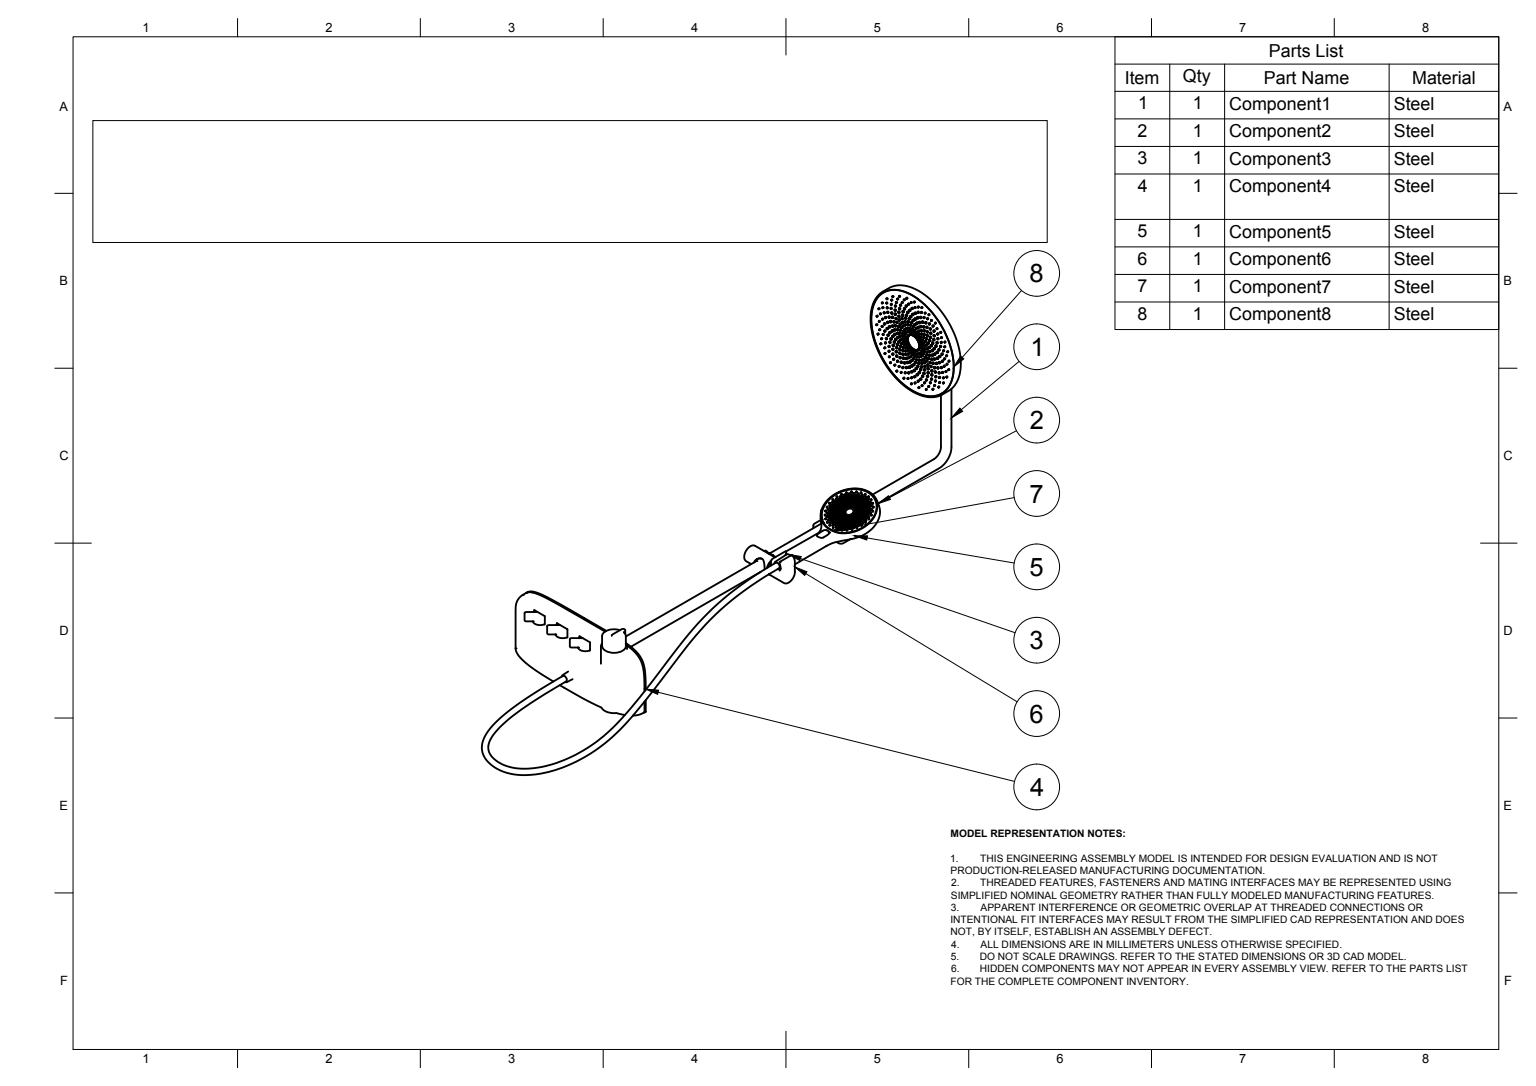
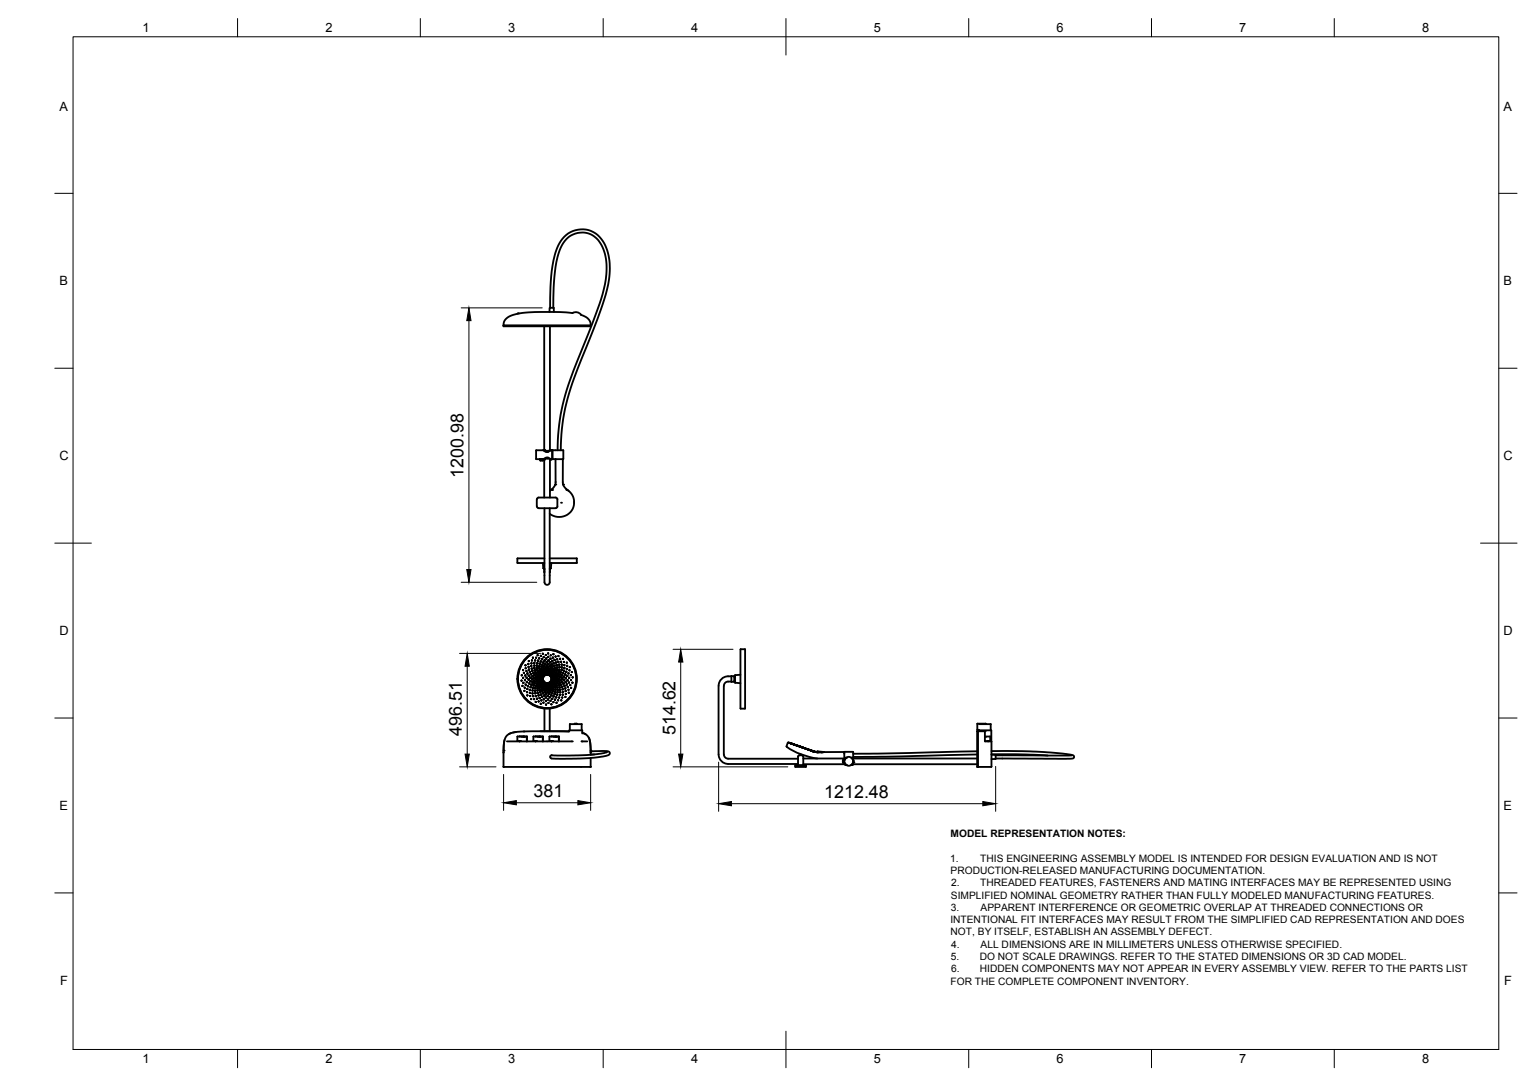
ISO-10303-21;
HEADER;
/* Generated by software containing ST-Developer
 * from STEP Tools, Inc. (www.steptools.com) 
 */

FILE_DESCRIPTION(
/* description */ ('STEP AP214'),
/* implementation_level */ '2;1');

FILE_NAME(
/* name */ 'MAS-616',
/* time_stamp */ '2026-10-06T11:02:40-07:00',
/* author */ (''),
/* organization */ (''),
/* preprocessor_version */ 'ST-DEVELOPER v20.2',
/* originating_system */ 'Autodesk Translation Framework v15.15.0.0',
/* authorisation */ '');

FILE_SCHEMA (('AUTOMOTIVE_DESIGN { 1 0 10303 214 3 1 1 }'));
ENDSEC;

DATA;
#10=MECHANICAL_DESIGN_GEOMETRIC_PRESENTATION_REPRESENTATION('',(#2936,#2937,
#2938,#2939,#2940,#2941,#2942,#2943),#130910);
#11=ITEM_DEFINED_TRANSFORMATION($,$,#45550,#51593);
#12=ITEM_DEFINED_TRANSFORMATION($,$,#45568,#51594);
#13=ITEM_DEFINED_TRANSFORMATION($,$,#48137,#51595);
#14=ITEM_DEFINED_TRANSFORMATION($,$,#48162,#51596);
#15=ITEM_DEFINED_TRANSFORMATION($,$,#48574,#51597);
#16=ITEM_DEFINED_TRANSFORMATION($,$,#48753,#51598);
#17=ITEM_DEFINED_TRANSFORMATION($,$,#48892,#51599);
#18=ITEM_DEFINED_TRANSFORMATION($,$,#48902,#51600);
#19=(
REPRESENTATION_RELATIONSHIP($,$,#130942,#130941)
REPRESENTATION_RELATIONSHIP_WITH_TRANSFORMATION(#11)
SHAPE_REPRESENTATION_RELATIONSHIP()
);
#20=(
REPRESENTATION_RELATIONSHIP($,$,#130943,#130941)
REPRESENTATION_RELATIONSHIP_WITH_TRANSFORMATION(#12)
SHAPE_REPRESENTATION_RELATIONSHIP()
);
#21=(
REPRESENTATION_RELATIONSHIP($,$,#130944,#130941)
REPRESENTATION_RELATIONSHIP_WITH_TRANSFORMATION(#13)
SHAPE_REPRESENTATION_RELATIONSHIP()
);
#22=(
REPRESENTATION_RELATIONSHIP($,$,#130945,#130941)
REPRESENTATION_RELATIONSHIP_WITH_TRANSFORMATION(#14)
SHAPE_REPRESENTATION_RELATIONSHIP()
);
#23=(
REPRESENTATION_RELATIONSHIP($,$,#130946,#130941)
REPRESENTATION_RELATIONSHIP_WITH_TRANSFORMATION(#15)
SHAPE_REPRESENTATION_RELATIONSHIP()
);
#24=(
REPRESENTATION_RELATIONSHIP($,$,#130947,#130941)
REPRESENTATION_RELATIONSHIP_WITH_TRANSFORMATION(#16)
SHAPE_REPRESENTATION_RELATIONSHIP()
);
#25=(
REPRESENTATION_RELATIONSHIP($,$,#130948,#130941)
REPRESENTATION_RELATIONSHIP_WITH_TRANSFORMATION(#17)
SHAPE_REPRESENTATION_RELATIONSHIP()
);
#26=(
REPRESENTATION_RELATIONSHIP($,$,#130949,#130941)
REPRESENTATION_RELATIONSHIP_WITH_TRANSFORMATION(#18)
SHAPE_REPRESENTATION_RELATIONSHIP()
);
#27=CONTEXT_DEPENDENT_SHAPE_REPRESENTATION(#19,#130933);
#28=CONTEXT_DEPENDENT_SHAPE_REPRESENTATION(#20,#130934);
#29=CONTEXT_DEPENDENT_SHAPE_REPRESENTATION(#21,#130935);
#30=CONTEXT_DEPENDENT_SHAPE_REPRESENTATION(#22,#130936);
#31=CONTEXT_DEPENDENT_SHAPE_REPRESENTATION(#23,#130937);
#32=CONTEXT_DEPENDENT_SHAPE_REPRESENTATION(#24,#130938);
#33=CONTEXT_DEPENDENT_SHAPE_REPRESENTATION(#25,#130939);
#34=CONTEXT_DEPENDENT_SHAPE_REPRESENTATION(#26,#130940);
#35=NEXT_ASSEMBLY_USAGE_OCCURRENCE('Component1:1','Component1:1',
'Component1:1',#130951,#130952,'Component1:1');
#36=NEXT_ASSEMBLY_USAGE_OCCURRENCE('Component2:1','Component2:1',
'Component2:1',#130951,#130953,'Component2:1');
#37=NEXT_ASSEMBLY_USAGE_OCCURRENCE('Component3:1','Component3:1',
'Component3:1',#130951,#130954,'Component3:1');
#38=NEXT_ASSEMBLY_USAGE_OCCURRENCE('Component4:1','Component4:1',
'Component4:1',#130951,#130955,'Component4:1');
#39=NEXT_ASSEMBLY_USAGE_OCCURRENCE('Component5:1','Component5:1',
'Component5:1',#130951,#130956,'Component5:1');
#40=NEXT_ASSEMBLY_USAGE_OCCURRENCE('Component6:1','Component6:1',
'Component6:1',#130951,#130957,'Component6:1');
#41=NEXT_ASSEMBLY_USAGE_OCCURRENCE('Component7:1','Component7:1',
'Component7:1',#130951,#130958,'Component7:1');
#42=NEXT_ASSEMBLY_USAGE_OCCURRENCE('Component8:1','Component8:1',
'Component8:1',#130951,#130959,'Component8:1');
#43=(
BOUNDED_CURVE()
B_SPLINE_CURVE(3,(#103309,#103310,#103311,#103312,#103313,#103314,#103315,
#103316,#103317,#103318,#103319,#103320,#103321,#103322,#103323,#103324,
#103325,#103326),.UNSPECIFIED.,.F.,.F.)
B_SPLINE_CURVE_WITH_KNOTS((4,2,2,2,2,2,2,2,4),(0.,0.392699081698724,0.785398163397448,
1.17809724509617,1.5707963267949,1.96349540849362,2.35619449019234,2.74889357189107,
3.14159265358979),.UNSPECIFIED.)
CURVE()
GEOMETRIC_REPRESENTATION_ITEM()
RATIONAL_B_SPLINE_CURVE((1.,1.,1.,1.,1.,1.,1.,1.,1.,1.,1.,1.,1.,1.,1.,1.,
1.,1.))
REPRESENTATION_ITEM('')
);
#44=(
BOUNDED_CURVE()
B_SPLINE_CURVE(3,(#103476,#103477,#103478,#103479,#103480,#103481,#103482,
#103483,#103484,#103485,#103486,#103487,#103488,#103489,#103490,#103491,
#103492,#103493),.UNSPECIFIED.,.F.,.F.)
B_SPLINE_CURVE_WITH_KNOTS((4,2,2,2,2,2,2,2,4),(3.14159265358979,3.53429173528852,
3.92699081698724,4.31968989868597,4.71238898038469,5.10508806208341,5.49778714378214,
5.89048622548086,6.28318530717959),.UNSPECIFIED.)
CURVE()
GEOMETRIC_REPRESENTATION_ITEM()
RATIONAL_B_SPLINE_CURVE((1.,1.,1.,1.,1.,1.,1.,1.,1.,1.,1.,1.,1.,1.,1.,1.,
1.,1.))
REPRESENTATION_ITEM('')
);
#45=B_SPLINE_SURFACE_WITH_KNOTS('',5,5,((#80582,#80583,#80584,#80585,#80586,
#80587),(#80588,#80589,#80590,#80591,#80592,#80593),(#80594,#80595,#80596,
#80597,#80598,#80599),(#80600,#80601,#80602,#80603,#80604,#80605),(#80606,
#80607,#80608,#80609,#80610,#80611),(#80612,#80613,#80614,#80615,#80616,
#80617),(#80618,#80619,#80620,#80621,#80622,#80623),(#80624,#80625,#80626,
#80627,#80628,#80629),(#80630,#80631,#80632,#80633,#80634,#80635),(#80636,
#80637,#80638,#80639,#80640,#80641),(#80642,#80643,#80644,#80645,#80646,
#80647),(#80648,#80649,#80650,#80651,#80652,#80653),(#80654,#80655,#80656,
#80657,#80658,#80659),(#80660,#80661,#80662,#80663,#80664,#80665),(#80666,
#80667,#80668,#80669,#80670,#80671),(#80672,#80673,#80674,#80675,#80676,
#80677),(#80678,#80679,#80680,#80681,#80682,#80683),(#80684,#80685,#80686,
#80687,#80688,#80689),(#80690,#80691,#80692,#80693,#80694,#80695),(#80696,
#80697,#80698,#80699,#80700,#80701),(#80702,#80703,#80704,#80705,#80706,
#80707),(#80708,#80709,#80710,#80711,#80712,#80713)),.UNSPECIFIED.,.F.,
 .F.,.F.,(6,4,4,4,4,6),(6,6),(0.,0.25,0.375,0.5,0.75,1.),(-5.17415755595432E-6,
1.),.UNSPECIFIED.);
#46=B_SPLINE_SURFACE_WITH_KNOTS('',5,5,((#80915,#80916,#80917,#80918,#80919,
#80920),(#80921,#80922,#80923,#80924,#80925,#80926),(#80927,#80928,#80929,
#80930,#80931,#80932),(#80933,#80934,#80935,#80936,#80937,#80938),(#80939,
#80940,#80941,#80942,#80943,#80944),(#80945,#80946,#80947,#80948,#80949,
#80950),(#80951,#80952,#80953,#80954,#80955,#80956),(#80957,#80958,#80959,
#80960,#80961,#80962),(#80963,#80964,#80965,#80966,#80967,#80968),(#80969,
#80970,#80971,#80972,#80973,#80974),(#80975,#80976,#80977,#80978,#80979,
#80980),(#80981,#80982,#80983,#80984,#80985,#80986),(#80987,#80988,#80989,
#80990,#80991,#80992),(#80993,#80994,#80995,#80996,#80997,#80998),(#80999,
#81000,#81001,#81002,#81003,#81004),(#81005,#81006,#81007,#81008,#81009,
#81010),(#81011,#81012,#81013,#81014,#81015,#81016),(#81017,#81018,#81019,
#81020,#81021,#81022),(#81023,#81024,#81025,#81026,#81027,#81028),(#81029,
#81030,#81031,#81032,#81033,#81034),(#81035,#81036,#81037,#81038,#81039,
#81040),(#81041,#81042,#81043,#81044,#81045,#81046)),.UNSPECIFIED.,.F.,
 .F.,.F.,(6,4,4,4,4,6),(6,6),(0.,0.25,0.5,0.625,0.75,1.),(-4.87729692394977E-6,
1.),.UNSPECIFIED.);
#47=B_SPLINE_SURFACE_WITH_KNOTS('',5,5,((#81337,#81338,#81339,#81340,#81341,
#81342),(#81343,#81344,#81345,#81346,#81347,#81348),(#81349,#81350,#81351,
#81352,#81353,#81354),(#81355,#81356,#81357,#81358,#81359,#81360),(#81361,
#81362,#81363,#81364,#81365,#81366),(#81367,#81368,#81369,#81370,#81371,
#81372),(#81373,#81374,#81375,#81376,#81377,#81378),(#81379,#81380,#81381,
#81382,#81383,#81384),(#81385,#81386,#81387,#81388,#81389,#81390),(#81391,
#81392,#81393,#81394,#81395,#81396),(#81397,#81398,#81399,#81400,#81401,
#81402),(#81403,#81404,#81405,#81406,#81407,#81408),(#81409,#81410,#81411,
#81412,#81413,#81414),(#81415,#81416,#81417,#81418,#81419,#81420),(#81421,
#81422,#81423,#81424,#81425,#81426),(#81427,#81428,#81429,#81430,#81431,
#81432),(#81433,#81434,#81435,#81436,#81437,#81438),(#81439,#81440,#81441,
#81442,#81443,#81444),(#81445,#81446,#81447,#81448,#81449,#81450),(#81451,
#81452,#81453,#81454,#81455,#81456),(#81457,#81458,#81459,#81460,#81461,
#81462),(#81463,#81464,#81465,#81466,#81467,#81468),(#81469,#81470,#81471,
#81472,#81473,#81474),(#81475,#81476,#81477,#81478,#81479,#81480),(#81481,
#81482,#81483,#81484,#81485,#81486),(#81487,#81488,#81489,#81490,#81491,
#81492),(#81493,#81494,#81495,#81496,#81497,#81498),(#81499,#81500,#81501,
#81502,#81503,#81504),(#81505,#81506,#81507,#81508,#81509,#81510),(#81511,
#81512,#81513,#81514,#81515,#81516),(#81517,#81518,#81519,#81520,#81521,
#81522),(#81523,#81524,#81525,#81526,#81527,#81528),(#81529,#81530,#81531,
#81532,#81533,#81534),(#81535,#81536,#81537,#81538,#81539,#81540),(#81541,
#81542,#81543,#81544,#81545,#81546),(#81547,#81548,#81549,#81550,#81551,
#81552),(#81553,#81554,#81555,#81556,#81557,#81558),(#81559,#81560,#81561,
#81562,#81563,#81564),(#81565,#81566,#81567,#81568,#81569,#81570),(#81571,
#81572,#81573,#81574,#81575,#81576),(#81577,#81578,#81579,#81580,#81581,
#81582),(#81583,#81584,#81585,#81586,#81587,#81588),(#81589,#81590,#81591,
#81592,#81593,#81594),(#81595,#81596,#81597,#81598,#81599,#81600),(#81601,
#81602,#81603,#81604,#81605,#81606),(#81607,#81608,#81609,#81610,#81611,
#81612)),.UNSPECIFIED.,.F.,.F.,.F.,(6,4,4,4,4,4,4,4,4,4,4,6),(6,6),(0.,
0.0625,0.125,0.25,0.3125,0.375,0.5,0.625,0.6875,0.75,0.875,1.),(0.,1.),
 .UNSPECIFIED.);
#48=B_SPLINE_SURFACE_WITH_KNOTS('',5,5,((#82412,#82413,#82414,#82415,#82416,
#82417),(#82418,#82419,#82420,#82421,#82422,#82423),(#82424,#82425,#82426,
#82427,#82428,#82429),(#82430,#82431,#82432,#82433,#82434,#82435),(#82436,
#82437,#82438,#82439,#82440,#82441),(#82442,#82443,#82444,#82445,#82446,
#82447),(#82448,#82449,#82450,#82451,#82452,#82453),(#82454,#82455,#82456,
#82457,#82458,#82459),(#82460,#82461,#82462,#82463,#82464,#82465),(#82466,
#82467,#82468,#82469,#82470,#82471)),.UNSPECIFIED.,.F.,.F.,.F.,(6,4,6),
(6,6),(0.,0.5,1.),(-3.3767936030343E-7,1.),.UNSPECIFIED.);
#49=B_SPLINE_SURFACE_WITH_KNOTS('',5,5,((#83493,#83494,#83495,#83496,#83497,
#83498),(#83499,#83500,#83501,#83502,#83503,#83504),(#83505,#83506,#83507,
#83508,#83509,#83510),(#83511,#83512,#83513,#83514,#83515,#83516),(#83517,
#83518,#83519,#83520,#83521,#83522),(#83523,#83524,#83525,#83526,#83527,
#83528),(#83529,#83530,#83531,#83532,#83533,#83534),(#83535,#83536,#83537,
#83538,#83539,#83540),(#83541,#83542,#83543,#83544,#83545,#83546),(#83547,
#83548,#83549,#83550,#83551,#83552)),.UNSPECIFIED.,.F.,.F.,.F.,(6,4,6),
(6,6),(0.,0.5,1.),(0.,1.),.UNSPECIFIED.);
#50=B_SPLINE_SURFACE_WITH_KNOTS('',3,1,((#87618,#87619),(#87620,#87621),
(#87622,#87623),(#87624,#87625)),.UNSPECIFIED.,.F.,.F.,.F.,(4,4),(2,2),
(0.0749476459249852,1.),(0.,0.360000000000005),.UNSPECIFIED.);
#51=B_SPLINE_SURFACE_WITH_KNOTS('',3,1,((#88063,#88064),(#88065,#88066),
(#88067,#88068),(#88069,#88070)),.UNSPECIFIED.,.F.,.F.,.F.,(4,4),(2,2),
(0.,0.925052354075012),(0.,0.360000000000003),.UNSPECIFIED.);
#52=B_SPLINE_SURFACE_WITH_KNOTS('',3,1,((#96549,#96550),(#96551,#96552),
(#96553,#96554),(#96555,#96556)),.UNSPECIFIED.,.F.,.F.,.F.,(4,4),(2,2),
(0.0749476459249852,1.),(0.,3.46611820003485),.UNSPECIFIED.);
#53=B_SPLINE_SURFACE_WITH_KNOTS('',3,1,((#96558,#96559),(#96560,#96561),
(#96562,#96563),(#96564,#96565)),.UNSPECIFIED.,.F.,.F.,.F.,(4,4),(2,2),
(0.309194334580351,0.92505235407501),(0.,1.8569103791729),.UNSPECIFIED.);
#54=B_SPLINE_SURFACE_WITH_KNOTS('',3,1,((#96571,#96572),(#96573,#96574),
(#96575,#96576),(#96577,#96578)),.UNSPECIFIED.,.F.,.F.,.F.,(4,4),(2,2),
(0.62139116379009,1.),(0.,13.1529900906224),.UNSPECIFIED.);
#55=B_SPLINE_SURFACE_WITH_KNOTS('',3,1,((#96579,#96580),(#96581,#96582),
(#96583,#96584),(#96585,#96586)),.UNSPECIFIED.,.F.,.F.,.F.,(4,4),(2,2),
(0.,1.),(0.,13.1529900906224),.UNSPECIFIED.);
#56=B_SPLINE_SURFACE_WITH_KNOTS('',3,1,((#96901,#96902),(#96903,#96904),
(#96905,#96906),(#96907,#96908)),.UNSPECIFIED.,.F.,.F.,.F.,(4,4),(2,2),
(0.,0.448741420101952),(0.,13.1529900906224),.UNSPECIFIED.);
#57=B_SPLINE_SURFACE_WITH_KNOTS('',3,1,((#96909,#96910),(#96911,#96912),
(#96913,#96914),(#96915,#96916)),.UNSPECIFIED.,.F.,.F.,.F.,(4,4),(2,2),
(0.,0.274332977827422),(0.,3.42421373123634),.UNSPECIFIED.);
#58=SPHERICAL_SURFACE('',#47449,40.9182954767619);
#59=SPHERICAL_SURFACE('',#47518,216.25);
#60=SPHERICAL_SURFACE('',#48303,0.5);
#61=SPHERICAL_SURFACE('',#48305,0.5);
#62=SPHERICAL_SURFACE('',#48314,0.5);
#63=SPHERICAL_SURFACE('',#48316,0.5);
#64=SPHERICAL_SURFACE('',#48525,1.);
#65=SPHERICAL_SURFACE('',#48533,1.);
#66=SPHERICAL_SURFACE('',#48870,0.5);
#67=SPHERICAL_SURFACE('',#48880,0.5);
#68=SPHERICAL_SURFACE('',#48882,0.5);
#69=SPHERICAL_SURFACE('',#48888,0.5);
#70=SPHERICAL_SURFACE('',#50902,14.1583614602198);
#71=CONICAL_SURFACE('',#47414,8.99091713639496,1.30899693899566);
#72=CONICAL_SURFACE('',#47466,6.3031389659941,0.785398163397445);
#73=CONICAL_SURFACE('',#47469,6.3031389659941,0.785398163397445);
#74=CONICAL_SURFACE('',#47523,22.9751982564137,0.00349065850398867);
#75=CONICAL_SURFACE('',#47530,22.9751982564137,0.00349065850398867);
#76=CONICAL_SURFACE('',#48147,9.47320447306899,0.0418325464020223);
#77=CONICAL_SURFACE('',#48154,8.94802844775792,0.0407936828678657);
#78=CONICAL_SURFACE('',#48628,2.99999999999998,0.78539816339745);
#79=CONICAL_SURFACE('',#48632,2.99999999999998,0.78539816339745);
#80=CONICAL_SURFACE('',#48637,3.00000000000006,0.785398163397453);
#81=CONICAL_SURFACE('',#48641,3.00000000000006,0.785398163397453);
#82=CONICAL_SURFACE('',#50915,18.5103550292801,0.080595262641945);
#83=FACE_BOUND('',#13544,.T.);
#84=FACE_BOUND('',#13545,.T.);
#85=FACE_BOUND('',#13546,.T.);
#86=FACE_BOUND('',#13547,.T.);
#87=FACE_BOUND('',#13548,.T.);
#88=FACE_BOUND('',#13549,.T.);
#89=FACE_BOUND('',#13550,.T.);
#90=FACE_BOUND('',#13551,.T.);
#91=FACE_BOUND('',#13552,.T.);
#92=FACE_BOUND('',#13553,.T.);
#93=FACE_BOUND('',#13554,.T.);
#94=FACE_BOUND('',#13555,.T.);
#95=FACE_BOUND('',#13556,.T.);
#96=FACE_BOUND('',#13557,.T.);
#97=FACE_BOUND('',#13558,.T.);
#98=FACE_BOUND('',#13559,.T.);
#99=FACE_BOUND('',#13560,.T.);
#100=FACE_BOUND('',#13561,.T.);
#101=FACE_BOUND('',#13562,.T.);
#102=FACE_BOUND('',#13563,.T.);
#103=FACE_BOUND('',#13564,.T.);
#104=FACE_BOUND('',#13565,.T.);
#105=FACE_BOUND('',#13566,.T.);
#106=FACE_BOUND('',#13567,.T.);
#107=FACE_BOUND('',#13568,.T.);
#108=FACE_BOUND('',#13569,.T.);
#109=FACE_BOUND('',#13570,.T.);
#110=FACE_BOUND('',#13571,.T.);
#111=FACE_BOUND('',#13572,.T.);
#112=FACE_BOUND('',#13573,.T.);
#113=FACE_BOUND('',#13574,.T.);
#114=FACE_BOUND('',#13575,.T.);
#115=FACE_BOUND('',#13576,.T.);
#116=FACE_BOUND('',#13577,.T.);
#117=FACE_BOUND('',#13578,.T.);
#118=FACE_BOUND('',#13579,.T.);
#119=FACE_BOUND('',#13580,.T.);
#120=FACE_BOUND('',#13581,.T.);
#121=FACE_BOUND('',#13582,.T.);
#122=FACE_BOUND('',#13583,.T.);
#123=FACE_BOUND('',#13584,.T.);
#124=FACE_BOUND('',#13585,.T.);
#125=FACE_BOUND('',#13586,.T.);
#126=FACE_BOUND('',#13587,.T.);
#127=FACE_BOUND('',#13588,.T.);
#128=FACE_BOUND('',#13589,.T.);
#129=FACE_BOUND('',#13590,.T.);
#130=FACE_BOUND('',#13591,.T.);
#131=FACE_BOUND('',#13605,.T.);
#132=FACE_BOUND('',#13670,.T.);
#133=FACE_BOUND('',#13671,.T.);
#134=FACE_BOUND('',#13672,.T.);
#135=FACE_BOUND('',#13673,.T.);
#136=FACE_BOUND('',#13674,.T.);
#137=FACE_BOUND('',#13675,.T.);
#138=FACE_BOUND('',#13676,.T.);
#139=FACE_BOUND('',#13677,.T.);
#140=FACE_BOUND('',#13678,.T.);
#141=FACE_BOUND('',#13679,.T.);
#142=FACE_BOUND('',#13680,.T.);
#143=FACE_BOUND('',#13681,.T.);
#144=FACE_BOUND('',#13682,.T.);
#145=FACE_BOUND('',#13683,.T.);
#146=FACE_BOUND('',#13684,.T.);
#147=FACE_BOUND('',#13685,.T.);
#148=FACE_BOUND('',#13686,.T.);
#149=FACE_BOUND('',#13687,.T.);
#150=FACE_BOUND('',#13689,.T.);
#151=FACE_BOUND('',#13690,.T.);
#152=FACE_BOUND('',#13691,.T.);
#153=FACE_BOUND('',#13692,.T.);
#154=FACE_BOUND('',#13693,.T.);
#155=FACE_BOUND('',#13694,.T.);
#156=FACE_BOUND('',#13695,.T.);
#157=FACE_BOUND('',#13696,.T.);
#158=FACE_BOUND('',#13697,.T.);
#159=FACE_BOUND('',#13698,.T.);
#160=FACE_BOUND('',#13699,.T.);
#161=FACE_BOUND('',#13700,.T.);
#162=FACE_BOUND('',#13701,.T.);
#163=FACE_BOUND('',#13702,.T.);
#164=FACE_BOUND('',#13703,.T.);
#165=FACE_BOUND('',#13704,.T.);
#166=FACE_BOUND('',#13705,.T.);
#167=FACE_BOUND('',#13706,.T.);
#168=FACE_BOUND('',#13707,.T.);
#169=FACE_BOUND('',#13708,.T.);
#170=FACE_BOUND('',#13709,.T.);
#171=FACE_BOUND('',#13710,.T.);
#172=FACE_BOUND('',#13711,.T.);
#173=FACE_BOUND('',#13712,.T.);
#174=FACE_BOUND('',#13713,.T.);
#175=FACE_BOUND('',#13714,.T.);
#176=FACE_BOUND('',#13715,.T.);
#177=FACE_BOUND('',#13716,.T.);
#178=FACE_BOUND('',#13717,.T.);
#179=FACE_BOUND('',#13718,.T.);
#180=FACE_BOUND('',#13719,.T.);
#181=FACE_BOUND('',#13720,.T.);
#182=FACE_BOUND('',#13721,.T.);
#183=FACE_BOUND('',#13722,.T.);
#184=FACE_BOUND('',#13723,.T.);
#185=FACE_BOUND('',#13724,.T.);
#186=FACE_BOUND('',#13725,.T.);
#187=FACE_BOUND('',#13726,.T.);
#188=FACE_BOUND('',#13727,.T.);
#189=FACE_BOUND('',#13728,.T.);
#190=FACE_BOUND('',#13729,.T.);
#191=FACE_BOUND('',#13730,.T.);
#192=FACE_BOUND('',#13731,.T.);
#193=FACE_BOUND('',#13732,.T.);
#194=FACE_BOUND('',#13733,.T.);
#195=FACE_BOUND('',#13734,.T.);
#196=FACE_BOUND('',#13735,.T.);
#197=FACE_BOUND('',#13736,.T.);
#198=FACE_BOUND('',#13737,.T.);
#199=FACE_BOUND('',#13738,.T.);
#200=FACE_BOUND('',#13739,.T.);
#201=FACE_BOUND('',#13740,.T.);
#202=FACE_BOUND('',#13741,.T.);
#203=FACE_BOUND('',#13742,.T.);
#204=FACE_BOUND('',#13743,.T.);
#205=FACE_BOUND('',#13744,.T.);
#206=FACE_BOUND('',#13745,.T.);
#207=FACE_BOUND('',#13746,.T.);
#208=FACE_BOUND('',#13747,.T.);
#209=FACE_BOUND('',#13748,.T.);
#210=FACE_BOUND('',#13749,.T.);
#211=FACE_BOUND('',#13750,.T.);
#212=FACE_BOUND('',#13751,.T.);
#213=FACE_BOUND('',#13752,.T.);
#214=FACE_BOUND('',#13753,.T.);
#215=FACE_BOUND('',#13754,.T.);
#216=FACE_BOUND('',#13755,.T.);
#217=FACE_BOUND('',#13756,.T.);
#218=FACE_BOUND('',#13757,.T.);
#219=FACE_BOUND('',#13758,.T.);
#220=FACE_BOUND('',#13759,.T.);
#221=FACE_BOUND('',#13760,.T.);
#222=FACE_BOUND('',#13761,.T.);
#223=FACE_BOUND('',#13762,.T.);
#224=FACE_BOUND('',#13763,.T.);
#225=FACE_BOUND('',#13764,.T.);
#226=FACE_BOUND('',#13765,.T.);
#227=FACE_BOUND('',#13766,.T.);
#228=FACE_BOUND('',#13767,.T.);
#229=FACE_BOUND('',#13768,.T.);
#230=FACE_BOUND('',#13769,.T.);
#231=FACE_BOUND('',#13770,.T.);
#232=FACE_BOUND('',#13771,.T.);
#233=FACE_BOUND('',#13772,.T.);
#234=FACE_BOUND('',#13773,.T.);
#235=FACE_BOUND('',#13774,.T.);
#236=FACE_BOUND('',#13775,.T.);
#237=FACE_BOUND('',#13776,.T.);
#238=FACE_BOUND('',#13777,.T.);
#239=FACE_BOUND('',#13778,.T.);
#240=FACE_BOUND('',#13779,.T.);
#241=FACE_BOUND('',#13780,.T.);
#242=FACE_BOUND('',#13781,.T.);
#243=FACE_BOUND('',#13782,.T.);
#244=FACE_BOUND('',#13783,.T.);
#245=FACE_BOUND('',#13784,.T.);
#246=FACE_BOUND('',#13785,.T.);
#247=FACE_BOUND('',#13786,.T.);
#248=FACE_BOUND('',#13787,.T.);
#249=FACE_BOUND('',#13788,.T.);
#250=FACE_BOUND('',#13789,.T.);
#251=FACE_BOUND('',#13790,.T.);
#252=FACE_BOUND('',#13791,.T.);
#253=FACE_BOUND('',#13792,.T.);
#254=FACE_BOUND('',#13793,.T.);
#255=FACE_BOUND('',#13794,.T.);
#256=FACE_BOUND('',#13795,.T.);
#257=FACE_BOUND('',#13796,.T.);
#258=FACE_BOUND('',#13797,.T.);
#259=FACE_BOUND('',#13798,.T.);
#260=FACE_BOUND('',#13799,.T.);
#261=FACE_BOUND('',#13800,.T.);
#262=FACE_BOUND('',#13801,.T.);
#263=FACE_BOUND('',#13802,.T.);
#264=FACE_BOUND('',#13803,.T.);
#265=FACE_BOUND('',#13804,.T.);
#266=FACE_BOUND('',#13805,.T.);
#267=FACE_BOUND('',#13806,.T.);
#268=FACE_BOUND('',#13807,.T.);
#269=FACE_BOUND('',#13808,.T.);
#270=FACE_BOUND('',#13809,.T.);
#271=FACE_BOUND('',#13810,.T.);
#272=FACE_BOUND('',#13811,.T.);
#273=FACE_BOUND('',#13812,.T.);
#274=FACE_BOUND('',#13813,.T.);
#275=FACE_BOUND('',#13814,.T.);
#276=FACE_BOUND('',#13815,.T.);
#277=FACE_BOUND('',#13816,.T.);
#278=FACE_BOUND('',#13817,.T.);
#279=FACE_BOUND('',#13818,.T.);
#280=FACE_BOUND('',#13819,.T.);
#281=FACE_BOUND('',#13820,.T.);
#282=FACE_BOUND('',#13821,.T.);
#283=FACE_BOUND('',#13822,.T.);
#284=FACE_BOUND('',#13823,.T.);
#285=FACE_BOUND('',#13824,.T.);
#286=FACE_BOUND('',#13825,.T.);
#287=FACE_BOUND('',#13826,.T.);
#288=FACE_BOUND('',#13827,.T.);
#289=FACE_BOUND('',#13828,.T.);
#290=FACE_BOUND('',#13829,.T.);
#291=FACE_BOUND('',#13830,.T.);
#292=FACE_BOUND('',#13831,.T.);
#293=FACE_BOUND('',#13832,.T.);
#294=FACE_BOUND('',#13833,.T.);
#295=FACE_BOUND('',#13834,.T.);
#296=FACE_BOUND('',#13835,.T.);
#297=FACE_BOUND('',#13836,.T.);
#298=FACE_BOUND('',#13837,.T.);
#299=FACE_BOUND('',#13838,.T.);
#300=FACE_BOUND('',#13839,.T.);
#301=FACE_BOUND('',#13840,.T.);
#302=FACE_BOUND('',#13841,.T.);
#303=FACE_BOUND('',#13842,.T.);
#304=FACE_BOUND('',#13843,.T.);
#305=FACE_BOUND('',#13844,.T.);
#306=FACE_BOUND('',#13845,.T.);
#307=FACE_BOUND('',#13846,.T.);
#308=FACE_BOUND('',#13847,.T.);
#309=FACE_BOUND('',#13848,.T.);
#310=FACE_BOUND('',#13849,.T.);
#311=FACE_BOUND('',#13850,.T.);
#312=FACE_BOUND('',#13851,.T.);
#313=FACE_BOUND('',#13852,.T.);
#314=FACE_BOUND('',#13853,.T.);
#315=FACE_BOUND('',#13854,.T.);
#316=FACE_BOUND('',#13855,.T.);
#317=FACE_BOUND('',#13856,.T.);
#318=FACE_BOUND('',#13857,.T.);
#319=FACE_BOUND('',#13858,.T.);
#320=FACE_BOUND('',#13859,.T.);
#321=FACE_BOUND('',#13860,.T.);
#322=FACE_BOUND('',#13861,.T.);
#323=FACE_BOUND('',#13862,.T.);
#324=FACE_BOUND('',#13863,.T.);
#325=FACE_BOUND('',#13864,.T.);
#326=FACE_BOUND('',#13865,.T.);
#327=FACE_BOUND('',#13866,.T.);
#328=FACE_BOUND('',#13867,.T.);
#329=FACE_BOUND('',#13868,.T.);
#330=FACE_BOUND('',#13869,.T.);
#331=FACE_BOUND('',#13870,.T.);
#332=FACE_BOUND('',#13871,.T.);
#333=FACE_BOUND('',#13872,.T.);
#334=FACE_BOUND('',#13873,.T.);
#335=FACE_BOUND('',#13874,.T.);
#336=FACE_BOUND('',#13875,.T.);
#337=FACE_BOUND('',#13876,.T.);
#338=FACE_BOUND('',#13877,.T.);
#339=FACE_BOUND('',#13878,.T.);
#340=FACE_BOUND('',#13879,.T.);
#341=FACE_BOUND('',#13880,.T.);
#342=FACE_BOUND('',#13881,.T.);
#343=FACE_BOUND('',#13882,.T.);
#344=FACE_BOUND('',#13883,.T.);
#345=FACE_BOUND('',#13884,.T.);
#346=FACE_BOUND('',#13885,.T.);
#347=FACE_BOUND('',#13886,.T.);
#348=FACE_BOUND('',#13887,.T.);
#349=FACE_BOUND('',#13888,.T.);
#350=FACE_BOUND('',#13889,.T.);
#351=FACE_BOUND('',#13890,.T.);
#352=FACE_BOUND('',#13891,.T.);
#353=FACE_BOUND('',#13892,.T.);
#354=FACE_BOUND('',#13893,.T.);
#355=FACE_BOUND('',#13894,.T.);
#356=FACE_BOUND('',#13895,.T.);
#357=FACE_BOUND('',#13896,.T.);
#358=FACE_BOUND('',#13897,.T.);
#359=FACE_BOUND('',#13898,.T.);
#360=FACE_BOUND('',#13899,.T.);
#361=FACE_BOUND('',#13900,.T.);
#362=FACE_BOUND('',#13901,.T.);
#363=FACE_BOUND('',#13902,.T.);
#364=FACE_BOUND('',#13903,.T.);
#365=FACE_BOUND('',#13904,.T.);
#366=FACE_BOUND('',#13905,.T.);
#367=FACE_BOUND('',#13906,.T.);
#368=FACE_BOUND('',#13907,.T.);
#369=FACE_BOUND('',#13908,.T.);
#370=FACE_BOUND('',#13909,.T.);
#371=FACE_BOUND('',#13910,.T.);
#372=FACE_BOUND('',#13911,.T.);
#373=FACE_BOUND('',#13912,.T.);
#374=FACE_BOUND('',#13913,.T.);
#375=FACE_BOUND('',#13914,.T.);
#376=FACE_BOUND('',#13915,.T.);
#377=FACE_BOUND('',#13916,.T.);
#378=FACE_BOUND('',#13917,.T.);
#379=FACE_BOUND('',#13918,.T.);
#380=FACE_BOUND('',#13919,.T.);
#381=FACE_BOUND('',#13920,.T.);
#382=FACE_BOUND('',#13921,.T.);
#383=FACE_BOUND('',#13922,.T.);
#384=FACE_BOUND('',#13923,.T.);
#385=FACE_BOUND('',#13924,.T.);
#386=FACE_BOUND('',#13933,.T.);
#387=FACE_BOUND('',#13936,.T.);
#388=FACE_BOUND('',#13939,.T.);
#389=FACE_BOUND('',#13942,.T.);
#390=FACE_BOUND('',#13945,.T.);
#391=FACE_BOUND('',#13948,.T.);
#392=FACE_BOUND('',#13951,.T.);
#393=FACE_BOUND('',#13954,.T.);
#394=FACE_BOUND('',#13957,.T.);
#395=FACE_BOUND('',#13960,.T.);
#396=FACE_BOUND('',#13963,.T.);
#397=FACE_BOUND('',#13966,.T.);
#398=FACE_BOUND('',#13969,.T.);
#399=FACE_BOUND('',#13972,.T.);
#400=FACE_BOUND('',#13975,.T.);
#401=FACE_BOUND('',#13978,.T.);
#402=FACE_BOUND('',#13981,.T.);
#403=FACE_BOUND('',#13984,.T.);
#404=FACE_BOUND('',#13987,.T.);
#405=FACE_BOUND('',#13990,.T.);
#406=FACE_BOUND('',#13993,.T.);
#407=FACE_BOUND('',#13996,.T.);
#408=FACE_BOUND('',#13999,.T.);
#409=FACE_BOUND('',#14002,.T.);
#410=FACE_BOUND('',#14005,.T.);
#411=FACE_BOUND('',#14008,.T.);
#412=FACE_BOUND('',#14011,.T.);
#413=FACE_BOUND('',#14014,.T.);
#414=FACE_BOUND('',#14017,.T.);
#415=FACE_BOUND('',#14020,.T.);
#416=FACE_BOUND('',#14023,.T.);
#417=FACE_BOUND('',#14026,.T.);
#418=FACE_BOUND('',#14029,.T.);
#419=FACE_BOUND('',#14032,.T.);
#420=FACE_BOUND('',#14035,.T.);
#421=FACE_BOUND('',#14038,.T.);
#422=FACE_BOUND('',#14041,.T.);
#423=FACE_BOUND('',#14044,.T.);
#424=FACE_BOUND('',#14047,.T.);
#425=FACE_BOUND('',#14050,.T.);
#426=FACE_BOUND('',#14053,.T.);
#427=FACE_BOUND('',#14056,.T.);
#428=FACE_BOUND('',#14059,.T.);
#429=FACE_BOUND('',#14062,.T.);
#430=FACE_BOUND('',#14065,.T.);
#431=FACE_BOUND('',#14068,.T.);
#432=FACE_BOUND('',#14071,.T.);
#433=FACE_BOUND('',#14074,.T.);
#434=FACE_BOUND('',#14077,.T.);
#435=FACE_BOUND('',#14080,.T.);
#436=FACE_BOUND('',#14083,.T.);
#437=FACE_BOUND('',#14086,.T.);
#438=FACE_BOUND('',#14089,.T.);
#439=FACE_BOUND('',#14092,.T.);
#440=FACE_BOUND('',#14095,.T.);
#441=FACE_BOUND('',#14098,.T.);
#442=FACE_BOUND('',#14101,.T.);
#443=FACE_BOUND('',#14104,.T.);
#444=FACE_BOUND('',#14107,.T.);
#445=FACE_BOUND('',#14110,.T.);
#446=FACE_BOUND('',#14113,.T.);
#447=FACE_BOUND('',#14116,.T.);
#448=FACE_BOUND('',#14119,.T.);
#449=FACE_BOUND('',#14122,.T.);
#450=FACE_BOUND('',#14125,.T.);
#451=FACE_BOUND('',#14128,.T.);
#452=FACE_BOUND('',#14131,.T.);
#453=FACE_BOUND('',#14134,.T.);
#454=FACE_BOUND('',#14137,.T.);
#455=FACE_BOUND('',#14140,.T.);
#456=FACE_BOUND('',#14143,.T.);
#457=FACE_BOUND('',#14146,.T.);
#458=FACE_BOUND('',#14149,.T.);
#459=FACE_BOUND('',#14152,.T.);
#460=FACE_BOUND('',#14155,.T.);
#461=FACE_BOUND('',#14158,.T.);
#462=FACE_BOUND('',#14161,.T.);
#463=FACE_BOUND('',#14164,.T.);
#464=FACE_BOUND('',#14167,.T.);
#465=FACE_BOUND('',#14170,.T.);
#466=FACE_BOUND('',#14173,.T.);
#467=FACE_BOUND('',#14176,.T.);
#468=FACE_BOUND('',#14179,.T.);
#469=FACE_BOUND('',#14182,.T.);
#470=FACE_BOUND('',#14185,.T.);
#471=FACE_BOUND('',#14188,.T.);
#472=FACE_BOUND('',#14191,.T.);
#473=FACE_BOUND('',#14194,.T.);
#474=FACE_BOUND('',#14197,.T.);
#475=FACE_BOUND('',#14200,.T.);
#476=FACE_BOUND('',#14203,.T.);
#477=FACE_BOUND('',#14206,.T.);
#478=FACE_BOUND('',#14209,.T.);
#479=FACE_BOUND('',#14212,.T.);
#480=FACE_BOUND('',#14215,.T.);
#481=FACE_BOUND('',#14218,.T.);
#482=FACE_BOUND('',#14221,.T.);
#483=FACE_BOUND('',#14224,.T.);
#484=FACE_BOUND('',#14227,.T.);
#485=FACE_BOUND('',#14230,.T.);
#486=FACE_BOUND('',#14233,.T.);
#487=FACE_BOUND('',#14236,.T.);
#488=FACE_BOUND('',#14239,.T.);
#489=FACE_BOUND('',#14242,.T.);
#490=FACE_BOUND('',#14245,.T.);
#491=FACE_BOUND('',#14248,.T.);
#492=FACE_BOUND('',#14251,.T.);
#493=FACE_BOUND('',#14254,.T.);
#494=FACE_BOUND('',#14257,.T.);
#495=FACE_BOUND('',#14260,.T.);
#496=FACE_BOUND('',#14263,.T.);
#497=FACE_BOUND('',#14266,.T.);
#498=FACE_BOUND('',#14269,.T.);
#499=FACE_BOUND('',#14272,.T.);
#500=FACE_BOUND('',#14275,.T.);
#501=FACE_BOUND('',#14278,.T.);
#502=FACE_BOUND('',#14281,.T.);
#503=FACE_BOUND('',#14284,.T.);
#504=FACE_BOUND('',#14287,.T.);
#505=FACE_BOUND('',#14290,.T.);
#506=FACE_BOUND('',#14293,.T.);
#507=FACE_BOUND('',#14296,.T.);
#508=FACE_BOUND('',#14299,.T.);
#509=FACE_BOUND('',#14302,.T.);
#510=FACE_BOUND('',#14305,.T.);
#511=FACE_BOUND('',#14308,.T.);
#512=FACE_BOUND('',#14311,.T.);
#513=FACE_BOUND('',#14314,.T.);
#514=FACE_BOUND('',#14317,.T.);
#515=FACE_BOUND('',#14320,.T.);
#516=FACE_BOUND('',#14323,.T.);
#517=FACE_BOUND('',#14326,.T.);
#518=FACE_BOUND('',#14329,.T.);
#519=FACE_BOUND('',#14332,.T.);
#520=FACE_BOUND('',#14335,.T.);
#521=FACE_BOUND('',#14338,.T.);
#522=FACE_BOUND('',#14341,.T.);
#523=FACE_BOUND('',#14344,.T.);
#524=FACE_BOUND('',#14347,.T.);
#525=FACE_BOUND('',#14350,.T.);
#526=FACE_BOUND('',#14353,.T.);
#527=FACE_BOUND('',#14356,.T.);
#528=FACE_BOUND('',#14359,.T.);
#529=FACE_BOUND('',#14362,.T.);
#530=FACE_BOUND('',#14365,.T.);
#531=FACE_BOUND('',#14368,.T.);
#532=FACE_BOUND('',#14371,.T.);
#533=FACE_BOUND('',#14374,.T.);
#534=FACE_BOUND('',#14377,.T.);
#535=FACE_BOUND('',#14380,.T.);
#536=FACE_BOUND('',#14383,.T.);
#537=FACE_BOUND('',#14386,.T.);
#538=FACE_BOUND('',#14389,.T.);
#539=FACE_BOUND('',#14392,.T.);
#540=FACE_BOUND('',#14395,.T.);
#541=FACE_BOUND('',#14398,.T.);
#542=FACE_BOUND('',#14401,.T.);
#543=FACE_BOUND('',#14404,.T.);
#544=FACE_BOUND('',#14407,.T.);
#545=FACE_BOUND('',#14410,.T.);
#546=FACE_BOUND('',#14413,.T.);
#547=FACE_BOUND('',#14416,.T.);
#548=FACE_BOUND('',#14419,.T.);
#549=FACE_BOUND('',#14422,.T.);
#550=FACE_BOUND('',#14425,.T.);
#551=FACE_BOUND('',#14428,.T.);
#552=FACE_BOUND('',#14431,.T.);
#553=FACE_BOUND('',#14434,.T.);
#554=FACE_BOUND('',#14437,.T.);
#555=FACE_BOUND('',#14440,.T.);
#556=FACE_BOUND('',#14443,.T.);
#557=FACE_BOUND('',#14446,.T.);
#558=FACE_BOUND('',#14449,.T.);
#559=FACE_BOUND('',#14452,.T.);
#560=FACE_BOUND('',#14455,.T.);
#561=FACE_BOUND('',#14458,.T.);
#562=FACE_BOUND('',#14461,.T.);
#563=FACE_BOUND('',#14464,.T.);
#564=FACE_BOUND('',#14467,.T.);
#565=FACE_BOUND('',#14470,.T.);
#566=FACE_BOUND('',#14473,.T.);
#567=FACE_BOUND('',#14476,.T.);
#568=FACE_BOUND('',#14479,.T.);
#569=FACE_BOUND('',#14482,.T.);
#570=FACE_BOUND('',#14485,.T.);
#571=FACE_BOUND('',#14488,.T.);
#572=FACE_BOUND('',#14491,.T.);
#573=FACE_BOUND('',#14494,.T.);
#574=FACE_BOUND('',#14497,.T.);
#575=FACE_BOUND('',#14500,.T.);
#576=FACE_BOUND('',#14503,.T.);
#577=FACE_BOUND('',#14506,.T.);
#578=FACE_BOUND('',#14509,.T.);
#579=FACE_BOUND('',#14512,.T.);
#580=FACE_BOUND('',#14515,.T.);
#581=FACE_BOUND('',#14518,.T.);
#582=FACE_BOUND('',#14521,.T.);
#583=FACE_BOUND('',#14524,.T.);
#584=FACE_BOUND('',#14527,.T.);
#585=FACE_BOUND('',#14530,.T.);
#586=FACE_BOUND('',#14533,.T.);
#587=FACE_BOUND('',#14536,.T.);
#588=FACE_BOUND('',#14539,.T.);
#589=FACE_BOUND('',#14542,.T.);
#590=FACE_BOUND('',#14545,.T.);
#591=FACE_BOUND('',#14548,.T.);
#592=FACE_BOUND('',#14551,.T.);
#593=FACE_BOUND('',#14554,.T.);
#594=FACE_BOUND('',#14557,.T.);
#595=FACE_BOUND('',#14560,.T.);
#596=FACE_BOUND('',#14563,.T.);
#597=FACE_BOUND('',#14566,.T.);
#598=FACE_BOUND('',#14569,.T.);
#599=FACE_BOUND('',#14572,.T.);
#600=FACE_BOUND('',#14575,.T.);
#601=FACE_BOUND('',#14578,.T.);
#602=FACE_BOUND('',#14581,.T.);
#603=FACE_BOUND('',#14584,.T.);
#604=FACE_BOUND('',#14587,.T.);
#605=FACE_BOUND('',#14590,.T.);
#606=FACE_BOUND('',#14593,.T.);
#607=FACE_BOUND('',#14596,.T.);
#608=FACE_BOUND('',#14599,.T.);
#609=FACE_BOUND('',#14602,.T.);
#610=FACE_BOUND('',#14605,.T.);
#611=FACE_BOUND('',#14608,.T.);
#612=FACE_BOUND('',#14611,.T.);
#613=FACE_BOUND('',#14614,.T.);
#614=FACE_BOUND('',#14617,.T.);
#615=FACE_BOUND('',#14620,.T.);
#616=FACE_BOUND('',#14623,.T.);
#617=FACE_BOUND('',#14626,.T.);
#618=FACE_BOUND('',#14629,.T.);
#619=FACE_BOUND('',#14632,.T.);
#620=FACE_BOUND('',#14635,.T.);
#621=FACE_BOUND('',#14638,.T.);
#622=FACE_BOUND('',#14641,.T.);
#623=FACE_BOUND('',#14644,.T.);
#624=FACE_BOUND('',#14647,.T.);
#625=FACE_BOUND('',#14650,.T.);
#626=FACE_BOUND('',#14653,.T.);
#627=FACE_BOUND('',#14656,.T.);
#628=FACE_BOUND('',#14659,.T.);
#629=FACE_BOUND('',#14662,.T.);
#630=FACE_BOUND('',#14665,.T.);
#631=FACE_BOUND('',#14668,.T.);
#632=FACE_BOUND('',#14671,.T.);
#633=FACE_BOUND('',#14674,.T.);
#634=FACE_BOUND('',#14677,.T.);
#635=FACE_BOUND('',#14680,.T.);
#636=FACE_BOUND('',#14683,.T.);
#637=FACE_BOUND('',#14686,.T.);
#638=FACE_BOUND('',#14689,.T.);
#639=FACE_BOUND('',#14692,.T.);
#640=FACE_BOUND('',#14695,.T.);
#641=FACE_BOUND('',#14698,.T.);
#642=FACE_BOUND('',#14701,.T.);
#643=FACE_BOUND('',#14704,.T.);
#644=FACE_BOUND('',#14707,.T.);
#645=FACE_BOUND('',#14710,.T.);
#646=FACE_BOUND('',#14713,.T.);
#647=FACE_BOUND('',#14716,.T.);
#648=FACE_BOUND('',#14719,.T.);
#649=FACE_BOUND('',#14722,.T.);
#650=FACE_BOUND('',#14725,.T.);
#651=FACE_BOUND('',#14728,.T.);
#652=FACE_BOUND('',#14731,.T.);
#653=FACE_BOUND('',#14734,.T.);
#654=FACE_BOUND('',#14737,.T.);
#655=FACE_BOUND('',#14740,.T.);
#656=FACE_BOUND('',#14743,.T.);
#657=FACE_BOUND('',#14746,.T.);
#658=FACE_BOUND('',#14749,.T.);
#659=FACE_BOUND('',#14752,.T.);
#660=FACE_BOUND('',#14755,.T.);
#661=FACE_BOUND('',#14758,.T.);
#662=FACE_BOUND('',#14761,.T.);
#663=FACE_BOUND('',#14764,.T.);
#664=FACE_BOUND('',#14767,.T.);
#665=FACE_BOUND('',#14770,.T.);
#666=FACE_BOUND('',#14773,.T.);
#667=FACE_BOUND('',#14776,.T.);
#668=FACE_BOUND('',#14779,.T.);
#669=FACE_BOUND('',#14782,.T.);
#670=FACE_BOUND('',#14785,.T.);
#671=FACE_BOUND('',#14788,.T.);
#672=FACE_BOUND('',#14791,.T.);
#673=FACE_BOUND('',#14794,.T.);
#674=FACE_BOUND('',#14797,.T.);
#675=FACE_BOUND('',#14800,.T.);
#676=FACE_BOUND('',#14803,.T.);
#677=FACE_BOUND('',#14806,.T.);
#678=FACE_BOUND('',#14809,.T.);
#679=FACE_BOUND('',#14812,.T.);
#680=FACE_BOUND('',#14815,.T.);
#681=FACE_BOUND('',#14818,.T.);
#682=FACE_BOUND('',#14821,.T.);
#683=FACE_BOUND('',#14824,.T.);
#684=FACE_BOUND('',#14827,.T.);
#685=FACE_BOUND('',#14830,.T.);
#686=FACE_BOUND('',#14833,.T.);
#687=FACE_BOUND('',#14836,.T.);
#688=FACE_BOUND('',#14839,.T.);
#689=FACE_BOUND('',#14842,.T.);
#690=FACE_BOUND('',#14845,.T.);
#691=FACE_BOUND('',#14848,.T.);
#692=FACE_BOUND('',#14851,.T.);
#693=FACE_BOUND('',#14854,.T.);
#694=FACE_BOUND('',#14857,.T.);
#695=FACE_BOUND('',#14860,.T.);
#696=FACE_BOUND('',#14863,.T.);
#697=FACE_BOUND('',#14866,.T.);
#698=FACE_BOUND('',#14869,.T.);
#699=FACE_BOUND('',#14872,.T.);
#700=FACE_BOUND('',#14875,.T.);
#701=FACE_BOUND('',#14878,.T.);
#702=FACE_BOUND('',#14881,.T.);
#703=FACE_BOUND('',#14884,.T.);
#704=FACE_BOUND('',#14887,.T.);
#705=FACE_BOUND('',#14890,.T.);
#706=FACE_BOUND('',#14893,.T.);
#707=FACE_BOUND('',#14896,.T.);
#708=FACE_BOUND('',#14899,.T.);
#709=FACE_BOUND('',#14901,.T.);
#710=FACE_BOUND('',#14904,.T.);
#711=FACE_BOUND('',#14907,.T.);
#712=FACE_BOUND('',#14910,.T.);
#713=FACE_BOUND('',#14913,.T.);
#714=FACE_BOUND('',#14916,.T.);
#715=FACE_BOUND('',#14926,.T.);
#716=FACE_BOUND('',#14930,.T.);
#717=FACE_BOUND('',#15125,.T.);
#718=FACE_BOUND('',#15135,.T.);
#719=FACE_BOUND('',#15136,.T.);
#720=FACE_BOUND('',#15137,.T.);
#721=FACE_BOUND('',#15164,.T.);
#722=FACE_BOUND('',#15172,.T.);
#723=FACE_BOUND('',#15175,.T.);
#724=FACE_BOUND('',#15265,.T.);
#725=FACE_BOUND('',#15266,.T.);
#726=FACE_BOUND('',#15267,.T.);
#727=FACE_BOUND('',#15278,.T.);
#728=FACE_BOUND('',#15280,.T.);
#729=FACE_BOUND('',#15289,.T.);
#730=FACE_BOUND('',#15291,.T.);
#731=FACE_BOUND('',#15335,.T.);
#732=FACE_BOUND('',#15338,.T.);
#733=FACE_BOUND('',#15339,.T.);
#734=FACE_BOUND('',#15340,.T.);
#735=FACE_BOUND('',#15341,.T.);
#736=FACE_BOUND('',#15342,.T.);
#737=FACE_BOUND('',#15343,.T.);
#738=FACE_BOUND('',#15344,.T.);
#739=FACE_BOUND('',#15345,.T.);
#740=FACE_BOUND('',#15346,.T.);
#741=FACE_BOUND('',#15347,.T.);
#742=FACE_BOUND('',#15348,.T.);
#743=FACE_BOUND('',#15349,.T.);
#744=FACE_BOUND('',#15350,.T.);
#745=FACE_BOUND('',#15351,.T.);
#746=FACE_BOUND('',#15352,.T.);
#747=FACE_BOUND('',#15353,.T.);
#748=FACE_BOUND('',#15354,.T.);
#749=FACE_BOUND('',#15355,.T.);
#750=FACE_BOUND('',#15356,.T.);
#751=FACE_BOUND('',#15357,.T.);
#752=FACE_BOUND('',#15358,.T.);
#753=FACE_BOUND('',#15359,.T.);
#754=FACE_BOUND('',#15360,.T.);
#755=FACE_BOUND('',#15361,.T.);
#756=FACE_BOUND('',#15362,.T.);
#757=FACE_BOUND('',#15363,.T.);
#758=FACE_BOUND('',#15364,.T.);
#759=FACE_BOUND('',#15365,.T.);
#760=FACE_BOUND('',#15366,.T.);
#761=FACE_BOUND('',#15367,.T.);
#762=FACE_BOUND('',#15368,.T.);
#763=FACE_BOUND('',#15369,.T.);
#764=FACE_BOUND('',#15370,.T.);
#765=FACE_BOUND('',#15371,.T.);
#766=FACE_BOUND('',#15372,.T.);
#767=FACE_BOUND('',#15373,.T.);
#768=FACE_BOUND('',#15374,.T.);
#769=FACE_BOUND('',#15375,.T.);
#770=FACE_BOUND('',#15376,.T.);
#771=FACE_BOUND('',#15377,.T.);
#772=FACE_BOUND('',#15378,.T.);
#773=FACE_BOUND('',#15379,.T.);
#774=FACE_BOUND('',#15380,.T.);
#775=FACE_BOUND('',#15381,.T.);
#776=FACE_BOUND('',#15382,.T.);
#777=FACE_BOUND('',#15383,.T.);
#778=FACE_BOUND('',#15384,.T.);
#779=FACE_BOUND('',#15385,.T.);
#780=FACE_BOUND('',#15386,.T.);
#781=FACE_BOUND('',#15387,.T.);
#782=FACE_BOUND('',#15388,.T.);
#783=FACE_BOUND('',#15389,.T.);
#784=FACE_BOUND('',#15390,.T.);
#785=FACE_BOUND('',#15391,.T.);
#786=FACE_BOUND('',#15392,.T.);
#787=FACE_BOUND('',#15393,.T.);
#788=FACE_BOUND('',#15394,.T.);
#789=FACE_BOUND('',#15395,.T.);
#790=FACE_BOUND('',#15396,.T.);
#791=FACE_BOUND('',#15397,.T.);
#792=FACE_BOUND('',#16183,.T.);
#793=FACE_BOUND('',#16193,.T.);
#794=FACE_BOUND('',#16196,.T.);
#795=FACE_BOUND('',#16198,.T.);
#796=FACE_BOUND('',#16200,.T.);
#797=FACE_BOUND('',#16203,.T.);
#798=FACE_BOUND('',#16205,.T.);
#799=FACE_BOUND('',#16206,.T.);
#800=FACE_BOUND('',#16207,.T.);
#801=FACE_BOUND('',#16208,.T.);
#802=FACE_BOUND('',#16209,.T.);
#803=FACE_BOUND('',#16210,.T.);
#804=FACE_BOUND('',#16211,.T.);
#805=FACE_BOUND('',#16212,.T.);
#806=FACE_BOUND('',#16213,.T.);
#807=FACE_BOUND('',#16214,.T.);
#808=FACE_BOUND('',#16215,.T.);
#809=FACE_BOUND('',#16216,.T.);
#810=FACE_BOUND('',#16217,.T.);
#811=FACE_BOUND('',#16218,.T.);
#812=FACE_BOUND('',#16219,.T.);
#813=FACE_BOUND('',#16220,.T.);
#814=FACE_BOUND('',#16221,.T.);
#815=FACE_BOUND('',#16222,.T.);
#816=FACE_BOUND('',#16223,.T.);
#817=FACE_BOUND('',#16224,.T.);
#818=FACE_BOUND('',#16225,.T.);
#819=FACE_BOUND('',#16226,.T.);
#820=FACE_BOUND('',#16227,.T.);
#821=FACE_BOUND('',#16228,.T.);
#822=FACE_BOUND('',#16229,.T.);
#823=FACE_BOUND('',#16230,.T.);
#824=FACE_BOUND('',#16231,.T.);
#825=FACE_BOUND('',#16232,.T.);
#826=FACE_BOUND('',#16233,.T.);
#827=FACE_BOUND('',#16234,.T.);
#828=FACE_BOUND('',#16235,.T.);
#829=FACE_BOUND('',#16236,.T.);
#830=FACE_BOUND('',#16237,.T.);
#831=FACE_BOUND('',#16238,.T.);
#832=FACE_BOUND('',#16239,.T.);
#833=FACE_BOUND('',#16240,.T.);
#834=FACE_BOUND('',#16241,.T.);
#835=FACE_BOUND('',#16242,.T.);
#836=FACE_BOUND('',#16243,.T.);
#837=FACE_BOUND('',#16244,.T.);
#838=FACE_BOUND('',#16245,.T.);
#839=FACE_BOUND('',#16246,.T.);
#840=FACE_BOUND('',#16247,.T.);
#841=FACE_BOUND('',#16248,.T.);
#842=FACE_BOUND('',#16249,.T.);
#843=FACE_BOUND('',#16250,.T.);
#844=FACE_BOUND('',#16251,.T.);
#845=FACE_BOUND('',#16252,.T.);
#846=FACE_BOUND('',#16253,.T.);
#847=FACE_BOUND('',#16254,.T.);
#848=FACE_BOUND('',#16255,.T.);
#849=FACE_BOUND('',#16256,.T.);
#850=FACE_BOUND('',#16257,.T.);
#851=FACE_BOUND('',#16258,.T.);
#852=FACE_BOUND('',#16259,.T.);
#853=FACE_BOUND('',#16260,.T.);
#854=FACE_BOUND('',#16261,.T.);
#855=FACE_BOUND('',#16262,.T.);
#856=FACE_BOUND('',#16263,.T.);
#857=FACE_BOUND('',#16264,.T.);
#858=FACE_BOUND('',#16265,.T.);
#859=FACE_BOUND('',#16266,.T.);
#860=FACE_BOUND('',#16267,.T.);
#861=FACE_BOUND('',#16268,.T.);
#862=FACE_BOUND('',#16269,.T.);
#863=FACE_BOUND('',#16270,.T.);
#864=FACE_BOUND('',#16271,.T.);
#865=FACE_BOUND('',#16272,.T.);
#866=FACE_BOUND('',#16273,.T.);
#867=FACE_BOUND('',#16274,.T.);
#868=FACE_BOUND('',#16275,.T.);
#869=FACE_BOUND('',#16276,.T.);
#870=FACE_BOUND('',#16277,.T.);
#871=FACE_BOUND('',#16278,.T.);
#872=FACE_BOUND('',#16279,.T.);
#873=FACE_BOUND('',#16280,.T.);
#874=FACE_BOUND('',#16281,.T.);
#875=FACE_BOUND('',#16282,.T.);
#876=FACE_BOUND('',#16283,.T.);
#877=FACE_BOUND('',#16284,.T.);
#878=FACE_BOUND('',#16285,.T.);
#879=FACE_BOUND('',#16286,.T.);
#880=FACE_BOUND('',#16287,.T.);
#881=FACE_BOUND('',#16288,.T.);
#882=FACE_BOUND('',#16289,.T.);
#883=FACE_BOUND('',#16290,.T.);
#884=FACE_BOUND('',#16291,.T.);
#885=FACE_BOUND('',#16292,.T.);
#886=FACE_BOUND('',#16293,.T.);
#887=FACE_BOUND('',#16294,.T.);
#888=FACE_BOUND('',#16295,.T.);
#889=FACE_BOUND('',#16296,.T.);
#890=FACE_BOUND('',#16297,.T.);
#891=FACE_BOUND('',#16298,.T.);
#892=FACE_BOUND('',#16299,.T.);
#893=FACE_BOUND('',#16300,.T.);
#894=FACE_BOUND('',#16301,.T.);
#895=FACE_BOUND('',#16302,.T.);
#896=FACE_BOUND('',#16303,.T.);
#897=FACE_BOUND('',#16304,.T.);
#898=FACE_BOUND('',#16305,.T.);
#899=FACE_BOUND('',#16306,.T.);
#900=FACE_BOUND('',#16307,.T.);
#901=FACE_BOUND('',#16308,.T.);
#902=FACE_BOUND('',#16309,.T.);
#903=FACE_BOUND('',#16310,.T.);
#904=FACE_BOUND('',#16311,.T.);
#905=FACE_BOUND('',#16312,.T.);
#906=FACE_BOUND('',#16313,.T.);
#907=FACE_BOUND('',#16314,.T.);
#908=FACE_BOUND('',#16315,.T.);
#909=FACE_BOUND('',#16316,.T.);
#910=FACE_BOUND('',#16317,.T.);
#911=FACE_BOUND('',#16318,.T.);
#912=FACE_BOUND('',#16319,.T.);
#913=FACE_BOUND('',#16320,.T.);
#914=FACE_BOUND('',#16321,.T.);
#915=FACE_BOUND('',#16322,.T.);
#916=FACE_BOUND('',#16323,.T.);
#917=FACE_BOUND('',#16324,.T.);
#918=FACE_BOUND('',#16325,.T.);
#919=FACE_BOUND('',#16326,.T.);
#920=FACE_BOUND('',#16327,.T.);
#921=FACE_BOUND('',#16328,.T.);
#922=FACE_BOUND('',#16329,.T.);
#923=FACE_BOUND('',#16330,.T.);
#924=FACE_BOUND('',#16331,.T.);
#925=FACE_BOUND('',#16332,.T.);
#926=FACE_BOUND('',#16333,.T.);
#927=FACE_BOUND('',#16334,.T.);
#928=FACE_BOUND('',#16335,.T.);
#929=FACE_BOUND('',#16336,.T.);
#930=FACE_BOUND('',#16337,.T.);
#931=FACE_BOUND('',#16338,.T.);
#932=FACE_BOUND('',#16339,.T.);
#933=FACE_BOUND('',#16340,.T.);
#934=FACE_BOUND('',#16341,.T.);
#935=FACE_BOUND('',#16342,.T.);
#936=FACE_BOUND('',#16343,.T.);
#937=FACE_BOUND('',#16344,.T.);
#938=FACE_BOUND('',#16345,.T.);
#939=FACE_BOUND('',#16346,.T.);
#940=FACE_BOUND('',#16347,.T.);
#941=FACE_BOUND('',#16348,.T.);
#942=FACE_BOUND('',#16349,.T.);
#943=FACE_BOUND('',#16350,.T.);
#944=FACE_BOUND('',#16351,.T.);
#945=FACE_BOUND('',#16352,.T.);
#946=FACE_BOUND('',#16353,.T.);
#947=FACE_BOUND('',#16354,.T.);
#948=FACE_BOUND('',#16355,.T.);
#949=FACE_BOUND('',#16356,.T.);
#950=FACE_BOUND('',#16357,.T.);
#951=FACE_BOUND('',#16358,.T.);
#952=FACE_BOUND('',#16359,.T.);
#953=FACE_BOUND('',#16360,.T.);
#954=FACE_BOUND('',#16361,.T.);
#955=FACE_BOUND('',#16362,.T.);
#956=FACE_BOUND('',#16363,.T.);
#957=FACE_BOUND('',#16364,.T.);
#958=FACE_BOUND('',#16365,.T.);
#959=FACE_BOUND('',#16366,.T.);
#960=FACE_BOUND('',#16367,.T.);
#961=FACE_BOUND('',#16368,.T.);
#962=FACE_BOUND('',#16369,.T.);
#963=FACE_BOUND('',#16370,.T.);
#964=FACE_BOUND('',#16371,.T.);
#965=FACE_BOUND('',#16372,.T.);
#966=FACE_BOUND('',#16373,.T.);
#967=FACE_BOUND('',#16374,.T.);
#968=FACE_BOUND('',#16375,.T.);
#969=FACE_BOUND('',#16376,.T.);
#970=FACE_BOUND('',#16377,.T.);
#971=FACE_BOUND('',#16378,.T.);
#972=FACE_BOUND('',#16379,.T.);
#973=FACE_BOUND('',#16380,.T.);
#974=FACE_BOUND('',#16381,.T.);
#975=FACE_BOUND('',#16382,.T.);
#976=FACE_BOUND('',#16383,.T.);
#977=FACE_BOUND('',#16384,.T.);
#978=FACE_BOUND('',#16385,.T.);
#979=FACE_BOUND('',#16386,.T.);
#980=FACE_BOUND('',#16387,.T.);
#981=FACE_BOUND('',#16388,.T.);
#982=FACE_BOUND('',#16389,.T.);
#983=FACE_BOUND('',#16390,.T.);
#984=FACE_BOUND('',#16391,.T.);
#985=FACE_BOUND('',#16392,.T.);
#986=FACE_BOUND('',#16393,.T.);
#987=FACE_BOUND('',#16394,.T.);
#988=FACE_BOUND('',#16395,.T.);
#989=FACE_BOUND('',#16396,.T.);
#990=FACE_BOUND('',#16397,.T.);
#991=FACE_BOUND('',#16398,.T.);
#992=FACE_BOUND('',#16399,.T.);
#993=FACE_BOUND('',#16400,.T.);
#994=FACE_BOUND('',#16401,.T.);
#995=FACE_BOUND('',#16402,.T.);
#996=FACE_BOUND('',#16403,.T.);
#997=FACE_BOUND('',#16404,.T.);
#998=FACE_BOUND('',#16405,.T.);
#999=FACE_BOUND('',#16406,.T.);
#1000=FACE_BOUND('',#16407,.T.);
#1001=FACE_BOUND('',#16408,.T.);
#1002=FACE_BOUND('',#16409,.T.);
#1003=FACE_BOUND('',#16410,.T.);
#1004=FACE_BOUND('',#16411,.T.);
#1005=FACE_BOUND('',#16412,.T.);
#1006=FACE_BOUND('',#16413,.T.);
#1007=FACE_BOUND('',#16414,.T.);
#1008=FACE_BOUND('',#16415,.T.);
#1009=FACE_BOUND('',#16416,.T.);
#1010=FACE_BOUND('',#16417,.T.);
#1011=FACE_BOUND('',#16418,.T.);
#1012=FACE_BOUND('',#16419,.T.);
#1013=FACE_BOUND('',#16420,.T.);
#1014=FACE_BOUND('',#16421,.T.);
#1015=FACE_BOUND('',#16422,.T.);
#1016=FACE_BOUND('',#16423,.T.);
#1017=FACE_BOUND('',#16424,.T.);
#1018=FACE_BOUND('',#16425,.T.);
#1019=FACE_BOUND('',#16426,.T.);
#1020=FACE_BOUND('',#16427,.T.);
#1021=FACE_BOUND('',#16428,.T.);
#1022=FACE_BOUND('',#16429,.T.);
#1023=FACE_BOUND('',#16430,.T.);
#1024=FACE_BOUND('',#16431,.T.);
#1025=FACE_BOUND('',#16432,.T.);
#1026=FACE_BOUND('',#16433,.T.);
#1027=FACE_BOUND('',#16434,.T.);
#1028=FACE_BOUND('',#16435,.T.);
#1029=FACE_BOUND('',#16436,.T.);
#1030=FACE_BOUND('',#16437,.T.);
#1031=FACE_BOUND('',#16438,.T.);
#1032=FACE_BOUND('',#16439,.T.);
#1033=FACE_BOUND('',#16440,.T.);
#1034=FACE_BOUND('',#16441,.T.);
#1035=FACE_BOUND('',#16442,.T.);
#1036=FACE_BOUND('',#16443,.T.);
#1037=FACE_BOUND('',#16444,.T.);
#1038=FACE_BOUND('',#16445,.T.);
#1039=FACE_BOUND('',#16446,.T.);
#1040=FACE_BOUND('',#16447,.T.);
#1041=FACE_BOUND('',#16448,.T.);
#1042=FACE_BOUND('',#16449,.T.);
#1043=FACE_BOUND('',#16450,.T.);
#1044=FACE_BOUND('',#16451,.T.);
#1045=FACE_BOUND('',#16452,.T.);
#1046=FACE_BOUND('',#16453,.T.);
#1047=FACE_BOUND('',#16454,.T.);
#1048=FACE_BOUND('',#16455,.T.);
#1049=FACE_BOUND('',#16456,.T.);
#1050=FACE_BOUND('',#16457,.T.);
#1051=FACE_BOUND('',#16458,.T.);
#1052=FACE_BOUND('',#16459,.T.);
#1053=FACE_BOUND('',#16460,.T.);
#1054=FACE_BOUND('',#16461,.T.);
#1055=FACE_BOUND('',#16462,.T.);
#1056=FACE_BOUND('',#16463,.T.);
#1057=FACE_BOUND('',#16464,.T.);
#1058=FACE_BOUND('',#16465,.T.);
#1059=FACE_BOUND('',#16466,.T.);
#1060=FACE_BOUND('',#16467,.T.);
#1061=FACE_BOUND('',#16468,.T.);
#1062=FACE_BOUND('',#16469,.T.);
#1063=FACE_BOUND('',#16470,.T.);
#1064=FACE_BOUND('',#16471,.T.);
#1065=FACE_BOUND('',#16472,.T.);
#1066=FACE_BOUND('',#16473,.T.);
#1067=FACE_BOUND('',#16474,.T.);
#1068=FACE_BOUND('',#16476,.T.);
#1069=FACE_BOUND('',#16477,.T.);
#1070=FACE_BOUND('',#16478,.T.);
#1071=FACE_BOUND('',#16479,.T.);
#1072=FACE_BOUND('',#16480,.T.);
#1073=FACE_BOUND('',#16481,.T.);
#1074=FACE_BOUND('',#16482,.T.);
#1075=FACE_BOUND('',#16483,.T.);
#1076=FACE_BOUND('',#16484,.T.);
#1077=FACE_BOUND('',#16485,.T.);
#1078=FACE_BOUND('',#16486,.T.);
#1079=FACE_BOUND('',#16487,.T.);
#1080=FACE_BOUND('',#16488,.T.);
#1081=FACE_BOUND('',#16489,.T.);
#1082=FACE_BOUND('',#16490,.T.);
#1083=FACE_BOUND('',#16491,.T.);
#1084=FACE_BOUND('',#16492,.T.);
#1085=FACE_BOUND('',#16493,.T.);
#1086=FACE_BOUND('',#16494,.T.);
#1087=FACE_BOUND('',#16495,.T.);
#1088=FACE_BOUND('',#16496,.T.);
#1089=FACE_BOUND('',#16497,.T.);
#1090=FACE_BOUND('',#16498,.T.);
#1091=FACE_BOUND('',#16499,.T.);
#1092=FACE_BOUND('',#16500,.T.);
#1093=FACE_BOUND('',#16501,.T.);
#1094=FACE_BOUND('',#16502,.T.);
#1095=FACE_BOUND('',#16503,.T.);
#1096=FACE_BOUND('',#16504,.T.);
#1097=FACE_BOUND('',#16505,.T.);
#1098=FACE_BOUND('',#16506,.T.);
#1099=FACE_BOUND('',#16507,.T.);
#1100=FACE_BOUND('',#16508,.T.);
#1101=FACE_BOUND('',#16509,.T.);
#1102=FACE_BOUND('',#16510,.T.);
#1103=FACE_BOUND('',#16511,.T.);
#1104=FACE_BOUND('',#16512,.T.);
#1105=FACE_BOUND('',#16513,.T.);
#1106=FACE_BOUND('',#16514,.T.);
#1107=FACE_BOUND('',#16515,.T.);
#1108=FACE_BOUND('',#16516,.T.);
#1109=FACE_BOUND('',#16517,.T.);
#1110=FACE_BOUND('',#16518,.T.);
#1111=FACE_BOUND('',#16519,.T.);
#1112=FACE_BOUND('',#16520,.T.);
#1113=FACE_BOUND('',#16521,.T.);
#1114=FACE_BOUND('',#16522,.T.);
#1115=FACE_BOUND('',#16523,.T.);
#1116=FACE_BOUND('',#16524,.T.);
#1117=FACE_BOUND('',#16525,.T.);
#1118=FACE_BOUND('',#16526,.T.);
#1119=FACE_BOUND('',#16527,.T.);
#1120=FACE_BOUND('',#16528,.T.);
#1121=FACE_BOUND('',#16529,.T.);
#1122=FACE_BOUND('',#16530,.T.);
#1123=FACE_BOUND('',#16531,.T.);
#1124=FACE_BOUND('',#16532,.T.);
#1125=FACE_BOUND('',#16533,.T.);
#1126=FACE_BOUND('',#16534,.T.);
#1127=FACE_BOUND('',#16535,.T.);
#1128=FACE_BOUND('',#16538,.T.);
#1129=FACE_BOUND('',#16541,.T.);
#1130=FACE_BOUND('',#16544,.T.);
#1131=FACE_BOUND('',#16547,.T.);
#1132=FACE_BOUND('',#16550,.T.);
#1133=FACE_BOUND('',#16553,.T.);
#1134=FACE_BOUND('',#16556,.T.);
#1135=FACE_BOUND('',#16559,.T.);
#1136=FACE_BOUND('',#16562,.T.);
#1137=FACE_BOUND('',#16565,.T.);
#1138=FACE_BOUND('',#16568,.T.);
#1139=FACE_BOUND('',#16571,.T.);
#1140=FACE_BOUND('',#16574,.T.);
#1141=FACE_BOUND('',#16577,.T.);
#1142=FACE_BOUND('',#16580,.T.);
#1143=FACE_BOUND('',#16583,.T.);
#1144=FACE_BOUND('',#16586,.T.);
#1145=FACE_BOUND('',#16589,.T.);
#1146=FACE_BOUND('',#16592,.T.);
#1147=FACE_BOUND('',#16595,.T.);
#1148=FACE_BOUND('',#16598,.T.);
#1149=FACE_BOUND('',#16601,.T.);
#1150=FACE_BOUND('',#16604,.T.);
#1151=FACE_BOUND('',#16607,.T.);
#1152=FACE_BOUND('',#16610,.T.);
#1153=FACE_BOUND('',#16613,.T.);
#1154=FACE_BOUND('',#16616,.T.);
#1155=FACE_BOUND('',#16619,.T.);
#1156=FACE_BOUND('',#16622,.T.);
#1157=FACE_BOUND('',#16625,.T.);
#1158=FACE_BOUND('',#16628,.T.);
#1159=FACE_BOUND('',#16631,.T.);
#1160=FACE_BOUND('',#16634,.T.);
#1161=FACE_BOUND('',#16637,.T.);
#1162=FACE_BOUND('',#16640,.T.);
#1163=FACE_BOUND('',#16643,.T.);
#1164=FACE_BOUND('',#16646,.T.);
#1165=FACE_BOUND('',#16649,.T.);
#1166=FACE_BOUND('',#16652,.T.);
#1167=FACE_BOUND('',#16655,.T.);
#1168=FACE_BOUND('',#16658,.T.);
#1169=FACE_BOUND('',#16661,.T.);
#1170=FACE_BOUND('',#16664,.T.);
#1171=FACE_BOUND('',#16667,.T.);
#1172=FACE_BOUND('',#16670,.T.);
#1173=FACE_BOUND('',#16673,.T.);
#1174=FACE_BOUND('',#16676,.T.);
#1175=FACE_BOUND('',#16679,.T.);
#1176=FACE_BOUND('',#16682,.T.);
#1177=FACE_BOUND('',#16685,.T.);
#1178=FACE_BOUND('',#16688,.T.);
#1179=FACE_BOUND('',#16691,.T.);
#1180=FACE_BOUND('',#16694,.T.);
#1181=FACE_BOUND('',#16697,.T.);
#1182=FACE_BOUND('',#16700,.T.);
#1183=FACE_BOUND('',#16703,.T.);
#1184=FACE_BOUND('',#16706,.T.);
#1185=FACE_BOUND('',#16709,.T.);
#1186=FACE_BOUND('',#16712,.T.);
#1187=FACE_BOUND('',#16715,.T.);
#1188=FACE_BOUND('',#16718,.T.);
#1189=FACE_BOUND('',#16721,.T.);
#1190=FACE_BOUND('',#16724,.T.);
#1191=FACE_BOUND('',#16727,.T.);
#1192=FACE_BOUND('',#16730,.T.);
#1193=FACE_BOUND('',#16733,.T.);
#1194=FACE_BOUND('',#16736,.T.);
#1195=FACE_BOUND('',#16739,.T.);
#1196=FACE_BOUND('',#16742,.T.);
#1197=FACE_BOUND('',#16745,.T.);
#1198=FACE_BOUND('',#16748,.T.);
#1199=FACE_BOUND('',#16751,.T.);
#1200=FACE_BOUND('',#16754,.T.);
#1201=FACE_BOUND('',#16757,.T.);
#1202=FACE_BOUND('',#16760,.T.);
#1203=FACE_BOUND('',#16763,.T.);
#1204=FACE_BOUND('',#16766,.T.);
#1205=FACE_BOUND('',#16769,.T.);
#1206=FACE_BOUND('',#16772,.T.);
#1207=FACE_BOUND('',#16775,.T.);
#1208=FACE_BOUND('',#16778,.T.);
#1209=FACE_BOUND('',#16781,.T.);
#1210=FACE_BOUND('',#16784,.T.);
#1211=FACE_BOUND('',#16787,.T.);
#1212=FACE_BOUND('',#16790,.T.);
#1213=FACE_BOUND('',#16793,.T.);
#1214=FACE_BOUND('',#16796,.T.);
#1215=FACE_BOUND('',#16799,.T.);
#1216=FACE_BOUND('',#16802,.T.);
#1217=FACE_BOUND('',#16805,.T.);
#1218=FACE_BOUND('',#16808,.T.);
#1219=FACE_BOUND('',#16811,.T.);
#1220=FACE_BOUND('',#16814,.T.);
#1221=FACE_BOUND('',#16817,.T.);
#1222=FACE_BOUND('',#16820,.T.);
#1223=FACE_BOUND('',#16823,.T.);
#1224=FACE_BOUND('',#16826,.T.);
#1225=FACE_BOUND('',#16829,.T.);
#1226=FACE_BOUND('',#16832,.T.);
#1227=FACE_BOUND('',#16835,.T.);
#1228=FACE_BOUND('',#16838,.T.);
#1229=FACE_BOUND('',#16841,.T.);
#1230=FACE_BOUND('',#16844,.T.);
#1231=FACE_BOUND('',#16847,.T.);
#1232=FACE_BOUND('',#16850,.T.);
#1233=FACE_BOUND('',#16853,.T.);
#1234=FACE_BOUND('',#16856,.T.);
#1235=FACE_BOUND('',#16859,.T.);
#1236=FACE_BOUND('',#16862,.T.);
#1237=FACE_BOUND('',#16865,.T.);
#1238=FACE_BOUND('',#16868,.T.);
#1239=FACE_BOUND('',#16871,.T.);
#1240=FACE_BOUND('',#16874,.T.);
#1241=FACE_BOUND('',#16877,.T.);
#1242=FACE_BOUND('',#16880,.T.);
#1243=FACE_BOUND('',#16883,.T.);
#1244=FACE_BOUND('',#16886,.T.);
#1245=FACE_BOUND('',#16889,.T.);
#1246=FACE_BOUND('',#16892,.T.);
#1247=FACE_BOUND('',#16895,.T.);
#1248=FACE_BOUND('',#16898,.T.);
#1249=FACE_BOUND('',#16901,.T.);
#1250=FACE_BOUND('',#16904,.T.);
#1251=FACE_BOUND('',#16907,.T.);
#1252=FACE_BOUND('',#16910,.T.);
#1253=FACE_BOUND('',#16913,.T.);
#1254=FACE_BOUND('',#16916,.T.);
#1255=FACE_BOUND('',#16919,.T.);
#1256=FACE_BOUND('',#16922,.T.);
#1257=FACE_BOUND('',#16925,.T.);
#1258=FACE_BOUND('',#16928,.T.);
#1259=FACE_BOUND('',#16931,.T.);
#1260=FACE_BOUND('',#16934,.T.);
#1261=FACE_BOUND('',#16937,.T.);
#1262=FACE_BOUND('',#16940,.T.);
#1263=FACE_BOUND('',#16943,.T.);
#1264=FACE_BOUND('',#16946,.T.);
#1265=FACE_BOUND('',#16949,.T.);
#1266=FACE_BOUND('',#16952,.T.);
#1267=FACE_BOUND('',#16955,.T.);
#1268=FACE_BOUND('',#16958,.T.);
#1269=FACE_BOUND('',#16961,.T.);
#1270=FACE_BOUND('',#16964,.T.);
#1271=FACE_BOUND('',#16967,.T.);
#1272=FACE_BOUND('',#16970,.T.);
#1273=FACE_BOUND('',#16973,.T.);
#1274=FACE_BOUND('',#16976,.T.);
#1275=FACE_BOUND('',#16979,.T.);
#1276=FACE_BOUND('',#16982,.T.);
#1277=FACE_BOUND('',#16985,.T.);
#1278=FACE_BOUND('',#16988,.T.);
#1279=FACE_BOUND('',#16991,.T.);
#1280=FACE_BOUND('',#16994,.T.);
#1281=FACE_BOUND('',#16997,.T.);
#1282=FACE_BOUND('',#17000,.T.);
#1283=FACE_BOUND('',#17003,.T.);
#1284=FACE_BOUND('',#17006,.T.);
#1285=FACE_BOUND('',#17009,.T.);
#1286=FACE_BOUND('',#17012,.T.);
#1287=FACE_BOUND('',#17015,.T.);
#1288=FACE_BOUND('',#17018,.T.);
#1289=FACE_BOUND('',#17021,.T.);
#1290=FACE_BOUND('',#17024,.T.);
#1291=FACE_BOUND('',#17027,.T.);
#1292=FACE_BOUND('',#17030,.T.);
#1293=FACE_BOUND('',#17033,.T.);
#1294=FACE_BOUND('',#17036,.T.);
#1295=FACE_BOUND('',#17039,.T.);
#1296=FACE_BOUND('',#17042,.T.);
#1297=FACE_BOUND('',#17045,.T.);
#1298=FACE_BOUND('',#17048,.T.);
#1299=FACE_BOUND('',#17051,.T.);
#1300=FACE_BOUND('',#17054,.T.);
#1301=FACE_BOUND('',#17057,.T.);
#1302=FACE_BOUND('',#17060,.T.);
#1303=FACE_BOUND('',#17063,.T.);
#1304=FACE_BOUND('',#17066,.T.);
#1305=FACE_BOUND('',#17069,.T.);
#1306=FACE_BOUND('',#17072,.T.);
#1307=FACE_BOUND('',#17075,.T.);
#1308=FACE_BOUND('',#17078,.T.);
#1309=FACE_BOUND('',#17081,.T.);
#1310=FACE_BOUND('',#17084,.T.);
#1311=FACE_BOUND('',#17087,.T.);
#1312=FACE_BOUND('',#17090,.T.);
#1313=FACE_BOUND('',#17093,.T.);
#1314=FACE_BOUND('',#17096,.T.);
#1315=FACE_BOUND('',#17099,.T.);
#1316=FACE_BOUND('',#17102,.T.);
#1317=FACE_BOUND('',#17105,.T.);
#1318=FACE_BOUND('',#17108,.T.);
#1319=FACE_BOUND('',#17111,.T.);
#1320=FACE_BOUND('',#17114,.T.);
#1321=FACE_BOUND('',#17117,.T.);
#1322=FACE_BOUND('',#17120,.T.);
#1323=FACE_BOUND('',#17123,.T.);
#1324=FACE_BOUND('',#17126,.T.);
#1325=FACE_BOUND('',#17129,.T.);
#1326=FACE_BOUND('',#17132,.T.);
#1327=FACE_BOUND('',#17135,.T.);
#1328=FACE_BOUND('',#17138,.T.);
#1329=FACE_BOUND('',#17141,.T.);
#1330=FACE_BOUND('',#17144,.T.);
#1331=FACE_BOUND('',#17147,.T.);
#1332=FACE_BOUND('',#17150,.T.);
#1333=FACE_BOUND('',#17153,.T.);
#1334=FACE_BOUND('',#17156,.T.);
#1335=FACE_BOUND('',#17159,.T.);
#1336=FACE_BOUND('',#17162,.T.);
#1337=FACE_BOUND('',#17165,.T.);
#1338=FACE_BOUND('',#17168,.T.);
#1339=FACE_BOUND('',#17171,.T.);
#1340=FACE_BOUND('',#17174,.T.);
#1341=FACE_BOUND('',#17177,.T.);
#1342=FACE_BOUND('',#17180,.T.);
#1343=FACE_BOUND('',#17183,.T.);
#1344=FACE_BOUND('',#17186,.T.);
#1345=FACE_BOUND('',#17189,.T.);
#1346=FACE_BOUND('',#17192,.T.);
#1347=FACE_BOUND('',#17195,.T.);
#1348=FACE_BOUND('',#17198,.T.);
#1349=FACE_BOUND('',#17201,.T.);
#1350=FACE_BOUND('',#17204,.T.);
#1351=FACE_BOUND('',#17207,.T.);
#1352=FACE_BOUND('',#17210,.T.);
#1353=FACE_BOUND('',#17213,.T.);
#1354=FACE_BOUND('',#17216,.T.);
#1355=FACE_BOUND('',#17219,.T.);
#1356=FACE_BOUND('',#17222,.T.);
#1357=FACE_BOUND('',#17225,.T.);
#1358=FACE_BOUND('',#17228,.T.);
#1359=FACE_BOUND('',#17231,.T.);
#1360=FACE_BOUND('',#17234,.T.);
#1361=FACE_BOUND('',#17237,.T.);
#1362=FACE_BOUND('',#17240,.T.);
#1363=FACE_BOUND('',#17243,.T.);
#1364=FACE_BOUND('',#17246,.T.);
#1365=FACE_BOUND('',#17249,.T.);
#1366=FACE_BOUND('',#17252,.T.);
#1367=FACE_BOUND('',#17255,.T.);
#1368=FACE_BOUND('',#17258,.T.);
#1369=FACE_BOUND('',#17261,.T.);
#1370=FACE_BOUND('',#17264,.T.);
#1371=FACE_BOUND('',#17267,.T.);
#1372=FACE_BOUND('',#17270,.T.);
#1373=FACE_BOUND('',#17273,.T.);
#1374=FACE_BOUND('',#17276,.T.);
#1375=FACE_BOUND('',#17279,.T.);
#1376=FACE_BOUND('',#17282,.T.);
#1377=FACE_BOUND('',#17285,.T.);
#1378=FACE_BOUND('',#17288,.T.);
#1379=FACE_BOUND('',#17291,.T.);
#1380=FACE_BOUND('',#17294,.T.);
#1381=FACE_BOUND('',#17297,.T.);
#1382=FACE_BOUND('',#17300,.T.);
#1383=FACE_BOUND('',#17303,.T.);
#1384=FACE_BOUND('',#17306,.T.);
#1385=FACE_BOUND('',#17309,.T.);
#1386=FACE_BOUND('',#17312,.T.);
#1387=FACE_BOUND('',#17315,.T.);
#1388=FACE_BOUND('',#17318,.T.);
#1389=FACE_BOUND('',#17321,.T.);
#1390=FACE_BOUND('',#17324,.T.);
#1391=FACE_BOUND('',#17327,.T.);
#1392=FACE_BOUND('',#17330,.T.);
#1393=FACE_BOUND('',#17333,.T.);
#1394=FACE_BOUND('',#17336,.T.);
#1395=FACE_BOUND('',#17339,.T.);
#1396=FACE_BOUND('',#17342,.T.);
#1397=FACE_BOUND('',#17345,.T.);
#1398=FACE_BOUND('',#17348,.T.);
#1399=FACE_BOUND('',#17351,.T.);
#1400=FACE_BOUND('',#17354,.T.);
#1401=FACE_BOUND('',#17357,.T.);
#1402=FACE_BOUND('',#17360,.T.);
#1403=FACE_BOUND('',#17363,.T.);
#1404=FACE_BOUND('',#17366,.T.);
#1405=FACE_BOUND('',#17369,.T.);
#1406=FACE_BOUND('',#17372,.T.);
#1407=FACE_BOUND('',#17375,.T.);
#1408=FACE_BOUND('',#17378,.T.);
#1409=FACE_BOUND('',#17381,.T.);
#1410=FACE_BOUND('',#17384,.T.);
#1411=FACE_BOUND('',#17387,.T.);
#1412=FACE_BOUND('',#17390,.T.);
#1413=FACE_BOUND('',#17393,.T.);
#1414=FACE_BOUND('',#17396,.T.);
#1415=FACE_BOUND('',#17399,.T.);
#1416=FACE_BOUND('',#17402,.T.);
#1417=FACE_BOUND('',#17405,.T.);
#1418=FACE_BOUND('',#17408,.T.);
#1419=FACE_BOUND('',#17411,.T.);
#1420=FACE_BOUND('',#17414,.T.);
#1421=FACE_BOUND('',#17417,.T.);
#1422=FACE_BOUND('',#17420,.T.);
#1423=FACE_BOUND('',#17423,.T.);
#1424=FACE_BOUND('',#17426,.T.);
#1425=FACE_BOUND('',#17429,.T.);
#1426=FACE_BOUND('',#17432,.T.);
#1427=FACE_BOUND('',#17435,.T.);
#1428=FACE_BOUND('',#17438,.T.);
#1429=FACE_BOUND('',#17441,.T.);
#1430=FACE_BOUND('',#17444,.T.);
#1431=FACE_BOUND('',#17447,.T.);
#1432=FACE_BOUND('',#17450,.T.);
#1433=FACE_BOUND('',#17453,.T.);
#1434=FACE_BOUND('',#17456,.T.);
#1435=FACE_BOUND('',#17459,.T.);
#1436=FACE_BOUND('',#17462,.T.);
#1437=FACE_BOUND('',#17465,.T.);
#1438=FACE_BOUND('',#17468,.T.);
#1439=FACE_BOUND('',#17471,.T.);
#1440=FACE_BOUND('',#17474,.T.);
#1441=FACE_BOUND('',#17477,.T.);
#1442=FACE_BOUND('',#17480,.T.);
#1443=FACE_BOUND('',#17483,.T.);
#1444=FACE_BOUND('',#17486,.T.);
#1445=FACE_BOUND('',#17489,.T.);
#1446=FACE_BOUND('',#17492,.T.);
#1447=FACE_BOUND('',#17495,.T.);
#1448=FACE_BOUND('',#17498,.T.);
#1449=FACE_BOUND('',#17501,.T.);
#1450=FACE_BOUND('',#17504,.T.);
#1451=FACE_BOUND('',#17507,.T.);
#1452=FACE_BOUND('',#17510,.T.);
#1453=FACE_BOUND('',#17513,.T.);
#1454=FACE_BOUND('',#17516,.T.);
#1455=FACE_BOUND('',#17519,.T.);
#1456=FACE_BOUND('',#17522,.T.);
#1457=FACE_BOUND('',#17525,.T.);
#1458=FACE_BOUND('',#17528,.T.);
#1459=FACE_BOUND('',#17531,.T.);
#1460=FACE_BOUND('',#17534,.T.);
#1461=FACE_BOUND('',#17537,.T.);
#1462=FACE_BOUND('',#17540,.T.);
#1463=FACE_BOUND('',#17543,.T.);
#1464=FACE_BOUND('',#17546,.T.);
#1465=FACE_BOUND('',#17549,.T.);
#1466=FACE_BOUND('',#17552,.T.);
#1467=FACE_BOUND('',#17555,.T.);
#1468=FACE_BOUND('',#17558,.T.);
#1469=FACE_BOUND('',#17561,.T.);
#1470=FACE_BOUND('',#17564,.T.);
#1471=FACE_BOUND('',#17567,.T.);
#1472=FACE_BOUND('',#17570,.T.);
#1473=FACE_BOUND('',#17573,.T.);
#1474=FACE_BOUND('',#17576,.T.);
#1475=FACE_BOUND('',#17579,.T.);
#1476=FACE_BOUND('',#17582,.T.);
#1477=FACE_BOUND('',#17585,.T.);
#1478=FACE_BOUND('',#17588,.T.);
#1479=FACE_BOUND('',#17591,.T.);
#1480=FACE_BOUND('',#17594,.T.);
#1481=FACE_BOUND('',#17597,.T.);
#1482=FACE_BOUND('',#17600,.T.);
#1483=FACE_BOUND('',#17603,.T.);
#1484=FACE_BOUND('',#17606,.T.);
#1485=FACE_BOUND('',#17609,.T.);
#1486=FACE_BOUND('',#17612,.T.);
#1487=FACE_BOUND('',#17615,.T.);
#1488=FACE_BOUND('',#17618,.T.);
#1489=FACE_BOUND('',#17621,.T.);
#1490=FACE_BOUND('',#17624,.T.);
#1491=FACE_BOUND('',#17627,.T.);
#1492=FACE_BOUND('',#17630,.T.);
#1493=FACE_BOUND('',#17633,.T.);
#1494=FACE_BOUND('',#17636,.T.);
#1495=FACE_BOUND('',#17639,.T.);
#1496=FACE_BOUND('',#17642,.T.);
#1497=FACE_BOUND('',#17645,.T.);
#1498=FACE_BOUND('',#17648,.T.);
#1499=FACE_BOUND('',#17651,.T.);
#1500=FACE_BOUND('',#17654,.T.);
#1501=FACE_BOUND('',#17657,.T.);
#1502=FACE_BOUND('',#17660,.T.);
#1503=FACE_BOUND('',#17663,.T.);
#1504=FACE_BOUND('',#17666,.T.);
#1505=FACE_BOUND('',#17669,.T.);
#1506=FACE_BOUND('',#17672,.T.);
#1507=FACE_BOUND('',#17675,.T.);
#1508=FACE_BOUND('',#17678,.T.);
#1509=FACE_BOUND('',#17681,.T.);
#1510=FACE_BOUND('',#17684,.T.);
#1511=FACE_BOUND('',#17687,.T.);
#1512=FACE_BOUND('',#17690,.T.);
#1513=FACE_BOUND('',#17693,.T.);
#1514=FACE_BOUND('',#17696,.T.);
#1515=FACE_BOUND('',#17699,.T.);
#1516=FACE_BOUND('',#17702,.T.);
#1517=(
BOUNDED_SURFACE()
B_SPLINE_SURFACE(2,2,((#77343,#77344,#77345,#77346,#77347,#77348,#77349,
#77350,#77351),(#77352,#77353,#77354,#77355,#77356,#77357,#77358,#77359,
#77360),(#77361,#77362,#77363,#77364,#77365,#77366,#77367,#77368,#77369)),
 .UNSPECIFIED.,.F.,.F.,.F.)
B_SPLINE_SURFACE_WITH_KNOTS((3,3),(3,2,2,2,3),(1.3311777581657,1.5707963267949),
(-2.52686466384705,-1.26345162727942,-3.85907117990136E-5,1.26337444585582,
2.52678748242345),.UNSPECIFIED.)
GEOMETRIC_REPRESENTATION_ITEM()
RATIONAL_B_SPLINE_SURFACE(((1.,0.807020945928444,1.,0.807020945928444,1.,
0.807020945928444,1.,0.807020945928444,1.),(0.992831448793889,0.801235774953152,
0.992831448793889,0.801235774953152,0.992831448793889,0.801235774953152,
0.992831448793889,0.801235774953152,0.992831448793889),(1.,0.807020945928444,
1.,0.807020945928444,1.,0.807020945928444,1.,0.807020945928444,1.)))
REPRESENTATION_ITEM('')
SURFACE()
);
#1518=(
BOUNDED_SURFACE()
B_SPLINE_SURFACE(2,3,((#77987,#77988,#77989,#77990),(#77991,#77992,#77993,
#77994),(#77995,#77996,#77997,#77998)),.UNSPECIFIED.,.F.,.F.,.F.)
B_SPLINE_SURFACE_WITH_KNOTS((3,3),(4,4),(0.122256864728636,0.285813497577799),
(0.,1.),.UNSPECIFIED.)
GEOMETRIC_REPRESENTATION_ITEM()
RATIONAL_B_SPLINE_SURFACE(((1.,0.999857188395218,0.999857188395218,1.),
(1.,0.999857188395218,0.999857188395218,1.),(1.,0.999857188395218,0.999857188395218,
1.)))
REPRESENTATION_ITEM('')
SURFACE()
);
#1519=(
BOUNDED_SURFACE()
B_SPLINE_SURFACE(3,2,((#78330,#78331,#78332),(#78333,#78334,#78335),(#78336,
#78337,#78338),(#78339,#78340,#78341),(#78342,#78343,#78344),(#78345,#78346,
#78347),(#78348,#78349,#78350),(#78351,#78352,#78353)),.UNSPECIFIED.,.F.,
 .F.,.F.)
B_SPLINE_SURFACE_WITH_KNOTS((4,2,2,4),(3,3),(-0.000825561057166025,0.00287128254447656,
0.00574256508895301,0.012310691235072),(0.,1.00082556105717),
 .UNSPECIFIED.)
GEOMETRIC_REPRESENTATION_ITEM()
RATIONAL_B_SPLINE_SURFACE(((1.,0.548378337711978,1.00074568251392),(1.,
0.548355519536473,1.00074572018951),(1.,0.548039556019421,1.00074624188386),
(1.,0.550338775294527,1.00074244559207),(1.,0.552341143417591,1.00073913943778),
(1.,0.563047839052552,1.00072146137585),(1.,0.577111435906181,1.00069824066007),
(1.,0.593159390799436,1.00067174352686)))
REPRESENTATION_ITEM('')
SURFACE()
);
#1520=(
BOUNDED_SURFACE()
B_SPLINE_SURFACE(3,2,((#78409,#78410,#78411),(#78412,#78413,#78414),(#78415,
#78416,#78417),(#78418,#78419,#78420),(#78421,#78422,#78423),(#78424,#78425,
#78426),(#78427,#78428,#78429),(#78430,#78431,#78432),(#78433,#78434,#78435),
(#78436,#78437,#78438),(#78439,#78440,#78441),(#78442,#78443,#78444),(#78445,
#78446,#78447),(#78448,#78449,#78450),(#78451,#78452,#78453),(#78454,#78455,
#78456),(#78457,#78458,#78459),(#78460,#78461,#78462),(#78463,#78464,#78465),
(#78466,#78467,#78468),(#78469,#78470,#78471),(#78472,#78473,#78474),(#78475,
#78476,#78477),(#78478,#78479,#78480),(#78481,#78482,#78483),(#78484,#78485,
#78486),(#78487,#78488,#78489),(#78490,#78491,#78492),(#78493,#78494,#78495),
(#78496,#78497,#78498),(#78499,#78500,#78501),(#78502,#78503,#78504),(#78505,
#78506,#78507),(#78508,#78509,#78510),(#78511,#78512,#78513),(#78514,#78515,
#78516),(#78517,#78518,#78519),(#78520,#78521,#78522),(#78523,#78524,#78525),
(#78526,#78527,#78528),(#78529,#78530,#78531),(#78532,#78533,#78534),(#78535,
#78536,#78537),(#78538,#78539,#78540),(#78541,#78542,#78543),(#78544,#78545,
#78546),(#78547,#78548,#78549),(#78550,#78551,#78552),(#78553,#78554,#78555),
(#78556,#78557,#78558)),.UNSPECIFIED.,.F.,.F.,.F.)
B_SPLINE_SURFACE_WITH_KNOTS((4,2,2,2,2,2,2,2,2,2,2,2,2,2,2,2,2,2,2,2,2,
2,2,2,4),(3,3),(-8.67361737988404E-19,0.00173990906147062,0.00260986359220593,
0.00347981812294124,0.00521972718441186,0.00608968171514717,0.00695963624588248,
0.00869954530735309,0.0095694998380884,0.0104394543688237,0.011309408899559,
0.0121793634302943,0.013919272491765,0.0147892270225003,0.0156591815532356,
0.0173990906147062,0.0182690451454415,0.0191389996761768,0.0200089542069121,
0.0208789087376474,0.022618817799118,0.0234887723298534,0.0243587268605887,
0.0260986359220593,0.0278385449835299),(0.,1.),.UNSPECIFIED.)
GEOMETRIC_REPRESENTATION_ITEM()
RATIONAL_B_SPLINE_SURFACE(((1.,0.587551834406292,1.),(1.,0.594699344437623,
1.),(1.,0.60382457287242,1.),(1.,0.618585716818677,1.),(1.,0.623688783259158,
1.),(1.,0.63402443640501,1.),(1.,0.639270861094579,1.),(1.,0.654612725815785,
1.),(1.,0.664393776262156,1.),(1.,0.677891309661685,1.),(1.,0.682215510713266,
1.),(1.,0.690382450875376,1.),(1.,0.694194502561824,1.),(1.,0.70485633352738,
1.),(1.,0.710933841358089,1.),(1.,0.718683431814466,1.),(1.,0.721040520492153,
1.),(1.,0.72523171526594,1.),(1.,0.727081934015882,1.),(1.,0.730342541173125,
1.),(1.,0.731752928390573,1.),(1.,0.734165338317436,1.),(1.,0.735170559598651,
1.),(1.,0.73756891973958,1.),(1.,0.738337302433501,1.),(1.,0.738350513419653,
1.),(1.,0.738161957403833,1.),(1.,0.737381790844921,1.),(1.,0.736790346153837,
1.),(1.,0.734428150437933,1.),(1.,0.732073793565705,1.),(1.,0.727166869065942,
1.),(1.,0.72528892033234,1.),(1.,0.721100474370705,1.),(1.,0.718783894149779,
1.),(1.,0.713670637512177,1.),(1.,0.710873855381012,1.),(1.,0.704754666210018,
1.),(1.,0.701414681407374,1.),(1.,0.690657616069657,1.),(1.,0.682568234525227,
1.),(1.,0.66911478968892,1.),(1.,0.664412058412855,1.),(1.,0.654618386970392,
1.),(1.,0.64955633063672,1.),(1.,0.634259701134918,1.),(1.,0.623798684793027,
1.),(1.,0.603998854527123,1.),(1.,0.594654550866798,1.),(1.,0.587551863023681,
1.)))
REPRESENTATION_ITEM('')
SURFACE()
);
#1521=(
BOUNDED_SURFACE()
B_SPLINE_SURFACE(3,2,((#78907,#78908,#78909),(#78910,#78911,#78912),(#78913,
#78914,#78915),(#78916,#78917,#78918),(#78919,#78920,#78921),(#78922,#78923,
#78924),(#78925,#78926,#78927),(#78928,#78929,#78930)),.UNSPECIFIED.,.F.,
 .F.,.F.)
B_SPLINE_SURFACE_WITH_KNOTS((4,2,2,4),(3,3),(-0.000839894778808834,0.00577703258153561,
0.00866554887230341,0.0123250319154216),(0.,1.00083989477881),
 .UNSPECIFIED.)
GEOMETRIC_REPRESENTATION_ITEM()
RATIONAL_B_SPLINE_SURFACE(((1.,0.59326054090623,1.00068323669606),(1.,0.577077765226871,
1.00071042035366),(1.,0.562913931262478,1.00073421261405),(1.,0.552227354080058,
1.0007521638148),(1.,0.550251225165873,1.00075548329552),(1.,0.548035546079893,
1.00075920517011),(1.,0.548356794981543,1.00075866553956),(1.,0.548365499452713,
1.00075865091788)))
REPRESENTATION_ITEM('')
SURFACE()
);
#1522=(
BOUNDED_SURFACE()
B_SPLINE_SURFACE(3,2,((#79061,#79062,#79063),(#79064,#79065,#79066),(#79067,
#79068,#79069),(#79070,#79071,#79072)),.UNSPECIFIED.,.F.,.F.,.F.)
B_SPLINE_SURFACE_WITH_KNOTS((4,4),(3,3),(0.,0.00312507179263297),(0.,1.),
 .UNSPECIFIED.)
GEOMETRIC_REPRESENTATION_ITEM()
RATIONAL_B_SPLINE_SURFACE(((1.,0.705667563680649,1.),(1.,0.683141011037701,
1.),(1.,0.667195074226265,1.),(1.,0.657315835427036,1.)))
REPRESENTATION_ITEM('')
SURFACE()
);
#1523=(
BOUNDED_SURFACE()
B_SPLINE_SURFACE(3,2,((#79086,#79087,#79088),(#79089,#79090,#79091),(#79092,
#79093,#79094),(#79095,#79096,#79097),(#79098,#79099,#79100),(#79101,#79102,
#79103),(#79104,#79105,#79106),(#79107,#79108,#79109),(#79110,#79111,#79112),
(#79113,#79114,#79115),(#79116,#79117,#79118),(#79119,#79120,#79121),(#79122,
#79123,#79124),(#79125,#79126,#79127),(#79128,#79129,#79130),(#79131,#79132,
#79133),(#79134,#79135,#79136),(#79137,#79138,#79139),(#79140,#79141,#79142),
(#79143,#79144,#79145),(#79146,#79147,#79148),(#79149,#79150,#79151),(#79152,
#79153,#79154),(#79155,#79156,#79157),(#79158,#79159,#79160),(#79161,#79162,
#79163),(#79164,#79165,#79166),(#79167,#79168,#79169),(#79170,#79171,#79172),
(#79173,#79174,#79175),(#79176,#79177,#79178),(#79179,#79180,#79181),(#79182,
#79183,#79184),(#79185,#79186,#79187),(#79188,#79189,#79190),(#79191,#79192,
#79193),(#79194,#79195,#79196),(#79197,#79198,#79199)),.UNSPECIFIED.,.F.,
 .F.,.F.)
B_SPLINE_SURFACE_WITH_KNOTS((4,2,2,2,2,2,2,2,2,2,2,2,2,2,2,2,2,2,4),(3,
3),(0.177629622043919,0.182227008052906,0.186824394061894,0.191421780070882,
0.19601916607987,0.200616552088858,0.205213938097846,0.209811324106834,
0.212110017111328,0.214408710115822,0.21900609612481,0.223603482133797,
0.228200868142785,0.230499561147279,0.232798254151773,0.237395640160761,
0.241993026169749,0.246590412178737,0.251187798187725),(-0.0011272803117177,
1.),.UNSPECIFIED.)
GEOMETRIC_REPRESENTATION_ITEM()
RATIONAL_B_SPLINE_SURFACE(((1.00066433836603,0.705335771802172,1.),(1.0006672369253,
0.704050129161315,1.),(1.00067174234902,0.702051769185273,1.),(1.00067937529164,
0.698666212576715,1.),(1.00068246888629,0.697294062890189,1.),(1.00068363404296,
0.696777263006209,1.),(1.00068168398229,0.697642203450054,1.),(1.00067057469206,
0.702569678060129,1.),(1.0006614418033,0.706620528884515,1.),(1.00063696614129,
0.717476596249883,1.),(1.0006216381699,0.724275247496527,1.),(1.00058883922152,
0.738823070267793,1.),(1.00057145082916,0.746535611763709,1.),(1.00054028106102,
0.760360819129251,1.),(1.00052657168104,0.766441551595995,1.),(1.00051230540889,
0.772769291024644,1.),(1.00050858517592,0.774419383257745,1.),(1.00050358230416,
0.776638384027486,1.),(1.00050231593974,0.777200074144778,1.),(1.00050237161857,
0.777175378053496,1.),(1.00050761438758,0.774849971960635,1.),(1.00052653204965,
0.766459129919287,1.),(1.00054018535901,0.760403267317986,1.),(1.00057139341204,
0.746561078861873,1.),(1.00058887691054,0.738806353479752,1.),(1.00061367660858,
0.727806561420185,1.),(1.00062171490961,0.724241209950337,1.),(1.00063661263986,
0.717633390187928,1.),(1.0006434784523,0.714588090641112,1.),(1.00066174186374,
0.706487438457221,1.),(1.00067070720977,0.702510900441748,1.),(1.00068161675471,
0.69767202193592,1.),(1.00068360383072,0.696790663504269,1.),(1.00068252855983,
0.697267594964546,1.),(1.00067947813414,0.698620597255677,1.),(1.00067181783581,
0.702018287367237,1.),(1.00066724002584,0.704048753932027,1.),(1.00066433837343,
0.705335768520302,1.)))
REPRESENTATION_ITEM('')
SURFACE()
);
#1524=(
BOUNDED_SURFACE()
B_SPLINE_SURFACE(3,2,((#79482,#79483,#79484),(#79485,#79486,#79487),(#79488,
#79489,#79490),(#79491,#79492,#79493)),.UNSPECIFIED.,.F.,.F.,.F.)
B_SPLINE_SURFACE_WITH_KNOTS((4,4),(3,3),(-2.75071984392645E-5,0.00458060955690249),
(0.,1.),.UNSPECIFIED.)
GEOMETRIC_REPRESENTATION_ITEM()
RATIONAL_B_SPLINE_SURFACE(((1.,0.641978469944238,1.),(1.,0.641650471821333,
1.),(1.,0.64244455436399,1.),(1.,0.657315835410222,1.)))
REPRESENTATION_ITEM('')
SURFACE()
);
#1525=(
BOUNDED_SURFACE()
B_SPLINE_SURFACE(3,2,((#79501,#79502,#79503),(#79504,#79505,#79506),(#79507,
#79508,#79509),(#79510,#79511,#79512)),.UNSPECIFIED.,.F.,.F.,.F.)
B_SPLINE_SURFACE_WITH_KNOTS((4,4),(3,3),(-2.46898855527089E-13,0.00312495174925659),
(0.,1.),.UNSPECIFIED.)
GEOMETRIC_REPRESENTATION_ITEM()
RATIONAL_B_SPLINE_SURFACE(((1.,0.657316968304524,1.),(1.,0.667197332814039,
1.),(1.,0.683144406660839,1.),(1.,0.7056675669599,1.)))
REPRESENTATION_ITEM('')
SURFACE()
);
#1526=(
BOUNDED_SURFACE()
B_SPLINE_SURFACE(3,2,((#79523,#79524,#79525),(#79526,#79527,#79528),(#79529,
#79530,#79531),(#79532,#79533,#79534)),.UNSPECIFIED.,.F.,.F.,.F.)
B_SPLINE_SURFACE_WITH_KNOTS((4,4),(3,3),(-2.7488975911652E-5,0.00458149598527533),
(0.,1.),.UNSPECIFIED.)
GEOMETRIC_REPRESENTATION_ITEM()
RATIONAL_B_SPLINE_SURFACE(((1.,0.641978587954326,1.),(1.,0.641650294890703,
1.),(1.,0.642442143358719,1.),(1.,0.657316968289027,1.)))
REPRESENTATION_ITEM('')
SURFACE()
);
#1527=(
BOUNDED_SURFACE()
B_SPLINE_SURFACE(3,2,((#79542,#79543,#79544),(#79545,#79546,#79547),(#79548,
#79549,#79550),(#79551,#79552,#79553),(#79554,#79555,#79556),(#79557,#79558,
#79559),(#79560,#79561,#79562),(#79563,#79564,#79565)),.UNSPECIFIED.,.F.,
 .F.,.F.)
B_SPLINE_SURFACE_WITH_KNOTS((4,2,2,4),(3,3),(0.,0.000314760444717589,0.000629520889435179,
0.00125904177887036),(0.,1.),.UNSPECIFIED.)
GEOMETRIC_REPRESENTATION_ITEM()
RATIONAL_B_SPLINE_SURFACE(((1.,0.705871570678672,1.),(1.,0.705832198773769,
1.),(1.,0.705802677875688,1.),(1.,0.705762810535011,1.),(1.,0.705752530546662,
1.),(1.,0.705752443860712,1.),(1.,0.705792484302677,1.),(1.,0.705871570678672,
1.)))
REPRESENTATION_ITEM('')
SURFACE()
);
#1528=(
BOUNDED_SURFACE()
B_SPLINE_SURFACE(3,2,((#79592,#79593,#79594),(#79595,#79596,#79597),(#79598,
#79599,#79600),(#79601,#79602,#79603),(#79604,#79605,#79606),(#79607,#79608,
#79609),(#79610,#79611,#79612),(#79613,#79614,#79615)),.UNSPECIFIED.,.F.,
 .F.,.F.)
B_SPLINE_SURFACE_WITH_KNOTS((4,2,2,4),(3,3),(0.,0.000314760444717589,0.000629520889435178,
0.00125904177887036),(0.,1.),.UNSPECIFIED.)
GEOMETRIC_REPRESENTATION_ITEM()
RATIONAL_B_SPLINE_SURFACE(((1.,0.705871570678664,1.),(1.,0.705832198778323,
1.),(1.,0.705802677887727,1.),(1.,0.705762810539017,1.),(1.,0.705752530546526,
1.),(1.,0.705752443861208,1.),(1.,0.705792484282721,1.),(1.,0.705871570678672,
1.)))
REPRESENTATION_ITEM('')
SURFACE()
);
#1529=(
BOUNDED_SURFACE()
B_SPLINE_SURFACE(3,2,((#79636,#79637,#79638),(#79639,#79640,#79641),(#79642,
#79643,#79644),(#79645,#79646,#79647),(#79648,#79649,#79650),(#79651,#79652,
#79653),(#79654,#79655,#79656),(#79657,#79658,#79659)),.UNSPECIFIED.,.F.,
 .F.,.F.)
B_SPLINE_SURFACE_WITH_KNOTS((4,2,2,4),(3,3),(0.,0.000314760444717595,0.000629520889435189,
0.00125904177887038),(0.,1.),.UNSPECIFIED.)
GEOMETRIC_REPRESENTATION_ITEM()
RATIONAL_B_SPLINE_SURFACE(((1.,0.705871570678672,1.),(1.,0.705832198778314,
1.),(1.,0.705802677887727,1.),(1.,0.705762810539017,1.),(1.,0.705752530546536,
1.),(1.,0.7057524438612,1.),(1.,0.705792484282725,1.),(1.,0.705871570678672,
1.)))
REPRESENTATION_ITEM('')
SURFACE()
);
#1530=(
BOUNDED_SURFACE()
B_SPLINE_SURFACE(3,2,((#79683,#79684,#79685),(#79686,#79687,#79688),(#79689,
#79690,#79691),(#79692,#79693,#79694),(#79695,#79696,#79697),(#79698,#79699,
#79700),(#79701,#79702,#79703),(#79704,#79705,#79706)),.UNSPECIFIED.,.F.,
 .F.,.F.)
B_SPLINE_SURFACE_WITH_KNOTS((4,2,2,4),(3,3),(-1.36609473733174E-17,0.000314760444717569,
0.000629520889435153,0.00125904177887032),(0.,1.),.UNSPECIFIED.)
GEOMETRIC_REPRESENTATION_ITEM()
RATIONAL_B_SPLINE_SURFACE(((1.,0.705871570678672,1.),(1.,0.705832198773852,
1.),(1.,0.705802677875577,1.),(1.,0.705762810535121,1.),(1.,0.705752530546451,
1.),(1.,0.705752443861133,1.),(1.,0.705792484302369,1.),(1.,0.705871570678672,
1.)))
REPRESENTATION_ITEM('')
SURFACE()
);
#1531=(
BOUNDED_SURFACE()
B_SPLINE_SURFACE(3,2,((#79724,#79725,#79726),(#79727,#79728,#79729),(#79730,
#79731,#79732),(#79733,#79734,#79735),(#79736,#79737,#79738),(#79739,#79740,
#79741),(#79742,#79743,#79744),(#79745,#79746,#79747),(#79748,#79749,#79750),
(#79751,#79752,#79753),(#79754,#79755,#79756),(#79757,#79758,#79759),(#79760,
#79761,#79762),(#79763,#79764,#79765)),.UNSPECIFIED.,.F.,.F.,.F.)
B_SPLINE_SURFACE_WITH_KNOTS((4,2,2,2,2,2,4),(3,3),(0.0964178567359105,0.0969969483064025,
0.097141430047764,0.0974303935304871,0.0980083204959333,0.0991641744268257,
0.101910812839202),(-0.0156147939957968,0.908717315728862),
 .UNSPECIFIED.)
GEOMETRIC_REPRESENTATION_ITEM()
RATIONAL_B_SPLINE_SURFACE(((1.01039996590636,0.697849574056477,0.945601885810221),
(1.00920776855038,0.732486508654537,0.951837799321068),(1.00928443570073,
0.730259096339428,0.951436783737236),(1.00928198827333,0.730330201498752,
0.951449585263377),(1.00928121023475,0.730352805869793,0.9514536548759),
(1.00927803608829,0.730445024412888,0.951470257582389),(1.00927479988541,
0.730539045882487,0.951487184881511),(1.00926195866405,0.73091212215395,
0.951554352238807),(1.00924922181827,0.731282165999437,0.951620973648653),
(1.00920031293424,0.73270311682538,0.951876796704491),(1.00915348816192,
0.734063517910211,0.952121718595055),(1.00896275601819,0.739604862851685,
0.953119363109207),(1.00877459790181,0.745071424523457,0.954103543902988),
(1.00857970487406,0.750733655715106,0.955122952358132)))
REPRESENTATION_ITEM('')
SURFACE()
);
#1532=(
BOUNDED_SURFACE()
B_SPLINE_SURFACE(3,2,((#79838,#79839,#79840),(#79841,#79842,#79843),(#79844,
#79845,#79846),(#79847,#79848,#79849),(#79850,#79851,#79852),(#79853,#79854,
#79855),(#79856,#79857,#79858),(#79859,#79860,#79861),(#79862,#79863,#79864),
(#79865,#79866,#79867),(#79868,#79869,#79870),(#79871,#79872,#79873),(#79874,
#79875,#79876),(#79877,#79878,#79879)),.UNSPECIFIED.,.F.,.F.,.F.)
B_SPLINE_SURFACE_WITH_KNOTS((4,2,2,2,2,2,4),(3,3),(0.0924478328249838,0.0927448966007841,
0.0928885691804298,0.0931759143397212,0.0937506046583039,0.0948999852954695,
0.0973806489601807),(0.0912830955164557,1.),.UNSPECIFIED.)
GEOMETRIC_REPRESENTATION_ITEM()
RATIONAL_B_SPLINE_SURFACE(((0.950792246120108,0.730466229253696,1.),(0.951545496940602,
0.734592134582775,1.),(0.951441568640601,0.734022870912366,1.),(0.951449313493617,
0.734065293077013,1.),(0.951453334853521,0.734087319936867,1.),(0.951469744567059,
0.734177203575482,1.),(0.951486478882703,0.734268865210911,1.),(0.951552891707438,
0.734632639162483,1.),(0.951618775955208,0.734993517851996,1.),(0.951871831973123,
0.736379623441885,1.),(0.9521141728944,0.737707037460359,1.),(0.95303809490497,
0.742767788332922,1.),(0.953900490476868,0.747491530264648,1.),(0.954811659448391,
0.752482426806707,1.)))
REPRESENTATION_ITEM('')
SURFACE()
);
#1533=(
BOUNDED_SURFACE()
B_SPLINE_SURFACE(3,2,((#79936,#79937,#79938),(#79939,#79940,#79941),(#79942,
#79943,#79944),(#79945,#79946,#79947),(#79948,#79949,#79950),(#79951,#79952,
#79953),(#79954,#79955,#79956),(#79957,#79958,#79959),(#79960,#79961,#79962),
(#79963,#79964,#79965),(#79966,#79967,#79968),(#79969,#79970,#79971),(#79972,
#79973,#79974),(#79975,#79976,#79977),(#79978,#79979,#79980),(#79981,#79982,
#79983),(#79984,#79985,#79986),(#79987,#79988,#79989),(#79990,#79991,#79992),
(#79993,#79994,#79995),(#79996,#79997,#79998),(#79999,#80000,#80001),(#80002,
#80003,#80004),(#80005,#80006,#80007),(#80008,#80009,#80010),(#80011,#80012,
#80013)),.UNSPECIFIED.,.F.,.F.,.F.)
B_SPLINE_SURFACE_WITH_KNOTS((4,2,2,2,2,2,2,2,2,2,2,2,4),(3,3),(0.0594208250393089,
0.0624427293703808,0.0654646337014528,0.0684865380325247,0.0715084423635966,
0.0745303466946686,0.0775522510257405,0.0835960596878844,0.0896398683500283,
0.0956836770121721,0.101727485674316,0.104749390005388,0.10777129433646),
(0.,1.),.UNSPECIFIED.)
GEOMETRIC_REPRESENTATION_ITEM()
RATIONAL_B_SPLINE_SURFACE(((1.,0.910520832001509,1.),(1.,0.9105597736334,
1.),(1.,0.910319336406336,1.),(1.,0.908142721689739,1.),(1.,0.906245529262798,
1.),(1.,0.901234434942702,1.),(1.,0.898144388409968,1.),(1.,0.891406127314929,
1.),(1.,0.887761424599258,1.),(1.,0.880392731230951,1.),(1.,0.876718575830069,
1.),(1.,0.869691185417515,1.),(1.,0.866327693994065,1.),(1.,0.856764909704854,
1.),(1.,0.851141864877978,1.),(1.,0.840201694261591,1.),(1.,0.834927827340277,
1.),(1.,0.822462805562699,1.),(1.,0.815237195282872,1.),(1.,0.796337704941202,
1.),(1.,0.784465640270227,1.),(1.,0.763309807388115,1.),(1.,0.755741399790356,
1.),(1.,0.740595302762885,1.),(1.,0.733036463112068,1.),(1.,0.726414797481264,
1.)))
REPRESENTATION_ITEM('')
SURFACE()
);
#1534=(
BOUNDED_SURFACE()
B_SPLINE_SURFACE(3,2,((#80259,#80260,#80261),(#80262,#80263,#80264),(#80265,
#80266,#80267),(#80268,#80269,#80270),(#80271,#80272,#80273),(#80274,#80275,
#80276),(#80277,#80278,#80279),(#80280,#80281,#80282),(#80283,#80284,#80285),
(#80286,#80287,#80288),(#80289,#80290,#80291),(#80292,#80293,#80294),(#80295,
#80296,#80297),(#80298,#80299,#80300),(#80301,#80302,#80303),(#80304,#80305,
#80306),(#80307,#80308,#80309),(#80310,#80311,#80312),(#80313,#80314,#80315),
(#80316,#80317,#80318),(#80319,#80320,#80321),(#80322,#80323,#80324),(#80325,
#80326,#80327),(#80328,#80329,#80330)),.UNSPECIFIED.,.F.,.F.,.F.)
B_SPLINE_SURFACE_WITH_KNOTS((4,2,2,2,2,2,2,2,2,2,2,4),(3,3),(0.0606605585620472,
0.0636555247412189,0.0666504909203906,0.0696454570995622,0.0726404232787339,
0.0786303556370772,0.0846202879954206,0.0906102203537639,0.0966001527121072,
0.102590085070451,0.105585051249622,0.108580017428794),(0.,1.),
 .UNSPECIFIED.)
GEOMETRIC_REPRESENTATION_ITEM()
RATIONAL_B_SPLINE_SURFACE(((1.,0.910520832008251,1.),(1.,0.910557149201625,
1.),(1.,0.910326426062521,1.),(1.,0.908197427220197,1.),(1.,0.906334049728144,
1.),(1.,0.901360304418425,1.),(1.,0.898273108952946,1.),(1.,0.891491725305196,
1.),(1.,0.887782421911941,1.),(1.,0.876777623836887,1.),(1.,0.869626693180036,
1.),(1.,0.856891658692805,1.),(1.,0.851262654293129,1.),(1.,0.8403112833867,
1.),(1.,0.835034820594825,1.),(1.,0.822574702116822,1.),(1.,0.815355066496494,
1.),(1.,0.796454715054513,1.),(1.,0.784574360623197,1.),(1.,0.763378174579001,
1.),(1.,0.755789676929053,1.),(1.,0.740619606484873,1.),(1.,0.733047686471531,
1.),(1.,0.726415577619866,1.)))
REPRESENTATION_ITEM('')
SURFACE()
);
#1535=(
BOUNDED_SURFACE()
B_SPLINE_SURFACE(3,2,((#82000,#82001,#82002),(#82003,#82004,#82005),(#82006,
#82007,#82008),(#82009,#82010,#82011)),.UNSPECIFIED.,.F.,.F.,.F.)
B_SPLINE_SURFACE_WITH_KNOTS((4,4),(3,3),(0.216396890133946,0.218669589029756),
(-1.61816610990125E-8,1.00000001618164),.UNSPECIFIED.)
GEOMETRIC_REPRESENTATION_ITEM()
RATIONAL_B_SPLINE_SURFACE(((1.00000000633075,0.804385064253204,1.00000000633074),
(1.0000000063304,0.804395878645463,1.00000000633039),(1.00000000633075,
0.804385034103866,1.00000000633074),(1.00000000632997,0.804409130794161,
1.00000000632996)))
REPRESENTATION_ITEM('')
SURFACE()
);
#1536=(
BOUNDED_SURFACE()
B_SPLINE_SURFACE(3,2,((#82049,#82050,#82051),(#82052,#82053,#82054),(#82055,
#82056,#82057),(#82058,#82059,#82060),(#82061,#82062,#82063),(#82064,#82065,
#82066),(#82067,#82068,#82069),(#82070,#82071,#82072),(#82073,#82074,#82075),
(#82076,#82077,#82078),(#82079,#82080,#82081),(#82082,#82083,#82084),(#82085,
#82086,#82087),(#82088,#82089,#82090),(#82091,#82092,#82093),(#82094,#82095,
#82096),(#82097,#82098,#82099),(#82100,#82101,#82102),(#82103,#82104,#82105),
(#82106,#82107,#82108),(#82109,#82110,#82111),(#82112,#82113,#82114),(#82115,
#82116,#82117),(#82118,#82119,#82120),(#82121,#82122,#82123),(#82124,#82125,
#82126),(#82127,#82128,#82129),(#82130,#82131,#82132),(#82133,#82134,#82135),
(#82136,#82137,#82138),(#82139,#82140,#82141),(#82142,#82143,#82144)),
 .UNSPECIFIED.,.F.,.F.,.F.)
B_SPLINE_SURFACE_WITH_KNOTS((4,2,2,2,2,2,2,2,2,2,2,2,2,2,2,4),(3,3),(0.0174491083826989,
0.0224393045100345,0.0274148701487939,0.0373660014263126,0.0473171327038314,
0.0572682639813502,0.0622438296201096,0.067219395258869,0.0721949608976284,
0.0771705265363878,0.0796583093557675,0.0821460921751472,0.0871216578139065,
0.0896094406332862,0.0920972234526659,0.0970881741758769),(-1.53850844515961E-5,
1.),.UNSPECIFIED.)
GEOMETRIC_REPRESENTATION_ITEM()
RATIONAL_B_SPLINE_SURFACE(((1.00000601573862,0.804494455691282,1.),(1.00000601347822,
0.804567916370663,1.),(1.00000598439474,0.80551310069534,1.),(1.00000592861333,
0.807325941125275,1.),(1.00000590213421,0.808186486425802,1.),(1.00000584309961,
0.8101050523979,1.),(1.00000582785138,0.810600604914554,1.),(1.00000576773212,
0.812554421336114,1.),(1.00000572109564,0.814070060616225,1.),(1.00000555112649,
0.819593889563631,1.),(1.00000542866216,0.823573859054488,1.),(1.00000517883153,
0.831693106854347,1.),(1.00000508467203,0.834753197277551,1.),(1.00000487522662,
0.841559965551597,1.),(1.00000475986163,0.845309213420213,1.),(1.00000450905516,
0.853460175211236,1.),(1.00000437351983,0.857864939115207,1.),(1.00000408592671,
0.867211430603691,1.),(1.00000393358681,0.872162326389599,1.),(1.00000370102243,
0.879720438187042,1.),(1.00000362262617,0.882268239125395,1.),(1.00000347023075,
0.887220939280501,1.),(1.00000339603593,0.889632197256966,1.),(1.00000318536523,
0.896478786368241,1.),(1.00000306133323,0.900509703409517,1.),(1.00000292228749,
0.90502855208934,1.),(1.00000288369192,0.906282870115633,1.),(1.00000282289798,
0.908258612681891,1.),(1.00000280075343,0.908978288843577,1.),(1.00000275537084,
0.910453178046207,1.),(1.00000275328214,0.910521058617971,1.),(1.000002752855,
0.910534940276836,0.999999999999999)))
REPRESENTATION_ITEM('')
SURFACE()
);
#1537=(
BOUNDED_SURFACE()
B_SPLINE_SURFACE(3,2,((#82158,#82159,#82160),(#82161,#82162,#82163),(#82164,
#82165,#82166),(#82167,#82168,#82169),(#82170,#82171,#82172),(#82173,#82174,
#82175),(#82176,#82177,#82178),(#82179,#82180,#82181),(#82182,#82183,#82184),
(#82185,#82186,#82187),(#82188,#82189,#82190),(#82191,#82192,#82193),(#82194,
#82195,#82196),(#82197,#82198,#82199),(#82200,#82201,#82202),(#82203,#82204,
#82205),(#82206,#82207,#82208),(#82209,#82210,#82211),(#82212,#82213,#82214),
(#82215,#82216,#82217),(#82218,#82219,#82220),(#82221,#82222,#82223),(#82224,
#82225,#82226),(#82227,#82228,#82229),(#82230,#82231,#82232),(#82233,#82234,
#82235),(#82236,#82237,#82238),(#82239,#82240,#82241),(#82242,#82243,#82244),
(#82245,#82246,#82247),(#82248,#82249,#82250),(#82251,#82252,#82253),(#82254,
#82255,#82256),(#82257,#82258,#82259),(#82260,#82261,#82262),(#82263,#82264,
#82265),(#82266,#82267,#82268),(#82269,#82270,#82271),(#82272,#82273,#82274),
(#82275,#82276,#82277),(#82278,#82279,#82280),(#82281,#82282,#82283)),
 .UNSPECIFIED.,.F.,.F.,.F.)
B_SPLINE_SURFACE_WITH_KNOTS((4,2,2,2,2,2,2,2,2,2,2,2,2,2,2,2,2,2,2,2,4),
(3,3),(0.0202219973471745,0.0205361900892103,0.0206932864602282,0.0208503828312461,
0.0214787683153177,0.0227355392834609,0.0252490812197474,0.0302761650923202,
0.0403303328374658,0.0503845005826114,0.060438668327757,0.0654657522003299,
0.0704928360729027,0.0755199199454755,0.0805470038180483,0.0830605457543347,
0.0855740876906211,0.0906011715631939,0.0956282554357667,0.0981417973720531,
0.10065533930834),(0.,1.),.UNSPECIFIED.)
GEOMETRIC_REPRESENTATION_ITEM()
RATIONAL_B_SPLINE_SURFACE(((1.,0.807165688592199,1.),(1.,0.806582212610433,
1.),(1.,0.805998311839245,1.),(1.,0.805121971305601,1.),(1.,0.804829775055439,
1.),(1.,0.804245234526162,1.),(1.,0.804494537678017,1.),(1.,0.804512504992895,
1.),(1.,0.804541617021244,1.),(1.,0.804665694249588,1.),(1.,0.804797226303217,
1.),(1.,0.805283123878148,1.),(1.,0.805724879158345,1.),(1.,0.807081366668598,
1.),(1.,0.807987348168922,1.),(1.,0.810007014899584,1.),(1.,0.810518600716015,
1.),(1.,0.812400911040395,1.),(1.,0.813844794272986,1.),(1.,0.819230623807962,
1.),(1.,0.823143123389045,1.),(1.,0.831181433207098,1.),(1.,0.834218469870357,
1.),(1.,0.840986673920921,1.),(1.,0.844720392224904,1.),(1.,0.852849711004914,
1.),(1.,0.85724827861479,1.),(1.,0.866596658340533,1.),(1.,0.871555644103613,
1.),(1.,0.879143902650669,1.),(1.,0.881695428003563,1.),(1.,0.886744320440305,
1.),(1.,0.88920804734286,1.),(1.,0.896192729532698,1.),(1.,0.900300234614913,
1.),(1.,0.906436112516518,1.),(1.,0.908421979022621,1.),(1.,0.909940953080824,
1.),(1.,0.910217476180097,1.),(1.,0.910507345346127,1.),(1.,0.910523722940057,
1.),(1.,0.910536186741694,1.)))
REPRESENTATION_ITEM('')
SURFACE()
);
#1538=(
BOUNDED_SURFACE()
B_SPLINE_SURFACE(3,2,((#82322,#82323,#82324),(#82325,#82326,#82327),(#82328,
#82329,#82330),(#82331,#82332,#82333)),.UNSPECIFIED.,.F.,.F.,.F.)
B_SPLINE_SURFACE_WITH_KNOTS((4,4),(3,3),(0.216508113827287,0.218767312738254),
(0.,1.),.UNSPECIFIED.)
GEOMETRIC_REPRESENTATION_ITEM()
RATIONAL_B_SPLINE_SURFACE(((1.,0.804378955100775,1.),(1.,0.804378707109012,
1.),(1.,0.804379610342439,1.),(1.,0.804401469359353,1.)))
REPRESENTATION_ITEM('')
SURFACE()
);
#1539=(
BOUNDED_SURFACE()
B_SPLINE_SURFACE(3,2,((#82334,#82335,#82336),(#82337,#82338,#82339),(#82340,
#82341,#82342),(#82343,#82344,#82345)),.UNSPECIFIED.,.F.,.F.,.F.)
B_SPLINE_SURFACE_WITH_KNOTS((4,4),(3,3),(0.10574004256303,0.205836563902916),
(-5.04238789072631E-7,1.00000050424698),.UNSPECIFIED.)
GEOMETRIC_REPRESENTATION_ITEM()
RATIONAL_B_SPLINE_SURFACE(((1.00000008857927,0.912165313998971,1.00000008858071),
(1.00000008909479,0.91165412809819,1.00000008909623),(1.00000008961932,
0.911134000853112,1.00000008962078),(1.00000009015337,0.910604444656701,
1.00000009015483)))
REPRESENTATION_ITEM('')
SURFACE()
);
#1540=(
BOUNDED_SURFACE()
B_SPLINE_SURFACE(3,2,((#82358,#82359,#82360),(#82361,#82362,#82363),(#82364,
#82365,#82366),(#82367,#82368,#82369)),.UNSPECIFIED.,.F.,.F.,.F.)
B_SPLINE_SURFACE_WITH_KNOTS((4,4),(3,3),(0.115644169265868,0.215740688922389),
(-5.04243592763465E-7,1.00000050424162),.UNSPECIFIED.)
GEOMETRIC_REPRESENTATION_ITEM()
RATIONAL_B_SPLINE_SURFACE(((1.00000009015423,0.910604444683308,1.00000009015387),
(1.00000008962018,0.911134000870471,1.00000008961982),(1.00000008909563,
0.911654128106663,1.00000008909529),(1.00000008858011,0.912165313998868,
1.00000008857976)))
REPRESENTATION_ITEM('')
SURFACE()
);
#1541=(
BOUNDED_SURFACE()
B_SPLINE_SURFACE(3,2,((#82378,#82379,#82380),(#82381,#82382,#82383),(#82384,
#82385,#82386),(#82387,#82388,#82389)),.UNSPECIFIED.,.F.,.F.,.F.)
B_SPLINE_SURFACE_WITH_KNOTS((4,4),(3,3),(0.10574004257307,0.205836562229605),
(-5.04246958612367E-7,1.00000050424698),.UNSPECIFIED.)
GEOMETRIC_REPRESENTATION_ITEM()
RATIONAL_B_SPLINE_SURFACE(((1.0000000885807,0.9121653139981,1.00000008858071),
(1.00000008909623,0.911654128105911,1.00000008909623),(1.00000008962077,
0.911134000869722,1.00000008962078),(1.00000009015483,0.910604444682528,
1.00000009015483)))
REPRESENTATION_ITEM('')
SURFACE()
);
#1542=(
BOUNDED_SURFACE()
B_SPLINE_SURFACE(3,2,((#82394,#82395,#82396),(#82397,#82398,#82399),(#82400,
#82401,#82402),(#82403,#82404,#82405)),.UNSPECIFIED.,.F.,.F.,.F.)
B_SPLINE_SURFACE_WITH_KNOTS((4,4),(3,3),(0.11564416787367,0.21574068893074),
(-5.04246457809262E-7,1.00000050424698),.UNSPECIFIED.)
GEOMETRIC_REPRESENTATION_ITEM()
RATIONAL_B_SPLINE_SURFACE(((1.00000009015474,0.910604444660476,1.00000009015483),
(1.00000008962069,0.911134000855317,1.00000008962078),(1.00000008909614,
0.911654128098913,1.00000008909623),(1.00000008858061,0.912165313998272,
1.00000008858071)))
REPRESENTATION_ITEM('')
SURFACE()
);
#1543=(
BOUNDED_SURFACE()
B_SPLINE_SURFACE(3,2,((#82662,#82663,#82664),(#82665,#82666,#82667),(#82668,
#82669,#82670),(#82671,#82672,#82673),(#82674,#82675,#82676),(#82677,#82678,
#82679),(#82680,#82681,#82682),(#82683,#82684,#82685),(#82686,#82687,#82688),
(#82689,#82690,#82691),(#82692,#82693,#82694),(#82695,#82696,#82697),(#82698,
#82699,#82700),(#82701,#82702,#82703),(#82704,#82705,#82706),(#82707,#82708,
#82709),(#82710,#82711,#82712),(#82713,#82714,#82715),(#82716,#82717,#82718),
(#82719,#82720,#82721),(#82722,#82723,#82724),(#82725,#82726,#82727),(#82728,
#82729,#82730),(#82731,#82732,#82733),(#82734,#82735,#82736),(#82737,#82738,
#82739),(#82740,#82741,#82742),(#82743,#82744,#82745),(#82746,#82747,#82748),
(#82749,#82750,#82751),(#82752,#82753,#82754),(#82755,#82756,#82757),(#82758,
#82759,#82760),(#82761,#82762,#82763),(#82764,#82765,#82766),(#82767,#82768,
#82769),(#82770,#82771,#82772),(#82773,#82774,#82775)),.UNSPECIFIED.,.F.,
 .F.,.F.)
B_SPLINE_SURFACE_WITH_KNOTS((4,2,2,2,2,2,2,2,2,2,2,2,2,2,2,2,2,2,4),(3,
3),(-0.000153005044684754,0.00487935154325309,0.00975870308650617,0.0146380546297593,
0.0195174061730123,0.0219570819446389,0.0243967577162654,0.0292761092595185,
0.0341554608027716,0.0390348123460247,0.0414744881176512,0.0439141638892778,
0.0487935154325309,0.0536728669757839,0.058552218519037,0.0634315700622901,
0.0683109216055432,0.0731902731487963,0.0782226297367341),(-0.0169255195142288,
1.00015300504468),.UNSPECIFIED.)
GEOMETRIC_REPRESENTATION_ITEM()
RATIONAL_B_SPLINE_SURFACE(((1.0100822613812,0.702111663841635,1.00008963941067),
(1.0100867902307,0.701977855424187,1.00008967967579),(1.01004679985172,
0.703159402599464,1.00008932412916),(1.00994454152905,0.706180705107466,
1.00008841497045),(1.00988572291064,0.707918547414101,1.00008789202564),
(1.00982367182762,0.709751895427783,1.00008734034161),(1.00982036137587,
0.70984970532654,1.00008731090904),(1.00991672914796,0.707002443764782,
1.00008816769602),(1.01001697409506,0.704040628020217,1.0000890589542),
(1.01025875007564,0.696897166662037,1.00009120853708),(1.0103545597349,
0.694066394982443,1.00009206036199),(1.01057160703966,0.68765356178565,
1.00009399008705),(1.01069283755543,0.684071710922103,1.00009506792382),
(1.01108293972011,0.672545835885354,1.00009853624574),(1.01137949432823,
0.663783896926268,1.00010117285466),(1.01194225591252,0.647156663644023,
1.00010617625765),(1.01220631384047,0.639354864639494,1.00010852394495),
(1.01258477234773,0.628173010611811,1.0001118887454),(1.01269712171499,
0.624853560260868,1.00011288762161),(1.01270485754633,0.624624999044277,
1.00011295639937),(1.0126812274977,0.625323167401867,1.00011274630924),
(1.01258396260394,0.628196935128459,1.00011188154612),(1.01251079042069,
0.630358864788737,1.00011123098658),(1.01223331549631,0.638557079497002,
1.00010876401139),(1.01197060246929,0.646319142346594,1.00010642828133),
(1.01140779312517,0.662947786730735,1.00010142445372),(1.01110987446146,
0.671750027784363,1.00009877571724),(1.01058580635657,0.687234031808314,
1.0000941163304),(1.01036033377541,0.693895796417769,1.00009211169785),
(1.0100292848136,0.703676898165709,1.00008916840639),(1.00992329109318,
0.706808565936043,1.00008822603699),(1.0098208881916,0.709834140141601,
1.00008731559285),(1.00982288319264,0.709775196268177,1.00008733333001),
(1.00988403419022,0.707968441985946,1.00008787701155),(1.00994325766289,
0.706218637942392,1.00008840355585),(1.01004641341464,0.703170820186587,
1.00008932069343),(1.010086856497,0.701975897534046,1.00008968026495),(1.01008225630153,
0.7021118139247,1.00008963936551)))
REPRESENTATION_ITEM('')
SURFACE()
);
#1544=(
BOUNDED_SURFACE()
B_SPLINE_SURFACE(3,2,((#82814,#82815,#82816),(#82817,#82818,#82819),(#82820,
#82821,#82822),(#82823,#82824,#82825),(#82826,#82827,#82828),(#82829,#82830,
#82831),(#82832,#82833,#82834),(#82835,#82836,#82837),(#82838,#82839,#82840),
(#82841,#82842,#82843),(#82844,#82845,#82846),(#82847,#82848,#82849),(#82850,
#82851,#82852),(#82853,#82854,#82855),(#82856,#82857,#82858),(#82859,#82860,
#82861),(#82862,#82863,#82864),(#82865,#82866,#82867),(#82868,#82869,#82870),
(#82871,#82872,#82873),(#82874,#82875,#82876),(#82877,#82878,#82879),(#82880,
#82881,#82882),(#82883,#82884,#82885),(#82886,#82887,#82888),(#82889,#82890,
#82891),(#82892,#82893,#82894),(#82895,#82896,#82897),(#82898,#82899,#82900),
(#82901,#82902,#82903),(#82904,#82905,#82906),(#82907,#82908,#82909),(#82910,
#82911,#82912),(#82913,#82914,#82915),(#82916,#82917,#82918),(#82919,#82920,
#82921),(#82922,#82923,#82924),(#82925,#82926,#82927),(#82928,#82929,#82930),
(#82931,#82932,#82933),(#82934,#82935,#82936),(#82937,#82938,#82939),(#82940,
#82941,#82942),(#82943,#82944,#82945),(#82946,#82947,#82948),(#82949,#82950,
#82951),(#82952,#82953,#82954),(#82955,#82956,#82957),(#82958,#82959,#82960),
(#82961,#82962,#82963),(#82964,#82965,#82966),(#82967,#82968,#82969),(#82970,
#82971,#82972),(#82973,#82974,#82975),(#82976,#82977,#82978),(#82979,#82980,
#82981),(#82982,#82983,#82984),(#82985,#82986,#82987),(#82988,#82989,#82990),
(#82991,#82992,#82993),(#82994,#82995,#82996),(#82997,#82998,#82999),(#83000,
#83001,#83002),(#83003,#83004,#83005),(#83006,#83007,#83008),(#83009,#83010,
#83011),(#83012,#83013,#83014),(#83015,#83016,#83017),(#83018,#83019,#83020),
(#83021,#83022,#83023),(#83024,#83025,#83026),(#83027,#83028,#83029),(#83030,
#83031,#83032),(#83033,#83034,#83035),(#83036,#83037,#83038),(#83039,#83040,
#83041),(#83042,#83043,#83044),(#83045,#83046,#83047),(#83048,#83049,#83050),
(#83051,#83052,#83053),(#83054,#83055,#83056),(#83057,#83058,#83059),(#83060,
#83061,#83062),(#83063,#83064,#83065)),.UNSPECIFIED.,.F.,.F.,.F.)
B_SPLINE_SURFACE_WITH_KNOTS((4,2,2,2,2,2,2,2,2,2,2,2,2,2,2,2,2,2,2,2,2,
2,2,2,2,2,2,2,2,2,2,2,2,2,2,2,2,2,2,2,2,4),(3,3),(0.143336734946112,0.145077233025809,
0.14676220431832,0.14844717561083,0.149289661257085,0.150132146903341,0.150974632549596,
0.151395875372724,0.151817118195851,0.152238361018979,0.152659603842107,
0.153080846665234,0.153502089488362,0.154344575134617,0.155187060780872,
0.156029546427128,0.156872032073383,0.158557003365894,0.160241974658404,
0.163611917243425,0.166981859828446,0.170351802413467,0.173721744998489,
0.17709168758351,0.180461630168531,0.182146601461041,0.183831572753552,
0.184674058399807,0.185516544046062,0.186359029692318,0.187201515338573,
0.187622758161701,0.188044000984828,0.188465243807956,0.188886486631084,
0.189728972277339,0.190571457923594,0.191413943569849,0.192256429216105,
0.193941400508615,0.195626371801126,0.197366417069027),(-5.55267871867606E-5,
1.),.UNSPECIFIED.)
GEOMETRIC_REPRESENTATION_ITEM()
RATIONAL_B_SPLINE_SURFACE(((1.0000007961373,0.992831051955489,1.),(1.00000079614004,
0.99283102735741,1.),(1.00000079610334,0.992831357779363,1.),(1.00000079553568,
0.992836469390048,1.),(1.00000079502573,0.992841061353999,1.),(1.00000079388901,
0.992851297090919,1.),(1.00000079321307,0.992857383722212,1.),(1.00000079328263,
0.992856757367858,1.),(1.00000079349646,0.992854831864327,1.),(1.00000079489792,
0.99284221223048,1.),(1.0000007960679,0.992831676885065,1.),(1.00000080065879,
0.992790337525115,1.),(1.00000080402759,0.99276000259259,1.),(1.00000081291108,
0.99268000979147,1.),(1.0000008165308,0.992647415417328,1.),(1.00000082570108,
0.992564840127059,1.),(1.00000083126436,0.992514744632364,1.),(1.00000084494363,
0.992391567460146,1.),(1.00000085308652,0.992318243506232,1.),(1.00000087193122,
0.992148553332822,1.),(1.00000088262546,0.992052255238254,1.),(1.00000090544812,
0.99184674487725,1.),(1.00000091755832,0.99173769661988,1.),(1.00000094174194,
0.9915199312853,1.),(1.00000095374568,0.991411841667855,1.),(1.0000009885794,
0.991098175741489,1.),(1.00000101018179,0.990903653484852,1.),(1.0000010498042,
0.990546867101254,1.),(1.00000106791611,0.990383775459736,1.),(1.00000110147245,
0.990081611875504,1.),(1.000001116925,0.989942466912265,1.),(1.00000114577958,
0.989682641089782,1.),(1.00000115917998,0.989561975013968,1.),(1.00000119692308,
0.989222111151196,1.),(1.00000121884368,0.98902472358164,1.),(1.0000012581359,
0.988670910349041,1.),(1.00000127548289,0.988514706508194,1.),(1.00000132214589,
0.98809452195995,1.),(1.00000134616352,0.987878251318118,1.),(1.0000013836916,
0.987540323616174,1.),(1.00000139708822,0.987419691529657,1.),(1.00000141461613,
0.987261858649905,1.),(1.00000141873575,0.987224762828979,1.),(1.00000141813951,
0.987230131741563,1.),(1.00000141342297,0.987272602591746,1.),(1.00000139474718,
0.987440771836899,1.),(1.00000138080777,0.987566291546218,1.),(1.00000134224022,
0.987913579257289,1.),(1.00000131768873,0.988134657203702,1.),(1.00000127005862,
0.98856355026087,1.),(1.00000125236095,0.988722911871249,1.),(1.00000121226484,
0.98908396376986,1.),(1.0000011898936,0.989285409256699,1.),(1.00000115132915,
0.989632669120568,1.),(1.00000113763001,0.989756025257267,1.),(1.00000110810876,
0.990021854183857,1.),(1.00000109228755,0.990164318811314,1.),(1.00000105790784,
0.990473896506666,1.),(1.00000103933542,0.990641134935092,1.),(1.00000099876335,
0.991006472756129,1.),(1.00000097663901,0.991205694949805,1.),(1.00000094145119,
0.991522549380576,1.),(1.00000092941198,0.991630958408669,1.),(1.00000090553833,
0.991845932574461,1.),(1.00000089369581,0.991952570533307,1.),(1.00000087196574,
0.992148242439595,1.),(1.00000086207814,0.992237276976211,1.),(1.00000084501282,
0.992390944434512,1.),(1.0000008378228,0.992455688157901,1.),(1.00000081985816,
0.992617453680996,1.),(1.00000081255367,0.992683228105805,1.),(1.0000008023705,
0.992774924164358,1.),(1.00000079947944,0.992800957134375,1.),(1.00000079555182,
0.992836324009601,1.),(1.00000079455633,0.992845288063244,1.),(1.00000079339196,
0.992855772879035,1.),(1.00000079324102,0.992857132057369,1.),(1.00000079329672,
0.992856630423569,1.),(1.00000079396815,0.992850584467251,1.),(1.00000079508137,
0.992840560290287,1.),(1.00000079556752,0.992836182715642,1.),(1.00000079610664,
0.99283132804581,1.),(1.00000079613978,0.992831029688952,1.),(1.00000079613732,
0.992831051827691,1.)))
REPRESENTATION_ITEM('')
SURFACE()
);
#1545=(
BOUNDED_SURFACE()
B_SPLINE_SURFACE(3,2,((#83553,#83554,#83555),(#83556,#83557,#83558),(#83559,
#83560,#83561),(#83562,#83563,#83564),(#83565,#83566,#83567),(#83568,#83569,
#83570),(#83571,#83572,#83573),(#83574,#83575,#83576),(#83577,#83578,#83579),
(#83580,#83581,#83582),(#83583,#83584,#83585),(#83586,#83587,#83588),(#83589,
#83590,#83591),(#83592,#83593,#83594),(#83595,#83596,#83597),(#83598,#83599,
#83600),(#83601,#83602,#83603),(#83604,#83605,#83606),(#83607,#83608,#83609),
(#83610,#83611,#83612),(#83613,#83614,#83615),(#83616,#83617,#83618),(#83619,
#83620,#83621),(#83622,#83623,#83624),(#83625,#83626,#83627),(#83628,#83629,
#83630),(#83631,#83632,#83633),(#83634,#83635,#83636),(#83637,#83638,#83639),
(#83640,#83641,#83642),(#83643,#83644,#83645),(#83646,#83647,#83648),(#83649,
#83650,#83651),(#83652,#83653,#83654),(#83655,#83656,#83657),(#83658,#83659,
#83660),(#83661,#83662,#83663),(#83664,#83665,#83666),(#83667,#83668,#83669),
(#83670,#83671,#83672),(#83673,#83674,#83675),(#83676,#83677,#83678),(#83679,
#83680,#83681),(#83682,#83683,#83684),(#83685,#83686,#83687),(#83688,#83689,
#83690)),.UNSPECIFIED.,.F.,.F.,.F.)
B_SPLINE_SURFACE_WITH_KNOTS((4,2,2,2,2,2,2,2,2,2,2,2,2,2,2,2,2,2,2,2,2,
2,4),(3,3),(0.,0.00173795884810334,0.00260693827215501,0.00347591769620668,
0.00521387654431002,0.00608285596836169,0.00695183539241337,0.00868979424051671,
0.01042775308862,0.0112967325126717,0.0121657119367234,0.0139036707848267,
0.0147726502088784,0.0156416296329301,0.0173795884810334,0.0191175473291368,
0.0199865267531884,0.0208555061772401,0.0225934650253434,0.0234624444493951,
0.0243314238734468,0.0260693827215501,0.0278073415696535),(0.,1.),
 .UNSPECIFIED.)
GEOMETRIC_REPRESENTATION_ITEM()
RATIONAL_B_SPLINE_SURFACE(((1.,0.548774182857018,1.),(1.,0.548893499031212,
1.),(1.,0.551454790284224,1.),(1.,0.558414139525284,1.),(1.,0.561252468336352,
1.),(1.,0.567859325258193,1.),(1.,0.571621573059519,1.),(1.,0.583808409735634,
1.),(1.,0.593194455071645,1.),(1.,0.608188368401722,1.),(1.,0.613360873897966,
1.),(1.,0.62366572039419,1.),(1.,0.628817963503084,1.),(1.,0.644073171070199,
1.),(1.,0.654001656968634,1.),(1.,0.67225025019413,1.),(1.,0.68032620635555,
1.),(1.,0.690419184626026,1.),(1.,0.693446892845268,1.),(1.,0.698746884637556,
1.),(1.,0.7010212029547,1.),(1.,0.70645959379097,1.),(1.,0.708316472383437,
1.),(1.,0.70835119300799,1.),(1.,0.70789791374197,1.),(1.,0.706062313929642,
1.),(1.,0.70469165429023,1.),(1.,0.699305887702423,1.),(1.,0.69401802314486,
1.),(1.,0.680392676022202,1.),(1.,0.672280667494579,1.),(1.,0.658740368498969,
1.),(1.,0.653997319012882,1.),(1.,0.644149376735424,1.),(1.,0.639064976044898,
1.),(1.,0.623754379898659,1.),(1.,0.613373212611566,1.),(1.,0.598394950949806,
1.),(1.,0.593477175295379,1.),(1.,0.584180333306127,1.),(1.,0.579796878582778,
1.),(1.,0.567666674638681,1.),(1.,0.560935688280663,1.),(1.,0.551485305881092,
1.),(1.,0.548874864843112,1.),(1.,0.548774182857018,1.)))
REPRESENTATION_ITEM('')
SURFACE()
);
#1546=(
BOUNDED_SURFACE()
B_SPLINE_SURFACE(2,3,((#84213,#84214,#84215,#84216),(#84217,#84218,#84219,
#84220),(#84221,#84222,#84223,#84224)),.UNSPECIFIED.,.F.,.F.,.F.)
B_SPLINE_SURFACE_WITH_KNOTS((3,3),(4,4),(0.119519500000458,0.283084102927177),
(0.,1.),.UNSPECIFIED.)
GEOMETRIC_REPRESENTATION_ITEM()
RATIONAL_B_SPLINE_SURFACE(((1.,0.999857616157758,0.999857616157758,1.),
(1.,0.999857616157758,0.999857616157758,1.),(1.,0.999857616157758,0.999857616157758,
1.)))
REPRESENTATION_ITEM('')
SURFACE()
);
#1547=(
BOUNDED_SURFACE()
B_SPLINE_SURFACE(2,3,((#84226,#84227,#84228,#84229),(#84230,#84231,#84232,
#84233),(#84234,#84235,#84236,#84237)),.UNSPECIFIED.,.F.,.F.,.F.)
B_SPLINE_SURFACE_WITH_KNOTS((3,3),(4,4),(0.446518847929411,0.592183392830318),
(0.,1.),.UNSPECIFIED.)
GEOMETRIC_REPRESENTATION_ITEM()
RATIONAL_B_SPLINE_SURFACE(((1.,0.999895190835713,0.999895190835713,1.),
(1.,0.999895190835713,0.999895190835713,1.),(1.,0.999895190835713,0.999895190835713,
1.)))
REPRESENTATION_ITEM('')
SURFACE()
);
#1548=(
BOUNDED_SURFACE()
B_SPLINE_SURFACE(2,3,((#84239,#84240,#84241,#84242),(#84243,#84244,#84245,
#84246),(#84247,#84248,#84249,#84250)),.UNSPECIFIED.,.F.,.F.,.F.)
B_SPLINE_SURFACE_WITH_KNOTS((3,3),(4,4),(0.444107179195925,0.589622570294522),
(0.,1.),.UNSPECIFIED.)
GEOMETRIC_REPRESENTATION_ITEM()
RATIONAL_B_SPLINE_SURFACE(((1.,0.999894134350414,0.999894134350414,1.),
(1.,0.999894134350414,0.999894134350414,1.),(1.,0.999894134350414,0.999894134350414,
1.)))
REPRESENTATION_ITEM('')
SURFACE()
);
#1549=(
BOUNDED_SURFACE()
B_SPLINE_SURFACE(2,3,((#84252,#84253,#84254,#84255),(#84256,#84257,#84258,
#84259),(#84260,#84261,#84262,#84263)),.UNSPECIFIED.,.F.,.F.,.F.)
B_SPLINE_SURFACE_WITH_KNOTS((3,3),(4,4),(0.116491116663128,0.280009921526958),
(0.,1.),.UNSPECIFIED.)
GEOMETRIC_REPRESENTATION_ITEM()
RATIONAL_B_SPLINE_SURFACE(((1.,0.999856284631683,0.999856284631683,1.),
(1.,0.999856284631683,0.999856284631683,1.),(1.,0.999856284631683,0.999856284631683,
1.)))
REPRESENTATION_ITEM('')
SURFACE()
);
#1550=(
BOUNDED_SURFACE()
B_SPLINE_SURFACE(2,3,((#84265,#84266,#84267,#84268),(#84269,#84270,#84271,
#84272),(#84273,#84274,#84275,#84276)),.UNSPECIFIED.,.F.,.F.,.F.)
B_SPLINE_SURFACE_WITH_KNOTS((3,3),(4,4),(0.4413524597824,0.586836701733118),
(0.,1.),.UNSPECIFIED.)
GEOMETRIC_REPRESENTATION_ITEM()
RATIONAL_B_SPLINE_SURFACE(((1.,0.99989457919486,0.99989457919486,1.),(1.,
0.99989457919486,0.99989457919486,1.),(1.,0.99989457919486,0.99989457919486,
1.)))
REPRESENTATION_ITEM('')
SURFACE()
);
#1551=(
BOUNDED_SURFACE()
B_SPLINE_SURFACE(2,3,((#84278,#84279,#84280,#84281),(#84282,#84283,#84284,
#84285),(#84286,#84287,#84288,#84289)),.UNSPECIFIED.,.F.,.F.,.F.)
B_SPLINE_SURFACE_WITH_KNOTS((3,3),(4,4),(0.11378820966997,0.27774209483516),
(0.,1.),.UNSPECIFIED.)
GEOMETRIC_REPRESENTATION_ITEM()
RATIONAL_B_SPLINE_SURFACE(((1.,0.99985641298154,0.99985641298154,1.),(1.,
0.99985641298154,0.99985641298154,1.),(1.,0.99985641298154,0.99985641298154,
1.)))
REPRESENTATION_ITEM('')
SURFACE()
);
#1552=(
BOUNDED_SURFACE()
B_SPLINE_SURFACE(2,3,((#84291,#84292,#84293,#84294),(#84295,#84296,#84297,
#84298),(#84299,#84300,#84301,#84302)),.UNSPECIFIED.,.F.,.F.,.F.)
B_SPLINE_SURFACE_WITH_KNOTS((3,3),(4,4),(0.439204842985634,0.585079578178692),
(0.,1.),.UNSPECIFIED.)
GEOMETRIC_REPRESENTATION_ITEM()
RATIONAL_B_SPLINE_SURFACE(((1.,0.999894006880548,0.999894006880548,1.),
(1.,0.999894006880548,0.999894006880548,1.),(1.,0.999894006880548,0.999894006880548,
1.)))
REPRESENTATION_ITEM('')
SURFACE()
);
#1553=(
BOUNDED_SURFACE()
B_SPLINE_SURFACE(2,3,((#84304,#84305,#84306,#84307),(#84308,#84309,#84310,
#84311),(#84312,#84313,#84314,#84315)),.UNSPECIFIED.,.F.,.F.,.F.)
B_SPLINE_SURFACE_WITH_KNOTS((3,3),(4,4),(0.111781170302558,0.275355623142002),
(0.,1.),.UNSPECIFIED.)
GEOMETRIC_REPRESENTATION_ITEM()
RATIONAL_B_SPLINE_SURFACE(((1.,0.999855716855875,0.999855716855875,1.),
(1.,0.999855716855875,0.999855716855875,1.),(1.,0.999855716855875,0.999855716855875,
1.)))
REPRESENTATION_ITEM('')
SURFACE()
);
#1554=(
BOUNDED_SURFACE()
B_SPLINE_SURFACE(2,3,((#84317,#84318,#84319,#84320),(#84321,#84322,#84323,
#84324),(#84325,#84326,#84327,#84328)),.UNSPECIFIED.,.F.,.F.,.F.)
B_SPLINE_SURFACE_WITH_KNOTS((3,3),(4,4),(0.437631507199148,0.58331506862024),
(0.,1.),.UNSPECIFIED.)
GEOMETRIC_REPRESENTATION_ITEM()
RATIONAL_B_SPLINE_SURFACE(((1.,0.999893875799735,0.999893875799735,1.),
(1.,0.999893875799735,0.999893875799735,1.),(1.,0.999893875799735,0.999893875799735,
1.)))
REPRESENTATION_ITEM('')
SURFACE()
);
#1555=(
BOUNDED_SURFACE()
B_SPLINE_SURFACE(2,3,((#84330,#84331,#84332,#84333),(#84334,#84335,#84336,
#84337),(#84338,#84339,#84340,#84341)),.UNSPECIFIED.,.F.,.F.,.F.)
B_SPLINE_SURFACE_WITH_KNOTS((3,3),(4,4),(0.109326350548543,0.273102821567692),
(0.,1.),.UNSPECIFIED.)
GEOMETRIC_REPRESENTATION_ITEM()
RATIONAL_B_SPLINE_SURFACE(((1.,0.999856457285684,0.999856457285684,1.),
(1.,0.999856457285684,0.999856457285684,1.),(1.,0.999856457285684,0.999856457285684,
1.)))
REPRESENTATION_ITEM('')
SURFACE()
);
#1556=(
BOUNDED_SURFACE()
B_SPLINE_SURFACE(2,3,((#84343,#84344,#84345,#84346),(#84347,#84348,#84349,
#84350),(#84351,#84352,#84353,#84354)),.UNSPECIFIED.,.F.,.F.,.F.)
B_SPLINE_SURFACE_WITH_KNOTS((3,3),(4,4),(0.4362431045186,0.582003553328225),
(0.,1.),.UNSPECIFIED.)
GEOMETRIC_REPRESENTATION_ITEM()
RATIONAL_B_SPLINE_SURFACE(((1.,0.999894314506178,0.999894314506178,1.),
(1.,0.999894314506178,0.999894314506178,1.),(1.,0.999894314506178,0.999894314506178,
1.)))
REPRESENTATION_ITEM('')
SURFACE()
);
#1557=(
BOUNDED_SURFACE()
B_SPLINE_SURFACE(2,3,((#84356,#84357,#84358,#84359),(#84360,#84361,#84362,
#84363),(#84364,#84365,#84366,#84367)),.UNSPECIFIED.,.F.,.F.,.F.)
B_SPLINE_SURFACE_WITH_KNOTS((3,3),(4,4),(0.107751460645953,0.271675591859108),
(0.,1.),.UNSPECIFIED.)
GEOMETRIC_REPRESENTATION_ITEM()
RATIONAL_B_SPLINE_SURFACE(((1.,0.999855488146839,0.999855488146839,1.),
(1.,0.999855488146839,0.999855488146839,1.),(1.,0.999855488146839,0.999855488146839,
1.)))
REPRESENTATION_ITEM('')
SURFACE()
);
#1558=(
BOUNDED_SURFACE()
B_SPLINE_SURFACE(2,3,((#84369,#84370,#84371,#84372),(#84373,#84374,#84375,
#84376),(#84377,#84378,#84379,#84380)),.UNSPECIFIED.,.F.,.F.,.F.)
B_SPLINE_SURFACE_WITH_KNOTS((3,3),(4,4),(0.435648728780737,0.581287225202112),
(0.,1.),.UNSPECIFIED.)
GEOMETRIC_REPRESENTATION_ITEM()
RATIONAL_B_SPLINE_SURFACE(((1.,0.999893801137434,0.999893801137434,1.),
(1.,0.999893801137434,0.999893801137434,1.),(1.,0.999893801137434,0.999893801137434,
1.)))
REPRESENTATION_ITEM('')
SURFACE()
);
#1559=(
BOUNDED_SURFACE()
B_SPLINE_SURFACE(2,3,((#84382,#84383,#84384,#84385),(#84386,#84387,#84388,
#84389),(#84390,#84391,#84392,#84393)),.UNSPECIFIED.,.F.,.F.,.F.)
B_SPLINE_SURFACE_WITH_KNOTS((3,3),(4,4),(0.106721261020608,0.270558651464622),
(0.,1.),.UNSPECIFIED.)
GEOMETRIC_REPRESENTATION_ITEM()
RATIONAL_B_SPLINE_SURFACE(((1.,0.999855390875252,0.999855390875252,1.),
(1.,0.999855390875252,0.999855390875252,1.),(1.,0.999855390875252,0.999855390875252,
1.)))
REPRESENTATION_ITEM('')
SURFACE()
);
#1560=(
BOUNDED_SURFACE()
B_SPLINE_SURFACE(2,3,((#84397,#84398,#84399,#84400),(#84401,#84402,#84403,
#84404),(#84405,#84406,#84407,#84408)),.UNSPECIFIED.,.F.,.F.,.F.)
B_SPLINE_SURFACE_WITH_KNOTS((3,3),(4,4),(0.435592989219888,0.580856308187753),
(0.,1.),.UNSPECIFIED.)
GEOMETRIC_REPRESENTATION_ITEM()
RATIONAL_B_SPLINE_SURFACE(((1.,0.999893836126727,0.999893836126727,1.),
(1.,0.999893836126727,0.999893836126727,1.),(1.,0.999893836126727,0.999893836126727,
1.)))
REPRESENTATION_ITEM('')
SURFACE()
);
#1561=(
BOUNDED_SURFACE()
B_SPLINE_SURFACE(2,3,((#84410,#84411,#84412,#84413),(#84414,#84415,#84416,
#84417),(#84418,#84419,#84420,#84421)),.UNSPECIFIED.,.F.,.F.,.F.)
B_SPLINE_SURFACE_WITH_KNOTS((3,3),(4,4),(0.106356611558605,0.270154561740801),
(0.,1.),.UNSPECIFIED.)
GEOMETRIC_REPRESENTATION_ITEM()
RATIONAL_B_SPLINE_SURFACE(((1.,0.999856152844613,0.999856152844613,1.),
(1.,0.999856152844613,0.999856152844613,1.),(1.,0.999856152844613,0.999856152844613,
1.)))
REPRESENTATION_ITEM('')
SURFACE()
);
#1562=(
BOUNDED_SURFACE()
B_SPLINE_SURFACE(2,3,((#84425,#84426,#84427,#84428),(#84429,#84430,#84431,
#84432),(#84433,#84434,#84435,#84436)),.UNSPECIFIED.,.F.,.F.,.F.)
B_SPLINE_SURFACE_WITH_KNOTS((3,3),(4,4),(0.435593699966305,0.581365752295347),
(0.,1.),.UNSPECIFIED.)
GEOMETRIC_REPRESENTATION_ITEM()
RATIONAL_B_SPLINE_SURFACE(((1.,0.999894372975926,0.999894372975926,1.),
(1.,0.999894372975926,0.999894372975926,1.),(1.,0.999894372975926,0.999894372975926,
1.)))
REPRESENTATION_ITEM('')
SURFACE()
);
#1563=(
BOUNDED_SURFACE()
B_SPLINE_SURFACE(2,3,((#84438,#84439,#84440,#84441),(#84442,#84443,#84444,
#84445),(#84446,#84447,#84448,#84449)),.UNSPECIFIED.,.F.,.F.,.F.)
B_SPLINE_SURFACE_WITH_KNOTS((3,3),(4,4),(0.10645020218376,0.269987102818262),
(0.,1.),.UNSPECIFIED.)
GEOMETRIC_REPRESENTATION_ITEM()
RATIONAL_B_SPLINE_SURFACE(((1.,0.999855425942098,0.999855425942098,1.),
(1.,0.999855425942098,0.999855425942098,1.),(1.,0.999855425942098,0.999855425942098,
1.)))
REPRESENTATION_ITEM('')
SURFACE()
);
#1564=(
BOUNDED_SURFACE()
B_SPLINE_SURFACE(2,3,((#84455,#84456,#84457,#84458),(#84459,#84460,#84461,
#84462),(#84463,#84464,#84465,#84466)),.UNSPECIFIED.,.F.,.F.,.F.)
B_SPLINE_SURFACE_WITH_KNOTS((3,3),(4,4),(0.43676522787172,0.582408838010634),
(0.,1.),.UNSPECIFIED.)
GEOMETRIC_REPRESENTATION_ITEM()
RATIONAL_B_SPLINE_SURFACE(((1.,0.999893765134106,0.999893765134106,1.),
(1.,0.999893765134106,0.999893765134106,1.),(1.,0.999893765134106,0.999893765134106,
1.)))
REPRESENTATION_ITEM('')
SURFACE()
);
#1565=(
BOUNDED_SURFACE()
B_SPLINE_SURFACE(2,3,((#84468,#84469,#84470,#84471),(#84472,#84473,#84474,
#84475),(#84476,#84477,#84478,#84479)),.UNSPECIFIED.,.F.,.F.,.F.)
B_SPLINE_SURFACE_WITH_KNOTS((3,3),(4,4),(0.106848672671777,0.270925177669003),
(0.,1.),.UNSPECIFIED.)
GEOMETRIC_REPRESENTATION_ITEM()
RATIONAL_B_SPLINE_SURFACE(((1.,0.999855651237632,0.999855651237632,1.),
(1.,0.999855651237632,0.999855651237632,1.),(1.,0.999855651237632,0.999855651237632,
1.)))
REPRESENTATION_ITEM('')
SURFACE()
);
#1566=(
BOUNDED_SURFACE()
B_SPLINE_SURFACE(2,3,((#84485,#84486,#84487,#84488),(#84489,#84490,#84491,
#84492),(#84493,#84494,#84495,#84496)),.UNSPECIFIED.,.F.,.F.,.F.)
B_SPLINE_SURFACE_WITH_KNOTS((3,3),(4,4),(0.437930879651441,0.583845036959533),
(0.,1.),.UNSPECIFIED.)
GEOMETRIC_REPRESENTATION_ITEM()
RATIONAL_B_SPLINE_SURFACE(((1.,0.999894219919845,0.999894219919845,1.),
(1.,0.999894219919845,0.999894219919845,1.),(1.,0.999894219919845,0.999894219919845,
1.)))
REPRESENTATION_ITEM('')
SURFACE()
);
#1567=(
BOUNDED_SURFACE()
B_SPLINE_SURFACE(2,3,((#84498,#84499,#84500,#84501),(#84502,#84503,#84504,
#84505),(#84506,#84507,#84508,#84509)),.UNSPECIFIED.,.F.,.F.,.F.)
B_SPLINE_SURFACE_WITH_KNOTS((3,3),(4,4),(0.108080512552553,0.271754524433647),
(0.,1.),.UNSPECIFIED.)
GEOMETRIC_REPRESENTATION_ITEM()
RATIONAL_B_SPLINE_SURFACE(((1.,0.999855950268206,0.999855950268206,1.),
(1.,0.999855950268206,0.999855950268206,1.),(1.,0.999855950268206,0.999855950268206,
1.)))
REPRESENTATION_ITEM('')
SURFACE()
);
#1568=(
BOUNDED_SURFACE()
B_SPLINE_SURFACE(2,3,((#84511,#84512,#84513,#84514),(#84515,#84516,#84517,
#84518),(#84519,#84520,#84521,#84522)),.UNSPECIFIED.,.F.,.F.,.F.)
B_SPLINE_SURFACE_WITH_KNOTS((3,3),(4,4),(0.439818550318335,0.585360171796468),
(0.,1.),.UNSPECIFIED.)
GEOMETRIC_REPRESENTATION_ITEM()
RATIONAL_B_SPLINE_SURFACE(((1.,0.999894184107649,0.999894184107649,1.),
(1.,0.999894184107649,0.999894184107649,1.),(1.,0.999894184107649,0.999894184107649,
1.)))
REPRESENTATION_ITEM('')
SURFACE()
);
#1569=(
BOUNDED_SURFACE()
B_SPLINE_SURFACE(2,3,((#84524,#84525,#84526,#84527),(#84528,#84529,#84530,
#84531),(#84532,#84533,#84534,#84535)),.UNSPECIFIED.,.F.,.F.,.F.)
B_SPLINE_SURFACE_WITH_KNOTS((3,3),(4,4),(0.110237303004777,0.27386314548445),
(0.,1.),.UNSPECIFIED.)
GEOMETRIC_REPRESENTATION_ITEM()
RATIONAL_B_SPLINE_SURFACE(((1.,0.999855610234961,0.999855610234961,1.),
(1.,0.999855610234961,0.999855610234961,1.),(1.,0.999855610234961,0.999855610234961,
1.)))
REPRESENTATION_ITEM('')
SURFACE()
);
#1570=(
BOUNDED_SURFACE()
B_SPLINE_SURFACE(2,3,((#84537,#84538,#84539,#84540),(#84541,#84542,#84543,
#84544),(#84545,#84546,#84547,#84548)),.UNSPECIFIED.,.F.,.F.,.F.)
B_SPLINE_SURFACE_WITH_KNOTS((3,3),(4,4),(0.442417506739257,0.587930688159455),
(0.,1.),.UNSPECIFIED.)
GEOMETRIC_REPRESENTATION_ITEM()
RATIONAL_B_SPLINE_SURFACE(((1.,0.999894126686531,0.999894126686531,1.),
(1.,0.999894126686531,0.999894126686531,1.),(1.,0.999894126686531,0.999894126686531,
1.)))
REPRESENTATION_ITEM('')
SURFACE()
);
#1571=(
BOUNDED_SURFACE()
B_SPLINE_SURFACE(2,3,((#84550,#84551,#84552,#84553),(#84554,#84555,#84556,
#84557),(#84558,#84559,#84560,#84561)),.UNSPECIFIED.,.F.,.F.,.F.)
B_SPLINE_SURFACE_WITH_KNOTS((3,3),(4,4),(0.112034372975308,0.275982742979846),
(0.,1.),.UNSPECIFIED.)
GEOMETRIC_REPRESENTATION_ITEM()
RATIONAL_B_SPLINE_SURFACE(((1.,0.99985664856181,0.99985664856181,1.),(1.,
0.99985664856181,0.99985664856181,1.),(1.,0.99985664856181,0.99985664856181,
1.)))
REPRESENTATION_ITEM('')
SURFACE()
);
#1572=(
BOUNDED_SURFACE()
B_SPLINE_SURFACE(2,3,((#84563,#84564,#84565,#84566),(#84567,#84568,#84569,
#84570),(#84571,#84572,#84573,#84574)),.UNSPECIFIED.,.F.,.F.,.F.)
B_SPLINE_SURFACE_WITH_KNOTS((3,3),(4,4),(0.444647530372542,0.590398629876671),
(0.,1.),.UNSPECIFIED.)
GEOMETRIC_REPRESENTATION_ITEM()
RATIONAL_B_SPLINE_SURFACE(((1.,0.999894743750065,0.999894743750065,1.),
(1.,0.999894743750065,0.999894743750065,1.),(1.,0.999894743750065,0.999894743750065,
1.)))
REPRESENTATION_ITEM('')
SURFACE()
);
#1573=(
BOUNDED_SURFACE()
B_SPLINE_SURFACE(2,3,((#84576,#84577,#84578,#84579),(#84580,#84581,#84582,
#84583),(#84584,#84585,#84586,#84587)),.UNSPECIFIED.,.F.,.F.,.F.)
B_SPLINE_SURFACE_WITH_KNOTS((3,3),(4,4),(0.114586911656446,0.278222488663965),
(0.,1.),.UNSPECIFIED.)
GEOMETRIC_REPRESENTATION_ITEM()
RATIONAL_B_SPLINE_SURFACE(((1.,0.99985598038009,0.99985598038009,1.),(1.,
0.99985598038009,0.99985598038009,1.),(1.,0.99985598038009,0.99985598038009,
1.)))
REPRESENTATION_ITEM('')
SURFACE()
);
#1574=(
BOUNDED_SURFACE()
B_SPLINE_SURFACE(2,3,((#84589,#84590,#84591,#84592),(#84593,#84594,#84595,
#84596),(#84597,#84598,#84599,#84600)),.UNSPECIFIED.,.F.,.F.,.F.)
B_SPLINE_SURFACE_WITH_KNOTS((3,3),(4,4),(0.447384652812814,0.592887765650982),
(0.,1.),.UNSPECIFIED.)
GEOMETRIC_REPRESENTATION_ITEM()
RATIONAL_B_SPLINE_SURFACE(((1.,0.999894664792425,0.999894664792425,1.),
(1.,0.999894664792425,0.999894664792425,1.),(1.,0.999894664792425,0.999894664792425,
1.)))
REPRESENTATION_ITEM('')
SURFACE()
);
#1575=(
BOUNDED_SURFACE()
B_SPLINE_SURFACE(2,3,((#84602,#84603,#84604,#84605),(#84606,#84607,#84608,
#84609),(#84610,#84611,#84612,#84613)),.UNSPECIFIED.,.F.,.F.,.F.)
B_SPLINE_SURFACE_WITH_KNOTS((3,3),(4,4),(0.117361364034985,0.281017412150302),
(0.,1.),.UNSPECIFIED.)
GEOMETRIC_REPRESENTATION_ITEM()
RATIONAL_B_SPLINE_SURFACE(((1.,0.99985654046593,0.99985654046593,1.),(1.,
0.99985654046593,0.99985654046593,1.),(1.,0.99985654046593,0.99985654046593,
1.)))
REPRESENTATION_ITEM('')
SURFACE()
);
#1576=(
BOUNDED_SURFACE()
B_SPLINE_SURFACE(2,3,((#84615,#84616,#84617,#84618),(#84619,#84620,#84621,
#84622),(#84623,#84624,#84625,#84626)),.UNSPECIFIED.,.F.,.F.,.F.)
B_SPLINE_SURFACE_WITH_KNOTS((3,3),(4,4),(0.450061410330926,0.59563674968253),
(0.,1.),.UNSPECIFIED.)
GEOMETRIC_REPRESENTATION_ITEM()
RATIONAL_B_SPLINE_SURFACE(((1.,0.999895034648578,0.999895034648578,1.),
(1.,0.999895034648578,0.999895034648578,1.),(1.,0.999895034648578,0.999895034648578,
1.)))
REPRESENTATION_ITEM('')
SURFACE()
);
#1577=(
BOUNDED_SURFACE()
B_SPLINE_SURFACE(2,3,((#84628,#84629,#84630,#84631),(#84632,#84633,#84634,
#84635),(#84636,#84637,#84638,#84639)),.UNSPECIFIED.,.F.,.F.,.F.)
B_SPLINE_SURFACE_WITH_KNOTS((3,3),(4,4),(0.120146383290712,0.283727976150696),
(0.,1.),.UNSPECIFIED.)
GEOMETRIC_REPRESENTATION_ITEM()
RATIONAL_B_SPLINE_SURFACE(((1.,0.999857826216213,0.999857826216213,1.),
(1.,0.999857826216213,0.999857826216213,1.),(1.,0.999857826216213,0.999857826216213,
1.)))
REPRESENTATION_ITEM('')
SURFACE()
);
#1578=(
BOUNDED_SURFACE()
B_SPLINE_SURFACE(2,3,((#84641,#84642,#84643,#84644),(#84645,#84646,#84647,
#84648),(#84649,#84650,#84651,#84652)),.UNSPECIFIED.,.F.,.F.,.F.)
B_SPLINE_SURFACE_WITH_KNOTS((3,3),(4,4),(0.452662415799281,0.598065007501956),
(0.,1.),.UNSPECIFIED.)
GEOMETRIC_REPRESENTATION_ITEM()
RATIONAL_B_SPLINE_SURFACE(((1.,0.999894544464411,0.999894544464411,1.),
(1.,0.999894544464411,0.999894544464411,1.),(1.,0.999894544464411,0.999894544464411,
1.)))
REPRESENTATION_ITEM('')
SURFACE()
);
#1579=(
BOUNDED_SURFACE()
B_SPLINE_SURFACE(2,3,((#84654,#84655,#84656,#84657),(#84658,#84659,#84660,
#84661),(#84662,#84663,#84664,#84665)),.UNSPECIFIED.,.F.,.F.,.F.)
B_SPLINE_SURFACE_WITH_KNOTS((3,3),(4,4),(0.123248945302883,0.286626574700324),
(0.,1.),.UNSPECIFIED.)
GEOMETRIC_REPRESENTATION_ITEM()
RATIONAL_B_SPLINE_SURFACE(((1.,0.999857334762909,0.999857334762909,1.),
(1.,0.999857334762909,0.999857334762909,1.),(1.,0.999857334762909,0.999857334762909,
1.)))
REPRESENTATION_ITEM('')
SURFACE()
);
#1580=(
BOUNDED_SURFACE()
B_SPLINE_SURFACE(2,3,((#84667,#84668,#84669,#84670),(#84671,#84672,#84673,
#84674),(#84675,#84676,#84677,#84678)),.UNSPECIFIED.,.F.,.F.,.F.)
B_SPLINE_SURFACE_WITH_KNOTS((3,3),(4,4),(0.455532155630731,0.600703145607525),
(0.,1.),.UNSPECIFIED.)
GEOMETRIC_REPRESENTATION_ITEM()
RATIONAL_B_SPLINE_SURFACE(((1.,0.999895073920667,0.999895073920667,1.),
(1.,0.999895073920667,0.999895073920667,1.),(1.,0.999895073920667,0.999895073920667,
1.)))
REPRESENTATION_ITEM('')
SURFACE()
);
#1581=(
BOUNDED_SURFACE()
B_SPLINE_SURFACE(2,3,((#84680,#84681,#84682,#84683),(#84684,#84685,#84686,
#84687),(#84688,#84689,#84690,#84691)),.UNSPECIFIED.,.F.,.F.,.F.)
B_SPLINE_SURFACE_WITH_KNOTS((3,3),(4,4),(0.125578640126081,0.289268722273738),
(0.,1.),.UNSPECIFIED.)
GEOMETRIC_REPRESENTATION_ITEM()
RATIONAL_B_SPLINE_SURFACE(((1.,0.999857143537026,0.999857143537026,1.),
(1.,0.999857143537026,0.999857143537026,1.),(1.,0.999857143537026,0.999857143537026,
1.)))
REPRESENTATION_ITEM('')
SURFACE()
);
#1582=(
BOUNDED_SURFACE()
B_SPLINE_SURFACE(2,3,((#84693,#84694,#84695,#84696),(#84697,#84698,#84699,
#84700),(#84701,#84702,#84703,#84704)),.UNSPECIFIED.,.F.,.F.,.F.)
B_SPLINE_SURFACE_WITH_KNOTS((3,3),(4,4),(0.45725674537802,0.602810602402847),
(0.,1.),.UNSPECIFIED.)
GEOMETRIC_REPRESENTATION_ITEM()
RATIONAL_B_SPLINE_SURFACE(((1.,0.999895364461255,0.999895364461255,1.),
(1.,0.999895364461255,0.999895364461255,1.),(1.,0.999895364461255,0.999895364461255,
1.)))
REPRESENTATION_ITEM('')
SURFACE()
);
#1583=(
BOUNDED_SURFACE()
B_SPLINE_SURFACE(2,3,((#84706,#84707,#84708,#84709),(#84710,#84711,#84712,
#84713),(#84714,#84715,#84716,#84717)),.UNSPECIFIED.,.F.,.F.,.F.)
B_SPLINE_SURFACE_WITH_KNOTS((3,3),(4,4),(0.128000754786,0.291182820426702),
(0.,1.),.UNSPECIFIED.)
GEOMETRIC_REPRESENTATION_ITEM()
RATIONAL_B_SPLINE_SURFACE(((1.,0.999856825985705,0.999856825985705,1.),
(1.,0.999856825985705,0.999856825985705,1.),(1.,0.999856825985705,0.999856825985705,
1.)))
REPRESENTATION_ITEM('')
SURFACE()
);
#1584=(
BOUNDED_SURFACE()
B_SPLINE_SURFACE(2,3,((#84719,#84720,#84721,#84722),(#84723,#84724,#84725,
#84726),(#84727,#84728,#84729,#84730)),.UNSPECIFIED.,.F.,.F.,.F.)
B_SPLINE_SURFACE_WITH_KNOTS((3,3),(4,4),(0.459038110287163,0.604290998985184),
(0.,1.),.UNSPECIFIED.)
GEOMETRIC_REPRESENTATION_ITEM()
RATIONAL_B_SPLINE_SURFACE(((1.,0.999895063286365,0.999895063286365,1.),
(1.,0.999895063286365,0.999895063286365,1.),(1.,0.999895063286365,0.999895063286365,
1.)))
REPRESENTATION_ITEM('')
SURFACE()
);
#1585=(
BOUNDED_SURFACE()
B_SPLINE_SURFACE(2,3,((#84732,#84733,#84734,#84735),(#84736,#84737,#84738,
#84739),(#84740,#84741,#84742,#84743)),.UNSPECIFIED.,.F.,.F.,.F.)
B_SPLINE_SURFACE_WITH_KNOTS((3,3),(4,4),(0.130338341892577,0.293624277563459),
(0.,1.),.UNSPECIFIED.)
GEOMETRIC_REPRESENTATION_ITEM()
RATIONAL_B_SPLINE_SURFACE(((1.,0.99985730936314,0.99985730936314,1.),(1.,
0.99985730936314,0.99985730936314,1.),(1.,0.99985730936314,0.99985730936314,
1.)))
REPRESENTATION_ITEM('')
SURFACE()
);
#1586=(
BOUNDED_SURFACE()
B_SPLINE_SURFACE(2,3,((#84745,#84746,#84747,#84748),(#84749,#84750,#84751,
#84752),(#84753,#84754,#84755,#84756)),.UNSPECIFIED.,.F.,.F.,.F.)
B_SPLINE_SURFACE_WITH_KNOTS((3,3),(4,4),(0.46039588922153,0.605713534640108),
(0.,1.),.UNSPECIFIED.)
GEOMETRIC_REPRESENTATION_ITEM()
RATIONAL_B_SPLINE_SURFACE(((1.,0.999895090466177,0.999895090466177,1.),
(1.,0.999895090466177,0.999895090466177,1.),(1.,0.999895090466177,0.999895090466177,
1.)))
REPRESENTATION_ITEM('')
SURFACE()
);
#1587=(
BOUNDED_SURFACE()
B_SPLINE_SURFACE(2,3,((#84758,#84759,#84760,#84761),(#84762,#84763,#84764,
#84765),(#84766,#84767,#84768,#84769)),.UNSPECIFIED.,.F.,.F.,.F.)
B_SPLINE_SURFACE_WITH_KNOTS((3,3),(4,4),(0.131726348549557,0.295159314599406),
(0.,1.),.UNSPECIFIED.)
GEOMETRIC_REPRESENTATION_ITEM()
RATIONAL_B_SPLINE_SURFACE(((1.,0.999857853682077,0.999857853682077,1.),
(1.,0.999857853682077,0.999857853682077,1.),(1.,0.999857853682077,0.999857853682077,
1.)))
REPRESENTATION_ITEM('')
SURFACE()
);
#1588=(
BOUNDED_SURFACE()
B_SPLINE_SURFACE(2,3,((#84771,#84772,#84773,#84774),(#84775,#84776,#84777,
#84778),(#84779,#84780,#84781,#84782)),.UNSPECIFIED.,.F.,.F.,.F.)
B_SPLINE_SURFACE_WITH_KNOTS((3,3),(4,4),(0.461107076972092,0.606286854344933),
(0.,1.),.UNSPECIFIED.)
GEOMETRIC_REPRESENTATION_ITEM()
RATIONAL_B_SPLINE_SURFACE(((1.,0.999895120190421,0.999895120190421,1.),
(1.,0.999895120190421,0.999895120190421,1.),(1.,0.999895120190421,0.999895120190421,
1.)))
REPRESENTATION_ITEM('')
SURFACE()
);
#1589=(
BOUNDED_SURFACE()
B_SPLINE_SURFACE(2,3,((#84784,#84785,#84786,#84787),(#84788,#84789,#84790,
#84791),(#84792,#84793,#84794,#84795)),.UNSPECIFIED.,.F.,.F.,.F.)
B_SPLINE_SURFACE_WITH_KNOTS((3,3),(4,4),(0.132862776548585,0.29611733043446),
(0.,1.),.UNSPECIFIED.)
GEOMETRIC_REPRESENTATION_ITEM()
RATIONAL_B_SPLINE_SURFACE(((1.,0.999857587798397,0.999857587798397,1.),
(1.,0.999857587798397,0.999857587798397,1.),(1.,0.999857587798397,0.999857587798397,
1.)))
REPRESENTATION_ITEM('')
SURFACE()
);
#1590=(
BOUNDED_SURFACE()
B_SPLINE_SURFACE(2,3,((#84797,#84798,#84799,#84800),(#84801,#84802,#84803,
#84804),(#84805,#84806,#84807,#84808)),.UNSPECIFIED.,.F.,.F.,.F.)
B_SPLINE_SURFACE_WITH_KNOTS((3,3),(4,4),(0.46154805509299,0.606328036429091),
(0.,1.),.UNSPECIFIED.)
GEOMETRIC_REPRESENTATION_ITEM()
RATIONAL_B_SPLINE_SURFACE(((1.,0.999895578580056,0.999895578580056,1.),
(1.,0.999895578580056,0.999895578580056,1.),(1.,0.999895578580056,0.999895578580056,
1.)))
REPRESENTATION_ITEM('')
SURFACE()
);
#1591=(
BOUNDED_SURFACE()
B_SPLINE_SURFACE(2,3,((#84810,#84811,#84812,#84813),(#84814,#84815,#84816,
#84817),(#84818,#84819,#84820,#84821)),.UNSPECIFIED.,.F.,.F.,.F.)
B_SPLINE_SURFACE_WITH_KNOTS((3,3),(4,4),(0.133282157276565,0.296502083979664),
(0.,1.),.UNSPECIFIED.)
GEOMETRIC_REPRESENTATION_ITEM()
RATIONAL_B_SPLINE_SURFACE(((1.,0.999857405537845,0.999857405537845,1.),
(1.,0.999857405537845,0.999857405537845,1.),(1.,0.999857405537845,0.999857405537845,
1.)))
REPRESENTATION_ITEM('')
SURFACE()
);
#1592=(
BOUNDED_SURFACE()
B_SPLINE_SURFACE(2,3,((#84823,#84824,#84825,#84826),(#84827,#84828,#84829,
#84830),(#84831,#84832,#84833,#84834)),.UNSPECIFIED.,.F.,.F.,.F.)
B_SPLINE_SURFACE_WITH_KNOTS((3,3),(4,4),(0.461051817256631,0.606319374173236),
(0.,1.),.UNSPECIFIED.)
GEOMETRIC_REPRESENTATION_ITEM()
RATIONAL_B_SPLINE_SURFACE(((1.,0.999895294476726,0.999895294476726,1.),
(1.,0.999895294476726,0.999895294476726,1.),(1.,0.999895294476726,0.999895294476726,
1.)))
REPRESENTATION_ITEM('')
SURFACE()
);
#1593=(
BOUNDED_SURFACE()
B_SPLINE_SURFACE(2,3,((#84836,#84837,#84838,#84839),(#84840,#84841,#84842,
#84843),(#84844,#84845,#84846,#84847)),.UNSPECIFIED.,.F.,.F.,.F.)
B_SPLINE_SURFACE_WITH_KNOTS((3,3),(4,4),(0.133462377346205,0.296408008484315),
(0.,1.),.UNSPECIFIED.)
GEOMETRIC_REPRESENTATION_ITEM()
RATIONAL_B_SPLINE_SURFACE(((1.,0.99985728327432,0.99985728327432,1.),(1.,
0.99985728327432,0.99985728327432,1.),(1.,0.99985728327432,0.99985728327432,
1.)))
REPRESENTATION_ITEM('')
SURFACE()
);
#1594=(
BOUNDED_SURFACE()
B_SPLINE_SURFACE(2,3,((#84849,#84850,#84851,#84852),(#84853,#84854,#84855,
#84856),(#84857,#84858,#84859,#84860)),.UNSPECIFIED.,.F.,.F.,.F.)
B_SPLINE_SURFACE_WITH_KNOTS((3,3),(4,4),(0.459951997369159,0.605164063679616),
(0.,1.),.UNSPECIFIED.)
GEOMETRIC_REPRESENTATION_ITEM()
RATIONAL_B_SPLINE_SURFACE(((1.,0.999894901788882,0.999894901788882,1.),
(1.,0.999894901788882,0.999894901788882,1.),(1.,0.999894901788882,0.999894901788882,
1.)))
REPRESENTATION_ITEM('')
SURFACE()
);
#1595=(
BOUNDED_SURFACE()
B_SPLINE_SURFACE(2,3,((#84862,#84863,#84864,#84865),(#84866,#84867,#84868,
#84869),(#84870,#84871,#84872,#84873)),.UNSPECIFIED.,.F.,.F.,.F.)
B_SPLINE_SURFACE_WITH_KNOTS((3,3),(4,4),(0.132492075185841,0.296014197565379),
(0.,1.),.UNSPECIFIED.)
GEOMETRIC_REPRESENTATION_ITEM()
RATIONAL_B_SPLINE_SURFACE(((1.,0.999857956642642,0.999857956642642,1.),
(1.,0.999857956642642,0.999857956642642,1.),(1.,0.999857956642642,0.999857956642642,
1.)))
REPRESENTATION_ITEM('')
SURFACE()
);
#1596=(
BOUNDED_SURFACE()
B_SPLINE_SURFACE(2,3,((#84875,#84876,#84877,#84878),(#84879,#84880,#84881,
#84882),(#84883,#84884,#84885,#84886)),.UNSPECIFIED.,.F.,.F.,.F.)
B_SPLINE_SURFACE_WITH_KNOTS((3,3),(4,4),(0.458503447428235,0.604044265656637),
(0.,1.),.UNSPECIFIED.)
GEOMETRIC_REPRESENTATION_ITEM()
RATIONAL_B_SPLINE_SURFACE(((1.,0.99989525299666,0.99989525299666,1.),(1.,
0.99989525299666,0.99989525299666,1.),(1.,0.99989525299666,0.99989525299666,
1.)))
REPRESENTATION_ITEM('')
SURFACE()
);
#1597=(
BOUNDED_SURFACE()
B_SPLINE_SURFACE(2,3,((#84888,#84889,#84890,#84891),(#84892,#84893,#84894,
#84895),(#84896,#84897,#84898,#84899)),.UNSPECIFIED.,.F.,.F.,.F.)
B_SPLINE_SURFACE_WITH_KNOTS((3,3),(4,4),(0.13173580484991,0.294818644607769),
(0.,1.),.UNSPECIFIED.)
GEOMETRIC_REPRESENTATION_ITEM()
RATIONAL_B_SPLINE_SURFACE(((1.,0.999857776424627,0.999857776424627,1.),
(1.,0.999857776424627,0.999857776424627,1.),(1.,0.999857776424627,0.999857776424627,
1.)))
REPRESENTATION_ITEM('')
SURFACE()
);
#1598=(
BOUNDED_SURFACE()
B_SPLINE_SURFACE(2,3,((#84901,#84902,#84903,#84904),(#84905,#84906,#84907,
#84908),(#84909,#84910,#84911,#84912)),.UNSPECIFIED.,.F.,.F.,.F.)
B_SPLINE_SURFACE_WITH_KNOTS((3,3),(4,4),(0.457070219990733,0.602201786761517),
(0.,1.),.UNSPECIFIED.)
GEOMETRIC_REPRESENTATION_ITEM()
RATIONAL_B_SPLINE_SURFACE(((1.,0.999895375004805,0.999895375004805,1.),
(1.,0.999895375004805,0.999895375004805,1.),(1.,0.999895375004805,0.999895375004805,
1.)))
REPRESENTATION_ITEM('')
SURFACE()
);
#1599=(
BOUNDED_SURFACE()
B_SPLINE_SURFACE(2,3,((#84914,#84915,#84916,#84917),(#84918,#84919,#84920,
#84921),(#84922,#84923,#84924,#84925)),.UNSPECIFIED.,.F.,.F.,.F.)
B_SPLINE_SURFACE_WITH_KNOTS((3,3),(4,4),(0.129525912426222,0.29278263731982),
(0.,1.),.UNSPECIFIED.)
GEOMETRIC_REPRESENTATION_ITEM()
RATIONAL_B_SPLINE_SURFACE(((1.,0.999856990812476,0.999856990812476,1.),
(1.,0.999856990812476,0.999856990812476,1.),(1.,0.999856990812476,0.999856990812476,
1.)))
REPRESENTATION_ITEM('')
SURFACE()
);
#1600=(
BOUNDED_SURFACE()
B_SPLINE_SURFACE(2,3,((#84927,#84928,#84929,#84930),(#84931,#84932,#84933,
#84934),(#84935,#84936,#84937,#84938)),.UNSPECIFIED.,.F.,.F.,.F.)
B_SPLINE_SURFACE_WITH_KNOTS((3,3),(4,4),(0.454381854054376,0.599708978407689),
(0.,1.),.UNSPECIFIED.)
GEOMETRIC_REPRESENTATION_ITEM()
RATIONAL_B_SPLINE_SURFACE(((1.,0.999894752812304,0.999894752812304,1.),
(1.,0.999894752812304,0.999894752812304,1.),(1.,0.999894752812304,0.999894752812304,
1.)))
REPRESENTATION_ITEM('')
SURFACE()
);
#1601=(
BOUNDED_SURFACE()
B_SPLINE_SURFACE(2,3,((#84940,#84941,#84942,#84943),(#84944,#84945,#84946,
#84947),(#84948,#84949,#84950,#84951)),.UNSPECIFIED.,.F.,.F.,.F.)
B_SPLINE_SURFACE_WITH_KNOTS((3,3),(4,4),(0.127384118218686,0.29096643518866),
(0.,1.),.UNSPECIFIED.)
GEOMETRIC_REPRESENTATION_ITEM()
RATIONAL_B_SPLINE_SURFACE(((1.,0.999857013359022,0.999857013359022,1.),
(1.,0.999857013359022,0.999857013359022,1.),(1.,0.999857013359022,0.999857013359022,
1.)))
REPRESENTATION_ITEM('')
SURFACE()
);
#1602=(
BOUNDED_SURFACE()
B_SPLINE_SURFACE(2,3,((#84953,#84954,#84955,#84956),(#84957,#84958,#84959,
#84960),(#84961,#84962,#84963,#84964)),.UNSPECIFIED.,.F.,.F.,.F.)
B_SPLINE_SURFACE_WITH_KNOTS((3,3),(4,4),(0.451885461485502,0.597476529771293),
(0.,1.),.UNSPECIFIED.)
GEOMETRIC_REPRESENTATION_ITEM()
RATIONAL_B_SPLINE_SURFACE(((1.,0.999894655481396,0.999894655481396,1.),
(1.,0.999894655481396,0.999894655481396,1.),(1.,0.999894655481396,0.999894655481396,
1.)))
REPRESENTATION_ITEM('')
SURFACE()
);
#1603=(
BOUNDED_SURFACE()
B_SPLINE_SURFACE(2,3,((#84966,#84967,#84968,#84969),(#84970,#84971,#84972,
#84973),(#84974,#84975,#84976,#84977)),.UNSPECIFIED.,.F.,.F.,.F.)
B_SPLINE_SURFACE_WITH_KNOTS((3,3),(4,4),(0.125053932102849,0.288479498956097),
(0.,1.),.UNSPECIFIED.)
GEOMETRIC_REPRESENTATION_ITEM()
RATIONAL_B_SPLINE_SURFACE(((1.,0.999857122345165,0.999857122345165,1.),
(1.,0.999857122345165,0.999857122345165,1.),(1.,0.999857122345165,0.999857122345165,
1.)))
REPRESENTATION_ITEM('')
SURFACE()
);
#1604=(
BOUNDED_SURFACE()
B_SPLINE_SURFACE(2,3,((#84979,#84980,#84981,#84982),(#84983,#84984,#84985,
#84986),(#84987,#84988,#84989,#84990)),.UNSPECIFIED.,.F.,.F.,.F.)
B_SPLINE_SURFACE_WITH_KNOTS((3,3),(4,4),(0.449312907381874,0.594798425786394),
(0.,1.),.UNSPECIFIED.)
GEOMETRIC_REPRESENTATION_ITEM()
RATIONAL_B_SPLINE_SURFACE(((1.,0.999894852716433,0.999894852716433,1.),
(1.,0.999894852716433,0.999894852716433,1.),(1.,0.999894852716433,0.999894852716433,
1.)))
REPRESENTATION_ITEM('')
SURFACE()
);
#1605=(
BOUNDED_SURFACE()
B_SPLINE_SURFACE(3,3,((#85020,#85021,#85022,#85023,#85024,#85025,#85026,
#85027,#85028,#85029,#85030,#85031,#85032,#85033,#85034,#85035,#85036,#85037,
#85038,#85039,#85040,#85041,#85042,#85043,#85044,#85045,#85046,#85047,#85048,
#85049,#85050,#85051,#85052,#85053,#85054,#85055,#85056,#85057,#85058,#85059,
#85060,#85061,#85062,#85063,#85064,#85065,#85066,#85067,#85068,#85069,#85070,
#85071,#85072,#85073),(#85074,#85075,#85076,#85077,#85078,#85079,#85080,
#85081,#85082,#85083,#85084,#85085,#85086,#85087,#85088,#85089,#85090,#85091,
#85092,#85093,#85094,#85095,#85096,#85097,#85098,#85099,#85100,#85101,#85102,
#85103,#85104,#85105,#85106,#85107,#85108,#85109,#85110,#85111,#85112,#85113,
#85114,#85115,#85116,#85117,#85118,#85119,#85120,#85121,#85122,#85123,#85124,
#85125,#85126,#85127),(#85128,#85129,#85130,#85131,#85132,#85133,#85134,
#85135,#85136,#85137,#85138,#85139,#85140,#85141,#85142,#85143,#85144,#85145,
#85146,#85147,#85148,#85149,#85150,#85151,#85152,#85153,#85154,#85155,#85156,
#85157,#85158,#85159,#85160,#85161,#85162,#85163,#85164,#85165,#85166,#85167,
#85168,#85169,#85170,#85171,#85172,#85173,#85174,#85175,#85176,#85177,#85178,
#85179,#85180,#85181),(#85182,#85183,#85184,#85185,#85186,#85187,#85188,
#85189,#85190,#85191,#85192,#85193,#85194,#85195,#85196,#85197,#85198,#85199,
#85200,#85201,#85202,#85203,#85204,#85205,#85206,#85207,#85208,#85209,#85210,
#85211,#85212,#85213,#85214,#85215,#85216,#85217,#85218,#85219,#85220,#85221,
#85222,#85223,#85224,#85225,#85226,#85227,#85228,#85229,#85230,#85231,#85232,
#85233,#85234,#85235),(#85236,#85237,#85238,#85239,#85240,#85241,#85242,
#85243,#85244,#85245,#85246,#85247,#85248,#85249,#85250,#85251,#85252,#85253,
#85254,#85255,#85256,#85257,#85258,#85259,#85260,#85261,#85262,#85263,#85264,
#85265,#85266,#85267,#85268,#85269,#85270,#85271,#85272,#85273,#85274,#85275,
#85276,#85277,#85278,#85279,#85280,#85281,#85282,#85283,#85284,#85285,#85286,
#85287,#85288,#85289),(#85290,#85291,#85292,#85293,#85294,#85295,#85296,
#85297,#85298,#85299,#85300,#85301,#85302,#85303,#85304,#85305,#85306,#85307,
#85308,#85309,#85310,#85311,#85312,#85313,#85314,#85315,#85316,#85317,#85318,
#85319,#85320,#85321,#85322,#85323,#85324,#85325,#85326,#85327,#85328,#85329,
#85330,#85331,#85332,#85333,#85334,#85335,#85336,#85337,#85338,#85339,#85340,
#85341,#85342,#85343),(#85344,#85345,#85346,#85347,#85348,#85349,#85350,
#85351,#85352,#85353,#85354,#85355,#85356,#85357,#85358,#85359,#85360,#85361,
#85362,#85363,#85364,#85365,#85366,#85367,#85368,#85369,#85370,#85371,#85372,
#85373,#85374,#85375,#85376,#85377,#85378,#85379,#85380,#85381,#85382,#85383,
#85384,#85385,#85386,#85387,#85388,#85389,#85390,#85391,#85392,#85393,#85394,
#85395,#85396,#85397)),.UNSPECIFIED.,.T.,.F.,.F.)
B_SPLINE_SURFACE_WITH_KNOTS((4,3,4),(4,2,2,2,2,2,2,2,2,2,2,2,2,2,2,2,2,
2,2,2,2,2,2,2,2,2,4),(0.,0.5,1.),(0.,0.00855967103632646,0.0171193420726529,
0.0342386841453058,0.0684773682906117,0.136954736581223,0.171193420726529,
0.205432104871835,0.239670789017141,0.273909473162447,0.302569805907928,
0.316899972280669,0.324065055467039,0.33123013865341,0.358116418237434,
0.385002697821458,0.438775256989507,0.492547816157555,0.546320375325604,
0.555016077087237,0.563711778848869,0.581103182372135,0.615885989418665,
0.711914492063999,0.807942994709333,0.903971497354666,1.),.UNSPECIFIED.)
GEOMETRIC_REPRESENTATION_ITEM()
RATIONAL_B_SPLINE_SURFACE(((1.,1.,1.,1.,1.,1.,1.,1.,1.,1.,1.,1.,1.,1.,1.,
1.,1.,1.,1.,1.,1.,1.,1.,1.,1.,1.,1.,1.,1.,1.,1.,1.,1.,1.,1.,1.,1.,1.,1.,
1.,1.,1.,1.,1.,1.,1.,1.,1.,1.,1.,1.,1.,1.,1.),(0.333333333333333,0.333333333333333,
0.333333333333333,0.333333333333333,0.333333333333333,0.333333333333333,
0.333333333333333,0.333333333333333,0.333333333333333,0.333333333333333,
0.333333333333333,0.333333333333333,0.333333333333333,0.333333333333333,
0.333333333333333,0.333333333333333,0.333333333333333,0.333333333333333,
0.333333333333333,0.333333333333333,0.333333333333333,0.333333333333333,
0.333333333333333,0.333333333333333,0.333333333333333,0.333333333333333,
0.333333333333333,0.333333333333333,0.333333333333333,0.333333333333333,
0.333333333333333,0.333333333333333,0.333333333333333,0.333333333333333,
0.333333333333333,0.333333333333333,0.333333333333333,0.333333333333333,
0.333333333333333,0.333333333333333,0.333333333333333,0.333333333333333,
0.333333333333333,0.333333333333333,0.333333333333333,0.333333333333333,
0.333333333333333,0.333333333333333,0.333333333333333,0.333333333333333,
0.333333333333333,0.333333333333333,0.333333333333333,0.333333333333333),
(0.333333333333333,0.333333333333333,0.333333333333333,0.333333333333333,
0.333333333333333,0.333333333333333,0.333333333333333,0.333333333333333,
0.333333333333333,0.333333333333333,0.333333333333333,0.333333333333333,
0.333333333333333,0.333333333333333,0.333333333333333,0.333333333333333,
0.333333333333333,0.333333333333333,0.333333333333333,0.333333333333333,
0.333333333333333,0.333333333333333,0.333333333333333,0.333333333333333,
0.333333333333333,0.333333333333333,0.333333333333333,0.333333333333333,
0.333333333333333,0.333333333333333,0.333333333333333,0.333333333333333,
0.333333333333333,0.333333333333333,0.333333333333333,0.333333333333333,
0.333333333333333,0.333333333333333,0.333333333333333,0.333333333333333,
0.333333333333333,0.333333333333333,0.333333333333333,0.333333333333333,
0.333333333333333,0.333333333333333,0.333333333333333,0.333333333333333,
0.333333333333333,0.333333333333333,0.333333333333333,0.333333333333333,
0.333333333333333,0.333333333333333),(1.,1.,1.,1.,1.,1.,1.,1.,1.,1.,1.,
1.,1.,1.,1.,1.,1.,1.,1.,1.,1.,1.,1.,1.,1.,1.,1.,1.,1.,1.,1.,1.,1.,1.,1.,
1.,1.,1.,1.,1.,1.,1.,1.,1.,1.,1.,1.,1.,1.,1.,1.,1.,1.,1.),(0.333333333333333,
0.333333333333333,0.333333333333333,0.333333333333333,0.333333333333333,
0.333333333333333,0.333333333333333,0.333333333333333,0.333333333333333,
0.333333333333333,0.333333333333333,0.333333333333333,0.333333333333333,
0.333333333333333,0.333333333333333,0.333333333333333,0.333333333333333,
0.333333333333333,0.333333333333333,0.333333333333333,0.333333333333333,
0.333333333333333,0.333333333333333,0.333333333333333,0.333333333333333,
0.333333333333333,0.333333333333333,0.333333333333333,0.333333333333333,
0.333333333333333,0.333333333333333,0.333333333333333,0.333333333333333,
0.333333333333333,0.333333333333333,0.333333333333333,0.333333333333333,
0.333333333333333,0.333333333333333,0.333333333333333,0.333333333333333,
0.333333333333333,0.333333333333333,0.333333333333333,0.333333333333333,
0.333333333333333,0.333333333333333,0.333333333333333,0.333333333333333,
0.333333333333333,0.333333333333333,0.333333333333333,0.333333333333333,
0.333333333333333),(0.333333333333333,0.333333333333333,0.333333333333333,
0.333333333333333,0.333333333333333,0.333333333333333,0.333333333333333,
0.333333333333333,0.333333333333333,0.333333333333333,0.333333333333333,
0.333333333333333,0.333333333333333,0.333333333333333,0.333333333333333,
0.333333333333333,0.333333333333333,0.333333333333333,0.333333333333333,
0.333333333333333,0.333333333333333,0.333333333333333,0.333333333333333,
0.333333333333333,0.333333333333333,0.333333333333333,0.333333333333333,
0.333333333333333,0.333333333333333,0.333333333333333,0.333333333333333,
0.333333333333333,0.333333333333333,0.333333333333333,0.333333333333333,
0.333333333333333,0.333333333333333,0.333333333333333,0.333333333333333,
0.333333333333333,0.333333333333333,0.333333333333333,0.333333333333333,
0.333333333333333,0.333333333333333,0.333333333333333,0.333333333333333,
0.333333333333333,0.333333333333333,0.333333333333333,0.333333333333333,
0.333333333333333,0.333333333333333,0.333333333333333),(1.,1.,1.,1.,1.,
1.,1.,1.,1.,1.,1.,1.,1.,1.,1.,1.,1.,1.,1.,1.,1.,1.,1.,1.,1.,1.,1.,1.,1.,
1.,1.,1.,1.,1.,1.,1.,1.,1.,1.,1.,1.,1.,1.,1.,1.,1.,1.,1.,1.,1.,1.,1.,1.,
1.)))
REPRESENTATION_ITEM('')
SURFACE()
);
#1606=(
BOUNDED_SURFACE()
B_SPLINE_SURFACE(3,3,((#85525,#85526,#85527,#85528,#85529,#85530,#85531,
#85532,#85533,#85534,#85535,#85536,#85537,#85538,#85539,#85540,#85541,#85542,
#85543,#85544,#85545,#85546,#85547,#85548,#85549,#85550,#85551,#85552,#85553,
#85554,#85555,#85556,#85557,#85558,#85559,#85560,#85561,#85562,#85563,#85564,
#85565,#85566,#85567,#85568,#85569,#85570,#85571,#85572,#85573,#85574,#85575,
#85576,#85577,#85578),(#85579,#85580,#85581,#85582,#85583,#85584,#85585,
#85586,#85587,#85588,#85589,#85590,#85591,#85592,#85593,#85594,#85595,#85596,
#85597,#85598,#85599,#85600,#85601,#85602,#85603,#85604,#85605,#85606,#85607,
#85608,#85609,#85610,#85611,#85612,#85613,#85614,#85615,#85616,#85617,#85618,
#85619,#85620,#85621,#85622,#85623,#85624,#85625,#85626,#85627,#85628,#85629,
#85630,#85631,#85632),(#85633,#85634,#85635,#85636,#85637,#85638,#85639,
#85640,#85641,#85642,#85643,#85644,#85645,#85646,#85647,#85648,#85649,#85650,
#85651,#85652,#85653,#85654,#85655,#85656,#85657,#85658,#85659,#85660,#85661,
#85662,#85663,#85664,#85665,#85666,#85667,#85668,#85669,#85670,#85671,#85672,
#85673,#85674,#85675,#85676,#85677,#85678,#85679,#85680,#85681,#85682,#85683,
#85684,#85685,#85686),(#85687,#85688,#85689,#85690,#85691,#85692,#85693,
#85694,#85695,#85696,#85697,#85698,#85699,#85700,#85701,#85702,#85703,#85704,
#85705,#85706,#85707,#85708,#85709,#85710,#85711,#85712,#85713,#85714,#85715,
#85716,#85717,#85718,#85719,#85720,#85721,#85722,#85723,#85724,#85725,#85726,
#85727,#85728,#85729,#85730,#85731,#85732,#85733,#85734,#85735,#85736,#85737,
#85738,#85739,#85740),(#85741,#85742,#85743,#85744,#85745,#85746,#85747,
#85748,#85749,#85750,#85751,#85752,#85753,#85754,#85755,#85756,#85757,#85758,
#85759,#85760,#85761,#85762,#85763,#85764,#85765,#85766,#85767,#85768,#85769,
#85770,#85771,#85772,#85773,#85774,#85775,#85776,#85777,#85778,#85779,#85780,
#85781,#85782,#85783,#85784,#85785,#85786,#85787,#85788,#85789,#85790,#85791,
#85792,#85793,#85794),(#85795,#85796,#85797,#85798,#85799,#85800,#85801,
#85802,#85803,#85804,#85805,#85806,#85807,#85808,#85809,#85810,#85811,#85812,
#85813,#85814,#85815,#85816,#85817,#85818,#85819,#85820,#85821,#85822,#85823,
#85824,#85825,#85826,#85827,#85828,#85829,#85830,#85831,#85832,#85833,#85834,
#85835,#85836,#85837,#85838,#85839,#85840,#85841,#85842,#85843,#85844,#85845,
#85846,#85847,#85848),(#85849,#85850,#85851,#85852,#85853,#85854,#85855,
#85856,#85857,#85858,#85859,#85860,#85861,#85862,#85863,#85864,#85865,#85866,
#85867,#85868,#85869,#85870,#85871,#85872,#85873,#85874,#85875,#85876,#85877,
#85878,#85879,#85880,#85881,#85882,#85883,#85884,#85885,#85886,#85887,#85888,
#85889,#85890,#85891,#85892,#85893,#85894,#85895,#85896,#85897,#85898,#85899,
#85900,#85901,#85902)),.UNSPECIFIED.,.T.,.F.,.F.)
B_SPLINE_SURFACE_WITH_KNOTS((4,3,4),(4,2,2,2,2,2,2,2,2,2,2,2,2,2,2,2,2,
2,2,2,2,2,2,2,2,2,4),(0.,0.5,1.),(0.,0.00855967103632646,0.0171193420726529,
0.0342386841453058,0.0684773682906117,0.136954736581223,0.171193420726529,
0.205432104871835,0.239670789017141,0.273909473162447,0.302569805907928,
0.316899972280669,0.324065055467039,0.33123013865341,0.358116418237434,
0.385002697821458,0.438775256989507,0.492547816157555,0.546320375325604,
0.555016077087237,0.563711778848869,0.581103182372135,0.615885989418665,
0.711914492063999,0.807942994709333,0.903971497354666,1.),.UNSPECIFIED.)
GEOMETRIC_REPRESENTATION_ITEM()
RATIONAL_B_SPLINE_SURFACE(((1.,1.,1.,1.,1.,1.,1.,1.,1.,1.,1.,1.,1.,1.,1.,
1.,1.,1.,1.,1.,1.,1.,1.,1.,1.,1.,1.,1.,1.,1.,1.,1.,1.,1.,1.,1.,1.,1.,1.,
1.,1.,1.,1.,1.,1.,1.,1.,1.,1.,1.,1.,1.,1.,1.),(0.333333333333333,0.333333333333333,
0.333333333333333,0.333333333333333,0.333333333333333,0.333333333333333,
0.333333333333333,0.333333333333333,0.333333333333333,0.333333333333333,
0.333333333333333,0.333333333333333,0.333333333333333,0.333333333333333,
0.333333333333333,0.333333333333333,0.333333333333333,0.333333333333333,
0.333333333333333,0.333333333333333,0.333333333333333,0.333333333333333,
0.333333333333333,0.333333333333333,0.333333333333333,0.333333333333333,
0.333333333333333,0.333333333333333,0.333333333333333,0.333333333333333,
0.333333333333333,0.333333333333333,0.333333333333333,0.333333333333333,
0.333333333333333,0.333333333333333,0.333333333333333,0.333333333333333,
0.333333333333333,0.333333333333333,0.333333333333333,0.333333333333333,
0.333333333333333,0.333333333333333,0.333333333333333,0.333333333333333,
0.333333333333333,0.333333333333333,0.333333333333333,0.333333333333333,
0.333333333333333,0.333333333333333,0.333333333333333,0.333333333333333),
(0.333333333333333,0.333333333333333,0.333333333333333,0.333333333333333,
0.333333333333333,0.333333333333333,0.333333333333333,0.333333333333333,
0.333333333333333,0.333333333333333,0.333333333333333,0.333333333333333,
0.333333333333333,0.333333333333333,0.333333333333333,0.333333333333333,
0.333333333333333,0.333333333333333,0.333333333333333,0.333333333333333,
0.333333333333333,0.333333333333333,0.333333333333333,0.333333333333333,
0.333333333333333,0.333333333333333,0.333333333333333,0.333333333333333,
0.333333333333333,0.333333333333333,0.333333333333333,0.333333333333333,
0.333333333333333,0.333333333333333,0.333333333333333,0.333333333333333,
0.333333333333333,0.333333333333333,0.333333333333333,0.333333333333333,
0.333333333333333,0.333333333333333,0.333333333333333,0.333333333333333,
0.333333333333333,0.333333333333333,0.333333333333333,0.333333333333333,
0.333333333333333,0.333333333333333,0.333333333333333,0.333333333333333,
0.333333333333333,0.333333333333333),(1.,1.,1.,1.,1.,1.,1.,1.,1.,1.,1.,
1.,1.,1.,1.,1.,1.,1.,1.,1.,1.,1.,1.,1.,1.,1.,1.,1.,1.,1.,1.,1.,1.,1.,1.,
1.,1.,1.,1.,1.,1.,1.,1.,1.,1.,1.,1.,1.,1.,1.,1.,1.,1.,1.),(0.333333333333333,
0.333333333333333,0.333333333333333,0.333333333333333,0.333333333333333,
0.333333333333333,0.333333333333333,0.333333333333333,0.333333333333333,
0.333333333333333,0.333333333333333,0.333333333333333,0.333333333333333,
0.333333333333333,0.333333333333333,0.333333333333333,0.333333333333333,
0.333333333333333,0.333333333333333,0.333333333333333,0.333333333333333,
0.333333333333333,0.333333333333333,0.333333333333333,0.333333333333333,
0.333333333333333,0.333333333333333,0.333333333333333,0.333333333333333,
0.333333333333333,0.333333333333333,0.333333333333333,0.333333333333333,
0.333333333333333,0.333333333333333,0.333333333333333,0.333333333333333,
0.333333333333333,0.333333333333333,0.333333333333333,0.333333333333333,
0.333333333333333,0.333333333333333,0.333333333333333,0.333333333333333,
0.333333333333333,0.333333333333333,0.333333333333333,0.333333333333333,
0.333333333333333,0.333333333333333,0.333333333333333,0.333333333333333,
0.333333333333333),(0.333333333333333,0.333333333333333,0.333333333333333,
0.333333333333333,0.333333333333333,0.333333333333333,0.333333333333333,
0.333333333333333,0.333333333333333,0.333333333333333,0.333333333333333,
0.333333333333333,0.333333333333333,0.333333333333333,0.333333333333333,
0.333333333333333,0.333333333333333,0.333333333333333,0.333333333333333,
0.333333333333333,0.333333333333333,0.333333333333333,0.333333333333333,
0.333333333333333,0.333333333333333,0.333333333333333,0.333333333333333,
0.333333333333333,0.333333333333333,0.333333333333333,0.333333333333333,
0.333333333333333,0.333333333333333,0.333333333333333,0.333333333333333,
0.333333333333333,0.333333333333333,0.333333333333333,0.333333333333333,
0.333333333333333,0.333333333333333,0.333333333333333,0.333333333333333,
0.333333333333333,0.333333333333333,0.333333333333333,0.333333333333333,
0.333333333333333,0.333333333333333,0.333333333333333,0.333333333333333,
0.333333333333333,0.333333333333333,0.333333333333333),(1.,1.,1.,1.,1.,
1.,1.,1.,1.,1.,1.,1.,1.,1.,1.,1.,1.,1.,1.,1.,1.,1.,1.,1.,1.,1.,1.,1.,1.,
1.,1.,1.,1.,1.,1.,1.,1.,1.,1.,1.,1.,1.,1.,1.,1.,1.,1.,1.,1.,1.,1.,1.,1.,
1.)))
REPRESENTATION_ITEM('')
SURFACE()
);
#1607=(
BOUNDED_SURFACE()
B_SPLINE_SURFACE(3,2,((#88517,#88518,#88519),(#88520,#88521,#88522),(#88523,
#88524,#88525),(#88526,#88527,#88528),(#88529,#88530,#88531),(#88532,#88533,
#88534),(#88535,#88536,#88537),(#88538,#88539,#88540),(#88541,#88542,#88543),
(#88544,#88545,#88546),(#88547,#88548,#88549),(#88550,#88551,#88552),(#88553,
#88554,#88555),(#88556,#88557,#88558),(#88559,#88560,#88561),(#88562,#88563,
#88564),(#88565,#88566,#88567),(#88568,#88569,#88570),(#88571,#88572,#88573),
(#88574,#88575,#88576),(#88577,#88578,#88579),(#88580,#88581,#88582),(#88583,
#88584,#88585),(#88586,#88587,#88588),(#88589,#88590,#88591),(#88592,#88593,
#88594),(#88595,#88596,#88597),(#88598,#88599,#88600),(#88601,#88602,#88603),
(#88604,#88605,#88606),(#88607,#88608,#88609),(#88610,#88611,#88612),(#88613,
#88614,#88615),(#88616,#88617,#88618),(#88619,#88620,#88621),(#88622,#88623,
#88624),(#88625,#88626,#88627),(#88628,#88629,#88630),(#88631,#88632,#88633),
(#88634,#88635,#88636),(#88637,#88638,#88639),(#88640,#88641,#88642),(#88643,
#88644,#88645),(#88646,#88647,#88648),(#88649,#88650,#88651),(#88652,#88653,
#88654),(#88655,#88656,#88657),(#88658,#88659,#88660),(#88661,#88662,#88663),
(#88664,#88665,#88666),(#88667,#88668,#88669),(#88670,#88671,#88672),(#88673,
#88674,#88675),(#88676,#88677,#88678),(#88679,#88680,#88681),(#88682,#88683,
#88684),(#88685,#88686,#88687),(#88688,#88689,#88690)),.UNSPECIFIED.,.F.,
 .F.,.F.)
B_SPLINE_SURFACE_WITH_KNOTS((4,2,2,2,2,2,2,2,2,2,2,2,2,2,2,2,2,2,2,2,2,
2,2,2,2,2,2,2,4),(3,3),(0.,0.0321349777273596,0.0642699554547192,0.080337444318399,
0.0964049331820788,0.112472422045759,0.128539910909438,0.136573655341278,
0.140590527557198,0.144607399773118,0.152641144204958,0.156658016420878,
0.160674888636798,0.168708633068638,0.172725505284558,0.174733941392518,
0.176742377500478,0.184776121932318,0.186784558040278,0.188792994148238,
0.192809866364158,0.200843610795998,0.204860483011918,0.208877355227837,
0.216911099659677,0.224944844091517,0.232978588523357,0.241012332955197,
0.25739509415827),(0.295972225728062,1.),.UNSPECIFIED.)
GEOMETRIC_REPRESENTATION_ITEM()
RATIONAL_B_SPLINE_SURFACE(((0.877938117508499,0.793795039059425,1.),(0.877938117508499,
0.793795039059425,1.),(0.877938117508498,0.793795039059421,1.),(0.877938117508498,
0.793795039059421,1.),(0.877938117508498,0.793795039059421,1.),(0.877938117508498,
0.793795039059421,1.),(0.877938117508498,0.793795039059421,1.),(0.877938117508498,
0.793795039059421,1.),(0.877938117508499,0.793795039059425,1.),(0.877938117508499,
0.793795039059425,1.),(0.877938117508489,0.793795039059407,1.),(0.877938117508489,
0.793795039059407,1.),(0.877938117508506,0.793795039059435,1.),(0.877938117508506,
0.793795039059435,1.),(0.877938117508499,0.793795039059425,1.),(0.877938117508499,
0.793795039059425,1.),(0.877938117508499,0.793795039059425,1.),(0.877938117508499,
0.793795039059425,1.),(0.877938117508498,0.793795039059421,1.),(0.877938117508498,
0.793795039059421,1.),(0.877938117508485,0.793795039059401,1.),(0.877938117508485,
0.793795039059401,1.),(0.877938117508505,0.793795039059434,1.),(0.877938117508505,
0.793795039059434,1.),(0.87793811750849,0.793795039059408,1.),(0.87793811750849,
0.793795039059408,1.),(0.87793811750849,0.793795039059409,1.),(0.87793811750849,
0.793795039059409,1.),(0.877938117508486,0.793795039059402,1.),(0.877938117508486,
0.793795039059402,1.),(0.877938117508504,0.793795039059432,1.),(0.877938117508504,
0.793795039059432,1.),(0.877938117508498,0.793795039059421,1.),(0.877938117508498,
0.793795039059421,1.),(0.877938117508506,0.793795039059436,1.),(0.877938117508506,
0.793795039059436,1.),(0.877938117508498,0.793795039059421,1.),(0.877938117508498,
0.793795039059421,1.),(0.877938117508493,0.793795039059414,1.),(0.877938117508493,
0.793795039059414,1.),(0.877938117508498,0.793795039059421,1.),(0.877938117508498,
0.793795039059421,1.),(0.877938117508498,0.793795039059421,1.),(0.877938117508498,
0.793795039059421,1.),(0.877938117508489,0.793795039059408,1.),(0.877938117508489,
0.793795039059408,1.),(0.877938117508506,0.793795039059435,1.),(0.877938117508506,
0.793795039059435,1.),(0.877938117508489,0.793795039059408,1.),(0.877938117508489,
0.793795039059408,1.),(0.877938117508498,0.793795039059421,1.),(0.877938117508498,
0.793795039059421,1.),(0.877938117508506,0.793795039059435,1.),(0.877938117508506,
0.793795039059435,1.),(0.877938117508506,0.793795039059435,1.),(0.877938117508506,
0.793795039059435,1.),(0.877938117508499,0.793795039059424,1.),(0.877938117508499,
0.793795039059425,1.)))
REPRESENTATION_ITEM('')
SURFACE()
);
#1608=(
BOUNDED_SURFACE()
B_SPLINE_SURFACE(3,2,((#88828,#88829,#88830),(#88831,#88832,#88833),(#88834,
#88835,#88836),(#88837,#88838,#88839),(#88840,#88841,#88842),(#88843,#88844,
#88845),(#88846,#88847,#88848),(#88849,#88850,#88851),(#88852,#88853,#88854),
(#88855,#88856,#88857),(#88858,#88859,#88860),(#88861,#88862,#88863),(#88864,
#88865,#88866),(#88867,#88868,#88869),(#88870,#88871,#88872),(#88873,#88874,
#88875),(#88876,#88877,#88878),(#88879,#88880,#88881),(#88882,#88883,#88884),
(#88885,#88886,#88887),(#88888,#88889,#88890),(#88891,#88892,#88893),(#88894,
#88895,#88896),(#88897,#88898,#88899),(#88900,#88901,#88902),(#88903,#88904,
#88905),(#88906,#88907,#88908),(#88909,#88910,#88911),(#88912,#88913,#88914),
(#88915,#88916,#88917),(#88918,#88919,#88920),(#88921,#88922,#88923),(#88924,
#88925,#88926),(#88927,#88928,#88929),(#88930,#88931,#88932),(#88933,#88934,
#88935),(#88936,#88937,#88938),(#88939,#88940,#88941),(#88942,#88943,#88944),
(#88945,#88946,#88947),(#88948,#88949,#88950),(#88951,#88952,#88953),(#88954,
#88955,#88956),(#88957,#88958,#88959),(#88960,#88961,#88962),(#88963,#88964,
#88965),(#88966,#88967,#88968),(#88969,#88970,#88971),(#88972,#88973,#88974),
(#88975,#88976,#88977),(#88978,#88979,#88980),(#88981,#88982,#88983),(#88984,
#88985,#88986),(#88987,#88988,#88989),(#88990,#88991,#88992),(#88993,#88994,
#88995)),.UNSPECIFIED.,.F.,.F.,.F.)
B_SPLINE_SURFACE_WITH_KNOTS((4,2,2,2,2,2,2,2,2,2,2,2,2,2,2,2,2,2,2,2,2,
2,2,2,2,2,2,4),(3,3),(0.,0.0161428187212414,0.0242142280818621,0.0322856374424828,
0.0403570468031035,0.0484284561637242,0.0564998655243449,0.0605355702046552,
0.0645712748849656,0.0686069795652759,0.0706248319054311,0.0726426842455863,
0.0807140936062069,0.0847497982865173,0.0867676506266725,0.0887855029668276,
0.0968569123274483,0.100892617007759,0.104928321688069,0.11299973104869,
0.12107114040931,0.129142549769931,0.145285368491173,0.161428187212414,
0.177571005933655,0.193713824654897,0.225999462097379,0.258285099539862),
(0.296287498067819,1.),.UNSPECIFIED.)
GEOMETRIC_REPRESENTATION_ITEM()
RATIONAL_B_SPLINE_SURFACE(((0.877862815112484,0.793887380189833,1.),(0.877862815112484,
0.793887380189833,1.),(0.877862815112466,0.793887380189802,1.),(0.877862815112466,
0.793887380189802,1.),(0.87786281511247,0.793887380189809,1.),(0.87786281511247,
0.793887380189809,1.),(0.877862815112476,0.793887380189819,1.),(0.877862815112476,
0.793887380189819,1.),(0.877862815112474,0.793887380189816,1.),(0.877862815112474,
0.793887380189816,1.),(0.877862815112474,0.793887380189816,1.),(0.877862815112474,
0.793887380189816,1.),(0.877862815112476,0.793887380189819,1.),(0.877862815112476,
0.793887380189819,1.),(0.877862815112474,0.793887380189816,1.),(0.877862815112474,
0.793887380189816,1.),(0.877862815112481,0.793887380189828,1.),(0.877862815112481,
0.793887380189828,1.),(0.877862815112485,0.793887380189834,1.),(0.877862815112485,
0.793887380189834,1.),(0.877862815112478,0.793887380189823,1.),(0.877862815112478,
0.793887380189823,1.),(0.877862815112464,0.7938873801898,1.),(0.877862815112464,
0.7938873801898,1.),(0.877862815112474,0.793887380189816,1.),(0.877862815112474,
0.793887380189816,1.),(0.877862815112474,0.793887380189816,1.),(0.877862815112474,
0.793887380189816,1.),(0.877862815112474,0.793887380189816,1.),(0.877862815112474,
0.793887380189816,1.),(0.877862815112474,0.793887380189816,1.),(0.877862815112474,
0.793887380189816,1.),(0.877862815112472,0.793887380189812,1.),(0.877862815112472,
0.793887380189812,1.),(0.877862815112482,0.793887380189829,1.),(0.877862815112482,
0.793887380189829,1.),(0.877862815112466,0.793887380189802,1.),(0.877862815112466,
0.793887380189802,1.),(0.877862815112476,0.793887380189819,1.),(0.877862815112476,
0.793887380189819,1.),(0.877862815112466,0.793887380189802,1.),(0.877862815112466,
0.793887380189802,1.),(0.877862815112474,0.793887380189816,1.),(0.877862815112474,
0.793887380189816,1.),(0.877862815112474,0.793887380189815,1.),(0.877862815112474,
0.793887380189815,1.),(0.877862815112484,0.793887380189833,1.),(0.877862815112484,
0.793887380189833,1.),(0.877862815112461,0.793887380189795,1.),(0.877862815112461,
0.793887380189795,1.),(0.877862815112466,0.793887380189802,1.),(0.877862815112466,
0.793887380189802,1.),(0.877862815112474,0.793887380189816,1.),(0.877862815112474,
0.793887380189816,1.),(0.877862815112476,0.793887380189819,1.),(0.877862815112476,
0.793887380189819,1.)))
REPRESENTATION_ITEM('')
SURFACE()
);
#1609=(
BOUNDED_SURFACE()
B_SPLINE_SURFACE(3,2,((#89355,#89356,#89357),(#89358,#89359,#89360),(#89361,
#89362,#89363),(#89364,#89365,#89366),(#89367,#89368,#89369),(#89370,#89371,
#89372),(#89373,#89374,#89375),(#89376,#89377,#89378),(#89379,#89380,#89381),
(#89382,#89383,#89384),(#89385,#89386,#89387),(#89388,#89389,#89390),(#89391,
#89392,#89393),(#89394,#89395,#89396),(#89397,#89398,#89399),(#89400,#89401,
#89402),(#89403,#89404,#89405),(#89406,#89407,#89408),(#89409,#89410,#89411),
(#89412,#89413,#89414),(#89415,#89416,#89417),(#89418,#89419,#89420),(#89421,
#89422,#89423),(#89424,#89425,#89426),(#89427,#89428,#89429),(#89430,#89431,
#89432),(#89433,#89434,#89435),(#89436,#89437,#89438),(#89439,#89440,#89441),
(#89442,#89443,#89444),(#89445,#89446,#89447),(#89448,#89449,#89450),(#89451,
#89452,#89453),(#89454,#89455,#89456),(#89457,#89458,#89459),(#89460,#89461,
#89462),(#89463,#89464,#89465),(#89466,#89467,#89468),(#89469,#89470,#89471),
(#89472,#89473,#89474),(#89475,#89476,#89477),(#89478,#89479,#89480),(#89481,
#89482,#89483),(#89484,#89485,#89486),(#89487,#89488,#89489),(#89490,#89491,
#89492),(#89493,#89494,#89495),(#89496,#89497,#89498),(#89499,#89500,#89501),
(#89502,#89503,#89504),(#89505,#89506,#89507),(#89508,#89509,#89510),(#89511,
#89512,#89513),(#89514,#89515,#89516),(#89517,#89518,#89519),(#89520,#89521,
#89522)),.UNSPECIFIED.,.F.,.F.,.F.)
B_SPLINE_SURFACE_WITH_KNOTS((4,2,2,2,2,2,2,2,2,2,2,2,2,2,2,2,2,2,2,2,2,
2,2,2,2,2,2,4),(3,3),(0.,0.0161428187212413,0.024214228081862,0.0322856374424827,
0.0403570468031034,0.048428456163724,0.0564998655243447,0.060535570204655,
0.0645712748849654,0.0686069795652757,0.0706248319054309,0.072642684245586,
0.0807140936062067,0.084749798286517,0.0867676506266722,0.0887855029668274,
0.0968569123274481,0.100892617007758,0.104928321688069,0.112999731048689,
0.12107114040931,0.129142549769931,0.145285368491172,0.161428187212413,
0.177571005933655,0.193713824654896,0.225999462097379,0.258285099539862),
(0.,1.),.UNSPECIFIED.)
GEOMETRIC_REPRESENTATION_ITEM()
RATIONAL_B_SPLINE_SURFACE(((1.,0.707106781186543,1.),(1.,0.707106781186543,
1.),(1.,0.707106781186528,1.),(1.,0.707106781186528,1.),(1.,0.707106781186548,
1.),(1.,0.707106781186548,1.),(1.,0.707106781186548,1.),(1.,0.707106781186548,
1.),(1.,0.707106781186533,1.),(1.,0.707106781186533,1.),(1.,0.707106781186557,
1.),(1.,0.707106781186557,1.),(1.,0.707106781186548,1.),(1.,0.707106781186548,
1.),(1.,0.707106781186548,1.),(1.,0.707106781186548,1.),(1.,0.707106781186548,
1.),(1.,0.707106781186548,1.),(1.,0.707106781186548,1.),(1.,0.707106781186548,
1.),(1.,0.707106781186564,1.),(1.,0.707106781186564,1.),(1.,0.707106781186562,
1.),(1.,0.707106781186562,1.),(1.,0.707106781186548,1.),(1.,0.707106781186548,
1.),(1.,0.707106781186559,1.),(1.,0.707106781186559,1.),(1.,0.707106781186537,
1.),(1.,0.707106781186537,1.),(1.,0.707106781186579,1.),(1.,0.707106781186579,
1.),(1.,0.707106781186543,1.),(1.,0.707106781186543,1.),(1.,0.707106781186548,
1.),(1.,0.707106781186548,1.),(1.,0.707106781186562,1.),(1.,0.707106781186562,
1.),(1.,0.707106781186533,1.),(1.,0.707106781186533,1.),(1.,0.707106781186562,
1.),(1.,0.707106781186562,1.),(1.,0.707106781186548,1.),(1.,0.707106781186548,
1.),(1.,0.707106781186548,1.),(1.,0.707106781186548,1.),(1.,0.707106781186547,
1.),(1.,0.707106781186547,1.),(1.,0.707106781186548,1.),(1.,0.707106781186548,
1.),(1.,0.707106781186548,1.),(1.,0.707106781186548,1.),(1.,0.707106781186543,
1.),(1.,0.707106781186543,1.),(1.,0.707106781186543,1.),(1.,0.707106781186543,
1.)))
REPRESENTATION_ITEM('')
SURFACE()
);
#1610=(
BOUNDED_SURFACE()
B_SPLINE_SURFACE(3,2,((#89524,#89525,#89526),(#89527,#89528,#89529),(#89530,
#89531,#89532),(#89533,#89534,#89535),(#89536,#89537,#89538),(#89539,#89540,
#89541),(#89542,#89543,#89544),(#89545,#89546,#89547),(#89548,#89549,#89550),
(#89551,#89552,#89553),(#89554,#89555,#89556),(#89557,#89558,#89559),(#89560,
#89561,#89562),(#89563,#89564,#89565),(#89566,#89567,#89568),(#89569,#89570,
#89571),(#89572,#89573,#89574),(#89575,#89576,#89577),(#89578,#89579,#89580),
(#89581,#89582,#89583),(#89584,#89585,#89586),(#89587,#89588,#89589),(#89590,
#89591,#89592),(#89593,#89594,#89595),(#89596,#89597,#89598),(#89599,#89600,
#89601),(#89602,#89603,#89604),(#89605,#89606,#89607),(#89608,#89609,#89610),
(#89611,#89612,#89613),(#89614,#89615,#89616),(#89617,#89618,#89619),(#89620,
#89621,#89622),(#89623,#89624,#89625),(#89626,#89627,#89628),(#89629,#89630,
#89631),(#89632,#89633,#89634),(#89635,#89636,#89637),(#89638,#89639,#89640),
(#89641,#89642,#89643),(#89644,#89645,#89646),(#89647,#89648,#89649),(#89650,
#89651,#89652),(#89653,#89654,#89655),(#89656,#89657,#89658),(#89659,#89660,
#89661),(#89662,#89663,#89664),(#89665,#89666,#89667),(#89668,#89669,#89670),
(#89671,#89672,#89673),(#89674,#89675,#89676),(#89677,#89678,#89679),(#89680,
#89681,#89682),(#89683,#89684,#89685),(#89686,#89687,#89688),(#89689,#89690,
#89691),(#89692,#89693,#89694),(#89695,#89696,#89697)),.UNSPECIFIED.,.F.,
 .F.,.F.)
B_SPLINE_SURFACE_WITH_KNOTS((4,2,2,2,2,2,2,2,2,2,2,2,2,2,2,2,2,2,2,2,2,
2,2,2,2,2,2,2,4),(3,3),(0.,0.0321349777273597,0.0642699554547194,0.0803374443183993,
0.0964049331820791,0.112472422045759,0.128539910909439,0.136573655341279,
0.140590527557199,0.144607399773119,0.152641144204959,0.156658016420879,
0.160674888636799,0.168708633068638,0.172725505284558,0.174733941392518,
0.176742377500478,0.184776121932318,0.186784558040278,0.188792994148238,
0.192809866364158,0.200843610795998,0.204860483011918,0.208877355227838,
0.216911099659678,0.224944844091518,0.232978588523358,0.241012332955198,
0.257079821818878),(0.,1.),.UNSPECIFIED.)
GEOMETRIC_REPRESENTATION_ITEM()
RATIONAL_B_SPLINE_SURFACE(((1.,0.707106781186543,1.),(1.,0.707106781186543,
1.),(1.,0.707106781186543,1.),(1.,0.707106781186543,1.),(1.,0.707106781186548,
1.),(1.,0.707106781186548,1.),(1.,0.707106781186548,1.),(1.,0.707106781186548,
1.),(1.,0.707106781186548,1.),(1.,0.707106781186548,1.),(1.,0.707106781186553,
1.),(1.,0.707106781186553,1.),(1.,0.707106781186567,1.),(1.,0.707106781186567,
1.),(1.,0.707106781186533,1.),(1.,0.707106781186533,1.),(1.,0.707106781186552,
1.),(1.,0.707106781186552,1.),(1.,0.707106781186572,1.),(1.,0.707106781186572,
1.),(1.,0.707106781186552,1.),(1.,0.707106781186552,1.),(1.,0.707106781186552,
1.),(1.,0.707106781186552,1.),(1.,0.707106781186561,1.),(1.,0.707106781186561,
1.),(1.,0.707106781186543,1.),(1.,0.707106781186543,1.),(1.,0.707106781186552,
1.),(1.,0.707106781186552,1.),(1.,0.707106781186558,1.),(1.,0.707106781186558,
1.),(1.,0.707106781186543,1.),(1.,0.707106781186543,1.),(1.,0.707106781186552,
1.),(1.,0.707106781186552,1.),(1.,0.707106781186532,1.),(1.,0.707106781186532,
1.),(1.,0.707106781186533,1.),(1.,0.707106781186533,1.),(1.,0.707106781186543,
1.),(1.,0.707106781186543,1.),(1.,0.707106781186543,1.),(1.,0.707106781186543,
1.),(1.,0.707106781186543,1.),(1.,0.707106781186543,1.),(1.,0.707106781186543,
1.),(1.,0.707106781186543,1.),(1.,0.707106781186538,1.),(1.,0.707106781186538,
1.),(1.,0.707106781186552,1.),(1.,0.707106781186552,1.),(1.,0.707106781186572,
1.),(1.,0.707106781186572,1.),(1.,0.707106781186552,1.),(1.,0.707106781186552,
1.),(1.,0.707106781186528,1.),(1.,0.707106781186528,1.)))
REPRESENTATION_ITEM('')
SURFACE()
);
#1611=(
BOUNDED_SURFACE()
B_SPLINE_SURFACE(3,2,((#89728,#89729,#89730),(#89731,#89732,#89733),(#89734,
#89735,#89736),(#89737,#89738,#89739),(#89740,#89741,#89742),(#89743,#89744,
#89745),(#89746,#89747,#89748),(#89749,#89750,#89751),(#89752,#89753,#89754),
(#89755,#89756,#89757),(#89758,#89759,#89760),(#89761,#89762,#89763)),
 .UNSPECIFIED.,.F.,.F.,.F.)
B_SPLINE_SURFACE_WITH_KNOTS((4,2,2,2,2,4),(3,3),(0.000926277054046903,0.00147787442090103,
0.00175367310432809,0.00202947178775516,0.00258106915460929,0.00313266652146341),
(0.,1.),.UNSPECIFIED.)
GEOMETRIC_REPRESENTATION_ITEM()
RATIONAL_B_SPLINE_SURFACE(((1.,0.775937515965206,1.),(1.,0.775965554436259,
1.),(1.,0.773720199380605,1.),(1.,0.767576773145645,1.),(1.,0.765096790635356,
1.),(1.,0.759365493434644,1.),(1.,0.756099558648518,1.),(1.,0.745708436761125,
1.),(1.,0.737726760693873,1.),(1.,0.721983931595965,1.),(1.,0.714015299600668,
1.),(1.,0.707106781186543,1.)))
REPRESENTATION_ITEM('')
SURFACE()
);
#1612=(
BOUNDED_SURFACE()
B_SPLINE_SURFACE(3,2,((#89809,#89810,#89811),(#89812,#89813,#89814),(#89815,
#89816,#89817),(#89818,#89819,#89820),(#89821,#89822,#89823),(#89824,#89825,
#89826),(#89827,#89828,#89829),(#89830,#89831,#89832),(#89833,#89834,#89835),
(#89836,#89837,#89838),(#89839,#89840,#89841),(#89842,#89843,#89844)),
 .UNSPECIFIED.,.F.,.F.,.F.)
B_SPLINE_SURFACE_WITH_KNOTS((4,2,2,2,2,4),(3,3),(0.000925070050461762,0.00147866127618651,
0.00175545688904888,0.00203225250191126,0.00258584372763601,0.00313943495336076),
(0.,1.),.UNSPECIFIED.)
GEOMETRIC_REPRESENTATION_ITEM()
RATIONAL_B_SPLINE_SURFACE(((1.,0.775937515965214,1.),(1.,0.775948908187678,
1.),(1.,0.7742815251738,1.),(1.,0.769435561772286,1.),(1.,0.767450319305812,
1.),(1.,0.762709308920971,1.),(1.,0.75994120696576,1.),(1.,0.750761268625032,
1.),(1.,0.743229618394193,1.),(1.,0.726398019745837,1.),(1.,0.716867225806667,
1.),(1.,0.707106781186526,1.)))
REPRESENTATION_ITEM('')
SURFACE()
);
#1613=(
BOUNDED_SURFACE()
B_SPLINE_SURFACE(3,2,((#89924,#89925,#89926),(#89927,#89928,#89929),(#89930,
#89931,#89932),(#89933,#89934,#89935),(#89936,#89937,#89938),(#89939,#89940,
#89941),(#89942,#89943,#89944),(#89945,#89946,#89947),(#89948,#89949,#89950),
(#89951,#89952,#89953),(#89954,#89955,#89956),(#89957,#89958,#89959)),
 .UNSPECIFIED.,.F.,.F.,.F.)
B_SPLINE_SURFACE_WITH_KNOTS((4,2,2,2,2,4),(3,3),(0.000954052972318673,0.00150562533929701,
0.00178141152278617,0.00205719770627534,0.00260877007325367,0.003160342440232),
(0.,1.),.UNSPECIFIED.)
GEOMETRIC_REPRESENTATION_ITEM()
RATIONAL_B_SPLINE_SURFACE(((1.,0.707106781186548,1.),(1.,0.714095715093505,
1.),(1.,0.721962502896922,1.),(1.,0.733852450860903,1.),(1.,0.737775695415353,
1.),(1.,0.745441210409867,1.),(1.,0.749210335263833,1.),(1.,0.759607646869478,
1.),(1.,0.765574863587299,1.),(1.,0.773709421852012,1.),(1.,0.775971965811445,
1.),(1.,0.775937515965212,1.)))
REPRESENTATION_ITEM('')
SURFACE()
);
#1614=(
BOUNDED_SURFACE()
B_SPLINE_SURFACE(3,2,((#90005,#90006,#90007),(#90008,#90009,#90010),(#90011,
#90012,#90013),(#90014,#90015,#90016),(#90017,#90018,#90019),(#90020,#90021,
#90022),(#90023,#90024,#90025),(#90026,#90027,#90028),(#90029,#90030,#90031),
(#90032,#90033,#90034),(#90035,#90036,#90037),(#90038,#90039,#90040)),
 .UNSPECIFIED.,.F.,.F.,.F.)
B_SPLINE_SURFACE_WITH_KNOTS((4,2,2,2,2,4),(3,3),(0.000982297288438947,0.0015357772992534,
0.00181251730466063,0.00208925731006786,0.00264273732088231,0.00319621733169676),
(0.,1.),.UNSPECIFIED.)
GEOMETRIC_REPRESENTATION_ITEM()
RATIONAL_B_SPLINE_SURFACE(((1.,0.707106781186548,1.),(1.,0.716971715675457,
1.),(1.,0.726372587537382,1.),(1.,0.739082989278526,1.),(1.,0.743030515251258,
1.),(1.,0.75040043255623,1.),(1.,0.753848954137035,1.),(1.,0.763039215535026,
1.),(1.,0.767853458839658,1.),(1.,0.774273736205767,1.),(1.,0.7759516406652,
1.),(1.,0.775937515965214,1.)))
REPRESENTATION_ITEM('')
SURFACE()
);
#1615=(
BOUNDED_SURFACE()
B_SPLINE_SURFACE(3,2,((#90152,#90153,#90154),(#90155,#90156,#90157),(#90158,
#90159,#90160),(#90161,#90162,#90163),(#90164,#90165,#90166),(#90167,#90168,
#90169),(#90170,#90171,#90172),(#90173,#90174,#90175),(#90176,#90177,#90178),
(#90179,#90180,#90181)),.UNSPECIFIED.,.F.,.F.,.F.)
B_SPLINE_SURFACE_WITH_KNOTS((4,2,2,2,4),(3,3),(0.000653855251160619,0.00105056734621481,
0.00144727944126899,0.00184399153632318,0.00224070363137736),(0.,1.),
 .UNSPECIFIED.)
GEOMETRIC_REPRESENTATION_ITEM()
RATIONAL_B_SPLINE_SURFACE(((1.,0.797116436093323,1.),(1.,0.797153870787656,
1.),(1.,0.794288909474886,1.),(1.,0.78384172562724,1.),(1.,0.776220388773547,
1.),(1.,0.758398453086649,1.),(1.,0.748065045409874,1.),(1.,0.727318436656279,
1.),(1.,0.716633802230093,1.),(1.,0.707106781186546,1.)))
REPRESENTATION_ITEM('')
SURFACE()
);
#1616=(
BOUNDED_SURFACE()
B_SPLINE_SURFACE(3,2,((#90227,#90228,#90229),(#90230,#90231,#90232),(#90233,
#90234,#90235),(#90236,#90237,#90238),(#90239,#90240,#90241),(#90242,#90243,
#90244),(#90245,#90246,#90247),(#90248,#90249,#90250),(#90251,#90252,#90253),
(#90254,#90255,#90256)),.UNSPECIFIED.,.F.,.F.,.F.)
B_SPLINE_SURFACE_WITH_KNOTS((4,2,2,2,4),(3,3),(0.000346079680846979,0.000742789375765937,
0.0011394990706849,0.00153620876560385,0.00193291846052281),(0.,1.),
 .UNSPECIFIED.)
GEOMETRIC_REPRESENTATION_ITEM()
RATIONAL_B_SPLINE_SURFACE(((1.,0.707106781186546,1.),(1.,0.716758952028491,
1.),(1.,0.727288011548078,1.),(1.,0.748184897298097,1.),(1.,0.758437122287583,
1.),(1.,0.776285930138696,1.),(1.,0.783895918656499,1.),(1.,0.794279688273945,
1.),(1.,0.797152913684426,1.),(1.,0.797116436093324,1.)))
REPRESENTATION_ITEM('')
SURFACE()
);
#1617=(
BOUNDED_SURFACE()
B_SPLINE_SURFACE(3,2,((#90319,#90320,#90321),(#90322,#90323,#90324),(#90325,
#90326,#90327),(#90328,#90329,#90330),(#90331,#90332,#90333),(#90334,#90335,
#90336),(#90337,#90338,#90339),(#90340,#90341,#90342),(#90343,#90344,#90345),
(#90346,#90347,#90348)),.UNSPECIFIED.,.F.,.F.,.F.)
B_SPLINE_SURFACE_WITH_KNOTS((4,2,2,2,4),(3,3),(0.000652435349851691,0.00105161226574612,
0.00145078918164054,0.00184996609753497,0.00224914301342939),(0.,1.),
 .UNSPECIFIED.)
GEOMETRIC_REPRESENTATION_ITEM()
RATIONAL_B_SPLINE_SURFACE(((1.,0.797116436093325,1.),(1.,0.797133991687376,
1.),(1.,0.794952627585106,1.),(1.,0.786540751799673,1.),(1.,0.780263959283907,
1.),(1.,0.764334803592024,1.),(1.,0.754537231252642,1.),(1.,0.73252430168142,
1.),(1.,0.720028936379281,1.),(1.,0.707106781186558,1.)))
REPRESENTATION_ITEM('')
SURFACE()
);
#1618=(
BOUNDED_SURFACE()
B_SPLINE_SURFACE(3,2,((#90394,#90395,#90396),(#90397,#90398,#90399),(#90400,
#90401,#90402),(#90403,#90404,#90405),(#90406,#90407,#90408),(#90409,#90410,
#90411),(#90412,#90413,#90414),(#90415,#90416,#90417),(#90418,#90419,#90420),
(#90421,#90422,#90423)),.UNSPECIFIED.,.F.,.F.,.F.)
B_SPLINE_SURFACE_WITH_KNOTS((4,2,2,2,4),(3,3),(0.000364014256986725,0.000763079051988796,
0.00116214384699087,0.00156120864199294,0.00196027343699501),(0.,1.),
 .UNSPECIFIED.)
GEOMETRIC_REPRESENTATION_ITEM()
RATIONAL_B_SPLINE_SURFACE(((1.,0.707106781186567,1.),(1.,0.720184284287166,
1.),(1.,0.73248314811275,1.),(1.,0.754654774294656,1.),(1.,0.764346716512339,
1.),(1.,0.780321857768423,1.),(1.,0.786575289610347,1.),(1.,0.794947899012155,
1.),(1.,0.797127700950814,1.),(1.,0.797116436093325,1.)))
REPRESENTATION_ITEM('')
SURFACE()
);
#1619=(
BOUNDED_SURFACE()
B_SPLINE_SURFACE(3,2,((#90516,#90517,#90518),(#90519,#90520,#90521),(#90522,
#90523,#90524),(#90525,#90526,#90527),(#90528,#90529,#90530),(#90531,#90532,
#90533),(#90534,#90535,#90536),(#90537,#90538,#90539),(#90540,#90541,#90542),
(#90543,#90544,#90545)),.UNSPECIFIED.,.F.,.F.,.F.)
B_SPLINE_SURFACE_WITH_KNOTS((4,2,2,2,4),(3,3),(0.000653855251160618,0.0010505673462148,
0.00144727944126899,0.00184399153632318,0.00224070363137736),(0.,1.),
 .UNSPECIFIED.)
GEOMETRIC_REPRESENTATION_ITEM()
RATIONAL_B_SPLINE_SURFACE(((1.,0.797116436093328,1.),(1.,0.797153870787879,
1.),(1.,0.794288909474585,1.),(1.,0.783841725627543,1.),(1.,0.776220388773417,
1.),(1.,0.758398453086769,1.),(1.,0.748065045410025,1.),(1.,0.727318436656137,
1.),(1.,0.7166338022302,1.),(1.,0.707106781186548,1.)))
REPRESENTATION_ITEM('')
SURFACE()
);
#1620=(
BOUNDED_SURFACE()
B_SPLINE_SURFACE(3,2,((#90591,#90592,#90593),(#90594,#90595,#90596),(#90597,
#90598,#90599),(#90600,#90601,#90602),(#90603,#90604,#90605),(#90606,#90607,
#90608),(#90609,#90610,#90611),(#90612,#90613,#90614),(#90615,#90616,#90617),
(#90618,#90619,#90620)),.UNSPECIFIED.,.F.,.F.,.F.)
B_SPLINE_SURFACE_WITH_KNOTS((4,2,2,2,4),(3,3),(0.000346079680846979,0.000742789375765937,
0.0011394990706849,0.00153620876560385,0.00193291846052281),(0.,1.),
 .UNSPECIFIED.)
GEOMETRIC_REPRESENTATION_ITEM()
RATIONAL_B_SPLINE_SURFACE(((1.,0.707106781186542,1.),(1.,0.716758952028229,
1.),(1.,0.727288011548429,1.),(1.,0.748184897297752,1.),(1.,0.758437122287011,
1.),(1.,0.776285930139258,1.),(1.,0.783895918655783,1.),(1.,0.794279688274653,
1.),(1.,0.797152913683895,1.),(1.,0.79711643609332,1.)))
REPRESENTATION_ITEM('')
SURFACE()
);
#1621=(
BOUNDED_SURFACE()
B_SPLINE_SURFACE(3,2,((#90683,#90684,#90685),(#90686,#90687,#90688),(#90689,
#90690,#90691),(#90692,#90693,#90694),(#90695,#90696,#90697),(#90698,#90699,
#90700),(#90701,#90702,#90703),(#90704,#90705,#90706),(#90707,#90708,#90709),
(#90710,#90711,#90712)),.UNSPECIFIED.,.F.,.F.,.F.)
B_SPLINE_SURFACE_WITH_KNOTS((4,2,2,2,4),(3,3),(0.000652435349851691,0.00105161226574612,
0.00145078918164054,0.00184996609753497,0.00224914301342939),(0.,1.),
 .UNSPECIFIED.)
GEOMETRIC_REPRESENTATION_ITEM()
RATIONAL_B_SPLINE_SURFACE(((1.,0.797116436093328,1.),(1.,0.797133991687402,
1.),(1.,0.79495262758507,1.),(1.,0.786540751799712,1.),(1.,0.780263959283842,
1.),(1.,0.764334803592092,1.),(1.,0.754537231252535,1.),(1.,0.732524301681536,
1.),(1.,0.720028936379193,1.),(1.,0.707106781186563,1.)))
REPRESENTATION_ITEM('')
SURFACE()
);
#1622=(
BOUNDED_SURFACE()
B_SPLINE_SURFACE(3,2,((#90758,#90759,#90760),(#90761,#90762,#90763),(#90764,
#90765,#90766),(#90767,#90768,#90769),(#90770,#90771,#90772),(#90773,#90774,
#90775),(#90776,#90777,#90778),(#90779,#90780,#90781),(#90782,#90783,#90784),
(#90785,#90786,#90787)),.UNSPECIFIED.,.F.,.F.,.F.)
B_SPLINE_SURFACE_WITH_KNOTS((4,2,2,2,4),(3,3),(0.000364014256986725,0.000763079051988796,
0.00116214384699087,0.00156120864199294,0.00196027343699501),(0.,1.),
 .UNSPECIFIED.)
GEOMETRIC_REPRESENTATION_ITEM()
RATIONAL_B_SPLINE_SURFACE(((1.,0.707106781186571,1.),(1.,0.72018428428724,
1.),(1.,0.732483148112645,1.),(1.,0.75465477429476,1.),(1.,0.764346716512432,
1.),(1.,0.780321857768337,1.),(1.,0.786575289610486,1.),(1.,0.794947899012013,
1.),(1.,0.797127700950917,1.),(1.,0.797116436093326,1.)))
REPRESENTATION_ITEM('')
SURFACE()
);
#1623=(
BOUNDED_SURFACE()
B_SPLINE_SURFACE(3,2,((#90880,#90881,#90882),(#90883,#90884,#90885),(#90886,
#90887,#90888),(#90889,#90890,#90891),(#90892,#90893,#90894),(#90895,#90896,
#90897),(#90898,#90899,#90900),(#90901,#90902,#90903),(#90904,#90905,#90906),
(#90907,#90908,#90909)),.UNSPECIFIED.,.F.,.F.,.F.)
B_SPLINE_SURFACE_WITH_KNOTS((4,2,2,2,4),(3,3),(0.000653855251160619,0.00105056734621481,
0.00144727944126899,0.00184399153632318,0.00224070363137737),(0.,1.),
 .UNSPECIFIED.)
GEOMETRIC_REPRESENTATION_ITEM()
RATIONAL_B_SPLINE_SURFACE(((1.,0.797116436093321,1.),(1.,0.797153870787877,
1.),(1.,0.794288909474591,1.),(1.,0.783841725627535,1.),(1.,0.776220388773692,
1.),(1.,0.7583984530865,1.),(1.,0.748065045409612,1.),(1.,0.727318436656547,
1.),(1.,0.716633802229892,1.),(1.,0.707106781186553,1.)))
REPRESENTATION_ITEM('')
SURFACE()
);
#1624=(
BOUNDED_SURFACE()
B_SPLINE_SURFACE(3,2,((#90955,#90956,#90957),(#90958,#90959,#90960),(#90961,
#90962,#90963),(#90964,#90965,#90966),(#90967,#90968,#90969),(#90970,#90971,
#90972),(#90973,#90974,#90975),(#90976,#90977,#90978),(#90979,#90980,#90981),
(#90982,#90983,#90984)),.UNSPECIFIED.,.F.,.F.,.F.)
B_SPLINE_SURFACE_WITH_KNOTS((4,2,2,2,4),(3,3),(0.000346079680846979,0.000742789375765937,
0.0011394990706849,0.00153620876560385,0.00193291846052281),(0.,1.),
 .UNSPECIFIED.)
GEOMETRIC_REPRESENTATION_ITEM()
RATIONAL_B_SPLINE_SURFACE(((1.,0.707106781186546,1.),(1.,0.716758952028333,
1.),(1.,0.727288011548303,1.),(1.,0.748184897297863,1.),(1.,0.758437122288391,
1.),(1.,0.776285930137885,1.),(1.,0.783895918656293,1.),(1.,0.79427968827415,
1.),(1.,0.797152913684263,1.),(1.,0.797116436093329,1.)))
REPRESENTATION_ITEM('')
SURFACE()
);
#1625=(
BOUNDED_SURFACE()
B_SPLINE_SURFACE(3,2,((#91047,#91048,#91049),(#91050,#91051,#91052),(#91053,
#91054,#91055),(#91056,#91057,#91058),(#91059,#91060,#91061),(#91062,#91063,
#91064),(#91065,#91066,#91067),(#91068,#91069,#91070),(#91071,#91072,#91073),
(#91074,#91075,#91076)),.UNSPECIFIED.,.F.,.F.,.F.)
B_SPLINE_SURFACE_WITH_KNOTS((4,2,2,2,4),(3,3),(0.000652435349851691,0.00105161226574612,
0.00145078918164054,0.00184996609753497,0.00224914301342939),(0.,1.),
 .UNSPECIFIED.)
GEOMETRIC_REPRESENTATION_ITEM()
RATIONAL_B_SPLINE_SURFACE(((1.,0.797116436093322,1.),(1.,0.79713399168744,
1.),(1.,0.794952627585016,1.),(1.,0.786540751799761,1.),(1.,0.780263959283671,
1.),(1.,0.764334803592261,1.),(1.,0.754537231253279,1.),(1.,0.732524301680786,
1.),(1.,0.720028936379745,1.),(1.,0.707106781186564,1.)))
REPRESENTATION_ITEM('')
SURFACE()
);
#1626=(
BOUNDED_SURFACE()
B_SPLINE_SURFACE(3,2,((#91122,#91123,#91124),(#91125,#91126,#91127),(#91128,
#91129,#91130),(#91131,#91132,#91133),(#91134,#91135,#91136),(#91137,#91138,
#91139),(#91140,#91141,#91142),(#91143,#91144,#91145),(#91146,#91147,#91148),
(#91149,#91150,#91151)),.UNSPECIFIED.,.F.,.F.,.F.)
B_SPLINE_SURFACE_WITH_KNOTS((4,2,2,2,4),(3,3),(0.000364014256986725,0.000763079051988796,
0.00116214384699087,0.00156120864199294,0.00196027343699501),(0.,1.),
 .UNSPECIFIED.)
GEOMETRIC_REPRESENTATION_ITEM()
RATIONAL_B_SPLINE_SURFACE(((1.,0.707106781186567,1.),(1.,0.720184284287246,
1.),(1.,0.732483148112649,1.),(1.,0.754654774294764,1.),(1.,0.76434671651307,
1.),(1.,0.780321857767699,1.),(1.,0.786575289610259,1.),(1.,0.79494789901223,
1.),(1.,0.797127700950757,1.),(1.,0.797116436093331,1.)))
REPRESENTATION_ITEM('')
SURFACE()
);
#1627=(
BOUNDED_SURFACE()
B_SPLINE_SURFACE(2,2,((#91239,#91240,#91241),(#91242,#91243,#91244),(#91245,
#91246,#91247)),.UNSPECIFIED.,.F.,.F.,.F.)
B_SPLINE_SURFACE_WITH_KNOTS((3,3),(3,3),(-1.11976951499864,0.),(0.,1.5707963267949),
 .UNSPECIFIED.)
GEOMETRIC_REPRESENTATION_ITEM()
RATIONAL_B_SPLINE_SURFACE(((1.,0.707106781186548,1.),(0.847316320613008,
0.599143116115493,0.847316320613008),(1.,0.707106781186548,1.)))
REPRESENTATION_ITEM('')
SURFACE()
);
#1628=(
BOUNDED_SURFACE()
B_SPLINE_SURFACE(3,2,((#91251,#91252,#91253),(#91254,#91255,#91256),(#91257,
#91258,#91259),(#91260,#91261,#91262),(#91263,#91264,#91265),(#91266,#91267,
#91268),(#91269,#91270,#91271),(#91272,#91273,#91274),(#91275,#91276,#91277),
(#91278,#91279,#91280),(#91281,#91282,#91283),(#91284,#91285,#91286),(#91287,
#91288,#91289),(#91290,#91291,#91292),(#91293,#91294,#91295),(#91296,#91297,
#91298),(#91299,#91300,#91301),(#91302,#91303,#91304),(#91305,#91306,#91307),
(#91308,#91309,#91310),(#91311,#91312,#91313),(#91314,#91315,#91316),(#91317,
#91318,#91319),(#91320,#91321,#91322),(#91323,#91324,#91325),(#91326,#91327,
#91328),(#91329,#91330,#91331),(#91332,#91333,#91334),(#91335,#91336,#91337),
(#91338,#91339,#91340),(#91341,#91342,#91343),(#91344,#91345,#91346),(#91347,
#91348,#91349),(#91350,#91351,#91352),(#91353,#91354,#91355),(#91356,#91357,
#91358),(#91359,#91360,#91361),(#91362,#91363,#91364),(#91365,#91366,#91367),
(#91368,#91369,#91370),(#91371,#91372,#91373),(#91374,#91375,#91376),(#91377,
#91378,#91379),(#91380,#91381,#91382),(#91383,#91384,#91385),(#91386,#91387,
#91388)),.UNSPECIFIED.,.F.,.F.,.F.)
B_SPLINE_SURFACE_WITH_KNOTS((4,2,2,2,2,2,2,2,2,2,2,2,2,2,2,2,2,2,2,2,2,
2,4),(3,3),(-0.000517275538890252,0.0157285769420072,0.0235928654130109,
0.0314571538840145,0.0393214423550181,0.0471857308260217,0.0550500192970254,
0.0570160914147763,0.0589821635325272,0.062914307768029,0.0707785962390326,
0.0727446683567835,0.0747107404745344,0.0786428847100362,0.082575028945538,
0.0845411010632889,0.0865071731810398,0.0943714616520435,0.102235750123047,
0.106167894358549,0.110100038594051,0.117964327065054,0.126345891074948),
(0.295770222528606,1.),.UNSPECIFIED.)
GEOMETRIC_REPRESENTATION_ITEM()
RATIONAL_B_SPLINE_SURFACE(((0.877986426924503,0.793735873692126,1.),(0.877986426924503,
0.793735873692126,1.),(0.877986426924503,0.793735873692126,1.),(0.877986426924503,
0.793735873692126,1.),(0.877986426924503,0.793735873692126,1.),(0.877986426924503,
0.793735873692126,1.),(0.877986426924503,0.793735873692126,1.),(0.877986426924503,
0.793735873692126,1.),(0.877986426924505,0.793735873692129,1.),(0.877986426924505,
0.793735873692129,1.),(0.877986426924511,0.793735873692139,1.),(0.877986426924511,
0.793735873692139,1.),(0.877986426924503,0.793735873692126,1.),(0.877986426924503,
0.793735873692126,1.),(0.877986426924503,0.793735873692126,1.),(0.877986426924503,
0.793735873692126,1.),(0.877986426924503,0.793735873692126,1.),(0.877986426924503,
0.793735873692126,1.),(0.877986426924503,0.793735873692126,1.),(0.877986426924503,
0.793735873692126,1.),(0.877986426924503,0.793735873692126,1.),(0.877986426924503,
0.793735873692126,1.),(0.877986426924492,0.793735873692107,1.),(0.877986426924492,
0.793735873692107,1.),(0.877986426924499,0.793735873692119,1.),(0.877986426924499,
0.793735873692119,1.),(0.877986426924505,0.793735873692129,1.),(0.877986426924505,
0.793735873692129,1.),(0.877986426924504,0.793735873692127,1.),(0.877986426924504,
0.793735873692127,1.),(0.877986426924488,0.793735873692099,1.),(0.877986426924488,
0.793735873692099,1.),(0.877986426924506,0.79373587369213,1.),(0.877986426924506,
0.79373587369213,1.),(0.877986426924503,0.793735873692126,1.),(0.877986426924503,
0.793735873692126,1.),(0.877986426924499,0.793735873692119,1.),(0.877986426924499,
0.793735873692119,1.),(0.877986426924503,0.793735873692126,1.),(0.877986426924503,
0.793735873692126,1.),(0.877986426924507,0.793735873692132,1.),(0.877986426924507,
0.793735873692132,1.),(0.877986426924503,0.793735873692126,1.),(0.877986426924503,
0.793735873692126,1.),(0.877986426924498,0.793735873692118,1.),(0.877986426924499,
0.793735873692119,1.)))
REPRESENTATION_ITEM('')
SURFACE()
);
#1629=(
BOUNDED_SURFACE()
B_SPLINE_SURFACE(3,2,((#91399,#91400,#91401),(#91402,#91403,#91404),(#91405,
#91406,#91407),(#91408,#91409,#91410),(#91411,#91412,#91413),(#91414,#91415,
#91416)),.UNSPECIFIED.,.F.,.F.,.F.)
B_SPLINE_SURFACE_WITH_KNOTS((4,2,4),(3,3),(0.,0.00187370917737372,0.00374741835474743),
(0.,0.715643358171679),.UNSPECIFIED.)
GEOMETRIC_REPRESENTATION_ITEM()
RATIONAL_B_SPLINE_SURFACE(((1.,0.868676996939189,0.925314863709635),(1.,
0.862154096139035,0.921605203376613),(1.,0.852620844137825,0.916183516327079),
(1.,0.826855889165617,0.901530644181569),(1.,0.81063530623189,0.892305783198504),
(1.,0.790392913302621,0.880793665446632)))
REPRESENTATION_ITEM('')
SURFACE()
);
#1630=(
BOUNDED_SURFACE()
B_SPLINE_SURFACE(2,2,((#91432,#91433,#91434),(#91435,#91436,#91437),(#91438,
#91439,#91440)),.UNSPECIFIED.,.F.,.F.,.F.)
B_SPLINE_SURFACE_WITH_KNOTS((3,3),(3,3),(-1.11976951499864,0.),(-1.5707963267949,
0.),.UNSPECIFIED.)
GEOMETRIC_REPRESENTATION_ITEM()
RATIONAL_B_SPLINE_SURFACE(((1.,0.707106781186548,1.),(0.847316320613008,
0.599143116115493,0.847316320613008),(1.,0.707106781186548,1.)))
REPRESENTATION_ITEM('')
SURFACE()
);
#1631=(
BOUNDED_SURFACE()
B_SPLINE_SURFACE(3,2,((#91444,#91445,#91446),(#91447,#91448,#91449),(#91450,
#91451,#91452),(#91453,#91454,#91455),(#91456,#91457,#91458),(#91459,#91460,
#91461)),.UNSPECIFIED.,.F.,.F.,.F.)
B_SPLINE_SURFACE_WITH_KNOTS((4,2,4),(3,3),(0.,0.00204073705610436,0.00408147411220872),
(0.,0.735738848586875),.UNSPECIFIED.)
GEOMETRIC_REPRESENTATION_ITEM()
RATIONAL_B_SPLINE_SURFACE(((1.,0.864989405740761,0.928643889816166),(1.,
0.872322079329199,0.932519371347001),(1.,0.875877893683041,0.934398698537716),
(1.,0.875878347808356,0.934398938553073),(1.,0.872319864193714,0.932518200598494),
(1.,0.864989405740073,0.928643889815803)))
REPRESENTATION_ITEM('')
SURFACE()
);
#1632=(
BOUNDED_SURFACE()
B_SPLINE_SURFACE(3,2,((#91474,#91475,#91476),(#91477,#91478,#91479),(#91480,
#91481,#91482),(#91483,#91484,#91485),(#91486,#91487,#91488),(#91489,#91490,
#91491)),.UNSPECIFIED.,.F.,.F.,.F.)
B_SPLINE_SURFACE_WITH_KNOTS((4,2,4),(3,3),(-4.33680868994202E-19,0.00187190510061502,
0.00374381020123004),(0.,0.715644139044445),.UNSPECIFIED.)
GEOMETRIC_REPRESENTATION_ITEM()
RATIONAL_B_SPLINE_SURFACE(((1.,0.790392684589732,0.880793862727862),(1.,
0.810642558292627,0.892310203269917),(1.,0.826863334737431,0.901535148972577),
(1.,0.852626485765744,0.916186954955745),(1.,0.862156703884265,0.921606901712117),
(1.,0.86867685364703,0.925314987310818)))
REPRESENTATION_ITEM('')
SURFACE()
);
#1633=(
BOUNDED_SURFACE()
B_SPLINE_SURFACE(3,2,((#91511,#91512,#91513),(#91514,#91515,#91516),(#91517,
#91518,#91519),(#91520,#91521,#91522),(#91523,#91524,#91525),(#91526,#91527,
#91528),(#91529,#91530,#91531),(#91532,#91533,#91534),(#91535,#91536,#91537),
(#91538,#91539,#91540),(#91541,#91542,#91543),(#91544,#91545,#91546),(#91547,
#91548,#91549),(#91550,#91551,#91552)),.UNSPECIFIED.,.F.,.F.,.F.)
B_SPLINE_SURFACE_WITH_KNOTS((4,2,2,2,2,2,4),(3,3),(-9.89281647458895E-5,
0.0149256238360901,0.0298512476721802,0.0447768715082703,0.0597024953443604,
0.0895537430165406,0.119503918899356),(0.296188569857101,1.),
 .UNSPECIFIED.)
GEOMETRIC_REPRESENTATION_ITEM()
RATIONAL_B_SPLINE_SURFACE(((0.877886431452041,0.793858404787744,1.),(0.877886431452041,
0.793858404787744,1.),(0.877886431452049,0.793858404787757,1.),(0.877886431452049,
0.793858404787757,1.),(0.877886431452045,0.79385840478775,1.),(0.877886431452045,
0.79385840478775,1.),(0.877886431452041,0.793858404787744,1.),(0.877886431452041,
0.793858404787744,1.),(0.877886431452041,0.793858404787744,1.),(0.877886431452041,
0.793858404787744,1.),(0.877886431452037,0.793858404787737,1.),(0.877886431452037,
0.793858404787737,1.),(0.877886431452041,0.793858404787744,1.),(0.877886431452041,
0.793858404787744,1.)))
REPRESENTATION_ITEM('')
SURFACE()
);
#1634=(
BOUNDED_SURFACE()
B_SPLINE_SURFACE(3,2,((#91583,#91584,#91585),(#91586,#91587,#91588),(#91589,
#91590,#91591),(#91592,#91593,#91594),(#91595,#91596,#91597),(#91598,#91599,
#91600),(#91601,#91602,#91603),(#91604,#91605,#91606),(#91607,#91608,#91609),
(#91610,#91611,#91612),(#91613,#91614,#91615),(#91616,#91617,#91618),(#91619,
#91620,#91621),(#91622,#91623,#91624),(#91625,#91626,#91627),(#91628,#91629,
#91630),(#91631,#91632,#91633),(#91634,#91635,#91636),(#91637,#91638,#91639),
(#91640,#91641,#91642),(#91643,#91644,#91645),(#91646,#91647,#91648),(#91649,
#91650,#91651),(#91652,#91653,#91654),(#91655,#91656,#91657),(#91658,#91659,
#91660),(#91661,#91662,#91663),(#91664,#91665,#91666),(#91667,#91668,#91669),
(#91670,#91671,#91672),(#91673,#91674,#91675),(#91676,#91677,#91678),(#91679,
#91680,#91681),(#91682,#91683,#91684),(#91685,#91686,#91687),(#91688,#91689,
#91690),(#91691,#91692,#91693),(#91694,#91695,#91696),(#91697,#91698,#91699),
(#91700,#91701,#91702),(#91703,#91704,#91705),(#91706,#91707,#91708),(#91709,
#91710,#91711),(#91712,#91713,#91714),(#91715,#91716,#91717),(#91718,#91719,
#91720),(#91721,#91722,#91723),(#91724,#91725,#91726),(#91727,#91728,#91729),
(#91730,#91731,#91732),(#91733,#91734,#91735),(#91736,#91737,#91738),(#91739,
#91740,#91741),(#91742,#91743,#91744),(#91745,#91746,#91747),(#91748,#91749,
#91750),(#91751,#91752,#91753),(#91754,#91755,#91756)),.UNSPECIFIED.,.F.,
 .F.,.F.)
B_SPLINE_SURFACE_WITH_KNOTS((4,2,2,2,2,2,2,2,2,2,2,2,2,2,2,2,2,2,2,2,2,
2,2,2,2,2,2,2,4),(3,3),(-0.000108339933889343,0.0321349777273597,0.0642699554547194,
0.0803374443183993,0.0964049331820792,0.112472422045759,0.128539910909439,
0.136573655341279,0.140590527557199,0.144607399773119,0.152641144204959,
0.156658016420879,0.160674888636799,0.168708633068639,0.172725505284558,
0.174733941392518,0.176742377500478,0.184776121932318,0.186784558040278,
0.188792994148238,0.192809866364158,0.200843610795998,0.204860483011918,
0.208877355227838,0.216911099659678,0.224944844091518,0.232978588523358,
0.241012332955198,0.257188161752767),(0.296179158133916,1.),
 .UNSPECIFIED.)
GEOMETRIC_REPRESENTATION_ITEM()
RATIONAL_B_SPLINE_SURFACE(((0.877888678834658,0.793855648157845,1.),(0.877888678834658,
0.793855648157845,1.),(0.877888678834658,0.793855648157845,1.),(0.877888678834658,
0.793855648157845,1.),(0.877888678834658,0.793855648157845,1.),(0.877888678834658,
0.793855648157845,1.),(0.877888678834658,0.793855648157845,1.),(0.877888678834658,
0.793855648157845,1.),(0.877888678834658,0.793855648157845,1.),(0.877888678834658,
0.793855648157845,1.),(0.877888678834658,0.793855648157846,1.),(0.877888678834658,
0.793855648157846,1.),(0.877888678834658,0.793855648157845,1.),(0.877888678834658,
0.793855648157845,1.),(0.877888678834649,0.793855648157832,1.),(0.877888678834649,
0.793855648157832,1.),(0.877888678834662,0.793855648157852,1.),(0.877888678834662,
0.793855648157852,1.),(0.87788867883467,0.793855648157866,1.),(0.87788867883467,
0.793855648157866,1.),(0.877888678834662,0.793855648157852,1.),(0.877888678834662,
0.793855648157852,1.),(0.877888678834658,0.793855648157845,1.),(0.877888678834658,
0.793855648157845,1.),(0.877888678834669,0.793855648157865,1.),(0.877888678834669,
0.793855648157865,1.),(0.877888678834662,0.793855648157852,1.),(0.877888678834662,
0.793855648157852,1.),(0.877888678834662,0.793855648157852,1.),(0.877888678834662,
0.793855648157852,1.),(0.877888678834667,0.793855648157861,1.),(0.877888678834667,
0.793855648157861,1.),(0.877888678834668,0.793855648157862,1.),(0.877888678834668,
0.793855648157862,1.),(0.877888678834658,0.793855648157845,1.),(0.877888678834658,
0.793855648157845,1.),(0.877888678834658,0.793855648157845,1.),(0.877888678834658,
0.793855648157845,1.),(0.877888678834658,0.793855648157845,1.),(0.877888678834658,
0.793855648157845,1.),(0.877888678834656,0.793855648157842,1.),(0.877888678834656,
0.793855648157842,1.),(0.877888678834663,0.793855648157855,1.),(0.877888678834663,
0.793855648157855,1.),(0.877888678834658,0.793855648157845,1.),(0.877888678834658,
0.793855648157845,1.),(0.877888678834662,0.793855648157852,1.),(0.877888678834662,
0.793855648157852,1.),(0.877888678834658,0.793855648157845,1.),(0.877888678834658,
0.793855648157845,1.),(0.877888678834662,0.793855648157852,1.),(0.877888678834662,
0.793855648157852,1.),(0.877888678834658,0.793855648157845,1.),(0.877888678834658,
0.793855648157845,1.),(0.877888678834664,0.793855648157856,1.),(0.877888678834664,
0.793855648157856,1.),(0.877888678834649,0.793855648157831,1.),(0.877888678834649,
0.793855648157831,1.)))
REPRESENTATION_ITEM('')
SURFACE()
);
#1635=(
BOUNDED_SURFACE()
B_SPLINE_SURFACE(3,2,((#91965,#91966,#91967),(#91968,#91969,#91970),(#91971,
#91972,#91973),(#91974,#91975,#91976),(#91977,#91978,#91979),(#91980,#91981,
#91982),(#91983,#91984,#91985),(#91986,#91987,#91988),(#91989,#91990,#91991),
(#91992,#91993,#91994),(#91995,#91996,#91997),(#91998,#91999,#92000),(#92001,
#92002,#92003),(#92004,#92005,#92006),(#92007,#92008,#92009),(#92010,#92011,
#92012),(#92013,#92014,#92015),(#92016,#92017,#92018),(#92019,#92020,#92021),
(#92022,#92023,#92024),(#92025,#92026,#92027),(#92028,#92029,#92030),(#92031,
#92032,#92033),(#92034,#92035,#92036),(#92037,#92038,#92039),(#92040,#92041,
#92042),(#92043,#92044,#92045),(#92046,#92047,#92048),(#92049,#92050,#92051),
(#92052,#92053,#92054),(#92055,#92056,#92057),(#92058,#92059,#92060),(#92061,
#92062,#92063),(#92064,#92065,#92066),(#92067,#92068,#92069),(#92070,#92071,
#92072),(#92073,#92074,#92075),(#92076,#92077,#92078),(#92079,#92080,#92081),
(#92082,#92083,#92084),(#92085,#92086,#92087),(#92088,#92089,#92090)),
 .UNSPECIFIED.,.F.,.F.,.F.)
B_SPLINE_SURFACE_WITH_KNOTS((4,2,2,2,2,2,2,2,2,2,2,2,2,2,2,2,2,2,2,2,4),
(3,3),(0.,0.0265419162547455,0.053083832509491,0.0796257487642365,0.0928967068916092,
0.106167665018982,0.119438623146355,0.132709581273727,0.139345060337414,
0.1459805394011,0.159251497528473,0.165886976592159,0.172522455655846,0.179157934719532,
0.185793413783218,0.189111153315062,0.192428892846905,0.199064371910591,
0.205699850974278,0.209017590506121,0.212335330037964),(0.,1.),
 .UNSPECIFIED.)
GEOMETRIC_REPRESENTATION_ITEM()
RATIONAL_B_SPLINE_SURFACE(((1.,0.707106781186547,1.),(1.,0.707106781186547,
1.),(1.,0.707106781186548,1.),(1.,0.707106781186548,1.),(1.,0.707106781186548,
1.),(1.,0.707106781186548,1.),(1.,0.707106781186543,1.),(1.,0.707106781186543,
1.),(1.,0.707106781186552,1.),(1.,0.707106781186552,1.),(1.,0.707106781186548,
1.),(1.,0.707106781186548,1.),(1.,0.707106781186548,1.),(1.,0.707106781186548,
1.),(1.,0.707106781186547,1.),(1.,0.707106781186547,1.),(1.,0.707106781186543,
1.),(1.,0.707106781186543,1.),(1.,0.707106781186548,1.),(1.,0.707106781186548,
1.),(1.,0.707106781186552,1.),(1.,0.707106781186552,1.),(1.,0.707106781186543,
1.),(1.,0.707106781186543,1.),(1.,0.707106781186547,1.),(1.,0.707106781186547,
1.),(1.,0.707106781186548,1.),(1.,0.707106781186548,1.),(1.,0.707106781186531,
1.),(1.,0.707106781186531,1.),(1.,0.707106781186543,1.),(1.,0.707106781186543,
1.),(1.,0.707106781186557,1.),(1.,0.707106781186557,1.),(1.,0.707106781186538,
1.),(1.,0.707106781186538,1.),(1.,0.707106781186548,1.),(1.,0.707106781186548,
1.),(1.,0.707106781186557,1.),(1.,0.707106781186557,1.),(1.,0.707106781186548,
1.),(1.,0.707106781186548,1.)))
REPRESENTATION_ITEM('')
SURFACE()
);
#1636=(
BOUNDED_SURFACE()
B_SPLINE_SURFACE(3,2,((#92408,#92409,#92410),(#92411,#92412,#92413),(#92414,
#92415,#92416),(#92417,#92418,#92419),(#92420,#92421,#92422),(#92423,#92424,
#92425),(#92426,#92427,#92428),(#92429,#92430,#92431),(#92432,#92433,#92434),
(#92435,#92436,#92437),(#92438,#92439,#92440),(#92441,#92442,#92443)),
 .UNSPECIFIED.,.F.,.F.,.F.)
B_SPLINE_SURFACE_WITH_KNOTS((4,2,2,2,2,4),(3,3),(0.,0.0276588530591966,
0.0553177061183932,0.0829765591775898,0.0968059857071881,0.110635412236786),
(0.,1.),.UNSPECIFIED.)
GEOMETRIC_REPRESENTATION_ITEM()
RATIONAL_B_SPLINE_SURFACE(((1.,0.707106781186547,1.),(1.,0.707106781186547,
1.),(1.,0.707106781186553,1.),(1.,0.707106781186553,1.),(1.,0.707106781186543,
1.),(1.,0.707106781186543,1.),(1.,0.707106781186548,1.),(1.,0.707106781186548,
1.),(1.,0.707106781186543,1.),(1.,0.707106781186543,1.),(1.,0.707106781186543,
1.),(1.,0.707106781186543,1.)))
REPRESENTATION_ITEM('')
SURFACE()
);
#1637=(
BOUNDED_SURFACE()
B_SPLINE_SURFACE(3,2,((#92543,#92544,#92545),(#92546,#92547,#92548),(#92549,
#92550,#92551),(#92552,#92553,#92554),(#92555,#92556,#92557),(#92558,#92559,
#92560),(#92561,#92562,#92563),(#92564,#92565,#92566),(#92567,#92568,#92569),
(#92570,#92571,#92572),(#92573,#92574,#92575),(#92576,#92577,#92578),(#92579,
#92580,#92581),(#92582,#92583,#92584)),.UNSPECIFIED.,.F.,.F.,.F.)
B_SPLINE_SURFACE_WITH_KNOTS((4,2,2,2,2,2,4),(3,3),(-2.75387351811318E-17,
0.000503019152578121,0.00100603830515627,0.00150905745773442,0.00201207661031257,
0.00301811491546887,0.00402415322062516),(0.,1.),.UNSPECIFIED.)
GEOMETRIC_REPRESENTATION_ITEM()
RATIONAL_B_SPLINE_SURFACE(((1.,0.947539216237274,1.),(1.,0.947529154337319,
1.),(1.,0.945092080349251,1.),(1.,0.936003138514207,1.),(1.,0.92961504518381,
1.),(1.,0.914166261177696,1.),(1.,0.905357494770243,1.),(1.,0.8860141198597,
1.),(1.,0.875396745378908,1.),(1.,0.842143074103383,1.),(1.,0.817763975573635,
1.),(1.,0.764845303360259,1.),(1.,0.736920996311044,1.),(1.,0.707106781186552,
1.)))
REPRESENTATION_ITEM('')
SURFACE()
);
#1638=(
BOUNDED_SURFACE()
B_SPLINE_SURFACE(3,2,((#92663,#92664,#92665),(#92666,#92667,#92668),(#92669,
#92670,#92671),(#92672,#92673,#92674),(#92675,#92676,#92677),(#92678,#92679,
#92680),(#92681,#92682,#92683),(#92684,#92685,#92686),(#92687,#92688,#92689),
(#92690,#92691,#92692),(#92693,#92694,#92695),(#92696,#92697,#92698),(#92699,
#92700,#92701),(#92702,#92703,#92704),(#92705,#92706,#92707),(#92708,#92709,
#92710),(#92711,#92712,#92713),(#92714,#92715,#92716),(#92717,#92718,#92719),
(#92720,#92721,#92722),(#92723,#92724,#92725),(#92726,#92727,#92728),(#92729,
#92730,#92731),(#92732,#92733,#92734),(#92735,#92736,#92737),(#92738,#92739,
#92740),(#92741,#92742,#92743),(#92744,#92745,#92746)),.UNSPECIFIED.,.F.,
 .F.,.F.)
B_SPLINE_SURFACE_WITH_KNOTS((4,2,2,2,2,2,2,2,2,2,2,2,2,4),(3,3),(0.,0.00784373710475995,
0.0117656056571399,0.0137265399333299,0.0156874742095199,0.0235312113142798,
0.0254921455904698,0.0274530798666598,0.0313749484190398,0.0392186855237997,
0.0431405540761797,0.0470624226285597,0.0549061597333196,0.0627498968380796),
(0.,1.),.UNSPECIFIED.)
GEOMETRIC_REPRESENTATION_ITEM()
RATIONAL_B_SPLINE_SURFACE(((1.,0.707106781186548,1.),(1.,0.707106781186548,
1.),(1.,0.707106781186548,1.),(1.,0.707106781186548,1.),(1.,0.707106781186548,
1.),(1.,0.707106781186548,1.),(1.,0.707106781186548,1.),(1.,0.707106781186548,
1.),(1.,0.707106781186539,1.),(1.,0.707106781186539,1.),(1.,0.707106781186558,
1.),(1.,0.707106781186558,1.),(1.,0.707106781186545,1.),(1.,0.707106781186545,
1.),(1.,0.70710678118655,1.),(1.,0.70710678118655,1.),(1.,0.707106781186557,
1.),(1.,0.707106781186557,1.),(1.,0.707106781186552,1.),(1.,0.707106781186552,
1.),(1.,0.707106781186543,1.),(1.,0.707106781186543,1.),(1.,0.707106781186538,
1.),(1.,0.707106781186538,1.),(1.,0.707106781186552,1.),(1.,0.707106781186552,
1.),(1.,0.707106781186552,1.),(1.,0.707106781186552,1.)))
REPRESENTATION_ITEM('')
SURFACE()
);
#1639=(
BOUNDED_SURFACE()
B_SPLINE_SURFACE(3,2,((#92883,#92884,#92885),(#92886,#92887,#92888),(#92889,
#92890,#92891),(#92892,#92893,#92894),(#92895,#92896,#92897),(#92898,#92899,
#92900),(#92901,#92902,#92903),(#92904,#92905,#92906),(#92907,#92908,#92909),
(#92910,#92911,#92912),(#92913,#92914,#92915),(#92916,#92917,#92918)),
 .UNSPECIFIED.,.F.,.F.,.F.)
B_SPLINE_SURFACE_WITH_KNOTS((4,2,2,2,2,4),(3,3),(-1.51788304147971E-17,
0.001026154090376,0.00205230818075201,0.00307846227112803,0.00359153931631603,
0.00410461636150404),(0.,1.),.UNSPECIFIED.)
GEOMETRIC_REPRESENTATION_ITEM()
RATIONAL_B_SPLINE_SURFACE(((1.,0.707106781186551,1.),(1.,0.737458539324085,
1.),(1.,0.765604818101815,1.),(1.,0.818578626740854,1.),(1.,0.843670764069377,
1.),(1.,0.88861714259258,1.),(1.,0.909068963683481,1.),(1.,0.932796796200486,
1.),(1.,0.939529068116547,1.),(1.,0.948990840857779,1.),(1.,0.951717595991349,
1.),(1.,0.951672260128341,1.)))
REPRESENTATION_ITEM('')
SURFACE()
);
#1640=(
BOUNDED_SURFACE()
B_SPLINE_SURFACE(3,2,((#93010,#93011,#93012),(#93013,#93014,#93015),(#93016,
#93017,#93018),(#93019,#93020,#93021),(#93022,#93023,#93024),(#93025,#93026,
#93027),(#93028,#93029,#93030),(#93031,#93032,#93033),(#93034,#93035,#93036),
(#93037,#93038,#93039),(#93040,#93041,#93042),(#93043,#93044,#93045),(#93046,
#93047,#93048),(#93049,#93050,#93051)),.UNSPECIFIED.,.F.,.F.,.F.)
B_SPLINE_SURFACE_WITH_KNOTS((4,2,2,2,2,2,4),(3,3),(-8.43509290193722E-17,
0.000727263540504352,0.00109089531075657,0.00145452708100879,0.00181815885126101,
0.00218179062151323,0.00290905416201766),(0.,1.),.UNSPECIFIED.)
GEOMETRIC_REPRESENTATION_ITEM()
RATIONAL_B_SPLINE_SURFACE(((1.,0.725721029069481,1.),(1.,0.724034693474907,
1.),(1.,0.721379296500622,1.),(1.,0.716422727384689,1.),(1.,0.714644097901878,
1.),(1.,0.710947104597259,1.),(1.,0.709008369219941,1.),(1.,0.705233944978655,
1.),(1.,0.703402722400818,1.),(1.,0.699997845626205,1.),(1.,0.698413596841744,
1.),(1.,0.694441904737375,1.),(1.,0.692773088959507,1.),(1.,0.69256010548478,
1.)))
REPRESENTATION_ITEM('')
SURFACE()
);
#1641=(
BOUNDED_SURFACE()
B_SPLINE_SURFACE(3,2,((#93095,#93096,#93097),(#93098,#93099,#93100),(#93101,
#93102,#93103),(#93104,#93105,#93106)),.UNSPECIFIED.,.F.,.F.,.F.)
B_SPLINE_SURFACE_WITH_KNOTS((4,4),(3,3),(-2.84494650060196E-16,0.00346720850760631),
(0.,1.),.UNSPECIFIED.)
GEOMETRIC_REPRESENTATION_ITEM()
RATIONAL_B_SPLINE_SURFACE(((1.,0.69256010548478,1.),(1.,0.692352515709661,
1.),(1.,0.693728033206585,1.),(1.,0.696613144076467,1.)))
REPRESENTATION_ITEM('')
SURFACE()
);
#1642=(
BOUNDED_SURFACE()
B_SPLINE_SURFACE(3,2,((#93116,#93117,#93118),(#93119,#93120,#93121),(#93122,
#93123,#93124),(#93125,#93126,#93127),(#93128,#93129,#93130),(#93131,#93132,
#93133),(#93134,#93135,#93136),(#93137,#93138,#93139)),.UNSPECIFIED.,.F.,
 .F.,.F.)
B_SPLINE_SURFACE_WITH_KNOTS((4,2,2,4),(3,3),(-2.56413813792822E-15,0.00117043131394467,
0.00175564697091828,0.0023408626278919),(0.,1.),.UNSPECIFIED.)
GEOMETRIC_REPRESENTATION_ITEM()
RATIONAL_B_SPLINE_SURFACE(((1.,0.829660876349343,1.),(1.,0.821608938591335,
1.),(1.,0.808805545265545,1.),(1.,0.782695994949833,1.),(1.,0.772729068233022,
1.),(1.,0.750888902265591,1.),(1.,0.738815967034684,1.),(1.,0.725721029069557,
1.)))
REPRESENTATION_ITEM('')
SURFACE()
);
#1643=(
BOUNDED_SURFACE()
B_SPLINE_SURFACE(3,2,((#93182,#93183,#93184),(#93185,#93186,#93187),(#93188,
#93189,#93190),(#93191,#93192,#93193),(#93194,#93195,#93196),(#93197,#93198,
#93199),(#93200,#93201,#93202),(#93203,#93204,#93205),(#93206,#93207,#93208),
(#93209,#93210,#93211),(#93212,#93213,#93214),(#93215,#93216,#93217),(#93218,
#93219,#93220),(#93221,#93222,#93223),(#93224,#93225,#93226),(#93227,#93228,
#93229),(#93230,#93231,#93232),(#93233,#93234,#93235),(#93236,#93237,#93238),
(#93239,#93240,#93241),(#93242,#93243,#93244),(#93245,#93246,#93247),(#93248,
#93249,#93250),(#93251,#93252,#93253),(#93254,#93255,#93256),(#93257,#93258,
#93259),(#93260,#93261,#93262),(#93263,#93264,#93265),(#93266,#93267,#93268),
(#93269,#93270,#93271)),.UNSPECIFIED.,.F.,.F.,.F.)
B_SPLINE_SURFACE_WITH_KNOTS((4,2,2,2,2,2,2,2,2,2,2,2,2,2,4),(3,3),(-2.39565312032397E-15,
0.00505776268902388,0.00758664403353702,0.0101155253780502,0.0151732880670764,
0.0177021694115896,0.0189666100838462,0.0202310507561027,0.025288813445129,
0.0278176947896421,0.0290821354618987,0.0303465761341553,0.0354043388231816,
0.0379332201676947,0.0404621015122078),(0.,1.),.UNSPECIFIED.)
GEOMETRIC_REPRESENTATION_ITEM()
RATIONAL_B_SPLINE_SURFACE(((1.,0.696613144076472,1.),(1.,0.696599130026136,
1.),(1.,0.696575727272268,1.),(1.,0.696538360390545,1.),(1.,0.696525560572403,
1.),(1.,0.696502310365975,1.),(1.,0.696491830261394,1.),(1.,0.696470340381519,
1.),(1.,0.696468946397757,1.),(1.,0.696519595395987,1.),(1.,0.696545414772987,
1.),(1.,0.696603616414338,1.),(1.,0.696626278754734,1.),(1.,0.696679373029936,
1.),(1.,0.696709897027162,1.),(1.,0.69688419627133,1.),(1.,0.697091091364156,
1.),(1.,0.697570485772635,1.),(1.,0.697758737895884,1.),(1.,0.698095724987984,
1.),(1.,0.698217184521284,1.),(1.,0.698480760086518,1.),(1.,0.698623206103489,
1.),(1.,0.699386462708979,1.),(1.,0.700161541053975,1.),(1.,0.701679166289421,
1.),(1.,0.702244592832563,1.),(1.,0.703518483373878,1.),(1.,0.704229250046039,
1.),(1.,0.705017710605485,1.)))
REPRESENTATION_ITEM('')
SURFACE()
);
#1644=(
BOUNDED_SURFACE()
B_SPLINE_SURFACE(3,2,((#93358,#93359,#93360),(#93361,#93362,#93363),(#93364,
#93365,#93366),(#93367,#93368,#93369),(#93370,#93371,#93372),(#93373,#93374,
#93375),(#93376,#93377,#93378),(#93379,#93380,#93381),(#93382,#93383,#93384),
(#93385,#93386,#93387),(#93388,#93389,#93390),(#93391,#93392,#93393)),
 .UNSPECIFIED.,.F.,.F.,.F.)
B_SPLINE_SURFACE_WITH_KNOTS((4,2,2,2,2,4),(3,3),(0.,0.00381964231177775,
0.0076392846235555,0.00954910577944438,0.0114589269353332,0.015278569247111),
(0.,1.),.UNSPECIFIED.)
GEOMETRIC_REPRESENTATION_ITEM()
RATIONAL_B_SPLINE_SURFACE(((1.,0.781244946784369,1.),(1.,0.781562440256923,
1.),(1.,0.783026424270278,1.),(1.,0.787952903484347,1.),(1.,0.791415097203598,
1.),(1.,0.797906633970797,1.),(1.,0.800295219844003,1.),(1.,0.805396324076371,
1.),(1.,0.808114271065591,1.),(1.,0.816694595542238,1.),(1.,0.822982727529132,
1.),(1.,0.829660876349356,1.)))
REPRESENTATION_ITEM('')
SURFACE()
);
#1645=(
BOUNDED_SURFACE()
B_SPLINE_SURFACE(3,2,((#93427,#93428,#93429),(#93430,#93431,#93432),(#93433,
#93434,#93435),(#93436,#93437,#93438),(#93439,#93440,#93441),(#93442,#93443,
#93444)),.UNSPECIFIED.,.F.,.F.,.F.)
B_SPLINE_SURFACE_WITH_KNOTS((4,2,4),(3,3),(0.00622093395683224,0.00836137417484186,
0.0105018143928515),(0.215795545199942,1.),.UNSPECIFIED.)
GEOMETRIC_REPRESENTATION_ITEM()
RATIONAL_B_SPLINE_SURFACE(((0.900161575810827,0.768673574571085,1.),(0.906212716749595,
0.782694116406556,1.),(0.909226759580194,0.789677677693251,1.),(0.909711211930778,
0.790800157654861,1.),(0.907180359960508,0.784936153446793,1.),(0.901691029052784,
0.772217329935776,1.)))
REPRESENTATION_ITEM('')
SURFACE()
);
#1646=(
BOUNDED_SURFACE()
B_SPLINE_SURFACE(3,2,((#93446,#93447,#93448),(#93449,#93450,#93451),(#93452,
#93453,#93454),(#93455,#93456,#93457),(#93458,#93459,#93460),(#93461,#93462,
#93463),(#93464,#93465,#93466),(#93467,#93468,#93469),(#93470,#93471,#93472),
(#93473,#93474,#93475),(#93476,#93477,#93478),(#93479,#93480,#93481),(#93482,
#93483,#93484),(#93485,#93486,#93487),(#93488,#93489,#93490),(#93491,#93492,
#93493),(#93494,#93495,#93496),(#93497,#93498,#93499),(#93500,#93501,#93502),
(#93503,#93504,#93505),(#93506,#93507,#93508),(#93509,#93510,#93511),(#93512,
#93513,#93514),(#93515,#93516,#93517)),.UNSPECIFIED.,.F.,.F.,.F.)
B_SPLINE_SURFACE_WITH_KNOTS((4,2,2,2,2,2,2,2,2,2,2,4),(3,3),(0.044623233310389,
0.0484077487639251,0.0503000064906932,0.0521922642174613,0.0559767796709975,
0.0578690373977656,0.0597612951245336,0.0635458105780698,0.067330326031606,
0.0692225837583741,0.0711148414851421,0.0748993569386783),(0.,1.),
 .UNSPECIFIED.)
GEOMETRIC_REPRESENTATION_ITEM()
RATIONAL_B_SPLINE_SURFACE(((1.,0.709536628273658,1.),(1.,0.711112477964268,
1.),(1.,0.712886961021962,1.),(1.,0.715904125550345,1.),(1.,0.716973272082696,
1.),(1.,0.71921250292588,1.),(1.,0.720383423890183,1.),(1.,0.724054149508398,
1.),(1.,0.726712444737782,1.),(1.,0.731025306021556,1.),(1.,0.732517045915888,
1.),(1.,0.735608355478324,1.),(1.,0.737211774675347,1.),(1.,0.742154682346366,
1.),(1.,0.74559035921566,1.),(1.,0.752655465612555,1.),(1.,0.756285259234572,
1.),(1.,0.761780390504015,1.),(1.,0.76362016208338,1.),(1.,0.767295160021535,
1.),(1.,0.769124263260604,1.),(1.,0.774512328170999,1.),(1.,0.77798836077047,
1.),(1.,0.781244946784368,1.)))
REPRESENTATION_ITEM('')
SURFACE()
);
#1647=(
BOUNDED_SURFACE()
B_SPLINE_SURFACE(3,2,((#93592,#93593,#93594),(#93595,#93596,#93597),(#93598,
#93599,#93600),(#93601,#93602,#93603),(#93604,#93605,#93606),(#93607,#93608,
#93609),(#93610,#93611,#93612),(#93613,#93614,#93615),(#93616,#93617,#93618),
(#93619,#93620,#93621),(#93622,#93623,#93624),(#93625,#93626,#93627),(#93628,
#93629,#93630),(#93631,#93632,#93633),(#93634,#93635,#93636),(#93637,#93638,
#93639),(#93640,#93641,#93642),(#93643,#93644,#93645),(#93646,#93647,#93648),
(#93649,#93650,#93651),(#93652,#93653,#93654),(#93655,#93656,#93657),(#93658,
#93659,#93660),(#93661,#93662,#93663),(#93664,#93665,#93666),(#93667,#93668,
#93669),(#93670,#93671,#93672),(#93673,#93674,#93675),(#93676,#93677,#93678),
(#93679,#93680,#93681),(#93682,#93683,#93684),(#93685,#93686,#93687),(#93688,
#93689,#93690),(#93691,#93692,#93693),(#93694,#93695,#93696),(#93697,#93698,
#93699),(#93700,#93701,#93702),(#93703,#93704,#93705),(#93706,#93707,#93708),
(#93709,#93710,#93711),(#93712,#93713,#93714),(#93715,#93716,#93717),(#93718,
#93719,#93720),(#93721,#93722,#93723),(#93724,#93725,#93726),(#93727,#93728,
#93729),(#93730,#93731,#93732),(#93733,#93734,#93735),(#93736,#93737,#93738),
(#93739,#93740,#93741),(#93742,#93743,#93744),(#93745,#93746,#93747)),
 .UNSPECIFIED.,.F.,.F.,.F.)
B_SPLINE_SURFACE_WITH_KNOTS((4,2,2,2,2,2,2,2,2,2,2,2,2,2,2,2,2,2,2,2,2,
2,2,2,2,4),(3,3),(0.,0.0246541424270968,0.0493082848541936,0.0739624272812903,
0.0862894984948387,0.0986165697083871,0.110943640921935,0.123270712135484,
0.129434247742258,0.135597783349032,0.141761318955806,0.144843086759194,
0.147924854562581,0.154088390169355,0.160251925776129,0.163333693579516,
0.16487457748121,0.166415461382903,0.172578996989677,0.175660764793065,
0.178742532596452,0.184906068203226,0.187987836006613,0.189528719908306,
0.19106960381,0.197233139416774),(0.,1.),.UNSPECIFIED.)
GEOMETRIC_REPRESENTATION_ITEM()
RATIONAL_B_SPLINE_SURFACE(((1.,0.709074301978794,1.),(1.,0.709074301978794,
1.),(1.,0.708963390930669,1.),(1.,0.710109418369442,1.),(1.,0.711345435969898,
1.),(1.,0.716322609340493,1.),(1.,0.720058949582277,1.),(1.,0.72837691193742,
1.),(1.,0.731601440707376,1.),(1.,0.739089721988529,1.),(1.,0.743354004659929,
1.),(1.,0.753044180212456,1.),(1.,0.758471196283739,1.),(1.,0.770572077971438,
1.),(1.,0.777247974837517,1.),(1.,0.788198389680482,1.),(1.,0.792007762550323,
1.),(1.,0.79989916400913,1.),(1.,0.803980722224322,1.),(1.,0.812377434705544,
1.),(1.,0.816692624895053,1.),(1.,0.82329981820533,1.),(1.,0.825524485365509,
1.),(1.,0.830009997246824,1.),(1.,0.832273217353446,1.),(1.,0.839066413030268,
1.),(1.,0.843609213674719,1.),(1.,0.852620563957069,1.),(1.,0.857088966114341,
1.),(1.,0.863655694461054,1.),(1.,0.86582194782431,1.),(1.,0.869027054063668,
1.),(1.,0.8700880407856,1.),(1.,0.872193462935808,1.),(1.,0.873239200602622,
1.),(1.,0.878385612494048,1.),(1.,0.882266154343622,1.),(1.,0.887638176463745,
1.),(1.,0.889353780493633,1.),(1.,0.892609052853279,1.),(1.,0.894152648985923,
1.),(1.,0.898377291742568,1.),(1.,0.900580262495945,1.),(1.,0.903583189673952,
1.),(1.,0.904578419755403,1.),(1.,0.906308844732561,1.),(1.,0.90692493411477,
1.),(1.,0.908224668315115,1.),(1.,0.90890921926144,1.),(1.,0.912472172767833,
1.),(1.,0.915754136767764,1.),(1.,0.918929033017135,1.)))
REPRESENTATION_ITEM('')
SURFACE()
);
#1648=(
BOUNDED_SURFACE()
B_SPLINE_SURFACE(3,2,((#94143,#94144,#94145),(#94146,#94147,#94148),(#94149,
#94150,#94151),(#94152,#94153,#94154),(#94155,#94156,#94157),(#94158,#94159,
#94160),(#94161,#94162,#94163),(#94164,#94165,#94166),(#94167,#94168,#94169),
(#94170,#94171,#94172),(#94173,#94174,#94175),(#94176,#94177,#94178),(#94179,
#94180,#94181),(#94182,#94183,#94184)),.UNSPECIFIED.,.F.,.F.,.F.)
B_SPLINE_SURFACE_WITH_KNOTS((4,2,2,2,2,2,4),(3,3),(0.00157084992542587,
0.00258948856452903,0.00355026347239947,0.00403065092633469,0.00451103838026991,
0.00499142583420513,0.00552967701937307),(0.,1.00005786373123),
 .UNSPECIFIED.)
GEOMETRIC_REPRESENTATION_ITEM()
RATIONAL_B_SPLINE_SURFACE(((1.,0.704737095511617,1.0000341700267),(1.,0.736101336346774,
1.00003054032269),(1.,0.764731830804985,1.00002722698822),(1.,0.815971505611802,
1.00002129715068),(1.,0.839121073814733,1.00001861810989),(1.,0.868723144579927,
1.00001519233736),(1.,0.877891123385711,1.00001413135044),(1.,0.893882869863667,
1.00001228066619),(1.,0.900743560306276,1.0000114866959),(1.,0.911766049485974,
1.0000102110912),(1.,0.915689588589873,1.00000975702997),(1.,0.920335904299819,
1.00000921932364),(1.,0.920452978363282,1.00000920577496),(1.,0.918312342823876,
1.00000945350528)))
REPRESENTATION_ITEM('')
SURFACE()
);
#1649=(
BOUNDED_SURFACE()
B_SPLINE_SURFACE(3,2,((#94281,#94282,#94283),(#94284,#94285,#94286),(#94287,
#94288,#94289),(#94290,#94291,#94292),(#94293,#94294,#94295),(#94296,#94297,
#94298),(#94299,#94300,#94301),(#94302,#94303,#94304),(#94305,#94306,#94307),
(#94308,#94309,#94310),(#94311,#94312,#94313),(#94314,#94315,#94316)),
 .UNSPECIFIED.,.F.,.F.,.F.)
B_SPLINE_SURFACE_WITH_KNOTS((4,2,2,2,2,4),(3,3),(0.,0.0240998197753932,
0.0481996395507863,0.0722994593261795,0.0843493692138761,0.0963992791015727),
(0.,1.),.UNSPECIFIED.)
GEOMETRIC_REPRESENTATION_ITEM()
RATIONAL_B_SPLINE_SURFACE(((1.,0.709074301978794,1.),(1.,0.709074301978794,
1.),(1.,0.708967090641946,1.),(1.,0.710030391587723,1.),(1.,0.711181727679598,
1.),(1.,0.715829967728869,1.),(1.,0.719322261302017,1.),(1.,0.727098307859076,
1.),(1.,0.730113359209246,1.),(1.,0.737118658661219,1.),(1.,0.741109043083379,
1.),(1.,0.745647926668359,1.)))
REPRESENTATION_ITEM('')
SURFACE()
);
#1650=(
BOUNDED_SURFACE()
B_SPLINE_SURFACE(3,2,((#94357,#94358,#94359),(#94360,#94361,#94362),(#94363,
#94364,#94365),(#94366,#94367,#94368)),.UNSPECIFIED.,.F.,.F.,.F.)
B_SPLINE_SURFACE_WITH_KNOTS((4,4),(3,3),(0.,0.000852897709755378),(0.,1.),
 .UNSPECIFIED.)
GEOMETRIC_REPRESENTATION_ITEM()
RATIONAL_B_SPLINE_SURFACE(((1.,0.707106781186548,1.),(1.,0.708115545993389,
1.),(1.,0.709103409674823,1.),(1.,0.710072428249471,1.)))
REPRESENTATION_ITEM('')
SURFACE()
);
#1651=(
BOUNDED_SURFACE()
B_SPLINE_SURFACE(3,2,((#94374,#94375,#94376),(#94377,#94378,#94379),(#94380,
#94381,#94382),(#94383,#94384,#94385),(#94386,#94387,#94388),(#94389,#94390,
#94391),(#94392,#94393,#94394),(#94395,#94396,#94397),(#94398,#94399,#94400),
(#94401,#94402,#94403),(#94404,#94405,#94406),(#94407,#94408,#94409),(#94410,
#94411,#94412),(#94413,#94414,#94415),(#94416,#94417,#94418),(#94419,#94420,
#94421)),.UNSPECIFIED.,.F.,.F.,.F.)
B_SPLINE_SURFACE_WITH_KNOTS((4,2,2,2,2,2,2,4),(3,3),(0.00112108086692784,
0.00160664620305947,0.00209221153919109,0.00257777687532272,0.00306334221145435,
0.00354890754758597,0.0040344728837176,0.00500560355598086),(0.,1.),
 .UNSPECIFIED.)
GEOMETRIC_REPRESENTATION_ITEM()
RATIONAL_B_SPLINE_SURFACE(((1.,0.918929033017135,1.),(1.,0.920406077770156,
1.),(1.,0.92007472019659,1.),(1.,0.915695855491378,1.),(1.,0.911745925902294,
1.),(1.,0.900758581231695,1.),(1.,0.893857751485131,1.),(1.,0.877902801467609,
1.),(1.,0.868723355189685,1.),(1.,0.849021030588752,1.),(1.,0.838418680991936,
1.),(1.,0.815752189451713,1.),(1.,0.803660285004169,1.),(1.,0.766185207769967,
1.),(1.,0.739276146867789,1.),(1.,0.710072428249468,1.)))
REPRESENTATION_ITEM('')
SURFACE()
);
#1652=(
BOUNDED_SURFACE()
B_SPLINE_SURFACE(3,2,((#94571,#94572,#94573),(#94574,#94575,#94576),(#94577,
#94578,#94579),(#94580,#94581,#94582),(#94583,#94584,#94585),(#94586,#94587,
#94588),(#94589,#94590,#94591),(#94592,#94593,#94594),(#94595,#94596,#94597),
(#94598,#94599,#94600),(#94601,#94602,#94603),(#94604,#94605,#94606),(#94607,
#94608,#94609),(#94610,#94611,#94612),(#94613,#94614,#94615),(#94616,#94617,
#94618),(#94619,#94620,#94621),(#94622,#94623,#94624),(#94625,#94626,#94627),
(#94628,#94629,#94630),(#94631,#94632,#94633),(#94634,#94635,#94636),(#94637,
#94638,#94639),(#94640,#94641,#94642),(#94643,#94644,#94645),(#94646,#94647,
#94648),(#94649,#94650,#94651),(#94652,#94653,#94654),(#94655,#94656,#94657),
(#94658,#94659,#94660),(#94661,#94662,#94663),(#94664,#94665,#94666)),
 .UNSPECIFIED.,.F.,.F.,.F.)
B_SPLINE_SURFACE_WITH_KNOTS((4,2,2,2,2,2,2,2,2,2,2,2,2,2,2,4),(3,3),(0.,
0.0224324402603045,0.044864880520609,0.0672973207809135,0.0785135409110657,
0.089729761041218,0.112162201301522,0.123378421431675,0.134594641561827,
0.140202751626903,0.145810861691979,0.157027081822131,0.168243301952284,
0.171047356984822,0.17385141201736,0.179459522082436),(0.,1.),
 .UNSPECIFIED.)
GEOMETRIC_REPRESENTATION_ITEM()
RATIONAL_B_SPLINE_SURFACE(((1.,0.707106781186547,1.),(1.,0.707106781186547,
1.),(1.,0.707106781186548,1.),(1.,0.707106781186548,1.),(1.,0.707106781186548,
1.),(1.,0.707106781186548,1.),(1.,0.707106781186548,1.),(1.,0.707106781186548,
1.),(1.,0.707106781186548,1.),(1.,0.707106781186548,1.),(1.,0.707106781186548,
1.),(1.,0.707106781186548,1.),(1.,0.707106781186548,1.),(1.,0.707106781186548,
1.),(1.,0.707106781186548,1.),(1.,0.707106781186548,1.),(1.,0.707106781186548,
1.),(1.,0.707106781186548,1.),(1.,0.707106781186548,1.),(1.,0.707106781186548,
1.),(1.,0.707106781186548,1.),(1.,0.707106781186548,1.),(1.,0.707106781186548,
1.),(1.,0.707106781186548,1.),(1.,0.707106781186548,1.),(1.,0.707106781186548,
1.),(1.,0.707106781186557,1.),(1.,0.707106781186557,1.),(1.,0.707106781186548,
1.),(1.,0.707106781186548,1.),(1.,0.707106781186554,1.),(1.,0.707106781186554,
1.)))
REPRESENTATION_ITEM('')
SURFACE()
);
#1653=(
BOUNDED_SURFACE()
B_SPLINE_SURFACE(3,2,((#94746,#94747,#94748),(#94749,#94750,#94751),(#94752,
#94753,#94754),(#94755,#94756,#94757)),.UNSPECIFIED.,.F.,.F.,.F.)
B_SPLINE_SURFACE_WITH_KNOTS((4,4),(3,3),(0.,0.000852980308014371),(0.,1.),
 .UNSPECIFIED.)
GEOMETRIC_REPRESENTATION_ITEM()
RATIONAL_B_SPLINE_SURFACE(((1.,0.70710678118654,1.),(1.,0.708115537335819,
1.),(1.,0.709103401373757,1.),(1.,0.710072428249464,1.)))
REPRESENTATION_ITEM('')
SURFACE()
);
#1654=(
BOUNDED_SURFACE()
B_SPLINE_SURFACE(3,2,((#94763,#94764,#94765),(#94766,#94767,#94768),(#94769,
#94770,#94771),(#94772,#94773,#94774),(#94775,#94776,#94777),(#94778,#94779,
#94780),(#94781,#94782,#94783),(#94784,#94785,#94786),(#94787,#94788,#94789),
(#94790,#94791,#94792)),.UNSPECIFIED.,.F.,.F.,.F.)
B_SPLINE_SURFACE_WITH_KNOTS((4,2,2,2,4),(3,3),(-9.09012448646607E-14,0.0074893773271988,
0.0149787546544885,0.0224681319817782,0.0299575093090679),(0.,1.),
 .UNSPECIFIED.)
GEOMETRIC_REPRESENTATION_ITEM()
RATIONAL_B_SPLINE_SURFACE(((1.,0.707106781186548,1.),(1.,0.707106781186548,
1.),(1.,0.707106781186553,1.),(1.,0.707106781186553,1.),(1.,0.707106781186547,
1.),(1.,0.707106781186547,1.),(1.,0.707106781186548,1.),(1.,0.707106781186548,
1.),(1.,0.707106781186548,1.),(1.,0.707106781186548,1.)))
REPRESENTATION_ITEM('')
SURFACE()
);
#1655=(
BOUNDED_SURFACE()
B_SPLINE_SURFACE(3,2,((#94873,#94874,#94875),(#94876,#94877,#94878),(#94879,
#94880,#94881),(#94882,#94883,#94884),(#94885,#94886,#94887),(#94888,#94889,
#94890),(#94891,#94892,#94893),(#94894,#94895,#94896),(#94897,#94898,#94899),
(#94900,#94901,#94902),(#94903,#94904,#94905),(#94906,#94907,#94908),(#94909,
#94910,#94911),(#94912,#94913,#94914),(#94915,#94916,#94917),(#94918,#94919,
#94920),(#94921,#94922,#94923),(#94924,#94925,#94926),(#94927,#94928,#94929),
(#94930,#94931,#94932),(#94933,#94934,#94935),(#94936,#94937,#94938),(#94939,
#94940,#94941),(#94942,#94943,#94944),(#94945,#94946,#94947),(#94948,#94949,
#94950),(#94951,#94952,#94953),(#94954,#94955,#94956),(#94957,#94958,#94959),
(#94960,#94961,#94962),(#94963,#94964,#94965),(#94966,#94967,#94968),(#94969,
#94970,#94971),(#94972,#94973,#94974),(#94975,#94976,#94977),(#94978,#94979,
#94980),(#94981,#94982,#94983),(#94984,#94985,#94986),(#94987,#94988,#94989),
(#94990,#94991,#94992),(#94993,#94994,#94995),(#94996,#94997,#94998),(#94999,
#95000,#95001),(#95002,#95003,#95004),(#95005,#95006,#95007),(#95008,#95009,
#95010),(#95011,#95012,#95013),(#95014,#95015,#95016),(#95017,#95018,#95019),
(#95020,#95021,#95022),(#95023,#95024,#95025),(#95026,#95027,#95028),(#95029,
#95030,#95031),(#95032,#95033,#95034),(#95035,#95036,#95037),(#95038,#95039,
#95040),(#95041,#95042,#95043),(#95044,#95045,#95046),(#95047,#95048,#95049),
(#95050,#95051,#95052),(#95053,#95054,#95055),(#95056,#95057,#95058),(#95059,
#95060,#95061),(#95062,#95063,#95064),(#95065,#95066,#95067),(#95068,#95069,
#95070),(#95071,#95072,#95073),(#95074,#95075,#95076),(#95077,#95078,#95079),
(#95080,#95081,#95082),(#95083,#95084,#95085),(#95086,#95087,#95088),(#95089,
#95090,#95091),(#95092,#95093,#95094),(#95095,#95096,#95097),(#95098,#95099,
#95100),(#95101,#95102,#95103),(#95104,#95105,#95106),(#95107,#95108,#95109),
(#95110,#95111,#95112),(#95113,#95114,#95115),(#95116,#95117,#95118),(#95119,
#95120,#95121),(#95122,#95123,#95124),(#95125,#95126,#95127),(#95128,#95129,
#95130),(#95131,#95132,#95133),(#95134,#95135,#95136),(#95137,#95138,#95139),
(#95140,#95141,#95142),(#95143,#95144,#95145),(#95146,#95147,#95148),(#95149,
#95150,#95151),(#95152,#95153,#95154),(#95155,#95156,#95157),(#95158,#95159,
#95160),(#95161,#95162,#95163),(#95164,#95165,#95166),(#95167,#95168,#95169),
(#95170,#95171,#95172),(#95173,#95174,#95175),(#95176,#95177,#95178),(#95179,
#95180,#95181),(#95182,#95183,#95184),(#95185,#95186,#95187),(#95188,#95189,
#95190),(#95191,#95192,#95193),(#95194,#95195,#95196),(#95197,#95198,#95199),
(#95200,#95201,#95202),(#95203,#95204,#95205),(#95206,#95207,#95208),(#95209,
#95210,#95211),(#95212,#95213,#95214),(#95215,#95216,#95217),(#95218,#95219,
#95220)),.UNSPECIFIED.,.F.,.F.,.F.)
B_SPLINE_SURFACE_WITH_KNOTS((4,2,2,2,2,2,2,2,2,2,2,2,2,2,2,2,2,2,2,2,2,
2,2,2,2,2,2,2,2,2,2,2,2,2,2,2,2,2,2,2,2,2,2,2,2,2,2,2,2,2,2,2,2,2,2,2,2,
4),(3,3),(-0.000159417639105601,5.25012345884415E-5,0.000105002469176911,
0.000210004938353849,0.000420009876707727,0.000840019753415481,0.00168003950683099,
0.00336007901366201,0.00504011852049303,0.00672015802732404,0.0100802370409861,
0.0134403160546481,0.0168003950683101,0.0201604740819722,0.0235205530956342,
0.0268806321092963,0.0302407111229583,0.0336007901366203,0.0369608691502824,
0.0403209481639444,0.0436810271776064,0.0453610666844374,0.0470411061912685,
0.0487211456980995,0.0504011852049305,0.051241204958346,0.0520812247117615,
0.052921244465177,0.0537612642185925,0.054601283972008,0.0550212938487158,
0.0554413037254236,0.0558613136021313,0.0562813234788391,0.0567013333555468,
0.0571213432322546,0.0579613629856701,0.0588013827390856,0.0596414024925011,
0.0604814222459166,0.0621614617527476,0.0638415012595786,0.0655215407664097,
0.0672015802732407,0.0705616592869027,0.0739217383005648,0.0772818173142268,
0.0806418963278888,0.0873620543552129,0.094082212382537,0.100802370409861,
0.107522528437185,0.120962844491833,0.134403160546481,0.14784347660113,
0.161283792655778,0.188164424765074,0.215204474513476),(0.,1.00049765253644),
 .UNSPECIFIED.)
GEOMETRIC_REPRESENTATION_ITEM()
RATIONAL_B_SPLINE_SURFACE(((1.,0.999949367340627,1.00000005039494),(1.,
1.00000292399598,0.999999997089732),(1.,1.00000065570695,0.999999999347372),
(1.,0.999995149653455,1.00000000482757),(1.,0.999993866690958,1.00000000610451),
(1.,0.999989925403203,1.0000000100273),(1.,0.999987096878001,1.00000001284254),
(1.,0.99997833469904,1.00000002156358),(1.,0.999972169356053,1.00000002769998),
(1.,0.999953092103803,1.00000004668767),(1.,0.999939523207601,1.00000006019286),
(1.,0.999896582312161,1.00000010293215),(1.,0.999865028402933,1.00000013433792),
(1.,0.99976109014112,1.00000023778819),(1.,0.999679452472188,1.00000031904258),
(1.,0.99948567066185,1.0000005119146),(1.,0.99937353290825,1.00000062352587),
(1.,0.999110700111499,1.00000088512469),(1.,0.998960025063699,1.00000103509233),
(1.,0.998434367260317,1.00000155828221),(1.,0.997987950051853,1.00000200260352),
(1.,0.996776052520384,1.00000320881128),(1.,0.996011341315486,1.00000396993222),
(1.,0.993955400376975,1.00000601622067),(1.,0.992659906297562,1.0000073056325),
(1.,0.989276125492113,1.0000106735267),(1.,0.987170900665479,1.00001276886765),
(1.,0.98215667507351,1.00001775955182),(1.,0.979261511224488,1.00002064112308),
(1.,0.973160709403129,1.00002671328208),(1.,0.969970805398307,1.00002988820972),
(1.,0.9635930773515,1.0000362359948),(1.,0.960398704296731,1.00003941537051),
(1.,0.954031963961403,1.00004575221946),(1.,0.95085609693907,1.00004891317602),
(1.,0.9444675189357,1.00005527176011),(1.,0.941254261837805,1.0000584699312),
(1.,0.934708472493586,1.00006498498854),(1.,0.931376690992807,1.00006830112757),
(1.,0.924480383729073,1.00007516505718),(1.,0.920918391836673,1.00007871032578),
(1.,0.915258653779197,1.00008434349178),(1.,0.913318538561208,1.0000862744983),
(1.,0.909289199099064,1.0000902849203),(1.,0.907200548321262,1.00009236376502),
(1.,0.902807624646881,1.00009673606423),(1.,0.900504791744677,1.0000990280855),
(1.,0.895564714735884,1.00010394496921),(1.,0.892926137783545,1.00010657115824),
(1.,0.888550840104385,1.00011092591421),(1.,0.887026301150163,1.00011244329557),
(1.,0.883791478576254,1.00011566293089),(1.,0.88208209272103,1.0001173642913),
(1.,0.878387519679857,1.00012104151859),(1.,0.876404617983387,1.00012301511071),
(1.,0.871992495379262,1.00012740651872),(1.,0.869569843109419,1.00012981779681),
(1.,0.863909422913507,1.00013545164175),(1.,0.860681833252753,1.00013866407811),
(1.,0.854578489267958,1.00014473876734),(1.,0.85234061153918,1.00014696613839),
(1.,0.847339711856798,1.00015194355922),(1.,0.844566230719838,1.00015470401906),
(1.,0.838556583919586,1.00016068545101),(1.,0.835325483162265,1.00016390138198),
(1.,0.828864063959496,1.00017033246529),(1.,0.825653137654185,1.00017352831653),
(1.,0.819601311538472,1.00017955172977),(1.,0.816754485958108,1.00018238518971),
(1.,0.811453866107576,1.00018766092354),(1.,0.808994767190061,1.00019010847716),
(1.,0.802099709928181,1.00019697116263),(1.,0.798172772551782,1.00020087966333),
(1.,0.791166169096681,1.00020785337129),(1.,0.788081780349506,1.00021092327906),
(1.,0.782459542826891,1.00021651912058),(1.,0.779924928789769,1.00021904183479),
(1.,0.775247221203772,1.00022369758088),(1.,0.773105531885213,1.00022582921512),
(1.,0.76712446186861,1.00023178220445),(1.,0.763721566682336,1.00023516912329),
(1.,0.757649562702981,1.00024121261966),(1.,0.754986501187558,1.00024386317829),
(1.,0.750176146086482,1.00024865094913),(1.,0.748029059539643,1.00025078795526),
(1.,0.744138354127913,1.00025466039409),(1.,0.742391880608881,1.00025639866805),
(1.,0.737599380181131,1.00026116866803),(1.,0.734992429078544,1.00026376337969),
(1.,0.730493964703101,1.0002682407241),(1.,0.728608199101415,1.00027011763617),
(1.,0.725314975577855,1.00027339539825),(1.,0.723909745358972,1.00027479403102),
(1.,0.721433553601674,1.00027725859724),(1.,0.720363611737886,1.0002783235158),
(1.,0.717515918379571,1.00028115783945),(1.,0.716092416594757,1.00028257465799),
(1.,0.713767134874405,1.00028488902269),(1.,0.712870679247257,1.00028578126952),
(1.,0.71140011759095,1.000287244927),(1.,0.710826151043487,1.00028781619881),
(1.,0.709874603825523,1.00028876327859),(1.,0.709498188857635,1.00028913792631),
(1.,0.708557794279807,1.00029007390581),(1.,0.708176463449255,1.00029045344632),
(1.,0.707619701944943,1.00029100759387),(1.,0.707449638803699,1.00029117685857),
(1.,0.707205802728201,1.00029141954986),(1.,0.707133872162536,1.00029149114271),
(1.,0.707034573241446,1.00029158997543),(1.,0.707007932052635,1.00029161649154),
(1.,0.706956830206343,1.00029166735347),(1.,0.706958779087662,1.00029166541374),
(1.,0.7069598146507,1.00029166438304),(1.,0.706961036516168,1.00029166316691),
(0.999999999999999,0.706961022005169,1.00029166318135)))
REPRESENTATION_ITEM('')
SURFACE()
);
#1656=(
BOUNDED_SURFACE()
B_SPLINE_SURFACE(3,2,((#95897,#95898,#95899),(#95900,#95901,#95902),(#95903,
#95904,#95905),(#95906,#95907,#95908),(#95909,#95910,#95911),(#95912,#95913,
#95914),(#95915,#95916,#95917),(#95918,#95919,#95920),(#95921,#95922,#95923),
(#95924,#95925,#95926),(#95927,#95928,#95929),(#95930,#95931,#95932),(#95933,
#95934,#95935),(#95936,#95937,#95938),(#95939,#95940,#95941),(#95942,#95943,
#95944),(#95945,#95946,#95947),(#95948,#95949,#95950),(#95951,#95952,#95953),
(#95954,#95955,#95956),(#95957,#95958,#95959),(#95960,#95961,#95962),(#95963,
#95964,#95965),(#95966,#95967,#95968),(#95969,#95970,#95971),(#95972,#95973,
#95974),(#95975,#95976,#95977),(#95978,#95979,#95980),(#95981,#95982,#95983),
(#95984,#95985,#95986),(#95987,#95988,#95989),(#95990,#95991,#95992),(#95993,
#95994,#95995),(#95996,#95997,#95998),(#95999,#96000,#96001),(#96002,#96003,
#96004),(#96005,#96006,#96007),(#96008,#96009,#96010),(#96011,#96012,#96013),
(#96014,#96015,#96016),(#96017,#96018,#96019),(#96020,#96021,#96022),(#96023,
#96024,#96025),(#96026,#96027,#96028),(#96029,#96030,#96031),(#96032,#96033,
#96034),(#96035,#96036,#96037),(#96038,#96039,#96040),(#96041,#96042,#96043),
(#96044,#96045,#96046),(#96047,#96048,#96049),(#96050,#96051,#96052),(#96053,
#96054,#96055),(#96056,#96057,#96058),(#96059,#96060,#96061),(#96062,#96063,
#96064),(#96065,#96066,#96067),(#96068,#96069,#96070),(#96071,#96072,#96073),
(#96074,#96075,#96076),(#96077,#96078,#96079),(#96080,#96081,#96082),(#96083,
#96084,#96085),(#96086,#96087,#96088),(#96089,#96090,#96091),(#96092,#96093,
#96094),(#96095,#96096,#96097),(#96098,#96099,#96100),(#96101,#96102,#96103),
(#96104,#96105,#96106),(#96107,#96108,#96109),(#96110,#96111,#96112),(#96113,
#96114,#96115),(#96116,#96117,#96118),(#96119,#96120,#96121),(#96122,#96123,
#96124),(#96125,#96126,#96127),(#96128,#96129,#96130),(#96131,#96132,#96133),
(#96134,#96135,#96136),(#96137,#96138,#96139),(#96140,#96141,#96142),(#96143,
#96144,#96145),(#96146,#96147,#96148),(#96149,#96150,#96151),(#96152,#96153,
#96154),(#96155,#96156,#96157),(#96158,#96159,#96160),(#96161,#96162,#96163),
(#96164,#96165,#96166),(#96167,#96168,#96169),(#96170,#96171,#96172),(#96173,
#96174,#96175),(#96176,#96177,#96178)),.UNSPECIFIED.,.F.,.F.,.F.)
B_SPLINE_SURFACE_WITH_KNOTS((4,2,2,2,2,2,2,2,2,2,2,2,2,2,2,2,2,2,2,2,2,
2,2,2,2,2,2,2,2,2,2,2,2,2,2,2,2,2,2,2,2,2,2,2,2,2,4),(3,3),(-0.000455987201348429,
6.77530739903753E-5,0.000135506147980765,0.000271012295961543,0.0005420245919231,
0.00108404918384621,0.00216809836769244,0.0043361967353849,0.00650429510307735,
0.00867239347076981,0.0130085902061547,0.0151766885738472,0.0173447869415396,
0.0195128853092321,0.0216809836769245,0.023849082044617,0.0260171804123094,
0.0303533771476944,0.0346895738830793,0.0390257706184642,0.0433619673538491,
0.0455300657215415,0.047698164089234,0.0498662624569264,0.0509503116407727,
0.0520343608246189,0.0531184100084651,0.0536604346003882,0.0542024591923114,
0.0547444837842345,0.055015496080196,0.0552865083761576,0.0555575206721191,
0.0558285329680807,0.0560995452640423,0.0563705575600038,0.0569125821519269,
0.05745460674385,0.0579966313357732,0.0585386559276963,0.0596227051115425,
0.0607067542953887,0.0617908034792349,0.0628748526630812,0.0650429510307736,
0.0672110493984661,0.0693791477661585),(-0.00105667980444056,1.),
 .UNSPECIFIED.)
GEOMETRIC_REPRESENTATION_ITEM()
RATIONAL_B_SPLINE_SURFACE(((1.00000122872547,0.999418591393398,1.),(0.999999970682267,
1.00001387257154,1.),(0.999999984891384,1.00000714909853,1.),(1.0000000133113,
0.999993701353975,1.),(1.0000000169606,0.999991974577991,1.),(1.00000002816705,
0.999986671909136,1.),(1.00000003618925,0.999982875963573,1.),(1.00000006084249,
0.99997121053403,1.),(1.00000007816967,0.99996301165573,1.),(1.00000013222322,
0.999937434583641,1.),(1.00000017108158,0.999919047579035,1.),(1.00000029529396,
0.999860272733172,1.),(1.00000038845866,0.999816189039171,1.),(1.00000070251841,
0.999667582170744,1.),(1.00000095771891,0.99954682633964,1.),(1.00000159059792,
0.999247360501307,1.),(1.00000196820243,0.999068685507852,1.),(1.0000028904322,
0.998632304607156,1.),(1.00000343484386,0.998374699769646,1.),(1.00000541275052,
0.99743879342894,1.),(1.00000717381538,0.996605492340337,1.),(1.00001110917801,
0.994743356518011,1.),(1.00001264120727,0.994018430551732,1.),(1.00001629437776,
0.992289822476323,1.),(1.00001841824292,0.991284851457104,1.),(1.00002338906489,
0.988932756739908,1.),(1.00002624044633,0.987583539396207,1.),(1.00003266989126,
0.984541253121083,1.),(1.00003624703493,0.982848619430627,1.),(1.00004391733999,
0.979219182668691,1.),(1.00004800332235,0.977285776567571,1.),(1.00005640354012,
0.973310959535482,1.),(1.00006071496906,0.97127087656586,1.),(1.00007372132053,
0.96511652809888,1.),(1.00008246110805,0.960981033372461,1.),(1.00009983287502,
0.952761056566164,1.),(1.00010849085217,0.94866427288905,1.),(1.00012601542624,
0.940371990780815,1.),(1.00013488263451,0.936176203071392,1.),(1.00015325734255,
0.927481654375009,1.),(1.00016275199041,0.922988974649895,1.),(1.0001780326614,
0.915758463134714,1.),(1.00018330226891,0.913264989006041,1.),(1.00019438183262,
0.90802235842585,1.),(1.00020018692943,0.905275501342365,1.),(1.00021268132342,
0.8993634010367,1.),(1.00021935337707,0.896206317112169,1.),(1.00023061024255,
0.890879790841062,1.),(1.00023457668858,0.889002946966943,1.),(1.0002430696063,
0.884984266152402,1.),(1.00024759861899,0.882841226853296,1.),(1.00025759604395,
0.878110642946419,1.),(1.00026304750707,0.875531118337484,1.),(1.00027254695219,
0.871036168645314,1.),(1.0002759382853,0.869431456840574,1.),(1.00028339567493,
0.865902767449779,1.),(1.00028745809758,0.863980509341721,1.),(1.00029664982192,
0.859631167041402,1.),(1.00030180427318,0.857192182572172,1.),(1.00031072607401,
0.852970562746628,1.),(1.00031389851946,0.851469424257118,1.),(1.0003207022979,
0.848250010763257,1.),(1.00032433622182,0.846530509782674,1.),(1.00033205991999,
0.842875808456326,1.),(1.00033615148806,0.840939759307718,1.),(1.00034464121058,
0.836922590395633,1.),(1.00034903560759,0.83484324857865,1.),(1.0003578501401,
0.830672385995587,1.),(1.00036226481903,0.828583447176264,1.),(1.00037087202048,
0.824510689556839,1.),(1.00037506411381,0.822527073841625,1.),(1.00038714159423,
0.816812248801122,1.),(1.00039451387087,0.81332383319144,1.),(1.00040797039675,
0.806956471094042,1.),(1.00041408703279,0.804062199804767,1.),(1.00042528086499,
0.798765499632482,1.),(1.00043037654998,0.796354322200385,1.),(1.00043983949878,
0.791876641849007,1.),(1.00044420538629,0.789810790164972,1.),(1.00045647509847,
0.78400500485181,1.),(1.0004635657767,0.780649836045255,1.),(1.00047637896645,
0.774586887889098,1.),(1.00048209039966,0.771884350569236,1.),(1.00049254768431,
0.766936170141906,1.),(1.00049728941638,0.764692476240422,1.),(1.00050605146711,
0.760546447002399,1.),(1.0005100700131,0.758644950456529,1.),(1.00052128416306,
0.753338636324398,1.),(1.00052765962714,0.750321892724031,1.),(1.00053892919238,
0.744989357174405,1.),(1.00054380318641,0.742683079527015,1.),(1.00055251252087,
0.73856199458653,1.),(1.00055634149899,0.736750197813865,1.),(1.00055979741554,
0.735114926399246,1.)))
REPRESENTATION_ITEM('')
SURFACE()
);
#1657=(
BOUNDED_SURFACE()
B_SPLINE_SURFACE(3,2,((#96588,#96589,#96590),(#96591,#96592,#96593),(#96594,
#96595,#96596),(#96597,#96598,#96599),(#96600,#96601,#96602),(#96603,#96604,
#96605),(#96606,#96607,#96608),(#96609,#96610,#96611),(#96612,#96613,#96614),
(#96615,#96616,#96617),(#96618,#96619,#96620),(#96621,#96622,#96623),(#96624,
#96625,#96626),(#96627,#96628,#96629),(#96630,#96631,#96632),(#96633,#96634,
#96635),(#96636,#96637,#96638),(#96639,#96640,#96641),(#96642,#96643,#96644),
(#96645,#96646,#96647),(#96648,#96649,#96650),(#96651,#96652,#96653),(#96654,
#96655,#96656),(#96657,#96658,#96659),(#96660,#96661,#96662),(#96663,#96664,
#96665)),.UNSPECIFIED.,.F.,.F.,.F.)
B_SPLINE_SURFACE_WITH_KNOTS((4,2,2,2,2,2,2,2,2,2,2,2,4),(3,3),(0.155017009813997,
0.160281319258347,0.165545628702697,0.170809938147046,0.173442092869221,
0.174758170230309,0.176074247591396,0.181338557035746,0.18397071175792,
0.185286789119008,0.186602866480095,0.191867175924445,0.19714352226199),
(0.,1.0000120368932),.UNSPECIFIED.)
GEOMETRIC_REPRESENTATION_ITEM()
RATIONAL_B_SPLINE_SURFACE(((1.,0.850111718516678,1.00000360837847),(1.,
0.853975052401841,1.0000035153734),(1.,0.85784940533772,1.00000342210305),
(1.,0.865373998108453,1.00000324095761),(1.,0.869032295171854,1.00000315288855),
(1.,0.876071575182358,1.00000298342643),(1.,0.87945336507496,1.00000290201394),
(1.,0.884260511104441,1.00000278628773),(1.,0.885818521137499,1.00000274878053),
(1.,0.888078501958785,1.00000269437424),(1.,0.888819457713693,1.00000267653663),
(1.,0.890260900245237,1.00000264183565),(1.,0.890962995541521,1.00000262493355),
(1.,0.894376106658767,1.00000254276705),(1.,0.896789199731204,1.00000248467476),
(1.,0.899867832814397,1.0000024105604),(1.,0.900801953241813,1.00000238807259),
(1.,0.9021344685165,1.0000023559939),(1.,0.902568647198769,1.00000234554158),
(1.,0.903435292916418,1.00000232467813),(1.,0.90386932572828,1.00000231422932),
(1.,0.906115157049724,1.00000226016365),(1.,0.908273545910519,1.00000220820306),
(1.,0.913356587833321,1.000002085835),(1.,0.916197241241691,1.00000201744971),
(1.,0.918946876765757,1.00000195125558)))
REPRESENTATION_ITEM('')
SURFACE()
);
#1658=(
BOUNDED_SURFACE()
B_SPLINE_SURFACE(3,2,((#96751,#96752,#96753),(#96754,#96755,#96756),(#96757,
#96758,#96759),(#96760,#96761,#96762),(#96763,#96764,#96765),(#96766,#96767,
#96768),(#96769,#96770,#96771),(#96772,#96773,#96774),(#96775,#96776,#96777),
(#96778,#96779,#96780),(#96781,#96782,#96783),(#96784,#96785,#96786)),
 .UNSPECIFIED.,.F.,.F.,.F.)
B_SPLINE_SURFACE_WITH_KNOTS((4,2,2,2,2,4),(3,3),(0.0678369045371883,0.0816632472223668,
0.0954895899075452,0.123142275277902,0.150794960648259,0.178447646018616),
(0.,1.),.UNSPECIFIED.)
GEOMETRIC_REPRESENTATION_ITEM()
RATIONAL_B_SPLINE_SURFACE(((1.,0.707106781186538,1.),(1.,0.707106781186538,
1.),(1.,0.707106781186548,1.),(1.,0.707106781186548,1.),(1.,0.707106781186548,
1.),(1.,0.707106781186548,1.),(1.,0.707106781186548,1.),(1.,0.707106781186548,
1.),(1.,0.707106781186547,1.),(1.,0.707106781186547,1.),(1.,0.707106781186547,
1.),(1.,0.707106781186547,1.)))
REPRESENTATION_ITEM('')
SURFACE()
);
#1659=(
BOUNDED_SURFACE()
B_SPLINE_SURFACE(3,2,((#96801,#96802,#96803),(#96804,#96805,#96806),(#96807,
#96808,#96809),(#96810,#96811,#96812),(#96813,#96814,#96815),(#96816,#96817,
#96818),(#96819,#96820,#96821),(#96822,#96823,#96824),(#96825,#96826,#96827),
(#96828,#96829,#96830),(#96831,#96832,#96833),(#96834,#96835,#96836),(#96837,
#96838,#96839),(#96840,#96841,#96842)),.UNSPECIFIED.,.F.,.F.,.F.)
B_SPLINE_SURFACE_WITH_KNOTS((4,2,2,2,2,2,4),(3,3),(0.118318550770891,0.130409364032191,
0.142500177293491,0.154590990554791,0.166681803816091,0.190863430338691,
0.215045056861291),(0.,0.0769991253144525),.UNSPECIFIED.)
GEOMETRIC_REPRESENTATION_ITEM()
RATIONAL_B_SPLINE_SURFACE(((1.,0.977533303103487,0.958526438226447),(1.,
0.977510801002336,0.958484899308358),(1.,0.977496043811651,0.958457657508537),
(1.,0.977474369053602,0.958417645867262),(1.,0.977467466178115,0.958404903147037),
(1.,0.977457506956036,0.958386518405656),(1.,0.977454497282011,0.958380962542142),
(1.,0.977450352423876,0.958373311126773),(1.,0.977449238571154,0.9583712549527),
(1.,0.97744714373703,0.958367387885243),(1.,0.977447298282621,0.958367673176674),
(1.,0.977447427205131,0.958367911167852),(1.,0.97744747834083,0.958368005564442),
(1.,0.97744747834083,0.958368005564442)))
REPRESENTATION_ITEM('')
SURFACE()
);
#1660=(
BOUNDED_SURFACE()
B_SPLINE_SURFACE(3,2,((#97421,#97422,#97423),(#97424,#97425,#97426),(#97427,
#97428,#97429),(#97430,#97431,#97432),(#97433,#97434,#97435),(#97436,#97437,
#97438),(#97439,#97440,#97441),(#97442,#97443,#97444),(#97445,#97446,#97447),
(#97448,#97449,#97450),(#97451,#97452,#97453),(#97454,#97455,#97456),(#97457,
#97458,#97459),(#97460,#97461,#97462),(#97463,#97464,#97465),(#97466,#97467,
#97468),(#97469,#97470,#97471),(#97472,#97473,#97474),(#97475,#97476,#97477),
(#97478,#97479,#97480),(#97481,#97482,#97483),(#97484,#97485,#97486),(#97487,
#97488,#97489),(#97490,#97491,#97492),(#97493,#97494,#97495),(#97496,#97497,
#97498),(#97499,#97500,#97501),(#97502,#97503,#97504),(#97505,#97506,#97507),
(#97508,#97509,#97510),(#97511,#97512,#97513),(#97514,#97515,#97516),(#97517,
#97518,#97519),(#97520,#97521,#97522),(#97523,#97524,#97525),(#97526,#97527,
#97528),(#97529,#97530,#97531),(#97532,#97533,#97534),(#97535,#97536,#97537),
(#97538,#97539,#97540),(#97541,#97542,#97543),(#97544,#97545,#97546),(#97547,
#97548,#97549),(#97550,#97551,#97552),(#97553,#97554,#97555),(#97556,#97557,
#97558),(#97559,#97560,#97561),(#97562,#97563,#97564),(#97565,#97566,#97567),
(#97568,#97569,#97570),(#97571,#97572,#97573),(#97574,#97575,#97576),(#97577,
#97578,#97579),(#97580,#97581,#97582),(#97583,#97584,#97585),(#97586,#97587,
#97588),(#97589,#97590,#97591),(#97592,#97593,#97594),(#97595,#97596,#97597),
(#97598,#97599,#97600)),.UNSPECIFIED.,.F.,.F.,.F.)
B_SPLINE_SURFACE_WITH_KNOTS((4,2,2,2,2,2,2,2,2,2,2,2,2,2,2,2,2,2,2,2,2,
2,2,2,2,2,2,2,2,4),(3,3),(-0.00058262743669386,0.00319856320703094,0.00399820400878867,
0.00479784481054641,0.00639712641406187,0.00719676721581961,0.00799640801757734,
0.00959568962109281,0.0111949712246083,0.0127942528281237,0.0159928160351547,
0.0175920976386702,0.0191913792421856,0.0223899424492166,0.023989224052732,
0.0255885056562475,0.027187787259763,0.0279874280615207,0.0287870688632784,
0.0319856320703094,0.0335849136738248,0.0351841952773403,0.0367834768808558,
0.0383827584843712,0.0399820400878867,0.0415813216914022,0.0447798848984331,
0.0463791665019486,0.047978448105464,0.0517596387491888),(0.,1.00058262743669),
 .UNSPECIFIED.)
GEOMETRIC_REPRESENTATION_ITEM()
RATIONAL_B_SPLINE_SURFACE(((1.,0.372615622620617,1.00073106270323),(1.,
0.349888963005402,1.0007575450541),(1.,0.33336913321619,1.00077679486627),
(1.,0.327705676201969,1.00078339423716),(1.,0.327251477944985,1.00078392349389),
(1.,0.327438578938257,1.00078370547354),(1.,0.328073122498965,1.00078296606857),
(1.,0.331521383799571,1.00077894796528),(1.,0.335886927429418,1.00077386099429),
(1.,0.345028662937665,1.00076320854244),(1.,0.348522443164058,1.00075913739801),
(1.,0.356175477316151,1.00075021966266),(1.,0.360329629032238,1.00074537901713),
(1.,0.373578575616019,1.00072994061756),(1.,0.383450575672534,1.00071843722138),
(1.,0.404468341585455,1.00069394616722),(1.,0.415617057266219,1.00068095507195),
(1.,0.438646408868145,1.00065412000776),(1.,0.450439636237964,1.00064037789209),
(1.,0.485738524418637,1.00059924569062),(1.,0.509290450787533,1.00057180169364),
(1.,0.543406923368721,1.0005320473077),(1.,0.554585702870248,1.00051902118041),
(1.,0.576402400431413,1.00049359916725),(1.,0.586915261405066,1.00048134900477),
(1.,0.616896247011513,1.00044641351518),(1.,0.634916789357006,1.00042541499039),
(1.,0.658271057878159,1.00039820131519),(1.,0.665440397537911,1.00038984720721),
(1.,0.678364602785122,1.00037478721406),(1.,0.684003905064955,1.00036821598959),
(1.,0.693490447304963,1.00035716175002),(1.,0.697353099044676,1.00035266077625),
(1.,0.701751933579305,1.00034753501288),(1.,0.702985302217132,1.00034609782406),
(1.,0.704968511748717,1.00034378687949),(1.,0.705717903905829,1.00034291364662),
(1.,0.708180950178283,1.00034004356995),(1.,0.706146530160687,1.00034241418779),
(1.,0.69729017361677,1.00035273410042),(1.,0.693336856914947,1.00035734072197),
(1.,0.683762701080569,1.00036849705371),(1.,0.678128040418911,1.00037506286951),
(1.,0.665292401063798,1.00039001966082),(1.,0.658088068918505,1.00039841454396),
(1.,0.642209400675926,1.00041691723951),(1.,0.633656376746873,1.00042688369233),
(1.,0.615478575266067,1.00044806546409),(1.,0.605853070392858,1.00045928163056),
(1.,0.585652603574339,1.00048282032296),(1.,0.575043134289062,1.00049518305875),
(1.,0.542192039840224,1.00053346295665),(1.,0.519160353863195,1.00056030074098),
(1.,0.483909414581263,1.00060137706977),(1.,0.472043707472279,1.0006152036428),
(1.,0.448330324994361,1.0006428357773),(1.,0.43649600801918,1.00065662577283),
(1.,0.398029999848111,1.00070144847631),(1.,0.372846379395456,1.00073079381277),
(1.,0.353825408000619,1.00075295809239)))
REPRESENTATION_ITEM('')
SURFACE()
);
#1661=(
BOUNDED_SURFACE()
B_SPLINE_SURFACE(3,2,((#97849,#97850,#97851),(#97852,#97853,#97854),(#97855,
#97856,#97857),(#97858,#97859,#97860),(#97861,#97862,#97863),(#97864,#97865,
#97866),(#97867,#97868,#97869),(#97870,#97871,#97872),(#97873,#97874,#97875),
(#97876,#97877,#97878),(#97879,#97880,#97881),(#97882,#97883,#97884),(#97885,
#97886,#97887),(#97888,#97889,#97890),(#97891,#97892,#97893),(#97894,#97895,
#97896),(#97897,#97898,#97899),(#97900,#97901,#97902),(#97903,#97904,#97905),
(#97906,#97907,#97908),(#97909,#97910,#97911),(#97912,#97913,#97914),(#97915,
#97916,#97917),(#97918,#97919,#97920),(#97921,#97922,#97923),(#97924,#97925,
#97926),(#97927,#97928,#97929),(#97930,#97931,#97932),(#97933,#97934,#97935),
(#97936,#97937,#97938),(#97939,#97940,#97941),(#97942,#97943,#97944),(#97945,
#97946,#97947),(#97948,#97949,#97950),(#97951,#97952,#97953),(#97954,#97955,
#97956),(#97957,#97958,#97959),(#97960,#97961,#97962),(#97963,#97964,#97965),
(#97966,#97967,#97968),(#97969,#97970,#97971),(#97972,#97973,#97974),(#97975,
#97976,#97977),(#97978,#97979,#97980),(#97981,#97982,#97983),(#97984,#97985,
#97986),(#97987,#97988,#97989),(#97990,#97991,#97992),(#97993,#97994,#97995),
(#97996,#97997,#97998),(#97999,#98000,#98001),(#98002,#98003,#98004)),
 .UNSPECIFIED.,.F.,.F.,.F.)
B_SPLINE_SURFACE_WITH_KNOTS((4,2,2,2,2,2,2,2,2,2,2,2,2,2,2,2,2,2,2,2,2,
2,2,2,2,4),(3,3),(0.,0.00315886476497431,0.00473829714746146,0.00631772952994861,
0.00789716191243577,0.00947659429492292,0.0126354590598972,0.0142148914423844,
0.0157943238248715,0.0189531885898458,0.0221120533548201,0.0236914857373073,
0.0252709181197944,0.0268503505022816,0.0284297828847688,0.0315886476497431,
0.0331680800322302,0.0347475124147174,0.0363269447972045,0.0379063771796917,
0.041065241944666,0.0426446743271531,0.0442241067096403,0.0473829714746146,
0.0489624038571017,0.0509081571689574),(-0.000366320929394054,1.),
 .UNSPECIFIED.)
GEOMETRIC_REPRESENTATION_ITEM()
RATIONAL_B_SPLINE_SURFACE(((1.00005042977931,0.931167215319011,1.),(1.00004802363142,
0.934451422823265,1.),(1.00004766638974,0.934939030352376,1.),(1.00005016915153,
0.931522952280194,1.),(1.00005152792892,0.92966832525533,1.),(1.00005514272126,
0.924734410684191,1.),(1.00005739708062,0.921657382894737,1.),(1.00006270960761,
0.914406190616929,1.),(1.00006578664498,0.910206270369143,1.),(1.00007258454286,
0.900927660639692,1.),(1.00007629268405,0.89586633205052,1.),(1.0000882084061,
0.879602284474657,1.),(1.00009720731593,0.867319462069032,1.),(1.00011185421907,
0.847327561573564,1.),(1.00011692583641,0.840405192509689,1.),(1.00012717668813,
0.826413565365098,1.),(1.00013237821318,0.819313882232296,1.),(1.00014804138246,
0.797934856318314,1.),(1.00015859373613,0.783531702112416,1.),(1.00017861952009,
0.756198041441388,1.),(1.00018776819113,0.743710806479728,1.),(1.00019903767144,
0.728328829354908,1.),(1.00020239085733,0.723751987553838,1.),(1.00020800234017,
0.716092743446008,1.),(1.00021021837205,0.713068029719533,1.),(1.00021337561237,
0.708758638603594,1.),(1.00021431665381,0.707474189140747,1.),(1.00021485246247,
0.70674285137928,1.),(1.0002144426404,0.707302227096993,1.),(1.00021115809343,
0.711785382037871,1.),(1.00020631623579,0.718394146723749,1.),(1.00019606386371,
0.732387849048684,1.),(1.0001921234338,0.737766233939451,1.),(1.0001836019673,
0.74939738277055,1.),(1.00017901501663,0.755658218975225,1.),(1.00016939628292,
0.768787053474939,1.),(1.00016436417741,0.775655491921232,1.),(1.00015402891774,
0.789762329443024,1.),(1.00014872894768,0.796996382481174,1.),(1.00013293409498,
0.818555146164889,1.),(1.00012245640244,0.832856393646782,1.),(1.00010747739276,
0.853301594132862,1.),(1.0001025893796,0.859973357550685,1.),(1.00009330215817,
0.872649703192738,1.),(1.00008888539535,0.878678246012862,1.),(1.00007641546784,
0.895698741577217,1.),(1.00006912991505,0.905642962900587,1.),(1.00006026267051,
0.917746072269067,1.),(1.00005766031332,0.921298090426901,1.),(1.00005289421335,
0.927803451699111,1.),(1.00005093853036,0.930472809118457,1.),(1.00004972550474,
0.932128496152477,1.)))
REPRESENTATION_ITEM('')
SURFACE()
);
#1662=(
BOUNDED_SURFACE()
B_SPLINE_SURFACE(3,2,((#98299,#98300,#98301),(#98302,#98303,#98304),(#98305,
#98306,#98307),(#98308,#98309,#98310),(#98311,#98312,#98313),(#98314,#98315,
#98316),(#98317,#98318,#98319),(#98320,#98321,#98322),(#98323,#98324,#98325),
(#98326,#98327,#98328),(#98329,#98330,#98331),(#98332,#98333,#98334),(#98335,
#98336,#98337),(#98338,#98339,#98340),(#98341,#98342,#98343),(#98344,#98345,
#98346),(#98347,#98348,#98349),(#98350,#98351,#98352),(#98353,#98354,#98355),
(#98356,#98357,#98358),(#98359,#98360,#98361),(#98362,#98363,#98364),(#98365,
#98366,#98367),(#98368,#98369,#98370),(#98371,#98372,#98373),(#98374,#98375,
#98376),(#98377,#98378,#98379),(#98380,#98381,#98382),(#98383,#98384,#98385),
(#98386,#98387,#98388),(#98389,#98390,#98391),(#98392,#98393,#98394),(#98395,
#98396,#98397),(#98398,#98399,#98400),(#98401,#98402,#98403),(#98404,#98405,
#98406),(#98407,#98408,#98409),(#98410,#98411,#98412),(#98413,#98414,#98415),
(#98416,#98417,#98418),(#98419,#98420,#98421),(#98422,#98423,#98424),(#98425,
#98426,#98427),(#98428,#98429,#98430),(#98431,#98432,#98433),(#98434,#98435,
#98436),(#98437,#98438,#98439),(#98440,#98441,#98442),(#98443,#98444,#98445),
(#98446,#98447,#98448)),.UNSPECIFIED.,.F.,.F.,.F.)
B_SPLINE_SURFACE_WITH_KNOTS((4,2,2,2,2,2,2,2,2,2,2,2,2,2,2,2,2,2,2,2,2,
2,2,2,4),(3,3),(0.,0.0025187116162184,0.00377806742432761,0.00503742323243681,
0.00629677904054601,0.00755613484865521,0.0100748464648736,0.0113342022729828,
0.012593558081092,0.0151122696973104,0.0163716255054196,0.0176309813135288,
0.018890337121638,0.0201496929297472,0.0226684045459656,0.0239277603540748,
0.025187116162184,0.0264464719702932,0.0277058277784024,0.0302245393946208,
0.0327432510108392,0.0352619626270576,0.0365213184351669,0.0377806742432761,
0.0402993858594945),(0.,1.),.UNSPECIFIED.)
GEOMETRIC_REPRESENTATION_ITEM()
RATIONAL_B_SPLINE_SURFACE(((1.,0.444837807664136,1.),(1.,0.443889729175589,
1.),(1.,0.447748071183855,1.),(1.,0.459453142902776,1.),(1.,0.464367346379585,
1.),(1.,0.475717163519536,1.),(1.,0.48211295799902,1.),(1.,0.495944712524718,
1.),(1.,0.503380981743553,1.),(1.,0.518962657925113,1.),(1.,0.527139185789211,
1.),(1.,0.551895636149689,1.),(1.,0.568781778812327,1.),(1.,0.593444445481799,
1.),(1.,0.601597343431266,1.),(1.,0.61732836948322,1.),(1.,0.624889681210996,
1.),(1.,0.646485984307859,1.),(1.,0.659441840352202,1.),(1.,0.675982223306384,
1.),(1.,0.68102172685123,1.),(1.,0.689763664719054,1.),(1.,0.693504359158594,
1.),(1.,0.69968025928586,1.),(1.,0.702115682658639,1.),(1.,0.705612781075522,
1.),(1.,0.706675637348199,1.),(1.,0.707648224727786,1.),(1.,0.705356532405246,
1.),(1.,0.697802511437167,1.),(1.,0.69458157237586,1.),(1.,0.686829651284654,
1.),(1.,0.682347030399091,1.),(1.,0.672289714801745,1.),(1.,0.666714572428337,
1.),(1.,0.654569105179005,1.),(1.,0.647967838573232,1.),(1.,0.627025457575446,
1.),(1.,0.611679454062546,1.),(1.,0.579351199094756,1.),(1.,0.56222647842645,
1.),(1.,0.529022354961919,1.),(1.,0.512804015742491,1.),(1.,0.490778638607675,
1.),(1.,0.48379298434534,1.),(1.,0.471266214350623,1.),(1.,0.46570913806108,
1.),(1.,0.451670624760032,1.),(1.,0.445830006853561,1.),(1.,0.444857616465186,
1.)))
REPRESENTATION_ITEM('')
SURFACE()
);
#1663=(
BOUNDED_SURFACE()
B_SPLINE_SURFACE(3,2,((#99274,#99275,#99276),(#99277,#99278,#99279),(#99280,
#99281,#99282),(#99283,#99284,#99285),(#99286,#99287,#99288),(#99289,#99290,
#99291),(#99292,#99293,#99294),(#99295,#99296,#99297),(#99298,#99299,#99300),
(#99301,#99302,#99303),(#99304,#99305,#99306),(#99307,#99308,#99309),(#99310,
#99311,#99312),(#99313,#99314,#99315),(#99316,#99317,#99318),(#99319,#99320,
#99321),(#99322,#99323,#99324),(#99325,#99326,#99327),(#99328,#99329,#99330),
(#99331,#99332,#99333),(#99334,#99335,#99336),(#99337,#99338,#99339),(#99340,
#99341,#99342),(#99343,#99344,#99345),(#99346,#99347,#99348),(#99349,#99350,
#99351),(#99352,#99353,#99354),(#99355,#99356,#99357),(#99358,#99359,#99360),
(#99361,#99362,#99363),(#99364,#99365,#99366),(#99367,#99368,#99369),(#99370,
#99371,#99372),(#99373,#99374,#99375),(#99376,#99377,#99378),(#99379,#99380,
#99381),(#99382,#99383,#99384),(#99385,#99386,#99387),(#99388,#99389,#99390),
(#99391,#99392,#99393),(#99394,#99395,#99396),(#99397,#99398,#99399),(#99400,
#99401,#99402),(#99403,#99404,#99405),(#99406,#99407,#99408),(#99409,#99410,
#99411)),.UNSPECIFIED.,.F.,.F.,.F.)
B_SPLINE_SURFACE_WITH_KNOTS((4,2,2,2,2,2,2,2,2,2,2,2,2,2,2,2,2,2,2,2,2,
2,4),(3,3),(0.,0.00125459591840773,0.0018818938776116,0.00250919183681547,
0.0037637877552232,0.00439108571442707,0.00501838367363094,0.00564568163283481,
0.00627297959203867,0.00752757551044641,0.00878217142885414,0.0100367673472619,
0.0106640653064657,0.0112913632656696,0.0125459591840773,0.0138005551024851,
0.0144278530616889,0.0150551510208928,0.0163097469393006,0.0169370448985044,
0.0175643428577083,0.018818938776116,0.0200735346945238),(0.,1.),
 .UNSPECIFIED.)
GEOMETRIC_REPRESENTATION_ITEM()
RATIONAL_B_SPLINE_SURFACE(((1.,0.753501700966988,1.),(1.,0.758919966590289,
1.),(1.,0.762624474007346,1.),(1.,0.765493967892479,1.),(1.,0.766001864196328,
1.),(1.,0.766081899420437,1.),(1.,0.765645177532698,1.),(1.,0.762965796826428,
1.),(1.,0.75937217675435,1.),(1.,0.751475581705692,1.),(1.,0.748410443135639,
1.),(1.,0.741628592661977,1.),(1.,0.737899758372927,1.),(1.,0.729842420453465,
1.),(1.,0.725513701271151,1.),(1.,0.716322621401233,1.),(1.,0.71144077787533,
1.),(1.,0.696381444937169,1.),(1.,0.685722488457871,1.),(1.,0.663879284854164,
1.),(1.,0.652645530876282,1.),(1.,0.631293420609983,1.),(1.,0.621067849093089,
1.),(1.,0.607073245214128,1.),(1.,0.602619800288969,1.),(1.,0.594464909703987,
1.),(1.,0.590739984910806,1.),(1.,0.580731511515441,1.),(1.,0.575617470391927,
1.),(1.,0.569031517938587,1.),(1.,0.567674325666079,1.),(1.,0.568262977064503,
1.),(1.,0.568891116188093,1.),(1.,0.570935397635918,1.),(1.,0.572362568136071,
1.),(1.,0.577560685048605,1.),(1.,0.582247188120323,1.),(1.,0.59023516464793,
1.),(1.,0.593074756205356,1.),(1.,0.598856135494127,1.),(1.,0.601790038290455,
1.),(1.,0.610522818926502,1.),(1.,0.616249874441583,1.),(1.,0.626614400505202,
1.),(1.,0.631088239307343,1.),(1.,0.634563057406884,1.)))
REPRESENTATION_ITEM('')
SURFACE()
);
#1664=(
BOUNDED_SURFACE()
B_SPLINE_SURFACE(3,2,((#99754,#99755,#99756),(#99757,#99758,#99759),(#99760,
#99761,#99762),(#99763,#99764,#99765),(#99766,#99767,#99768),(#99769,#99770,
#99771),(#99772,#99773,#99774),(#99775,#99776,#99777),(#99778,#99779,#99780),
(#99781,#99782,#99783),(#99784,#99785,#99786),(#99787,#99788,#99789),(#99790,
#99791,#99792),(#99793,#99794,#99795),(#99796,#99797,#99798),(#99799,#99800,
#99801),(#99802,#99803,#99804),(#99805,#99806,#99807),(#99808,#99809,#99810),
(#99811,#99812,#99813),(#99814,#99815,#99816),(#99817,#99818,#99819),(#99820,
#99821,#99822),(#99823,#99824,#99825),(#99826,#99827,#99828),(#99829,#99830,
#99831),(#99832,#99833,#99834),(#99835,#99836,#99837),(#99838,#99839,#99840),
(#99841,#99842,#99843),(#99844,#99845,#99846),(#99847,#99848,#99849),(#99850,
#99851,#99852),(#99853,#99854,#99855),(#99856,#99857,#99858),(#99859,#99860,
#99861),(#99862,#99863,#99864),(#99865,#99866,#99867),(#99868,#99869,#99870),
(#99871,#99872,#99873),(#99874,#99875,#99876),(#99877,#99878,#99879),(#99880,
#99881,#99882),(#99883,#99884,#99885),(#99886,#99887,#99888),(#99889,#99890,
#99891),(#99892,#99893,#99894),(#99895,#99896,#99897),(#99898,#99899,#99900),
(#99901,#99902,#99903),(#99904,#99905,#99906),(#99907,#99908,#99909),(#99910,
#99911,#99912),(#99913,#99914,#99915)),.UNSPECIFIED.,.F.,.F.,.F.)
B_SPLINE_SURFACE_WITH_KNOTS((4,2,2,2,2,2,2,2,2,2,2,2,2,2,2,2,2,2,2,2,2,
2,2,2,2,2,4),(3,3),(-7.78153428745613E-5,0.00257554787859691,0.00386332181789536,
0.00515109575719382,0.00643886969649227,0.00772664363579073,0.0103021915143876,
0.0115899654536861,0.0128777393929845,0.0154532872715815,0.0167410612108799,
0.0180288351501784,0.0193166090894768,0.0206043830287753,0.0231799309073722,
0.0244677048466706,0.0257554787859691,0.0270432527252676,0.028331026664566,
0.0309065745431629,0.0321943484824614,0.0334821224217598,0.0347698963610583,
0.0360576703003567,0.0386332181789536,0.0399209921182521,0.0412865814003949),
(-5.57615391788296E-5,1.00007781534287),.UNSPECIFIED.)
GEOMETRIC_REPRESENTATION_ITEM()
RATIONAL_B_SPLINE_SURFACE(((1.00006499666788,0.417145519460541,1.00009070498426),
(1.00006613373744,0.406948903154154,1.00009229180215),(1.00006666002296,
0.402229463167758,1.00009302625088),(1.00006643124968,0.404280976494946,
1.00009270699026),(1.00006619616633,0.406389075066969,1.00009237892372),
(1.00006542207527,0.413330699283567,1.00009129865423),(1.00006489161556,
0.418087571101604,1.00009055838029),(1.00006360370812,0.429636818858515,
1.00008876106317),(1.00006284644101,0.436427575124811,1.00008770427205),
(1.00006116075035,0.451543924676617,1.00008535183539),(1.00006022957763,
0.459894171148586,1.00008405235327),(1.00005731845811,0.485999494820791,
1.0000799897904),(1.00005520865809,0.504919024658453,1.00007704549518),
(1.00005200598796,0.533638814326789,1.00007257606387),(1.00005092886496,
0.543297862838644,1.00007107290335),(1.00004879117353,0.562467507505169,
1.00006808968476),(1.00004774201681,0.571875769700711,1.00006662555212),
(1.00004468046442,0.599330092951599,1.00006235305522),(1.00004275366152,
0.616608604952205,1.0000596641385),(1.00004012772931,0.640156525218429,
1.00005599956388),(1.00003929341804,0.647638171228524,1.00005483525511),
(1.00003776153149,0.661375289848644,1.00005269745713),(1.00003706001501,
0.667666105061143,1.00005171846784),(1.00003579596344,0.679001426435143,
1.00004995444238),(1.00003523337831,0.684046381465567,1.00004916933635),
(1.00003426031965,0.692772237972241,1.00004781140104),(1.00003384837915,
0.696466294543873,1.00004723652454),(1.00003288787868,0.705079536093434,
1.0000458961146),(1.00003260121688,0.707650161916355,1.00004549606865),
(1.00003271698939,0.706611977550149,1.00004565763299),(1.0000328491286,
0.705427025561222,1.00004584203759),(1.0000332924415,0.701451638594737,
1.00004646069529),(1.00003360204356,0.6986752970103,1.00004689275514),(1.00003438648853,
0.691640824637982,1.00004798747386),(1.00003486136748,0.687382370582247,
1.00004865018302),(1.00003596953549,0.677444927484954,1.00005019666787),
(1.0000366053434,0.671743350745739,1.00005108395868),(1.00003869257694,
0.653026184786068,1.00005399676162),(1.00004033354564,0.638310877237478,
1.00005628678732),(1.00004309135935,0.613580315885842,1.00006013540692),
(1.00004405946053,0.604898915345222,1.0000614864239),(1.00004604481265,
0.587095366038472,1.00006425704798),(1.00004706626934,0.577935502541562,
1.00006568252433),(1.00004914915559,0.559257320686793,1.00006858926048),
(1.00005021068348,0.549738120586547,1.00007007065751),(1.00005235335541,
0.530523813480548,1.00007306082655),(1.00005343979317,0.520781235371959,
1.00007457698611),(1.00005663467271,0.492131307351429,1.00007903554542),
(1.00005869139382,0.4736877601911,1.00008190576725),(1.00006143077889,0.449122456788815,
1.00008572866908),(1.00006228506745,0.44146166545061,1.00008692085681),
(1.00006386334166,0.427308567599321,1.0000891233903),(1.00006457824779,
0.420897681437532,1.00009012106528),(1.00006512941961,0.415955074725545,
1.00009089024365)))
REPRESENTATION_ITEM('')
SURFACE()
);
#1665=(
BOUNDED_SURFACE()
B_SPLINE_SURFACE(3,2,((#100046,#100047,#100048),(#100049,#100050,#100051),
(#100052,#100053,#100054),(#100055,#100056,#100057),(#100058,#100059,#100060),
(#100061,#100062,#100063),(#100064,#100065,#100066),(#100067,#100068,#100069),
(#100070,#100071,#100072),(#100073,#100074,#100075),(#100076,#100077,#100078),
(#100079,#100080,#100081),(#100082,#100083,#100084),(#100085,#100086,#100087),
(#100088,#100089,#100090),(#100091,#100092,#100093),(#100094,#100095,#100096),
(#100097,#100098,#100099),(#100100,#100101,#100102),(#100103,#100104,#100105),
(#100106,#100107,#100108),(#100109,#100110,#100111),(#100112,#100113,#100114),
(#100115,#100116,#100117),(#100118,#100119,#100120),(#100121,#100122,#100123),
(#100124,#100125,#100126),(#100127,#100128,#100129),(#100130,#100131,#100132),
(#100133,#100134,#100135),(#100136,#100137,#100138),(#100139,#100140,#100141),
(#100142,#100143,#100144),(#100145,#100146,#100147),(#100148,#100149,#100150),
(#100151,#100152,#100153),(#100154,#100155,#100156),(#100157,#100158,#100159),
(#100160,#100161,#100162),(#100163,#100164,#100165),(#100166,#100167,#100168),
(#100169,#100170,#100171),(#100172,#100173,#100174),(#100175,#100176,#100177),
(#100178,#100179,#100180),(#100181,#100182,#100183),(#100184,#100185,#100186),
(#100187,#100188,#100189),(#100190,#100191,#100192),(#100193,#100194,#100195),
(#100196,#100197,#100198),(#100199,#100200,#100201),(#100202,#100203,#100204),
(#100205,#100206,#100207)),.UNSPECIFIED.,.F.,.F.,.F.)
B_SPLINE_SURFACE_WITH_KNOTS((4,2,2,2,2,2,2,2,2,2,2,2,2,2,2,2,2,2,2,2,2,
2,2,2,2,2,4),(3,3),(-7.78153430528562E-5,0.00257554787859691,0.00386332181789536,
0.00515109575719382,0.00643886969649227,0.00772664363579073,0.0103021915143876,
0.0115899654536861,0.0128777393929845,0.0154532872715815,0.0167410612108799,
0.0180288351501784,0.0193166090894768,0.0206043830287753,0.0231799309073722,
0.0244677048466706,0.0257554787859691,0.0270432527252676,0.028331026664566,
0.0309065745431629,0.0321943484824614,0.0334821224217598,0.0347698963610583,
0.0360576703003567,0.0386332181789536,0.0399209921182521,0.0412865814005733),
(-5.57615387946816E-5,1.00007781534305),.UNSPECIFIED.)
GEOMETRIC_REPRESENTATION_ITEM()
RATIONAL_B_SPLINE_SURFACE(((1.00006499666744,0.417145519462717,1.00009070498446),
(1.00006613373698,0.406948903154911,1.00009229180236),(1.0000666600225,
0.402229463167788,1.00009302625109),(1.00006643124922,0.404280976495069,
1.00009270699047),(1.00006619616587,0.406389075067091,1.00009237892394),
(1.00006542207482,0.413330699283688,1.00009129865444),(1.00006489161511,
0.418087571101724,1.0000905583805),(1.00006360370768,0.429636818858632,
1.00008876106337),(1.00006284644058,0.436427575124927,1.00008770427225),
(1.00006116074993,0.45154392467673,1.00008535183558),(1.00006022957721,
0.459894171148698,1.00008405235346),(1.00005731845772,0.485999494820897,
1.00007998979058),(1.00005520865771,0.504919024658555,1.00007704549536),
(1.0000520059876,0.533638814326885,1.00007257606403),(1.00005092886461,
0.543297862838738,1.00007107290351),(1.00004879117319,0.562467507505259,
1.00006808968492),(1.00004774201649,0.571875769700799,1.00006662555227),
(1.00004468046411,0.599330092951681,1.00006235305536),(1.00004275366122,
0.616608604952284,1.00005966413864),(1.00004012772903,0.640156525218503,
1.00005599956401),(1.00003929341777,0.647638171228596,1.00005483525523),
(1.00003776153123,0.661375289848713,1.00005269745725),(1.00003706001475,
0.667666105061211,1.00005171846796),(1.00003579596319,0.679001426435209,
1.00004995444249),(1.00003523337806,0.684046381465632,1.00004916933646),
(1.00003426031941,0.692772237972305,1.00004781140115),(1.00003384837891,
0.696466294543935,1.00004723652465),(1.00003288787845,0.705079536093495,
1.00004589611471),(1.00003260121666,0.707650161916415,1.00004549606876),
(1.00003271698917,0.706611977550209,1.00004565763309),(1.00003284912838,
0.705427025561283,1.0000458420377),(1.00003329244127,0.701451638594799,
1.0000464606954),(1.00003360204333,0.698675297010362,1.00004689275525),
(1.00003438648829,0.691640824638045,1.00004798747396),(1.00003486136724,
0.687382370582311,1.00004865018313),(1.00003596953524,0.677444927485021,
1.00005019666798),(1.00003660534315,0.671743350745806,1.0000510839588),
(1.00003869257667,0.653026184786139,1.00005399676175),(1.00004033354536,
0.638310877237552,1.00005628678745),(1.00004309135906,0.613580315885922,
1.00006013540706),(1.00004405946023,0.604898915345303,1.00006148642404),
(1.00004604481234,0.587095366038557,1.00006425704813),(1.00004706626902,
0.577935502541649,1.00006568252448),(1.00004914915525,0.559257320686884,
1.00006858926064),(1.00005021068313,0.54973812058664,1.00007007065767),
(1.00005235335505,0.530523813480645,1.00007306082672),(1.0000534397928,
0.520781235372058,1.00007457698628),(1.00005663467232,0.492131307351533,
1.0000790355456),(1.00005869139341,0.473687760191208,1.00008190576744),
(1.00006143077847,0.449122456788928,1.00008572866928),(1.00006228506702,
0.441461665450725,1.000086920857),(1.00006386334123,0.427308567598488,1.00008912339051),
(1.00006457824735,0.420897681435977,1.00009012106548),(1.00006512941917,
0.415955074723729,1.00009089024386)))
REPRESENTATION_ITEM('')
SURFACE()
);
#1666=(
BOUNDED_SURFACE()
B_SPLINE_SURFACE(3,2,((#101435,#101436,#101437),(#101438,#101439,#101440),
(#101441,#101442,#101443),(#101444,#101445,#101446),(#101447,#101448,#101449),
(#101450,#101451,#101452),(#101453,#101454,#101455),(#101456,#101457,#101458),
(#101459,#101460,#101461),(#101462,#101463,#101464),(#101465,#101466,#101467),
(#101468,#101469,#101470),(#101471,#101472,#101473),(#101474,#101475,#101476),
(#101477,#101478,#101479),(#101480,#101481,#101482),(#101483,#101484,#101485),
(#101486,#101487,#101488),(#101489,#101490,#101491),(#101492,#101493,#101494),
(#101495,#101496,#101497),(#101498,#101499,#101500),(#101501,#101502,#101503),
(#101504,#101505,#101506),(#101507,#101508,#101509),(#101510,#101511,#101512),
(#101513,#101514,#101515),(#101516,#101517,#101518),(#101519,#101520,#101521),
(#101522,#101523,#101524),(#101525,#101526,#101527),(#101528,#101529,#101530),
(#101531,#101532,#101533),(#101534,#101535,#101536),(#101537,#101538,#101539),
(#101540,#101541,#101542),(#101543,#101544,#101545),(#101546,#101547,#101548),
(#101549,#101550,#101551),(#101552,#101553,#101554),(#101555,#101556,#101557),
(#101558,#101559,#101560),(#101561,#101562,#101563),(#101564,#101565,#101566),
(#101567,#101568,#101569),(#101570,#101571,#101572),(#101573,#101574,#101575),
(#101576,#101577,#101578),(#101579,#101580,#101581),(#101582,#101583,#101584),
(#101585,#101586,#101587),(#101588,#101589,#101590),(#101591,#101592,#101593),
(#101594,#101595,#101596),(#101597,#101598,#101599),(#101600,#101601,#101602),
(#101603,#101604,#101605),(#101606,#101607,#101608),(#101609,#101610,#101611),
(#101612,#101613,#101614)),.UNSPECIFIED.,.F.,.F.,.F.)
B_SPLINE_SURFACE_WITH_KNOTS((4,2,2,2,2,2,2,2,2,2,2,2,2,2,2,2,2,2,2,2,2,
2,2,2,2,2,2,2,2,4),(3,3),(-0.000582627436703559,0.00319856320703094,0.00399820400878867,
0.00479784481054641,0.00639712641406187,0.00719676721581961,0.00799640801757734,
0.00959568962109281,0.0111949712246083,0.0127942528281237,0.0159928160351547,
0.0175920976386702,0.0191913792421856,0.0223899424492166,0.023989224052732,
0.0255885056562475,0.027187787259763,0.0279874280615207,0.0287870688632784,
0.0319856320703094,0.0335849136738248,0.0351841952773403,0.0367834768808558,
0.0383827584843712,0.0399820400878867,0.0415813216914022,0.0447798848984331,
0.0463791665019486,0.047978448105464,0.0517596387491986),(-0.000582627436703563,
1.),.UNSPECIFIED.)
GEOMETRIC_REPRESENTATION_ITEM()
RATIONAL_B_SPLINE_SURFACE(((1.00073106270324,0.372615622620786,1.),(1.00075754505411,
0.34988896300548,1.),(1.00077679486628,0.333369133216196,1.),(1.00078339423717,
0.327705676201963,1.),(1.0007839234939,0.327251477944978,1.),(1.00078370547356,
0.327438578938251,1.),(1.00078296606858,0.328073122498959,1.),(1.0007789479653,
0.331521383799564,1.),(1.00077386099431,0.335886927429411,1.),(1.00076320854245,
0.345028662937659,1.),(1.00075913739802,0.348522443164051,1.),(1.00075021966268,
0.356175477316145,1.),(1.00074537901714,0.360329629032232,1.),(1.00072994061757,
0.373578575616013,1.),(1.00071843722139,0.383450575672528,1.),(1.00069394616724,
0.404468341585449,1.),(1.00068095507196,0.415617057266214,1.),(1.00065412000777,
0.438646408868139,1.),(1.0006403778921,0.450439636237959,1.),(1.00059924569063,
0.485738524418632,1.),(1.00057180169365,0.509290450787528,1.),(1.00053204730771,
0.543406923368716,1.),(1.00051902118042,0.554585702870244,1.),(1.00049359916726,
0.576402400431409,1.),(1.00048134900478,0.586915261405062,1.),(1.00044641351519,
0.616896247011509,1.),(1.0004254149904,0.634916789357002,1.),(1.00039820131519,
0.658271057878156,1.),(1.00038984720721,0.665440397537908,1.),(1.00037478721406,
0.678364602785118,1.),(1.0003682159896,0.684003905064952,1.),(1.00035716175002,
0.69349044730496,1.),(1.00035266077626,0.697353099044673,1.),(1.00034753501288,
0.701751933579303,1.),(1.00034609782407,0.702985302217129,1.),(1.00034378687949,
0.704968511748714,1.),(1.00034291364663,0.705717903905826,1.),(1.00034004356996,
0.70818095017828,1.),(1.0003424141878,0.706146530160684,1.),(1.00035273410042,
0.697290173616767,1.),(1.00035734072197,0.693336856914944,1.),(1.00036849705372,
0.683762701080566,1.),(1.00037506286951,0.678128040418907,1.),(1.00039001966083,
0.665292401063795,1.),(1.00039841454397,0.658088068918501,1.),(1.00041691723952,
0.642209400675922,1.),(1.00042688369234,0.633656376746869,1.),(1.0004480654641,
0.615478575266063,1.),(1.00045928163056,0.605853070392854,1.),(1.00048282032297,
0.585652603574335,1.),(1.00049518305876,0.575043134289058,1.),(1.00053346295666,
0.542192039840219,1.),(1.00056030074099,0.51916035386319,1.),(1.00060137706978,
0.483909414581257,1.),(1.00061520364281,0.472043707472274,1.),(1.00064283577731,
0.448330324994356,1.),(1.00065662577284,0.436496008019175,1.),(1.00070144847632,
0.398029999848035,1.),(1.00073079381278,0.37284637939532,1.),(1.0007529580924,
0.353825408000466,1.)))
REPRESENTATION_ITEM('')
SURFACE()
);
#1667=(
BOUNDED_SURFACE()
B_SPLINE_SURFACE(3,2,((#101803,#101804,#101805),(#101806,#101807,#101808),
(#101809,#101810,#101811),(#101812,#101813,#101814),(#101815,#101816,#101817),
(#101818,#101819,#101820),(#101821,#101822,#101823),(#101824,#101825,#101826),
(#101827,#101828,#101829),(#101830,#101831,#101832),(#101833,#101834,#101835),
(#101836,#101837,#101838),(#101839,#101840,#101841),(#101842,#101843,#101844),
(#101845,#101846,#101847),(#101848,#101849,#101850),(#101851,#101852,#101853),
(#101854,#101855,#101856),(#101857,#101858,#101859),(#101860,#101861,#101862),
(#101863,#101864,#101865),(#101866,#101867,#101868),(#101869,#101870,#101871),
(#101872,#101873,#101874),(#101875,#101876,#101877),(#101878,#101879,#101880),
(#101881,#101882,#101883),(#101884,#101885,#101886),(#101887,#101888,#101889),
(#101890,#101891,#101892),(#101893,#101894,#101895),(#101896,#101897,#101898),
(#101899,#101900,#101901),(#101902,#101903,#101904),(#101905,#101906,#101907),
(#101908,#101909,#101910),(#101911,#101912,#101913),(#101914,#101915,#101916),
(#101917,#101918,#101919),(#101920,#101921,#101922),(#101923,#101924,#101925),
(#101926,#101927,#101928),(#101929,#101930,#101931),(#101932,#101933,#101934),
(#101935,#101936,#101937),(#101938,#101939,#101940),(#101941,#101942,#101943),
(#101944,#101945,#101946),(#101947,#101948,#101949),(#101950,#101951,#101952),
(#101953,#101954,#101955),(#101956,#101957,#101958)),.UNSPECIFIED.,.F.,
 .F.,.F.)
B_SPLINE_SURFACE_WITH_KNOTS((4,2,2,2,2,2,2,2,2,2,2,2,2,2,2,2,2,2,2,2,2,
2,2,2,2,4),(3,3),(0.,0.00315886476497431,0.00473829714746146,0.00631772952994861,
0.00789716191243577,0.00947659429492292,0.0126354590598972,0.0142148914423844,
0.0157943238248715,0.0189531885898458,0.0221120533548201,0.0236914857373073,
0.0252709181197944,0.0268503505022816,0.0284297828847688,0.0315886476497431,
0.0331680800322302,0.0347475124147174,0.0363269447972045,0.0379063771796917,
0.041065241944666,0.0426446743271531,0.0442241067096403,0.0473829714746146,
0.0489624038571017,0.0509081571686288),(0.,1.00036632092907),
 .UNSPECIFIED.)
GEOMETRIC_REPRESENTATION_ITEM()
RATIONAL_B_SPLINE_SURFACE(((1.,0.931167215319034,1.00005042977927),(1.,
0.934451422823286,1.00004802363138),(1.,0.934939030352398,1.00004766638969),
(1.,0.931522952280216,1.00005016915148),(1.,0.929668325255353,1.00005152792887),
(1.,0.924734410684215,1.00005514272121),(1.,0.921657382894763,1.00005739708057),
(1.,0.914406190616957,1.00006270960755),(1.,0.910206270369172,1.00006578664493),
(1.,0.900927660639724,1.0000725845428),(1.,0.895866332050554,1.00007629268398),
(1.,0.879602284474697,1.00008820840602),(1.,0.867319462069075,1.00009720731585),
(1.,0.847327561573614,1.00011185421897),(1.,0.840405192509742,1.00011692583631),
(1.,0.826413565365155,1.00012717668802),(1.,0.819313882232356,1.00013237821306),
(1.,0.797934856318381,1.00014804138233),(1.,0.783531702112487,1.00015859373599),
(1.,0.756198041441468,1.00017861951993),(1.,0.743710806479812,1.00018776819096),
(1.,0.728328829354997,1.00019903767126),(1.,0.723751987553928,1.00020239085714),
(1.,0.716092743446101,1.00020800233998),(1.,0.713068029719627,1.00021021837186),
(1.,0.708758638603689,1.00021337561218),(1.,0.707474189140843,1.00021431665362),
(1.,0.706742851379377,1.00021485246228),(1.,0.70730222709709,1.00021444264021),
(1.,0.711785382037965,1.00021115809324),(1.,0.718394146723841,1.0002063162356),
(1.,0.732387849048772,1.00019606386353),(1.,0.737766233939537,1.00019212343363),
(1.,0.749397382770632,1.00018360196714),(1.,0.755658218975305,1.00017901501647),
(1.,0.768787053475015,1.00016939628277),(1.,0.775655491921306,1.00016436417726),
(1.,0.789762329443093,1.00015402891761),(1.,0.79699638248124,1.00014872894755),
(1.,0.818555146164949,1.00013293409486),(1.,0.832856393646837,1.00012245640233),
(1.,0.85330159413291,1.00010747739266),(1.,0.859973357550731,1.00010258937951),
(1.,0.872649703192779,1.00009330215809),(1.,0.878678246012902,1.00008888539527),
(1.,0.895698741577251,1.00007641546778),(1.,0.905642962900618,1.00006912991499),
(1.,0.917746072269094,1.00006026267045),(1.,0.921298090426927,1.00005766031327),
(1.,0.927803451698529,1.0000528942133),(1.,0.930472809117578,1.00005093853032),
(1.,0.93212849615166,1.00004972550469)))
REPRESENTATION_ITEM('')
SURFACE()
);
#1668=(
BOUNDED_SURFACE()
B_SPLINE_SURFACE(3,2,((#102253,#102254,#102255),(#102256,#102257,#102258),
(#102259,#102260,#102261),(#102262,#102263,#102264),(#102265,#102266,#102267),
(#102268,#102269,#102270),(#102271,#102272,#102273),(#102274,#102275,#102276),
(#102277,#102278,#102279),(#102280,#102281,#102282),(#102283,#102284,#102285),
(#102286,#102287,#102288),(#102289,#102290,#102291),(#102292,#102293,#102294),
(#102295,#102296,#102297),(#102298,#102299,#102300),(#102301,#102302,#102303),
(#102304,#102305,#102306),(#102307,#102308,#102309),(#102310,#102311,#102312),
(#102313,#102314,#102315),(#102316,#102317,#102318),(#102319,#102320,#102321),
(#102322,#102323,#102324),(#102325,#102326,#102327),(#102328,#102329,#102330),
(#102331,#102332,#102333),(#102334,#102335,#102336),(#102337,#102338,#102339),
(#102340,#102341,#102342),(#102343,#102344,#102345),(#102346,#102347,#102348),
(#102349,#102350,#102351),(#102352,#102353,#102354),(#102355,#102356,#102357),
(#102358,#102359,#102360),(#102361,#102362,#102363),(#102364,#102365,#102366),
(#102367,#102368,#102369),(#102370,#102371,#102372),(#102373,#102374,#102375),
(#102376,#102377,#102378),(#102379,#102380,#102381),(#102382,#102383,#102384),
(#102385,#102386,#102387),(#102388,#102389,#102390),(#102391,#102392,#102393),
(#102394,#102395,#102396),(#102397,#102398,#102399),(#102400,#102401,#102402)),
 .UNSPECIFIED.,.F.,.F.,.F.)
B_SPLINE_SURFACE_WITH_KNOTS((4,2,2,2,2,2,2,2,2,2,2,2,2,2,2,2,2,2,2,2,2,
2,2,2,4),(3,3),(0.,0.0025187116162184,0.00377806742432761,0.00503742323243681,
0.00629677904054601,0.00755613484865521,0.0100748464648736,0.0113342022729828,
0.012593558081092,0.0151122696973104,0.0163716255054196,0.0176309813135288,
0.018890337121638,0.0201496929297472,0.0226684045459656,0.0239277603540748,
0.025187116162184,0.0264464719702932,0.0277058277784024,0.0302245393946208,
0.0327432510108392,0.0352619626270576,0.0365213184351669,0.0377806742432761,
0.0402993858594945),(0.,1.),.UNSPECIFIED.)
GEOMETRIC_REPRESENTATION_ITEM()
RATIONAL_B_SPLINE_SURFACE(((1.,0.444837807664136,1.),(1.,0.443889729175589,
1.),(1.,0.447748071183855,1.),(1.,0.459453142902776,1.),(1.,0.464367346379585,
1.),(1.,0.475717163519536,1.),(1.,0.48211295799902,1.),(1.,0.495944712524718,
1.),(1.,0.503380981743553,1.),(1.,0.518962657925113,1.),(1.,0.527139185789211,
1.),(1.,0.551895636149689,1.),(1.,0.568781778812327,1.),(1.,0.593444445481799,
1.),(1.,0.601597343431266,1.),(1.,0.61732836948322,1.),(1.,0.624889681210996,
1.),(1.,0.646485984307859,1.),(1.,0.659441840352202,1.),(1.,0.675982223306384,
1.),(1.,0.68102172685123,1.),(1.,0.689763664719054,1.),(1.,0.693504359158594,
1.),(1.,0.69968025928586,1.),(1.,0.702115682658639,1.),(1.,0.705612781075522,
1.),(1.,0.706675637348199,1.),(1.,0.707648224727786,1.),(1.,0.705356532405246,
1.),(1.,0.697802511437167,1.),(1.,0.69458157237586,1.),(1.,0.686829651284654,
1.),(1.,0.682347030399091,1.),(1.,0.672289714801745,1.),(1.,0.666714572428337,
1.),(1.,0.654569105179005,1.),(1.,0.647967838573232,1.),(1.,0.627025457575446,
1.),(1.,0.611679454062546,1.),(1.,0.579351199094756,1.),(1.,0.56222647842645,
1.),(1.,0.529022354961919,1.),(1.,0.512804015742491,1.),(1.,0.490778638607675,
1.),(1.,0.48379298434534,1.),(1.,0.471266214350623,1.),(1.,0.46570913806108,
1.),(1.,0.451670624760032,1.),(1.,0.445830006853561,1.),(1.,0.444857616465186,
1.)))
REPRESENTATION_ITEM('')
SURFACE()
);
#1669=(
BOUNDED_SURFACE()
B_SPLINE_SURFACE(3,2,((#103225,#103226,#103227),(#103228,#103229,#103230),
(#103231,#103232,#103233),(#103234,#103235,#103236),(#103237,#103238,#103239),
(#103240,#103241,#103242),(#103243,#103244,#103245),(#103246,#103247,#103248),
(#103249,#103250,#103251),(#103252,#103253,#103254),(#103255,#103256,#103257),
(#103258,#103259,#103260),(#103261,#103262,#103263),(#103264,#103265,#103266),
(#103267,#103268,#103269),(#103270,#103271,#103272),(#103273,#103274,#103275),
(#103276,#103277,#103278)),.UNSPECIFIED.,.F.,.F.,.F.)
B_SPLINE_SURFACE_WITH_KNOTS((4,2,2,2,2,2,2,2,4),(3,3),(0.,0.392699081698724,
0.785398163397448,1.17809724509617,1.5707963267949,1.96349540849362,2.35619449019234,
2.74889357189107,3.14159265358979),(0.,1.),.UNSPECIFIED.)
GEOMETRIC_REPRESENTATION_ITEM()
RATIONAL_B_SPLINE_SURFACE(((1.,0.766044443118988,1.),(1.,0.766049891332403,
1.),(1.,0.764573371724783,1.),(1.,0.758863530286151,1.),(1.,0.754625142483316,
1.),(1.,0.74389933443991,1.),(1.,0.737413012003865,1.),(1.,0.723033687231336,
1.),(1.,0.715143224098042,1.),(1.,0.699070338275054,1.),(1.,0.690892921248369,
1.),(1.,0.675524086364245,1.),(1.,0.668340746363067,1.),(1.,0.656206116553444,
1.),(1.,0.651264584058791,1.),(1.,0.644551763110563,1.),(1.,0.642777121345109,
1.),(1.,0.642787609686527,1.)))
REPRESENTATION_ITEM('')
SURFACE()
);
#1670=(
BOUNDED_SURFACE()
B_SPLINE_SURFACE(3,2,((#103526,#103527,#103528),(#103529,#103530,#103531),
(#103532,#103533,#103534),(#103535,#103536,#103537),(#103538,#103539,#103540),
(#103541,#103542,#103543),(#103544,#103545,#103546),(#103547,#103548,#103549),
(#103550,#103551,#103552),(#103553,#103554,#103555),(#103556,#103557,#103558),
(#103559,#103560,#103561),(#103562,#103563,#103564),(#103565,#103566,#103567),
(#103568,#103569,#103570),(#103571,#103572,#103573),(#103574,#103575,#103576),
(#103577,#103578,#103579)),.UNSPECIFIED.,.F.,.F.,.F.)
B_SPLINE_SURFACE_WITH_KNOTS((4,2,2,2,2,2,2,2,4),(3,3),(3.14159265358979,
3.53429173528852,3.92699081698724,4.31968989868597,4.71238898038469,5.10508806208341,
5.49778714378214,5.89048622548086,6.28318530717959),(0.,1.),
 .UNSPECIFIED.)
GEOMETRIC_REPRESENTATION_ITEM()
RATIONAL_B_SPLINE_SURFACE(((1.,0.642787609686527,1.),(1.,0.642777121345374,
1.),(1.,0.64455176311021,1.),(1.,0.651264584059143,1.),(1.,0.656206116553373,
1.),(1.,0.668340746363138,1.),(1.,0.675524086364297,1.),(1.,0.690892921248316,
1.),(1.,0.699070338275045,1.),(1.,0.71514322409805,1.),(1.,0.723033687231423,
1.),(1.,0.737413012003777,1.),(1.,0.74389933443967,1.),(1.,0.754625142483555,
1.),(1.,0.758863530286359,1.),(1.,0.764573371724574,1.),(1.,0.76604989133256,
1.),(1.,0.766044443118988,1.)))
REPRESENTATION_ITEM('')
SURFACE()
);
#1671=(
BOUNDED_SURFACE()
B_SPLINE_SURFACE(3,2,((#104053,#104054,#104055),(#104056,#104057,#104058),
(#104059,#104060,#104061),(#104062,#104063,#104064),(#104065,#104066,#104067),
(#104068,#104069,#104070),(#104071,#104072,#104073),(#104074,#104075,#104076),
(#104077,#104078,#104079),(#104080,#104081,#104082),(#104083,#104084,#104085),
(#104086,#104087,#104088),(#104089,#104090,#104091),(#104092,#104093,#104094),
(#104095,#104096,#104097),(#104098,#104099,#104100),(#104101,#104102,#104103),
(#104104,#104105,#104106),(#104107,#104108,#104109),(#104110,#104111,#104112),
(#104113,#104114,#104115),(#104116,#104117,#104118),(#104119,#104120,#104121),
(#104122,#104123,#104124),(#104125,#104126,#104127),(#104128,#104129,#104130),
(#104131,#104132,#104133),(#104134,#104135,#104136),(#104137,#104138,#104139),
(#104140,#104141,#104142),(#104143,#104144,#104145),(#104146,#104147,#104148),
(#104149,#104150,#104151),(#104152,#104153,#104154),(#104155,#104156,#104157),
(#104158,#104159,#104160),(#104161,#104162,#104163),(#104164,#104165,#104166),
(#104167,#104168,#104169),(#104170,#104171,#104172),(#104173,#104174,#104175),
(#104176,#104177,#104178),(#104179,#104180,#104181),(#104182,#104183,#104184),
(#104185,#104186,#104187),(#104188,#104189,#104190),(#104191,#104192,#104193),
(#104194,#104195,#104196),(#104197,#104198,#104199),(#104200,#104201,#104202)),
 .UNSPECIFIED.,.F.,.F.,.F.)
B_SPLINE_SURFACE_WITH_KNOTS((4,2,2,2,2,2,2,2,2,2,2,2,2,2,2,2,2,2,2,2,2,
2,2,2,4),(3,3),(0.0401498964591801,0.0428180974757128,0.044077453283822,
0.0453368090919312,0.0478555207081496,0.0503742323243681,0.0516335881324773,
0.0528929439405865,0.0554116555568049,0.0566710113649141,0.0579303671730233,
0.0604490787892417,0.0617084345973509,0.0629677904054601,0.0642271462135693,
0.0654865020216785,0.0680052136378969,0.0692645694460061,0.0705239252541153,
0.0717832810622245,0.0730426368703337,0.0755613484865521,0.0768207042946613,
0.0780800601027705,0.0807482611193032),(-0.000149489400314319,1.00005043309073),
 .UNSPECIFIED.)
GEOMETRIC_REPRESENTATION_ITEM()
RATIONAL_B_SPLINE_SURFACE(((1.00016593113143,0.444979039486126,1.00005597447691),
(1.00016643634691,0.443289150557816,1.00005614490407),(1.00016529660589,
0.447101455982151,1.00005576042886),(1.00016168673046,0.459176083043693,
1.00005454268938),(1.00016023845558,0.464020399532478,1.00005405413471),
(1.0001568480558,0.475360905223927,1.00005291043219),(1.00015492735237,
0.481785442045407,1.00005226251055),(1.00014872412617,0.502534535585041,
1.00005016994155),(1.00014399003011,0.518369554110557,1.00004857296244),
(1.00013406108711,0.551580751016643,1.00004522357655),(1.00012899351324,
0.568531215324515,1.00004351410351),(1.00012163222129,0.593153908442809,
1.00004103087771),(1.00011921529229,0.601238263928208,1.00004021556153),
(1.00011450349337,0.616998701048742,1.00003862610404),(1.00011220865661,
0.624674671757922,1.00003785197391),(1.00010570995292,0.646412104231448,
1.00003565972984),(1.00010183928869,0.659359040447713,1.00003435401702),
(1.00009691980327,0.675814165548792,1.00003269449948),(1.00009542797567,
0.680804160975152,1.00003219125293),(1.0000927816452,0.689655838565047,
1.00003129855147),(1.00009164983775,0.693441607130467,1.00003091675252),
(1.0000888664481,0.702751732254162,1.00002997781612),(1.00008780970836,
0.706286407750837,1.00002962134019),(1.000087517189,0.707264852088577,1.000029522663),
(1.00008764050632,0.706852369539625,1.00002956426232),(1.00008831781664,
0.704586842745149,1.0000297927432),(1.00008886935843,0.702741997522547,
1.00002997879788),(1.00009037928611,0.697691459383048,1.00003048815023),
(1.00009133772998,0.694485572475585,1.00003081146747),(1.00009365026412,
0.686750406029988,1.00003159156755),(1.00009500848198,0.682207320168808,
1.00003204974277),(1.00009954618833,0.667029203085519,1.00003358047265),
(1.0001032112903,0.654769849490324,1.000034816842),(1.00010947933538,0.633803944091153,
1.00003693127671),(1.00011169564763,0.626390629056982,1.00003767891772),
(1.0001162633142,0.61111229843889,1.00003921975424),(1.00011862464285,0.603213919841106,
1.00004001631445),(1.00012345746406,0.587048676802423,1.00004164659706),
(1.00012592916457,0.578781116742047,1.00004248038963),(1.00013093264633,
0.562045033359206,1.00004416824212),(1.00013347588336,0.553538191714369,
1.0000450261665),(1.00014096760153,0.528479237548492,1.0000475533897),(1.00014581500858,
0.512265206506655,1.00004918859264),(1.00015235765643,0.490380785760463,
1.00005139566065),(1.00015441501403,0.483499156141063,1.0000520896806),
(1.00015816391477,0.470959505082299,1.00005335431825),(1.00015984343524,
0.465341698114523,1.00005392088029),(1.00016419732593,0.450778423751254,
1.0000553896026),(1.00016593013437,0.44498237454662,1.00005597414056),(1.00016604025919,
0.444614019388471,1.00005601128959)))
REPRESENTATION_ITEM('')
SURFACE()
);
#1672=(
BOUNDED_SURFACE()
B_SPLINE_SURFACE(3,2,((#104203,#104204,#104205),(#104206,#104207,#104208),
(#104209,#104210,#104211),(#104212,#104213,#104214),(#104215,#104216,#104217),
(#104218,#104219,#104220),(#104221,#104222,#104223),(#104224,#104225,#104226),
(#104227,#104228,#104229),(#104230,#104231,#104232),(#104233,#104234,#104235),
(#104236,#104237,#104238),(#104239,#104240,#104241),(#104242,#104243,#104244),
(#104245,#104246,#104247),(#104248,#104249,#104250),(#104251,#104252,#104253),
(#104254,#104255,#104256),(#104257,#104258,#104259),(#104260,#104261,#104262),
(#104263,#104264,#104265),(#104266,#104267,#104268),(#104269,#104270,#104271),
(#104272,#104273,#104274),(#104275,#104276,#104277),(#104278,#104279,#104280),
(#104281,#104282,#104283),(#104284,#104285,#104286),(#104287,#104288,#104289),
(#104290,#104291,#104292),(#104293,#104294,#104295),(#104296,#104297,#104298),
(#104299,#104300,#104301),(#104302,#104303,#104304),(#104305,#104306,#104307),
(#104308,#104309,#104310),(#104311,#104312,#104313),(#104314,#104315,#104316),
(#104317,#104318,#104319),(#104320,#104321,#104322),(#104323,#104324,#104325),
(#104326,#104327,#104328),(#104329,#104330,#104331),(#104332,#104333,#104334),
(#104335,#104336,#104337),(#104338,#104339,#104340),(#104341,#104342,#104343),
(#104344,#104345,#104346),(#104347,#104348,#104349),(#104350,#104351,#104352),
(#104353,#104354,#104355),(#104356,#104357,#104358),(#104359,#104360,#104361),
(#104362,#104363,#104364),(#104365,#104366,#104367),(#104368,#104369,#104370),
(#104371,#104372,#104373),(#104374,#104375,#104376)),.UNSPECIFIED.,.F.,
 .F.,.F.)
B_SPLINE_SURFACE_WITH_KNOTS((4,2,2,2,2,2,2,2,2,2,2,2,2,2,2,2,2,2,2,2,2,
2,2,2,2,2,2,2,4),(3,3),(0.0492257416356437,0.05212126862205,0.0537007010045366,
0.0568595657695099,0.0576492819607532,0.0584389981519965,0.0600184305344832,
0.0615978629169698,0.0631772952994565,0.0663361600644298,0.0679155924469164,
0.0694950248294031,0.0726538895943764,0.0734436057856197,0.074233321976863,
0.0758127543593496,0.0773921867418363,0.0781819029330796,0.0789716191243229,
0.0821304838892962,0.0852893486542695,0.0868687810367562,0.0884482134192428,
0.0900276458017295,0.0916070781842161,0.0947659429491894,0.096345375331676,
0.0979248077141627,0.102399767083081),(-0.00131609460394527,1.),
 .UNSPECIFIED.)
GEOMETRIC_REPRESENTATION_ITEM()
RATIONAL_B_SPLINE_SURFACE(((1.00019594420023,0.925558466828159,1.),(1.00018290788058,
0.930511119781782,1.),(1.0001751814063,0.933446499297356,1.),(1.00017321277706,
0.934194404970496,1.),(1.0001744476356,0.933725267517896,1.),(1.00018352032596,
0.930278444495986,1.),(1.00019661401617,0.925303995782883,1.),(1.00022056253643,
0.916205667977813,1.),(1.00022574524419,0.914236695630683,1.),(1.00023669726237,
0.910075893610628,1.),(1.00024248153479,0.907878379693053,1.),(1.00026068949453,
0.90096095913229,1.),(1.00027396619521,0.89591698256937,1.),(1.00030249814301,
0.885077356102603,1.),(1.00031775500613,0.879281092265426,1.),(1.0003500033902,
0.867029547437474,1.),(1.00036707393448,0.860544244548642,1.),(1.00041973886326,
0.840536211453396,1.),(1.00045688450781,0.826424139102216,1.),(1.00051343672853,
0.804939277545135,1.),(1.00053242174643,0.797726643344391,1.),(1.00057017087807,
0.783385299064109,1.),(1.00058872431045,0.776336629339777,1.),(1.00064219262702,
0.756023379667273,1.),(1.00067513352966,0.743508738794324,1.),(1.00070920004036,
0.730566466029059,1.),(1.00071565293189,0.728114935756786,1.),(1.00072756192772,
0.723590566538064,1.),(1.0007330434182,0.721508083078691,1.),(1.00074797494598,
0.715835418009637,1.),(1.00075591036059,0.712820659575825,1.),(1.000767275578,
0.708502878251978,1.),(1.00077070476305,0.707200090045197,1.),(1.00077216358358,
0.706645866767436,1.),(1.00077203127614,0.706696131940276,1.),(1.00077052239234,
0.707269374848357,1.),(1.00076915238989,0.707789855080943,1.),(1.00075935410316,
0.711512340799273,1.),(1.00074204927767,0.718086649909378,1.),(1.00069241079651,
0.736944899541594,1.),(1.00066105961441,0.748855586662284,1.),(1.00060901661395,
0.768627341787248,1.),(1.00059072235101,0.77557754995927,1.),(1.00055350269926,
0.789717738526475,1.),(1.00053461513014,0.796893350775199,1.),(1.00049682155246,
0.81125158063532,1.),(1.00047791391785,0.818434816002099,1.),(1.00044051452833,
0.832643289086462,1.),(1.00042195785068,0.839693191730224,1.),(1.0003679404696,
0.860215037543297,1.),(1.00033443596869,0.87294379610312,1.),(1.00028952640061,
0.890005475388769,1.),(1.00027544616487,0.895354724483665,1.),(1.00024937271555,
0.905260338122725,1.),(1.00023733657422,0.909833011429418,1.),(1.00019681928589,
0.925226011375529,1.),(1.00017807148057,0.932348525694257,1.),(1.00017411585802,
0.93385131376765,1.)))
REPRESENTATION_ITEM('')
SURFACE()
);
#1673=(
BOUNDED_SURFACE()
B_SPLINE_SURFACE(3,2,((#104377,#104378,#104379),(#104380,#104381,#104382),
(#104383,#104384,#104385),(#104386,#104387,#104388),(#104389,#104390,#104391),
(#104392,#104393,#104394),(#104395,#104396,#104397),(#104398,#104399,#104400),
(#104401,#104402,#104403),(#104404,#104405,#104406),(#104407,#104408,#104409),
(#104410,#104411,#104412),(#104413,#104414,#104415),(#104416,#104417,#104418),
(#104419,#104420,#104421),(#104422,#104423,#104424),(#104425,#104426,#104427),
(#104428,#104429,#104430),(#104431,#104432,#104433),(#104434,#104435,#104436),
(#104437,#104438,#104439),(#104440,#104441,#104442),(#104443,#104444,#104445),
(#104446,#104447,#104448),(#104449,#104450,#104451),(#104452,#104453,#104454),
(#104455,#104456,#104457),(#104458,#104459,#104460),(#104461,#104462,#104463),
(#104464,#104465,#104466),(#104467,#104468,#104469),(#104470,#104471,#104472),
(#104473,#104474,#104475),(#104476,#104477,#104478),(#104479,#104480,#104481),
(#104482,#104483,#104484),(#104485,#104486,#104487),(#104488,#104489,#104490),
(#104491,#104492,#104493),(#104494,#104495,#104496),(#104497,#104498,#104499),
(#104500,#104501,#104502),(#104503,#104504,#104505),(#104506,#104507,#104508),
(#104509,#104510,#104511),(#104512,#104513,#104514),(#104515,#104516,#104517),
(#104518,#104519,#104520),(#104521,#104522,#104523),(#104524,#104525,#104526),
(#104527,#104528,#104529),(#104530,#104531,#104532),(#104533,#104534,#104535),
(#104536,#104537,#104538),(#104539,#104540,#104541),(#104542,#104543,#104544)),
 .UNSPECIFIED.,.F.,.F.,.F.)
B_SPLINE_SURFACE_WITH_KNOTS((4,2,2,2,2,2,2,2,2,2,2,2,2,2,2,2,2,2,2,2,2,
2,2,2,2,2,2,4),(3,3),(0.0511475161399861,0.0543755745194946,0.0559748561230095,
0.0575741377265244,0.0591734193300392,0.0607727009335541,0.062371982537069,
0.0639712641405839,0.0671698273476136,0.0687691089511285,0.0703683905546434,
0.0735669537616731,0.0743665945634306,0.075166235365188,0.0767655169687029,
0.0783647985722178,0.0799640801757326,0.0831626433827624,0.0839622841845198,
0.0847619249862773,0.0863612065897922,0.087960488193307,0.0895597697968219,
0.0911590514003368,0.0927583330038517,0.0959568962108814,0.0991554594179112,
0.102525861223953),(0.,1.00017183859901),.UNSPECIFIED.)
GEOMETRIC_REPRESENTATION_ITEM()
RATIONAL_B_SPLINE_SURFACE(((0.999999999999999,0.363791624139497,1.00021865031197),
(1.,0.345907098152807,1.00022479681575),(1.,0.333093359896291,1.00022920060541),
(1.,0.326997783970327,1.00023129551587),(1.,0.327177805749954,1.00023123364649),
(1.,0.331655133124558,1.00022969489116),(1.,0.33594526264938,1.00022822047147),
(1.,0.347973250814003,1.0002240867262),(1.,0.355767139651311,1.00022140814432),
(1.,0.373420234385515,1.00021534117819),(1.,0.383300909504948,1.00021194541545),
(1.,0.404353607436141,1.00020471008321),(1.,0.415539518961281,1.00020086574048),
(1.,0.438608462395935,1.00019293747064),(1.,0.450347915466347,1.0001889028883),
(1.,0.48562633119133,1.00017677850123),(1.,0.509203616458581,1.0001686755259),
(1.,0.543403436110305,1.00015692182771),(1.,0.554652013302503,1.00015305594821),
(1.,0.576466905683596,1.00014555866713),(1.,0.58694153284502,1.00014195877661),
(1.,0.616911695858428,1.00013165871496),(1.,0.634969557244847,1.00012545263976),
(1.,0.654503005935658,1.00011873943885),(1.,0.65825654007911,1.00011744943475),
(1.,0.665435063621704,1.00011498233989),(1.,0.668871309120368,1.00011380138067),
(1.,0.678546034793369,1.00011047639806),(1.,0.684157382338495,1.00010854790585),
(1.,0.693634268435882,1.00010529091619),(1.,0.697500232426135,1.00010396227252),
(1.,0.703370534929454,1.00010194478341),(1.,0.705371444929301,1.00010125711626),
(1.,0.708290812429381,1.00010025379622),(1.,0.706260755280861,1.00010095148057),
(1.,0.69882470043928,1.00010350708307),(1.,0.697084750890873,1.00010410506405),
(1.,0.693165330790786,1.00010545207937),(1.,0.690982356485942,1.00010620231786),
(1.,0.68379338348011,1.00010867300396),(1.,0.678148780393404,1.00011061292534),
(1.,0.665272843129722,1.00011503809138),(1.,0.658004130630274,1.00011753618212),
(1.,0.642133827810631,1.00012299044333),(1.,0.6335794985508,1.00012593037124),
(1.,0.615382081200458,1.00013218440864),(1.,0.605738300581893,1.00013549875614),
(1.,0.585480053220422,1.00014246105383),(1.,0.57481870187419,1.00014612511719),
(1.,0.54200218601379,1.00015740340541),(1.,0.51896068005778,1.00016532224562),
(1.,0.471865311436787,1.00018150784994),(1.,0.447600125261933,1.00018984724114),
(1.,0.400739305781053,1.00020595223628),(1.,0.378121326325834,1.00021372552008),
(1.,0.360032870100529,1.00021994211003)))
REPRESENTATION_ITEM('')
SURFACE()
);
#1674=(
BOUNDED_SURFACE()
B_SPLINE_SURFACE(3,2,((#104546,#104547,#104548),(#104549,#104550,#104551),
(#104552,#104553,#104554),(#104555,#104556,#104557),(#104558,#104559,#104560),
(#104561,#104562,#104563),(#104564,#104565,#104566),(#104567,#104568,#104569),
(#104570,#104571,#104572),(#104573,#104574,#104575),(#104576,#104577,#104578),
(#104579,#104580,#104581),(#104582,#104583,#104584),(#104585,#104586,#104587),
(#104588,#104589,#104590),(#104591,#104592,#104593),(#104594,#104595,#104596),
(#104597,#104598,#104599),(#104600,#104601,#104602),(#104603,#104604,#104605),
(#104606,#104607,#104608),(#104609,#104610,#104611),(#104612,#104613,#104614),
(#104615,#104616,#104617),(#104618,#104619,#104620),(#104621,#104622,#104623),
(#104624,#104625,#104626),(#104627,#104628,#104629),(#104630,#104631,#104632),
(#104633,#104634,#104635),(#104636,#104637,#104638),(#104639,#104640,#104641),
(#104642,#104643,#104644),(#104645,#104646,#104647),(#104648,#104649,#104650),
(#104651,#104652,#104653),(#104654,#104655,#104656),(#104657,#104658,#104659),
(#104660,#104661,#104662),(#104663,#104664,#104665),(#104666,#104667,#104668),
(#104669,#104670,#104671),(#104672,#104673,#104674),(#104675,#104676,#104677),
(#104678,#104679,#104680),(#104681,#104682,#104683),(#104684,#104685,#104686),
(#104687,#104688,#104689),(#104690,#104691,#104692),(#104693,#104694,#104695)),
 .UNSPECIFIED.,.F.,.F.,.F.)
B_SPLINE_SURFACE_WITH_KNOTS((4,2,2,2,2,2,2,2,2,2,2,2,2,2,2,2,2,2,2,2,2,
2,2,2,4),(3,3),(0.0411832956025613,0.0424965399968198,0.0437843139361192,
0.0463598618147179,0.0476476357540172,0.0489354096933166,0.0515109575719153,
0.054086505450514,0.0553742793898133,0.0566620533291127,0.0592376012077114,
0.0618131490863101,0.0631009230256095,0.0643886969649088,0.0656764709042082,
0.0669642448435075,0.0695397927221063,0.0708275666614056,0.072115340600705,
0.0734031145400043,0.0746908884793037,0.0772664363579024,0.0785542102972017,
0.0798419842365011,0.0824175321150998),(-2.54704549892859E-5,1.),
 .UNSPECIFIED.)
GEOMETRIC_REPRESENTATION_ITEM()
RATIONAL_B_SPLINE_SURFACE(((1.00002969011113,0.41716567016007,1.),(1.00002994384796,
0.412184667121395,1.),(1.0000301347314,0.408437513003748,1.),(1.00003036746518,
0.403868812055419,1.),(1.00003041084928,0.403017156769614,1.),(1.00003031596223,
0.404879845196922,1.),(1.00002995641597,0.411937949549854,1.),(1.00002907725759,
0.42919634528864,1.),(1.0000287281148,0.436050223421914,1.),(1.0000279625118,
0.45107946022051,1.),(1.00002754420566,0.459291055676708,1.),(1.00002621873246,
0.485310873574663,1.),(1.00002523535442,0.504615162293121,1.),(1.00002327853494,
0.543028678709834,1.),(1.00002229863343,0.562264721202267,1.),(1.00002088610616,
0.58999346174123,1.),(1.00002042575008,0.599030522075286,1.),(1.00001954857755,
0.616249934281681,1.),(1.00001912948864,0.624476895847254,1.),(1.00001793948785,
0.647837310828753,1.),(1.0000172350414,0.661666008506602,1.),(1.00001606044591,
0.68472400830539,1.),(1.00001561170694,0.693533018117966,1.),(1.00001517175011,
0.702169629233436,1.),(1.00001506362195,0.704292248448626,1.),(1.00001493152404,
0.706885408022375,1.),(1.0000149083449,0.70734042817065,1.),(1.00001494501072,
0.706620656543938,1.),(1.00001500486264,0.705445728351282,1.),(1.00001520669394,
0.701483661229885,1.),(1.00001534974885,0.698675409330837,1.),(1.00001589553929,
0.687961222177015,1.),(1.0000164072945,0.677915166725478,1.),(1.00001736385409,
0.659137339788157,1.),(1.00001771630397,0.652218541517549,1.),(1.00001846671731,
0.637487486635047,1.),(1.00001886535688,0.629661957539986,1.),(1.00001970257416,
0.613226890341952,1.),(1.0000201411837,0.604616727276649,1.),(1.00002105184036,
0.586740001976879,1.),(1.00002152598384,0.577432286849769,1.),(1.00002296522561,
0.549179124901904,1.),(1.00002395181897,0.529811717588144,1.),(1.00002540634078,
0.501258599676148,1.),(1.00002588670869,0.491828695166698,1.),(1.00002682175625,
0.473473162191487,1.),(1.000027272038,0.464633866720484,1.),(1.0000285273913,
0.439990543645249,1.),(1.00002924391365,0.425924788916652,1.),(1.00002973290203,
0.416325659622527,1.)))
REPRESENTATION_ITEM('')
SURFACE()
);
#1675=(
BOUNDED_SURFACE()
B_SPLINE_SURFACE(3,2,((#104696,#104697,#104698),(#104699,#104700,#104701),
(#104702,#104703,#104704),(#104705,#104706,#104707),(#104708,#104709,#104710),
(#104711,#104712,#104713),(#104714,#104715,#104716),(#104717,#104718,#104719),
(#104720,#104721,#104722),(#104723,#104724,#104725),(#104726,#104727,#104728),
(#104729,#104730,#104731),(#104732,#104733,#104734),(#104735,#104736,#104737),
(#104738,#104739,#104740),(#104741,#104742,#104743),(#104744,#104745,#104746),
(#104747,#104748,#104749),(#104750,#104751,#104752),(#104753,#104754,#104755),
(#104756,#104757,#104758),(#104759,#104760,#104761),(#104762,#104763,#104764),
(#104765,#104766,#104767),(#104768,#104769,#104770),(#104771,#104772,#104773),
(#104774,#104775,#104776),(#104777,#104778,#104779),(#104780,#104781,#104782),
(#104783,#104784,#104785),(#104786,#104787,#104788),(#104789,#104790,#104791),
(#104792,#104793,#104794),(#104795,#104796,#104797),(#104798,#104799,#104800),
(#104801,#104802,#104803),(#104804,#104805,#104806),(#104807,#104808,#104809),
(#104810,#104811,#104812),(#104813,#104814,#104815),(#104816,#104817,#104818),
(#104819,#104820,#104821),(#104822,#104823,#104824),(#104825,#104826,#104827),
(#104828,#104829,#104830),(#104831,#104832,#104833),(#104834,#104835,#104836),
(#104837,#104838,#104839),(#104840,#104841,#104842),(#104843,#104844,#104845)),
 .UNSPECIFIED.,.F.,.F.,.F.)
B_SPLINE_SURFACE_WITH_KNOTS((4,2,2,2,2,2,2,2,2,2,2,2,2,2,2,2,2,2,2,2,2,
2,2,2,4),(3,3),(0.0411832956025262,0.0424965399968198,0.0437843139361192,
0.0463598618147179,0.0476476357540172,0.0489354096933166,0.0515109575719153,
0.054086505450514,0.0553742793898133,0.0566620533291127,0.0592376012077114,
0.0618131490863101,0.0631009230256095,0.0643886969649088,0.0656764709042082,
0.0669642448435075,0.0695397927221063,0.0708275666614056,0.072115340600705,
0.0734031145400043,0.0746908884793037,0.0772664363579024,0.0785542102972017,
0.0798419842365011,0.0824175321150998),(-2.54704550244023E-5,1.),
 .UNSPECIFIED.)
GEOMETRIC_REPRESENTATION_ITEM()
RATIONAL_B_SPLINE_SURFACE(((1.00002969011117,0.417165670160449,1.),(1.000029943848,
0.412184667121575,1.),(1.00003013473144,0.408437513003789,1.),(1.00003036746522,
0.403868812055398,1.),(1.00003041084932,0.403017156769593,1.),(1.00003031596227,
0.404879845196902,1.),(1.00002995641602,0.411937949549833,1.),(1.00002907725763,
0.42919634528862,1.),(1.00002872811484,0.436050223421894,1.),(1.00002796251184,
0.451079460220491,1.),(1.0000275442057,0.459291055676689,1.),(1.00002621873249,
0.485310873574645,1.),(1.00002523535446,0.504615162293104,1.),(1.00002327853497,
0.543028678709818,1.),(1.00002229863346,0.562264721202251,1.),(1.00002088610619,
0.589993461741216,1.),(1.00002042575011,0.599030522075271,1.),(1.00001954857758,
0.616249934281668,1.),(1.00001912948867,0.624476895847241,1.),(1.00001793948787,
0.64783731082874,1.),(1.00001723504143,0.66166600850659,1.),(1.00001606044593,
0.684724008305379,1.),(1.00001561170696,0.693533018117955,1.),(1.00001517175013,
0.702169629233425,1.),(1.00001506362197,0.704292248448615,1.),(1.00001493152406,
0.706885408022364,1.),(1.00001490834492,0.70734042817064,1.),(1.00001494501075,
0.706620656543927,1.),(1.00001500486266,0.705445728351272,1.),(1.00001520669396,
0.701483661229874,1.),(1.00001534974887,0.698675409330827,1.),(1.00001589553931,
0.687961222177005,1.),(1.00001640729452,0.677915166725467,1.),(1.00001736385411,
0.659137339788145,1.),(1.00001771630399,0.652218541517537,1.),(1.00001846671733,
0.637487486635034,1.),(1.00001886535691,0.629661957539973,1.),(1.00001970257419,
0.613226890341938,1.),(1.00002014118373,0.604616727276635,1.),(1.00002105184039,
0.586740001976865,1.),(1.00002152598387,0.577432286849754,1.),(1.00002296522565,
0.549179124901888,1.),(1.000023951819,0.529811717588127,1.),(1.00002540634081,
0.50125859967613,1.),(1.00002588670873,0.49182869516668,1.),(1.00002682175628,
0.473473162191469,1.),(1.00002727203804,0.464633866720466,1.),(1.00002852739134,
0.439990543645229,1.),(1.00002924391369,0.425924788916632,1.),(1.00002973290207,
0.416325659622506,1.)))
REPRESENTATION_ITEM('')
SURFACE()
);
#1676=(
BOUNDED_SURFACE()
B_SPLINE_SURFACE(3,2,((#105057,#105058,#105059),(#105060,#105061,#105062),
(#105063,#105064,#105065),(#105066,#105067,#105068),(#105069,#105070,#105071),
(#105072,#105073,#105074),(#105075,#105076,#105077),(#105078,#105079,#105080),
(#105081,#105082,#105083),(#105084,#105085,#105086),(#105087,#105088,#105089),
(#105090,#105091,#105092),(#105093,#105094,#105095),(#105096,#105097,#105098),
(#105099,#105100,#105101),(#105102,#105103,#105104),(#105105,#105106,#105107),
(#105108,#105109,#105110),(#105111,#105112,#105113),(#105114,#105115,#105116),
(#105117,#105118,#105119),(#105120,#105121,#105122),(#105123,#105124,#105125),
(#105126,#105127,#105128),(#105129,#105130,#105131),(#105132,#105133,#105134),
(#105135,#105136,#105137),(#105138,#105139,#105140),(#105141,#105142,#105143),
(#105144,#105145,#105146),(#105147,#105148,#105149),(#105150,#105151,#105152),
(#105153,#105154,#105155),(#105156,#105157,#105158),(#105159,#105160,#105161),
(#105162,#105163,#105164),(#105165,#105166,#105167),(#105168,#105169,#105170),
(#105171,#105172,#105173),(#105174,#105175,#105176),(#105177,#105178,#105179),
(#105180,#105181,#105182)),.UNSPECIFIED.,.F.,.F.,.F.)
B_SPLINE_SURFACE_WITH_KNOTS((4,2,2,2,2,2,2,2,2,2,2,2,2,2,2,2,2,2,2,2,4),
(3,3),(0.0200568639003605,0.0213281306129126,0.0225827265313192,0.0232100244905226,
0.0238373224497259,0.0250919183681325,0.0263465142865391,0.0269738122457424,
0.0276011102049457,0.0288557061233524,0.030110302041759,0.0313648979601656,
0.0326194938785723,0.0332467918377756,0.0338740897969789,0.0351286857153855,
0.0363832816337921,0.0376378775521988,0.0382651755114021,0.0388924734706054,
0.040147069389012),(-1.6670794163376E-5,1.),.UNSPECIFIED.)
GEOMETRIC_REPRESENTATION_ITEM()
RATIONAL_B_SPLINE_SURFACE(((1.00001218909147,0.634417792362364,1.),(1.00001207070658,
0.637968459699978,1.),(1.00001198539686,0.640527117559773,1.),(1.00001190087293,
0.643062207776934,1.),(1.00001189940874,0.643106122556049,1.),(1.00001195795143,
0.641350276625085,1.),(1.00001198783686,0.640453935716271,1.),(1.0000120665277,
0.638093795110533,1.),(1.00001211511354,0.636636580788178,1.),(1.00001228558705,
0.631523641684606,1.),(1.0000124323333,0.627122344191632,1.),(1.00001277455001,
0.616858384702073,1.),(1.00001296504766,0.611144870017612,1.),(1.00001325563189,
0.602429501679159,1.),(1.00001335337752,0.599497858598228,1.),(1.00001354628551,
0.593712051753561,1.),(1.0000136417071,0.590850112792402,1.),(1.00001391054031,
0.582787113346938,1.),(1.00001406873562,0.578042429230547,1.),(1.00001430529436,
0.570947423996434,1.),(1.00001438238684,0.568635222351684,1.),(1.00001441730522,
0.56758793028365,1.),(1.00001437708325,0.568794290657144,1.),(1.00001416717897,
0.575089859693509,1.),(1.0000139997862,0.580110399619696,1.),(1.00001367027674,
0.589993235888577,1.),(1.00001354728695,0.593682016041953,1.),(1.00001327743302,
0.601775629678951,1.),(1.0000131303487,0.606187066817002,1.),(1.00001266743157,
0.620071142126849,1.),(1.00001232742341,0.630268861450101,1.),(1.00001161384565,
0.6516708939964,1.),(1.0000112397551,0.662890831923292,1.),(1.00001051322695,
0.684681280272715,1.),(1.0000101570569,0.69536373622251,1.),(1.00000965159222,
0.710523921999963,1.),(1.00000948811148,0.715427130046569,1.),(1.00000918068499,
0.724647641305723,1.),(1.00000903576729,0.728994095987094,1.),(1.00000863062084,
0.741145479997482,1.),(1.00000839984957,0.748066904027392,1.),(1.00000821878182,
0.753497591644584,1.)))
REPRESENTATION_ITEM('')
SURFACE()
);
#1677=(
BOUNDED_SURFACE()
B_SPLINE_SURFACE(3,2,((#105445,#105446,#105447),(#105448,#105449,#105450),
(#105451,#105452,#105453),(#105454,#105455,#105456),(#105457,#105458,#105459),
(#105460,#105461,#105462),(#105463,#105464,#105465),(#105466,#105467,#105468),
(#105469,#105470,#105471),(#105472,#105473,#105474),(#105475,#105476,#105477),
(#105478,#105479,#105480),(#105481,#105482,#105483),(#105484,#105485,#105486),
(#105487,#105488,#105489),(#105490,#105491,#105492),(#105493,#105494,#105495),
(#105496,#105497,#105498),(#105499,#105500,#105501),(#105502,#105503,#105504),
(#105505,#105506,#105507),(#105508,#105509,#105510),(#105511,#105512,#105513),
(#105514,#105515,#105516),(#105517,#105518,#105519),(#105520,#105521,#105522),
(#105523,#105524,#105525),(#105526,#105527,#105528),(#105529,#105530,#105531),
(#105532,#105533,#105534),(#105535,#105536,#105537),(#105538,#105539,#105540),
(#105541,#105542,#105543),(#105544,#105545,#105546),(#105547,#105548,#105549),
(#105550,#105551,#105552),(#105553,#105554,#105555),(#105556,#105557,#105558),
(#105559,#105560,#105561),(#105562,#105563,#105564),(#105565,#105566,#105567),
(#105568,#105569,#105570),(#105571,#105572,#105573),(#105574,#105575,#105576),
(#105577,#105578,#105579),(#105580,#105581,#105582),(#105583,#105584,#105585),
(#105586,#105587,#105588),(#105589,#105590,#105591),(#105592,#105593,#105594)),
 .UNSPECIFIED.,.F.,.F.,.F.)
B_SPLINE_SURFACE_WITH_KNOTS((4,2,2,2,2,2,2,2,2,2,2,2,2,2,2,2,2,2,2,2,2,
2,2,2,4),(3,3),(0.0401498964592781,0.0428180974757128,0.044077453283822,
0.0453368090919312,0.0478555207081496,0.0503742323243681,0.0516335881324773,
0.0528929439405865,0.0554116555568049,0.0566710113649141,0.0579303671730233,
0.0604490787892417,0.0617084345973509,0.0629677904054601,0.0642271462135693,
0.0654865020216785,0.0680052136378969,0.0692645694460061,0.0705239252541153,
0.0717832810622245,0.0730426368703337,0.0755613484865521,0.0768207042946613,
0.0780800601027705,0.0807482611192052),(-5.04330907357126E-5,1.00014948940022),
 .UNSPECIFIED.)
GEOMETRIC_REPRESENTATION_ITEM()
RATIONAL_B_SPLINE_SURFACE(((1.00005597447691,0.444979039485992,1.00016593113132),
(1.00005614490408,0.443289150558148,1.0001664363468),(1.00005576042886,
0.447101455982505,1.00016529660579),(1.00005454268939,0.459176083043744,
1.00016168673036),(1.00005405413472,0.464020399532528,1.00016023845548),
(1.00005291043219,0.475360905223976,1.0001568480557),(1.00005226251056,
0.481785442045456,1.00015492735227),(1.00005016994156,0.502534535585088,
1.00014872412607),(1.00004857296245,0.518369554110602,1.00014399003002),
(1.00004522357656,0.551580751016686,1.00013406108703),(1.00004351410351,
0.568531215324555,1.00012899351315),(1.00004103087771,0.593153908442847,
1.00012163222121),(1.00004021556153,0.601238263928246,1.00011921529221),
(1.00003862610404,0.616998701048778,1.0001145034933),(1.00003785197391,
0.624674671757957,1.00011220865653),(1.00003565972984,0.646412104231481,
1.00010570995285),(1.00003435401702,0.659359040447745,1.00010183928863),
(1.00003269449948,0.675814165548823,1.00009691980321),(1.00003219125293,
0.680804160975182,1.00009542797561),(1.00003129855147,0.689655838565076,
1.00009278164514),(1.00003091675253,0.693441607130496,1.00009164983769),
(1.00002997781612,0.70275173225419,1.00008886644804),(1.0000296213402,0.706286407750865,
1.0000878097083),(1.000029522663,0.707264852088604,1.00008751718895),(1.00002956426232,
0.706852369539653,1.00008764050626),(1.0000297927432,0.704586842745177,
1.00008831781658),(1.00002997879788,0.702741997522575,1.00008886935837),
(1.00003048815023,0.697691459383076,1.00009037928605),(1.00003081146747,
0.694485572475614,1.00009133772992),(1.00003159156755,0.686750406030017,
1.00009365026406),(1.00003204974278,0.682207320168837,1.00009500848191),
(1.00003358047265,0.66702920308555,1.00009954618827),(1.000034816842,0.654769849490357,
1.00010321129023),(1.00003693127672,0.633803944091187,1.00010947933531),
(1.00003767891773,0.626390629057017,1.00011169564756),(1.00003921975424,
0.611112298438927,1.00011626331412),(1.00004001631445,0.603213919841143,
1.00011862464277),(1.00004164659707,0.587048676802461,1.00012345746397),
(1.00004248038963,0.578781116742087,1.00012592916449),(1.00004416824212,
0.562045033359247,1.00013093264624),(1.0000450261665,0.553538191714411,
1.00013347588327),(1.00004755338971,0.528479237548537,1.00014096760144),
(1.00004918859265,0.512265206506701,1.00014581500849),(1.00005139566065,
0.490380785760511,1.00015235765633),(1.0000520896806,0.483499156141111,
1.00015441501393),(1.00005335431826,0.470959505082348,1.00015816391466),
(1.0000539208803,0.465341698114573,1.00015984343514),(1.0000553896026,0.450778423751669,
1.00016419732582),(1.00005597414057,0.444982374547099,1.00016593013426),
(1.00005601128959,0.444614019388563,1.00016604025909)))
REPRESENTATION_ITEM('')
SURFACE()
);
#1678=(
BOUNDED_SURFACE()
B_SPLINE_SURFACE(3,2,((#105595,#105596,#105597),(#105598,#105599,#105600),
(#105601,#105602,#105603),(#105604,#105605,#105606),(#105607,#105608,#105609),
(#105610,#105611,#105612),(#105613,#105614,#105615),(#105616,#105617,#105618),
(#105619,#105620,#105621),(#105622,#105623,#105624),(#105625,#105626,#105627),
(#105628,#105629,#105630),(#105631,#105632,#105633),(#105634,#105635,#105636),
(#105637,#105638,#105639),(#105640,#105641,#105642),(#105643,#105644,#105645),
(#105646,#105647,#105648),(#105649,#105650,#105651),(#105652,#105653,#105654),
(#105655,#105656,#105657),(#105658,#105659,#105660),(#105661,#105662,#105663),
(#105664,#105665,#105666),(#105667,#105668,#105669),(#105670,#105671,#105672),
(#105673,#105674,#105675),(#105676,#105677,#105678),(#105679,#105680,#105681),
(#105682,#105683,#105684),(#105685,#105686,#105687),(#105688,#105689,#105690),
(#105691,#105692,#105693),(#105694,#105695,#105696),(#105697,#105698,#105699),
(#105700,#105701,#105702),(#105703,#105704,#105705),(#105706,#105707,#105708),
(#105709,#105710,#105711),(#105712,#105713,#105714),(#105715,#105716,#105717),
(#105718,#105719,#105720),(#105721,#105722,#105723),(#105724,#105725,#105726),
(#105727,#105728,#105729),(#105730,#105731,#105732),(#105733,#105734,#105735),
(#105736,#105737,#105738),(#105739,#105740,#105741),(#105742,#105743,#105744),
(#105745,#105746,#105747),(#105748,#105749,#105750),(#105751,#105752,#105753),
(#105754,#105755,#105756),(#105757,#105758,#105759),(#105760,#105761,#105762),
(#105763,#105764,#105765),(#105766,#105767,#105768)),.UNSPECIFIED.,.F.,
 .F.,.F.)
B_SPLINE_SURFACE_WITH_KNOTS((4,2,2,2,2,2,2,2,2,2,2,2,2,2,2,2,2,2,2,2,2,
2,2,2,2,2,2,2,4),(3,3),(0.0492257416375651,0.05212126862205,0.0537007010045366,
0.0568595657695099,0.0576492819607532,0.0584389981519965,0.0600184305344832,
0.0615978629169698,0.0631772952994565,0.0663361600644298,0.0679155924469164,
0.0694950248294031,0.0726538895943764,0.0734436057856197,0.074233321976863,
0.0758127543593496,0.0773921867418363,0.0781819029330796,0.0789716191243229,
0.0821304838892962,0.0852893486542695,0.0868687810367562,0.0884482134192428,
0.0900276458017295,0.0916070781842161,0.0947659429491894,0.096345375331676,
0.0979248077141627,0.10239976708116),(0.,1.00131609460202),
 .UNSPECIFIED.)
GEOMETRIC_REPRESENTATION_ITEM()
RATIONAL_B_SPLINE_SURFACE(((1.,0.925558466838161,1.00019594419992),(1.,
0.930511119785811,1.0001829078803),(1.,0.933446499297804,1.00017518140604),
(1.,0.934194404970622,1.0001732127768),(1.,0.933725267518023,1.00017444763534),
(1.,0.93027844449612,1.00018352032569),(1.,0.925303995783027,1.00019661401589),
(1.,0.916205667977974,1.00022056253611),(1.,0.914236695630848,1.00022574524386),
(1.,0.910075893610801,1.00023669726202),(1.,0.907878379693229,1.00024248153443),
(1.,0.90096095913248,1.00026068949415),(1.,0.895916982569569,1.00027396619481),
(1.,0.885077356102823,1.00030249814257),(1.,0.879281092265658,1.00031775500566),
(1.,0.867029547437729,1.00035000338969),(1.,0.86054424454891,1.00036707393394),
(1.,0.840536211453702,1.00041973886265),(1.,0.826424139102549,1.00045688450714),
(1.,0.804939277545509,1.00051343672778),(1.,0.797726643344779,1.00053242174565),
(1.,0.783385299064525,1.00057017087724),(1.,0.776336629340206,1.00058872430959),
(1.,0.756023379667741,1.00064219262608),(1.,0.743508738794816,1.00067513352868),
(1.,0.730566466029576,1.00070920003933),(1.,0.728114935757307,1.00071565293084),
(1.,0.723590566538595,1.00072756192665),(1.,0.721508083079225,1.00073304341713),
(1.,0.715835418010182,1.00074797494489),(1.,0.712820659576376,1.00075591035949),
(1.,0.708502878252537,1.00076727557687),(1.,0.707200090045759,1.00077070476193),
(1.,0.706645866767999,1.00077216358246),(1.,0.706696131940839,1.00077203127501),
(1.,0.707269374848919,1.00077052239122),(1.,0.707789855081503,1.00076915238877),
(1.,0.711512340799826,1.00075935410205),(1.,0.718086649909919,1.00074204927658),
(1.,0.736944899542099,1.0006924107955),(1.,0.748855586662766,1.00066105961344),
(1.,0.768627341787692,1.00060901661306),(1.,0.7755775499597,1.00059072235014),
(1.,0.789717738526879,1.00055350269845),(1.,0.796893350775588,1.00053461512936),
(1.,0.811251580635682,1.00049682155173),(1.,0.818434816002448,1.00047791391715),
(1.,0.832643289086783,1.00044051452769),(1.,0.839693191730531,1.00042195785006),
(1.,0.860215037543565,1.00036794046907),(1.,0.872943796103364,1.0003344359682),
(1.,0.89000547538898,1.00028952640019),(1.,0.895354724483866,1.00027544616447),
(1.,0.905260338122907,1.00024937271519),(1.,0.909833011429591,1.00023733657388),
(1.,0.925226011370787,1.00019681928561),(1.,0.93234852568827,1.00017807148032),
(1.,0.933851313765841,1.00017411585777)))
REPRESENTATION_ITEM('')
SURFACE()
);
#1679=(
BOUNDED_SURFACE()
B_SPLINE_SURFACE(3,2,((#105769,#105770,#105771),(#105772,#105773,#105774),
(#105775,#105776,#105777),(#105778,#105779,#105780),(#105781,#105782,#105783),
(#105784,#105785,#105786),(#105787,#105788,#105789),(#105790,#105791,#105792),
(#105793,#105794,#105795),(#105796,#105797,#105798),(#105799,#105800,#105801),
(#105802,#105803,#105804),(#105805,#105806,#105807),(#105808,#105809,#105810),
(#105811,#105812,#105813),(#105814,#105815,#105816),(#105817,#105818,#105819),
(#105820,#105821,#105822),(#105823,#105824,#105825),(#105826,#105827,#105828),
(#105829,#105830,#105831),(#105832,#105833,#105834),(#105835,#105836,#105837),
(#105838,#105839,#105840),(#105841,#105842,#105843),(#105844,#105845,#105846),
(#105847,#105848,#105849),(#105850,#105851,#105852),(#105853,#105854,#105855),
(#105856,#105857,#105858),(#105859,#105860,#105861),(#105862,#105863,#105864),
(#105865,#105866,#105867),(#105868,#105869,#105870),(#105871,#105872,#105873),
(#105874,#105875,#105876),(#105877,#105878,#105879),(#105880,#105881,#105882),
(#105883,#105884,#105885),(#105886,#105887,#105888),(#105889,#105890,#105891),
(#105892,#105893,#105894),(#105895,#105896,#105897),(#105898,#105899,#105900),
(#105901,#105902,#105903),(#105904,#105905,#105906),(#105907,#105908,#105909),
(#105910,#105911,#105912),(#105913,#105914,#105915),(#105916,#105917,#105918),
(#105919,#105920,#105921),(#105922,#105923,#105924),(#105925,#105926,#105927),
(#105928,#105929,#105930),(#105931,#105932,#105933),(#105934,#105935,#105936)),
 .UNSPECIFIED.,.F.,.F.,.F.)
B_SPLINE_SURFACE_WITH_KNOTS((4,2,2,2,2,2,2,2,2,2,2,2,2,2,2,2,2,2,2,2,2,
2,2,2,2,2,2,4),(3,3),(0.0511475161397767,0.0543755745194946,0.0559748561230095,
0.0575741377265244,0.0591734193300392,0.0607727009335541,0.062371982537069,
0.0639712641405839,0.0671698273476136,0.0687691089511285,0.0703683905546434,
0.0735669537616731,0.0743665945634306,0.075166235365188,0.0767655169687029,
0.0783647985722178,0.0799640801757326,0.0831626433827624,0.0839622841845198,
0.0847619249862773,0.0863612065897922,0.087960488193307,0.0895597697968219,
0.0911590514003368,0.0927583330038517,0.0959568962108814,0.0991554594179112,
0.102525861223878),(-0.000171838598937368,1.),.UNSPECIFIED.)
GEOMETRIC_REPRESENTATION_ITEM()
RATIONAL_B_SPLINE_SURFACE(((1.00021865031188,0.363791624143024,1.),(1.00022479681566,
0.345907098154518,1.),(1.00022920060531,0.333093359896605,1.),(1.00023129551577,
0.326997783970377,1.),(1.00023123364639,0.327177805750004,1.),(1.00022969489106,
0.331655133124608,1.),(1.00022822047137,0.33594526264943,1.),(1.0002240867261,
0.347973250814052,1.),(1.00022140814422,0.35576713965136,1.),(1.00021534117809,
0.373420234385561,1.),(1.00021194541535,0.383300909504994,1.),(1.00020471008312,
0.404353607436186,1.),(1.00020086574039,0.415539518961325,1.),(1.00019293747055,
0.438608462395977,1.),(1.00018890288822,0.450347915466388,1.),(1.00017677850116,
0.485626331191368,1.),(1.00016867552582,0.509203616458618,1.),(1.00015692182764,
0.543403436110339,1.),(1.00015305594815,0.554652013302536,1.),(1.00014555866706,
0.576466905683628,1.),(1.00014195877655,0.586941532845051,1.),(1.00013165871491,
0.616911695858456,1.),(1.0001254526397,0.634969557244874,1.),(1.00011873943879,
0.654503005935684,1.),(1.0001174494347,0.658256540079135,1.),(1.00011498233984,
0.665435063621729,1.),(1.00011380138062,0.668871309120393,1.),(1.00011047639801,
0.678546034793393,1.),(1.00010854790581,0.684157382338519,1.),(1.00010529091615,
0.693634268435905,1.),(1.00010396227248,0.697500232426158,1.),(1.00010194478336,
0.703370534929476,1.),(1.00010125711622,0.705371444929324,1.),(1.00010025379618,
0.708290812429403,1.),(1.00010095148053,0.706260755280883,1.),(1.00010350708302,
0.698824700439302,1.),(1.00010410506401,0.697084750890896,1.),(1.00010545207932,
0.693165330790809,1.),(1.00010620231782,0.690982356485965,1.),(1.00010867300391,
0.683793383480134,1.),(1.00011061292529,0.678148780393428,1.),(1.00011503809133,
0.665272843129747,1.),(1.00011753618207,0.658004130630299,1.),(1.00012299044327,
0.642133827810658,1.),(1.00012593037118,0.633579498550827,1.),(1.00013218440859,
0.615382081200487,1.),(1.00013549875609,0.605738300581923,1.),(1.00014246105377,
0.585480053220453,1.),(1.00014612511713,0.574818701874222,1.),(1.00015740340534,
0.542002186013824,1.),(1.00016532224555,0.518960680057816,1.),(1.00018150784987,
0.471865311436827,1.),(1.00018984724106,0.447600125261974,1.),(1.00020595223619,
0.400739305781631,1.),(1.00021372551999,0.378121326326883,1.),(1.00021994210994,
0.36003287010178,1.)))
REPRESENTATION_ITEM('')
SURFACE()
);
#1680=(
BOUNDED_SURFACE()
B_SPLINE_SURFACE(3,2,((#106162,#106163,#106164),(#106165,#106166,#106167),
(#106168,#106169,#106170),(#106171,#106172,#106173),(#106174,#106175,#106176),
(#106177,#106178,#106179),(#106180,#106181,#106182),(#106183,#106184,#106185),
(#106186,#106187,#106188),(#106189,#106190,#106191),(#106192,#106193,#106194),
(#106195,#106196,#106197)),.UNSPECIFIED.,.F.,.F.,.F.)
B_SPLINE_SURFACE_WITH_KNOTS((4,2,2,2,2,4),(3,3),(0.0020168056312046,0.00318801267491835,
0.00435921971863209,0.00670163380605957,0.00904404789348706,0.0113864619809145),
(0.,1.),.UNSPECIFIED.)
GEOMETRIC_REPRESENTATION_ITEM()
RATIONAL_B_SPLINE_SURFACE(((1.,0.707106781186548,1.),(1.,0.734176096219266,
1.),(1.,0.758590233751572,1.),(1.,0.803187254291515,1.),(1.,0.823368840149339,
1.),(1.,0.878495386168538,1.),(1.,0.908178291941153,1.),(1.,0.954777204682283,
1.),(1.,0.971753344320815,1.),(1.,0.994387335841996,1.),(1.,0.999999540046553,
1.),(1.,1.,1.)))
REPRESENTATION_ITEM('')
SURFACE()
);
#1681=(
BOUNDED_SURFACE()
B_SPLINE_SURFACE(3,2,((#106201,#106202,#106203),(#106204,#106205,#106206),
(#106207,#106208,#106209),(#106210,#106211,#106212),(#106213,#106214,#106215),
(#106216,#106217,#106218),(#106219,#106220,#106221),(#106222,#106223,#106224),
(#106225,#106226,#106227),(#106228,#106229,#106230),(#106231,#106232,#106233),
(#106234,#106235,#106236)),.UNSPECIFIED.,.F.,.F.,.F.)
B_SPLINE_SURFACE_WITH_KNOTS((4,2,2,2,2,4),(3,3),(0.00201680563120466,0.00318801267491843,
0.00435921971863221,0.00670163380605975,0.0090440478934873,0.0113864619809148),
(0.,1.),.UNSPECIFIED.)
GEOMETRIC_REPRESENTATION_ITEM()
RATIONAL_B_SPLINE_SURFACE(((1.,0.707106781186548,1.),(1.,0.734176096219302,
1.),(1.,0.758590233751572,1.),(1.,0.803187254291516,1.),(1.,0.823368840149552,
1.),(1.,0.878495386168105,1.),(1.,0.908178291940607,1.),(1.,0.954777204682866,
1.),(1.,0.971753344320825,1.),(1.,0.994387335842007,1.),(1.,0.999999540046577,
1.),(1.,1.,1.)))
REPRESENTATION_ITEM('')
SURFACE()
);
#1682=(
BOUNDED_SURFACE()
B_SPLINE_SURFACE(3,2,((#106403,#106404,#106405),(#106406,#106407,#106408),
(#106409,#106410,#106411),(#106412,#106413,#106414),(#106415,#106416,#106417),
(#106418,#106419,#106420),(#106421,#106422,#106423),(#106424,#106425,#106426),
(#106427,#106428,#106429),(#106430,#106431,#106432)),.UNSPECIFIED.,.F.,
 .F.,.F.)
B_SPLINE_SURFACE_WITH_KNOTS((4,2,2,2,4),(3,3),(0.,0.000214020122328381,
0.000428040244656761,0.000642060366985142,0.000856080489313522),(0.,1.),
 .UNSPECIFIED.)
GEOMETRIC_REPRESENTATION_ITEM()
RATIONAL_B_SPLINE_SURFACE(((1.,0.707106781186548,1.),(1.,0.68347722662262,
1.),(1.,0.659481175544654,1.),(1.,0.610508879439021,1.),(1.,0.585996172067873,
1.),(1.,0.540858044367121,1.),(1.,0.519989927806179,1.),(1.,0.489650895143399,
1.),(1.,0.480786371092266,1.),(1.,0.480804881866771,1.)))
REPRESENTATION_ITEM('')
SURFACE()
);
#1683=(
BOUNDED_SURFACE()
B_SPLINE_SURFACE(3,2,((#106441,#106442,#106443),(#106444,#106445,#106446),
(#106447,#106448,#106449),(#106450,#106451,#106452),(#106453,#106454,#106455),
(#106456,#106457,#106458),(#106459,#106460,#106461),(#106462,#106463,#106464),
(#106465,#106466,#106467),(#106468,#106469,#106470),(#106471,#106472,#106473),
(#106474,#106475,#106476),(#106477,#106478,#106479),(#106480,#106481,#106482)),
 .UNSPECIFIED.,.F.,.F.,.F.)
B_SPLINE_SURFACE_WITH_KNOTS((4,2,2,2,2,2,4),(3,3),(-8.59074174355445E-5,
0.000107384271794359,0.000214768543588717,0.000322152815383076,0.000429537087177435,
0.000644305630766152,0.000944981591790375),(-0.00127279735662637,1.),
 .UNSPECIFIED.)
GEOMETRIC_REPRESENTATION_ITEM()
RATIONAL_B_SPLINE_SURFACE(((1.0013127144284,0.484319156713673,1.),(1.00132886473298,
0.477974743557733,1.),(1.0013261987696,0.47902202864576,1.),(1.00129711892767,
0.490445623210585,1.),(1.00128159687351,0.496543237288905,1.),(1.00124353256439,
0.511496249612038,1.),(1.00122061910444,0.520497470359364,1.),(1.00117008762078,
0.540348031566809,1.),(1.0011427053451,0.551104761827022,1.),(1.00105582580784,
0.585234129241031,1.),(1.00099333442134,0.609782964990972,1.),(1.00084281910852,
0.668910724817792,1.),(1.00075790617431,0.70226754071777,1.),(1.00067489566942,
0.734877014827455,1.)))
REPRESENTATION_ITEM('')
SURFACE()
);
#1684=(
BOUNDED_SURFACE()
B_SPLINE_SURFACE(3,2,((#106494,#106495,#106496),(#106497,#106498,#106499),
(#106500,#106501,#106502),(#106503,#106504,#106505),(#106506,#106507,#106508),
(#106509,#106510,#106511),(#106512,#106513,#106514),(#106515,#106516,#106517),
(#106518,#106519,#106520),(#106521,#106522,#106523)),.UNSPECIFIED.,.F.,
 .F.,.F.)
B_SPLINE_SURFACE_WITH_KNOTS((4,2,2,2,4),(3,3),(0.,0.000214020122328381,
0.000428040244656761,0.000642060366985142,0.000856080489313522),(0.,1.),
 .UNSPECIFIED.)
GEOMETRIC_REPRESENTATION_ITEM()
RATIONAL_B_SPLINE_SURFACE(((1.,0.707106781186548,1.),(1.,0.68347722662262,
1.),(1.,0.659481175544654,1.),(1.,0.610508879439021,1.),(1.,0.585996172067677,
1.),(1.,0.540858044367307,1.),(1.,0.519989927806563,1.),(1.,0.489650895143026,
1.),(1.,0.480786371092547,1.),(1.,0.480804881866766,1.)))
REPRESENTATION_ITEM('')
SURFACE()
);
#1685=(
BOUNDED_SURFACE()
B_SPLINE_SURFACE(3,2,((#106531,#106532,#106533),(#106534,#106535,#106536),
(#106537,#106538,#106539),(#106540,#106541,#106542),(#106543,#106544,#106545),
(#106546,#106547,#106548),(#106549,#106550,#106551),(#106552,#106553,#106554),
(#106555,#106556,#106557),(#106558,#106559,#106560),(#106561,#106562,#106563),
(#106564,#106565,#106566),(#106567,#106568,#106569),(#106570,#106571,#106572)),
 .UNSPECIFIED.,.F.,.F.,.F.)
B_SPLINE_SURFACE_WITH_KNOTS((4,2,2,2,2,2,4),(3,3),(-8.59074174354856E-5,
0.000107384271794357,0.000214768543588714,0.000322152815383071,0.000429537087177428,
0.000644305630766142,0.00094498159179036),(0.,1.00128352994005),
 .UNSPECIFIED.)
GEOMETRIC_REPRESENTATION_ITEM()
RATIONAL_B_SPLINE_SURFACE(((1.,0.484313629162157,1.00132379779329),(1.,
0.477969147999695,1.00134008445634),(1.,0.47901644431411,1.00133739598399),
(1.,0.490440161327499,1.00130807061837),(1.,0.496537840765783,1.00129241751012),
(1.,0.511491013369546,1.00125403182065),(1.,0.520492330600339,1.00123092490032),
(1.,0.540343104584769,1.00117996677483),(1.,0.551099950145726,1.00115235330815),
(1.,0.585229683390388,1.00106474023922),(1.,0.609778782278141,1.00100172123238),
(1.,0.668907175891151,1.00084993510536),(1.,0.702264349342087,1.00076430524368),
(1.,0.734874172989235,1.0006805938737)))
REPRESENTATION_ITEM('')
SURFACE()
);
#1686=(
BOUNDED_SURFACE()
B_SPLINE_SURFACE(2,3,((#106592,#106593,#106594,#106595),(#106596,#106597,
#106598,#106599),(#106600,#106601,#106602,#106603)),.UNSPECIFIED.,.F.,.F.,
 .F.)
B_SPLINE_SURFACE_WITH_KNOTS((3,3),(4,4),(0.,0.976475345222878),(0.,1.),
 .UNSPECIFIED.)
GEOMETRIC_REPRESENTATION_ITEM()
RATIONAL_B_SPLINE_SURFACE(((1.,0.333333333333333,0.333333333333333,1.),
(1.,0.333333333333333,0.333333333333333,1.),(1.,0.333333333333333,0.333333333333333,
1.)))
REPRESENTATION_ITEM('')
SURFACE()
);
#1687=(
BOUNDED_SURFACE()
B_SPLINE_SURFACE(3,3,((#128284,#128285,#128286,#128287),(#128288,#128289,
#128290,#128291),(#128292,#128293,#128294,#128295),(#128296,#128297,#128298,
#128299)),.UNSPECIFIED.,.F.,.F.,.F.)
B_SPLINE_SURFACE_WITH_KNOTS((4,4),(4,4),(0.847987177476328,0.924268857153948),
(0.,1.),.UNSPECIFIED.)
GEOMETRIC_REPRESENTATION_ITEM()
RATIONAL_B_SPLINE_SURFACE(((1.,0.999906698612453,0.999906698612453,1.),
(1.,0.999906698612453,0.999906698612453,1.),(1.,0.999906698612453,0.999906698612453,
1.),(1.,0.999906698612453,0.999906698612453,1.)))
REPRESENTATION_ITEM('')
SURFACE()
);
#1688=(
BOUNDED_SURFACE()
B_SPLINE_SURFACE(2,3,((#128308,#128309,#128310,#128311),(#128312,#128313,
#128314,#128315),(#128316,#128317,#128318,#128319)),.UNSPECIFIED.,.F.,.F.,
 .F.)
B_SPLINE_SURFACE_WITH_KNOTS((3,3),(4,4),(0.,0.976475345222877),(0.,1.),
 .UNSPECIFIED.)
GEOMETRIC_REPRESENTATION_ITEM()
RATIONAL_B_SPLINE_SURFACE(((1.,0.333333333333333,0.333333333333333,1.),
(1.,0.333333333333333,0.333333333333333,1.),(1.,0.333333333333333,0.333333333333333,
1.)))
REPRESENTATION_ITEM('')
SURFACE()
);
#1689=(
BOUNDED_SURFACE()
B_SPLINE_SURFACE(3,3,((#128861,#128862,#128863,#128864),(#128865,#128866,
#128867,#128868),(#128869,#128870,#128871,#128872),(#128873,#128874,#128875,
#128876)),.UNSPECIFIED.,.F.,.F.,.F.)
B_SPLINE_SURFACE_WITH_KNOTS((4,4),(4,4),(0.485044458534508,0.53777950288349),
(0.,1.),.UNSPECIFIED.)
GEOMETRIC_REPRESENTATION_ITEM()
RATIONAL_B_SPLINE_SURFACE(((1.,0.999962226576742,0.999962226576742,1.),
(1.,0.999962226576742,0.999962226576742,1.),(1.,0.999962226576742,0.999962226576742,
1.),(1.,0.999962226576742,0.999962226576742,1.)))
REPRESENTATION_ITEM('')
SURFACE()
);
#1690=(
BOUNDED_SURFACE()
B_SPLINE_SURFACE(3,3,((#128878,#128879,#128880,#128881),(#128882,#128883,
#128884,#128885),(#128886,#128887,#128888,#128889),(#128890,#128891,#128892,
#128893)),.UNSPECIFIED.,.F.,.F.,.F.)
B_SPLINE_SURFACE_WITH_KNOTS((4,4),(4,4),(0.320611406771219,0.371419418548152),
(0.,1.),.UNSPECIFIED.)
GEOMETRIC_REPRESENTATION_ITEM()
RATIONAL_B_SPLINE_SURFACE(((1.,0.999967235134602,0.999967235134602,1.),
(1.,0.999967235134602,0.999967235134602,1.),(1.,0.999967235134602,0.999967235134602,
1.),(1.,0.999967235134602,0.999967235134602,1.)))
REPRESENTATION_ITEM('')
SURFACE()
);
#1691=(
BOUNDED_SURFACE()
B_SPLINE_SURFACE(3,3,((#128895,#128896,#128897,#128898),(#128899,#128900,
#128901,#128902),(#128903,#128904,#128905,#128906),(#128907,#128908,#128909,
#128910)),.UNSPECIFIED.,.F.,.F.,.F.)
B_SPLINE_SURFACE_WITH_KNOTS((4,4),(4,4),(0.675456663809549,0.739075881246651),
(0.,1.),.UNSPECIFIED.)
GEOMETRIC_REPRESENTATION_ITEM()
RATIONAL_B_SPLINE_SURFACE(((1.,0.999940066556315,0.999940066556315,1.),
(1.,0.999940066556315,0.999940066556315,1.),(1.,0.999940066556315,0.999940066556315,
1.),(1.,0.999940066556315,0.999940066556315,1.)))
REPRESENTATION_ITEM('')
SURFACE()
);
#1692=(
BOUNDED_SURFACE()
B_SPLINE_SURFACE(3,3,((#128912,#128913,#128914,#128915),(#128916,#128917,
#128918,#128919),(#128920,#128921,#128922,#128923),(#128924,#128925,#128926,
#128927)),.UNSPECIFIED.,.F.,.F.,.F.)
B_SPLINE_SURFACE_WITH_KNOTS((4,4),(4,4),(0.848056712870581,0.924286002747189),
(0.,1.),.UNSPECIFIED.)
GEOMETRIC_REPRESENTATION_ITEM()
RATIONAL_B_SPLINE_SURFACE(((1.,0.999906141303136,0.999906141303136,1.),
(1.,0.999906141303136,0.999906141303136,1.),(1.,0.999906141303136,0.999906141303136,
1.),(1.,0.999906141303136,0.999906141303136,1.)))
REPRESENTATION_ITEM('')
SURFACE()
);
#1693=(
BOUNDED_SURFACE()
B_SPLINE_SURFACE(3,3,((#128929,#128930,#128931,#128932),(#128933,#128934,
#128935,#128936),(#128937,#128938,#128939,#128940),(#128941,#128942,#128943,
#128944)),.UNSPECIFIED.,.F.,.F.,.F.)
B_SPLINE_SURFACE_WITH_KNOTS((4,4),(4,4),(0.320500925502344,0.371279762151148),
(0.,1.),.UNSPECIFIED.)
GEOMETRIC_REPRESENTATION_ITEM()
RATIONAL_B_SPLINE_SURFACE(((1.,0.999967409032415,0.999967409032415,1.),
(1.,0.999967409032415,0.999967409032415,1.),(1.,0.999967409032415,0.999967409032415,
1.),(1.,0.999967409032415,0.999967409032415,1.)))
REPRESENTATION_ITEM('')
SURFACE()
);
#1694=(
BOUNDED_SURFACE()
B_SPLINE_SURFACE(3,3,((#128946,#128947,#128948,#128949),(#128950,#128951,
#128952,#128953),(#128954,#128955,#128956,#128957),(#128958,#128959,#128960,
#128961)),.UNSPECIFIED.,.F.,.F.,.F.)
B_SPLINE_SURFACE_WITH_KNOTS((4,4),(4,4),(0.485038746158877,0.537899824885899),
(0.,1.),.UNSPECIFIED.)
GEOMETRIC_REPRESENTATION_ITEM()
RATIONAL_B_SPLINE_SURFACE(((1.,0.999962208905504,0.999962208905504,1.),
(1.,0.999962208905504,0.999962208905504,1.),(1.,0.999962208905504,0.999962208905504,
1.),(1.,0.999962208905504,0.999962208905504,1.)))
REPRESENTATION_ITEM('')
SURFACE()
);
#1695=(
BOUNDED_SURFACE()
B_SPLINE_SURFACE(3,3,((#128963,#128964,#128965,#128966),(#128967,#128968,
#128969,#128970),(#128971,#128972,#128973,#128974),(#128975,#128976,#128977,
#128978)),.UNSPECIFIED.,.F.,.F.,.F.)
B_SPLINE_SURFACE_WITH_KNOTS((4,4),(4,4),(0.675591945838646,0.739081108319602),
(0.,1.),.UNSPECIFIED.)
GEOMETRIC_REPRESENTATION_ITEM()
RATIONAL_B_SPLINE_SURFACE(((1.,0.999939919244887,0.999939919244887,1.),
(1.,0.999939919244887,0.999939919244887,1.),(1.,0.999939919244887,0.999939919244887,
1.),(1.,0.999939919244887,0.999939919244887,1.)))
REPRESENTATION_ITEM('')
SURFACE()
);
#1696=(
BOUNDED_SURFACE()
B_SPLINE_SURFACE(3,3,((#128980,#128981,#128982,#128983),(#128984,#128985,
#128986,#128987),(#128988,#128989,#128990,#128991),(#128992,#128993,#128994,
#128995)),.UNSPECIFIED.,.F.,.F.,.F.)
B_SPLINE_SURFACE_WITH_KNOTS((4,4),(4,4),(0.847948073492975,0.924101847380027),
(0.,1.),.UNSPECIFIED.)
GEOMETRIC_REPRESENTATION_ITEM()
RATIONAL_B_SPLINE_SURFACE(((1.,0.999906397449935,0.999906397449935,1.),
(1.,0.999906397449935,0.999906397449935,1.),(1.,0.999906397449935,0.999906397449935,
1.),(1.,0.999906397449935,0.999906397449935,1.)))
REPRESENTATION_ITEM('')
SURFACE()
);
#1697=(
BOUNDED_SURFACE()
B_SPLINE_SURFACE(3,3,((#128997,#128998,#128999,#129000),(#129001,#129002,
#129003,#129004),(#129005,#129006,#129007,#129008),(#129009,#129010,#129011,
#129012)),.UNSPECIFIED.,.F.,.F.,.F.)
B_SPLINE_SURFACE_WITH_KNOTS((4,4),(4,4),(0.320502373890073,0.371416725883164),
(0.,1.),.UNSPECIFIED.)
GEOMETRIC_REPRESENTATION_ITEM()
RATIONAL_B_SPLINE_SURFACE(((1.,0.999967412958646,0.999967412958646,1.),
(1.,0.999967412958646,0.999967412958646,1.),(1.,0.999967412958646,0.999967412958646,
1.),(1.,0.999967412958646,0.999967412958646,1.)))
REPRESENTATION_ITEM('')
SURFACE()
);
#1698=(
BOUNDED_SURFACE()
B_SPLINE_SURFACE(3,3,((#129014,#129015,#129016,#129017),(#129018,#129019,
#129020,#129021),(#129022,#129023,#129024,#129025),(#129026,#129027,#129028,
#129029)),.UNSPECIFIED.,.F.,.F.,.F.)
B_SPLINE_SURFACE_WITH_KNOTS((4,4),(4,4),(0.485176572716987,0.537896306928668),
(0.,1.),.UNSPECIFIED.)
GEOMETRIC_REPRESENTATION_ITEM()
RATIONAL_B_SPLINE_SURFACE(((1.,0.999962047914293,0.999962047914293,1.),
(1.,0.999962047914293,0.999962047914293,1.),(1.,0.999962047914293,0.999962047914293,
1.),(1.,0.999962047914293,0.999962047914293,1.)))
REPRESENTATION_ITEM('')
SURFACE()
);
#1699=(
BOUNDED_SURFACE()
B_SPLINE_SURFACE(3,3,((#129031,#129032,#129033,#129034),(#129035,#129036,
#129037,#129038),(#129039,#129040,#129041,#129042),(#129043,#129044,#129045,
#129046)),.UNSPECIFIED.,.F.,.F.,.F.)
B_SPLINE_SURFACE_WITH_KNOTS((4,4),(4,4),(0.675443757413942,0.738914540526937),
(0.,1.),.UNSPECIFIED.)
GEOMETRIC_REPRESENTATION_ITEM()
RATIONAL_B_SPLINE_SURFACE(((1.,0.999940218802441,0.999940218802441,1.),
(1.,0.999940218802441,0.999940218802441,1.),(1.,0.999940218802441,0.999940218802441,
1.),(1.,0.999940218802441,0.999940218802441,1.)))
REPRESENTATION_ITEM('')
SURFACE()
);
#1700=(
BOUNDED_SURFACE()
B_SPLINE_SURFACE(3,3,((#129048,#129049,#129050,#129051),(#129052,#129053,
#129054,#129055),(#129056,#129057,#129058,#129059),(#129060,#129061,#129062,
#129063)),.UNSPECIFIED.,.F.,.F.,.F.)
B_SPLINE_SURFACE_WITH_KNOTS((4,4),(4,4),(0.847942166937427,0.924299897199325),
(0.,1.),.UNSPECIFIED.)
GEOMETRIC_REPRESENTATION_ITEM()
RATIONAL_B_SPLINE_SURFACE(((1.,0.999906256993129,0.999906256993129,1.),
(1.,0.999906256993129,0.999906256993129,1.),(1.,0.999906256993129,0.999906256993129,
1.),(1.,0.999906256993129,0.999906256993129,1.)))
REPRESENTATION_ITEM('')
SURFACE()
);
#1701=(
BOUNDED_SURFACE()
B_SPLINE_SURFACE(3,3,((#129065,#129066,#129067,#129068),(#129069,#129070,
#129071,#129072),(#129073,#129074,#129075,#129076),(#129077,#129078,#129079,
#129080)),.UNSPECIFIED.,.F.,.F.,.F.)
B_SPLINE_SURFACE_WITH_KNOTS((4,4),(4,4),(0.320591553275913,0.371408509515467),
(0.,1.),.UNSPECIFIED.)
GEOMETRIC_REPRESENTATION_ITEM()
RATIONAL_B_SPLINE_SURFACE(((1.,0.999967222717093,0.999967222717093,1.),
(1.,0.999967222717093,0.999967222717093,1.),(1.,0.999967222717093,0.999967222717093,
1.),(1.,0.999967222717093,0.999967222717093,1.)))
REPRESENTATION_ITEM('')
SURFACE()
);
#1702=(
BOUNDED_SURFACE()
B_SPLINE_SURFACE(3,3,((#129082,#129083,#129084,#129085),(#129086,#129087,
#129088,#129089),(#129090,#129091,#129092,#129093),(#129094,#129095,#129096,
#129097)),.UNSPECIFIED.,.F.,.F.,.F.)
B_SPLINE_SURFACE_WITH_KNOTS((4,4),(4,4),(0.485044526648914,0.537808799135296),
(0.,1.),.UNSPECIFIED.)
GEOMETRIC_REPRESENTATION_ITEM()
RATIONAL_B_SPLINE_SURFACE(((1.,0.999962197880072,0.999962197880072,1.),
(1.,0.999962197880072,0.999962197880072,1.),(1.,0.999962197880072,0.999962197880072,
1.),(1.,0.999962197880072,0.999962197880072,1.)))
REPRESENTATION_ITEM('')
SURFACE()
);
#1703=(
BOUNDED_SURFACE()
B_SPLINE_SURFACE(3,3,((#129099,#129100,#129101,#129102),(#129103,#129104,
#129105,#129106),(#129107,#129108,#129109,#129110),(#129111,#129112,#129113,
#129114)),.UNSPECIFIED.,.F.,.F.,.F.)
B_SPLINE_SURFACE_WITH_KNOTS((4,4),(4,4),(0.675446956850003,0.739072743686735),
(0.,1.),.UNSPECIFIED.)
GEOMETRIC_REPRESENTATION_ITEM()
RATIONAL_B_SPLINE_SURFACE(((1.,0.999940262362188,0.999940262362188,1.),
(1.,0.999940262362188,0.999940262362188,1.),(1.,0.999940262362188,0.999940262362188,
1.),(1.,0.999940262362188,0.999940262362188,1.)))
REPRESENTATION_ITEM('')
SURFACE()
);
#1704=(
BOUNDED_SURFACE()
B_SPLINE_SURFACE(3,3,((#129116,#129117,#129118,#129119),(#129120,#129121,
#129122,#129123),(#129124,#129125,#129126,#129127),(#129128,#129129,#129130,
#129131)),.UNSPECIFIED.,.F.,.F.,.F.)
B_SPLINE_SURFACE_WITH_KNOTS((4,4),(4,4),(0.848119490523076,0.924292153421624),
(0.,1.),.UNSPECIFIED.)
GEOMETRIC_REPRESENTATION_ITEM()
RATIONAL_B_SPLINE_SURFACE(((1.,0.999905838370628,0.999905838370628,1.),
(1.,0.999905838370628,0.999905838370628,1.),(1.,0.999905838370628,0.999905838370628,
1.),(1.,0.999905838370628,0.999905838370628,1.)))
REPRESENTATION_ITEM('')
SURFACE()
);
#1705=(
BOUNDED_SURFACE()
B_SPLINE_SURFACE(3,3,((#129133,#129134,#129135,#129136),(#129137,#129138,
#129139,#129140),(#129141,#129142,#129143,#129144),(#129145,#129146,#129147,
#129148)),.UNSPECIFIED.,.F.,.F.,.F.)
B_SPLINE_SURFACE_WITH_KNOTS((4,4),(4,4),(0.320518889190736,0.371365428236457),
(0.,1.),.UNSPECIFIED.)
GEOMETRIC_REPRESENTATION_ITEM()
RATIONAL_B_SPLINE_SURFACE(((1.,0.999967318979484,0.999967318979484,1.),
(1.,0.999967318979484,0.999967318979484,1.),(1.,0.999967318979484,0.999967318979484,
1.),(1.,0.999967318979484,0.999967318979484,1.)))
REPRESENTATION_ITEM('')
SURFACE()
);
#1706=(
BOUNDED_SURFACE()
B_SPLINE_SURFACE(3,3,((#129150,#129151,#129152,#129153),(#129154,#129155,
#129156,#129157),(#129158,#129159,#129160,#129161),(#129162,#129163,#129164,
#129165)),.UNSPECIFIED.,.F.,.F.,.F.)
B_SPLINE_SURFACE_WITH_KNOTS((4,4),(4,4),(0.485053151926106,0.537874785203655),
(0.,1.),.UNSPECIFIED.)
GEOMETRIC_REPRESENTATION_ITEM()
RATIONAL_B_SPLINE_SURFACE(((1.,0.999962225139893,0.999962225139893,1.),
(1.,0.999962225139893,0.999962225139893,1.),(1.,0.999962225139893,0.999962225139893,
1.),(1.,0.999962225139893,0.999962225139893,1.)))
REPRESENTATION_ITEM('')
SURFACE()
);
#1707=(
BOUNDED_SURFACE()
B_SPLINE_SURFACE(3,3,((#129167,#129168,#129169,#129170),(#129171,#129172,
#129173,#129174),(#129175,#129176,#129177,#129178),(#129179,#129180,#129181,
#129182)),.UNSPECIFIED.,.F.,.F.,.F.)
B_SPLINE_SURFACE_WITH_KNOTS((4,4),(4,4),(0.675540106157524,0.739058970060862),
(0.,1.),.UNSPECIFIED.)
GEOMETRIC_REPRESENTATION_ITEM()
RATIONAL_B_SPLINE_SURFACE(((1.,0.999939959405442,0.999939959405442,1.),
(1.,0.999939959405442,0.999939959405442,1.),(1.,0.999939959405442,0.999939959405442,
1.),(1.,0.999939959405442,0.999939959405442,1.)))
REPRESENTATION_ITEM('')
SURFACE()
);
#1708=(
BOUNDED_SURFACE()
B_SPLINE_SURFACE(3,3,((#129184,#129185,#129186,#129187),(#129188,#129189,
#129190,#129191),(#129192,#129193,#129194,#129195),(#129196,#129197,#129198,
#129199)),.UNSPECIFIED.,.F.,.F.,.F.)
B_SPLINE_SURFACE_WITH_KNOTS((4,4),(4,4),(0.847959162456777,0.924189890634277),
(0.,1.),.UNSPECIFIED.)
GEOMETRIC_REPRESENTATION_ITEM()
RATIONAL_B_SPLINE_SURFACE(((1.,0.999906054677511,0.999906054677511,1.),
(1.,0.999906054677511,0.999906054677511,1.),(1.,0.999906054677511,0.999906054677511,
1.),(1.,0.999906054677511,0.999906054677511,1.)))
REPRESENTATION_ITEM('')
SURFACE()
);
#1709=(
BOUNDED_SURFACE()
B_SPLINE_SURFACE(3,3,((#129201,#129202,#129203,#129204),(#129205,#129206,
#129207,#129208),(#129209,#129210,#129211,#129212),(#129213,#129214,#129215,
#129216)),.UNSPECIFIED.,.F.,.F.,.F.)
B_SPLINE_SURFACE_WITH_KNOTS((4,4),(4,4),(0.320639964684793,0.371314507617759),
(0.,1.),.UNSPECIFIED.)
GEOMETRIC_REPRESENTATION_ITEM()
RATIONAL_B_SPLINE_SURFACE(((1.,0.999967350702174,0.999967350702174,1.),
(1.,0.999967350702174,0.999967350702174,1.),(1.,0.999967350702174,0.999967350702174,
1.),(1.,0.999967350702174,0.999967350702174,1.)))
REPRESENTATION_ITEM('')
SURFACE()
);
#1710=(
BOUNDED_SURFACE()
B_SPLINE_SURFACE(3,3,((#129218,#129219,#129220,#129221),(#129222,#129223,
#129224,#129225),(#129226,#129227,#129228,#129229),(#129230,#129231,#129232,
#129233)),.UNSPECIFIED.,.F.,.F.,.F.)
B_SPLINE_SURFACE_WITH_KNOTS((4,4),(4,4),(0.485088192372813,0.537796433966225),
(0.,1.),.UNSPECIFIED.)
GEOMETRIC_REPRESENTATION_ITEM()
RATIONAL_B_SPLINE_SURFACE(((1.,0.999962120409815,0.999962120409815,1.),
(1.,0.999962120409815,0.999962120409815,1.),(1.,0.999962120409815,0.999962120409815,
1.),(1.,0.999962120409815,0.999962120409815,1.)))
REPRESENTATION_ITEM('')
SURFACE()
);
#1711=(
BOUNDED_SURFACE()
B_SPLINE_SURFACE(3,3,((#129235,#129236,#129237,#129238),(#129239,#129240,
#129241,#129242),(#129243,#129244,#129245,#129246),(#129247,#129248,#129249,
#129250)),.UNSPECIFIED.,.F.,.F.,.F.)
B_SPLINE_SURFACE_WITH_KNOTS((4,4),(4,4),(0.675478450031988,0.739029557635334),
(0.,1.),.UNSPECIFIED.)
GEOMETRIC_REPRESENTATION_ITEM()
RATIONAL_B_SPLINE_SURFACE(((1.,0.999940036715462,0.999940036715462,1.),
(1.,0.999940036715462,0.999940036715462,1.),(1.,0.999940036715462,0.999940036715462,
1.),(1.,0.999940036715462,0.999940036715462,1.)))
REPRESENTATION_ITEM('')
SURFACE()
);
#1712=(
BOUNDED_SURFACE()
B_SPLINE_SURFACE(3,3,((#129252,#129253,#129254,#129255),(#129256,#129257,
#129258,#129259),(#129260,#129261,#129262,#129263),(#129264,#129265,#129266,
#129267)),.UNSPECIFIED.,.F.,.F.,.F.)
B_SPLINE_SURFACE_WITH_KNOTS((4,4),(4,4),(0.847977146575099,0.924247070973153),
(0.,1.),.UNSPECIFIED.)
GEOMETRIC_REPRESENTATION_ITEM()
RATIONAL_B_SPLINE_SURFACE(((1.,0.9999062633542,0.9999062633542,1.),(1.,
0.9999062633542,0.9999062633542,1.),(1.,0.9999062633542,0.9999062633542,
1.),(1.,0.9999062633542,0.9999062633542,1.)))
REPRESENTATION_ITEM('')
SURFACE()
);
#1713=(
BOUNDED_SURFACE()
B_SPLINE_SURFACE(3,3,((#129269,#129270,#129271,#129272),(#129273,#129274,
#129275,#129276),(#129277,#129278,#129279,#129280),(#129281,#129282,#129283,
#129284)),.UNSPECIFIED.,.F.,.F.,.F.)
B_SPLINE_SURFACE_WITH_KNOTS((4,4),(4,4),(0.320583334123496,0.371380663507137),
(0.,1.),.UNSPECIFIED.)
GEOMETRIC_REPRESENTATION_ITEM()
RATIONAL_B_SPLINE_SURFACE(((1.,0.99996730938274,0.99996730938274,1.),(1.,
0.99996730938274,0.99996730938274,1.),(1.,0.99996730938274,0.99996730938274,
1.),(1.,0.99996730938274,0.99996730938274,1.)))
REPRESENTATION_ITEM('')
SURFACE()
);
#1714=(
BOUNDED_SURFACE()
B_SPLINE_SURFACE(3,3,((#129286,#129287,#129288,#129289),(#129290,#129291,
#129292,#129293),(#129294,#129295,#129296,#129297),(#129298,#129299,#129300,
#129301)),.UNSPECIFIED.,.F.,.F.,.F.)
B_SPLINE_SURFACE_WITH_KNOTS((4,4),(4,4),(0.485126102700377,0.537860300944991),
(0.,1.),.UNSPECIFIED.)
GEOMETRIC_REPRESENTATION_ITEM()
RATIONAL_B_SPLINE_SURFACE(((1.,0.999962137299808,0.999962137299808,1.),
(1.,0.999962137299808,0.999962137299808,1.),(1.,0.999962137299808,0.999962137299808,
1.),(1.,0.999962137299808,0.999962137299808,1.)))
REPRESENTATION_ITEM('')
SURFACE()
);
#1715=(
BOUNDED_SURFACE()
B_SPLINE_SURFACE(3,3,((#129303,#129304,#129305,#129306),(#129307,#129308,
#129309,#129310),(#129311,#129312,#129313,#129314),(#129315,#129316,#129317,
#129318)),.UNSPECIFIED.,.F.,.F.,.F.)
B_SPLINE_SURFACE_WITH_KNOTS((4,4),(4,4),(0.675620555481706,0.738956525898373),
(0.,1.),.UNSPECIFIED.)
GEOMETRIC_REPRESENTATION_ITEM()
RATIONAL_B_SPLINE_SURFACE(((1.,0.999940072974474,0.999940072974474,1.),
(1.,0.999940072974474,0.999940072974474,1.),(1.,0.999940072974474,0.999940072974474,
1.),(1.,0.999940072974474,0.999940072974474,1.)))
REPRESENTATION_ITEM('')
SURFACE()
);
#1716=(
BOUNDED_SURFACE()
B_SPLINE_SURFACE(3,3,((#129320,#129321,#129322,#129323),(#129324,#129325,
#129326,#129327),(#129328,#129329,#129330,#129331),(#129332,#129333,#129334,
#129335)),.UNSPECIFIED.,.F.,.F.,.F.)
B_SPLINE_SURFACE_WITH_KNOTS((4,4),(4,4),(0.84799244392776,0.924142505922786),
(0.,1.),.UNSPECIFIED.)
GEOMETRIC_REPRESENTATION_ITEM()
RATIONAL_B_SPLINE_SURFACE(((1.,0.999906153501141,0.999906153501141,1.),
(1.,0.999906153501141,0.999906153501141,1.),(1.,0.999906153501141,0.999906153501141,
1.),(1.,0.999906153501141,0.999906153501141,1.)))
REPRESENTATION_ITEM('')
SURFACE()
);
#1717=(
BOUNDED_SURFACE()
B_SPLINE_SURFACE(3,3,((#129337,#129338,#129339,#129340),(#129341,#129342,
#129343,#129344),(#129345,#129346,#129347,#129348),(#129349,#129350,#129351,
#129352)),.UNSPECIFIED.,.F.,.F.,.F.)
B_SPLINE_SURFACE_WITH_KNOTS((4,4),(4,4),(0.320518100436019,0.371362835533565),
(0.,1.),.UNSPECIFIED.)
GEOMETRIC_REPRESENTATION_ITEM()
RATIONAL_B_SPLINE_SURFACE(((1.,0.999967298407033,0.999967298407033,1.),
(1.,0.999967298407033,0.999967298407033,1.),(1.,0.999967298407033,0.999967298407033,
1.),(1.,0.999967298407033,0.999967298407033,1.)))
REPRESENTATION_ITEM('')
SURFACE()
);
#1718=(
BOUNDED_SURFACE()
B_SPLINE_SURFACE(3,3,((#129354,#129355,#129356,#129357),(#129358,#129359,
#129360,#129361),(#129362,#129363,#129364,#129365),(#129366,#129367,#129368,
#129369)),.UNSPECIFIED.,.F.,.F.,.F.)
B_SPLINE_SURFACE_WITH_KNOTS((4,4),(4,4),(0.485111695336929,0.537875420193652),
(0.,1.),.UNSPECIFIED.)
GEOMETRIC_REPRESENTATION_ITEM()
RATIONAL_B_SPLINE_SURFACE(((1.,0.999962111917502,0.999962111917502,1.),
(1.,0.999962111917502,0.999962111917502,1.),(1.,0.999962111917502,0.999962111917502,
1.),(1.,0.999962111917502,0.999962111917502,1.)))
REPRESENTATION_ITEM('')
SURFACE()
);
#1719=(
BOUNDED_SURFACE()
B_SPLINE_SURFACE(3,3,((#129371,#129372,#129373,#129374),(#129375,#129376,
#129377,#129378),(#129379,#129380,#129381,#129382),(#129383,#129384,#129385,
#129386)),.UNSPECIFIED.,.F.,.F.,.F.)
B_SPLINE_SURFACE_WITH_KNOTS((4,4),(4,4),(0.67554330969252,0.739050792335592),
(0.,1.),.UNSPECIFIED.)
GEOMETRIC_REPRESENTATION_ITEM()
RATIONAL_B_SPLINE_SURFACE(((1.,0.999940183216014,0.999940183216014,1.),
(1.,0.999940183216014,0.999940183216014,1.),(1.,0.999940183216014,0.999940183216014,
1.),(1.,0.999940183216014,0.999940183216014,1.)))
REPRESENTATION_ITEM('')
SURFACE()
);
#1720=(
BOUNDED_SURFACE()
B_SPLINE_SURFACE(3,3,((#129388,#129389,#129390,#129391),(#129392,#129393,
#129394,#129395),(#129396,#129397,#129398,#129399),(#129400,#129401,#129402,
#129403)),.UNSPECIFIED.,.F.,.F.,.F.)
B_SPLINE_SURFACE_WITH_KNOTS((4,4),(4,4),(0.848082295900864,0.924212909944339),
(0.,1.),.UNSPECIFIED.)
GEOMETRIC_REPRESENTATION_ITEM()
RATIONAL_B_SPLINE_SURFACE(((1.,0.999906015094081,0.999906015094081,1.),
(1.,0.999906015094081,0.999906015094081,1.),(1.,0.999906015094081,0.999906015094081,
1.),(1.,0.999906015094081,0.999906015094081,1.)))
REPRESENTATION_ITEM('')
SURFACE()
);
#1721=(
BOUNDED_SURFACE()
B_SPLINE_SURFACE(3,3,((#129405,#129406,#129407,#129408),(#129409,#129410,
#129411,#129412),(#129413,#129414,#129415,#129416),(#129417,#129418,#129419,
#129420)),.UNSPECIFIED.,.F.,.F.,.F.)
B_SPLINE_SURFACE_WITH_KNOTS((4,4),(4,4),(0.320600960423681,0.371411458072819),
(0.,1.),.UNSPECIFIED.)
GEOMETRIC_REPRESENTATION_ITEM()
RATIONAL_B_SPLINE_SURFACE(((1.,0.999967243891018,0.999967243891018,1.),
(1.,0.999967243891018,0.999967243891018,1.),(1.,0.999967243891018,0.999967243891018,
1.),(1.,0.999967243891018,0.999967243891018,1.)))
REPRESENTATION_ITEM('')
SURFACE()
);
#1722=(
BOUNDED_SURFACE()
B_SPLINE_SURFACE(3,3,((#129422,#129423,#129424,#129425),(#129426,#129427,
#129428,#129429),(#129430,#129431,#129432,#129433),(#129434,#129435,#129436,
#129437)),.UNSPECIFIED.,.F.,.F.,.F.)
B_SPLINE_SURFACE_WITH_KNOTS((4,4),(4,4),(0.48504256867854,0.537887934754555),
(0.,1.),.UNSPECIFIED.)
GEOMETRIC_REPRESENTATION_ITEM()
RATIONAL_B_SPLINE_SURFACE(((1.,0.999962231855016,0.999962231855016,1.),
(1.,0.999962231855016,0.999962231855016,1.),(1.,0.999962231855016,0.999962231855016,
1.),(1.,0.999962231855016,0.999962231855016,1.)))
REPRESENTATION_ITEM('')
SURFACE()
);
#1723=(
BOUNDED_SURFACE()
B_SPLINE_SURFACE(3,3,((#129439,#129440,#129441,#129442),(#129443,#129444,
#129445,#129446),(#129447,#129448,#129449,#129450),(#129451,#129452,#129453,
#129454)),.UNSPECIFIED.,.F.,.F.,.F.)
B_SPLINE_SURFACE_WITH_KNOTS((4,4),(4,4),(0.675450724081424,0.73897092350891),
(0.,1.),.UNSPECIFIED.)
GEOMETRIC_REPRESENTATION_ITEM()
RATIONAL_B_SPLINE_SURFACE(((1.,0.99994009649207,0.99994009649207,1.),(1.,
0.99994009649207,0.99994009649207,1.),(1.,0.99994009649207,0.99994009649207,
1.),(1.,0.99994009649207,0.99994009649207,1.)))
REPRESENTATION_ITEM('')
SURFACE()
);
#1724=(
BOUNDED_SURFACE()
B_SPLINE_SURFACE(3,3,((#129456,#129457,#129458,#129459),(#129460,#129461,
#129462,#129463),(#129464,#129465,#129466,#129467),(#129468,#129469,#129470,
#129471)),.UNSPECIFIED.,.F.,.F.,.F.)
B_SPLINE_SURFACE_WITH_KNOTS((4,4),(4,4),(0.848090733102027,0.924284397580542),
(0.,1.),.UNSPECIFIED.)
GEOMETRIC_REPRESENTATION_ITEM()
RATIONAL_B_SPLINE_SURFACE(((1.,0.999905868674041,0.999905868674041,1.),
(1.,0.999905868674041,0.999905868674041,1.),(1.,0.999905868674041,0.999905868674041,
1.),(1.,0.999905868674041,0.999905868674041,1.)))
REPRESENTATION_ITEM('')
SURFACE()
);
#1725=(
BOUNDED_SURFACE()
B_SPLINE_SURFACE(3,3,((#129473,#129474,#129475,#129476),(#129477,#129478,
#129479,#129480),(#129481,#129482,#129483,#129484),(#129485,#129486,#129487,
#129488)),.UNSPECIFIED.,.F.,.F.,.F.)
B_SPLINE_SURFACE_WITH_KNOTS((4,4),(4,4),(0.320500281417297,0.37141920772819),
(0.,1.),.UNSPECIFIED.)
GEOMETRIC_REPRESENTATION_ITEM()
RATIONAL_B_SPLINE_SURFACE(((1.,0.999967398958956,0.999967398958956,1.),
(1.,0.999967398958956,0.999967398958956,1.),(1.,0.999967398958956,0.999967398958956,
1.),(1.,0.999967398958956,0.999967398958956,1.)))
REPRESENTATION_ITEM('')
SURFACE()
);
#1726=(
BOUNDED_SURFACE()
B_SPLINE_SURFACE(3,3,((#129490,#129491,#129492,#129493),(#129494,#129495,
#129496,#129497),(#129498,#129499,#129500,#129501),(#129502,#129503,#129504,
#129505)),.UNSPECIFIED.,.F.,.F.,.F.)
B_SPLINE_SURFACE_WITH_KNOTS((4,4),(4,4),(0.485039113478553,0.537770836541586),
(0.,1.),.UNSPECIFIED.)
GEOMETRIC_REPRESENTATION_ITEM()
RATIONAL_B_SPLINE_SURFACE(((1.,0.999962216400084,0.999962216400084,1.),
(1.,0.999962216400084,0.999962216400084,1.),(1.,0.999962216400084,0.999962216400084,
1.),(1.,0.999962216400084,0.999962216400084,1.)))
REPRESENTATION_ITEM('')
SURFACE()
);
#1727=(
BOUNDED_SURFACE()
B_SPLINE_SURFACE(3,3,((#129507,#129508,#129509,#129510),(#129511,#129512,
#129513,#129514),(#129515,#129516,#129517,#129518),(#129519,#129520,#129521,
#129522)),.UNSPECIFIED.,.F.,.F.,.F.)
B_SPLINE_SURFACE_WITH_KNOTS((4,4),(4,4),(0.675616885244456,0.739079678101414),
(0.,1.),.UNSPECIFIED.)
GEOMETRIC_REPRESENTATION_ITEM()
RATIONAL_B_SPLINE_SURFACE(((1.,0.999939908563371,0.999939908563371,1.),
(1.,0.999939908563371,0.999939908563371,1.),(1.,0.999939908563371,0.999939908563371,
1.),(1.,0.999939908563371,0.999939908563371,1.)))
REPRESENTATION_ITEM('')
SURFACE()
);
#1728=(
BOUNDED_SURFACE()
B_SPLINE_SURFACE(3,3,((#129524,#129525,#129526,#129527),(#129528,#129529,
#129530,#129531),(#129532,#129533,#129534,#129535),(#129536,#129537,#129538,
#129539)),.UNSPECIFIED.,.F.,.F.,.F.)
B_SPLINE_SURFACE_WITH_KNOTS((4,4),(4,4),(0.847942523738152,0.924296420006828),
(0.,1.),.UNSPECIFIED.)
GEOMETRIC_REPRESENTATION_ITEM()
RATIONAL_B_SPLINE_SURFACE(((1.,0.999906356251184,0.999906356251184,1.),
(1.,0.999906356251184,0.999906356251184,1.),(1.,0.999906356251184,0.999906356251184,
1.),(1.,0.999906356251184,0.999906356251184,1.)))
REPRESENTATION_ITEM('')
SURFACE()
);
#1729=(
BOUNDED_SURFACE()
B_SPLINE_SURFACE(3,3,((#129541,#129542,#129543,#129544),(#129545,#129546,
#129547,#129548),(#129549,#129550,#129551,#129552),(#129553,#129554,#129555,
#129556)),.UNSPECIFIED.,.F.,.F.,.F.)
B_SPLINE_SURFACE_WITH_KNOTS((4,4),(4,4),(0.320503220290746,0.371278341845292),
(0.,1.),.UNSPECIFIED.)
GEOMETRIC_REPRESENTATION_ITEM()
RATIONAL_B_SPLINE_SURFACE(((1.,0.999967413248699,0.999967413248699,1.),
(1.,0.999967413248699,0.999967413248699,1.),(1.,0.999967413248699,0.999967413248699,
1.),(1.,0.999967413248699,0.999967413248699,1.)))
REPRESENTATION_ITEM('')
SURFACE()
);
#1730=(
BOUNDED_SURFACE()
B_SPLINE_SURFACE(3,3,((#129558,#129559,#129560,#129561),(#129562,#129563,
#129564,#129565),(#129566,#129567,#129568,#129569),(#129570,#129571,#129572,
#129573)),.UNSPECIFIED.,.F.,.F.,.F.)
B_SPLINE_SURFACE_WITH_KNOTS((4,4),(4,4),(0.485167461585208,0.537898795794421),
(0.,1.),.UNSPECIFIED.)
GEOMETRIC_REPRESENTATION_ITEM()
RATIONAL_B_SPLINE_SURFACE(((1.,0.999962048910248,0.999962048910248,1.),
(1.,0.999962048910248,0.999962048910248,1.),(1.,0.999962048910248,0.999962048910248,
1.),(1.,0.999962048910248,0.999962048910248,1.)))
REPRESENTATION_ITEM('')
SURFACE()
);
#1731=(
BOUNDED_SURFACE()
B_SPLINE_SURFACE(3,3,((#129575,#129576,#129577,#129578),(#129579,#129580,
#129581,#129582),(#129583,#129584,#129585,#129586),(#129587,#129588,#129589,
#129590)),.UNSPECIFIED.,.F.,.F.,.F.)
B_SPLINE_SURFACE_WITH_KNOTS((4,4),(4,4),(0.675444558331159,0.739082790885492),
(0.,1.),.UNSPECIFIED.)
GEOMETRIC_REPRESENTATION_ITEM()
RATIONAL_B_SPLINE_SURFACE(((1.,0.999940167892219,0.999940167892219,1.),
(1.,0.999940167892219,0.999940167892219,1.),(1.,0.999940167892219,0.999940167892219,
1.),(1.,0.999940167892219,0.999940167892219,1.)))
REPRESENTATION_ITEM('')
SURFACE()
);
#1732=(
BOUNDED_SURFACE()
B_SPLINE_SURFACE(3,3,((#129592,#129593,#129594,#129595),(#129596,#129597,
#129598,#129599),(#129600,#129601,#129602,#129603),(#129604,#129605,#129606,
#129607)),.UNSPECIFIED.,.F.,.F.,.F.)
B_SPLINE_SURFACE_WITH_KNOTS((4,4),(4,4),(0.847944615083763,0.924067134683459),
(0.,1.),.UNSPECIFIED.)
GEOMETRIC_REPRESENTATION_ITEM()
RATIONAL_B_SPLINE_SURFACE(((1.,0.999906379098947,0.999906379098947,1.),
(1.,0.999906379098947,0.999906379098947,1.),(1.,0.999906379098947,0.999906379098947,
1.),(1.,0.999906379098947,0.999906379098947,1.)))
REPRESENTATION_ITEM('')
SURFACE()
);
#1733=(
BOUNDED_SURFACE()
B_SPLINE_SURFACE(3,3,((#129609,#129610,#129611,#129612),(#129613,#129614,
#129615,#129616),(#129617,#129618,#129619,#129620),(#129621,#129622,#129623,
#129624)),.UNSPECIFIED.,.F.,.F.,.F.)
B_SPLINE_SURFACE_WITH_KNOTS((4,4),(4,4),(0.320579981379885,0.371413971104649),
(0.,1.),.UNSPECIFIED.)
GEOMETRIC_REPRESENTATION_ITEM()
RATIONAL_B_SPLINE_SURFACE(((1.,0.999967229881466,0.999967229881466,1.),
(1.,0.999967229881466,0.999967229881466,1.),(1.,0.999967229881466,0.999967229881466,
1.),(1.,0.999967229881466,0.999967229881466,1.)))
REPRESENTATION_ITEM('')
SURFACE()
);
#1734=(
BOUNDED_SURFACE()
B_SPLINE_SURFACE(3,3,((#129626,#129627,#129628,#129629),(#129630,#129631,
#129632,#129633),(#129634,#129635,#129636,#129637),(#129638,#129639,#129640,
#129641)),.UNSPECIFIED.,.F.,.F.,.F.)
B_SPLINE_SURFACE_WITH_KNOTS((4,4),(4,4),(0.485048076032685,0.537894489611572),
(0.,1.),.UNSPECIFIED.)
GEOMETRIC_REPRESENTATION_ITEM()
RATIONAL_B_SPLINE_SURFACE(((1.,0.999962180624942,0.999962180624942,1.),
(1.,0.999962180624942,0.999962180624942,1.),(1.,0.999962180624942,0.999962180624942,
1.),(1.,0.999962180624942,0.999962180624942,1.)))
REPRESENTATION_ITEM('')
SURFACE()
);
#1735=(
BOUNDED_SURFACE()
B_SPLINE_SURFACE(3,3,((#129643,#129644,#129645,#129646),(#129647,#129648,
#129649,#129650),(#129651,#129652,#129653,#129654),(#129655,#129656,#129657,
#129658)),.UNSPECIFIED.,.F.,.F.,.F.)
B_SPLINE_SURFACE_WITH_KNOTS((4,4),(4,4),(0.675453398131279,0.738944677678275),
(0.,1.),.UNSPECIFIED.)
GEOMETRIC_REPRESENTATION_ITEM()
RATIONAL_B_SPLINE_SURFACE(((1.,0.9999402244459,0.9999402244459,1.),(1.,
0.9999402244459,0.9999402244459,1.),(1.,0.9999402244459,0.9999402244459,
1.),(1.,0.9999402244459,0.9999402244459,1.)))
REPRESENTATION_ITEM('')
SURFACE()
);
#1736=(
BOUNDED_SURFACE()
B_SPLINE_SURFACE(3,3,((#129660,#129661,#129662,#129663),(#129664,#129665,
#129666,#129667),(#129668,#129669,#129670,#129671),(#129672,#129673,#129674,
#129675)),.UNSPECIFIED.,.F.,.F.,.F.)
B_SPLINE_SURFACE_WITH_KNOTS((4,4),(4,4),(0.848081923661779,0.924293307560431),
(0.,1.),.UNSPECIFIED.)
GEOMETRIC_REPRESENTATION_ITEM()
RATIONAL_B_SPLINE_SURFACE(((1.,0.999905876932681,0.999905876932681,1.),
(1.,0.999905876932681,0.999905876932681,1.),(1.,0.999905876932681,0.999905876932681,
1.),(1.,0.999905876932681,0.999905876932681,1.)))
REPRESENTATION_ITEM('')
SURFACE()
);
#1737=(
BOUNDED_SURFACE()
B_SPLINE_SURFACE(3,3,((#129677,#129678,#129679,#129680),(#129681,#129682,
#129683,#129684),(#129685,#129686,#129687,#129688),(#129689,#129690,#129691,
#129692)),.UNSPECIFIED.,.F.,.F.,.F.)
B_SPLINE_SURFACE_WITH_KNOTS((4,4),(4,4),(0.320532095739598,0.371399682963038),
(0.,1.),.UNSPECIFIED.)
GEOMETRIC_REPRESENTATION_ITEM()
RATIONAL_B_SPLINE_SURFACE(((1.,0.999967407141921,0.999967407141921,1.),
(1.,0.999967407141921,0.999967407141921,1.),(1.,0.999967407141921,0.999967407141921,
1.),(1.,0.999967407141921,0.999967407141921,1.)))
REPRESENTATION_ITEM('')
SURFACE()
);
#1738=(
BOUNDED_SURFACE()
B_SPLINE_SURFACE(3,3,((#129694,#129695,#129696,#129697),(#129698,#129699,
#129700,#129701),(#129702,#129703,#129704,#129705),(#129706,#129707,#129708,
#129709)),.UNSPECIFIED.,.F.,.F.,.F.)
B_SPLINE_SURFACE_WITH_KNOTS((4,4),(4,4),(0.485063242836078,0.537827571850851),
(0.,1.),.UNSPECIFIED.)
GEOMETRIC_REPRESENTATION_ITEM()
RATIONAL_B_SPLINE_SURFACE(((1.,0.999962210107628,0.999962210107628,1.),
(1.,0.999962210107628,0.999962210107628,1.),(1.,0.999962210107628,0.999962210107628,
1.),(1.,0.999962210107628,0.999962210107628,1.)))
REPRESENTATION_ITEM('')
SURFACE()
);
#1739=(
BOUNDED_SURFACE()
B_SPLINE_SURFACE(3,3,((#129711,#129712,#129713,#129714),(#129715,#129716,
#129717,#129718),(#129719,#129720,#129721,#129722),(#129723,#129724,#129725,
#129726)),.UNSPECIFIED.,.F.,.F.,.F.)
B_SPLINE_SURFACE_WITH_KNOTS((4,4),(4,4),(0.675517041172354,0.739061923565337),
(0.,1.),.UNSPECIFIED.)
GEOMETRIC_REPRESENTATION_ITEM()
RATIONAL_B_SPLINE_SURFACE(((1.,0.999940001666099,0.999940001666099,1.),
(1.,0.999940001666099,0.999940001666099,1.),(1.,0.999940001666099,0.999940001666099,
1.),(1.,0.999940001666099,0.999940001666099,1.)))
REPRESENTATION_ITEM('')
SURFACE()
);
#1740=(
BOUNDED_SURFACE()
B_SPLINE_SURFACE(3,3,((#129728,#129729,#129730,#129731),(#129732,#129733,
#129734,#129735),(#129736,#129737,#129738,#129739),(#129740,#129741,#129742,
#129743)),.UNSPECIFIED.,.F.,.F.,.F.)
B_SPLINE_SURFACE_WITH_KNOTS((4,4),(4,4),(0.847973179754561,0.924280871374564),
(0.,1.),.UNSPECIFIED.)
GEOMETRIC_REPRESENTATION_ITEM()
RATIONAL_B_SPLINE_SURFACE(((1.,0.999906008444178,0.999906008444178,1.),
(1.,0.999906008444178,0.999906008444178,1.),(1.,0.999906008444178,0.999906008444178,
1.),(1.,0.999906008444178,0.999906008444178,1.)))
REPRESENTATION_ITEM('')
SURFACE()
);
#1741=(
BOUNDED_SURFACE()
B_SPLINE_SURFACE(3,3,((#129745,#129746,#129747,#129748),(#129749,#129750,
#129751,#129752),(#129753,#129754,#129755,#129756),(#129757,#129758,#129759,
#129760)),.UNSPECIFIED.,.F.,.F.,.F.)
B_SPLINE_SURFACE_WITH_KNOTS((4,4),(4,4),(0.320557075856707,0.371389535077562),
(0.,1.),.UNSPECIFIED.)
GEOMETRIC_REPRESENTATION_ITEM()
RATIONAL_B_SPLINE_SURFACE(((1.,0.999967354745893,0.999967354745893,1.),
(1.,0.999967354745893,0.999967354745893,1.),(1.,0.999967354745893,0.999967354745893,
1.),(1.,0.999967354745893,0.999967354745893,1.)))
REPRESENTATION_ITEM('')
SURFACE()
);
#1742=(
BOUNDED_SURFACE()
B_SPLINE_SURFACE(3,3,((#129762,#129763,#129764,#129765),(#129766,#129767,
#129768,#129769),(#129770,#129771,#129772,#129773),(#129774,#129775,#129776,
#129777)),.UNSPECIFIED.,.F.,.F.,.F.)
B_SPLINE_SURFACE_WITH_KNOTS((4,4),(4,4),(0.485068338493211,0.537857806791834),
(0.,1.),.UNSPECIFIED.)
GEOMETRIC_REPRESENTATION_ITEM()
RATIONAL_B_SPLINE_SURFACE(((1.,0.999962427563455,0.999962427563455,1.),
(1.,0.999962427563455,0.999962427563455,1.),(1.,0.999962427563455,0.999962427563455,
1.),(1.,0.999962427563455,0.999962427563455,1.)))
REPRESENTATION_ITEM('')
SURFACE()
);
#1743=(
BOUNDED_SURFACE()
B_SPLINE_SURFACE(3,3,((#129779,#129780,#129781,#129782),(#129783,#129784,
#129785,#129786),(#129787,#129788,#129789,#129790),(#129791,#129792,#129793,
#129794)),.UNSPECIFIED.,.F.,.F.,.F.)
B_SPLINE_SURFACE_WITH_KNOTS((4,4),(4,4),(0.675489981246965,0.739042440925566),
(0.,1.),.UNSPECIFIED.)
GEOMETRIC_REPRESENTATION_ITEM()
RATIONAL_B_SPLINE_SURFACE(((1.,0.999940192796421,0.999940192796421,1.),
(1.,0.999940192796421,0.999940192796421,1.),(1.,0.999940192796421,0.999940192796421,
1.),(1.,0.999940192796421,0.999940192796421,1.)))
REPRESENTATION_ITEM('')
SURFACE()
);
#1744=(
BOUNDED_SURFACE()
B_SPLINE_SURFACE(3,3,((#129796,#129797,#129798,#129799),(#129800,#129801,
#129802,#129803),(#129804,#129805,#129806,#129807),(#129808,#129809,#129810,
#129811)),.UNSPECIFIED.,.F.,.F.,.F.)
B_SPLINE_SURFACE_WITH_KNOTS((4,4),(4,4),(0.847997664137825,0.924222883197149),
(0.,1.),.UNSPECIFIED.)
GEOMETRIC_REPRESENTATION_ITEM()
RATIONAL_B_SPLINE_SURFACE(((1.,0.999906130607457,0.999906130607457,1.),
(1.,0.999906130607457,0.999906130607457,1.),(1.,0.999906130607457,0.999906130607457,
1.),(1.,0.999906130607457,0.999906130607457,1.)))
REPRESENTATION_ITEM('')
SURFACE()
);
#1745=(
BOUNDED_SURFACE()
B_SPLINE_SURFACE(3,3,((#129813,#129814,#129815,#129816),(#129817,#129818,
#129819,#129820),(#129821,#129822,#129823,#129824),(#129825,#129826,#129827,
#129828)),.UNSPECIFIED.,.F.,.F.,.F.)
B_SPLINE_SURFACE_WITH_KNOTS((4,4),(4,4),(0.320507814263771,0.371406373023686),
(0.,1.),.UNSPECIFIED.)
GEOMETRIC_REPRESENTATION_ITEM()
RATIONAL_B_SPLINE_SURFACE(((1.,0.999967375144329,0.999967375144329,1.),
(1.,0.999967375144329,0.999967375144329,1.),(1.,0.999967375144329,0.999967375144329,
1.),(1.,0.999967375144329,0.999967375144329,1.)))
REPRESENTATION_ITEM('')
SURFACE()
);
#1746=(
BOUNDED_SURFACE()
B_SPLINE_SURFACE(3,3,((#129830,#129831,#129832,#129833),(#129834,#129835,
#129836,#129837),(#129838,#129839,#129840,#129841),(#129842,#129843,#129844,
#129845)),.UNSPECIFIED.,.F.,.F.,.F.)
B_SPLINE_SURFACE_WITH_KNOTS((4,4),(4,4),(0.485052737431369,0.53783191570572),
(0.,1.),.UNSPECIFIED.)
GEOMETRIC_REPRESENTATION_ITEM()
RATIONAL_B_SPLINE_SURFACE(((1.,0.999962226594182,0.999962226594182,1.),
(1.,0.999962226594182,0.999962226594182,1.),(1.,0.999962226594182,0.999962226594182,
1.),(1.,0.999962226594182,0.999962226594182,1.)))
REPRESENTATION_ITEM('')
SURFACE()
);
#1747=(
BOUNDED_SURFACE()
B_SPLINE_SURFACE(3,3,((#129847,#129848,#129849,#129850),(#129851,#129852,
#129853,#129854),(#129855,#129856,#129857,#129858),(#129859,#129860,#129861,
#129862)),.UNSPECIFIED.,.F.,.F.,.F.)
B_SPLINE_SURFACE_WITH_KNOTS((4,4),(4,4),(0.675526759490361,0.739051034903929),
(0.,1.),.UNSPECIFIED.)
GEOMETRIC_REPRESENTATION_ITEM()
RATIONAL_B_SPLINE_SURFACE(((1.,0.999940214293996,0.999940214293996,1.),
(1.,0.999940214293996,0.999940214293996,1.),(1.,0.999940214293996,0.999940214293996,
1.),(1.,0.999940214293996,0.999940214293996,1.)))
REPRESENTATION_ITEM('')
SURFACE()
);
#1748=(
BOUNDED_SURFACE()
B_SPLINE_SURFACE(3,3,((#129864,#129865,#129866,#129867),(#129868,#129869,
#129870,#129871),(#129872,#129873,#129874,#129875),(#129876,#129877,#129878,
#129879)),.UNSPECIFIED.,.F.,.F.,.F.)
B_SPLINE_SURFACE_WITH_KNOTS((4,4),(4,4),(0.847972351420996,0.924252627795196),
(0.,1.),.UNSPECIFIED.)
GEOMETRIC_REPRESENTATION_ITEM()
RATIONAL_B_SPLINE_SURFACE(((1.,0.999906726046663,0.999906726046663,1.),
(1.,0.999906726046663,0.999906726046663,1.),(1.,0.999906726046663,0.999906726046663,
1.),(1.,0.999906726046663,0.999906726046663,1.)))
REPRESENTATION_ITEM('')
SURFACE()
);
#1749=(
BOUNDED_SURFACE()
B_SPLINE_SURFACE(3,3,((#129881,#129882,#129883,#129884),(#129885,#129886,
#129887,#129888),(#129889,#129890,#129891,#129892),(#129893,#129894,#129895,
#129896)),.UNSPECIFIED.,.F.,.F.,.F.)
B_SPLINE_SURFACE_WITH_KNOTS((4,4),(4,4),(0.320502655600432,0.371307521287429),
(0.,1.),.UNSPECIFIED.)
GEOMETRIC_REPRESENTATION_ITEM()
RATIONAL_B_SPLINE_SURFACE(((1.,0.999967242859915,0.999967242859915,1.),
(1.,0.999967242859915,0.999967242859915,1.),(1.,0.999967242859915,0.999967242859915,
1.),(1.,0.999967242859915,0.999967242859915,1.)))
REPRESENTATION_ITEM('')
SURFACE()
);
#1750=(
BOUNDED_SURFACE()
B_SPLINE_SURFACE(3,3,((#129898,#129899,#129900,#129901),(#129902,#129903,
#129904,#129905),(#129906,#129907,#129908,#129909),(#129910,#129911,#129912,
#129913)),.UNSPECIFIED.,.F.,.F.,.F.)
B_SPLINE_SURFACE_WITH_KNOTS((4,4),(4,4),(0.485155008733541,0.537892550151409),
(0.,1.),.UNSPECIFIED.)
GEOMETRIC_REPRESENTATION_ITEM()
RATIONAL_B_SPLINE_SURFACE(((1.,0.999962141529141,0.999962141529141,1.),
(1.,0.999962141529141,0.999962141529141,1.),(1.,0.999962141529141,0.999962141529141,
1.),(1.,0.999962141529141,0.999962141529141,1.)))
REPRESENTATION_ITEM('')
SURFACE()
);
#1751=(
BOUNDED_SURFACE()
B_SPLINE_SURFACE(3,3,((#129915,#129916,#129917,#129918),(#129919,#129920,
#129921,#129922),(#129923,#129924,#129925,#129926),(#129927,#129928,#129929,
#129930)),.UNSPECIFIED.,.F.,.F.,.F.)
B_SPLINE_SURFACE_WITH_KNOTS((4,4),(4,4),(0.675449354058364,0.739068188298896),
(0.,1.),.UNSPECIFIED.)
GEOMETRIC_REPRESENTATION_ITEM()
RATIONAL_B_SPLINE_SURFACE(((1.,0.999940252055417,0.999940252055417,1.),
(1.,0.999940252055417,0.999940252055417,1.),(1.,0.999940252055417,0.999940252055417,
1.),(1.,0.999940252055417,0.999940252055417,1.)))
REPRESENTATION_ITEM('')
SURFACE()
);
#1752=(
BOUNDED_SURFACE()
B_SPLINE_SURFACE(3,3,((#129932,#129933,#129934,#129935),(#129936,#129937,
#129938,#129939),(#129940,#129941,#129942,#129943),(#129944,#129945,#129946,
#129947)),.UNSPECIFIED.,.F.,.F.,.F.)
B_SPLINE_SURFACE_WITH_KNOTS((4,4),(4,4),(0.847955892602436,0.924180945781555),
(0.,1.),.UNSPECIFIED.)
GEOMETRIC_REPRESENTATION_ITEM()
RATIONAL_B_SPLINE_SURFACE(((1.,0.999906284659141,0.999906284659141,1.),
(1.,0.999906284659141,0.999906284659141,1.),(1.,0.999906284659141,0.999906284659141,
1.),(1.,0.999906284659141,0.999906284659141,1.)))
REPRESENTATION_ITEM('')
SURFACE()
);
#1753=(
BOUNDED_SURFACE()
B_SPLINE_SURFACE(3,3,((#129949,#129950,#129951,#129952),(#129953,#129954,
#129955,#129956),(#129957,#129958,#129959,#129960),(#129961,#129962,#129963,
#129964)),.UNSPECIFIED.,.F.,.F.,.F.)
B_SPLINE_SURFACE_WITH_KNOTS((4,4),(4,4),(0.320636407294544,0.371421293305274),
(0.,1.),.UNSPECIFIED.)
GEOMETRIC_REPRESENTATION_ITEM()
RATIONAL_B_SPLINE_SURFACE(((1.,0.999967341957925,0.999967341957925,1.),
(1.,0.999967341957925,0.999967341957925,1.),(1.,0.999967341957925,0.999967341957925,
1.),(1.,0.999967341957925,0.999967341957925,1.)))
REPRESENTATION_ITEM('')
SURFACE()
);
#1754=(
BOUNDED_SURFACE()
B_SPLINE_SURFACE(3,3,((#129966,#129967,#129968,#129969),(#129970,#129971,
#129972,#129973),(#129974,#129975,#129976,#129977),(#129978,#129979,#129980,
#129981)),.UNSPECIFIED.,.F.,.F.,.F.)
B_SPLINE_SURFACE_WITH_KNOTS((4,4),(4,4),(0.485037430561784,0.537898553504801),
(0.,1.),.UNSPECIFIED.)
GEOMETRIC_REPRESENTATION_ITEM()
RATIONAL_B_SPLINE_SURFACE(((1.,0.999962289386236,0.999962289386236,1.),
(1.,0.999962289386236,0.999962289386236,1.),(1.,0.999962289386236,0.999962289386236,
1.),(1.,0.999962289386236,0.999962289386236,1.)))
REPRESENTATION_ITEM('')
SURFACE()
);
#1755=(
BOUNDED_SURFACE()
B_SPLINE_SURFACE(3,3,((#129983,#129984,#129985,#129986),(#129987,#129988,
#129989,#129990),(#129991,#129992,#129993,#129994),(#129995,#129996,#129997,
#129998)),.UNSPECIFIED.,.F.,.F.,.F.)
B_SPLINE_SURFACE_WITH_KNOTS((4,4),(4,4),(0.675444462502036,0.738927835629777),
(0.,1.),.UNSPECIFIED.)
GEOMETRIC_REPRESENTATION_ITEM()
RATIONAL_B_SPLINE_SURFACE(((1.,0.999939938463589,0.999939938463589,1.),
(1.,0.999939938463589,0.999939938463589,1.),(1.,0.999939938463589,0.999939938463589,
1.),(1.,0.999939938463589,0.999939938463589,1.)))
REPRESENTATION_ITEM('')
SURFACE()
);
#1756=(
BOUNDED_SURFACE()
B_SPLINE_SURFACE(3,3,((#130000,#130001,#130002,#130003),(#130004,#130005,
#130006,#130007),(#130008,#130009,#130010,#130011),(#130012,#130013,#130014,
#130015)),.UNSPECIFIED.,.F.,.F.,.F.)
B_SPLINE_SURFACE_WITH_KNOTS((4,4),(4,4),(0.848132173016768,0.924294320658525),
(0.,1.),.UNSPECIFIED.)
GEOMETRIC_REPRESENTATION_ITEM()
RATIONAL_B_SPLINE_SURFACE(((1.,0.999906066464898,0.999906066464898,1.),
(1.,0.999906066464898,0.999906066464898,1.),(1.,0.999906066464898,0.999906066464898,
1.),(1.,0.999906066464898,0.999906066464898,1.)))
REPRESENTATION_ITEM('')
SURFACE()
);
#1757=(
BOUNDED_SURFACE()
B_SPLINE_SURFACE(3,3,((#130017,#130018,#130019,#130020),(#130021,#130022,
#130023,#130024),(#130025,#130026,#130027,#130028),(#130029,#130030,#130031,
#130032)),.UNSPECIFIED.,.F.,.F.,.F.)
B_SPLINE_SURFACE_WITH_KNOTS((4,4),(4,4),(0.320505725021218,0.371419722674487),
(0.,1.),.UNSPECIFIED.)
GEOMETRIC_REPRESENTATION_ITEM()
RATIONAL_B_SPLINE_SURFACE(((1.,0.999967360975282,0.999967360975282,1.),
(1.,0.999967360975282,0.999967360975282,1.),(1.,0.999967360975282,0.999967360975282,
1.),(1.,0.999967360975282,0.999967360975282,1.)))
REPRESENTATION_ITEM('')
SURFACE()
);
#1758=(
BOUNDED_SURFACE()
B_SPLINE_SURFACE(3,3,((#130034,#130035,#130036,#130037),(#130038,#130039,
#130040,#130041),(#130042,#130043,#130044,#130045),(#130046,#130047,#130048,
#130049)),.UNSPECIFIED.,.F.,.F.,.F.)
B_SPLINE_SURFACE_WITH_KNOTS((4,4),(4,4),(0.485041236272929,0.537757161067977),
(0.,1.),.UNSPECIFIED.)
GEOMETRIC_REPRESENTATION_ITEM()
RATIONAL_B_SPLINE_SURFACE(((1.,0.999962057900831,0.999962057900831,1.),
(1.,0.999962057900831,0.999962057900831,1.),(1.,0.999962057900831,0.999962057900831,
1.),(1.,0.999962057900831,0.999962057900831,1.)))
REPRESENTATION_ITEM('')
SURFACE()
);
#1759=(
BOUNDED_SURFACE()
B_SPLINE_SURFACE(3,3,((#130051,#130052,#130053,#130054),(#130055,#130056,
#130057,#130058),(#130059,#130060,#130061,#130062),(#130063,#130064,#130065,
#130066)),.UNSPECIFIED.,.F.,.F.,.F.)
B_SPLINE_SURFACE_WITH_KNOTS((4,4),(4,4),(0.675602722634434,0.739081859127056),
(0.,1.),.UNSPECIFIED.)
GEOMETRIC_REPRESENTATION_ITEM()
RATIONAL_B_SPLINE_SURFACE(((1.,0.99994018156245,0.99994018156245,1.),(1.,
0.99994018156245,0.99994018156245,1.),(1.,0.99994018156245,0.99994018156245,
1.),(1.,0.99994018156245,0.99994018156245,1.)))
REPRESENTATION_ITEM('')
SURFACE()
);
#1760=(
BOUNDED_SURFACE()
B_SPLINE_SURFACE(3,3,((#130068,#130069,#130070,#130071),(#130072,#130073,
#130074,#130075),(#130076,#130077,#130078,#130079),(#130080,#130081,#130082,
#130083)),.UNSPECIFIED.,.F.,.F.,.F.)
B_SPLINE_SURFACE_WITH_KNOTS((4,4),(4,4),(0.847942716817777,0.924300472680093),
(0.,1.),.UNSPECIFIED.)
GEOMETRIC_REPRESENTATION_ITEM()
RATIONAL_B_SPLINE_SURFACE(((1.,0.99990624222844,0.99990624222844,1.),(1.,
0.99990624222844,0.99990624222844,1.),(1.,0.99990624222844,0.99990624222844,
1.),(1.,0.99990624222844,0.99990624222844,1.)))
REPRESENTATION_ITEM('')
SURFACE()
);
#1761=(
BOUNDED_SURFACE()
B_SPLINE_SURFACE(3,3,((#130085,#130086,#130087,#130088),(#130089,#130090,
#130091,#130092),(#130093,#130094,#130095,#130096),(#130097,#130098,#130099,
#130100)),.UNSPECIFIED.,.F.,.F.,.F.)
B_SPLINE_SURFACE_WITH_KNOTS((4,4),(4,4),(0.320514009564598,0.371328550441877),
(0.,1.),.UNSPECIFIED.)
GEOMETRIC_REPRESENTATION_ITEM()
RATIONAL_B_SPLINE_SURFACE(((1.,0.999967231313903,0.999967231313903,1.),
(1.,0.999967231313903,0.999967231313903,1.),(1.,0.999967231313903,0.999967231313903,
1.),(1.,0.999967231313903,0.999967231313903,1.)))
REPRESENTATION_ITEM('')
SURFACE()
);
#1762=(
BOUNDED_SURFACE()
B_SPLINE_SURFACE(3,3,((#130102,#130103,#130104,#130105),(#130106,#130107,
#130108,#130109),(#130110,#130111,#130112,#130113),(#130114,#130115,#130116,
#130117)),.UNSPECIFIED.,.F.,.F.,.F.)
B_SPLINE_SURFACE_WITH_KNOTS((4,4),(4,4),(0.48512402908949,0.537892318607367),
(0.,1.),.UNSPECIFIED.)
GEOMETRIC_REPRESENTATION_ITEM()
RATIONAL_B_SPLINE_SURFACE(((1.,0.999962289571751,0.999962289571751,1.),
(1.,0.999962289571751,0.999962289571751,1.),(1.,0.999962289571751,0.999962289571751,
1.),(1.,0.999962289571751,0.999962289571751,1.)))
REPRESENTATION_ITEM('')
SURFACE()
);
#1763=(
BOUNDED_SURFACE()
B_SPLINE_SURFACE(3,3,((#130119,#130120,#130121,#130122),(#130123,#130124,
#130125,#130126),(#130127,#130128,#130129,#130130),(#130131,#130132,#130133,
#130134)),.UNSPECIFIED.,.F.,.F.,.F.)
B_SPLINE_SURFACE_WITH_KNOTS((4,4),(4,4),(0.675452991908006,0.739078420574732),
(0.,1.),.UNSPECIFIED.)
GEOMETRIC_REPRESENTATION_ITEM()
RATIONAL_B_SPLINE_SURFACE(((1.,0.999940089902897,0.999940089902897,1.),
(1.,0.999940089902897,0.999940089902897,1.),(1.,0.999940089902897,0.999940089902897,
1.),(1.,0.999940089902897,0.999940089902897,1.)))
REPRESENTATION_ITEM('')
SURFACE()
);
#1764=(
BOUNDED_SURFACE()
B_SPLINE_SURFACE(3,3,((#130136,#130137,#130138,#130139),(#130140,#130141,
#130142,#130143),(#130144,#130145,#130146,#130147),(#130148,#130149,#130150,
#130151)),.UNSPECIFIED.,.F.,.F.,.F.)
B_SPLINE_SURFACE_WITH_KNOTS((4,4),(4,4),(0.847950520319574,0.924115043194035),
(0.,1.),.UNSPECIFIED.)
GEOMETRIC_REPRESENTATION_ITEM()
RATIONAL_B_SPLINE_SURFACE(((1.,0.999905876767882,0.999905876767882,1.),
(1.,0.999905876767882,0.999905876767882,1.),(1.,0.999905876767882,0.999905876767882,
1.),(1.,0.999905876767882,0.999905876767882,1.)))
REPRESENTATION_ITEM('')
SURFACE()
);
#1765=(
BOUNDED_SURFACE()
B_SPLINE_SURFACE(3,3,((#130153,#130154,#130155,#130156),(#130157,#130158,
#130159,#130160),(#130161,#130162,#130163,#130164),(#130165,#130166,#130167,
#130168)),.UNSPECIFIED.,.F.,.F.,.F.)
B_SPLINE_SURFACE_WITH_KNOTS((4,4),(4,4),(0.320554317164351,0.371402703199328),
(0.,1.),.UNSPECIFIED.)
GEOMETRIC_REPRESENTATION_ITEM()
RATIONAL_B_SPLINE_SURFACE(((1.,0.999967393810812,0.999967393810812,1.),
(1.,0.999967393810812,0.999967393810812,1.),(1.,0.999967393810812,0.999967393810812,
1.),(1.,0.999967393810812,0.999967393810812,1.)))
REPRESENTATION_ITEM('')
SURFACE()
);
#1766=(
BOUNDED_SURFACE()
B_SPLINE_SURFACE(3,3,((#130170,#130171,#130172,#130173),(#130174,#130175,
#130176,#130177),(#130178,#130179,#130180,#130181),(#130182,#130183,#130184,
#130185)),.UNSPECIFIED.,.F.,.F.,.F.)
B_SPLINE_SURFACE_WITH_KNOTS((4,4),(4,4),(0.485062342489115,0.537883560988347),
(0.,1.),.UNSPECIFIED.)
GEOMETRIC_REPRESENTATION_ITEM()
RATIONAL_B_SPLINE_SURFACE(((1.,0.999962138574809,0.999962138574809,1.),
(1.,0.999962138574809,0.999962138574809,1.),(1.,0.999962138574809,0.999962138574809,
1.),(1.,0.999962138574809,0.999962138574809,1.)))
REPRESENTATION_ITEM('')
SURFACE()
);
#1767=(
BOUNDED_SURFACE()
B_SPLINE_SURFACE(3,3,((#130187,#130188,#130189,#130190),(#130191,#130192,
#130193,#130194),(#130195,#130196,#130197,#130198),(#130199,#130200,#130201,
#130202)),.UNSPECIFIED.,.F.,.F.,.F.)
B_SPLINE_SURFACE_WITH_KNOTS((4,4),(4,4),(0.675466656549766,0.738982296165968),
(0.,1.),.UNSPECIFIED.)
GEOMETRIC_REPRESENTATION_ITEM()
RATIONAL_B_SPLINE_SURFACE(((1.,0.999939980433748,0.999939980433748,1.),
(1.,0.999939980433748,0.999939980433748,1.),(1.,0.999939980433748,0.999939980433748,
1.),(1.,0.999939980433748,0.999939980433748,1.)))
REPRESENTATION_ITEM('')
SURFACE()
);
#1768=(
BOUNDED_SURFACE()
B_SPLINE_SURFACE(3,3,((#130204,#130205,#130206,#130207),(#130208,#130209,
#130210,#130211),(#130212,#130213,#130214,#130215),(#130216,#130217,#130218,
#130219)),.UNSPECIFIED.,.F.,.F.,.F.)
B_SPLINE_SURFACE_WITH_KNOTS((4,4),(4,4),(0.84804648712844,0.924282372382723),
(0.,1.),.UNSPECIFIED.)
GEOMETRIC_REPRESENTATION_ITEM()
RATIONAL_B_SPLINE_SURFACE(((1.,0.999906415714148,0.999906415714148,1.),
(1.,0.999906415714148,0.999906415714148,1.),(1.,0.999906415714148,0.999906415714148,
1.),(1.,0.999906415714148,0.999906415714148,1.)))
REPRESENTATION_ITEM('')
SURFACE()
);
#1769=(
BOUNDED_SURFACE()
B_SPLINE_SURFACE(3,3,((#130221,#130222,#130223,#130224),(#130225,#130226,
#130227,#130228),(#130229,#130230,#130231,#130232),(#130233,#130234,#130235,
#130236)),.UNSPECIFIED.,.F.,.F.,.F.)
B_SPLINE_SURFACE_WITH_KNOTS((4,4),(4,4),(0.320604734130633,0.371278297272317),
(0.,1.),.UNSPECIFIED.)
GEOMETRIC_REPRESENTATION_ITEM()
RATIONAL_B_SPLINE_SURFACE(((1.,0.999967281636602,0.999967281636602,1.),
(1.,0.999967281636602,0.999967281636602,1.),(1.,0.999967281636602,0.999967281636602,
1.),(1.,0.999967281636602,0.999967281636602,1.)))
REPRESENTATION_ITEM('')
SURFACE()
);
#1770=(
BOUNDED_SURFACE()
B_SPLINE_SURFACE(3,3,((#130238,#130239,#130240,#130241),(#130242,#130243,
#130244,#130245),(#130246,#130247,#130248,#130249),(#130250,#130251,#130252,
#130253)),.UNSPECIFIED.,.F.,.F.,.F.)
B_SPLINE_SURFACE_WITH_KNOTS((4,4),(4,4),(0.485137973433402,0.537847298674517),
(0.,1.),.UNSPECIFIED.)
GEOMETRIC_REPRESENTATION_ITEM()
RATIONAL_B_SPLINE_SURFACE(((1.,0.99996212094789,0.99996212094789,1.),(1.,
0.99996212094789,0.99996212094789,1.),(1.,0.99996212094789,0.99996212094789,
1.),(1.,0.99996212094789,0.99996212094789,1.)))
REPRESENTATION_ITEM('')
SURFACE()
);
#1771=(
BOUNDED_SURFACE()
B_SPLINE_SURFACE(3,3,((#130255,#130256,#130257,#130258),(#130259,#130260,
#130261,#130262),(#130263,#130264,#130265,#130266),(#130267,#130268,#130269,
#130270)),.UNSPECIFIED.,.F.,.F.,.F.)
B_SPLINE_SURFACE_WITH_KNOTS((4,4),(4,4),(0.675493277798674,0.739045612587958),
(0.,1.),.UNSPECIFIED.)
GEOMETRIC_REPRESENTATION_ITEM()
RATIONAL_B_SPLINE_SURFACE(((1.,0.999940222070666,0.999940222070666,1.),
(1.,0.999940222070666,0.999940222070666,1.),(1.,0.999940222070666,0.999940222070666,
1.),(1.,0.999940222070666,0.999940222070666,1.)))
REPRESENTATION_ITEM('')
SURFACE()
);
#1772=(
BOUNDED_SURFACE()
B_SPLINE_SURFACE(3,3,((#130272,#130273,#130274,#130275),(#130276,#130277,
#130278,#130279),(#130280,#130281,#130282,#130283),(#130284,#130285,#130286,
#130287)),.UNSPECIFIED.,.F.,.F.,.F.)
B_SPLINE_SURFACE_WITH_KNOTS((4,4),(4,4),(0.84799348482738,0.92426372810007),
(0.,1.),.UNSPECIFIED.)
GEOMETRIC_REPRESENTATION_ITEM()
RATIONAL_B_SPLINE_SURFACE(((1.,0.999905944721945,0.999905944721945,1.),
(1.,0.999905944721945,0.999905944721945,1.),(1.,0.999905944721945,0.999905944721945,
1.),(1.,0.999905944721945,0.999905944721945,1.)))
REPRESENTATION_ITEM('')
SURFACE()
);
#1773=(
BOUNDED_SURFACE()
B_SPLINE_SURFACE(3,3,((#130289,#130290,#130291,#130292),(#130293,#130294,
#130295,#130296),(#130297,#130298,#130299,#130300),(#130301,#130302,#130303,
#130304)),.UNSPECIFIED.,.F.,.F.,.F.)
B_SPLINE_SURFACE_WITH_KNOTS((4,4),(4,4),(0.3205402280231,0.371335872514157),
(0.,1.),.UNSPECIFIED.)
GEOMETRIC_REPRESENTATION_ITEM()
RATIONAL_B_SPLINE_SURFACE(((1.,0.99996727377962,0.99996727377962,1.),(1.,
0.99996727377962,0.99996727377962,1.),(1.,0.99996727377962,0.99996727377962,
1.),(1.,0.99996727377962,0.99996727377962,1.)))
REPRESENTATION_ITEM('')
SURFACE()
);
#1774=(
BOUNDED_SURFACE()
B_SPLINE_SURFACE(3,3,((#130306,#130307,#130308,#130309),(#130310,#130311,
#130312,#130313),(#130314,#130315,#130316,#130317),(#130318,#130319,#130320,
#130321)),.UNSPECIFIED.,.F.,.F.,.F.)
B_SPLINE_SURFACE_WITH_KNOTS((4,4),(4,4),(0.485075837246189,0.537808186355769),
(0.,1.),.UNSPECIFIED.)
GEOMETRIC_REPRESENTATION_ITEM()
RATIONAL_B_SPLINE_SURFACE(((1.,0.999962230795869,0.999962230795869,1.),
(1.,0.999962230795869,0.999962230795869,1.),(1.,0.999962230795869,0.999962230795869,
1.),(1.,0.999962230795869,0.999962230795869,1.)))
REPRESENTATION_ITEM('')
SURFACE()
);
#1775=(
BOUNDED_SURFACE()
B_SPLINE_SURFACE(3,3,((#130323,#130324,#130325,#130326),(#130327,#130328,
#130329,#130330),(#130331,#130332,#130333,#130334),(#130335,#130336,#130337,
#130338)),.UNSPECIFIED.,.F.,.F.,.F.)
B_SPLINE_SURFACE_WITH_KNOTS((4,4),(4,4),(0.675564486464684,0.738898139890546),
(0.,1.),.UNSPECIFIED.)
GEOMETRIC_REPRESENTATION_ITEM()
RATIONAL_B_SPLINE_SURFACE(((1.,0.999939996666824,0.999939996666824,1.),
(1.,0.999939996666824,0.999939996666824,1.),(1.,0.999939996666824,0.999939996666824,
1.),(1.,0.999939996666824,0.999939996666824,1.)))
REPRESENTATION_ITEM('')
SURFACE()
);
#1776=(
BOUNDED_SURFACE()
B_SPLINE_SURFACE(3,3,((#130340,#130341,#130342,#130343),(#130344,#130345,
#130346,#130347),(#130348,#130349,#130350,#130351),(#130352,#130353,#130354,
#130355)),.UNSPECIFIED.,.F.,.F.,.F.)
B_SPLINE_SURFACE_WITH_KNOTS((4,4),(4,4),(0.84809304582895,0.924247716835722),
(0.,1.),.UNSPECIFIED.)
GEOMETRIC_REPRESENTATION_ITEM()
RATIONAL_B_SPLINE_SURFACE(((1.,0.999905933509504,0.999905933509504,1.),
(1.,0.999905933509504,0.999905933509504,1.),(1.,0.999905933509504,0.999905933509504,
1.),(1.,0.999905933509504,0.999905933509504,1.)))
REPRESENTATION_ITEM('')
SURFACE()
);
#1777=(
BOUNDED_SURFACE()
B_SPLINE_SURFACE(3,3,((#130357,#130358,#130359,#130360),(#130361,#130362,
#130363,#130364),(#130365,#130366,#130367,#130368),(#130369,#130370,#130371,
#130372)),.UNSPECIFIED.,.F.,.F.,.F.)
B_SPLINE_SURFACE_WITH_KNOTS((4,4),(4,4),(0.320557294445702,0.371402834588606),
(0.,1.),.UNSPECIFIED.)
GEOMETRIC_REPRESENTATION_ITEM()
RATIONAL_B_SPLINE_SURFACE(((1.,0.999967373265669,0.999967373265669,1.),
(1.,0.999967373265669,0.999967373265669,1.),(1.,0.999967373265669,0.999967373265669,
1.),(1.,0.999967373265669,0.999967373265669,1.)))
REPRESENTATION_ITEM('')
SURFACE()
);
#1778=(
BOUNDED_SURFACE()
B_SPLINE_SURFACE(3,3,((#130374,#130375,#130376,#130377),(#130378,#130379,
#130380,#130381),(#130382,#130383,#130384,#130385),(#130386,#130387,#130388,
#130389)),.UNSPECIFIED.,.F.,.F.,.F.)
B_SPLINE_SURFACE_WITH_KNOTS((4,4),(4,4),(0.485061470768506,0.537824685725865),
(0.,1.),.UNSPECIFIED.)
GEOMETRIC_REPRESENTATION_ITEM()
RATIONAL_B_SPLINE_SURFACE(((1.,0.999962123207486,0.999962123207486,1.),
(1.,0.999962123207486,0.999962123207486,1.),(1.,0.999962123207486,0.999962123207486,
1.),(1.,0.999962123207486,0.999962123207486,1.)))
REPRESENTATION_ITEM('')
SURFACE()
);
#1779=(
BOUNDED_SURFACE()
B_SPLINE_SURFACE(3,3,((#130391,#130392,#130393,#130394),(#130395,#130396,
#130397,#130398),(#130399,#130400,#130401,#130402),(#130403,#130404,#130405,
#130406)),.UNSPECIFIED.,.F.,.F.,.F.)
B_SPLINE_SURFACE_WITH_KNOTS((4,4),(4,4),(0.675473799809187,0.738977929617164),
(0.,1.),.UNSPECIFIED.)
GEOMETRIC_REPRESENTATION_ITEM()
RATIONAL_B_SPLINE_SURFACE(((1.,0.999940012441812,0.999940012441812,1.),
(1.,0.999940012441812,0.999940012441812,1.),(1.,0.999940012441812,0.999940012441812,
1.),(1.,0.999940012441812,0.999940012441812,1.)))
REPRESENTATION_ITEM('')
SURFACE()
);
#1780=(
BOUNDED_SURFACE()
B_SPLINE_SURFACE(3,3,((#130408,#130409,#130410,#130411),(#130412,#130413,
#130414,#130415),(#130416,#130417,#130418,#130419),(#130420,#130421,#130422,
#130423)),.UNSPECIFIED.,.F.,.F.,.F.)
B_SPLINE_SURFACE_WITH_KNOTS((4,4),(4,4),(0.848025753359781,0.924153418178438),
(0.,1.),.UNSPECIFIED.)
GEOMETRIC_REPRESENTATION_ITEM()
RATIONAL_B_SPLINE_SURFACE(((1.,0.99990637728161,0.99990637728161,1.),(1.,
0.99990637728161,0.99990637728161,1.),(1.,0.99990637728161,0.99990637728161,
1.),(1.,0.99990637728161,0.99990637728161,1.)))
REPRESENTATION_ITEM('')
SURFACE()
);
#1781=(
BOUNDED_SURFACE()
B_SPLINE_SURFACE(3,3,((#130425,#130426,#130427,#130428),(#130429,#130430,
#130431,#130432),(#130433,#130434,#130435,#130436),(#130437,#130438,#130439,
#130440)),.UNSPECIFIED.,.F.,.F.,.F.)
B_SPLINE_SURFACE_WITH_KNOTS((4,4),(4,4),(0.320510703809115,0.371320148131838),
(0.,1.),.UNSPECIFIED.)
GEOMETRIC_REPRESENTATION_ITEM()
RATIONAL_B_SPLINE_SURFACE(((1.,0.999967253008905,0.999967253008905,1.),
(1.,0.999967253008905,0.999967253008905,1.),(1.,0.999967253008905,0.999967253008905,
1.),(1.,0.999967253008905,0.999967253008905,1.)))
REPRESENTATION_ITEM('')
SURFACE()
);
#1782=(
BOUNDED_SURFACE()
B_SPLINE_SURFACE(3,3,((#130442,#130443,#130444,#130445),(#130446,#130447,
#130448,#130449),(#130450,#130451,#130452,#130453),(#130454,#130455,#130456,
#130457)),.UNSPECIFIED.,.F.,.F.,.F.)
B_SPLINE_SURFACE_WITH_KNOTS((4,4),(4,4),(0.485049233505636,0.537894115044618),
(0.,1.),.UNSPECIFIED.)
GEOMETRIC_REPRESENTATION_ITEM()
RATIONAL_B_SPLINE_SURFACE(((1.,0.999962145144179,0.999962145144179,1.),
(1.,0.999962145144179,0.999962145144179,1.),(1.,0.999962145144179,0.999962145144179,
1.),(1.,0.999962145144179,0.999962145144179,1.)))
REPRESENTATION_ITEM('')
SURFACE()
);
#1783=(
BOUNDED_SURFACE()
B_SPLINE_SURFACE(3,3,((#130459,#130460,#130461,#130462),(#130463,#130464,
#130465,#130466),(#130467,#130468,#130469,#130470),(#130471,#130472,#130473,
#130474)),.UNSPECIFIED.,.F.,.F.,.F.)
B_SPLINE_SURFACE_WITH_KNOTS((4,4),(4,4),(0.67554993384203,0.739074174432657),
(0.,1.),.UNSPECIFIED.)
GEOMETRIC_REPRESENTATION_ITEM()
RATIONAL_B_SPLINE_SURFACE(((1.,0.999940279534679,0.999940279534679,1.),
(1.,0.999940279534679,0.999940279534679,1.),(1.,0.999940279534679,0.999940279534679,
1.),(1.,0.999940279534679,0.999940279534679,1.)))
REPRESENTATION_ITEM('')
SURFACE()
);
#1784=(
BOUNDED_SURFACE()
B_SPLINE_SURFACE(3,3,((#130476,#130477,#130478,#130479),(#130480,#130481,
#130482,#130483),(#130484,#130485,#130486,#130487),(#130488,#130489,#130490,
#130491)),.UNSPECIFIED.,.F.,.F.,.F.)
B_SPLINE_SURFACE_WITH_KNOTS((4,4),(4,4),(0.847957765543921,0.924145861363742),
(0.,1.),.UNSPECIFIED.)
GEOMETRIC_REPRESENTATION_ITEM()
RATIONAL_B_SPLINE_SURFACE(((1.,0.9999059073186,0.9999059073186,1.),(1.,
0.9999059073186,0.9999059073186,1.),(1.,0.9999059073186,0.9999059073186,
1.),(1.,0.9999059073186,0.9999059073186,1.)))
REPRESENTATION_ITEM('')
SURFACE()
);
#1785=(
BOUNDED_SURFACE()
B_SPLINE_SURFACE(3,3,((#130493,#130494,#130495,#130496),(#130497,#130498,
#130499,#130500),(#130501,#130502,#130503,#130504),(#130505,#130506,#130507,
#130508)),.UNSPECIFIED.,.F.,.F.,.F.)
B_SPLINE_SURFACE_WITH_KNOTS((4,4),(4,4),(0.320502991162247,0.371421831902603),
(0.,1.),.UNSPECIFIED.)
GEOMETRIC_REPRESENTATION_ITEM()
RATIONAL_B_SPLINE_SURFACE(((1.,0.999967329307079,0.999967329307079,1.),
(1.,0.999967329307079,0.999967329307079,1.),(1.,0.999967329307079,0.999967329307079,
1.),(1.,0.999967329307079,0.999967329307079,1.)))
REPRESENTATION_ITEM('')
SURFACE()
);
#1786=(
BOUNDED_SURFACE()
B_SPLINE_SURFACE(3,3,((#130510,#130511,#130512,#130513),(#130514,#130515,
#130516,#130517),(#130518,#130519,#130520,#130521),(#130522,#130523,#130524,
#130525)),.UNSPECIFIED.,.F.,.F.,.F.)
B_SPLINE_SURFACE_WITH_KNOTS((4,4),(4,4),(0.485162005966803,0.537898074092653),
(0.,1.),.UNSPECIFIED.)
GEOMETRIC_REPRESENTATION_ITEM()
RATIONAL_B_SPLINE_SURFACE(((1.,0.999962283120094,0.999962283120094,1.),
(1.,0.999962283120094,0.999962283120094,1.),(1.,0.999962283120094,0.999962283120094,
1.),(1.,0.999962283120094,0.999962283120094,1.)))
REPRESENTATION_ITEM('')
SURFACE()
);
#1787=(
BOUNDED_SURFACE()
B_SPLINE_SURFACE(3,3,((#130527,#130528,#130529,#130530),(#130531,#130532,
#130533,#130534),(#130535,#130536,#130537,#130538),(#130539,#130540,#130541,
#130542)),.UNSPECIFIED.,.F.,.F.,.F.)
B_SPLINE_SURFACE_WITH_KNOTS((4,4),(4,4),(0.675446019028147,0.738904200659153),
(0.,1.),.UNSPECIFIED.)
GEOMETRIC_REPRESENTATION_ITEM()
RATIONAL_B_SPLINE_SURFACE(((1.,0.999939928462316,0.999939928462316,1.),
(1.,0.999939928462316,0.999939928462316,1.),(1.,0.999939928462316,0.999939928462316,
1.),(1.,0.999939928462316,0.999939928462316,1.)))
REPRESENTATION_ITEM('')
SURFACE()
);
#1788=(
BOUNDED_SURFACE()
B_SPLINE_SURFACE(3,3,((#130544,#130545,#130546,#130547),(#130548,#130549,
#130550,#130551),(#130552,#130553,#130554,#130555),(#130556,#130557,#130558,
#130559)),.UNSPECIFIED.,.F.,.F.,.F.)
B_SPLINE_SURFACE_WITH_KNOTS((4,4),(4,4),(0.847946092181821,0.924299972364549),
(0.,1.),.UNSPECIFIED.)
GEOMETRIC_REPRESENTATION_ITEM()
RATIONAL_B_SPLINE_SURFACE(((1.,0.999906151714093,0.999906151714093,1.),
(1.,0.999906151714093,0.999906151714093,1.),(1.,0.999906151714093,0.999906151714093,
1.),(1.,0.999906151714093,0.999906151714093,1.)))
REPRESENTATION_ITEM('')
SURFACE()
);
#1789=(
BOUNDED_SURFACE()
B_SPLINE_SURFACE(3,3,((#130561,#130562,#130563,#130564),(#130565,#130566,
#130567,#130568),(#130569,#130570,#130571,#130572),(#130573,#130574,#130575,
#130576)),.UNSPECIFIED.,.F.,.F.,.F.)
B_SPLINE_SURFACE_WITH_KNOTS((4,4),(4,4),(0.320639346010966,0.371419107445367),
(0.,1.),.UNSPECIFIED.)
GEOMETRIC_REPRESENTATION_ITEM()
RATIONAL_B_SPLINE_SURFACE(((1.,0.999967363082376,0.999967363082376,1.),
(1.,0.999967363082376,0.999967363082376,1.),(1.,0.999967363082376,0.999967363082376,
1.),(1.,0.999967363082376,0.999967363082376,1.)))
REPRESENTATION_ITEM('')
SURFACE()
);
#1790=(
BOUNDED_SURFACE()
B_SPLINE_SURFACE(3,3,((#130578,#130579,#130580,#130581),(#130582,#130583,
#130584,#130585),(#130586,#130587,#130588,#130589),(#130590,#130591,#130592,
#130593)),.UNSPECIFIED.,.F.,.F.,.F.)
B_SPLINE_SURFACE_WITH_KNOTS((4,4),(4,4),(0.485038469133326,0.53776448421819),
(0.,1.),.UNSPECIFIED.)
GEOMETRIC_REPRESENTATION_ITEM()
RATIONAL_B_SPLINE_SURFACE(((1.,0.999962058707067,0.999962058707067,1.),
(1.,0.999962058707067,0.999962058707067,1.),(1.,0.999962058707067,0.999962058707067,
1.),(1.,0.999962058707067,0.999962058707067,1.)))
REPRESENTATION_ITEM('')
SURFACE()
);
#1791=(
BOUNDED_SURFACE()
B_SPLINE_SURFACE(3,3,((#130595,#130596,#130597,#130598),(#130599,#130600,
#130601,#130602),(#130603,#130604,#130605,#130606),(#130607,#130608,#130609,
#130610)),.UNSPECIFIED.,.F.,.F.,.F.)
B_SPLINE_SURFACE_WITH_KNOTS((4,4),(4,4),(0.675442877290701,0.739081132522842),
(0.,1.),.UNSPECIFIED.)
GEOMETRIC_REPRESENTATION_ITEM()
RATIONAL_B_SPLINE_SURFACE(((1.,0.999940234359194,0.999940234359194,1.),
(1.,0.999940234359194,0.999940234359194,1.),(1.,0.999940234359194,0.999940234359194,
1.),(1.,0.999940234359194,0.999940234359194,1.)))
REPRESENTATION_ITEM('')
SURFACE()
);
#1792=(
BOUNDED_SURFACE()
B_SPLINE_SURFACE(3,3,((#130612,#130613,#130614,#130615),(#130616,#130617,
#130618,#130619),(#130620,#130621,#130622,#130623),(#130624,#130625,#130626,
#130627)),.UNSPECIFIED.,.F.,.F.,.F.)
B_SPLINE_SURFACE_WITH_KNOTS((4,4),(4,4),(0.848165051389747,0.924298160543409),
(0.,1.),.UNSPECIFIED.)
GEOMETRIC_REPRESENTATION_ITEM()
RATIONAL_B_SPLINE_SURFACE(((1.,0.999906139404426,0.999906139404426,1.),
(1.,0.999906139404426,0.999906139404426,1.),(1.,0.999906139404426,0.999906139404426,
1.),(1.,0.999906139404426,0.999906139404426,1.)))
REPRESENTATION_ITEM('')
SURFACE()
);
#1793=(
BOUNDED_SURFACE()
B_SPLINE_SURFACE(3,3,((#130629,#130630,#130631,#130632),(#130633,#130634,
#130635,#130636),(#130637,#130638,#130639,#130640),(#130641,#130642,#130643,
#130644)),.UNSPECIFIED.,.F.,.F.,.F.)
B_SPLINE_SURFACE_WITH_KNOTS((4,4),(4,4),(0.32050822714455,0.371339675656775),
(0.,1.),.UNSPECIFIED.)
GEOMETRIC_REPRESENTATION_ITEM()
RATIONAL_B_SPLINE_SURFACE(((1.,0.999967238121568,0.999967238121568,1.),
(1.,0.999967238121568,0.999967238121568,1.),(1.,0.999967238121568,0.999967238121568,
1.),(1.,0.999967238121568,0.999967238121568,1.)))
REPRESENTATION_ITEM('')
SURFACE()
);
#1794=(
BOUNDED_SURFACE()
B_SPLINE_SURFACE(3,3,((#130646,#130647,#130648,#130649),(#130650,#130651,
#130652,#130653),(#130654,#130655,#130656,#130657),(#130658,#130659,#130660,
#130661)),.UNSPECIFIED.,.F.,.F.,.F.)
B_SPLINE_SURFACE_WITH_KNOTS((4,4),(4,4),(0.48504281620503,0.537888955734494),
(0.,1.),.UNSPECIFIED.)
GEOMETRIC_REPRESENTATION_ITEM()
RATIONAL_B_SPLINE_SURFACE(((1.,0.999962273981182,0.999962273981182,1.),
(1.,0.999962273981182,0.999962273981182,1.),(1.,0.999962273981182,0.999962273981182,
1.),(1.,0.999962273981182,0.999962273981182,1.)))
REPRESENTATION_ITEM('')
SURFACE()
);
#1795=(
BOUNDED_SURFACE()
B_SPLINE_SURFACE(3,3,((#130663,#130664,#130665,#130666),(#130667,#130668,
#130669,#130670),(#130671,#130672,#130673,#130674),(#130675,#130676,#130677,
#130678)),.UNSPECIFIED.,.F.,.F.,.F.)
B_SPLINE_SURFACE_WITH_KNOTS((4,4),(4,4),(0.675575393990298,0.739072202256826),
(0.,1.),.UNSPECIFIED.)
GEOMETRIC_REPRESENTATION_ITEM()
RATIONAL_B_SPLINE_SURFACE(((1.,0.999940054601015,0.999940054601015,1.),
(1.,0.999940054601015,0.999940054601015,1.),(1.,0.999940054601015,0.999940054601015,
1.),(1.,0.999940054601015,0.999940054601015,1.)))
REPRESENTATION_ITEM('')
SURFACE()
);
#1796=(
BOUNDED_SURFACE()
B_SPLINE_SURFACE(3,3,((#130680,#130681,#130682,#130683),(#130684,#130685,
#130686,#130687),(#130688,#130689,#130690,#130691),(#130692,#130693,#130694,
#130695)),.UNSPECIFIED.,.F.,.F.,.F.)
B_SPLINE_SURFACE_WITH_KNOTS((4,4),(4,4),(0.847948974964019,0.924153056993776),
(0.,1.),.UNSPECIFIED.)
GEOMETRIC_REPRESENTATION_ITEM()
RATIONAL_B_SPLINE_SURFACE(((1.,0.999905914043422,0.999905914043422,1.),
(1.,0.999905914043422,0.999905914043422,1.),(1.,0.999905914043422,0.999905914043422,
1.),(1.,0.999905914043422,0.999905914043422,1.)))
REPRESENTATION_ITEM('')
SURFACE()
);
#1797=(
BOUNDED_SURFACE()
B_SPLINE_SURFACE(3,3,((#130697,#130698,#130699,#130700),(#130701,#130702,
#130703,#130704),(#130705,#130706,#130707,#130708),(#130709,#130710,#130711,
#130712)),.UNSPECIFIED.,.F.,.F.,.F.)
B_SPLINE_SURFACE_WITH_KNOTS((4,4),(4,4),(0.320522498194537,0.37138906164921),
(0.,1.),.UNSPECIFIED.)
GEOMETRIC_REPRESENTATION_ITEM()
RATIONAL_B_SPLINE_SURFACE(((1.,0.999967455651376,0.999967455651376,1.),
(1.,0.999967455651376,0.999967455651376,1.),(1.,0.999967455651376,0.999967455651376,
1.),(1.,0.999967455651376,0.999967455651376,1.)))
REPRESENTATION_ITEM('')
SURFACE()
);
#1798=(
BOUNDED_SURFACE()
B_SPLINE_SURFACE(3,3,((#130714,#130715,#130716,#130717),(#130718,#130719,
#130720,#130721),(#130722,#130723,#130724,#130725),(#130726,#130727,#130728,
#130729)),.UNSPECIFIED.,.F.,.F.,.F.)
B_SPLINE_SURFACE_WITH_KNOTS((4,4),(4,4),(0.485106664599375,0.537873353821538),
(0.,1.),.UNSPECIFIED.)
GEOMETRIC_REPRESENTATION_ITEM()
RATIONAL_B_SPLINE_SURFACE(((1.,0.999962124007028,0.999962124007028,1.),
(1.,0.999962124007028,0.999962124007028,1.),(1.,0.999962124007028,0.999962124007028,
1.),(1.,0.999962124007028,0.999962124007028,1.)))
REPRESENTATION_ITEM('')
SURFACE()
);
#1799=(
BOUNDED_SURFACE()
B_SPLINE_SURFACE(3,3,((#130731,#130732,#130733,#130734),(#130735,#130736,
#130737,#130738),(#130739,#130740,#130741,#130742),(#130743,#130744,#130745,
#130746)),.UNSPECIFIED.,.F.,.F.,.F.)
B_SPLINE_SURFACE_WITH_KNOTS((4,4),(4,4),(0.675463196603712,0.739005452081438),
(0.,1.),.UNSPECIFIED.)
GEOMETRIC_REPRESENTATION_ITEM()
RATIONAL_B_SPLINE_SURFACE(((1.,0.999940012325831,0.999940012325831,1.),
(1.,0.999940012325831,0.999940012325831,1.),(1.,0.999940012325831,0.999940012325831,
1.),(1.,0.999940012325831,0.999940012325831,1.)))
REPRESENTATION_ITEM('')
SURFACE()
);
#1800=(
BOUNDED_SURFACE()
B_SPLINE_SURFACE(3,3,((#130748,#130749,#130750,#130751),(#130752,#130753,
#130754,#130755),(#130756,#130757,#130758,#130759),(#130760,#130761,#130762,
#130763)),.UNSPECIFIED.,.F.,.F.,.F.)
B_SPLINE_SURFACE_WITH_KNOTS((4,4),(4,4),(0.847961069051777,0.924267936729202),
(0.,1.),.UNSPECIFIED.)
GEOMETRIC_REPRESENTATION_ITEM()
RATIONAL_B_SPLINE_SURFACE(((1.,0.999906371282588,0.999906371282588,1.),
(1.,0.999906371282588,0.999906371282588,1.),(1.,0.999906371282588,0.999906371282588,
1.),(1.,0.999906371282588,0.999906371282588,1.)))
REPRESENTATION_ITEM('')
SURFACE()
);
#1801=(
BOUNDED_SURFACE()
B_SPLINE_SURFACE(3,3,((#130765,#130766,#130767,#130768),(#130769,#130770,
#130771,#130772),(#130773,#130774,#130775,#130776),(#130777,#130778,#130779,
#130780)),.UNSPECIFIED.,.F.,.F.,.F.)
B_SPLINE_SURFACE_WITH_KNOTS((4,4),(4,4),(0.320531188332224,0.371363614789913),
(0.,1.),.UNSPECIFIED.)
GEOMETRIC_REPRESENTATION_ITEM()
RATIONAL_B_SPLINE_SURFACE(((1.,0.999967376576078,0.999967376576078,1.),
(1.,0.999967376576078,0.999967376576078,1.),(1.,0.999967376576078,0.999967376576078,
1.),(1.,0.999967376576078,0.999967376576078,1.)))
REPRESENTATION_ITEM('')
SURFACE()
);
#1802=(
BOUNDED_SURFACE()
B_SPLINE_SURFACE(3,3,((#130782,#130783,#130784,#130785),(#130786,#130787,
#130788,#130789),(#130790,#130791,#130792,#130793),(#130794,#130795,#130796,
#130797)),.UNSPECIFIED.,.F.,.F.,.F.)
B_SPLINE_SURFACE_WITH_KNOTS((4,4),(4,4),(0.485078772666084,0.537867979489318),
(0.,1.),.UNSPECIFIED.)
GEOMETRIC_REPRESENTATION_ITEM()
RATIONAL_B_SPLINE_SURFACE(((1.,0.999962406883938,0.999962406883938,1.),
(1.,0.999962406883938,0.999962406883938,1.),(1.,0.999962406883938,0.999962406883938,
1.),(1.,0.999962406883938,0.999962406883938,1.)))
REPRESENTATION_ITEM('')
SURFACE()
);
#1803=(
BOUNDED_SURFACE()
B_SPLINE_SURFACE(3,3,((#130799,#130800,#130801,#130802),(#130803,#130804,
#130805,#130806),(#130807,#130808,#130809,#130810),(#130811,#130812,#130813,
#130814)),.UNSPECIFIED.,.F.,.F.,.F.)
B_SPLINE_SURFACE_WITH_KNOTS((4,4),(4,4),(0.675482427883467,0.739033730461373),
(0.,1.),.UNSPECIFIED.)
GEOMETRIC_REPRESENTATION_ITEM()
RATIONAL_B_SPLINE_SURFACE(((1.,0.999940312318114,0.999940312318114,1.),
(1.,0.999940312318114,0.999940312318114,1.),(1.,0.999940312318114,0.999940312318114,
1.),(1.,0.999940312318114,0.999940312318114,1.)))
REPRESENTATION_ITEM('')
SURFACE()
);
#1804=(
BOUNDED_SURFACE()
B_SPLINE_SURFACE(3,3,((#130816,#130817,#130818,#130819),(#130820,#130821,
#130822,#130823),(#130824,#130825,#130826,#130827),(#130828,#130829,#130830,
#130831)),.UNSPECIFIED.,.F.,.F.,.F.)
B_SPLINE_SURFACE_WITH_KNOTS((4,4),(4,4),(0.848015663369457,0.924242408791934),
(0.,1.),.UNSPECIFIED.)
GEOMETRIC_REPRESENTATION_ITEM()
RATIONAL_B_SPLINE_SURFACE(((1.,0.999905933188592,0.999905933188592,1.),
(1.,0.999905933188592,0.999905933188592,1.),(1.,0.999905933188592,0.999905933188592,
1.),(1.,0.999905933188592,0.999905933188592,1.)))
REPRESENTATION_ITEM('')
SURFACE()
);
#1805=(
BOUNDED_SURFACE()
B_SPLINE_SURFACE(3,3,((#130833,#130834,#130835,#130836),(#130837,#130838,
#130839,#130840),(#130841,#130842,#130843,#130844),(#130845,#130846,#130847,
#130848)),.UNSPECIFIED.,.F.,.F.,.F.)
B_SPLINE_SURFACE_WITH_KNOTS((4,4),(4,4),(0.320515186267197,0.371414001692915),
(0.,1.),.UNSPECIFIED.)
GEOMETRIC_REPRESENTATION_ITEM()
RATIONAL_B_SPLINE_SURFACE(((1.,0.999967299513002,0.999967299513002,1.),
(1.,0.999967299513002,0.999967299513002,1.),(1.,0.999967299513002,0.999967299513002,
1.),(1.,0.999967299513002,0.999967299513002,1.)))
REPRESENTATION_ITEM('')
SURFACE()
);
#1806=(
BOUNDED_SURFACE()
B_SPLINE_SURFACE(3,3,((#130850,#130851,#130852,#130853),(#130854,#130855,
#130856,#130857),(#130858,#130859,#130860,#130861),(#130862,#130863,#130864,
#130865)),.UNSPECIFIED.,.F.,.F.,.F.)
B_SPLINE_SURFACE_WITH_KNOTS((4,4),(4,4),(0.485104001865671,0.537883970557087),
(0.,1.),.UNSPECIFIED.)
GEOMETRIC_REPRESENTATION_ITEM()
RATIONAL_B_SPLINE_SURFACE(((1.,0.999962204175861,0.999962204175861,1.),
(1.,0.999962204175861,0.999962204175861,1.),(1.,0.999962204175861,0.999962204175861,
1.),(1.,0.999962204175861,0.999962204175861,1.)))
REPRESENTATION_ITEM('')
SURFACE()
);
#1807=(
BOUNDED_SURFACE()
B_SPLINE_SURFACE(3,3,((#130867,#130868,#130869,#130870),(#130871,#130872,
#130873,#130874),(#130875,#130876,#130877,#130878),(#130879,#130880,#130881,
#130882)),.UNSPECIFIED.,.F.,.F.,.F.)
B_SPLINE_SURFACE_WITH_KNOTS((4,4),(4,4),(0.675472893615401,0.738995723881163),
(0.,1.),.UNSPECIFIED.)
GEOMETRIC_REPRESENTATION_ITEM()
RATIONAL_B_SPLINE_SURFACE(((1.,0.999940268417788,0.999940268417788,1.),
(1.,0.999940268417788,0.999940268417788,1.),(1.,0.999940268417788,0.999940268417788,
1.),(1.,0.999940268417788,0.999940268417788,1.)))
REPRESENTATION_ITEM('')
SURFACE()
);
#1808=B_SPLINE_CURVE_WITH_KNOTS('',3,(#65625,#65626,#65627,#65628,#65629,
#65630,#65631,#65632,#65633,#65634,#65635,#65636,#65637,#65638,#65639,#65640,
#65641,#65642,#65643,#65644,#65645),.UNSPECIFIED.,.F.,.F.,(4,2,2,2,2,2,
2,2,3,4),(-0.301207075635748,-0.262710648076985,-0.224963089028706,-0.187920887348923,
-0.151298118741226,-0.114507144214601,-0.0770611386627541,-0.0389186460799617,
0.,0.000154759158804522),.UNSPECIFIED.);
#1809=B_SPLINE_CURVE_WITH_KNOTS('',3,(#65648,#65649,#65650,#65651,#65652,
#65653,#65654,#65655,#65656,#65657,#65658,#65659,#65660,#65661,#65662,#65663,
#65664,#65665,#65666,#65667,#65668,#65669,#65670,#65671,#65672,#65673,#65674,
#65675,#65676,#65677,#65678,#65679,#65680,#65681,#65682,#65683),
 .UNSPECIFIED.,.T.,.F.,(4,2,2,2,2,2,2,2,2,2,2,2,2,2,2,2,2,4),(0.,0.0355202696276814,
0.0730229242192624,0.109881947978595,0.147332215352117,0.185244244852364,
0.223245130807779,0.259644256147526,0.294838797511801,0.330228485407574,
0.366554345821638,0.404791218300025,0.442165216596553,0.480056587425708,
0.518291371447407,0.552548743077857,0.58852966840272,0.599949959198704),
 .UNSPECIFIED.);
#1810=B_SPLINE_CURVE_WITH_KNOTS('',3,(#65684,#65685,#65686,#65687,#65688,
#65689,#65690,#65691,#65692,#65693,#65694,#65695,#65696,#65697,#65698,#65699,
#65700,#65701,#65702,#65703),.UNSPECIFIED.,.F.,.F.,(4,2,2,2,2,2,2,2,2,4),
(0.000154759158804522,0.0372889614373737,0.0752199300055963,0.112924529730869,
0.149859365579758,0.187155736640999,0.224850670418274,0.262646502930588,
0.300853550272872,0.301114086264827),.UNSPECIFIED.);
#1811=B_SPLINE_CURVE_WITH_KNOTS('',3,(#65709,#65710,#65711,#65712,#65713,
#65714,#65715,#65716,#65717,#65718,#65719,#65720,#65721,#65722,#65723,#65724,
#65725,#65726,#65727,#65728,#65729,#65730,#65731,#65732,#65733,#65734,#65735,
#65736,#65737,#65738,#65739,#65740,#65741,#65742),.UNSPECIFIED.,.T.,.F.,
(4,2,2,2,2,2,2,2,2,2,2,2,2,2,2,2,4),(-0.31764321474939,-0.297585218798245,
-0.277672851988763,-0.258107799080609,-0.238754678175866,-0.21934156864919,
-0.199630721249192,-0.179486526168813,-0.159056300074024,-0.13875563311955,
-0.118621969325576,-0.0989972178555827,-0.0795589853250667,-0.0601192898607882,
-0.040316055511345,-0.0202331842178355,0.),.UNSPECIFIED.);
#1812=B_SPLINE_CURVE_WITH_KNOTS('',3,(#65746,#65747,#65748,#65749,#65750,
#65751,#65752,#65753,#65754,#65755,#65756,#65757,#65758,#65759,#65760,#65761,
#65762,#65763,#65764,#65765),.UNSPECIFIED.,.F.,.F.,(4,2,2,2,2,2,2,2,2,4),
(-0.322456793629602,-0.321930945694818,-0.281120714431957,-0.240874004386435,
-0.200756138465722,-0.160810087223787,-0.12089229981328,-0.0807982385809383,
-0.0404605678798725,-5.67197663269965E-6),.UNSPECIFIED.);
#1813=B_SPLINE_CURVE_WITH_KNOTS('',3,(#65768,#65769,#65770,#65771,#65772,
#65773,#65774,#65775,#65776,#65777,#65778,#65779,#65780,#65781,#65782,#65783,
#65784,#65785,#65786,#65787,#65788,#65789,#65790,#65791,#65792,#65793,#65794,
#65795,#65796,#65797,#65798,#65799,#65800,#65801,#65802,#65803),
 .UNSPECIFIED.,.T.,.F.,(4,2,2,2,2,2,2,2,2,2,2,2,2,2,2,2,2,4),(0.,0.0399541104209996,
0.0799101633968203,0.120042188030658,0.160349494009884,0.200700062460061,
0.240669149748206,0.281146928547698,0.321688268052451,0.361827692829584,
0.401937446248238,0.441912733331546,0.482224630786286,0.523014478227826,
0.563360237934725,0.603655558776063,0.623959945525968,0.644496878439197),
 .UNSPECIFIED.);
#1814=B_SPLINE_CURVE_WITH_KNOTS('',3,(#65804,#65805,#65806,#65807,#65808,
#65809,#65810,#65811,#65812,#65813,#65814,#65815,#65816,#65817,#65818,#65819,
#65820,#65821,#65822,#65823,#65824),.UNSPECIFIED.,.F.,.F.,(4,3,2,2,2,2,
2,2,2,4),(-5.67197663269965E-6,0.,0.0395310619276315,0.0803390393793353,
0.120710239662218,0.161056371560083,0.201562793815772,0.242068779839465,
0.282414440590624,0.322260650653274),.UNSPECIFIED.);
#1815=B_SPLINE_CURVE_WITH_KNOTS('',3,(#65830,#65831,#65832,#65833,#65834,
#65835,#65836,#65837,#65838,#65839,#65840,#65841,#65842,#65843,#65844,#65845,
#65846,#65847,#65848,#65849,#65850,#65851,#65852,#65853,#65854,#65855,#65856,
#65857,#65858,#65859,#65860,#65861,#65862,#65863),.UNSPECIFIED.,.T.,.F.,
(4,2,2,2,2,2,2,2,2,2,2,2,2,2,2,2,4),(-0.315589981954352,-0.297256657266753,
-0.277538667548594,-0.257873603172813,-0.238278181150012,-0.218708538295045,
-0.199094835855894,-0.179399406131129,-0.159642486979386,-0.139670907982114,
-0.119619104317766,-0.0996819381389054,-0.0797621233342936,-0.0598091169008165,
-0.039854339317345,-0.0199328473099917,0.),.UNSPECIFIED.);
#1816=B_SPLINE_CURVE_WITH_KNOTS('',3,(#65867,#65868,#65869,#65870,#65871,
#65872,#65873,#65874,#65875,#65876,#65877,#65878,#65879,#65880,#65881,#65882,
#65883,#65884,#65885,#65886,#65887,#65888,#65889),.UNSPECIFIED.,.F.,.F.,
(4,2,2,2,2,2,2,2,2,3,4),(-0.301165935385473,-0.300788234391116,-0.262281544053756,
-0.22421926833655,-0.186818821875507,-0.15004770924054,-0.113427897963337,
-0.0763613905919923,-0.0385473925034182,0.,0.000181127945344951),
 .UNSPECIFIED.);
#1817=B_SPLINE_CURVE_WITH_KNOTS('',3,(#65892,#65893,#65894,#65895,#65896,
#65897,#65898,#65899,#65900,#65901,#65902,#65903,#65904,#65905,#65906,#65907,
#65908,#65909,#65910,#65911,#65912,#65913,#65914,#65915,#65916,#65917,#65918,
#65919,#65920,#65921,#65922,#65923,#65924,#65925,#65926,#65927),
 .UNSPECIFIED.,.T.,.F.,(4,2,2,2,2,2,2,2,2,2,2,2,2,2,2,2,2,4),(0.,0.0355202696276384,
0.0730229242190651,0.109881947978276,0.14733221535191,0.18524424485214,
0.223245130807427,0.259644256147236,0.294838797511598,0.330228485407464,
0.366554345821612,0.4047912183001,0.442165216596848,0.480056587426246,0.518291371448191,
0.552548743078774,0.588529668403866,0.599949959199946),.UNSPECIFIED.);
#1818=B_SPLINE_CURVE_WITH_KNOTS('',3,(#65928,#65929,#65930,#65931,#65932,
#65933,#65934,#65935,#65936,#65937,#65938,#65939,#65940,#65941,#65942,#65943,
#65944,#65945),.UNSPECIFIED.,.F.,.F.,(4,2,2,2,2,2,2,2,4),(0.000181127945344951,
0.0376469167067535,0.0758399504044883,0.113626377029077,0.151312096065185,
0.18817171823677,0.225871250407431,0.263579914127532,0.301176733243773),
 .UNSPECIFIED.);
#1819=B_SPLINE_CURVE_WITH_KNOTS('',3,(#65951,#65952,#65953,#65954,#65955,
#65956,#65957,#65958,#65959,#65960,#65961,#65962,#65963,#65964,#65965,#65966,
#65967,#65968,#65969,#65970,#65971,#65972,#65973,#65974,#65975,#65976,#65977,
#65978,#65979,#65980,#65981,#65982,#65983,#65984),.UNSPECIFIED.,.T.,.F.,
(4,2,2,2,2,2,2,2,2,2,2,2,2,2,2,2,4),(-0.317651970798428,-0.29815178689123,
-0.277708377482877,-0.257961131709923,-0.238526287372716,-0.219184977021519,
-0.19965572209791,-0.179773340350517,-0.159321772514999,-0.13892751869627,
-0.118697905777899,-0.0986211371345974,-0.0791085006013058,-0.0596989356638533,
-0.0401874040480438,-0.0201536713619323,0.),.UNSPECIFIED.);
#1820=B_SPLINE_CURVE_WITH_KNOTS('',3,(#65988,#65989,#65990,#65991,#65992,
#65993,#65994,#65995,#65996,#65997,#65998,#65999,#66000,#66001,#66002,#66003,
#66004,#66005,#66006,#66007),.UNSPECIFIED.,.F.,.F.,(4,2,2,2,2,2,2,2,2,4),
(-0.322457248719835,-0.321529294029697,-0.281003068363887,-0.240747294879843,
-0.20053995746929,-0.160507771051919,-0.120603186514104,-0.0806274654213206,
-0.0404172639125648,-3.12966711858995E-5),.UNSPECIFIED.);
#1821=B_SPLINE_CURVE_WITH_KNOTS('',3,(#66010,#66011,#66012,#66013,#66014,
#66015,#66016,#66017,#66018,#66019,#66020,#66021,#66022,#66023,#66024,#66025,
#66026,#66027,#66028,#66029,#66030,#66031,#66032,#66033,#66034,#66035,#66036,
#66037,#66038,#66039,#66040,#66041,#66042,#66043,#66044,#66045),
 .UNSPECIFIED.,.T.,.F.,(4,2,2,2,2,2,2,2,2,2,2,2,2,2,2,2,2,4),(0.,0.0399541104211576,
0.0799101633974278,0.120042188031722,0.160349494011448,0.20070006246199,
0.240669149750381,0.281146928550143,0.321688268055072,0.361827692832458,
0.401937446251656,0.44191273333538,0.482224630790607,0.523014478232421,
0.563360237939489,0.603655558781071,0.623959945531265,0.644496878444614),
 .UNSPECIFIED.);
#1822=B_SPLINE_CURVE_WITH_KNOTS('',3,(#66046,#66047,#66048,#66049,#66050,
#66051,#66052,#66053,#66054,#66055,#66056,#66057,#66058,#66059,#66060,#66061,
#66062,#66063,#66064,#66065,#66066),.UNSPECIFIED.,.F.,.F.,(4,3,2,2,2,2,
2,2,2,4),(-3.12966711858995E-5,0.,0.0394735202592785,0.0806056751944302,
0.121148951974962,0.161462087232505,0.201894298596311,0.242442947719733,
0.282882236373443,0.322267164573172),.UNSPECIFIED.);
#1823=B_SPLINE_CURVE_WITH_KNOTS('',3,(#66072,#66073,#66074,#66075,#66076,
#66077,#66078,#66079,#66080,#66081,#66082,#66083,#66084,#66085,#66086,#66087,
#66088,#66089,#66090,#66091,#66092,#66093,#66094,#66095,#66096,#66097,#66098,
#66099,#66100,#66101,#66102,#66103,#66104,#66105),.UNSPECIFIED.,.T.,.F.,
(4,2,2,2,2,2,2,2,2,2,2,2,2,2,2,2,4),(-0.315593239578836,-0.297155229491326,
-0.277429616910152,-0.257728814722726,-0.238097547859077,-0.218523354285244,
-0.198942519291424,-0.179292718177143,-0.159563077843648,-0.139793456325068,
-0.119664685919836,-0.0996815350600369,-0.0797642526410489,-0.0598256812499414,
-0.0398597186100538,-0.0199163208441135,0.),.UNSPECIFIED.);
#1824=B_SPLINE_CURVE_WITH_KNOTS('',3,(#66109,#66110,#66111,#66112,#66113,
#66114,#66115,#66116,#66117,#66118,#66119,#66120,#66121,#66122,#66123,#66124,
#66125,#66126,#66127,#66128,#66129,#66130,#66131),.UNSPECIFIED.,.F.,.F.,
(4,2,2,2,2,2,2,2,2,3,4),(-0.301161917452386,-0.300838295583177,-0.262579133327298,
-0.223756342411398,-0.185991834148995,-0.14894433741301,-0.112334627077444,
-0.0755690315276266,-0.0381431397130738,0.,0.000141379885012664),
 .UNSPECIFIED.);
#1825=B_SPLINE_CURVE_WITH_KNOTS('',3,(#66134,#66135,#66136,#66137,#66138,
#66139,#66140,#66141,#66142,#66143,#66144,#66145,#66146,#66147,#66148,#66149,
#66150,#66151,#66152,#66153,#66154,#66155,#66156,#66157,#66158,#66159,#66160,
#66161,#66162,#66163,#66164,#66165,#66166,#66167,#66168,#66169),
 .UNSPECIFIED.,.T.,.F.,(4,2,2,2,2,2,2,2,2,2,2,2,2,2,2,2,2,4),(0.,0.035520269627735,
0.0730229242195194,0.109881947979011,0.147332215352631,0.185244244852754,
0.223245130808132,0.259644256148007,0.294838797512386,0.330228485408292,
0.366554345822388,0.404791218300835,0.442165216597801,0.480056587427053,
0.518291371449001,0.552548743079509,0.588529668404388,0.599949959200391),
 .UNSPECIFIED.);
#1826=B_SPLINE_CURVE_WITH_KNOTS('',3,(#66170,#66171,#66172,#66173,#66174,
#66175,#66176,#66177,#66178,#66179,#66180,#66181,#66182,#66183,#66184,#66185,
#66186,#66187),.UNSPECIFIED.,.F.,.F.,(4,2,2,2,2,2,2,2,4),(0.000141379885012664,
0.0375906403896581,0.0761417945336856,0.114138356543264,0.151831601486628,
0.188756872156502,0.226035096963817,0.263685590536988,0.301167081091413),
 .UNSPECIFIED.);
#1827=B_SPLINE_CURVE_WITH_KNOTS('',3,(#66193,#66194,#66195,#66196,#66197,
#66198,#66199,#66200,#66201,#66202,#66203,#66204,#66205,#66206,#66207,#66208,
#66209,#66210,#66211,#66212,#66213,#66214,#66215,#66216,#66217,#66218,#66219,
#66220,#66221,#66222,#66223,#66224,#66225,#66226),.UNSPECIFIED.,.T.,.F.,
(4,2,2,2,2,2,2,2,2,2,2,2,2,2,2,2,4),(-0.317642803625192,-0.297848684457,
-0.277420857385532,-0.257494471404098,-0.237922107431991,-0.218574026097491,
-0.199176141984307,-0.179480980704758,-0.159354591123693,-0.138883902901578,
-0.118529867925916,-0.0983635747576582,-0.0787362066700163,-0.0593026472197343,
-0.0398721579205076,-0.0200860310405472,0.),.UNSPECIFIED.);
#1828=B_SPLINE_CURVE_WITH_KNOTS('',3,(#66230,#66231,#66232,#66233,#66234,
#66235,#66236,#66237,#66238,#66239,#66240,#66241,#66242,#66243,#66244,#66245,
#66246,#66247,#66248,#66249,#66250,#66251,#66252),.UNSPECIFIED.,.F.,.F.,
(4,2,2,2,2,2,2,2,2,3,4),(-0.322302397770585,-0.321865205480829,-0.281475562271467,
-0.240625403307893,-0.200376862230115,-0.160259298530777,-0.120320752093,
-0.0804184780332567,-0.0403383378354368,0.,0.000100255797653548),
 .UNSPECIFIED.);
#1829=B_SPLINE_CURVE_WITH_KNOTS('',3,(#66255,#66256,#66257,#66258,#66259,
#66260,#66261,#66262,#66263,#66264,#66265,#66266,#66267,#66268,#66269,#66270,
#66271,#66272,#66273,#66274,#66275,#66276,#66277,#66278,#66279,#66280,#66281,
#66282,#66283,#66284,#66285,#66286,#66287,#66288,#66289,#66290),
 .UNSPECIFIED.,.T.,.F.,(4,2,2,2,2,2,2,2,2,2,2,2,2,2,2,2,2,4),(0.,0.0399541104210705,
0.0799101633969787,0.120042188030797,0.160349494010289,0.200700062460403,
0.240669149748371,0.281146928547758,0.321688268052559,0.361827692829776,
0.401937446248424,0.441912733331591,0.482224630786227,0.523014478227558,
0.56336023793413,0.603655558775227,0.623959945525105,0.64449687843833),
 .UNSPECIFIED.);
#1830=B_SPLINE_CURVE_WITH_KNOTS('',3,(#66291,#66292,#66293,#66294,#66295,
#66296,#66297,#66298,#66299,#66300,#66301,#66302,#66303,#66304,#66305,#66306,
#66307,#66308),.UNSPECIFIED.,.F.,.F.,(4,2,2,2,2,2,2,2,4),(0.000100255797653548,
0.0395671716758544,0.0800121271978018,0.120938471359253,0.16136281430439,
0.201675954298304,0.242101002732803,0.282537408146094,0.322421957479456),
 .UNSPECIFIED.);
#1831=B_SPLINE_CURVE_WITH_KNOTS('',3,(#66314,#66315,#66316,#66317,#66318,
#66319,#66320,#66321,#66322,#66323,#66324,#66325,#66326,#66327,#66328,#66329,
#66330,#66331,#66332,#66333,#66334,#66335,#66336,#66337,#66338,#66339,#66340,
#66341,#66342,#66343,#66344,#66345,#66346,#66347),.UNSPECIFIED.,.T.,.F.,
(4,2,2,2,2,2,2,2,2,2,2,2,2,2,2,2,4),(-0.315594444981776,-0.297150257709209,
-0.277089673960405,-0.257371001063089,-0.237708755743781,-0.218118780490078,
-0.198554739122427,-0.178943293168605,-0.159244534976724,-0.139480293177502,
-0.119705544795745,-0.0996065223937357,-0.0796463317455234,-0.0597393894595519,
-0.0398237825108839,-0.019905987916103,0.),.UNSPECIFIED.);
#1832=B_SPLINE_CURVE_WITH_KNOTS('',3,(#66351,#66352,#66353,#66354,#66355,
#66356,#66357,#66358,#66359,#66360,#66361,#66362,#66363,#66364,#66365,#66366,
#66367,#66368,#66369,#66370,#66371,#66372,#66373),.UNSPECIFIED.,.F.,.F.,
(4,2,2,2,2,2,2,2,2,3,4),(-0.301138647978451,-0.300148980683225,-0.262187460405049,
-0.223694248594581,-0.185606204515038,-0.148180061349361,-0.111404035321645,
-0.0748077387741857,-0.0377816370688137,0.,9.36180134758838E-5),
 .UNSPECIFIED.);
#1833=B_SPLINE_CURVE_WITH_KNOTS('',3,(#66376,#66377,#66378,#66379,#66380,
#66381,#66382,#66383,#66384,#66385,#66386,#66387,#66388,#66389,#66390,#66391,
#66392,#66393,#66394,#66395,#66396,#66397,#66398,#66399,#66400,#66401,#66402,
#66403,#66404,#66405,#66406,#66407,#66408,#66409,#66410,#66411),
 .UNSPECIFIED.,.T.,.F.,(4,2,2,2,2,2,2,2,2,2,2,2,2,2,2,2,2,4),(0.,0.0355202696276501,
0.0730229242191375,0.109881947978365,0.147332215351896,0.185244244852142,
0.223245130807564,0.259644256147409,0.294838797511695,0.330228485407438,
0.366554345821406,0.404791218299827,0.442165216596728,0.48005658742597,
0.518291371447828,0.552548743078327,0.588529668403252,0.599949959199292),
 .UNSPECIFIED.);
#1834=B_SPLINE_CURVE_WITH_KNOTS('',3,(#66412,#66413,#66414,#66415,#66416,
#66417,#66418,#66419,#66420,#66421,#66422,#66423,#66424,#66425,#66426,#66427,
#66428,#66429),.UNSPECIFIED.,.F.,.F.,(4,2,2,2,2,2,2,2,4),(9.36180134758838E-5,
0.0374299437225984,0.0762103935681948,0.114435762991268,0.152233330864938,
0.189908215887392,0.226754855658746,0.264441309346417,0.301150344435867),
 .UNSPECIFIED.);
#1835=B_SPLINE_CURVE_WITH_KNOTS('',3,(#66435,#66436,#66437,#66438,#66439,
#66440,#66441,#66442,#66443,#66444,#66445,#66446,#66447,#66448,#66449,#66450,
#66451,#66452,#66453,#66454,#66455,#66456,#66457,#66458,#66459,#66460,#66461,
#66462,#66463,#66464,#66465,#66466,#66467,#66468),.UNSPECIFIED.,.T.,.F.,
(4,2,2,2,2,2,2,2,2,2,2,2,2,2,2,2,4),(-0.317624209562258,-0.298289597345508,
-0.277972697831312,-0.257527888571395,-0.237763251490301,-0.218322761768441,
-0.198992662014899,-0.179486146547689,-0.159624742417884,-0.139172721329641,
-0.118765873430163,-0.0985217268535809,-0.0784385072884339,-0.0589223902968011,
-0.0395209714294252,-0.0200261862458832,0.),.UNSPECIFIED.);
#1836=B_SPLINE_CURVE_WITH_KNOTS('',3,(#66472,#66473,#66474,#66475,#66476,
#66477,#66478,#66479,#66480,#66481,#66482,#66483,#66484,#66485,#66486,#66487,
#66488,#66489,#66490,#66491,#66492,#66493,#66494),.UNSPECIFIED.,.F.,.F.,
(4,2,2,2,2,2,2,2,2,3,4),(-0.322297560764302,-0.321398021306828,-0.281085553827047,
-0.240561930877692,-0.200304325379963,-0.16008994753857,-0.120052587150318,
-0.0801539535150511,-0.0401950225836323,0.,7.70459312222638E-5),
 .UNSPECIFIED.);
#1837=B_SPLINE_CURVE_WITH_KNOTS('',3,(#66497,#66498,#66499,#66500,#66501,
#66502,#66503,#66504,#66505,#66506,#66507,#66508,#66509,#66510,#66511,#66512,
#66513,#66514,#66515,#66516,#66517,#66518,#66519,#66520,#66521,#66522,#66523,
#66524,#66525,#66526,#66527,#66528,#66529,#66530,#66531,#66532),
 .UNSPECIFIED.,.T.,.F.,(4,2,2,2,2,2,2,2,2,2,2,2,2,2,2,2,2,4),(0.,0.0399541104210288,
0.0799101633969753,0.120042188031154,0.160349494011009,0.200700062461553,
0.240669149749968,0.281146928549773,0.321688268054745,0.361827692832095,
0.401937446251242,0.441912733335269,0.482224630790471,0.523014478232509,
0.563360237939814,0.603655558781587,0.623959945531849,0.644496878445225),
 .UNSPECIFIED.);
#1838=B_SPLINE_CURVE_WITH_KNOTS('',3,(#66533,#66534,#66535,#66536,#66537,
#66538,#66539,#66540,#66541,#66542,#66543,#66544,#66545,#66546,#66547,#66548,
#66549,#66550),.UNSPECIFIED.,.F.,.F.,(4,2,2,2,2,2,2,2,4),(7.70459312222638E-5,
0.0397955677791879,0.0802687034398072,0.121068716980965,0.161667866029956,
0.201985897549818,0.242384262176046,0.282897418235116,0.322422982766503),
 .UNSPECIFIED.);
#1839=B_SPLINE_CURVE_WITH_KNOTS('',3,(#66556,#66557,#66558,#66559,#66560,
#66561,#66562,#66563,#66564,#66565,#66566,#66567,#66568,#66569,#66570,#66571,
#66572,#66573,#66574,#66575,#66576,#66577,#66578,#66579,#66580,#66581,#66582,
#66583,#66584,#66585,#66586,#66587,#66588,#66589),.UNSPECIFIED.,.T.,.F.,
(4,2,2,2,2,2,2,2,2,2,2,2,2,2,2,2,4),(-0.315594596112197,-0.297212238945519,
-0.277244382715483,-0.257516629840736,-0.237813342886634,-0.218181203303342,
-0.198609433310666,-0.179033482143113,-0.159387625583977,-0.139657909631806,
-0.119884576737678,-0.0997305737884784,-0.0797274953574875,-0.0598072340293335,
-0.0398813658942522,-0.0199326208918523,0.),.UNSPECIFIED.);
#1840=B_SPLINE_CURVE_WITH_KNOTS('',3,(#66593,#66594,#66595,#66596,#66597,
#66598,#66599,#66600,#66601,#66602,#66603,#66604,#66605,#66606,#66607,#66608,
#66609,#66610,#66611,#66612,#66613,#66614,#66615),.UNSPECIFIED.,.F.,.F.,
(4,2,2,2,2,2,2,2,2,3,4),(-0.301061346698403,-0.300154233107256,-0.262390271276384,
-0.224265876054378,-0.185595957927573,-0.147776554844827,-0.110684741630273,
-0.0740733635944757,-0.0373547309855255,0.,9.9963037913639E-5),
 .UNSPECIFIED.);
#1841=B_SPLINE_CURVE_WITH_KNOTS('',3,(#66618,#66619,#66620,#66621,#66622,
#66623,#66624,#66625,#66626,#66627,#66628,#66629,#66630,#66631,#66632,#66633,
#66634,#66635,#66636,#66637,#66638,#66639,#66640,#66641,#66642,#66643,#66644,
#66645,#66646,#66647,#66648,#66649,#66650,#66651,#66652,#66653),
 .UNSPECIFIED.,.T.,.F.,(4,2,2,2,2,2,2,2,2,2,2,2,2,2,2,2,2,4),(0.,0.0355202696277959,
0.0730229242197281,0.109881947979451,0.14733221535353,0.185244244854458,
0.223245130810672,0.259644256151418,0.294838797516899,0.330228485413916,
0.366554345829066,0.404791218309081,0.442165216607522,0.480056587438502,
0.518291371462249,0.552548743094609,0.588529668421804,0.59994995921808),
 .UNSPECIFIED.);
#1842=B_SPLINE_CURVE_WITH_KNOTS('',3,(#66654,#66655,#66656,#66657,#66658,
#66659,#66660,#66661,#66662,#66663,#66664,#66665,#66666,#66667,#66668,#66669,
#66670,#66671),.UNSPECIFIED.,.F.,.F.,(4,2,2,2,2,2,2,2,4),(9.9963037913639E-5,
0.0375956597039427,0.0765101512186815,0.114950962752918,0.152884443087743,
0.190596119807599,0.227522757249408,0.264361209646464,0.301167798081618),
 .UNSPECIFIED.);
#1843=B_SPLINE_CURVE_WITH_KNOTS('',3,(#66677,#66678,#66679,#66680,#66681,
#66682,#66683,#66684,#66685,#66686,#66687,#66688,#66689,#66690,#66691,#66692,
#66693,#66694,#66695,#66696,#66697,#66698,#66699,#66700,#66701,#66702,#66703,
#66704,#66705,#66706,#66707,#66708,#66709,#66710),.UNSPECIFIED.,.T.,.F.,
(4,2,2,2,2,2,2,2,2,2,2,2,2,2,2,2,4),(-0.317595599740568,-0.297703490970376,
-0.277509143763147,-0.257154452491718,-0.237202102860055,-0.217609159241214,
-0.198259786702619,-0.178882547663072,-0.159219940579443,-0.139111795431245,
-0.118694444304224,-0.0983996654619764,-0.0782652805385247,-0.0586175735931439,
-0.0391812471909454,-0.0197681563368876,0.),.UNSPECIFIED.);
#1844=B_SPLINE_CURVE_WITH_KNOTS('',3,(#66714,#66715,#66716,#66717,#66718,
#66719,#66720,#66721,#66722,#66723,#66724,#66725,#66726,#66727,#66728,#66729,
#66730,#66731,#66732,#66733,#66734,#66735,#66736),.UNSPECIFIED.,.F.,.F.,
(4,2,2,2,2,2,2,2,2,3,4),(-0.322354039166853,-0.321726786837625,-0.28131793661759,
-0.241002699918155,-0.200356598490939,-0.160084029752791,-0.119921696599811,
-0.0799481541673699,-0.0400452631944034,0.,7.17856074681361E-6),
 .UNSPECIFIED.);
#1845=B_SPLINE_CURVE_WITH_KNOTS('',3,(#66739,#66740,#66741,#66742,#66743,
#66744,#66745,#66746,#66747,#66748,#66749,#66750,#66751,#66752,#66753,#66754,
#66755,#66756,#66757,#66758,#66759,#66760,#66761,#66762,#66763,#66764,#66765,
#66766,#66767,#66768,#66769,#66770,#66771,#66772,#66773,#66774),
 .UNSPECIFIED.,.T.,.F.,(4,2,2,2,2,2,2,2,2,2,2,2,2,2,2,2,2,4),(0.,0.0399541104211525,
0.0799101633973132,0.120042188031252,0.160349494010639,0.200700062460746,
0.24066914974878,0.281146928548183,0.321688268052773,0.361827692829693,
0.401937446248195,0.441912733331337,0.482224630785847,0.523014478227025,
0.563360237933407,0.603655558774048,0.623959945523888,0.644496878437146),
 .UNSPECIFIED.);
#1846=B_SPLINE_CURVE_WITH_KNOTS('',3,(#66775,#66776,#66777,#66778,#66779,
#66780,#66781,#66782,#66783,#66784,#66785,#66786,#66787,#66788,#66789,#66790,
#66791,#66792),.UNSPECIFIED.,.F.,.F.,(4,2,2,2,2,2,2,2,4),(7.17856074681361E-6,
0.0390237938020301,0.0794667944515802,0.120295929995562,0.16108166723615,
0.201434585894493,0.241793385121914,0.282373009958602,0.322362267042215),
 .UNSPECIFIED.);
#1847=B_SPLINE_CURVE_WITH_KNOTS('',3,(#66798,#66799,#66800,#66801,#66802,
#66803,#66804,#66805,#66806,#66807,#66808,#66809,#66810,#66811,#66812,#66813,
#66814,#66815,#66816,#66817,#66818,#66819,#66820,#66821,#66822,#66823,#66824,
#66825,#66826,#66827,#66828,#66829,#66830,#66831),.UNSPECIFIED.,.T.,.F.,
(4,2,2,2,2,2,2,2,2,2,2,2,2,2,2,2,4),(-0.315594622373487,-0.297533870662118,
-0.277622157510714,-0.257651723875446,-0.237921713542688,-0.218237311660376,
-0.198628601130043,-0.179061340536985,-0.159464238093167,-0.139788278396831,
-0.120041716967774,-0.0998694200192435,-0.0798494940937937,-0.0599296759610903,
-0.0399990336273364,-0.0200054074132563,0.),.UNSPECIFIED.);
#1848=B_SPLINE_CURVE_WITH_KNOTS('',3,(#66835,#66836,#66837,#66838,#66839,
#66840,#66841,#66842,#66843,#66844,#66845,#66846,#66847,#66848,#66849,#66850,
#66851,#66852,#66853,#66854),.UNSPECIFIED.,.F.,.F.,(4,2,2,2,2,2,2,2,2,4),
(-0.301147961624379,-0.300062316631199,-0.262394637047186,-0.224420968944876,
-0.185887448097902,-0.1477829056142,-0.110335991047362,-0.0735563535339244,
-0.036984133703636,-4.35690811094724E-5),.UNSPECIFIED.);
#1849=B_SPLINE_CURVE_WITH_KNOTS('',3,(#66857,#66858,#66859,#66860,#66861,
#66862,#66863,#66864,#66865,#66866,#66867,#66868,#66869,#66870,#66871,#66872,
#66873,#66874,#66875,#66876,#66877,#66878,#66879,#66880,#66881,#66882,#66883,
#66884,#66885,#66886,#66887,#66888,#66889,#66890,#66891,#66892),
 .UNSPECIFIED.,.T.,.F.,(4,2,2,2,2,2,2,2,2,2,2,2,2,2,2,2,2,4),(0.,0.0355202696275203,
0.0730229242186996,0.109881947977571,0.147332215350384,0.185244244849724,
0.223245130804017,0.259644256142594,0.294838797505521,0.330228485399748,
0.366554345812062,0.40479121828863,0.442165216583351,0.48005658741036,0.518291371429938,
0.552548743058257,0.588529668380768,0.599949959176512),.UNSPECIFIED.);
#1850=B_SPLINE_CURVE_WITH_KNOTS('',3,(#66893,#66894,#66895,#66896,#66897,
#66898,#66899,#66900,#66901,#66902,#66903,#66904,#66905,#66906,#66907,#66908,
#66909,#66910,#66911,#66912,#66913),.UNSPECIFIED.,.F.,.F.,(4,3,2,2,2,2,
2,2,2,4),(-4.35690811094724E-5,0.,0.0365327773178391,0.0750112777319575,
0.113889864865708,0.152210652521084,0.190038882754267,0.227668024742707,
0.264502667827508,0.301030361353156),.UNSPECIFIED.);
#1851=B_SPLINE_CURVE_WITH_KNOTS('',3,(#66919,#66920,#66921,#66922,#66923,
#66924,#66925,#66926,#66927,#66928,#66929,#66930,#66931,#66932,#66933,#66934,
#66935,#66936,#66937,#66938,#66939,#66940,#66941,#66942,#66943,#66944,#66945,
#66946,#66947,#66948,#66949,#66950,#66951,#66952),.UNSPECIFIED.,.T.,.F.,
(4,2,2,2,2,2,2,2,2,2,2,2,2,2,2,2,4),(-0.31757151244209,-0.298332728669395,
-0.27818234576115,-0.2578362591579,-0.23736096878236,-0.217588804779534,
-0.198148148450172,-0.178828387511107,-0.159338797938639,-0.139491768304976,
-0.119229310805976,-0.098777940027667,-0.078489708879422,-0.0583916924149346,
-0.0388763803889898,-0.0194825025044759,0.),.UNSPECIFIED.);
#1852=B_SPLINE_CURVE_WITH_KNOTS('',3,(#66956,#66957,#66958,#66959,#66960,
#66961,#66962,#66963,#66964,#66965,#66966,#66967,#66968,#66969,#66970,#66971,
#66972,#66973,#66974,#66975),.UNSPECIFIED.,.F.,.F.,(4,2,2,2,2,2,2,2,2,4),
(-0.322405728416197,-0.321546706061062,-0.281198364753022,-0.2408951979842,
-0.200323869063384,-0.160069256043837,-0.119861454351153,-0.0798327506359469,
-0.0399463257727349,-5.45498490094123E-5),.UNSPECIFIED.);
#1853=B_SPLINE_CURVE_WITH_KNOTS('',3,(#66978,#66979,#66980,#66981,#66982,
#66983,#66984,#66985,#66986,#66987,#66988,#66989,#66990,#66991,#66992,#66993,
#66994,#66995,#66996,#66997,#66998,#66999,#67000,#67001,#67002,#67003,#67004,
#67005,#67006,#67007,#67008,#67009,#67010,#67011,#67012,#67013),
 .UNSPECIFIED.,.T.,.F.,(4,2,2,2,2,2,2,2,2,2,2,2,2,2,2,2,2,4),(0.,0.0399541104209913,
0.0799101633967558,0.120042188030517,0.1603494940098,0.200700062459717,
0.240669149747544,0.281146928546853,0.321688268051145,0.361827692827755,
0.401937446246095,0.4419127333289,0.482224630783017,0.523014478224009,0.563360237930216,
0.603655558770796,0.623959945520647,0.644496878433936),.UNSPECIFIED.);
#1854=B_SPLINE_CURVE_WITH_KNOTS('',3,(#67014,#67015,#67016,#67017,#67018,
#67019,#67020,#67021,#67022,#67023,#67024,#67025,#67026,#67027,#67028,#67029,
#67030,#67031,#67032,#67033,#67034),.UNSPECIFIED.,.F.,.F.,(4,3,2,2,2,2,
2,2,2,4),(-5.45498490094123E-5,0.,0.0396635395521475,0.080088963912866,
0.12057975818371,0.161389406329886,0.202107242285931,0.242444716121441,
0.282765523937027,0.322306952019563),.UNSPECIFIED.);
#1855=B_SPLINE_CURVE_WITH_KNOTS('',3,(#67040,#67041,#67042,#67043,#67044,
#67045,#67046,#67047,#67048,#67049,#67050,#67051,#67052,#67053,#67054,#67055,
#67056,#67057,#67058,#67059,#67060,#67061,#67062,#67063,#67064,#67065,#67066,
#67067,#67068,#67069,#67070,#67071,#67072,#67073),.UNSPECIFIED.,.T.,.F.,
(4,2,2,2,2,2,2,2,2,2,2,2,2,2,2,2,4),(-0.315593063776311,-0.29700803323264,
-0.277101906790985,-0.25710555612465,-0.237377416904486,-0.217678261420823,
-0.198052738861469,-0.178487401632928,-0.158914692523433,-0.139266634878621,
-0.119529894293757,-0.0997490751108272,-0.0797713096896962,-0.05971623206454,
-0.0397855249884807,-0.0198939142348958,0.),.UNSPECIFIED.);
#1856=B_SPLINE_CURVE_WITH_KNOTS('',3,(#67077,#67078,#67079,#67080,#67081,
#67082,#67083,#67084,#67085,#67086,#67087,#67088,#67089,#67090,#67091,#67092,
#67093,#67094,#67095,#67096),.UNSPECIFIED.,.F.,.F.,(4,2,2,2,2,2,2,2,2,4),
(-0.301118946487766,-0.300527485838102,-0.262862138850157,-0.22510653196151,
-0.186960746251741,-0.148254876835345,-0.110408214249886,-0.0732924492929095,
-0.0366839954349046,-4.93896356226975E-5),.UNSPECIFIED.);
#1857=B_SPLINE_CURVE_WITH_KNOTS('',3,(#67099,#67100,#67101,#67102,#67103,
#67104,#67105,#67106,#67107,#67108,#67109,#67110,#67111,#67112,#67113,#67114,
#67115,#67116,#67117,#67118,#67119,#67120,#67121,#67122,#67123,#67124,#67125,
#67126,#67127,#67128,#67129,#67130,#67131,#67132,#67133,#67134),
 .UNSPECIFIED.,.T.,.F.,(4,2,2,2,2,2,2,2,2,2,2,2,2,2,2,2,2,4),(0.,0.0355202696277843,
0.0730229242196146,0.10988194797903,0.147332215352703,0.185244244852949,
0.223245130808307,0.25964425614813,0.294838797512346,0.330228485408035,
0.366554345822135,0.404791218300662,0.442165216597325,0.480056587426433,
0.51829137144813,0.552548743078511,0.588529668403261,0.599949959199294),
 .UNSPECIFIED.);
#1858=B_SPLINE_CURVE_WITH_KNOTS('',3,(#67135,#67136,#67137,#67138,#67139,
#67140,#67141,#67142,#67143,#67144,#67145,#67146,#67147,#67148,#67149,#67150,
#67151,#67152,#67153,#67154,#67155),.UNSPECIFIED.,.F.,.F.,(4,3,2,2,2,2,
2,2,2,4),(-4.93896356226975E-5,0.,0.0365695267012744,0.074616322225757,
0.113601961148227,0.152149562549399,0.190151155062694,0.227853759249584,
0.264779511262172,0.301013530103241),.UNSPECIFIED.);
#1859=B_SPLINE_CURVE_WITH_KNOTS('',3,(#67161,#67162,#67163,#67164,#67165,
#67166,#67167,#67168,#67169,#67170,#67171,#67172,#67173,#67174,#67175,#67176,
#67177,#67178,#67179,#67180,#67181,#67182,#67183,#67184,#67185,#67186,#67187,
#67188,#67189,#67190,#67191,#67192,#67193,#67194),.UNSPECIFIED.,.T.,.F.,
(4,2,2,2,2,2,2,2,2,2,2,2,2,2,2,2,4),(-0.317551766644571,-0.298486525081855,
-0.278428882026584,-0.258221088221274,-0.237842005071232,-0.217867604593861,
-0.198254586659461,-0.178902478996899,-0.159544153524827,-0.139911897737489,
-0.119838709236774,-0.0993894180525655,-0.0790440450201523,-0.0588750365855975,
-0.0388400330894688,-0.0194039455565196,0.),.UNSPECIFIED.);
#1860=B_SPLINE_CURVE_WITH_KNOTS('',3,(#67198,#67199,#67200,#67201,#67202,
#67203,#67204,#67205,#67206,#67207,#67208,#67209,#67210,#67211,#67212,#67213,
#67214,#67215,#67216,#67217),.UNSPECIFIED.,.F.,.F.,(4,2,2,2,2,2,2,2,2,4),
(-0.322355554522363,-0.322178904200381,-0.281704619582365,-0.241356636912598,
-0.201005058459337,-0.16025826339261,-0.119996742027504,-0.0798488072456165,
-0.0398898126128195,-2.20474994749807E-6),.UNSPECIFIED.);
#1861=B_SPLINE_CURVE_WITH_KNOTS('',3,(#67220,#67221,#67222,#67223,#67224,
#67225,#67226,#67227,#67228,#67229,#67230,#67231,#67232,#67233,#67234,#67235,
#67236,#67237,#67238,#67239,#67240,#67241,#67242,#67243,#67244,#67245,#67246,
#67247,#67248,#67249,#67250,#67251,#67252,#67253,#67254,#67255),
 .UNSPECIFIED.,.T.,.F.,(4,2,2,2,2,2,2,2,2,2,2,2,2,2,2,2,2,4),(0.,0.0399541104211012,
0.0799101633971579,0.120042188031192,0.160349494010781,0.200700062461153,
0.240669149749436,0.281146928549182,0.321688268054342,0.361827692831924,
0.401937446250896,0.441912733334278,0.482224630789236,0.523014478230996,
0.563360237938004,0.603655558779501,0.623959945529625,0.644496878442948),
 .UNSPECIFIED.);
#1862=B_SPLINE_CURVE_WITH_KNOTS('',3,(#67256,#67257,#67258,#67259,#67260,
#67261,#67262,#67263,#67264,#67265,#67266,#67267,#67268,#67269,#67270,#67271,
#67272,#67273,#67274,#67275,#67276),.UNSPECIFIED.,.F.,.F.,(4,3,2,2,2,2,
2,2,2,4),(-2.20474994749807E-6,0.,0.0391360015106571,0.0794317419925186,
0.119897010292482,0.160355079753466,0.201332782499759,0.241783415181495,
0.282097330185288,0.32235683326756),.UNSPECIFIED.);
#1863=B_SPLINE_CURVE_WITH_KNOTS('',3,(#67282,#67283,#67284,#67285,#67286,
#67287,#67288,#67289,#67290,#67291,#67292,#67293,#67294,#67295,#67296,#67297,
#67298,#67299,#67300,#67301,#67302,#67303,#67304,#67305,#67306,#67307,#67308,
#67309,#67310,#67311,#67312,#67313,#67314,#67315),.UNSPECIFIED.,.T.,.F.,
(4,2,2,2,2,2,2,2,2,2,2,2,2,2,2,2,4),(-0.315592915588056,-0.297157230115009,
-0.277242481766554,-0.257314550571046,-0.237282993015635,-0.217557856490286,
-0.197884126696601,-0.178286261599438,-0.158724647806166,-0.139124925349899,
-0.119439049162832,-0.0996807653366323,-0.0799033227642352,-0.0598016412664598,
-0.0398382198951536,-0.0199265333829655,0.),.UNSPECIFIED.);
#1864=B_SPLINE_CURVE_WITH_KNOTS('',3,(#67319,#67320,#67321,#67322,#67323,
#67324,#67325,#67326,#67327,#67328,#67329,#67330,#67331,#67332,#67333,#67334,
#67335,#67336,#67337,#67338),.UNSPECIFIED.,.F.,.F.,(4,2,2,2,2,2,2,2,2,4),
(-0.301058381607661,-0.300695934659419,-0.263083586410712,-0.225429745929767,
-0.187495787142987,-0.149014527999422,-0.110874845528449,-0.0733724375687369,
-0.0365583584387441,-2.17004182293026E-6),.UNSPECIFIED.);
#1865=B_SPLINE_CURVE_WITH_KNOTS('',3,(#67341,#67342,#67343,#67344,#67345,
#67346,#67347,#67348,#67349,#67350,#67351,#67352,#67353,#67354,#67355,#67356,
#67357,#67358,#67359,#67360,#67361,#67362,#67363,#67364,#67365,#67366,#67367,
#67368,#67369,#67370,#67371,#67372,#67373,#67374,#67375,#67376),
 .UNSPECIFIED.,.T.,.F.,(4,2,2,2,2,2,2,2,2,2,2,2,2,2,2,2,2,4),(0.,0.0355202696277563,
0.0730229242195573,0.109881947979313,0.147332215353586,0.185244244854587,
0.223245130811004,0.259644256151833,0.294838797517268,0.330228485414355,
0.366554345829942,0.404791218310431,0.442165216609281,0.480056587440684,
0.518291371464912,0.552548743097934,0.588529668425773,0.599949959222132),
 .UNSPECIFIED.);
#1866=B_SPLINE_CURVE_WITH_KNOTS('',3,(#67377,#67378,#67379,#67380,#67381,
#67382,#67383,#67384,#67385,#67386,#67387,#67388,#67389,#67390,#67391,#67392,
#67393,#67394,#67395,#67396,#67397),.UNSPECIFIED.,.F.,.F.,(4,3,2,2,2,2,
2,2,2,4),(-2.17004182293026E-6,0.,0.0357498274067009,0.0734077363203498,
0.111837190993789,0.150741885695325,0.189101783842794,0.226953230384565,
0.264585676093243,0.301058061735977),.UNSPECIFIED.);
#1867=B_SPLINE_CURVE_WITH_KNOTS('',3,(#67403,#67404,#67405,#67406,#67407,
#67408,#67409,#67410,#67411,#67412,#67413,#67414,#67415,#67416,#67417,#67418,
#67419,#67420,#67421,#67422,#67423,#67424,#67425,#67426,#67427,#67428,#67429,
#67430,#67431,#67432,#67433,#67434,#67435,#67436),.UNSPECIFIED.,.T.,.F.,
(4,2,2,2,2,2,2,2,2,2,2,2,2,2,2,2,4),(-0.31754433338207,-0.298803281332166,
-0.278807800538721,-0.258673081016315,-0.238343826302372,-0.217876028762562,
-0.19807748660554,-0.178620027297595,-0.159304922169407,-0.139840169793005,
-0.120023736794459,-0.0997855989498413,-0.0793300681815676,-0.0590301788462695,
-0.0389218783466252,-0.0193925721148871,0.),.UNSPECIFIED.);
#1868=B_SPLINE_CURVE_WITH_KNOTS('',3,(#67440,#67441,#67442,#67443,#67444,
#67445,#67446,#67447,#67448,#67449,#67450,#67451,#67452,#67453,#67454,#67455,
#67456,#67457,#67458,#67459),.UNSPECIFIED.,.F.,.F.,(4,2,2,2,2,2,2,2,2,4),
(-0.322354756361963,-0.322205918870643,-0.281689949818391,-0.241237699113221,
-0.20092186741425,-0.160456629709274,-0.120204465960691,-0.0799716249211841,
-0.039906809364872,-5.39397368838195E-6),.UNSPECIFIED.);
#1869=B_SPLINE_CURVE_WITH_KNOTS('',3,(#67462,#67463,#67464,#67465,#67466,
#67467,#67468,#67469,#67470,#67471,#67472,#67473,#67474,#67475,#67476,#67477,
#67478,#67479,#67480,#67481,#67482,#67483,#67484,#67485,#67486,#67487,#67488,
#67489,#67490,#67491,#67492,#67493,#67494,#67495,#67496,#67497),
 .UNSPECIFIED.,.T.,.F.,(4,2,2,2,2,2,2,2,2,2,2,2,2,2,2,2,2,4),(0.,0.0399541104210428,
0.0799101633969861,0.120042188031056,0.160349494010698,0.200700062460998,
0.240669149749349,0.281146928549081,0.321688268054021,0.361827692831356,
0.401937446250295,0.44191273333395,0.482224630789036,0.52301447823097,0.563360237938078,
0.603655558779622,0.623959945529193,0.644496878442225),.UNSPECIFIED.);
#1870=B_SPLINE_CURVE_WITH_KNOTS('',3,(#67498,#67499,#67500,#67501,#67502,
#67503,#67504,#67505,#67506,#67507,#67508,#67509,#67510,#67511,#67512,#67513,
#67514,#67515,#67516,#67517,#67518),.UNSPECIFIED.,.F.,.F.,(4,3,2,2,2,2,
2,2,2,4),(-5.39397368838195E-6,0.,0.0393075887039707,0.0794597964783887,
0.119850067157852,0.160325694985967,0.201138041009554,0.241798684361789,
0.282127159463835,0.322359660598591),.UNSPECIFIED.);
#1871=B_SPLINE_CURVE_WITH_KNOTS('',3,(#67524,#67525,#67526,#67527,#67528,
#67529,#67530,#67531,#67532,#67533,#67534,#67535,#67536,#67537,#67538,#67539,
#67540,#67541,#67542,#67543,#67544,#67545,#67546,#67547,#67548,#67549,#67550,
#67551,#67552,#67553,#67554,#67555,#67556,#67557),.UNSPECIFIED.,.T.,.F.,
(4,2,2,2,2,2,2,2,2,2,2,2,2,2,2,2,4),(-0.315593410768126,-0.29754747075378,
-0.277605746518463,-0.257690189723362,-0.237736453581343,-0.217652321280653,
-0.197942437206122,-0.178301549934773,-0.15872624759116,-0.139155513391519,
-0.119520099622689,-0.099798701851234,-0.080027130270589,-0.0598618542633545,
-0.0398484241333443,-0.0199251752696053,0.),.UNSPECIFIED.);
#1872=B_SPLINE_CURVE_WITH_KNOTS('',3,(#67561,#67562,#67563,#67564,#67565,
#67566,#67567,#67568,#67569,#67570,#67571,#67572,#67573,#67574,#67575,#67576,
#67577,#67578,#67579,#67580,#67581),.UNSPECIFIED.,.F.,.F.,(4,2,2,2,2,2,
2,2,3,4),(-0.300978142018712,-0.263914525329246,-0.226284750703183,-0.188545296544232,
-0.150403990415101,-0.111688584966917,-0.0737943243144371,-0.0366264406025384,
0.,8.00110665434538E-5),.UNSPECIFIED.);
#1873=B_SPLINE_CURVE_WITH_KNOTS('',3,(#67584,#67585,#67586,#67587,#67588,
#67589,#67590,#67591,#67592,#67593,#67594,#67595,#67596,#67597,#67598,#67599,
#67600,#67601,#67602,#67603,#67604,#67605,#67606,#67607,#67608,#67609,#67610,
#67611,#67612,#67613,#67614,#67615,#67616,#67617,#67618,#67619),
 .UNSPECIFIED.,.T.,.F.,(4,2,2,2,2,2,2,2,2,2,2,2,2,2,2,2,2,4),(0.,0.0355202696274643,
0.0730229242183205,0.109881947976405,0.147332215348248,0.185244244846206,
0.223245130798705,0.259644256135453,0.294838797496282,0.330228485388232,
0.366554345798093,0.404791218271537,0.442165216563109,0.480056587386566,
0.518291371402324,0.55254874302685,0.58852966834476,0.599949959139978),
 .UNSPECIFIED.);
#1874=B_SPLINE_CURVE_WITH_KNOTS('',3,(#67620,#67621,#67622,#67623,#67624,
#67625,#67626,#67627,#67628,#67629,#67630,#67631,#67632,#67633,#67634,#67635,
#67636,#67637,#67638,#67639),.UNSPECIFIED.,.F.,.F.,(4,2,2,2,2,2,2,2,2,4),
(8.00110665434538E-5,0.0353108547782378,0.0725312692972248,0.110518938547593,
0.149564323404323,0.188222355253345,0.226307975094044,0.264023560479495,
0.300970351665515,0.301144794938351),.UNSPECIFIED.);
#1875=B_SPLINE_CURVE_WITH_KNOTS('',3,(#67645,#67646,#67647,#67648,#67649,
#67650,#67651,#67652,#67653,#67654,#67655,#67656,#67657,#67658,#67659,#67660,
#67661,#67662,#67663,#67664,#67665,#67666,#67667,#67668,#67669,#67670,#67671,
#67672,#67673,#67674,#67675,#67676,#67677,#67678),.UNSPECIFIED.,.T.,.F.,
(4,2,2,2,2,2,2,2,2,2,2,2,2,2,2,2,4),(-0.31754678186458,-0.298854543535332,
-0.279132590217806,-0.25908366028776,-0.238869461524636,-0.218473096805952,
-0.198477657185613,-0.17884202633409,-0.159481005232111,-0.140133917139174,
-0.120526215304075,-0.100546056505587,-0.0800747095050212,-0.0596878946432227,
-0.0394856419211679,-0.019444442213569,0.),.UNSPECIFIED.);
#1876=B_SPLINE_CURVE_WITH_KNOTS('',3,(#67682,#67683,#67684,#67685,#67686,
#67687,#67688,#67689,#67690,#67691,#67692,#67693,#67694,#67695,#67696,#67697,
#67698,#67699),.UNSPECIFIED.,.F.,.F.,(4,2,2,2,2,2,2,2,4),(-0.322410599568958,
-0.282381736564621,-0.241782820187053,-0.201359211265473,-0.161045994561305,
-0.120443581321846,-0.0801730862382622,-0.0399924380800003,-6.45926737957721E-5),
 .UNSPECIFIED.);
#1877=B_SPLINE_CURVE_WITH_KNOTS('',3,(#67702,#67703,#67704,#67705,#67706,
#67707,#67708,#67709,#67710,#67711,#67712,#67713,#67714,#67715,#67716,#67717,
#67718,#67719,#67720,#67721,#67722,#67723,#67724,#67725,#67726,#67727,#67728,
#67729,#67730,#67731,#67732,#67733,#67734,#67735,#67736,#67737),
 .UNSPECIFIED.,.T.,.F.,(4,2,2,2,2,2,2,2,2,2,2,2,2,2,2,2,2,4),(0.,0.0399541104209861,
0.0799101633967313,0.120042188030496,0.160349494009841,0.200700062459914,
0.240669149747714,0.281146928546904,0.321688268051343,0.361827692828311,
0.401937446247057,0.441912733330249,0.482224630784895,0.523014478226398,
0.563360237933181,0.603655558774504,0.623959945523992,0.644496878437005),
 .UNSPECIFIED.);
#1878=B_SPLINE_CURVE_WITH_KNOTS('',3,(#67738,#67739,#67740,#67741,#67742,
#67743,#67744,#67745,#67746,#67747,#67748,#67749,#67750,#67751,#67752,#67753,
#67754,#67755,#67756,#67757,#67758,#67759,#67760),.UNSPECIFIED.,.F.,.F.,
(4,3,2,2,2,2,2,2,2,2,4),(-6.45926737957721E-5,0.,0.0390108812553356,0.0790243539467953,
0.119283184671902,0.159719989985786,0.200170808743092,0.241073441282928,
0.281478872292121,0.321809987466221,0.322307943731577),.UNSPECIFIED.);
#1879=B_SPLINE_CURVE_WITH_KNOTS('',3,(#67766,#67767,#67768,#67769,#67770,
#67771,#67772,#67773,#67774,#67775,#67776,#67777,#67778,#67779,#67780,#67781,
#67782,#67783,#67784,#67785,#67786,#67787,#67788,#67789,#67790,#67791,#67792,
#67793,#67794,#67795,#67796,#67797,#67798,#67799),.UNSPECIFIED.,.T.,.F.,
(4,2,2,2,2,2,2,2,2,2,2,2,2,2,2,2,4),(-0.31559325345182,-0.297317730854205,
-0.277323673584106,-0.257372580958333,-0.237457900008399,-0.217484430544864,
-0.197755119221471,-0.178067553902672,-0.158455097163848,-0.138887603657002,
-0.119294455824915,-0.0996233242918477,-0.0798789996652367,-0.0599063556623395,
-0.0398565846628778,-0.0199228180997341,0.),.UNSPECIFIED.);
#1880=B_SPLINE_CURVE_WITH_KNOTS('',3,(#67803,#67804,#67805,#67806,#67807,
#67808,#67809,#67810,#67811,#67812,#67813,#67814,#67815,#67816,#67817,#67818,
#67819,#67820,#67821,#67822,#67823,#67824,#67825),.UNSPECIFIED.,.F.,.F.,
(4,2,2,2,2,2,2,2,2,3,4),(-0.301050544014646,-0.300701045912431,-0.263849573346669,
-0.226560847894422,-0.188894701836328,-0.151018078542583,-0.112639483085741,
-0.0744561853366415,-0.0368753905065712,0.,7.74278383810611E-6),
 .UNSPECIFIED.);
#1881=B_SPLINE_CURVE_WITH_KNOTS('',3,(#67828,#67829,#67830,#67831,#67832,
#67833,#67834,#67835,#67836,#67837,#67838,#67839,#67840,#67841,#67842,#67843,
#67844,#67845,#67846,#67847,#67848,#67849,#67850,#67851,#67852,#67853,#67854,
#67855,#67856,#67857,#67858,#67859,#67860,#67861,#67862,#67863),
 .UNSPECIFIED.,.T.,.F.,(4,2,2,2,2,2,2,2,2,2,2,2,2,2,2,2,2,4),(0.,0.0355202696275411,
0.0730229242188105,0.10988194797803,0.147332215351439,0.185244244851336,
0.223245130806424,0.259644256145998,0.294838797510073,0.330228485405602,
0.366554345819332,0.404791218297467,0.442165216593924,0.480056587422867,
0.518291371444443,0.552548743074661,0.588529668399372,0.599949959195358),
 .UNSPECIFIED.);
#1882=B_SPLINE_CURVE_WITH_KNOTS('',3,(#67864,#67865,#67866,#67867,#67868,
#67869,#67870,#67871,#67872,#67873,#67874,#67875,#67876,#67877,#67878,#67879,
#67880,#67881),.UNSPECIFIED.,.F.,.F.,(4,2,2,2,2,2,2,2,4),(7.74278383810611E-6,
0.0358556004554429,0.0727165890303891,0.110307479935514,0.148690120729207,
0.187575552003323,0.225931327919466,0.263793633053924,0.301107698759479),
 .UNSPECIFIED.);
#1883=B_SPLINE_CURVE_WITH_KNOTS('',3,(#67887,#67888,#67889,#67890,#67891,
#67892,#67893,#67894,#67895,#67896,#67897,#67898,#67899,#67900,#67901,#67902,
#67903,#67904,#67905,#67906,#67907,#67908,#67909,#67910,#67911,#67912,#67913,
#67914,#67915,#67916,#67917,#67918,#67919,#67920),.UNSPECIFIED.,.T.,.F.,
(4,2,2,2,2,2,2,2,2,2,2,2,2,2,2,2,4),(-0.317562554188654,-0.298753170810319,
-0.279306735529762,-0.259305046894606,-0.239193146172324,-0.21890439655601,
-0.198468405269086,-0.178635579958314,-0.159150751579314,-0.139831347137531,
-0.120387634799293,-0.100604124620228,-0.0803902771831579,-0.0599545013953302,
-0.0396660633012328,-0.0195543258745943,0.),.UNSPECIFIED.);
#1884=B_SPLINE_CURVE_WITH_KNOTS('',3,(#67924,#67925,#67926,#67927,#67928,
#67929,#67930,#67931,#67932,#67933,#67934,#67935,#67936,#67937,#67938,#67939,
#67940,#67941),.UNSPECIFIED.,.F.,.F.,(4,2,2,2,2,2,2,2,4),(-0.322408809219383,
-0.282264936011648,-0.241770195002564,-0.201321774169933,-0.161005070722384,
-0.120554276389559,-0.0803107265542591,-0.0400757886480797,-8.3535166333862E-5),
 .UNSPECIFIED.);
#1885=B_SPLINE_CURVE_WITH_KNOTS('',3,(#67944,#67945,#67946,#67947,#67948,
#67949,#67950,#67951,#67952,#67953,#67954,#67955,#67956,#67957,#67958,#67959,
#67960,#67961,#67962,#67963,#67964,#67965,#67966,#67967,#67968,#67969,#67970,
#67971,#67972,#67973,#67974,#67975,#67976,#67977,#67978,#67979),
 .UNSPECIFIED.,.T.,.F.,(4,2,2,2,2,2,2,2,2,2,2,2,2,2,2,2,2,4),(0.,0.0399541104210371,
0.0799101633969276,0.120042188030811,0.160349494010247,0.200700062460135,
0.240669149748269,0.281146928547783,0.321688268052386,0.361827692829341,
0.401937446247806,0.441912733330861,0.48222463078534,0.5230144782264,0.563360237932858,
0.603655558773727,0.623959945523498,0.644496878436718),.UNSPECIFIED.);
#1886=B_SPLINE_CURVE_WITH_KNOTS('',3,(#67980,#67981,#67982,#67983,#67984,
#67985,#67986,#67987,#67988,#67989,#67990,#67991,#67992,#67993,#67994,#67995,
#67996,#67997,#67998,#67999,#68000,#68001,#68002),.UNSPECIFIED.,.F.,.F.,
(4,3,2,2,2,2,2,2,2,2,4),(-8.3535166333862E-5,0.,0.0393019758222067,0.0792300811977625,
0.119369024266062,0.159749636133907,0.200224937322439,0.241039083207198,
0.281753542603645,0.322095726126061,0.322313417546895),.UNSPECIFIED.);
#1887=B_SPLINE_CURVE_WITH_KNOTS('',3,(#68008,#68009,#68010,#68011,#68012,
#68013,#68014,#68015,#68016,#68017,#68018,#68019,#68020,#68021,#68022,#68023,
#68024,#68025,#68026,#68027,#68028,#68029,#68030,#68031,#68032,#68033,#68034,
#68035,#68036,#68037,#68038,#68039,#68040,#68041),.UNSPECIFIED.,.T.,.F.,
(4,2,2,2,2,2,2,2,2,2,2,2,2,2,2,2,4),(-0.315593216159719,-0.297386462000642,
-0.277445073116452,-0.257509675245072,-0.23759598204093,-0.217641702014589,
-0.197556079016382,-0.177846611841745,-0.158203876776851,-0.138626450407983,
-0.119055296324289,-0.0994213253944243,-0.0797018271356818,-0.0599314841789836,
-0.0399559588412318,-0.0199275817504349,0.),.UNSPECIFIED.);
#1888=B_SPLINE_CURVE_WITH_KNOTS('',3,(#68045,#68046,#68047,#68048,#68049,
#68050,#68051,#68052,#68053,#68054,#68055,#68056,#68057,#68058,#68059,#68060,
#68061,#68062),.UNSPECIFIED.,.F.,.F.,(4,2,2,2,2,2,2,2,4),(-0.301100921471536,
-0.264139472742094,-0.227310847047349,-0.18966289503287,-0.151936985647909,
-0.113847516176928,-0.0751904625710873,-0.0372387069697444,-4.04142026933364E-5),
 .UNSPECIFIED.);
#1889=B_SPLINE_CURVE_WITH_KNOTS('',3,(#68065,#68066,#68067,#68068,#68069,
#68070,#68071,#68072,#68073,#68074,#68075,#68076,#68077,#68078,#68079,#68080,
#68081,#68082,#68083,#68084,#68085,#68086,#68087,#68088,#68089,#68090,#68091,
#68092,#68093,#68094,#68095,#68096,#68097,#68098,#68099,#68100),
 .UNSPECIFIED.,.T.,.F.,(4,2,2,2,2,2,2,2,2,2,2,2,2,2,2,2,2,4),(0.,0.0355202696276432,
0.0730229242191987,0.10988194797855,0.14733221535206,0.185244244852172,
0.223245130807611,0.259644256147649,0.294838797512173,0.330228485408115,
0.366554345822225,0.404791218300779,0.442165216597644,0.48005658742687,
0.518291371448558,0.552548743079322,0.588529668404772,0.59994995920088),
 .UNSPECIFIED.);
#1890=B_SPLINE_CURVE_WITH_KNOTS('',3,(#68101,#68102,#68103,#68104,#68105,
#68106,#68107,#68108,#68109,#68110,#68111,#68112,#68113,#68114,#68115,#68116,
#68117,#68118,#68119,#68120,#68121,#68122,#68123),.UNSPECIFIED.,.F.,.F.,
(4,3,2,2,2,2,2,2,2,2,4),(-4.04142026933364E-5,0.,0.03615915200202,0.0727912610659081,
0.109971042269411,0.147916803776992,0.186554927423317,0.225238144277993,
0.263352588611955,0.301088646814997,0.301107134483528),.UNSPECIFIED.);
#1891=B_SPLINE_CURVE_WITH_KNOTS('',3,(#68129,#68130,#68131,#68132,#68133,
#68134,#68135,#68136,#68137,#68138,#68139,#68140,#68141,#68142,#68143,#68144,
#68145,#68146,#68147,#68148,#68149,#68150,#68151,#68152,#68153,#68154,#68155,
#68156,#68157,#68158,#68159,#68160,#68161,#68162),.UNSPECIFIED.,.T.,.F.,
(4,2,2,2,2,2,2,2,2,2,2,2,2,2,2,2,4),(-0.317584181788589,-0.298794557913286,
-0.279396413811771,-0.259685398425666,-0.239643320269254,-0.219448537685349,
-0.199071862622537,-0.179049482147542,-0.159380904563574,-0.140000463388759,
-0.120658150946535,-0.101075283083877,-0.0811229435079882,-0.0606564184644852,
-0.0402655107884883,-0.0200531994927753,0.),.UNSPECIFIED.);
#1892=B_SPLINE_CURVE_WITH_KNOTS('',3,(#68166,#68167,#68168,#68169,#68170,
#68171,#68172,#68173,#68174,#68175,#68176,#68177,#68178,#68179,#68180,#68181,
#68182,#68183),.UNSPECIFIED.,.F.,.F.,(4,2,2,2,2,2,2,2,4),(-0.322367453094563,
-0.282589671050591,-0.242222087757724,-0.201802504566437,-0.161472574115384,
-0.121132041451418,-0.0804114872777562,-0.0401588574067352,-6.49995567824529E-5),
 .UNSPECIFIED.);
#1893=B_SPLINE_CURVE_WITH_KNOTS('',3,(#68186,#68187,#68188,#68189,#68190,
#68191,#68192,#68193,#68194,#68195,#68196,#68197,#68198,#68199,#68200,#68201,
#68202,#68203,#68204,#68205,#68206,#68207,#68208,#68209,#68210,#68211,#68212,
#68213,#68214,#68215,#68216,#68217,#68218,#68219,#68220,#68221),
 .UNSPECIFIED.,.T.,.F.,(4,2,2,2,2,2,2,2,2,2,2,2,2,2,2,2,2,4),(0.,0.0399541104210577,
0.0799101633970396,0.120042188031162,0.160349494011025,0.200700062461786,
0.240669149750123,0.281146928549829,0.321688268054903,0.361827692832479,
0.401937446251727,0.441912733335557,0.482224630790908,0.523014478233397,
0.563360237941084,0.603655558783352,0.623959945533176,0.644496878446289),
 .UNSPECIFIED.);
#1894=B_SPLINE_CURVE_WITH_KNOTS('',3,(#68222,#68223,#68224,#68225,#68226,
#68227,#68228,#68229,#68230,#68231,#68232,#68233,#68234,#68235,#68236,#68237,
#68238,#68239,#68240,#68241,#68242,#68243,#68244),.UNSPECIFIED.,.F.,.F.,
(4,3,2,2,2,2,2,2,2,2,4),(-6.49995567824529E-5,0.,0.0390494216426324,0.0789385757792174,
0.118952328471186,0.159225359712887,0.199685658614001,0.240152451429887,
0.281286390433688,0.321830207846101,0.322355904221303),.UNSPECIFIED.);
#1895=B_SPLINE_CURVE_WITH_KNOTS('',3,(#68250,#68251,#68252,#68253,#68254,
#68255,#68256,#68257,#68258,#68259,#68260,#68261,#68262,#68263,#68264,#68265,
#68266,#68267,#68268,#68269,#68270,#68271,#68272,#68273,#68274,#68275,#68276,
#68277,#68278,#68279,#68280,#68281,#68282,#68283),.UNSPECIFIED.,.T.,.F.,
(4,2,2,2,2,2,2,2,2,2,2,2,2,2,2,2,4),(-0.315592124455107,-0.297184981883786,
-0.277286589738207,-0.257382966676634,-0.237485648421939,-0.217559378959289,
-0.19751848279024,-0.177796769809496,-0.158121997499943,-0.138520769293498,
-0.118957847887096,-0.0993605170780253,-0.0796782175625232,-0.0599216742760547,
-0.0401442832093851,-0.0199940413345806,0.),.UNSPECIFIED.);
#1896=B_SPLINE_CURVE_WITH_KNOTS('',3,(#68287,#68288,#68289,#68290,#68291,
#68292,#68293,#68294,#68295,#68296,#68297,#68298,#68299,#68300,#68301,#68302,
#68303,#68304),.UNSPECIFIED.,.F.,.F.,(4,2,2,2,2,2,2,2,4),(-0.301134002178748,
-0.264338890436258,-0.227452398713043,-0.190161791067931,-0.152441756292719,
-0.114634728995588,-0.0764184751015692,-0.0376670804260189,-7.69005437173066E-5),
 .UNSPECIFIED.);
#1897=B_SPLINE_CURVE_WITH_KNOTS('',3,(#68307,#68308,#68309,#68310,#68311,
#68312,#68313,#68314,#68315,#68316,#68317,#68318,#68319,#68320,#68321,#68322,
#68323,#68324,#68325,#68326,#68327,#68328,#68329,#68330,#68331,#68332,#68333,
#68334,#68335,#68336,#68337,#68338,#68339,#68340,#68341,#68342),
 .UNSPECIFIED.,.T.,.F.,(4,2,2,2,2,2,2,2,2,2,2,2,2,2,2,2,2,4),(0.,0.0355202696275121,
0.0730229242186736,0.109881947977543,0.147332215350511,0.185244244850115,
0.223245130804628,0.259644256143591,0.29483879750692,0.330228485401583,
0.366554345814411,0.404791218291486,0.442165216586747,0.480056587414318,
0.518291371434548,0.552548743063418,0.588529668386507,0.599949959182332),
 .UNSPECIFIED.);
#1898=B_SPLINE_CURVE_WITH_KNOTS('',3,(#68343,#68344,#68345,#68346,#68347,
#68348,#68349,#68350,#68351,#68352,#68353,#68354,#68355,#68356,#68357,#68358,
#68359,#68360,#68361,#68362,#68363,#68364,#68365),.UNSPECIFIED.,.F.,.F.,
(4,3,2,2,2,2,2,2,2,2,4),(-7.69005437173066E-5,0.,0.0360098100406934,0.0725977261367332,
0.109413926555899,0.146922956928712,0.185251849369556,0.224065827656858,
0.262360606682867,0.300207053497309,0.301127729713689),.UNSPECIFIED.);
#1899=B_SPLINE_CURVE_WITH_KNOTS('',3,(#68371,#68372,#68373,#68374,#68375,
#68376,#68377,#68378,#68379,#68380,#68381,#68382,#68383,#68384,#68385,#68386,
#68387,#68388,#68389,#68390,#68391,#68392,#68393,#68394,#68395,#68396,#68397,
#68398,#68399,#68400,#68401,#68402,#68403,#68404),.UNSPECIFIED.,.T.,.F.,
(4,2,2,2,2,2,2,2,2,2,2,2,2,2,2,2,4),(-0.317612772210092,-0.29817683215515,
-0.278761042396339,-0.259321595298189,-0.239494618350438,-0.219410736380407,
-0.199190916813444,-0.178820497886802,-0.158948070546673,-0.139427101945941,
-0.120094699680415,-0.100667107706439,-0.0809176240818496,-0.0607258855069793,
-0.0403404075805791,-0.0200982006130535,0.),.UNSPECIFIED.);
#1900=B_SPLINE_CURVE_WITH_KNOTS('',3,(#68408,#68409,#68410,#68411,#68412,
#68413,#68414,#68415,#68416,#68417,#68418,#68419,#68420,#68421,#68422,#68423,
#68424,#68425,#68426,#68427,#68428),.UNSPECIFIED.,.F.,.F.,(4,2,2,2,2,2,
2,2,3,4),(-0.322272493248835,-0.283311097305131,-0.242918471103494,-0.202337942338775,
-0.161792707575712,-0.121445031217079,-0.0810725197347086,-0.0402471007473572,
0.,8.22734960809895E-6),.UNSPECIFIED.);
#1901=B_SPLINE_CURVE_WITH_KNOTS('',3,(#68431,#68432,#68433,#68434,#68435,
#68436,#68437,#68438,#68439,#68440,#68441,#68442,#68443,#68444,#68445,#68446,
#68447,#68448,#68449,#68450,#68451,#68452,#68453,#68454,#68455,#68456,#68457,
#68458,#68459,#68460,#68461,#68462,#68463,#68464,#68465,#68466),
 .UNSPECIFIED.,.T.,.F.,(4,2,2,2,2,2,2,2,2,2,2,2,2,2,2,2,2,4),(0.,0.0399541104210513,
0.0799101633969759,0.120042188030928,0.160349494010625,0.200700062460617,
0.240669149748604,0.281146928548014,0.321688268052903,0.361827692830282,
0.401937446249133,0.441912733332665,0.482224630787743,0.523014478229303,
0.563360237936166,0.603655558777767,0.623959945527549,0.644496878440685),
 .UNSPECIFIED.);
#1902=B_SPLINE_CURVE_WITH_KNOTS('',3,(#68467,#68468,#68469,#68470,#68471,
#68472,#68473,#68474,#68475,#68476,#68477,#68478,#68479,#68480,#68481,#68482,
#68483,#68484,#68485,#68486),.UNSPECIFIED.,.F.,.F.,(4,2,2,2,2,2,2,2,2,4),
(8.22734960809895E-6,0.0388137442425556,0.0787567868575889,0.118683761763293,
0.158793716743972,0.19913884956911,0.239593065809621,0.280403847371113,
0.321081099617034,0.322446122896613),.UNSPECIFIED.);
#1903=B_SPLINE_CURVE_WITH_KNOTS('',3,(#68492,#68493,#68494,#68495,#68496,
#68497,#68498,#68499,#68500,#68501,#68502,#68503,#68504,#68505,#68506,#68507,
#68508,#68509,#68510,#68511,#68512,#68513,#68514,#68515,#68516,#68517,#68518,
#68519,#68520,#68521,#68522,#68523,#68524,#68525),.UNSPECIFIED.,.T.,.F.,
(4,2,2,2,2,2,2,2,2,2,2,2,2,2,2,2,4),(-0.315589991769754,-0.297543654155397,
-0.277607478676899,-0.257621899085537,-0.237642557654303,-0.21771469574947,
-0.197788689069841,-0.177759014798792,-0.158043966994748,-0.138388532458108,
-0.118799826628472,-0.0992263512383482,-0.0796005434512017,-0.0598945213917012,
-0.04013518410926,-0.0199929772862508,0.),.UNSPECIFIED.);
#1904=B_SPLINE_CURVE_WITH_KNOTS('',3,(#68529,#68530,#68531,#68532,#68533,
#68534,#68535,#68536,#68537,#68538,#68539,#68540,#68541,#68542,#68543,#68544,
#68545,#68546),.UNSPECIFIED.,.F.,.F.,(4,2,2,2,2,2,2,2,4),(-0.301156891144586,
-0.264547753021578,-0.226893649082149,-0.190048717511566,-0.152393534543418,
-0.114675560216569,-0.0766170892067709,-0.0379948570526523,-0.000119814599371271),
 .UNSPECIFIED.);
#1905=B_SPLINE_CURVE_WITH_KNOTS('',3,(#68549,#68550,#68551,#68552,#68553,
#68554,#68555,#68556,#68557,#68558,#68559,#68560,#68561,#68562,#68563,#68564,
#68565,#68566,#68567,#68568,#68569,#68570,#68571,#68572,#68573,#68574,#68575,
#68576,#68577,#68578,#68579,#68580,#68581,#68582,#68583,#68584),
 .UNSPECIFIED.,.T.,.F.,(4,2,2,2,2,2,2,2,2,2,2,2,2,2,2,2,2,4),(0.,0.0355202696278532,
0.0730229242199749,0.109881947980052,0.147332215354528,0.185244244855757,
0.223245130812486,0.259644256153658,0.294838797519483,0.330228485416982,
0.366554345832849,0.40479121831343,0.44216521661239,0.480056587444108,0.518291371468795,
0.552548743101786,0.588529668429641,0.599949959225988),.UNSPECIFIED.);
#1906=B_SPLINE_CURVE_WITH_KNOTS('',3,(#68585,#68586,#68587,#68588,#68589,
#68590,#68591,#68592,#68593,#68594,#68595,#68596,#68597,#68598,#68599,#68600,
#68601,#68602,#68603,#68604,#68605,#68606,#68607),.UNSPECIFIED.,.F.,.F.,
(4,3,2,2,2,2,2,2,2,2,4),(-0.000119814599371271,0.,0.0361408497492226,0.0728594924793139,
0.109485135803451,0.14661099959075,0.18449654911239,0.223091526309962,0.261828300698411,
0.299996368157121,0.301150010874056),.UNSPECIFIED.);
#1907=B_SPLINE_CURVE_WITH_KNOTS('',3,(#68613,#68614,#68615,#68616,#68617,
#68618,#68619,#68620,#68621,#68622,#68623,#68624,#68625,#68626,#68627,#68628,
#68629,#68630,#68631,#68632,#68633,#68634,#68635,#68636,#68637,#68638,#68639,
#68640,#68641,#68642,#68643,#68644,#68645,#68646),.UNSPECIFIED.,.T.,.F.,
(4,2,2,2,2,2,2,2,2,2,2,2,2,2,2,2,4),(-0.317634341816681,-0.298273465275683,
-0.278787654783001,-0.25938260516859,-0.239674569645085,-0.219635485556022,
-0.199447957928304,-0.179077235091592,-0.159038453352017,-0.139345729329634,
-0.119946990249479,-0.100601607582497,-0.0810308238562121,-0.06109602261861,
-0.0406271433249967,-0.0202254737216437,0.),.UNSPECIFIED.);
#1908=B_SPLINE_CURVE_WITH_KNOTS('',3,(#68650,#68651,#68652,#68653,#68654,
#68655,#68656,#68657,#68658,#68659,#68660,#68661,#68662,#68663,#68664,#68665,
#68666,#68667),.UNSPECIFIED.,.F.,.F.,(4,2,2,2,2,2,2,2,4),(-0.322263458289222,
-0.282900889548461,-0.242587226965438,-0.202121378962893,-0.161558213341175,
-0.121131727269642,-0.0808194109808987,-0.0402525098016497,-1.03876710068041E-5),
 .UNSPECIFIED.);
#1909=B_SPLINE_CURVE_WITH_KNOTS('',3,(#68670,#68671,#68672,#68673,#68674,
#68675,#68676,#68677,#68678,#68679,#68680,#68681,#68682,#68683,#68684,#68685,
#68686,#68687,#68688,#68689,#68690,#68691,#68692,#68693,#68694,#68695,#68696,
#68697,#68698,#68699,#68700,#68701,#68702,#68703,#68704,#68705),
 .UNSPECIFIED.,.T.,.F.,(4,2,2,2,2,2,2,2,2,2,2,2,2,2,2,2,2,4),(0.,0.0399541104210523,
0.0799101633969911,0.120042188030941,0.160349494010304,0.200700062459907,
0.240669149747547,0.281146928546813,0.321688268051475,0.361827692828482,
0.401937446246947,0.441912733330034,0.482224630784599,0.523014478226203,
0.563360237932926,0.603655558773891,0.623959945523787,0.644496878437038),
 .UNSPECIFIED.);
#1910=B_SPLINE_CURVE_WITH_KNOTS('',3,(#68706,#68707,#68708,#68709,#68710,
#68711,#68712,#68713,#68714,#68715,#68716,#68717,#68718,#68719,#68720,#68721,
#68722,#68723,#68724,#68725,#68726,#68727,#68728),.UNSPECIFIED.,.F.,.F.,
(4,3,2,2,2,2,2,2,2,2,4),(-1.03876710068041E-5,0.,0.0392625678077015,0.0792796756538265,
0.119187885161736,0.159187268402346,0.199422118099274,0.239844848466983,
0.280293454869346,0.321327404961611,0.322443487755003),.UNSPECIFIED.);
#1911=B_SPLINE_CURVE_WITH_KNOTS('',3,(#68734,#68735,#68736,#68737,#68738,
#68739,#68740,#68741,#68742,#68743,#68744,#68745,#68746,#68747,#68748,#68749,
#68750,#68751,#68752,#68753,#68754,#68755,#68756,#68757,#68758,#68759,#68760,
#68761,#68762,#68763,#68764,#68765,#68766,#68767),.UNSPECIFIED.,.T.,.F.,
(4,2,2,2,2,2,2,2,2,2,2,2,2,2,2,2,4),(-0.315584858250283,-0.297326864181455,
-0.27741097433004,-0.257461582863128,-0.237487701039889,-0.217544474680261,
-0.197628413501937,-0.177651504562011,-0.157929072796535,-0.138241416178837,
-0.118623507039874,-0.0990510100831163,-0.0794575655906757,-0.0597904016325671,
-0.0400512984940925,-0.0200862920905489,0.),.UNSPECIFIED.);
#1912=B_SPLINE_CURVE_WITH_KNOTS('',3,(#68771,#68772,#68773,#68774,#68775,
#68776,#68777,#68778,#68779,#68780,#68781,#68782,#68783,#68784,#68785,#68786,
#68787,#68788),.UNSPECIFIED.,.F.,.F.,(4,2,2,2,2,2,2,2,4),(-0.301172697629259,
-0.264933081927209,-0.227255014847489,-0.190345810670057,-0.152699661165205,
-0.115048750531758,-0.077207473536471,-0.0388798599000017,-0.000160983825265968),
 .UNSPECIFIED.);
#1913=B_SPLINE_CURVE_WITH_KNOTS('',3,(#68791,#68792,#68793,#68794,#68795,
#68796,#68797,#68798,#68799,#68800,#68801,#68802,#68803,#68804,#68805,#68806,
#68807,#68808,#68809,#68810,#68811,#68812,#68813,#68814,#68815,#68816,#68817,
#68818,#68819,#68820,#68821,#68822,#68823,#68824,#68825,#68826),
 .UNSPECIFIED.,.T.,.F.,(4,2,2,2,2,2,2,2,2,2,2,2,2,2,2,2,2,4),(0.,0.0355202696277295,
0.0730229242194867,0.109881947979006,0.147332215352552,0.185244244852634,
0.223245130807763,0.259644256147242,0.294838797511455,0.330228485407204,
0.366554345821095,0.404791218299421,0.44216521659611,0.480056587425235,
0.518291371446824,0.552548743077254,0.588529668402066,0.599949959198078),
 .UNSPECIFIED.);
#1914=B_SPLINE_CURVE_WITH_KNOTS('',3,(#68827,#68828,#68829,#68830,#68831,
#68832,#68833,#68834,#68835,#68836,#68837,#68838,#68839,#68840,#68841,#68842,
#68843,#68844,#68845,#68846,#68847,#68848,#68849),.UNSPECIFIED.,.F.,.F.,
(4,3,2,2,2,2,2,2,2,2,4),(-0.000160983825265968,0.,0.0358793027228612,0.0728886733477424,
0.10949360406576,0.14629244320943,0.183767821004726,0.2219434550389,0.260934846486396,
0.299438510889526,0.301156987828858),.UNSPECIFIED.);
#1915=B_SPLINE_CURVE_WITH_KNOTS('',3,(#68855,#68856,#68857,#68858,#68859,
#68860,#68861,#68862,#68863,#68864,#68865,#68866,#68867,#68868,#68869,#68870,
#68871,#68872,#68873,#68874,#68875,#68876,#68877,#68878,#68879,#68880,#68881,
#68882,#68883,#68884,#68885,#68886,#68887,#68888),.UNSPECIFIED.,.T.,.F.,
(4,2,2,2,2,2,2,2,2,2,2,2,2,2,2,2,4),(-0.317647719239506,-0.298200520794536,
-0.278596926941396,-0.25917026528438,-0.239726352873434,-0.21973739477608,
-0.199634745171728,-0.179348387513285,-0.158901547715117,-0.139020909227822,
-0.119487985266671,-0.100147621029955,-0.0807199456085233,-0.060975594285225,
-0.0408050752255367,-0.0203363613524164,0.),.UNSPECIFIED.);
#1916=B_SPLINE_CURVE_WITH_KNOTS('',3,(#68892,#68893,#68894,#68895,#68896,
#68897,#68898,#68899,#68900,#68901,#68902,#68903,#68904,#68905,#68906,#68907,
#68908,#68909),.UNSPECIFIED.,.F.,.F.,(4,2,2,2,2,2,2,2,4),(-0.322308096898006,
-0.283403399723437,-0.243105674074854,-0.202689452701646,-0.162028412209055,
-0.121388392100284,-0.0810028958206459,-0.0406912162856388,-6.69647710747405E-5),
 .UNSPECIFIED.);
#1917=B_SPLINE_CURVE_WITH_KNOTS('',3,(#68912,#68913,#68914,#68915,#68916,
#68917,#68918,#68919,#68920,#68921,#68922,#68923,#68924,#68925,#68926,#68927,
#68928,#68929,#68930,#68931,#68932,#68933,#68934,#68935,#68936,#68937,#68938,
#68939,#68940,#68941,#68942,#68943,#68944,#68945,#68946,#68947),
 .UNSPECIFIED.,.T.,.F.,(4,2,2,2,2,2,2,2,2,2,2,2,2,2,2,2,2,4),(0.,0.0399541104210872,
0.0799101633970701,0.120042188030963,0.160349494010509,0.200700062460821,
0.240669149749049,0.281146928548708,0.32168826805372,0.361827692831149,
0.401937446250155,0.441912733333774,0.482224630788839,0.523014478230791,
0.563360237937848,0.603655558779499,0.623959945529538,0.644496878442784),
 .UNSPECIFIED.);
#1918=B_SPLINE_CURVE_WITH_KNOTS('',3,(#68948,#68949,#68950,#68951,#68952,
#68953,#68954,#68955,#68956,#68957,#68958,#68959,#68960,#68961,#68962,#68963,
#68964,#68965,#68966,#68967,#68968,#68969,#68970),.UNSPECIFIED.,.F.,.F.,
(4,3,2,2,2,2,2,2,2,2,4),(-6.69647710747405E-5,0.,0.0389899751502963,0.0791272762346116,
0.119095234364202,0.159026497444346,0.199115825652264,0.239429199251524,
0.279858625606866,0.320661061518468,0.322378864463958),.UNSPECIFIED.);
#1919=B_SPLINE_CURVE_WITH_KNOTS('',3,(#68976,#68977,#68978,#68979,#68980,
#68981,#68982,#68983,#68984,#68985,#68986,#68987,#68988,#68989,#68990,#68991,
#68992,#68993,#68994,#68995,#68996,#68997,#68998,#68999,#69000,#69001,#69002,
#69003,#69004,#69005,#69006,#69007,#69008,#69009),.UNSPECIFIED.,.T.,.F.,
(4,2,2,2,2,2,2,2,2,2,2,2,2,2,2,2,4),(-0.315576748184792,-0.297053244765837,
-0.277151967701907,-0.257199189469323,-0.237571593074575,-0.217547892466614,
-0.197602911587109,-0.177701138303981,-0.157724828227981,-0.138006616652287,
-0.118340280590273,-0.0987405684270933,-0.079163582765697,-0.0595443936454144,
-0.0398513567435344,-0.0201041897531687,0.),.UNSPECIFIED.);
#1920=B_SPLINE_CURVE_WITH_KNOTS('',3,(#69013,#69014,#69015,#69016,#69017,
#69018,#69019,#69020,#69021,#69022,#69023,#69024,#69025,#69026,#69027,#69028,
#69029,#69030),.UNSPECIFIED.,.F.,.F.,(4,2,2,2,2,2,2,2,4),(-0.301120281951729,
-0.263576382922298,-0.225818802173902,-0.188754997605974,-0.151895401076345,
-0.114142761407066,-0.0764203504572131,-0.0384663620558447,-0.000147603040413052),
 .UNSPECIFIED.);
#1921=B_SPLINE_CURVE_WITH_KNOTS('',3,(#69033,#69034,#69035,#69036,#69037,
#69038,#69039,#69040,#69041,#69042,#69043,#69044,#69045,#69046,#69047,#69048,
#69049,#69050,#69051,#69052,#69053,#69054,#69055,#69056,#69057,#69058,#69059,
#69060,#69061,#69062,#69063,#69064,#69065,#69066,#69067,#69068),
 .UNSPECIFIED.,.T.,.F.,(4,2,2,2,2,2,2,2,2,2,2,2,2,2,2,2,2,4),(0.,0.0355202696276992,
0.0730229242193473,0.109881947978628,0.147332215351885,0.185244244851691,
0.223245130806753,0.259644256146375,0.294838797510505,0.330228485406038,
0.366554345819724,0.404791218297806,0.442165216594333,0.480056587423189,
0.518291371444511,0.552548743074586,0.588529668399033,0.599949959194981),
 .UNSPECIFIED.);
#1922=B_SPLINE_CURVE_WITH_KNOTS('',3,(#69069,#69070,#69071,#69072,#69073,
#69074,#69075,#69076,#69077,#69078,#69079,#69080,#69081,#69082,#69083,#69084,
#69085,#69086,#69087,#69088,#69089,#69090,#69091),.UNSPECIFIED.,.F.,.F.,
(4,3,2,2,2,2,2,2,2,2,4),(-0.000147603040413052,0.,0.0377539037831993,0.0751281221644984,
0.111887841210243,0.148520861419402,0.185616402493165,0.223453147294145,
0.262021736554917,0.300656505695179,0.301204822429525),.UNSPECIFIED.);
#1923=B_SPLINE_CURVE_WITH_KNOTS('',3,(#69097,#69098,#69099,#69100,#69101,
#69102,#69103,#69104,#69105,#69106,#69107,#69108,#69109,#69110,#69111,#69112,
#69113,#69114,#69115,#69116,#69117,#69118,#69119,#69120,#69121,#69122,#69123,
#69124,#69125,#69126,#69127,#69128,#69129,#69130),.UNSPECIFIED.,.T.,.F.,
(4,2,2,2,2,2,2,2,2,2,2,2,2,2,2,2,4),(-0.31764769122437,-0.298126594757583,
-0.278061059087757,-0.25855168614256,-0.239139946378455,-0.219621724224507,
-0.199578995246519,-0.179441223078379,-0.159144891999467,-0.138727517362643,
-0.119005202378359,-0.0995832877709888,-0.080234028709081,-0.060680702994594,
-0.0407740894175593,-0.0203443038622857,0.),.UNSPECIFIED.);
#1924=B_SPLINE_CURVE_WITH_KNOTS('',3,(#69134,#69135,#69136,#69137,#69138,
#69139,#69140,#69141,#69142,#69143,#69144,#69145,#69146,#69147,#69148,#69149,
#69150,#69151),.UNSPECIFIED.,.F.,.F.,(4,2,2,2,2,2,2,2,4),(-0.322294993083104,
-0.283085587582025,-0.242573319111423,-0.202265149720554,-0.161825459085777,
-0.121278611006667,-0.0808520831048596,-0.0405436064875047,-6.00049658257628E-5),
 .UNSPECIFIED.);
#1925=B_SPLINE_CURVE_WITH_KNOTS('',3,(#69154,#69155,#69156,#69157,#69158,
#69159,#69160,#69161,#69162,#69163,#69164,#69165,#69166,#69167,#69168,#69169,
#69170,#69171,#69172,#69173,#69174,#69175,#69176,#69177,#69178,#69179,#69180,
#69181,#69182,#69183,#69184,#69185,#69186,#69187,#69188,#69189),
 .UNSPECIFIED.,.T.,.F.,(4,2,2,2,2,2,2,2,2,2,2,2,2,2,2,2,2,4),(0.,0.0399541104211089,
0.0799101633971605,0.120042188031111,0.160349494010587,0.200700062460756,
0.240669149748765,0.281146928548236,0.321688268053059,0.361827692830262,
0.401937446248863,0.441912733332053,0.482224630786682,0.523014478228254,
0.563360237935002,0.603655558776195,0.623959945526125,0.644496878439372),
 .UNSPECIFIED.);
#1926=B_SPLINE_CURVE_WITH_KNOTS('',3,(#69190,#69191,#69192,#69193,#69194,
#69195,#69196,#69197,#69198,#69199,#69200,#69201,#69202,#69203,#69204,#69205,
#69206,#69207,#69208,#69209,#69210,#69211,#69212),.UNSPECIFIED.,.F.,.F.,
(4,3,2,2,2,2,2,2,2,2,4),(-6.00049658257628E-5,0.,0.0392897850588587,0.079479345871773,
0.119504351273332,0.159417323923056,0.199410327075563,0.239631683305099,
0.280043161873825,0.320485699897508,0.322364974673507),.UNSPECIFIED.);
#1927=B_SPLINE_CURVE_WITH_KNOTS('',3,(#69218,#69219,#69220,#69221,#69222,
#69223,#69224,#69225,#69226,#69227,#69228,#69229,#69230,#69231,#69232,#69233,
#69234,#69235,#69236,#69237,#69238,#69239,#69240,#69241,#69242,#69243,#69244,
#69245,#69246,#69247,#69248,#69249,#69250,#69251),.UNSPECIFIED.,.T.,.F.,
(4,2,2,2,2,2,2,2,2,2,2,2,2,2,2,2,4),(-0.315565835813836,-0.296977761293976,
-0.27700797437709,-0.257093427677873,-0.237151911102798,-0.217186116270328,
-0.197247154373207,-0.177332194059719,-0.157355502362145,-0.137638223444148,
-0.117952752060795,-0.098333751530719,-0.078758992743179,-0.0591645986628483,
-0.039498859894482,-0.0197630645862081,0.),.UNSPECIFIED.);
#1928=B_SPLINE_CURVE_WITH_KNOTS('',3,(#69255,#69256,#69257,#69258,#69259,
#69260,#69261,#69262,#69263,#69264,#69265,#69266,#69267,#69268,#69269,#69270,
#69271,#69272),.UNSPECIFIED.,.F.,.F.,(4,2,2,2,2,2,2,2,4),(-0.301047223106738,
-0.263578632733685,-0.225649522088337,-0.18795353439141,-0.151022848397426,
-0.113722078451354,-0.076039607899864,-0.0382349400305562,-9.66538702340807E-5),
 .UNSPECIFIED.);
#1929=B_SPLINE_CURVE_WITH_KNOTS('',3,(#69275,#69276,#69277,#69278,#69279,
#69280,#69281,#69282,#69283,#69284,#69285,#69286,#69287,#69288,#69289,#69290,
#69291,#69292,#69293,#69294,#69295,#69296,#69297,#69298,#69299,#69300,#69301,
#69302,#69303,#69304,#69305,#69306,#69307,#69308,#69309,#69310),
 .UNSPECIFIED.,.T.,.F.,(4,2,2,2,2,2,2,2,2,2,2,2,2,2,2,2,2,4),(0.,0.0355202696276597,
0.0730229242192084,0.109881947978522,0.147332215351905,0.185244244851805,
0.223245130806825,0.259644256146175,0.29483879750995,0.330228485405148,
0.366554345818643,0.404791218296623,0.442165216592673,0.480056587420968,
0.518291371441852,0.552548743071643,0.588529668395749,0.599949959191659),
 .UNSPECIFIED.);
#1930=B_SPLINE_CURVE_WITH_KNOTS('',3,(#69311,#69312,#69313,#69314,#69315,
#69316,#69317,#69318,#69319,#69320,#69321,#69322,#69323,#69324,#69325,#69326,
#69327,#69328,#69329,#69330,#69331,#69332,#69333),.UNSPECIFIED.,.F.,.F.,
(4,3,2,2,2,2,2,2,2,2,4),(-9.66538702340807E-5,0.,0.0375393633518907,0.0752835051296635,
0.112326473702278,0.148951470060482,0.18574314538863,0.223186825882593,
0.261324249138133,0.300258541488849,0.301234911690416),.UNSPECIFIED.);
#1931=B_SPLINE_CURVE_WITH_KNOTS('',3,(#69339,#69340,#69341,#69342,#69343,
#69344,#69345,#69346,#69347,#69348,#69349,#69350,#69351,#69352,#69353,#69354,
#69355,#69356,#69357,#69358,#69359,#69360,#69361,#69362,#69363,#69364,#69365,
#69366,#69367,#69368,#69369,#69370,#69371,#69372),.UNSPECIFIED.,.T.,.F.,
(4,2,2,2,2,2,2,2,2,2,2,2,2,2,2,2,4),(-0.317629464904961,-0.297714272038367,
-0.277577500901888,-0.257956254729707,-0.238517861015399,-0.219074978638032,
-0.199269307107419,-0.179183937587056,-0.158941321785611,-0.138538737217386,
-0.11863886681209,-0.099083234988701,-0.0797310797511626,-0.0603101816157416,
-0.0405879439157434,-0.0204362250140278,0.),.UNSPECIFIED.);
#1932=B_SPLINE_CURVE_WITH_KNOTS('',3,(#69376,#69377,#69378,#69379,#69380,
#69381,#69382,#69383,#69384,#69385,#69386,#69387,#69388,#69389,#69390,#69391,
#69392,#69393),.UNSPECIFIED.,.F.,.F.,(4,2,2,2,2,2,2,2,4),(-0.322273280496128,
-0.283164066278084,-0.242313649635905,-0.201927757921193,-0.161607273321421,
-0.121157355445028,-0.080708923195034,-0.0403897617268959,-4.12631041346659E-5),
 .UNSPECIFIED.);
#1933=B_SPLINE_CURVE_WITH_KNOTS('',3,(#69396,#69397,#69398,#69399,#69400,
#69401,#69402,#69403,#69404,#69405,#69406,#69407,#69408,#69409,#69410,#69411,
#69412,#69413,#69414,#69415,#69416,#69417,#69418,#69419,#69420,#69421,#69422,
#69423,#69424,#69425,#69426,#69427,#69428,#69429,#69430,#69431),
 .UNSPECIFIED.,.T.,.F.,(4,2,2,2,2,2,2,2,2,2,2,2,2,2,2,2,2,4),(0.,0.0399541104210812,
0.0799101633970315,0.120042188030822,0.160349494010275,0.200700062460568,
0.240669149748756,0.281146928548416,0.321688268053484,0.361827692830935,
0.401937446249939,0.441912733333782,0.482224630788817,0.523014478230698,
0.563360237937675,0.603655558779108,0.623959945529211,0.644496878442527),
 .UNSPECIFIED.);
#1934=B_SPLINE_CURVE_WITH_KNOTS('',3,(#69432,#69433,#69434,#69435,#69436,
#69437,#69438,#69439,#69440,#69441,#69442,#69443,#69444,#69445,#69446,#69447,
#69448,#69449,#69450,#69451,#69452,#69453,#69454),.UNSPECIFIED.,.F.,.F.,
(4,3,2,2,2,2,2,2,2,2,4),(-4.12631041346659E-5,0.,0.0399675679442238,0.0801897951235173,
0.120290688199724,0.160233372859482,0.200158067921408,0.240260671009271,
0.280600379519264,0.321053048499667,0.322354423090216),.UNSPECIFIED.);
#1935=B_SPLINE_CURVE_WITH_KNOTS('',3,(#69460,#69461,#69462,#69463,#69464,
#69465,#69466,#69467,#69468,#69469,#69470,#69471,#69472,#69473,#69474,#69475,
#69476,#69477,#69478,#69479,#69480,#69481,#69482,#69483,#69484,#69485,#69486,
#69487,#69488,#69489,#69490,#69491,#69492,#69493),.UNSPECIFIED.,.T.,.F.,
(4,2,2,2,2,2,2,2,2,2,2,2,2,2,2,2,4),(-0.315553268146494,-0.297304300154847,
-0.277232874841197,-0.257288395179118,-0.237380069391282,-0.217453712880523,
-0.197526993272217,-0.177618574645662,-0.157675821289914,-0.137607666323394,
-0.117904352341964,-0.0982559940572506,-0.0786687230926247,-0.0590935104011807,
-0.0394653656100249,-0.0197579638748003,0.),.UNSPECIFIED.);
#1936=B_SPLINE_CURVE_WITH_KNOTS('',3,(#69497,#69498,#69499,#69500,#69501,
#69502,#69503,#69504,#69505,#69506,#69507,#69508,#69509,#69510,#69511,#69512,
#69513,#69514),.UNSPECIFIED.,.F.,.F.,(4,2,2,2,2,2,2,2,4),(-0.301109175947192,
-0.262812042982321,-0.224724316953933,-0.186970956972154,-0.149886488164483,
-0.11301762842648,-0.0756285515230846,-0.0379138418272327,-0.000181832202353105),
 .UNSPECIFIED.);
#1937=B_SPLINE_CURVE_WITH_KNOTS('',3,(#69517,#69518,#69519,#69520,#69521,
#69522,#69523,#69524,#69525,#69526,#69527,#69528,#69529,#69530,#69531,#69532,
#69533,#69534,#69535,#69536,#69537,#69538,#69539,#69540,#69541,#69542,#69543,
#69544,#69545,#69546,#69547,#69548,#69549,#69550,#69551,#69552),
 .UNSPECIFIED.,.T.,.F.,(4,2,2,2,2,2,2,2,2,2,2,2,2,2,2,2,2,4),(0.,0.0355202696277283,
0.0730229242195419,0.109881947979107,0.147332215352648,0.185244244852912,
0.223245130808583,0.25964425614879,0.294838797513527,0.330228485409711,
0.366554345824243,0.404791218303629,0.442165216601193,0.480056587431119,
0.518291371453736,0.552548743085037,0.588529668410891,0.59994995920701),
 .UNSPECIFIED.);
#1938=B_SPLINE_CURVE_WITH_KNOTS('',3,(#69553,#69554,#69555,#69556,#69557,
#69558,#69559,#69560,#69561,#69562,#69563,#69564,#69565,#69566,#69567,#69568,
#69569,#69570,#69571,#69572,#69573,#69574,#69575,#69576,#69577),
 .UNSPECIFIED.,.F.,.F.,(4,3,2,2,2,2,2,2,2,2,2,4),(-0.000181832202353105,
0.,9.38366536167301E-5,0.0385047798493244,0.0765518818810497,0.113953342602953,
0.150737446188046,0.187371554731283,0.224440136490084,0.262235508831512,
0.300767100191795,0.301097788245665),.UNSPECIFIED.);
#1939=B_SPLINE_CURVE_WITH_KNOTS('',3,(#69583,#69584,#69585,#69586,#69587,
#69588,#69589,#69590,#69591,#69592,#69593,#69594,#69595,#69596,#69597,#69598,
#69599,#69600,#69601,#69602,#69603,#69604,#69605,#69606,#69607,#69608,#69609,
#69610,#69611,#69612,#69613,#69614,#69615,#69616),.UNSPECIFIED.,.T.,.F.,
(4,2,2,2,2,2,2,2,2,2,2,2,2,2,2,2,4),(-0.317594533089036,-0.297902075164115,
-0.277717583659871,-0.257653287417695,-0.238130426363534,-0.218714109872533,
-0.199204998726052,-0.179166112450341,-0.159044764786859,-0.138770672776784,
-0.118368847123579,-0.0986295682412476,-0.0791930104351003,-0.0598423732615011,
-0.0403036962525294,-0.0204206770504485,0.),.UNSPECIFIED.);
#1940=B_SPLINE_CURVE_WITH_KNOTS('',3,(#69620,#69621,#69622,#69623,#69624,
#69625,#69626,#69627,#69628,#69629,#69630,#69631,#69632,#69633,#69634,#69635,
#69636,#69637,#69638,#69639,#69640),.UNSPECIFIED.,.F.,.F.,(4,2,2,2,2,2,
2,2,3,4),(-0.322212451494843,-0.283737281153516,-0.242722123714327,-0.202268209971048,
-0.161970355596362,-0.121472143151954,-0.0808174241678842,-0.0403032184405623,
0.,3.41805086617603E-5),.UNSPECIFIED.);
#1941=B_SPLINE_CURVE_WITH_KNOTS('',3,(#69643,#69644,#69645,#69646,#69647,
#69648,#69649,#69650,#69651,#69652,#69653,#69654,#69655,#69656,#69657,#69658,
#69659,#69660,#69661,#69662,#69663,#69664,#69665,#69666,#69667,#69668,#69669,
#69670,#69671,#69672,#69673,#69674,#69675,#69676,#69677,#69678),
 .UNSPECIFIED.,.T.,.F.,(4,2,2,2,2,2,2,2,2,2,2,2,2,2,2,2,2,4),(0.,0.0399541104211557,
0.0799101633973391,0.120042188031283,0.160349494010752,0.200700062461029,
0.240669149749152,0.281146928548658,0.321688268053438,0.361827692830745,
0.401937446249819,0.441912733333285,0.482224630788115,0.523014478229936,
0.563360237936776,0.603655558778112,0.623959945528129,0.644496878441407),
 .UNSPECIFIED.);
#1942=B_SPLINE_CURVE_WITH_KNOTS('',3,(#69679,#69680,#69681,#69682,#69683,
#69684,#69685,#69686,#69687,#69688,#69689,#69690,#69691,#69692,#69693,#69694,
#69695,#69696,#69697,#69698),.UNSPECIFIED.,.F.,.F.,(4,2,2,2,2,2,2,2,2,4),
(3.41805086617603E-5,0.0394732086774792,0.079701088033428,0.119906369771394,
0.159959613748505,0.199889421771116,0.239872401764791,0.280061608671928,
0.320438058972153,0.32238398619812),.UNSPECIFIED.);
#1943=B_SPLINE_CURVE_WITH_KNOTS('',3,(#69704,#69705,#69706,#69707,#69708,
#69709,#69710,#69711,#69712,#69713,#69714,#69715,#69716,#69717,#69718,#69719,
#69720,#69721,#69722,#69723,#69724,#69725,#69726,#69727,#69728,#69729,#69730,
#69731,#69732,#69733,#69734,#69735,#69736,#69737),.UNSPECIFIED.,.T.,.F.,
(4,2,2,2,2,2,2,2,2,2,2,2,2,2,2,2,4),(-0.315539422451451,-0.29764665964427,
-0.277579650597126,-0.25764437253977,-0.237734954471469,-0.217762026234666,
-0.19774279120852,-0.17776218314531,-0.157848862492919,-0.137922119941295,
-0.117871746268506,-0.0981780349529489,-0.078545939200476,-0.0589630124018614,
-0.0393717766439356,-0.0197194318849499,0.),.UNSPECIFIED.);
#1944=B_SPLINE_CURVE_WITH_KNOTS('',3,(#69741,#69742,#69743,#69744,#69745,
#69746,#69747,#69748,#69749,#69750,#69751,#69752,#69753,#69754,#69755,#69756,
#69757,#69758),.UNSPECIFIED.,.F.,.F.,(4,2,2,2,2,2,2,2,4),(-0.301006762787625,
-0.264925988556105,-0.226376240130882,-0.188384262261974,-0.150702655161475,
-0.113069725454281,-0.0754287199925444,-0.0377927671943644,-6.79809902074358E-5),
 .UNSPECIFIED.);
#1945=B_SPLINE_CURVE_WITH_KNOTS('',3,(#69761,#69762,#69763,#69764,#69765,
#69766,#69767,#69768,#69769,#69770,#69771,#69772,#69773,#69774,#69775,#69776,
#69777,#69778,#69779,#69780,#69781,#69782,#69783,#69784,#69785,#69786,#69787,
#69788,#69789,#69790,#69791,#69792,#69793,#69794,#69795,#69796),
 .UNSPECIFIED.,.T.,.F.,(4,2,2,2,2,2,2,2,2,2,2,2,2,2,2,2,2,4),(0.,0.0355202696277629,
0.0730229242196933,0.109881947979405,0.147332215353019,0.185244244853643,
0.223245130809453,0.259644256149627,0.294838797514426,0.330228485410828,
0.366554345825704,0.404791218305273,0.442165216603097,0.480056587433275,
0.518291371456087,0.552548743087593,0.58852966841366,0.599949959209818),
 .UNSPECIFIED.);
#1946=B_SPLINE_CURVE_WITH_KNOTS('',3,(#69797,#69798,#69799,#69800,#69801,
#69802,#69803,#69804,#69805,#69806,#69807,#69808,#69809,#69810,#69811,#69812,
#69813,#69814,#69815,#69816,#69817,#69818,#69819),.UNSPECIFIED.,.F.,.F.,
(4,3,2,2,2,2,2,2,2,2,4),(-6.79809902074358E-5,0.,0.0356803651782013,0.0744612460975631,
0.112238318105394,0.14932462663091,0.185963804099021,0.222722923188193,
0.260104146420146,0.298186022335344,0.301109163651249),.UNSPECIFIED.);
#1947=B_SPLINE_CURVE_WITH_KNOTS('',3,(#69825,#69826,#69827,#69828,#69829,
#69830,#69831,#69832,#69833,#69834,#69835,#69836,#69837,#69838,#69839,#69840,
#69841,#69842,#69843,#69844,#69845,#69846,#69847,#69848,#69849,#69850,#69851,
#69852,#69853,#69854,#69855,#69856,#69857,#69858),.UNSPECIFIED.,.T.,.F.,
(4,2,2,2,2,2,2,2,2,2,2,2,2,2,2,2,4),(-0.317546919319209,-0.298237181118452,
-0.27788599623212,-0.257722699827236,-0.237703531338022,-0.218259701974539,
-0.198818616029039,-0.178839663119116,-0.158758082875245,-0.138499360197678,
-0.118073251856203,-0.0981722626108359,-0.0786104829396448,-0.0592550425800418,
-0.0398390935163074,-0.0201296135639513,0.),.UNSPECIFIED.);
#1948=B_SPLINE_CURVE_WITH_KNOTS('',3,(#69862,#69863,#69864,#69865,#69866,
#69867,#69868,#69869,#69870,#69871,#69872,#69873,#69874,#69875,#69876,#69877,
#69878,#69879),.UNSPECIFIED.,.F.,.F.,(4,2,2,2,2,2,2,2,4),(-0.322300981754088,
-0.28318251522055,-0.242774753788783,-0.201858981303984,-0.16144569609712,
-0.121144311498917,-0.0807322407035335,-0.0403094094323443,-4.72125003703735E-5),
 .UNSPECIFIED.);
#1949=B_SPLINE_CURVE_WITH_KNOTS('',3,(#69882,#69883,#69884,#69885,#69886,
#69887,#69888,#69889,#69890,#69891,#69892,#69893,#69894,#69895,#69896,#69897,
#69898,#69899,#69900,#69901,#69902,#69903,#69904,#69905,#69906,#69907,#69908,
#69909,#69910,#69911,#69912,#69913,#69914,#69915,#69916,#69917),
 .UNSPECIFIED.,.T.,.F.,(4,2,2,2,2,2,2,2,2,2,2,2,2,2,2,2,2,4),(0.,0.0399541104209768,
0.0799101633966359,0.120042188030262,0.160349494009563,0.200700062459491,
0.240669149747351,0.281146928546543,0.321688268050956,0.361827692827786,
0.401937446246216,0.441912733329095,0.482224630783251,0.523014478224417,
0.563360237930717,0.603655558771478,0.623959945521238,0.644496878434432),
 .UNSPECIFIED.);
#1950=B_SPLINE_CURVE_WITH_KNOTS('',3,(#69918,#69919,#69920,#69921,#69922,
#69923,#69924,#69925,#69926,#69927,#69928,#69929,#69930,#69931,#69932,#69933,
#69934,#69935,#69936,#69937,#69938,#69939,#69940),.UNSPECIFIED.,.F.,.F.,
(4,3,2,2,2,2,2,2,2,2,4),(-4.72125003703735E-5,0.,0.0401541608355253,0.0803379018857595,
0.120550355458553,0.160650987023366,0.200596462646156,0.2405175782139,0.280609074525696,
0.320937808358075,0.322266789344037),.UNSPECIFIED.);
#1951=B_SPLINE_CURVE_WITH_KNOTS('',3,(#69946,#69947,#69948,#69949,#69950,
#69951,#69952,#69953,#69954,#69955,#69956,#69957,#69958,#69959,#69960,#69961,
#69962,#69963,#69964,#69965,#69966,#69967,#69968,#69969,#69970,#69971,#69972,
#69973,#69974,#69975,#69976,#69977,#69978,#69979),.UNSPECIFIED.,.T.,.F.,
(4,2,2,2,2,2,2,2,2,2,2,2,2,2,2,2,4),(-0.31552451047958,-0.297280907827344,
-0.277523391905511,-0.257428902418356,-0.237473497248995,-0.217571624881194,
-0.197661500232289,-0.177749354472922,-0.157848485240125,-0.137907777204664,
-0.117838620146662,-0.09813907693786,-0.0784912592307547,-0.0589032081742604,
-0.0393286932776206,-0.0197035504924225,0.),.UNSPECIFIED.);
#1952=B_SPLINE_CURVE_WITH_KNOTS('',3,(#69983,#69984,#69985,#69986,#69987,
#69988,#69989,#69990,#69991,#69992,#69993,#69994,#69995,#69996,#69997,#69998,
#69999,#70000),.UNSPECIFIED.,.F.,.F.,(4,2,2,2,2,2,2,2,4),(-0.301015621190795,
-0.26464913614506,-0.225860948774485,-0.187630348606652,-0.149844101969181,
-0.112198999979826,-0.0753249907283473,-0.037674212913492,-9.15455865655557E-5),
 .UNSPECIFIED.);
#1953=B_SPLINE_CURVE_WITH_KNOTS('',3,(#70003,#70004,#70005,#70006,#70007,
#70008,#70009,#70010,#70011,#70012,#70013,#70014,#70015,#70016,#70017,#70018,
#70019,#70020,#70021,#70022,#70023,#70024,#70025,#70026,#70027,#70028,#70029,
#70030,#70031,#70032,#70033,#70034,#70035,#70036,#70037,#70038),
 .UNSPECIFIED.,.T.,.F.,(4,2,2,2,2,2,2,2,2,2,2,2,2,2,2,2,2,4),(0.,0.0355202696278056,
0.0730229242197536,0.109881947979361,0.147332215353219,0.185244244853985,
0.223245130809959,0.259644256150568,0.29483879751575,0.330228485412583,
0.366554345827937,0.404791218307693,0.442165216605726,0.48005658743653,
0.518291371460154,0.552548743092215,0.588529668419006,0.599949959215237),
 .UNSPECIFIED.);
#1954=B_SPLINE_CURVE_WITH_KNOTS('',3,(#70039,#70040,#70041,#70042,#70043,
#70044,#70045,#70046,#70047,#70048,#70049,#70050,#70051,#70052,#70053,#70054,
#70055,#70056,#70057,#70058,#70059,#70060,#70061),.UNSPECIFIED.,.F.,.F.,
(4,3,2,2,2,2,2,2,2,2,4),(-9.15455865655557E-5,0.,0.0367498513809987,0.0752209939176623,
0.113273329807805,0.15070796959203,0.187516731080181,0.224138077913942,
0.261156975549728,0.298894829763992,0.300991424502598),.UNSPECIFIED.);
#1955=B_SPLINE_CURVE_WITH_KNOTS('',3,(#70067,#70068,#70069,#70070,#70071,
#70072,#70073,#70074,#70075,#70076,#70077,#70078,#70079,#70080,#70081,#70082,
#70083,#70084,#70085,#70086,#70087,#70088,#70089,#70090,#70091,#70092,#70093,
#70094,#70095,#70096,#70097,#70098,#70099,#70100),.UNSPECIFIED.,.T.,.F.,
(4,2,2,2,2,2,2,2,2,2,2,2,2,2,2,2,4),(-0.317488428877463,-0.298036515488589,
-0.277628055879793,-0.25738424350405,-0.237308164390969,-0.21778572227554,
-0.198368809302504,-0.178862365231032,-0.158846741703291,-0.138701111469329,
-0.11837423341009,-0.0979264050779261,-0.078190697669169,-0.0587545592685796,
-0.0394060149601878,-0.0198735656069791,0.),.UNSPECIFIED.);
#1956=B_SPLINE_CURVE_WITH_KNOTS('',3,(#70104,#70105,#70106,#70107,#70108,
#70109,#70110,#70111,#70112,#70113,#70114,#70115,#70116,#70117,#70118,#70119,
#70120,#70121),.UNSPECIFIED.,.F.,.F.,(4,2,2,2,2,2,2,2,4),(-0.322341080919583,
-0.283397192137026,-0.242965114707,-0.202207166282649,-0.161620101984401,
-0.12131449207317,-0.0809262451179171,-0.0404192807283227,-7.52860376557503E-5),
 .UNSPECIFIED.);
#1957=B_SPLINE_CURVE_WITH_KNOTS('',3,(#70124,#70125,#70126,#70127,#70128,
#70129,#70130,#70131,#70132,#70133,#70134,#70135,#70136,#70137,#70138,#70139,
#70140,#70141,#70142,#70143,#70144,#70145,#70146,#70147,#70148,#70149,#70150,
#70151,#70152,#70153,#70154,#70155,#70156,#70157,#70158,#70159,#70160,#70161,
#70162,#70163,#70164,#70165,#70166,#70167,#70168,#70169,#70170,#70171),
 .UNSPECIFIED.,.T.,.F.,(4,2,2,2,2,2,2,2,2,2,2,2,2,2,2,2,2,2,2,2,2,2,2,4),
(0.,0.0335113392274846,0.0695662695919637,0.108091819664512,0.148791621535511,
0.188697016176582,0.228911969541493,0.248549485762229,0.261288477298313,
0.266974681879587,0.279405337299656,0.297653721121311,0.335724703623805,
0.370458461479632,0.40772209622371,0.447602408687505,0.488121713087397,
0.527106132404311,0.559214002352181,0.575561093124945,0.587383293115077,
0.599420863476123,0.616221156668834,0.644049639714414),.UNSPECIFIED.);
#1958=B_SPLINE_CURVE_WITH_KNOTS('',3,(#70172,#70173,#70174,#70175,#70176,
#70177,#70178,#70179,#70180,#70181,#70182,#70183,#70184,#70185,#70186,#70187,
#70188,#70189,#70190,#70191,#70192,#70193,#70194),.UNSPECIFIED.,.F.,.F.,
(4,3,2,2,2,2,2,2,2,2,4),(-7.52860376557503E-5,0.,0.0397392322804878,0.0802354008620384,
0.120447425093409,0.16063007506737,0.200664146488323,0.240582108771279,
0.280562031686767,0.320758571866905,0.322205986735066),.UNSPECIFIED.);
#1959=B_SPLINE_CURVE_WITH_KNOTS('',3,(#70200,#70201,#70202,#70203,#70204,
#70205,#70206,#70207,#70208,#70209,#70210,#70211,#70212,#70213,#70214,#70215,
#70216,#70217,#70218,#70219,#70220,#70221,#70222,#70223,#70224,#70225,#70226,
#70227,#70228,#70229,#70230,#70231,#70232,#70233),.UNSPECIFIED.,.T.,.F.,
(4,2,2,2,2,2,2,2,2,2,2,2,2,2,2,2,4),(-0.315511801736032,-0.297322926516652,
-0.277567954138442,-0.257424067681664,-0.237430365844225,-0.217516351887858,
-0.197593634790712,-0.177646959906082,-0.157717567973084,-0.137807467592321,
-0.117838533294104,-0.0981312561837001,-0.0784480093982619,-0.0588252961267834,
-0.0392478427160484,-0.0196569263325427,0.),.UNSPECIFIED.);
#1960=B_SPLINE_CURVE_WITH_KNOTS('',3,(#70237,#70238,#70239,#70240,#70241,
#70242,#70243,#70244,#70245,#70246,#70247,#70248,#70249,#70250,#70251,#70252,
#70253,#70254),.UNSPECIFIED.,.F.,.F.,(4,2,2,2,2,2,2,2,4),(-0.301008850825269,
-0.26442428051724,-0.225539555035701,-0.187129468600546,-0.14922300031385,
-0.111530253351743,-0.0745692246178906,-0.0377021715762848,-9.92896090334623E-5),
 .UNSPECIFIED.);
#1961=B_SPLINE_CURVE_WITH_KNOTS('',3,(#70257,#70258,#70259,#70260,#70261,
#70262,#70263,#70264,#70265,#70266,#70267,#70268,#70269,#70270,#70271,#70272,
#70273,#70274,#70275,#70276,#70277,#70278,#70279,#70280,#70281,#70282,#70283,
#70284,#70285,#70286,#70287,#70288,#70289,#70290,#70291,#70292),
 .UNSPECIFIED.,.T.,.F.,(4,2,2,2,2,2,2,2,2,2,2,2,2,2,2,2,2,4),(0.,0.0355202696276149,
0.0730229242189981,0.109881947977939,0.147332215351036,0.185244244850885,
0.223245130805628,0.259644256144758,0.294838797508318,0.330228485403177,
0.366554345816096,0.404791218293387,0.442165216588983,0.480056587416825,
0.51829137143723,0.552548743066467,0.588529668389975,0.599949959185819),
 .UNSPECIFIED.);
#1962=B_SPLINE_CURVE_WITH_KNOTS('',3,(#70293,#70294,#70295,#70296,#70297,
#70298,#70299,#70300,#70301,#70302,#70303,#70304,#70305,#70306,#70307,#70308,
#70309,#70310,#70311,#70312,#70313,#70314,#70315),.UNSPECIFIED.,.F.,.F.,
(4,3,2,2,2,2,2,2,2,2,4),(-9.92896090334623E-5,0.,0.0371215071931662,0.0751963489563421,
0.113814279468518,0.151609467281234,0.18872289670269,0.22537433686428,0.262116084041776,
0.299451874579786,0.3008946113259),.UNSPECIFIED.);
#1963=B_SPLINE_CURVE_WITH_KNOTS('',3,(#70321,#70322,#70323,#70324,#70325,
#70326,#70327,#70328,#70329,#70330,#70331,#70332,#70333,#70334,#70335,#70336,
#70337,#70338,#70339,#70340,#70341,#70342,#70343,#70344,#70345,#70346,#70347,
#70348,#70349,#70350,#70351,#70352,#70353,#70354),.UNSPECIFIED.,.T.,.F.,
(4,2,2,2,2,2,2,2,2,2,2,2,2,2,2,2,4),(-0.31742888296956,-0.297614680988988,
-0.277216006988426,-0.256943128376054,-0.236826826287557,-0.217180233857531,
-0.197728370920642,-0.178297477151747,-0.158518654238573,-0.138464191712988,
-0.118284269507906,-0.0979458955695503,-0.078023359766043,-0.0584366788244967,
-0.0390722257779513,-0.0196727140138107,0.),.UNSPECIFIED.);
#1964=B_SPLINE_CURVE_WITH_KNOTS('',3,(#70360,#70361,#70362,#70363,#70364,
#70365,#70366,#70367,#70368,#70369,#70370,#70371,#70372,#70373,#70374,#70375,
#70376,#70377,#70378,#70379,#70380,#70381,#70382,#70383,#70384,#70385,#70386,
#70387,#70388,#70389,#70390,#70391,#70392,#70393,#70394,#70395,#70396,#70397,
#70398,#70399,#70400,#70401,#70402,#70403),.UNSPECIFIED.,.T.,.F.,(4,2,2,
2,2,2,2,2,2,2,2,2,2,2,2,2,2,2,2,2,2,4),(0.,0.0127770956840893,0.0401769293152859,
0.0780448846179358,0.139821331639922,0.195108267791615,0.25352997178776,
0.31553240477771,0.376490923311257,0.438446166471974,0.474035280748466,
0.500390883434378,0.526892757452704,0.56201393628215,0.624036266196096,
0.678511078694792,0.736162275713911,0.797543466099766,0.858642911548674,
0.920080478592296,0.956389836746744,0.97628076565265),.UNSPECIFIED.);
#1965=B_SPLINE_CURVE_WITH_KNOTS('',3,(#70415,#70416,#70417,#70418,#70419,
#70420,#70421,#70422,#70423,#70424,#70425,#70426,#70427,#70428,#70429,#70430,
#70431,#70432,#70433,#70434,#70435,#70436,#70437,#70438,#70439,#70440,#70441,
#70442,#70443,#70444,#70445,#70446,#70447,#70448,#70449,#70450,#70451,#70452,
#70453,#70454,#70455,#70456,#70457,#70458,#70459,#70460),.UNSPECIFIED.,
 .T.,.F.,(4,2,2,2,2,2,2,2,2,2,2,2,2,2,2,2,2,2,2,2,2,2,4),(0.,0.00956491245687488,
0.030883344589073,0.0618829516961483,0.112184753046831,0.156999876022228,
0.204430459079411,0.254727738816217,0.304367474343013,0.353938489206773,
0.383699609227687,0.404561462882039,0.414031956382108,0.435291839053782,
0.466616523466818,0.517017233475614,0.561720661065273,0.609373928277655,
0.659517635087295,0.708833303469572,0.754032026996831,0.78008309963919,
0.793860837770021),.UNSPECIFIED.);
#1966=B_SPLINE_CURVE_WITH_KNOTS('',3,(#70470,#70471,#70472,#70473,#70474,
#70475,#70476,#70477,#70478,#70479,#70480,#70481,#70482,#70483,#70484,#70485,
#70486,#70487),.UNSPECIFIED.,.F.,.F.,(4,2,2,2,2,2,2,2,4),(-0.32228159478291,
-0.283799439738403,-0.243381635204158,-0.202597493718955,-0.161764444001045,
-0.121394670185239,-0.0810652882896529,-0.0405499785426211,-6.66314878022331E-6),
 .UNSPECIFIED.);
#1967=B_SPLINE_CURVE_WITH_KNOTS('',3,(#70490,#70491,#70492,#70493,#70494,
#70495,#70496,#70497,#70498,#70499,#70500,#70501,#70502,#70503,#70504,#70505,
#70506,#70507,#70508,#70509,#70510,#70511,#70512,#70513,#70514,#70515,#70516,
#70517,#70518,#70519,#70520,#70521,#70522,#70523,#70524,#70525,#70526,#70527,
#70528,#70529,#70530,#70531,#70532,#70533,#70534,#70535,#70536,#70537,#70538,
#70539,#70540,#70541),.UNSPECIFIED.,.T.,.F.,(4,2,2,2,2,2,2,2,2,2,2,2,2,
2,2,2,2,2,2,2,2,2,2,2,2,4),(0.,0.0282895937381302,0.0604612061645479,0.0955483414317913,
0.133156791658192,0.173259107140958,0.2138054447814,0.252451243352889,0.283476215783229,
0.297624487910025,0.307274542296832,0.311654955761004,0.321804811499666,
0.337921929043092,0.375015994336447,0.40903555725717,0.446013229785303,
0.486013466010895,0.526529373075068,0.564703570234459,0.599506180594163,
0.613229117562791,0.622237737759,0.626302999451298,0.635646637048587,0.644410107943693),
 .UNSPECIFIED.);
#1968=B_SPLINE_CURVE_WITH_KNOTS('',3,(#70542,#70543,#70544,#70545,#70546,
#70547,#70548,#70549,#70550,#70551,#70552,#70553,#70554,#70555,#70556,#70557,
#70558,#70559,#70560,#70561,#70562,#70563,#70564),.UNSPECIFIED.,.F.,.F.,
(4,3,2,2,2,2,2,2,2,2,4),(-6.66314878022331E-6,0.,0.0391495632548314,0.0794647813952141,
0.120127711159877,0.160348499619285,0.200480693554725,0.240456530427129,
0.280381832209827,0.32044609784586,0.322252227541039),.UNSPECIFIED.);
#1969=B_SPLINE_CURVE_WITH_KNOTS('',3,(#70570,#70571,#70572,#70573,#70574,
#70575,#70576,#70577,#70578,#70579,#70580,#70581,#70582,#70583,#70584,#70585,
#70586,#70587,#70588,#70589,#70590,#70591,#70592,#70593,#70594,#70595,#70596,
#70597,#70598,#70599,#70600,#70601,#70602,#70603),.UNSPECIFIED.,.T.,.F.,
(4,2,2,2,2,2,2,2,2,2,2,2,2,2,2,2,4),(-0.315502449039155,-0.297515748826024,
-0.277778880448211,-0.257824981175595,-0.237783331527644,-0.217855184230197,
-0.197937909351415,-0.177974799956127,-0.158002028094032,-0.138072732783704,
-0.118158524215663,-0.0981590114967407,-0.0784549137780755,-0.0587934272076247,
-0.0391924430371145,-0.0196151302800391,0.),.UNSPECIFIED.);
#1970=B_SPLINE_CURVE_WITH_KNOTS('',3,(#70607,#70608,#70609,#70610,#70611,
#70612,#70613,#70614,#70615,#70616,#70617,#70618,#70619,#70620,#70621,#70622,
#70623,#70624,#70625,#70626,#70627),.UNSPECIFIED.,.F.,.F.,(4,2,2,2,2,2,
2,2,3,4),(-0.300867269446679,-0.266056862620371,-0.227808585743502,-0.188962005203739,
-0.150665481576804,-0.11285491655002,-0.0752335214926206,-0.037614382743869,
0.,4.23225959967841E-5),.UNSPECIFIED.);
#1971=B_SPLINE_CURVE_WITH_KNOTS('',3,(#70630,#70631,#70632,#70633,#70634,
#70635,#70636,#70637,#70638,#70639,#70640,#70641,#70642,#70643,#70644,#70645,
#70646,#70647,#70648,#70649,#70650,#70651,#70652,#70653,#70654,#70655,#70656,
#70657,#70658,#70659,#70660,#70661,#70662,#70663,#70664,#70665,#70666,#70667,
#70668,#70669,#70670,#70671,#70672,#70673,#70674,#70675,#70676,#70677,#70678,
#70679,#70680,#70681,#70682,#70683),.UNSPECIFIED.,.T.,.F.,(4,2,2,2,2,2,
2,2,2,2,2,2,2,2,2,2,2,2,2,2,2,2,2,2,2,2,4),(0.,0.029081491771507,0.0612502674553373,
0.0961097574703367,0.133607299680108,0.171385053584874,0.206641008499803,
0.237112772984767,0.249042656047471,0.256728934232189,0.260169709018563,
0.267882879740654,0.279907399797955,0.312932772577639,0.343668137806066,
0.377290154421155,0.413624402754248,0.451812104238219,0.488740715671467,
0.523779739364488,0.54324113697516,0.552348398814064,0.556143993023423,
0.559504603731152,0.5668581250006,0.578100823004826,0.599543898462904),
 .UNSPECIFIED.);
#1972=B_SPLINE_CURVE_WITH_KNOTS('',3,(#70684,#70685,#70686,#70687,#70688,
#70689,#70690,#70691,#70692,#70693,#70694,#70695,#70696,#70697,#70698,#70699,
#70700,#70701,#70702,#70703),.UNSPECIFIED.,.F.,.F.,(4,2,2,2,2,2,2,2,2,4),
(4.23225959967841E-5,0.0357919825936412,0.0736951427824967,0.11213398720573,
0.150200682323832,0.187678724930752,0.224519795797413,0.261130708849028,
0.29809507630152,0.300954458020331),.UNSPECIFIED.);
#1973=B_SPLINE_CURVE_WITH_KNOTS('',3,(#70709,#70710,#70711,#70712,#70713,
#70714,#70715,#70716,#70717,#70718,#70719,#70720,#70721,#70722,#70723,#70724,
#70725,#70726,#70727,#70728,#70729,#70730,#70731,#70732,#70733,#70734,#70735,
#70736,#70737,#70738,#70739,#70740,#70741,#70742),.UNSPECIFIED.,.T.,.F.,
(4,2,2,2,2,2,2,2,2,2,2,2,2,2,2,2,4),(-0.317382584107991,-0.298404141251476,
-0.278172891490457,-0.257747654398373,-0.237483739094739,-0.217400881549399,
-0.197870634374672,-0.178454632462585,-0.158961383169832,-0.138962436628909,
-0.118826492452815,-0.0985020845516959,-0.0780507441744616,-0.0583017008699032,
-0.0388560211137377,-0.0195122248887286,0.),.UNSPECIFIED.);
#1974=B_SPLINE_CURVE_WITH_KNOTS('',3,(#70748,#70749,#70750,#70751,#70752,
#70753,#70754,#70755,#70756,#70757,#70758,#70759,#70760,#70761,#70762,#70763,
#70764,#70765,#70766,#70767,#70768,#70769,#70770,#70771,#70772,#70773,#70774,
#70775,#70776,#70777,#70778,#70779,#70780,#70781,#70782,#70783,#70784,#70785,
#70786,#70787,#70788,#70789,#70790,#70791,#70792,#70793,#70794,#70795),
 .UNSPECIFIED.,.T.,.F.,(4,2,2,2,2,2,2,2,2,2,2,2,2,2,2,2,2,2,2,2,2,2,2,4),
(0.,0.0282046675723413,0.0672171199264202,0.129041618802007,0.184527661316184,
0.24325253918707,0.304784892317842,0.365588080179233,0.423060617652659,
0.457593113565745,0.47215336749717,0.485219180055195,0.513137775499108,
0.551542455419591,0.613353262192266,0.66846001838336,0.726644630290134,
0.788438287740315,0.849529302645522,0.908974797531781,0.944754831213901,
0.959764451759562,0.967998471593533,0.976310474265571),.UNSPECIFIED.);
#1975=B_SPLINE_CURVE_WITH_KNOTS('',3,(#70807,#70808,#70809,#70810,#70811,
#70812,#70813,#70814,#70815,#70816,#70817,#70818,#70819,#70820,#70821,#70822,
#70823,#70824,#70825,#70826,#70827,#70828,#70829,#70830,#70831,#70832,#70833,
#70834,#70835,#70836,#70837,#70838,#70839,#70840,#70841,#70842,#70843,#70844,
#70845,#70846,#70847,#70848,#70849,#70850,#70851,#70852),.UNSPECIFIED.,
 .T.,.F.,(4,2,2,2,2,2,2,2,2,2,2,2,2,2,2,2,2,2,2,2,2,2,4),(0.,0.0111055104419066,
0.0368929406912385,0.074670643681405,0.125120054145412,0.171409106180065,
0.220390846274497,0.270537305216151,0.319819552908647,0.35954184970516,
0.386169475565741,0.397831092450577,0.408798696086061,0.434213522740755,
0.471993677197715,0.522392420649816,0.568316684839256,0.617007335876734,
0.66731342361697,0.716761752372739,0.755752478614718,0.782476626020418,
0.794702189516223),.UNSPECIFIED.);
#1976=B_SPLINE_CURVE_WITH_KNOTS('',3,(#70862,#70863,#70864,#70865,#70866,
#70867,#70868,#70869,#70870,#70871,#70872,#70873,#70874,#70875,#70876,#70877,
#70878,#70879,#70880,#70881,#70882),.UNSPECIFIED.,.F.,.F.,(4,2,2,2,2,2,
2,2,3,4),(-0.322218774969075,-0.28335234068869,-0.24295415460927,-0.202510991809381,
-0.161749409589793,-0.121051618638299,-0.0807274114131348,-0.0404085956102785,
0.,5.45605715912487E-5),.UNSPECIFIED.);
#1977=B_SPLINE_CURVE_WITH_KNOTS('',3,(#70885,#70886,#70887,#70888,#70889,
#70890,#70891,#70892,#70893,#70894,#70895,#70896,#70897,#70898,#70899,#70900,
#70901,#70902,#70903,#70904,#70905,#70906,#70907,#70908,#70909,#70910,#70911,
#70912,#70913,#70914,#70915,#70916,#70917,#70918,#70919,#70920,#70921,#70922,
#70923,#70924,#70925,#70926,#70927,#70928,#70929,#70930),.UNSPECIFIED.,
 .T.,.F.,(4,2,2,2,2,2,2,2,2,2,2,2,2,2,2,2,2,2,2,2,2,2,4),(0.,0.00873810502121739,
0.0297335652237157,0.0616990112040461,0.0970631346087308,0.134531567849255,
0.174349671243284,0.215481948596841,0.255760444392016,0.290213292281182,
0.312334523108192,0.321849300142609,0.33060135081765,0.350070743937972,
0.378009519424791,0.418839524570214,0.455810185569734,0.495264052732823,
0.536510600809825,0.576903924585634,0.610567503992075,0.632496660166461,
0.646225650111759),.UNSPECIFIED.);
#1978=B_SPLINE_CURVE_WITH_KNOTS('',3,(#70931,#70932,#70933,#70934,#70935,
#70936,#70937,#70938,#70939,#70940,#70941,#70942,#70943,#70944,#70945,#70946,
#70947,#70948,#70949,#70950),.UNSPECIFIED.,.F.,.F.,(4,2,2,2,2,2,2,2,2,4),
(5.45605715912487E-5,0.039878400931096,0.0801684025650735,0.120697106682991,
0.160900180797334,0.201072985262158,0.241099781645388,0.281010189203807,
0.320981648387607,0.322308412283677),.UNSPECIFIED.);
#1979=B_SPLINE_CURVE_WITH_KNOTS('',3,(#70956,#70957,#70958,#70959,#70960,
#70961,#70962,#70963,#70964,#70965,#70966,#70967,#70968,#70969,#70970,#70971,
#70972,#70973,#70974,#70975,#70976,#70977,#70978,#70979,#70980,#70981,#70982,
#70983,#70984,#70985,#70986,#70987,#70988,#70989),.UNSPECIFIED.,.T.,.F.,
(4,2,2,2,2,2,2,2,2,2,2,2,2,2,2,2,4),(-0.315496151749696,-0.297141575074231,
-0.277415457408466,-0.25765681663082,-0.237703025077304,-0.217662758313652,
-0.197739942938581,-0.177848166453009,-0.157949624971573,-0.138056146550069,
-0.118152621681464,-0.0981620045445807,-0.0784580509416342,-0.058779887561761,
-0.039162115708029,-0.0195886853957665,0.),.UNSPECIFIED.);
#1980=B_SPLINE_CURVE_WITH_KNOTS('',3,(#70993,#70994,#70995,#70996,#70997,
#70998,#70999,#71000,#71001,#71002,#71003,#71004,#71005,#71006,#71007,#71008,
#71009,#71010,#71011,#71012,#71013),.UNSPECIFIED.,.F.,.F.,(4,2,2,2,2,2,
2,2,3,4),(-0.300833207677732,-0.264750113783143,-0.226774592484691,-0.187880911782623,
-0.149445134550555,-0.111523025139705,-0.0738351531346529,-0.0368602858553398,
0.,4.89537572855928E-5),.UNSPECIFIED.);
#1981=B_SPLINE_CURVE_WITH_KNOTS('',3,(#71016,#71017,#71018,#71019,#71020,
#71021,#71022,#71023,#71024,#71025,#71026,#71027,#71028,#71029,#71030,#71031,
#71032,#71033,#71034,#71035,#71036,#71037,#71038,#71039,#71040,#71041,#71042,
#71043,#71044,#71045,#71046,#71047,#71048,#71049,#71050,#71051,#71052,#71053,
#71054,#71055,#71056,#71057,#71058,#71059,#71060,#71061,#71062,#71063,#71064,
#71065),.UNSPECIFIED.,.T.,.F.,(4,2,2,2,2,2,2,2,2,2,2,2,2,2,2,2,2,2,2,2,
2,2,2,2,4),(0.,0.0174902552738314,0.0550858062300793,0.0874413426616621,
0.122435820544715,0.160114672538892,0.198542604931461,0.235366820436462,
0.265053282103129,0.280633075883739,0.29213323641515,0.297515032600734,
0.310503863061896,0.331904262314661,0.369614127865018,0.402708235043435,
0.438605222741391,0.477283719499992,0.515058936087459,0.552237125762763,
0.571453983183572,0.583426564445621,0.588721291414423,0.593833968276376,
0.601312691951912),.UNSPECIFIED.);
#1982=B_SPLINE_CURVE_WITH_KNOTS('',3,(#71066,#71067,#71068,#71069,#71070,
#71071,#71072,#71073,#71074,#71075,#71076,#71077,#71078,#71079,#71080,#71081,
#71082,#71083,#71084,#71085),.UNSPECIFIED.,.F.,.F.,(4,2,2,2,2,2,2,2,2,4),
(4.89537572855928E-5,0.0370578863318484,0.0747718108286307,0.112802698338598,
0.151373421073754,0.189198820460287,0.226350822172125,0.263015487542908,
0.299729496728428,0.30092650203114),.UNSPECIFIED.);
#1983=B_SPLINE_CURVE_WITH_KNOTS('',3,(#71091,#71092,#71093,#71094,#71095,
#71096,#71097,#71098,#71099,#71100,#71101,#71102,#71103,#71104,#71105,#71106,
#71107,#71108,#71109,#71110,#71111,#71112,#71113,#71114,#71115,#71116,#71117,
#71118,#71119,#71120,#71121,#71122,#71123,#71124),.UNSPECIFIED.,.T.,.F.,
(4,2,2,2,2,2,2,2,2,2,2,2,2,2,2,2,4),(-0.317346030989117,-0.297995934362178,
-0.277928934514266,-0.25753190568753,-0.237254031147267,-0.217134005118395,
-0.197471893982024,-0.178012846903565,-0.158589272536198,-0.138829010197109,
-0.118785798049446,-0.0986237170224576,-0.0783022451151404,-0.0583630651928147,
-0.0387567340203183,-0.0193856473349845,0.),.UNSPECIFIED.);
#1984=B_SPLINE_CURVE_WITH_KNOTS('',3,(#71130,#71131,#71132,#71133,#71134,
#71135,#71136,#71137,#71138,#71139,#71140,#71141,#71142,#71143,#71144,#71145,
#71146,#71147,#71148,#71149,#71150,#71151,#71152,#71153,#71154,#71155,#71156,
#71157,#71158,#71159,#71160,#71161,#71162,#71163,#71164,#71165,#71166,#71167,
#71168,#71169,#71170,#71171,#71172,#71173,#71174,#71175,#71176,#71177),
 .UNSPECIFIED.,.T.,.F.,(4,2,2,2,2,2,2,2,2,2,2,2,2,2,2,2,2,2,2,2,2,2,2,4),
(0.,0.0228087393460127,0.0549366750067231,0.105316123466778,0.150464710355334,
0.198392767561193,0.248535673308152,0.297889317955252,0.342588836115512,
0.369689349930825,0.38118255907791,0.391575762926861,0.41409606552552,0.445762906742391,
0.49601844873358,0.540990902106172,0.5885466312523,0.639053432053313,0.688811270073417,
0.738067260149195,0.767321634856702,0.778057915095754,0.786088157672185,
0.794230570233434),.UNSPECIFIED.);
#1985=B_SPLINE_CURVE_WITH_KNOTS('',3,(#71187,#71188,#71189,#71190,#71191,
#71192,#71193,#71194,#71195,#71196,#71197,#71198,#71199,#71200,#71201,#71202,
#71203,#71204),.UNSPECIFIED.,.F.,.F.,(4,2,2,2,2,2,2,2,4),(-0.322324642448947,
-0.283170110480757,-0.242893701651131,-0.20248068587249,-0.162079642170941,
-0.121214233737345,-0.0808314172024501,-0.0405092858788416,-5.16185884715199E-5),
 .UNSPECIFIED.);
#1986=B_SPLINE_CURVE_WITH_KNOTS('',3,(#71207,#71208,#71209,#71210,#71211,
#71212,#71213,#71214,#71215,#71216,#71217,#71218,#71219,#71220,#71221,#71222,
#71223,#71224,#71225,#71226,#71227,#71228,#71229,#71230,#71231,#71232,#71233,
#71234,#71235,#71236,#71237,#71238,#71239,#71240,#71241,#71242,#71243,#71244,
#71245,#71246,#71247,#71248,#71249,#71250,#71251,#71252),.UNSPECIFIED.,
 .T.,.F.,(4,2,2,2,2,2,2,2,2,2,2,2,2,2,2,2,2,2,2,2,2,2,4),(0.,0.0199662620991212,
0.0456036708902883,0.0866788818107017,0.123725228190072,0.163049723108265,
0.204263320607153,0.244685065062753,0.282205616781563,0.306135095944507,
0.316400114302969,0.325778046773526,0.346228604908454,0.374648057812432,
0.415526278856,0.452824745585227,0.492421691123166,0.533724430707627,0.574202604793491,
0.609288763055298,0.632836882279711,0.639650492487668,0.646612817989489),
 .UNSPECIFIED.);
#1987=B_SPLINE_CURVE_WITH_KNOTS('',3,(#71253,#71254,#71255,#71256,#71257,
#71258,#71259,#71260,#71261,#71262,#71263,#71264,#71265,#71266,#71267,#71268,
#71269,#71270,#71271,#71272,#71273,#71274,#71275),.UNSPECIFIED.,.F.,.F.,
(4,3,2,2,2,2,2,2,2,2,4),(-5.16185884715199E-5,0.,0.0397076196931033,0.0800974819415304,
0.12040505293073,0.161034734354159,0.201254995785147,0.241394874061776,
0.281378594841956,0.321302725625809,0.322201573923194),.UNSPECIFIED.);
#1988=B_SPLINE_CURVE_WITH_KNOTS('',3,(#71281,#71282,#71283,#71284,#71285,
#71286,#71287,#71288,#71289,#71290,#71291,#71292,#71293,#71294,#71295,#71296,
#71297,#71298,#71299,#71300,#71301,#71302,#71303,#71304,#71305,#71306,#71307,
#71308,#71309,#71310,#71311,#71312,#71313,#71314),.UNSPECIFIED.,.T.,.F.,
(4,2,2,2,2,2,2,2,2,2,2,2,2,2,2,2,4),(-0.315495812936942,-0.297578610010775,
-0.277904381048878,-0.25817151629882,-0.238219344577973,-0.218169621207347,
-0.198238419757734,-0.17832335818959,-0.158361527849011,-0.138384955393027,
-0.11845118141045,-0.0985400198722068,-0.0785529006156278,-0.0588481937293625,
-0.0391823435752262,-0.0195772166611429,0.),.UNSPECIFIED.);
#1989=B_SPLINE_CURVE_WITH_KNOTS('',3,(#71318,#71319,#71320,#71321,#71322,
#71323,#71324,#71325,#71326,#71327,#71328,#71329,#71330,#71331,#71332,#71333,
#71334,#71335,#71336,#71337,#71338),.UNSPECIFIED.,.F.,.F.,(4,2,2,2,2,2,
2,2,3,4),(-0.300885931061383,-0.266181870099638,-0.228550611403087,-0.190322958570215,
-0.151381013671441,-0.112981195344573,-0.0751269286008902,-0.0375398082342578,
0.,1.71168970408003E-6),.UNSPECIFIED.);
#1990=B_SPLINE_CURVE_WITH_KNOTS('',3,(#71341,#71342,#71343,#71344,#71345,
#71346,#71347,#71348,#71349,#71350,#71351,#71352,#71353,#71354,#71355,#71356,
#71357,#71358,#71359,#71360,#71361,#71362,#71363,#71364,#71365,#71366,#71367,
#71368,#71369,#71370,#71371,#71372,#71373,#71374,#71375,#71376,#71377,#71378,
#71379,#71380,#71381,#71382,#71383,#71384),.UNSPECIFIED.,.T.,.F.,(4,2,2,
2,2,2,2,2,2,2,2,2,2,2,2,2,2,2,2,2,2,4),(0.,0.0203990498424528,0.0469460048503852,
0.0848738261531423,0.120105716086176,0.157717798457702,0.196702634118489,
0.234570083384929,0.26706804740395,0.289415373886137,0.299224543866209,
0.308435731691215,0.329423643581651,0.359480802783041,0.392724216440543,
0.428045328293282,0.465901370645603,0.504950277233587,0.542785883592349,
0.572721848192345,0.594147464046836,0.603455879224188),.UNSPECIFIED.);
#1991=B_SPLINE_CURVE_WITH_KNOTS('',3,(#71385,#71386,#71387,#71388,#71389,
#71390,#71391,#71392,#71393,#71394,#71395,#71396,#71397,#71398,#71399,#71400,
#71401,#71402,#71403,#71404),.UNSPECIFIED.,.F.,.F.,(4,2,2,2,2,2,2,2,2,4),
(1.71168970408003E-6,0.03560475636088,0.0732078587183183,0.111112077341659,
0.149581682513832,0.187656524414964,0.225160409956919,0.262020719057387,
0.298624458310984,0.300851400504656),.UNSPECIFIED.);
#1992=B_SPLINE_CURVE_WITH_KNOTS('',3,(#71410,#71411,#71412,#71413,#71414,
#71415,#71416,#71417,#71418,#71419,#71420,#71421,#71422,#71423,#71424,#71425,
#71426,#71427,#71428,#71429,#71430,#71431,#71432,#71433,#71434,#71435,#71436,
#71437,#71438,#71439,#71440,#71441,#71442,#71443),.UNSPECIFIED.,.T.,.F.,
(4,2,2,2,2,2,2,2,2,2,2,2,2,2,2,2,4),(-0.317333830607944,-0.299024107107697,
-0.279222039008183,-0.259023226107041,-0.238552477892511,-0.218235524773687,
-0.198127155821481,-0.178585612581037,-0.15916910395986,-0.139501687049666,
-0.119527020809853,-0.0993901227013666,-0.0790439448424767,-0.0585635571160489,
-0.0387971326001783,-0.0193396977379661,0.),.UNSPECIFIED.);
#1993=B_SPLINE_CURVE_WITH_KNOTS('',3,(#71449,#71450,#71451,#71452,#71453,
#71454,#71455,#71456,#71457,#71458,#71459,#71460,#71461,#71462,#71463,#71464,
#71465,#71466,#71467,#71468,#71469,#71470,#71471,#71472,#71473,#71474,#71475,
#71476,#71477,#71478,#71479,#71480,#71481,#71482,#71483,#71484,#71485,#71486,
#71487,#71488,#71489,#71490,#71491,#71492,#71493,#71494,#71495,#71496,#71497,
#71498),.UNSPECIFIED.,.T.,.F.,(4,2,2,2,2,2,2,2,2,2,2,2,2,2,2,2,2,2,2,2,
2,2,2,2,4),(0.,0.015737764201583,0.0227091894460013,0.0379800462074193,
0.0610465319914851,0.109245059961081,0.151423734853957,0.196523645677437,
0.244746836023321,0.294515239039496,0.343325882195566,0.373646972099584,
0.391245029174184,0.398851690056153,0.40592016688941,0.42227530229542,0.447514818143624,
0.497644663183851,0.54189375504281,0.588933970108545,0.63880092723784,0.688513444191969,
0.736651553710438,0.778315039794088,0.793270637567377),.UNSPECIFIED.);
#1994=B_SPLINE_CURVE_WITH_KNOTS('',3,(#71508,#71509,#71510,#71511,#71512,
#71513,#71514,#71515,#71516,#71517,#71518,#71519,#71520,#71521,#71522,#71523,
#71524,#71525,#71526,#71527,#71528),.UNSPECIFIED.,.F.,.F.,(4,2,2,2,2,2,
2,2,3,4),(-0.322273947232433,-0.283099340074154,-0.242930612661278,-0.202553329014119,
-0.162116370789489,-0.121350728416329,-0.0806718074596314,-0.0403491998561452,
0.,4.9818029130011E-6),.UNSPECIFIED.);
#1995=B_SPLINE_CURVE_WITH_KNOTS('',3,(#71531,#71532,#71533,#71534,#71535,
#71536,#71537,#71538,#71539,#71540,#71541,#71542,#71543,#71544,#71545,#71546,
#71547,#71548,#71549,#71550,#71551,#71552,#71553,#71554,#71555,#71556,#71557,
#71558,#71559,#71560,#71561,#71562,#71563,#71564,#71565,#71566,#71567,#71568,
#71569,#71570,#71571,#71572,#71573,#71574,#71575,#71576,#71577,#71578),
 .UNSPECIFIED.,.T.,.F.,(4,2,2,2,2,2,2,2,2,2,2,2,2,2,2,2,2,2,2,2,2,2,2,4),
(0.,0.00669853431147558,0.012713180910249,0.0259817703783651,0.0457978017341711,
0.0862472748334269,0.121364061808267,0.159062921898553,0.19950502707867,
0.239781234850052,0.279191609031118,0.303790559229149,0.318543386024955,
0.331106263508047,0.345588545654211,0.368909480379511,0.409771179994493,
0.445823314050088,0.48429238576702,0.525273376653319,0.565632394938103,
0.604062186616965,0.630829326260229,0.644914916016497),.UNSPECIFIED.);
#1996=B_SPLINE_CURVE_WITH_KNOTS('',3,(#71579,#71580,#71581,#71582,#71583,
#71584,#71585,#71586,#71587,#71588,#71589,#71590,#71591,#71592,#71593,#71594,
#71595,#71596,#71597,#71598),.UNSPECIFIED.,.F.,.F.,(4,2,2,2,2,2,2,2,2,4),
(4.9818029130011E-6,0.0399314412331601,0.0803482982070822,0.12064699164969,
0.161109119663353,0.201310573704939,0.241498999732639,0.28154854111158,
0.3214703171836,0.322256971972009),.UNSPECIFIED.);
#1997=B_SPLINE_CURVE_WITH_KNOTS('',3,(#71604,#71605,#71606,#71607,#71608,
#71609,#71610,#71611,#71612,#71613,#71614,#71615,#71616,#71617,#71618,#71619,
#71620,#71621,#71622,#71623,#71624,#71625,#71626,#71627,#71628,#71629,#71630,
#71631,#71632,#71633,#71634,#71635,#71636,#71637),.UNSPECIFIED.,.T.,.F.,
(4,2,2,2,2,2,2,2,2,2,2,2,2,2,2,2,4),(-0.315499076058523,-0.2972402057324,
-0.277597963621351,-0.257882336638775,-0.238128502172578,-0.21817417918185,
-0.198149453137237,-0.178227840344242,-0.15831825446875,-0.1383881085649,
-0.118467083477265,-0.0985607662514616,-0.0785988845860134,-0.0588944188066577,
-0.0392078558436279,-0.0195791697313611,0.),.UNSPECIFIED.);
#1998=B_SPLINE_CURVE_WITH_KNOTS('',3,(#71641,#71642,#71643,#71644,#71645,
#71646,#71647,#71648,#71649,#71650,#71651,#71652,#71653,#71654,#71655,#71656,
#71657,#71658),.UNSPECIFIED.,.F.,.F.,(4,2,2,2,2,2,2,2,4),(-0.300918316190137,
-0.265745760462606,-0.228515752189276,-0.190575887865076,-0.151992690861013,
-0.113365511833562,-0.0753078026554617,-0.0376144696996458,-2.55858819131527E-5),
 .UNSPECIFIED.);
#1999=B_SPLINE_CURVE_WITH_KNOTS('',3,(#71661,#71662,#71663,#71664,#71665,
#71666,#71667,#71668,#71669,#71670,#71671,#71672,#71673,#71674,#71675,#71676,
#71677,#71678,#71679,#71680,#71681,#71682,#71683,#71684,#71685,#71686,#71687,
#71688,#71689,#71690,#71691,#71692,#71693,#71694,#71695,#71696,#71697,#71698,
#71699,#71700,#71701,#71702,#71703,#71704,#71705,#71706),.UNSPECIFIED.,
 .T.,.F.,(4,2,2,2,2,2,2,2,2,2,2,2,2,2,2,2,2,2,2,2,2,2,4),(0.,0.00760469797038185,
0.0225312774191947,0.0419560879026201,0.0780731809945311,0.111552300436574,
0.147532803522562,0.185950797597975,0.223692437106523,0.260678361683232,
0.284505934676511,0.300664678877027,0.307944044053357,0.323797732599743,
0.34634348054576,0.384453328157906,0.418674376842058,0.455279169648842,
0.4942078035792,0.531921981089708,0.568780963126567,0.59189655980923,0.602188976422285),
 .UNSPECIFIED.);
#2000=B_SPLINE_CURVE_WITH_KNOTS('',3,(#71707,#71708,#71709,#71710,#71711,
#71712,#71713,#71714,#71715,#71716,#71717,#71718,#71719,#71720,#71721,#71722,
#71723,#71724,#71725,#71726,#71727,#71728,#71729),.UNSPECIFIED.,.F.,.F.,
(4,3,2,2,2,2,2,2,2,2,4),(-2.55858819131527E-5,0.,0.035530362708851,0.0731447096843527,
0.110848045581484,0.148930238186376,0.187583389005476,0.22544323105114,
0.262636684542578,0.299315223853983,0.300828949622202),.UNSPECIFIED.);
#2001=B_SPLINE_CURVE_WITH_KNOTS('',3,(#71735,#71736,#71737,#71738,#71739,
#71740,#71741,#71742,#71743,#71744,#71745,#71746,#71747,#71748,#71749,#71750,
#71751,#71752,#71753,#71754,#71755,#71756,#71757,#71758,#71759,#71760,#71761,
#71762,#71763,#71764,#71765,#71766,#71767,#71768),.UNSPECIFIED.,.T.,.F.,
(4,2,2,2,2,2,2,2,2,2,2,2,2,2,2,2,4),(-0.317339667561293,-0.298795703489905,
-0.279184279507441,-0.259230080396284,-0.238777447832178,-0.218410892308438,
-0.198226466872123,-0.17819786279233,-0.158733004447799,-0.139311936420403,
-0.119571300281915,-0.0995322929494558,-0.0793315274247309,-0.0589518315551108,
-0.0389982306107753,-0.0193762192206639,0.),.UNSPECIFIED.);
#2002=B_SPLINE_CURVE_WITH_KNOTS('',3,(#71772,#71773,#71774,#71775,#71776,
#71777,#71778,#71779,#71780,#71781,#71782,#71783,#71784,#71785,#71786,#71787,
#71788,#71789,#71790,#71791,#71792),.UNSPECIFIED.,.F.,.F.,(4,2,2,2,2,2,
2,2,3,4),(-0.322274258494419,-0.282879524331831,-0.242837204088746,-0.202563596153524,
-0.162140589147018,-0.121726321036062,-0.0807483977258747,-0.0403043194683415,
0.,1.88449534006124E-5),.UNSPECIFIED.);
#2003=B_SPLINE_CURVE_WITH_KNOTS('',3,(#71795,#71796,#71797,#71798,#71799,
#71800,#71801,#71802,#71803,#71804,#71805,#71806,#71807,#71808,#71809,#71810,
#71811,#71812,#71813,#71814,#71815,#71816,#71817,#71818,#71819,#71820,#71821,
#71822,#71823,#71824,#71825,#71826,#71827,#71828,#71829,#71830,#71831,#71832,
#71833,#71834,#71835,#71836,#71837,#71838,#71839,#71840,#71841,#71842,#71843,
#71844,#71845,#71846),.UNSPECIFIED.,.T.,.F.,(4,2,2,2,2,2,2,2,2,2,2,2,2,
2,2,2,2,2,2,2,2,2,2,2,2,4),(0.,0.0269134229306956,0.0409782021484428,0.0467989934801527,
0.0519956902626756,0.0634124484114814,0.0804691074750597,0.117157819874466,
0.151328717625095,0.188057436113526,0.227289028229523,0.267875360744782,
0.307235789391439,0.342887885734985,0.359578238118146,0.370976269015013,
0.376151692845378,0.388053248420623,0.406799989243721,0.44617600536186,
0.481057576445251,0.518571261952553,0.558803877079373,0.59508754338857,
0.616643521243479,0.643958608562694),.UNSPECIFIED.);
#2004=B_SPLINE_CURVE_WITH_KNOTS('',3,(#71847,#71848,#71849,#71850,#71851,
#71852,#71853,#71854,#71855,#71856,#71857,#71858,#71859,#71860,#71861,#71862,
#71863,#71864,#71865,#71866),.UNSPECIFIED.,.F.,.F.,(4,2,2,2,2,2,2,2,2,4),
(1.88449534006124E-5,0.0395684033320943,0.0800690626690298,0.120435494836762,
0.160752649183436,0.201406338324787,0.241624765872817,0.281764951499659,
0.321747064678894,0.322268162535351),.UNSPECIFIED.);
#2005=B_SPLINE_CURVE_WITH_KNOTS('',3,(#71872,#71873,#71874,#71875,#71876,
#71877,#71878,#71879,#71880,#71881,#71882,#71883,#71884,#71885,#71886,#71887,
#71888,#71889,#71890,#71891,#71892,#71893,#71894,#71895,#71896,#71897,#71898,
#71899,#71900,#71901,#71902,#71903,#71904,#71905),.UNSPECIFIED.,.T.,.F.,
(4,2,2,2,2,2,2,2,2,2,2,2,2,2,2,2,4),(-0.315507475062968,-0.297429255241995,
-0.27782589295879,-0.258150653180531,-0.238413338898343,-0.218658308519064,
-0.198562599760213,-0.178604336309516,-0.158695105820558,-0.138763144550359,
-0.118818027328735,-0.0988989879663173,-0.0789817611557068,-0.0589745295578617,
-0.0392695744228467,-0.0196038790058241,0.),.UNSPECIFIED.);
#2006=B_SPLINE_CURVE_WITH_KNOTS('',3,(#71909,#71910,#71911,#71912,#71913,
#71914,#71915,#71916,#71917,#71918,#71919,#71920,#71921,#71922,#71923,#71924,
#71925,#71926),.UNSPECIFIED.,.F.,.F.,(4,2,2,2,2,2,2,2,4),(-0.300983756064892,
-0.265266012119335,-0.228384761090753,-0.190829162479439,-0.152502737010859,
-0.113726790690218,-0.0754803593170012,-0.0376768011524792,-5.89284099797474E-5),
 .UNSPECIFIED.);
#2007=B_SPLINE_CURVE_WITH_KNOTS('',3,(#71929,#71930,#71931,#71932,#71933,
#71934,#71935,#71936,#71937,#71938,#71939,#71940,#71941,#71942,#71943,#71944,
#71945,#71946,#71947,#71948,#71949,#71950,#71951,#71952,#71953,#71954,#71955,
#71956,#71957,#71958,#71959,#71960,#71961,#71962,#71963,#71964,#71965,#71966,
#71967,#71968,#71969,#71970,#71971,#71972,#71973,#71974,#71975,#71976,#71977,
#71978,#71979,#71980,#71981,#71982,#71983,#71984),.UNSPECIFIED.,.T.,.F.,
(4,2,2,2,2,2,2,2,2,2,2,2,2,2,2,2,2,2,2,2,2,2,2,2,2,2,2,4),(0.,0.0195543842904808,
0.027312393989098,0.0324982300196665,0.0348519738504469,0.0403876189278208,
0.0496853599646738,0.082443001531438,0.112274367628169,0.145234456597813,
0.180889844249304,0.219274867422076,0.256429259960666,0.288239963951727,
0.314854389628641,0.324153776360445,0.329896973336055,0.332440267879227,
0.338012281194982,0.34657211619618,0.37067856846271,0.39932757792812,0.431417294726784,
0.466348706046538,0.50396323936281,0.542162628101251,0.565650967054169,
0.599691088329776),.UNSPECIFIED.);
#2008=B_SPLINE_CURVE_WITH_KNOTS('',3,(#71985,#71986,#71987,#71988,#71989,
#71990,#71991,#71992,#71993,#71994,#71995,#71996,#71997,#71998,#71999,#72000,
#72001,#72002,#72003,#72004,#72005,#72006,#72007),.UNSPECIFIED.,.F.,.F.,
(4,3,2,2,2,2,2,2,2,2,4),(-5.89284099797474E-5,0.,0.0356142768925199,0.072932941351032,
0.110609867053781,0.148407439096288,0.186642520710408,0.225409711009659,
0.2629940508189,0.299916704084242,0.300810914179693),.UNSPECIFIED.);
#2009=B_SPLINE_CURVE_WITH_KNOTS('',3,(#72013,#72014,#72015,#72016,#72017,
#72018,#72019,#72020,#72021,#72022,#72023,#72024,#72025,#72026,#72027,#72028,
#72029,#72030,#72031,#72032,#72033,#72034,#72035,#72036,#72037,#72038,#72039,
#72040,#72041,#72042,#72043,#72044,#72045,#72046),.UNSPECIFIED.,.T.,.F.,
(4,2,2,2,2,2,2,2,2,2,2,2,2,2,2,2,4),(-0.317367226772087,-0.29856007747775,
-0.279107507122395,-0.259344623570977,-0.239162101406073,-0.218785432411179,
-0.198555314522819,-0.178473874575583,-0.15889896570101,-0.139474421591269,
-0.120014537391426,-0.100004403392165,-0.0799235976831349,-0.0596943289774754,
-0.0393180790414062,-0.0194978929382608,0.),.UNSPECIFIED.);
#2010=B_SPLINE_CURVE_WITH_KNOTS('',3,(#72050,#72051,#72052,#72053,#72054,
#72055,#72056,#72057,#72058,#72059,#72060,#72061,#72062,#72063,#72064,#72065,
#72066,#72067,#72068,#72069,#72070),.UNSPECIFIED.,.F.,.F.,(4,2,2,2,2,2,
2,2,3,4),(-0.322235936119025,-0.282555513840953,-0.242603866140275,-0.202466099519466,
-0.162118431397947,-0.121692507545716,-0.0809194365641546,-0.0403047888943224,
0.,8.24103542715754E-5),.UNSPECIFIED.);
#2011=B_SPLINE_CURVE_WITH_KNOTS('',3,(#72073,#72074,#72075,#72076,#72077,
#72078,#72079,#72080,#72081,#72082,#72083,#72084,#72085,#72086,#72087,#72088,
#72089,#72090,#72091,#72092,#72093,#72094,#72095,#72096,#72097,#72098,#72099,
#72100,#72101,#72102,#72103,#72104,#72105,#72106,#72107,#72108),
 .UNSPECIFIED.,.T.,.F.,(4,2,2,2,2,2,2,2,2,2,2,2,2,2,2,2,2,4),(0.,0.0399541104210797,
0.0799101633971029,0.120042188031122,0.160349494010668,0.200700062460712,
0.24066914974901,0.281146928548852,0.321688268053878,0.361827692831203,
0.401937446249913,0.441912733333203,0.482224630787991,0.523014478229367,
0.563360237936025,0.603655558777084,0.623959945526864,0.644496878440061),
 .UNSPECIFIED.);
#2012=B_SPLINE_CURVE_WITH_KNOTS('',3,(#72109,#72110,#72111,#72112,#72113,
#72114,#72115,#72116,#72117,#72118,#72119,#72120,#72121,#72122,#72123,#72124,
#72125,#72126,#72127,#72128),.UNSPECIFIED.,.F.,.F.,(4,2,2,2,2,2,2,2,2,4),
(8.24103542715754E-5,0.0391110548112336,0.0796930627605846,0.12022456504364,
0.160555221999647,0.200926013596631,0.241765756700222,0.281979900518358,
0.322064242067825,0.322325169710773),.UNSPECIFIED.);
#2013=B_SPLINE_CURVE_WITH_KNOTS('',3,(#72134,#72135,#72136,#72137,#72138,
#72139,#72140,#72141,#72142,#72143,#72144,#72145,#72146,#72147,#72148,#72149,
#72150,#72151,#72152,#72153,#72154,#72155,#72156,#72157,#72158,#72159,#72160,
#72161,#72162,#72163,#72164,#72165,#72166,#72167),.UNSPECIFIED.,.T.,.F.,
(4,2,2,2,2,2,2,2,2,2,2,2,2,2,2,2,4),(-0.315519596162171,-0.297809213750164,
-0.278229052184091,-0.258601131851469,-0.238901505305988,-0.219155579631688,
-0.19901849790277,-0.179030986117222,-0.15911985913336,-0.139182788191571,
-0.11919620309571,-0.0992213413463237,-0.0793002802766647,-0.0593770243920267,
-0.0393451090122846,-0.0196454507796741,0.),.UNSPECIFIED.);
#2014=B_SPLINE_CURVE_WITH_KNOTS('',3,(#72171,#72172,#72173,#72174,#72175,
#72176,#72177,#72178,#72179,#72180,#72181,#72182,#72183,#72184,#72185,#72186,
#72187,#72188),.UNSPECIFIED.,.F.,.F.,(4,2,2,2,2,2,2,2,4),(-0.300994263979636,
-0.264790681083084,-0.228121553138037,-0.190934646109778,-0.153029416903194,
-0.114459349502728,-0.0758034579641479,-0.0377146753865591,-9.89973092749212E-6),
 .UNSPECIFIED.);
#2015=B_SPLINE_CURVE_WITH_KNOTS('',3,(#72191,#72192,#72193,#72194,#72195,
#72196,#72197,#72198,#72199,#72200,#72201,#72202,#72203,#72204,#72205,#72206,
#72207,#72208,#72209,#72210,#72211,#72212,#72213,#72214,#72215,#72216,#72217,
#72218,#72219,#72220,#72221,#72222,#72223,#72224,#72225,#72226,#72227,#72228,
#72229,#72230,#72231,#72232,#72233,#72234,#72235,#72236,#72237,#72238,#72239,
#72240),.UNSPECIFIED.,.T.,.F.,(4,2,2,2,2,2,2,2,2,2,2,2,2,2,2,2,2,2,2,2,
2,2,2,2,4),(0.,0.0307690129943918,0.0457737289117332,0.0564496066162463,
0.067013357847641,0.0815094903801632,0.112271321654035,0.143533118871858,
0.177384865979269,0.213742800882818,0.251861559810511,0.288869905007967,
0.326261511254301,0.342991018079337,0.354087677704956,0.359080348486155,
0.370267767881213,0.38720643207021,0.422871977549177,0.455142045306466,
0.489970533764269,0.527422511009619,0.559321254860859,0.577641902721842,
0.599527726299083),.UNSPECIFIED.);
#2016=B_SPLINE_CURVE_WITH_KNOTS('',3,(#72241,#72242,#72243,#72244,#72245,
#72246,#72247,#72248,#72249,#72250,#72251,#72252,#72253,#72254,#72255,#72256,
#72257,#72258,#72259,#72260,#72261,#72262,#72263),.UNSPECIFIED.,.F.,.F.,
(4,3,2,2,2,2,2,2,2,2,4),(-9.89973092749212E-6,0.,0.0355811345666444,0.073230471527062,
0.110862998883392,0.148561283179237,0.186608826750277,0.225220645754983,
0.263129936848216,0.300376106774349,0.300875213706327),.UNSPECIFIED.);
#2017=B_SPLINE_CURVE_WITH_KNOTS('',3,(#72269,#72270,#72271,#72272,#72273,
#72274,#72275,#72276,#72277,#72278,#72279,#72280,#72281,#72282,#72283,#72284,
#72285,#72286,#72287,#72288,#72289,#72290,#72291,#72292,#72293,#72294,#72295,
#72296,#72297,#72298,#72299,#72300,#72301,#72302),.UNSPECIFIED.,.T.,.F.,
(4,2,2,2,2,2,2,2,2,2,2,2,2,2,2,2,4),(-0.317410329630175,-0.298796136347515,
-0.279435032432556,-0.259850090267512,-0.239920497281374,-0.219468774491086,
-0.199092484550111,-0.178893042770457,-0.158849925953669,-0.139369604600803,
-0.119951222078813,-0.100224265505886,-0.0801908841414913,-0.0600071079341823,
-0.0396435087199044,-0.0196564465565322,0.),.UNSPECIFIED.);
#2018=B_SPLINE_CURVE_WITH_KNOTS('',3,(#72306,#72307,#72308,#72309,#72310,
#72311,#72312,#72313,#72314,#72315,#72316,#72317,#72318,#72319,#72320,#72321,
#72322,#72323,#72324,#72325,#72326),.UNSPECIFIED.,.F.,.F.,(4,2,2,2,2,2,
2,2,3,4),(-0.322296005070645,-0.282691705710254,-0.242785602353315,-0.202757253805612,
-0.162487760230491,-0.122052055744033,-0.0816187550391033,-0.0405188529317101,
0.,6.19087250895434E-5),.UNSPECIFIED.);
#2019=B_SPLINE_CURVE_WITH_KNOTS('',3,(#72329,#72330,#72331,#72332,#72333,
#72334,#72335,#72336,#72337,#72338,#72339,#72340,#72341,#72342,#72343,#72344,
#72345,#72346,#72347,#72348,#72349,#72350,#72351,#72352,#72353,#72354,#72355,
#72356,#72357,#72358,#72359,#72360,#72361,#72362,#72363,#72364),
 .UNSPECIFIED.,.T.,.F.,(4,2,2,2,2,2,2,2,2,2,2,2,2,2,2,2,2,4),(0.,0.0399541104210688,
0.079910163397041,0.120042188031002,0.160349494010565,0.200700062460793,
0.240669149749168,0.281146928548791,0.321688268053567,0.361827692830774,
0.401937446249555,0.441912733332932,0.482224630787771,0.52301447822922,
0.563360237936112,0.603655558777431,0.623959945527353,0.644496878440584),
 .UNSPECIFIED.);
#2020=B_SPLINE_CURVE_WITH_KNOTS('',3,(#72365,#72366,#72367,#72368,#72369,
#72370,#72371,#72372,#72373,#72374,#72375,#72376,#72377,#72378,#72379,#72380,
#72381,#72382,#72383,#72384),.UNSPECIFIED.,.F.,.F.,(4,2,2,2,2,2,2,2,2,4),
(6.19087250895434E-5,0.0393985606342027,0.0797735668134333,0.120209511040999,
0.160547540179541,0.200870649931096,0.241547367613034,0.281769090282563,
0.321913645565474,0.322291378416777),.UNSPECIFIED.);
#2021=B_SPLINE_CURVE_WITH_KNOTS('',3,(#72390,#72391,#72392,#72393,#72394,
#72395,#72396,#72397,#72398,#72399,#72400,#72401,#72402,#72403,#72404,#72405,
#72406,#72407,#72408,#72409,#72410,#72411,#72412,#72413,#72414,#72415,#72416,
#72417,#72418,#72419,#72420,#72421,#72422,#72423),.UNSPECIFIED.,.T.,.F.,
(4,2,2,2,2,2,2,2,2,2,2,2,2,2,2,2,4),(-0.315533165774014,-0.297436528606874,
-0.277865413070616,-0.258265642221209,-0.238590196427937,-0.218847406594884,
-0.199084884742368,-0.178940376230227,-0.158949603464515,-0.139041131952,
-0.119136887716367,-0.0992245788045587,-0.0793233934924771,-0.0594023812818215,
-0.0393747941743775,-0.0196670977017911,0.),.UNSPECIFIED.);
#2022=B_SPLINE_CURVE_WITH_KNOTS('',3,(#72427,#72428,#72429,#72430,#72431,
#72432,#72433,#72434,#72435,#72436,#72437,#72438,#72439,#72440,#72441,#72442,
#72443,#72444,#72445,#72446,#72447),.UNSPECIFIED.,.F.,.F.,(4,2,2,2,2,2,
2,2,3,4),(-0.30096860817143,-0.264198560924269,-0.227582862782118,-0.19073044092391,
-0.153208886894111,-0.115042102447996,-0.0761891983612259,-0.0378539075755994,
0.,0.000101239354754264),.UNSPECIFIED.);
#2023=B_SPLINE_CURVE_WITH_KNOTS('',3,(#72450,#72451,#72452,#72453,#72454,
#72455,#72456,#72457,#72458,#72459,#72460,#72461,#72462,#72463,#72464,#72465,
#72466,#72467,#72468,#72469,#72470,#72471,#72472,#72473,#72474,#72475,#72476,
#72477,#72478,#72479,#72480,#72481,#72482,#72483,#72484,#72485),
 .UNSPECIFIED.,.T.,.F.,(4,2,2,2,2,2,2,2,2,2,2,2,2,2,2,2,2,4),(0.,0.0355202696275906,
0.0730229242189133,0.109881947977843,0.147332215350788,0.185244244850189,
0.223245130804677,0.259644256143498,0.29483879750671,0.330228485401298,
0.366554345813953,0.404791218290754,0.442165216585822,0.480056587413159,
0.518291371432835,0.552548743061451,0.588529668384299,0.599949959180055),
 .UNSPECIFIED.);
#2024=B_SPLINE_CURVE_WITH_KNOTS('',3,(#72486,#72487,#72488,#72489,#72490,
#72491,#72492,#72493,#72494,#72495,#72496,#72497,#72498,#72499,#72500,#72501,
#72502,#72503,#72504,#72505),.UNSPECIFIED.,.F.,.F.,(4,2,2,2,2,2,2,2,2,4),
(0.000101239354754264,0.036436712581457,0.0733520329498323,0.110663930226565,
0.14833558961367,0.186139232912933,0.224385561227797,0.263172520415901,
0.300809097706522,0.30100062624167),.UNSPECIFIED.);
#2025=B_SPLINE_CURVE_WITH_KNOTS('',3,(#72511,#72512,#72513,#72514,#72515,
#72516,#72517,#72518,#72519,#72520,#72521,#72522,#72523,#72524,#72525,#72526,
#72527,#72528,#72529,#72530,#72531,#72532,#72533,#72534,#72535,#72536,#72537,
#72538,#72539,#72540,#72541,#72542,#72543,#72544),.UNSPECIFIED.,.T.,.F.,
(4,2,2,2,2,2,2,2,2,2,2,2,2,2,2,2,4),(-0.317465401521424,-0.298534881991798,
-0.279185985931209,-0.259748990694432,-0.24000764059935,-0.219844234330012,
-0.199433889771009,-0.179162910845198,-0.159055689337048,-0.13946094284028,
-0.120029518902961,-0.100576113834194,-0.0805716695602433,-0.060486845933592,
-0.0402456000833756,-0.0198516982892401,0.),.UNSPECIFIED.);
#2026=B_SPLINE_CURVE_WITH_KNOTS('',3,(#72548,#72549,#72550,#72551,#72552,
#72553,#72554,#72555,#72556,#72557,#72558,#72559,#72560,#72561,#72562,#72563,
#72564,#72565,#72566,#72567),.UNSPECIFIED.,.F.,.F.,(4,2,2,2,2,2,2,2,2,4),
(-0.32240779513704,-0.322309948170045,-0.282207124514264,-0.242258251398018,
-0.202316548946315,-0.162196977851497,-0.121858894724617,-0.0814269356067834,
-0.0406404219381981,-1.19643287557059E-5),.UNSPECIFIED.);
#2027=B_SPLINE_CURVE_WITH_KNOTS('',3,(#72570,#72571,#72572,#72573,#72574,
#72575,#72576,#72577,#72578,#72579,#72580,#72581,#72582,#72583,#72584,#72585,
#72586,#72587,#72588,#72589,#72590,#72591,#72592,#72593,#72594,#72595,#72596,
#72597,#72598,#72599,#72600,#72601,#72602,#72603,#72604,#72605),
 .UNSPECIFIED.,.T.,.F.,(4,2,2,2,2,2,2,2,2,2,2,2,2,2,2,2,2,4),(0.,0.0399541104211151,
0.0799101633971823,0.120042188031122,0.160349494010512,0.200700062460637,
0.240669149748722,0.281146928548262,0.321688268053098,0.361827692830207,
0.401937446248661,0.441912733331772,0.482224630786321,0.523014478227461,
0.563360237933615,0.603655558774151,0.623959945524341,0.64449687843778),
 .UNSPECIFIED.);
#2028=B_SPLINE_CURVE_WITH_KNOTS('',3,(#72606,#72607,#72608,#72609,#72610,
#72611,#72612,#72613,#72614,#72615,#72616,#72617,#72618,#72619,#72620,#72621,
#72622,#72623,#72624,#72625,#72626),.UNSPECIFIED.,.F.,.F.,(4,3,2,2,2,2,
2,2,2,4),(-1.19643287557059E-5,0.,0.0390447294337543,0.0794373447788432,
0.120030120161568,0.160589432579093,0.200937759073155,0.241289481748733,
0.282079104740989,0.322210485893345),.UNSPECIFIED.);
#2029=B_SPLINE_CURVE_WITH_KNOTS('',3,(#72632,#72633,#72634,#72635,#72636,
#72637,#72638,#72639,#72640,#72641,#72642,#72643,#72644,#72645,#72646,#72647,
#72648,#72649,#72650,#72651,#72652,#72653,#72654,#72655,#72656,#72657,#72658,
#72659,#72660,#72661,#72662,#72663,#72664,#72665),.UNSPECIFIED.,.T.,.F.,
(4,2,2,2,2,2,2,2,2,2,2,2,2,2,2,2,4),(-0.315548571684421,-0.297773351174838,
-0.278176003062129,-0.258598189537295,-0.238976726468293,-0.219281852001301,
-0.199535221016545,-0.179391819962517,-0.159399197996224,-0.139486889367128,
-0.11954902226534,-0.0995560164366063,-0.0795697129165012,-0.059641377251603,
-0.0397234123798072,-0.0197072139785503,0.),.UNSPECIFIED.);
#2030=B_SPLINE_CURVE_WITH_KNOTS('',3,(#72669,#72670,#72671,#72672,#72673,
#72674,#72675,#72676,#72677,#72678,#72679,#72680,#72681,#72682,#72683,#72684,
#72685,#72686,#72687,#72688,#72689,#72690,#72691),.UNSPECIFIED.,.F.,.F.,
(4,2,2,2,2,2,2,2,2,3,4),(-0.301044807969637,-0.301018227949179,-0.263705218785146,
-0.226969493307541,-0.190315888874966,-0.153176105293676,-0.115309971137163,
-0.0767479418711244,-0.0380966018702412,0.,0.000121343267829525),
 .UNSPECIFIED.);
#2031=B_SPLINE_CURVE_WITH_KNOTS('',3,(#72694,#72695,#72696,#72697,#72698,
#72699,#72700,#72701,#72702,#72703,#72704,#72705,#72706,#72707,#72708,#72709,
#72710,#72711,#72712,#72713,#72714,#72715,#72716,#72717,#72718,#72719,#72720,
#72721,#72722,#72723,#72724,#72725,#72726,#72727,#72728,#72729),
 .UNSPECIFIED.,.T.,.F.,(4,2,2,2,2,2,2,2,2,2,2,2,2,2,2,2,2,4),(0.,0.035520269627724,
0.0730229242195072,0.109881947979195,0.147332215353038,0.185244244853688,
0.223245130809801,0.259644256150227,0.294838797515063,0.330228485411425,
0.366554345826138,0.404791218305404,0.442165216602898,0.480056587432884,
0.518291371455665,0.55254874308709,0.588529668413202,0.599949959209379),
 .UNSPECIFIED.);
#2032=B_SPLINE_CURVE_WITH_KNOTS('',3,(#72730,#72731,#72732,#72733,#72734,
#72735,#72736,#72737,#72738,#72739,#72740,#72741,#72742,#72743,#72744,#72745,
#72746,#72747),.UNSPECIFIED.,.F.,.F.,(4,2,2,2,2,2,2,2,4),(0.000121343267829525,
0.0366203311667738,0.0742978920120693,0.111163641608319,0.148850930352528,
0.186555371217545,0.224549916816768,0.263085201813925,0.301031791575559),
 .UNSPECIFIED.);
#2033=B_SPLINE_CURVE_WITH_KNOTS('',3,(#72753,#72754,#72755,#72756,#72757,
#72758,#72759,#72760,#72761,#72762,#72763,#72764,#72765,#72766,#72767,#72768,
#72769,#72770,#72771,#72772,#72773,#72774,#72775,#72776,#72777,#72778,#72779,
#72780,#72781,#72782,#72783,#72784,#72785,#72786),.UNSPECIFIED.,.T.,.F.,
(4,2,2,2,2,2,2,2,2,2,2,2,2,2,2,2,4),(-0.317520789214244,-0.298884746791165,
-0.279463280388508,-0.260109693987934,-0.240554297200441,-0.220653647372428,
-0.200213118904547,-0.179844668128175,-0.159642952730947,-0.139584427087022,
-0.120082689424148,-0.100665871473826,-0.0809522571001296,-0.0609189321719877,
-0.0407632761903409,-0.0204362576967705,0.),.UNSPECIFIED.);
#2034=B_SPLINE_CURVE_WITH_KNOTS('',3,(#72790,#72791,#72792,#72793,#72794,
#72795,#72796,#72797,#72798,#72799,#72800,#72801,#72802,#72803,#72804,#72805,
#72806,#72807,#72808,#72809,#72810,#72811,#72812),.UNSPECIFIED.,.F.,.F.,
(4,2,2,2,2,2,2,2,2,3,4),(-0.322425076967677,-0.32231349089565,-0.282145629075095,
-0.242145113385566,-0.202238999895162,-0.162228469192213,-0.121978668171416,
-0.0815481694877585,-0.0411040729638831,0.,7.74523776212593E-6),
 .UNSPECIFIED.);
#2035=B_SPLINE_CURVE_WITH_KNOTS('',3,(#72815,#72816,#72817,#72818,#72819,
#72820,#72821,#72822,#72823,#72824,#72825,#72826,#72827,#72828,#72829,#72830,
#72831,#72832,#72833,#72834,#72835,#72836,#72837,#72838,#72839,#72840,#72841,
#72842,#72843,#72844,#72845,#72846,#72847,#72848,#72849,#72850),
 .UNSPECIFIED.,.T.,.F.,(4,2,2,2,2,2,2,2,2,2,2,2,2,2,2,2,2,4),(0.,0.0399541104210824,
0.0799101633971159,0.120042188031233,0.160349494011014,0.200700062461302,
0.240669149749529,0.281146928549236,0.321688268054275,0.361827692831736,
0.401937446250701,0.441912733334188,0.482224630789035,0.523014478230616,
0.56336023793752,0.603655558779058,0.623959945529218,0.644496878442553),
 .UNSPECIFIED.);
#2036=B_SPLINE_CURVE_WITH_KNOTS('',3,(#72851,#72852,#72853,#72854,#72855,
#72856,#72857,#72858,#72859,#72860,#72861,#72862,#72863,#72864,#72865,#72866,
#72867,#72868),.UNSPECIFIED.,.F.,.F.,(4,2,2,2,2,2,2,2,4),(7.74523776212593E-6,
0.0396065933934371,0.0799124406986436,0.120313242028674,0.160793977016685,
0.201168607760791,0.24148430748624,0.282102424584037,0.322225812953619),
 .UNSPECIFIED.);
#2037=B_SPLINE_CURVE_WITH_KNOTS('',3,(#72874,#72875,#72876,#72877,#72878,
#72879,#72880,#72881,#72882,#72883,#72884,#72885,#72886,#72887,#72888,#72889,
#72890,#72891,#72892,#72893,#72894,#72895,#72896,#72897,#72898,#72899,#72900,
#72901,#72902,#72903,#72904,#72905,#72906,#72907),.UNSPECIFIED.,.T.,.F.,
(4,2,2,2,2,2,2,2,2,2,2,2,2,2,2,2,4),(-0.315562181390567,-0.297399338673171,
-0.277783079139259,-0.258210583754242,-0.238617327429595,-0.218950639127311,
-0.19921201502306,-0.179446456268321,-0.159308096556667,-0.139319421594417,
-0.119405860207257,-0.0994866391650725,-0.0795530415751003,-0.0596365801854092,
-0.0397191192000682,-0.0197147983578177,0.),.UNSPECIFIED.);
#2038=B_SPLINE_CURVE_WITH_KNOTS('',3,(#72911,#72912,#72913,#72914,#72915,
#72916,#72917,#72918,#72919,#72920,#72921,#72922,#72923,#72924,#72925,#72926,
#72927,#72928,#72929,#72930,#72931),.UNSPECIFIED.,.F.,.F.,(4,2,2,2,2,2,
2,2,3,4),(-0.301143817833422,-0.263550055241862,-0.226554857552283,-0.189938047509704,
-0.153112323520037,-0.115617591452942,-0.0774492295109371,-0.0384767409856328,
0.,0.000115639545563484),.UNSPECIFIED.);
#2039=B_SPLINE_CURVE_WITH_KNOTS('',3,(#72934,#72935,#72936,#72937,#72938,
#72939,#72940,#72941,#72942,#72943,#72944,#72945,#72946,#72947,#72948,#72949,
#72950,#72951,#72952,#72953,#72954,#72955,#72956,#72957,#72958,#72959,#72960,
#72961,#72962,#72963,#72964,#72965,#72966,#72967,#72968,#72969),
 .UNSPECIFIED.,.T.,.F.,(4,2,2,2,2,2,2,2,2,2,2,2,2,2,2,2,2,4),(0.,0.0355202696276797,
0.0730229242192678,0.109881947978633,0.147332215352278,0.185244244852624,
0.223245130807942,0.259644256147764,0.294838797512181,0.330228485408057,
0.366554345822135,0.404791218300789,0.442165216597746,0.480056587427034,
0.518291371449068,0.552548743079712,0.588529668404829,0.599949959200832),
 .UNSPECIFIED.);
#2040=B_SPLINE_CURVE_WITH_KNOTS('',3,(#72970,#72971,#72972,#72973,#72974,
#72975,#72976,#72977,#72978,#72979,#72980,#72981,#72982,#72983,#72984,#72985,
#72986,#72987,#72988,#72989),.UNSPECIFIED.,.F.,.F.,(4,2,2,2,2,2,2,2,2,4),
(0.000115639545563484,0.0353759396023698,0.0730488697140438,0.110680865125456,
0.14831820650525,0.185958002516291,0.223780919085869,0.262084290340789,
0.300943211829805,0.301033737001698),.UNSPECIFIED.);
#2041=B_SPLINE_CURVE_WITH_KNOTS('',3,(#72995,#72996,#72997,#72998,#72999,
#73000,#73001,#73002,#73003,#73004,#73005,#73006,#73007,#73008,#73009,#73010,
#73011,#73012,#73013,#73014,#73015,#73016,#73017,#73018,#73019,#73020,#73021,
#73022,#73023,#73024,#73025,#73026,#73027,#73028),.UNSPECIFIED.,.T.,.F.,
(4,2,2,2,2,2,2,2,2,2,2,2,2,2,2,2,4),(-0.317575567098843,-0.298445182096447,
-0.278896806076191,-0.259545627203428,-0.240120965983672,-0.220394138326682,
-0.200247246637959,-0.179781459930513,-0.159442591673954,-0.13929341444518,
-0.11968545437467,-0.100250205219309,-0.080800551891539,-0.0608164077051777,
-0.0407200069083776,-0.020440667324873,0.),.UNSPECIFIED.);
#2042=B_SPLINE_CURVE_WITH_KNOTS('',3,(#73032,#73033,#73034,#73035,#73036,
#73037,#73038,#73039,#73040,#73041,#73042,#73043,#73044,#73045,#73046,#73047,
#73048,#73049,#73050,#73051,#73052,#73053,#73054),.UNSPECIFIED.,.F.,.F.,
(4,2,2,2,2,2,2,2,2,3,4),(-0.301177822624064,-0.30086554318467,-0.262823177269621,
-0.225437092346638,-0.188664030260345,-0.152025487199693,-0.114937899685909,
-0.0771209266757964,-0.0385646913814458,0.,0.000147036074768649),
 .UNSPECIFIED.);
#2043=B_SPLINE_CURVE_WITH_KNOTS('',3,(#73057,#73058,#73059,#73060,#73061,
#73062,#73063,#73064,#73065,#73066,#73067,#73068,#73069,#73070,#73071,#73072,
#73073,#73074,#73075,#73076,#73077,#73078,#73079,#73080,#73081,#73082,#73083,
#73084,#73085,#73086,#73087,#73088,#73089,#73090,#73091,#73092),
 .UNSPECIFIED.,.T.,.F.,(4,2,2,2,2,2,2,2,2,2,2,2,2,2,2,2,2,4),(0.,0.0355202696277128,
0.0730229242193518,0.109881947978684,0.147332215352392,0.185244244852654,
0.223245130808227,0.259644256148146,0.294838797512514,0.330228485408397,
0.366554345822571,0.404791218301228,0.442165216598115,0.480056587427485,
0.518291371449575,0.552548743080241,0.588529668405412,0.599949959201459),
 .UNSPECIFIED.);
#2044=B_SPLINE_CURVE_WITH_KNOTS('',3,(#73093,#73094,#73095,#73096,#73097,
#73098,#73099,#73100,#73101,#73102,#73103,#73104,#73105,#73106,#73107,#73108,
#73109,#73110,#73111,#73112),.UNSPECIFIED.,.F.,.F.,(4,2,2,2,2,2,2,2,2,4),
(0.000147036074768649,0.0002632003303773,0.0382957067158387,0.076039995313587,
0.11311569401633,0.149980240799155,0.1873806962898,0.225106586749685,0.26300984239388,
0.301085178106991),.UNSPECIFIED.);
#2045=B_SPLINE_CURVE_WITH_KNOTS('',3,(#73118,#73119,#73120,#73121,#73122,
#73123,#73124,#73125,#73126,#73127,#73128,#73129,#73130,#73131,#73132,#73133,
#73134,#73135,#73136,#73137,#73138,#73139,#73140,#73141,#73142,#73143,#73144,
#73145,#73146,#73147,#73148,#73149,#73150,#73151),.UNSPECIFIED.,.T.,.F.,
(4,2,2,2,2,2,2,2,2,2,2,2,2,2,2,2,4),(-0.317617838667146,-0.297749119122409,
-0.27801232301177,-0.25857847777276,-0.239227863669495,-0.219685791919498,
-0.199797683321152,-0.179390605497121,-0.159080534568315,-0.138922841472281,
-0.118864173739561,-0.0993487487947275,-0.0799339791397019,-0.0604183948867128,
-0.0403723235572229,-0.0202583353081762,0.),.UNSPECIFIED.);
#2046=B_SPLINE_CURVE_WITH_KNOTS('',3,(#73155,#73156,#73157,#73158,#73159,
#73160,#73161,#73162,#73163,#73164,#73165,#73166,#73167,#73168,#73169,#73170,
#73171,#73172,#73173,#73174,#73175,#73176,#73177),.UNSPECIFIED.,.F.,.F.,
(4,2,2,2,2,2,2,2,2,3,4),(-0.322386353128523,-0.321924747431815,-0.281676040704693,
-0.241548845237877,-0.201587824271888,-0.16165494878838,-0.121556749590579,
-0.081233967950947,-0.0408003840156776,0.,6.67458284606265E-5),
 .UNSPECIFIED.);
#2047=B_SPLINE_CURVE_WITH_KNOTS('',3,(#73180,#73181,#73182,#73183,#73184,
#73185,#73186,#73187,#73188,#73189,#73190,#73191,#73192,#73193,#73194,#73195,
#73196,#73197,#73198,#73199,#73200,#73201,#73202,#73203,#73204,#73205,#73206,
#73207,#73208,#73209,#73210,#73211,#73212,#73213,#73214,#73215),
 .UNSPECIFIED.,.T.,.F.,(4,2,2,2,2,2,2,2,2,2,2,2,2,2,2,2,2,4),(0.,0.0399541104211141,
0.0799101633971717,0.120042188031049,0.160349494010557,0.200700062460784,
0.240669149748917,0.281146928548468,0.321688268053327,0.361827692830636,
0.401937446249474,0.441912733332744,0.482224630787451,0.523014478229153,
0.56336023793604,0.603655558777477,0.623959945527602,0.644496878440942),
 .UNSPECIFIED.);
#2048=B_SPLINE_CURVE_WITH_KNOTS('',3,(#73216,#73217,#73218,#73219,#73220,
#73221,#73222,#73223,#73224,#73225,#73226,#73227,#73228,#73229,#73230,#73231,
#73232,#73233),.UNSPECIFIED.,.F.,.F.,(4,2,2,2,2,2,2,2,4),(6.67458284606265E-5,
0.0393826488471203,0.0796914813289635,0.120093624542018,0.160725370013617,
0.201339688030563,0.24171722174321,0.282040571557513,0.322293513905308),
 .UNSPECIFIED.);
#2049=B_SPLINE_CURVE_WITH_KNOTS('',3,(#73239,#73240,#73241,#73242,#73243,
#73244,#73245,#73246,#73247,#73248,#73249,#73250,#73251,#73252,#73253,#73254,
#73255,#73256,#73257,#73258,#73259,#73260,#73261,#73262,#73263,#73264,#73265,
#73266,#73267,#73268,#73269,#73270,#73271,#73272),.UNSPECIFIED.,.T.,.F.,
(4,2,2,2,2,2,2,2,2,2,2,2,2,2,2,2,4),(-0.315575068397107,-0.297725501979271,
-0.278054313638465,-0.258450452345541,-0.238874557421568,-0.219261153221667,
-0.199573893731351,-0.179829007564642,-0.159694178352794,-0.139711485464633,
-0.119804488965712,-0.0998605425660636,-0.0798476482302862,-0.0598364031986145,
-0.0398950310581945,-0.0199874120120488,0.),.UNSPECIFIED.);
#2050=B_SPLINE_CURVE_WITH_KNOTS('',3,(#73375,#73376,#73377,#73378,#73379,
#73380,#73381,#73382,#73383,#73384,#73385,#73386,#73387,#73388,#73389,#73390,
#73391,#73392,#73393,#73394,#73395,#73396,#73397,#73398,#73399),
 .UNSPECIFIED.,.F.,.F.,(4,2,2,2,3,2,2,2,2,2,2,4),(-0.163168148872215,-0.149527097306421,
-0.099418871001962,-0.0495338134349146,0.,0.0181167695460887,0.0672138706813057,
0.116111680955948,0.165495495020991,0.211936470057348,0.257662170504295,
0.287380385163945),.UNSPECIFIED.);
#2051=B_SPLINE_CURVE_WITH_KNOTS('',3,(#73402,#73403,#73404,#73405,#73406,
#73407,#73408,#73409),.UNSPECIFIED.,.F.,.F.,(4,2,2,4),(-0.287435863143152,
-0.242415728675084,-0.196766145639793,-0.163168148872215),.UNSPECIFIED.);
#2052=B_SPLINE_CURVE_WITH_KNOTS('',3,(#73518,#73519,#73520,#73521,#73522,
#73523,#73524,#73525,#73526,#73527,#73528,#73529,#73530,#73531,#73532,#73533,
#73534,#73535,#73536,#73537,#73538,#73539,#73540),.UNSPECIFIED.,.F.,.F.,
(4,2,2,3,2,2,2,2,2,2,4),(-0.136734216111625,-0.0994188710018493,-0.0495338134348796,
0.,0.0181167695462525,0.0672138706826966,0.11611168095846,0.165495495024581,
0.211936470061975,0.257662170509725,0.287380385169817),.UNSPECIFIED.);
#2053=B_SPLINE_CURVE_WITH_KNOTS('',3,(#73543,#73544,#73545,#73546,#73547,
#73548,#73549,#73550,#73551,#73552),.UNSPECIFIED.,.F.,.F.,(4,2,2,2,4),(-0.287435863144066,
-0.242415728675624,-0.196766145640031,-0.149527097306449,-0.136734216111625),
 .UNSPECIFIED.);
#2054=B_SPLINE_CURVE_WITH_KNOTS('',3,(#73649,#73650,#73651,#73652,#73653,
#73654,#73655,#73656,#73657,#73658,#73659,#73660,#73661,#73662,#73663,#73664,
#73665,#73666,#73667,#73668,#73669,#73670,#73671),.UNSPECIFIED.,.F.,.F.,
(4,2,2,3,2,2,2,2,2,2,4),(-0.110237651798014,-0.0994188710015688,-0.0495338134348444,
0.,0.018116769546061,0.0672138706809179,0.116111680955262,0.165495495019963,
0.21193647005629,0.257662170503162,0.287380385162707),.UNSPECIFIED.);
#2055=B_SPLINE_CURVE_WITH_KNOTS('',3,(#73674,#73675,#73676,#73677,#73678,
#73679,#73680,#73681,#73682,#73683),.UNSPECIFIED.,.F.,.F.,(4,2,2,2,4),(-0.287435863141549,
-0.242415728673738,-0.196766145638641,-0.149527097305494,-0.110237651798014),
 .UNSPECIFIED.);
#2056=B_SPLINE_CURVE_WITH_KNOTS('',3,(#73792,#73793,#73794,#73795,#73796,
#73797,#73798,#73799,#73800,#73801,#73802,#73803,#73804,#73805,#73806,#73807,
#73808,#73809,#73810,#73811,#73812),.UNSPECIFIED.,.F.,.F.,(4,2,3,2,2,2,
2,2,2,4),(-0.0838008711994917,-0.0495338134349723,0.,0.0181167695463933,
0.0672138706835067,0.116111680959761,0.165495495026224,0.211936470064241,
0.25766217051282,0.287380385173364),.UNSPECIFIED.);
#2057=B_SPLINE_CURVE_WITH_KNOTS('',3,(#73815,#73816,#73817,#73818,#73819,
#73820,#73821,#73822,#73823,#73824,#73825,#73826),.UNSPECIFIED.,.F.,.F.,
(4,2,2,2,2,4),(-0.28743586314397,-0.242415728675305,-0.196766145639633,
-0.149527097306083,-0.0994188710019063,-0.0838008711994917),
 .UNSPECIFIED.);
#2058=B_SPLINE_CURVE_WITH_KNOTS('',3,(#73935,#73936,#73937,#73938,#73939,
#73940,#73941,#73942,#73943,#73944,#73945,#73946,#73947,#73948,#73949,#73950,
#73951,#73952,#73953,#73954,#73955),.UNSPECIFIED.,.F.,.F.,(4,2,3,2,2,2,
2,2,2,4),(-0.0573096617767208,-0.0495338134349582,0.,0.0181167695464065,
0.067213870683422,0.11611168095957,0.165495495026031,0.211936470063854,
0.257662170511938,0.287380385172065),.UNSPECIFIED.);
#2059=B_SPLINE_CURVE_WITH_KNOTS('',3,(#73958,#73959,#73960,#73961,#73962,
#73963,#73964,#73965,#73966,#73967,#73968,#73969),.UNSPECIFIED.,.F.,.F.,
(4,2,2,2,2,4),(-0.287435863144792,-0.24241572867618,-0.196766145640472,
-0.149527097306765,-0.0994188710021029,-0.0573096617767208),
 .UNSPECIFIED.);
#2060=B_SPLINE_CURVE_WITH_KNOTS('',3,(#74078,#74079,#74080,#74081,#74082,
#74083,#74084,#74085,#74086,#74087,#74088,#74089,#74090,#74091,#74092,#74093,
#74094,#74095,#74096),.UNSPECIFIED.,.F.,.F.,(4,3,2,2,2,2,2,2,4),(-0.030871330269263,
0.,0.0181167695458699,0.0672138706791213,0.116111680952223,0.165495495015657,
0.211936470050785,0.257662170496474,0.287380385155237),.UNSPECIFIED.);
#2061=B_SPLINE_CURVE_WITH_KNOTS('',3,(#74099,#74100,#74101,#74102,#74103,
#74104,#74105,#74106,#74107,#74108,#74109,#74110,#74111,#74112),
 .UNSPECIFIED.,.F.,.F.,(4,2,2,2,2,2,4),(-0.287435863140128,-0.242415728672749,
-0.196766145638088,-0.149527097305286,-0.0994188710013708,-0.0495338134347677,
-0.030871330269263),.UNSPECIFIED.);
#2062=B_SPLINE_CURVE_WITH_KNOTS('',3,(#74221,#74222,#74223,#74224,#74225,
#74226,#74227,#74228,#74229,#74230,#74231,#74232,#74233,#74234,#74235,#74236,
#74237,#74238,#74239),.UNSPECIFIED.,.F.,.F.,(4,3,2,2,2,2,2,2,4),(-0.0043909955767957,
0.,0.0181167695464896,0.0672138706846621,0.116111680961959,0.165495495029324,
0.211936470068035,0.257662170516974,0.287380385177773),.UNSPECIFIED.);
#2063=B_SPLINE_CURVE_WITH_KNOTS('',3,(#74242,#74243,#74244,#74245,#74246,
#74247,#74248,#74249,#74250,#74251,#74252,#74253,#74254,#74255),
 .UNSPECIFIED.,.F.,.F.,(4,2,2,2,2,2,4),(-0.287435863146267,-0.242415728677103,
-0.196766145640964,-0.149527097306892,-0.0994188710022298,-0.0495338134350148,
-0.0043909955767957),.UNSPECIFIED.);
#2064=B_SPLINE_CURVE_WITH_KNOTS('',3,(#74352,#74353,#74354,#74355,#74356,
#74357,#74358,#74359,#74360,#74361,#74362,#74363,#74364,#74365),
 .UNSPECIFIED.,.F.,.F.,(4,2,2,2,2,2,4),(0.0219992412523513,0.0672138706833701,
0.116111680959517,0.165495495025897,0.211936470063604,0.257662170511581,
0.287380385171759),.UNSPECIFIED.);
#2065=B_SPLINE_CURVE_WITH_KNOTS('',3,(#74368,#74369,#74370,#74371,#74372,
#74373,#74374,#74375,#74376,#74377,#74378,#74379,#74380,#74381,#74382,#74383,
#74384,#74385,#74386),.UNSPECIFIED.,.F.,.F.,(4,2,2,2,2,2,3,2,4),(-0.287435863143863,
-0.242415728675397,-0.196766145639793,-0.149527097306269,-0.0994188710018298,
-0.0495338134348875,0.,0.0181167695463815,0.0219992412523513),
 .UNSPECIFIED.);
#2066=B_SPLINE_CURVE_WITH_KNOTS('',3,(#74495,#74496,#74497,#74498,#74499,
#74500,#74501,#74502,#74503,#74504,#74505,#74506,#74507,#74508),
 .UNSPECIFIED.,.F.,.F.,(4,2,2,2,2,2,4),(0.0484769366691737,0.0672138706802703,
0.116111680953911,0.165495495018043,0.211936470053924,0.2576621705003,0.287380385159541),
 .UNSPECIFIED.);
#2067=B_SPLINE_CURVE_WITH_KNOTS('',3,(#74511,#74512,#74513,#74514,#74515,
#74516,#74517,#74518,#74519,#74520,#74521,#74522,#74523,#74524,#74525,#74526,
#74527,#74528,#74529),.UNSPECIFIED.,.F.,.F.,(4,2,2,2,2,2,3,2,4),(-0.28743586314069,
-0.242415728673121,-0.196766145638307,-0.149527097305332,-0.0994188710013639,
-0.0495338134347652,0.,0.0181167695459964,0.0484769366691737),
 .UNSPECIFIED.);
#2068=B_SPLINE_CURVE_WITH_KNOTS('',3,(#74638,#74639,#74640,#74641,#74642,
#74643,#74644,#74645,#74646,#74647,#74648,#74649),.UNSPECIFIED.,.F.,.F.,
(4,2,2,2,2,4),(0.074915383377095,0.116111680950963,0.165495495013905,0.211936470048695,
0.257662170494074,0.287380385152742),.UNSPECIFIED.);
#2069=B_SPLINE_CURVE_WITH_KNOTS('',3,(#74652,#74653,#74654,#74655,#74656,
#74657,#74658,#74659,#74660,#74661,#74662,#74663,#74664,#74665,#74666,#74667,
#74668,#74669,#74670,#74671,#74672),.UNSPECIFIED.,.F.,.F.,(4,2,2,2,2,2,
3,2,2,4),(-0.287435863139544,-0.242415728672318,-0.196766145637718,-0.149527097305004,
-0.099418871001249,-0.0495338134347465,0.,0.0181167695457953,0.067213870678527,
0.074915383377095),.UNSPECIFIED.);
#2070=B_SPLINE_CURVE_WITH_KNOTS('',3,(#74781,#74782,#74783,#74784,#74785,
#74786,#74787,#74788,#74789,#74790,#74791,#74792),.UNSPECIFIED.,.F.,.F.,
(4,2,2,2,2,4),(0.101402925040076,0.116111680956364,0.165495495021304,0.211936470057817,
0.257662170504839,0.287380385164579),.UNSPECIFIED.);
#2071=B_SPLINE_CURVE_WITH_KNOTS('',3,(#74795,#74796,#74797,#74798,#74799,
#74800,#74801,#74802,#74803,#74804,#74805,#74806,#74807,#74808,#74809,#74810,
#74811,#74812,#74813,#74814,#74815),.UNSPECIFIED.,.F.,.F.,(4,2,2,2,2,2,
3,2,2,4),(-0.28743586314205,-0.242415728673942,-0.196766145638722,-0.14952709730564,
-0.0994188710015697,-0.0495338134348303,0.,0.0181167695460824,0.0672138706815053,
0.101402925040076),.UNSPECIFIED.);
#2072=B_SPLINE_CURVE_WITH_KNOTS('',3,(#74924,#74925,#74926,#74927,#74928,
#74929,#74930,#74931,#74932,#74933),.UNSPECIFIED.,.F.,.F.,(4,2,2,2,4),(0.127838203298608,
0.165495495016154,0.211936470051326,0.257662170497038,0.287380385156003),
 .UNSPECIFIED.);
#2073=B_SPLINE_CURVE_WITH_KNOTS('',3,(#74936,#74937,#74938,#74939,#74940,
#74941,#74942,#74943,#74944,#74945,#74946,#74947,#74948,#74949,#74950,#74951,
#74952,#74953,#74954,#74955,#74956,#74957,#74958),.UNSPECIFIED.,.F.,.F.,
(4,2,2,2,2,2,3,2,2,2,4),(-0.287435863140559,-0.242415728672966,-0.196766145638107,
-0.149527097305205,-0.0994188710012938,-0.0495338134347454,0.,0.0181167695458621,
0.0672138706792296,0.116111680952409,0.127838203298608),.UNSPECIFIED.);
#2074=B_SPLINE_CURVE_WITH_KNOTS('',3,(#75055,#75056,#75057,#75058,#75059,
#75060,#75061,#75062,#75063,#75064),.UNSPECIFIED.,.F.,.F.,(4,2,2,2,4),(0.154331148598444,
0.165495495019413,0.211936470055537,0.257662170502203,0.287380385161736),
 .UNSPECIFIED.);
#2075=B_SPLINE_CURVE_WITH_KNOTS('',3,(#75067,#75068,#75069,#75070,#75071,
#75072,#75073,#75074,#75075,#75076,#75077,#75078,#75079,#75080,#75081,#75082,
#75083,#75084,#75085,#75086,#75087,#75088,#75089),.UNSPECIFIED.,.F.,.F.,
(4,2,2,2,2,2,3,2,2,2,4),(-0.2874358631423,-0.242415728674201,-0.196766145638911,
-0.149527097305732,-0.0994188710014949,-0.0495338134347817,0.,0.018116769546075,
0.0672138706808332,0.116111680954877,0.154331148598444),.UNSPECIFIED.);
#2076=B_SPLINE_CURVE_WITH_KNOTS('',3,(#75198,#75199,#75200,#75201,#75202,
#75203,#75204,#75205),.UNSPECIFIED.,.F.,.F.,(4,2,2,4),(0.180763661414687,
0.211936470057055,0.257662170504015,0.287380385163549),.UNSPECIFIED.);
#2077=B_SPLINE_CURVE_WITH_KNOTS('',3,(#75208,#75209,#75210,#75211,#75212,
#75213,#75214,#75215,#75216,#75217,#75218,#75219,#75220,#75221,#75222,#75223,
#75224,#75225,#75226,#75227,#75228,#75229,#75230,#75231,#75232),
 .UNSPECIFIED.,.F.,.F.,(4,2,2,2,2,2,3,2,2,2,2,4),(-0.287435863142792,-0.242415728674566,
-0.196766145639177,-0.149527097305729,-0.0994188710016275,-0.0495338134348599,
0.,0.0181167695461263,0.0672138706812888,0.116111680955793,0.165495495020501,
0.180763661414687),.UNSPECIFIED.);
#2078=B_SPLINE_CURVE_WITH_KNOTS('',3,(#75341,#75342,#75343,#75344,#75345,
#75346,#75347,#75348),.UNSPECIFIED.,.F.,.F.,(4,2,2,4),(0.20723494990689,
0.211936470059604,0.25766217050719,0.28738038516735),.UNSPECIFIED.);
#2079=B_SPLINE_CURVE_WITH_KNOTS('',3,(#75351,#75352,#75353,#75354,#75355,
#75356,#75357,#75358,#75359,#75360,#75361,#75362,#75363,#75364,#75365,#75366,
#75367,#75368,#75369,#75370,#75371,#75372,#75373,#75374,#75375),
 .UNSPECIFIED.,.F.,.F.,(4,2,2,2,2,2,3,2,2,2,2,4),(-0.287435863143056,-0.242415728674689,
-0.196766145639263,-0.14952709730598,-0.099418871001769,-0.0495338134348932,
0.,0.0181167695462657,0.0672138706821976,0.116111680957489,0.165495495022889,
0.20723494990689),.UNSPECIFIED.);
#2080=B_SPLINE_CURVE_WITH_KNOTS('',3,(#75484,#75485,#75486,#75487,#75488,
#75489),.UNSPECIFIED.,.F.,.F.,(4,2,4),(0.233673284093007,0.257662170504296,
0.287380385164373),.UNSPECIFIED.);
#2081=B_SPLINE_CURVE_WITH_KNOTS('',3,(#75492,#75493,#75494,#75495,#75496,
#75497,#75498,#75499,#75500,#75501,#75502,#75503,#75504,#75505,#75506,#75507,
#75508,#75509,#75510,#75511,#75512,#75513,#75514,#75515,#75516,#75517,#75518),
 .UNSPECIFIED.,.F.,.F.,(4,2,2,2,2,2,3,2,2,2,2,2,4),(-0.287435863141504,
-0.242415728674061,-0.196766145638992,-0.149527097305872,-0.0994188710018303,
-0.0495338134349093,0.,0.0181167695460408,0.0672138706811696,0.116111680955736,
0.165495495020723,0.211936470057386,0.233673284093007),.UNSPECIFIED.);
#2082=B_SPLINE_CURVE_WITH_KNOTS('',3,(#75627,#75628,#75629,#75630),
 .UNSPECIFIED.,.F.,.F.,(4,4),(0.260117487351587,0.287380385169054),
 .UNSPECIFIED.);
#2083=B_SPLINE_CURVE_WITH_KNOTS('',3,(#75633,#75634,#75635,#75636,#75637,
#75638,#75639,#75640,#75641,#75642,#75643,#75644,#75645,#75646,#75647,#75648,
#75649,#75650,#75651,#75652,#75653,#75654,#75655,#75656,#75657,#75658,#75659,
#75660,#75661),.UNSPECIFIED.,.F.,.F.,(4,2,2,2,2,2,3,2,2,2,2,2,2,4),(-0.287435863143853,
-0.242415728675398,-0.19676614563975,-0.149527097306065,-0.0994188710017117,
-0.0495338134348613,0.,0.0181167695462665,0.0672138706825982,0.116111680958237,
0.165495495023962,0.211936470061099,0.257662170508858,0.260117487351587),
 .UNSPECIFIED.);
#2084=B_SPLINE_CURVE_WITH_KNOTS('',3,(#75758,#75759,#75760,#75761),
 .UNSPECIFIED.,.F.,.F.,(4,4),(0.286585728945047,0.287380385163699),
 .UNSPECIFIED.);
#2085=B_SPLINE_CURVE_WITH_KNOTS('',3,(#75764,#75765,#75766,#75767,#75768,
#75769,#75770,#75771,#75772,#75773,#75774,#75775,#75776,#75777,#75778,#75779,
#75780,#75781,#75782,#75783,#75784,#75785,#75786,#75787,#75788,#75789,#75790,
#75791,#75792),.UNSPECIFIED.,.F.,.F.,(4,2,2,2,2,2,3,2,2,2,2,2,2,4),(-0.287435863142645,
-0.242415728674694,-0.196766145639482,-0.149527097306091,-0.099418871001846,
-0.0495338134349094,0.,0.0181167695460932,0.0672138706811363,0.116111680955706,
0.165495495020644,0.211936470057252,0.257662170504159,0.286585728945047),
 .UNSPECIFIED.);
#2086=B_SPLINE_CURVE_WITH_KNOTS('',3,(#75903,#75904,#75905,#75906,#75907,
#75908,#75909,#75910,#75911,#75912,#75913,#75914,#75915,#75916,#75917,#75918,
#75919,#75920,#75921,#75922,#75923,#75924,#75925,#75926,#75927,#75928,#75929,
#75930,#75931),.UNSPECIFIED.,.F.,.F.,(4,2,2,2,2,2,2,3,2,2,2,2,2,4),(0.50632031739344,
0.53603853205329,0.581764232500794,0.628205207537996,0.677589021603566,
0.726486831878774,0.775583933014714,0.793700702560937,0.843234515995651,
0.893119573562134,0.94322779986628,0.990466848199578,1.0361164312349,1.08113656570317),
 .UNSPECIFIED.);
#2087=B_SPLINE_CURVE_WITH_KNOTS('',3,(#76031,#76032,#76033,#76034,#76035,
#76036,#76037,#76038,#76039,#76040,#76041,#76042),.UNSPECIFIED.,.F.,.F.,
(4,2,2,2,2,4),(0.,0.0190658252712468,0.0452304041939831,0.0568941639977528,
0.0817283147450615,0.110084577318765),.UNSPECIFIED.);
#2088=B_SPLINE_CURVE_WITH_KNOTS('',3,(#76058,#76059,#76060,#76061,#76062,
#76063,#76064,#76065,#76066,#76067,#76068,#76069,#76070,#76071,#76072,#76073,
#76074,#76075,#76076,#76077,#76078,#76079,#76080,#76081,#76082,#76083,#76084,
#76085,#76086,#76087,#76088,#76089,#76090,#76091,#76092,#76093),
 .UNSPECIFIED.,.F.,.F.,(4,2,2,2,2,2,2,2,2,2,2,2,2,2,2,2,2,4),(0.,0.0308101291271131,
0.0585102160249069,0.107376034221475,0.153242377810569,0.196274905402532,
0.246470222643019,0.271920550681864,0.288008391296742,0.294995460635489,
0.310418509414427,0.333264464530267,0.381330610566836,0.423929647067707,
0.469249423768235,0.517202341943224,0.551749790166704,0.59009865246996),
 .UNSPECIFIED.);
#2089=B_SPLINE_CURVE_WITH_KNOTS('',3,(#76181,#76182,#76183,#76184,#76185,
#76186,#76187,#76188,#76189,#76190,#76191,#76192,#76193,#76194),
 .UNSPECIFIED.,.F.,.F.,(4,2,2,2,2,2,4),(0.,0.0755351073398052,0.117972466547439,
0.150106900517715,0.182308953145744,0.22500423988959,0.300408947780656),
 .UNSPECIFIED.);
#2090=B_SPLINE_CURVE_WITH_KNOTS('',3,(#76366,#76367,#76368,#76369,#76370,
#76371,#76372,#76373,#76374,#76375,#76376,#76377,#76378,#76379,#76380,#76381,
#76382,#76383,#76384,#76385,#76386,#76387,#76388,#76389),.UNSPECIFIED.,
 .F.,.F.,(4,2,2,2,2,2,2,2,2,2,2,4),(0.,0.0432252777893914,0.0917875128943153,
0.153562045824851,0.189491598602029,0.215103697999651,0.226790580176592,
0.253342417228272,0.292964110987221,0.354939922037077,0.394370298538859,
0.430153691883516),.UNSPECIFIED.);
#2091=B_SPLINE_CURVE_WITH_KNOTS('',3,(#76597,#76598,#76599,#76600,#76601,
#76602,#76603,#76604,#76605,#76606),.UNSPECIFIED.,.F.,.F.,(4,2,2,2,4),(0.115471253326685,
0.14952709730731,0.196766145641448,0.242415728677503,0.287435863146423),
 .UNSPECIFIED.);
#2092=B_SPLINE_CURVE_WITH_KNOTS('',3,(#76608,#76609,#76610,#76611,#76612,
#76613,#76614,#76615,#76616,#76617,#76618,#76619,#76620,#76621,#76622,#76623,
#76624,#76625,#76626,#76627,#76628,#76629,#76630,#76631,#76632,#76633,#76634,
#76635),.UNSPECIFIED.,.F.,.F.,(4,2,2,2,2,2,2,2,2,2,2,2,2,4),(0.,0.0337497043514118,
0.064125244377998,0.112622372775232,0.158167577684873,0.200871358502125,
0.246447408502993,0.269509078364172,0.2859826603936,0.293562975218655,0.311533142617737,
0.3405100735619,0.374412159077522,0.401781469644215),.UNSPECIFIED.);
#2093=B_SPLINE_CURVE_WITH_KNOTS('',3,(#76747,#76748,#76749,#76750,#76751,
#76752,#76753,#76754,#76755,#76756,#76757,#76758,#76759,#76760,#76761,#76762,
#76763,#76764,#76765,#76766,#76767,#76768,#76769,#76770,#76771,#76772,#76773,
#76774,#76775),.UNSPECIFIED.,.F.,.F.,(4,2,2,2,2,2,2,3,2,2,2,2,2,4),(0.506320317396995,
0.536038532057083,0.581764232504992,0.628205207542535,0.677589021608681,
0.726486831884498,0.775583933021264,0.793700702567583,0.843234516002442,
0.893119573569278,0.943227799873571,0.990466848207139,1.03611643124272,
1.08113656571108),.UNSPECIFIED.);
#2094=B_SPLINE_CURVE_WITH_KNOTS('',3,(#76885,#76886,#76887,#76888,#76889,
#76890,#76891,#76892,#76893,#76894,#76895,#76896,#76897,#76898,#76899,#76900,
#76901,#76902,#76903,#76904,#76905,#76906,#76907,#76908,#76909,#76910,#76911,
#76912,#76913),.UNSPECIFIED.,.F.,.F.,(4,2,2,2,2,2,3,2,2,2,2,2,2,4),(-0.268990399052299,
-0.242415728673278,-0.196766145638393,-0.149527097305505,-0.0994188710015041,
-0.0495338134348189,0.,0.0181167695460229,0.0672138706805404,0.116111680954595,
0.165495495019033,0.211936470055113,0.257662170501655,0.287380385160891),
 .UNSPECIFIED.);
#2095=B_SPLINE_CURVE_WITH_KNOTS('',3,(#76916,#76917,#76918,#76919),
 .UNSPECIFIED.,.F.,.F.,(4,4),(-0.287435863140965,-0.268990399052299),
 .UNSPECIFIED.);
#2096=B_SPLINE_CURVE_WITH_KNOTS('',3,(#77016,#77017,#77018,#77019,#77020,
#77021,#77022,#77023,#77024,#77025,#77026,#77027,#77028,#77029,#77030,#77031,
#77032,#77033,#77034,#77035,#77036,#77037,#77038,#77039,#77040,#77041,#77042,
#77043,#77044),.UNSPECIFIED.,.F.,.F.,(4,2,2,2,2,2,3,2,2,2,2,2,2,4),(-0.242533959473534,
-0.242415728674442,-0.196766145639165,-0.149527097305957,-0.099418871001771,
-0.0495338134348831,0.,0.0181167695462372,0.067213870681872,0.116111680956732,
0.165495495021875,0.211936470058645,0.257662170505937,0.287380385164999),
 .UNSPECIFIED.);
#2097=B_SPLINE_CURVE_WITH_KNOTS('',3,(#77047,#77048,#77049,#77050),
 .UNSPECIFIED.,.F.,.F.,(4,4),(-0.287435863143146,-0.242533959473534),
 .UNSPECIFIED.);
#2098=B_SPLINE_CURVE_WITH_KNOTS('',3,(#77159,#77160,#77161,#77162,#77163,
#77164,#77165,#77166,#77167,#77168,#77169,#77170,#77171,#77172,#77173,#77174,
#77175,#77176,#77177,#77178,#77179,#77180,#77181,#77182,#77183,#77184,#77185),
 .UNSPECIFIED.,.F.,.F.,(4,2,2,2,2,3,2,2,2,2,2,2,4),(-0.216081250737383,
-0.196766145639079,-0.149527097305844,-0.0994188710017439,-0.0495338134348963,
0.,0.0181167695460728,0.067213870681023,0.116111680955563,0.165495495020394,
0.211936470056958,0.25766217050386,0.287380385163262),.UNSPECIFIED.);
#2099=B_SPLINE_CURVE_WITH_KNOTS('',3,(#77188,#77189,#77190,#77191,#77192,
#77193),.UNSPECIFIED.,.F.,.F.,(4,2,4),(-0.287435863142567,-0.242415728674427,
-0.216081250737383),.UNSPECIFIED.);
#2100=B_SPLINE_CURVE_WITH_KNOTS('',3,(#77302,#77303,#77304,#77305,#77306,
#77307,#77308,#77309,#77310,#77311,#77312,#77313,#77314,#77315,#77316,#77317,
#77318,#77319,#77320,#77321,#77322,#77323,#77324,#77325,#77326),
 .UNSPECIFIED.,.F.,.F.,(4,2,2,2,3,2,2,2,2,2,2,4),(-0.189647450541698,-0.149527097305893,
-0.0994188710016985,-0.0495338134348624,0.,0.0181167695462411,0.0672138706819809,
0.11611168095712,0.165495495022401,0.211936470059391,0.25766217050701,0.287380385166855),
 .UNSPECIFIED.);
#2101=B_SPLINE_CURVE_WITH_KNOTS('',3,(#77329,#77330,#77331,#77332,#77333,
#77334,#77335,#77336),.UNSPECIFIED.,.F.,.F.,(4,2,2,4),(-0.287435863142678,
-0.242415728674601,-0.19676614563926,-0.189647450541698),.UNSPECIFIED.);
#2102=B_SPLINE_CURVE_WITH_KNOTS('',3,(#77403,#77404,#77405,#77406,#77407,
#77408,#77409,#77410,#77411,#77412,#77413,#77414,#77415,#77416,#77417,#77418,
#77419,#77420,#77421,#77422,#77423,#77424,#77425),.UNSPECIFIED.,.F.,.F.,
(4,2,2,2,2,2,3,2,2,2,4),(0.46489444415617,0.482224630787222,0.523014478228721,
0.563360237935425,0.603655558776688,0.623959945526705,0.644496878439993,
0.684450988861052,0.72440704183694,0.76453906647082,0.78715174771853),
 .UNSPECIFIED.);
#2103=B_SPLINE_CURVE_WITH_KNOTS('',3,(#77426,#77427,#77428,#77429,#77430,
#77431,#77432,#77433,#77434,#77435,#77436,#77437,#77438,#77439,#77440,#77441,
#77442,#77443,#77444,#77445),.UNSPECIFIED.,.F.,.F.,(4,2,2,2,2,2,2,2,2,4),
(0.78715174771853,0.804846372450503,0.845196940900909,0.88516602818916,
0.925643806988713,0.96618514649351,1.00632457127068,1.04643432468934,1.08640961177265,
1.10939132259616),.UNSPECIFIED.);
#2104=B_SPLINE_CURVE_WITH_KNOTS('',3,(#77453,#77454,#77455,#77456),
 .UNSPECIFIED.,.F.,.F.,(4,4),(0.,0.000964377926953999),.UNSPECIFIED.);
#2105=B_SPLINE_CURVE_WITH_KNOTS('',3,(#77458,#77459,#77460,#77461),
 .UNSPECIFIED.,.F.,.F.,(4,4),(0.000964426268463036,0.0153569489639517),
 .UNSPECIFIED.);
#2106=B_SPLINE_CURVE_WITH_KNOTS('',3,(#77463,#77464,#77465,#77466,#77467,
#77468,#77469,#77470,#77471,#77472,#77473,#77474,#77475,#77476,#77477,#77478,
#77479,#77480,#77481,#77482,#77483,#77484,#77485,#77486,#77487,#77488,#77489,
#77490,#77491,#77492,#77493,#77494,#77495,#77496,#77497,#77498,#77499,#77500,
#77501,#77502,#77503,#77504,#77505,#77506,#77507,#77508,#77509,#77510,#77511,
#77512,#77513,#77514,#77515,#77516,#77517,#77518,#77519,#77520,#77521,#77522,
#77523,#77524,#77525,#77526,#77527,#77528,#77529,#77530,#77531,#77532,#77533,
#77534,#77535,#77536,#77537,#77538,#77539,#77540,#77541,#77542,#77543,#77544,
#77545,#77546,#77547,#77548,#77549,#77550,#77551,#77552,#77553,#77554,#77555,
#77556,#77557,#77558,#77559,#77560,#77561,#77562,#77563,#77564,#77565,#77566,
#77567,#77568,#77569,#77570,#77571,#77572,#77573,#77574,#77575,#77576,#77577,
#77578,#77579,#77580,#77581,#77582,#77583,#77584,#77585,#77586,#77587,#77588,
#77589,#77590,#77591,#77592,#77593,#77594,#77595,#77596,#77597,#77598,#77599,
#77600,#77601,#77602,#77603,#77604,#77605,#77606,#77607,#77608,#77609,#77610,
#77611,#77612,#77613,#77614,#77615,#77616,#77617,#77618,#77619,#77620,#77621,
#77622),.UNSPECIFIED.,.F.,.F.,(4,3,3,3,3,3,3,3,3,3,3,3,3,3,3,3,3,3,3,3,
3,3,3,3,3,3,3,3,3,3,3,3,3,3,3,3,3,3,3,3,3,3,3,3,3,3,3,3,3,3,3,3,3,4),(0.0153569489639517,
0.0219282083148865,0.0294333381847798,0.0381269700773983,0.0456471396536513,
0.0550333230967721,0.0644194943084723,0.0738056535444641,0.0831918010597966,
0.0925779371097566,0.101964061949826,0.111350175835289,0.120736279021378,
0.130122371763683,0.139508454317902,0.148894526938201,0.158280589880695,
0.167666643401077,0.177052687754107,0.186438723195174,0.196237513095298,
0.205730090811043,0.21511647703801,0.224502831755281,0.233889155984714,
0.243275450747821,0.252661717066159,0.262047955961215,0.271434168454673,
0.280820355568032,0.290206518322942,0.29959265774067,0.308978774842652,
0.318364870650084,0.327750946184637,0.337137002467656,0.346523040520444,
0.356115350487863,0.365501714783882,0.374888018497213,0.384274265714455,
0.39366046052189,0.403046607005449,0.412432709250706,0.42181877134353,0.431591424925482,
0.440977743225469,0.450363950600201,0.459750063393973,0.469064457894216,
0.47842434354882,0.48778780374317,0.497151365244305,0.499999999999145),
 .UNSPECIFIED.);
#2107=B_SPLINE_CURVE_WITH_KNOTS('',3,(#77624,#77625,#77626,#77627,#77628,
#77629,#77630,#77631,#77632,#77633,#77634,#77635,#77636,#77637,#77638,#77639,
#77640,#77641,#77642,#77643,#77644,#77645,#77646,#77647,#77648,#77649,#77650,
#77651,#77652,#77653,#77654,#77655,#77656,#77657,#77658,#77659,#77660,#77661,
#77662,#77663,#77664,#77665,#77666,#77667,#77668,#77669,#77670,#77671,#77672,
#77673,#77674,#77675,#77676,#77677,#77678,#77679,#77680,#77681,#77682,#77683,
#77684,#77685,#77686,#77687,#77688,#77689,#77690,#77691,#77692,#77693,#77694,
#77695,#77696,#77697,#77698,#77699,#77700,#77701,#77702,#77703,#77704,#77705,
#77706,#77707,#77708,#77709,#77710,#77711,#77712,#77713,#77714,#77715,#77716,
#77717,#77718,#77719,#77720,#77721,#77722,#77723,#77724,#77725,#77726,#77727,
#77728,#77729,#77730,#77731,#77732,#77733,#77734,#77735,#77736,#77737,#77738,
#77739,#77740,#77741,#77742,#77743,#77744,#77745,#77746,#77747,#77748,#77749,
#77750,#77751,#77752,#77753,#77754,#77755,#77756,#77757,#77758,#77759,#77760,
#77761,#77762,#77763,#77764,#77765,#77766,#77767,#77768,#77769,#77770,#77771,
#77772,#77773,#77774,#77775,#77776,#77777,#77778,#77779,#77780,#77781,#77782,
#77783),.UNSPECIFIED.,.F.,.F.,(4,3,3,3,3,3,3,3,3,3,3,3,3,3,3,3,3,3,3,3,
3,3,3,3,3,3,3,3,3,3,3,3,3,3,3,3,3,3,3,3,3,3,3,3,3,3,3,3,3,3,3,3,3,4),(0.499999999999145,
0.509363634815052,0.518727213283903,0.528087636608761,0.537479514573638,
0.546865650705078,0.556251775624736,0.565637889587881,0.575023992849933,
0.584410085666254,0.593796168292422,0.60318224098332,0.612568303994555,
0.621954357581328,0.631340401999322,0.64072643750358,0.650527332785632,
0.66002195009012,0.669408336532774,0.678794691458984,0.688181015890325,
0.697567310848398,0.706953577354932,0.716339816431409,0.725726029099394,
0.735112216380421,0.744498379295462,0.753884518867239,0.763270636116398,
0.772656732063998,0.78204280773193,0.791428864141412,0.800814902313632,
0.810411163827108,0.819797528518683,0.829183832601694,0.838570080162811,
0.847956275288611,0.857342422064618,0.866728524576365,0.876114586909905,
0.885894649362323,0.895280968320628,0.904667176263448,0.914053289534979,
0.923439324478087,0.932825563338133,0.942211619595582,0.951597722715543,
0.954355086529251,0.963248944870356,0.971455195139771,0.978625769560708,
0.984645425631258),.UNSPECIFIED.);
#2108=B_SPLINE_CURVE_WITH_KNOTS('',3,(#77785,#77786,#77787,#77788),
 .UNSPECIFIED.,.F.,.F.,(4,4),(0.984645425631258,0.999035201896067),
 .UNSPECIFIED.);
#2109=B_SPLINE_CURVE_WITH_KNOTS('',3,(#77790,#77791,#77792,#77793),
 .UNSPECIFIED.,.F.,.F.,(4,4),(0.999035250238492,1.),.UNSPECIFIED.);
#2110=B_SPLINE_CURVE_WITH_KNOTS('',3,(#77818,#77819,#77820,#77821,#77822,
#77823,#77824,#77825,#77826,#77827),.UNSPECIFIED.,.F.,.F.,(4,2,2,2,4),(0.,
0.221863776616433,0.443727553232867,0.6655913298493,0.887455106465734),
 .UNSPECIFIED.);
#2111=B_SPLINE_CURVE_WITH_KNOTS('',3,(#77830,#77831,#77832,#77833,#77834,
#77835,#77836,#77837,#77838,#77839),.UNSPECIFIED.,.F.,.F.,(4,2,2,2,4),(0.,
0.22177646038554,0.443552920771081,0.665329381156621,0.887105841542162),
 .UNSPECIFIED.);
#2112=B_SPLINE_CURVE_WITH_KNOTS('',3,(#77861,#77862,#77863,#77864,#77865,
#77866,#77867,#77868,#77869,#77870,#77871,#77872,#77873,#77874,#77875,#77876,
#77877,#77878,#77879,#77880,#77881,#77882,#77883,#77884,#77885,#77886,#77887,
#77888,#77889,#77890,#77891),.UNSPECIFIED.,.F.,.F.,(4,3,3,3,3,3,3,3,3,3,
4),(0.0219302008781805,0.110889998370047,0.208167498777535,0.309406295627344,
0.422707248982262,0.5,0.625,0.72740110002725,0.823316949159066,0.912880322251734,
1.),.UNSPECIFIED.);
#2113=B_SPLINE_CURVE_WITH_KNOTS('',3,(#77908,#77909,#77910,#77911,#77912,
#77913,#77914,#77915,#77916,#77917,#77918,#77919,#77920,#77921,#77922,#77923,
#77924,#77925,#77926,#77927,#77928,#77929,#77930,#77931,#77932,#77933,#77934,
#77935,#77936,#77937,#77938,#77939,#77940,#77941),.UNSPECIFIED.,.T.,.F.,
(4,2,2,2,2,2,2,2,2,2,2,2,2,2,2,2,4),(-0.315583874891462,-0.29738266229352,
-0.27768463654161,-0.258053667090507,-0.238476218724991,-0.218890293083453,
-0.199237519662791,-0.179509847947857,-0.159745824539116,-0.139647939264777,
-0.119687705010333,-0.0997724646185103,-0.0798173438841853,-0.0598300512340101,
-0.0398741605185745,-0.0199587807235321,0.),.UNSPECIFIED.);
#2114=B_SPLINE_CURVE_WITH_KNOTS('',3,(#77945,#77946,#77947,#77948,#77949,
#77950,#77951,#77952,#77953,#77954,#77955,#77956,#77957,#77958,#77959,#77960,
#77961,#77962,#77963,#77964,#77965,#77966,#77967),.UNSPECIFIED.,.F.,.F.,
(4,2,2,2,2,2,2,2,2,3,4),(-0.322394442933457,-0.321463867844831,-0.281213098456134,
-0.241013349314738,-0.200984471704924,-0.161071936773251,-0.121080015185152,
-0.080858754962794,-0.0404461452144988,0.,6.19698534856371E-5),
 .UNSPECIFIED.);
#2115=B_SPLINE_CURVE_WITH_KNOTS('',3,(#77969,#77970,#77971,#77972,#77973,
#77974,#77975,#77976,#77977,#77978,#77979,#77980,#77981,#77982,#77983,#77984,
#77985,#77986),.UNSPECIFIED.,.F.,.F.,(4,2,2,2,2,2,2,2,4),(6.19698534856371E-5,
0.04009610250426,0.0805804917540971,0.120891813402526,0.161364748502932,
0.201955855009439,0.242412218648003,0.282721308068169,0.322308248865181),
 .UNSPECIFIED.);
#2116=B_SPLINE_CURVE_WITH_KNOTS('',3,(#78006,#78007,#78008,#78009,#78010,
#78011,#78012,#78013,#78014,#78015,#78016,#78017,#78018,#78019,#78020,#78021,
#78022,#78023,#78024,#78025,#78026,#78027),.UNSPECIFIED.,.F.,.F.,(4,3,3,
3,3,3,3,4),(0.000407408283309958,0.00497275683192009,0.005742565261487,
0.00594626923060788,0.00861384760452239,0.00871569970425684,0.0108497382981234,
0.0114851301779058),.UNSPECIFIED.);
#2117=B_SPLINE_CURVE_WITH_KNOTS('',3,(#78031,#78032,#78033,#78034,#78035,
#78036,#78037,#78038),.UNSPECIFIED.,.F.,.F.,(4,2,2,4),(-0.0450504263378443,
-0.043734901660658,-0.0225288176281075,0.),.UNSPECIFIED.);
#2118=B_SPLINE_CURVE_WITH_KNOTS('',3,(#78047,#78048,#78049,#78050,#78051,
#78052,#78053,#78054,#78055,#78056,#78057,#78058,#78059,#78060,#78061,#78062,
#78063,#78064,#78065,#78066,#78067,#78068),.UNSPECIFIED.,.F.,.F.,(4,3,3,
3,3,3,3,4),(2.91329505494903E-9,0.000660163016541207,0.00123543637619839,
0.0017900655732896,0.00185315456429469,0.00211503954798182,0.00237836381180336,
0.00247087275239099),.UNSPECIFIED.);
#2119=B_SPLINE_CURVE_WITH_KNOTS('',3,(#78072,#78073,#78074,#78075,#78076,
#78077,#78078,#78079,#78080,#78081,#78082,#78083,#78084,#78085,#78086,#78087,
#78088,#78089),.UNSPECIFIED.,.F.,.F.,(4,2,2,2,2,2,2,2,4),(-0.31597704258338,
-0.275100125004532,-0.244154449549492,-0.223290285080556,-0.213738196895435,
-0.192181551009235,-0.15769667845806,-0.0892749983694439,-1.39001374278569E-6),
 .UNSPECIFIED.);
#2120=B_SPLINE_CURVE_WITH_KNOTS('',3,(#78105,#78106,#78107,#78108,#78109,
#78110),.UNSPECIFIED.,.F.,.F.,(4,2,4),(1.13372962259874E-5,0.075979708245961,
0.132752016386919),.UNSPECIFIED.);
#2121=B_SPLINE_CURVE_WITH_KNOTS('',3,(#78116,#78117,#78118,#78119,#78120,
#78121,#78122,#78123,#78124,#78125,#78126,#78127,#78128,#78129,#78130,#78131,
#78132,#78133,#78134),.UNSPECIFIED.,.F.,.F.,(4,3,3,3,3,3,4),(0.,0.00276943641060585,
0.00281960538769298,0.00553887282121171,0.00570812155224864,0.0103685864131738,
0.0110777456424234),.UNSPECIFIED.);
#2122=B_SPLINE_CURVE_WITH_KNOTS('',3,(#78136,#78137,#78138,#78139,#78140,
#78141,#78142,#78143,#78144,#78145),.UNSPECIFIED.,.F.,.F.,(4,3,3,4),(5.53618044130801E-9,
0.000299661069992586,0.000432086313124671,0.000450310767172612),
 .UNSPECIFIED.);
#2123=B_SPLINE_CURVE_WITH_KNOTS('',3,(#78171,#78172,#78173,#78174,#78175,
#78176,#78177,#78178,#78179,#78180,#78181,#78182,#78183),.UNSPECIFIED.,
 .F.,.F.,(4,3,3,3,4),(2.55408693138011E-10,0.000328350173161266,0.00065542770044065,
0.000980575591406873,0.00121964937926107),.UNSPECIFIED.);
#2124=B_SPLINE_CURVE_WITH_KNOTS('',3,(#78191,#78192,#78193,#78194,#78195,
#78196),.UNSPECIFIED.,.F.,.F.,(4,2,4),(-0.12344151138567,-0.0612593453644722,
-1.69855123624801E-5),.UNSPECIFIED.);
#2125=B_SPLINE_CURVE_WITH_KNOTS('',3,(#78197,#78198,#78199,#78200,#78201,
#78202,#78203,#78204,#78205,#78206,#78207,#78208,#78209,#78210,#78211,#78212,
#78213,#78214,#78215,#78216,#78217,#78218,#78219,#78220,#78221,#78222,#78223,
#78224,#78225,#78226,#78227,#78228,#78229,#78230,#78231,#78232,#78233,#78234,
#78235,#78236,#78237,#78238,#78239,#78240,#78241,#78242,#78243,#78244,#78245,
#78246,#78247,#78248,#78249,#78250,#78251,#78252,#78253,#78254,#78255,#78256,
#78257,#78258,#78259,#78260,#78261,#78262,#78263,#78264,#78265,#78266,#78267,
#78268,#78269,#78270,#78271,#78272,#78273,#78274,#78275,#78276,#78277,#78278,
#78279,#78280,#78281,#78282,#78283,#78284,#78285,#78286,#78287,#78288,#78289,
#78290,#78291,#78292,#78293),.UNSPECIFIED.,.F.,.F.,(4,3,3,3,3,3,3,3,3,3,
3,3,3,3,3,3,3,3,3,3,3,3,3,3,3,3,3,3,3,3,3,3,4),(0.00488558905517301,0.0051934316125717,
0.00550131709313176,0.0056266698314079,0.00611648667187354,0.00636775060764279,
0.00686005421483842,0.00735498318747559,0.00784991216011275,0.00819113275196426,
0.00853283329082221,0.00859099293634774,0.00908351642592215,0.00933207371258273,
0.00982197624572552,0.0103181057553891,0.0108142352650527,0.0113008118805492,
0.0117986043490359,0.0122963968175226,0.0127889568608241,0.0130374775937576,
0.0133803810095318,0.0137227757530312,0.0137785583699925,0.0142670392354198,
0.0147638795789411,0.0152607199224624,0.0157505715721473,0.0160018006986973,
0.0163098524339766,0.016617784004579,0.016742881472115),.UNSPECIFIED.);
#2126=B_SPLINE_CURVE_WITH_KNOTS('',3,(#78306,#78307,#78308,#78309,#78310,
#78311,#78312,#78313,#78314,#78315,#78316,#78317,#78318,#78319,#78320,#78321,
#78322,#78323),.UNSPECIFIED.,.F.,.F.,(4,2,2,2,2,2,2,2,4),(-0.314107268919085,
-0.223401463457807,-0.156175714250431,-0.122651406592743,-0.10167412033179,
-0.092313374585261,-0.0715343781050509,-0.0401556420432856,-1.88820737717577E-5),
 .UNSPECIFIED.);
#2127=B_SPLINE_CURVE_WITH_KNOTS('',3,(#78357,#78358,#78359,#78360),
 .UNSPECIFIED.,.F.,.F.,(4,4),(0.,0.000407408044724523),.UNSPECIFIED.);
#2128=B_SPLINE_CURVE_WITH_KNOTS('',3,(#78363,#78364,#78365,#78366,#78367,
#78368,#78369,#78370,#78371,#78372,#78373,#78374,#78375,#78376,#78377,#78378,
#78379,#78380,#78381,#78382,#78383,#78384,#78385,#78386,#78387,#78388,#78389,
#78390,#78391,#78392,#78393,#78394,#78395,#78396,#78397,#78398,#78399,#78400,
#78401,#78402,#78403,#78404,#78405,#78406,#78407,#78408),.UNSPECIFIED.,
 .F.,.F.,(4,3,3,3,3,3,3,3,3,3,3,3,3,3,3,4),(1.47097541858838E-9,0.000771492196635795,
0.00152729150168422,0.00226483520945305,0.00286070517058098,0.00360261249656041,
0.00434678131828715,0.0050965673029855,0.00572141034116197,0.00654881697400354,
0.00740654146015019,0.00829947330035251,0.00925690323311813,0.010261775897808,
0.0113497658956453,0.0114428206823239),.UNSPECIFIED.);
#2129=B_SPLINE_CURVE_WITH_KNOTS('',3,(#78562,#78563,#78564,#78565,#78566,
#78567,#78568,#78569,#78570,#78571,#78572,#78573,#78574,#78575,#78576,#78577,
#78578,#78579,#78580,#78581,#78582,#78583,#78584,#78585,#78586,#78587,#78588,
#78589,#78590,#78591,#78592,#78593,#78594,#78595,#78596,#78597,#78598,#78599,
#78600,#78601,#78602,#78603,#78604,#78605,#78606,#78607,#78608,#78609,#78610,
#78611,#78612,#78613,#78614,#78615,#78616,#78617,#78618,#78619,#78620,#78621,
#78622,#78623,#78624,#78625,#78626,#78627,#78628,#78629,#78630,#78631,#78632,
#78633,#78634,#78635,#78636,#78637,#78638,#78639,#78640,#78641,#78642,#78643,
#78644,#78645,#78646,#78647,#78648,#78649,#78650,#78651,#78652,#78653,#78654,
#78655,#78656,#78657,#78658,#78659,#78660,#78661,#78662,#78663,#78664,#78665,
#78666,#78667,#78668,#78669,#78670,#78671,#78672,#78673,#78674,#78675,#78676,
#78677,#78678,#78679,#78680,#78681,#78682,#78683,#78684,#78685,#78686,#78687,
#78688,#78689,#78690,#78691,#78692,#78693,#78694,#78695,#78696,#78697,#78698,
#78699,#78700,#78701,#78702,#78703,#78704,#78705,#78706,#78707,#78708,#78709,
#78710,#78711,#78712,#78713,#78714,#78715,#78716,#78717,#78718,#78719,#78720,
#78721,#78722,#78723,#78724,#78725,#78726,#78727,#78728,#78729,#78730,#78731,
#78732,#78733,#78734,#78735,#78736,#78737,#78738,#78739),.UNSPECIFIED.,
 .F.,.F.,(4,3,3,3,3,3,3,3,3,3,3,3,3,3,3,3,3,3,3,3,3,3,3,3,3,3,3,3,3,3,3,
3,3,3,3,3,3,3,3,3,3,3,3,3,3,3,3,3,3,3,3,3,3,3,3,3,3,3,3,4),(0.,0.000926416342889362,
0.00173634802732097,0.00175238767688987,0.00260794610843211,0.00262858151533464,
0.00340413825758895,0.00348157049108613,0.00350477535377941,0.00497295805954557,
0.00523349326742887,0.00525716303066868,0.00611135611184734,0.0069897893210327,
0.00700955070755794,0.00850723651272925,0.00874742345145967,0.0087619383844472,
0.00962649083989963,0.00963813222289174,0.0105052986518987,0.0105143260613363,
0.0113839108634704,0.0113905198997808,0.0122624548555008,0.0122667137382254,
0.0135264537493205,0.0140191014151145,0.014019137693761,0.0148952952535591,
0.014897467492945,0.0157714890920036,0.0157758871470558,0.0169878014714307,
0.0175238767688928,0.0175330131040703,0.0184000706073373,0.0184119417422983,
0.0192762644457819,0.0192908621262671,0.0201524582842264,0.0201697828683268,
0.0208826521471334,0.0210286521226709,0.0210487131721851,0.0221316423632042,
0.02278103979956,0.0228048120482523,0.0236572336380045,0.0236815439919199,
0.024533427476449,0.0245569736992918,0.0257675221065015,0.0262858151533381,
0.0263020749158942,0.0267918500587691,0.0271620089917824,0.0275476169326534,
0.0279235134160577,0.0280382028302268),.UNSPECIFIED.);
#2130=B_SPLINE_CURVE_WITH_KNOTS('',3,(#78740,#78741,#78742,#78743,#78744,
#78745,#78746,#78747,#78748,#78749,#78750,#78751,#78752,#78753,#78754,#78755,
#78756,#78757,#78758,#78759,#78760,#78761,#78762,#78763,#78764,#78765,#78766,
#78767,#78768,#78769,#78770,#78771,#78772,#78773,#78774,#78775,#78776,#78777,
#78778,#78779,#78780,#78781,#78782,#78783,#78784,#78785,#78786,#78787,#78788,
#78789,#78790,#78791,#78792,#78793,#78794,#78795,#78796,#78797,#78798,#78799,
#78800,#78801,#78802,#78803,#78804,#78805,#78806,#78807,#78808,#78809,#78810,
#78811,#78812,#78813,#78814,#78815,#78816,#78817,#78818,#78819,#78820,#78821,
#78822,#78823,#78824,#78825,#78826,#78827,#78828,#78829,#78830,#78831,#78832,
#78833,#78834,#78835,#78836,#78837,#78838,#78839,#78840,#78841,#78842,#78843,
#78844,#78845,#78846,#78847,#78848,#78849,#78850,#78851,#78852,#78853,#78854,
#78855,#78856,#78857,#78858,#78859,#78860,#78861,#78862,#78863,#78864,#78865,
#78866,#78867,#78868,#78869,#78870,#78871,#78872,#78873,#78874,#78875,#78876,
#78877,#78878,#78879,#78880,#78881,#78882,#78883,#78884,#78885,#78886,#78887,
#78888,#78889,#78890,#78891,#78892,#78893,#78894,#78895,#78896,#78897,#78898,
#78899,#78900,#78901,#78902),.UNSPECIFIED.,.F.,.F.,(4,3,3,3,3,3,3,3,3,3,
3,3,3,3,3,3,3,3,3,3,3,3,3,3,3,3,3,3,3,3,3,3,3,3,3,3,3,3,3,3,3,3,3,3,3,3,
3,3,3,3,3,3,3,3,4),(0.,0.000368128432020981,0.000744995308322254,0.000832257560475207,
0.0013051293478806,0.00166426378958133,0.00166451512095041,0.00296289381169945,
0.00332903024190082,0.00333012447958715,0.00416335856250361,0.00499354536285123,
0.00499658605666537,0.00656887393213025,0.00665806048380164,0.00666253488292151,
0.00749031804427697,0.00749514135964159,0.0083225756047523,0.00832744533043317,
0.00915483316522763,0.0091594350159297,0.00998709072570296,0.00999111303251047,
0.0116516058466535,0.0116538603965027,0.0124838634071288,0.0124849548202084,
0.0133160095344897,0.0133161209676041,0.0148710898848926,0.0149782215041487,
0.0149806360885546,0.0158094588117832,0.0158128936490299,0.0166409414709503,
0.0166451512095052,0.0174726683061663,0.0174774087699804,0.0183046496274646,
0.0183096663304557,0.0199695592386629,0.0199741814514062,0.0208024587002455,
0.021635565418514,0.0216386965723568,0.0231473042510861,0.0233019830100467,
0.0233032116933073,0.0241350880431039,0.0241354692537826,0.0249677268142579,
0.0249679138728332,0.0260382453062477,0.0266322419352084),.UNSPECIFIED.);
#2131=B_SPLINE_CURVE_WITH_KNOTS('',3,(#78933,#78934,#78935,#78936,#78937,
#78938,#78939,#78940,#78941,#78942,#78943,#78944,#78945,#78946,#78947,#78948,
#78949,#78950,#78951,#78952,#78953,#78954,#78955,#78956,#78957,#78958,#78959,
#78960,#78961,#78962,#78963,#78964,#78965,#78966,#78967,#78968,#78969,#78970,
#78971,#78972,#78973,#78974,#78975,#78976,#78977,#78978),.UNSPECIFIED.,
 .F.,.F.,(4,3,3,3,3,3,3,3,3,3,3,3,3,3,3,4),(0.,0.00106719154926921,0.00206281499229115,
0.00297783614552313,0.00385877869507663,0.00471036156803993,0.00552671449927665,
0.00572149247899258,0.00647690763549953,0.00722797363372799,0.00797355695846304,
0.00858223871848886,0.00932082492988301,0.0100699874777538,0.0108423688248513,
0.0114429849579852),.UNSPECIFIED.);
#2132=B_SPLINE_CURVE_WITH_KNOTS('',3,(#78979,#78980,#78981,#78982),
 .UNSPECIFIED.,.F.,.F.,(4,4),(0.011077745885897,0.0114851542376453),
 .UNSPECIFIED.);
#2133=B_SPLINE_CURVE_WITH_KNOTS('',3,(#78988,#78989,#78990,#78991,#78992,
#78993,#78994,#78995,#78996,#78997,#78998,#78999,#79000,#79001,#79002,#79003,
#79004,#79005,#79006,#79007,#79008,#79009,#79010,#79011,#79012,#79013,#79014,
#79015,#79016,#79017,#79018,#79019,#79020,#79021,#79022,#79023,#79024,#79025,
#79026,#79027,#79028,#79029,#79030,#79031,#79032,#79033,#79034,#79035,#79036,
#79037,#79038,#79039,#79040,#79041,#79042,#79043,#79044,#79045,#79046,#79047,
#79048,#79049,#79050,#79051,#79052,#79053,#79054,#79055,#79056,#79057,#79058,
#79059,#79060),.UNSPECIFIED.,.F.,.F.,(4,3,3,3,3,3,3,3,3,3,3,3,3,3,3,3,3,
3,3,3,3,3,3,3,4),(0.00723577310341842,0.00746729739937353,0.00813249812078954,
0.00829755964440309,0.00874410725636207,0.00949827503482505,0.00995736819421411,
0.010252442813288,0.0113395003728997,0.0116156878478535,0.011760778370214,
0.0124443236839924,0.0132691139271399,0.0132728091843271,0.0147774494840659,
0.0149301313935435,0.0155316172625289,0.0157589738467299,0.0162857850409919,
0.0165883666173337,0.0177941205979179,0.0182480168910559,0.018548288376381,
0.0191055922868745,0.0193024561548439),.UNSPECIFIED.);
#2134=B_SPLINE_CURVE_WITH_KNOTS('',3,(#79076,#79077,#79078,#79079),
 .UNSPECIFIED.,.F.,.F.,(4,4),(0.,0.00312907272408999),.UNSPECIFIED.);
#2135=B_SPLINE_CURVE_WITH_KNOTS('',3,(#79082,#79083,#79084,#79085),
 .UNSPECIFIED.,.F.,.F.,(4,4),(0.,1.),.UNSPECIFIED.);
#2136=B_SPLINE_CURVE_WITH_KNOTS('',3,(#79204,#79205,#79206,#79207,#79208,
#79209,#79210,#79211,#79212,#79213,#79214,#79215,#79216,#79217,#79218,#79219,
#79220,#79221,#79222,#79223,#79224,#79225,#79226,#79227,#79228),
 .UNSPECIFIED.,.F.,.F.,(4,3,3,3,3,3,3,3,4),(0.,0.125,0.25,0.258487929334817,
0.437367182643581,0.5,0.562763102241527,0.867038912738001,0.999999776819451),
 .UNSPECIFIED.);
#2137=B_SPLINE_CURVE_WITH_KNOTS('',3,(#79230,#79231,#79232,#79233,#79234,
#79235,#79236,#79237,#79238,#79239,#79240,#79241,#79242,#79243,#79244,#79245,
#79246,#79247,#79248,#79249,#79250,#79251,#79252,#79253,#79254,#79255,#79256,
#79257,#79258,#79259,#79260,#79261,#79262,#79263,#79264,#79265,#79266,#79267,
#79268,#79269,#79270,#79271,#79272,#79273,#79274,#79275,#79276,#79277,#79278,
#79279,#79280,#79281,#79282,#79283,#79284,#79285,#79286,#79287,#79288,#79289,
#79290,#79291,#79292,#79293,#79294,#79295,#79296,#79297,#79298,#79299),
 .UNSPECIFIED.,.F.,.F.,(4,3,3,3,3,3,3,3,3,3,3,3,3,3,3,3,3,3,3,3,3,3,3,4),
(0.,0.0141557809778879,0.0625000000000003,0.0746323172226332,0.125000000000001,
0.13511093095757,0.250000000000001,0.256066251541517,0.375000000000001,
0.3770215763065,0.487187056529488,0.497976862476372,0.500000000000001,0.558454572926683,
0.562500000000001,0.618932222315836,0.625000000000001,0.739887548974724,
0.750000000000001,0.860842875279398,0.875,0.941938525686023,0.981797501825127,
0.999999999378131),.UNSPECIFIED.);
#2138=B_SPLINE_CURVE_WITH_KNOTS('',3,(#79300,#79301,#79302,#79303,#79304,
#79305,#79306,#79307,#79308,#79309,#79310,#79311,#79312,#79313,#79314,#79315,
#79316,#79317,#79318,#79319,#79320,#79321),.UNSPECIFIED.,.F.,.F.,(4,3,3,
3,3,3,3,4),(1.32021523337872E-9,0.130874672952653,0.432343443865136,0.500000000000005,
0.733812423852511,0.750000000000002,0.964531007757503,0.999999999999006),
 .UNSPECIFIED.);
#2139=B_SPLINE_CURVE_WITH_KNOTS('',3,(#79322,#79323,#79324,#79325,#79326,
#79327,#79328,#79329,#79330,#79331,#79332,#79333,#79334,#79335,#79336,#79337,
#79338,#79339,#79340,#79341,#79342,#79343,#79344,#79345,#79346,#79347,#79348,
#79349,#79350,#79351,#79352,#79353,#79354,#79355,#79356,#79357,#79358,#79359,
#79360,#79361,#79362,#79363,#79364,#79365,#79366,#79367,#79368,#79369,#79370,
#79371,#79372,#79373,#79374,#79375,#79376,#79377,#79378,#79379,#79380,#79381,
#79382,#79383,#79384,#79385,#79386,#79387,#79388,#79389,#79390,#79391,#79392,
#79393,#79394,#79395,#79396,#79397,#79398,#79399,#79400,#79401,#79402,#79403,
#79404,#79405,#79406,#79407,#79408,#79409,#79410,#79411,#79412,#79413,#79414,
#79415,#79416,#79417,#79418,#79419,#79420,#79421,#79422,#79423,#79424,#79425,
#79426,#79427,#79428,#79429,#79430,#79431,#79432,#79433,#79434,#79435,#79436,
#79437,#79438,#79439,#79440,#79441,#79442,#79443,#79444,#79445,#79446,#79447,
#79448,#79449,#79450,#79451,#79452,#79453,#79454,#79455,#79456,#79457,#79458,
#79459,#79460,#79461,#79462,#79463,#79464,#79465,#79466,#79467,#79468,#79469,
#79470,#79471,#79472,#79473,#79474,#79475,#79476,#79477,#79478,#79479,#79480,
#79481),.UNSPECIFIED.,.F.,.F.,(4,3,3,3,3,3,3,3,3,3,3,3,3,3,3,3,3,3,3,3,
3,3,3,3,3,3,3,3,3,3,3,3,3,3,3,3,3,3,3,3,3,3,3,3,3,3,3,3,3,3,3,3,3,4),(2.91264979220492E-15,
0.00300575703219071,0.00458596257778495,0.00462972345140002,0.00757533490906404,
0.00918741237741677,0.00925944690279713,0.0126379912408766,0.0138046411776548,
0.0138891703541942,0.0172144086662736,0.0184304802702438,0.0185188938055914,
0.0219135792309688,0.023059852717408,0.0231486172569885,0.026176380485865,
0.0276962761650712,0.0277783407083856,0.0309338119603887,0.0323414639693572,
0.0324080641597827,0.0344028998389768,0.0346670786726838,0.0347229258854812,
0.0365283926285558,0.036993641415406,0.0370377876111798,0.040278050293859,
0.041644475594072,0.0416675110625769,0.0449242871498441,0.0462888090190751,
0.046297234513974,0.0493505573314523,0.0509248440873743,0.0509269579653712,
0.0532400429443998,0.0532418196910697,0.0555542205796149,0.0555566814167682,
0.0588514339459642,0.0601819075336434,0.0601864048681651,0.0640737496238627,
0.0648116186367275,0.064816128319562,0.0689095202840357,0.0694454977932579,
0.0694458517709589,0.0709188654315961,0.0723842403891683,0.0737814416001958,
0.0740755752223558),.UNSPECIFIED.);
#2140=B_SPLINE_CURVE_WITH_KNOTS('',3,(#79494,#79495,#79496,#79497,#79498,
#79499,#79500),.UNSPECIFIED.,.F.,.F.,(4,3,4),(0.,0.00276685003849761,0.00458363052137194),
 .UNSPECIFIED.);
#2141=B_SPLINE_CURVE_WITH_KNOTS('',3,(#79515,#79516,#79517,#79518),
 .UNSPECIFIED.,.F.,.F.,(4,4),(0.,1.),.UNSPECIFIED.);
#2142=B_SPLINE_CURVE_WITH_KNOTS('',3,(#79519,#79520,#79521,#79522),
 .UNSPECIFIED.,.F.,.F.,(4,4),(0.,0.00312895336538498),.UNSPECIFIED.);
#2143=B_SPLINE_CURVE_WITH_KNOTS('',3,(#79535,#79536,#79537,#79538,#79539,
#79540,#79541),.UNSPECIFIED.,.F.,.F.,(4,3,4),(5.87409092738369E-11,0.00293217098656389,
0.00458274107704695),.UNSPECIFIED.);
#2144=B_SPLINE_CURVE_WITH_KNOTS('',3,(#79570,#79571,#79572,#79573,#79574,
#79575,#79576,#79577,#79578,#79579,#79580,#79581,#79582,#79583,#79584,#79585),
 .UNSPECIFIED.,.F.,.F.,(4,3,3,3,3,4),(0.,0.000314760444717577,0.000629520889435155,
0.000835315943262965,0.00104717886106664,0.00125904177887031),
 .UNSPECIFIED.);
#2145=B_SPLINE_CURVE_WITH_KNOTS('',3,(#79619,#79620,#79621,#79622,#79623,
#79624,#79625,#79626,#79627,#79628,#79629,#79630,#79631,#79632,#79633,#79634),
 .UNSPECIFIED.,.F.,.F.,(4,3,3,3,3,4),(0.,0.000314760444717579,0.000629520889435158,
0.000835315943339465,0.00104717886110491,0.00125904177887035),
 .UNSPECIFIED.);
#2146=B_SPLINE_CURVE_WITH_KNOTS('',3,(#79661,#79662,#79663,#79664,#79665,
#79666,#79667,#79668,#79669,#79670,#79671,#79672,#79673,#79674,#79675,#79676),
 .UNSPECIFIED.,.F.,.F.,(4,3,3,3,3,4),(0.,0.000314760444717591,0.000629520889435182,
0.000835315943223551,0.00104717886104696,0.00125904177887036),
 .UNSPECIFIED.);
#2147=B_SPLINE_CURVE_WITH_KNOTS('',3,(#79708,#79709,#79710,#79711,#79712,
#79713,#79714,#79715,#79716,#79717,#79718,#79719,#79720,#79721,#79722,#79723),
 .UNSPECIFIED.,.F.,.F.,(4,3,3,3,3,4),(0.,0.000314760444717582,0.000629520889435164,
0.000835315943184375,0.00104717886102734,0.0012590417788703),
 .UNSPECIFIED.);
#2148=B_SPLINE_CURVE_WITH_KNOTS('',3,(#79767,#79768,#79769,#79770,#79771,
#79772,#79773,#79774,#79775,#79776,#79777,#79778,#79779,#79780,#79781,#79782,
#79783,#79784,#79785,#79786,#79787,#79788,#79789,#79790,#79791,#79792,#79793,
#79794,#79795,#79796,#79797,#79798,#79799,#79800,#79801,#79802,#79803,#79804,
#79805,#79806,#79807,#79808,#79809,#79810,#79811,#79812,#79813,#79814,#79815),
 .UNSPECIFIED.,.F.,.F.,(4,3,3,3,3,3,3,3,3,3,3,3,3,3,3,3,4),(6.4247391107438E-15,
0.0672804347847839,0.137054964536528,0.212077380895502,0.227495036868895,
0.298907893425271,0.372169120979542,0.447629859322508,0.454990073737789,
0.529338104220492,0.605911607413588,0.6782088495798,0.682485110606684,0.757595417712821,
0.829409200582694,0.897759011016633,0.909980147475578),.UNSPECIFIED.);
#2149=B_SPLINE_CURVE_WITH_KNOTS('',3,(#79816,#79817,#79818,#79819,#79820,
#79821,#79822,#79823,#79824,#79825,#79826,#79827,#79828,#79829,#79830,#79831,
#79832,#79833,#79834,#79835,#79836,#79837),.UNSPECIFIED.,.F.,.F.,(4,3,3,
3,3,3,3,4),(0.,0.000855980888566154,0.00166641330334462,0.00241857507887524,
0.00314395788179104,0.00384525579784931,0.00451678851924274,0.0046334773523488),
 .UNSPECIFIED.);
#2150=B_SPLINE_CURVE_WITH_KNOTS('',3,(#79882,#79883,#79884,#79885,#79886,
#79887,#79888,#79889,#79890,#79891,#79892,#79893,#79894,#79895,#79896,#79897,
#79898,#79899,#79900,#79901,#79902,#79903,#79904,#79905,#79906),
 .UNSPECIFIED.,.F.,.F.,(4,3,3,3,3,3,3,3,4),(-6.00000001243266E-8,0.000118874083410464,
0.00026625895319811,0.000560941736381697,0.00114958238230934,0.00232100875268056,
0.00261300899752845,0.003820437717179,0.00463423520310888),
 .UNSPECIFIED.);
#2151=B_SPLINE_CURVE_WITH_KNOTS('',3,(#79909,#79910,#79911,#79912,#79913,
#79914),.UNSPECIFIED.,.F.,.F.,(4,2,4),(0.00373703492180183,0.0175573755935873,
0.0313777749446053),.UNSPECIFIED.);
#2152=B_SPLINE_CURVE_WITH_KNOTS('',3,(#79916,#79917,#79918,#79919,#79920,
#79921,#79922),.UNSPECIFIED.,.F.,.F.,(4,3,4),(0.,0.00190419423264558,0.00234423638057238),
 .UNSPECIFIED.);
#2153=B_SPLINE_CURVE_WITH_KNOTS('',3,(#79926,#79927,#79928,#79929),
 .UNSPECIFIED.,.F.,.F.,(4,4),(0.,0.00234424630178264),.UNSPECIFIED.);
#2154=B_SPLINE_CURVE_WITH_KNOTS('',3,(#79930,#79931,#79932,#79933,#79934,
#79935),.UNSPECIFIED.,.F.,.F.,(4,2,4),(0.00236563017817001,0.0161860243951214,
0.0300063042511233),.UNSPECIFIED.);
#2155=B_SPLINE_CURVE_WITH_KNOTS('',3,(#80015,#80016,#80017,#80018,#80019,
#80020,#80021,#80022,#80023,#80024,#80025,#80026,#80027,#80028,#80029,#80030,
#80031,#80032,#80033,#80034,#80035,#80036,#80037,#80038,#80039,#80040,#80041,
#80042,#80043,#80044,#80045,#80046,#80047,#80048,#80049,#80050,#80051,#80052,
#80053,#80054,#80055,#80056,#80057,#80058,#80059,#80060,#80061,#80062,#80063,
#80064,#80065,#80066,#80067,#80068,#80069,#80070,#80071,#80072,#80073,#80074,
#80075,#80076,#80077,#80078,#80079,#80080,#80081,#80082,#80083,#80084,#80085,
#80086,#80087,#80088,#80089,#80090,#80091,#80092,#80093,#80094,#80095,#80096,
#80097,#80098,#80099,#80100,#80101,#80102,#80103,#80104,#80105,#80106,#80107,
#80108,#80109,#80110,#80111,#80112,#80113,#80114,#80115,#80116,#80117,#80118,
#80119,#80120,#80121,#80122,#80123,#80124,#80125,#80126,#80127,#80128,#80129),
 .UNSPECIFIED.,.F.,.F.,(4,3,3,3,3,3,3,3,3,3,3,3,3,3,3,3,3,3,3,3,3,3,3,3,
3,3,3,3,3,3,3,3,3,3,3,3,3,3,4),(0.00311905352256314,0.0053801116275994,
0.00602984295399501,0.00807521049387905,0.00859175969223719,0.0109929812518547,
0.0120513367482218,0.0140644658619112,0.0165539281004915,0.0180279533176651,
0.0195371720315853,0.0213524177914092,0.0222735251164223,0.0239416797884228,
0.0250098782012593,0.0268439228031144,0.0286311930298163,0.0297781443204118,
0.0304825843709334,0.0326614314275284,0.0332189374557705,0.0342821935385057,
0.0345871139981891,0.0355175999826488,0.0359552905406078,0.0371490638991439,
0.03834283725768,0.0394975346329774,0.0406635361544574,0.0411512932950454,
0.0414279967102819,0.0423661024051587,0.0433094733853823,0.0439784633754719,
0.0441643497951191,0.0449939343403188,0.0457876834631741,0.0465442361737627,
0.0469007028799563),.UNSPECIFIED.);
#2156=B_SPLINE_CURVE_WITH_KNOTS('',3,(#80131,#80132,#80133,#80134,#80135,
#80136,#80137,#80138,#80139,#80140,#80141,#80142,#80143,#80144,#80145,#80146,
#80147,#80148,#80149,#80150,#80151,#80152,#80153,#80154,#80155,#80156,#80157,
#80158,#80159,#80160,#80161,#80162,#80163,#80164,#80165,#80166,#80167,#80168,
#80169,#80170,#80171,#80172,#80173,#80174,#80175,#80176,#80177,#80178,#80179,
#80180,#80181,#80182,#80183,#80184,#80185,#80186,#80187,#80188,#80189,#80190,
#80191,#80192,#80193,#80194,#80195,#80196,#80197,#80198,#80199,#80200,#80201,
#80202,#80203,#80204,#80205,#80206,#80207,#80208,#80209,#80210,#80211,#80212,
#80213,#80214,#80215,#80216,#80217,#80218,#80219,#80220,#80221,#80222,#80223,
#80224,#80225,#80226,#80227,#80228,#80229,#80230,#80231,#80232,#80233,#80234,
#80235,#80236,#80237,#80238,#80239,#80240,#80241,#80242,#80243,#80244,#80245,
#80246,#80247,#80248,#80249,#80250,#80251,#80252,#80253,#80254,#80255,#80256,
#80257),.UNSPECIFIED.,.F.,.F.,(4,3,3,3,3,3,3,3,3,3,3,3,3,3,3,3,3,3,3,3,
3,3,3,3,3,3,3,3,3,3,3,3,3,3,3,3,3,3,3,3,3,3,4),(0.,0.000768003065203817,
0.00156145589592255,0.00241145844771756,0.00290679751418499,0.00294209519057979,
0.00392936817884266,0.0049005686379947,0.00578940001938904,0.00581359502836999,
0.00691978270676153,0.00802064641753534,0.00861020326582181,0.00872039254255498,
0.00999358199255706,0.011283185442689,0.0114371426134103,0.01162719005674,
0.0129550959660898,0.0142810553350758,0.0157391861777158,0.0171489834289433,
0.01744078508511,0.0191831843701593,0.0210590838955528,0.0229349834209464,
0.0232543801134799,0.0252635651010464,0.0273699950355587,0.028769893630631,
0.0290679751418499,0.0320087732834693,0.0346366633260412,0.0348815701702199,
0.0373829744484225,0.0398598781887525,0.0405367165403877,0.0406951651985899,
0.0429951987229959,0.0435089813873852,0.0436019627127749,0.0450961502804854,
0.0465087602269599),.UNSPECIFIED.);
#2157=B_SPLINE_CURVE_WITH_KNOTS('',3,(#80332,#80333,#80334,#80335,#80336,
#80337,#80338,#80339,#80340,#80341,#80342,#80343,#80344,#80345,#80346,#80347,
#80348,#80349,#80350,#80351,#80352,#80353,#80354,#80355,#80356,#80357,#80358,
#80359,#80360,#80361,#80362,#80363,#80364,#80365,#80366,#80367,#80368,#80369,
#80370,#80371,#80372,#80373,#80374,#80375,#80376,#80377,#80378,#80379,#80380,
#80381,#80382,#80383,#80384,#80385,#80386,#80387,#80388,#80389,#80390,#80391,
#80392,#80393,#80394,#80395,#80396,#80397,#80398,#80399,#80400,#80401,#80402,
#80403,#80404,#80405,#80406,#80407,#80408,#80409,#80410,#80411,#80412,#80413,
#80414,#80415,#80416,#80417,#80418,#80419,#80420,#80421,#80422,#80423,#80424,
#80425,#80426,#80427,#80428,#80429,#80430,#80431,#80432,#80433,#80434,#80435,
#80436,#80437,#80438,#80439,#80440,#80441,#80442,#80443,#80444,#80445,#80446,
#80447,#80448,#80449),.UNSPECIFIED.,.F.,.F.,(4,3,3,3,3,3,3,3,3,3,3,3,3,
3,3,3,3,3,3,3,3,3,3,3,3,3,3,3,3,3,3,3,3,3,3,3,3,3,3,4),(0.,0.000726143059507885,
0.00147913467854374,0.00229201659693578,0.00272869752028247,0.00289529540141928,
0.00384720949917479,0.00478654822520129,0.00545739504056494,0.00570254014808291,
0.00675424881063688,0.00778705433857549,0.00818609256084741,0.00849911281909295,
0.00934447282246815,0.00955044132098881,0.0104584755543277,0.0109147900811302,
0.0113219360486972,0.0135942089848239,0.0157324884413447,0.0163721851216964,
0.0170495208719571,0.0188101707222918,0.0206158981728578,0.0218295801622627,
0.0228747183578681,0.0245582776825458,0.0263139312909912,0.0272869752028289,
0.02877680882973,0.0313209150461057,0.032744370243395,0.0347410550859414,
0.037138016640503,0.0382017652839612,0.0403769928727384,0.0407493932180728,
0.0431136999609109,0.0436591603245274),.UNSPECIFIED.);
#2158=B_SPLINE_CURVE_WITH_KNOTS('',3,(#80452,#80453,#80454,#80455,#80456,
#80457,#80458,#80459,#80460,#80461,#80462,#80463,#80464,#80465,#80466,#80467,
#80468,#80469,#80470,#80471,#80472,#80473,#80474,#80475,#80476,#80477,#80478,
#80479,#80480,#80481,#80482,#80483,#80484,#80485,#80486,#80487,#80488,#80489,
#80490,#80491,#80492,#80493,#80494,#80495,#80496,#80497,#80498,#80499,#80500,
#80501,#80502,#80503,#80504,#80505,#80506,#80507,#80508,#80509,#80510,#80511,
#80512,#80513,#80514,#80515,#80516,#80517,#80518,#80519,#80520,#80521,#80522,
#80523,#80524,#80525,#80526,#80527,#80528,#80529,#80530,#80531,#80532,#80533,
#80534,#80535,#80536,#80537,#80538,#80539,#80540,#80541,#80542,#80543,#80544,
#80545,#80546,#80547,#80548,#80549,#80550,#80551,#80552,#80553,#80554,#80555,
#80556,#80557,#80558,#80559,#80560,#80561,#80562,#80563,#80564,#80565,#80566,
#80567,#80568,#80569,#80570,#80571,#80572,#80573,#80574,#80575,#80576,#80577,
#80578,#80579,#80580,#80581),.UNSPECIFIED.,.F.,.F.,(4,3,3,3,3,3,3,3,3,3,
3,3,3,3,3,3,3,3,3,3,3,3,3,3,3,3,3,3,3,3,3,3,3,3,3,3,3,3,3,3,3,3,3,4),(0.,
0.0014880631106233,0.00289325796053988,0.00298895696726662,0.00546149369419472,
0.00578651592107976,0.00595032476225151,0.00839147043197193,0.0108596509061964,
0.0115730318421595,0.0118288390287403,0.014754677083364,0.0173595477632393,
0.0176745278189992,0.0196969647367931,0.0216224066731238,0.0231460636843191,
0.0234885065984452,0.0252834612916259,0.0271080204485124,0.0287938721334718,
0.0289325796053988,0.0292532769261303,0.030987394920195,0.0326942847566698,
0.0343658661896815,0.0347190955264786,0.034944203878361,0.035728171147985,
0.0361657245067487,0.0376123534870188,0.0377582145051172,0.0387818159471292,
0.0398198044369845,0.0405056114475593,0.0405598044644439,0.0415184848666389,
0.0425122980456137,0.0433815323903777,0.0433988694080998,0.0442301226091971,
0.0450135032249515,0.0457477991098854,0.0462921273686404),.UNSPECIFIED.);
#2159=B_SPLINE_CURVE_WITH_KNOTS('',3,(#80715,#80716,#80717,#80718,#80719,
#80720,#80721,#80722,#80723,#80724,#80725,#80726,#80727,#80728,#80729,#80730,
#80731,#80732,#80733,#80734,#80735,#80736,#80737,#80738,#80739,#80740,#80741,
#80742,#80743,#80744,#80745,#80746,#80747,#80748,#80749,#80750,#80751,#80752,
#80753,#80754,#80755,#80756,#80757,#80758,#80759,#80760,#80761,#80762,#80763,
#80764,#80765,#80766,#80767,#80768,#80769,#80770,#80771,#80772,#80773,#80774,
#80775,#80776,#80777,#80778,#80779,#80780,#80781,#80782,#80783,#80784,#80785,
#80786,#80787,#80788,#80789,#80790,#80791,#80792,#80793,#80794,#80795,#80796,
#80797,#80798,#80799,#80800,#80801,#80802,#80803,#80804,#80805,#80806,#80807,
#80808,#80809,#80810,#80811,#80812,#80813,#80814,#80815,#80816,#80817,#80818,
#80819,#80820,#80821,#80822,#80823,#80824,#80825,#80826,#80827,#80828,#80829,
#80830,#80831,#80832,#80833,#80834,#80835,#80836,#80837,#80838,#80839,#80840,
#80841,#80842,#80843,#80844,#80845,#80846,#80847,#80848,#80849,#80850,#80851,
#80852,#80853,#80854,#80855,#80856,#80857,#80858,#80859,#80860,#80861,#80862,
#80863,#80864,#80865,#80866,#80867,#80868,#80869,#80870,#80871,#80872,#80873,
#80874,#80875,#80876,#80877,#80878,#80879,#80880,#80881,#80882,#80883,#80884,
#80885,#80886,#80887,#80888,#80889,#80890,#80891,#80892,#80893,#80894,#80895,
#80896,#80897,#80898,#80899,#80900,#80901,#80902,#80903,#80904,#80905,#80906,
#80907,#80908,#80909,#80910,#80911,#80912,#80913),.UNSPECIFIED.,.F.,.F.,
(4,3,3,3,3,3,3,3,3,3,3,3,3,3,3,3,3,3,3,3,3,3,3,3,3,3,3,3,3,3,3,3,3,3,3,
3,3,3,3,3,3,3,3,3,3,3,3,3,3,3,3,3,3,3,3,3,3,3,3,3,3,3,3,3,3,3,4),(-5.59795119973968E-8,
3.77153166948725E-5,5.42420177488181E-5,0.000132553837957507,0.000150709093707369,
0.000302142533558002,0.000604345067115865,0.000786478784293366,0.0012087501342316,
0.00205947175303894,0.00241756026846307,0.00432788328869313,0.00460569556319153,
0.00483518053692602,0.00765167798628207,0.0096704210738519,0.00968212413977662,
0.0121986817239082,0.0147309548882147,0.0172905697838751,0.0193409021477037,
0.0197246627808341,0.0225497079721102,0.0254165723872828,0.0283511952458422,
0.0290113832215555,0.0296334023415766,0.032598479695546,0.0356401719954766,
0.0384990492010592,0.0386818642954072,0.0394311552495718,0.0420390225446679,
0.0435171048323331,0.0442854463712337,0.0465596741328543,0.048352345369259,
0.0491025292327438,0.0511450575694643,0.0530508480161911,0.0531875859061849,
0.0538733380029565,0.0557095849073245,0.0575121872200063,0.0580228264431107,
0.0585879878559654,0.0604404467115735,0.0609228364106318,0.0616492568458051,
0.0628580669800366,0.0632453611893526,0.0645539017016228,0.0658671302108557,
0.0671869467768509,0.0676933075169628,0.0678750498154547,0.0692097954598117,
0.0705855751610864,0.0720100465266797,0.0725285480538889,0.0725479710459296,
0.0738436643829537,0.0749312406649937,0.0749461683223518,0.0759822319304995,
0.0769769212816998,0.0773637885908147),.UNSPECIFIED.);
#2160=B_SPLINE_CURVE_WITH_KNOTS('',3,(#81049,#81050,#81051,#81052,#81053,
#81054,#81055,#81056,#81057,#81058,#81059,#81060,#81061,#81062,#81063,#81064,
#81065,#81066,#81067,#81068,#81069,#81070,#81071,#81072,#81073,#81074,#81075,
#81076,#81077,#81078,#81079,#81080,#81081,#81082,#81083,#81084,#81085,#81086,
#81087,#81088),.UNSPECIFIED.,.F.,.F.,(4,2,2,2,2,2,2,2,2,2,2,2,2,2,2,2,2,
2,2,4),(0.,0.00488270447985229,0.00732405671977861,0.00976540895970492,
0.0146481134395579,0.0170894656794843,0.0183101417994474,0.0195308179194105,
0.0244135223992626,0.0292962268791146,0.0341789313589667,0.0390616358388187,
0.0488270447985229,0.058592453758227,0.0683578627179311,0.073240567197783,
0.0756819194377091,0.0769025955576723,0.0775129336176539,0.0781232716776354),
 .UNSPECIFIED.);
#2161=B_SPLINE_CURVE_WITH_KNOTS('',3,(#81092,#81093,#81094,#81095,#81096,
#81097,#81098,#81099,#81100,#81101,#81102,#81103,#81104,#81105,#81106,#81107,
#81108,#81109,#81110,#81111,#81112,#81113,#81114,#81115,#81116,#81117,#81118,
#81119,#81120,#81121,#81122,#81123,#81124,#81125,#81126,#81127,#81128,#81129,
#81130,#81131,#81132,#81133,#81134,#81135,#81136,#81137,#81138,#81139,#81140,
#81141,#81142,#81143,#81144,#81145,#81146,#81147,#81148,#81149,#81150,#81151,
#81152,#81153,#81154,#81155,#81156,#81157,#81158,#81159,#81160,#81161,#81162,
#81163,#81164,#81165,#81166,#81167,#81168,#81169,#81170,#81171,#81172,#81173,
#81174,#81175,#81176,#81177,#81178,#81179,#81180,#81181,#81182,#81183,#81184,
#81185,#81186,#81187,#81188,#81189,#81190,#81191,#81192,#81193,#81194,#81195,
#81196,#81197,#81198,#81199,#81200,#81201,#81202,#81203,#81204,#81205,#81206,
#81207,#81208,#81209,#81210,#81211,#81212,#81213,#81214,#81215,#81216,#81217,
#81218,#81219,#81220,#81221,#81222,#81223,#81224,#81225,#81226,#81227,#81228,
#81229,#81230,#81231,#81232,#81233,#81234,#81235,#81236,#81237,#81238,#81239,
#81240,#81241,#81242,#81243,#81244,#81245,#81246,#81247,#81248,#81249,#81250,
#81251,#81252,#81253,#81254,#81255,#81256,#81257,#81258,#81259,#81260,#81261,
#81262,#81263,#81264,#81265,#81266,#81267,#81268,#81269,#81270,#81271,#81272,
#81273,#81274,#81275,#81276,#81277,#81278,#81279,#81280,#81281,#81282,#81283,
#81284,#81285,#81286,#81287,#81288,#81289,#81290,#81291,#81292,#81293,#81294,
#81295,#81296,#81297,#81298,#81299,#81300,#81301,#81302,#81303,#81304,#81305,
#81306,#81307,#81308,#81309,#81310,#81311,#81312,#81313,#81314,#81315,#81316,
#81317,#81318,#81319,#81320,#81321,#81322,#81323,#81324,#81325,#81326,#81327,
#81328,#81329,#81330,#81331,#81332,#81333,#81334,#81335),.UNSPECIFIED.,
 .F.,.F.,(4,3,3,3,3,3,3,3,3,3,3,3,3,3,3,3,3,3,3,3,3,3,3,3,3,3,3,3,3,3,3,
3,3,3,3,3,3,3,3,3,3,3,3,3,3,3,3,3,3,3,3,3,3,3,3,3,3,3,3,3,3,3,3,3,3,3,3,
3,3,3,3,3,3,3,3,3,3,3,3,3,3,4),(0.0138213625150584,0.0153557252057815,0.016967809312913,
0.0186005460987653,0.0203100782662155,0.0218040616343076,0.0236391782065667,
0.0256135223282299,0.0278020457228518,0.0297867607535567,0.0324211420232949,
0.0346222226998159,0.0366314376259851,0.0385183080194414,0.0402765202164955,
0.0419783697096923,0.0436039474387354,0.0449779475927287,0.0457521589920549,
0.0471616940402511,0.0485724556204019,0.0499853340506432,0.0513995226194317,
0.0528159415151625,0.0537348581113041,0.0551463951926526,0.0565385724899381,
0.0577262076709287,0.0590012271883266,0.060299813065953,0.0613266973480848,
0.0617175572305534,0.0633557013899515,0.0649958419736401,0.0666385396463259,
0.0682825571558663,0.0699276823934046,0.0715737010877966,0.0732206481682718,
0.0748679134463574,0.0765153305568312,0.0776771708855837,0.0776829554690519,
0.0798220465852468,0.0820269821662078,0.0841070044248161,0.0856656545883011,
0.0875503928177031,0.0892804802057929,0.0909480261844515,0.0925357499280549,
0.0936483537075503,0.0940287551521221,0.095402302693789,0.0968005776623906,
0.0982387635443414,0.0997005647312465,0.10119455705148,0.1016310528268,
0.103158876473257,0.10470000813583,0.105775168386768,0.10731195168399,0.107618077166237,
0.108766337718664,0.109613751946049,0.110371017456633,0.112612002482226,
0.11491420298544,0.117283745588801,0.119769286762534,0.122334997043814,
0.125039715440694,0.125579150184548,0.128267344839129,0.129570499744172,
0.131236775216371,0.132915090511205,0.133561849303797,0.136328208654542,
0.139188103873677,0.14154453702431),.UNSPECIFIED.);
#2162=B_SPLINE_CURVE_WITH_KNOTS('',3,(#81614,#81615,#81616,#81617),
 .UNSPECIFIED.,.F.,.F.,(4,4),(0.,0.00229184701740597),.UNSPECIFIED.);
#2163=B_SPLINE_CURVE_WITH_KNOTS('',3,(#81619,#81620,#81621,#81622,#81623,
#81624,#81625),.UNSPECIFIED.,.F.,.F.,(4,3,4),(-5.9999999698125E-8,0.00114592679117705,
0.0022919135823538),.UNSPECIFIED.);
#2164=B_SPLINE_CURVE_WITH_KNOTS('',3,(#81627,#81628,#81629,#81630,#81631,
#81632,#81633,#81634,#81635,#81636,#81637,#81638,#81639,#81640,#81641,#81642,
#81643,#81644,#81645,#81646,#81647,#81648,#81649,#81650,#81651,#81652,#81653,
#81654,#81655,#81656,#81657,#81658,#81659,#81660,#81661,#81662,#81663,#81664,
#81665,#81666,#81667,#81668,#81669,#81670,#81671,#81672,#81673,#81674,#81675,
#81676,#81677,#81678,#81679,#81680,#81681,#81682,#81683,#81684,#81685,#81686,
#81687,#81688,#81689,#81690,#81691,#81692,#81693,#81694,#81695,#81696,#81697,
#81698,#81699,#81700,#81701,#81702,#81703,#81704,#81705,#81706,#81707,#81708,
#81709,#81710,#81711,#81712,#81713,#81714,#81715,#81716,#81717,#81718,#81719,
#81720,#81721,#81722,#81723,#81724,#81725,#81726,#81727,#81728,#81729,#81730,
#81731,#81732,#81733,#81734,#81735,#81736,#81737,#81738,#81739,#81740,#81741,
#81742,#81743,#81744,#81745,#81746,#81747,#81748,#81749,#81750,#81751,#81752,
#81753,#81754,#81755,#81756,#81757,#81758,#81759,#81760,#81761,#81762,#81763,
#81764,#81765,#81766,#81767,#81768,#81769,#81770,#81771,#81772,#81773,#81774,
#81775,#81776,#81777),.UNSPECIFIED.,.F.,.F.,(4,3,3,3,3,3,3,3,3,3,3,3,3,
3,3,3,3,3,3,3,3,3,3,3,3,3,3,3,3,3,3,3,3,3,3,3,3,3,3,3,3,3,3,3,3,3,3,3,3,
3,4),(0.,0.00254964314673973,0.00496070222628838,0.00501980874154407,0.00826545197487785,
0.00992140445257675,0.0100311925058059,0.0136136254161935,0.0174983629157502,
0.0198428089051537,0.0200323843653405,0.0251558497217403,0.0297642133577307,
0.0300168623559456,0.0348512400831266,0.0388899647682047,0.0396856178103077,
0.0399877547963082,0.0442724564177337,0.0446463200365963,0.044965125921608,
0.0478278095482398,0.0496070222628849,0.0499357590496292,0.0522517417694013,
0.0543924576210147,0.0545677244891735,0.0548913186057754,0.0568663425859277,
0.0587651627048331,0.0595284267154621,0.0598185736751817,0.0612486302751543,
0.0620087778286062,0.0622677632564443,0.0638697876314808,0.0644891289417504,
0.0647077384064401,0.0662847719523633,0.0678876752602966,0.0694498311680387,
0.0695699086585862,0.0710966014883998,0.0719301822811829,0.0720034895600447,
0.0734239213479113,0.074410533394327,0.0744472360436,0.0763835183275585,
0.077890280957556,0.079371235620615),.UNSPECIFIED.);
#2165=B_SPLINE_CURVE_WITH_KNOTS('',5,(#81779,#81780,#81781,#81782,#81783,
#81784,#81785,#81786,#81787,#81788,#81789,#81790,#81791,#81792,#81793,#81794,
#81795,#81796,#81797),.UNSPECIFIED.,.F.,.F.,(6,1,2,3,3,3,1,6),(0.026904580241564,
0.0624999999998681,0.124999999999887,0.249999999999925,0.500000000000001,
0.750000000000077,0.875000000000115,0.97309541975779),.UNSPECIFIED.);
#2166=B_SPLINE_CURVE_WITH_KNOTS('',3,(#81798,#81799,#81800,#81801,#81802,
#81803,#81804,#81805,#81806,#81807,#81808,#81809,#81810,#81811,#81812,#81813,
#81814,#81815,#81816,#81817,#81818,#81819,#81820,#81821,#81822,#81823,#81824,
#81825,#81826,#81827,#81828,#81829,#81830,#81831,#81832,#81833,#81834,#81835,
#81836,#81837,#81838,#81839,#81840,#81841,#81842,#81843,#81844,#81845,#81846,
#81847,#81848,#81849,#81850,#81851,#81852,#81853,#81854,#81855,#81856,#81857,
#81858,#81859,#81860,#81861,#81862,#81863,#81864,#81865,#81866,#81867,#81868,
#81869,#81870,#81871,#81872,#81873,#81874,#81875,#81876,#81877,#81878,#81879,
#81880,#81881,#81882,#81883,#81884,#81885,#81886,#81887,#81888,#81889,#81890,
#81891,#81892,#81893,#81894,#81895,#81896,#81897,#81898,#81899,#81900,#81901,
#81902,#81903,#81904,#81905,#81906,#81907,#81908,#81909,#81910,#81911,#81912,
#81913,#81914,#81915,#81916,#81917,#81918,#81919,#81920,#81921,#81922,#81923,
#81924,#81925,#81926,#81927,#81928,#81929,#81930,#81931,#81932,#81933,#81934,
#81935,#81936,#81937,#81938,#81939,#81940,#81941,#81942,#81943,#81944,#81945,
#81946,#81947,#81948,#81949,#81950,#81951,#81952,#81953,#81954,#81955,#81956,
#81957,#81958,#81959,#81960),.UNSPECIFIED.,.F.,.F.,(4,3,3,3,3,3,3,3,3,3,
3,3,3,3,3,3,3,3,3,3,3,3,3,3,3,3,3,3,3,3,3,3,3,3,3,3,3,3,3,3,3,3,3,3,3,3,
3,3,3,3,3,3,3,3,4),(0.,0.00140947603978418,0.0024756341357668,0.00248033423984031,
0.00401846206250739,0.00494329357891454,0.00495126827153361,0.00676698994228475,
0.00838410792447671,0.00982709094185986,0.00990253654306755,0.0114864206850264,
0.0130928099150335,0.0146991991450405,0.0148538048146015,0.0167010364617009,
0.0171457642489763,0.0173294389503683,0.0194739265126486,0.0196023111933348,
0.0198050730861351,0.0217052560346576,0.0236804462177422,0.0245443401511237,
0.0247563413576684,0.0269124535382796,0.0291847695784314,0.0295139096563174,
0.0297076096292018,0.0325507544885065,0.034497823346557,0.0346588779007351,
0.0378033430080754,0.0394883310170963,0.0396101461722684,0.0429789048814282,
0.0468219392681408,0.049498571171444,0.0495126827153351,0.0556179629347513,
0.0594152192584017,0.0595245880574298,0.0637007112342887,0.0643664875299352,
0.0666105083933754,0.0686940084843271,0.0693177558014686,0.0695562768533866,
0.0719529892403943,0.0742690240730021,0.0746112540765943,0.0771545039955694,
0.0784302024647239,0.0790690551790372,0.0792202923445355),.UNSPECIFIED.);
#2167=B_SPLINE_CURVE_WITH_KNOTS('',3,(#81962,#81963,#81964,#81965,#81966,
#81967,#81968,#81969,#81970,#81971,#81972,#81973,#81974,#81975,#81976,#81977,
#81978,#81979,#81980,#81981,#81982,#81983,#81984,#81985,#81986,#81987,#81988,
#81989,#81990,#81991,#81992,#81993,#81994,#81995,#81996,#81997,#81998),
 .UNSPECIFIED.,.F.,.F.,(4,3,3,3,3,3,3,3,3,3,3,3,4),(0.,0.0797408492149254,
0.161855164948292,0.248717931187981,0.338623906203558,0.432533374925927,
0.5,0.594371835892723,0.686236776709294,0.772607332273767,0.856209295506246,
0.93626015886546,1.),.UNSPECIFIED.);
#2168=B_SPLINE_CURVE_WITH_KNOTS('',3,(#82012,#82013,#82014,#82015,#82016,
#82017,#82018,#82019,#82020,#82021,#82022,#82023,#82024,#82025,#82026,#82027,
#82028,#82029,#82030,#82031,#82032,#82033,#82034,#82035,#82036,#82037,#82038,
#82039,#82040,#82041,#82042,#82043,#82044,#82045,#82046,#82047,#82048),
 .UNSPECIFIED.,.F.,.F.,(4,3,3,3,3,3,3,3,3,3,3,3,4),(0.,0.0797761540364943,
0.161934993682177,0.248863688029891,0.338853887792259,0.432867845144356,
0.5,0.594694033641728,0.686818625637526,0.773322404313094,0.857008887365513,
0.937104727272101,1.),.UNSPECIFIED.);
#2169=B_SPLINE_CURVE_WITH_KNOTS('',3,(#82147,#82148,#82149,#82150),
 .UNSPECIFIED.,.F.,.F.,(4,4),(0.,0.0994990093838759),.UNSPECIFIED.);
#2170=B_SPLINE_CURVE_WITH_KNOTS('',3,(#82151,#82152,#82153,#82154,#82155,
#82156,#82157),.UNSPECIFIED.,.F.,.F.,(4,3,4),(0.000501749122919644,0.0788687616003136,
0.100000758506779),.UNSPECIFIED.);
#2171=B_SPLINE_CURVE_WITH_KNOTS('',3,(#82285,#82286,#82287,#82288,#82289,
#82290,#82291,#82292,#82293,#82294,#82295,#82296,#82297,#82298,#82299,#82300,
#82301,#82302,#82303,#82304,#82305,#82306,#82307,#82308,#82309,#82310,#82311,
#82312,#82313,#82314,#82315,#82316,#82317,#82318,#82319,#82320,#82321),
 .UNSPECIFIED.,.F.,.F.,(4,3,3,3,3,3,3,3,3,3,3,3,4),(0.,0.0798162266516071,
0.161952526089989,0.248677675875237,0.338294947140869,0.431635010482063,
0.5,0.593343691841967,0.684478682447239,0.770593179237603,0.854107271329051,
0.934207928070758,1.),.UNSPECIFIED.);
#2172=B_SPLINE_CURVE_WITH_KNOTS('',3,(#82346,#82347,#82348,#82349),
 .UNSPECIFIED.,.F.,.F.,(4,4),(0.000501748999621204,0.100000733467173),
 .UNSPECIFIED.);
#2173=B_SPLINE_CURVE_WITH_KNOTS('',3,(#82350,#82351,#82352,#82353,#82354,
#82355,#82356),.UNSPECIFIED.,.F.,.F.,(4,3,4),(0.,0.0156807264631829,0.0994990093838759),
 .UNSPECIFIED.);
#2174=B_SPLINE_CURVE_WITH_KNOTS('',3,(#82370,#82371,#82372,#82373),
 .UNSPECIFIED.,.F.,.F.,(4,4),(0.000501749122919617,0.100000758506779),
 .UNSPECIFIED.);
#2175=B_SPLINE_CURVE_WITH_KNOTS('',3,(#82374,#82375,#82376,#82377),
 .UNSPECIFIED.,.F.,.F.,(4,4),(0.,0.0994989844675695),.UNSPECIFIED.);
#2176=B_SPLINE_CURVE_WITH_KNOTS('',3,(#82390,#82391,#82392,#82393),
 .UNSPECIFIED.,.F.,.F.,(4,4),(0.000501748999621204,0.100000733467173),
 .UNSPECIFIED.);
#2177=B_SPLINE_CURVE_WITH_KNOTS('',3,(#82406,#82407,#82408,#82409),
 .UNSPECIFIED.,.F.,.F.,(4,4),(0.,0.0994989844675695),.UNSPECIFIED.);
#2178=B_SPLINE_CURVE_WITH_KNOTS('',3,(#82475,#82476,#82477,#82478,#82479,
#82480,#82481,#82482,#82483,#82484,#82485,#82486,#82487,#82488,#82489,#82490,
#82491,#82492,#82493,#82494,#82495,#82496,#82497,#82498,#82499,#82500,#82501,
#82502,#82503,#82504,#82505,#82506,#82507,#82508,#82509,#82510,#82511,#82512,
#82513,#82514,#82515,#82516,#82517,#82518,#82519,#82520,#82521,#82522,#82523,
#82524,#82525,#82526,#82527,#82528,#82529,#82530,#82531,#82532,#82533,#82534,
#82535,#82536,#82537,#82538,#82539,#82540,#82541,#82542,#82543,#82544,#82545,
#82546,#82547,#82548,#82549,#82550,#82551,#82552,#82553,#82554,#82555,#82556,
#82557,#82558,#82559,#82560,#82561,#82562,#82563,#82564,#82565,#82566,#82567,
#82568,#82569,#82570,#82571,#82572,#82573,#82574,#82575,#82576,#82577,#82578,
#82579,#82580,#82581,#82582,#82583,#82584,#82585,#82586,#82587,#82588,#82589,
#82590,#82591,#82592,#82593,#82594,#82595,#82596,#82597,#82598,#82599,#82600,
#82601,#82602,#82603,#82604,#82605,#82606,#82607,#82608,#82609,#82610,#82611,
#82612,#82613,#82614,#82615,#82616,#82617,#82618,#82619,#82620,#82621,#82622,
#82623,#82624,#82625,#82626,#82627,#82628,#82629,#82630,#82631,#82632,#82633,
#82634,#82635,#82636,#82637,#82638,#82639,#82640,#82641,#82642,#82643,#82644,
#82645,#82646,#82647,#82648,#82649,#82650,#82651,#82652,#82653,#82654,#82655,
#82656,#82657,#82658,#82659,#82660,#82661),.UNSPECIFIED.,.F.,.F.,(4,3,3,
3,3,3,3,3,3,3,3,3,3,3,3,3,3,3,3,3,3,3,3,3,3,3,3,3,3,3,3,3,3,3,3,3,3,3,3,
3,3,3,3,3,3,3,3,3,3,3,3,3,3,3,3,3,3,3,3,3,3,3,4),(0.,0.00129806474652078,
0.00173826111454353,0.00175748537690092,0.00253439280672143,0.00260848340217944,
0.00263622806535153,0.00347971001178824,0.00351497075380215,0.00459045036182651,
0.00522713955700752,0.00527245613070368,0.00593919936703502,0.00610334028621381,
0.00615119881915445,0.00698136154947715,0.00702994150760521,0.00761773897739526,
0.00790868419605598,0.00836503337917805,0.00874285200622063,0.00878742688450675,
0.0102952263202082,0.0105106640972962,0.0105449122614081,0.0113430190056926,
0.0113966380311906,0.0114236549498588,0.0122838726044989,0.0123023976383095,
0.0140595560052317,0.0140598830152109,0.014764174565025,0.0149386257036616,
0.0149478752944383,0.0158173683921124,0.0158357198344066,0.0169081214885754,
0.0175748537690138,0.0176088189027247,0.0187941931735089,0.0193323391459153,
0.0193769020438058,0.0202110818343661,0.020258524249687,0.0209265199003004,
0.021089824522817,0.0211384645734138,0.0221119423053973,0.0228473098997184,
0.022892870910804,0.0236593526447152,0.0237260525881691,0.0237673174050347,
0.0246047952766199,0.0246402836506722,0.0258895920454538,0.0263622806535216,
0.0263820780204341,0.0268115506812034,0.0272410233419727,0.0276803946861982,
0.0281197660304237),.UNSPECIFIED.);
#2179=B_SPLINE_CURVE_WITH_KNOTS('',3,(#82776,#82777,#82778,#82779,#82780,
#82781,#82782,#82783,#82784,#82785,#82786,#82787,#82788,#82789,#82790,#82791,
#82792,#82793,#82794,#82795,#82796,#82797,#82798,#82799,#82800,#82801,#82802,
#82803,#82804,#82805,#82806,#82807,#82808,#82809,#82810,#82811,#82812,#82813),
 .UNSPECIFIED.,.F.,.F.,(4,2,2,2,2,2,2,2,2,2,2,2,2,2,2,2,2,2,4),(1.69183768239892E-7,
0.0048773097517895,0.00975461950357901,0.0146319292553685,0.019509239007158,
0.0219478938830527,0.0243865487589474,0.0292638585107367,0.034141168262526,
0.0390184780143152,0.0414571328902099,0.0438957877661045,0.0487730975178938,
0.0536504072696831,0.0585277170214724,0.0634050267732618,0.0682823365250511,
0.0731596462768404,0.078036786716835),.UNSPECIFIED.);
#2180=B_SPLINE_CURVE_WITH_KNOTS('',3,(#83066,#83067,#83068,#83069,#83070,
#83071,#83072,#83073,#83074,#83075,#83076,#83077,#83078,#83079,#83080,#83081,
#83082,#83083,#83084,#83085,#83086,#83087,#83088,#83089,#83090),
 .UNSPECIFIED.,.F.,.F.,(4,3,3,3,3,3,3,3,4),(0.0299184616875247,0.0303501458310297,
0.0337269825420159,0.0352479488762528,0.037103821794114,0.0379126924706169,
0.0387922400745739,0.0404806582791753,0.0405774360649809),.UNSPECIFIED.);
#2181=B_SPLINE_CURVE_WITH_KNOTS('',3,(#83091,#83092,#83093,#83094,#83095,
#83096,#83097,#83098,#83099,#83100,#83101,#83102,#83103,#83104,#83105,#83106),
 .UNSPECIFIED.,.F.,.F.,(4,3,3,3,3,4),(0.0170041804055748,0.0202196292169069,
0.0221201639002461,0.0235964706859312,0.0269733085854605,0.0272361473949173),
 .UNSPECIFIED.);
#2182=B_SPLINE_CURVE_WITH_KNOTS('',3,(#83107,#83108,#83109,#83110,#83111,
#83112,#83113,#83114,#83115,#83116,#83117,#83118,#83119,#83120,#83121,#83122,
#83123,#83124,#83125,#83126,#83127,#83128,#83129,#83130,#83131,#83132,#83133,
#83134,#83135,#83136,#83137,#83138,#83139,#83140,#83141,#83142,#83143,#83144,
#83145,#83146,#83147,#83148,#83149,#83150,#83151,#83152,#83153,#83154,#83155,
#83156,#83157,#83158,#83159,#83160,#83161,#83162,#83163,#83164,#83165,#83166,
#83167,#83168,#83169,#83170,#83171,#83172,#83173,#83174,#83175,#83176),
 .UNSPECIFIED.,.F.,.F.,(4,3,3,3,3,3,3,3,3,3,3,3,3,3,3,3,3,3,3,3,3,3,3,4),
(0.0019251675425492,0.00334378906625673,0.00447186156832812,0.00493983969368741,
0.00502452477533919,0.00586801927215848,0.00644718237437487,0.00671228437311717,
0.00755649345598186,0.00795452505506233,0.00840082127134725,0.00882308249445703,
0.00924513359857515,0.00946186773574978,0.00966686202115364,0.0100888830220607,
0.0108460286904892,0.0109333300155275,0.0109692104164372,0.0117775399721665,
0.0124765530971247,0.0126217496304117,0.0134659578750993,0.0139838957778122),
 .UNSPECIFIED.);
#2183=B_SPLINE_CURVE_WITH_KNOTS('',3,(#83177,#83178,#83179,#83180,#83181,
#83182,#83183,#83184,#83185,#83186,#83187,#83188,#83189,#83190,#83191,#83192,
#83193,#83194,#83195,#83196,#83197,#83198,#83199,#83200,#83201,#83202,#83203,
#83204,#83205,#83206,#83207,#83208,#83209,#83210,#83211,#83212,#83213,#83214,
#83215,#83216,#83217,#83218,#83219,#83220,#83221,#83222,#83223,#83224,#83225,
#83226,#83227,#83228,#83229,#83230,#83231,#83232,#83233,#83234,#83235,#83236,
#83237,#83238,#83239,#83240,#83241,#83242,#83243,#83244,#83245,#83246,#83247,
#83248,#83249,#83250,#83251,#83252,#83253,#83254,#83255,#83256,#83257,#83258,
#83259,#83260,#83261,#83262,#83263,#83264,#83265,#83266,#83267,#83268,#83269,
#83270,#83271,#83272,#83273,#83274,#83275,#83276,#83277,#83278,#83279,#83280,
#83281,#83282,#83283,#83284,#83285,#83286,#83287,#83288,#83289,#83290,#83291,
#83292,#83293,#83294,#83295,#83296,#83297,#83298,#83299,#83300,#83301,#83302,
#83303,#83304,#83305,#83306,#83307,#83308,#83309,#83310,#83311,#83312,#83313,
#83314,#83315,#83316,#83317,#83318,#83319,#83320,#83321,#83322,#83323,#83324,
#83325,#83326,#83327,#83328,#83329,#83330,#83331,#83332,#83333,#83334,#83335,
#83336,#83337,#83338,#83339,#83340,#83341,#83342,#83343,#83344,#83345,#83346,
#83347,#83348,#83349,#83350,#83351,#83352,#83353,#83354,#83355,#83356,#83357,
#83358,#83359,#83360,#83361,#83362,#83363,#83364,#83365,#83366,#83367,#83368,
#83369,#83370,#83371,#83372,#83373,#83374,#83375,#83376,#83377,#83378,#83379,
#83380,#83381,#83382,#83383,#83384,#83385,#83386,#83387,#83388,#83389,#83390,
#83391,#83392,#83393,#83394,#83395,#83396,#83397,#83398,#83399,#83400,#83401,
#83402,#83403,#83404,#83405,#83406,#83407,#83408,#83409,#83410,#83411,#83412,
#83413,#83414,#83415,#83416,#83417,#83418,#83419,#83420,#83421,#83422,#83423,
#83424,#83425,#83426,#83427,#83428,#83429,#83430,#83431,#83432),
 .UNSPECIFIED.,.F.,.F.,(4,3,3,3,3,3,3,3,3,3,3,3,3,3,3,3,3,3,3,3,3,3,3,3,
3,3,3,3,3,3,3,3,3,3,3,3,3,3,3,3,3,3,3,3,3,3,3,3,3,3,3,3,3,3,3,3,3,3,3,3,
3,3,3,3,3,3,3,3,3,3,3,3,3,3,3,3,3,3,3,3,3,3,3,3,3,4),(0.,0.000671271444715106,
0.00133573398492509,0.00199656612730211,0.00267564160261107,0.00334004269519932,
0.00402645536186862,0.00471286802853793,0.00547920794335988,0.00628429962118388,
0.00716079437273603,0.00808586384770316,0.00908883320141247,0.00942573605707585,
0.0104652026191,0.0115317045578357,0.0126000266263672,0.013666613817005,
0.0141386040856138,0.0151515096840178,0.0161699677133158,0.0171934455273772,
0.018228269718743,0.0188514721141517,0.0197328956913815,0.0206287034168766,
0.0212079061284207,0.0222544789108859,0.0233470560080171,0.0235643401426896,
0.0246626218613768,0.0258454200191195,0.0271492080637942,0.0282772081712275,
0.0296408732222399,0.030981969144124,0.0322417032554741,0.0329900761997653,
0.0341682932068998,0.0352934947584113,0.0363996004210637,0.0374869166232296,
0.0377029442283032,0.0378307562325676,0.0389450672375698,0.0400593782425721,
0.0410084966162602,0.0419734390593707,0.0424158122568411,0.0436667633990814,
0.0449613146661833,0.046274937431326,0.0471286802853789,0.048395788287793,
0.0495938760100985,0.0507177121620077,0.0518415483139168,0.0529519305126435,
0.0540079497098051,0.0550392316356208,0.0560406255956614,0.0565544163424547,
0.0575733034733135,0.0585697691399218,0.0589108503567236,0.0597776382715151,
0.0606400134853726,0.0612672843709925,0.0623243005149662,0.0633870339544853,
0.0644492360151451,0.0654931261235198,0.0659801523995304,0.0669869888480002,
0.0679134967430172,0.0687682851712823,0.0695816398702095,0.0703432939240617,
0.0706930204280682,0.0713654965182033,0.0720302304898885,0.0726900854517225,
0.0733690266256629,0.0740291640074781,0.074717507077481,0.0754058501474839),
 .UNSPECIFIED.);
#2184=B_SPLINE_CURVE_WITH_KNOTS('',3,(#83433,#83434,#83435,#83436,#83437,
#83438,#83439,#83440,#83441,#83442,#83443,#83444,#83445,#83446,#83447,#83448,
#83449,#83450,#83451,#83452,#83453,#83454),.UNSPECIFIED.,.F.,.F.,(4,3,3,
3,3,3,3,4),(0.0477477555525722,0.0480785186018883,0.0489227697563253,0.0493078116841327,
0.0506111708367689,0.0508678770957731,0.0522995954683137,0.0539880079190539),
 .UNSPECIFIED.);
#2185=B_SPLINE_CURVE_WITH_KNOTS('',3,(#83455,#83456,#83457,#83458,#83459,
#83460,#83461,#83462,#83463,#83464,#83465,#83466,#83467,#83468,#83469,#83470,
#83471,#83472,#83473,#83474,#83475,#83476,#83477,#83478,#83479,#83480,#83481,
#83482,#83483,#83484,#83485,#83486,#83487,#83488),.UNSPECIFIED.,.F.,.F.,
(4,3,3,3,3,3,3,3,3,3,3,4),(0.0416412057894145,0.0421690766487205,0.0427185744702001,
0.0430132854152916,0.0437959431509857,0.0438574958856639,0.0442796014294634,
0.0447017045928652,0.0448733118317713,0.0451238084081384,0.0455459138152578,
0.0459506805125569),.UNSPECIFIED.);
#2186=B_SPLINE_CURVE_WITH_KNOTS('',3,(#85402,#85403,#85404,#85405,#85406,
#85407,#85408,#85409,#85410,#85411,#85412,#85413,#85414,#85415,#85416,#85417,
#85418,#85419,#85420,#85421,#85422,#85423,#85424,#85425,#85426,#85427,#85428,
#85429,#85430,#85431,#85432,#85433,#85434,#85435,#85436,#85437,#85438,#85439,
#85440,#85441,#85442,#85443,#85444,#85445,#85446,#85447,#85448,#85449,#85450,
#85451,#85452,#85453,#85454,#85455),.UNSPECIFIED.,.F.,.F.,(4,2,2,2,2,2,
2,2,2,2,2,2,2,2,2,2,2,2,2,2,2,2,2,2,2,2,4),(0.,0.00855967103632646,0.0171193420726529,
0.0342386841453058,0.0684773682906117,0.136954736581223,0.171193420726529,
0.205432104871835,0.239670789017141,0.273909473162447,0.302569805907928,
0.316899972280669,0.324065055467039,0.33123013865341,0.358116418237434,
0.385002697821458,0.438775256989507,0.492547816157555,0.546320375325604,
0.555016077087237,0.563711778848869,0.581103182372135,0.615885989418665,
0.711914492063999,0.807942994709333,0.903971497354666,1.),.UNSPECIFIED.);
#2187=B_SPLINE_CURVE_WITH_KNOTS('',3,(#85458,#85459,#85460,#85461,#85462,
#85463,#85464,#85465,#85466,#85467,#85468,#85469,#85470,#85471,#85472,#85473,
#85474,#85475,#85476,#85477,#85478,#85479,#85480,#85481,#85482,#85483,#85484,
#85485,#85486,#85487,#85488,#85489,#85490,#85491,#85492,#85493,#85494,#85495,
#85496,#85497,#85498,#85499,#85500,#85501,#85502,#85503,#85504,#85505,#85506,
#85507,#85508,#85509,#85510,#85511),.UNSPECIFIED.,.F.,.F.,(4,2,2,2,2,2,
2,2,2,2,2,2,2,2,2,2,2,2,2,2,2,2,2,2,2,2,4),(0.,0.00855967103632646,0.0171193420726529,
0.0342386841453058,0.0684773682906117,0.136954736581223,0.171193420726529,
0.205432104871835,0.239670789017141,0.273909473162447,0.302569805907928,
0.316899972280669,0.324065055467039,0.33123013865341,0.358116418237434,
0.385002697821458,0.438775256989507,0.492547816157555,0.546320375325604,
0.555016077087237,0.563711778848869,0.581103182372135,0.615885989418665,
0.711914492063999,0.807942994709333,0.903971497354666,1.),.UNSPECIFIED.);
#2188=B_SPLINE_CURVE_WITH_KNOTS('',3,(#85962,#85963,#85964,#85965,#85966,
#85967,#85968,#85969,#85970,#85971,#85972,#85973,#85974,#85975,#85976,#85977,
#85978,#85979,#85980,#85981,#85982,#85983,#85984,#85985,#85986,#85987,#85988,
#85989,#85990,#85991,#85992,#85993,#85994,#85995,#85996,#85997,#85998,#85999,
#86000,#86001,#86002,#86003,#86004,#86005,#86006,#86007,#86008,#86009,#86010,
#86011,#86012,#86013,#86014,#86015,#86016),.UNSPECIFIED.,.F.,.F.,(4,3,3,
3,3,3,3,3,3,3,3,3,3,3,3,3,3,3,4),(0.000201753170275764,0.000391372308539321,
0.000584482554336057,0.000714496028078632,0.0008767415620752,0.0010625312444393,
0.00107365626679827,0.00127227482719147,0.00143589683236403,0.00155172995387464,
0.00173223334765279,0.00179960500601608,0.00198632247061839,0.00216599342059071,
0.00222671834567407,0.00240462689396127,0.00258342197686667,0.00276178812585047,
0.00290170673747351),.UNSPECIFIED.);
#2189=B_SPLINE_CURVE_WITH_KNOTS('',3,(#86022,#86023,#86024,#86025,#86026,
#86027,#86028,#86029,#86030,#86031,#86032,#86033,#86034,#86035,#86036,#86037,
#86038,#86039,#86040,#86041,#86042,#86043,#86044,#86045,#86046,#86047,#86048,
#86049,#86050,#86051,#86052,#86053,#86054,#86055,#86056,#86057,#86058,#86059,
#86060,#86061,#86062,#86063,#86064,#86065,#86066,#86067,#86068,#86069,#86070,
#86071,#86072,#86073,#86074,#86075,#86076,#86077,#86078,#86079),
 .UNSPECIFIED.,.F.,.F.,(4,3,3,3,3,3,3,3,3,3,3,3,3,3,3,3,3,3,3,4),(0.,0.000522356852536227,
0.000973581345339098,0.000984510290454162,0.00147422172391699,0.00195092533138153,
0.00196902058090832,0.00225002553935448,0.00244233119126233,0.00246127572613544,
0.00274151904332241,0.00293687568327876,0.00295353087136256,0.00317316065111924,
0.00336741647887176,0.00343557230408307,0.00344578601658967,0.00363646086434783,
0.00381869545059764,0.00393804116181679),.UNSPECIFIED.);
#2190=B_SPLINE_CURVE_WITH_KNOTS('',3,(#86087,#86088,#86089,#86090,#86091,
#86092,#86093,#86094,#86095,#86096,#86097,#86098,#86099,#86100,#86101,#86102,
#86103,#86104,#86105,#86106,#86107,#86108,#86109,#86110,#86111,#86112,#86113,
#86114,#86115,#86116,#86117,#86118,#86119,#86120,#86121,#86122,#86123,#86124,
#86125,#86126,#86127,#86128,#86129,#86130,#86131,#86132,#86133,#86134,#86135,
#86136,#86137,#86138,#86139,#86140,#86141),.UNSPECIFIED.,.F.,.F.,(4,3,3,
3,3,3,3,3,3,3,3,3,3,3,3,3,3,3,4),(0.,0.000132978696347368,0.000270241287995725,
0.000411196528084791,0.000507024332052189,0.000517726876311709,0.000779514505849355,
0.00101404866410438,0.00103112302519988,0.00132345052735938,0.00162877172921639,
0.0019603915463655,0.00202809732820876,0.00204614960503823,0.0024101150598867,
0.0028021558357775,0.00304214599231314,0.0030527561475232,0.00405619465641752),
 .UNSPECIFIED.);
#2191=B_SPLINE_CURVE_WITH_KNOTS('',3,(#86147,#86148,#86149,#86150,#86151,
#86152,#86153,#86154,#86155,#86156,#86157,#86158,#86159,#86160,#86161,#86162,
#86163,#86164,#86165,#86166,#86167,#86168,#86169,#86170,#86171,#86172,#86173,
#86174,#86175,#86176,#86177,#86178,#86179,#86180,#86181,#86182,#86183),
 .UNSPECIFIED.,.F.,.F.,(4,3,3,3,3,3,3,3,3,3,3,3,4),(0.,0.000314989845557401,
0.000586378060207524,0.000591775134429816,0.000903988302624528,0.00117275612041505,
0.00118112606261453,0.00147953454208657,0.00175913418062257,0.00192133188362462,
0.00208133452678515,0.00223644178065543,0.0023455122408301),
 .UNSPECIFIED.);
#2192=B_SPLINE_CURVE_WITH_KNOTS('',3,(#86190,#86191,#86192,#86193,#86194,
#86195,#86196,#86197,#86198,#86199,#86200,#86201),.UNSPECIFIED.,.F.,.F.,
(4,2,2,2,2,4),(0.00051471383035223,0.0041158554304885,0.00591642623055662,
0.00771699703062475,0.0113181386307609,0.0149192802308972),
 .UNSPECIFIED.);
#2193=B_SPLINE_CURVE_WITH_KNOTS('',3,(#86203,#86204,#86205,#86206,#86207,
#86208,#86209,#86210,#86211,#86212,#86213,#86214,#86215,#86216,#86217,#86218,
#86219,#86220,#86221,#86222,#86223,#86224,#86225,#86226,#86227,#86228,#86229,
#86230,#86231,#86232,#86233,#86234,#86235,#86236,#86237,#86238,#86239,#86240,
#86241,#86242,#86243,#86244,#86245,#86246,#86247,#86248,#86249,#86250,#86251,
#86252,#86253,#86254,#86255,#86256,#86257,#86258,#86259,#86260,#86261,#86262,
#86263,#86264,#86265,#86266),.UNSPECIFIED.,.F.,.F.,(4,3,3,3,3,3,3,3,3,3,
3,3,3,3,3,3,3,3,3,3,3,4),(0.,0.00369526538577179,0.0036953789086402,0.00554306836296028,
0.00554307302616271,0.00739075781728036,0.00739094612820333,0.0110861367259205,
0.0110867689982037,0.0147815156345607,0.0147825819056023,0.0166292050888808,
0.0166304351141471,0.018476894543201,0.0184782074975879,0.0221722734518412,
0.0221734986832148,0.0240199629061612,0.0240210156826648,0.0258676523604813,
0.025868445268313,0.0295630312691215),.UNSPECIFIED.);
#2194=B_SPLINE_CURVE_WITH_KNOTS('',3,(#86268,#86269,#86270,#86271,#86272,
#86273),.UNSPECIFIED.,.F.,.F.,(4,2,4),(0.,0.00201691944843358,0.00403383889686717),
 .UNSPECIFIED.);
#2195=B_SPLINE_CURVE_WITH_KNOTS('',3,(#86275,#86276,#86277,#86278,#86279,
#86280,#86281,#86282,#86283,#86284,#86285,#86286,#86287,#86288,#86289,#86290,
#86291,#86292,#86293,#86294,#86295,#86296,#86297,#86298,#86299,#86300,#86301,
#86302,#86303,#86304,#86305,#86306,#86307,#86308,#86309,#86310,#86311,#86312,
#86313,#86314,#86315,#86316,#86317,#86318,#86319,#86320,#86321,#86322,#86323,
#86324,#86325,#86326,#86327,#86328,#86329,#86330,#86331,#86332,#86333,#86334,
#86335,#86336,#86337,#86338,#86339,#86340,#86341,#86342,#86343,#86344,#86345,
#86346,#86347,#86348,#86349,#86350,#86351,#86352,#86353,#86354,#86355,#86356,
#86357,#86358,#86359,#86360,#86361,#86362,#86363,#86364,#86365,#86366,#86367,
#86368),.UNSPECIFIED.,.F.,.F.,(4,3,3,3,3,3,3,3,3,3,3,3,3,3,3,3,3,3,3,3,
3,3,3,3,3,3,3,3,3,3,3,4),(0.0336249043084812,0.0343340923276341,0.0348588967541102,
0.0357053672787823,0.0360928891997393,0.0360932923083427,0.0385608740909975,
0.0385615770429876,0.0434968438735138,0.043497886927775,0.0447308363191429,
0.0447319180031058,0.045964828764772,0.0459659358769334,0.0484328136560302,
0.0484339372781486,0.0533687834385465,0.0533698239727818,0.0546027758841757,
0.0546037755549375,0.0558367683298048,0.055837722246927,0.058304753221063,
0.0583056028338379,0.0632407230035794,0.0632413203753338,0.0657087078948376,
0.0657091630133129,0.0681766927860958,0.0681770006224813,0.0720142225821143,
0.0731126625686122),.UNSPECIFIED.);
#2196=B_SPLINE_CURVE_WITH_KNOTS('',3,(#86370,#86371,#86372,#86373,#86374,
#86375,#86376),.UNSPECIFIED.,.F.,.F.,(4,3,4),(0.,0.0026726882593627,0.00335009582233665),
 .UNSPECIFIED.);
#2197=B_SPLINE_CURVE_WITH_KNOTS('',3,(#86389,#86390,#86391,#86392,#86393,
#86394,#86395,#86396,#86397,#86398),.UNSPECIFIED.,.F.,.F.,(4,2,2,2,4),(0.,
0.0376344322078685,0.075268864415737,0.113378213559111,0.151487562702486),
 .UNSPECIFIED.);
#2198=B_SPLINE_CURVE_WITH_KNOTS('',3,(#86402,#86403,#86404,#86405,#86406,
#86407,#86408,#86409,#86410,#86411),.UNSPECIFIED.,.F.,.F.,(4,2,2,2,4),(0.455861178528749,
0.493970527672123,0.532079876815497,0.569714309023366,0.607348741231234),
 .UNSPECIFIED.);
#2199=B_SPLINE_CURVE_WITH_KNOTS('',3,(#86420,#86421,#86422,#86423,#86424,
#86425,#86426,#86427,#86428,#86429),.UNSPECIFIED.,.F.,.F.,(4,2,2,2,4),(0.,
0.0376344322078685,0.075268864415737,0.113378213559111,0.151487562702485),
 .UNSPECIFIED.);
#2200=B_SPLINE_CURVE_WITH_KNOTS('',3,(#86433,#86434,#86435,#86436,#86437,
#86438,#86439,#86440,#86441,#86442),.UNSPECIFIED.,.F.,.F.,(4,2,2,2,4),(0.455861178528749,
0.493970527672123,0.532079876815497,0.569714309023366,0.607348741231234),
 .UNSPECIFIED.);
#2201=B_SPLINE_CURVE_WITH_KNOTS('',3,(#86451,#86452,#86453,#86454,#86455,
#86456,#86457,#86458,#86459,#86460),.UNSPECIFIED.,.F.,.F.,(4,2,2,2,4),(0.,
0.0376344322078685,0.075268864415737,0.113378213559111,0.151487562702486),
 .UNSPECIFIED.);
#2202=B_SPLINE_CURVE_WITH_KNOTS('',3,(#86464,#86465,#86466,#86467,#86468,
#86469,#86470,#86471,#86472,#86473),.UNSPECIFIED.,.F.,.F.,(4,2,2,2,4),(0.455861178528749,
0.493970527672123,0.532079876815497,0.569714309023366,0.607348741231234),
 .UNSPECIFIED.);
#2203=B_SPLINE_CURVE_WITH_KNOTS('',3,(#86486,#86487,#86488,#86489,#86490,
#86491,#86492,#86493,#86494,#86495,#86496,#86497,#86498,#86499,#86500,#86501,
#86502,#86503,#86504,#86505,#86506,#86507,#86508,#86509,#86510,#86511,#86512,
#86513,#86514,#86515,#86516,#86517,#86518,#86519,#86520,#86521,#86522,#86523,
#86524,#86525,#86526,#86527,#86528,#86529,#86530,#86531,#86532,#86533,#86534),
 .UNSPECIFIED.,.F.,.F.,(4,3,3,3,3,3,3,3,3,3,3,3,3,3,3,3,4),(0.,0.000109821895971414,
0.000223718409793574,0.000340120943679785,0.000386128285975577,0.000392555857712287,
0.000584663348330143,0.000759528189981808,0.000776770838947999,0.000785111715424574,
0.000978472745646417,0.00117183377586826,0.00117766757313686,0.00129027810656827,
0.00140353834105485,0.00151434258567243,0.00157022343084915),
 .UNSPECIFIED.);
#2204=B_SPLINE_CURVE_WITH_KNOTS('',3,(#86538,#86539,#86540,#86541,#86542,
#86543,#86544,#86545,#86546,#86547,#86548,#86549,#86550,#86551,#86552,#86553,
#86554,#86555,#86556,#86557,#86558,#86559,#86560,#86561,#86562,#86563,#86564,
#86565,#86566,#86567,#86568,#86569,#86570,#86571,#86572,#86573,#86574,#86575,
#86576,#86577,#86578,#86579,#86580,#86581,#86582,#86583,#86584,#86585,#86586,
#86587,#86588,#86589,#86590,#86591,#86592,#86593,#86594,#86595),
 .UNSPECIFIED.,.F.,.F.,(4,3,3,3,3,3,3,3,3,3,3,3,3,3,3,3,3,3,3,4),(0.,0.000111469447673193,
0.000178663865080732,0.000294336346988578,0.000331041450458318,0.000388183044974913,
0.000398191848878749,0.000413182492575923,0.000536788127134726,0.000600678349583499,
0.000694426278087287,0.000788174206591076,0.000795149710050332,0.000971945613108558,
0.00115606563722798,0.00118226130988662,0.00118727564039461,0.00131748712639905,
0.00144691776979061,0.00157634841318217),.UNSPECIFIED.);
#2205=B_SPLINE_CURVE_WITH_KNOTS('',3,(#86617,#86618,#86619,#86620,#86621,
#86622,#86623,#86624,#86625,#86626,#86627,#86628,#86629,#86630,#86631,#86632,
#86633,#86634,#86635,#86636,#86637,#86638,#86639,#86640,#86641,#86642,#86643,
#86644,#86645,#86646,#86647,#86648,#86649,#86650,#86651,#86652,#86653,#86654,
#86655,#86656,#86657,#86658,#86659),.UNSPECIFIED.,.F.,.F.,(4,3,3,3,3,3,
3,3,3,3,3,3,3,3,4),(0.,9.24121435778908E-5,0.000182286807566461,0.00022129722760121,
0.000307679864338664,0.000389567696567305,0.000421720982923359,0.000436387456642549,
0.000526984691978052,0.000610982297301783,0.000642714900038087,0.000669097214438017,
0.000737690381912385,0.000803424779895835,0.000843441965846719),
 .UNSPECIFIED.);
#2206=B_SPLINE_CURVE_WITH_KNOTS('',3,(#86662,#86663,#86664,#86665,#86666,
#86667,#86668,#86669,#86670,#86671,#86672,#86673,#86674,#86675,#86676,#86677,
#86678,#86679,#86680,#86681,#86682,#86683,#86684,#86685,#86686,#86687,#86688,
#86689,#86690,#86691,#86692,#86693,#86694,#86695,#86696,#86697,#86698,#86699,
#86700,#86701,#86702,#86703,#86704,#86705,#86706,#86707),.UNSPECIFIED.,
 .F.,.F.,(4,3,3,3,3,3,3,3,3,3,3,3,3,3,3,4),(0.,6.65927751009938E-5,0.000136207087983939,
0.00015351019459415,0.000200453902910958,0.000220309690001092,0.000313539212629657,
0.000400256492199074,0.000406768735258222,0.000420708176221917,0.000497485021765038,
0.000579980519596234,0.000621930854547057,0.000707656251985938,0.000795542926537232,
0.000841416352443835),.UNSPECIFIED.);
#2207=B_SPLINE_CURVE_WITH_KNOTS('',3,(#86729,#86730,#86731,#86732,#86733,
#86734,#86735,#86736,#86737,#86738,#86739,#86740,#86741,#86742,#86743,#86744,
#86745,#86746,#86747,#86748,#86749,#86750,#86751,#86752,#86753,#86754,#86755,
#86756,#86757,#86758,#86759,#86760,#86761,#86762,#86763,#86764,#86765,#86766,
#86767,#86768,#86769,#86770,#86771,#86772,#86773,#86774,#86775,#86776,#86777),
 .UNSPECIFIED.,.F.,.F.,(4,3,3,3,3,3,3,3,3,3,3,3,3,3,3,3,4),(0.,0.000109821895962571,
0.000223718409775525,0.000340120943651616,0.000386128285975588,0.000392555857712286,
0.000584663348330096,0.000759528190225243,0.000776770838947905,0.000785111715424573,
0.000978472745646407,0.00117183377586824,0.00117766757313686,0.00129027810657364,
0.00140353834106094,0.00151434258567274,0.00157022343084915),
 .UNSPECIFIED.);
#2208=B_SPLINE_CURVE_WITH_KNOTS('',3,(#86781,#86782,#86783,#86784,#86785,
#86786,#86787,#86788,#86789,#86790,#86791,#86792,#86793,#86794,#86795,#86796,
#86797,#86798,#86799,#86800,#86801,#86802,#86803,#86804,#86805,#86806,#86807,
#86808,#86809,#86810,#86811,#86812,#86813,#86814,#86815,#86816,#86817,#86818,
#86819,#86820,#86821,#86822,#86823,#86824,#86825,#86826,#86827,#86828,#86829,
#86830,#86831,#86832,#86833,#86834,#86835,#86836,#86837,#86838),
 .UNSPECIFIED.,.F.,.F.,(4,3,3,3,3,3,3,3,3,3,3,3,3,3,3,3,3,3,3,4),(0.,0.00011146944768469,
0.000178663865080786,0.000294336346967297,0.000331041450458361,0.000388183044974952,
0.000398191848878757,0.00041318249257596,0.00053678812714408,0.000600678349583523,
0.000694426278087305,0.000788174206591086,0.000795149710050351,0.000971945613065413,
0.00115606563713422,0.00118226130988663,0.00118727564039461,0.00131748712642929,
0.00144691776980573,0.00157634841318217),.UNSPECIFIED.);
#2209=B_SPLINE_CURVE_WITH_KNOTS('',3,(#86860,#86861,#86862,#86863,#86864,
#86865,#86866,#86867,#86868,#86869,#86870,#86871,#86872,#86873,#86874,#86875,
#86876,#86877,#86878,#86879,#86880,#86881,#86882,#86883,#86884,#86885,#86886,
#86887,#86888,#86889,#86890,#86891,#86892,#86893,#86894,#86895,#86896,#86897,
#86898,#86899,#86900,#86901,#86902),.UNSPECIFIED.,.F.,.F.,(4,3,3,3,3,3,
3,3,3,3,3,3,3,3,4),(0.,9.2412143565261E-5,0.000182286807543989,0.000221297227600963,
0.000307679864329089,0.000389567696548903,0.000421720982923359,0.000436387456642595,
0.00052698469192393,0.000610982297301772,0.000642714900038126,0.000669097214438008,
0.000737690381855536,0.000803424779780432,0.000843441965846718),
 .UNSPECIFIED.);
#2210=B_SPLINE_CURVE_WITH_KNOTS('',3,(#86905,#86906,#86907,#86908,#86909,
#86910,#86911,#86912,#86913,#86914,#86915,#86916,#86917,#86918,#86919,#86920,
#86921,#86922,#86923,#86924,#86925,#86926,#86927,#86928,#86929,#86930,#86931,
#86932,#86933,#86934,#86935,#86936,#86937,#86938,#86939,#86940,#86941,#86942,
#86943,#86944,#86945,#86946,#86947,#86948,#86949,#86950),.UNSPECIFIED.,
 .F.,.F.,(4,3,3,3,3,3,3,3,3,3,3,3,3,3,3,4),(0.,6.65927750353964E-5,0.00013620708785258,
0.000153510194594128,0.000200453902910995,0.000220309690001075,0.000313539212629635,
0.000400256492216322,0.000406768735258194,0.000420708176221917,0.00049748502176149,
0.000579980519588019,0.000621930854547426,0.000707656251980385,0.000795542926521112,
0.000841416352443835),.UNSPECIFIED.);
#2211=B_SPLINE_CURVE_WITH_KNOTS('',3,(#86972,#86973,#86974,#86975,#86976,
#86977,#86978,#86979,#86980,#86981,#86982,#86983,#86984,#86985,#86986,#86987,
#86988,#86989,#86990,#86991,#86992,#86993,#86994,#86995,#86996,#86997,#86998,
#86999,#87000,#87001,#87002,#87003,#87004,#87005,#87006,#87007,#87008,#87009,
#87010,#87011,#87012,#87013,#87014,#87015,#87016,#87017,#87018,#87019,#87020),
 .UNSPECIFIED.,.F.,.F.,(4,3,3,3,3,3,3,3,3,3,3,3,3,3,3,3,4),(0.,0.000109821895955179,
0.000223718409760101,0.000340120943627297,0.000386128285975582,0.000392555857712287,
0.000584663348330105,0.000759528190240281,0.000776770838947923,0.000785111715424574,
0.000978472745646415,0.00117183377586826,0.00117766757313686,0.0012902781065717,
0.00140353834105677,0.00151434258566574,0.00157022343084915),
 .UNSPECIFIED.);
#2212=B_SPLINE_CURVE_WITH_KNOTS('',3,(#87024,#87025,#87026,#87027,#87028,
#87029,#87030,#87031,#87032,#87033,#87034,#87035,#87036,#87037,#87038,#87039,
#87040,#87041,#87042,#87043,#87044,#87045,#87046,#87047,#87048,#87049,#87050,
#87051,#87052,#87053,#87054,#87055,#87056,#87057,#87058,#87059,#87060,#87061,
#87062,#87063,#87064,#87065,#87066,#87067,#87068,#87069,#87070,#87071,#87072,
#87073,#87074,#87075,#87076,#87077,#87078,#87079,#87080,#87081),
 .UNSPECIFIED.,.F.,.F.,(4,3,3,3,3,3,3,3,3,3,3,3,3,3,3,3,3,3,3,4),(0.,0.000111469447679236,
0.000178663865080771,0.000294336346982952,0.000331041450458349,0.000388183044974941,
0.000398191848878742,0.00041318249257595,0.000536788127148723,0.000600678349583517,
0.000694426278087301,0.000788174206591084,0.000795149710050379,0.000971945613071812,
0.00115606563714846,0.00118226130988662,0.00118727564039459,0.00131748712641446,
0.00144691776979831,0.00157634841318216),.UNSPECIFIED.);
#2213=B_SPLINE_CURVE_WITH_KNOTS('',3,(#87103,#87104,#87105,#87106,#87107,
#87108,#87109,#87110,#87111,#87112,#87113,#87114,#87115,#87116,#87117,#87118,
#87119,#87120,#87121,#87122,#87123,#87124,#87125,#87126,#87127,#87128,#87129,
#87130,#87131,#87132,#87133,#87134,#87135,#87136,#87137,#87138,#87139,#87140,
#87141,#87142,#87143,#87144,#87145),.UNSPECIFIED.,.F.,.F.,(4,3,3,3,3,3,
3,3,3,3,3,3,3,3,4),(0.,9.24121435661261E-5,0.000182286807546301,0.000221297227601306,
0.00030767986433129,0.000389567696553656,0.000421720982923359,0.000436387456642586,
0.000526984691977222,0.000610982297301761,0.000642714900038117,0.000669097214438,
0.000737690381925544,0.000803424779913494,0.000843441965846718),
 .UNSPECIFIED.);
#2214=B_SPLINE_CURVE_WITH_KNOTS('',3,(#87148,#87149,#87150,#87151,#87152,
#87153,#87154,#87155,#87156,#87157,#87158,#87159,#87160,#87161,#87162,#87163,
#87164,#87165,#87166,#87167,#87168,#87169,#87170,#87171,#87172,#87173,#87174,
#87175,#87176,#87177,#87178,#87179,#87180,#87181,#87182,#87183,#87184,#87185,
#87186,#87187,#87188,#87189,#87190,#87191,#87192,#87193),.UNSPECIFIED.,
 .F.,.F.,(4,3,3,3,3,3,3,3,3,3,3,3,3,3,3,4),(0.,6.65927750433562E-5,0.000136207087870291,
0.000153510194594151,0.000200453902910911,0.000220309690001092,0.000313539212629646,
0.000400256492213659,0.000406768735258199,0.000420708176221917,0.000497485021762217,
0.000579980519589639,0.000621930854547661,0.000707656251980853,0.000795542926521681,
0.000841416352443835),.UNSPECIFIED.);
#2215=B_SPLINE_CURVE_WITH_KNOTS('',3,(#87214,#87215,#87216,#87217,#87218,
#87219,#87220,#87221,#87222,#87223,#87224,#87225,#87226,#87227,#87228,#87229,
#87230,#87231,#87232,#87233,#87234,#87235,#87236,#87237,#87238,#87239,#87240,
#87241,#87242,#87243,#87244,#87245,#87246,#87247,#87248,#87249,#87250,#87251,
#87252,#87253,#87254,#87255,#87256,#87257,#87258,#87259,#87260,#87261,#87262,
#87263,#87264,#87265,#87266,#87267,#87268,#87269,#87270,#87271),
 .UNSPECIFIED.,.F.,.F.,(4,3,3,3,3,3,3,3,3,3,3,3,3,3,3,3,3,3,3,4),(0.,0.000142427063094415,
0.000289764879815003,0.0004406238037737,0.000539597691306959,0.000547604890660785,
0.000777640858258875,0.000994951020817798,0.0010850065158908,0.00109520978132157,
0.00129973831583479,0.00135974988827171,0.00136901222665201,0.0016002541036825,
0.00163575977437615,0.00164281467198245,0.00178996226046791,0.00193796990731151,
0.00208341869133047,0.00219041956264326),.UNSPECIFIED.);
#2216=B_SPLINE_CURVE_WITH_KNOTS('',3,(#87275,#87276,#87277,#87278,#87279,
#87280,#87281,#87282,#87283,#87284,#87285,#87286,#87287,#87288,#87289,#87290,
#87291,#87292,#87293,#87294,#87295,#87296,#87297,#87298,#87299,#87300,#87301,
#87302,#87303,#87304,#87305,#87306,#87307,#87308,#87309,#87310,#87311,#87312,
#87313,#87314,#87315,#87316,#87317,#87318,#87319,#87320,#87321,#87322,#87323,
#87324,#87325,#87326,#87327,#87328,#87329),.UNSPECIFIED.,.F.,.F.,(4,3,3,
3,3,3,3,3,3,3,3,3,3,3,3,3,3,3,4),(0.,0.000149745139195585,0.000303435116966849,
0.000457535596445036,0.00054874626362146,0.00055385056701855,0.000825671547130735,
0.00109749252724292,0.00110571813660245,0.0012824107487252,0.00137186565905368,
0.00137959364926584,0.00162472087354463,0.00164623879086444,0.00165222802848104,
0.00181217997322851,0.00197175562074787,0.00212790425251907,0.00219498505448598),
 .UNSPECIFIED.);
#2217=B_SPLINE_CURVE_WITH_KNOTS('',3,(#87335,#87336,#87337,#87338,#87339,
#87340,#87341,#87342,#87343,#87344,#87345,#87346,#87347,#87348,#87349,#87350,
#87351,#87352,#87353,#87354,#87355,#87356,#87357,#87358,#87359,#87360,#87361,
#87362,#87363,#87364,#87365,#87366,#87367,#87368,#87369,#87370,#87371,#87372,
#87373,#87374,#87375,#87376,#87377,#87378,#87379,#87380,#87381,#87382,#87383),
 .UNSPECIFIED.,.F.,.F.,(4,3,3,3,3,3,3,3,3,3,3,3,3,3,3,3,4),(0.,8.13766152637004E-5,
0.000166095243180767,0.000231150059491329,0.000279600583482743,0.000370403859907583,
0.000403777499519012,0.000524287940974636,0.000564363768371529,0.000576404939546696,
0.000685318810052787,0.000709431730850445,0.000855957854003566,0.000864607409320044,
0.000958227502067959,0.00105551869058068,0.00115280987909339),
 .UNSPECIFIED.);
#2218=B_SPLINE_CURVE_WITH_KNOTS('',3,(#87386,#87387,#87388,#87389,#87390,
#87391,#87392,#87393,#87394,#87395,#87396,#87397,#87398,#87399,#87400,#87401,
#87402,#87403,#87404,#87405,#87406,#87407,#87408,#87409,#87410,#87411,#87412,
#87413,#87414,#87415,#87416,#87417,#87418,#87419,#87420,#87421,#87422,#87423,
#87424,#87425,#87426,#87427,#87428),.UNSPECIFIED.,.F.,.F.,(4,3,3,3,3,3,
3,3,3,3,3,3,3,3,4),(0.,9.08098863106932E-5,0.000185034709549021,0.000277456643574092,
0.000285171347001819,0.000417664071564358,0.000524072108197603,0.00055944501884406,
0.000570342694003638,0.000673602018050586,0.000783825143420611,0.000848914171300631,
0.000962109447417837,0.00107297388323492,0.00114068538800723),
 .UNSPECIFIED.);
#2219=B_SPLINE_CURVE_WITH_KNOTS('',3,(#87434,#87435,#87436,#87437,#87438,
#87439,#87440,#87441,#87442,#87443,#87444,#87445,#87446,#87447,#87448,#87449,
#87450,#87451,#87452,#87453,#87454,#87455,#87456,#87457,#87458,#87459,#87460,
#87461,#87462,#87463,#87464,#87465,#87466,#87467,#87468,#87469,#87470,#87471,
#87472,#87473,#87474,#87475,#87476,#87477,#87478,#87479,#87480,#87481,#87482,
#87483,#87484,#87485,#87486,#87487,#87488,#87489,#87490,#87491,#87492,#87493,
#87494,#87495,#87496,#87497,#87498,#87499,#87500,#87501,#87502,#87503,#87504,
#87505,#87506,#87507,#87508,#87509,#87510,#87511,#87512,#87513,#87514,#87515,
#87516,#87517,#87518),.UNSPECIFIED.,.F.,.F.,(4,3,3,3,3,3,3,3,3,3,3,3,3,
3,3,3,3,3,3,3,3,3,3,3,3,3,3,3,4),(0.,0.015926332992886,0.023889499489329,
0.031852665985772,0.039815832482215,0.0477789989786579,0.0517605822268794,
0.0557421654751008,0.0637053319715438,0.0676869152197653,0.0696777068438761,
0.0716684984679868,0.0796316649644298,0.0816224565885406,0.0836132482126513,
0.0875948314608729,0.0955579979573159,0.0995395812055374,0.103521164453759,
0.111484330950202,0.115465914198423,0.119447497446645,0.127410663943087,
0.143336996935973,0.159263329928859,0.175189662921744,0.19111599591463,
0.222968661900401,0.254821327886172),.UNSPECIFIED.);
#2220=B_SPLINE_CURVE_WITH_KNOTS('',3,(#87520,#87521,#87522,#87523,#87524,
#87525,#87526,#87527,#87528,#87529,#87530,#87531,#87532,#87533,#87534,#87535,
#87536,#87537,#87538,#87539,#87540,#87541,#87542,#87543,#87544,#87545,#87546,
#87547,#87548,#87549,#87550,#87551,#87552,#87553,#87554,#87555,#87556,#87557,
#87558,#87559,#87560,#87561,#87562,#87563,#87564,#87565,#87566,#87567,#87568,
#87569,#87570,#87571,#87572,#87573,#87574,#87575,#87576,#87577,#87578,#87579,
#87580,#87581,#87582,#87583,#87584,#87585,#87586,#87587,#87588,#87589,#87590,
#87591,#87592,#87593,#87594,#87595,#87596,#87597,#87598,#87599,#87600,#87601),
 .UNSPECIFIED.,.F.,.F.,(4,3,3,3,3,3,3,3,3,3,3,3,3,3,3,3,3,3,3,3,3,3,3,3,
3,3,3,4),(0.,0.0319823773664769,0.0639647547329538,0.0799559434161923,0.0959471320994307,
0.111938320782669,0.127929509465908,0.135925103807527,0.143920698149146,
0.151916292490765,0.155914089661575,0.159911886832385,0.167907481174004,
0.169906379759409,0.171905278344814,0.175903075515623,0.183898669857243,
0.185897568442648,0.187896467028052,0.191894264198862,0.195892061369672,
0.199889858540482,0.207885452882102,0.215881047223722,0.223876641565341,
0.231872235906961,0.239867830248581,0.25585901893182),.UNSPECIFIED.);
#2221=B_SPLINE_CURVE_WITH_KNOTS('',3,(#87629,#87630,#87631,#87632,#87633,
#87634,#87635,#87636,#87637,#87638,#87639,#87640,#87641,#87642,#87643,#87644,
#87645,#87646,#87647,#87648,#87649,#87650,#87651,#87652,#87653,#87654,#87655,
#87656,#87657,#87658,#87659,#87660,#87661,#87662,#87663,#87664,#87665,#87666,
#87667,#87668,#87669,#87670,#87671,#87672,#87673,#87674,#87675,#87676,#87677,
#87678,#87679,#87680,#87681,#87682,#87683,#87684,#87685,#87686,#87687,#87688,
#87689,#87690,#87691,#87692,#87693,#87694,#87695,#87696,#87697,#87698,#87699,
#87700,#87701,#87702,#87703,#87704,#87705,#87706,#87707,#87708,#87709,#87710,
#87711,#87712,#87713,#87714,#87715,#87716,#87717,#87718,#87719,#87720,#87721,
#87722,#87723,#87724,#87725,#87726,#87727,#87728,#87729,#87730,#87731,#87732,
#87733,#87734,#87735,#87736,#87737,#87738,#87739,#87740,#87741,#87742,#87743,
#87744,#87745,#87746,#87747,#87748,#87749,#87750,#87751,#87752,#87753,#87754,
#87755,#87756,#87757,#87758,#87759,#87760,#87761,#87762,#87763,#87764,#87765,
#87766,#87767,#87768,#87769,#87770,#87771,#87772,#87773,#87774,#87775,#87776,
#87777,#87778,#87779,#87780,#87781,#87782,#87783,#87784,#87785,#87786,#87787,
#87788,#87789,#87790,#87791,#87792,#87793,#87794,#87795,#87796,#87797,#87798,
#87799,#87800,#87801,#87802,#87803,#87804,#87805,#87806,#87807,#87808,#87809,
#87810,#87811,#87812,#87813,#87814,#87815,#87816,#87817,#87818,#87819,#87820,
#87821,#87822,#87823,#87824,#87825,#87826,#87827,#87828,#87829,#87830),
 .UNSPECIFIED.,.F.,.F.,(4,3,3,3,3,3,3,3,3,3,3,3,3,3,3,3,3,3,3,3,3,3,3,3,
3,3,3,3,3,3,3,3,3,3,3,3,3,3,3,3,3,3,3,3,3,3,3,3,3,3,3,3,3,3,3,3,3,3,3,3,
3,3,3,3,3,3,3,4),(0.,0.0321347663513911,0.0495590544123357,0.0642731458325226,
0.08034498525143,0.0862931788198439,0.096420051205167,0.104175959222532,
0.112500619108118,0.118863546557499,0.127099328679868,0.128591290601529,
0.134437145537029,0.13664323902993,0.137833345962692,0.140671729597307,
0.141438649477965,0.144702441480307,0.145881989700091,0.150173982122068,
0.15277262499039,0.153697717723032,0.156609795436613,0.156813504295752,
0.157452006785746,0.160140339134182,0.160859452487887,0.161815966928969,
0.165392978615863,0.168754753105444,0.168969990302757,0.172572899244027,
0.173035427576007,0.17347524134314,0.174874914490513,0.175070484733593,
0.175252929180179,0.175430745910084,0.176752761163085,0.177106662985369,
0.177544810736285,0.180196510461824,0.182865217256473,0.185255162170941,
0.187290885676172,0.188723431177471,0.189325249765294,0.191782739905368,
0.193388999062593,0.196260693769467,0.199201867815336,0.201293292290039,
0.201495395322361,0.203648653929001,0.205190627207978,0.20553912739097,
0.208511016314483,0.20957779685043,0.213946752277146,0.217643568734126,
0.223067791290745,0.225698462781859,0.232343117717054,0.23374618069259,
0.240117376236147,0.24178905493371,0.252643459611325,0.257865728390371),
 .UNSPECIFIED.);
#2222=B_SPLINE_CURVE_WITH_KNOTS('',3,(#87831,#87832,#87833,#87834,#87835,
#87836,#87837,#87838,#87839,#87840,#87841,#87842,#87843,#87844,#87845,#87846,
#87847,#87848,#87849,#87850,#87851,#87852,#87853,#87854,#87855,#87856,#87857,
#87858,#87859,#87860,#87861,#87862,#87863,#87864,#87865,#87866,#87867,#87868,
#87869,#87870,#87871,#87872,#87873,#87874,#87875,#87876,#87877,#87878,#87879,
#87880,#87881,#87882,#87883,#87884,#87885,#87886,#87887,#87888,#87889,#87890,
#87891,#87892,#87893,#87894,#87895,#87896,#87897,#87898,#87899,#87900,#87901,
#87902,#87903,#87904,#87905,#87906,#87907,#87908,#87909,#87910,#87911,#87912,
#87913,#87914,#87915,#87916,#87917,#87918,#87919,#87920,#87921,#87922,#87923,
#87924,#87925,#87926,#87927,#87928,#87929,#87930,#87931,#87932,#87933,#87934,
#87935,#87936,#87937,#87938,#87939,#87940,#87941,#87942,#87943,#87944,#87945,
#87946,#87947,#87948,#87949,#87950,#87951,#87952,#87953,#87954,#87955,#87956,
#87957,#87958,#87959,#87960,#87961,#87962,#87963,#87964,#87965,#87966,#87967,
#87968,#87969,#87970,#87971,#87972,#87973,#87974,#87975,#87976,#87977,#87978,
#87979,#87980,#87981,#87982,#87983,#87984,#87985,#87986,#87987,#87988,#87989,
#87990,#87991,#87992,#87993,#87994,#87995,#87996,#87997,#87998,#87999,#88000,
#88001,#88002,#88003,#88004,#88005,#88006,#88007,#88008,#88009,#88010,#88011,
#88012,#88013,#88014,#88015,#88016,#88017,#88018,#88019,#88020,#88021,#88022,
#88023,#88024,#88025,#88026,#88027,#88028,#88029,#88030,#88031,#88032,#88033,
#88034,#88035,#88036,#88037,#88038,#88039,#88040,#88041,#88042,#88043,#88044,
#88045,#88046,#88047,#88048,#88049,#88050,#88051,#88052,#88053),
 .UNSPECIFIED.,.F.,.F.,(4,3,3,3,3,3,3,3,3,3,3,3,3,3,3,3,3,3,3,3,3,3,3,3,
3,3,3,3,3,3,3,3,3,3,3,3,3,3,3,3,3,3,3,3,3,3,3,3,3,3,3,3,3,3,3,3,3,3,3,3,
3,3,3,3,3,3,3,3,3,3,3,3,3,3,4),(1.38777878078145E-17,0.0106941639093447,
0.0161523461777034,0.0227402015251543,0.024233158169914,0.0280246446205861,
0.032318957692043,0.0343085312999032,0.039439559310476,0.040412204119208,
0.0438163939820961,0.0480516959393415,0.0485168201369417,0.0521392406465668,
0.0556011264251879,0.0566387545963194,0.0595190127146115,0.0607085988403213,
0.0641053404658499,0.0647854729869067,0.0683552918842684,0.0688694798512335,
0.0705958462991164,0.0709138855415459,0.0721915283538115,0.0729595587907659,
0.0756454538405821,0.0783958280485235,0.0811462022564649,0.083190893065739,
0.084213238470376,0.0847448494708462,0.085235583875013,0.0862567993079951,
0.0867688029516202,0.0869883753967039,0.0871941013119647,0.0872780147409773,
0.0882984146107854,0.0889848264050506,0.0893188144805935,0.0925804399340324,
0.095871378192766,0.0974647550772858,0.0994966706183769,0.100770759871012,
0.101528586159468,0.103558015878763,0.104572730738411,0.105084838473142,
0.105497282385778,0.105587445598059,0.109640760080191,0.111667417321258,
0.11305254753347,0.113694074562324,0.119113264047518,0.121790080016155,
0.128084746183264,0.129879086061019,0.138165401946804,0.144801674340403,
0.146044239431815,0.15806298841324,0.162199498439194,0.170274193011518,
0.174902658669718,0.177996378870079,0.178348887583842,0.189957445534057,
0.19449377824725,0.210635725330604,0.221799181517672,0.226777672413958,
0.259058112487482),.UNSPECIFIED.);
#2223=B_SPLINE_CURVE_WITH_KNOTS('',3,(#88071,#88072,#88073,#88074,#88075,
#88076,#88077,#88078,#88079,#88080,#88081,#88082,#88083,#88084,#88085,#88086,
#88087,#88088,#88089,#88090,#88091,#88092,#88093,#88094,#88095,#88096,#88097,
#88098,#88099,#88100,#88101,#88102,#88103,#88104,#88105,#88106,#88107,#88108,
#88109,#88110,#88111,#88112,#88113,#88114,#88115,#88116,#88117,#88118,#88119,
#88120,#88121,#88122,#88123,#88124,#88125,#88126,#88127,#88128,#88129,#88130,
#88131,#88132,#88133,#88134,#88135,#88136,#88137,#88138,#88139,#88140,#88141,
#88142,#88143,#88144,#88145,#88146,#88147,#88148,#88149,#88150,#88151,#88152,
#88153,#88154,#88155,#88156,#88157,#88158,#88159,#88160,#88161,#88162,#88163,
#88164,#88165,#88166,#88167,#88168,#88169,#88170,#88171,#88172,#88173,#88174,
#88175,#88176,#88177,#88178,#88179,#88180,#88181,#88182,#88183,#88184,#88185,
#88186,#88187,#88188,#88189,#88190,#88191,#88192,#88193,#88194,#88195,#88196,
#88197,#88198,#88199,#88200,#88201,#88202,#88203,#88204,#88205,#88206,#88207,
#88208,#88209,#88210,#88211,#88212,#88213,#88214,#88215,#88216,#88217,#88218,
#88219,#88220,#88221,#88222,#88223,#88224,#88225,#88226,#88227,#88228,#88229,
#88230,#88231,#88232,#88233,#88234,#88235,#88236,#88237,#88238,#88239,#88240,
#88241,#88242,#88243,#88244,#88245,#88246,#88247,#88248,#88249,#88250,#88251,
#88252,#88253,#88254,#88255,#88256,#88257,#88258,#88259,#88260,#88261,#88262,
#88263,#88264,#88265,#88266,#88267,#88268,#88269,#88270,#88271,#88272,#88273,
#88274,#88275,#88276,#88277,#88278,#88279,#88280,#88281,#88282,#88283,#88284,
#88285,#88286,#88287,#88288,#88289,#88290,#88291,#88292,#88293),
 .UNSPECIFIED.,.F.,.F.,(4,3,3,3,3,3,3,3,3,3,3,3,3,3,3,3,3,3,3,3,3,3,3,3,
3,3,3,3,3,3,3,3,3,3,3,3,3,3,3,3,3,3,3,3,3,3,3,3,3,3,3,3,3,3,3,3,3,3,3,3,
3,3,3,3,3,3,3,3,3,3,3,3,3,3,4),(0.,0.0106941636076985,0.0161523461777031,
0.0227402277212279,0.0242331581699135,0.028024634482012,0.0323189576920425,
0.0343085308806789,0.0394395588329036,0.0404122041192073,0.043816391934837,
0.0480516939348734,0.048516820136941,0.0521392405666208,0.0556011263566289,
0.0566387545963185,0.059519013554307,0.0607085988403205,0.0641053384666623,
0.0647854729869058,0.0683553012725267,0.0688694798512329,0.0705958456560103,
0.0709138855415449,0.0721915282587155,0.0729595587907649,0.0756454538060452,
0.078395828031255,0.0811462022564647,0.0831908930657383,0.0842132384703751,
0.0847448494807507,0.0852355838750119,0.0862567993079953,0.0867688029457022,
0.0869883753565705,0.0871941012416039,0.0872780147409787,0.0882984146107866,
0.0889848263941232,0.0893188144805945,0.0925804399957425,0.0958713775988918,
0.0974647550772867,0.0994966706183765,0.100770759912968,0.101528586159466,
0.10355801587876,0.104572730738408,0.105084838501772,0.105497282404785,
0.105587445598055,0.109640760080188,0.111667417321254,0.113052547649134,
0.113694074562321,0.119113264976225,0.121790080016154,0.128084747049764,
0.129879086061018,0.138165402400325,0.14480167568036,0.146044239431815,
0.158062989096084,0.162199498439194,0.170274193011518,0.174902656539617,
0.17799637619432,0.178348887583842,0.189957483032288,0.194493778247249,
0.210635725330603,0.22179915802068,0.226777672413957,0.259058112487481),
 .UNSPECIFIED.);
#2224=B_SPLINE_CURVE_WITH_KNOTS('',3,(#88294,#88295,#88296,#88297,#88298,
#88299,#88300,#88301,#88302,#88303,#88304,#88305,#88306,#88307,#88308,#88309,
#88310,#88311,#88312,#88313,#88314,#88315,#88316,#88317,#88318,#88319,#88320,
#88321,#88322,#88323,#88324,#88325,#88326,#88327,#88328,#88329,#88330,#88331,
#88332,#88333,#88334,#88335,#88336,#88337,#88338,#88339,#88340,#88341,#88342,
#88343,#88344,#88345,#88346,#88347,#88348,#88349,#88350,#88351,#88352,#88353,
#88354,#88355,#88356,#88357,#88358,#88359,#88360,#88361,#88362,#88363,#88364,
#88365,#88366,#88367,#88368,#88369,#88370,#88371,#88372,#88373,#88374,#88375,
#88376,#88377,#88378,#88379,#88380,#88381,#88382,#88383,#88384,#88385,#88386,
#88387,#88388,#88389,#88390,#88391,#88392,#88393,#88394,#88395,#88396,#88397,
#88398,#88399,#88400,#88401,#88402,#88403,#88404,#88405,#88406,#88407,#88408,
#88409,#88410,#88411,#88412,#88413,#88414,#88415,#88416,#88417,#88418,#88419,
#88420,#88421,#88422,#88423,#88424,#88425,#88426,#88427,#88428,#88429,#88430,
#88431,#88432,#88433,#88434,#88435,#88436,#88437,#88438,#88439,#88440,#88441,
#88442,#88443,#88444,#88445,#88446,#88447,#88448,#88449,#88450,#88451,#88452,
#88453,#88454,#88455,#88456,#88457,#88458,#88459,#88460,#88461,#88462,#88463,
#88464,#88465,#88466,#88467,#88468,#88469,#88470,#88471,#88472,#88473,#88474,
#88475,#88476,#88477,#88478,#88479,#88480,#88481,#88482,#88483,#88484,#88485,
#88486,#88487,#88488,#88489,#88490,#88491,#88492,#88493,#88494,#88495),
 .UNSPECIFIED.,.F.,.F.,(4,3,3,3,3,3,3,3,3,3,3,3,3,3,3,3,3,3,3,3,3,3,3,3,
3,3,3,3,3,3,3,3,3,3,3,3,3,3,3,3,3,3,3,3,3,3,3,3,3,3,3,3,3,3,3,3,3,3,3,3,
3,3,3,3,3,3,3,4),(6.16297582203915E-33,0.0321347663513911,0.0495589744394204,
0.0642731458325225,0.0803449852514303,0.0862931668316303,0.0964200512051673,
0.104175946597151,0.112500619108118,0.11886353125611,0.127099313737542,
0.12859129060153,0.134437149230977,0.136643239029932,0.137833345642357,
0.140671729597306,0.14143864949136,0.144702441480305,0.145881990070148,
0.150173982655845,0.152772624990387,0.15369771794186,0.156609795765364,
0.156813504295751,0.157452006799269,0.160140339164123,0.160859452487887,
0.161815966913,0.165392978607879,0.168754753103115,0.168969990302757,0.17257289992554,
0.173035427576007,0.173475241346685,0.174874914500988,0.175070484733593,
0.17525292917881,0.175430745909119,0.176752761147611,0.177106662985368,
0.177544810722352,0.180196510450715,0.18286521724812,0.185255162170942,
0.187290885676172,0.188723431189574,0.189325249765294,0.191782743547589,
0.193388999062593,0.196260694481045,0.199201866898202,0.201293290007858,
0.201495395322361,0.203648653861136,0.205190627103753,0.20553912739097,
0.208511015022924,0.20957779685043,0.213946752579418,0.217643568734125,
0.223067792625719,0.225698462781859,0.232343125900126,0.23374618069259,
0.240117367875956,0.24178905493371,0.252643459758372,0.257865728390371),
 .UNSPECIFIED.);
#2225=B_SPLINE_CURVE_WITH_KNOTS('',3,(#88693,#88694,#88695,#88696,#88697,
#88698,#88699,#88700,#88701,#88702,#88703,#88704,#88705,#88706,#88707,#88708,
#88709,#88710,#88711,#88712,#88713,#88714,#88715,#88716,#88717,#88718,#88719,
#88720,#88721,#88722,#88723,#88724,#88725,#88726,#88727,#88728,#88729,#88730,
#88731,#88732),.UNSPECIFIED.,.F.,.F.,(4,3,3,3,3,3,3,3,3,3,3,3,3,4),(0.000395514605004968,
0.00735803993026417,0.0147386515350848,0.0193564268053037,0.0234273968067644,
0.0287669019918199,0.0316481254819651,0.0395037906813469,0.0451972349114162,
0.0555782389740722,0.060131141684423,0.0877234345305647,0.0899989552304367,
0.11986676877645),.UNSPECIFIED.);
#2226=B_SPLINE_CURVE_WITH_KNOTS('',3,(#88734,#88735,#88736,#88737),
 .UNSPECIFIED.,.F.,.F.,(4,4),(3.69657704960075E-5,0.00377790776151813),
 .UNSPECIFIED.);
#2227=B_SPLINE_CURVE_WITH_KNOTS('',3,(#88739,#88740,#88741,#88742,#88743,
#88744,#88745,#88746,#88747,#88748,#88749,#88750,#88751,#88752,#88753,#88754,
#88755,#88756),.UNSPECIFIED.,.F.,.F.,(4,2,2,2,2,2,2,2,4),(3.84557724733612E-8,
0.0945840906584437,0.156697190455936,0.184260984131437,0.204445099552682,
0.225130065891661,0.254993330497327,0.329798839730618,0.408766486569211),
 .UNSPECIFIED.);
#2228=B_SPLINE_CURVE_WITH_KNOTS('',3,(#88758,#88759,#88760,#88761,#88762,
#88763,#88764,#88765,#88766,#88767,#88768,#88769,#88770,#88771,#88772,#88773,
#88774,#88775,#88776,#88777,#88778,#88779,#88780,#88781,#88782),
 .UNSPECIFIED.,.F.,.F.,(4,3,3,3,3,3,3,3,4),(5.10853787706198E-5,0.00062493792641946,
0.000987407891113938,0.00133852883324268,0.00149214424542401,0.00192050093150165,
0.00259944460152424,0.00332768414277843,0.00379637501318569),
 .UNSPECIFIED.);
#2229=B_SPLINE_CURVE_WITH_KNOTS('',3,(#88784,#88785,#88786,#88787,#88788,
#88789,#88790,#88791,#88792,#88793,#88794,#88795,#88796,#88797,#88798,#88799,
#88800,#88801,#88802,#88803,#88804,#88805,#88806,#88807,#88808,#88809,#88810,
#88811,#88812,#88813,#88814,#88815,#88816,#88817,#88818,#88819,#88820,#88821,
#88822,#88823,#88824,#88825),.UNSPECIFIED.,.F.,.F.,(4,2,2,2,2,2,2,2,2,2,
2,2,2,2,2,2,2,2,2,2,4),(0.00244866002632205,0.0182112504277692,0.0260925456284927,
0.0339738408292162,0.0418551360299397,0.0497364312306633,0.0576177264313868,
0.0654990216321103,0.0694396692324721,0.0733803168328338,0.0773209644331956,
0.0792912882333765,0.0812616120335574,0.0891429072342809,0.0930835548346426,
0.0970242024350043,0.104905497635728,0.112786792836451,0.116727440436813,
0.120668088037175,0.128549383237898),.UNSPECIFIED.);
#2230=B_SPLINE_CURVE_WITH_KNOTS('',3,(#88997,#88998,#88999,#89000,#89001,
#89002,#89003,#89004,#89005,#89006,#89007,#89008,#89009,#89010,#89011,#89012,
#89013,#89014,#89015,#89016,#89017,#89018,#89019,#89020,#89021,#89022,#89023,
#89024,#89025,#89026,#89027,#89028,#89029,#89030,#89031,#89032,#89033,#89034,
#89035,#89036,#89037,#89038,#89039,#89040,#89041,#89042,#89043,#89044,#89045,
#89046,#89047,#89048,#89049,#89050,#89051,#89052,#89053,#89054,#89055,#89056,
#89057,#89058,#89059,#89060,#89061,#89062,#89063,#89064,#89065,#89066,#89067,
#89068,#89069,#89070,#89071,#89072,#89073,#89074,#89075,#89076,#89077,#89078,
#89079,#89080,#89081,#89082,#89083,#89084,#89085,#89086,#89087,#89088,#89089,
#89090,#89091,#89092,#89093,#89094,#89095,#89096,#89097,#89098,#89099,#89100,
#89101,#89102,#89103,#89104,#89105,#89106,#89107,#89108,#89109,#89110,#89111,
#89112,#89113,#89114,#89115,#89116,#89117,#89118,#89119,#89120,#89121,#89122,
#89123,#89124,#89125,#89126,#89127,#89128,#89129,#89130,#89131,#89132,#89133,
#89134,#89135,#89136,#89137,#89138,#89139,#89140,#89141,#89142,#89143,#89144,
#89145,#89146,#89147,#89148,#89149,#89150,#89151,#89152,#89153,#89154,#89155,
#89156,#89157,#89158,#89159,#89160,#89161,#89162,#89163,#89164,#89165,#89166,
#89167,#89168,#89169,#89170,#89171,#89172,#89173,#89174,#89175,#89176,#89177,
#89178,#89179,#89180,#89181,#89182,#89183,#89184,#89185,#89186,#89187,#89188,
#89189,#89190,#89191,#89192,#89193,#89194,#89195,#89196,#89197,#89198,#89199,
#89200,#89201,#89202,#89203,#89204,#89205,#89206,#89207,#89208,#89209,#89210,
#89211,#89212,#89213,#89214,#89215,#89216,#89217,#89218,#89219,#89220,#89221,
#89222,#89223,#89224,#89225,#89226,#89227,#89228,#89229,#89230,#89231,#89232,
#89233,#89234,#89235,#89236,#89237,#89238,#89239,#89240,#89241,#89242,#89243,
#89244,#89245,#89246,#89247,#89248,#89249,#89250,#89251,#89252,#89253,#89254,
#89255,#89256,#89257,#89258,#89259,#89260,#89261,#89262,#89263,#89264),
 .UNSPECIFIED.,.F.,.F.,(4,3,3,3,3,3,3,3,3,3,3,3,3,3,3,3,3,3,3,3,3,3,3,3,
3,3,3,3,3,3,3,3,3,3,3,3,3,3,3,3,3,3,3,3,3,3,3,3,3,3,3,3,3,3,3,3,3,3,3,3,
3,3,3,3,3,3,3,3,3,3,3,3,3,3,3,3,3,3,3,3,3,3,3,3,3,3,3,3,3,4),(0.00290000689679031,
0.0348826539958882,0.0350963826156628,0.0668668642324351,0.0672927583345353,
0.082860078071171,0.0833909461939715,0.0945706526654511,0.0988570416155822,
0.0994891340534077,0.110217632937352,0.114848443355895,0.115587321912844,
0.123621459932078,0.130825599159465,0.13168550977228,0.137907945927169,
0.138805785100152,0.139734603701998,0.142569338258938,0.145202261479709,
0.146788974383255,0.147783697631716,0.151528124751556,0.154835996905122,
0.155832791561434,0.157625464684268,0.158877559866273,0.159857338526293,
0.161374923374203,0.162784053106398,0.162892508222113,0.163881885491152,
0.166084679257195,0.168252123500641,0.170375742136789,0.170967585801291,
0.17193097942087,0.172948658231983,0.17300624347377,0.174025064253037,0.174961804199926,
0.175043885032305,0.175955526385729,0.176776567282671,0.177588295814947,
0.177967799868159,0.179058628275698,0.179980073350588,0.181933154415629,
0.183873304502664,0.185793614314497,0.187147307106593,0.188029167280306,
0.188897271074614,0.189178590123301,0.190041440762736,0.191196751699605,
0.192053714245165,0.194476618658257,0.195242705240045,0.196078261210024,
0.197610910808871,0.199202289441857,0.199305039765874,0.200979572980401,
0.20270812750911,0.203367880943842,0.204127355139742,0.205268535517417,
0.206139628622172,0.208151902104601,0.210715513500852,0.211463812165016,
0.21217644906946,0.215080533727073,0.218147052981163,0.219623796694952,
0.220225542999178,0.223743899304297,0.227811751274587,0.228274636928896,
0.234017162824901,0.235987273171213,0.236323730858614,0.243348196588658,
0.244153738737961,0.244372824788332,0.25381684351193,0.260471012647768),
 .UNSPECIFIED.);
#2231=B_SPLINE_CURVE_WITH_KNOTS('',3,(#89277,#89278,#89279,#89280,#89281,
#89282),.UNSPECIFIED.,.F.,.F.,(4,2,4),(-0.370409044038645,-0.349794382456071,
-0.288542083039148),.UNSPECIFIED.);
#2232=B_SPLINE_CURVE_WITH_KNOTS('',3,(#89290,#89291,#89292,#89293,#89294,
#89295,#89296,#89297),.UNSPECIFIED.,.F.,.F.,(4,2,2,4),(-0.28854208306912,
-0.285779192265103,-0.236097520538759,-0.207305103379315),.UNSPECIFIED.);
#2233=B_SPLINE_CURVE_WITH_KNOTS('',3,(#89301,#89302,#89303,#89304,#89305,
#89306),.UNSPECIFIED.,.F.,.F.,(4,2,4),(-0.370409029704745,-0.349794370647721,
-0.288542073385836),.UNSPECIFIED.);
#2234=B_SPLINE_CURVE_WITH_KNOTS('',3,(#89311,#89312,#89313,#89314,#89315,
#89316,#89317,#89318),.UNSPECIFIED.,.F.,.F.,(4,2,2,4),(-0.288542084579862,
-0.285779193751398,-0.236097521603963,-0.20730510422017),.UNSPECIFIED.);
#2235=B_SPLINE_CURVE_WITH_KNOTS('',3,(#89321,#89322,#89323,#89324,#89325,
#89326),.UNSPECIFIED.,.F.,.F.,(4,2,4),(0.0586376217690057,0.0656506321388606,
0.0726636425083133),.UNSPECIFIED.);
#2236=B_SPLINE_CURVE_WITH_KNOTS('',3,(#89329,#89330,#89331,#89332,#89333,
#89334),.UNSPECIFIED.,.F.,.F.,(4,2,4),(0.0586376217689954,0.0656506321388567,
0.0726636425085365),.UNSPECIFIED.);
#2237=B_SPLINE_CURVE_WITH_KNOTS('',3,(#89766,#89767,#89768,#89769,#89770,
#89771,#89772,#89773,#89774,#89775,#89776,#89777,#89778,#89779,#89780,#89781,
#89782,#89783,#89784,#89785,#89786,#89787,#89788,#89789,#89790,#89791,#89792,
#89793,#89794,#89795,#89796,#89797,#89798,#89799,#89800,#89801,#89802,#89803,
#89804,#89805,#89806,#89807,#89808),.UNSPECIFIED.,.F.,.F.,(4,3,3,3,3,3,
3,3,3,3,3,3,3,3,4),(0.,8.9705753555212E-5,0.000183089135322613,0.000276472517090014,
0.000281553305630493,0.000416119195405342,0.000530992189354976,0.000557015156113086,
0.000563106611260986,0.000666450358589742,0.000774434672098113,0.000842506489703533,
0.000949864819656856,0.00104944593936403,0.00112621322252192),
 .UNSPECIFIED.);
#2238=B_SPLINE_CURVE_WITH_KNOTS('',3,(#89847,#89848,#89849,#89850,#89851,
#89852,#89853,#89854,#89855,#89856,#89857,#89858,#89859,#89860,#89861,#89862,
#89863,#89864,#89865,#89866,#89867,#89868,#89869,#89870,#89871,#89872,#89873,
#89874,#89875,#89876,#89877,#89878,#89879,#89880,#89881,#89882,#89883,#89884,
#89885,#89886,#89887,#89888,#89889,#89890,#89891,#89892,#89893,#89894,#89895,
#89896,#89897,#89898,#89899,#89900,#89901),.UNSPECIFIED.,.F.,.F.,(4,3,3,
3,3,3,3,3,3,3,3,3,3,3,3,3,3,3,4),(0.,0.000143392181484494,0.000291008849434949,
0.000439783745059069,0.000555292712107868,0.000556789243875147,0.00099691583468798,
0.00111258082262434,0.00111357848775029,0.0013912248898476,0.00139197310968786,
0.00166986892675867,0.00167036773162542,0.00178582121038124,0.00190189432266007,
0.00194876235356299,0.00206633842710468,0.00218183211487081,0.00222715697550056),
 .UNSPECIFIED.);
#2239=B_SPLINE_CURVE_WITH_KNOTS('',3,(#89962,#89963,#89964,#89965,#89966,
#89967,#89968,#89969,#89970,#89971,#89972,#89973,#89974,#89975,#89976,#89977,
#89978,#89979,#89980,#89981,#89982,#89983,#89984,#89985,#89986,#89987,#89988,
#89989,#89990,#89991,#89992,#89993,#89994,#89995,#89996,#89997,#89998,#89999,
#90000,#90001,#90002,#90003,#90004),.UNSPECIFIED.,.F.,.F.,(4,3,3,3,3,3,
3,3,3,3,3,3,3,3,4),(0.,9.05348581213434E-5,0.000186230685823136,0.000281926513524929,
0.000285981344804193,0.000428798602281781,0.000551039228772444,0.000563853027049858,
0.000571011012586812,0.000700764976115681,0.000820908721173626,0.000852457805291007,
0.000968426992556637,0.00107689164183138,0.00112770605409983),
 .UNSPECIFIED.);
#2240=B_SPLINE_CURVE_WITH_KNOTS('',3,(#90043,#90044,#90045,#90046,#90047,
#90048,#90049,#90050,#90051,#90052,#90053,#90054,#90055,#90056,#90057,#90058,
#90059,#90060,#90061,#90062,#90063,#90064,#90065,#90066,#90067,#90068,#90069,
#90070,#90071,#90072,#90073,#90074,#90075,#90076,#90077,#90078,#90079,#90080,
#90081,#90082,#90083,#90084,#90085,#90086,#90087,#90088,#90089,#90090,#90091,
#90092,#90093,#90094,#90095,#90096,#90097,#90098,#90099,#90100,#90101,#90102,
#90103),.UNSPECIFIED.,.F.,.F.,(4,3,3,3,3,3,3,3,3,3,3,3,3,3,3,3,3,3,3,3,
4),(0.,0.000156013234498623,0.00031658985362754,0.000479148774670394,0.000556927769468564,
0.00055839865504465,0.000679544683456882,0.000802052832349284,0.000837597982566976,
0.000954893942540085,0.00107174028492991,0.00111581667603572,0.0011167973100893,
0.00139526120827785,0.00139599663761163,0.00167470569152652,0.00167519596513395,
0.00183768579152785,0.0020007981043495,0.00216182265289023,0.00223359462017865),
 .UNSPECIFIED.);
#2241=B_SPLINE_CURVE_WITH_KNOTS('',3,(#90184,#90185,#90186,#90187,#90188,
#90189,#90190,#90191,#90192,#90193,#90194,#90195,#90196,#90197,#90198,#90199,
#90200,#90201,#90202,#90203,#90204,#90205,#90206,#90207,#90208,#90209,#90210,
#90211,#90212,#90213,#90214,#90215,#90216,#90217,#90218,#90219,#90220,#90221,
#90222,#90223,#90224,#90225,#90226),.UNSPECIFIED.,.F.,.F.,(4,3,3,3,3,3,
3,3,3,3,3,3,3,3,4),(0.,6.67265512522049E-5,0.000136622019400954,0.000153029544754912,
0.00019924472822554,0.000217818617549667,0.000312328270306139,0.000403808730923921,
0.000412185835933932,0.000489165233070777,0.00057076509789447,0.000614356689352663,
0.000696473891804212,0.000772875577879106,0.000824371671867865),
 .UNSPECIFIED.);
#2242=B_SPLINE_CURVE_WITH_KNOTS('',3,(#90259,#90260,#90261,#90262,#90263,
#90264,#90265,#90266,#90267,#90268,#90269,#90270,#90271,#90272,#90273,#90274,
#90275,#90276,#90277,#90278,#90279,#90280,#90281,#90282,#90283,#90284,#90285,
#90286,#90287,#90288,#90289,#90290,#90291,#90292,#90293,#90294,#90295,#90296,
#90297,#90298),.UNSPECIFIED.,.F.,.F.,(4,3,3,3,3,3,3,3,3,3,3,3,3,4),(0.,
8.52389357182548E-5,0.000172733323547372,0.000211640487491587,0.000298212835710885,
0.000380876745557343,0.000413153329460335,0.000422318843197918,0.000516826234508421,
0.000606276517040864,0.000627441770070006,0.00071476091751551,0.000798063637109017,
0.00082630665892067),.UNSPECIFIED.);
#2243=B_SPLINE_CURVE_WITH_KNOTS('',3,(#90351,#90352,#90353,#90354,#90355,
#90356,#90357,#90358,#90359,#90360,#90361,#90362,#90363,#90364,#90365,#90366,
#90367,#90368,#90369,#90370,#90371,#90372,#90373,#90374,#90375,#90376,#90377,
#90378,#90379,#90380,#90381,#90382,#90383,#90384,#90385,#90386,#90387,#90388,
#90389,#90390),.UNSPECIFIED.,.F.,.F.,(4,3,3,3,3,3,3,3,3,3,3,3,3,4),(0.,
0.00011221574809149,0.000227726453824885,0.000343358926450897,0.000400006487034198,
0.000401026826947022,0.000801373468181378,0.000802053653894043,0.00120274039453808,
0.00120308048084106,0.00131908058326075,0.001435186796666,0.00154804834527591,
0.00160410730778809),.UNSPECIFIED.);
#2244=B_SPLINE_CURVE_WITH_KNOTS('',3,(#90426,#90427,#90428,#90429,#90430,
#90431,#90432,#90433,#90434,#90435,#90436,#90437,#90438,#90439,#90440,#90441,
#90442,#90443,#90444,#90445,#90446,#90447,#90448,#90449,#90450,#90451,#90452,
#90453,#90454,#90455,#90456,#90457,#90458,#90459,#90460,#90461,#90462,#90463,
#90464,#90465,#90466,#90467,#90468,#90469,#90470,#90471,#90472,#90473,#90474,
#90475,#90476,#90477,#90478,#90479,#90480),.UNSPECIFIED.,.F.,.F.,(4,3,3,
3,3,3,3,3,3,3,3,3,3,3,3,3,3,3,4),(0.,0.000114915791844144,0.000172822750101235,
0.000292298157290126,0.00033117836085677,0.000390561714890095,0.000402052540286958,
0.000416541932279675,0.000550281559212149,0.000611393562701525,0.000745898236157288,
0.000805581435491517,0.000806245193123375,0.00116372865527049,0.00120903591007228,
0.00120936778968506,0.0013421660310875,0.00147732820866712,0.00161249038624675),
 .UNSPECIFIED.);
#2245=B_SPLINE_CURVE_WITH_KNOTS('',3,(#90548,#90549,#90550,#90551,#90552,
#90553,#90554,#90555,#90556,#90557,#90558,#90559,#90560,#90561,#90562,#90563,
#90564,#90565,#90566,#90567,#90568,#90569,#90570,#90571,#90572,#90573,#90574,
#90575,#90576,#90577,#90578,#90579,#90580,#90581,#90582,#90583,#90584,#90585,
#90586,#90587,#90588,#90589,#90590),.UNSPECIFIED.,.F.,.F.,(4,3,3,3,3,3,
3,3,3,3,3,3,3,3,4),(0.,6.67265512633752E-5,0.000136622019425751,0.000153029544754895,
0.000199244728225524,0.000217818617549654,0.000312328270310071,0.000403808730923931,
0.000412185835933931,0.000489165233073854,0.000570765097900325,0.0006143566893525,
0.000696473891807362,0.000772875577886235,0.000824371671867863),
 .UNSPECIFIED.);
#2246=B_SPLINE_CURVE_WITH_KNOTS('',3,(#90623,#90624,#90625,#90626,#90627,
#90628,#90629,#90630,#90631,#90632,#90633,#90634,#90635,#90636,#90637,#90638,
#90639,#90640,#90641,#90642,#90643,#90644,#90645,#90646,#90647,#90648,#90649,
#90650,#90651,#90652,#90653,#90654,#90655,#90656,#90657,#90658,#90659,#90660,
#90661,#90662),.UNSPECIFIED.,.F.,.F.,(4,3,3,3,3,3,3,3,3,3,3,3,3,4),(0.,
8.52389357147525E-5,0.000172733323539415,0.000211640487491721,0.000298212835707085,
0.000380876745550233,0.000413153329460335,0.000422318843197926,0.000516826234503452,
0.000606276517025046,0.000627441770069871,0.000714760917507696,0.000798063637099582,
0.00082630665892067),.UNSPECIFIED.);
#2247=B_SPLINE_CURVE_WITH_KNOTS('',3,(#90715,#90716,#90717,#90718,#90719,
#90720,#90721,#90722,#90723,#90724,#90725,#90726,#90727,#90728,#90729,#90730,
#90731,#90732,#90733,#90734,#90735,#90736,#90737,#90738,#90739,#90740,#90741,
#90742,#90743,#90744,#90745,#90746,#90747,#90748,#90749,#90750,#90751,#90752,
#90753,#90754),.UNSPECIFIED.,.F.,.F.,(4,3,3,3,3,3,3,3,3,3,3,3,3,4),(0.,
0.000112215748106196,0.000227726453854894,0.000343358926496841,0.000400006487034196,
0.000401026826947021,0.000801373468181415,0.000802053653894042,0.00120274039453804,
0.00120308048084106,0.00131908058325572,0.00143518679665637,0.00154804834526206,
0.00160410730778808),.UNSPECIFIED.);
#2248=B_SPLINE_CURVE_WITH_KNOTS('',3,(#90790,#90791,#90792,#90793,#90794,
#90795,#90796,#90797,#90798,#90799,#90800,#90801,#90802,#90803,#90804,#90805,
#90806,#90807,#90808,#90809,#90810,#90811,#90812,#90813,#90814,#90815,#90816,
#90817,#90818,#90819,#90820,#90821,#90822,#90823,#90824,#90825,#90826,#90827,
#90828,#90829,#90830,#90831,#90832,#90833,#90834,#90835,#90836,#90837,#90838,
#90839,#90840,#90841,#90842,#90843,#90844),.UNSPECIFIED.,.F.,.F.,(4,3,3,
3,3,3,3,3,3,3,3,3,3,3,3,3,3,3,4),(0.,0.000114915791837638,0.000172822750101249,
0.000292298157306797,0.00033117836085678,0.000390561714890105,0.000402052540286979,
0.000416541932279684,0.000550281559217109,0.00061139356270153,0.000745898236163757,
0.00080558143549149,0.000806245193123376,0.00116372865379815,0.00120903591007227,
0.00120936778968506,0.00134216603106807,0.00147732820865741,0.00161249038624675),
 .UNSPECIFIED.);
#2249=B_SPLINE_CURVE_WITH_KNOTS('',3,(#90912,#90913,#90914,#90915,#90916,
#90917,#90918,#90919,#90920,#90921,#90922,#90923,#90924,#90925,#90926,#90927,
#90928,#90929,#90930,#90931,#90932,#90933,#90934,#90935,#90936,#90937,#90938,
#90939,#90940,#90941,#90942,#90943,#90944,#90945,#90946,#90947,#90948,#90949,
#90950,#90951,#90952,#90953,#90954),.UNSPECIFIED.,.F.,.F.,(4,3,3,3,3,3,
3,3,3,3,3,3,3,3,4),(0.,6.67265512482609E-5,0.000136622019394041,0.000153029544754874,
0.000199244728225511,0.000217818617549638,0.000312328270301001,0.000403808730923887,
0.000412185835933931,0.000489165233063715,0.000570765097881359,0.000614356689352532,
0.00069647389179857,0.000772875577868274,0.000824371671867862),
 .UNSPECIFIED.);
#2250=B_SPLINE_CURVE_WITH_KNOTS('',3,(#90987,#90988,#90989,#90990,#90991,
#90992,#90993,#90994,#90995,#90996,#90997,#90998,#90999,#91000,#91001,#91002,
#91003,#91004,#91005,#91006,#91007,#91008,#91009,#91010,#91011,#91012,#91013,
#91014,#91015,#91016,#91017,#91018,#91019,#91020,#91021,#91022,#91023,#91024,
#91025,#91026),.UNSPECIFIED.,.F.,.F.,(4,3,3,3,3,3,3,3,3,3,3,3,3,4),(0.,
8.5238935718577E-5,0.000172733323546976,0.000211640487491245,0.000298212835710136,
0.000380876745556722,0.000413153329460335,0.000422318843197919,0.000516826234506355,
0.000606276517037616,0.000627441770070124,0.000714760917514443,0.000798063637110687,
0.00082630665892067),.UNSPECIFIED.);
#2251=B_SPLINE_CURVE_WITH_KNOTS('',3,(#91079,#91080,#91081,#91082,#91083,
#91084,#91085,#91086,#91087,#91088,#91089,#91090,#91091,#91092,#91093,#91094,
#91095,#91096,#91097,#91098,#91099,#91100,#91101,#91102,#91103,#91104,#91105,
#91106,#91107,#91108,#91109,#91110,#91111,#91112,#91113,#91114,#91115,#91116,
#91117,#91118),.UNSPECIFIED.,.F.,.F.,(4,3,3,3,3,3,3,3,3,3,3,3,3,4),(0.,
0.000112215748089412,0.000227726453820774,0.000343358926444529,0.000400006487034207,
0.000401026826947022,0.000801373468181404,0.000802053653894045,0.00120274039453804,
0.00120308048084107,0.00131908058325539,0.00143518679665721,0.00154804834526584,
0.00160410730778809),.UNSPECIFIED.);
#2252=B_SPLINE_CURVE_WITH_KNOTS('',3,(#91154,#91155,#91156,#91157,#91158,
#91159,#91160,#91161,#91162,#91163,#91164,#91165,#91166,#91167,#91168,#91169,
#91170,#91171,#91172,#91173,#91174,#91175,#91176,#91177,#91178,#91179,#91180,
#91181,#91182,#91183,#91184,#91185,#91186,#91187,#91188,#91189,#91190,#91191,
#91192,#91193,#91194,#91195,#91196,#91197,#91198,#91199,#91200,#91201,#91202,
#91203,#91204,#91205,#91206,#91207,#91208),.UNSPECIFIED.,.F.,.F.,(4,3,3,
3,3,3,3,3,3,3,3,3,3,3,3,3,3,3,4),(0.,0.000114915791794343,0.000172822750101289,
0.000292298157340931,0.000331178360856813,0.000390561714890135,0.00040205254028697,
0.000416541932279713,0.00055028155921315,0.000611393562701549,0.000745898236154648,
0.000805581435491558,0.000806245193123386,0.00116372865600683,0.00120903591007228,
0.00120936778968507,0.00134216603108612,0.00147732820866644,0.00161249038624675),
 .UNSPECIFIED.);
#2253=B_SPLINE_CURVE_WITH_KNOTS('',3,(#91391,#91392,#91393,#91394),
 .UNSPECIFIED.,.F.,.F.,(4,4),(-0.92505235407501,-0.312867444040557),
 .UNSPECIFIED.);
#2254=B_SPLINE_CURVE_WITH_KNOTS('',3,(#91419,#91420,#91421,#91422,#91423,
#91424,#91425,#91426,#91427,#91428,#91429,#91430,#91431),.UNSPECIFIED.,
 .F.,.F.,(4,3,3,3,4),(2.77555756156289E-17,0.00107584967114952,0.00186640722503582,
0.00326502442945365,0.00374644515873592),.UNSPECIFIED.);
#2255=B_SPLINE_CURVE_WITH_KNOTS('',3,(#91464,#91465,#91466,#91467,#91468,
#91469),.UNSPECIFIED.,.F.,.F.,(4,2,4),(0.,0.00205629279785326,0.00411258559570652),
 .UNSPECIFIED.);
#2256=B_SPLINE_CURVE_WITH_KNOTS('',3,(#91494,#91495,#91496,#91497,#91498,
#91499,#91500,#91501,#91502,#91503,#91504,#91505,#91506),.UNSPECIFIED.,
 .F.,.F.,(4,3,3,3,4),(0.,0.00135643839013762,0.00187754543955613,0.00293345159169245,
0.00374102163234538),.UNSPECIFIED.);
#2257=B_SPLINE_CURVE_WITH_KNOTS('',3,(#91555,#91556,#91557,#91558,#91559,
#91560,#91561,#91562,#91563,#91564,#91565,#91566,#91567,#91568,#91569,#91570,
#91571,#91572,#91573,#91574,#91575,#91576,#91577,#91578,#91579,#91580,#91581,
#91582),.UNSPECIFIED.,.F.,.F.,(4,3,3,3,3,3,3,3,3,4),(0.,0.00952633528178463,
0.0149413816810589,0.027827346998543,0.0298764199626499,0.044807721980472,
0.0597366932955049,0.0825180253977875,0.0895905783515619,0.119441539355168),
 .UNSPECIFIED.);
#2258=B_SPLINE_CURVE_WITH_KNOTS('',3,(#91757,#91758,#91759,#91760,#91761,
#91762,#91763,#91764,#91765,#91766,#91767,#91768,#91769,#91770,#91771,#91772,
#91773,#91774,#91775,#91776,#91777,#91778,#91779,#91780,#91781,#91782,#91783,
#91784,#91785,#91786,#91787,#91788,#91789,#91790,#91791,#91792,#91793,#91794,
#91795,#91796,#91797,#91798,#91799,#91800,#91801,#91802,#91803,#91804,#91805,
#91806,#91807,#91808,#91809,#91810,#91811,#91812,#91813,#91814,#91815,#91816,
#91817,#91818,#91819,#91820,#91821,#91822,#91823,#91824,#91825,#91826,#91827,
#91828,#91829,#91830,#91831,#91832,#91833,#91834,#91835,#91836,#91837,#91838,
#91839,#91840,#91841,#91842,#91843,#91844,#91845,#91846,#91847,#91848,#91849,
#91850,#91851,#91852,#91853,#91854,#91855,#91856,#91857,#91858,#91859,#91860,
#91861,#91862,#91863,#91864,#91865,#91866,#91867,#91868,#91869,#91870,#91871,
#91872,#91873,#91874,#91875,#91876,#91877,#91878,#91879,#91880,#91881,#91882,
#91883,#91884,#91885,#91886,#91887,#91888,#91889,#91890,#91891,#91892,#91893,
#91894,#91895,#91896,#91897,#91898,#91899,#91900,#91901,#91902,#91903,#91904,
#91905,#91906,#91907,#91908,#91909,#91910,#91911,#91912,#91913,#91914,#91915,
#91916,#91917,#91918,#91919,#91920,#91921,#91922,#91923,#91924,#91925,#91926,
#91927,#91928,#91929,#91930,#91931,#91932,#91933,#91934,#91935,#91936,#91937,
#91938,#91939,#91940,#91941,#91942,#91943,#91944,#91945,#91946,#91947,#91948,
#91949,#91950,#91951,#91952,#91953,#91954,#91955,#91956,#91957,#91958),
 .UNSPECIFIED.,.F.,.F.,(4,3,3,3,3,3,3,3,3,3,3,3,3,3,3,3,3,3,3,3,3,3,3,3,
3,3,3,3,3,3,3,3,3,3,3,3,3,3,3,3,3,3,3,3,3,3,3,3,3,3,3,3,3,3,3,3,3,3,3,3,
3,3,3,3,3,3,3,4),(0.,0.0321347663513911,0.0495590971962858,0.0642731458325224,
0.0803449852514299,0.0862931845746985,0.0964200512051668,0.10417597746563,
0.112500619108118,0.1188635453537,0.127099327263411,0.12859129060153,0.134437158235721,
0.136643239029931,0.137833345921669,0.140671729597307,0.141438649477679,
0.144702441480307,0.145881989724134,0.150173982146214,0.15277262499039,
0.153697717707011,0.156609795439022,0.156813504295751,0.157452006796345,
0.160140339175471,0.160859452487887,0.161815966934324,0.165392978618541,
0.168754753030431,0.168969990302759,0.172572893113886,0.173035427576006,
0.17347524133991,0.174874914476304,0.175070484733593,0.17525292917978,0.175430745909724,
0.176752761166982,0.177106662985369,0.177544810746771,0.180196510508637,
0.182865217339906,0.185255162170942,0.187290885676172,0.188723430659198,
0.189325249765294,0.191782738213962,0.193388999062593,0.196260696109834,
0.199201866293497,0.201293287365534,0.201495395322362,0.203648653252632,
0.205190626206137,0.20553912739097,0.208511013889035,0.20957779685043,0.213946752682742,
0.217643568734126,0.2230677928992,0.22569846278186,0.23234312451842,0.233746180692591,
0.24011738396337,0.24178905493371,0.25264345913106,0.257865728390371),
 .UNSPECIFIED.);
#2259=B_SPLINE_CURVE_WITH_KNOTS('',3,(#92094,#92095,#92096,#92097,#92098,
#92099,#92100,#92101,#92102,#92103,#92104,#92105,#92106,#92107,#92108,#92109,
#92110,#92111,#92112,#92113,#92114,#92115,#92116,#92117,#92118,#92119,#92120,
#92121,#92122,#92123,#92124,#92125,#92126,#92127,#92128,#92129,#92130,#92131,
#92132,#92133,#92134,#92135,#92136,#92137,#92138,#92139,#92140,#92141,#92142,
#92143,#92144,#92145,#92146,#92147,#92148,#92149,#92150,#92151,#92152,#92153,
#92154,#92155,#92156,#92157,#92158,#92159,#92160,#92161,#92162,#92163,#92164,
#92165,#92166,#92167,#92168,#92169,#92170,#92171,#92172,#92173,#92174,#92175,
#92176,#92177,#92178,#92179,#92180,#92181,#92182,#92183,#92184,#92185,#92186,
#92187,#92188,#92189,#92190,#92191,#92192,#92193,#92194,#92195,#92196,#92197,
#92198,#92199,#92200,#92201,#92202,#92203,#92204,#92205,#92206,#92207,#92208,
#92209,#92210,#92211,#92212,#92213,#92214,#92215,#92216,#92217,#92218,#92219,
#92220,#92221,#92222,#92223,#92224,#92225,#92226,#92227,#92228,#92229,#92230,
#92231,#92232,#92233,#92234,#92235,#92236,#92237,#92238,#92239,#92240,#92241,
#92242,#92243,#92244,#92245,#92246,#92247,#92248,#92249,#92250,#92251,#92252,
#92253,#92254,#92255,#92256,#92257,#92258,#92259,#92260,#92261,#92262,#92263,
#92264,#92265,#92266,#92267,#92268,#92269,#92270,#92271,#92272,#92273,#92274,
#92275,#92276,#92277,#92278,#92279,#92280,#92281,#92282,#92283,#92284,#92285,
#92286,#92287,#92288,#92289,#92290,#92291,#92292,#92293,#92294,#92295,#92296,
#92297,#92298,#92299,#92300,#92301,#92302,#92303,#92304,#92305,#92306,#92307,
#92308,#92309,#92310,#92311,#92312,#92313,#92314,#92315,#92316,#92317,#92318,
#92319,#92320,#92321,#92322,#92323,#92324,#92325,#92326,#92327,#92328,#92329,
#92330,#92331,#92332,#92333,#92334,#92335,#92336,#92337,#92338,#92339,#92340,
#92341,#92342,#92343),.UNSPECIFIED.,.F.,.F.,(4,3,3,3,3,3,3,3,3,3,3,3,3,
3,3,3,3,3,3,3,3,3,3,3,3,3,3,3,3,3,3,3,3,3,3,3,3,3,3,3,3,3,3,3,3,3,3,3,3,
3,3,3,3,3,3,3,3,3,3,3,3,3,3,3,3,3,3,3,3,3,3,3,3,3,3,3,3,3,3,3,3,3,3,4),
(-5.99999999961901E-8,0.00205213753470555,0.00346047691825982,0.00549976480516702,
0.00684933075492668,0.00692828170882304,0.00947037504164401,0.0116737828388313,
0.0127754867374249,0.0134477508061639,0.0137277075245536,0.0138771906360185,
0.0147454865964315,0.0152762362074286,0.0156228660994763,0.0176161119027071,
0.0192198351110147,0.0202986140975471,0.0208235583193224,0.0225611142429988,
0.0236071707918062,0.0239227132772834,0.0242885895794692,0.025152866209584,
0.0255712676146208,0.0266029893184477,0.0268886660138179,0.0271218002136788,
0.0272592346694993,0.0277456960999287,0.0299580577697661,0.032296502762021,
0.0335558689820468,0.0343992850002989,0.0346349477542758,0.0377731272866975,
0.040976446705338,0.0414941580473473,0.0449116181533913,0.0473261513120718,
0.0480896243204303,0.0483290782594353,0.0500331936258331,0.0510138895980884,
0.0534411134522563,0.0551455397250265,0.0597641814744442,0.0642522681203356,
0.0665629408104305,0.0677395126638232,0.0685561850589512,0.068740354766227,
0.0721325097284016,0.073828587209489,0.0746119055671886,0.0750773246746244,
0.0755246646905763,0.0789136615920156,0.0808492608585523,0.082302658493455,
0.0899824409819067,0.095845006466064,0.102609655818586,0.106117423701975,
0.108183528611815,0.109374305171108,0.116134326690507,0.119525294284937,
0.122087358326956,0.122894348209906,0.12964774211714,0.133677826490132,
0.136177104645105,0.136401136024373,0.147704077365847,0.15553974506886,
0.159457578920367,0.161717990371485,0.163099656918869,0.163375412771874,
0.181117111195966,0.190331075834418,0.210237730720008,0.217279461675811),
 .UNSPECIFIED.);
#2260=B_SPLINE_CURVE_WITH_KNOTS('',3,(#92344,#92345,#92346,#92347,#92348,
#92349,#92350,#92351,#92352,#92353,#92354,#92355,#92356,#92357,#92358,#92359,
#92360,#92361,#92362,#92363,#92364,#92365,#92366,#92367,#92368,#92369,#92370,
#92371,#92372,#92373,#92374,#92375,#92376,#92377,#92378,#92379,#92380,#92381,
#92382,#92383,#92384,#92385,#92386,#92387,#92388,#92389,#92390,#92391,#92392,
#92393,#92394,#92395,#92396,#92397,#92398,#92399,#92400,#92401,#92402,#92403,
#92404,#92405,#92406,#92407),.UNSPECIFIED.,.F.,.F.,(4,3,3,3,3,3,3,3,3,3,
3,3,3,3,3,3,3,3,3,3,3,4),(0.,0.0265419162547455,0.0530838325094911,0.0796257487642366,
0.0928967068916094,0.106167665018982,0.119438623146355,0.132709581273728,
0.139345060337414,0.145980539401101,0.159251497528473,0.16588697659216,
0.172522455655846,0.179157934719533,0.185793413783219,0.189111153315062,
0.192428892846905,0.199064371910592,0.205699850974278,0.209017590506122,
0.21076098823351,0.212335330037965),.UNSPECIFIED.);
#2261=B_SPLINE_CURVE_WITH_KNOTS('',3,(#92447,#92448,#92449,#92450,#92451,
#92452,#92453,#92454,#92455,#92456,#92457,#92458,#92459,#92460,#92461,#92462,
#92463,#92464,#92465,#92466,#92467,#92468,#92469,#92470,#92471,#92472,#92473,
#92474,#92475,#92476,#92477,#92478,#92479,#92480,#92481,#92482,#92483,#92484,
#92485,#92486,#92487,#92488,#92489),.UNSPECIFIED.,.F.,.F.,(4,3,3,3,3,3,
3,3,3,3,3,3,3,3,4),(0.,0.0174818147702963,0.0276661561951365,0.0466085742141883,
0.0553487132947371,0.0706615640779338,0.083047726575705,0.0850821797454832,
0.0909913302116415,0.0939459054447206,0.0954294830608625,0.0964768515157899,
0.0969004806777997,0.107725903082733,0.110740358368174),.UNSPECIFIED.);
#2262=B_SPLINE_CURVE_WITH_KNOTS('',3,(#92490,#92491,#92492,#92493,#92494,
#92495,#92496,#92497,#92498,#92499,#92500,#92501,#92502,#92503,#92504,#92505,
#92506,#92507,#92508,#92509,#92510,#92511,#92512,#92513,#92514,#92515,#92516,
#92517,#92518,#92519,#92520,#92521,#92522,#92523),.UNSPECIFIED.,.F.,.F.,
(4,3,3,3,3,3,3,3,3,3,3,4),(0.,0.00853528476678784,0.0138219837281452,0.0138424585775806,
0.0212354389568398,0.0276642139270636,0.0276849171551612,0.0553560321602673,
0.0553698343103225,0.0830478503904525,0.0830547514654838,0.110739668620645),
 .UNSPECIFIED.);
#2263=B_SPLINE_CURVE_WITH_KNOTS('',3,(#92587,#92588,#92589,#92590,#92591,
#92592,#92593,#92594,#92595,#92596,#92597,#92598,#92599,#92600,#92601,#92602,
#92603,#92604,#92605,#92606,#92607,#92608,#92609,#92610,#92611,#92612,#92613,
#92614,#92615,#92616,#92617,#92618,#92619,#92620,#92621,#92622,#92623,#92624,
#92625,#92626,#92627,#92628,#92629,#92630,#92631,#92632,#92633,#92634,#92635,
#92636,#92637,#92638,#92639,#92640,#92641,#92642,#92643,#92644,#92645,#92646,
#92647,#92648,#92649,#92650,#92651,#92652,#92653,#92654,#92655,#92656,#92657,
#92658,#92659,#92660,#92661,#92662),.UNSPECIFIED.,.F.,.F.,(4,3,3,3,3,3,
3,3,3,3,3,3,3,3,3,3,3,3,3,3,3,3,3,3,3,4),(2.00078531959267E-15,6.27245974407096E-5,
0.00012523366663523,0.000168194487246218,0.000208019821857731,0.000263919656744897,
0.000292924598205694,0.000363889403564607,0.000377194267852935,0.000453363357768638,
0.000533936193646606,0.000576783819641349,0.000670776831385002,0.000735149291962565,
0.000856545197961509,0.000932596455777723,0.00105992985614175,0.00120019572685142,
0.00131573376212713,0.00147029858392507,0.00170701877802783,0.00195809484060081,
0.00211995765409861,0.00220544787588757,0.00284725701195324,0.00294057482639061),
 .UNSPECIFIED.);
#2264=B_SPLINE_CURVE_WITH_KNOTS('',3,(#92750,#92751,#92752,#92753,#92754,
#92755,#92756,#92757,#92758,#92759,#92760,#92761,#92762,#92763,#92764,#92765,
#92766,#92767,#92768,#92769,#92770,#92771,#92772,#92773,#92774,#92775,#92776,
#92777),.UNSPECIFIED.,.F.,.F.,(4,2,2,2,2,2,2,2,2,2,2,2,2,4),(1.73472347597681E-18,
0.00801632890443165,0.0160326578088633,0.0200408222610791,0.0240489867132949,
0.0320653156177267,0.0360734800699425,0.0380775622960505,0.0400816445221584,
0.0480979734265901,0.0501020556526981,0.052106137878806,0.0561143023310219,
0.0641306312354537),.UNSPECIFIED.);
#2265=B_SPLINE_CURVE_WITH_KNOTS('',3,(#92778,#92779,#92780,#92781,#92782,
#92783,#92784,#92785,#92786,#92787,#92788,#92789,#92790,#92791,#92792,#92793,
#92794,#92795,#92796,#92797,#92798,#92799,#92800,#92801,#92802,#92803,#92804,
#92805,#92806,#92807,#92808,#92809,#92810,#92811,#92812,#92813,#92814,#92815,
#92816,#92817,#92818,#92819,#92820,#92821,#92822,#92823,#92824,#92825,#92826,
#92827,#92828,#92829,#92830,#92831,#92832,#92833,#92834,#92835,#92836,#92837,
#92838,#92839,#92840,#92841,#92842,#92843,#92844,#92845,#92846,#92847,#92848,
#92849,#92850,#92851,#92852,#92853,#92854,#92855,#92856,#92857,#92858,#92859,
#92860,#92861,#92862,#92863,#92864,#92865,#92866,#92867,#92868,#92869,#92870,
#92871),.UNSPECIFIED.,.F.,.F.,(4,3,3,3,3,3,3,3,3,3,3,3,3,3,3,3,3,3,3,3,
3,3,3,3,3,3,3,3,3,3,3,4),(0.,0.00674763364146324,0.00782968911952726,0.00784373710529933,
0.0117445336792909,0.0117656056534845,0.0137019559591727,0.0137265401335389,
0.0156593782390545,0.0156874742092816,0.0234890673585819,0.0235312113204749,
0.0254464896384637,0.0254921454471888,0.0274039119183456,0.0274530829252165,
0.0303049604471932,0.0313187564781093,0.0313749484131831,0.0391484455976365,
0.0392186860654585,0.0416267378991184,0.0430632901574002,0.0431404818311709,
0.0469781347171638,0.0470560909016423,0.0506039903695911,0.0542607409119146,
0.0548078238366911,0.0548609217456285,0.0590992763654095,0.0626375129562184),
 .UNSPECIFIED.);
#2266=B_SPLINE_CURVE_WITH_KNOTS('',3,(#92921,#92922,#92923,#92924,#92925,
#92926,#92927,#92928,#92929,#92930,#92931,#92932,#92933,#92934,#92935,#92936,
#92937,#92938,#92939,#92940,#92941,#92942,#92943,#92944,#92945,#92946,#92947,
#92948,#92949,#92950,#92951,#92952,#92953,#92954,#92955,#92956,#92957,#92958,
#92959,#92960,#92961,#92962,#92963,#92964,#92965,#92966,#92967,#92968,#92969,
#92970,#92971,#92972,#92973,#92974,#92975,#92976,#92977,#92978,#92979,#92980,
#92981,#92982,#92983,#92984,#92985,#92986,#92987,#92988,#92989,#92990,#92991,
#92992,#92993),.UNSPECIFIED.,.F.,.F.,(4,3,3,3,3,3,3,3,3,3,3,3,3,3,3,3,3,
3,3,3,3,3,3,3,4),(2.53193767630367E-8,0.000761602148823654,0.000848295295233062,
0.00109951708486985,0.00132392636131809,0.0015232042976473,0.00168207255245941,
0.00185215920385473,0.00190400537205915,0.00204222878317895,0.00217140981375754,
0.00228480644647099,0.00238367032878988,0.00244986162048359,0.0025321966759578,
0.00260949404176403,0.00266560752088284,0.00272802392810674,0.00276080778948581,
0.0027758345451979,0.00282959836697759,0.00285600805808879,0.00290360819239027,
0.00297598425714359,0.00304640859529444),.UNSPECIFIED.);
#2267=B_SPLINE_CURVE_WITH_KNOTS('',3,(#93054,#93055,#93056,#93057,#93058,
#93059,#93060,#93061,#93062,#93063,#93064,#93065,#93066,#93067,#93068,#93069,
#93070,#93071,#93072,#93073,#93074,#93075,#93076,#93077,#93078,#93079,#93080,
#93081,#93082,#93083,#93084,#93085,#93086,#93087,#93088,#93089,#93090),
 .UNSPECIFIED.,.F.,.F.,(4,3,3,3,3,3,3,3,3,3,3,3,4),(1.83990108477198E-9,
0.000128387533529865,0.00025794985788125,0.000364723131813831,0.000364936417772228,
0.000547613913069482,0.000729446263627662,0.000730277175766961,0.000912528804080312,
0.00109439518681158,0.00127664385703345,0.00144798651104331,0.00145889252725532),
 .UNSPECIFIED.);
#2268=B_SPLINE_CURVE_WITH_KNOTS('',3,(#93109,#93110,#93111,#93112,#93113,
#93114,#93115),.UNSPECIFIED.,.F.,.F.,(4,3,4),(2.41016821063581E-15,0.00262158494557133,
0.00335832469594566),.UNSPECIFIED.);
#2269=B_SPLINE_CURVE_WITH_KNOTS('',3,(#93142,#93143,#93144,#93145,#93146,
#93147,#93148,#93149,#93150,#93151,#93152,#93153,#93154,#93155,#93156,#93157,
#93158,#93159,#93160,#93161,#93162,#93163,#93164,#93165,#93166,#93167,#93168,
#93169,#93170,#93171,#93172,#93173,#93174,#93175,#93176,#93177,#93178,#93179,
#93180,#93181),.UNSPECIFIED.,.F.,.F.,(4,3,3,3,3,3,3,3,3,3,3,3,3,4),(4.75463922286045E-13,
0.000114874771772721,0.000233668770413462,0.00035889395548095,0.000488266865941692,
0.000623835778388218,0.000646036121242161,0.000676434176771284,0.000814383672645379,
0.00095995065267877,0.000993298115721985,0.00115816801506027,0.00133156200529955,
0.00135286835354256),.UNSPECIFIED.);
#2270=B_SPLINE_CURVE_WITH_KNOTS('',3,(#93273,#93274,#93275,#93276,#93277,
#93278,#93279,#93280,#93281,#93282,#93283,#93284,#93285,#93286,#93287,#93288,
#93289,#93290,#93291,#93292,#93293,#93294,#93295,#93296,#93297,#93298,#93299,
#93300,#93301,#93302,#93303,#93304,#93305,#93306,#93307,#93308,#93309,#93310,
#93311,#93312,#93313,#93314,#93315,#93316,#93317,#93318,#93319,#93320,#93321,
#93322,#93323,#93324,#93325,#93326,#93327,#93328,#93329,#93330,#93331,#93332,
#93333,#93334,#93335,#93336,#93337,#93338,#93339,#93340,#93341,#93342,#93343,
#93344,#93345,#93346,#93347,#93348,#93349,#93350,#93351,#93352,#93353,#93354,
#93355,#93356,#93357),.UNSPECIFIED.,.F.,.F.,(4,3,3,3,3,3,3,3,3,3,3,3,3,
3,3,3,3,3,3,3,3,3,3,3,3,3,3,3,4),(1.04083408558608E-17,0.00306132087462231,
0.00458763228313725,0.00505755460700053,0.00737727473051059,0.00758657165052886,
0.0091752645662745,0.0101149087127913,0.0114690807078431,0.0137628968494117,
0.0151702835088379,0.0176976693841385,0.0183505291325489,0.0189612134424709,
0.0202246504480127,0.0206443452741175,0.0227077461535235,0.0229381614156862,
0.0252770618598094,0.0275257936988233,0.0278023764522136,0.0290648438726516,
0.0298196098403919,0.0303268301110632,0.0318006663681232,0.0321134259819605,
0.0348081739351341,0.0353740968812584,0.0367010582650977),.UNSPECIFIED.);
#2271=B_SPLINE_CURVE_WITH_KNOTS('',3,(#93396,#93397,#93398,#93399,#93400,
#93401,#93402,#93403,#93404,#93405,#93406,#93407,#93408,#93409,#93410,#93411,
#93412,#93413,#93414,#93415,#93416,#93417,#93418,#93419,#93420,#93421,#93422,
#93423,#93424,#93425,#93426),.UNSPECIFIED.,.F.,.F.,(4,3,3,3,3,3,3,3,3,3,
4),(1.38777878078145E-17,0.00369677025853092,0.00369698575261873,0.00739308614352542,
0.00739397150523745,0.00924116752762853,0.00924246438154679,0.0110896622905033,
0.0110909572578561,0.0145604524022874,0.0147879430104749),.UNSPECIFIED.);
#2272=B_SPLINE_CURVE_WITH_KNOTS('',3,(#93518,#93519,#93520,#93521,#93522,
#93523,#93524,#93525,#93526,#93527,#93528,#93529,#93530,#93531,#93532,#93533,
#93534,#93535,#93536,#93537,#93538,#93539,#93540,#93541,#93542,#93543,#93544,
#93545,#93546,#93547,#93548,#93549,#93550,#93551,#93552,#93553,#93554,#93555,
#93556,#93557,#93558,#93559,#93560,#93561,#93562,#93563,#93564,#93565,#93566,
#93567,#93568,#93569,#93570,#93571,#93572,#93573,#93574,#93575,#93576,#93577,
#93578,#93579,#93580,#93581,#93582,#93583,#93584,#93585,#93586,#93587,#93588,
#93589,#93590),.UNSPECIFIED.,.F.,.F.,(4,3,3,3,3,3,3,3,3,3,3,3,3,3,3,3,3,
3,3,3,3,3,3,3,4),(0.0483087273746794,0.0483353046476464,0.0499595272800289,
0.0502196409139219,0.0516103271853785,0.052103792003993,0.0549119269960775,
0.0558715388891371,0.0575187227537936,0.0577552750749259,0.0582135268067766,
0.0592308700721096,0.0596389008572866,0.0598643267121261,0.0615151266174756,
0.063406623077028,0.0671759109819169,0.0681183262388737,0.0690610075966447,
0.0697691261442232,0.0708751300026104,0.0709471315103791,0.0714199260495728,
0.0743329760918185,0.0747215258602685),.UNSPECIFIED.);
#2273=B_SPLINE_CURVE_WITH_KNOTS('',3,(#93752,#93753,#93754,#93755,#93756,
#93757,#93758,#93759,#93760,#93761,#93762,#93763,#93764,#93765,#93766,#93767,
#93768,#93769,#93770,#93771,#93772,#93773,#93774,#93775,#93776,#93777,#93778,
#93779,#93780,#93781,#93782,#93783,#93784,#93785,#93786,#93787,#93788,#93789,
#93790,#93791,#93792,#93793,#93794,#93795,#93796,#93797,#93798,#93799,#93800,
#93801,#93802,#93803,#93804,#93805,#93806,#93807,#93808,#93809,#93810,#93811,
#93812,#93813,#93814,#93815,#93816,#93817,#93818,#93819,#93820,#93821,#93822,
#93823,#93824,#93825,#93826,#93827,#93828,#93829,#93830,#93831,#93832,#93833,
#93834,#93835,#93836,#93837,#93838,#93839,#93840,#93841,#93842,#93843,#93844,
#93845,#93846,#93847,#93848,#93849,#93850,#93851,#93852,#93853,#93854,#93855,
#93856,#93857,#93858,#93859,#93860,#93861,#93862,#93863,#93864,#93865,#93866,
#93867,#93868,#93869,#93870,#93871,#93872,#93873,#93874,#93875,#93876,#93877,
#93878,#93879,#93880,#93881,#93882,#93883,#93884,#93885,#93886,#93887,#93888,
#93889,#93890,#93891,#93892,#93893,#93894,#93895,#93896,#93897,#93898,#93899,
#93900,#93901,#93902,#93903,#93904,#93905,#93906,#93907,#93908,#93909,#93910,
#93911,#93912,#93913,#93914,#93915,#93916,#93917,#93918,#93919,#93920,#93921,
#93922,#93923,#93924,#93925,#93926,#93927,#93928,#93929,#93930,#93931,#93932,
#93933,#93934,#93935,#93936,#93937,#93938,#93939,#93940,#93941,#93942,#93943,
#93944,#93945,#93946,#93947,#93948,#93949,#93950,#93951,#93952,#93953,#93954,
#93955,#93956,#93957,#93958,#93959,#93960,#93961,#93962,#93963,#93964,#93965),
 .UNSPECIFIED.,.F.,.F.,(4,3,3,3,3,3,3,3,3,3,3,3,3,3,3,3,3,3,3,3,3,3,3,3,
3,3,3,3,3,3,3,3,3,3,3,3,3,3,3,3,3,3,3,3,3,3,3,3,3,3,3,3,3,3,3,3,3,3,3,3,
3,3,3,3,3,3,3,3,3,3,3,4),(0.,0.0016184602718221,0.00319828590087957,0.004726552519676,
0.0062296665305914,0.00624571575272172,0.0077129297625436,0.00780714469090215,
0.00780777507546303,0.00880374169768939,0.00936857362908258,0.00939497775797128,
0.0110637108063712,0.0124914315054434,0.0125796213647023,0.014886037330468,
0.0172473351707312,0.0187371472581651,0.0189513025431913,0.0199039933520977,
0.0202985761963456,0.0213604955378055,0.021860005134526,0.0221313353710413,
0.023934479755877,0.0249828630108868,0.0253066784590323,0.0290723120433818,
0.0312285787636085,0.0316436340020624,0.0332250107158749,0.0343514366399693,
0.0348052706445514,0.0374742945163301,0.0379625216831405,0.0417199791548649,
0.0437200102690518,0.0442643097824748,0.0482414580560455,0.0499657260217734,
0.0505499917372572,0.0530885838981343,0.053687282245013,0.0562114417744951,
0.0568213808126068,0.0613502593264657,0.0624571575272168,0.0630810366667805,
0.0680308152815377,0.0687028732799386,0.0693306751795749,0.0735190343863351,
0.0749485890326603,0.0755720956952829,0.0811367906296009,0.0871241069005245,
0.0874400205381038,0.0880368539666603,0.0960156407501182,0.0999314520435472,
0.100484493326179,0.110352684692032,0.112422883548991,0.112920779842532,
0.124914315054434,0.125349598801627,0.142221446158236,0.149897178065321,
0.150194407331914,0.174880041076208,0.175030605012004,0.199862904087095),
 .UNSPECIFIED.);
#2274=B_SPLINE_CURVE_WITH_KNOTS('',3,(#93968,#93969,#93970,#93971,#93972,
#93973,#93974,#93975,#93976,#93977,#93978,#93979,#93980,#93981,#93982,#93983,
#93984,#93985,#93986,#93987,#93988,#93989,#93990,#93991,#93992,#93993,#93994,
#93995,#93996,#93997,#93998,#93999,#94000,#94001,#94002,#94003,#94004,#94005,
#94006,#94007,#94008,#94009,#94010,#94011,#94012,#94013,#94014,#94015,#94016,
#94017,#94018,#94019,#94020,#94021,#94022,#94023,#94024,#94025,#94026,#94027,
#94028,#94029,#94030,#94031,#94032,#94033,#94034,#94035,#94036,#94037,#94038,
#94039,#94040,#94041,#94042,#94043,#94044,#94045,#94046,#94047,#94048,#94049,
#94050,#94051,#94052,#94053,#94054,#94055,#94056,#94057,#94058,#94059,#94060,
#94061,#94062,#94063,#94064,#94065,#94066,#94067,#94068,#94069,#94070,#94071,
#94072,#94073,#94074,#94075,#94076,#94077,#94078,#94079,#94080,#94081,#94082,
#94083,#94084,#94085,#94086,#94087,#94088,#94089,#94090,#94091,#94092,#94093,
#94094,#94095,#94096,#94097,#94098,#94099,#94100,#94101,#94102,#94103,#94104,
#94105,#94106,#94107,#94108,#94109,#94110,#94111,#94112,#94113,#94114,#94115,
#94116,#94117,#94118,#94119,#94120,#94121,#94122,#94123,#94124,#94125,#94126,
#94127,#94128,#94129,#94130,#94131,#94132,#94133,#94134,#94135,#94136,#94137,
#94138,#94139,#94140,#94141,#94142),.UNSPECIFIED.,.F.,.F.,(4,3,3,3,3,3,
3,3,3,3,3,3,3,3,3,3,3,3,3,3,3,3,3,3,3,3,3,3,3,3,3,3,3,3,3,3,3,3,3,3,3,3,
3,3,3,3,3,3,3,3,3,3,3,3,3,3,3,3,4),(0.,0.0246446543849258,0.0246541408539193,
0.0492893087698515,0.0493082813931077,0.0739339631547773,0.0739624219187268,
0.0862562903472402,0.0862894922015488,0.0985786175397031,0.0986165624711814,
0.110900944732166,0.110943632741705,0.123223271924629,0.123270703016623,
0.12938443552086,0.129434238115484,0.135545599117092,0.135597773279537,
0.141706762713323,0.141761308417236,0.144787344511439,0.144843075947332,
0.147867926309555,0.147924844511973,0.15366260629182,0.154029089905786,
0.154088378680815,0.160190253502018,0.160251913829296,0.163270835300134,
0.163333681393769,0.164811126199191,0.164874564889871,0.166351417098249,
0.166415452062168,0.170160979779983,0.17251258069448,0.172578984095756,
0.175593162492596,0.175660751383538,0.177765246175035,0.178673744290712,
0.178742525402502,0.181788716644722,0.184834907886943,0.184906054338471,
0.187915489685058,0.187987822676343,0.189057434582198,0.189455780584116,
0.189527858303638,0.190809262316065,0.190996071483174,0.191062726298861,
0.192788975213052,0.194560412577886,0.196416249655382,0.197157235079405),
 .UNSPECIFIED.);
#2275=B_SPLINE_CURVE_WITH_KNOTS('',3,(#94188,#94189,#94190,#94191,#94192,
#94193,#94194,#94195,#94196,#94197,#94198,#94199,#94200,#94201,#94202,#94203,
#94204,#94205,#94206,#94207,#94208,#94209,#94210,#94211,#94212,#94213,#94214,
#94215,#94216,#94217,#94218,#94219,#94220,#94221,#94222,#94223,#94224,#94225,
#94226,#94227,#94228,#94229,#94230,#94231,#94232,#94233,#94234,#94235,#94236,
#94237,#94238,#94239,#94240,#94241,#94242,#94243,#94244,#94245,#94246,#94247,
#94248,#94249,#94250,#94251,#94252,#94253,#94254,#94255,#94256,#94257,#94258,
#94259,#94260,#94261,#94262,#94263,#94264,#94265,#94266),.UNSPECIFIED.,
 .F.,.F.,(4,3,3,3,3,3,3,3,3,3,3,3,3,3,3,3,3,3,3,3,3,3,3,3,3,3,4),(0.,0.000336250842231429,
0.000672501684462858,0.000787345219381404,0.000973846749200159,0.00114945806151638,
0.0013133825161952,0.00134500336892572,0.00148679920422429,0.00153267447151819,
0.00165410437577115,0.00168125421115719,0.00178334395389124,0.00187375941124646,
0.00197323383655314,0.00201750505338867,0.00209923935339125,0.00218097365339383,
0.00225620497656911,0.00232840090118059,0.00235375589562014,0.00242936444625713,
0.00244707680874984,0.00251502720952607,0.0025826808988154,0.00265019823541125,
0.00269000673785162),.UNSPECIFIED.);
#2276=B_SPLINE_CURVE_WITH_KNOTS('',3,(#94267,#94268,#94269,#94270,#94271,
#94272,#94273,#94274,#94275,#94276,#94277,#94278,#94279,#94280),
 .UNSPECIFIED.,.F.,.F.,(4,2,2,2,2,2,4),(0.,0.000499758886231802,0.000999517772463604,
0.00149927665869541,0.00199903554492721,0.00299855331739082,0.00399807108985443),
 .UNSPECIFIED.);
#2277=B_SPLINE_CURVE_WITH_KNOTS('',3,(#94317,#94318,#94319,#94320,#94321,
#94322,#94323,#94324,#94325,#94326,#94327,#94328,#94329,#94330,#94331,#94332,
#94333,#94334,#94335,#94336,#94337,#94338,#94339,#94340,#94341,#94342,#94343,
#94344),.UNSPECIFIED.,.F.,.F.,(4,3,3,3,3,3,3,3,3,4),(0.102333040030003,
0.113924927639759,0.114433131497043,0.126097619555127,0.126533222964083,
0.150443003704343,0.150733405898164,0.174788387734704,0.174933588832244,
0.199133771766325),.UNSPECIFIED.);
#2278=B_SPLINE_CURVE_WITH_KNOTS('',3,(#94345,#94346,#94347,#94348,#94349,
#94350,#94351,#94352,#94353,#94354,#94355,#94356),.UNSPECIFIED.,.F.,.F.,
(4,2,2,2,2,4),(6.16297582203915E-33,0.0239358211212684,0.0478716422425369,
0.0718074633638053,0.0837753739244396,0.0957432844850738),.UNSPECIFIED.);
#2279=B_SPLINE_CURVE_WITH_KNOTS('',3,(#94426,#94427,#94428,#94429,#94430,
#94431,#94432,#94433,#94434,#94435,#94436,#94437,#94438,#94439,#94440,#94441,
#94442,#94443,#94444,#94445,#94446,#94447,#94448,#94449,#94450,#94451,#94452,
#94453,#94454,#94455,#94456,#94457,#94458,#94459,#94460,#94461,#94462,#94463,
#94464,#94465,#94466,#94467,#94468,#94469,#94470,#94471,#94472,#94473,#94474,
#94475,#94476,#94477,#94478,#94479,#94480,#94481,#94482,#94483,#94484,#94485,
#94486,#94487,#94488,#94489,#94490,#94491,#94492,#94493,#94494,#94495,#94496,
#94497,#94498,#94499,#94500,#94501,#94502,#94503,#94504,#94505,#94506,#94507),
 .UNSPECIFIED.,.F.,.F.,(4,3,3,3,3,3,3,3,3,3,3,3,3,3,3,3,3,3,3,3,3,3,3,3,
3,3,3,4),(0.,0.000336813957898486,0.000673627915796972,0.000788294450931827,
0.000965405233874476,0.0011241828986832,0.00117000317678504,0.00133401990639404,
0.00134725583159394,0.00149483781156424,0.00153477011657144,0.00165318596336469,
0.00168406978949244,0.00178416166633809,0.00187612406911513,0.00197204161846305,
0.00202088374739094,0.00210969879246536,0.00218359020102549,0.00227031653218695,
0.00231573286521894,0.00235731345133549,0.0023805412898631,0.00245198186431492,
0.00252610468423863,0.00259198145108106,0.00265777781837003,0.00269451166318783),
 .UNSPECIFIED.);
#2280=B_SPLINE_CURVE_WITH_KNOTS('',3,(#94510,#94511,#94512,#94513,#94514,
#94515,#94516,#94517,#94518,#94519,#94520,#94521,#94522,#94523,#94524,#94525,
#94526,#94527,#94528,#94529,#94530,#94531,#94532,#94533,#94534,#94535,#94536,
#94537,#94538,#94539,#94540,#94541,#94542,#94543,#94544,#94545,#94546,#94547,
#94548,#94549,#94550,#94551,#94552,#94553,#94554,#94555,#94556,#94557,#94558,
#94559,#94560,#94561,#94562,#94563,#94564,#94565,#94566,#94567,#94568,#94569,
#94570),.UNSPECIFIED.,.F.,.F.,(4,3,3,3,3,3,3,3,3,3,3,3,3,3,3,3,3,3,3,3,
4),(0.,0.000740904719734282,0.000992426177924283,0.000994381157584888,0.00134969342662063,
0.00148863926688639,0.00149340155200891,0.00198485235584851,0.00199238270471871,
0.00229592938464614,0.00249083959038169,0.00275696980167887,0.00297727853377274,
0.00298709774675677,0.00319310808437571,0.00338978198634247,0.00347349162273481,
0.00348023433971105,0.00372496952570397,0.00395655830428439,0.00396970471169688),
 .UNSPECIFIED.);
#2281=B_SPLINE_CURVE_WITH_KNOTS('',3,(#94670,#94671,#94672,#94673,#94674,
#94675,#94676,#94677,#94678,#94679,#94680,#94681,#94682,#94683,#94684,#94685,
#94686,#94687,#94688,#94689,#94690,#94691,#94692,#94693,#94694,#94695,#94696,
#94697,#94698,#94699,#94700,#94701,#94702,#94703,#94704,#94705,#94706,#94707,
#94708,#94709,#94710,#94711,#94712,#94713,#94714,#94715),.UNSPECIFIED.,
 .F.,.F.,(4,3,3,3,3,3,3,3,3,3,3,3,3,3,3,4),(0.,0.0056591289497744,0.00848869342466156,
0.0113182578995487,0.0226365157990974,0.033954773698646,0.0396139026484203,
0.0452730315981947,0.0565912894977434,0.0679095473972921,0.0905460631963896,
0.101864321095938,0.113182578995487,0.135819094794585,0.158455610593682,
0.18109212639278),.UNSPECIFIED.);
#2282=B_SPLINE_CURVE_WITH_KNOTS('',3,(#94716,#94717,#94718,#94719,#94720,
#94721,#94722,#94723,#94724,#94725,#94726,#94727,#94728,#94729,#94730,#94731,
#94732,#94733,#94734,#94735,#94736,#94737,#94738,#94739,#94740,#94741,#94742,
#94743,#94744,#94745),.UNSPECIFIED.,.F.,.F.,(4,2,2,2,2,2,2,2,2,2,2,2,2,
2,4),(0.,0.0225170076686272,0.0450340153372545,0.0675510230058817,0.0788095268401953,
0.0900680306745089,0.112585038343136,0.12384354217745,0.135102046011763,
0.146360549846077,0.15761905368039,0.168877557514704,0.171692183473282,
0.174506809431861,0.180136061349017),.UNSPECIFIED.);
#2283=B_SPLINE_CURVE_WITH_KNOTS('',3,(#94793,#94794,#94795,#94796,#94797,
#94798,#94799,#94800,#94801,#94802,#94803,#94804,#94805,#94806,#94807,#94808,
#94809,#94810,#94811,#94812,#94813,#94814,#94815,#94816,#94817,#94818,#94819,
#94820),.UNSPECIFIED.,.F.,.F.,(4,3,3,3,3,3,3,3,3,4),(0.152124875880697,
0.156978231818529,0.158991212459818,0.164515562446826,0.165857549038938,
0.170542889642604,0.172052891500496,0.172723885618059,0.177134015604045,
0.17959022219718),.UNSPECIFIED.);
#2284=B_SPLINE_CURVE_WITH_KNOTS('',3,(#94821,#94822,#94823,#94824,#94825,
#94826,#94827,#94828,#94829,#94830),.UNSPECIFIED.,.F.,.F.,(4,2,2,2,4),(6.20633538311818E-17,
0.00753427253238126,0.0150685450647625,0.0226028175971437,0.0301370901295249),
 .UNSPECIFIED.);
#2285=B_SPLINE_CURVE_WITH_KNOTS('',3,(#94834,#94835,#94836,#94837,#94838,
#94839,#94840,#94841,#94842,#94843,#94844,#94845,#94846,#94847,#94848,#94849,
#94850,#94851,#94852,#94853,#94854,#94855,#94856,#94857,#94858,#94859,#94860,
#94861,#94862,#94863,#94864),.UNSPECIFIED.,.F.,.F.,(4,3,3,3,3,3,3,3,3,3,
4),(0.,0.0270705423331218,0.0278297418200406,0.0541410846662436,0.0556594833976957,
0.0812116269993654,0.083489181931652,0.0930720176545818,0.0947468981659263,
0.0974041311753799,0.108282169332487),.UNSPECIFIED.);
#2286=B_SPLINE_CURVE_WITH_KNOTS('',3,(#95223,#95224,#95225,#95226,#95227,
#95228,#95229,#95230,#95231,#95232,#95233,#95234,#95235,#95236,#95237,#95238,
#95239,#95240,#95241,#95242,#95243,#95244,#95245,#95246,#95247,#95248,#95249,
#95250,#95251,#95252,#95253,#95254,#95255,#95256,#95257,#95258,#95259,#95260,
#95261,#95262,#95263,#95264,#95265,#95266,#95267,#95268,#95269,#95270,#95271,
#95272,#95273,#95274,#95275,#95276,#95277,#95278,#95279,#95280,#95281,#95282,
#95283,#95284,#95285,#95286,#95287,#95288,#95289,#95290,#95291,#95292,#95293,
#95294,#95295,#95296,#95297,#95298,#95299,#95300,#95301,#95302,#95303,#95304,
#95305,#95306,#95307,#95308,#95309,#95310,#95311,#95312,#95313,#95314,#95315,
#95316,#95317,#95318,#95319,#95320,#95321,#95322,#95323,#95324,#95325,#95326,
#95327,#95328,#95329,#95330,#95331,#95332,#95333,#95334,#95335,#95336,#95337,
#95338,#95339,#95340,#95341,#95342,#95343,#95344,#95345,#95346,#95347,#95348,
#95349,#95350,#95351,#95352,#95353,#95354,#95355,#95356,#95357,#95358,#95359,
#95360,#95361,#95362,#95363,#95364,#95365,#95366,#95367,#95368,#95369,#95370,
#95371,#95372,#95373,#95374,#95375,#95376,#95377,#95378,#95379,#95380,#95381,
#95382,#95383,#95384,#95385,#95386,#95387,#95388,#95389,#95390,#95391,#95392,
#95393,#95394,#95395,#95396,#95397,#95398,#95399,#95400,#95401,#95402,#95403,
#95404,#95405,#95406,#95407,#95408,#95409,#95410,#95411,#95412,#95413,#95414,
#95415,#95416,#95417,#95418,#95419,#95420,#95421,#95422,#95423,#95424,#95425,
#95426,#95427,#95428,#95429,#95430,#95431,#95432,#95433,#95434,#95435,#95436,
#95437,#95438,#95439,#95440,#95441,#95442,#95443,#95444,#95445,#95446,#95447,
#95448,#95449,#95450,#95451,#95452,#95453,#95454,#95455,#95456,#95457,#95458,
#95459,#95460,#95461,#95462,#95463,#95464,#95465,#95466,#95467,#95468,#95469,
#95470,#95471,#95472,#95473,#95474,#95475,#95476,#95477,#95478,#95479,#95480,
#95481,#95482,#95483,#95484,#95485,#95486,#95487,#95488,#95489,#95490,#95491,
#95492,#95493,#95494,#95495,#95496,#95497,#95498,#95499,#95500,#95501,#95502,
#95503,#95504,#95505,#95506,#95507,#95508,#95509,#95510,#95511,#95512,#95513,
#95514,#95515,#95516,#95517,#95518,#95519,#95520,#95521,#95522,#95523,#95524,
#95525,#95526,#95527,#95528,#95529,#95530,#95531,#95532,#95533,#95534,#95535,
#95536,#95537,#95538,#95539,#95540,#95541,#95542,#95543,#95544,#95545,#95546,
#95547,#95548,#95549,#95550,#95551,#95552,#95553,#95554,#95555,#95556,#95557,
#95558,#95559,#95560,#95561,#95562,#95563,#95564,#95565,#95566,#95567,#95568,
#95569,#95570,#95571,#95572,#95573,#95574,#95575,#95576,#95577,#95578,#95579,
#95580,#95581,#95582,#95583,#95584,#95585,#95586,#95587,#95588,#95589,#95590,
#95591,#95592,#95593,#95594,#95595,#95596,#95597,#95598,#95599,#95600,#95601),
 .UNSPECIFIED.,.F.,.F.,(4,3,3,3,3,3,3,3,3,3,3,3,3,3,3,3,3,3,3,3,3,3,3,3,
3,3,3,3,3,3,3,3,3,3,3,3,3,3,3,3,3,3,3,3,3,3,3,3,3,3,3,3,3,3,3,3,3,3,3,3,
3,3,3,3,3,3,3,3,3,3,3,3,3,3,3,3,3,3,3,3,3,3,3,3,3,3,3,3,3,3,3,3,3,3,3,3,
3,3,3,3,3,3,3,3,3,3,3,3,3,3,3,3,3,3,3,3,3,3,3,3,3,3,3,3,3,3,4),(0.,6.3863872932077E-5,
0.000127727745864154,0.000255455491728355,0.000510910983456715,0.00102182196691343,
0.00204364393382687,0.00395866138431376,0.00408728786765373,0.00729301756278118,
0.00817457573530746,0.0109725858555631,0.0137315028763566,0.0163491514706149,
0.0188948101717854,0.0214185435272282,0.0239103168830918,0.0245237272059223,
0.0268730591163259,0.0292008190500179,0.0314952438282925,0.0326983029412297,
0.0348110563874667,0.0369036365300053,0.0389623250662188,0.0408728786765371,
0.042768391397286,0.0446313687617704,0.0464752601039315,0.0482907238196907,
0.0490474544118446,0.0507095387659064,0.0523399285160803,0.0539528973554379,
0.055587463751295,0.057222030147152,0.0585122437009908,0.0597920455722731,
0.0610597218698551,0.0613093180148057,0.0631588971570508,0.0649809589485905,
0.0653966058824594,0.0672599831382585,0.0691003001841124,0.0694838937501131,
0.0704474234477631,0.0714030435344079,0.0723553074864157,0.0733045284193833,
0.0735711816177668,0.0751256651782625,0.0766739942267828,0.0776584694854205,
0.079205276027418,0.0807467960809093,0.0817457573530743,0.0833266384402915,
0.0837894012869011,0.0846318113552563,0.0854751143109977,0.0858330452207279,
0.087426131113557,0.0890419747830855,0.0899203330883816,0.0914954629283162,
0.0931453244021594,0.0947560270353013,0.0964254679294951,0.0980949088236888,
0.100273110033121,0.102182196691342,0.103761745158836,0.105357246450793,
0.106269484558996,0.108028728367388,0.109807518376732,0.111597064178548,
0.113402460236553,0.114444060294304,0.11648770422813,0.118525317988821,
0.12058098272364,0.122618636029611,0.124886611197948,0.12716589682006,0.129461943442204,
0.130793211764918,0.134072565285742,0.137393966194065,0.138967787500226,
0.141523871414855,0.144091743727972,0.146675795174257,0.147142363235533,
0.149988497106441,0.152848718747428,0.155730243243085,0.158623557998049,
0.16153491316658,0.163491514706148,0.16674704306941,0.170024638087439,0.173314174255391,
0.176623301543565,0.179840666176763,0.183487414628456,0.187155087402397,
0.190834713137538,0.19453197048957,0.196189817647378,0.200362893445446,
0.204549745330657,0.208750511135911,0.212965303417563,0.217201799274002,
0.221450368174175,0.225717874822285,0.228888120588607,0.233645051531473,
0.238413896994045,0.243200551547939,0.245237272059222,0.250355598656634,
0.255485848524186,0.260633046954424,0.261586423529837),.UNSPECIFIED.);
#2287=B_SPLINE_CURVE_WITH_KNOTS('',3,(#95602,#95603,#95604,#95605,#95606,
#95607,#95608,#95609,#95610,#95611,#95612,#95613,#95614,#95615,#95616,#95617,
#95618,#95619,#95620,#95621,#95622,#95623,#95624,#95625,#95626,#95627,#95628,
#95629,#95630,#95631,#95632,#95633,#95634,#95635,#95636,#95637,#95638,#95639,
#95640,#95641,#95642,#95643,#95644,#95645,#95646,#95647,#95648,#95649,#95650,
#95651,#95652,#95653,#95654,#95655,#95656,#95657,#95658,#95659,#95660,#95661,
#95662,#95663,#95664,#95665,#95666,#95667,#95668,#95669,#95670,#95671,#95672,
#95673,#95674,#95675,#95676,#95677,#95678,#95679,#95680,#95681,#95682,#95683,
#95684,#95685,#95686,#95687,#95688,#95689,#95690,#95691,#95692,#95693,#95694,
#95695,#95696,#95697,#95698,#95699,#95700,#95701,#95702,#95703,#95704,#95705,
#95706,#95707,#95708,#95709,#95710,#95711,#95712,#95713,#95714,#95715,#95716,
#95717,#95718,#95719,#95720,#95721,#95722,#95723,#95724,#95725,#95726,#95727,
#95728,#95729,#95730,#95731,#95732,#95733,#95734,#95735,#95736,#95737,#95738,
#95739,#95740,#95741,#95742,#95743,#95744,#95745,#95746,#95747,#95748,#95749,
#95750,#95751,#95752,#95753,#95754,#95755,#95756,#95757,#95758,#95759,#95760,
#95761,#95762,#95763,#95764,#95765,#95766,#95767,#95768,#95769,#95770,#95771,
#95772,#95773,#95774,#95775,#95776,#95777,#95778,#95779,#95780,#95781,#95782,
#95783,#95784,#95785,#95786,#95787,#95788,#95789,#95790,#95791,#95792,#95793,
#95794,#95795,#95796,#95797,#95798,#95799,#95800,#95801,#95802,#95803,#95804,
#95805,#95806,#95807,#95808,#95809,#95810,#95811,#95812,#95813,#95814,#95815,
#95816,#95817,#95818,#95819,#95820,#95821,#95822,#95823,#95824,#95825,#95826,
#95827,#95828,#95829,#95830,#95831,#95832,#95833,#95834,#95835,#95836,#95837,
#95838,#95839,#95840,#95841,#95842,#95843,#95844,#95845,#95846,#95847,#95848,
#95849,#95850,#95851,#95852,#95853,#95854,#95855,#95856,#95857,#95858,#95859,
#95860,#95861,#95862,#95863,#95864,#95865,#95866,#95867,#95868,#95869,#95870,
#95871,#95872,#95873,#95874,#95875,#95876,#95877,#95878,#95879,#95880,#95881,
#95882,#95883,#95884,#95885,#95886,#95887,#95888,#95889,#95890,#95891,#95892,
#95893,#95894,#95895,#95896),.UNSPECIFIED.,.F.,.F.,(4,3,3,3,3,3,3,3,3,3,
3,3,3,3,3,3,3,3,3,3,3,3,3,3,3,3,3,3,3,3,3,3,3,3,3,3,3,3,3,3,3,3,3,3,3,3,
3,3,3,3,3,3,3,3,3,3,3,3,3,3,3,3,3,3,3,3,3,3,3,3,3,3,3,3,3,3,3,3,3,3,3,3,
3,3,3,3,3,3,3,3,3,3,3,3,3,3,3,3,4),(0.1827680134667,0.1837097763468,0.183788376881043,
0.1848114574746,0.185834538068157,0.186450425254853,0.187665846450934,0.187847001796835,
0.189183047116277,0.189834967005636,0.190132837043007,0.191684431947844,
0.193343346752475,0.193763845867017,0.195709116538605,0.197497660619314,
0.197664069537048,0.199428846362787,0.201037120742463,0.201573334879782,
0.203004814586262,0.204361491262147,0.20486248419562,0.205540372303086,
0.206882660228423,0.208197711507143,0.208544895983774,0.209619358449715,
0.211014679742743,0.212227307771927,0.213385155422244,0.213865693507827,
0.214928865854929,0.215909719560081,0.217074197422792,0.218129218846608,
0.218238675285504,0.219212653160603,0.219592131348234,0.220477427707672,
0.221340257489479,0.222173866721717,0.222523667053981,0.223274543136388,
0.224537890016825,0.225767044721813,0.226557950821135,0.226956954924541,
0.227791691781628,0.228649200114669,0.228798160818618,0.229998539586015,
0.230362152850368,0.230639366712694,0.231774149191568,0.232961266775828,
0.234037876499932,0.234321778500848,0.235846026650995,0.236162984394925,
0.236957113549215,0.237648448805943,0.238004190289001,0.238546786721677,
0.23892479323604,0.239291967104069,0.239471814281867,0.239740665904253,
0.239845396183078,0.240033003014875,0.240209425489808,0.240305697656597,
0.240424316420931,0.240595157775524,0.240755298158673,0.240765999130116,
0.240868186286462,0.240934658995761,0.241007569397729,0.241076617911449,
0.241145342671251,0.241214156232952,0.241226300603636,0.241227953670809,
0.241269769601594,0.241310756863425,0.241351708284969,0.241393277997084,
0.241408856129991,0.24144045251339,0.241456451340395,0.241496529999511,
0.241528523246559,0.241561898975136,0.241571526708775,0.241603871867202,
0.241636532552263,0.241670569204549,0.241686602077155),.UNSPECIFIED.);
#2288=B_SPLINE_CURVE_WITH_KNOTS('',3,(#96180,#96181,#96182,#96183,#96184,
#96185,#96186,#96187,#96188,#96189,#96190,#96191,#96192,#96193,#96194,#96195,
#96196,#96197,#96198,#96199,#96200,#96201,#96202,#96203,#96204,#96205,#96206,
#96207,#96208,#96209,#96210,#96211,#96212,#96213,#96214,#96215,#96216,#96217,
#96218,#96219,#96220,#96221,#96222,#96223,#96224,#96225,#96226,#96227,#96228,
#96229,#96230,#96231,#96232,#96233,#96234,#96235,#96236,#96237),
 .UNSPECIFIED.,.F.,.F.,(4,2,2,2,2,2,2,2,2,2,2,2,2,2,2,2,2,2,2,2,2,2,2,2,
2,2,2,2,4),(0.152635115845842,0.155960973078063,0.159286830310285,0.165938544774729,
0.172590259239172,0.175916116471394,0.179241973703615,0.185893688168059,
0.18755661678417,0.189219545400281,0.192545402632502,0.199197117096946,
0.202522974329168,0.20584883156139,0.212500546025834,0.219152260490277,
0.225803974954721,0.232455689419165,0.239107403883608,0.245759118348052,
0.252410832812496,0.255736690044718,0.257399618660829,0.258231082968884,
0.258646815122912,0.258854681199926,0.258958614238433,0.259010580757686,
0.25906254727694),.UNSPECIFIED.);
#2289=B_SPLINE_CURVE_WITH_KNOTS('',3,(#96238,#96239,#96240,#96241,#96242,
#96243,#96244,#96245,#96246,#96247,#96248,#96249,#96250,#96251,#96252,#96253,
#96254,#96255,#96256,#96257,#96258,#96259,#96260,#96261,#96262,#96263),
 .UNSPECIFIED.,.F.,.F.,(4,2,2,2,2,2,2,2,2,2,2,2,4),(0.155674698583529,0.158344544285759,
0.161014389987988,0.166354081392447,0.171693772796906,0.174363618499135,
0.177033464201365,0.182373155605823,0.185043001308053,0.186377924159168,
0.187712847010282,0.193052538414741,0.1983922298192),.UNSPECIFIED.);
#2290=B_SPLINE_CURVE_WITH_KNOTS('',3,(#96265,#96266,#96267,#96268,#96269,
#96270,#96271,#96272,#96273,#96274,#96275,#96276,#96277,#96278,#96279,#96280,
#96281,#96282,#96283,#96284,#96285,#96286,#96287,#96288,#96289,#96290,#96291,
#96292,#96293,#96294,#96295,#96296,#96297,#96298,#96299,#96300,#96301,#96302,
#96303,#96304,#96305,#96306,#96307,#96308,#96309,#96310,#96311,#96312,#96313,
#96314,#96315,#96316,#96317,#96318,#96319,#96320,#96321,#96322,#96323,#96324,
#96325,#96326,#96327,#96328,#96329,#96330,#96331,#96332,#96333,#96334,#96335,
#96336,#96337,#96338,#96339,#96340,#96341,#96342,#96343,#96344,#96345,#96346,
#96347,#96348,#96349,#96350,#96351,#96352,#96353,#96354,#96355,#96356,#96357,
#96358,#96359,#96360,#96361,#96362,#96363,#96364,#96365,#96366,#96367,#96368,
#96369,#96370,#96371,#96372,#96373,#96374,#96375,#96376,#96377,#96378,#96379,
#96380,#96381,#96382,#96383,#96384,#96385,#96386,#96387,#96388,#96389,#96390,
#96391,#96392,#96393,#96394,#96395,#96396,#96397,#96398,#96399,#96400,#96401,
#96402,#96403,#96404,#96405,#96406,#96407,#96408,#96409,#96410,#96411,#96412,
#96413,#96414,#96415,#96416,#96417,#96418,#96419,#96420,#96421,#96422,#96423,
#96424,#96425,#96426,#96427,#96428,#96429,#96430,#96431,#96432,#96433,#96434,
#96435,#96436,#96437,#96438,#96439,#96440,#96441,#96442,#96443,#96444,#96445,
#96446,#96447,#96448,#96449,#96450,#96451,#96452,#96453,#96454,#96455,#96456,
#96457,#96458,#96459,#96460,#96461,#96462,#96463,#96464,#96465,#96466,#96467,
#96468,#96469,#96470,#96471,#96472,#96473,#96474,#96475,#96476,#96477,#96478,
#96479,#96480,#96481,#96482,#96483,#96484,#96485,#96486,#96487,#96488,#96489,
#96490,#96491,#96492,#96493,#96494,#96495,#96496,#96497,#96498,#96499,#96500,
#96501,#96502,#96503,#96504,#96505,#96506,#96507,#96508,#96509,#96510,#96511,
#96512,#96513,#96514,#96515,#96516,#96517,#96518,#96519,#96520,#96521,#96522,
#96523,#96524,#96525,#96526,#96527,#96528,#96529,#96530,#96531,#96532,#96533,
#96534,#96535,#96536,#96537,#96538,#96539,#96540,#96541,#96542,#96543,#96544),
 .UNSPECIFIED.,.F.,.F.,(4,3,3,3,3,3,3,3,3,3,3,3,3,3,3,3,3,3,3,3,3,3,3,3,
3,3,3,3,3,3,3,3,3,3,3,3,3,3,3,3,3,3,3,3,3,3,3,3,3,3,3,3,3,3,3,3,3,3,3,3,
3,3,3,3,3,3,3,3,3,3,3,3,3,3,3,3,3,3,3,3,3,3,3,3,3,3,3,3,3,3,3,3,3,4),(-5.99999997357394E-8,
4.38639073236214E-5,9.45970100728408E-5,0.000143126291908774,0.000186981185804612,
0.000191655573744707,0.000238520430505583,0.000270886863781888,0.000302536470316016,
0.000334074906589417,0.000343491009070944,0.000385878567015112,0.000429046783158217,
0.000477100861010902,0.00053209145428618,0.000565495260578844,0.000644015141512509,
0.000724439418075443,0.000806876778552401,0.00089462570938181,0.000937236773082297,
0.000954261722021523,0.00108689662222606,0.00122328225306106,0.00136816856359854,
0.00143142258303214,0.00159703908410309,0.00182842102722904,0.00190858344404277,
0.00248987825450814,0.00283814937392281,0.002862905166064,0.0032727783285689,
0.00369274471980585,0.00381722688808523,0.00453462896213004,0.0052489820951574,
0.00572587033212766,0.00670618958050466,0.00763451377617009,0.00765380603805355,
0.00886989494599809,0.0100859838539426,0.0112427315510617,0.0114518006642549,
0.012508327049095,0.0135431991630298,0.01455216354716,0.0150992258566461,
0.0152690875523398,0.0165866437037344,0.0177273665533294,0.0189215940108622,
0.0190863744404246,0.0201406885427821,0.0204648227868727,0.0213971958834355,
0.0223802573823971,0.0229036613285095,0.0233008123087915,0.0243620918098927,
0.0255722010062106,0.0261934427647077,0.0267209482165943,0.0279206208184966,
0.0290918341054633,0.0303053741212861,0.0305382351046792,0.0319468973072417,
0.0336437380028234,0.034355521992764,0.0357530268846585,0.0371798114132647,
0.0374722459149548,0.0381728088808489,0.0396630234973826,0.0412451663134016,
0.0428139984561576,0.0446963350828273,0.0458073826570186,0.0478860358725533,
0.0480757277027665,0.0499768000329801,0.0516885463137229,0.0533471197081705,
0.0534419564331883,0.0548581550144974,0.0560142987512958,0.0572592433212732,
0.058412277998669,0.058721495098687,0.0597401974867129,0.0607272993377569,
0.0610765302093581),.UNSPECIFIED.);
#2291=B_SPLINE_CURVE_WITH_KNOTS('',3,(#96666,#96667,#96668,#96669,#96670,
#96671,#96672,#96673,#96674,#96675,#96676,#96677,#96678,#96679,#96680,#96681,
#96682,#96683,#96684,#96685,#96686,#96687,#96688,#96689,#96690,#96691,#96692,
#96693,#96694,#96695,#96696,#96697,#96698,#96699,#96700,#96701,#96702,#96703,
#96704,#96705,#96706,#96707,#96708,#96709,#96710,#96711,#96712,#96713,#96714,
#96715,#96716,#96717,#96718,#96719,#96720,#96721,#96722,#96723,#96724,#96725,
#96726,#96727,#96728,#96729,#96730,#96731,#96732,#96733,#96734,#96735,#96736,
#96737,#96738,#96739,#96740,#96741,#96742,#96743,#96744,#96745,#96746,#96747),
 .UNSPECIFIED.,.F.,.F.,(4,3,3,3,3,3,3,3,3,3,3,3,3,3,3,3,3,3,3,3,3,3,3,3,
3,3,3,4),(0.,0.00184488703262337,0.00351661220106541,0.00518833736950746,
0.00531158003263634,0.00840640040076616,0.0103766747390149,0.0106295342414134,
0.0119592317531148,0.0129708434237686,0.0132884192546281,0.0148093646562269,
0.0155650121085223,0.0159474718369938,0.0207533494780297,0.0212654877795165,
0.0225952604584355,0.0233475181627834,0.0239242929808601,0.0254892764424578,
0.025941686847537,0.0265833716869893,0.0311300242170443,0.0319013210682786,
0.0363183615865516,0.0372192739307114,0.041056774429001,0.0415066989560588),
 .UNSPECIFIED.);
#2292=B_SPLINE_CURVE_WITH_KNOTS('',3,(#96787,#96788,#96789,#96790,#96791,
#96792,#96793,#96794,#96795,#96796,#96797,#96798),.UNSPECIFIED.,.F.,.F.,
(4,2,2,2,2,4),(0.0690311453325833,0.082781586176973,0.0965320270213627,
0.124032908710142,0.151533790398921,0.179034672087701),.UNSPECIFIED.);
#2293=B_SPLINE_CURVE_WITH_KNOTS('',3,(#96843,#96844,#96845,#96846,#96847,
#96848,#96849,#96850,#96851,#96852,#96853,#96854,#96855,#96856,#96857,#96858,
#96859,#96860,#96861,#96862,#96863,#96864,#96865,#96866,#96867,#96868,#96869,
#96870,#96871,#96872,#96873,#96874,#96875,#96876,#96877,#96878,#96879,#96880,
#96881,#96882,#96883,#96884,#96885,#96886,#96887,#96888,#96889,#96890,#96891,
#96892,#96893,#96894,#96895,#96896,#96897,#96898,#96899,#96900),
 .UNSPECIFIED.,.F.,.F.,(4,3,3,3,3,3,3,3,3,3,3,3,3,3,3,3,3,3,3,4),(6.16297582203915E-33,
0.0119699703913031,0.022367524718284,0.0239399407826063,0.0240424455537452,
0.0334984644888833,0.0423205469418825,0.0479759496178658,0.0480848911074903,
0.055447210326906,0.0600524042179919,0.0667007954868039,0.0721273366612355,
0.0721894789266184,0.0776788850245133,0.0829468346892967,0.0844114653878106,
0.0892194993938014,0.0938779179888398,0.0961697822083357),.UNSPECIFIED.);
#2294=B_SPLINE_CURVE_WITH_KNOTS('',3,(#97323,#97324,#97325,#97326,#97327,
#97328,#97329,#97330,#97331,#97332,#97333,#97334,#97335,#97336,#97337,#97338,
#97339,#97340,#97341,#97342,#97343,#97344,#97345,#97346,#97347,#97348,#97349,
#97350,#97351,#97352,#97353,#97354,#97355,#97356,#97357,#97358,#97359),
 .UNSPECIFIED.,.F.,.F.,(4,3,3,3,3,3,3,3,3,3,3,3,4),(-2.78934132800095E-5,
0.00121588438262122,0.00221227975556897,0.00221609308686091,0.00384184723093993,
0.00445245292441795,0.00445837553689522,0.00611808335700871,0.00669262609326693,
0.00669744820440185,0.00781574891708038,0.00880510804235627,0.00893279926211591),
 .UNSPECIFIED.);
#2295=B_SPLINE_CURVE_WITH_KNOTS('',3,(#97363,#97364,#97365,#97366,#97367,
#97368,#97369,#97370,#97371,#97372,#97373,#97374,#97375,#97376,#97377,#97378,
#97379,#97380,#97381,#97382,#97383,#97384,#97385,#97386,#97387,#97388,#97389,
#97390,#97391,#97392,#97393,#97394,#97395,#97396,#97397,#97398,#97399,#97400,
#97401,#97402,#97403,#97404,#97405),.UNSPECIFIED.,.F.,.F.,(4,3,3,3,3,3,
3,3,3,3,3,3,3,3,4),(0.,0.000981863058810054,0.00110848267565544,0.00221820625791767,
0.00222304486987606,0.00387027745216958,0.00444010558372466,0.00444608973975211,
0.00605994093001663,0.00666519007157424,0.00666913460962817,0.00778065704456617,
0.00833641826203515,0.00866716277185096,0.00889217947950412),
 .UNSPECIFIED.);
#2296=B_SPLINE_CURVE_WITH_KNOTS('',3,(#97603,#97604,#97605,#97606,#97607,
#97608,#97609,#97610,#97611,#97612,#97613,#97614,#97615,#97616,#97617,#97618,
#97619,#97620,#97621,#97622,#97623,#97624,#97625,#97626,#97627,#97628,#97629,
#97630,#97631,#97632,#97633,#97634,#97635,#97636,#97637,#97638,#97639,#97640,
#97641,#97642,#97643,#97644,#97645,#97646,#97647,#97648,#97649,#97650,#97651,
#97652,#97653,#97654,#97655,#97656,#97657,#97658,#97659,#97660,#97661,#97662,
#97663,#97664,#97665,#97666,#97667,#97668,#97669,#97670,#97671,#97672,#97673,
#97674,#97675,#97676,#97677,#97678,#97679,#97680,#97681,#97682,#97683,#97684,
#97685,#97686,#97687,#97688,#97689,#97690,#97691,#97692,#97693,#97694,#97695,
#97696,#97697,#97698,#97699,#97700,#97701,#97702,#97703,#97704,#97705,#97706,
#97707,#97708,#97709,#97710,#97711,#97712,#97713,#97714,#97715,#97716,#97717,
#97718,#97719,#97720,#97721,#97722,#97723,#97724,#97725,#97726,#97727,#97728,
#97729,#97730,#97731,#97732,#97733,#97734,#97735,#97736,#97737,#97738,#97739,
#97740,#97741,#97742,#97743,#97744,#97745,#97746,#97747,#97748,#97749,#97750,
#97751,#97752,#97753,#97754,#97755,#97756,#97757,#97758,#97759,#97760,#97761,
#97762,#97763,#97764,#97765,#97766,#97767,#97768,#97769,#97770,#97771,#97772,
#97773,#97774,#97775,#97776,#97777),.UNSPECIFIED.,.F.,.F.,(4,3,3,3,3,3,
3,3,3,3,3,3,3,3,3,3,3,3,3,3,3,3,3,3,3,3,3,3,3,3,3,3,3,3,3,3,3,3,3,3,3,3,
3,3,3,3,3,3,3,3,3,3,3,3,3,3,3,3,4),(0.,7.00136229228457E-5,0.000880271419196664,
0.0019798005518509,0.00250406869828295,0.00300266268960072,0.00331712911283043,
0.00413059578319972,0.00532772256795508,0.0057574742158991,0.00600532537920143,
0.00738304200408563,0.00900794430850163,0.00900798806880215,0.0112899391799351,
0.0120106507584029,0.012257034623011,0.0135119821032032,0.0138815868497288,
0.0147250110536992,0.0150133134480036,0.0155067088258864,0.0168452146168024,
0.0180159761376041,0.0187586550708965,0.0195173074824044,0.0203855296680284,
0.0210186388272047,0.0220135800001955,0.0236425023713016,0.0240213015168053,
0.0244570699511878,0.0252717472664166,0.0255226328616056,0.0270239642064059,
0.0285252955512062,0.0285300848199135,0.0293428874314649,0.0300266268960065,
0.0301588925271162,0.0313458910919412,0.0317871551652159,0.033029289585607,
0.0334140923804464,0.0345306209304072,0.0350404780787164,0.0360319522752075,
0.0366663282699642,0.0375332836200077,0.0382915981957547,0.039034614964808,
0.0412861444649818,0.0415405183457811,0.0420372776544085,0.0431651404778179,
0.0447901356468785,0.045039940344009,0.0470573761230531,0.0480426030336095),
 .UNSPECIFIED.);
#2297=B_SPLINE_CURVE_WITH_KNOTS('',3,(#97781,#97782,#97783,#97784,#97785,
#97786,#97787,#97788,#97789,#97790,#97791,#97792,#97793,#97794,#97795,#97796,
#97797,#97798,#97799,#97800,#97801,#97802,#97803,#97804,#97805,#97806,#97807,
#97808,#97809,#97810,#97811,#97812,#97813,#97814,#97815,#97816,#97817,#97818,
#97819,#97820,#97821,#97822,#97823,#97824,#97825,#97826,#97827,#97828,#97829,
#97830,#97831,#97832,#97833,#97834,#97835,#97836,#97837,#97838),
 .UNSPECIFIED.,.F.,.F.,(4,2,2,2,2,2,2,2,2,2,2,2,2,2,2,2,2,2,2,2,2,2,2,2,
2,2,2,2,4),(0.0557463281926296,0.0589772878231815,0.0605927676384573,0.0622082474537332,
0.0654392070842851,0.067054686899561,0.068670166714837,0.0702856465301129,
0.0719011263453888,0.0735166061606648,0.0751320859759407,0.0783630456064926,
0.0791707855141306,0.0799785254217686,0.0815940052370446,0.0832094850523206,
0.0848249648675966,0.0880559244981484,0.0896714043134243,0.0912868841287003,
0.0945178437592521,0.096133323574528,0.0977488033898038,0.0993642832050797,
0.100979763020356,0.102595242835631,0.103402982743269,0.104210722650907,
0.107441682281459),.UNSPECIFIED.);
#2298=B_SPLINE_CURVE_WITH_KNOTS('',3,(#97841,#97842,#97843,#97844,#97845,
#97846,#97847,#97848),.UNSPECIFIED.,.F.,.F.,(4,2,2,4),(0.100097362857501,
0.102091718402555,0.103088896175082,0.104086073947609),.UNSPECIFIED.);
#2299=B_SPLINE_CURVE_WITH_KNOTS('',3,(#98007,#98008,#98009,#98010,#98011,
#98012,#98013,#98014,#98015,#98016,#98017,#98018,#98019,#98020,#98021,#98022,
#98023,#98024,#98025,#98026,#98027,#98028,#98029,#98030,#98031,#98032,#98033,
#98034,#98035,#98036,#98037,#98038,#98039,#98040,#98041,#98042,#98043,#98044,
#98045,#98046,#98047,#98048,#98049,#98050,#98051,#98052,#98053,#98054,#98055,
#98056,#98057,#98058,#98059,#98060),.UNSPECIFIED.,.F.,.F.,(4,2,2,2,2,2,
2,2,2,2,2,2,2,2,2,2,2,2,2,2,2,2,2,2,2,2,4),(0.,0.00156341081501294,0.00312682163002588,
0.00469023244503882,0.00625364326005176,0.00938046489007764,0.0109438757050905,
0.0125072865201034,0.0156341081501293,0.0171975189651422,0.0187609297801551,
0.021887751410181,0.0226694568176875,0.023451162225194,0.0250145730402071,
0.0265779838552202,0.0281413946702332,0.0312682163002594,0.0328316271152726,
0.0343950379302857,0.037521859560312,0.0406486811903383,0.0422120920053514,
0.0437755028203645,0.0469023244503908,0.0484657352654039,0.050029146080417),
 .UNSPECIFIED.);
#2300=B_SPLINE_CURVE_WITH_KNOTS('',3,(#98064,#98065,#98066,#98067,#98068,
#98069,#98070,#98071,#98072,#98073,#98074,#98075,#98076,#98077,#98078,#98079,
#98080,#98081,#98082,#98083,#98084,#98085,#98086,#98087,#98088,#98089,#98090,
#98091,#98092,#98093,#98094,#98095,#98096,#98097,#98098,#98099,#98100,#98101,
#98102,#98103,#98104,#98105,#98106,#98107,#98108,#98109,#98110,#98111,#98112,
#98113,#98114,#98115,#98116,#98117,#98118,#98119,#98120,#98121,#98122,#98123,
#98124,#98125,#98126,#98127,#98128,#98129,#98130,#98131,#98132,#98133,#98134,
#98135,#98136,#98137,#98138,#98139,#98140,#98141,#98142,#98143,#98144,#98145,
#98146,#98147,#98148,#98149,#98150,#98151,#98152,#98153,#98154,#98155,#98156,
#98157,#98158,#98159,#98160,#98161,#98162,#98163,#98164,#98165,#98166,#98167,
#98168,#98169,#98170,#98171,#98172,#98173,#98174,#98175,#98176,#98177,#98178,
#98179,#98180,#98181,#98182,#98183,#98184,#98185,#98186,#98187,#98188,#98189,
#98190,#98191,#98192,#98193,#98194,#98195,#98196,#98197,#98198,#98199,#98200,
#98201,#98202,#98203,#98204,#98205,#98206,#98207,#98208,#98209,#98210,#98211,
#98212,#98213,#98214,#98215,#98216,#98217,#98218,#98219,#98220,#98221,#98222,
#98223,#98224,#98225,#98226,#98227,#98228,#98229,#98230,#98231,#98232,#98233,
#98234,#98235,#98236,#98237,#98238,#98239,#98240,#98241,#98242,#98243,#98244,
#98245,#98246,#98247,#98248,#98249,#98250,#98251,#98252,#98253,#98254,#98255,
#98256,#98257,#98258,#98259,#98260,#98261,#98262,#98263,#98264,#98265,#98266,
#98267,#98268,#98269,#98270,#98271,#98272,#98273,#98274,#98275,#98276,#98277,
#98278,#98279,#98280,#98281,#98282,#98283,#98284,#98285,#98286),
 .UNSPECIFIED.,.F.,.F.,(4,3,3,3,3,3,3,3,3,3,3,3,3,3,3,3,3,3,3,3,3,3,3,3,
3,3,3,3,3,3,3,3,3,3,3,3,3,3,3,3,3,3,3,3,3,3,3,3,3,3,3,3,3,3,3,3,3,3,3,3,
3,3,3,3,3,3,3,3,3,3,3,3,3,3,4),(0.0536197899396224,0.0552276244004005,0.0552355709876449,
0.0564636360418572,0.056836730186764,0.0568513520356673,0.0585010989847782,
0.0600604289236084,0.0600829141317123,0.0616747375677009,0.0616986951797348,
0.0631694062564205,0.0632905117196436,0.0633144762277572,0.0653332916269836,
0.0665264501713466,0.0665460383238021,0.0680226211562579,0.0681465613676236,
0.0681618193718244,0.06976797630888,0.0697776004198467,0.0713906714255839,
0.0713933814678691,0.0730091625158914,0.0730146093723317,0.0752607556615613,
0.0762407246119361,0.0762648548190899,0.0777231476585644,0.0778565056599585,
0.0778906973850273,0.0791924472927823,0.0794722867079808,0.0795162256569394,
0.0810880677560031,0.0811414459847621,0.0823878645715334,0.0827038488040255,
0.082765970222281,0.0844200933214001,0.0859354109000701,0.0860114915248442,
0.0868961672851169,0.0875511919480923,0.0887466775681185,0.0891669729961145,
0.0892519026800105,0.0907827540441368,0.090869989342466,0.0922381233776412,
0.092398535092159,0.0924866314778508,0.0942502320947687,0.0956300971882036,
0.0957154955381664,0.0971616980108514,0.0972458782362259,0.0973274461005371,
0.0983010085687395,0.0988616592842482,0.0989376222126474,0.0999829246183408,
0.10047744033227,0.100546243852972,0.101152494922683,0.101724341209355,
0.102093221380293,0.102150357244739,0.102702522250809,0.102901111904304,
0.103522312960999,0.103709002428315,0.104937728080031,0.105324783476337),
 .UNSPECIFIED.);
#2301=B_SPLINE_CURVE_WITH_KNOTS('',3,(#98289,#98290,#98291,#98292,#98293,
#98294,#98295,#98296,#98297,#98298),.UNSPECIFIED.,.F.,.F.,(4,3,3,4),(0.101994009991496,
0.102941137438368,0.103427904624697,0.103888264885239),.UNSPECIFIED.);
#2302=B_SPLINE_CURVE_WITH_KNOTS('',3,(#98451,#98452,#98453,#98454,#98455,
#98456,#98457,#98458,#98459,#98460,#98461,#98462,#98463,#98464,#98465,#98466,
#98467,#98468,#98469,#98470,#98471,#98472,#98473,#98474,#98475,#98476,#98477,
#98478,#98479,#98480,#98481,#98482,#98483,#98484,#98485,#98486,#98487,#98488,
#98489,#98490,#98491,#98492,#98493,#98494,#98495,#98496,#98497,#98498,#98499,
#98500,#98501,#98502,#98503,#98504,#98505,#98506,#98507,#98508,#98509,#98510,
#98511,#98512,#98513,#98514,#98515,#98516,#98517,#98518,#98519,#98520,#98521,
#98522,#98523,#98524,#98525,#98526,#98527,#98528,#98529,#98530,#98531,#98532,
#98533,#98534,#98535,#98536,#98537,#98538,#98539,#98540,#98541,#98542,#98543,
#98544,#98545,#98546,#98547,#98548,#98549,#98550,#98551,#98552,#98553,#98554,
#98555,#98556,#98557,#98558,#98559,#98560,#98561,#98562,#98563,#98564,#98565,
#98566,#98567,#98568,#98569,#98570,#98571,#98572,#98573,#98574,#98575,#98576,
#98577,#98578,#98579,#98580,#98581,#98582,#98583,#98584,#98585,#98586,#98587,
#98588,#98589,#98590,#98591,#98592,#98593,#98594,#98595,#98596,#98597,#98598,
#98599,#98600,#98601,#98602,#98603,#98604,#98605,#98606,#98607,#98608,#98609,
#98610,#98611,#98612,#98613,#98614,#98615,#98616,#98617,#98618,#98619,#98620,
#98621,#98622,#98623,#98624,#98625,#98626,#98627,#98628,#98629,#98630,#98631,
#98632,#98633,#98634,#98635,#98636,#98637,#98638,#98639,#98640,#98641,#98642,
#98643,#98644,#98645,#98646,#98647,#98648,#98649,#98650,#98651,#98652,#98653,
#98654,#98655,#98656,#98657,#98658,#98659,#98660,#98661,#98662,#98663,#98664),
 .UNSPECIFIED.,.F.,.F.,(4,3,3,3,3,3,3,3,3,3,3,3,3,3,3,3,3,3,3,3,3,3,3,3,
3,3,3,3,3,3,3,3,3,3,3,3,3,3,3,3,3,3,3,3,3,3,3,3,3,3,3,3,3,3,3,3,3,3,3,3,
3,3,3,3,3,3,3,3,3,3,3,4),(0.,0.000919480979115724,0.00186665391132834,0.00222303890370072,
0.00246023501007185,0.00308006741790905,0.00345996891983424,0.00369035251510777,
0.00469778641362988,0.00492047002014368,0.00577875096527111,0.00593619564291903,
0.0061505875251796,0.00691217011934619,0.00717505541494653,0.00738070503021552,
0.00841742521904112,0.00946182449544975,0.00965322408999175,0.00984094004028725,
0.0105271968013281,0.0108924604402717,0.0110710575453231,0.0121313588744037,
0.012301175050359,0.0135614282722711,0.014608084951402,0.0147614100604307,
0.0155427428163806,0.0158457881834858,0.0159915275654665,0.0170831200839182,
0.0172216450705023,0.0180163683085217,0.0183201098374356,0.0184517625755382,
0.0191739816007994,0.0195568018131331,0.019681880080574,0.0208560722381215,
0.022030264395669,0.0221421150906457,0.0229078739324747,0.0232673524625759,
0.0233722325956815,0.0245048134750372,0.0246023501007174,0.0254360756730852,
0.0257427490373535,0.0258324676057532,0.026634352472142,0.0269811460780055,
0.027062585110789,0.0284787188530985,0.0294588729843419,0.0295228201208608,
0.0310014861472265,0.0319371442892161,0.0319830551309325,0.0335148785821422,
0.0344145418676413,0.0344432901410042,0.0353749506244627,0.0356525636344977,
0.0356734076460401,0.0368901184213511,0.036903525151076,0.0375185839035939,
0.0381336426561119,0.0385671407304436,0.0389938437394034,0.0393637601611478),
 .UNSPECIFIED.);
#2303=B_SPLINE_CURVE_WITH_KNOTS('',3,(#98668,#98669,#98670,#98671,#98672,
#98673,#98674,#98675,#98676,#98677,#98678,#98679,#98680,#98681,#98682,#98683,
#98684,#98685,#98686,#98687,#98688,#98689,#98690,#98691,#98692,#98693,#98694,
#98695,#98696,#98697,#98698,#98699,#98700,#98701,#98702,#98703,#98704,#98705,
#98706,#98707,#98708,#98709,#98710,#98711,#98712,#98713,#98714,#98715,#98716,
#98717,#98718,#98719,#98720,#98721,#98722,#98723,#98724,#98725,#98726,#98727,
#98728,#98729,#98730,#98731,#98732,#98733,#98734,#98735,#98736,#98737,#98738,
#98739,#98740,#98741,#98742,#98743,#98744,#98745,#98746,#98747,#98748,#98749,
#98750,#98751,#98752,#98753,#98754,#98755,#98756,#98757,#98758,#98759,#98760,
#98761,#98762,#98763,#98764,#98765,#98766,#98767,#98768,#98769,#98770,#98771,
#98772,#98773,#98774,#98775,#98776,#98777,#98778,#98779,#98780,#98781,#98782,
#98783,#98784,#98785,#98786,#98787,#98788,#98789,#98790,#98791,#98792,#98793,
#98794,#98795,#98796,#98797,#98798,#98799,#98800,#98801,#98802,#98803,#98804,
#98805,#98806,#98807,#98808,#98809,#98810,#98811,#98812,#98813,#98814,#98815,
#98816,#98817,#98818,#98819,#98820,#98821,#98822,#98823,#98824,#98825,#98826,
#98827,#98828,#98829,#98830,#98831,#98832,#98833,#98834,#98835,#98836,#98837,
#98838,#98839,#98840,#98841,#98842,#98843,#98844,#98845,#98846,#98847,#98848,
#98849,#98850,#98851,#98852,#98853,#98854,#98855,#98856,#98857,#98858,#98859,
#98860,#98861,#98862,#98863,#98864,#98865,#98866),.UNSPECIFIED.,.F.,.F.,
(4,3,3,3,3,3,3,3,3,3,3,3,3,3,3,3,3,3,3,3,3,3,3,3,3,3,3,3,3,3,3,3,3,3,3,
3,3,3,3,3,3,3,3,3,3,3,3,3,3,3,3,3,3,3,3,3,3,3,3,3,3,3,3,3,3,3,4),(0.0415609574076441,
0.0419999079181991,0.0424456108255438,0.0428514400237989,0.0434891733075762,
0.0441269065913535,0.0441419226399537,0.0454112381061315,0.0454324052561084,
0.0465323604471359,0.0466965822688831,0.0467228878722632,0.0484820040278885,
0.0492715033675918,0.0493038531045728,0.0507359116685006,0.0518516607057079,
0.0518848183368824,0.0535408116929441,0.0544369446773842,0.054465783569192,
0.0555110612925173,0.0557314168323167,0.0557562661853469,0.0570268987744937,
0.0570467488015017,0.0580899941195753,0.0583234009749456,0.0583372314176566,
0.0593028016533825,0.0596206777396424,0.0596277140338114,0.0622086792661211,
0.0622163187211141,0.063499161882276,0.0635142754825525,0.0647896444984309,
0.0648116296745799,0.0660801271145858,0.0661083966471777,0.0673706097307407,
0.0674045134523431,0.0688635319843868,0.0699515749630503,0.0699933139595394,
0.0712420575792051,0.0712859635838355,0.0722808578694621,0.0725325401953599,
0.0725774037566074,0.0740349703453863,0.0751135054276695,0.0751563211290189,
0.0761837854504516,0.0764039880438243,0.0764437283836802,0.07758048125962,
0.0776944706599792,0.0777298862469095,0.078984953276134,0.0790147568862244,
0.0801773798799933,0.0802754358922888,0.0802979121042526,0.0811942832430352,
0.082067096754397,0.0828564011245984),.UNSPECIFIED.);
#2304=B_SPLINE_CURVE_WITH_KNOTS('',3,(#98873,#98874,#98875,#98876,#98877,
#98878,#98879,#98880,#98881,#98882,#98883,#98884,#98885,#98886,#98887,#98888,
#98889,#98890,#98891,#98892,#98893,#98894,#98895,#98896,#98897,#98898),
 .UNSPECIFIED.,.F.,.F.,(4,2,2,2,2,2,2,2,2,2,2,2,4),(0.,0.24105520274149,
0.482110405482979,0.964220810965958,1.44228868010388,1.68132261467284,1.9203565492418,
2.15939048381076,2.39842441837972,2.87649228751764,3.35860269300062,3.59965789574211,
3.8407130984836),.UNSPECIFIED.);
#2305=B_SPLINE_CURVE_WITH_KNOTS('',3,(#98902,#98903,#98904,#98905,#98906,
#98907,#98908,#98909,#98910,#98911,#98912,#98913,#98914,#98915,#98916,#98917,
#98918,#98919,#98920,#98921,#98922,#98923,#98924,#98925,#98926,#98927,#98928,
#98929,#98930,#98931,#98932,#98933,#98934,#98935,#98936,#98937,#98938,#98939,
#98940,#98941,#98942,#98943,#98944,#98945,#98946,#98947,#98948,#98949,#98950,
#98951,#98952,#98953),.UNSPECIFIED.,.F.,.F.,(4,2,2,2,2,2,2,2,2,2,2,2,2,
2,2,2,2,2,2,2,2,2,2,2,2,4),(0.0396248818917768,0.0420848252462827,0.0433147969235357,
0.0445447686007886,0.0457747402780416,0.0470047119552946,0.0494646553098004,
0.0506946269870533,0.0519245986643062,0.0543845420188121,0.055614513696065,
0.0568444853733179,0.0593044287278237,0.0605344004050766,0.0617643720823295,
0.0629943437595824,0.0642243154368353,0.0666842587913412,0.0679142304685941,
0.069144202145847,0.0703741738231,0.0716041455003529,0.0740640888548589,
0.075294060532112,0.076524032209365,0.078983975563871),.UNSPECIFIED.);
#2306=B_SPLINE_CURVE_WITH_KNOTS('',3,(#98954,#98955,#98956,#98957,#98958,
#98959,#98960,#98961,#98962,#98963,#98964,#98965,#98966,#98967,#98968,#98969,
#98970,#98971,#98972,#98973,#98974,#98975,#98976,#98977,#98978,#98979),
 .UNSPECIFIED.,.F.,.F.,(4,2,2,2,2,2,2,2,2,2,2,2,4),(3.8407130984836,4.08176830122509,
4.32282350396658,4.80493390944956,5.28300177858748,5.52203571315644,5.7610696477254,
6.00010358229436,6.23913751686332,6.71720538600124,7.19931579148422,7.4403709942257,
7.68142619696719),.UNSPECIFIED.);
#2307=B_SPLINE_CURVE_WITH_KNOTS('',3,(#98982,#98983,#98984,#98985,#98986,
#98987,#98988,#98989,#98990,#98991,#98992,#98993,#98994,#98995,#98996,#98997,
#98998,#98999,#99000,#99001,#99002,#99003,#99004,#99005,#99006,#99007,#99008,
#99009,#99010,#99011,#99012,#99013,#99014,#99015,#99016,#99017,#99018,#99019,
#99020,#99021,#99022,#99023,#99024,#99025,#99026,#99027,#99028,#99029,#99030,
#99031,#99032,#99033,#99034,#99035,#99036,#99037,#99038,#99039,#99040,#99041,
#99042,#99043,#99044,#99045,#99046,#99047,#99048,#99049,#99050,#99051,#99052,
#99053,#99054,#99055,#99056,#99057,#99058,#99059,#99060,#99061,#99062,#99063,
#99064,#99065,#99066,#99067,#99068,#99069,#99070,#99071,#99072,#99073,#99074,
#99075,#99076,#99077,#99078,#99079,#99080,#99081,#99082,#99083,#99084,#99085,
#99086,#99087,#99088,#99089,#99090,#99091,#99092,#99093,#99094,#99095,#99096,
#99097,#99098,#99099,#99100,#99101,#99102,#99103,#99104,#99105,#99106,#99107,
#99108,#99109,#99110,#99111,#99112,#99113,#99114,#99115,#99116,#99117,#99118,
#99119,#99120,#99121,#99122,#99123,#99124,#99125,#99126,#99127,#99128,#99129,
#99130,#99131,#99132,#99133,#99134,#99135,#99136,#99137,#99138,#99139,#99140,
#99141,#99142,#99143,#99144,#99145,#99146,#99147,#99148,#99149,#99150,#99151,
#99152,#99153,#99154,#99155,#99156,#99157,#99158,#99159,#99160,#99161,#99162,
#99163,#99164,#99165,#99166,#99167,#99168,#99169,#99170,#99171,#99172,#99173,
#99174,#99175,#99176,#99177,#99178,#99179,#99180,#99181,#99182,#99183,#99184,
#99185,#99186),.UNSPECIFIED.,.F.,.F.,(4,3,3,3,3,3,3,3,3,3,3,3,3,3,3,3,3,
3,3,3,3,3,3,3,3,3,3,3,3,3,3,3,3,3,3,3,3,3,3,3,3,3,3,3,3,3,3,3,3,3,3,3,3,
3,3,3,3,3,3,3,3,3,3,3,3,3,3,3,4),(0.051952788832463,0.0523437358727679,
0.0530396348010571,0.0532815940436916,0.0535165769936827,0.0550803651549024,
0.0565315459304904,0.0566441533161221,0.0573435791058262,0.0581553062489573,
0.0582079414773418,0.0597781972481067,0.0613355177997813,0.0614004919138027,
0.0627595431985349,0.0628993059610011,0.0630224461823626,0.0644630941222208,
0.0662665572770309,0.0675906704446604,0.0678890579253496,0.0688036127964488,
0.0691544586058802,0.0695121857757964,0.0705623247810647,0.0707182467671,
0.0722820349283198,0.0727603963114584,0.0735729358548261,0.0738458230895395,
0.0743855823551034,0.0760111644019605,0.0769733994119791,0.0775954188217194,
0.0776371348320698,0.077755293492589,0.0783329590758319,0.0784502993253913,
0.078537187573199,0.079263366729678,0.0801009757344188,0.0816647638956387,
0.0825143971297319,0.0832285520568585,0.0853698372313069,0.0857634780397393,
0.0863561283792982,0.0870860429658391,0.087387128745137,0.087919916540518,
0.0890096229688163,0.0894837047017378,0.0904433744731794,0.0906319233369377,
0.0910474928629577,0.0918522904268007,0.0922540308854936,0.0926112810241775,
0.0947257451244876,0.0954981621844028,0.095738857346617,0.0966800930537362,
0.0971208482525779,0.0973026455078367,0.0981728563859435,0.0987443411160432,
0.0988664336690564,0.100855253342667,0.101994009991496),.UNSPECIFIED.);
#2308=B_SPLINE_CURVE_WITH_KNOTS('',3,(#99189,#99190,#99191,#99192,#99193,
#99194,#99195,#99196,#99197,#99198),.UNSPECIFIED.,.F.,.F.,(4,2,2,2,4),(0.0480426030336095,
0.0490467205767583,0.050050838119907,0.0510549556630558,0.0520590732062046),
 .UNSPECIFIED.);
#2309=B_SPLINE_CURVE_WITH_KNOTS('',3,(#99199,#99200,#99201,#99202,#99203,
#99204,#99205,#99206,#99207,#99208,#99209,#99210,#99211,#99212,#99213,#99214,
#99215,#99216,#99217,#99218,#99219,#99220,#99221,#99222,#99223,#99224,#99225,
#99226,#99227,#99228,#99229,#99230,#99231,#99232,#99233,#99234,#99235,#99236,
#99237,#99238,#99239,#99240,#99241,#99242,#99243,#99244,#99245,#99246,#99247,
#99248),.UNSPECIFIED.,.F.,.F.,(4,2,2,2,2,2,2,2,2,2,2,2,2,2,2,2,2,2,2,2,
2,2,2,2,4),(0.0520590732062046,0.0550614663094106,0.0558120645852121,0.0565626628610136,
0.0580638594126164,0.0595650559642193,0.0610662525158222,0.0640686456190281,
0.0655698421706311,0.0670710387222342,0.0700734318254403,0.0715746283770435,
0.0730758249286465,0.0760782180318527,0.0775794145834557,0.0790806111350588,
0.0805818076866618,0.0820830042382648,0.0850853973414709,0.0880877904446769,
0.0910901835478829,0.094092576651089,0.095593773202692,0.097094969754295,
0.100097362857501),.UNSPECIFIED.);
#2310=B_SPLINE_CURVE_WITH_KNOTS('',3,(#99249,#99250,#99251,#99252,#99253,
#99254,#99255,#99256,#99257,#99258,#99259,#99260,#99261,#99262,#99263,#99264,
#99265,#99266,#99267,#99268,#99269,#99270,#99271,#99272,#99273),
 .UNSPECIFIED.,.F.,.F.,(4,3,3,3,3,3,3,3,4),(0.050029146080417,0.0504604958563201,
0.0505100567684285,0.0509435518624639,0.05099096745644,0.0514718781444515,
0.0516554513507709,0.0517123334884572,0.0519527888232233),.UNSPECIFIED.);
#2311=B_SPLINE_CURVE_WITH_KNOTS('',3,(#99414,#99415,#99416,#99417,#99418,
#99419,#99420,#99421,#99422,#99423,#99424,#99425,#99426,#99427,#99428,#99429,
#99430,#99431,#99432,#99433,#99434,#99435,#99436,#99437,#99438,#99439,#99440,
#99441,#99442,#99443,#99444,#99445,#99446,#99447,#99448,#99449,#99450,#99451,
#99452,#99453,#99454,#99455,#99456,#99457,#99458,#99459,#99460,#99461,#99462,
#99463,#99464,#99465,#99466,#99467,#99468,#99469,#99470,#99471,#99472,#99473,
#99474,#99475,#99476,#99477,#99478,#99479,#99480,#99481,#99482,#99483,#99484,
#99485,#99486,#99487,#99488,#99489,#99490,#99491,#99492,#99493,#99494,#99495,
#99496,#99497,#99498,#99499,#99500,#99501,#99502,#99503,#99504,#99505,#99506,
#99507,#99508,#99509,#99510,#99511,#99512,#99513,#99514,#99515,#99516,#99517,
#99518,#99519,#99520,#99521,#99522,#99523,#99524,#99525,#99526,#99527,#99528,
#99529,#99530,#99531,#99532,#99533,#99534,#99535,#99536,#99537,#99538,#99539,
#99540,#99541,#99542,#99543,#99544,#99545,#99546,#99547,#99548,#99549,#99550,
#99551,#99552,#99553,#99554,#99555,#99556,#99557,#99558),.UNSPECIFIED.,
 .F.,.F.,(4,3,3,3,3,3,3,3,3,3,3,3,3,3,3,3,3,3,3,3,3,3,3,3,3,3,3,3,3,3,3,
3,3,3,3,3,3,3,3,3,3,3,3,3,3,3,3,3,4),(0.0203612017522921,0.0208877325613553,
0.0214142633704186,0.0215214199490211,0.0222272019780885,0.022467324988545,
0.0226816347878761,0.0232615135447818,0.0235203866066714,0.0238415310374913,
0.0244196285836592,0.0245734482247979,0.0250017753684234,0.0250999790338611,
0.0254745069658603,0.0255817617933977,0.0256265098429244,0.0261621061518675,
0.0266795714610508,0.027093539205275,0.0273236651342074,0.0277326330791773,
0.0284867951362316,0.0287856946973038,0.0290694919072253,0.0296527825000932,
0.0298387563154302,0.030424002716454,0.0308207212525154,0.0308918179335567,
0.0314448180467838,0.0319448795516832,0.0319897325623951,0.0328989778740624,
0.0329979411698097,0.033158038557521,0.0337415514971665,0.0340510027879362,
0.0343244349253117,0.034906676680582,0.0351040644060626,0.0354884218747967,
0.0359549037492386,0.0361571260241891,0.0364421515354402,0.0366539939248379,
0.0369320907835768,0.0371958940818509,0.0372101876423156),.UNSPECIFIED.);
#2312=B_SPLINE_CURVE_WITH_KNOTS('',3,(#99562,#99563,#99564,#99565,#99566,
#99567,#99568,#99569,#99570,#99571,#99572,#99573,#99574,#99575,#99576,#99577,
#99578,#99579,#99580,#99581,#99582,#99583,#99584,#99585,#99586,#99587,#99588,
#99589,#99590,#99591,#99592,#99593,#99594,#99595,#99596,#99597,#99598,#99599,
#99600,#99601,#99602,#99603,#99604,#99605,#99606,#99607,#99608,#99609,#99610,
#99611,#99612,#99613,#99614,#99615,#99616,#99617,#99618,#99619,#99620,#99621,
#99622,#99623,#99624,#99625,#99626,#99627,#99628,#99629,#99630,#99631,#99632,
#99633,#99634,#99635,#99636,#99637,#99638,#99639,#99640,#99641,#99642,#99643,
#99644,#99645,#99646,#99647,#99648,#99649,#99650,#99651,#99652,#99653,#99654,
#99655,#99656,#99657,#99658,#99659,#99660,#99661,#99662,#99663,#99664,#99665,
#99666,#99667,#99668,#99669,#99670,#99671,#99672,#99673,#99674,#99675,#99676,
#99677,#99678,#99679,#99680,#99681,#99682,#99683,#99684,#99685,#99686,#99687,
#99688,#99689,#99690,#99691,#99692,#99693,#99694,#99695,#99696,#99697,#99698,
#99699,#99700,#99701,#99702,#99703,#99704,#99705,#99706,#99707,#99708,#99709,
#99710,#99711,#99712,#99713,#99714,#99715,#99716,#99717,#99718,#99719,#99720,
#99721,#99722,#99723,#99724,#99725,#99726,#99727,#99728,#99729,#99730,#99731,
#99732,#99733,#99734,#99735,#99736,#99737,#99738,#99739,#99740,#99741,#99742,
#99743,#99744,#99745),.UNSPECIFIED.,.F.,.F.,(4,3,3,3,3,3,3,3,3,3,3,3,3,
3,3,3,3,3,3,3,3,3,3,3,3,3,3,3,3,3,3,3,3,3,3,3,3,3,3,3,3,3,3,3,3,3,3,3,3,
3,3,3,3,3,3,3,3,3,3,3,3,4),(0.0393915580945953,0.0406020192817889,0.0406842633633433,
0.0406958727203922,0.0411897366401807,0.041347511295112,0.0417997522419474,
0.0419769686320912,0.042001060508596,0.0427295402264934,0.0432696739008392,
0.0433092324285996,0.0438450851123192,0.0439160265352132,0.043962195669524,
0.0444511285765506,0.0445623791695872,0.044613777558144,0.0452087318039612,
0.0452639875668987,0.0457762976609016,0.0458550844383352,0.0459128163539046,
0.0466311140589519,0.0471477897070833,0.047205819393466,0.047825754424214,
0.0484404949758313,0.0484929313137353,0.0492161864185054,0.0497332002445794,
0.0497750420548443,0.0502299672427955,0.0503795528789534,0.0504143578583252,
0.0509624748546795,0.0510259055133274,0.0510532316307843,0.0523186107820755,
0.0523300368138618,0.053160842001516,0.0536076953320472,0.0536113160508235,
0.0542478903539933,0.0542576686851976,0.0547677584017706,0.0548891050414737,
0.0549040213195716,0.0557559568875907,0.0561762838139536,0.0561967265883197,
0.0567415483777051,0.0568222920920382,0.0568430792226938,0.0574699119703464,
0.0574894318570679,0.0582050150642818,0.0587698423842959,0.058782137125816,
0.0593635404971942,0.0599514576204697,0.0600748423945641),.UNSPECIFIED.);
#2313=B_SPLINE_CURVE_WITH_KNOTS('',3,(#99748,#99749,#99750,#99751,#99752,
#99753),.UNSPECIFIED.,.F.,.F.,(4,2,4),(1.4304896245382E-17,0.000879674198175861,
0.00175934839635171),.UNSPECIFIED.);
#2314=B_SPLINE_CURVE_WITH_KNOTS('',3,(#99918,#99919,#99920,#99921,#99922,
#99923,#99924,#99925,#99926,#99927,#99928,#99929,#99930,#99931,#99932,#99933,
#99934,#99935,#99936,#99937,#99938,#99939,#99940,#99941,#99942,#99943,#99944,
#99945,#99946,#99947,#99948,#99949,#99950,#99951,#99952,#99953,#99954,#99955,
#99956,#99957,#99958,#99959,#99960,#99961,#99962,#99963,#99964,#99965,#99966,
#99967,#99968,#99969,#99970,#99971),.UNSPECIFIED.,.F.,.F.,(4,2,2,2,2,2,
2,2,2,2,2,2,2,2,2,2,2,2,2,2,2,2,2,2,2,2,4),(0.0425666836577637,0.0437586716581344,
0.0449506596585051,0.0473346356592465,0.0485266236596173,0.0497186116599881,
0.0521025876607297,0.0532945756611006,0.0544865636614714,0.0556785516618422,
0.056870539662213,0.0592545156629546,0.0604465036633254,0.0616384916636961,
0.0628304796640669,0.0640224676644376,0.066406443665179,0.0675984316655497,
0.0687904196659204,0.0711743956666619,0.0723663836670326,0.0735583716674033,
0.0759423476681446,0.0771343356685152,0.0783263236688858,0.0795183116692565,
0.0807102996696271),.UNSPECIFIED.);
#2315=B_SPLINE_CURVE_WITH_KNOTS('',3,(#99975,#99976,#99977,#99978,#99979,
#99980,#99981,#99982,#99983,#99984,#99985,#99986,#99987,#99988,#99989,#99990,
#99991,#99992,#99993,#99994,#99995,#99996,#99997,#99998,#99999,#100000,
#100001,#100002,#100003,#100004,#100005,#100006,#100007,#100008,#100009,
#100010,#100011,#100012,#100013,#100014,#100015,#100016,#100017,#100018,
#100019,#100020,#100021,#100022,#100023,#100024,#100025,#100026,#100027,
#100028,#100029,#100030),.UNSPECIFIED.,.F.,.F.,(4,2,2,2,2,2,2,2,2,2,2,2,
2,2,2,2,2,2,2,2,2,2,2,2,2,2,2,4),(0.0826968326824961,0.0840239767822064,
0.0853511208819168,0.0866782649816271,0.0880054090813374,0.0893325531810478,
0.0906596972807581,0.0933139854801787,0.0946411295798889,0.0959682736795991,
0.0986225618790196,0.0999497059787299,0.10127685007844,0.10260399417815,
0.103931138277861,0.106585426477281,0.107912570576991,0.109239714676702,
0.110566858776412,0.111894002876122,0.114548291075542,0.115875435175253,
0.117202579274963,0.118529723374673,0.119856867474383,0.122511155673804,
0.123838299773514,0.125165443873224),.UNSPECIFIED.);
#2316=B_SPLINE_CURVE_WITH_KNOTS('',3,(#100033,#100034,#100035,#100036,#100037,
#100038,#100039,#100040,#100041,#100042,#100043,#100044,#100045),
 .UNSPECIFIED.,.F.,.F.,(4,3,3,3,4),(5.74602846774033E-18,0.00103091965574787,
0.00109496199515262,0.00213421079951866,0.00218992399030524),
 .UNSPECIFIED.);
#2317=B_SPLINE_CURVE_WITH_KNOTS('',3,(#100210,#100211,#100212,#100213,#100214,
#100215,#100216,#100217,#100218,#100219,#100220,#100221,#100222,#100223,
#100224,#100225,#100226,#100227,#100228,#100229,#100230,#100231,#100232,
#100233,#100234,#100235,#100236,#100237,#100238,#100239,#100240,#100241,
#100242,#100243,#100244,#100245,#100246,#100247,#100248,#100249,#100250,
#100251,#100252,#100253,#100254,#100255,#100256,#100257,#100258,#100259,
#100260,#100261,#100262,#100263),.UNSPECIFIED.,.F.,.F.,(4,2,2,2,2,2,2,2,
2,2,2,2,2,2,2,2,2,2,2,2,2,2,2,2,2,2,4),(0.0425666836577637,0.0437586716581344,
0.0449506596585051,0.0473346356592465,0.0485266236596173,0.0497186116599881,
0.0521025876607297,0.0532945756611006,0.0544865636614714,0.0556785516618422,
0.056870539662213,0.0592545156629546,0.0604465036633254,0.0616384916636961,
0.0628304796640669,0.0640224676644376,0.066406443665179,0.0675984316655497,
0.0687904196659204,0.0711743956666619,0.0723663836670326,0.0735583716674033,
0.0759423476681446,0.0771343356685152,0.0783263236688858,0.0795183116692565,
0.0807102996696271),.UNSPECIFIED.);
#2318=B_SPLINE_CURVE_WITH_KNOTS('',3,(#100267,#100268,#100269,#100270,#100271,
#100272,#100273,#100274,#100275,#100276,#100277,#100278,#100279,#100280,
#100281,#100282,#100283,#100284,#100285,#100286,#100287,#100288,#100289,
#100290,#100291,#100292,#100293,#100294,#100295,#100296,#100297,#100298,
#100299,#100300,#100301,#100302,#100303,#100304,#100305,#100306,#100307,
#100308,#100309,#100310,#100311,#100312,#100313,#100314,#100315,#100316,
#100317,#100318,#100319,#100320,#100321,#100322),.UNSPECIFIED.,.F.,.F.,
(4,2,2,2,2,2,2,2,2,2,2,2,2,2,2,2,2,2,2,2,2,2,2,2,2,2,2,4),(0.0826968326824961,
0.0840239767822064,0.0853511208819168,0.0866782649816271,0.0880054090813374,
0.0893325531810478,0.0906596972807581,0.0933139854801787,0.0946411295798889,
0.0959682736795991,0.0986225618790196,0.0999497059787299,0.10127685007844,
0.10260399417815,0.103931138277861,0.106585426477281,0.107912570576991,
0.109239714676702,0.110566858776412,0.111894002876122,0.114548291075542,
0.115875435175253,0.117202579274963,0.118529723374673,0.119856867474383,
0.122511155673804,0.123838299773514,0.125165443873224),.UNSPECIFIED.);
#2319=B_SPLINE_CURVE_WITH_KNOTS('',3,(#100325,#100326,#100327,#100328,#100329,
#100330,#100331,#100332,#100333,#100334,#100335,#100336,#100337),
 .UNSPECIFIED.,.F.,.F.,(4,3,3,3,4),(5.74602846774033E-18,0.00103091965584011,
0.00109496199515262,0.00213421079971333,0.00218992399030524),
 .UNSPECIFIED.);
#2320=B_SPLINE_CURVE_WITH_KNOTS('',3,(#100352,#100353,#100354,#100355,#100356,
#100357,#100358,#100359,#100360,#100361,#100362,#100363,#100364,#100365,
#100366,#100367,#100368,#100369,#100370,#100371,#100372,#100373,#100374,
#100375,#100376,#100377,#100378,#100379,#100380,#100381,#100382,#100383,
#100384,#100385,#100386,#100387,#100388,#100389,#100390,#100391,#100392,
#100393,#100394,#100395,#100396,#100397,#100398,#100399,#100400,#100401,
#100402,#100403,#100404,#100405,#100406,#100407,#100408,#100409,#100410,
#100411,#100412,#100413,#100414,#100415,#100416,#100417,#100418,#100419,
#100420,#100421,#100422,#100423,#100424,#100425,#100426,#100427,#100428,
#100429,#100430,#100431,#100432,#100433,#100434,#100435,#100436,#100437,
#100438,#100439,#100440,#100441,#100442,#100443,#100444,#100445,#100446,
#100447,#100448,#100449,#100450,#100451,#100452,#100453,#100454,#100455,
#100456,#100457,#100458,#100459,#100460,#100461,#100462,#100463,#100464,
#100465,#100466,#100467,#100468,#100469,#100470,#100471,#100472,#100473,
#100474,#100475,#100476,#100477,#100478,#100479,#100480,#100481,#100482,
#100483,#100484,#100485,#100486,#100487,#100488,#100489,#100490,#100491,
#100492,#100493,#100494,#100495,#100496,#100497,#100498,#100499,#100500,
#100501,#100502,#100503,#100504,#100505,#100506,#100507,#100508,#100509,
#100510,#100511,#100512,#100513,#100514,#100515,#100516,#100517,#100518,
#100519,#100520,#100521,#100522,#100523,#100524,#100525,#100526,#100527,
#100528,#100529,#100530,#100531,#100532,#100533,#100534,#100535,#100536,
#100537,#100538,#100539,#100540,#100541,#100542,#100543,#100544),
 .UNSPECIFIED.,.F.,.F.,(4,3,3,3,3,3,3,3,3,3,3,3,3,3,3,3,3,3,3,3,3,3,3,3,
3,3,3,3,3,3,3,3,3,3,3,3,3,3,3,3,3,3,3,3,3,3,3,3,3,3,3,3,3,3,3,3,3,3,3,3,
3,3,3,3,4),(0.00218992399030524,0.00308955832189556,0.004018478740376,0.00457303964936322,
0.00471820601332814,0.00528919436517401,0.00576459747889221,0.00599015957137656,
0.0064977592807818,0.00695615530842121,0.00724973709061845,0.00855234536231135,
0.0093392709674792,0.00977080820653486,0.0105308287970081,0.0110350977515803,
0.0117223866265371,0.012299424271805,0.0131312412090355,0.0135628412595257,
0.0141055022855951,0.0148235883463824,0.0156561031455178,0.0164886179446531,
0.0171451126945242,0.0173447902188242,0.0176801757741821,0.0181792030037352,
0.0186034896216875,0.0188717336037111,0.0196753837693712,0.0198625075997739,
0.0206539618856476,0.0211202966732222,0.0212548492627691,0.0219966235055716,
0.0223781033376274,0.0231455767622806,0.0236379649218272,0.0245470980206528,
0.0248989158279885,0.0258457255439288,0.0260210805808852,0.0274226554767584,
0.0284041962399432,0.0286863596781406,0.0299508419517926,0.0307873118990013,
0.0320722689041744,0.0324806915917337,0.0331704275580593,0.0337099622359248,
0.0342395035047979,0.0343619853875884,0.0350082143941416,0.0355535432171174,
0.0362707981721182,0.0367451010466465,0.0372671387162966,0.0375316513660662,
0.0379366588761756,0.0389074701956465,0.0398687342463795,0.0400497152061118,
0.0403197745314809),.UNSPECIFIED.);
#2321=B_SPLINE_CURVE_WITH_KNOTS('',3,(#100547,#100548,#100549,#100550,#100551,
#100552),.UNSPECIFIED.,.F.,.F.,(4,2,4),(0.0403197745352163,0.04144322909649,
0.0425666836577637),.UNSPECIFIED.);
#2322=B_SPLINE_CURVE_WITH_KNOTS('',3,(#100553,#100554,#100555,#100556,#100557,
#100558,#100559,#100560,#100561,#100562,#100563,#100564,#100565,#100566,
#100567,#100568,#100569,#100570,#100571,#100572,#100573,#100574,#100575,
#100576,#100577,#100578,#100579,#100580,#100581,#100582,#100583,#100584,
#100585,#100586,#100587,#100588,#100589,#100590,#100591,#100592,#100593,
#100594,#100595,#100596,#100597,#100598,#100599,#100600,#100601,#100602,
#100603,#100604,#100605,#100606,#100607,#100608,#100609,#100610,#100611,
#100612,#100613,#100614,#100615,#100616,#100617,#100618,#100619,#100620,
#100621,#100622,#100623,#100624,#100625,#100626,#100627,#100628,#100629,
#100630,#100631,#100632,#100633,#100634,#100635,#100636,#100637,#100638,
#100639,#100640,#100641,#100642,#100643,#100644,#100645,#100646,#100647,
#100648,#100649,#100650,#100651,#100652,#100653,#100654,#100655,#100656,
#100657,#100658,#100659,#100660,#100661,#100662,#100663,#100664,#100665,
#100666,#100667,#100668,#100669,#100670,#100671,#100672,#100673,#100674,
#100675,#100676,#100677,#100678,#100679,#100680,#100681,#100682,#100683,
#100684,#100685,#100686,#100687,#100688,#100689,#100690,#100691,#100692,
#100693,#100694,#100695,#100696,#100697,#100698,#100699,#100700,#100701,
#100702,#100703,#100704,#100705,#100706,#100707,#100708,#100709,#100710,
#100711,#100712,#100713,#100714,#100715,#100716,#100717,#100718,#100719,
#100720,#100721,#100722,#100723,#100724,#100725,#100726,#100727,#100728,
#100729,#100730,#100731,#100732,#100733,#100734,#100735,#100736,#100737,
#100738,#100739,#100740,#100741,#100742,#100743,#100744,#100745),
 .UNSPECIFIED.,.F.,.F.,(4,3,3,3,3,3,3,3,3,3,3,3,3,3,3,3,3,3,3,3,3,3,3,3,
3,3,3,3,3,3,3,3,3,3,3,3,3,3,3,3,3,3,3,3,3,3,3,3,3,3,3,3,3,3,3,3,3,3,3,3,
3,3,3,3,4),(0.00218992399030524,0.00308955832192262,0.00401847874043237,
0.0045730396493621,0.00471820601332802,0.00528919436515712,0.00576459747889057,
0.00599015957137656,0.00649775928078463,0.00695615530841904,0.00724973709061851,
0.00855234536240134,0.00933927096747599,0.00977080820653491,0.0105308287970044,
0.0110350977515804,0.0117223866265329,0.0122994242718053,0.0131312412090609,
0.0135628412595259,0.0141055022855899,0.0148235883463828,0.0156561031455148,
0.0164886179446468,0.0171451126945234,0.0173447902188245,0.0176801757741753,
0.0181792030037235,0.0186034896216878,0.0188717336037037,0.0196753837693461,
0.0198625075997741,0.0206539618856354,0.0211202966732224,0.0212548492627606,
0.0219966235055572,0.0223781033376276,0.0231455767622747,0.0236379649218175,
0.0245470980206775,0.0248989158279887,0.0258457255439675,0.0260210805808744,
0.0274226554767585,0.0284041962399313,0.0286863596781406,0.0299508419517927,
0.0307873118989883,0.0320722689041961,0.0324806915917337,0.0331704275580452,
0.0337099622359205,0.0342395035047928,0.0343619853875737,0.0350082143941417,
0.0355535432171022,0.0362707981721182,0.0367451010466307,0.0372671387162828,
0.0375316513660662,0.0379366588761592,0.0389074701956399,0.0398687342463254,
0.0400497152061118,0.0403197745314634),.UNSPECIFIED.);
#2323=B_SPLINE_CURVE_WITH_KNOTS('',3,(#100746,#100747,#100748,#100749,#100750,
#100751),.UNSPECIFIED.,.F.,.F.,(4,2,4),(0.0403197745352337,0.0414432290964987,
0.0425666836577637),.UNSPECIFIED.);
#2324=B_SPLINE_CURVE_WITH_KNOTS('',3,(#100754,#100755,#100756,#100757,#100758,
#100759,#100760,#100761,#100762,#100763,#100764,#100765,#100766,#100767,
#100768,#100769,#100770,#100771,#100772,#100773,#100774,#100775,#100776,
#100777,#100778,#100779,#100780,#100781,#100782,#100783,#100784,#100785,
#100786,#100787,#100788,#100789,#100790,#100791,#100792,#100793,#100794,
#100795,#100796,#100797,#100798,#100799,#100800,#100801,#100802,#100803,
#100804,#100805,#100806,#100807,#100808,#100809,#100810,#100811,#100812,
#100813,#100814,#100815,#100816,#100817,#100818,#100819,#100820,#100821,
#100822,#100823,#100824,#100825,#100826,#100827,#100828,#100829,#100830,
#100831,#100832,#100833,#100834,#100835,#100836,#100837,#100838,#100839,
#100840,#100841,#100842,#100843,#100844,#100845,#100846,#100847,#100848,
#100849,#100850,#100851,#100852,#100853,#100854,#100855,#100856,#100857,
#100858,#100859,#100860,#100861,#100862,#100863,#100864,#100865,#100866,
#100867,#100868,#100869,#100870,#100871,#100872,#100873,#100874,#100875,
#100876,#100877,#100878,#100879,#100880,#100881,#100882,#100883,#100884,
#100885,#100886,#100887,#100888,#100889,#100890,#100891,#100892,#100893,
#100894,#100895,#100896,#100897,#100898,#100899,#100900,#100901,#100902,
#100903,#100904,#100905,#100906,#100907,#100908,#100909,#100910,#100911,
#100912,#100913,#100914,#100915,#100916,#100917,#100918,#100919,#100920,
#100921,#100922,#100923,#100924,#100925,#100926,#100927,#100928,#100929,
#100930,#100931,#100932,#100933,#100934,#100935,#100936,#100937,#100938,
#100939,#100940,#100941,#100942,#100943,#100944,#100945,#100946,#100947,
#100948,#100949,#100950,#100951,#100952,#100953,#100954,#100955,#100956,
#100957,#100958,#100959,#100960,#100961,#100962,#100963,#100964,#100965,
#100966,#100967,#100968,#100969,#100970,#100971,#100972,#100973),
 .UNSPECIFIED.,.F.,.F.,(4,3,3,3,3,3,3,3,3,3,3,3,3,3,3,3,3,3,3,3,3,3,3,3,
3,3,3,3,3,3,3,3,3,3,3,3,3,3,3,3,3,3,3,3,3,3,3,3,3,3,3,3,3,3,3,3,3,3,3,3,
3,3,3,3,3,3,3,3,3,3,3,3,3,4),(0.00398066249725657,0.00520970825651315,0.00650636077682542,
0.00721601660321733,0.00723521461508359,0.00790676989862768,0.00859462407436548,
0.0088336936561977,0.00953736387305569,0.010259563370406,0.0104513707091781,
0.0104840369026883,0.0122603887891099,0.0136867248151388,0.0137089680572726,
0.0147832361856882,0.0153044018681193,0.0153241614395351,0.0169220789210998,
0.0169382407877385,0.0185397559740803,0.0185508989686889,0.0201574330270607,
0.0201622062086101,0.0217724235733863,0.0217751100800412,0.0225771129414008,
0.0225839486065314,0.0233815379211718,0.0233927871330216,0.0251680184799019,
0.0265986566873695,0.0266281412389824,0.0276739747417877,0.0282071183667835,
0.0282458182919628,0.0298163947543849,0.0298634953449433,0.0314265764578142,
0.0314811723979237,0.0322320258870935,0.033037874608938,0.0330988494509041,
0.0353209486500281,0.0362648283008095,0.0363342035568649,0.0372867356601343,
0.0378804048033753,0.0379518806098454,0.0388901500916239,0.0394973460129241,
0.0395695576628258,0.0417194838636053,0.0427357414432794,0.0428049117687866,
0.0443574142826654,0.0459808396568091,0.0460402658747474,0.0470431195999113,
0.0476060477279055,0.0476579429277278,0.0487984511437497,0.0492332173564472,
0.0492756199807082,0.0505099933557396,0.0508616218729735,0.0520424580018409,
0.0524903086159866,0.0525109740866689,0.0535033159543337,0.0541286511396493,
0.0546624608776011,0.0552149480467196,0.0557463281926296),.UNSPECIFIED.);
#2325=B_SPLINE_CURVE_WITH_KNOTS('',3,(#100976,#100977,#100978,#100979,#100980,
#100981,#100982,#100983,#100984,#100985,#100986,#100987,#100988,#100989,
#100990,#100991,#100992,#100993,#100994,#100995,#100996,#100997,#100998,
#100999,#101000,#101001,#101002,#101003,#101004,#101005,#101006,#101007,
#101008,#101009,#101010,#101011,#101012,#101013,#101014,#101015,#101016,
#101017,#101018,#101019,#101020,#101021,#101022,#101023,#101024,#101025,
#101026,#101027,#101028,#101029,#101030,#101031,#101032,#101033,#101034,
#101035,#101036,#101037,#101038,#101039,#101040,#101041,#101042,#101043,
#101044,#101045,#101046,#101047,#101048,#101049,#101050,#101051,#101052,
#101053,#101054,#101055,#101056,#101057,#101058,#101059,#101060,#101061,
#101062,#101063,#101064,#101065,#101066,#101067,#101068,#101069,#101070,
#101071,#101072,#101073,#101074,#101075,#101076,#101077,#101078,#101079,
#101080,#101081,#101082,#101083,#101084,#101085,#101086,#101087,#101088,
#101089,#101090,#101091,#101092,#101093,#101094,#101095,#101096,#101097,
#101098,#101099,#101100,#101101,#101102,#101103,#101104,#101105,#101106,
#101107,#101108,#101109,#101110,#101111,#101112,#101113,#101114,#101115,
#101116,#101117,#101118,#101119,#101120,#101121,#101122,#101123,#101124,
#101125,#101126,#101127,#101128,#101129,#101130,#101131,#101132,#101133,
#101134,#101135,#101136,#101137,#101138,#101139,#101140,#101141,#101142,
#101143,#101144,#101145,#101146,#101147,#101148,#101149,#101150,#101151,
#101152,#101153,#101154,#101155,#101156,#101157,#101158,#101159,#101160,
#101161,#101162,#101163,#101164,#101165,#101166,#101167,#101168,#101169,
#101170,#101171,#101172,#101173,#101174,#101175,#101176,#101177,#101178,
#101179,#101180,#101181,#101182,#101183,#101184,#101185,#101186,#101187,
#101188,#101189,#101190,#101191,#101192,#101193,#101194,#101195),
 .UNSPECIFIED.,.F.,.F.,(4,3,3,3,3,3,3,3,3,3,3,3,3,3,3,3,3,3,3,3,3,3,3,3,
3,3,3,3,3,3,3,3,3,3,3,3,3,3,3,3,3,3,3,3,3,3,3,3,3,3,3,3,3,3,3,3,3,3,3,3,
3,3,3,3,3,3,3,3,3,3,3,3,3,4),(0.00398066249725657,0.00520970825644499,0.00650636077671913,
0.00721601660321733,0.00723521461508372,0.00790676989864398,0.00859462407441027,
0.0088336936561977,0.00953736387311957,0.0102595633704823,0.0104513707091781,
0.0104840369026883,0.0122603887890039,0.0136867248151388,0.0137089680572725,
0.0147832361856785,0.0153044018681193,0.015324161439535,0.0169220789210998,
0.0169382407877384,0.0185397559740803,0.0185508989686889,0.0201574330270607,
0.0201622062086101,0.0217724235733863,0.0217751100800412,0.0225771129414007,
0.0225839486065314,0.0233815379211717,0.0233927871330216,0.0251680184799104,
0.0265986566873695,0.0266281412389824,0.027673974741794,0.0282071183667836,
0.0282458182919628,0.0298163947543848,0.0298634953449433,0.0314265764578142,
0.0314811723979237,0.0322320258870934,0.0330378746089379,0.0330988494509041,
0.0353209486498751,0.0362648283008094,0.0363342035568649,0.0372867356600656,
0.0378804048033753,0.0379518806098454,0.0388901500916096,0.0394973460129241,
0.0395695576628258,0.0417194838637361,0.0427357414432794,0.0428049117687866,
0.0443574142826654,0.045980839656809,0.0460402658747474,0.0470431195998788,
0.0476060477279055,0.0476579429277278,0.0487984511436461,0.0492332173564472,
0.0492756199807082,0.0505099933557137,0.0508616218729735,0.0520424580018639,
0.0524903086159865,0.0525109740866689,0.0535033159542304,0.0541286511396493,
0.0546624608775954,0.0552149480467123,0.0557463281926296),.UNSPECIFIED.);
#2326=B_SPLINE_CURVE_WITH_KNOTS('',3,(#101196,#101197,#101198,#101199,#101200,
#101201,#101202,#101203,#101204,#101205,#101206,#101207,#101208,#101209,
#101210,#101211,#101212,#101213,#101214,#101215,#101216,#101217,#101218,
#101219,#101220,#101221,#101222,#101223,#101224,#101225,#101226,#101227,
#101228,#101229,#101230,#101231,#101232,#101233,#101234,#101235,#101236,
#101237,#101238,#101239,#101240,#101241,#101242,#101243,#101244,#101245,
#101246,#101247,#101248,#101249,#101250,#101251,#101252,#101253),
 .UNSPECIFIED.,.F.,.F.,(4,2,2,2,2,2,2,2,2,2,2,2,2,2,2,2,2,2,2,2,2,2,2,2,
2,2,2,2,4),(0.0557463281926296,0.0589772878231815,0.0605927676384573,0.0622082474537332,
0.0654392070842851,0.067054686899561,0.068670166714837,0.0702856465301129,
0.0719011263453888,0.0735166061606648,0.0751320859759407,0.0783630456064926,
0.0791707855141306,0.0799785254217686,0.0815940052370446,0.0832094850523206,
0.0848249648675966,0.0880559244981484,0.0896714043134243,0.0912868841287003,
0.0945178437592521,0.096133323574528,0.0977488033898038,0.0993642832050797,
0.100979763020356,0.102595242835631,0.103402982743269,0.104210722650907,
0.107441682281459),.UNSPECIFIED.);
#2327=B_SPLINE_CURVE_WITH_KNOTS('',3,(#101254,#101255,#101256,#101257,#101258,
#101259,#101260,#101261,#101262,#101263,#101264,#101265,#101266,#101267,
#101268,#101269,#101270,#101271,#101272,#101273,#101274,#101275,#101276,
#101277,#101278,#101279,#101280,#101281,#101282,#101283,#101284,#101285,
#101286,#101287,#101288,#101289,#101290,#101291,#101292,#101293,#101294,
#101295,#101296,#101297,#101298,#101299,#101300,#101301,#101302,#101303,
#101304,#101305,#101306,#101307,#101308,#101309,#101310,#101311,#101312,
#101313,#101314,#101315,#101316,#101317,#101318,#101319,#101320,#101321,
#101322,#101323,#101324,#101325,#101326,#101327,#101328,#101329,#101330,
#101331,#101332,#101333,#101334,#101335,#101336,#101337,#101338,#101339,
#101340,#101341,#101342,#101343,#101344,#101345,#101346,#101347,#101348,
#101349,#101350,#101351,#101352,#101353,#101354,#101355,#101356,#101357,
#101358,#101359,#101360,#101361,#101362,#101363,#101364,#101365,#101366,
#101367,#101368,#101369,#101370,#101371,#101372,#101373,#101374,#101375,
#101376,#101377,#101378,#101379,#101380,#101381,#101382,#101383,#101384,
#101385,#101386,#101387,#101388,#101389,#101390,#101391,#101392,#101393,
#101394,#101395,#101396,#101397,#101398,#101399,#101400,#101401,#101402,
#101403,#101404,#101405,#101406,#101407,#101408,#101409,#101410,#101411,
#101412,#101413,#101414,#101415,#101416,#101417,#101418,#101419,#101420,
#101421,#101422,#101423,#101424,#101425,#101426,#101427,#101428,#101429,
#101430,#101431,#101432,#101433,#101434),.UNSPECIFIED.,.F.,.F.,(4,3,3,3,
3,3,3,3,3,3,3,3,3,3,3,3,3,3,3,3,3,3,3,3,3,3,3,3,3,3,3,3,3,3,3,3,3,3,3,3,
3,3,3,3,3,3,3,3,3,3,3,3,3,3,3,3,3,3,3,3,4),(0.0187002242979963,0.0189846710771926,
0.0192766768141431,0.01934682847914,0.0196838394086382,0.0199934326602836,
0.0200088365092078,0.0211598636679579,0.021286641022571,0.0213183403852421,
0.0219730079604549,0.0225798493848584,0.0226270459403006,0.0237548263912282,
0.0238730577471458,0.0239321804060318,0.0248848375890449,0.0251662661094332,
0.0252323362288836,0.0258128702905769,0.0258800535176497,0.0263231529799011,
0.0264594744717206,0.0265261910961018,0.0271926230304998,0.0277526828340081,
0.0278136196686285,0.0283474366902465,0.0288971381406126,0.0290458911962956,
0.0290951190771367,0.0297446067327393,0.0303390995585831,0.0303729190324874,
0.0306881476849833,0.0309857037397268,0.0313980451165654,0.0316323079208706,
0.0316493951147151,0.0322789121020143,0.0322880973836838,0.0328405965385594,
0.0329255162831581,0.0329273016035652,0.0340932297430462,0.034209139758673,
0.0342187246454456,0.0345492922426382,0.0348653288265893,0.0351986616609935,
0.0354959079175446,0.035511933007733,0.0365799882698762,0.0367886773665346,
0.0368051413700205,0.0374373369862022,0.0374517455511642,0.0380873647343798,
0.0380983497323079,0.0391442500642898,0.0393915580945953),.UNSPECIFIED.);
#2328=B_SPLINE_CURVE_WITH_KNOTS('',3,(#101618,#101619,#101620,#101621,#101622,
#101623,#101624,#101625,#101626,#101627,#101628,#101629,#101630,#101631,
#101632,#101633,#101634,#101635,#101636,#101637,#101638,#101639,#101640,
#101641,#101642,#101643,#101644,#101645,#101646,#101647,#101648,#101649,
#101650,#101651,#101652,#101653,#101654,#101655,#101656,#101657,#101658,
#101659,#101660,#101661,#101662,#101663,#101664,#101665,#101666,#101667,
#101668,#101669,#101670,#101671,#101672,#101673,#101674,#101675,#101676,
#101677,#101678,#101679,#101680,#101681,#101682,#101683,#101684,#101685,
#101686,#101687,#101688,#101689,#101690,#101691,#101692,#101693,#101694,
#101695,#101696,#101697,#101698,#101699,#101700,#101701,#101702,#101703,
#101704,#101705,#101706,#101707,#101708,#101709,#101710,#101711,#101712,
#101713,#101714,#101715,#101716,#101717,#101718,#101719,#101720,#101721,
#101722,#101723,#101724,#101725,#101726,#101727,#101728,#101729,#101730,
#101731,#101732,#101733,#101734,#101735,#101736,#101737,#101738,#101739,
#101740,#101741,#101742,#101743,#101744,#101745,#101746,#101747,#101748,
#101749,#101750,#101751,#101752,#101753,#101754,#101755,#101756,#101757,
#101758,#101759,#101760,#101761,#101762,#101763,#101764,#101765,#101766,
#101767,#101768,#101769,#101770,#101771,#101772,#101773,#101774,#101775,
#101776,#101777,#101778,#101779,#101780,#101781,#101782,#101783,#101784,
#101785,#101786,#101787,#101788,#101789,#101790,#101791,#101792),
 .UNSPECIFIED.,.F.,.F.,(4,3,3,3,3,3,3,3,3,3,3,3,3,3,3,3,3,3,3,3,3,3,3,3,
3,3,3,3,3,3,3,3,3,3,3,3,3,3,3,3,3,3,3,3,3,3,3,3,3,3,3,3,3,3,3,3,3,3,4),
(0.,7.00136229228461E-5,0.000880271419196672,0.00197980055185577,0.00250406869828298,
0.00300266268960072,0.00331712911283045,0.00413059578319974,0.00532772256794858,
0.0057574742158991,0.00600532537920143,0.00738304200408561,0.00900794430850162,
0.00900798806880215,0.0112899391783712,0.0120106507584029,0.0122570346230108,
0.0135119821032032,0.0138815868497288,0.0147250110537092,0.0150133134480036,
0.0155067088258865,0.016845214616771,0.0180159761376041,0.0187586550708964,
0.0195173074824044,0.0203855296680284,0.0210186388272047,0.0220135800001955,
0.0236425023713017,0.0240213015168053,0.0244570699511879,0.0252717472664166,
0.0255226328616056,0.0270239642064059,0.0285252955512062,0.0285300848199135,
0.0293428874314582,0.0300266268960065,0.0301588925271162,0.0313458910919184,
0.031787155165216,0.033029289585607,0.0334140923804464,0.0345306209304072,
0.0350404780787163,0.0360319522752075,0.0366663282699641,0.0375332836200077,
0.0382915981957545,0.039034614964808,0.0412861444660561,0.041540518345781,
0.0420372776544085,0.0431651404778179,0.0447901356468785,0.045039940344009,
0.0470573761227504,0.0480426030336095),.UNSPECIFIED.);
#2329=B_SPLINE_CURVE_WITH_KNOTS('',3,(#101794,#101795,#101796,#101797,#101798,
#101799,#101800,#101801),.UNSPECIFIED.,.F.,.F.,(4,2,2,4),(0.100097362857501,
0.102091718402555,0.103088896175082,0.104086073947609),.UNSPECIFIED.);
#2330=B_SPLINE_CURVE_WITH_KNOTS('',3,(#101961,#101962,#101963,#101964,#101965,
#101966,#101967,#101968,#101969,#101970,#101971,#101972,#101973,#101974,
#101975,#101976,#101977,#101978,#101979,#101980,#101981,#101982,#101983,
#101984,#101985,#101986,#101987,#101988,#101989,#101990,#101991,#101992,
#101993,#101994,#101995,#101996,#101997,#101998,#101999,#102000,#102001,
#102002,#102003,#102004,#102005,#102006,#102007,#102008,#102009,#102010,
#102011,#102012,#102013,#102014,#102015,#102016,#102017,#102018,#102019,
#102020,#102021,#102022,#102023,#102024,#102025,#102026,#102027,#102028,
#102029,#102030,#102031,#102032,#102033,#102034,#102035,#102036,#102037,
#102038,#102039,#102040,#102041,#102042,#102043,#102044,#102045,#102046,
#102047,#102048,#102049,#102050,#102051,#102052,#102053,#102054,#102055,
#102056,#102057,#102058,#102059,#102060,#102061,#102062,#102063,#102064,
#102065,#102066,#102067,#102068,#102069,#102070,#102071,#102072,#102073,
#102074,#102075,#102076,#102077,#102078,#102079,#102080,#102081,#102082,
#102083,#102084,#102085,#102086,#102087,#102088,#102089,#102090,#102091,
#102092,#102093,#102094,#102095,#102096,#102097,#102098,#102099,#102100,
#102101,#102102,#102103,#102104,#102105,#102106,#102107,#102108,#102109,
#102110,#102111,#102112,#102113,#102114,#102115,#102116,#102117,#102118,
#102119,#102120,#102121,#102122,#102123,#102124,#102125,#102126,#102127,
#102128,#102129,#102130,#102131,#102132,#102133,#102134,#102135,#102136,
#102137,#102138,#102139,#102140,#102141,#102142,#102143,#102144,#102145,
#102146,#102147,#102148,#102149,#102150,#102151,#102152,#102153,#102154,
#102155,#102156,#102157,#102158,#102159,#102160,#102161,#102162,#102163,
#102164,#102165,#102166,#102167,#102168,#102169,#102170,#102171,#102172,
#102173,#102174,#102175,#102176,#102177,#102178,#102179,#102180,#102181,
#102182,#102183),.UNSPECIFIED.,.F.,.F.,(4,3,3,3,3,3,3,3,3,3,3,3,3,3,3,3,
3,3,3,3,3,3,3,3,3,3,3,3,3,3,3,3,3,3,3,3,3,3,3,3,3,3,3,3,3,3,3,3,3,3,3,3,
3,3,3,3,3,3,3,3,3,3,3,3,3,3,3,3,3,3,3,3,3,3,4),(0.0536197899396224,0.0552276244004006,
0.0552355709876449,0.0564636360413837,0.056836730186764,0.0568513520356673,
0.0585010989846075,0.0600604289236084,0.0600829141317123,0.0616747375677009,
0.0616986951797348,0.0631694062564402,0.0632905117196437,0.0633144762277572,
0.0653332916274416,0.0665264501713466,0.0665460383238021,0.0680226211568013,
0.0681465613676236,0.0681618193718244,0.0697679763088799,0.0697776004198467,
0.0713906714255839,0.0713933814678691,0.0730091625158914,0.0730146093723318,
0.0752607556604403,0.0762407246119361,0.0762648548190898,0.0777231476585592,
0.0778565056599585,0.0778906973850273,0.0791924472928067,0.0794722867079808,
0.0795162256569394,0.0810880677560031,0.0811414459847621,0.0823878645714303,
0.0827038488040255,0.082765970222281,0.0844200933214862,0.0859354109000701,
0.0860114915248442,0.0868961672850943,0.0875511919480923,0.0887466775684487,
0.0891669729961145,0.0892519026800103,0.0907827540441368,0.090869989342466,
0.0922381233782822,0.092398535092159,0.0924866314778507,0.0942502320947376,
0.0956300971882036,0.0957154955381666,0.0971616980126198,0.0972458782362259,
0.097327446100537,0.0983010085687495,0.0988616592842482,0.0989376222126474,
0.0999829246184123,0.10047744033227,0.100546243852972,0.101152494922671,
0.101724341209343,0.102093221380293,0.102150357244739,0.102702522250806,
0.102901111904304,0.103522312960998,0.103709002428315,0.104937728080333,
0.105324783476337),.UNSPECIFIED.);
#2331=B_SPLINE_CURVE_WITH_KNOTS('',3,(#102187,#102188,#102189,#102190,#102191,
#102192,#102193,#102194,#102195,#102196,#102197,#102198,#102199,#102200,
#102201,#102202,#102203,#102204,#102205,#102206,#102207,#102208,#102209,
#102210,#102211,#102212,#102213,#102214,#102215,#102216,#102217,#102218,
#102219,#102220,#102221,#102222,#102223,#102224,#102225,#102226,#102227,
#102228,#102229,#102230,#102231,#102232,#102233,#102234,#102235,#102236,
#102237,#102238,#102239,#102240),.UNSPECIFIED.,.F.,.F.,(4,2,2,2,2,2,2,2,
2,2,2,2,2,2,2,2,2,2,2,2,2,2,2,2,2,2,4),(0.,0.00156341081501294,0.00312682163002588,
0.00469023244503882,0.00625364326005176,0.00938046489007764,0.0109438757050905,
0.0125072865201034,0.0156341081501293,0.0171975189651422,0.0187609297801551,
0.021887751410181,0.0226694568176875,0.023451162225194,0.0250145730402071,
0.0265779838552202,0.0281413946702332,0.0312682163002594,0.0328316271152726,
0.0343950379302857,0.037521859560312,0.0406486811903383,0.0422120920053514,
0.0437755028203645,0.0469023244503908,0.0484657352654039,0.050029146080417),
 .UNSPECIFIED.);
#2332=B_SPLINE_CURVE_WITH_KNOTS('',3,(#102242,#102243,#102244,#102245,#102246,
#102247,#102248,#102249,#102250,#102251),.UNSPECIFIED.,.F.,.F.,(4,3,3,4),
(0.101994009991496,0.102941137438368,0.1034279046247,0.103888264885239),
 .UNSPECIFIED.);
#2333=B_SPLINE_CURVE_WITH_KNOTS('',3,(#102405,#102406,#102407,#102408,#102409,
#102410,#102411,#102412,#102413,#102414,#102415,#102416,#102417,#102418,
#102419,#102420,#102421,#102422,#102423,#102424,#102425,#102426,#102427,
#102428,#102429,#102430,#102431,#102432,#102433,#102434,#102435,#102436,
#102437,#102438,#102439,#102440,#102441,#102442,#102443,#102444,#102445,
#102446,#102447,#102448,#102449,#102450,#102451,#102452,#102453,#102454,
#102455,#102456,#102457,#102458,#102459,#102460,#102461,#102462,#102463,
#102464,#102465,#102466,#102467,#102468,#102469,#102470,#102471,#102472,
#102473,#102474,#102475,#102476,#102477,#102478,#102479,#102480,#102481,
#102482,#102483,#102484,#102485,#102486,#102487,#102488,#102489,#102490,
#102491,#102492,#102493,#102494,#102495,#102496,#102497,#102498,#102499,
#102500,#102501,#102502,#102503,#102504,#102505,#102506,#102507,#102508,
#102509,#102510,#102511,#102512,#102513,#102514,#102515,#102516,#102517,
#102518,#102519,#102520,#102521,#102522,#102523,#102524,#102525,#102526,
#102527,#102528,#102529,#102530,#102531,#102532,#102533,#102534,#102535,
#102536,#102537,#102538,#102539,#102540,#102541,#102542,#102543,#102544,
#102545,#102546,#102547,#102548,#102549,#102550,#102551,#102552,#102553,
#102554,#102555,#102556,#102557,#102558,#102559,#102560,#102561,#102562,
#102563,#102564,#102565,#102566,#102567,#102568,#102569,#102570,#102571,
#102572,#102573,#102574,#102575,#102576,#102577,#102578,#102579,#102580,
#102581,#102582,#102583,#102584,#102585,#102586,#102587,#102588,#102589,
#102590,#102591,#102592,#102593,#102594,#102595,#102596,#102597,#102598,
#102599,#102600,#102601,#102602,#102603),.UNSPECIFIED.,.F.,.F.,(4,3,3,3,
3,3,3,3,3,3,3,3,3,3,3,3,3,3,3,3,3,3,3,3,3,3,3,3,3,3,3,3,3,3,3,3,3,3,3,3,
3,3,3,3,3,3,3,3,3,3,3,3,3,3,3,3,3,3,3,3,3,3,3,3,3,3,4),(0.0415609574076441,
0.0419999079181986,0.0424456108255441,0.0428514400237989,0.0434891733075762,
0.0441269065913535,0.0441419226399537,0.0454112381061315,0.0454324052561084,
0.0465323604473209,0.0466965822688831,0.0467228878722632,0.0484820040281491,
0.0492715033675918,0.0493038531045728,0.050735911668559,0.0518516607057079,
0.0518848183368824,0.0535408116928349,0.0544369446773842,0.054465783569192,
0.0555110612923409,0.0557314168323167,0.0557562661853469,0.0570268987744937,
0.0570467488015017,0.0580899941196728,0.0583234009749456,0.0583372314176566,
0.0593028016534022,0.0596206777396424,0.0596277140338114,0.0622086792661211,
0.0622163187211141,0.063499161882276,0.0635142754825525,0.0647896444984309,
0.0648116296745799,0.0660801271145858,0.0661083966471777,0.0673706097307407,
0.0674045134523431,0.0688635319844597,0.0699515749630503,0.0699933139595394,
0.0712420575792051,0.0712859635838356,0.0722808578696521,0.0725325401953599,
0.0725774037566074,0.0740349703455224,0.0751135054276695,0.0751563211290189,
0.0761837854504818,0.0764039880438243,0.0764437283836802,0.0775804812596956,
0.0776944706599792,0.0777298862469096,0.078984953276134,0.0790147568862244,
0.0801773798800301,0.0802754358922888,0.0802979121042526,0.0811942832430378,
0.0820670967544178,0.0828564011245984),.UNSPECIFIED.);
#2334=B_SPLINE_CURVE_WITH_KNOTS('',3,(#102607,#102608,#102609,#102610,#102611,
#102612,#102613,#102614,#102615,#102616,#102617,#102618,#102619,#102620,
#102621,#102622,#102623,#102624,#102625,#102626,#102627,#102628,#102629,
#102630,#102631,#102632,#102633,#102634,#102635,#102636,#102637,#102638,
#102639,#102640,#102641,#102642,#102643,#102644,#102645,#102646,#102647,
#102648,#102649,#102650,#102651,#102652,#102653,#102654,#102655,#102656,
#102657,#102658,#102659,#102660,#102661,#102662,#102663,#102664,#102665,
#102666,#102667,#102668,#102669,#102670,#102671,#102672,#102673,#102674,
#102675,#102676,#102677,#102678,#102679,#102680,#102681,#102682,#102683,
#102684,#102685,#102686,#102687,#102688,#102689,#102690,#102691,#102692,
#102693,#102694,#102695,#102696,#102697,#102698,#102699,#102700,#102701,
#102702,#102703,#102704,#102705,#102706,#102707,#102708,#102709,#102710,
#102711,#102712,#102713,#102714,#102715,#102716,#102717,#102718,#102719,
#102720,#102721,#102722,#102723,#102724,#102725,#102726,#102727,#102728,
#102729,#102730,#102731,#102732,#102733,#102734,#102735,#102736,#102737,
#102738,#102739,#102740,#102741,#102742,#102743,#102744,#102745,#102746,
#102747,#102748,#102749,#102750,#102751,#102752,#102753,#102754,#102755,
#102756,#102757,#102758,#102759,#102760,#102761,#102762,#102763,#102764,
#102765,#102766,#102767,#102768,#102769,#102770,#102771,#102772,#102773,
#102774,#102775,#102776,#102777,#102778,#102779,#102780,#102781,#102782,
#102783,#102784,#102785,#102786,#102787,#102788,#102789,#102790,#102791,
#102792,#102793,#102794,#102795,#102796,#102797,#102798,#102799,#102800,
#102801,#102802,#102803,#102804,#102805,#102806,#102807,#102808,#102809,
#102810,#102811,#102812,#102813,#102814,#102815,#102816,#102817,#102818,
#102819,#102820),.UNSPECIFIED.,.F.,.F.,(4,3,3,3,3,3,3,3,3,3,3,3,3,3,3,3,
3,3,3,3,3,3,3,3,3,3,3,3,3,3,3,3,3,3,3,3,3,3,3,3,3,3,3,3,3,3,3,3,3,3,3,3,
3,3,3,3,3,3,3,3,3,3,3,3,3,3,3,3,3,3,3,4),(0.,0.000919480979116562,0.00186665391132835,
0.00222303890370072,0.00246023501007185,0.00308006741789906,0.00345996891983423,
0.00369035251510777,0.00469778641362987,0.00492047002014368,0.00577875096523307,
0.00593619564291911,0.0061505875251796,0.00691217011921717,0.00717505541494648,
0.00738070503021552,0.00841742521903872,0.00946182449544707,0.00965322408999174,
0.00984094004028725,0.010527196801318,0.0108924604402717,0.0110710575453231,
0.0121313588744037,0.012301175050359,0.0135614282722574,0.014608084951402,
0.0147614100604307,0.0155427428164244,0.0158457881834858,0.0159915275654665,
0.0170831200839182,0.0172216450705023,0.0180163683085078,0.0183201098374356,
0.0184517625755382,0.0191739816007739,0.0195568018131331,0.019681880080574,
0.0208560722381215,0.022030264395669,0.0221421150906457,0.0229078739325012,
0.0232673524625759,0.0233722325956815,0.0245048134750371,0.0246023501007174,
0.0254360756729617,0.0257427490373535,0.0258324676057532,0.026634352472116,
0.0269811460780054,0.027062585110789,0.028478718853076,0.0294588729843419,
0.0295228201208608,0.0310014861472409,0.0319371442892162,0.0319830551309325,
0.0335148785822243,0.0344145418676412,0.0344432901410042,0.0353749506243358,
0.0356525636344977,0.0356734076460401,0.0368901184213511,0.036903525151076,
0.0375185839035939,0.0381336426561119,0.0385671407304433,0.0389938437394035,
0.0393637601611478),.UNSPECIFIED.);
#2335=B_SPLINE_CURVE_WITH_KNOTS('',3,(#102826,#102827,#102828,#102829,#102830,
#102831,#102832,#102833,#102834,#102835,#102836,#102837,#102838,#102839,
#102840,#102841,#102842,#102843,#102844,#102845,#102846,#102847,#102848,
#102849,#102850,#102851,#102852,#102853,#102854,#102855,#102856,#102857,
#102858,#102859,#102860,#102861,#102862,#102863,#102864,#102865,#102866,
#102867,#102868,#102869,#102870,#102871,#102872,#102873,#102874,#102875),
 .UNSPECIFIED.,.T.,.F.,(4,2,2,2,2,2,2,2,2,2,2,2,2,2,2,2,2,2,2,2,2,2,2,2,
4),(-7.68142619696719,-7.4403709942257,-7.19931579148422,-6.71720538600124,
-6.23913751686332,-6.00010358229436,-5.7610696477254,-5.52203571315644,
-5.28300177858748,-4.80493390944956,-4.32282350396658,-4.08176830122509,
-3.8407130984836,-3.59965789574211,-3.35860269300062,-2.87649228751764,
-2.39842441837972,-2.15939048381076,-1.9203565492418,-1.68132261467284,
-1.44228868010388,-0.964220810965958,-0.482110405482979,-0.24105520274149,
0.),.UNSPECIFIED.);
#2336=B_SPLINE_CURVE_WITH_KNOTS('',3,(#102878,#102879,#102880,#102881,#102882,
#102883,#102884,#102885,#102886,#102887,#102888,#102889,#102890,#102891,
#102892,#102893,#102894,#102895,#102896,#102897,#102898,#102899,#102900,
#102901,#102902,#102903,#102904,#102905,#102906,#102907,#102908,#102909,
#102910,#102911,#102912,#102913,#102914,#102915,#102916,#102917,#102918,
#102919,#102920,#102921,#102922,#102923,#102924,#102925,#102926,#102927,
#102928,#102929),.UNSPECIFIED.,.F.,.F.,(4,2,2,2,2,2,2,2,2,2,2,2,2,2,2,2,
2,2,2,2,2,2,2,2,2,4),(0.0396248818917468,0.0420848252462546,0.0433147969235084,
0.0445447686007623,0.0457747402780162,0.04700471195527,0.0494646553097779,
0.0506946269870318,0.0519245986642857,0.0543845420187934,0.0556145136960473,
0.0568444853733012,0.059304428727809,0.0605344004050629,0.0617643720823168,
0.0629943437595707,0.0642243154368246,0.0666842587913323,0.0679142304685862,
0.0691442021458401,0.0703741738230939,0.0716041455003478,0.0740640888548556,
0.0752940605321094,0.0765240322093633,0.078983975563871),.UNSPECIFIED.);
#2337=B_SPLINE_CURVE_WITH_KNOTS('',3,(#102933,#102934,#102935,#102936,#102937,
#102938,#102939,#102940,#102941,#102942,#102943,#102944,#102945,#102946,
#102947,#102948,#102949,#102950,#102951,#102952,#102953,#102954,#102955,
#102956,#102957),.UNSPECIFIED.,.F.,.F.,(4,3,3,3,3,3,3,3,4),(0.050029146080417,
0.0504604958563081,0.0505100567684285,0.0509435518624711,0.05099096745644,
0.0514718781444515,0.0516554513507709,0.0517123334884572,0.0519527888232233),
 .UNSPECIFIED.);
#2338=B_SPLINE_CURVE_WITH_KNOTS('',3,(#102960,#102961,#102962,#102963,#102964,
#102965,#102966,#102967,#102968,#102969,#102970,#102971,#102972,#102973,
#102974,#102975,#102976,#102977,#102978,#102979,#102980,#102981,#102982,
#102983,#102984,#102985,#102986,#102987,#102988,#102989,#102990,#102991,
#102992,#102993,#102994,#102995,#102996,#102997,#102998,#102999,#103000,
#103001,#103002,#103003,#103004,#103005,#103006,#103007,#103008,#103009),
 .UNSPECIFIED.,.F.,.F.,(4,2,2,2,2,2,2,2,2,2,2,2,2,2,2,2,2,2,2,2,2,2,2,2,
4),(0.0520590732062046,0.0550614663094106,0.0558120645852121,0.0565626628610136,
0.0580638594126165,0.0595650559642194,0.0610662525158222,0.0640686456190281,
0.0655698421706312,0.0670710387222342,0.0700734318254404,0.0715746283770435,
0.0730758249286466,0.0760782180318527,0.0775794145834557,0.0790806111350588,
0.0805818076866618,0.0820830042382649,0.0850853973414709,0.0880877904446769,
0.0910901835478829,0.094092576651089,0.095593773202692,0.097094969754295,
0.100097362857501),.UNSPECIFIED.);
#2339=B_SPLINE_CURVE_WITH_KNOTS('',3,(#103010,#103011,#103012,#103013,#103014,
#103015,#103016,#103017,#103018,#103019),.UNSPECIFIED.,.F.,.F.,(4,2,2,2,
4),(0.0480426030336095,0.0490467205767583,0.050050838119907,0.0510549556630558,
0.0520590732062046),.UNSPECIFIED.);
#2340=B_SPLINE_CURVE_WITH_KNOTS('',3,(#103020,#103021,#103022,#103023,#103024,
#103025,#103026,#103027,#103028,#103029,#103030,#103031,#103032,#103033,
#103034,#103035,#103036,#103037,#103038,#103039,#103040,#103041,#103042,
#103043,#103044,#103045,#103046,#103047,#103048,#103049,#103050,#103051,
#103052,#103053,#103054,#103055,#103056,#103057,#103058,#103059,#103060,
#103061,#103062,#103063,#103064,#103065,#103066,#103067,#103068,#103069,
#103070,#103071,#103072,#103073,#103074,#103075,#103076,#103077,#103078,
#103079,#103080,#103081,#103082,#103083,#103084,#103085,#103086,#103087,
#103088,#103089,#103090,#103091,#103092,#103093,#103094,#103095,#103096,
#103097,#103098,#103099,#103100,#103101,#103102,#103103,#103104,#103105,
#103106,#103107,#103108,#103109,#103110,#103111,#103112,#103113,#103114,
#103115,#103116,#103117,#103118,#103119,#103120,#103121,#103122,#103123,
#103124,#103125,#103126,#103127,#103128,#103129,#103130,#103131,#103132,
#103133,#103134,#103135,#103136,#103137,#103138,#103139,#103140,#103141,
#103142,#103143,#103144,#103145,#103146,#103147,#103148,#103149,#103150,
#103151,#103152,#103153,#103154,#103155,#103156,#103157,#103158,#103159,
#103160,#103161,#103162,#103163,#103164,#103165,#103166,#103167,#103168,
#103169,#103170,#103171,#103172,#103173,#103174,#103175,#103176,#103177,
#103178,#103179,#103180,#103181,#103182,#103183,#103184,#103185,#103186,
#103187,#103188,#103189,#103190,#103191,#103192,#103193,#103194,#103195,
#103196,#103197,#103198,#103199,#103200,#103201,#103202,#103203,#103204,
#103205,#103206,#103207,#103208,#103209,#103210,#103211,#103212,#103213,
#103214,#103215,#103216,#103217,#103218,#103219,#103220,#103221,#103222,
#103223,#103224),.UNSPECIFIED.,.F.,.F.,(4,3,3,3,3,3,3,3,3,3,3,3,3,3,3,3,
3,3,3,3,3,3,3,3,3,3,3,3,3,3,3,3,3,3,3,3,3,3,3,3,3,3,3,3,3,3,3,3,3,3,3,3,
3,3,3,3,3,3,3,3,3,3,3,3,3,3,3,3,4),(0.051952788832463,0.0523437358727679,
0.0530396348010499,0.0532815940436916,0.0535165769936827,0.0550803651549024,
0.0565315459304904,0.0566441533161221,0.0573435791058262,0.0581553062489572,
0.0582079414773418,0.0597781972481066,0.0613355177997813,0.0614004919138027,
0.0627595431987245,0.0628993059610011,0.0630224461823624,0.0644630941222208,
0.066266557277031,0.0675906704446604,0.0678890579253495,0.0688036127964717,
0.0691544586058802,0.0695121857757964,0.0705623247811663,0.0707182467671,
0.0722820349283198,0.0727603963114585,0.0735729358548261,0.0738458230895395,
0.0743855823551034,0.0760111644019604,0.0769733994119791,0.0775954188216906,
0.0776371348320698,0.077755293492589,0.0783329590757904,0.0784502993253913,
0.078537187573199,0.079263366729678,0.0801009757344188,0.0816647638956387,
0.0825143971297319,0.0832285520568585,0.0853698372315117,0.0857634780397394,
0.0863561283792982,0.0870860429658589,0.087387128745137,0.087919916540518,
0.0890096229688163,0.0894837047017378,0.0904433744732693,0.0906319233369378,
0.0910474928629577,0.0918522904268146,0.0922540308854937,0.0926112810241775,
0.0947257451253502,0.0954981621844028,0.095738857346617,0.0966800930537847,
0.0971208482525778,0.0973026455078367,0.098172856385979,0.0987443411160432,
0.0988664336690564,0.100855253343851,0.101994009991496),.UNSPECIFIED.);
#2341=B_SPLINE_CURVE_WITH_KNOTS('',3,(#103281,#103282,#103283,#103284,#103285,
#103286,#103287,#103288,#103289,#103290,#103291,#103292,#103293,#103294,
#103295,#103296,#103297,#103298,#103299,#103300,#103301,#103302,#103303,
#103304,#103305),.UNSPECIFIED.,.F.,.F.,(4,3,3,3,3,3,3,3,4),(3.14159265358979,
3.53429173528852,3.92699081698724,4.31968989868597,4.71238898038469,5.10508806208341,
5.49778714378214,5.89048622548086,6.28318530717959),.UNSPECIFIED.);
#2342=B_SPLINE_CURVE_WITH_KNOTS('',3,(#103330,#103331,#103332,#103333,#103334,
#103335,#103336,#103337,#103338,#103339,#103340,#103341,#103342,#103343,
#103344,#103345,#103346,#103347,#103348,#103349,#103350,#103351,#103352,
#103353,#103354,#103355,#103356,#103357,#103358,#103359,#103360,#103361,
#103362,#103363,#103364,#103365,#103366,#103367,#103368,#103369,#103370,
#103371,#103372,#103373,#103374,#103375,#103376,#103377,#103378,#103379,
#103380,#103381,#103382,#103383,#103384,#103385,#103386,#103387,#103388,
#103389,#103390,#103391,#103392,#103393,#103394,#103395,#103396,#103397,
#103398,#103399,#103400,#103401,#103402,#103403,#103404,#103405,#103406,
#103407,#103408,#103409,#103410,#103411,#103412,#103413,#103414,#103415,
#103416,#103417,#103418,#103419,#103420,#103421,#103422,#103423,#103424,
#103425,#103426,#103427,#103428,#103429,#103430,#103431,#103432,#103433,
#103434,#103435,#103436,#103437,#103438,#103439,#103440,#103441,#103442,
#103443,#103444,#103445,#103446,#103447,#103448,#103449,#103450,#103451,
#103452,#103453,#103454,#103455,#103456,#103457,#103458,#103459,#103460,
#103461,#103462,#103463,#103464,#103465,#103466,#103467,#103468,#103469,
#103470,#103471,#103472,#103473,#103474),.UNSPECIFIED.,.F.,.F.,(4,3,3,3,
3,3,3,3,3,3,3,3,3,3,3,3,3,3,3,3,3,3,3,3,3,3,3,3,3,3,3,3,3,3,3,3,3,3,3,3,
3,3,3,3,3,3,3,3,4),(0.00175934839635171,0.00264937165101398,0.00281190034136253,
0.0029216913114692,0.00345298327300805,0.00350284378635125,0.00386445228637335,
0.00408494443402798,0.0045643909026228,0.0050528930166323,0.00525444258302874,
0.00573754835263548,0.00596955617639502,0.00642216793328342,0.00688988455817184,
0.00702210812140589,0.00759015068768004,0.00807466006641675,0.00817328490518593,
0.00875592930808911,0.00912721201142762,0.00950595668589702,0.00965348798393305,
0.0099194404906703,0.0101797639564385,0.0106406398760054,0.0110804857260411,
0.0112323159014494,0.0116411351505613,0.0120566663811269,0.0122406856381238,
0.0122848678464602,0.0133374197914711,0.013400690819128,0.0139807325781765,
0.014389971736482,0.014560858934484,0.0150704291285518,0.0154425236814929,
0.015721211993778,0.0159687996539983,0.0164950756265037,0.0168813629537642,
0.0174094393522003,0.0174613379315374,0.0175476275715146,0.0180410999382036,
0.0185583303726384,0.0186001795165254),.UNSPECIFIED.);
#2343=B_SPLINE_CURVE_WITH_KNOTS('',3,(#103494,#103495,#103496,#103497,#103498,
#103499),.UNSPECIFIED.,.F.,.F.,(4,2,4),(0.0186001795165254,0.0194806906344087,
0.0203612017522921),.UNSPECIFIED.);
#2344=B_SPLINE_CURVE_WITH_KNOTS('',3,(#103501,#103502,#103503,#103504,#103505,
#103506,#103507,#103508,#103509,#103510,#103511,#103512,#103513,#103514,
#103515,#103516,#103517,#103518,#103519,#103520,#103521,#103522,#103523,
#103524,#103525),.UNSPECIFIED.,.F.,.F.,(4,3,3,3,3,3,3,3,4),(0.,0.392699081698723,
0.785398163397448,1.17809724509617,1.5707963267949,1.96349540849362,2.35619449019234,
2.74889357189107,3.14159265358979),.UNSPECIFIED.);
#2345=B_SPLINE_CURVE_WITH_KNOTS('',3,(#103581,#103582,#103583,#103584,#103585,
#103586,#103587,#103588,#103589,#103590,#103591,#103592,#103593,#103594,
#103595,#103596,#103597,#103598,#103599,#103600,#103601,#103602,#103603,
#103604,#103605,#103606,#103607,#103608,#103609,#103610,#103611,#103612,
#103613,#103614,#103615,#103616,#103617,#103618,#103619,#103620,#103621,
#103622,#103623,#103624,#103625,#103626,#103627,#103628,#103629,#103630,
#103631,#103632,#103633,#103634,#103635,#103636,#103637,#103638,#103639,
#103640,#103641,#103642,#103643,#103644,#103645,#103646,#103647,#103648,
#103649,#103650,#103651,#103652,#103653,#103654,#103655,#103656,#103657,
#103658,#103659,#103660,#103661,#103662,#103663,#103664,#103665,#103666,
#103667,#103668,#103669,#103670,#103671,#103672,#103673,#103674,#103675,
#103676,#103677,#103678,#103679,#103680,#103681,#103682,#103683,#103684,
#103685,#103686,#103687,#103688,#103689,#103690,#103691,#103692,#103693,
#103694,#103695,#103696,#103697,#103698,#103699,#103700,#103701,#103702,
#103703,#103704,#103705,#103706,#103707,#103708,#103709,#103710,#103711,
#103712,#103713,#103714,#103715,#103716,#103717,#103718,#103719,#103720,
#103721,#103722,#103723,#103724,#103725,#103726,#103727,#103728,#103729,
#103730,#103731,#103732,#103733,#103734,#103735,#103736,#103737,#103738,
#103739,#103740,#103741,#103742,#103743,#103744,#103745,#103746,#103747,
#103748,#103749,#103750,#103751,#103752,#103753,#103754,#103755,#103756,
#103757,#103758,#103759,#103760,#103761,#103762,#103763,#103764,#103765,
#103766,#103767,#103768,#103769,#103770,#103771,#103772,#103773,#103774,
#103775,#103776,#103777,#103778,#103779,#103780,#103781,#103782,#103783,
#103784,#103785,#103786,#103787,#103788,#103789,#103790,#103791),
 .UNSPECIFIED.,.F.,.F.,(4,3,3,3,3,3,3,3,3,3,3,3,3,3,3,3,3,3,3,3,3,3,3,3,
3,3,3,3,3,3,3,3,3,3,3,3,3,3,3,3,3,3,3,3,3,3,3,3,3,3,3,3,3,3,3,3,3,3,3,3,
3,3,3,3,3,3,3,3,3,3,4),(0.040185803323384,0.0413856421772186,0.0414967660328816,
0.0415142729908562,0.0422433040571364,0.0428064492703943,0.0428427426583284,
0.0441360070801344,0.0454292715019403,0.0454996819932728,0.0464712818980196,
0.0467431693953829,0.046828151660745,0.0477888706112027,0.0480601760161093,
0.0481566213282172,0.0494297557376454,0.0505688592524304,0.0507028901470736,
0.0508135606631617,0.05208542808009,0.0533572954970183,0.0534704999981061,
0.0543381547764814,0.0546885729894539,0.0547989696655784,0.0560224031717165,
0.0561274393330507,0.0570603085182229,0.0579546885749173,0.0586976832404988,
0.0587843786679952,0.0596803976577506,0.0605641633514876,0.0613811379148684,
0.0614413180029398,0.0626283973946032,0.0627251289020388,0.062769787670412,
0.0640695304066911,0.0640982573378843,0.0654135246131901,0.0654267270053565,
0.06664916102305,0.0667551966728288,0.0667570806288456,0.0685560798819261,
0.0694121360077733,0.069439147524414,0.0705885834253151,0.0707406056752456,
0.0707771747906088,0.0719257582233479,0.0720690753427178,0.072112636943896,
0.0733975450101901,0.0734454921936495,0.0745326321982652,0.0747260146776624,
0.0747757157272833,0.0763275630104522,0.0773829540126069,0.0774278153549588,
0.0787114236800792,0.0787493996324898,0.0798784815282868,0.0800398933475515,
0.0800679872775242,0.0812906359372778,0.0824788066968498,0.0826968326824961),
 .UNSPECIFIED.);
#2346=B_SPLINE_CURVE_WITH_KNOTS('',3,(#103793,#103794,#103795,#103796,#103797,
#103798,#103799,#103800,#103801,#103802,#103803,#103804,#103805,#103806,
#103807,#103808,#103809,#103810,#103811,#103812,#103813,#103814,#103815,
#103816,#103817,#103818,#103819,#103820,#103821,#103822,#103823,#103824,
#103825,#103826,#103827,#103828,#103829,#103830,#103831,#103832,#103833,
#103834,#103835,#103836,#103837,#103838,#103839,#103840,#103841,#103842,
#103843,#103844,#103845,#103846,#103847,#103848,#103849,#103850,#103851,
#103852,#103853,#103854,#103855,#103856,#103857,#103858,#103859,#103860,
#103861,#103862,#103863,#103864,#103865,#103866,#103867,#103868,#103869,
#103870,#103871,#103872,#103873,#103874,#103875,#103876,#103877,#103878,
#103879,#103880,#103881,#103882,#103883,#103884,#103885,#103886,#103887,
#103888,#103889,#103890,#103891,#103892,#103893,#103894,#103895,#103896,
#103897,#103898,#103899,#103900,#103901,#103902,#103903,#103904,#103905,
#103906,#103907,#103908,#103909,#103910,#103911,#103912,#103913,#103914,
#103915,#103916,#103917,#103918,#103919,#103920,#103921,#103922,#103923,
#103924,#103925,#103926,#103927,#103928,#103929,#103930,#103931,#103932,
#103933,#103934,#103935,#103936,#103937,#103938,#103939,#103940,#103941,
#103942,#103943,#103944,#103945,#103946,#103947,#103948,#103949,#103950,
#103951,#103952,#103953,#103954,#103955,#103956,#103957,#103958,#103959,
#103960,#103961,#103962,#103963,#103964,#103965,#103966,#103967,#103968,
#103969,#103970,#103971,#103972,#103973,#103974,#103975,#103976,#103977,
#103978,#103979,#103980,#103981,#103982,#103983,#103984,#103985,#103986,
#103987,#103988,#103989,#103990,#103991,#103992,#103993,#103994,#103995,
#103996,#103997,#103998,#103999,#104000),.UNSPECIFIED.,.F.,.F.,(4,3,3,3,
3,3,3,3,3,3,3,3,3,3,3,3,3,3,3,3,3,3,3,3,3,3,3,3,3,3,3,3,3,3,3,3,3,3,3,3,
3,3,3,3,3,3,3,3,3,3,3,3,3,3,3,3,3,3,3,3,3,3,3,3,3,3,3,3,3,4),(0.00187081090387685,
0.00271260435667731,0.00362268902859222,0.00470889615954381,0.0051051220936109,
0.00599081910916758,0.00672227768847788,0.00778276880661964,0.00833943328334486,
0.00942599481829403,0.0104998696456864,0.0115737444730788,0.0123823222705124,
0.0131909000679459,0.0142060282593073,0.014808055662813,0.01570812992925,
0.0164252112576801,0.0170970893496278,0.0177619833705879,0.0180423668525471,
0.0190026734096154,0.019950368561138,0.0208795972594237,0.0212766780422811,
0.0222765344942613,0.0232692933815865,0.0242499722556784,0.0245109892320151,
0.0253195670294486,0.025748847290095,0.0261281448268821,0.0270598184241075,
0.027745300421749,0.0287399757306573,0.029362456016616,0.0299897241643628,
0.0306190954857662,0.030979611611483,0.0318533830950452,0.032738324644238,
0.0336403396115833,0.034213922801217,0.0352558542716105,0.035831078396084,
0.0367181867272328,0.0374482339909511,0.038496060625361,0.0395893029030231,
0.0406825451806851,0.0413774134031154,0.0420918307001871,0.0422997007755522,
0.0433943605093511,0.0439168563704194,0.0450236020511531,0.0455340119652865,
0.04634258976272,0.0470220692265429,0.0471511675601536,0.048029000435268,
0.0488603746190341,0.0496350381747758,0.050385478749888,0.0511032328730903,
0.0517960284135848,0.0520026343447552,0.0527090367424346,0.0534533603415312,
0.0536197899396224),.UNSPECIFIED.);
#2347=B_SPLINE_CURVE_WITH_KNOTS('',3,(#104001,#104002,#104003,#104004,#104005,
#104006,#104007,#104008,#104009,#104010,#104011,#104012,#104013,#104014,
#104015,#104016,#104017,#104018,#104019,#104020,#104021,#104022,#104023,
#104024,#104025,#104026,#104027,#104028,#104029,#104030,#104031,#104032,
#104033,#104034,#104035,#104036,#104037,#104038,#104039,#104040,#104041,
#104042,#104043,#104044,#104045,#104046,#104047,#104048,#104049,#104050,
#104051,#104052),.UNSPECIFIED.,.F.,.F.,(4,2,2,2,2,2,2,2,2,2,2,2,2,2,2,2,
2,2,2,2,2,2,2,2,2,4),(0.000252666121810611,0.00283443432717517,0.00412531842985747,
0.00541620253253977,0.00799797073790439,0.00928885484058674,0.0105797389432691,
0.0118706230459514,0.0131615071486338,0.0157432753539985,0.0170341594566808,
0.018325043559363,0.0196159276620453,0.0209068117647276,0.0234885799700922,
0.0247794640727745,0.0260703481754568,0.0286521163808214,0.0299430004835037,
0.031233884586186,0.0338156527915506,0.0363974209969151,0.0376883050995973,
0.0389791892022796,0.0402700733049619,0.0415609574076441),.UNSPECIFIED.);
#2348=B_SPLINE_CURVE_WITH_KNOTS('',3,(#104846,#104847,#104848,#104849,#104850,
#104851,#104852,#104853,#104854,#104855,#104856,#104857,#104858,#104859,
#104860,#104861,#104862,#104863,#104864,#104865,#104866,#104867,#104868,
#104869,#104870,#104871,#104872,#104873,#104874,#104875,#104876,#104877,
#104878,#104879,#104880,#104881,#104882,#104883,#104884,#104885,#104886,
#104887,#104888,#104889,#104890,#104891,#104892,#104893,#104894,#104895,
#104896,#104897,#104898,#104899,#104900,#104901,#104902,#104903,#104904,
#104905,#104906,#104907,#104908,#104909,#104910,#104911,#104912,#104913,
#104914,#104915,#104916,#104917,#104918,#104919,#104920,#104921,#104922,
#104923,#104924,#104925,#104926,#104927,#104928,#104929,#104930,#104931,
#104932,#104933,#104934,#104935,#104936,#104937,#104938,#104939,#104940,
#104941,#104942,#104943,#104944,#104945,#104946,#104947,#104948,#104949,
#104950,#104951,#104952,#104953,#104954,#104955,#104956,#104957,#104958,
#104959,#104960,#104961,#104962,#104963,#104964,#104965,#104966,#104967,
#104968,#104969,#104970,#104971,#104972,#104973,#104974,#104975,#104976,
#104977,#104978,#104979,#104980,#104981,#104982,#104983,#104984,#104985,
#104986,#104987,#104988,#104989,#104990,#104991,#104992,#104993,#104994,
#104995,#104996,#104997,#104998,#104999,#105000,#105001,#105002,#105003,
#105004,#105005,#105006,#105007,#105008,#105009,#105010,#105011,#105012,
#105013,#105014,#105015,#105016,#105017,#105018,#105019,#105020,#105021,
#105022,#105023,#105024,#105025,#105026,#105027,#105028,#105029,#105030,
#105031,#105032,#105033,#105034,#105035,#105036,#105037,#105038,#105039,
#105040,#105041,#105042,#105043,#105044,#105045,#105046,#105047,#105048,
#105049,#105050,#105051,#105052,#105053,#105054,#105055,#105056),
 .UNSPECIFIED.,.F.,.F.,(4,3,3,3,3,3,3,3,3,3,3,3,3,3,3,3,3,3,3,3,3,3,3,3,
3,3,3,3,3,3,3,3,3,3,3,3,3,3,3,3,3,3,3,3,3,3,3,3,3,3,3,3,3,3,3,3,3,3,3,3,
3,3,3,3,3,3,3,3,3,3,4),(0.040185803323384,0.041385642177111,0.0414967660328816,
0.0415142729908562,0.0422433040571271,0.0428064492703943,0.0428427426583284,
0.0441360070801344,0.0454292715019403,0.0454996819932728,0.0464712818980038,
0.046743169395383,0.046828151660745,0.0477888706109921,0.0480601760161093,
0.0481566213282172,0.0494297557376455,0.050568859252351,0.0507028901470738,
0.0508135606631617,0.05208542808009,0.0533572954970184,0.0534704999981061,
0.0543381547765564,0.0546885729894539,0.0547989696655784,0.0560224031717167,
0.0561274393330507,0.0570603085182185,0.0579546885749104,0.0586976832404988,
0.0587843786679952,0.0596803976577581,0.0605641633515005,0.0613811379148684,
0.0614413180029398,0.062628397394844,0.0627251289020388,0.062769787670412,
0.0640695304066911,0.0640982573378843,0.0654135246131901,0.0654267270053565,
0.0666491610230946,0.0667551966728288,0.0667570806288456,0.0685560798820927,
0.0694121360077733,0.069439147524414,0.0705885834257307,0.0707406056752456,
0.0707771747906088,0.071925758222996,0.0720690753427178,0.072112636943896,
0.0733975450101901,0.0734454921936494,0.0745326321983655,0.0747260146776624,
0.0747757157272833,0.0763275630090201,0.0773829540126069,0.0774278153549589,
0.0787114236800792,0.0787493996324898,0.0798784815281566,0.0800398933475515,
0.0800679872775241,0.0812906359372127,0.0824788066966756,0.0826968326824961),
 .UNSPECIFIED.);
#2349=B_SPLINE_CURVE_WITH_KNOTS('',3,(#105185,#105186,#105187,#105188,#105189,
#105190,#105191,#105192,#105193,#105194,#105195,#105196,#105197,#105198,
#105199,#105200,#105201,#105202,#105203,#105204,#105205,#105206,#105207,
#105208,#105209,#105210,#105211,#105212,#105213,#105214,#105215,#105216,
#105217,#105218,#105219,#105220,#105221,#105222,#105223,#105224,#105225,
#105226,#105227,#105228,#105229,#105230,#105231,#105232,#105233,#105234,
#105235,#105236,#105237,#105238,#105239,#105240,#105241,#105242,#105243,
#105244,#105245,#105246,#105247,#105248,#105249,#105250,#105251,#105252,
#105253,#105254,#105255,#105256,#105257,#105258,#105259,#105260,#105261,
#105262,#105263,#105264,#105265,#105266,#105267,#105268,#105269,#105270,
#105271,#105272,#105273,#105274,#105275,#105276,#105277,#105278,#105279,
#105280,#105281,#105282,#105283,#105284,#105285,#105286,#105287,#105288,
#105289,#105290,#105291,#105292,#105293,#105294,#105295,#105296,#105297,
#105298,#105299,#105300,#105301,#105302,#105303,#105304,#105305,#105306,
#105307,#105308,#105309,#105310,#105311,#105312,#105313,#105314,#105315,
#105316,#105317,#105318,#105319,#105320,#105321,#105322,#105323,#105324,
#105325,#105326,#105327,#105328,#105329,#105330,#105331,#105332,#105333,
#105334,#105335,#105336,#105337,#105338,#105339,#105340,#105341,#105342,
#105343,#105344,#105345,#105346,#105347,#105348,#105349,#105350,#105351,
#105352,#105353,#105354,#105355,#105356,#105357,#105358,#105359,#105360,
#105361,#105362,#105363,#105364,#105365,#105366,#105367,#105368,#105369,
#105370,#105371,#105372,#105373,#105374,#105375,#105376,#105377,#105378,
#105379,#105380,#105381,#105382,#105383,#105384,#105385,#105386,#105387,
#105388,#105389,#105390,#105391,#105392),.UNSPECIFIED.,.F.,.F.,(4,3,3,3,
3,3,3,3,3,3,3,3,3,3,3,3,3,3,3,3,3,3,3,3,3,3,3,3,3,3,3,3,3,3,3,3,3,3,3,3,
3,3,3,3,3,3,3,3,3,3,3,3,3,3,3,3,3,3,3,3,3,3,3,3,3,3,3,3,3,4),(0.00187081090387685,
0.00271260435668075,0.00362268902859932,0.0047088961595475,0.0051051220936109,
0.00599081910917896,0.00672227768847788,0.00778276880660481,0.00833943328334486,
0.00942599481828414,0.0104998696456815,0.0115737444730788,0.0123823222705124,
0.0131909000679459,0.0142060282592838,0.014808055662813,0.0157081299291953,
0.0164252112576801,0.0170970893496155,0.0177619833705849,0.0180423668525471,
0.0190026734096196,0.0199503685611344,0.0208795972594173,0.0212766780422811,
0.0222765344942665,0.0232692933815988,0.0242499722556933,0.0245109892320151,
0.0253195670294486,0.0257488472900959,0.0261281448268821,0.0270598184241087,
0.027745300421749,0.0287399757306378,0.029362456016616,0.0299897241643665,
0.0306190954857663,0.030979611611483,0.0318533830950635,0.0327383246442732,
0.0336403396115905,0.034213922801217,0.0352558542716055,0.035831078396084,
0.0367181867272809,0.0374482339909511,0.0384960606253587,0.0395893029030219,
0.0406825451806851,0.0413774134031492,0.0420918307002056,0.0422997007755522,
0.0433943605093599,0.0439168563704194,0.045023602051156,0.0455340119652865,
0.04634258976272,0.0470220692264879,0.0471511675601536,0.04802900043527,
0.0488603746190379,0.0496350381747814,0.050385478749888,0.0511032328730951,
0.0517960284135882,0.0520026343447552,0.0527090367424356,0.0534533603415317,
0.0536197899396224),.UNSPECIFIED.);
#2350=B_SPLINE_CURVE_WITH_KNOTS('',3,(#105393,#105394,#105395,#105396,#105397,
#105398,#105399,#105400,#105401,#105402,#105403,#105404,#105405,#105406,
#105407,#105408,#105409,#105410,#105411,#105412,#105413,#105414,#105415,
#105416,#105417,#105418,#105419,#105420,#105421,#105422,#105423,#105424,
#105425,#105426,#105427,#105428,#105429,#105430,#105431,#105432,#105433,
#105434,#105435,#105436,#105437,#105438,#105439,#105440,#105441,#105442,
#105443,#105444),.UNSPECIFIED.,.F.,.F.,(4,2,2,2,2,2,2,2,2,2,2,2,2,2,2,2,
2,2,2,2,2,2,2,2,2,4),(0.000252666121810611,0.00283443432717517,0.00412531842985747,
0.00541620253253977,0.00799797073790439,0.00928885484058674,0.0105797389432691,
0.0118706230459514,0.0131615071486338,0.0157432753539985,0.0170341594566808,
0.018325043559363,0.0196159276620453,0.0209068117647276,0.0234885799700922,
0.0247794640727745,0.0260703481754568,0.0286521163808214,0.0299430004835037,
0.031233884586186,0.0338156527915506,0.0363974209969151,0.0376883050995973,
0.0389791892022796,0.0402700733049619,0.0415609574076441),.UNSPECIFIED.);
#2351=B_SPLINE_CURVE_WITH_KNOTS('',3,(#105992,#105993,#105994,#105995,#105996,
#105997),.UNSPECIFIED.,.F.,.F.,(4,2,4),(0.,0.000429537087177428,0.000859074174354856),
 .UNSPECIFIED.);
#2352=B_SPLINE_CURVE_WITH_KNOTS('',3,(#106005,#106006,#106007,#106008,#106009,
#106010,#106011,#106012,#106013,#106014,#106015,#106016,#106017,#106018,
#106019,#106020,#106021,#106022,#106023,#106024,#106025,#106026),
 .UNSPECIFIED.,.F.,.F.,(4,3,3,3,3,3,3,4),(1.38777878078145E-17,0.000188059268556367,
0.000214020122328391,0.000428040244656768,0.000642060366985145,0.000721468200741508,
0.000798165243973893,0.000856080489313522),.UNSPECIFIED.);
#2353=B_SPLINE_CURVE_WITH_KNOTS('',3,(#106031,#106032,#106033,#106034,#106035,
#106036,#106037,#106038,#106039,#106040,#106041,#106042,#106043,#106044,
#106045,#106046,#106047,#106048,#106049,#106050,#106051,#106052),
 .UNSPECIFIED.,.F.,.F.,(4,3,3,3,3,3,3,4),(0.,7.79304036744801E-5,0.000158641952040327,
0.00021866555281504,0.000437331105630081,0.000655996658445121,0.000848137862261846,
0.000874662211260162),.UNSPECIFIED.);
#2354=B_SPLINE_CURVE_WITH_KNOTS('',3,(#106060,#106061,#106062,#106063,#106064,
#106065),.UNSPECIFIED.,.F.,.F.,(4,2,4),(1.38777878078145E-17,0.000428854539313667,
0.00085770907862732),.UNSPECIFIED.);
#2355=B_SPLINE_CURVE_WITH_KNOTS('',3,(#106068,#106069,#106070,#106071,#106072,
#106073,#106074,#106075,#106076,#106077,#106078,#106079,#106080,#106081,
#106082,#106083,#106084,#106085,#106086,#106087,#106088,#106089,#106090,
#106091,#106092,#106093,#106094,#106095,#106096,#106097,#106098,#106099,
#106100,#106101,#106102,#106103,#106104,#106105,#106106,#106107,#106108,
#106109,#106110,#106111,#106112,#106113,#106114,#106115,#106116),
 .UNSPECIFIED.,.F.,.F.,(4,3,3,3,3,3,3,3,3,3,3,3,3,3,3,3,4),(0.,0.000172655359583005,
0.000214472733930129,0.000345356453129998,0.00040194427569836,0.000426371089395591,
0.000551635597584684,0.000633757499696936,0.000803888551396719,0.000836019899938085,
0.00100450939519915,0.00116399791926213,0.00120583282709508,0.00122724609507386,
0.00139282382099101,0.00156108680528541,0.00160777710279344),
 .UNSPECIFIED.);
#2356=B_SPLINE_CURVE_WITH_KNOTS('',3,(#106119,#106120,#106121,#106122,#106123,
#106124,#106125,#106126,#106127,#106128,#106129,#106130,#106131,#106132,
#106133,#106134,#106135,#106136,#106137,#106138,#106139,#106140,#106141,
#106142,#106143,#106144,#106145,#106146,#106147,#106148,#106149,#106150,
#106151,#106152,#106153,#106154,#106155,#106156,#106157,#106158,#106159,
#106160,#106161),.UNSPECIFIED.,.F.,.F.,(4,3,3,3,3,3,3,3,3,3,3,3,3,3,4),
(0.,0.00097071180919006,0.00109494777504685,0.00211704535126196,0.00219853891044863,
0.00223735799194462,0.00296830632650111,0.00376840487765825,0.00443540273119751,
0.00447471598388924,0.00577557119702807,0.00668663775574798,0.00671207397583386,
0.00820153167491206,0.00894943196777848),.UNSPECIFIED.);
#2357=B_SPLINE_CURVE_WITH_KNOTS('',3,(#106237,#106238,#106239,#106240,#106241,
#106242,#106243,#106244,#106245,#106246,#106247,#106248,#106249,#106250,
#106251,#106252,#106253,#106254,#106255,#106256,#106257,#106258,#106259,
#106260,#106261,#106262,#106263,#106264,#106265,#106266,#106267,#106268,
#106269,#106270,#106271,#106272,#106273,#106274,#106275,#106276,#106277,
#106278,#106279),.UNSPECIFIED.,.F.,.F.,(4,3,3,3,3,3,3,3,3,3,3,3,3,3,4),
(0.,0.000970711791819082,0.0010949477750237,0.00211704534669127,0.00219853891044869,
0.00223735799194468,0.00296830632781392,0.0037684048802517,0.00443540273119768,
0.00447471598388935,0.00577557115859329,0.0066866377557481,0.00671207397583403,
0.00820153142505179,0.00894943196777871),.UNSPECIFIED.);
#2358=B_SPLINE_CURVE_WITH_KNOTS('',3,(#106281,#106282,#106283,#106284,#106285,
#106286,#106287,#106288,#106289,#106290,#106291,#106292,#106293,#106294,
#106295,#106296,#106297,#106298,#106299,#106300,#106301,#106302,#106303,
#106304,#106305,#106306,#106307,#106308,#106309,#106310,#106311,#106312,
#106313,#106314,#106315,#106316,#106317,#106318,#106319,#106320,#106321,
#106322,#106323,#106324,#106325,#106326,#106327,#106328,#106329,#106330,
#106331,#106332,#106333,#106334,#106335),.UNSPECIFIED.,.F.,.F.,(4,3,3,3,
3,3,3,3,3,3,3,3,3,3,3,3,3,3,4),(0.,0.00011263901958812,0.000224528452761069,
0.000335876538867614,0.000378780084712497,0.000403082142219989,0.000535803330753571,
0.000671115250426468,0.000770572167488891,0.000806164284439978,0.000922051893666942,
0.000990761403542633,0.00108645700528024,0.00114554120348879,0.00118215260701784,
0.00126269703837782,0.00139376821745601,0.00152129814935798,0.00161232856888021),
 .UNSPECIFIED.);
#2359=B_SPLINE_CURVE_WITH_KNOTS('',3,(#106339,#106340,#106341,#106342,#106343,
#106344,#106345,#106346,#106347,#106348,#106349,#106350,#106351,#106352,
#106353,#106354,#106355,#106356,#106357,#106358,#106359,#106360,#106361,
#106362,#106363,#106364,#106365,#106366,#106367,#106368,#106369,#106370,
#106371,#106372,#106373,#106374,#106375,#106376,#106377,#106378,#106379,
#106380,#106381,#106382,#106383,#106384,#106385,#106386,#106387),
 .UNSPECIFIED.,.F.,.F.,(4,3,3,3,3,3,3,3,3,3,3,3,3,3,3,3,4),(0.,0.000167524699450898,
0.000332355096398968,0.00037843928853009,0.000399734851137576,0.000557949097585033,
0.000724839875838272,0.000767514974710719,0.000799469702275151,0.000968665570301764,
0.001093241519164,0.00117491201007438,0.00119920455341273,0.00132936882535921,
0.00138564559355697,0.00155735189376102,0.0015989394045503),
 .UNSPECIFIED.);
#2360=B_SPLINE_CURVE_WITH_KNOTS('',3,(#106393,#106394,#106395,#106396,#106397,
#106398,#106399,#106400,#106401,#106402),.UNSPECIFIED.,.F.,.F.,(4,2,2,2,
4),(0.,0.000406430200333951,0.000812860400667902,0.00121929060100185,0.0016257208013358),
 .UNSPECIFIED.);
#2361=B_SPLINE_CURVE_WITH_KNOTS('',2,(#106608,#106609,#106610),
 .UNSPECIFIED.,.F.,.F.,(3,3),(0.,0.976475345222877),.UNSPECIFIED.);
#2362=B_SPLINE_CURVE_WITH_KNOTS('',2,(#106613,#106614,#106615),
 .UNSPECIFIED.,.F.,.F.,(3,3),(0.,0.976475345222875),.UNSPECIFIED.);
#2363=B_SPLINE_CURVE_WITH_KNOTS('',3,(#106618,#106619,#106620,#106621,#106622,
#106623,#106624,#106625,#106626,#106627,#106628,#106629,#106630,#106631,
#106632,#106633,#106634,#106635,#106636,#106637,#106638,#106639,#106640,
#106641,#106642,#106643,#106644,#106645,#106646,#106647),.UNSPECIFIED.,
 .F.,.F.,(4,2,2,2,2,2,2,2,2,2,2,2,2,2,4),(0.344961523665507,0.345864796648895,
0.383397870327102,0.424095939866412,0.467988143099323,0.511077186362632,
0.54898968974865,0.584500295299886,0.594525424662999,0.600320181695393,
0.604744384514621,0.610406509282569,0.620117456540854,0.65644704575773,
0.689892766641171),.UNSPECIFIED.);
#2364=B_SPLINE_CURVE_WITH_KNOTS('',3,(#106648,#106649,#106650,#106651,#106652,
#106653,#106654,#106655,#106656,#106657,#106658,#106659,#106660,#106661,
#106662,#106663,#106664,#106665,#106666,#106667,#106668,#106669,#106670,
#106671,#106672,#106673,#106674,#106675,#106676,#106677,#106678),
 .UNSPECIFIED.,.F.,.F.,(4,3,2,2,2,2,2,2,2,2,2,2,2,2,4),(0.689892766641171,
0.689896902267116,0.727453888182981,0.768250651128135,0.812331190066408,
0.855408230286001,0.893310548156423,0.92927077257846,0.939389872106851,
0.945235691660359,0.949698027562582,0.955408685939896,0.965204348659296,
1.00190831825778,1.03485842593262),.UNSPECIFIED.);
#2365=B_SPLINE_CURVE_WITH_KNOTS('',3,(#106681,#106682,#106683,#106684,#106685,
#106686,#106687,#106688,#106689,#106690,#106691,#106692,#106693,#106694,
#106695,#106696,#106697,#106698,#106699,#106700,#106701,#106702,#106703,
#106704,#106705,#106706,#106707,#106708,#106709,#106710),.UNSPECIFIED.,
 .F.,.F.,(4,2,2,2,2,2,2,2,2,2,2,2,2,2,4),(0.345009231853205,0.378244613783399,
0.420328023332794,0.464149227428814,0.506016437255813,0.543856281234535,
0.565813314722034,0.573688761513894,0.578687760592208,0.583312543899507,
0.589347859881529,0.601974028845171,0.645360854368571,0.669727951332881,
0.689924578750462),.UNSPECIFIED.);
#2366=B_SPLINE_CURVE_WITH_KNOTS('',3,(#106711,#106712,#106713,#106714,#106715,
#106716,#106717,#106718,#106719,#106720,#106721,#106722,#106723,#106724,
#106725,#106726,#106727,#106728,#106729,#106730,#106731,#106732,#106733,
#106734,#106735,#106736,#106737,#106738,#106739,#106740,#106741,#106742,
#106743),.UNSPECIFIED.,.F.,.F.,(4,3,2,2,2,2,2,2,2,2,2,2,2,2,2,4),(0.689924578750462,
0.68993991408243,0.729536128270215,0.772335318064264,0.815994793172523,
0.857023119234385,0.897080615078242,0.913006093260828,0.919873093228367,
0.924198675336843,0.928927860867944,0.935400644318752,0.950143092826215,
0.993632031191612,1.02921319219025,1.03494914593564),.UNSPECIFIED.);
#2367=B_SPLINE_CURVE_WITH_KNOTS('',3,(#106746,#106747,#106748,#106749,#106750,
#106751,#106752,#106753,#106754,#106755,#106756,#106757,#106758,#106759,
#106760,#106761,#106762,#106763,#106764,#106765,#106766,#106767,#106768,
#106769,#106770,#106771,#106772,#106773,#106774,#106775),.UNSPECIFIED.,
 .F.,.F.,(4,2,2,2,2,2,2,2,2,2,2,2,2,2,4),(0.346938551924172,0.378440651179373,
0.421240632795595,0.464958543144959,0.506100204098339,0.54769824656266,
0.561705730881516,0.567440855372351,0.572216908670401,0.577088174639597,
0.584110215881562,0.601759745786392,0.645470178035154,0.67174709596461,
0.693868053317107),.UNSPECIFIED.);
#2368=B_SPLINE_CURVE_WITH_KNOTS('',3,(#106776,#106777,#106778,#106779,#106780,
#106781,#106782,#106783,#106784,#106785,#106786,#106787,#106788,#106789,
#106790,#106791,#106792,#106793,#106794,#106795,#106796,#106797,#106798,
#106799,#106800,#106801,#106802,#106803,#106804,#106805,#106806,#106807,
#106808),.UNSPECIFIED.,.F.,.F.,(4,3,2,2,2,2,2,2,2,2,2,2,2,2,2,4),(0.693868053317107,
0.693886488938521,0.734477998053822,0.778249159437278,0.82165549791726,
0.860952275386496,0.900557922887624,0.9098397687485,0.915807211744923,0.920529512902708,
0.925787413564647,0.934409438144411,0.963342903225506,0.99595895476539,
1.03255538373466,1.04082504086269),.UNSPECIFIED.);
#2369=B_SPLINE_CURVE_WITH_KNOTS('',3,(#106811,#106812,#106813,#106814,#106815,
#106816,#106817,#106818,#106819,#106820,#106821,#106822,#106823,#106824,
#106825,#106826,#106827,#106828,#106829,#106830,#106831,#106832,#106833,
#106834,#106835,#106836,#106837,#106838,#106839,#106840),.UNSPECIFIED.,
 .F.,.F.,(4,2,2,2,2,2,2,2,2,2,2,2,2,2,4),(0.40209989847735,0.40660288487618,
0.45450907004254,0.50530634558164,0.554814904564047,0.59717232465397,0.631280174008838,
0.641914587848182,0.648218209580416,0.653710157873207,0.660536877518756,
0.673512975029444,0.724577287352579,0.76556777577582,0.80412687291917),
 .UNSPECIFIED.);
#2370=B_SPLINE_CURVE_WITH_KNOTS('',3,(#106841,#106842,#106843,#106844,#106845,
#106846,#106847,#106848,#106849,#106850,#106851,#106852,#106853,#106854,
#106855,#106856,#106857,#106858,#106859,#106860,#106861,#106862,#106863,
#106864,#106865,#106866,#106867,#106868,#106869,#106870,#106871),
 .UNSPECIFIED.,.F.,.F.,(4,3,2,2,2,2,2,2,2,2,2,2,2,2,4),(0.80412687291917,
0.804148773323481,0.852022764489678,0.902845917375077,0.952486292226827,
0.993805484048557,1.03219252264168,1.04331428445352,1.04983910175525,1.0553827665417,
1.06210101783198,1.07437911638428,1.12547022180492,1.16619918742605,1.20624867180083),
 .UNSPECIFIED.);
#2371=B_SPLINE_CURVE_WITH_KNOTS('',3,(#106874,#106875,#106876,#106877,#106878,
#106879,#106880,#106881,#106882,#106883,#106884,#106885,#106886,#106887,
#106888,#106889,#106890,#106891,#106892,#106893,#106894,#106895,#106896,
#106897,#106898,#106899,#106900,#106901,#106902,#106903),.UNSPECIFIED.,
 .F.,.F.,(4,2,2,2,2,2,2,2,2,2,2,2,2,2,4),(0.465633214662796,0.465954622179084,
0.521966589812807,0.580586441169497,0.637296003323887,0.689137640373933,
0.718928717554103,0.730000425807782,0.737142867836688,0.743827353101546,
0.75265656150245,0.771478832925962,0.830418451259722,0.87860301952136,0.931247240689163),
 .UNSPECIFIED.);
#2372=B_SPLINE_CURVE_WITH_KNOTS('',3,(#106904,#106905,#106906,#106907,#106908,
#106909,#106910,#106911,#106912,#106913,#106914,#106915,#106916,#106917,
#106918,#106919,#106920,#106921,#106922,#106923,#106924,#106925,#106926,
#106927,#106928,#106929,#106930,#106931,#106932,#106933,#106934),
 .UNSPECIFIED.,.F.,.F.,(4,3,2,2,2,2,2,2,2,2,2,2,2,2,4),(0.931247240689163,
0.931260314529748,0.987731629074412,1.04629867668198,1.1027854627381,1.15459842582523,
1.18443011275622,1.19558842708719,1.20281567458219,1.20960223615331,1.21860242711111,
1.23793740883115,1.29692637503074,1.34499044045235,1.39689352919254),
 .UNSPECIFIED.);
#2373=B_SPLINE_CURVE_WITH_KNOTS('',3,(#106937,#106938,#106939,#106940,#106941,
#106942,#106943,#106944,#106945,#106946,#106947,#106948,#106949,#106950,
#106951,#106952,#106953,#106954,#106955,#106956,#106957,#106958,#106959,
#106960,#106961,#106962,#106963,#106964,#106965,#106966),.UNSPECIFIED.,
 .F.,.F.,(4,2,2,2,2,2,2,2,2,2,2,2,2,2,4),(0.465633282607765,0.476375394601976,
0.528663123786714,0.584725991294486,0.64333981569091,0.700032605532688,
0.75318841685325,0.780812469598235,0.792201294755606,0.799151250192924,
0.806562525317479,0.816363786652937,0.837233438559275,0.896272823761712,
0.931207257834669),.UNSPECIFIED.);
#2374=B_SPLINE_CURVE_WITH_KNOTS('',3,(#106967,#106968,#106969,#106970,#106971,
#106972,#106973,#106974,#106975,#106976,#106977,#106978,#106979,#106980,
#106981,#106982,#106983,#106984,#106985,#106986,#106987,#106988,#106989,
#106990,#106991,#106992,#106993,#106994,#106995,#106996,#106997),
 .UNSPECIFIED.,.F.,.F.,(4,3,2,2,2,2,2,2,2,2,2,2,2,2,4),(0.931207257834669,
0.931212131173444,0.982986506311894,1.03869641281129,1.09737760956241,1.15460057349639,
1.20473347532919,1.24264303882272,1.25581895302213,1.26401634376283,1.27147456569156,
1.28101576638611,1.3002403817436,1.35942112225154,1.39684541378121),
 .UNSPECIFIED.);
#2375=B_SPLINE_CURVE_WITH_KNOTS('',3,(#107000,#107001,#107002,#107003,#107004,
#107005,#107006,#107007,#107008,#107009,#107010,#107011,#107012,#107013,
#107014,#107015,#107016,#107017,#107018,#107019,#107020,#107021,#107022,
#107023,#107024,#107025,#107026,#107027,#107028,#107029),.UNSPECIFIED.,
 .F.,.F.,(4,2,2,2,2,2,2,2,2,2,2,2,2,2,4),(0.402110712104017,0.41872237939637,
0.463540332761411,0.511693032899096,0.562458220229975,0.611784757547159,
0.655989679395872,0.685075113511474,0.695759884692332,0.702594719239558,
0.708942989788131,0.717248297339878,0.734614608729777,0.757078010388911,
0.804098343149695),.UNSPECIFIED.);
#2376=B_SPLINE_CURVE_WITH_KNOTS('',3,(#107030,#107031,#107032,#107033,#107034,
#107035,#107036,#107037,#107038,#107039,#107040,#107041,#107042,#107043,
#107044,#107045,#107046,#107047,#107048,#107049,#107050,#107051,#107052,
#107053,#107054,#107055,#107056,#107057,#107058,#107059,#107060),
 .UNSPECIFIED.,.F.,.F.,(4,3,2,2,2,2,2,2,2,2,2,2,2,2,4),(0.804098343149695,
0.804102668688614,0.84772337182573,0.894852633655198,0.945590312254206,
0.995686686428953,1.04088233415374,1.08317466217842,1.0957257184503,1.10311305075802,
1.10939434530366,1.11700267358253,1.1308607530412,1.18173687996318,1.20621338079263),
 .UNSPECIFIED.);
#2377=B_SPLINE_CURVE_WITH_KNOTS('',3,(#107063,#107064,#107065,#107066,#107067,
#107068,#107069,#107070,#107071,#107072,#107073,#107074,#107075,#107076,
#107077,#107078,#107079,#107080,#107081,#107082,#107083,#107084,#107085,
#107086,#107087,#107088,#107089,#107090,#107091,#107092),.UNSPECIFIED.,
 .F.,.F.,(4,2,2,2,2,2,2,2,2,2,2,2,2,2,4),(0.346992260168847,0.349530800286321,
0.38627866048027,0.426164077376898,0.469071116498728,0.512754181117553,
0.553769559902602,0.597242326448665,0.60786359204204,0.614714583583491,
0.620138976121923,0.626171706766658,0.636023024924637,0.668251949000156,
0.693906585258332),.UNSPECIFIED.);
#2378=B_SPLINE_CURVE_WITH_KNOTS('',3,(#107093,#107094,#107095,#107096,#107097,
#107098,#107099,#107100,#107101,#107102,#107103,#107104,#107105,#107106,
#107107,#107108,#107109,#107110,#107111,#107112,#107113,#107114,#107115,
#107116,#107117,#107118,#107119,#107120,#107121,#107122,#107123),
 .UNSPECIFIED.,.F.,.F.,(4,3,2,2,2,2,2,2,2,2,2,2,2,2,4),(0.693906585258332,
0.693912249614694,0.730513622803473,0.770348783422489,0.813285096596775,
0.857012732304838,0.898242274447473,0.940578720860681,0.953105519851957,
0.959832426695438,0.965425958564593,0.971115461808322,0.979275907192453,
0.999461241194498,1.04090450978354),.UNSPECIFIED.);
#2379=B_SPLINE_CURVE_WITH_KNOTS('',3,(#107126,#107127,#107128,#107129,#107130,
#107131,#107132,#107133,#107134,#107135,#107136,#107137,#107138,#107139,
#107140,#107141,#107142,#107143,#107144,#107145,#107146,#107147,#107148,
#107149,#107150,#107151,#107152,#107153,#107154,#107155),.UNSPECIFIED.,
 .F.,.F.,(4,2,2,2,2,2,2,2,2,2,2,2,2,2,4),(0.344951413336473,0.351263812252431,
0.387082240635607,0.426231505582015,0.468477015007063,0.512252444209689,
0.553957162909252,0.593842901031732,0.61206567233696,0.620069861726783,
0.62514830287496,0.630721476371493,0.638371191430603,0.655771612190609,
0.689837953066993),.UNSPECIFIED.);
#2380=B_SPLINE_CURVE_WITH_KNOTS('',3,(#107156,#107157,#107158,#107159,#107160,
#107161,#107162,#107163,#107164,#107165,#107166,#107167,#107168,#107169,
#107170,#107171,#107172,#107173,#107174,#107175,#107176,#107177,#107178,
#107179,#107180,#107181,#107182,#107183,#107184,#107185,#107186),
 .UNSPECIFIED.,.F.,.F.,(4,3,2,2,2,2,2,2,2,2,2,2,2,2,4),(0.689837953066993,
0.689842314231483,0.725044567858473,0.763732437183778,0.805601673607611,
0.849510712956202,0.891773097528399,0.92955257745313,0.954274008555207,
0.963486286429678,0.969426005177119,0.974977209335325,0.982290928535058,
0.997772229719781,1.03479372756796),.UNSPECIFIED.);
#2381=B_SPLINE_CURVE_WITH_KNOTS('',3,(#107189,#107190,#107191,#107192,#107193,
#107194,#107195,#107196,#107197,#107198,#107199,#107200,#107201,#107202,
#107203,#107204,#107205,#107206,#107207,#107208,#107209,#107210,#107211,
#107212,#107213,#107214,#107215,#107216,#107217,#107218),.UNSPECIFIED.,
 .F.,.F.,(4,2,2,2,2,2,2,2,2,2,2,2,2,2,4),(0.465611109415691,0.467801168335867,
0.521727320971316,0.579585905539099,0.637746437962676,0.691244410595713,
0.743421186764121,0.756490984203512,0.765054461682126,0.771929024386779,
0.779678856588505,0.792584330974367,0.837109914470849,0.88241247221796,
0.931180169103219),.UNSPECIFIED.);
#2382=B_SPLINE_CURVE_WITH_KNOTS('',3,(#107219,#107220,#107221,#107222,#107223,
#107224,#107225,#107226,#107227,#107228,#107229,#107230,#107231,#107232,
#107233,#107234,#107235,#107236,#107237,#107238,#107239,#107240,#107241,
#107242,#107243,#107244,#107245,#107246,#107247,#107248,#107249),
 .UNSPECIFIED.,.F.,.F.,(4,3,2,2,2,2,2,2,2,2,2,2,2,2,4),(0.931180169103219,
0.931190700960073,0.985359391461488,1.04360629966377,1.1017009783728,1.15517235673943,
1.20857836605825,1.22186490429068,1.23055817840862,1.23753111124902,1.24538769484831,
1.25846672994737,1.30364877307048,1.34893703322522,1.39680181037576),
 .UNSPECIFIED.);
#2383=B_SPLINE_CURVE_WITH_KNOTS('',3,(#107252,#107253,#107254,#107255,#107256,
#107257,#107258,#107259,#107260,#107261,#107262,#107263,#107264,#107265,
#107266,#107267,#107268,#107269,#107270,#107271,#107272,#107273,#107274,
#107275,#107276,#107277,#107278,#107279,#107280,#107281),.UNSPECIFIED.,
 .F.,.F.,(4,2,2,2,2,2,2,2,2,2,2,2,2,2,4),(0.402104921302211,0.40543549785947,
0.451285049701036,0.500507144213953,0.551060081418048,0.599064996386686,
0.647473246556257,0.664439861589408,0.672224467659491,0.678150589012572,
0.684415149542514,0.693989426680647,0.721067191394358,0.757870178076073,
0.804134169471361),.UNSPECIFIED.);
#2384=B_SPLINE_CURVE_WITH_KNOTS('',3,(#107282,#107283,#107284,#107285,#107286,
#107287,#107288,#107289,#107290,#107291,#107292,#107293,#107294,#107295,
#107296,#107297,#107298,#107299,#107300,#107301,#107302,#107303,#107304,
#107305,#107306,#107307,#107308,#107309,#107310,#107311,#107312),
 .UNSPECIFIED.,.F.,.F.,(4,3,2,2,2,2,2,2,2,2,2,2,2,2,4),(0.804134169471361,
0.804148839679616,0.849980894175911,0.899293831723779,0.949871636716832,
0.998054666218493,1.04512970460772,1.06464658368308,1.07326751351405,1.07931411697895,
1.08546450846965,1.09429459053202,1.11625370584153,1.16727831526251,1.20625376098183),
 .UNSPECIFIED.);
#2385=B_SPLINE_CURVE_WITH_KNOTS('',3,(#107315,#107316,#107317,#107318,#107319,
#107320,#107321,#107322,#107323,#107324,#107325,#107326,#107327,#107328,
#107329,#107330,#107331,#107332,#107333,#107334,#107335,#107336,#107337,
#107338,#107339,#107340,#107341,#107342,#107343,#107344,#107345,#107346),
 .UNSPECIFIED.,.F.,.F.,(4,2,2,2,2,2,2,2,2,2,2,2,2,2,2,4),(0.346968393948669,
0.349681440565168,0.38848093502615,0.43028464532601,0.474246146607666,0.516732383605594,
0.554321336137149,0.579626948171219,0.588407112189454,0.593879794000829,
0.598870391068503,0.605276295008421,0.618284444515363,0.634910302035259,
0.666887126081608,0.693786984354256),.UNSPECIFIED.);
#2386=B_SPLINE_CURVE_WITH_KNOTS('',3,(#107347,#107348,#107349,#107350,#107351,
#107352,#107353,#107354,#107355,#107356,#107357,#107358,#107359,#107360,
#107361,#107362,#107363,#107364,#107365,#107366,#107367,#107368,#107369,
#107370,#107371,#107372,#107373,#107374,#107375,#107376,#107377),
 .UNSPECIFIED.,.F.,.F.,(4,3,2,2,2,2,2,2,2,2,2,2,2,2,4),(0.693786984354256,
0.693797831240842,0.732509231161277,0.774310918514032,0.818303801091492,
0.860899596877086,0.89782782159184,0.925658037889556,0.934852364047167,
0.940451300977366,0.945471484446629,0.951800265319109,0.964281244127681,
1.00801838154444,1.04076622518951),.UNSPECIFIED.);
#2387=B_SPLINE_CURVE_WITH_KNOTS('',3,(#107380,#107381,#107382,#107383,#107384,
#107385,#107386,#107387,#107388,#107389,#107390,#107391,#107392,#107393,
#107394,#107395,#107396,#107397,#107398,#107399,#107400,#107401,#107402,
#107403,#107404,#107405,#107406,#107407,#107408,#107409),.UNSPECIFIED.,
 .F.,.F.,(4,2,2,2,2,2,2,2,2,2,2,2,2,2,4),(0.235057050857596,0.292167847167887,
0.348533232507195,0.401524038651083,0.427641552568632,0.43803416448635,
0.444965886579442,0.451624678980447,0.460685531955045,0.481055806932457,
0.540180732620175,0.588617276937645,0.641338245174112,0.698017197142133,
0.700679974573688),.UNSPECIFIED.);
#2388=B_SPLINE_CURVE_WITH_KNOTS('',3,(#107410,#107411,#107412,#107413,#107414,
#107415,#107416,#107417,#107418,#107419,#107420,#107421,#107422,#107423,
#107424,#107425,#107426,#107427,#107428,#107429,#107430,#107431,#107432,
#107433,#107434,#107435,#107436,#107437,#107438,#107439,#107440,#107441,
#107442),.UNSPECIFIED.,.F.,.F.,(4,2,2,2,2,2,2,2,2,3,2,2,2,2,2,4),(0.700679974573688,
0.75654544780487,0.81278852129577,0.865332254711976,0.892716069810879,0.903401685258624,
0.910463492023461,0.917199943822292,0.92629568345056,0.93118074096206,0.964614669288399,
1.00756753716764,1.05596925831,1.1084746812396,1.1647789115579,1.16623779181966),
 .UNSPECIFIED.);
#2389=B_SPLINE_CURVE_WITH_KNOTS('',3,(#107445,#107446,#107447,#107448,#107449,
#107450,#107451,#107452,#107453,#107454,#107455,#107456,#107457,#107458,
#107459,#107460,#107461,#107462,#107463,#107464,#107465,#107466,#107467,
#107468,#107469,#107470,#107471,#107472),.UNSPECIFIED.,.F.,.F.,(4,2,2,2,
2,2,2,2,2,2,2,2,2,4),(0.402076330997609,0.452506126987892,0.501960460596592,
0.544174046662978,0.578024001620107,0.588408509033419,0.594526453801688,
0.599886720261833,0.606484916474157,0.61902420194864,0.670057777031238,
0.710940214646799,0.755738002101945,0.804142170440177),.UNSPECIFIED.);
#2390=B_SPLINE_CURVE_WITH_KNOTS('',3,(#107473,#107474,#107475,#107476,#107477,
#107478,#107479,#107480,#107481,#107482,#107483,#107484,#107485,#107486,
#107487,#107488,#107489,#107490,#107491,#107492,#107493,#107494,#107495,
#107496,#107497,#107498,#107499,#107500,#107501,#107502,#107503,#107504,
#107505),.UNSPECIFIED.,.F.,.F.,(4,3,2,2,2,2,2,2,2,2,2,2,2,2,2,4),(0.804142170440177,
0.80418148149889,0.854955500213731,0.904274720656576,0.946542921138172,
0.980094405895,0.990499100597637,0.996663986623071,1.0020365722695,1.00872009768154,
1.02145302090351,1.07252538866429,1.11332010049143,1.15793086937237,1.20589739254531,
1.2062578124965),.UNSPECIFIED.);
#2391=B_SPLINE_CURVE_WITH_KNOTS('',3,(#107508,#107509,#107510,#107511,#107512,
#107513,#107514,#107515,#107516,#107517,#107518,#107519,#107520,#107521,
#107522,#107523,#107524,#107525,#107526,#107527,#107528,#107529,#107530,
#107531,#107532,#107533,#107534,#107535,#107536,#107537),.UNSPECIFIED.,
 .F.,.F.,(4,2,2,2,2,2,2,2,2,2,2,2,2,2,4),(0.346941605198609,0.373567910257419,
0.417315713383248,0.458600424228201,0.499168359176905,0.514509718036955,
0.521095418591649,0.525235214587882,0.529755122461575,0.535931877421553,
0.549970599447536,0.593803901426271,0.629554481206799,0.663265304325165,
0.693877848521967),.UNSPECIFIED.);
#2392=B_SPLINE_CURVE_WITH_KNOTS('',3,(#107538,#107539,#107540,#107541,#107542,
#107543,#107544,#107545,#107546,#107547,#107548,#107549,#107550,#107551,
#107552,#107553,#107554,#107555,#107556,#107557,#107558,#107559,#107560,
#107561,#107562,#107563,#107564,#107565,#107566,#107567,#107568,#107569,
#107570),.UNSPECIFIED.,.F.,.F.,(4,3,2,2,2,2,2,2,2,2,2,2,2,2,2,4),(0.693877848521967,
0.693902648209849,0.738154480356306,0.781315453318249,0.81887107307235,
0.855429713474733,0.86408961971932,0.869698324340631,0.874166418409527,
0.879174671198948,0.887469616252308,0.916149834072149,0.948595112072686,
0.985080349849095,1.02476161037089,1.04084425340846),.UNSPECIFIED.);
#2393=B_SPLINE_CURVE_WITH_KNOTS('',3,(#107573,#107574,#107575,#107576,#107577,
#107578,#107579,#107580,#107581,#107582,#107583,#107584,#107585,#107586,
#107587,#107588,#107589,#107590,#107591,#107592,#107593,#107594,#107595,
#107596,#107597,#107598,#107599,#107600,#107601,#107602),.UNSPECIFIED.,
 .F.,.F.,(4,2,2,2,2,2,2,2,2,2,2,2,2,2,4),(0.345013218218888,0.376774001203925,
0.42054829328545,0.462160314370201,0.500129576849606,0.520667701551143,
0.52798814139206,0.532626762104135,0.536915397032792,0.542511761139062,
0.554238383666024,0.597657877890008,0.632740518823297,0.662888343785372,
0.689951584416554),.UNSPECIFIED.);
#2394=B_SPLINE_CURVE_WITH_KNOTS('',3,(#107603,#107604,#107605,#107606,#107607,
#107608,#107609,#107610,#107611,#107612,#107613,#107614,#107615,#107616,
#107617,#107618,#107619,#107620,#107621,#107622,#107623,#107624,#107625,
#107626,#107627,#107628,#107629,#107630,#107631,#107632,#107633,#107634,
#107635),.UNSPECIFIED.,.F.,.F.,(4,3,2,2,2,2,2,2,2,2,2,2,2,2,2,4),(0.689951584416554,
0.690031175819254,0.733367493896147,0.77682341922442,0.816779853506336,
0.859352194286298,0.869120219591277,0.874371575626691,0.878753589986668,
0.883235408613554,0.889725075757398,0.906246615748049,0.949592112952706,
0.985377265897947,1.02453248644676,1.03504439403814),.UNSPECIFIED.);
#2395=B_SPLINE_CURVE_WITH_KNOTS('',3,(#107638,#107639,#107640,#107641,#107642,
#107643,#107644,#107645,#107646,#107647,#107648,#107649,#107650,#107651,
#107652,#107653,#107654,#107655,#107656,#107657,#107658,#107659,#107660,
#107661,#107662,#107663,#107664,#107665,#107666,#107667),.UNSPECIFIED.,
 .F.,.F.,(4,2,2,2,2,2,2,2,2,2,2,2,2,2,4),(0.465678353925176,0.47947283256797,
0.538189478865465,0.595588351848854,0.645484311587241,0.685163547761563,
0.697581925416736,0.704952011159827,0.711377663530687,0.719369776764823,
0.734570748252662,0.793813012992343,0.841382671384268,0.888689663004795,
0.931208999842379),.UNSPECIFIED.);
#2396=B_SPLINE_CURVE_WITH_KNOTS('',3,(#107668,#107669,#107670,#107671,#107672,
#107673,#107674,#107675,#107676,#107677,#107678,#107679,#107680,#107681,
#107682,#107683,#107684,#107685,#107686,#107687,#107688,#107689,#107690,
#107691,#107692,#107693,#107694,#107695,#107696,#107697,#107698),
 .UNSPECIFIED.,.F.,.F.,(4,3,2,2,2,2,2,2,2,2,2,2,2,2,4),(0.931208999842379,
0.931226011304187,0.990115852016496,1.04793975658026,1.09935327814772,1.14838855309107,
1.16193535150595,1.16970866979478,1.17627256265779,1.18405220552771,1.19799767304289,
1.25690684108002,1.30400469548165,1.35545656622951,1.39690436522936),
 .UNSPECIFIED.);
#2397=B_SPLINE_CURVE_WITH_KNOTS('',3,(#107701,#107702,#107703,#107704,#107705,
#107706,#107707,#107708,#107709,#107710,#107711,#107712,#107713,#107714,
#107715,#107716,#107717,#107718,#107719,#107720,#107721,#107722,#107723,
#107724,#107725,#107726,#107727,#107728,#107729,#107730),.UNSPECIFIED.,
 .F.,.F.,(4,2,2,2,2,2,2,2,2,2,2,2,2,2,4),(0.345014549679634,0.386080567219748,
0.430067136651455,0.472735539508552,0.507148500076332,0.54032355653713,
0.549335158653087,0.554493138732614,0.558409474651096,0.563401158008921,
0.571922511028402,0.603836011650846,0.636683621167115,0.665362157489524,
0.689861699781107),.UNSPECIFIED.);
#2398=B_SPLINE_CURVE_WITH_KNOTS('',3,(#107731,#107732,#107733,#107734,#107735,
#107736,#107737,#107738,#107739,#107740,#107741,#107742,#107743,#107744,
#107745,#107746,#107747,#107748,#107749,#107750,#107751,#107752,#107753,
#107754,#107755,#107756,#107757,#107758,#107759,#107760,#107761,#107762,
#107763),.UNSPECIFIED.,.F.,.F.,(4,3,2,2,2,2,2,2,2,2,2,2,2,2,2,4),(0.689861699781107,
0.689885375867946,0.731365309643938,0.775350418287857,0.81793713912826,
0.854547668609502,0.885597013512973,0.894397666004993,0.899531658955586,
0.903879917755934,0.909136579589272,0.918721215817642,0.961979632551239,
0.996553294581035,1.0346901002883,1.03489992554758),.UNSPECIFIED.);
#2399=B_SPLINE_CURVE_WITH_KNOTS('',3,(#107766,#107767,#107768,#107769,#107770,
#107771,#107772,#107773,#107774,#107775,#107776,#107777,#107778,#107779,
#107780,#107781,#107782,#107783,#107784,#107785,#107786,#107787,#107788,
#107789,#107790,#107791,#107792,#107793,#107794,#107795),.UNSPECIFIED.,
 .F.,.F.,(4,2,2,2,2,2,2,2,2,2,2,2,2,2,4),(0.346984223850431,0.383731720043479,
0.427698885613696,0.470189395445113,0.506972584188474,0.533779035203666,
0.542258080208027,0.547330337125225,0.551374818695336,0.556768695551526,
0.566676832623525,0.610454623908707,0.645453349283034,0.670975380391931,
0.693877493439465),.UNSPECIFIED.);
#2400=B_SPLINE_CURVE_WITH_KNOTS('',3,(#107796,#107797,#107798,#107799,#107800,
#107801,#107802,#107803,#107804,#107805,#107806,#107807,#107808,#107809,
#107810,#107811,#107812,#107813,#107814,#107815,#107816,#107817,#107818,
#107819,#107820,#107821,#107822,#107823,#107824,#107825,#107826,#107827,
#107828),.UNSPECIFIED.,.F.,.F.,(4,3,2,2,2,2,2,2,2,2,2,2,2,2,2,4),(0.693877493439465,
0.693901141466938,0.73629287301764,0.780170172633046,0.82212462450606,0.860287561330358,
0.882073393862794,0.889866480431594,0.894811040195521,0.899385691506485,
0.905358118387944,0.917873381778568,0.961665207927685,0.997075301414317,
1.03584749510858,1.04088536531737),.UNSPECIFIED.);
#2401=B_SPLINE_CURVE_WITH_KNOTS('',3,(#107831,#107832,#107833,#107834,#107835,
#107836,#107837,#107838,#107839,#107840,#107841,#107842,#107843,#107844,
#107845,#107846,#107847,#107848,#107849,#107850,#107851,#107852,#107853,
#107854,#107855,#107856,#107857,#107858,#107859,#107860),.UNSPECIFIED.,
 .F.,.F.,(4,2,2,2,2,2,2,2,2,2,2,2,2,2,4),(0.402049162873731,0.433559116857739,
0.484300694332918,0.533445518859648,0.576861073004399,0.606036271221772,
0.615810656424386,0.621810686769589,0.627224521241337,0.634098780951983,
0.64782988545491,0.698680764045257,0.739769115378164,0.773562070585536,
0.804032136336491),.UNSPECIFIED.);
#2402=B_SPLINE_CURVE_WITH_KNOTS('',3,(#107861,#107862,#107863,#107864,#107865,
#107866,#107867,#107868,#107869,#107870,#107871,#107872,#107873,#107874,
#107875,#107876,#107877,#107878,#107879,#107880,#107881,#107882,#107883,
#107884,#107885,#107886,#107887,#107888,#107889,#107890,#107891,#107892,
#107893),.UNSPECIFIED.,.F.,.F.,(4,3,2,2,2,2,2,2,2,2,2,2,2,2,2,4),(0.804032136336491,
0.804062641115949,0.85398261454777,0.904386995172918,0.951492381667235,
1.00139949755574,1.01359242137182,1.02087251185226,1.02641430638157,1.03227768692638,
1.04126037251219,1.06694413485489,1.1031299344385,1.14435539546706,1.18931296399841,
1.20611180398968),.UNSPECIFIED.);
#2403=B_SPLINE_CURVE_WITH_KNOTS('',3,(#107896,#107897,#107898,#107899,#107900,
#107901,#107902,#107903,#107904,#107905,#107906,#107907,#107908,#107909,
#107910,#107911,#107912,#107913,#107914,#107915,#107916,#107917,#107918,
#107919,#107920,#107921,#107922,#107923),.UNSPECIFIED.,.F.,.F.,(4,2,2,2,
2,2,2,2,2,2,2,2,2,4),(0.346923834548804,0.347492471562536,0.358682387319118,
0.381656594144265,0.4255057126124,0.463082280883045,0.503624903071197,0.547176174235262,
0.590646242398574,0.630908946566644,0.663727463065525,0.677240358541954,
0.686199062140188,0.693838455970793),.UNSPECIFIED.);
#2404=B_SPLINE_CURVE_WITH_KNOTS('',3,(#107924,#107925,#107926,#107927,#107928,
#107929,#107930,#107931,#107932,#107933,#107934,#107935,#107936,#107937,
#107938,#107939,#107940,#107941,#107942,#107943,#107944,#107945,#107946,
#107947,#107948,#107949),.UNSPECIFIED.,.F.,.F.,(4,2,2,2,2,2,2,2,2,2,2,2,
4),(0.693839419404206,0.704606750411996,0.725889158263226,0.769735770694385,
0.807180923266053,0.847680428772612,0.891263177530282,0.934787064816284,
0.975315507846382,1.00980363380315,1.02369855675641,1.03279737143398,1.0407622905196),
 .UNSPECIFIED.);
#2405=B_SPLINE_CURVE_WITH_KNOTS('',3,(#107952,#107953,#107954,#107955,#107956,
#107957,#107958,#107959,#107960,#107961,#107962,#107963,#107964,#107965,
#107966,#107967,#107968,#107969,#107970,#107971,#107972,#107973,#107974,
#107975,#107976,#107977,#107978,#107979),.UNSPECIFIED.,.F.,.F.,(4,2,2,2,
2,2,2,2,2,2,2,2,2,4),(0.402045801646055,0.426921368863666,0.477783146629179,
0.521019108342606,0.567585276430284,0.617510190643648,0.66788189707345,
0.715127898259456,0.756057910476084,0.771905472506671,0.782049634113368,
0.791401874899713,0.803445023961482,0.804097435867718),.UNSPECIFIED.);
#2406=B_SPLINE_CURVE_WITH_KNOTS('',3,(#107980,#107981,#107982,#107983,#107984,
#107985,#107986,#107987,#107988,#107989,#107990,#107991,#107992,#107993,
#107994,#107995,#107996,#107997,#107998,#107999,#108000,#108001,#108002,
#108003,#108004,#108005,#108006,#108007,#108008,#108009,#108010),
 .UNSPECIFIED.,.F.,.F.,(4,3,2,2,2,2,2,2,2,2,2,2,2,2,4),(0.804097435867718,
0.804103776346135,0.829254561954751,0.880091094347011,0.923508652442152,
0.970360729707258,1.02070692826603,1.07099893487689,1.11789119350307,1.1582226578329,
1.17400850621127,1.18420897271328,1.19368863158308,1.20600944477179,1.20614957799219),
 .UNSPECIFIED.);
#2407=B_SPLINE_CURVE_WITH_KNOTS('',3,(#108013,#108014,#108015,#108016,#108017,
#108018,#108019,#108020,#108021,#108022,#108023,#108024,#108025,#108026,
#108027,#108028,#108029,#108030,#108031,#108032,#108033,#108034,#108035,
#108036,#108037,#108038,#108039,#108040,#108041,#108042,#108043),
 .UNSPECIFIED.,.F.,.F.,(4,2,2,2,2,2,2,2,2,2,2,2,2,3,4),(0.465705745830445,
0.470774723111983,0.52973002499315,0.578949941471191,0.632027677515685,
0.688850530102868,0.747336217373916,0.803360293533464,0.858785062007324,
0.878232653829143,0.889966032860068,0.900224687334042,0.912925016678726,
0.931340862153995,0.931356284564515),.UNSPECIFIED.);
#2408=B_SPLINE_CURVE_WITH_KNOTS('',3,(#108044,#108045,#108046,#108047,#108048,
#108049,#108050,#108051,#108052,#108053,#108054,#108055,#108056,#108057,
#108058,#108059,#108060,#108061,#108062,#108063,#108064,#108065,#108066,
#108067,#108068,#108069),.UNSPECIFIED.,.F.,.F.,(4,2,2,2,2,2,2,2,2,2,2,2,
4),(0.931356284564515,0.99029013163098,1.03925563042585,1.09229320421292,
1.1492159206642,1.20771402926609,1.26396011211653,1.32304991410423,1.34320598478706,
1.35520274265849,1.3656980982517,1.37850099915017,1.39704660798444),
 .UNSPECIFIED.);
#2409=B_SPLINE_CURVE_WITH_KNOTS('',3,(#108072,#108073,#108074,#108075,#108076,
#108077,#108078,#108079,#108080,#108081,#108082,#108083,#108084,#108085,
#108086,#108087,#108088,#108089,#108090,#108091,#108092,#108093,#108094,
#108095,#108096,#108097,#108098,#108099,#108100,#108101,#108102),
 .UNSPECIFIED.,.F.,.F.,(4,2,2,2,2,2,2,2,2,2,2,2,2,3,4),(0.465625642587795,
0.46963582819796,0.486523139143415,0.521324663550571,0.580567805094179,
0.631598103689096,0.68626244179692,0.744842955132037,0.802806095596914,
0.856101750172039,0.894199625898987,0.912116560013009,0.92483196746483,
0.93121746950414,0.931219179268937),.UNSPECIFIED.);
#2410=B_SPLINE_CURVE_WITH_KNOTS('',3,(#108103,#108104,#108105,#108106,#108107,
#108108,#108109,#108110,#108111,#108112,#108113,#108114,#108115,#108116,
#108117,#108118,#108119,#108120,#108121,#108122,#108123,#108124,#108125,
#108126,#108127,#108128),.UNSPECIFIED.,.F.,.F.,(4,2,2,2,2,2,2,2,2,2,2,2,
4),(0.931219179268937,0.945898873169598,0.971610242714637,1.03089218876425,
1.08093500745788,1.13484629914441,1.19265752748803,1.25095610952642,1.30630408366767,
1.3543436424464,1.37459191685001,1.38807682528934,1.39684311209194),
 .UNSPECIFIED.);
#2411=B_SPLINE_CURVE_WITH_KNOTS('',3,(#108131,#108132,#108133,#108134,#108135,
#108136,#108137,#108138,#108139,#108140,#108141,#108142,#108143,#108144,
#108145,#108146,#108147,#108148,#108149,#108150,#108151,#108152,#108153,
#108154,#108155,#108156,#108157,#108158,#108159,#108160),.UNSPECIFIED.,
 .F.,.F.,(4,2,2,2,2,2,2,2,2,2,2,2,2,2,4),(0.344929353748955,0.356066387985214,
0.389855717107168,0.427273389355083,0.46783456176705,0.511548842370844,
0.554747413930576,0.593618559643077,0.627942429506497,0.63944129776671,
0.646393342871627,0.651954413439602,0.659369265155035,0.672885808948647,
0.689779825813832),.UNSPECIFIED.);
#2412=B_SPLINE_CURVE_WITH_KNOTS('',3,(#108161,#108162,#108163,#108164,#108165,
#108166,#108167,#108168,#108169,#108170,#108171,#108172,#108173,#108174,
#108175,#108176,#108177,#108178,#108179,#108180,#108181,#108182,#108183,
#108184,#108185,#108186,#108187,#108188,#108189,#108190,#108191),
 .UNSPECIFIED.,.F.,.F.,(4,3,2,2,2,2,2,2,2,2,2,2,2,2,4),(0.689779825813832,
0.689781272935385,0.722061177204161,0.758341904221671,0.797942076641633,
0.840714760187093,0.884384308283039,0.925587030298816,0.968028390553152,
0.980740789559616,0.988792848857853,0.995059183993389,1.00190661459628,
1.01279771322258,1.03471062668434),.UNSPECIFIED.);
#2413=B_SPLINE_CURVE_WITH_KNOTS('',3,(#108194,#108195,#108196,#108197,#108198,
#108199,#108200,#108201,#108202,#108203,#108204,#108205,#108206,#108207,
#108208,#108209,#108210,#108211,#108212,#108213,#108214,#108215,#108216,
#108217,#108218,#108219,#108220,#108221,#108222,#108223),.UNSPECIFIED.,
 .F.,.F.,(4,2,2,2,2,2,2,2,2,2,2,2,2,2,4),(0.346946091970032,0.362169661154315,
0.397913330429784,0.436911788404973,0.478890702759673,0.522820047512213,
0.565181015061556,0.604959042354894,0.625937529042244,0.635004093110909,
0.640690484113908,0.646869824701532,0.655230741674527,0.673680600425937,
0.693804801232447),.UNSPECIFIED.);
#2414=B_SPLINE_CURVE_WITH_KNOTS('',3,(#108224,#108225,#108226,#108227,#108228,
#108229,#108230,#108231,#108232,#108233,#108234,#108235,#108236,#108237,
#108238,#108239,#108240,#108241,#108242,#108243,#108244,#108245,#108246,
#108247,#108248,#108249,#108250,#108251,#108252,#108253,#108254),
 .UNSPECIFIED.,.F.,.F.,(4,3,2,2,2,2,2,2,2,2,2,2,2,2,4),(0.693804801232447,
0.693806115099353,0.727855665576057,0.765538671741975,0.806334052799794,
0.850308183137197,0.893628499506294,0.932649719620875,0.967659922220942,
0.979166044414383,0.986074731355195,0.991577842716568,0.998889785880524,
1.01215643999181,1.04075220706938),.UNSPECIFIED.);
#2415=B_SPLINE_CURVE_WITH_KNOTS('',3,(#108257,#108258,#108259,#108260,#108261,
#108262,#108263,#108264,#108265,#108266,#108267,#108268,#108269,#108270,
#108271,#108272,#108273,#108274,#108275,#108276,#108277,#108278,#108279,
#108280,#108281,#108282,#108283,#108284,#108285,#108286),.UNSPECIFIED.,
 .F.,.F.,(4,2,2,2,2,2,2,2,2,2,2,2,2,2,4),(0.402056392934123,0.415725541001598,
0.458014623602486,0.503818281659996,0.552968951849433,0.603544598861705,
0.651759339635257,0.701442307487862,0.717795138271998,0.726389516260717,
0.733336281403097,0.741203550532206,0.754346536834056,0.799145653455496,
0.804125925786716),.UNSPECIFIED.);
#2416=B_SPLINE_CURVE_WITH_KNOTS('',3,(#108287,#108288,#108289,#108290,#108291,
#108292,#108293,#108294,#108295,#108296,#108297,#108298,#108299,#108300,
#108301,#108302,#108303,#108304,#108305,#108306,#108307,#108308,#108309,
#108310,#108311,#108312,#108313,#108314,#108315,#108316,#108317),
 .UNSPECIFIED.,.F.,.F.,(4,3,2,2,2,2,2,2,2,2,2,2,2,2,4),(0.804125925786716,
0.804128615238701,0.845155185705043,0.890014570959388,0.93831179499375,
0.989084952746491,1.03844854652443,1.08299792990404,1.11259388513163,1.12407593396706,
1.13161574664347,1.13875379755981,1.14828275904418,1.16884243501129,1.20618500817282),
 .UNSPECIFIED.);
#2417=B_SPLINE_CURVE_WITH_KNOTS('',3,(#108320,#108321,#108322,#108323,#108324,
#108325,#108326,#108327,#108328,#108329,#108330,#108331,#108332,#108333,
#108334,#108335,#108336,#108337,#108338,#108339,#108340,#108341,#108342,
#108343,#108344,#108345,#108346,#108347,#108348,#108349),.UNSPECIFIED.,
 .F.,.F.,(4,2,2,2,2,2,2,2,2,2,2,2,2,2,4),(0.465633555653808,0.48902304098224,
0.539900733776193,0.594559743378545,0.653268263770176,0.711087177306013,
0.762115182186353,0.805365665617788,0.820017835174731,0.828957198199194,
0.836960392683509,0.847007604204608,0.866574886846893,0.891177068870352,
0.931115281912586),.UNSPECIFIED.);
#2418=B_SPLINE_CURVE_WITH_KNOTS('',3,(#108350,#108351,#108352,#108353,#108354,
#108355,#108356,#108357,#108358,#108359,#108360,#108361,#108362,#108363,
#108364,#108365,#108366,#108367,#108368,#108369,#108370,#108371,#108372,
#108373,#108374,#108375,#108376,#108377,#108378,#108379,#108380),
 .UNSPECIFIED.,.F.,.F.,(4,3,2,2,2,2,2,2,2,2,2,2,2,2,4),(0.931115281912586,
0.931118834265423,0.980185404156724,1.03339735797292,1.09056474151636,1.14899276356096,
1.20469552616681,1.26194703525585,1.28158858556552,1.29173091397475,1.29984279634438,
1.30894160242414,1.32394974737251,1.3737045459604,1.39675238991923),
 .UNSPECIFIED.);
#2419=B_SPLINE_CURVE_WITH_KNOTS('',3,(#108383,#108384,#108385,#108386,#108387,
#108388,#108389,#108390,#108391,#108392,#108393,#108394,#108395,#108396,
#108397,#108398,#108399,#108400,#108401,#108402,#108403,#108404,#108405,
#108406,#108407,#108408,#108409,#108410,#108411,#108412,#108413),
 .UNSPECIFIED.,.F.,.F.,(4,2,2,2,2,2,2,2,2,2,2,2,2,3,4),(0.465589681684986,
0.496128546877633,0.544999613356941,0.597826659970873,0.65441740735428,
0.712942957110809,0.769128685328421,0.827041610036713,0.844828954473707,
0.856270447579278,0.865269152346198,0.875183138738762,0.891087651752675,
0.931218391145373,0.931220143022425),.UNSPECIFIED.);
#2420=B_SPLINE_CURVE_WITH_KNOTS('',3,(#108414,#108415,#108416,#108417,#108418,
#108419,#108420,#108421,#108422,#108423,#108424,#108425,#108426,#108427,
#108428,#108429,#108430,#108431,#108432,#108433,#108434,#108435,#108436,
#108437,#108438,#108439,#108440,#108441),.UNSPECIFIED.,.F.,.F.,(4,2,2,2,
2,2,2,2,2,2,2,2,2,4),(0.931220143022425,0.976984089799801,1.02746543549214,
1.08190728792339,1.14042373752107,1.19843917110758,1.25168121512924,1.29873019007383,
1.31517435472236,1.3252999622728,1.33441215374149,1.34589730846604,1.36832488468541,
1.39680807283036),.UNSPECIFIED.);
#2421=B_SPLINE_CURVE_WITH_KNOTS('',3,(#108444,#108445,#108446,#108447,#108448,
#108449,#108450,#108451,#108452,#108453,#108454,#108455,#108456,#108457,
#108458,#108459,#108460,#108461,#108462,#108463,#108464,#108465,#108466,
#108467,#108468,#108469,#108470,#108471),.UNSPECIFIED.,.F.,.F.,(4,2,2,2,
2,2,2,2,2,2,2,2,2,4),(0.402063646876575,0.441646596742676,0.483924716415397,
0.529687053017377,0.578771335705642,0.62936790151733,0.677767564968129,
0.728753561348022,0.744574570083672,0.753834238490205,0.760926103248254,
0.769993393033367,0.785403526963908,0.804156206519059),.UNSPECIFIED.);
#2422=B_SPLINE_CURVE_WITH_KNOTS('',3,(#108472,#108473,#108474,#108475,#108476,
#108477,#108478,#108479,#108480,#108481,#108482,#108483,#108484,#108485,
#108486,#108487,#108488,#108489,#108490,#108491,#108492,#108493,#108494,
#108495,#108496,#108497,#108498,#108499,#108500,#108501,#108502),
 .UNSPECIFIED.,.F.,.F.,(4,3,2,2,2,2,2,2,2,2,2,2,2,2,4),(0.804156206519059,
0.804157258093312,0.854950961196192,0.898407721114375,0.945342475157257,
0.995820010661875,1.0460439587594,1.0923382436039,1.13368877110193,1.14817489104761,
1.15708729909082,1.16509903970329,1.17518134959325,1.19480243396671,1.20622090496989),
 .UNSPECIFIED.);
#2423=B_SPLINE_CURVE_WITH_KNOTS('',3,(#108505,#108506,#108507,#108508,#108509,
#108510,#108511,#108512,#108513,#108514,#108515,#108516,#108517,#108518,
#108519,#108520,#108521,#108522,#108523,#108524,#108525,#108526,#108527,
#108528,#108529,#108530,#108531,#108532),.UNSPECIFIED.,.F.,.F.,(4,2,2,2,
2,2,2,2,2,2,2,2,2,4),(0.346979838988578,0.389336004351652,0.425577187134249,
0.46496713826328,0.507320727156668,0.55117060783772,0.593174276350411,0.635676681418817,
0.651757495702357,0.660344238561706,0.667330683117476,0.675272687128708,
0.688553176936598,0.693939839454841),.UNSPECIFIED.);
#2424=B_SPLINE_CURVE_WITH_KNOTS('',3,(#108533,#108534,#108535,#108536,#108537,
#108538,#108539,#108540,#108541,#108542,#108543,#108544,#108545,#108546,
#108547,#108548,#108549,#108550,#108551,#108552,#108553,#108554,#108555,
#108556,#108557,#108558,#108559,#108560),.UNSPECIFIED.,.F.,.F.,(4,2,2,2,
2,2,2,2,2,2,2,2,2,4),(0.693940241893941,0.737947156937577,0.774444412995097,
0.814135349753758,0.856885167708674,0.900674824035094,0.942337766572511,
0.986246565510725,1.00029536137702,1.0084596027801,1.01549910539396,1.02397712029396,
1.03938606723986,1.04092008088252),.UNSPECIFIED.);
#2425=B_SPLINE_CURVE_WITH_KNOTS('',3,(#108563,#108564,#108565,#108566,#108567,
#108568,#108569,#108570,#108571,#108572,#108573,#108574,#108575,#108576,
#108577,#108578,#108579,#108580,#108581,#108582,#108583,#108584,#108585,
#108586,#108587,#108588,#108589,#108590),.UNSPECIFIED.,.F.,.F.,(4,2,2,2,
2,2,2,2,2,2,2,2,2,4),(0.344885080154984,0.354876053781735,0.398358879728667,
0.434465989334581,0.473802837102125,0.516196923660638,0.55993729649274,
0.601593803249262,0.644356926525559,0.659194193979544,0.667768322580426,
0.674987214089382,0.683465605510929,0.689844673350394),.UNSPECIFIED.);
#2426=B_SPLINE_CURVE_WITH_KNOTS('',3,(#108591,#108592,#108593,#108594,#108595,
#108596,#108597,#108598,#108599,#108600,#108601,#108602,#108603,#108604,
#108605,#108606,#108607,#108608,#108609,#108610,#108611,#108612,#108613,
#108614,#108615,#108616,#108617,#108618,#108619,#108620,#108621),
 .UNSPECIFIED.,.F.,.F.,(4,3,2,2,2,2,2,2,2,2,2,2,2,2,4),(0.689844673350394,
0.689846634861934,0.715465196018713,0.748402202680178,0.785108152470509,
0.825054217672711,0.868162581283261,0.911721478265126,0.952519282856293,
0.99187467863693,1.00547719556773,1.01371135701474,1.02028401069715,1.02900997080457,
1.03473171501692),.UNSPECIFIED.);
#2427=B_SPLINE_CURVE_WITH_KNOTS('',3,(#108624,#108625,#108626,#108627,#108628,
#108629,#108630,#108631,#108632,#108633,#108634,#108635,#108636,#108637,
#108638,#108639,#108640,#108641,#108642,#108643,#108644,#108645,#108646,
#108647,#108648,#108649,#108650,#108651,#108652,#108653),.UNSPECIFIED.,
 .F.,.F.,(4,2,2,2,2,2,2,2,2,2,2,2,2,2,4),(0.23513087161813,0.257665545269238,
0.314319195769947,0.366535179018702,0.395398201653438,0.406406232789782,
0.413600810132003,0.42040112084831,0.429482432095946,0.449207525765485,
0.508236859979792,0.556589804879141,0.609236088900844,0.665834302352657,
0.700744682332408),.UNSPECIFIED.);
#2428=B_SPLINE_CURVE_WITH_KNOTS('',3,(#108654,#108655,#108656,#108657,#108658,
#108659,#108660,#108661,#108662,#108663,#108664,#108665,#108666,#108667,
#108668,#108669,#108670,#108671,#108672,#108673,#108674,#108675,#108676,
#108677,#108678,#108679,#108680,#108681,#108682,#108683,#108684,#108685,
#108686),.UNSPECIFIED.,.F.,.F.,(4,2,2,2,2,2,2,2,2,2,3,2,2,2,2,4),(0.700744682332408,
0.724377815208848,0.780725936511176,0.833217266124318,0.86120641695614,
0.872169246047208,0.879420403240007,0.886340189619999,0.895684963280036,
0.916407130769888,0.931141466796302,0.973719157965918,1.02185187591133,
1.07413019711891,1.13019606874401,1.16627233841443),.UNSPECIFIED.);
#2429=B_SPLINE_CURVE_WITH_KNOTS('',3,(#108689,#108690,#108691,#108692,#108693,
#108694,#108695,#108696,#108697,#108698,#108699,#108700,#108701,#108702,
#108703,#108704,#108705,#108706,#108707,#108708,#108709,#108710,#108711,
#108712,#108713,#108714,#108715,#108716,#108717,#108718),.UNSPECIFIED.,
 .F.,.F.,(4,2,2,2,2,2,2,2,2,2,2,2,2,2,4),(0.402049576064962,0.442924940773306,
0.490985398883326,0.538391239477101,0.556366477228441,0.564315810841895,
0.569899087317611,0.575587236270038,0.583774297354325,0.604278587837761,
0.655331441968366,0.69752209930774,0.743402415341105,0.773581410804251,
0.804039827553986),.UNSPECIFIED.);
#2430=B_SPLINE_CURVE_WITH_KNOTS('',3,(#108719,#108720,#108721,#108722,#108723,
#108724,#108725,#108726,#108727,#108728,#108729,#108730,#108731,#108732,
#108733,#108734,#108735,#108736,#108737,#108738,#108739,#108740,#108741,
#108742,#108743,#108744,#108745,#108746,#108747,#108748,#108749,#108750,
#108751),.UNSPECIFIED.,.F.,.F.,(4,3,2,2,2,2,2,2,2,2,2,2,2,2,2,4),(0.804039827553986,
0.804063550621079,0.854373442811622,0.900881225382939,0.949678790887404,
0.96080284686332,0.967871450737339,0.973410881050953,0.979522490884367,
0.989418941157237,1.02159380938173,1.05923062921021,1.10145952242515,1.14725276098453,
1.19642197418901,1.20611312668604),.UNSPECIFIED.);
#2431=B_SPLINE_CURVE_WITH_KNOTS('',3,(#108754,#108755,#108756,#108757,#108758,
#108759,#108760,#108761,#108762,#108763,#108764,#108765,#108766,#108767,
#108768,#108769,#108770,#108771,#108772,#108773,#108774,#108775,#108776,
#108777,#108778,#108779,#108780,#108781,#108782,#108783),.UNSPECIFIED.,
 .F.,.F.,(4,2,2,2,2,2,2,2,2,2,2,2,2,2,4),(0.346993950805442,0.380996151679775,
0.423508224638363,0.460147398068903,0.487374610716494,0.495858524682818,
0.500900558944594,0.505305062634139,0.51079885501452,0.52131419844937,0.565233428154864,
0.600368372516561,0.638991123740337,0.66668600193962,0.693883548523562),
 .UNSPECIFIED.);
#2432=B_SPLINE_CURVE_WITH_KNOTS('',3,(#108784,#108785,#108786,#108787,#108788,
#108789,#108790,#108791,#108792,#108793,#108794,#108795,#108796,#108797,
#108798,#108799,#108800,#108801,#108802,#108803,#108804,#108805,#108806,
#108807,#108808,#108809,#108810,#108811,#108812,#108813,#108814,#108815,
#108816),.UNSPECIFIED.,.F.,.F.,(4,3,2,2,2,2,2,2,2,2,2,2,2,2,2,4),(0.693883548523562,
0.693911449692292,0.737714685061078,0.779272180174301,0.818589460670165,
0.836942720435357,0.844132912473772,0.848432810651463,0.852961474627973,
0.858870645041464,0.871244658654114,0.915042137758771,0.950422336714534,
0.989171528292634,1.03093524701467,1.04090540049773),.UNSPECIFIED.);
#2433=B_SPLINE_CURVE_WITH_KNOTS('',3,(#108819,#108820,#108821,#108822,#108823,
#108824,#108825,#108826,#108827,#108828,#108829,#108830,#108831,#108832,
#108833,#108834,#108835,#108836,#108837,#108838,#108839,#108840,#108841,
#108842,#108843,#108844,#108845,#108846,#108847,#108848),.UNSPECIFIED.,
 .F.,.F.,(4,2,2,2,2,2,2,2,2,2,2,2,2,2,4),(0.3449473234351,0.383972379609475,
0.426630739903034,0.463495506028656,0.49478654096451,0.503410679492906,
0.508385006664272,0.512183429878956,0.517050806941317,0.525433985800617,
0.557706502535248,0.590555291519674,0.627396944749139,0.659553333722666,
0.68982195704123),.UNSPECIFIED.);
#2434=B_SPLINE_CURVE_WITH_KNOTS('',3,(#108849,#108850,#108851,#108852,#108853,
#108854,#108855,#108856,#108857,#108858,#108859,#108860,#108861,#108862,
#108863,#108864,#108865,#108866,#108867,#108868,#108869,#108870,#108871,
#108872,#108873,#108874,#108875,#108876,#108877,#108878,#108879,#108880,
#108881),.UNSPECIFIED.,.F.,.F.,(4,3,2,2,2,2,2,2,2,2,2,2,2,2,2,4),(0.68982195704123,
0.689915857735377,0.733838749870872,0.776100520611407,0.811923867201258,
0.840265609412777,0.848576158635835,0.853501218510488,0.857761720827947,
0.862941916004609,0.872615795928119,0.915883691423952,0.950464809790433,
0.988612423914805,1.02990109317486,1.03486318117048),.UNSPECIFIED.);
#2435=B_SPLINE_CURVE_WITH_KNOTS('',3,(#108884,#108885,#108886,#108887,#108888,
#108889,#108890,#108891,#108892,#108893,#108894,#108895,#108896,#108897,
#108898,#108899,#108900,#108901,#108902,#108903,#108904,#108905,#108906,
#108907,#108908,#108909,#108910,#108911,#108912,#108913,#108914),
 .UNSPECIFIED.,.F.,.F.,(4,2,2,2,2,2,2,2,2,2,2,2,2,3,4),(0.344948818872903,
0.34648558610318,0.35379420124694,0.363486809549799,0.380807029707963,0.424289830006885,
0.460871612859494,0.500666448418649,0.543589083599318,0.587222639540401,
0.628438882135512,0.668029692054682,0.682703378839969,0.689884357221945,
0.689885383506442),.UNSPECIFIED.);
#2436=B_SPLINE_CURVE_WITH_KNOTS('',3,(#108915,#108916,#108917,#108918,#108919,
#108920,#108921,#108922,#108923,#108924,#108925,#108926,#108927,#108928,
#108929,#108930,#108931,#108932,#108933,#108934,#108935,#108936,#108937,
#108938,#108939,#108940),.UNSPECIFIED.,.F.,.F.,(4,2,2,2,2,2,2,2,2,2,2,2,
4),(0.689885383506442,0.698053478442917,0.707526032156531,0.723721892194936,
0.767089663931964,0.803365942675116,0.842817653261609,0.885307866396609,
0.929024686839016,0.970639482202589,1.01223872953034,1.02722931611229,1.03483317609485),
 .UNSPECIFIED.);
#2437=B_SPLINE_CURVE_WITH_KNOTS('',3,(#108943,#108944,#108945,#108946,#108947,
#108948,#108949,#108950,#108951,#108952,#108953,#108954,#108955,#108956,
#108957,#108958,#108959,#108960,#108961,#108962,#108963,#108964,#108965,
#108966,#108967,#108968,#108969,#108970),.UNSPECIFIED.,.F.,.F.,(4,2,2,2,
2,2,2,2,2,2,2,2,2,4),(0.344882043626189,0.352989105107807,0.363926627501424,
0.3711716185643,0.378060236624948,0.387276828919064,0.407094714992322,0.450659584359954,
0.487474857318371,0.527535978355668,0.570775578744059,0.614277204715927,
0.65477324729973,0.689797023258215),.UNSPECIFIED.);
#2438=B_SPLINE_CURVE_WITH_KNOTS('',3,(#108971,#108972,#108973,#108974,#108975,
#108976,#108977,#108978,#108979,#108980,#108981,#108982,#108983,#108984,
#108985,#108986,#108987,#108988,#108989,#108990,#108991,#108992,#108993,
#108994,#108995,#108996,#108997,#108998),.UNSPECIFIED.,.F.,.F.,(4,2,2,2,
2,2,2,2,2,2,2,2,2,4),(0.689797333961378,0.703450158460547,0.71220221069754,
0.719066574503029,0.726610076636724,0.738671816952097,0.775294349047951,
0.80986862415414,0.847901887648394,0.889027092265501,0.933366718957538,
0.976197876803047,1.01535724395698,1.0346790668844),.UNSPECIFIED.);
#2439=B_SPLINE_CURVE_WITH_KNOTS('',3,(#109001,#109002,#109003,#109004,#109005,
#109006,#109007,#109008,#109009,#109010,#109011,#109012,#109013,#109014,
#109015,#109016,#109017,#109018,#109019,#109020,#109021,#109022,#109023,
#109024,#109025,#109026,#109027,#109028),.UNSPECIFIED.,.F.,.F.,(4,2,2,2,
2,2,2,2,2,2,2,2,2,4),(0.346869666639179,0.354370653515026,0.362541062299255,
0.370355651574061,0.38085124734922,0.403385681755292,0.447233199907815,
0.484762146264627,0.52536318975603,0.569075144213089,0.612537491684678,
0.652657149294534,0.687070443946799,0.693791313456527),.UNSPECIFIED.);
#2440=B_SPLINE_CURVE_WITH_KNOTS('',3,(#109029,#109030,#109031,#109032,#109033,
#109034,#109035,#109036,#109037,#109038,#109039,#109040,#109041,#109042,
#109043,#109044,#109045,#109046,#109047,#109048,#109049,#109050,#109051,
#109052,#109053,#109054,#109055,#109056,#109057,#109058,#109059),
 .UNSPECIFIED.,.F.,.F.,(4,3,2,2,2,2,2,2,2,2,2,2,2,2,4),(0.693791313456527,
0.693794119363892,0.704023311866356,0.711876653713803,0.720190462252714,
0.732808907987192,0.766691935276412,0.80138404315909,0.839422665010973,
0.880425923133339,0.924528249546443,0.967721377887932,1.00633946370428,
1.03596310622201,1.04066378600307),.UNSPECIFIED.);
#2441=B_SPLINE_CURVE_WITH_KNOTS('',3,(#109062,#109063,#109064,#109065,#109066,
#109067,#109068,#109069,#109070,#109071,#109072,#109073,#109074,#109075,
#109076,#109077,#109078,#109079,#109080,#109081,#109082,#109083,#109084,
#109085,#109086,#109087,#109088,#109089,#109090,#109091,#109092),
 .UNSPECIFIED.,.F.,.F.,(4,2,2,2,2,2,2,2,2,2,2,2,2,3,4),(0.402095295909212,
0.405579891764716,0.415766170466332,0.4284730590739,0.45249443113515,0.503327000412256,
0.546700481715136,0.593473225181061,0.643696040678488,0.694046096415582,
0.741373026361261,0.781608430858166,0.798286582163595,0.804144678533662,
0.804146349058566),.UNSPECIFIED.);
#2442=B_SPLINE_CURVE_WITH_KNOTS('',3,(#109093,#109094,#109095,#109096,#109097,
#109098,#109099,#109100,#109101,#109102,#109103,#109104,#109105,#109106,
#109107,#109108,#109109,#109110,#109111,#109112,#109113,#109114,#109115,
#109116,#109117,#109118),.UNSPECIFIED.,.F.,.F.,(4,2,2,2,2,2,2,2,2,2,2,2,
4),(0.804146349058566,0.814450657715169,0.825919625880521,0.844245346091432,
0.89509135649372,0.937392406014544,0.983081672039519,1.03202864527732,1.0826698233326,
1.13145421224722,1.18006724600391,1.19837326252841,1.20623997444287),
 .UNSPECIFIED.);
#2443=B_SPLINE_CURVE_WITH_KNOTS('',3,(#109121,#109122,#109123,#109124,#109125,
#109126,#109127,#109128,#109129,#109130,#109131,#109132,#109133,#109134,
#109135,#109136,#109137,#109138,#109139,#109140,#109141,#109142,#109143,
#109144,#109145,#109146,#109147,#109148,#109149,#109150),.UNSPECIFIED.,
 .F.,.F.,(4,2,2,2,2,2,2,2,2,2,2,2,2,2,4),(0.465630957639009,0.481933210616303,
0.535242614313078,0.563024946110058,0.574648402499332,0.581809656529143,
0.589496546094033,0.599743139456495,0.621829787220229,0.680864997484433,
0.729716870256327,0.782756962199145,0.83974870019235,0.881827618684303,
0.931138912205881),.UNSPECIFIED.);
#2444=B_SPLINE_CURVE_WITH_KNOTS('',3,(#109151,#109152,#109153,#109154,#109155,
#109156,#109157,#109158,#109159,#109160,#109161,#109162,#109163,#109164,
#109165,#109166,#109167,#109168,#109169,#109170,#109171,#109172,#109173,
#109174,#109175,#109176,#109177,#109178,#109179,#109180,#109181),
 .UNSPECIFIED.,.F.,.F.,(4,3,2,2,2,2,2,2,2,2,2,2,2,2,4),(0.931138912205881,
0.931141638331543,0.980504007870222,1.02323155336671,1.0374278068647,1.0460417539728,
1.05373254085545,1.06337028302394,1.08213318737524,1.14131516052482,1.18943829620451,
1.24168287524649,1.29769743121417,1.35631949893545,1.39677259597055),
 .UNSPECIFIED.);
#2445=B_SPLINE_CURVE_WITH_KNOTS('',3,(#109184,#109185,#109186,#109187,#109188,
#109189,#109190,#109191,#109192,#109193,#109194,#109195,#109196,#109197,
#109198,#109199,#109200,#109201,#109202,#109203,#109204,#109205,#109206,
#109207,#109208,#109209,#109210,#109211,#109212,#109213),.UNSPECIFIED.,
 .F.,.F.,(4,2,2,2,2,2,2,2,2,2,2,2,2,2,4),(0.402124309272361,0.421627341777243,
0.464872714227461,0.496765510113577,0.507624575968613,0.514319250314185,
0.520371390461007,0.528062884199748,0.543405344995164,0.594209088483205,
0.635662749000266,0.680906583862294,0.729607600766311,0.764590820032904,
0.804073160672369),.UNSPECIFIED.);
#2446=B_SPLINE_CURVE_WITH_KNOTS('',3,(#109214,#109215,#109216,#109217,#109218,
#109219,#109220,#109221,#109222,#109223,#109224,#109225,#109226,#109227,
#109228,#109229,#109230,#109231,#109232,#109233,#109234,#109235,#109236,
#109237,#109238,#109239,#109240,#109241,#109242,#109243,#109244),
 .UNSPECIFIED.,.F.,.F.,(4,3,2,2,2,2,2,2,2,2,2,2,2,2,4),(0.804073160672369,
0.804085254144401,0.850050308649933,0.895243952982647,0.907843732340252,
0.915061602581693,0.921143593411249,0.928331556329836,0.94114401239225,
0.991985862136534,1.0328415254673,1.0774801344348,1.12546183964273,1.17625016754876,
1.20620956341676),.UNSPECIFIED.);
#2447=B_SPLINE_CURVE_WITH_KNOTS('',3,(#109247,#109248,#109249,#109250,#109251,
#109252,#109253,#109254,#109255,#109256,#109257,#109258,#109259,#109260,
#109261,#109262,#109263,#109264,#109265,#109266,#109267,#109268,#109269,
#109270,#109271,#109272,#109273,#109274,#109275,#109276),.UNSPECIFIED.,
 .F.,.F.,(4,2,2,2,2,2,2,2,2,2,2,2,2,2,4),(0.346994532186391,0.382164652532166,
0.420784033011186,0.442103361704628,0.45010253341702,0.455291674197675,
0.460170465296368,0.466649939984645,0.480606624884645,0.524360787319406,
0.560151349727645,0.599306476742075,0.64155218827536,0.666590950965648,
0.693872421523419),.UNSPECIFIED.);
#2448=B_SPLINE_CURVE_WITH_KNOTS('',3,(#109277,#109278,#109279,#109280,#109281,
#109282,#109283,#109284,#109285,#109286,#109287,#109288,#109289,#109290,
#109291,#109292,#109293,#109294,#109295,#109296,#109297,#109298,#109299,
#109300,#109301,#109302,#109303,#109304,#109305,#109306,#109307,#109308,
#109309),.UNSPECIFIED.,.F.,.F.,(4,3,2,2,2,2,2,2,2,2,2,2,2,2,2,4),(0.693872421523419,
0.693884091081668,0.7351695103979,0.776128574475123,0.791745968454944,0.797891390586484,
0.802453862835923,0.807407685914084,0.814124184856907,0.829141438103611,
0.872882271954203,0.908751433499746,0.947896971802218,0.990049089273971,
1.03394297490375,1.04087862326806),.UNSPECIFIED.);
#2449=B_SPLINE_CURVE_WITH_KNOTS('',3,(#109312,#109313,#109314,#109315,#109316,
#109317,#109318,#109319,#109320,#109321,#109322,#109323,#109324,#109325,
#109326,#109327,#109328,#109329,#109330,#109331,#109332,#109333,#109334,
#109335,#109336,#109337,#109338,#109339,#109340,#109341),.UNSPECIFIED.,
 .F.,.F.,(4,2,2,2,2,2,2,2,2,2,2,2,2,2,4),(0.344999942815522,0.381943582058605,
0.418154029345294,0.44831722446467,0.45712008470837,0.462312727341851,0.46678675019175,
0.472201183473186,0.482227764720134,0.525498069008382,0.560258776784043,
0.598611000252602,0.640171561678573,0.664290716544723,0.68990424298228),
 .UNSPECIFIED.);
#2450=B_SPLINE_CURVE_WITH_KNOTS('',3,(#109342,#109343,#109344,#109345,#109346,
#109347,#109348,#109349,#109350,#109351,#109352,#109353,#109354,#109355,
#109356,#109357,#109358,#109359,#109360,#109361,#109362,#109363,#109364,
#109365,#109366,#109367,#109368,#109369,#109370,#109371,#109372,#109373,
#109374),.UNSPECIFIED.,.F.,.F.,(4,3,2,2,2,2,2,2,2,2,2,2,2,2,2,4),(0.68990424298228,
0.689921489597089,0.732017271454668,0.768741909879443,0.794320223466152,
0.802659448183967,0.807720878420951,0.811799401099935,0.817294338043404,
0.827565067504058,0.870910623355331,0.90565267068528,0.943924419349473,
0.985327674934479,1.0292961171375,1.03492143241261),.UNSPECIFIED.);
#2451=B_SPLINE_CURVE_WITH_KNOTS('',3,(#109377,#109378,#109379,#109380,#109381,
#109382,#109383,#109384,#109385,#109386,#109387,#109388,#109389,#109390,
#109391,#109392,#109393,#109394,#109395,#109396,#109397,#109398,#109399,
#109400,#109401,#109402,#109403,#109404,#109405,#109406),.UNSPECIFIED.,
 .F.,.F.,(4,2,2,2,2,2,2,2,2,2,2,2,2,2,4),(0.235147519047353,0.270079203343737,
0.321248161065438,0.360484158913179,0.373462373146903,0.381345721820111,
0.388394617326011,0.397247094673285,0.414563352645265,0.473778780166836,
0.521797219958211,0.574157167267294,0.630455746779035,0.689053581599555,
0.700757096167161),.UNSPECIFIED.);
#2452=B_SPLINE_CURVE_WITH_KNOTS('',3,(#109407,#109408,#109409,#109410,#109411,
#109412,#109413,#109414,#109415,#109416,#109417,#109418,#109419,#109420,
#109421,#109422,#109423,#109424,#109425,#109426,#109427,#109428,#109429,
#109430,#109431,#109432,#109433,#109434,#109435,#109436,#109437),
 .UNSPECIFIED.,.F.,.F.,(4,2,2,2,2,2,2,2,2,3,2,2,2,2,4),(0.700757096167161,
0.74574592571697,0.797562147829136,0.828614623243329,0.840400148080654,
0.848080143967425,0.855320592607384,0.864958909385184,0.885761885582985,
0.931172598139542,0.978100519054367,1.02940050406239,1.0844850950303,1.1437492669342,
1.16632011718689),.UNSPECIFIED.);
#2453=B_SPLINE_CURVE_WITH_KNOTS('',3,(#109440,#109441,#109442,#109443,#109444,
#109445,#109446,#109447,#109448,#109449,#109450,#109451,#109452,#109453,
#109454,#109455,#109456,#109457,#109458,#109459,#109460,#109461,#109462,
#109463,#109464,#109465,#109466,#109467,#109468,#109469),.UNSPECIFIED.,
 .F.,.F.,(4,2,2,2,2,2,2,2,2,2,2,2,2,2,4),(0.402068706671266,0.403065557403745,
0.452265829927698,0.495942952564712,0.525036207784967,0.535088757160506,
0.541344128236347,0.547042238725329,0.554348485704057,0.569162218753928,
0.619983909342393,0.661298627530047,0.706438874571811,0.755042332304185,
0.804117029823683),.UNSPECIFIED.);
#2454=B_SPLINE_CURVE_WITH_KNOTS('',3,(#109470,#109471,#109472,#109473,#109474,
#109475,#109476,#109477,#109478,#109479,#109480,#109481,#109482,#109483,
#109484,#109485,#109486,#109487,#109488,#109489,#109490,#109491,#109492,
#109493,#109494,#109495,#109496,#109497,#109498,#109499,#109500),
 .UNSPECIFIED.,.F.,.F.,(4,3,2,2,2,2,2,2,2,2,2,2,2,2,4),(0.804117029823683,
0.804148478785509,0.853289954180878,0.89669726254831,0.926741624702312,
0.936995948249101,0.943342218262998,0.949101125759267,0.956456433532982,
0.971280891051743,1.02210639107617,1.06328898116581,1.10820381165191,1.15646537383303,
1.20621718545677),.UNSPECIFIED.);
#2455=B_SPLINE_CURVE_WITH_KNOTS('',3,(#109503,#109504,#109505,#109506,#109507,
#109508,#109509,#109510,#109511,#109512,#109513,#109514,#109515,#109516,
#109517,#109518,#109519,#109520,#109521,#109522,#109523,#109524,#109525,
#109526,#109527,#109528,#109529,#109530,#109531,#109532,#109533,#109534),
 .UNSPECIFIED.,.F.,.F.,(4,2,2,2,2,2,2,2,2,2,2,2,2,2,2,4),(0.347000201591407,
0.349957219711082,0.39293291266258,0.428785611965772,0.46239565443992,0.47172731156569,
0.477108289343941,0.481213483526896,0.486467015331691,0.495487378786048,
0.529647560730359,0.56320586320055,0.600581178594504,0.641128658155968,
0.667016278770337,0.69380582230332),.UNSPECIFIED.);
#2456=B_SPLINE_CURVE_WITH_KNOTS('',3,(#109535,#109536,#109537,#109538,#109539,
#109540,#109541,#109542,#109543,#109544,#109545,#109546,#109547,#109548,
#109549,#109550,#109551,#109552,#109553,#109554,#109555,#109556,#109557,
#109558,#109559,#109560,#109561,#109562,#109563,#109564,#109565),
 .UNSPECIFIED.,.F.,.F.,(4,3,2,2,2,2,2,2,2,2,2,2,2,2,4),(0.69380582230332,
0.693823417159995,0.736887921450666,0.77375096897562,0.8088488216942,0.818398781231576,
0.823859998204031,0.828463261660433,0.833911929852199,0.843668681036052,
0.885405269817422,0.920052462661799,0.958204970860161,0.99939121812381,
1.0408236187514),.UNSPECIFIED.);
#2457=B_SPLINE_CURVE_WITH_KNOTS('',3,(#109568,#109569,#109570,#109571,#109572,
#109573,#109574,#109575,#109576,#109577,#109578,#109579,#109580,#109581,
#109582,#109583,#109584,#109585,#109586,#109587,#109588,#109589,#109590,
#109591,#109592,#109593,#109594,#109595,#109596,#109597),.UNSPECIFIED.,
 .F.,.F.,(4,2,2,2,2,2,2,2,2,2,2,2,2,2,4),(0.344994788972036,0.371998850508981,
0.41383828389175,0.451257335147389,0.473742260370782,0.481413353641608,
0.486172059564842,0.490502237936666,0.496054570065859,0.50734469069417,
0.5507443601542,0.585751946465345,0.624314672083482,0.657180388120093,0.689930754578743),
 .UNSPECIFIED.);
#2458=B_SPLINE_CURVE_WITH_KNOTS('',3,(#109598,#109599,#109600,#109601,#109602,
#109603,#109604,#109605,#109606,#109607,#109608,#109609,#109610,#109611,
#109612,#109613,#109614,#109615,#109616,#109617,#109618,#109619,#109620,
#109621,#109622,#109623,#109624,#109625,#109626,#109627,#109628,#109629,
#109630),.UNSPECIFIED.,.F.,.F.,(4,3,2,2,2,2,2,2,2,2,2,2,2,2,2,4),(0.689930754578743,
0.68995605109708,0.733315175883505,0.772752808703065,0.814476102512377,
0.823487197603381,0.829129592965408,0.833502545720314,0.838281230189835,
0.845927355678044,0.870210369956026,0.901450945282902,0.937040898848585,
0.976028236344697,1.01813254197155,1.03495084006912),.UNSPECIFIED.);
#2459=B_SPLINE_CURVE_WITH_KNOTS('',3,(#109633,#109634,#109635,#109636,#109637,
#109638,#109639,#109640,#109641,#109642,#109643,#109644,#109645,#109646,
#109647,#109648,#109649,#109650,#109651,#109652,#109653,#109654,#109655,
#109656,#109657,#109658,#109659,#109660,#109661,#109662,#109663,#109664),
 .UNSPECIFIED.,.F.,.F.,(4,2,2,2,2,2,2,2,2,2,2,2,2,2,2,4),(0.344971545335952,
0.345545647028644,0.384764681179798,0.40424327008886,0.412309880833698,
0.417253957091865,0.422545454073276,0.429579981909098,0.444717699179436,
0.488060634823621,0.523877930949446,0.563102095839794,0.605510165502449,
0.643225963532927,0.664545274820508,0.689824776316506),.UNSPECIFIED.);
#2460=B_SPLINE_CURVE_WITH_KNOTS('',3,(#109665,#109666,#109667,#109668,#109669,
#109670,#109671,#109672,#109673,#109674,#109675,#109676,#109677,#109678,
#109679,#109680,#109681,#109682,#109683,#109684,#109685,#109686,#109687,
#109688,#109689,#109690,#109691,#109692,#109693,#109694,#109695),
 .UNSPECIFIED.,.F.,.F.,(4,3,2,2,2,2,2,2,2,2,2,2,2,2,4),(0.689824776316506,
0.689830282259499,0.728867836398559,0.74884817389962,0.757049758657684,
0.762048740226498,0.767378328492543,0.77442980694277,0.789487509518511,
0.832830212937649,0.868546979352336,0.907616287512977,0.949786922410696,
0.993585378979441,1.03480182759545),.UNSPECIFIED.);
#2461=B_SPLINE_CURVE_WITH_KNOTS('',3,(#109698,#109699,#109700,#109701,#109702,
#109703,#109704,#109705,#109706,#109707,#109708,#109709,#109710,#109711,
#109712,#109713,#109714,#109715,#109716,#109717,#109718,#109719,#109720,
#109721,#109722,#109723,#109724,#109725,#109726,#109727),.UNSPECIFIED.,
 .F.,.F.,(4,2,2,2,2,2,2,2,2,2,2,2,2,2,4),(0.346991000077703,0.369652304047158,
0.393534285289892,0.402847338016846,0.408986699981362,0.414819000879822,
0.422638624902608,0.439658747555291,0.483358554520194,0.51977654113599,
0.559441391326081,0.602191731812778,0.641992454894118,0.665097906765919,
0.693832015935598),.UNSPECIFIED.);
#2462=B_SPLINE_CURVE_WITH_KNOTS('',3,(#109728,#109729,#109730,#109731,#109732,
#109733,#109734,#109735,#109736,#109737,#109738,#109739,#109740,#109741,
#109742,#109743,#109744,#109745,#109746,#109747,#109748,#109749,#109750,
#109751,#109752,#109753,#109754,#109755,#109756,#109757,#109758),
 .UNSPECIFIED.,.F.,.F.,(4,3,2,2,2,2,2,2,2,2,2,2,2,2,4),(0.693832015935598,
0.693838450061331,0.735157906153247,0.747030826425598,0.753866318900802,
0.759637840977357,0.766464847112779,0.778622940969573,0.82230777596829,
0.857791368445199,0.896584070116107,0.938366691203684,0.982333997742008,
1.02487382026543,1.04082945013903),.UNSPECIFIED.);
#2463=B_SPLINE_CURVE_WITH_KNOTS('',3,(#109761,#109762,#109763,#109764,#109765,
#109766,#109767,#109768,#109769,#109770,#109771,#109772,#109773,#109774,
#109775,#109776,#109777,#109778,#109779,#109780,#109781,#109782,#109783,
#109784,#109785,#109786,#109787,#109788,#109789,#109790),.UNSPECIFIED.,
 .F.,.F.,(4,2,2,2,2,2,2,2,2,2,2,2,2,2,4),(0.402070660444346,0.430721222203059,
0.448436737907617,0.457639121252569,0.465012884527248,0.473287523239665,
0.486915648254195,0.531388130722923,0.571962836637525,0.616435337523612,
0.664342021409311,0.715164441118493,0.752777285105839,0.775342417317356,
0.803996534145188),.UNSPECIFIED.);
#2464=B_SPLINE_CURVE_WITH_KNOTS('',3,(#109791,#109792,#109793,#109794,#109795,
#109796,#109797,#109798,#109799,#109800,#109801,#109802,#109803,#109804,
#109805,#109806,#109807,#109808,#109809,#109810,#109811,#109812,#109813,
#109814,#109815,#109816,#109817,#109818),.UNSPECIFIED.,.F.,.F.,(4,2,2,2,
2,2,2,2,2,2,2,2,2,4),(0.80399666330925,0.840948073023333,0.85411547906342,
0.862340222843209,0.869827285138543,0.879389422933621,0.898503079269372,
0.949541782070688,0.991673901808353,1.03732980012108,1.08631662695951,1.13693275473247,
1.18540913330378,1.20606719458953),.UNSPECIFIED.);
#2465=B_SPLINE_CURVE_WITH_KNOTS('',3,(#109821,#109822,#109823,#109824,#109825,
#109826,#109827,#109828,#109829,#109830,#109831,#109832,#109833,#109834,
#109835,#109836,#109837,#109838,#109839,#109840,#109841,#109842,#109843,
#109844,#109845,#109846,#109847,#109848,#109849,#109850,#109851),
 .UNSPECIFIED.,.F.,.F.,(4,2,2,2,2,2,2,2,2,2,2,2,2,3,4),(0.46556985358348,
0.477882011556651,0.488346204604764,0.499686903254209,0.514866865476111,
0.547047227056689,0.606163109414153,0.656953163861814,0.711606625070641,
0.770301819100196,0.828283906607871,0.881749498431883,0.924288167774753,
0.931164974956878,0.931170439482049),.UNSPECIFIED.);
#2466=B_SPLINE_CURVE_WITH_KNOTS('',3,(#109852,#109853,#109854,#109855,#109856,
#109857,#109858,#109859,#109860,#109861,#109862,#109863,#109864,#109865,
#109866,#109867,#109868,#109869,#109870,#109871,#109872,#109873,#109874,
#109875,#109876,#109877,#109878,#109879),.UNSPECIFIED.,.F.,.F.,(4,2,2,2,
2,2,2,2,2,2,2,2,2,4),(0.931170439482049,0.946077334530951,0.957538186455137,
0.969659736733055,0.987988431122021,1.03634818069539,1.08369048993003,1.13512985187121,
1.19024389724709,1.24943791437987,1.30707512832393,1.36096869048164,1.39504142334864,
1.39673482854036),.UNSPECIFIED.);
#2467=B_SPLINE_CURVE_WITH_KNOTS('',3,(#109882,#109883,#109884,#109885,#109886,
#109887,#109888,#109889,#109890,#109891,#109892,#109893,#109894,#109895,
#109896,#109897,#109898,#109899,#109900,#109901,#109902,#109903,#109904,
#109905,#109906,#109907,#109908,#109909),.UNSPECIFIED.,.F.,.F.,(4,2,2,2,
2,2,2,2,2,2,2,2,2,4),(0.402035858284301,0.415800106188637,0.426509562079159,
0.43449821732174,0.44316499473855,0.454821097473714,0.479978494161069,0.530831774585308,
0.574142313470446,0.620921348665322,0.671202766396292,0.721509774951859,
0.768376054624899,0.804067995108011),.UNSPECIFIED.);
#2468=B_SPLINE_CURVE_WITH_KNOTS('',3,(#109910,#109911,#109912,#109913,#109914,
#109915,#109916,#109917,#109918,#109919,#109920,#109921,#109922,#109923,
#109924,#109925,#109926,#109927,#109928,#109929,#109930,#109931,#109932,
#109933,#109934,#109935,#109936,#109937),.UNSPECIFIED.,.F.,.F.,(4,2,2,2,
2,2,2,2,2,2,2,2,2,4),(0.804068015337196,0.820830037169018,0.831725865127309,
0.840355281596958,0.849911251608451,0.865314090182635,0.912359544350536,
0.953570658305018,0.998400421083362,1.04651355615953,1.09728907212346,1.14674897700792,
1.19347446440925,1.20610385339231),.UNSPECIFIED.);
#2469=B_SPLINE_CURVE_WITH_KNOTS('',3,(#109940,#109941,#109942,#109943,#109944,
#109945,#109946,#109947,#109948,#109949,#109950,#109951,#109952,#109953,
#109954,#109955,#109956,#109957,#109958,#109959,#109960,#109961,#109962,
#109963,#109964,#109965,#109966,#109967,#109968,#109969),.UNSPECIFIED.,
 .F.,.F.,(4,2,2,2,2,2,2,2,2,2,2,2,2,2,4),(0.34693956539501,0.36351871144698,
0.376402246255229,0.383922554697919,0.390434897410649,0.398320444565317,
0.41279772900145,0.456696958114542,0.492818163098098,0.532197319465947,
0.574634286636639,0.61850585479356,0.649183604204981,0.668216244832537,
0.693788573117956),.UNSPECIFIED.);
#2470=B_SPLINE_CURVE_WITH_KNOTS('',3,(#109970,#109971,#109972,#109973,#109974,
#109975,#109976,#109977,#109978,#109979,#109980,#109981,#109982,#109983,
#109984,#109985,#109986,#109987,#109988,#109989,#109990,#109991,#109992,
#109993,#109994,#109995,#109996,#109997),.UNSPECIFIED.,.F.,.F.,(4,2,2,2,
2,2,2,2,2,2,2,2,2,4),(0.693788666223921,0.716636792221272,0.726516620727249,
0.732704302176124,0.739415944795447,0.748466294242799,0.768259990862704,
0.812205377250718,0.849077532443543,0.88904156018983,0.932010512859336,
0.975680172894089,1.01671881686369,1.04072813851297),.UNSPECIFIED.);
#2471=B_SPLINE_CURVE_WITH_KNOTS('',3,(#110000,#110001,#110002,#110003,#110004,
#110005,#110006,#110007,#110008,#110009,#110010,#110011,#110012,#110013,
#110014,#110015,#110016,#110017,#110018,#110019,#110020,#110021,#110022,
#110023,#110024,#110025,#110026,#110027,#110028,#110029),.UNSPECIFIED.,
 .F.,.F.,(4,2,2,2,2,2,2,2,2,2,2,2,2,2,4),(0.344949052494914,0.36277009235622,
0.381467624672727,0.388884092762833,0.394389517740211,0.400354875245585,
0.408399545858477,0.426069166833454,0.469389147836557,0.505710222697627,
0.545356716966147,0.588183386073944,0.630668972094002,0.656032036251321,
0.6898186201039),.UNSPECIFIED.);
#2472=B_SPLINE_CURVE_WITH_KNOTS('',3,(#110030,#110031,#110032,#110033,#110034,
#110035,#110036,#110037,#110038,#110039,#110040,#110041,#110042,#110043,
#110044,#110045,#110046,#110047,#110048,#110049,#110050,#110051,#110052,
#110053,#110054,#110055,#110056,#110057,#110058,#110059,#110060),
 .UNSPECIFIED.,.F.,.F.,(4,3,2,2,2,2,2,2,2,2,2,2,2,2,4),(0.6898186201039,
0.689820287363217,0.720993326898501,0.731680371989911,0.738253283448811,
0.744176013144634,0.751666615512782,0.766445212379684,0.809788249849371,
0.845546547900242,0.884630535928773,0.926803266506532,0.970599772849603,
1.01242230839075,1.03476933985813),.UNSPECIFIED.);
#2473=B_SPLINE_CURVE_WITH_KNOTS('',3,(#110063,#110064,#110065,#110066,#110067,
#110068,#110069,#110070,#110071,#110072,#110073,#110074,#110075,#110076,
#110077,#110078,#110079,#110080,#110081,#110082,#110083,#110084,#110085,
#110086,#110087,#110088,#110089,#110090,#110091,#110092),.UNSPECIFIED.,
 .F.,.F.,(4,2,2,2,2,2,2,2,2,2,2,2,2,2,4),(0.344940008736965,0.378978791644863,
0.42186508520073,0.431590749918263,0.437742985858769,0.442544553022841,
0.44782033022748,0.456311381108014,0.48343211103597,0.515569701577298,0.551845082220461,
0.591482902943101,0.634321511103674,0.660439052235908,0.689822751077019),
 .UNSPECIFIED.);
#2474=B_SPLINE_CURVE_WITH_KNOTS('',3,(#110093,#110094,#110095,#110096,#110097,
#110098,#110099,#110100,#110101,#110102,#110103,#110104,#110105,#110106,
#110107,#110108,#110109,#110110,#110111,#110112,#110113,#110114,#110115,
#110116,#110117,#110118,#110119,#110120,#110121,#110122,#110123,#110124,
#110125),.UNSPECIFIED.,.F.,.F.,(4,3,2,2,2,2,2,2,2,2,2,2,2,2,2,4),(0.689822751077019,
0.689835002982984,0.728744495340446,0.76747936074641,0.776814384144543,
0.782869367749044,0.787694633017288,0.793101248828574,0.802041370620515,
0.832608555074118,0.865362173435765,0.902043132002549,0.941969769687353,
0.985027673395759,1.02852816507098,1.03477501171995),.UNSPECIFIED.);
#2475=B_SPLINE_CURVE_WITH_KNOTS('',3,(#110128,#110129,#110130,#110131,#110132,
#110133,#110134,#110135,#110136,#110137,#110138,#110139,#110140,#110141,
#110142,#110143,#110144,#110145,#110146,#110147,#110148,#110149,#110150,
#110151,#110152,#110153,#110154,#110155,#110156,#110157,#110158,#110159,
#110160),.UNSPECIFIED.,.F.,.F.,(4,2,2,2,2,2,2,2,2,2,2,2,2,2,3,4),(0.347023138138081,
0.354237651152506,0.392088742983375,0.417111712806915,0.426077762137051,
0.43174994473942,0.436977598867684,0.44376256853267,0.45778036032763,0.501521672898848,
0.537374603000262,0.576570640714205,0.618850505784507,0.653291130836709,
0.693855228776299,0.693903487772775),.UNSPECIFIED.);
#2476=B_SPLINE_CURVE_WITH_KNOTS('',3,(#110161,#110162,#110163,#110164,#110165,
#110166,#110167,#110168,#110169,#110170,#110171,#110172,#110173,#110174,
#110175,#110176,#110177,#110178,#110179,#110180,#110181,#110182,#110183,
#110184,#110185,#110186,#110187,#110188),.UNSPECIFIED.,.F.,.F.,(4,2,2,2,
2,2,2,2,2,2,2,2,2,4),(0.693903487772775,0.729687754639204,0.761874414282563,
0.771942093684843,0.777899539963646,0.783079765382483,0.789502118333581,
0.801642899823187,0.845596548586892,0.881045805067327,0.91982886691259,
0.961612807804786,1.00557856818985,1.04087836691438),.UNSPECIFIED.);
#2477=B_SPLINE_CURVE_WITH_KNOTS('',3,(#110191,#110192,#110193,#110194,#110195,
#110196,#110197,#110198,#110199,#110200,#110201,#110202,#110203,#110204,
#110205,#110206,#110207,#110208,#110209,#110210,#110211,#110212,#110213,
#110214,#110215,#110216,#110217,#110218,#110219,#110220),.UNSPECIFIED.,
 .F.,.F.,(4,2,2,2,2,2,2,2,2,2,2,2,2,2,4),(0.402082644734097,0.408816886367671,
0.457317700146456,0.475413758181528,0.484000465094417,0.490648854483846,
0.497776850058018,0.508849809023471,0.540995027585967,0.579223696731807,
0.621922224793676,0.668212867966239,0.718001195146057,0.756613895926381,
0.804035907610257),.UNSPECIFIED.);
#2478=B_SPLINE_CURVE_WITH_KNOTS('',3,(#110221,#110222,#110223,#110224,#110225,
#110226,#110227,#110228,#110229,#110230,#110231,#110232,#110233,#110234,
#110235,#110236,#110237,#110238,#110239,#110240,#110241,#110242,#110243,
#110244,#110245,#110246,#110247,#110248,#110249,#110250,#110251),
 .UNSPECIFIED.,.F.,.F.,(4,3,2,2,2,2,2,2,2,2,2,2,2,2,4),(0.804035907610257,
0.804040984651415,0.850086369432104,0.873922371268176,0.884014085041587,
0.89028098025585,0.897048185533734,0.906140890385097,0.926032251354922,
0.977055761637495,1.0191917936117,1.06487574383506,1.11390884249085,1.16451044494518,
1.20612362938551),.UNSPECIFIED.);
#2479=B_SPLINE_CURVE_WITH_KNOTS('',3,(#110254,#110255,#110256,#110257,#110258,
#110259,#110260,#110261,#110262,#110263,#110264,#110265,#110266,#110267,
#110268,#110269,#110270,#110271,#110272,#110273,#110274,#110275,#110276,
#110277,#110278,#110279,#110280,#110281,#110282,#110283,#110284,#110285,
#110286),.UNSPECIFIED.,.F.,.F.,(4,2,2,2,2,2,2,2,2,2,2,2,2,2,3,4),(0.465697318151285,
0.500096550816189,0.530152083768842,0.542887027000964,0.550777921662509,
0.55927272797757,0.570621274065763,0.595067159352315,0.65402940437608,0.703342238243548,
0.756754657905659,0.814127098826639,0.865095529254773,0.894692705834994,
0.931141236328648,0.931163109251236),.UNSPECIFIED.);
#2480=B_SPLINE_CURVE_WITH_KNOTS('',3,(#110287,#110288,#110289,#110290,#110291,
#110292,#110293,#110294,#110295,#110296,#110297,#110298,#110299,#110300,
#110301,#110302,#110303,#110304,#110305,#110306,#110307,#110308,#110309,
#110310,#110311,#110312,#110313,#110314),.UNSPECIFIED.,.F.,.F.,(4,2,2,2,
2,2,2,2,2,2,2,2,2,4),(0.931163109251236,0.986893757473382,1.00378700412891,
1.01368892697709,1.02129904029214,1.03107558281521,1.04786913337837,1.10678708647645,
1.15462078504369,1.20659986804395,1.26232717177621,1.32099255779553,1.37806644213216,
1.39683855447993),.UNSPECIFIED.);
#2481=B_SPLINE_CURVE_WITH_KNOTS('',3,(#110317,#110318,#110319,#110320,#110321,
#110322,#110323,#110324,#110325,#110326,#110327,#110328,#110329,#110330,
#110331,#110332,#110333,#110334,#110335,#110336,#110337,#110338,#110339,
#110340,#110341,#110342,#110343,#110344),.UNSPECIFIED.,.F.,.F.,(4,2,2,2,
2,2,2,2,2,2,2,2,2,4),(0.4655389112447,0.488133130774159,0.506318884175181,
0.517142152662043,0.526626059065126,0.538230532411421,0.559797581148832,
0.618783918753435,0.667805538713148,0.720924860650082,0.777953615959564,
0.83642444066412,0.875349746240229,0.93113996876562),.UNSPECIFIED.);
#2482=B_SPLINE_CURVE_WITH_KNOTS('',3,(#110345,#110346,#110347,#110348,#110349,
#110350,#110351,#110352,#110353,#110354,#110355,#110356,#110357,#110358,
#110359,#110360,#110361,#110362,#110363,#110364,#110365,#110366,#110367,
#110368,#110369,#110370,#110371,#110372),.UNSPECIFIED.,.F.,.F.,(4,2,2,2,
2,2,2,2,2,2,2,2,2,4),(0.93113999918218,0.963154453507864,0.977016717729584,
0.986854762909184,0.996911582350658,1.01135266092654,1.04654269594155,1.09119591127059,
1.14061195756702,1.19389677378683,1.25097456683904,1.30939222705096,1.3649241947938,
1.39667888001032),.UNSPECIFIED.);
#2483=B_SPLINE_CURVE_WITH_KNOTS('',3,(#110382,#110383,#110384,#110385,#110386,
#110387,#110388,#110389,#110390,#110391,#110392,#110393,#110394,#110395,
#110396,#110397,#110398,#110399,#110400,#110401,#110402,#110403,#110404,
#110405,#110406,#110407,#110408,#110409,#110410,#110411,#110412,#110413,
#110414,#110415,#110416,#110417,#110418,#110419),.UNSPECIFIED.,.T.,.F.,
(4,2,2,2,2,2,2,2,2,2,2,2,2,2,2,2,2,2,4),(0.,0.0253587207966879,0.0757398285085816,
0.126070132097997,0.176266080606921,0.226299383634684,0.276249073740046,
0.326254642699978,0.376402382431699,0.401502370508004,0.426571573512854,
0.477394582349303,0.528028902540467,0.57881116631453,0.629741966063948,
0.68057107151679,0.731217559248426,0.7819629019431,0.804608887664541),
 .UNSPECIFIED.);
#2484=B_SPLINE_CURVE_WITH_KNOTS('',3,(#110423,#110424,#110425,#110426,#110427,
#110428,#110429,#110430,#110431,#110432,#110433,#110434,#110435,#110436,
#110437,#110438,#110439,#110440,#110441,#110442,#110443,#110444,#110445),
 .UNSPECIFIED.,.F.,.F.,(4,2,2,2,2,2,2,2,2,3,4),(0.213085231160066,0.229427465846964,
0.256360845004798,0.282978089057426,0.309527611387396,0.336016212989723,
0.362490334276596,0.389007528718512,0.415593427837248,0.42617576632081,
0.42617835082105),.UNSPECIFIED.);
#2485=B_SPLINE_CURVE_WITH_KNOTS('',3,(#110449,#110450,#110451,#110452,#110453,
#110454,#110455,#110456,#110457,#110458,#110459,#110460,#110461,#110462,
#110463,#110464,#110465,#110466,#110467,#110468),.UNSPECIFIED.,.F.,.F.,
(4,2,2,2,2,2,2,2,2,4),(0.42617835082105,0.439441496185428,0.466455555306613,
0.493421519222728,0.520432879955794,0.547485339174318,0.574506555632534,
0.6014753733821,0.628473697232218,0.639260997480876),.UNSPECIFIED.);
#2486=B_SPLINE_CURVE_WITH_KNOTS('',3,(#110472,#110473,#110474,#110475,#110476,
#110477,#110478,#110479,#110480,#110481,#110482,#110483,#110484,#110485,
#110486,#110487,#110488,#110489,#110490,#110491,#110492,#110493,#110494,
#110495,#110496,#110497,#110498,#110499,#110500,#110501,#110502,#110503,
#110504,#110505,#110506,#110507,#110508,#110509),.UNSPECIFIED.,.T.,.F.,
(4,2,2,2,2,2,2,2,2,2,2,2,2,2,2,2,2,2,4),(0.,0.0215934538029461,0.0661140688763958,
0.109673264959663,0.152976786454784,0.196013449229872,0.238933453610375,
0.281964346413397,0.325260417404302,0.347000989066419,0.368728099328494,
0.412825446316775,0.456665802011567,0.500491031429621,0.544396329252895,
0.587414183713088,0.631225382181991,0.675103653567844,0.694395412341892),
 .UNSPECIFIED.);
#2487=B_SPLINE_CURVE_WITH_KNOTS('',3,(#110513,#110514,#110515,#110516,#110517,
#110518,#110519,#110520,#110521,#110522,#110523,#110524,#110525,#110526,
#110527,#110528,#110529,#110530,#110531,#110532,#110533,#110534),
 .UNSPECIFIED.,.F.,.F.,(4,2,2,2,2,2,2,2,2,2,4),(0.157591377093445,0.158341318200066,
0.16816064064739,0.188318306898892,0.2082429048757,0.227875908952582,0.247403814330963,
0.266900129823757,0.28645832978064,0.306134210260318,0.315207466804691),
 .UNSPECIFIED.);
#2488=B_SPLINE_CURVE_WITH_KNOTS('',3,(#110538,#110539,#110540,#110541,#110542,
#110543,#110544,#110545,#110546,#110547,#110548,#110549,#110550,#110551,
#110552,#110553,#110554,#110555,#110556,#110557,#110558,#110559,#110560),
 .UNSPECIFIED.,.F.,.F.,(4,3,2,2,2,2,2,2,2,2,4),(0.315207466804691,0.315229215381257,
0.325074413465618,0.345142403734454,0.36514541055531,0.385129442882843,
0.404649613884746,0.424165788062158,0.443755125331743,0.463768996929674,
0.472820592474702),.UNSPECIFIED.);
#2489=B_SPLINE_CURVE_WITH_KNOTS('',3,(#110564,#110565,#110566,#110567,#110568,
#110569,#110570,#110571,#110572,#110573,#110574,#110575,#110576,#110577,
#110578,#110579,#110580,#110581,#110582,#110583,#110584,#110585,#110586,
#110587,#110588,#110589,#110590,#110591,#110592,#110593,#110594,#110595,
#110596,#110597,#110598,#110599,#110600,#110601),.UNSPECIFIED.,.T.,.F.,
(4,2,2,2,2,2,2,2,2,2,2,2,2,2,2,2,2,2,4),(0.,0.0214612457013718,0.0430041716204019,
0.0873575122693011,0.130712730392479,0.173621420731722,0.2161633020124,
0.258638327861848,0.301388430216311,0.344585415156887,0.366255653226389,
0.387851313185509,0.431696072327512,0.475306021742627,0.518888272730588,
0.561418888334619,0.604005607771101,0.647584473031916,0.690474393099494),
 .UNSPECIFIED.);
#2490=B_SPLINE_CURVE_WITH_KNOTS('',3,(#110605,#110606,#110607,#110608,#110609,
#110610,#110611,#110612,#110613,#110614,#110615,#110616,#110617,#110618,
#110619,#110620,#110621,#110622,#110623,#110624,#110625,#110626,#110627,
#110628,#110629),.UNSPECIFIED.,.F.,.F.,(4,2,2,2,2,2,2,2,2,2,3,4),(0.155294477826636,
0.155659400125146,0.165338299598688,0.175034361113789,0.194920097606448,
0.214541319872842,0.233821348963659,0.252953941695607,0.272074687541761,
0.29132605951052,0.310584998214978,0.310589086453876),.UNSPECIFIED.);
#2491=B_SPLINE_CURVE_WITH_KNOTS('',3,(#110633,#110634,#110635,#110636,#110637,
#110638,#110639,#110640,#110641,#110642,#110643,#110644,#110645,#110646,
#110647,#110648,#110649,#110650,#110651,#110652),.UNSPECIFIED.,.F.,.F.,
(4,2,2,2,2,2,2,2,2,4),(0.310589086453876,0.320305218454811,0.330010867645859,
0.349792458885214,0.369503570696552,0.388938417010325,0.408070037520553,
0.427213089555852,0.446492546606876,0.465879476041615),.UNSPECIFIED.);
#2492=B_SPLINE_CURVE_WITH_KNOTS('',3,(#110656,#110657,#110658,#110659,#110660,
#110661,#110662,#110663,#110664,#110665,#110666,#110667,#110668,#110669,
#110670,#110671,#110672,#110673,#110674,#110675,#110676,#110677,#110678,
#110679,#110680,#110681,#110682,#110683,#110684,#110685,#110686,#110687,
#110688,#110689,#110690,#110691,#110692,#110693),.UNSPECIFIED.,.T.,.F.,
(4,2,2,2,2,2,2,2,2,2,2,2,2,2,2,2,2,2,4),(0.,0.0582499854078214,0.116522238011401,
0.174719222883445,0.232763101450122,0.290685326407376,0.348596993560137,
0.406576740290978,0.435566714351364,0.494495631365087,0.552987315365781,
0.611558833999642,0.670345355331475,0.729066826381109,0.78756171029075,
0.846156998753239,0.874931172542359,0.903174012205886,0.93172187928848),
 .UNSPECIFIED.);
#2493=B_SPLINE_CURVE_WITH_KNOTS('',3,(#110697,#110698,#110699,#110700,#110701,
#110702,#110703,#110704,#110705,#110706,#110707,#110708,#110709,#110710,
#110711,#110712,#110713,#110714,#110715,#110716,#110717,#110718),
 .UNSPECIFIED.,.F.,.F.,(4,2,2,2,2,2,2,2,2,2,4),(0.276825859161365,0.297043390131478,
0.331626580694953,0.366194217943258,0.400710187129129,0.435170426794847,
0.469611031748545,0.504073425287484,0.521299803107865,0.537372852441424,
0.55357036764084),.UNSPECIFIED.);
#2494=B_SPLINE_CURVE_WITH_KNOTS('',3,(#110722,#110723,#110724,#110725,#110726,
#110727,#110728,#110729,#110730,#110731,#110732,#110733,#110734,#110735,
#110736,#110737,#110738,#110739,#110740,#110741),.UNSPECIFIED.,.F.,.F.,
(4,2,2,2,2,2,2,2,2,4),(0.553570660833043,0.588585516849723,0.623535548686362,
0.658551470263866,0.693596719240443,0.728577625844064,0.763532714810859,
0.798639038192274,0.816043463348951,0.830396226802205),.UNSPECIFIED.);
#2495=B_SPLINE_CURVE_WITH_KNOTS('',3,(#110745,#110746,#110747,#110748,#110749,
#110750,#110751,#110752,#110753,#110754,#110755,#110756,#110757,#110758,
#110759,#110760,#110761,#110762,#110763,#110764,#110765,#110766,#110767,
#110768,#110769,#110770,#110771,#110772,#110773,#110774,#110775,#110776,
#110777,#110778,#110779,#110780),.UNSPECIFIED.,.T.,.F.,(4,2,2,2,2,2,2,2,
2,2,2,2,2,2,2,2,2,4),(0.,0.0503768236674881,0.100697265705858,0.150882364943078,
0.200910039641612,0.250863071799662,0.300878991841609,0.351037208469142,
0.376138911045814,0.401180140933725,0.45196140826745,0.502592407894745,
0.553406592994723,0.60437887729313,0.655232719281932,0.70587844620255,0.756604415957716,
0.804713332817945),.UNSPECIFIED.);
#2496=B_SPLINE_CURVE_WITH_KNOTS('',3,(#110784,#110785,#110786,#110787,#110788,
#110789,#110790,#110791,#110792,#110793,#110794,#110795,#110796,#110797,
#110798,#110799,#110800,#110801,#110802,#110803,#110804,#110805,#110806,
#110807,#110808),.UNSPECIFIED.,.F.,.F.,(4,2,2,2,2,2,2,2,2,2,3,4),(0.213125454324095,
0.215371214439484,0.242304080051861,0.26891712435903,0.295463050658844,
0.321950717827531,0.348427104398956,0.374948460855996,0.401537986608032,
0.413805283512627,0.426168952202461,0.426174000047882),.UNSPECIFIED.);
#2497=B_SPLINE_CURVE_WITH_KNOTS('',3,(#110812,#110813,#110814,#110815,#110816,
#110817,#110818,#110819,#110820,#110821,#110822,#110823,#110824,#110825,
#110826,#110827,#110828,#110829),.UNSPECIFIED.,.F.,.F.,(4,2,2,2,2,2,2,2,
4),(0.426174000047882,0.453163023079439,0.480127907810925,0.507155788480461,
0.533952061349386,0.560478308801999,0.587447628308409,0.614431474663807,
0.639294406526556),.UNSPECIFIED.);
#2498=B_SPLINE_CURVE_WITH_KNOTS('',3,(#110833,#110834,#110835,#110836,#110837,
#110838,#110839,#110840,#110841,#110842,#110843,#110844,#110845,#110846,
#110847,#110848,#110849,#110850,#110851,#110852,#110853,#110854,#110855,
#110856,#110857,#110858,#110859,#110860,#110861,#110862,#110863,#110864,
#110865,#110866,#110867,#110868,#110869,#110870),.UNSPECIFIED.,.T.,.F.,
(4,2,2,2,2,2,2,2,2,2,2,2,2,2,2,2,2,2,4),(0.,0.0444221121400932,0.0879541817963996,
0.131227015999418,0.174246979918824,0.217174048974236,0.260231920457301,
0.303559228338858,0.325306871790306,0.346970541213297,0.390946973288773,
0.434747171355873,0.478633478836622,0.521609326830897,0.564635515872938,
0.608480355472813,0.652299252145619,0.673231330408672,0.694389830450528),
 .UNSPECIFIED.);
#2499=B_SPLINE_CURVE_WITH_KNOTS('',3,(#110874,#110875,#110876,#110877,#110878,
#110879,#110880,#110881,#110882,#110883,#110884,#110885,#110886,#110887,
#110888,#110889,#110890,#110891,#110892,#110893,#110894,#110895),
 .UNSPECIFIED.,.F.,.F.,(4,2,2,2,2,2,2,2,2,2,4),(0.157589267359033,0.158005279271924,
0.178114857305211,0.198037545113508,0.217659078264535,0.237181560870524,
0.256681548189167,0.276250496936562,0.295938152700304,0.305537860047768,
0.315206514186509),.UNSPECIFIED.);
#2500=B_SPLINE_CURVE_WITH_KNOTS('',3,(#110899,#110900,#110901,#110902,#110903,
#110904,#110905,#110906,#110907,#110908,#110909,#110910,#110911,#110912,
#110913,#110914,#110915,#110916,#110917,#110918,#110919,#110920,#110921),
 .UNSPECIFIED.,.F.,.F.,(4,3,2,2,2,2,2,2,2,2,4),(0.315206514186509,0.315228106062157,
0.335243855233202,0.355229872898987,0.375034891987949,0.39454965103334,
0.414070002826143,0.43367079485033,0.453658486096216,0.463440026256045,
0.472817373421189),.UNSPECIFIED.);
#2501=B_SPLINE_CURVE_WITH_KNOTS('',3,(#110925,#110926,#110927,#110928,#110929,
#110930,#110931,#110932,#110933,#110934,#110935,#110936,#110937,#110938,
#110939,#110940,#110941,#110942,#110943,#110944,#110945,#110946,#110947,
#110948,#110949,#110950,#110951,#110952,#110953,#110954,#110955,#110956,
#110957,#110958,#110959,#110960,#110961,#110962),.UNSPECIFIED.,.T.,.F.,
(4,2,2,2,2,2,2,2,2,2,2,2,2,2,2,2,2,2,4),(0.,0.0215520464773449,0.065916778292889,
0.109258524694745,0.152151785274527,0.194685629726144,0.237165327483375,
0.279930295138766,0.323143228583621,0.344811565913954,0.366403507243528,
0.410241083863158,0.453847992476275,0.497429011858637,0.539957033885482,
0.582551741103232,0.626132369502366,0.6698761895927,0.69048940316824),
 .UNSPECIFIED.);
#2502=B_SPLINE_CURVE_WITH_KNOTS('',3,(#110966,#110967,#110968,#110969,#110970,
#110971,#110972,#110973,#110974,#110975,#110976,#110977,#110978,#110979,
#110980,#110981,#110982,#110983,#110984,#110985,#110986,#110987),
 .UNSPECIFIED.,.F.,.F.,(4,2,2,2,2,2,2,2,2,2,4),(0.15527235737458,0.15562510787596,
0.165323609967748,0.185212103287073,0.204826616573261,0.224100586518285,
0.243230509120738,0.26235370154504,0.28161134459152,0.30106539687992,0.31057081404642),
 .UNSPECIFIED.);
#2503=B_SPLINE_CURVE_WITH_KNOTS('',3,(#110991,#110992,#110993,#110994,#110995,
#110996,#110997,#110998,#110999,#111000,#111001,#111002,#111003,#111004,
#111005,#111006,#111007,#111008,#111009,#111010,#111011,#111012,#111013),
 .UNSPECIFIED.,.F.,.F.,(4,3,2,2,2,2,2,2,2,2,4),(0.31057081404642,0.310589850236165,
0.32029547338224,0.340076326550382,0.359786151240218,0.379216021927432,
0.398345929856394,0.417491927740968,0.436777439352559,0.456533677744053,
0.465862207610745),.UNSPECIFIED.);
#2504=B_SPLINE_CURVE_WITH_KNOTS('',3,(#111017,#111018,#111019,#111020,#111021,
#111022,#111023,#111024,#111025,#111026,#111027,#111028,#111029,#111030,
#111031,#111032,#111033,#111034,#111035,#111036,#111037,#111038,#111039,
#111040,#111041,#111042,#111043,#111044,#111045,#111046,#111047,#111048,
#111049,#111050,#111051,#111052,#111053,#111054),.UNSPECIFIED.,.T.,.F.,
(4,2,2,2,2,2,2,2,2,2,2,2,2,2,2,2,2,2,4),(0.,0.0582371853616322,0.116450034307396,
0.174555153981211,0.23253603852723,0.290470301636954,0.348447688277155,
0.377437572006861,0.406430276039093,0.465167898343824,0.523607434262112,
0.582288349171024,0.641268831623812,0.700144809512642,0.758670415181914,
0.817168437078618,0.845875575798632,0.875163161983379,0.931710252415266),
 .UNSPECIFIED.);
#2505=B_SPLINE_CURVE_WITH_KNOTS('',3,(#111058,#111059,#111060,#111061,#111062,
#111063,#111064,#111065,#111066,#111067,#111068,#111069,#111070,#111071,
#111072,#111073,#111074,#111075,#111076,#111077,#111078,#111079,#111080,
#111081,#111082),.UNSPECIFIED.,.F.,.F.,(4,2,2,2,2,2,2,2,2,2,3,4),(0.276799012407407,
0.279373782652995,0.313936794852817,0.348484301688893,0.382991613305011,
0.417459748808092,0.45192017602727,0.48640262407376,0.50363241062791,0.520852093736164,
0.553556515029853,0.55355923315894),.UNSPECIFIED.);
#2506=B_SPLINE_CURVE_WITH_KNOTS('',3,(#111086,#111087,#111088,#111089,#111090,
#111091,#111092,#111093,#111094,#111095,#111096,#111097,#111098,#111099,
#111100,#111101,#111102,#111103,#111104,#111105),.UNSPECIFIED.,.F.,.F.,
(4,2,2,2,2,2,2,2,2,4),(0.55355923315894,0.588486820049772,0.623528572740515,
0.658687237671087,0.693800354600396,0.728770060347164,0.763712953575019,
0.780829430331441,0.798001660236641,0.83035552743726),.UNSPECIFIED.);
#2507=B_SPLINE_CURVE_WITH_KNOTS('',3,(#111109,#111110,#111111,#111112,#111113,
#111114,#111115,#111116,#111117,#111118,#111119,#111120,#111121,#111122,
#111123,#111124,#111125,#111126,#111127,#111128,#111129,#111130,#111131,
#111132,#111133,#111134,#111135,#111136,#111137,#111138,#111139,#111140,
#111141,#111142,#111143,#111144),.UNSPECIFIED.,.T.,.F.,(4,2,2,2,2,2,2,2,
2,2,2,2,2,2,2,2,2,4),(0.,0.0503765293579072,0.100656386784499,0.150767302359921,
0.200734910020674,0.250685919670086,0.300751653603399,0.35095811132866,
0.376056517716232,0.426926457491189,0.477568603688572,0.528302799585843,
0.579143561840979,0.629894549187007,0.680535051806248,0.73136306480552,
0.782694491287284,0.80473018173603),.UNSPECIFIED.);
#2508=B_SPLINE_CURVE_WITH_KNOTS('',3,(#111148,#111149,#111150,#111151,#111152,
#111153,#111154,#111155,#111156,#111157,#111158,#111159,#111160,#111161,
#111162,#111163,#111164,#111165,#111166,#111167),.UNSPECIFIED.,.F.,.F.,
(4,2,2,2,2,2,2,2,2,4),(0.213098726156546,0.215970507757757,0.242617902005601,
0.269207806476468,0.295724361337248,0.322195200337876,0.348679383881839,
0.375225908894206,0.401835845995312,0.426189984379948),.UNSPECIFIED.);
#2509=B_SPLINE_CURVE_WITH_KNOTS('',3,(#111171,#111172,#111173,#111174,#111175,
#111176,#111177,#111178,#111179,#111180,#111181,#111182,#111183,#111184,
#111185,#111186,#111187,#111188,#111189,#111190,#111191),.UNSPECIFIED.,
 .F.,.F.,(4,3,2,2,2,2,2,2,2,4),(0.426189984379948,0.426215668917109,0.453208711882292,
0.480176759933483,0.507173805734186,0.534171874901274,0.561140699681476,
0.588130649676459,0.615239336311902,0.639314395073655),.UNSPECIFIED.);
#2510=B_SPLINE_CURVE_WITH_KNOTS('',3,(#111195,#111196,#111197,#111198,#111199,
#111200,#111201,#111202,#111203,#111204,#111205,#111206,#111207,#111208,
#111209,#111210,#111211,#111212,#111213,#111214,#111215,#111216,#111217,
#111218,#111219,#111220,#111221,#111222,#111223,#111224,#111225,#111226,
#111227,#111228,#111229,#111230,#111231,#111232),.UNSPECIFIED.,.T.,.F.,
(4,2,2,2,2,2,2,2,2,2,2,2,2,2,2,2,2,2,4),(0.,0.0436396354015875,0.0870799379946624,
0.130235175112472,0.173181603494129,0.216128697217889,0.259286147781706,
0.302719831957823,0.324465331746154,0.368595894415476,0.412446137360158,
0.456247245545887,0.500100201234702,0.543937122812399,0.58773303976263,
0.63165494060563,0.653207446330335,0.673701504443971,0.694392975330147),
 .UNSPECIFIED.);
#2511=B_SPLINE_CURVE_WITH_KNOTS('',3,(#111236,#111237,#111238,#111239,#111240,
#111241,#111242,#111243,#111244,#111245,#111246,#111247,#111248,#111249,
#111250,#111251,#111252,#111253,#111254,#111255,#111256,#111257),
 .UNSPECIFIED.,.F.,.F.,(4,2,2,2,2,2,2,2,2,2,4),(0.157608270286503,0.168928237568431,
0.188674330321961,0.208302465762515,0.227826612069672,0.247322672121388,
0.266884223982705,0.286564705052486,0.296430638563966,0.305790479364867,
0.315202716294224),.UNSPECIFIED.);
#2512=B_SPLINE_CURVE_WITH_KNOTS('',3,(#111261,#111262,#111263,#111264,#111265,
#111266,#111267,#111268,#111269,#111270,#111271,#111272,#111273,#111274,
#111275,#111276,#111277,#111278,#111279,#111280,#111281,#111282,#111283),
 .UNSPECIFIED.,.F.,.F.,(4,3,2,2,2,2,2,2,2,2,4),(0.315202716294224,0.315228523372249,
0.335270894652026,0.355254388730732,0.375013449023108,0.394520810149056,
0.414067151678346,0.434066258167069,0.454138928812652,0.463973627677658,
0.472836793658752),.UNSPECIFIED.);
#2513=B_SPLINE_CURVE_WITH_KNOTS('',3,(#111287,#111288,#111289,#111290,#111291,
#111292,#111293,#111294,#111295,#111296,#111297,#111298,#111299,#111300,
#111301,#111302,#111303,#111304,#111305,#111306,#111307,#111308,#111309,
#111310,#111311,#111312,#111313,#111314,#111315,#111316,#111317,#111318,
#111319,#111320,#111321,#111322,#111323,#111324),.UNSPECIFIED.,.T.,.F.,
(4,2,2,2,2,2,2,2,2,2,2,2,2,2,2,2,2,2,4),(0.,0.044308474695846,0.0876221732407881,
0.13048794984384,0.173010584725196,0.215501776298411,0.258294467524509,
0.301535055508773,0.323165493512123,0.34471113614295,0.38847500202065,0.432069843045601,
0.475261647497953,0.517783869440572,0.560390231176503,0.603979847218741,
0.647677207401233,0.668966276445715,0.690485997484513),.UNSPECIFIED.);
#2514=B_SPLINE_CURVE_WITH_KNOTS('',3,(#111328,#111329,#111330,#111331,#111332,
#111333,#111334,#111335,#111336,#111337,#111338,#111339,#111340,#111341,
#111342,#111343,#111344,#111345,#111346,#111347,#111348,#111349),
 .UNSPECIFIED.,.F.,.F.,(4,2,2,2,2,2,2,2,2,2,4),(0.155266549715351,0.155540359583602,
0.175401508132681,0.195010291008741,0.214273102592753,0.233399032217858,
0.252527597849283,0.271796998188979,0.291262445086705,0.300880271086537,
0.310565043388772),.UNSPECIFIED.);
#2515=B_SPLINE_CURVE_WITH_KNOTS('',3,(#111353,#111354,#111355,#111356,#111357,
#111358,#111359,#111360,#111361,#111362,#111363,#111364,#111365,#111366,
#111367,#111368,#111369,#111370,#111371,#111372,#111373,#111374,#111375),
 .UNSPECIFIED.,.F.,.F.,(4,3,2,2,2,2,2,2,2,2,4),(0.310565043388772,0.310589642487775,
0.330339397260518,0.350044366011474,0.369470075015529,0.388596515754746,
0.407748711655326,0.427046686185302,0.446782028837706,0.456448834828453,
0.465856192203126),.UNSPECIFIED.);
#2516=B_SPLINE_CURVE_WITH_KNOTS('',3,(#111379,#111380,#111381,#111382,#111383,
#111384,#111385,#111386,#111387,#111388,#111389,#111390,#111391,#111392,
#111393,#111394,#111395,#111396,#111397,#111398,#111399,#111400,#111401,
#111402,#111403,#111404,#111405,#111406,#111407,#111408,#111409,#111410,
#111411,#111412,#111413,#111414,#111415,#111416),.UNSPECIFIED.,.T.,.F.,
(4,2,2,2,2,2,2,2,2,2,2,2,2,2,2,2,2,2,4),(0.,0.0582746652411334,0.116465563883562,
0.174498657639209,0.232413193768181,0.290323519241188,0.348304847203968,
0.37729479476534,0.436198928686154,0.49468657172654,0.553261258987217,0.612031433556264,
0.670719397047039,0.729201952557845,0.787836578600544,0.816640912143595,
0.845923968771257,0.90415568160122,0.931717558493197),.UNSPECIFIED.);
#2517=B_SPLINE_CURVE_WITH_KNOTS('',3,(#111420,#111421,#111422,#111423,#111424,
#111425,#111426,#111427,#111428,#111429,#111430,#111431,#111432,#111433,
#111434,#111435,#111436,#111437,#111438,#111439,#111440,#111441),
 .UNSPECIFIED.,.F.,.F.,(4,2,2,2,2,2,2,2,2,2,4),(0.276824259036896,0.296611116807084,
0.331178721594792,0.365691854475663,0.400148469904013,0.434586793442788,
0.469048541672308,0.486274882510752,0.503503889308575,0.53860420639192,
0.553568065350035),.UNSPECIFIED.);
#2518=B_SPLINE_CURVE_WITH_KNOTS('',3,(#111445,#111446,#111447,#111448,#111449,
#111450,#111451,#111452,#111453,#111454,#111455,#111456,#111457,#111458,
#111459,#111460,#111461,#111462,#111463,#111464),.UNSPECIFIED.,.F.,.F.,
(4,2,2,2,2,2,2,2,2,4),(0.553568655458047,0.588517511821428,0.623525749772073,
0.658555918364597,0.693525509166112,0.728486932769869,0.763618198128497,
0.781022020612757,0.815594259375338,0.830392914494943),.UNSPECIFIED.);
#2519=B_SPLINE_CURVE_WITH_KNOTS('',3,(#111468,#111469,#111470,#111471,#111472,
#111473,#111474,#111475,#111476,#111477,#111478,#111479,#111480,#111481,
#111482,#111483,#111484,#111485,#111486,#111487,#111488,#111489,#111490,
#111491,#111492,#111493,#111494,#111495,#111496,#111497,#111498,#111499,
#111500,#111501,#111502,#111503),.UNSPECIFIED.,.T.,.F.,(4,2,2,2,2,2,2,2,
2,2,2,2,2,2,2,2,2,4),(0.,0.0503397569852893,0.100535814375046,0.150559311436999,
0.20049644388078,0.250492956056916,0.300635695532588,0.325734796020786,
0.350832855894969,0.401702116132417,0.452343313876895,0.503069511784625,
0.553891621921385,0.60462388767292,0.655263863923187,0.706116496828786,
0.757483229007975,0.804696187913725),.UNSPECIFIED.);
#2520=B_SPLINE_CURVE_WITH_KNOTS('',3,(#111507,#111508,#111509,#111510,#111511,
#111512,#111513,#111514,#111515,#111516,#111517,#111518,#111519,#111520,
#111521,#111522,#111523,#111524,#111525,#111526,#111527,#111528,#111529),
 .UNSPECIFIED.,.F.,.F.,(4,2,2,2,2,2,2,2,2,3,4),(0.213084510884075,0.228781186975439,
0.255371494150004,0.281887710763666,0.308357606751256,0.334840690693978,
0.361386330906224,0.387995767314121,0.41510213099284,0.426162916715676,
0.426168100816612),.UNSPECIFIED.);
#2521=B_SPLINE_CURVE_WITH_KNOTS('',3,(#111533,#111534,#111535,#111536,#111537,
#111538,#111539,#111540,#111541,#111542,#111543,#111544,#111545,#111546,
#111547,#111548,#111549,#111550,#111551,#111552),.UNSPECIFIED.,.F.,.F.,
(4,2,2,2,2,2,2,2,2,4),(0.426168100816612,0.453130885029272,0.480106246397837,
0.507100150030191,0.53407533862366,0.561043554729105,0.588091928815527,
0.601349529885376,0.628296013507661,0.639247427599751),.UNSPECIFIED.);
#2522=B_SPLINE_CURVE_WITH_KNOTS('',3,(#111556,#111557,#111558,#111559,#111560,
#111561,#111562,#111563,#111564,#111565,#111566,#111567,#111568,#111569,
#111570,#111571,#111572,#111573,#111574,#111575,#111576,#111577,#111578,
#111579,#111580,#111581,#111582,#111583,#111584,#111585,#111586,#111587,
#111588,#111589,#111590,#111591,#111592,#111593),.UNSPECIFIED.,.T.,.F.,
(4,2,2,2,2,2,2,2,2,2,2,2,2,2,2,2,2,2,4),(0.,0.0435250099426588,0.0867875676414407,
0.129798831049099,0.172723528677881,0.215785743787518,0.259119343545877,
0.280868720015448,0.302536290796754,0.346522406274042,0.390327377842269,
0.434204529765891,0.477178955585274,0.520208273340797,0.564038055478109,
0.607876492390102,0.6293685607735,0.650934887956273,0.694354039347353),
 .UNSPECIFIED.);
#2523=B_SPLINE_CURVE_WITH_KNOTS('',3,(#111597,#111598,#111599,#111600,#111601,
#111602,#111603,#111604,#111605,#111606,#111607,#111608,#111609,#111610,
#111611,#111612,#111613,#111614,#111615,#111616,#111617,#111618,#111619,
#111620,#111621),.UNSPECIFIED.,.F.,.F.,(4,2,2,2,2,2,2,2,2,2,3,4),(0.157609960982023,
0.158131914212271,0.178047596316255,0.197664157824957,0.21718321769825,
0.236683024193072,0.256254661663229,0.275945553163195,0.2857852745923,0.295605663211171,
0.315211906754256,0.315215197496655),.UNSPECIFIED.);
#2524=B_SPLINE_CURVE_WITH_KNOTS('',3,(#111625,#111626,#111627,#111628,#111629,
#111630,#111631,#111632,#111633,#111634,#111635,#111636,#111637,#111638,
#111639,#111640,#111641,#111642,#111643,#111644),.UNSPECIFIED.,.F.,.F.,
(4,2,2,2,2,2,2,2,2,4),(0.315215197496655,0.335200466876354,0.354999433605467,
0.374512449736718,0.394033699253622,0.413636951394353,0.433631734481444,
0.443418967878,0.453219950155937,0.472821867736279),.UNSPECIFIED.);
#2525=B_SPLINE_CURVE_WITH_KNOTS('',3,(#111648,#111649,#111650,#111651,#111652,
#111653,#111654,#111655,#111656,#111657,#111658,#111659,#111660,#111661,
#111662,#111663,#111664,#111665,#111666,#111667,#111668,#111669,#111670,
#111671,#111672,#111673,#111674,#111675,#111676,#111677,#111678,#111679,
#111680,#111681,#111682,#111683,#111684,#111685),.UNSPECIFIED.,.T.,.F.,
(4,2,2,2,2,2,2,2,2,2,2,2,2,2,2,2,2,2,4),(0.,0.0435158903681535,0.0866337303822979,
0.129311950410083,0.17176772862335,0.214353892471028,0.257343254730134,
0.300752733852546,0.322381697566155,0.366274614380129,0.409883810353136,
0.453406609581401,0.495934191090317,0.538530090897993,0.582105934721859,
0.625923161624818,0.64744336097096,0.66884623605417,0.69046738873967),
 .UNSPECIFIED.);
#2526=B_SPLINE_CURVE_WITH_KNOTS('',3,(#111689,#111690,#111691,#111692,#111693,
#111694,#111695,#111696,#111697,#111698,#111699,#111700,#111701,#111702,
#111703,#111704,#111705,#111706,#111707,#111708,#111709,#111710,#111711,
#111712,#111713),.UNSPECIFIED.,.F.,.F.,(4,2,2,2,2,2,2,2,2,2,3,4),(0.15531487351589,
0.166145970728797,0.185609441146789,0.204874632650298,0.223999607628438,
0.243124535499743,0.262389220003626,0.281850923436399,0.291587450265206,
0.301045446444696,0.310583538395292,0.310587695933181),.UNSPECIFIED.);
#2527=B_SPLINE_CURVE_WITH_KNOTS('',3,(#111717,#111718,#111719,#111720,#111721,
#111722,#111723,#111724,#111725,#111726,#111727,#111728,#111729,#111730,
#111731,#111732,#111733,#111734,#111735,#111736),.UNSPECIFIED.,.F.,.F.,
(4,2,2,2,2,2,2,2,2,4),(0.310587695933181,0.330338548490155,0.35001160002629,
0.36918336873163,0.388303018538272,0.407509226017143,0.427247589363119,
0.447088430248727,0.456810155929384,0.465898411911182),.UNSPECIFIED.);
#2528=B_SPLINE_CURVE_WITH_KNOTS('',3,(#111740,#111741,#111742,#111743,#111744,
#111745,#111746,#111747,#111748,#111749,#111750,#111751,#111752,#111753,
#111754,#111755,#111756,#111757,#111758,#111759,#111760,#111761,#111762,
#111763,#111764,#111765,#111766,#111767,#111768,#111769,#111770,#111771,
#111772,#111773,#111774,#111775,#111776,#111777),.UNSPECIFIED.,.T.,.F.,
(4,2,2,2,2,2,2,2,2,2,2,2,2,2,2,2,2,2,4),(0.,0.0579456402909644,0.0869299048751541,
0.115920063309306,0.174806990420041,0.233290522899272,0.291875001059739,
0.350660758745357,0.409359852180272,0.467844120994597,0.526472280441444,
0.555272349874393,0.584555610575361,0.642786260517934,0.701059261140235,
0.759300709458156,0.817409370762721,0.875368479051853,0.931707159703552),
 .UNSPECIFIED.);
#2529=B_SPLINE_CURVE_WITH_KNOTS('',3,(#111781,#111782,#111783,#111784,#111785,
#111786,#111787,#111788,#111789,#111790,#111791,#111792,#111793,#111794,
#111795,#111796,#111797,#111798,#111799,#111800),.UNSPECIFIED.,.F.,.F.,
(4,2,2,2,2,2,2,2,2,4),(1.00000028111068E-6,0.0347832075796592,0.0692716651495764,
0.103819772803296,0.13840130343469,0.172863389577014,0.190089620355572,
0.207318502211029,0.242417063886181,0.276778761880576),.UNSPECIFIED.);
#2530=B_SPLINE_CURVE_WITH_KNOTS('',3,(#111804,#111805,#111806,#111807,#111808,
#111809,#111810,#111811,#111812,#111813,#111814,#111815,#111816,#111817,
#111818,#111819,#111820,#111821,#111822,#111823,#111824,#111825,#111826,
#111827,#111828,#111829,#111830,#111831,#111832,#111833,#111834,#111835,
#111836,#111837,#111838,#111839,#111840,#111841,#111842,#111843,#111844,
#111845,#111846,#111847,#111848,#111849,#111850,#111851,#111852,#111853,
#111854,#111855,#111856,#111857,#111858,#111859,#111860,#111861,#111862,
#111863,#111864,#111865,#111866,#111867,#111868,#111869,#111870,#111871,
#111872,#111873,#111874,#111875,#111876,#111877,#111878,#111879,#111880,
#111881,#111882),.UNSPECIFIED.,.F.,.F.,(4,3,3,3,3,3,3,3,3,3,3,3,3,3,3,3,
3,3,3,3,3,3,3,3,3,3,4),(0.00274647550789723,0.00284764836235053,0.00294876159984055,
0.00304994614202459,0.00308970325655458,0.00318942908487613,0.00328907626887442,
0.00338877449852303,0.00343293100521208,0.00354315533571446,0.00365327844248592,
0.00376338004483701,0.00377615875386958,0.0039686408465685,0.00411938650252707,
0.00426424510927638,0.00441595944867224,0.00446261425118457,0.00458541711012655,
0.00470860724668196,0.00480584199984207,0.00493281230714532,0.00505965424824699,
0.00518600265972549,0.00531190386550827,0.00543695346148025,0.00549229749715719),
 .UNSPECIFIED.);
#2531=B_SPLINE_CURVE_WITH_KNOTS('',3,(#111886,#111887,#111888,#111889,#111890,
#111891,#111892,#111893,#111894,#111895,#111896,#111897,#111898,#111899,
#111900,#111901,#111902,#111903,#111904,#111905,#111906,#111907,#111908,
#111909,#111910,#111911,#111912,#111913,#111914,#111915,#111916,#111917,
#111918,#111919,#111920,#111921),.UNSPECIFIED.,.T.,.F.,(4,2,2,2,2,2,2,2,
2,2,2,2,2,2,2,2,2,4),(0.,0.050238053143519,0.100318703593234,0.150284930734814,
0.200263745526201,0.250367992087392,0.30059723478709,0.351510110444586,
0.402132532931605,0.452865784267353,0.503834596479786,0.554795405381783,
0.605516639507723,0.656143227180573,0.680951395143589,0.705853156657982,
0.756739251203461,0.804680497302985),.UNSPECIFIED.);
#2532=B_SPLINE_CURVE_WITH_KNOTS('',3,(#111925,#111926,#111927,#111928,#111929,
#111930,#111931,#111932,#111933,#111934,#111935,#111936,#111937,#111938,
#111939,#111940,#111941,#111942,#111943,#111944,#111945,#111946,#111947),
 .UNSPECIFIED.,.F.,.F.,(4,2,2,2,2,2,2,2,2,3,4),(0.2131238921346,0.214468422234068,
0.241041142260569,0.267548108379182,0.294021969529815,0.320519566555282,
0.347081755444668,0.373699970899426,0.400716003372662,0.426139175217478,
0.426214998931696),.UNSPECIFIED.);
#2533=B_SPLINE_CURVE_WITH_KNOTS('',3,(#111951,#111952,#111953,#111954,#111955,
#111956,#111957,#111958,#111959,#111960,#111961,#111962,#111963,#111964,
#111965,#111966,#111967,#111968,#111969,#111970),.UNSPECIFIED.,.F.,.F.,
(4,2,2,2,2,2,2,2,2,4),(0.426214998931696,0.453141486117911,0.479941628222141,
0.506446749253699,0.533446181809698,0.560399835109198,0.573588277851575,
0.586799440471832,0.61397554918602,0.639263067352078),.UNSPECIFIED.);
#2534=B_SPLINE_CURVE_WITH_KNOTS('',3,(#111974,#111975,#111976,#111977,#111978,
#111979,#111980,#111981,#111982,#111983,#111984,#111985,#111986,#111987,
#111988,#111989,#111990,#111991,#111992,#111993,#111994,#111995,#111996,
#111997,#111998,#111999,#112000,#112001,#112002,#112003,#112004,#112005,
#112006,#112007,#112008,#112009,#112010,#112011),.UNSPECIFIED.,.T.,.F.,
(4,2,2,2,2,2,2,2,2,2,2,2,2,2,2,2,2,2,4),(0.,0.0434332594561585,0.0865773364499496,
0.129513968405876,0.17245727714254,0.215616554324647,0.259052653928386,
0.280820020239544,0.324985455094301,0.368839855016106,0.412603610869772,
0.456387211561026,0.500159730990598,0.543941426909056,0.587917004107691,
0.609507132339805,0.631194826658406,0.675273884169567,0.694350838467621),
 .UNSPECIFIED.);
#2535=B_SPLINE_CURVE_WITH_KNOTS('',3,(#112015,#112016,#112017,#112018,#112019,
#112020,#112021,#112022,#112023,#112024,#112025,#112026,#112027,#112028,
#112029,#112030,#112031,#112032,#112033,#112034,#112035,#112036),
 .UNSPECIFIED.,.F.,.F.,(4,2,2,2,2,2,2,2,2,2,4),(0.157597789128493,0.169083802496607,
0.18870673517436,0.208226233094476,0.227720441582404,0.247283245699002,
0.266966206820028,0.276841811354643,0.286707833757665,0.306807298818768,
0.315181555765077),.UNSPECIFIED.);
#2536=B_SPLINE_CURVE_WITH_KNOTS('',3,(#112040,#112041,#112042,#112043,#112044,
#112045,#112046,#112047,#112048,#112049,#112050,#112051,#112052,#112053,
#112054,#112055,#112056,#112057,#112058,#112059,#112060,#112061,#112062),
 .UNSPECIFIED.,.F.,.F.,(4,3,2,2,2,2,2,2,2,2,4),(0.315181555765077,0.315211081404571,
0.335185778257555,0.355123769487627,0.374629687959294,0.394580515763128,
0.414589339174075,0.43469511893165,0.44454832600833,0.46455224696731,0.472808870533064),
 .UNSPECIFIED.);
#2537=B_SPLINE_CURVE_WITH_KNOTS('',3,(#112066,#112067,#112068,#112069,#112070,
#112071,#112072,#112073,#112074,#112075,#112076,#112077,#112078,#112079,
#112080,#112081,#112082,#112083,#112084,#112085,#112086,#112087,#112088,
#112089,#112090,#112091,#112092,#112093,#112094,#112095,#112096,#112097,
#112098,#112099,#112100,#112101),.UNSPECIFIED.,.T.,.F.,(4,2,2,2,2,2,2,2,
2,2,2,2,2,2,2,2,2,4),(0.,0.0433164111904613,0.0861802904256355,0.128695730684266,
0.17117710467452,0.213959992111218,0.257192364442634,0.278872188929985,
0.300475215881829,0.344325448282991,0.387923981596494,0.43146876574843,
0.473989434020882,0.516592272710811,0.560170910964625,0.603968557707506,
0.648131236112833,0.690514011068081),.UNSPECIFIED.);
#2538=B_SPLINE_CURVE_WITH_KNOTS('',3,(#112105,#112106,#112107,#112108,#112109,
#112110,#112111,#112112,#112113,#112114,#112115,#112116,#112117,#112118,
#112119,#112120,#112121,#112122,#112123,#112124,#112125,#112126),
 .UNSPECIFIED.,.F.,.F.,(4,2,2,2,2,2,2,2,2,2,4),(0.155287089809751,0.156239702321605,
0.175693722579379,0.194950054784518,0.214071007842835,0.233198182186066,
0.252469243668368,0.271936827701031,0.281664497015936,0.291376767571409,
0.310561645694942),.UNSPECIFIED.);
#2539=B_SPLINE_CURVE_WITH_KNOTS('',3,(#112130,#112131,#112132,#112133,#112134,
#112135,#112136,#112137,#112138,#112139,#112140,#112141,#112142,#112143,
#112144,#112145,#112146,#112147,#112148,#112149,#112150),.UNSPECIFIED.,
 .F.,.F.,(4,3,2,2,2,2,2,2,2,4),(0.310561645694942,0.310600891687435,0.330305486834909,
0.349720687016697,0.368845270661463,0.387995078999074,0.40729029280085,
0.427067810869433,0.446935487204266,0.465887981497185),.UNSPECIFIED.);
#2540=B_SPLINE_CURVE_WITH_KNOTS('',3,(#112154,#112155,#112156,#112157,#112158,
#112159,#112160,#112161,#112162,#112163,#112164,#112165,#112166,#112167,
#112168,#112169,#112170,#112171,#112172,#112173,#112174,#112175,#112176,
#112177,#112178,#112179,#112180,#112181,#112182,#112183,#112184,#112185,
#112186,#112187,#112188,#112189,#112190,#112191),.UNSPECIFIED.,.T.,.F.,
(4,2,2,2,2,2,2,2,2,2,2,2,2,2,2,2,2,2,4),(0.,0.0580082234967378,0.0870003549736756,
0.145722824454584,0.204170932747089,0.262860983195594,0.32181813325465,
0.380645368506535,0.439147647867318,0.497686767907287,0.526427549115819,
0.555714243195097,0.61393184666816,0.672175661372658,0.730386137666084,
0.78847933364516,0.846448163441301,0.904377989258386,0.93172076410077),
 .UNSPECIFIED.);
#2541=B_SPLINE_CURVE_WITH_KNOTS('',3,(#112195,#112196,#112197,#112198,#112199,
#112200,#112201,#112202,#112203,#112204,#112205,#112206,#112207,#112208,
#112209,#112210,#112211,#112212,#112213,#112214,#112215,#112216),
 .UNSPECIFIED.,.F.,.F.,(4,2,2,2,2,2,2,2,2,2,4),(0.276825419382499,0.296324142535683,
0.330827915139416,0.365291806459535,0.399749802742698,0.434231353821986,
0.451460874855943,0.468676585515715,0.503676193620126,0.538615895182268,
0.553565879266481),.UNSPECIFIED.);
#2542=B_SPLINE_CURVE_WITH_KNOTS('',3,(#112220,#112221,#112222,#112223,#112224,
#112225,#112226,#112227,#112228,#112229,#112230,#112231,#112232,#112233,
#112234,#112235,#112236,#112237,#112238,#112239),.UNSPECIFIED.,.F.,.F.,
(4,2,2,2,2,2,2,2,2,4),(0.553566629579059,0.588673847195773,0.623808685061497,
0.658827117911204,0.693760556057172,0.728808292162389,0.74621422278564,
0.780776959390752,0.815342636920125,0.830391298648981),.UNSPECIFIED.);
#2543=B_SPLINE_CURVE_WITH_KNOTS('',3,(#112243,#112244,#112245,#112246,#112247,
#112248,#112249,#112250,#112251,#112252,#112253,#112254,#112255,#112256,
#112257,#112258,#112259,#112260,#112261,#112262,#112263,#112264,#112265,
#112266,#112267,#112268,#112269,#112270,#112271,#112272,#112273,#112274,
#112275,#112276,#112277,#112278),.UNSPECIFIED.,.T.,.F.,(4,2,2,2,2,2,2,2,
2,2,2,2,2,2,2,2,2,4),(0.,0.0501941079062752,0.100208029985453,0.150133961016788,
0.200122562975031,0.250261040409613,0.300503454318807,0.351402927886362,
0.402040021073659,0.452714837694694,0.503452587635481,0.55411839025828,
0.604764231782756,0.655704733278668,0.681060469351491,0.731450356759017,
0.781833273489143,0.804680564507272),.UNSPECIFIED.);
#2544=B_SPLINE_CURVE_WITH_KNOTS('',3,(#112282,#112283,#112284,#112285,#112286,
#112287,#112288,#112289,#112290,#112291,#112292,#112293,#112294,#112295,
#112296,#112297,#112298,#112299,#112300,#112301,#112302,#112303,#112304,
#112305,#112306),.UNSPECIFIED.,.F.,.F.,(4,2,2,2,2,2,2,2,2,2,3,4),(0.213115940430313,
0.228240783603859,0.25475654265634,0.281222254477514,0.307699372237131,
0.334239639354176,0.347526280393058,0.360821523860804,0.387448044952019,
0.41444762115626,0.42607809063124,0.426122798621427),.UNSPECIFIED.);
#2545=B_SPLINE_CURVE_WITH_KNOTS('',3,(#112310,#112311,#112312,#112313,#112314,
#112315,#112316,#112317,#112318,#112319,#112320,#112321,#112322,#112323,
#112324,#112325,#112326,#112327,#112328,#112329),.UNSPECIFIED.,.F.,.F.,
(4,2,2,2,2,2,2,2,2,4),(0.426122798621427,0.453022011122751,0.479971032167598,
0.506914688870937,0.533886525204312,0.560974013753547,0.574405821463177,
0.601073035300724,0.627725348855489,0.639194031061553),.UNSPECIFIED.);
#2546=B_SPLINE_CURVE_WITH_KNOTS('',3,(#112333,#112334,#112335,#112336,#112337,
#112338,#112339,#112340,#112341,#112342,#112343,#112344,#112345,#112346,
#112347,#112348,#112349,#112350,#112351,#112352,#112353,#112354,#112355,
#112356,#112357,#112358,#112359,#112360,#112361,#112362,#112363,#112364,
#112365,#112366,#112367,#112368,#112369,#112370),.UNSPECIFIED.,.T.,.F.,
(4,2,2,2,2,2,2,2,2,2,2,2,2,2,2,2,2,2,4),(0.,0.0432546244612286,0.086255807439944,
0.129173083664551,0.172232566355353,0.215565601873972,0.23731502413423,
0.259009358276642,0.30304397619408,0.346860989813651,0.390696968675583,
0.434168192850255,0.477198720502358,0.521002216775895,0.564898011457953,
0.586432590869027,0.608052372281735,0.652125519462753,0.694293106594506),
 .UNSPECIFIED.);
#2547=B_SPLINE_CURVE_WITH_KNOTS('',3,(#112374,#112375,#112376,#112377,#112378,
#112379,#112380,#112381,#112382,#112383,#112384,#112385,#112386,#112387,
#112388,#112389,#112390,#112391,#112392,#112393,#112394,#112395),
 .UNSPECIFIED.,.F.,.F.,(4,2,2,2,2,2,2,2,2,2,4),(0.157571090181139,0.158533388827235,
0.178145141731992,0.197659871594592,0.217157670328134,0.236729740971422,
0.256421770612226,0.266273321120224,0.276108275501286,0.296155698892633,
0.315156398956201),.UNSPECIFIED.);
#2548=B_SPLINE_CURVE_WITH_KNOTS('',3,(#112399,#112400,#112401,#112402,#112403,
#112404,#112405,#112406,#112407,#112408,#112409,#112410,#112411,#112412,
#112413,#112414,#112415,#112416,#112417,#112418,#112419,#112420,#112421),
 .UNSPECIFIED.,.F.,.F.,(4,3,2,2,2,2,2,2,2,2,4),(0.315156398956201,0.315184248085558,
0.33516826884962,0.354679961794265,0.37420007938843,0.394184451236293,0.414202323850884,
0.4240062685368,0.433828109433089,0.453986817846637,0.472755338266697),
 .UNSPECIFIED.);
#2549=B_SPLINE_CURVE_WITH_KNOTS('',3,(#112425,#112426,#112427,#112428,#112429,
#112430,#112431,#112432,#112433,#112434,#112435,#112436,#112437,#112438,
#112439,#112440,#112441,#112442,#112443,#112444,#112445,#112446,#112447,
#112448,#112449,#112450,#112451,#112452,#112453,#112454,#112455,#112456,
#112457,#112458,#112459,#112460),.UNSPECIFIED.,.T.,.F.,(4,2,2,2,2,2,2,2,
2,2,2,2,2,2,2,2,2,4),(0.,0.0430585199525399,0.0856946946073311,0.128146367850984,
0.170765293674358,0.21380192121876,0.258059130523452,0.279602698825103,
0.32336245007672,0.366948239185581,0.41010425798879,0.452616352668395,0.495235832149333,
0.53881891492568,0.582560673493689,0.626639303656973,0.670992351859876,
0.690486283458249),.UNSPECIFIED.);
#2550=B_SPLINE_CURVE_WITH_KNOTS('',3,(#112464,#112465,#112466,#112467,#112468,
#112469,#112470,#112471,#112472,#112473,#112474,#112475,#112476,#112477,
#112478,#112479,#112480,#112481,#112482,#112483,#112484,#112485,#112486),
 .UNSPECIFIED.,.F.,.F.,(4,2,2,2,2,2,2,2,2,3,4),(0.15531757295188,0.156219469888912,
0.175559071474778,0.194724030140012,0.21382905049678,0.233024066023952,
0.252406525118312,0.272263835569533,0.292052092223187,0.310621714473832,
0.310623433033234),.UNSPECIFIED.);
#2551=B_SPLINE_CURVE_WITH_KNOTS('',3,(#112490,#112491,#112492,#112493,#112494,
#112495,#112496,#112497,#112498,#112499,#112500,#112501,#112502,#112503,
#112504,#112505,#112506,#112507),.UNSPECIFIED.,.F.,.F.,(4,2,2,2,2,2,2,2,
4),(0.310623433033234,0.330112775227974,0.349270594235827,0.36839029551999,
0.387608771293272,0.407326728692038,0.42711301933763,0.446969017839007,
0.465939287425712),.UNSPECIFIED.);
#2552=B_SPLINE_CURVE_WITH_KNOTS('',3,(#112511,#112512,#112513,#112514,#112515,
#112516,#112517,#112518,#112519,#112520,#112521,#112522,#112523,#112524,
#112525,#112526,#112527,#112528,#112529,#112530,#112531,#112532,#112533,
#112534,#112535,#112536,#112537,#112538,#112539,#112540,#112541,#112542,
#112543,#112544,#112545,#112546),.UNSPECIFIED.,.T.,.F.,(4,2,2,2,2,2,2,2,
2,2,2,2,2,2,2,2,2,4),(0.,0.0580987417317566,0.116047179752343,0.173942504194012,
0.231890034901526,0.260874895236775,0.289864886177479,0.348715623176785,
0.40719421054338,0.465783055157053,0.524545288006566,0.583199724794616,
0.641672766601171,0.700361462609497,0.759142645252055,0.817380642606661,
0.875659937599892,0.931838431390136),.UNSPECIFIED.);
#2553=B_SPLINE_CURVE_WITH_KNOTS('',3,(#112550,#112551,#112552,#112553,#112554,
#112555,#112556,#112557,#112558,#112559,#112560,#112561,#112562,#112563,
#112564,#112565,#112566,#112567,#112568,#112569,#112570,#112571),
 .UNSPECIFIED.,.F.,.F.,(4,2,2,2,2,2,2,2,2,2,4),(0.139807847310764,0.172892344288993,
0.207349020107777,0.241786047442339,0.276246202522754,0.293472315492746,
0.31070131942903,0.345811547283687,0.380767382220101,0.41573982156058,0.416591164797455),
 .UNSPECIFIED.);
#2554=B_SPLINE_CURVE_WITH_KNOTS('',3,(#112575,#112576,#112577,#112578,#112579,
#112580,#112581,#112582,#112583,#112584,#112585,#112586,#112587,#112588,
#112589,#112590,#112591,#112592,#112593,#112594,#112595,#112596,#112597),
 .UNSPECIFIED.,.F.,.F.,(4,2,2,2,3,2,2,2,2,2,4),(0.416591164797455,0.450764532772226,
0.485758661251731,0.52070521808968,0.553554982405065,0.570960064057211,
0.588202925424454,0.622775829172639,0.657363001084429,0.691932699501471,
0.69336282971583),.UNSPECIFIED.);
#2555=B_SPLINE_CURVE_WITH_KNOTS('',3,(#112601,#112602,#112603,#112604,#112605,
#112606,#112607,#112608,#112609,#112610,#112611,#112612,#112613,#112614,
#112615,#112616,#112617,#112618,#112619,#112620,#112621,#112622,#112623,
#112624,#112625,#112626,#112627,#112628,#112629,#112630,#112631,#112632,
#112633,#112634,#112635,#112636),.UNSPECIFIED.,.T.,.F.,(4,2,2,2,2,2,2,2,
2,2,2,2,2,2,2,2,2,4),(0.,0.0500751837172648,0.100032835755184,0.150004622813311,
0.200104477996478,0.250330155712872,0.301275718890895,0.351916973449905,
0.402634777221146,0.453544462099944,0.504429457760046,0.555113620900938,
0.605779259382996,0.630621781652347,0.655571265702426,0.706455348933985,
0.756802298634988,0.804652792367142),.UNSPECIFIED.);
#2556=B_SPLINE_CURVE_WITH_KNOTS('',3,(#112640,#112641,#112642,#112643,#112644,
#112645,#112646,#112647,#112648,#112649,#112650,#112651,#112652,#112653,
#112654,#112655,#112656,#112657,#112658,#112659,#112660,#112661,#112662,
#112663,#112664),.UNSPECIFIED.,.F.,.F.,(4,2,2,2,2,2,2,2,2,2,3,4),(0.213076432906529,
0.214625312887961,0.241130224916482,0.267600798364176,0.294095401469753,
0.320655354479264,0.333945803383919,0.347229432506566,0.374268970490067,
0.401233145512626,0.426062397290551,0.426094069355307),.UNSPECIFIED.);
#2557=B_SPLINE_CURVE_WITH_KNOTS('',3,(#112668,#112669,#112670,#112671,#112672,
#112673,#112674,#112675,#112676,#112677,#112678,#112679,#112680,#112681,
#112682,#112683,#112684,#112685,#112686,#112687),.UNSPECIFIED.,.F.,.F.,
(4,2,2,2,2,2,2,2,2,4),(0.426094069355307,0.453108809523285,0.480148392673564,
0.507128954570031,0.534100718191605,0.547305148979544,0.560538665060336,
0.58748104776454,0.614114710291041,0.63913883019708),.UNSPECIFIED.);
#2558=B_SPLINE_CURVE_WITH_KNOTS('',3,(#112691,#112692,#112693,#112694,#112695,
#112696,#112697,#112698,#112699,#112700,#112701,#112702,#112703,#112704,
#112705,#112706,#112707,#112708,#112709,#112710,#112711,#112712,#112713,
#112714,#112715,#112716,#112717,#112718,#112719,#112720,#112721,#112722,
#112723,#112724,#112725,#112726,#112727,#112728),.UNSPECIFIED.,.T.,.F.,
(4,2,2,2,2,2,2,2,2,2,2,2,2,2,2,2,2,2,4),(0.,0.0431036505402475,0.086030227698429,
0.12899757453654,0.172198322896197,0.215665127366231,0.237347439199144,
0.28136115483838,0.325171935923412,0.369015030741623,0.412483731024054,
0.455518305292952,0.499321306509743,0.54321713079997,0.564752036213917,
0.58637219462266,0.63043986218883,0.673944869558154,0.694276631667984),
 .UNSPECIFIED.);
#2559=B_SPLINE_CURVE_WITH_KNOTS('',3,(#112732,#112733,#112734,#112735,#112736,
#112737,#112738,#112739,#112740,#112741,#112742,#112743,#112744,#112745,
#112746,#112747,#112748,#112749,#112750,#112751,#112752,#112753),
 .UNSPECIFIED.,.F.,.F.,(4,2,2,2,2,2,2,2,2,2,4),(0.157610394168263,0.167948182018796,
0.187461103302467,0.206959039117144,0.226532732494941,0.246226517887538,
0.256075595964361,0.265907492794962,0.285949702319035,0.305941086537169,
0.315175721481595),.UNSPECIFIED.);
#2560=B_SPLINE_CURVE_WITH_KNOTS('',3,(#112757,#112758,#112759,#112760,#112761,
#112762,#112763,#112764,#112765,#112766,#112767,#112768,#112769,#112770,
#112771,#112772,#112773,#112774,#112775,#112776),.UNSPECIFIED.,.F.,.F.,
(4,2,2,2,2,2,2,2,2,4),(0.315176131159691,0.334712905302903,0.354217365440266,
0.373772274158537,0.393765409621518,0.413813284197024,0.423632882046344,
0.443787520663527,0.46351526610713,0.472786115649858),.UNSPECIFIED.);
#2561=B_SPLINE_CURVE_WITH_KNOTS('',3,(#112780,#112781,#112782,#112783,#112784,
#112785,#112786,#112787,#112788,#112789,#112790,#112791,#112792,#112793,
#112794,#112795,#112796,#112797,#112798,#112799,#112800,#112801,#112802,
#112803,#112804,#112805,#112806,#112807,#112808,#112809,#112810,#112811,
#112812,#112813,#112814,#112815,#112816,#112817),.UNSPECIFIED.,.T.,.F.,
(4,2,2,2,2,2,2,2,2,2,2,2,2,2,2,2,2,2,4),(0.,0.0428352656493673,0.0853323262706088,
0.12781305629003,0.170609089855836,0.213855236814163,0.23554467169079,0.257156357809307,
0.301012526245623,0.344596881047352,0.388103409972812,0.43061567105667,
0.473223348968646,0.51680383210501,0.56065107298488,0.582188244212754,0.626563562308793,
0.67003492597377,0.69032599641099),.UNSPECIFIED.);
#2562=B_SPLINE_CURVE_WITH_KNOTS('',3,(#112821,#112822,#112823,#112824,#112825,
#112826,#112827,#112828,#112829,#112830,#112831,#112832,#112833,#112834,
#112835,#112836,#112837,#112838,#112839,#112840),.UNSPECIFIED.,.F.,.F.,
(4,2,2,2,2,2,2,2,2,4),(0.155279913630204,0.16580783098891,0.184973337282856,
0.204075159603871,0.223264401799693,0.242640837393322,0.262555404900247,
0.282398648796319,0.3021371068126,0.310566010568874),.UNSPECIFIED.);
#2563=B_SPLINE_CURVE_WITH_KNOTS('',3,(#112844,#112845,#112846,#112847,#112848,
#112849,#112850,#112851,#112852,#112853,#112854,#112855,#112856,#112857,
#112858,#112859,#112860,#112861,#112862,#112863),.UNSPECIFIED.,.F.,.F.,
(4,2,2,2,2,2,2,2,2,4),(0.31056680619282,0.329971810180022,0.349091924172357,
0.368241538651675,0.387939228916316,0.407735663979358,0.417440913787486,
0.437356634777529,0.457031325949547,0.465846719823024),.UNSPECIFIED.);
#2564=B_SPLINE_CURVE_WITH_KNOTS('',3,(#112868,#112869,#112870,#112871,#112872,
#112873,#112874,#112875,#112876,#112877,#112878,#112879,#112880,#112881,
#112882,#112883,#112884,#112885,#112886,#112887,#112888,#112889,#112890,
#112891,#112892,#112893,#112894,#112895,#112896,#112897,#112898,#112899,
#112900,#112901,#112902,#112903,#112904,#112905,#112906,#112907,#112908,
#112909,#112910,#112911,#112912,#112913,#112914,#112915,#112916,#112917,
#112918,#112919,#112920,#112921,#112922,#112923,#112924,#112925,#112926,
#112927,#112928,#112929,#112930,#112931,#112932,#112933,#112934,#112935,
#112936,#112937,#112938,#112939,#112940,#112941,#112942,#112943,#112944,
#112945,#112946,#112947,#112948,#112949,#112950,#112951,#112952,#112953,
#112954,#112955,#112956,#112957,#112958,#112959,#112960,#112961,#112962,
#112963,#112964,#112965,#112966,#112967,#112968,#112969,#112970,#112971,
#112972,#112973,#112974,#112975,#112976,#112977,#112978,#112979,#112980,
#112981,#112982,#112983,#112984,#112985,#112986,#112987,#112988,#112989,
#112990,#112991),.UNSPECIFIED.,.F.,.F.,(4,3,3,3,3,3,3,3,3,3,3,3,3,3,3,3,
3,3,3,3,3,3,3,3,3,3,3,3,3,3,3,3,3,3,3,3,3,3,3,3,3,4),(0.,0.000132727827510117,
0.000266773740721149,0.000288916803381741,0.000405384809022413,0.000521742841023505,
0.000577833606763482,0.000712486468141431,0.000847464610128366,0.000866750410145223,
0.000975173680697608,0.00108362607993552,0.00115566721352696,0.00130437632058373,
0.00145300072902973,0.00160173866912145,0.00173350082029021,0.0018816218515353,
0.00202963491476389,0.00217772706204638,0.00231133442705345,0.00242041547284975,
0.0025294417699843,0.00260025123043525,0.0027352309774238,0.00287005073028349,
0.00288916803381705,0.00300322542298272,0.00311737920790335,0.00317808483719885,
0.00331233809713726,0.00344542767765184,0.00346700164058064,0.00367446908522699,
0.00389243458456527,0.00404483524734448,0.00417937562109319,0.00431434174898983,
0.00433375205072634,0.00444167959104199,0.00454961794032719,0.00462266885410819),
 .UNSPECIFIED.);
#2565=B_SPLINE_CURVE_WITH_KNOTS('',3,(#112992,#112993,#112994,#112995,#112996,
#112997,#112998,#112999,#113000,#113001,#113002,#113003,#113004,#113005,
#113006,#113007,#113008,#113009,#113010,#113011,#113012,#113013),
 .UNSPECIFIED.,.F.,.F.,(4,2,2,2,2,2,2,2,2,2,4),(1.00000008493243E-6,0.029653429365995,
0.0602604700157899,0.11533078437385,0.17381113667683,0.232718531946666,
0.29151133439998,0.349760765588745,0.405060944992747,0.435860211986261,
0.465679959802954),.UNSPECIFIED.);
#2566=B_SPLINE_CURVE_WITH_KNOTS('',3,(#113017,#113018,#113019,#113020,#113021,
#113022,#113023,#113024,#113025,#113026,#113027,#113028,#113029,#113030,
#113031,#113032,#113033,#113034,#113035,#113036,#113037,#113038),
 .UNSPECIFIED.,.F.,.F.,(4,2,2,2,2,2,2,2,2,2,4),(0.139778603637599,0.155618232301033,
0.190078361151525,0.224525782933454,0.258996784686075,0.276224747417236,
0.293454286943181,0.328509035327943,0.363455338377977,0.398466352212045,
0.416560896929866),.UNSPECIFIED.);
#2567=B_SPLINE_CURVE_WITH_KNOTS('',3,(#113042,#113043,#113044,#113045,#113046,
#113047,#113048,#113049,#113050,#113051,#113052,#113053,#113054,#113055,
#113056,#113057,#113058,#113059,#113060,#113061,#113062,#113063,#113064),
 .UNSPECIFIED.,.F.,.F.,(4,2,2,2,2,3,2,2,2,2,4),(0.416560896929866,0.433550062973671,
0.468586736901151,0.503537705167099,0.538545078807563,0.553571177289101,
0.5709760822326,0.605544501529132,0.640121440384529,0.674680233623428,0.6933497809267),
 .UNSPECIFIED.);
#2568=B_SPLINE_CURVE_WITH_KNOTS('',3,(#113068,#113069,#113070,#113071,#113072,
#113073,#113074,#113075,#113076,#113077,#113078,#113079,#113080,#113081,
#113082,#113083,#113084,#113085,#113086,#113087,#113088,#113089,#113090,
#113091,#113092,#113093,#113094,#113095,#113096,#113097,#113098,#113099,
#113100,#113101,#113102,#113103),.UNSPECIFIED.,.T.,.F.,(4,2,2,2,2,2,2,2,
2,2,2,2,2,2,2,2,2,4),(0.,0.0500013751008811,0.0999335696666295,0.149942216996394,
0.200099464079681,0.250344942531881,0.301166873531067,0.35180215134918,
0.402535817466994,0.453341707681982,0.504043858657694,0.554688223342568,
0.605603037386339,0.630958857926489,0.681344686655627,0.731710165394641,
0.781959095477368,0.8046581519998),.UNSPECIFIED.);
#2569=B_SPLINE_CURVE_WITH_KNOTS('',3,(#113107,#113108,#113109,#113110,#113111,
#113112,#113113,#113114,#113115,#113116,#113117,#113118,#113119,#113120,
#113121,#113122,#113123,#113124,#113125,#113126,#113127,#113128,#113129,
#113130,#113131),.UNSPECIFIED.,.F.,.F.,(4,2,2,2,2,2,2,2,2,2,3,4),(0.21306639715026,
0.227818517188535,0.254284620692242,0.280769692590348,0.307320004030579,
0.320608781865553,0.333904721980843,0.360999127823795,0.387980630115309,
0.414943709069341,0.426070661041189,0.426071735170524),.UNSPECIFIED.);
#2570=B_SPLINE_CURVE_WITH_KNOTS('',3,(#113135,#113136,#113137,#113138,#113139,
#113140,#113141,#113142,#113143,#113144,#113145,#113146,#113147,#113148,
#113149,#113150,#113151,#113152,#113153,#113154),.UNSPECIFIED.,.F.,.F.,
(4,2,2,2,2,2,2,2,2,4),(0.426071735170524,0.453056419326165,0.480023136717187,
0.506993993658203,0.534059802781662,0.547491641042938,0.574156120741799,
0.600799182590686,0.627381165688696,0.639137058191448),.UNSPECIFIED.);
#2571=B_SPLINE_CURVE_WITH_KNOTS('',3,(#113158,#113159,#113160,#113161,#113162,
#113163,#113164,#113165,#113166,#113167,#113168,#113169,#113170,#113171,
#113172,#113173,#113174,#113175,#113176,#113177,#113178,#113179,#113180,
#113181,#113182,#113183,#113184,#113185,#113186,#113187,#113188,#113189,
#113190,#113191,#113192,#113193,#113194,#113195),.UNSPECIFIED.,.T.,.F.,
(4,2,2,2,2,2,2,2,2,2,2,2,2,2,2,2,2,2,4),(0.,0.0429891853374796,0.0859005999535319,
0.128961697155561,0.172298985504059,0.194049435970534,0.215763342582676,
0.259828801018375,0.30364808584257,0.34744608553005,0.391291350030285,0.435107609405515,
0.478899297207649,0.522858735862178,0.544436771053145,0.566107742248526,
0.610164662353544,0.653665850718197,0.694242334530551),.UNSPECIFIED.);
#2572=B_SPLINE_CURVE_WITH_KNOTS('',3,(#113199,#113200,#113201,#113202,#113203,
#113204,#113205,#113206,#113207,#113208,#113209,#113210,#113211,#113212,
#113213,#113214,#113215,#113216,#113217,#113218,#113219,#113220),
 .UNSPECIFIED.,.F.,.F.,(4,2,2,2,2,2,2,2,2,2,4),(0.157585769628841,0.158225301867115,
0.177736895355939,0.197232454756444,0.216803549637752,0.236495203073658,
0.246357547652047,0.256205161209479,0.276272029703586,0.296265613933276,
0.315159925279468),.UNSPECIFIED.);
#2573=B_SPLINE_CURVE_WITH_KNOTS('',3,(#113224,#113225,#113226,#113227,#113228,
#113229,#113230,#113231,#113232,#113233,#113234,#113235,#113236,#113237,
#113238,#113239,#113240,#113241,#113242,#113243),.UNSPECIFIED.,.F.,.F.,
(4,2,2,2,2,2,2,2,2,4),(0.315160050285981,0.334670430203605,0.354189141254802,
0.374168068425965,0.394206586146733,0.404024624906889,0.413863252447633,
0.434047259293593,0.453776342647583,0.47274569490831),.UNSPECIFIED.);
#2574=B_SPLINE_CURVE_WITH_KNOTS('',3,(#113247,#113248,#113249,#113250,#113251,
#113252,#113253,#113254,#113255,#113256,#113257,#113258,#113259,#113260,
#113261,#113262,#113263,#113264,#113265,#113266,#113267,#113268,#113269,
#113270,#113271,#113272,#113273,#113274,#113275,#113276,#113277,#113278,
#113279,#113280,#113281,#113282),.UNSPECIFIED.,.T.,.F.,(4,2,2,2,2,2,2,2,
2,2,2,2,2,2,2,2,2,4),(0.,0.0426100058611737,0.0850537338212922,0.127683673144397,
0.170738592765703,0.21499975720634,0.258917600876533,0.302551931591063,
0.346114098909498,0.388667892881555,0.431196440879394,0.473979898101083,
0.517628800858337,0.539043319669517,0.560533654325841,0.604811095552307,
0.648250315521968,0.690350009265023),.UNSPECIFIED.);
#2575=B_SPLINE_CURVE_WITH_KNOTS('',3,(#113286,#113287,#113288,#113289,#113290,
#113291,#113292,#113293,#113294,#113295,#113296,#113297,#113298,#113299,
#113300,#113301,#113302,#113303,#113304,#113305),.UNSPECIFIED.,.F.,.F.,
(4,2,2,2,2,2,2,2,2,4),(0.155247189447164,0.15543816107154,0.174597755768616,
0.193700166759114,0.212895298509184,0.232278832018566,0.252145502041954,
0.271941852319901,0.291661619042685,0.310534450795838),.UNSPECIFIED.);
#2576=B_SPLINE_CURVE_WITH_KNOTS('',3,(#113309,#113310,#113311,#113312,#113313,
#113314,#113315,#113316,#113317,#113318,#113319,#113320,#113321,#113322,
#113323,#113324,#113325,#113326,#113327,#113328),.UNSPECIFIED.,.F.,.F.,
(4,2,2,2,2,2,2,2,2,4),(0.310534954456055,0.329684905209518,0.348803441508971,
0.368026285193018,0.387750202801044,0.397415039714546,0.407097339812214,
0.426966474822227,0.446639471435926,0.465781640243002),.UNSPECIFIED.);
#2577=B_SPLINE_CURVE_WITH_KNOTS('',3,(#113331,#113332,#113333,#113334,#113335,
#113336,#113337,#113338,#113339,#113340,#113341,#113342,#113343,#113344,
#113345,#113346,#113347,#113348,#113349,#113350,#113351,#113352,#113353,
#113354,#113355,#113356,#113357,#113358,#113359,#113360,#113361,#113362,
#113363,#113364,#113365,#113366,#113367,#113368,#113369,#113370,#113371,
#113372,#113373,#113374,#113375,#113376,#113377,#113378,#113379,#113380,
#113381,#113382),.UNSPECIFIED.,.T.,.F.,(4,2,2,2,2,2,2,2,2,2,2,2,2,2,2,2,
2,2,2,2,2,2,2,2,2,4),(0.,0.0149121900649762,0.0263730121522091,0.0384946282833061,
0.0568236080976033,0.105185035310543,0.15252757552285,0.203967129899997,
0.259081364502726,0.318275621652717,0.375912708112063,0.429806971717993,
0.463877271061734,0.477882387809619,0.488346463978146,0.499687248960309,
0.514867691809364,0.547050340458692,0.606166413599678,0.656956780260717,
0.711610535401277,0.770306075356335,0.828288024650288,0.881752841068639,
0.924288918494816,0.931164985314503),.UNSPECIFIED.);
#2578=B_SPLINE_CURVE_WITH_KNOTS('',3,(#113385,#113386,#113387,#113388,#113389,
#113390,#113391,#113392,#113393,#113394,#113395,#113396,#113397,#113398,
#113399,#113400,#113401,#113402,#113403,#113404,#113405,#113406,#113407,
#113408,#113409,#113410,#113411,#113412,#113413,#113414,#113415,#113416,
#113417,#113418,#113419,#113420),.UNSPECIFIED.,.T.,.F.,(4,2,2,2,2,2,2,2,
2,2,2,2,2,2,2,2,2,4),(0.,0.0579392178980262,0.115832358242759,0.173782569200263,
0.202768105596445,0.231758126402807,0.290580147948642,0.349055239233202,
0.407648475424486,0.466395965739747,0.525022431850849,0.583492702203568,
0.642227911139218,0.701011634440832,0.759255031074558,0.817537947627413,
0.875769434518001,0.931837689371155),.UNSPECIFIED.);
#2579=B_SPLINE_CURVE_WITH_KNOTS('',3,(#113424,#113425,#113426,#113427,#113428,
#113429,#113430,#113431,#113432,#113433,#113434,#113435,#113436,#113437,
#113438,#113439,#113440,#113441,#113442,#113443,#113444,#113445),
 .UNSPECIFIED.,.F.,.F.,(4,2,2,2,2,2,2,2,2,2,4),(0.139755173621917,0.172696789744073,
0.207132505990929,0.241593382301936,0.258819812106426,0.276048929239917,
0.311151713616841,0.346105311669953,0.381075529717181,0.41609094289428,
0.416542789415429),.UNSPECIFIED.);
#2580=B_SPLINE_CURVE_WITH_KNOTS('',3,(#113449,#113450,#113451,#113452,#113453,
#113454,#113455,#113456,#113457,#113458,#113459,#113460,#113461,#113462,
#113463,#113464,#113465,#113466,#113467,#113468,#113469),.UNSPECIFIED.,
 .F.,.F.,(4,2,2,2,3,2,2,2,2,4),(0.416542789415429,0.451073116937688,0.486019624601739,
0.521078658759031,0.553639441035905,0.588214628645733,0.622803758665613,
0.657372419330951,0.691883255250138,0.693394614657822),.UNSPECIFIED.);
#2581=B_SPLINE_CURVE_WITH_KNOTS('',3,(#113472,#113473,#113474,#113475,#113476,
#113477,#113478,#113479,#113480,#113481,#113482,#113483,#113484,#113485,
#113486,#113487,#113488,#113489,#113490,#113491,#113492,#113493,#113494,
#113495,#113496,#113497,#113498,#113499,#113500,#113501,#113502,#113503,
#113504,#113505,#113506,#113507,#113508,#113509,#113510,#113511,#113512,
#113513,#113514,#113515,#113516,#113517,#113518,#113519,#113520,#113521),
 .UNSPECIFIED.,.T.,.F.,(4,2,2,2,2,2,2,2,2,2,2,2,2,2,2,2,2,2,2,2,2,2,2,2,
4),(0.,0.0103059827755144,0.021774930988132,0.0401005683710028,0.090946545392836,
0.133247576820222,0.17893682677858,0.227883783029288,0.278524964641298,
0.327309372403573,0.37592257094133,0.394228620230764,0.40557993585886,0.415766213194267,
0.428473089004967,0.452494405415434,0.503326975354497,0.546700448497774,
0.593473184390451,0.643695991372201,0.694046049974661,0.741372994330537,
0.781608468235862,0.798286634292714,0.804144679584088),.UNSPECIFIED.);
#2582=B_SPLINE_CURVE_WITH_KNOTS('',3,(#113524,#113525,#113526,#113527,#113528,
#113529,#113530,#113531,#113532,#113533,#113534,#113535,#113536,#113537,
#113538,#113539,#113540,#113541,#113542,#113543,#113544,#113545,#113546,
#113547,#113548,#113549,#113550,#113551,#113552,#113553,#113554,#113555,
#113556,#113557,#113558,#113559,#113560,#113561),.UNSPECIFIED.,.T.,.F.,
(4,2,2,2,2,2,2,2,2,2,2,2,2,2,2,2,2,2,4),(0.,0.0499381989460856,0.0998725123828674,
0.149935465327738,0.175016839438851,0.20011500129057,0.250360066695874,
0.301079010812412,0.351683677823475,0.402342546584077,0.452986451623471,
0.503593628908851,0.55440362747551,0.579355474490794,0.604708961736832,
0.655104047538882,0.705491754668316,0.755762117527372,0.80452176568964),
 .UNSPECIFIED.);
#2583=B_SPLINE_CURVE_WITH_KNOTS('',3,(#113565,#113566,#113567,#113568,#113569,
#113570,#113571,#113572,#113573,#113574,#113575,#113576,#113577,#113578,
#113579,#113580,#113581,#113582,#113583,#113584,#113585,#113586),
 .UNSPECIFIED.,.F.,.F.,(4,2,2,2,2,2,2,2,2,2,4),(0.213036061661774,0.214062815800093,
0.240524020727665,0.266997646133557,0.29353628989623,0.306823019148326,
0.320117997400603,0.346744786261035,0.373746339552302,0.400671850422301,
0.426054641361433),.UNSPECIFIED.);
#2584=B_SPLINE_CURVE_WITH_KNOTS('',3,(#113590,#113591,#113592,#113593,#113594,
#113595,#113596,#113597,#113598,#113599,#113600,#113601,#113602,#113603,
#113604,#113605,#113606,#113607,#113608,#113609),.UNSPECIFIED.,.F.,.F.,
(4,2,2,2,2,2,2,2,2,4),(0.426054687950607,0.452967716227119,0.479908637510472,
0.506954984943613,0.520385011281766,0.533687129977179,0.560356541301992,
0.587011391805014,0.613604928441249,0.639090749612381),.UNSPECIFIED.);
#2585=B_SPLINE_CURVE_WITH_KNOTS('',3,(#113613,#113614,#113615,#113616,#113617,
#113618,#113619,#113620,#113621,#113622,#113623,#113624,#113625,#113626,
#113627,#113628,#113629,#113630,#113631,#113632,#113633,#113634,#113635,
#113636,#113637,#113638,#113639,#113640,#113641,#113642,#113643,#113644,
#113645,#113646,#113647,#113648,#113649,#113650),.UNSPECIFIED.,.T.,.F.,
(4,2,2,2,2,2,2,2,2,2,2,2,2,2,2,2,2,2,4),(0.,0.0429187561003746,0.0858896515884315,
0.129100841751142,0.172575064704186,0.194263906971067,0.238287259078713,
0.282096822611242,0.325917945154874,0.369798678855887,0.413639582963019,
0.457434972396386,0.501380295514906,0.52294868181926,0.544607783282859,
0.588658005732957,0.63214369771093,0.675352452131438,0.694246639445642),
 .UNSPECIFIED.);
#2586=B_SPLINE_CURVE_WITH_KNOTS('',3,(#113654,#113655,#113656,#113657,#113658,
#113659,#113660,#113661,#113662,#113663,#113664,#113665,#113666,#113667,
#113668,#113669,#113670,#113671,#113672,#113673,#113674,#113675),
 .UNSPECIFIED.,.F.,.F.,(4,2,2,2,2,2,2,2,2,2,4),(0.157602878251341,0.167966818930531,
0.187464755105539,0.207042369642738,0.226740593720201,0.236595153449156,
0.246433052495769,0.266483796840619,0.286473869825833,0.306251221539351,
0.31516019215871),.UNSPECIFIED.);
#2587=B_SPLINE_CURVE_WITH_KNOTS('',3,(#113679,#113680,#113681,#113682,#113683,
#113684,#113685,#113686,#113687,#113688,#113689,#113690,#113691,#113692,
#113693,#113694,#113695,#113696,#113697,#113698),.UNSPECIFIED.,.F.,.F.,
(4,2,2,2,2,2,2,2,2,4),(0.315160208779593,0.334664476111517,0.354222134261767,
0.374222014056629,0.394291801029766,0.40412343171917,0.424295177671824,
0.44401709971294,0.463618758444822,0.472763087030934),.UNSPECIFIED.);
#2588=B_SPLINE_CURVE_WITH_KNOTS('',3,(#113702,#113703,#113704,#113705,#113706,
#113707,#113708,#113709,#113710,#113711,#113712,#113713,#113714,#113715,
#113716,#113717,#113718,#113719,#113720,#113721,#113722,#113723,#113724,
#113725,#113726,#113727,#113728,#113729,#113730,#113731,#113732,#113733,
#113734,#113735,#113736,#113737),.UNSPECIFIED.,.T.,.F.,(4,2,2,2,2,2,2,2,
2,2,2,2,2,2,2,2,2,4),(0.,0.0424789666300493,0.0849679774709149,0.127790667162137,
0.171061745642256,0.215259555594848,0.259077282811308,0.302642339527092,
0.346144078161022,0.38864715447244,0.431272128189375,0.474862210112901,
0.518734949851575,0.54028507684164,0.584672370605554,0.628106698383023,
0.671112016502596,0.690344504645899),.UNSPECIFIED.);
#2589=B_SPLINE_CURVE_WITH_KNOTS('',3,(#113741,#113742,#113743,#113744,#113745,
#113746,#113747,#113748,#113749,#113750,#113751,#113752,#113753,#113754,
#113755,#113756,#113757,#113758,#113759,#113760,#113761,#113762),
 .UNSPECIFIED.,.F.,.F.,(4,2,2,2,2,2,2,2,2,2,4),(0.155262427717209,0.165532373530381,
0.184632674841114,0.203829217875136,0.223215778643951,0.232952142141799,
0.24268393600619,0.262519622819918,0.282251093096163,0.301905988234787,
0.310480476684161),.UNSPECIFIED.);
#2590=B_SPLINE_CURVE_WITH_KNOTS('',3,(#113766,#113767,#113768,#113769,#113770,
#113771,#113772,#113773,#113774,#113775,#113776,#113777,#113778,#113779,
#113780,#113781,#113782,#113783,#113784,#113785),.UNSPECIFIED.,.F.,.F.,
(4,2,2,2,2,2,2,2,2,4),(0.310481108556768,0.329596553706086,0.348750568027949,
0.368451085094143,0.388251140444173,0.39795747456272,0.417871174091899,
0.437531059277961,0.456858480786928,0.465742904401369),.UNSPECIFIED.);
#2591=B_SPLINE_CURVE_WITH_KNOTS('',3,(#113788,#113789,#113790,#113791,#113792,
#113793,#113794,#113795,#113796,#113797,#113798,#113799,#113800,#113801,
#113802,#113803,#113804,#113805,#113806,#113807,#113808,#113809,#113810,
#113811,#113812,#113813,#113814,#113815,#113816,#113817,#113818,#113819,
#113820,#113821,#113822,#113823,#113824,#113825,#113826,#113827,#113828,
#113829,#113830,#113831,#113832,#113833,#113834,#113835,#113836,#113837,
#113838,#113839),.UNSPECIFIED.,.T.,.F.,(4,2,2,2,2,2,2,2,2,2,2,2,2,2,2,2,
2,2,2,2,2,2,2,2,2,4),(0.,0.0320144497702016,0.0458767136401181,0.0557147592155635,
0.0657715796145349,0.0802126605367964,0.115402705682847,0.160055925397762,
0.209471976042195,0.262756796732718,0.319834594604882,0.378252258368803,
0.433784228024685,0.488133124396683,0.506318876043764,0.517142144121038,
0.526626050564159,0.538230524464352,0.559797575654237,0.61878391320983,
0.667805533571324,0.720924855856359,0.777953611535871,0.836424436159223,
0.875349742476717,0.931139968817718),.UNSPECIFIED.);
#2592=B_SPLINE_CURVE_WITH_KNOTS('',3,(#113842,#113843,#113844,#113845,#113846,
#113847,#113848,#113849,#113850,#113851,#113852,#113853,#113854,#113855,
#113856,#113857,#113858,#113859,#113860,#113861,#113862,#113863,#113864,
#113865,#113866,#113867,#113868,#113869,#113870,#113871,#113872,#113873,
#113874,#113875,#113876,#113877),.UNSPECIFIED.,.T.,.F.,(4,2,2,2,2,2,2,2,
2,2,2,2,2,2,2,2,2,4),(0.,0.057912290383271,0.115844267345691,0.173845899019275,
0.202836343323089,0.261569328211721,0.320036860000859,0.378698392235191,
0.437537296788471,0.496221105841023,0.554691820018049,0.613381775757485,
0.672164534867042,0.730400175357851,0.788666822605191,0.846880699532441,
0.904953792012004,0.931852649550286),.UNSPECIFIED.);
#2593=B_SPLINE_CURVE_WITH_KNOTS('',3,(#113881,#113882,#113883,#113884,#113885,
#113886,#113887,#113888,#113889,#113890,#113891,#113892,#113893,#113894,
#113895,#113896,#113897,#113898,#113899,#113900),.UNSPECIFIED.,.F.,.F.,
(4,2,2,2,2,2,2,2,2,4),(0.139754715013795,0.172609259421165,0.207064650854054,
0.24155037115346,0.258779798092583,0.293833199650583,0.328780765782036,
0.363788421544044,0.398858105741495,0.416586635623603),.UNSPECIFIED.);
#2594=B_SPLINE_CURVE_WITH_KNOTS('',3,(#113904,#113905,#113906,#113907,#113908,
#113909,#113910,#113911,#113912,#113913,#113914,#113915,#113916,#113917,
#113918,#113919,#113920,#113921,#113922,#113923,#113924,#113925,#113926),
 .UNSPECIFIED.,.F.,.F.,(4,2,2,2,2,3,2,2,2,2,4),(0.416586635623603,0.433877760225201,
0.468826219581986,0.503854463105767,0.538780024933523,0.553655470180159,
0.588232581400899,0.6228064666686,0.657341280871621,0.691819483465528,0.693410185193954),
 .UNSPECIFIED.);
#2595=B_SPLINE_CURVE_WITH_KNOTS('',3,(#113929,#113930,#113931,#113932,#113933,
#113934,#113935,#113936,#113937,#113938,#113939,#113940,#113941,#113942,
#113943,#113944,#113945,#113946,#113947,#113948,#113949,#113950,#113951,
#113952,#113953,#113954,#113955,#113956,#113957,#113958,#113959,#113960,
#113961,#113962,#113963,#113964,#113965,#113966,#113967,#113968,#113969,
#113970,#113971,#113972,#113973,#113974,#113975,#113976,#113977,#113978,
#113979,#113980),.UNSPECIFIED.,.T.,.F.,(4,2,2,2,2,2,2,2,2,2,2,2,2,2,2,2,
2,2,2,2,2,2,2,2,2,4),(0.,0.0167619929348656,0.0276578117894851,0.0362872275608602,
0.0458432035478929,0.061246066336341,0.108291688612086,0.149502826269685,
0.194332609410432,0.242445764956923,0.293221281057508,0.342681173875022,
0.389406729870615,0.415800156239406,0.426509574580191,0.434498220080772,
0.44316500485031,0.454821148519414,0.479978746987761,0.530832024838283,
0.57414259102436,0.620921651218219,0.671203097113141,0.72151009555737,0.768376318472014,
0.804067995997234),.UNSPECIFIED.);
#2596=B_SPLINE_CURVE_WITH_KNOTS('',3,(#113983,#113984,#113985,#113986,#113987,
#113988,#113989,#113990,#113991,#113992,#113993,#113994,#113995,#113996,
#113997,#113998,#113999,#114000,#114001,#114002,#114003,#114004,#114005,
#114006,#114007,#114008,#114009,#114010,#114011,#114012,#114013,#114014,
#114015,#114016,#114017,#114018,#114019,#114020),.UNSPECIFIED.,.T.,.F.,
(4,2,2,2,2,2,2,2,2,2,2,2,2,2,2,2,2,2,4),(0.,0.0499483525656873,0.099989590289901,
0.150174211793659,0.175276943687537,0.226175081735644,0.276808377411066,
0.32754657529046,0.378464849820159,0.429330158496053,0.479996567083159,
0.530683580160234,0.5555461562912,0.580523336179942,0.631403252897784,0.681741873714619,
0.731957307096482,0.782008216404938,0.804543742961689),.UNSPECIFIED.);
#2597=B_SPLINE_CURVE_WITH_KNOTS('',3,(#114024,#114025,#114026,#114027,#114028,
#114029,#114030,#114031,#114032,#114033,#114034,#114035,#114036,#114037,
#114038,#114039,#114040,#114041,#114042,#114043,#114044,#114045),
 .UNSPECIFIED.,.F.,.F.,(4,2,2,2,2,2,2,2,2,2,4),(0.21306486411963,0.227332866823859,
0.253831618810689,0.280397178858473,0.293689043125694,0.306966278490336,
0.33399561376579,0.360958674455788,0.387958258092557,0.415007997854744,
0.426072187027784),.UNSPECIFIED.);
#2598=B_SPLINE_CURVE_WITH_KNOTS('',3,(#114049,#114050,#114051,#114052,#114053,
#114054,#114055,#114056,#114057,#114058,#114059,#114060,#114061,#114062,
#114063,#114064,#114065,#114066,#114067,#114068),.UNSPECIFIED.,.F.,.F.,
(4,2,2,2,2,2,2,2,2,4),(0.426072562334217,0.453077952711787,0.480040917586814,
0.507059803852167,0.520299739781239,0.547239747248079,0.573869121368994,
0.600435778555616,0.62693553674137,0.639137426453847),.UNSPECIFIED.);
#2599=B_SPLINE_CURVE_WITH_KNOTS('',3,(#114071,#114072,#114073,#114074,#114075,
#114076,#114077,#114078,#114079,#114080,#114081,#114082,#114083,#114084,
#114085,#114086,#114087,#114088,#114089,#114090,#114091,#114092,#114093,
#114094,#114095,#114096,#114097,#114098,#114099,#114100,#114101,#114102,
#114103,#114104,#114105,#114106,#114107,#114108,#114109,#114110,#114111,
#114112,#114113,#114114,#114115,#114116,#114117,#114118,#114119,#114120,
#114121,#114122),.UNSPECIFIED.,.T.,.F.,(4,2,2,2,2,2,2,2,2,2,2,2,2,2,2,2,
2,2,2,2,2,2,2,2,2,4),(0.,0.0102292473935223,0.018082598833696,0.0263963859846061,
0.0390147385032582,0.0728971977507561,0.107589219061119,0.145627768693997,
0.186630958119302,0.230733204186149,0.273926375893012,0.312544707081939,
0.342168896043744,0.354370671563563,0.362541105016026,0.370355680991137,
0.380851202731197,0.403385275933281,0.447232798198564,0.484761694810815,
0.525362691985882,0.569074594761023,0.612536964225629,0.652656732784191,
0.687070434853681,0.693794119617982),.UNSPECIFIED.);
#2600=B_SPLINE_CURVE_WITH_KNOTS('',3,(#114125,#114126,#114127,#114128,#114129,
#114130,#114131,#114132,#114133,#114134,#114135,#114136,#114137,#114138,
#114139,#114140,#114141,#114142,#114143,#114144,#114145,#114146,#114147,
#114148,#114149,#114150,#114151,#114152,#114153,#114154,#114155,#114156,
#114157,#114158,#114159,#114160),.UNSPECIFIED.,.T.,.F.,(4,2,2,2,2,2,2,2,
2,2,2,2,2,2,2,2,2,4),(0.,0.0429106502366654,0.0859817598443145,0.129331618969271,
0.151085232625045,0.172807852044397,0.21688288321358,0.260697808811353,
0.304470070080087,0.348270726520065,0.392048555605167,0.435841729163604,
0.479853272526997,0.524250865104275,0.567905223640583,0.611392741401498,
0.654598658582422,0.694333300491708),.UNSPECIFIED.);
#2601=B_SPLINE_CURVE_WITH_KNOTS('',3,(#114164,#114165,#114166,#114167,#114168,
#114169,#114170,#114171,#114172,#114173,#114174,#114175,#114176,#114177,
#114178,#114179,#114180,#114181,#114182,#114183,#114184,#114185),
 .UNSPECIFIED.,.F.,.F.,(4,2,2,2,2,2,2,2,2,2,4),(0.157555629279167,0.158070011383171,
0.177565895247574,0.197140695879063,0.216836715527659,0.226706323780034,
0.236561509314436,0.256637830271492,0.276629064151961,0.296577893477034,
0.315128960060253),.UNSPECIFIED.);
#2602=B_SPLINE_CURVE_WITH_KNOTS('',3,(#114189,#114190,#114191,#114192,#114193,
#114194,#114195,#114196,#114197,#114198,#114199,#114200,#114201,#114202,
#114203,#114204,#114205,#114206,#114207,#114208,#114209,#114210,#114211),
 .UNSPECIFIED.,.F.,.F.,(4,3,2,2,2,2,2,2,2,2,4),(0.315128960060253,0.31515595446884,
0.334676647783077,0.354656565529836,0.374714656610475,0.384544781031409,
0.394396710796161,0.41438903597914,0.434114151291953,0.453717853798424,
0.472711583748007),.UNSPECIFIED.);
#2603=B_SPLINE_CURVE_WITH_KNOTS('',3,(#114214,#114215,#114216,#114217,#114218,
#114219,#114220,#114221,#114222,#114223,#114224,#114225,#114226,#114227,
#114228,#114229,#114230,#114231,#114232,#114233,#114234,#114235,#114236,
#114237,#114238,#114239,#114240,#114241,#114242,#114243,#114244,#114245,
#114246,#114247,#114248,#114249,#114250,#114251,#114252,#114253,#114254,
#114255,#114256,#114257,#114258,#114259,#114260,#114261,#114262,#114263),
 .UNSPECIFIED.,.T.,.F.,(4,2,2,2,2,2,2,2,2,2,2,2,2,2,2,2,2,2,2,2,2,2,2,2,
4),(0.,0.00816912193231024,0.0176416594614524,0.0338374510674327,0.0772052149196674,
0.113481480317982,0.152933178844101,0.195423379618985,0.239140203807657,
0.28075501503573,0.3223543759762,0.3373449838732,0.346485616157516,0.353794230672201,
0.363486832242064,0.380807023601717,0.424289821313145,0.460871598877258,
0.500666429588826,0.54358905970758,0.587222617397712,0.628438867274253,
0.668029721109657,0.682703416332507,0.689884358287045),.UNSPECIFIED.);
#2604=B_SPLINE_CURVE_WITH_KNOTS('',3,(#114266,#114267,#114268,#114269,#114270,
#114271,#114272,#114273,#114274,#114275,#114276,#114277,#114278,#114279,
#114280,#114281,#114282,#114283,#114284,#114285,#114286,#114287,#114288,
#114289,#114290,#114291,#114292,#114293,#114294,#114295,#114296,#114297,
#114298,#114299,#114300,#114301,#114302,#114303),.UNSPECIFIED.,.T.,.F.,
(4,2,2,2,2,2,2,2,2,2,2,2,2,2,2,2,2,2,4),(0.,0.0424329954915689,0.0850548921633571,
0.128105489804561,0.149803496669879,0.171520604045967,0.215603286957798,
0.259291508388645,0.302760327587543,0.3461701106744,0.388697344372228,0.432199116431131,
0.47596752314268,0.497471190734652,0.519075683971176,0.563108028735137,
0.606545409681133,0.649549890723535,0.690224907908624),.UNSPECIFIED.);
#2605=B_SPLINE_CURVE_WITH_KNOTS('',3,(#114307,#114308,#114309,#114310,#114311,
#114312,#114313,#114314,#114315,#114316,#114317,#114318,#114319,#114320,
#114321,#114322,#114323,#114324,#114325,#114326,#114327,#114328),
 .UNSPECIFIED.,.F.,.F.,(4,2,2,2,2,2,2,2,2,2,4),(0.155239472480513,0.155629710387306,
0.174728016684647,0.193920885494023,0.213303831703006,0.223055692389348,
0.23280748114644,0.252679804558889,0.272421255492315,0.292053011218848,
0.310471145323146),.UNSPECIFIED.);
#2606=B_SPLINE_CURVE_WITH_KNOTS('',3,(#114332,#114333,#114334,#114335,#114336,
#114337,#114338,#114339,#114340,#114341,#114342,#114343,#114344,#114345,
#114346,#114347,#114348,#114349,#114350,#114351),.UNSPECIFIED.,.F.,.F.,
(4,2,2,2,2,2,2,2,2,4),(0.310471318769338,0.329587743034597,0.348807224721795,
0.368577426857687,0.378277472762051,0.388005564817206,0.407959259227537,
0.427615216256153,0.44694589841925,0.465710791249851),.UNSPECIFIED.);
#2607=B_SPLINE_CURVE_WITH_KNOTS('',3,(#114354,#114355,#114356,#114357,#114358,
#114359,#114360,#114361,#114362,#114363,#114364,#114365,#114366,#114367,
#114368,#114369,#114370,#114371,#114372,#114373,#114374,#114375,#114376,
#114377,#114378,#114379,#114380,#114381,#114382,#114383,#114384,#114385,
#114386,#114387,#114388,#114389,#114390,#114391,#114392,#114393,#114394,
#114395,#114396,#114397,#114398,#114399,#114400,#114401,#114402,#114403,
#114404,#114405),.UNSPECIFIED.,.T.,.F.,(4,2,2,2,2,2,2,2,2,2,2,2,2,2,2,2,
2,2,2,2,2,2,2,2,2,4),(0.,0.0525083345848551,0.108779286030152,0.167362101081689,
0.223884663346406,0.279431074018823,0.303364169525237,0.314486881214728,
0.322976133922097,0.331946667594864,0.345595995515426,0.383174082493277,
0.427903989648404,0.477632626158776,0.531410548614856,0.589183859623761,
0.647452074973242,0.702210239020413,0.756794536135306,0.773516436584552,
0.783377035922492,0.791753189623331,0.801870707780898,0.820156312424674,
0.879246497783655,0.931260216792454),.UNSPECIFIED.);
#2608=B_SPLINE_CURVE_WITH_KNOTS('',3,(#114408,#114409,#114410,#114411,#114412,
#114413,#114414,#114415,#114416,#114417,#114418,#114419,#114420,#114421,
#114422,#114423,#114424,#114425,#114426,#114427,#114428,#114429,#114430,
#114431,#114432,#114433,#114434,#114435,#114436,#114437,#114438,#114439,
#114440,#114441),.UNSPECIFIED.,.T.,.F.,(4,2,2,2,2,2,2,2,2,2,2,2,2,2,2,2,
4),(0.,0.0579319231973149,0.115920382400655,0.17394883011719,0.232575230845978,
0.29104002295107,0.349793697557817,0.408751929036138,0.467508142527154,
0.525973906050046,0.58459684254218,0.643901563943303,0.702126116460104,
0.760371269954299,0.818562878710026,0.876625675277847,0.931980461253038),
 .UNSPECIFIED.);
#2609=B_SPLINE_CURVE_WITH_KNOTS('',3,(#114445,#114446,#114447,#114448,#114449,
#114450,#114451,#114452,#114453,#114454,#114455,#114456,#114457,#114458,
#114459,#114460,#114461,#114462,#114463,#114464),.UNSPECIFIED.,.F.,.F.,
(4,2,2,2,2,2,2,2,2,4),(0.139799730781408,0.172534688541551,0.20701737584227,
0.224247110424717,0.241456599860779,0.27645017850127,0.311393660872747,
0.346452033300128,0.381592642182531,0.416592031663367),.UNSPECIFIED.);
#2610=B_SPLINE_CURVE_WITH_KNOTS('',3,(#114468,#114469,#114470,#114471,#114472,
#114473,#114474,#114475,#114476,#114477,#114478,#114479,#114480,#114481,
#114482,#114483,#114484,#114485,#114486,#114487,#114488,#114489,#114490),
 .UNSPECIFIED.,.F.,.F.,(4,2,2,2,2,3,2,2,2,2,4),(0.416592031663367,0.416659563180101,
0.451607079053152,0.486590699737675,0.521807059609053,0.553638721576443,
0.588205308843122,0.62275164209292,0.657252949664438,0.691715150272187,
0.693438452357851),.UNSPECIFIED.);
#2611=B_SPLINE_CURVE_WITH_KNOTS('',3,(#114493,#114494,#114495,#114496,#114497,
#114498,#114499,#114500,#114501,#114502,#114503,#114504,#114505,#114506,
#114507,#114508,#114509,#114510,#114511,#114512,#114513,#114514,#114515,
#114516,#114517,#114518,#114519,#114520,#114521,#114522,#114523,#114524,
#114525,#114526,#114527,#114528,#114529,#114530,#114531,#114532,#114533,
#114534,#114535,#114536,#114537,#114538,#114539,#114540,#114541,#114542,
#114543,#114544,#114545,#114546),.UNSPECIFIED.,.T.,.F.,(4,2,2,2,2,2,2,2,
2,2,2,2,2,2,2,2,2,2,2,2,2,2,2,2,2,2,4),(0.,0.0369491160369705,0.0501161427537167,
0.0583408003539779,0.0658278867613358,0.0753901969450591,0.0945046567240877,
0.145543352718396,0.187675607865597,0.233331625629896,0.282318578506677,
0.332934697685839,0.381410945852096,0.430720162800404,0.448434472729937,
0.45763659248232,0.465010329741499,0.473285136007353,0.486913981469558,
0.531392119941888,0.57196763051739,0.616440783205194,0.66434809866151,0.715170452984358,
0.752780603211039,0.775344267167268,0.803996562106116),.UNSPECIFIED.);
#2612=B_SPLINE_CURVE_WITH_KNOTS('',3,(#114549,#114550,#114551,#114552,#114553,
#114554,#114555,#114556,#114557,#114558,#114559,#114560,#114561,#114562,
#114563,#114564,#114565,#114566,#114567,#114568,#114569,#114570,#114571,
#114572,#114573,#114574,#114575,#114576,#114577,#114578,#114579,#114580,
#114581,#114582,#114583,#114584,#114585,#114586),.UNSPECIFIED.,.T.,.F.,
(4,2,2,2,2,2,2,2,2,2,2,2,2,2,2,2,2,2,4),(0.,0.0499637560937677,0.100062844084125,
0.125152294272686,0.150253945446171,0.201248481135741,0.251911968622351,
0.30259118437123,0.353387136819273,0.404139339396542,0.454777727746519,
0.505547296964785,0.530469187635523,0.555824699095162,0.606213141707336,
0.656572148122596,0.706804639103619,0.75685973914386,0.804538060714784),
 .UNSPECIFIED.);
#2613=B_SPLINE_CURVE_WITH_KNOTS('',3,(#114590,#114591,#114592,#114593,#114594,
#114595,#114596,#114597,#114598,#114599,#114600,#114601,#114602,#114603,
#114604,#114605,#114606,#114607,#114608,#114609,#114610,#114611),
 .UNSPECIFIED.,.F.,.F.,(4,2,2,2,2,2,2,2,2,2,4),(0.213035334055591,0.213498058337152,
0.239986509786572,0.266541736009027,0.279831953885245,0.293128400800926,
0.320214748878366,0.347192802047242,0.374155977515257,0.401138870741644,
0.42606188797298),.UNSPECIFIED.);
#2614=B_SPLINE_CURVE_WITH_KNOTS('',3,(#114615,#114616,#114617,#114618,#114619,
#114620,#114621,#114622,#114623,#114624,#114625,#114626,#114627,#114628,
#114629,#114630,#114631,#114632,#114633,#114634),.UNSPECIFIED.,.F.,.F.,
(4,2,2,2,2,2,2,2,2,4),(0.42606268775071,0.453023220919234,0.480038654483965,
0.493275670389338,0.506707490462197,0.533372517385062,0.560013344973749,
0.586590984961471,0.613095139159837,0.639098021806301),.UNSPECIFIED.);
#2615=B_SPLINE_CURVE_WITH_KNOTS('',3,(#114637,#114638,#114639,#114640,#114641,
#114642,#114643,#114644,#114645,#114646,#114647,#114648,#114649,#114650,
#114651,#114652,#114653,#114654,#114655,#114656,#114657,#114658,#114659,
#114660,#114661,#114662,#114663,#114664,#114665,#114666,#114667,#114668,
#114669,#114670,#114671,#114672,#114673,#114674,#114675,#114676,#114677,
#114678,#114679,#114680,#114681,#114682,#114683,#114684,#114685,#114686,
#114687,#114688,#114689,#114690),.UNSPECIFIED.,.T.,.F.,(4,2,2,2,2,2,2,2,
2,2,2,2,2,2,2,2,2,2,2,2,2,2,2,2,2,2,4),(0.,0.0228480468435155,0.0327278613357826,
0.0389155412692941,0.0456271880868092,0.0546775533820688,0.0744713233992156,
0.118416720185575,0.155288894882617,0.195252941934963,0.238221915332059,
0.281891583999893,0.322930222568161,0.363518611295154,0.3764021328255,0.383922438192359,
0.390434781093071,0.398320332011738,0.412797633133752,0.456696864945195,
0.492818073211253,0.532197232422632,0.574634202506513,0.618505769963775,
0.64918353719598,0.668216196324756,0.693788572706354),.UNSPECIFIED.);
#2616=B_SPLINE_CURVE_WITH_KNOTS('',3,(#114693,#114694,#114695,#114696,#114697,
#114698,#114699,#114700,#114701,#114702,#114703,#114704,#114705,#114706,
#114707,#114708,#114709,#114710,#114711,#114712,#114713,#114714,#114715,
#114716,#114717,#114718,#114719,#114720,#114721,#114722,#114723,#114724,
#114725,#114726,#114727,#114728),.UNSPECIFIED.,.T.,.F.,(4,2,2,2,2,2,2,2,
2,2,2,2,2,2,2,2,2,4),(0.,0.0429881271999506,0.0862259450153807,0.12971880175422,
0.151383394484505,0.195368245878792,0.239171549410387,0.283012428053759,
0.32647532705118,0.370326496748914,0.414125196034328,0.458075699664007,
0.502382022531898,0.546417694371204,0.589878387317715,0.633059308295633,
0.676015445526238,0.694361023560929),.UNSPECIFIED.);
#2617=B_SPLINE_CURVE_WITH_KNOTS('',3,(#114732,#114733,#114734,#114735,#114736,
#114737,#114738,#114739,#114740,#114741,#114742,#114743,#114744,#114745,
#114746,#114747,#114748,#114749,#114750,#114751,#114752,#114753),
 .UNSPECIFIED.,.F.,.F.,(4,2,2,2,2,2,2,2,2,2,4),(0.157606273259384,0.167943647681616,
0.187531534785128,0.207239841218768,0.217088558581301,0.226918881348354,
0.246957240578774,0.266944508893794,0.286716039025147,0.306221084842367,
0.315164770989864),.UNSPECIFIED.);
#2618=B_SPLINE_CURVE_WITH_KNOTS('',3,(#114757,#114758,#114759,#114760,#114761,
#114762,#114763,#114764,#114765,#114766,#114767,#114768,#114769,#114770,
#114771,#114772,#114773,#114774,#114775,#114776),.UNSPECIFIED.,.F.,.F.,
(4,2,2,2,2,2,2,2,2,4),(0.315165008584859,0.33473120703126,0.354732300285761,
0.374800531585434,0.384630520973591,0.404797893462523,0.42451030767009,
0.444102244164262,0.463606440620998,0.472771281844243),.UNSPECIFIED.);
#2619=B_SPLINE_CURVE_WITH_KNOTS('',3,(#114779,#114780,#114781,#114782,#114783,
#114784,#114785,#114786,#114787,#114788,#114789,#114790,#114791,#114792,
#114793,#114794,#114795,#114796,#114797,#114798,#114799,#114800,#114801,
#114802,#114803,#114804,#114805,#114806,#114807,#114808,#114809,#114810,
#114811,#114812,#114813,#114814,#114815,#114816,#114817,#114818,#114819,
#114820,#114821,#114822,#114823,#114824,#114825,#114826,#114827,#114828,
#114829,#114830),.UNSPECIFIED.,.T.,.F.,(4,2,2,2,2,2,2,2,2,2,2,2,2,2,2,2,
2,2,2,2,2,2,2,2,2,4),(0.,0.0136527846687363,0.0224048280718145,0.0292691959298057,
0.0368127137003927,0.0488745028759635,0.085497339849254,0.12007168662968,
0.158105018498429,0.199230292707366,0.243569997033518,0.286401168138391,
0.325560442066355,0.352989103119234,0.363926580530411,0.371171561415239,
0.378060184528038,0.387276805864347,0.407094836053811,0.450659703174363,
0.487474997610149,0.527536138269538,0.570775759477264,0.614277377050491,
0.654773380862052,0.689797023507),.UNSPECIFIED.);
#2620=B_SPLINE_CURVE_WITH_KNOTS('',3,(#114833,#114834,#114835,#114836,#114837,
#114838,#114839,#114840,#114841,#114842,#114843,#114844,#114845,#114846,
#114847,#114848,#114849,#114850,#114851,#114852,#114853,#114854,#114855,
#114856,#114857,#114858,#114859,#114860,#114861,#114862,#114863,#114864,
#114865,#114866,#114867,#114868,#114869,#114870),.UNSPECIFIED.,.T.,.F.,
(4,2,2,2,2,2,2,2,2,2,2,2,2,2,2,2,2,2,4),(0.,0.0425200356386948,0.0854005081350503,
0.128721173636264,0.150328968556923,0.194198532515018,0.237811372563917,
0.281382187239665,0.323917849204456,0.36645979650346,0.41002400041801,0.45368714777466,
0.475110659146658,0.496611135342448,0.540900250276031,0.584295227160176,
0.627255306982154,0.669821335667285,0.690233235741649),.UNSPECIFIED.);
#2621=B_SPLINE_CURVE_WITH_KNOTS('',3,(#114874,#114875,#114876,#114877,#114878,
#114879,#114880,#114881,#114882,#114883,#114884,#114885,#114886,#114887,
#114888,#114889,#114890,#114891,#114892,#114893,#114894,#114895),
 .UNSPECIFIED.,.F.,.F.,(4,2,2,2,2,2,2,2,2,2,4),(0.155262278701396,0.165381853607852,
0.184598949561035,0.204009403841683,0.213725435380747,0.223428918096119,
0.243208588599942,0.262918832679783,0.282370974502219,0.301506216814708,
0.310476735734228),.UNSPECIFIED.);
#2622=B_SPLINE_CURVE_WITH_KNOTS('',3,(#114899,#114900,#114901,#114902,#114903,
#114904,#114905,#114906,#114907,#114908,#114909,#114910,#114911,#114912,
#114913,#114914,#114915,#114916,#114917,#114918),.UNSPECIFIED.,.F.,.F.,
(4,2,2,2,2,2,2,2,2,4),(0.310476868687956,0.329646504529723,0.349347797550038,
0.369112205680196,0.378795195849324,0.3986619979492,0.418308071473111,0.437611587488503,
0.456753059132737,0.465739147389351),.UNSPECIFIED.);
#2623=B_SPLINE_CURVE_WITH_KNOTS('',3,(#114921,#114922,#114923,#114924,#114925,
#114926,#114927,#114928,#114929,#114930,#114931,#114932,#114933,#114934,
#114935,#114936,#114937,#114938,#114939,#114940,#114941,#114942,#114943,
#114944,#114945,#114946,#114947,#114948,#114949,#114950,#114951,#114952,
#114953,#114954,#114955,#114956,#114957,#114958,#114959,#114960,#114961,
#114962,#114963,#114964,#114965,#114966,#114967,#114968,#114969,#114970,
#114971,#114972,#114973,#114974),.UNSPECIFIED.,.T.,.F.,(4,2,2,2,2,2,2,2,
2,2,2,2,2,2,2,2,2,2,2,2,2,2,2,2,2,2,4),(0.,0.0493622911687678,0.0920897389128855,
0.106285977716751,0.114899921438983,0.122590708880221,0.132228456506715,
0.150991386280156,0.210173358576881,0.25829649839813,0.310541080858129,
0.366555640333151,0.425177707499093,0.481933053819406,0.535242472646899,
0.563024761787985,0.574648209252878,0.581809461553343,0.589496352209351,
0.59974295206476,0.621829632667757,0.680864842162272,0.729716719843076,
0.782756815964081,0.839748558376594,0.881827529122477,0.931141638313032),
 .UNSPECIFIED.);
#2624=B_SPLINE_CURVE_WITH_KNOTS('',3,(#114977,#114978,#114979,#114980,#114981,
#114982,#114983,#114984,#114985,#114986,#114987,#114988,#114989,#114990,
#114991,#114992,#114993,#114994,#114995,#114996,#114997,#114998,#114999,
#115000,#115001,#115002,#115003,#115004,#115005,#115006,#115007,#115008,
#115009,#115010,#115011,#115012),.UNSPECIFIED.,.T.,.F.,(4,2,2,2,2,2,2,2,
2,2,2,2,2,2,2,2,2,4),(0.,0.0579192164299872,0.115915121999537,0.173939752951927,
0.232491074358606,0.290999738521068,0.349702831816148,0.408399067865895,
0.466900664533333,0.525466259798678,0.554212336114783,0.612999379812414,
0.671249213282526,0.729534399890861,0.787757602555752,0.845825377259922,
0.903751470504909,0.931850859346782),.UNSPECIFIED.);
#2625=B_SPLINE_CURVE_WITH_KNOTS('',3,(#115016,#115017,#115018,#115019,#115020,
#115021,#115022,#115023,#115024,#115025,#115026,#115027,#115028,#115029,
#115030,#115031,#115032,#115033,#115034,#115035),.UNSPECIFIED.,.F.,.F.,
(4,2,2,2,2,2,2,2,2,4),(0.139799547746219,0.172474352311618,0.206955199528419,
0.241453517992284,0.276447794358104,0.311395446051869,0.346393507325481,
0.381392485264966,0.416340784159462,0.416668190260015),.UNSPECIFIED.);
#2626=B_SPLINE_CURVE_WITH_KNOTS('',3,(#115039,#115040,#115041,#115042,#115043,
#115044,#115045,#115046,#115047,#115048,#115049,#115050,#115051,#115052,
#115053,#115054,#115055,#115056,#115057,#115058,#115059),.UNSPECIFIED.,
 .F.,.F.,(4,2,2,2,3,2,2,2,2,4),(0.416668190260015,0.451332143736155,0.486542632424401,
0.521110864132053,0.553717878818723,0.588300910930042,0.622838001130257,
0.657310553681014,0.691745956896247,0.693517426564942),.UNSPECIFIED.);
#2627=B_SPLINE_CURVE_WITH_KNOTS('',3,(#115062,#115063,#115064,#115065,#115066,
#115067,#115068,#115069,#115070,#115071,#115072,#115073,#115074,#115075,
#115076,#115077,#115078,#115079,#115080,#115081,#115082,#115083,#115084,
#115085,#115086,#115087,#115088,#115089,#115090,#115091,#115092,#115093,
#115094,#115095,#115096,#115097,#115098,#115099,#115100,#115101,#115102,
#115103,#115104,#115105,#115106,#115107,#115108,#115109,#115110,#115111,
#115112,#115113,#115114,#115115),.UNSPECIFIED.,.T.,.F.,(4,2,2,2,2,2,2,2,
2,2,2,2,2,2,2,2,2,2,2,2,2,2,2,2,2,2,4),(0.,0.0460454477309475,0.0698812709915654,
0.0799729491598215,0.0862398375617845,0.0930070476114817,0.102099779915382,
0.12199128194129,0.173014803100763,0.21515085683549,0.260834825677685,0.309867943965691,
0.360469541845697,0.408816940310194,0.457317861799748,0.475413690833949,
0.484000351732,0.490648733697361,0.497776749178407,0.508849795549764,0.540995625074898,
0.579224411541502,0.621923026586917,0.668213746346409,0.718002156860292,
0.756614424716887,0.804040984351295),.UNSPECIFIED.);
#2628=B_SPLINE_CURVE_WITH_KNOTS('',3,(#115118,#115119,#115120,#115121,#115122,
#115123,#115124,#115125,#115126,#115127,#115128,#115129,#115130,#115131,
#115132,#115133,#115134,#115135,#115136,#115137,#115138,#115139,#115140,
#115141,#115142,#115143,#115144,#115145,#115146,#115147,#115148,#115149,
#115150,#115151,#115152,#115153,#115154,#115155),.UNSPECIFIED.,.T.,.F.,
(4,2,2,2,2,2,2,2,2,2,2,2,2,2,2,2,2,2,4),(0.,0.0500536302415826,0.100248886721465,
0.125348489355815,0.176214379653189,0.226845565123319,0.277601849505133,
0.328529501083987,0.379384828230058,0.430042925474586,0.480747127831807,
0.505624113439625,0.530982199089092,0.581360554251538,0.631694084279792,
0.681899084709615,0.731940525776284,0.781889300824048,0.804562731596483),
 .UNSPECIFIED.);
#2629=B_SPLINE_CURVE_WITH_KNOTS('',3,(#115159,#115160,#115161,#115162,#115163,
#115164,#115165,#115166,#115167,#115168,#115169,#115170,#115171,#115172,
#115173,#115174,#115175,#115176,#115177,#115178,#115179,#115180),
 .UNSPECIFIED.,.F.,.F.,(4,2,2,2,2,2,2,2,2,2,4),(0.21303360006203,0.226832685951809,
0.253402905279486,0.266696066155347,0.279968866775037,0.306991635605764,
0.333954950569698,0.360959243335334,0.388011844627178,0.415040640294028,
0.426047300578329),.UNSPECIFIED.);
#2630=B_SPLINE_CURVE_WITH_KNOTS('',3,(#115184,#115185,#115186,#115187,#115188,
#115189,#115190,#115191,#115192,#115193,#115194,#115195,#115196,#115197,
#115198,#115199,#115200,#115201,#115202,#115203,#115204,#115205,#115206),
 .UNSPECIFIED.,.F.,.F.,(4,3,2,2,2,2,2,2,2,2,4),(0.426047300578329,0.426084033079102,
0.453047560010972,0.4800723465664,0.493315909525459,0.520255179816914,0.5468823927282,
0.573445726460533,0.599943230326549,0.626413995982194,0.639117633141133),
 .UNSPECIFIED.);
#2631=B_SPLINE_CURVE_WITH_KNOTS('',3,(#115209,#115210,#115211,#115212,#115213,
#115214,#115215,#115216,#115217,#115218,#115219,#115220,#115221,#115222,
#115223,#115224,#115225,#115226,#115227,#115228,#115229,#115230,#115231,
#115232,#115233,#115234,#115235,#115236,#115237,#115238,#115239,#115240,
#115241,#115242,#115243,#115244,#115245,#115246,#115247,#115248,#115249,
#115250,#115251,#115252,#115253,#115254,#115255,#115256,#115257,#115258,
#115259,#115260,#115261,#115262),.UNSPECIFIED.,.T.,.F.,(4,2,2,2,2,2,2,2,
2,2,2,2,2,2,2,2,2,2,2,2,2,2,2,2,2,2,4),(0.,0.0413227067380907,0.0531960655412227,
0.060031662678502,0.0658031849778232,0.07263008717472,0.0847877219638444,
0.128472435213838,0.163955924831537,0.202748540799982,0.24453107733556,
0.288498399386162,0.331038302481138,0.369654939117629,0.393537949750696,
0.40285118334134,0.408990585916016,0.414822866875922,0.422642375189097,
0.439661907426131,0.483361718793369,0.519779614744175,0.559444385853513,
0.602194643829491,0.641994578407272,0.665099346451145,0.693838467012807),
 .UNSPECIFIED.);
#2632=B_SPLINE_CURVE_WITH_KNOTS('',3,(#115265,#115266,#115267,#115268,#115269,
#115270,#115271,#115272,#115273,#115274,#115275,#115276,#115277,#115278,
#115279,#115280,#115281,#115282,#115283,#115284,#115285,#115286,#115287,
#115288,#115289,#115290,#115291,#115292,#115293,#115294,#115295,#115296,
#115297,#115298,#115299,#115300),.UNSPECIFIED.,.T.,.F.,(4,2,2,2,2,2,2,2,
2,2,2,2,2,2,2,2,2,4),(0.,0.0431187333258002,0.0865147403830464,0.108243472874369,
0.12987976773851,0.173823473750012,0.217625265484648,0.261500895168154,
0.30446942925918,0.347533682276283,0.391335394292735,0.435259987839497,
0.479528027047697,0.523564188295094,0.567017611697541,0.610192543513944,
0.65314862373146,0.69437312784443),.UNSPECIFIED.);
#2633=B_SPLINE_CURVE_WITH_KNOTS('',3,(#115304,#115305,#115306,#115307,#115308,
#115309,#115310,#115311,#115312,#115313,#115314,#115315,#115316,#115317,
#115318,#115319,#115320,#115321,#115322,#115323,#115324,#115325,#115326),
 .UNSPECIFIED.,.F.,.F.,(4,2,2,2,2,2,2,2,2,3,4),(0.157667239710267,0.158554027511542,
0.17815254113598,0.1978706695312,0.217965348217132,0.237985776857621,0.257972625908517,
0.277739830800538,0.297244191330894,0.315264873286815,0.315290356393478),
 .UNSPECIFIED.);
#2634=B_SPLINE_CURVE_WITH_KNOTS('',3,(#115330,#115331,#115332,#115333,#115334,
#115335,#115336,#115337,#115338,#115339,#115340,#115341,#115342,#115343,
#115344,#115345,#115346,#115347),.UNSPECIFIED.,.F.,.F.,(4,2,2,2,2,2,2,2,
4),(0.315290356393478,0.335251799150366,0.35527186304086,0.37536599132469,
0.395521932534894,0.415225521851564,0.434809279024896,0.454311174901168,
0.472932112997082),.UNSPECIFIED.);
#2635=B_SPLINE_CURVE_WITH_KNOTS('',3,(#115350,#115351,#115352,#115353,#115354,
#115355,#115356,#115357,#115358,#115359,#115360,#115361,#115362,#115363,
#115364,#115365,#115366,#115367,#115368,#115369,#115370,#115371,#115372,
#115373,#115374,#115375,#115376,#115377,#115378,#115379,#115380,#115381,
#115382,#115383,#115384,#115385,#115386,#115387,#115388,#115389,#115390,
#115391,#115392,#115393,#115394,#115395,#115396,#115397,#115398,#115399,
#115400,#115401,#115402,#115403),.UNSPECIFIED.,.T.,.F.,(4,2,2,2,2,2,2,2,
2,2,2,2,2,2,2,2,2,2,2,2,2,2,2,2,2,2,4),(0.,0.0311731506870284,0.0418602132086393,
0.048433128696634,0.0543558575881586,0.0618464529327373,0.0766250168557595,
0.119968052551404,0.155726344679955,0.19481032757455,0.236983053010675,
0.280779560740691,0.322602102638611,0.362770152170366,0.381467742535013,
0.388884220477945,0.394389648003183,0.400355003625582,0.408399663589159,
0.426069229886513,0.469389210961475,0.505710277303957,0.545356763992023,
0.588183425258028,0.630669016411542,0.656032073470706,0.689820287540479),
 .UNSPECIFIED.);
#2636=B_SPLINE_CURVE_WITH_KNOTS('',3,(#115406,#115407,#115408,#115409,#115410,
#115411,#115412,#115413,#115414,#115415,#115416,#115417,#115418,#115419,
#115420,#115421,#115422,#115423,#115424,#115425,#115426,#115427,#115428,
#115429,#115430,#115431,#115432,#115433,#115434,#115435,#115436,#115437,
#115438,#115439,#115440,#115441,#115442,#115443),.UNSPECIFIED.,.T.,.F.,
(4,2,2,2,2,2,2,2,2,2,2,2,2,2,2,2,2,2,4),(0.,0.0426685344635419,0.0857754965458324,
0.107489611928664,0.129156562111911,0.173132822929053,0.216777258109929,
0.260284069552824,0.303288551242756,0.345834109097685,0.389370602799947,
0.433121652565274,0.454607365601712,0.476184832899817,0.520605100709639,
0.564002866904102,0.606959572147738,0.649520039161279,0.690276797053979),
 .UNSPECIFIED.);
#2637=B_SPLINE_CURVE_WITH_KNOTS('',3,(#115447,#115448,#115449,#115450,#115451,
#115452,#115453,#115454,#115455,#115456,#115457,#115458,#115459,#115460,
#115461,#115462,#115463,#115464,#115465,#115466,#115467,#115468,#115469,
#115470,#115471),.UNSPECIFIED.,.F.,.F.,(4,2,2,2,2,2,2,2,2,2,3,4),(0.155275981907625,
0.155530727882454,0.174743293281782,0.194149185772797,0.203888255648882,
0.213620765996803,0.233452450372135,0.253177159350054,0.272625126802198,
0.29176374553163,0.310495193130836,0.310519740065872),.UNSPECIFIED.);
#2638=B_SPLINE_CURVE_WITH_KNOTS('',3,(#115475,#115476,#115477,#115478,#115479,
#115480,#115481,#115482,#115483,#115484,#115485,#115486,#115487,#115488,
#115489,#115490,#115491,#115492,#115493,#115494),.UNSPECIFIED.,.F.,.F.,
(4,2,2,2,2,2,2,2,2,4),(0.310519740065872,0.329735065471992,0.349497188529111,
0.359187916628613,0.368901622450452,0.388823108609513,0.408466318982931,
0.427776988505657,0.446921682939557,0.465771175038461),.UNSPECIFIED.);
#2639=B_SPLINE_CURVE_WITH_KNOTS('',3,(#115497,#115498,#115499,#115500,#115501,
#115502,#115503,#115504,#115505,#115506,#115507,#115508,#115509,#115510,
#115511,#115512,#115513,#115514,#115515,#115516,#115517,#115518,#115519,
#115520,#115521,#115522,#115523,#115524,#115525,#115526,#115527,#115528,
#115529,#115530,#115531,#115532,#115533,#115534,#115535,#115536,#115537,
#115538,#115539,#115540,#115541,#115542,#115543,#115544,#115545,#115546,
#115547,#115548,#115549,#115550,#115551,#115552),.UNSPECIFIED.,.T.,.F.,
(4,2,2,2,2,2,2,2,2,2,2,2,2,2,2,2,2,2,2,2,2,2,2,2,2,2,2,4),(0.,0.0556753555883514,
0.111295357417788,0.132652566908597,0.14142414914753,0.1487293705942,0.156174104643047,
0.166882176783822,0.193563212831233,0.2306943281175,0.277656076892647,0.328982761782772,
0.384093225685445,0.443390367350251,0.500873838595757,0.551867915029868,
0.590932224647382,0.603885289668247,0.611762893866178,0.618812845921861,
0.627674925944102,0.645036014643981,0.704250219211749,0.752276706881969,
0.804643362721499,0.860948773120595,0.894503008286371,0.931042954406025),
 .UNSPECIFIED.);
#2640=B_SPLINE_CURVE_WITH_KNOTS('',3,(#115555,#115556,#115557,#115558,#115559,
#115560,#115561,#115562,#115563,#115564,#115565,#115566,#115567,#115568,
#115569,#115570,#115571,#115572,#115573,#115574,#115575,#115576,#115577,
#115578,#115579,#115580,#115581,#115582,#115583,#115584,#115585,#115586,
#115587,#115588,#115589,#115590),.UNSPECIFIED.,.T.,.F.,(4,2,2,2,2,2,2,2,
2,2,2,2,2,2,2,2,2,4),(0.,0.0579994311336097,0.116029404790947,0.174596164903087,
0.233073341184589,0.291880997534754,0.350877078588918,0.409632811124117,
0.468086866237769,0.526716683879389,0.555532242001599,0.614327126259762,
0.672562416696001,0.730782847087877,0.788903549501615,0.84689624499945,
0.904830147920778,0.931861761959869),.UNSPECIFIED.);
#2641=B_SPLINE_CURVE_WITH_KNOTS('',3,(#115594,#115595,#115596,#115597,#115598,
#115599,#115600,#115601,#115602,#115603,#115604,#115605,#115606,#115607,
#115608,#115609,#115610,#115611),.UNSPECIFIED.,.F.,.F.,(4,2,2,2,2,2,2,2,
4),(0.139799327221814,0.172451176872989,0.206950960902435,0.241917535014109,
0.276864920489073,0.311948417753927,0.347111913059652,0.382185271834272,
0.416673693505186),.UNSPECIFIED.);
#2642=B_SPLINE_CURVE_WITH_KNOTS('',3,(#115615,#115616,#115617,#115618,#115619,
#115620,#115621,#115622,#115623,#115624,#115625,#115626,#115627,#115628,
#115629,#115630,#115631,#115632,#115633,#115634,#115635,#115636,#115637,
#115638,#115639),.UNSPECIFIED.,.F.,.F.,(4,2,2,2,2,2,3,2,2,2,2,4),(0.416673693505186,
0.417127062322145,0.452103545097567,0.469249909212646,0.504177842204279,
0.538741036337965,0.553651070766805,0.588191271421502,0.622688360343799,
0.657151199404152,0.691614448294263,0.693450397988619),.UNSPECIFIED.);
#2643=B_SPLINE_CURVE_WITH_KNOTS('',3,(#115642,#115643,#115644,#115645,#115646,
#115647,#115648,#115649,#115650,#115651,#115652,#115653,#115654,#115655,
#115656,#115657,#115658,#115659,#115660,#115661,#115662,#115663,#115664,
#115665,#115666,#115667,#115668,#115669,#115670,#115671,#115672,#115673,
#115674,#115675,#115676,#115677,#115678,#115679,#115680,#115681,#115682,
#115683,#115684,#115685,#115686,#115687,#115688,#115689,#115690,#115691,
#115692,#115693,#115694,#115695),.UNSPECIFIED.,.T.,.F.,(4,2,2,2,2,2,2,2,
2,2,2,2,2,2,2,2,2,2,2,2,2,2,2,2,2,2,4),(0.,0.0459650663680729,0.0911587487632471,
0.103758532892469,0.11097640426392,0.117058395098765,0.124246356906787,
0.137058808038479,0.187900652546287,0.228756314324871,0.273394922041315,
0.32137662602244,0.372164954082387,0.421627383459268,0.464872751605755,
0.4967655638021,0.507624632110352,0.514319307018795,0.520371447043926,0.528062939766105,
0.543405395719753,0.594209139288907,0.635662798972432,0.680906633143842,
0.729607649348098,0.764590848895352,0.804085254219191),.UNSPECIFIED.);
#2644=B_SPLINE_CURVE_WITH_KNOTS('',3,(#115698,#115699,#115700,#115701,#115702,
#115703,#115704,#115705,#115706,#115707,#115708,#115709,#115710,#115711,
#115712,#115713,#115714,#115715,#115716,#115717,#115718,#115719,#115720,
#115721,#115722,#115723,#115724,#115725,#115726,#115727,#115728,#115729,
#115730,#115731,#115732,#115733,#115734,#115735),.UNSPECIFIED.,.T.,.F.,
(4,2,2,2,2,2,2,2,2,2,2,2,2,2,2,2,2,2,4),(0.,0.050121484155583,0.075216166844529,
0.100319777381396,0.151235204038981,0.20188109216132,0.252602851798492,
0.30345847426458,0.3542470207301,0.404892138611418,0.455654054509687,0.480571332706012,
0.505928132668391,0.556314256329173,0.606659368692688,0.656872239708216,
0.706914001750365,0.756857068749588,0.804567373387168),.UNSPECIFIED.);
#2645=B_SPLINE_CURVE_WITH_KNOTS('',3,(#115739,#115740,#115741,#115742,#115743,
#115744,#115745,#115746,#115747,#115748,#115749,#115750,#115751,#115752,
#115753,#115754,#115755,#115756,#115757,#115758,#115759,#115760),
 .UNSPECIFIED.,.F.,.F.,(4,2,2,2,2,2,2,2,2,2,4),(0.213043644044945,0.213108864360279,
0.23967407776299,0.252966657113423,0.266258274056565,0.293313125821752,
0.320284000338968,0.347266237832029,0.374279444703112,0.401275655429572,
0.426078427446025),.UNSPECIFIED.);
#2646=B_SPLINE_CURVE_WITH_KNOTS('',3,(#115764,#115765,#115766,#115767,#115768,
#115769,#115770,#115771,#115772,#115773,#115774,#115775,#115776,#115777,
#115778,#115779,#115780,#115781,#115782,#115783),.UNSPECIFIED.,.F.,.F.,
(4,2,2,2,2,2,2,2,2,4),(0.426078993093609,0.453084151464664,0.466313597304974,
0.479578787641244,0.506518893015236,0.533152886075883,0.559722291205634,
0.586222004888706,0.612690373328852,0.639122637138555),.UNSPECIFIED.);
#2647=B_SPLINE_CURVE_WITH_KNOTS('',3,(#115786,#115787,#115788,#115789,#115790,
#115791,#115792,#115793,#115794,#115795,#115796,#115797,#115798,#115799,
#115800,#115801,#115802,#115803,#115804,#115805,#115806,#115807,#115808,
#115809,#115810,#115811,#115812,#115813,#115814,#115815,#115816,#115817,
#115818,#115819,#115820,#115821,#115822,#115823,#115824,#115825,#115826,
#115827,#115828,#115829,#115830,#115831,#115832,#115833,#115834,#115835,
#115836,#115837,#115838,#115839),.UNSPECIFIED.,.T.,.F.,(4,2,2,2,2,2,2,2,
2,2,2,2,2,2,2,2,2,2,2,2,2,2,2,2,2,2,4),(0.,0.0358323773236018,0.0680188975168841,
0.0780865576065245,0.0840439994585673,0.0892242253478545,0.0956465843966478,
0.107787393851632,0.151741050997288,0.187190313612102,0.225973380531026,
0.267757326418516,0.311723085858284,0.354237392706437,0.392088501575104,
0.417111408422495,0.426077447776635,0.431749628100514,0.436977282925462,
0.443762257478613,0.457780073244758,0.501521385415829,0.537374319538356,
0.576570360647237,0.618850229147283,0.653290957580071,0.693855228535154),
 .UNSPECIFIED.);
#2648=B_SPLINE_CURVE_WITH_KNOTS('',3,(#115842,#115843,#115844,#115845,#115846,
#115847,#115848,#115849,#115850,#115851,#115852,#115853,#115854,#115855,
#115856,#115857,#115858,#115859,#115860,#115861,#115862,#115863,#115864,
#115865,#115866,#115867,#115868,#115869,#115870,#115871,#115872,#115873,
#115874,#115875,#115876,#115877),.UNSPECIFIED.,.T.,.F.,(4,2,2,2,2,2,2,2,
2,2,2,2,2,2,2,2,2,4),(0.,0.0432393772392339,0.0867357606147896,0.108454670231706,
0.152516802376092,0.196322221380555,0.240080495751704,0.283855323105076,
0.327612995695394,0.371423848910237,0.415499999521694,0.437148924076865,
0.481248840441568,0.524832181184604,0.568165199922297,0.611217062785529,
0.654126345857691,0.694403285213169),.UNSPECIFIED.);
#2649=B_SPLINE_CURVE_WITH_KNOTS('',3,(#115881,#115882,#115883,#115884,#115885,
#115886,#115887,#115888,#115889,#115890,#115891,#115892,#115893,#115894,
#115895,#115896,#115897,#115898,#115899,#115900),.UNSPECIFIED.,.F.,.F.,
(4,2,2,2,2,2,2,2,2,4),(0.157626892744907,0.158356648238268,0.178006478909925,
0.197765608415954,0.217893227495238,0.237918399467858,0.257873965262179,
0.277802919510397,0.297312155754085,0.315258042050784),.UNSPECIFIED.);
#2650=B_SPLINE_CURVE_WITH_KNOTS('',3,(#115904,#115905,#115906,#115907,#115908,
#115909,#115910,#115911,#115912,#115913,#115914,#115915,#115916,#115917,
#115918,#115919,#115920,#115921,#115922,#115923,#115924),.UNSPECIFIED.,
 .F.,.F.,(4,3,2,2,2,2,2,2,2,4),(0.315258042050784,0.315279326727019,0.335308798957692,
0.35544106154069,0.375647730314253,0.395414743460894,0.415069475378914,
0.434609381924642,0.454099654500455,0.472906219471926),.UNSPECIFIED.);
#2651=B_SPLINE_CURVE_WITH_KNOTS('',3,(#115927,#115928,#115929,#115930,#115931,
#115932,#115933,#115934,#115935,#115936,#115937,#115938,#115939,#115940,
#115941,#115942,#115943,#115944,#115945,#115946,#115947,#115948,#115949,
#115950,#115951,#115952,#115953,#115954,#115955,#115956,#115957,#115958,
#115959,#115960,#115961,#115962,#115963,#115964,#115965,#115966,#115967,
#115968,#115969,#115970,#115971,#115972,#115973,#115974,#115975,#115976,
#115977,#115978,#115979,#115980,#115981,#115982),.UNSPECIFIED.,.T.,.F.,
(4,2,2,2,2,2,2,2,2,2,2,2,2,2,2,2,2,2,2,2,2,2,2,2,2,2,2,4),(0.,0.0390375792045744,
0.0590178458522155,0.0672194166711689,0.0722183955160815,0.0775479853100994,
0.0845994732587413,0.0996572237805605,0.14299992688214,0.178716701234394,
0.217786016234129,0.259956657972089,0.303755112722266,0.345545654433592,
0.38476471673647,0.404243229009083,0.412309823986064,0.417253897181447,
0.422545396002088,0.429579934992201,0.444717708915258,0.488060644137423,
0.523877949673102,0.563102122736068,0.605510200655335,0.643225976330391,
0.664545279498856,0.689830282636683),.UNSPECIFIED.);
#2652=B_SPLINE_CURVE_WITH_KNOTS('',3,(#115985,#115986,#115987,#115988,#115989,
#115990,#115991,#115992,#115993,#115994,#115995,#115996,#115997,#115998,
#115999,#116000,#116001,#116002,#116003,#116004,#116005,#116006,#116007,
#116008,#116009,#116010,#116011,#116012,#116013,#116014,#116015,#116016,
#116017,#116018,#116019,#116020,#116021,#116022),.UNSPECIFIED.,.T.,.F.,
(4,2,2,2,2,2,2,2,2,2,2,2,2,2,2,2,2,2,4),(0.,0.0429286760162795,0.0862893470429538,
0.107869956323031,0.15168893150141,0.195288381210701,0.238885645590843,
0.281412823568044,0.323975646504692,0.367552260777747,0.411219341914282,
0.432643267861024,0.454142634616226,0.498425946874695,0.541789855901478,
0.584712513093188,0.627258856393838,0.669718871101792,0.69031086887045),
 .UNSPECIFIED.);
#2653=B_SPLINE_CURVE_WITH_KNOTS('',3,(#116026,#116027,#116028,#116029,#116030,
#116031,#116032,#116033,#116034,#116035,#116036,#116037,#116038,#116039,
#116040,#116041,#116042,#116043,#116044,#116045,#116046,#116047),
 .UNSPECIFIED.,.F.,.F.,(4,2,2,2,2,2,2,2,2,2,4),(0.155281525707715,0.165407413678005,
0.184837154921267,0.194547083649518,0.204241569791125,0.224004541735763,
0.243710040103625,0.263152667016854,0.282283166620068,0.301416643807714,
0.310510623695354),.UNSPECIFIED.);
#2654=B_SPLINE_CURVE_WITH_KNOTS('',3,(#116051,#116052,#116053,#116054,#116055,
#116056,#116057,#116058,#116059,#116060,#116061,#116062,#116063,#116064,
#116065,#116066,#116067,#116068,#116069,#116070),.UNSPECIFIED.,.F.,.F.,
(4,2,2,2,2,2,2,2,2,4),(0.310510783932394,0.33021534549801,0.349975556798286,
0.359654748676357,0.37951365110717,0.399147572564983,0.418436153684863,
0.43757097487398,0.456683395879265,0.465792149403069),.UNSPECIFIED.);
#2655=B_SPLINE_CURVE_WITH_KNOTS('',3,(#116073,#116074,#116075,#116076,#116077,
#116078,#116079,#116080,#116081,#116082,#116083,#116084,#116085,#116086,
#116087,#116088,#116089,#116090,#116091,#116092,#116093,#116094,#116095,
#116096,#116097,#116098,#116099,#116100,#116101,#116102,#116103,#116104,
#116105,#116106,#116107,#116108,#116109,#116110,#116111,#116112,#116113,
#116114,#116115,#116116,#116117,#116118,#116119,#116120,#116121,#116122,
#116123,#116124,#116125,#116126),.UNSPECIFIED.,.T.,.F.,(4,2,2,2,2,2,2,2,
2,2,2,2,2,2,2,2,2,2,2,2,2,2,2,2,2,2,4),(0.,0.0577066589623385,0.108220241511108,
0.155025064619134,0.168566924488323,0.176486388257448,0.183196502035754,
0.19130287220519,0.206035894029007,0.26494305616825,0.312215986498219,0.36379987608317,
0.419167761629723,0.477871964115765,0.535180527979754,0.584787120836968,
0.622981568939877,0.63542970577016,0.642952510898312,0.648987621127709,
0.657075914044929,0.672025070963926,0.731047633253834,0.778568461524894,
0.83053501913079,0.880505757758383,0.931203521812045),.UNSPECIFIED.);
#2656=B_SPLINE_CURVE_WITH_KNOTS('',3,(#116129,#116130,#116131,#116132,#116133,
#116134,#116135,#116136,#116137,#116138,#116139,#116140,#116141,#116142,
#116143,#116144,#116145,#116146,#116147,#116148,#116149,#116150,#116151,
#116152,#116153,#116154,#116155,#116156,#116157,#116158,#116159,#116160,
#116161,#116162,#116163,#116164),.UNSPECIFIED.,.T.,.F.,(4,2,2,2,2,2,2,2,
2,2,2,2,2,2,2,2,2,4),(0.,0.0580062210999761,0.116027500581797,0.174539501268387,
0.233085095091822,0.291851800270691,0.350586183609165,0.4090941168664,0.467658902805053,
0.496406714569538,0.525691391466127,0.583914495393509,0.642183460479962,
0.700438611055605,0.758574908135443,0.816555683924175,0.874457701625133,
0.931848830026075),.UNSPECIFIED.);
#2657=B_SPLINE_CURVE_WITH_KNOTS('',3,(#116168,#116169,#116170,#116171,#116172,
#116173,#116174,#116175,#116176,#116177,#116178,#116179,#116180,#116181,
#116182,#116183,#116184,#116185),.UNSPECIFIED.,.F.,.F.,(4,2,2,2,2,2,2,2,
4),(0.139756359393238,0.172379146205813,0.206875888117782,0.241848498189916,
0.276811650419912,0.311843728956546,0.346869648108179,0.381826442196638,
0.416625798777337),.UNSPECIFIED.);
#2658=B_SPLINE_CURVE_WITH_KNOTS('',3,(#116189,#116190,#116191,#116192,#116193,
#116194,#116195,#116196,#116197,#116198,#116199,#116200,#116201,#116202,
#116203,#116204,#116205,#116206,#116207,#116208,#116209,#116210,#116211,
#116212,#116213),.UNSPECIFIED.,.F.,.F.,(4,2,2,2,2,2,3,2,2,2,2,4),(0.416625798777337,
0.416811988200141,0.433955298027859,0.4513600485358,0.48592734829649,0.520509887106317,
0.553630915158508,0.588160307888751,0.622630239726201,0.657069905215908,
0.69152400979313,0.693387274551746),.UNSPECIFIED.);
#2659=B_SPLINE_CURVE_WITH_KNOTS('',3,(#116216,#116217,#116218,#116219,#116220,
#116221,#116222,#116223,#116224,#116225,#116226,#116227,#116228,#116229,
#116230,#116231,#116232,#116233,#116234,#116235,#116236,#116237,#116238,
#116239,#116240,#116241,#116242,#116243,#116244,#116245,#116246,#116247,
#116248,#116249,#116250,#116251,#116252,#116253,#116254,#116255,#116256,
#116257,#116258,#116259,#116260,#116261,#116262,#116263,#116264,#116265,
#116266,#116267,#116268,#116269),.UNSPECIFIED.,.T.,.F.,(4,2,2,2,2,2,2,2,
2,2,2,2,2,2,2,2,2,2,2,2,2,2,2,2,2,2,4),(0.,0.0491414753089632,0.0925487839832437,
0.122593144975948,0.132847468349746,0.139193738324383,0.14495264583004,
0.152307953678182,0.167132411558137,0.217957911591671,0.25914050175531,
0.304055332305895,0.35231689455287,0.403065556918838,0.452265829412814,
0.495942952242087,0.525036206824292,0.535088756106163,0.54134412715987,
0.547042237653256,0.554348484673671,0.56916221793295,0.619983908515213,
0.661298626737727,0.706438873808049,0.755042331569686,0.804148478915545),
 .UNSPECIFIED.);
#2660=B_SPLINE_CURVE_WITH_KNOTS('',3,(#116272,#116273,#116274,#116275,#116276,
#116277,#116278,#116279,#116280,#116281,#116282,#116283,#116284,#116285,
#116286,#116287,#116288,#116289,#116290,#116291,#116292,#116293,#116294,
#116295,#116296,#116297,#116298,#116299,#116300,#116301,#116302,#116303,
#116304,#116305,#116306,#116307,#116308,#116309),.UNSPECIFIED.,.T.,.F.,
(4,2,2,2,2,2,2,2,2,2,2,2,2,2,2,2,2,2,4),(0.,0.0501833807776728,0.0752864723656921,
0.12626759651476,0.176927418053835,0.227597522568229,0.278358481987529,
0.329065980432407,0.379699791417318,0.430534861965737,0.455501787095014,
0.480856165965872,0.531251764035078,0.581611739513776,0.63183513372458,
0.681877255988317,0.731811481032622,0.781785602018675,0.804591288052395),
 .UNSPECIFIED.);
#2661=B_SPLINE_CURVE_WITH_KNOTS('',3,(#116313,#116314,#116315,#116316,#116317,
#116318,#116319,#116320,#116321,#116322,#116323,#116324,#116325,#116326,
#116327,#116328,#116329,#116330,#116331,#116332,#116333,#116334),
 .UNSPECIFIED.,.F.,.F.,(4,2,2,2,2,2,2,2,2,2,4),(0.213057265421291,0.226444841366151,
0.239736816501714,0.253034106200005,0.280126668221598,0.3071042938041,0.334056714793563,
0.36101913045305,0.387974252130544,0.414936420729693,0.42607613571615),
 .UNSPECIFIED.);
#2662=B_SPLINE_CURVE_WITH_KNOTS('',3,(#116338,#116339,#116340,#116341,#116342,
#116343,#116344,#116345,#116346,#116347,#116348,#116349,#116350,#116351,
#116352,#116353,#116354,#116355,#116356,#116357,#116358,#116359,#116360),
 .UNSPECIFIED.,.F.,.F.,(4,3,2,2,2,2,2,2,2,2,4),(0.42607613571615,0.426097060646127,
0.453209656703842,0.466641094363468,0.493308893322814,0.519950454049193,
0.546525916596096,0.57302682164241,0.599491300460783,0.625982272547063,
0.639154326067418),.UNSPECIFIED.);
#2663=B_SPLINE_CURVE_WITH_KNOTS('',3,(#116363,#116364,#116365,#116366,#116367,
#116368,#116369,#116370,#116371,#116372,#116373,#116374,#116375,#116376,
#116377,#116378,#116379,#116380,#116381,#116382,#116383,#116384,#116385,
#116386,#116387,#116388,#116389,#116390,#116391,#116392,#116393,#116394,
#116395,#116396,#116397,#116398,#116399,#116400,#116401,#116402,#116403,
#116404,#116405,#116406,#116407,#116408,#116409,#116410,#116411,#116412,
#116413,#116414,#116415,#116416,#116417,#116418),.UNSPECIFIED.,.T.,.F.,
(4,2,2,2,2,2,2,2,2,2,2,2,2,2,2,2,2,2,2,2,2,2,2,2,2,2,2,4),(0.,0.041285253628399,
0.0822448660680709,0.0978610724808867,0.10400629769675,0.108568719624014,
0.113522581485496,0.120239297953382,0.13525770505281,0.178998524482636,
0.214867867279051,0.254013558218206,0.296165829644769,0.340059680648694,
0.382165264453309,0.420785265606447,0.442102674108075,0.450101530221598,
0.455290600040355,0.460169421252104,0.466649080514575,0.480606708590981,
0.524360856110365,0.560151574991358,0.599306833792761,0.6415526782016,0.666591170965427,
0.693884097625634),.UNSPECIFIED.);
#2664=B_SPLINE_CURVE_WITH_KNOTS('',3,(#116421,#116422,#116423,#116424,#116425,
#116426,#116427,#116428,#116429,#116430,#116431,#116432,#116433,#116434,
#116435,#116436,#116437,#116438,#116439,#116440,#116441,#116442,#116443,
#116444,#116445,#116446,#116447,#116448,#116449,#116450,#116451,#116452,
#116453,#116454,#116455,#116456),.UNSPECIFIED.,.T.,.F.,(4,2,2,2,2,2,2,2,
2,2,2,2,2,2,2,2,2,4),(0.,0.043430317645468,0.0876189818453222,0.131490406017855,
0.17529842262449,0.219243734427261,0.262215746345614,0.305308136875401,
0.34910933896524,0.393004507675874,0.414540236113842,0.45894962553968,0.502489821198032,
0.545774652003282,0.588801627501863,0.63172385035613,0.674765513237447,
0.694442278112711),.UNSPECIFIED.);
#2665=B_SPLINE_CURVE_WITH_KNOTS('',3,(#116460,#116461,#116462,#116463,#116464,
#116465,#116466,#116467,#116468,#116469,#116470,#116471,#116472,#116473,
#116474,#116475,#116476,#116477,#116478,#116479),.UNSPECIFIED.,.F.,.F.,
(4,2,2,2,2,2,2,2,2,4),(0.157627193529841,0.167716827321412,0.187814282331985,
0.207836144110288,0.227821673078062,0.247827083298905,0.267342985260238,
0.28685856777808,0.306450487286998,0.315250728700652),.UNSPECIFIED.);
#2666=B_SPLINE_CURVE_WITH_KNOTS('',3,(#116483,#116484,#116485,#116486,#116487,
#116488,#116489,#116490,#116491,#116492,#116493,#116494,#116495,#116496,
#116497,#116498,#116499,#116500,#116501,#116502,#116503,#116504,#116505),
 .UNSPECIFIED.,.F.,.F.,(4,3,2,2,2,2,2,2,2,2,4),(0.315250728700652,0.315252659637721,
0.335252771579398,0.345044128740003,0.365147854527748,0.385081661646758,
0.404715888785962,0.424245396326341,0.443741595607751,0.463297264804012,
0.472879853167562),.UNSPECIFIED.);
#2667=B_SPLINE_CURVE_WITH_KNOTS('',3,(#116508,#116509,#116510,#116511,#116512,
#116513,#116514,#116515,#116516,#116517,#116518,#116519,#116520,#116521,
#116522,#116523,#116524,#116525,#116526,#116527,#116528,#116529,#116530,
#116531,#116532,#116533,#116534,#116535,#116536,#116537,#116538,#116539,
#116540,#116541,#116542,#116543,#116544,#116545,#116546,#116547,#116548,
#116549,#116550,#116551,#116552,#116553,#116554,#116555,#116556,#116557,
#116558,#116559,#116560,#116561,#116562,#116563),.UNSPECIFIED.,.T.,.F.,
(4,2,2,2,2,2,2,2,2,2,2,2,2,2,2,2,2,2,2,2,2,2,2,2,2,2,2,4),(0.,0.0389094768208776,
0.077644299909024,0.0869793188239608,0.0930343010064621,0.0978595661268027,
0.103266182813461,0.112206308441846,0.142773526660472,0.175527151159333,
0.212208114415353,0.252134756286138,0.29519266441111,0.338693154248625,
0.378978774214529,0.421865026269376,0.431590686763012,0.437742921379179,
0.442544488371915,0.447820266261681,0.456311320145132,0.483432074234788,
0.51556966970483,0.551845054032032,0.591482878005452,0.63432148952688,0.660439037839305,
0.689835002387049),.UNSPECIFIED.);
#2668=B_SPLINE_CURVE_WITH_KNOTS('',3,(#116566,#116567,#116568,#116569,#116570,
#116571,#116572,#116573,#116574,#116575,#116576,#116577,#116578,#116579,
#116580,#116581,#116582,#116583,#116584,#116585,#116586,#116587,#116588,
#116589,#116590,#116591,#116592,#116593,#116594,#116595,#116596,#116597,
#116598,#116599,#116600,#116601,#116602,#116603),.UNSPECIFIED.,.T.,.F.,
(4,2,2,2,2,2,2,2,2,2,2,2,2,2,2,2,2,2,4),(0.,0.0431561762404372,0.0648561590452176,
0.0864916690642867,0.130405697248895,0.174030302676733,0.217566990876258,
0.260102189498512,0.302668301258938,0.346227368299971,0.389977906413364,
0.411459041889591,0.433027647489369,0.477425144947406,0.520797890347173,
0.563724989172446,0.606272249689026,0.648733187794411,0.690383069014513),
 .UNSPECIFIED.);
#2669=B_SPLINE_CURVE_WITH_KNOTS('',3,(#116607,#116608,#116609,#116610,#116611,
#116612,#116613,#116614,#116615,#116616,#116617,#116618,#116619,#116620,
#116621,#116622,#116623,#116624,#116625,#116626,#116627,#116628),
 .UNSPECIFIED.,.F.,.F.,(4,2,2,2,2,2,2,2,2,2,4),(0.155275319539932,0.155472519940377,
0.174899463638446,0.184631482355954,0.194352939394403,0.214162137141302,
0.233879076545751,0.253319079372333,0.272453534450712,0.291587356219028,
0.310541455171113),.UNSPECIFIED.);
#2670=B_SPLINE_CURVE_WITH_KNOTS('',3,(#116632,#116633,#116634,#116635,#116636,
#116637,#116638,#116639,#116640,#116641,#116642,#116643,#116644,#116645,
#116646,#116647,#116648,#116649,#116650,#116651,#116652,#116653,#116654),
 .UNSPECIFIED.,.F.,.F.,(4,3,2,2,2,2,2,2,2,2,4),(0.310541455171113,0.310542742432682,
0.330303977577274,0.339991361015711,0.349699012642844,0.369606133275464,
0.389237991660081,0.408533484226866,0.42767172155954,0.446783628648094,
0.465818061972614),.UNSPECIFIED.);
#2671=B_SPLINE_CURVE_WITH_KNOTS('',3,(#116657,#116658,#116659,#116660,#116661,
#116662,#116663,#116664,#116665,#116666,#116667,#116668,#116669,#116670,
#116671,#116672,#116673,#116674,#116675,#116676,#116677,#116678,#116679,
#116680,#116681,#116682,#116683,#116684,#116685,#116686,#116687,#116688,
#116689,#116690,#116691,#116692,#116693,#116694,#116695,#116696,#116697,
#116698,#116699,#116700,#116701,#116702,#116703,#116704,#116705,#116706,
#116707,#116708,#116709,#116710,#116711,#116712),.UNSPECIFIED.,.T.,.F.,
(4,2,2,2,2,2,2,2,2,2,2,2,2,2,2,2,2,2,2,2,2,2,2,2,2,2,2,4),(0.,0.0584891512695919,
0.114492542178861,0.167895255153171,0.192926962144756,0.203201312515091,
0.209475661727826,0.216178889385321,0.225078797588162,0.244244249149783,
0.303228610481566,0.351253205348421,0.40344779802583,0.459430920400994,
0.518055048404651,0.574790904207356,0.626379818080268,0.656739046234691,
0.667820528375868,0.674906502512356,0.681494594812286,0.690134018443859,
0.708330275060749,0.767556059783576,0.81565597509107,0.86809846809008,0.89975349026725,
0.931147159319543),.UNSPECIFIED.);
#2672=B_SPLINE_CURVE_WITH_KNOTS('',3,(#116715,#116716,#116717,#116718,#116719,
#116720,#116721,#116722,#116723,#116724,#116725,#116726,#116727,#116728,
#116729,#116730,#116731,#116732,#116733,#116734,#116735,#116736,#116737,
#116738,#116739,#116740,#116741,#116742,#116743,#116744,#116745,#116746,
#116747,#116748,#116749,#116750),.UNSPECIFIED.,.T.,.F.,(4,2,2,2,2,2,2,2,
2,2,2,2,2,2,2,2,2,4),(0.,0.0580273876658578,0.116624709778379,0.175109980248094,
0.233875067237791,0.292781005354475,0.351458258505243,0.409917402953638,
0.468652301333266,0.497938514908916,0.556156374039708,0.614407784487279,
0.672639310224047,0.730758072220705,0.788738683692563,0.846658543028034,
0.904617546167748,0.931861050654944),.UNSPECIFIED.);
#2673=B_SPLINE_CURVE_WITH_KNOTS('',3,(#116754,#116755,#116756,#116757,#116758,
#116759,#116760,#116761,#116762,#116763,#116764,#116765,#116766,#116767,
#116768,#116769,#116770,#116771),.UNSPECIFIED.,.F.,.F.,(4,2,2,2,2,2,2,2,
4),(0.13975667624528,0.172385107747455,0.207377997148642,0.242328900489864,
0.277382835898854,0.312493359299448,0.347523544103189,0.382466335247368,
0.416631398225218),.UNSPECIFIED.);
#2674=B_SPLINE_CURVE_WITH_KNOTS('',3,(#116775,#116776,#116777,#116778,#116779,
#116780,#116781,#116782,#116783,#116784,#116785,#116786,#116787,#116788,
#116789,#116790,#116791,#116792,#116793,#116794,#116795,#116796,#116797,
#116798,#116799),.UNSPECIFIED.,.F.,.F.,(4,2,2,2,2,2,3,2,2,2,2,4),(0.416631398225218,
0.417494170154389,0.434899729575189,0.469463645133473,0.504035272545212,
0.538595601414024,0.55364530802227,0.588140235067004,0.6225958952251,0.657050905834583,
0.691532621286376,0.69340198426755),.UNSPECIFIED.);
#2675=B_SPLINE_CURVE_WITH_KNOTS('',3,(#116802,#116803,#116804,#116805,#116806,
#116807,#116808,#116809,#116810,#116811,#116812,#116813,#116814,#116815,
#116816,#116817,#116818,#116819,#116820,#116821,#116822,#116823,#116824,
#116825,#116826,#116827,#116828,#116829,#116830,#116831,#116832,#116833,
#116834,#116835,#116836,#116837,#116838,#116839,#116840,#116841,#116842,
#116843,#116844,#116845,#116846,#116847,#116848,#116849,#116850,#116851,
#116852,#116853,#116854,#116855,#116856,#116857),.UNSPECIFIED.,.T.,.F.,
(4,2,2,2,2,2,2,2,2,2,2,2,2,2,2,2,2,2,2,2,2,2,2,2,2,2,2,4),(0.,0.050309885077182,
0.0968176213990348,0.14561500811571,0.156739046106578,0.163807644338246,
0.16934707395481,0.175458686824546,0.185355150398173,0.217530128519313,
0.25516696991148,0.297395878474636,0.343189130145614,0.392358357282366,
0.442924870955592,0.490985306930195,0.538391227704406,0.55636629273847,
0.564315592840812,0.569898862718201,0.575587019218597,0.583774116525507,
0.604278624054994,0.655331471969062,0.697522159209062,0.743402500798943,
0.773581445154641,0.804063549998697),.UNSPECIFIED.);
#2676=B_SPLINE_CURVE_WITH_KNOTS('',3,(#116860,#116861,#116862,#116863,#116864,
#116865,#116866,#116867,#116868,#116869,#116870,#116871,#116872,#116873,
#116874,#116875,#116876,#116877,#116878,#116879,#116880,#116881,#116882,
#116883,#116884,#116885,#116886,#116887,#116888,#116889,#116890,#116891,
#116892,#116893,#116894,#116895),.UNSPECIFIED.,.T.,.F.,(4,2,2,2,2,2,2,2,
2,2,2,2,2,2,2,2,2,4),(0.,0.0251012805543509,0.0501415752591219,0.100917082239335,
0.151542035486755,0.202362336623636,0.253360602597951,0.304245574169001,
0.354898572509294,0.405593370032142,0.45672129467809,0.507094850947286,
0.557408623612551,0.607586772950294,0.657611039698548,0.707566257516175,
0.757588498528219,0.804710998356802),.UNSPECIFIED.);
#2677=B_SPLINE_CURVE_WITH_KNOTS('',3,(#116899,#116900,#116901,#116902,#116903,
#116904,#116905,#116906,#116907,#116908,#116909,#116910,#116911,#116912,
#116913,#116914,#116915,#116916,#116917,#116918),.UNSPECIFIED.,.F.,.F.,
(4,2,2,2,2,2,2,2,2,4),(0.213045309439027,0.225903171160768,0.23915487036106,
0.266145051380448,0.293105692945154,0.320136249990941,0.34662148809123,
0.373143786348127,0.400118964953456,0.426087518215633),.UNSPECIFIED.);
#2678=B_SPLINE_CURVE_WITH_KNOTS('',3,(#116922,#116923,#116924,#116925,#116926,
#116927,#116928,#116929,#116930,#116931,#116932,#116933,#116934,#116935,
#116936,#116937,#116938,#116939,#116940,#116941,#116942,#116943,#116944,
#116945,#116946),.UNSPECIFIED.,.F.,.F.,(4,3,2,2,2,2,2,2,2,2,2,4),(0.426087518215633,
0.426092043059227,0.439294541944362,0.452527327986773,0.479465410345481,
0.506084663851214,0.532639176079408,0.559132814855581,0.58560811112673,
0.612122033742717,0.638703850902336,0.639137352498254),.UNSPECIFIED.);
#2679=B_SPLINE_CURVE_WITH_KNOTS('',3,(#116949,#116950,#116951,#116952,#116953,
#116954,#116955,#116956,#116957,#116958,#116959,#116960,#116961,#116962,
#116963,#116964,#116965,#116966,#116967,#116968,#116969,#116970,#116971,
#116972,#116973,#116974,#116975,#116976,#116977,#116978,#116979,#116980,
#116981,#116982,#116983,#116984,#116985,#116986,#116987,#116988,#116989,
#116990,#116991,#116992,#116993,#116994,#116995,#116996,#116997,#116998,
#116999,#117000,#117001,#117002,#117003,#117004),.UNSPECIFIED.,.T.,.F.,
(4,2,2,2,2,2,2,2,2,2,2,2,2,2,2,2,2,2,2,2,2,2,2,2,2,2,2,4),(0.,0.04306450588528,
0.0799275659781319,0.115025434929688,0.124575396355486,0.130036613772263,
0.134639877230734,0.140088544983391,0.149845294197815,0.191581859546887,
0.22622904912325,0.264381554721172,0.305567799522646,0.349957215317373,
0.392932910186313,0.428785627015779,0.462395684866412,0.471727343819009,
0.477108322028563,0.481213516207419,0.486467047619745,0.495487409345996,
0.529647573843035,0.563205873397388,0.600581186566829,0.641128664104466,
0.667016282704079,0.693823417143794),.UNSPECIFIED.);
#2680=B_SPLINE_CURVE_WITH_KNOTS('',3,(#117007,#117008,#117009,#117010,#117011,
#117012,#117013,#117014,#117015,#117016,#117017,#117018,#117019,#117020,
#117021,#117022,#117023,#117024,#117025,#117026,#117027,#117028,#117029,
#117030,#117031,#117032,#117033,#117034,#117035,#117036,#117037,#117038,
#117039,#117040,#117041,#117042),.UNSPECIFIED.,.T.,.F.,(4,2,2,2,2,2,2,2,
2,2,2,2,2,2,2,2,2,4),(0.,0.0435201388237783,0.0876896865062443,0.131556050902525,
0.175347888012368,0.219184263957841,0.263011932322101,0.306802442037427,
0.350712621875749,0.372257866489833,0.393892414057866,0.437988072782709,
0.481550707432859,0.524854944245018,0.567888576652302,0.610803761428183,
0.653830385515191,0.69446576879133),.UNSPECIFIED.);
#2681=B_SPLINE_CURVE_WITH_KNOTS('',3,(#117046,#117047,#117048,#117049,#117050,
#117051,#117052,#117053,#117054,#117055,#117056,#117057,#117058,#117059,
#117060,#117061,#117062,#117063,#117064,#117065,#117066),.UNSPECIFIED.,
 .F.,.F.,(4,2,2,2,2,2,2,2,3,4),(0.157656823790096,0.177236697355346,0.197336849182283,
0.217351967607823,0.237321518579206,0.256846128436631,0.276358786518457,
0.296332744546969,0.315265150459455,0.315307705902751),.UNSPECIFIED.);
#2682=B_SPLINE_CURVE_WITH_KNOTS('',3,(#117070,#117071,#117072,#117073,#117074,
#117075,#117076,#117077,#117078,#117079,#117080,#117081,#117082,#117083,
#117084,#117085,#117086,#117087,#117088,#117089,#117090,#117091),
 .UNSPECIFIED.,.F.,.F.,(4,2,2,2,2,2,2,2,2,2,4),(0.315307705902751,0.325075072158519,
0.33490628806666,0.355089026447615,0.374851285877192,0.394499906238306,
0.4140370791025,0.433530763726022,0.453075863775059,0.472735940924408,0.472921974249551),
 .UNSPECIFIED.);
#2683=B_SPLINE_CURVE_WITH_KNOTS('',3,(#117094,#117095,#117096,#117097,#117098,
#117099,#117100,#117101,#117102,#117103,#117104,#117105,#117106,#117107,
#117108,#117109,#117110,#117111,#117112,#117113,#117114,#117115,#117116,
#117117,#117118,#117119,#117120,#117121,#117122,#117123,#117124,#117125,
#117126,#117127,#117128,#117129,#117130,#117131,#117132,#117133,#117134,
#117135,#117136,#117137,#117138,#117139,#117140,#117141,#117142,#117143,
#117144,#117145,#117146,#117147,#117148,#117149),.UNSPECIFIED.,.T.,.F.,
(4,2,2,2,2,2,2,2,2,2,2,2,2,2,2,2,2,2,2,2,2,2,2,2,2,2,2,4),(0.,0.0420957482556104,
0.0788204825590171,0.10439842115468,0.112737593521854,0.117799011810767,
0.121877536406845,0.127372490945778,0.137643300991004,0.180988892763695,
0.215730960955723,0.25400272679975,0.295405998843111,0.339374438240802,
0.381943378576841,0.418153695727972,0.448316824505312,0.457119676510764,
0.462312317182371,0.466786340130831,0.472200775743362,0.482227367612323,
0.525497676632813,0.560258387201869,0.598610612973799,0.640171176621586,
0.664290506141458,0.689921488883007),.UNSPECIFIED.);
#2684=B_SPLINE_CURVE_WITH_KNOTS('',3,(#117152,#117153,#117154,#117155,#117156,
#117157,#117158,#117159,#117160,#117161,#117162,#117163,#117164,#117165,
#117166,#117167,#117168,#117169,#117170,#117171,#117172,#117173,#117174,
#117175,#117176,#117177,#117178,#117179,#117180,#117181,#117182,#117183,
#117184,#117185,#117186,#117187,#117188,#117189),.UNSPECIFIED.,.T.,.F.,
(4,2,2,2,2,2,2,2,2,2,2,2,2,2,2,2,2,2,4),(0.,0.0433710488880423,0.0650253824547739,
0.108968254486875,0.152596643322638,0.196107206689574,0.238642946636128,
0.281214225978943,0.32477135649117,0.368564045409551,0.390072545346376,
0.411672777792178,0.455677790431156,0.499049066862304,0.541971910087472,
0.584515751159163,0.626977488416304,0.669703944754416,0.690418361534604),
 .UNSPECIFIED.);
#2685=B_SPLINE_CURVE_WITH_KNOTS('',3,(#117193,#117194,#117195,#117196,#117197,
#117198,#117199,#117200,#117201,#117202,#117203,#117204,#117205,#117206,
#117207,#117208,#117209,#117210,#117211,#117212,#117213,#117214),
 .UNSPECIFIED.,.F.,.F.,(4,2,2,2,2,2,2,2,2,2,4),(0.155304109067118,0.165313690891263,
0.175054466501976,0.184785723582231,0.204609586111903,0.224327485013603,
0.243761651045815,0.262895169247043,0.282030889979258,0.301296683977728,
0.310555525369536),.UNSPECIFIED.);
#2686=B_SPLINE_CURVE_WITH_KNOTS('',3,(#117218,#117219,#117220,#117221,#117222,
#117223,#117224,#117225,#117226,#117227,#117228,#117229,#117230,#117231,
#117232,#117233,#117234,#117235,#117236,#117237,#117238,#117239,#117240),
 .UNSPECIFIED.,.F.,.F.,(4,3,2,2,2,2,2,2,2,2,4),(0.310555525369536,0.31055833948538,
0.330390740094614,0.340111031893878,0.360037161153345,0.37966238872268,
0.398954774450647,0.418091310700888,0.437204580349564,0.456440316485847,
0.465862448552498),.UNSPECIFIED.);
#2687=B_SPLINE_CURVE_WITH_KNOTS('',3,(#117243,#117244,#117245,#117246,#117247,
#117248,#117249,#117250,#117251,#117252,#117253,#117254,#117255,#117256,
#117257,#117258,#117259,#117260,#117261,#117262,#117263,#117264,#117265,
#117266,#117267,#117268,#117269,#117270,#117271,#117272,#117273,#117274,
#117275,#117276,#117277,#117278,#117279,#117280,#117281,#117282,#117283,
#117284,#117285,#117286,#117287,#117288,#117289,#117290,#117291,#117292,
#117293,#117294,#117295,#117296),.UNSPECIFIED.,.T.,.F.,(4,2,2,2,2,2,2,2,
2,2,2,2,2,2,2,2,2,2,2,2,2,2,2,2,2,2,4),(0.,0.0588899148675681,0.116713784598351,
0.168127032983557,0.217161756198921,0.230708488164785,0.238481790712691,
0.245045683531671,0.252825342057254,0.266770879667179,0.325680310196297,
0.372778207213426,0.424230111324823,0.479472421391073,0.538189063657707,
0.59558791103362,0.645483611950939,0.685162679203097,0.697581033759298,
0.704951114140878,0.711376767007497,0.719368887500008,0.734569892864707,
0.793812168199268,0.841381833347496,0.888689256421084,0.931225999577531),
 .UNSPECIFIED.);
#2688=B_SPLINE_CURVE_WITH_KNOTS('',3,(#117299,#117300,#117301,#117302,#117303,
#117304,#117305,#117306,#117307,#117308,#117309,#117310,#117311,#117312,
#117313,#117314,#117315,#117316,#117317,#117318,#117319,#117320,#117321,
#117322,#117323,#117324,#117325,#117326,#117327,#117328,#117329,#117330,
#117331,#117332,#117333,#117334,#117335,#117336),.UNSPECIFIED.,.T.,.F.,
(4,2,2,2,2,2,2,2,2,2,2,2,2,2,2,2,2,2,4),(0.,0.0586869128804075,0.117101756083158,
0.175809300555675,0.234870079029752,0.293836105351144,0.352394127952532,
0.410832470887651,0.439493106921451,0.468301655288093,0.527096860275995,
0.585318822752492,0.643517734326523,0.701618600084167,0.759606971398693,
0.817555987879628,0.875547839400924,0.903528726059672,0.931729138475359),
 .UNSPECIFIED.);
#2689=B_SPLINE_CURVE_WITH_KNOTS('',3,(#117340,#117341,#117342,#117343,#117344,
#117345,#117346,#117347,#117348,#117349,#117350,#117351,#117352,#117353,
#117354,#117355,#117356,#117357,#117358,#117359),.UNSPECIFIED.,.F.,.F.,
(4,2,2,2,2,2,2,2,2,4),(0.139842570142282,0.172920078696101,0.207831273050215,
0.242880597158898,0.278083844108549,0.3132558378693,0.348251982782376,0.383159208999535,
0.400246012749396,0.416635718978169),.UNSPECIFIED.);
#2690=B_SPLINE_CURVE_WITH_KNOTS('',3,(#117363,#117364,#117365,#117366,#117367,
#117368,#117369,#117370,#117371,#117372,#117373,#117374,#117375,#117376,
#117377,#117378,#117379,#117380,#117381,#117382,#117383,#117384,#117385),
 .UNSPECIFIED.,.F.,.F.,(4,2,2,2,2,3,2,2,2,2,4),(0.416635718978169,0.417378505027386,
0.45230554511966,0.486859439730073,0.521400572944025,0.553633145844837,
0.588108965928037,0.622576103225218,0.657062747984201,0.691566133172587,
0.69347571598712),.UNSPECIFIED.);
#2691=B_SPLINE_CURVE_WITH_KNOTS('',3,(#117388,#117389,#117390,#117391,#117392,
#117393,#117394,#117395,#117396,#117397,#117398,#117399,#117400,#117401,
#117402,#117403,#117404,#117405,#117406,#117407,#117408,#117409,#117410,
#117411,#117412,#117413,#117414,#117415,#117416,#117417,#117418,#117419,
#117420,#117421,#117422,#117423,#117424,#117425,#117426,#117427,#117428,
#117429,#117430,#117431,#117432,#117433,#117434,#117435,#117436,#117437,
#117438,#117439,#117440,#117441),.UNSPECIFIED.,.T.,.F.,(4,2,2,2,2,2,2,2,
2,2,2,2,2,2,2,2,2,2,2,2,2,2,2,2,2,2,4),(0.,0.0507741420462431,0.100094123453666,
0.142359412560989,0.175922593461849,0.186328843425225,0.19249408395989,
0.197866628454765,0.204549652896258,0.217280256032914,0.268351707683292,
0.309145879302129,0.353756216170168,0.401722317023322,0.45251258636343,
0.501967269874822,0.544179399225482,0.578035171108809,0.588420444970115,
0.594538564389574,0.599898813169662,0.60649676894749,0.619034943707488,
0.670068082662381,0.710950255764047,0.755747830094524,0.804181423392594),
 .UNSPECIFIED.);
#2692=B_SPLINE_CURVE_WITH_KNOTS('',3,(#117444,#117445,#117446,#117447,#117448,
#117449,#117450,#117451,#117452,#117453,#117454,#117455,#117456,#117457,
#117458,#117459,#117460,#117461,#117462,#117463,#117464,#117465,#117466,
#117467,#117468,#117469,#117470,#117471,#117472,#117473,#117474,#117475,
#117476,#117477,#117478,#117479),.UNSPECIFIED.,.T.,.F.,(4,2,2,2,2,2,2,2,
2,2,2,2,2,2,2,2,2,4),(0.,0.0250756242963306,0.0759095369482803,0.126546430158223,
0.177318372769854,0.228228295543835,0.279038395635305,0.329682630992297,
0.380447242003444,0.431684110304875,0.482066275987924,0.532392855418118,
0.582579304112608,0.632602831630785,0.68254973102261,0.73256082187328,0.782716074484924,
0.804734027170493),.UNSPECIFIED.);
#2693=B_SPLINE_CURVE_WITH_KNOTS('',3,(#117483,#117484,#117485,#117486,#117487,
#117488,#117489,#117490,#117491,#117492,#117493,#117494,#117495,#117496,
#117497,#117498,#117499,#117500,#117501,#117502),.UNSPECIFIED.,.F.,.F.,
(4,2,2,2,2,2,2,2,2,4),(0.213048682846188,0.226000664813719,0.253024885755239,
0.279991915565222,0.306995259686518,0.334036256070164,0.361049651624042,
0.388018253154667,0.415023294971757,0.426106451248178),.UNSPECIFIED.);
#2694=B_SPLINE_CURVE_WITH_KNOTS('',3,(#117506,#117507,#117508,#117509,#117510,
#117511,#117512,#117513,#117514,#117515,#117516,#117517,#117518,#117519,
#117520,#117521,#117522,#117523,#117524,#117525,#117526,#117527,#117528,
#117529,#117530),.UNSPECIFIED.,.F.,.F.,(4,3,2,2,2,2,2,2,2,2,2,4),(0.426106451248178,
0.426109299341064,0.43936868528645,0.466306397762246,0.492932086443071,
0.519491619644926,0.545986019938596,0.57245772480979,0.598965803631853,
0.625542456621915,0.638837591160798,0.639157982187252),.UNSPECIFIED.);
#2695=B_SPLINE_CURVE_WITH_KNOTS('',3,(#117533,#117534,#117535,#117536,#117537,
#117538,#117539,#117540,#117541,#117542,#117543,#117544,#117545,#117546,
#117547,#117548,#117549,#117550,#117551,#117552,#117553,#117554,#117555,
#117556,#117557,#117558,#117559,#117560,#117561,#117562,#117563,#117564,
#117565,#117566,#117567,#117568,#117569,#117570,#117571,#117572,#117573,
#117574,#117575,#117576,#117577,#117578,#117579,#117580,#117581,#117582,
#117583,#117584,#117585,#117586,#117587,#117588),.UNSPECIFIED.,.T.,.F.,
(4,2,2,2,2,2,2,2,2,2,2,2,2,2,2,2,2,2,2,2,2,2,2,2,2,2,2,4),(0.,0.0438032399281999,
0.0853607593781,0.124677963323405,0.143031430545011,0.150221652844284,0.154521557014495,
0.159050218307573,0.16495937041696,0.17733329248977,0.221130773605562,0.256510956710958,
0.295260135268376,0.337023841203116,0.380996197810603,0.423508283158955,
0.460147416455634,0.487374794940251,0.495858730912228,0.500900770187446,
0.505305273252891,0.510799058391344,0.521314368148725,0.565233583186423,
0.600368519153137,0.638991263532745,0.66668607501751,0.693911448956519),
 .UNSPECIFIED.);
#2696=B_SPLINE_CURVE_WITH_KNOTS('',3,(#117591,#117592,#117593,#117594,#117595,
#117596,#117597,#117598,#117599,#117600,#117601,#117602,#117603,#117604,
#117605,#117606,#117607,#117608,#117609,#117610,#117611,#117612,#117613,
#117614,#117615,#117616,#117617,#117618,#117619,#117620,#117621,#117622,
#117623,#117624,#117625,#117626,#117627,#117628),.UNSPECIFIED.,.T.,.F.,
(4,2,2,2,2,2,2,2,2,2,2,2,2,2,2,2,2,2,4),(0.,0.021720404281955,0.0658046663067377,
0.109640478743245,0.153471770102935,0.196955906477114,0.239974074579092,
0.283788922227855,0.327660640057054,0.349176397554091,0.370772527384884,
0.415295853168791,0.458843328684095,0.502130984362252,0.545156609874512,
0.588077379151349,0.631120466938282,0.674432102515339,0.694392108277034),
 .UNSPECIFIED.);
#2697=B_SPLINE_CURVE_WITH_KNOTS('',3,(#117632,#117633,#117634,#117635,#117636,
#117637,#117638,#117639,#117640,#117641,#117642,#117643,#117644,#117645,
#117646,#117647,#117648,#117649,#117650,#117651,#117652,#117653,#117654,
#117655,#117656),.UNSPECIFIED.,.F.,.F.,(4,2,2,2,2,2,2,2,2,2,3,4),(0.157639235373943,
0.157642233535094,0.167484880448895,0.187547965451918,0.207549295069419,
0.227535872366622,0.24705560360124,0.266571987452983,0.286162045201152,
0.306173181062702,0.315228898222867,0.315250512378167),.UNSPECIFIED.);
#2698=B_SPLINE_CURVE_WITH_KNOTS('',3,(#117660,#117661,#117662,#117663,#117664,
#117665,#117666,#117667,#117668,#117669,#117670,#117671,#117672,#117673,
#117674,#117675,#117676,#117677,#117678,#117679),.UNSPECIFIED.,.F.,.F.,
(4,2,2,2,2,2,2,2,2,4),(0.315250512378167,0.325044189685063,0.345194921525286,
0.365124037617517,0.38476096157514,0.404291501464033,0.423787526395124,
0.443342675224153,0.463014699867811,0.47286813359681),.UNSPECIFIED.);
#2699=B_SPLINE_CURVE_WITH_KNOTS('',3,(#117682,#117683,#117684,#117685,#117686,
#117687,#117688,#117689,#117690,#117691,#117692,#117693,#117694,#117695,
#117696,#117697,#117698,#117699,#117700,#117701,#117702,#117703,#117704,
#117705,#117706,#117707,#117708,#117709,#117710,#117711,#117712,#117713,
#117714,#117715,#117716,#117717,#117718,#117719,#117720,#117721,#117722,
#117723,#117724,#117725,#117726,#117727,#117728,#117729,#117730,#117731,
#117732,#117733,#117734,#117735,#117736,#117737),.UNSPECIFIED.,.T.,.F.,
(4,2,2,2,2,2,2,2,2,2,2,2,2,2,2,2,2,2,2,2,2,2,2,2,2,2,2,4),(0.,0.043359114946712,
0.0827966930249876,0.124519807183276,0.133530885608685,0.139173275794822,
0.143546227845922,0.14832491485639,0.155971051546056,0.180254156404085,
0.211494752418665,0.247084720750642,0.286072070810718,0.328176388927468,
0.371998745260341,0.413838162940434,0.451257260030457,0.473742030125035,
0.481413100726095,0.486171801486404,0.490501981131898,0.496054323204978,
0.5073444923318,0.550744168012344,0.585751764291186,0.624314498227347,0.65718029277283,
0.689956049972293),.UNSPECIFIED.);
#2700=B_SPLINE_CURVE_WITH_KNOTS('',3,(#117740,#117741,#117742,#117743,#117744,
#117745,#117746,#117747,#117748,#117749,#117750,#117751,#117752,#117753,
#117754,#117755,#117756,#117757,#117758,#117759,#117760,#117761,#117762,
#117763,#117764,#117765,#117766,#117767,#117768,#117769,#117770,#117771,
#117772,#117773,#117774,#117775,#117776,#117777),.UNSPECIFIED.,.T.,.F.,
(4,2,2,2,2,2,2,2,2,2,2,2,2,2,2,2,2,2,4),(0.,0.0216485531474219,0.0432173037461375,
0.0870175786107822,0.130618682039334,0.174231294254911,0.216757996492257,
0.259351610024986,0.30293769448103,0.34664050390938,0.368085861126179,0.389609200257064,
0.433928919817407,0.477263108896134,0.520150204902444,0.562682206963715,
0.605164701416418,0.64793524162617,0.690474681070088),.UNSPECIFIED.);
#2701=B_SPLINE_CURVE_WITH_KNOTS('',3,(#117781,#117782,#117783,#117784,#117785,
#117786,#117787,#117788,#117789,#117790,#117791,#117792,#117793,#117794,
#117795,#117796,#117797,#117798,#117799,#117800),.UNSPECIFIED.,.F.,.F.,
(4,2,2,2,2,2,2,2,2,4),(0.155292405987498,0.164791612401374,0.174486676683334,
0.194251067647735,0.213959456186071,0.233396530522292,0.252527635537242,
0.271671379434195,0.290952375222479,0.310581312971656),.UNSPECIFIED.);
#2702=B_SPLINE_CURVE_WITH_KNOTS('',3,(#117804,#117805,#117806,#117807,#117808,
#117809,#117810,#117811,#117812,#117813,#117814,#117815,#117816,#117817,
#117818,#117819,#117820,#117821,#117822,#117823,#117824,#117825,#117826,
#117827,#117828),.UNSPECIFIED.,.F.,.F.,(4,3,2,2,2,2,2,2,2,2,2,4),(0.310581312971656,
0.310585453103689,0.320254584528652,0.329939011021033,0.349806464126837,
0.369431787280329,0.38871220797298,0.407845471371859,0.426966696725866,
0.446218186332258,0.465665653817226,0.465877859091187),.UNSPECIFIED.);
#2703=B_SPLINE_CURVE_WITH_KNOTS('',3,(#117831,#117832,#117833,#117834,#117835,
#117836,#117837,#117838,#117839,#117840,#117841,#117842,#117843,#117844,
#117845,#117846,#117847,#117848,#117849,#117850,#117851,#117852,#117853,
#117854,#117855,#117856,#117857,#117858,#117859,#117860,#117861,#117862,
#117863,#117864,#117865,#117866,#117867,#117868,#117869,#117870,#117871,
#117872,#117873,#117874,#117875,#117876,#117877,#117878,#117879,#117880,
#117881,#117882,#117883,#117884),.UNSPECIFIED.,.T.,.F.,(4,2,2,2,2,2,2,2,
2,2,2,2,2,2,2,2,2,2,2,2,2,2,2,2,2,2,4),(0.,0.0564712967416743,0.115038347531717,
0.171525153227716,0.223338045127873,0.253169957371529,0.264328308664071,
0.271555564478627,0.278342122584976,0.287342292159235,0.306677164918464,
0.365666117627072,0.413730164621536,0.465954645778289,0.521966597945684,
0.580586451721482,0.637296030517189,0.689137603931885,0.718928884525764,
0.730000625988998,0.737143075518541,0.743827557819252,0.752656747560013,
0.771478924689879,0.830418531004859,0.878603082634546,0.931260313331436),
 .UNSPECIFIED.);
#2704=B_SPLINE_CURVE_WITH_KNOTS('',3,(#117888,#117889,#117890,#117891,#117892,
#117893,#117894,#117895,#117896,#117897,#117898,#117899,#117900,#117901,
#117902,#117903,#117904,#117905,#117906,#117907,#117908,#117909,#117910,
#117911,#117912,#117913,#117914,#117915,#117916,#117917,#117918,#117919,
#117920,#117921,#117922,#117923,#117924,#117925,#117926,#117927,#117928,
#117929,#117930,#117931,#117932,#117933,#117934,#117935,#117936,#117937,
#117938,#117939,#117940,#117941,#117942,#117943,#117944,#117945,#117946,
#117947,#117948,#117949,#117950,#117951,#117952,#117953,#117954,#117955,
#117956,#117957,#117958,#117959,#117960,#117961,#117962,#117963,#117964,
#117965,#117966,#117967,#117968,#117969,#117970,#117971,#117972,#117973,
#117974,#117975,#117976,#117977,#117978,#117979,#117980,#117981,#117982,
#117983,#117984,#117985,#117986,#117987,#117988,#117989,#117990,#117991,
#117992,#117993,#117994,#117995,#117996,#117997,#117998,#117999,#118000,
#118001,#118002,#118003,#118004,#118005,#118006,#118007,#118008,#118009,
#118010,#118011),.UNSPECIFIED.,.F.,.F.,(4,3,3,3,3,3,3,3,3,3,3,3,3,3,3,3,
3,3,3,3,3,3,3,3,3,3,3,3,3,3,3,3,3,3,3,3,3,3,3,3,3,4),(0.,0.000132780866822235,
0.000266873743469484,0.000288904340061033,0.000405509517205523,0.000522002177348785,
0.000577808680122067,0.000712482869108472,0.00084747631154527,0.0008667130201831,
0.000975050275463839,0.00108341287396082,0.00115561736024413,0.00130428113167908,
0.00145285915006363,0.00160154905450121,0.00173342604036622,0.00188138755364419,
0.00202924107209608,0.00217717427357142,0.00231123472048831,0.00242030735385376,
0.0025293260926867,0.00260013906054927,0.00273508332987814,0.00286987804292202,
0.00288904340061024,0.00300313603185183,0.0031173273659021,0.0031779477406712,
0.00331220596338911,0.00344530795511321,0.00346685208073216,0.00367373680256345,
0.00389128296162316,0.004044660760854,0.00417924015261657,0.00431424687026292,
0.00433356510091496,0.00444155537662282,0.00454955744617284,0.00462246944097592),
 .UNSPECIFIED.);
#2705=B_SPLINE_CURVE_WITH_KNOTS('',3,(#118012,#118013,#118014,#118015,#118016,
#118017,#118018,#118019,#118020,#118021,#118022,#118023,#118024,#118025,
#118026,#118027,#118028,#118029,#118030,#118031),.UNSPECIFIED.,.F.,.F.,
(4,2,2,2,2,2,2,2,2,4),(1.00000017144998E-6,0.0589091086023463,0.116821182098481,
0.174782248585886,0.232882215848222,0.290811365541089,0.348733625156973,
0.406721474339845,0.436820554289351,0.465866613116424),.UNSPECIFIED.);
#2706=B_SPLINE_CURVE_WITH_KNOTS('',3,(#118035,#118036,#118037,#118038,#118039,
#118040,#118041,#118042,#118043,#118044,#118045,#118046,#118047,#118048,
#118049,#118050,#118051,#118052,#118053,#118054,#118055,#118056),
 .UNSPECIFIED.,.F.,.F.,(4,2,2,2,2,2,2,2,2,2,4),(0.139811245314732,0.155709821294679,
0.1906606447556,0.225651069631098,0.260726976222177,0.295779710904132,0.330740401449915,
0.365720622817098,0.38286162399923,0.4002666603197,0.416590733425148),
 .UNSPECIFIED.);
#2707=B_SPLINE_CURVE_WITH_KNOTS('',3,(#118060,#118061,#118062,#118063,#118064,
#118065,#118066,#118067,#118068,#118069,#118070,#118071,#118072,#118073,
#118074,#118075,#118076,#118077,#118078,#118079,#118080,#118081,#118082),
 .UNSPECIFIED.,.F.,.F.,(4,2,2,2,2,3,2,2,2,2,4),(0.416590733425148,0.434833062902334,
0.469409572199181,0.503972722175614,0.538489176242052,0.553563397262184,
0.588014339663571,0.62246556895172,0.656945200368898,0.674174237448786,
0.693374642576916),.UNSPECIFIED.);
#2708=B_SPLINE_CURVE_WITH_KNOTS('',3,(#118085,#118086,#118087,#118088,#118089,
#118090,#118091,#118092,#118093,#118094,#118095,#118096,#118097,#118098,
#118099,#118100,#118101,#118102,#118103,#118104,#118105,#118106,#118107,
#118108,#118109,#118110,#118111,#118112,#118113,#118114,#118115,#118116,
#118117,#118118,#118119,#118120,#118121,#118122,#118123,#118124,#118125,
#118126,#118127,#118128,#118129,#118130,#118131,#118132,#118133,#118134,
#118135,#118136,#118137,#118138,#118139,#118140),.UNSPECIFIED.,.T.,.F.,
(4,2,2,2,2,2,2,2,2,2,2,2,2,2,2,2,2,2,2,2,2,2,2,2,2,2,2,4),(0.,0.0499191511799086,
0.100323798483693,0.147430853941386,0.19733219387334,0.209533422841237,
0.21681600564989,0.222358234196958,0.228220671789085,0.23719913857369,0.262853256702964,
0.299031751002697,0.340252278981359,0.385205828086949,0.433510601774857,
0.484252817009215,0.533401629552871,0.576802914325161,0.606031391015876,
0.615813482963946,0.621815274859459,0.627228741894021,0.63409986671774,
0.647815955990171,0.69869320668563,0.739781768645123,0.773567944088127,
0.804062709433453),.UNSPECIFIED.);
#2709=B_SPLINE_CURVE_WITH_KNOTS('',3,(#118143,#118144,#118145,#118146,#118147,
#118148,#118149,#118150,#118151,#118152,#118153,#118154,#118155,#118156,
#118157,#118158,#118159,#118160,#118161,#118162,#118163,#118164,#118165,
#118166,#118167,#118168,#118169,#118170,#118171,#118172,#118173,#118174,
#118175,#118176,#118177,#118178),.UNSPECIFIED.,.T.,.F.,(4,2,2,2,2,2,2,2,
2,2,2,2,2,2,2,2,2,4),(0.,0.0508102428370469,0.101446446049902,0.15223400388986,
0.203157794195011,0.253970631498262,0.304612808351331,0.355379759922047,
0.406622741889554,0.45700292782468,0.507323471911212,0.557501934458369,
0.607520193736365,0.657468271381405,0.707486102342854,0.75764833283291,
0.781103021944058,0.80473316872163),.UNSPECIFIED.);
#2710=B_SPLINE_CURVE_WITH_KNOTS('',3,(#118182,#118183,#118184,#118185,#118186,
#118187,#118188,#118189,#118190,#118191,#118192,#118193,#118194,#118195,
#118196,#118197,#118198,#118199,#118200,#118201,#118202),.UNSPECIFIED.,
 .F.,.F.,(4,2,2,2,2,2,2,2,3,4),(0.213076350460928,0.239748662991589,0.266715218453498,
0.293725024577096,0.32077322414254,0.347789969932072,0.37475820239879,0.401761549963476,
0.426157396856437,0.426182397841807),.UNSPECIFIED.);
#2711=B_SPLINE_CURVE_WITH_KNOTS('',3,(#118206,#118207,#118208,#118209,#118210,
#118211,#118212,#118213,#118214,#118215,#118216,#118217,#118218,#118219,
#118220,#118221,#118222,#118223,#118224,#118225,#118226,#118227),
 .UNSPECIFIED.,.F.,.F.,(4,2,2,2,2,2,2,2,2,2,4),(0.426182397841807,0.453093828382958,
0.479716429177484,0.506272416039609,0.532764847505401,0.559237494928504,
0.585748871646683,0.612328914248202,0.625624663661876,0.638890854983996,
0.639233747317365),.UNSPECIFIED.);
#2712=B_SPLINE_CURVE_WITH_KNOTS('',3,(#118230,#118231,#118232,#118233,#118234,
#118235,#118236,#118237,#118238,#118239,#118240,#118241,#118242,#118243,
#118244,#118245,#118246,#118247,#118248,#118249,#118250,#118251,#118252,
#118253,#118254,#118255,#118256,#118257,#118258,#118259,#118260,#118261,
#118262,#118263,#118264,#118265,#118266,#118267,#118268,#118269,#118270,
#118271,#118272,#118273,#118274,#118275,#118276,#118277,#118278,#118279,
#118280,#118281,#118282,#118283,#118284,#118285),.UNSPECIFIED.,.T.,.F.,
(4,2,2,2,2,2,2,2,2,2,2,2,2,2,2,2,2,2,2,2,2,2,2,2,2,2,2,4),(0.,0.0442480422944534,
0.0874111550741445,0.124982769447723,0.161567305412722,0.17022981975583,
0.175839348378204,0.18030752670857,0.185315270085969,0.193607980645255,
0.222268058354423,0.254709421019499,0.291191815675512,0.330870616067579,
0.373576985297977,0.417325574307142,0.458614686770495,0.499167985772272,
0.514540802408916,0.521132469232114,0.525273371147843,0.529792346622681,
0.535963995927171,0.549975098997772,0.593804620572848,0.629550277964284,
0.663265595848305,0.693902648410645),.UNSPECIFIED.);
#2713=B_SPLINE_CURVE_WITH_KNOTS('',3,(#118288,#118289,#118290,#118291,#118292,
#118293,#118294,#118295,#118296,#118297,#118298,#118299,#118300,#118301,
#118302,#118303,#118304,#118305,#118306,#118307,#118308,#118309,#118310,
#118311,#118312,#118313,#118314,#118315,#118316,#118317,#118318,#118319,
#118320,#118321,#118322,#118323,#118324,#118325),.UNSPECIFIED.,.T.,.F.,
(4,2,2,2,2,2,2,2,2,2,2,2,2,2,2,2,2,2,4),(0.,0.0439639503368589,0.0877604826916409,
0.131653516194325,0.174628164548689,0.217655865061386,0.261503244306837,
0.305316782533662,0.326788961668223,0.348329007627559,0.39274923929494,
0.436273490381119,0.479536625012623,0.522550458846832,0.565478794845261,
0.608544620564116,0.651881382844738,0.673041580934267,0.69438925335854),
 .UNSPECIFIED.);
#2714=B_SPLINE_CURVE_WITH_KNOTS('',3,(#118329,#118330,#118331,#118332,#118333,
#118334,#118335,#118336,#118337,#118338,#118339,#118340,#118341,#118342,
#118343,#118344,#118345,#118346,#118347,#118348),.UNSPECIFIED.,.F.,.F.,
(4,2,2,2,2,2,2,2,2,4),(0.157613569881594,0.177590621004305,0.197575064366368,
0.21738044374067,0.236894863818513,0.256415359500327,0.276016696532489,
0.296001655089685,0.305565247158479,0.315223462967867),.UNSPECIFIED.);
#2715=B_SPLINE_CURVE_WITH_KNOTS('',3,(#118352,#118353,#118354,#118355,#118356,
#118357,#118358,#118359,#118360,#118361,#118362,#118363,#118364,#118365,
#118366,#118367,#118368,#118369,#118370,#118371,#118372,#118373,#118374,
#118375,#118376),.UNSPECIFIED.,.F.,.F.,(4,3,2,2,2,2,2,2,2,2,2,4),(0.315223462967867,
0.315228090781128,0.335331383930744,0.355256493204118,0.374879646147263,
0.394403179322639,0.413902980207927,0.433470625988996,0.453156745636569,
0.462992521725115,0.472807666153366,0.472841660662722),.UNSPECIFIED.);
#2716=B_SPLINE_CURVE_WITH_KNOTS('',3,(#118379,#118380,#118381,#118382,#118383,
#118384,#118385,#118386,#118387,#118388,#118389,#118390,#118391,#118392,
#118393,#118394,#118395,#118396,#118397,#118398,#118399,#118400,#118401,
#118402,#118403,#118404,#118405,#118406,#118407,#118408,#118409,#118410,
#118411,#118412,#118413,#118414,#118415,#118416,#118417,#118418,#118419,
#118420,#118421,#118422,#118423,#118424,#118425,#118426,#118427,#118428,
#118429,#118430,#118431,#118432,#118433,#118434),.UNSPECIFIED.,.T.,.F.,
(4,2,2,2,2,2,2,2,2,2,2,2,2,2,2,2,2,2,2,2,2,2,2,2,2,2,2,4),(0.,0.0439238371863919,
0.0861902321541546,0.122000766940326,0.150399248999695,0.158716774702034,
0.16364349810409,0.167903904328712,0.173082066416487,0.182746594055837,
0.22600984128997,0.260588517680107,0.298734181935875,0.340021026144596,
0.384008664161648,0.426668835524534,0.460906519679387,0.494393680768921,
0.502475247123739,0.507752815267995,0.511987106073311,0.516766095538759,
0.524760138175885,0.553180307333632,0.585302647338573,0.621597531052235,
0.656973501569907,0.689916370643902),.UNSPECIFIED.);
#2717=B_SPLINE_CURVE_WITH_KNOTS('',3,(#118437,#118438,#118439,#118440,#118441,
#118442,#118443,#118444,#118445,#118446,#118447,#118448,#118449,#118450,
#118451,#118452,#118453,#118454,#118455,#118456,#118457,#118458,#118459,
#118460,#118461,#118462,#118463,#118464,#118465,#118466,#118467,#118468,
#118469,#118470,#118471,#118472,#118473,#118474),.UNSPECIFIED.,.T.,.F.,
(4,2,2,2,2,2,2,2,2,2,2,2,2,2,2,2,2,2,4),(0.,0.0215971103688694,0.0654425307483053,
0.109049877051987,0.152622345814217,0.195150110292293,0.237745904043596,
0.28132562175596,0.325081612743124,0.346562119435945,0.368126525189833,
0.412507376679562,0.455838675269931,0.498719845806797,0.54124703606024,
0.583729631416507,0.626505135491807,0.669729282213455,0.690488132151514),
 .UNSPECIFIED.);
#2718=B_SPLINE_CURVE_WITH_KNOTS('',3,(#118478,#118479,#118480,#118481,#118482,
#118483,#118484,#118485,#118486,#118487,#118488,#118489,#118490,#118491,
#118492,#118493,#118494,#118495,#118496,#118497,#118498,#118499,#118500),
 .UNSPECIFIED.,.F.,.F.,(4,2,2,2,2,2,2,2,2,3,4),(0.155318197570125,0.164879844339497,
0.184666529440326,0.204377543531482,0.223808485417644,0.242939179394705,
0.262083926601905,0.281366837067981,0.301126438334268,0.310590172209869,
0.310609150032715),.UNSPECIFIED.);
#2719=B_SPLINE_CURVE_WITH_KNOTS('',3,(#118504,#118505,#118506,#118507,#118508,
#118509,#118510,#118511,#118512,#118513,#118514,#118515,#118516,#118517,
#118518,#118519,#118520,#118521,#118522,#118523,#118524,#118525),
 .UNSPECIFIED.,.F.,.F.,(4,2,2,2,2,2,2,2,2,2,4),(0.310609150032715,0.320291308615886,
0.340184624148909,0.359802870962863,0.379081454733931,0.398213338810906,
0.417334739031231,0.436587884463708,0.456037397362742,0.46576085708419,
0.465908369779994),.UNSPECIFIED.);
#2720=B_SPLINE_CURVE_WITH_KNOTS('',3,(#118528,#118529,#118530,#118531,#118532,
#118533,#118534,#118535,#118536,#118537,#118538,#118539,#118540,#118541,
#118542,#118543,#118544,#118545,#118546,#118547,#118548,#118549,#118550,
#118551,#118552,#118553,#118554,#118555,#118556,#118557,#118558,#118559,
#118560,#118561,#118562,#118563,#118564,#118565,#118566,#118567,#118568,
#118569,#118570,#118571,#118572,#118573,#118574,#118575,#118576,#118577,
#118578,#118579,#118580,#118581),.UNSPECIFIED.,.T.,.F.,(4,2,2,2,2,2,2,2,
2,2,2,2,2,2,2,2,2,2,2,2,2,2,2,2,2,2,4),(0.,0.0541686820922835,0.112415580690374,
0.170510262941422,0.223981665771125,0.277387759445974,0.290674307093365,
0.299367584212841,0.306340517334599,0.31419709898001,0.327276125557507,
0.372458093488531,0.417746341578146,0.467801168688974,0.521727313250452,
0.579585888464177,0.637746424232553,0.691244422142438,0.743421281273534,
0.756491088086435,0.765054568557719,0.771929131539263,0.77967896178005,
0.792584427627161,0.837109936091434,0.882412481374293,0.931190701269262),
 .UNSPECIFIED.);
#2721=B_SPLINE_CURVE_WITH_KNOTS('',3,(#118585,#118586,#118587,#118588,#118589,
#118590,#118591,#118592,#118593,#118594,#118595,#118596,#118597,#118598,
#118599,#118600,#118601,#118602,#118603,#118604,#118605,#118606,#118607,
#118608,#118609,#118610,#118611,#118612,#118613,#118614,#118615,#118616,
#118617,#118618,#118619,#118620,#118621,#118622,#118623,#118624,#118625,
#118626,#118627,#118628,#118629,#118630,#118631,#118632,#118633,#118634,
#118635,#118636,#118637,#118638,#118639,#118640,#118641,#118642,#118643,
#118644,#118645,#118646,#118647,#118648,#118649,#118650,#118651,#118652,
#118653,#118654,#118655,#118656,#118657,#118658,#118659,#118660,#118661,
#118662,#118663,#118664,#118665,#118666,#118667,#118668,#118669,#118670,
#118671,#118672,#118673,#118674,#118675,#118676,#118677,#118678,#118679,
#118680,#118681,#118682,#118683,#118684,#118685,#118686,#118687,#118688,
#118689,#118690,#118691,#118692,#118693,#118694,#118695,#118696,#118697,
#118698,#118699,#118700,#118701,#118702,#118703,#118704,#118705,#118706,
#118707,#118708),.UNSPECIFIED.,.F.,.F.,(4,3,3,3,3,3,3,3,3,3,3,3,3,3,3,3,
3,3,3,3,3,3,3,3,3,3,3,3,3,3,3,3,3,3,3,3,3,3,3,3,3,4),(0.,0.00013277251793653,
0.000266857202581178,0.000288907094292459,0.000405479252460701,0.000521939192059059,
0.000577814188584917,0.000712479190419921,0.000847463317123744,0.000866721282877376,
0.00097506874242616,0.00108344212283471,0.00115562837716983,0.00130427764647303,
0.00145284128808089,0.00160151709564146,0.00173344256575487,0.00188142671647943,
0.00202930303207845,0.00217725917594754,0.0023112567543399,0.00242030890240509,
0.00252930785338822,0.00260016384863234,0.0027351175251363,0.00286991989522071,
0.00288907094292478,0.00300323587270697,0.00311750014522043,0.00317797803721722,
0.00331224152428824,0.00344534695923621,0.00346688513150965,0.00367342646213443,
0.00389049440139844,0.00404469932009453,0.00417928189170992,0.00431428786646436,
0.00433360641438694,0.00444159423475505,0.00454959321591867,0.00462251350867935),
 .UNSPECIFIED.);
#2722=B_SPLINE_CURVE_WITH_KNOTS('',3,(#118709,#118710,#118711,#118712,#118713,
#118714,#118715,#118716,#118717,#118718,#118719,#118720,#118721,#118722,
#118723,#118724,#118725,#118726,#118727,#118728),.UNSPECIFIED.,.F.,.F.,
(4,2,2,2,2,2,2,2,2,4),(1.0000001659162E-6,0.0587516845672802,0.116678515181389,
0.174707853111328,0.232881544735254,0.29079726537627,0.3487559236141,0.377742355197926,
0.423463627058049,0.465815224763171),.UNSPECIFIED.);
#2723=B_SPLINE_CURVE_WITH_KNOTS('',3,(#118732,#118733,#118734,#118735,#118736,
#118737,#118738,#118739,#118740,#118741,#118742,#118743,#118744,#118745,
#118746,#118747,#118748,#118749,#118750,#118751),.UNSPECIFIED.,.F.,.F.,
(4,2,2,2,2,2,2,2,2,4),(0.139779656786197,0.173396151004641,0.208397696003322,
0.243489615098716,0.27855188804276,0.313513313892874,0.348489752671695,
0.365628705522415,0.383033972564603,0.416570719226277),.UNSPECIFIED.);
#2724=B_SPLINE_CURVE_WITH_KNOTS('',3,(#118755,#118756,#118757,#118758,#118759,
#118760,#118761,#118762,#118763,#118764,#118765,#118766,#118767,#118768,
#118769,#118770,#118771,#118772,#118773,#118774,#118775,#118776,#118777,
#118778,#118779),.UNSPECIFIED.,.F.,.F.,(4,2,2,2,2,3,2,2,2,2,2,4),(0.416570719226277,
0.417599765181018,0.45217391626731,0.486733498952397,0.521247003328364,
0.553550457873372,0.587998762871438,0.622466686453937,0.639693726684147,
0.656923100441351,0.692000901398468,0.69333011465957),.UNSPECIFIED.);
#2725=B_SPLINE_CURVE_WITH_KNOTS('',3,(#118782,#118783,#118784,#118785,#118786,
#118787,#118788,#118789,#118790,#118791,#118792,#118793,#118794,#118795,
#118796,#118797,#118798,#118799,#118800,#118801,#118802,#118803,#118804,
#118805,#118806,#118807,#118808,#118809,#118810,#118811,#118812,#118813,
#118814,#118815,#118816,#118817,#118818,#118819,#118820,#118821,#118822,
#118823,#118824,#118825,#118826,#118827,#118828,#118829,#118830,#118831,
#118832,#118833,#118834,#118835),.UNSPECIFIED.,.T.,.F.,(4,2,2,2,2,2,2,2,
2,2,2,2,2,2,2,2,2,2,2,2,2,2,2,2,2,2,4),(0.,0.0478739945692769,0.0986971471010809,
0.148337519565137,0.189656688812435,0.228043708382913,0.239165467815064,
0.245690284550349,0.251233949360227,0.25795220129384,0.270230302745385,
0.321321411721412,0.362050378315662,0.406602849867675,0.454509035792872,
0.505306311247286,0.554814869634011,0.597172283297015,0.631280129484872,
0.641914542897276,0.648218164531197,0.653710112834502,0.660536832617733,
0.673512930764169,0.724577243318909,0.765567731891649,0.804148773373606),
 .UNSPECIFIED.);
#2726=B_SPLINE_CURVE_WITH_KNOTS('',3,(#118838,#118839,#118840,#118841,#118842,
#118843,#118844,#118845,#118846,#118847,#118848,#118849,#118850,#118851,
#118852,#118853,#118854,#118855,#118856,#118857,#118858,#118859,#118860,
#118861,#118862,#118863,#118864,#118865,#118866,#118867,#118868,#118869,
#118870,#118871),.UNSPECIFIED.,.T.,.F.,(4,2,2,2,2,2,2,2,2,2,2,2,2,2,2,2,
4),(0.,0.0507036982380927,0.101367967769165,0.15217435009708,0.202988254858527,
0.253660615022253,0.304349675621658,0.355417624755026,0.406309245550189,
0.456681959570615,0.506950514497502,0.557047627860013,0.607008171588907,
0.65696367342519,0.707040719162867,0.757254767928788,0.80482271556345),
 .UNSPECIFIED.);
#2727=B_SPLINE_CURVE_WITH_KNOTS('',3,(#118875,#118876,#118877,#118878,#118879,
#118880,#118881,#118882,#118883,#118884,#118885,#118886,#118887,#118888,
#118889,#118890,#118891,#118892,#118893,#118894,#118895,#118896,#118897),
 .UNSPECIFIED.,.F.,.F.,(4,2,2,2,2,2,2,2,2,3,4),(0.213107054482159,0.226203862898588,
0.253173118245501,0.28015352143344,0.307156285370326,0.334139138956564,
0.361106824850293,0.38814457612529,0.415330879616146,0.42617130555841,0.426197129198138),
 .UNSPECIFIED.);
#2728=B_SPLINE_CURVE_WITH_KNOTS('',3,(#118901,#118902,#118903,#118904,#118905,
#118906,#118907,#118908,#118909,#118910,#118911,#118912,#118913,#118914,
#118915,#118916,#118917,#118918,#118919,#118920),.UNSPECIFIED.,.F.,.F.,
(4,2,2,2,2,2,2,2,2,4),(0.426197129198138,0.452822943590338,0.479420811937044,
0.505945019640447,0.532418265293895,0.558897919334064,0.58543642024838,
0.612041061741514,0.625328210873673,0.639278360040569),.UNSPECIFIED.);
#2729=B_SPLINE_CURVE_WITH_KNOTS('',3,(#118923,#118924,#118925,#118926,#118927,
#118928,#118929,#118930,#118931,#118932,#118933,#118934,#118935,#118936,
#118937,#118938,#118939,#118940,#118941,#118942,#118943,#118944,#118945,
#118946,#118947,#118948,#118949,#118950,#118951,#118952,#118953,#118954,
#118955,#118956,#118957,#118958,#118959,#118960,#118961,#118962,#118963,
#118964,#118965,#118966,#118967,#118968,#118969,#118970,#118971,#118972,
#118973,#118974,#118975,#118976,#118977,#118978),.UNSPECIFIED.,.T.,.F.,
(4,2,2,2,2,2,2,2,2,2,2,2,2,2,2,2,2,2,2,2,2,2,2,2,2,2,2,4),(0.,0.0423917071008588,
0.0862690124816813,0.128223494874909,0.166386336836243,0.188172470137429,
0.195965603192946,0.200910173484711,0.205484821318604,0.211457224587722,
0.223972369869265,0.267764198510775,0.303174271614316,0.341946448532938,
0.383731798431802,0.42769896692924,0.470189492903271,0.506972629115825,
0.533779293250024,0.542258367054284,0.547330630539367,0.55137511128395,
0.556768979326987,0.566677076478627,0.610454812685682,0.645453523164812,
0.670975464062507,0.69390114019026),.UNSPECIFIED.);
#2730=B_SPLINE_CURVE_WITH_KNOTS('',3,(#118981,#118982,#118983,#118984,#118985,
#118986,#118987,#118988,#118989,#118990,#118991,#118992,#118993,#118994,
#118995,#118996,#118997,#118998,#118999,#119000,#119001,#119002,#119003,
#119004,#119005,#119006,#119007,#119008,#119009,#119010,#119011,#119012,
#119013,#119014,#119015,#119016,#119017,#119018),.UNSPECIFIED.,.T.,.F.,
(4,2,2,2,2,2,2,2,2,2,2,2,2,2,2,2,2,2,4),(0.,0.0439285969839785,0.0877338055835913,
0.131600288228661,0.174581723094377,0.218417405783077,0.262237812383161,
0.306273059701853,0.327893564393435,0.371979478856129,0.415515580695926,
0.458786565242884,0.501799585059231,0.544720010296071,0.587775168317762,
0.631102572848802,0.652852121001093,0.673538591001646,0.694388197397481),
 .UNSPECIFIED.);
#2731=B_SPLINE_CURVE_WITH_KNOTS('',3,(#119022,#119023,#119024,#119025,#119026,
#119027,#119028,#119029,#119030,#119031,#119032,#119033,#119034,#119035,
#119036,#119037,#119038,#119039,#119040,#119041,#119042,#119043,#119044,
#119045,#119046),.UNSPECIFIED.,.F.,.F.,(4,2,2,2,2,2,2,2,2,2,3,4),(0.157664314186863,
0.167520999539812,0.187522964929857,0.207504733138004,0.227022893262324,
0.246540738053684,0.266134356212337,0.286153085842429,0.295957890558149,
0.30554520497725,0.315225351986019,0.315251153228398),.UNSPECIFIED.);
#2732=B_SPLINE_CURVE_WITH_KNOTS('',3,(#119050,#119051,#119052,#119053,#119054,
#119055,#119056,#119057,#119058,#119059,#119060,#119061,#119062,#119063,
#119064,#119065,#119066,#119067,#119068,#119069),.UNSPECIFIED.,.F.,.F.,
(4,2,2,2,2,2,2,2,2,4),(0.315251153228398,0.335201080329252,0.354894727899546,
0.374468684471932,0.393968635000947,0.413485447868118,0.433100328931788,
0.452833383067246,0.462678741523263,0.472889666172882),.UNSPECIFIED.);
#2733=B_SPLINE_CURVE_WITH_KNOTS('',3,(#119072,#119073,#119074,#119075,#119076,
#119077,#119078,#119079,#119080,#119081,#119082,#119083,#119084,#119085,
#119086,#119087,#119088,#119089,#119090,#119091,#119092,#119093,#119094,
#119095,#119096,#119097,#119098,#119099,#119100,#119101,#119102,#119103,
#119104,#119105,#119106,#119107,#119108,#119109,#119110,#119111,#119112,
#119113,#119114,#119115,#119116,#119117,#119118,#119119,#119120,#119121,
#119122,#119123,#119124,#119125,#119126,#119127),.UNSPECIFIED.,.T.,.F.,
(4,2,2,2,2,2,2,2,2,2,2,2,2,2,2,2,2,2,2,2,2,2,2,2,2,2,2,4),(0.,0.0433357033279547,
0.0867918942096803,0.12674974376004,0.169317740075874,0.179091766390012,
0.184344749294548,0.188727191507819,0.193208494521891,0.199695700510524,
0.216202111608105,0.259547133084174,0.295329969828243,0.334483203156315,
0.376753899026277,0.420528758464677,0.462143525407209,0.500104687054551,
0.520667413014844,0.527991625556146,0.532631100199553,0.536919456730402,
0.542513918627149,0.554231014573357,0.597650721490353,0.632731625953485,
0.662884793490238,0.690031112817339),.UNSPECIFIED.);
#2734=B_SPLINE_CURVE_WITH_KNOTS('',3,(#119130,#119131,#119132,#119133,#119134,
#119135,#119136,#119137,#119138,#119139,#119140,#119141,#119142,#119143,
#119144,#119145,#119146,#119147,#119148,#119149,#119150,#119151,#119152,
#119153,#119154,#119155,#119156,#119157,#119158,#119159,#119160,#119161,
#119162,#119163,#119164,#119165,#119166,#119167),.UNSPECIFIED.,.T.,.F.,
(4,2,2,2,2,2,2,2,2,2,2,2,2,2,2,2,2,2,4),(0.,0.0437846598539115,0.0873818383118426,
0.130569174600926,0.173091910935896,0.215698254859366,0.25928498636956,
0.303005395562776,0.324461683296978,0.345997226871332,0.390332486539213,
0.433644313592107,0.476506969627738,0.519027119267212,0.561518089693932,
0.604312670966229,0.647555474893121,0.668924190877181,0.690483896486725),
 .UNSPECIFIED.);
#2735=B_SPLINE_CURVE_WITH_KNOTS('',3,(#119171,#119172,#119173,#119174,#119175,
#119176,#119177,#119178,#119179,#119180,#119181,#119182,#119183,#119184,
#119185,#119186,#119187,#119188,#119189,#119190,#119191,#119192,#119193),
 .UNSPECIFIED.,.F.,.F.,(4,2,2,2,2,2,2,2,2,3,4),(0.155323839065176,0.174895282975292,
0.194601807476139,0.214028772431744,0.233156373086578,0.252306343141429,
0.271599920800694,0.291343602566944,0.300917682052659,0.310590124203141,
0.310614889159676),.UNSPECIFIED.);
#2736=B_SPLINE_CURVE_WITH_KNOTS('',3,(#119197,#119198,#119199,#119200,#119201,
#119202,#119203,#119204,#119205,#119206,#119207,#119208,#119209,#119210,
#119211,#119212,#119213,#119214,#119215,#119216,#119217,#119218),
 .UNSPECIFIED.,.F.,.F.,(4,2,2,2,2,2,2,2,2,2,4),(0.310614889159676,0.330461615882692,
0.350073356350718,0.369341148381857,0.38846889618466,0.407595133318853,
0.426859384772424,0.446319865203601,0.45603054018867,0.465724013336885,
0.465913963268316),.UNSPECIFIED.);
#2737=B_SPLINE_CURVE_WITH_KNOTS('',3,(#119222,#119223,#119224,#119225,#119226,
#119227,#119228,#119229,#119230,#119231,#119232,#119233,#119234,#119235,
#119236,#119237,#119238,#119239,#119240,#119241,#119242,#119243,#119244,
#119245,#119246,#119247,#119248,#119249,#119250,#119251),.UNSPECIFIED.,
 .F.,.F.,(4,2,2,2,2,2,2,2,2,2,2,2,2,2,4),(1.00000010940975E-6,0.0384609387804645,
0.0726049480932644,0.12998621409426,0.183385238805886,0.232646795046144,
0.285302749131523,0.314403553947751,0.326074174045375,0.333858467758951,
0.341326316436165,0.351457949388285,0.37402026617642,0.433053304401173,
0.465421514323042),.UNSPECIFIED.);
#2738=B_SPLINE_CURVE_WITH_KNOTS('',3,(#119255,#119256,#119257,#119258,#119259,
#119260,#119261,#119262,#119263,#119264,#119265,#119266,#119267,#119268,
#119269,#119270,#119271,#119272,#119273,#119274,#119275,#119276,#119277,
#119278,#119279,#119280,#119281,#119282,#119283,#119284,#119285,#119286,
#119287,#119288,#119289,#119290,#119291,#119292,#119293,#119294,#119295,
#119296,#119297,#119298,#119299,#119300,#119301,#119302,#119303,#119304,
#119305,#119306,#119307,#119308,#119309,#119310,#119311,#119312,#119313,
#119314,#119315,#119316,#119317,#119318,#119319,#119320,#119321,#119322,
#119323,#119324,#119325,#119326,#119327,#119328,#119329,#119330,#119331,
#119332,#119333,#119334,#119335,#119336,#119337,#119338,#119339,#119340,
#119341,#119342,#119343,#119344,#119345,#119346,#119347,#119348,#119349,
#119350,#119351,#119352,#119353,#119354,#119355,#119356,#119357,#119358,
#119359,#119360,#119361,#119362,#119363,#119364,#119365,#119366,#119367,
#119368,#119369,#119370,#119371,#119372,#119373,#119374,#119375,#119376,
#119377,#119378),.UNSPECIFIED.,.F.,.F.,(4,3,3,3,3,3,3,3,3,3,3,3,3,3,3,3,
3,3,3,3,3,3,3,3,3,3,3,3,3,3,3,3,3,3,3,3,3,3,3,3,3,4),(0.,0.00013276129913434,
0.000266835524831858,0.000288910361442746,0.00040545879614334,0.000521895356260907,
0.000577820722885491,0.00071247778923503,0.000847454257176977,0.000866731084328237,
0.000975087715605292,0.00108347076913653,0.00115564144577098,0.00130428008995543,
0.00145283323966009,0.00160149883572666,0.00173346216865647,0.00188146410637275,
0.00202935838489384,0.00217733269970768,0.00231128289154197,0.00242032515157694,
0.00252931477079484,0.00260019325298471,0.00273515651973894,0.00286996752096618,
0.00288910361442745,0.0030033190459749,0.00311763416070541,0.00317801397587019,
0.00331228109060909,0.00344538869240954,0.00346692433731293,0.00367323273482719,
0.00388991397652125,0.00404474506019841,0.00417932605144588,0.00431432738910213,
0.00433365542164112,0.00444162789512621,0.0045496106988975,0.00462256578308383),
 .UNSPECIFIED.);
#2739=B_SPLINE_CURVE_WITH_KNOTS('',3,(#119379,#119380,#119381,#119382,#119383,
#119384,#119385,#119386,#119387,#119388,#119389,#119390,#119391,#119392,
#119393,#119394,#119395,#119396,#119397,#119398),.UNSPECIFIED.,.F.,.F.,
(4,2,2,2,2,2,2,2,2,4),(1.00000016868767E-6,0.0585541366944336,0.116515904932218,
0.174631749418359,0.232879705095392,0.290789101013029,0.348769985500845,
0.377759774398062,0.42345230050058,0.465809052198513),.UNSPECIFIED.);
#2740=B_SPLINE_CURVE_WITH_KNOTS('',3,(#119399,#119400,#119401,#119402,#119403,
#119404,#119405,#119406,#119407,#119408,#119409,#119410,#119411,#119412,
#119413,#119414,#119415,#119416,#119417,#119418,#119419,#119420,#119421,
#119422,#119423,#119424,#119425,#119426,#119427,#119428,#119429,#119430,
#119431,#119432,#119433,#119434,#119435,#119436,#119437,#119438,#119439,
#119440,#119441,#119442,#119443,#119444,#119445,#119446,#119447,#119448,
#119449,#119450,#119451,#119452,#119453,#119454,#119455,#119456,#119457,
#119458,#119459,#119460,#119461,#119462,#119463,#119464,#119465,#119466,
#119467,#119468,#119469,#119470,#119471,#119472,#119473,#119474,#119475,
#119476,#119477,#119478,#119479,#119480,#119481,#119482,#119483,#119484,
#119485,#119486,#119487,#119488,#119489,#119490,#119491,#119492,#119493,
#119494,#119495,#119496,#119497,#119498,#119499,#119500,#119501,#119502,
#119503,#119504,#119505,#119506,#119507,#119508,#119509,#119510,#119511,
#119512,#119513,#119514,#119515,#119516,#119517,#119518,#119519,#119520,
#119521,#119522),.UNSPECIFIED.,.F.,.F.,(4,3,3,3,3,3,3,3,3,3,3,3,3,3,3,3,
3,3,3,3,3,3,3,3,3,3,3,3,3,3,3,3,3,3,3,3,3,3,3,3,3,4),(0.,0.000132745935003127,
0.000266814935045813,0.000288919615584892,0.000405543240980673,0.00052205660558132,
0.000577839231169785,0.000712522167078833,0.000847534928045407,0.000866758846754677,
0.00097514847331441,0.00108356503212164,0.00115567846233957,0.00130446679715503,
0.00145316983239142,0.00160198502321772,0.00173351769350932,0.00188149019865714,
0.00202935391483387,0.0021772961594043,0.00231135692467908,0.00242052512897724,
0.00252963569872571,0.00260027654026395,0.00273521641874506,0.00287000951803308,
0.00288919615584882,0.00300295417106767,0.00311680707883515,0.00317811577143369,
0.00331235835362441,0.00344545082104483,0.00346703538701856,0.003675605881335,
0.0038952874317491,0.0040448746181883,0.00417940787509396,0.00431437880260212,
0.00433379423377317,0.0044417693386194,0.00454975693031286,0.00462271384935804),
 .UNSPECIFIED.);
#2741=B_SPLINE_CURVE_WITH_KNOTS('',3,(#119526,#119527,#119528,#119529,#119530,
#119531,#119532,#119533,#119534,#119535,#119536,#119537,#119538,#119539,
#119540,#119541,#119542,#119543,#119544,#119545,#119546,#119547),
 .UNSPECIFIED.,.F.,.F.,(4,2,2,2,2,2,2,2,2,2,4),(0.139827597716775,0.156235126594654,
0.191204336808387,0.226231673968276,0.261235307761556,0.296182933144171,
0.33120275340376,0.34837260812873,0.365776511367808,0.400348110030799,0.41660864742562),
 .UNSPECIFIED.);
#2742=B_SPLINE_CURVE_WITH_KNOTS('',3,(#119551,#119552,#119553,#119554,#119555,
#119556,#119557,#119558,#119559,#119560,#119561,#119562,#119563,#119564,
#119565,#119566,#119567,#119568,#119569,#119570,#119571,#119572,#119573),
 .UNSPECIFIED.,.F.,.F.,(4,2,2,2,2,3,2,2,2,2,4),(0.41660864742562,0.434934002630221,
0.469503712280229,0.504019646860705,0.538477704551985,0.553565728510636,
0.588009075052285,0.622483929180438,0.639712551567059,0.67484049808458,
0.69339332622741),.UNSPECIFIED.);
#2743=B_SPLINE_CURVE_WITH_KNOTS('',3,(#119576,#119577,#119578,#119579,#119580,
#119581,#119582,#119583,#119584,#119585,#119586,#119587,#119588,#119589,
#119590,#119591,#119592,#119593,#119594,#119595,#119596,#119597,#119598,
#119599,#119600,#119601,#119602,#119603,#119604,#119605,#119606,#119607,
#119608,#119609,#119610,#119611,#119612,#119613,#119614,#119615,#119616,
#119617,#119618,#119619,#119620,#119621,#119622,#119623,#119624,#119625,
#119626,#119627,#119628,#119629),.UNSPECIFIED.,.T.,.F.,(4,2,2,2,2,2,2,2,
2,2,2,2,2,2,2,2,2,2,2,2,2,2,2,2,2,2,4),(0.,0.0458320233936563,0.0951449281800662,
0.145722741215669,0.193905817750798,0.24098068927026,0.260497956547193,
0.269118961822078,0.275165580221845,0.281315954994347,0.290145956654934,
0.312104595695031,0.36312921663319,0.405435175946239,0.451284673710212,
0.500506710518771,0.551059662709869,0.599064670783345,0.647472573581018,
0.664439886250511,0.672224627284561,0.67815077226323,0.684415281967539,
0.693989332263362,0.721065537010137,0.757868161553381,0.80414884601772),
 .UNSPECIFIED.);
#2744=B_SPLINE_CURVE_WITH_KNOTS('',3,(#119632,#119633,#119634,#119635,#119636,
#119637,#119638,#119639,#119640,#119641,#119642,#119643,#119644,#119645,
#119646,#119647,#119648,#119649,#119650,#119651,#119652,#119653,#119654,
#119655,#119656,#119657,#119658,#119659,#119660,#119661,#119662,#119663,
#119664,#119665,#119666,#119667),.UNSPECIFIED.,.T.,.F.,(4,2,2,2,2,2,2,2,
2,2,2,2,2,2,2,2,2,4),(0.,0.0506382155192934,0.101412301739861,0.152300545666833,
0.203076346321417,0.253714832497476,0.304525318114152,0.329477947350912,
0.380367701352928,0.430730790890535,0.480986961082011,0.531075489416336,
0.581036229250358,0.631000474534633,0.681089122694047,0.731309856554222,
0.782321329423195,0.804714418336591),.UNSPECIFIED.);
#2745=B_SPLINE_CURVE_WITH_KNOTS('',3,(#119671,#119672,#119673,#119674,#119675,
#119676,#119677,#119678,#119679,#119680,#119681,#119682,#119683,#119684,
#119685,#119686,#119687,#119688,#119689,#119690),.UNSPECIFIED.,.F.,.F.,
(4,2,2,2,2,2,2,2,2,4),(0.213039430164029,0.239784499091426,0.266784297866583,
0.29381362797788,0.320813732727093,0.347781018775311,0.374802890367102,
0.388043853196362,0.414989929726265,0.426095694247663),.UNSPECIFIED.);
#2746=B_SPLINE_CURVE_WITH_KNOTS('',3,(#119694,#119695,#119696,#119697,#119698,
#119699,#119700,#119701,#119702,#119703,#119704,#119705,#119706,#119707,
#119708,#119709,#119710,#119711,#119712,#119713,#119714,#119715,#119716,
#119717,#119718),.UNSPECIFIED.,.F.,.F.,(4,3,2,2,2,2,2,2,2,2,2,4),(0.426095694247663,
0.426100860962362,0.452722929227169,0.479276968030936,0.505766829860246,
0.532237790565919,0.55874892707621,0.585329286001983,0.59862501203735,0.611895650008454,
0.638918112912157,0.639140291126391),.UNSPECIFIED.);
#2747=B_SPLINE_CURVE_WITH_KNOTS('',3,(#119721,#119722,#119723,#119724,#119725,
#119726,#119727,#119728,#119729,#119730,#119731,#119732,#119733,#119734,
#119735,#119736,#119737,#119738,#119739,#119740,#119741,#119742,#119743,
#119744,#119745,#119746,#119747,#119748,#119749,#119750,#119751,#119752,
#119753,#119754,#119755,#119756,#119757,#119758,#119759,#119760,#119761,
#119762,#119763,#119764,#119765,#119766,#119767,#119768,#119769,#119770,
#119771,#119772,#119773,#119774,#119775,#119776),.UNSPECIFIED.,.T.,.F.,
(4,2,2,2,2,2,2,2,2,2,2,2,2,2,2,2,2,2,2,2,2,2,2,2,2,2,2,4),(0.,0.0405914926291309,
0.0843626355691103,0.127768982513206,0.167065813577391,0.206671614216115,
0.215953475712915,0.221920923639481,0.226643225345449,0.231901123126324,
0.240523135098381,0.269456491599303,0.302072522394008,0.338668936139127,
0.378440679256369,0.421240646865564,0.46495856166125,0.50610024767708,0.547698204088174,
0.561705855753858,0.567441009098402,0.572217070056482,0.577088327121725,
0.584110325732133,0.60175959891513,0.645470033107342,0.671747046627922,
0.693886489051851),.UNSPECIFIED.);
#2748=B_SPLINE_CURVE_WITH_KNOTS('',3,(#119779,#119780,#119781,#119782,#119783,
#119784,#119785,#119786,#119787,#119788,#119789,#119790,#119791,#119792,
#119793,#119794,#119795,#119796,#119797,#119798,#119799,#119800,#119801,
#119802,#119803,#119804,#119805,#119806,#119807,#119808,#119809,#119810,
#119811,#119812,#119813,#119814,#119815,#119816),.UNSPECIFIED.,.T.,.F.,
(4,2,2,2,2,2,2,2,2,2,2,2,2,2,2,2,2,2,4),(0.,0.0438175087151928,0.0876691144818819,
0.131147129449532,0.174176486018958,0.217992008349161,0.261863242175615,
0.283379432303044,0.304976216118143,0.349059089995391,0.392583706563762,
0.435842850089949,0.478849630518895,0.52177211286288,0.564835596442599,
0.608171918261097,0.629922691866238,0.651607491185624,0.694352304660229),
 .UNSPECIFIED.);
#2749=B_SPLINE_CURVE_WITH_KNOTS('',3,(#119820,#119821,#119822,#119823,#119824,
#119825,#119826,#119827,#119828,#119829,#119830,#119831,#119832,#119833,
#119834,#119835,#119836,#119837,#119838,#119839),.UNSPECIFIED.,.F.,.F.,
(4,2,2,2,2,2,2,2,2,4),(0.157606167153757,0.177533160499949,0.197526249232083,
0.21704082507597,0.236560887844295,0.256160878575661,0.27616865652419,0.285965370433475,
0.29577830412786,0.315209094655922),.UNSPECIFIED.);
#2750=B_SPLINE_CURVE_WITH_KNOTS('',3,(#119843,#119844,#119845,#119846,#119847,
#119848,#119849,#119850,#119851,#119852,#119853,#119854,#119855,#119856,
#119857,#119858,#119859,#119860,#119861,#119862,#119863,#119864,#119865,
#119866,#119867),.UNSPECIFIED.,.F.,.F.,(4,3,2,2,2,2,2,2,2,2,2,4),(0.315209094655922,
0.315212335396961,0.335131144657127,0.354754972246871,0.374277570779983,
0.39377515829634,0.413340082716485,0.433023708581587,0.442873251294654,
0.452706286471694,0.472750995875536,0.472818502550718),.UNSPECIFIED.);
#2751=B_SPLINE_CURVE_WITH_KNOTS('',3,(#119870,#119871,#119872,#119873,#119874,
#119875,#119876,#119877,#119878,#119879,#119880,#119881,#119882,#119883,
#119884,#119885,#119886,#119887,#119888,#119889,#119890,#119891,#119892,
#119893,#119894,#119895,#119896,#119897,#119898,#119899,#119900,#119901,
#119902,#119903,#119904,#119905,#119906,#119907,#119908,#119909,#119910,
#119911,#119912,#119913,#119914,#119915,#119916,#119917,#119918,#119919,
#119920,#119921,#119922,#119923,#119924,#119925),.UNSPECIFIED.,.T.,.F.,
(4,2,2,2,2,2,2,2,2,2,2,2,2,2,2,2,2,2,2,2,2,2,2,2,2,2,2,4),(0.,0.0414795115022862,
0.0854646868492746,0.128051759118891,0.164665226970607,0.195716497055745,
0.204517379482455,0.209651426874716,0.213999683797992,0.219256285248534,
0.228840648703378,0.272097887192487,0.306671347087566,0.344807987469752,
0.386083672854091,0.430070266056682,0.472738795403928,0.507152959663538,
0.540328694973379,0.549340374995075,0.554498373378035,0.558414709258595,
0.563406376511839,0.571927658782594,0.603840451269834,0.636687933284218,
0.665364108131361,0.689885376340169),.UNSPECIFIED.);
#2752=B_SPLINE_CURVE_WITH_KNOTS('',3,(#119928,#119929,#119930,#119931,#119932,
#119933,#119934,#119935,#119936,#119937,#119938,#119939,#119940,#119941,
#119942,#119943,#119944,#119945,#119946,#119947,#119948,#119949,#119950,
#119951,#119952,#119953,#119954,#119955,#119956,#119957,#119958,#119959,
#119960,#119961,#119962,#119963),.UNSPECIFIED.,.T.,.F.,(4,2,2,2,2,2,2,2,
2,2,2,2,2,2,2,2,2,4),(0.,0.0437203941025976,0.0872619187212367,0.130314443853127,
0.172840099632362,0.216371752952188,0.260051472953626,0.304070571832068,
0.348437356049367,0.39193122891185,0.435014940311694,0.477666783665775,
0.520120318579686,0.562730177846754,0.605754886603923,0.649188896287545,
0.669804552140718,0.690576832826956),.UNSPECIFIED.);
#2753=B_SPLINE_CURVE_WITH_KNOTS('',3,(#119967,#119968,#119969,#119970,#119971,
#119972,#119973,#119974,#119975,#119976,#119977,#119978,#119979,#119980,
#119981,#119982,#119983,#119984,#119985,#119986),.UNSPECIFIED.,.F.,.F.,
(4,2,2,2,2,2,2,2,2,4),(0.155313790581586,0.165349433967049,0.185058166819829,
0.204477450512361,0.223605464026358,0.242753401686118,0.262450452504133,
0.282242587220628,0.302131095225523,0.310630462500323),.UNSPECIFIED.);
#2754=B_SPLINE_CURVE_WITH_KNOTS('',3,(#119990,#119991,#119992,#119993,#119994,
#119995,#119996,#119997,#119998,#119999,#120000,#120001,#120002,#120003,
#120004,#120005,#120006,#120007,#120008,#120009,#120010,#120011,#120012),
 .UNSPECIFIED.,.F.,.F.,(4,3,2,2,2,2,2,2,2,2,4),(0.310630462500323,0.310634616707648,
0.330337216979212,0.349710864965688,0.368898762124798,0.388004166232081,
0.407178443301545,0.426532516796507,0.446452164049864,0.4561765436671,0.465948407289234),
 .UNSPECIFIED.);
#2755=B_SPLINE_CURVE_WITH_KNOTS('',3,(#120015,#120016,#120017,#120018,#120019,
#120020,#120021,#120022,#120023,#120024,#120025,#120026,#120027,#120028,
#120029,#120030,#120031,#120032,#120033,#120034,#120035,#120036,#120037,
#120038,#120039,#120040,#120041,#120042,#120043,#120044,#120045,#120046,
#120047,#120048,#120049,#120050,#120051,#120052,#120053,#120054,#120055,
#120056,#120057,#120058,#120059,#120060,#120061,#120062,#120063,#120064,
#120065,#120066,#120067,#120068),.UNSPECIFIED.,.T.,.F.,(4,2,2,2,2,2,2,2,
2,2,2,2,2,2,2,2,2,2,2,2,2,2,2,2,2,2,4),(0.,0.0540423596745269,0.106458768986388,
0.122382214139942,0.131786992503092,0.139792246283686,0.149487906352155,
0.167103867927491,0.226190960021578,0.274156863496862,0.326257305107725,
0.382114137371328,0.440761445270956,0.497701345644869,0.55092190315513,
0.580002255699023,0.59223296424121,0.599783921991879,0.607895871128139,
0.6187122561808,0.641990799106262,0.70098574657611,0.750074000444414,0.803304704986148,
0.860492178265741,0.893904470056555,0.931148964406098),.UNSPECIFIED.);
#2756=B_SPLINE_CURVE_WITH_KNOTS('',3,(#120071,#120072,#120073,#120074,#120075,
#120076,#120077,#120078,#120079,#120080,#120081,#120082,#120083,#120084,
#120085,#120086,#120087,#120088,#120089,#120090,#120091,#120092,#120093,
#120094,#120095,#120096,#120097,#120098,#120099,#120100,#120101,#120102,
#120103,#120104,#120105,#120106,#120107,#120108),.UNSPECIFIED.,.T.,.F.,
(4,2,2,2,2,2,2,2,2,2,2,2,2,2,2,2,2,2,4),(0.,0.0586300084882738,0.117483040973624,
0.17622629878783,0.234715123518207,0.293318069965833,0.322102318538047,
0.351386546001824,0.409612976636273,0.467874879536276,0.526102208109452,
0.584201159872194,0.642161284355705,0.700072909012953,0.758033873788971,
0.787020936942943,0.816011821099062,0.874804862256184,0.931703358703855),
 .UNSPECIFIED.);
#2757=B_SPLINE_CURVE_WITH_KNOTS('',3,(#120112,#120113,#120114,#120115,#120116,
#120117,#120118,#120119,#120120,#120121,#120122,#120123,#120124,#120125,
#120126,#120127,#120128,#120129,#120130,#120131),.UNSPECIFIED.,.F.,.F.,
(4,2,2,2,2,2,2,2,2,4),(0.139767201099283,0.173948087346139,0.209027502769792,
0.244070694700763,0.279025309570312,0.31402030403869,0.331173399059848,
0.348578268416969,0.38314632638829,0.416559483837296),.UNSPECIFIED.);
#2758=B_SPLINE_CURVE_WITH_KNOTS('',3,(#120135,#120136,#120137,#120138,#120139,
#120140,#120141,#120142,#120143,#120144,#120145,#120146,#120147,#120148,
#120149,#120150,#120151,#120152,#120153,#120154,#120155,#120156,#120157,
#120158,#120159),.UNSPECIFIED.,.F.,.F.,(4,2,2,2,2,3,2,2,2,2,2,4),(0.416559483837296,
0.417723433981753,0.452283374405963,0.486794062508417,0.521254824770743,
0.553553763071154,0.588021449246394,0.605248660316662,0.622478045168663,
0.657553404742335,0.692501114966837,0.693320964170437),.UNSPECIFIED.);
#2759=B_SPLINE_CURVE_WITH_KNOTS('',3,(#120162,#120163,#120164,#120165,#120166,
#120167,#120168,#120169,#120170,#120171,#120172,#120173,#120174,#120175,
#120176,#120177,#120178,#120179,#120180,#120181,#120182,#120183,#120184,
#120185,#120186,#120187,#120188,#120189,#120190,#120191,#120192,#120193,
#120194,#120195,#120196,#120197,#120198,#120199,#120200,#120201,#120202,
#120203,#120204,#120205,#120206,#120207,#120208,#120209,#120210,#120211,
#120212,#120213,#120214,#120215),.UNSPECIFIED.,.T.,.F.,(4,2,2,2,2,2,2,2,
2,2,2,2,2,2,2,2,2,2,2,2,2,2,2,2,2,2,4),(0.,0.0436206699491311,0.090749901183791,
0.14148754427114,0.191583934327092,0.236779691637168,0.279072297635201,
0.291623391075206,0.299010732283145,0.305292026455287,0.312900344618033,
0.326758378813266,0.377634492790539,0.418722650965157,0.463540596216931,
0.511693288303611,0.562458476750911,0.611785021190842,0.655989914646358,
0.685075451837005,0.695760239918773,0.702595078313781,0.70894334751278,
0.717248646167864,0.734614913634257,0.7570782451133,0.804102668187989),
 .UNSPECIFIED.);
#2760=B_SPLINE_CURVE_WITH_KNOTS('',3,(#120218,#120219,#120220,#120221,#120222,
#120223,#120224,#120225,#120226,#120227,#120228,#120229,#120230,#120231,
#120232,#120233,#120234,#120235,#120236,#120237,#120238,#120239,#120240,
#120241,#120242,#120243,#120244,#120245,#120246,#120247,#120248,#120249,
#120250,#120251,#120252,#120253),.UNSPECIFIED.,.T.,.F.,(4,2,2,2,2,2,2,2,
2,2,2,2,2,2,2,2,2,4),(0.,0.0507228794267668,0.10166597248895,0.1526015226544,
0.20331343587648,0.253951968982878,0.27876966200945,0.303684210636509,0.354570883308706,
0.404917178454264,0.455153400555304,0.505229442536965,0.555191945447311,
0.605170640049558,0.655277164146098,0.705507445865675,0.756424092950211,
0.804681319466827),.UNSPECIFIED.);
#2761=B_SPLINE_CURVE_WITH_KNOTS('',3,(#120257,#120258,#120259,#120260,#120261,
#120262,#120263,#120264,#120265,#120266,#120267,#120268,#120269,#120270,
#120271,#120272,#120273,#120274,#120275,#120276,#120277,#120278),
 .UNSPECIFIED.,.F.,.F.,(4,2,2,2,2,2,2,2,2,2,4),(0.213065565020054,0.2132216265088,
0.240218856302912,0.267018454471732,0.293523298289317,0.320516778459753,
0.34747669940655,0.360670422284557,0.373888860401591,0.401079646648718,
0.426100077448779),.UNSPECIFIED.);
#2762=B_SPLINE_CURVE_WITH_KNOTS('',3,(#120282,#120283,#120284,#120285,#120286,
#120287,#120288,#120289,#120290,#120291,#120292,#120293,#120294,#120295,
#120296,#120297,#120298,#120299,#120300,#120301,#120302),.UNSPECIFIED.,
 .F.,.F.,(4,3,2,2,2,2,2,2,2,4),(0.426100077448779,0.426138379615387,0.452716978378953,
0.479228067467344,0.505701620846424,0.532194452261604,0.558750452815834,
0.585365281292561,0.612400917766107,0.639203944635441),.UNSPECIFIED.);
#2763=B_SPLINE_CURVE_WITH_KNOTS('',3,(#120305,#120306,#120307,#120308,#120309,
#120310,#120311,#120312,#120313,#120314,#120315,#120316,#120317,#120318,
#120319,#120320,#120321,#120322,#120323,#120324,#120325,#120326,#120327,
#120328,#120329,#120330,#120331,#120332,#120333,#120334,#120335,#120336,
#120337,#120338,#120339,#120340,#120341,#120342,#120343,#120344,#120345,
#120346,#120347,#120348,#120349,#120350,#120351,#120352,#120353,#120354,
#120355,#120356,#120357,#120358,#120359,#120360),.UNSPECIFIED.,.T.,.F.,
(4,2,2,2,2,2,2,2,2,2,2,2,2,2,2,2,2,2,2,2,2,2,2,2,2,2,2,4),(0.,0.0387113895615106,
0.0805130667469615,0.124505950972711,0.167101755822628,0.204029948058607,
0.231860291834698,0.241054636366574,0.246653577504196,0.251673760202214,
0.25800253399371,0.270483479280963,0.314220613655029,0.349681497508595,
0.388480986665803,0.430284691736075,0.474246193962455,0.516732436076201,
0.554321371029958,0.579627049069653,0.588407223118832,0.593879907222584,
0.598870503701298,0.605276403150402,0.618284530922307,0.634910354183487,
0.666887166430965,0.693797831079255),.UNSPECIFIED.);
#2764=B_SPLINE_CURVE_WITH_KNOTS('',3,(#120363,#120364,#120365,#120366,#120367,
#120368,#120369,#120370,#120371,#120372,#120373,#120374,#120375,#120376,
#120377,#120378,#120379,#120380,#120381,#120382,#120383,#120384,#120385,
#120386,#120387,#120388,#120389,#120390,#120391,#120392,#120393,#120394,
#120395,#120396,#120397,#120398,#120399,#120400),.UNSPECIFIED.,.T.,.F.,
(4,2,2,2,2,2,2,2,2,2,2,2,2,2,2,2,2,2,4),(0.,0.0437823947455483,0.0875527147869647,
0.131334832842352,0.175097356688018,0.218947594184666,0.263105738677232,
0.284797487459486,0.32887262269309,0.37240987695627,0.415675530898497,0.458678387410487,
0.501589552021586,0.544639998300872,0.587966065552883,0.609716214397085,
0.631470618066917,0.675605980504124,0.694348679609398),.UNSPECIFIED.);
#2765=B_SPLINE_CURVE_WITH_KNOTS('',3,(#120404,#120405,#120406,#120407,#120408,
#120409,#120410,#120411,#120412,#120413,#120414,#120415,#120416,#120417,
#120418,#120419,#120420,#120421,#120422,#120423,#120424,#120425,#120426,
#120427,#120428),.UNSPECIFIED.,.F.,.F.,(4,2,2,2,2,2,2,2,2,2,3,4),(0.157655388235319,
0.167606622324439,0.18755797051286,0.207290121019144,0.226806056807627,
0.246779384867164,0.266832954580611,0.276661997683397,0.286514670215304,
0.30652070403251,0.315210277187737,0.315239843192017),.UNSPECIFIED.);
#2766=B_SPLINE_CURVE_WITH_KNOTS('',3,(#120432,#120433,#120434,#120435,#120436,
#120437,#120438,#120439,#120440,#120441,#120442,#120443,#120444,#120445,
#120446,#120447,#120448,#120449,#120450,#120451),.UNSPECIFIED.,.F.,.F.,
(4,2,2,2,2,2,2,2,2,4),(0.315239843192017,0.334905849086587,0.354479560933382,
0.37397666178475,0.393489039425844,0.413099451365576,0.432829362268491,
0.442698129027635,0.462806348593131,0.472865665423056),.UNSPECIFIED.);
#2767=B_SPLINE_CURVE_WITH_KNOTS('',3,(#120454,#120455,#120456,#120457,#120458,
#120459,#120460,#120461,#120462,#120463,#120464,#120465,#120466,#120467,
#120468,#120469,#120470,#120471,#120472,#120473,#120474,#120475,#120476,
#120477,#120478,#120479,#120480,#120481,#120482,#120483,#120484,#120485,
#120486,#120487,#120488,#120489,#120490,#120491,#120492,#120493,#120494,
#120495,#120496,#120497,#120498,#120499,#120500,#120501,#120502,#120503,
#120504,#120505,#120506,#120507,#120508,#120509),.UNSPECIFIED.,.T.,.F.,
(4,2,2,2,2,2,2,2,2,2,2,2,2,2,2,2,2,2,2,2,2,2,2,2,2,2,2,4),(0.,0.039596158659987,
0.0823952911968967,0.126054785698637,0.167083206104417,0.207140413493102,
0.223066542451077,0.229933665475212,0.234259270307438,0.238988436149959,
0.245461112639432,0.260202981801162,0.303691845955503,0.339272904760605,
0.378244153279671,0.420327476204424,0.464148702486995,0.506016018533843,
0.543855540127323,0.565813628575552,0.573689239620962,0.578688275946453,
0.583313046972282,0.589348279542586,0.601974032650628,0.645360865220518,
0.669727977192671,0.689939909009643),.UNSPECIFIED.);
#2768=B_SPLINE_CURVE_WITH_KNOTS('',3,(#120512,#120513,#120514,#120515,#120516,
#120517,#120518,#120519,#120520,#120521,#120522,#120523,#120524,#120525,
#120526,#120527,#120528,#120529,#120530,#120531,#120532,#120533,#120534,
#120535,#120536,#120537,#120538,#120539,#120540,#120541,#120542,#120543,
#120544,#120545,#120546,#120547),.UNSPECIFIED.,.T.,.F.,(4,2,2,2,2,2,2,2,
2,2,2,2,2,2,2,2,2,4),(0.,0.0435930401462006,0.0871572230823697,0.129674587861441,
0.172285514734114,0.215867409321496,0.259652335979,0.303793851724133,0.347750906264732,
0.391036793565589,0.433869767017643,0.476371911416724,0.518865596090745,
0.561678995218631,0.604941064761695,0.62660055680218,0.648177684239587,
0.690509480107086),.UNSPECIFIED.);
#2769=B_SPLINE_CURVE_WITH_KNOTS('',3,(#120551,#120552,#120553,#120554,#120555,
#120556,#120557,#120558,#120559,#120560,#120561,#120562,#120563,#120564,
#120565,#120566,#120567,#120568,#120569,#120570,#120571,#120572,#120573),
 .UNSPECIFIED.,.F.,.F.,(4,2,2,2,2,2,2,2,2,3,4),(0.15531965076079,0.174754840487143,
0.19417250033404,0.213297327409549,0.232446865721418,0.251741462324811,
0.271508668310458,0.281196368653977,0.290901690065796,0.310557892572504,
0.310597054279583),.UNSPECIFIED.);
#2770=B_SPLINE_CURVE_WITH_KNOTS('',3,(#120577,#120578,#120579,#120580,#120581,
#120582,#120583,#120584,#120585,#120586,#120587,#120588,#120589,#120590,
#120591,#120592,#120593,#120594,#120595,#120596,#120597,#120598),
 .UNSPECIFIED.,.F.,.F.,(4,2,2,2,2,2,2,2,2,2,4),(0.310597054279583,0.330158543285891,
0.349421041224732,0.36854476073145,0.38766961382693,0.406934670947526,0.426396249473789,
0.436119083138285,0.445826468337623,0.465607794634539,0.465877543333294),
 .UNSPECIFIED.);
#2771=B_SPLINE_CURVE_WITH_KNOTS('',3,(#120601,#120602,#120603,#120604,#120605,
#120606,#120607,#120608,#120609,#120610,#120611,#120612,#120613,#120614,
#120615,#120616,#120617,#120618,#120619,#120620,#120621,#120622,#120623,
#120624,#120625,#120626,#120627,#120628,#120629,#120630,#120631,#120632,
#120633,#120634,#120635,#120636,#120637,#120638,#120639,#120640,#120641,
#120642,#120643,#120644,#120645,#120646,#120647,#120648,#120649,#120650,
#120651,#120652),.UNSPECIFIED.,.T.,.F.,(4,2,2,2,2,2,2,2,2,2,2,2,2,2,2,2,
2,2,2,2,2,2,2,2,2,4),(0.,0.0457657280663599,0.0962470966331294,0.150688970124808,
0.209205444217228,0.267220868171189,0.320462850227009,0.367511629141848,
0.383955761133481,0.39408136108263,0.403193554022451,0.414678721773825,
0.437106357996681,0.496128410031509,0.544999485599928,0.597826540018831,
0.654417295736584,0.712942843780337,0.769128561133749,0.827041531221436,
0.84482879582721,0.856270263279855,0.865268964852738,0.875182965117314,
0.891087537723763,0.931218391002395),.UNSPECIFIED.);
#2772=B_SPLINE_CURVE_WITH_KNOTS('',3,(#120655,#120656,#120657,#120658,#120659,
#120660,#120661,#120662,#120663,#120664,#120665,#120666,#120667,#120668,
#120669,#120670,#120671,#120672,#120673,#120674,#120675,#120676,#120677,
#120678,#120679,#120680,#120681,#120682,#120683,#120684,#120685,#120686,
#120687,#120688,#120689,#120690,#120691,#120692),.UNSPECIFIED.,.T.,.F.,
(4,2,2,2,2,2,2,2,2,2,2,2,2,2,2,2,2,2,4),(0.,0.058920779517719,0.117921436837851,
0.176593233578414,0.235023562463093,0.293771351172449,0.323059071245716,
0.381271618805364,0.439504199673013,0.497700513711045,0.555783874858827,
0.613753712690792,0.671694751020526,0.729686214224615,0.758678280096495,
0.787653234155945,0.846285702672291,0.904728850431761,0.931714763997535),
 .UNSPECIFIED.);
#2773=B_SPLINE_CURVE_WITH_KNOTS('',3,(#120696,#120697,#120698,#120699,#120700,
#120701,#120702,#120703,#120704,#120705,#120706,#120707,#120708,#120709,
#120710,#120711,#120712,#120713,#120714,#120715,#120716,#120717),
 .UNSPECIFIED.,.F.,.F.,(4,2,2,2,2,2,2,2,2,2,4),(0.13982808209604,0.156684952645851,
0.191864559984887,0.226983871072615,0.261948168518473,0.296885504504634,
0.314000364276795,0.331172042431347,0.366100387596459,0.400659900140943,
0.416615012156061),.UNSPECIFIED.);
#2774=B_SPLINE_CURVE_WITH_KNOTS('',3,(#120721,#120722,#120723,#120724,#120725,
#120726,#120727,#120728,#120729,#120730,#120731,#120732,#120733,#120734,
#120735,#120736,#120737,#120738,#120739,#120740,#120741,#120742,#120743),
 .UNSPECIFIED.,.F.,.F.,(4,2,2,2,2,3,2,2,2,2,4),(0.416615012156061,0.435202420474221,
0.469705730447166,0.504173728227007,0.53863810543123,0.553572697693693,
0.588069349484204,0.605280113114109,0.640265555971116,0.675195238381487,
0.693400779789733),.UNSPECIFIED.);
#2775=B_SPLINE_CURVE_WITH_KNOTS('',3,(#120746,#120747,#120748,#120749,#120750,
#120751,#120752,#120753,#120754,#120755,#120756,#120757,#120758,#120759,
#120760,#120761,#120762,#120763,#120764,#120765,#120766,#120767,#120768,
#120769,#120770,#120771,#120772,#120773,#120774,#120775,#120776,#120777,
#120778,#120779,#120780,#120781,#120782,#120783,#120784,#120785,#120786,
#120787,#120788,#120789,#120790,#120791,#120792,#120793,#120794,#120795,
#120796,#120797,#120798,#120799),.UNSPECIFIED.,.T.,.F.,(4,2,2,2,2,2,2,2,
2,2,2,2,2,2,2,2,2,2,2,2,2,2,2,2,2,2,4),(0.,0.0410256960338938,0.0858843637209721,
0.134180876844018,0.184954132352005,0.234318315071286,0.278865232377034,
0.308469870893335,0.319953448457986,0.327493605622781,0.334631495158405,
0.344159506408106,0.364714387064434,0.415726230703315,0.458014625617533,
0.503817689631654,0.552967727939839,0.603543528547655,0.651759195827544,
0.701438514782395,0.717798245396003,0.726394137160027,0.733341030655905,
0.741207260526554,0.754345756228916,0.799107153766506,0.804128273467629),
 .UNSPECIFIED.);
#2776=B_SPLINE_CURVE_WITH_KNOTS('',3,(#120802,#120803,#120804,#120805,#120806,
#120807,#120808,#120809,#120810,#120811,#120812,#120813,#120814,#120815,
#120816,#120817,#120818,#120819,#120820,#120821,#120822,#120823,#120824,
#120825,#120826,#120827,#120828,#120829,#120830,#120831,#120832,#120833,
#120834,#120835,#120836,#120837),.UNSPECIFIED.,.T.,.F.,(4,2,2,2,2,2,2,2,
2,2,2,2,2,2,2,2,2,4),(0.,0.050671481475036,0.101404234134367,0.152066263127611,
0.202712434371903,0.253657694987048,0.279013189545143,0.32940308141885,
0.379786196260612,0.430059917310446,0.480151651481399,0.530099594615151,
0.580042077960693,0.630109747347428,0.680318594563881,0.730564119609313,
0.781277800571749,0.80467565281243),.UNSPECIFIED.);
#2777=B_SPLINE_CURVE_WITH_KNOTS('',3,(#120841,#120842,#120843,#120844,#120845,
#120846,#120847,#120848,#120849,#120850,#120851,#120852,#120853,#120854,
#120855,#120856,#120857,#120858,#120859,#120860,#120861,#120862),
 .UNSPECIFIED.,.F.,.F.,(4,2,2,2,2,2,2,2,2,2,4),(0.213054899584985,0.213240549849428,
0.240182910677569,0.267129686203949,0.294071943340295,0.321044789490067,
0.348135746666136,0.361567634376776,0.388235323149757,0.414887993400968,
0.426100610580404),.UNSPECIFIED.);
#2778=B_SPLINE_CURVE_WITH_KNOTS('',3,(#120866,#120867,#120868,#120869,#120870,
#120871,#120872,#120873,#120874,#120875,#120876,#120877,#120878,#120879,
#120880,#120881,#120882,#120883,#120884,#120885,#120886),.UNSPECIFIED.,
 .F.,.F.,(4,3,2,2,2,2,2,2,2,4),(0.426100610580404,0.426145242037738,0.452705254015028,
0.47919324694378,0.505655512683507,0.532155454420269,0.558727065325242,
0.585349496759048,0.612421136299796,0.639200141622723),.UNSPECIFIED.);
#2779=B_SPLINE_CURVE_WITH_KNOTS('',3,(#120889,#120890,#120891,#120892,#120893,
#120894,#120895,#120896,#120897,#120898,#120899,#120900,#120901,#120902,
#120903,#120904,#120905,#120906,#120907,#120908,#120909,#120910,#120911,
#120912,#120913,#120914,#120915,#120916,#120917,#120918,#120919,#120920,
#120921,#120922,#120923,#120924,#120925,#120926,#120927,#120928,#120929,
#120930,#120931,#120932,#120933,#120934,#120935,#120936,#120937,#120938,
#120939,#120940,#120941,#120942),.UNSPECIFIED.,.T.,.F.,(4,2,2,2,2,2,2,2,
2,2,2,2,2,2,2,2,2,2,2,2,2,2,2,2,2,2,4),(0.,0.0366013559564401,0.0764365014300665,
0.119372798610828,0.16310043928206,0.204330007717561,0.246666363043394,
0.259193316849719,0.265920265998224,0.271513809212394,0.277203299739624,
0.285363684119845,0.305548661058766,0.349530477740465,0.38627829019971,
0.426163665012696,0.469070659303587,0.51275373872358,0.553769200036606,
0.597242402126746,0.607863717680535,0.614714725095663,0.620139119416996,
0.626171840821019,0.636023118823449,0.668251715399877,0.693912250555093),
 .UNSPECIFIED.);
#2780=B_SPLINE_CURVE_WITH_KNOTS('',3,(#120945,#120946,#120947,#120948,#120949,
#120950,#120951,#120952,#120953,#120954,#120955,#120956,#120957,#120958,
#120959,#120960,#120961,#120962,#120963,#120964,#120965,#120966,#120967,
#120968,#120969,#120970,#120971,#120972,#120973,#120974,#120975,#120976,
#120977,#120978,#120979,#120980,#120981,#120982),.UNSPECIFIED.,.T.,.F.,
(4,2,2,2,2,2,2,2,2,2,2,2,2,2,2,2,2,2,4),(0.,0.043813290614458,0.0876872070663863,
0.13153218183437,0.175328457737809,0.2192572073628,0.240814554252403,0.26246165039269,
0.306530340064736,0.350044147248009,0.393286106662586,0.43627728806497,
0.479194135759194,0.522262928847021,0.565607803967553,0.587360629268619,
0.609062896535199,0.653109830395691,0.69429306613882),.UNSPECIFIED.);
#2781=B_SPLINE_CURVE_WITH_KNOTS('',3,(#120986,#120987,#120988,#120989,#120990,
#120991,#120992,#120993,#120994,#120995,#120996,#120997,#120998,#120999,
#121000,#121001,#121002,#121003,#121004,#121005,#121006,#121007,#121008,
#121009,#121010),.UNSPECIFIED.,.F.,.F.,(4,2,2,2,2,2,2,2,2,2,3,4),(0.157621952213009,
0.157653184764648,0.17762672741589,0.197139809159047,0.216658658704082,
0.236639750750289,0.256668741552331,0.266480438865674,0.27631172587911,
0.29648603104283,0.31518544605496,0.315213231454912),.UNSPECIFIED.);
#2782=B_SPLINE_CURVE_WITH_KNOTS('',3,(#121014,#121015,#121016,#121017,#121018,
#121019,#121020,#121021,#121022,#121023,#121024,#121025,#121026,#121027,
#121028,#121029,#121030,#121031,#121032,#121033),.UNSPECIFIED.,.F.,.F.,
(4,2,2,2,2,2,2,2,2,4),(0.315213231454912,0.334806435763938,0.354325740797582,
0.373820720858293,0.393384197724592,0.413067020071531,0.422927128560577,
0.432773257208208,0.452840403179137,0.472807398267969),.UNSPECIFIED.);
#2783=B_SPLINE_CURVE_WITH_KNOTS('',3,(#121036,#121037,#121038,#121039,#121040,
#121041,#121042,#121043,#121044,#121045,#121046,#121047,#121048,#121049,
#121050,#121051,#121052,#121053,#121054,#121055,#121056,#121057,#121058,
#121059,#121060,#121061,#121062,#121063,#121064,#121065,#121066,#121067,
#121068,#121069,#121070,#121071,#121072,#121073,#121074,#121075,#121076,
#121077,#121078,#121079,#121080,#121081,#121082,#121083,#121084,#121085,
#121086,#121087,#121088,#121089),.UNSPECIFIED.,.T.,.F.,(4,2,2,2,2,2,2,2,
2,2,2,2,2,2,2,2,2,2,2,2,2,2,2,2,2,2,4),(0.,0.037556946163732,0.078353672010978,
0.122434169468536,0.165511233753611,0.20341370217087,0.239374223192113,
0.249493359317307,0.255339187545231,0.259801523354461,0.265512173804729,
0.275307801757659,0.312011429228339,0.345864756632766,0.383397787727872,
0.424095817779774,0.467987976817719,0.511077045633704,0.548989716122193,
0.584500641602089,0.594525810714392,0.60032057717742,0.604744779895977,
0.610406896041102,0.620117805489341,0.656447023762833,0.689896900949306),
 .UNSPECIFIED.);
#2784=B_SPLINE_CURVE_WITH_KNOTS('',3,(#121092,#121093,#121094,#121095,#121096,
#121097,#121098,#121099,#121100,#121101,#121102,#121103,#121104,#121105,
#121106,#121107,#121108,#121109,#121110,#121111,#121112,#121113,#121114,
#121115,#121116,#121117,#121118,#121119,#121120,#121121,#121122,#121123,
#121124,#121125),.UNSPECIFIED.,.T.,.F.,(4,2,2,2,2,2,2,2,2,2,2,2,2,2,2,2,
4),(0.,0.043596439164069,0.0861642710137229,0.128693297937725,0.171468209427599,
0.2150813225096,0.258933409386575,0.303127744859599,0.346899194209671,0.389933113733483,
0.432552889836591,0.475005878811627,0.517643008156437,0.560703769720036,
0.604908662276928,0.648772568902826,0.690554784558767),.UNSPECIFIED.);
#2785=B_SPLINE_CURVE_WITH_KNOTS('',3,(#121129,#121130,#121131,#121132,#121133,
#121134,#121135,#121136,#121137,#121138,#121139,#121140,#121141,#121142,
#121143,#121144,#121145,#121146,#121147,#121148),.UNSPECIFIED.,.F.,.F.,
(4,2,2,2,2,2,2,2,2,4),(0.15526622356778,0.16514719842404,0.184370089139019,
0.203490683518605,0.222647435046449,0.241956293352432,0.261690989855888,
0.28149517603416,0.301354306664443,0.31055959145846),.UNSPECIFIED.);
#2786=B_SPLINE_CURVE_WITH_KNOTS('',3,(#121152,#121153,#121154,#121155,#121156,
#121157,#121158,#121159,#121160,#121161,#121162,#121163,#121164,#121165,
#121166,#121167,#121168,#121169,#121170,#121171,#121172,#121173,#121174),
 .UNSPECIFIED.,.F.,.F.,(4,3,2,2,2,2,2,2,2,2,4),(0.31055959145846,0.310586625858458,
0.329931516356413,0.349100382910039,0.368205489314063,0.387396736722476,
0.406773990247626,0.426614881078628,0.436294287031581,0.456033588890424,
0.465852849426238),.UNSPECIFIED.);
#2787=B_SPLINE_CURVE_WITH_KNOTS('',3,(#121177,#121178,#121179,#121180,#121181,
#121182,#121183,#121184,#121185,#121186,#121187,#121188,#121189,#121190,
#121191,#121192,#121193,#121194,#121195,#121196,#121197,#121198,#121199,
#121200,#121201,#121202,#121203,#121204,#121205,#121206,#121207,#121208,
#121209,#121210,#121211,#121212,#121213,#121214,#121215,#121216,#121217,
#121218,#121219,#121220,#121221,#121222,#121223,#121224,#121225,#121226),
 .UNSPECIFIED.,.T.,.F.,(4,2,2,2,2,2,2,2,2,2,2,2,2,2,2,2,2,2,2,2,2,2,2,2,
4),(0.,0.0589492574510598,0.107914736457218,0.160952293016516,0.217874991214115,
0.276373103612947,0.332619207687263,0.391709189818869,0.41186529192147,
0.423862057197878,0.434357412140907,0.447160303263547,0.470774846569851,
0.529730149181218,0.578950059106104,0.63202778938777,0.688850635712996,
0.747336324371342,0.803360408965686,0.858785238766215,0.878232841788907,
0.889966223471808,0.900224877634544,0.912925203241937,0.931340863912512),
 .UNSPECIFIED.);
#2788=B_SPLINE_CURVE_WITH_KNOTS('',3,(#121229,#121230,#121231,#121232,#121233,
#121234,#121235,#121236,#121237,#121238,#121239,#121240,#121241,#121242,
#121243,#121244,#121245,#121246,#121247,#121248,#121249,#121250,#121251,
#121252,#121253,#121254,#121255,#121256,#121257,#121258,#121259,#121260,
#121261,#121262,#121263,#121264),.UNSPECIFIED.,.T.,.F.,(4,2,2,2,2,2,2,2,
2,2,2,2,2,2,2,2,2,4),(0.,0.058754774143773,0.117403197632285,0.175875621269893,
0.234569790357621,0.293351237166583,0.351590064970777,0.409870781021814,
0.468108002533021,0.526201151535928,0.584144950061525,0.642039413541678,
0.699988642810973,0.728973944077931,0.75796401140306,0.816798564560837,
0.87527518388624,0.931839180559051),.UNSPECIFIED.);
#2789=B_SPLINE_CURVE_WITH_KNOTS('',3,(#121268,#121269,#121270,#121271,#121272,
#121273,#121274,#121275,#121276,#121277,#121278,#121279,#121280,#121281,
#121282,#121283,#121284,#121285),.UNSPECIFIED.,.F.,.F.,(4,2,2,2,2,2,2,2,
4),(0.139818026634276,0.174512333238167,0.209502003810185,0.244448225294873,
0.279493276844203,0.314418985135482,0.348993948138227,0.383582033172368,
0.416694165602581),.UNSPECIFIED.);
#2790=B_SPLINE_CURVE_WITH_KNOTS('',3,(#121289,#121290,#121291,#121292,#121293,
#121294,#121295,#121296,#121297,#121298,#121299,#121300,#121301,#121302,
#121303,#121304,#121305,#121306,#121307,#121308,#121309,#121310,#121311,
#121312,#121313),.UNSPECIFIED.,.F.,.F.,(4,2,2,2,2,3,2,2,2,2,2,4),(0.416694165602581,
0.418149030337749,0.452658452441695,0.487111215703082,0.521548035500538,
0.55363961027923,0.570865744607261,0.588094764652048,0.6232050832238,0.658160766047363,
0.693131459530335,0.693457636913506),.UNSPECIFIED.);
#2791=B_SPLINE_CURVE_WITH_KNOTS('',3,(#121316,#121317,#121318,#121319,#121320,
#121321,#121322,#121323,#121324,#121325,#121326,#121327,#121328,#121329,
#121330,#121331,#121332,#121333,#121334,#121335,#121336,#121337,#121338,
#121339,#121340,#121341,#121342,#121343,#121344,#121345,#121346,#121347,
#121348,#121349,#121350,#121351,#121352,#121353,#121354,#121355,#121356,
#121357,#121358,#121359,#121360,#121361,#121362,#121363,#121364,#121365,
#121366,#121367),.UNSPECIFIED.,.T.,.F.,(4,2,2,2,2,2,2,2,2,2,2,2,2,2,2,2,
2,2,2,2,2,2,2,2,2,4),(0.,0.0507937034377209,0.0942504582104237,0.141185207519934,
0.191662737622325,0.241886687841347,0.288180985331185,0.32953155683084,
0.344017684193696,0.352930093965412,0.360941834251172,0.371024141212346,
0.390645212147654,0.441646633380299,0.483924750998178,0.529687085817695,
0.578771366615263,0.629367932882979,0.677767598915435,0.728753614508766,
0.744574626260671,0.753834295400635,0.760926160148939,0.769993449257638,
0.785403580290456,0.804157258531139),.UNSPECIFIED.);
#2792=B_SPLINE_CURVE_WITH_KNOTS('',3,(#121370,#121371,#121372,#121373,#121374,
#121375,#121376,#121377,#121378,#121379,#121380,#121381,#121382,#121383,
#121384,#121385,#121386,#121387,#121388,#121389,#121390,#121391,#121392,
#121393,#121394,#121395,#121396,#121397,#121398,#121399,#121400,#121401,
#121402,#121403,#121404,#121405),.UNSPECIFIED.,.T.,.F.,(4,2,2,2,2,2,2,2,
2,2,2,2,2,2,2,2,2,4),(0.,0.050833907134388,0.101649533693549,0.152311708696542,
0.203013209115999,0.227882884844094,0.252867746078267,0.303753702130619,
0.354114469975017,0.404361960576347,0.454437938512487,0.504389486437119,
0.554352331677784,0.604444370792824,0.654665986279593,0.705665420859672,
0.75632877106835,0.804655263691419),.UNSPECIFIED.);
#2793=B_SPLINE_CURVE_WITH_KNOTS('',3,(#121409,#121410,#121411,#121412,#121413,
#121414,#121415,#121416,#121417,#121418,#121419,#121420,#121421,#121422,
#121423,#121424,#121425,#121426,#121427,#121428,#121429,#121430),
 .UNSPECIFIED.,.F.,.F.,(4,2,2,2,2,2,2,2,2,2,4),(0.213066841557169,0.213662545774583,
0.240669569811573,0.267670841941382,0.294638476552452,0.321631963442581,
0.334853033549719,0.348108184038777,0.375050927422802,0.401690612064548,
0.426093389507995),.UNSPECIFIED.);
#2794=B_SPLINE_CURVE_WITH_KNOTS('',3,(#121434,#121435,#121436,#121437,#121438,
#121439,#121440,#121441,#121442,#121443,#121444,#121445,#121446,#121447,
#121448,#121449,#121450,#121451,#121452,#121453,#121454),.UNSPECIFIED.,
 .F.,.F.,(4,3,2,2,2,2,2,2,2,4),(0.426093389507995,0.426125083936875,0.452637149993507,
0.479106168396101,0.505591290010395,0.532139726713557,0.558750010866693,
0.585835324843181,0.612814653428274,0.639191925494045),.UNSPECIFIED.);
#2795=B_SPLINE_CURVE_WITH_KNOTS('',3,(#121457,#121458,#121459,#121460,#121461,
#121462,#121463,#121464,#121465,#121466,#121467,#121468,#121469,#121470,
#121471,#121472,#121473,#121474,#121475,#121476,#121477,#121478,#121479,
#121480,#121481,#121482,#121483,#121484,#121485,#121486,#121487,#121488,
#121489,#121490,#121491,#121492,#121493,#121494,#121495,#121496,#121497,
#121498,#121499,#121500,#121501,#121502,#121503,#121504,#121505,#121506,
#121507,#121508,#121509,#121510),.UNSPECIFIED.,.T.,.F.,(4,2,2,2,2,2,2,2,
2,2,2,2,2,2,2,2,2,2,2,2,2,2,2,2,2,2,4),(0.,0.0340495896964589,0.0717326270132875,
0.11252803704836,0.156502200310784,0.199822500511049,0.238843623221006,
0.273853576148806,0.285359660224145,0.292268338347826,0.297771450755393,
0.305083405497963,0.318350110983871,0.362169458367038,0.397913138379148,
0.436911605435009,0.478890528871826,0.522819871797262,0.565180829903189,
0.6049588927033,0.625937273272207,0.635003816763026,0.640690203873801,0.646869547498752,
0.655230481335403,0.673680426876438,0.693806114392571),.UNSPECIFIED.);
#2796=B_SPLINE_CURVE_WITH_KNOTS('',3,(#121513,#121514,#121515,#121516,#121517,
#121518,#121519,#121520,#121521,#121522,#121523,#121524,#121525,#121526,
#121527,#121528,#121529,#121530,#121531,#121532,#121533,#121534,#121535,
#121536,#121537,#121538,#121539,#121540,#121541,#121542,#121543,#121544,
#121545,#121546,#121547,#121548,#121549,#121550),.UNSPECIFIED.,.T.,.F.,
(4,2,2,2,2,2,2,2,2,2,2,2,2,2,2,2,2,2,4),(0.,0.0439347739032266,0.0869159744428171,
0.13077627881111,0.174581205598091,0.218579365897418,0.240178093592474,
0.284240919487602,0.327731207437498,0.370950319256991,0.413931398391036,
0.456855715235624,0.499944459043748,0.543309401480821,0.565046800844102,
0.586695146990834,0.630653497733593,0.674454613655654,0.694278240948528),
 .UNSPECIFIED.);
#2797=B_SPLINE_CURVE_WITH_KNOTS('',3,(#121554,#121555,#121556,#121557,#121558,
#121559,#121560,#121561,#121562,#121563,#121564,#121565,#121566,#121567,
#121568,#121569,#121570,#121571,#121572,#121573,#121574,#121575),
 .UNSPECIFIED.,.F.,.F.,(4,2,2,2,2,2,2,2,2,2,4),(0.157610631276741,0.167958486015372,
0.187466426098309,0.206990222488691,0.22660072328568,0.246603187530971,
0.256396456163226,0.266205345368447,0.286342556288682,0.306065981237513,
0.315177053872359),.UNSPECIFIED.);
#2798=B_SPLINE_CURVE_WITH_KNOTS('',3,(#121579,#121580,#121581,#121582,#121583,
#121584,#121585,#121586,#121587,#121588,#121589,#121590,#121591,#121592,
#121593,#121594,#121595,#121596,#121597,#121598),.UNSPECIFIED.,.F.,.F.,
(4,2,2,2,2,2,2,2,2,4),(0.315177875652213,0.334731312382099,0.354225127407107,
0.373752029378928,0.393385414052036,0.413517586583673,0.423338460875682,
0.443362292717093,0.463349884707035,0.472788506928953),.UNSPECIFIED.);
#2799=B_SPLINE_CURVE_WITH_KNOTS('',3,(#121601,#121602,#121603,#121604,#121605,
#121606,#121607,#121608,#121609,#121610,#121611,#121612,#121613,#121614,
#121615,#121616,#121617,#121618,#121619,#121620,#121621,#121622,#121623,
#121624,#121625,#121626,#121627,#121628,#121629,#121630,#121631,#121632,
#121633,#121634,#121635,#121636,#121637,#121638,#121639,#121640,#121641,
#121642,#121643,#121644,#121645,#121646,#121647,#121648,#121649,#121650,
#121651,#121652,#121653,#121654),.UNSPECIFIED.,.T.,.F.,(4,2,2,2,2,2,2,2,
2,2,2,2,2,2,2,2,2,2,2,2,2,2,2,2,2,2,4),(0.,0.0352022673375941,0.0738901483084225,
0.1157593961888,0.159668433184647,0.201930806507174,0.239710322409318,0.264431621656874,
0.2736438776145,0.279583591391943,0.285134797469431,0.292448528839575,0.307929890803635,
0.351263787235359,0.387082225605215,0.426231499198338,0.468477017309043,
0.512252444068684,0.553957151412746,0.593842927431791,0.612065599873391,
0.620069770023004,0.625148207635513,0.630721384385979,0.638371116778437,
0.655771630237812,0.689842314476748),.UNSPECIFIED.);
#2800=B_SPLINE_CURVE_WITH_KNOTS('',3,(#121657,#121658,#121659,#121660,#121661,
#121662,#121663,#121664,#121665,#121666,#121667,#121668,#121669,#121670,
#121671,#121672,#121673,#121674,#121675,#121676,#121677,#121678,#121679,
#121680,#121681,#121682,#121683,#121684,#121685,#121686,#121687,#121688,
#121689,#121690,#121691,#121692),.UNSPECIFIED.,.T.,.F.,(4,2,2,2,2,2,2,2,
2,2,2,2,2,2,2,2,2,4),(0.,0.0435016177078772,0.0860121887793504,0.12862128786204,
0.172202755572531,0.216057150084804,0.237598491123779,0.281980320515373,
0.325446999346799,0.368494831481356,0.411117560750869,0.453561023893441,
0.496180500458554,0.539222786240642,0.58266489810085,0.626698842331351,
0.67038314380947,0.690425413549481),.UNSPECIFIED.);
#2801=B_SPLINE_CURVE_WITH_KNOTS('',3,(#121696,#121697,#121698,#121699,#121700,
#121701,#121702,#121703,#121704,#121705,#121706,#121707,#121708,#121709,
#121710,#121711,#121712,#121713,#121714,#121715,#121716,#121717),
 .UNSPECIFIED.,.F.,.F.,(4,2,2,2,2,2,2,2,2,2,4),(0.155304341878299,0.155614346327306,
0.175017713542264,0.194137740808806,0.213289212695199,0.232988751462658,
0.252789069790465,0.262496324252049,0.282415062372032,0.302087245052277,
0.310566042860497),.UNSPECIFIED.);
#2802=B_SPLINE_CURVE_WITH_KNOTS('',3,(#121721,#121722,#121723,#121724,#121725,
#121726,#121727,#121728,#121729,#121730,#121731,#121732,#121733,#121734,
#121735,#121736,#121737,#121738),.UNSPECIFIED.,.F.,.F.,(4,2,2,2,2,2,2,2,
4),(0.310566841812876,0.329820690946879,0.348938270234188,0.368061455771084,
0.38732839010858,0.406792237945073,0.426685381368033,0.446482972279099,
0.465870384738796),.UNSPECIFIED.);
#2803=B_SPLINE_CURVE_WITH_KNOTS('',3,(#121741,#121742,#121743,#121744,#121745,
#121746,#121747,#121748,#121749,#121750,#121751,#121752,#121753,#121754,
#121755,#121756,#121757,#121758,#121759,#121760,#121761,#121762,#121763,
#121764,#121765,#121766,#121767,#121768,#121769,#121770,#121771,#121772,
#121773,#121774,#121775,#121776,#121777,#121778,#121779,#121780,#121781,
#121782,#121783,#121784,#121785,#121786,#121787,#121788,#121789,#121790),
 .UNSPECIFIED.,.T.,.F.,(4,2,2,2,2,2,2,2,2,2,2,2,2,2,2,2,2,2,2,2,2,2,2,2,
4),(0.,0.0146814900877869,0.0403932201823766,0.0996751527325199,0.149718027008705,
0.203629369858852,0.261440655475543,0.319739221183558,0.375087111970191,
0.423126186803048,0.443374355706851,0.456859239591619,0.469635723415156,
0.486523100520705,0.521324927686473,0.580568089427896,0.631598426631969,
0.686262802022563,0.744843360768508,0.802806482356597,0.856102034365298,
0.894199591680106,0.912116451169146,0.924831843263324,0.931217467582355),
 .UNSPECIFIED.);
#2804=B_SPLINE_CURVE_WITH_KNOTS('',3,(#121793,#121794,#121795,#121796,#121797,
#121798,#121799,#121800,#121801,#121802,#121803,#121804,#121805,#121806,
#121807,#121808,#121809,#121810,#121811,#121812,#121813,#121814,#121815,
#121816,#121817,#121818,#121819,#121820,#121821,#121822,#121823,#121824,
#121825,#121826,#121827,#121828),.UNSPECIFIED.,.T.,.F.,(4,2,2,2,2,2,2,2,
2,2,2,2,2,2,2,2,2,4),(0.,0.0587304660413623,0.117261312681522,0.175782378681062,
0.234811396887744,0.293027463812867,0.351294329347738,0.409567101310013,
0.467736885839166,0.525743559075219,0.583645163091547,0.641559649632323,
0.699549298941314,0.728539390326633,0.78735949377363,0.845834430734695,
0.904430972318154,0.93184955269919),.UNSPECIFIED.);
#2805=B_SPLINE_CURVE_WITH_KNOTS('',3,(#121832,#121833,#121834,#121835,#121836,
#121837,#121838,#121839,#121840,#121841,#121842,#121843,#121844,#121845,
#121846,#121847,#121848,#121849,#121850,#121851),.UNSPECIFIED.,.F.,.F.,
(4,2,2,2,2,2,2,2,2,4),(0.139782642488671,0.157277236176017,0.192263350991827,
0.227209833005202,0.262263155174017,0.297189356143265,0.331765243145084,
0.366353631343455,0.40091932638502,0.416650087036247),.UNSPECIFIED.);
#2806=B_SPLINE_CURVE_WITH_KNOTS('',3,(#121855,#121856,#121857,#121858,#121859,
#121860,#121861,#121862,#121863,#121864,#121865,#121866,#121867,#121868,
#121869,#121870,#121871,#121872,#121873,#121874,#121875,#121876,#121877),
 .UNSPECIFIED.,.F.,.F.,(4,2,2,2,2,3,2,2,2,2,4),(0.416650087036247,0.43542645929999,
0.469877637670099,0.504314536277139,0.538777951627268,0.553655749381749,
0.57088485344067,0.605987902900473,0.640941818311758,0.675913700988461,
0.693438391870421),.UNSPECIFIED.);
#2807=B_SPLINE_CURVE_WITH_KNOTS('',3,(#121880,#121881,#121882,#121883,#121884,
#121885,#121886,#121887,#121888,#121889,#121890,#121891,#121892,#121893,
#121894,#121895,#121896,#121897,#121898,#121899,#121900,#121901,#121902,
#121903,#121904,#121905,#121906,#121907,#121908,#121909,#121910,#121911,
#121912,#121913,#121914,#121915,#121916,#121917,#121918,#121919,#121920,
#121921,#121922,#121923,#121924,#121925,#121926,#121927,#121928,#121929,
#121930,#121931),.UNSPECIFIED.,.T.,.F.,(4,2,2,2,2,2,2,2,2,2,2,2,2,2,2,2,
2,2,2,2,2,2,2,2,2,4),(0.,0.0251512584232482,0.0759877853106741,0.119405408870884,
0.16625754672263,0.216603813925032,0.266895795796829,0.313787921137438,
0.354118828253151,0.36990456778704,0.380105008924405,0.389584676639667,
0.401905547614001,0.426921516051744,0.477783291068181,0.521019289601979,
0.567585491492379,0.617510443801545,0.667882138154644,0.715128069050405,
0.756057760669801,0.771905259786264,0.782049406675469,0.791401652048583,
0.803444832488867,0.804103777769588),.UNSPECIFIED.);
#2808=B_SPLINE_CURVE_WITH_KNOTS('',3,(#121934,#121935,#121936,#121937,#121938,
#121939,#121940,#121941,#121942,#121943,#121944,#121945,#121946,#121947,
#121948,#121949,#121950,#121951,#121952,#121953,#121954,#121955,#121956,
#121957,#121958,#121959,#121960,#121961,#121962,#121963,#121964,#121965,
#121966,#121967,#121968,#121969,#121970,#121971),.UNSPECIFIED.,.T.,.F.,
(4,2,2,2,2,2,2,2,2,2,2,2,2,2,2,2,2,2,4),(0.,0.0508792217220559,0.10162781996598,
0.15226341389946,0.203118878795053,0.22810150196294,0.278985025900999,0.329338017561462,
0.379573992903277,0.429640500475744,0.479590456671073,0.529560364764325,
0.579662501253364,0.604751617442169,0.629853487047417,0.680809050484543,
0.731459039231061,0.782167614091922,0.804545530220026),.UNSPECIFIED.);
#2809=B_SPLINE_CURVE_WITH_KNOTS('',3,(#121975,#121976,#121977,#121978,#121979,
#121980,#121981,#121982,#121983,#121984,#121985,#121986,#121987,#121988,
#121989,#121990,#121991,#121992,#121993,#121994,#121995,#121996),
 .UNSPECIFIED.,.F.,.F.,(4,2,2,2,2,2,2,2,2,2,4),(0.213062544082035,0.227396210814127,
0.254408164208183,0.281378412056288,0.308367215720059,0.32158497568968,
0.334835900148672,0.361777221247026,0.388412697486444,0.414986226725616,
0.426072215562033),.UNSPECIFIED.);
#2810=B_SPLINE_CURVE_WITH_KNOTS('',3,(#122000,#122001,#122002,#122003,#122004,
#122005,#122006,#122007,#122008,#122009,#122010,#122011,#122012,#122013,
#122014,#122015,#122016,#122017,#122018,#122019),.UNSPECIFIED.,.F.,.F.,
(4,2,2,2,2,2,2,2,2,4),(0.426073055069735,0.45255530258914,0.479026549487086,
0.50554445216474,0.532131476024713,0.545427554156093,0.572495206369301,
0.599468234270871,0.626448478859957,0.63913559915177),.UNSPECIFIED.);
#2811=B_SPLINE_CURVE_WITH_KNOTS('',3,(#122022,#122023,#122024,#122025,#122026,
#122027,#122028,#122029,#122030,#122031,#122032,#122033,#122034,#122035,
#122036,#122037,#122038,#122039,#122040,#122041,#122042,#122043,#122044,
#122045,#122046,#122047,#122048,#122049,#122050,#122051,#122052,#122053,
#122054,#122055,#122056,#122057,#122058,#122059,#122060,#122061,#122062,
#122063,#122064,#122065,#122066,#122067,#122068,#122069,#122070,#122071,
#122072,#122073),.UNSPECIFIED.,.T.,.F.,(4,2,2,2,2,2,2,2,2,2,2,2,2,2,2,2,
2,2,2,2,2,2,2,2,2,4),(0.,0.0440069107173191,0.0805041598387523,0.120195090458515,
0.162944901989734,0.206734560097777,0.248397511361373,0.29230637149236,
0.306355177191658,0.314519420881693,0.321558923387898,0.3300369356061,0.34544587077815,
0.38933609730284,0.425577319914237,0.464967314809013,0.507320950852571,
0.551170882890177,0.593174602554415,0.635677047601321,0.651757900842182,
0.660344658217508,0.667331111227712,0.675273121184593,0.688553612441433,
0.693940242356045),.UNSPECIFIED.);
#2812=B_SPLINE_CURVE_WITH_KNOTS('',3,(#122076,#122077,#122078,#122079,#122080,
#122081,#122082,#122083,#122084,#122085,#122086,#122087,#122088,#122089,
#122090,#122091,#122092,#122093,#122094,#122095,#122096,#122097,#122098,
#122099,#122100,#122101,#122102,#122103,#122104,#122105,#122106,#122107,
#122108,#122109,#122110,#122111,#122112,#122113),.UNSPECIFIED.,.T.,.F.,
(4,2,2,2,2,2,2,2,2,2,2,2,2,2,2,2,2,2,4),(0.,0.0438389442248891,0.0876506808071734,
0.131441119700838,0.175401927756875,0.196981044998168,0.218653481449126,
0.262711426228952,0.306215256616897,0.349443427925576,0.392423288200706,
0.435336799977891,0.478410083186314,0.521761202550275,0.543514873045346,
0.565221898322078,0.609273798985652,0.65308768053503,0.694240451037776),
 .UNSPECIFIED.);
#2813=B_SPLINE_CURVE_WITH_KNOTS('',3,(#122117,#122118,#122119,#122120,#122121,
#122122,#122123,#122124,#122125,#122126,#122127,#122128,#122129,#122130,
#122131,#122132,#122133,#122134,#122135,#122136,#122137,#122138),
 .UNSPECIFIED.,.F.,.F.,(4,2,2,2,2,2,2,2,2,2,4),(0.157584368232204,0.158006990486079,
0.177516943435242,0.19703668521392,0.217016218832852,0.237058339849597,
0.246878518641527,0.256719439219093,0.276906190297129,0.296633512619878,
0.315161445165693),.UNSPECIFIED.);
#2814=B_SPLINE_CURVE_WITH_KNOTS('',3,(#122142,#122143,#122144,#122145,#122146,
#122147,#122148,#122149,#122150,#122151,#122152,#122153,#122154,#122155,
#122156,#122157,#122158,#122159,#122160,#122161),.UNSPECIFIED.,.F.,.F.,
(4,2,2,2,2,2,2,2,2,4),(0.315161496914806,0.334675383606245,0.35416969963247,
0.373736756484906,0.393424082824057,0.403288169457306,0.413138376950184,
0.433210368829472,0.453206070159705,0.47274586514701),.UNSPECIFIED.);
#2815=B_SPLINE_CURVE_WITH_KNOTS('',3,(#122164,#122165,#122166,#122167,#122168,
#122169,#122170,#122171,#122172,#122173,#122174,#122175,#122176,#122177,
#122178,#122179,#122180,#122181,#122182,#122183,#122184,#122185,#122186,
#122187,#122188,#122189,#122190,#122191,#122192,#122193,#122194,#122195,
#122196,#122197,#122198,#122199,#122200,#122201,#122202,#122203,#122204,
#122205,#122206,#122207,#122208,#122209,#122210,#122211,#122212,#122213,
#122214,#122215,#122216,#122217),.UNSPECIFIED.,.T.,.F.,(4,2,2,2,2,2,2,2,
2,2,2,2,2,2,2,2,2,2,2,2,2,2,2,2,2,2,4),(0.,0.0322798876799803,0.0685606018541347,
0.108160762822184,0.150933434540211,0.194602986518808,0.23580572634401,
0.278247026689384,0.290959529057898,0.299011621102778,0.305277960644338,
0.312125374882226,0.323016402638355,0.356065834727992,0.389855079384049,
0.427272683016013,0.46783379181312,0.511548002156746,0.554746610986197,
0.593617964666262,0.627942371636709,0.639441324513358,0.646393389257674,
0.651954457241392,0.65936928222828,0.672885707450089,0.689781272001862),
 .UNSPECIFIED.);
#2816=B_SPLINE_CURVE_WITH_KNOTS('',3,(#122220,#122221,#122222,#122223,#122224,
#122225,#122226,#122227,#122228,#122229,#122230,#122231,#122232,#122233,
#122234,#122235,#122236,#122237,#122238,#122239,#122240,#122241,#122242,
#122243,#122244,#122245,#122246,#122247,#122248,#122249,#122250,#122251,
#122252,#122253,#122254,#122255),.UNSPECIFIED.,.T.,.F.,(4,2,2,2,2,2,2,2,
2,2,2,2,2,2,2,2,2,4),(0.,0.0430238998492563,0.0855495432772724,0.129093659280037,
0.172765482913272,0.194198251448662,0.215713043540718,0.260038404831785,
0.303483524869659,0.346505583580621,0.38911120796889,0.431553960019549,
0.474187363803603,0.517247893807355,0.560698863378657,0.604659525929812,
0.648310276563095,0.69036198545067),.UNSPECIFIED.);
#2817=B_SPLINE_CURVE_WITH_KNOTS('',3,(#122259,#122260,#122261,#122262,#122263,
#122264,#122265,#122266,#122267,#122268,#122269,#122270,#122271,#122272,
#122273,#122274,#122275,#122276,#122277,#122278,#122279,#122280),
 .UNSPECIFIED.,.F.,.F.,(4,2,2,2,2,2,2,2,2,2,4),(0.155290377429681,0.155736107592449,
0.17488551807521,0.194003788295001,0.213226575722084,0.232961080634223,
0.242634223098727,0.252327558687821,0.272217875481461,0.291885970236276,
0.310528859738257),.UNSPECIFIED.);
#2818=B_SPLINE_CURVE_WITH_KNOTS('',3,(#122284,#122285,#122286,#122287,#122288,
#122289,#122290,#122291,#122292,#122293,#122294,#122295,#122296,#122297,
#122298,#122299,#122300,#122301),.UNSPECIFIED.,.F.,.F.,(4,2,2,2,2,2,2,2,
4),(0.310529493700324,0.329692092162944,0.348793029124575,0.3679828392031,
0.387359973042316,0.407247623417337,0.427064981708464,0.446792783922369,
0.465819871130005),.UNSPECIFIED.);
#2819=B_SPLINE_CURVE_WITH_KNOTS('',3,(#122305,#122306,#122307,#122308,#122309,
#122310,#122311,#122312,#122313,#122314,#122315,#122316,#122317,#122318,
#122319,#122320,#122321,#122322,#122323,#122324,#122325,#122326,#122327,
#122328,#122329,#122330,#122331,#122332,#122333,#122334,#122335,#122336,
#122337,#122338,#122339,#122340),.UNSPECIFIED.,.T.,.F.,(4,2,2,2,2,2,2,2,
2,2,2,2,2,2,2,2,2,4),(0.,0.0586757670894926,0.117148553828277,0.175835299561973,
0.234617343239876,0.292853783791768,0.35112523429996,0.40934790866558,0.467429051180109,
0.525371799214443,0.583276714932037,0.641239111551701,0.670226582819686,
0.699216950303947,0.757975002952515,0.816444247800303,0.875085664577425,
0.931838732230833),.UNSPECIFIED.);
#2820=B_SPLINE_CURVE_WITH_KNOTS('',3,(#122344,#122345,#122346,#122347,#122348,
#122349,#122350,#122351,#122352,#122353,#122354,#122355,#122356,#122357,
#122358,#122359,#122360,#122361,#122362,#122363),.UNSPECIFIED.,.F.,.F.,
(4,2,2,2,2,2,2,2,2,4),(0.139760712682487,0.140067134145623,0.175076082565958,
0.210024263823074,0.245061416664295,0.27998722238202,0.314560327877607,
0.349142502650659,0.383701322132445,0.416632407884874),.UNSPECIFIED.);
#2821=B_SPLINE_CURVE_WITH_KNOTS('',3,(#122367,#122368,#122369,#122370,#122371,
#122372,#122373,#122374,#122375,#122376,#122377,#122378,#122379,#122380,
#122381,#122382,#122383,#122384,#122385,#122386,#122387,#122388,#122389),
 .UNSPECIFIED.,.F.,.F.,(4,2,2,2,2,2,3,2,2,2,4),(0.416632407884874,0.418204784014263,
0.452657939033403,0.487101288526142,0.521571286252258,0.537552757131005,
0.553655480527853,0.588723712999936,0.623672800339298,0.658668999727483,
0.69341619321034),.UNSPECIFIED.);
#2822=B_SPLINE_CURVE_WITH_KNOTS('',3,(#122393,#122394,#122395,#122396,#122397,
#122398,#122399,#122400,#122401,#122402,#122403,#122404,#122405,#122406,
#122407,#122408,#122409,#122410,#122411,#122412,#122413,#122414,#122415,
#122416,#122417,#122418,#122419,#122420,#122421,#122422,#122423,#122424,
#122425,#122426,#122427,#122428,#122429,#122430),.UNSPECIFIED.,.T.,.F.,
(4,2,2,2,2,2,2,2,2,2,2,2,2,2,2,2,2,2,4),(0.,0.050673276883592,0.101289176630062,
0.152081759329459,0.177020645452896,0.202374739783901,0.252767720361165,
0.303150046715415,0.353415021404996,0.403493331193659,0.45343162999718,
0.503373416551825,0.553446254375365,0.578529932675748,0.603629101080887,
0.653871646642357,0.704574133420325,0.75519545932242,0.804523692757691),
 .UNSPECIFIED.);
#2823=B_SPLINE_CURVE_WITH_KNOTS('',3,(#122434,#122435,#122436,#122437,#122438,
#122439,#122440,#122441,#122442,#122443,#122444,#122445,#122446,#122447,
#122448,#122449,#122450,#122451,#122452,#122453,#122454,#122455,#122456,
#122457,#122458),.UNSPECIFIED.,.F.,.F.,(4,2,2,2,2,2,2,2,2,2,3,4),(0.213033721720665,
0.213549478728336,0.24047802645704,0.267424502166104,0.294464476694524,
0.307719796467723,0.321150652985462,0.347819019993753,0.374470148743606,
0.401059222374504,0.426055563255932,0.426056605130622),.UNSPECIFIED.);
#2824=B_SPLINE_CURVE_WITH_KNOTS('',3,(#122462,#122463,#122464,#122465,#122466,
#122467,#122468,#122469,#122470,#122471,#122472,#122473,#122474,#122475,
#122476,#122477,#122478,#122479,#122480,#122481),.UNSPECIFIED.,.F.,.F.,
(4,2,2,2,2,2,2,2,2,4),(0.426056605130622,0.452518691987417,0.478993507171365,
0.50553229834979,0.5188187144497,0.532113581809939,0.5587398015711,0.585740731909802,
0.612676088223349,0.639089284976597),.UNSPECIFIED.);
#2825=B_SPLINE_CURVE_WITH_KNOTS('',3,(#122484,#122485,#122486,#122487,#122488,
#122489,#122490,#122491,#122492,#122493,#122494,#122495,#122496,#122497,
#122498,#122499,#122500,#122501,#122502,#122503,#122504,#122505,#122506,
#122507,#122508,#122509,#122510,#122511,#122512,#122513,#122514,#122515,
#122516,#122517,#122518,#122519,#122520,#122521,#122522,#122523,#122524,
#122525,#122526,#122527,#122528,#122529,#122530,#122531,#122532,#122533),
 .UNSPECIFIED.,.T.,.F.,(4,2,2,2,2,2,2,2,2,2,2,2,2,2,2,2,2,2,2,2,2,2,2,2,
4),(0.,0.0107674088208145,0.032050092364627,0.0758968238756297,0.113342112075795,
0.153841759557963,0.197424662011024,0.24094865716672,0.281477151458961,
0.315965112974783,0.329860021699639,0.338958849354584,0.347492432482236,
0.358682378546163,0.381656726340758,0.425505843569457,0.463082431170076,
0.503625071404071,0.547176362783087,0.590646422407844,0.630909084266853,
0.663727441955104,0.677240304474487,0.686199000451462,0.693838454416704),
 .UNSPECIFIED.);
#2826=B_SPLINE_CURVE_WITH_KNOTS('',3,(#122536,#122537,#122538,#122539,#122540,
#122541,#122542,#122543,#122544,#122545,#122546,#122547,#122548,#122549,
#122550,#122551,#122552,#122553,#122554,#122555,#122556,#122557,#122558,
#122559,#122560,#122561,#122562,#122563,#122564,#122565,#122566,#122567,
#122568,#122569,#122570,#122571,#122572,#122573),.UNSPECIFIED.,.T.,.F.,
(4,2,2,2,2,2,2,2,2,2,2,2,2,2,2,2,2,2,4),(0.,0.0438243930740146,0.0876062081298315,
0.131457732547539,0.175607022982147,0.197291180384503,0.241342381381052,
0.284837958123228,0.328055583488919,0.371028367060835,0.413942440611152,
0.457022969056832,0.500382292840913,0.522137595971807,0.543841887873517,
0.587887555125371,0.631697460152709,0.675489393505295,0.694245519838248),
 .UNSPECIFIED.);
#2827=B_SPLINE_CURVE_WITH_KNOTS('',3,(#122577,#122578,#122579,#122580,#122581,
#122582,#122583,#122584,#122585,#122586,#122587,#122588,#122589,#122590,
#122591,#122592,#122593,#122594,#122595,#122596,#122597,#122598),
 .UNSPECIFIED.,.F.,.F.,(4,2,2,2,2,2,2,2,2,2,4),(0.157602387106129,0.167770702836318,
0.187291656000666,0.207271901672337,0.227319605740903,0.237143104959657,
0.246987541016024,0.267178023530022,0.286901794386752,0.306504569661967,
0.315162938093162),.UNSPECIFIED.);
#2828=B_SPLINE_CURVE_WITH_KNOTS('',3,(#122602,#122603,#122604,#122605,#122606,
#122607,#122608,#122609,#122610,#122611,#122612,#122613,#122614,#122615,
#122616,#122617,#122618,#122619,#122620,#122621),.UNSPECIFIED.,.F.,.F.,
(4,2,2,2,2,2,2,2,2,4),(0.315162961924269,0.334653864296084,0.354176529092422,
0.373805857336121,0.393549777338162,0.403400597304252,0.423472399890395,
0.443466235193495,0.463424991039942,0.472765325199292),.UNSPECIFIED.);
#2829=B_SPLINE_CURVE_WITH_KNOTS('',3,(#122624,#122625,#122626,#122627,#122628,
#122629,#122630,#122631,#122632,#122633,#122634,#122635,#122636,#122637,
#122638,#122639,#122640,#122641,#122642,#122643,#122644,#122645,#122646,
#122647,#122648,#122649,#122650,#122651,#122652,#122653,#122654,#122655,
#122656,#122657,#122658,#122659,#122660,#122661,#122662,#122663,#122664,
#122665,#122666,#122667,#122668,#122669,#122670,#122671,#122672,#122673,
#122674,#122675),.UNSPECIFIED.,.T.,.F.,(4,2,2,2,2,2,2,2,2,2,2,2,2,2,2,2,
2,2,2,2,2,2,2,2,2,4),(0.,0.0256189301624599,0.0585560093974178,0.0952620183024296,
0.135208137493268,0.178316557997087,0.221875433422912,0.262673142368552,
0.302028045604151,0.315630477424899,0.323864618891318,0.33043727500203,
0.3391632615135,0.354876094361664,0.398358935388055,0.434466067107987,0.473802934543292,
0.516197041102924,0.559937408000424,0.601593888860772,0.644357103880208,
0.659194186873084,0.667768270573467,0.674987161506823,0.683465595734622,
0.689846633560524),.UNSPECIFIED.);
#2830=B_SPLINE_CURVE_WITH_KNOTS('',3,(#122678,#122679,#122680,#122681,#122682,
#122683,#122684,#122685,#122686,#122687,#122688,#122689,#122690,#122691,
#122692,#122693,#122694,#122695,#122696,#122697,#122698,#122699,#122700,
#122701,#122702,#122703,#122704,#122705,#122706,#122707,#122708,#122709,
#122710,#122711,#122712,#122713,#122714,#122715),.UNSPECIFIED.,.T.,.F.,
(4,2,2,2,2,2,2,2,2,2,2,2,2,2,2,2,2,2,4),(0.,0.0425025968360725,0.0851241096660763,
0.128708281636964,0.17255349411788,0.19408748717439,0.238446766102907,0.281883879757632,
0.324894484406876,0.367490323725331,0.409929583877134,0.452566309918705,
0.495632893687133,0.517333643790689,0.538995930030127,0.58297389480917,
0.626627855561898,0.670154211137559,0.690235808572164),.UNSPECIFIED.);
#2831=B_SPLINE_CURVE_WITH_KNOTS('',3,(#122719,#122720,#122721,#122722,#122723,
#122724,#122725,#122726,#122727,#122728,#122729,#122730,#122731,#122732,
#122733,#122734,#122735,#122736,#122737,#122738,#122739,#122740),
 .UNSPECIFIED.,.F.,.F.,(4,2,2,2,2,2,2,2,2,2,4),(0.155260120941377,0.165093014777806,
0.184211383687861,0.203435996037152,0.223178890816999,0.232858171175101,
0.242559308220261,0.262463457205943,0.282125538253841,0.301453343875752,
0.31047848171439),.UNSPECIFIED.);
#2832=B_SPLINE_CURVE_WITH_KNOTS('',3,(#122744,#122745,#122746,#122747,#122748,
#122749,#122750,#122751,#122752,#122753,#122754,#122755,#122756,#122757,
#122758,#122759,#122760,#122761,#122762,#122763),.UNSPECIFIED.,.F.,.F.,
(4,2,2,2,2,2,2,2,2,4),(0.310479060901921,0.329589414222322,0.348718434799171,
0.367999675413274,0.387476460125835,0.39720372215973,0.417032430741726,
0.436763267001542,0.456424627637958,0.465739181843299),.UNSPECIFIED.);
#2833=B_SPLINE_CURVE_WITH_KNOTS('',3,(#122767,#122768,#122769,#122770,#122771,
#122772,#122773,#122774,#122775,#122776,#122777,#122778,#122779,#122780,
#122781,#122782,#122783,#122784,#122785,#122786,#122787,#122788,#122789,
#122790,#122791,#122792,#122793,#122794,#122795,#122796,#122797,#122798,
#122799,#122800),.UNSPECIFIED.,.T.,.F.,(4,2,2,2,2,2,2,2,2,2,2,2,2,2,2,2,
4),(0.,0.0585926765660801,0.117060852770377,0.175963863544342,0.234757324802159,
0.292998945417122,0.351235837265488,0.409377235300801,0.467380436815063,
0.525306461368404,0.583257580760452,0.641271299034342,0.700216836299,0.75869435519625,
0.817268571442382,0.876149337626487,0.931978006137413),.UNSPECIFIED.);
#2834=B_SPLINE_CURVE_WITH_KNOTS('',3,(#122804,#122805,#122806,#122807,#122808,
#122809,#122810,#122811,#122812,#122813,#122814,#122815,#122816,#122817,
#122818,#122819,#122820,#122821,#122822,#122823),.UNSPECIFIED.,.F.,.F.,
(4,2,2,2,2,2,2,2,2,4),(0.139772579008333,0.140146289744173,0.17514281240646,
0.210084776298185,0.245174835201649,0.28010335525236,0.314672240383326,
0.34923361254127,0.383757569691577,0.416643770851934),.UNSPECIFIED.);
#2835=B_SPLINE_CURVE_WITH_KNOTS('',3,(#122827,#122828,#122829,#122830,#122831,
#122832,#122833,#122834,#122835,#122836,#122837,#122838,#122839,#122840,
#122841,#122842,#122843,#122844,#122845,#122846,#122847),.UNSPECIFIED.,
 .F.,.F.,(4,2,2,2,2,3,2,2,2,4),(0.416643770851934,0.418233336826679,0.452686571599011,
0.487154891484257,0.521648920350911,0.553720957181638,0.588667950785789,
0.623652766915587,0.658756034818722,0.693493536189971),.UNSPECIFIED.);
#2836=B_SPLINE_CURVE_WITH_KNOTS('',3,(#122851,#122852,#122853,#122854,#122855,
#122856,#122857,#122858,#122859,#122860,#122861,#122862,#122863,#122864,
#122865,#122866,#122867,#122868,#122869,#122870,#122871,#122872,#122873,
#122874,#122875,#122876,#122877,#122878,#122879,#122880,#122881,#122882,
#122883,#122884,#122885,#122886,#122887,#122888),.UNSPECIFIED.,.T.,.F.,
(4,2,2,2,2,2,2,2,2,2,2,2,2,2,2,2,2,2,4),(0.,0.0507229383181265,0.101364562659594,
0.152264741697718,0.177621136402009,0.228004403729544,0.278358115075993,
0.328590359266365,0.378650356083607,0.428595870888352,0.478566224724603,
0.528671625350514,0.553761862420612,0.578863709834058,0.62981803707715,
0.680469487571423,0.731173027366969,0.782017463135863,0.804541332944367),
 .UNSPECIFIED.);
#2837=B_SPLINE_CURVE_WITH_KNOTS('',3,(#122892,#122893,#122894,#122895,#122896,
#122897,#122898,#122899,#122900,#122901,#122902,#122903,#122904,#122905,
#122906,#122907,#122908,#122909,#122910,#122911,#122912,#122913,#122914,
#122915,#122916),.UNSPECIFIED.,.F.,.F.,(4,2,2,2,2,2,2,2,2,2,3,4),(0.213066867406632,
0.227903691482098,0.254869439722097,0.28187163635418,0.295099259249335,
0.308362448361286,0.335302105137811,0.361936581907251,0.38850722497422,
0.415007489812642,0.426072923770395,0.426074041187361),.UNSPECIFIED.);
#2838=B_SPLINE_CURVE_WITH_KNOTS('',3,(#122920,#122921,#122922,#122923,#122924,
#122925,#122926,#122927,#122928,#122929,#122930,#122931,#122932,#122933,
#122934,#122935,#122936,#122937,#122938,#122939),.UNSPECIFIED.,.F.,.F.,
(4,2,2,2,2,2,2,2,2,4),(0.426074041187361,0.452544161682515,0.479064421758956,
0.505653908774553,0.51895026828597,0.546020643171311,0.572994766851648,
0.599970746744037,0.626979273531269,0.639139791177027),.UNSPECIFIED.);
#2839=B_SPLINE_CURVE_WITH_KNOTS('',3,(#122943,#122944,#122945,#122946,#122947,
#122948,#122949,#122950,#122951,#122952,#122953,#122954,#122955,#122956,
#122957,#122958,#122959,#122960,#122961,#122962,#122963,#122964,#122965,
#122966,#122967,#122968,#122969,#122970,#122971,#122972,#122973,#122974,
#122975,#122976,#122977,#122978,#122979,#122980),.UNSPECIFIED.,.T.,.F.,
(4,2,2,2,2,2,2,2,2,2,2,2,2,2,2,2,2,2,4),(0.,0.0437776276195715,0.0875679900144141,
0.131571445742023,0.153177954178476,0.175159227728739,0.218816832071539,
0.262314817569206,0.305533297393407,0.348505149880481,0.39141745318968,
0.43449638406335,0.477854755514743,0.499610120533722,0.52132723824042,0.565391550289609,
0.609202037344911,0.652974164254737,0.694228661865369),.UNSPECIFIED.);
#2840=B_SPLINE_CURVE_WITH_KNOTS('',3,(#122984,#122985,#122986,#122987,#122988,
#122989,#122990,#122991,#122992,#122993,#122994,#122995,#122996,#122997,
#122998,#122999,#123000,#123001,#123002,#123003,#123004,#123005),
 .UNSPECIFIED.,.F.,.F.,(4,2,2,2,2,2,2,2,2,2,4),(0.157582047532889,0.158016502864322,
0.177538316893226,0.197519409217786,0.217579884773166,0.227411236627675,
0.237264279446347,0.257255031976338,0.276977952611641,0.296579243132181,
0.315156893082293),.UNSPECIFIED.);
#2841=B_SPLINE_CURVE_WITH_KNOTS('',3,(#123009,#123010,#123011,#123012,#123013,
#123014,#123015,#123016,#123017,#123018,#123019,#123020,#123021,#123022,
#123023,#123024,#123025,#123026,#123027,#123028),.UNSPECIFIED.,.F.,.F.,
(4,2,2,2,2,2,2,2,2,4),(0.315157288501979,0.334652252907642,0.354224086191744,
0.373916998640349,0.383787341684051,0.393643851193707,0.413723260089021,
0.433716344820741,0.453665515143594,0.472739336034868),.UNSPECIFIED.);
#2842=B_SPLINE_CURVE_WITH_KNOTS('',3,(#123032,#123033,#123034,#123035,#123036,
#123037,#123038,#123039,#123040,#123041,#123042,#123043,#123044,#123045,
#123046,#123047,#123048,#123049,#123050,#123051,#123052,#123053,#123054,
#123055,#123056,#123057,#123058,#123059,#123060,#123061,#123062,#123063,
#123064,#123065,#123066,#123067,#123068,#123069),.UNSPECIFIED.,.T.,.F.,
(4,2,2,2,2,2,2,2,2,2,2,2,2,2,2,2,2,2,4),(0.,0.0425264858563654,0.0860379263816963,
0.129775411807249,0.151257181847517,0.172834633622422,0.217270439947479,
0.26070584185836,0.303710158081262,0.346298776724129,0.388734672817207,
0.431373528152147,0.474445047486068,0.496148628393663,0.517840489242917,
0.561870047910052,0.60553584876945,0.649023088411614,0.690222497519466),
 .UNSPECIFIED.);
#2843=B_SPLINE_CURVE_WITH_KNOTS('',3,(#123073,#123074,#123075,#123076,#123077,
#123078,#123079,#123080,#123081,#123082,#123083,#123084,#123085,#123086,
#123087,#123088,#123089,#123090,#123091,#123092,#123093,#123094),
 .UNSPECIFIED.,.F.,.F.,(4,2,2,2,2,2,2,2,2,2,4),(0.155239240071724,0.155545159095705,
0.174663418665415,0.193888856365997,0.213651467942332,0.223344964073576,
0.233063963677857,0.252999263159233,0.272652527427125,0.291976817994604,
0.310472561331592),.UNSPECIFIED.);
#2844=B_SPLINE_CURVE_WITH_KNOTS('',3,(#123098,#123099,#123100,#123101,#123102,
#123103,#123104,#123105,#123106,#123107,#123108,#123109,#123110,#123111,
#123112,#123113,#123114,#123115,#123116,#123117),.UNSPECIFIED.,.F.,.F.,
(4,2,2,2,2,2,2,2,2,4),(0.310472731789002,0.329571781965114,0.348764795900237,
0.368147384944638,0.377891730151636,0.387634194863333,0.407490285800687,
0.427228176729605,0.4468714803911,0.465711801403316),.UNSPECIFIED.);
#2845=B_SPLINE_CURVE_WITH_KNOTS('',3,(#123121,#123122,#123123,#123124,#123125,
#123126,#123127,#123128,#123129,#123130,#123131,#123132,#123133,#123134,
#123135,#123136,#123137,#123138,#123139,#123140,#123141,#123142,#123143,
#123144,#123145,#123146,#123147,#123148,#123149,#123150,#123151,#123152,
#123153,#123154),.UNSPECIFIED.,.T.,.F.,(4,2,2,2,2,2,2,2,2,2,2,2,2,2,2,2,
4),(0.,0.0584699775520228,0.117165575370348,0.175948938510645,0.234185086571246,
0.292451210877633,0.350662965265276,0.408733587688452,0.466673944838772,
0.524585872842989,0.582557670909233,0.640581469672834,0.699285196519633,
0.757754370947284,0.816432379354141,0.875275608146019,0.931978925642126),
 .UNSPECIFIED.);
#2846=B_SPLINE_CURVE_WITH_KNOTS('',3,(#123158,#123159,#123160,#123161,#123162,
#123163,#123164,#123165,#123166,#123167,#123168,#123169,#123170,#123171,
#123172,#123173,#123174,#123175,#123176,#123177),.UNSPECIFIED.,.F.,.F.,
(4,2,2,2,2,2,2,2,2,4),(0.139770748206514,0.140049608785387,0.174997299730298,
0.210031400032424,0.244957219954342,0.279529040299516,0.314107503356081,
0.348661078446231,0.383160589516241,0.416637496476957),.UNSPECIFIED.);
#2847=B_SPLINE_CURVE_WITH_KNOTS('',3,(#123181,#123182,#123183,#123184,#123185,
#123186,#123187,#123188,#123189,#123190,#123191,#123192,#123193,#123194,
#123195,#123196,#123197,#123198,#123199,#123200,#123201),.UNSPECIFIED.,
 .F.,.F.,(4,2,2,2,2,3,2,2,2,4),(0.416637496476957,0.417613792200944,0.452061028986347,
0.486535436540338,0.521032083188937,0.553718729366543,0.588666002789255,
0.623678907144246,0.658750981999921,0.693489477573057),.UNSPECIFIED.);
#2848=B_SPLINE_CURVE_WITH_KNOTS('',3,(#123205,#123206,#123207,#123208,#123209,
#123210,#123211,#123212,#123213,#123214,#123215,#123216,#123217,#123218,
#123219,#123220,#123221,#123222,#123223,#123224,#123225,#123226,#123227,
#123228,#123229,#123230,#123231,#123232,#123233,#123234,#123235,#123236,
#123237,#123238,#123239,#123240,#123241,#123242),.UNSPECIFIED.,.T.,.F.,
(4,2,2,2,2,2,2,2,2,2,2,2,2,2,2,2,2,2,4),(0.,0.050638733810621,0.101400253214682,
0.12631607681873,0.151671805389745,0.202060284621524,0.252423238238989,
0.302663024997971,0.352724854939833,0.402666384079521,0.452629817735602,
0.502729034043684,0.52781857736665,0.552920189788985,0.603916159489469,
0.654579944565998,0.705256808810519,0.7560470808032,0.804537568823649),
 .UNSPECIFIED.);
#2849=B_SPLINE_CURVE_WITH_KNOTS('',3,(#123246,#123247,#123248,#123249,#123250,
#123251,#123252,#123253,#123254,#123255,#123256,#123257,#123258,#123259,
#123260,#123261,#123262,#123263,#123264,#123265,#123266,#123267),
 .UNSPECIFIED.,.F.,.F.,(4,2,2,2,2,2,2,2,2,2,4),(0.213045628511085,0.214611385801652,
0.241571963452503,0.268595658943336,0.281838232681206,0.29526966423576,
0.321934713953309,0.348573294216842,0.375146966582712,0.401647612531603,
0.426064000816764),.UNSPECIFIED.);
#2850=B_SPLINE_CURVE_WITH_KNOTS('',3,(#123271,#123272,#123273,#123274,#123275,
#123276,#123277,#123278,#123279,#123280,#123281,#123282,#123283,#123284,
#123285,#123286,#123287,#123288,#123289,#123290),.UNSPECIFIED.,.F.,.F.,
(4,2,2,2,2,2,2,2,2,4),(0.426064655025976,0.452551754020046,0.479105237030249,
0.492395062055931,0.505691423761415,0.532783295767128,0.55976324004501,
0.586724469365241,0.613704084643966,0.639109629327848),.UNSPECIFIED.);
#2851=B_SPLINE_CURVE_WITH_KNOTS('',3,(#123294,#123295,#123296,#123297,#123298,
#123299,#123300,#123301,#123302,#123303,#123304,#123305,#123306,#123307,
#123308,#123309,#123310,#123311,#123312,#123313,#123314,#123315,#123316,
#123317,#123318,#123319,#123320,#123321,#123322,#123323,#123324,#123325,
#123326,#123327,#123328,#123329),.UNSPECIFIED.,.T.,.F.,(4,2,2,2,2,2,2,2,
2,2,2,2,2,2,2,2,2,4),(0.,0.043833939544088,0.0876547626552344,0.13171418373345,
0.176143188576216,0.219711530800857,0.263036228023697,0.306089647100756,
0.349005450632323,0.392008244919775,0.435266561780069,0.478772277691574,
0.500403324464899,0.544338765949995,0.588137875440213,0.63201610258223,
0.674982061745284,0.694353973193238),.UNSPECIFIED.);
#2852=B_SPLINE_CURVE_WITH_KNOTS('',3,(#123333,#123334,#123335,#123336,#123337,
#123338,#123339,#123340,#123341,#123342,#123343,#123344,#123345,#123346,
#123347,#123348,#123349,#123350,#123351,#123352),.UNSPECIFIED.,.F.,.F.,
(4,2,2,2,2,2,2,2,2,4),(0.157606283114567,0.167956263024278,0.18794232221838,
0.20795897095516,0.228048601843927,0.248201222227485,0.26790407483132,0.287487183630145,
0.306988348642051,0.31521639087299),.UNSPECIFIED.);
#2853=B_SPLINE_CURVE_WITH_KNOTS('',3,(#123356,#123357,#123358,#123359,#123360,
#123361,#123362,#123363,#123364,#123365,#123366,#123367,#123368,#123369,
#123370,#123371,#123372,#123373,#123374,#123375),.UNSPECIFIED.,.F.,.F.,
(4,2,2,2,2,2,2,2,2,4),(0.315216519374046,0.334753816642054,0.354403128902944,
0.374535263751892,0.384354671581488,0.404377048151514,0.424363772031088,
0.444136761249955,0.463641311616163,0.472822673987557),.UNSPECIFIED.);
#2854=B_SPLINE_CURVE_WITH_KNOTS('',3,(#123379,#123380,#123381,#123382,#123383,
#123384,#123385,#123386,#123387,#123388,#123389,#123390,#123391,#123392,
#123393,#123394,#123395,#123396,#123397,#123398,#123399,#123400,#123401,
#123402,#123403,#123404,#123405,#123406,#123407,#123408,#123409,#123410,
#123411,#123412,#123413,#123414,#123415,#123416),.UNSPECIFIED.,.T.,.F.,
(4,2,2,2,2,2,2,2,2,2,2,2,2,2,2,2,2,2,4),(0.,0.0426485590853426,0.0862402884782325,
0.130075390184566,0.151600424496342,0.195934123792694,0.239336229067572,
0.282303133840975,0.324871762696591,0.367316422243404,0.409987876619906,
0.453097218074252,0.474786527840847,0.496414747803411,0.540321419594795,
0.583944828411629,0.62749138901914,0.670027574651375,0.69023199317909),
 .UNSPECIFIED.);
#2855=B_SPLINE_CURVE_WITH_KNOTS('',3,(#123420,#123421,#123422,#123423,#123424,
#123425,#123426,#123427,#123428,#123429,#123430,#123431,#123432,#123433,
#123434,#123435,#123436,#123437,#123438,#123439,#123440,#123441),
 .UNSPECIFIED.,.F.,.F.,(4,2,2,2,2,2,2,2,2,2,4),(0.155261651907409,0.16527671528697,
0.184519016768904,0.204259152541559,0.213934192699869,0.223628296706432,
0.24351518419013,0.263160537961134,0.282467130496838,0.301609884756148,
0.310478261413411),.UNSPECIFIED.);
#2856=B_SPLINE_CURVE_WITH_KNOTS('',3,(#123445,#123446,#123447,#123448,#123449,
#123450,#123451,#123452,#123453,#123454,#123455,#123456,#123457,#123458,
#123459,#123460,#123461,#123462,#123463,#123464),.UNSPECIFIED.,.F.,.F.,
(4,2,2,2,2,2,2,2,2,4),(0.310478282765048,0.329618019148117,0.348918877254669,
0.368809358815657,0.378523932330328,0.398324219984893,0.418040807624495,
0.43749361537484,0.456631081663014,0.46573991332082),.UNSPECIFIED.);
#2857=B_SPLINE_CURVE_WITH_KNOTS('',3,(#123468,#123469,#123470,#123471,#123472,
#123473,#123474,#123475,#123476,#123477,#123478,#123479,#123480,#123481,
#123482,#123483,#123484,#123485,#123486,#123487,#123488,#123489,#123490,
#123491,#123492,#123493,#123494,#123495,#123496,#123497,#123498,#123499,
#123500,#123501),.UNSPECIFIED.,.T.,.F.,(4,2,2,2,2,2,2,2,2,2,2,2,2,2,2,2,
4),(0.,0.058563364489267,0.117704649598256,0.175927357335253,0.234203267650359,
0.29247366123109,0.350626680658072,0.408614250475086,0.466507970326649,
0.524426802488493,0.582422733706092,0.640447373658858,0.698997907681633,
0.757505974204621,0.816205252734419,0.874894888625525,0.931980995563416),
 .UNSPECIFIED.);
#2858=B_SPLINE_CURVE_WITH_KNOTS('',3,(#123505,#123506,#123507,#123508,#123509,
#123510,#123511,#123512,#123513,#123514,#123515,#123516,#123517,#123518,
#123519,#123520,#123521,#123522,#123523,#123524),.UNSPECIFIED.,.F.,.F.,
(4,2,2,2,2,2,2,2,2,4),(0.139768652132161,0.139884269762596,0.174878693268074,
0.2100959056963,0.244664521169186,0.279252724422164,0.313834457306522,0.348367398742558,
0.382835795250566,0.416634411007083),.UNSPECIFIED.);
#2859=B_SPLINE_CURVE_WITH_KNOTS('',3,(#123528,#123529,#123530,#123531,#123532,
#123533,#123534,#123535,#123536,#123537,#123538,#123539,#123540,#123541,
#123542,#123543,#123544,#123545,#123546,#123547,#123548),.UNSPECIFIED.,
 .F.,.F.,(4,2,2,2,2,3,2,2,2,4),(0.416634411007083,0.417269899088962,0.451717700829539,
0.48620037123172,0.520698761065574,0.55371684967054,0.588663626154184,0.623659124796111,
0.658654452558276,0.693485501802701),.UNSPECIFIED.);
#2860=B_SPLINE_CURVE_WITH_KNOTS('',3,(#123552,#123553,#123554,#123555,#123556,
#123557,#123558,#123559,#123560,#123561,#123562,#123563,#123564,#123565,
#123566,#123567,#123568,#123569,#123570,#123571,#123572,#123573,#123574,
#123575,#123576,#123577,#123578,#123579,#123580,#123581,#123582,#123583,
#123584,#123585,#123586,#123587,#123588,#123589),.UNSPECIFIED.,.T.,.F.,
(4,2,2,2,2,2,2,2,2,2,2,2,2,2,2,2,2,2,4),(0.,0.0506163528267545,0.101414878043581,
0.126365601401302,0.177244213141222,0.227568438122892,0.277767225411541,
0.327809330368101,0.377764479210017,0.427767296504768,0.477908463703247,
0.503005947479194,0.52806740581208,0.578867942145032,0.62948374284351,0.680281858769973,
0.73128102309058,0.782192581946867,0.804565921037956),.UNSPECIFIED.);
#2861=B_SPLINE_CURVE_WITH_KNOTS('',3,(#123593,#123594,#123595,#123596,#123597,
#123598,#123599,#123600,#123601,#123602,#123603,#123604,#123605,#123606,
#123607,#123608,#123609,#123610,#123611,#123612,#123613,#123614,#123615,
#123616,#123617),.UNSPECIFIED.,.F.,.F.,(4,2,2,2,2,2,2,2,2,2,3,4),(0.213105558873963,
0.227668433906905,0.254627533146885,0.267825149105576,0.281051705768159,
0.307989464834126,0.334608596622551,0.36116368773351,0.387657442427522,
0.414131180745578,0.426078364283007,0.426115006982538),.UNSPECIFIED.);
#2862=B_SPLINE_CURVE_WITH_KNOTS('',3,(#123621,#123622,#123623,#123624,#123625,
#123626,#123627,#123628,#123629,#123630,#123631,#123632,#123633,#123634,
#123635,#123636,#123637,#123638,#123639,#123640),.UNSPECIFIED.,.F.,.F.,
(4,2,2,2,2,2,2,2,2,4),(0.426115006982538,0.452619111505283,0.479224276888074,
0.492480316918045,0.51947355541356,0.546429257856091,0.573453669608358,
0.600249948544724,0.626767102937182,0.63918392315697),.UNSPECIFIED.);
#2863=B_SPLINE_CURVE_WITH_KNOTS('',3,(#123644,#123645,#123646,#123647,#123648,
#123649,#123650,#123651,#123652,#123653,#123654,#123655,#123656,#123657,
#123658,#123659,#123660,#123661,#123662,#123663,#123664,#123665,#123666,
#123667,#123668,#123669,#123670,#123671,#123672,#123673,#123674,#123675,
#123676,#123677,#123678,#123679),.UNSPECIFIED.,.T.,.F.,(4,2,2,2,2,2,2,2,
2,2,2,2,2,2,2,2,2,4),(0.,0.0438004959938472,0.0877618839639682,0.132083039219552,
0.176121014722894,0.219586138844758,0.262771060863382,0.305729705032781,
0.348658957103483,0.391776284984157,0.435171792857276,0.456919677130482,
0.478577335014969,0.522551998360091,0.566354050965616,0.610193917091003,
0.654085372794423,0.694370484526123),.UNSPECIFIED.);
#2864=B_SPLINE_CURVE_WITH_KNOTS('',3,(#123683,#123684,#123685,#123686,#123687,
#123688,#123689,#123690,#123691,#123692,#123693,#123694,#123695,#123696,
#123697,#123698,#123699,#123700,#123701,#123702),.UNSPECIFIED.,.F.,.F.,
(4,2,2,2,2,2,2,2,2,4),(0.157563609058178,0.15782359728517,0.17781025817529,
0.197849116873822,0.217969925178253,0.238143964435893,0.257850129783055,
0.277435616699145,0.296937498491984,0.315195637226173),.UNSPECIFIED.);
#2865=B_SPLINE_CURVE_WITH_KNOTS('',3,(#123706,#123707,#123708,#123709,#123710,
#123711,#123712,#123713,#123714,#123715,#123716,#123717,#123718,#123719,
#123720,#123721,#123722,#123723,#123724,#123725,#123726,#123727,#123728),
 .UNSPECIFIED.,.F.,.F.,(4,3,2,2,2,2,2,2,2,2,4),(0.315195637226173,0.315221189479864,
0.334810208300643,0.354519738182407,0.364371264592903,0.374204660308851,
0.394247715670578,0.414236021170778,0.434007786695688,0.453513973251726,
0.472784798538042),.UNSPECIFIED.);
#2866=B_SPLINE_CURVE_WITH_KNOTS('',3,(#123732,#123733,#123734,#123735,#123736,
#123737,#123738,#123739,#123740,#123741,#123742,#123743,#123744,#123745,
#123746,#123747,#123748,#123749,#123750,#123751,#123752,#123753,#123754,
#123755,#123756,#123757,#123758,#123759,#123760,#123761,#123762,#123763,
#123764,#123765,#123766,#123767,#123768,#123769),.UNSPECIFIED.,.T.,.F.,
(4,2,2,2,2,2,2,2,2,2,2,2,2,2,2,2,2,2,4),(0.,0.0435335379564071,0.0872805418243845,
0.10876424930064,0.130340015627335,0.1747602629752,0.218165610708909,0.261131650700908,
0.3036977785209,0.346142301938299,0.38881760853067,0.431932992538991,0.453649473472543,
0.475314817814312,0.519285676559382,0.562925631864407,0.606429094795108,
0.649431149953087,0.69027309180811),.UNSPECIFIED.);
#2867=B_SPLINE_CURVE_WITH_KNOTS('',3,(#123773,#123774,#123775,#123776,#123777,
#123778,#123779,#123780,#123781,#123782,#123783,#123784,#123785,#123786,
#123787,#123788,#123789,#123790,#123791,#123792,#123793,#123794),
 .UNSPECIFIED.,.F.,.F.,(4,2,2,2,2,2,2,2,2,2,4),(0.155223965039871,0.155362142301834,
0.174603165145324,0.194367025915675,0.204058790757966,0.213773625392455,
0.233696561634035,0.253338083772129,0.272647283209335,0.291791090103793,
0.31047162775744),.UNSPECIFIED.);
#2868=B_SPLINE_CURVE_WITH_KNOTS('',3,(#123798,#123799,#123800,#123801,#123802,
#123803,#123804,#123805,#123806,#123807,#123808,#123809,#123810,#123811,
#123812,#123813,#123814,#123815,#123816,#123817,#123818,#123819,#123820),
 .UNSPECIFIED.,.F.,.F.,(4,3,2,2,2,2,2,2,2,2,4),(0.31047162775744,0.310496225533347,
0.329706636164436,0.349109981103316,0.358849708851866,0.368583376798189,
0.38841786259702,0.408144271063843,0.427594276693172,0.446734179455907,
0.465720190573218),.UNSPECIFIED.);
#2869=B_SPLINE_CURVE_WITH_KNOTS('',3,(#123824,#123825,#123826,#123827,#123828,
#123829,#123830,#123831,#123832,#123833,#123834,#123835,#123836,#123837,
#123838,#123839,#123840,#123841,#123842,#123843,#123844,#123845,#123846,
#123847,#123848,#123849,#123850,#123851,#123852,#123853,#123854,#123855,
#123856,#123857,#123858,#123859),.UNSPECIFIED.,.T.,.F.,(4,2,2,2,2,2,2,2,
2,2,2,2,2,2,2,2,2,4),(0.,0.0586079814967797,0.0874078554054557,0.146201962571134,
0.204435711225752,0.262657544525573,0.320782955246569,0.378780112689523,
0.436715022410588,0.494682759830729,0.552706578295632,0.611539730354419,
0.669983012530477,0.728607350829478,0.787564378993769,0.846487759981544,
0.905061888398866,0.931862013437082),.UNSPECIFIED.);
#2870=B_SPLINE_CURVE_WITH_KNOTS('',3,(#123863,#123864,#123865,#123866,#123867,
#123868,#123869,#123870,#123871,#123872,#123873,#123874,#123875,#123876,
#123877,#123878,#123879,#123880,#123881,#123882,#123883,#123884),
 .UNSPECIFIED.,.F.,.F.,(4,2,2,2,2,2,2,2,2,2,4),(0.139816053457858,0.140268245540218,
0.175242647417502,0.192387726565067,0.227315557315772,0.261878269111605,
0.29643087927095,0.330947507666127,0.365421949126044,0.399880936816061,
0.416635497165623),.UNSPECIFIED.);
#2871=B_SPLINE_CURVE_WITH_KNOTS('',3,(#123888,#123889,#123890,#123891,#123892,
#123893,#123894,#123895,#123896,#123897,#123898,#123899,#123900,#123901,
#123902,#123903,#123904,#123905,#123906,#123907,#123908),.UNSPECIFIED.,
 .F.,.F.,(4,2,2,2,2,3,2,2,2,4),(0.416635497165623,0.434357841681837,0.468856471627119,
0.503897324003799,0.53882431509626,0.553651505064719,0.588736869748285,
0.623903021104051,0.658978159339036,0.693467558522578),.UNSPECIFIED.);
#2872=B_SPLINE_CURVE_WITH_KNOTS('',3,(#123912,#123913,#123914,#123915,#123916,
#123917,#123918,#123919,#123920,#123921,#123922,#123923,#123924,#123925,
#123926,#123927,#123928,#123929,#123930,#123931,#123932,#123933,#123934,
#123935,#123936,#123937,#123938,#123939,#123940,#123941,#123942,#123943,
#123944,#123945,#123946,#123947,#123948,#123949),.UNSPECIFIED.,.T.,.F.,
(4,2,2,2,2,2,2,2,2,2,2,2,2,2,2,2,2,2,4),(0.,0.0507410411059291,0.0756428906135374,
0.101000376964068,0.151385667510921,0.201733650877737,0.251953710970444,
0.302003032346441,0.35194855798103,0.401931246270778,0.452052993923605,
0.477147607318242,0.502251198424077,0.553162007043944,0.603806479049535,
0.6545319614579,0.705395871704498,0.756192455948636,0.804565083083937),
 .UNSPECIFIED.);
#2873=B_SPLINE_CURVE_WITH_KNOTS('',3,(#123953,#123954,#123955,#123956,#123957,
#123958,#123959,#123960,#123961,#123962,#123963,#123964,#123965,#123966,
#123967,#123968,#123969,#123970,#123971,#123972,#123973,#123974),
 .UNSPECIFIED.,.F.,.F.,(4,2,2,2,2,2,2,2,2,2,4),(0.213054244451595,0.215140827835265,
0.242150406659373,0.25538302799454,0.268815218273894,0.295477383870316,
0.322106682092898,0.348669736568472,0.375165012920701,0.401633838738512,
0.426079206306101),.UNSPECIFIED.);
#2874=B_SPLINE_CURVE_WITH_KNOTS('',3,(#123978,#123979,#123980,#123981,#123982,
#123983,#123984,#123985,#123986,#123987,#123988,#123989,#123990,#123991,
#123992,#123993,#123994,#123995,#123996,#123997),.UNSPECIFIED.,.F.,.F.,
(4,2,2,2,2,2,2,2,2,4),(0.426079625809021,0.452645595099671,0.465938337013661,
0.479227879223233,0.506279278725265,0.533249557531349,0.560234630804096,
0.587252678468645,0.614252916234622,0.639133450757696),.UNSPECIFIED.);
#2875=B_SPLINE_CURVE_WITH_KNOTS('',3,(#124001,#124002,#124003,#124004,#124005,
#124006,#124007,#124008,#124009,#124010,#124011,#124012,#124013,#124014,
#124015,#124016,#124017,#124018,#124019,#124020,#124021,#124022,#124023,
#124024,#124025,#124026,#124027,#124028,#124029,#124030,#124031,#124032,
#124033,#124034,#124035,#124036),.UNSPECIFIED.,.T.,.F.,(4,2,2,2,2,2,2,2,
2,2,2,2,2,2,2,2,2,4),(0.,0.0439031127094954,0.065447765592922,0.109902791721661,
0.153561484989613,0.19704719047054,0.240247824587854,0.28320987925128,0.326130003594881,
0.369231772635403,0.412614437139118,0.456180877068987,0.500239656278008,
0.544042664929523,0.587798556171279,0.631569949867552,0.67532475002012,
0.694414801328956),.UNSPECIFIED.);
#2876=B_SPLINE_CURVE_WITH_KNOTS('',3,(#124040,#124041,#124042,#124043,#124044,
#124045,#124046,#124047,#124048,#124049,#124050,#124051,#124052,#124053,
#124054,#124055,#124056,#124057,#124058,#124059,#124060,#124061,#124062,
#124063,#124064),.UNSPECIFIED.,.F.,.F.,(4,2,2,2,2,2,2,2,2,2,3,4),(0.157670270859278,
0.158917049885251,0.178952570765188,0.188772784740277,0.198617965338202,
0.218827169194992,0.238590756353538,0.258240538801305,0.277776837156618,
0.29726705640842,0.315235161822161,0.315256462625511),.UNSPECIFIED.);
#2877=B_SPLINE_CURVE_WITH_KNOTS('',3,(#124068,#124069,#124070,#124071,#124072,
#124073,#124074,#124075,#124076,#124077,#124078,#124079,#124080,#124081,
#124082,#124083,#124084,#124085),.UNSPECIFIED.,.F.,.F.,(4,2,2,2,2,2,2,2,
4),(0.315256462625511,0.334880195493556,0.354636232285665,0.374768960524188,
0.394798226033378,0.414755231257366,0.434683621715996,0.454191919873264,
0.472905432681439),.UNSPECIFIED.);
#2878=B_SPLINE_CURVE_WITH_KNOTS('',3,(#124089,#124090,#124091,#124092,#124093,
#124094,#124095,#124096,#124097,#124098,#124099,#124100,#124101,#124102,
#124103,#124104,#124105,#124106,#124107,#124108,#124109,#124110,#124111,
#124112,#124113,#124114,#124115,#124116,#124117,#124118,#124119,#124120,
#124121,#124122,#124123,#124124,#124125,#124126),.UNSPECIFIED.,.T.,.F.,
(4,2,2,2,2,2,2,2,2,2,2,2,2,2,2,2,2,2,4),(0.,0.0435871080099574,0.0873540036482257,
0.108835854513303,0.153089303041548,0.196450323283551,0.239370816524269,
0.281917126448144,0.324379281818892,0.367100824058561,0.410266027335005,
0.431906304365628,0.453468385800544,0.497254546642128,0.540844614594443,
0.584460030183684,0.626983036772123,0.669548662465944,0.690304813988971),
 .UNSPECIFIED.);
#2879=B_SPLINE_CURVE_WITH_KNOTS('',3,(#124130,#124131,#124132,#124133,#124134,
#124135,#124136,#124137,#124138,#124139,#124140,#124141,#124142,#124143,
#124144,#124145,#124146,#124147,#124148,#124149,#124150,#124151),
 .UNSPECIFIED.,.F.,.F.,(4,2,2,2,2,2,2,2,2,2,4),(0.155277913628404,0.165292665851862,
0.185011545100367,0.19466938884267,0.204340835104207,0.224186417404708,
0.24382080194478,0.263107290942695,0.282241250383083,0.301354342848805,
0.31051158851085),.UNSPECIFIED.);
#2880=B_SPLINE_CURVE_WITH_KNOTS('',3,(#124155,#124156,#124157,#124158,#124159,
#124160,#124161,#124162,#124163,#124164,#124165,#124166,#124167,#124168,
#124169,#124170,#124171,#124172,#124173,#124174),.UNSPECIFIED.,.F.,.F.,
(4,2,2,2,2,2,2,2,2,4),(0.310511631495674,0.329840353193037,0.349688712066573,
0.359376076106975,0.37912670235507,0.398829574981945,0.418273867256278,
0.437404148789155,0.4565385186502,0.465789545124077),.UNSPECIFIED.);
#2881=B_SPLINE_CURVE_WITH_KNOTS('',3,(#124178,#124179,#124180,#124181,#124182,
#124183,#124184,#124185,#124186,#124187,#124188,#124189,#124190,#124191,
#124192,#124193,#124194,#124195,#124196,#124197,#124198,#124199,#124200,
#124201,#124202,#124203,#124204,#124205,#124206,#124207,#124208,#124209,
#124210,#124211,#124212,#124213),.UNSPECIFIED.,.T.,.F.,(4,2,2,2,2,2,2,2,
2,2,2,2,2,2,2,2,2,4),(0.,0.0287048976197577,0.0579909299519489,0.116207370107013,
0.174459798915435,0.232700244737173,0.290833045742682,0.348822778718614,
0.406740374765474,0.46469012417934,0.522704198390246,0.581625693995376,
0.640106014433827,0.698690856835086,0.757547003621423,0.816366942407726,
0.874903135177207,0.931848802228483),.UNSPECIFIED.);
#2882=B_SPLINE_CURVE_WITH_KNOTS('',3,(#124217,#124218,#124219,#124220,#124221,
#124222,#124223,#124224,#124225,#124226,#124227,#124228,#124229,#124230,
#124231,#124232,#124233,#124234,#124235,#124236,#124237,#124238),
 .UNSPECIFIED.,.F.,.F.,(4,2,2,2,2,2,2,2,2,2,4),(0.276840898672623,0.279628334212692,
0.296758473080632,0.314164071599323,0.348729292078658,0.38330329595071,
0.41786548372865,0.452383753230674,0.486851783291951,0.521300673093516,
0.55360078593496),.UNSPECIFIED.);
#2883=B_SPLINE_CURVE_WITH_KNOTS('',3,(#124242,#124243,#124244,#124245,#124246,
#124247,#124248,#124249,#124250,#124251,#124252,#124253,#124254,#124255,
#124256,#124257,#124258,#124259,#124260,#124261,#124262),.UNSPECIFIED.,
 .F.,.F.,(4,3,2,2,2,2,2,2,2,4),(0.55360078593496,0.55363816449267,0.588131209987963,
0.623227027140864,0.658175347111053,0.693169329612643,0.728259424581328,
0.763330988935877,0.798299689355572,0.830479063165293),.UNSPECIFIED.);
#2884=B_SPLINE_CURVE_WITH_KNOTS('',3,(#124266,#124267,#124268,#124269,#124270,
#124271,#124272,#124273,#124274,#124275,#124276,#124277,#124278,#124279,
#124280,#124281,#124282,#124283,#124284,#124285,#124286,#124287,#124288,
#124289,#124290,#124291,#124292,#124293,#124294,#124295,#124296,#124297,
#124298,#124299,#124300,#124301,#124302,#124303),.UNSPECIFIED.,.T.,.F.,
(4,2,2,2,2,2,2,2,2,2,2,2,2,2,2,2,2,2,4),(0.,0.0510429338667782,0.076397917131576,
0.126793391862614,0.177157527703175,0.227388740140887,0.277437957066358,
0.327373639274449,0.377342839915421,0.427453608676605,0.452546874856284,
0.477649776776157,0.528631836304232,0.579291425945068,0.6299594819957,0.68071679986447,
0.731420932397828,0.78205413142032,0.80458996698247),.UNSPECIFIED.);
#2885=B_SPLINE_CURVE_WITH_KNOTS('',3,(#124307,#124308,#124309,#124310,#124311,
#124312,#124313,#124314,#124315,#124316,#124317,#124318,#124319,#124320,
#124321,#124322,#124323,#124324,#124325,#124326,#124327,#124328,#124329,
#124330,#124331),.UNSPECIFIED.,.F.,.F.,(4,2,2,2,2,2,2,2,2,2,3,4),(0.213098728070289,
0.228843062715118,0.242103271971766,0.255533998221794,0.282201549216426,
0.308839793496936,0.335409925514743,0.361906495950229,0.3883705405282,0.414865169494334,
0.42609769849922,0.426118424467579),.UNSPECIFIED.);
#2886=B_SPLINE_CURVE_WITH_KNOTS('',3,(#124335,#124336,#124337,#124338,#124339,
#124340,#124341,#124342,#124343,#124344,#124345,#124346,#124347,#124348,
#124349,#124350,#124351,#124352,#124353,#124354),.UNSPECIFIED.,.F.,.F.,
(4,2,2,2,2,2,2,2,2,4),(0.426118424467579,0.452690856909965,0.465988190892994,
0.493083182685766,0.520061578949307,0.547013033000589,0.573973789465176,
0.600927728790317,0.627889696575217,0.639196426569509),.UNSPECIFIED.);
#2887=B_SPLINE_CURVE_WITH_KNOTS('',3,(#124358,#124359,#124360,#124361,#124362,
#124363,#124364,#124365,#124366,#124367,#124368,#124369,#124370,#124371,
#124372,#124373,#124374,#124375,#124376,#124377,#124378,#124379,#124380,
#124381,#124382,#124383,#124384,#124385,#124386,#124387,#124388,#124389,
#124390,#124391,#124392,#124393),.UNSPECIFIED.,.T.,.F.,(4,2,2,2,2,2,2,2,
2,2,2,2,2,2,2,2,2,4),(0.,0.0439191898210743,0.0654694974190781,0.109907007449981,
0.153463834912755,0.196769506044468,0.239810145530631,0.282730920257517,
0.325757072673901,0.369045496294376,0.412571123326874,0.45662283646866,
0.500442890777996,0.544288582176787,0.587775210315516,0.63078465200412,
0.674618447999147,0.694439725374071),.UNSPECIFIED.);
#2888=B_SPLINE_CURVE_WITH_KNOTS('',3,(#124397,#124398,#124399,#124400,#124401,
#124402,#124403,#124404,#124405,#124406,#124407,#124408,#124409,#124410,
#124411,#124412,#124413,#124414,#124415,#124416,#124417,#124418,#124419,
#124420,#124421),.UNSPECIFIED.,.F.,.F.,(4,2,2,2,2,2,2,2,2,2,3,4),(0.157675809345969,
0.158611419670666,0.178629032205577,0.188431328274174,0.208556988599352,
0.228485012656645,0.248116540522748,0.267643763056576,0.287139442297717,
0.306696505525884,0.315254903066365,0.315278867342973),.UNSPECIFIED.);
#2889=B_SPLINE_CURVE_WITH_KNOTS('',3,(#124425,#124426,#124427,#124428,#124429,
#124430,#124431,#124432,#124433,#124434,#124435,#124436,#124437,#124438,
#124439,#124440,#124441,#124442),.UNSPECIFIED.,.F.,.F.,(4,2,2,2,2,2,2,2,
4),(0.315278867342973,0.334979822168361,0.355060989011452,0.375072649078575,
0.395061815886258,0.414829311844664,0.43433498391426,0.453877529419646,
0.472930712412335),.UNSPECIFIED.);
#2890=B_SPLINE_CURVE_WITH_KNOTS('',3,(#124446,#124447,#124448,#124449,#124450,
#124451,#124452,#124453,#124454,#124455,#124456,#124457,#124458,#124459,
#124460,#124461,#124462,#124463,#124464,#124465,#124466,#124467,#124468,
#124469,#124470,#124471,#124472,#124473,#124474,#124475,#124476,#124477,
#124478,#124479,#124480,#124481,#124482,#124483),.UNSPECIFIED.,.T.,.F.,
(4,2,2,2,2,2,2,2,2,2,2,2,2,2,2,2,2,2,4),(0.,0.0437215782121247,0.0651830243893058,
0.0867281067522949,0.131089093155095,0.174465295391611,0.217398166083778,
0.259950071597516,0.302411478707208,0.345128929837316,0.38829073955286,
0.409975559561997,0.43159220439922,0.475473805177582,0.5190906858709,0.562648790415719,
0.605181447805459,0.647749615983058,0.690381534302931),.UNSPECIFIED.);
#2891=B_SPLINE_CURVE_WITH_KNOTS('',3,(#124487,#124488,#124489,#124490,#124491,
#124492,#124493,#124494,#124495,#124496,#124497,#124498,#124499,#124500,
#124501,#124502,#124503,#124504,#124505,#124506,#124507,#124508,#124509,
#124510,#124511),.UNSPECIFIED.,.F.,.F.,(4,2,2,2,2,2,2,2,2,2,3,4),(0.155271413259303,
0.155351020020443,0.175102755092281,0.184783290700741,0.194482425574497,
0.21437504374942,0.2340065060019,0.253298723705622,0.272435688303237,0.291548990163982,
0.31054439799597,0.310545731557595),.UNSPECIFIED.);
#2892=B_SPLINE_CURVE_WITH_KNOTS('',3,(#124515,#124516,#124517,#124518,#124519,
#124520,#124521,#124522,#124523,#124524,#124525,#124526,#124527,#124528,
#124529,#124530,#124531,#124532,#124533,#124534),.UNSPECIFIED.,.F.,.F.,
(4,2,2,2,2,2,2,2,2,4),(0.310545731557595,0.329972473025655,0.339697811404467,
0.349411125640383,0.369206800889191,0.388921424958359,0.408363687262648,
0.427498048467781,0.446632485253342,0.465815811255273),.UNSPECIFIED.);
#2893=B_SPLINE_CURVE_WITH_KNOTS('',3,(#124538,#124539,#124540,#124541,#124542,
#124543,#124544,#124545,#124546,#124547,#124548,#124549,#124550,#124551,
#124552,#124553,#124554,#124555,#124556,#124557,#124558,#124559,#124560,
#124561,#124562,#124563,#124564,#124565,#124566,#124567,#124568,#124569,
#124570,#124571,#124572,#124573),.UNSPECIFIED.,.T.,.F.,(4,2,2,2,2,2,2,2,
2,2,2,2,2,2,2,2,2,4),(0.,0.0292857032011709,0.0875046671306897,0.145761743962781,
0.204003525537326,0.262132469964737,0.320116278552626,0.378029949376738,
0.435978624454139,0.493992508043103,0.552906912724376,0.611388834361421,
0.669975114270796,0.728816779746512,0.787608935744797,0.846130493044841,
0.904669723525998,0.931860524916837),.UNSPECIFIED.);
#2894=B_SPLINE_CURVE_WITH_KNOTS('',3,(#124577,#124578,#124579,#124580,#124581,
#124582,#124583,#124584,#124585,#124586,#124587,#124588,#124589,#124590,
#124591,#124592,#124593,#124594,#124595,#124596,#124597,#124598),
 .UNSPECIFIED.,.F.,.F.,(4,2,2,2,2,2,2,2,2,2,4),(0.276760272839279,0.279486310257967,
0.296891678680277,0.331458165558293,0.366034485059258,0.400597852950089,
0.43511518918133,0.469581034947741,0.504027951985929,0.538494797944952,
0.553534858849661),.UNSPECIFIED.);
#2895=B_SPLINE_CURVE_WITH_KNOTS('',3,(#124602,#124603,#124604,#124605,#124606,
#124607,#124608,#124609,#124610,#124611,#124612,#124613,#124614,#124615,
#124616,#124617,#124618,#124619,#124620,#124621,#124622,#124623,#124624),
 .UNSPECIFIED.,.F.,.F.,(4,3,2,2,2,2,2,2,2,2,4),(0.553534858849661,0.553571407556779,
0.57080071510399,0.605899668347728,0.640850429205566,0.675842030038425,
0.710921555264802,0.745979016681533,0.780941869360024,0.815919166540209,
0.830331680396058),.UNSPECIFIED.);
#2896=B_SPLINE_CURVE_WITH_KNOTS('',3,(#124628,#124629,#124630,#124631,#124632,
#124633,#124634,#124635,#124636,#124637,#124638,#124639,#124640,#124641,
#124642,#124643,#124644,#124645,#124646,#124647,#124648,#124649,#124650,
#124651,#124652,#124653,#124654,#124655,#124656,#124657,#124658,#124659,
#124660,#124661,#124662,#124663,#124664,#124665),.UNSPECIFIED.,.T.,.F.,
(4,2,2,2,2,2,2,2,2,2,2,2,2,2,2,2,2,2,4),(0.,0.0248933932359958,0.0502522570920565,
0.100634389368853,0.150969557978298,0.201172913172633,0.251211890868952,
0.301161391274955,0.351160968415509,0.401301682580004,0.42640034086851,
0.451484147713581,0.502328460810631,0.552963491530814,0.603732474844502,
0.654653180071778,0.705482878991501,0.756131972743015,0.804589874132826),
 .UNSPECIFIED.);
#2897=B_SPLINE_CURVE_WITH_KNOTS('',3,(#124669,#124670,#124671,#124672,#124673,
#124674,#124675,#124676,#124677,#124678,#124679,#124680,#124681,#124682,
#124683,#124684,#124685,#124686,#124687,#124688,#124689,#124690,#124691),
 .UNSPECIFIED.,.F.,.F.,(4,2,2,2,2,2,2,2,2,3,4),(0.213062242779274,0.215594286347048,
0.242723114912628,0.26965769329563,0.296277525050163,0.322829978657394,
0.349320058762837,0.375793067010212,0.402307147515523,0.42615612595573,
0.426158064897884),.UNSPECIFIED.);
#2898=B_SPLINE_CURVE_WITH_KNOTS('',3,(#124695,#124696,#124697,#124698,#124699,
#124700,#124701,#124702,#124703,#124704,#124705,#124706,#124707,#124708,
#124709,#124710,#124711,#124712,#124713,#124714),.UNSPECIFIED.,.F.,.F.,
(4,2,2,2,2,2,2,2,2,4),(0.426158064897884,0.439451111668312,0.452721748725907,
0.479742872920943,0.50670905019566,0.533715458489057,0.56076305839436,0.587782693638629,
0.614752016947225,0.639218368735004),.UNSPECIFIED.);
#2899=B_SPLINE_CURVE_WITH_KNOTS('',3,(#124718,#124719,#124720,#124721,#124722,
#124723,#124724,#124725,#124726,#124727,#124728,#124729,#124730,#124731,
#124732,#124733,#124734,#124735,#124736,#124737,#124738,#124739,#124740,
#124741,#124742,#124743,#124744,#124745,#124746,#124747,#124748,#124749,
#124750,#124751,#124752,#124753,#124754,#124755),.UNSPECIFIED.,.T.,.F.,
(4,2,2,2,2,2,2,2,2,2,2,2,2,2,2,2,2,2,4),(0.,0.0439678896202485,0.0655655029275496,
0.110009025062157,0.15338644656328,0.196316281992617,0.238864267606157,
0.281325189401524,0.324046767682901,0.36721469666785,0.388931797762863,
0.410585946819287,0.454527722035373,0.498154390781355,0.54166243443166,
0.584196741622454,0.62676799340196,0.670324587180314,0.690419290830314),
 .UNSPECIFIED.);
#2900=B_SPLINE_CURVE_WITH_KNOTS('',3,(#124759,#124760,#124761,#124762,#124763,
#124764,#124765,#124766,#124767,#124768,#124769,#124770,#124771,#124772,
#124773,#124774,#124775,#124776,#124777,#124778,#124779,#124780,#124781,
#124782,#124783),.UNSPECIFIED.,.F.,.F.,(4,2,2,2,2,2,2,2,2,2,3,4),(0.155303368541285,
0.165953518380685,0.175653526394182,0.185375252576559,0.20530184599077,
0.224787768869467,0.24407598561316,0.263210264313593,0.282324346612549,
0.301563317562167,0.310561428945123,0.310564213819402),.UNSPECIFIED.);
#2901=B_SPLINE_CURVE_WITH_KNOTS('',3,(#124787,#124788,#124789,#124790,#124791,
#124792,#124793,#124794,#124795,#124796,#124797,#124798,#124799,#124800,
#124801,#124802,#124803,#124804,#124805,#124806),.UNSPECIFIED.,.F.,.F.,
(4,2,2,2,2,2,2,2,2,4),(0.310564213819402,0.330488585935209,0.340220314466039,
0.360044613831472,0.379762342175092,0.399195717228921,0.41832915217723,
0.437465757350788,0.456733128657656,0.465864797486408),.UNSPECIFIED.);
#2902=B_SPLINE_CURVE_WITH_KNOTS('',3,(#124810,#124811,#124812,#124813,#124814,
#124815,#124816,#124817,#124818,#124819,#124820,#124821,#124822,#124823,
#124824,#124825,#124826,#124827,#124828,#124829,#124830,#124831,#124832,
#124833,#124834,#124835,#124836,#124837,#124838,#124839,#124840,#124841,
#124842,#124843,#124844,#124845),.UNSPECIFIED.,.T.,.F.,(4,2,2,2,2,2,2,2,
2,2,2,2,2,2,2,2,2,4),(0.,0.0215162851055023,0.0431138208697561,0.0876446091306586,
0.131214824931109,0.174533219411644,0.217580020450594,0.260498958605342,
0.303517942761,0.346798698928251,0.390321256126534,0.434453407875001,0.478306337336134,
0.522117779247078,0.565997578097342,0.60900882863582,0.65281351297531,0.694470762403534),
 .UNSPECIFIED.);
#2903=B_SPLINE_CURVE_WITH_KNOTS('',3,(#124849,#124850,#124851,#124852,#124853,
#124854,#124855,#124856,#124857,#124858,#124859,#124860,#124861,#124862,
#124863,#124864,#124865,#124866,#124867,#124868,#124869,#124870),
 .UNSPECIFIED.,.F.,.F.,(4,2,2,2,2,2,2,2,2,2,4),(0.157596843449002,0.158418367788362,
0.168222589374335,0.178045702719235,0.198211232858027,0.217965980314702,
0.237605523059871,0.2571371745784,0.276632033627272,0.296184226993561,0.315204316067632),
 .UNSPECIFIED.);
#2904=B_SPLINE_CURVE_WITH_KNOTS('',3,(#124874,#124875,#124876,#124877,#124878,
#124879,#124880,#124881,#124882,#124883,#124884,#124885,#124886,#124887,
#124888,#124889,#124890,#124891,#124892,#124893,#124894,#124895,#124896),
 .UNSPECIFIED.,.F.,.F.,(4,3,2,2,2,2,2,2,2,2,4),(0.315204316067632,0.315219848506788,
0.325082339394274,0.33493357406727,0.355013881071206,0.375021647425745,
0.395000614069428,0.41452308079024,0.434037261815992,0.45362137049485,0.47281669195579),
 .UNSPECIFIED.);
#2905=B_SPLINE_CURVE_WITH_KNOTS('',3,(#128198,#128199,#128200,#128201,#128202,
#128203,#128204,#128205,#128206,#128207,#128208,#128209,#128210,#128211,
#128212,#128213,#128214,#128215,#128216,#128217,#128218,#128219),
 .UNSPECIFIED.,.F.,.F.,(4,2,2,2,2,2,2,2,2,2,4),(0.276798234884123,0.279451999398466,
0.314379791973188,0.348934706381492,0.383475726766096,0.417982346714956,
0.45245551940928,0.486923657573857,0.521413018577935,0.537430969346281,
0.553574548070559),.UNSPECIFIED.);
#2906=B_SPLINE_CURVE_WITH_KNOTS('',3,(#128223,#128224,#128225,#128226,#128227,
#128228,#128229,#128230,#128231,#128232,#128233,#128234,#128235,#128236,
#128237,#128238,#128239,#128240,#128241,#128242),.UNSPECIFIED.,.F.,.F.,
(4,2,2,2,2,2,2,2,2,4),(0.553575400065736,0.58855639024539,0.623472209566331,
0.658530105742964,0.693733478557596,0.728894593312329,0.763880944627597,
0.798792653463988,0.815885151458029,0.830372782954682),.UNSPECIFIED.);
#2907=B_SPLINE_CURVE_WITH_KNOTS('',3,(#128246,#128247,#128248,#128249,#128250,
#128251,#128252,#128253,#128254,#128255,#128256,#128257,#128258,#128259,
#128260,#128261,#128262,#128263,#128264,#128265,#128266,#128267,#128268,
#128269,#128270,#128271,#128272,#128273,#128274,#128275,#128276,#128277,
#128278,#128279,#128280,#128281,#128282,#128283),.UNSPECIFIED.,.T.,.F.,
(4,2,2,2,2,2,2,2,2,2,2,2,2,2,2,2,2,2,4),(0.,0.0587946924940988,0.117017440565929,
0.175220198207046,0.233326761370365,0.29131841207302,0.349265888456903,
0.40725387524115,0.436245732062709,0.465239839112465,0.523939722158812,
0.582356104658916,0.641055278220904,0.700106923889623,0.75907025217679,
0.817630646713495,0.876070888006275,0.903750502884322,0.931728974146718),
 .UNSPECIFIED.);
#2908=ORIENTED_CLOSED_SHELL('',*,#45449,.F.);
#2909=ORIENTED_CLOSED_SHELL('',*,#45450,.F.);
#2910=ORIENTED_CLOSED_SHELL('',*,#45453,.F.);
#2911=ORIENTED_CLOSED_SHELL('',*,#45454,.F.);
#2912=ELLIPSE('',#45570,8.34154176961301,8.30313896599411);
#2913=ELLIPSE('',#45577,8.31271199747688,8.30313896599411);
#2914=ELLIPSE('',#45578,8.3415417696134,8.3031389659941);
#2915=ELLIPSE('',#47457,8.31271199747759,8.3031389659941);
#2916=ELLIPSE('',#47528,19.6143071532144,16.9851908864685);
#2917=ELLIPSE('',#47529,19.614307153188,16.9851908864196);
#2918=BREP_WITH_VOIDS('Body1',#45451,(#2908,#2909));
#2919=BREP_WITH_VOIDS('Body1',#45455,(#2910,#2911));
#2920=SHAPE_REPRESENTATION_RELATIONSHIP('SRR','None',#130942,#2928);
#2921=SHAPE_REPRESENTATION_RELATIONSHIP('SRR','None',#130943,#2929);
#2922=SHAPE_REPRESENTATION_RELATIONSHIP('SRR','None',#130944,#2930);
#2923=SHAPE_REPRESENTATION_RELATIONSHIP('SRR','None',#130945,#2931);
#2924=SHAPE_REPRESENTATION_RELATIONSHIP('SRR','None',#130946,#2932);
#2925=SHAPE_REPRESENTATION_RELATIONSHIP('SRR','None',#130947,#2933);
#2926=SHAPE_REPRESENTATION_RELATIONSHIP('SRR','None',#130948,#2934);
#2927=SHAPE_REPRESENTATION_RELATIONSHIP('SRR','None',#130949,#2935);
#2928=ADVANCED_BREP_SHAPE_REPRESENTATION('',(#2944),#130902);
#2929=ADVANCED_BREP_SHAPE_REPRESENTATION('',(#2918),#130903);
#2930=ADVANCED_BREP_SHAPE_REPRESENTATION('',(#2945),#130904);
#2931=ADVANCED_BREP_SHAPE_REPRESENTATION('',(#2919),#130905);
#2932=ADVANCED_BREP_SHAPE_REPRESENTATION('',(#2946),#130906);
#2933=ADVANCED_BREP_SHAPE_REPRESENTATION('',(#2947),#130907);
#2934=ADVANCED_BREP_SHAPE_REPRESENTATION('',(#2948),#130908);
#2935=ADVANCED_BREP_SHAPE_REPRESENTATION('',(#2949),#130909);
#2936=STYLED_ITEM('',(#130991),#2944);
#2937=STYLED_ITEM('',(#130991),#2918);
#2938=STYLED_ITEM('',(#130991),#2945);
#2939=STYLED_ITEM('',(#130991),#2919);
#2940=STYLED_ITEM('',(#130991),#2946);
#2941=STYLED_ITEM('',(#130991),#2947);
#2942=STYLED_ITEM('',(#130991),#2948);
#2943=STYLED_ITEM('',(#130991),#2949);
#2944=MANIFOLD_SOLID_BREP('Body1',#45448);
#2945=MANIFOLD_SOLID_BREP('Body1',#45452);
#2946=MANIFOLD_SOLID_BREP('Body1',#45456);
#2947=MANIFOLD_SOLID_BREP('Body1',#45457);
#2948=MANIFOLD_SOLID_BREP('Body1',#45458);
#2949=MANIFOLD_SOLID_BREP('Body1',#45459);
#2950=PLANE('',#45566);
#2951=PLANE('',#45567);
#2952=PLANE('',#45569);
#2953=PLANE('',#45571);
#2954=PLANE('',#45574);
#2955=PLANE('',#45575);
#2956=PLANE('',#45579);
#2957=PLANE('',#45580);
#2958=PLANE('',#45581);
#2959=PLANE('',#47448);
#2960=PLANE('',#47450);
#2961=PLANE('',#47461);
#2962=PLANE('',#47462);
#2963=PLANE('',#47465);
#2964=PLANE('',#47472);
#2965=PLANE('',#47525);
#2966=PLANE('',#47526);
#2967=PLANE('',#47527);
#2968=PLANE('',#47531);
#2969=PLANE('',#47532);
#2970=PLANE('',#47535);
#2971=PLANE('',#47536);
#2972=PLANE('',#47538);
#2973=PLANE('',#47539);
#2974=PLANE('',#47540);
#2975=PLANE('',#47541);
#2976=PLANE('',#47542);
#2977=PLANE('',#47543);
#2978=PLANE('',#47544);
#2979=PLANE('',#47545);
#2980=PLANE('',#47546);
#2981=PLANE('',#47547);
#2982=PLANE('',#47548);
#2983=PLANE('',#47549);
#2984=PLANE('',#47550);
#2985=PLANE('',#47551);
#2986=PLANE('',#47552);
#2987=PLANE('',#47553);
#2988=PLANE('',#47554);
#2989=PLANE('',#47555);
#2990=PLANE('',#47556);
#2991=PLANE('',#47557);
#2992=PLANE('',#47558);
#2993=PLANE('',#47559);
#2994=PLANE('',#47560);
#2995=PLANE('',#47561);
#2996=PLANE('',#47562);
#2997=PLANE('',#47563);
#2998=PLANE('',#47564);
#2999=PLANE('',#47565);
#3000=PLANE('',#47566);
#3001=PLANE('',#47567);
#3002=PLANE('',#47568);
#3003=PLANE('',#47569);
#3004=PLANE('',#47570);
#3005=PLANE('',#47571);
#3006=PLANE('',#47572);
#3007=PLANE('',#47573);
#3008=PLANE('',#47574);
#3009=PLANE('',#47575);
#3010=PLANE('',#47576);
#3011=PLANE('',#47577);
#3012=PLANE('',#47578);
#3013=PLANE('',#47579);
#3014=PLANE('',#47580);
#3015=PLANE('',#47581);
#3016=PLANE('',#47582);
#3017=PLANE('',#47583);
#3018=PLANE('',#47584);
#3019=PLANE('',#47585);
#3020=PLANE('',#47586);
#3021=PLANE('',#47587);
#3022=PLANE('',#47588);
#3023=PLANE('',#47589);
#3024=PLANE('',#47590);
#3025=PLANE('',#47591);
#3026=PLANE('',#47592);
#3027=PLANE('',#47593);
#3028=PLANE('',#47594);
#3029=PLANE('',#47595);
#3030=PLANE('',#47596);
#3031=PLANE('',#47597);
#3032=PLANE('',#47598);
#3033=PLANE('',#47599);
#3034=PLANE('',#47600);
#3035=PLANE('',#47601);
#3036=PLANE('',#47602);
#3037=PLANE('',#47603);
#3038=PLANE('',#47604);
#3039=PLANE('',#47605);
#3040=PLANE('',#47606);
#3041=PLANE('',#47607);
#3042=PLANE('',#47608);
#3043=PLANE('',#47609);
#3044=PLANE('',#47610);
#3045=PLANE('',#47611);
#3046=PLANE('',#47612);
#3047=PLANE('',#47613);
#3048=PLANE('',#47614);
#3049=PLANE('',#47615);
#3050=PLANE('',#47616);
#3051=PLANE('',#47617);
#3052=PLANE('',#47618);
#3053=PLANE('',#47619);
#3054=PLANE('',#47620);
#3055=PLANE('',#47621);
#3056=PLANE('',#47622);
#3057=PLANE('',#47623);
#3058=PLANE('',#47624);
#3059=PLANE('',#47625);
#3060=PLANE('',#47626);
#3061=PLANE('',#47627);
#3062=PLANE('',#47628);
#3063=PLANE('',#47629);
#3064=PLANE('',#47630);
#3065=PLANE('',#47631);
#3066=PLANE('',#47632);
#3067=PLANE('',#47633);
#3068=PLANE('',#47634);
#3069=PLANE('',#47635);
#3070=PLANE('',#47636);
#3071=PLANE('',#47637);
#3072=PLANE('',#47638);
#3073=PLANE('',#47639);
#3074=PLANE('',#47640);
#3075=PLANE('',#47641);
#3076=PLANE('',#47642);
#3077=PLANE('',#47643);
#3078=PLANE('',#47644);
#3079=PLANE('',#47645);
#3080=PLANE('',#47646);
#3081=PLANE('',#47647);
#3082=PLANE('',#47648);
#3083=PLANE('',#47649);
#3084=PLANE('',#47650);
#3085=PLANE('',#47651);
#3086=PLANE('',#47652);
#3087=PLANE('',#47653);
#3088=PLANE('',#47654);
#3089=PLANE('',#47655);
#3090=PLANE('',#47656);
#3091=PLANE('',#47657);
#3092=PLANE('',#47658);
#3093=PLANE('',#47659);
#3094=PLANE('',#47660);
#3095=PLANE('',#47661);
#3096=PLANE('',#47662);
#3097=PLANE('',#47663);
#3098=PLANE('',#47664);
#3099=PLANE('',#47665);
#3100=PLANE('',#47666);
#3101=PLANE('',#47667);
#3102=PLANE('',#47668);
#3103=PLANE('',#47669);
#3104=PLANE('',#47670);
#3105=PLANE('',#47671);
#3106=PLANE('',#47672);
#3107=PLANE('',#47673);
#3108=PLANE('',#47674);
#3109=PLANE('',#47675);
#3110=PLANE('',#47676);
#3111=PLANE('',#47677);
#3112=PLANE('',#47678);
#3113=PLANE('',#47679);
#3114=PLANE('',#47680);
#3115=PLANE('',#47681);
#3116=PLANE('',#47682);
#3117=PLANE('',#47683);
#3118=PLANE('',#47684);
#3119=PLANE('',#47685);
#3120=PLANE('',#47686);
#3121=PLANE('',#47687);
#3122=PLANE('',#47688);
#3123=PLANE('',#47689);
#3124=PLANE('',#47690);
#3125=PLANE('',#47691);
#3126=PLANE('',#47692);
#3127=PLANE('',#47693);
#3128=PLANE('',#47694);
#3129=PLANE('',#47695);
#3130=PLANE('',#47696);
#3131=PLANE('',#47697);
#3132=PLANE('',#47698);
#3133=PLANE('',#47699);
#3134=PLANE('',#47700);
#3135=PLANE('',#47701);
#3136=PLANE('',#47702);
#3137=PLANE('',#47703);
#3138=PLANE('',#47704);
#3139=PLANE('',#47705);
#3140=PLANE('',#47706);
#3141=PLANE('',#47707);
#3142=PLANE('',#47708);
#3143=PLANE('',#47709);
#3144=PLANE('',#47710);
#3145=PLANE('',#47711);
#3146=PLANE('',#47712);
#3147=PLANE('',#47713);
#3148=PLANE('',#47714);
#3149=PLANE('',#47715);
#3150=PLANE('',#47716);
#3151=PLANE('',#47717);
#3152=PLANE('',#47718);
#3153=PLANE('',#47719);
#3154=PLANE('',#47720);
#3155=PLANE('',#47721);
#3156=PLANE('',#47722);
#3157=PLANE('',#47723);
#3158=PLANE('',#47724);
#3159=PLANE('',#47725);
#3160=PLANE('',#47726);
#3161=PLANE('',#47727);
#3162=PLANE('',#47728);
#3163=PLANE('',#47729);
#3164=PLANE('',#47730);
#3165=PLANE('',#47731);
#3166=PLANE('',#47732);
#3167=PLANE('',#47733);
#3168=PLANE('',#47734);
#3169=PLANE('',#47735);
#3170=PLANE('',#47736);
#3171=PLANE('',#47737);
#3172=PLANE('',#47738);
#3173=PLANE('',#47739);
#3174=PLANE('',#47740);
#3175=PLANE('',#47741);
#3176=PLANE('',#47742);
#3177=PLANE('',#47743);
#3178=PLANE('',#47744);
#3179=PLANE('',#47745);
#3180=PLANE('',#47746);
#3181=PLANE('',#47747);
#3182=PLANE('',#47748);
#3183=PLANE('',#47749);
#3184=PLANE('',#47750);
#3185=PLANE('',#47751);
#3186=PLANE('',#47752);
#3187=PLANE('',#47753);
#3188=PLANE('',#47754);
#3189=PLANE('',#47755);
#3190=PLANE('',#47756);
#3191=PLANE('',#47757);
#3192=PLANE('',#47758);
#3193=PLANE('',#47759);
#3194=PLANE('',#47760);
#3195=PLANE('',#47761);
#3196=PLANE('',#47762);
#3197=PLANE('',#47763);
#3198=PLANE('',#47764);
#3199=PLANE('',#47765);
#3200=PLANE('',#47766);
#3201=PLANE('',#47767);
#3202=PLANE('',#47768);
#3203=PLANE('',#47769);
#3204=PLANE('',#47770);
#3205=PLANE('',#47771);
#3206=PLANE('',#47772);
#3207=PLANE('',#47773);
#3208=PLANE('',#47774);
#3209=PLANE('',#47775);
#3210=PLANE('',#47776);
#3211=PLANE('',#47777);
#3212=PLANE('',#47778);
#3213=PLANE('',#47779);
#3214=PLANE('',#47780);
#3215=PLANE('',#47781);
#3216=PLANE('',#47782);
#3217=PLANE('',#47783);
#3218=PLANE('',#47784);
#3219=PLANE('',#47785);
#3220=PLANE('',#47786);
#3221=PLANE('',#47787);
#3222=PLANE('',#47788);
#3223=PLANE('',#47789);
#3224=PLANE('',#47790);
#3225=PLANE('',#47791);
#3226=PLANE('',#47792);
#3227=PLANE('',#47793);
#3228=PLANE('',#47794);
#3229=PLANE('',#47795);
#3230=PLANE('',#47796);
#3231=PLANE('',#47797);
#3232=PLANE('',#47798);
#3233=PLANE('',#47799);
#3234=PLANE('',#47800);
#3235=PLANE('',#47801);
#3236=PLANE('',#47802);
#3237=PLANE('',#47803);
#3238=PLANE('',#47804);
#3239=PLANE('',#47805);
#3240=PLANE('',#47806);
#3241=PLANE('',#47807);
#3242=PLANE('',#47808);
#3243=PLANE('',#47809);
#3244=PLANE('',#47810);
#3245=PLANE('',#47811);
#3246=PLANE('',#47812);
#3247=PLANE('',#47813);
#3248=PLANE('',#47814);
#3249=PLANE('',#47815);
#3250=PLANE('',#47816);
#3251=PLANE('',#47817);
#3252=PLANE('',#47818);
#3253=PLANE('',#47819);
#3254=PLANE('',#47820);
#3255=PLANE('',#47821);
#3256=PLANE('',#47822);
#3257=PLANE('',#47823);
#3258=PLANE('',#47824);
#3259=PLANE('',#47825);
#3260=PLANE('',#47826);
#3261=PLANE('',#47827);
#3262=PLANE('',#47828);
#3263=PLANE('',#47829);
#3264=PLANE('',#47830);
#3265=PLANE('',#47831);
#3266=PLANE('',#47832);
#3267=PLANE('',#47833);
#3268=PLANE('',#47834);
#3269=PLANE('',#47835);
#3270=PLANE('',#47836);
#3271=PLANE('',#47837);
#3272=PLANE('',#47838);
#3273=PLANE('',#47839);
#3274=PLANE('',#47840);
#3275=PLANE('',#47841);
#3276=PLANE('',#47842);
#3277=PLANE('',#47843);
#3278=PLANE('',#47844);
#3279=PLANE('',#47845);
#3280=PLANE('',#47846);
#3281=PLANE('',#47847);
#3282=PLANE('',#47848);
#3283=PLANE('',#47849);
#3284=PLANE('',#47850);
#3285=PLANE('',#47851);
#3286=PLANE('',#47852);
#3287=PLANE('',#47853);
#3288=PLANE('',#47854);
#3289=PLANE('',#47855);
#3290=PLANE('',#47856);
#3291=PLANE('',#47857);
#3292=PLANE('',#47858);
#3293=PLANE('',#47859);
#3294=PLANE('',#47860);
#3295=PLANE('',#47861);
#3296=PLANE('',#47862);
#3297=PLANE('',#47863);
#3298=PLANE('',#47864);
#3299=PLANE('',#47865);
#3300=PLANE('',#47866);
#3301=PLANE('',#47867);
#3302=PLANE('',#47868);
#3303=PLANE('',#47869);
#3304=PLANE('',#47870);
#3305=PLANE('',#47871);
#3306=PLANE('',#47872);
#3307=PLANE('',#47873);
#3308=PLANE('',#47874);
#3309=PLANE('',#47875);
#3310=PLANE('',#47876);
#3311=PLANE('',#47877);
#3312=PLANE('',#47878);
#3313=PLANE('',#47879);
#3314=PLANE('',#47880);
#3315=PLANE('',#47881);
#3316=PLANE('',#47882);
#3317=PLANE('',#47883);
#3318=PLANE('',#47884);
#3319=PLANE('',#47885);
#3320=PLANE('',#47886);
#3321=PLANE('',#47887);
#3322=PLANE('',#47888);
#3323=PLANE('',#47889);
#3324=PLANE('',#47890);
#3325=PLANE('',#47891);
#3326=PLANE('',#47892);
#3327=PLANE('',#47893);
#3328=PLANE('',#47894);
#3329=PLANE('',#47895);
#3330=PLANE('',#47896);
#3331=PLANE('',#47897);
#3332=PLANE('',#47898);
#3333=PLANE('',#47899);
#3334=PLANE('',#47900);
#3335=PLANE('',#47901);
#3336=PLANE('',#47902);
#3337=PLANE('',#47903);
#3338=PLANE('',#47904);
#3339=PLANE('',#47905);
#3340=PLANE('',#47906);
#3341=PLANE('',#47907);
#3342=PLANE('',#47908);
#3343=PLANE('',#47909);
#3344=PLANE('',#47910);
#3345=PLANE('',#47911);
#3346=PLANE('',#47912);
#3347=PLANE('',#47913);
#3348=PLANE('',#47914);
#3349=PLANE('',#47915);
#3350=PLANE('',#47916);
#3351=PLANE('',#47917);
#3352=PLANE('',#47918);
#3353=PLANE('',#47919);
#3354=PLANE('',#47920);
#3355=PLANE('',#47921);
#3356=PLANE('',#47922);
#3357=PLANE('',#47923);
#3358=PLANE('',#47924);
#3359=PLANE('',#47925);
#3360=PLANE('',#47926);
#3361=PLANE('',#47927);
#3362=PLANE('',#47928);
#3363=PLANE('',#47929);
#3364=PLANE('',#47930);
#3365=PLANE('',#47931);
#3366=PLANE('',#47932);
#3367=PLANE('',#47933);
#3368=PLANE('',#47934);
#3369=PLANE('',#47935);
#3370=PLANE('',#47936);
#3371=PLANE('',#47937);
#3372=PLANE('',#47938);
#3373=PLANE('',#47939);
#3374=PLANE('',#47940);
#3375=PLANE('',#47941);
#3376=PLANE('',#47942);
#3377=PLANE('',#47943);
#3378=PLANE('',#47944);
#3379=PLANE('',#47945);
#3380=PLANE('',#47946);
#3381=PLANE('',#47947);
#3382=PLANE('',#47948);
#3383=PLANE('',#47949);
#3384=PLANE('',#47950);
#3385=PLANE('',#47951);
#3386=PLANE('',#47952);
#3387=PLANE('',#47953);
#3388=PLANE('',#47954);
#3389=PLANE('',#47955);
#3390=PLANE('',#47956);
#3391=PLANE('',#47957);
#3392=PLANE('',#47958);
#3393=PLANE('',#47959);
#3394=PLANE('',#47960);
#3395=PLANE('',#47961);
#3396=PLANE('',#47962);
#3397=PLANE('',#47963);
#3398=PLANE('',#47964);
#3399=PLANE('',#47965);
#3400=PLANE('',#47966);
#3401=PLANE('',#47967);
#3402=PLANE('',#47968);
#3403=PLANE('',#47969);
#3404=PLANE('',#47970);
#3405=PLANE('',#47971);
#3406=PLANE('',#47972);
#3407=PLANE('',#47973);
#3408=PLANE('',#47974);
#3409=PLANE('',#47975);
#3410=PLANE('',#47976);
#3411=PLANE('',#47977);
#3412=PLANE('',#47978);
#3413=PLANE('',#47979);
#3414=PLANE('',#47980);
#3415=PLANE('',#47981);
#3416=PLANE('',#47982);
#3417=PLANE('',#47983);
#3418=PLANE('',#47984);
#3419=PLANE('',#47985);
#3420=PLANE('',#47986);
#3421=PLANE('',#47987);
#3422=PLANE('',#47988);
#3423=PLANE('',#47989);
#3424=PLANE('',#47990);
#3425=PLANE('',#47991);
#3426=PLANE('',#47992);
#3427=PLANE('',#47993);
#3428=PLANE('',#47994);
#3429=PLANE('',#47995);
#3430=PLANE('',#47996);
#3431=PLANE('',#47997);
#3432=PLANE('',#47998);
#3433=PLANE('',#47999);
#3434=PLANE('',#48000);
#3435=PLANE('',#48001);
#3436=PLANE('',#48002);
#3437=PLANE('',#48003);
#3438=PLANE('',#48004);
#3439=PLANE('',#48005);
#3440=PLANE('',#48006);
#3441=PLANE('',#48007);
#3442=PLANE('',#48008);
#3443=PLANE('',#48009);
#3444=PLANE('',#48010);
#3445=PLANE('',#48011);
#3446=PLANE('',#48012);
#3447=PLANE('',#48013);
#3448=PLANE('',#48014);
#3449=PLANE('',#48015);
#3450=PLANE('',#48016);
#3451=PLANE('',#48017);
#3452=PLANE('',#48018);
#3453=PLANE('',#48019);
#3454=PLANE('',#48020);
#3455=PLANE('',#48021);
#3456=PLANE('',#48022);
#3457=PLANE('',#48023);
#3458=PLANE('',#48024);
#3459=PLANE('',#48025);
#3460=PLANE('',#48026);
#3461=PLANE('',#48027);
#3462=PLANE('',#48028);
#3463=PLANE('',#48029);
#3464=PLANE('',#48030);
#3465=PLANE('',#48031);
#3466=PLANE('',#48032);
#3467=PLANE('',#48033);
#3468=PLANE('',#48034);
#3469=PLANE('',#48035);
#3470=PLANE('',#48036);
#3471=PLANE('',#48037);
#3472=PLANE('',#48038);
#3473=PLANE('',#48039);
#3474=PLANE('',#48040);
#3475=PLANE('',#48041);
#3476=PLANE('',#48042);
#3477=PLANE('',#48043);
#3478=PLANE('',#48044);
#3479=PLANE('',#48045);
#3480=PLANE('',#48046);
#3481=PLANE('',#48047);
#3482=PLANE('',#48048);
#3483=PLANE('',#48049);
#3484=PLANE('',#48050);
#3485=PLANE('',#48051);
#3486=PLANE('',#48052);
#3487=PLANE('',#48053);
#3488=PLANE('',#48054);
#3489=PLANE('',#48055);
#3490=PLANE('',#48056);
#3491=PLANE('',#48057);
#3492=PLANE('',#48058);
#3493=PLANE('',#48059);
#3494=PLANE('',#48060);
#3495=PLANE('',#48061);
#3496=PLANE('',#48062);
#3497=PLANE('',#48063);
#3498=PLANE('',#48064);
#3499=PLANE('',#48065);
#3500=PLANE('',#48066);
#3501=PLANE('',#48067);
#3502=PLANE('',#48068);
#3503=PLANE('',#48069);
#3504=PLANE('',#48070);
#3505=PLANE('',#48071);
#3506=PLANE('',#48072);
#3507=PLANE('',#48073);
#3508=PLANE('',#48074);
#3509=PLANE('',#48075);
#3510=PLANE('',#48076);
#3511=PLANE('',#48077);
#3512=PLANE('',#48078);
#3513=PLANE('',#48079);
#3514=PLANE('',#48080);
#3515=PLANE('',#48081);
#3516=PLANE('',#48082);
#3517=PLANE('',#48083);
#3518=PLANE('',#48084);
#3519=PLANE('',#48085);
#3520=PLANE('',#48086);
#3521=PLANE('',#48087);
#3522=PLANE('',#48088);
#3523=PLANE('',#48089);
#3524=PLANE('',#48090);
#3525=PLANE('',#48091);
#3526=PLANE('',#48092);
#3527=PLANE('',#48093);
#3528=PLANE('',#48094);
#3529=PLANE('',#48095);
#3530=PLANE('',#48096);
#3531=PLANE('',#48097);
#3532=PLANE('',#48098);
#3533=PLANE('',#48099);
#3534=PLANE('',#48100);
#3535=PLANE('',#48101);
#3536=PLANE('',#48102);
#3537=PLANE('',#48103);
#3538=PLANE('',#48104);
#3539=PLANE('',#48105);
#3540=PLANE('',#48106);
#3541=PLANE('',#48107);
#3542=PLANE('',#48108);
#3543=PLANE('',#48109);
#3544=PLANE('',#48110);
#3545=PLANE('',#48111);
#3546=PLANE('',#48112);
#3547=PLANE('',#48113);
#3548=PLANE('',#48114);
#3549=PLANE('',#48115);
#3550=PLANE('',#48116);
#3551=PLANE('',#48117);
#3552=PLANE('',#48118);
#3553=PLANE('',#48119);
#3554=PLANE('',#48120);
#3555=PLANE('',#48121);
#3556=PLANE('',#48122);
#3557=PLANE('',#48123);
#3558=PLANE('',#48124);
#3559=PLANE('',#48125);
#3560=PLANE('',#48126);
#3561=PLANE('',#48127);
#3562=PLANE('',#48128);
#3563=PLANE('',#48129);
#3564=PLANE('',#48130);
#3565=PLANE('',#48131);
#3566=PLANE('',#48132);
#3567=PLANE('',#48133);
#3568=PLANE('',#48134);
#3569=PLANE('',#48135);
#3570=PLANE('',#48136);
#3571=PLANE('',#48156);
#3572=PLANE('',#48157);
#3573=PLANE('',#48160);
#3574=PLANE('',#48161);
#3575=PLANE('',#48166);
#3576=PLANE('',#48170);
#3577=PLANE('',#48171);
#3578=PLANE('',#48172);
#3579=PLANE('',#48173);
#3580=PLANE('',#48176);
#3581=PLANE('',#48179);
#3582=PLANE('',#48182);
#3583=PLANE('',#48275);
#3584=PLANE('',#48284);
#3585=PLANE('',#48285);
#3586=PLANE('',#48286);
#3587=PLANE('',#48365);
#3588=PLANE('',#48366);
#3589=PLANE('',#48369);
#3590=PLANE('',#48370);
#3591=PLANE('',#48371);
#3592=PLANE('',#48400);
#3593=PLANE('',#48401);
#3594=PLANE('',#48403);
#3595=PLANE('',#48404);
#3596=PLANE('',#48405);
#3597=PLANE('',#48434);
#3598=PLANE('',#48435);
#3599=PLANE('',#48437);
#3600=PLANE('',#48438);
#3601=PLANE('',#48439);
#3602=PLANE('',#48468);
#3603=PLANE('',#48469);
#3604=PLANE('',#48471);
#3605=PLANE('',#48472);
#3606=PLANE('',#48473);
#3607=PLANE('',#48474);
#3608=PLANE('',#48475);
#3609=PLANE('',#48476);
#3610=PLANE('',#48544);
#3611=PLANE('',#48557);
#3612=PLANE('',#48563);
#3613=PLANE('',#48564);
#3614=PLANE('',#48565);
#3615=PLANE('',#48567);
#3616=PLANE('',#48568);
#3617=PLANE('',#48573);
#3618=PLANE('',#48578);
#3619=PLANE('',#48591);
#3620=PLANE('',#48592);
#3621=PLANE('',#48593);
#3622=PLANE('',#48594);
#3623=PLANE('',#48595);
#3624=PLANE('',#48600);
#3625=PLANE('',#48601);
#3626=PLANE('',#48604);
#3627=PLANE('',#48605);
#3628=PLANE('',#48608);
#3629=PLANE('',#48627);
#3630=PLANE('',#48631);
#3631=PLANE('',#48635);
#3632=PLANE('',#48636);
#3633=PLANE('',#48640);
#3634=PLANE('',#48644);
#3635=PLANE('',#48825);
#3636=PLANE('',#48828);
#3637=PLANE('',#48834);
#3638=PLANE('',#48837);
#3639=PLANE('',#48843);
#3640=PLANE('',#48844);
#3641=PLANE('',#48847);
#3642=PLANE('',#48848);
#3643=PLANE('',#48899);
#3644=PLANE('',#48900);
#3645=PLANE('',#48901);
#3646=PLANE('',#50926);
#3647=PLANE('',#50927);
#3648=PLANE('',#50928);
#3649=PLANE('',#50929);
#3650=PLANE('',#50930);
#3651=PLANE('',#50931);
#3652=PLANE('',#50932);
#3653=PLANE('',#50934);
#3654=PLANE('',#50935);
#3655=PLANE('',#50936);
#3656=PLANE('',#50937);
#3657=PLANE('',#50938);
#3658=PLANE('',#50939);
#3659=PLANE('',#50940);
#3660=PLANE('',#50941);
#3661=PLANE('',#50942);
#3662=PLANE('',#50943);
#3663=PLANE('',#50944);
#3664=PLANE('',#50945);
#3665=PLANE('',#50946);
#3666=PLANE('',#50947);
#3667=PLANE('',#50948);
#3668=PLANE('',#50949);
#3669=PLANE('',#50950);
#3670=PLANE('',#50951);
#3671=PLANE('',#50952);
#3672=PLANE('',#50953);
#3673=PLANE('',#50954);
#3674=PLANE('',#50955);
#3675=PLANE('',#50956);
#3676=PLANE('',#50957);
#3677=PLANE('',#50958);
#3678=PLANE('',#50959);
#3679=PLANE('',#50960);
#3680=PLANE('',#50961);
#3681=PLANE('',#50962);
#3682=PLANE('',#50963);
#3683=PLANE('',#50964);
#3684=PLANE('',#50965);
#3685=PLANE('',#50966);
#3686=PLANE('',#50967);
#3687=PLANE('',#50968);
#3688=PLANE('',#50969);
#3689=PLANE('',#50970);
#3690=PLANE('',#50971);
#3691=PLANE('',#50972);
#3692=PLANE('',#50973);
#3693=PLANE('',#50974);
#3694=PLANE('',#50975);
#3695=PLANE('',#50976);
#3696=PLANE('',#50977);
#3697=PLANE('',#50978);
#3698=PLANE('',#50979);
#3699=PLANE('',#50980);
#3700=PLANE('',#50981);
#3701=PLANE('',#50982);
#3702=PLANE('',#50983);
#3703=PLANE('',#50984);
#3704=PLANE('',#50985);
#3705=PLANE('',#50986);
#3706=PLANE('',#50987);
#3707=PLANE('',#50988);
#3708=PLANE('',#50989);
#3709=PLANE('',#50990);
#3710=PLANE('',#50991);
#3711=PLANE('',#50992);
#3712=PLANE('',#50993);
#3713=PLANE('',#50994);
#3714=PLANE('',#50995);
#3715=PLANE('',#50996);
#3716=PLANE('',#50997);
#3717=PLANE('',#50998);
#3718=PLANE('',#50999);
#3719=PLANE('',#51000);
#3720=PLANE('',#51001);
#3721=PLANE('',#51002);
#3722=PLANE('',#51003);
#3723=PLANE('',#51004);
#3724=PLANE('',#51005);
#3725=PLANE('',#51006);
#3726=PLANE('',#51007);
#3727=PLANE('',#51008);
#3728=PLANE('',#51009);
#3729=PLANE('',#51010);
#3730=PLANE('',#51011);
#3731=PLANE('',#51012);
#3732=PLANE('',#51013);
#3733=PLANE('',#51014);
#3734=PLANE('',#51015);
#3735=PLANE('',#51016);
#3736=PLANE('',#51017);
#3737=PLANE('',#51018);
#3738=PLANE('',#51019);
#3739=PLANE('',#51020);
#3740=PLANE('',#51021);
#3741=PLANE('',#51022);
#3742=PLANE('',#51023);
#3743=PLANE('',#51024);
#3744=PLANE('',#51025);
#3745=PLANE('',#51026);
#3746=PLANE('',#51027);
#3747=PLANE('',#51028);
#3748=PLANE('',#51029);
#3749=PLANE('',#51030);
#3750=PLANE('',#51031);
#3751=PLANE('',#51032);
#3752=PLANE('',#51033);
#3753=PLANE('',#51034);
#3754=PLANE('',#51035);
#3755=PLANE('',#51036);
#3756=PLANE('',#51037);
#3757=PLANE('',#51038);
#3758=PLANE('',#51039);
#3759=PLANE('',#51040);
#3760=PLANE('',#51041);
#3761=PLANE('',#51042);
#3762=PLANE('',#51043);
#3763=PLANE('',#51044);
#3764=PLANE('',#51045);
#3765=PLANE('',#51046);
#3766=PLANE('',#51047);
#3767=PLANE('',#51048);
#3768=PLANE('',#51049);
#3769=PLANE('',#51050);
#3770=PLANE('',#51051);
#3771=PLANE('',#51052);
#3772=PLANE('',#51053);
#3773=PLANE('',#51054);
#3774=PLANE('',#51055);
#3775=PLANE('',#51056);
#3776=PLANE('',#51057);
#3777=PLANE('',#51058);
#3778=PLANE('',#51059);
#3779=PLANE('',#51060);
#3780=PLANE('',#51061);
#3781=PLANE('',#51062);
#3782=PLANE('',#51063);
#3783=PLANE('',#51064);
#3784=PLANE('',#51065);
#3785=PLANE('',#51066);
#3786=PLANE('',#51067);
#3787=PLANE('',#51068);
#3788=PLANE('',#51069);
#3789=PLANE('',#51070);
#3790=PLANE('',#51071);
#3791=PLANE('',#51072);
#3792=PLANE('',#51073);
#3793=PLANE('',#51074);
#3794=PLANE('',#51075);
#3795=PLANE('',#51076);
#3796=PLANE('',#51077);
#3797=PLANE('',#51078);
#3798=PLANE('',#51079);
#3799=PLANE('',#51080);
#3800=PLANE('',#51081);
#3801=PLANE('',#51082);
#3802=PLANE('',#51083);
#3803=PLANE('',#51084);
#3804=PLANE('',#51085);
#3805=PLANE('',#51086);
#3806=PLANE('',#51087);
#3807=PLANE('',#51088);
#3808=PLANE('',#51089);
#3809=PLANE('',#51090);
#3810=PLANE('',#51091);
#3811=PLANE('',#51092);
#3812=PLANE('',#51093);
#3813=PLANE('',#51094);
#3814=PLANE('',#51095);
#3815=PLANE('',#51096);
#3816=PLANE('',#51097);
#3817=PLANE('',#51098);
#3818=PLANE('',#51099);
#3819=PLANE('',#51100);
#3820=PLANE('',#51101);
#3821=PLANE('',#51102);
#3822=PLANE('',#51103);
#3823=PLANE('',#51104);
#3824=PLANE('',#51105);
#3825=PLANE('',#51106);
#3826=PLANE('',#51107);
#3827=PLANE('',#51108);
#3828=PLANE('',#51109);
#3829=PLANE('',#51110);
#3830=PLANE('',#51111);
#3831=PLANE('',#51112);
#3832=PLANE('',#51113);
#3833=PLANE('',#51114);
#3834=PLANE('',#51115);
#3835=PLANE('',#51116);
#3836=PLANE('',#51117);
#3837=PLANE('',#51118);
#3838=PLANE('',#51119);
#3839=PLANE('',#51120);
#3840=PLANE('',#51121);
#3841=PLANE('',#51122);
#3842=PLANE('',#51123);
#3843=PLANE('',#51124);
#3844=PLANE('',#51125);
#3845=PLANE('',#51126);
#3846=PLANE('',#51127);
#3847=PLANE('',#51128);
#3848=PLANE('',#51129);
#3849=PLANE('',#51130);
#3850=PLANE('',#51131);
#3851=PLANE('',#51132);
#3852=PLANE('',#51133);
#3853=PLANE('',#51134);
#3854=PLANE('',#51135);
#3855=PLANE('',#51136);
#3856=PLANE('',#51137);
#3857=PLANE('',#51138);
#3858=PLANE('',#51139);
#3859=PLANE('',#51140);
#3860=PLANE('',#51141);
#3861=PLANE('',#51142);
#3862=PLANE('',#51143);
#3863=PLANE('',#51144);
#3864=PLANE('',#51145);
#3865=PLANE('',#51146);
#3866=PLANE('',#51147);
#3867=PLANE('',#51148);
#3868=PLANE('',#51149);
#3869=PLANE('',#51150);
#3870=PLANE('',#51151);
#3871=PLANE('',#51152);
#3872=PLANE('',#51153);
#3873=PLANE('',#51154);
#3874=PLANE('',#51155);
#3875=PLANE('',#51156);
#3876=PLANE('',#51157);
#3877=PLANE('',#51158);
#3878=PLANE('',#51159);
#3879=PLANE('',#51160);
#3880=PLANE('',#51161);
#3881=PLANE('',#51162);
#3882=PLANE('',#51163);
#3883=PLANE('',#51164);
#3884=PLANE('',#51165);
#3885=PLANE('',#51166);
#3886=PLANE('',#51167);
#3887=PLANE('',#51168);
#3888=PLANE('',#51169);
#3889=PLANE('',#51170);
#3890=PLANE('',#51171);
#3891=PLANE('',#51172);
#3892=PLANE('',#51173);
#3893=PLANE('',#51174);
#3894=PLANE('',#51175);
#3895=PLANE('',#51176);
#3896=PLANE('',#51177);
#3897=PLANE('',#51178);
#3898=PLANE('',#51179);
#3899=PLANE('',#51180);
#3900=PLANE('',#51181);
#3901=PLANE('',#51182);
#3902=PLANE('',#51183);
#3903=PLANE('',#51184);
#3904=PLANE('',#51185);
#3905=PLANE('',#51186);
#3906=PLANE('',#51187);
#3907=PLANE('',#51188);
#3908=PLANE('',#51189);
#3909=PLANE('',#51190);
#3910=PLANE('',#51191);
#3911=PLANE('',#51192);
#3912=PLANE('',#51193);
#3913=PLANE('',#51194);
#3914=PLANE('',#51195);
#3915=PLANE('',#51196);
#3916=PLANE('',#51197);
#3917=PLANE('',#51198);
#3918=PLANE('',#51199);
#3919=PLANE('',#51200);
#3920=PLANE('',#51201);
#3921=PLANE('',#51202);
#3922=PLANE('',#51203);
#3923=PLANE('',#51204);
#3924=PLANE('',#51205);
#3925=PLANE('',#51206);
#3926=PLANE('',#51207);
#3927=PLANE('',#51208);
#3928=PLANE('',#51209);
#3929=PLANE('',#51210);
#3930=PLANE('',#51211);
#3931=PLANE('',#51212);
#3932=PLANE('',#51213);
#3933=PLANE('',#51214);
#3934=PLANE('',#51215);
#3935=PLANE('',#51216);
#3936=PLANE('',#51217);
#3937=PLANE('',#51218);
#3938=PLANE('',#51219);
#3939=PLANE('',#51220);
#3940=PLANE('',#51221);
#3941=PLANE('',#51222);
#3942=PLANE('',#51223);
#3943=PLANE('',#51224);
#3944=PLANE('',#51225);
#3945=PLANE('',#51226);
#3946=PLANE('',#51227);
#3947=PLANE('',#51228);
#3948=PLANE('',#51229);
#3949=PLANE('',#51230);
#3950=PLANE('',#51231);
#3951=PLANE('',#51232);
#3952=PLANE('',#51233);
#3953=PLANE('',#51234);
#3954=PLANE('',#51235);
#3955=PLANE('',#51236);
#3956=PLANE('',#51237);
#3957=PLANE('',#51238);
#3958=PLANE('',#51239);
#3959=PLANE('',#51240);
#3960=PLANE('',#51241);
#3961=PLANE('',#51242);
#3962=PLANE('',#51243);
#3963=PLANE('',#51244);
#3964=PLANE('',#51245);
#3965=PLANE('',#51246);
#3966=PLANE('',#51247);
#3967=PLANE('',#51248);
#3968=PLANE('',#51249);
#3969=PLANE('',#51250);
#3970=PLANE('',#51251);
#3971=PLANE('',#51252);
#3972=PLANE('',#51253);
#3973=PLANE('',#51254);
#3974=PLANE('',#51255);
#3975=PLANE('',#51256);
#3976=PLANE('',#51257);
#3977=PLANE('',#51258);
#3978=PLANE('',#51259);
#3979=PLANE('',#51260);
#3980=PLANE('',#51261);
#3981=PLANE('',#51262);
#3982=PLANE('',#51263);
#3983=PLANE('',#51264);
#3984=PLANE('',#51265);
#3985=PLANE('',#51266);
#3986=PLANE('',#51267);
#3987=PLANE('',#51268);
#3988=PLANE('',#51269);
#3989=PLANE('',#51270);
#3990=PLANE('',#51271);
#3991=PLANE('',#51272);
#3992=PLANE('',#51273);
#3993=PLANE('',#51274);
#3994=PLANE('',#51275);
#3995=PLANE('',#51276);
#3996=PLANE('',#51277);
#3997=PLANE('',#51278);
#3998=PLANE('',#51279);
#3999=PLANE('',#51280);
#4000=PLANE('',#51281);
#4001=PLANE('',#51282);
#4002=PLANE('',#51283);
#4003=PLANE('',#51284);
#4004=PLANE('',#51285);
#4005=PLANE('',#51286);
#4006=PLANE('',#51287);
#4007=PLANE('',#51288);
#4008=PLANE('',#51289);
#4009=PLANE('',#51290);
#4010=PLANE('',#51291);
#4011=PLANE('',#51292);
#4012=PLANE('',#51293);
#4013=PLANE('',#51294);
#4014=PLANE('',#51295);
#4015=PLANE('',#51296);
#4016=PLANE('',#51297);
#4017=PLANE('',#51298);
#4018=PLANE('',#51299);
#4019=PLANE('',#51300);
#4020=PLANE('',#51301);
#4021=PLANE('',#51302);
#4022=PLANE('',#51303);
#4023=PLANE('',#51304);
#4024=PLANE('',#51305);
#4025=PLANE('',#51306);
#4026=PLANE('',#51307);
#4027=PLANE('',#51308);
#4028=PLANE('',#51309);
#4029=PLANE('',#51310);
#4030=PLANE('',#51311);
#4031=PLANE('',#51312);
#4032=PLANE('',#51313);
#4033=PLANE('',#51314);
#4034=PLANE('',#51315);
#4035=PLANE('',#51316);
#4036=PLANE('',#51317);
#4037=PLANE('',#51318);
#4038=PLANE('',#51319);
#4039=PLANE('',#51320);
#4040=PLANE('',#51321);
#4041=PLANE('',#51322);
#4042=PLANE('',#51323);
#4043=PLANE('',#51324);
#4044=PLANE('',#51325);
#4045=PLANE('',#51326);
#4046=PLANE('',#51327);
#4047=PLANE('',#51328);
#4048=PLANE('',#51329);
#4049=PLANE('',#51330);
#4050=PLANE('',#51331);
#4051=PLANE('',#51332);
#4052=PLANE('',#51333);
#4053=PLANE('',#51334);
#4054=PLANE('',#51335);
#4055=PLANE('',#51336);
#4056=PLANE('',#51337);
#4057=PLANE('',#51338);
#4058=PLANE('',#51339);
#4059=PLANE('',#51340);
#4060=PLANE('',#51341);
#4061=PLANE('',#51342);
#4062=PLANE('',#51343);
#4063=PLANE('',#51344);
#4064=PLANE('',#51345);
#4065=PLANE('',#51346);
#4066=PLANE('',#51347);
#4067=PLANE('',#51348);
#4068=PLANE('',#51349);
#4069=PLANE('',#51350);
#4070=PLANE('',#51351);
#4071=PLANE('',#51352);
#4072=PLANE('',#51353);
#4073=PLANE('',#51354);
#4074=PLANE('',#51355);
#4075=PLANE('',#51356);
#4076=PLANE('',#51357);
#4077=PLANE('',#51358);
#4078=PLANE('',#51359);
#4079=PLANE('',#51360);
#4080=PLANE('',#51361);
#4081=PLANE('',#51362);
#4082=PLANE('',#51363);
#4083=PLANE('',#51364);
#4084=PLANE('',#51365);
#4085=PLANE('',#51366);
#4086=PLANE('',#51367);
#4087=PLANE('',#51368);
#4088=PLANE('',#51369);
#4089=PLANE('',#51370);
#4090=PLANE('',#51371);
#4091=PLANE('',#51372);
#4092=PLANE('',#51373);
#4093=PLANE('',#51374);
#4094=PLANE('',#51375);
#4095=PLANE('',#51376);
#4096=PLANE('',#51377);
#4097=PLANE('',#51378);
#4098=PLANE('',#51379);
#4099=PLANE('',#51380);
#4100=PLANE('',#51381);
#4101=PLANE('',#51382);
#4102=PLANE('',#51383);
#4103=PLANE('',#51384);
#4104=PLANE('',#51385);
#4105=PLANE('',#51386);
#4106=PLANE('',#51387);
#4107=PLANE('',#51388);
#4108=PLANE('',#51389);
#4109=PLANE('',#51390);
#4110=PLANE('',#51391);
#4111=PLANE('',#51392);
#4112=PLANE('',#51393);
#4113=PLANE('',#51394);
#4114=PLANE('',#51395);
#4115=PLANE('',#51396);
#4116=PLANE('',#51397);
#4117=PLANE('',#51398);
#4118=PLANE('',#51399);
#4119=PLANE('',#51400);
#4120=PLANE('',#51401);
#4121=PLANE('',#51402);
#4122=PLANE('',#51403);
#4123=PLANE('',#51404);
#4124=PLANE('',#51405);
#4125=PLANE('',#51406);
#4126=PLANE('',#51407);
#4127=PLANE('',#51408);
#4128=PLANE('',#51409);
#4129=PLANE('',#51410);
#4130=PLANE('',#51411);
#4131=PLANE('',#51412);
#4132=PLANE('',#51413);
#4133=PLANE('',#51414);
#4134=PLANE('',#51415);
#4135=PLANE('',#51416);
#4136=PLANE('',#51417);
#4137=PLANE('',#51418);
#4138=PLANE('',#51419);
#4139=PLANE('',#51420);
#4140=PLANE('',#51421);
#4141=PLANE('',#51422);
#4142=PLANE('',#51423);
#4143=PLANE('',#51424);
#4144=PLANE('',#51425);
#4145=PLANE('',#51426);
#4146=PLANE('',#51427);
#4147=PLANE('',#51428);
#4148=PLANE('',#51429);
#4149=PLANE('',#51430);
#4150=PLANE('',#51431);
#4151=PLANE('',#51432);
#4152=PLANE('',#51433);
#4153=PLANE('',#51434);
#4154=PLANE('',#51435);
#4155=PLANE('',#51436);
#4156=PLANE('',#51437);
#4157=PLANE('',#51438);
#4158=PLANE('',#51439);
#4159=PLANE('',#51440);
#4160=PLANE('',#51441);
#4161=PLANE('',#51442);
#4162=PLANE('',#51443);
#4163=PLANE('',#51444);
#4164=PLANE('',#51445);
#4165=PLANE('',#51446);
#4166=PLANE('',#51447);
#4167=PLANE('',#51448);
#4168=PLANE('',#51449);
#4169=PLANE('',#51450);
#4170=PLANE('',#51451);
#4171=PLANE('',#51452);
#4172=PLANE('',#51453);
#4173=PLANE('',#51454);
#4174=PLANE('',#51455);
#4175=PLANE('',#51456);
#4176=PLANE('',#51457);
#4177=PLANE('',#51458);
#4178=PLANE('',#51459);
#4179=PLANE('',#51460);
#4180=PLANE('',#51461);
#4181=PLANE('',#51462);
#4182=PLANE('',#51463);
#4183=PLANE('',#51464);
#4184=PLANE('',#51465);
#4185=PLANE('',#51466);
#4186=PLANE('',#51467);
#4187=PLANE('',#51468);
#4188=PLANE('',#51469);
#4189=PLANE('',#51470);
#4190=PLANE('',#51471);
#4191=PLANE('',#51472);
#4192=PLANE('',#51473);
#4193=PLANE('',#51474);
#4194=PLANE('',#51475);
#4195=PLANE('',#51476);
#4196=PLANE('',#51477);
#4197=PLANE('',#51478);
#4198=PLANE('',#51479);
#4199=PLANE('',#51480);
#4200=PLANE('',#51481);
#4201=PLANE('',#51482);
#4202=PLANE('',#51483);
#4203=PLANE('',#51484);
#4204=PLANE('',#51485);
#4205=PLANE('',#51486);
#4206=PLANE('',#51487);
#4207=PLANE('',#51488);
#4208=PLANE('',#51489);
#4209=PLANE('',#51490);
#4210=PLANE('',#51491);
#4211=PLANE('',#51492);
#4212=PLANE('',#51493);
#4213=PLANE('',#51494);
#4214=PLANE('',#51495);
#4215=PLANE('',#51496);
#4216=PLANE('',#51497);
#4217=PLANE('',#51498);
#4218=PLANE('',#51499);
#4219=PLANE('',#51500);
#4220=PLANE('',#51501);
#4221=PLANE('',#51502);
#4222=PLANE('',#51503);
#4223=PLANE('',#51504);
#4224=PLANE('',#51505);
#4225=PLANE('',#51506);
#4226=PLANE('',#51507);
#4227=PLANE('',#51508);
#4228=PLANE('',#51509);
#4229=PLANE('',#51510);
#4230=PLANE('',#51511);
#4231=PLANE('',#51512);
#4232=PLANE('',#51513);
#4233=PLANE('',#51514);
#4234=PLANE('',#51515);
#4235=PLANE('',#51516);
#4236=PLANE('',#51517);
#4237=PLANE('',#51518);
#4238=PLANE('',#51519);
#4239=PLANE('',#51520);
#4240=PLANE('',#51521);
#4241=PLANE('',#51522);
#4242=PLANE('',#51523);
#4243=PLANE('',#51524);
#4244=PLANE('',#51525);
#4245=PLANE('',#51526);
#4246=PLANE('',#51527);
#4247=PLANE('',#51528);
#4248=PLANE('',#51529);
#4249=PLANE('',#51530);
#4250=PLANE('',#51531);
#4251=PLANE('',#51532);
#4252=PLANE('',#51533);
#4253=PLANE('',#51534);
#4254=PLANE('',#51535);
#4255=PLANE('',#51536);
#4256=PLANE('',#51537);
#4257=PLANE('',#51538);
#4258=PLANE('',#51539);
#4259=PLANE('',#51540);
#4260=PLANE('',#51541);
#4261=PLANE('',#51542);
#4262=PLANE('',#51543);
#4263=PLANE('',#51544);
#4264=PLANE('',#51545);
#4265=PLANE('',#51546);
#4266=PLANE('',#51547);
#4267=PLANE('',#51548);
#4268=PLANE('',#51549);
#4269=PLANE('',#51550);
#4270=PLANE('',#51551);
#4271=PLANE('',#51552);
#4272=PLANE('',#51553);
#4273=PLANE('',#51554);
#4274=PLANE('',#51555);
#4275=PLANE('',#51556);
#4276=PLANE('',#51557);
#4277=PLANE('',#51558);
#4278=PLANE('',#51559);
#4279=PLANE('',#51560);
#4280=PLANE('',#51561);
#4281=PLANE('',#51562);
#4282=PLANE('',#51563);
#4283=PLANE('',#51564);
#4284=PLANE('',#51565);
#4285=PLANE('',#51566);
#4286=PLANE('',#51567);
#4287=PLANE('',#51568);
#4288=PLANE('',#51569);
#4289=PLANE('',#51570);
#4290=PLANE('',#51571);
#4291=PLANE('',#51572);
#4292=PLANE('',#51573);
#4293=PLANE('',#51574);
#4294=PLANE('',#51575);
#4295=PLANE('',#51576);
#4296=PLANE('',#51577);
#4297=PLANE('',#51578);
#4298=PLANE('',#51579);
#4299=PLANE('',#51580);
#4300=PLANE('',#51581);
#4301=PLANE('',#51582);
#4302=PLANE('',#51583);
#4303=PLANE('',#51584);
#4304=PLANE('',#51585);
#4305=PLANE('',#51586);
#4306=PLANE('',#51587);
#4307=PLANE('',#51588);
#4308=PLANE('',#51589);
#4309=PLANE('',#51590);
#4310=PLANE('',#51591);
#4311=PLANE('',#51592);
#4312=LINE('',#65500,#6086);
#4313=LINE('',#65502,#6087);
#4314=LINE('',#65505,#6088);
#4315=LINE('',#65513,#6089);
#4316=LINE('',#65517,#6090);
#4317=LINE('',#65518,#6091);
#4318=LINE('',#65521,#6092);
#4319=LINE('',#65524,#6093);
#4320=LINE('',#65526,#6094);
#4321=LINE('',#65527,#6095);
#4322=LINE('',#65533,#6096);
#4323=LINE('',#65537,#6097);
#4324=LINE('',#65541,#6098);
#4325=LINE('',#65542,#6099);
#4326=LINE('',#65545,#6100);
#4327=LINE('',#65546,#6101);
#4328=LINE('',#65554,#6102);
#4329=LINE('',#65560,#6103);
#4330=LINE('',#65566,#6104);
#4331=LINE('',#65572,#6105);
#4332=LINE('',#65578,#6106);
#4333=LINE('',#65584,#6107);
#4334=LINE('',#65590,#6108);
#4335=LINE('',#65596,#6109);
#4336=LINE('',#65602,#6110);
#4337=LINE('',#65608,#6111);
#4338=LINE('',#65614,#6112);
#4339=LINE('',#65620,#6113);
#4340=LINE('',#65647,#6114);
#4341=LINE('',#65708,#6115);
#4342=LINE('',#65767,#6116);
#4343=LINE('',#65829,#6117);
#4344=LINE('',#65891,#6118);
#4345=LINE('',#65950,#6119);
#4346=LINE('',#66009,#6120);
#4347=LINE('',#66071,#6121);
#4348=LINE('',#66133,#6122);
#4349=LINE('',#66192,#6123);
#4350=LINE('',#66254,#6124);
#4351=LINE('',#66313,#6125);
#4352=LINE('',#66375,#6126);
#4353=LINE('',#66434,#6127);
#4354=LINE('',#66496,#6128);
#4355=LINE('',#66555,#6129);
#4356=LINE('',#66617,#6130);
#4357=LINE('',#66676,#6131);
#4358=LINE('',#66738,#6132);
#4359=LINE('',#66797,#6133);
#4360=LINE('',#66856,#6134);
#4361=LINE('',#66918,#6135);
#4362=LINE('',#66977,#6136);
#4363=LINE('',#67039,#6137);
#4364=LINE('',#67098,#6138);
#4365=LINE('',#67160,#6139);
#4366=LINE('',#67219,#6140);
#4367=LINE('',#67281,#6141);
#4368=LINE('',#67340,#6142);
#4369=LINE('',#67402,#6143);
#4370=LINE('',#67461,#6144);
#4371=LINE('',#67523,#6145);
#4372=LINE('',#67583,#6146);
#4373=LINE('',#67644,#6147);
#4374=LINE('',#67701,#6148);
#4375=LINE('',#67765,#6149);
#4376=LINE('',#67827,#6150);
#4377=LINE('',#67886,#6151);
#4378=LINE('',#67943,#6152);
#4379=LINE('',#68007,#6153);
#4380=LINE('',#68064,#6154);
#4381=LINE('',#68128,#6155);
#4382=LINE('',#68185,#6156);
#4383=LINE('',#68249,#6157);
#4384=LINE('',#68306,#6158);
#4385=LINE('',#68370,#6159);
#4386=LINE('',#68430,#6160);
#4387=LINE('',#68491,#6161);
#4388=LINE('',#68548,#6162);
#4389=LINE('',#68612,#6163);
#4390=LINE('',#68669,#6164);
#4391=LINE('',#68733,#6165);
#4392=LINE('',#68790,#6166);
#4393=LINE('',#68854,#6167);
#4394=LINE('',#68911,#6168);
#4395=LINE('',#68975,#6169);
#4396=LINE('',#69032,#6170);
#4397=LINE('',#69096,#6171);
#4398=LINE('',#69153,#6172);
#4399=LINE('',#69217,#6173);
#4400=LINE('',#69274,#6174);
#4401=LINE('',#69338,#6175);
#4402=LINE('',#69395,#6176);
#4403=LINE('',#69459,#6177);
#4404=LINE('',#69516,#6178);
#4405=LINE('',#69582,#6179);
#4406=LINE('',#69642,#6180);
#4407=LINE('',#69703,#6181);
#4408=LINE('',#69760,#6182);
#4409=LINE('',#69824,#6183);
#4410=LINE('',#69881,#6184);
#4411=LINE('',#69945,#6185);
#4412=LINE('',#70002,#6186);
#4413=LINE('',#70066,#6187);
#4414=LINE('',#70123,#6188);
#4415=LINE('',#70199,#6189);
#4416=LINE('',#70256,#6190);
#4417=LINE('',#70320,#6191);
#4418=LINE('',#70359,#6192);
#4419=LINE('',#70408,#6193);
#4420=LINE('',#70414,#6194);
#4421=LINE('',#70465,#6195);
#4422=LINE('',#70489,#6196);
#4423=LINE('',#70569,#6197);
#4424=LINE('',#70629,#6198);
#4425=LINE('',#70708,#6199);
#4426=LINE('',#70747,#6200);
#4427=LINE('',#70800,#6201);
#4428=LINE('',#70806,#6202);
#4429=LINE('',#70857,#6203);
#4430=LINE('',#70884,#6204);
#4431=LINE('',#70955,#6205);
#4432=LINE('',#71015,#6206);
#4433=LINE('',#71090,#6207);
#4434=LINE('',#71129,#6208);
#4435=LINE('',#71182,#6209);
#4436=LINE('',#71206,#6210);
#4437=LINE('',#71280,#6211);
#4438=LINE('',#71340,#6212);
#4439=LINE('',#71409,#6213);
#4440=LINE('',#71448,#6214);
#4441=LINE('',#71503,#6215);
#4442=LINE('',#71530,#6216);
#4443=LINE('',#71603,#6217);
#4444=LINE('',#71660,#6218);
#4445=LINE('',#71734,#6219);
#4446=LINE('',#71794,#6220);
#4447=LINE('',#71871,#6221);
#4448=LINE('',#71928,#6222);
#4449=LINE('',#72012,#6223);
#4450=LINE('',#72072,#6224);
#4451=LINE('',#72133,#6225);
#4452=LINE('',#72190,#6226);
#4453=LINE('',#72268,#6227);
#4454=LINE('',#72328,#6228);
#4455=LINE('',#72389,#6229);
#4456=LINE('',#72449,#6230);
#4457=LINE('',#72510,#6231);
#4458=LINE('',#72569,#6232);
#4459=LINE('',#72631,#6233);
#4460=LINE('',#72693,#6234);
#4461=LINE('',#72752,#6235);
#4462=LINE('',#72814,#6236);
#4463=LINE('',#72873,#6237);
#4464=LINE('',#72933,#6238);
#4465=LINE('',#72994,#6239);
#4466=LINE('',#73056,#6240);
#4467=LINE('',#73117,#6241);
#4468=LINE('',#73179,#6242);
#4469=LINE('',#73238,#6243);
#4470=LINE('',#73277,#6244);
#4471=LINE('',#73283,#6245);
#4472=LINE('',#73289,#6246);
#4473=LINE('',#73295,#6247);
#4474=LINE('',#73301,#6248);
#4475=LINE('',#73307,#6249);
#4476=LINE('',#73313,#6250);
#4477=LINE('',#73319,#6251);
#4478=LINE('',#73325,#6252);
#4479=LINE('',#73331,#6253);
#4480=LINE('',#73337,#6254);
#4481=LINE('',#73343,#6255);
#4482=LINE('',#73349,#6256);
#4483=LINE('',#73355,#6257);
#4484=LINE('',#73361,#6258);
#4485=LINE('',#73367,#6259);
#4486=LINE('',#73373,#6260);
#4487=LINE('',#73414,#6261);
#4488=LINE('',#73420,#6262);
#4489=LINE('',#73426,#6263);
#4490=LINE('',#73432,#6264);
#4491=LINE('',#73438,#6265);
#4492=LINE('',#73444,#6266);
#4493=LINE('',#73450,#6267);
#4494=LINE('',#73456,#6268);
#4495=LINE('',#73462,#6269);
#4496=LINE('',#73468,#6270);
#4497=LINE('',#73474,#6271);
#4498=LINE('',#73480,#6272);
#4499=LINE('',#73486,#6273);
#4500=LINE('',#73492,#6274);
#4501=LINE('',#73498,#6275);
#4502=LINE('',#73504,#6276);
#4503=LINE('',#73510,#6277);
#4504=LINE('',#73516,#6278);
#4505=LINE('',#73557,#6279);
#4506=LINE('',#73563,#6280);
#4507=LINE('',#73569,#6281);
#4508=LINE('',#73575,#6282);
#4509=LINE('',#73581,#6283);
#4510=LINE('',#73587,#6284);
#4511=LINE('',#73593,#6285);
#4512=LINE('',#73599,#6286);
#4513=LINE('',#73605,#6287);
#4514=LINE('',#73611,#6288);
#4515=LINE('',#73617,#6289);
#4516=LINE('',#73623,#6290);
#4517=LINE('',#73629,#6291);
#4518=LINE('',#73635,#6292);
#4519=LINE('',#73641,#6293);
#4520=LINE('',#73647,#6294);
#4521=LINE('',#73688,#6295);
#4522=LINE('',#73694,#6296);
#4523=LINE('',#73700,#6297);
#4524=LINE('',#73706,#6298);
#4525=LINE('',#73712,#6299);
#4526=LINE('',#73718,#6300);
#4527=LINE('',#73724,#6301);
#4528=LINE('',#73730,#6302);
#4529=LINE('',#73736,#6303);
#4530=LINE('',#73742,#6304);
#4531=LINE('',#73748,#6305);
#4532=LINE('',#73754,#6306);
#4533=LINE('',#73760,#6307);
#4534=LINE('',#73766,#6308);
#4535=LINE('',#73772,#6309);
#4536=LINE('',#73778,#6310);
#4537=LINE('',#73784,#6311);
#4538=LINE('',#73790,#6312);
#4539=LINE('',#73831,#6313);
#4540=LINE('',#73837,#6314);
#4541=LINE('',#73843,#6315);
#4542=LINE('',#73849,#6316);
#4543=LINE('',#73855,#6317);
#4544=LINE('',#73861,#6318);
#4545=LINE('',#73867,#6319);
#4546=LINE('',#73873,#6320);
#4547=LINE('',#73879,#6321);
#4548=LINE('',#73885,#6322);
#4549=LINE('',#73891,#6323);
#4550=LINE('',#73897,#6324);
#4551=LINE('',#73903,#6325);
#4552=LINE('',#73909,#6326);
#4553=LINE('',#73915,#6327);
#4554=LINE('',#73921,#6328);
#4555=LINE('',#73927,#6329);
#4556=LINE('',#73933,#6330);
#4557=LINE('',#73974,#6331);
#4558=LINE('',#73980,#6332);
#4559=LINE('',#73986,#6333);
#4560=LINE('',#73992,#6334);
#4561=LINE('',#73998,#6335);
#4562=LINE('',#74004,#6336);
#4563=LINE('',#74010,#6337);
#4564=LINE('',#74016,#6338);
#4565=LINE('',#74022,#6339);
#4566=LINE('',#74028,#6340);
#4567=LINE('',#74034,#6341);
#4568=LINE('',#74040,#6342);
#4569=LINE('',#74046,#6343);
#4570=LINE('',#74052,#6344);
#4571=LINE('',#74058,#6345);
#4572=LINE('',#74064,#6346);
#4573=LINE('',#74070,#6347);
#4574=LINE('',#74076,#6348);
#4575=LINE('',#74117,#6349);
#4576=LINE('',#74123,#6350);
#4577=LINE('',#74129,#6351);
#4578=LINE('',#74135,#6352);
#4579=LINE('',#74141,#6353);
#4580=LINE('',#74147,#6354);
#4581=LINE('',#74153,#6355);
#4582=LINE('',#74159,#6356);
#4583=LINE('',#74165,#6357);
#4584=LINE('',#74171,#6358);
#4585=LINE('',#74177,#6359);
#4586=LINE('',#74183,#6360);
#4587=LINE('',#74189,#6361);
#4588=LINE('',#74195,#6362);
#4589=LINE('',#74201,#6363);
#4590=LINE('',#74207,#6364);
#4591=LINE('',#74213,#6365);
#4592=LINE('',#74219,#6366);
#4593=LINE('',#74260,#6367);
#4594=LINE('',#74266,#6368);
#4595=LINE('',#74272,#6369);
#4596=LINE('',#74278,#6370);
#4597=LINE('',#74284,#6371);
#4598=LINE('',#74290,#6372);
#4599=LINE('',#74296,#6373);
#4600=LINE('',#74302,#6374);
#4601=LINE('',#74308,#6375);
#4602=LINE('',#74314,#6376);
#4603=LINE('',#74320,#6377);
#4604=LINE('',#74326,#6378);
#4605=LINE('',#74332,#6379);
#4606=LINE('',#74338,#6380);
#4607=LINE('',#74344,#6381);
#4608=LINE('',#74350,#6382);
#4609=LINE('',#74391,#6383);
#4610=LINE('',#74397,#6384);
#4611=LINE('',#74403,#6385);
#4612=LINE('',#74409,#6386);
#4613=LINE('',#74415,#6387);
#4614=LINE('',#74421,#6388);
#4615=LINE('',#74427,#6389);
#4616=LINE('',#74433,#6390);
#4617=LINE('',#74439,#6391);
#4618=LINE('',#74445,#6392);
#4619=LINE('',#74451,#6393);
#4620=LINE('',#74457,#6394);
#4621=LINE('',#74463,#6395);
#4622=LINE('',#74469,#6396);
#4623=LINE('',#74475,#6397);
#4624=LINE('',#74481,#6398);
#4625=LINE('',#74487,#6399);
#4626=LINE('',#74493,#6400);
#4627=LINE('',#74534,#6401);
#4628=LINE('',#74540,#6402);
#4629=LINE('',#74546,#6403);
#4630=LINE('',#74552,#6404);
#4631=LINE('',#74558,#6405);
#4632=LINE('',#74564,#6406);
#4633=LINE('',#74570,#6407);
#4634=LINE('',#74576,#6408);
#4635=LINE('',#74582,#6409);
#4636=LINE('',#74588,#6410);
#4637=LINE('',#74594,#6411);
#4638=LINE('',#74600,#6412);
#4639=LINE('',#74606,#6413);
#4640=LINE('',#74612,#6414);
#4641=LINE('',#74618,#6415);
#4642=LINE('',#74624,#6416);
#4643=LINE('',#74630,#6417);
#4644=LINE('',#74636,#6418);
#4645=LINE('',#74677,#6419);
#4646=LINE('',#74683,#6420);
#4647=LINE('',#74689,#6421);
#4648=LINE('',#74695,#6422);
#4649=LINE('',#74701,#6423);
#4650=LINE('',#74707,#6424);
#4651=LINE('',#74713,#6425);
#4652=LINE('',#74719,#6426);
#4653=LINE('',#74725,#6427);
#4654=LINE('',#74731,#6428);
#4655=LINE('',#74737,#6429);
#4656=LINE('',#74743,#6430);
#4657=LINE('',#74749,#6431);
#4658=LINE('',#74755,#6432);
#4659=LINE('',#74761,#6433);
#4660=LINE('',#74767,#6434);
#4661=LINE('',#74773,#6435);
#4662=LINE('',#74779,#6436);
#4663=LINE('',#74820,#6437);
#4664=LINE('',#74826,#6438);
#4665=LINE('',#74832,#6439);
#4666=LINE('',#74838,#6440);
#4667=LINE('',#74844,#6441);
#4668=LINE('',#74850,#6442);
#4669=LINE('',#74856,#6443);
#4670=LINE('',#74862,#6444);
#4671=LINE('',#74868,#6445);
#4672=LINE('',#74874,#6446);
#4673=LINE('',#74880,#6447);
#4674=LINE('',#74886,#6448);
#4675=LINE('',#74892,#6449);
#4676=LINE('',#74898,#6450);
#4677=LINE('',#74904,#6451);
#4678=LINE('',#74910,#6452);
#4679=LINE('',#74916,#6453);
#4680=LINE('',#74922,#6454);
#4681=LINE('',#74963,#6455);
#4682=LINE('',#74969,#6456);
#4683=LINE('',#74975,#6457);
#4684=LINE('',#74981,#6458);
#4685=LINE('',#74987,#6459);
#4686=LINE('',#74993,#6460);
#4687=LINE('',#74999,#6461);
#4688=LINE('',#75005,#6462);
#4689=LINE('',#75011,#6463);
#4690=LINE('',#75017,#6464);
#4691=LINE('',#75023,#6465);
#4692=LINE('',#75029,#6466);
#4693=LINE('',#75035,#6467);
#4694=LINE('',#75041,#6468);
#4695=LINE('',#75047,#6469);
#4696=LINE('',#75053,#6470);
#4697=LINE('',#75094,#6471);
#4698=LINE('',#75100,#6472);
#4699=LINE('',#75106,#6473);
#4700=LINE('',#75112,#6474);
#4701=LINE('',#75118,#6475);
#4702=LINE('',#75124,#6476);
#4703=LINE('',#75130,#6477);
#4704=LINE('',#75136,#6478);
#4705=LINE('',#75142,#6479);
#4706=LINE('',#75148,#6480);
#4707=LINE('',#75154,#6481);
#4708=LINE('',#75160,#6482);
#4709=LINE('',#75166,#6483);
#4710=LINE('',#75172,#6484);
#4711=LINE('',#75178,#6485);
#4712=LINE('',#75184,#6486);
#4713=LINE('',#75190,#6487);
#4714=LINE('',#75196,#6488);
#4715=LINE('',#75237,#6489);
#4716=LINE('',#75243,#6490);
#4717=LINE('',#75249,#6491);
#4718=LINE('',#75255,#6492);
#4719=LINE('',#75261,#6493);
#4720=LINE('',#75267,#6494);
#4721=LINE('',#75273,#6495);
#4722=LINE('',#75279,#6496);
#4723=LINE('',#75285,#6497);
#4724=LINE('',#75291,#6498);
#4725=LINE('',#75297,#6499);
#4726=LINE('',#75303,#6500);
#4727=LINE('',#75309,#6501);
#4728=LINE('',#75315,#6502);
#4729=LINE('',#75321,#6503);
#4730=LINE('',#75327,#6504);
#4731=LINE('',#75333,#6505);
#4732=LINE('',#75339,#6506);
#4733=LINE('',#75380,#6507);
#4734=LINE('',#75386,#6508);
#4735=LINE('',#75392,#6509);
#4736=LINE('',#75398,#6510);
#4737=LINE('',#75404,#6511);
#4738=LINE('',#75410,#6512);
#4739=LINE('',#75416,#6513);
#4740=LINE('',#75422,#6514);
#4741=LINE('',#75428,#6515);
#4742=LINE('',#75434,#6516);
#4743=LINE('',#75440,#6517);
#4744=LINE('',#75446,#6518);
#4745=LINE('',#75452,#6519);
#4746=LINE('',#75458,#6520);
#4747=LINE('',#75464,#6521);
#4748=LINE('',#75470,#6522);
#4749=LINE('',#75476,#6523);
#4750=LINE('',#75482,#6524);
#4751=LINE('',#75523,#6525);
#4752=LINE('',#75529,#6526);
#4753=LINE('',#75535,#6527);
#4754=LINE('',#75541,#6528);
#4755=LINE('',#75547,#6529);
#4756=LINE('',#75553,#6530);
#4757=LINE('',#75559,#6531);
#4758=LINE('',#75565,#6532);
#4759=LINE('',#75571,#6533);
#4760=LINE('',#75577,#6534);
#4761=LINE('',#75583,#6535);
#4762=LINE('',#75589,#6536);
#4763=LINE('',#75595,#6537);
#4764=LINE('',#75601,#6538);
#4765=LINE('',#75607,#6539);
#4766=LINE('',#75613,#6540);
#4767=LINE('',#75619,#6541);
#4768=LINE('',#75625,#6542);
#4769=LINE('',#75666,#6543);
#4770=LINE('',#75672,#6544);
#4771=LINE('',#75678,#6545);
#4772=LINE('',#75684,#6546);
#4773=LINE('',#75690,#6547);
#4774=LINE('',#75696,#6548);
#4775=LINE('',#75702,#6549);
#4776=LINE('',#75708,#6550);
#4777=LINE('',#75714,#6551);
#4778=LINE('',#75720,#6552);
#4779=LINE('',#75726,#6553);
#4780=LINE('',#75732,#6554);
#4781=LINE('',#75738,#6555);
#4782=LINE('',#75744,#6556);
#4783=LINE('',#75750,#6557);
#4784=LINE('',#75756,#6558);
#4785=LINE('',#75797,#6559);
#4786=LINE('',#75803,#6560);
#4787=LINE('',#75809,#6561);
#4788=LINE('',#75815,#6562);
#4789=LINE('',#75821,#6563);
#4790=LINE('',#75827,#6564);
#4791=LINE('',#75833,#6565);
#4792=LINE('',#75839,#6566);
#4793=LINE('',#75845,#6567);
#4794=LINE('',#75851,#6568);
#4795=LINE('',#75857,#6569);
#4796=LINE('',#75863,#6570);
#4797=LINE('',#75869,#6571);
#4798=LINE('',#75875,#6572);
#4799=LINE('',#75881,#6573);
#4800=LINE('',#75887,#6574);
#4801=LINE('',#75893,#6575);
#4802=LINE('',#75899,#6576);
#4803=LINE('',#75937,#6577);
#4804=LINE('',#75943,#6578);
#4805=LINE('',#75949,#6579);
#4806=LINE('',#75955,#6580);
#4807=LINE('',#75961,#6581);
#4808=LINE('',#75967,#6582);
#4809=LINE('',#75973,#6583);
#4810=LINE('',#75979,#6584);
#4811=LINE('',#75985,#6585);
#4812=LINE('',#75991,#6586);
#4813=LINE('',#75997,#6587);
#4814=LINE('',#76003,#6588);
#4815=LINE('',#76009,#6589);
#4816=LINE('',#76015,#6590);
#4817=LINE('',#76021,#6591);
#4818=LINE('',#76027,#6592);
#4819=LINE('',#76048,#6593);
#4820=LINE('',#76054,#6594);
#4821=LINE('',#76099,#6595);
#4822=LINE('',#76105,#6596);
#4823=LINE('',#76111,#6597);
#4824=LINE('',#76117,#6598);
#4825=LINE('',#76123,#6599);
#4826=LINE('',#76129,#6600);
#4827=LINE('',#76135,#6601);
#4828=LINE('',#76141,#6602);
#4829=LINE('',#76147,#6603);
#4830=LINE('',#76153,#6604);
#4831=LINE('',#76159,#6605);
#4832=LINE('',#76165,#6606);
#4833=LINE('',#76171,#6607);
#4834=LINE('',#76177,#6608);
#4835=LINE('',#76200,#6609);
#4836=LINE('',#76206,#6610);
#4837=LINE('',#76212,#6611);
#4838=LINE('',#76218,#6612);
#4839=LINE('',#76224,#6613);
#4840=LINE('',#76230,#6614);
#4841=LINE('',#76236,#6615);
#4842=LINE('',#76242,#6616);
#4843=LINE('',#76248,#6617);
#4844=LINE('',#76254,#6618);
#4845=LINE('',#76260,#6619);
#4846=LINE('',#76266,#6620);
#4847=LINE('',#76272,#6621);
#4848=LINE('',#76278,#6622);
#4849=LINE('',#76284,#6623);
#4850=LINE('',#76290,#6624);
#4851=LINE('',#76296,#6625);
#4852=LINE('',#76302,#6626);
#4853=LINE('',#76308,#6627);
#4854=LINE('',#76314,#6628);
#4855=LINE('',#76320,#6629);
#4856=LINE('',#76326,#6630);
#4857=LINE('',#76332,#6631);
#4858=LINE('',#76338,#6632);
#4859=LINE('',#76344,#6633);
#4860=LINE('',#76350,#6634);
#4861=LINE('',#76356,#6635);
#4862=LINE('',#76362,#6636);
#4863=LINE('',#76395,#6637);
#4864=LINE('',#76401,#6638);
#4865=LINE('',#76407,#6639);
#4866=LINE('',#76413,#6640);
#4867=LINE('',#76419,#6641);
#4868=LINE('',#76425,#6642);
#4869=LINE('',#76431,#6643);
#4870=LINE('',#76437,#6644);
#4871=LINE('',#76443,#6645);
#4872=LINE('',#76449,#6646);
#4873=LINE('',#76455,#6647);
#4874=LINE('',#76461,#6648);
#4875=LINE('',#76467,#6649);
#4876=LINE('',#76473,#6650);
#4877=LINE('',#76479,#6651);
#4878=LINE('',#76485,#6652);
#4879=LINE('',#76491,#6653);
#4880=LINE('',#76497,#6654);
#4881=LINE('',#76503,#6655);
#4882=LINE('',#76509,#6656);
#4883=LINE('',#76515,#6657);
#4884=LINE('',#76521,#6658);
#4885=LINE('',#76527,#6659);
#4886=LINE('',#76533,#6660);
#4887=LINE('',#76539,#6661);
#4888=LINE('',#76545,#6662);
#4889=LINE('',#76551,#6663);
#4890=LINE('',#76557,#6664);
#4891=LINE('',#76563,#6665);
#4892=LINE('',#76569,#6666);
#4893=LINE('',#76575,#6667);
#4894=LINE('',#76581,#6668);
#4895=LINE('',#76587,#6669);
#4896=LINE('',#76593,#6670);
#4897=LINE('',#76641,#6671);
#4898=LINE('',#76647,#6672);
#4899=LINE('',#76653,#6673);
#4900=LINE('',#76659,#6674);
#4901=LINE('',#76665,#6675);
#4902=LINE('',#76671,#6676);
#4903=LINE('',#76677,#6677);
#4904=LINE('',#76683,#6678);
#4905=LINE('',#76689,#6679);
#4906=LINE('',#76695,#6680);
#4907=LINE('',#76701,#6681);
#4908=LINE('',#76707,#6682);
#4909=LINE('',#76713,#6683);
#4910=LINE('',#76719,#6684);
#4911=LINE('',#76725,#6685);
#4912=LINE('',#76731,#6686);
#4913=LINE('',#76737,#6687);
#4914=LINE('',#76743,#6688);
#4915=LINE('',#76781,#6689);
#4916=LINE('',#76787,#6690);
#4917=LINE('',#76793,#6691);
#4918=LINE('',#76799,#6692);
#4919=LINE('',#76805,#6693);
#4920=LINE('',#76811,#6694);
#4921=LINE('',#76817,#6695);
#4922=LINE('',#76823,#6696);
#4923=LINE('',#76829,#6697);
#4924=LINE('',#76835,#6698);
#4925=LINE('',#76841,#6699);
#4926=LINE('',#76847,#6700);
#4927=LINE('',#76853,#6701);
#4928=LINE('',#76859,#6702);
#4929=LINE('',#76865,#6703);
#4930=LINE('',#76871,#6704);
#4931=LINE('',#76877,#6705);
#4932=LINE('',#76883,#6706);
#4933=LINE('',#76924,#6707);
#4934=LINE('',#76930,#6708);
#4935=LINE('',#76936,#6709);
#4936=LINE('',#76942,#6710);
#4937=LINE('',#76948,#6711);
#4938=LINE('',#76954,#6712);
#4939=LINE('',#76960,#6713);
#4940=LINE('',#76966,#6714);
#4941=LINE('',#76972,#6715);
#4942=LINE('',#76978,#6716);
#4943=LINE('',#76984,#6717);
#4944=LINE('',#76990,#6718);
#4945=LINE('',#76996,#6719);
#4946=LINE('',#77002,#6720);
#4947=LINE('',#77008,#6721);
#4948=LINE('',#77014,#6722);
#4949=LINE('',#77055,#6723);
#4950=LINE('',#77061,#6724);
#4951=LINE('',#77067,#6725);
#4952=LINE('',#77073,#6726);
#4953=LINE('',#77079,#6727);
#4954=LINE('',#77085,#6728);
#4955=LINE('',#77091,#6729);
#4956=LINE('',#77097,#6730);
#4957=LINE('',#77103,#6731);
#4958=LINE('',#77109,#6732);
#4959=LINE('',#77115,#6733);
#4960=LINE('',#77121,#6734);
#4961=LINE('',#77127,#6735);
#4962=LINE('',#77133,#6736);
#4963=LINE('',#77139,#6737);
#4964=LINE('',#77145,#6738);
#4965=LINE('',#77151,#6739);
#4966=LINE('',#77157,#6740);
#4967=LINE('',#77198,#6741);
#4968=LINE('',#77204,#6742);
#4969=LINE('',#77210,#6743);
#4970=LINE('',#77216,#6744);
#4971=LINE('',#77222,#6745);
#4972=LINE('',#77228,#6746);
#4973=LINE('',#77234,#6747);
#4974=LINE('',#77240,#6748);
#4975=LINE('',#77246,#6749);
#4976=LINE('',#77252,#6750);
#4977=LINE('',#77258,#6751);
#4978=LINE('',#77264,#6752);
#4979=LINE('',#77270,#6753);
#4980=LINE('',#77276,#6754);
#4981=LINE('',#77282,#6755);
#4982=LINE('',#77288,#6756);
#4983=LINE('',#77294,#6757);
#4984=LINE('',#77300,#6758);
#4985=LINE('',#77341,#6759);
#4986=LINE('',#77800,#6760);
#4987=LINE('',#77856,#6761);
#4988=LINE('',#77859,#6762);
#4989=LINE('',#77897,#6763);
#4990=LINE('',#77907,#6764);
#4991=LINE('',#77968,#6765);
#4992=LINE('',#78004,#6766);
#4993=LINE('',#78029,#6767);
#4994=LINE('',#78040,#6768);
#4995=LINE('',#78041,#6769);
#4996=LINE('',#78069,#6770);
#4997=LINE('',#78096,#6771);
#4998=LINE('',#78099,#6772);
#4999=LINE('',#78102,#6773);
#5000=LINE('',#78115,#6774);
#5001=LINE('',#78135,#6775);
#5002=LINE('',#78149,#6776);
#5003=LINE('',#78153,#6777);
#5004=LINE('',#78158,#6778);
#5005=LINE('',#78160,#6779);
#5006=LINE('',#78161,#6780);
#5007=LINE('',#78162,#6781);
#5008=LINE('',#78166,#6782);
#5009=LINE('',#78187,#6783);
#5010=LINE('',#78295,#6784);
#5011=LINE('',#78296,#6785);
#5012=LINE('',#78906,#6786);
#5013=LINE('',#78986,#6787);
#5014=LINE('',#79681,#6788);
#5015=LINE('',#79682,#6789);
#5016=LINE('',#80914,#6790);
#5017=LINE('',#81048,#6791);
#5018=LINE('',#83692,#6792);
#5019=LINE('',#83694,#6793);
#5020=LINE('',#85019,#6794);
#5021=LINE('',#85521,#6795);
#5022=LINE('',#85910,#6796);
#5023=LINE('',#85914,#6797);
#5024=LINE('',#85919,#6798);
#5025=LINE('',#85920,#6799);
#5026=LINE('',#85921,#6800);
#5027=LINE('',#85925,#6801);
#5028=LINE('',#85929,#6802);
#5029=LINE('',#85930,#6803);
#5030=LINE('',#85938,#6804);
#5031=LINE('',#85941,#6805);
#5032=LINE('',#85944,#6806);
#5033=LINE('',#85946,#6807);
#5034=LINE('',#85947,#6808);
#5035=LINE('',#85951,#6809);
#5036=LINE('',#85954,#6810);
#5037=LINE('',#85955,#6811);
#5038=LINE('',#86018,#6812);
#5039=LINE('',#86081,#6813);
#5040=LINE('',#86085,#6814);
#5041=LINE('',#86145,#6815);
#5042=LINE('',#86187,#6816);
#5043=LINE('',#86387,#6817);
#5044=LINE('',#86412,#6818);
#5045=LINE('',#86418,#6819);
#5046=LINE('',#86443,#6820);
#5047=LINE('',#86449,#6821);
#5048=LINE('',#86474,#6822);
#5049=LINE('',#86480,#6823);
#5050=LINE('',#86484,#6824);
#5051=LINE('',#86597,#6825);
#5052=LINE('',#86605,#6826);
#5053=LINE('',#86608,#6827);
#5054=LINE('',#86723,#6828);
#5055=LINE('',#86727,#6829);
#5056=LINE('',#86840,#6830);
#5057=LINE('',#86848,#6831);
#5058=LINE('',#86851,#6832);
#5059=LINE('',#86966,#6833);
#5060=LINE('',#86970,#6834);
#5061=LINE('',#87083,#6835);
#5062=LINE('',#87091,#6836);
#5063=LINE('',#87094,#6837);
#5064=LINE('',#87208,#6838);
#5065=LINE('',#87212,#6839);
#5066=LINE('',#87331,#6840);
#5067=LINE('',#87605,#6841);
#5068=LINE('',#87607,#6842);
#5069=LINE('',#87608,#6843);
#5070=LINE('',#87612,#6844);
#5071=LINE('',#87616,#6845);
#5072=LINE('',#87628,#6846);
#5073=LINE('',#88057,#6847);
#5074=LINE('',#88061,#6848);
#5075=LINE('',#88499,#6849);
#5076=LINE('',#88501,#6850);
#5077=LINE('',#88503,#6851);
#5078=LINE('',#88504,#6852);
#5079=LINE('',#88507,#6853);
#5080=LINE('',#88509,#6854);
#5081=LINE('',#88510,#6855);
#5082=LINE('',#88514,#6856);
#5083=LINE('',#88515,#6857);
#5084=LINE('',#88516,#6858);
#5085=LINE('',#89284,#6859);
#5086=LINE('',#89287,#6860);
#5087=LINE('',#89319,#6861);
#5088=LINE('',#89711,#6862);
#5089=LINE('',#89712,#6863);
#5090=LINE('',#89717,#6864);
#5091=LINE('',#89718,#6865);
#5092=LINE('',#89726,#6866);
#5093=LINE('',#89906,#6867);
#5094=LINE('',#89907,#6868);
#5095=LINE('',#89916,#6869);
#5096=LINE('',#89917,#6870);
#5097=LINE('',#90113,#6871);
#5098=LINE('',#90114,#6872);
#5099=LINE('',#90116,#6873);
#5100=LINE('',#90118,#6874);
#5101=LINE('',#90119,#6875);
#5102=LINE('',#90123,#6876);
#5103=LINE('',#90124,#6877);
#5104=LINE('',#90126,#6878);
#5105=LINE('',#90127,#6879);
#5106=LINE('',#90135,#6880);
#5107=LINE('',#90136,#6881);
#5108=LINE('',#90144,#6882);
#5109=LINE('',#90145,#6883);
#5110=LINE('',#90302,#6884);
#5111=LINE('',#90307,#6885);
#5112=LINE('',#90308,#6886);
#5113=LINE('',#90313,#6887);
#5114=LINE('',#90314,#6888);
#5115=LINE('',#90318,#6889);
#5116=LINE('',#90482,#6890);
#5117=LINE('',#90483,#6891);
#5118=LINE('',#90485,#6892);
#5119=LINE('',#90486,#6893);
#5120=LINE('',#90490,#6894);
#5121=LINE('',#90491,#6895);
#5122=LINE('',#90499,#6896);
#5123=LINE('',#90500,#6897);
#5124=LINE('',#90508,#6898);
#5125=LINE('',#90509,#6899);
#5126=LINE('',#90666,#6900);
#5127=LINE('',#90671,#6901);
#5128=LINE('',#90672,#6902);
#5129=LINE('',#90677,#6903);
#5130=LINE('',#90678,#6904);
#5131=LINE('',#90682,#6905);
#5132=LINE('',#90846,#6906);
#5133=LINE('',#90847,#6907);
#5134=LINE('',#90849,#6908);
#5135=LINE('',#90850,#6909);
#5136=LINE('',#90854,#6910);
#5137=LINE('',#90855,#6911);
#5138=LINE('',#90863,#6912);
#5139=LINE('',#90864,#6913);
#5140=LINE('',#90872,#6914);
#5141=LINE('',#90873,#6915);
#5142=LINE('',#91030,#6916);
#5143=LINE('',#91035,#6917);
#5144=LINE('',#91036,#6918);
#5145=LINE('',#91041,#6919);
#5146=LINE('',#91042,#6920);
#5147=LINE('',#91046,#6921);
#5148=LINE('',#91210,#6922);
#5149=LINE('',#91211,#6923);
#5150=LINE('',#91213,#6924);
#5151=LINE('',#91214,#6925);
#5152=LINE('',#91218,#6926);
#5153=LINE('',#91219,#6927);
#5154=LINE('',#91224,#6928);
#5155=LINE('',#91226,#6929);
#5156=LINE('',#91228,#6930);
#5157=LINE('',#91234,#6931);
#5158=LINE('',#91398,#6932);
#5159=LINE('',#91473,#6933);
#5160=LINE('',#91961,#6934);
#5161=LINE('',#91963,#6935);
#5162=LINE('',#92536,#6936);
#5163=LINE('',#92875,#6937);
#5164=LINE('',#92881,#6938);
#5165=LINE('',#92882,#6939);
#5166=LINE('',#93005,#6940);
#5167=LINE('',#93094,#6941);
#5168=LINE('',#94832,#6942);
#5169=LINE('',#94833,#6943);
#5170=LINE('',#94865,#6944);
#5171=LINE('',#94866,#6945);
#5172=LINE('',#94869,#6946);
#5173=LINE('',#94871,#6947);
#5174=LINE('',#96547,#6948);
#5175=LINE('',#96548,#6949);
#5176=LINE('',#96557,#6950);
#5177=LINE('',#96568,#6951);
#5178=LINE('',#96570,#6952);
#5179=LINE('',#96587,#6953);
#5180=LINE('',#96749,#6954);
#5181=LINE('',#96750,#6955);
#5182=LINE('',#96918,#6956);
#5183=LINE('',#96920,#6957);
#5184=LINE('',#96922,#6958);
#5185=LINE('',#96924,#6959);
#5186=LINE('',#96931,#6960);
#5187=LINE('',#96938,#6961);
#5188=LINE('',#96942,#6962);
#5189=LINE('',#96946,#6963);
#5190=LINE('',#96949,#6964);
#5191=LINE('',#96952,#6965);
#5192=LINE('',#96956,#6966);
#5193=LINE('',#96960,#6967);
#5194=LINE('',#96964,#6968);
#5195=LINE('',#96968,#6969);
#5196=LINE('',#96972,#6970);
#5197=LINE('',#96976,#6971);
#5198=LINE('',#96980,#6972);
#5199=LINE('',#96985,#6973);
#5200=LINE('',#96987,#6974);
#5201=LINE('',#96989,#6975);
#5202=LINE('',#96990,#6976);
#5203=LINE('',#96994,#6977);
#5204=LINE('',#96996,#6978);
#5205=LINE('',#96998,#6979);
#5206=LINE('',#96999,#6980);
#5207=LINE('',#97003,#6981);
#5208=LINE('',#97005,#6982);
#5209=LINE('',#97007,#6983);
#5210=LINE('',#97008,#6984);
#5211=LINE('',#97012,#6985);
#5212=LINE('',#97014,#6986);
#5213=LINE('',#97016,#6987);
#5214=LINE('',#97017,#6988);
#5215=LINE('',#97023,#6989);
#5216=LINE('',#97027,#6990);
#5217=LINE('',#97031,#6991);
#5218=LINE('',#97034,#6992);
#5219=LINE('',#97038,#6993);
#5220=LINE('',#97040,#6994);
#5221=LINE('',#97042,#6995);
#5222=LINE('',#97043,#6996);
#5223=LINE('',#97047,#6997);
#5224=LINE('',#97049,#6998);
#5225=LINE('',#97051,#6999);
#5226=LINE('',#97055,#7000);
#5227=LINE('',#97060,#7001);
#5228=LINE('',#97062,#7002);
#5229=LINE('',#97064,#7003);
#5230=LINE('',#97065,#7004);
#5231=LINE('',#97069,#7005);
#5232=LINE('',#97071,#7006);
#5233=LINE('',#97073,#7007);
#5234=LINE('',#97077,#7008);
#5235=LINE('',#97082,#7009);
#5236=LINE('',#97084,#7010);
#5237=LINE('',#97086,#7011);
#5238=LINE('',#97087,#7012);
#5239=LINE('',#97109,#7013);
#5240=LINE('',#97111,#7014);
#5241=LINE('',#97113,#7015);
#5242=LINE('',#97114,#7016);
#5243=LINE('',#97118,#7017);
#5244=LINE('',#97124,#7018);
#5245=LINE('',#97125,#7019);
#5246=LINE('',#97126,#7020);
#5247=LINE('',#97130,#7021);
#5248=LINE('',#97135,#7022);
#5249=LINE('',#97137,#7023);
#5250=LINE('',#97138,#7024);
#5251=LINE('',#97142,#7025);
#5252=LINE('',#97144,#7026);
#5253=LINE('',#97146,#7027);
#5254=LINE('',#97147,#7028);
#5255=LINE('',#97151,#7029);
#5256=LINE('',#97157,#7030);
#5257=LINE('',#97158,#7031);
#5258=LINE('',#97159,#7032);
#5259=LINE('',#97163,#7033);
#5260=LINE('',#97168,#7034);
#5261=LINE('',#97170,#7035);
#5262=LINE('',#97171,#7036);
#5263=LINE('',#97319,#7037);
#5264=LINE('',#97321,#7038);
#5265=LINE('',#97406,#7039);
#5266=LINE('',#97420,#7040);
#5267=LINE('',#98900,#7041);
#5268=LINE('',#99188,#7042);
#5269=LINE('',#100546,#7043);
#5270=LINE('',#100753,#7044);
#5271=LINE('',#102877,#7045);
#5272=LINE('',#102959,#7046);
#5273=LINE('',#103475,#7047);
#5274=LINE('',#105942,#7048);
#5275=LINE('',#105945,#7049);
#5276=LINE('',#105948,#7050);
#5277=LINE('',#105951,#7051);
#5278=LINE('',#105953,#7052);
#5279=LINE('',#105956,#7053);
#5280=LINE('',#105961,#7054);
#5281=LINE('',#105963,#7055);
#5282=LINE('',#105966,#7056);
#5283=LINE('',#105967,#7057);
#5284=LINE('',#105973,#7058);
#5285=LINE('',#105976,#7059);
#5286=LINE('',#105978,#7060);
#5287=LINE('',#105979,#7061);
#5288=LINE('',#105984,#7062);
#5289=LINE('',#105985,#7063);
#5290=LINE('',#105987,#7064);
#5291=LINE('',#105988,#7065);
#5292=LINE('',#105999,#7066);
#5293=LINE('',#106001,#7067);
#5294=LINE('',#106003,#7068);
#5295=LINE('',#106027,#7069);
#5296=LINE('',#106054,#7070);
#5297=LINE('',#106056,#7071);
#5298=LINE('',#106058,#7072);
#5299=LINE('',#106066,#7073);
#5300=LINE('',#106580,#7074);
#5301=LINE('',#106586,#7075);
#5302=LINE('',#110381,#7076);
#5303=LINE('',#110447,#7077);
#5304=LINE('',#110471,#7078);
#5305=LINE('',#110536,#7079);
#5306=LINE('',#110563,#7080);
#5307=LINE('',#110631,#7081);
#5308=LINE('',#110655,#7082);
#5309=LINE('',#110720,#7083);
#5310=LINE('',#110744,#7084);
#5311=LINE('',#110810,#7085);
#5312=LINE('',#110832,#7086);
#5313=LINE('',#110897,#7087);
#5314=LINE('',#110924,#7088);
#5315=LINE('',#110989,#7089);
#5316=LINE('',#111016,#7090);
#5317=LINE('',#111084,#7091);
#5318=LINE('',#111108,#7092);
#5319=LINE('',#111169,#7093);
#5320=LINE('',#111194,#7094);
#5321=LINE('',#111259,#7095);
#5322=LINE('',#111286,#7096);
#5323=LINE('',#111351,#7097);
#5324=LINE('',#111378,#7098);
#5325=LINE('',#111443,#7099);
#5326=LINE('',#111467,#7100);
#5327=LINE('',#111531,#7101);
#5328=LINE('',#111555,#7102);
#5329=LINE('',#111623,#7103);
#5330=LINE('',#111647,#7104);
#5331=LINE('',#111715,#7105);
#5332=LINE('',#111739,#7106);
#5333=LINE('',#111802,#7107);
#5334=LINE('',#111885,#7108);
#5335=LINE('',#111949,#7109);
#5336=LINE('',#111973,#7110);
#5337=LINE('',#112038,#7111);
#5338=LINE('',#112065,#7112);
#5339=LINE('',#112128,#7113);
#5340=LINE('',#112153,#7114);
#5341=LINE('',#112218,#7115);
#5342=LINE('',#112242,#7116);
#5343=LINE('',#112308,#7117);
#5344=LINE('',#112332,#7118);
#5345=LINE('',#112397,#7119);
#5346=LINE('',#112424,#7120);
#5347=LINE('',#112488,#7121);
#5348=LINE('',#112510,#7122);
#5349=LINE('',#112573,#7123);
#5350=LINE('',#112600,#7124);
#5351=LINE('',#112666,#7125);
#5352=LINE('',#112690,#7126);
#5353=LINE('',#112755,#7127);
#5354=LINE('',#112779,#7128);
#5355=LINE('',#112842,#7129);
#5356=LINE('',#112866,#7130);
#5357=LINE('',#113040,#7131);
#5358=LINE('',#113067,#7132);
#5359=LINE('',#113133,#7133);
#5360=LINE('',#113157,#7134);
#5361=LINE('',#113222,#7135);
#5362=LINE('',#113246,#7136);
#5363=LINE('',#113307,#7137);
#5364=LINE('',#113384,#7138);
#5365=LINE('',#113447,#7139);
#5366=LINE('',#113523,#7140);
#5367=LINE('',#113588,#7141);
#5368=LINE('',#113612,#7142);
#5369=LINE('',#113677,#7143);
#5370=LINE('',#113701,#7144);
#5371=LINE('',#113764,#7145);
#5372=LINE('',#113841,#7146);
#5373=LINE('',#113902,#7147);
#5374=LINE('',#113982,#7148);
#5375=LINE('',#114047,#7149);
#5376=LINE('',#114124,#7150);
#5377=LINE('',#114187,#7151);
#5378=LINE('',#114265,#7152);
#5379=LINE('',#114330,#7153);
#5380=LINE('',#114407,#7154);
#5381=LINE('',#114466,#7155);
#5382=LINE('',#114548,#7156);
#5383=LINE('',#114613,#7157);
#5384=LINE('',#114692,#7158);
#5385=LINE('',#114755,#7159);
#5386=LINE('',#114832,#7160);
#5387=LINE('',#114897,#7161);
#5388=LINE('',#114976,#7162);
#5389=LINE('',#115037,#7163);
#5390=LINE('',#115117,#7164);
#5391=LINE('',#115182,#7165);
#5392=LINE('',#115264,#7166);
#5393=LINE('',#115328,#7167);
#5394=LINE('',#115405,#7168);
#5395=LINE('',#115473,#7169);
#5396=LINE('',#115554,#7170);
#5397=LINE('',#115613,#7171);
#5398=LINE('',#115697,#7172);
#5399=LINE('',#115762,#7173);
#5400=LINE('',#115841,#7174);
#5401=LINE('',#115902,#7175);
#5402=LINE('',#115984,#7176);
#5403=LINE('',#116049,#7177);
#5404=LINE('',#116128,#7178);
#5405=LINE('',#116187,#7179);
#5406=LINE('',#116271,#7180);
#5407=LINE('',#116336,#7181);
#5408=LINE('',#116420,#7182);
#5409=LINE('',#116481,#7183);
#5410=LINE('',#116565,#7184);
#5411=LINE('',#116630,#7185);
#5412=LINE('',#116714,#7186);
#5413=LINE('',#116773,#7187);
#5414=LINE('',#116859,#7188);
#5415=LINE('',#116920,#7189);
#5416=LINE('',#117006,#7190);
#5417=LINE('',#117068,#7191);
#5418=LINE('',#117151,#7192);
#5419=LINE('',#117216,#7193);
#5420=LINE('',#117298,#7194);
#5421=LINE('',#117361,#7195);
#5422=LINE('',#117443,#7196);
#5423=LINE('',#117504,#7197);
#5424=LINE('',#117590,#7198);
#5425=LINE('',#117658,#7199);
#5426=LINE('',#117739,#7200);
#5427=LINE('',#117802,#7201);
#5428=LINE('',#117886,#7202);
#5429=LINE('',#118058,#7203);
#5430=LINE('',#118142,#7204);
#5431=LINE('',#118204,#7205);
#5432=LINE('',#118287,#7206);
#5433=LINE('',#118350,#7207);
#5434=LINE('',#118436,#7208);
#5435=LINE('',#118502,#7209);
#5436=LINE('',#118583,#7210);
#5437=LINE('',#118753,#7211);
#5438=LINE('',#118837,#7212);
#5439=LINE('',#118899,#7213);
#5440=LINE('',#118980,#7214);
#5441=LINE('',#119048,#7215);
#5442=LINE('',#119129,#7216);
#5443=LINE('',#119195,#7217);
#5444=LINE('',#119253,#7218);
#5445=LINE('',#119549,#7219);
#5446=LINE('',#119631,#7220);
#5447=LINE('',#119692,#7221);
#5448=LINE('',#119778,#7222);
#5449=LINE('',#119841,#7223);
#5450=LINE('',#119927,#7224);
#5451=LINE('',#119988,#7225);
#5452=LINE('',#120070,#7226);
#5453=LINE('',#120133,#7227);
#5454=LINE('',#120217,#7228);
#5455=LINE('',#120280,#7229);
#5456=LINE('',#120362,#7230);
#5457=LINE('',#120430,#7231);
#5458=LINE('',#120511,#7232);
#5459=LINE('',#120575,#7233);
#5460=LINE('',#120654,#7234);
#5461=LINE('',#120719,#7235);
#5462=LINE('',#120801,#7236);
#5463=LINE('',#120864,#7237);
#5464=LINE('',#120944,#7238);
#5465=LINE('',#121012,#7239);
#5466=LINE('',#121091,#7240);
#5467=LINE('',#121150,#7241);
#5468=LINE('',#121228,#7242);
#5469=LINE('',#121287,#7243);
#5470=LINE('',#121369,#7244);
#5471=LINE('',#121432,#7245);
#5472=LINE('',#121512,#7246);
#5473=LINE('',#121577,#7247);
#5474=LINE('',#121656,#7248);
#5475=LINE('',#121719,#7249);
#5476=LINE('',#121792,#7250);
#5477=LINE('',#121853,#7251);
#5478=LINE('',#121933,#7252);
#5479=LINE('',#121998,#7253);
#5480=LINE('',#122075,#7254);
#5481=LINE('',#122140,#7255);
#5482=LINE('',#122219,#7256);
#5483=LINE('',#122282,#7257);
#5484=LINE('',#122304,#7258);
#5485=LINE('',#122365,#7259);
#5486=LINE('',#122392,#7260);
#5487=LINE('',#122460,#7261);
#5488=LINE('',#122535,#7262);
#5489=LINE('',#122600,#7263);
#5490=LINE('',#122677,#7264);
#5491=LINE('',#122742,#7265);
#5492=LINE('',#122766,#7266);
#5493=LINE('',#122825,#7267);
#5494=LINE('',#122850,#7268);
#5495=LINE('',#122918,#7269);
#5496=LINE('',#122942,#7270);
#5497=LINE('',#123007,#7271);
#5498=LINE('',#123031,#7272);
#5499=LINE('',#123096,#7273);
#5500=LINE('',#123120,#7274);
#5501=LINE('',#123179,#7275);
#5502=LINE('',#123204,#7276);
#5503=LINE('',#123269,#7277);
#5504=LINE('',#123293,#7278);
#5505=LINE('',#123354,#7279);
#5506=LINE('',#123378,#7280);
#5507=LINE('',#123443,#7281);
#5508=LINE('',#123467,#7282);
#5509=LINE('',#123526,#7283);
#5510=LINE('',#123551,#7284);
#5511=LINE('',#123619,#7285);
#5512=LINE('',#123643,#7286);
#5513=LINE('',#123704,#7287);
#5514=LINE('',#123731,#7288);
#5515=LINE('',#123796,#7289);
#5516=LINE('',#123823,#7290);
#5517=LINE('',#123886,#7291);
#5518=LINE('',#123911,#7292);
#5519=LINE('',#123976,#7293);
#5520=LINE('',#124000,#7294);
#5521=LINE('',#124066,#7295);
#5522=LINE('',#124088,#7296);
#5523=LINE('',#124153,#7297);
#5524=LINE('',#124177,#7298);
#5525=LINE('',#124240,#7299);
#5526=LINE('',#124265,#7300);
#5527=LINE('',#124333,#7301);
#5528=LINE('',#124357,#7302);
#5529=LINE('',#124423,#7303);
#5530=LINE('',#124445,#7304);
#5531=LINE('',#124513,#7305);
#5532=LINE('',#124537,#7306);
#5533=LINE('',#124600,#7307);
#5534=LINE('',#124627,#7308);
#5535=LINE('',#124693,#7309);
#5536=LINE('',#124717,#7310);
#5537=LINE('',#124785,#7311);
#5538=LINE('',#124809,#7312);
#5539=LINE('',#124872,#7313);
#5540=LINE('',#124901,#7314);
#5541=LINE('',#124907,#7315);
#5542=LINE('',#124913,#7316);
#5543=LINE('',#124919,#7317);
#5544=LINE('',#124925,#7318);
#5545=LINE('',#124931,#7319);
#5546=LINE('',#124937,#7320);
#5547=LINE('',#124943,#7321);
#5548=LINE('',#124949,#7322);
#5549=LINE('',#124955,#7323);
#5550=LINE('',#124961,#7324);
#5551=LINE('',#124967,#7325);
#5552=LINE('',#124973,#7326);
#5553=LINE('',#124979,#7327);
#5554=LINE('',#124985,#7328);
#5555=LINE('',#124991,#7329);
#5556=LINE('',#124997,#7330);
#5557=LINE('',#125003,#7331);
#5558=LINE('',#125009,#7332);
#5559=LINE('',#125015,#7333);
#5560=LINE('',#125021,#7334);
#5561=LINE('',#125027,#7335);
#5562=LINE('',#125033,#7336);
#5563=LINE('',#125039,#7337);
#5564=LINE('',#125045,#7338);
#5565=LINE('',#125051,#7339);
#5566=LINE('',#125057,#7340);
#5567=LINE('',#125063,#7341);
#5568=LINE('',#125069,#7342);
#5569=LINE('',#125075,#7343);
#5570=LINE('',#125081,#7344);
#5571=LINE('',#125087,#7345);
#5572=LINE('',#125093,#7346);
#5573=LINE('',#125099,#7347);
#5574=LINE('',#125105,#7348);
#5575=LINE('',#125111,#7349);
#5576=LINE('',#125117,#7350);
#5577=LINE('',#125123,#7351);
#5578=LINE('',#125129,#7352);
#5579=LINE('',#125135,#7353);
#5580=LINE('',#125141,#7354);
#5581=LINE('',#125147,#7355);
#5582=LINE('',#125153,#7356);
#5583=LINE('',#125159,#7357);
#5584=LINE('',#125165,#7358);
#5585=LINE('',#125171,#7359);
#5586=LINE('',#125177,#7360);
#5587=LINE('',#125183,#7361);
#5588=LINE('',#125189,#7362);
#5589=LINE('',#125195,#7363);
#5590=LINE('',#125201,#7364);
#5591=LINE('',#125207,#7365);
#5592=LINE('',#125213,#7366);
#5593=LINE('',#125219,#7367);
#5594=LINE('',#125225,#7368);
#5595=LINE('',#125231,#7369);
#5596=LINE('',#125237,#7370);
#5597=LINE('',#125243,#7371);
#5598=LINE('',#125249,#7372);
#5599=LINE('',#125255,#7373);
#5600=LINE('',#125261,#7374);
#5601=LINE('',#125267,#7375);
#5602=LINE('',#125273,#7376);
#5603=LINE('',#125279,#7377);
#5604=LINE('',#125285,#7378);
#5605=LINE('',#125291,#7379);
#5606=LINE('',#125297,#7380);
#5607=LINE('',#125303,#7381);
#5608=LINE('',#125309,#7382);
#5609=LINE('',#125315,#7383);
#5610=LINE('',#125321,#7384);
#5611=LINE('',#125327,#7385);
#5612=LINE('',#125333,#7386);
#5613=LINE('',#125339,#7387);
#5614=LINE('',#125345,#7388);
#5615=LINE('',#125351,#7389);
#5616=LINE('',#125357,#7390);
#5617=LINE('',#125363,#7391);
#5618=LINE('',#125369,#7392);
#5619=LINE('',#125375,#7393);
#5620=LINE('',#125381,#7394);
#5621=LINE('',#125387,#7395);
#5622=LINE('',#125393,#7396);
#5623=LINE('',#125399,#7397);
#5624=LINE('',#125405,#7398);
#5625=LINE('',#125411,#7399);
#5626=LINE('',#125417,#7400);
#5627=LINE('',#125423,#7401);
#5628=LINE('',#125429,#7402);
#5629=LINE('',#125435,#7403);
#5630=LINE('',#125441,#7404);
#5631=LINE('',#125447,#7405);
#5632=LINE('',#125453,#7406);
#5633=LINE('',#125459,#7407);
#5634=LINE('',#125465,#7408);
#5635=LINE('',#125471,#7409);
#5636=LINE('',#125477,#7410);
#5637=LINE('',#125483,#7411);
#5638=LINE('',#125489,#7412);
#5639=LINE('',#125495,#7413);
#5640=LINE('',#125501,#7414);
#5641=LINE('',#125507,#7415);
#5642=LINE('',#125513,#7416);
#5643=LINE('',#125519,#7417);
#5644=LINE('',#125525,#7418);
#5645=LINE('',#125531,#7419);
#5646=LINE('',#125537,#7420);
#5647=LINE('',#125543,#7421);
#5648=LINE('',#125549,#7422);
#5649=LINE('',#125555,#7423);
#5650=LINE('',#125561,#7424);
#5651=LINE('',#125567,#7425);
#5652=LINE('',#125573,#7426);
#5653=LINE('',#125579,#7427);
#5654=LINE('',#125585,#7428);
#5655=LINE('',#125591,#7429);
#5656=LINE('',#125597,#7430);
#5657=LINE('',#125603,#7431);
#5658=LINE('',#125609,#7432);
#5659=LINE('',#125615,#7433);
#5660=LINE('',#125621,#7434);
#5661=LINE('',#125627,#7435);
#5662=LINE('',#125633,#7436);
#5663=LINE('',#125639,#7437);
#5664=LINE('',#125645,#7438);
#5665=LINE('',#125651,#7439);
#5666=LINE('',#125657,#7440);
#5667=LINE('',#125663,#7441);
#5668=LINE('',#125669,#7442);
#5669=LINE('',#125675,#7443);
#5670=LINE('',#125681,#7444);
#5671=LINE('',#125687,#7445);
#5672=LINE('',#125693,#7446);
#5673=LINE('',#125699,#7447);
#5674=LINE('',#125705,#7448);
#5675=LINE('',#125711,#7449);
#5676=LINE('',#125717,#7450);
#5677=LINE('',#125723,#7451);
#5678=LINE('',#125729,#7452);
#5679=LINE('',#125735,#7453);
#5680=LINE('',#125741,#7454);
#5681=LINE('',#125747,#7455);
#5682=LINE('',#125753,#7456);
#5683=LINE('',#125759,#7457);
#5684=LINE('',#125765,#7458);
#5685=LINE('',#125771,#7459);
#5686=LINE('',#125777,#7460);
#5687=LINE('',#125783,#7461);
#5688=LINE('',#125789,#7462);
#5689=LINE('',#125795,#7463);
#5690=LINE('',#125801,#7464);
#5691=LINE('',#125807,#7465);
#5692=LINE('',#125813,#7466);
#5693=LINE('',#125819,#7467);
#5694=LINE('',#125825,#7468);
#5695=LINE('',#125831,#7469);
#5696=LINE('',#125837,#7470);
#5697=LINE('',#125843,#7471);
#5698=LINE('',#125849,#7472);
#5699=LINE('',#125855,#7473);
#5700=LINE('',#125861,#7474);
#5701=LINE('',#125867,#7475);
#5702=LINE('',#125873,#7476);
#5703=LINE('',#125879,#7477);
#5704=LINE('',#125885,#7478);
#5705=LINE('',#125891,#7479);
#5706=LINE('',#125897,#7480);
#5707=LINE('',#125903,#7481);
#5708=LINE('',#125909,#7482);
#5709=LINE('',#125915,#7483);
#5710=LINE('',#125921,#7484);
#5711=LINE('',#125927,#7485);
#5712=LINE('',#125933,#7486);
#5713=LINE('',#125939,#7487);
#5714=LINE('',#125945,#7488);
#5715=LINE('',#125951,#7489);
#5716=LINE('',#125957,#7490);
#5717=LINE('',#125963,#7491);
#5718=LINE('',#125969,#7492);
#5719=LINE('',#125975,#7493);
#5720=LINE('',#125981,#7494);
#5721=LINE('',#125987,#7495);
#5722=LINE('',#125993,#7496);
#5723=LINE('',#125999,#7497);
#5724=LINE('',#126005,#7498);
#5725=LINE('',#126011,#7499);
#5726=LINE('',#126017,#7500);
#5727=LINE('',#126023,#7501);
#5728=LINE('',#126029,#7502);
#5729=LINE('',#126035,#7503);
#5730=LINE('',#126041,#7504);
#5731=LINE('',#126047,#7505);
#5732=LINE('',#126053,#7506);
#5733=LINE('',#126059,#7507);
#5734=LINE('',#126065,#7508);
#5735=LINE('',#126071,#7509);
#5736=LINE('',#126077,#7510);
#5737=LINE('',#126083,#7511);
#5738=LINE('',#126089,#7512);
#5739=LINE('',#126095,#7513);
#5740=LINE('',#126101,#7514);
#5741=LINE('',#126107,#7515);
#5742=LINE('',#126113,#7516);
#5743=LINE('',#126119,#7517);
#5744=LINE('',#126125,#7518);
#5745=LINE('',#126131,#7519);
#5746=LINE('',#126137,#7520);
#5747=LINE('',#126143,#7521);
#5748=LINE('',#126149,#7522);
#5749=LINE('',#126155,#7523);
#5750=LINE('',#126161,#7524);
#5751=LINE('',#126167,#7525);
#5752=LINE('',#126173,#7526);
#5753=LINE('',#126179,#7527);
#5754=LINE('',#126185,#7528);
#5755=LINE('',#126191,#7529);
#5756=LINE('',#126197,#7530);
#5757=LINE('',#126203,#7531);
#5758=LINE('',#126209,#7532);
#5759=LINE('',#126215,#7533);
#5760=LINE('',#126221,#7534);
#5761=LINE('',#126227,#7535);
#5762=LINE('',#126233,#7536);
#5763=LINE('',#126239,#7537);
#5764=LINE('',#126245,#7538);
#5765=LINE('',#126251,#7539);
#5766=LINE('',#126257,#7540);
#5767=LINE('',#126263,#7541);
#5768=LINE('',#126269,#7542);
#5769=LINE('',#126275,#7543);
#5770=LINE('',#126281,#7544);
#5771=LINE('',#126287,#7545);
#5772=LINE('',#126293,#7546);
#5773=LINE('',#126299,#7547);
#5774=LINE('',#126305,#7548);
#5775=LINE('',#126311,#7549);
#5776=LINE('',#126317,#7550);
#5777=LINE('',#126323,#7551);
#5778=LINE('',#126329,#7552);
#5779=LINE('',#126335,#7553);
#5780=LINE('',#126341,#7554);
#5781=LINE('',#126347,#7555);
#5782=LINE('',#126353,#7556);
#5783=LINE('',#126359,#7557);
#5784=LINE('',#126365,#7558);
#5785=LINE('',#126371,#7559);
#5786=LINE('',#126377,#7560);
#5787=LINE('',#126383,#7561);
#5788=LINE('',#126389,#7562);
#5789=LINE('',#126395,#7563);
#5790=LINE('',#126401,#7564);
#5791=LINE('',#126407,#7565);
#5792=LINE('',#126413,#7566);
#5793=LINE('',#126419,#7567);
#5794=LINE('',#126425,#7568);
#5795=LINE('',#126431,#7569);
#5796=LINE('',#126437,#7570);
#5797=LINE('',#126443,#7571);
#5798=LINE('',#126449,#7572);
#5799=LINE('',#126455,#7573);
#5800=LINE('',#126461,#7574);
#5801=LINE('',#126467,#7575);
#5802=LINE('',#126473,#7576);
#5803=LINE('',#126479,#7577);
#5804=LINE('',#126485,#7578);
#5805=LINE('',#126491,#7579);
#5806=LINE('',#126497,#7580);
#5807=LINE('',#126503,#7581);
#5808=LINE('',#126509,#7582);
#5809=LINE('',#126515,#7583);
#5810=LINE('',#126521,#7584);
#5811=LINE('',#126527,#7585);
#5812=LINE('',#126533,#7586);
#5813=LINE('',#126539,#7587);
#5814=LINE('',#126545,#7588);
#5815=LINE('',#126551,#7589);
#5816=LINE('',#126557,#7590);
#5817=LINE('',#126563,#7591);
#5818=LINE('',#126569,#7592);
#5819=LINE('',#126575,#7593);
#5820=LINE('',#126581,#7594);
#5821=LINE('',#126587,#7595);
#5822=LINE('',#126593,#7596);
#5823=LINE('',#126599,#7597);
#5824=LINE('',#126605,#7598);
#5825=LINE('',#126611,#7599);
#5826=LINE('',#126617,#7600);
#5827=LINE('',#126623,#7601);
#5828=LINE('',#126629,#7602);
#5829=LINE('',#126635,#7603);
#5830=LINE('',#126641,#7604);
#5831=LINE('',#126647,#7605);
#5832=LINE('',#126653,#7606);
#5833=LINE('',#126659,#7607);
#5834=LINE('',#126665,#7608);
#5835=LINE('',#126671,#7609);
#5836=LINE('',#126677,#7610);
#5837=LINE('',#126683,#7611);
#5838=LINE('',#126689,#7612);
#5839=LINE('',#126695,#7613);
#5840=LINE('',#126701,#7614);
#5841=LINE('',#126707,#7615);
#5842=LINE('',#126713,#7616);
#5843=LINE('',#126719,#7617);
#5844=LINE('',#126725,#7618);
#5845=LINE('',#126731,#7619);
#5846=LINE('',#126737,#7620);
#5847=LINE('',#126743,#7621);
#5848=LINE('',#126749,#7622);
#5849=LINE('',#126755,#7623);
#5850=LINE('',#126761,#7624);
#5851=LINE('',#126767,#7625);
#5852=LINE('',#126773,#7626);
#5853=LINE('',#126779,#7627);
#5854=LINE('',#126785,#7628);
#5855=LINE('',#126791,#7629);
#5856=LINE('',#126797,#7630);
#5857=LINE('',#126803,#7631);
#5858=LINE('',#126809,#7632);
#5859=LINE('',#126815,#7633);
#5860=LINE('',#126821,#7634);
#5861=LINE('',#126827,#7635);
#5862=LINE('',#126833,#7636);
#5863=LINE('',#126839,#7637);
#5864=LINE('',#126845,#7638);
#5865=LINE('',#126851,#7639);
#5866=LINE('',#126857,#7640);
#5867=LINE('',#126863,#7641);
#5868=LINE('',#126869,#7642);
#5869=LINE('',#126875,#7643);
#5870=LINE('',#126881,#7644);
#5871=LINE('',#126887,#7645);
#5872=LINE('',#126893,#7646);
#5873=LINE('',#126899,#7647);
#5874=LINE('',#126905,#7648);
#5875=LINE('',#126911,#7649);
#5876=LINE('',#126917,#7650);
#5877=LINE('',#126923,#7651);
#5878=LINE('',#126929,#7652);
#5879=LINE('',#126935,#7653);
#5880=LINE('',#126941,#7654);
#5881=LINE('',#126947,#7655);
#5882=LINE('',#126953,#7656);
#5883=LINE('',#126959,#7657);
#5884=LINE('',#126965,#7658);
#5885=LINE('',#126971,#7659);
#5886=LINE('',#126977,#7660);
#5887=LINE('',#126983,#7661);
#5888=LINE('',#126989,#7662);
#5889=LINE('',#126995,#7663);
#5890=LINE('',#127001,#7664);
#5891=LINE('',#127007,#7665);
#5892=LINE('',#127013,#7666);
#5893=LINE('',#127019,#7667);
#5894=LINE('',#127025,#7668);
#5895=LINE('',#127031,#7669);
#5896=LINE('',#127037,#7670);
#5897=LINE('',#127043,#7671);
#5898=LINE('',#127049,#7672);
#5899=LINE('',#127055,#7673);
#5900=LINE('',#127061,#7674);
#5901=LINE('',#127067,#7675);
#5902=LINE('',#127073,#7676);
#5903=LINE('',#127079,#7677);
#5904=LINE('',#127085,#7678);
#5905=LINE('',#127091,#7679);
#5906=LINE('',#127097,#7680);
#5907=LINE('',#127103,#7681);
#5908=LINE('',#127109,#7682);
#5909=LINE('',#127115,#7683);
#5910=LINE('',#127121,#7684);
#5911=LINE('',#127127,#7685);
#5912=LINE('',#127133,#7686);
#5913=LINE('',#127139,#7687);
#5914=LINE('',#127145,#7688);
#5915=LINE('',#127151,#7689);
#5916=LINE('',#127157,#7690);
#5917=LINE('',#127163,#7691);
#5918=LINE('',#127169,#7692);
#5919=LINE('',#127175,#7693);
#5920=LINE('',#127181,#7694);
#5921=LINE('',#127187,#7695);
#5922=LINE('',#127193,#7696);
#5923=LINE('',#127199,#7697);
#5924=LINE('',#127205,#7698);
#5925=LINE('',#127211,#7699);
#5926=LINE('',#127217,#7700);
#5927=LINE('',#127223,#7701);
#5928=LINE('',#127229,#7702);
#5929=LINE('',#127235,#7703);
#5930=LINE('',#127241,#7704);
#5931=LINE('',#127247,#7705);
#5932=LINE('',#127253,#7706);
#5933=LINE('',#127259,#7707);
#5934=LINE('',#127265,#7708);
#5935=LINE('',#127271,#7709);
#5936=LINE('',#127277,#7710);
#5937=LINE('',#127283,#7711);
#5938=LINE('',#127289,#7712);
#5939=LINE('',#127295,#7713);
#5940=LINE('',#127301,#7714);
#5941=LINE('',#127307,#7715);
#5942=LINE('',#127313,#7716);
#5943=LINE('',#127319,#7717);
#5944=LINE('',#127325,#7718);
#5945=LINE('',#127331,#7719);
#5946=LINE('',#127337,#7720);
#5947=LINE('',#127343,#7721);
#5948=LINE('',#127349,#7722);
#5949=LINE('',#127355,#7723);
#5950=LINE('',#127361,#7724);
#5951=LINE('',#127367,#7725);
#5952=LINE('',#127373,#7726);
#5953=LINE('',#127379,#7727);
#5954=LINE('',#127385,#7728);
#5955=LINE('',#127391,#7729);
#5956=LINE('',#127397,#7730);
#5957=LINE('',#127403,#7731);
#5958=LINE('',#127409,#7732);
#5959=LINE('',#127415,#7733);
#5960=LINE('',#127421,#7734);
#5961=LINE('',#127427,#7735);
#5962=LINE('',#127433,#7736);
#5963=LINE('',#127439,#7737);
#5964=LINE('',#127445,#7738);
#5965=LINE('',#127451,#7739);
#5966=LINE('',#127457,#7740);
#5967=LINE('',#127463,#7741);
#5968=LINE('',#127469,#7742);
#5969=LINE('',#127475,#7743);
#5970=LINE('',#127481,#7744);
#5971=LINE('',#127487,#7745);
#5972=LINE('',#127493,#7746);
#5973=LINE('',#127499,#7747);
#5974=LINE('',#127505,#7748);
#5975=LINE('',#127511,#7749);
#5976=LINE('',#127517,#7750);
#5977=LINE('',#127523,#7751);
#5978=LINE('',#127529,#7752);
#5979=LINE('',#127535,#7753);
#5980=LINE('',#127541,#7754);
#5981=LINE('',#127547,#7755);
#5982=LINE('',#127553,#7756);
#5983=LINE('',#127559,#7757);
#5984=LINE('',#127565,#7758);
#5985=LINE('',#127571,#7759);
#5986=LINE('',#127577,#7760);
#5987=LINE('',#127583,#7761);
#5988=LINE('',#127589,#7762);
#5989=LINE('',#127595,#7763);
#5990=LINE('',#127601,#7764);
#5991=LINE('',#127607,#7765);
#5992=LINE('',#127613,#7766);
#5993=LINE('',#127619,#7767);
#5994=LINE('',#127625,#7768);
#5995=LINE('',#127631,#7769);
#5996=LINE('',#127637,#7770);
#5997=LINE('',#127643,#7771);
#5998=LINE('',#127649,#7772);
#5999=LINE('',#127655,#7773);
#6000=LINE('',#127661,#7774);
#6001=LINE('',#127667,#7775);
#6002=LINE('',#127673,#7776);
#6003=LINE('',#127679,#7777);
#6004=LINE('',#127685,#7778);
#6005=LINE('',#127691,#7779);
#6006=LINE('',#127697,#7780);
#6007=LINE('',#127703,#7781);
#6008=LINE('',#127709,#7782);
#6009=LINE('',#127715,#7783);
#6010=LINE('',#127721,#7784);
#6011=LINE('',#127727,#7785);
#6012=LINE('',#127733,#7786);
#6013=LINE('',#127739,#7787);
#6014=LINE('',#127745,#7788);
#6015=LINE('',#127751,#7789);
#6016=LINE('',#127757,#7790);
#6017=LINE('',#127763,#7791);
#6018=LINE('',#127769,#7792);
#6019=LINE('',#127775,#7793);
#6020=LINE('',#127781,#7794);
#6021=LINE('',#127787,#7795);
#6022=LINE('',#127793,#7796);
#6023=LINE('',#127799,#7797);
#6024=LINE('',#127805,#7798);
#6025=LINE('',#127811,#7799);
#6026=LINE('',#127817,#7800);
#6027=LINE('',#127823,#7801);
#6028=LINE('',#127829,#7802);
#6029=LINE('',#127835,#7803);
#6030=LINE('',#127841,#7804);
#6031=LINE('',#127847,#7805);
#6032=LINE('',#127853,#7806);
#6033=LINE('',#127859,#7807);
#6034=LINE('',#127865,#7808);
#6035=LINE('',#127871,#7809);
#6036=LINE('',#127877,#7810);
#6037=LINE('',#127883,#7811);
#6038=LINE('',#127889,#7812);
#6039=LINE('',#127895,#7813);
#6040=LINE('',#127901,#7814);
#6041=LINE('',#127907,#7815);
#6042=LINE('',#127913,#7816);
#6043=LINE('',#127919,#7817);
#6044=LINE('',#127925,#7818);
#6045=LINE('',#127931,#7819);
#6046=LINE('',#127937,#7820);
#6047=LINE('',#127943,#7821);
#6048=LINE('',#127949,#7822);
#6049=LINE('',#127955,#7823);
#6050=LINE('',#127961,#7824);
#6051=LINE('',#127967,#7825);
#6052=LINE('',#127973,#7826);
#6053=LINE('',#127979,#7827);
#6054=LINE('',#127985,#7828);
#6055=LINE('',#127991,#7829);
#6056=LINE('',#127997,#7830);
#6057=LINE('',#128003,#7831);
#6058=LINE('',#128009,#7832);
#6059=LINE('',#128015,#7833);
#6060=LINE('',#128021,#7834);
#6061=LINE('',#128027,#7835);
#6062=LINE('',#128033,#7836);
#6063=LINE('',#128039,#7837);
#6064=LINE('',#128045,#7838);
#6065=LINE('',#128051,#7839);
#6066=LINE('',#128057,#7840);
#6067=LINE('',#128063,#7841);
#6068=LINE('',#128069,#7842);
#6069=LINE('',#128075,#7843);
#6070=LINE('',#128081,#7844);
#6071=LINE('',#128087,#7845);
#6072=LINE('',#128093,#7846);
#6073=LINE('',#128099,#7847);
#6074=LINE('',#128105,#7848);
#6075=LINE('',#128111,#7849);
#6076=LINE('',#128117,#7850);
#6077=LINE('',#128123,#7851);
#6078=LINE('',#128129,#7852);
#6079=LINE('',#128135,#7853);
#6080=LINE('',#128144,#7854);
#6081=LINE('',#128161,#7855);
#6082=LINE('',#128184,#7856);
#6083=LINE('',#128194,#7857);
#6084=LINE('',#128221,#7858);
#6085=LINE('',#128245,#7859);
#6086=VECTOR('',#51629,11.5);
#6087=VECTOR('',#51632,11.5);
#6088=VECTOR('',#51635,11.5);
#6089=VECTOR('',#51646,1000.);
#6090=VECTOR('',#51649,1000.);
#6091=VECTOR('',#51650,1000.);
#6092=VECTOR('',#51653,1000.);
#6093=VECTOR('',#51656,1000.);
#6094=VECTOR('',#51659,1000.);
#6095=VECTOR('',#51660,1000.);
#6096=VECTOR('',#51667,1000.);
#6097=VECTOR('',#51670,1000.);
#6098=VECTOR('',#51675,1000.);
#6099=VECTOR('',#51676,1000.);
#6100=VECTOR('',#51679,1000.);
#6101=VECTOR('',#51680,1000.);
#6102=VECTOR('',#51691,0.500000000000054);
#6103=VECTOR('',#51698,1.81285717707168);
#6104=VECTOR('',#51705,0.500000000000054);
#6105=VECTOR('',#51712,1.81285717707167);
#6106=VECTOR('',#51719,0.500000000000054);
#6107=VECTOR('',#51726,1.81285717707166);
#6108=VECTOR('',#51733,0.499999999999939);
#6109=VECTOR('',#51740,1.81285717707156);
#6110=VECTOR('',#51747,0.499999999999935);
#6111=VECTOR('',#51754,1.81285717707156);
#6112=VECTOR('',#51761,0.499999999999944);
#6113=VECTOR('',#51768,1.81285717707167);
#6114=VECTOR('',#51773,0.948084450180161);
#6115=VECTOR('',#51778,0.500000000000054);
#6116=VECTOR('',#51781,1.02140828085145);
#6117=VECTOR('',#51786,0.500000000000054);
#6118=VECTOR('',#51789,0.948084450180157);
#6119=VECTOR('',#51794,0.500000000000054);
#6120=VECTOR('',#51797,1.02140828085145);
#6121=VECTOR('',#51802,0.500000000000054);
#6122=VECTOR('',#51805,0.948084450180157);
#6123=VECTOR('',#51810,0.500000000000054);
#6124=VECTOR('',#51813,1.02140828085145);
#6125=VECTOR('',#51818,0.499999999999944);
#6126=VECTOR('',#51821,0.948084450180161);
#6127=VECTOR('',#51826,0.499999999999944);
#6128=VECTOR('',#51829,1.02140828085144);
#6129=VECTOR('',#51834,0.500000000000058);
#6130=VECTOR('',#51837,0.948084450180162);
#6131=VECTOR('',#51842,0.500000000000058);
#6132=VECTOR('',#51845,1.02140828085145);
#6133=VECTOR('',#51850,0.500000000000058);
#6134=VECTOR('',#51853,0.948084450180161);
#6135=VECTOR('',#51858,0.500000000000172);
#6136=VECTOR('',#51861,1.02140828085157);
#6137=VECTOR('',#51866,0.499999999999935);
#6138=VECTOR('',#51869,0.948084450180161);
#6139=VECTOR('',#51874,0.500000000000058);
#6140=VECTOR('',#51877,1.02140828085134);
#6141=VECTOR('',#51882,0.499999999999935);
#6142=VECTOR('',#51885,0.948084450180275);
#6143=VECTOR('',#51890,0.500000000000058);
#6144=VECTOR('',#51893,1.02140828085134);
#6145=VECTOR('',#51898,0.500000000000058);
#6146=VECTOR('',#51901,0.948084450180152);
#6147=VECTOR('',#51906,0.499999999999944);
#6148=VECTOR('',#51909,1.02140828085157);
#6149=VECTOR('',#51914,0.500000000000067);
#6150=VECTOR('',#51917,0.948084450180047);
#6151=VECTOR('',#51922,0.499999999999935);
#6152=VECTOR('',#51925,1.02140828085145);
#6153=VECTOR('',#51930,0.499999999999935);
#6154=VECTOR('',#51933,0.94808445018017);
#6155=VECTOR('',#51938,0.500000000000058);
#6156=VECTOR('',#51941,1.02140828085121);
#6157=VECTOR('',#51946,0.499999999999944);
#6158=VECTOR('',#51949,0.948084450180161);
#6159=VECTOR('',#51954,0.499999999999944);
#6160=VECTOR('',#51957,1.02140828085145);
#6161=VECTOR('',#51962,0.499999999999939);
#6162=VECTOR('',#51965,0.948084450180161);
#6163=VECTOR('',#51970,0.500000000000167);
#6164=VECTOR('',#51973,1.02140828085134);
#6165=VECTOR('',#51978,0.499999999999944);
#6166=VECTOR('',#51981,0.948084450180275);
#6167=VECTOR('',#51986,0.500000000000054);
#6168=VECTOR('',#51989,1.02140828085134);
#6169=VECTOR('',#51994,0.49999999999994);
#6170=VECTOR('',#51997,0.948084450180161);
#6171=VECTOR('',#52002,0.500000000000054);
#6172=VECTOR('',#52005,1.02140828085145);
#6173=VECTOR('',#52010,0.500000000000054);
#6174=VECTOR('',#52013,0.948084450180157);
#6175=VECTOR('',#52018,0.500000000000049);
#6176=VECTOR('',#52021,1.02140828085145);
#6177=VECTOR('',#52026,0.500000000000054);
#6178=VECTOR('',#52029,0.948084450180157);
#6179=VECTOR('',#52034,0.500000000000054);
#6180=VECTOR('',#52037,1.02140828085134);
#6181=VECTOR('',#52042,0.500000000000049);
#6182=VECTOR('',#52045,0.948084450180157);
#6183=VECTOR('',#52050,0.500000000000049);
#6184=VECTOR('',#52053,1.02140828085145);
#6185=VECTOR('',#52058,0.500000000000058);
#6186=VECTOR('',#52061,0.948084450180161);
#6187=VECTOR('',#52066,0.499999999999944);
#6188=VECTOR('',#52069,1.02140828085133);
#6189=VECTOR('',#52074,0.499999999999935);
#6190=VECTOR('',#52077,0.948084450180047);
#6191=VECTOR('',#52082,0.499999999999944);
#6192=VECTOR('',#52087,1.54967110260237);
#6193=VECTOR('',#52092,0.49999999999994);
#6194=VECTOR('',#52099,1.25936103546568);
#6195=VECTOR('',#52104,0.500000000000049);
#6196=VECTOR('',#52109,1.02140828085145);
#6197=VECTOR('',#52114,0.49999999999994);
#6198=VECTOR('',#52117,0.948084450179934);
#6199=VECTOR('',#52122,0.49999999999994);
#6200=VECTOR('',#52127,1.54967110260249);
#6201=VECTOR('',#52132,0.499999999999944);
#6202=VECTOR('',#52139,1.25936103546569);
#6203=VECTOR('',#52144,0.500000000000058);
#6204=VECTOR('',#52149,1.02140828085145);
#6205=VECTOR('',#52154,0.500000000000058);
#6206=VECTOR('',#52157,0.948084450180166);
#6207=VECTOR('',#52162,0.500000000000054);
#6208=VECTOR('',#52167,1.25936103546568);
#6209=VECTOR('',#52172,0.500000000000054);
#6210=VECTOR('',#52177,1.02140828085145);
#6211=VECTOR('',#52182,0.500000000000058);
#6212=VECTOR('',#52185,0.948084450180275);
#6213=VECTOR('',#52190,0.500000000000058);
#6214=VECTOR('',#52195,1.25936103546568);
#6215=VECTOR('',#52200,0.49999999999994);
#6216=VECTOR('',#52205,1.02140828085145);
#6217=VECTOR('',#52210,0.500000000000058);
#6218=VECTOR('',#52213,0.948084450180162);
#6219=VECTOR('',#52218,0.49999999999994);
#6220=VECTOR('',#52221,1.02140828085133);
#6221=VECTOR('',#52226,0.499999999999944);
#6222=VECTOR('',#52229,0.948084450180166);
#6223=VECTOR('',#52234,0.499999999999944);
#6224=VECTOR('',#52237,1.02140828085146);
#6225=VECTOR('',#52242,0.500000000000058);
#6226=VECTOR('',#52245,0.948084450180161);
#6227=VECTOR('',#52250,0.500000000000054);
#6228=VECTOR('',#52253,1.02140828085144);
#6229=VECTOR('',#52258,0.499999999999944);
#6230=VECTOR('',#52261,0.948084450180157);
#6231=VECTOR('',#52266,0.500000000000063);
#6232=VECTOR('',#52269,1.02140828085156);
#6233=VECTOR('',#52274,0.49999999999994);
#6234=VECTOR('',#52277,0.948084450180161);
#6235=VECTOR('',#52282,0.500000000000054);
#6236=VECTOR('',#52285,1.02140828085134);
#6237=VECTOR('',#52290,0.500000000000054);
#6238=VECTOR('',#52293,0.948084450180157);
#6239=VECTOR('',#52298,0.49999999999994);
#6240=VECTOR('',#52301,0.948084450180161);
#6241=VECTOR('',#52306,0.500000000000054);
#6242=VECTOR('',#52309,1.02140828085134);
#6243=VECTOR('',#52314,0.499999999999944);
#6244=VECTOR('',#52319,1.0588834746273);
#6245=VECTOR('',#52326,0.500000000000054);
#6246=VECTOR('',#52333,1.29583333162394);
#6247=VECTOR('',#52340,0.500000000000054);
#6248=VECTOR('',#52347,1.60653900437062);
#6249=VECTOR('',#52354,0.500000000000054);
#6250=VECTOR('',#52361,1.82809807486272);
#6251=VECTOR('',#52368,0.499999999999944);
#6252=VECTOR('',#52375,1.85841829658605);
#6253=VECTOR('',#52382,0.500000000000054);
#6254=VECTOR('',#52389,1.81285717707166);
#6255=VECTOR('',#52396,0.500000000000054);
#6256=VECTOR('',#52403,1.91146602029503);
#6257=VECTOR('',#52410,0.500000000000054);
#6258=VECTOR('',#52417,1.54967110260249);
#6259=VECTOR('',#52424,0.499999999999944);
#6260=VECTOR('',#52431,1.25936103546568);
#6261=VECTOR('',#52438,0.500000000000054);
#6262=VECTOR('',#52445,1.0588834746273);
#6263=VECTOR('',#52452,0.500000000000054);
#6264=VECTOR('',#52459,1.29583333162394);
#6265=VECTOR('',#52466,0.499999999999944);
#6266=VECTOR('',#52473,1.60653900437062);
#6267=VECTOR('',#52480,0.500000000000054);
#6268=VECTOR('',#52487,1.82809807486272);
#6269=VECTOR('',#52494,0.499999999999944);
#6270=VECTOR('',#52501,1.85841829658605);
#6271=VECTOR('',#52508,0.499999999999944);
#6272=VECTOR('',#52515,1.81285717707166);
#6273=VECTOR('',#52522,0.499999999999944);
#6274=VECTOR('',#52529,1.91146602029502);
#6275=VECTOR('',#52536,0.500000000000054);
#6276=VECTOR('',#52543,1.54967110260249);
#6277=VECTOR('',#52550,0.499999999999944);
#6278=VECTOR('',#52557,1.25936103546569);
#6279=VECTOR('',#52564,0.500000000000054);
#6280=VECTOR('',#52571,1.0588834746273);
#6281=VECTOR('',#52578,0.499999999999935);
#6282=VECTOR('',#52585,1.29583333162394);
#6283=VECTOR('',#52592,0.500000000000054);
#6284=VECTOR('',#52599,1.60653900437051);
#6285=VECTOR('',#52606,0.499999999999935);
#6286=VECTOR('',#52613,1.82809807486262);
#6287=VECTOR('',#52620,0.500000000000049);
#6288=VECTOR('',#52627,1.85841829658605);
#6289=VECTOR('',#52634,0.500000000000054);
#6290=VECTOR('',#52641,1.91146602029503);
#6291=VECTOR('',#52648,0.500000000000049);
#6292=VECTOR('',#52655,1.54967110260249);
#6293=VECTOR('',#52662,0.500000000000058);
#6294=VECTOR('',#52669,1.25936103546568);
#6295=VECTOR('',#52676,0.500000000000049);
#6296=VECTOR('',#52683,1.05888347462729);
#6297=VECTOR('',#52690,0.500000000000049);
#6298=VECTOR('',#52697,1.29583333162383);
#6299=VECTOR('',#52704,0.499999999999826);
#6300=VECTOR('',#52711,1.60653900437051);
#6301=VECTOR('',#52718,0.500000000000054);
#6302=VECTOR('',#52725,1.82809807486273);
#6303=VECTOR('',#52732,0.500000000000049);
#6304=VECTOR('',#52739,1.85841829658606);
#6305=VECTOR('',#52746,0.500000000000049);
#6306=VECTOR('',#52753,1.81285717707167);
#6307=VECTOR('',#52760,0.499999999999944);
#6308=VECTOR('',#52767,1.91146602029503);
#6309=VECTOR('',#52774,0.500000000000058);
#6310=VECTOR('',#52781,1.5496711026026);
#6311=VECTOR('',#52788,0.500000000000058);
#6312=VECTOR('',#52795,1.25936103546569);
#6313=VECTOR('',#52802,0.500000000000049);
#6314=VECTOR('',#52809,1.05888347462741);
#6315=VECTOR('',#52816,0.500000000000054);
#6316=VECTOR('',#52823,1.29583333162417);
#6317=VECTOR('',#52830,0.500000000000177);
#6318=VECTOR('',#52837,1.60653900437062);
#6319=VECTOR('',#52844,0.500000000000063);
#6320=VECTOR('',#52851,1.82809807486272);
#6321=VECTOR('',#52858,0.500000000000054);
#6322=VECTOR('',#52865,1.85841829658605);
#6323=VECTOR('',#52872,0.499999999999935);
#6324=VECTOR('',#52879,1.81285717707167);
#6325=VECTOR('',#52886,0.499999999999944);
#6326=VECTOR('',#52893,1.91146602029502);
#6327=VECTOR('',#52900,0.499999999999935);
#6328=VECTOR('',#52907,1.54967110260249);
#6329=VECTOR('',#52914,0.499999999999935);
#6330=VECTOR('',#52921,1.25936103546568);
#6331=VECTOR('',#52928,0.500000000000058);
#6332=VECTOR('',#52935,1.05888347462741);
#6333=VECTOR('',#52942,0.500000000000054);
#6334=VECTOR('',#52949,1.29583333162394);
#6335=VECTOR('',#52956,0.49999999999994);
#6336=VECTOR('',#52963,1.60653900437051);
#6337=VECTOR('',#52970,0.49999999999994);
#6338=VECTOR('',#52977,1.82809807486272);
#6339=VECTOR('',#52984,0.499999999999935);
#6340=VECTOR('',#52991,1.85841829658605);
#6341=VECTOR('',#52998,0.500000000000049);
#6342=VECTOR('',#53005,1.81285717707144);
#6343=VECTOR('',#53012,0.499999999999821);
#6344=VECTOR('',#53019,1.9114660202949);
#6345=VECTOR('',#53026,0.499999999999935);
#6346=VECTOR('',#53033,1.54967110260237);
#6347=VECTOR('',#53040,0.500000000000049);
#6348=VECTOR('',#53047,1.25936103546556);
#6349=VECTOR('',#53054,0.499999999999821);
#6350=VECTOR('',#53061,1.0588834746273);
#6351=VECTOR('',#53068,0.500000000000058);
#6352=VECTOR('',#53075,1.29583333162394);
#6353=VECTOR('',#53082,0.500000000000058);
#6354=VECTOR('',#53089,1.60653900437062);
#6355=VECTOR('',#53096,0.499999999999944);
#6356=VECTOR('',#53103,1.82809807486284);
#6357=VECTOR('',#53110,0.500000000000172);
#6358=VECTOR('',#53117,1.85841829658605);
#6359=VECTOR('',#53124,0.500000000000058);
#6360=VECTOR('',#53131,1.81285717707155);
#6361=VECTOR('',#53138,0.500000000000058);
#6362=VECTOR('',#53145,1.91146602029503);
#6363=VECTOR('',#53152,0.499999999999944);
#6364=VECTOR('',#53159,1.5496711026025);
#6365=VECTOR('',#53166,0.499999999999944);
#6366=VECTOR('',#53173,1.2593610354658);
#6367=VECTOR('',#53180,0.500000000000172);
#6368=VECTOR('',#53187,1.0588834746273);
#6369=VECTOR('',#53194,0.49999999999994);
#6370=VECTOR('',#53201,1.29583333162394);
#6371=VECTOR('',#53208,0.499999999999944);
#6372=VECTOR('',#53215,1.60653900437051);
#6373=VECTOR('',#53222,0.499999999999944);
#6374=VECTOR('',#53229,1.82809807486261);
#6375=VECTOR('',#53236,0.49999999999994);
#6376=VECTOR('',#53243,1.85841829658593);
#6377=VECTOR('',#53250,0.49999999999994);
#6378=VECTOR('',#53257,1.91146602029514);
#6379=VECTOR('',#53264,0.500000000000058);
#6380=VECTOR('',#53271,1.54967110260249);
#6381=VECTOR('',#53278,0.499999999999935);
#6382=VECTOR('',#53285,1.25936103546568);
#6383=VECTOR('',#53292,0.499999999999944);
#6384=VECTOR('',#53299,1.05888347462741);
#6385=VECTOR('',#53306,0.500000000000058);
#6386=VECTOR('',#53313,1.29583333162394);
#6387=VECTOR('',#53320,0.49999999999994);
#6388=VECTOR('',#53327,1.60653900437051);
#6389=VECTOR('',#53334,0.500000000000058);
#6390=VECTOR('',#53341,1.82809807486273);
#6391=VECTOR('',#53348,0.500000000000058);
#6392=VECTOR('',#53355,1.85841829658593);
#6393=VECTOR('',#53362,0.500000000000058);
#6394=VECTOR('',#53369,1.81285717707167);
#6395=VECTOR('',#53376,0.500000000000058);
#6396=VECTOR('',#53383,1.91146602029491);
#6397=VECTOR('',#53390,0.499999999999944);
#6398=VECTOR('',#53397,1.54967110260237);
#6399=VECTOR('',#53404,0.499999999999935);
#6400=VECTOR('',#53411,1.25936103546569);
#6401=VECTOR('',#53418,0.500000000000058);
#6402=VECTOR('',#53425,1.05888347462741);
#6403=VECTOR('',#53432,0.500000000000054);
#6404=VECTOR('',#53439,1.29583333162383);
#6405=VECTOR('',#53446,0.500000000000054);
#6406=VECTOR('',#53453,1.60653900437062);
#6407=VECTOR('',#53460,0.499999999999935);
#6408=VECTOR('',#53467,1.82809807486272);
#6409=VECTOR('',#53474,0.499999999999935);
#6410=VECTOR('',#53481,1.85841829658616);
#6411=VECTOR('',#53488,0.500000000000054);
#6412=VECTOR('',#53495,1.81285717707168);
#6413=VECTOR('',#53502,0.500000000000054);
#6414=VECTOR('',#53509,1.91146602029514);
#6415=VECTOR('',#53516,0.500000000000054);
#6416=VECTOR('',#53523,1.5496711026025);
#6417=VECTOR('',#53530,0.500000000000049);
#6418=VECTOR('',#53537,1.25936103546568);
#6419=VECTOR('',#53544,0.500000000000049);
#6420=VECTOR('',#53551,1.05888347462729);
#6421=VECTOR('',#53558,0.500000000000058);
#6422=VECTOR('',#53565,1.29583333162394);
#6423=VECTOR('',#53572,0.49999999999994);
#6424=VECTOR('',#53579,1.60653900437051);
#6425=VECTOR('',#53586,0.49999999999994);
#6426=VECTOR('',#53593,1.82809807486273);
#6427=VECTOR('',#53600,0.49999999999994);
#6428=VECTOR('',#53607,1.85841829658616);
#6429=VECTOR('',#53614,0.500000000000054);
#6430=VECTOR('',#53621,1.81285717707166);
#6431=VECTOR('',#53628,0.499999999999821);
#6432=VECTOR('',#53635,1.91146602029503);
#6433=VECTOR('',#53642,0.499999999999821);
#6434=VECTOR('',#53649,1.54967110260249);
#6435=VECTOR('',#53656,0.500000000000054);
#6436=VECTOR('',#53663,1.25936103546579);
#6437=VECTOR('',#53670,0.500000000000058);
#6438=VECTOR('',#53677,1.0588834746273);
#6439=VECTOR('',#53684,0.500000000000058);
#6440=VECTOR('',#53691,1.29583333162395);
#6441=VECTOR('',#53698,0.499999999999935);
#6442=VECTOR('',#53705,1.60653900437051);
#6443=VECTOR('',#53712,0.500000000000054);
#6444=VECTOR('',#53719,1.82809807486273);
#6445=VECTOR('',#53726,0.500000000000063);
#6446=VECTOR('',#53733,1.85841829658605);
#6447=VECTOR('',#53740,0.499999999999821);
#6448=VECTOR('',#53747,1.81285717707144);
#6449=VECTOR('',#53754,0.499999999999821);
#6450=VECTOR('',#53761,1.91146602029503);
#6451=VECTOR('',#53768,0.500000000000054);
#6452=VECTOR('',#53775,1.54967110260249);
#6453=VECTOR('',#53782,0.499999999999944);
#6454=VECTOR('',#53789,1.25936103546568);
#6455=VECTOR('',#53796,0.499999999999944);
#6456=VECTOR('',#53803,1.0588834746273);
#6457=VECTOR('',#53810,0.500000000000054);
#6458=VECTOR('',#53817,1.29583333162382);
#6459=VECTOR('',#53824,0.499999999999826);
#6460=VECTOR('',#53831,1.60653900437062);
#6461=VECTOR('',#53838,0.500000000000058);
#6462=VECTOR('',#53845,1.82809807486272);
#6463=VECTOR('',#53852,0.499999999999944);
#6464=VECTOR('',#53859,1.85841829658605);
#6465=VECTOR('',#53866,0.49999999999994);
#6466=VECTOR('',#53873,1.9114660202949);
#6467=VECTOR('',#53880,0.499999999999821);
#6468=VECTOR('',#53887,1.54967110260249);
#6469=VECTOR('',#53894,0.500000000000054);
#6470=VECTOR('',#53901,1.25936103546569);
#6471=VECTOR('',#53908,0.49999999999994);
#6472=VECTOR('',#53915,1.05888347462729);
#6473=VECTOR('',#53922,0.500000000000054);
#6474=VECTOR('',#53929,1.29583333162371);
#6475=VECTOR('',#53936,0.499999999999935);
#6476=VECTOR('',#53943,1.60653900437051);
#6477=VECTOR('',#53950,0.499999999999944);
#6478=VECTOR('',#53957,1.82809807486262);
#6479=VECTOR('',#53964,0.500000000000058);
#6480=VECTOR('',#53971,1.85841829658605);
#6481=VECTOR('',#53978,0.499999999999944);
#6482=VECTOR('',#53985,1.81285717707166);
#6483=VECTOR('',#53992,0.499999999999944);
#6484=VECTOR('',#53999,1.91146602029514);
#6485=VECTOR('',#54006,0.500000000000054);
#6486=VECTOR('',#54013,1.54967110260238);
#6487=VECTOR('',#54020,0.499999999999935);
#6488=VECTOR('',#54027,1.25936103546568);
#6489=VECTOR('',#54034,0.49999999999994);
#6490=VECTOR('',#54041,1.0588834746273);
#6491=VECTOR('',#54048,0.499999999999944);
#6492=VECTOR('',#54055,1.29583333162395);
#6493=VECTOR('',#54062,0.500000000000054);
#6494=VECTOR('',#54069,1.60653900437063);
#6495=VECTOR('',#54076,0.500000000000054);
#6496=VECTOR('',#54083,1.82809807486273);
#6497=VECTOR('',#54090,0.500000000000058);
#6498=VECTOR('',#54097,1.85841829658594);
#6499=VECTOR('',#54104,0.49999999999994);
#6500=VECTOR('',#54111,1.81285717707156);
#6501=VECTOR('',#54118,0.500000000000058);
#6502=VECTOR('',#54125,1.91146602029491);
#6503=VECTOR('',#54132,0.500000000000054);
#6504=VECTOR('',#54139,1.54967110260249);
#6505=VECTOR('',#54146,0.499999999999944);
#6506=VECTOR('',#54153,1.25936103546568);
#6507=VECTOR('',#54160,0.500000000000058);
#6508=VECTOR('',#54167,1.0588834746273);
#6509=VECTOR('',#54174,0.500000000000054);
#6510=VECTOR('',#54181,1.29583333162394);
#6511=VECTOR('',#54188,0.500000000000054);
#6512=VECTOR('',#54195,1.60653900437062);
#6513=VECTOR('',#54202,0.500000000000054);
#6514=VECTOR('',#54209,1.82809807486272);
#6515=VECTOR('',#54216,0.499999999999944);
#6516=VECTOR('',#54223,1.85841829658605);
#6517=VECTOR('',#54230,0.500000000000054);
#6518=VECTOR('',#54237,1.81285717707167);
#6519=VECTOR('',#54244,0.500000000000054);
#6520=VECTOR('',#54251,1.91146602029503);
#6521=VECTOR('',#54258,0.500000000000049);
#6522=VECTOR('',#54265,1.54967110260249);
#6523=VECTOR('',#54272,0.499999999999944);
#6524=VECTOR('',#54279,1.25936103546569);
#6525=VECTOR('',#54286,0.500000000000054);
#6526=VECTOR('',#54293,1.0588834746274);
#6527=VECTOR('',#54300,0.499999999999944);
#6528=VECTOR('',#54307,1.29583333162394);
#6529=VECTOR('',#54314,0.500000000000054);
#6530=VECTOR('',#54321,1.60653900437062);
#6531=VECTOR('',#54328,0.500000000000054);
#6532=VECTOR('',#54335,1.82809807486272);
#6533=VECTOR('',#54342,0.500000000000054);
#6534=VECTOR('',#54349,1.85841829658605);
#6535=VECTOR('',#54356,0.500000000000049);
#6536=VECTOR('',#54363,1.81285717707167);
#6537=VECTOR('',#54370,0.500000000000054);
#6538=VECTOR('',#54377,1.91146602029502);
#6539=VECTOR('',#54384,0.500000000000054);
#6540=VECTOR('',#54391,1.54967110260249);
#6541=VECTOR('',#54398,0.500000000000054);
#6542=VECTOR('',#54405,1.25936103546568);
#6543=VECTOR('',#54412,0.499999999999944);
#6544=VECTOR('',#54419,1.05888347462741);
#6545=VECTOR('',#54426,0.500000000000054);
#6546=VECTOR('',#54433,1.29583333162394);
#6547=VECTOR('',#54440,0.500000000000054);
#6548=VECTOR('',#54447,1.60653900437062);
#6549=VECTOR('',#54454,0.500000000000054);
#6550=VECTOR('',#54461,1.82809807486261);
#6551=VECTOR('',#54468,0.49999999999994);
#6552=VECTOR('',#54475,1.85841829658605);
#6553=VECTOR('',#54482,0.500000000000054);
#6554=VECTOR('',#54489,1.91146602029503);
#6555=VECTOR('',#54496,0.500000000000054);
#6556=VECTOR('',#54503,1.54967110260249);
#6557=VECTOR('',#54510,0.500000000000054);
#6558=VECTOR('',#54517,1.25936103546568);
#6559=VECTOR('',#54524,0.500000000000054);
#6560=VECTOR('',#54531,1.05888347462729);
#6561=VECTOR('',#54538,0.499999999999935);
#6562=VECTOR('',#54545,1.29583333162395);
#6563=VECTOR('',#54552,0.500000000000063);
#6564=VECTOR('',#54559,1.60653900437062);
#6565=VECTOR('',#54566,0.500000000000054);
#6566=VECTOR('',#54573,1.82809807486273);
#6567=VECTOR('',#54580,0.500000000000058);
#6568=VECTOR('',#54587,1.85841829658605);
#6569=VECTOR('',#54594,0.49999999999994);
#6570=VECTOR('',#54601,1.81285717707167);
#6571=VECTOR('',#54608,0.49999999999994);
#6572=VECTOR('',#54615,1.91146602029491);
#6573=VECTOR('',#54622,0.499999999999826);
#6574=VECTOR('',#54629,1.54967110260249);
#6575=VECTOR('',#54636,0.500000000000054);
#6576=VECTOR('',#54643,1.2593610354658);
#6577=VECTOR('',#54652,0.500000000000058);
#6578=VECTOR('',#54659,1.0588834746273);
#6579=VECTOR('',#54666,0.499999999999935);
#6580=VECTOR('',#54673,1.29583333162395);
#6581=VECTOR('',#54680,0.500000000000054);
#6582=VECTOR('',#54687,1.60653900437074);
#6583=VECTOR('',#54694,0.500000000000058);
#6584=VECTOR('',#54701,1.82809807486272);
#6585=VECTOR('',#54708,0.500000000000054);
#6586=VECTOR('',#54715,1.85841829658616);
#6587=VECTOR('',#54722,0.500000000000167);
#6588=VECTOR('',#54729,1.81285717707155);
#6589=VECTOR('',#54736,0.499999999999935);
#6590=VECTOR('',#54743,1.91146602029503);
#6591=VECTOR('',#54750,0.500000000000054);
#6592=VECTOR('',#54757,1.54967110260249);
#6593=VECTOR('',#54766,0.49999999999994);
#6594=VECTOR('',#54773,1.25936103546556);
#6595=VECTOR('',#54782,0.499999999999821);
#6596=VECTOR('',#54789,1.05888347462729);
#6597=VECTOR('',#54796,0.500000000000058);
#6598=VECTOR('',#54803,1.29583333162382);
#6599=VECTOR('',#54810,0.500000000000054);
#6600=VECTOR('',#54817,1.60653900437074);
#6601=VECTOR('',#54824,0.500000000000063);
#6602=VECTOR('',#54831,1.82809807486272);
#6603=VECTOR('',#54838,0.500000000000054);
#6604=VECTOR('',#54845,1.85841829658605);
#6605=VECTOR('',#54852,0.500000000000049);
#6606=VECTOR('',#54859,1.81285717707166);
#6607=VECTOR('',#54866,0.500000000000049);
#6608=VECTOR('',#54873,1.91146602029503);
#6609=VECTOR('',#54882,0.500000000000054);
#6610=VECTOR('',#54889,1.0588834746273);
#6611=VECTOR('',#54896,0.500000000000058);
#6612=VECTOR('',#54903,1.29583333162395);
#6613=VECTOR('',#54910,0.500000000000058);
#6614=VECTOR('',#54917,1.60653900437063);
#6615=VECTOR('',#54924,0.500000000000058);
#6616=VECTOR('',#54931,1.82809807486273);
#6617=VECTOR('',#54938,0.49999999999994);
#6618=VECTOR('',#54945,1.85841829658605);
#6619=VECTOR('',#54952,0.499999999999935);
#6620=VECTOR('',#54959,1.81285717707167);
#6621=VECTOR('',#54966,0.499999999999944);
#6622=VECTOR('',#54973,1.91146602029503);
#6623=VECTOR('',#54980,0.500000000000167);
#6624=VECTOR('',#54987,1.0588834746273);
#6625=VECTOR('',#54994,0.499999999999944);
#6626=VECTOR('',#55001,1.29583333162394);
#6627=VECTOR('',#55008,0.500000000000054);
#6628=VECTOR('',#55015,1.60653900437062);
#6629=VECTOR('',#55022,0.499999999999944);
#6630=VECTOR('',#55029,1.82809807486273);
#6631=VECTOR('',#55036,0.499999999999944);
#6632=VECTOR('',#55043,1.85841829658605);
#6633=VECTOR('',#55050,0.499999999999944);
#6634=VECTOR('',#55057,1.91146602029503);
#6635=VECTOR('',#55064,0.500000000000058);
#6636=VECTOR('',#55071,1.54967110260249);
#6637=VECTOR('',#55080,0.49999999999994);
#6638=VECTOR('',#55087,1.05888347462741);
#6639=VECTOR('',#55094,0.49999999999994);
#6640=VECTOR('',#55101,1.29583333162394);
#6641=VECTOR('',#55108,0.49999999999994);
#6642=VECTOR('',#55115,1.60653900437063);
#6643=VECTOR('',#55122,0.500000000000058);
#6644=VECTOR('',#55129,1.82809807486273);
#6645=VECTOR('',#55136,0.500000000000058);
#6646=VECTOR('',#55143,1.85841829658593);
#6647=VECTOR('',#55150,0.49999999999994);
#6648=VECTOR('',#55157,1.81285717707155);
#6649=VECTOR('',#55164,0.49999999999994);
#6650=VECTOR('',#55171,1.91146602029503);
#6651=VECTOR('',#55178,0.49999999999994);
#6652=VECTOR('',#55185,1.54967110260237);
#6653=VECTOR('',#55192,0.49999999999994);
#6654=VECTOR('',#55199,1.05888347462729);
#6655=VECTOR('',#55206,0.500000000000054);
#6656=VECTOR('',#55213,1.29583333162383);
#6657=VECTOR('',#55220,0.500000000000054);
#6658=VECTOR('',#55227,1.60653900437051);
#6659=VECTOR('',#55234,0.499999999999935);
#6660=VECTOR('',#55241,1.82809807486262);
#6661=VECTOR('',#55248,0.500000000000063);
#6662=VECTOR('',#55255,1.85841829658605);
#6663=VECTOR('',#55262,0.500000000000054);
#6664=VECTOR('',#55269,1.81285717707166);
#6665=VECTOR('',#55276,0.499999999999935);
#6666=VECTOR('',#55283,1.9114660202949);
#6667=VECTOR('',#55290,0.499999999999935);
#6668=VECTOR('',#55297,1.54967110260238);
#6669=VECTOR('',#55304,0.499999999999935);
#6670=VECTOR('',#55311,1.25936103546556);
#6671=VECTOR('',#55320,0.499999999999935);
#6672=VECTOR('',#55327,1.05888347462741);
#6673=VECTOR('',#55334,0.500000000000058);
#6674=VECTOR('',#55341,1.29583333162406);
#6675=VECTOR('',#55348,0.49999999999994);
#6676=VECTOR('',#55355,1.60653900437063);
#6677=VECTOR('',#55362,0.500000000000058);
#6678=VECTOR('',#55369,1.82809807486262);
#6679=VECTOR('',#55376,0.49999999999994);
#6680=VECTOR('',#55383,1.85841829658593);
#6681=VECTOR('',#55390,0.49999999999994);
#6682=VECTOR('',#55397,1.81285717707179);
#6683=VECTOR('',#55404,0.49999999999994);
#6684=VECTOR('',#55411,1.91146602029502);
#6685=VECTOR('',#55418,0.49999999999994);
#6686=VECTOR('',#55425,1.54967110260249);
#6687=VECTOR('',#55432,0.500000000000058);
#6688=VECTOR('',#55439,1.25936103546569);
#6689=VECTOR('',#55448,0.499999999999935);
#6690=VECTOR('',#55455,1.0588834746273);
#6691=VECTOR('',#55462,0.500000000000054);
#6692=VECTOR('',#55469,1.29583333162406);
#6693=VECTOR('',#55476,0.500000000000177);
#6694=VECTOR('',#55483,1.60653900437051);
#6695=VECTOR('',#55490,0.49999999999994);
#6696=VECTOR('',#55497,1.82809807486261);
#6697=VECTOR('',#55504,0.499999999999944);
#6698=VECTOR('',#55511,1.85841829658594);
#6699=VECTOR('',#55518,0.49999999999994);
#6700=VECTOR('',#55525,1.81285717707156);
#6701=VECTOR('',#55532,0.499999999999944);
#6702=VECTOR('',#55539,1.91146602029503);
#6703=VECTOR('',#55546,0.500000000000054);
#6704=VECTOR('',#55553,1.5496711026026);
#6705=VECTOR('',#55560,0.500000000000058);
#6706=VECTOR('',#55567,1.2593610354658);
#6707=VECTOR('',#55574,0.500000000000063);
#6708=VECTOR('',#55581,1.05888347462741);
#6709=VECTOR('',#55588,0.49999999999994);
#6710=VECTOR('',#55595,1.29583333162395);
#6711=VECTOR('',#55602,0.500000000000054);
#6712=VECTOR('',#55609,1.60653900437063);
#6713=VECTOR('',#55616,0.500000000000167);
#6714=VECTOR('',#55623,1.82809807486262);
#6715=VECTOR('',#55630,0.499999999999944);
#6716=VECTOR('',#55637,1.85841829658605);
#6717=VECTOR('',#55644,0.499999999999944);
#6718=VECTOR('',#55651,1.91146602029502);
#6719=VECTOR('',#55658,0.499999999999944);
#6720=VECTOR('',#55665,1.5496711026026);
#6721=VECTOR('',#55672,0.500000000000054);
#6722=VECTOR('',#55679,1.25936103546567);
#6723=VECTOR('',#55686,0.49999999999994);
#6724=VECTOR('',#55693,1.05888347462741);
#6725=VECTOR('',#55700,0.500000000000054);
#6726=VECTOR('',#55707,1.29583333162394);
#6727=VECTOR('',#55714,0.49999999999994);
#6728=VECTOR('',#55721,1.6065390043705);
#6729=VECTOR('',#55728,0.49999999999994);
#6730=VECTOR('',#55735,1.82809807486261);
#6731=VECTOR('',#55742,0.500000000000054);
#6732=VECTOR('',#55749,1.85841829658593);
#6733=VECTOR('',#55756,0.49999999999994);
#6734=VECTOR('',#55763,1.81285717707167);
#6735=VECTOR('',#55770,0.500000000000058);
#6736=VECTOR('',#55777,1.91146602029503);
#6737=VECTOR('',#55784,0.500000000000054);
#6738=VECTOR('',#55791,1.54967110260249);
#6739=VECTOR('',#55798,0.500000000000058);
#6740=VECTOR('',#55805,1.25936103546568);
#6741=VECTOR('',#55812,0.49999999999994);
#6742=VECTOR('',#55819,1.0588834746273);
#6743=VECTOR('',#55826,0.500000000000054);
#6744=VECTOR('',#55833,1.29583333162383);
#6745=VECTOR('',#55840,0.499999999999935);
#6746=VECTOR('',#55847,1.60653900437062);
#6747=VECTOR('',#55854,0.500000000000058);
#6748=VECTOR('',#55861,1.82809807486272);
#6749=VECTOR('',#55868,0.500000000000058);
#6750=VECTOR('',#55875,1.85841829658594);
#6751=VECTOR('',#55882,0.499999999999826);
#6752=VECTOR('',#55889,1.81285717707156);
#6753=VECTOR('',#55896,0.499999999999944);
#6754=VECTOR('',#55903,1.91146602029502);
#6755=VECTOR('',#55910,0.499999999999935);
#6756=VECTOR('',#55917,1.54967110260249);
#6757=VECTOR('',#55924,0.500000000000054);
#6758=VECTOR('',#55931,1.25936103546568);
#6759=VECTOR('',#55938,0.500000000000054);
#6760=VECTOR('',#56009,8.99091713639496);
#6761=VECTOR('',#56050,1000.);
#6762=VECTOR('',#56053,1000.);
#6763=VECTOR('',#56062,8.99091713639503);
#6764=VECTOR('',#56075,0.500000000000054);
#6765=VECTOR('',#56078,1.02140828085145);
#6766=VECTOR('',#56085,1000.);
#6767=VECTOR('',#56086,10.);
#6768=VECTOR('',#56087,1000.);
#6769=VECTOR('',#56088,1000.);
#6770=VECTOR('',#56093,1000.);
#6771=VECTOR('',#56102,1000.);
#6772=VECTOR('',#56105,1000.);
#6773=VECTOR('',#56108,1000.);
#6774=VECTOR('',#56115,10.);
#6775=VECTOR('',#56116,1000.);
#6776=VECTOR('',#56119,1000.);
#6777=VECTOR('',#56122,1000.);
#6778=VECTOR('',#56127,1000.);
#6779=VECTOR('',#56128,1000.);
#6780=VECTOR('',#56129,1000.);
#6781=VECTOR('',#56130,1000.);
#6782=VECTOR('',#56133,1000.);
#6783=VECTOR('',#56142,1000.);
#6784=VECTOR('',#56147,1000.);
#6785=VECTOR('',#56148,1000.);
#6786=VECTOR('',#56189,10.);
#6787=VECTOR('',#56196,10.);
#6788=VECTOR('',#56229,1000.);
#6789=VECTOR('',#56230,1000.);
#6790=VECTOR('',#56243,10.);
#6791=VECTOR('',#56244,10.);
#6792=VECTOR('',#56281,1000.);
#6793=VECTOR('',#56284,1000.);
#6794=VECTOR('',#57507,9.47320447306899);
#6795=VECTOR('',#57524,8.94802844775792);
#6796=VECTOR('',#57541,1000.);
#6797=VECTOR('',#57544,1000.);
#6798=VECTOR('',#57549,1000.);
#6799=VECTOR('',#57550,1000.);
#6800=VECTOR('',#57551,1000.);
#6801=VECTOR('',#57554,1000.);
#6802=VECTOR('',#57561,1000.);
#6803=VECTOR('',#57562,1000.);
#6804=VECTOR('',#57571,1000.);
#6805=VECTOR('',#57574,1000.);
#6806=VECTOR('',#57577,1000.);
#6807=VECTOR('',#57578,1000.);
#6808=VECTOR('',#57579,1000.);
#6809=VECTOR('',#57584,1000.);
#6810=VECTOR('',#57587,1000.);
#6811=VECTOR('',#57588,1000.);
#6812=VECTOR('',#57597,1000.);
#6813=VECTOR('',#57600,1000.);
#6814=VECTOR('',#57603,1000.);
#6815=VECTOR('',#57606,1000.);
#6816=VECTOR('',#57609,28.5226030790361);
#6817=VECTOR('',#57624,1000.);
#6818=VECTOR('',#57627,1000.);
#6819=VECTOR('',#57632,1000.);
#6820=VECTOR('',#57635,1000.);
#6821=VECTOR('',#57640,1000.);
#6822=VECTOR('',#57643,1000.);
#6823=VECTOR('',#57648,16.);
#6824=VECTOR('',#57651,1000.);
#6825=VECTOR('',#57654,1000.);
#6826=VECTOR('',#57663,1000.);
#6827=VECTOR('',#57666,1000.);
#6828=VECTOR('',#57697,16.);
#6829=VECTOR('',#57700,1000.);
#6830=VECTOR('',#57703,1000.);
#6831=VECTOR('',#57712,1000.);
#6832=VECTOR('',#57715,1000.);
#6833=VECTOR('',#57746,16.);
#6834=VECTOR('',#57749,1000.);
#6835=VECTOR('',#57752,1000.);
#6836=VECTOR('',#57761,1000.);
#6837=VECTOR('',#57764,1000.);
#6838=VECTOR('',#57795,26.0226030790361);
#6839=VECTOR('',#57798,1000.);
#6840=VECTOR('',#57801,1000.);
#6841=VECTOR('',#57814,1000.);
#6842=VECTOR('',#57815,1000.);
#6843=VECTOR('',#57816,1000.);
#6844=VECTOR('',#57819,1000.);
#6845=VECTOR('',#57822,1000.);
#6846=VECTOR('',#57825,1000.);
#6847=VECTOR('',#57828,1000.);
#6848=VECTOR('',#57831,1000.);
#6849=VECTOR('',#57836,1000.);
#6850=VECTOR('',#57837,1000.);
#6851=VECTOR('',#57838,1000.);
#6852=VECTOR('',#57839,1000.);
#6853=VECTOR('',#57842,1000.);
#6854=VECTOR('',#57843,1000.);
#6855=VECTOR('',#57844,1000.);
#6856=VECTOR('',#57847,1000.);
#6857=VECTOR('',#57848,1000.);
#6858=VECTOR('',#57849,1000.);
#6859=VECTOR('',#57872,1000.);
#6860=VECTOR('',#57875,1000.);
#6861=VECTOR('',#57884,1000.);
#6862=VECTOR('',#57947,1000.);
#6863=VECTOR('',#57948,1000.);
#6864=VECTOR('',#57953,1000.);
#6865=VECTOR('',#57954,1000.);
#6866=VECTOR('',#57965,1000.);
#6867=VECTOR('',#57976,1000.);
#6868=VECTOR('',#57977,1000.);
#6869=VECTOR('',#57988,1000.);
#6870=VECTOR('',#57989,1000.);
#6871=VECTOR('',#58014,1000.);
#6872=VECTOR('',#58015,1000.);
#6873=VECTOR('',#58018,1000.);
#6874=VECTOR('',#58021,1000.);
#6875=VECTOR('',#58022,1000.);
#6876=VECTOR('',#58029,1000.);
#6877=VECTOR('',#58030,1000.);
#6878=VECTOR('',#58033,1000.);
#6879=VECTOR('',#58034,1000.);
#6880=VECTOR('',#58045,1000.);
#6881=VECTOR('',#58046,1000.);
#6882=VECTOR('',#58057,1000.);
#6883=VECTOR('',#58058,1000.);
#6884=VECTOR('',#58075,1000.);
#6885=VECTOR('',#58080,1000.);
#6886=VECTOR('',#58081,1000.);
#6887=VECTOR('',#58086,1000.);
#6888=VECTOR('',#58087,1000.);
#6889=VECTOR('',#58092,1000.);
#6890=VECTOR('',#58105,1000.);
#6891=VECTOR('',#58106,1000.);
#6892=VECTOR('',#58109,1000.);
#6893=VECTOR('',#58110,1000.);
#6894=VECTOR('',#58117,1000.);
#6895=VECTOR('',#58118,1000.);
#6896=VECTOR('',#58129,1000.);
#6897=VECTOR('',#58130,1000.);
#6898=VECTOR('',#58141,1000.);
#6899=VECTOR('',#58142,1000.);
#6900=VECTOR('',#58159,1000.);
#6901=VECTOR('',#58164,1000.);
#6902=VECTOR('',#58165,1000.);
#6903=VECTOR('',#58170,1000.);
#6904=VECTOR('',#58171,1000.);
#6905=VECTOR('',#58176,1000.);
#6906=VECTOR('',#58189,1000.);
#6907=VECTOR('',#58190,1000.);
#6908=VECTOR('',#58193,1000.);
#6909=VECTOR('',#58194,1000.);
#6910=VECTOR('',#58201,1000.);
#6911=VECTOR('',#58202,1000.);
#6912=VECTOR('',#58213,1000.);
#6913=VECTOR('',#58214,1000.);
#6914=VECTOR('',#58225,1000.);
#6915=VECTOR('',#58226,1000.);
#6916=VECTOR('',#58243,1000.);
#6917=VECTOR('',#58248,1000.);
#6918=VECTOR('',#58249,1000.);
#6919=VECTOR('',#58254,1000.);
#6920=VECTOR('',#58255,1000.);
#6921=VECTOR('',#58260,1000.);
#6922=VECTOR('',#58273,1000.);
#6923=VECTOR('',#58274,1000.);
#6924=VECTOR('',#58277,1000.);
#6925=VECTOR('',#58278,1000.);
#6926=VECTOR('',#58285,1000.);
#6927=VECTOR('',#58286,1000.);
#6928=VECTOR('',#58295,1000.);
#6929=VECTOR('',#58298,1000.);
#6930=VECTOR('',#58301,1000.);
#6931=VECTOR('',#58308,1000.);
#6932=VECTOR('',#58325,1000.);
#6933=VECTOR('',#58338,1000.);
#6934=VECTOR('',#58351,1000.);
#6935=VECTOR('',#58352,1000.);
#6936=VECTOR('',#58377,1000.);
#6937=VECTOR('',#58394,1000.);
#6938=VECTOR('',#58403,1000.);
#6939=VECTOR('',#58404,1000.);
#6940=VECTOR('',#58423,1000.);
#6941=VECTOR('',#58436,1000.);
#6942=VECTOR('',#58475,1000.);
#6943=VECTOR('',#58476,1000.);
#6944=VECTOR('',#58477,1000.);
#6945=VECTOR('',#58478,1000.);
#6946=VECTOR('',#58481,1000.);
#6947=VECTOR('',#58482,1000.);
#6948=VECTOR('',#58491,1000.);
#6949=VECTOR('',#58492,1000.);
#6950=VECTOR('',#58493,1000.);
#6951=VECTOR('',#58498,1000.);
#6952=VECTOR('',#58501,1000.);
#6953=VECTOR('',#58502,1000.);
#6954=VECTOR('',#58505,1000.);
#6955=VECTOR('',#58506,1000.);
#6956=VECTOR('',#58513,1000.);
#6957=VECTOR('',#58516,1000.);
#6958=VECTOR('',#58519,1000.);
#6959=VECTOR('',#58522,1000.);
#6960=VECTOR('',#58531,12.);
#6961=VECTOR('',#58538,1000.);
#6962=VECTOR('',#58541,1000.);
#6963=VECTOR('',#58544,1000.);
#6964=VECTOR('',#58547,1000.);
#6965=VECTOR('',#58548,1000.);
#6966=VECTOR('',#58551,1000.);
#6967=VECTOR('',#58554,1000.);
#6968=VECTOR('',#58557,1000.);
#6969=VECTOR('',#58560,1000.);
#6970=VECTOR('',#58563,1000.);
#6971=VECTOR('',#58566,1000.);
#6972=VECTOR('',#58569,1000.);
#6973=VECTOR('',#58574,1000.);
#6974=VECTOR('',#58575,1000.);
#6975=VECTOR('',#58576,1000.);
#6976=VECTOR('',#58577,1000.);
#6977=VECTOR('',#58580,1000.);
#6978=VECTOR('',#58581,1000.);
#6979=VECTOR('',#58582,1000.);
#6980=VECTOR('',#58583,1000.);
#6981=VECTOR('',#58586,1000.);
#6982=VECTOR('',#58587,1000.);
#6983=VECTOR('',#58588,1000.);
#6984=VECTOR('',#58589,1000.);
#6985=VECTOR('',#58592,1000.);
#6986=VECTOR('',#58593,1000.);
#6987=VECTOR('',#58594,1000.);
#6988=VECTOR('',#58595,1000.);
#6989=VECTOR('',#58600,1000.);
#6990=VECTOR('',#58603,1000.);
#6991=VECTOR('',#58606,1000.);
#6992=VECTOR('',#58609,1000.);
#6993=VECTOR('',#58612,1000.);
#6994=VECTOR('',#58613,1000.);
#6995=VECTOR('',#58614,1000.);
#6996=VECTOR('',#58615,1000.);
#6997=VECTOR('',#58618,1000.);
#6998=VECTOR('',#58619,1000.);
#6999=VECTOR('',#58620,1000.);
#7000=VECTOR('',#58623,1000.);
#7001=VECTOR('',#58628,1000.);
#7002=VECTOR('',#58629,1000.);
#7003=VECTOR('',#58630,1000.);
#7004=VECTOR('',#58631,1000.);
#7005=VECTOR('',#58634,1000.);
#7006=VECTOR('',#58635,1000.);
#7007=VECTOR('',#58636,1000.);
#7008=VECTOR('',#58639,1000.);
#7009=VECTOR('',#58644,1000.);
#7010=VECTOR('',#58645,1000.);
#7011=VECTOR('',#58646,1000.);
#7012=VECTOR('',#58647,1000.);
#7013=VECTOR('',#58686,1000.);
#7014=VECTOR('',#58687,1000.);
#7015=VECTOR('',#58688,1000.);
#7016=VECTOR('',#58689,1000.);
#7017=VECTOR('',#58692,1000.);
#7018=VECTOR('',#58699,1000.);
#7019=VECTOR('',#58700,1000.);
#7020=VECTOR('',#58701,1000.);
#7021=VECTOR('',#58704,1000.);
#7022=VECTOR('',#58711,1000.);
#7023=VECTOR('',#58712,1000.);
#7024=VECTOR('',#58713,1000.);
#7025=VECTOR('',#58716,1000.);
#7026=VECTOR('',#58717,1000.);
#7027=VECTOR('',#58718,1000.);
#7028=VECTOR('',#58719,1000.);
#7029=VECTOR('',#58722,1000.);
#7030=VECTOR('',#58729,1000.);
#7031=VECTOR('',#58730,1000.);
#7032=VECTOR('',#58731,1000.);
#7033=VECTOR('',#58734,1000.);
#7034=VECTOR('',#58741,1000.);
#7035=VECTOR('',#58742,1000.);
#7036=VECTOR('',#58743,1000.);
#7037=VECTOR('',#59006,19.4499999999999);
#7038=VECTOR('',#59007,1000.);
#7039=VECTOR('',#59010,1000.);
#7040=VECTOR('',#59029,19.45);
#7041=VECTOR('',#59046,12.3);
#7042=VECTOR('',#59051,15.7183063441034);
#7043=VECTOR('',#59082,12.2808574779498);
#7044=VECTOR('',#59085,19.45);
#7045=VECTOR('',#59102,12.3);
#7046=VECTOR('',#59107,15.7183063441034);
#7047=VECTOR('',#59114,5.84048589276829);
#7048=VECTOR('',#59131,1000.);
#7049=VECTOR('',#59134,1000.);
#7050=VECTOR('',#59137,1000.);
#7051=VECTOR('',#59140,1000.);
#7052=VECTOR('',#59141,1000.);
#7053=VECTOR('',#59144,1000.);
#7054=VECTOR('',#59149,1000.);
#7055=VECTOR('',#59150,1000.);
#7056=VECTOR('',#59153,1000.);
#7057=VECTOR('',#59154,1000.);
#7058=VECTOR('',#59159,1000.);
#7059=VECTOR('',#59162,1000.);
#7060=VECTOR('',#59165,1000.);
#7061=VECTOR('',#59166,1000.);
#7062=VECTOR('',#59171,1000.);
#7063=VECTOR('',#59172,1000.);
#7064=VECTOR('',#59175,1000.);
#7065=VECTOR('',#59176,1000.);
#7066=VECTOR('',#59179,1000.);
#7067=VECTOR('',#59180,1000.);
#7068=VECTOR('',#59181,1000.);
#7069=VECTOR('',#59182,1000.);
#7070=VECTOR('',#59185,1000.);
#7071=VECTOR('',#59186,1000.);
#7072=VECTOR('',#59187,1000.);
#7073=VECTOR('',#59188,1000.);
#7074=VECTOR('',#59281,11.5);
#7075=VECTOR('',#59288,12.5);
#7076=VECTOR('',#59313,1.27544412113617);
#7077=VECTOR('',#59316,0.675444121136126);
#7078=VECTOR('',#59321,1.09883113599246);
#7079=VECTOR('',#59324,0.498831135992472);
#7080=VECTOR('',#59329,1.09054074872833);
#7081=VECTOR('',#59332,0.490540748728341);
#7082=VECTOR('',#59337,1.47830313219327);
#7083=VECTOR('',#59340,0.878303132193281);
#7084=VECTOR('',#59345,1.27544412113612);
#7085=VECTOR('',#59348,0.675444121136182);
#7086=VECTOR('',#59353,1.09883113599246);
#7087=VECTOR('',#59356,0.498831135992472);
#7088=VECTOR('',#59361,1.09054074872833);
#7089=VECTOR('',#59364,0.490540748728341);
#7090=VECTOR('',#59369,1.47830313219333);
#7091=VECTOR('',#59372,0.878303132193337);
#7092=VECTOR('',#59377,1.27544412113617);
#7093=VECTOR('',#59380,0.675444121136126);
#7094=VECTOR('',#59385,1.09883113599246);
#7095=VECTOR('',#59388,0.498831135992472);
#7096=VECTOR('',#59393,1.09054074872833);
#7097=VECTOR('',#59396,0.490540748728341);
#7098=VECTOR('',#59401,1.47830313219327);
#7099=VECTOR('',#59404,0.878303132193281);
#7100=VECTOR('',#59409,1.27544412113617);
#7101=VECTOR('',#59412,0.675444121136126);
#7102=VECTOR('',#59417,1.09883113599246);
#7103=VECTOR('',#59420,0.498831135992472);
#7104=VECTOR('',#59425,1.09054074872833);
#7105=VECTOR('',#59428,0.490540748728285);
#7106=VECTOR('',#59433,1.47830313219327);
#7107=VECTOR('',#59436,0.878303132193226);
#7108=VECTOR('',#59441,1.27544412113617);
#7109=VECTOR('',#59444,0.675444121136182);
#7110=VECTOR('',#59449,1.09883113599246);
#7111=VECTOR('',#59452,0.498831135992472);
#7112=VECTOR('',#59457,1.09054074872833);
#7113=VECTOR('',#59460,0.490540748728341);
#7114=VECTOR('',#59465,1.47830313219333);
#7115=VECTOR('',#59468,0.878303132193281);
#7116=VECTOR('',#59473,1.27544412113612);
#7117=VECTOR('',#59476,0.675444121136182);
#7118=VECTOR('',#59481,1.09883113599241);
#7119=VECTOR('',#59484,0.498831135992472);
#7120=VECTOR('',#59489,1.09054074872839);
#7121=VECTOR('',#59492,0.490540748728341);
#7122=VECTOR('',#59497,1.47830313219333);
#7123=VECTOR('',#59500,0.878303132193281);
#7124=VECTOR('',#59505,1.27544412113612);
#7125=VECTOR('',#59508,0.675444121136182);
#7126=VECTOR('',#59513,1.09883113599252);
#7127=VECTOR('',#59516,0.498831135992583);
#7128=VECTOR('',#59521,1.09054074872827);
#7129=VECTOR('',#59524,0.490540748728341);
#7130=VECTOR('',#59529,1.47830313219321);
#7131=VECTOR('',#59532,0.87830313219317);
#7132=VECTOR('',#59537,1.27544412113612);
#7133=VECTOR('',#59540,0.675444121136071);
#7134=VECTOR('',#59545,1.09883113599252);
#7135=VECTOR('',#59548,0.498831135992472);
#7136=VECTOR('',#59553,1.09054074872839);
#7137=VECTOR('',#59556,0.490540748728341);
#7138=VECTOR('',#59561,1.47830313219321);
#7139=VECTOR('',#59564,0.87830313219317);
#7140=VECTOR('',#59569,1.27544412113612);
#7141=VECTOR('',#59572,0.675444121136071);
#7142=VECTOR('',#59577,1.09883113599241);
#7143=VECTOR('',#59580,0.498831135992361);
#7144=VECTOR('',#59585,1.09054074872839);
#7145=VECTOR('',#59588,0.490540748728341);
#7146=VECTOR('',#59593,1.47830313219333);
#7147=VECTOR('',#59596,0.878303132193281);
#7148=VECTOR('',#59601,1.27544412113612);
#7149=VECTOR('',#59604,0.675444121136182);
#7150=VECTOR('',#59609,1.09883113599252);
#7151=VECTOR('',#59612,0.498831135992472);
#7152=VECTOR('',#59617,1.09054074872827);
#7153=VECTOR('',#59620,0.49054074872823);
#7154=VECTOR('',#59625,1.47830313219333);
#7155=VECTOR('',#59628,0.878303132193281);
#7156=VECTOR('',#59633,1.27544412113623);
#7157=VECTOR('',#59636,0.675444121136182);
#7158=VECTOR('',#59641,1.09883113599252);
#7159=VECTOR('',#59644,0.498831135992472);
#7160=VECTOR('',#59649,1.09054074872827);
#7161=VECTOR('',#59652,0.490540748728341);
#7162=VECTOR('',#59657,1.47830313219333);
#7163=VECTOR('',#59660,0.878303132193281);
#7164=VECTOR('',#59665,1.27544412113617);
#7165=VECTOR('',#59668,0.675444121136126);
#7166=VECTOR('',#59673,1.09883113599252);
#7167=VECTOR('',#59676,0.498831135992472);
#7168=VECTOR('',#59681,1.09054074872839);
#7169=VECTOR('',#59684,0.490540748728341);
#7170=VECTOR('',#59689,1.47830313219327);
#7171=VECTOR('',#59692,0.878303132193281);
#7172=VECTOR('',#59697,1.27544412113617);
#7173=VECTOR('',#59700,0.675444121136182);
#7174=VECTOR('',#59705,1.09883113599246);
#7175=VECTOR('',#59708,0.498831135992417);
#7176=VECTOR('',#59713,1.09054074872827);
#7177=VECTOR('',#59716,0.490540748728341);
#7178=VECTOR('',#59721,1.47830313219327);
#7179=VECTOR('',#59724,0.878303132193281);
#7180=VECTOR('',#59729,1.27544412113612);
#7181=VECTOR('',#59732,0.675444121136126);
#7182=VECTOR('',#59737,1.09883113599241);
#7183=VECTOR('',#59740,0.498831135992417);
#7184=VECTOR('',#59745,1.09054074872839);
#7185=VECTOR('',#59748,0.490540748728341);
#7186=VECTOR('',#59753,1.47830313219333);
#7187=VECTOR('',#59756,0.878303132193337);
#7188=VECTOR('',#59761,1.27544412113617);
#7189=VECTOR('',#59764,0.675444121136182);
#7190=VECTOR('',#59769,1.09883113599246);
#7191=VECTOR('',#59772,0.498831135992417);
#7192=VECTOR('',#59777,1.09054074872833);
#7193=VECTOR('',#59780,0.490540748728341);
#7194=VECTOR('',#59785,1.47830313219333);
#7195=VECTOR('',#59788,0.878303132193337);
#7196=VECTOR('',#59793,1.27544412113617);
#7197=VECTOR('',#59796,0.675444121136126);
#7198=VECTOR('',#59801,1.09883113599246);
#7199=VECTOR('',#59804,0.498831135992472);
#7200=VECTOR('',#59809,1.09054074872833);
#7201=VECTOR('',#59812,0.490540748728341);
#7202=VECTOR('',#59817,1.47830313219333);
#7203=VECTOR('',#59820,0.878303132193281);
#7204=VECTOR('',#59825,1.27544412113617);
#7205=VECTOR('',#59828,0.675444121136182);
#7206=VECTOR('',#59833,1.09883113599246);
#7207=VECTOR('',#59836,0.498831135992472);
#7208=VECTOR('',#59841,1.09054074872833);
#7209=VECTOR('',#59844,0.490540748728341);
#7210=VECTOR('',#59849,1.47830313219333);
#7211=VECTOR('',#59852,0.878303132193281);
#7212=VECTOR('',#59857,1.27544412113617);
#7213=VECTOR('',#59860,0.675444121136182);
#7214=VECTOR('',#59865,1.09883113599246);
#7215=VECTOR('',#59868,0.498831135992472);
#7216=VECTOR('',#59873,1.09054074872833);
#7217=VECTOR('',#59876,0.490540748728341);
#7218=VECTOR('',#59881,1.47830313219333);
#7219=VECTOR('',#59884,0.878303132193281);
#7220=VECTOR('',#59889,1.27544412113612);
#7221=VECTOR('',#59892,0.675444121136126);
#7222=VECTOR('',#59897,1.09883113599252);
#7223=VECTOR('',#59900,0.498831135992472);
#7224=VECTOR('',#59905,1.09054074872833);
#7225=VECTOR('',#59908,0.490540748728341);
#7226=VECTOR('',#59913,1.47830313219333);
#7227=VECTOR('',#59916,0.878303132193337);
#7228=VECTOR('',#59921,1.27544412113617);
#7229=VECTOR('',#59924,0.675444121136126);
#7230=VECTOR('',#59929,1.09883113599246);
#7231=VECTOR('',#59932,0.498831135992472);
#7232=VECTOR('',#59937,1.09054074872833);
#7233=VECTOR('',#59940,0.490540748728341);
#7234=VECTOR('',#59945,1.47830313219327);
#7235=VECTOR('',#59948,0.878303132193281);
#7236=VECTOR('',#59953,1.27544412113617);
#7237=VECTOR('',#59956,0.675444121136182);
#7238=VECTOR('',#59961,1.09883113599246);
#7239=VECTOR('',#59964,0.498831135992472);
#7240=VECTOR('',#59969,1.09054074872827);
#7241=VECTOR('',#59972,0.490540748728341);
#7242=VECTOR('',#59977,1.47830313219327);
#7243=VECTOR('',#59980,0.878303132193281);
#7244=VECTOR('',#59985,1.27544412113617);
#7245=VECTOR('',#59988,0.675444121136126);
#7246=VECTOR('',#59993,1.09883113599241);
#7247=VECTOR('',#59996,0.498831135992472);
#7248=VECTOR('',#60001,1.09054074872827);
#7249=VECTOR('',#60004,0.490540748728341);
#7250=VECTOR('',#60009,1.47830313219327);
#7251=VECTOR('',#60012,0.878303132193281);
#7252=VECTOR('',#60017,1.27544412113617);
#7253=VECTOR('',#60020,0.675444121136126);
#7254=VECTOR('',#60025,1.09883113599252);
#7255=VECTOR('',#60028,0.498831135992472);
#7256=VECTOR('',#60033,1.09054074872839);
#7257=VECTOR('',#60036,0.490540748728396);
#7258=VECTOR('',#60041,1.47830313219327);
#7259=VECTOR('',#60044,0.878303132193281);
#7260=VECTOR('',#60049,1.27544412113612);
#7261=VECTOR('',#60052,0.675444121136126);
#7262=VECTOR('',#60057,1.09883113599241);
#7263=VECTOR('',#60060,0.498831135992417);
#7264=VECTOR('',#60065,1.09054074872833);
#7265=VECTOR('',#60068,0.490540748728341);
#7266=VECTOR('',#60073,1.47830313219327);
#7267=VECTOR('',#60076,0.878303132193281);
#7268=VECTOR('',#60081,1.27544412113617);
#7269=VECTOR('',#60084,0.675444121136126);
#7270=VECTOR('',#60089,1.09883113599241);
#7271=VECTOR('',#60092,0.498831135992472);
#7272=VECTOR('',#60097,1.09054074872839);
#7273=VECTOR('',#60100,0.490540748728396);
#7274=VECTOR('',#60105,1.47830313219327);
#7275=VECTOR('',#60108,0.878303132193281);
#7276=VECTOR('',#60113,1.27544412113617);
#7277=VECTOR('',#60116,0.675444121136182);
#7278=VECTOR('',#60121,1.09883113599246);
#7279=VECTOR('',#60124,0.498831135992528);
#7280=VECTOR('',#60129,1.09054074872833);
#7281=VECTOR('',#60132,0.490540748728341);
#7282=VECTOR('',#60137,1.47830313219333);
#7283=VECTOR('',#60140,0.878303132193337);
#7284=VECTOR('',#60145,1.27544412113617);
#7285=VECTOR('',#60148,0.675444121136126);
#7286=VECTOR('',#60153,1.09883113599246);
#7287=VECTOR('',#60156,0.498831135992472);
#7288=VECTOR('',#60161,1.09054074872839);
#7289=VECTOR('',#60164,0.490540748728285);
#7290=VECTOR('',#60169,1.47830313219327);
#7291=VECTOR('',#60172,0.878303132193281);
#7292=VECTOR('',#60177,1.27544412113617);
#7293=VECTOR('',#60180,0.675444121136126);
#7294=VECTOR('',#60185,1.09883113599246);
#7295=VECTOR('',#60188,0.498831135992528);
#7296=VECTOR('',#60193,1.09054074872833);
#7297=VECTOR('',#60196,0.490540748728341);
#7298=VECTOR('',#60201,1.47830313219333);
#7299=VECTOR('',#60204,0.878303132193337);
#7300=VECTOR('',#60209,1.27544412113617);
#7301=VECTOR('',#60212,0.675444121136182);
#7302=VECTOR('',#60217,1.09883113599246);
#7303=VECTOR('',#60220,0.498831135992472);
#7304=VECTOR('',#60225,1.09054074872833);
#7305=VECTOR('',#60228,0.490540748728285);
#7306=VECTOR('',#60233,1.47830313219327);
#7307=VECTOR('',#60236,0.878303132193281);
#7308=VECTOR('',#60241,1.27544412113617);
#7309=VECTOR('',#60244,0.675444121136126);
#7310=VECTOR('',#60249,1.09054074872833);
#7311=VECTOR('',#60252,0.490540748728341);
#7312=VECTOR('',#60257,1.09883113599252);
#7313=VECTOR('',#60260,0.498831135992472);
#7314=VECTOR('',#60267,1.10035806567471);
#7315=VECTOR('',#60274,0.500358065674722);
#7316=VECTOR('',#60281,1.21403156673711);
#7317=VECTOR('',#60288,0.614031566737117);
#7318=VECTOR('',#60295,1.32880796357332);
#7319=VECTOR('',#60302,0.72880796357333);
#7320=VECTOR('',#60309,1.46111700181689);
#7321=VECTOR('',#60316,0.861117001816902);
#7322=VECTOR('',#60323,1.6204820426246);
#7323=VECTOR('',#60330,1.02048204262462);
#7324=VECTOR('',#60337,1.70100022308284);
#7325=VECTOR('',#60344,1.10100022308285);
#7326=VECTOR('',#60351,1.72127463204352);
#7327=VECTOR('',#60358,1.12127463204348);
#7328=VECTOR('',#60365,1.78199265440493);
#7329=VECTOR('',#60372,1.18199265440494);
#7330=VECTOR('',#60379,1.66088080992077);
#7331=VECTOR('',#60386,1.06088080992078);
#7332=VECTOR('',#60393,1.10035806567471);
#7333=VECTOR('',#60400,0.500358065674722);
#7334=VECTOR('',#60407,1.21403156673716);
#7335=VECTOR('',#60414,0.614031566737117);
#7336=VECTOR('',#60421,1.32880796357332);
#7337=VECTOR('',#60428,0.728807963573275);
#7338=VECTOR('',#60435,1.46111700181689);
#7339=VECTOR('',#60442,0.861117001816902);
#7340=VECTOR('',#60449,1.6204820426246);
#7341=VECTOR('',#60456,1.02048204262462);
#7342=VECTOR('',#60463,1.70100022308284);
#7343=VECTOR('',#60470,1.10100022308285);
#7344=VECTOR('',#60477,1.72127463204347);
#7345=VECTOR('',#60484,1.12127463204348);
#7346=VECTOR('',#60491,1.78199265440493);
#7347=VECTOR('',#60498,1.18199265440494);
#7348=VECTOR('',#60505,1.66088080992077);
#7349=VECTOR('',#60512,1.06088080992078);
#7350=VECTOR('',#60519,1.10035806567471);
#7351=VECTOR('',#60526,0.500358065674722);
#7352=VECTOR('',#60533,1.21403156673716);
#7353=VECTOR('',#60540,0.614031566737117);
#7354=VECTOR('',#60547,1.32880796357326);
#7355=VECTOR('',#60554,0.72880796357333);
#7356=VECTOR('',#60561,1.46111700181689);
#7357=VECTOR('',#60568,0.861117001816902);
#7358=VECTOR('',#60575,1.6204820426246);
#7359=VECTOR('',#60582,1.02048204262456);
#7360=VECTOR('',#60589,1.70100022308284);
#7361=VECTOR('',#60596,1.10100022308285);
#7362=VECTOR('',#60603,1.72127463204347);
#7363=VECTOR('',#60610,1.12127463204348);
#7364=VECTOR('',#60617,1.78199265440493);
#7365=VECTOR('',#60624,1.18199265440494);
#7366=VECTOR('',#60631,1.66088080992077);
#7367=VECTOR('',#60638,1.06088080992078);
#7368=VECTOR('',#60645,1.10035806567471);
#7369=VECTOR('',#60652,0.500358065674666);
#7370=VECTOR('',#60659,1.21403156673711);
#7371=VECTOR('',#60666,0.614031566737172);
#7372=VECTOR('',#60673,1.32880796357332);
#7373=VECTOR('',#60680,0.72880796357333);
#7374=VECTOR('',#60687,1.46111700181689);
#7375=VECTOR('',#60694,0.861117001816847);
#7376=VECTOR('',#60701,1.6204820426246);
#7377=VECTOR('',#60708,1.02048204262462);
#7378=VECTOR('',#60715,1.70100022308284);
#7379=VECTOR('',#60722,1.10100022308285);
#7380=VECTOR('',#60729,1.72127463204347);
#7381=VECTOR('',#60736,1.12127463204353);
#7382=VECTOR('',#60743,1.78199265440498);
#7383=VECTOR('',#60750,1.18199265440494);
#7384=VECTOR('',#60757,1.66088080992083);
#7385=VECTOR('',#60764,1.06088080992078);
#7386=VECTOR('',#60771,1.10035806567477);
#7387=VECTOR('',#60778,0.500358065674777);
#7388=VECTOR('',#60785,1.21403156673711);
#7389=VECTOR('',#60792,0.614031566737172);
#7390=VECTOR('',#60799,1.32880796357326);
#7391=VECTOR('',#60806,0.72880796357333);
#7392=VECTOR('',#60813,1.46111700181684);
#7393=VECTOR('',#60820,0.861117001816847);
#7394=VECTOR('',#60827,1.6204820426246);
#7395=VECTOR('',#60834,1.02048204262462);
#7396=VECTOR('',#60841,1.70100022308278);
#7397=VECTOR('',#60848,1.1010002230829);
#7398=VECTOR('',#60855,1.72127463204347);
#7399=VECTOR('',#60862,1.12127463204342);
#7400=VECTOR('',#60869,1.78199265440487);
#7401=VECTOR('',#60876,1.18199265440488);
#7402=VECTOR('',#60883,1.66088080992077);
#7403=VECTOR('',#60890,1.06088080992078);
#7404=VECTOR('',#60897,1.10035806567466);
#7405=VECTOR('',#60904,0.500358065674722);
#7406=VECTOR('',#60911,1.21403156673716);
#7407=VECTOR('',#60918,0.614031566737117);
#7408=VECTOR('',#60925,1.32880796357326);
#7409=VECTOR('',#60932,0.728807963573275);
#7410=VECTOR('',#60939,1.46111700181684);
#7411=VECTOR('',#60946,0.861117001816847);
#7412=VECTOR('',#60953,1.6204820426246);
#7413=VECTOR('',#60960,1.02048204262456);
#7414=VECTOR('',#60967,1.70100022308284);
#7415=VECTOR('',#60974,1.10100022308279);
#7416=VECTOR('',#60981,1.72127463204347);
#7417=VECTOR('',#60988,1.12127463204348);
#7418=VECTOR('',#60995,1.78199265440493);
#7419=VECTOR('',#61002,1.18199265440494);
#7420=VECTOR('',#61009,1.66088080992088);
#7421=VECTOR('',#61016,1.06088080992084);
#7422=VECTOR('',#61023,1.10035806567466);
#7423=VECTOR('',#61030,0.500358065674666);
#7424=VECTOR('',#61037,1.21403156673716);
#7425=VECTOR('',#61044,0.614031566737172);
#7426=VECTOR('',#61051,1.32880796357332);
#7427=VECTOR('',#61058,0.728807963573275);
#7428=VECTOR('',#61065,1.46111700181689);
#7429=VECTOR('',#61072,0.861117001816847);
#7430=VECTOR('',#61079,1.6204820426246);
#7431=VECTOR('',#61086,1.02048204262456);
#7432=VECTOR('',#61093,1.70100022308284);
#7433=VECTOR('',#61100,1.10100022308285);
#7434=VECTOR('',#61107,1.72127463204352);
#7435=VECTOR('',#61114,1.12127463204348);
#7436=VECTOR('',#61121,1.78199265440493);
#7437=VECTOR('',#61128,1.18199265440494);
#7438=VECTOR('',#61135,1.66088080992077);
#7439=VECTOR('',#61142,1.06088080992073);
#7440=VECTOR('',#61149,1.10035806567471);
#7441=VECTOR('',#61156,0.500358065674722);
#7442=VECTOR('',#61163,1.21403156673716);
#7443=VECTOR('',#61170,0.614031566737117);
#7444=VECTOR('',#61177,1.32880796357332);
#7445=VECTOR('',#61184,0.72880796357333);
#7446=VECTOR('',#61191,1.46111700181689);
#7447=VECTOR('',#61198,0.861117001816902);
#7448=VECTOR('',#61205,1.6204820426246);
#7449=VECTOR('',#61212,1.02048204262456);
#7450=VECTOR('',#61219,1.70100022308278);
#7451=VECTOR('',#61226,1.10100022308285);
#7452=VECTOR('',#61233,1.72127463204347);
#7453=VECTOR('',#61240,1.12127463204348);
#7454=VECTOR('',#61247,1.78199265440493);
#7455=VECTOR('',#61254,1.18199265440494);
#7456=VECTOR('',#61261,1.66088080992077);
#7457=VECTOR('',#61268,1.06088080992073);
#7458=VECTOR('',#61275,1.10035806567471);
#7459=VECTOR('',#61282,0.500358065674722);
#7460=VECTOR('',#61289,1.21403156673711);
#7461=VECTOR('',#61296,0.614031566737117);
#7462=VECTOR('',#61303,1.32880796357332);
#7463=VECTOR('',#61310,0.72880796357333);
#7464=VECTOR('',#61317,1.46111700181689);
#7465=VECTOR('',#61324,0.861117001816902);
#7466=VECTOR('',#61331,1.6204820426246);
#7467=VECTOR('',#61338,1.02048204262456);
#7468=VECTOR('',#61345,1.70100022308284);
#7469=VECTOR('',#61352,1.10100022308285);
#7470=VECTOR('',#61359,1.72127463204352);
#7471=VECTOR('',#61366,1.12127463204348);
#7472=VECTOR('',#61373,1.78199265440487);
#7473=VECTOR('',#61380,1.18199265440488);
#7474=VECTOR('',#61387,1.66088080992088);
#7475=VECTOR('',#61394,1.06088080992073);
#7476=VECTOR('',#61401,1.10035806567471);
#7477=VECTOR('',#61408,0.500358065674666);
#7478=VECTOR('',#61415,1.21403156673716);
#7479=VECTOR('',#61422,0.614031566737172);
#7480=VECTOR('',#61429,1.32880796357338);
#7481=VECTOR('',#61436,0.72880796357333);
#7482=VECTOR('',#61443,1.46111700181689);
#7483=VECTOR('',#61450,0.861117001816902);
#7484=VECTOR('',#61457,1.6204820426246);
#7485=VECTOR('',#61464,1.02048204262456);
#7486=VECTOR('',#61471,1.70100022308284);
#7487=VECTOR('',#61478,1.10100022308285);
#7488=VECTOR('',#61485,1.72127463204352);
#7489=VECTOR('',#61492,1.12127463204348);
#7490=VECTOR('',#61499,1.78199265440498);
#7491=VECTOR('',#61506,1.181992654405);
#7492=VECTOR('',#61513,1.66088080992077);
#7493=VECTOR('',#61520,1.06088080992073);
#7494=VECTOR('',#61527,1.10035806567471);
#7495=VECTOR('',#61534,0.500358065674722);
#7496=VECTOR('',#61541,1.21403156673705);
#7497=VECTOR('',#61548,0.614031566737117);
#7498=VECTOR('',#61555,1.32880796357338);
#7499=VECTOR('',#61562,0.72880796357333);
#7500=VECTOR('',#61569,1.46111700181689);
#7501=VECTOR('',#61576,0.861117001816902);
#7502=VECTOR('',#61583,1.6204820426246);
#7503=VECTOR('',#61590,1.02048204262462);
#7504=VECTOR('',#61597,1.70100022308278);
#7505=VECTOR('',#61604,1.10100022308279);
#7506=VECTOR('',#61611,1.72127463204352);
#7507=VECTOR('',#61618,1.12127463204348);
#7508=VECTOR('',#61625,1.78199265440493);
#7509=VECTOR('',#61632,1.18199265440494);
#7510=VECTOR('',#61639,1.66088080992077);
#7511=VECTOR('',#61646,1.06088080992078);
#7512=VECTOR('',#61653,1.10035806567471);
#7513=VECTOR('',#61660,0.500358065674722);
#7514=VECTOR('',#61667,1.21403156673711);
#7515=VECTOR('',#61674,0.614031566737117);
#7516=VECTOR('',#61681,1.32880796357332);
#7517=VECTOR('',#61688,0.72880796357333);
#7518=VECTOR('',#61695,1.46111700181689);
#7519=VECTOR('',#61702,0.861117001816902);
#7520=VECTOR('',#61709,1.62048204262455);
#7521=VECTOR('',#61716,1.02048204262462);
#7522=VECTOR('',#61723,1.70100022308278);
#7523=VECTOR('',#61730,1.10100022308279);
#7524=VECTOR('',#61737,1.72127463204347);
#7525=VECTOR('',#61744,1.12127463204353);
#7526=VECTOR('',#61751,1.78199265440487);
#7527=VECTOR('',#61758,1.18199265440494);
#7528=VECTOR('',#61765,1.66088080992077);
#7529=VECTOR('',#61772,1.06088080992078);
#7530=VECTOR('',#61779,1.10035806567471);
#7531=VECTOR('',#61786,0.500358065674777);
#7532=VECTOR('',#61793,1.21403156673711);
#7533=VECTOR('',#61800,0.614031566737117);
#7534=VECTOR('',#61807,1.32880796357332);
#7535=VECTOR('',#61814,0.728807963573275);
#7536=VECTOR('',#61821,1.46111700181695);
#7537=VECTOR('',#61828,0.861117001816902);
#7538=VECTOR('',#61835,1.6204820426246);
#7539=VECTOR('',#61842,1.02048204262462);
#7540=VECTOR('',#61849,1.70100022308284);
#7541=VECTOR('',#61856,1.10100022308285);
#7542=VECTOR('',#61863,1.72127463204347);
#7543=VECTOR('',#61870,1.12127463204348);
#7544=VECTOR('',#61877,1.78199265440493);
#7545=VECTOR('',#61884,1.18199265440488);
#7546=VECTOR('',#61891,1.66088080992077);
#7547=VECTOR('',#61898,1.06088080992078);
#7548=VECTOR('',#61905,1.10035806567471);
#7549=VECTOR('',#61912,0.500358065674722);
#7550=VECTOR('',#61919,1.21403156673711);
#7551=VECTOR('',#61926,0.614031566737117);
#7552=VECTOR('',#61933,1.32880796357332);
#7553=VECTOR('',#61940,0.72880796357333);
#7554=VECTOR('',#61947,1.46111700181689);
#7555=VECTOR('',#61954,0.861117001816902);
#7556=VECTOR('',#61961,1.62048204262455);
#7557=VECTOR('',#61968,1.02048204262456);
#7558=VECTOR('',#61975,1.70100022308284);
#7559=VECTOR('',#61982,1.10100022308285);
#7560=VECTOR('',#61989,1.72127463204347);
#7561=VECTOR('',#61996,1.12127463204348);
#7562=VECTOR('',#62003,1.78199265440493);
#7563=VECTOR('',#62010,1.18199265440494);
#7564=VECTOR('',#62017,1.66088080992077);
#7565=VECTOR('',#62024,1.06088080992078);
#7566=VECTOR('',#62031,1.10035806567471);
#7567=VECTOR('',#62038,0.500358065674722);
#7568=VECTOR('',#62045,1.21403156673711);
#7569=VECTOR('',#62052,0.614031566737117);
#7570=VECTOR('',#62059,1.32880796357326);
#7571=VECTOR('',#62066,0.728807963573275);
#7572=VECTOR('',#62073,1.46111700181689);
#7573=VECTOR('',#62080,0.861117001816902);
#7574=VECTOR('',#62087,1.6204820426246);
#7575=VECTOR('',#62094,1.02048204262456);
#7576=VECTOR('',#62101,1.70100022308284);
#7577=VECTOR('',#62108,1.10100022308285);
#7578=VECTOR('',#62115,1.72127463204352);
#7579=VECTOR('',#62122,1.12127463204348);
#7580=VECTOR('',#62129,1.78199265440498);
#7581=VECTOR('',#62136,1.18199265440494);
#7582=VECTOR('',#62143,1.66088080992083);
#7583=VECTOR('',#62150,1.06088080992078);
#7584=VECTOR('',#62157,1.10035806567471);
#7585=VECTOR('',#62164,0.500358065674722);
#7586=VECTOR('',#62171,1.21403156673711);
#7587=VECTOR('',#62178,0.614031566737117);
#7588=VECTOR('',#62185,1.32880796357332);
#7589=VECTOR('',#62192,0.72880796357333);
#7590=VECTOR('',#62199,1.46111700181689);
#7591=VECTOR('',#62206,0.861117001816847);
#7592=VECTOR('',#62213,1.6204820426246);
#7593=VECTOR('',#62220,1.02048204262462);
#7594=VECTOR('',#62227,1.70100022308284);
#7595=VECTOR('',#62234,1.10100022308279);
#7596=VECTOR('',#62241,1.72127463204347);
#7597=VECTOR('',#62248,1.12127463204353);
#7598=VECTOR('',#62255,1.78199265440493);
#7599=VECTOR('',#62262,1.18199265440494);
#7600=VECTOR('',#62269,1.66088080992077);
#7601=VECTOR('',#62276,1.06088080992078);
#7602=VECTOR('',#62283,1.10035806567471);
#7603=VECTOR('',#62290,0.500358065674722);
#7604=VECTOR('',#62297,1.21403156673711);
#7605=VECTOR('',#62304,0.614031566737117);
#7606=VECTOR('',#62311,1.32880796357332);
#7607=VECTOR('',#62318,0.72880796357333);
#7608=VECTOR('',#62325,1.46111700181689);
#7609=VECTOR('',#62332,0.861117001816902);
#7610=VECTOR('',#62339,1.6204820426246);
#7611=VECTOR('',#62346,1.02048204262462);
#7612=VECTOR('',#62353,1.70100022308284);
#7613=VECTOR('',#62360,1.10100022308285);
#7614=VECTOR('',#62367,1.72127463204347);
#7615=VECTOR('',#62374,1.12127463204348);
#7616=VECTOR('',#62381,1.78199265440493);
#7617=VECTOR('',#62388,1.18199265440494);
#7618=VECTOR('',#62395,1.66088080992077);
#7619=VECTOR('',#62402,1.06088080992078);
#7620=VECTOR('',#62409,1.10035806567471);
#7621=VECTOR('',#62416,0.500358065674666);
#7622=VECTOR('',#62423,1.21403156673716);
#7623=VECTOR('',#62430,0.614031566737117);
#7624=VECTOR('',#62437,1.32880796357332);
#7625=VECTOR('',#62444,0.72880796357333);
#7626=VECTOR('',#62451,1.46111700181689);
#7627=VECTOR('',#62458,0.861117001816902);
#7628=VECTOR('',#62465,1.6204820426246);
#7629=VECTOR('',#62472,1.02048204262462);
#7630=VECTOR('',#62479,1.70100022308284);
#7631=VECTOR('',#62486,1.10100022308285);
#7632=VECTOR('',#62493,1.72127463204352);
#7633=VECTOR('',#62500,1.12127463204353);
#7634=VECTOR('',#62507,1.78199265440493);
#7635=VECTOR('',#62514,1.18199265440494);
#7636=VECTOR('',#62521,1.66088080992077);
#7637=VECTOR('',#62528,1.06088080992078);
#7638=VECTOR('',#62535,1.10035806567471);
#7639=VECTOR('',#62542,0.500358065674666);
#7640=VECTOR('',#62549,1.21403156673716);
#7641=VECTOR('',#62556,0.614031566737172);
#7642=VECTOR('',#62563,1.32880796357326);
#7643=VECTOR('',#62570,0.728807963573275);
#7644=VECTOR('',#62577,1.46111700181689);
#7645=VECTOR('',#62584,0.861117001816847);
#7646=VECTOR('',#62591,1.62048204262455);
#7647=VECTOR('',#62598,1.02048204262462);
#7648=VECTOR('',#62605,1.70100022308284);
#7649=VECTOR('',#62612,1.10100022308279);
#7650=VECTOR('',#62619,1.72127463204352);
#7651=VECTOR('',#62626,1.12127463204348);
#7652=VECTOR('',#62633,1.78199265440493);
#7653=VECTOR('',#62640,1.18199265440494);
#7654=VECTOR('',#62647,1.66088080992083);
#7655=VECTOR('',#62654,1.06088080992078);
#7656=VECTOR('',#62661,1.10035806567471);
#7657=VECTOR('',#62668,0.500358065674722);
#7658=VECTOR('',#62675,1.21403156673716);
#7659=VECTOR('',#62682,0.614031566737172);
#7660=VECTOR('',#62689,1.32880796357326);
#7661=VECTOR('',#62696,0.72880796357333);
#7662=VECTOR('',#62703,1.46111700181689);
#7663=VECTOR('',#62710,0.861117001816902);
#7664=VECTOR('',#62717,1.6204820426246);
#7665=VECTOR('',#62724,1.02048204262456);
#7666=VECTOR('',#62731,1.70100022308278);
#7667=VECTOR('',#62738,1.10100022308279);
#7668=VECTOR('',#62745,1.72127463204347);
#7669=VECTOR('',#62752,1.12127463204348);
#7670=VECTOR('',#62759,1.78199265440493);
#7671=VECTOR('',#62766,1.18199265440494);
#7672=VECTOR('',#62773,1.66088080992077);
#7673=VECTOR('',#62780,1.06088080992084);
#7674=VECTOR('',#62787,1.10035806567471);
#7675=VECTOR('',#62794,0.500358065674722);
#7676=VECTOR('',#62801,1.21403156673716);
#7677=VECTOR('',#62808,0.614031566737117);
#7678=VECTOR('',#62815,1.32880796357338);
#7679=VECTOR('',#62822,0.728807963573386);
#7680=VECTOR('',#62829,1.46111700181695);
#7681=VECTOR('',#62836,0.861117001816902);
#7682=VECTOR('',#62843,1.6204820426246);
#7683=VECTOR('',#62850,1.02048204262456);
#7684=VECTOR('',#62857,1.70100022308284);
#7685=VECTOR('',#62864,1.10100022308279);
#7686=VECTOR('',#62871,1.72127463204352);
#7687=VECTOR('',#62878,1.12127463204348);
#7688=VECTOR('',#62885,1.78199265440493);
#7689=VECTOR('',#62892,1.18199265440494);
#7690=VECTOR('',#62899,1.66088080992083);
#7691=VECTOR('',#62906,1.06088080992078);
#7692=VECTOR('',#62913,1.10035806567466);
#7693=VECTOR('',#62920,0.500358065674666);
#7694=VECTOR('',#62927,1.21403156673716);
#7695=VECTOR('',#62934,0.614031566737172);
#7696=VECTOR('',#62941,1.32880796357326);
#7697=VECTOR('',#62948,0.728807963573275);
#7698=VECTOR('',#62955,1.46111700181689);
#7699=VECTOR('',#62962,0.861117001816847);
#7700=VECTOR('',#62969,1.6204820426246);
#7701=VECTOR('',#62976,1.02048204262456);
#7702=VECTOR('',#62983,1.70100022308284);
#7703=VECTOR('',#62990,1.10100022308285);
#7704=VECTOR('',#62997,1.72127463204352);
#7705=VECTOR('',#63004,1.12127463204348);
#7706=VECTOR('',#63011,1.78199265440498);
#7707=VECTOR('',#63018,1.18199265440494);
#7708=VECTOR('',#63025,1.66088080992077);
#7709=VECTOR('',#63032,1.06088080992078);
#7710=VECTOR('',#63039,1.10035806567471);
#7711=VECTOR('',#63046,0.500358065674666);
#7712=VECTOR('',#63053,1.21403156673716);
#7713=VECTOR('',#63060,0.614031566737117);
#7714=VECTOR('',#63067,1.32880796357332);
#7715=VECTOR('',#63074,0.72880796357333);
#7716=VECTOR('',#63081,1.46111700181689);
#7717=VECTOR('',#63088,0.861117001816902);
#7718=VECTOR('',#63095,1.62048204262455);
#7719=VECTOR('',#63102,1.02048204262456);
#7720=VECTOR('',#63109,1.70100022308278);
#7721=VECTOR('',#63116,1.10100022308285);
#7722=VECTOR('',#63123,1.72127463204347);
#7723=VECTOR('',#63130,1.12127463204348);
#7724=VECTOR('',#63137,1.78199265440493);
#7725=VECTOR('',#63144,1.18199265440488);
#7726=VECTOR('',#63151,1.66088080992083);
#7727=VECTOR('',#63158,1.06088080992078);
#7728=VECTOR('',#63165,1.10035806567471);
#7729=VECTOR('',#63172,0.500358065674666);
#7730=VECTOR('',#63179,1.21403156673716);
#7731=VECTOR('',#63186,0.614031566737117);
#7732=VECTOR('',#63193,1.32880796357332);
#7733=VECTOR('',#63200,0.72880796357333);
#7734=VECTOR('',#63207,1.46111700181689);
#7735=VECTOR('',#63214,0.861117001816902);
#7736=VECTOR('',#63221,1.6204820426246);
#7737=VECTOR('',#63228,1.02048204262462);
#7738=VECTOR('',#63235,1.70100022308284);
#7739=VECTOR('',#63242,1.10100022308285);
#7740=VECTOR('',#63249,1.72127463204352);
#7741=VECTOR('',#63256,1.12127463204353);
#7742=VECTOR('',#63263,1.78199265440493);
#7743=VECTOR('',#63270,1.18199265440488);
#7744=VECTOR('',#63277,1.66088080992077);
#7745=VECTOR('',#63284,1.06088080992078);
#7746=VECTOR('',#63291,1.10035806567477);
#7747=VECTOR('',#63298,0.500358065674722);
#7748=VECTOR('',#63305,1.21403156673711);
#7749=VECTOR('',#63312,0.614031566737061);
#7750=VECTOR('',#63319,1.32880796357332);
#7751=VECTOR('',#63326,0.728807963573275);
#7752=VECTOR('',#63333,1.46111700181684);
#7753=VECTOR('',#63340,0.861117001816847);
#7754=VECTOR('',#63347,1.6204820426246);
#7755=VECTOR('',#63354,1.02048204262456);
#7756=VECTOR('',#63361,1.70100022308278);
#7757=VECTOR('',#63368,1.10100022308279);
#7758=VECTOR('',#63375,1.72127463204352);
#7759=VECTOR('',#63382,1.12127463204353);
#7760=VECTOR('',#63389,1.78199265440493);
#7761=VECTOR('',#63396,1.18199265440494);
#7762=VECTOR('',#63403,1.66088080992077);
#7763=VECTOR('',#63410,1.06088080992073);
#7764=VECTOR('',#63417,1.10035806567471);
#7765=VECTOR('',#63424,0.500358065674722);
#7766=VECTOR('',#63431,1.21403156673711);
#7767=VECTOR('',#63438,0.614031566737117);
#7768=VECTOR('',#63445,1.32880796357332);
#7769=VECTOR('',#63452,0.728807963573275);
#7770=VECTOR('',#63459,1.46111700181684);
#7771=VECTOR('',#63466,0.861117001816902);
#7772=VECTOR('',#63473,1.6204820426246);
#7773=VECTOR('',#63480,1.02048204262462);
#7774=VECTOR('',#63487,1.70100022308289);
#7775=VECTOR('',#63494,1.10100022308285);
#7776=VECTOR('',#63501,1.72127463204347);
#7777=VECTOR('',#63508,1.12127463204342);
#7778=VECTOR('',#63515,1.78199265440498);
#7779=VECTOR('',#63522,1.18199265440494);
#7780=VECTOR('',#63529,1.66088080992077);
#7781=VECTOR('',#63536,1.06088080992078);
#7782=VECTOR('',#63543,1.10035806567471);
#7783=VECTOR('',#63550,0.500358065674666);
#7784=VECTOR('',#63557,1.21403156673711);
#7785=VECTOR('',#63564,0.614031566737117);
#7786=VECTOR('',#63571,1.32880796357332);
#7787=VECTOR('',#63578,0.72880796357333);
#7788=VECTOR('',#63585,1.46111700181684);
#7789=VECTOR('',#63592,0.861117001816847);
#7790=VECTOR('',#63599,1.6204820426246);
#7791=VECTOR('',#63606,1.02048204262456);
#7792=VECTOR('',#63613,1.70100022308284);
#7793=VECTOR('',#63620,1.10100022308285);
#7794=VECTOR('',#63627,1.72127463204347);
#7795=VECTOR('',#63634,1.12127463204353);
#7796=VECTOR('',#63641,1.78199265440498);
#7797=VECTOR('',#63648,1.18199265440494);
#7798=VECTOR('',#63655,1.66088080992083);
#7799=VECTOR('',#63662,1.06088080992078);
#7800=VECTOR('',#63669,1.10035806567477);
#7801=VECTOR('',#63676,0.500358065674777);
#7802=VECTOR('',#63683,1.21403156673705);
#7803=VECTOR('',#63690,0.614031566737117);
#7804=VECTOR('',#63697,1.32880796357326);
#7805=VECTOR('',#63704,0.728807963573275);
#7806=VECTOR('',#63711,1.46111700181684);
#7807=VECTOR('',#63718,0.861117001816847);
#7808=VECTOR('',#63725,1.6204820426246);
#7809=VECTOR('',#63732,1.02048204262462);
#7810=VECTOR('',#63739,1.70100022308278);
#7811=VECTOR('',#63746,1.10100022308285);
#7812=VECTOR('',#63753,1.72127463204347);
#7813=VECTOR('',#63760,1.12127463204353);
#7814=VECTOR('',#63767,1.78199265440493);
#7815=VECTOR('',#63774,1.18199265440494);
#7816=VECTOR('',#63781,1.66088080992077);
#7817=VECTOR('',#63788,1.06088080992078);
#7818=VECTOR('',#63795,1.10035806567471);
#7819=VECTOR('',#63802,0.500358065674722);
#7820=VECTOR('',#63809,1.21403156673716);
#7821=VECTOR('',#63816,0.614031566737117);
#7822=VECTOR('',#63823,1.32880796357332);
#7823=VECTOR('',#63830,0.72880796357333);
#7824=VECTOR('',#63837,1.46111700181689);
#7825=VECTOR('',#63844,0.861117001816902);
#7826=VECTOR('',#63851,1.6204820426246);
#7827=VECTOR('',#63858,1.02048204262462);
#7828=VECTOR('',#63865,1.70100022308284);
#7829=VECTOR('',#63872,1.10100022308285);
#7830=VECTOR('',#63879,1.72127463204352);
#7831=VECTOR('',#63886,1.12127463204348);
#7832=VECTOR('',#63893,1.78199265440493);
#7833=VECTOR('',#63900,1.18199265440488);
#7834=VECTOR('',#63907,1.66088080992088);
#7835=VECTOR('',#63914,1.06088080992084);
#7836=VECTOR('',#63921,1.10035806567471);
#7837=VECTOR('',#63928,0.500358065674722);
#7838=VECTOR('',#63935,1.21403156673716);
#7839=VECTOR('',#63942,0.614031566737117);
#7840=VECTOR('',#63949,1.32880796357332);
#7841=VECTOR('',#63956,0.72880796357333);
#7842=VECTOR('',#63963,1.46111700181689);
#7843=VECTOR('',#63970,0.861117001816902);
#7844=VECTOR('',#63977,1.6204820426246);
#7845=VECTOR('',#63984,1.02048204262462);
#7846=VECTOR('',#63991,1.70100022308284);
#7847=VECTOR('',#63998,1.10100022308285);
#7848=VECTOR('',#64005,1.72127463204352);
#7849=VECTOR('',#64012,1.12127463204348);
#7850=VECTOR('',#64019,1.78199265440493);
#7851=VECTOR('',#64026,1.18199265440494);
#7852=VECTOR('',#64033,1.66088080992077);
#7853=VECTOR('',#64040,1.06088080992078);
#7854=VECTOR('',#64053,127.41606204049);
#7855=VECTOR('',#64076,12.3670707361132);
#7856=VECTOR('',#64107,18.5103550292801);
#7857=VECTOR('',#64120,130.);
#7858=VECTOR('',#64123,0.878303132193281);
#7859=VECTOR('',#64128,1.47830313219333);
#7860=CYLINDRICAL_SURFACE('',#45561,11.5);
#7861=CYLINDRICAL_SURFACE('',#45563,11.5);
#7862=CYLINDRICAL_SURFACE('',#45564,11.5);
#7863=CYLINDRICAL_SURFACE('',#45573,8.3031389659941);
#7864=CYLINDRICAL_SURFACE('',#45576,8.3031389659941);
#7865=CYLINDRICAL_SURFACE('',#45583,8.3031389659941);
#7866=CYLINDRICAL_SURFACE('',#45584,0.500000000000054);
#7867=CYLINDRICAL_SURFACE('',#45587,1.81285717707168);
#7868=CYLINDRICAL_SURFACE('',#45590,0.500000000000054);
#7869=CYLINDRICAL_SURFACE('',#45593,1.81285717707167);
#7870=CYLINDRICAL_SURFACE('',#45596,0.500000000000054);
#7871=CYLINDRICAL_SURFACE('',#45599,1.81285717707166);
#7872=CYLINDRICAL_SURFACE('',#45602,0.499999999999939);
#7873=CYLINDRICAL_SURFACE('',#45605,1.81285717707156);
#7874=CYLINDRICAL_SURFACE('',#45608,0.499999999999935);
#7875=CYLINDRICAL_SURFACE('',#45611,1.81285717707156);
#7876=CYLINDRICAL_SURFACE('',#45614,0.499999999999944);
#7877=CYLINDRICAL_SURFACE('',#45617,1.81285717707167);
#7878=CYLINDRICAL_SURFACE('',#45620,0.948084450180161);
#7879=CYLINDRICAL_SURFACE('',#45621,0.500000000000054);
#7880=CYLINDRICAL_SURFACE('',#45623,1.02140828085145);
#7881=CYLINDRICAL_SURFACE('',#45624,0.500000000000054);
#7882=CYLINDRICAL_SURFACE('',#45626,0.948084450180157);
#7883=CYLINDRICAL_SURFACE('',#45627,0.500000000000054);
#7884=CYLINDRICAL_SURFACE('',#45629,1.02140828085145);
#7885=CYLINDRICAL_SURFACE('',#45630,0.500000000000054);
#7886=CYLINDRICAL_SURFACE('',#45632,0.948084450180157);
#7887=CYLINDRICAL_SURFACE('',#45633,0.500000000000054);
#7888=CYLINDRICAL_SURFACE('',#45635,1.02140828085145);
#7889=CYLINDRICAL_SURFACE('',#45636,0.499999999999944);
#7890=CYLINDRICAL_SURFACE('',#45638,0.948084450180161);
#7891=CYLINDRICAL_SURFACE('',#45639,0.499999999999944);
#7892=CYLINDRICAL_SURFACE('',#45641,1.02140828085144);
#7893=CYLINDRICAL_SURFACE('',#45642,0.500000000000058);
#7894=CYLINDRICAL_SURFACE('',#45644,0.948084450180161);
#7895=CYLINDRICAL_SURFACE('',#45645,0.500000000000058);
#7896=CYLINDRICAL_SURFACE('',#45647,1.02140828085145);
#7897=CYLINDRICAL_SURFACE('',#45648,0.500000000000058);
#7898=CYLINDRICAL_SURFACE('',#45650,0.948084450180161);
#7899=CYLINDRICAL_SURFACE('',#45651,0.500000000000172);
#7900=CYLINDRICAL_SURFACE('',#45653,1.02140828085157);
#7901=CYLINDRICAL_SURFACE('',#45654,0.499999999999935);
#7902=CYLINDRICAL_SURFACE('',#45656,0.948084450180161);
#7903=CYLINDRICAL_SURFACE('',#45657,0.500000000000058);
#7904=CYLINDRICAL_SURFACE('',#45659,1.02140828085134);
#7905=CYLINDRICAL_SURFACE('',#45660,0.499999999999935);
#7906=CYLINDRICAL_SURFACE('',#45662,0.948084450180275);
#7907=CYLINDRICAL_SURFACE('',#45663,0.500000000000058);
#7908=CYLINDRICAL_SURFACE('',#45665,1.02140828085134);
#7909=CYLINDRICAL_SURFACE('',#45666,0.500000000000058);
#7910=CYLINDRICAL_SURFACE('',#45668,0.948084450180152);
#7911=CYLINDRICAL_SURFACE('',#45669,0.499999999999944);
#7912=CYLINDRICAL_SURFACE('',#45671,1.02140828085157);
#7913=CYLINDRICAL_SURFACE('',#45672,0.500000000000067);
#7914=CYLINDRICAL_SURFACE('',#45674,0.948084450180047);
#7915=CYLINDRICAL_SURFACE('',#45675,0.499999999999935);
#7916=CYLINDRICAL_SURFACE('',#45677,1.02140828085145);
#7917=CYLINDRICAL_SURFACE('',#45678,0.499999999999935);
#7918=CYLINDRICAL_SURFACE('',#45680,0.94808445018017);
#7919=CYLINDRICAL_SURFACE('',#45681,0.500000000000058);
#7920=CYLINDRICAL_SURFACE('',#45683,1.02140828085121);
#7921=CYLINDRICAL_SURFACE('',#45684,0.499999999999944);
#7922=CYLINDRICAL_SURFACE('',#45686,0.948084450180161);
#7923=CYLINDRICAL_SURFACE('',#45687,0.499999999999944);
#7924=CYLINDRICAL_SURFACE('',#45689,1.02140828085145);
#7925=CYLINDRICAL_SURFACE('',#45690,0.499999999999939);
#7926=CYLINDRICAL_SURFACE('',#45692,0.948084450180161);
#7927=CYLINDRICAL_SURFACE('',#45693,0.500000000000167);
#7928=CYLINDRICAL_SURFACE('',#45695,1.02140828085134);
#7929=CYLINDRICAL_SURFACE('',#45696,0.499999999999944);
#7930=CYLINDRICAL_SURFACE('',#45698,0.948084450180275);
#7931=CYLINDRICAL_SURFACE('',#45699,0.500000000000054);
#7932=CYLINDRICAL_SURFACE('',#45701,1.02140828085134);
#7933=CYLINDRICAL_SURFACE('',#45702,0.499999999999939);
#7934=CYLINDRICAL_SURFACE('',#45704,0.948084450180161);
#7935=CYLINDRICAL_SURFACE('',#45705,0.500000000000054);
#7936=CYLINDRICAL_SURFACE('',#45707,1.02140828085145);
#7937=CYLINDRICAL_SURFACE('',#45708,0.500000000000054);
#7938=CYLINDRICAL_SURFACE('',#45710,0.948084450180157);
#7939=CYLINDRICAL_SURFACE('',#45711,0.500000000000049);
#7940=CYLINDRICAL_SURFACE('',#45713,1.02140828085145);
#7941=CYLINDRICAL_SURFACE('',#45714,0.500000000000054);
#7942=CYLINDRICAL_SURFACE('',#45716,0.948084450180157);
#7943=CYLINDRICAL_SURFACE('',#45717,0.500000000000054);
#7944=CYLINDRICAL_SURFACE('',#45719,1.02140828085134);
#7945=CYLINDRICAL_SURFACE('',#45720,0.500000000000049);
#7946=CYLINDRICAL_SURFACE('',#45722,0.948084450180157);
#7947=CYLINDRICAL_SURFACE('',#45723,0.500000000000049);
#7948=CYLINDRICAL_SURFACE('',#45725,1.02140828085145);
#7949=CYLINDRICAL_SURFACE('',#45726,0.500000000000058);
#7950=CYLINDRICAL_SURFACE('',#45728,0.948084450180161);
#7951=CYLINDRICAL_SURFACE('',#45729,0.499999999999944);
#7952=CYLINDRICAL_SURFACE('',#45731,1.02140828085133);
#7953=CYLINDRICAL_SURFACE('',#45732,0.499999999999935);
#7954=CYLINDRICAL_SURFACE('',#45734,0.948084450180047);
#7955=CYLINDRICAL_SURFACE('',#45735,0.499999999999944);
#7956=CYLINDRICAL_SURFACE('',#45737,1.54967110260237);
#7957=CYLINDRICAL_SURFACE('',#45739,0.499999999999939);
#7958=CYLINDRICAL_SURFACE('',#45742,1.25936103546568);
#7959=CYLINDRICAL_SURFACE('',#45744,0.500000000000049);
#7960=CYLINDRICAL_SURFACE('',#45747,1.02140828085145);
#7961=CYLINDRICAL_SURFACE('',#45748,0.499999999999939);
#7962=CYLINDRICAL_SURFACE('',#45750,0.948084450179933);
#7963=CYLINDRICAL_SURFACE('',#45751,0.499999999999939);
#7964=CYLINDRICAL_SURFACE('',#45753,1.54967110260249);
#7965=CYLINDRICAL_SURFACE('',#45755,0.499999999999944);
#7966=CYLINDRICAL_SURFACE('',#45758,1.25936103546569);
#7967=CYLINDRICAL_SURFACE('',#45760,0.500000000000058);
#7968=CYLINDRICAL_SURFACE('',#45763,1.02140828085145);
#7969=CYLINDRICAL_SURFACE('',#45764,0.500000000000058);
#7970=CYLINDRICAL_SURFACE('',#45766,0.948084450180166);
#7971=CYLINDRICAL_SURFACE('',#45767,0.500000000000054);
#7972=CYLINDRICAL_SURFACE('',#45769,1.25936103546568);
#7973=CYLINDRICAL_SURFACE('',#45771,0.500000000000054);
#7974=CYLINDRICAL_SURFACE('',#45774,1.02140828085145);
#7975=CYLINDRICAL_SURFACE('',#45775,0.500000000000058);
#7976=CYLINDRICAL_SURFACE('',#45777,0.948084450180275);
#7977=CYLINDRICAL_SURFACE('',#45778,0.500000000000058);
#7978=CYLINDRICAL_SURFACE('',#45780,1.25936103546568);
#7979=CYLINDRICAL_SURFACE('',#45782,0.499999999999939);
#7980=CYLINDRICAL_SURFACE('',#45785,1.02140828085145);
#7981=CYLINDRICAL_SURFACE('',#45786,0.500000000000058);
#7982=CYLINDRICAL_SURFACE('',#45788,0.948084450180161);
#7983=CYLINDRICAL_SURFACE('',#45789,0.499999999999939);
#7984=CYLINDRICAL_SURFACE('',#45791,1.02140828085133);
#7985=CYLINDRICAL_SURFACE('',#45792,0.499999999999944);
#7986=CYLINDRICAL_SURFACE('',#45794,0.948084450180166);
#7987=CYLINDRICAL_SURFACE('',#45795,0.499999999999944);
#7988=CYLINDRICAL_SURFACE('',#45797,1.02140828085146);
#7989=CYLINDRICAL_SURFACE('',#45798,0.500000000000058);
#7990=CYLINDRICAL_SURFACE('',#45800,0.948084450180161);
#7991=CYLINDRICAL_SURFACE('',#45801,0.500000000000054);
#7992=CYLINDRICAL_SURFACE('',#45803,1.02140828085144);
#7993=CYLINDRICAL_SURFACE('',#45804,0.499999999999944);
#7994=CYLINDRICAL_SURFACE('',#45806,0.948084450180157);
#7995=CYLINDRICAL_SURFACE('',#45807,0.500000000000063);
#7996=CYLINDRICAL_SURFACE('',#45809,1.02140828085156);
#7997=CYLINDRICAL_SURFACE('',#45810,0.499999999999939);
#7998=CYLINDRICAL_SURFACE('',#45812,0.948084450180161);
#7999=CYLINDRICAL_SURFACE('',#45813,0.500000000000054);
#8000=CYLINDRICAL_SURFACE('',#45815,1.02140828085134);
#8001=CYLINDRICAL_SURFACE('',#45816,0.500000000000054);
#8002=CYLINDRICAL_SURFACE('',#45818,0.948084450180157);
#8003=CYLINDRICAL_SURFACE('',#45819,0.499999999999939);
#8004=CYLINDRICAL_SURFACE('',#45821,0.948084450180161);
#8005=CYLINDRICAL_SURFACE('',#45822,0.500000000000054);
#8006=CYLINDRICAL_SURFACE('',#45824,1.02140828085134);
#8007=CYLINDRICAL_SURFACE('',#45825,0.499999999999944);
#8008=CYLINDRICAL_SURFACE('',#45827,1.0588834746273);
#8009=CYLINDRICAL_SURFACE('',#45830,0.500000000000054);
#8010=CYLINDRICAL_SURFACE('',#45833,1.29583333162394);
#8011=CYLINDRICAL_SURFACE('',#45836,0.500000000000054);
#8012=CYLINDRICAL_SURFACE('',#45839,1.60653900437062);
#8013=CYLINDRICAL_SURFACE('',#45842,0.500000000000054);
#8014=CYLINDRICAL_SURFACE('',#45845,1.82809807486272);
#8015=CYLINDRICAL_SURFACE('',#45848,0.499999999999944);
#8016=CYLINDRICAL_SURFACE('',#45851,1.85841829658605);
#8017=CYLINDRICAL_SURFACE('',#45854,0.500000000000054);
#8018=CYLINDRICAL_SURFACE('',#45857,1.81285717707166);
#8019=CYLINDRICAL_SURFACE('',#45860,0.500000000000054);
#8020=CYLINDRICAL_SURFACE('',#45863,1.91146602029503);
#8021=CYLINDRICAL_SURFACE('',#45866,0.500000000000054);
#8022=CYLINDRICAL_SURFACE('',#45869,1.54967110260249);
#8023=CYLINDRICAL_SURFACE('',#45872,0.499999999999944);
#8024=CYLINDRICAL_SURFACE('',#45875,1.25936103546568);
#8025=CYLINDRICAL_SURFACE('',#45878,0.500000000000054);
#8026=CYLINDRICAL_SURFACE('',#45881,1.0588834746273);
#8027=CYLINDRICAL_SURFACE('',#45884,0.500000000000054);
#8028=CYLINDRICAL_SURFACE('',#45887,1.29583333162394);
#8029=CYLINDRICAL_SURFACE('',#45890,0.499999999999944);
#8030=CYLINDRICAL_SURFACE('',#45893,1.60653900437062);
#8031=CYLINDRICAL_SURFACE('',#45896,0.500000000000054);
#8032=CYLINDRICAL_SURFACE('',#45899,1.82809807486272);
#8033=CYLINDRICAL_SURFACE('',#45902,0.499999999999944);
#8034=CYLINDRICAL_SURFACE('',#45905,1.85841829658605);
#8035=CYLINDRICAL_SURFACE('',#45908,0.499999999999944);
#8036=CYLINDRICAL_SURFACE('',#45911,1.81285717707166);
#8037=CYLINDRICAL_SURFACE('',#45914,0.499999999999944);
#8038=CYLINDRICAL_SURFACE('',#45917,1.91146602029502);
#8039=CYLINDRICAL_SURFACE('',#45920,0.500000000000054);
#8040=CYLINDRICAL_SURFACE('',#45923,1.54967110260249);
#8041=CYLINDRICAL_SURFACE('',#45926,0.499999999999944);
#8042=CYLINDRICAL_SURFACE('',#45929,1.25936103546569);
#8043=CYLINDRICAL_SURFACE('',#45932,0.500000000000054);
#8044=CYLINDRICAL_SURFACE('',#45935,1.0588834746273);
#8045=CYLINDRICAL_SURFACE('',#45938,0.499999999999935);
#8046=CYLINDRICAL_SURFACE('',#45941,1.29583333162394);
#8047=CYLINDRICAL_SURFACE('',#45944,0.500000000000054);
#8048=CYLINDRICAL_SURFACE('',#45947,1.60653900437051);
#8049=CYLINDRICAL_SURFACE('',#45950,0.499999999999935);
#8050=CYLINDRICAL_SURFACE('',#45953,1.82809807486262);
#8051=CYLINDRICAL_SURFACE('',#45956,0.500000000000049);
#8052=CYLINDRICAL_SURFACE('',#45959,1.85841829658605);
#8053=CYLINDRICAL_SURFACE('',#45962,0.500000000000054);
#8054=CYLINDRICAL_SURFACE('',#45965,1.91146602029503);
#8055=CYLINDRICAL_SURFACE('',#45968,0.500000000000049);
#8056=CYLINDRICAL_SURFACE('',#45971,1.54967110260249);
#8057=CYLINDRICAL_SURFACE('',#45974,0.500000000000058);
#8058=CYLINDRICAL_SURFACE('',#45977,1.25936103546568);
#8059=CYLINDRICAL_SURFACE('',#45980,0.500000000000049);
#8060=CYLINDRICAL_SURFACE('',#45983,1.05888347462729);
#8061=CYLINDRICAL_SURFACE('',#45986,0.500000000000049);
#8062=CYLINDRICAL_SURFACE('',#45989,1.29583333162383);
#8063=CYLINDRICAL_SURFACE('',#45992,0.499999999999826);
#8064=CYLINDRICAL_SURFACE('',#45995,1.60653900437051);
#8065=CYLINDRICAL_SURFACE('',#45998,0.500000000000054);
#8066=CYLINDRICAL_SURFACE('',#46001,1.82809807486273);
#8067=CYLINDRICAL_SURFACE('',#46004,0.500000000000049);
#8068=CYLINDRICAL_SURFACE('',#46007,1.85841829658605);
#8069=CYLINDRICAL_SURFACE('',#46010,0.500000000000049);
#8070=CYLINDRICAL_SURFACE('',#46013,1.81285717707167);
#8071=CYLINDRICAL_SURFACE('',#46016,0.499999999999944);
#8072=CYLINDRICAL_SURFACE('',#46019,1.91146602029503);
#8073=CYLINDRICAL_SURFACE('',#46022,0.500000000000058);
#8074=CYLINDRICAL_SURFACE('',#46025,1.5496711026026);
#8075=CYLINDRICAL_SURFACE('',#46028,0.500000000000058);
#8076=CYLINDRICAL_SURFACE('',#46031,1.25936103546569);
#8077=CYLINDRICAL_SURFACE('',#46034,0.500000000000049);
#8078=CYLINDRICAL_SURFACE('',#46037,1.05888347462741);
#8079=CYLINDRICAL_SURFACE('',#46040,0.500000000000054);
#8080=CYLINDRICAL_SURFACE('',#46043,1.29583333162417);
#8081=CYLINDRICAL_SURFACE('',#46046,0.500000000000177);
#8082=CYLINDRICAL_SURFACE('',#46049,1.60653900437062);
#8083=CYLINDRICAL_SURFACE('',#46052,0.500000000000063);
#8084=CYLINDRICAL_SURFACE('',#46055,1.82809807486272);
#8085=CYLINDRICAL_SURFACE('',#46058,0.500000000000054);
#8086=CYLINDRICAL_SURFACE('',#46061,1.85841829658605);
#8087=CYLINDRICAL_SURFACE('',#46064,0.499999999999935);
#8088=CYLINDRICAL_SURFACE('',#46067,1.81285717707167);
#8089=CYLINDRICAL_SURFACE('',#46070,0.499999999999944);
#8090=CYLINDRICAL_SURFACE('',#46073,1.91146602029502);
#8091=CYLINDRICAL_SURFACE('',#46076,0.499999999999935);
#8092=CYLINDRICAL_SURFACE('',#46079,1.54967110260249);
#8093=CYLINDRICAL_SURFACE('',#46082,0.499999999999935);
#8094=CYLINDRICAL_SURFACE('',#46085,1.25936103546568);
#8095=CYLINDRICAL_SURFACE('',#46088,0.500000000000058);
#8096=CYLINDRICAL_SURFACE('',#46091,1.05888347462741);
#8097=CYLINDRICAL_SURFACE('',#46094,0.500000000000054);
#8098=CYLINDRICAL_SURFACE('',#46097,1.29583333162394);
#8099=CYLINDRICAL_SURFACE('',#46100,0.499999999999939);
#8100=CYLINDRICAL_SURFACE('',#46103,1.60653900437051);
#8101=CYLINDRICAL_SURFACE('',#46106,0.499999999999939);
#8102=CYLINDRICAL_SURFACE('',#46109,1.82809807486272);
#8103=CYLINDRICAL_SURFACE('',#46112,0.499999999999935);
#8104=CYLINDRICAL_SURFACE('',#46115,1.85841829658605);
#8105=CYLINDRICAL_SURFACE('',#46118,0.500000000000049);
#8106=CYLINDRICAL_SURFACE('',#46121,1.81285717707144);
#8107=CYLINDRICAL_SURFACE('',#46124,0.499999999999821);
#8108=CYLINDRICAL_SURFACE('',#46127,1.9114660202949);
#8109=CYLINDRICAL_SURFACE('',#46130,0.499999999999935);
#8110=CYLINDRICAL_SURFACE('',#46133,1.54967110260237);
#8111=CYLINDRICAL_SURFACE('',#46136,0.500000000000049);
#8112=CYLINDRICAL_SURFACE('',#46139,1.25936103546556);
#8113=CYLINDRICAL_SURFACE('',#46142,0.499999999999821);
#8114=CYLINDRICAL_SURFACE('',#46145,1.0588834746273);
#8115=CYLINDRICAL_SURFACE('',#46148,0.500000000000058);
#8116=CYLINDRICAL_SURFACE('',#46151,1.29583333162394);
#8117=CYLINDRICAL_SURFACE('',#46154,0.500000000000058);
#8118=CYLINDRICAL_SURFACE('',#46157,1.60653900437062);
#8119=CYLINDRICAL_SURFACE('',#46160,0.499999999999944);
#8120=CYLINDRICAL_SURFACE('',#46163,1.82809807486284);
#8121=CYLINDRICAL_SURFACE('',#46166,0.500000000000172);
#8122=CYLINDRICAL_SURFACE('',#46169,1.85841829658605);
#8123=CYLINDRICAL_SURFACE('',#46172,0.500000000000058);
#8124=CYLINDRICAL_SURFACE('',#46175,1.81285717707155);
#8125=CYLINDRICAL_SURFACE('',#46178,0.500000000000058);
#8126=CYLINDRICAL_SURFACE('',#46181,1.91146602029503);
#8127=CYLINDRICAL_SURFACE('',#46184,0.499999999999944);
#8128=CYLINDRICAL_SURFACE('',#46187,1.5496711026025);
#8129=CYLINDRICAL_SURFACE('',#46190,0.499999999999944);
#8130=CYLINDRICAL_SURFACE('',#46193,1.2593610354658);
#8131=CYLINDRICAL_SURFACE('',#46196,0.500000000000172);
#8132=CYLINDRICAL_SURFACE('',#46199,1.0588834746273);
#8133=CYLINDRICAL_SURFACE('',#46202,0.499999999999939);
#8134=CYLINDRICAL_SURFACE('',#46205,1.29583333162394);
#8135=CYLINDRICAL_SURFACE('',#46208,0.499999999999944);
#8136=CYLINDRICAL_SURFACE('',#46211,1.60653900437051);
#8137=CYLINDRICAL_SURFACE('',#46214,0.499999999999944);
#8138=CYLINDRICAL_SURFACE('',#46217,1.82809807486261);
#8139=CYLINDRICAL_SURFACE('',#46220,0.499999999999939);
#8140=CYLINDRICAL_SURFACE('',#46223,1.85841829658593);
#8141=CYLINDRICAL_SURFACE('',#46226,0.499999999999939);
#8142=CYLINDRICAL_SURFACE('',#46229,1.91146602029514);
#8143=CYLINDRICAL_SURFACE('',#46232,0.500000000000058);
#8144=CYLINDRICAL_SURFACE('',#46235,1.54967110260249);
#8145=CYLINDRICAL_SURFACE('',#46238,0.499999999999935);
#8146=CYLINDRICAL_SURFACE('',#46241,1.25936103546568);
#8147=CYLINDRICAL_SURFACE('',#46244,0.499999999999944);
#8148=CYLINDRICAL_SURFACE('',#46247,1.05888347462741);
#8149=CYLINDRICAL_SURFACE('',#46250,0.500000000000058);
#8150=CYLINDRICAL_SURFACE('',#46253,1.29583333162394);
#8151=CYLINDRICAL_SURFACE('',#46256,0.499999999999939);
#8152=CYLINDRICAL_SURFACE('',#46259,1.60653900437051);
#8153=CYLINDRICAL_SURFACE('',#46262,0.500000000000058);
#8154=CYLINDRICAL_SURFACE('',#46265,1.82809807486273);
#8155=CYLINDRICAL_SURFACE('',#46268,0.500000000000058);
#8156=CYLINDRICAL_SURFACE('',#46271,1.85841829658593);
#8157=CYLINDRICAL_SURFACE('',#46274,0.500000000000058);
#8158=CYLINDRICAL_SURFACE('',#46277,1.81285717707167);
#8159=CYLINDRICAL_SURFACE('',#46280,0.500000000000058);
#8160=CYLINDRICAL_SURFACE('',#46283,1.91146602029491);
#8161=CYLINDRICAL_SURFACE('',#46286,0.499999999999944);
#8162=CYLINDRICAL_SURFACE('',#46289,1.54967110260237);
#8163=CYLINDRICAL_SURFACE('',#46292,0.499999999999935);
#8164=CYLINDRICAL_SURFACE('',#46295,1.25936103546569);
#8165=CYLINDRICAL_SURFACE('',#46298,0.500000000000058);
#8166=CYLINDRICAL_SURFACE('',#46301,1.05888347462741);
#8167=CYLINDRICAL_SURFACE('',#46304,0.500000000000054);
#8168=CYLINDRICAL_SURFACE('',#46307,1.29583333162383);
#8169=CYLINDRICAL_SURFACE('',#46310,0.500000000000054);
#8170=CYLINDRICAL_SURFACE('',#46313,1.60653900437062);
#8171=CYLINDRICAL_SURFACE('',#46316,0.499999999999935);
#8172=CYLINDRICAL_SURFACE('',#46319,1.82809807486272);
#8173=CYLINDRICAL_SURFACE('',#46322,0.499999999999935);
#8174=CYLINDRICAL_SURFACE('',#46325,1.85841829658616);
#8175=CYLINDRICAL_SURFACE('',#46328,0.500000000000054);
#8176=CYLINDRICAL_SURFACE('',#46331,1.81285717707168);
#8177=CYLINDRICAL_SURFACE('',#46334,0.500000000000054);
#8178=CYLINDRICAL_SURFACE('',#46337,1.91146602029514);
#8179=CYLINDRICAL_SURFACE('',#46340,0.500000000000054);
#8180=CYLINDRICAL_SURFACE('',#46343,1.5496711026025);
#8181=CYLINDRICAL_SURFACE('',#46346,0.500000000000049);
#8182=CYLINDRICAL_SURFACE('',#46349,1.25936103546568);
#8183=CYLINDRICAL_SURFACE('',#46352,0.500000000000049);
#8184=CYLINDRICAL_SURFACE('',#46355,1.05888347462729);
#8185=CYLINDRICAL_SURFACE('',#46358,0.500000000000058);
#8186=CYLINDRICAL_SURFACE('',#46361,1.29583333162394);
#8187=CYLINDRICAL_SURFACE('',#46364,0.499999999999939);
#8188=CYLINDRICAL_SURFACE('',#46367,1.60653900437051);
#8189=CYLINDRICAL_SURFACE('',#46370,0.499999999999939);
#8190=CYLINDRICAL_SURFACE('',#46373,1.82809807486273);
#8191=CYLINDRICAL_SURFACE('',#46376,0.499999999999939);
#8192=CYLINDRICAL_SURFACE('',#46379,1.85841829658616);
#8193=CYLINDRICAL_SURFACE('',#46382,0.500000000000054);
#8194=CYLINDRICAL_SURFACE('',#46385,1.81285717707166);
#8195=CYLINDRICAL_SURFACE('',#46388,0.499999999999821);
#8196=CYLINDRICAL_SURFACE('',#46391,1.91146602029503);
#8197=CYLINDRICAL_SURFACE('',#46394,0.499999999999821);
#8198=CYLINDRICAL_SURFACE('',#46397,1.54967110260249);
#8199=CYLINDRICAL_SURFACE('',#46400,0.500000000000054);
#8200=CYLINDRICAL_SURFACE('',#46403,1.25936103546579);
#8201=CYLINDRICAL_SURFACE('',#46406,0.500000000000058);
#8202=CYLINDRICAL_SURFACE('',#46409,1.0588834746273);
#8203=CYLINDRICAL_SURFACE('',#46412,0.500000000000058);
#8204=CYLINDRICAL_SURFACE('',#46415,1.29583333162395);
#8205=CYLINDRICAL_SURFACE('',#46418,0.499999999999935);
#8206=CYLINDRICAL_SURFACE('',#46421,1.60653900437051);
#8207=CYLINDRICAL_SURFACE('',#46424,0.500000000000054);
#8208=CYLINDRICAL_SURFACE('',#46427,1.82809807486273);
#8209=CYLINDRICAL_SURFACE('',#46430,0.500000000000063);
#8210=CYLINDRICAL_SURFACE('',#46433,1.85841829658605);
#8211=CYLINDRICAL_SURFACE('',#46436,0.499999999999821);
#8212=CYLINDRICAL_SURFACE('',#46439,1.81285717707144);
#8213=CYLINDRICAL_SURFACE('',#46442,0.499999999999821);
#8214=CYLINDRICAL_SURFACE('',#46445,1.91146602029503);
#8215=CYLINDRICAL_SURFACE('',#46448,0.500000000000054);
#8216=CYLINDRICAL_SURFACE('',#46451,1.54967110260249);
#8217=CYLINDRICAL_SURFACE('',#46454,0.499999999999944);
#8218=CYLINDRICAL_SURFACE('',#46457,1.25936103546568);
#8219=CYLINDRICAL_SURFACE('',#46460,0.499999999999944);
#8220=CYLINDRICAL_SURFACE('',#46463,1.0588834746273);
#8221=CYLINDRICAL_SURFACE('',#46466,0.500000000000054);
#8222=CYLINDRICAL_SURFACE('',#46469,1.29583333162382);
#8223=CYLINDRICAL_SURFACE('',#46472,0.499999999999826);
#8224=CYLINDRICAL_SURFACE('',#46475,1.60653900437062);
#8225=CYLINDRICAL_SURFACE('',#46478,0.500000000000058);
#8226=CYLINDRICAL_SURFACE('',#46481,1.82809807486272);
#8227=CYLINDRICAL_SURFACE('',#46484,0.499999999999944);
#8228=CYLINDRICAL_SURFACE('',#46487,1.85841829658605);
#8229=CYLINDRICAL_SURFACE('',#46490,0.499999999999939);
#8230=CYLINDRICAL_SURFACE('',#46493,1.9114660202949);
#8231=CYLINDRICAL_SURFACE('',#46496,0.499999999999821);
#8232=CYLINDRICAL_SURFACE('',#46499,1.54967110260249);
#8233=CYLINDRICAL_SURFACE('',#46502,0.500000000000054);
#8234=CYLINDRICAL_SURFACE('',#46505,1.25936103546569);
#8235=CYLINDRICAL_SURFACE('',#46508,0.499999999999939);
#8236=CYLINDRICAL_SURFACE('',#46511,1.05888347462729);
#8237=CYLINDRICAL_SURFACE('',#46514,0.500000000000054);
#8238=CYLINDRICAL_SURFACE('',#46517,1.29583333162371);
#8239=CYLINDRICAL_SURFACE('',#46520,0.499999999999935);
#8240=CYLINDRICAL_SURFACE('',#46523,1.60653900437051);
#8241=CYLINDRICAL_SURFACE('',#46526,0.499999999999944);
#8242=CYLINDRICAL_SURFACE('',#46529,1.82809807486262);
#8243=CYLINDRICAL_SURFACE('',#46532,0.500000000000058);
#8244=CYLINDRICAL_SURFACE('',#46535,1.85841829658605);
#8245=CYLINDRICAL_SURFACE('',#46538,0.499999999999944);
#8246=CYLINDRICAL_SURFACE('',#46541,1.81285717707166);
#8247=CYLINDRICAL_SURFACE('',#46544,0.499999999999944);
#8248=CYLINDRICAL_SURFACE('',#46547,1.91146602029514);
#8249=CYLINDRICAL_SURFACE('',#46550,0.500000000000054);
#8250=CYLINDRICAL_SURFACE('',#46553,1.54967110260238);
#8251=CYLINDRICAL_SURFACE('',#46556,0.499999999999935);
#8252=CYLINDRICAL_SURFACE('',#46559,1.25936103546568);
#8253=CYLINDRICAL_SURFACE('',#46562,0.499999999999939);
#8254=CYLINDRICAL_SURFACE('',#46565,1.0588834746273);
#8255=CYLINDRICAL_SURFACE('',#46568,0.499999999999944);
#8256=CYLINDRICAL_SURFACE('',#46571,1.29583333162395);
#8257=CYLINDRICAL_SURFACE('',#46574,0.500000000000054);
#8258=CYLINDRICAL_SURFACE('',#46577,1.60653900437063);
#8259=CYLINDRICAL_SURFACE('',#46580,0.500000000000054);
#8260=CYLINDRICAL_SURFACE('',#46583,1.82809807486273);
#8261=CYLINDRICAL_SURFACE('',#46586,0.500000000000058);
#8262=CYLINDRICAL_SURFACE('',#46589,1.85841829658594);
#8263=CYLINDRICAL_SURFACE('',#46592,0.499999999999939);
#8264=CYLINDRICAL_SURFACE('',#46595,1.81285717707156);
#8265=CYLINDRICAL_SURFACE('',#46598,0.500000000000058);
#8266=CYLINDRICAL_SURFACE('',#46601,1.91146602029491);
#8267=CYLINDRICAL_SURFACE('',#46604,0.500000000000054);
#8268=CYLINDRICAL_SURFACE('',#46607,1.54967110260249);
#8269=CYLINDRICAL_SURFACE('',#46610,0.499999999999944);
#8270=CYLINDRICAL_SURFACE('',#46613,1.25936103546568);
#8271=CYLINDRICAL_SURFACE('',#46616,0.500000000000058);
#8272=CYLINDRICAL_SURFACE('',#46619,1.0588834746273);
#8273=CYLINDRICAL_SURFACE('',#46622,0.500000000000054);
#8274=CYLINDRICAL_SURFACE('',#46625,1.29583333162394);
#8275=CYLINDRICAL_SURFACE('',#46628,0.500000000000054);
#8276=CYLINDRICAL_SURFACE('',#46631,1.60653900437062);
#8277=CYLINDRICAL_SURFACE('',#46634,0.500000000000054);
#8278=CYLINDRICAL_SURFACE('',#46637,1.82809807486272);
#8279=CYLINDRICAL_SURFACE('',#46640,0.499999999999944);
#8280=CYLINDRICAL_SURFACE('',#46643,1.85841829658605);
#8281=CYLINDRICAL_SURFACE('',#46646,0.500000000000054);
#8282=CYLINDRICAL_SURFACE('',#46649,1.81285717707167);
#8283=CYLINDRICAL_SURFACE('',#46652,0.500000000000054);
#8284=CYLINDRICAL_SURFACE('',#46655,1.91146602029503);
#8285=CYLINDRICAL_SURFACE('',#46658,0.500000000000049);
#8286=CYLINDRICAL_SURFACE('',#46661,1.54967110260249);
#8287=CYLINDRICAL_SURFACE('',#46664,0.499999999999944);
#8288=CYLINDRICAL_SURFACE('',#46667,1.25936103546569);
#8289=CYLINDRICAL_SURFACE('',#46670,0.500000000000054);
#8290=CYLINDRICAL_SURFACE('',#46673,1.0588834746274);
#8291=CYLINDRICAL_SURFACE('',#46676,0.499999999999944);
#8292=CYLINDRICAL_SURFACE('',#46679,1.29583333162394);
#8293=CYLINDRICAL_SURFACE('',#46682,0.500000000000054);
#8294=CYLINDRICAL_SURFACE('',#46685,1.60653900437062);
#8295=CYLINDRICAL_SURFACE('',#46688,0.500000000000054);
#8296=CYLINDRICAL_SURFACE('',#46691,1.82809807486272);
#8297=CYLINDRICAL_SURFACE('',#46694,0.500000000000054);
#8298=CYLINDRICAL_SURFACE('',#46697,1.85841829658605);
#8299=CYLINDRICAL_SURFACE('',#46700,0.500000000000049);
#8300=CYLINDRICAL_SURFACE('',#46703,1.81285717707167);
#8301=CYLINDRICAL_SURFACE('',#46706,0.500000000000054);
#8302=CYLINDRICAL_SURFACE('',#46709,1.91146602029502);
#8303=CYLINDRICAL_SURFACE('',#46712,0.500000000000054);
#8304=CYLINDRICAL_SURFACE('',#46715,1.54967110260249);
#8305=CYLINDRICAL_SURFACE('',#46718,0.500000000000054);
#8306=CYLINDRICAL_SURFACE('',#46721,1.25936103546568);
#8307=CYLINDRICAL_SURFACE('',#46724,0.499999999999944);
#8308=CYLINDRICAL_SURFACE('',#46727,1.05888347462741);
#8309=CYLINDRICAL_SURFACE('',#46730,0.500000000000054);
#8310=CYLINDRICAL_SURFACE('',#46733,1.29583333162394);
#8311=CYLINDRICAL_SURFACE('',#46736,0.500000000000054);
#8312=CYLINDRICAL_SURFACE('',#46739,1.60653900437062);
#8313=CYLINDRICAL_SURFACE('',#46742,0.500000000000054);
#8314=CYLINDRICAL_SURFACE('',#46745,1.82809807486262);
#8315=CYLINDRICAL_SURFACE('',#46748,0.499999999999939);
#8316=CYLINDRICAL_SURFACE('',#46751,1.85841829658605);
#8317=CYLINDRICAL_SURFACE('',#46754,0.500000000000054);
#8318=CYLINDRICAL_SURFACE('',#46757,1.91146602029503);
#8319=CYLINDRICAL_SURFACE('',#46760,0.500000000000054);
#8320=CYLINDRICAL_SURFACE('',#46763,1.54967110260249);
#8321=CYLINDRICAL_SURFACE('',#46766,0.500000000000054);
#8322=CYLINDRICAL_SURFACE('',#46769,1.25936103546568);
#8323=CYLINDRICAL_SURFACE('',#46772,0.500000000000054);
#8324=CYLINDRICAL_SURFACE('',#46775,1.05888347462729);
#8325=CYLINDRICAL_SURFACE('',#46778,0.499999999999935);
#8326=CYLINDRICAL_SURFACE('',#46781,1.29583333162395);
#8327=CYLINDRICAL_SURFACE('',#46784,0.500000000000063);
#8328=CYLINDRICAL_SURFACE('',#46787,1.60653900437062);
#8329=CYLINDRICAL_SURFACE('',#46790,0.500000000000054);
#8330=CYLINDRICAL_SURFACE('',#46793,1.82809807486273);
#8331=CYLINDRICAL_SURFACE('',#46796,0.500000000000058);
#8332=CYLINDRICAL_SURFACE('',#46799,1.85841829658605);
#8333=CYLINDRICAL_SURFACE('',#46802,0.499999999999939);
#8334=CYLINDRICAL_SURFACE('',#46805,1.81285717707167);
#8335=CYLINDRICAL_SURFACE('',#46808,0.499999999999939);
#8336=CYLINDRICAL_SURFACE('',#46811,1.91146602029491);
#8337=CYLINDRICAL_SURFACE('',#46814,0.499999999999826);
#8338=CYLINDRICAL_SURFACE('',#46817,1.54967110260249);
#8339=CYLINDRICAL_SURFACE('',#46820,0.500000000000054);
#8340=CYLINDRICAL_SURFACE('',#46823,1.2593610354658);
#8341=CYLINDRICAL_SURFACE('',#46827,0.500000000000058);
#8342=CYLINDRICAL_SURFACE('',#46830,1.0588834746273);
#8343=CYLINDRICAL_SURFACE('',#46833,0.499999999999935);
#8344=CYLINDRICAL_SURFACE('',#46836,1.29583333162395);
#8345=CYLINDRICAL_SURFACE('',#46839,0.500000000000054);
#8346=CYLINDRICAL_SURFACE('',#46842,1.60653900437074);
#8347=CYLINDRICAL_SURFACE('',#46845,0.500000000000058);
#8348=CYLINDRICAL_SURFACE('',#46848,1.82809807486272);
#8349=CYLINDRICAL_SURFACE('',#46851,0.500000000000054);
#8350=CYLINDRICAL_SURFACE('',#46854,1.85841829658616);
#8351=CYLINDRICAL_SURFACE('',#46857,0.500000000000167);
#8352=CYLINDRICAL_SURFACE('',#46860,1.81285717707155);
#8353=CYLINDRICAL_SURFACE('',#46863,0.499999999999935);
#8354=CYLINDRICAL_SURFACE('',#46866,1.91146602029503);
#8355=CYLINDRICAL_SURFACE('',#46869,0.500000000000054);
#8356=CYLINDRICAL_SURFACE('',#46872,1.54967110260249);
#8357=CYLINDRICAL_SURFACE('',#46876,0.499999999999939);
#8358=CYLINDRICAL_SURFACE('',#46879,1.25936103546556);
#8359=CYLINDRICAL_SURFACE('',#46883,0.499999999999821);
#8360=CYLINDRICAL_SURFACE('',#46886,1.05888347462729);
#8361=CYLINDRICAL_SURFACE('',#46889,0.500000000000058);
#8362=CYLINDRICAL_SURFACE('',#46892,1.29583333162382);
#8363=CYLINDRICAL_SURFACE('',#46895,0.500000000000054);
#8364=CYLINDRICAL_SURFACE('',#46898,1.60653900437074);
#8365=CYLINDRICAL_SURFACE('',#46901,0.500000000000063);
#8366=CYLINDRICAL_SURFACE('',#46904,1.82809807486272);
#8367=CYLINDRICAL_SURFACE('',#46907,0.500000000000054);
#8368=CYLINDRICAL_SURFACE('',#46910,1.85841829658605);
#8369=CYLINDRICAL_SURFACE('',#46913,0.500000000000049);
#8370=CYLINDRICAL_SURFACE('',#46916,1.81285717707166);
#8371=CYLINDRICAL_SURFACE('',#46919,0.500000000000049);
#8372=CYLINDRICAL_SURFACE('',#46922,1.91146602029503);
#8373=CYLINDRICAL_SURFACE('',#46926,0.500000000000054);
#8374=CYLINDRICAL_SURFACE('',#46929,1.0588834746273);
#8375=CYLINDRICAL_SURFACE('',#46932,0.500000000000058);
#8376=CYLINDRICAL_SURFACE('',#46935,1.29583333162395);
#8377=CYLINDRICAL_SURFACE('',#46938,0.500000000000058);
#8378=CYLINDRICAL_SURFACE('',#46941,1.60653900437063);
#8379=CYLINDRICAL_SURFACE('',#46944,0.500000000000058);
#8380=CYLINDRICAL_SURFACE('',#46947,1.82809807486273);
#8381=CYLINDRICAL_SURFACE('',#46950,0.499999999999939);
#8382=CYLINDRICAL_SURFACE('',#46953,1.85841829658605);
#8383=CYLINDRICAL_SURFACE('',#46956,0.499999999999935);
#8384=CYLINDRICAL_SURFACE('',#46959,1.81285717707167);
#8385=CYLINDRICAL_SURFACE('',#46962,0.499999999999944);
#8386=CYLINDRICAL_SURFACE('',#46965,1.91146602029503);
#8387=CYLINDRICAL_SURFACE('',#46968,0.500000000000167);
#8388=CYLINDRICAL_SURFACE('',#46971,1.0588834746273);
#8389=CYLINDRICAL_SURFACE('',#46974,0.499999999999944);
#8390=CYLINDRICAL_SURFACE('',#46977,1.29583333162394);
#8391=CYLINDRICAL_SURFACE('',#46980,0.500000000000054);
#8392=CYLINDRICAL_SURFACE('',#46983,1.60653900437062);
#8393=CYLINDRICAL_SURFACE('',#46986,0.499999999999944);
#8394=CYLINDRICAL_SURFACE('',#46989,1.82809807486273);
#8395=CYLINDRICAL_SURFACE('',#46992,0.499999999999944);
#8396=CYLINDRICAL_SURFACE('',#46995,1.85841829658605);
#8397=CYLINDRICAL_SURFACE('',#46998,0.499999999999944);
#8398=CYLINDRICAL_SURFACE('',#47001,1.91146602029503);
#8399=CYLINDRICAL_SURFACE('',#47004,0.500000000000058);
#8400=CYLINDRICAL_SURFACE('',#47007,1.54967110260249);
#8401=CYLINDRICAL_SURFACE('',#47011,0.499999999999939);
#8402=CYLINDRICAL_SURFACE('',#47014,1.05888347462741);
#8403=CYLINDRICAL_SURFACE('',#47017,0.499999999999939);
#8404=CYLINDRICAL_SURFACE('',#47020,1.29583333162394);
#8405=CYLINDRICAL_SURFACE('',#47023,0.499999999999939);
#8406=CYLINDRICAL_SURFACE('',#47026,1.60653900437063);
#8407=CYLINDRICAL_SURFACE('',#47029,0.500000000000058);
#8408=CYLINDRICAL_SURFACE('',#47032,1.82809807486273);
#8409=CYLINDRICAL_SURFACE('',#47035,0.500000000000058);
#8410=CYLINDRICAL_SURFACE('',#47038,1.85841829658593);
#8411=CYLINDRICAL_SURFACE('',#47041,0.499999999999939);
#8412=CYLINDRICAL_SURFACE('',#47044,1.81285717707155);
#8413=CYLINDRICAL_SURFACE('',#47047,0.499999999999939);
#8414=CYLINDRICAL_SURFACE('',#47050,1.91146602029503);
#8415=CYLINDRICAL_SURFACE('',#47053,0.499999999999939);
#8416=CYLINDRICAL_SURFACE('',#47056,1.54967110260237);
#8417=CYLINDRICAL_SURFACE('',#47059,0.499999999999939);
#8418=CYLINDRICAL_SURFACE('',#47062,1.05888347462729);
#8419=CYLINDRICAL_SURFACE('',#47065,0.500000000000054);
#8420=CYLINDRICAL_SURFACE('',#47068,1.29583333162383);
#8421=CYLINDRICAL_SURFACE('',#47071,0.500000000000054);
#8422=CYLINDRICAL_SURFACE('',#47074,1.60653900437051);
#8423=CYLINDRICAL_SURFACE('',#47077,0.499999999999935);
#8424=CYLINDRICAL_SURFACE('',#47080,1.82809807486262);
#8425=CYLINDRICAL_SURFACE('',#47083,0.500000000000063);
#8426=CYLINDRICAL_SURFACE('',#47086,1.85841829658605);
#8427=CYLINDRICAL_SURFACE('',#47089,0.500000000000054);
#8428=CYLINDRICAL_SURFACE('',#47092,1.81285717707166);
#8429=CYLINDRICAL_SURFACE('',#47095,0.499999999999935);
#8430=CYLINDRICAL_SURFACE('',#47098,1.9114660202949);
#8431=CYLINDRICAL_SURFACE('',#47101,0.499999999999935);
#8432=CYLINDRICAL_SURFACE('',#47104,1.54967110260238);
#8433=CYLINDRICAL_SURFACE('',#47107,0.499999999999935);
#8434=CYLINDRICAL_SURFACE('',#47110,1.25936103546556);
#8435=CYLINDRICAL_SURFACE('',#47114,0.499999999999935);
#8436=CYLINDRICAL_SURFACE('',#47117,1.05888347462741);
#8437=CYLINDRICAL_SURFACE('',#47120,0.500000000000058);
#8438=CYLINDRICAL_SURFACE('',#47123,1.29583333162406);
#8439=CYLINDRICAL_SURFACE('',#47126,0.499999999999939);
#8440=CYLINDRICAL_SURFACE('',#47129,1.60653900437063);
#8441=CYLINDRICAL_SURFACE('',#47132,0.500000000000058);
#8442=CYLINDRICAL_SURFACE('',#47135,1.82809807486262);
#8443=CYLINDRICAL_SURFACE('',#47138,0.499999999999939);
#8444=CYLINDRICAL_SURFACE('',#47141,1.85841829658593);
#8445=CYLINDRICAL_SURFACE('',#47144,0.499999999999939);
#8446=CYLINDRICAL_SURFACE('',#47147,1.81285717707179);
#8447=CYLINDRICAL_SURFACE('',#47150,0.499999999999939);
#8448=CYLINDRICAL_SURFACE('',#47153,1.91146602029502);
#8449=CYLINDRICAL_SURFACE('',#47156,0.499999999999939);
#8450=CYLINDRICAL_SURFACE('',#47159,1.54967110260249);
#8451=CYLINDRICAL_SURFACE('',#47162,0.500000000000058);
#8452=CYLINDRICAL_SURFACE('',#47165,1.25936103546569);
#8453=CYLINDRICAL_SURFACE('',#47169,0.499999999999935);
#8454=CYLINDRICAL_SURFACE('',#47172,1.0588834746273);
#8455=CYLINDRICAL_SURFACE('',#47175,0.500000000000054);
#8456=CYLINDRICAL_SURFACE('',#47178,1.29583333162406);
#8457=CYLINDRICAL_SURFACE('',#47181,0.500000000000177);
#8458=CYLINDRICAL_SURFACE('',#47184,1.60653900437051);
#8459=CYLINDRICAL_SURFACE('',#47187,0.499999999999939);
#8460=CYLINDRICAL_SURFACE('',#47190,1.82809807486261);
#8461=CYLINDRICAL_SURFACE('',#47193,0.499999999999944);
#8462=CYLINDRICAL_SURFACE('',#47196,1.85841829658594);
#8463=CYLINDRICAL_SURFACE('',#47199,0.499999999999939);
#8464=CYLINDRICAL_SURFACE('',#47202,1.81285717707156);
#8465=CYLINDRICAL_SURFACE('',#47205,0.499999999999944);
#8466=CYLINDRICAL_SURFACE('',#47208,1.91146602029503);
#8467=CYLINDRICAL_SURFACE('',#47211,0.500000000000054);
#8468=CYLINDRICAL_SURFACE('',#47214,1.5496711026026);
#8469=CYLINDRICAL_SURFACE('',#47217,0.500000000000058);
#8470=CYLINDRICAL_SURFACE('',#47220,1.2593610354658);
#8471=CYLINDRICAL_SURFACE('',#47223,0.500000000000063);
#8472=CYLINDRICAL_SURFACE('',#47226,1.05888347462741);
#8473=CYLINDRICAL_SURFACE('',#47229,0.499999999999939);
#8474=CYLINDRICAL_SURFACE('',#47232,1.29583333162395);
#8475=CYLINDRICAL_SURFACE('',#47235,0.500000000000054);
#8476=CYLINDRICAL_SURFACE('',#47238,1.60653900437063);
#8477=CYLINDRICAL_SURFACE('',#47241,0.500000000000167);
#8478=CYLINDRICAL_SURFACE('',#47244,1.82809807486262);
#8479=CYLINDRICAL_SURFACE('',#47247,0.499999999999944);
#8480=CYLINDRICAL_SURFACE('',#47250,1.85841829658605);
#8481=CYLINDRICAL_SURFACE('',#47253,0.499999999999944);
#8482=CYLINDRICAL_SURFACE('',#47256,1.91146602029502);
#8483=CYLINDRICAL_SURFACE('',#47259,0.499999999999944);
#8484=CYLINDRICAL_SURFACE('',#47262,1.5496711026026);
#8485=CYLINDRICAL_SURFACE('',#47265,0.500000000000054);
#8486=CYLINDRICAL_SURFACE('',#47268,1.25936103546567);
#8487=CYLINDRICAL_SURFACE('',#47271,0.499999999999939);
#8488=CYLINDRICAL_SURFACE('',#47274,1.05888347462741);
#8489=CYLINDRICAL_SURFACE('',#47277,0.500000000000054);
#8490=CYLINDRICAL_SURFACE('',#47280,1.29583333162394);
#8491=CYLINDRICAL_SURFACE('',#47283,0.499999999999939);
#8492=CYLINDRICAL_SURFACE('',#47286,1.6065390043705);
#8493=CYLINDRICAL_SURFACE('',#47289,0.499999999999939);
#8494=CYLINDRICAL_SURFACE('',#47292,1.82809807486262);
#8495=CYLINDRICAL_SURFACE('',#47295,0.500000000000054);
#8496=CYLINDRICAL_SURFACE('',#47298,1.85841829658593);
#8497=CYLINDRICAL_SURFACE('',#47301,0.499999999999939);
#8498=CYLINDRICAL_SURFACE('',#47304,1.81285717707167);
#8499=CYLINDRICAL_SURFACE('',#47307,0.500000000000058);
#8500=CYLINDRICAL_SURFACE('',#47310,1.91146602029503);
#8501=CYLINDRICAL_SURFACE('',#47313,0.500000000000054);
#8502=CYLINDRICAL_SURFACE('',#47316,1.54967110260249);
#8503=CYLINDRICAL_SURFACE('',#47319,0.500000000000058);
#8504=CYLINDRICAL_SURFACE('',#47322,1.25936103546568);
#8505=CYLINDRICAL_SURFACE('',#47325,0.499999999999939);
#8506=CYLINDRICAL_SURFACE('',#47328,1.0588834746273);
#8507=CYLINDRICAL_SURFACE('',#47331,0.500000000000054);
#8508=CYLINDRICAL_SURFACE('',#47334,1.29583333162383);
#8509=CYLINDRICAL_SURFACE('',#47337,0.499999999999935);
#8510=CYLINDRICAL_SURFACE('',#47340,1.60653900437062);
#8511=CYLINDRICAL_SURFACE('',#47343,0.500000000000058);
#8512=CYLINDRICAL_SURFACE('',#47346,1.82809807486272);
#8513=CYLINDRICAL_SURFACE('',#47349,0.500000000000058);
#8514=CYLINDRICAL_SURFACE('',#47352,1.85841829658594);
#8515=CYLINDRICAL_SURFACE('',#47355,0.499999999999826);
#8516=CYLINDRICAL_SURFACE('',#47358,1.81285717707156);
#8517=CYLINDRICAL_SURFACE('',#47361,0.499999999999944);
#8518=CYLINDRICAL_SURFACE('',#47364,1.91146602029502);
#8519=CYLINDRICAL_SURFACE('',#47367,0.499999999999935);
#8520=CYLINDRICAL_SURFACE('',#47370,1.54967110260249);
#8521=CYLINDRICAL_SURFACE('',#47373,0.500000000000054);
#8522=CYLINDRICAL_SURFACE('',#47376,1.25936103546568);
#8523=CYLINDRICAL_SURFACE('',#47379,0.500000000000054);
#8524=CYLINDRICAL_SURFACE('',#47433,0.5);
#8525=CYLINDRICAL_SURFACE('',#47439,8.99091713639503);
#8526=CYLINDRICAL_SURFACE('',#47445,0.500000000000054);
#8527=CYLINDRICAL_SURFACE('',#47447,1.02140828085145);
#8528=CYLINDRICAL_SURFACE('',#47451,8.3031389659941);
#8529=CYLINDRICAL_SURFACE('',#47456,8.3031389659941);
#8530=CYLINDRICAL_SURFACE('',#47459,8.3031389659941);
#8531=CYLINDRICAL_SURFACE('',#47476,0.999999999999995);
#8532=CYLINDRICAL_SURFACE('',#47478,0.999999999999995);
#8533=CYLINDRICAL_SURFACE('',#47483,0.999999999999995);
#8534=CYLINDRICAL_SURFACE('',#47485,0.999999999999995);
#8535=CYLINDRICAL_SURFACE('',#47491,0.500000017388205);
#8536=CYLINDRICAL_SURFACE('',#47494,0.500000017611928);
#8537=CYLINDRICAL_SURFACE('',#47496,8.3031389659941);
#8538=CYLINDRICAL_SURFACE('',#47510,0.5);
#8539=CYLINDRICAL_SURFACE('',#47514,65.);
#8540=CYLINDRICAL_SURFACE('',#47537,8.3031389659941);
#8541=CYLINDRICAL_SURFACE('',#48163,0.500000000000028);
#8542=CYLINDRICAL_SURFACE('',#48167,0.499999999999973);
#8543=CYLINDRICAL_SURFACE('',#48177,0.499999999999973);
#8544=CYLINDRICAL_SURFACE('',#48180,0.500000000000028);
#8545=CYLINDRICAL_SURFACE('',#48183,28.5226030790361);
#8546=CYLINDRICAL_SURFACE('',#48193,16.5);
#8547=CYLINDRICAL_SURFACE('',#48196,16.5);
#8548=CYLINDRICAL_SURFACE('',#48199,16.5);
#8549=CYLINDRICAL_SURFACE('',#48202,16.);
#8550=CYLINDRICAL_SURFACE('',#48208,3.96802221877415);
#8551=CYLINDRICAL_SURFACE('',#48224,16.);
#8552=CYLINDRICAL_SURFACE('',#48230,3.96802221877416);
#8553=CYLINDRICAL_SURFACE('',#48246,16.);
#8554=CYLINDRICAL_SURFACE('',#48252,3.96802221877416);
#8555=CYLINDRICAL_SURFACE('',#48268,26.0226030790361);
#8556=CYLINDRICAL_SURFACE('',#48278,30.);
#8557=CYLINDRICAL_SURFACE('',#48281,30.);
#8558=CYLINDRICAL_SURFACE('',#48296,0.5);
#8559=CYLINDRICAL_SURFACE('',#48298,0.5);
#8560=CYLINDRICAL_SURFACE('',#48300,0.5);
#8561=CYLINDRICAL_SURFACE('',#48307,0.5);
#8562=CYLINDRICAL_SURFACE('',#48309,0.5);
#8563=CYLINDRICAL_SURFACE('',#48311,0.5);
#8564=CYLINDRICAL_SURFACE('',#48318,0.5);
#8565=CYLINDRICAL_SURFACE('',#48320,0.5);
#8566=CYLINDRICAL_SURFACE('',#48332,0.700000000000006);
#8567=CYLINDRICAL_SURFACE('',#48334,0.700000000000006);
#8568=CYLINDRICAL_SURFACE('',#48339,0.700000000000006);
#8569=CYLINDRICAL_SURFACE('',#48344,0.700000000000006);
#8570=CYLINDRICAL_SURFACE('',#48349,0.700000000000006);
#8571=CYLINDRICAL_SURFACE('',#48362,0.700000000000006);
#8572=CYLINDRICAL_SURFACE('',#48363,0.700000000000006);
#8573=CYLINDRICAL_SURFACE('',#48364,0.700000000000006);
#8574=CYLINDRICAL_SURFACE('',#48367,4.75563473233925);
#8575=CYLINDRICAL_SURFACE('',#48368,4.75563473233925);
#8576=CYLINDRICAL_SURFACE('',#48372,0.499999999999998);
#8577=CYLINDRICAL_SURFACE('',#48378,0.499999999999998);
#8578=CYLINDRICAL_SURFACE('',#48385,0.5);
#8579=CYLINDRICAL_SURFACE('',#48387,0.499999999999998);
#8580=CYLINDRICAL_SURFACE('',#48389,0.499999999999998);
#8581=CYLINDRICAL_SURFACE('',#48391,0.5);
#8582=CYLINDRICAL_SURFACE('',#48398,0.499999999999998);
#8583=CYLINDRICAL_SURFACE('',#48399,0.499999999999998);
#8584=CYLINDRICAL_SURFACE('',#48402,3.96802221877416);
#8585=CYLINDRICAL_SURFACE('',#48406,0.499999999999998);
#8586=CYLINDRICAL_SURFACE('',#48412,0.499999999999998);
#8587=CYLINDRICAL_SURFACE('',#48419,0.5);
#8588=CYLINDRICAL_SURFACE('',#48421,0.499999999999998);
#8589=CYLINDRICAL_SURFACE('',#48423,0.499999999999998);
#8590=CYLINDRICAL_SURFACE('',#48425,0.5);
#8591=CYLINDRICAL_SURFACE('',#48432,0.5);
#8592=CYLINDRICAL_SURFACE('',#48433,0.499999999999998);
#8593=CYLINDRICAL_SURFACE('',#48436,3.96802221877416);
#8594=CYLINDRICAL_SURFACE('',#48440,0.500000000000003);
#8595=CYLINDRICAL_SURFACE('',#48446,0.500000000000003);
#8596=CYLINDRICAL_SURFACE('',#48453,0.5);
#8597=CYLINDRICAL_SURFACE('',#48455,0.500000000000003);
#8598=CYLINDRICAL_SURFACE('',#48457,0.500000000000003);
#8599=CYLINDRICAL_SURFACE('',#48459,0.5);
#8600=CYLINDRICAL_SURFACE('',#48466,0.500000000000003);
#8601=CYLINDRICAL_SURFACE('',#48467,0.500000000000003);
#8602=CYLINDRICAL_SURFACE('',#48470,3.96802221877415);
#8603=CYLINDRICAL_SURFACE('',#48477,0.5);
#8604=CYLINDRICAL_SURFACE('',#48486,0.5);
#8605=CYLINDRICAL_SURFACE('',#48492,0.5);
#8606=CYLINDRICAL_SURFACE('',#48499,1.);
#8607=CYLINDRICAL_SURFACE('',#48510,1.);
#8608=CYLINDRICAL_SURFACE('',#48518,1.);
#8609=CYLINDRICAL_SURFACE('',#48523,1.);
#8610=CYLINDRICAL_SURFACE('',#48531,1.);
#8611=CYLINDRICAL_SURFACE('',#48537,1.);
#8612=CYLINDRICAL_SURFACE('',#48558,30.);
#8613=CYLINDRICAL_SURFACE('',#48562,30.);
#8614=CYLINDRICAL_SURFACE('',#48566,1.);
#8615=CYLINDRICAL_SURFACE('',#48569,1.);
#8616=CYLINDRICAL_SURFACE('',#48570,1.);
#8617=CYLINDRICAL_SURFACE('',#48571,1.);
#8618=CYLINDRICAL_SURFACE('',#48572,1.);
#8619=CYLINDRICAL_SURFACE('',#48575,12.);
#8620=CYLINDRICAL_SURFACE('',#48609,8.00000000000001);
#8621=CYLINDRICAL_SURFACE('',#48612,8.00000000000001);
#8622=CYLINDRICAL_SURFACE('',#48615,8.);
#8623=CYLINDRICAL_SURFACE('',#48618,8.);
#8624=CYLINDRICAL_SURFACE('',#48621,8.);
#8625=CYLINDRICAL_SURFACE('',#48624,8.);
#8626=CYLINDRICAL_SURFACE('',#48645,1.);
#8627=CYLINDRICAL_SURFACE('',#48652,1.);
#8628=CYLINDRICAL_SURFACE('',#48654,1.);
#8629=CYLINDRICAL_SURFACE('',#48660,1.);
#8630=CYLINDRICAL_SURFACE('',#48661,1.);
#8631=CYLINDRICAL_SURFACE('',#48668,1.);
#8632=CYLINDRICAL_SURFACE('',#48670,1.);
#8633=CYLINDRICAL_SURFACE('',#48676,1.);
#8634=CYLINDRICAL_SURFACE('',#48677,1.);
#8635=CYLINDRICAL_SURFACE('',#48682,1.);
#8636=CYLINDRICAL_SURFACE('',#48686,1.);
#8637=CYLINDRICAL_SURFACE('',#48688,1.);
#8638=CYLINDRICAL_SURFACE('',#48693,1.);
#8639=CYLINDRICAL_SURFACE('',#48697,1.);
#8640=CYLINDRICAL_SURFACE('',#48699,1.);
#8641=CYLINDRICAL_SURFACE('',#48704,1.);
#8642=CYLINDRICAL_SURFACE('',#48708,1.);
#8643=CYLINDRICAL_SURFACE('',#48710,1.);
#8644=CYLINDRICAL_SURFACE('',#48715,1.);
#8645=CYLINDRICAL_SURFACE('',#48719,1.);
#8646=CYLINDRICAL_SURFACE('',#48724,1.99999999999999);
#8647=CYLINDRICAL_SURFACE('',#48726,2.);
#8648=CYLINDRICAL_SURFACE('',#48732,2.);
#8649=CYLINDRICAL_SURFACE('',#48734,1.99999999999999);
#8650=CYLINDRICAL_SURFACE('',#48740,1.99999999999999);
#8651=CYLINDRICAL_SURFACE('',#48742,2.);
#8652=CYLINDRICAL_SURFACE('',#48748,2.);
#8653=CYLINDRICAL_SURFACE('',#48750,1.99999999999999);
#8654=CYLINDRICAL_SURFACE('',#48775,19.4499999999999);
#8655=CYLINDRICAL_SURFACE('',#48785,19.45);
#8656=CYLINDRICAL_SURFACE('',#48793,12.3);
#8657=CYLINDRICAL_SURFACE('',#48795,15.7183063441034);
#8658=CYLINDRICAL_SURFACE('',#48810,12.2808574779498);
#8659=CYLINDRICAL_SURFACE('',#48811,19.45);
#8660=CYLINDRICAL_SURFACE('',#48819,12.3);
#8661=CYLINDRICAL_SURFACE('',#48821,15.7183063441034);
#8662=CYLINDRICAL_SURFACE('',#48824,5.84048589276829);
#8663=CYLINDRICAL_SURFACE('',#48826,19.45);
#8664=CYLINDRICAL_SURFACE('',#48827,21.0115219102092);
#8665=CYLINDRICAL_SURFACE('',#48829,19.45);
#8666=CYLINDRICAL_SURFACE('',#48830,21.0115219102092);
#8667=CYLINDRICAL_SURFACE('',#48831,18.1223816084529);
#8668=CYLINDRICAL_SURFACE('',#48840,18.1223816084529);
#8669=CYLINDRICAL_SURFACE('',#48846,12.2099993856753);
#8670=CYLINDRICAL_SURFACE('',#48851,1.);
#8671=CYLINDRICAL_SURFACE('',#48857,1.);
#8672=CYLINDRICAL_SURFACE('',#48860,1.);
#8673=CYLINDRICAL_SURFACE('',#48861,1.);
#8674=CYLINDRICAL_SURFACE('',#48866,0.5);
#8675=CYLINDRICAL_SURFACE('',#48868,0.5);
#8676=CYLINDRICAL_SURFACE('',#48873,0.5);
#8677=CYLINDRICAL_SURFACE('',#48875,0.5);
#8678=CYLINDRICAL_SURFACE('',#48877,0.5);
#8679=CYLINDRICAL_SURFACE('',#48884,0.5);
#8680=CYLINDRICAL_SURFACE('',#48886,0.5);
#8681=CYLINDRICAL_SURFACE('',#48891,0.5);
#8682=CYLINDRICAL_SURFACE('',#48893,11.5);
#8683=CYLINDRICAL_SURFACE('',#48896,12.5);
#8684=CYLINDRICAL_SURFACE('',#48909,1.27544412113617);
#8685=CYLINDRICAL_SURFACE('',#48910,0.675444121136126);
#8686=CYLINDRICAL_SURFACE('',#48912,1.09883113599246);
#8687=CYLINDRICAL_SURFACE('',#48913,0.498831135992472);
#8688=CYLINDRICAL_SURFACE('',#48915,1.09054074872833);
#8689=CYLINDRICAL_SURFACE('',#48916,0.490540748728341);
#8690=CYLINDRICAL_SURFACE('',#48918,1.47830313219327);
#8691=CYLINDRICAL_SURFACE('',#48919,0.878303132193281);
#8692=CYLINDRICAL_SURFACE('',#48921,1.27544412113612);
#8693=CYLINDRICAL_SURFACE('',#48922,0.675444121136182);
#8694=CYLINDRICAL_SURFACE('',#48924,1.09883113599246);
#8695=CYLINDRICAL_SURFACE('',#48925,0.498831135992472);
#8696=CYLINDRICAL_SURFACE('',#48927,1.09054074872833);
#8697=CYLINDRICAL_SURFACE('',#48928,0.490540748728341);
#8698=CYLINDRICAL_SURFACE('',#48930,1.47830313219333);
#8699=CYLINDRICAL_SURFACE('',#48931,0.878303132193337);
#8700=CYLINDRICAL_SURFACE('',#48933,1.27544412113617);
#8701=CYLINDRICAL_SURFACE('',#48934,0.675444121136126);
#8702=CYLINDRICAL_SURFACE('',#48936,1.09883113599246);
#8703=CYLINDRICAL_SURFACE('',#48937,0.498831135992472);
#8704=CYLINDRICAL_SURFACE('',#48939,1.09054074872833);
#8705=CYLINDRICAL_SURFACE('',#48940,0.490540748728341);
#8706=CYLINDRICAL_SURFACE('',#48942,1.47830313219327);
#8707=CYLINDRICAL_SURFACE('',#48943,0.878303132193281);
#8708=CYLINDRICAL_SURFACE('',#48945,1.27544412113617);
#8709=CYLINDRICAL_SURFACE('',#48946,0.675444121136126);
#8710=CYLINDRICAL_SURFACE('',#48948,1.09883113599246);
#8711=CYLINDRICAL_SURFACE('',#48949,0.498831135992472);
#8712=CYLINDRICAL_SURFACE('',#48951,1.09054074872833);
#8713=CYLINDRICAL_SURFACE('',#48952,0.490540748728285);
#8714=CYLINDRICAL_SURFACE('',#48954,1.47830313219327);
#8715=CYLINDRICAL_SURFACE('',#48955,0.878303132193226);
#8716=CYLINDRICAL_SURFACE('',#48957,1.27544412113617);
#8717=CYLINDRICAL_SURFACE('',#48958,0.675444121136182);
#8718=CYLINDRICAL_SURFACE('',#48960,1.09883113599246);
#8719=CYLINDRICAL_SURFACE('',#48961,0.498831135992472);
#8720=CYLINDRICAL_SURFACE('',#48963,1.09054074872833);
#8721=CYLINDRICAL_SURFACE('',#48964,0.490540748728341);
#8722=CYLINDRICAL_SURFACE('',#48966,1.47830313219333);
#8723=CYLINDRICAL_SURFACE('',#48967,0.878303132193281);
#8724=CYLINDRICAL_SURFACE('',#48969,1.27544412113612);
#8725=CYLINDRICAL_SURFACE('',#48970,0.675444121136182);
#8726=CYLINDRICAL_SURFACE('',#48972,1.09883113599241);
#8727=CYLINDRICAL_SURFACE('',#48973,0.498831135992472);
#8728=CYLINDRICAL_SURFACE('',#48975,1.09054074872839);
#8729=CYLINDRICAL_SURFACE('',#48976,0.490540748728341);
#8730=CYLINDRICAL_SURFACE('',#48978,1.47830313219333);
#8731=CYLINDRICAL_SURFACE('',#48979,0.878303132193281);
#8732=CYLINDRICAL_SURFACE('',#48981,1.27544412113612);
#8733=CYLINDRICAL_SURFACE('',#48982,0.675444121136182);
#8734=CYLINDRICAL_SURFACE('',#48984,1.09883113599252);
#8735=CYLINDRICAL_SURFACE('',#48985,0.498831135992583);
#8736=CYLINDRICAL_SURFACE('',#48987,1.09054074872827);
#8737=CYLINDRICAL_SURFACE('',#48988,0.490540748728341);
#8738=CYLINDRICAL_SURFACE('',#48990,1.47830313219321);
#8739=CYLINDRICAL_SURFACE('',#48991,0.87830313219317);
#8740=CYLINDRICAL_SURFACE('',#48993,1.27544412113612);
#8741=CYLINDRICAL_SURFACE('',#48994,0.675444121136071);
#8742=CYLINDRICAL_SURFACE('',#48996,1.09883113599252);
#8743=CYLINDRICAL_SURFACE('',#48997,0.498831135992472);
#8744=CYLINDRICAL_SURFACE('',#48999,1.09054074872839);
#8745=CYLINDRICAL_SURFACE('',#49000,0.490540748728341);
#8746=CYLINDRICAL_SURFACE('',#49002,1.47830313219321);
#8747=CYLINDRICAL_SURFACE('',#49003,0.87830313219317);
#8748=CYLINDRICAL_SURFACE('',#49005,1.27544412113612);
#8749=CYLINDRICAL_SURFACE('',#49006,0.675444121136071);
#8750=CYLINDRICAL_SURFACE('',#49008,1.09883113599241);
#8751=CYLINDRICAL_SURFACE('',#49009,0.498831135992361);
#8752=CYLINDRICAL_SURFACE('',#49011,1.09054074872839);
#8753=CYLINDRICAL_SURFACE('',#49012,0.490540748728341);
#8754=CYLINDRICAL_SURFACE('',#49014,1.47830313219333);
#8755=CYLINDRICAL_SURFACE('',#49015,0.878303132193281);
#8756=CYLINDRICAL_SURFACE('',#49017,1.27544412113612);
#8757=CYLINDRICAL_SURFACE('',#49018,0.675444121136182);
#8758=CYLINDRICAL_SURFACE('',#49020,1.09883113599252);
#8759=CYLINDRICAL_SURFACE('',#49021,0.498831135992472);
#8760=CYLINDRICAL_SURFACE('',#49023,1.09054074872827);
#8761=CYLINDRICAL_SURFACE('',#49024,0.49054074872823);
#8762=CYLINDRICAL_SURFACE('',#49026,1.47830313219333);
#8763=CYLINDRICAL_SURFACE('',#49027,0.878303132193281);
#8764=CYLINDRICAL_SURFACE('',#49029,1.27544412113623);
#8765=CYLINDRICAL_SURFACE('',#49030,0.675444121136182);
#8766=CYLINDRICAL_SURFACE('',#49032,1.09883113599252);
#8767=CYLINDRICAL_SURFACE('',#49033,0.498831135992472);
#8768=CYLINDRICAL_SURFACE('',#49035,1.09054074872827);
#8769=CYLINDRICAL_SURFACE('',#49036,0.490540748728341);
#8770=CYLINDRICAL_SURFACE('',#49038,1.47830313219333);
#8771=CYLINDRICAL_SURFACE('',#49039,0.878303132193281);
#8772=CYLINDRICAL_SURFACE('',#49041,1.27544412113617);
#8773=CYLINDRICAL_SURFACE('',#49042,0.675444121136126);
#8774=CYLINDRICAL_SURFACE('',#49044,1.09883113599252);
#8775=CYLINDRICAL_SURFACE('',#49045,0.498831135992472);
#8776=CYLINDRICAL_SURFACE('',#49047,1.09054074872839);
#8777=CYLINDRICAL_SURFACE('',#49048,0.490540748728341);
#8778=CYLINDRICAL_SURFACE('',#49050,1.47830313219327);
#8779=CYLINDRICAL_SURFACE('',#49051,0.878303132193281);
#8780=CYLINDRICAL_SURFACE('',#49053,1.27544412113617);
#8781=CYLINDRICAL_SURFACE('',#49054,0.675444121136182);
#8782=CYLINDRICAL_SURFACE('',#49056,1.09883113599246);
#8783=CYLINDRICAL_SURFACE('',#49057,0.498831135992417);
#8784=CYLINDRICAL_SURFACE('',#49059,1.09054074872827);
#8785=CYLINDRICAL_SURFACE('',#49060,0.490540748728341);
#8786=CYLINDRICAL_SURFACE('',#49062,1.47830313219327);
#8787=CYLINDRICAL_SURFACE('',#49063,0.878303132193281);
#8788=CYLINDRICAL_SURFACE('',#49065,1.27544412113612);
#8789=CYLINDRICAL_SURFACE('',#49066,0.675444121136126);
#8790=CYLINDRICAL_SURFACE('',#49068,1.09883113599241);
#8791=CYLINDRICAL_SURFACE('',#49069,0.498831135992417);
#8792=CYLINDRICAL_SURFACE('',#49071,1.09054074872839);
#8793=CYLINDRICAL_SURFACE('',#49072,0.490540748728341);
#8794=CYLINDRICAL_SURFACE('',#49074,1.47830313219333);
#8795=CYLINDRICAL_SURFACE('',#49075,0.878303132193337);
#8796=CYLINDRICAL_SURFACE('',#49077,1.27544412113617);
#8797=CYLINDRICAL_SURFACE('',#49078,0.675444121136182);
#8798=CYLINDRICAL_SURFACE('',#49080,1.09883113599246);
#8799=CYLINDRICAL_SURFACE('',#49081,0.498831135992417);
#8800=CYLINDRICAL_SURFACE('',#49083,1.09054074872833);
#8801=CYLINDRICAL_SURFACE('',#49084,0.490540748728341);
#8802=CYLINDRICAL_SURFACE('',#49086,1.47830313219333);
#8803=CYLINDRICAL_SURFACE('',#49087,0.878303132193337);
#8804=CYLINDRICAL_SURFACE('',#49089,1.27544412113617);
#8805=CYLINDRICAL_SURFACE('',#49090,0.675444121136126);
#8806=CYLINDRICAL_SURFACE('',#49092,1.09883113599246);
#8807=CYLINDRICAL_SURFACE('',#49093,0.498831135992472);
#8808=CYLINDRICAL_SURFACE('',#49095,1.09054074872833);
#8809=CYLINDRICAL_SURFACE('',#49096,0.490540748728341);
#8810=CYLINDRICAL_SURFACE('',#49098,1.47830313219333);
#8811=CYLINDRICAL_SURFACE('',#49099,0.878303132193281);
#8812=CYLINDRICAL_SURFACE('',#49101,1.27544412113617);
#8813=CYLINDRICAL_SURFACE('',#49102,0.675444121136182);
#8814=CYLINDRICAL_SURFACE('',#49104,1.09883113599246);
#8815=CYLINDRICAL_SURFACE('',#49105,0.498831135992472);
#8816=CYLINDRICAL_SURFACE('',#49107,1.09054074872833);
#8817=CYLINDRICAL_SURFACE('',#49108,0.490540748728341);
#8818=CYLINDRICAL_SURFACE('',#49110,1.47830313219333);
#8819=CYLINDRICAL_SURFACE('',#49111,0.878303132193281);
#8820=CYLINDRICAL_SURFACE('',#49113,1.27544412113617);
#8821=CYLINDRICAL_SURFACE('',#49114,0.675444121136182);
#8822=CYLINDRICAL_SURFACE('',#49116,1.09883113599246);
#8823=CYLINDRICAL_SURFACE('',#49117,0.498831135992472);
#8824=CYLINDRICAL_SURFACE('',#49119,1.09054074872833);
#8825=CYLINDRICAL_SURFACE('',#49120,0.490540748728341);
#8826=CYLINDRICAL_SURFACE('',#49122,1.47830313219333);
#8827=CYLINDRICAL_SURFACE('',#49123,0.878303132193281);
#8828=CYLINDRICAL_SURFACE('',#49125,1.27544412113612);
#8829=CYLINDRICAL_SURFACE('',#49126,0.675444121136126);
#8830=CYLINDRICAL_SURFACE('',#49128,1.09883113599252);
#8831=CYLINDRICAL_SURFACE('',#49129,0.498831135992472);
#8832=CYLINDRICAL_SURFACE('',#49131,1.09054074872833);
#8833=CYLINDRICAL_SURFACE('',#49132,0.490540748728341);
#8834=CYLINDRICAL_SURFACE('',#49134,1.47830313219333);
#8835=CYLINDRICAL_SURFACE('',#49135,0.878303132193337);
#8836=CYLINDRICAL_SURFACE('',#49137,1.27544412113617);
#8837=CYLINDRICAL_SURFACE('',#49138,0.675444121136126);
#8838=CYLINDRICAL_SURFACE('',#49140,1.09883113599246);
#8839=CYLINDRICAL_SURFACE('',#49141,0.498831135992472);
#8840=CYLINDRICAL_SURFACE('',#49143,1.09054074872833);
#8841=CYLINDRICAL_SURFACE('',#49144,0.490540748728341);
#8842=CYLINDRICAL_SURFACE('',#49146,1.47830313219327);
#8843=CYLINDRICAL_SURFACE('',#49147,0.878303132193281);
#8844=CYLINDRICAL_SURFACE('',#49149,1.27544412113617);
#8845=CYLINDRICAL_SURFACE('',#49150,0.675444121136182);
#8846=CYLINDRICAL_SURFACE('',#49152,1.09883113599246);
#8847=CYLINDRICAL_SURFACE('',#49153,0.498831135992472);
#8848=CYLINDRICAL_SURFACE('',#49155,1.09054074872827);
#8849=CYLINDRICAL_SURFACE('',#49156,0.490540748728341);
#8850=CYLINDRICAL_SURFACE('',#49158,1.47830313219327);
#8851=CYLINDRICAL_SURFACE('',#49159,0.878303132193281);
#8852=CYLINDRICAL_SURFACE('',#49161,1.27544412113617);
#8853=CYLINDRICAL_SURFACE('',#49162,0.675444121136126);
#8854=CYLINDRICAL_SURFACE('',#49164,1.09883113599241);
#8855=CYLINDRICAL_SURFACE('',#49165,0.498831135992472);
#8856=CYLINDRICAL_SURFACE('',#49167,1.09054074872827);
#8857=CYLINDRICAL_SURFACE('',#49168,0.490540748728341);
#8858=CYLINDRICAL_SURFACE('',#49170,1.47830313219327);
#8859=CYLINDRICAL_SURFACE('',#49171,0.878303132193281);
#8860=CYLINDRICAL_SURFACE('',#49173,1.27544412113617);
#8861=CYLINDRICAL_SURFACE('',#49174,0.675444121136126);
#8862=CYLINDRICAL_SURFACE('',#49176,1.09883113599252);
#8863=CYLINDRICAL_SURFACE('',#49177,0.498831135992472);
#8864=CYLINDRICAL_SURFACE('',#49179,1.09054074872839);
#8865=CYLINDRICAL_SURFACE('',#49180,0.490540748728396);
#8866=CYLINDRICAL_SURFACE('',#49182,1.47830313219327);
#8867=CYLINDRICAL_SURFACE('',#49183,0.878303132193281);
#8868=CYLINDRICAL_SURFACE('',#49185,1.27544412113612);
#8869=CYLINDRICAL_SURFACE('',#49186,0.675444121136126);
#8870=CYLINDRICAL_SURFACE('',#49188,1.09883113599241);
#8871=CYLINDRICAL_SURFACE('',#49189,0.498831135992417);
#8872=CYLINDRICAL_SURFACE('',#49191,1.09054074872833);
#8873=CYLINDRICAL_SURFACE('',#49192,0.490540748728341);
#8874=CYLINDRICAL_SURFACE('',#49194,1.47830313219327);
#8875=CYLINDRICAL_SURFACE('',#49195,0.878303132193281);
#8876=CYLINDRICAL_SURFACE('',#49197,1.27544412113617);
#8877=CYLINDRICAL_SURFACE('',#49198,0.675444121136126);
#8878=CYLINDRICAL_SURFACE('',#49200,1.09883113599241);
#8879=CYLINDRICAL_SURFACE('',#49201,0.498831135992472);
#8880=CYLINDRICAL_SURFACE('',#49203,1.09054074872839);
#8881=CYLINDRICAL_SURFACE('',#49204,0.490540748728396);
#8882=CYLINDRICAL_SURFACE('',#49206,1.47830313219327);
#8883=CYLINDRICAL_SURFACE('',#49207,0.878303132193281);
#8884=CYLINDRICAL_SURFACE('',#49209,1.27544412113617);
#8885=CYLINDRICAL_SURFACE('',#49210,0.675444121136182);
#8886=CYLINDRICAL_SURFACE('',#49212,1.09883113599246);
#8887=CYLINDRICAL_SURFACE('',#49213,0.498831135992528);
#8888=CYLINDRICAL_SURFACE('',#49215,1.09054074872833);
#8889=CYLINDRICAL_SURFACE('',#49216,0.490540748728341);
#8890=CYLINDRICAL_SURFACE('',#49218,1.47830313219333);
#8891=CYLINDRICAL_SURFACE('',#49219,0.878303132193337);
#8892=CYLINDRICAL_SURFACE('',#49221,1.27544412113617);
#8893=CYLINDRICAL_SURFACE('',#49222,0.675444121136126);
#8894=CYLINDRICAL_SURFACE('',#49224,1.09883113599246);
#8895=CYLINDRICAL_SURFACE('',#49225,0.498831135992472);
#8896=CYLINDRICAL_SURFACE('',#49227,1.09054074872839);
#8897=CYLINDRICAL_SURFACE('',#49228,0.490540748728285);
#8898=CYLINDRICAL_SURFACE('',#49230,1.47830313219327);
#8899=CYLINDRICAL_SURFACE('',#49231,0.878303132193281);
#8900=CYLINDRICAL_SURFACE('',#49233,1.27544412113617);
#8901=CYLINDRICAL_SURFACE('',#49234,0.675444121136126);
#8902=CYLINDRICAL_SURFACE('',#49236,1.09883113599246);
#8903=CYLINDRICAL_SURFACE('',#49237,0.498831135992528);
#8904=CYLINDRICAL_SURFACE('',#49239,1.09054074872833);
#8905=CYLINDRICAL_SURFACE('',#49240,0.490540748728341);
#8906=CYLINDRICAL_SURFACE('',#49242,1.47830313219333);
#8907=CYLINDRICAL_SURFACE('',#49243,0.878303132193337);
#8908=CYLINDRICAL_SURFACE('',#49245,1.27544412113617);
#8909=CYLINDRICAL_SURFACE('',#49246,0.675444121136182);
#8910=CYLINDRICAL_SURFACE('',#49248,1.09883113599246);
#8911=CYLINDRICAL_SURFACE('',#49249,0.498831135992472);
#8912=CYLINDRICAL_SURFACE('',#49251,1.09054074872833);
#8913=CYLINDRICAL_SURFACE('',#49252,0.490540748728285);
#8914=CYLINDRICAL_SURFACE('',#49254,1.47830313219327);
#8915=CYLINDRICAL_SURFACE('',#49255,0.878303132193281);
#8916=CYLINDRICAL_SURFACE('',#49257,1.27544412113617);
#8917=CYLINDRICAL_SURFACE('',#49258,0.675444121136126);
#8918=CYLINDRICAL_SURFACE('',#49260,1.09054074872833);
#8919=CYLINDRICAL_SURFACE('',#49261,0.490540748728341);
#8920=CYLINDRICAL_SURFACE('',#49263,1.09883113599252);
#8921=CYLINDRICAL_SURFACE('',#49264,0.498831135992472);
#8922=CYLINDRICAL_SURFACE('',#49266,1.10035806567471);
#8923=CYLINDRICAL_SURFACE('',#49269,0.500358065674722);
#8924=CYLINDRICAL_SURFACE('',#49272,1.21403156673711);
#8925=CYLINDRICAL_SURFACE('',#49275,0.614031566737117);
#8926=CYLINDRICAL_SURFACE('',#49278,1.32880796357332);
#8927=CYLINDRICAL_SURFACE('',#49281,0.72880796357333);
#8928=CYLINDRICAL_SURFACE('',#49284,1.46111700181689);
#8929=CYLINDRICAL_SURFACE('',#49287,0.861117001816902);
#8930=CYLINDRICAL_SURFACE('',#49290,1.6204820426246);
#8931=CYLINDRICAL_SURFACE('',#49293,1.02048204262462);
#8932=CYLINDRICAL_SURFACE('',#49296,1.70100022308284);
#8933=CYLINDRICAL_SURFACE('',#49299,1.10100022308285);
#8934=CYLINDRICAL_SURFACE('',#49302,1.72127463204352);
#8935=CYLINDRICAL_SURFACE('',#49305,1.12127463204348);
#8936=CYLINDRICAL_SURFACE('',#49308,1.78199265440493);
#8937=CYLINDRICAL_SURFACE('',#49311,1.18199265440494);
#8938=CYLINDRICAL_SURFACE('',#49314,1.66088080992077);
#8939=CYLINDRICAL_SURFACE('',#49317,1.06088080992078);
#8940=CYLINDRICAL_SURFACE('',#49320,1.10035806567471);
#8941=CYLINDRICAL_SURFACE('',#49323,0.500358065674722);
#8942=CYLINDRICAL_SURFACE('',#49326,1.21403156673716);
#8943=CYLINDRICAL_SURFACE('',#49329,0.614031566737117);
#8944=CYLINDRICAL_SURFACE('',#49332,1.32880796357332);
#8945=CYLINDRICAL_SURFACE('',#49335,0.728807963573275);
#8946=CYLINDRICAL_SURFACE('',#49338,1.46111700181689);
#8947=CYLINDRICAL_SURFACE('',#49341,0.861117001816902);
#8948=CYLINDRICAL_SURFACE('',#49344,1.6204820426246);
#8949=CYLINDRICAL_SURFACE('',#49347,1.02048204262462);
#8950=CYLINDRICAL_SURFACE('',#49350,1.70100022308284);
#8951=CYLINDRICAL_SURFACE('',#49353,1.10100022308285);
#8952=CYLINDRICAL_SURFACE('',#49356,1.72127463204347);
#8953=CYLINDRICAL_SURFACE('',#49359,1.12127463204348);
#8954=CYLINDRICAL_SURFACE('',#49362,1.78199265440493);
#8955=CYLINDRICAL_SURFACE('',#49365,1.18199265440494);
#8956=CYLINDRICAL_SURFACE('',#49368,1.66088080992077);
#8957=CYLINDRICAL_SURFACE('',#49371,1.06088080992078);
#8958=CYLINDRICAL_SURFACE('',#49374,1.10035806567471);
#8959=CYLINDRICAL_SURFACE('',#49377,0.500358065674722);
#8960=CYLINDRICAL_SURFACE('',#49380,1.21403156673716);
#8961=CYLINDRICAL_SURFACE('',#49383,0.614031566737117);
#8962=CYLINDRICAL_SURFACE('',#49386,1.32880796357326);
#8963=CYLINDRICAL_SURFACE('',#49389,0.72880796357333);
#8964=CYLINDRICAL_SURFACE('',#49392,1.46111700181689);
#8965=CYLINDRICAL_SURFACE('',#49395,0.861117001816902);
#8966=CYLINDRICAL_SURFACE('',#49398,1.6204820426246);
#8967=CYLINDRICAL_SURFACE('',#49401,1.02048204262456);
#8968=CYLINDRICAL_SURFACE('',#49404,1.70100022308284);
#8969=CYLINDRICAL_SURFACE('',#49407,1.10100022308285);
#8970=CYLINDRICAL_SURFACE('',#49410,1.72127463204347);
#8971=CYLINDRICAL_SURFACE('',#49413,1.12127463204348);
#8972=CYLINDRICAL_SURFACE('',#49416,1.78199265440493);
#8973=CYLINDRICAL_SURFACE('',#49419,1.18199265440494);
#8974=CYLINDRICAL_SURFACE('',#49422,1.66088080992077);
#8975=CYLINDRICAL_SURFACE('',#49425,1.06088080992078);
#8976=CYLINDRICAL_SURFACE('',#49428,1.10035806567471);
#8977=CYLINDRICAL_SURFACE('',#49431,0.500358065674666);
#8978=CYLINDRICAL_SURFACE('',#49434,1.21403156673711);
#8979=CYLINDRICAL_SURFACE('',#49437,0.614031566737172);
#8980=CYLINDRICAL_SURFACE('',#49440,1.32880796357332);
#8981=CYLINDRICAL_SURFACE('',#49443,0.72880796357333);
#8982=CYLINDRICAL_SURFACE('',#49446,1.46111700181689);
#8983=CYLINDRICAL_SURFACE('',#49449,0.861117001816847);
#8984=CYLINDRICAL_SURFACE('',#49452,1.6204820426246);
#8985=CYLINDRICAL_SURFACE('',#49455,1.02048204262462);
#8986=CYLINDRICAL_SURFACE('',#49458,1.70100022308284);
#8987=CYLINDRICAL_SURFACE('',#49461,1.10100022308285);
#8988=CYLINDRICAL_SURFACE('',#49464,1.72127463204347);
#8989=CYLINDRICAL_SURFACE('',#49467,1.12127463204353);
#8990=CYLINDRICAL_SURFACE('',#49470,1.78199265440498);
#8991=CYLINDRICAL_SURFACE('',#49473,1.18199265440494);
#8992=CYLINDRICAL_SURFACE('',#49476,1.66088080992083);
#8993=CYLINDRICAL_SURFACE('',#49479,1.06088080992078);
#8994=CYLINDRICAL_SURFACE('',#49482,1.10035806567477);
#8995=CYLINDRICAL_SURFACE('',#49485,0.500358065674777);
#8996=CYLINDRICAL_SURFACE('',#49488,1.21403156673711);
#8997=CYLINDRICAL_SURFACE('',#49491,0.614031566737172);
#8998=CYLINDRICAL_SURFACE('',#49494,1.32880796357326);
#8999=CYLINDRICAL_SURFACE('',#49497,0.72880796357333);
#9000=CYLINDRICAL_SURFACE('',#49500,1.46111700181684);
#9001=CYLINDRICAL_SURFACE('',#49503,0.861117001816847);
#9002=CYLINDRICAL_SURFACE('',#49506,1.6204820426246);
#9003=CYLINDRICAL_SURFACE('',#49509,1.02048204262462);
#9004=CYLINDRICAL_SURFACE('',#49512,1.70100022308278);
#9005=CYLINDRICAL_SURFACE('',#49515,1.1010002230829);
#9006=CYLINDRICAL_SURFACE('',#49518,1.72127463204347);
#9007=CYLINDRICAL_SURFACE('',#49521,1.12127463204342);
#9008=CYLINDRICAL_SURFACE('',#49524,1.78199265440487);
#9009=CYLINDRICAL_SURFACE('',#49527,1.18199265440488);
#9010=CYLINDRICAL_SURFACE('',#49530,1.66088080992077);
#9011=CYLINDRICAL_SURFACE('',#49533,1.06088080992078);
#9012=CYLINDRICAL_SURFACE('',#49536,1.10035806567466);
#9013=CYLINDRICAL_SURFACE('',#49539,0.500358065674722);
#9014=CYLINDRICAL_SURFACE('',#49542,1.21403156673716);
#9015=CYLINDRICAL_SURFACE('',#49545,0.614031566737117);
#9016=CYLINDRICAL_SURFACE('',#49548,1.32880796357326);
#9017=CYLINDRICAL_SURFACE('',#49551,0.728807963573275);
#9018=CYLINDRICAL_SURFACE('',#49554,1.46111700181684);
#9019=CYLINDRICAL_SURFACE('',#49557,0.861117001816847);
#9020=CYLINDRICAL_SURFACE('',#49560,1.6204820426246);
#9021=CYLINDRICAL_SURFACE('',#49563,1.02048204262456);
#9022=CYLINDRICAL_SURFACE('',#49566,1.70100022308284);
#9023=CYLINDRICAL_SURFACE('',#49569,1.10100022308279);
#9024=CYLINDRICAL_SURFACE('',#49572,1.72127463204347);
#9025=CYLINDRICAL_SURFACE('',#49575,1.12127463204348);
#9026=CYLINDRICAL_SURFACE('',#49578,1.78199265440493);
#9027=CYLINDRICAL_SURFACE('',#49581,1.18199265440494);
#9028=CYLINDRICAL_SURFACE('',#49584,1.66088080992088);
#9029=CYLINDRICAL_SURFACE('',#49587,1.06088080992084);
#9030=CYLINDRICAL_SURFACE('',#49590,1.10035806567466);
#9031=CYLINDRICAL_SURFACE('',#49593,0.500358065674666);
#9032=CYLINDRICAL_SURFACE('',#49596,1.21403156673716);
#9033=CYLINDRICAL_SURFACE('',#49599,0.614031566737172);
#9034=CYLINDRICAL_SURFACE('',#49602,1.32880796357332);
#9035=CYLINDRICAL_SURFACE('',#49605,0.728807963573275);
#9036=CYLINDRICAL_SURFACE('',#49608,1.46111700181689);
#9037=CYLINDRICAL_SURFACE('',#49611,0.861117001816847);
#9038=CYLINDRICAL_SURFACE('',#49614,1.6204820426246);
#9039=CYLINDRICAL_SURFACE('',#49617,1.02048204262456);
#9040=CYLINDRICAL_SURFACE('',#49620,1.70100022308284);
#9041=CYLINDRICAL_SURFACE('',#49623,1.10100022308285);
#9042=CYLINDRICAL_SURFACE('',#49626,1.72127463204352);
#9043=CYLINDRICAL_SURFACE('',#49629,1.12127463204348);
#9044=CYLINDRICAL_SURFACE('',#49632,1.78199265440493);
#9045=CYLINDRICAL_SURFACE('',#49635,1.18199265440494);
#9046=CYLINDRICAL_SURFACE('',#49638,1.66088080992077);
#9047=CYLINDRICAL_SURFACE('',#49641,1.06088080992073);
#9048=CYLINDRICAL_SURFACE('',#49644,1.10035806567471);
#9049=CYLINDRICAL_SURFACE('',#49647,0.500358065674722);
#9050=CYLINDRICAL_SURFACE('',#49650,1.21403156673716);
#9051=CYLINDRICAL_SURFACE('',#49653,0.614031566737117);
#9052=CYLINDRICAL_SURFACE('',#49656,1.32880796357332);
#9053=CYLINDRICAL_SURFACE('',#49659,0.72880796357333);
#9054=CYLINDRICAL_SURFACE('',#49662,1.46111700181689);
#9055=CYLINDRICAL_SURFACE('',#49665,0.861117001816902);
#9056=CYLINDRICAL_SURFACE('',#49668,1.6204820426246);
#9057=CYLINDRICAL_SURFACE('',#49671,1.02048204262456);
#9058=CYLINDRICAL_SURFACE('',#49674,1.70100022308278);
#9059=CYLINDRICAL_SURFACE('',#49677,1.10100022308285);
#9060=CYLINDRICAL_SURFACE('',#49680,1.72127463204347);
#9061=CYLINDRICAL_SURFACE('',#49683,1.12127463204348);
#9062=CYLINDRICAL_SURFACE('',#49686,1.78199265440493);
#9063=CYLINDRICAL_SURFACE('',#49689,1.18199265440494);
#9064=CYLINDRICAL_SURFACE('',#49692,1.66088080992077);
#9065=CYLINDRICAL_SURFACE('',#49695,1.06088080992073);
#9066=CYLINDRICAL_SURFACE('',#49698,1.10035806567471);
#9067=CYLINDRICAL_SURFACE('',#49701,0.500358065674722);
#9068=CYLINDRICAL_SURFACE('',#49704,1.21403156673711);
#9069=CYLINDRICAL_SURFACE('',#49707,0.614031566737117);
#9070=CYLINDRICAL_SURFACE('',#49710,1.32880796357332);
#9071=CYLINDRICAL_SURFACE('',#49713,0.72880796357333);
#9072=CYLINDRICAL_SURFACE('',#49716,1.46111700181689);
#9073=CYLINDRICAL_SURFACE('',#49719,0.861117001816902);
#9074=CYLINDRICAL_SURFACE('',#49722,1.6204820426246);
#9075=CYLINDRICAL_SURFACE('',#49725,1.02048204262456);
#9076=CYLINDRICAL_SURFACE('',#49728,1.70100022308284);
#9077=CYLINDRICAL_SURFACE('',#49731,1.10100022308285);
#9078=CYLINDRICAL_SURFACE('',#49734,1.72127463204352);
#9079=CYLINDRICAL_SURFACE('',#49737,1.12127463204348);
#9080=CYLINDRICAL_SURFACE('',#49740,1.78199265440487);
#9081=CYLINDRICAL_SURFACE('',#49743,1.18199265440488);
#9082=CYLINDRICAL_SURFACE('',#49746,1.66088080992088);
#9083=CYLINDRICAL_SURFACE('',#49749,1.06088080992073);
#9084=CYLINDRICAL_SURFACE('',#49752,1.10035806567471);
#9085=CYLINDRICAL_SURFACE('',#49755,0.500358065674666);
#9086=CYLINDRICAL_SURFACE('',#49758,1.21403156673716);
#9087=CYLINDRICAL_SURFACE('',#49761,0.614031566737172);
#9088=CYLINDRICAL_SURFACE('',#49764,1.32880796357338);
#9089=CYLINDRICAL_SURFACE('',#49767,0.72880796357333);
#9090=CYLINDRICAL_SURFACE('',#49770,1.46111700181689);
#9091=CYLINDRICAL_SURFACE('',#49773,0.861117001816902);
#9092=CYLINDRICAL_SURFACE('',#49776,1.6204820426246);
#9093=CYLINDRICAL_SURFACE('',#49779,1.02048204262456);
#9094=CYLINDRICAL_SURFACE('',#49782,1.70100022308284);
#9095=CYLINDRICAL_SURFACE('',#49785,1.10100022308285);
#9096=CYLINDRICAL_SURFACE('',#49788,1.72127463204352);
#9097=CYLINDRICAL_SURFACE('',#49791,1.12127463204348);
#9098=CYLINDRICAL_SURFACE('',#49794,1.78199265440498);
#9099=CYLINDRICAL_SURFACE('',#49797,1.181992654405);
#9100=CYLINDRICAL_SURFACE('',#49800,1.66088080992077);
#9101=CYLINDRICAL_SURFACE('',#49803,1.06088080992073);
#9102=CYLINDRICAL_SURFACE('',#49806,1.10035806567471);
#9103=CYLINDRICAL_SURFACE('',#49809,0.500358065674722);
#9104=CYLINDRICAL_SURFACE('',#49812,1.21403156673705);
#9105=CYLINDRICAL_SURFACE('',#49815,0.614031566737117);
#9106=CYLINDRICAL_SURFACE('',#49818,1.32880796357338);
#9107=CYLINDRICAL_SURFACE('',#49821,0.72880796357333);
#9108=CYLINDRICAL_SURFACE('',#49824,1.46111700181689);
#9109=CYLINDRICAL_SURFACE('',#49827,0.861117001816902);
#9110=CYLINDRICAL_SURFACE('',#49830,1.6204820426246);
#9111=CYLINDRICAL_SURFACE('',#49833,1.02048204262462);
#9112=CYLINDRICAL_SURFACE('',#49836,1.70100022308278);
#9113=CYLINDRICAL_SURFACE('',#49839,1.10100022308279);
#9114=CYLINDRICAL_SURFACE('',#49842,1.72127463204352);
#9115=CYLINDRICAL_SURFACE('',#49845,1.12127463204348);
#9116=CYLINDRICAL_SURFACE('',#49848,1.78199265440493);
#9117=CYLINDRICAL_SURFACE('',#49851,1.18199265440494);
#9118=CYLINDRICAL_SURFACE('',#49854,1.66088080992077);
#9119=CYLINDRICAL_SURFACE('',#49857,1.06088080992078);
#9120=CYLINDRICAL_SURFACE('',#49860,1.10035806567471);
#9121=CYLINDRICAL_SURFACE('',#49863,0.500358065674722);
#9122=CYLINDRICAL_SURFACE('',#49866,1.21403156673711);
#9123=CYLINDRICAL_SURFACE('',#49869,0.614031566737117);
#9124=CYLINDRICAL_SURFACE('',#49872,1.32880796357332);
#9125=CYLINDRICAL_SURFACE('',#49875,0.72880796357333);
#9126=CYLINDRICAL_SURFACE('',#49878,1.46111700181689);
#9127=CYLINDRICAL_SURFACE('',#49881,0.861117001816902);
#9128=CYLINDRICAL_SURFACE('',#49884,1.62048204262455);
#9129=CYLINDRICAL_SURFACE('',#49887,1.02048204262462);
#9130=CYLINDRICAL_SURFACE('',#49890,1.70100022308278);
#9131=CYLINDRICAL_SURFACE('',#49893,1.10100022308279);
#9132=CYLINDRICAL_SURFACE('',#49896,1.72127463204347);
#9133=CYLINDRICAL_SURFACE('',#49899,1.12127463204353);
#9134=CYLINDRICAL_SURFACE('',#49902,1.78199265440487);
#9135=CYLINDRICAL_SURFACE('',#49905,1.18199265440494);
#9136=CYLINDRICAL_SURFACE('',#49908,1.66088080992077);
#9137=CYLINDRICAL_SURFACE('',#49911,1.06088080992078);
#9138=CYLINDRICAL_SURFACE('',#49914,1.10035806567471);
#9139=CYLINDRICAL_SURFACE('',#49917,0.500358065674777);
#9140=CYLINDRICAL_SURFACE('',#49920,1.21403156673711);
#9141=CYLINDRICAL_SURFACE('',#49923,0.614031566737117);
#9142=CYLINDRICAL_SURFACE('',#49926,1.32880796357332);
#9143=CYLINDRICAL_SURFACE('',#49929,0.728807963573275);
#9144=CYLINDRICAL_SURFACE('',#49932,1.46111700181695);
#9145=CYLINDRICAL_SURFACE('',#49935,0.861117001816902);
#9146=CYLINDRICAL_SURFACE('',#49938,1.6204820426246);
#9147=CYLINDRICAL_SURFACE('',#49941,1.02048204262462);
#9148=CYLINDRICAL_SURFACE('',#49944,1.70100022308284);
#9149=CYLINDRICAL_SURFACE('',#49947,1.10100022308285);
#9150=CYLINDRICAL_SURFACE('',#49950,1.72127463204347);
#9151=CYLINDRICAL_SURFACE('',#49953,1.12127463204348);
#9152=CYLINDRICAL_SURFACE('',#49956,1.78199265440493);
#9153=CYLINDRICAL_SURFACE('',#49959,1.18199265440488);
#9154=CYLINDRICAL_SURFACE('',#49962,1.66088080992077);
#9155=CYLINDRICAL_SURFACE('',#49965,1.06088080992078);
#9156=CYLINDRICAL_SURFACE('',#49968,1.10035806567471);
#9157=CYLINDRICAL_SURFACE('',#49971,0.500358065674722);
#9158=CYLINDRICAL_SURFACE('',#49974,1.21403156673711);
#9159=CYLINDRICAL_SURFACE('',#49977,0.614031566737117);
#9160=CYLINDRICAL_SURFACE('',#49980,1.32880796357332);
#9161=CYLINDRICAL_SURFACE('',#49983,0.72880796357333);
#9162=CYLINDRICAL_SURFACE('',#49986,1.46111700181689);
#9163=CYLINDRICAL_SURFACE('',#49989,0.861117001816902);
#9164=CYLINDRICAL_SURFACE('',#49992,1.62048204262455);
#9165=CYLINDRICAL_SURFACE('',#49995,1.02048204262456);
#9166=CYLINDRICAL_SURFACE('',#49998,1.70100022308284);
#9167=CYLINDRICAL_SURFACE('',#50001,1.10100022308285);
#9168=CYLINDRICAL_SURFACE('',#50004,1.72127463204347);
#9169=CYLINDRICAL_SURFACE('',#50007,1.12127463204348);
#9170=CYLINDRICAL_SURFACE('',#50010,1.78199265440493);
#9171=CYLINDRICAL_SURFACE('',#50013,1.18199265440494);
#9172=CYLINDRICAL_SURFACE('',#50016,1.66088080992077);
#9173=CYLINDRICAL_SURFACE('',#50019,1.06088080992078);
#9174=CYLINDRICAL_SURFACE('',#50022,1.10035806567471);
#9175=CYLINDRICAL_SURFACE('',#50025,0.500358065674722);
#9176=CYLINDRICAL_SURFACE('',#50028,1.21403156673711);
#9177=CYLINDRICAL_SURFACE('',#50031,0.614031566737117);
#9178=CYLINDRICAL_SURFACE('',#50034,1.32880796357326);
#9179=CYLINDRICAL_SURFACE('',#50037,0.728807963573275);
#9180=CYLINDRICAL_SURFACE('',#50040,1.46111700181689);
#9181=CYLINDRICAL_SURFACE('',#50043,0.861117001816902);
#9182=CYLINDRICAL_SURFACE('',#50046,1.6204820426246);
#9183=CYLINDRICAL_SURFACE('',#50049,1.02048204262456);
#9184=CYLINDRICAL_SURFACE('',#50052,1.70100022308284);
#9185=CYLINDRICAL_SURFACE('',#50055,1.10100022308285);
#9186=CYLINDRICAL_SURFACE('',#50058,1.72127463204352);
#9187=CYLINDRICAL_SURFACE('',#50061,1.12127463204348);
#9188=CYLINDRICAL_SURFACE('',#50064,1.78199265440498);
#9189=CYLINDRICAL_SURFACE('',#50067,1.18199265440494);
#9190=CYLINDRICAL_SURFACE('',#50070,1.66088080992083);
#9191=CYLINDRICAL_SURFACE('',#50073,1.06088080992078);
#9192=CYLINDRICAL_SURFACE('',#50076,1.10035806567471);
#9193=CYLINDRICAL_SURFACE('',#50079,0.500358065674722);
#9194=CYLINDRICAL_SURFACE('',#50082,1.21403156673711);
#9195=CYLINDRICAL_SURFACE('',#50085,0.614031566737117);
#9196=CYLINDRICAL_SURFACE('',#50088,1.32880796357332);
#9197=CYLINDRICAL_SURFACE('',#50091,0.72880796357333);
#9198=CYLINDRICAL_SURFACE('',#50094,1.46111700181689);
#9199=CYLINDRICAL_SURFACE('',#50097,0.861117001816847);
#9200=CYLINDRICAL_SURFACE('',#50100,1.6204820426246);
#9201=CYLINDRICAL_SURFACE('',#50103,1.02048204262462);
#9202=CYLINDRICAL_SURFACE('',#50106,1.70100022308284);
#9203=CYLINDRICAL_SURFACE('',#50109,1.10100022308279);
#9204=CYLINDRICAL_SURFACE('',#50112,1.72127463204347);
#9205=CYLINDRICAL_SURFACE('',#50115,1.12127463204353);
#9206=CYLINDRICAL_SURFACE('',#50118,1.78199265440493);
#9207=CYLINDRICAL_SURFACE('',#50121,1.18199265440494);
#9208=CYLINDRICAL_SURFACE('',#50124,1.66088080992077);
#9209=CYLINDRICAL_SURFACE('',#50127,1.06088080992078);
#9210=CYLINDRICAL_SURFACE('',#50130,1.10035806567471);
#9211=CYLINDRICAL_SURFACE('',#50133,0.500358065674722);
#9212=CYLINDRICAL_SURFACE('',#50136,1.21403156673711);
#9213=CYLINDRICAL_SURFACE('',#50139,0.614031566737117);
#9214=CYLINDRICAL_SURFACE('',#50142,1.32880796357332);
#9215=CYLINDRICAL_SURFACE('',#50145,0.72880796357333);
#9216=CYLINDRICAL_SURFACE('',#50148,1.46111700181689);
#9217=CYLINDRICAL_SURFACE('',#50151,0.861117001816902);
#9218=CYLINDRICAL_SURFACE('',#50154,1.6204820426246);
#9219=CYLINDRICAL_SURFACE('',#50157,1.02048204262462);
#9220=CYLINDRICAL_SURFACE('',#50160,1.70100022308284);
#9221=CYLINDRICAL_SURFACE('',#50163,1.10100022308285);
#9222=CYLINDRICAL_SURFACE('',#50166,1.72127463204347);
#9223=CYLINDRICAL_SURFACE('',#50169,1.12127463204348);
#9224=CYLINDRICAL_SURFACE('',#50172,1.78199265440493);
#9225=CYLINDRICAL_SURFACE('',#50175,1.18199265440494);
#9226=CYLINDRICAL_SURFACE('',#50178,1.66088080992077);
#9227=CYLINDRICAL_SURFACE('',#50181,1.06088080992078);
#9228=CYLINDRICAL_SURFACE('',#50184,1.10035806567471);
#9229=CYLINDRICAL_SURFACE('',#50187,0.500358065674666);
#9230=CYLINDRICAL_SURFACE('',#50190,1.21403156673716);
#9231=CYLINDRICAL_SURFACE('',#50193,0.614031566737117);
#9232=CYLINDRICAL_SURFACE('',#50196,1.32880796357332);
#9233=CYLINDRICAL_SURFACE('',#50199,0.72880796357333);
#9234=CYLINDRICAL_SURFACE('',#50202,1.46111700181689);
#9235=CYLINDRICAL_SURFACE('',#50205,0.861117001816902);
#9236=CYLINDRICAL_SURFACE('',#50208,1.6204820426246);
#9237=CYLINDRICAL_SURFACE('',#50211,1.02048204262462);
#9238=CYLINDRICAL_SURFACE('',#50214,1.70100022308284);
#9239=CYLINDRICAL_SURFACE('',#50217,1.10100022308285);
#9240=CYLINDRICAL_SURFACE('',#50220,1.72127463204352);
#9241=CYLINDRICAL_SURFACE('',#50223,1.12127463204353);
#9242=CYLINDRICAL_SURFACE('',#50226,1.78199265440493);
#9243=CYLINDRICAL_SURFACE('',#50229,1.18199265440494);
#9244=CYLINDRICAL_SURFACE('',#50232,1.66088080992077);
#9245=CYLINDRICAL_SURFACE('',#50235,1.06088080992078);
#9246=CYLINDRICAL_SURFACE('',#50238,1.10035806567471);
#9247=CYLINDRICAL_SURFACE('',#50241,0.500358065674666);
#9248=CYLINDRICAL_SURFACE('',#50244,1.21403156673716);
#9249=CYLINDRICAL_SURFACE('',#50247,0.614031566737172);
#9250=CYLINDRICAL_SURFACE('',#50250,1.32880796357326);
#9251=CYLINDRICAL_SURFACE('',#50253,0.728807963573275);
#9252=CYLINDRICAL_SURFACE('',#50256,1.46111700181689);
#9253=CYLINDRICAL_SURFACE('',#50259,0.861117001816847);
#9254=CYLINDRICAL_SURFACE('',#50262,1.62048204262455);
#9255=CYLINDRICAL_SURFACE('',#50265,1.02048204262462);
#9256=CYLINDRICAL_SURFACE('',#50268,1.70100022308284);
#9257=CYLINDRICAL_SURFACE('',#50271,1.10100022308279);
#9258=CYLINDRICAL_SURFACE('',#50274,1.72127463204352);
#9259=CYLINDRICAL_SURFACE('',#50277,1.12127463204348);
#9260=CYLINDRICAL_SURFACE('',#50280,1.78199265440493);
#9261=CYLINDRICAL_SURFACE('',#50283,1.18199265440494);
#9262=CYLINDRICAL_SURFACE('',#50286,1.66088080992083);
#9263=CYLINDRICAL_SURFACE('',#50289,1.06088080992078);
#9264=CYLINDRICAL_SURFACE('',#50292,1.10035806567471);
#9265=CYLINDRICAL_SURFACE('',#50295,0.500358065674722);
#9266=CYLINDRICAL_SURFACE('',#50298,1.21403156673716);
#9267=CYLINDRICAL_SURFACE('',#50301,0.614031566737172);
#9268=CYLINDRICAL_SURFACE('',#50304,1.32880796357326);
#9269=CYLINDRICAL_SURFACE('',#50307,0.72880796357333);
#9270=CYLINDRICAL_SURFACE('',#50310,1.46111700181689);
#9271=CYLINDRICAL_SURFACE('',#50313,0.861117001816902);
#9272=CYLINDRICAL_SURFACE('',#50316,1.6204820426246);
#9273=CYLINDRICAL_SURFACE('',#50319,1.02048204262456);
#9274=CYLINDRICAL_SURFACE('',#50322,1.70100022308278);
#9275=CYLINDRICAL_SURFACE('',#50325,1.10100022308279);
#9276=CYLINDRICAL_SURFACE('',#50328,1.72127463204347);
#9277=CYLINDRICAL_SURFACE('',#50331,1.12127463204348);
#9278=CYLINDRICAL_SURFACE('',#50334,1.78199265440493);
#9279=CYLINDRICAL_SURFACE('',#50337,1.18199265440494);
#9280=CYLINDRICAL_SURFACE('',#50340,1.66088080992077);
#9281=CYLINDRICAL_SURFACE('',#50343,1.06088080992084);
#9282=CYLINDRICAL_SURFACE('',#50346,1.10035806567471);
#9283=CYLINDRICAL_SURFACE('',#50349,0.500358065674722);
#9284=CYLINDRICAL_SURFACE('',#50352,1.21403156673716);
#9285=CYLINDRICAL_SURFACE('',#50355,0.614031566737117);
#9286=CYLINDRICAL_SURFACE('',#50358,1.32880796357338);
#9287=CYLINDRICAL_SURFACE('',#50361,0.728807963573386);
#9288=CYLINDRICAL_SURFACE('',#50364,1.46111700181695);
#9289=CYLINDRICAL_SURFACE('',#50367,0.861117001816902);
#9290=CYLINDRICAL_SURFACE('',#50370,1.6204820426246);
#9291=CYLINDRICAL_SURFACE('',#50373,1.02048204262456);
#9292=CYLINDRICAL_SURFACE('',#50376,1.70100022308284);
#9293=CYLINDRICAL_SURFACE('',#50379,1.10100022308279);
#9294=CYLINDRICAL_SURFACE('',#50382,1.72127463204352);
#9295=CYLINDRICAL_SURFACE('',#50385,1.12127463204348);
#9296=CYLINDRICAL_SURFACE('',#50388,1.78199265440493);
#9297=CYLINDRICAL_SURFACE('',#50391,1.18199265440494);
#9298=CYLINDRICAL_SURFACE('',#50394,1.66088080992083);
#9299=CYLINDRICAL_SURFACE('',#50397,1.06088080992078);
#9300=CYLINDRICAL_SURFACE('',#50400,1.10035806567466);
#9301=CYLINDRICAL_SURFACE('',#50403,0.500358065674666);
#9302=CYLINDRICAL_SURFACE('',#50406,1.21403156673716);
#9303=CYLINDRICAL_SURFACE('',#50409,0.614031566737172);
#9304=CYLINDRICAL_SURFACE('',#50412,1.32880796357326);
#9305=CYLINDRICAL_SURFACE('',#50415,0.728807963573275);
#9306=CYLINDRICAL_SURFACE('',#50418,1.46111700181689);
#9307=CYLINDRICAL_SURFACE('',#50421,0.861117001816847);
#9308=CYLINDRICAL_SURFACE('',#50424,1.6204820426246);
#9309=CYLINDRICAL_SURFACE('',#50427,1.02048204262456);
#9310=CYLINDRICAL_SURFACE('',#50430,1.70100022308284);
#9311=CYLINDRICAL_SURFACE('',#50433,1.10100022308285);
#9312=CYLINDRICAL_SURFACE('',#50436,1.72127463204352);
#9313=CYLINDRICAL_SURFACE('',#50439,1.12127463204348);
#9314=CYLINDRICAL_SURFACE('',#50442,1.78199265440498);
#9315=CYLINDRICAL_SURFACE('',#50445,1.18199265440494);
#9316=CYLINDRICAL_SURFACE('',#50448,1.66088080992077);
#9317=CYLINDRICAL_SURFACE('',#50451,1.06088080992078);
#9318=CYLINDRICAL_SURFACE('',#50454,1.10035806567471);
#9319=CYLINDRICAL_SURFACE('',#50457,0.500358065674666);
#9320=CYLINDRICAL_SURFACE('',#50460,1.21403156673716);
#9321=CYLINDRICAL_SURFACE('',#50463,0.614031566737117);
#9322=CYLINDRICAL_SURFACE('',#50466,1.32880796357332);
#9323=CYLINDRICAL_SURFACE('',#50469,0.72880796357333);
#9324=CYLINDRICAL_SURFACE('',#50472,1.46111700181689);
#9325=CYLINDRICAL_SURFACE('',#50475,0.861117001816902);
#9326=CYLINDRICAL_SURFACE('',#50478,1.62048204262455);
#9327=CYLINDRICAL_SURFACE('',#50481,1.02048204262456);
#9328=CYLINDRICAL_SURFACE('',#50484,1.70100022308278);
#9329=CYLINDRICAL_SURFACE('',#50487,1.10100022308285);
#9330=CYLINDRICAL_SURFACE('',#50490,1.72127463204347);
#9331=CYLINDRICAL_SURFACE('',#50493,1.12127463204348);
#9332=CYLINDRICAL_SURFACE('',#50496,1.78199265440493);
#9333=CYLINDRICAL_SURFACE('',#50499,1.18199265440488);
#9334=CYLINDRICAL_SURFACE('',#50502,1.66088080992083);
#9335=CYLINDRICAL_SURFACE('',#50505,1.06088080992078);
#9336=CYLINDRICAL_SURFACE('',#50508,1.10035806567471);
#9337=CYLINDRICAL_SURFACE('',#50511,0.500358065674666);
#9338=CYLINDRICAL_SURFACE('',#50514,1.21403156673716);
#9339=CYLINDRICAL_SURFACE('',#50517,0.614031566737117);
#9340=CYLINDRICAL_SURFACE('',#50520,1.32880796357332);
#9341=CYLINDRICAL_SURFACE('',#50523,0.72880796357333);
#9342=CYLINDRICAL_SURFACE('',#50526,1.46111700181689);
#9343=CYLINDRICAL_SURFACE('',#50529,0.861117001816902);
#9344=CYLINDRICAL_SURFACE('',#50532,1.6204820426246);
#9345=CYLINDRICAL_SURFACE('',#50535,1.02048204262462);
#9346=CYLINDRICAL_SURFACE('',#50538,1.70100022308284);
#9347=CYLINDRICAL_SURFACE('',#50541,1.10100022308285);
#9348=CYLINDRICAL_SURFACE('',#50544,1.72127463204352);
#9349=CYLINDRICAL_SURFACE('',#50547,1.12127463204353);
#9350=CYLINDRICAL_SURFACE('',#50550,1.78199265440493);
#9351=CYLINDRICAL_SURFACE('',#50553,1.18199265440488);
#9352=CYLINDRICAL_SURFACE('',#50556,1.66088080992077);
#9353=CYLINDRICAL_SURFACE('',#50559,1.06088080992078);
#9354=CYLINDRICAL_SURFACE('',#50562,1.10035806567477);
#9355=CYLINDRICAL_SURFACE('',#50565,0.500358065674722);
#9356=CYLINDRICAL_SURFACE('',#50568,1.21403156673711);
#9357=CYLINDRICAL_SURFACE('',#50571,0.614031566737061);
#9358=CYLINDRICAL_SURFACE('',#50574,1.32880796357332);
#9359=CYLINDRICAL_SURFACE('',#50577,0.728807963573275);
#9360=CYLINDRICAL_SURFACE('',#50580,1.46111700181684);
#9361=CYLINDRICAL_SURFACE('',#50583,0.861117001816847);
#9362=CYLINDRICAL_SURFACE('',#50586,1.6204820426246);
#9363=CYLINDRICAL_SURFACE('',#50589,1.02048204262456);
#9364=CYLINDRICAL_SURFACE('',#50592,1.70100022308278);
#9365=CYLINDRICAL_SURFACE('',#50595,1.10100022308279);
#9366=CYLINDRICAL_SURFACE('',#50598,1.72127463204352);
#9367=CYLINDRICAL_SURFACE('',#50601,1.12127463204353);
#9368=CYLINDRICAL_SURFACE('',#50604,1.78199265440493);
#9369=CYLINDRICAL_SURFACE('',#50607,1.18199265440494);
#9370=CYLINDRICAL_SURFACE('',#50610,1.66088080992077);
#9371=CYLINDRICAL_SURFACE('',#50613,1.06088080992073);
#9372=CYLINDRICAL_SURFACE('',#50616,1.10035806567471);
#9373=CYLINDRICAL_SURFACE('',#50619,0.500358065674722);
#9374=CYLINDRICAL_SURFACE('',#50622,1.21403156673711);
#9375=CYLINDRICAL_SURFACE('',#50625,0.614031566737117);
#9376=CYLINDRICAL_SURFACE('',#50628,1.32880796357332);
#9377=CYLINDRICAL_SURFACE('',#50631,0.728807963573275);
#9378=CYLINDRICAL_SURFACE('',#50634,1.46111700181684);
#9379=CYLINDRICAL_SURFACE('',#50637,0.861117001816902);
#9380=CYLINDRICAL_SURFACE('',#50640,1.6204820426246);
#9381=CYLINDRICAL_SURFACE('',#50643,1.02048204262462);
#9382=CYLINDRICAL_SURFACE('',#50646,1.70100022308289);
#9383=CYLINDRICAL_SURFACE('',#50649,1.10100022308285);
#9384=CYLINDRICAL_SURFACE('',#50652,1.72127463204347);
#9385=CYLINDRICAL_SURFACE('',#50655,1.12127463204342);
#9386=CYLINDRICAL_SURFACE('',#50658,1.78199265440498);
#9387=CYLINDRICAL_SURFACE('',#50661,1.18199265440494);
#9388=CYLINDRICAL_SURFACE('',#50664,1.66088080992077);
#9389=CYLINDRICAL_SURFACE('',#50667,1.06088080992078);
#9390=CYLINDRICAL_SURFACE('',#50670,1.10035806567471);
#9391=CYLINDRICAL_SURFACE('',#50673,0.500358065674666);
#9392=CYLINDRICAL_SURFACE('',#50676,1.21403156673711);
#9393=CYLINDRICAL_SURFACE('',#50679,0.614031566737117);
#9394=CYLINDRICAL_SURFACE('',#50682,1.32880796357332);
#9395=CYLINDRICAL_SURFACE('',#50685,0.72880796357333);
#9396=CYLINDRICAL_SURFACE('',#50688,1.46111700181684);
#9397=CYLINDRICAL_SURFACE('',#50691,0.861117001816847);
#9398=CYLINDRICAL_SURFACE('',#50694,1.6204820426246);
#9399=CYLINDRICAL_SURFACE('',#50697,1.02048204262456);
#9400=CYLINDRICAL_SURFACE('',#50700,1.70100022308284);
#9401=CYLINDRICAL_SURFACE('',#50703,1.10100022308285);
#9402=CYLINDRICAL_SURFACE('',#50706,1.72127463204347);
#9403=CYLINDRICAL_SURFACE('',#50709,1.12127463204353);
#9404=CYLINDRICAL_SURFACE('',#50712,1.78199265440498);
#9405=CYLINDRICAL_SURFACE('',#50715,1.18199265440494);
#9406=CYLINDRICAL_SURFACE('',#50718,1.66088080992083);
#9407=CYLINDRICAL_SURFACE('',#50721,1.06088080992078);
#9408=CYLINDRICAL_SURFACE('',#50724,1.10035806567477);
#9409=CYLINDRICAL_SURFACE('',#50727,0.500358065674777);
#9410=CYLINDRICAL_SURFACE('',#50730,1.21403156673705);
#9411=CYLINDRICAL_SURFACE('',#50733,0.614031566737117);
#9412=CYLINDRICAL_SURFACE('',#50736,1.32880796357326);
#9413=CYLINDRICAL_SURFACE('',#50739,0.728807963573275);
#9414=CYLINDRICAL_SURFACE('',#50742,1.46111700181684);
#9415=CYLINDRICAL_SURFACE('',#50745,0.861117001816847);
#9416=CYLINDRICAL_SURFACE('',#50748,1.6204820426246);
#9417=CYLINDRICAL_SURFACE('',#50751,1.02048204262462);
#9418=CYLINDRICAL_SURFACE('',#50754,1.70100022308278);
#9419=CYLINDRICAL_SURFACE('',#50757,1.10100022308285);
#9420=CYLINDRICAL_SURFACE('',#50760,1.72127463204347);
#9421=CYLINDRICAL_SURFACE('',#50763,1.12127463204353);
#9422=CYLINDRICAL_SURFACE('',#50766,1.78199265440493);
#9423=CYLINDRICAL_SURFACE('',#50769,1.18199265440494);
#9424=CYLINDRICAL_SURFACE('',#50772,1.66088080992077);
#9425=CYLINDRICAL_SURFACE('',#50775,1.06088080992078);
#9426=CYLINDRICAL_SURFACE('',#50778,1.10035806567471);
#9427=CYLINDRICAL_SURFACE('',#50781,0.500358065674722);
#9428=CYLINDRICAL_SURFACE('',#50784,1.21403156673716);
#9429=CYLINDRICAL_SURFACE('',#50787,0.614031566737117);
#9430=CYLINDRICAL_SURFACE('',#50790,1.32880796357332);
#9431=CYLINDRICAL_SURFACE('',#50793,0.72880796357333);
#9432=CYLINDRICAL_SURFACE('',#50796,1.46111700181689);
#9433=CYLINDRICAL_SURFACE('',#50799,0.861117001816902);
#9434=CYLINDRICAL_SURFACE('',#50802,1.6204820426246);
#9435=CYLINDRICAL_SURFACE('',#50805,1.02048204262462);
#9436=CYLINDRICAL_SURFACE('',#50808,1.70100022308284);
#9437=CYLINDRICAL_SURFACE('',#50811,1.10100022308285);
#9438=CYLINDRICAL_SURFACE('',#50814,1.72127463204352);
#9439=CYLINDRICAL_SURFACE('',#50817,1.12127463204348);
#9440=CYLINDRICAL_SURFACE('',#50820,1.78199265440493);
#9441=CYLINDRICAL_SURFACE('',#50823,1.18199265440488);
#9442=CYLINDRICAL_SURFACE('',#50826,1.66088080992088);
#9443=CYLINDRICAL_SURFACE('',#50829,1.06088080992084);
#9444=CYLINDRICAL_SURFACE('',#50832,1.10035806567471);
#9445=CYLINDRICAL_SURFACE('',#50835,0.500358065674722);
#9446=CYLINDRICAL_SURFACE('',#50838,1.21403156673716);
#9447=CYLINDRICAL_SURFACE('',#50841,0.614031566737117);
#9448=CYLINDRICAL_SURFACE('',#50844,1.32880796357332);
#9449=CYLINDRICAL_SURFACE('',#50847,0.72880796357333);
#9450=CYLINDRICAL_SURFACE('',#50850,1.46111700181689);
#9451=CYLINDRICAL_SURFACE('',#50853,0.861117001816902);
#9452=CYLINDRICAL_SURFACE('',#50856,1.6204820426246);
#9453=CYLINDRICAL_SURFACE('',#50859,1.02048204262462);
#9454=CYLINDRICAL_SURFACE('',#50862,1.70100022308284);
#9455=CYLINDRICAL_SURFACE('',#50865,1.10100022308285);
#9456=CYLINDRICAL_SURFACE('',#50868,1.72127463204352);
#9457=CYLINDRICAL_SURFACE('',#50871,1.12127463204348);
#9458=CYLINDRICAL_SURFACE('',#50874,1.78199265440493);
#9459=CYLINDRICAL_SURFACE('',#50877,1.18199265440494);
#9460=CYLINDRICAL_SURFACE('',#50880,1.66088080992077);
#9461=CYLINDRICAL_SURFACE('',#50883,1.06088080992078);
#9462=CYLINDRICAL_SURFACE('',#50890,127.41606204049);
#9463=CYLINDRICAL_SURFACE('',#50901,12.3670707361132);
#9464=CYLINDRICAL_SURFACE('',#50922,130.);
#9465=CYLINDRICAL_SURFACE('',#50923,0.878303132193281);
#9466=CYLINDRICAL_SURFACE('',#50925,1.47830313219333);
#9467=FACE_OUTER_BOUND('',#12868,.T.);
#9468=FACE_OUTER_BOUND('',#12869,.T.);
#9469=FACE_OUTER_BOUND('',#12870,.T.);
#9470=FACE_OUTER_BOUND('',#12871,.T.);
#9471=FACE_OUTER_BOUND('',#12872,.T.);
#9472=FACE_OUTER_BOUND('',#12873,.T.);
#9473=FACE_OUTER_BOUND('',#12874,.T.);
#9474=FACE_OUTER_BOUND('',#12875,.T.);
#9475=FACE_OUTER_BOUND('',#12876,.T.);
#9476=FACE_OUTER_BOUND('',#12877,.T.);
#9477=FACE_OUTER_BOUND('',#12878,.T.);
#9478=FACE_OUTER_BOUND('',#12879,.T.);
#9479=FACE_OUTER_BOUND('',#12880,.T.);
#9480=FACE_OUTER_BOUND('',#12881,.T.);
#9481=FACE_OUTER_BOUND('',#12882,.T.);
#9482=FACE_OUTER_BOUND('',#12883,.T.);
#9483=FACE_OUTER_BOUND('',#12884,.T.);
#9484=FACE_OUTER_BOUND('',#12885,.T.);
#9485=FACE_OUTER_BOUND('',#12886,.T.);
#9486=FACE_OUTER_BOUND('',#12887,.T.);
#9487=FACE_OUTER_BOUND('',#12888,.T.);
#9488=FACE_OUTER_BOUND('',#12889,.T.);
#9489=FACE_OUTER_BOUND('',#12890,.T.);
#9490=FACE_OUTER_BOUND('',#12891,.T.);
#9491=FACE_OUTER_BOUND('',#12892,.T.);
#9492=FACE_OUTER_BOUND('',#12893,.T.);
#9493=FACE_OUTER_BOUND('',#12894,.T.);
#9494=FACE_OUTER_BOUND('',#12895,.T.);
#9495=FACE_OUTER_BOUND('',#12896,.T.);
#9496=FACE_OUTER_BOUND('',#12897,.T.);
#9497=FACE_OUTER_BOUND('',#12898,.T.);
#9498=FACE_OUTER_BOUND('',#12899,.T.);
#9499=FACE_OUTER_BOUND('',#12900,.T.);
#9500=FACE_OUTER_BOUND('',#12901,.T.);
#9501=FACE_OUTER_BOUND('',#12902,.T.);
#9502=FACE_OUTER_BOUND('',#12903,.T.);
#9503=FACE_OUTER_BOUND('',#12904,.T.);
#9504=FACE_OUTER_BOUND('',#12905,.T.);
#9505=FACE_OUTER_BOUND('',#12906,.T.);
#9506=FACE_OUTER_BOUND('',#12907,.T.);
#9507=FACE_OUTER_BOUND('',#12908,.T.);
#9508=FACE_OUTER_BOUND('',#12909,.T.);
#9509=FACE_OUTER_BOUND('',#12910,.T.);
#9510=FACE_OUTER_BOUND('',#12911,.T.);
#9511=FACE_OUTER_BOUND('',#12912,.T.);
#9512=FACE_OUTER_BOUND('',#12913,.T.);
#9513=FACE_OUTER_BOUND('',#12914,.T.);
#9514=FACE_OUTER_BOUND('',#12915,.T.);
#9515=FACE_OUTER_BOUND('',#12916,.T.);
#9516=FACE_OUTER_BOUND('',#12917,.T.);
#9517=FACE_OUTER_BOUND('',#12918,.T.);
#9518=FACE_OUTER_BOUND('',#12919,.T.);
#9519=FACE_OUTER_BOUND('',#12920,.T.);
#9520=FACE_OUTER_BOUND('',#12921,.T.);
#9521=FACE_OUTER_BOUND('',#12922,.T.);
#9522=FACE_OUTER_BOUND('',#12923,.T.);
#9523=FACE_OUTER_BOUND('',#12924,.T.);
#9524=FACE_OUTER_BOUND('',#12925,.T.);
#9525=FACE_OUTER_BOUND('',#12926,.T.);
#9526=FACE_OUTER_BOUND('',#12927,.T.);
#9527=FACE_OUTER_BOUND('',#12928,.T.);
#9528=FACE_OUTER_BOUND('',#12929,.T.);
#9529=FACE_OUTER_BOUND('',#12930,.T.);
#9530=FACE_OUTER_BOUND('',#12931,.T.);
#9531=FACE_OUTER_BOUND('',#12932,.T.);
#9532=FACE_OUTER_BOUND('',#12933,.T.);
#9533=FACE_OUTER_BOUND('',#12934,.T.);
#9534=FACE_OUTER_BOUND('',#12935,.T.);
#9535=FACE_OUTER_BOUND('',#12936,.T.);
#9536=FACE_OUTER_BOUND('',#12937,.T.);
#9537=FACE_OUTER_BOUND('',#12938,.T.);
#9538=FACE_OUTER_BOUND('',#12939,.T.);
#9539=FACE_OUTER_BOUND('',#12940,.T.);
#9540=FACE_OUTER_BOUND('',#12941,.T.);
#9541=FACE_OUTER_BOUND('',#12942,.T.);
#9542=FACE_OUTER_BOUND('',#12943,.T.);
#9543=FACE_OUTER_BOUND('',#12944,.T.);
#9544=FACE_OUTER_BOUND('',#12945,.T.);
#9545=FACE_OUTER_BOUND('',#12946,.T.);
#9546=FACE_OUTER_BOUND('',#12947,.T.);
#9547=FACE_OUTER_BOUND('',#12948,.T.);
#9548=FACE_OUTER_BOUND('',#12949,.T.);
#9549=FACE_OUTER_BOUND('',#12950,.T.);
#9550=FACE_OUTER_BOUND('',#12951,.T.);
#9551=FACE_OUTER_BOUND('',#12952,.T.);
#9552=FACE_OUTER_BOUND('',#12953,.T.);
#9553=FACE_OUTER_BOUND('',#12954,.T.);
#9554=FACE_OUTER_BOUND('',#12955,.T.);
#9555=FACE_OUTER_BOUND('',#12956,.T.);
#9556=FACE_OUTER_BOUND('',#12957,.T.);
#9557=FACE_OUTER_BOUND('',#12958,.T.);
#9558=FACE_OUTER_BOUND('',#12959,.T.);
#9559=FACE_OUTER_BOUND('',#12960,.T.);
#9560=FACE_OUTER_BOUND('',#12961,.T.);
#9561=FACE_OUTER_BOUND('',#12962,.T.);
#9562=FACE_OUTER_BOUND('',#12963,.T.);
#9563=FACE_OUTER_BOUND('',#12964,.T.);
#9564=FACE_OUTER_BOUND('',#12965,.T.);
#9565=FACE_OUTER_BOUND('',#12966,.T.);
#9566=FACE_OUTER_BOUND('',#12967,.T.);
#9567=FACE_OUTER_BOUND('',#12968,.T.);
#9568=FACE_OUTER_BOUND('',#12969,.T.);
#9569=FACE_OUTER_BOUND('',#12970,.T.);
#9570=FACE_OUTER_BOUND('',#12971,.T.);
#9571=FACE_OUTER_BOUND('',#12972,.T.);
#9572=FACE_OUTER_BOUND('',#12973,.T.);
#9573=FACE_OUTER_BOUND('',#12974,.T.);
#9574=FACE_OUTER_BOUND('',#12975,.T.);
#9575=FACE_OUTER_BOUND('',#12976,.T.);
#9576=FACE_OUTER_BOUND('',#12977,.T.);
#9577=FACE_OUTER_BOUND('',#12978,.T.);
#9578=FACE_OUTER_BOUND('',#12979,.T.);
#9579=FACE_OUTER_BOUND('',#12980,.T.);
#9580=FACE_OUTER_BOUND('',#12981,.T.);
#9581=FACE_OUTER_BOUND('',#12982,.T.);
#9582=FACE_OUTER_BOUND('',#12983,.T.);
#9583=FACE_OUTER_BOUND('',#12984,.T.);
#9584=FACE_OUTER_BOUND('',#12985,.T.);
#9585=FACE_OUTER_BOUND('',#12986,.T.);
#9586=FACE_OUTER_BOUND('',#12987,.T.);
#9587=FACE_OUTER_BOUND('',#12988,.T.);
#9588=FACE_OUTER_BOUND('',#12989,.T.);
#9589=FACE_OUTER_BOUND('',#12990,.T.);
#9590=FACE_OUTER_BOUND('',#12991,.T.);
#9591=FACE_OUTER_BOUND('',#12992,.T.);
#9592=FACE_OUTER_BOUND('',#12993,.T.);
#9593=FACE_OUTER_BOUND('',#12994,.T.);
#9594=FACE_OUTER_BOUND('',#12995,.T.);
#9595=FACE_OUTER_BOUND('',#12996,.T.);
#9596=FACE_OUTER_BOUND('',#12997,.T.);
#9597=FACE_OUTER_BOUND('',#12998,.T.);
#9598=FACE_OUTER_BOUND('',#12999,.T.);
#9599=FACE_OUTER_BOUND('',#13000,.T.);
#9600=FACE_OUTER_BOUND('',#13001,.T.);
#9601=FACE_OUTER_BOUND('',#13002,.T.);
#9602=FACE_OUTER_BOUND('',#13003,.T.);
#9603=FACE_OUTER_BOUND('',#13004,.T.);
#9604=FACE_OUTER_BOUND('',#13005,.T.);
#9605=FACE_OUTER_BOUND('',#13006,.T.);
#9606=FACE_OUTER_BOUND('',#13007,.T.);
#9607=FACE_OUTER_BOUND('',#13008,.T.);
#9608=FACE_OUTER_BOUND('',#13009,.T.);
#9609=FACE_OUTER_BOUND('',#13010,.T.);
#9610=FACE_OUTER_BOUND('',#13011,.T.);
#9611=FACE_OUTER_BOUND('',#13012,.T.);
#9612=FACE_OUTER_BOUND('',#13013,.T.);
#9613=FACE_OUTER_BOUND('',#13014,.T.);
#9614=FACE_OUTER_BOUND('',#13015,.T.);
#9615=FACE_OUTER_BOUND('',#13016,.T.);
#9616=FACE_OUTER_BOUND('',#13017,.T.);
#9617=FACE_OUTER_BOUND('',#13018,.T.);
#9618=FACE_OUTER_BOUND('',#13019,.T.);
#9619=FACE_OUTER_BOUND('',#13020,.T.);
#9620=FACE_OUTER_BOUND('',#13021,.T.);
#9621=FACE_OUTER_BOUND('',#13022,.T.);
#9622=FACE_OUTER_BOUND('',#13023,.T.);
#9623=FACE_OUTER_BOUND('',#13024,.T.);
#9624=FACE_OUTER_BOUND('',#13025,.T.);
#9625=FACE_OUTER_BOUND('',#13026,.T.);
#9626=FACE_OUTER_BOUND('',#13027,.T.);
#9627=FACE_OUTER_BOUND('',#13028,.T.);
#9628=FACE_OUTER_BOUND('',#13029,.T.);
#9629=FACE_OUTER_BOUND('',#13030,.T.);
#9630=FACE_OUTER_BOUND('',#13031,.T.);
#9631=FACE_OUTER_BOUND('',#13032,.T.);
#9632=FACE_OUTER_BOUND('',#13033,.T.);
#9633=FACE_OUTER_BOUND('',#13034,.T.);
#9634=FACE_OUTER_BOUND('',#13035,.T.);
#9635=FACE_OUTER_BOUND('',#13036,.T.);
#9636=FACE_OUTER_BOUND('',#13037,.T.);
#9637=FACE_OUTER_BOUND('',#13038,.T.);
#9638=FACE_OUTER_BOUND('',#13039,.T.);
#9639=FACE_OUTER_BOUND('',#13040,.T.);
#9640=FACE_OUTER_BOUND('',#13041,.T.);
#9641=FACE_OUTER_BOUND('',#13042,.T.);
#9642=FACE_OUTER_BOUND('',#13043,.T.);
#9643=FACE_OUTER_BOUND('',#13044,.T.);
#9644=FACE_OUTER_BOUND('',#13045,.T.);
#9645=FACE_OUTER_BOUND('',#13046,.T.);
#9646=FACE_OUTER_BOUND('',#13047,.T.);
#9647=FACE_OUTER_BOUND('',#13048,.T.);
#9648=FACE_OUTER_BOUND('',#13049,.T.);
#9649=FACE_OUTER_BOUND('',#13050,.T.);
#9650=FACE_OUTER_BOUND('',#13051,.T.);
#9651=FACE_OUTER_BOUND('',#13052,.T.);
#9652=FACE_OUTER_BOUND('',#13053,.T.);
#9653=FACE_OUTER_BOUND('',#13054,.T.);
#9654=FACE_OUTER_BOUND('',#13055,.T.);
#9655=FACE_OUTER_BOUND('',#13056,.T.);
#9656=FACE_OUTER_BOUND('',#13057,.T.);
#9657=FACE_OUTER_BOUND('',#13058,.T.);
#9658=FACE_OUTER_BOUND('',#13059,.T.);
#9659=FACE_OUTER_BOUND('',#13060,.T.);
#9660=FACE_OUTER_BOUND('',#13061,.T.);
#9661=FACE_OUTER_BOUND('',#13062,.T.);
#9662=FACE_OUTER_BOUND('',#13063,.T.);
#9663=FACE_OUTER_BOUND('',#13064,.T.);
#9664=FACE_OUTER_BOUND('',#13065,.T.);
#9665=FACE_OUTER_BOUND('',#13066,.T.);
#9666=FACE_OUTER_BOUND('',#13067,.T.);
#9667=FACE_OUTER_BOUND('',#13068,.T.);
#9668=FACE_OUTER_BOUND('',#13069,.T.);
#9669=FACE_OUTER_BOUND('',#13070,.T.);
#9670=FACE_OUTER_BOUND('',#13071,.T.);
#9671=FACE_OUTER_BOUND('',#13072,.T.);
#9672=FACE_OUTER_BOUND('',#13073,.T.);
#9673=FACE_OUTER_BOUND('',#13074,.T.);
#9674=FACE_OUTER_BOUND('',#13075,.T.);
#9675=FACE_OUTER_BOUND('',#13076,.T.);
#9676=FACE_OUTER_BOUND('',#13077,.T.);
#9677=FACE_OUTER_BOUND('',#13078,.T.);
#9678=FACE_OUTER_BOUND('',#13079,.T.);
#9679=FACE_OUTER_BOUND('',#13080,.T.);
#9680=FACE_OUTER_BOUND('',#13081,.T.);
#9681=FACE_OUTER_BOUND('',#13082,.T.);
#9682=FACE_OUTER_BOUND('',#13083,.T.);
#9683=FACE_OUTER_BOUND('',#13084,.T.);
#9684=FACE_OUTER_BOUND('',#13085,.T.);
#9685=FACE_OUTER_BOUND('',#13086,.T.);
#9686=FACE_OUTER_BOUND('',#13087,.T.);
#9687=FACE_OUTER_BOUND('',#13088,.T.);
#9688=FACE_OUTER_BOUND('',#13089,.T.);
#9689=FACE_OUTER_BOUND('',#13090,.T.);
#9690=FACE_OUTER_BOUND('',#13091,.T.);
#9691=FACE_OUTER_BOUND('',#13092,.T.);
#9692=FACE_OUTER_BOUND('',#13093,.T.);
#9693=FACE_OUTER_BOUND('',#13094,.T.);
#9694=FACE_OUTER_BOUND('',#13095,.T.);
#9695=FACE_OUTER_BOUND('',#13096,.T.);
#9696=FACE_OUTER_BOUND('',#13097,.T.);
#9697=FACE_OUTER_BOUND('',#13098,.T.);
#9698=FACE_OUTER_BOUND('',#13099,.T.);
#9699=FACE_OUTER_BOUND('',#13100,.T.);
#9700=FACE_OUTER_BOUND('',#13101,.T.);
#9701=FACE_OUTER_BOUND('',#13102,.T.);
#9702=FACE_OUTER_BOUND('',#13103,.T.);
#9703=FACE_OUTER_BOUND('',#13104,.T.);
#9704=FACE_OUTER_BOUND('',#13105,.T.);
#9705=FACE_OUTER_BOUND('',#13106,.T.);
#9706=FACE_OUTER_BOUND('',#13107,.T.);
#9707=FACE_OUTER_BOUND('',#13108,.T.);
#9708=FACE_OUTER_BOUND('',#13109,.T.);
#9709=FACE_OUTER_BOUND('',#13110,.T.);
#9710=FACE_OUTER_BOUND('',#13111,.T.);
#9711=FACE_OUTER_BOUND('',#13112,.T.);
#9712=FACE_OUTER_BOUND('',#13113,.T.);
#9713=FACE_OUTER_BOUND('',#13114,.T.);
#9714=FACE_OUTER_BOUND('',#13115,.T.);
#9715=FACE_OUTER_BOUND('',#13116,.T.);
#9716=FACE_OUTER_BOUND('',#13117,.T.);
#9717=FACE_OUTER_BOUND('',#13118,.T.);
#9718=FACE_OUTER_BOUND('',#13119,.T.);
#9719=FACE_OUTER_BOUND('',#13120,.T.);
#9720=FACE_OUTER_BOUND('',#13121,.T.);
#9721=FACE_OUTER_BOUND('',#13122,.T.);
#9722=FACE_OUTER_BOUND('',#13123,.T.);
#9723=FACE_OUTER_BOUND('',#13124,.T.);
#9724=FACE_OUTER_BOUND('',#13125,.T.);
#9725=FACE_OUTER_BOUND('',#13126,.T.);
#9726=FACE_OUTER_BOUND('',#13127,.T.);
#9727=FACE_OUTER_BOUND('',#13128,.T.);
#9728=FACE_OUTER_BOUND('',#13129,.T.);
#9729=FACE_OUTER_BOUND('',#13130,.T.);
#9730=FACE_OUTER_BOUND('',#13131,.T.);
#9731=FACE_OUTER_BOUND('',#13132,.T.);
#9732=FACE_OUTER_BOUND('',#13133,.T.);
#9733=FACE_OUTER_BOUND('',#13134,.T.);
#9734=FACE_OUTER_BOUND('',#13135,.T.);
#9735=FACE_OUTER_BOUND('',#13136,.T.);
#9736=FACE_OUTER_BOUND('',#13137,.T.);
#9737=FACE_OUTER_BOUND('',#13138,.T.);
#9738=FACE_OUTER_BOUND('',#13139,.T.);
#9739=FACE_OUTER_BOUND('',#13140,.T.);
#9740=FACE_OUTER_BOUND('',#13141,.T.);
#9741=FACE_OUTER_BOUND('',#13142,.T.);
#9742=FACE_OUTER_BOUND('',#13143,.T.);
#9743=FACE_OUTER_BOUND('',#13144,.T.);
#9744=FACE_OUTER_BOUND('',#13145,.T.);
#9745=FACE_OUTER_BOUND('',#13146,.T.);
#9746=FACE_OUTER_BOUND('',#13147,.T.);
#9747=FACE_OUTER_BOUND('',#13148,.T.);
#9748=FACE_OUTER_BOUND('',#13149,.T.);
#9749=FACE_OUTER_BOUND('',#13150,.T.);
#9750=FACE_OUTER_BOUND('',#13151,.T.);
#9751=FACE_OUTER_BOUND('',#13152,.T.);
#9752=FACE_OUTER_BOUND('',#13153,.T.);
#9753=FACE_OUTER_BOUND('',#13154,.T.);
#9754=FACE_OUTER_BOUND('',#13155,.T.);
#9755=FACE_OUTER_BOUND('',#13156,.T.);
#9756=FACE_OUTER_BOUND('',#13157,.T.);
#9757=FACE_OUTER_BOUND('',#13158,.T.);
#9758=FACE_OUTER_BOUND('',#13159,.T.);
#9759=FACE_OUTER_BOUND('',#13160,.T.);
#9760=FACE_OUTER_BOUND('',#13161,.T.);
#9761=FACE_OUTER_BOUND('',#13162,.T.);
#9762=FACE_OUTER_BOUND('',#13163,.T.);
#9763=FACE_OUTER_BOUND('',#13164,.T.);
#9764=FACE_OUTER_BOUND('',#13165,.T.);
#9765=FACE_OUTER_BOUND('',#13166,.T.);
#9766=FACE_OUTER_BOUND('',#13167,.T.);
#9767=FACE_OUTER_BOUND('',#13168,.T.);
#9768=FACE_OUTER_BOUND('',#13169,.T.);
#9769=FACE_OUTER_BOUND('',#13170,.T.);
#9770=FACE_OUTER_BOUND('',#13171,.T.);
#9771=FACE_OUTER_BOUND('',#13172,.T.);
#9772=FACE_OUTER_BOUND('',#13173,.T.);
#9773=FACE_OUTER_BOUND('',#13174,.T.);
#9774=FACE_OUTER_BOUND('',#13175,.T.);
#9775=FACE_OUTER_BOUND('',#13176,.T.);
#9776=FACE_OUTER_BOUND('',#13177,.T.);
#9777=FACE_OUTER_BOUND('',#13178,.T.);
#9778=FACE_OUTER_BOUND('',#13179,.T.);
#9779=FACE_OUTER_BOUND('',#13180,.T.);
#9780=FACE_OUTER_BOUND('',#13181,.T.);
#9781=FACE_OUTER_BOUND('',#13182,.T.);
#9782=FACE_OUTER_BOUND('',#13183,.T.);
#9783=FACE_OUTER_BOUND('',#13184,.T.);
#9784=FACE_OUTER_BOUND('',#13185,.T.);
#9785=FACE_OUTER_BOUND('',#13186,.T.);
#9786=FACE_OUTER_BOUND('',#13187,.T.);
#9787=FACE_OUTER_BOUND('',#13188,.T.);
#9788=FACE_OUTER_BOUND('',#13189,.T.);
#9789=FACE_OUTER_BOUND('',#13190,.T.);
#9790=FACE_OUTER_BOUND('',#13191,.T.);
#9791=FACE_OUTER_BOUND('',#13192,.T.);
#9792=FACE_OUTER_BOUND('',#13193,.T.);
#9793=FACE_OUTER_BOUND('',#13194,.T.);
#9794=FACE_OUTER_BOUND('',#13195,.T.);
#9795=FACE_OUTER_BOUND('',#13196,.T.);
#9796=FACE_OUTER_BOUND('',#13197,.T.);
#9797=FACE_OUTER_BOUND('',#13198,.T.);
#9798=FACE_OUTER_BOUND('',#13199,.T.);
#9799=FACE_OUTER_BOUND('',#13200,.T.);
#9800=FACE_OUTER_BOUND('',#13201,.T.);
#9801=FACE_OUTER_BOUND('',#13202,.T.);
#9802=FACE_OUTER_BOUND('',#13203,.T.);
#9803=FACE_OUTER_BOUND('',#13204,.T.);
#9804=FACE_OUTER_BOUND('',#13205,.T.);
#9805=FACE_OUTER_BOUND('',#13206,.T.);
#9806=FACE_OUTER_BOUND('',#13207,.T.);
#9807=FACE_OUTER_BOUND('',#13208,.T.);
#9808=FACE_OUTER_BOUND('',#13209,.T.);
#9809=FACE_OUTER_BOUND('',#13210,.T.);
#9810=FACE_OUTER_BOUND('',#13211,.T.);
#9811=FACE_OUTER_BOUND('',#13212,.T.);
#9812=FACE_OUTER_BOUND('',#13213,.T.);
#9813=FACE_OUTER_BOUND('',#13214,.T.);
#9814=FACE_OUTER_BOUND('',#13215,.T.);
#9815=FACE_OUTER_BOUND('',#13216,.T.);
#9816=FACE_OUTER_BOUND('',#13217,.T.);
#9817=FACE_OUTER_BOUND('',#13218,.T.);
#9818=FACE_OUTER_BOUND('',#13219,.T.);
#9819=FACE_OUTER_BOUND('',#13220,.T.);
#9820=FACE_OUTER_BOUND('',#13221,.T.);
#9821=FACE_OUTER_BOUND('',#13222,.T.);
#9822=FACE_OUTER_BOUND('',#13223,.T.);
#9823=FACE_OUTER_BOUND('',#13224,.T.);
#9824=FACE_OUTER_BOUND('',#13225,.T.);
#9825=FACE_OUTER_BOUND('',#13226,.T.);
#9826=FACE_OUTER_BOUND('',#13227,.T.);
#9827=FACE_OUTER_BOUND('',#13228,.T.);
#9828=FACE_OUTER_BOUND('',#13229,.T.);
#9829=FACE_OUTER_BOUND('',#13230,.T.);
#9830=FACE_OUTER_BOUND('',#13231,.T.);
#9831=FACE_OUTER_BOUND('',#13232,.T.);
#9832=FACE_OUTER_BOUND('',#13233,.T.);
#9833=FACE_OUTER_BOUND('',#13234,.T.);
#9834=FACE_OUTER_BOUND('',#13235,.T.);
#9835=FACE_OUTER_BOUND('',#13236,.T.);
#9836=FACE_OUTER_BOUND('',#13237,.T.);
#9837=FACE_OUTER_BOUND('',#13238,.T.);
#9838=FACE_OUTER_BOUND('',#13239,.T.);
#9839=FACE_OUTER_BOUND('',#13240,.T.);
#9840=FACE_OUTER_BOUND('',#13241,.T.);
#9841=FACE_OUTER_BOUND('',#13242,.T.);
#9842=FACE_OUTER_BOUND('',#13243,.T.);
#9843=FACE_OUTER_BOUND('',#13244,.T.);
#9844=FACE_OUTER_BOUND('',#13245,.T.);
#9845=FACE_OUTER_BOUND('',#13246,.T.);
#9846=FACE_OUTER_BOUND('',#13247,.T.);
#9847=FACE_OUTER_BOUND('',#13248,.T.);
#9848=FACE_OUTER_BOUND('',#13249,.T.);
#9849=FACE_OUTER_BOUND('',#13250,.T.);
#9850=FACE_OUTER_BOUND('',#13251,.T.);
#9851=FACE_OUTER_BOUND('',#13252,.T.);
#9852=FACE_OUTER_BOUND('',#13253,.T.);
#9853=FACE_OUTER_BOUND('',#13254,.T.);
#9854=FACE_OUTER_BOUND('',#13255,.T.);
#9855=FACE_OUTER_BOUND('',#13256,.T.);
#9856=FACE_OUTER_BOUND('',#13257,.T.);
#9857=FACE_OUTER_BOUND('',#13258,.T.);
#9858=FACE_OUTER_BOUND('',#13259,.T.);
#9859=FACE_OUTER_BOUND('',#13260,.T.);
#9860=FACE_OUTER_BOUND('',#13261,.T.);
#9861=FACE_OUTER_BOUND('',#13262,.T.);
#9862=FACE_OUTER_BOUND('',#13263,.T.);
#9863=FACE_OUTER_BOUND('',#13264,.T.);
#9864=FACE_OUTER_BOUND('',#13265,.T.);
#9865=FACE_OUTER_BOUND('',#13266,.T.);
#9866=FACE_OUTER_BOUND('',#13267,.T.);
#9867=FACE_OUTER_BOUND('',#13268,.T.);
#9868=FACE_OUTER_BOUND('',#13269,.T.);
#9869=FACE_OUTER_BOUND('',#13270,.T.);
#9870=FACE_OUTER_BOUND('',#13271,.T.);
#9871=FACE_OUTER_BOUND('',#13272,.T.);
#9872=FACE_OUTER_BOUND('',#13273,.T.);
#9873=FACE_OUTER_BOUND('',#13274,.T.);
#9874=FACE_OUTER_BOUND('',#13275,.T.);
#9875=FACE_OUTER_BOUND('',#13276,.T.);
#9876=FACE_OUTER_BOUND('',#13277,.T.);
#9877=FACE_OUTER_BOUND('',#13278,.T.);
#9878=FACE_OUTER_BOUND('',#13279,.T.);
#9879=FACE_OUTER_BOUND('',#13280,.T.);
#9880=FACE_OUTER_BOUND('',#13281,.T.);
#9881=FACE_OUTER_BOUND('',#13282,.T.);
#9882=FACE_OUTER_BOUND('',#13283,.T.);
#9883=FACE_OUTER_BOUND('',#13284,.T.);
#9884=FACE_OUTER_BOUND('',#13285,.T.);
#9885=FACE_OUTER_BOUND('',#13286,.T.);
#9886=FACE_OUTER_BOUND('',#13287,.T.);
#9887=FACE_OUTER_BOUND('',#13288,.T.);
#9888=FACE_OUTER_BOUND('',#13289,.T.);
#9889=FACE_OUTER_BOUND('',#13290,.T.);
#9890=FACE_OUTER_BOUND('',#13291,.T.);
#9891=FACE_OUTER_BOUND('',#13292,.T.);
#9892=FACE_OUTER_BOUND('',#13293,.T.);
#9893=FACE_OUTER_BOUND('',#13294,.T.);
#9894=FACE_OUTER_BOUND('',#13295,.T.);
#9895=FACE_OUTER_BOUND('',#13296,.T.);
#9896=FACE_OUTER_BOUND('',#13297,.T.);
#9897=FACE_OUTER_BOUND('',#13298,.T.);
#9898=FACE_OUTER_BOUND('',#13299,.T.);
#9899=FACE_OUTER_BOUND('',#13300,.T.);
#9900=FACE_OUTER_BOUND('',#13301,.T.);
#9901=FACE_OUTER_BOUND('',#13302,.T.);
#9902=FACE_OUTER_BOUND('',#13303,.T.);
#9903=FACE_OUTER_BOUND('',#13304,.T.);
#9904=FACE_OUTER_BOUND('',#13305,.T.);
#9905=FACE_OUTER_BOUND('',#13306,.T.);
#9906=FACE_OUTER_BOUND('',#13307,.T.);
#9907=FACE_OUTER_BOUND('',#13308,.T.);
#9908=FACE_OUTER_BOUND('',#13309,.T.);
#9909=FACE_OUTER_BOUND('',#13310,.T.);
#9910=FACE_OUTER_BOUND('',#13311,.T.);
#9911=FACE_OUTER_BOUND('',#13312,.T.);
#9912=FACE_OUTER_BOUND('',#13313,.T.);
#9913=FACE_OUTER_BOUND('',#13314,.T.);
#9914=FACE_OUTER_BOUND('',#13315,.T.);
#9915=FACE_OUTER_BOUND('',#13316,.T.);
#9916=FACE_OUTER_BOUND('',#13317,.T.);
#9917=FACE_OUTER_BOUND('',#13318,.T.);
#9918=FACE_OUTER_BOUND('',#13319,.T.);
#9919=FACE_OUTER_BOUND('',#13320,.T.);
#9920=FACE_OUTER_BOUND('',#13321,.T.);
#9921=FACE_OUTER_BOUND('',#13322,.T.);
#9922=FACE_OUTER_BOUND('',#13323,.T.);
#9923=FACE_OUTER_BOUND('',#13324,.T.);
#9924=FACE_OUTER_BOUND('',#13325,.T.);
#9925=FACE_OUTER_BOUND('',#13326,.T.);
#9926=FACE_OUTER_BOUND('',#13327,.T.);
#9927=FACE_OUTER_BOUND('',#13328,.T.);
#9928=FACE_OUTER_BOUND('',#13329,.T.);
#9929=FACE_OUTER_BOUND('',#13330,.T.);
#9930=FACE_OUTER_BOUND('',#13331,.T.);
#9931=FACE_OUTER_BOUND('',#13332,.T.);
#9932=FACE_OUTER_BOUND('',#13333,.T.);
#9933=FACE_OUTER_BOUND('',#13334,.T.);
#9934=FACE_OUTER_BOUND('',#13335,.T.);
#9935=FACE_OUTER_BOUND('',#13336,.T.);
#9936=FACE_OUTER_BOUND('',#13337,.T.);
#9937=FACE_OUTER_BOUND('',#13338,.T.);
#9938=FACE_OUTER_BOUND('',#13339,.T.);
#9939=FACE_OUTER_BOUND('',#13340,.T.);
#9940=FACE_OUTER_BOUND('',#13341,.T.);
#9941=FACE_OUTER_BOUND('',#13342,.T.);
#9942=FACE_OUTER_BOUND('',#13343,.T.);
#9943=FACE_OUTER_BOUND('',#13344,.T.);
#9944=FACE_OUTER_BOUND('',#13345,.T.);
#9945=FACE_OUTER_BOUND('',#13346,.T.);
#9946=FACE_OUTER_BOUND('',#13347,.T.);
#9947=FACE_OUTER_BOUND('',#13348,.T.);
#9948=FACE_OUTER_BOUND('',#13349,.T.);
#9949=FACE_OUTER_BOUND('',#13350,.T.);
#9950=FACE_OUTER_BOUND('',#13351,.T.);
#9951=FACE_OUTER_BOUND('',#13352,.T.);
#9952=FACE_OUTER_BOUND('',#13353,.T.);
#9953=FACE_OUTER_BOUND('',#13354,.T.);
#9954=FACE_OUTER_BOUND('',#13355,.T.);
#9955=FACE_OUTER_BOUND('',#13356,.T.);
#9956=FACE_OUTER_BOUND('',#13357,.T.);
#9957=FACE_OUTER_BOUND('',#13358,.T.);
#9958=FACE_OUTER_BOUND('',#13359,.T.);
#9959=FACE_OUTER_BOUND('',#13360,.T.);
#9960=FACE_OUTER_BOUND('',#13361,.T.);
#9961=FACE_OUTER_BOUND('',#13362,.T.);
#9962=FACE_OUTER_BOUND('',#13363,.T.);
#9963=FACE_OUTER_BOUND('',#13364,.T.);
#9964=FACE_OUTER_BOUND('',#13365,.T.);
#9965=FACE_OUTER_BOUND('',#13366,.T.);
#9966=FACE_OUTER_BOUND('',#13367,.T.);
#9967=FACE_OUTER_BOUND('',#13368,.T.);
#9968=FACE_OUTER_BOUND('',#13369,.T.);
#9969=FACE_OUTER_BOUND('',#13370,.T.);
#9970=FACE_OUTER_BOUND('',#13371,.T.);
#9971=FACE_OUTER_BOUND('',#13372,.T.);
#9972=FACE_OUTER_BOUND('',#13373,.T.);
#9973=FACE_OUTER_BOUND('',#13374,.T.);
#9974=FACE_OUTER_BOUND('',#13375,.T.);
#9975=FACE_OUTER_BOUND('',#13376,.T.);
#9976=FACE_OUTER_BOUND('',#13377,.T.);
#9977=FACE_OUTER_BOUND('',#13378,.T.);
#9978=FACE_OUTER_BOUND('',#13379,.T.);
#9979=FACE_OUTER_BOUND('',#13380,.T.);
#9980=FACE_OUTER_BOUND('',#13381,.T.);
#9981=FACE_OUTER_BOUND('',#13382,.T.);
#9982=FACE_OUTER_BOUND('',#13383,.T.);
#9983=FACE_OUTER_BOUND('',#13384,.T.);
#9984=FACE_OUTER_BOUND('',#13385,.T.);
#9985=FACE_OUTER_BOUND('',#13386,.T.);
#9986=FACE_OUTER_BOUND('',#13387,.T.);
#9987=FACE_OUTER_BOUND('',#13388,.T.);
#9988=FACE_OUTER_BOUND('',#13389,.T.);
#9989=FACE_OUTER_BOUND('',#13390,.T.);
#9990=FACE_OUTER_BOUND('',#13391,.T.);
#9991=FACE_OUTER_BOUND('',#13392,.T.);
#9992=FACE_OUTER_BOUND('',#13393,.T.);
#9993=FACE_OUTER_BOUND('',#13394,.T.);
#9994=FACE_OUTER_BOUND('',#13395,.T.);
#9995=FACE_OUTER_BOUND('',#13396,.T.);
#9996=FACE_OUTER_BOUND('',#13397,.T.);
#9997=FACE_OUTER_BOUND('',#13398,.T.);
#9998=FACE_OUTER_BOUND('',#13399,.T.);
#9999=FACE_OUTER_BOUND('',#13400,.T.);
#10000=FACE_OUTER_BOUND('',#13401,.T.);
#10001=FACE_OUTER_BOUND('',#13402,.T.);
#10002=FACE_OUTER_BOUND('',#13403,.T.);
#10003=FACE_OUTER_BOUND('',#13404,.T.);
#10004=FACE_OUTER_BOUND('',#13405,.T.);
#10005=FACE_OUTER_BOUND('',#13406,.T.);
#10006=FACE_OUTER_BOUND('',#13407,.T.);
#10007=FACE_OUTER_BOUND('',#13408,.T.);
#10008=FACE_OUTER_BOUND('',#13409,.T.);
#10009=FACE_OUTER_BOUND('',#13410,.T.);
#10010=FACE_OUTER_BOUND('',#13411,.T.);
#10011=FACE_OUTER_BOUND('',#13412,.T.);
#10012=FACE_OUTER_BOUND('',#13413,.T.);
#10013=FACE_OUTER_BOUND('',#13414,.T.);
#10014=FACE_OUTER_BOUND('',#13415,.T.);
#10015=FACE_OUTER_BOUND('',#13416,.T.);
#10016=FACE_OUTER_BOUND('',#13417,.T.);
#10017=FACE_OUTER_BOUND('',#13418,.T.);
#10018=FACE_OUTER_BOUND('',#13419,.T.);
#10019=FACE_OUTER_BOUND('',#13420,.T.);
#10020=FACE_OUTER_BOUND('',#13421,.T.);
#10021=FACE_OUTER_BOUND('',#13422,.T.);
#10022=FACE_OUTER_BOUND('',#13423,.T.);
#10023=FACE_OUTER_BOUND('',#13424,.T.);
#10024=FACE_OUTER_BOUND('',#13425,.T.);
#10025=FACE_OUTER_BOUND('',#13426,.T.);
#10026=FACE_OUTER_BOUND('',#13427,.T.);
#10027=FACE_OUTER_BOUND('',#13428,.T.);
#10028=FACE_OUTER_BOUND('',#13429,.T.);
#10029=FACE_OUTER_BOUND('',#13430,.T.);
#10030=FACE_OUTER_BOUND('',#13431,.T.);
#10031=FACE_OUTER_BOUND('',#13432,.T.);
#10032=FACE_OUTER_BOUND('',#13433,.T.);
#10033=FACE_OUTER_BOUND('',#13434,.T.);
#10034=FACE_OUTER_BOUND('',#13435,.T.);
#10035=FACE_OUTER_BOUND('',#13436,.T.);
#10036=FACE_OUTER_BOUND('',#13437,.T.);
#10037=FACE_OUTER_BOUND('',#13438,.T.);
#10038=FACE_OUTER_BOUND('',#13439,.T.);
#10039=FACE_OUTER_BOUND('',#13440,.T.);
#10040=FACE_OUTER_BOUND('',#13441,.T.);
#10041=FACE_OUTER_BOUND('',#13442,.T.);
#10042=FACE_OUTER_BOUND('',#13443,.T.);
#10043=FACE_OUTER_BOUND('',#13444,.T.);
#10044=FACE_OUTER_BOUND('',#13445,.T.);
#10045=FACE_OUTER_BOUND('',#13446,.T.);
#10046=FACE_OUTER_BOUND('',#13447,.T.);
#10047=FACE_OUTER_BOUND('',#13448,.T.);
#10048=FACE_OUTER_BOUND('',#13449,.T.);
#10049=FACE_OUTER_BOUND('',#13450,.T.);
#10050=FACE_OUTER_BOUND('',#13451,.T.);
#10051=FACE_OUTER_BOUND('',#13452,.T.);
#10052=FACE_OUTER_BOUND('',#13453,.T.);
#10053=FACE_OUTER_BOUND('',#13454,.T.);
#10054=FACE_OUTER_BOUND('',#13455,.T.);
#10055=FACE_OUTER_BOUND('',#13456,.T.);
#10056=FACE_OUTER_BOUND('',#13457,.T.);
#10057=FACE_OUTER_BOUND('',#13458,.T.);
#10058=FACE_OUTER_BOUND('',#13459,.T.);
#10059=FACE_OUTER_BOUND('',#13460,.T.);
#10060=FACE_OUTER_BOUND('',#13461,.T.);
#10061=FACE_OUTER_BOUND('',#13462,.T.);
#10062=FACE_OUTER_BOUND('',#13463,.T.);
#10063=FACE_OUTER_BOUND('',#13464,.T.);
#10064=FACE_OUTER_BOUND('',#13465,.T.);
#10065=FACE_OUTER_BOUND('',#13466,.T.);
#10066=FACE_OUTER_BOUND('',#13467,.T.);
#10067=FACE_OUTER_BOUND('',#13468,.T.);
#10068=FACE_OUTER_BOUND('',#13469,.T.);
#10069=FACE_OUTER_BOUND('',#13470,.T.);
#10070=FACE_OUTER_BOUND('',#13471,.T.);
#10071=FACE_OUTER_BOUND('',#13472,.T.);
#10072=FACE_OUTER_BOUND('',#13473,.T.);
#10073=FACE_OUTER_BOUND('',#13474,.T.);
#10074=FACE_OUTER_BOUND('',#13475,.T.);
#10075=FACE_OUTER_BOUND('',#13476,.T.);
#10076=FACE_OUTER_BOUND('',#13477,.T.);
#10077=FACE_OUTER_BOUND('',#13478,.T.);
#10078=FACE_OUTER_BOUND('',#13479,.T.);
#10079=FACE_OUTER_BOUND('',#13480,.T.);
#10080=FACE_OUTER_BOUND('',#13481,.T.);
#10081=FACE_OUTER_BOUND('',#13482,.T.);
#10082=FACE_OUTER_BOUND('',#13483,.T.);
#10083=FACE_OUTER_BOUND('',#13484,.T.);
#10084=FACE_OUTER_BOUND('',#13485,.T.);
#10085=FACE_OUTER_BOUND('',#13486,.T.);
#10086=FACE_OUTER_BOUND('',#13487,.T.);
#10087=FACE_OUTER_BOUND('',#13488,.T.);
#10088=FACE_OUTER_BOUND('',#13489,.T.);
#10089=FACE_OUTER_BOUND('',#13490,.T.);
#10090=FACE_OUTER_BOUND('',#13491,.T.);
#10091=FACE_OUTER_BOUND('',#13492,.T.);
#10092=FACE_OUTER_BOUND('',#13493,.T.);
#10093=FACE_OUTER_BOUND('',#13494,.T.);
#10094=FACE_OUTER_BOUND('',#13495,.T.);
#10095=FACE_OUTER_BOUND('',#13496,.T.);
#10096=FACE_OUTER_BOUND('',#13497,.T.);
#10097=FACE_OUTER_BOUND('',#13498,.T.);
#10098=FACE_OUTER_BOUND('',#13499,.T.);
#10099=FACE_OUTER_BOUND('',#13500,.T.);
#10100=FACE_OUTER_BOUND('',#13501,.T.);
#10101=FACE_OUTER_BOUND('',#13502,.T.);
#10102=FACE_OUTER_BOUND('',#13503,.T.);
#10103=FACE_OUTER_BOUND('',#13504,.T.);
#10104=FACE_OUTER_BOUND('',#13505,.T.);
#10105=FACE_OUTER_BOUND('',#13506,.T.);
#10106=FACE_OUTER_BOUND('',#13507,.T.);
#10107=FACE_OUTER_BOUND('',#13508,.T.);
#10108=FACE_OUTER_BOUND('',#13509,.T.);
#10109=FACE_OUTER_BOUND('',#13510,.T.);
#10110=FACE_OUTER_BOUND('',#13511,.T.);
#10111=FACE_OUTER_BOUND('',#13512,.T.);
#10112=FACE_OUTER_BOUND('',#13513,.T.);
#10113=FACE_OUTER_BOUND('',#13514,.T.);
#10114=FACE_OUTER_BOUND('',#13515,.T.);
#10115=FACE_OUTER_BOUND('',#13516,.T.);
#10116=FACE_OUTER_BOUND('',#13517,.T.);
#10117=FACE_OUTER_BOUND('',#13518,.T.);
#10118=FACE_OUTER_BOUND('',#13519,.T.);
#10119=FACE_OUTER_BOUND('',#13520,.T.);
#10120=FACE_OUTER_BOUND('',#13521,.T.);
#10121=FACE_OUTER_BOUND('',#13522,.T.);
#10122=FACE_OUTER_BOUND('',#13523,.T.);
#10123=FACE_OUTER_BOUND('',#13524,.T.);
#10124=FACE_OUTER_BOUND('',#13525,.T.);
#10125=FACE_OUTER_BOUND('',#13526,.T.);
#10126=FACE_OUTER_BOUND('',#13527,.T.);
#10127=FACE_OUTER_BOUND('',#13528,.T.);
#10128=FACE_OUTER_BOUND('',#13529,.T.);
#10129=FACE_OUTER_BOUND('',#13530,.T.);
#10130=FACE_OUTER_BOUND('',#13531,.T.);
#10131=FACE_OUTER_BOUND('',#13532,.T.);
#10132=FACE_OUTER_BOUND('',#13533,.T.);
#10133=FACE_OUTER_BOUND('',#13534,.T.);
#10134=FACE_OUTER_BOUND('',#13535,.T.);
#10135=FACE_OUTER_BOUND('',#13536,.T.);
#10136=FACE_OUTER_BOUND('',#13537,.T.);
#10137=FACE_OUTER_BOUND('',#13538,.T.);
#10138=FACE_OUTER_BOUND('',#13539,.T.);
#10139=FACE_OUTER_BOUND('',#13540,.T.);
#10140=FACE_OUTER_BOUND('',#13541,.T.);
#10141=FACE_OUTER_BOUND('',#13542,.T.);
#10142=FACE_OUTER_BOUND('',#13543,.T.);
#10143=FACE_OUTER_BOUND('',#13592,.T.);
#10144=FACE_OUTER_BOUND('',#13593,.T.);
#10145=FACE_OUTER_BOUND('',#13594,.T.);
#10146=FACE_OUTER_BOUND('',#13595,.T.);
#10147=FACE_OUTER_BOUND('',#13596,.T.);
#10148=FACE_OUTER_BOUND('',#13597,.T.);
#10149=FACE_OUTER_BOUND('',#13598,.T.);
#10150=FACE_OUTER_BOUND('',#13599,.T.);
#10151=FACE_OUTER_BOUND('',#13600,.T.);
#10152=FACE_OUTER_BOUND('',#13601,.T.);
#10153=FACE_OUTER_BOUND('',#13602,.T.);
#10154=FACE_OUTER_BOUND('',#13603,.T.);
#10155=FACE_OUTER_BOUND('',#13604,.T.);
#10156=FACE_OUTER_BOUND('',#13606,.T.);
#10157=FACE_OUTER_BOUND('',#13607,.T.);
#10158=FACE_OUTER_BOUND('',#13608,.T.);
#10159=FACE_OUTER_BOUND('',#13609,.T.);
#10160=FACE_OUTER_BOUND('',#13610,.T.);
#10161=FACE_OUTER_BOUND('',#13611,.T.);
#10162=FACE_OUTER_BOUND('',#13612,.T.);
#10163=FACE_OUTER_BOUND('',#13613,.T.);
#10164=FACE_OUTER_BOUND('',#13614,.T.);
#10165=FACE_OUTER_BOUND('',#13615,.T.);
#10166=FACE_OUTER_BOUND('',#13616,.T.);
#10167=FACE_OUTER_BOUND('',#13617,.T.);
#10168=FACE_OUTER_BOUND('',#13618,.T.);
#10169=FACE_OUTER_BOUND('',#13619,.T.);
#10170=FACE_OUTER_BOUND('',#13620,.T.);
#10171=FACE_OUTER_BOUND('',#13621,.T.);
#10172=FACE_OUTER_BOUND('',#13622,.T.);
#10173=FACE_OUTER_BOUND('',#13623,.T.);
#10174=FACE_OUTER_BOUND('',#13624,.T.);
#10175=FACE_OUTER_BOUND('',#13625,.T.);
#10176=FACE_OUTER_BOUND('',#13626,.T.);
#10177=FACE_OUTER_BOUND('',#13627,.T.);
#10178=FACE_OUTER_BOUND('',#13628,.T.);
#10179=FACE_OUTER_BOUND('',#13629,.T.);
#10180=FACE_OUTER_BOUND('',#13630,.T.);
#10181=FACE_OUTER_BOUND('',#13631,.T.);
#10182=FACE_OUTER_BOUND('',#13632,.T.);
#10183=FACE_OUTER_BOUND('',#13633,.T.);
#10184=FACE_OUTER_BOUND('',#13634,.T.);
#10185=FACE_OUTER_BOUND('',#13635,.T.);
#10186=FACE_OUTER_BOUND('',#13636,.T.);
#10187=FACE_OUTER_BOUND('',#13637,.T.);
#10188=FACE_OUTER_BOUND('',#13638,.T.);
#10189=FACE_OUTER_BOUND('',#13639,.T.);
#10190=FACE_OUTER_BOUND('',#13640,.T.);
#10191=FACE_OUTER_BOUND('',#13641,.T.);
#10192=FACE_OUTER_BOUND('',#13642,.T.);
#10193=FACE_OUTER_BOUND('',#13643,.T.);
#10194=FACE_OUTER_BOUND('',#13644,.T.);
#10195=FACE_OUTER_BOUND('',#13645,.T.);
#10196=FACE_OUTER_BOUND('',#13646,.T.);
#10197=FACE_OUTER_BOUND('',#13647,.T.);
#10198=FACE_OUTER_BOUND('',#13648,.T.);
#10199=FACE_OUTER_BOUND('',#13649,.T.);
#10200=FACE_OUTER_BOUND('',#13650,.T.);
#10201=FACE_OUTER_BOUND('',#13651,.T.);
#10202=FACE_OUTER_BOUND('',#13652,.T.);
#10203=FACE_OUTER_BOUND('',#13653,.T.);
#10204=FACE_OUTER_BOUND('',#13654,.T.);
#10205=FACE_OUTER_BOUND('',#13655,.T.);
#10206=FACE_OUTER_BOUND('',#13656,.T.);
#10207=FACE_OUTER_BOUND('',#13657,.T.);
#10208=FACE_OUTER_BOUND('',#13658,.T.);
#10209=FACE_OUTER_BOUND('',#13659,.T.);
#10210=FACE_OUTER_BOUND('',#13660,.T.);
#10211=FACE_OUTER_BOUND('',#13661,.T.);
#10212=FACE_OUTER_BOUND('',#13662,.T.);
#10213=FACE_OUTER_BOUND('',#13663,.T.);
#10214=FACE_OUTER_BOUND('',#13664,.T.);
#10215=FACE_OUTER_BOUND('',#13665,.T.);
#10216=FACE_OUTER_BOUND('',#13666,.T.);
#10217=FACE_OUTER_BOUND('',#13667,.T.);
#10218=FACE_OUTER_BOUND('',#13668,.T.);
#10219=FACE_OUTER_BOUND('',#13669,.T.);
#10220=FACE_OUTER_BOUND('',#13688,.T.);
#10221=FACE_OUTER_BOUND('',#13925,.T.);
#10222=FACE_OUTER_BOUND('',#13926,.T.);
#10223=FACE_OUTER_BOUND('',#13927,.T.);
#10224=FACE_OUTER_BOUND('',#13928,.T.);
#10225=FACE_OUTER_BOUND('',#13929,.T.);
#10226=FACE_OUTER_BOUND('',#13930,.T.);
#10227=FACE_OUTER_BOUND('',#13931,.T.);
#10228=FACE_OUTER_BOUND('',#13932,.T.);
#10229=FACE_OUTER_BOUND('',#13934,.T.);
#10230=FACE_OUTER_BOUND('',#13935,.T.);
#10231=FACE_OUTER_BOUND('',#13937,.T.);
#10232=FACE_OUTER_BOUND('',#13938,.T.);
#10233=FACE_OUTER_BOUND('',#13940,.T.);
#10234=FACE_OUTER_BOUND('',#13941,.T.);
#10235=FACE_OUTER_BOUND('',#13943,.T.);
#10236=FACE_OUTER_BOUND('',#13944,.T.);
#10237=FACE_OUTER_BOUND('',#13946,.T.);
#10238=FACE_OUTER_BOUND('',#13947,.T.);
#10239=FACE_OUTER_BOUND('',#13949,.T.);
#10240=FACE_OUTER_BOUND('',#13950,.T.);
#10241=FACE_OUTER_BOUND('',#13952,.T.);
#10242=FACE_OUTER_BOUND('',#13953,.T.);
#10243=FACE_OUTER_BOUND('',#13955,.T.);
#10244=FACE_OUTER_BOUND('',#13956,.T.);
#10245=FACE_OUTER_BOUND('',#13958,.T.);
#10246=FACE_OUTER_BOUND('',#13959,.T.);
#10247=FACE_OUTER_BOUND('',#13961,.T.);
#10248=FACE_OUTER_BOUND('',#13962,.T.);
#10249=FACE_OUTER_BOUND('',#13964,.T.);
#10250=FACE_OUTER_BOUND('',#13965,.T.);
#10251=FACE_OUTER_BOUND('',#13967,.T.);
#10252=FACE_OUTER_BOUND('',#13968,.T.);
#10253=FACE_OUTER_BOUND('',#13970,.T.);
#10254=FACE_OUTER_BOUND('',#13971,.T.);
#10255=FACE_OUTER_BOUND('',#13973,.T.);
#10256=FACE_OUTER_BOUND('',#13974,.T.);
#10257=FACE_OUTER_BOUND('',#13976,.T.);
#10258=FACE_OUTER_BOUND('',#13977,.T.);
#10259=FACE_OUTER_BOUND('',#13979,.T.);
#10260=FACE_OUTER_BOUND('',#13980,.T.);
#10261=FACE_OUTER_BOUND('',#13982,.T.);
#10262=FACE_OUTER_BOUND('',#13983,.T.);
#10263=FACE_OUTER_BOUND('',#13985,.T.);
#10264=FACE_OUTER_BOUND('',#13986,.T.);
#10265=FACE_OUTER_BOUND('',#13988,.T.);
#10266=FACE_OUTER_BOUND('',#13989,.T.);
#10267=FACE_OUTER_BOUND('',#13991,.T.);
#10268=FACE_OUTER_BOUND('',#13992,.T.);
#10269=FACE_OUTER_BOUND('',#13994,.T.);
#10270=FACE_OUTER_BOUND('',#13995,.T.);
#10271=FACE_OUTER_BOUND('',#13997,.T.);
#10272=FACE_OUTER_BOUND('',#13998,.T.);
#10273=FACE_OUTER_BOUND('',#14000,.T.);
#10274=FACE_OUTER_BOUND('',#14001,.T.);
#10275=FACE_OUTER_BOUND('',#14003,.T.);
#10276=FACE_OUTER_BOUND('',#14004,.T.);
#10277=FACE_OUTER_BOUND('',#14006,.T.);
#10278=FACE_OUTER_BOUND('',#14007,.T.);
#10279=FACE_OUTER_BOUND('',#14009,.T.);
#10280=FACE_OUTER_BOUND('',#14010,.T.);
#10281=FACE_OUTER_BOUND('',#14012,.T.);
#10282=FACE_OUTER_BOUND('',#14013,.T.);
#10283=FACE_OUTER_BOUND('',#14015,.T.);
#10284=FACE_OUTER_BOUND('',#14016,.T.);
#10285=FACE_OUTER_BOUND('',#14018,.T.);
#10286=FACE_OUTER_BOUND('',#14019,.T.);
#10287=FACE_OUTER_BOUND('',#14021,.T.);
#10288=FACE_OUTER_BOUND('',#14022,.T.);
#10289=FACE_OUTER_BOUND('',#14024,.T.);
#10290=FACE_OUTER_BOUND('',#14025,.T.);
#10291=FACE_OUTER_BOUND('',#14027,.T.);
#10292=FACE_OUTER_BOUND('',#14028,.T.);
#10293=FACE_OUTER_BOUND('',#14030,.T.);
#10294=FACE_OUTER_BOUND('',#14031,.T.);
#10295=FACE_OUTER_BOUND('',#14033,.T.);
#10296=FACE_OUTER_BOUND('',#14034,.T.);
#10297=FACE_OUTER_BOUND('',#14036,.T.);
#10298=FACE_OUTER_BOUND('',#14037,.T.);
#10299=FACE_OUTER_BOUND('',#14039,.T.);
#10300=FACE_OUTER_BOUND('',#14040,.T.);
#10301=FACE_OUTER_BOUND('',#14042,.T.);
#10302=FACE_OUTER_BOUND('',#14043,.T.);
#10303=FACE_OUTER_BOUND('',#14045,.T.);
#10304=FACE_OUTER_BOUND('',#14046,.T.);
#10305=FACE_OUTER_BOUND('',#14048,.T.);
#10306=FACE_OUTER_BOUND('',#14049,.T.);
#10307=FACE_OUTER_BOUND('',#14051,.T.);
#10308=FACE_OUTER_BOUND('',#14052,.T.);
#10309=FACE_OUTER_BOUND('',#14054,.T.);
#10310=FACE_OUTER_BOUND('',#14055,.T.);
#10311=FACE_OUTER_BOUND('',#14057,.T.);
#10312=FACE_OUTER_BOUND('',#14058,.T.);
#10313=FACE_OUTER_BOUND('',#14060,.T.);
#10314=FACE_OUTER_BOUND('',#14061,.T.);
#10315=FACE_OUTER_BOUND('',#14063,.T.);
#10316=FACE_OUTER_BOUND('',#14064,.T.);
#10317=FACE_OUTER_BOUND('',#14066,.T.);
#10318=FACE_OUTER_BOUND('',#14067,.T.);
#10319=FACE_OUTER_BOUND('',#14069,.T.);
#10320=FACE_OUTER_BOUND('',#14070,.T.);
#10321=FACE_OUTER_BOUND('',#14072,.T.);
#10322=FACE_OUTER_BOUND('',#14073,.T.);
#10323=FACE_OUTER_BOUND('',#14075,.T.);
#10324=FACE_OUTER_BOUND('',#14076,.T.);
#10325=FACE_OUTER_BOUND('',#14078,.T.);
#10326=FACE_OUTER_BOUND('',#14079,.T.);
#10327=FACE_OUTER_BOUND('',#14081,.T.);
#10328=FACE_OUTER_BOUND('',#14082,.T.);
#10329=FACE_OUTER_BOUND('',#14084,.T.);
#10330=FACE_OUTER_BOUND('',#14085,.T.);
#10331=FACE_OUTER_BOUND('',#14087,.T.);
#10332=FACE_OUTER_BOUND('',#14088,.T.);
#10333=FACE_OUTER_BOUND('',#14090,.T.);
#10334=FACE_OUTER_BOUND('',#14091,.T.);
#10335=FACE_OUTER_BOUND('',#14093,.T.);
#10336=FACE_OUTER_BOUND('',#14094,.T.);
#10337=FACE_OUTER_BOUND('',#14096,.T.);
#10338=FACE_OUTER_BOUND('',#14097,.T.);
#10339=FACE_OUTER_BOUND('',#14099,.T.);
#10340=FACE_OUTER_BOUND('',#14100,.T.);
#10341=FACE_OUTER_BOUND('',#14102,.T.);
#10342=FACE_OUTER_BOUND('',#14103,.T.);
#10343=FACE_OUTER_BOUND('',#14105,.T.);
#10344=FACE_OUTER_BOUND('',#14106,.T.);
#10345=FACE_OUTER_BOUND('',#14108,.T.);
#10346=FACE_OUTER_BOUND('',#14109,.T.);
#10347=FACE_OUTER_BOUND('',#14111,.T.);
#10348=FACE_OUTER_BOUND('',#14112,.T.);
#10349=FACE_OUTER_BOUND('',#14114,.T.);
#10350=FACE_OUTER_BOUND('',#14115,.T.);
#10351=FACE_OUTER_BOUND('',#14117,.T.);
#10352=FACE_OUTER_BOUND('',#14118,.T.);
#10353=FACE_OUTER_BOUND('',#14120,.T.);
#10354=FACE_OUTER_BOUND('',#14121,.T.);
#10355=FACE_OUTER_BOUND('',#14123,.T.);
#10356=FACE_OUTER_BOUND('',#14124,.T.);
#10357=FACE_OUTER_BOUND('',#14126,.T.);
#10358=FACE_OUTER_BOUND('',#14127,.T.);
#10359=FACE_OUTER_BOUND('',#14129,.T.);
#10360=FACE_OUTER_BOUND('',#14130,.T.);
#10361=FACE_OUTER_BOUND('',#14132,.T.);
#10362=FACE_OUTER_BOUND('',#14133,.T.);
#10363=FACE_OUTER_BOUND('',#14135,.T.);
#10364=FACE_OUTER_BOUND('',#14136,.T.);
#10365=FACE_OUTER_BOUND('',#14138,.T.);
#10366=FACE_OUTER_BOUND('',#14139,.T.);
#10367=FACE_OUTER_BOUND('',#14141,.T.);
#10368=FACE_OUTER_BOUND('',#14142,.T.);
#10369=FACE_OUTER_BOUND('',#14144,.T.);
#10370=FACE_OUTER_BOUND('',#14145,.T.);
#10371=FACE_OUTER_BOUND('',#14147,.T.);
#10372=FACE_OUTER_BOUND('',#14148,.T.);
#10373=FACE_OUTER_BOUND('',#14150,.T.);
#10374=FACE_OUTER_BOUND('',#14151,.T.);
#10375=FACE_OUTER_BOUND('',#14153,.T.);
#10376=FACE_OUTER_BOUND('',#14154,.T.);
#10377=FACE_OUTER_BOUND('',#14156,.T.);
#10378=FACE_OUTER_BOUND('',#14157,.T.);
#10379=FACE_OUTER_BOUND('',#14159,.T.);
#10380=FACE_OUTER_BOUND('',#14160,.T.);
#10381=FACE_OUTER_BOUND('',#14162,.T.);
#10382=FACE_OUTER_BOUND('',#14163,.T.);
#10383=FACE_OUTER_BOUND('',#14165,.T.);
#10384=FACE_OUTER_BOUND('',#14166,.T.);
#10385=FACE_OUTER_BOUND('',#14168,.T.);
#10386=FACE_OUTER_BOUND('',#14169,.T.);
#10387=FACE_OUTER_BOUND('',#14171,.T.);
#10388=FACE_OUTER_BOUND('',#14172,.T.);
#10389=FACE_OUTER_BOUND('',#14174,.T.);
#10390=FACE_OUTER_BOUND('',#14175,.T.);
#10391=FACE_OUTER_BOUND('',#14177,.T.);
#10392=FACE_OUTER_BOUND('',#14178,.T.);
#10393=FACE_OUTER_BOUND('',#14180,.T.);
#10394=FACE_OUTER_BOUND('',#14181,.T.);
#10395=FACE_OUTER_BOUND('',#14183,.T.);
#10396=FACE_OUTER_BOUND('',#14184,.T.);
#10397=FACE_OUTER_BOUND('',#14186,.T.);
#10398=FACE_OUTER_BOUND('',#14187,.T.);
#10399=FACE_OUTER_BOUND('',#14189,.T.);
#10400=FACE_OUTER_BOUND('',#14190,.T.);
#10401=FACE_OUTER_BOUND('',#14192,.T.);
#10402=FACE_OUTER_BOUND('',#14193,.T.);
#10403=FACE_OUTER_BOUND('',#14195,.T.);
#10404=FACE_OUTER_BOUND('',#14196,.T.);
#10405=FACE_OUTER_BOUND('',#14198,.T.);
#10406=FACE_OUTER_BOUND('',#14199,.T.);
#10407=FACE_OUTER_BOUND('',#14201,.T.);
#10408=FACE_OUTER_BOUND('',#14202,.T.);
#10409=FACE_OUTER_BOUND('',#14204,.T.);
#10410=FACE_OUTER_BOUND('',#14205,.T.);
#10411=FACE_OUTER_BOUND('',#14207,.T.);
#10412=FACE_OUTER_BOUND('',#14208,.T.);
#10413=FACE_OUTER_BOUND('',#14210,.T.);
#10414=FACE_OUTER_BOUND('',#14211,.T.);
#10415=FACE_OUTER_BOUND('',#14213,.T.);
#10416=FACE_OUTER_BOUND('',#14214,.T.);
#10417=FACE_OUTER_BOUND('',#14216,.T.);
#10418=FACE_OUTER_BOUND('',#14217,.T.);
#10419=FACE_OUTER_BOUND('',#14219,.T.);
#10420=FACE_OUTER_BOUND('',#14220,.T.);
#10421=FACE_OUTER_BOUND('',#14222,.T.);
#10422=FACE_OUTER_BOUND('',#14223,.T.);
#10423=FACE_OUTER_BOUND('',#14225,.T.);
#10424=FACE_OUTER_BOUND('',#14226,.T.);
#10425=FACE_OUTER_BOUND('',#14228,.T.);
#10426=FACE_OUTER_BOUND('',#14229,.T.);
#10427=FACE_OUTER_BOUND('',#14231,.T.);
#10428=FACE_OUTER_BOUND('',#14232,.T.);
#10429=FACE_OUTER_BOUND('',#14234,.T.);
#10430=FACE_OUTER_BOUND('',#14235,.T.);
#10431=FACE_OUTER_BOUND('',#14237,.T.);
#10432=FACE_OUTER_BOUND('',#14238,.T.);
#10433=FACE_OUTER_BOUND('',#14240,.T.);
#10434=FACE_OUTER_BOUND('',#14241,.T.);
#10435=FACE_OUTER_BOUND('',#14243,.T.);
#10436=FACE_OUTER_BOUND('',#14244,.T.);
#10437=FACE_OUTER_BOUND('',#14246,.T.);
#10438=FACE_OUTER_BOUND('',#14247,.T.);
#10439=FACE_OUTER_BOUND('',#14249,.T.);
#10440=FACE_OUTER_BOUND('',#14250,.T.);
#10441=FACE_OUTER_BOUND('',#14252,.T.);
#10442=FACE_OUTER_BOUND('',#14253,.T.);
#10443=FACE_OUTER_BOUND('',#14255,.T.);
#10444=FACE_OUTER_BOUND('',#14256,.T.);
#10445=FACE_OUTER_BOUND('',#14258,.T.);
#10446=FACE_OUTER_BOUND('',#14259,.T.);
#10447=FACE_OUTER_BOUND('',#14261,.T.);
#10448=FACE_OUTER_BOUND('',#14262,.T.);
#10449=FACE_OUTER_BOUND('',#14264,.T.);
#10450=FACE_OUTER_BOUND('',#14265,.T.);
#10451=FACE_OUTER_BOUND('',#14267,.T.);
#10452=FACE_OUTER_BOUND('',#14268,.T.);
#10453=FACE_OUTER_BOUND('',#14270,.T.);
#10454=FACE_OUTER_BOUND('',#14271,.T.);
#10455=FACE_OUTER_BOUND('',#14273,.T.);
#10456=FACE_OUTER_BOUND('',#14274,.T.);
#10457=FACE_OUTER_BOUND('',#14276,.T.);
#10458=FACE_OUTER_BOUND('',#14277,.T.);
#10459=FACE_OUTER_BOUND('',#14279,.T.);
#10460=FACE_OUTER_BOUND('',#14280,.T.);
#10461=FACE_OUTER_BOUND('',#14282,.T.);
#10462=FACE_OUTER_BOUND('',#14283,.T.);
#10463=FACE_OUTER_BOUND('',#14285,.T.);
#10464=FACE_OUTER_BOUND('',#14286,.T.);
#10465=FACE_OUTER_BOUND('',#14288,.T.);
#10466=FACE_OUTER_BOUND('',#14289,.T.);
#10467=FACE_OUTER_BOUND('',#14291,.T.);
#10468=FACE_OUTER_BOUND('',#14292,.T.);
#10469=FACE_OUTER_BOUND('',#14294,.T.);
#10470=FACE_OUTER_BOUND('',#14295,.T.);
#10471=FACE_OUTER_BOUND('',#14297,.T.);
#10472=FACE_OUTER_BOUND('',#14298,.T.);
#10473=FACE_OUTER_BOUND('',#14300,.T.);
#10474=FACE_OUTER_BOUND('',#14301,.T.);
#10475=FACE_OUTER_BOUND('',#14303,.T.);
#10476=FACE_OUTER_BOUND('',#14304,.T.);
#10477=FACE_OUTER_BOUND('',#14306,.T.);
#10478=FACE_OUTER_BOUND('',#14307,.T.);
#10479=FACE_OUTER_BOUND('',#14309,.T.);
#10480=FACE_OUTER_BOUND('',#14310,.T.);
#10481=FACE_OUTER_BOUND('',#14312,.T.);
#10482=FACE_OUTER_BOUND('',#14313,.T.);
#10483=FACE_OUTER_BOUND('',#14315,.T.);
#10484=FACE_OUTER_BOUND('',#14316,.T.);
#10485=FACE_OUTER_BOUND('',#14318,.T.);
#10486=FACE_OUTER_BOUND('',#14319,.T.);
#10487=FACE_OUTER_BOUND('',#14321,.T.);
#10488=FACE_OUTER_BOUND('',#14322,.T.);
#10489=FACE_OUTER_BOUND('',#14324,.T.);
#10490=FACE_OUTER_BOUND('',#14325,.T.);
#10491=FACE_OUTER_BOUND('',#14327,.T.);
#10492=FACE_OUTER_BOUND('',#14328,.T.);
#10493=FACE_OUTER_BOUND('',#14330,.T.);
#10494=FACE_OUTER_BOUND('',#14331,.T.);
#10495=FACE_OUTER_BOUND('',#14333,.T.);
#10496=FACE_OUTER_BOUND('',#14334,.T.);
#10497=FACE_OUTER_BOUND('',#14336,.T.);
#10498=FACE_OUTER_BOUND('',#14337,.T.);
#10499=FACE_OUTER_BOUND('',#14339,.T.);
#10500=FACE_OUTER_BOUND('',#14340,.T.);
#10501=FACE_OUTER_BOUND('',#14342,.T.);
#10502=FACE_OUTER_BOUND('',#14343,.T.);
#10503=FACE_OUTER_BOUND('',#14345,.T.);
#10504=FACE_OUTER_BOUND('',#14346,.T.);
#10505=FACE_OUTER_BOUND('',#14348,.T.);
#10506=FACE_OUTER_BOUND('',#14349,.T.);
#10507=FACE_OUTER_BOUND('',#14351,.T.);
#10508=FACE_OUTER_BOUND('',#14352,.T.);
#10509=FACE_OUTER_BOUND('',#14354,.T.);
#10510=FACE_OUTER_BOUND('',#14355,.T.);
#10511=FACE_OUTER_BOUND('',#14357,.T.);
#10512=FACE_OUTER_BOUND('',#14358,.T.);
#10513=FACE_OUTER_BOUND('',#14360,.T.);
#10514=FACE_OUTER_BOUND('',#14361,.T.);
#10515=FACE_OUTER_BOUND('',#14363,.T.);
#10516=FACE_OUTER_BOUND('',#14364,.T.);
#10517=FACE_OUTER_BOUND('',#14366,.T.);
#10518=FACE_OUTER_BOUND('',#14367,.T.);
#10519=FACE_OUTER_BOUND('',#14369,.T.);
#10520=FACE_OUTER_BOUND('',#14370,.T.);
#10521=FACE_OUTER_BOUND('',#14372,.T.);
#10522=FACE_OUTER_BOUND('',#14373,.T.);
#10523=FACE_OUTER_BOUND('',#14375,.T.);
#10524=FACE_OUTER_BOUND('',#14376,.T.);
#10525=FACE_OUTER_BOUND('',#14378,.T.);
#10526=FACE_OUTER_BOUND('',#14379,.T.);
#10527=FACE_OUTER_BOUND('',#14381,.T.);
#10528=FACE_OUTER_BOUND('',#14382,.T.);
#10529=FACE_OUTER_BOUND('',#14384,.T.);
#10530=FACE_OUTER_BOUND('',#14385,.T.);
#10531=FACE_OUTER_BOUND('',#14387,.T.);
#10532=FACE_OUTER_BOUND('',#14388,.T.);
#10533=FACE_OUTER_BOUND('',#14390,.T.);
#10534=FACE_OUTER_BOUND('',#14391,.T.);
#10535=FACE_OUTER_BOUND('',#14393,.T.);
#10536=FACE_OUTER_BOUND('',#14394,.T.);
#10537=FACE_OUTER_BOUND('',#14396,.T.);
#10538=FACE_OUTER_BOUND('',#14397,.T.);
#10539=FACE_OUTER_BOUND('',#14399,.T.);
#10540=FACE_OUTER_BOUND('',#14400,.T.);
#10541=FACE_OUTER_BOUND('',#14402,.T.);
#10542=FACE_OUTER_BOUND('',#14403,.T.);
#10543=FACE_OUTER_BOUND('',#14405,.T.);
#10544=FACE_OUTER_BOUND('',#14406,.T.);
#10545=FACE_OUTER_BOUND('',#14408,.T.);
#10546=FACE_OUTER_BOUND('',#14409,.T.);
#10547=FACE_OUTER_BOUND('',#14411,.T.);
#10548=FACE_OUTER_BOUND('',#14412,.T.);
#10549=FACE_OUTER_BOUND('',#14414,.T.);
#10550=FACE_OUTER_BOUND('',#14415,.T.);
#10551=FACE_OUTER_BOUND('',#14417,.T.);
#10552=FACE_OUTER_BOUND('',#14418,.T.);
#10553=FACE_OUTER_BOUND('',#14420,.T.);
#10554=FACE_OUTER_BOUND('',#14421,.T.);
#10555=FACE_OUTER_BOUND('',#14423,.T.);
#10556=FACE_OUTER_BOUND('',#14424,.T.);
#10557=FACE_OUTER_BOUND('',#14426,.T.);
#10558=FACE_OUTER_BOUND('',#14427,.T.);
#10559=FACE_OUTER_BOUND('',#14429,.T.);
#10560=FACE_OUTER_BOUND('',#14430,.T.);
#10561=FACE_OUTER_BOUND('',#14432,.T.);
#10562=FACE_OUTER_BOUND('',#14433,.T.);
#10563=FACE_OUTER_BOUND('',#14435,.T.);
#10564=FACE_OUTER_BOUND('',#14436,.T.);
#10565=FACE_OUTER_BOUND('',#14438,.T.);
#10566=FACE_OUTER_BOUND('',#14439,.T.);
#10567=FACE_OUTER_BOUND('',#14441,.T.);
#10568=FACE_OUTER_BOUND('',#14442,.T.);
#10569=FACE_OUTER_BOUND('',#14444,.T.);
#10570=FACE_OUTER_BOUND('',#14445,.T.);
#10571=FACE_OUTER_BOUND('',#14447,.T.);
#10572=FACE_OUTER_BOUND('',#14448,.T.);
#10573=FACE_OUTER_BOUND('',#14450,.T.);
#10574=FACE_OUTER_BOUND('',#14451,.T.);
#10575=FACE_OUTER_BOUND('',#14453,.T.);
#10576=FACE_OUTER_BOUND('',#14454,.T.);
#10577=FACE_OUTER_BOUND('',#14456,.T.);
#10578=FACE_OUTER_BOUND('',#14457,.T.);
#10579=FACE_OUTER_BOUND('',#14459,.T.);
#10580=FACE_OUTER_BOUND('',#14460,.T.);
#10581=FACE_OUTER_BOUND('',#14462,.T.);
#10582=FACE_OUTER_BOUND('',#14463,.T.);
#10583=FACE_OUTER_BOUND('',#14465,.T.);
#10584=FACE_OUTER_BOUND('',#14466,.T.);
#10585=FACE_OUTER_BOUND('',#14468,.T.);
#10586=FACE_OUTER_BOUND('',#14469,.T.);
#10587=FACE_OUTER_BOUND('',#14471,.T.);
#10588=FACE_OUTER_BOUND('',#14472,.T.);
#10589=FACE_OUTER_BOUND('',#14474,.T.);
#10590=FACE_OUTER_BOUND('',#14475,.T.);
#10591=FACE_OUTER_BOUND('',#14477,.T.);
#10592=FACE_OUTER_BOUND('',#14478,.T.);
#10593=FACE_OUTER_BOUND('',#14480,.T.);
#10594=FACE_OUTER_BOUND('',#14481,.T.);
#10595=FACE_OUTER_BOUND('',#14483,.T.);
#10596=FACE_OUTER_BOUND('',#14484,.T.);
#10597=FACE_OUTER_BOUND('',#14486,.T.);
#10598=FACE_OUTER_BOUND('',#14487,.T.);
#10599=FACE_OUTER_BOUND('',#14489,.T.);
#10600=FACE_OUTER_BOUND('',#14490,.T.);
#10601=FACE_OUTER_BOUND('',#14492,.T.);
#10602=FACE_OUTER_BOUND('',#14493,.T.);
#10603=FACE_OUTER_BOUND('',#14495,.T.);
#10604=FACE_OUTER_BOUND('',#14496,.T.);
#10605=FACE_OUTER_BOUND('',#14498,.T.);
#10606=FACE_OUTER_BOUND('',#14499,.T.);
#10607=FACE_OUTER_BOUND('',#14501,.T.);
#10608=FACE_OUTER_BOUND('',#14502,.T.);
#10609=FACE_OUTER_BOUND('',#14504,.T.);
#10610=FACE_OUTER_BOUND('',#14505,.T.);
#10611=FACE_OUTER_BOUND('',#14507,.T.);
#10612=FACE_OUTER_BOUND('',#14508,.T.);
#10613=FACE_OUTER_BOUND('',#14510,.T.);
#10614=FACE_OUTER_BOUND('',#14511,.T.);
#10615=FACE_OUTER_BOUND('',#14513,.T.);
#10616=FACE_OUTER_BOUND('',#14514,.T.);
#10617=FACE_OUTER_BOUND('',#14516,.T.);
#10618=FACE_OUTER_BOUND('',#14517,.T.);
#10619=FACE_OUTER_BOUND('',#14519,.T.);
#10620=FACE_OUTER_BOUND('',#14520,.T.);
#10621=FACE_OUTER_BOUND('',#14522,.T.);
#10622=FACE_OUTER_BOUND('',#14523,.T.);
#10623=FACE_OUTER_BOUND('',#14525,.T.);
#10624=FACE_OUTER_BOUND('',#14526,.T.);
#10625=FACE_OUTER_BOUND('',#14528,.T.);
#10626=FACE_OUTER_BOUND('',#14529,.T.);
#10627=FACE_OUTER_BOUND('',#14531,.T.);
#10628=FACE_OUTER_BOUND('',#14532,.T.);
#10629=FACE_OUTER_BOUND('',#14534,.T.);
#10630=FACE_OUTER_BOUND('',#14535,.T.);
#10631=FACE_OUTER_BOUND('',#14537,.T.);
#10632=FACE_OUTER_BOUND('',#14538,.T.);
#10633=FACE_OUTER_BOUND('',#14540,.T.);
#10634=FACE_OUTER_BOUND('',#14541,.T.);
#10635=FACE_OUTER_BOUND('',#14543,.T.);
#10636=FACE_OUTER_BOUND('',#14544,.T.);
#10637=FACE_OUTER_BOUND('',#14546,.T.);
#10638=FACE_OUTER_BOUND('',#14547,.T.);
#10639=FACE_OUTER_BOUND('',#14549,.T.);
#10640=FACE_OUTER_BOUND('',#14550,.T.);
#10641=FACE_OUTER_BOUND('',#14552,.T.);
#10642=FACE_OUTER_BOUND('',#14553,.T.);
#10643=FACE_OUTER_BOUND('',#14555,.T.);
#10644=FACE_OUTER_BOUND('',#14556,.T.);
#10645=FACE_OUTER_BOUND('',#14558,.T.);
#10646=FACE_OUTER_BOUND('',#14559,.T.);
#10647=FACE_OUTER_BOUND('',#14561,.T.);
#10648=FACE_OUTER_BOUND('',#14562,.T.);
#10649=FACE_OUTER_BOUND('',#14564,.T.);
#10650=FACE_OUTER_BOUND('',#14565,.T.);
#10651=FACE_OUTER_BOUND('',#14567,.T.);
#10652=FACE_OUTER_BOUND('',#14568,.T.);
#10653=FACE_OUTER_BOUND('',#14570,.T.);
#10654=FACE_OUTER_BOUND('',#14571,.T.);
#10655=FACE_OUTER_BOUND('',#14573,.T.);
#10656=FACE_OUTER_BOUND('',#14574,.T.);
#10657=FACE_OUTER_BOUND('',#14576,.T.);
#10658=FACE_OUTER_BOUND('',#14577,.T.);
#10659=FACE_OUTER_BOUND('',#14579,.T.);
#10660=FACE_OUTER_BOUND('',#14580,.T.);
#10661=FACE_OUTER_BOUND('',#14582,.T.);
#10662=FACE_OUTER_BOUND('',#14583,.T.);
#10663=FACE_OUTER_BOUND('',#14585,.T.);
#10664=FACE_OUTER_BOUND('',#14586,.T.);
#10665=FACE_OUTER_BOUND('',#14588,.T.);
#10666=FACE_OUTER_BOUND('',#14589,.T.);
#10667=FACE_OUTER_BOUND('',#14591,.T.);
#10668=FACE_OUTER_BOUND('',#14592,.T.);
#10669=FACE_OUTER_BOUND('',#14594,.T.);
#10670=FACE_OUTER_BOUND('',#14595,.T.);
#10671=FACE_OUTER_BOUND('',#14597,.T.);
#10672=FACE_OUTER_BOUND('',#14598,.T.);
#10673=FACE_OUTER_BOUND('',#14600,.T.);
#10674=FACE_OUTER_BOUND('',#14601,.T.);
#10675=FACE_OUTER_BOUND('',#14603,.T.);
#10676=FACE_OUTER_BOUND('',#14604,.T.);
#10677=FACE_OUTER_BOUND('',#14606,.T.);
#10678=FACE_OUTER_BOUND('',#14607,.T.);
#10679=FACE_OUTER_BOUND('',#14609,.T.);
#10680=FACE_OUTER_BOUND('',#14610,.T.);
#10681=FACE_OUTER_BOUND('',#14612,.T.);
#10682=FACE_OUTER_BOUND('',#14613,.T.);
#10683=FACE_OUTER_BOUND('',#14615,.T.);
#10684=FACE_OUTER_BOUND('',#14616,.T.);
#10685=FACE_OUTER_BOUND('',#14618,.T.);
#10686=FACE_OUTER_BOUND('',#14619,.T.);
#10687=FACE_OUTER_BOUND('',#14621,.T.);
#10688=FACE_OUTER_BOUND('',#14622,.T.);
#10689=FACE_OUTER_BOUND('',#14624,.T.);
#10690=FACE_OUTER_BOUND('',#14625,.T.);
#10691=FACE_OUTER_BOUND('',#14627,.T.);
#10692=FACE_OUTER_BOUND('',#14628,.T.);
#10693=FACE_OUTER_BOUND('',#14630,.T.);
#10694=FACE_OUTER_BOUND('',#14631,.T.);
#10695=FACE_OUTER_BOUND('',#14633,.T.);
#10696=FACE_OUTER_BOUND('',#14634,.T.);
#10697=FACE_OUTER_BOUND('',#14636,.T.);
#10698=FACE_OUTER_BOUND('',#14637,.T.);
#10699=FACE_OUTER_BOUND('',#14639,.T.);
#10700=FACE_OUTER_BOUND('',#14640,.T.);
#10701=FACE_OUTER_BOUND('',#14642,.T.);
#10702=FACE_OUTER_BOUND('',#14643,.T.);
#10703=FACE_OUTER_BOUND('',#14645,.T.);
#10704=FACE_OUTER_BOUND('',#14646,.T.);
#10705=FACE_OUTER_BOUND('',#14648,.T.);
#10706=FACE_OUTER_BOUND('',#14649,.T.);
#10707=FACE_OUTER_BOUND('',#14651,.T.);
#10708=FACE_OUTER_BOUND('',#14652,.T.);
#10709=FACE_OUTER_BOUND('',#14654,.T.);
#10710=FACE_OUTER_BOUND('',#14655,.T.);
#10711=FACE_OUTER_BOUND('',#14657,.T.);
#10712=FACE_OUTER_BOUND('',#14658,.T.);
#10713=FACE_OUTER_BOUND('',#14660,.T.);
#10714=FACE_OUTER_BOUND('',#14661,.T.);
#10715=FACE_OUTER_BOUND('',#14663,.T.);
#10716=FACE_OUTER_BOUND('',#14664,.T.);
#10717=FACE_OUTER_BOUND('',#14666,.T.);
#10718=FACE_OUTER_BOUND('',#14667,.T.);
#10719=FACE_OUTER_BOUND('',#14669,.T.);
#10720=FACE_OUTER_BOUND('',#14670,.T.);
#10721=FACE_OUTER_BOUND('',#14672,.T.);
#10722=FACE_OUTER_BOUND('',#14673,.T.);
#10723=FACE_OUTER_BOUND('',#14675,.T.);
#10724=FACE_OUTER_BOUND('',#14676,.T.);
#10725=FACE_OUTER_BOUND('',#14678,.T.);
#10726=FACE_OUTER_BOUND('',#14679,.T.);
#10727=FACE_OUTER_BOUND('',#14681,.T.);
#10728=FACE_OUTER_BOUND('',#14682,.T.);
#10729=FACE_OUTER_BOUND('',#14684,.T.);
#10730=FACE_OUTER_BOUND('',#14685,.T.);
#10731=FACE_OUTER_BOUND('',#14687,.T.);
#10732=FACE_OUTER_BOUND('',#14688,.T.);
#10733=FACE_OUTER_BOUND('',#14690,.T.);
#10734=FACE_OUTER_BOUND('',#14691,.T.);
#10735=FACE_OUTER_BOUND('',#14693,.T.);
#10736=FACE_OUTER_BOUND('',#14694,.T.);
#10737=FACE_OUTER_BOUND('',#14696,.T.);
#10738=FACE_OUTER_BOUND('',#14697,.T.);
#10739=FACE_OUTER_BOUND('',#14699,.T.);
#10740=FACE_OUTER_BOUND('',#14700,.T.);
#10741=FACE_OUTER_BOUND('',#14702,.T.);
#10742=FACE_OUTER_BOUND('',#14703,.T.);
#10743=FACE_OUTER_BOUND('',#14705,.T.);
#10744=FACE_OUTER_BOUND('',#14706,.T.);
#10745=FACE_OUTER_BOUND('',#14708,.T.);
#10746=FACE_OUTER_BOUND('',#14709,.T.);
#10747=FACE_OUTER_BOUND('',#14711,.T.);
#10748=FACE_OUTER_BOUND('',#14712,.T.);
#10749=FACE_OUTER_BOUND('',#14714,.T.);
#10750=FACE_OUTER_BOUND('',#14715,.T.);
#10751=FACE_OUTER_BOUND('',#14717,.T.);
#10752=FACE_OUTER_BOUND('',#14718,.T.);
#10753=FACE_OUTER_BOUND('',#14720,.T.);
#10754=FACE_OUTER_BOUND('',#14721,.T.);
#10755=FACE_OUTER_BOUND('',#14723,.T.);
#10756=FACE_OUTER_BOUND('',#14724,.T.);
#10757=FACE_OUTER_BOUND('',#14726,.T.);
#10758=FACE_OUTER_BOUND('',#14727,.T.);
#10759=FACE_OUTER_BOUND('',#14729,.T.);
#10760=FACE_OUTER_BOUND('',#14730,.T.);
#10761=FACE_OUTER_BOUND('',#14732,.T.);
#10762=FACE_OUTER_BOUND('',#14733,.T.);
#10763=FACE_OUTER_BOUND('',#14735,.T.);
#10764=FACE_OUTER_BOUND('',#14736,.T.);
#10765=FACE_OUTER_BOUND('',#14738,.T.);
#10766=FACE_OUTER_BOUND('',#14739,.T.);
#10767=FACE_OUTER_BOUND('',#14741,.T.);
#10768=FACE_OUTER_BOUND('',#14742,.T.);
#10769=FACE_OUTER_BOUND('',#14744,.T.);
#10770=FACE_OUTER_BOUND('',#14745,.T.);
#10771=FACE_OUTER_BOUND('',#14747,.T.);
#10772=FACE_OUTER_BOUND('',#14748,.T.);
#10773=FACE_OUTER_BOUND('',#14750,.T.);
#10774=FACE_OUTER_BOUND('',#14751,.T.);
#10775=FACE_OUTER_BOUND('',#14753,.T.);
#10776=FACE_OUTER_BOUND('',#14754,.T.);
#10777=FACE_OUTER_BOUND('',#14756,.T.);
#10778=FACE_OUTER_BOUND('',#14757,.T.);
#10779=FACE_OUTER_BOUND('',#14759,.T.);
#10780=FACE_OUTER_BOUND('',#14760,.T.);
#10781=FACE_OUTER_BOUND('',#14762,.T.);
#10782=FACE_OUTER_BOUND('',#14763,.T.);
#10783=FACE_OUTER_BOUND('',#14765,.T.);
#10784=FACE_OUTER_BOUND('',#14766,.T.);
#10785=FACE_OUTER_BOUND('',#14768,.T.);
#10786=FACE_OUTER_BOUND('',#14769,.T.);
#10787=FACE_OUTER_BOUND('',#14771,.T.);
#10788=FACE_OUTER_BOUND('',#14772,.T.);
#10789=FACE_OUTER_BOUND('',#14774,.T.);
#10790=FACE_OUTER_BOUND('',#14775,.T.);
#10791=FACE_OUTER_BOUND('',#14777,.T.);
#10792=FACE_OUTER_BOUND('',#14778,.T.);
#10793=FACE_OUTER_BOUND('',#14780,.T.);
#10794=FACE_OUTER_BOUND('',#14781,.T.);
#10795=FACE_OUTER_BOUND('',#14783,.T.);
#10796=FACE_OUTER_BOUND('',#14784,.T.);
#10797=FACE_OUTER_BOUND('',#14786,.T.);
#10798=FACE_OUTER_BOUND('',#14787,.T.);
#10799=FACE_OUTER_BOUND('',#14789,.T.);
#10800=FACE_OUTER_BOUND('',#14790,.T.);
#10801=FACE_OUTER_BOUND('',#14792,.T.);
#10802=FACE_OUTER_BOUND('',#14793,.T.);
#10803=FACE_OUTER_BOUND('',#14795,.T.);
#10804=FACE_OUTER_BOUND('',#14796,.T.);
#10805=FACE_OUTER_BOUND('',#14798,.T.);
#10806=FACE_OUTER_BOUND('',#14799,.T.);
#10807=FACE_OUTER_BOUND('',#14801,.T.);
#10808=FACE_OUTER_BOUND('',#14802,.T.);
#10809=FACE_OUTER_BOUND('',#14804,.T.);
#10810=FACE_OUTER_BOUND('',#14805,.T.);
#10811=FACE_OUTER_BOUND('',#14807,.T.);
#10812=FACE_OUTER_BOUND('',#14808,.T.);
#10813=FACE_OUTER_BOUND('',#14810,.T.);
#10814=FACE_OUTER_BOUND('',#14811,.T.);
#10815=FACE_OUTER_BOUND('',#14813,.T.);
#10816=FACE_OUTER_BOUND('',#14814,.T.);
#10817=FACE_OUTER_BOUND('',#14816,.T.);
#10818=FACE_OUTER_BOUND('',#14817,.T.);
#10819=FACE_OUTER_BOUND('',#14819,.T.);
#10820=FACE_OUTER_BOUND('',#14820,.T.);
#10821=FACE_OUTER_BOUND('',#14822,.T.);
#10822=FACE_OUTER_BOUND('',#14823,.T.);
#10823=FACE_OUTER_BOUND('',#14825,.T.);
#10824=FACE_OUTER_BOUND('',#14826,.T.);
#10825=FACE_OUTER_BOUND('',#14828,.T.);
#10826=FACE_OUTER_BOUND('',#14829,.T.);
#10827=FACE_OUTER_BOUND('',#14831,.T.);
#10828=FACE_OUTER_BOUND('',#14832,.T.);
#10829=FACE_OUTER_BOUND('',#14834,.T.);
#10830=FACE_OUTER_BOUND('',#14835,.T.);
#10831=FACE_OUTER_BOUND('',#14837,.T.);
#10832=FACE_OUTER_BOUND('',#14838,.T.);
#10833=FACE_OUTER_BOUND('',#14840,.T.);
#10834=FACE_OUTER_BOUND('',#14841,.T.);
#10835=FACE_OUTER_BOUND('',#14843,.T.);
#10836=FACE_OUTER_BOUND('',#14844,.T.);
#10837=FACE_OUTER_BOUND('',#14846,.T.);
#10838=FACE_OUTER_BOUND('',#14847,.T.);
#10839=FACE_OUTER_BOUND('',#14849,.T.);
#10840=FACE_OUTER_BOUND('',#14850,.T.);
#10841=FACE_OUTER_BOUND('',#14852,.T.);
#10842=FACE_OUTER_BOUND('',#14853,.T.);
#10843=FACE_OUTER_BOUND('',#14855,.T.);
#10844=FACE_OUTER_BOUND('',#14856,.T.);
#10845=FACE_OUTER_BOUND('',#14858,.T.);
#10846=FACE_OUTER_BOUND('',#14859,.T.);
#10847=FACE_OUTER_BOUND('',#14861,.T.);
#10848=FACE_OUTER_BOUND('',#14862,.T.);
#10849=FACE_OUTER_BOUND('',#14864,.T.);
#10850=FACE_OUTER_BOUND('',#14865,.T.);
#10851=FACE_OUTER_BOUND('',#14867,.T.);
#10852=FACE_OUTER_BOUND('',#14868,.T.);
#10853=FACE_OUTER_BOUND('',#14870,.T.);
#10854=FACE_OUTER_BOUND('',#14871,.T.);
#10855=FACE_OUTER_BOUND('',#14873,.T.);
#10856=FACE_OUTER_BOUND('',#14874,.T.);
#10857=FACE_OUTER_BOUND('',#14876,.T.);
#10858=FACE_OUTER_BOUND('',#14877,.T.);
#10859=FACE_OUTER_BOUND('',#14879,.T.);
#10860=FACE_OUTER_BOUND('',#14880,.T.);
#10861=FACE_OUTER_BOUND('',#14882,.T.);
#10862=FACE_OUTER_BOUND('',#14883,.T.);
#10863=FACE_OUTER_BOUND('',#14885,.T.);
#10864=FACE_OUTER_BOUND('',#14886,.T.);
#10865=FACE_OUTER_BOUND('',#14888,.T.);
#10866=FACE_OUTER_BOUND('',#14889,.T.);
#10867=FACE_OUTER_BOUND('',#14891,.T.);
#10868=FACE_OUTER_BOUND('',#14892,.T.);
#10869=FACE_OUTER_BOUND('',#14894,.T.);
#10870=FACE_OUTER_BOUND('',#14895,.T.);
#10871=FACE_OUTER_BOUND('',#14897,.T.);
#10872=FACE_OUTER_BOUND('',#14898,.T.);
#10873=FACE_OUTER_BOUND('',#14900,.T.);
#10874=FACE_OUTER_BOUND('',#14902,.T.);
#10875=FACE_OUTER_BOUND('',#14903,.T.);
#10876=FACE_OUTER_BOUND('',#14905,.T.);
#10877=FACE_OUTER_BOUND('',#14906,.T.);
#10878=FACE_OUTER_BOUND('',#14908,.T.);
#10879=FACE_OUTER_BOUND('',#14909,.T.);
#10880=FACE_OUTER_BOUND('',#14911,.T.);
#10881=FACE_OUTER_BOUND('',#14912,.T.);
#10882=FACE_OUTER_BOUND('',#14914,.T.);
#10883=FACE_OUTER_BOUND('',#14915,.T.);
#10884=FACE_OUTER_BOUND('',#14917,.T.);
#10885=FACE_OUTER_BOUND('',#14918,.T.);
#10886=FACE_OUTER_BOUND('',#14919,.T.);
#10887=FACE_OUTER_BOUND('',#14920,.T.);
#10888=FACE_OUTER_BOUND('',#14921,.T.);
#10889=FACE_OUTER_BOUND('',#14922,.T.);
#10890=FACE_OUTER_BOUND('',#14923,.T.);
#10891=FACE_OUTER_BOUND('',#14924,.T.);
#10892=FACE_OUTER_BOUND('',#14925,.T.);
#10893=FACE_OUTER_BOUND('',#14927,.T.);
#10894=FACE_OUTER_BOUND('',#14928,.T.);
#10895=FACE_OUTER_BOUND('',#14929,.T.);
#10896=FACE_OUTER_BOUND('',#14931,.T.);
#10897=FACE_OUTER_BOUND('',#14932,.T.);
#10898=FACE_OUTER_BOUND('',#14933,.T.);
#10899=FACE_OUTER_BOUND('',#14934,.T.);
#10900=FACE_OUTER_BOUND('',#14935,.T.);
#10901=FACE_OUTER_BOUND('',#14936,.T.);
#10902=FACE_OUTER_BOUND('',#14937,.T.);
#10903=FACE_OUTER_BOUND('',#14938,.T.);
#10904=FACE_OUTER_BOUND('',#14939,.T.);
#10905=FACE_OUTER_BOUND('',#14940,.T.);
#10906=FACE_OUTER_BOUND('',#14941,.T.);
#10907=FACE_OUTER_BOUND('',#14942,.T.);
#10908=FACE_OUTER_BOUND('',#14943,.T.);
#10909=FACE_OUTER_BOUND('',#14944,.T.);
#10910=FACE_OUTER_BOUND('',#14945,.T.);
#10911=FACE_OUTER_BOUND('',#14946,.T.);
#10912=FACE_OUTER_BOUND('',#14947,.T.);
#10913=FACE_OUTER_BOUND('',#14948,.T.);
#10914=FACE_OUTER_BOUND('',#14949,.T.);
#10915=FACE_OUTER_BOUND('',#14950,.T.);
#10916=FACE_OUTER_BOUND('',#14951,.T.);
#10917=FACE_OUTER_BOUND('',#14952,.T.);
#10918=FACE_OUTER_BOUND('',#14953,.T.);
#10919=FACE_OUTER_BOUND('',#14954,.T.);
#10920=FACE_OUTER_BOUND('',#14955,.T.);
#10921=FACE_OUTER_BOUND('',#14956,.T.);
#10922=FACE_OUTER_BOUND('',#14957,.T.);
#10923=FACE_OUTER_BOUND('',#14958,.T.);
#10924=FACE_OUTER_BOUND('',#14959,.T.);
#10925=FACE_OUTER_BOUND('',#14960,.T.);
#10926=FACE_OUTER_BOUND('',#14961,.T.);
#10927=FACE_OUTER_BOUND('',#14962,.T.);
#10928=FACE_OUTER_BOUND('',#14963,.T.);
#10929=FACE_OUTER_BOUND('',#14964,.T.);
#10930=FACE_OUTER_BOUND('',#14965,.T.);
#10931=FACE_OUTER_BOUND('',#14966,.T.);
#10932=FACE_OUTER_BOUND('',#14967,.T.);
#10933=FACE_OUTER_BOUND('',#14968,.T.);
#10934=FACE_OUTER_BOUND('',#14969,.T.);
#10935=FACE_OUTER_BOUND('',#14970,.T.);
#10936=FACE_OUTER_BOUND('',#14971,.T.);
#10937=FACE_OUTER_BOUND('',#14972,.T.);
#10938=FACE_OUTER_BOUND('',#14973,.T.);
#10939=FACE_OUTER_BOUND('',#14974,.T.);
#10940=FACE_OUTER_BOUND('',#14975,.T.);
#10941=FACE_OUTER_BOUND('',#14976,.T.);
#10942=FACE_OUTER_BOUND('',#14977,.T.);
#10943=FACE_OUTER_BOUND('',#14978,.T.);
#10944=FACE_OUTER_BOUND('',#14979,.T.);
#10945=FACE_OUTER_BOUND('',#14980,.T.);
#10946=FACE_OUTER_BOUND('',#14981,.T.);
#10947=FACE_OUTER_BOUND('',#14982,.T.);
#10948=FACE_OUTER_BOUND('',#14983,.T.);
#10949=FACE_OUTER_BOUND('',#14984,.T.);
#10950=FACE_OUTER_BOUND('',#14985,.T.);
#10951=FACE_OUTER_BOUND('',#14986,.T.);
#10952=FACE_OUTER_BOUND('',#14987,.T.);
#10953=FACE_OUTER_BOUND('',#14988,.T.);
#10954=FACE_OUTER_BOUND('',#14989,.T.);
#10955=FACE_OUTER_BOUND('',#14990,.T.);
#10956=FACE_OUTER_BOUND('',#14991,.T.);
#10957=FACE_OUTER_BOUND('',#14992,.T.);
#10958=FACE_OUTER_BOUND('',#14993,.T.);
#10959=FACE_OUTER_BOUND('',#14994,.T.);
#10960=FACE_OUTER_BOUND('',#14995,.T.);
#10961=FACE_OUTER_BOUND('',#14996,.T.);
#10962=FACE_OUTER_BOUND('',#14997,.T.);
#10963=FACE_OUTER_BOUND('',#14998,.T.);
#10964=FACE_OUTER_BOUND('',#14999,.T.);
#10965=FACE_OUTER_BOUND('',#15000,.T.);
#10966=FACE_OUTER_BOUND('',#15001,.T.);
#10967=FACE_OUTER_BOUND('',#15002,.T.);
#10968=FACE_OUTER_BOUND('',#15003,.T.);
#10969=FACE_OUTER_BOUND('',#15004,.T.);
#10970=FACE_OUTER_BOUND('',#15005,.T.);
#10971=FACE_OUTER_BOUND('',#15006,.T.);
#10972=FACE_OUTER_BOUND('',#15007,.T.);
#10973=FACE_OUTER_BOUND('',#15008,.T.);
#10974=FACE_OUTER_BOUND('',#15009,.T.);
#10975=FACE_OUTER_BOUND('',#15010,.T.);
#10976=FACE_OUTER_BOUND('',#15011,.T.);
#10977=FACE_OUTER_BOUND('',#15012,.T.);
#10978=FACE_OUTER_BOUND('',#15013,.T.);
#10979=FACE_OUTER_BOUND('',#15014,.T.);
#10980=FACE_OUTER_BOUND('',#15015,.T.);
#10981=FACE_OUTER_BOUND('',#15016,.T.);
#10982=FACE_OUTER_BOUND('',#15017,.T.);
#10983=FACE_OUTER_BOUND('',#15018,.T.);
#10984=FACE_OUTER_BOUND('',#15019,.T.);
#10985=FACE_OUTER_BOUND('',#15020,.T.);
#10986=FACE_OUTER_BOUND('',#15021,.T.);
#10987=FACE_OUTER_BOUND('',#15022,.T.);
#10988=FACE_OUTER_BOUND('',#15023,.T.);
#10989=FACE_OUTER_BOUND('',#15024,.T.);
#10990=FACE_OUTER_BOUND('',#15025,.T.);
#10991=FACE_OUTER_BOUND('',#15026,.T.);
#10992=FACE_OUTER_BOUND('',#15027,.T.);
#10993=FACE_OUTER_BOUND('',#15028,.T.);
#10994=FACE_OUTER_BOUND('',#15029,.T.);
#10995=FACE_OUTER_BOUND('',#15030,.T.);
#10996=FACE_OUTER_BOUND('',#15031,.T.);
#10997=FACE_OUTER_BOUND('',#15032,.T.);
#10998=FACE_OUTER_BOUND('',#15033,.T.);
#10999=FACE_OUTER_BOUND('',#15034,.T.);
#11000=FACE_OUTER_BOUND('',#15035,.T.);
#11001=FACE_OUTER_BOUND('',#15036,.T.);
#11002=FACE_OUTER_BOUND('',#15037,.T.);
#11003=FACE_OUTER_BOUND('',#15038,.T.);
#11004=FACE_OUTER_BOUND('',#15039,.T.);
#11005=FACE_OUTER_BOUND('',#15040,.T.);
#11006=FACE_OUTER_BOUND('',#15041,.T.);
#11007=FACE_OUTER_BOUND('',#15042,.T.);
#11008=FACE_OUTER_BOUND('',#15043,.T.);
#11009=FACE_OUTER_BOUND('',#15044,.T.);
#11010=FACE_OUTER_BOUND('',#15045,.T.);
#11011=FACE_OUTER_BOUND('',#15046,.T.);
#11012=FACE_OUTER_BOUND('',#15047,.T.);
#11013=FACE_OUTER_BOUND('',#15048,.T.);
#11014=FACE_OUTER_BOUND('',#15049,.T.);
#11015=FACE_OUTER_BOUND('',#15050,.T.);
#11016=FACE_OUTER_BOUND('',#15051,.T.);
#11017=FACE_OUTER_BOUND('',#15052,.T.);
#11018=FACE_OUTER_BOUND('',#15053,.T.);
#11019=FACE_OUTER_BOUND('',#15054,.T.);
#11020=FACE_OUTER_BOUND('',#15055,.T.);
#11021=FACE_OUTER_BOUND('',#15056,.T.);
#11022=FACE_OUTER_BOUND('',#15057,.T.);
#11023=FACE_OUTER_BOUND('',#15058,.T.);
#11024=FACE_OUTER_BOUND('',#15059,.T.);
#11025=FACE_OUTER_BOUND('',#15060,.T.);
#11026=FACE_OUTER_BOUND('',#15061,.T.);
#11027=FACE_OUTER_BOUND('',#15062,.T.);
#11028=FACE_OUTER_BOUND('',#15063,.T.);
#11029=FACE_OUTER_BOUND('',#15064,.T.);
#11030=FACE_OUTER_BOUND('',#15065,.T.);
#11031=FACE_OUTER_BOUND('',#15066,.T.);
#11032=FACE_OUTER_BOUND('',#15067,.T.);
#11033=FACE_OUTER_BOUND('',#15068,.T.);
#11034=FACE_OUTER_BOUND('',#15069,.T.);
#11035=FACE_OUTER_BOUND('',#15070,.T.);
#11036=FACE_OUTER_BOUND('',#15071,.T.);
#11037=FACE_OUTER_BOUND('',#15072,.T.);
#11038=FACE_OUTER_BOUND('',#15073,.T.);
#11039=FACE_OUTER_BOUND('',#15074,.T.);
#11040=FACE_OUTER_BOUND('',#15075,.T.);
#11041=FACE_OUTER_BOUND('',#15076,.T.);
#11042=FACE_OUTER_BOUND('',#15077,.T.);
#11043=FACE_OUTER_BOUND('',#15078,.T.);
#11044=FACE_OUTER_BOUND('',#15079,.T.);
#11045=FACE_OUTER_BOUND('',#15080,.T.);
#11046=FACE_OUTER_BOUND('',#15081,.T.);
#11047=FACE_OUTER_BOUND('',#15082,.T.);
#11048=FACE_OUTER_BOUND('',#15083,.T.);
#11049=FACE_OUTER_BOUND('',#15084,.T.);
#11050=FACE_OUTER_BOUND('',#15085,.T.);
#11051=FACE_OUTER_BOUND('',#15086,.T.);
#11052=FACE_OUTER_BOUND('',#15087,.T.);
#11053=FACE_OUTER_BOUND('',#15088,.T.);
#11054=FACE_OUTER_BOUND('',#15089,.T.);
#11055=FACE_OUTER_BOUND('',#15090,.T.);
#11056=FACE_OUTER_BOUND('',#15091,.T.);
#11057=FACE_OUTER_BOUND('',#15092,.T.);
#11058=FACE_OUTER_BOUND('',#15093,.T.);
#11059=FACE_OUTER_BOUND('',#15094,.T.);
#11060=FACE_OUTER_BOUND('',#15095,.T.);
#11061=FACE_OUTER_BOUND('',#15096,.T.);
#11062=FACE_OUTER_BOUND('',#15097,.T.);
#11063=FACE_OUTER_BOUND('',#15098,.T.);
#11064=FACE_OUTER_BOUND('',#15099,.T.);
#11065=FACE_OUTER_BOUND('',#15100,.T.);
#11066=FACE_OUTER_BOUND('',#15101,.T.);
#11067=FACE_OUTER_BOUND('',#15102,.T.);
#11068=FACE_OUTER_BOUND('',#15103,.T.);
#11069=FACE_OUTER_BOUND('',#15104,.T.);
#11070=FACE_OUTER_BOUND('',#15105,.T.);
#11071=FACE_OUTER_BOUND('',#15106,.T.);
#11072=FACE_OUTER_BOUND('',#15107,.T.);
#11073=FACE_OUTER_BOUND('',#15108,.T.);
#11074=FACE_OUTER_BOUND('',#15109,.T.);
#11075=FACE_OUTER_BOUND('',#15110,.T.);
#11076=FACE_OUTER_BOUND('',#15111,.T.);
#11077=FACE_OUTER_BOUND('',#15112,.T.);
#11078=FACE_OUTER_BOUND('',#15113,.T.);
#11079=FACE_OUTER_BOUND('',#15114,.T.);
#11080=FACE_OUTER_BOUND('',#15115,.T.);
#11081=FACE_OUTER_BOUND('',#15116,.T.);
#11082=FACE_OUTER_BOUND('',#15117,.T.);
#11083=FACE_OUTER_BOUND('',#15118,.T.);
#11084=FACE_OUTER_BOUND('',#15119,.T.);
#11085=FACE_OUTER_BOUND('',#15120,.T.);
#11086=FACE_OUTER_BOUND('',#15121,.T.);
#11087=FACE_OUTER_BOUND('',#15122,.T.);
#11088=FACE_OUTER_BOUND('',#15123,.T.);
#11089=FACE_OUTER_BOUND('',#15124,.T.);
#11090=FACE_OUTER_BOUND('',#15126,.T.);
#11091=FACE_OUTER_BOUND('',#15127,.T.);
#11092=FACE_OUTER_BOUND('',#15128,.T.);
#11093=FACE_OUTER_BOUND('',#15129,.T.);
#11094=FACE_OUTER_BOUND('',#15130,.T.);
#11095=FACE_OUTER_BOUND('',#15131,.T.);
#11096=FACE_OUTER_BOUND('',#15132,.T.);
#11097=FACE_OUTER_BOUND('',#15133,.T.);
#11098=FACE_OUTER_BOUND('',#15134,.T.);
#11099=FACE_OUTER_BOUND('',#15138,.T.);
#11100=FACE_OUTER_BOUND('',#15139,.T.);
#11101=FACE_OUTER_BOUND('',#15140,.T.);
#11102=FACE_OUTER_BOUND('',#15141,.T.);
#11103=FACE_OUTER_BOUND('',#15142,.T.);
#11104=FACE_OUTER_BOUND('',#15143,.T.);
#11105=FACE_OUTER_BOUND('',#15144,.T.);
#11106=FACE_OUTER_BOUND('',#15145,.T.);
#11107=FACE_OUTER_BOUND('',#15146,.T.);
#11108=FACE_OUTER_BOUND('',#15147,.T.);
#11109=FACE_OUTER_BOUND('',#15148,.T.);
#11110=FACE_OUTER_BOUND('',#15149,.T.);
#11111=FACE_OUTER_BOUND('',#15150,.T.);
#11112=FACE_OUTER_BOUND('',#15151,.T.);
#11113=FACE_OUTER_BOUND('',#15152,.T.);
#11114=FACE_OUTER_BOUND('',#15153,.T.);
#11115=FACE_OUTER_BOUND('',#15154,.T.);
#11116=FACE_OUTER_BOUND('',#15155,.T.);
#11117=FACE_OUTER_BOUND('',#15156,.T.);
#11118=FACE_OUTER_BOUND('',#15157,.T.);
#11119=FACE_OUTER_BOUND('',#15158,.T.);
#11120=FACE_OUTER_BOUND('',#15159,.T.);
#11121=FACE_OUTER_BOUND('',#15160,.T.);
#11122=FACE_OUTER_BOUND('',#15161,.T.);
#11123=FACE_OUTER_BOUND('',#15162,.T.);
#11124=FACE_OUTER_BOUND('',#15163,.T.);
#11125=FACE_OUTER_BOUND('',#15165,.T.);
#11126=FACE_OUTER_BOUND('',#15166,.T.);
#11127=FACE_OUTER_BOUND('',#15167,.T.);
#11128=FACE_OUTER_BOUND('',#15168,.T.);
#11129=FACE_OUTER_BOUND('',#15169,.T.);
#11130=FACE_OUTER_BOUND('',#15170,.T.);
#11131=FACE_OUTER_BOUND('',#15171,.T.);
#11132=FACE_OUTER_BOUND('',#15173,.T.);
#11133=FACE_OUTER_BOUND('',#15174,.T.);
#11134=FACE_OUTER_BOUND('',#15176,.T.);
#11135=FACE_OUTER_BOUND('',#15177,.T.);
#11136=FACE_OUTER_BOUND('',#15178,.T.);
#11137=FACE_OUTER_BOUND('',#15179,.T.);
#11138=FACE_OUTER_BOUND('',#15180,.T.);
#11139=FACE_OUTER_BOUND('',#15181,.T.);
#11140=FACE_OUTER_BOUND('',#15182,.T.);
#11141=FACE_OUTER_BOUND('',#15183,.T.);
#11142=FACE_OUTER_BOUND('',#15184,.T.);
#11143=FACE_OUTER_BOUND('',#15185,.T.);
#11144=FACE_OUTER_BOUND('',#15186,.T.);
#11145=FACE_OUTER_BOUND('',#15187,.T.);
#11146=FACE_OUTER_BOUND('',#15188,.T.);
#11147=FACE_OUTER_BOUND('',#15189,.T.);
#11148=FACE_OUTER_BOUND('',#15190,.T.);
#11149=FACE_OUTER_BOUND('',#15191,.T.);
#11150=FACE_OUTER_BOUND('',#15192,.T.);
#11151=FACE_OUTER_BOUND('',#15193,.T.);
#11152=FACE_OUTER_BOUND('',#15194,.T.);
#11153=FACE_OUTER_BOUND('',#15195,.T.);
#11154=FACE_OUTER_BOUND('',#15196,.T.);
#11155=FACE_OUTER_BOUND('',#15197,.T.);
#11156=FACE_OUTER_BOUND('',#15198,.T.);
#11157=FACE_OUTER_BOUND('',#15199,.T.);
#11158=FACE_OUTER_BOUND('',#15200,.T.);
#11159=FACE_OUTER_BOUND('',#15201,.T.);
#11160=FACE_OUTER_BOUND('',#15202,.T.);
#11161=FACE_OUTER_BOUND('',#15203,.T.);
#11162=FACE_OUTER_BOUND('',#15204,.T.);
#11163=FACE_OUTER_BOUND('',#15205,.T.);
#11164=FACE_OUTER_BOUND('',#15206,.T.);
#11165=FACE_OUTER_BOUND('',#15207,.T.);
#11166=FACE_OUTER_BOUND('',#15208,.T.);
#11167=FACE_OUTER_BOUND('',#15209,.T.);
#11168=FACE_OUTER_BOUND('',#15210,.T.);
#11169=FACE_OUTER_BOUND('',#15211,.T.);
#11170=FACE_OUTER_BOUND('',#15212,.T.);
#11171=FACE_OUTER_BOUND('',#15213,.T.);
#11172=FACE_OUTER_BOUND('',#15214,.T.);
#11173=FACE_OUTER_BOUND('',#15215,.T.);
#11174=FACE_OUTER_BOUND('',#15216,.T.);
#11175=FACE_OUTER_BOUND('',#15217,.T.);
#11176=FACE_OUTER_BOUND('',#15218,.T.);
#11177=FACE_OUTER_BOUND('',#15219,.T.);
#11178=FACE_OUTER_BOUND('',#15220,.T.);
#11179=FACE_OUTER_BOUND('',#15221,.T.);
#11180=FACE_OUTER_BOUND('',#15222,.T.);
#11181=FACE_OUTER_BOUND('',#15223,.T.);
#11182=FACE_OUTER_BOUND('',#15224,.T.);
#11183=FACE_OUTER_BOUND('',#15225,.T.);
#11184=FACE_OUTER_BOUND('',#15226,.T.);
#11185=FACE_OUTER_BOUND('',#15227,.T.);
#11186=FACE_OUTER_BOUND('',#15228,.T.);
#11187=FACE_OUTER_BOUND('',#15229,.T.);
#11188=FACE_OUTER_BOUND('',#15230,.T.);
#11189=FACE_OUTER_BOUND('',#15231,.T.);
#11190=FACE_OUTER_BOUND('',#15232,.T.);
#11191=FACE_OUTER_BOUND('',#15233,.T.);
#11192=FACE_OUTER_BOUND('',#15234,.T.);
#11193=FACE_OUTER_BOUND('',#15235,.T.);
#11194=FACE_OUTER_BOUND('',#15236,.T.);
#11195=FACE_OUTER_BOUND('',#15237,.T.);
#11196=FACE_OUTER_BOUND('',#15238,.T.);
#11197=FACE_OUTER_BOUND('',#15239,.T.);
#11198=FACE_OUTER_BOUND('',#15240,.T.);
#11199=FACE_OUTER_BOUND('',#15241,.T.);
#11200=FACE_OUTER_BOUND('',#15242,.T.);
#11201=FACE_OUTER_BOUND('',#15243,.T.);
#11202=FACE_OUTER_BOUND('',#15244,.T.);
#11203=FACE_OUTER_BOUND('',#15245,.T.);
#11204=FACE_OUTER_BOUND('',#15246,.T.);
#11205=FACE_OUTER_BOUND('',#15247,.T.);
#11206=FACE_OUTER_BOUND('',#15248,.T.);
#11207=FACE_OUTER_BOUND('',#15249,.T.);
#11208=FACE_OUTER_BOUND('',#15250,.T.);
#11209=FACE_OUTER_BOUND('',#15251,.T.);
#11210=FACE_OUTER_BOUND('',#15252,.T.);
#11211=FACE_OUTER_BOUND('',#15253,.T.);
#11212=FACE_OUTER_BOUND('',#15254,.T.);
#11213=FACE_OUTER_BOUND('',#15255,.T.);
#11214=FACE_OUTER_BOUND('',#15256,.T.);
#11215=FACE_OUTER_BOUND('',#15257,.T.);
#11216=FACE_OUTER_BOUND('',#15258,.T.);
#11217=FACE_OUTER_BOUND('',#15259,.T.);
#11218=FACE_OUTER_BOUND('',#15260,.T.);
#11219=FACE_OUTER_BOUND('',#15261,.T.);
#11220=FACE_OUTER_BOUND('',#15262,.T.);
#11221=FACE_OUTER_BOUND('',#15263,.T.);
#11222=FACE_OUTER_BOUND('',#15264,.T.);
#11223=FACE_OUTER_BOUND('',#15268,.T.);
#11224=FACE_OUTER_BOUND('',#15269,.T.);
#11225=FACE_OUTER_BOUND('',#15270,.T.);
#11226=FACE_OUTER_BOUND('',#15271,.T.);
#11227=FACE_OUTER_BOUND('',#15272,.T.);
#11228=FACE_OUTER_BOUND('',#15273,.T.);
#11229=FACE_OUTER_BOUND('',#15274,.T.);
#11230=FACE_OUTER_BOUND('',#15275,.T.);
#11231=FACE_OUTER_BOUND('',#15276,.T.);
#11232=FACE_OUTER_BOUND('',#15277,.T.);
#11233=FACE_OUTER_BOUND('',#15279,.T.);
#11234=FACE_OUTER_BOUND('',#15281,.T.);
#11235=FACE_OUTER_BOUND('',#15282,.T.);
#11236=FACE_OUTER_BOUND('',#15283,.T.);
#11237=FACE_OUTER_BOUND('',#15284,.T.);
#11238=FACE_OUTER_BOUND('',#15285,.T.);
#11239=FACE_OUTER_BOUND('',#15286,.T.);
#11240=FACE_OUTER_BOUND('',#15287,.T.);
#11241=FACE_OUTER_BOUND('',#15288,.T.);
#11242=FACE_OUTER_BOUND('',#15290,.T.);
#11243=FACE_OUTER_BOUND('',#15292,.T.);
#11244=FACE_OUTER_BOUND('',#15293,.T.);
#11245=FACE_OUTER_BOUND('',#15294,.T.);
#11246=FACE_OUTER_BOUND('',#15295,.T.);
#11247=FACE_OUTER_BOUND('',#15296,.T.);
#11248=FACE_OUTER_BOUND('',#15297,.T.);
#11249=FACE_OUTER_BOUND('',#15298,.T.);
#11250=FACE_OUTER_BOUND('',#15299,.T.);
#11251=FACE_OUTER_BOUND('',#15300,.T.);
#11252=FACE_OUTER_BOUND('',#15301,.T.);
#11253=FACE_OUTER_BOUND('',#15302,.T.);
#11254=FACE_OUTER_BOUND('',#15303,.T.);
#11255=FACE_OUTER_BOUND('',#15304,.T.);
#11256=FACE_OUTER_BOUND('',#15305,.T.);
#11257=FACE_OUTER_BOUND('',#15306,.T.);
#11258=FACE_OUTER_BOUND('',#15307,.T.);
#11259=FACE_OUTER_BOUND('',#15308,.T.);
#11260=FACE_OUTER_BOUND('',#15309,.T.);
#11261=FACE_OUTER_BOUND('',#15310,.T.);
#11262=FACE_OUTER_BOUND('',#15311,.T.);
#11263=FACE_OUTER_BOUND('',#15312,.T.);
#11264=FACE_OUTER_BOUND('',#15313,.T.);
#11265=FACE_OUTER_BOUND('',#15314,.T.);
#11266=FACE_OUTER_BOUND('',#15315,.T.);
#11267=FACE_OUTER_BOUND('',#15316,.T.);
#11268=FACE_OUTER_BOUND('',#15317,.T.);
#11269=FACE_OUTER_BOUND('',#15318,.T.);
#11270=FACE_OUTER_BOUND('',#15319,.T.);
#11271=FACE_OUTER_BOUND('',#15320,.T.);
#11272=FACE_OUTER_BOUND('',#15321,.T.);
#11273=FACE_OUTER_BOUND('',#15322,.T.);
#11274=FACE_OUTER_BOUND('',#15323,.T.);
#11275=FACE_OUTER_BOUND('',#15324,.T.);
#11276=FACE_OUTER_BOUND('',#15325,.T.);
#11277=FACE_OUTER_BOUND('',#15326,.T.);
#11278=FACE_OUTER_BOUND('',#15327,.T.);
#11279=FACE_OUTER_BOUND('',#15328,.T.);
#11280=FACE_OUTER_BOUND('',#15329,.T.);
#11281=FACE_OUTER_BOUND('',#15330,.T.);
#11282=FACE_OUTER_BOUND('',#15331,.T.);
#11283=FACE_OUTER_BOUND('',#15332,.T.);
#11284=FACE_OUTER_BOUND('',#15333,.T.);
#11285=FACE_OUTER_BOUND('',#15334,.T.);
#11286=FACE_OUTER_BOUND('',#15336,.T.);
#11287=FACE_OUTER_BOUND('',#15337,.T.);
#11288=FACE_OUTER_BOUND('',#15398,.T.);
#11289=FACE_OUTER_BOUND('',#15399,.T.);
#11290=FACE_OUTER_BOUND('',#15400,.T.);
#11291=FACE_OUTER_BOUND('',#15401,.T.);
#11292=FACE_OUTER_BOUND('',#15402,.T.);
#11293=FACE_OUTER_BOUND('',#15403,.T.);
#11294=FACE_OUTER_BOUND('',#15404,.T.);
#11295=FACE_OUTER_BOUND('',#15405,.T.);
#11296=FACE_OUTER_BOUND('',#15406,.T.);
#11297=FACE_OUTER_BOUND('',#15407,.T.);
#11298=FACE_OUTER_BOUND('',#15408,.T.);
#11299=FACE_OUTER_BOUND('',#15409,.T.);
#11300=FACE_OUTER_BOUND('',#15410,.T.);
#11301=FACE_OUTER_BOUND('',#15411,.T.);
#11302=FACE_OUTER_BOUND('',#15412,.T.);
#11303=FACE_OUTER_BOUND('',#15413,.T.);
#11304=FACE_OUTER_BOUND('',#15414,.T.);
#11305=FACE_OUTER_BOUND('',#15415,.T.);
#11306=FACE_OUTER_BOUND('',#15416,.T.);
#11307=FACE_OUTER_BOUND('',#15417,.T.);
#11308=FACE_OUTER_BOUND('',#15418,.T.);
#11309=FACE_OUTER_BOUND('',#15419,.T.);
#11310=FACE_OUTER_BOUND('',#15420,.T.);
#11311=FACE_OUTER_BOUND('',#15421,.T.);
#11312=FACE_OUTER_BOUND('',#15422,.T.);
#11313=FACE_OUTER_BOUND('',#15423,.T.);
#11314=FACE_OUTER_BOUND('',#15424,.T.);
#11315=FACE_OUTER_BOUND('',#15425,.T.);
#11316=FACE_OUTER_BOUND('',#15426,.T.);
#11317=FACE_OUTER_BOUND('',#15427,.T.);
#11318=FACE_OUTER_BOUND('',#15428,.T.);
#11319=FACE_OUTER_BOUND('',#15429,.T.);
#11320=FACE_OUTER_BOUND('',#15430,.T.);
#11321=FACE_OUTER_BOUND('',#15431,.T.);
#11322=FACE_OUTER_BOUND('',#15432,.T.);
#11323=FACE_OUTER_BOUND('',#15433,.T.);
#11324=FACE_OUTER_BOUND('',#15434,.T.);
#11325=FACE_OUTER_BOUND('',#15435,.T.);
#11326=FACE_OUTER_BOUND('',#15436,.T.);
#11327=FACE_OUTER_BOUND('',#15437,.T.);
#11328=FACE_OUTER_BOUND('',#15438,.T.);
#11329=FACE_OUTER_BOUND('',#15439,.T.);
#11330=FACE_OUTER_BOUND('',#15440,.T.);
#11331=FACE_OUTER_BOUND('',#15441,.T.);
#11332=FACE_OUTER_BOUND('',#15442,.T.);
#11333=FACE_OUTER_BOUND('',#15443,.T.);
#11334=FACE_OUTER_BOUND('',#15444,.T.);
#11335=FACE_OUTER_BOUND('',#15445,.T.);
#11336=FACE_OUTER_BOUND('',#15446,.T.);
#11337=FACE_OUTER_BOUND('',#15447,.T.);
#11338=FACE_OUTER_BOUND('',#15448,.T.);
#11339=FACE_OUTER_BOUND('',#15449,.T.);
#11340=FACE_OUTER_BOUND('',#15450,.T.);
#11341=FACE_OUTER_BOUND('',#15451,.T.);
#11342=FACE_OUTER_BOUND('',#15452,.T.);
#11343=FACE_OUTER_BOUND('',#15453,.T.);
#11344=FACE_OUTER_BOUND('',#15454,.T.);
#11345=FACE_OUTER_BOUND('',#15455,.T.);
#11346=FACE_OUTER_BOUND('',#15456,.T.);
#11347=FACE_OUTER_BOUND('',#15457,.T.);
#11348=FACE_OUTER_BOUND('',#15458,.T.);
#11349=FACE_OUTER_BOUND('',#15459,.T.);
#11350=FACE_OUTER_BOUND('',#15460,.T.);
#11351=FACE_OUTER_BOUND('',#15461,.T.);
#11352=FACE_OUTER_BOUND('',#15462,.T.);
#11353=FACE_OUTER_BOUND('',#15463,.T.);
#11354=FACE_OUTER_BOUND('',#15464,.T.);
#11355=FACE_OUTER_BOUND('',#15465,.T.);
#11356=FACE_OUTER_BOUND('',#15466,.T.);
#11357=FACE_OUTER_BOUND('',#15467,.T.);
#11358=FACE_OUTER_BOUND('',#15468,.T.);
#11359=FACE_OUTER_BOUND('',#15469,.T.);
#11360=FACE_OUTER_BOUND('',#15470,.T.);
#11361=FACE_OUTER_BOUND('',#15471,.T.);
#11362=FACE_OUTER_BOUND('',#15472,.T.);
#11363=FACE_OUTER_BOUND('',#15473,.T.);
#11364=FACE_OUTER_BOUND('',#15474,.T.);
#11365=FACE_OUTER_BOUND('',#15475,.T.);
#11366=FACE_OUTER_BOUND('',#15476,.T.);
#11367=FACE_OUTER_BOUND('',#15477,.T.);
#11368=FACE_OUTER_BOUND('',#15478,.T.);
#11369=FACE_OUTER_BOUND('',#15479,.T.);
#11370=FACE_OUTER_BOUND('',#15480,.T.);
#11371=FACE_OUTER_BOUND('',#15481,.T.);
#11372=FACE_OUTER_BOUND('',#15482,.T.);
#11373=FACE_OUTER_BOUND('',#15483,.T.);
#11374=FACE_OUTER_BOUND('',#15484,.T.);
#11375=FACE_OUTER_BOUND('',#15485,.T.);
#11376=FACE_OUTER_BOUND('',#15486,.T.);
#11377=FACE_OUTER_BOUND('',#15487,.T.);
#11378=FACE_OUTER_BOUND('',#15488,.T.);
#11379=FACE_OUTER_BOUND('',#15489,.T.);
#11380=FACE_OUTER_BOUND('',#15490,.T.);
#11381=FACE_OUTER_BOUND('',#15491,.T.);
#11382=FACE_OUTER_BOUND('',#15492,.T.);
#11383=FACE_OUTER_BOUND('',#15493,.T.);
#11384=FACE_OUTER_BOUND('',#15494,.T.);
#11385=FACE_OUTER_BOUND('',#15495,.T.);
#11386=FACE_OUTER_BOUND('',#15496,.T.);
#11387=FACE_OUTER_BOUND('',#15497,.T.);
#11388=FACE_OUTER_BOUND('',#15498,.T.);
#11389=FACE_OUTER_BOUND('',#15499,.T.);
#11390=FACE_OUTER_BOUND('',#15500,.T.);
#11391=FACE_OUTER_BOUND('',#15501,.T.);
#11392=FACE_OUTER_BOUND('',#15502,.T.);
#11393=FACE_OUTER_BOUND('',#15503,.T.);
#11394=FACE_OUTER_BOUND('',#15504,.T.);
#11395=FACE_OUTER_BOUND('',#15505,.T.);
#11396=FACE_OUTER_BOUND('',#15506,.T.);
#11397=FACE_OUTER_BOUND('',#15507,.T.);
#11398=FACE_OUTER_BOUND('',#15508,.T.);
#11399=FACE_OUTER_BOUND('',#15509,.T.);
#11400=FACE_OUTER_BOUND('',#15510,.T.);
#11401=FACE_OUTER_BOUND('',#15511,.T.);
#11402=FACE_OUTER_BOUND('',#15512,.T.);
#11403=FACE_OUTER_BOUND('',#15513,.T.);
#11404=FACE_OUTER_BOUND('',#15514,.T.);
#11405=FACE_OUTER_BOUND('',#15515,.T.);
#11406=FACE_OUTER_BOUND('',#15516,.T.);
#11407=FACE_OUTER_BOUND('',#15517,.T.);
#11408=FACE_OUTER_BOUND('',#15518,.T.);
#11409=FACE_OUTER_BOUND('',#15519,.T.);
#11410=FACE_OUTER_BOUND('',#15520,.T.);
#11411=FACE_OUTER_BOUND('',#15521,.T.);
#11412=FACE_OUTER_BOUND('',#15522,.T.);
#11413=FACE_OUTER_BOUND('',#15523,.T.);
#11414=FACE_OUTER_BOUND('',#15524,.T.);
#11415=FACE_OUTER_BOUND('',#15525,.T.);
#11416=FACE_OUTER_BOUND('',#15526,.T.);
#11417=FACE_OUTER_BOUND('',#15527,.T.);
#11418=FACE_OUTER_BOUND('',#15528,.T.);
#11419=FACE_OUTER_BOUND('',#15529,.T.);
#11420=FACE_OUTER_BOUND('',#15530,.T.);
#11421=FACE_OUTER_BOUND('',#15531,.T.);
#11422=FACE_OUTER_BOUND('',#15532,.T.);
#11423=FACE_OUTER_BOUND('',#15533,.T.);
#11424=FACE_OUTER_BOUND('',#15534,.T.);
#11425=FACE_OUTER_BOUND('',#15535,.T.);
#11426=FACE_OUTER_BOUND('',#15536,.T.);
#11427=FACE_OUTER_BOUND('',#15537,.T.);
#11428=FACE_OUTER_BOUND('',#15538,.T.);
#11429=FACE_OUTER_BOUND('',#15539,.T.);
#11430=FACE_OUTER_BOUND('',#15540,.T.);
#11431=FACE_OUTER_BOUND('',#15541,.T.);
#11432=FACE_OUTER_BOUND('',#15542,.T.);
#11433=FACE_OUTER_BOUND('',#15543,.T.);
#11434=FACE_OUTER_BOUND('',#15544,.T.);
#11435=FACE_OUTER_BOUND('',#15545,.T.);
#11436=FACE_OUTER_BOUND('',#15546,.T.);
#11437=FACE_OUTER_BOUND('',#15547,.T.);
#11438=FACE_OUTER_BOUND('',#15548,.T.);
#11439=FACE_OUTER_BOUND('',#15549,.T.);
#11440=FACE_OUTER_BOUND('',#15550,.T.);
#11441=FACE_OUTER_BOUND('',#15551,.T.);
#11442=FACE_OUTER_BOUND('',#15552,.T.);
#11443=FACE_OUTER_BOUND('',#15553,.T.);
#11444=FACE_OUTER_BOUND('',#15554,.T.);
#11445=FACE_OUTER_BOUND('',#15555,.T.);
#11446=FACE_OUTER_BOUND('',#15556,.T.);
#11447=FACE_OUTER_BOUND('',#15557,.T.);
#11448=FACE_OUTER_BOUND('',#15558,.T.);
#11449=FACE_OUTER_BOUND('',#15559,.T.);
#11450=FACE_OUTER_BOUND('',#15560,.T.);
#11451=FACE_OUTER_BOUND('',#15561,.T.);
#11452=FACE_OUTER_BOUND('',#15562,.T.);
#11453=FACE_OUTER_BOUND('',#15563,.T.);
#11454=FACE_OUTER_BOUND('',#15564,.T.);
#11455=FACE_OUTER_BOUND('',#15565,.T.);
#11456=FACE_OUTER_BOUND('',#15566,.T.);
#11457=FACE_OUTER_BOUND('',#15567,.T.);
#11458=FACE_OUTER_BOUND('',#15568,.T.);
#11459=FACE_OUTER_BOUND('',#15569,.T.);
#11460=FACE_OUTER_BOUND('',#15570,.T.);
#11461=FACE_OUTER_BOUND('',#15571,.T.);
#11462=FACE_OUTER_BOUND('',#15572,.T.);
#11463=FACE_OUTER_BOUND('',#15573,.T.);
#11464=FACE_OUTER_BOUND('',#15574,.T.);
#11465=FACE_OUTER_BOUND('',#15575,.T.);
#11466=FACE_OUTER_BOUND('',#15576,.T.);
#11467=FACE_OUTER_BOUND('',#15577,.T.);
#11468=FACE_OUTER_BOUND('',#15578,.T.);
#11469=FACE_OUTER_BOUND('',#15579,.T.);
#11470=FACE_OUTER_BOUND('',#15580,.T.);
#11471=FACE_OUTER_BOUND('',#15581,.T.);
#11472=FACE_OUTER_BOUND('',#15582,.T.);
#11473=FACE_OUTER_BOUND('',#15583,.T.);
#11474=FACE_OUTER_BOUND('',#15584,.T.);
#11475=FACE_OUTER_BOUND('',#15585,.T.);
#11476=FACE_OUTER_BOUND('',#15586,.T.);
#11477=FACE_OUTER_BOUND('',#15587,.T.);
#11478=FACE_OUTER_BOUND('',#15588,.T.);
#11479=FACE_OUTER_BOUND('',#15589,.T.);
#11480=FACE_OUTER_BOUND('',#15590,.T.);
#11481=FACE_OUTER_BOUND('',#15591,.T.);
#11482=FACE_OUTER_BOUND('',#15592,.T.);
#11483=FACE_OUTER_BOUND('',#15593,.T.);
#11484=FACE_OUTER_BOUND('',#15594,.T.);
#11485=FACE_OUTER_BOUND('',#15595,.T.);
#11486=FACE_OUTER_BOUND('',#15596,.T.);
#11487=FACE_OUTER_BOUND('',#15597,.T.);
#11488=FACE_OUTER_BOUND('',#15598,.T.);
#11489=FACE_OUTER_BOUND('',#15599,.T.);
#11490=FACE_OUTER_BOUND('',#15600,.T.);
#11491=FACE_OUTER_BOUND('',#15601,.T.);
#11492=FACE_OUTER_BOUND('',#15602,.T.);
#11493=FACE_OUTER_BOUND('',#15603,.T.);
#11494=FACE_OUTER_BOUND('',#15604,.T.);
#11495=FACE_OUTER_BOUND('',#15605,.T.);
#11496=FACE_OUTER_BOUND('',#15606,.T.);
#11497=FACE_OUTER_BOUND('',#15607,.T.);
#11498=FACE_OUTER_BOUND('',#15608,.T.);
#11499=FACE_OUTER_BOUND('',#15609,.T.);
#11500=FACE_OUTER_BOUND('',#15610,.T.);
#11501=FACE_OUTER_BOUND('',#15611,.T.);
#11502=FACE_OUTER_BOUND('',#15612,.T.);
#11503=FACE_OUTER_BOUND('',#15613,.T.);
#11504=FACE_OUTER_BOUND('',#15614,.T.);
#11505=FACE_OUTER_BOUND('',#15615,.T.);
#11506=FACE_OUTER_BOUND('',#15616,.T.);
#11507=FACE_OUTER_BOUND('',#15617,.T.);
#11508=FACE_OUTER_BOUND('',#15618,.T.);
#11509=FACE_OUTER_BOUND('',#15619,.T.);
#11510=FACE_OUTER_BOUND('',#15620,.T.);
#11511=FACE_OUTER_BOUND('',#15621,.T.);
#11512=FACE_OUTER_BOUND('',#15622,.T.);
#11513=FACE_OUTER_BOUND('',#15623,.T.);
#11514=FACE_OUTER_BOUND('',#15624,.T.);
#11515=FACE_OUTER_BOUND('',#15625,.T.);
#11516=FACE_OUTER_BOUND('',#15626,.T.);
#11517=FACE_OUTER_BOUND('',#15627,.T.);
#11518=FACE_OUTER_BOUND('',#15628,.T.);
#11519=FACE_OUTER_BOUND('',#15629,.T.);
#11520=FACE_OUTER_BOUND('',#15630,.T.);
#11521=FACE_OUTER_BOUND('',#15631,.T.);
#11522=FACE_OUTER_BOUND('',#15632,.T.);
#11523=FACE_OUTER_BOUND('',#15633,.T.);
#11524=FACE_OUTER_BOUND('',#15634,.T.);
#11525=FACE_OUTER_BOUND('',#15635,.T.);
#11526=FACE_OUTER_BOUND('',#15636,.T.);
#11527=FACE_OUTER_BOUND('',#15637,.T.);
#11528=FACE_OUTER_BOUND('',#15638,.T.);
#11529=FACE_OUTER_BOUND('',#15639,.T.);
#11530=FACE_OUTER_BOUND('',#15640,.T.);
#11531=FACE_OUTER_BOUND('',#15641,.T.);
#11532=FACE_OUTER_BOUND('',#15642,.T.);
#11533=FACE_OUTER_BOUND('',#15643,.T.);
#11534=FACE_OUTER_BOUND('',#15644,.T.);
#11535=FACE_OUTER_BOUND('',#15645,.T.);
#11536=FACE_OUTER_BOUND('',#15646,.T.);
#11537=FACE_OUTER_BOUND('',#15647,.T.);
#11538=FACE_OUTER_BOUND('',#15648,.T.);
#11539=FACE_OUTER_BOUND('',#15649,.T.);
#11540=FACE_OUTER_BOUND('',#15650,.T.);
#11541=FACE_OUTER_BOUND('',#15651,.T.);
#11542=FACE_OUTER_BOUND('',#15652,.T.);
#11543=FACE_OUTER_BOUND('',#15653,.T.);
#11544=FACE_OUTER_BOUND('',#15654,.T.);
#11545=FACE_OUTER_BOUND('',#15655,.T.);
#11546=FACE_OUTER_BOUND('',#15656,.T.);
#11547=FACE_OUTER_BOUND('',#15657,.T.);
#11548=FACE_OUTER_BOUND('',#15658,.T.);
#11549=FACE_OUTER_BOUND('',#15659,.T.);
#11550=FACE_OUTER_BOUND('',#15660,.T.);
#11551=FACE_OUTER_BOUND('',#15661,.T.);
#11552=FACE_OUTER_BOUND('',#15662,.T.);
#11553=FACE_OUTER_BOUND('',#15663,.T.);
#11554=FACE_OUTER_BOUND('',#15664,.T.);
#11555=FACE_OUTER_BOUND('',#15665,.T.);
#11556=FACE_OUTER_BOUND('',#15666,.T.);
#11557=FACE_OUTER_BOUND('',#15667,.T.);
#11558=FACE_OUTER_BOUND('',#15668,.T.);
#11559=FACE_OUTER_BOUND('',#15669,.T.);
#11560=FACE_OUTER_BOUND('',#15670,.T.);
#11561=FACE_OUTER_BOUND('',#15671,.T.);
#11562=FACE_OUTER_BOUND('',#15672,.T.);
#11563=FACE_OUTER_BOUND('',#15673,.T.);
#11564=FACE_OUTER_BOUND('',#15674,.T.);
#11565=FACE_OUTER_BOUND('',#15675,.T.);
#11566=FACE_OUTER_BOUND('',#15676,.T.);
#11567=FACE_OUTER_BOUND('',#15677,.T.);
#11568=FACE_OUTER_BOUND('',#15678,.T.);
#11569=FACE_OUTER_BOUND('',#15679,.T.);
#11570=FACE_OUTER_BOUND('',#15680,.T.);
#11571=FACE_OUTER_BOUND('',#15681,.T.);
#11572=FACE_OUTER_BOUND('',#15682,.T.);
#11573=FACE_OUTER_BOUND('',#15683,.T.);
#11574=FACE_OUTER_BOUND('',#15684,.T.);
#11575=FACE_OUTER_BOUND('',#15685,.T.);
#11576=FACE_OUTER_BOUND('',#15686,.T.);
#11577=FACE_OUTER_BOUND('',#15687,.T.);
#11578=FACE_OUTER_BOUND('',#15688,.T.);
#11579=FACE_OUTER_BOUND('',#15689,.T.);
#11580=FACE_OUTER_BOUND('',#15690,.T.);
#11581=FACE_OUTER_BOUND('',#15691,.T.);
#11582=FACE_OUTER_BOUND('',#15692,.T.);
#11583=FACE_OUTER_BOUND('',#15693,.T.);
#11584=FACE_OUTER_BOUND('',#15694,.T.);
#11585=FACE_OUTER_BOUND('',#15695,.T.);
#11586=FACE_OUTER_BOUND('',#15696,.T.);
#11587=FACE_OUTER_BOUND('',#15697,.T.);
#11588=FACE_OUTER_BOUND('',#15698,.T.);
#11589=FACE_OUTER_BOUND('',#15699,.T.);
#11590=FACE_OUTER_BOUND('',#15700,.T.);
#11591=FACE_OUTER_BOUND('',#15701,.T.);
#11592=FACE_OUTER_BOUND('',#15702,.T.);
#11593=FACE_OUTER_BOUND('',#15703,.T.);
#11594=FACE_OUTER_BOUND('',#15704,.T.);
#11595=FACE_OUTER_BOUND('',#15705,.T.);
#11596=FACE_OUTER_BOUND('',#15706,.T.);
#11597=FACE_OUTER_BOUND('',#15707,.T.);
#11598=FACE_OUTER_BOUND('',#15708,.T.);
#11599=FACE_OUTER_BOUND('',#15709,.T.);
#11600=FACE_OUTER_BOUND('',#15710,.T.);
#11601=FACE_OUTER_BOUND('',#15711,.T.);
#11602=FACE_OUTER_BOUND('',#15712,.T.);
#11603=FACE_OUTER_BOUND('',#15713,.T.);
#11604=FACE_OUTER_BOUND('',#15714,.T.);
#11605=FACE_OUTER_BOUND('',#15715,.T.);
#11606=FACE_OUTER_BOUND('',#15716,.T.);
#11607=FACE_OUTER_BOUND('',#15717,.T.);
#11608=FACE_OUTER_BOUND('',#15718,.T.);
#11609=FACE_OUTER_BOUND('',#15719,.T.);
#11610=FACE_OUTER_BOUND('',#15720,.T.);
#11611=FACE_OUTER_BOUND('',#15721,.T.);
#11612=FACE_OUTER_BOUND('',#15722,.T.);
#11613=FACE_OUTER_BOUND('',#15723,.T.);
#11614=FACE_OUTER_BOUND('',#15724,.T.);
#11615=FACE_OUTER_BOUND('',#15725,.T.);
#11616=FACE_OUTER_BOUND('',#15726,.T.);
#11617=FACE_OUTER_BOUND('',#15727,.T.);
#11618=FACE_OUTER_BOUND('',#15728,.T.);
#11619=FACE_OUTER_BOUND('',#15729,.T.);
#11620=FACE_OUTER_BOUND('',#15730,.T.);
#11621=FACE_OUTER_BOUND('',#15731,.T.);
#11622=FACE_OUTER_BOUND('',#15732,.T.);
#11623=FACE_OUTER_BOUND('',#15733,.T.);
#11624=FACE_OUTER_BOUND('',#15734,.T.);
#11625=FACE_OUTER_BOUND('',#15735,.T.);
#11626=FACE_OUTER_BOUND('',#15736,.T.);
#11627=FACE_OUTER_BOUND('',#15737,.T.);
#11628=FACE_OUTER_BOUND('',#15738,.T.);
#11629=FACE_OUTER_BOUND('',#15739,.T.);
#11630=FACE_OUTER_BOUND('',#15740,.T.);
#11631=FACE_OUTER_BOUND('',#15741,.T.);
#11632=FACE_OUTER_BOUND('',#15742,.T.);
#11633=FACE_OUTER_BOUND('',#15743,.T.);
#11634=FACE_OUTER_BOUND('',#15744,.T.);
#11635=FACE_OUTER_BOUND('',#15745,.T.);
#11636=FACE_OUTER_BOUND('',#15746,.T.);
#11637=FACE_OUTER_BOUND('',#15747,.T.);
#11638=FACE_OUTER_BOUND('',#15748,.T.);
#11639=FACE_OUTER_BOUND('',#15749,.T.);
#11640=FACE_OUTER_BOUND('',#15750,.T.);
#11641=FACE_OUTER_BOUND('',#15751,.T.);
#11642=FACE_OUTER_BOUND('',#15752,.T.);
#11643=FACE_OUTER_BOUND('',#15753,.T.);
#11644=FACE_OUTER_BOUND('',#15754,.T.);
#11645=FACE_OUTER_BOUND('',#15755,.T.);
#11646=FACE_OUTER_BOUND('',#15756,.T.);
#11647=FACE_OUTER_BOUND('',#15757,.T.);
#11648=FACE_OUTER_BOUND('',#15758,.T.);
#11649=FACE_OUTER_BOUND('',#15759,.T.);
#11650=FACE_OUTER_BOUND('',#15760,.T.);
#11651=FACE_OUTER_BOUND('',#15761,.T.);
#11652=FACE_OUTER_BOUND('',#15762,.T.);
#11653=FACE_OUTER_BOUND('',#15763,.T.);
#11654=FACE_OUTER_BOUND('',#15764,.T.);
#11655=FACE_OUTER_BOUND('',#15765,.T.);
#11656=FACE_OUTER_BOUND('',#15766,.T.);
#11657=FACE_OUTER_BOUND('',#15767,.T.);
#11658=FACE_OUTER_BOUND('',#15768,.T.);
#11659=FACE_OUTER_BOUND('',#15769,.T.);
#11660=FACE_OUTER_BOUND('',#15770,.T.);
#11661=FACE_OUTER_BOUND('',#15771,.T.);
#11662=FACE_OUTER_BOUND('',#15772,.T.);
#11663=FACE_OUTER_BOUND('',#15773,.T.);
#11664=FACE_OUTER_BOUND('',#15774,.T.);
#11665=FACE_OUTER_BOUND('',#15775,.T.);
#11666=FACE_OUTER_BOUND('',#15776,.T.);
#11667=FACE_OUTER_BOUND('',#15777,.T.);
#11668=FACE_OUTER_BOUND('',#15778,.T.);
#11669=FACE_OUTER_BOUND('',#15779,.T.);
#11670=FACE_OUTER_BOUND('',#15780,.T.);
#11671=FACE_OUTER_BOUND('',#15781,.T.);
#11672=FACE_OUTER_BOUND('',#15782,.T.);
#11673=FACE_OUTER_BOUND('',#15783,.T.);
#11674=FACE_OUTER_BOUND('',#15784,.T.);
#11675=FACE_OUTER_BOUND('',#15785,.T.);
#11676=FACE_OUTER_BOUND('',#15786,.T.);
#11677=FACE_OUTER_BOUND('',#15787,.T.);
#11678=FACE_OUTER_BOUND('',#15788,.T.);
#11679=FACE_OUTER_BOUND('',#15789,.T.);
#11680=FACE_OUTER_BOUND('',#15790,.T.);
#11681=FACE_OUTER_BOUND('',#15791,.T.);
#11682=FACE_OUTER_BOUND('',#15792,.T.);
#11683=FACE_OUTER_BOUND('',#15793,.T.);
#11684=FACE_OUTER_BOUND('',#15794,.T.);
#11685=FACE_OUTER_BOUND('',#15795,.T.);
#11686=FACE_OUTER_BOUND('',#15796,.T.);
#11687=FACE_OUTER_BOUND('',#15797,.T.);
#11688=FACE_OUTER_BOUND('',#15798,.T.);
#11689=FACE_OUTER_BOUND('',#15799,.T.);
#11690=FACE_OUTER_BOUND('',#15800,.T.);
#11691=FACE_OUTER_BOUND('',#15801,.T.);
#11692=FACE_OUTER_BOUND('',#15802,.T.);
#11693=FACE_OUTER_BOUND('',#15803,.T.);
#11694=FACE_OUTER_BOUND('',#15804,.T.);
#11695=FACE_OUTER_BOUND('',#15805,.T.);
#11696=FACE_OUTER_BOUND('',#15806,.T.);
#11697=FACE_OUTER_BOUND('',#15807,.T.);
#11698=FACE_OUTER_BOUND('',#15808,.T.);
#11699=FACE_OUTER_BOUND('',#15809,.T.);
#11700=FACE_OUTER_BOUND('',#15810,.T.);
#11701=FACE_OUTER_BOUND('',#15811,.T.);
#11702=FACE_OUTER_BOUND('',#15812,.T.);
#11703=FACE_OUTER_BOUND('',#15813,.T.);
#11704=FACE_OUTER_BOUND('',#15814,.T.);
#11705=FACE_OUTER_BOUND('',#15815,.T.);
#11706=FACE_OUTER_BOUND('',#15816,.T.);
#11707=FACE_OUTER_BOUND('',#15817,.T.);
#11708=FACE_OUTER_BOUND('',#15818,.T.);
#11709=FACE_OUTER_BOUND('',#15819,.T.);
#11710=FACE_OUTER_BOUND('',#15820,.T.);
#11711=FACE_OUTER_BOUND('',#15821,.T.);
#11712=FACE_OUTER_BOUND('',#15822,.T.);
#11713=FACE_OUTER_BOUND('',#15823,.T.);
#11714=FACE_OUTER_BOUND('',#15824,.T.);
#11715=FACE_OUTER_BOUND('',#15825,.T.);
#11716=FACE_OUTER_BOUND('',#15826,.T.);
#11717=FACE_OUTER_BOUND('',#15827,.T.);
#11718=FACE_OUTER_BOUND('',#15828,.T.);
#11719=FACE_OUTER_BOUND('',#15829,.T.);
#11720=FACE_OUTER_BOUND('',#15830,.T.);
#11721=FACE_OUTER_BOUND('',#15831,.T.);
#11722=FACE_OUTER_BOUND('',#15832,.T.);
#11723=FACE_OUTER_BOUND('',#15833,.T.);
#11724=FACE_OUTER_BOUND('',#15834,.T.);
#11725=FACE_OUTER_BOUND('',#15835,.T.);
#11726=FACE_OUTER_BOUND('',#15836,.T.);
#11727=FACE_OUTER_BOUND('',#15837,.T.);
#11728=FACE_OUTER_BOUND('',#15838,.T.);
#11729=FACE_OUTER_BOUND('',#15839,.T.);
#11730=FACE_OUTER_BOUND('',#15840,.T.);
#11731=FACE_OUTER_BOUND('',#15841,.T.);
#11732=FACE_OUTER_BOUND('',#15842,.T.);
#11733=FACE_OUTER_BOUND('',#15843,.T.);
#11734=FACE_OUTER_BOUND('',#15844,.T.);
#11735=FACE_OUTER_BOUND('',#15845,.T.);
#11736=FACE_OUTER_BOUND('',#15846,.T.);
#11737=FACE_OUTER_BOUND('',#15847,.T.);
#11738=FACE_OUTER_BOUND('',#15848,.T.);
#11739=FACE_OUTER_BOUND('',#15849,.T.);
#11740=FACE_OUTER_BOUND('',#15850,.T.);
#11741=FACE_OUTER_BOUND('',#15851,.T.);
#11742=FACE_OUTER_BOUND('',#15852,.T.);
#11743=FACE_OUTER_BOUND('',#15853,.T.);
#11744=FACE_OUTER_BOUND('',#15854,.T.);
#11745=FACE_OUTER_BOUND('',#15855,.T.);
#11746=FACE_OUTER_BOUND('',#15856,.T.);
#11747=FACE_OUTER_BOUND('',#15857,.T.);
#11748=FACE_OUTER_BOUND('',#15858,.T.);
#11749=FACE_OUTER_BOUND('',#15859,.T.);
#11750=FACE_OUTER_BOUND('',#15860,.T.);
#11751=FACE_OUTER_BOUND('',#15861,.T.);
#11752=FACE_OUTER_BOUND('',#15862,.T.);
#11753=FACE_OUTER_BOUND('',#15863,.T.);
#11754=FACE_OUTER_BOUND('',#15864,.T.);
#11755=FACE_OUTER_BOUND('',#15865,.T.);
#11756=FACE_OUTER_BOUND('',#15866,.T.);
#11757=FACE_OUTER_BOUND('',#15867,.T.);
#11758=FACE_OUTER_BOUND('',#15868,.T.);
#11759=FACE_OUTER_BOUND('',#15869,.T.);
#11760=FACE_OUTER_BOUND('',#15870,.T.);
#11761=FACE_OUTER_BOUND('',#15871,.T.);
#11762=FACE_OUTER_BOUND('',#15872,.T.);
#11763=FACE_OUTER_BOUND('',#15873,.T.);
#11764=FACE_OUTER_BOUND('',#15874,.T.);
#11765=FACE_OUTER_BOUND('',#15875,.T.);
#11766=FACE_OUTER_BOUND('',#15876,.T.);
#11767=FACE_OUTER_BOUND('',#15877,.T.);
#11768=FACE_OUTER_BOUND('',#15878,.T.);
#11769=FACE_OUTER_BOUND('',#15879,.T.);
#11770=FACE_OUTER_BOUND('',#15880,.T.);
#11771=FACE_OUTER_BOUND('',#15881,.T.);
#11772=FACE_OUTER_BOUND('',#15882,.T.);
#11773=FACE_OUTER_BOUND('',#15883,.T.);
#11774=FACE_OUTER_BOUND('',#15884,.T.);
#11775=FACE_OUTER_BOUND('',#15885,.T.);
#11776=FACE_OUTER_BOUND('',#15886,.T.);
#11777=FACE_OUTER_BOUND('',#15887,.T.);
#11778=FACE_OUTER_BOUND('',#15888,.T.);
#11779=FACE_OUTER_BOUND('',#15889,.T.);
#11780=FACE_OUTER_BOUND('',#15890,.T.);
#11781=FACE_OUTER_BOUND('',#15891,.T.);
#11782=FACE_OUTER_BOUND('',#15892,.T.);
#11783=FACE_OUTER_BOUND('',#15893,.T.);
#11784=FACE_OUTER_BOUND('',#15894,.T.);
#11785=FACE_OUTER_BOUND('',#15895,.T.);
#11786=FACE_OUTER_BOUND('',#15896,.T.);
#11787=FACE_OUTER_BOUND('',#15897,.T.);
#11788=FACE_OUTER_BOUND('',#15898,.T.);
#11789=FACE_OUTER_BOUND('',#15899,.T.);
#11790=FACE_OUTER_BOUND('',#15900,.T.);
#11791=FACE_OUTER_BOUND('',#15901,.T.);
#11792=FACE_OUTER_BOUND('',#15902,.T.);
#11793=FACE_OUTER_BOUND('',#15903,.T.);
#11794=FACE_OUTER_BOUND('',#15904,.T.);
#11795=FACE_OUTER_BOUND('',#15905,.T.);
#11796=FACE_OUTER_BOUND('',#15906,.T.);
#11797=FACE_OUTER_BOUND('',#15907,.T.);
#11798=FACE_OUTER_BOUND('',#15908,.T.);
#11799=FACE_OUTER_BOUND('',#15909,.T.);
#11800=FACE_OUTER_BOUND('',#15910,.T.);
#11801=FACE_OUTER_BOUND('',#15911,.T.);
#11802=FACE_OUTER_BOUND('',#15912,.T.);
#11803=FACE_OUTER_BOUND('',#15913,.T.);
#11804=FACE_OUTER_BOUND('',#15914,.T.);
#11805=FACE_OUTER_BOUND('',#15915,.T.);
#11806=FACE_OUTER_BOUND('',#15916,.T.);
#11807=FACE_OUTER_BOUND('',#15917,.T.);
#11808=FACE_OUTER_BOUND('',#15918,.T.);
#11809=FACE_OUTER_BOUND('',#15919,.T.);
#11810=FACE_OUTER_BOUND('',#15920,.T.);
#11811=FACE_OUTER_BOUND('',#15921,.T.);
#11812=FACE_OUTER_BOUND('',#15922,.T.);
#11813=FACE_OUTER_BOUND('',#15923,.T.);
#11814=FACE_OUTER_BOUND('',#15924,.T.);
#11815=FACE_OUTER_BOUND('',#15925,.T.);
#11816=FACE_OUTER_BOUND('',#15926,.T.);
#11817=FACE_OUTER_BOUND('',#15927,.T.);
#11818=FACE_OUTER_BOUND('',#15928,.T.);
#11819=FACE_OUTER_BOUND('',#15929,.T.);
#11820=FACE_OUTER_BOUND('',#15930,.T.);
#11821=FACE_OUTER_BOUND('',#15931,.T.);
#11822=FACE_OUTER_BOUND('',#15932,.T.);
#11823=FACE_OUTER_BOUND('',#15933,.T.);
#11824=FACE_OUTER_BOUND('',#15934,.T.);
#11825=FACE_OUTER_BOUND('',#15935,.T.);
#11826=FACE_OUTER_BOUND('',#15936,.T.);
#11827=FACE_OUTER_BOUND('',#15937,.T.);
#11828=FACE_OUTER_BOUND('',#15938,.T.);
#11829=FACE_OUTER_BOUND('',#15939,.T.);
#11830=FACE_OUTER_BOUND('',#15940,.T.);
#11831=FACE_OUTER_BOUND('',#15941,.T.);
#11832=FACE_OUTER_BOUND('',#15942,.T.);
#11833=FACE_OUTER_BOUND('',#15943,.T.);
#11834=FACE_OUTER_BOUND('',#15944,.T.);
#11835=FACE_OUTER_BOUND('',#15945,.T.);
#11836=FACE_OUTER_BOUND('',#15946,.T.);
#11837=FACE_OUTER_BOUND('',#15947,.T.);
#11838=FACE_OUTER_BOUND('',#15948,.T.);
#11839=FACE_OUTER_BOUND('',#15949,.T.);
#11840=FACE_OUTER_BOUND('',#15950,.T.);
#11841=FACE_OUTER_BOUND('',#15951,.T.);
#11842=FACE_OUTER_BOUND('',#15952,.T.);
#11843=FACE_OUTER_BOUND('',#15953,.T.);
#11844=FACE_OUTER_BOUND('',#15954,.T.);
#11845=FACE_OUTER_BOUND('',#15955,.T.);
#11846=FACE_OUTER_BOUND('',#15956,.T.);
#11847=FACE_OUTER_BOUND('',#15957,.T.);
#11848=FACE_OUTER_BOUND('',#15958,.T.);
#11849=FACE_OUTER_BOUND('',#15959,.T.);
#11850=FACE_OUTER_BOUND('',#15960,.T.);
#11851=FACE_OUTER_BOUND('',#15961,.T.);
#11852=FACE_OUTER_BOUND('',#15962,.T.);
#11853=FACE_OUTER_BOUND('',#15963,.T.);
#11854=FACE_OUTER_BOUND('',#15964,.T.);
#11855=FACE_OUTER_BOUND('',#15965,.T.);
#11856=FACE_OUTER_BOUND('',#15966,.T.);
#11857=FACE_OUTER_BOUND('',#15967,.T.);
#11858=FACE_OUTER_BOUND('',#15968,.T.);
#11859=FACE_OUTER_BOUND('',#15969,.T.);
#11860=FACE_OUTER_BOUND('',#15970,.T.);
#11861=FACE_OUTER_BOUND('',#15971,.T.);
#11862=FACE_OUTER_BOUND('',#15972,.T.);
#11863=FACE_OUTER_BOUND('',#15973,.T.);
#11864=FACE_OUTER_BOUND('',#15974,.T.);
#11865=FACE_OUTER_BOUND('',#15975,.T.);
#11866=FACE_OUTER_BOUND('',#15976,.T.);
#11867=FACE_OUTER_BOUND('',#15977,.T.);
#11868=FACE_OUTER_BOUND('',#15978,.T.);
#11869=FACE_OUTER_BOUND('',#15979,.T.);
#11870=FACE_OUTER_BOUND('',#15980,.T.);
#11871=FACE_OUTER_BOUND('',#15981,.T.);
#11872=FACE_OUTER_BOUND('',#15982,.T.);
#11873=FACE_OUTER_BOUND('',#15983,.T.);
#11874=FACE_OUTER_BOUND('',#15984,.T.);
#11875=FACE_OUTER_BOUND('',#15985,.T.);
#11876=FACE_OUTER_BOUND('',#15986,.T.);
#11877=FACE_OUTER_BOUND('',#15987,.T.);
#11878=FACE_OUTER_BOUND('',#15988,.T.);
#11879=FACE_OUTER_BOUND('',#15989,.T.);
#11880=FACE_OUTER_BOUND('',#15990,.T.);
#11881=FACE_OUTER_BOUND('',#15991,.T.);
#11882=FACE_OUTER_BOUND('',#15992,.T.);
#11883=FACE_OUTER_BOUND('',#15993,.T.);
#11884=FACE_OUTER_BOUND('',#15994,.T.);
#11885=FACE_OUTER_BOUND('',#15995,.T.);
#11886=FACE_OUTER_BOUND('',#15996,.T.);
#11887=FACE_OUTER_BOUND('',#15997,.T.);
#11888=FACE_OUTER_BOUND('',#15998,.T.);
#11889=FACE_OUTER_BOUND('',#15999,.T.);
#11890=FACE_OUTER_BOUND('',#16000,.T.);
#11891=FACE_OUTER_BOUND('',#16001,.T.);
#11892=FACE_OUTER_BOUND('',#16002,.T.);
#11893=FACE_OUTER_BOUND('',#16003,.T.);
#11894=FACE_OUTER_BOUND('',#16004,.T.);
#11895=FACE_OUTER_BOUND('',#16005,.T.);
#11896=FACE_OUTER_BOUND('',#16006,.T.);
#11897=FACE_OUTER_BOUND('',#16007,.T.);
#11898=FACE_OUTER_BOUND('',#16008,.T.);
#11899=FACE_OUTER_BOUND('',#16009,.T.);
#11900=FACE_OUTER_BOUND('',#16010,.T.);
#11901=FACE_OUTER_BOUND('',#16011,.T.);
#11902=FACE_OUTER_BOUND('',#16012,.T.);
#11903=FACE_OUTER_BOUND('',#16013,.T.);
#11904=FACE_OUTER_BOUND('',#16014,.T.);
#11905=FACE_OUTER_BOUND('',#16015,.T.);
#11906=FACE_OUTER_BOUND('',#16016,.T.);
#11907=FACE_OUTER_BOUND('',#16017,.T.);
#11908=FACE_OUTER_BOUND('',#16018,.T.);
#11909=FACE_OUTER_BOUND('',#16019,.T.);
#11910=FACE_OUTER_BOUND('',#16020,.T.);
#11911=FACE_OUTER_BOUND('',#16021,.T.);
#11912=FACE_OUTER_BOUND('',#16022,.T.);
#11913=FACE_OUTER_BOUND('',#16023,.T.);
#11914=FACE_OUTER_BOUND('',#16024,.T.);
#11915=FACE_OUTER_BOUND('',#16025,.T.);
#11916=FACE_OUTER_BOUND('',#16026,.T.);
#11917=FACE_OUTER_BOUND('',#16027,.T.);
#11918=FACE_OUTER_BOUND('',#16028,.T.);
#11919=FACE_OUTER_BOUND('',#16029,.T.);
#11920=FACE_OUTER_BOUND('',#16030,.T.);
#11921=FACE_OUTER_BOUND('',#16031,.T.);
#11922=FACE_OUTER_BOUND('',#16032,.T.);
#11923=FACE_OUTER_BOUND('',#16033,.T.);
#11924=FACE_OUTER_BOUND('',#16034,.T.);
#11925=FACE_OUTER_BOUND('',#16035,.T.);
#11926=FACE_OUTER_BOUND('',#16036,.T.);
#11927=FACE_OUTER_BOUND('',#16037,.T.);
#11928=FACE_OUTER_BOUND('',#16038,.T.);
#11929=FACE_OUTER_BOUND('',#16039,.T.);
#11930=FACE_OUTER_BOUND('',#16040,.T.);
#11931=FACE_OUTER_BOUND('',#16041,.T.);
#11932=FACE_OUTER_BOUND('',#16042,.T.);
#11933=FACE_OUTER_BOUND('',#16043,.T.);
#11934=FACE_OUTER_BOUND('',#16044,.T.);
#11935=FACE_OUTER_BOUND('',#16045,.T.);
#11936=FACE_OUTER_BOUND('',#16046,.T.);
#11937=FACE_OUTER_BOUND('',#16047,.T.);
#11938=FACE_OUTER_BOUND('',#16048,.T.);
#11939=FACE_OUTER_BOUND('',#16049,.T.);
#11940=FACE_OUTER_BOUND('',#16050,.T.);
#11941=FACE_OUTER_BOUND('',#16051,.T.);
#11942=FACE_OUTER_BOUND('',#16052,.T.);
#11943=FACE_OUTER_BOUND('',#16053,.T.);
#11944=FACE_OUTER_BOUND('',#16054,.T.);
#11945=FACE_OUTER_BOUND('',#16055,.T.);
#11946=FACE_OUTER_BOUND('',#16056,.T.);
#11947=FACE_OUTER_BOUND('',#16057,.T.);
#11948=FACE_OUTER_BOUND('',#16058,.T.);
#11949=FACE_OUTER_BOUND('',#16059,.T.);
#11950=FACE_OUTER_BOUND('',#16060,.T.);
#11951=FACE_OUTER_BOUND('',#16061,.T.);
#11952=FACE_OUTER_BOUND('',#16062,.T.);
#11953=FACE_OUTER_BOUND('',#16063,.T.);
#11954=FACE_OUTER_BOUND('',#16064,.T.);
#11955=FACE_OUTER_BOUND('',#16065,.T.);
#11956=FACE_OUTER_BOUND('',#16066,.T.);
#11957=FACE_OUTER_BOUND('',#16067,.T.);
#11958=FACE_OUTER_BOUND('',#16068,.T.);
#11959=FACE_OUTER_BOUND('',#16069,.T.);
#11960=FACE_OUTER_BOUND('',#16070,.T.);
#11961=FACE_OUTER_BOUND('',#16071,.T.);
#11962=FACE_OUTER_BOUND('',#16072,.T.);
#11963=FACE_OUTER_BOUND('',#16073,.T.);
#11964=FACE_OUTER_BOUND('',#16074,.T.);
#11965=FACE_OUTER_BOUND('',#16075,.T.);
#11966=FACE_OUTER_BOUND('',#16076,.T.);
#11967=FACE_OUTER_BOUND('',#16077,.T.);
#11968=FACE_OUTER_BOUND('',#16078,.T.);
#11969=FACE_OUTER_BOUND('',#16079,.T.);
#11970=FACE_OUTER_BOUND('',#16080,.T.);
#11971=FACE_OUTER_BOUND('',#16081,.T.);
#11972=FACE_OUTER_BOUND('',#16082,.T.);
#11973=FACE_OUTER_BOUND('',#16083,.T.);
#11974=FACE_OUTER_BOUND('',#16084,.T.);
#11975=FACE_OUTER_BOUND('',#16085,.T.);
#11976=FACE_OUTER_BOUND('',#16086,.T.);
#11977=FACE_OUTER_BOUND('',#16087,.T.);
#11978=FACE_OUTER_BOUND('',#16088,.T.);
#11979=FACE_OUTER_BOUND('',#16089,.T.);
#11980=FACE_OUTER_BOUND('',#16090,.T.);
#11981=FACE_OUTER_BOUND('',#16091,.T.);
#11982=FACE_OUTER_BOUND('',#16092,.T.);
#11983=FACE_OUTER_BOUND('',#16093,.T.);
#11984=FACE_OUTER_BOUND('',#16094,.T.);
#11985=FACE_OUTER_BOUND('',#16095,.T.);
#11986=FACE_OUTER_BOUND('',#16096,.T.);
#11987=FACE_OUTER_BOUND('',#16097,.T.);
#11988=FACE_OUTER_BOUND('',#16098,.T.);
#11989=FACE_OUTER_BOUND('',#16099,.T.);
#11990=FACE_OUTER_BOUND('',#16100,.T.);
#11991=FACE_OUTER_BOUND('',#16101,.T.);
#11992=FACE_OUTER_BOUND('',#16102,.T.);
#11993=FACE_OUTER_BOUND('',#16103,.T.);
#11994=FACE_OUTER_BOUND('',#16104,.T.);
#11995=FACE_OUTER_BOUND('',#16105,.T.);
#11996=FACE_OUTER_BOUND('',#16106,.T.);
#11997=FACE_OUTER_BOUND('',#16107,.T.);
#11998=FACE_OUTER_BOUND('',#16108,.T.);
#11999=FACE_OUTER_BOUND('',#16109,.T.);
#12000=FACE_OUTER_BOUND('',#16110,.T.);
#12001=FACE_OUTER_BOUND('',#16111,.T.);
#12002=FACE_OUTER_BOUND('',#16112,.T.);
#12003=FACE_OUTER_BOUND('',#16113,.T.);
#12004=FACE_OUTER_BOUND('',#16114,.T.);
#12005=FACE_OUTER_BOUND('',#16115,.T.);
#12006=FACE_OUTER_BOUND('',#16116,.T.);
#12007=FACE_OUTER_BOUND('',#16117,.T.);
#12008=FACE_OUTER_BOUND('',#16118,.T.);
#12009=FACE_OUTER_BOUND('',#16119,.T.);
#12010=FACE_OUTER_BOUND('',#16120,.T.);
#12011=FACE_OUTER_BOUND('',#16121,.T.);
#12012=FACE_OUTER_BOUND('',#16122,.T.);
#12013=FACE_OUTER_BOUND('',#16123,.T.);
#12014=FACE_OUTER_BOUND('',#16124,.T.);
#12015=FACE_OUTER_BOUND('',#16125,.T.);
#12016=FACE_OUTER_BOUND('',#16126,.T.);
#12017=FACE_OUTER_BOUND('',#16127,.T.);
#12018=FACE_OUTER_BOUND('',#16128,.T.);
#12019=FACE_OUTER_BOUND('',#16129,.T.);
#12020=FACE_OUTER_BOUND('',#16130,.T.);
#12021=FACE_OUTER_BOUND('',#16131,.T.);
#12022=FACE_OUTER_BOUND('',#16132,.T.);
#12023=FACE_OUTER_BOUND('',#16133,.T.);
#12024=FACE_OUTER_BOUND('',#16134,.T.);
#12025=FACE_OUTER_BOUND('',#16135,.T.);
#12026=FACE_OUTER_BOUND('',#16136,.T.);
#12027=FACE_OUTER_BOUND('',#16137,.T.);
#12028=FACE_OUTER_BOUND('',#16138,.T.);
#12029=FACE_OUTER_BOUND('',#16139,.T.);
#12030=FACE_OUTER_BOUND('',#16140,.T.);
#12031=FACE_OUTER_BOUND('',#16141,.T.);
#12032=FACE_OUTER_BOUND('',#16142,.T.);
#12033=FACE_OUTER_BOUND('',#16143,.T.);
#12034=FACE_OUTER_BOUND('',#16144,.T.);
#12035=FACE_OUTER_BOUND('',#16145,.T.);
#12036=FACE_OUTER_BOUND('',#16146,.T.);
#12037=FACE_OUTER_BOUND('',#16147,.T.);
#12038=FACE_OUTER_BOUND('',#16148,.T.);
#12039=FACE_OUTER_BOUND('',#16149,.T.);
#12040=FACE_OUTER_BOUND('',#16150,.T.);
#12041=FACE_OUTER_BOUND('',#16151,.T.);
#12042=FACE_OUTER_BOUND('',#16152,.T.);
#12043=FACE_OUTER_BOUND('',#16153,.T.);
#12044=FACE_OUTER_BOUND('',#16154,.T.);
#12045=FACE_OUTER_BOUND('',#16155,.T.);
#12046=FACE_OUTER_BOUND('',#16156,.T.);
#12047=FACE_OUTER_BOUND('',#16157,.T.);
#12048=FACE_OUTER_BOUND('',#16158,.T.);
#12049=FACE_OUTER_BOUND('',#16159,.T.);
#12050=FACE_OUTER_BOUND('',#16160,.T.);
#12051=FACE_OUTER_BOUND('',#16161,.T.);
#12052=FACE_OUTER_BOUND('',#16162,.T.);
#12053=FACE_OUTER_BOUND('',#16163,.T.);
#12054=FACE_OUTER_BOUND('',#16164,.T.);
#12055=FACE_OUTER_BOUND('',#16165,.T.);
#12056=FACE_OUTER_BOUND('',#16166,.T.);
#12057=FACE_OUTER_BOUND('',#16167,.T.);
#12058=FACE_OUTER_BOUND('',#16168,.T.);
#12059=FACE_OUTER_BOUND('',#16169,.T.);
#12060=FACE_OUTER_BOUND('',#16170,.T.);
#12061=FACE_OUTER_BOUND('',#16171,.T.);
#12062=FACE_OUTER_BOUND('',#16172,.T.);
#12063=FACE_OUTER_BOUND('',#16173,.T.);
#12064=FACE_OUTER_BOUND('',#16174,.T.);
#12065=FACE_OUTER_BOUND('',#16175,.T.);
#12066=FACE_OUTER_BOUND('',#16176,.T.);
#12067=FACE_OUTER_BOUND('',#16177,.T.);
#12068=FACE_OUTER_BOUND('',#16178,.T.);
#12069=FACE_OUTER_BOUND('',#16179,.T.);
#12070=FACE_OUTER_BOUND('',#16180,.T.);
#12071=FACE_OUTER_BOUND('',#16181,.T.);
#12072=FACE_OUTER_BOUND('',#16182,.T.);
#12073=FACE_OUTER_BOUND('',#16184,.T.);
#12074=FACE_OUTER_BOUND('',#16185,.T.);
#12075=FACE_OUTER_BOUND('',#16186,.T.);
#12076=FACE_OUTER_BOUND('',#16187,.T.);
#12077=FACE_OUTER_BOUND('',#16188,.T.);
#12078=FACE_OUTER_BOUND('',#16189,.T.);
#12079=FACE_OUTER_BOUND('',#16190,.T.);
#12080=FACE_OUTER_BOUND('',#16191,.T.);
#12081=FACE_OUTER_BOUND('',#16192,.T.);
#12082=FACE_OUTER_BOUND('',#16194,.T.);
#12083=FACE_OUTER_BOUND('',#16195,.T.);
#12084=FACE_OUTER_BOUND('',#16197,.T.);
#12085=FACE_OUTER_BOUND('',#16199,.T.);
#12086=FACE_OUTER_BOUND('',#16201,.T.);
#12087=FACE_OUTER_BOUND('',#16202,.T.);
#12088=FACE_OUTER_BOUND('',#16204,.T.);
#12089=FACE_OUTER_BOUND('',#16475,.T.);
#12090=FACE_OUTER_BOUND('',#16536,.T.);
#12091=FACE_OUTER_BOUND('',#16537,.T.);
#12092=FACE_OUTER_BOUND('',#16539,.T.);
#12093=FACE_OUTER_BOUND('',#16540,.T.);
#12094=FACE_OUTER_BOUND('',#16542,.T.);
#12095=FACE_OUTER_BOUND('',#16543,.T.);
#12096=FACE_OUTER_BOUND('',#16545,.T.);
#12097=FACE_OUTER_BOUND('',#16546,.T.);
#12098=FACE_OUTER_BOUND('',#16548,.T.);
#12099=FACE_OUTER_BOUND('',#16549,.T.);
#12100=FACE_OUTER_BOUND('',#16551,.T.);
#12101=FACE_OUTER_BOUND('',#16552,.T.);
#12102=FACE_OUTER_BOUND('',#16554,.T.);
#12103=FACE_OUTER_BOUND('',#16555,.T.);
#12104=FACE_OUTER_BOUND('',#16557,.T.);
#12105=FACE_OUTER_BOUND('',#16558,.T.);
#12106=FACE_OUTER_BOUND('',#16560,.T.);
#12107=FACE_OUTER_BOUND('',#16561,.T.);
#12108=FACE_OUTER_BOUND('',#16563,.T.);
#12109=FACE_OUTER_BOUND('',#16564,.T.);
#12110=FACE_OUTER_BOUND('',#16566,.T.);
#12111=FACE_OUTER_BOUND('',#16567,.T.);
#12112=FACE_OUTER_BOUND('',#16569,.T.);
#12113=FACE_OUTER_BOUND('',#16570,.T.);
#12114=FACE_OUTER_BOUND('',#16572,.T.);
#12115=FACE_OUTER_BOUND('',#16573,.T.);
#12116=FACE_OUTER_BOUND('',#16575,.T.);
#12117=FACE_OUTER_BOUND('',#16576,.T.);
#12118=FACE_OUTER_BOUND('',#16578,.T.);
#12119=FACE_OUTER_BOUND('',#16579,.T.);
#12120=FACE_OUTER_BOUND('',#16581,.T.);
#12121=FACE_OUTER_BOUND('',#16582,.T.);
#12122=FACE_OUTER_BOUND('',#16584,.T.);
#12123=FACE_OUTER_BOUND('',#16585,.T.);
#12124=FACE_OUTER_BOUND('',#16587,.T.);
#12125=FACE_OUTER_BOUND('',#16588,.T.);
#12126=FACE_OUTER_BOUND('',#16590,.T.);
#12127=FACE_OUTER_BOUND('',#16591,.T.);
#12128=FACE_OUTER_BOUND('',#16593,.T.);
#12129=FACE_OUTER_BOUND('',#16594,.T.);
#12130=FACE_OUTER_BOUND('',#16596,.T.);
#12131=FACE_OUTER_BOUND('',#16597,.T.);
#12132=FACE_OUTER_BOUND('',#16599,.T.);
#12133=FACE_OUTER_BOUND('',#16600,.T.);
#12134=FACE_OUTER_BOUND('',#16602,.T.);
#12135=FACE_OUTER_BOUND('',#16603,.T.);
#12136=FACE_OUTER_BOUND('',#16605,.T.);
#12137=FACE_OUTER_BOUND('',#16606,.T.);
#12138=FACE_OUTER_BOUND('',#16608,.T.);
#12139=FACE_OUTER_BOUND('',#16609,.T.);
#12140=FACE_OUTER_BOUND('',#16611,.T.);
#12141=FACE_OUTER_BOUND('',#16612,.T.);
#12142=FACE_OUTER_BOUND('',#16614,.T.);
#12143=FACE_OUTER_BOUND('',#16615,.T.);
#12144=FACE_OUTER_BOUND('',#16617,.T.);
#12145=FACE_OUTER_BOUND('',#16618,.T.);
#12146=FACE_OUTER_BOUND('',#16620,.T.);
#12147=FACE_OUTER_BOUND('',#16621,.T.);
#12148=FACE_OUTER_BOUND('',#16623,.T.);
#12149=FACE_OUTER_BOUND('',#16624,.T.);
#12150=FACE_OUTER_BOUND('',#16626,.T.);
#12151=FACE_OUTER_BOUND('',#16627,.T.);
#12152=FACE_OUTER_BOUND('',#16629,.T.);
#12153=FACE_OUTER_BOUND('',#16630,.T.);
#12154=FACE_OUTER_BOUND('',#16632,.T.);
#12155=FACE_OUTER_BOUND('',#16633,.T.);
#12156=FACE_OUTER_BOUND('',#16635,.T.);
#12157=FACE_OUTER_BOUND('',#16636,.T.);
#12158=FACE_OUTER_BOUND('',#16638,.T.);
#12159=FACE_OUTER_BOUND('',#16639,.T.);
#12160=FACE_OUTER_BOUND('',#16641,.T.);
#12161=FACE_OUTER_BOUND('',#16642,.T.);
#12162=FACE_OUTER_BOUND('',#16644,.T.);
#12163=FACE_OUTER_BOUND('',#16645,.T.);
#12164=FACE_OUTER_BOUND('',#16647,.T.);
#12165=FACE_OUTER_BOUND('',#16648,.T.);
#12166=FACE_OUTER_BOUND('',#16650,.T.);
#12167=FACE_OUTER_BOUND('',#16651,.T.);
#12168=FACE_OUTER_BOUND('',#16653,.T.);
#12169=FACE_OUTER_BOUND('',#16654,.T.);
#12170=FACE_OUTER_BOUND('',#16656,.T.);
#12171=FACE_OUTER_BOUND('',#16657,.T.);
#12172=FACE_OUTER_BOUND('',#16659,.T.);
#12173=FACE_OUTER_BOUND('',#16660,.T.);
#12174=FACE_OUTER_BOUND('',#16662,.T.);
#12175=FACE_OUTER_BOUND('',#16663,.T.);
#12176=FACE_OUTER_BOUND('',#16665,.T.);
#12177=FACE_OUTER_BOUND('',#16666,.T.);
#12178=FACE_OUTER_BOUND('',#16668,.T.);
#12179=FACE_OUTER_BOUND('',#16669,.T.);
#12180=FACE_OUTER_BOUND('',#16671,.T.);
#12181=FACE_OUTER_BOUND('',#16672,.T.);
#12182=FACE_OUTER_BOUND('',#16674,.T.);
#12183=FACE_OUTER_BOUND('',#16675,.T.);
#12184=FACE_OUTER_BOUND('',#16677,.T.);
#12185=FACE_OUTER_BOUND('',#16678,.T.);
#12186=FACE_OUTER_BOUND('',#16680,.T.);
#12187=FACE_OUTER_BOUND('',#16681,.T.);
#12188=FACE_OUTER_BOUND('',#16683,.T.);
#12189=FACE_OUTER_BOUND('',#16684,.T.);
#12190=FACE_OUTER_BOUND('',#16686,.T.);
#12191=FACE_OUTER_BOUND('',#16687,.T.);
#12192=FACE_OUTER_BOUND('',#16689,.T.);
#12193=FACE_OUTER_BOUND('',#16690,.T.);
#12194=FACE_OUTER_BOUND('',#16692,.T.);
#12195=FACE_OUTER_BOUND('',#16693,.T.);
#12196=FACE_OUTER_BOUND('',#16695,.T.);
#12197=FACE_OUTER_BOUND('',#16696,.T.);
#12198=FACE_OUTER_BOUND('',#16698,.T.);
#12199=FACE_OUTER_BOUND('',#16699,.T.);
#12200=FACE_OUTER_BOUND('',#16701,.T.);
#12201=FACE_OUTER_BOUND('',#16702,.T.);
#12202=FACE_OUTER_BOUND('',#16704,.T.);
#12203=FACE_OUTER_BOUND('',#16705,.T.);
#12204=FACE_OUTER_BOUND('',#16707,.T.);
#12205=FACE_OUTER_BOUND('',#16708,.T.);
#12206=FACE_OUTER_BOUND('',#16710,.T.);
#12207=FACE_OUTER_BOUND('',#16711,.T.);
#12208=FACE_OUTER_BOUND('',#16713,.T.);
#12209=FACE_OUTER_BOUND('',#16714,.T.);
#12210=FACE_OUTER_BOUND('',#16716,.T.);
#12211=FACE_OUTER_BOUND('',#16717,.T.);
#12212=FACE_OUTER_BOUND('',#16719,.T.);
#12213=FACE_OUTER_BOUND('',#16720,.T.);
#12214=FACE_OUTER_BOUND('',#16722,.T.);
#12215=FACE_OUTER_BOUND('',#16723,.T.);
#12216=FACE_OUTER_BOUND('',#16725,.T.);
#12217=FACE_OUTER_BOUND('',#16726,.T.);
#12218=FACE_OUTER_BOUND('',#16728,.T.);
#12219=FACE_OUTER_BOUND('',#16729,.T.);
#12220=FACE_OUTER_BOUND('',#16731,.T.);
#12221=FACE_OUTER_BOUND('',#16732,.T.);
#12222=FACE_OUTER_BOUND('',#16734,.T.);
#12223=FACE_OUTER_BOUND('',#16735,.T.);
#12224=FACE_OUTER_BOUND('',#16737,.T.);
#12225=FACE_OUTER_BOUND('',#16738,.T.);
#12226=FACE_OUTER_BOUND('',#16740,.T.);
#12227=FACE_OUTER_BOUND('',#16741,.T.);
#12228=FACE_OUTER_BOUND('',#16743,.T.);
#12229=FACE_OUTER_BOUND('',#16744,.T.);
#12230=FACE_OUTER_BOUND('',#16746,.T.);
#12231=FACE_OUTER_BOUND('',#16747,.T.);
#12232=FACE_OUTER_BOUND('',#16749,.T.);
#12233=FACE_OUTER_BOUND('',#16750,.T.);
#12234=FACE_OUTER_BOUND('',#16752,.T.);
#12235=FACE_OUTER_BOUND('',#16753,.T.);
#12236=FACE_OUTER_BOUND('',#16755,.T.);
#12237=FACE_OUTER_BOUND('',#16756,.T.);
#12238=FACE_OUTER_BOUND('',#16758,.T.);
#12239=FACE_OUTER_BOUND('',#16759,.T.);
#12240=FACE_OUTER_BOUND('',#16761,.T.);
#12241=FACE_OUTER_BOUND('',#16762,.T.);
#12242=FACE_OUTER_BOUND('',#16764,.T.);
#12243=FACE_OUTER_BOUND('',#16765,.T.);
#12244=FACE_OUTER_BOUND('',#16767,.T.);
#12245=FACE_OUTER_BOUND('',#16768,.T.);
#12246=FACE_OUTER_BOUND('',#16770,.T.);
#12247=FACE_OUTER_BOUND('',#16771,.T.);
#12248=FACE_OUTER_BOUND('',#16773,.T.);
#12249=FACE_OUTER_BOUND('',#16774,.T.);
#12250=FACE_OUTER_BOUND('',#16776,.T.);
#12251=FACE_OUTER_BOUND('',#16777,.T.);
#12252=FACE_OUTER_BOUND('',#16779,.T.);
#12253=FACE_OUTER_BOUND('',#16780,.T.);
#12254=FACE_OUTER_BOUND('',#16782,.T.);
#12255=FACE_OUTER_BOUND('',#16783,.T.);
#12256=FACE_OUTER_BOUND('',#16785,.T.);
#12257=FACE_OUTER_BOUND('',#16786,.T.);
#12258=FACE_OUTER_BOUND('',#16788,.T.);
#12259=FACE_OUTER_BOUND('',#16789,.T.);
#12260=FACE_OUTER_BOUND('',#16791,.T.);
#12261=FACE_OUTER_BOUND('',#16792,.T.);
#12262=FACE_OUTER_BOUND('',#16794,.T.);
#12263=FACE_OUTER_BOUND('',#16795,.T.);
#12264=FACE_OUTER_BOUND('',#16797,.T.);
#12265=FACE_OUTER_BOUND('',#16798,.T.);
#12266=FACE_OUTER_BOUND('',#16800,.T.);
#12267=FACE_OUTER_BOUND('',#16801,.T.);
#12268=FACE_OUTER_BOUND('',#16803,.T.);
#12269=FACE_OUTER_BOUND('',#16804,.T.);
#12270=FACE_OUTER_BOUND('',#16806,.T.);
#12271=FACE_OUTER_BOUND('',#16807,.T.);
#12272=FACE_OUTER_BOUND('',#16809,.T.);
#12273=FACE_OUTER_BOUND('',#16810,.T.);
#12274=FACE_OUTER_BOUND('',#16812,.T.);
#12275=FACE_OUTER_BOUND('',#16813,.T.);
#12276=FACE_OUTER_BOUND('',#16815,.T.);
#12277=FACE_OUTER_BOUND('',#16816,.T.);
#12278=FACE_OUTER_BOUND('',#16818,.T.);
#12279=FACE_OUTER_BOUND('',#16819,.T.);
#12280=FACE_OUTER_BOUND('',#16821,.T.);
#12281=FACE_OUTER_BOUND('',#16822,.T.);
#12282=FACE_OUTER_BOUND('',#16824,.T.);
#12283=FACE_OUTER_BOUND('',#16825,.T.);
#12284=FACE_OUTER_BOUND('',#16827,.T.);
#12285=FACE_OUTER_BOUND('',#16828,.T.);
#12286=FACE_OUTER_BOUND('',#16830,.T.);
#12287=FACE_OUTER_BOUND('',#16831,.T.);
#12288=FACE_OUTER_BOUND('',#16833,.T.);
#12289=FACE_OUTER_BOUND('',#16834,.T.);
#12290=FACE_OUTER_BOUND('',#16836,.T.);
#12291=FACE_OUTER_BOUND('',#16837,.T.);
#12292=FACE_OUTER_BOUND('',#16839,.T.);
#12293=FACE_OUTER_BOUND('',#16840,.T.);
#12294=FACE_OUTER_BOUND('',#16842,.T.);
#12295=FACE_OUTER_BOUND('',#16843,.T.);
#12296=FACE_OUTER_BOUND('',#16845,.T.);
#12297=FACE_OUTER_BOUND('',#16846,.T.);
#12298=FACE_OUTER_BOUND('',#16848,.T.);
#12299=FACE_OUTER_BOUND('',#16849,.T.);
#12300=FACE_OUTER_BOUND('',#16851,.T.);
#12301=FACE_OUTER_BOUND('',#16852,.T.);
#12302=FACE_OUTER_BOUND('',#16854,.T.);
#12303=FACE_OUTER_BOUND('',#16855,.T.);
#12304=FACE_OUTER_BOUND('',#16857,.T.);
#12305=FACE_OUTER_BOUND('',#16858,.T.);
#12306=FACE_OUTER_BOUND('',#16860,.T.);
#12307=FACE_OUTER_BOUND('',#16861,.T.);
#12308=FACE_OUTER_BOUND('',#16863,.T.);
#12309=FACE_OUTER_BOUND('',#16864,.T.);
#12310=FACE_OUTER_BOUND('',#16866,.T.);
#12311=FACE_OUTER_BOUND('',#16867,.T.);
#12312=FACE_OUTER_BOUND('',#16869,.T.);
#12313=FACE_OUTER_BOUND('',#16870,.T.);
#12314=FACE_OUTER_BOUND('',#16872,.T.);
#12315=FACE_OUTER_BOUND('',#16873,.T.);
#12316=FACE_OUTER_BOUND('',#16875,.T.);
#12317=FACE_OUTER_BOUND('',#16876,.T.);
#12318=FACE_OUTER_BOUND('',#16878,.T.);
#12319=FACE_OUTER_BOUND('',#16879,.T.);
#12320=FACE_OUTER_BOUND('',#16881,.T.);
#12321=FACE_OUTER_BOUND('',#16882,.T.);
#12322=FACE_OUTER_BOUND('',#16884,.T.);
#12323=FACE_OUTER_BOUND('',#16885,.T.);
#12324=FACE_OUTER_BOUND('',#16887,.T.);
#12325=FACE_OUTER_BOUND('',#16888,.T.);
#12326=FACE_OUTER_BOUND('',#16890,.T.);
#12327=FACE_OUTER_BOUND('',#16891,.T.);
#12328=FACE_OUTER_BOUND('',#16893,.T.);
#12329=FACE_OUTER_BOUND('',#16894,.T.);
#12330=FACE_OUTER_BOUND('',#16896,.T.);
#12331=FACE_OUTER_BOUND('',#16897,.T.);
#12332=FACE_OUTER_BOUND('',#16899,.T.);
#12333=FACE_OUTER_BOUND('',#16900,.T.);
#12334=FACE_OUTER_BOUND('',#16902,.T.);
#12335=FACE_OUTER_BOUND('',#16903,.T.);
#12336=FACE_OUTER_BOUND('',#16905,.T.);
#12337=FACE_OUTER_BOUND('',#16906,.T.);
#12338=FACE_OUTER_BOUND('',#16908,.T.);
#12339=FACE_OUTER_BOUND('',#16909,.T.);
#12340=FACE_OUTER_BOUND('',#16911,.T.);
#12341=FACE_OUTER_BOUND('',#16912,.T.);
#12342=FACE_OUTER_BOUND('',#16914,.T.);
#12343=FACE_OUTER_BOUND('',#16915,.T.);
#12344=FACE_OUTER_BOUND('',#16917,.T.);
#12345=FACE_OUTER_BOUND('',#16918,.T.);
#12346=FACE_OUTER_BOUND('',#16920,.T.);
#12347=FACE_OUTER_BOUND('',#16921,.T.);
#12348=FACE_OUTER_BOUND('',#16923,.T.);
#12349=FACE_OUTER_BOUND('',#16924,.T.);
#12350=FACE_OUTER_BOUND('',#16926,.T.);
#12351=FACE_OUTER_BOUND('',#16927,.T.);
#12352=FACE_OUTER_BOUND('',#16929,.T.);
#12353=FACE_OUTER_BOUND('',#16930,.T.);
#12354=FACE_OUTER_BOUND('',#16932,.T.);
#12355=FACE_OUTER_BOUND('',#16933,.T.);
#12356=FACE_OUTER_BOUND('',#16935,.T.);
#12357=FACE_OUTER_BOUND('',#16936,.T.);
#12358=FACE_OUTER_BOUND('',#16938,.T.);
#12359=FACE_OUTER_BOUND('',#16939,.T.);
#12360=FACE_OUTER_BOUND('',#16941,.T.);
#12361=FACE_OUTER_BOUND('',#16942,.T.);
#12362=FACE_OUTER_BOUND('',#16944,.T.);
#12363=FACE_OUTER_BOUND('',#16945,.T.);
#12364=FACE_OUTER_BOUND('',#16947,.T.);
#12365=FACE_OUTER_BOUND('',#16948,.T.);
#12366=FACE_OUTER_BOUND('',#16950,.T.);
#12367=FACE_OUTER_BOUND('',#16951,.T.);
#12368=FACE_OUTER_BOUND('',#16953,.T.);
#12369=FACE_OUTER_BOUND('',#16954,.T.);
#12370=FACE_OUTER_BOUND('',#16956,.T.);
#12371=FACE_OUTER_BOUND('',#16957,.T.);
#12372=FACE_OUTER_BOUND('',#16959,.T.);
#12373=FACE_OUTER_BOUND('',#16960,.T.);
#12374=FACE_OUTER_BOUND('',#16962,.T.);
#12375=FACE_OUTER_BOUND('',#16963,.T.);
#12376=FACE_OUTER_BOUND('',#16965,.T.);
#12377=FACE_OUTER_BOUND('',#16966,.T.);
#12378=FACE_OUTER_BOUND('',#16968,.T.);
#12379=FACE_OUTER_BOUND('',#16969,.T.);
#12380=FACE_OUTER_BOUND('',#16971,.T.);
#12381=FACE_OUTER_BOUND('',#16972,.T.);
#12382=FACE_OUTER_BOUND('',#16974,.T.);
#12383=FACE_OUTER_BOUND('',#16975,.T.);
#12384=FACE_OUTER_BOUND('',#16977,.T.);
#12385=FACE_OUTER_BOUND('',#16978,.T.);
#12386=FACE_OUTER_BOUND('',#16980,.T.);
#12387=FACE_OUTER_BOUND('',#16981,.T.);
#12388=FACE_OUTER_BOUND('',#16983,.T.);
#12389=FACE_OUTER_BOUND('',#16984,.T.);
#12390=FACE_OUTER_BOUND('',#16986,.T.);
#12391=FACE_OUTER_BOUND('',#16987,.T.);
#12392=FACE_OUTER_BOUND('',#16989,.T.);
#12393=FACE_OUTER_BOUND('',#16990,.T.);
#12394=FACE_OUTER_BOUND('',#16992,.T.);
#12395=FACE_OUTER_BOUND('',#16993,.T.);
#12396=FACE_OUTER_BOUND('',#16995,.T.);
#12397=FACE_OUTER_BOUND('',#16996,.T.);
#12398=FACE_OUTER_BOUND('',#16998,.T.);
#12399=FACE_OUTER_BOUND('',#16999,.T.);
#12400=FACE_OUTER_BOUND('',#17001,.T.);
#12401=FACE_OUTER_BOUND('',#17002,.T.);
#12402=FACE_OUTER_BOUND('',#17004,.T.);
#12403=FACE_OUTER_BOUND('',#17005,.T.);
#12404=FACE_OUTER_BOUND('',#17007,.T.);
#12405=FACE_OUTER_BOUND('',#17008,.T.);
#12406=FACE_OUTER_BOUND('',#17010,.T.);
#12407=FACE_OUTER_BOUND('',#17011,.T.);
#12408=FACE_OUTER_BOUND('',#17013,.T.);
#12409=FACE_OUTER_BOUND('',#17014,.T.);
#12410=FACE_OUTER_BOUND('',#17016,.T.);
#12411=FACE_OUTER_BOUND('',#17017,.T.);
#12412=FACE_OUTER_BOUND('',#17019,.T.);
#12413=FACE_OUTER_BOUND('',#17020,.T.);
#12414=FACE_OUTER_BOUND('',#17022,.T.);
#12415=FACE_OUTER_BOUND('',#17023,.T.);
#12416=FACE_OUTER_BOUND('',#17025,.T.);
#12417=FACE_OUTER_BOUND('',#17026,.T.);
#12418=FACE_OUTER_BOUND('',#17028,.T.);
#12419=FACE_OUTER_BOUND('',#17029,.T.);
#12420=FACE_OUTER_BOUND('',#17031,.T.);
#12421=FACE_OUTER_BOUND('',#17032,.T.);
#12422=FACE_OUTER_BOUND('',#17034,.T.);
#12423=FACE_OUTER_BOUND('',#17035,.T.);
#12424=FACE_OUTER_BOUND('',#17037,.T.);
#12425=FACE_OUTER_BOUND('',#17038,.T.);
#12426=FACE_OUTER_BOUND('',#17040,.T.);
#12427=FACE_OUTER_BOUND('',#17041,.T.);
#12428=FACE_OUTER_BOUND('',#17043,.T.);
#12429=FACE_OUTER_BOUND('',#17044,.T.);
#12430=FACE_OUTER_BOUND('',#17046,.T.);
#12431=FACE_OUTER_BOUND('',#17047,.T.);
#12432=FACE_OUTER_BOUND('',#17049,.T.);
#12433=FACE_OUTER_BOUND('',#17050,.T.);
#12434=FACE_OUTER_BOUND('',#17052,.T.);
#12435=FACE_OUTER_BOUND('',#17053,.T.);
#12436=FACE_OUTER_BOUND('',#17055,.T.);
#12437=FACE_OUTER_BOUND('',#17056,.T.);
#12438=FACE_OUTER_BOUND('',#17058,.T.);
#12439=FACE_OUTER_BOUND('',#17059,.T.);
#12440=FACE_OUTER_BOUND('',#17061,.T.);
#12441=FACE_OUTER_BOUND('',#17062,.T.);
#12442=FACE_OUTER_BOUND('',#17064,.T.);
#12443=FACE_OUTER_BOUND('',#17065,.T.);
#12444=FACE_OUTER_BOUND('',#17067,.T.);
#12445=FACE_OUTER_BOUND('',#17068,.T.);
#12446=FACE_OUTER_BOUND('',#17070,.T.);
#12447=FACE_OUTER_BOUND('',#17071,.T.);
#12448=FACE_OUTER_BOUND('',#17073,.T.);
#12449=FACE_OUTER_BOUND('',#17074,.T.);
#12450=FACE_OUTER_BOUND('',#17076,.T.);
#12451=FACE_OUTER_BOUND('',#17077,.T.);
#12452=FACE_OUTER_BOUND('',#17079,.T.);
#12453=FACE_OUTER_BOUND('',#17080,.T.);
#12454=FACE_OUTER_BOUND('',#17082,.T.);
#12455=FACE_OUTER_BOUND('',#17083,.T.);
#12456=FACE_OUTER_BOUND('',#17085,.T.);
#12457=FACE_OUTER_BOUND('',#17086,.T.);
#12458=FACE_OUTER_BOUND('',#17088,.T.);
#12459=FACE_OUTER_BOUND('',#17089,.T.);
#12460=FACE_OUTER_BOUND('',#17091,.T.);
#12461=FACE_OUTER_BOUND('',#17092,.T.);
#12462=FACE_OUTER_BOUND('',#17094,.T.);
#12463=FACE_OUTER_BOUND('',#17095,.T.);
#12464=FACE_OUTER_BOUND('',#17097,.T.);
#12465=FACE_OUTER_BOUND('',#17098,.T.);
#12466=FACE_OUTER_BOUND('',#17100,.T.);
#12467=FACE_OUTER_BOUND('',#17101,.T.);
#12468=FACE_OUTER_BOUND('',#17103,.T.);
#12469=FACE_OUTER_BOUND('',#17104,.T.);
#12470=FACE_OUTER_BOUND('',#17106,.T.);
#12471=FACE_OUTER_BOUND('',#17107,.T.);
#12472=FACE_OUTER_BOUND('',#17109,.T.);
#12473=FACE_OUTER_BOUND('',#17110,.T.);
#12474=FACE_OUTER_BOUND('',#17112,.T.);
#12475=FACE_OUTER_BOUND('',#17113,.T.);
#12476=FACE_OUTER_BOUND('',#17115,.T.);
#12477=FACE_OUTER_BOUND('',#17116,.T.);
#12478=FACE_OUTER_BOUND('',#17118,.T.);
#12479=FACE_OUTER_BOUND('',#17119,.T.);
#12480=FACE_OUTER_BOUND('',#17121,.T.);
#12481=FACE_OUTER_BOUND('',#17122,.T.);
#12482=FACE_OUTER_BOUND('',#17124,.T.);
#12483=FACE_OUTER_BOUND('',#17125,.T.);
#12484=FACE_OUTER_BOUND('',#17127,.T.);
#12485=FACE_OUTER_BOUND('',#17128,.T.);
#12486=FACE_OUTER_BOUND('',#17130,.T.);
#12487=FACE_OUTER_BOUND('',#17131,.T.);
#12488=FACE_OUTER_BOUND('',#17133,.T.);
#12489=FACE_OUTER_BOUND('',#17134,.T.);
#12490=FACE_OUTER_BOUND('',#17136,.T.);
#12491=FACE_OUTER_BOUND('',#17137,.T.);
#12492=FACE_OUTER_BOUND('',#17139,.T.);
#12493=FACE_OUTER_BOUND('',#17140,.T.);
#12494=FACE_OUTER_BOUND('',#17142,.T.);
#12495=FACE_OUTER_BOUND('',#17143,.T.);
#12496=FACE_OUTER_BOUND('',#17145,.T.);
#12497=FACE_OUTER_BOUND('',#17146,.T.);
#12498=FACE_OUTER_BOUND('',#17148,.T.);
#12499=FACE_OUTER_BOUND('',#17149,.T.);
#12500=FACE_OUTER_BOUND('',#17151,.T.);
#12501=FACE_OUTER_BOUND('',#17152,.T.);
#12502=FACE_OUTER_BOUND('',#17154,.T.);
#12503=FACE_OUTER_BOUND('',#17155,.T.);
#12504=FACE_OUTER_BOUND('',#17157,.T.);
#12505=FACE_OUTER_BOUND('',#17158,.T.);
#12506=FACE_OUTER_BOUND('',#17160,.T.);
#12507=FACE_OUTER_BOUND('',#17161,.T.);
#12508=FACE_OUTER_BOUND('',#17163,.T.);
#12509=FACE_OUTER_BOUND('',#17164,.T.);
#12510=FACE_OUTER_BOUND('',#17166,.T.);
#12511=FACE_OUTER_BOUND('',#17167,.T.);
#12512=FACE_OUTER_BOUND('',#17169,.T.);
#12513=FACE_OUTER_BOUND('',#17170,.T.);
#12514=FACE_OUTER_BOUND('',#17172,.T.);
#12515=FACE_OUTER_BOUND('',#17173,.T.);
#12516=FACE_OUTER_BOUND('',#17175,.T.);
#12517=FACE_OUTER_BOUND('',#17176,.T.);
#12518=FACE_OUTER_BOUND('',#17178,.T.);
#12519=FACE_OUTER_BOUND('',#17179,.T.);
#12520=FACE_OUTER_BOUND('',#17181,.T.);
#12521=FACE_OUTER_BOUND('',#17182,.T.);
#12522=FACE_OUTER_BOUND('',#17184,.T.);
#12523=FACE_OUTER_BOUND('',#17185,.T.);
#12524=FACE_OUTER_BOUND('',#17187,.T.);
#12525=FACE_OUTER_BOUND('',#17188,.T.);
#12526=FACE_OUTER_BOUND('',#17190,.T.);
#12527=FACE_OUTER_BOUND('',#17191,.T.);
#12528=FACE_OUTER_BOUND('',#17193,.T.);
#12529=FACE_OUTER_BOUND('',#17194,.T.);
#12530=FACE_OUTER_BOUND('',#17196,.T.);
#12531=FACE_OUTER_BOUND('',#17197,.T.);
#12532=FACE_OUTER_BOUND('',#17199,.T.);
#12533=FACE_OUTER_BOUND('',#17200,.T.);
#12534=FACE_OUTER_BOUND('',#17202,.T.);
#12535=FACE_OUTER_BOUND('',#17203,.T.);
#12536=FACE_OUTER_BOUND('',#17205,.T.);
#12537=FACE_OUTER_BOUND('',#17206,.T.);
#12538=FACE_OUTER_BOUND('',#17208,.T.);
#12539=FACE_OUTER_BOUND('',#17209,.T.);
#12540=FACE_OUTER_BOUND('',#17211,.T.);
#12541=FACE_OUTER_BOUND('',#17212,.T.);
#12542=FACE_OUTER_BOUND('',#17214,.T.);
#12543=FACE_OUTER_BOUND('',#17215,.T.);
#12544=FACE_OUTER_BOUND('',#17217,.T.);
#12545=FACE_OUTER_BOUND('',#17218,.T.);
#12546=FACE_OUTER_BOUND('',#17220,.T.);
#12547=FACE_OUTER_BOUND('',#17221,.T.);
#12548=FACE_OUTER_BOUND('',#17223,.T.);
#12549=FACE_OUTER_BOUND('',#17224,.T.);
#12550=FACE_OUTER_BOUND('',#17226,.T.);
#12551=FACE_OUTER_BOUND('',#17227,.T.);
#12552=FACE_OUTER_BOUND('',#17229,.T.);
#12553=FACE_OUTER_BOUND('',#17230,.T.);
#12554=FACE_OUTER_BOUND('',#17232,.T.);
#12555=FACE_OUTER_BOUND('',#17233,.T.);
#12556=FACE_OUTER_BOUND('',#17235,.T.);
#12557=FACE_OUTER_BOUND('',#17236,.T.);
#12558=FACE_OUTER_BOUND('',#17238,.T.);
#12559=FACE_OUTER_BOUND('',#17239,.T.);
#12560=FACE_OUTER_BOUND('',#17241,.T.);
#12561=FACE_OUTER_BOUND('',#17242,.T.);
#12562=FACE_OUTER_BOUND('',#17244,.T.);
#12563=FACE_OUTER_BOUND('',#17245,.T.);
#12564=FACE_OUTER_BOUND('',#17247,.T.);
#12565=FACE_OUTER_BOUND('',#17248,.T.);
#12566=FACE_OUTER_BOUND('',#17250,.T.);
#12567=FACE_OUTER_BOUND('',#17251,.T.);
#12568=FACE_OUTER_BOUND('',#17253,.T.);
#12569=FACE_OUTER_BOUND('',#17254,.T.);
#12570=FACE_OUTER_BOUND('',#17256,.T.);
#12571=FACE_OUTER_BOUND('',#17257,.T.);
#12572=FACE_OUTER_BOUND('',#17259,.T.);
#12573=FACE_OUTER_BOUND('',#17260,.T.);
#12574=FACE_OUTER_BOUND('',#17262,.T.);
#12575=FACE_OUTER_BOUND('',#17263,.T.);
#12576=FACE_OUTER_BOUND('',#17265,.T.);
#12577=FACE_OUTER_BOUND('',#17266,.T.);
#12578=FACE_OUTER_BOUND('',#17268,.T.);
#12579=FACE_OUTER_BOUND('',#17269,.T.);
#12580=FACE_OUTER_BOUND('',#17271,.T.);
#12581=FACE_OUTER_BOUND('',#17272,.T.);
#12582=FACE_OUTER_BOUND('',#17274,.T.);
#12583=FACE_OUTER_BOUND('',#17275,.T.);
#12584=FACE_OUTER_BOUND('',#17277,.T.);
#12585=FACE_OUTER_BOUND('',#17278,.T.);
#12586=FACE_OUTER_BOUND('',#17280,.T.);
#12587=FACE_OUTER_BOUND('',#17281,.T.);
#12588=FACE_OUTER_BOUND('',#17283,.T.);
#12589=FACE_OUTER_BOUND('',#17284,.T.);
#12590=FACE_OUTER_BOUND('',#17286,.T.);
#12591=FACE_OUTER_BOUND('',#17287,.T.);
#12592=FACE_OUTER_BOUND('',#17289,.T.);
#12593=FACE_OUTER_BOUND('',#17290,.T.);
#12594=FACE_OUTER_BOUND('',#17292,.T.);
#12595=FACE_OUTER_BOUND('',#17293,.T.);
#12596=FACE_OUTER_BOUND('',#17295,.T.);
#12597=FACE_OUTER_BOUND('',#17296,.T.);
#12598=FACE_OUTER_BOUND('',#17298,.T.);
#12599=FACE_OUTER_BOUND('',#17299,.T.);
#12600=FACE_OUTER_BOUND('',#17301,.T.);
#12601=FACE_OUTER_BOUND('',#17302,.T.);
#12602=FACE_OUTER_BOUND('',#17304,.T.);
#12603=FACE_OUTER_BOUND('',#17305,.T.);
#12604=FACE_OUTER_BOUND('',#17307,.T.);
#12605=FACE_OUTER_BOUND('',#17308,.T.);
#12606=FACE_OUTER_BOUND('',#17310,.T.);
#12607=FACE_OUTER_BOUND('',#17311,.T.);
#12608=FACE_OUTER_BOUND('',#17313,.T.);
#12609=FACE_OUTER_BOUND('',#17314,.T.);
#12610=FACE_OUTER_BOUND('',#17316,.T.);
#12611=FACE_OUTER_BOUND('',#17317,.T.);
#12612=FACE_OUTER_BOUND('',#17319,.T.);
#12613=FACE_OUTER_BOUND('',#17320,.T.);
#12614=FACE_OUTER_BOUND('',#17322,.T.);
#12615=FACE_OUTER_BOUND('',#17323,.T.);
#12616=FACE_OUTER_BOUND('',#17325,.T.);
#12617=FACE_OUTER_BOUND('',#17326,.T.);
#12618=FACE_OUTER_BOUND('',#17328,.T.);
#12619=FACE_OUTER_BOUND('',#17329,.T.);
#12620=FACE_OUTER_BOUND('',#17331,.T.);
#12621=FACE_OUTER_BOUND('',#17332,.T.);
#12622=FACE_OUTER_BOUND('',#17334,.T.);
#12623=FACE_OUTER_BOUND('',#17335,.T.);
#12624=FACE_OUTER_BOUND('',#17337,.T.);
#12625=FACE_OUTER_BOUND('',#17338,.T.);
#12626=FACE_OUTER_BOUND('',#17340,.T.);
#12627=FACE_OUTER_BOUND('',#17341,.T.);
#12628=FACE_OUTER_BOUND('',#17343,.T.);
#12629=FACE_OUTER_BOUND('',#17344,.T.);
#12630=FACE_OUTER_BOUND('',#17346,.T.);
#12631=FACE_OUTER_BOUND('',#17347,.T.);
#12632=FACE_OUTER_BOUND('',#17349,.T.);
#12633=FACE_OUTER_BOUND('',#17350,.T.);
#12634=FACE_OUTER_BOUND('',#17352,.T.);
#12635=FACE_OUTER_BOUND('',#17353,.T.);
#12636=FACE_OUTER_BOUND('',#17355,.T.);
#12637=FACE_OUTER_BOUND('',#17356,.T.);
#12638=FACE_OUTER_BOUND('',#17358,.T.);
#12639=FACE_OUTER_BOUND('',#17359,.T.);
#12640=FACE_OUTER_BOUND('',#17361,.T.);
#12641=FACE_OUTER_BOUND('',#17362,.T.);
#12642=FACE_OUTER_BOUND('',#17364,.T.);
#12643=FACE_OUTER_BOUND('',#17365,.T.);
#12644=FACE_OUTER_BOUND('',#17367,.T.);
#12645=FACE_OUTER_BOUND('',#17368,.T.);
#12646=FACE_OUTER_BOUND('',#17370,.T.);
#12647=FACE_OUTER_BOUND('',#17371,.T.);
#12648=FACE_OUTER_BOUND('',#17373,.T.);
#12649=FACE_OUTER_BOUND('',#17374,.T.);
#12650=FACE_OUTER_BOUND('',#17376,.T.);
#12651=FACE_OUTER_BOUND('',#17377,.T.);
#12652=FACE_OUTER_BOUND('',#17379,.T.);
#12653=FACE_OUTER_BOUND('',#17380,.T.);
#12654=FACE_OUTER_BOUND('',#17382,.T.);
#12655=FACE_OUTER_BOUND('',#17383,.T.);
#12656=FACE_OUTER_BOUND('',#17385,.T.);
#12657=FACE_OUTER_BOUND('',#17386,.T.);
#12658=FACE_OUTER_BOUND('',#17388,.T.);
#12659=FACE_OUTER_BOUND('',#17389,.T.);
#12660=FACE_OUTER_BOUND('',#17391,.T.);
#12661=FACE_OUTER_BOUND('',#17392,.T.);
#12662=FACE_OUTER_BOUND('',#17394,.T.);
#12663=FACE_OUTER_BOUND('',#17395,.T.);
#12664=FACE_OUTER_BOUND('',#17397,.T.);
#12665=FACE_OUTER_BOUND('',#17398,.T.);
#12666=FACE_OUTER_BOUND('',#17400,.T.);
#12667=FACE_OUTER_BOUND('',#17401,.T.);
#12668=FACE_OUTER_BOUND('',#17403,.T.);
#12669=FACE_OUTER_BOUND('',#17404,.T.);
#12670=FACE_OUTER_BOUND('',#17406,.T.);
#12671=FACE_OUTER_BOUND('',#17407,.T.);
#12672=FACE_OUTER_BOUND('',#17409,.T.);
#12673=FACE_OUTER_BOUND('',#17410,.T.);
#12674=FACE_OUTER_BOUND('',#17412,.T.);
#12675=FACE_OUTER_BOUND('',#17413,.T.);
#12676=FACE_OUTER_BOUND('',#17415,.T.);
#12677=FACE_OUTER_BOUND('',#17416,.T.);
#12678=FACE_OUTER_BOUND('',#17418,.T.);
#12679=FACE_OUTER_BOUND('',#17419,.T.);
#12680=FACE_OUTER_BOUND('',#17421,.T.);
#12681=FACE_OUTER_BOUND('',#17422,.T.);
#12682=FACE_OUTER_BOUND('',#17424,.T.);
#12683=FACE_OUTER_BOUND('',#17425,.T.);
#12684=FACE_OUTER_BOUND('',#17427,.T.);
#12685=FACE_OUTER_BOUND('',#17428,.T.);
#12686=FACE_OUTER_BOUND('',#17430,.T.);
#12687=FACE_OUTER_BOUND('',#17431,.T.);
#12688=FACE_OUTER_BOUND('',#17433,.T.);
#12689=FACE_OUTER_BOUND('',#17434,.T.);
#12690=FACE_OUTER_BOUND('',#17436,.T.);
#12691=FACE_OUTER_BOUND('',#17437,.T.);
#12692=FACE_OUTER_BOUND('',#17439,.T.);
#12693=FACE_OUTER_BOUND('',#17440,.T.);
#12694=FACE_OUTER_BOUND('',#17442,.T.);
#12695=FACE_OUTER_BOUND('',#17443,.T.);
#12696=FACE_OUTER_BOUND('',#17445,.T.);
#12697=FACE_OUTER_BOUND('',#17446,.T.);
#12698=FACE_OUTER_BOUND('',#17448,.T.);
#12699=FACE_OUTER_BOUND('',#17449,.T.);
#12700=FACE_OUTER_BOUND('',#17451,.T.);
#12701=FACE_OUTER_BOUND('',#17452,.T.);
#12702=FACE_OUTER_BOUND('',#17454,.T.);
#12703=FACE_OUTER_BOUND('',#17455,.T.);
#12704=FACE_OUTER_BOUND('',#17457,.T.);
#12705=FACE_OUTER_BOUND('',#17458,.T.);
#12706=FACE_OUTER_BOUND('',#17460,.T.);
#12707=FACE_OUTER_BOUND('',#17461,.T.);
#12708=FACE_OUTER_BOUND('',#17463,.T.);
#12709=FACE_OUTER_BOUND('',#17464,.T.);
#12710=FACE_OUTER_BOUND('',#17466,.T.);
#12711=FACE_OUTER_BOUND('',#17467,.T.);
#12712=FACE_OUTER_BOUND('',#17469,.T.);
#12713=FACE_OUTER_BOUND('',#17470,.T.);
#12714=FACE_OUTER_BOUND('',#17472,.T.);
#12715=FACE_OUTER_BOUND('',#17473,.T.);
#12716=FACE_OUTER_BOUND('',#17475,.T.);
#12717=FACE_OUTER_BOUND('',#17476,.T.);
#12718=FACE_OUTER_BOUND('',#17478,.T.);
#12719=FACE_OUTER_BOUND('',#17479,.T.);
#12720=FACE_OUTER_BOUND('',#17481,.T.);
#12721=FACE_OUTER_BOUND('',#17482,.T.);
#12722=FACE_OUTER_BOUND('',#17484,.T.);
#12723=FACE_OUTER_BOUND('',#17485,.T.);
#12724=FACE_OUTER_BOUND('',#17487,.T.);
#12725=FACE_OUTER_BOUND('',#17488,.T.);
#12726=FACE_OUTER_BOUND('',#17490,.T.);
#12727=FACE_OUTER_BOUND('',#17491,.T.);
#12728=FACE_OUTER_BOUND('',#17493,.T.);
#12729=FACE_OUTER_BOUND('',#17494,.T.);
#12730=FACE_OUTER_BOUND('',#17496,.T.);
#12731=FACE_OUTER_BOUND('',#17497,.T.);
#12732=FACE_OUTER_BOUND('',#17499,.T.);
#12733=FACE_OUTER_BOUND('',#17500,.T.);
#12734=FACE_OUTER_BOUND('',#17502,.T.);
#12735=FACE_OUTER_BOUND('',#17503,.T.);
#12736=FACE_OUTER_BOUND('',#17505,.T.);
#12737=FACE_OUTER_BOUND('',#17506,.T.);
#12738=FACE_OUTER_BOUND('',#17508,.T.);
#12739=FACE_OUTER_BOUND('',#17509,.T.);
#12740=FACE_OUTER_BOUND('',#17511,.T.);
#12741=FACE_OUTER_BOUND('',#17512,.T.);
#12742=FACE_OUTER_BOUND('',#17514,.T.);
#12743=FACE_OUTER_BOUND('',#17515,.T.);
#12744=FACE_OUTER_BOUND('',#17517,.T.);
#12745=FACE_OUTER_BOUND('',#17518,.T.);
#12746=FACE_OUTER_BOUND('',#17520,.T.);
#12747=FACE_OUTER_BOUND('',#17521,.T.);
#12748=FACE_OUTER_BOUND('',#17523,.T.);
#12749=FACE_OUTER_BOUND('',#17524,.T.);
#12750=FACE_OUTER_BOUND('',#17526,.T.);
#12751=FACE_OUTER_BOUND('',#17527,.T.);
#12752=FACE_OUTER_BOUND('',#17529,.T.);
#12753=FACE_OUTER_BOUND('',#17530,.T.);
#12754=FACE_OUTER_BOUND('',#17532,.T.);
#12755=FACE_OUTER_BOUND('',#17533,.T.);
#12756=FACE_OUTER_BOUND('',#17535,.T.);
#12757=FACE_OUTER_BOUND('',#17536,.T.);
#12758=FACE_OUTER_BOUND('',#17538,.T.);
#12759=FACE_OUTER_BOUND('',#17539,.T.);
#12760=FACE_OUTER_BOUND('',#17541,.T.);
#12761=FACE_OUTER_BOUND('',#17542,.T.);
#12762=FACE_OUTER_BOUND('',#17544,.T.);
#12763=FACE_OUTER_BOUND('',#17545,.T.);
#12764=FACE_OUTER_BOUND('',#17547,.T.);
#12765=FACE_OUTER_BOUND('',#17548,.T.);
#12766=FACE_OUTER_BOUND('',#17550,.T.);
#12767=FACE_OUTER_BOUND('',#17551,.T.);
#12768=FACE_OUTER_BOUND('',#17553,.T.);
#12769=FACE_OUTER_BOUND('',#17554,.T.);
#12770=FACE_OUTER_BOUND('',#17556,.T.);
#12771=FACE_OUTER_BOUND('',#17557,.T.);
#12772=FACE_OUTER_BOUND('',#17559,.T.);
#12773=FACE_OUTER_BOUND('',#17560,.T.);
#12774=FACE_OUTER_BOUND('',#17562,.T.);
#12775=FACE_OUTER_BOUND('',#17563,.T.);
#12776=FACE_OUTER_BOUND('',#17565,.T.);
#12777=FACE_OUTER_BOUND('',#17566,.T.);
#12778=FACE_OUTER_BOUND('',#17568,.T.);
#12779=FACE_OUTER_BOUND('',#17569,.T.);
#12780=FACE_OUTER_BOUND('',#17571,.T.);
#12781=FACE_OUTER_BOUND('',#17572,.T.);
#12782=FACE_OUTER_BOUND('',#17574,.T.);
#12783=FACE_OUTER_BOUND('',#17575,.T.);
#12784=FACE_OUTER_BOUND('',#17577,.T.);
#12785=FACE_OUTER_BOUND('',#17578,.T.);
#12786=FACE_OUTER_BOUND('',#17580,.T.);
#12787=FACE_OUTER_BOUND('',#17581,.T.);
#12788=FACE_OUTER_BOUND('',#17583,.T.);
#12789=FACE_OUTER_BOUND('',#17584,.T.);
#12790=FACE_OUTER_BOUND('',#17586,.T.);
#12791=FACE_OUTER_BOUND('',#17587,.T.);
#12792=FACE_OUTER_BOUND('',#17589,.T.);
#12793=FACE_OUTER_BOUND('',#17590,.T.);
#12794=FACE_OUTER_BOUND('',#17592,.T.);
#12795=FACE_OUTER_BOUND('',#17593,.T.);
#12796=FACE_OUTER_BOUND('',#17595,.T.);
#12797=FACE_OUTER_BOUND('',#17596,.T.);
#12798=FACE_OUTER_BOUND('',#17598,.T.);
#12799=FACE_OUTER_BOUND('',#17599,.T.);
#12800=FACE_OUTER_BOUND('',#17601,.T.);
#12801=FACE_OUTER_BOUND('',#17602,.T.);
#12802=FACE_OUTER_BOUND('',#17604,.T.);
#12803=FACE_OUTER_BOUND('',#17605,.T.);
#12804=FACE_OUTER_BOUND('',#17607,.T.);
#12805=FACE_OUTER_BOUND('',#17608,.T.);
#12806=FACE_OUTER_BOUND('',#17610,.T.);
#12807=FACE_OUTER_BOUND('',#17611,.T.);
#12808=FACE_OUTER_BOUND('',#17613,.T.);
#12809=FACE_OUTER_BOUND('',#17614,.T.);
#12810=FACE_OUTER_BOUND('',#17616,.T.);
#12811=FACE_OUTER_BOUND('',#17617,.T.);
#12812=FACE_OUTER_BOUND('',#17619,.T.);
#12813=FACE_OUTER_BOUND('',#17620,.T.);
#12814=FACE_OUTER_BOUND('',#17622,.T.);
#12815=FACE_OUTER_BOUND('',#17623,.T.);
#12816=FACE_OUTER_BOUND('',#17625,.T.);
#12817=FACE_OUTER_BOUND('',#17626,.T.);
#12818=FACE_OUTER_BOUND('',#17628,.T.);
#12819=FACE_OUTER_BOUND('',#17629,.T.);
#12820=FACE_OUTER_BOUND('',#17631,.T.);
#12821=FACE_OUTER_BOUND('',#17632,.T.);
#12822=FACE_OUTER_BOUND('',#17634,.T.);
#12823=FACE_OUTER_BOUND('',#17635,.T.);
#12824=FACE_OUTER_BOUND('',#17637,.T.);
#12825=FACE_OUTER_BOUND('',#17638,.T.);
#12826=FACE_OUTER_BOUND('',#17640,.T.);
#12827=FACE_OUTER_BOUND('',#17641,.T.);
#12828=FACE_OUTER_BOUND('',#17643,.T.);
#12829=FACE_OUTER_BOUND('',#17644,.T.);
#12830=FACE_OUTER_BOUND('',#17646,.T.);
#12831=FACE_OUTER_BOUND('',#17647,.T.);
#12832=FACE_OUTER_BOUND('',#17649,.T.);
#12833=FACE_OUTER_BOUND('',#17650,.T.);
#12834=FACE_OUTER_BOUND('',#17652,.T.);
#12835=FACE_OUTER_BOUND('',#17653,.T.);
#12836=FACE_OUTER_BOUND('',#17655,.T.);
#12837=FACE_OUTER_BOUND('',#17656,.T.);
#12838=FACE_OUTER_BOUND('',#17658,.T.);
#12839=FACE_OUTER_BOUND('',#17659,.T.);
#12840=FACE_OUTER_BOUND('',#17661,.T.);
#12841=FACE_OUTER_BOUND('',#17662,.T.);
#12842=FACE_OUTER_BOUND('',#17664,.T.);
#12843=FACE_OUTER_BOUND('',#17665,.T.);
#12844=FACE_OUTER_BOUND('',#17667,.T.);
#12845=FACE_OUTER_BOUND('',#17668,.T.);
#12846=FACE_OUTER_BOUND('',#17670,.T.);
#12847=FACE_OUTER_BOUND('',#17671,.T.);
#12848=FACE_OUTER_BOUND('',#17673,.T.);
#12849=FACE_OUTER_BOUND('',#17674,.T.);
#12850=FACE_OUTER_BOUND('',#17676,.T.);
#12851=FACE_OUTER_BOUND('',#17677,.T.);
#12852=FACE_OUTER_BOUND('',#17679,.T.);
#12853=FACE_OUTER_BOUND('',#17680,.T.);
#12854=FACE_OUTER_BOUND('',#17682,.T.);
#12855=FACE_OUTER_BOUND('',#17683,.T.);
#12856=FACE_OUTER_BOUND('',#17685,.T.);
#12857=FACE_OUTER_BOUND('',#17686,.T.);
#12858=FACE_OUTER_BOUND('',#17688,.T.);
#12859=FACE_OUTER_BOUND('',#17689,.T.);
#12860=FACE_OUTER_BOUND('',#17691,.T.);
#12861=FACE_OUTER_BOUND('',#17692,.T.);
#12862=FACE_OUTER_BOUND('',#17694,.T.);
#12863=FACE_OUTER_BOUND('',#17695,.T.);
#12864=FACE_OUTER_BOUND('',#17697,.T.);
#12865=FACE_OUTER_BOUND('',#17698,.T.);
#12866=FACE_OUTER_BOUND('',#17700,.T.);
#12867=FACE_OUTER_BOUND('',#17701,.T.);
#12868=EDGE_LOOP('',(#30316,#30317,#30318,#30319,#30320));
#12869=EDGE_LOOP('',(#30321,#30322,#30323,#30324,#30325));
#12870=EDGE_LOOP('',(#30326,#30327,#30328,#30329));
#12871=EDGE_LOOP('',(#30330,#30331,#30332,#30333,#30334,#30335));
#12872=EDGE_LOOP('',(#30336,#30337,#30338,#30339));
#12873=EDGE_LOOP('',(#30340));
#12874=EDGE_LOOP('',(#30341));
#12875=EDGE_LOOP('',(#30342,#30343,#30344,#30345));
#12876=EDGE_LOOP('',(#30346,#30347,#30348,#30349));
#12877=EDGE_LOOP('',(#30350,#30351,#30352,#30353));
#12878=EDGE_LOOP('',(#30354,#30355,#30356));
#12879=EDGE_LOOP('',(#30357,#30358,#30359));
#12880=EDGE_LOOP('',(#30360,#30361,#30362,#30363));
#12881=EDGE_LOOP('',(#30364,#30365,#30366));
#12882=EDGE_LOOP('',(#30367,#30368,#30369));
#12883=EDGE_LOOP('',(#30370,#30371,#30372,#30373));
#12884=EDGE_LOOP('',(#30374,#30375,#30376,#30377));
#12885=EDGE_LOOP('',(#30378,#30379,#30380,#30381));
#12886=EDGE_LOOP('',(#30382,#30383,#30384,#30385));
#12887=EDGE_LOOP('',(#30386,#30387,#30388,#30389));
#12888=EDGE_LOOP('',(#30390,#30391,#30392,#30393));
#12889=EDGE_LOOP('',(#30394,#30395,#30396,#30397));
#12890=EDGE_LOOP('',(#30398,#30399,#30400,#30401));
#12891=EDGE_LOOP('',(#30402,#30403,#30404,#30405));
#12892=EDGE_LOOP('',(#30406,#30407,#30408,#30409));
#12893=EDGE_LOOP('',(#30410,#30411,#30412,#30413));
#12894=EDGE_LOOP('',(#30414,#30415,#30416,#30417));
#12895=EDGE_LOOP('',(#30418,#30419,#30420,#30421));
#12896=EDGE_LOOP('',(#30422,#30423,#30424,#30425));
#12897=EDGE_LOOP('',(#30426,#30427,#30428,#30429,#30430));
#12898=EDGE_LOOP('',(#30431,#30432,#30433,#30434));
#12899=EDGE_LOOP('',(#30435,#30436,#30437,#30438,#30439));
#12900=EDGE_LOOP('',(#30440,#30441,#30442,#30443));
#12901=EDGE_LOOP('',(#30444,#30445,#30446,#30447,#30448));
#12902=EDGE_LOOP('',(#30449,#30450,#30451,#30452));
#12903=EDGE_LOOP('',(#30453,#30454,#30455,#30456,#30457));
#12904=EDGE_LOOP('',(#30458,#30459,#30460,#30461));
#12905=EDGE_LOOP('',(#30462,#30463,#30464,#30465,#30466));
#12906=EDGE_LOOP('',(#30467,#30468,#30469,#30470));
#12907=EDGE_LOOP('',(#30471,#30472,#30473,#30474,#30475));
#12908=EDGE_LOOP('',(#30476,#30477,#30478,#30479));
#12909=EDGE_LOOP('',(#30480,#30481,#30482,#30483,#30484));
#12910=EDGE_LOOP('',(#30485,#30486,#30487,#30488));
#12911=EDGE_LOOP('',(#30489,#30490,#30491,#30492,#30493));
#12912=EDGE_LOOP('',(#30494,#30495,#30496,#30497));
#12913=EDGE_LOOP('',(#30498,#30499,#30500,#30501,#30502));
#12914=EDGE_LOOP('',(#30503,#30504,#30505,#30506));
#12915=EDGE_LOOP('',(#30507,#30508,#30509,#30510,#30511));
#12916=EDGE_LOOP('',(#30512,#30513,#30514,#30515));
#12917=EDGE_LOOP('',(#30516,#30517,#30518,#30519,#30520));
#12918=EDGE_LOOP('',(#30521,#30522,#30523,#30524));
#12919=EDGE_LOOP('',(#30525,#30526,#30527,#30528,#30529));
#12920=EDGE_LOOP('',(#30530,#30531,#30532,#30533));
#12921=EDGE_LOOP('',(#30534,#30535,#30536,#30537,#30538));
#12922=EDGE_LOOP('',(#30539,#30540,#30541,#30542));
#12923=EDGE_LOOP('',(#30543,#30544,#30545,#30546,#30547));
#12924=EDGE_LOOP('',(#30548,#30549,#30550,#30551));
#12925=EDGE_LOOP('',(#30552,#30553,#30554,#30555,#30556));
#12926=EDGE_LOOP('',(#30557,#30558,#30559,#30560));
#12927=EDGE_LOOP('',(#30561,#30562,#30563,#30564,#30565));
#12928=EDGE_LOOP('',(#30566,#30567,#30568,#30569));
#12929=EDGE_LOOP('',(#30570,#30571,#30572,#30573,#30574));
#12930=EDGE_LOOP('',(#30575,#30576,#30577,#30578));
#12931=EDGE_LOOP('',(#30579,#30580,#30581,#30582,#30583));
#12932=EDGE_LOOP('',(#30584,#30585,#30586,#30587));
#12933=EDGE_LOOP('',(#30588,#30589,#30590,#30591,#30592));
#12934=EDGE_LOOP('',(#30593,#30594,#30595,#30596));
#12935=EDGE_LOOP('',(#30597,#30598,#30599,#30600,#30601));
#12936=EDGE_LOOP('',(#30602,#30603,#30604,#30605));
#12937=EDGE_LOOP('',(#30606,#30607,#30608,#30609,#30610));
#12938=EDGE_LOOP('',(#30611,#30612,#30613,#30614));
#12939=EDGE_LOOP('',(#30615,#30616,#30617,#30618,#30619));
#12940=EDGE_LOOP('',(#30620,#30621,#30622,#30623));
#12941=EDGE_LOOP('',(#30624,#30625,#30626,#30627,#30628));
#12942=EDGE_LOOP('',(#30629,#30630,#30631,#30632));
#12943=EDGE_LOOP('',(#30633,#30634,#30635,#30636,#30637));
#12944=EDGE_LOOP('',(#30638,#30639,#30640,#30641));
#12945=EDGE_LOOP('',(#30642,#30643,#30644,#30645,#30646));
#12946=EDGE_LOOP('',(#30647,#30648,#30649,#30650));
#12947=EDGE_LOOP('',(#30651,#30652,#30653,#30654,#30655));
#12948=EDGE_LOOP('',(#30656,#30657,#30658,#30659));
#12949=EDGE_LOOP('',(#30660,#30661,#30662,#30663,#30664));
#12950=EDGE_LOOP('',(#30665,#30666,#30667,#30668));
#12951=EDGE_LOOP('',(#30669,#30670,#30671,#30672,#30673));
#12952=EDGE_LOOP('',(#30674,#30675,#30676,#30677));
#12953=EDGE_LOOP('',(#30678,#30679,#30680,#30681,#30682));
#12954=EDGE_LOOP('',(#30683,#30684,#30685,#30686));
#12955=EDGE_LOOP('',(#30687,#30688,#30689,#30690,#30691));
#12956=EDGE_LOOP('',(#30692,#30693,#30694,#30695));
#12957=EDGE_LOOP('',(#30696,#30697,#30698,#30699,#30700));
#12958=EDGE_LOOP('',(#30701,#30702,#30703,#30704));
#12959=EDGE_LOOP('',(#30705,#30706,#30707,#30708,#30709));
#12960=EDGE_LOOP('',(#30710,#30711,#30712,#30713));
#12961=EDGE_LOOP('',(#30714,#30715,#30716,#30717,#30718));
#12962=EDGE_LOOP('',(#30719,#30720,#30721,#30722));
#12963=EDGE_LOOP('',(#30723,#30724,#30725,#30726,#30727));
#12964=EDGE_LOOP('',(#30728,#30729,#30730,#30731));
#12965=EDGE_LOOP('',(#30732,#30733,#30734,#30735,#30736));
#12966=EDGE_LOOP('',(#30737,#30738,#30739,#30740));
#12967=EDGE_LOOP('',(#30741,#30742,#30743,#30744,#30745));
#12968=EDGE_LOOP('',(#30746,#30747,#30748,#30749));
#12969=EDGE_LOOP('',(#30750,#30751,#30752,#30753,#30754));
#12970=EDGE_LOOP('',(#30755,#30756,#30757,#30758));
#12971=EDGE_LOOP('',(#30759,#30760,#30761,#30762,#30763));
#12972=EDGE_LOOP('',(#30764,#30765,#30766,#30767));
#12973=EDGE_LOOP('',(#30768,#30769,#30770,#30771,#30772));
#12974=EDGE_LOOP('',(#30773,#30774,#30775,#30776));
#12975=EDGE_LOOP('',(#30777,#30778,#30779,#30780));
#12976=EDGE_LOOP('',(#30781,#30782,#30783,#30784));
#12977=EDGE_LOOP('',(#30785,#30786,#30787,#30788));
#12978=EDGE_LOOP('',(#30789,#30790,#30791,#30792));
#12979=EDGE_LOOP('',(#30793,#30794,#30795,#30796,#30797));
#12980=EDGE_LOOP('',(#30798,#30799,#30800,#30801));
#12981=EDGE_LOOP('',(#30802,#30803,#30804,#30805,#30806));
#12982=EDGE_LOOP('',(#30807,#30808,#30809,#30810));
#12983=EDGE_LOOP('',(#30811,#30812,#30813,#30814));
#12984=EDGE_LOOP('',(#30815,#30816,#30817,#30818));
#12985=EDGE_LOOP('',(#30819,#30820,#30821,#30822));
#12986=EDGE_LOOP('',(#30823,#30824,#30825,#30826));
#12987=EDGE_LOOP('',(#30827,#30828,#30829,#30830,#30831));
#12988=EDGE_LOOP('',(#30832,#30833,#30834,#30835));
#12989=EDGE_LOOP('',(#30836,#30837,#30838,#30839,#30840));
#12990=EDGE_LOOP('',(#30841,#30842,#30843,#30844));
#12991=EDGE_LOOP('',(#30845,#30846,#30847,#30848));
#12992=EDGE_LOOP('',(#30849,#30850,#30851,#30852));
#12993=EDGE_LOOP('',(#30853,#30854,#30855,#30856,#30857));
#12994=EDGE_LOOP('',(#30858,#30859,#30860,#30861));
#12995=EDGE_LOOP('',(#30862,#30863,#30864,#30865,#30866));
#12996=EDGE_LOOP('',(#30867,#30868,#30869,#30870));
#12997=EDGE_LOOP('',(#30871,#30872,#30873,#30874));
#12998=EDGE_LOOP('',(#30875,#30876,#30877,#30878));
#12999=EDGE_LOOP('',(#30879,#30880,#30881,#30882,#30883));
#13000=EDGE_LOOP('',(#30884,#30885,#30886,#30887));
#13001=EDGE_LOOP('',(#30888,#30889,#30890,#30891,#30892));
#13002=EDGE_LOOP('',(#30893,#30894,#30895,#30896));
#13003=EDGE_LOOP('',(#30897,#30898,#30899,#30900,#30901));
#13004=EDGE_LOOP('',(#30902,#30903,#30904,#30905));
#13005=EDGE_LOOP('',(#30906,#30907,#30908,#30909,#30910));
#13006=EDGE_LOOP('',(#30911,#30912,#30913,#30914));
#13007=EDGE_LOOP('',(#30915,#30916,#30917,#30918,#30919));
#13008=EDGE_LOOP('',(#30920,#30921,#30922,#30923));
#13009=EDGE_LOOP('',(#30924,#30925,#30926,#30927,#30928));
#13010=EDGE_LOOP('',(#30929,#30930,#30931,#30932));
#13011=EDGE_LOOP('',(#30933,#30934,#30935,#30936,#30937));
#13012=EDGE_LOOP('',(#30938,#30939,#30940,#30941));
#13013=EDGE_LOOP('',(#30942,#30943,#30944,#30945,#30946));
#13014=EDGE_LOOP('',(#30947,#30948,#30949,#30950));
#13015=EDGE_LOOP('',(#30951,#30952,#30953,#30954,#30955));
#13016=EDGE_LOOP('',(#30956,#30957,#30958,#30959));
#13017=EDGE_LOOP('',(#30960,#30961,#30962,#30963,#30964));
#13018=EDGE_LOOP('',(#30965,#30966,#30967,#30968));
#13019=EDGE_LOOP('',(#30969,#30970,#30971,#30972,#30973));
#13020=EDGE_LOOP('',(#30974,#30975,#30976,#30977));
#13021=EDGE_LOOP('',(#30978,#30979,#30980,#30981,#30982));
#13022=EDGE_LOOP('',(#30983,#30984,#30985,#30986));
#13023=EDGE_LOOP('',(#30987,#30988,#30989,#30990,#30991));
#13024=EDGE_LOOP('',(#30992,#30993,#30994,#30995));
#13025=EDGE_LOOP('',(#30996,#30997,#30998,#30999,#31000));
#13026=EDGE_LOOP('',(#31001,#31002,#31003,#31004));
#13027=EDGE_LOOP('',(#31005,#31006,#31007,#31008));
#13028=EDGE_LOOP('',(#31009,#31010,#31011,#31012));
#13029=EDGE_LOOP('',(#31013,#31014,#31015,#31016));
#13030=EDGE_LOOP('',(#31017,#31018,#31019,#31020));
#13031=EDGE_LOOP('',(#31021,#31022,#31023,#31024));
#13032=EDGE_LOOP('',(#31025,#31026,#31027,#31028));
#13033=EDGE_LOOP('',(#31029,#31030,#31031,#31032));
#13034=EDGE_LOOP('',(#31033,#31034,#31035,#31036));
#13035=EDGE_LOOP('',(#31037,#31038,#31039,#31040));
#13036=EDGE_LOOP('',(#31041,#31042,#31043,#31044));
#13037=EDGE_LOOP('',(#31045,#31046,#31047,#31048));
#13038=EDGE_LOOP('',(#31049,#31050,#31051,#31052));
#13039=EDGE_LOOP('',(#31053,#31054,#31055,#31056));
#13040=EDGE_LOOP('',(#31057,#31058,#31059,#31060));
#13041=EDGE_LOOP('',(#31061,#31062,#31063,#31064));
#13042=EDGE_LOOP('',(#31065,#31066,#31067,#31068));
#13043=EDGE_LOOP('',(#31069,#31070,#31071,#31072,#31073,#31074));
#13044=EDGE_LOOP('',(#31075,#31076,#31077,#31078));
#13045=EDGE_LOOP('',(#31079,#31080,#31081,#31082));
#13046=EDGE_LOOP('',(#31083,#31084,#31085,#31086));
#13047=EDGE_LOOP('',(#31087,#31088,#31089,#31090));
#13048=EDGE_LOOP('',(#31091,#31092,#31093,#31094));
#13049=EDGE_LOOP('',(#31095,#31096,#31097,#31098));
#13050=EDGE_LOOP('',(#31099,#31100,#31101,#31102));
#13051=EDGE_LOOP('',(#31103,#31104,#31105,#31106));
#13052=EDGE_LOOP('',(#31107,#31108,#31109,#31110));
#13053=EDGE_LOOP('',(#31111,#31112,#31113,#31114));
#13054=EDGE_LOOP('',(#31115,#31116,#31117,#31118));
#13055=EDGE_LOOP('',(#31119,#31120,#31121,#31122));
#13056=EDGE_LOOP('',(#31123,#31124,#31125,#31126));
#13057=EDGE_LOOP('',(#31127,#31128,#31129,#31130));
#13058=EDGE_LOOP('',(#31131,#31132,#31133,#31134));
#13059=EDGE_LOOP('',(#31135,#31136,#31137,#31138));
#13060=EDGE_LOOP('',(#31139,#31140,#31141,#31142));
#13061=EDGE_LOOP('',(#31143,#31144,#31145,#31146,#31147,#31148));
#13062=EDGE_LOOP('',(#31149,#31150,#31151,#31152));
#13063=EDGE_LOOP('',(#31153,#31154,#31155,#31156));
#13064=EDGE_LOOP('',(#31157,#31158,#31159,#31160));
#13065=EDGE_LOOP('',(#31161,#31162,#31163,#31164));
#13066=EDGE_LOOP('',(#31165,#31166,#31167,#31168));
#13067=EDGE_LOOP('',(#31169,#31170,#31171,#31172));
#13068=EDGE_LOOP('',(#31173,#31174,#31175,#31176));
#13069=EDGE_LOOP('',(#31177,#31178,#31179,#31180));
#13070=EDGE_LOOP('',(#31181,#31182,#31183,#31184));
#13071=EDGE_LOOP('',(#31185,#31186,#31187,#31188));
#13072=EDGE_LOOP('',(#31189,#31190,#31191,#31192));
#13073=EDGE_LOOP('',(#31193,#31194,#31195,#31196));
#13074=EDGE_LOOP('',(#31197,#31198,#31199,#31200));
#13075=EDGE_LOOP('',(#31201,#31202,#31203,#31204));
#13076=EDGE_LOOP('',(#31205,#31206,#31207,#31208));
#13077=EDGE_LOOP('',(#31209,#31210,#31211,#31212,#31213,#31214));
#13078=EDGE_LOOP('',(#31215,#31216,#31217,#31218));
#13079=EDGE_LOOP('',(#31219,#31220,#31221,#31222));
#13080=EDGE_LOOP('',(#31223,#31224,#31225,#31226));
#13081=EDGE_LOOP('',(#31227,#31228,#31229,#31230));
#13082=EDGE_LOOP('',(#31231,#31232,#31233,#31234));
#13083=EDGE_LOOP('',(#31235,#31236,#31237,#31238));
#13084=EDGE_LOOP('',(#31239,#31240,#31241,#31242));
#13085=EDGE_LOOP('',(#31243,#31244,#31245,#31246));
#13086=EDGE_LOOP('',(#31247,#31248,#31249,#31250));
#13087=EDGE_LOOP('',(#31251,#31252,#31253,#31254));
#13088=EDGE_LOOP('',(#31255,#31256,#31257,#31258));
#13089=EDGE_LOOP('',(#31259,#31260,#31261,#31262));
#13090=EDGE_LOOP('',(#31263,#31264,#31265,#31266));
#13091=EDGE_LOOP('',(#31267,#31268,#31269,#31270));
#13092=EDGE_LOOP('',(#31271,#31272,#31273,#31274));
#13093=EDGE_LOOP('',(#31275,#31276,#31277,#31278));
#13094=EDGE_LOOP('',(#31279,#31280,#31281,#31282));
#13095=EDGE_LOOP('',(#31283,#31284,#31285,#31286,#31287,#31288));
#13096=EDGE_LOOP('',(#31289,#31290,#31291,#31292));
#13097=EDGE_LOOP('',(#31293,#31294,#31295,#31296));
#13098=EDGE_LOOP('',(#31297,#31298,#31299,#31300));
#13099=EDGE_LOOP('',(#31301,#31302,#31303,#31304));
#13100=EDGE_LOOP('',(#31305,#31306,#31307,#31308));
#13101=EDGE_LOOP('',(#31309,#31310,#31311,#31312));
#13102=EDGE_LOOP('',(#31313,#31314,#31315,#31316));
#13103=EDGE_LOOP('',(#31317,#31318,#31319,#31320));
#13104=EDGE_LOOP('',(#31321,#31322,#31323,#31324));
#13105=EDGE_LOOP('',(#31325,#31326,#31327,#31328));
#13106=EDGE_LOOP('',(#31329,#31330,#31331,#31332));
#13107=EDGE_LOOP('',(#31333,#31334,#31335,#31336));
#13108=EDGE_LOOP('',(#31337,#31338,#31339,#31340));
#13109=EDGE_LOOP('',(#31341,#31342,#31343,#31344));
#13110=EDGE_LOOP('',(#31345,#31346,#31347,#31348));
#13111=EDGE_LOOP('',(#31349,#31350,#31351,#31352));
#13112=EDGE_LOOP('',(#31353,#31354,#31355,#31356));
#13113=EDGE_LOOP('',(#31357,#31358,#31359,#31360,#31361,#31362));
#13114=EDGE_LOOP('',(#31363,#31364,#31365,#31366));
#13115=EDGE_LOOP('',(#31367,#31368,#31369,#31370));
#13116=EDGE_LOOP('',(#31371,#31372,#31373,#31374));
#13117=EDGE_LOOP('',(#31375,#31376,#31377,#31378));
#13118=EDGE_LOOP('',(#31379,#31380,#31381,#31382));
#13119=EDGE_LOOP('',(#31383,#31384,#31385,#31386));
#13120=EDGE_LOOP('',(#31387,#31388,#31389,#31390));
#13121=EDGE_LOOP('',(#31391,#31392,#31393,#31394));
#13122=EDGE_LOOP('',(#31395,#31396,#31397,#31398));
#13123=EDGE_LOOP('',(#31399,#31400,#31401,#31402));
#13124=EDGE_LOOP('',(#31403,#31404,#31405,#31406));
#13125=EDGE_LOOP('',(#31407,#31408,#31409,#31410));
#13126=EDGE_LOOP('',(#31411,#31412,#31413,#31414));
#13127=EDGE_LOOP('',(#31415,#31416,#31417,#31418));
#13128=EDGE_LOOP('',(#31419,#31420,#31421,#31422));
#13129=EDGE_LOOP('',(#31423,#31424,#31425,#31426));
#13130=EDGE_LOOP('',(#31427,#31428,#31429,#31430));
#13131=EDGE_LOOP('',(#31431,#31432,#31433,#31434,#31435,#31436));
#13132=EDGE_LOOP('',(#31437,#31438,#31439,#31440));
#13133=EDGE_LOOP('',(#31441,#31442,#31443,#31444));
#13134=EDGE_LOOP('',(#31445,#31446,#31447,#31448));
#13135=EDGE_LOOP('',(#31449,#31450,#31451,#31452));
#13136=EDGE_LOOP('',(#31453,#31454,#31455,#31456));
#13137=EDGE_LOOP('',(#31457,#31458,#31459,#31460));
#13138=EDGE_LOOP('',(#31461,#31462,#31463,#31464));
#13139=EDGE_LOOP('',(#31465,#31466,#31467,#31468));
#13140=EDGE_LOOP('',(#31469,#31470,#31471,#31472));
#13141=EDGE_LOOP('',(#31473,#31474,#31475,#31476));
#13142=EDGE_LOOP('',(#31477,#31478,#31479,#31480));
#13143=EDGE_LOOP('',(#31481,#31482,#31483,#31484));
#13144=EDGE_LOOP('',(#31485,#31486,#31487,#31488));
#13145=EDGE_LOOP('',(#31489,#31490,#31491,#31492));
#13146=EDGE_LOOP('',(#31493,#31494,#31495,#31496));
#13147=EDGE_LOOP('',(#31497,#31498,#31499,#31500));
#13148=EDGE_LOOP('',(#31501,#31502,#31503,#31504));
#13149=EDGE_LOOP('',(#31505,#31506,#31507,#31508,#31509,#31510));
#13150=EDGE_LOOP('',(#31511,#31512,#31513,#31514));
#13151=EDGE_LOOP('',(#31515,#31516,#31517,#31518));
#13152=EDGE_LOOP('',(#31519,#31520,#31521,#31522));
#13153=EDGE_LOOP('',(#31523,#31524,#31525,#31526));
#13154=EDGE_LOOP('',(#31527,#31528,#31529,#31530));
#13155=EDGE_LOOP('',(#31531,#31532,#31533,#31534));
#13156=EDGE_LOOP('',(#31535,#31536,#31537,#31538));
#13157=EDGE_LOOP('',(#31539,#31540,#31541,#31542));
#13158=EDGE_LOOP('',(#31543,#31544,#31545,#31546));
#13159=EDGE_LOOP('',(#31547,#31548,#31549,#31550));
#13160=EDGE_LOOP('',(#31551,#31552,#31553,#31554));
#13161=EDGE_LOOP('',(#31555,#31556,#31557,#31558));
#13162=EDGE_LOOP('',(#31559,#31560,#31561,#31562));
#13163=EDGE_LOOP('',(#31563,#31564,#31565,#31566));
#13164=EDGE_LOOP('',(#31567,#31568,#31569,#31570));
#13165=EDGE_LOOP('',(#31571,#31572,#31573,#31574,#31575,#31576));
#13166=EDGE_LOOP('',(#31577,#31578,#31579,#31580));
#13167=EDGE_LOOP('',(#31581,#31582,#31583,#31584));
#13168=EDGE_LOOP('',(#31585,#31586,#31587,#31588));
#13169=EDGE_LOOP('',(#31589,#31590,#31591,#31592));
#13170=EDGE_LOOP('',(#31593,#31594,#31595,#31596));
#13171=EDGE_LOOP('',(#31597,#31598,#31599,#31600));
#13172=EDGE_LOOP('',(#31601,#31602,#31603,#31604));
#13173=EDGE_LOOP('',(#31605,#31606,#31607,#31608));
#13174=EDGE_LOOP('',(#31609,#31610,#31611,#31612));
#13175=EDGE_LOOP('',(#31613,#31614,#31615,#31616));
#13176=EDGE_LOOP('',(#31617,#31618,#31619,#31620));
#13177=EDGE_LOOP('',(#31621,#31622,#31623,#31624));
#13178=EDGE_LOOP('',(#31625,#31626,#31627,#31628));
#13179=EDGE_LOOP('',(#31629,#31630,#31631,#31632));
#13180=EDGE_LOOP('',(#31633,#31634,#31635,#31636));
#13181=EDGE_LOOP('',(#31637,#31638,#31639,#31640));
#13182=EDGE_LOOP('',(#31641,#31642,#31643,#31644));
#13183=EDGE_LOOP('',(#31645,#31646,#31647,#31648,#31649,#31650));
#13184=EDGE_LOOP('',(#31651,#31652,#31653,#31654));
#13185=EDGE_LOOP('',(#31655,#31656,#31657,#31658));
#13186=EDGE_LOOP('',(#31659,#31660,#31661,#31662));
#13187=EDGE_LOOP('',(#31663,#31664,#31665,#31666));
#13188=EDGE_LOOP('',(#31667,#31668,#31669,#31670));
#13189=EDGE_LOOP('',(#31671,#31672,#31673,#31674));
#13190=EDGE_LOOP('',(#31675,#31676,#31677,#31678));
#13191=EDGE_LOOP('',(#31679,#31680,#31681,#31682));
#13192=EDGE_LOOP('',(#31683,#31684,#31685,#31686));
#13193=EDGE_LOOP('',(#31687,#31688,#31689,#31690));
#13194=EDGE_LOOP('',(#31691,#31692,#31693,#31694));
#13195=EDGE_LOOP('',(#31695,#31696,#31697,#31698));
#13196=EDGE_LOOP('',(#31699,#31700,#31701,#31702));
#13197=EDGE_LOOP('',(#31703,#31704,#31705,#31706));
#13198=EDGE_LOOP('',(#31707,#31708,#31709,#31710));
#13199=EDGE_LOOP('',(#31711,#31712,#31713,#31714));
#13200=EDGE_LOOP('',(#31715,#31716,#31717,#31718));
#13201=EDGE_LOOP('',(#31719,#31720,#31721,#31722,#31723,#31724));
#13202=EDGE_LOOP('',(#31725,#31726,#31727,#31728));
#13203=EDGE_LOOP('',(#31729,#31730,#31731,#31732));
#13204=EDGE_LOOP('',(#31733,#31734,#31735,#31736));
#13205=EDGE_LOOP('',(#31737,#31738,#31739,#31740));
#13206=EDGE_LOOP('',(#31741,#31742,#31743,#31744));
#13207=EDGE_LOOP('',(#31745,#31746,#31747,#31748));
#13208=EDGE_LOOP('',(#31749,#31750,#31751,#31752));
#13209=EDGE_LOOP('',(#31753,#31754,#31755,#31756));
#13210=EDGE_LOOP('',(#31757,#31758,#31759,#31760));
#13211=EDGE_LOOP('',(#31761,#31762,#31763,#31764));
#13212=EDGE_LOOP('',(#31765,#31766,#31767,#31768));
#13213=EDGE_LOOP('',(#31769,#31770,#31771,#31772));
#13214=EDGE_LOOP('',(#31773,#31774,#31775,#31776));
#13215=EDGE_LOOP('',(#31777,#31778,#31779,#31780));
#13216=EDGE_LOOP('',(#31781,#31782,#31783,#31784));
#13217=EDGE_LOOP('',(#31785,#31786,#31787,#31788));
#13218=EDGE_LOOP('',(#31789,#31790,#31791,#31792));
#13219=EDGE_LOOP('',(#31793,#31794,#31795,#31796,#31797,#31798));
#13220=EDGE_LOOP('',(#31799,#31800,#31801,#31802));
#13221=EDGE_LOOP('',(#31803,#31804,#31805,#31806));
#13222=EDGE_LOOP('',(#31807,#31808,#31809,#31810));
#13223=EDGE_LOOP('',(#31811,#31812,#31813,#31814));
#13224=EDGE_LOOP('',(#31815,#31816,#31817,#31818));
#13225=EDGE_LOOP('',(#31819,#31820,#31821,#31822));
#13226=EDGE_LOOP('',(#31823,#31824,#31825,#31826));
#13227=EDGE_LOOP('',(#31827,#31828,#31829,#31830));
#13228=EDGE_LOOP('',(#31831,#31832,#31833,#31834));
#13229=EDGE_LOOP('',(#31835,#31836,#31837,#31838));
#13230=EDGE_LOOP('',(#31839,#31840,#31841,#31842));
#13231=EDGE_LOOP('',(#31843,#31844,#31845,#31846));
#13232=EDGE_LOOP('',(#31847,#31848,#31849,#31850));
#13233=EDGE_LOOP('',(#31851,#31852,#31853,#31854));
#13234=EDGE_LOOP('',(#31855,#31856,#31857,#31858));
#13235=EDGE_LOOP('',(#31859,#31860,#31861,#31862));
#13236=EDGE_LOOP('',(#31863,#31864,#31865,#31866));
#13237=EDGE_LOOP('',(#31867,#31868,#31869,#31870,#31871,#31872));
#13238=EDGE_LOOP('',(#31873,#31874,#31875,#31876));
#13239=EDGE_LOOP('',(#31877,#31878,#31879,#31880));
#13240=EDGE_LOOP('',(#31881,#31882,#31883,#31884));
#13241=EDGE_LOOP('',(#31885,#31886,#31887,#31888));
#13242=EDGE_LOOP('',(#31889,#31890,#31891,#31892));
#13243=EDGE_LOOP('',(#31893,#31894,#31895,#31896));
#13244=EDGE_LOOP('',(#31897,#31898,#31899,#31900));
#13245=EDGE_LOOP('',(#31901,#31902,#31903,#31904));
#13246=EDGE_LOOP('',(#31905,#31906,#31907,#31908));
#13247=EDGE_LOOP('',(#31909,#31910,#31911,#31912));
#13248=EDGE_LOOP('',(#31913,#31914,#31915,#31916));
#13249=EDGE_LOOP('',(#31917,#31918,#31919,#31920));
#13250=EDGE_LOOP('',(#31921,#31922,#31923,#31924));
#13251=EDGE_LOOP('',(#31925,#31926,#31927,#31928));
#13252=EDGE_LOOP('',(#31929,#31930,#31931,#31932));
#13253=EDGE_LOOP('',(#31933,#31934,#31935,#31936,#31937,#31938));
#13254=EDGE_LOOP('',(#31939,#31940,#31941,#31942));
#13255=EDGE_LOOP('',(#31943,#31944,#31945,#31946));
#13256=EDGE_LOOP('',(#31947,#31948,#31949,#31950));
#13257=EDGE_LOOP('',(#31951,#31952,#31953,#31954));
#13258=EDGE_LOOP('',(#31955,#31956,#31957,#31958));
#13259=EDGE_LOOP('',(#31959,#31960,#31961,#31962));
#13260=EDGE_LOOP('',(#31963,#31964,#31965,#31966));
#13261=EDGE_LOOP('',(#31967,#31968,#31969,#31970));
#13262=EDGE_LOOP('',(#31971,#31972,#31973,#31974));
#13263=EDGE_LOOP('',(#31975,#31976,#31977,#31978));
#13264=EDGE_LOOP('',(#31979,#31980,#31981,#31982));
#13265=EDGE_LOOP('',(#31983,#31984,#31985,#31986));
#13266=EDGE_LOOP('',(#31987,#31988,#31989,#31990));
#13267=EDGE_LOOP('',(#31991,#31992,#31993,#31994));
#13268=EDGE_LOOP('',(#31995,#31996,#31997,#31998));
#13269=EDGE_LOOP('',(#31999,#32000,#32001,#32002));
#13270=EDGE_LOOP('',(#32003,#32004,#32005,#32006));
#13271=EDGE_LOOP('',(#32007,#32008,#32009,#32010,#32011,#32012));
#13272=EDGE_LOOP('',(#32013,#32014,#32015,#32016));
#13273=EDGE_LOOP('',(#32017,#32018,#32019,#32020));
#13274=EDGE_LOOP('',(#32021,#32022,#32023,#32024));
#13275=EDGE_LOOP('',(#32025,#32026,#32027,#32028));
#13276=EDGE_LOOP('',(#32029,#32030,#32031,#32032));
#13277=EDGE_LOOP('',(#32033,#32034,#32035,#32036));
#13278=EDGE_LOOP('',(#32037,#32038,#32039,#32040));
#13279=EDGE_LOOP('',(#32041,#32042,#32043,#32044));
#13280=EDGE_LOOP('',(#32045,#32046,#32047,#32048));
#13281=EDGE_LOOP('',(#32049,#32050,#32051,#32052));
#13282=EDGE_LOOP('',(#32053,#32054,#32055,#32056));
#13283=EDGE_LOOP('',(#32057,#32058,#32059,#32060));
#13284=EDGE_LOOP('',(#32061,#32062,#32063,#32064));
#13285=EDGE_LOOP('',(#32065,#32066,#32067,#32068));
#13286=EDGE_LOOP('',(#32069,#32070,#32071,#32072));
#13287=EDGE_LOOP('',(#32073,#32074,#32075,#32076));
#13288=EDGE_LOOP('',(#32077,#32078,#32079,#32080));
#13289=EDGE_LOOP('',(#32081,#32082,#32083,#32084,#32085,#32086));
#13290=EDGE_LOOP('',(#32087,#32088,#32089,#32090));
#13291=EDGE_LOOP('',(#32091,#32092,#32093,#32094));
#13292=EDGE_LOOP('',(#32095,#32096,#32097,#32098));
#13293=EDGE_LOOP('',(#32099,#32100,#32101,#32102));
#13294=EDGE_LOOP('',(#32103,#32104,#32105,#32106));
#13295=EDGE_LOOP('',(#32107,#32108,#32109,#32110));
#13296=EDGE_LOOP('',(#32111,#32112,#32113,#32114));
#13297=EDGE_LOOP('',(#32115,#32116,#32117,#32118));
#13298=EDGE_LOOP('',(#32119,#32120,#32121,#32122));
#13299=EDGE_LOOP('',(#32123,#32124,#32125,#32126));
#13300=EDGE_LOOP('',(#32127,#32128,#32129,#32130));
#13301=EDGE_LOOP('',(#32131,#32132,#32133,#32134));
#13302=EDGE_LOOP('',(#32135,#32136,#32137,#32138));
#13303=EDGE_LOOP('',(#32139,#32140,#32141,#32142));
#13304=EDGE_LOOP('',(#32143,#32144,#32145,#32146));
#13305=EDGE_LOOP('',(#32147,#32148,#32149,#32150));
#13306=EDGE_LOOP('',(#32151,#32152,#32153,#32154));
#13307=EDGE_LOOP('',(#32155,#32156,#32157,#32158,#32159,#32160));
#13308=EDGE_LOOP('',(#32161,#32162,#32163,#32164));
#13309=EDGE_LOOP('',(#32165,#32166,#32167,#32168));
#13310=EDGE_LOOP('',(#32169,#32170,#32171,#32172));
#13311=EDGE_LOOP('',(#32173,#32174,#32175,#32176));
#13312=EDGE_LOOP('',(#32177,#32178,#32179,#32180));
#13313=EDGE_LOOP('',(#32181,#32182,#32183,#32184));
#13314=EDGE_LOOP('',(#32185,#32186,#32187,#32188));
#13315=EDGE_LOOP('',(#32189,#32190,#32191,#32192));
#13316=EDGE_LOOP('',(#32193,#32194,#32195,#32196));
#13317=EDGE_LOOP('',(#32197,#32198,#32199,#32200));
#13318=EDGE_LOOP('',(#32201,#32202,#32203,#32204));
#13319=EDGE_LOOP('',(#32205,#32206,#32207,#32208));
#13320=EDGE_LOOP('',(#32209,#32210,#32211,#32212));
#13321=EDGE_LOOP('',(#32213,#32214,#32215,#32216));
#13322=EDGE_LOOP('',(#32217,#32218,#32219,#32220));
#13323=EDGE_LOOP('',(#32221,#32222,#32223,#32224));
#13324=EDGE_LOOP('',(#32225,#32226,#32227,#32228));
#13325=EDGE_LOOP('',(#32229,#32230,#32231,#32232,#32233,#32234));
#13326=EDGE_LOOP('',(#32235,#32236,#32237,#32238));
#13327=EDGE_LOOP('',(#32239,#32240,#32241,#32242));
#13328=EDGE_LOOP('',(#32243,#32244,#32245,#32246));
#13329=EDGE_LOOP('',(#32247,#32248,#32249,#32250));
#13330=EDGE_LOOP('',(#32251,#32252,#32253,#32254));
#13331=EDGE_LOOP('',(#32255,#32256,#32257,#32258));
#13332=EDGE_LOOP('',(#32259,#32260,#32261,#32262));
#13333=EDGE_LOOP('',(#32263,#32264,#32265,#32266));
#13334=EDGE_LOOP('',(#32267,#32268,#32269,#32270));
#13335=EDGE_LOOP('',(#32271,#32272,#32273,#32274));
#13336=EDGE_LOOP('',(#32275,#32276,#32277,#32278));
#13337=EDGE_LOOP('',(#32279,#32280,#32281,#32282));
#13338=EDGE_LOOP('',(#32283,#32284,#32285,#32286));
#13339=EDGE_LOOP('',(#32287,#32288,#32289,#32290));
#13340=EDGE_LOOP('',(#32291,#32292,#32293,#32294));
#13341=EDGE_LOOP('',(#32295,#32296,#32297,#32298,#32299,#32300));
#13342=EDGE_LOOP('',(#32301,#32302,#32303,#32304));
#13343=EDGE_LOOP('',(#32305,#32306,#32307,#32308));
#13344=EDGE_LOOP('',(#32309,#32310,#32311,#32312));
#13345=EDGE_LOOP('',(#32313,#32314,#32315,#32316));
#13346=EDGE_LOOP('',(#32317,#32318,#32319,#32320));
#13347=EDGE_LOOP('',(#32321,#32322,#32323,#32324));
#13348=EDGE_LOOP('',(#32325,#32326,#32327,#32328));
#13349=EDGE_LOOP('',(#32329,#32330,#32331,#32332));
#13350=EDGE_LOOP('',(#32333,#32334,#32335,#32336));
#13351=EDGE_LOOP('',(#32337,#32338,#32339,#32340));
#13352=EDGE_LOOP('',(#32341,#32342,#32343,#32344));
#13353=EDGE_LOOP('',(#32345,#32346,#32347,#32348));
#13354=EDGE_LOOP('',(#32349,#32350,#32351,#32352));
#13355=EDGE_LOOP('',(#32353,#32354,#32355,#32356));
#13356=EDGE_LOOP('',(#32357,#32358,#32359,#32360));
#13357=EDGE_LOOP('',(#32361,#32362,#32363,#32364));
#13358=EDGE_LOOP('',(#32365,#32366,#32367,#32368));
#13359=EDGE_LOOP('',(#32369,#32370,#32371,#32372,#32373,#32374));
#13360=EDGE_LOOP('',(#32375,#32376,#32377,#32378));
#13361=EDGE_LOOP('',(#32379,#32380,#32381,#32382));
#13362=EDGE_LOOP('',(#32383,#32384,#32385,#32386));
#13363=EDGE_LOOP('',(#32387,#32388,#32389,#32390));
#13364=EDGE_LOOP('',(#32391,#32392,#32393,#32394));
#13365=EDGE_LOOP('',(#32395,#32396,#32397,#32398));
#13366=EDGE_LOOP('',(#32399,#32400,#32401,#32402));
#13367=EDGE_LOOP('',(#32403,#32404,#32405,#32406));
#13368=EDGE_LOOP('',(#32407,#32408,#32409,#32410));
#13369=EDGE_LOOP('',(#32411,#32412,#32413,#32414));
#13370=EDGE_LOOP('',(#32415,#32416,#32417,#32418));
#13371=EDGE_LOOP('',(#32419,#32420,#32421,#32422));
#13372=EDGE_LOOP('',(#32423,#32424,#32425,#32426));
#13373=EDGE_LOOP('',(#32427,#32428,#32429,#32430));
#13374=EDGE_LOOP('',(#32431,#32432,#32433,#32434));
#13375=EDGE_LOOP('',(#32435,#32436,#32437,#32438,#32439,#32440));
#13376=EDGE_LOOP('',(#32441,#32442,#32443,#32444));
#13377=EDGE_LOOP('',(#32445,#32446,#32447,#32448,#32449,#32450));
#13378=EDGE_LOOP('',(#32451,#32452,#32453,#32454));
#13379=EDGE_LOOP('',(#32455,#32456,#32457,#32458));
#13380=EDGE_LOOP('',(#32459,#32460,#32461,#32462));
#13381=EDGE_LOOP('',(#32463,#32464,#32465,#32466));
#13382=EDGE_LOOP('',(#32467,#32468,#32469,#32470));
#13383=EDGE_LOOP('',(#32471,#32472,#32473,#32474));
#13384=EDGE_LOOP('',(#32475,#32476,#32477,#32478));
#13385=EDGE_LOOP('',(#32479,#32480,#32481,#32482));
#13386=EDGE_LOOP('',(#32483,#32484,#32485,#32486));
#13387=EDGE_LOOP('',(#32487,#32488,#32489,#32490));
#13388=EDGE_LOOP('',(#32491,#32492,#32493,#32494));
#13389=EDGE_LOOP('',(#32495,#32496,#32497,#32498));
#13390=EDGE_LOOP('',(#32499,#32500,#32501,#32502));
#13391=EDGE_LOOP('',(#32503,#32504,#32505,#32506,#32507,#32508));
#13392=EDGE_LOOP('',(#32509,#32510,#32511,#32512));
#13393=EDGE_LOOP('',(#32513,#32514,#32515,#32516));
#13394=EDGE_LOOP('',(#32517,#32518,#32519,#32520));
#13395=EDGE_LOOP('',(#32521,#32522,#32523,#32524));
#13396=EDGE_LOOP('',(#32525,#32526,#32527,#32528));
#13397=EDGE_LOOP('',(#32529,#32530,#32531,#32532));
#13398=EDGE_LOOP('',(#32533,#32534,#32535,#32536));
#13399=EDGE_LOOP('',(#32537,#32538,#32539,#32540));
#13400=EDGE_LOOP('',(#32541,#32542,#32543,#32544));
#13401=EDGE_LOOP('',(#32545,#32546,#32547,#32548));
#13402=EDGE_LOOP('',(#32549,#32550,#32551,#32552));
#13403=EDGE_LOOP('',(#32553,#32554,#32555,#32556));
#13404=EDGE_LOOP('',(#32557,#32558,#32559,#32560));
#13405=EDGE_LOOP('',(#32561,#32562,#32563,#32564));
#13406=EDGE_LOOP('',(#32565,#32566,#32567,#32568));
#13407=EDGE_LOOP('',(#32569,#32570,#32571,#32572));
#13408=EDGE_LOOP('',(#32573,#32574,#32575,#32576));
#13409=EDGE_LOOP('',(#32577,#32578,#32579,#32580));
#13410=EDGE_LOOP('',(#32581,#32582,#32583,#32584));
#13411=EDGE_LOOP('',(#32585,#32586,#32587,#32588));
#13412=EDGE_LOOP('',(#32589,#32590,#32591,#32592));
#13413=EDGE_LOOP('',(#32593,#32594,#32595,#32596));
#13414=EDGE_LOOP('',(#32597,#32598,#32599,#32600));
#13415=EDGE_LOOP('',(#32601,#32602,#32603,#32604));
#13416=EDGE_LOOP('',(#32605,#32606,#32607,#32608));
#13417=EDGE_LOOP('',(#32609,#32610,#32611,#32612));
#13418=EDGE_LOOP('',(#32613,#32614,#32615,#32616));
#13419=EDGE_LOOP('',(#32617,#32618,#32619,#32620,#32621,#32622));
#13420=EDGE_LOOP('',(#32623,#32624,#32625,#32626));
#13421=EDGE_LOOP('',(#32627,#32628,#32629,#32630));
#13422=EDGE_LOOP('',(#32631,#32632,#32633,#32634));
#13423=EDGE_LOOP('',(#32635,#32636,#32637,#32638));
#13424=EDGE_LOOP('',(#32639,#32640,#32641,#32642));
#13425=EDGE_LOOP('',(#32643,#32644,#32645,#32646));
#13426=EDGE_LOOP('',(#32647,#32648,#32649,#32650));
#13427=EDGE_LOOP('',(#32651,#32652,#32653,#32654));
#13428=EDGE_LOOP('',(#32655,#32656,#32657,#32658));
#13429=EDGE_LOOP('',(#32659,#32660,#32661,#32662));
#13430=EDGE_LOOP('',(#32663,#32664,#32665,#32666));
#13431=EDGE_LOOP('',(#32667,#32668,#32669,#32670));
#13432=EDGE_LOOP('',(#32671,#32672,#32673,#32674));
#13433=EDGE_LOOP('',(#32675,#32676,#32677,#32678));
#13434=EDGE_LOOP('',(#32679,#32680,#32681,#32682));
#13435=EDGE_LOOP('',(#32683,#32684,#32685,#32686));
#13436=EDGE_LOOP('',(#32687,#32688,#32689,#32690));
#13437=EDGE_LOOP('',(#32691,#32692,#32693,#32694));
#13438=EDGE_LOOP('',(#32695,#32696,#32697,#32698));
#13439=EDGE_LOOP('',(#32699,#32700,#32701,#32702));
#13440=EDGE_LOOP('',(#32703,#32704,#32705,#32706));
#13441=EDGE_LOOP('',(#32707,#32708,#32709,#32710));
#13442=EDGE_LOOP('',(#32711,#32712,#32713,#32714));
#13443=EDGE_LOOP('',(#32715,#32716,#32717,#32718));
#13444=EDGE_LOOP('',(#32719,#32720,#32721,#32722));
#13445=EDGE_LOOP('',(#32723,#32724,#32725,#32726));
#13446=EDGE_LOOP('',(#32727,#32728,#32729,#32730));
#13447=EDGE_LOOP('',(#32731,#32732,#32733,#32734));
#13448=EDGE_LOOP('',(#32735,#32736,#32737,#32738));
#13449=EDGE_LOOP('',(#32739,#32740,#32741,#32742));
#13450=EDGE_LOOP('',(#32743,#32744,#32745,#32746));
#13451=EDGE_LOOP('',(#32747,#32748,#32749,#32750));
#13452=EDGE_LOOP('',(#32751,#32752,#32753,#32754));
#13453=EDGE_LOOP('',(#32755,#32756,#32757,#32758,#32759,#32760,#32761));
#13454=EDGE_LOOP('',(#32762,#32763,#32764,#32765));
#13455=EDGE_LOOP('',(#32766,#32767,#32768,#32769));
#13456=EDGE_LOOP('',(#32770,#32771,#32772,#32773));
#13457=EDGE_LOOP('',(#32774,#32775,#32776,#32777));
#13458=EDGE_LOOP('',(#32778,#32779,#32780,#32781));
#13459=EDGE_LOOP('',(#32782,#32783,#32784,#32785));
#13460=EDGE_LOOP('',(#32786,#32787,#32788,#32789));
#13461=EDGE_LOOP('',(#32790,#32791,#32792,#32793));
#13462=EDGE_LOOP('',(#32794,#32795,#32796,#32797));
#13463=EDGE_LOOP('',(#32798,#32799,#32800,#32801));
#13464=EDGE_LOOP('',(#32802,#32803,#32804,#32805));
#13465=EDGE_LOOP('',(#32806,#32807,#32808,#32809));
#13466=EDGE_LOOP('',(#32810,#32811,#32812,#32813));
#13467=EDGE_LOOP('',(#32814,#32815,#32816,#32817));
#13468=EDGE_LOOP('',(#32818,#32819,#32820,#32821));
#13469=EDGE_LOOP('',(#32822,#32823,#32824,#32825));
#13470=EDGE_LOOP('',(#32826,#32827,#32828,#32829));
#13471=EDGE_LOOP('',(#32830,#32831,#32832,#32833,#32834,#32835));
#13472=EDGE_LOOP('',(#32836,#32837,#32838,#32839));
#13473=EDGE_LOOP('',(#32840,#32841,#32842,#32843));
#13474=EDGE_LOOP('',(#32844,#32845,#32846,#32847));
#13475=EDGE_LOOP('',(#32848,#32849,#32850,#32851));
#13476=EDGE_LOOP('',(#32852,#32853,#32854,#32855));
#13477=EDGE_LOOP('',(#32856,#32857,#32858,#32859));
#13478=EDGE_LOOP('',(#32860,#32861,#32862,#32863));
#13479=EDGE_LOOP('',(#32864,#32865,#32866,#32867));
#13480=EDGE_LOOP('',(#32868,#32869,#32870,#32871));
#13481=EDGE_LOOP('',(#32872,#32873,#32874,#32875));
#13482=EDGE_LOOP('',(#32876,#32877,#32878,#32879));
#13483=EDGE_LOOP('',(#32880,#32881,#32882,#32883));
#13484=EDGE_LOOP('',(#32884,#32885,#32886,#32887));
#13485=EDGE_LOOP('',(#32888,#32889,#32890,#32891));
#13486=EDGE_LOOP('',(#32892,#32893,#32894,#32895));
#13487=EDGE_LOOP('',(#32896,#32897,#32898,#32899));
#13488=EDGE_LOOP('',(#32900,#32901,#32902,#32903));
#13489=EDGE_LOOP('',(#32904,#32905,#32906,#32907,#32908,#32909));
#13490=EDGE_LOOP('',(#32910,#32911,#32912,#32913));
#13491=EDGE_LOOP('',(#32914,#32915,#32916,#32917));
#13492=EDGE_LOOP('',(#32918,#32919,#32920,#32921));
#13493=EDGE_LOOP('',(#32922,#32923,#32924,#32925));
#13494=EDGE_LOOP('',(#32926,#32927,#32928,#32929));
#13495=EDGE_LOOP('',(#32930,#32931,#32932,#32933));
#13496=EDGE_LOOP('',(#32934,#32935,#32936,#32937));
#13497=EDGE_LOOP('',(#32938,#32939,#32940,#32941));
#13498=EDGE_LOOP('',(#32942,#32943,#32944,#32945));
#13499=EDGE_LOOP('',(#32946,#32947,#32948,#32949));
#13500=EDGE_LOOP('',(#32950,#32951,#32952,#32953));
#13501=EDGE_LOOP('',(#32954,#32955,#32956,#32957));
#13502=EDGE_LOOP('',(#32958,#32959,#32960,#32961));
#13503=EDGE_LOOP('',(#32962,#32963,#32964,#32965));
#13504=EDGE_LOOP('',(#32966,#32967,#32968,#32969));
#13505=EDGE_LOOP('',(#32970,#32971,#32972,#32973,#32974,#32975));
#13506=EDGE_LOOP('',(#32976,#32977,#32978,#32979));
#13507=EDGE_LOOP('',(#32980,#32981,#32982,#32983));
#13508=EDGE_LOOP('',(#32984,#32985,#32986,#32987));
#13509=EDGE_LOOP('',(#32988,#32989,#32990,#32991));
#13510=EDGE_LOOP('',(#32992,#32993,#32994,#32995));
#13511=EDGE_LOOP('',(#32996,#32997,#32998,#32999));
#13512=EDGE_LOOP('',(#33000,#33001,#33002,#33003));
#13513=EDGE_LOOP('',(#33004,#33005,#33006,#33007));
#13514=EDGE_LOOP('',(#33008,#33009,#33010,#33011));
#13515=EDGE_LOOP('',(#33012,#33013,#33014,#33015));
#13516=EDGE_LOOP('',(#33016,#33017,#33018,#33019));
#13517=EDGE_LOOP('',(#33020,#33021,#33022,#33023));
#13518=EDGE_LOOP('',(#33024,#33025,#33026,#33027));
#13519=EDGE_LOOP('',(#33028,#33029,#33030,#33031));
#13520=EDGE_LOOP('',(#33032,#33033,#33034,#33035));
#13521=EDGE_LOOP('',(#33036,#33037,#33038,#33039));
#13522=EDGE_LOOP('',(#33040,#33041,#33042,#33043));
#13523=EDGE_LOOP('',(#33044,#33045,#33046,#33047,#33048,#33049));
#13524=EDGE_LOOP('',(#33050,#33051,#33052,#33053));
#13525=EDGE_LOOP('',(#33054,#33055,#33056,#33057));
#13526=EDGE_LOOP('',(#33058,#33059,#33060,#33061));
#13527=EDGE_LOOP('',(#33062,#33063,#33064,#33065));
#13528=EDGE_LOOP('',(#33066,#33067,#33068,#33069));
#13529=EDGE_LOOP('',(#33070,#33071,#33072,#33073));
#13530=EDGE_LOOP('',(#33074,#33075,#33076,#33077));
#13531=EDGE_LOOP('',(#33078,#33079,#33080,#33081));
#13532=EDGE_LOOP('',(#33082,#33083,#33084,#33085));
#13533=EDGE_LOOP('',(#33086,#33087,#33088,#33089));
#13534=EDGE_LOOP('',(#33090,#33091,#33092,#33093));
#13535=EDGE_LOOP('',(#33094,#33095,#33096,#33097));
#13536=EDGE_LOOP('',(#33098,#33099,#33100,#33101));
#13537=EDGE_LOOP('',(#33102,#33103,#33104,#33105));
#13538=EDGE_LOOP('',(#33106,#33107,#33108,#33109));
#13539=EDGE_LOOP('',(#33110,#33111,#33112,#33113));
#13540=EDGE_LOOP('',(#33114,#33115,#33116,#33117));
#13541=EDGE_LOOP('',(#33118,#33119,#33120,#33121,#33122,#33123));
#13542=EDGE_LOOP('',(#33124,#33125,#33126,#33127));
#13543=EDGE_LOOP('',(#33128,#33129,#33130,#33131,#33132,#33133,#33134,#33135,
#33136,#33137,#33138,#33139,#33140,#33141,#33142,#33143,#33144,#33145,#33146,
#33147,#33148,#33149,#33150,#33151,#33152,#33153,#33154,#33155,#33156,#33157,
#33158,#33159,#33160,#33161,#33162,#33163,#33164,#33165,#33166,#33167,#33168,
#33169,#33170,#33171,#33172,#33173,#33174,#33175,#33176,#33177,#33178,#33179,
#33180,#33181,#33182,#33183,#33184,#33185,#33186,#33187,#33188,#33189,#33190,
#33191,#33192,#33193,#33194,#33195,#33196,#33197,#33198,#33199,#33200,#33201,
#33202));
#13544=EDGE_LOOP('',(#33203));
#13545=EDGE_LOOP('',(#33204));
#13546=EDGE_LOOP('',(#33205));
#13547=EDGE_LOOP('',(#33206));
#13548=EDGE_LOOP('',(#33207));
#13549=EDGE_LOOP('',(#33208));
#13550=EDGE_LOOP('',(#33209));
#13551=EDGE_LOOP('',(#33210));
#13552=EDGE_LOOP('',(#33211));
#13553=EDGE_LOOP('',(#33212,#33213));
#13554=EDGE_LOOP('',(#33214));
#13555=EDGE_LOOP('',(#33215));
#13556=EDGE_LOOP('',(#33216));
#13557=EDGE_LOOP('',(#33217));
#13558=EDGE_LOOP('',(#33218));
#13559=EDGE_LOOP('',(#33219));
#13560=EDGE_LOOP('',(#33220));
#13561=EDGE_LOOP('',(#33221));
#13562=EDGE_LOOP('',(#33222));
#13563=EDGE_LOOP('',(#33223));
#13564=EDGE_LOOP('',(#33224));
#13565=EDGE_LOOP('',(#33225));
#13566=EDGE_LOOP('',(#33226));
#13567=EDGE_LOOP('',(#33227));
#13568=EDGE_LOOP('',(#33228));
#13569=EDGE_LOOP('',(#33229));
#13570=EDGE_LOOP('',(#33230));
#13571=EDGE_LOOP('',(#33231));
#13572=EDGE_LOOP('',(#33232));
#13573=EDGE_LOOP('',(#33233));
#13574=EDGE_LOOP('',(#33234));
#13575=EDGE_LOOP('',(#33235));
#13576=EDGE_LOOP('',(#33236));
#13577=EDGE_LOOP('',(#33237));
#13578=EDGE_LOOP('',(#33238));
#13579=EDGE_LOOP('',(#33239));
#13580=EDGE_LOOP('',(#33240));
#13581=EDGE_LOOP('',(#33241));
#13582=EDGE_LOOP('',(#33242));
#13583=EDGE_LOOP('',(#33243));
#13584=EDGE_LOOP('',(#33244));
#13585=EDGE_LOOP('',(#33245));
#13586=EDGE_LOOP('',(#33246));
#13587=EDGE_LOOP('',(#33247));
#13588=EDGE_LOOP('',(#33248));
#13589=EDGE_LOOP('',(#33249));
#13590=EDGE_LOOP('',(#33250));
#13591=EDGE_LOOP('',(#33251));
#13592=EDGE_LOOP('',(#33252,#33253,#33254,#33255,#33256,#33257,#33258,#33259,
#33260));
#13593=EDGE_LOOP('',(#33261,#33262,#33263,#33264,#33265));
#13594=EDGE_LOOP('',(#33266,#33267,#33268,#33269));
#13595=EDGE_LOOP('',(#33270,#33271,#33272,#33273,#33274,#33275));
#13596=EDGE_LOOP('',(#33276,#33277,#33278,#33279));
#13597=EDGE_LOOP('',(#33280,#33281,#33282,#33283));
#13598=EDGE_LOOP('',(#33284,#33285,#33286,#33287,#33288));
#13599=EDGE_LOOP('',(#33289,#33290,#33291,#33292,#33293));
#13600=EDGE_LOOP('',(#33294,#33295,#33296,#33297,#33298,#33299));
#13601=EDGE_LOOP('',(#33300,#33301,#33302,#33303,#33304));
#13602=EDGE_LOOP('',(#33305,#33306,#33307,#33308));
#13603=EDGE_LOOP('',(#33309,#33310,#33311,#33312,#33313,#33314));
#13604=EDGE_LOOP('',(#33315,#33316));
#13605=EDGE_LOOP('',(#33317));
#13606=EDGE_LOOP('',(#33318));
#13607=EDGE_LOOP('',(#33319));
#13608=EDGE_LOOP('',(#33320,#33321,#33322,#33323,#33324,#33325));
#13609=EDGE_LOOP('',(#33326,#33327,#33328));
#13610=EDGE_LOOP('',(#33329,#33330,#33331,#33332));
#13611=EDGE_LOOP('',(#33333,#33334,#33335,#33336,#33337,#33338));
#13612=EDGE_LOOP('',(#33339,#33340,#33341));
#13613=EDGE_LOOP('',(#33342,#33343,#33344,#33345,#33346,#33347));
#13614=EDGE_LOOP('',(#33348,#33349,#33350,#33351));
#13615=EDGE_LOOP('',(#33352,#33353,#33354,#33355));
#13616=EDGE_LOOP('',(#33356,#33357,#33358,#33359));
#13617=EDGE_LOOP('',(#33360,#33361,#33362,#33363,#33364,#33365,#33366,#33367));
#13618=EDGE_LOOP('',(#33368,#33369,#33370,#33371));
#13619=EDGE_LOOP('',(#33372,#33373,#33374,#33375));
#13620=EDGE_LOOP('',(#33376,#33377,#33378,#33379));
#13621=EDGE_LOOP('',(#33380,#33381,#33382,#33383));
#13622=EDGE_LOOP('',(#33384,#33385,#33386,#33387));
#13623=EDGE_LOOP('',(#33388,#33389,#33390,#33391));
#13624=EDGE_LOOP('',(#33392,#33393,#33394,#33395));
#13625=EDGE_LOOP('',(#33396,#33397,#33398,#33399));
#13626=EDGE_LOOP('',(#33400,#33401,#33402,#33403));
#13627=EDGE_LOOP('',(#33404,#33405,#33406,#33407,#33408));
#13628=EDGE_LOOP('',(#33409,#33410,#33411,#33412));
#13629=EDGE_LOOP('',(#33413,#33414,#33415,#33416));
#13630=EDGE_LOOP('',(#33417,#33418,#33419,#33420,#33421));
#13631=EDGE_LOOP('',(#33422,#33423,#33424,#33425));
#13632=EDGE_LOOP('',(#33426,#33427));
#13633=EDGE_LOOP('',(#33428,#33429,#33430,#33431,#33432));
#13634=EDGE_LOOP('',(#33433,#33434,#33435,#33436,#33437,#33438));
#13635=EDGE_LOOP('',(#33439,#33440,#33441,#33442));
#13636=EDGE_LOOP('',(#33443,#33444,#33445,#33446,#33447));
#13637=EDGE_LOOP('',(#33448,#33449,#33450,#33451));
#13638=EDGE_LOOP('',(#33452,#33453,#33454,#33455));
#13639=EDGE_LOOP('',(#33456,#33457,#33458,#33459));
#13640=EDGE_LOOP('',(#33460,#33461,#33462,#33463));
#13641=EDGE_LOOP('',(#33464,#33465,#33466,#33467,#33468));
#13642=EDGE_LOOP('',(#33469,#33470,#33471,#33472));
#13643=EDGE_LOOP('',(#33473,#33474,#33475,#33476));
#13644=EDGE_LOOP('',(#33477,#33478,#33479,#33480));
#13645=EDGE_LOOP('',(#33481,#33482,#33483,#33484));
#13646=EDGE_LOOP('',(#33485,#33486,#33487,#33488,#33489,#33490));
#13647=EDGE_LOOP('',(#33491,#33492,#33493,#33494,#33495));
#13648=EDGE_LOOP('',(#33496,#33497,#33498,#33499,#33500));
#13649=EDGE_LOOP('',(#33501,#33502,#33503,#33504,#33505));
#13650=EDGE_LOOP('',(#33506,#33507,#33508,#33509,#33510));
#13651=EDGE_LOOP('',(#33511,#33512));
#13652=EDGE_LOOP('',(#33513,#33514,#33515,#33516,#33517,#33518));
#13653=EDGE_LOOP('',(#33519,#33520,#33521,#33522));
#13654=EDGE_LOOP('',(#33523,#33524,#33525,#33526));
#13655=EDGE_LOOP('',(#33527,#33528,#33529,#33530));
#13656=EDGE_LOOP('',(#33531,#33532,#33533,#33534));
#13657=EDGE_LOOP('',(#33535,#33536,#33537,#33538));
#13658=EDGE_LOOP('',(#33539,#33540,#33541,#33542));
#13659=EDGE_LOOP('',(#33543,#33544,#33545,#33546));
#13660=EDGE_LOOP('',(#33547,#33548,#33549,#33550,#33551,#33552,#33553,#33554));
#13661=EDGE_LOOP('',(#33555,#33556,#33557,#33558));
#13662=EDGE_LOOP('',(#33559,#33560,#33561,#33562));
#13663=EDGE_LOOP('',(#33563,#33564,#33565,#33566));
#13664=EDGE_LOOP('',(#33567,#33568,#33569,#33570));
#13665=EDGE_LOOP('',(#33571,#33572,#33573,#33574));
#13666=EDGE_LOOP('',(#33575,#33576,#33577,#33578,#33579,#33580,#33581,#33582));
#13667=EDGE_LOOP('',(#33583,#33584,#33585,#33586,#33587,#33588,#33589,#33590));
#13668=EDGE_LOOP('',(#33591,#33592,#33593,#33594,#33595,#33596,#33597,#33598));
#13669=EDGE_LOOP('',(#33599,#33600,#33601,#33602,#33603,#33604,#33605,#33606,
#33607,#33608,#33609,#33610,#33611));
#13670=EDGE_LOOP('',(#33612));
#13671=EDGE_LOOP('',(#33613));
#13672=EDGE_LOOP('',(#33614));
#13673=EDGE_LOOP('',(#33615));
#13674=EDGE_LOOP('',(#33616));
#13675=EDGE_LOOP('',(#33617));
#13676=EDGE_LOOP('',(#33618));
#13677=EDGE_LOOP('',(#33619));
#13678=EDGE_LOOP('',(#33620));
#13679=EDGE_LOOP('',(#33621));
#13680=EDGE_LOOP('',(#33622));
#13681=EDGE_LOOP('',(#33623));
#13682=EDGE_LOOP('',(#33624));
#13683=EDGE_LOOP('',(#33625));
#13684=EDGE_LOOP('',(#33626));
#13685=EDGE_LOOP('',(#33627));
#13686=EDGE_LOOP('',(#33628));
#13687=EDGE_LOOP('',(#33629));
#13688=EDGE_LOOP('',(#33630,#33631,#33632,#33633,#33634,#33635,#33636,#33637,
#33638,#33639,#33640,#33641,#33642,#33643,#33644,#33645,#33646,#33647,#33648,
#33649,#33650,#33651,#33652,#33653,#33654,#33655,#33656,#33657,#33658,#33659,
#33660,#33661,#33662,#33663,#33664,#33665,#33666,#33667,#33668,#33669,#33670,
#33671,#33672,#33673,#33674,#33675,#33676,#33677,#33678,#33679,#33680,#33681,
#33682,#33683,#33684,#33685,#33686,#33687,#33688,#33689,#33690,#33691,#33692,
#33693,#33694,#33695));
#13689=EDGE_LOOP('',(#33696));
#13690=EDGE_LOOP('',(#33697));
#13691=EDGE_LOOP('',(#33698));
#13692=EDGE_LOOP('',(#33699));
#13693=EDGE_LOOP('',(#33700));
#13694=EDGE_LOOP('',(#33701));
#13695=EDGE_LOOP('',(#33702));
#13696=EDGE_LOOP('',(#33703));
#13697=EDGE_LOOP('',(#33704));
#13698=EDGE_LOOP('',(#33705));
#13699=EDGE_LOOP('',(#33706));
#13700=EDGE_LOOP('',(#33707));
#13701=EDGE_LOOP('',(#33708));
#13702=EDGE_LOOP('',(#33709));
#13703=EDGE_LOOP('',(#33710));
#13704=EDGE_LOOP('',(#33711));
#13705=EDGE_LOOP('',(#33712));
#13706=EDGE_LOOP('',(#33713));
#13707=EDGE_LOOP('',(#33714));
#13708=EDGE_LOOP('',(#33715));
#13709=EDGE_LOOP('',(#33716));
#13710=EDGE_LOOP('',(#33717));
#13711=EDGE_LOOP('',(#33718));
#13712=EDGE_LOOP('',(#33719));
#13713=EDGE_LOOP('',(#33720));
#13714=EDGE_LOOP('',(#33721));
#13715=EDGE_LOOP('',(#33722));
#13716=EDGE_LOOP('',(#33723));
#13717=EDGE_LOOP('',(#33724));
#13718=EDGE_LOOP('',(#33725));
#13719=EDGE_LOOP('',(#33726));
#13720=EDGE_LOOP('',(#33727));
#13721=EDGE_LOOP('',(#33728));
#13722=EDGE_LOOP('',(#33729));
#13723=EDGE_LOOP('',(#33730));
#13724=EDGE_LOOP('',(#33731));
#13725=EDGE_LOOP('',(#33732));
#13726=EDGE_LOOP('',(#33733));
#13727=EDGE_LOOP('',(#33734));
#13728=EDGE_LOOP('',(#33735));
#13729=EDGE_LOOP('',(#33736));
#13730=EDGE_LOOP('',(#33737));
#13731=EDGE_LOOP('',(#33738));
#13732=EDGE_LOOP('',(#33739));
#13733=EDGE_LOOP('',(#33740));
#13734=EDGE_LOOP('',(#33741));
#13735=EDGE_LOOP('',(#33742));
#13736=EDGE_LOOP('',(#33743));
#13737=EDGE_LOOP('',(#33744));
#13738=EDGE_LOOP('',(#33745));
#13739=EDGE_LOOP('',(#33746));
#13740=EDGE_LOOP('',(#33747));
#13741=EDGE_LOOP('',(#33748));
#13742=EDGE_LOOP('',(#33749));
#13743=EDGE_LOOP('',(#33750));
#13744=EDGE_LOOP('',(#33751));
#13745=EDGE_LOOP('',(#33752));
#13746=EDGE_LOOP('',(#33753));
#13747=EDGE_LOOP('',(#33754));
#13748=EDGE_LOOP('',(#33755));
#13749=EDGE_LOOP('',(#33756));
#13750=EDGE_LOOP('',(#33757));
#13751=EDGE_LOOP('',(#33758));
#13752=EDGE_LOOP('',(#33759));
#13753=EDGE_LOOP('',(#33760));
#13754=EDGE_LOOP('',(#33761));
#13755=EDGE_LOOP('',(#33762));
#13756=EDGE_LOOP('',(#33763));
#13757=EDGE_LOOP('',(#33764));
#13758=EDGE_LOOP('',(#33765));
#13759=EDGE_LOOP('',(#33766));
#13760=EDGE_LOOP('',(#33767));
#13761=EDGE_LOOP('',(#33768));
#13762=EDGE_LOOP('',(#33769));
#13763=EDGE_LOOP('',(#33770));
#13764=EDGE_LOOP('',(#33771));
#13765=EDGE_LOOP('',(#33772));
#13766=EDGE_LOOP('',(#33773));
#13767=EDGE_LOOP('',(#33774));
#13768=EDGE_LOOP('',(#33775));
#13769=EDGE_LOOP('',(#33776));
#13770=EDGE_LOOP('',(#33777));
#13771=EDGE_LOOP('',(#33778));
#13772=EDGE_LOOP('',(#33779));
#13773=EDGE_LOOP('',(#33780));
#13774=EDGE_LOOP('',(#33781));
#13775=EDGE_LOOP('',(#33782));
#13776=EDGE_LOOP('',(#33783));
#13777=EDGE_LOOP('',(#33784));
#13778=EDGE_LOOP('',(#33785));
#13779=EDGE_LOOP('',(#33786));
#13780=EDGE_LOOP('',(#33787));
#13781=EDGE_LOOP('',(#33788));
#13782=EDGE_LOOP('',(#33789));
#13783=EDGE_LOOP('',(#33790));
#13784=EDGE_LOOP('',(#33791));
#13785=EDGE_LOOP('',(#33792));
#13786=EDGE_LOOP('',(#33793));
#13787=EDGE_LOOP('',(#33794));
#13788=EDGE_LOOP('',(#33795));
#13789=EDGE_LOOP('',(#33796));
#13790=EDGE_LOOP('',(#33797));
#13791=EDGE_LOOP('',(#33798));
#13792=EDGE_LOOP('',(#33799));
#13793=EDGE_LOOP('',(#33800));
#13794=EDGE_LOOP('',(#33801));
#13795=EDGE_LOOP('',(#33802));
#13796=EDGE_LOOP('',(#33803));
#13797=EDGE_LOOP('',(#33804));
#13798=EDGE_LOOP('',(#33805));
#13799=EDGE_LOOP('',(#33806));
#13800=EDGE_LOOP('',(#33807));
#13801=EDGE_LOOP('',(#33808));
#13802=EDGE_LOOP('',(#33809));
#13803=EDGE_LOOP('',(#33810));
#13804=EDGE_LOOP('',(#33811));
#13805=EDGE_LOOP('',(#33812));
#13806=EDGE_LOOP('',(#33813));
#13807=EDGE_LOOP('',(#33814));
#13808=EDGE_LOOP('',(#33815));
#13809=EDGE_LOOP('',(#33816));
#13810=EDGE_LOOP('',(#33817));
#13811=EDGE_LOOP('',(#33818));
#13812=EDGE_LOOP('',(#33819));
#13813=EDGE_LOOP('',(#33820));
#13814=EDGE_LOOP('',(#33821));
#13815=EDGE_LOOP('',(#33822));
#13816=EDGE_LOOP('',(#33823));
#13817=EDGE_LOOP('',(#33824));
#13818=EDGE_LOOP('',(#33825));
#13819=EDGE_LOOP('',(#33826));
#13820=EDGE_LOOP('',(#33827));
#13821=EDGE_LOOP('',(#33828));
#13822=EDGE_LOOP('',(#33829));
#13823=EDGE_LOOP('',(#33830));
#13824=EDGE_LOOP('',(#33831));
#13825=EDGE_LOOP('',(#33832));
#13826=EDGE_LOOP('',(#33833));
#13827=EDGE_LOOP('',(#33834));
#13828=EDGE_LOOP('',(#33835));
#13829=EDGE_LOOP('',(#33836));
#13830=EDGE_LOOP('',(#33837));
#13831=EDGE_LOOP('',(#33838));
#13832=EDGE_LOOP('',(#33839));
#13833=EDGE_LOOP('',(#33840));
#13834=EDGE_LOOP('',(#33841));
#13835=EDGE_LOOP('',(#33842));
#13836=EDGE_LOOP('',(#33843));
#13837=EDGE_LOOP('',(#33844));
#13838=EDGE_LOOP('',(#33845));
#13839=EDGE_LOOP('',(#33846));
#13840=EDGE_LOOP('',(#33847));
#13841=EDGE_LOOP('',(#33848));
#13842=EDGE_LOOP('',(#33849));
#13843=EDGE_LOOP('',(#33850));
#13844=EDGE_LOOP('',(#33851));
#13845=EDGE_LOOP('',(#33852));
#13846=EDGE_LOOP('',(#33853));
#13847=EDGE_LOOP('',(#33854));
#13848=EDGE_LOOP('',(#33855));
#13849=EDGE_LOOP('',(#33856));
#13850=EDGE_LOOP('',(#33857));
#13851=EDGE_LOOP('',(#33858));
#13852=EDGE_LOOP('',(#33859));
#13853=EDGE_LOOP('',(#33860));
#13854=EDGE_LOOP('',(#33861));
#13855=EDGE_LOOP('',(#33862));
#13856=EDGE_LOOP('',(#33863));
#13857=EDGE_LOOP('',(#33864));
#13858=EDGE_LOOP('',(#33865));
#13859=EDGE_LOOP('',(#33866));
#13860=EDGE_LOOP('',(#33867));
#13861=EDGE_LOOP('',(#33868));
#13862=EDGE_LOOP('',(#33869));
#13863=EDGE_LOOP('',(#33870));
#13864=EDGE_LOOP('',(#33871));
#13865=EDGE_LOOP('',(#33872));
#13866=EDGE_LOOP('',(#33873));
#13867=EDGE_LOOP('',(#33874));
#13868=EDGE_LOOP('',(#33875));
#13869=EDGE_LOOP('',(#33876));
#13870=EDGE_LOOP('',(#33877));
#13871=EDGE_LOOP('',(#33878));
#13872=EDGE_LOOP('',(#33879));
#13873=EDGE_LOOP('',(#33880));
#13874=EDGE_LOOP('',(#33881));
#13875=EDGE_LOOP('',(#33882));
#13876=EDGE_LOOP('',(#33883));
#13877=EDGE_LOOP('',(#33884));
#13878=EDGE_LOOP('',(#33885));
#13879=EDGE_LOOP('',(#33886));
#13880=EDGE_LOOP('',(#33887));
#13881=EDGE_LOOP('',(#33888));
#13882=EDGE_LOOP('',(#33889));
#13883=EDGE_LOOP('',(#33890));
#13884=EDGE_LOOP('',(#33891));
#13885=EDGE_LOOP('',(#33892));
#13886=EDGE_LOOP('',(#33893));
#13887=EDGE_LOOP('',(#33894));
#13888=EDGE_LOOP('',(#33895));
#13889=EDGE_LOOP('',(#33896));
#13890=EDGE_LOOP('',(#33897));
#13891=EDGE_LOOP('',(#33898));
#13892=EDGE_LOOP('',(#33899));
#13893=EDGE_LOOP('',(#33900));
#13894=EDGE_LOOP('',(#33901));
#13895=EDGE_LOOP('',(#33902));
#13896=EDGE_LOOP('',(#33903));
#13897=EDGE_LOOP('',(#33904));
#13898=EDGE_LOOP('',(#33905));
#13899=EDGE_LOOP('',(#33906));
#13900=EDGE_LOOP('',(#33907));
#13901=EDGE_LOOP('',(#33908));
#13902=EDGE_LOOP('',(#33909));
#13903=EDGE_LOOP('',(#33910));
#13904=EDGE_LOOP('',(#33911));
#13905=EDGE_LOOP('',(#33912));
#13906=EDGE_LOOP('',(#33913));
#13907=EDGE_LOOP('',(#33914));
#13908=EDGE_LOOP('',(#33915));
#13909=EDGE_LOOP('',(#33916));
#13910=EDGE_LOOP('',(#33917));
#13911=EDGE_LOOP('',(#33918));
#13912=EDGE_LOOP('',(#33919));
#13913=EDGE_LOOP('',(#33920));
#13914=EDGE_LOOP('',(#33921));
#13915=EDGE_LOOP('',(#33922));
#13916=EDGE_LOOP('',(#33923));
#13917=EDGE_LOOP('',(#33924));
#13918=EDGE_LOOP('',(#33925));
#13919=EDGE_LOOP('',(#33926));
#13920=EDGE_LOOP('',(#33927));
#13921=EDGE_LOOP('',(#33928));
#13922=EDGE_LOOP('',(#33929));
#13923=EDGE_LOOP('',(#33930));
#13924=EDGE_LOOP('',(#33931));
#13925=EDGE_LOOP('',(#33932,#33933,#33934,#33935));
#13926=EDGE_LOOP('',(#33936,#33937,#33938,#33939));
#13927=EDGE_LOOP('',(#33940,#33941,#33942,#33943,#33944,#33945,#33946,#33947,
#33948,#33949,#33950,#33951));
#13928=EDGE_LOOP('',(#33952,#33953,#33954));
#13929=EDGE_LOOP('',(#33955,#33956,#33957));
#13930=EDGE_LOOP('',(#33958,#33959,#33960,#33961));
#13931=EDGE_LOOP('',(#33962));
#13932=EDGE_LOOP('',(#33963));
#13933=EDGE_LOOP('',(#33964));
#13934=EDGE_LOOP('',(#33965));
#13935=EDGE_LOOP('',(#33966));
#13936=EDGE_LOOP('',(#33967));
#13937=EDGE_LOOP('',(#33968));
#13938=EDGE_LOOP('',(#33969));
#13939=EDGE_LOOP('',(#33970));
#13940=EDGE_LOOP('',(#33971));
#13941=EDGE_LOOP('',(#33972));
#13942=EDGE_LOOP('',(#33973));
#13943=EDGE_LOOP('',(#33974));
#13944=EDGE_LOOP('',(#33975));
#13945=EDGE_LOOP('',(#33976));
#13946=EDGE_LOOP('',(#33977));
#13947=EDGE_LOOP('',(#33978));
#13948=EDGE_LOOP('',(#33979));
#13949=EDGE_LOOP('',(#33980));
#13950=EDGE_LOOP('',(#33981));
#13951=EDGE_LOOP('',(#33982));
#13952=EDGE_LOOP('',(#33983));
#13953=EDGE_LOOP('',(#33984));
#13954=EDGE_LOOP('',(#33985));
#13955=EDGE_LOOP('',(#33986));
#13956=EDGE_LOOP('',(#33987));
#13957=EDGE_LOOP('',(#33988));
#13958=EDGE_LOOP('',(#33989));
#13959=EDGE_LOOP('',(#33990));
#13960=EDGE_LOOP('',(#33991));
#13961=EDGE_LOOP('',(#33992));
#13962=EDGE_LOOP('',(#33993));
#13963=EDGE_LOOP('',(#33994));
#13964=EDGE_LOOP('',(#33995));
#13965=EDGE_LOOP('',(#33996));
#13966=EDGE_LOOP('',(#33997));
#13967=EDGE_LOOP('',(#33998));
#13968=EDGE_LOOP('',(#33999));
#13969=EDGE_LOOP('',(#34000));
#13970=EDGE_LOOP('',(#34001));
#13971=EDGE_LOOP('',(#34002));
#13972=EDGE_LOOP('',(#34003));
#13973=EDGE_LOOP('',(#34004));
#13974=EDGE_LOOP('',(#34005));
#13975=EDGE_LOOP('',(#34006));
#13976=EDGE_LOOP('',(#34007));
#13977=EDGE_LOOP('',(#34008));
#13978=EDGE_LOOP('',(#34009));
#13979=EDGE_LOOP('',(#34010));
#13980=EDGE_LOOP('',(#34011));
#13981=EDGE_LOOP('',(#34012));
#13982=EDGE_LOOP('',(#34013));
#13983=EDGE_LOOP('',(#34014));
#13984=EDGE_LOOP('',(#34015));
#13985=EDGE_LOOP('',(#34016));
#13986=EDGE_LOOP('',(#34017));
#13987=EDGE_LOOP('',(#34018));
#13988=EDGE_LOOP('',(#34019));
#13989=EDGE_LOOP('',(#34020));
#13990=EDGE_LOOP('',(#34021));
#13991=EDGE_LOOP('',(#34022));
#13992=EDGE_LOOP('',(#34023));
#13993=EDGE_LOOP('',(#34024));
#13994=EDGE_LOOP('',(#34025));
#13995=EDGE_LOOP('',(#34026));
#13996=EDGE_LOOP('',(#34027));
#13997=EDGE_LOOP('',(#34028));
#13998=EDGE_LOOP('',(#34029));
#13999=EDGE_LOOP('',(#34030));
#14000=EDGE_LOOP('',(#34031));
#14001=EDGE_LOOP('',(#34032));
#14002=EDGE_LOOP('',(#34033));
#14003=EDGE_LOOP('',(#34034));
#14004=EDGE_LOOP('',(#34035));
#14005=EDGE_LOOP('',(#34036));
#14006=EDGE_LOOP('',(#34037));
#14007=EDGE_LOOP('',(#34038));
#14008=EDGE_LOOP('',(#34039));
#14009=EDGE_LOOP('',(#34040));
#14010=EDGE_LOOP('',(#34041));
#14011=EDGE_LOOP('',(#34042));
#14012=EDGE_LOOP('',(#34043));
#14013=EDGE_LOOP('',(#34044));
#14014=EDGE_LOOP('',(#34045));
#14015=EDGE_LOOP('',(#34046));
#14016=EDGE_LOOP('',(#34047));
#14017=EDGE_LOOP('',(#34048));
#14018=EDGE_LOOP('',(#34049));
#14019=EDGE_LOOP('',(#34050));
#14020=EDGE_LOOP('',(#34051));
#14021=EDGE_LOOP('',(#34052));
#14022=EDGE_LOOP('',(#34053));
#14023=EDGE_LOOP('',(#34054));
#14024=EDGE_LOOP('',(#34055));
#14025=EDGE_LOOP('',(#34056));
#14026=EDGE_LOOP('',(#34057));
#14027=EDGE_LOOP('',(#34058));
#14028=EDGE_LOOP('',(#34059));
#14029=EDGE_LOOP('',(#34060));
#14030=EDGE_LOOP('',(#34061));
#14031=EDGE_LOOP('',(#34062));
#14032=EDGE_LOOP('',(#34063));
#14033=EDGE_LOOP('',(#34064));
#14034=EDGE_LOOP('',(#34065));
#14035=EDGE_LOOP('',(#34066));
#14036=EDGE_LOOP('',(#34067));
#14037=EDGE_LOOP('',(#34068));
#14038=EDGE_LOOP('',(#34069));
#14039=EDGE_LOOP('',(#34070));
#14040=EDGE_LOOP('',(#34071));
#14041=EDGE_LOOP('',(#34072));
#14042=EDGE_LOOP('',(#34073));
#14043=EDGE_LOOP('',(#34074));
#14044=EDGE_LOOP('',(#34075));
#14045=EDGE_LOOP('',(#34076));
#14046=EDGE_LOOP('',(#34077));
#14047=EDGE_LOOP('',(#34078));
#14048=EDGE_LOOP('',(#34079));
#14049=EDGE_LOOP('',(#34080));
#14050=EDGE_LOOP('',(#34081));
#14051=EDGE_LOOP('',(#34082));
#14052=EDGE_LOOP('',(#34083));
#14053=EDGE_LOOP('',(#34084));
#14054=EDGE_LOOP('',(#34085));
#14055=EDGE_LOOP('',(#34086));
#14056=EDGE_LOOP('',(#34087));
#14057=EDGE_LOOP('',(#34088));
#14058=EDGE_LOOP('',(#34089));
#14059=EDGE_LOOP('',(#34090));
#14060=EDGE_LOOP('',(#34091));
#14061=EDGE_LOOP('',(#34092));
#14062=EDGE_LOOP('',(#34093));
#14063=EDGE_LOOP('',(#34094));
#14064=EDGE_LOOP('',(#34095));
#14065=EDGE_LOOP('',(#34096));
#14066=EDGE_LOOP('',(#34097));
#14067=EDGE_LOOP('',(#34098));
#14068=EDGE_LOOP('',(#34099));
#14069=EDGE_LOOP('',(#34100));
#14070=EDGE_LOOP('',(#34101));
#14071=EDGE_LOOP('',(#34102));
#14072=EDGE_LOOP('',(#34103));
#14073=EDGE_LOOP('',(#34104));
#14074=EDGE_LOOP('',(#34105));
#14075=EDGE_LOOP('',(#34106));
#14076=EDGE_LOOP('',(#34107));
#14077=EDGE_LOOP('',(#34108));
#14078=EDGE_LOOP('',(#34109));
#14079=EDGE_LOOP('',(#34110));
#14080=EDGE_LOOP('',(#34111));
#14081=EDGE_LOOP('',(#34112));
#14082=EDGE_LOOP('',(#34113));
#14083=EDGE_LOOP('',(#34114));
#14084=EDGE_LOOP('',(#34115));
#14085=EDGE_LOOP('',(#34116));
#14086=EDGE_LOOP('',(#34117));
#14087=EDGE_LOOP('',(#34118));
#14088=EDGE_LOOP('',(#34119));
#14089=EDGE_LOOP('',(#34120));
#14090=EDGE_LOOP('',(#34121));
#14091=EDGE_LOOP('',(#34122));
#14092=EDGE_LOOP('',(#34123));
#14093=EDGE_LOOP('',(#34124));
#14094=EDGE_LOOP('',(#34125));
#14095=EDGE_LOOP('',(#34126));
#14096=EDGE_LOOP('',(#34127));
#14097=EDGE_LOOP('',(#34128));
#14098=EDGE_LOOP('',(#34129));
#14099=EDGE_LOOP('',(#34130));
#14100=EDGE_LOOP('',(#34131));
#14101=EDGE_LOOP('',(#34132));
#14102=EDGE_LOOP('',(#34133));
#14103=EDGE_LOOP('',(#34134));
#14104=EDGE_LOOP('',(#34135));
#14105=EDGE_LOOP('',(#34136));
#14106=EDGE_LOOP('',(#34137));
#14107=EDGE_LOOP('',(#34138));
#14108=EDGE_LOOP('',(#34139));
#14109=EDGE_LOOP('',(#34140));
#14110=EDGE_LOOP('',(#34141));
#14111=EDGE_LOOP('',(#34142));
#14112=EDGE_LOOP('',(#34143));
#14113=EDGE_LOOP('',(#34144));
#14114=EDGE_LOOP('',(#34145));
#14115=EDGE_LOOP('',(#34146));
#14116=EDGE_LOOP('',(#34147));
#14117=EDGE_LOOP('',(#34148));
#14118=EDGE_LOOP('',(#34149));
#14119=EDGE_LOOP('',(#34150));
#14120=EDGE_LOOP('',(#34151));
#14121=EDGE_LOOP('',(#34152));
#14122=EDGE_LOOP('',(#34153));
#14123=EDGE_LOOP('',(#34154));
#14124=EDGE_LOOP('',(#34155));
#14125=EDGE_LOOP('',(#34156));
#14126=EDGE_LOOP('',(#34157));
#14127=EDGE_LOOP('',(#34158));
#14128=EDGE_LOOP('',(#34159));
#14129=EDGE_LOOP('',(#34160));
#14130=EDGE_LOOP('',(#34161));
#14131=EDGE_LOOP('',(#34162));
#14132=EDGE_LOOP('',(#34163));
#14133=EDGE_LOOP('',(#34164));
#14134=EDGE_LOOP('',(#34165));
#14135=EDGE_LOOP('',(#34166));
#14136=EDGE_LOOP('',(#34167));
#14137=EDGE_LOOP('',(#34168));
#14138=EDGE_LOOP('',(#34169));
#14139=EDGE_LOOP('',(#34170));
#14140=EDGE_LOOP('',(#34171));
#14141=EDGE_LOOP('',(#34172));
#14142=EDGE_LOOP('',(#34173));
#14143=EDGE_LOOP('',(#34174));
#14144=EDGE_LOOP('',(#34175));
#14145=EDGE_LOOP('',(#34176));
#14146=EDGE_LOOP('',(#34177));
#14147=EDGE_LOOP('',(#34178));
#14148=EDGE_LOOP('',(#34179));
#14149=EDGE_LOOP('',(#34180));
#14150=EDGE_LOOP('',(#34181));
#14151=EDGE_LOOP('',(#34182));
#14152=EDGE_LOOP('',(#34183));
#14153=EDGE_LOOP('',(#34184));
#14154=EDGE_LOOP('',(#34185));
#14155=EDGE_LOOP('',(#34186));
#14156=EDGE_LOOP('',(#34187));
#14157=EDGE_LOOP('',(#34188));
#14158=EDGE_LOOP('',(#34189));
#14159=EDGE_LOOP('',(#34190));
#14160=EDGE_LOOP('',(#34191));
#14161=EDGE_LOOP('',(#34192));
#14162=EDGE_LOOP('',(#34193));
#14163=EDGE_LOOP('',(#34194));
#14164=EDGE_LOOP('',(#34195));
#14165=EDGE_LOOP('',(#34196));
#14166=EDGE_LOOP('',(#34197));
#14167=EDGE_LOOP('',(#34198));
#14168=EDGE_LOOP('',(#34199));
#14169=EDGE_LOOP('',(#34200));
#14170=EDGE_LOOP('',(#34201));
#14171=EDGE_LOOP('',(#34202));
#14172=EDGE_LOOP('',(#34203));
#14173=EDGE_LOOP('',(#34204));
#14174=EDGE_LOOP('',(#34205));
#14175=EDGE_LOOP('',(#34206));
#14176=EDGE_LOOP('',(#34207));
#14177=EDGE_LOOP('',(#34208));
#14178=EDGE_LOOP('',(#34209));
#14179=EDGE_LOOP('',(#34210));
#14180=EDGE_LOOP('',(#34211));
#14181=EDGE_LOOP('',(#34212));
#14182=EDGE_LOOP('',(#34213));
#14183=EDGE_LOOP('',(#34214));
#14184=EDGE_LOOP('',(#34215));
#14185=EDGE_LOOP('',(#34216));
#14186=EDGE_LOOP('',(#34217));
#14187=EDGE_LOOP('',(#34218));
#14188=EDGE_LOOP('',(#34219));
#14189=EDGE_LOOP('',(#34220));
#14190=EDGE_LOOP('',(#34221));
#14191=EDGE_LOOP('',(#34222));
#14192=EDGE_LOOP('',(#34223));
#14193=EDGE_LOOP('',(#34224));
#14194=EDGE_LOOP('',(#34225));
#14195=EDGE_LOOP('',(#34226));
#14196=EDGE_LOOP('',(#34227));
#14197=EDGE_LOOP('',(#34228));
#14198=EDGE_LOOP('',(#34229));
#14199=EDGE_LOOP('',(#34230));
#14200=EDGE_LOOP('',(#34231));
#14201=EDGE_LOOP('',(#34232));
#14202=EDGE_LOOP('',(#34233));
#14203=EDGE_LOOP('',(#34234));
#14204=EDGE_LOOP('',(#34235));
#14205=EDGE_LOOP('',(#34236));
#14206=EDGE_LOOP('',(#34237));
#14207=EDGE_LOOP('',(#34238));
#14208=EDGE_LOOP('',(#34239));
#14209=EDGE_LOOP('',(#34240));
#14210=EDGE_LOOP('',(#34241));
#14211=EDGE_LOOP('',(#34242));
#14212=EDGE_LOOP('',(#34243));
#14213=EDGE_LOOP('',(#34244));
#14214=EDGE_LOOP('',(#34245));
#14215=EDGE_LOOP('',(#34246));
#14216=EDGE_LOOP('',(#34247));
#14217=EDGE_LOOP('',(#34248));
#14218=EDGE_LOOP('',(#34249));
#14219=EDGE_LOOP('',(#34250));
#14220=EDGE_LOOP('',(#34251));
#14221=EDGE_LOOP('',(#34252));
#14222=EDGE_LOOP('',(#34253));
#14223=EDGE_LOOP('',(#34254));
#14224=EDGE_LOOP('',(#34255));
#14225=EDGE_LOOP('',(#34256));
#14226=EDGE_LOOP('',(#34257));
#14227=EDGE_LOOP('',(#34258));
#14228=EDGE_LOOP('',(#34259));
#14229=EDGE_LOOP('',(#34260));
#14230=EDGE_LOOP('',(#34261));
#14231=EDGE_LOOP('',(#34262));
#14232=EDGE_LOOP('',(#34263));
#14233=EDGE_LOOP('',(#34264));
#14234=EDGE_LOOP('',(#34265));
#14235=EDGE_LOOP('',(#34266));
#14236=EDGE_LOOP('',(#34267));
#14237=EDGE_LOOP('',(#34268));
#14238=EDGE_LOOP('',(#34269));
#14239=EDGE_LOOP('',(#34270));
#14240=EDGE_LOOP('',(#34271));
#14241=EDGE_LOOP('',(#34272));
#14242=EDGE_LOOP('',(#34273));
#14243=EDGE_LOOP('',(#34274));
#14244=EDGE_LOOP('',(#34275));
#14245=EDGE_LOOP('',(#34276));
#14246=EDGE_LOOP('',(#34277));
#14247=EDGE_LOOP('',(#34278));
#14248=EDGE_LOOP('',(#34279));
#14249=EDGE_LOOP('',(#34280));
#14250=EDGE_LOOP('',(#34281));
#14251=EDGE_LOOP('',(#34282));
#14252=EDGE_LOOP('',(#34283));
#14253=EDGE_LOOP('',(#34284));
#14254=EDGE_LOOP('',(#34285));
#14255=EDGE_LOOP('',(#34286));
#14256=EDGE_LOOP('',(#34287));
#14257=EDGE_LOOP('',(#34288));
#14258=EDGE_LOOP('',(#34289));
#14259=EDGE_LOOP('',(#34290));
#14260=EDGE_LOOP('',(#34291));
#14261=EDGE_LOOP('',(#34292));
#14262=EDGE_LOOP('',(#34293));
#14263=EDGE_LOOP('',(#34294));
#14264=EDGE_LOOP('',(#34295));
#14265=EDGE_LOOP('',(#34296));
#14266=EDGE_LOOP('',(#34297));
#14267=EDGE_LOOP('',(#34298));
#14268=EDGE_LOOP('',(#34299));
#14269=EDGE_LOOP('',(#34300));
#14270=EDGE_LOOP('',(#34301));
#14271=EDGE_LOOP('',(#34302));
#14272=EDGE_LOOP('',(#34303));
#14273=EDGE_LOOP('',(#34304));
#14274=EDGE_LOOP('',(#34305));
#14275=EDGE_LOOP('',(#34306));
#14276=EDGE_LOOP('',(#34307));
#14277=EDGE_LOOP('',(#34308));
#14278=EDGE_LOOP('',(#34309));
#14279=EDGE_LOOP('',(#34310));
#14280=EDGE_LOOP('',(#34311));
#14281=EDGE_LOOP('',(#34312));
#14282=EDGE_LOOP('',(#34313));
#14283=EDGE_LOOP('',(#34314));
#14284=EDGE_LOOP('',(#34315));
#14285=EDGE_LOOP('',(#34316));
#14286=EDGE_LOOP('',(#34317));
#14287=EDGE_LOOP('',(#34318));
#14288=EDGE_LOOP('',(#34319));
#14289=EDGE_LOOP('',(#34320));
#14290=EDGE_LOOP('',(#34321));
#14291=EDGE_LOOP('',(#34322));
#14292=EDGE_LOOP('',(#34323));
#14293=EDGE_LOOP('',(#34324));
#14294=EDGE_LOOP('',(#34325));
#14295=EDGE_LOOP('',(#34326));
#14296=EDGE_LOOP('',(#34327));
#14297=EDGE_LOOP('',(#34328));
#14298=EDGE_LOOP('',(#34329));
#14299=EDGE_LOOP('',(#34330));
#14300=EDGE_LOOP('',(#34331));
#14301=EDGE_LOOP('',(#34332));
#14302=EDGE_LOOP('',(#34333));
#14303=EDGE_LOOP('',(#34334));
#14304=EDGE_LOOP('',(#34335));
#14305=EDGE_LOOP('',(#34336));
#14306=EDGE_LOOP('',(#34337));
#14307=EDGE_LOOP('',(#34338));
#14308=EDGE_LOOP('',(#34339));
#14309=EDGE_LOOP('',(#34340));
#14310=EDGE_LOOP('',(#34341));
#14311=EDGE_LOOP('',(#34342));
#14312=EDGE_LOOP('',(#34343));
#14313=EDGE_LOOP('',(#34344));
#14314=EDGE_LOOP('',(#34345));
#14315=EDGE_LOOP('',(#34346));
#14316=EDGE_LOOP('',(#34347));
#14317=EDGE_LOOP('',(#34348));
#14318=EDGE_LOOP('',(#34349));
#14319=EDGE_LOOP('',(#34350));
#14320=EDGE_LOOP('',(#34351));
#14321=EDGE_LOOP('',(#34352));
#14322=EDGE_LOOP('',(#34353));
#14323=EDGE_LOOP('',(#34354));
#14324=EDGE_LOOP('',(#34355));
#14325=EDGE_LOOP('',(#34356));
#14326=EDGE_LOOP('',(#34357));
#14327=EDGE_LOOP('',(#34358));
#14328=EDGE_LOOP('',(#34359));
#14329=EDGE_LOOP('',(#34360));
#14330=EDGE_LOOP('',(#34361));
#14331=EDGE_LOOP('',(#34362));
#14332=EDGE_LOOP('',(#34363));
#14333=EDGE_LOOP('',(#34364));
#14334=EDGE_LOOP('',(#34365));
#14335=EDGE_LOOP('',(#34366));
#14336=EDGE_LOOP('',(#34367));
#14337=EDGE_LOOP('',(#34368));
#14338=EDGE_LOOP('',(#34369));
#14339=EDGE_LOOP('',(#34370));
#14340=EDGE_LOOP('',(#34371));
#14341=EDGE_LOOP('',(#34372));
#14342=EDGE_LOOP('',(#34373));
#14343=EDGE_LOOP('',(#34374));
#14344=EDGE_LOOP('',(#34375));
#14345=EDGE_LOOP('',(#34376));
#14346=EDGE_LOOP('',(#34377));
#14347=EDGE_LOOP('',(#34378));
#14348=EDGE_LOOP('',(#34379));
#14349=EDGE_LOOP('',(#34380));
#14350=EDGE_LOOP('',(#34381));
#14351=EDGE_LOOP('',(#34382));
#14352=EDGE_LOOP('',(#34383));
#14353=EDGE_LOOP('',(#34384));
#14354=EDGE_LOOP('',(#34385));
#14355=EDGE_LOOP('',(#34386));
#14356=EDGE_LOOP('',(#34387));
#14357=EDGE_LOOP('',(#34388));
#14358=EDGE_LOOP('',(#34389));
#14359=EDGE_LOOP('',(#34390));
#14360=EDGE_LOOP('',(#34391));
#14361=EDGE_LOOP('',(#34392));
#14362=EDGE_LOOP('',(#34393));
#14363=EDGE_LOOP('',(#34394));
#14364=EDGE_LOOP('',(#34395));
#14365=EDGE_LOOP('',(#34396));
#14366=EDGE_LOOP('',(#34397));
#14367=EDGE_LOOP('',(#34398));
#14368=EDGE_LOOP('',(#34399));
#14369=EDGE_LOOP('',(#34400));
#14370=EDGE_LOOP('',(#34401));
#14371=EDGE_LOOP('',(#34402));
#14372=EDGE_LOOP('',(#34403));
#14373=EDGE_LOOP('',(#34404));
#14374=EDGE_LOOP('',(#34405));
#14375=EDGE_LOOP('',(#34406));
#14376=EDGE_LOOP('',(#34407));
#14377=EDGE_LOOP('',(#34408));
#14378=EDGE_LOOP('',(#34409));
#14379=EDGE_LOOP('',(#34410));
#14380=EDGE_LOOP('',(#34411));
#14381=EDGE_LOOP('',(#34412));
#14382=EDGE_LOOP('',(#34413));
#14383=EDGE_LOOP('',(#34414));
#14384=EDGE_LOOP('',(#34415));
#14385=EDGE_LOOP('',(#34416));
#14386=EDGE_LOOP('',(#34417));
#14387=EDGE_LOOP('',(#34418));
#14388=EDGE_LOOP('',(#34419));
#14389=EDGE_LOOP('',(#34420));
#14390=EDGE_LOOP('',(#34421));
#14391=EDGE_LOOP('',(#34422));
#14392=EDGE_LOOP('',(#34423));
#14393=EDGE_LOOP('',(#34424));
#14394=EDGE_LOOP('',(#34425));
#14395=EDGE_LOOP('',(#34426));
#14396=EDGE_LOOP('',(#34427));
#14397=EDGE_LOOP('',(#34428));
#14398=EDGE_LOOP('',(#34429));
#14399=EDGE_LOOP('',(#34430));
#14400=EDGE_LOOP('',(#34431));
#14401=EDGE_LOOP('',(#34432));
#14402=EDGE_LOOP('',(#34433));
#14403=EDGE_LOOP('',(#34434));
#14404=EDGE_LOOP('',(#34435));
#14405=EDGE_LOOP('',(#34436));
#14406=EDGE_LOOP('',(#34437));
#14407=EDGE_LOOP('',(#34438));
#14408=EDGE_LOOP('',(#34439));
#14409=EDGE_LOOP('',(#34440));
#14410=EDGE_LOOP('',(#34441));
#14411=EDGE_LOOP('',(#34442));
#14412=EDGE_LOOP('',(#34443));
#14413=EDGE_LOOP('',(#34444));
#14414=EDGE_LOOP('',(#34445));
#14415=EDGE_LOOP('',(#34446));
#14416=EDGE_LOOP('',(#34447));
#14417=EDGE_LOOP('',(#34448));
#14418=EDGE_LOOP('',(#34449));
#14419=EDGE_LOOP('',(#34450));
#14420=EDGE_LOOP('',(#34451));
#14421=EDGE_LOOP('',(#34452));
#14422=EDGE_LOOP('',(#34453));
#14423=EDGE_LOOP('',(#34454));
#14424=EDGE_LOOP('',(#34455));
#14425=EDGE_LOOP('',(#34456));
#14426=EDGE_LOOP('',(#34457));
#14427=EDGE_LOOP('',(#34458));
#14428=EDGE_LOOP('',(#34459));
#14429=EDGE_LOOP('',(#34460));
#14430=EDGE_LOOP('',(#34461));
#14431=EDGE_LOOP('',(#34462));
#14432=EDGE_LOOP('',(#34463));
#14433=EDGE_LOOP('',(#34464));
#14434=EDGE_LOOP('',(#34465));
#14435=EDGE_LOOP('',(#34466));
#14436=EDGE_LOOP('',(#34467));
#14437=EDGE_LOOP('',(#34468));
#14438=EDGE_LOOP('',(#34469));
#14439=EDGE_LOOP('',(#34470));
#14440=EDGE_LOOP('',(#34471));
#14441=EDGE_LOOP('',(#34472));
#14442=EDGE_LOOP('',(#34473));
#14443=EDGE_LOOP('',(#34474));
#14444=EDGE_LOOP('',(#34475));
#14445=EDGE_LOOP('',(#34476));
#14446=EDGE_LOOP('',(#34477));
#14447=EDGE_LOOP('',(#34478));
#14448=EDGE_LOOP('',(#34479));
#14449=EDGE_LOOP('',(#34480));
#14450=EDGE_LOOP('',(#34481));
#14451=EDGE_LOOP('',(#34482));
#14452=EDGE_LOOP('',(#34483));
#14453=EDGE_LOOP('',(#34484));
#14454=EDGE_LOOP('',(#34485));
#14455=EDGE_LOOP('',(#34486));
#14456=EDGE_LOOP('',(#34487));
#14457=EDGE_LOOP('',(#34488));
#14458=EDGE_LOOP('',(#34489));
#14459=EDGE_LOOP('',(#34490));
#14460=EDGE_LOOP('',(#34491));
#14461=EDGE_LOOP('',(#34492));
#14462=EDGE_LOOP('',(#34493));
#14463=EDGE_LOOP('',(#34494));
#14464=EDGE_LOOP('',(#34495));
#14465=EDGE_LOOP('',(#34496));
#14466=EDGE_LOOP('',(#34497));
#14467=EDGE_LOOP('',(#34498));
#14468=EDGE_LOOP('',(#34499));
#14469=EDGE_LOOP('',(#34500));
#14470=EDGE_LOOP('',(#34501));
#14471=EDGE_LOOP('',(#34502));
#14472=EDGE_LOOP('',(#34503));
#14473=EDGE_LOOP('',(#34504));
#14474=EDGE_LOOP('',(#34505));
#14475=EDGE_LOOP('',(#34506));
#14476=EDGE_LOOP('',(#34507));
#14477=EDGE_LOOP('',(#34508));
#14478=EDGE_LOOP('',(#34509));
#14479=EDGE_LOOP('',(#34510));
#14480=EDGE_LOOP('',(#34511));
#14481=EDGE_LOOP('',(#34512));
#14482=EDGE_LOOP('',(#34513));
#14483=EDGE_LOOP('',(#34514));
#14484=EDGE_LOOP('',(#34515));
#14485=EDGE_LOOP('',(#34516));
#14486=EDGE_LOOP('',(#34517));
#14487=EDGE_LOOP('',(#34518));
#14488=EDGE_LOOP('',(#34519));
#14489=EDGE_LOOP('',(#34520));
#14490=EDGE_LOOP('',(#34521));
#14491=EDGE_LOOP('',(#34522));
#14492=EDGE_LOOP('',(#34523));
#14493=EDGE_LOOP('',(#34524));
#14494=EDGE_LOOP('',(#34525));
#14495=EDGE_LOOP('',(#34526));
#14496=EDGE_LOOP('',(#34527));
#14497=EDGE_LOOP('',(#34528));
#14498=EDGE_LOOP('',(#34529));
#14499=EDGE_LOOP('',(#34530));
#14500=EDGE_LOOP('',(#34531));
#14501=EDGE_LOOP('',(#34532));
#14502=EDGE_LOOP('',(#34533));
#14503=EDGE_LOOP('',(#34534));
#14504=EDGE_LOOP('',(#34535));
#14505=EDGE_LOOP('',(#34536));
#14506=EDGE_LOOP('',(#34537));
#14507=EDGE_LOOP('',(#34538));
#14508=EDGE_LOOP('',(#34539));
#14509=EDGE_LOOP('',(#34540));
#14510=EDGE_LOOP('',(#34541));
#14511=EDGE_LOOP('',(#34542));
#14512=EDGE_LOOP('',(#34543));
#14513=EDGE_LOOP('',(#34544));
#14514=EDGE_LOOP('',(#34545));
#14515=EDGE_LOOP('',(#34546));
#14516=EDGE_LOOP('',(#34547));
#14517=EDGE_LOOP('',(#34548));
#14518=EDGE_LOOP('',(#34549));
#14519=EDGE_LOOP('',(#34550));
#14520=EDGE_LOOP('',(#34551));
#14521=EDGE_LOOP('',(#34552));
#14522=EDGE_LOOP('',(#34553));
#14523=EDGE_LOOP('',(#34554));
#14524=EDGE_LOOP('',(#34555));
#14525=EDGE_LOOP('',(#34556));
#14526=EDGE_LOOP('',(#34557));
#14527=EDGE_LOOP('',(#34558));
#14528=EDGE_LOOP('',(#34559));
#14529=EDGE_LOOP('',(#34560));
#14530=EDGE_LOOP('',(#34561));
#14531=EDGE_LOOP('',(#34562));
#14532=EDGE_LOOP('',(#34563));
#14533=EDGE_LOOP('',(#34564));
#14534=EDGE_LOOP('',(#34565));
#14535=EDGE_LOOP('',(#34566));
#14536=EDGE_LOOP('',(#34567));
#14537=EDGE_LOOP('',(#34568));
#14538=EDGE_LOOP('',(#34569));
#14539=EDGE_LOOP('',(#34570));
#14540=EDGE_LOOP('',(#34571));
#14541=EDGE_LOOP('',(#34572));
#14542=EDGE_LOOP('',(#34573));
#14543=EDGE_LOOP('',(#34574));
#14544=EDGE_LOOP('',(#34575));
#14545=EDGE_LOOP('',(#34576));
#14546=EDGE_LOOP('',(#34577));
#14547=EDGE_LOOP('',(#34578));
#14548=EDGE_LOOP('',(#34579));
#14549=EDGE_LOOP('',(#34580));
#14550=EDGE_LOOP('',(#34581));
#14551=EDGE_LOOP('',(#34582));
#14552=EDGE_LOOP('',(#34583));
#14553=EDGE_LOOP('',(#34584));
#14554=EDGE_LOOP('',(#34585));
#14555=EDGE_LOOP('',(#34586));
#14556=EDGE_LOOP('',(#34587));
#14557=EDGE_LOOP('',(#34588));
#14558=EDGE_LOOP('',(#34589));
#14559=EDGE_LOOP('',(#34590));
#14560=EDGE_LOOP('',(#34591));
#14561=EDGE_LOOP('',(#34592));
#14562=EDGE_LOOP('',(#34593));
#14563=EDGE_LOOP('',(#34594));
#14564=EDGE_LOOP('',(#34595));
#14565=EDGE_LOOP('',(#34596));
#14566=EDGE_LOOP('',(#34597));
#14567=EDGE_LOOP('',(#34598));
#14568=EDGE_LOOP('',(#34599));
#14569=EDGE_LOOP('',(#34600));
#14570=EDGE_LOOP('',(#34601));
#14571=EDGE_LOOP('',(#34602));
#14572=EDGE_LOOP('',(#34603));
#14573=EDGE_LOOP('',(#34604));
#14574=EDGE_LOOP('',(#34605));
#14575=EDGE_LOOP('',(#34606));
#14576=EDGE_LOOP('',(#34607));
#14577=EDGE_LOOP('',(#34608));
#14578=EDGE_LOOP('',(#34609));
#14579=EDGE_LOOP('',(#34610));
#14580=EDGE_LOOP('',(#34611));
#14581=EDGE_LOOP('',(#34612));
#14582=EDGE_LOOP('',(#34613));
#14583=EDGE_LOOP('',(#34614));
#14584=EDGE_LOOP('',(#34615));
#14585=EDGE_LOOP('',(#34616));
#14586=EDGE_LOOP('',(#34617));
#14587=EDGE_LOOP('',(#34618));
#14588=EDGE_LOOP('',(#34619));
#14589=EDGE_LOOP('',(#34620));
#14590=EDGE_LOOP('',(#34621));
#14591=EDGE_LOOP('',(#34622));
#14592=EDGE_LOOP('',(#34623));
#14593=EDGE_LOOP('',(#34624));
#14594=EDGE_LOOP('',(#34625));
#14595=EDGE_LOOP('',(#34626));
#14596=EDGE_LOOP('',(#34627));
#14597=EDGE_LOOP('',(#34628));
#14598=EDGE_LOOP('',(#34629));
#14599=EDGE_LOOP('',(#34630));
#14600=EDGE_LOOP('',(#34631));
#14601=EDGE_LOOP('',(#34632));
#14602=EDGE_LOOP('',(#34633));
#14603=EDGE_LOOP('',(#34634));
#14604=EDGE_LOOP('',(#34635));
#14605=EDGE_LOOP('',(#34636));
#14606=EDGE_LOOP('',(#34637));
#14607=EDGE_LOOP('',(#34638));
#14608=EDGE_LOOP('',(#34639));
#14609=EDGE_LOOP('',(#34640));
#14610=EDGE_LOOP('',(#34641));
#14611=EDGE_LOOP('',(#34642));
#14612=EDGE_LOOP('',(#34643));
#14613=EDGE_LOOP('',(#34644));
#14614=EDGE_LOOP('',(#34645));
#14615=EDGE_LOOP('',(#34646));
#14616=EDGE_LOOP('',(#34647));
#14617=EDGE_LOOP('',(#34648));
#14618=EDGE_LOOP('',(#34649));
#14619=EDGE_LOOP('',(#34650));
#14620=EDGE_LOOP('',(#34651));
#14621=EDGE_LOOP('',(#34652));
#14622=EDGE_LOOP('',(#34653));
#14623=EDGE_LOOP('',(#34654));
#14624=EDGE_LOOP('',(#34655));
#14625=EDGE_LOOP('',(#34656));
#14626=EDGE_LOOP('',(#34657));
#14627=EDGE_LOOP('',(#34658));
#14628=EDGE_LOOP('',(#34659));
#14629=EDGE_LOOP('',(#34660));
#14630=EDGE_LOOP('',(#34661));
#14631=EDGE_LOOP('',(#34662));
#14632=EDGE_LOOP('',(#34663));
#14633=EDGE_LOOP('',(#34664));
#14634=EDGE_LOOP('',(#34665));
#14635=EDGE_LOOP('',(#34666));
#14636=EDGE_LOOP('',(#34667));
#14637=EDGE_LOOP('',(#34668));
#14638=EDGE_LOOP('',(#34669));
#14639=EDGE_LOOP('',(#34670));
#14640=EDGE_LOOP('',(#34671));
#14641=EDGE_LOOP('',(#34672));
#14642=EDGE_LOOP('',(#34673));
#14643=EDGE_LOOP('',(#34674));
#14644=EDGE_LOOP('',(#34675));
#14645=EDGE_LOOP('',(#34676));
#14646=EDGE_LOOP('',(#34677));
#14647=EDGE_LOOP('',(#34678));
#14648=EDGE_LOOP('',(#34679));
#14649=EDGE_LOOP('',(#34680));
#14650=EDGE_LOOP('',(#34681));
#14651=EDGE_LOOP('',(#34682));
#14652=EDGE_LOOP('',(#34683));
#14653=EDGE_LOOP('',(#34684));
#14654=EDGE_LOOP('',(#34685));
#14655=EDGE_LOOP('',(#34686));
#14656=EDGE_LOOP('',(#34687));
#14657=EDGE_LOOP('',(#34688));
#14658=EDGE_LOOP('',(#34689));
#14659=EDGE_LOOP('',(#34690));
#14660=EDGE_LOOP('',(#34691));
#14661=EDGE_LOOP('',(#34692));
#14662=EDGE_LOOP('',(#34693));
#14663=EDGE_LOOP('',(#34694));
#14664=EDGE_LOOP('',(#34695));
#14665=EDGE_LOOP('',(#34696));
#14666=EDGE_LOOP('',(#34697));
#14667=EDGE_LOOP('',(#34698));
#14668=EDGE_LOOP('',(#34699));
#14669=EDGE_LOOP('',(#34700));
#14670=EDGE_LOOP('',(#34701));
#14671=EDGE_LOOP('',(#34702));
#14672=EDGE_LOOP('',(#34703));
#14673=EDGE_LOOP('',(#34704));
#14674=EDGE_LOOP('',(#34705));
#14675=EDGE_LOOP('',(#34706));
#14676=EDGE_LOOP('',(#34707));
#14677=EDGE_LOOP('',(#34708));
#14678=EDGE_LOOP('',(#34709));
#14679=EDGE_LOOP('',(#34710));
#14680=EDGE_LOOP('',(#34711));
#14681=EDGE_LOOP('',(#34712));
#14682=EDGE_LOOP('',(#34713));
#14683=EDGE_LOOP('',(#34714));
#14684=EDGE_LOOP('',(#34715));
#14685=EDGE_LOOP('',(#34716));
#14686=EDGE_LOOP('',(#34717));
#14687=EDGE_LOOP('',(#34718));
#14688=EDGE_LOOP('',(#34719));
#14689=EDGE_LOOP('',(#34720));
#14690=EDGE_LOOP('',(#34721));
#14691=EDGE_LOOP('',(#34722));
#14692=EDGE_LOOP('',(#34723));
#14693=EDGE_LOOP('',(#34724));
#14694=EDGE_LOOP('',(#34725));
#14695=EDGE_LOOP('',(#34726));
#14696=EDGE_LOOP('',(#34727));
#14697=EDGE_LOOP('',(#34728));
#14698=EDGE_LOOP('',(#34729));
#14699=EDGE_LOOP('',(#34730));
#14700=EDGE_LOOP('',(#34731));
#14701=EDGE_LOOP('',(#34732));
#14702=EDGE_LOOP('',(#34733));
#14703=EDGE_LOOP('',(#34734));
#14704=EDGE_LOOP('',(#34735));
#14705=EDGE_LOOP('',(#34736));
#14706=EDGE_LOOP('',(#34737,#34738));
#14707=EDGE_LOOP('',(#34739));
#14708=EDGE_LOOP('',(#34740));
#14709=EDGE_LOOP('',(#34741,#34742));
#14710=EDGE_LOOP('',(#34743));
#14711=EDGE_LOOP('',(#34744));
#14712=EDGE_LOOP('',(#34745,#34746));
#14713=EDGE_LOOP('',(#34747));
#14714=EDGE_LOOP('',(#34748));
#14715=EDGE_LOOP('',(#34749,#34750));
#14716=EDGE_LOOP('',(#34751));
#14717=EDGE_LOOP('',(#34752));
#14718=EDGE_LOOP('',(#34753,#34754));
#14719=EDGE_LOOP('',(#34755));
#14720=EDGE_LOOP('',(#34756));
#14721=EDGE_LOOP('',(#34757,#34758));
#14722=EDGE_LOOP('',(#34759));
#14723=EDGE_LOOP('',(#34760));
#14724=EDGE_LOOP('',(#34761,#34762));
#14725=EDGE_LOOP('',(#34763));
#14726=EDGE_LOOP('',(#34764));
#14727=EDGE_LOOP('',(#34765,#34766));
#14728=EDGE_LOOP('',(#34767));
#14729=EDGE_LOOP('',(#34768));
#14730=EDGE_LOOP('',(#34769,#34770));
#14731=EDGE_LOOP('',(#34771));
#14732=EDGE_LOOP('',(#34772));
#14733=EDGE_LOOP('',(#34773,#34774));
#14734=EDGE_LOOP('',(#34775));
#14735=EDGE_LOOP('',(#34776));
#14736=EDGE_LOOP('',(#34777,#34778));
#14737=EDGE_LOOP('',(#34779));
#14738=EDGE_LOOP('',(#34780));
#14739=EDGE_LOOP('',(#34781,#34782));
#14740=EDGE_LOOP('',(#34783));
#14741=EDGE_LOOP('',(#34784));
#14742=EDGE_LOOP('',(#34785,#34786));
#14743=EDGE_LOOP('',(#34787));
#14744=EDGE_LOOP('',(#34788));
#14745=EDGE_LOOP('',(#34789,#34790));
#14746=EDGE_LOOP('',(#34791));
#14747=EDGE_LOOP('',(#34792));
#14748=EDGE_LOOP('',(#34793));
#14749=EDGE_LOOP('',(#34794));
#14750=EDGE_LOOP('',(#34795));
#14751=EDGE_LOOP('',(#34796,#34797));
#14752=EDGE_LOOP('',(#34798));
#14753=EDGE_LOOP('',(#34799));
#14754=EDGE_LOOP('',(#34800,#34801));
#14755=EDGE_LOOP('',(#34802));
#14756=EDGE_LOOP('',(#34803));
#14757=EDGE_LOOP('',(#34804));
#14758=EDGE_LOOP('',(#34805));
#14759=EDGE_LOOP('',(#34806));
#14760=EDGE_LOOP('',(#34807,#34808));
#14761=EDGE_LOOP('',(#34809));
#14762=EDGE_LOOP('',(#34810));
#14763=EDGE_LOOP('',(#34811,#34812));
#14764=EDGE_LOOP('',(#34813));
#14765=EDGE_LOOP('',(#34814));
#14766=EDGE_LOOP('',(#34815));
#14767=EDGE_LOOP('',(#34816));
#14768=EDGE_LOOP('',(#34817));
#14769=EDGE_LOOP('',(#34818));
#14770=EDGE_LOOP('',(#34819));
#14771=EDGE_LOOP('',(#34820));
#14772=EDGE_LOOP('',(#34821,#34822));
#14773=EDGE_LOOP('',(#34823));
#14774=EDGE_LOOP('',(#34824));
#14775=EDGE_LOOP('',(#34825,#34826));
#14776=EDGE_LOOP('',(#34827));
#14777=EDGE_LOOP('',(#34828));
#14778=EDGE_LOOP('',(#34829));
#14779=EDGE_LOOP('',(#34830));
#14780=EDGE_LOOP('',(#34831));
#14781=EDGE_LOOP('',(#34832));
#14782=EDGE_LOOP('',(#34833));
#14783=EDGE_LOOP('',(#34834));
#14784=EDGE_LOOP('',(#34835,#34836));
#14785=EDGE_LOOP('',(#34837));
#14786=EDGE_LOOP('',(#34838));
#14787=EDGE_LOOP('',(#34839,#34840));
#14788=EDGE_LOOP('',(#34841));
#14789=EDGE_LOOP('',(#34842));
#14790=EDGE_LOOP('',(#34843,#34844));
#14791=EDGE_LOOP('',(#34845));
#14792=EDGE_LOOP('',(#34846));
#14793=EDGE_LOOP('',(#34847,#34848));
#14794=EDGE_LOOP('',(#34849));
#14795=EDGE_LOOP('',(#34850));
#14796=EDGE_LOOP('',(#34851,#34852));
#14797=EDGE_LOOP('',(#34853));
#14798=EDGE_LOOP('',(#34854));
#14799=EDGE_LOOP('',(#34855,#34856));
#14800=EDGE_LOOP('',(#34857));
#14801=EDGE_LOOP('',(#34858));
#14802=EDGE_LOOP('',(#34859,#34860));
#14803=EDGE_LOOP('',(#34861));
#14804=EDGE_LOOP('',(#34862));
#14805=EDGE_LOOP('',(#34863,#34864));
#14806=EDGE_LOOP('',(#34865));
#14807=EDGE_LOOP('',(#34866));
#14808=EDGE_LOOP('',(#34867,#34868));
#14809=EDGE_LOOP('',(#34869));
#14810=EDGE_LOOP('',(#34870));
#14811=EDGE_LOOP('',(#34871,#34872));
#14812=EDGE_LOOP('',(#34873));
#14813=EDGE_LOOP('',(#34874));
#14814=EDGE_LOOP('',(#34875,#34876));
#14815=EDGE_LOOP('',(#34877));
#14816=EDGE_LOOP('',(#34878));
#14817=EDGE_LOOP('',(#34879,#34880));
#14818=EDGE_LOOP('',(#34881));
#14819=EDGE_LOOP('',(#34882));
#14820=EDGE_LOOP('',(#34883,#34884));
#14821=EDGE_LOOP('',(#34885));
#14822=EDGE_LOOP('',(#34886));
#14823=EDGE_LOOP('',(#34887,#34888));
#14824=EDGE_LOOP('',(#34889));
#14825=EDGE_LOOP('',(#34890));
#14826=EDGE_LOOP('',(#34891,#34892));
#14827=EDGE_LOOP('',(#34893));
#14828=EDGE_LOOP('',(#34894));
#14829=EDGE_LOOP('',(#34895,#34896));
#14830=EDGE_LOOP('',(#34897));
#14831=EDGE_LOOP('',(#34898));
#14832=EDGE_LOOP('',(#34899,#34900));
#14833=EDGE_LOOP('',(#34901));
#14834=EDGE_LOOP('',(#34902));
#14835=EDGE_LOOP('',(#34903,#34904));
#14836=EDGE_LOOP('',(#34905));
#14837=EDGE_LOOP('',(#34906));
#14838=EDGE_LOOP('',(#34907,#34908));
#14839=EDGE_LOOP('',(#34909));
#14840=EDGE_LOOP('',(#34910));
#14841=EDGE_LOOP('',(#34911,#34912));
#14842=EDGE_LOOP('',(#34913));
#14843=EDGE_LOOP('',(#34914));
#14844=EDGE_LOOP('',(#34915,#34916));
#14845=EDGE_LOOP('',(#34917));
#14846=EDGE_LOOP('',(#34918));
#14847=EDGE_LOOP('',(#34919,#34920));
#14848=EDGE_LOOP('',(#34921));
#14849=EDGE_LOOP('',(#34922));
#14850=EDGE_LOOP('',(#34923,#34924));
#14851=EDGE_LOOP('',(#34925));
#14852=EDGE_LOOP('',(#34926));
#14853=EDGE_LOOP('',(#34927,#34928));
#14854=EDGE_LOOP('',(#34929));
#14855=EDGE_LOOP('',(#34930));
#14856=EDGE_LOOP('',(#34931,#34932));
#14857=EDGE_LOOP('',(#34933));
#14858=EDGE_LOOP('',(#34934));
#14859=EDGE_LOOP('',(#34935,#34936));
#14860=EDGE_LOOP('',(#34937));
#14861=EDGE_LOOP('',(#34938));
#14862=EDGE_LOOP('',(#34939,#34940));
#14863=EDGE_LOOP('',(#34941));
#14864=EDGE_LOOP('',(#34942));
#14865=EDGE_LOOP('',(#34943,#34944));
#14866=EDGE_LOOP('',(#34945));
#14867=EDGE_LOOP('',(#34946));
#14868=EDGE_LOOP('',(#34947,#34948));
#14869=EDGE_LOOP('',(#34949));
#14870=EDGE_LOOP('',(#34950));
#14871=EDGE_LOOP('',(#34951,#34952));
#14872=EDGE_LOOP('',(#34953));
#14873=EDGE_LOOP('',(#34954));
#14874=EDGE_LOOP('',(#34955,#34956));
#14875=EDGE_LOOP('',(#34957));
#14876=EDGE_LOOP('',(#34958));
#14877=EDGE_LOOP('',(#34959,#34960));
#14878=EDGE_LOOP('',(#34961));
#14879=EDGE_LOOP('',(#34962));
#14880=EDGE_LOOP('',(#34963,#34964));
#14881=EDGE_LOOP('',(#34965));
#14882=EDGE_LOOP('',(#34966));
#14883=EDGE_LOOP('',(#34967,#34968));
#14884=EDGE_LOOP('',(#34969));
#14885=EDGE_LOOP('',(#34970));
#14886=EDGE_LOOP('',(#34971,#34972));
#14887=EDGE_LOOP('',(#34973));
#14888=EDGE_LOOP('',(#34974));
#14889=EDGE_LOOP('',(#34975,#34976));
#14890=EDGE_LOOP('',(#34977));
#14891=EDGE_LOOP('',(#34978));
#14892=EDGE_LOOP('',(#34979,#34980));
#14893=EDGE_LOOP('',(#34981));
#14894=EDGE_LOOP('',(#34982));
#14895=EDGE_LOOP('',(#34983,#34984));
#14896=EDGE_LOOP('',(#34985));
#14897=EDGE_LOOP('',(#34986));
#14898=EDGE_LOOP('',(#34987,#34988));
#14899=EDGE_LOOP('',(#34989));
#14900=EDGE_LOOP('',(#34990));
#14901=EDGE_LOOP('',(#34991));
#14902=EDGE_LOOP('',(#34992));
#14903=EDGE_LOOP('',(#34993));
#14904=EDGE_LOOP('',(#34994));
#14905=EDGE_LOOP('',(#34995));
#14906=EDGE_LOOP('',(#34996));
#14907=EDGE_LOOP('',(#34997));
#14908=EDGE_LOOP('',(#34998));
#14909=EDGE_LOOP('',(#34999));
#14910=EDGE_LOOP('',(#35000));
#14911=EDGE_LOOP('',(#35001));
#14912=EDGE_LOOP('',(#35002));
#14913=EDGE_LOOP('',(#35003));
#14914=EDGE_LOOP('',(#35004));
#14915=EDGE_LOOP('',(#35005));
#14916=EDGE_LOOP('',(#35006));
#14917=EDGE_LOOP('',(#35007));
#14918=EDGE_LOOP('',(#35008,#35009,#35010,#35011,#35012));
#14919=EDGE_LOOP('',(#35013,#35014,#35015,#35016));
#14920=EDGE_LOOP('',(#35017,#35018,#35019,#35020,#35021));
#14921=EDGE_LOOP('',(#35022,#35023,#35024,#35025));
#14922=EDGE_LOOP('',(#35026,#35027,#35028,#35029));
#14923=EDGE_LOOP('',(#35030,#35031,#35032,#35033));
#14924=EDGE_LOOP('',(#35034));
#14925=EDGE_LOOP('',(#35035));
#14926=EDGE_LOOP('',(#35036,#35037));
#14927=EDGE_LOOP('',(#35038,#35039,#35040,#35041));
#14928=EDGE_LOOP('',(#35042));
#14929=EDGE_LOOP('',(#35043));
#14930=EDGE_LOOP('',(#35044,#35045));
#14931=EDGE_LOOP('',(#35046,#35047,#35048,#35049));
#14932=EDGE_LOOP('',(#35050,#35051,#35052,#35053));
#14933=EDGE_LOOP('',(#35054,#35055,#35056,#35057));
#14934=EDGE_LOOP('',(#35058,#35059,#35060,#35061));
#14935=EDGE_LOOP('',(#35062,#35063,#35064,#35065));
#14936=EDGE_LOOP('',(#35066,#35067,#35068,#35069));
#14937=EDGE_LOOP('',(#35070,#35071,#35072,#35073));
#14938=EDGE_LOOP('',(#35074,#35075,#35076,#35077));
#14939=EDGE_LOOP('',(#35078,#35079,#35080,#35081));
#14940=EDGE_LOOP('',(#35082,#35083,#35084,#35085));
#14941=EDGE_LOOP('',(#35086,#35087,#35088,#35089));
#14942=EDGE_LOOP('',(#35090,#35091,#35092,#35093));
#14943=EDGE_LOOP('',(#35094,#35095,#35096,#35097,#35098,#35099,#35100,#35101,
#35102,#35103,#35104,#35105,#35106,#35107,#35108,#35109,#35110,#35111,#35112,
#35113,#35114));
#14944=EDGE_LOOP('',(#35115,#35116,#35117,#35118));
#14945=EDGE_LOOP('',(#35119,#35120,#35121,#35122,#35123,#35124));
#14946=EDGE_LOOP('',(#35125,#35126,#35127,#35128,#35129,#35130));
#14947=EDGE_LOOP('',(#35131,#35132,#35133,#35134,#35135,#35136));
#14948=EDGE_LOOP('',(#35137,#35138,#35139,#35140,#35141,#35142,#35143,#35144,
#35145,#35146,#35147));
#14949=EDGE_LOOP('',(#35148,#35149,#35150,#35151));
#14950=EDGE_LOOP('',(#35152,#35153,#35154,#35155));
#14951=EDGE_LOOP('',(#35156,#35157,#35158,#35159,#35160));
#14952=EDGE_LOOP('',(#35161,#35162,#35163,#35164));
#14953=EDGE_LOOP('',(#35165,#35166,#35167,#35168,#35169));
#14954=EDGE_LOOP('',(#35170,#35171,#35172,#35173,#35174,#35175,#35176,#35177,
#35178,#35179,#35180));
#14955=EDGE_LOOP('',(#35181,#35182,#35183,#35184));
#14956=EDGE_LOOP('',(#35185,#35186,#35187,#35188));
#14957=EDGE_LOOP('',(#35189,#35190,#35191,#35192,#35193));
#14958=EDGE_LOOP('',(#35194,#35195,#35196,#35197));
#14959=EDGE_LOOP('',(#35198,#35199,#35200,#35201,#35202));
#14960=EDGE_LOOP('',(#35203,#35204,#35205,#35206,#35207,#35208,#35209,#35210,
#35211,#35212,#35213));
#14961=EDGE_LOOP('',(#35214,#35215,#35216,#35217));
#14962=EDGE_LOOP('',(#35218,#35219,#35220,#35221));
#14963=EDGE_LOOP('',(#35222,#35223,#35224,#35225,#35226));
#14964=EDGE_LOOP('',(#35227,#35228,#35229,#35230));
#14965=EDGE_LOOP('',(#35231,#35232,#35233,#35234,#35235));
#14966=EDGE_LOOP('',(#35236,#35237,#35238,#35239,#35240,#35241,#35242,#35243,
#35244,#35245));
#14967=EDGE_LOOP('',(#35246,#35247,#35248,#35249,#35250));
#14968=EDGE_LOOP('',(#35251,#35252,#35253,#35254,#35255,#35256,#35257));
#14969=EDGE_LOOP('',(#35258,#35259,#35260,#35261));
#14970=EDGE_LOOP('',(#35262,#35263,#35264,#35265));
#14971=EDGE_LOOP('',(#35266,#35267,#35268,#35269));
#14972=EDGE_LOOP('',(#35270,#35271,#35272,#35273));
#14973=EDGE_LOOP('',(#35274,#35275,#35276,#35277));
#14974=EDGE_LOOP('',(#35278,#35279,#35280,#35281));
#14975=EDGE_LOOP('',(#35282,#35283,#35284,#35285));
#14976=EDGE_LOOP('',(#35286,#35287,#35288,#35289,#35290,#35291,#35292,#35293));
#14977=EDGE_LOOP('',(#35294,#35295,#35296,#35297));
#14978=EDGE_LOOP('',(#35298,#35299,#35300,#35301));
#14979=EDGE_LOOP('',(#35302,#35303,#35304,#35305));
#14980=EDGE_LOOP('',(#35306,#35307,#35308,#35309,#35310));
#14981=EDGE_LOOP('',(#35311,#35312,#35313,#35314,#35315));
#14982=EDGE_LOOP('',(#35316,#35317,#35318,#35319,#35320,#35321));
#14983=EDGE_LOOP('',(#35322,#35323,#35324,#35325));
#14984=EDGE_LOOP('',(#35326,#35327,#35328,#35329));
#14985=EDGE_LOOP('',(#35330,#35331,#35332,#35333));
#14986=EDGE_LOOP('',(#35334,#35335,#35336,#35337));
#14987=EDGE_LOOP('',(#35338,#35339,#35340,#35341));
#14988=EDGE_LOOP('',(#35342,#35343,#35344));
#14989=EDGE_LOOP('',(#35345,#35346,#35347));
#14990=EDGE_LOOP('',(#35348,#35349,#35350,#35351));
#14991=EDGE_LOOP('',(#35352,#35353,#35354,#35355));
#14992=EDGE_LOOP('',(#35356,#35357,#35358,#35359));
#14993=EDGE_LOOP('',(#35360,#35361,#35362,#35363));
#14994=EDGE_LOOP('',(#35364,#35365,#35366,#35367));
#14995=EDGE_LOOP('',(#35368,#35369,#35370,#35371));
#14996=EDGE_LOOP('',(#35372,#35373,#35374,#35375));
#14997=EDGE_LOOP('',(#35376,#35377,#35378,#35379));
#14998=EDGE_LOOP('',(#35380,#35381,#35382,#35383));
#14999=EDGE_LOOP('',(#35384,#35385,#35386,#35387));
#15000=EDGE_LOOP('',(#35388,#35389,#35390,#35391));
#15001=EDGE_LOOP('',(#35392,#35393,#35394,#35395));
#15002=EDGE_LOOP('',(#35396,#35397,#35398,#35399));
#15003=EDGE_LOOP('',(#35400,#35401,#35402,#35403));
#15004=EDGE_LOOP('',(#35404,#35405,#35406,#35407));
#15005=EDGE_LOOP('',(#35408,#35409,#35410,#35411));
#15006=EDGE_LOOP('',(#35412,#35413,#35414,#35415));
#15007=EDGE_LOOP('',(#35416,#35417,#35418,#35419));
#15008=EDGE_LOOP('',(#35420,#35421,#35422,#35423));
#15009=EDGE_LOOP('',(#35424,#35425,#35426,#35427));
#15010=EDGE_LOOP('',(#35428,#35429,#35430,#35431));
#15011=EDGE_LOOP('',(#35432,#35433,#35434,#35435));
#15012=EDGE_LOOP('',(#35436,#35437,#35438,#35439));
#15013=EDGE_LOOP('',(#35440,#35441,#35442,#35443));
#15014=EDGE_LOOP('',(#35444,#35445,#35446,#35447));
#15015=EDGE_LOOP('',(#35448,#35449,#35450,#35451));
#15016=EDGE_LOOP('',(#35452,#35453,#35454,#35455));
#15017=EDGE_LOOP('',(#35456,#35457,#35458,#35459,#35460,#35461,#35462));
#15018=EDGE_LOOP('',(#35463,#35464,#35465,#35466,#35467,#35468,#35469));
#15019=EDGE_LOOP('',(#35470,#35471,#35472,#35473));
#15020=EDGE_LOOP('',(#35474,#35475,#35476,#35477));
#15021=EDGE_LOOP('',(#35478,#35479,#35480,#35481));
#15022=EDGE_LOOP('',(#35482,#35483,#35484,#35485));
#15023=EDGE_LOOP('',(#35486,#35487,#35488,#35489));
#15024=EDGE_LOOP('',(#35490,#35491,#35492,#35493));
#15025=EDGE_LOOP('',(#35494,#35495,#35496,#35497));
#15026=EDGE_LOOP('',(#35498,#35499,#35500,#35501));
#15027=EDGE_LOOP('',(#35502,#35503,#35504,#35505));
#15028=EDGE_LOOP('',(#35506,#35507,#35508,#35509));
#15029=EDGE_LOOP('',(#35510,#35511,#35512,#35513));
#15030=EDGE_LOOP('',(#35514,#35515,#35516,#35517));
#15031=EDGE_LOOP('',(#35518,#35519,#35520,#35521));
#15032=EDGE_LOOP('',(#35522,#35523,#35524,#35525));
#15033=EDGE_LOOP('',(#35526,#35527,#35528,#35529));
#15034=EDGE_LOOP('',(#35530,#35531,#35532,#35533));
#15035=EDGE_LOOP('',(#35534,#35535,#35536,#35537));
#15036=EDGE_LOOP('',(#35538,#35539,#35540,#35541));
#15037=EDGE_LOOP('',(#35542,#35543,#35544,#35545));
#15038=EDGE_LOOP('',(#35546,#35547,#35548,#35549,#35550,#35551,#35552));
#15039=EDGE_LOOP('',(#35553,#35554,#35555,#35556,#35557,#35558,#35559));
#15040=EDGE_LOOP('',(#35560,#35561,#35562,#35563));
#15041=EDGE_LOOP('',(#35564,#35565,#35566,#35567));
#15042=EDGE_LOOP('',(#35568,#35569,#35570,#35571));
#15043=EDGE_LOOP('',(#35572,#35573,#35574,#35575));
#15044=EDGE_LOOP('',(#35576,#35577,#35578,#35579));
#15045=EDGE_LOOP('',(#35580,#35581,#35582,#35583));
#15046=EDGE_LOOP('',(#35584,#35585,#35586,#35587));
#15047=EDGE_LOOP('',(#35588,#35589,#35590,#35591));
#15048=EDGE_LOOP('',(#35592,#35593,#35594,#35595));
#15049=EDGE_LOOP('',(#35596,#35597,#35598,#35599));
#15050=EDGE_LOOP('',(#35600,#35601,#35602,#35603));
#15051=EDGE_LOOP('',(#35604,#35605,#35606,#35607));
#15052=EDGE_LOOP('',(#35608,#35609,#35610,#35611));
#15053=EDGE_LOOP('',(#35612,#35613,#35614,#35615));
#15054=EDGE_LOOP('',(#35616,#35617,#35618,#35619));
#15055=EDGE_LOOP('',(#35620,#35621,#35622,#35623));
#15056=EDGE_LOOP('',(#35624,#35625,#35626,#35627));
#15057=EDGE_LOOP('',(#35628,#35629,#35630,#35631));
#15058=EDGE_LOOP('',(#35632,#35633,#35634,#35635));
#15059=EDGE_LOOP('',(#35636,#35637,#35638,#35639,#35640,#35641,#35642));
#15060=EDGE_LOOP('',(#35643,#35644,#35645,#35646,#35647,#35648,#35649));
#15061=EDGE_LOOP('',(#35650,#35651,#35652,#35653));
#15062=EDGE_LOOP('',(#35654,#35655,#35656,#35657));
#15063=EDGE_LOOP('',(#35658,#35659,#35660,#35661));
#15064=EDGE_LOOP('',(#35662,#35663,#35664,#35665));
#15065=EDGE_LOOP('',(#35666,#35667,#35668,#35669));
#15066=EDGE_LOOP('',(#35670,#35671,#35672,#35673));
#15067=EDGE_LOOP('',(#35674,#35675,#35676,#35677));
#15068=EDGE_LOOP('',(#35678,#35679,#35680,#35681));
#15069=EDGE_LOOP('',(#35682,#35683,#35684,#35685));
#15070=EDGE_LOOP('',(#35686,#35687,#35688,#35689));
#15071=EDGE_LOOP('',(#35690,#35691,#35692,#35693));
#15072=EDGE_LOOP('',(#35694,#35695,#35696,#35697));
#15073=EDGE_LOOP('',(#35698,#35699,#35700,#35701));
#15074=EDGE_LOOP('',(#35702,#35703,#35704,#35705));
#15075=EDGE_LOOP('',(#35706,#35707,#35708,#35709));
#15076=EDGE_LOOP('',(#35710,#35711,#35712,#35713));
#15077=EDGE_LOOP('',(#35714,#35715,#35716,#35717));
#15078=EDGE_LOOP('',(#35718,#35719,#35720,#35721));
#15079=EDGE_LOOP('',(#35722,#35723,#35724,#35725));
#15080=EDGE_LOOP('',(#35726,#35727,#35728,#35729,#35730,#35731,#35732));
#15081=EDGE_LOOP('',(#35733,#35734,#35735,#35736,#35737,#35738,#35739));
#15082=EDGE_LOOP('',(#35740,#35741,#35742,#35743));
#15083=EDGE_LOOP('',(#35744,#35745));
#15084=EDGE_LOOP('',(#35746,#35747));
#15085=EDGE_LOOP('',(#35748,#35749));
#15086=EDGE_LOOP('',(#35750,#35751,#35752,#35753));
#15087=EDGE_LOOP('',(#35754,#35755,#35756,#35757));
#15088=EDGE_LOOP('',(#35758,#35759,#35760,#35761,#35762,#35763));
#15089=EDGE_LOOP('',(#35764,#35765,#35766,#35767));
#15090=EDGE_LOOP('',(#35768,#35769,#35770,#35771));
#15091=EDGE_LOOP('',(#35772,#35773,#35774,#35775));
#15092=EDGE_LOOP('',(#35776,#35777,#35778,#35779,#35780,#35781));
#15093=EDGE_LOOP('',(#35782,#35783,#35784,#35785));
#15094=EDGE_LOOP('',(#35786,#35787,#35788,#35789));
#15095=EDGE_LOOP('',(#35790,#35791,#35792,#35793));
#15096=EDGE_LOOP('',(#35794,#35795,#35796,#35797));
#15097=EDGE_LOOP('',(#35798,#35799,#35800,#35801));
#15098=EDGE_LOOP('',(#35802,#35803,#35804,#35805));
#15099=EDGE_LOOP('',(#35806,#35807,#35808,#35809));
#15100=EDGE_LOOP('',(#35810,#35811,#35812,#35813));
#15101=EDGE_LOOP('',(#35814,#35815,#35816,#35817));
#15102=EDGE_LOOP('',(#35818,#35819,#35820,#35821));
#15103=EDGE_LOOP('',(#35822,#35823,#35824,#35825));
#15104=EDGE_LOOP('',(#35826,#35827,#35828,#35829));
#15105=EDGE_LOOP('',(#35830,#35831,#35832,#35833));
#15106=EDGE_LOOP('',(#35834,#35835,#35836,#35837));
#15107=EDGE_LOOP('',(#35838,#35839,#35840,#35841));
#15108=EDGE_LOOP('',(#35842,#35843,#35844,#35845));
#15109=EDGE_LOOP('',(#35846,#35847,#35848,#35849));
#15110=EDGE_LOOP('',(#35850,#35851,#35852,#35853));
#15111=EDGE_LOOP('',(#35854,#35855,#35856,#35857));
#15112=EDGE_LOOP('',(#35858,#35859,#35860));
#15113=EDGE_LOOP('',(#35861,#35862,#35863,#35864));
#15114=EDGE_LOOP('',(#35865,#35866,#35867,#35868));
#15115=EDGE_LOOP('',(#35869,#35870,#35871));
#15116=EDGE_LOOP('',(#35872,#35873,#35874,#35875,#35876));
#15117=EDGE_LOOP('',(#35877,#35878,#35879,#35880));
#15118=EDGE_LOOP('',(#35881,#35882,#35883,#35884));
#15119=EDGE_LOOP('',(#35885,#35886,#35887,#35888));
#15120=EDGE_LOOP('',(#35889,#35890,#35891,#35892,#35893));
#15121=EDGE_LOOP('',(#35894,#35895,#35896,#35897,#35898));
#15122=EDGE_LOOP('',(#35899,#35900,#35901,#35902));
#15123=EDGE_LOOP('',(#35903,#35904,#35905,#35906,#35907));
#15124=EDGE_LOOP('',(#35908));
#15125=EDGE_LOOP('',(#35909));
#15126=EDGE_LOOP('',(#35910,#35911,#35912,#35913));
#15127=EDGE_LOOP('',(#35914,#35915,#35916,#35917));
#15128=EDGE_LOOP('',(#35918,#35919,#35920,#35921));
#15129=EDGE_LOOP('',(#35922,#35923,#35924,#35925));
#15130=EDGE_LOOP('',(#35926,#35927,#35928,#35929));
#15131=EDGE_LOOP('',(#35930,#35931,#35932,#35933));
#15132=EDGE_LOOP('',(#35934,#35935,#35936,#35937));
#15133=EDGE_LOOP('',(#35938,#35939,#35940,#35941));
#15134=EDGE_LOOP('',(#35942,#35943,#35944,#35945,#35946,#35947,#35948,#35949,
#35950,#35951,#35952));
#15135=EDGE_LOOP('',(#35953));
#15136=EDGE_LOOP('',(#35954));
#15137=EDGE_LOOP('',(#35955));
#15138=EDGE_LOOP('',(#35956,#35957,#35958,#35959));
#15139=EDGE_LOOP('',(#35960,#35961,#35962,#35963,#35964,#35965,#35966));
#15140=EDGE_LOOP('',(#35967,#35968,#35969,#35970,#35971,#35972,#35973));
#15141=EDGE_LOOP('',(#35974,#35975,#35976,#35977));
#15142=EDGE_LOOP('',(#35978,#35979,#35980,#35981));
#15143=EDGE_LOOP('',(#35982,#35983,#35984,#35985));
#15144=EDGE_LOOP('',(#35986,#35987,#35988,#35989,#35990,#35991,#35992,#35993,
#35994));
#15145=EDGE_LOOP('',(#35995,#35996,#35997,#35998));
#15146=EDGE_LOOP('',(#35999,#36000,#36001,#36002));
#15147=EDGE_LOOP('',(#36003,#36004,#36005,#36006,#36007));
#15148=EDGE_LOOP('',(#36008,#36009,#36010,#36011,#36012));
#15149=EDGE_LOOP('',(#36013,#36014,#36015,#36016));
#15150=EDGE_LOOP('',(#36017,#36018,#36019,#36020));
#15151=EDGE_LOOP('',(#36021,#36022,#36023,#36024));
#15152=EDGE_LOOP('',(#36025,#36026,#36027,#36028));
#15153=EDGE_LOOP('',(#36029,#36030,#36031));
#15154=EDGE_LOOP('',(#36032,#36033,#36034,#36035));
#15155=EDGE_LOOP('',(#36036,#36037,#36038,#36039));
#15156=EDGE_LOOP('',(#36040,#36041,#36042,#36043));
#15157=EDGE_LOOP('',(#36044,#36045,#36046,#36047));
#15158=EDGE_LOOP('',(#36048,#36049,#36050,#36051));
#15159=EDGE_LOOP('',(#36052,#36053,#36054,#36055));
#15160=EDGE_LOOP('',(#36056,#36057,#36058,#36059));
#15161=EDGE_LOOP('',(#36060,#36061,#36062,#36063,#36064,#36065,#36066,#36067,
#36068,#36069,#36070,#36071,#36072,#36073,#36074,#36075));
#15162=EDGE_LOOP('',(#36076,#36077,#36078,#36079));
#15163=EDGE_LOOP('',(#36080,#36081,#36082,#36083,#36084,#36085,#36086,#36087));
#15164=EDGE_LOOP('',(#36088,#36089,#36090,#36091,#36092,#36093,#36094,#36095,
#36096,#36097,#36098,#36099,#36100,#36101,#36102,#36103));
#15165=EDGE_LOOP('',(#36104,#36105,#36106,#36107));
#15166=EDGE_LOOP('',(#36108,#36109,#36110,#36111));
#15167=EDGE_LOOP('',(#36112,#36113,#36114,#36115));
#15168=EDGE_LOOP('',(#36116,#36117,#36118,#36119));
#15169=EDGE_LOOP('',(#36120,#36121,#36122,#36123,#36124,#36125,#36126,#36127));
#15170=EDGE_LOOP('',(#36128,#36129,#36130,#36131));
#15171=EDGE_LOOP('',(#36132,#36133,#36134,#36135,#36136,#36137));
#15172=EDGE_LOOP('',(#36138));
#15173=EDGE_LOOP('',(#36139,#36140,#36141,#36142));
#15174=EDGE_LOOP('',(#36143,#36144,#36145,#36146,#36147,#36148));
#15175=EDGE_LOOP('',(#36149));
#15176=EDGE_LOOP('',(#36150,#36151,#36152,#36153));
#15177=EDGE_LOOP('',(#36154,#36155,#36156,#36157));
#15178=EDGE_LOOP('',(#36158,#36159,#36160,#36161));
#15179=EDGE_LOOP('',(#36162,#36163,#36164,#36165));
#15180=EDGE_LOOP('',(#36166,#36167,#36168,#36169));
#15181=EDGE_LOOP('',(#36170,#36171,#36172,#36173));
#15182=EDGE_LOOP('',(#36174,#36175,#36176,#36177));
#15183=EDGE_LOOP('',(#36178,#36179,#36180,#36181));
#15184=EDGE_LOOP('',(#36182,#36183,#36184,#36185));
#15185=EDGE_LOOP('',(#36186,#36187,#36188,#36189));
#15186=EDGE_LOOP('',(#36190,#36191,#36192,#36193));
#15187=EDGE_LOOP('',(#36194,#36195,#36196,#36197));
#15188=EDGE_LOOP('',(#36198,#36199,#36200,#36201));
#15189=EDGE_LOOP('',(#36202,#36203,#36204,#36205));
#15190=EDGE_LOOP('',(#36206,#36207,#36208,#36209));
#15191=EDGE_LOOP('',(#36210,#36211,#36212,#36213));
#15192=EDGE_LOOP('',(#36214,#36215,#36216,#36217));
#15193=EDGE_LOOP('',(#36218,#36219,#36220,#36221));
#15194=EDGE_LOOP('',(#36222,#36223,#36224,#36225));
#15195=EDGE_LOOP('',(#36226,#36227,#36228,#36229));
#15196=EDGE_LOOP('',(#36230,#36231,#36232,#36233));
#15197=EDGE_LOOP('',(#36234,#36235,#36236,#36237));
#15198=EDGE_LOOP('',(#36238,#36239,#36240,#36241));
#15199=EDGE_LOOP('',(#36242,#36243,#36244,#36245));
#15200=EDGE_LOOP('',(#36246,#36247,#36248,#36249));
#15201=EDGE_LOOP('',(#36250,#36251,#36252,#36253));
#15202=EDGE_LOOP('',(#36254,#36255,#36256,#36257));
#15203=EDGE_LOOP('',(#36258,#36259,#36260,#36261));
#15204=EDGE_LOOP('',(#36262,#36263,#36264,#36265));
#15205=EDGE_LOOP('',(#36266,#36267,#36268,#36269));
#15206=EDGE_LOOP('',(#36270,#36271,#36272,#36273));
#15207=EDGE_LOOP('',(#36274,#36275,#36276,#36277));
#15208=EDGE_LOOP('',(#36278,#36279,#36280,#36281));
#15209=EDGE_LOOP('',(#36282,#36283,#36284,#36285));
#15210=EDGE_LOOP('',(#36286,#36287,#36288,#36289));
#15211=EDGE_LOOP('',(#36290,#36291,#36292,#36293));
#15212=EDGE_LOOP('',(#36294,#36295,#36296,#36297));
#15213=EDGE_LOOP('',(#36298,#36299,#36300,#36301));
#15214=EDGE_LOOP('',(#36302,#36303,#36304,#36305));
#15215=EDGE_LOOP('',(#36306,#36307,#36308,#36309));
#15216=EDGE_LOOP('',(#36310,#36311,#36312,#36313));
#15217=EDGE_LOOP('',(#36314,#36315,#36316,#36317));
#15218=EDGE_LOOP('',(#36318,#36319,#36320,#36321));
#15219=EDGE_LOOP('',(#36322,#36323,#36324,#36325));
#15220=EDGE_LOOP('',(#36326,#36327,#36328,#36329));
#15221=EDGE_LOOP('',(#36330,#36331,#36332,#36333));
#15222=EDGE_LOOP('',(#36334,#36335,#36336,#36337));
#15223=EDGE_LOOP('',(#36338,#36339,#36340,#36341));
#15224=EDGE_LOOP('',(#36342,#36343,#36344,#36345));
#15225=EDGE_LOOP('',(#36346,#36347,#36348,#36349));
#15226=EDGE_LOOP('',(#36350,#36351,#36352,#36353));
#15227=EDGE_LOOP('',(#36354,#36355,#36356,#36357));
#15228=EDGE_LOOP('',(#36358,#36359,#36360,#36361));
#15229=EDGE_LOOP('',(#36362,#36363,#36364,#36365));
#15230=EDGE_LOOP('',(#36366,#36367,#36368,#36369));
#15231=EDGE_LOOP('',(#36370,#36371,#36372,#36373));
#15232=EDGE_LOOP('',(#36374,#36375,#36376,#36377));
#15233=EDGE_LOOP('',(#36378,#36379,#36380,#36381));
#15234=EDGE_LOOP('',(#36382,#36383,#36384,#36385));
#15235=EDGE_LOOP('',(#36386,#36387,#36388,#36389));
#15236=EDGE_LOOP('',(#36390,#36391,#36392,#36393));
#15237=EDGE_LOOP('',(#36394,#36395,#36396,#36397));
#15238=EDGE_LOOP('',(#36398,#36399,#36400,#36401));
#15239=EDGE_LOOP('',(#36402,#36403,#36404,#36405));
#15240=EDGE_LOOP('',(#36406,#36407,#36408,#36409));
#15241=EDGE_LOOP('',(#36410,#36411,#36412,#36413));
#15242=EDGE_LOOP('',(#36414,#36415,#36416,#36417));
#15243=EDGE_LOOP('',(#36418,#36419,#36420,#36421));
#15244=EDGE_LOOP('',(#36422,#36423,#36424,#36425));
#15245=EDGE_LOOP('',(#36426,#36427,#36428,#36429,#36430));
#15246=EDGE_LOOP('',(#36431,#36432,#36433,#36434));
#15247=EDGE_LOOP('',(#36435,#36436,#36437,#36438));
#15248=EDGE_LOOP('',(#36439,#36440,#36441,#36442,#36443));
#15249=EDGE_LOOP('',(#36444,#36445,#36446,#36447,#36448,#36449,#36450,#36451,
#36452,#36453,#36454));
#15250=EDGE_LOOP('',(#36455,#36456,#36457,#36458,#36459));
#15251=EDGE_LOOP('',(#36460,#36461,#36462,#36463));
#15252=EDGE_LOOP('',(#36464,#36465,#36466,#36467,#36468));
#15253=EDGE_LOOP('',(#36469,#36470,#36471,#36472,#36473));
#15254=EDGE_LOOP('',(#36474,#36475,#36476,#36477,#36478));
#15255=EDGE_LOOP('',(#36479,#36480,#36481,#36482,#36483));
#15256=EDGE_LOOP('',(#36484,#36485,#36486,#36487,#36488,#36489,#36490,#36491));
#15257=EDGE_LOOP('',(#36492,#36493,#36494,#36495,#36496,#36497,#36498,#36499,
#36500,#36501));
#15258=EDGE_LOOP('',(#36502,#36503,#36504,#36505,#36506));
#15259=EDGE_LOOP('',(#36507,#36508,#36509,#36510,#36511));
#15260=EDGE_LOOP('',(#36512,#36513,#36514,#36515,#36516));
#15261=EDGE_LOOP('',(#36517,#36518,#36519,#36520));
#15262=EDGE_LOOP('',(#36521,#36522,#36523,#36524,#36525));
#15263=EDGE_LOOP('',(#36526,#36527,#36528,#36529,#36530,#36531,#36532,#36533,
#36534,#36535));
#15264=EDGE_LOOP('',(#36536,#36537,#36538,#36539,#36540));
#15265=EDGE_LOOP('',(#36541,#36542));
#15266=EDGE_LOOP('',(#36543,#36544));
#15267=EDGE_LOOP('',(#36545,#36546));
#15268=EDGE_LOOP('',(#36547,#36548,#36549,#36550,#36551));
#15269=EDGE_LOOP('',(#36552,#36553,#36554,#36555,#36556));
#15270=EDGE_LOOP('',(#36557,#36558,#36559,#36560,#36561));
#15271=EDGE_LOOP('',(#36562,#36563,#36564,#36565,#36566,#36567,#36568));
#15272=EDGE_LOOP('',(#36569,#36570,#36571,#36572,#36573,#36574,#36575,#36576,
#36577,#36578));
#15273=EDGE_LOOP('',(#36579,#36580,#36581,#36582));
#15274=EDGE_LOOP('',(#36583,#36584,#36585,#36586,#36587,#36588,#36589,#36590));
#15275=EDGE_LOOP('',(#36591,#36592));
#15276=EDGE_LOOP('',(#36593,#36594,#36595,#36596));
#15277=EDGE_LOOP('',(#36597,#36598));
#15278=EDGE_LOOP('',(#36599));
#15279=EDGE_LOOP('',(#36600,#36601));
#15280=EDGE_LOOP('',(#36602,#36603));
#15281=EDGE_LOOP('',(#36604,#36605,#36606,#36607,#36608));
#15282=EDGE_LOOP('',(#36609,#36610,#36611,#36612,#36613));
#15283=EDGE_LOOP('',(#36614,#36615,#36616,#36617,#36618));
#15284=EDGE_LOOP('',(#36619));
#15285=EDGE_LOOP('',(#36620,#36621,#36622,#36623,#36624));
#15286=EDGE_LOOP('',(#36625,#36626,#36627,#36628,#36629));
#15287=EDGE_LOOP('',(#36630,#36631,#36632,#36633,#36634));
#15288=EDGE_LOOP('',(#36635,#36636));
#15289=EDGE_LOOP('',(#36637,#36638));
#15290=EDGE_LOOP('',(#36639,#36640));
#15291=EDGE_LOOP('',(#36641,#36642));
#15292=EDGE_LOOP('',(#36643,#36644,#36645,#36646,#36647));
#15293=EDGE_LOOP('',(#36648,#36649,#36650,#36651,#36652));
#15294=EDGE_LOOP('',(#36653,#36654,#36655,#36656,#36657));
#15295=EDGE_LOOP('',(#36658,#36659,#36660,#36661));
#15296=EDGE_LOOP('',(#36662,#36663,#36664,#36665,#36666,#36667,#36668,#36669));
#15297=EDGE_LOOP('',(#36670,#36671,#36672,#36673,#36674,#36675,#36676,#36677));
#15298=EDGE_LOOP('',(#36678,#36679,#36680,#36681));
#15299=EDGE_LOOP('',(#36682,#36683,#36684,#36685));
#15300=EDGE_LOOP('',(#36686,#36687,#36688,#36689));
#15301=EDGE_LOOP('',(#36690,#36691,#36692,#36693));
#15302=EDGE_LOOP('',(#36694,#36695,#36696,#36697,#36698,#36699));
#15303=EDGE_LOOP('',(#36700,#36701,#36702,#36703,#36704,#36705));
#15304=EDGE_LOOP('',(#36706,#36707,#36708,#36709));
#15305=EDGE_LOOP('',(#36710,#36711,#36712,#36713));
#15306=EDGE_LOOP('',(#36714,#36715,#36716));
#15307=EDGE_LOOP('',(#36717,#36718,#36719,#36720));
#15308=EDGE_LOOP('',(#36721,#36722,#36723));
#15309=EDGE_LOOP('',(#36724,#36725,#36726,#36727));
#15310=EDGE_LOOP('',(#36728,#36729,#36730,#36731));
#15311=EDGE_LOOP('',(#36732,#36733,#36734,#36735));
#15312=EDGE_LOOP('',(#36736,#36737,#36738,#36739));
#15313=EDGE_LOOP('',(#36740,#36741,#36742,#36743));
#15314=EDGE_LOOP('',(#36744,#36745,#36746,#36747));
#15315=EDGE_LOOP('',(#36748,#36749,#36750,#36751));
#15316=EDGE_LOOP('',(#36752,#36753,#36754,#36755));
#15317=EDGE_LOOP('',(#36756,#36757,#36758,#36759));
#15318=EDGE_LOOP('',(#36760,#36761,#36762));
#15319=EDGE_LOOP('',(#36763,#36764,#36765,#36766));
#15320=EDGE_LOOP('',(#36767,#36768,#36769,#36770));
#15321=EDGE_LOOP('',(#36771,#36772,#36773,#36774));
#15322=EDGE_LOOP('',(#36775,#36776,#36777,#36778));
#15323=EDGE_LOOP('',(#36779,#36780,#36781));
#15324=EDGE_LOOP('',(#36782,#36783,#36784));
#15325=EDGE_LOOP('',(#36785,#36786,#36787,#36788));
#15326=EDGE_LOOP('',(#36789,#36790,#36791,#36792));
#15327=EDGE_LOOP('',(#36793,#36794,#36795,#36796));
#15328=EDGE_LOOP('',(#36797,#36798,#36799));
#15329=EDGE_LOOP('',(#36800,#36801,#36802,#36803));
#15330=EDGE_LOOP('',(#36804,#36805,#36806,#36807));
#15331=EDGE_LOOP('',(#36808,#36809,#36810,#36811));
#15332=EDGE_LOOP('',(#36812,#36813,#36814,#36815));
#15333=EDGE_LOOP('',(#36816));
#15334=EDGE_LOOP('',(#36817));
#15335=EDGE_LOOP('',(#36818));
#15336=EDGE_LOOP('',(#36819));
#15337=EDGE_LOOP('',(#36820,#36821,#36822,#36823));
#15338=EDGE_LOOP('',(#36824,#36825));
#15339=EDGE_LOOP('',(#36826,#36827));
#15340=EDGE_LOOP('',(#36828,#36829));
#15341=EDGE_LOOP('',(#36830,#36831));
#15342=EDGE_LOOP('',(#36832,#36833));
#15343=EDGE_LOOP('',(#36834,#36835));
#15344=EDGE_LOOP('',(#36836,#36837));
#15345=EDGE_LOOP('',(#36838,#36839));
#15346=EDGE_LOOP('',(#36840,#36841));
#15347=EDGE_LOOP('',(#36842,#36843));
#15348=EDGE_LOOP('',(#36844,#36845));
#15349=EDGE_LOOP('',(#36846,#36847));
#15350=EDGE_LOOP('',(#36848,#36849));
#15351=EDGE_LOOP('',(#36850,#36851));
#15352=EDGE_LOOP('',(#36852,#36853));
#15353=EDGE_LOOP('',(#36854,#36855));
#15354=EDGE_LOOP('',(#36856,#36857));
#15355=EDGE_LOOP('',(#36858,#36859));
#15356=EDGE_LOOP('',(#36860,#36861));
#15357=EDGE_LOOP('',(#36862,#36863));
#15358=EDGE_LOOP('',(#36864,#36865));
#15359=EDGE_LOOP('',(#36866,#36867));
#15360=EDGE_LOOP('',(#36868,#36869));
#15361=EDGE_LOOP('',(#36870,#36871));
#15362=EDGE_LOOP('',(#36872,#36873));
#15363=EDGE_LOOP('',(#36874,#36875));
#15364=EDGE_LOOP('',(#36876,#36877));
#15365=EDGE_LOOP('',(#36878,#36879));
#15366=EDGE_LOOP('',(#36880,#36881));
#15367=EDGE_LOOP('',(#36882,#36883));
#15368=EDGE_LOOP('',(#36884,#36885));
#15369=EDGE_LOOP('',(#36886,#36887));
#15370=EDGE_LOOP('',(#36888,#36889));
#15371=EDGE_LOOP('',(#36890,#36891));
#15372=EDGE_LOOP('',(#36892,#36893));
#15373=EDGE_LOOP('',(#36894,#36895));
#15374=EDGE_LOOP('',(#36896,#36897));
#15375=EDGE_LOOP('',(#36898,#36899));
#15376=EDGE_LOOP('',(#36900,#36901));
#15377=EDGE_LOOP('',(#36902,#36903));
#15378=EDGE_LOOP('',(#36904,#36905));
#15379=EDGE_LOOP('',(#36906,#36907));
#15380=EDGE_LOOP('',(#36908,#36909));
#15381=EDGE_LOOP('',(#36910,#36911));
#15382=EDGE_LOOP('',(#36912,#36913));
#15383=EDGE_LOOP('',(#36914,#36915));
#15384=EDGE_LOOP('',(#36916,#36917));
#15385=EDGE_LOOP('',(#36918,#36919));
#15386=EDGE_LOOP('',(#36920,#36921));
#15387=EDGE_LOOP('',(#36922,#36923));
#15388=EDGE_LOOP('',(#36924,#36925));
#15389=EDGE_LOOP('',(#36926,#36927));
#15390=EDGE_LOOP('',(#36928,#36929));
#15391=EDGE_LOOP('',(#36930,#36931));
#15392=EDGE_LOOP('',(#36932,#36933));
#15393=EDGE_LOOP('',(#36934,#36935));
#15394=EDGE_LOOP('',(#36936,#36937));
#15395=EDGE_LOOP('',(#36938,#36939));
#15396=EDGE_LOOP('',(#36940,#36941));
#15397=EDGE_LOOP('',(#36942,#36943));
#15398=EDGE_LOOP('',(#36944,#36945,#36946,#36947));
#15399=EDGE_LOOP('',(#36948,#36949,#36950,#36951,#36952));
#15400=EDGE_LOOP('',(#36953,#36954,#36955,#36956,#36957));
#15401=EDGE_LOOP('',(#36958,#36959,#36960,#36961,#36962));
#15402=EDGE_LOOP('',(#36963,#36964,#36965,#36966,#36967));
#15403=EDGE_LOOP('',(#36968,#36969,#36970,#36971,#36972));
#15404=EDGE_LOOP('',(#36973,#36974,#36975,#36976,#36977));
#15405=EDGE_LOOP('',(#36978,#36979,#36980,#36981,#36982));
#15406=EDGE_LOOP('',(#36983,#36984,#36985,#36986,#36987));
#15407=EDGE_LOOP('',(#36988,#36989,#36990,#36991,#36992));
#15408=EDGE_LOOP('',(#36993,#36994,#36995,#36996,#36997));
#15409=EDGE_LOOP('',(#36998,#36999,#37000,#37001,#37002));
#15410=EDGE_LOOP('',(#37003,#37004,#37005,#37006,#37007));
#15411=EDGE_LOOP('',(#37008,#37009,#37010,#37011,#37012));
#15412=EDGE_LOOP('',(#37013,#37014,#37015,#37016,#37017));
#15413=EDGE_LOOP('',(#37018,#37019,#37020,#37021,#37022));
#15414=EDGE_LOOP('',(#37023,#37024,#37025,#37026,#37027));
#15415=EDGE_LOOP('',(#37028,#37029,#37030,#37031,#37032));
#15416=EDGE_LOOP('',(#37033,#37034,#37035,#37036,#37037));
#15417=EDGE_LOOP('',(#37038,#37039,#37040,#37041,#37042));
#15418=EDGE_LOOP('',(#37043,#37044,#37045,#37046,#37047));
#15419=EDGE_LOOP('',(#37048,#37049,#37050,#37051,#37052));
#15420=EDGE_LOOP('',(#37053,#37054,#37055,#37056,#37057));
#15421=EDGE_LOOP('',(#37058,#37059,#37060,#37061,#37062));
#15422=EDGE_LOOP('',(#37063,#37064,#37065,#37066,#37067));
#15423=EDGE_LOOP('',(#37068,#37069,#37070,#37071,#37072));
#15424=EDGE_LOOP('',(#37073,#37074,#37075,#37076,#37077));
#15425=EDGE_LOOP('',(#37078,#37079,#37080,#37081,#37082));
#15426=EDGE_LOOP('',(#37083,#37084,#37085,#37086,#37087));
#15427=EDGE_LOOP('',(#37088,#37089,#37090,#37091,#37092));
#15428=EDGE_LOOP('',(#37093,#37094,#37095,#37096,#37097));
#15429=EDGE_LOOP('',(#37098,#37099,#37100,#37101,#37102));
#15430=EDGE_LOOP('',(#37103,#37104,#37105,#37106,#37107));
#15431=EDGE_LOOP('',(#37108,#37109,#37110,#37111,#37112));
#15432=EDGE_LOOP('',(#37113,#37114,#37115,#37116,#37117));
#15433=EDGE_LOOP('',(#37118,#37119,#37120,#37121,#37122));
#15434=EDGE_LOOP('',(#37123,#37124,#37125,#37126,#37127));
#15435=EDGE_LOOP('',(#37128,#37129,#37130,#37131,#37132));
#15436=EDGE_LOOP('',(#37133,#37134,#37135,#37136,#37137));
#15437=EDGE_LOOP('',(#37138,#37139,#37140,#37141,#37142));
#15438=EDGE_LOOP('',(#37143,#37144,#37145,#37146,#37147));
#15439=EDGE_LOOP('',(#37148,#37149,#37150,#37151,#37152));
#15440=EDGE_LOOP('',(#37153,#37154,#37155,#37156,#37157));
#15441=EDGE_LOOP('',(#37158,#37159,#37160,#37161,#37162));
#15442=EDGE_LOOP('',(#37163,#37164,#37165,#37166,#37167));
#15443=EDGE_LOOP('',(#37168,#37169,#37170,#37171,#37172));
#15444=EDGE_LOOP('',(#37173,#37174,#37175,#37176,#37177));
#15445=EDGE_LOOP('',(#37178,#37179,#37180,#37181,#37182));
#15446=EDGE_LOOP('',(#37183,#37184,#37185,#37186,#37187));
#15447=EDGE_LOOP('',(#37188,#37189,#37190,#37191,#37192));
#15448=EDGE_LOOP('',(#37193,#37194,#37195,#37196,#37197));
#15449=EDGE_LOOP('',(#37198,#37199,#37200,#37201,#37202));
#15450=EDGE_LOOP('',(#37203,#37204,#37205,#37206,#37207));
#15451=EDGE_LOOP('',(#37208,#37209,#37210,#37211,#37212));
#15452=EDGE_LOOP('',(#37213,#37214,#37215,#37216,#37217));
#15453=EDGE_LOOP('',(#37218,#37219,#37220,#37221,#37222,#37223));
#15454=EDGE_LOOP('',(#37224,#37225,#37226,#37227,#37228));
#15455=EDGE_LOOP('',(#37229,#37230,#37231,#37232,#37233));
#15456=EDGE_LOOP('',(#37234,#37235,#37236,#37237,#37238));
#15457=EDGE_LOOP('',(#37239,#37240,#37241,#37242,#37243));
#15458=EDGE_LOOP('',(#37244,#37245,#37246,#37247,#37248));
#15459=EDGE_LOOP('',(#37249,#37250,#37251,#37252,#37253));
#15460=EDGE_LOOP('',(#37254,#37255,#37256,#37257,#37258));
#15461=EDGE_LOOP('',(#37259,#37260,#37261,#37262));
#15462=EDGE_LOOP('',(#37263,#37264,#37265,#37266,#37267));
#15463=EDGE_LOOP('',(#37268,#37269,#37270,#37271));
#15464=EDGE_LOOP('',(#37272,#37273,#37274,#37275,#37276));
#15465=EDGE_LOOP('',(#37277,#37278,#37279,#37280,#37281));
#15466=EDGE_LOOP('',(#37282,#37283,#37284,#37285,#37286));
#15467=EDGE_LOOP('',(#37287,#37288,#37289,#37290,#37291));
#15468=EDGE_LOOP('',(#37292,#37293,#37294,#37295,#37296));
#15469=EDGE_LOOP('',(#37297,#37298,#37299,#37300));
#15470=EDGE_LOOP('',(#37301,#37302,#37303,#37304,#37305));
#15471=EDGE_LOOP('',(#37306,#37307,#37308,#37309));
#15472=EDGE_LOOP('',(#37310,#37311,#37312,#37313,#37314));
#15473=EDGE_LOOP('',(#37315,#37316,#37317,#37318));
#15474=EDGE_LOOP('',(#37319,#37320,#37321,#37322,#37323));
#15475=EDGE_LOOP('',(#37324,#37325,#37326,#37327));
#15476=EDGE_LOOP('',(#37328,#37329,#37330,#37331,#37332));
#15477=EDGE_LOOP('',(#37333,#37334,#37335,#37336));
#15478=EDGE_LOOP('',(#37337,#37338,#37339,#37340,#37341));
#15479=EDGE_LOOP('',(#37342,#37343,#37344,#37345));
#15480=EDGE_LOOP('',(#37346,#37347,#37348,#37349,#37350));
#15481=EDGE_LOOP('',(#37351,#37352,#37353,#37354));
#15482=EDGE_LOOP('',(#37355,#37356,#37357,#37358,#37359));
#15483=EDGE_LOOP('',(#37360,#37361,#37362,#37363));
#15484=EDGE_LOOP('',(#37364,#37365,#37366,#37367,#37368));
#15485=EDGE_LOOP('',(#37369,#37370,#37371,#37372));
#15486=EDGE_LOOP('',(#37373,#37374,#37375,#37376,#37377));
#15487=EDGE_LOOP('',(#37378,#37379,#37380,#37381));
#15488=EDGE_LOOP('',(#37382,#37383,#37384,#37385,#37386));
#15489=EDGE_LOOP('',(#37387,#37388,#37389,#37390));
#15490=EDGE_LOOP('',(#37391,#37392,#37393,#37394,#37395));
#15491=EDGE_LOOP('',(#37396,#37397,#37398,#37399));
#15492=EDGE_LOOP('',(#37400,#37401,#37402,#37403,#37404));
#15493=EDGE_LOOP('',(#37405,#37406,#37407,#37408));
#15494=EDGE_LOOP('',(#37409,#37410,#37411,#37412,#37413));
#15495=EDGE_LOOP('',(#37414,#37415,#37416,#37417));
#15496=EDGE_LOOP('',(#37418,#37419,#37420,#37421,#37422));
#15497=EDGE_LOOP('',(#37423,#37424,#37425,#37426));
#15498=EDGE_LOOP('',(#37427,#37428,#37429,#37430,#37431));
#15499=EDGE_LOOP('',(#37432,#37433,#37434,#37435));
#15500=EDGE_LOOP('',(#37436,#37437,#37438,#37439,#37440));
#15501=EDGE_LOOP('',(#37441,#37442,#37443,#37444));
#15502=EDGE_LOOP('',(#37445,#37446,#37447,#37448,#37449));
#15503=EDGE_LOOP('',(#37450,#37451,#37452,#37453));
#15504=EDGE_LOOP('',(#37454,#37455,#37456,#37457,#37458));
#15505=EDGE_LOOP('',(#37459,#37460,#37461,#37462));
#15506=EDGE_LOOP('',(#37463,#37464,#37465,#37466,#37467));
#15507=EDGE_LOOP('',(#37468,#37469,#37470,#37471));
#15508=EDGE_LOOP('',(#37472,#37473,#37474,#37475,#37476));
#15509=EDGE_LOOP('',(#37477,#37478,#37479,#37480));
#15510=EDGE_LOOP('',(#37481,#37482,#37483,#37484,#37485));
#15511=EDGE_LOOP('',(#37486,#37487,#37488,#37489));
#15512=EDGE_LOOP('',(#37490,#37491,#37492,#37493,#37494));
#15513=EDGE_LOOP('',(#37495,#37496,#37497,#37498));
#15514=EDGE_LOOP('',(#37499,#37500,#37501,#37502,#37503));
#15515=EDGE_LOOP('',(#37504,#37505,#37506,#37507));
#15516=EDGE_LOOP('',(#37508,#37509,#37510,#37511,#37512));
#15517=EDGE_LOOP('',(#37513,#37514,#37515,#37516));
#15518=EDGE_LOOP('',(#37517,#37518,#37519,#37520,#37521));
#15519=EDGE_LOOP('',(#37522,#37523,#37524,#37525));
#15520=EDGE_LOOP('',(#37526,#37527,#37528,#37529,#37530));
#15521=EDGE_LOOP('',(#37531,#37532,#37533,#37534));
#15522=EDGE_LOOP('',(#37535,#37536,#37537,#37538,#37539));
#15523=EDGE_LOOP('',(#37540,#37541,#37542,#37543));
#15524=EDGE_LOOP('',(#37544,#37545,#37546,#37547,#37548));
#15525=EDGE_LOOP('',(#37549,#37550,#37551,#37552,#37553));
#15526=EDGE_LOOP('',(#37554,#37555,#37556,#37557,#37558));
#15527=EDGE_LOOP('',(#37559,#37560,#37561,#37562));
#15528=EDGE_LOOP('',(#37563,#37564,#37565,#37566,#37567));
#15529=EDGE_LOOP('',(#37568,#37569,#37570,#37571));
#15530=EDGE_LOOP('',(#37572,#37573,#37574,#37575,#37576));
#15531=EDGE_LOOP('',(#37577,#37578,#37579,#37580));
#15532=EDGE_LOOP('',(#37581,#37582,#37583,#37584,#37585));
#15533=EDGE_LOOP('',(#37586,#37587,#37588,#37589,#37590));
#15534=EDGE_LOOP('',(#37591,#37592,#37593,#37594,#37595));
#15535=EDGE_LOOP('',(#37596,#37597,#37598,#37599));
#15536=EDGE_LOOP('',(#37600,#37601,#37602,#37603,#37604));
#15537=EDGE_LOOP('',(#37605,#37606,#37607,#37608));
#15538=EDGE_LOOP('',(#37609,#37610,#37611,#37612,#37613));
#15539=EDGE_LOOP('',(#37614,#37615,#37616,#37617));
#15540=EDGE_LOOP('',(#37618,#37619,#37620,#37621,#37622));
#15541=EDGE_LOOP('',(#37623,#37624,#37625,#37626,#37627,#37628));
#15542=EDGE_LOOP('',(#37629,#37630,#37631,#37632,#37633));
#15543=EDGE_LOOP('',(#37634,#37635,#37636,#37637));
#15544=EDGE_LOOP('',(#37638,#37639,#37640,#37641,#37642));
#15545=EDGE_LOOP('',(#37643,#37644,#37645,#37646));
#15546=EDGE_LOOP('',(#37647,#37648,#37649,#37650,#37651));
#15547=EDGE_LOOP('',(#37652,#37653,#37654,#37655));
#15548=EDGE_LOOP('',(#37656,#37657,#37658,#37659,#37660));
#15549=EDGE_LOOP('',(#37661,#37662,#37663,#37664));
#15550=EDGE_LOOP('',(#37665,#37666,#37667,#37668,#37669));
#15551=EDGE_LOOP('',(#37670,#37671,#37672,#37673));
#15552=EDGE_LOOP('',(#37674,#37675,#37676,#37677,#37678));
#15553=EDGE_LOOP('',(#37679,#37680,#37681,#37682));
#15554=EDGE_LOOP('',(#37683,#37684,#37685,#37686,#37687));
#15555=EDGE_LOOP('',(#37688,#37689,#37690,#37691));
#15556=EDGE_LOOP('',(#37692,#37693,#37694,#37695,#37696));
#15557=EDGE_LOOP('',(#37697,#37698,#37699,#37700));
#15558=EDGE_LOOP('',(#37701,#37702,#37703,#37704,#37705));
#15559=EDGE_LOOP('',(#37706,#37707,#37708,#37709));
#15560=EDGE_LOOP('',(#37710,#37711,#37712,#37713,#37714));
#15561=EDGE_LOOP('',(#37715,#37716,#37717,#37718));
#15562=EDGE_LOOP('',(#37719,#37720,#37721,#37722,#37723));
#15563=EDGE_LOOP('',(#37724,#37725,#37726,#37727));
#15564=EDGE_LOOP('',(#37728,#37729,#37730,#37731,#37732));
#15565=EDGE_LOOP('',(#37733,#37734,#37735,#37736));
#15566=EDGE_LOOP('',(#37737,#37738,#37739,#37740,#37741));
#15567=EDGE_LOOP('',(#37742,#37743,#37744,#37745));
#15568=EDGE_LOOP('',(#37746,#37747,#37748,#37749,#37750));
#15569=EDGE_LOOP('',(#37751,#37752,#37753,#37754));
#15570=EDGE_LOOP('',(#37755,#37756,#37757,#37758,#37759));
#15571=EDGE_LOOP('',(#37760,#37761,#37762,#37763));
#15572=EDGE_LOOP('',(#37764,#37765,#37766,#37767,#37768));
#15573=EDGE_LOOP('',(#37769,#37770,#37771,#37772));
#15574=EDGE_LOOP('',(#37773,#37774,#37775,#37776,#37777));
#15575=EDGE_LOOP('',(#37778,#37779,#37780,#37781));
#15576=EDGE_LOOP('',(#37782,#37783,#37784,#37785,#37786));
#15577=EDGE_LOOP('',(#37787,#37788,#37789,#37790));
#15578=EDGE_LOOP('',(#37791,#37792,#37793,#37794,#37795));
#15579=EDGE_LOOP('',(#37796,#37797,#37798,#37799));
#15580=EDGE_LOOP('',(#37800,#37801,#37802,#37803,#37804));
#15581=EDGE_LOOP('',(#37805,#37806,#37807,#37808,#37809));
#15582=EDGE_LOOP('',(#37810,#37811,#37812,#37813,#37814));
#15583=EDGE_LOOP('',(#37815,#37816,#37817,#37818,#37819));
#15584=EDGE_LOOP('',(#37820,#37821,#37822,#37823,#37824));
#15585=EDGE_LOOP('',(#37825,#37826,#37827,#37828));
#15586=EDGE_LOOP('',(#37829,#37830,#37831,#37832,#37833));
#15587=EDGE_LOOP('',(#37834,#37835,#37836,#37837));
#15588=EDGE_LOOP('',(#37838,#37839,#37840,#37841,#37842));
#15589=EDGE_LOOP('',(#37843,#37844,#37845,#37846,#37847));
#15590=EDGE_LOOP('',(#37848,#37849,#37850,#37851,#37852));
#15591=EDGE_LOOP('',(#37853,#37854,#37855,#37856,#37857));
#15592=EDGE_LOOP('',(#37858,#37859,#37860,#37861,#37862));
#15593=EDGE_LOOP('',(#37863,#37864,#37865,#37866,#37867));
#15594=EDGE_LOOP('',(#37868,#37869,#37870,#37871,#37872));
#15595=EDGE_LOOP('',(#37873,#37874,#37875,#37876,#37877));
#15596=EDGE_LOOP('',(#37878,#37879,#37880,#37881,#37882));
#15597=EDGE_LOOP('',(#37883,#37884,#37885,#37886,#37887));
#15598=EDGE_LOOP('',(#37888,#37889,#37890,#37891,#37892));
#15599=EDGE_LOOP('',(#37893,#37894,#37895,#37896,#37897));
#15600=EDGE_LOOP('',(#37898,#37899,#37900,#37901,#37902));
#15601=EDGE_LOOP('',(#37903,#37904,#37905,#37906,#37907));
#15602=EDGE_LOOP('',(#37908,#37909,#37910,#37911,#37912));
#15603=EDGE_LOOP('',(#37913,#37914,#37915,#37916,#37917));
#15604=EDGE_LOOP('',(#37918,#37919,#37920,#37921,#37922));
#15605=EDGE_LOOP('',(#37923,#37924,#37925,#37926,#37927));
#15606=EDGE_LOOP('',(#37928,#37929,#37930,#37931,#37932));
#15607=EDGE_LOOP('',(#37933,#37934,#37935,#37936,#37937));
#15608=EDGE_LOOP('',(#37938,#37939,#37940,#37941,#37942));
#15609=EDGE_LOOP('',(#37943,#37944,#37945,#37946,#37947));
#15610=EDGE_LOOP('',(#37948,#37949,#37950,#37951,#37952));
#15611=EDGE_LOOP('',(#37953,#37954,#37955,#37956,#37957));
#15612=EDGE_LOOP('',(#37958,#37959,#37960,#37961,#37962));
#15613=EDGE_LOOP('',(#37963,#37964,#37965,#37966,#37967));
#15614=EDGE_LOOP('',(#37968,#37969,#37970,#37971,#37972));
#15615=EDGE_LOOP('',(#37973,#37974,#37975,#37976,#37977));
#15616=EDGE_LOOP('',(#37978,#37979,#37980,#37981,#37982));
#15617=EDGE_LOOP('',(#37983,#37984,#37985,#37986,#37987));
#15618=EDGE_LOOP('',(#37988,#37989,#37990,#37991,#37992));
#15619=EDGE_LOOP('',(#37993,#37994,#37995,#37996,#37997));
#15620=EDGE_LOOP('',(#37998,#37999,#38000,#38001,#38002));
#15621=EDGE_LOOP('',(#38003,#38004,#38005,#38006,#38007));
#15622=EDGE_LOOP('',(#38008,#38009,#38010,#38011,#38012));
#15623=EDGE_LOOP('',(#38013,#38014,#38015,#38016,#38017));
#15624=EDGE_LOOP('',(#38018,#38019,#38020,#38021,#38022));
#15625=EDGE_LOOP('',(#38023,#38024,#38025,#38026,#38027));
#15626=EDGE_LOOP('',(#38028,#38029,#38030,#38031,#38032));
#15627=EDGE_LOOP('',(#38033,#38034,#38035,#38036,#38037));
#15628=EDGE_LOOP('',(#38038,#38039,#38040,#38041,#38042));
#15629=EDGE_LOOP('',(#38043,#38044,#38045,#38046,#38047));
#15630=EDGE_LOOP('',(#38048,#38049,#38050,#38051,#38052));
#15631=EDGE_LOOP('',(#38053,#38054,#38055,#38056,#38057));
#15632=EDGE_LOOP('',(#38058,#38059,#38060,#38061,#38062));
#15633=EDGE_LOOP('',(#38063,#38064,#38065,#38066,#38067));
#15634=EDGE_LOOP('',(#38068,#38069,#38070,#38071,#38072));
#15635=EDGE_LOOP('',(#38073,#38074,#38075,#38076,#38077));
#15636=EDGE_LOOP('',(#38078,#38079,#38080,#38081,#38082));
#15637=EDGE_LOOP('',(#38083,#38084,#38085,#38086));
#15638=EDGE_LOOP('',(#38087,#38088,#38089,#38090));
#15639=EDGE_LOOP('',(#38091,#38092,#38093,#38094));
#15640=EDGE_LOOP('',(#38095,#38096,#38097,#38098));
#15641=EDGE_LOOP('',(#38099,#38100,#38101,#38102));
#15642=EDGE_LOOP('',(#38103,#38104,#38105,#38106));
#15643=EDGE_LOOP('',(#38107,#38108,#38109,#38110));
#15644=EDGE_LOOP('',(#38111,#38112,#38113,#38114));
#15645=EDGE_LOOP('',(#38115,#38116,#38117,#38118));
#15646=EDGE_LOOP('',(#38119,#38120,#38121,#38122));
#15647=EDGE_LOOP('',(#38123,#38124,#38125,#38126));
#15648=EDGE_LOOP('',(#38127,#38128,#38129,#38130));
#15649=EDGE_LOOP('',(#38131,#38132,#38133,#38134));
#15650=EDGE_LOOP('',(#38135,#38136,#38137,#38138));
#15651=EDGE_LOOP('',(#38139,#38140,#38141,#38142));
#15652=EDGE_LOOP('',(#38143,#38144,#38145,#38146));
#15653=EDGE_LOOP('',(#38147,#38148,#38149,#38150));
#15654=EDGE_LOOP('',(#38151,#38152,#38153,#38154));
#15655=EDGE_LOOP('',(#38155,#38156,#38157,#38158));
#15656=EDGE_LOOP('',(#38159,#38160,#38161,#38162));
#15657=EDGE_LOOP('',(#38163,#38164,#38165,#38166));
#15658=EDGE_LOOP('',(#38167,#38168,#38169,#38170));
#15659=EDGE_LOOP('',(#38171,#38172,#38173,#38174));
#15660=EDGE_LOOP('',(#38175,#38176,#38177,#38178));
#15661=EDGE_LOOP('',(#38179,#38180,#38181,#38182));
#15662=EDGE_LOOP('',(#38183,#38184,#38185,#38186));
#15663=EDGE_LOOP('',(#38187,#38188,#38189,#38190));
#15664=EDGE_LOOP('',(#38191,#38192,#38193,#38194));
#15665=EDGE_LOOP('',(#38195,#38196,#38197,#38198));
#15666=EDGE_LOOP('',(#38199,#38200,#38201,#38202));
#15667=EDGE_LOOP('',(#38203,#38204,#38205,#38206));
#15668=EDGE_LOOP('',(#38207,#38208,#38209,#38210));
#15669=EDGE_LOOP('',(#38211,#38212,#38213,#38214));
#15670=EDGE_LOOP('',(#38215,#38216,#38217,#38218));
#15671=EDGE_LOOP('',(#38219,#38220,#38221,#38222));
#15672=EDGE_LOOP('',(#38223,#38224,#38225,#38226));
#15673=EDGE_LOOP('',(#38227,#38228,#38229,#38230));
#15674=EDGE_LOOP('',(#38231,#38232,#38233,#38234));
#15675=EDGE_LOOP('',(#38235,#38236,#38237,#38238));
#15676=EDGE_LOOP('',(#38239,#38240,#38241,#38242));
#15677=EDGE_LOOP('',(#38243,#38244,#38245,#38246));
#15678=EDGE_LOOP('',(#38247,#38248,#38249,#38250));
#15679=EDGE_LOOP('',(#38251,#38252,#38253,#38254));
#15680=EDGE_LOOP('',(#38255,#38256,#38257,#38258));
#15681=EDGE_LOOP('',(#38259,#38260,#38261,#38262));
#15682=EDGE_LOOP('',(#38263,#38264,#38265,#38266));
#15683=EDGE_LOOP('',(#38267,#38268,#38269,#38270));
#15684=EDGE_LOOP('',(#38271,#38272,#38273,#38274));
#15685=EDGE_LOOP('',(#38275,#38276,#38277,#38278));
#15686=EDGE_LOOP('',(#38279,#38280,#38281,#38282));
#15687=EDGE_LOOP('',(#38283,#38284,#38285,#38286));
#15688=EDGE_LOOP('',(#38287,#38288,#38289,#38290));
#15689=EDGE_LOOP('',(#38291,#38292,#38293,#38294));
#15690=EDGE_LOOP('',(#38295,#38296,#38297,#38298));
#15691=EDGE_LOOP('',(#38299,#38300,#38301,#38302));
#15692=EDGE_LOOP('',(#38303,#38304,#38305,#38306));
#15693=EDGE_LOOP('',(#38307,#38308,#38309,#38310));
#15694=EDGE_LOOP('',(#38311,#38312,#38313,#38314));
#15695=EDGE_LOOP('',(#38315,#38316,#38317,#38318));
#15696=EDGE_LOOP('',(#38319,#38320,#38321,#38322));
#15697=EDGE_LOOP('',(#38323,#38324,#38325,#38326));
#15698=EDGE_LOOP('',(#38327,#38328,#38329,#38330));
#15699=EDGE_LOOP('',(#38331,#38332,#38333,#38334));
#15700=EDGE_LOOP('',(#38335,#38336,#38337,#38338));
#15701=EDGE_LOOP('',(#38339,#38340,#38341,#38342));
#15702=EDGE_LOOP('',(#38343,#38344,#38345,#38346));
#15703=EDGE_LOOP('',(#38347,#38348,#38349,#38350));
#15704=EDGE_LOOP('',(#38351,#38352,#38353,#38354));
#15705=EDGE_LOOP('',(#38355,#38356,#38357,#38358));
#15706=EDGE_LOOP('',(#38359,#38360,#38361,#38362));
#15707=EDGE_LOOP('',(#38363,#38364,#38365,#38366));
#15708=EDGE_LOOP('',(#38367,#38368,#38369,#38370));
#15709=EDGE_LOOP('',(#38371,#38372,#38373,#38374));
#15710=EDGE_LOOP('',(#38375,#38376,#38377,#38378));
#15711=EDGE_LOOP('',(#38379,#38380,#38381,#38382));
#15712=EDGE_LOOP('',(#38383,#38384,#38385,#38386));
#15713=EDGE_LOOP('',(#38387,#38388,#38389,#38390));
#15714=EDGE_LOOP('',(#38391,#38392,#38393,#38394));
#15715=EDGE_LOOP('',(#38395,#38396,#38397,#38398));
#15716=EDGE_LOOP('',(#38399,#38400,#38401,#38402));
#15717=EDGE_LOOP('',(#38403,#38404,#38405,#38406));
#15718=EDGE_LOOP('',(#38407,#38408,#38409,#38410));
#15719=EDGE_LOOP('',(#38411,#38412,#38413,#38414));
#15720=EDGE_LOOP('',(#38415,#38416,#38417,#38418));
#15721=EDGE_LOOP('',(#38419,#38420,#38421,#38422));
#15722=EDGE_LOOP('',(#38423,#38424,#38425,#38426));
#15723=EDGE_LOOP('',(#38427,#38428,#38429,#38430));
#15724=EDGE_LOOP('',(#38431,#38432,#38433,#38434));
#15725=EDGE_LOOP('',(#38435,#38436,#38437,#38438));
#15726=EDGE_LOOP('',(#38439,#38440,#38441,#38442));
#15727=EDGE_LOOP('',(#38443,#38444,#38445,#38446));
#15728=EDGE_LOOP('',(#38447,#38448,#38449,#38450));
#15729=EDGE_LOOP('',(#38451,#38452,#38453,#38454));
#15730=EDGE_LOOP('',(#38455,#38456,#38457,#38458));
#15731=EDGE_LOOP('',(#38459,#38460,#38461,#38462));
#15732=EDGE_LOOP('',(#38463,#38464,#38465,#38466));
#15733=EDGE_LOOP('',(#38467,#38468,#38469,#38470));
#15734=EDGE_LOOP('',(#38471,#38472,#38473,#38474));
#15735=EDGE_LOOP('',(#38475,#38476,#38477,#38478));
#15736=EDGE_LOOP('',(#38479,#38480,#38481,#38482));
#15737=EDGE_LOOP('',(#38483,#38484,#38485,#38486));
#15738=EDGE_LOOP('',(#38487,#38488,#38489,#38490));
#15739=EDGE_LOOP('',(#38491,#38492,#38493,#38494));
#15740=EDGE_LOOP('',(#38495,#38496,#38497,#38498));
#15741=EDGE_LOOP('',(#38499,#38500,#38501,#38502));
#15742=EDGE_LOOP('',(#38503,#38504,#38505,#38506));
#15743=EDGE_LOOP('',(#38507,#38508,#38509,#38510));
#15744=EDGE_LOOP('',(#38511,#38512,#38513,#38514));
#15745=EDGE_LOOP('',(#38515,#38516,#38517,#38518));
#15746=EDGE_LOOP('',(#38519,#38520,#38521,#38522));
#15747=EDGE_LOOP('',(#38523,#38524,#38525,#38526));
#15748=EDGE_LOOP('',(#38527,#38528,#38529,#38530));
#15749=EDGE_LOOP('',(#38531,#38532,#38533,#38534));
#15750=EDGE_LOOP('',(#38535,#38536,#38537,#38538));
#15751=EDGE_LOOP('',(#38539,#38540,#38541,#38542));
#15752=EDGE_LOOP('',(#38543,#38544,#38545,#38546));
#15753=EDGE_LOOP('',(#38547,#38548,#38549,#38550));
#15754=EDGE_LOOP('',(#38551,#38552,#38553,#38554));
#15755=EDGE_LOOP('',(#38555,#38556,#38557,#38558));
#15756=EDGE_LOOP('',(#38559,#38560,#38561,#38562));
#15757=EDGE_LOOP('',(#38563,#38564,#38565,#38566));
#15758=EDGE_LOOP('',(#38567,#38568,#38569,#38570));
#15759=EDGE_LOOP('',(#38571,#38572,#38573,#38574));
#15760=EDGE_LOOP('',(#38575,#38576,#38577,#38578));
#15761=EDGE_LOOP('',(#38579,#38580,#38581,#38582));
#15762=EDGE_LOOP('',(#38583,#38584,#38585,#38586));
#15763=EDGE_LOOP('',(#38587,#38588,#38589,#38590));
#15764=EDGE_LOOP('',(#38591,#38592,#38593,#38594));
#15765=EDGE_LOOP('',(#38595,#38596,#38597,#38598));
#15766=EDGE_LOOP('',(#38599,#38600,#38601,#38602));
#15767=EDGE_LOOP('',(#38603,#38604,#38605,#38606));
#15768=EDGE_LOOP('',(#38607,#38608,#38609,#38610));
#15769=EDGE_LOOP('',(#38611,#38612,#38613,#38614));
#15770=EDGE_LOOP('',(#38615,#38616,#38617,#38618));
#15771=EDGE_LOOP('',(#38619,#38620,#38621,#38622));
#15772=EDGE_LOOP('',(#38623,#38624,#38625,#38626));
#15773=EDGE_LOOP('',(#38627,#38628,#38629,#38630));
#15774=EDGE_LOOP('',(#38631,#38632,#38633,#38634));
#15775=EDGE_LOOP('',(#38635,#38636,#38637,#38638));
#15776=EDGE_LOOP('',(#38639,#38640,#38641,#38642));
#15777=EDGE_LOOP('',(#38643,#38644,#38645,#38646));
#15778=EDGE_LOOP('',(#38647,#38648,#38649,#38650));
#15779=EDGE_LOOP('',(#38651,#38652,#38653,#38654));
#15780=EDGE_LOOP('',(#38655,#38656,#38657,#38658));
#15781=EDGE_LOOP('',(#38659,#38660,#38661,#38662));
#15782=EDGE_LOOP('',(#38663,#38664,#38665,#38666));
#15783=EDGE_LOOP('',(#38667,#38668,#38669,#38670));
#15784=EDGE_LOOP('',(#38671,#38672,#38673,#38674));
#15785=EDGE_LOOP('',(#38675,#38676,#38677,#38678));
#15786=EDGE_LOOP('',(#38679,#38680,#38681,#38682));
#15787=EDGE_LOOP('',(#38683,#38684,#38685,#38686));
#15788=EDGE_LOOP('',(#38687,#38688,#38689,#38690));
#15789=EDGE_LOOP('',(#38691,#38692,#38693,#38694));
#15790=EDGE_LOOP('',(#38695,#38696,#38697,#38698));
#15791=EDGE_LOOP('',(#38699,#38700,#38701,#38702));
#15792=EDGE_LOOP('',(#38703,#38704,#38705,#38706));
#15793=EDGE_LOOP('',(#38707,#38708,#38709,#38710));
#15794=EDGE_LOOP('',(#38711,#38712,#38713,#38714));
#15795=EDGE_LOOP('',(#38715,#38716,#38717,#38718));
#15796=EDGE_LOOP('',(#38719,#38720,#38721,#38722));
#15797=EDGE_LOOP('',(#38723,#38724,#38725,#38726));
#15798=EDGE_LOOP('',(#38727,#38728,#38729,#38730));
#15799=EDGE_LOOP('',(#38731,#38732,#38733,#38734));
#15800=EDGE_LOOP('',(#38735,#38736,#38737,#38738));
#15801=EDGE_LOOP('',(#38739,#38740,#38741,#38742));
#15802=EDGE_LOOP('',(#38743,#38744,#38745,#38746));
#15803=EDGE_LOOP('',(#38747,#38748,#38749,#38750));
#15804=EDGE_LOOP('',(#38751,#38752,#38753,#38754));
#15805=EDGE_LOOP('',(#38755,#38756,#38757,#38758));
#15806=EDGE_LOOP('',(#38759,#38760,#38761,#38762));
#15807=EDGE_LOOP('',(#38763,#38764,#38765,#38766));
#15808=EDGE_LOOP('',(#38767,#38768,#38769,#38770));
#15809=EDGE_LOOP('',(#38771,#38772,#38773,#38774));
#15810=EDGE_LOOP('',(#38775,#38776,#38777,#38778));
#15811=EDGE_LOOP('',(#38779,#38780,#38781,#38782));
#15812=EDGE_LOOP('',(#38783,#38784,#38785,#38786));
#15813=EDGE_LOOP('',(#38787,#38788,#38789,#38790));
#15814=EDGE_LOOP('',(#38791,#38792,#38793,#38794));
#15815=EDGE_LOOP('',(#38795,#38796,#38797,#38798));
#15816=EDGE_LOOP('',(#38799,#38800,#38801,#38802));
#15817=EDGE_LOOP('',(#38803,#38804,#38805,#38806));
#15818=EDGE_LOOP('',(#38807,#38808,#38809,#38810));
#15819=EDGE_LOOP('',(#38811,#38812,#38813,#38814));
#15820=EDGE_LOOP('',(#38815,#38816,#38817,#38818));
#15821=EDGE_LOOP('',(#38819,#38820,#38821,#38822));
#15822=EDGE_LOOP('',(#38823,#38824,#38825,#38826));
#15823=EDGE_LOOP('',(#38827,#38828,#38829,#38830));
#15824=EDGE_LOOP('',(#38831,#38832,#38833,#38834));
#15825=EDGE_LOOP('',(#38835,#38836,#38837,#38838));
#15826=EDGE_LOOP('',(#38839,#38840,#38841,#38842));
#15827=EDGE_LOOP('',(#38843,#38844,#38845,#38846));
#15828=EDGE_LOOP('',(#38847,#38848,#38849,#38850));
#15829=EDGE_LOOP('',(#38851,#38852,#38853,#38854));
#15830=EDGE_LOOP('',(#38855,#38856,#38857,#38858));
#15831=EDGE_LOOP('',(#38859,#38860,#38861,#38862));
#15832=EDGE_LOOP('',(#38863,#38864,#38865,#38866));
#15833=EDGE_LOOP('',(#38867,#38868,#38869,#38870));
#15834=EDGE_LOOP('',(#38871,#38872,#38873,#38874));
#15835=EDGE_LOOP('',(#38875,#38876,#38877,#38878));
#15836=EDGE_LOOP('',(#38879,#38880,#38881,#38882));
#15837=EDGE_LOOP('',(#38883,#38884,#38885,#38886));
#15838=EDGE_LOOP('',(#38887,#38888,#38889,#38890));
#15839=EDGE_LOOP('',(#38891,#38892,#38893,#38894));
#15840=EDGE_LOOP('',(#38895,#38896,#38897,#38898));
#15841=EDGE_LOOP('',(#38899,#38900,#38901,#38902));
#15842=EDGE_LOOP('',(#38903,#38904,#38905,#38906));
#15843=EDGE_LOOP('',(#38907,#38908,#38909,#38910));
#15844=EDGE_LOOP('',(#38911,#38912,#38913,#38914));
#15845=EDGE_LOOP('',(#38915,#38916,#38917,#38918));
#15846=EDGE_LOOP('',(#38919,#38920,#38921,#38922));
#15847=EDGE_LOOP('',(#38923,#38924,#38925,#38926));
#15848=EDGE_LOOP('',(#38927,#38928,#38929,#38930));
#15849=EDGE_LOOP('',(#38931,#38932,#38933,#38934));
#15850=EDGE_LOOP('',(#38935,#38936,#38937,#38938));
#15851=EDGE_LOOP('',(#38939,#38940,#38941,#38942));
#15852=EDGE_LOOP('',(#38943,#38944,#38945,#38946));
#15853=EDGE_LOOP('',(#38947,#38948,#38949,#38950));
#15854=EDGE_LOOP('',(#38951,#38952,#38953,#38954));
#15855=EDGE_LOOP('',(#38955,#38956,#38957,#38958));
#15856=EDGE_LOOP('',(#38959,#38960,#38961,#38962));
#15857=EDGE_LOOP('',(#38963,#38964,#38965,#38966));
#15858=EDGE_LOOP('',(#38967,#38968,#38969,#38970));
#15859=EDGE_LOOP('',(#38971,#38972,#38973,#38974));
#15860=EDGE_LOOP('',(#38975,#38976,#38977,#38978));
#15861=EDGE_LOOP('',(#38979,#38980,#38981,#38982));
#15862=EDGE_LOOP('',(#38983,#38984,#38985,#38986));
#15863=EDGE_LOOP('',(#38987,#38988,#38989,#38990));
#15864=EDGE_LOOP('',(#38991,#38992,#38993,#38994));
#15865=EDGE_LOOP('',(#38995,#38996,#38997,#38998));
#15866=EDGE_LOOP('',(#38999,#39000,#39001,#39002));
#15867=EDGE_LOOP('',(#39003,#39004,#39005,#39006));
#15868=EDGE_LOOP('',(#39007,#39008,#39009,#39010));
#15869=EDGE_LOOP('',(#39011,#39012,#39013,#39014));
#15870=EDGE_LOOP('',(#39015,#39016,#39017,#39018));
#15871=EDGE_LOOP('',(#39019,#39020,#39021,#39022));
#15872=EDGE_LOOP('',(#39023,#39024,#39025,#39026));
#15873=EDGE_LOOP('',(#39027,#39028,#39029,#39030));
#15874=EDGE_LOOP('',(#39031,#39032,#39033,#39034));
#15875=EDGE_LOOP('',(#39035,#39036,#39037,#39038));
#15876=EDGE_LOOP('',(#39039,#39040,#39041,#39042));
#15877=EDGE_LOOP('',(#39043,#39044,#39045,#39046));
#15878=EDGE_LOOP('',(#39047,#39048,#39049,#39050));
#15879=EDGE_LOOP('',(#39051,#39052,#39053,#39054));
#15880=EDGE_LOOP('',(#39055,#39056,#39057,#39058));
#15881=EDGE_LOOP('',(#39059,#39060,#39061,#39062));
#15882=EDGE_LOOP('',(#39063,#39064,#39065,#39066));
#15883=EDGE_LOOP('',(#39067,#39068,#39069,#39070));
#15884=EDGE_LOOP('',(#39071,#39072,#39073,#39074));
#15885=EDGE_LOOP('',(#39075,#39076,#39077,#39078));
#15886=EDGE_LOOP('',(#39079,#39080,#39081,#39082));
#15887=EDGE_LOOP('',(#39083,#39084,#39085,#39086));
#15888=EDGE_LOOP('',(#39087,#39088,#39089,#39090));
#15889=EDGE_LOOP('',(#39091,#39092,#39093,#39094));
#15890=EDGE_LOOP('',(#39095,#39096,#39097,#39098));
#15891=EDGE_LOOP('',(#39099,#39100,#39101,#39102));
#15892=EDGE_LOOP('',(#39103,#39104,#39105,#39106));
#15893=EDGE_LOOP('',(#39107,#39108,#39109,#39110));
#15894=EDGE_LOOP('',(#39111,#39112,#39113,#39114));
#15895=EDGE_LOOP('',(#39115,#39116,#39117,#39118));
#15896=EDGE_LOOP('',(#39119,#39120,#39121,#39122));
#15897=EDGE_LOOP('',(#39123,#39124,#39125,#39126));
#15898=EDGE_LOOP('',(#39127,#39128,#39129,#39130));
#15899=EDGE_LOOP('',(#39131,#39132,#39133,#39134));
#15900=EDGE_LOOP('',(#39135,#39136,#39137,#39138));
#15901=EDGE_LOOP('',(#39139,#39140,#39141,#39142));
#15902=EDGE_LOOP('',(#39143,#39144,#39145,#39146));
#15903=EDGE_LOOP('',(#39147,#39148,#39149,#39150));
#15904=EDGE_LOOP('',(#39151,#39152,#39153,#39154));
#15905=EDGE_LOOP('',(#39155,#39156,#39157,#39158));
#15906=EDGE_LOOP('',(#39159,#39160,#39161,#39162));
#15907=EDGE_LOOP('',(#39163,#39164,#39165,#39166));
#15908=EDGE_LOOP('',(#39167,#39168,#39169,#39170));
#15909=EDGE_LOOP('',(#39171,#39172,#39173,#39174));
#15910=EDGE_LOOP('',(#39175,#39176,#39177,#39178));
#15911=EDGE_LOOP('',(#39179,#39180,#39181,#39182));
#15912=EDGE_LOOP('',(#39183,#39184,#39185,#39186));
#15913=EDGE_LOOP('',(#39187,#39188,#39189,#39190));
#15914=EDGE_LOOP('',(#39191,#39192,#39193,#39194));
#15915=EDGE_LOOP('',(#39195,#39196,#39197,#39198));
#15916=EDGE_LOOP('',(#39199,#39200,#39201,#39202));
#15917=EDGE_LOOP('',(#39203,#39204,#39205,#39206));
#15918=EDGE_LOOP('',(#39207,#39208,#39209,#39210));
#15919=EDGE_LOOP('',(#39211,#39212,#39213,#39214));
#15920=EDGE_LOOP('',(#39215,#39216,#39217,#39218));
#15921=EDGE_LOOP('',(#39219,#39220,#39221,#39222));
#15922=EDGE_LOOP('',(#39223,#39224,#39225,#39226));
#15923=EDGE_LOOP('',(#39227,#39228,#39229,#39230));
#15924=EDGE_LOOP('',(#39231,#39232,#39233,#39234));
#15925=EDGE_LOOP('',(#39235,#39236,#39237,#39238));
#15926=EDGE_LOOP('',(#39239,#39240,#39241,#39242));
#15927=EDGE_LOOP('',(#39243,#39244,#39245,#39246));
#15928=EDGE_LOOP('',(#39247,#39248,#39249,#39250));
#15929=EDGE_LOOP('',(#39251,#39252,#39253,#39254));
#15930=EDGE_LOOP('',(#39255,#39256,#39257,#39258));
#15931=EDGE_LOOP('',(#39259,#39260,#39261,#39262));
#15932=EDGE_LOOP('',(#39263,#39264,#39265,#39266));
#15933=EDGE_LOOP('',(#39267,#39268,#39269,#39270));
#15934=EDGE_LOOP('',(#39271,#39272,#39273,#39274));
#15935=EDGE_LOOP('',(#39275,#39276,#39277,#39278));
#15936=EDGE_LOOP('',(#39279,#39280,#39281,#39282));
#15937=EDGE_LOOP('',(#39283,#39284,#39285,#39286));
#15938=EDGE_LOOP('',(#39287,#39288,#39289,#39290));
#15939=EDGE_LOOP('',(#39291,#39292,#39293,#39294));
#15940=EDGE_LOOP('',(#39295,#39296,#39297,#39298));
#15941=EDGE_LOOP('',(#39299,#39300,#39301,#39302));
#15942=EDGE_LOOP('',(#39303,#39304,#39305,#39306));
#15943=EDGE_LOOP('',(#39307,#39308,#39309,#39310));
#15944=EDGE_LOOP('',(#39311,#39312,#39313,#39314));
#15945=EDGE_LOOP('',(#39315,#39316,#39317,#39318));
#15946=EDGE_LOOP('',(#39319,#39320,#39321,#39322));
#15947=EDGE_LOOP('',(#39323,#39324,#39325,#39326));
#15948=EDGE_LOOP('',(#39327,#39328,#39329,#39330));
#15949=EDGE_LOOP('',(#39331,#39332,#39333,#39334));
#15950=EDGE_LOOP('',(#39335,#39336,#39337,#39338));
#15951=EDGE_LOOP('',(#39339,#39340,#39341,#39342));
#15952=EDGE_LOOP('',(#39343,#39344,#39345,#39346));
#15953=EDGE_LOOP('',(#39347,#39348,#39349,#39350));
#15954=EDGE_LOOP('',(#39351,#39352,#39353,#39354));
#15955=EDGE_LOOP('',(#39355,#39356,#39357,#39358));
#15956=EDGE_LOOP('',(#39359,#39360,#39361,#39362));
#15957=EDGE_LOOP('',(#39363,#39364,#39365,#39366));
#15958=EDGE_LOOP('',(#39367,#39368,#39369,#39370));
#15959=EDGE_LOOP('',(#39371,#39372,#39373,#39374));
#15960=EDGE_LOOP('',(#39375,#39376,#39377,#39378));
#15961=EDGE_LOOP('',(#39379,#39380,#39381,#39382));
#15962=EDGE_LOOP('',(#39383,#39384,#39385,#39386));
#15963=EDGE_LOOP('',(#39387,#39388,#39389,#39390));
#15964=EDGE_LOOP('',(#39391,#39392,#39393,#39394));
#15965=EDGE_LOOP('',(#39395,#39396,#39397,#39398));
#15966=EDGE_LOOP('',(#39399,#39400,#39401,#39402));
#15967=EDGE_LOOP('',(#39403,#39404,#39405,#39406));
#15968=EDGE_LOOP('',(#39407,#39408,#39409,#39410));
#15969=EDGE_LOOP('',(#39411,#39412,#39413,#39414));
#15970=EDGE_LOOP('',(#39415,#39416,#39417,#39418));
#15971=EDGE_LOOP('',(#39419,#39420,#39421,#39422));
#15972=EDGE_LOOP('',(#39423,#39424,#39425,#39426));
#15973=EDGE_LOOP('',(#39427,#39428,#39429,#39430));
#15974=EDGE_LOOP('',(#39431,#39432,#39433,#39434));
#15975=EDGE_LOOP('',(#39435,#39436,#39437,#39438));
#15976=EDGE_LOOP('',(#39439,#39440,#39441,#39442));
#15977=EDGE_LOOP('',(#39443,#39444,#39445,#39446));
#15978=EDGE_LOOP('',(#39447,#39448,#39449,#39450));
#15979=EDGE_LOOP('',(#39451,#39452,#39453,#39454));
#15980=EDGE_LOOP('',(#39455,#39456,#39457,#39458));
#15981=EDGE_LOOP('',(#39459,#39460,#39461,#39462));
#15982=EDGE_LOOP('',(#39463,#39464,#39465,#39466));
#15983=EDGE_LOOP('',(#39467,#39468,#39469,#39470));
#15984=EDGE_LOOP('',(#39471,#39472,#39473,#39474));
#15985=EDGE_LOOP('',(#39475,#39476,#39477,#39478));
#15986=EDGE_LOOP('',(#39479,#39480,#39481,#39482));
#15987=EDGE_LOOP('',(#39483,#39484,#39485,#39486));
#15988=EDGE_LOOP('',(#39487,#39488,#39489,#39490));
#15989=EDGE_LOOP('',(#39491,#39492,#39493,#39494));
#15990=EDGE_LOOP('',(#39495,#39496,#39497,#39498));
#15991=EDGE_LOOP('',(#39499,#39500,#39501,#39502));
#15992=EDGE_LOOP('',(#39503,#39504,#39505,#39506));
#15993=EDGE_LOOP('',(#39507,#39508,#39509,#39510));
#15994=EDGE_LOOP('',(#39511,#39512,#39513,#39514));
#15995=EDGE_LOOP('',(#39515,#39516,#39517,#39518));
#15996=EDGE_LOOP('',(#39519,#39520,#39521,#39522));
#15997=EDGE_LOOP('',(#39523,#39524,#39525,#39526));
#15998=EDGE_LOOP('',(#39527,#39528,#39529,#39530));
#15999=EDGE_LOOP('',(#39531,#39532,#39533,#39534));
#16000=EDGE_LOOP('',(#39535,#39536,#39537,#39538));
#16001=EDGE_LOOP('',(#39539,#39540,#39541,#39542));
#16002=EDGE_LOOP('',(#39543,#39544,#39545,#39546));
#16003=EDGE_LOOP('',(#39547,#39548,#39549,#39550));
#16004=EDGE_LOOP('',(#39551,#39552,#39553,#39554));
#16005=EDGE_LOOP('',(#39555,#39556,#39557,#39558));
#16006=EDGE_LOOP('',(#39559,#39560,#39561,#39562));
#16007=EDGE_LOOP('',(#39563,#39564,#39565,#39566));
#16008=EDGE_LOOP('',(#39567,#39568,#39569,#39570));
#16009=EDGE_LOOP('',(#39571,#39572,#39573,#39574));
#16010=EDGE_LOOP('',(#39575,#39576,#39577,#39578));
#16011=EDGE_LOOP('',(#39579,#39580,#39581,#39582));
#16012=EDGE_LOOP('',(#39583,#39584,#39585,#39586));
#16013=EDGE_LOOP('',(#39587,#39588,#39589,#39590));
#16014=EDGE_LOOP('',(#39591,#39592,#39593,#39594));
#16015=EDGE_LOOP('',(#39595,#39596,#39597,#39598));
#16016=EDGE_LOOP('',(#39599,#39600,#39601,#39602));
#16017=EDGE_LOOP('',(#39603,#39604,#39605,#39606));
#16018=EDGE_LOOP('',(#39607,#39608,#39609,#39610));
#16019=EDGE_LOOP('',(#39611,#39612,#39613,#39614));
#16020=EDGE_LOOP('',(#39615,#39616,#39617,#39618));
#16021=EDGE_LOOP('',(#39619,#39620,#39621,#39622));
#16022=EDGE_LOOP('',(#39623,#39624,#39625,#39626));
#16023=EDGE_LOOP('',(#39627,#39628,#39629,#39630));
#16024=EDGE_LOOP('',(#39631,#39632,#39633,#39634));
#16025=EDGE_LOOP('',(#39635,#39636,#39637,#39638));
#16026=EDGE_LOOP('',(#39639,#39640,#39641,#39642));
#16027=EDGE_LOOP('',(#39643,#39644,#39645,#39646));
#16028=EDGE_LOOP('',(#39647,#39648,#39649,#39650));
#16029=EDGE_LOOP('',(#39651,#39652,#39653,#39654));
#16030=EDGE_LOOP('',(#39655,#39656,#39657,#39658));
#16031=EDGE_LOOP('',(#39659,#39660,#39661,#39662));
#16032=EDGE_LOOP('',(#39663,#39664,#39665,#39666));
#16033=EDGE_LOOP('',(#39667,#39668,#39669,#39670));
#16034=EDGE_LOOP('',(#39671,#39672,#39673,#39674));
#16035=EDGE_LOOP('',(#39675,#39676,#39677,#39678));
#16036=EDGE_LOOP('',(#39679,#39680,#39681,#39682));
#16037=EDGE_LOOP('',(#39683,#39684,#39685,#39686));
#16038=EDGE_LOOP('',(#39687,#39688,#39689,#39690));
#16039=EDGE_LOOP('',(#39691,#39692,#39693,#39694));
#16040=EDGE_LOOP('',(#39695,#39696,#39697,#39698));
#16041=EDGE_LOOP('',(#39699,#39700,#39701,#39702));
#16042=EDGE_LOOP('',(#39703,#39704,#39705,#39706));
#16043=EDGE_LOOP('',(#39707,#39708,#39709,#39710));
#16044=EDGE_LOOP('',(#39711,#39712,#39713,#39714));
#16045=EDGE_LOOP('',(#39715,#39716,#39717,#39718));
#16046=EDGE_LOOP('',(#39719,#39720,#39721,#39722));
#16047=EDGE_LOOP('',(#39723,#39724,#39725,#39726));
#16048=EDGE_LOOP('',(#39727,#39728,#39729,#39730));
#16049=EDGE_LOOP('',(#39731,#39732,#39733,#39734));
#16050=EDGE_LOOP('',(#39735,#39736,#39737,#39738));
#16051=EDGE_LOOP('',(#39739,#39740,#39741,#39742));
#16052=EDGE_LOOP('',(#39743,#39744,#39745,#39746));
#16053=EDGE_LOOP('',(#39747,#39748,#39749,#39750));
#16054=EDGE_LOOP('',(#39751,#39752,#39753,#39754));
#16055=EDGE_LOOP('',(#39755,#39756,#39757,#39758));
#16056=EDGE_LOOP('',(#39759,#39760,#39761,#39762));
#16057=EDGE_LOOP('',(#39763,#39764,#39765,#39766));
#16058=EDGE_LOOP('',(#39767,#39768,#39769,#39770));
#16059=EDGE_LOOP('',(#39771,#39772,#39773,#39774));
#16060=EDGE_LOOP('',(#39775,#39776,#39777,#39778));
#16061=EDGE_LOOP('',(#39779,#39780,#39781,#39782));
#16062=EDGE_LOOP('',(#39783,#39784,#39785,#39786));
#16063=EDGE_LOOP('',(#39787,#39788,#39789,#39790));
#16064=EDGE_LOOP('',(#39791,#39792,#39793,#39794));
#16065=EDGE_LOOP('',(#39795,#39796,#39797,#39798));
#16066=EDGE_LOOP('',(#39799,#39800,#39801,#39802));
#16067=EDGE_LOOP('',(#39803,#39804,#39805,#39806));
#16068=EDGE_LOOP('',(#39807,#39808,#39809,#39810));
#16069=EDGE_LOOP('',(#39811,#39812,#39813,#39814));
#16070=EDGE_LOOP('',(#39815,#39816,#39817,#39818));
#16071=EDGE_LOOP('',(#39819,#39820,#39821,#39822));
#16072=EDGE_LOOP('',(#39823,#39824,#39825,#39826));
#16073=EDGE_LOOP('',(#39827,#39828,#39829,#39830));
#16074=EDGE_LOOP('',(#39831,#39832,#39833,#39834));
#16075=EDGE_LOOP('',(#39835,#39836,#39837,#39838));
#16076=EDGE_LOOP('',(#39839,#39840,#39841,#39842));
#16077=EDGE_LOOP('',(#39843,#39844,#39845,#39846));
#16078=EDGE_LOOP('',(#39847,#39848,#39849,#39850));
#16079=EDGE_LOOP('',(#39851,#39852,#39853,#39854));
#16080=EDGE_LOOP('',(#39855,#39856,#39857,#39858));
#16081=EDGE_LOOP('',(#39859,#39860,#39861,#39862));
#16082=EDGE_LOOP('',(#39863,#39864,#39865,#39866));
#16083=EDGE_LOOP('',(#39867,#39868,#39869,#39870));
#16084=EDGE_LOOP('',(#39871,#39872,#39873,#39874));
#16085=EDGE_LOOP('',(#39875,#39876,#39877,#39878));
#16086=EDGE_LOOP('',(#39879,#39880,#39881,#39882));
#16087=EDGE_LOOP('',(#39883,#39884,#39885,#39886));
#16088=EDGE_LOOP('',(#39887,#39888,#39889,#39890));
#16089=EDGE_LOOP('',(#39891,#39892,#39893,#39894));
#16090=EDGE_LOOP('',(#39895,#39896,#39897,#39898));
#16091=EDGE_LOOP('',(#39899,#39900,#39901,#39902));
#16092=EDGE_LOOP('',(#39903,#39904,#39905,#39906));
#16093=EDGE_LOOP('',(#39907,#39908,#39909,#39910));
#16094=EDGE_LOOP('',(#39911,#39912,#39913,#39914));
#16095=EDGE_LOOP('',(#39915,#39916,#39917,#39918));
#16096=EDGE_LOOP('',(#39919,#39920,#39921,#39922));
#16097=EDGE_LOOP('',(#39923,#39924,#39925,#39926));
#16098=EDGE_LOOP('',(#39927,#39928,#39929,#39930));
#16099=EDGE_LOOP('',(#39931,#39932,#39933,#39934));
#16100=EDGE_LOOP('',(#39935,#39936,#39937,#39938));
#16101=EDGE_LOOP('',(#39939,#39940,#39941,#39942));
#16102=EDGE_LOOP('',(#39943,#39944,#39945,#39946));
#16103=EDGE_LOOP('',(#39947,#39948,#39949,#39950));
#16104=EDGE_LOOP('',(#39951,#39952,#39953,#39954));
#16105=EDGE_LOOP('',(#39955,#39956,#39957,#39958));
#16106=EDGE_LOOP('',(#39959,#39960,#39961,#39962));
#16107=EDGE_LOOP('',(#39963,#39964,#39965,#39966));
#16108=EDGE_LOOP('',(#39967,#39968,#39969,#39970));
#16109=EDGE_LOOP('',(#39971,#39972,#39973,#39974));
#16110=EDGE_LOOP('',(#39975,#39976,#39977,#39978));
#16111=EDGE_LOOP('',(#39979,#39980,#39981,#39982));
#16112=EDGE_LOOP('',(#39983,#39984,#39985,#39986));
#16113=EDGE_LOOP('',(#39987,#39988,#39989,#39990));
#16114=EDGE_LOOP('',(#39991,#39992,#39993,#39994));
#16115=EDGE_LOOP('',(#39995,#39996,#39997,#39998));
#16116=EDGE_LOOP('',(#39999,#40000,#40001,#40002));
#16117=EDGE_LOOP('',(#40003,#40004,#40005,#40006));
#16118=EDGE_LOOP('',(#40007,#40008,#40009,#40010));
#16119=EDGE_LOOP('',(#40011,#40012,#40013,#40014));
#16120=EDGE_LOOP('',(#40015,#40016,#40017,#40018));
#16121=EDGE_LOOP('',(#40019,#40020,#40021,#40022));
#16122=EDGE_LOOP('',(#40023,#40024,#40025,#40026));
#16123=EDGE_LOOP('',(#40027,#40028,#40029,#40030));
#16124=EDGE_LOOP('',(#40031,#40032,#40033,#40034));
#16125=EDGE_LOOP('',(#40035,#40036,#40037,#40038));
#16126=EDGE_LOOP('',(#40039,#40040,#40041,#40042));
#16127=EDGE_LOOP('',(#40043,#40044,#40045,#40046));
#16128=EDGE_LOOP('',(#40047,#40048,#40049,#40050));
#16129=EDGE_LOOP('',(#40051,#40052,#40053,#40054));
#16130=EDGE_LOOP('',(#40055,#40056,#40057,#40058));
#16131=EDGE_LOOP('',(#40059,#40060,#40061,#40062));
#16132=EDGE_LOOP('',(#40063,#40064,#40065,#40066));
#16133=EDGE_LOOP('',(#40067,#40068,#40069,#40070));
#16134=EDGE_LOOP('',(#40071,#40072,#40073,#40074));
#16135=EDGE_LOOP('',(#40075,#40076,#40077,#40078));
#16136=EDGE_LOOP('',(#40079,#40080,#40081,#40082));
#16137=EDGE_LOOP('',(#40083,#40084,#40085,#40086));
#16138=EDGE_LOOP('',(#40087,#40088,#40089,#40090));
#16139=EDGE_LOOP('',(#40091,#40092,#40093,#40094));
#16140=EDGE_LOOP('',(#40095,#40096,#40097,#40098));
#16141=EDGE_LOOP('',(#40099,#40100,#40101,#40102));
#16142=EDGE_LOOP('',(#40103,#40104,#40105,#40106));
#16143=EDGE_LOOP('',(#40107,#40108,#40109,#40110));
#16144=EDGE_LOOP('',(#40111,#40112,#40113,#40114));
#16145=EDGE_LOOP('',(#40115,#40116,#40117,#40118));
#16146=EDGE_LOOP('',(#40119,#40120,#40121,#40122));
#16147=EDGE_LOOP('',(#40123,#40124,#40125,#40126));
#16148=EDGE_LOOP('',(#40127,#40128,#40129,#40130));
#16149=EDGE_LOOP('',(#40131,#40132,#40133,#40134));
#16150=EDGE_LOOP('',(#40135,#40136,#40137,#40138));
#16151=EDGE_LOOP('',(#40139,#40140,#40141,#40142));
#16152=EDGE_LOOP('',(#40143,#40144,#40145,#40146));
#16153=EDGE_LOOP('',(#40147,#40148,#40149,#40150));
#16154=EDGE_LOOP('',(#40151,#40152,#40153,#40154));
#16155=EDGE_LOOP('',(#40155,#40156,#40157,#40158));
#16156=EDGE_LOOP('',(#40159,#40160,#40161,#40162));
#16157=EDGE_LOOP('',(#40163,#40164,#40165,#40166));
#16158=EDGE_LOOP('',(#40167,#40168,#40169,#40170));
#16159=EDGE_LOOP('',(#40171,#40172,#40173,#40174));
#16160=EDGE_LOOP('',(#40175,#40176,#40177,#40178));
#16161=EDGE_LOOP('',(#40179,#40180,#40181,#40182));
#16162=EDGE_LOOP('',(#40183,#40184,#40185,#40186));
#16163=EDGE_LOOP('',(#40187,#40188,#40189,#40190));
#16164=EDGE_LOOP('',(#40191,#40192,#40193,#40194));
#16165=EDGE_LOOP('',(#40195,#40196,#40197,#40198));
#16166=EDGE_LOOP('',(#40199,#40200,#40201,#40202));
#16167=EDGE_LOOP('',(#40203,#40204,#40205,#40206));
#16168=EDGE_LOOP('',(#40207,#40208,#40209,#40210));
#16169=EDGE_LOOP('',(#40211,#40212,#40213,#40214));
#16170=EDGE_LOOP('',(#40215,#40216,#40217,#40218));
#16171=EDGE_LOOP('',(#40219,#40220,#40221,#40222));
#16172=EDGE_LOOP('',(#40223,#40224,#40225,#40226));
#16173=EDGE_LOOP('',(#40227,#40228,#40229,#40230));
#16174=EDGE_LOOP('',(#40231,#40232,#40233,#40234));
#16175=EDGE_LOOP('',(#40235,#40236,#40237,#40238));
#16176=EDGE_LOOP('',(#40239,#40240,#40241,#40242));
#16177=EDGE_LOOP('',(#40243,#40244,#40245,#40246,#40247));
#16178=EDGE_LOOP('',(#40248,#40249,#40250,#40251));
#16179=EDGE_LOOP('',(#40252,#40253,#40254,#40255,#40256));
#16180=EDGE_LOOP('',(#40257,#40258,#40259,#40260));
#16181=EDGE_LOOP('',(#40261,#40262,#40263,#40264,#40265));
#16182=EDGE_LOOP('',(#40266));
#16183=EDGE_LOOP('',(#40267));
#16184=EDGE_LOOP('',(#40268,#40269,#40270,#40271));
#16185=EDGE_LOOP('',(#40272,#40273,#40274,#40275));
#16186=EDGE_LOOP('',(#40276,#40277,#40278,#40279));
#16187=EDGE_LOOP('',(#40280,#40281,#40282,#40283));
#16188=EDGE_LOOP('',(#40284,#40285,#40286,#40287,#40288));
#16189=EDGE_LOOP('',(#40289,#40290,#40291,#40292,#40293));
#16190=EDGE_LOOP('',(#40294,#40295,#40296,#40297,#40298));
#16191=EDGE_LOOP('',(#40299,#40300,#40301,#40302,#40303));
#16192=EDGE_LOOP('',(#40304));
#16193=EDGE_LOOP('',(#40305,#40306));
#16194=EDGE_LOOP('',(#40307));
#16195=EDGE_LOOP('',(#40308));
#16196=EDGE_LOOP('',(#40309));
#16197=EDGE_LOOP('',(#40310));
#16198=EDGE_LOOP('',(#40311));
#16199=EDGE_LOOP('',(#40312));
#16200=EDGE_LOOP('',(#40313));
#16201=EDGE_LOOP('',(#40314));
#16202=EDGE_LOOP('',(#40315));
#16203=EDGE_LOOP('',(#40316));
#16204=EDGE_LOOP('',(#40317,#40318));
#16205=EDGE_LOOP('',(#40319));
#16206=EDGE_LOOP('',(#40320));
#16207=EDGE_LOOP('',(#40321));
#16208=EDGE_LOOP('',(#40322));
#16209=EDGE_LOOP('',(#40323));
#16210=EDGE_LOOP('',(#40324));
#16211=EDGE_LOOP('',(#40325));
#16212=EDGE_LOOP('',(#40326));
#16213=EDGE_LOOP('',(#40327));
#16214=EDGE_LOOP('',(#40328));
#16215=EDGE_LOOP('',(#40329));
#16216=EDGE_LOOP('',(#40330));
#16217=EDGE_LOOP('',(#40331));
#16218=EDGE_LOOP('',(#40332));
#16219=EDGE_LOOP('',(#40333));
#16220=EDGE_LOOP('',(#40334));
#16221=EDGE_LOOP('',(#40335));
#16222=EDGE_LOOP('',(#40336));
#16223=EDGE_LOOP('',(#40337));
#16224=EDGE_LOOP('',(#40338));
#16225=EDGE_LOOP('',(#40339));
#16226=EDGE_LOOP('',(#40340));
#16227=EDGE_LOOP('',(#40341));
#16228=EDGE_LOOP('',(#40342));
#16229=EDGE_LOOP('',(#40343));
#16230=EDGE_LOOP('',(#40344));
#16231=EDGE_LOOP('',(#40345));
#16232=EDGE_LOOP('',(#40346));
#16233=EDGE_LOOP('',(#40347));
#16234=EDGE_LOOP('',(#40348));
#16235=EDGE_LOOP('',(#40349));
#16236=EDGE_LOOP('',(#40350));
#16237=EDGE_LOOP('',(#40351));
#16238=EDGE_LOOP('',(#40352));
#16239=EDGE_LOOP('',(#40353));
#16240=EDGE_LOOP('',(#40354));
#16241=EDGE_LOOP('',(#40355));
#16242=EDGE_LOOP('',(#40356));
#16243=EDGE_LOOP('',(#40357));
#16244=EDGE_LOOP('',(#40358));
#16245=EDGE_LOOP('',(#40359));
#16246=EDGE_LOOP('',(#40360));
#16247=EDGE_LOOP('',(#40361));
#16248=EDGE_LOOP('',(#40362));
#16249=EDGE_LOOP('',(#40363));
#16250=EDGE_LOOP('',(#40364));
#16251=EDGE_LOOP('',(#40365));
#16252=EDGE_LOOP('',(#40366));
#16253=EDGE_LOOP('',(#40367));
#16254=EDGE_LOOP('',(#40368));
#16255=EDGE_LOOP('',(#40369));
#16256=EDGE_LOOP('',(#40370));
#16257=EDGE_LOOP('',(#40371));
#16258=EDGE_LOOP('',(#40372));
#16259=EDGE_LOOP('',(#40373));
#16260=EDGE_LOOP('',(#40374));
#16261=EDGE_LOOP('',(#40375));
#16262=EDGE_LOOP('',(#40376));
#16263=EDGE_LOOP('',(#40377));
#16264=EDGE_LOOP('',(#40378));
#16265=EDGE_LOOP('',(#40379));
#16266=EDGE_LOOP('',(#40380));
#16267=EDGE_LOOP('',(#40381));
#16268=EDGE_LOOP('',(#40382));
#16269=EDGE_LOOP('',(#40383));
#16270=EDGE_LOOP('',(#40384));
#16271=EDGE_LOOP('',(#40385));
#16272=EDGE_LOOP('',(#40386));
#16273=EDGE_LOOP('',(#40387));
#16274=EDGE_LOOP('',(#40388));
#16275=EDGE_LOOP('',(#40389));
#16276=EDGE_LOOP('',(#40390));
#16277=EDGE_LOOP('',(#40391));
#16278=EDGE_LOOP('',(#40392));
#16279=EDGE_LOOP('',(#40393));
#16280=EDGE_LOOP('',(#40394));
#16281=EDGE_LOOP('',(#40395));
#16282=EDGE_LOOP('',(#40396));
#16283=EDGE_LOOP('',(#40397));
#16284=EDGE_LOOP('',(#40398));
#16285=EDGE_LOOP('',(#40399));
#16286=EDGE_LOOP('',(#40400));
#16287=EDGE_LOOP('',(#40401));
#16288=EDGE_LOOP('',(#40402));
#16289=EDGE_LOOP('',(#40403));
#16290=EDGE_LOOP('',(#40404));
#16291=EDGE_LOOP('',(#40405));
#16292=EDGE_LOOP('',(#40406));
#16293=EDGE_LOOP('',(#40407));
#16294=EDGE_LOOP('',(#40408));
#16295=EDGE_LOOP('',(#40409));
#16296=EDGE_LOOP('',(#40410));
#16297=EDGE_LOOP('',(#40411));
#16298=EDGE_LOOP('',(#40412));
#16299=EDGE_LOOP('',(#40413));
#16300=EDGE_LOOP('',(#40414));
#16301=EDGE_LOOP('',(#40415));
#16302=EDGE_LOOP('',(#40416));
#16303=EDGE_LOOP('',(#40417));
#16304=EDGE_LOOP('',(#40418));
#16305=EDGE_LOOP('',(#40419));
#16306=EDGE_LOOP('',(#40420));
#16307=EDGE_LOOP('',(#40421));
#16308=EDGE_LOOP('',(#40422));
#16309=EDGE_LOOP('',(#40423));
#16310=EDGE_LOOP('',(#40424));
#16311=EDGE_LOOP('',(#40425));
#16312=EDGE_LOOP('',(#40426));
#16313=EDGE_LOOP('',(#40427));
#16314=EDGE_LOOP('',(#40428));
#16315=EDGE_LOOP('',(#40429));
#16316=EDGE_LOOP('',(#40430));
#16317=EDGE_LOOP('',(#40431));
#16318=EDGE_LOOP('',(#40432));
#16319=EDGE_LOOP('',(#40433));
#16320=EDGE_LOOP('',(#40434));
#16321=EDGE_LOOP('',(#40435));
#16322=EDGE_LOOP('',(#40436));
#16323=EDGE_LOOP('',(#40437));
#16324=EDGE_LOOP('',(#40438));
#16325=EDGE_LOOP('',(#40439));
#16326=EDGE_LOOP('',(#40440));
#16327=EDGE_LOOP('',(#40441));
#16328=EDGE_LOOP('',(#40442));
#16329=EDGE_LOOP('',(#40443));
#16330=EDGE_LOOP('',(#40444));
#16331=EDGE_LOOP('',(#40445));
#16332=EDGE_LOOP('',(#40446));
#16333=EDGE_LOOP('',(#40447));
#16334=EDGE_LOOP('',(#40448));
#16335=EDGE_LOOP('',(#40449));
#16336=EDGE_LOOP('',(#40450));
#16337=EDGE_LOOP('',(#40451));
#16338=EDGE_LOOP('',(#40452));
#16339=EDGE_LOOP('',(#40453));
#16340=EDGE_LOOP('',(#40454));
#16341=EDGE_LOOP('',(#40455));
#16342=EDGE_LOOP('',(#40456));
#16343=EDGE_LOOP('',(#40457));
#16344=EDGE_LOOP('',(#40458));
#16345=EDGE_LOOP('',(#40459));
#16346=EDGE_LOOP('',(#40460));
#16347=EDGE_LOOP('',(#40461));
#16348=EDGE_LOOP('',(#40462));
#16349=EDGE_LOOP('',(#40463));
#16350=EDGE_LOOP('',(#40464));
#16351=EDGE_LOOP('',(#40465));
#16352=EDGE_LOOP('',(#40466));
#16353=EDGE_LOOP('',(#40467));
#16354=EDGE_LOOP('',(#40468));
#16355=EDGE_LOOP('',(#40469));
#16356=EDGE_LOOP('',(#40470));
#16357=EDGE_LOOP('',(#40471));
#16358=EDGE_LOOP('',(#40472));
#16359=EDGE_LOOP('',(#40473));
#16360=EDGE_LOOP('',(#40474));
#16361=EDGE_LOOP('',(#40475));
#16362=EDGE_LOOP('',(#40476));
#16363=EDGE_LOOP('',(#40477));
#16364=EDGE_LOOP('',(#40478));
#16365=EDGE_LOOP('',(#40479));
#16366=EDGE_LOOP('',(#40480));
#16367=EDGE_LOOP('',(#40481));
#16368=EDGE_LOOP('',(#40482));
#16369=EDGE_LOOP('',(#40483));
#16370=EDGE_LOOP('',(#40484));
#16371=EDGE_LOOP('',(#40485));
#16372=EDGE_LOOP('',(#40486));
#16373=EDGE_LOOP('',(#40487));
#16374=EDGE_LOOP('',(#40488));
#16375=EDGE_LOOP('',(#40489));
#16376=EDGE_LOOP('',(#40490));
#16377=EDGE_LOOP('',(#40491));
#16378=EDGE_LOOP('',(#40492));
#16379=EDGE_LOOP('',(#40493));
#16380=EDGE_LOOP('',(#40494));
#16381=EDGE_LOOP('',(#40495));
#16382=EDGE_LOOP('',(#40496));
#16383=EDGE_LOOP('',(#40497));
#16384=EDGE_LOOP('',(#40498));
#16385=EDGE_LOOP('',(#40499));
#16386=EDGE_LOOP('',(#40500));
#16387=EDGE_LOOP('',(#40501));
#16388=EDGE_LOOP('',(#40502));
#16389=EDGE_LOOP('',(#40503));
#16390=EDGE_LOOP('',(#40504));
#16391=EDGE_LOOP('',(#40505));
#16392=EDGE_LOOP('',(#40506));
#16393=EDGE_LOOP('',(#40507));
#16394=EDGE_LOOP('',(#40508));
#16395=EDGE_LOOP('',(#40509));
#16396=EDGE_LOOP('',(#40510));
#16397=EDGE_LOOP('',(#40511));
#16398=EDGE_LOOP('',(#40512));
#16399=EDGE_LOOP('',(#40513));
#16400=EDGE_LOOP('',(#40514));
#16401=EDGE_LOOP('',(#40515));
#16402=EDGE_LOOP('',(#40516));
#16403=EDGE_LOOP('',(#40517));
#16404=EDGE_LOOP('',(#40518));
#16405=EDGE_LOOP('',(#40519));
#16406=EDGE_LOOP('',(#40520));
#16407=EDGE_LOOP('',(#40521));
#16408=EDGE_LOOP('',(#40522));
#16409=EDGE_LOOP('',(#40523));
#16410=EDGE_LOOP('',(#40524));
#16411=EDGE_LOOP('',(#40525));
#16412=EDGE_LOOP('',(#40526));
#16413=EDGE_LOOP('',(#40527));
#16414=EDGE_LOOP('',(#40528));
#16415=EDGE_LOOP('',(#40529));
#16416=EDGE_LOOP('',(#40530));
#16417=EDGE_LOOP('',(#40531));
#16418=EDGE_LOOP('',(#40532));
#16419=EDGE_LOOP('',(#40533));
#16420=EDGE_LOOP('',(#40534));
#16421=EDGE_LOOP('',(#40535));
#16422=EDGE_LOOP('',(#40536));
#16423=EDGE_LOOP('',(#40537));
#16424=EDGE_LOOP('',(#40538));
#16425=EDGE_LOOP('',(#40539));
#16426=EDGE_LOOP('',(#40540));
#16427=EDGE_LOOP('',(#40541));
#16428=EDGE_LOOP('',(#40542));
#16429=EDGE_LOOP('',(#40543));
#16430=EDGE_LOOP('',(#40544));
#16431=EDGE_LOOP('',(#40545));
#16432=EDGE_LOOP('',(#40546));
#16433=EDGE_LOOP('',(#40547));
#16434=EDGE_LOOP('',(#40548));
#16435=EDGE_LOOP('',(#40549));
#16436=EDGE_LOOP('',(#40550));
#16437=EDGE_LOOP('',(#40551));
#16438=EDGE_LOOP('',(#40552));
#16439=EDGE_LOOP('',(#40553));
#16440=EDGE_LOOP('',(#40554));
#16441=EDGE_LOOP('',(#40555));
#16442=EDGE_LOOP('',(#40556));
#16443=EDGE_LOOP('',(#40557));
#16444=EDGE_LOOP('',(#40558));
#16445=EDGE_LOOP('',(#40559));
#16446=EDGE_LOOP('',(#40560));
#16447=EDGE_LOOP('',(#40561));
#16448=EDGE_LOOP('',(#40562));
#16449=EDGE_LOOP('',(#40563));
#16450=EDGE_LOOP('',(#40564));
#16451=EDGE_LOOP('',(#40565));
#16452=EDGE_LOOP('',(#40566));
#16453=EDGE_LOOP('',(#40567));
#16454=EDGE_LOOP('',(#40568));
#16455=EDGE_LOOP('',(#40569));
#16456=EDGE_LOOP('',(#40570));
#16457=EDGE_LOOP('',(#40571));
#16458=EDGE_LOOP('',(#40572));
#16459=EDGE_LOOP('',(#40573));
#16460=EDGE_LOOP('',(#40574));
#16461=EDGE_LOOP('',(#40575));
#16462=EDGE_LOOP('',(#40576));
#16463=EDGE_LOOP('',(#40577));
#16464=EDGE_LOOP('',(#40578));
#16465=EDGE_LOOP('',(#40579));
#16466=EDGE_LOOP('',(#40580));
#16467=EDGE_LOOP('',(#40581));
#16468=EDGE_LOOP('',(#40582));
#16469=EDGE_LOOP('',(#40583));
#16470=EDGE_LOOP('',(#40584));
#16471=EDGE_LOOP('',(#40585));
#16472=EDGE_LOOP('',(#40586));
#16473=EDGE_LOOP('',(#40587));
#16474=EDGE_LOOP('',(#40588));
#16475=EDGE_LOOP('',(#40589,#40590,#40591,#40592));
#16476=EDGE_LOOP('',(#40593));
#16477=EDGE_LOOP('',(#40594));
#16478=EDGE_LOOP('',(#40595));
#16479=EDGE_LOOP('',(#40596));
#16480=EDGE_LOOP('',(#40597));
#16481=EDGE_LOOP('',(#40598));
#16482=EDGE_LOOP('',(#40599));
#16483=EDGE_LOOP('',(#40600));
#16484=EDGE_LOOP('',(#40601));
#16485=EDGE_LOOP('',(#40602));
#16486=EDGE_LOOP('',(#40603));
#16487=EDGE_LOOP('',(#40604));
#16488=EDGE_LOOP('',(#40605));
#16489=EDGE_LOOP('',(#40606));
#16490=EDGE_LOOP('',(#40607));
#16491=EDGE_LOOP('',(#40608));
#16492=EDGE_LOOP('',(#40609));
#16493=EDGE_LOOP('',(#40610));
#16494=EDGE_LOOP('',(#40611));
#16495=EDGE_LOOP('',(#40612));
#16496=EDGE_LOOP('',(#40613));
#16497=EDGE_LOOP('',(#40614));
#16498=EDGE_LOOP('',(#40615));
#16499=EDGE_LOOP('',(#40616));
#16500=EDGE_LOOP('',(#40617));
#16501=EDGE_LOOP('',(#40618));
#16502=EDGE_LOOP('',(#40619));
#16503=EDGE_LOOP('',(#40620));
#16504=EDGE_LOOP('',(#40621));
#16505=EDGE_LOOP('',(#40622));
#16506=EDGE_LOOP('',(#40623));
#16507=EDGE_LOOP('',(#40624));
#16508=EDGE_LOOP('',(#40625));
#16509=EDGE_LOOP('',(#40626));
#16510=EDGE_LOOP('',(#40627));
#16511=EDGE_LOOP('',(#40628));
#16512=EDGE_LOOP('',(#40629));
#16513=EDGE_LOOP('',(#40630));
#16514=EDGE_LOOP('',(#40631));
#16515=EDGE_LOOP('',(#40632));
#16516=EDGE_LOOP('',(#40633));
#16517=EDGE_LOOP('',(#40634));
#16518=EDGE_LOOP('',(#40635));
#16519=EDGE_LOOP('',(#40636));
#16520=EDGE_LOOP('',(#40637,#40638));
#16521=EDGE_LOOP('',(#40639));
#16522=EDGE_LOOP('',(#40640));
#16523=EDGE_LOOP('',(#40641));
#16524=EDGE_LOOP('',(#40642));
#16525=EDGE_LOOP('',(#40643));
#16526=EDGE_LOOP('',(#40644));
#16527=EDGE_LOOP('',(#40645));
#16528=EDGE_LOOP('',(#40646));
#16529=EDGE_LOOP('',(#40647));
#16530=EDGE_LOOP('',(#40648));
#16531=EDGE_LOOP('',(#40649));
#16532=EDGE_LOOP('',(#40650));
#16533=EDGE_LOOP('',(#40651));
#16534=EDGE_LOOP('',(#40652));
#16535=EDGE_LOOP('',(#40653));
#16536=EDGE_LOOP('',(#40654));
#16537=EDGE_LOOP('',(#40655));
#16538=EDGE_LOOP('',(#40656));
#16539=EDGE_LOOP('',(#40657));
#16540=EDGE_LOOP('',(#40658));
#16541=EDGE_LOOP('',(#40659));
#16542=EDGE_LOOP('',(#40660));
#16543=EDGE_LOOP('',(#40661));
#16544=EDGE_LOOP('',(#40662));
#16545=EDGE_LOOP('',(#40663));
#16546=EDGE_LOOP('',(#40664));
#16547=EDGE_LOOP('',(#40665));
#16548=EDGE_LOOP('',(#40666));
#16549=EDGE_LOOP('',(#40667));
#16550=EDGE_LOOP('',(#40668));
#16551=EDGE_LOOP('',(#40669));
#16552=EDGE_LOOP('',(#40670));
#16553=EDGE_LOOP('',(#40671));
#16554=EDGE_LOOP('',(#40672));
#16555=EDGE_LOOP('',(#40673));
#16556=EDGE_LOOP('',(#40674));
#16557=EDGE_LOOP('',(#40675));
#16558=EDGE_LOOP('',(#40676));
#16559=EDGE_LOOP('',(#40677));
#16560=EDGE_LOOP('',(#40678));
#16561=EDGE_LOOP('',(#40679));
#16562=EDGE_LOOP('',(#40680));
#16563=EDGE_LOOP('',(#40681));
#16564=EDGE_LOOP('',(#40682));
#16565=EDGE_LOOP('',(#40683));
#16566=EDGE_LOOP('',(#40684));
#16567=EDGE_LOOP('',(#40685));
#16568=EDGE_LOOP('',(#40686));
#16569=EDGE_LOOP('',(#40687));
#16570=EDGE_LOOP('',(#40688));
#16571=EDGE_LOOP('',(#40689));
#16572=EDGE_LOOP('',(#40690));
#16573=EDGE_LOOP('',(#40691));
#16574=EDGE_LOOP('',(#40692));
#16575=EDGE_LOOP('',(#40693));
#16576=EDGE_LOOP('',(#40694));
#16577=EDGE_LOOP('',(#40695));
#16578=EDGE_LOOP('',(#40696));
#16579=EDGE_LOOP('',(#40697));
#16580=EDGE_LOOP('',(#40698));
#16581=EDGE_LOOP('',(#40699));
#16582=EDGE_LOOP('',(#40700));
#16583=EDGE_LOOP('',(#40701));
#16584=EDGE_LOOP('',(#40702));
#16585=EDGE_LOOP('',(#40703));
#16586=EDGE_LOOP('',(#40704));
#16587=EDGE_LOOP('',(#40705));
#16588=EDGE_LOOP('',(#40706));
#16589=EDGE_LOOP('',(#40707));
#16590=EDGE_LOOP('',(#40708));
#16591=EDGE_LOOP('',(#40709));
#16592=EDGE_LOOP('',(#40710));
#16593=EDGE_LOOP('',(#40711));
#16594=EDGE_LOOP('',(#40712));
#16595=EDGE_LOOP('',(#40713));
#16596=EDGE_LOOP('',(#40714));
#16597=EDGE_LOOP('',(#40715));
#16598=EDGE_LOOP('',(#40716));
#16599=EDGE_LOOP('',(#40717));
#16600=EDGE_LOOP('',(#40718));
#16601=EDGE_LOOP('',(#40719));
#16602=EDGE_LOOP('',(#40720));
#16603=EDGE_LOOP('',(#40721));
#16604=EDGE_LOOP('',(#40722));
#16605=EDGE_LOOP('',(#40723));
#16606=EDGE_LOOP('',(#40724));
#16607=EDGE_LOOP('',(#40725));
#16608=EDGE_LOOP('',(#40726));
#16609=EDGE_LOOP('',(#40727));
#16610=EDGE_LOOP('',(#40728));
#16611=EDGE_LOOP('',(#40729));
#16612=EDGE_LOOP('',(#40730));
#16613=EDGE_LOOP('',(#40731));
#16614=EDGE_LOOP('',(#40732));
#16615=EDGE_LOOP('',(#40733));
#16616=EDGE_LOOP('',(#40734));
#16617=EDGE_LOOP('',(#40735));
#16618=EDGE_LOOP('',(#40736));
#16619=EDGE_LOOP('',(#40737));
#16620=EDGE_LOOP('',(#40738));
#16621=EDGE_LOOP('',(#40739));
#16622=EDGE_LOOP('',(#40740));
#16623=EDGE_LOOP('',(#40741));
#16624=EDGE_LOOP('',(#40742));
#16625=EDGE_LOOP('',(#40743));
#16626=EDGE_LOOP('',(#40744));
#16627=EDGE_LOOP('',(#40745));
#16628=EDGE_LOOP('',(#40746));
#16629=EDGE_LOOP('',(#40747));
#16630=EDGE_LOOP('',(#40748));
#16631=EDGE_LOOP('',(#40749));
#16632=EDGE_LOOP('',(#40750));
#16633=EDGE_LOOP('',(#40751));
#16634=EDGE_LOOP('',(#40752));
#16635=EDGE_LOOP('',(#40753));
#16636=EDGE_LOOP('',(#40754));
#16637=EDGE_LOOP('',(#40755));
#16638=EDGE_LOOP('',(#40756));
#16639=EDGE_LOOP('',(#40757));
#16640=EDGE_LOOP('',(#40758));
#16641=EDGE_LOOP('',(#40759));
#16642=EDGE_LOOP('',(#40760));
#16643=EDGE_LOOP('',(#40761));
#16644=EDGE_LOOP('',(#40762));
#16645=EDGE_LOOP('',(#40763));
#16646=EDGE_LOOP('',(#40764));
#16647=EDGE_LOOP('',(#40765));
#16648=EDGE_LOOP('',(#40766));
#16649=EDGE_LOOP('',(#40767));
#16650=EDGE_LOOP('',(#40768));
#16651=EDGE_LOOP('',(#40769));
#16652=EDGE_LOOP('',(#40770));
#16653=EDGE_LOOP('',(#40771));
#16654=EDGE_LOOP('',(#40772));
#16655=EDGE_LOOP('',(#40773));
#16656=EDGE_LOOP('',(#40774));
#16657=EDGE_LOOP('',(#40775));
#16658=EDGE_LOOP('',(#40776));
#16659=EDGE_LOOP('',(#40777));
#16660=EDGE_LOOP('',(#40778));
#16661=EDGE_LOOP('',(#40779));
#16662=EDGE_LOOP('',(#40780));
#16663=EDGE_LOOP('',(#40781));
#16664=EDGE_LOOP('',(#40782));
#16665=EDGE_LOOP('',(#40783));
#16666=EDGE_LOOP('',(#40784));
#16667=EDGE_LOOP('',(#40785));
#16668=EDGE_LOOP('',(#40786));
#16669=EDGE_LOOP('',(#40787));
#16670=EDGE_LOOP('',(#40788));
#16671=EDGE_LOOP('',(#40789));
#16672=EDGE_LOOP('',(#40790));
#16673=EDGE_LOOP('',(#40791));
#16674=EDGE_LOOP('',(#40792));
#16675=EDGE_LOOP('',(#40793));
#16676=EDGE_LOOP('',(#40794));
#16677=EDGE_LOOP('',(#40795));
#16678=EDGE_LOOP('',(#40796));
#16679=EDGE_LOOP('',(#40797));
#16680=EDGE_LOOP('',(#40798));
#16681=EDGE_LOOP('',(#40799));
#16682=EDGE_LOOP('',(#40800));
#16683=EDGE_LOOP('',(#40801));
#16684=EDGE_LOOP('',(#40802));
#16685=EDGE_LOOP('',(#40803));
#16686=EDGE_LOOP('',(#40804));
#16687=EDGE_LOOP('',(#40805));
#16688=EDGE_LOOP('',(#40806));
#16689=EDGE_LOOP('',(#40807));
#16690=EDGE_LOOP('',(#40808));
#16691=EDGE_LOOP('',(#40809));
#16692=EDGE_LOOP('',(#40810));
#16693=EDGE_LOOP('',(#40811));
#16694=EDGE_LOOP('',(#40812));
#16695=EDGE_LOOP('',(#40813));
#16696=EDGE_LOOP('',(#40814));
#16697=EDGE_LOOP('',(#40815));
#16698=EDGE_LOOP('',(#40816));
#16699=EDGE_LOOP('',(#40817));
#16700=EDGE_LOOP('',(#40818));
#16701=EDGE_LOOP('',(#40819));
#16702=EDGE_LOOP('',(#40820));
#16703=EDGE_LOOP('',(#40821));
#16704=EDGE_LOOP('',(#40822));
#16705=EDGE_LOOP('',(#40823));
#16706=EDGE_LOOP('',(#40824));
#16707=EDGE_LOOP('',(#40825));
#16708=EDGE_LOOP('',(#40826));
#16709=EDGE_LOOP('',(#40827));
#16710=EDGE_LOOP('',(#40828));
#16711=EDGE_LOOP('',(#40829));
#16712=EDGE_LOOP('',(#40830));
#16713=EDGE_LOOP('',(#40831));
#16714=EDGE_LOOP('',(#40832));
#16715=EDGE_LOOP('',(#40833));
#16716=EDGE_LOOP('',(#40834));
#16717=EDGE_LOOP('',(#40835));
#16718=EDGE_LOOP('',(#40836));
#16719=EDGE_LOOP('',(#40837));
#16720=EDGE_LOOP('',(#40838));
#16721=EDGE_LOOP('',(#40839));
#16722=EDGE_LOOP('',(#40840));
#16723=EDGE_LOOP('',(#40841));
#16724=EDGE_LOOP('',(#40842));
#16725=EDGE_LOOP('',(#40843));
#16726=EDGE_LOOP('',(#40844));
#16727=EDGE_LOOP('',(#40845));
#16728=EDGE_LOOP('',(#40846));
#16729=EDGE_LOOP('',(#40847));
#16730=EDGE_LOOP('',(#40848));
#16731=EDGE_LOOP('',(#40849));
#16732=EDGE_LOOP('',(#40850));
#16733=EDGE_LOOP('',(#40851));
#16734=EDGE_LOOP('',(#40852));
#16735=EDGE_LOOP('',(#40853));
#16736=EDGE_LOOP('',(#40854));
#16737=EDGE_LOOP('',(#40855));
#16738=EDGE_LOOP('',(#40856));
#16739=EDGE_LOOP('',(#40857));
#16740=EDGE_LOOP('',(#40858));
#16741=EDGE_LOOP('',(#40859));
#16742=EDGE_LOOP('',(#40860));
#16743=EDGE_LOOP('',(#40861));
#16744=EDGE_LOOP('',(#40862));
#16745=EDGE_LOOP('',(#40863));
#16746=EDGE_LOOP('',(#40864));
#16747=EDGE_LOOP('',(#40865));
#16748=EDGE_LOOP('',(#40866));
#16749=EDGE_LOOP('',(#40867));
#16750=EDGE_LOOP('',(#40868));
#16751=EDGE_LOOP('',(#40869));
#16752=EDGE_LOOP('',(#40870));
#16753=EDGE_LOOP('',(#40871));
#16754=EDGE_LOOP('',(#40872));
#16755=EDGE_LOOP('',(#40873));
#16756=EDGE_LOOP('',(#40874));
#16757=EDGE_LOOP('',(#40875));
#16758=EDGE_LOOP('',(#40876));
#16759=EDGE_LOOP('',(#40877));
#16760=EDGE_LOOP('',(#40878));
#16761=EDGE_LOOP('',(#40879));
#16762=EDGE_LOOP('',(#40880));
#16763=EDGE_LOOP('',(#40881));
#16764=EDGE_LOOP('',(#40882));
#16765=EDGE_LOOP('',(#40883));
#16766=EDGE_LOOP('',(#40884));
#16767=EDGE_LOOP('',(#40885));
#16768=EDGE_LOOP('',(#40886));
#16769=EDGE_LOOP('',(#40887));
#16770=EDGE_LOOP('',(#40888));
#16771=EDGE_LOOP('',(#40889));
#16772=EDGE_LOOP('',(#40890));
#16773=EDGE_LOOP('',(#40891));
#16774=EDGE_LOOP('',(#40892));
#16775=EDGE_LOOP('',(#40893));
#16776=EDGE_LOOP('',(#40894));
#16777=EDGE_LOOP('',(#40895));
#16778=EDGE_LOOP('',(#40896));
#16779=EDGE_LOOP('',(#40897));
#16780=EDGE_LOOP('',(#40898));
#16781=EDGE_LOOP('',(#40899));
#16782=EDGE_LOOP('',(#40900));
#16783=EDGE_LOOP('',(#40901));
#16784=EDGE_LOOP('',(#40902));
#16785=EDGE_LOOP('',(#40903));
#16786=EDGE_LOOP('',(#40904));
#16787=EDGE_LOOP('',(#40905));
#16788=EDGE_LOOP('',(#40906));
#16789=EDGE_LOOP('',(#40907));
#16790=EDGE_LOOP('',(#40908));
#16791=EDGE_LOOP('',(#40909));
#16792=EDGE_LOOP('',(#40910));
#16793=EDGE_LOOP('',(#40911));
#16794=EDGE_LOOP('',(#40912));
#16795=EDGE_LOOP('',(#40913));
#16796=EDGE_LOOP('',(#40914));
#16797=EDGE_LOOP('',(#40915));
#16798=EDGE_LOOP('',(#40916));
#16799=EDGE_LOOP('',(#40917));
#16800=EDGE_LOOP('',(#40918));
#16801=EDGE_LOOP('',(#40919));
#16802=EDGE_LOOP('',(#40920));
#16803=EDGE_LOOP('',(#40921));
#16804=EDGE_LOOP('',(#40922));
#16805=EDGE_LOOP('',(#40923));
#16806=EDGE_LOOP('',(#40924));
#16807=EDGE_LOOP('',(#40925));
#16808=EDGE_LOOP('',(#40926));
#16809=EDGE_LOOP('',(#40927));
#16810=EDGE_LOOP('',(#40928));
#16811=EDGE_LOOP('',(#40929));
#16812=EDGE_LOOP('',(#40930));
#16813=EDGE_LOOP('',(#40931));
#16814=EDGE_LOOP('',(#40932));
#16815=EDGE_LOOP('',(#40933));
#16816=EDGE_LOOP('',(#40934));
#16817=EDGE_LOOP('',(#40935));
#16818=EDGE_LOOP('',(#40936));
#16819=EDGE_LOOP('',(#40937));
#16820=EDGE_LOOP('',(#40938));
#16821=EDGE_LOOP('',(#40939));
#16822=EDGE_LOOP('',(#40940));
#16823=EDGE_LOOP('',(#40941));
#16824=EDGE_LOOP('',(#40942));
#16825=EDGE_LOOP('',(#40943));
#16826=EDGE_LOOP('',(#40944));
#16827=EDGE_LOOP('',(#40945));
#16828=EDGE_LOOP('',(#40946));
#16829=EDGE_LOOP('',(#40947));
#16830=EDGE_LOOP('',(#40948));
#16831=EDGE_LOOP('',(#40949));
#16832=EDGE_LOOP('',(#40950));
#16833=EDGE_LOOP('',(#40951));
#16834=EDGE_LOOP('',(#40952));
#16835=EDGE_LOOP('',(#40953));
#16836=EDGE_LOOP('',(#40954));
#16837=EDGE_LOOP('',(#40955));
#16838=EDGE_LOOP('',(#40956));
#16839=EDGE_LOOP('',(#40957));
#16840=EDGE_LOOP('',(#40958));
#16841=EDGE_LOOP('',(#40959));
#16842=EDGE_LOOP('',(#40960));
#16843=EDGE_LOOP('',(#40961));
#16844=EDGE_LOOP('',(#40962));
#16845=EDGE_LOOP('',(#40963));
#16846=EDGE_LOOP('',(#40964));
#16847=EDGE_LOOP('',(#40965));
#16848=EDGE_LOOP('',(#40966));
#16849=EDGE_LOOP('',(#40967));
#16850=EDGE_LOOP('',(#40968));
#16851=EDGE_LOOP('',(#40969));
#16852=EDGE_LOOP('',(#40970));
#16853=EDGE_LOOP('',(#40971));
#16854=EDGE_LOOP('',(#40972));
#16855=EDGE_LOOP('',(#40973));
#16856=EDGE_LOOP('',(#40974));
#16857=EDGE_LOOP('',(#40975));
#16858=EDGE_LOOP('',(#40976));
#16859=EDGE_LOOP('',(#40977));
#16860=EDGE_LOOP('',(#40978));
#16861=EDGE_LOOP('',(#40979));
#16862=EDGE_LOOP('',(#40980));
#16863=EDGE_LOOP('',(#40981));
#16864=EDGE_LOOP('',(#40982));
#16865=EDGE_LOOP('',(#40983));
#16866=EDGE_LOOP('',(#40984));
#16867=EDGE_LOOP('',(#40985));
#16868=EDGE_LOOP('',(#40986));
#16869=EDGE_LOOP('',(#40987));
#16870=EDGE_LOOP('',(#40988));
#16871=EDGE_LOOP('',(#40989));
#16872=EDGE_LOOP('',(#40990));
#16873=EDGE_LOOP('',(#40991));
#16874=EDGE_LOOP('',(#40992));
#16875=EDGE_LOOP('',(#40993));
#16876=EDGE_LOOP('',(#40994));
#16877=EDGE_LOOP('',(#40995));
#16878=EDGE_LOOP('',(#40996));
#16879=EDGE_LOOP('',(#40997));
#16880=EDGE_LOOP('',(#40998));
#16881=EDGE_LOOP('',(#40999));
#16882=EDGE_LOOP('',(#41000));
#16883=EDGE_LOOP('',(#41001));
#16884=EDGE_LOOP('',(#41002));
#16885=EDGE_LOOP('',(#41003));
#16886=EDGE_LOOP('',(#41004));
#16887=EDGE_LOOP('',(#41005));
#16888=EDGE_LOOP('',(#41006));
#16889=EDGE_LOOP('',(#41007));
#16890=EDGE_LOOP('',(#41008));
#16891=EDGE_LOOP('',(#41009));
#16892=EDGE_LOOP('',(#41010));
#16893=EDGE_LOOP('',(#41011));
#16894=EDGE_LOOP('',(#41012));
#16895=EDGE_LOOP('',(#41013));
#16896=EDGE_LOOP('',(#41014));
#16897=EDGE_LOOP('',(#41015));
#16898=EDGE_LOOP('',(#41016));
#16899=EDGE_LOOP('',(#41017));
#16900=EDGE_LOOP('',(#41018));
#16901=EDGE_LOOP('',(#41019));
#16902=EDGE_LOOP('',(#41020));
#16903=EDGE_LOOP('',(#41021));
#16904=EDGE_LOOP('',(#41022));
#16905=EDGE_LOOP('',(#41023));
#16906=EDGE_LOOP('',(#41024));
#16907=EDGE_LOOP('',(#41025));
#16908=EDGE_LOOP('',(#41026));
#16909=EDGE_LOOP('',(#41027));
#16910=EDGE_LOOP('',(#41028));
#16911=EDGE_LOOP('',(#41029));
#16912=EDGE_LOOP('',(#41030));
#16913=EDGE_LOOP('',(#41031));
#16914=EDGE_LOOP('',(#41032));
#16915=EDGE_LOOP('',(#41033));
#16916=EDGE_LOOP('',(#41034));
#16917=EDGE_LOOP('',(#41035));
#16918=EDGE_LOOP('',(#41036));
#16919=EDGE_LOOP('',(#41037));
#16920=EDGE_LOOP('',(#41038));
#16921=EDGE_LOOP('',(#41039));
#16922=EDGE_LOOP('',(#41040));
#16923=EDGE_LOOP('',(#41041));
#16924=EDGE_LOOP('',(#41042));
#16925=EDGE_LOOP('',(#41043));
#16926=EDGE_LOOP('',(#41044));
#16927=EDGE_LOOP('',(#41045));
#16928=EDGE_LOOP('',(#41046));
#16929=EDGE_LOOP('',(#41047));
#16930=EDGE_LOOP('',(#41048));
#16931=EDGE_LOOP('',(#41049));
#16932=EDGE_LOOP('',(#41050));
#16933=EDGE_LOOP('',(#41051));
#16934=EDGE_LOOP('',(#41052));
#16935=EDGE_LOOP('',(#41053));
#16936=EDGE_LOOP('',(#41054));
#16937=EDGE_LOOP('',(#41055));
#16938=EDGE_LOOP('',(#41056));
#16939=EDGE_LOOP('',(#41057));
#16940=EDGE_LOOP('',(#41058));
#16941=EDGE_LOOP('',(#41059));
#16942=EDGE_LOOP('',(#41060));
#16943=EDGE_LOOP('',(#41061));
#16944=EDGE_LOOP('',(#41062));
#16945=EDGE_LOOP('',(#41063));
#16946=EDGE_LOOP('',(#41064));
#16947=EDGE_LOOP('',(#41065));
#16948=EDGE_LOOP('',(#41066));
#16949=EDGE_LOOP('',(#41067));
#16950=EDGE_LOOP('',(#41068));
#16951=EDGE_LOOP('',(#41069));
#16952=EDGE_LOOP('',(#41070));
#16953=EDGE_LOOP('',(#41071));
#16954=EDGE_LOOP('',(#41072));
#16955=EDGE_LOOP('',(#41073));
#16956=EDGE_LOOP('',(#41074));
#16957=EDGE_LOOP('',(#41075));
#16958=EDGE_LOOP('',(#41076));
#16959=EDGE_LOOP('',(#41077));
#16960=EDGE_LOOP('',(#41078));
#16961=EDGE_LOOP('',(#41079));
#16962=EDGE_LOOP('',(#41080));
#16963=EDGE_LOOP('',(#41081));
#16964=EDGE_LOOP('',(#41082));
#16965=EDGE_LOOP('',(#41083));
#16966=EDGE_LOOP('',(#41084));
#16967=EDGE_LOOP('',(#41085));
#16968=EDGE_LOOP('',(#41086));
#16969=EDGE_LOOP('',(#41087));
#16970=EDGE_LOOP('',(#41088));
#16971=EDGE_LOOP('',(#41089));
#16972=EDGE_LOOP('',(#41090));
#16973=EDGE_LOOP('',(#41091));
#16974=EDGE_LOOP('',(#41092));
#16975=EDGE_LOOP('',(#41093));
#16976=EDGE_LOOP('',(#41094));
#16977=EDGE_LOOP('',(#41095));
#16978=EDGE_LOOP('',(#41096));
#16979=EDGE_LOOP('',(#41097));
#16980=EDGE_LOOP('',(#41098));
#16981=EDGE_LOOP('',(#41099));
#16982=EDGE_LOOP('',(#41100));
#16983=EDGE_LOOP('',(#41101));
#16984=EDGE_LOOP('',(#41102));
#16985=EDGE_LOOP('',(#41103));
#16986=EDGE_LOOP('',(#41104));
#16987=EDGE_LOOP('',(#41105));
#16988=EDGE_LOOP('',(#41106));
#16989=EDGE_LOOP('',(#41107));
#16990=EDGE_LOOP('',(#41108));
#16991=EDGE_LOOP('',(#41109));
#16992=EDGE_LOOP('',(#41110));
#16993=EDGE_LOOP('',(#41111));
#16994=EDGE_LOOP('',(#41112));
#16995=EDGE_LOOP('',(#41113));
#16996=EDGE_LOOP('',(#41114));
#16997=EDGE_LOOP('',(#41115));
#16998=EDGE_LOOP('',(#41116));
#16999=EDGE_LOOP('',(#41117));
#17000=EDGE_LOOP('',(#41118));
#17001=EDGE_LOOP('',(#41119));
#17002=EDGE_LOOP('',(#41120));
#17003=EDGE_LOOP('',(#41121));
#17004=EDGE_LOOP('',(#41122));
#17005=EDGE_LOOP('',(#41123));
#17006=EDGE_LOOP('',(#41124));
#17007=EDGE_LOOP('',(#41125));
#17008=EDGE_LOOP('',(#41126));
#17009=EDGE_LOOP('',(#41127));
#17010=EDGE_LOOP('',(#41128));
#17011=EDGE_LOOP('',(#41129));
#17012=EDGE_LOOP('',(#41130));
#17013=EDGE_LOOP('',(#41131));
#17014=EDGE_LOOP('',(#41132));
#17015=EDGE_LOOP('',(#41133));
#17016=EDGE_LOOP('',(#41134));
#17017=EDGE_LOOP('',(#41135));
#17018=EDGE_LOOP('',(#41136));
#17019=EDGE_LOOP('',(#41137));
#17020=EDGE_LOOP('',(#41138));
#17021=EDGE_LOOP('',(#41139));
#17022=EDGE_LOOP('',(#41140));
#17023=EDGE_LOOP('',(#41141));
#17024=EDGE_LOOP('',(#41142));
#17025=EDGE_LOOP('',(#41143));
#17026=EDGE_LOOP('',(#41144));
#17027=EDGE_LOOP('',(#41145));
#17028=EDGE_LOOP('',(#41146));
#17029=EDGE_LOOP('',(#41147));
#17030=EDGE_LOOP('',(#41148));
#17031=EDGE_LOOP('',(#41149));
#17032=EDGE_LOOP('',(#41150));
#17033=EDGE_LOOP('',(#41151));
#17034=EDGE_LOOP('',(#41152));
#17035=EDGE_LOOP('',(#41153));
#17036=EDGE_LOOP('',(#41154));
#17037=EDGE_LOOP('',(#41155));
#17038=EDGE_LOOP('',(#41156));
#17039=EDGE_LOOP('',(#41157));
#17040=EDGE_LOOP('',(#41158));
#17041=EDGE_LOOP('',(#41159));
#17042=EDGE_LOOP('',(#41160));
#17043=EDGE_LOOP('',(#41161));
#17044=EDGE_LOOP('',(#41162));
#17045=EDGE_LOOP('',(#41163));
#17046=EDGE_LOOP('',(#41164));
#17047=EDGE_LOOP('',(#41165));
#17048=EDGE_LOOP('',(#41166));
#17049=EDGE_LOOP('',(#41167));
#17050=EDGE_LOOP('',(#41168));
#17051=EDGE_LOOP('',(#41169));
#17052=EDGE_LOOP('',(#41170));
#17053=EDGE_LOOP('',(#41171));
#17054=EDGE_LOOP('',(#41172));
#17055=EDGE_LOOP('',(#41173));
#17056=EDGE_LOOP('',(#41174));
#17057=EDGE_LOOP('',(#41175));
#17058=EDGE_LOOP('',(#41176));
#17059=EDGE_LOOP('',(#41177));
#17060=EDGE_LOOP('',(#41178));
#17061=EDGE_LOOP('',(#41179));
#17062=EDGE_LOOP('',(#41180));
#17063=EDGE_LOOP('',(#41181));
#17064=EDGE_LOOP('',(#41182));
#17065=EDGE_LOOP('',(#41183));
#17066=EDGE_LOOP('',(#41184));
#17067=EDGE_LOOP('',(#41185));
#17068=EDGE_LOOP('',(#41186));
#17069=EDGE_LOOP('',(#41187));
#17070=EDGE_LOOP('',(#41188));
#17071=EDGE_LOOP('',(#41189));
#17072=EDGE_LOOP('',(#41190));
#17073=EDGE_LOOP('',(#41191));
#17074=EDGE_LOOP('',(#41192));
#17075=EDGE_LOOP('',(#41193));
#17076=EDGE_LOOP('',(#41194));
#17077=EDGE_LOOP('',(#41195));
#17078=EDGE_LOOP('',(#41196));
#17079=EDGE_LOOP('',(#41197));
#17080=EDGE_LOOP('',(#41198));
#17081=EDGE_LOOP('',(#41199));
#17082=EDGE_LOOP('',(#41200));
#17083=EDGE_LOOP('',(#41201));
#17084=EDGE_LOOP('',(#41202));
#17085=EDGE_LOOP('',(#41203));
#17086=EDGE_LOOP('',(#41204));
#17087=EDGE_LOOP('',(#41205));
#17088=EDGE_LOOP('',(#41206));
#17089=EDGE_LOOP('',(#41207));
#17090=EDGE_LOOP('',(#41208));
#17091=EDGE_LOOP('',(#41209));
#17092=EDGE_LOOP('',(#41210));
#17093=EDGE_LOOP('',(#41211));
#17094=EDGE_LOOP('',(#41212));
#17095=EDGE_LOOP('',(#41213));
#17096=EDGE_LOOP('',(#41214));
#17097=EDGE_LOOP('',(#41215));
#17098=EDGE_LOOP('',(#41216));
#17099=EDGE_LOOP('',(#41217));
#17100=EDGE_LOOP('',(#41218));
#17101=EDGE_LOOP('',(#41219));
#17102=EDGE_LOOP('',(#41220));
#17103=EDGE_LOOP('',(#41221));
#17104=EDGE_LOOP('',(#41222));
#17105=EDGE_LOOP('',(#41223));
#17106=EDGE_LOOP('',(#41224));
#17107=EDGE_LOOP('',(#41225));
#17108=EDGE_LOOP('',(#41226));
#17109=EDGE_LOOP('',(#41227));
#17110=EDGE_LOOP('',(#41228));
#17111=EDGE_LOOP('',(#41229));
#17112=EDGE_LOOP('',(#41230));
#17113=EDGE_LOOP('',(#41231));
#17114=EDGE_LOOP('',(#41232));
#17115=EDGE_LOOP('',(#41233));
#17116=EDGE_LOOP('',(#41234));
#17117=EDGE_LOOP('',(#41235));
#17118=EDGE_LOOP('',(#41236));
#17119=EDGE_LOOP('',(#41237));
#17120=EDGE_LOOP('',(#41238));
#17121=EDGE_LOOP('',(#41239));
#17122=EDGE_LOOP('',(#41240));
#17123=EDGE_LOOP('',(#41241));
#17124=EDGE_LOOP('',(#41242));
#17125=EDGE_LOOP('',(#41243));
#17126=EDGE_LOOP('',(#41244));
#17127=EDGE_LOOP('',(#41245));
#17128=EDGE_LOOP('',(#41246));
#17129=EDGE_LOOP('',(#41247));
#17130=EDGE_LOOP('',(#41248));
#17131=EDGE_LOOP('',(#41249));
#17132=EDGE_LOOP('',(#41250));
#17133=EDGE_LOOP('',(#41251));
#17134=EDGE_LOOP('',(#41252));
#17135=EDGE_LOOP('',(#41253));
#17136=EDGE_LOOP('',(#41254));
#17137=EDGE_LOOP('',(#41255));
#17138=EDGE_LOOP('',(#41256));
#17139=EDGE_LOOP('',(#41257));
#17140=EDGE_LOOP('',(#41258));
#17141=EDGE_LOOP('',(#41259));
#17142=EDGE_LOOP('',(#41260));
#17143=EDGE_LOOP('',(#41261));
#17144=EDGE_LOOP('',(#41262));
#17145=EDGE_LOOP('',(#41263));
#17146=EDGE_LOOP('',(#41264));
#17147=EDGE_LOOP('',(#41265));
#17148=EDGE_LOOP('',(#41266));
#17149=EDGE_LOOP('',(#41267));
#17150=EDGE_LOOP('',(#41268));
#17151=EDGE_LOOP('',(#41269));
#17152=EDGE_LOOP('',(#41270));
#17153=EDGE_LOOP('',(#41271));
#17154=EDGE_LOOP('',(#41272));
#17155=EDGE_LOOP('',(#41273));
#17156=EDGE_LOOP('',(#41274));
#17157=EDGE_LOOP('',(#41275));
#17158=EDGE_LOOP('',(#41276));
#17159=EDGE_LOOP('',(#41277));
#17160=EDGE_LOOP('',(#41278));
#17161=EDGE_LOOP('',(#41279));
#17162=EDGE_LOOP('',(#41280));
#17163=EDGE_LOOP('',(#41281));
#17164=EDGE_LOOP('',(#41282));
#17165=EDGE_LOOP('',(#41283));
#17166=EDGE_LOOP('',(#41284));
#17167=EDGE_LOOP('',(#41285));
#17168=EDGE_LOOP('',(#41286));
#17169=EDGE_LOOP('',(#41287));
#17170=EDGE_LOOP('',(#41288));
#17171=EDGE_LOOP('',(#41289));
#17172=EDGE_LOOP('',(#41290));
#17173=EDGE_LOOP('',(#41291));
#17174=EDGE_LOOP('',(#41292));
#17175=EDGE_LOOP('',(#41293));
#17176=EDGE_LOOP('',(#41294));
#17177=EDGE_LOOP('',(#41295));
#17178=EDGE_LOOP('',(#41296));
#17179=EDGE_LOOP('',(#41297));
#17180=EDGE_LOOP('',(#41298));
#17181=EDGE_LOOP('',(#41299));
#17182=EDGE_LOOP('',(#41300));
#17183=EDGE_LOOP('',(#41301));
#17184=EDGE_LOOP('',(#41302));
#17185=EDGE_LOOP('',(#41303));
#17186=EDGE_LOOP('',(#41304));
#17187=EDGE_LOOP('',(#41305));
#17188=EDGE_LOOP('',(#41306));
#17189=EDGE_LOOP('',(#41307));
#17190=EDGE_LOOP('',(#41308));
#17191=EDGE_LOOP('',(#41309));
#17192=EDGE_LOOP('',(#41310));
#17193=EDGE_LOOP('',(#41311));
#17194=EDGE_LOOP('',(#41312));
#17195=EDGE_LOOP('',(#41313));
#17196=EDGE_LOOP('',(#41314));
#17197=EDGE_LOOP('',(#41315));
#17198=EDGE_LOOP('',(#41316));
#17199=EDGE_LOOP('',(#41317));
#17200=EDGE_LOOP('',(#41318));
#17201=EDGE_LOOP('',(#41319));
#17202=EDGE_LOOP('',(#41320));
#17203=EDGE_LOOP('',(#41321));
#17204=EDGE_LOOP('',(#41322));
#17205=EDGE_LOOP('',(#41323));
#17206=EDGE_LOOP('',(#41324));
#17207=EDGE_LOOP('',(#41325));
#17208=EDGE_LOOP('',(#41326));
#17209=EDGE_LOOP('',(#41327));
#17210=EDGE_LOOP('',(#41328));
#17211=EDGE_LOOP('',(#41329));
#17212=EDGE_LOOP('',(#41330));
#17213=EDGE_LOOP('',(#41331));
#17214=EDGE_LOOP('',(#41332));
#17215=EDGE_LOOP('',(#41333));
#17216=EDGE_LOOP('',(#41334));
#17217=EDGE_LOOP('',(#41335));
#17218=EDGE_LOOP('',(#41336));
#17219=EDGE_LOOP('',(#41337));
#17220=EDGE_LOOP('',(#41338));
#17221=EDGE_LOOP('',(#41339));
#17222=EDGE_LOOP('',(#41340));
#17223=EDGE_LOOP('',(#41341));
#17224=EDGE_LOOP('',(#41342));
#17225=EDGE_LOOP('',(#41343));
#17226=EDGE_LOOP('',(#41344));
#17227=EDGE_LOOP('',(#41345));
#17228=EDGE_LOOP('',(#41346));
#17229=EDGE_LOOP('',(#41347));
#17230=EDGE_LOOP('',(#41348));
#17231=EDGE_LOOP('',(#41349));
#17232=EDGE_LOOP('',(#41350));
#17233=EDGE_LOOP('',(#41351));
#17234=EDGE_LOOP('',(#41352));
#17235=EDGE_LOOP('',(#41353));
#17236=EDGE_LOOP('',(#41354));
#17237=EDGE_LOOP('',(#41355));
#17238=EDGE_LOOP('',(#41356));
#17239=EDGE_LOOP('',(#41357));
#17240=EDGE_LOOP('',(#41358));
#17241=EDGE_LOOP('',(#41359));
#17242=EDGE_LOOP('',(#41360));
#17243=EDGE_LOOP('',(#41361));
#17244=EDGE_LOOP('',(#41362));
#17245=EDGE_LOOP('',(#41363));
#17246=EDGE_LOOP('',(#41364));
#17247=EDGE_LOOP('',(#41365));
#17248=EDGE_LOOP('',(#41366));
#17249=EDGE_LOOP('',(#41367));
#17250=EDGE_LOOP('',(#41368));
#17251=EDGE_LOOP('',(#41369));
#17252=EDGE_LOOP('',(#41370));
#17253=EDGE_LOOP('',(#41371));
#17254=EDGE_LOOP('',(#41372));
#17255=EDGE_LOOP('',(#41373));
#17256=EDGE_LOOP('',(#41374));
#17257=EDGE_LOOP('',(#41375));
#17258=EDGE_LOOP('',(#41376));
#17259=EDGE_LOOP('',(#41377));
#17260=EDGE_LOOP('',(#41378));
#17261=EDGE_LOOP('',(#41379));
#17262=EDGE_LOOP('',(#41380));
#17263=EDGE_LOOP('',(#41381));
#17264=EDGE_LOOP('',(#41382));
#17265=EDGE_LOOP('',(#41383));
#17266=EDGE_LOOP('',(#41384));
#17267=EDGE_LOOP('',(#41385));
#17268=EDGE_LOOP('',(#41386));
#17269=EDGE_LOOP('',(#41387));
#17270=EDGE_LOOP('',(#41388));
#17271=EDGE_LOOP('',(#41389));
#17272=EDGE_LOOP('',(#41390));
#17273=EDGE_LOOP('',(#41391));
#17274=EDGE_LOOP('',(#41392));
#17275=EDGE_LOOP('',(#41393));
#17276=EDGE_LOOP('',(#41394));
#17277=EDGE_LOOP('',(#41395));
#17278=EDGE_LOOP('',(#41396));
#17279=EDGE_LOOP('',(#41397));
#17280=EDGE_LOOP('',(#41398));
#17281=EDGE_LOOP('',(#41399));
#17282=EDGE_LOOP('',(#41400));
#17283=EDGE_LOOP('',(#41401));
#17284=EDGE_LOOP('',(#41402));
#17285=EDGE_LOOP('',(#41403));
#17286=EDGE_LOOP('',(#41404));
#17287=EDGE_LOOP('',(#41405));
#17288=EDGE_LOOP('',(#41406));
#17289=EDGE_LOOP('',(#41407));
#17290=EDGE_LOOP('',(#41408));
#17291=EDGE_LOOP('',(#41409));
#17292=EDGE_LOOP('',(#41410));
#17293=EDGE_LOOP('',(#41411));
#17294=EDGE_LOOP('',(#41412));
#17295=EDGE_LOOP('',(#41413));
#17296=EDGE_LOOP('',(#41414));
#17297=EDGE_LOOP('',(#41415));
#17298=EDGE_LOOP('',(#41416));
#17299=EDGE_LOOP('',(#41417));
#17300=EDGE_LOOP('',(#41418));
#17301=EDGE_LOOP('',(#41419));
#17302=EDGE_LOOP('',(#41420));
#17303=EDGE_LOOP('',(#41421));
#17304=EDGE_LOOP('',(#41422));
#17305=EDGE_LOOP('',(#41423));
#17306=EDGE_LOOP('',(#41424));
#17307=EDGE_LOOP('',(#41425));
#17308=EDGE_LOOP('',(#41426));
#17309=EDGE_LOOP('',(#41427));
#17310=EDGE_LOOP('',(#41428));
#17311=EDGE_LOOP('',(#41429));
#17312=EDGE_LOOP('',(#41430));
#17313=EDGE_LOOP('',(#41431));
#17314=EDGE_LOOP('',(#41432));
#17315=EDGE_LOOP('',(#41433));
#17316=EDGE_LOOP('',(#41434));
#17317=EDGE_LOOP('',(#41435));
#17318=EDGE_LOOP('',(#41436));
#17319=EDGE_LOOP('',(#41437));
#17320=EDGE_LOOP('',(#41438));
#17321=EDGE_LOOP('',(#41439));
#17322=EDGE_LOOP('',(#41440));
#17323=EDGE_LOOP('',(#41441));
#17324=EDGE_LOOP('',(#41442));
#17325=EDGE_LOOP('',(#41443));
#17326=EDGE_LOOP('',(#41444));
#17327=EDGE_LOOP('',(#41445));
#17328=EDGE_LOOP('',(#41446));
#17329=EDGE_LOOP('',(#41447));
#17330=EDGE_LOOP('',(#41448));
#17331=EDGE_LOOP('',(#41449));
#17332=EDGE_LOOP('',(#41450));
#17333=EDGE_LOOP('',(#41451));
#17334=EDGE_LOOP('',(#41452));
#17335=EDGE_LOOP('',(#41453));
#17336=EDGE_LOOP('',(#41454));
#17337=EDGE_LOOP('',(#41455));
#17338=EDGE_LOOP('',(#41456));
#17339=EDGE_LOOP('',(#41457));
#17340=EDGE_LOOP('',(#41458));
#17341=EDGE_LOOP('',(#41459));
#17342=EDGE_LOOP('',(#41460));
#17343=EDGE_LOOP('',(#41461));
#17344=EDGE_LOOP('',(#41462));
#17345=EDGE_LOOP('',(#41463));
#17346=EDGE_LOOP('',(#41464));
#17347=EDGE_LOOP('',(#41465));
#17348=EDGE_LOOP('',(#41466,#41467));
#17349=EDGE_LOOP('',(#41468));
#17350=EDGE_LOOP('',(#41469));
#17351=EDGE_LOOP('',(#41470,#41471));
#17352=EDGE_LOOP('',(#41472));
#17353=EDGE_LOOP('',(#41473));
#17354=EDGE_LOOP('',(#41474,#41475));
#17355=EDGE_LOOP('',(#41476));
#17356=EDGE_LOOP('',(#41477));
#17357=EDGE_LOOP('',(#41478,#41479));
#17358=EDGE_LOOP('',(#41480));
#17359=EDGE_LOOP('',(#41481));
#17360=EDGE_LOOP('',(#41482,#41483));
#17361=EDGE_LOOP('',(#41484));
#17362=EDGE_LOOP('',(#41485));
#17363=EDGE_LOOP('',(#41486,#41487));
#17364=EDGE_LOOP('',(#41488));
#17365=EDGE_LOOP('',(#41489));
#17366=EDGE_LOOP('',(#41490,#41491));
#17367=EDGE_LOOP('',(#41492));
#17368=EDGE_LOOP('',(#41493));
#17369=EDGE_LOOP('',(#41494,#41495));
#17370=EDGE_LOOP('',(#41496));
#17371=EDGE_LOOP('',(#41497));
#17372=EDGE_LOOP('',(#41498,#41499));
#17373=EDGE_LOOP('',(#41500));
#17374=EDGE_LOOP('',(#41501));
#17375=EDGE_LOOP('',(#41502,#41503));
#17376=EDGE_LOOP('',(#41504));
#17377=EDGE_LOOP('',(#41505));
#17378=EDGE_LOOP('',(#41506,#41507));
#17379=EDGE_LOOP('',(#41508));
#17380=EDGE_LOOP('',(#41509));
#17381=EDGE_LOOP('',(#41510,#41511));
#17382=EDGE_LOOP('',(#41512));
#17383=EDGE_LOOP('',(#41513));
#17384=EDGE_LOOP('',(#41514,#41515));
#17385=EDGE_LOOP('',(#41516));
#17386=EDGE_LOOP('',(#41517));
#17387=EDGE_LOOP('',(#41518,#41519));
#17388=EDGE_LOOP('',(#41520));
#17389=EDGE_LOOP('',(#41521));
#17390=EDGE_LOOP('',(#41522,#41523));
#17391=EDGE_LOOP('',(#41524));
#17392=EDGE_LOOP('',(#41525));
#17393=EDGE_LOOP('',(#41526,#41527));
#17394=EDGE_LOOP('',(#41528));
#17395=EDGE_LOOP('',(#41529));
#17396=EDGE_LOOP('',(#41530,#41531));
#17397=EDGE_LOOP('',(#41532));
#17398=EDGE_LOOP('',(#41533));
#17399=EDGE_LOOP('',(#41534,#41535));
#17400=EDGE_LOOP('',(#41536));
#17401=EDGE_LOOP('',(#41537));
#17402=EDGE_LOOP('',(#41538,#41539));
#17403=EDGE_LOOP('',(#41540));
#17404=EDGE_LOOP('',(#41541));
#17405=EDGE_LOOP('',(#41542,#41543));
#17406=EDGE_LOOP('',(#41544));
#17407=EDGE_LOOP('',(#41545));
#17408=EDGE_LOOP('',(#41546,#41547));
#17409=EDGE_LOOP('',(#41548));
#17410=EDGE_LOOP('',(#41549));
#17411=EDGE_LOOP('',(#41550,#41551));
#17412=EDGE_LOOP('',(#41552));
#17413=EDGE_LOOP('',(#41553));
#17414=EDGE_LOOP('',(#41554,#41555));
#17415=EDGE_LOOP('',(#41556));
#17416=EDGE_LOOP('',(#41557));
#17417=EDGE_LOOP('',(#41558,#41559));
#17418=EDGE_LOOP('',(#41560));
#17419=EDGE_LOOP('',(#41561));
#17420=EDGE_LOOP('',(#41562,#41563));
#17421=EDGE_LOOP('',(#41564));
#17422=EDGE_LOOP('',(#41565));
#17423=EDGE_LOOP('',(#41566,#41567));
#17424=EDGE_LOOP('',(#41568));
#17425=EDGE_LOOP('',(#41569));
#17426=EDGE_LOOP('',(#41570,#41571));
#17427=EDGE_LOOP('',(#41572));
#17428=EDGE_LOOP('',(#41573));
#17429=EDGE_LOOP('',(#41574,#41575));
#17430=EDGE_LOOP('',(#41576));
#17431=EDGE_LOOP('',(#41577));
#17432=EDGE_LOOP('',(#41578,#41579));
#17433=EDGE_LOOP('',(#41580));
#17434=EDGE_LOOP('',(#41581));
#17435=EDGE_LOOP('',(#41582,#41583));
#17436=EDGE_LOOP('',(#41584));
#17437=EDGE_LOOP('',(#41585));
#17438=EDGE_LOOP('',(#41586,#41587));
#17439=EDGE_LOOP('',(#41588));
#17440=EDGE_LOOP('',(#41589));
#17441=EDGE_LOOP('',(#41590,#41591));
#17442=EDGE_LOOP('',(#41592));
#17443=EDGE_LOOP('',(#41593));
#17444=EDGE_LOOP('',(#41594,#41595));
#17445=EDGE_LOOP('',(#41596));
#17446=EDGE_LOOP('',(#41597));
#17447=EDGE_LOOP('',(#41598,#41599));
#17448=EDGE_LOOP('',(#41600));
#17449=EDGE_LOOP('',(#41601));
#17450=EDGE_LOOP('',(#41602,#41603));
#17451=EDGE_LOOP('',(#41604));
#17452=EDGE_LOOP('',(#41605));
#17453=EDGE_LOOP('',(#41606,#41607));
#17454=EDGE_LOOP('',(#41608));
#17455=EDGE_LOOP('',(#41609));
#17456=EDGE_LOOP('',(#41610,#41611));
#17457=EDGE_LOOP('',(#41612));
#17458=EDGE_LOOP('',(#41613));
#17459=EDGE_LOOP('',(#41614,#41615));
#17460=EDGE_LOOP('',(#41616));
#17461=EDGE_LOOP('',(#41617));
#17462=EDGE_LOOP('',(#41618,#41619));
#17463=EDGE_LOOP('',(#41620));
#17464=EDGE_LOOP('',(#41621));
#17465=EDGE_LOOP('',(#41622,#41623));
#17466=EDGE_LOOP('',(#41624));
#17467=EDGE_LOOP('',(#41625));
#17468=EDGE_LOOP('',(#41626,#41627));
#17469=EDGE_LOOP('',(#41628));
#17470=EDGE_LOOP('',(#41629));
#17471=EDGE_LOOP('',(#41630,#41631));
#17472=EDGE_LOOP('',(#41632));
#17473=EDGE_LOOP('',(#41633));
#17474=EDGE_LOOP('',(#41634,#41635));
#17475=EDGE_LOOP('',(#41636));
#17476=EDGE_LOOP('',(#41637));
#17477=EDGE_LOOP('',(#41638,#41639));
#17478=EDGE_LOOP('',(#41640));
#17479=EDGE_LOOP('',(#41641));
#17480=EDGE_LOOP('',(#41642,#41643));
#17481=EDGE_LOOP('',(#41644));
#17482=EDGE_LOOP('',(#41645));
#17483=EDGE_LOOP('',(#41646,#41647));
#17484=EDGE_LOOP('',(#41648));
#17485=EDGE_LOOP('',(#41649));
#17486=EDGE_LOOP('',(#41650,#41651));
#17487=EDGE_LOOP('',(#41652));
#17488=EDGE_LOOP('',(#41653,#41654));
#17489=EDGE_LOOP('',(#41655,#41656));
#17490=EDGE_LOOP('',(#41657));
#17491=EDGE_LOOP('',(#41658));
#17492=EDGE_LOOP('',(#41659,#41660));
#17493=EDGE_LOOP('',(#41661));
#17494=EDGE_LOOP('',(#41662));
#17495=EDGE_LOOP('',(#41663,#41664));
#17496=EDGE_LOOP('',(#41665));
#17497=EDGE_LOOP('',(#41666));
#17498=EDGE_LOOP('',(#41667,#41668));
#17499=EDGE_LOOP('',(#41669));
#17500=EDGE_LOOP('',(#41670,#41671));
#17501=EDGE_LOOP('',(#41672,#41673));
#17502=EDGE_LOOP('',(#41674));
#17503=EDGE_LOOP('',(#41675));
#17504=EDGE_LOOP('',(#41676,#41677));
#17505=EDGE_LOOP('',(#41678));
#17506=EDGE_LOOP('',(#41679));
#17507=EDGE_LOOP('',(#41680,#41681));
#17508=EDGE_LOOP('',(#41682));
#17509=EDGE_LOOP('',(#41683));
#17510=EDGE_LOOP('',(#41684,#41685));
#17511=EDGE_LOOP('',(#41686));
#17512=EDGE_LOOP('',(#41687,#41688));
#17513=EDGE_LOOP('',(#41689,#41690));
#17514=EDGE_LOOP('',(#41691));
#17515=EDGE_LOOP('',(#41692));
#17516=EDGE_LOOP('',(#41693,#41694));
#17517=EDGE_LOOP('',(#41695));
#17518=EDGE_LOOP('',(#41696));
#17519=EDGE_LOOP('',(#41697,#41698));
#17520=EDGE_LOOP('',(#41699));
#17521=EDGE_LOOP('',(#41700));
#17522=EDGE_LOOP('',(#41701,#41702));
#17523=EDGE_LOOP('',(#41703));
#17524=EDGE_LOOP('',(#41704));
#17525=EDGE_LOOP('',(#41705,#41706));
#17526=EDGE_LOOP('',(#41707));
#17527=EDGE_LOOP('',(#41708));
#17528=EDGE_LOOP('',(#41709,#41710));
#17529=EDGE_LOOP('',(#41711));
#17530=EDGE_LOOP('',(#41712));
#17531=EDGE_LOOP('',(#41713,#41714));
#17532=EDGE_LOOP('',(#41715));
#17533=EDGE_LOOP('',(#41716));
#17534=EDGE_LOOP('',(#41717,#41718));
#17535=EDGE_LOOP('',(#41719));
#17536=EDGE_LOOP('',(#41720));
#17537=EDGE_LOOP('',(#41721,#41722));
#17538=EDGE_LOOP('',(#41723));
#17539=EDGE_LOOP('',(#41724));
#17540=EDGE_LOOP('',(#41725,#41726));
#17541=EDGE_LOOP('',(#41727));
#17542=EDGE_LOOP('',(#41728));
#17543=EDGE_LOOP('',(#41729,#41730));
#17544=EDGE_LOOP('',(#41731));
#17545=EDGE_LOOP('',(#41732));
#17546=EDGE_LOOP('',(#41733,#41734));
#17547=EDGE_LOOP('',(#41735));
#17548=EDGE_LOOP('',(#41736));
#17549=EDGE_LOOP('',(#41737,#41738));
#17550=EDGE_LOOP('',(#41739));
#17551=EDGE_LOOP('',(#41740));
#17552=EDGE_LOOP('',(#41741,#41742));
#17553=EDGE_LOOP('',(#41743));
#17554=EDGE_LOOP('',(#41744));
#17555=EDGE_LOOP('',(#41745,#41746));
#17556=EDGE_LOOP('',(#41747));
#17557=EDGE_LOOP('',(#41748));
#17558=EDGE_LOOP('',(#41749,#41750));
#17559=EDGE_LOOP('',(#41751));
#17560=EDGE_LOOP('',(#41752));
#17561=EDGE_LOOP('',(#41753,#41754));
#17562=EDGE_LOOP('',(#41755));
#17563=EDGE_LOOP('',(#41756));
#17564=EDGE_LOOP('',(#41757,#41758));
#17565=EDGE_LOOP('',(#41759));
#17566=EDGE_LOOP('',(#41760));
#17567=EDGE_LOOP('',(#41761,#41762));
#17568=EDGE_LOOP('',(#41763));
#17569=EDGE_LOOP('',(#41764));
#17570=EDGE_LOOP('',(#41765,#41766));
#17571=EDGE_LOOP('',(#41767));
#17572=EDGE_LOOP('',(#41768));
#17573=EDGE_LOOP('',(#41769,#41770));
#17574=EDGE_LOOP('',(#41771));
#17575=EDGE_LOOP('',(#41772));
#17576=EDGE_LOOP('',(#41773,#41774));
#17577=EDGE_LOOP('',(#41775));
#17578=EDGE_LOOP('',(#41776));
#17579=EDGE_LOOP('',(#41777,#41778));
#17580=EDGE_LOOP('',(#41779));
#17581=EDGE_LOOP('',(#41780));
#17582=EDGE_LOOP('',(#41781,#41782));
#17583=EDGE_LOOP('',(#41783));
#17584=EDGE_LOOP('',(#41784));
#17585=EDGE_LOOP('',(#41785,#41786));
#17586=EDGE_LOOP('',(#41787));
#17587=EDGE_LOOP('',(#41788));
#17588=EDGE_LOOP('',(#41789,#41790));
#17589=EDGE_LOOP('',(#41791));
#17590=EDGE_LOOP('',(#41792));
#17591=EDGE_LOOP('',(#41793,#41794));
#17592=EDGE_LOOP('',(#41795));
#17593=EDGE_LOOP('',(#41796));
#17594=EDGE_LOOP('',(#41797,#41798));
#17595=EDGE_LOOP('',(#41799));
#17596=EDGE_LOOP('',(#41800));
#17597=EDGE_LOOP('',(#41801,#41802));
#17598=EDGE_LOOP('',(#41803));
#17599=EDGE_LOOP('',(#41804));
#17600=EDGE_LOOP('',(#41805,#41806));
#17601=EDGE_LOOP('',(#41807));
#17602=EDGE_LOOP('',(#41808));
#17603=EDGE_LOOP('',(#41809,#41810));
#17604=EDGE_LOOP('',(#41811));
#17605=EDGE_LOOP('',(#41812));
#17606=EDGE_LOOP('',(#41813,#41814));
#17607=EDGE_LOOP('',(#41815));
#17608=EDGE_LOOP('',(#41816));
#17609=EDGE_LOOP('',(#41817,#41818));
#17610=EDGE_LOOP('',(#41819));
#17611=EDGE_LOOP('',(#41820));
#17612=EDGE_LOOP('',(#41821,#41822));
#17613=EDGE_LOOP('',(#41823));
#17614=EDGE_LOOP('',(#41824));
#17615=EDGE_LOOP('',(#41825,#41826));
#17616=EDGE_LOOP('',(#41827));
#17617=EDGE_LOOP('',(#41828));
#17618=EDGE_LOOP('',(#41829,#41830));
#17619=EDGE_LOOP('',(#41831));
#17620=EDGE_LOOP('',(#41832,#41833));
#17621=EDGE_LOOP('',(#41834,#41835));
#17622=EDGE_LOOP('',(#41836));
#17623=EDGE_LOOP('',(#41837));
#17624=EDGE_LOOP('',(#41838,#41839));
#17625=EDGE_LOOP('',(#41840));
#17626=EDGE_LOOP('',(#41841));
#17627=EDGE_LOOP('',(#41842,#41843));
#17628=EDGE_LOOP('',(#41844));
#17629=EDGE_LOOP('',(#41845));
#17630=EDGE_LOOP('',(#41846,#41847));
#17631=EDGE_LOOP('',(#41848));
#17632=EDGE_LOOP('',(#41849));
#17633=EDGE_LOOP('',(#41850,#41851));
#17634=EDGE_LOOP('',(#41852));
#17635=EDGE_LOOP('',(#41853));
#17636=EDGE_LOOP('',(#41854,#41855));
#17637=EDGE_LOOP('',(#41856));
#17638=EDGE_LOOP('',(#41857));
#17639=EDGE_LOOP('',(#41858,#41859));
#17640=EDGE_LOOP('',(#41860));
#17641=EDGE_LOOP('',(#41861));
#17642=EDGE_LOOP('',(#41862,#41863));
#17643=EDGE_LOOP('',(#41864));
#17644=EDGE_LOOP('',(#41865));
#17645=EDGE_LOOP('',(#41866,#41867));
#17646=EDGE_LOOP('',(#41868));
#17647=EDGE_LOOP('',(#41869));
#17648=EDGE_LOOP('',(#41870,#41871));
#17649=EDGE_LOOP('',(#41872));
#17650=EDGE_LOOP('',(#41873));
#17651=EDGE_LOOP('',(#41874,#41875));
#17652=EDGE_LOOP('',(#41876));
#17653=EDGE_LOOP('',(#41877));
#17654=EDGE_LOOP('',(#41878,#41879));
#17655=EDGE_LOOP('',(#41880));
#17656=EDGE_LOOP('',(#41881));
#17657=EDGE_LOOP('',(#41882,#41883));
#17658=EDGE_LOOP('',(#41884));
#17659=EDGE_LOOP('',(#41885));
#17660=EDGE_LOOP('',(#41886,#41887));
#17661=EDGE_LOOP('',(#41888));
#17662=EDGE_LOOP('',(#41889));
#17663=EDGE_LOOP('',(#41890,#41891));
#17664=EDGE_LOOP('',(#41892));
#17665=EDGE_LOOP('',(#41893));
#17666=EDGE_LOOP('',(#41894,#41895));
#17667=EDGE_LOOP('',(#41896));
#17668=EDGE_LOOP('',(#41897));
#17669=EDGE_LOOP('',(#41898,#41899));
#17670=EDGE_LOOP('',(#41900));
#17671=EDGE_LOOP('',(#41901));
#17672=EDGE_LOOP('',(#41902,#41903));
#17673=EDGE_LOOP('',(#41904));
#17674=EDGE_LOOP('',(#41905));
#17675=EDGE_LOOP('',(#41906,#41907));
#17676=EDGE_LOOP('',(#41908));
#17677=EDGE_LOOP('',(#41909));
#17678=EDGE_LOOP('',(#41910,#41911));
#17679=EDGE_LOOP('',(#41912));
#17680=EDGE_LOOP('',(#41913));
#17681=EDGE_LOOP('',(#41914,#41915));
#17682=EDGE_LOOP('',(#41916));
#17683=EDGE_LOOP('',(#41917));
#17684=EDGE_LOOP('',(#41918,#41919));
#17685=EDGE_LOOP('',(#41920));
#17686=EDGE_LOOP('',(#41921));
#17687=EDGE_LOOP('',(#41922,#41923));
#17688=EDGE_LOOP('',(#41924));
#17689=EDGE_LOOP('',(#41925));
#17690=EDGE_LOOP('',(#41926,#41927));
#17691=EDGE_LOOP('',(#41928));
#17692=EDGE_LOOP('',(#41929));
#17693=EDGE_LOOP('',(#41930,#41931));
#17694=EDGE_LOOP('',(#41932));
#17695=EDGE_LOOP('',(#41933));
#17696=EDGE_LOOP('',(#41934,#41935));
#17697=EDGE_LOOP('',(#41936));
#17698=EDGE_LOOP('',(#41937));
#17699=EDGE_LOOP('',(#41938,#41939));
#17700=EDGE_LOOP('',(#41940));
#17701=EDGE_LOOP('',(#41941));
#17702=EDGE_LOOP('',(#41942,#41943));
#17703=CIRCLE('',#45552,11.5);
#17704=CIRCLE('',#45553,18.5);
#17705=CIRCLE('',#45554,11.5000000000001);
#17706=CIRCLE('',#45555,11.5000000000001);
#17707=CIRCLE('',#45557,11.5000000000001);
#17708=CIRCLE('',#45558,18.4999999999957);
#17709=CIRCLE('',#45559,11.5);
#17710=CIRCLE('',#45560,11.5000000000001);
#17711=CIRCLE('',#45562,11.5);
#17712=CIRCLE('',#45565,11.5);
#17713=CIRCLE('',#45572,8.3031389659941);
#17714=CIRCLE('',#45582,8.3031389659941);
#17715=CIRCLE('',#45585,0.500000000000054);
#17716=CIRCLE('',#45586,0.500000000000054);
#17717=CIRCLE('',#45588,1.81285717707167);
#17718=CIRCLE('',#45589,1.81285717707168);
#17719=CIRCLE('',#45591,0.500000000000054);
#17720=CIRCLE('',#45592,0.500000000000054);
#17721=CIRCLE('',#45594,1.81285717707167);
#17722=CIRCLE('',#45595,1.81285717707167);
#17723=CIRCLE('',#45597,0.500000000000054);
#17724=CIRCLE('',#45598,0.500000000000054);
#17725=CIRCLE('',#45600,1.81285717707166);
#17726=CIRCLE('',#45601,1.81285717707166);
#17727=CIRCLE('',#45603,0.499999999999939);
#17728=CIRCLE('',#45604,0.499999999999935);
#17729=CIRCLE('',#45606,1.81285717707155);
#17730=CIRCLE('',#45607,1.81285717707156);
#17731=CIRCLE('',#45609,0.499999999999935);
#17732=CIRCLE('',#45610,0.499999999999935);
#17733=CIRCLE('',#45612,1.81285717707155);
#17734=CIRCLE('',#45613,1.81285717707155);
#17735=CIRCLE('',#45615,0.499999999999944);
#17736=CIRCLE('',#45616,0.499999999999944);
#17737=CIRCLE('',#45618,1.81285717707167);
#17738=CIRCLE('',#45619,1.81285717707167);
#17739=CIRCLE('',#45622,0.500000000000053);
#17740=CIRCLE('',#45625,0.500000000000049);
#17741=CIRCLE('',#45628,0.500000000000049);
#17742=CIRCLE('',#45631,0.500000000000049);
#17743=CIRCLE('',#45634,0.500000000000049);
#17744=CIRCLE('',#45637,0.499999999999944);
#17745=CIRCLE('',#45640,0.499999999999944);
#17746=CIRCLE('',#45643,0.500000000000058);
#17747=CIRCLE('',#45646,0.500000000000058);
#17748=CIRCLE('',#45649,0.500000000000058);
#17749=CIRCLE('',#45652,0.500000000000172);
#17750=CIRCLE('',#45655,0.499999999999935);
#17751=CIRCLE('',#45658,0.500000000000058);
#17752=CIRCLE('',#45661,0.499999999999935);
#17753=CIRCLE('',#45664,0.500000000000058);
#17754=CIRCLE('',#45667,0.500000000000058);
#17755=CIRCLE('',#45670,0.499999999999944);
#17756=CIRCLE('',#45673,0.500000000000067);
#17757=CIRCLE('',#45676,0.499999999999935);
#17758=CIRCLE('',#45679,0.499999999999935);
#17759=CIRCLE('',#45682,0.500000000000058);
#17760=CIRCLE('',#45685,0.499999999999944);
#17761=CIRCLE('',#45688,0.499999999999944);
#17762=CIRCLE('',#45691,0.499999999999944);
#17763=CIRCLE('',#45694,0.500000000000172);
#17764=CIRCLE('',#45697,0.499999999999944);
#17765=CIRCLE('',#45700,0.500000000000049);
#17766=CIRCLE('',#45703,0.499999999999939);
#17767=CIRCLE('',#45706,0.500000000000053);
#17768=CIRCLE('',#45709,0.500000000000053);
#17769=CIRCLE('',#45712,0.500000000000049);
#17770=CIRCLE('',#45715,0.500000000000053);
#17771=CIRCLE('',#45718,0.500000000000053);
#17772=CIRCLE('',#45721,0.500000000000049);
#17773=CIRCLE('',#45724,0.500000000000049);
#17774=CIRCLE('',#45727,0.500000000000063);
#17775=CIRCLE('',#45730,0.499999999999944);
#17776=CIRCLE('',#45733,0.499999999999935);
#17777=CIRCLE('',#45736,0.499999999999944);
#17778=CIRCLE('',#45738,1.54967110260237);
#17779=CIRCLE('',#45740,0.499999999999939);
#17780=CIRCLE('',#45741,0.499999999999939);
#17781=CIRCLE('',#45743,1.25936103546568);
#17782=CIRCLE('',#45745,0.500000000000049);
#17783=CIRCLE('',#45746,0.500000000000049);
#17784=CIRCLE('',#45749,0.499999999999939);
#17785=CIRCLE('',#45752,0.499999999999939);
#17786=CIRCLE('',#45754,1.54967110260249);
#17787=CIRCLE('',#45756,0.499999999999944);
#17788=CIRCLE('',#45757,0.499999999999944);
#17789=CIRCLE('',#45759,1.25936103546569);
#17790=CIRCLE('',#45761,0.500000000000058);
#17791=CIRCLE('',#45762,0.500000000000058);
#17792=CIRCLE('',#45765,0.500000000000058);
#17793=CIRCLE('',#45768,0.500000000000053);
#17794=CIRCLE('',#45770,1.25936103546568);
#17795=CIRCLE('',#45772,0.500000000000053);
#17796=CIRCLE('',#45773,0.500000000000049);
#17797=CIRCLE('',#45776,0.500000000000058);
#17798=CIRCLE('',#45779,0.500000000000058);
#17799=CIRCLE('',#45781,1.25936103546568);
#17800=CIRCLE('',#45783,0.499999999999939);
#17801=CIRCLE('',#45784,0.499999999999939);
#17802=CIRCLE('',#45787,0.500000000000058);
#17803=CIRCLE('',#45790,0.499999999999939);
#17804=CIRCLE('',#45793,0.499999999999944);
#17805=CIRCLE('',#45796,0.499999999999944);
#17806=CIRCLE('',#45799,0.500000000000058);
#17807=CIRCLE('',#45802,0.500000000000053);
#17808=CIRCLE('',#45805,0.499999999999944);
#17809=CIRCLE('',#45808,0.500000000000063);
#17810=CIRCLE('',#45811,0.499999999999939);
#17811=CIRCLE('',#45814,0.500000000000053);
#17812=CIRCLE('',#45817,0.500000000000053);
#17813=CIRCLE('',#45820,0.499999999999939);
#17814=CIRCLE('',#45823,0.500000000000053);
#17815=CIRCLE('',#45826,0.499999999999944);
#17816=CIRCLE('',#45828,1.05888347462729);
#17817=CIRCLE('',#45829,1.05888347462729);
#17818=CIRCLE('',#45831,0.500000000000049);
#17819=CIRCLE('',#45832,0.500000000000049);
#17820=CIRCLE('',#45834,1.29583333162394);
#17821=CIRCLE('',#45835,1.29583333162394);
#17822=CIRCLE('',#45837,0.500000000000049);
#17823=CIRCLE('',#45838,0.500000000000049);
#17824=CIRCLE('',#45840,1.60653900437062);
#17825=CIRCLE('',#45841,1.60653900437062);
#17826=CIRCLE('',#45843,0.500000000000049);
#17827=CIRCLE('',#45844,0.500000000000049);
#17828=CIRCLE('',#45846,1.82809807486272);
#17829=CIRCLE('',#45847,1.82809807486272);
#17830=CIRCLE('',#45849,0.499999999999944);
#17831=CIRCLE('',#45850,0.499999999999944);
#17832=CIRCLE('',#45852,1.85841829658605);
#17833=CIRCLE('',#45853,1.85841829658605);
#17834=CIRCLE('',#45855,0.500000000000049);
#17835=CIRCLE('',#45856,0.500000000000049);
#17836=CIRCLE('',#45858,1.81285717707166);
#17837=CIRCLE('',#45859,1.81285717707167);
#17838=CIRCLE('',#45861,0.500000000000049);
#17839=CIRCLE('',#45862,0.500000000000049);
#17840=CIRCLE('',#45864,1.91146602029503);
#17841=CIRCLE('',#45865,1.91146602029503);
#17842=CIRCLE('',#45867,0.500000000000049);
#17843=CIRCLE('',#45868,0.500000000000049);
#17844=CIRCLE('',#45870,1.54967110260248);
#17845=CIRCLE('',#45871,1.54967110260249);
#17846=CIRCLE('',#45873,0.499999999999944);
#17847=CIRCLE('',#45874,0.499999999999944);
#17848=CIRCLE('',#45876,1.25936103546569);
#17849=CIRCLE('',#45877,1.25936103546556);
#17850=CIRCLE('',#45879,0.500000000000049);
#17851=CIRCLE('',#45880,0.500000000000049);
#17852=CIRCLE('',#45882,1.0588834746273);
#17853=CIRCLE('',#45883,1.0588834746273);
#17854=CIRCLE('',#45885,0.500000000000049);
#17855=CIRCLE('',#45886,0.500000000000049);
#17856=CIRCLE('',#45888,1.29583333162394);
#17857=CIRCLE('',#45889,1.29583333162394);
#17858=CIRCLE('',#45891,0.499999999999944);
#17859=CIRCLE('',#45892,0.499999999999944);
#17860=CIRCLE('',#45894,1.60653900437062);
#17861=CIRCLE('',#45895,1.60653900437062);
#17862=CIRCLE('',#45897,0.500000000000058);
#17863=CIRCLE('',#45898,0.500000000000058);
#17864=CIRCLE('',#45900,1.82809807486272);
#17865=CIRCLE('',#45901,1.82809807486272);
#17866=CIRCLE('',#45903,0.499999999999944);
#17867=CIRCLE('',#45904,0.499999999999944);
#17868=CIRCLE('',#45906,1.85841829658605);
#17869=CIRCLE('',#45907,1.85841829658605);
#17870=CIRCLE('',#45909,0.499999999999944);
#17871=CIRCLE('',#45910,0.499999999999944);
#17872=CIRCLE('',#45912,1.81285717707166);
#17873=CIRCLE('',#45913,1.81285717707167);
#17874=CIRCLE('',#45915,0.499999999999944);
#17875=CIRCLE('',#45916,0.499999999999944);
#17876=CIRCLE('',#45918,1.91146602029502);
#17877=CIRCLE('',#45919,1.91146602029503);
#17878=CIRCLE('',#45921,0.500000000000049);
#17879=CIRCLE('',#45922,0.500000000000049);
#17880=CIRCLE('',#45924,1.54967110260249);
#17881=CIRCLE('',#45925,1.54967110260249);
#17882=CIRCLE('',#45927,0.499999999999944);
#17883=CIRCLE('',#45928,0.499999999999944);
#17884=CIRCLE('',#45930,1.25936103546569);
#17885=CIRCLE('',#45931,1.25936103546556);
#17886=CIRCLE('',#45933,0.500000000000049);
#17887=CIRCLE('',#45934,0.500000000000049);
#17888=CIRCLE('',#45936,1.05888347462729);
#17889=CIRCLE('',#45937,1.05888347462729);
#17890=CIRCLE('',#45939,0.499999999999935);
#17891=CIRCLE('',#45940,0.499999999999935);
#17892=CIRCLE('',#45942,1.29583333162394);
#17893=CIRCLE('',#45943,1.29583333162394);
#17894=CIRCLE('',#45945,0.500000000000058);
#17895=CIRCLE('',#45946,0.500000000000058);
#17896=CIRCLE('',#45948,1.60653900437051);
#17897=CIRCLE('',#45949,1.60653900437051);
#17898=CIRCLE('',#45951,0.499999999999935);
#17899=CIRCLE('',#45952,0.499999999999935);
#17900=CIRCLE('',#45954,1.82809807486262);
#17901=CIRCLE('',#45955,1.82809807486262);
#17902=CIRCLE('',#45957,0.500000000000049);
#17903=CIRCLE('',#45958,0.500000000000049);
#17904=CIRCLE('',#45960,1.85841829658605);
#17905=CIRCLE('',#45961,1.85841829658605);
#17906=CIRCLE('',#45963,0.500000000000049);
#17907=CIRCLE('',#45964,0.500000000000049);
#17908=CIRCLE('',#45966,1.91146602029503);
#17909=CIRCLE('',#45967,1.91146602029503);
#17910=CIRCLE('',#45969,0.500000000000049);
#17911=CIRCLE('',#45970,0.500000000000049);
#17912=CIRCLE('',#45972,1.54967110260249);
#17913=CIRCLE('',#45973,1.54967110260249);
#17914=CIRCLE('',#45975,0.500000000000058);
#17915=CIRCLE('',#45976,0.500000000000058);
#17916=CIRCLE('',#45978,1.25936103546568);
#17917=CIRCLE('',#45979,1.25936103546556);
#17918=CIRCLE('',#45981,0.500000000000049);
#17919=CIRCLE('',#45982,0.500000000000049);
#17920=CIRCLE('',#45984,1.05888347462729);
#17921=CIRCLE('',#45985,1.05888347462729);
#17922=CIRCLE('',#45987,0.500000000000049);
#17923=CIRCLE('',#45988,0.500000000000049);
#17924=CIRCLE('',#45990,1.29583333162382);
#17925=CIRCLE('',#45991,1.29583333162382);
#17926=CIRCLE('',#45993,0.499999999999821);
#17927=CIRCLE('',#45994,0.499999999999821);
#17928=CIRCLE('',#45996,1.6065390043705);
#17929=CIRCLE('',#45997,1.60653900437051);
#17930=CIRCLE('',#45999,0.500000000000058);
#17931=CIRCLE('',#46000,0.500000000000058);
#17932=CIRCLE('',#46002,1.82809807486273);
#17933=CIRCLE('',#46003,1.82809807486273);
#17934=CIRCLE('',#46005,0.500000000000049);
#17935=CIRCLE('',#46006,0.500000000000049);
#17936=CIRCLE('',#46008,1.85841829658605);
#17937=CIRCLE('',#46009,1.85841829658605);
#17938=CIRCLE('',#46011,0.500000000000049);
#17939=CIRCLE('',#46012,0.500000000000049);
#17940=CIRCLE('',#46014,1.81285717707167);
#17941=CIRCLE('',#46015,1.81285717707167);
#17942=CIRCLE('',#46017,0.499999999999944);
#17943=CIRCLE('',#46018,0.499999999999944);
#17944=CIRCLE('',#46020,1.91146602029503);
#17945=CIRCLE('',#46021,1.91146602029503);
#17946=CIRCLE('',#46023,0.500000000000058);
#17947=CIRCLE('',#46024,0.500000000000058);
#17948=CIRCLE('',#46026,1.5496711026026);
#17949=CIRCLE('',#46027,1.5496711026026);
#17950=CIRCLE('',#46029,0.500000000000058);
#17951=CIRCLE('',#46030,0.500000000000058);
#17952=CIRCLE('',#46032,1.25936103546569);
#17953=CIRCLE('',#46033,1.25936103546568);
#17954=CIRCLE('',#46035,0.500000000000049);
#17955=CIRCLE('',#46036,0.500000000000049);
#17956=CIRCLE('',#46038,1.05888347462741);
#17957=CIRCLE('',#46039,1.05888347462741);
#17958=CIRCLE('',#46041,0.500000000000049);
#17959=CIRCLE('',#46042,0.500000000000049);
#17960=CIRCLE('',#46044,1.29583333162417);
#17961=CIRCLE('',#46045,1.29583333162417);
#17962=CIRCLE('',#46047,0.500000000000172);
#17963=CIRCLE('',#46048,0.500000000000172);
#17964=CIRCLE('',#46050,1.60653900437062);
#17965=CIRCLE('',#46051,1.60653900437062);
#17966=CIRCLE('',#46053,0.500000000000058);
#17967=CIRCLE('',#46054,0.500000000000058);
#17968=CIRCLE('',#46056,1.82809807486272);
#17969=CIRCLE('',#46057,1.82809807486272);
#17970=CIRCLE('',#46059,0.500000000000049);
#17971=CIRCLE('',#46060,0.500000000000049);
#17972=CIRCLE('',#46062,1.85841829658604);
#17973=CIRCLE('',#46063,1.85841829658605);
#17974=CIRCLE('',#46065,0.499999999999935);
#17975=CIRCLE('',#46066,0.499999999999935);
#17976=CIRCLE('',#46068,1.81285717707167);
#17977=CIRCLE('',#46069,1.81285717707167);
#17978=CIRCLE('',#46071,0.499999999999944);
#17979=CIRCLE('',#46072,0.499999999999944);
#17980=CIRCLE('',#46074,1.91146602029502);
#17981=CIRCLE('',#46075,1.91146602029502);
#17982=CIRCLE('',#46077,0.499999999999935);
#17983=CIRCLE('',#46078,0.499999999999935);
#17984=CIRCLE('',#46080,1.54967110260249);
#17985=CIRCLE('',#46081,1.54967110260249);
#17986=CIRCLE('',#46083,0.499999999999935);
#17987=CIRCLE('',#46084,0.499999999999935);
#17988=CIRCLE('',#46086,1.25936103546568);
#17989=CIRCLE('',#46087,1.25936103546568);
#17990=CIRCLE('',#46089,0.500000000000058);
#17991=CIRCLE('',#46090,0.500000000000058);
#17992=CIRCLE('',#46092,1.05888347462741);
#17993=CIRCLE('',#46093,1.05888347462741);
#17994=CIRCLE('',#46095,0.500000000000049);
#17995=CIRCLE('',#46096,0.500000000000049);
#17996=CIRCLE('',#46098,1.29583333162394);
#17997=CIRCLE('',#46099,1.29583333162394);
#17998=CIRCLE('',#46101,0.499999999999935);
#17999=CIRCLE('',#46102,0.499999999999935);
#18000=CIRCLE('',#46104,1.60653900437051);
#18001=CIRCLE('',#46105,1.60653900437051);
#18002=CIRCLE('',#46107,0.499999999999935);
#18003=CIRCLE('',#46108,0.499999999999935);
#18004=CIRCLE('',#46110,1.82809807486272);
#18005=CIRCLE('',#46111,1.82809807486273);
#18006=CIRCLE('',#46113,0.499999999999935);
#18007=CIRCLE('',#46114,0.499999999999935);
#18008=CIRCLE('',#46116,1.85841829658605);
#18009=CIRCLE('',#46117,1.85841829658605);
#18010=CIRCLE('',#46119,0.500000000000049);
#18011=CIRCLE('',#46120,0.500000000000049);
#18012=CIRCLE('',#46122,1.81285717707144);
#18013=CIRCLE('',#46123,1.81285717707144);
#18014=CIRCLE('',#46125,0.499999999999821);
#18015=CIRCLE('',#46126,0.499999999999821);
#18016=CIRCLE('',#46128,1.9114660202949);
#18017=CIRCLE('',#46129,1.9114660202949);
#18018=CIRCLE('',#46131,0.499999999999935);
#18019=CIRCLE('',#46132,0.499999999999935);
#18020=CIRCLE('',#46134,1.54967110260237);
#18021=CIRCLE('',#46135,1.54967110260237);
#18022=CIRCLE('',#46137,0.500000000000049);
#18023=CIRCLE('',#46138,0.500000000000049);
#18024=CIRCLE('',#46140,1.25936103546556);
#18025=CIRCLE('',#46141,1.25936103546568);
#18026=CIRCLE('',#46143,0.499999999999821);
#18027=CIRCLE('',#46144,0.499999999999821);
#18028=CIRCLE('',#46146,1.05888347462729);
#18029=CIRCLE('',#46147,1.0588834746273);
#18030=CIRCLE('',#46149,0.500000000000058);
#18031=CIRCLE('',#46150,0.500000000000058);
#18032=CIRCLE('',#46152,1.29583333162394);
#18033=CIRCLE('',#46153,1.29583333162394);
#18034=CIRCLE('',#46155,0.500000000000058);
#18035=CIRCLE('',#46156,0.500000000000058);
#18036=CIRCLE('',#46158,1.60653900437062);
#18037=CIRCLE('',#46159,1.60653900437062);
#18038=CIRCLE('',#46161,0.499999999999944);
#18039=CIRCLE('',#46162,0.499999999999944);
#18040=CIRCLE('',#46164,1.82809807486284);
#18041=CIRCLE('',#46165,1.82809807486284);
#18042=CIRCLE('',#46167,0.500000000000172);
#18043=CIRCLE('',#46168,0.500000000000172);
#18044=CIRCLE('',#46170,1.85841829658606);
#18045=CIRCLE('',#46171,1.85841829658606);
#18046=CIRCLE('',#46173,0.500000000000058);
#18047=CIRCLE('',#46174,0.500000000000058);
#18048=CIRCLE('',#46176,1.81285717707155);
#18049=CIRCLE('',#46177,1.81285717707155);
#18050=CIRCLE('',#46179,0.500000000000058);
#18051=CIRCLE('',#46180,0.500000000000058);
#18052=CIRCLE('',#46182,1.91146602029503);
#18053=CIRCLE('',#46183,1.91146602029503);
#18054=CIRCLE('',#46185,0.499999999999944);
#18055=CIRCLE('',#46186,0.499999999999944);
#18056=CIRCLE('',#46188,1.54967110260249);
#18057=CIRCLE('',#46189,1.5496711026025);
#18058=CIRCLE('',#46191,0.499999999999944);
#18059=CIRCLE('',#46192,0.499999999999944);
#18060=CIRCLE('',#46194,1.2593610354658);
#18061=CIRCLE('',#46195,1.25936103546556);
#18062=CIRCLE('',#46197,0.500000000000172);
#18063=CIRCLE('',#46198,0.500000000000172);
#18064=CIRCLE('',#46200,1.05888347462729);
#18065=CIRCLE('',#46201,1.05888347462729);
#18066=CIRCLE('',#46203,0.499999999999939);
#18067=CIRCLE('',#46204,0.499999999999935);
#18068=CIRCLE('',#46206,1.29583333162394);
#18069=CIRCLE('',#46207,1.29583333162394);
#18070=CIRCLE('',#46209,0.499999999999944);
#18071=CIRCLE('',#46210,0.499999999999944);
#18072=CIRCLE('',#46212,1.60653900437051);
#18073=CIRCLE('',#46213,1.60653900437051);
#18074=CIRCLE('',#46215,0.499999999999944);
#18075=CIRCLE('',#46216,0.499999999999944);
#18076=CIRCLE('',#46218,1.82809807486262);
#18077=CIRCLE('',#46219,1.82809807486262);
#18078=CIRCLE('',#46221,0.499999999999935);
#18079=CIRCLE('',#46222,0.499999999999935);
#18080=CIRCLE('',#46224,1.85841829658593);
#18081=CIRCLE('',#46225,1.85841829658593);
#18082=CIRCLE('',#46227,0.499999999999935);
#18083=CIRCLE('',#46228,0.499999999999935);
#18084=CIRCLE('',#46230,1.91146602029514);
#18085=CIRCLE('',#46231,1.91146602029514);
#18086=CIRCLE('',#46233,0.500000000000058);
#18087=CIRCLE('',#46234,0.500000000000058);
#18088=CIRCLE('',#46236,1.54967110260249);
#18089=CIRCLE('',#46237,1.54967110260249);
#18090=CIRCLE('',#46239,0.499999999999935);
#18091=CIRCLE('',#46240,0.499999999999935);
#18092=CIRCLE('',#46242,1.25936103546568);
#18093=CIRCLE('',#46243,1.2593610354658);
#18094=CIRCLE('',#46245,0.499999999999944);
#18095=CIRCLE('',#46246,0.499999999999944);
#18096=CIRCLE('',#46248,1.05888347462742);
#18097=CIRCLE('',#46249,1.05888347462742);
#18098=CIRCLE('',#46251,0.500000000000058);
#18099=CIRCLE('',#46252,0.500000000000058);
#18100=CIRCLE('',#46254,1.29583333162394);
#18101=CIRCLE('',#46255,1.29583333162395);
#18102=CIRCLE('',#46257,0.499999999999939);
#18103=CIRCLE('',#46258,0.499999999999944);
#18104=CIRCLE('',#46260,1.60653900437051);
#18105=CIRCLE('',#46261,1.60653900437051);
#18106=CIRCLE('',#46263,0.500000000000058);
#18107=CIRCLE('',#46264,0.500000000000058);
#18108=CIRCLE('',#46266,1.82809807486273);
#18109=CIRCLE('',#46267,1.82809807486273);
#18110=CIRCLE('',#46269,0.500000000000058);
#18111=CIRCLE('',#46270,0.500000000000058);
#18112=CIRCLE('',#46272,1.85841829658593);
#18113=CIRCLE('',#46273,1.85841829658594);
#18114=CIRCLE('',#46275,0.500000000000058);
#18115=CIRCLE('',#46276,0.500000000000058);
#18116=CIRCLE('',#46278,1.81285717707167);
#18117=CIRCLE('',#46279,1.81285717707167);
#18118=CIRCLE('',#46281,0.500000000000058);
#18119=CIRCLE('',#46282,0.500000000000058);
#18120=CIRCLE('',#46284,1.91146602029491);
#18121=CIRCLE('',#46285,1.91146602029491);
#18122=CIRCLE('',#46287,0.499999999999944);
#18123=CIRCLE('',#46288,0.499999999999944);
#18124=CIRCLE('',#46290,1.54967110260237);
#18125=CIRCLE('',#46291,1.54967110260237);
#18126=CIRCLE('',#46293,0.499999999999935);
#18127=CIRCLE('',#46294,0.499999999999935);
#18128=CIRCLE('',#46296,1.25936103546568);
#18129=CIRCLE('',#46297,1.25936103546556);
#18130=CIRCLE('',#46299,0.500000000000058);
#18131=CIRCLE('',#46300,0.500000000000058);
#18132=CIRCLE('',#46302,1.05888347462741);
#18133=CIRCLE('',#46303,1.05888347462741);
#18134=CIRCLE('',#46305,0.500000000000053);
#18135=CIRCLE('',#46306,0.500000000000058);
#18136=CIRCLE('',#46308,1.29583333162383);
#18137=CIRCLE('',#46309,1.29583333162383);
#18138=CIRCLE('',#46311,0.500000000000053);
#18139=CIRCLE('',#46312,0.500000000000058);
#18140=CIRCLE('',#46314,1.60653900437062);
#18141=CIRCLE('',#46315,1.60653900437062);
#18142=CIRCLE('',#46317,0.499999999999935);
#18143=CIRCLE('',#46318,0.499999999999935);
#18144=CIRCLE('',#46320,1.82809807486272);
#18145=CIRCLE('',#46321,1.82809807486272);
#18146=CIRCLE('',#46323,0.499999999999935);
#18147=CIRCLE('',#46324,0.499999999999935);
#18148=CIRCLE('',#46326,1.85841829658616);
#18149=CIRCLE('',#46327,1.85841829658616);
#18150=CIRCLE('',#46329,0.500000000000058);
#18151=CIRCLE('',#46330,0.500000000000058);
#18152=CIRCLE('',#46332,1.81285717707168);
#18153=CIRCLE('',#46333,1.81285717707168);
#18154=CIRCLE('',#46335,0.500000000000058);
#18155=CIRCLE('',#46336,0.500000000000049);
#18156=CIRCLE('',#46338,1.91146602029513);
#18157=CIRCLE('',#46339,1.91146602029514);
#18158=CIRCLE('',#46341,0.500000000000058);
#18159=CIRCLE('',#46342,0.500000000000058);
#18160=CIRCLE('',#46344,1.54967110260249);
#18161=CIRCLE('',#46345,1.5496711026025);
#18162=CIRCLE('',#46347,0.500000000000049);
#18163=CIRCLE('',#46348,0.500000000000049);
#18164=CIRCLE('',#46350,1.25936103546568);
#18165=CIRCLE('',#46351,1.25936103546568);
#18166=CIRCLE('',#46353,0.500000000000049);
#18167=CIRCLE('',#46354,0.500000000000049);
#18168=CIRCLE('',#46356,1.05888347462729);
#18169=CIRCLE('',#46357,1.05888347462729);
#18170=CIRCLE('',#46359,0.500000000000058);
#18171=CIRCLE('',#46360,0.500000000000058);
#18172=CIRCLE('',#46362,1.29583333162394);
#18173=CIRCLE('',#46363,1.29583333162394);
#18174=CIRCLE('',#46365,0.499999999999939);
#18175=CIRCLE('',#46366,0.499999999999944);
#18176=CIRCLE('',#46368,1.6065390043705);
#18177=CIRCLE('',#46369,1.60653900437051);
#18178=CIRCLE('',#46371,0.499999999999939);
#18179=CIRCLE('',#46372,0.499999999999944);
#18180=CIRCLE('',#46374,1.82809807486273);
#18181=CIRCLE('',#46375,1.82809807486273);
#18182=CIRCLE('',#46377,0.499999999999939);
#18183=CIRCLE('',#46378,0.499999999999935);
#18184=CIRCLE('',#46380,1.85841829658616);
#18185=CIRCLE('',#46381,1.85841829658616);
#18186=CIRCLE('',#46383,0.500000000000058);
#18187=CIRCLE('',#46384,0.500000000000049);
#18188=CIRCLE('',#46386,1.81285717707166);
#18189=CIRCLE('',#46387,1.81285717707167);
#18190=CIRCLE('',#46389,0.499999999999821);
#18191=CIRCLE('',#46390,0.499999999999821);
#18192=CIRCLE('',#46392,1.91146602029503);
#18193=CIRCLE('',#46393,1.91146602029503);
#18194=CIRCLE('',#46395,0.499999999999821);
#18195=CIRCLE('',#46396,0.499999999999821);
#18196=CIRCLE('',#46398,1.54967110260248);
#18197=CIRCLE('',#46399,1.54967110260248);
#18198=CIRCLE('',#46401,0.500000000000058);
#18199=CIRCLE('',#46402,0.500000000000058);
#18200=CIRCLE('',#46404,1.25936103546579);
#18201=CIRCLE('',#46405,1.25936103546568);
#18202=CIRCLE('',#46407,0.500000000000058);
#18203=CIRCLE('',#46408,0.500000000000058);
#18204=CIRCLE('',#46410,1.0588834746273);
#18205=CIRCLE('',#46411,1.0588834746273);
#18206=CIRCLE('',#46413,0.500000000000058);
#18207=CIRCLE('',#46414,0.500000000000058);
#18208=CIRCLE('',#46416,1.29583333162395);
#18209=CIRCLE('',#46417,1.29583333162395);
#18210=CIRCLE('',#46419,0.499999999999935);
#18211=CIRCLE('',#46420,0.499999999999935);
#18212=CIRCLE('',#46422,1.60653900437051);
#18213=CIRCLE('',#46423,1.60653900437051);
#18214=CIRCLE('',#46425,0.500000000000053);
#18215=CIRCLE('',#46426,0.500000000000049);
#18216=CIRCLE('',#46428,1.82809807486273);
#18217=CIRCLE('',#46429,1.82809807486273);
#18218=CIRCLE('',#46431,0.500000000000063);
#18219=CIRCLE('',#46432,0.500000000000058);
#18220=CIRCLE('',#46434,1.85841829658604);
#18221=CIRCLE('',#46435,1.85841829658605);
#18222=CIRCLE('',#46437,0.499999999999821);
#18223=CIRCLE('',#46438,0.499999999999821);
#18224=CIRCLE('',#46440,1.81285717707144);
#18225=CIRCLE('',#46441,1.81285717707144);
#18226=CIRCLE('',#46443,0.499999999999821);
#18227=CIRCLE('',#46444,0.499999999999821);
#18228=CIRCLE('',#46446,1.91146602029503);
#18229=CIRCLE('',#46447,1.91146602029503);
#18230=CIRCLE('',#46449,0.500000000000058);
#18231=CIRCLE('',#46450,0.500000000000058);
#18232=CIRCLE('',#46452,1.54967110260248);
#18233=CIRCLE('',#46453,1.54967110260249);
#18234=CIRCLE('',#46455,0.499999999999944);
#18235=CIRCLE('',#46456,0.499999999999944);
#18236=CIRCLE('',#46458,1.25936103546569);
#18237=CIRCLE('',#46459,1.25936103546568);
#18238=CIRCLE('',#46461,0.499999999999944);
#18239=CIRCLE('',#46462,0.499999999999944);
#18240=CIRCLE('',#46464,1.0588834746273);
#18241=CIRCLE('',#46465,1.0588834746273);
#18242=CIRCLE('',#46467,0.500000000000053);
#18243=CIRCLE('',#46468,0.500000000000054);
#18244=CIRCLE('',#46470,1.29583333162382);
#18245=CIRCLE('',#46471,1.29583333162382);
#18246=CIRCLE('',#46473,0.499999999999826);
#18247=CIRCLE('',#46474,0.499999999999826);
#18248=CIRCLE('',#46476,1.60653900437062);
#18249=CIRCLE('',#46477,1.60653900437062);
#18250=CIRCLE('',#46479,0.500000000000058);
#18251=CIRCLE('',#46480,0.500000000000058);
#18252=CIRCLE('',#46482,1.82809807486273);
#18253=CIRCLE('',#46483,1.82809807486272);
#18254=CIRCLE('',#46485,0.499999999999944);
#18255=CIRCLE('',#46486,0.499999999999944);
#18256=CIRCLE('',#46488,1.85841829658604);
#18257=CIRCLE('',#46489,1.85841829658605);
#18258=CIRCLE('',#46491,0.499999999999939);
#18259=CIRCLE('',#46492,0.499999999999939);
#18260=CIRCLE('',#46494,1.9114660202949);
#18261=CIRCLE('',#46495,1.9114660202949);
#18262=CIRCLE('',#46497,0.499999999999821);
#18263=CIRCLE('',#46498,0.499999999999821);
#18264=CIRCLE('',#46500,1.54967110260249);
#18265=CIRCLE('',#46501,1.54967110260249);
#18266=CIRCLE('',#46503,0.500000000000053);
#18267=CIRCLE('',#46504,0.500000000000049);
#18268=CIRCLE('',#46506,1.25936103546569);
#18269=CIRCLE('',#46507,1.25936103546556);
#18270=CIRCLE('',#46509,0.499999999999935);
#18271=CIRCLE('',#46510,0.499999999999935);
#18272=CIRCLE('',#46512,1.05888347462729);
#18273=CIRCLE('',#46513,1.05888347462729);
#18274=CIRCLE('',#46515,0.500000000000053);
#18275=CIRCLE('',#46516,0.500000000000054);
#18276=CIRCLE('',#46518,1.29583333162382);
#18277=CIRCLE('',#46519,1.29583333162371);
#18278=CIRCLE('',#46521,0.499999999999935);
#18279=CIRCLE('',#46522,0.499999999999935);
#18280=CIRCLE('',#46524,1.60653900437051);
#18281=CIRCLE('',#46525,1.60653900437051);
#18282=CIRCLE('',#46527,0.499999999999944);
#18283=CIRCLE('',#46528,0.499999999999939);
#18284=CIRCLE('',#46530,1.82809807486262);
#18285=CIRCLE('',#46531,1.82809807486262);
#18286=CIRCLE('',#46533,0.500000000000058);
#18287=CIRCLE('',#46534,0.500000000000058);
#18288=CIRCLE('',#46536,1.85841829658605);
#18289=CIRCLE('',#46537,1.85841829658605);
#18290=CIRCLE('',#46539,0.499999999999944);
#18291=CIRCLE('',#46540,0.499999999999939);
#18292=CIRCLE('',#46542,1.81285717707166);
#18293=CIRCLE('',#46543,1.81285717707166);
#18294=CIRCLE('',#46545,0.499999999999944);
#18295=CIRCLE('',#46546,0.499999999999944);
#18296=CIRCLE('',#46548,1.91146602029514);
#18297=CIRCLE('',#46549,1.91146602029514);
#18298=CIRCLE('',#46551,0.500000000000053);
#18299=CIRCLE('',#46552,0.500000000000054);
#18300=CIRCLE('',#46554,1.54967110260238);
#18301=CIRCLE('',#46555,1.54967110260238);
#18302=CIRCLE('',#46557,0.499999999999935);
#18303=CIRCLE('',#46558,0.499999999999935);
#18304=CIRCLE('',#46560,1.25936103546569);
#18305=CIRCLE('',#46561,1.25936103546579);
#18306=CIRCLE('',#46563,0.499999999999939);
#18307=CIRCLE('',#46564,0.499999999999944);
#18308=CIRCLE('',#46566,1.0588834746273);
#18309=CIRCLE('',#46567,1.0588834746273);
#18310=CIRCLE('',#46569,0.499999999999944);
#18311=CIRCLE('',#46570,0.499999999999944);
#18312=CIRCLE('',#46572,1.29583333162395);
#18313=CIRCLE('',#46573,1.29583333162395);
#18314=CIRCLE('',#46575,0.500000000000053);
#18315=CIRCLE('',#46576,0.500000000000054);
#18316=CIRCLE('',#46578,1.60653900437062);
#18317=CIRCLE('',#46579,1.60653900437063);
#18318=CIRCLE('',#46581,0.500000000000053);
#18319=CIRCLE('',#46582,0.500000000000054);
#18320=CIRCLE('',#46584,1.82809807486273);
#18321=CIRCLE('',#46585,1.82809807486273);
#18322=CIRCLE('',#46587,0.500000000000058);
#18323=CIRCLE('',#46588,0.500000000000058);
#18324=CIRCLE('',#46590,1.85841829658593);
#18325=CIRCLE('',#46591,1.85841829658594);
#18326=CIRCLE('',#46593,0.499999999999939);
#18327=CIRCLE('',#46594,0.499999999999939);
#18328=CIRCLE('',#46596,1.81285717707155);
#18329=CIRCLE('',#46597,1.81285717707156);
#18330=CIRCLE('',#46599,0.500000000000058);
#18331=CIRCLE('',#46600,0.500000000000058);
#18332=CIRCLE('',#46602,1.91146602029491);
#18333=CIRCLE('',#46603,1.91146602029491);
#18334=CIRCLE('',#46605,0.500000000000053);
#18335=CIRCLE('',#46606,0.500000000000054);
#18336=CIRCLE('',#46608,1.54967110260249);
#18337=CIRCLE('',#46609,1.54967110260249);
#18338=CIRCLE('',#46611,0.499999999999944);
#18339=CIRCLE('',#46612,0.499999999999944);
#18340=CIRCLE('',#46614,1.25936103546568);
#18341=CIRCLE('',#46615,1.25936103546569);
#18342=CIRCLE('',#46617,0.500000000000058);
#18343=CIRCLE('',#46618,0.500000000000058);
#18344=CIRCLE('',#46620,1.0588834746273);
#18345=CIRCLE('',#46621,1.0588834746273);
#18346=CIRCLE('',#46623,0.500000000000053);
#18347=CIRCLE('',#46624,0.500000000000054);
#18348=CIRCLE('',#46626,1.29583333162394);
#18349=CIRCLE('',#46627,1.29583333162394);
#18350=CIRCLE('',#46629,0.500000000000053);
#18351=CIRCLE('',#46630,0.500000000000054);
#18352=CIRCLE('',#46632,1.60653900437062);
#18353=CIRCLE('',#46633,1.60653900437062);
#18354=CIRCLE('',#46635,0.500000000000053);
#18355=CIRCLE('',#46636,0.500000000000054);
#18356=CIRCLE('',#46638,1.82809807486273);
#18357=CIRCLE('',#46639,1.82809807486272);
#18358=CIRCLE('',#46641,0.499999999999944);
#18359=CIRCLE('',#46642,0.499999999999944);
#18360=CIRCLE('',#46644,1.85841829658605);
#18361=CIRCLE('',#46645,1.85841829658605);
#18362=CIRCLE('',#46647,0.500000000000053);
#18363=CIRCLE('',#46648,0.500000000000054);
#18364=CIRCLE('',#46650,1.81285717707167);
#18365=CIRCLE('',#46651,1.81285717707167);
#18366=CIRCLE('',#46653,0.500000000000053);
#18367=CIRCLE('',#46654,0.500000000000054);
#18368=CIRCLE('',#46656,1.91146602029503);
#18369=CIRCLE('',#46657,1.91146602029503);
#18370=CIRCLE('',#46659,0.500000000000049);
#18371=CIRCLE('',#46660,0.500000000000049);
#18372=CIRCLE('',#46662,1.54967110260249);
#18373=CIRCLE('',#46663,1.54967110260249);
#18374=CIRCLE('',#46665,0.499999999999944);
#18375=CIRCLE('',#46666,0.499999999999944);
#18376=CIRCLE('',#46668,1.25936103546568);
#18377=CIRCLE('',#46669,1.25936103546568);
#18378=CIRCLE('',#46671,0.500000000000053);
#18379=CIRCLE('',#46672,0.500000000000054);
#18380=CIRCLE('',#46674,1.0588834746274);
#18381=CIRCLE('',#46675,1.0588834746274);
#18382=CIRCLE('',#46677,0.499999999999944);
#18383=CIRCLE('',#46678,0.499999999999944);
#18384=CIRCLE('',#46680,1.29583333162394);
#18385=CIRCLE('',#46681,1.29583333162394);
#18386=CIRCLE('',#46683,0.500000000000053);
#18387=CIRCLE('',#46684,0.500000000000054);
#18388=CIRCLE('',#46686,1.60653900437062);
#18389=CIRCLE('',#46687,1.60653900437062);
#18390=CIRCLE('',#46689,0.500000000000053);
#18391=CIRCLE('',#46690,0.500000000000054);
#18392=CIRCLE('',#46692,1.82809807486272);
#18393=CIRCLE('',#46693,1.82809807486272);
#18394=CIRCLE('',#46695,0.500000000000053);
#18395=CIRCLE('',#46696,0.500000000000054);
#18396=CIRCLE('',#46698,1.85841829658605);
#18397=CIRCLE('',#46699,1.85841829658605);
#18398=CIRCLE('',#46701,0.500000000000049);
#18399=CIRCLE('',#46702,0.500000000000049);
#18400=CIRCLE('',#46704,1.81285717707167);
#18401=CIRCLE('',#46705,1.81285717707167);
#18402=CIRCLE('',#46707,0.500000000000053);
#18403=CIRCLE('',#46708,0.500000000000054);
#18404=CIRCLE('',#46710,1.91146602029502);
#18405=CIRCLE('',#46711,1.91146602029502);
#18406=CIRCLE('',#46713,0.500000000000053);
#18407=CIRCLE('',#46714,0.500000000000049);
#18408=CIRCLE('',#46716,1.54967110260249);
#18409=CIRCLE('',#46717,1.54967110260249);
#18410=CIRCLE('',#46719,0.500000000000053);
#18411=CIRCLE('',#46720,0.500000000000049);
#18412=CIRCLE('',#46722,1.25936103546568);
#18413=CIRCLE('',#46723,1.25936103546557);
#18414=CIRCLE('',#46725,0.499999999999944);
#18415=CIRCLE('',#46726,0.499999999999944);
#18416=CIRCLE('',#46728,1.0588834746274);
#18417=CIRCLE('',#46729,1.05888347462741);
#18418=CIRCLE('',#46731,0.500000000000053);
#18419=CIRCLE('',#46732,0.500000000000054);
#18420=CIRCLE('',#46734,1.29583333162394);
#18421=CIRCLE('',#46735,1.29583333162394);
#18422=CIRCLE('',#46737,0.500000000000053);
#18423=CIRCLE('',#46738,0.500000000000054);
#18424=CIRCLE('',#46740,1.60653900437062);
#18425=CIRCLE('',#46741,1.60653900437062);
#18426=CIRCLE('',#46743,0.500000000000053);
#18427=CIRCLE('',#46744,0.500000000000054);
#18428=CIRCLE('',#46746,1.82809807486262);
#18429=CIRCLE('',#46747,1.82809807486262);
#18430=CIRCLE('',#46749,0.499999999999939);
#18431=CIRCLE('',#46750,0.499999999999939);
#18432=CIRCLE('',#46752,1.85841829658605);
#18433=CIRCLE('',#46753,1.85841829658605);
#18434=CIRCLE('',#46755,0.500000000000053);
#18435=CIRCLE('',#46756,0.500000000000054);
#18436=CIRCLE('',#46758,1.91146602029503);
#18437=CIRCLE('',#46759,1.91146602029503);
#18438=CIRCLE('',#46761,0.500000000000053);
#18439=CIRCLE('',#46762,0.500000000000054);
#18440=CIRCLE('',#46764,1.54967110260249);
#18441=CIRCLE('',#46765,1.54967110260249);
#18442=CIRCLE('',#46767,0.500000000000053);
#18443=CIRCLE('',#46768,0.500000000000054);
#18444=CIRCLE('',#46770,1.25936103546568);
#18445=CIRCLE('',#46771,1.25936103546568);
#18446=CIRCLE('',#46773,0.500000000000053);
#18447=CIRCLE('',#46774,0.500000000000054);
#18448=CIRCLE('',#46776,1.05888347462729);
#18449=CIRCLE('',#46777,1.05888347462729);
#18450=CIRCLE('',#46779,0.499999999999935);
#18451=CIRCLE('',#46780,0.499999999999935);
#18452=CIRCLE('',#46782,1.29583333162395);
#18453=CIRCLE('',#46783,1.29583333162395);
#18454=CIRCLE('',#46785,0.500000000000063);
#18455=CIRCLE('',#46786,0.500000000000063);
#18456=CIRCLE('',#46788,1.60653900437062);
#18457=CIRCLE('',#46789,1.60653900437062);
#18458=CIRCLE('',#46791,0.500000000000053);
#18459=CIRCLE('',#46792,0.500000000000054);
#18460=CIRCLE('',#46794,1.82809807486273);
#18461=CIRCLE('',#46795,1.82809807486273);
#18462=CIRCLE('',#46797,0.500000000000058);
#18463=CIRCLE('',#46798,0.500000000000058);
#18464=CIRCLE('',#46800,1.85841829658605);
#18465=CIRCLE('',#46801,1.85841829658605);
#18466=CIRCLE('',#46803,0.499999999999939);
#18467=CIRCLE('',#46804,0.499999999999939);
#18468=CIRCLE('',#46806,1.81285717707167);
#18469=CIRCLE('',#46807,1.81285717707167);
#18470=CIRCLE('',#46809,0.499999999999939);
#18471=CIRCLE('',#46810,0.499999999999939);
#18472=CIRCLE('',#46812,1.91146602029491);
#18473=CIRCLE('',#46813,1.91146602029491);
#18474=CIRCLE('',#46815,0.499999999999826);
#18475=CIRCLE('',#46816,0.499999999999826);
#18476=CIRCLE('',#46818,1.5496711026025);
#18477=CIRCLE('',#46819,1.54967110260249);
#18478=CIRCLE('',#46821,0.500000000000053);
#18479=CIRCLE('',#46822,0.500000000000054);
#18480=CIRCLE('',#46824,1.25936103546579);
#18481=CIRCLE('',#46825,1.25936103546568);
#18482=CIRCLE('',#46826,1.25936103546568);
#18483=CIRCLE('',#46828,0.500000000000063);
#18484=CIRCLE('',#46829,0.500000000000058);
#18485=CIRCLE('',#46831,1.0588834746273);
#18486=CIRCLE('',#46832,1.0588834746273);
#18487=CIRCLE('',#46834,0.499999999999935);
#18488=CIRCLE('',#46835,0.499999999999935);
#18489=CIRCLE('',#46837,1.29583333162395);
#18490=CIRCLE('',#46838,1.29583333162395);
#18491=CIRCLE('',#46840,0.500000000000053);
#18492=CIRCLE('',#46841,0.500000000000054);
#18493=CIRCLE('',#46843,1.60653900437074);
#18494=CIRCLE('',#46844,1.60653900437074);
#18495=CIRCLE('',#46846,0.500000000000058);
#18496=CIRCLE('',#46847,0.500000000000058);
#18497=CIRCLE('',#46849,1.82809807486273);
#18498=CIRCLE('',#46850,1.82809807486272);
#18499=CIRCLE('',#46852,0.500000000000053);
#18500=CIRCLE('',#46853,0.500000000000054);
#18501=CIRCLE('',#46855,1.85841829658616);
#18502=CIRCLE('',#46856,1.85841829658616);
#18503=CIRCLE('',#46858,0.500000000000167);
#18504=CIRCLE('',#46859,0.500000000000167);
#18505=CIRCLE('',#46861,1.81285717707155);
#18506=CIRCLE('',#46862,1.81285717707155);
#18507=CIRCLE('',#46864,0.499999999999935);
#18508=CIRCLE('',#46865,0.499999999999935);
#18509=CIRCLE('',#46867,1.91146602029503);
#18510=CIRCLE('',#46868,1.91146602029503);
#18511=CIRCLE('',#46870,0.500000000000053);
#18512=CIRCLE('',#46871,0.500000000000054);
#18513=CIRCLE('',#46873,1.54967110260249);
#18514=CIRCLE('',#46874,1.54967110260249);
#18515=CIRCLE('',#46875,1.54967110260249);
#18516=CIRCLE('',#46877,0.499999999999939);
#18517=CIRCLE('',#46878,0.499999999999939);
#18518=CIRCLE('',#46880,1.25936103546556);
#18519=CIRCLE('',#46881,1.25936103546568);
#18520=CIRCLE('',#46882,1.25936103546568);
#18521=CIRCLE('',#46884,0.499999999999821);
#18522=CIRCLE('',#46885,0.499999999999821);
#18523=CIRCLE('',#46887,1.05888347462729);
#18524=CIRCLE('',#46888,1.05888347462729);
#18525=CIRCLE('',#46890,0.500000000000058);
#18526=CIRCLE('',#46891,0.500000000000058);
#18527=CIRCLE('',#46893,1.29583333162382);
#18528=CIRCLE('',#46894,1.29583333162382);
#18529=CIRCLE('',#46896,0.500000000000053);
#18530=CIRCLE('',#46897,0.500000000000054);
#18531=CIRCLE('',#46899,1.60653900437074);
#18532=CIRCLE('',#46900,1.60653900437074);
#18533=CIRCLE('',#46902,0.500000000000063);
#18534=CIRCLE('',#46903,0.500000000000063);
#18535=CIRCLE('',#46905,1.82809807486273);
#18536=CIRCLE('',#46906,1.82809807486272);
#18537=CIRCLE('',#46908,0.500000000000053);
#18538=CIRCLE('',#46909,0.500000000000054);
#18539=CIRCLE('',#46911,1.85841829658605);
#18540=CIRCLE('',#46912,1.85841829658605);
#18541=CIRCLE('',#46914,0.500000000000049);
#18542=CIRCLE('',#46915,0.500000000000049);
#18543=CIRCLE('',#46917,1.81285717707166);
#18544=CIRCLE('',#46918,1.81285717707166);
#18545=CIRCLE('',#46920,0.500000000000049);
#18546=CIRCLE('',#46921,0.500000000000049);
#18547=CIRCLE('',#46923,1.91146602029503);
#18548=CIRCLE('',#46924,1.91146602029503);
#18549=CIRCLE('',#46925,1.91146602029503);
#18550=CIRCLE('',#46927,0.500000000000053);
#18551=CIRCLE('',#46928,0.500000000000054);
#18552=CIRCLE('',#46930,1.0588834746274);
#18553=CIRCLE('',#46931,1.0588834746274);
#18554=CIRCLE('',#46933,0.500000000000058);
#18555=CIRCLE('',#46934,0.500000000000058);
#18556=CIRCLE('',#46936,1.29583333162394);
#18557=CIRCLE('',#46937,1.29583333162395);
#18558=CIRCLE('',#46939,0.500000000000058);
#18559=CIRCLE('',#46940,0.500000000000058);
#18560=CIRCLE('',#46942,1.60653900437063);
#18561=CIRCLE('',#46943,1.60653900437063);
#18562=CIRCLE('',#46945,0.500000000000058);
#18563=CIRCLE('',#46946,0.500000000000058);
#18564=CIRCLE('',#46948,1.82809807486273);
#18565=CIRCLE('',#46949,1.82809807486273);
#18566=CIRCLE('',#46951,0.499999999999939);
#18567=CIRCLE('',#46952,0.499999999999939);
#18568=CIRCLE('',#46954,1.85841829658605);
#18569=CIRCLE('',#46955,1.85841829658605);
#18570=CIRCLE('',#46957,0.499999999999935);
#18571=CIRCLE('',#46958,0.499999999999935);
#18572=CIRCLE('',#46960,1.81285717707167);
#18573=CIRCLE('',#46961,1.81285717707167);
#18574=CIRCLE('',#46963,0.499999999999944);
#18575=CIRCLE('',#46964,0.499999999999944);
#18576=CIRCLE('',#46966,1.91146602029514);
#18577=CIRCLE('',#46967,1.91146602029503);
#18578=CIRCLE('',#46969,0.500000000000167);
#18579=CIRCLE('',#46970,0.500000000000167);
#18580=CIRCLE('',#46972,1.05888347462729);
#18581=CIRCLE('',#46973,1.0588834746273);
#18582=CIRCLE('',#46975,0.499999999999944);
#18583=CIRCLE('',#46976,0.499999999999944);
#18584=CIRCLE('',#46978,1.29583333162394);
#18585=CIRCLE('',#46979,1.29583333162394);
#18586=CIRCLE('',#46981,0.500000000000053);
#18587=CIRCLE('',#46982,0.500000000000049);
#18588=CIRCLE('',#46984,1.60653900437062);
#18589=CIRCLE('',#46985,1.60653900437062);
#18590=CIRCLE('',#46987,0.499999999999944);
#18591=CIRCLE('',#46988,0.499999999999944);
#18592=CIRCLE('',#46990,1.82809807486273);
#18593=CIRCLE('',#46991,1.82809807486273);
#18594=CIRCLE('',#46993,0.499999999999944);
#18595=CIRCLE('',#46994,0.499999999999944);
#18596=CIRCLE('',#46996,1.85841829658605);
#18597=CIRCLE('',#46997,1.85841829658605);
#18598=CIRCLE('',#46999,0.499999999999944);
#18599=CIRCLE('',#47000,0.499999999999944);
#18600=CIRCLE('',#47002,1.91146602029502);
#18601=CIRCLE('',#47003,1.91146602029503);
#18602=CIRCLE('',#47005,0.500000000000058);
#18603=CIRCLE('',#47006,0.500000000000054);
#18604=CIRCLE('',#47008,1.54967110260249);
#18605=CIRCLE('',#47009,1.54967110260261);
#18606=CIRCLE('',#47010,1.54967110260261);
#18607=CIRCLE('',#47012,0.499999999999939);
#18608=CIRCLE('',#47013,0.499999999999939);
#18609=CIRCLE('',#47015,1.05888347462741);
#18610=CIRCLE('',#47016,1.05888347462741);
#18611=CIRCLE('',#47018,0.499999999999939);
#18612=CIRCLE('',#47019,0.499999999999939);
#18613=CIRCLE('',#47021,1.29583333162394);
#18614=CIRCLE('',#47022,1.29583333162394);
#18615=CIRCLE('',#47024,0.499999999999939);
#18616=CIRCLE('',#47025,0.499999999999939);
#18617=CIRCLE('',#47027,1.60653900437063);
#18618=CIRCLE('',#47028,1.60653900437063);
#18619=CIRCLE('',#47030,0.500000000000058);
#18620=CIRCLE('',#47031,0.500000000000058);
#18621=CIRCLE('',#47033,1.82809807486273);
#18622=CIRCLE('',#47034,1.82809807486273);
#18623=CIRCLE('',#47036,0.500000000000058);
#18624=CIRCLE('',#47037,0.500000000000058);
#18625=CIRCLE('',#47039,1.85841829658593);
#18626=CIRCLE('',#47040,1.85841829658593);
#18627=CIRCLE('',#47042,0.499999999999939);
#18628=CIRCLE('',#47043,0.499999999999939);
#18629=CIRCLE('',#47045,1.81285717707154);
#18630=CIRCLE('',#47046,1.81285717707155);
#18631=CIRCLE('',#47048,0.499999999999939);
#18632=CIRCLE('',#47049,0.499999999999939);
#18633=CIRCLE('',#47051,1.91146602029503);
#18634=CIRCLE('',#47052,1.91146602029503);
#18635=CIRCLE('',#47054,0.499999999999939);
#18636=CIRCLE('',#47055,0.499999999999939);
#18637=CIRCLE('',#47057,1.54967110260237);
#18638=CIRCLE('',#47058,1.54967110260237);
#18639=CIRCLE('',#47060,0.499999999999939);
#18640=CIRCLE('',#47061,0.499999999999939);
#18641=CIRCLE('',#47063,1.05888347462729);
#18642=CIRCLE('',#47064,1.05888347462729);
#18643=CIRCLE('',#47066,0.500000000000053);
#18644=CIRCLE('',#47067,0.500000000000054);
#18645=CIRCLE('',#47069,1.29583333162383);
#18646=CIRCLE('',#47070,1.29583333162383);
#18647=CIRCLE('',#47072,0.500000000000053);
#18648=CIRCLE('',#47073,0.500000000000054);
#18649=CIRCLE('',#47075,1.60653900437051);
#18650=CIRCLE('',#47076,1.60653900437051);
#18651=CIRCLE('',#47078,0.499999999999935);
#18652=CIRCLE('',#47079,0.499999999999935);
#18653=CIRCLE('',#47081,1.82809807486262);
#18654=CIRCLE('',#47082,1.82809807486262);
#18655=CIRCLE('',#47084,0.500000000000063);
#18656=CIRCLE('',#47085,0.500000000000063);
#18657=CIRCLE('',#47087,1.85841829658605);
#18658=CIRCLE('',#47088,1.85841829658605);
#18659=CIRCLE('',#47090,0.500000000000053);
#18660=CIRCLE('',#47091,0.500000000000054);
#18661=CIRCLE('',#47093,1.81285717707166);
#18662=CIRCLE('',#47094,1.81285717707166);
#18663=CIRCLE('',#47096,0.499999999999935);
#18664=CIRCLE('',#47097,0.499999999999935);
#18665=CIRCLE('',#47099,1.9114660202949);
#18666=CIRCLE('',#47100,1.9114660202949);
#18667=CIRCLE('',#47102,0.499999999999935);
#18668=CIRCLE('',#47103,0.499999999999935);
#18669=CIRCLE('',#47105,1.54967110260248);
#18670=CIRCLE('',#47106,1.54967110260249);
#18671=CIRCLE('',#47108,0.499999999999935);
#18672=CIRCLE('',#47109,0.499999999999935);
#18673=CIRCLE('',#47111,1.25936103546556);
#18674=CIRCLE('',#47112,1.25936103546569);
#18675=CIRCLE('',#47113,1.25936103546569);
#18676=CIRCLE('',#47115,0.499999999999935);
#18677=CIRCLE('',#47116,0.499999999999935);
#18678=CIRCLE('',#47118,1.05888347462741);
#18679=CIRCLE('',#47119,1.05888347462741);
#18680=CIRCLE('',#47121,0.500000000000058);
#18681=CIRCLE('',#47122,0.500000000000058);
#18682=CIRCLE('',#47124,1.29583333162406);
#18683=CIRCLE('',#47125,1.29583333162406);
#18684=CIRCLE('',#47127,0.499999999999939);
#18685=CIRCLE('',#47128,0.499999999999944);
#18686=CIRCLE('',#47130,1.60653900437063);
#18687=CIRCLE('',#47131,1.60653900437063);
#18688=CIRCLE('',#47133,0.500000000000058);
#18689=CIRCLE('',#47134,0.500000000000058);
#18690=CIRCLE('',#47136,1.82809807486262);
#18691=CIRCLE('',#47137,1.82809807486262);
#18692=CIRCLE('',#47139,0.499999999999939);
#18693=CIRCLE('',#47140,0.499999999999939);
#18694=CIRCLE('',#47142,1.85841829658593);
#18695=CIRCLE('',#47143,1.85841829658593);
#18696=CIRCLE('',#47145,0.499999999999939);
#18697=CIRCLE('',#47146,0.499999999999939);
#18698=CIRCLE('',#47148,1.81285717707178);
#18699=CIRCLE('',#47149,1.81285717707179);
#18700=CIRCLE('',#47151,0.499999999999939);
#18701=CIRCLE('',#47152,0.499999999999939);
#18702=CIRCLE('',#47154,1.91146602029502);
#18703=CIRCLE('',#47155,1.91146602029502);
#18704=CIRCLE('',#47157,0.499999999999939);
#18705=CIRCLE('',#47158,0.499999999999939);
#18706=CIRCLE('',#47160,1.54967110260249);
#18707=CIRCLE('',#47161,1.54967110260249);
#18708=CIRCLE('',#47163,0.500000000000058);
#18709=CIRCLE('',#47164,0.500000000000058);
#18710=CIRCLE('',#47166,1.25936103546568);
#18711=CIRCLE('',#47167,1.25936103546556);
#18712=CIRCLE('',#47168,1.25936103546556);
#18713=CIRCLE('',#47170,0.499999999999935);
#18714=CIRCLE('',#47171,0.499999999999935);
#18715=CIRCLE('',#47173,1.05888347462729);
#18716=CIRCLE('',#47174,1.0588834746273);
#18717=CIRCLE('',#47176,0.500000000000053);
#18718=CIRCLE('',#47177,0.500000000000058);
#18719=CIRCLE('',#47179,1.29583333162406);
#18720=CIRCLE('',#47180,1.29583333162406);
#18721=CIRCLE('',#47182,0.500000000000177);
#18722=CIRCLE('',#47183,0.500000000000181);
#18723=CIRCLE('',#47185,1.60653900437051);
#18724=CIRCLE('',#47186,1.60653900437051);
#18725=CIRCLE('',#47188,0.499999999999939);
#18726=CIRCLE('',#47189,0.499999999999944);
#18727=CIRCLE('',#47191,1.82809807486261);
#18728=CIRCLE('',#47192,1.82809807486261);
#18729=CIRCLE('',#47194,0.499999999999944);
#18730=CIRCLE('',#47195,0.499999999999944);
#18731=CIRCLE('',#47197,1.85841829658594);
#18732=CIRCLE('',#47198,1.85841829658594);
#18733=CIRCLE('',#47200,0.499999999999939);
#18734=CIRCLE('',#47201,0.499999999999939);
#18735=CIRCLE('',#47203,1.81285717707156);
#18736=CIRCLE('',#47204,1.81285717707156);
#18737=CIRCLE('',#47206,0.499999999999944);
#18738=CIRCLE('',#47207,0.499999999999939);
#18739=CIRCLE('',#47209,1.91146602029503);
#18740=CIRCLE('',#47210,1.91146602029503);
#18741=CIRCLE('',#47212,0.500000000000053);
#18742=CIRCLE('',#47213,0.500000000000054);
#18743=CIRCLE('',#47215,1.5496711026026);
#18744=CIRCLE('',#47216,1.5496711026026);
#18745=CIRCLE('',#47218,0.500000000000058);
#18746=CIRCLE('',#47219,0.500000000000058);
#18747=CIRCLE('',#47221,1.2593610354658);
#18748=CIRCLE('',#47222,1.25936103546556);
#18749=CIRCLE('',#47224,0.500000000000063);
#18750=CIRCLE('',#47225,0.500000000000063);
#18751=CIRCLE('',#47227,1.05888347462741);
#18752=CIRCLE('',#47228,1.05888347462741);
#18753=CIRCLE('',#47230,0.499999999999939);
#18754=CIRCLE('',#47231,0.499999999999944);
#18755=CIRCLE('',#47233,1.29583333162395);
#18756=CIRCLE('',#47234,1.29583333162395);
#18757=CIRCLE('',#47236,0.500000000000053);
#18758=CIRCLE('',#47237,0.500000000000049);
#18759=CIRCLE('',#47239,1.60653900437063);
#18760=CIRCLE('',#47240,1.60653900437063);
#18761=CIRCLE('',#47242,0.500000000000167);
#18762=CIRCLE('',#47243,0.500000000000172);
#18763=CIRCLE('',#47245,1.82809807486262);
#18764=CIRCLE('',#47246,1.82809807486262);
#18765=CIRCLE('',#47248,0.499999999999944);
#18766=CIRCLE('',#47249,0.499999999999944);
#18767=CIRCLE('',#47251,1.85841829658604);
#18768=CIRCLE('',#47252,1.85841829658605);
#18769=CIRCLE('',#47254,0.499999999999944);
#18770=CIRCLE('',#47255,0.499999999999944);
#18771=CIRCLE('',#47257,1.91146602029502);
#18772=CIRCLE('',#47258,1.91146602029502);
#18773=CIRCLE('',#47260,0.499999999999944);
#18774=CIRCLE('',#47261,0.499999999999944);
#18775=CIRCLE('',#47263,1.5496711026026);
#18776=CIRCLE('',#47264,1.5496711026026);
#18777=CIRCLE('',#47266,0.500000000000053);
#18778=CIRCLE('',#47267,0.500000000000049);
#18779=CIRCLE('',#47269,1.25936103546567);
#18780=CIRCLE('',#47270,1.25936103546556);
#18781=CIRCLE('',#47272,0.499999999999939);
#18782=CIRCLE('',#47273,0.499999999999939);
#18783=CIRCLE('',#47275,1.05888347462741);
#18784=CIRCLE('',#47276,1.05888347462741);
#18785=CIRCLE('',#47278,0.500000000000053);
#18786=CIRCLE('',#47279,0.500000000000049);
#18787=CIRCLE('',#47281,1.29583333162394);
#18788=CIRCLE('',#47282,1.29583333162394);
#18789=CIRCLE('',#47284,0.499999999999939);
#18790=CIRCLE('',#47285,0.499999999999944);
#18791=CIRCLE('',#47287,1.6065390043705);
#18792=CIRCLE('',#47288,1.6065390043705);
#18793=CIRCLE('',#47290,0.499999999999939);
#18794=CIRCLE('',#47291,0.499999999999935);
#18795=CIRCLE('',#47293,1.82809807486262);
#18796=CIRCLE('',#47294,1.82809807486262);
#18797=CIRCLE('',#47296,0.500000000000053);
#18798=CIRCLE('',#47297,0.500000000000058);
#18799=CIRCLE('',#47299,1.85841829658593);
#18800=CIRCLE('',#47300,1.85841829658593);
#18801=CIRCLE('',#47302,0.499999999999939);
#18802=CIRCLE('',#47303,0.499999999999944);
#18803=CIRCLE('',#47305,1.81285717707167);
#18804=CIRCLE('',#47306,1.81285717707168);
#18805=CIRCLE('',#47308,0.500000000000058);
#18806=CIRCLE('',#47309,0.500000000000058);
#18807=CIRCLE('',#47311,1.91146602029503);
#18808=CIRCLE('',#47312,1.91146602029503);
#18809=CIRCLE('',#47314,0.500000000000053);
#18810=CIRCLE('',#47315,0.500000000000049);
#18811=CIRCLE('',#47317,1.54967110260249);
#18812=CIRCLE('',#47318,1.54967110260249);
#18813=CIRCLE('',#47320,0.500000000000058);
#18814=CIRCLE('',#47321,0.500000000000058);
#18815=CIRCLE('',#47323,1.25936103546568);
#18816=CIRCLE('',#47324,1.25936103546557);
#18817=CIRCLE('',#47326,0.499999999999939);
#18818=CIRCLE('',#47327,0.499999999999939);
#18819=CIRCLE('',#47329,1.05888347462729);
#18820=CIRCLE('',#47330,1.05888347462729);
#18821=CIRCLE('',#47332,0.500000000000053);
#18822=CIRCLE('',#47333,0.500000000000049);
#18823=CIRCLE('',#47335,1.29583333162382);
#18824=CIRCLE('',#47336,1.29583333162382);
#18825=CIRCLE('',#47338,0.499999999999935);
#18826=CIRCLE('',#47339,0.499999999999935);
#18827=CIRCLE('',#47341,1.60653900437062);
#18828=CIRCLE('',#47342,1.60653900437062);
#18829=CIRCLE('',#47344,0.500000000000058);
#18830=CIRCLE('',#47345,0.500000000000058);
#18831=CIRCLE('',#47347,1.82809807486272);
#18832=CIRCLE('',#47348,1.82809807486272);
#18833=CIRCLE('',#47350,0.500000000000058);
#18834=CIRCLE('',#47351,0.500000000000058);
#18835=CIRCLE('',#47353,1.85841829658594);
#18836=CIRCLE('',#47354,1.85841829658594);
#18837=CIRCLE('',#47356,0.49999999999983);
#18838=CIRCLE('',#47357,0.49999999999983);
#18839=CIRCLE('',#47359,1.81285717707166);
#18840=CIRCLE('',#47360,1.81285717707156);
#18841=CIRCLE('',#47362,0.499999999999944);
#18842=CIRCLE('',#47363,0.499999999999944);
#18843=CIRCLE('',#47365,1.91146602029502);
#18844=CIRCLE('',#47366,1.91146602029502);
#18845=CIRCLE('',#47368,0.499999999999939);
#18846=CIRCLE('',#47369,0.499999999999935);
#18847=CIRCLE('',#47371,1.5496711026025);
#18848=CIRCLE('',#47372,1.5496711026025);
#18849=CIRCLE('',#47374,0.500000000000053);
#18850=CIRCLE('',#47375,0.500000000000058);
#18851=CIRCLE('',#47377,1.25936103546568);
#18852=CIRCLE('',#47378,1.25936103546568);
#18853=CIRCLE('',#47380,0.500000000000053);
#18854=CIRCLE('',#47381,0.500000000000058);
#18855=CIRCLE('',#47382,61.7766775875802);
#18856=CIRCLE('',#47383,69.9999992709118);
#18857=CIRCLE('',#47384,45.1634298617437);
#18858=CIRCLE('',#47385,45.1634298617437);
#18859=CIRCLE('',#47386,45.1634298617437);
#18860=CIRCLE('',#47387,45.1634298617437);
#18861=CIRCLE('',#47388,45.1634298617437);
#18862=CIRCLE('',#47389,45.1634298617437);
#18863=CIRCLE('',#47390,45.1634298617437);
#18864=CIRCLE('',#47391,45.1634298617437);
#18865=CIRCLE('',#47392,45.1634298617437);
#18866=CIRCLE('',#47393,45.1634298617437);
#18867=CIRCLE('',#47394,45.1634298617437);
#18868=CIRCLE('',#47395,45.1634298617437);
#18869=CIRCLE('',#47396,45.1634298617437);
#18870=CIRCLE('',#47397,45.1634298617437);
#18871=CIRCLE('',#47398,45.1634298617437);
#18872=CIRCLE('',#47399,45.1634298617437);
#18873=CIRCLE('',#47400,45.1634298617437);
#18874=CIRCLE('',#47401,45.1634298617437);
#18875=CIRCLE('',#47402,45.1634298617437);
#18876=CIRCLE('',#47403,45.1634298617437);
#18877=CIRCLE('',#47404,45.1634298617437);
#18878=CIRCLE('',#47405,45.1634298617437);
#18879=CIRCLE('',#47406,45.1634298617437);
#18880=CIRCLE('',#47407,45.1634298617437);
#18881=CIRCLE('',#47408,45.1634298617437);
#18882=CIRCLE('',#47409,69.9999999999885);
#18883=CIRCLE('',#47411,62.7000000000001);
#18884=CIRCLE('',#47412,0.299999997585228);
#18885=CIRCLE('',#47413,0.299999997585552);
#18886=CIRCLE('',#47415,9.13915332737463);
#18887=CIRCLE('',#47416,10.7297759926639);
#18888=CIRCLE('',#47417,9.13915332737463);
#18889=CIRCLE('',#47419,1.);
#18890=CIRCLE('',#47420,10.9885950377664);
#18891=CIRCLE('',#47422,0.2);
#18892=CIRCLE('',#47423,8.99091713639504);
#18893=CIRCLE('',#47424,8.99091713639504);
#18894=CIRCLE('',#47426,63.3529411764695);
#18895=CIRCLE('',#47427,65.);
#18896=CIRCLE('',#47429,22.9734468277121);
#18897=CIRCLE('',#47430,0.500000000000003);
#18898=CIRCLE('',#47431,22.4734498738832);
#18899=CIRCLE('',#47432,0.499999999999997);
#18900=CIRCLE('',#47434,0.5);
#18901=CIRCLE('',#47435,0.5);
#18902=CIRCLE('',#47436,0.5);
#18903=CIRCLE('',#47438,0.300000458890413);
#18904=CIRCLE('',#47440,8.99091713639514);
#18905=CIRCLE('',#47441,8.99091713639514);
#18906=CIRCLE('',#47443,0.2);
#18907=CIRCLE('',#47444,8.83409633647444);
#18908=CIRCLE('',#47446,0.500000000000053);
#18909=CIRCLE('',#47452,8.3031389659941);
#18910=CIRCLE('',#47454,0.999999999999995);
#18911=CIRCLE('',#47455,8.01024574718068);
#18912=CIRCLE('',#47458,8.3031389659941);
#18913=CIRCLE('',#47460,8.3031389659941);
#18914=CIRCLE('',#47463,5.888925403621);
#18915=CIRCLE('',#47464,5.888925403621);
#18916=CIRCLE('',#47467,6.59603218480755);
#18917=CIRCLE('',#47468,8.01024574718068);
#18918=CIRCLE('',#47470,6.59603218480755);
#18919=CIRCLE('',#47471,8.01024574718068);
#18920=CIRCLE('',#47474,0.999999999999995);
#18921=CIRCLE('',#47475,0.999999999999995);
#18922=CIRCLE('',#47477,0.999999999999995);
#18923=CIRCLE('',#47479,0.999999999999995);
#18924=CIRCLE('',#47482,0.999999999999995);
#18925=CIRCLE('',#47484,0.999999999999995);
#18926=CIRCLE('',#47486,0.999999999999995);
#18927=CIRCLE('',#47488,0.500000000000008);
#18928=CIRCLE('',#47489,0.500000000000007);
#18929=CIRCLE('',#47490,0.500000000000004);
#18930=CIRCLE('',#47492,0.499999999999999);
#18931=CIRCLE('',#47493,0.500000411450474);
#18932=CIRCLE('',#47495,0.499999999999999);
#18933=CIRCLE('',#47497,0.299999999999944);
#18934=CIRCLE('',#47498,0.299999999999994);
#18935=CIRCLE('',#47499,0.30000000000002);
#18936=CIRCLE('',#47500,0.300000000000048);
#18937=CIRCLE('',#47501,1.99999248610074);
#18938=CIRCLE('',#47502,0.500000000000003);
#18939=CIRCLE('',#47504,0.500000000000003);
#18940=CIRCLE('',#47505,22.4734498738832);
#18941=CIRCLE('',#47506,22.9734468277121);
#18942=CIRCLE('',#47507,0.5);
#18943=CIRCLE('',#47508,1.99999248601366);
#18944=CIRCLE('',#47509,1.9999924861154);
#18945=CIRCLE('',#47511,0.5);
#18946=CIRCLE('',#47512,1.99999248606425);
#18947=CIRCLE('',#47513,2.00000000000005);
#18948=CIRCLE('',#47515,65.);
#18949=CIRCLE('',#47516,1.9999999999645);
#18950=CIRCLE('',#47517,2.);
#18951=CIRCLE('',#47519,63.5880980163361);
#18952=CIRCLE('',#47521,2.00000590977433);
#18953=CIRCLE('',#47522,1.99999999999992);
#18954=CIRCLE('',#47524,1.99999999997966);
#18955=CIRCLE('',#47533,146.40821343272);
#18956=CIRCLE('',#47534,146.408212929521);
#18957=CIRCLE('',#48139,10.9781962809611);
#18958=CIRCLE('',#48140,10.9781962809611);
#18959=CIRCLE('',#48141,0.5);
#18960=CIRCLE('',#48142,10.4786337076502);
#18961=CIRCLE('',#48144,9.49325771931311);
#18962=CIRCLE('',#48145,0.5);
#18963=CIRCLE('',#48146,8.99369514600215);
#18964=CIRCLE('',#48148,6.99999999999999);
#18965=CIRCLE('',#48149,6.99999999999999);
#18966=CIRCLE('',#48151,8.98718018777775);
#18967=CIRCLE('',#48152,1.);
#18968=CIRCLE('',#48153,7.98801213467717);
#18969=CIRCLE('',#48155,10.);
#18970=CIRCLE('',#48158,6.99999999999999);
#18971=CIRCLE('',#48159,6.99999999999999);
#18972=CIRCLE('',#48164,0.500000000000028);
#18973=CIRCLE('',#48165,0.500000000000028);
#18974=CIRCLE('',#48168,0.499999999999973);
#18975=CIRCLE('',#48169,0.499999999999973);
#18976=CIRCLE('',#48174,0.500000000000028);
#18977=CIRCLE('',#48175,0.499999999999973);
#18978=CIRCLE('',#48178,0.499999999999973);
#18979=CIRCLE('',#48181,0.500000000000028);
#18980=CIRCLE('',#48184,28.5226030790361);
#18981=CIRCLE('',#48185,28.5226030790361);
#18982=CIRCLE('',#48186,28.5226030790361);
#18983=CIRCLE('',#48187,27.5913762017691);
#18984=CIRCLE('',#48188,28.5226030790361);
#18985=CIRCLE('',#48189,1.86064640637173);
#18986=CIRCLE('',#48191,1.);
#18987=CIRCLE('',#48192,27.5226030790361);
#18988=CIRCLE('',#48194,16.5);
#18989=CIRCLE('',#48195,16.5);
#18990=CIRCLE('',#48197,16.5);
#18991=CIRCLE('',#48198,16.5);
#18992=CIRCLE('',#48200,16.5);
#18993=CIRCLE('',#48201,16.5);
#18994=CIRCLE('',#48203,16.);
#18995=CIRCLE('',#48204,16.);
#18996=CIRCLE('',#48205,16.);
#18997=CIRCLE('',#48206,16.);
#18998=CIRCLE('',#48207,16.);
#18999=CIRCLE('',#48209,3.96802221877415);
#19000=CIRCLE('',#48210,3.96802221877415);
#19001=CIRCLE('',#48212,0.5);
#19002=CIRCLE('',#48213,4.46802221877415);
#19003=CIRCLE('',#48214,0.5);
#19004=CIRCLE('',#48216,15.5);
#19005=CIRCLE('',#48218,0.5);
#19006=CIRCLE('',#48219,3.46802221877415);
#19007=CIRCLE('',#48220,0.5);
#19008=CIRCLE('',#48222,0.5);
#19009=CIRCLE('',#48223,15.5);
#19010=CIRCLE('',#48225,16.);
#19011=CIRCLE('',#48226,16.);
#19012=CIRCLE('',#48227,16.);
#19013=CIRCLE('',#48228,16.);
#19014=CIRCLE('',#48229,16.);
#19015=CIRCLE('',#48231,3.96802221877416);
#19016=CIRCLE('',#48232,3.96802221877416);
#19017=CIRCLE('',#48234,0.5);
#19018=CIRCLE('',#48235,4.46802221877416);
#19019=CIRCLE('',#48236,0.5);
#19020=CIRCLE('',#48238,15.5);
#19021=CIRCLE('',#48240,0.5);
#19022=CIRCLE('',#48241,3.46802221877416);
#19023=CIRCLE('',#48242,0.5);
#19024=CIRCLE('',#48244,0.5);
#19025=CIRCLE('',#48245,15.5);
#19026=CIRCLE('',#48247,16.);
#19027=CIRCLE('',#48248,16.);
#19028=CIRCLE('',#48249,16.);
#19029=CIRCLE('',#48250,16.);
#19030=CIRCLE('',#48251,16.);
#19031=CIRCLE('',#48253,3.96802221877416);
#19032=CIRCLE('',#48254,3.96802221877416);
#19033=CIRCLE('',#48256,0.5);
#19034=CIRCLE('',#48257,4.46802221877416);
#19035=CIRCLE('',#48258,0.5);
#19036=CIRCLE('',#48260,15.5);
#19037=CIRCLE('',#48262,0.5);
#19038=CIRCLE('',#48263,3.46802221877416);
#19039=CIRCLE('',#48264,0.5);
#19040=CIRCLE('',#48266,0.5);
#19041=CIRCLE('',#48267,15.5);
#19042=CIRCLE('',#48269,26.0226030790361);
#19043=CIRCLE('',#48270,26.0226030790361);
#19044=CIRCLE('',#48271,26.0226030790361);
#19045=CIRCLE('',#48272,26.0226030790361);
#19046=CIRCLE('',#48274,25.3226030790361);
#19047=CIRCLE('',#48276,29.5);
#19048=CIRCLE('',#48277,29.5);
#19049=CIRCLE('',#48279,30.);
#19050=CIRCLE('',#48280,30.);
#19051=CIRCLE('',#48282,30.);
#19052=CIRCLE('',#48283,30.);
#19053=CIRCLE('',#48287,0.500000000000003);
#19054=CIRCLE('',#48288,0.5);
#19055=CIRCLE('',#48289,0.500000000000003);
#19056=CIRCLE('',#48291,29.7179449471771);
#19057=CIRCLE('',#48292,0.5);
#19058=CIRCLE('',#48294,29.7179449471771);
#19059=CIRCLE('',#48295,0.5);
#19060=CIRCLE('',#48297,0.5);
#19061=CIRCLE('',#48299,0.5);
#19062=CIRCLE('',#48301,0.5);
#19063=CIRCLE('',#48302,0.5);
#19064=CIRCLE('',#48304,0.5);
#19065=CIRCLE('',#48306,0.5);
#19066=CIRCLE('',#48308,0.5);
#19067=CIRCLE('',#48310,0.5);
#19068=CIRCLE('',#48312,0.5);
#19069=CIRCLE('',#48313,0.5);
#19070=CIRCLE('',#48315,0.5);
#19071=CIRCLE('',#48317,0.5);
#19072=CIRCLE('',#48319,0.5);
#19073=CIRCLE('',#48321,0.5);
#19074=CIRCLE('',#48323,0.500000000000003);
#19075=CIRCLE('',#48325,0.500000000000003);
#19076=CIRCLE('',#48326,0.5);
#19077=CIRCLE('',#48328,0.700000000000006);
#19078=CIRCLE('',#48329,4.75563473233925);
#19079=CIRCLE('',#48330,0.700000000000006);
#19080=CIRCLE('',#48331,4.05563473233925);
#19081=CIRCLE('',#48333,0.700000000000006);
#19082=CIRCLE('',#48335,0.700000000000006);
#19083=CIRCLE('',#48337,4.75563473233925);
#19084=CIRCLE('',#48338,4.05563473233925);
#19085=CIRCLE('',#48340,0.700000000000006);
#19086=CIRCLE('',#48341,0.700000000000006);
#19087=CIRCLE('',#48342,0.699999999999998);
#19088=CIRCLE('',#48343,0.700000000000006);
#19089=CIRCLE('',#48345,0.700000000000006);
#19090=CIRCLE('',#48347,0.7);
#19091=CIRCLE('',#48348,26.7226030790361);
#19092=CIRCLE('',#48350,0.700000000000006);
#19093=CIRCLE('',#48352,0.700000000000006);
#19094=CIRCLE('',#48353,4.05563473233925);
#19095=CIRCLE('',#48354,4.75563473233925);
#19096=CIRCLE('',#48355,0.700000000000006);
#19097=CIRCLE('',#48356,0.700000000000006);
#19098=CIRCLE('',#48357,0.700000000000006);
#19099=CIRCLE('',#48359,0.700000000000006);
#19100=CIRCLE('',#48360,4.75563473233925);
#19101=CIRCLE('',#48361,5.45563473233926);
#19102=CIRCLE('',#48373,0.499999999999999);
#19103=CIRCLE('',#48375,0.5);
#19104=CIRCLE('',#48376,3.96802221877416);
#19105=CIRCLE('',#48377,3.46802221877416);
#19106=CIRCLE('',#48380,0.500000000000001);
#19107=CIRCLE('',#48381,0.5);
#19108=CIRCLE('',#48382,16.5);
#19109=CIRCLE('',#48383,0.5);
#19110=CIRCLE('',#48384,0.5);
#19111=CIRCLE('',#48386,0.5);
#19112=CIRCLE('',#48388,0.499999999999999);
#19113=CIRCLE('',#48390,0.5);
#19114=CIRCLE('',#48392,0.5);
#19115=CIRCLE('',#48393,0.499999999999999);
#19116=CIRCLE('',#48395,3.96802221877416);
#19117=CIRCLE('',#48396,3.46802221877416);
#19118=CIRCLE('',#48397,0.499999999999998);
#19119=CIRCLE('',#48407,0.500000000000001);
#19120=CIRCLE('',#48409,0.500000000000003);
#19121=CIRCLE('',#48410,3.96802221877416);
#19122=CIRCLE('',#48411,3.46802221877416);
#19123=CIRCLE('',#48414,0.499999999999999);
#19124=CIRCLE('',#48415,0.5);
#19125=CIRCLE('',#48416,16.5);
#19126=CIRCLE('',#48417,0.5);
#19127=CIRCLE('',#48418,0.5);
#19128=CIRCLE('',#48420,0.5);
#19129=CIRCLE('',#48422,0.500000000000002);
#19130=CIRCLE('',#48424,0.5);
#19131=CIRCLE('',#48426,0.5);
#19132=CIRCLE('',#48427,0.500000000000003);
#19133=CIRCLE('',#48429,3.96802221877416);
#19134=CIRCLE('',#48430,3.46802221877416);
#19135=CIRCLE('',#48431,0.5);
#19136=CIRCLE('',#48441,0.500000000000001);
#19137=CIRCLE('',#48443,0.500000000000003);
#19138=CIRCLE('',#48444,3.96802221877415);
#19139=CIRCLE('',#48445,3.46802221877417);
#19140=CIRCLE('',#48448,0.499999999999999);
#19141=CIRCLE('',#48449,0.5);
#19142=CIRCLE('',#48450,16.5);
#19143=CIRCLE('',#48451,0.5);
#19144=CIRCLE('',#48452,0.5);
#19145=CIRCLE('',#48454,0.5);
#19146=CIRCLE('',#48456,0.500000000000002);
#19147=CIRCLE('',#48458,0.5);
#19148=CIRCLE('',#48460,0.5);
#19149=CIRCLE('',#48461,0.499999999999997);
#19150=CIRCLE('',#48463,3.96802221877415);
#19151=CIRCLE('',#48464,3.46802221877417);
#19152=CIRCLE('',#48465,0.5);
#19153=CIRCLE('',#48478,0.5);
#19154=CIRCLE('',#48479,0.5);
#19155=CIRCLE('',#48481,0.500000000000003);
#19156=CIRCLE('',#48482,30.);
#19157=CIRCLE('',#48483,1.);
#19158=CIRCLE('',#48484,0.5);
#19159=CIRCLE('',#48485,0.499999999999988);
#19160=CIRCLE('',#48487,0.5);
#19161=CIRCLE('',#48488,0.500000000000011);
#19162=CIRCLE('',#48489,0.5);
#19163=CIRCLE('',#48490,1.);
#19164=CIRCLE('',#48491,0.499999999999989);
#19165=CIRCLE('',#48493,0.5);
#19166=CIRCLE('',#48494,0.499999999999993);
#19167=CIRCLE('',#48496,0.500000000000003);
#19168=CIRCLE('',#48497,30.);
#19169=CIRCLE('',#48498,0.5);
#19170=CIRCLE('',#48500,1.);
#19171=CIRCLE('',#48501,1.);
#19172=CIRCLE('',#48502,1.);
#19173=CIRCLE('',#48504,1.);
#19174=CIRCLE('',#48505,1.);
#19175=CIRCLE('',#48506,2.);
#19176=CIRCLE('',#48508,0.999999999999994);
#19177=CIRCLE('',#48509,27.5226030790361);
#19178=CIRCLE('',#48511,1.);
#19179=CIRCLE('',#48513,1.);
#19180=CIRCLE('',#48514,1.);
#19181=CIRCLE('',#48515,2.);
#19182=CIRCLE('',#48516,0.999999999999999);
#19183=CIRCLE('',#48517,1.);
#19184=CIRCLE('',#48519,1.);
#19185=CIRCLE('',#48521,1.);
#19186=CIRCLE('',#48522,29.5226030790361);
#19187=CIRCLE('',#48524,0.999999999999999);
#19188=CIRCLE('',#48526,1.);
#19189=CIRCLE('',#48527,1.);
#19190=CIRCLE('',#48529,1.);
#19191=CIRCLE('',#48530,29.5226030790361);
#19192=CIRCLE('',#48532,1.);
#19193=CIRCLE('',#48534,1.);
#19194=CIRCLE('',#48535,1.);
#19195=CIRCLE('',#48536,1.00000000000001);
#19196=CIRCLE('',#48538,1.);
#19197=CIRCLE('',#48539,1.00000000000001);
#19198=CIRCLE('',#48540,1.);
#19199=CIRCLE('',#48541,0.99999999999999);
#19200=CIRCLE('',#48542,1.00000000000001);
#19201=CIRCLE('',#48543,0.999999999999988);
#19202=CIRCLE('',#48545,1.);
#19203=CIRCLE('',#48546,1.);
#19204=CIRCLE('',#48547,1.00000000000001);
#19205=CIRCLE('',#48548,1.);
#19206=CIRCLE('',#48549,32.4650886384815);
#19207=CIRCLE('',#48550,33.3654637529391);
#19208=CIRCLE('',#48551,0.999999999999998);
#19209=CIRCLE('',#48552,1.);
#19210=CIRCLE('',#48553,1.);
#19211=CIRCLE('',#48554,1.);
#19212=CIRCLE('',#48555,33.3726238561351);
#19213=CIRCLE('',#48556,32.4650889393932);
#19214=CIRCLE('',#48559,30.);
#19215=CIRCLE('',#48560,30.);
#19216=CIRCLE('',#48561,30.);
#19217=CIRCLE('',#48576,12.);
#19218=CIRCLE('',#48577,12.);
#19219=CIRCLE('',#48579,7.);
#19220=CIRCLE('',#48580,7.);
#19221=CIRCLE('',#48581,7.);
#19222=CIRCLE('',#48582,7.);
#19223=CIRCLE('',#48583,3.);
#19224=CIRCLE('',#48584,3.);
#19225=CIRCLE('',#48585,3.);
#19226=CIRCLE('',#48586,3.);
#19227=CIRCLE('',#48587,3.);
#19228=CIRCLE('',#48588,3.);
#19229=CIRCLE('',#48589,3.);
#19230=CIRCLE('',#48590,3.);
#19231=CIRCLE('',#48596,7.);
#19232=CIRCLE('',#48597,7.);
#19233=CIRCLE('',#48598,7.);
#19234=CIRCLE('',#48599,7.);
#19235=CIRCLE('',#48602,2.58578643762686);
#19236=CIRCLE('',#48603,2.58578643762686);
#19237=CIRCLE('',#48606,2.58578643762694);
#19238=CIRCLE('',#48607,2.58578643762694);
#19239=CIRCLE('',#48610,8.00000000000001);
#19240=CIRCLE('',#48611,8.00000000000001);
#19241=CIRCLE('',#48613,8.00000000000001);
#19242=CIRCLE('',#48614,8.00000000000001);
#19243=CIRCLE('',#48616,8.);
#19244=CIRCLE('',#48617,8.);
#19245=CIRCLE('',#48619,8.);
#19246=CIRCLE('',#48620,8.);
#19247=CIRCLE('',#48622,8.);
#19248=CIRCLE('',#48623,8.);
#19249=CIRCLE('',#48625,8.);
#19250=CIRCLE('',#48626,8.);
#19251=CIRCLE('',#48629,7.70710678118658);
#19252=CIRCLE('',#48630,3.29289321881343);
#19253=CIRCLE('',#48633,7.70710678118658);
#19254=CIRCLE('',#48634,3.29289321881343);
#19255=CIRCLE('',#48638,3.29289321881349);
#19256=CIRCLE('',#48639,7.70710678118658);
#19257=CIRCLE('',#48642,3.29289321881349);
#19258=CIRCLE('',#48643,7.70710678118658);
#19259=CIRCLE('',#48646,1.);
#19260=CIRCLE('',#48647,1.);
#19261=CIRCLE('',#48649,1.);
#19262=CIRCLE('',#48651,1.);
#19263=CIRCLE('',#48653,1.);
#19264=CIRCLE('',#48655,1.);
#19265=CIRCLE('',#48657,1.);
#19266=CIRCLE('',#48659,1.);
#19267=CIRCLE('',#48662,1.);
#19268=CIRCLE('',#48663,1.);
#19269=CIRCLE('',#48665,1.);
#19270=CIRCLE('',#48667,1.);
#19271=CIRCLE('',#48669,1.);
#19272=CIRCLE('',#48671,1.);
#19273=CIRCLE('',#48673,1.);
#19274=CIRCLE('',#48675,1.);
#19275=CIRCLE('',#48678,1.);
#19276=CIRCLE('',#48679,1.);
#19277=CIRCLE('',#48681,1.);
#19278=CIRCLE('',#48683,1.);
#19279=CIRCLE('',#48685,1.);
#19280=CIRCLE('',#48687,1.);
#19281=CIRCLE('',#48689,1.);
#19282=CIRCLE('',#48690,1.);
#19283=CIRCLE('',#48692,1.);
#19284=CIRCLE('',#48694,1.);
#19285=CIRCLE('',#48696,1.);
#19286=CIRCLE('',#48698,1.);
#19287=CIRCLE('',#48700,1.);
#19288=CIRCLE('',#48701,1.);
#19289=CIRCLE('',#48703,1.);
#19290=CIRCLE('',#48705,1.);
#19291=CIRCLE('',#48707,1.);
#19292=CIRCLE('',#48709,1.);
#19293=CIRCLE('',#48711,1.);
#19294=CIRCLE('',#48712,1.);
#19295=CIRCLE('',#48714,1.);
#19296=CIRCLE('',#48716,1.);
#19297=CIRCLE('',#48718,1.);
#19298=CIRCLE('',#48720,1.);
#19299=CIRCLE('',#48722,2.);
#19300=CIRCLE('',#48723,1.99999999999997);
#19301=CIRCLE('',#48725,2.00000000000002);
#19302=CIRCLE('',#48727,2.);
#19303=CIRCLE('',#48729,2.);
#19304=CIRCLE('',#48731,2.00000000000001);
#19305=CIRCLE('',#48733,2.);
#19306=CIRCLE('',#48735,2.00000000000002);
#19307=CIRCLE('',#48737,2.00000000000001);
#19308=CIRCLE('',#48739,2.);
#19309=CIRCLE('',#48741,2.00000000000002);
#19310=CIRCLE('',#48743,2.);
#19311=CIRCLE('',#48745,2.);
#19312=CIRCLE('',#48747,2.00000000000001);
#19313=CIRCLE('',#48749,2.);
#19314=CIRCLE('',#48751,2.00000000000002);
#19315=CIRCLE('',#48755,19.4499999999999);
#19316=CIRCLE('',#48756,19.4499999999999);
#19317=CIRCLE('',#48757,0.5);
#19318=CIRCLE('',#48758,18.95);
#19319=CIRCLE('',#48760,12.2099993856753);
#19320=CIRCLE('',#48761,0.500000000000003);
#19321=CIRCLE('',#48762,12.7099993856753);
#19322=CIRCLE('',#48763,0.500000000000003);
#19323=CIRCLE('',#48765,12.7099993856753);
#19324=CIRCLE('',#48766,0.500000000000003);
#19325=CIRCLE('',#48767,12.2099993856753);
#19326=CIRCLE('',#48768,0.500000000000003);
#19327=CIRCLE('',#48770,19.4499999999999);
#19328=CIRCLE('',#48771,1.);
#19329=CIRCLE('',#48772,18.4499999999999);
#19330=CIRCLE('',#48773,1.);
#19331=CIRCLE('',#48774,19.4499999999999);
#19332=CIRCLE('',#48776,19.4499999999999);
#19333=CIRCLE('',#48778,0.5);
#19334=CIRCLE('',#48779,19.45);
#19335=CIRCLE('',#48780,19.45);
#19336=CIRCLE('',#48782,18.95);
#19337=CIRCLE('',#48783,0.5);
#19338=CIRCLE('',#48784,19.45);
#19339=CIRCLE('',#48786,0.250000000000021);
#19340=CIRCLE('',#48787,0.250000000000041);
#19341=CIRCLE('',#48788,0.249999999999985);
#19342=CIRCLE('',#48789,0.250000000000026);
#19343=CIRCLE('',#48790,0.249999999999998);
#19344=CIRCLE('',#48791,0.249999999999995);
#19345=CIRCLE('',#48792,9.76525702848835);
#19346=CIRCLE('',#48794,9.76341648719587);
#19347=CIRCLE('',#48796,0.500000000000001);
#19348=CIRCLE('',#48797,0.500000000000002);
#19349=CIRCLE('',#48798,0.500000000000001);
#19350=CIRCLE('',#48799,0.499999999999998);
#19351=CIRCLE('',#48800,0.500000000000001);
#19352=CIRCLE('',#48801,0.499999999999998);
#19353=CIRCLE('',#48803,19.45);
#19354=CIRCLE('',#48804,0.5);
#19355=CIRCLE('',#48806,19.45);
#19356=CIRCLE('',#48807,19.45);
#19357=CIRCLE('',#48808,1.);
#19358=CIRCLE('',#48809,18.45);
#19359=CIRCLE('',#48812,0.250000000000021);
#19360=CIRCLE('',#48813,0.250000000000042);
#19361=CIRCLE('',#48814,0.249999999999985);
#19362=CIRCLE('',#48815,0.250000000000026);
#19363=CIRCLE('',#48816,0.249999999999998);
#19364=CIRCLE('',#48817,9.76525702848803);
#19365=CIRCLE('',#48818,0.249999999999995);
#19366=CIRCLE('',#48820,9.76341648759087);
#19367=CIRCLE('',#48822,1.);
#19368=CIRCLE('',#48823,1.);
#19369=CIRCLE('',#48832,18.1223816084529);
#19370=CIRCLE('',#48833,18.1223816084529);
#19371=CIRCLE('',#48835,17.1223816084529);
#19372=CIRCLE('',#48836,17.1223816084529);
#19373=CIRCLE('',#48838,17.1223816084529);
#19374=CIRCLE('',#48839,17.1223816084529);
#19375=CIRCLE('',#48841,18.1223816084529);
#19376=CIRCLE('',#48842,18.1223816084529);
#19377=CIRCLE('',#48845,20.4499999999999);
#19378=CIRCLE('',#48850,1.);
#19379=CIRCLE('',#48852,1.00000000000002);
#19380=CIRCLE('',#48854,1.00000000000002);
#19381=CIRCLE('',#48856,1.);
#19382=CIRCLE('',#48859,1.);
#19383=CIRCLE('',#48862,1.);
#19384=CIRCLE('',#48864,0.5);
#19385=CIRCLE('',#48865,0.5);
#19386=CIRCLE('',#48867,0.5);
#19387=CIRCLE('',#48869,0.5);
#19388=CIRCLE('',#48871,0.5);
#19389=CIRCLE('',#48872,0.5);
#19390=CIRCLE('',#48874,0.5);
#19391=CIRCLE('',#48876,0.5);
#19392=CIRCLE('',#48878,0.5);
#19393=CIRCLE('',#48879,0.499999999999994);
#19394=CIRCLE('',#48881,0.5);
#19395=CIRCLE('',#48883,0.5);
#19396=CIRCLE('',#48885,0.5);
#19397=CIRCLE('',#48887,0.5);
#19398=CIRCLE('',#48889,0.5);
#19399=CIRCLE('',#48890,0.5);
#19400=CIRCLE('',#48894,11.5);
#19401=CIRCLE('',#48895,11.5);
#19402=CIRCLE('',#48897,12.5);
#19403=CIRCLE('',#48898,12.5);
#19404=CIRCLE('',#48903,85.1127409318642);
#19405=CIRCLE('',#48904,126.822029782344);
#19406=CIRCLE('',#48906,8.51742334960548);
#19407=CIRCLE('',#48907,0.5);
#19408=CIRCLE('',#48908,8.81821463020444);
#19409=CIRCLE('',#48911,0.675444121136126);
#19410=CIRCLE('',#48914,0.498831135992472);
#19411=CIRCLE('',#48917,0.490540748728341);
#19412=CIRCLE('',#48920,0.878303132193281);
#19413=CIRCLE('',#48923,0.675444121136182);
#19414=CIRCLE('',#48926,0.498831135992472);
#19415=CIRCLE('',#48929,0.490540748728341);
#19416=CIRCLE('',#48932,0.878303132193337);
#19417=CIRCLE('',#48935,0.675444121136126);
#19418=CIRCLE('',#48938,0.498831135992472);
#19419=CIRCLE('',#48941,0.490540748728341);
#19420=CIRCLE('',#48944,0.878303132193281);
#19421=CIRCLE('',#48947,0.675444121136126);
#19422=CIRCLE('',#48950,0.498831135992472);
#19423=CIRCLE('',#48953,0.490540748728285);
#19424=CIRCLE('',#48956,0.878303132193226);
#19425=CIRCLE('',#48959,0.675444121136182);
#19426=CIRCLE('',#48962,0.498831135992472);
#19427=CIRCLE('',#48965,0.490540748728341);
#19428=CIRCLE('',#48968,0.878303132193281);
#19429=CIRCLE('',#48971,0.675444121136182);
#19430=CIRCLE('',#48974,0.498831135992472);
#19431=CIRCLE('',#48977,0.490540748728341);
#19432=CIRCLE('',#48980,0.878303132193281);
#19433=CIRCLE('',#48983,0.675444121136182);
#19434=CIRCLE('',#48986,0.498831135992583);
#19435=CIRCLE('',#48989,0.490540748728341);
#19436=CIRCLE('',#48992,0.87830313219317);
#19437=CIRCLE('',#48995,0.675444121136071);
#19438=CIRCLE('',#48998,0.498831135992472);
#19439=CIRCLE('',#49001,0.490540748728341);
#19440=CIRCLE('',#49004,0.87830313219317);
#19441=CIRCLE('',#49007,0.675444121136071);
#19442=CIRCLE('',#49010,0.498831135992361);
#19443=CIRCLE('',#49013,0.490540748728341);
#19444=CIRCLE('',#49016,0.878303132193281);
#19445=CIRCLE('',#49019,0.675444121136182);
#19446=CIRCLE('',#49022,0.498831135992472);
#19447=CIRCLE('',#49025,0.49054074872823);
#19448=CIRCLE('',#49028,0.878303132193337);
#19449=CIRCLE('',#49031,0.675444121136182);
#19450=CIRCLE('',#49034,0.498831135992472);
#19451=CIRCLE('',#49037,0.490540748728341);
#19452=CIRCLE('',#49040,0.878303132193281);
#19453=CIRCLE('',#49043,0.675444121136126);
#19454=CIRCLE('',#49046,0.498831135992472);
#19455=CIRCLE('',#49049,0.490540748728341);
#19456=CIRCLE('',#49052,0.878303132193281);
#19457=CIRCLE('',#49055,0.675444121136182);
#19458=CIRCLE('',#49058,0.498831135992417);
#19459=CIRCLE('',#49061,0.490540748728341);
#19460=CIRCLE('',#49064,0.878303132193281);
#19461=CIRCLE('',#49067,0.675444121136126);
#19462=CIRCLE('',#49070,0.498831135992417);
#19463=CIRCLE('',#49073,0.490540748728341);
#19464=CIRCLE('',#49076,0.878303132193337);
#19465=CIRCLE('',#49079,0.675444121136182);
#19466=CIRCLE('',#49082,0.498831135992417);
#19467=CIRCLE('',#49085,0.490540748728341);
#19468=CIRCLE('',#49088,0.878303132193337);
#19469=CIRCLE('',#49091,0.675444121136126);
#19470=CIRCLE('',#49094,0.498831135992472);
#19471=CIRCLE('',#49097,0.490540748728341);
#19472=CIRCLE('',#49100,0.878303132193281);
#19473=CIRCLE('',#49103,0.675444121136182);
#19474=CIRCLE('',#49106,0.498831135992472);
#19475=CIRCLE('',#49109,0.490540748728341);
#19476=CIRCLE('',#49112,0.878303132193281);
#19477=CIRCLE('',#49115,0.675444121136182);
#19478=CIRCLE('',#49118,0.498831135992472);
#19479=CIRCLE('',#49121,0.490540748728341);
#19480=CIRCLE('',#49124,0.878303132193281);
#19481=CIRCLE('',#49127,0.675444121136126);
#19482=CIRCLE('',#49130,0.498831135992472);
#19483=CIRCLE('',#49133,0.490540748728341);
#19484=CIRCLE('',#49136,0.878303132193337);
#19485=CIRCLE('',#49139,0.675444121136126);
#19486=CIRCLE('',#49142,0.498831135992472);
#19487=CIRCLE('',#49145,0.490540748728341);
#19488=CIRCLE('',#49148,0.878303132193281);
#19489=CIRCLE('',#49151,0.675444121136182);
#19490=CIRCLE('',#49154,0.498831135992472);
#19491=CIRCLE('',#49157,0.490540748728341);
#19492=CIRCLE('',#49160,0.878303132193281);
#19493=CIRCLE('',#49163,0.675444121136126);
#19494=CIRCLE('',#49166,0.498831135992472);
#19495=CIRCLE('',#49169,0.490540748728341);
#19496=CIRCLE('',#49172,0.878303132193281);
#19497=CIRCLE('',#49175,0.675444121136126);
#19498=CIRCLE('',#49178,0.498831135992472);
#19499=CIRCLE('',#49181,0.490540748728396);
#19500=CIRCLE('',#49184,0.878303132193281);
#19501=CIRCLE('',#49187,0.675444121136126);
#19502=CIRCLE('',#49190,0.498831135992417);
#19503=CIRCLE('',#49193,0.490540748728341);
#19504=CIRCLE('',#49196,0.878303132193281);
#19505=CIRCLE('',#49199,0.675444121136126);
#19506=CIRCLE('',#49202,0.498831135992472);
#19507=CIRCLE('',#49205,0.490540748728396);
#19508=CIRCLE('',#49208,0.878303132193281);
#19509=CIRCLE('',#49211,0.675444121136182);
#19510=CIRCLE('',#49214,0.498831135992528);
#19511=CIRCLE('',#49217,0.490540748728341);
#19512=CIRCLE('',#49220,0.878303132193337);
#19513=CIRCLE('',#49223,0.675444121136126);
#19514=CIRCLE('',#49226,0.498831135992472);
#19515=CIRCLE('',#49229,0.490540748728285);
#19516=CIRCLE('',#49232,0.878303132193281);
#19517=CIRCLE('',#49235,0.675444121136126);
#19518=CIRCLE('',#49238,0.498831135992528);
#19519=CIRCLE('',#49241,0.490540748728341);
#19520=CIRCLE('',#49244,0.878303132193337);
#19521=CIRCLE('',#49247,0.675444121136182);
#19522=CIRCLE('',#49250,0.498831135992472);
#19523=CIRCLE('',#49253,0.490540748728285);
#19524=CIRCLE('',#49256,0.878303132193281);
#19525=CIRCLE('',#49259,0.675444121136126);
#19526=CIRCLE('',#49262,0.490540748728341);
#19527=CIRCLE('',#49265,0.498831135992472);
#19528=CIRCLE('',#49267,1.10035806567471);
#19529=CIRCLE('',#49268,1.10035806567471);
#19530=CIRCLE('',#49270,0.500358065674722);
#19531=CIRCLE('',#49271,0.500358065674722);
#19532=CIRCLE('',#49273,1.21403156673711);
#19533=CIRCLE('',#49274,1.21403156673711);
#19534=CIRCLE('',#49276,0.614031566737117);
#19535=CIRCLE('',#49277,0.614031566737117);
#19536=CIRCLE('',#49279,1.32880796357332);
#19537=CIRCLE('',#49280,1.32880796357332);
#19538=CIRCLE('',#49282,0.72880796357333);
#19539=CIRCLE('',#49283,0.72880796357333);
#19540=CIRCLE('',#49285,1.46111700181689);
#19541=CIRCLE('',#49286,1.46111700181689);
#19542=CIRCLE('',#49288,0.861117001816902);
#19543=CIRCLE('',#49289,0.861117001816902);
#19544=CIRCLE('',#49291,1.6204820426246);
#19545=CIRCLE('',#49292,1.6204820426246);
#19546=CIRCLE('',#49294,1.02048204262462);
#19547=CIRCLE('',#49295,1.02048204262462);
#19548=CIRCLE('',#49297,1.70100022308284);
#19549=CIRCLE('',#49298,1.70100022308284);
#19550=CIRCLE('',#49300,1.10100022308285);
#19551=CIRCLE('',#49301,1.10100022308285);
#19552=CIRCLE('',#49303,1.72127463204352);
#19553=CIRCLE('',#49304,1.72127463204352);
#19554=CIRCLE('',#49306,1.12127463204348);
#19555=CIRCLE('',#49307,1.12127463204348);
#19556=CIRCLE('',#49309,1.78199265440493);
#19557=CIRCLE('',#49310,1.78199265440493);
#19558=CIRCLE('',#49312,1.18199265440494);
#19559=CIRCLE('',#49313,1.18199265440494);
#19560=CIRCLE('',#49315,1.66088080992077);
#19561=CIRCLE('',#49316,1.66088080992077);
#19562=CIRCLE('',#49318,1.06088080992078);
#19563=CIRCLE('',#49319,1.06088080992078);
#19564=CIRCLE('',#49321,1.10035806567471);
#19565=CIRCLE('',#49322,1.10035806567471);
#19566=CIRCLE('',#49324,0.500358065674722);
#19567=CIRCLE('',#49325,0.500358065674722);
#19568=CIRCLE('',#49327,1.21403156673716);
#19569=CIRCLE('',#49328,1.21403156673716);
#19570=CIRCLE('',#49330,0.614031566737117);
#19571=CIRCLE('',#49331,0.614031566737117);
#19572=CIRCLE('',#49333,1.32880796357332);
#19573=CIRCLE('',#49334,1.32880796357332);
#19574=CIRCLE('',#49336,0.728807963573275);
#19575=CIRCLE('',#49337,0.728807963573275);
#19576=CIRCLE('',#49339,1.46111700181689);
#19577=CIRCLE('',#49340,1.46111700181689);
#19578=CIRCLE('',#49342,0.861117001816902);
#19579=CIRCLE('',#49343,0.861117001816902);
#19580=CIRCLE('',#49345,1.6204820426246);
#19581=CIRCLE('',#49346,1.6204820426246);
#19582=CIRCLE('',#49348,1.02048204262462);
#19583=CIRCLE('',#49349,1.02048204262462);
#19584=CIRCLE('',#49351,1.70100022308284);
#19585=CIRCLE('',#49352,1.70100022308284);
#19586=CIRCLE('',#49354,1.10100022308285);
#19587=CIRCLE('',#49355,1.10100022308285);
#19588=CIRCLE('',#49357,1.72127463204347);
#19589=CIRCLE('',#49358,1.72127463204347);
#19590=CIRCLE('',#49360,1.12127463204348);
#19591=CIRCLE('',#49361,1.12127463204348);
#19592=CIRCLE('',#49363,1.78199265440493);
#19593=CIRCLE('',#49364,1.78199265440493);
#19594=CIRCLE('',#49366,1.18199265440494);
#19595=CIRCLE('',#49367,1.18199265440494);
#19596=CIRCLE('',#49369,1.66088080992077);
#19597=CIRCLE('',#49370,1.66088080992077);
#19598=CIRCLE('',#49372,1.06088080992078);
#19599=CIRCLE('',#49373,1.06088080992078);
#19600=CIRCLE('',#49375,1.10035806567471);
#19601=CIRCLE('',#49376,1.10035806567471);
#19602=CIRCLE('',#49378,0.500358065674722);
#19603=CIRCLE('',#49379,0.500358065674722);
#19604=CIRCLE('',#49381,1.21403156673716);
#19605=CIRCLE('',#49382,1.21403156673716);
#19606=CIRCLE('',#49384,0.614031566737117);
#19607=CIRCLE('',#49385,0.614031566737117);
#19608=CIRCLE('',#49387,1.32880796357326);
#19609=CIRCLE('',#49388,1.32880796357326);
#19610=CIRCLE('',#49390,0.72880796357333);
#19611=CIRCLE('',#49391,0.72880796357333);
#19612=CIRCLE('',#49393,1.46111700181689);
#19613=CIRCLE('',#49394,1.46111700181689);
#19614=CIRCLE('',#49396,0.861117001816902);
#19615=CIRCLE('',#49397,0.861117001816902);
#19616=CIRCLE('',#49399,1.6204820426246);
#19617=CIRCLE('',#49400,1.6204820426246);
#19618=CIRCLE('',#49402,1.02048204262456);
#19619=CIRCLE('',#49403,1.02048204262456);
#19620=CIRCLE('',#49405,1.70100022308284);
#19621=CIRCLE('',#49406,1.70100022308284);
#19622=CIRCLE('',#49408,1.10100022308285);
#19623=CIRCLE('',#49409,1.10100022308285);
#19624=CIRCLE('',#49411,1.72127463204347);
#19625=CIRCLE('',#49412,1.72127463204347);
#19626=CIRCLE('',#49414,1.12127463204348);
#19627=CIRCLE('',#49415,1.12127463204348);
#19628=CIRCLE('',#49417,1.78199265440493);
#19629=CIRCLE('',#49418,1.78199265440493);
#19630=CIRCLE('',#49420,1.18199265440494);
#19631=CIRCLE('',#49421,1.18199265440494);
#19632=CIRCLE('',#49423,1.66088080992077);
#19633=CIRCLE('',#49424,1.66088080992077);
#19634=CIRCLE('',#49426,1.06088080992078);
#19635=CIRCLE('',#49427,1.06088080992078);
#19636=CIRCLE('',#49429,1.10035806567471);
#19637=CIRCLE('',#49430,1.10035806567471);
#19638=CIRCLE('',#49432,0.500358065674666);
#19639=CIRCLE('',#49433,0.500358065674666);
#19640=CIRCLE('',#49435,1.21403156673711);
#19641=CIRCLE('',#49436,1.21403156673711);
#19642=CIRCLE('',#49438,0.614031566737172);
#19643=CIRCLE('',#49439,0.614031566737172);
#19644=CIRCLE('',#49441,1.32880796357332);
#19645=CIRCLE('',#49442,1.32880796357332);
#19646=CIRCLE('',#49444,0.72880796357333);
#19647=CIRCLE('',#49445,0.72880796357333);
#19648=CIRCLE('',#49447,1.46111700181689);
#19649=CIRCLE('',#49448,1.46111700181689);
#19650=CIRCLE('',#49450,0.861117001816847);
#19651=CIRCLE('',#49451,0.861117001816847);
#19652=CIRCLE('',#49453,1.6204820426246);
#19653=CIRCLE('',#49454,1.6204820426246);
#19654=CIRCLE('',#49456,1.02048204262462);
#19655=CIRCLE('',#49457,1.02048204262462);
#19656=CIRCLE('',#49459,1.70100022308284);
#19657=CIRCLE('',#49460,1.70100022308284);
#19658=CIRCLE('',#49462,1.10100022308285);
#19659=CIRCLE('',#49463,1.10100022308285);
#19660=CIRCLE('',#49465,1.72127463204347);
#19661=CIRCLE('',#49466,1.72127463204347);
#19662=CIRCLE('',#49468,1.12127463204353);
#19663=CIRCLE('',#49469,1.12127463204353);
#19664=CIRCLE('',#49471,1.78199265440498);
#19665=CIRCLE('',#49472,1.78199265440498);
#19666=CIRCLE('',#49474,1.18199265440494);
#19667=CIRCLE('',#49475,1.18199265440494);
#19668=CIRCLE('',#49477,1.66088080992083);
#19669=CIRCLE('',#49478,1.66088080992083);
#19670=CIRCLE('',#49480,1.06088080992078);
#19671=CIRCLE('',#49481,1.06088080992078);
#19672=CIRCLE('',#49483,1.10035806567477);
#19673=CIRCLE('',#49484,1.10035806567477);
#19674=CIRCLE('',#49486,0.500358065674777);
#19675=CIRCLE('',#49487,0.500358065674777);
#19676=CIRCLE('',#49489,1.21403156673711);
#19677=CIRCLE('',#49490,1.21403156673711);
#19678=CIRCLE('',#49492,0.614031566737172);
#19679=CIRCLE('',#49493,0.614031566737172);
#19680=CIRCLE('',#49495,1.32880796357326);
#19681=CIRCLE('',#49496,1.32880796357326);
#19682=CIRCLE('',#49498,0.72880796357333);
#19683=CIRCLE('',#49499,0.72880796357333);
#19684=CIRCLE('',#49501,1.46111700181684);
#19685=CIRCLE('',#49502,1.46111700181684);
#19686=CIRCLE('',#49504,0.861117001816847);
#19687=CIRCLE('',#49505,0.861117001816847);
#19688=CIRCLE('',#49507,1.6204820426246);
#19689=CIRCLE('',#49508,1.6204820426246);
#19690=CIRCLE('',#49510,1.02048204262462);
#19691=CIRCLE('',#49511,1.02048204262462);
#19692=CIRCLE('',#49513,1.70100022308278);
#19693=CIRCLE('',#49514,1.70100022308278);
#19694=CIRCLE('',#49516,1.1010002230829);
#19695=CIRCLE('',#49517,1.1010002230829);
#19696=CIRCLE('',#49519,1.72127463204347);
#19697=CIRCLE('',#49520,1.72127463204347);
#19698=CIRCLE('',#49522,1.12127463204342);
#19699=CIRCLE('',#49523,1.12127463204342);
#19700=CIRCLE('',#49525,1.78199265440487);
#19701=CIRCLE('',#49526,1.78199265440487);
#19702=CIRCLE('',#49528,1.18199265440488);
#19703=CIRCLE('',#49529,1.18199265440488);
#19704=CIRCLE('',#49531,1.66088080992077);
#19705=CIRCLE('',#49532,1.66088080992077);
#19706=CIRCLE('',#49534,1.06088080992078);
#19707=CIRCLE('',#49535,1.06088080992078);
#19708=CIRCLE('',#49537,1.10035806567466);
#19709=CIRCLE('',#49538,1.10035806567466);
#19710=CIRCLE('',#49540,0.500358065674722);
#19711=CIRCLE('',#49541,0.500358065674722);
#19712=CIRCLE('',#49543,1.21403156673716);
#19713=CIRCLE('',#49544,1.21403156673716);
#19714=CIRCLE('',#49546,0.614031566737117);
#19715=CIRCLE('',#49547,0.614031566737117);
#19716=CIRCLE('',#49549,1.32880796357326);
#19717=CIRCLE('',#49550,1.32880796357326);
#19718=CIRCLE('',#49552,0.728807963573275);
#19719=CIRCLE('',#49553,0.728807963573275);
#19720=CIRCLE('',#49555,1.46111700181684);
#19721=CIRCLE('',#49556,1.46111700181684);
#19722=CIRCLE('',#49558,0.861117001816847);
#19723=CIRCLE('',#49559,0.861117001816847);
#19724=CIRCLE('',#49561,1.6204820426246);
#19725=CIRCLE('',#49562,1.6204820426246);
#19726=CIRCLE('',#49564,1.02048204262456);
#19727=CIRCLE('',#49565,1.02048204262456);
#19728=CIRCLE('',#49567,1.70100022308284);
#19729=CIRCLE('',#49568,1.70100022308284);
#19730=CIRCLE('',#49570,1.10100022308279);
#19731=CIRCLE('',#49571,1.10100022308279);
#19732=CIRCLE('',#49573,1.72127463204347);
#19733=CIRCLE('',#49574,1.72127463204347);
#19734=CIRCLE('',#49576,1.12127463204348);
#19735=CIRCLE('',#49577,1.12127463204348);
#19736=CIRCLE('',#49579,1.78199265440493);
#19737=CIRCLE('',#49580,1.78199265440493);
#19738=CIRCLE('',#49582,1.18199265440494);
#19739=CIRCLE('',#49583,1.18199265440494);
#19740=CIRCLE('',#49585,1.66088080992088);
#19741=CIRCLE('',#49586,1.66088080992083);
#19742=CIRCLE('',#49588,1.06088080992084);
#19743=CIRCLE('',#49589,1.06088080992084);
#19744=CIRCLE('',#49591,1.10035806567466);
#19745=CIRCLE('',#49592,1.10035806567466);
#19746=CIRCLE('',#49594,0.500358065674666);
#19747=CIRCLE('',#49595,0.500358065674666);
#19748=CIRCLE('',#49597,1.21403156673716);
#19749=CIRCLE('',#49598,1.21403156673716);
#19750=CIRCLE('',#49600,0.614031566737172);
#19751=CIRCLE('',#49601,0.614031566737172);
#19752=CIRCLE('',#49603,1.32880796357332);
#19753=CIRCLE('',#49604,1.32880796357332);
#19754=CIRCLE('',#49606,0.728807963573275);
#19755=CIRCLE('',#49607,0.728807963573275);
#19756=CIRCLE('',#49609,1.46111700181689);
#19757=CIRCLE('',#49610,1.46111700181689);
#19758=CIRCLE('',#49612,0.861117001816847);
#19759=CIRCLE('',#49613,0.861117001816847);
#19760=CIRCLE('',#49615,1.6204820426246);
#19761=CIRCLE('',#49616,1.6204820426246);
#19762=CIRCLE('',#49618,1.02048204262456);
#19763=CIRCLE('',#49619,1.02048204262456);
#19764=CIRCLE('',#49621,1.70100022308284);
#19765=CIRCLE('',#49622,1.70100022308284);
#19766=CIRCLE('',#49624,1.10100022308285);
#19767=CIRCLE('',#49625,1.10100022308285);
#19768=CIRCLE('',#49627,1.72127463204352);
#19769=CIRCLE('',#49628,1.72127463204352);
#19770=CIRCLE('',#49630,1.12127463204348);
#19771=CIRCLE('',#49631,1.12127463204348);
#19772=CIRCLE('',#49633,1.78199265440493);
#19773=CIRCLE('',#49634,1.78199265440498);
#19774=CIRCLE('',#49636,1.18199265440494);
#19775=CIRCLE('',#49637,1.18199265440494);
#19776=CIRCLE('',#49639,1.66088080992077);
#19777=CIRCLE('',#49640,1.66088080992077);
#19778=CIRCLE('',#49642,1.06088080992073);
#19779=CIRCLE('',#49643,1.06088080992073);
#19780=CIRCLE('',#49645,1.10035806567471);
#19781=CIRCLE('',#49646,1.10035806567471);
#19782=CIRCLE('',#49648,0.500358065674722);
#19783=CIRCLE('',#49649,0.500358065674722);
#19784=CIRCLE('',#49651,1.21403156673716);
#19785=CIRCLE('',#49652,1.21403156673716);
#19786=CIRCLE('',#49654,0.614031566737117);
#19787=CIRCLE('',#49655,0.614031566737117);
#19788=CIRCLE('',#49657,1.32880796357332);
#19789=CIRCLE('',#49658,1.32880796357332);
#19790=CIRCLE('',#49660,0.72880796357333);
#19791=CIRCLE('',#49661,0.72880796357333);
#19792=CIRCLE('',#49663,1.46111700181689);
#19793=CIRCLE('',#49664,1.46111700181689);
#19794=CIRCLE('',#49666,0.861117001816902);
#19795=CIRCLE('',#49667,0.861117001816902);
#19796=CIRCLE('',#49669,1.6204820426246);
#19797=CIRCLE('',#49670,1.6204820426246);
#19798=CIRCLE('',#49672,1.02048204262456);
#19799=CIRCLE('',#49673,1.02048204262456);
#19800=CIRCLE('',#49675,1.70100022308278);
#19801=CIRCLE('',#49676,1.70100022308278);
#19802=CIRCLE('',#49678,1.10100022308285);
#19803=CIRCLE('',#49679,1.10100022308285);
#19804=CIRCLE('',#49681,1.72127463204347);
#19805=CIRCLE('',#49682,1.72127463204347);
#19806=CIRCLE('',#49684,1.12127463204348);
#19807=CIRCLE('',#49685,1.12127463204348);
#19808=CIRCLE('',#49687,1.78199265440493);
#19809=CIRCLE('',#49688,1.78199265440493);
#19810=CIRCLE('',#49690,1.18199265440494);
#19811=CIRCLE('',#49691,1.18199265440494);
#19812=CIRCLE('',#49693,1.66088080992077);
#19813=CIRCLE('',#49694,1.66088080992077);
#19814=CIRCLE('',#49696,1.06088080992073);
#19815=CIRCLE('',#49697,1.06088080992073);
#19816=CIRCLE('',#49699,1.10035806567471);
#19817=CIRCLE('',#49700,1.10035806567471);
#19818=CIRCLE('',#49702,0.500358065674722);
#19819=CIRCLE('',#49703,0.500358065674722);
#19820=CIRCLE('',#49705,1.21403156673711);
#19821=CIRCLE('',#49706,1.21403156673711);
#19822=CIRCLE('',#49708,0.614031566737117);
#19823=CIRCLE('',#49709,0.614031566737117);
#19824=CIRCLE('',#49711,1.32880796357332);
#19825=CIRCLE('',#49712,1.32880796357332);
#19826=CIRCLE('',#49714,0.72880796357333);
#19827=CIRCLE('',#49715,0.72880796357333);
#19828=CIRCLE('',#49717,1.46111700181689);
#19829=CIRCLE('',#49718,1.46111700181689);
#19830=CIRCLE('',#49720,0.861117001816902);
#19831=CIRCLE('',#49721,0.861117001816902);
#19832=CIRCLE('',#49723,1.6204820426246);
#19833=CIRCLE('',#49724,1.6204820426246);
#19834=CIRCLE('',#49726,1.02048204262456);
#19835=CIRCLE('',#49727,1.02048204262456);
#19836=CIRCLE('',#49729,1.70100022308284);
#19837=CIRCLE('',#49730,1.70100022308284);
#19838=CIRCLE('',#49732,1.10100022308285);
#19839=CIRCLE('',#49733,1.10100022308285);
#19840=CIRCLE('',#49735,1.72127463204352);
#19841=CIRCLE('',#49736,1.72127463204352);
#19842=CIRCLE('',#49738,1.12127463204348);
#19843=CIRCLE('',#49739,1.12127463204348);
#19844=CIRCLE('',#49741,1.78199265440487);
#19845=CIRCLE('',#49742,1.78199265440487);
#19846=CIRCLE('',#49744,1.18199265440488);
#19847=CIRCLE('',#49745,1.18199265440488);
#19848=CIRCLE('',#49747,1.66088080992088);
#19849=CIRCLE('',#49748,1.66088080992088);
#19850=CIRCLE('',#49750,1.06088080992073);
#19851=CIRCLE('',#49751,1.06088080992073);
#19852=CIRCLE('',#49753,1.10035806567471);
#19853=CIRCLE('',#49754,1.10035806567471);
#19854=CIRCLE('',#49756,0.500358065674666);
#19855=CIRCLE('',#49757,0.500358065674666);
#19856=CIRCLE('',#49759,1.21403156673716);
#19857=CIRCLE('',#49760,1.21403156673716);
#19858=CIRCLE('',#49762,0.614031566737172);
#19859=CIRCLE('',#49763,0.614031566737172);
#19860=CIRCLE('',#49765,1.32880796357338);
#19861=CIRCLE('',#49766,1.32880796357338);
#19862=CIRCLE('',#49768,0.72880796357333);
#19863=CIRCLE('',#49769,0.72880796357333);
#19864=CIRCLE('',#49771,1.46111700181689);
#19865=CIRCLE('',#49772,1.46111700181689);
#19866=CIRCLE('',#49774,0.861117001816902);
#19867=CIRCLE('',#49775,0.861117001816902);
#19868=CIRCLE('',#49777,1.6204820426246);
#19869=CIRCLE('',#49778,1.6204820426246);
#19870=CIRCLE('',#49780,1.02048204262456);
#19871=CIRCLE('',#49781,1.02048204262456);
#19872=CIRCLE('',#49783,1.70100022308284);
#19873=CIRCLE('',#49784,1.70100022308284);
#19874=CIRCLE('',#49786,1.10100022308285);
#19875=CIRCLE('',#49787,1.10100022308285);
#19876=CIRCLE('',#49789,1.72127463204352);
#19877=CIRCLE('',#49790,1.72127463204352);
#19878=CIRCLE('',#49792,1.12127463204348);
#19879=CIRCLE('',#49793,1.12127463204348);
#19880=CIRCLE('',#49795,1.78199265440498);
#19881=CIRCLE('',#49796,1.78199265440498);
#19882=CIRCLE('',#49798,1.181992654405);
#19883=CIRCLE('',#49799,1.181992654405);
#19884=CIRCLE('',#49801,1.66088080992077);
#19885=CIRCLE('',#49802,1.66088080992077);
#19886=CIRCLE('',#49804,1.06088080992073);
#19887=CIRCLE('',#49805,1.06088080992073);
#19888=CIRCLE('',#49807,1.10035806567471);
#19889=CIRCLE('',#49808,1.10035806567471);
#19890=CIRCLE('',#49810,0.500358065674722);
#19891=CIRCLE('',#49811,0.500358065674722);
#19892=CIRCLE('',#49813,1.21403156673705);
#19893=CIRCLE('',#49814,1.21403156673705);
#19894=CIRCLE('',#49816,0.614031566737117);
#19895=CIRCLE('',#49817,0.614031566737117);
#19896=CIRCLE('',#49819,1.32880796357338);
#19897=CIRCLE('',#49820,1.32880796357338);
#19898=CIRCLE('',#49822,0.72880796357333);
#19899=CIRCLE('',#49823,0.72880796357333);
#19900=CIRCLE('',#49825,1.46111700181689);
#19901=CIRCLE('',#49826,1.46111700181689);
#19902=CIRCLE('',#49828,0.861117001816902);
#19903=CIRCLE('',#49829,0.861117001816902);
#19904=CIRCLE('',#49831,1.6204820426246);
#19905=CIRCLE('',#49832,1.6204820426246);
#19906=CIRCLE('',#49834,1.02048204262462);
#19907=CIRCLE('',#49835,1.02048204262462);
#19908=CIRCLE('',#49837,1.70100022308278);
#19909=CIRCLE('',#49838,1.70100022308278);
#19910=CIRCLE('',#49840,1.10100022308279);
#19911=CIRCLE('',#49841,1.10100022308279);
#19912=CIRCLE('',#49843,1.72127463204352);
#19913=CIRCLE('',#49844,1.72127463204352);
#19914=CIRCLE('',#49846,1.12127463204348);
#19915=CIRCLE('',#49847,1.12127463204348);
#19916=CIRCLE('',#49849,1.78199265440493);
#19917=CIRCLE('',#49850,1.78199265440493);
#19918=CIRCLE('',#49852,1.18199265440494);
#19919=CIRCLE('',#49853,1.18199265440494);
#19920=CIRCLE('',#49855,1.66088080992077);
#19921=CIRCLE('',#49856,1.66088080992077);
#19922=CIRCLE('',#49858,1.06088080992078);
#19923=CIRCLE('',#49859,1.06088080992078);
#19924=CIRCLE('',#49861,1.10035806567471);
#19925=CIRCLE('',#49862,1.10035806567471);
#19926=CIRCLE('',#49864,0.500358065674722);
#19927=CIRCLE('',#49865,0.500358065674722);
#19928=CIRCLE('',#49867,1.21403156673711);
#19929=CIRCLE('',#49868,1.21403156673711);
#19930=CIRCLE('',#49870,0.614031566737117);
#19931=CIRCLE('',#49871,0.614031566737117);
#19932=CIRCLE('',#49873,1.32880796357332);
#19933=CIRCLE('',#49874,1.32880796357332);
#19934=CIRCLE('',#49876,0.72880796357333);
#19935=CIRCLE('',#49877,0.72880796357333);
#19936=CIRCLE('',#49879,1.46111700181689);
#19937=CIRCLE('',#49880,1.46111700181689);
#19938=CIRCLE('',#49882,0.861117001816902);
#19939=CIRCLE('',#49883,0.861117001816902);
#19940=CIRCLE('',#49885,1.62048204262455);
#19941=CIRCLE('',#49886,1.62048204262455);
#19942=CIRCLE('',#49888,1.02048204262462);
#19943=CIRCLE('',#49889,1.02048204262462);
#19944=CIRCLE('',#49891,1.70100022308278);
#19945=CIRCLE('',#49892,1.70100022308278);
#19946=CIRCLE('',#49894,1.10100022308279);
#19947=CIRCLE('',#49895,1.10100022308279);
#19948=CIRCLE('',#49897,1.72127463204347);
#19949=CIRCLE('',#49898,1.72127463204347);
#19950=CIRCLE('',#49900,1.12127463204353);
#19951=CIRCLE('',#49901,1.12127463204353);
#19952=CIRCLE('',#49903,1.78199265440487);
#19953=CIRCLE('',#49904,1.78199265440487);
#19954=CIRCLE('',#49906,1.18199265440494);
#19955=CIRCLE('',#49907,1.18199265440494);
#19956=CIRCLE('',#49909,1.66088080992077);
#19957=CIRCLE('',#49910,1.66088080992077);
#19958=CIRCLE('',#49912,1.06088080992078);
#19959=CIRCLE('',#49913,1.06088080992078);
#19960=CIRCLE('',#49915,1.10035806567471);
#19961=CIRCLE('',#49916,1.10035806567471);
#19962=CIRCLE('',#49918,0.500358065674777);
#19963=CIRCLE('',#49919,0.500358065674777);
#19964=CIRCLE('',#49921,1.21403156673711);
#19965=CIRCLE('',#49922,1.21403156673711);
#19966=CIRCLE('',#49924,0.614031566737117);
#19967=CIRCLE('',#49925,0.614031566737117);
#19968=CIRCLE('',#49927,1.32880796357332);
#19969=CIRCLE('',#49928,1.32880796357332);
#19970=CIRCLE('',#49930,0.728807963573275);
#19971=CIRCLE('',#49931,0.728807963573275);
#19972=CIRCLE('',#49933,1.46111700181695);
#19973=CIRCLE('',#49934,1.46111700181695);
#19974=CIRCLE('',#49936,0.861117001816902);
#19975=CIRCLE('',#49937,0.861117001816902);
#19976=CIRCLE('',#49939,1.6204820426246);
#19977=CIRCLE('',#49940,1.6204820426246);
#19978=CIRCLE('',#49942,1.02048204262462);
#19979=CIRCLE('',#49943,1.02048204262462);
#19980=CIRCLE('',#49945,1.70100022308284);
#19981=CIRCLE('',#49946,1.70100022308284);
#19982=CIRCLE('',#49948,1.10100022308285);
#19983=CIRCLE('',#49949,1.10100022308285);
#19984=CIRCLE('',#49951,1.72127463204347);
#19985=CIRCLE('',#49952,1.72127463204347);
#19986=CIRCLE('',#49954,1.12127463204348);
#19987=CIRCLE('',#49955,1.12127463204348);
#19988=CIRCLE('',#49957,1.78199265440493);
#19989=CIRCLE('',#49958,1.78199265440493);
#19990=CIRCLE('',#49960,1.18199265440488);
#19991=CIRCLE('',#49961,1.18199265440488);
#19992=CIRCLE('',#49963,1.66088080992077);
#19993=CIRCLE('',#49964,1.66088080992077);
#19994=CIRCLE('',#49966,1.06088080992078);
#19995=CIRCLE('',#49967,1.06088080992078);
#19996=CIRCLE('',#49969,1.10035806567471);
#19997=CIRCLE('',#49970,1.10035806567471);
#19998=CIRCLE('',#49972,0.500358065674722);
#19999=CIRCLE('',#49973,0.500358065674722);
#20000=CIRCLE('',#49975,1.21403156673711);
#20001=CIRCLE('',#49976,1.21403156673711);
#20002=CIRCLE('',#49978,0.614031566737117);
#20003=CIRCLE('',#49979,0.614031566737117);
#20004=CIRCLE('',#49981,1.32880796357332);
#20005=CIRCLE('',#49982,1.32880796357332);
#20006=CIRCLE('',#49984,0.72880796357333);
#20007=CIRCLE('',#49985,0.72880796357333);
#20008=CIRCLE('',#49987,1.46111700181689);
#20009=CIRCLE('',#49988,1.46111700181689);
#20010=CIRCLE('',#49990,0.861117001816902);
#20011=CIRCLE('',#49991,0.861117001816902);
#20012=CIRCLE('',#49993,1.62048204262455);
#20013=CIRCLE('',#49994,1.62048204262455);
#20014=CIRCLE('',#49996,1.02048204262456);
#20015=CIRCLE('',#49997,1.02048204262456);
#20016=CIRCLE('',#49999,1.70100022308284);
#20017=CIRCLE('',#50000,1.70100022308284);
#20018=CIRCLE('',#50002,1.10100022308285);
#20019=CIRCLE('',#50003,1.10100022308285);
#20020=CIRCLE('',#50005,1.72127463204347);
#20021=CIRCLE('',#50006,1.72127463204347);
#20022=CIRCLE('',#50008,1.12127463204348);
#20023=CIRCLE('',#50009,1.12127463204348);
#20024=CIRCLE('',#50011,1.78199265440493);
#20025=CIRCLE('',#50012,1.78199265440493);
#20026=CIRCLE('',#50014,1.18199265440494);
#20027=CIRCLE('',#50015,1.18199265440494);
#20028=CIRCLE('',#50017,1.66088080992077);
#20029=CIRCLE('',#50018,1.66088080992077);
#20030=CIRCLE('',#50020,1.06088080992078);
#20031=CIRCLE('',#50021,1.06088080992078);
#20032=CIRCLE('',#50023,1.10035806567471);
#20033=CIRCLE('',#50024,1.10035806567471);
#20034=CIRCLE('',#50026,0.500358065674722);
#20035=CIRCLE('',#50027,0.500358065674722);
#20036=CIRCLE('',#50029,1.21403156673711);
#20037=CIRCLE('',#50030,1.21403156673711);
#20038=CIRCLE('',#50032,0.614031566737117);
#20039=CIRCLE('',#50033,0.614031566737117);
#20040=CIRCLE('',#50035,1.32880796357326);
#20041=CIRCLE('',#50036,1.32880796357326);
#20042=CIRCLE('',#50038,0.728807963573275);
#20043=CIRCLE('',#50039,0.728807963573275);
#20044=CIRCLE('',#50041,1.46111700181689);
#20045=CIRCLE('',#50042,1.46111700181689);
#20046=CIRCLE('',#50044,0.861117001816902);
#20047=CIRCLE('',#50045,0.861117001816902);
#20048=CIRCLE('',#50047,1.6204820426246);
#20049=CIRCLE('',#50048,1.6204820426246);
#20050=CIRCLE('',#50050,1.02048204262456);
#20051=CIRCLE('',#50051,1.02048204262456);
#20052=CIRCLE('',#50053,1.70100022308284);
#20053=CIRCLE('',#50054,1.70100022308284);
#20054=CIRCLE('',#50056,1.10100022308285);
#20055=CIRCLE('',#50057,1.10100022308285);
#20056=CIRCLE('',#50059,1.72127463204352);
#20057=CIRCLE('',#50060,1.72127463204352);
#20058=CIRCLE('',#50062,1.12127463204348);
#20059=CIRCLE('',#50063,1.12127463204348);
#20060=CIRCLE('',#50065,1.78199265440498);
#20061=CIRCLE('',#50066,1.78199265440498);
#20062=CIRCLE('',#50068,1.18199265440494);
#20063=CIRCLE('',#50069,1.18199265440494);
#20064=CIRCLE('',#50071,1.66088080992083);
#20065=CIRCLE('',#50072,1.66088080992083);
#20066=CIRCLE('',#50074,1.06088080992078);
#20067=CIRCLE('',#50075,1.06088080992078);
#20068=CIRCLE('',#50077,1.10035806567471);
#20069=CIRCLE('',#50078,1.10035806567471);
#20070=CIRCLE('',#50080,0.500358065674722);
#20071=CIRCLE('',#50081,0.500358065674722);
#20072=CIRCLE('',#50083,1.21403156673711);
#20073=CIRCLE('',#50084,1.21403156673711);
#20074=CIRCLE('',#50086,0.614031566737117);
#20075=CIRCLE('',#50087,0.614031566737117);
#20076=CIRCLE('',#50089,1.32880796357332);
#20077=CIRCLE('',#50090,1.32880796357332);
#20078=CIRCLE('',#50092,0.72880796357333);
#20079=CIRCLE('',#50093,0.72880796357333);
#20080=CIRCLE('',#50095,1.46111700181689);
#20081=CIRCLE('',#50096,1.46111700181689);
#20082=CIRCLE('',#50098,0.861117001816847);
#20083=CIRCLE('',#50099,0.861117001816847);
#20084=CIRCLE('',#50101,1.6204820426246);
#20085=CIRCLE('',#50102,1.6204820426246);
#20086=CIRCLE('',#50104,1.02048204262462);
#20087=CIRCLE('',#50105,1.02048204262462);
#20088=CIRCLE('',#50107,1.70100022308284);
#20089=CIRCLE('',#50108,1.70100022308284);
#20090=CIRCLE('',#50110,1.10100022308279);
#20091=CIRCLE('',#50111,1.10100022308279);
#20092=CIRCLE('',#50113,1.72127463204347);
#20093=CIRCLE('',#50114,1.72127463204347);
#20094=CIRCLE('',#50116,1.12127463204353);
#20095=CIRCLE('',#50117,1.12127463204353);
#20096=CIRCLE('',#50119,1.78199265440493);
#20097=CIRCLE('',#50120,1.78199265440493);
#20098=CIRCLE('',#50122,1.18199265440494);
#20099=CIRCLE('',#50123,1.18199265440494);
#20100=CIRCLE('',#50125,1.66088080992077);
#20101=CIRCLE('',#50126,1.66088080992077);
#20102=CIRCLE('',#50128,1.06088080992078);
#20103=CIRCLE('',#50129,1.06088080992078);
#20104=CIRCLE('',#50131,1.10035806567471);
#20105=CIRCLE('',#50132,1.10035806567471);
#20106=CIRCLE('',#50134,0.500358065674722);
#20107=CIRCLE('',#50135,0.500358065674722);
#20108=CIRCLE('',#50137,1.21403156673711);
#20109=CIRCLE('',#50138,1.21403156673711);
#20110=CIRCLE('',#50140,0.614031566737117);
#20111=CIRCLE('',#50141,0.614031566737117);
#20112=CIRCLE('',#50143,1.32880796357332);
#20113=CIRCLE('',#50144,1.32880796357332);
#20114=CIRCLE('',#50146,0.72880796357333);
#20115=CIRCLE('',#50147,0.72880796357333);
#20116=CIRCLE('',#50149,1.46111700181689);
#20117=CIRCLE('',#50150,1.46111700181689);
#20118=CIRCLE('',#50152,0.861117001816902);
#20119=CIRCLE('',#50153,0.861117001816902);
#20120=CIRCLE('',#50155,1.6204820426246);
#20121=CIRCLE('',#50156,1.6204820426246);
#20122=CIRCLE('',#50158,1.02048204262462);
#20123=CIRCLE('',#50159,1.02048204262462);
#20124=CIRCLE('',#50161,1.70100022308284);
#20125=CIRCLE('',#50162,1.70100022308284);
#20126=CIRCLE('',#50164,1.10100022308285);
#20127=CIRCLE('',#50165,1.10100022308285);
#20128=CIRCLE('',#50167,1.72127463204347);
#20129=CIRCLE('',#50168,1.72127463204347);
#20130=CIRCLE('',#50170,1.12127463204348);
#20131=CIRCLE('',#50171,1.12127463204348);
#20132=CIRCLE('',#50173,1.78199265440493);
#20133=CIRCLE('',#50174,1.78199265440493);
#20134=CIRCLE('',#50176,1.18199265440494);
#20135=CIRCLE('',#50177,1.18199265440494);
#20136=CIRCLE('',#50179,1.66088080992077);
#20137=CIRCLE('',#50180,1.66088080992077);
#20138=CIRCLE('',#50182,1.06088080992078);
#20139=CIRCLE('',#50183,1.06088080992078);
#20140=CIRCLE('',#50185,1.10035806567471);
#20141=CIRCLE('',#50186,1.10035806567471);
#20142=CIRCLE('',#50188,0.500358065674666);
#20143=CIRCLE('',#50189,0.500358065674666);
#20144=CIRCLE('',#50191,1.21403156673716);
#20145=CIRCLE('',#50192,1.21403156673716);
#20146=CIRCLE('',#50194,0.614031566737117);
#20147=CIRCLE('',#50195,0.614031566737117);
#20148=CIRCLE('',#50197,1.32880796357332);
#20149=CIRCLE('',#50198,1.32880796357332);
#20150=CIRCLE('',#50200,0.72880796357333);
#20151=CIRCLE('',#50201,0.72880796357333);
#20152=CIRCLE('',#50203,1.46111700181689);
#20153=CIRCLE('',#50204,1.46111700181689);
#20154=CIRCLE('',#50206,0.861117001816902);
#20155=CIRCLE('',#50207,0.861117001816902);
#20156=CIRCLE('',#50209,1.6204820426246);
#20157=CIRCLE('',#50210,1.6204820426246);
#20158=CIRCLE('',#50212,1.02048204262462);
#20159=CIRCLE('',#50213,1.02048204262462);
#20160=CIRCLE('',#50215,1.70100022308284);
#20161=CIRCLE('',#50216,1.70100022308284);
#20162=CIRCLE('',#50218,1.10100022308285);
#20163=CIRCLE('',#50219,1.10100022308285);
#20164=CIRCLE('',#50221,1.72127463204352);
#20165=CIRCLE('',#50222,1.72127463204352);
#20166=CIRCLE('',#50224,1.12127463204353);
#20167=CIRCLE('',#50225,1.12127463204353);
#20168=CIRCLE('',#50227,1.78199265440493);
#20169=CIRCLE('',#50228,1.78199265440493);
#20170=CIRCLE('',#50230,1.18199265440494);
#20171=CIRCLE('',#50231,1.18199265440494);
#20172=CIRCLE('',#50233,1.66088080992077);
#20173=CIRCLE('',#50234,1.66088080992077);
#20174=CIRCLE('',#50236,1.06088080992078);
#20175=CIRCLE('',#50237,1.06088080992078);
#20176=CIRCLE('',#50239,1.10035806567471);
#20177=CIRCLE('',#50240,1.10035806567471);
#20178=CIRCLE('',#50242,0.500358065674666);
#20179=CIRCLE('',#50243,0.500358065674666);
#20180=CIRCLE('',#50245,1.21403156673716);
#20181=CIRCLE('',#50246,1.21403156673716);
#20182=CIRCLE('',#50248,0.614031566737172);
#20183=CIRCLE('',#50249,0.614031566737172);
#20184=CIRCLE('',#50251,1.32880796357326);
#20185=CIRCLE('',#50252,1.32880796357326);
#20186=CIRCLE('',#50254,0.728807963573275);
#20187=CIRCLE('',#50255,0.728807963573275);
#20188=CIRCLE('',#50257,1.46111700181689);
#20189=CIRCLE('',#50258,1.46111700181689);
#20190=CIRCLE('',#50260,0.861117001816847);
#20191=CIRCLE('',#50261,0.861117001816847);
#20192=CIRCLE('',#50263,1.62048204262455);
#20193=CIRCLE('',#50264,1.62048204262455);
#20194=CIRCLE('',#50266,1.02048204262462);
#20195=CIRCLE('',#50267,1.02048204262462);
#20196=CIRCLE('',#50269,1.70100022308284);
#20197=CIRCLE('',#50270,1.70100022308284);
#20198=CIRCLE('',#50272,1.10100022308279);
#20199=CIRCLE('',#50273,1.10100022308279);
#20200=CIRCLE('',#50275,1.72127463204352);
#20201=CIRCLE('',#50276,1.72127463204352);
#20202=CIRCLE('',#50278,1.12127463204348);
#20203=CIRCLE('',#50279,1.12127463204348);
#20204=CIRCLE('',#50281,1.78199265440493);
#20205=CIRCLE('',#50282,1.78199265440493);
#20206=CIRCLE('',#50284,1.18199265440494);
#20207=CIRCLE('',#50285,1.18199265440494);
#20208=CIRCLE('',#50287,1.66088080992083);
#20209=CIRCLE('',#50288,1.66088080992083);
#20210=CIRCLE('',#50290,1.06088080992078);
#20211=CIRCLE('',#50291,1.06088080992078);
#20212=CIRCLE('',#50293,1.10035806567471);
#20213=CIRCLE('',#50294,1.10035806567471);
#20214=CIRCLE('',#50296,0.500358065674722);
#20215=CIRCLE('',#50297,0.500358065674722);
#20216=CIRCLE('',#50299,1.21403156673716);
#20217=CIRCLE('',#50300,1.21403156673716);
#20218=CIRCLE('',#50302,0.614031566737172);
#20219=CIRCLE('',#50303,0.614031566737172);
#20220=CIRCLE('',#50305,1.32880796357326);
#20221=CIRCLE('',#50306,1.32880796357326);
#20222=CIRCLE('',#50308,0.72880796357333);
#20223=CIRCLE('',#50309,0.72880796357333);
#20224=CIRCLE('',#50311,1.46111700181689);
#20225=CIRCLE('',#50312,1.46111700181689);
#20226=CIRCLE('',#50314,0.861117001816902);
#20227=CIRCLE('',#50315,0.861117001816902);
#20228=CIRCLE('',#50317,1.6204820426246);
#20229=CIRCLE('',#50318,1.6204820426246);
#20230=CIRCLE('',#50320,1.02048204262456);
#20231=CIRCLE('',#50321,1.02048204262456);
#20232=CIRCLE('',#50323,1.70100022308278);
#20233=CIRCLE('',#50324,1.70100022308278);
#20234=CIRCLE('',#50326,1.10100022308279);
#20235=CIRCLE('',#50327,1.10100022308279);
#20236=CIRCLE('',#50329,1.72127463204347);
#20237=CIRCLE('',#50330,1.72127463204347);
#20238=CIRCLE('',#50332,1.12127463204348);
#20239=CIRCLE('',#50333,1.12127463204348);
#20240=CIRCLE('',#50335,1.78199265440493);
#20241=CIRCLE('',#50336,1.78199265440493);
#20242=CIRCLE('',#50338,1.18199265440494);
#20243=CIRCLE('',#50339,1.18199265440494);
#20244=CIRCLE('',#50341,1.66088080992077);
#20245=CIRCLE('',#50342,1.66088080992077);
#20246=CIRCLE('',#50344,1.06088080992084);
#20247=CIRCLE('',#50345,1.06088080992084);
#20248=CIRCLE('',#50347,1.10035806567471);
#20249=CIRCLE('',#50348,1.10035806567471);
#20250=CIRCLE('',#50350,0.500358065674722);
#20251=CIRCLE('',#50351,0.500358065674722);
#20252=CIRCLE('',#50353,1.21403156673716);
#20253=CIRCLE('',#50354,1.21403156673716);
#20254=CIRCLE('',#50356,0.614031566737117);
#20255=CIRCLE('',#50357,0.614031566737117);
#20256=CIRCLE('',#50359,1.32880796357338);
#20257=CIRCLE('',#50360,1.32880796357338);
#20258=CIRCLE('',#50362,0.728807963573386);
#20259=CIRCLE('',#50363,0.728807963573386);
#20260=CIRCLE('',#50365,1.46111700181695);
#20261=CIRCLE('',#50366,1.46111700181695);
#20262=CIRCLE('',#50368,0.861117001816902);
#20263=CIRCLE('',#50369,0.861117001816902);
#20264=CIRCLE('',#50371,1.6204820426246);
#20265=CIRCLE('',#50372,1.6204820426246);
#20266=CIRCLE('',#50374,1.02048204262456);
#20267=CIRCLE('',#50375,1.02048204262456);
#20268=CIRCLE('',#50377,1.70100022308284);
#20269=CIRCLE('',#50378,1.70100022308284);
#20270=CIRCLE('',#50380,1.10100022308279);
#20271=CIRCLE('',#50381,1.10100022308279);
#20272=CIRCLE('',#50383,1.72127463204352);
#20273=CIRCLE('',#50384,1.72127463204352);
#20274=CIRCLE('',#50386,1.12127463204348);
#20275=CIRCLE('',#50387,1.12127463204348);
#20276=CIRCLE('',#50389,1.78199265440493);
#20277=CIRCLE('',#50390,1.78199265440493);
#20278=CIRCLE('',#50392,1.18199265440494);
#20279=CIRCLE('',#50393,1.18199265440494);
#20280=CIRCLE('',#50395,1.66088080992083);
#20281=CIRCLE('',#50396,1.66088080992083);
#20282=CIRCLE('',#50398,1.06088080992078);
#20283=CIRCLE('',#50399,1.06088080992078);
#20284=CIRCLE('',#50401,1.10035806567466);
#20285=CIRCLE('',#50402,1.10035806567466);
#20286=CIRCLE('',#50404,0.500358065674666);
#20287=CIRCLE('',#50405,0.500358065674666);
#20288=CIRCLE('',#50407,1.21403156673716);
#20289=CIRCLE('',#50408,1.21403156673716);
#20290=CIRCLE('',#50410,0.614031566737172);
#20291=CIRCLE('',#50411,0.614031566737172);
#20292=CIRCLE('',#50413,1.32880796357326);
#20293=CIRCLE('',#50414,1.32880796357326);
#20294=CIRCLE('',#50416,0.728807963573275);
#20295=CIRCLE('',#50417,0.728807963573275);
#20296=CIRCLE('',#50419,1.46111700181689);
#20297=CIRCLE('',#50420,1.46111700181689);
#20298=CIRCLE('',#50422,0.861117001816847);
#20299=CIRCLE('',#50423,0.861117001816847);
#20300=CIRCLE('',#50425,1.6204820426246);
#20301=CIRCLE('',#50426,1.6204820426246);
#20302=CIRCLE('',#50428,1.02048204262456);
#20303=CIRCLE('',#50429,1.02048204262456);
#20304=CIRCLE('',#50431,1.70100022308284);
#20305=CIRCLE('',#50432,1.70100022308284);
#20306=CIRCLE('',#50434,1.10100022308285);
#20307=CIRCLE('',#50435,1.10100022308285);
#20308=CIRCLE('',#50437,1.72127463204352);
#20309=CIRCLE('',#50438,1.72127463204352);
#20310=CIRCLE('',#50440,1.12127463204348);
#20311=CIRCLE('',#50441,1.12127463204348);
#20312=CIRCLE('',#50443,1.78199265440498);
#20313=CIRCLE('',#50444,1.78199265440498);
#20314=CIRCLE('',#50446,1.18199265440494);
#20315=CIRCLE('',#50447,1.18199265440494);
#20316=CIRCLE('',#50449,1.66088080992077);
#20317=CIRCLE('',#50450,1.66088080992077);
#20318=CIRCLE('',#50452,1.06088080992078);
#20319=CIRCLE('',#50453,1.06088080992078);
#20320=CIRCLE('',#50455,1.10035806567471);
#20321=CIRCLE('',#50456,1.10035806567471);
#20322=CIRCLE('',#50458,0.500358065674666);
#20323=CIRCLE('',#50459,0.500358065674666);
#20324=CIRCLE('',#50461,1.21403156673716);
#20325=CIRCLE('',#50462,1.21403156673716);
#20326=CIRCLE('',#50464,0.614031566737117);
#20327=CIRCLE('',#50465,0.614031566737117);
#20328=CIRCLE('',#50467,1.32880796357332);
#20329=CIRCLE('',#50468,1.32880796357332);
#20330=CIRCLE('',#50470,0.72880796357333);
#20331=CIRCLE('',#50471,0.72880796357333);
#20332=CIRCLE('',#50473,1.46111700181689);
#20333=CIRCLE('',#50474,1.46111700181689);
#20334=CIRCLE('',#50476,0.861117001816902);
#20335=CIRCLE('',#50477,0.861117001816902);
#20336=CIRCLE('',#50479,1.62048204262455);
#20337=CIRCLE('',#50480,1.62048204262455);
#20338=CIRCLE('',#50482,1.02048204262456);
#20339=CIRCLE('',#50483,1.02048204262456);
#20340=CIRCLE('',#50485,1.70100022308278);
#20341=CIRCLE('',#50486,1.70100022308278);
#20342=CIRCLE('',#50488,1.10100022308285);
#20343=CIRCLE('',#50489,1.10100022308285);
#20344=CIRCLE('',#50491,1.72127463204347);
#20345=CIRCLE('',#50492,1.72127463204347);
#20346=CIRCLE('',#50494,1.12127463204348);
#20347=CIRCLE('',#50495,1.12127463204348);
#20348=CIRCLE('',#50497,1.78199265440493);
#20349=CIRCLE('',#50498,1.78199265440493);
#20350=CIRCLE('',#50500,1.18199265440488);
#20351=CIRCLE('',#50501,1.18199265440488);
#20352=CIRCLE('',#50503,1.66088080992083);
#20353=CIRCLE('',#50504,1.66088080992083);
#20354=CIRCLE('',#50506,1.06088080992078);
#20355=CIRCLE('',#50507,1.06088080992078);
#20356=CIRCLE('',#50509,1.10035806567471);
#20357=CIRCLE('',#50510,1.10035806567471);
#20358=CIRCLE('',#50512,0.500358065674666);
#20359=CIRCLE('',#50513,0.500358065674666);
#20360=CIRCLE('',#50515,1.21403156673716);
#20361=CIRCLE('',#50516,1.21403156673716);
#20362=CIRCLE('',#50518,0.614031566737117);
#20363=CIRCLE('',#50519,0.614031566737117);
#20364=CIRCLE('',#50521,1.32880796357332);
#20365=CIRCLE('',#50522,1.32880796357332);
#20366=CIRCLE('',#50524,0.72880796357333);
#20367=CIRCLE('',#50525,0.72880796357333);
#20368=CIRCLE('',#50527,1.46111700181689);
#20369=CIRCLE('',#50528,1.46111700181689);
#20370=CIRCLE('',#50530,0.861117001816902);
#20371=CIRCLE('',#50531,0.861117001816902);
#20372=CIRCLE('',#50533,1.6204820426246);
#20373=CIRCLE('',#50534,1.6204820426246);
#20374=CIRCLE('',#50536,1.02048204262462);
#20375=CIRCLE('',#50537,1.02048204262462);
#20376=CIRCLE('',#50539,1.70100022308284);
#20377=CIRCLE('',#50540,1.70100022308284);
#20378=CIRCLE('',#50542,1.10100022308285);
#20379=CIRCLE('',#50543,1.10100022308285);
#20380=CIRCLE('',#50545,1.72127463204352);
#20381=CIRCLE('',#50546,1.72127463204352);
#20382=CIRCLE('',#50548,1.12127463204353);
#20383=CIRCLE('',#50549,1.12127463204353);
#20384=CIRCLE('',#50551,1.78199265440493);
#20385=CIRCLE('',#50552,1.78199265440493);
#20386=CIRCLE('',#50554,1.18199265440488);
#20387=CIRCLE('',#50555,1.18199265440488);
#20388=CIRCLE('',#50557,1.66088080992077);
#20389=CIRCLE('',#50558,1.66088080992077);
#20390=CIRCLE('',#50560,1.06088080992078);
#20391=CIRCLE('',#50561,1.06088080992078);
#20392=CIRCLE('',#50563,1.10035806567477);
#20393=CIRCLE('',#50564,1.10035806567477);
#20394=CIRCLE('',#50566,0.500358065674722);
#20395=CIRCLE('',#50567,0.500358065674722);
#20396=CIRCLE('',#50569,1.21403156673711);
#20397=CIRCLE('',#50570,1.21403156673711);
#20398=CIRCLE('',#50572,0.614031566737061);
#20399=CIRCLE('',#50573,0.614031566737061);
#20400=CIRCLE('',#50575,1.32880796357332);
#20401=CIRCLE('',#50576,1.32880796357332);
#20402=CIRCLE('',#50578,0.728807963573275);
#20403=CIRCLE('',#50579,0.728807963573275);
#20404=CIRCLE('',#50581,1.46111700181684);
#20405=CIRCLE('',#50582,1.46111700181684);
#20406=CIRCLE('',#50584,0.861117001816847);
#20407=CIRCLE('',#50585,0.861117001816847);
#20408=CIRCLE('',#50587,1.6204820426246);
#20409=CIRCLE('',#50588,1.6204820426246);
#20410=CIRCLE('',#50590,1.02048204262456);
#20411=CIRCLE('',#50591,1.02048204262456);
#20412=CIRCLE('',#50593,1.70100022308278);
#20413=CIRCLE('',#50594,1.70100022308278);
#20414=CIRCLE('',#50596,1.10100022308279);
#20415=CIRCLE('',#50597,1.10100022308279);
#20416=CIRCLE('',#50599,1.72127463204352);
#20417=CIRCLE('',#50600,1.72127463204352);
#20418=CIRCLE('',#50602,1.12127463204353);
#20419=CIRCLE('',#50603,1.12127463204353);
#20420=CIRCLE('',#50605,1.78199265440493);
#20421=CIRCLE('',#50606,1.78199265440493);
#20422=CIRCLE('',#50608,1.18199265440494);
#20423=CIRCLE('',#50609,1.18199265440494);
#20424=CIRCLE('',#50611,1.66088080992077);
#20425=CIRCLE('',#50612,1.66088080992077);
#20426=CIRCLE('',#50614,1.06088080992073);
#20427=CIRCLE('',#50615,1.06088080992073);
#20428=CIRCLE('',#50617,1.10035806567471);
#20429=CIRCLE('',#50618,1.10035806567471);
#20430=CIRCLE('',#50620,0.500358065674722);
#20431=CIRCLE('',#50621,0.500358065674722);
#20432=CIRCLE('',#50623,1.21403156673711);
#20433=CIRCLE('',#50624,1.21403156673711);
#20434=CIRCLE('',#50626,0.614031566737117);
#20435=CIRCLE('',#50627,0.614031566737117);
#20436=CIRCLE('',#50629,1.32880796357332);
#20437=CIRCLE('',#50630,1.32880796357332);
#20438=CIRCLE('',#50632,0.728807963573275);
#20439=CIRCLE('',#50633,0.728807963573275);
#20440=CIRCLE('',#50635,1.46111700181684);
#20441=CIRCLE('',#50636,1.46111700181684);
#20442=CIRCLE('',#50638,0.861117001816902);
#20443=CIRCLE('',#50639,0.861117001816902);
#20444=CIRCLE('',#50641,1.6204820426246);
#20445=CIRCLE('',#50642,1.6204820426246);
#20446=CIRCLE('',#50644,1.02048204262462);
#20447=CIRCLE('',#50645,1.02048204262462);
#20448=CIRCLE('',#50647,1.70100022308289);
#20449=CIRCLE('',#50648,1.70100022308289);
#20450=CIRCLE('',#50650,1.10100022308285);
#20451=CIRCLE('',#50651,1.10100022308285);
#20452=CIRCLE('',#50653,1.72127463204347);
#20453=CIRCLE('',#50654,1.72127463204347);
#20454=CIRCLE('',#50656,1.12127463204342);
#20455=CIRCLE('',#50657,1.12127463204342);
#20456=CIRCLE('',#50659,1.78199265440498);
#20457=CIRCLE('',#50660,1.78199265440498);
#20458=CIRCLE('',#50662,1.18199265440494);
#20459=CIRCLE('',#50663,1.18199265440494);
#20460=CIRCLE('',#50665,1.66088080992077);
#20461=CIRCLE('',#50666,1.66088080992077);
#20462=CIRCLE('',#50668,1.06088080992078);
#20463=CIRCLE('',#50669,1.06088080992078);
#20464=CIRCLE('',#50671,1.10035806567471);
#20465=CIRCLE('',#50672,1.10035806567471);
#20466=CIRCLE('',#50674,0.500358065674666);
#20467=CIRCLE('',#50675,0.500358065674666);
#20468=CIRCLE('',#50677,1.21403156673711);
#20469=CIRCLE('',#50678,1.21403156673711);
#20470=CIRCLE('',#50680,0.614031566737117);
#20471=CIRCLE('',#50681,0.614031566737117);
#20472=CIRCLE('',#50683,1.32880796357332);
#20473=CIRCLE('',#50684,1.32880796357332);
#20474=CIRCLE('',#50686,0.72880796357333);
#20475=CIRCLE('',#50687,0.72880796357333);
#20476=CIRCLE('',#50689,1.46111700181684);
#20477=CIRCLE('',#50690,1.46111700181684);
#20478=CIRCLE('',#50692,0.861117001816847);
#20479=CIRCLE('',#50693,0.861117001816847);
#20480=CIRCLE('',#50695,1.6204820426246);
#20481=CIRCLE('',#50696,1.6204820426246);
#20482=CIRCLE('',#50698,1.02048204262456);
#20483=CIRCLE('',#50699,1.02048204262456);
#20484=CIRCLE('',#50701,1.70100022308284);
#20485=CIRCLE('',#50702,1.70100022308284);
#20486=CIRCLE('',#50704,1.10100022308285);
#20487=CIRCLE('',#50705,1.10100022308285);
#20488=CIRCLE('',#50707,1.72127463204347);
#20489=CIRCLE('',#50708,1.72127463204347);
#20490=CIRCLE('',#50710,1.12127463204353);
#20491=CIRCLE('',#50711,1.12127463204353);
#20492=CIRCLE('',#50713,1.78199265440498);
#20493=CIRCLE('',#50714,1.78199265440498);
#20494=CIRCLE('',#50716,1.18199265440494);
#20495=CIRCLE('',#50717,1.18199265440494);
#20496=CIRCLE('',#50719,1.66088080992083);
#20497=CIRCLE('',#50720,1.66088080992083);
#20498=CIRCLE('',#50722,1.06088080992078);
#20499=CIRCLE('',#50723,1.06088080992078);
#20500=CIRCLE('',#50725,1.10035806567477);
#20501=CIRCLE('',#50726,1.10035806567477);
#20502=CIRCLE('',#50728,0.500358065674777);
#20503=CIRCLE('',#50729,0.500358065674777);
#20504=CIRCLE('',#50731,1.21403156673705);
#20505=CIRCLE('',#50732,1.21403156673705);
#20506=CIRCLE('',#50734,0.614031566737117);
#20507=CIRCLE('',#50735,0.614031566737117);
#20508=CIRCLE('',#50737,1.32880796357326);
#20509=CIRCLE('',#50738,1.32880796357326);
#20510=CIRCLE('',#50740,0.728807963573275);
#20511=CIRCLE('',#50741,0.728807963573275);
#20512=CIRCLE('',#50743,1.46111700181684);
#20513=CIRCLE('',#50744,1.46111700181684);
#20514=CIRCLE('',#50746,0.861117001816847);
#20515=CIRCLE('',#50747,0.861117001816847);
#20516=CIRCLE('',#50749,1.6204820426246);
#20517=CIRCLE('',#50750,1.6204820426246);
#20518=CIRCLE('',#50752,1.02048204262462);
#20519=CIRCLE('',#50753,1.02048204262462);
#20520=CIRCLE('',#50755,1.70100022308278);
#20521=CIRCLE('',#50756,1.70100022308278);
#20522=CIRCLE('',#50758,1.10100022308285);
#20523=CIRCLE('',#50759,1.10100022308285);
#20524=CIRCLE('',#50761,1.72127463204347);
#20525=CIRCLE('',#50762,1.72127463204347);
#20526=CIRCLE('',#50764,1.12127463204353);
#20527=CIRCLE('',#50765,1.12127463204353);
#20528=CIRCLE('',#50767,1.78199265440493);
#20529=CIRCLE('',#50768,1.78199265440493);
#20530=CIRCLE('',#50770,1.18199265440494);
#20531=CIRCLE('',#50771,1.18199265440494);
#20532=CIRCLE('',#50773,1.66088080992077);
#20533=CIRCLE('',#50774,1.66088080992077);
#20534=CIRCLE('',#50776,1.06088080992078);
#20535=CIRCLE('',#50777,1.06088080992078);
#20536=CIRCLE('',#50779,1.10035806567471);
#20537=CIRCLE('',#50780,1.10035806567471);
#20538=CIRCLE('',#50782,0.500358065674722);
#20539=CIRCLE('',#50783,0.500358065674722);
#20540=CIRCLE('',#50785,1.21403156673716);
#20541=CIRCLE('',#50786,1.21403156673716);
#20542=CIRCLE('',#50788,0.614031566737117);
#20543=CIRCLE('',#50789,0.614031566737117);
#20544=CIRCLE('',#50791,1.32880796357332);
#20545=CIRCLE('',#50792,1.32880796357332);
#20546=CIRCLE('',#50794,0.72880796357333);
#20547=CIRCLE('',#50795,0.72880796357333);
#20548=CIRCLE('',#50797,1.46111700181689);
#20549=CIRCLE('',#50798,1.46111700181689);
#20550=CIRCLE('',#50800,0.861117001816902);
#20551=CIRCLE('',#50801,0.861117001816902);
#20552=CIRCLE('',#50803,1.6204820426246);
#20553=CIRCLE('',#50804,1.6204820426246);
#20554=CIRCLE('',#50806,1.02048204262462);
#20555=CIRCLE('',#50807,1.02048204262462);
#20556=CIRCLE('',#50809,1.70100022308284);
#20557=CIRCLE('',#50810,1.70100022308284);
#20558=CIRCLE('',#50812,1.10100022308285);
#20559=CIRCLE('',#50813,1.10100022308285);
#20560=CIRCLE('',#50815,1.72127463204352);
#20561=CIRCLE('',#50816,1.72127463204352);
#20562=CIRCLE('',#50818,1.12127463204348);
#20563=CIRCLE('',#50819,1.12127463204348);
#20564=CIRCLE('',#50821,1.78199265440493);
#20565=CIRCLE('',#50822,1.78199265440493);
#20566=CIRCLE('',#50824,1.18199265440488);
#20567=CIRCLE('',#50825,1.18199265440488);
#20568=CIRCLE('',#50827,1.66088080992088);
#20569=CIRCLE('',#50828,1.66088080992088);
#20570=CIRCLE('',#50830,1.06088080992084);
#20571=CIRCLE('',#50831,1.06088080992084);
#20572=CIRCLE('',#50833,1.10035806567471);
#20573=CIRCLE('',#50834,1.10035806567471);
#20574=CIRCLE('',#50836,0.500358065674722);
#20575=CIRCLE('',#50837,0.500358065674722);
#20576=CIRCLE('',#50839,1.21403156673716);
#20577=CIRCLE('',#50840,1.21403156673716);
#20578=CIRCLE('',#50842,0.614031566737117);
#20579=CIRCLE('',#50843,0.614031566737117);
#20580=CIRCLE('',#50845,1.32880796357332);
#20581=CIRCLE('',#50846,1.32880796357332);
#20582=CIRCLE('',#50848,0.72880796357333);
#20583=CIRCLE('',#50849,0.72880796357333);
#20584=CIRCLE('',#50851,1.46111700181689);
#20585=CIRCLE('',#50852,1.46111700181689);
#20586=CIRCLE('',#50854,0.861117001816902);
#20587=CIRCLE('',#50855,0.861117001816902);
#20588=CIRCLE('',#50857,1.6204820426246);
#20589=CIRCLE('',#50858,1.6204820426246);
#20590=CIRCLE('',#50860,1.02048204262462);
#20591=CIRCLE('',#50861,1.02048204262462);
#20592=CIRCLE('',#50863,1.70100022308284);
#20593=CIRCLE('',#50864,1.70100022308284);
#20594=CIRCLE('',#50866,1.10100022308285);
#20595=CIRCLE('',#50867,1.10100022308285);
#20596=CIRCLE('',#50869,1.72127463204352);
#20597=CIRCLE('',#50870,1.72127463204352);
#20598=CIRCLE('',#50872,1.12127463204348);
#20599=CIRCLE('',#50873,1.12127463204348);
#20600=CIRCLE('',#50875,1.78199265440493);
#20601=CIRCLE('',#50876,1.78199265440493);
#20602=CIRCLE('',#50878,1.18199265440494);
#20603=CIRCLE('',#50879,1.18199265440494);
#20604=CIRCLE('',#50881,1.66088080992077);
#20605=CIRCLE('',#50882,1.66088080992077);
#20606=CIRCLE('',#50884,1.06088080992078);
#20607=CIRCLE('',#50885,1.06088080992078);
#20608=CIRCLE('',#50887,0.5);
#20609=CIRCLE('',#50888,127.41606204049);
#20610=CIRCLE('',#50889,126.822029782344);
#20611=CIRCLE('',#50891,127.41606204049);
#20612=CIRCLE('',#50893,11.8670707361131);
#20613=CIRCLE('',#50894,0.5);
#20614=CIRCLE('',#50895,12.3670707361131);
#20615=CIRCLE('',#50896,12.3670707361131);
#20616=CIRCLE('',#50898,11.8670707361131);
#20617=CIRCLE('',#50899,0.5);
#20618=CIRCLE('',#50900,12.3670707361132);
#20619=CIRCLE('',#50903,11.0429795822116);
#20620=CIRCLE('',#50905,16.6476722933764);
#20621=CIRCLE('',#50906,0.5);
#20622=CIRCLE('',#50907,16.1492953136407);
#20623=CIRCLE('',#50909,130.);
#20624=CIRCLE('',#50910,1.);
#20625=CIRCLE('',#50911,129.);
#20626=CIRCLE('',#50913,1.);
#20627=CIRCLE('',#50914,127.91606204049);
#20628=CIRCLE('',#50916,18.5103550292801);
#20629=CIRCLE('',#50918,130.);
#20630=CIRCLE('',#50919,130.);
#20631=CIRCLE('',#50920,1.);
#20632=CIRCLE('',#50921,129.);
#20633=CIRCLE('',#50924,0.878303132193281);
#20634=CIRCLE('',#50933,85.1127409318642);
#20635=VERTEX_POINT('',#65482);
#20636=VERTEX_POINT('',#65484);
#20637=VERTEX_POINT('',#65486);
#20638=VERTEX_POINT('',#65490);
#20639=VERTEX_POINT('',#65491);
#20640=VERTEX_POINT('',#65493);
#20641=VERTEX_POINT('',#65498);
#20642=VERTEX_POINT('',#65504);
#20643=VERTEX_POINT('',#65511);
#20644=VERTEX_POINT('',#65512);
#20645=VERTEX_POINT('',#65514);
#20646=VERTEX_POINT('',#65516);
#20647=VERTEX_POINT('',#65520);
#20648=VERTEX_POINT('',#65522);
#20649=VERTEX_POINT('',#65531);
#20650=VERTEX_POINT('',#65532);
#20651=VERTEX_POINT('',#65534);
#20652=VERTEX_POINT('',#65536);
#20653=VERTEX_POINT('',#65540);
#20654=VERTEX_POINT('',#65544);
#20655=VERTEX_POINT('',#65551);
#20656=VERTEX_POINT('',#65553);
#20657=VERTEX_POINT('',#65557);
#20658=VERTEX_POINT('',#65559);
#20659=VERTEX_POINT('',#65563);
#20660=VERTEX_POINT('',#65565);
#20661=VERTEX_POINT('',#65569);
#20662=VERTEX_POINT('',#65571);
#20663=VERTEX_POINT('',#65575);
#20664=VERTEX_POINT('',#65577);
#20665=VERTEX_POINT('',#65581);
#20666=VERTEX_POINT('',#65583);
#20667=VERTEX_POINT('',#65587);
#20668=VERTEX_POINT('',#65589);
#20669=VERTEX_POINT('',#65593);
#20670=VERTEX_POINT('',#65595);
#20671=VERTEX_POINT('',#65599);
#20672=VERTEX_POINT('',#65601);
#20673=VERTEX_POINT('',#65605);
#20674=VERTEX_POINT('',#65607);
#20675=VERTEX_POINT('',#65611);
#20676=VERTEX_POINT('',#65613);
#20677=VERTEX_POINT('',#65617);
#20678=VERTEX_POINT('',#65619);
#20679=VERTEX_POINT('',#65623);
#20680=VERTEX_POINT('',#65624);
#20681=VERTEX_POINT('',#65646);
#20682=VERTEX_POINT('',#65705);
#20683=VERTEX_POINT('',#65707);
#20684=VERTEX_POINT('',#65744);
#20685=VERTEX_POINT('',#65745);
#20686=VERTEX_POINT('',#65766);
#20687=VERTEX_POINT('',#65826);
#20688=VERTEX_POINT('',#65828);
#20689=VERTEX_POINT('',#65865);
#20690=VERTEX_POINT('',#65866);
#20691=VERTEX_POINT('',#65890);
#20692=VERTEX_POINT('',#65947);
#20693=VERTEX_POINT('',#65949);
#20694=VERTEX_POINT('',#65986);
#20695=VERTEX_POINT('',#65987);
#20696=VERTEX_POINT('',#66008);
#20697=VERTEX_POINT('',#66068);
#20698=VERTEX_POINT('',#66070);
#20699=VERTEX_POINT('',#66107);
#20700=VERTEX_POINT('',#66108);
#20701=VERTEX_POINT('',#66132);
#20702=VERTEX_POINT('',#66189);
#20703=VERTEX_POINT('',#66191);
#20704=VERTEX_POINT('',#66228);
#20705=VERTEX_POINT('',#66229);
#20706=VERTEX_POINT('',#66253);
#20707=VERTEX_POINT('',#66310);
#20708=VERTEX_POINT('',#66312);
#20709=VERTEX_POINT('',#66349);
#20710=VERTEX_POINT('',#66350);
#20711=VERTEX_POINT('',#66374);
#20712=VERTEX_POINT('',#66431);
#20713=VERTEX_POINT('',#66433);
#20714=VERTEX_POINT('',#66470);
#20715=VERTEX_POINT('',#66471);
#20716=VERTEX_POINT('',#66495);
#20717=VERTEX_POINT('',#66552);
#20718=VERTEX_POINT('',#66554);
#20719=VERTEX_POINT('',#66591);
#20720=VERTEX_POINT('',#66592);
#20721=VERTEX_POINT('',#66616);
#20722=VERTEX_POINT('',#66673);
#20723=VERTEX_POINT('',#66675);
#20724=VERTEX_POINT('',#66712);
#20725=VERTEX_POINT('',#66713);
#20726=VERTEX_POINT('',#66737);
#20727=VERTEX_POINT('',#66794);
#20728=VERTEX_POINT('',#66796);
#20729=VERTEX_POINT('',#66833);
#20730=VERTEX_POINT('',#66834);
#20731=VERTEX_POINT('',#66855);
#20732=VERTEX_POINT('',#66915);
#20733=VERTEX_POINT('',#66917);
#20734=VERTEX_POINT('',#66954);
#20735=VERTEX_POINT('',#66955);
#20736=VERTEX_POINT('',#66976);
#20737=VERTEX_POINT('',#67036);
#20738=VERTEX_POINT('',#67038);
#20739=VERTEX_POINT('',#67075);
#20740=VERTEX_POINT('',#67076);
#20741=VERTEX_POINT('',#67097);
#20742=VERTEX_POINT('',#67157);
#20743=VERTEX_POINT('',#67159);
#20744=VERTEX_POINT('',#67196);
#20745=VERTEX_POINT('',#67197);
#20746=VERTEX_POINT('',#67218);
#20747=VERTEX_POINT('',#67278);
#20748=VERTEX_POINT('',#67280);
#20749=VERTEX_POINT('',#67317);
#20750=VERTEX_POINT('',#67318);
#20751=VERTEX_POINT('',#67339);
#20752=VERTEX_POINT('',#67399);
#20753=VERTEX_POINT('',#67401);
#20754=VERTEX_POINT('',#67438);
#20755=VERTEX_POINT('',#67439);
#20756=VERTEX_POINT('',#67460);
#20757=VERTEX_POINT('',#67520);
#20758=VERTEX_POINT('',#67522);
#20759=VERTEX_POINT('',#67559);
#20760=VERTEX_POINT('',#67560);
#20761=VERTEX_POINT('',#67582);
#20762=VERTEX_POINT('',#67641);
#20763=VERTEX_POINT('',#67643);
#20764=VERTEX_POINT('',#67680);
#20765=VERTEX_POINT('',#67681);
#20766=VERTEX_POINT('',#67700);
#20767=VERTEX_POINT('',#67762);
#20768=VERTEX_POINT('',#67764);
#20769=VERTEX_POINT('',#67801);
#20770=VERTEX_POINT('',#67802);
#20771=VERTEX_POINT('',#67826);
#20772=VERTEX_POINT('',#67883);
#20773=VERTEX_POINT('',#67885);
#20774=VERTEX_POINT('',#67922);
#20775=VERTEX_POINT('',#67923);
#20776=VERTEX_POINT('',#67942);
#20777=VERTEX_POINT('',#68004);
#20778=VERTEX_POINT('',#68006);
#20779=VERTEX_POINT('',#68043);
#20780=VERTEX_POINT('',#68044);
#20781=VERTEX_POINT('',#68063);
#20782=VERTEX_POINT('',#68125);
#20783=VERTEX_POINT('',#68127);
#20784=VERTEX_POINT('',#68164);
#20785=VERTEX_POINT('',#68165);
#20786=VERTEX_POINT('',#68184);
#20787=VERTEX_POINT('',#68246);
#20788=VERTEX_POINT('',#68248);
#20789=VERTEX_POINT('',#68285);
#20790=VERTEX_POINT('',#68286);
#20791=VERTEX_POINT('',#68305);
#20792=VERTEX_POINT('',#68367);
#20793=VERTEX_POINT('',#68369);
#20794=VERTEX_POINT('',#68406);
#20795=VERTEX_POINT('',#68407);
#20796=VERTEX_POINT('',#68429);
#20797=VERTEX_POINT('',#68488);
#20798=VERTEX_POINT('',#68490);
#20799=VERTEX_POINT('',#68527);
#20800=VERTEX_POINT('',#68528);
#20801=VERTEX_POINT('',#68547);
#20802=VERTEX_POINT('',#68609);
#20803=VERTEX_POINT('',#68611);
#20804=VERTEX_POINT('',#68648);
#20805=VERTEX_POINT('',#68649);
#20806=VERTEX_POINT('',#68668);
#20807=VERTEX_POINT('',#68730);
#20808=VERTEX_POINT('',#68732);
#20809=VERTEX_POINT('',#68769);
#20810=VERTEX_POINT('',#68770);
#20811=VERTEX_POINT('',#68789);
#20812=VERTEX_POINT('',#68851);
#20813=VERTEX_POINT('',#68853);
#20814=VERTEX_POINT('',#68890);
#20815=VERTEX_POINT('',#68891);
#20816=VERTEX_POINT('',#68910);
#20817=VERTEX_POINT('',#68972);
#20818=VERTEX_POINT('',#68974);
#20819=VERTEX_POINT('',#69011);
#20820=VERTEX_POINT('',#69012);
#20821=VERTEX_POINT('',#69031);
#20822=VERTEX_POINT('',#69093);
#20823=VERTEX_POINT('',#69095);
#20824=VERTEX_POINT('',#69132);
#20825=VERTEX_POINT('',#69133);
#20826=VERTEX_POINT('',#69152);
#20827=VERTEX_POINT('',#69214);
#20828=VERTEX_POINT('',#69216);
#20829=VERTEX_POINT('',#69253);
#20830=VERTEX_POINT('',#69254);
#20831=VERTEX_POINT('',#69273);
#20832=VERTEX_POINT('',#69335);
#20833=VERTEX_POINT('',#69337);
#20834=VERTEX_POINT('',#69374);
#20835=VERTEX_POINT('',#69375);
#20836=VERTEX_POINT('',#69394);
#20837=VERTEX_POINT('',#69456);
#20838=VERTEX_POINT('',#69458);
#20839=VERTEX_POINT('',#69495);
#20840=VERTEX_POINT('',#69496);
#20841=VERTEX_POINT('',#69515);
#20842=VERTEX_POINT('',#69579);
#20843=VERTEX_POINT('',#69581);
#20844=VERTEX_POINT('',#69618);
#20845=VERTEX_POINT('',#69619);
#20846=VERTEX_POINT('',#69641);
#20847=VERTEX_POINT('',#69700);
#20848=VERTEX_POINT('',#69702);
#20849=VERTEX_POINT('',#69739);
#20850=VERTEX_POINT('',#69740);
#20851=VERTEX_POINT('',#69759);
#20852=VERTEX_POINT('',#69821);
#20853=VERTEX_POINT('',#69823);
#20854=VERTEX_POINT('',#69860);
#20855=VERTEX_POINT('',#69861);
#20856=VERTEX_POINT('',#69880);
#20857=VERTEX_POINT('',#69942);
#20858=VERTEX_POINT('',#69944);
#20859=VERTEX_POINT('',#69981);
#20860=VERTEX_POINT('',#69982);
#20861=VERTEX_POINT('',#70001);
#20862=VERTEX_POINT('',#70063);
#20863=VERTEX_POINT('',#70065);
#20864=VERTEX_POINT('',#70102);
#20865=VERTEX_POINT('',#70103);
#20866=VERTEX_POINT('',#70122);
#20867=VERTEX_POINT('',#70196);
#20868=VERTEX_POINT('',#70198);
#20869=VERTEX_POINT('',#70235);
#20870=VERTEX_POINT('',#70236);
#20871=VERTEX_POINT('',#70255);
#20872=VERTEX_POINT('',#70317);
#20873=VERTEX_POINT('',#70319);
#20874=VERTEX_POINT('',#70356);
#20875=VERTEX_POINT('',#70358);
#20876=VERTEX_POINT('',#70405);
#20877=VERTEX_POINT('',#70407);
#20878=VERTEX_POINT('',#70411);
#20879=VERTEX_POINT('',#70413);
#20880=VERTEX_POINT('',#70462);
#20881=VERTEX_POINT('',#70464);
#20882=VERTEX_POINT('',#70468);
#20883=VERTEX_POINT('',#70469);
#20884=VERTEX_POINT('',#70488);
#20885=VERTEX_POINT('',#70566);
#20886=VERTEX_POINT('',#70568);
#20887=VERTEX_POINT('',#70605);
#20888=VERTEX_POINT('',#70606);
#20889=VERTEX_POINT('',#70628);
#20890=VERTEX_POINT('',#70705);
#20891=VERTEX_POINT('',#70707);
#20892=VERTEX_POINT('',#70744);
#20893=VERTEX_POINT('',#70746);
#20894=VERTEX_POINT('',#70797);
#20895=VERTEX_POINT('',#70799);
#20896=VERTEX_POINT('',#70803);
#20897=VERTEX_POINT('',#70805);
#20898=VERTEX_POINT('',#70854);
#20899=VERTEX_POINT('',#70856);
#20900=VERTEX_POINT('',#70860);
#20901=VERTEX_POINT('',#70861);
#20902=VERTEX_POINT('',#70883);
#20903=VERTEX_POINT('',#70952);
#20904=VERTEX_POINT('',#70954);
#20905=VERTEX_POINT('',#70991);
#20906=VERTEX_POINT('',#70992);
#20907=VERTEX_POINT('',#71014);
#20908=VERTEX_POINT('',#71087);
#20909=VERTEX_POINT('',#71089);
#20910=VERTEX_POINT('',#71126);
#20911=VERTEX_POINT('',#71128);
#20912=VERTEX_POINT('',#71179);
#20913=VERTEX_POINT('',#71181);
#20914=VERTEX_POINT('',#71185);
#20915=VERTEX_POINT('',#71186);
#20916=VERTEX_POINT('',#71205);
#20917=VERTEX_POINT('',#71277);
#20918=VERTEX_POINT('',#71279);
#20919=VERTEX_POINT('',#71316);
#20920=VERTEX_POINT('',#71317);
#20921=VERTEX_POINT('',#71339);
#20922=VERTEX_POINT('',#71406);
#20923=VERTEX_POINT('',#71408);
#20924=VERTEX_POINT('',#71445);
#20925=VERTEX_POINT('',#71447);
#20926=VERTEX_POINT('',#71500);
#20927=VERTEX_POINT('',#71502);
#20928=VERTEX_POINT('',#71506);
#20929=VERTEX_POINT('',#71507);
#20930=VERTEX_POINT('',#71529);
#20931=VERTEX_POINT('',#71600);
#20932=VERTEX_POINT('',#71602);
#20933=VERTEX_POINT('',#71639);
#20934=VERTEX_POINT('',#71640);
#20935=VERTEX_POINT('',#71659);
#20936=VERTEX_POINT('',#71731);
#20937=VERTEX_POINT('',#71733);
#20938=VERTEX_POINT('',#71770);
#20939=VERTEX_POINT('',#71771);
#20940=VERTEX_POINT('',#71793);
#20941=VERTEX_POINT('',#71868);
#20942=VERTEX_POINT('',#71870);
#20943=VERTEX_POINT('',#71907);
#20944=VERTEX_POINT('',#71908);
#20945=VERTEX_POINT('',#71927);
#20946=VERTEX_POINT('',#72009);
#20947=VERTEX_POINT('',#72011);
#20948=VERTEX_POINT('',#72048);
#20949=VERTEX_POINT('',#72049);
#20950=VERTEX_POINT('',#72071);
#20951=VERTEX_POINT('',#72130);
#20952=VERTEX_POINT('',#72132);
#20953=VERTEX_POINT('',#72169);
#20954=VERTEX_POINT('',#72170);
#20955=VERTEX_POINT('',#72189);
#20956=VERTEX_POINT('',#72265);
#20957=VERTEX_POINT('',#72267);
#20958=VERTEX_POINT('',#72304);
#20959=VERTEX_POINT('',#72305);
#20960=VERTEX_POINT('',#72327);
#20961=VERTEX_POINT('',#72386);
#20962=VERTEX_POINT('',#72388);
#20963=VERTEX_POINT('',#72425);
#20964=VERTEX_POINT('',#72426);
#20965=VERTEX_POINT('',#72448);
#20966=VERTEX_POINT('',#72507);
#20967=VERTEX_POINT('',#72509);
#20968=VERTEX_POINT('',#72546);
#20969=VERTEX_POINT('',#72547);
#20970=VERTEX_POINT('',#72568);
#20971=VERTEX_POINT('',#72628);
#20972=VERTEX_POINT('',#72630);
#20973=VERTEX_POINT('',#72667);
#20974=VERTEX_POINT('',#72668);
#20975=VERTEX_POINT('',#72692);
#20976=VERTEX_POINT('',#72749);
#20977=VERTEX_POINT('',#72751);
#20978=VERTEX_POINT('',#72788);
#20979=VERTEX_POINT('',#72789);
#20980=VERTEX_POINT('',#72813);
#20981=VERTEX_POINT('',#72870);
#20982=VERTEX_POINT('',#72872);
#20983=VERTEX_POINT('',#72909);
#20984=VERTEX_POINT('',#72910);
#20985=VERTEX_POINT('',#72932);
#20986=VERTEX_POINT('',#72991);
#20987=VERTEX_POINT('',#72993);
#20988=VERTEX_POINT('',#73030);
#20989=VERTEX_POINT('',#73031);
#20990=VERTEX_POINT('',#73055);
#20991=VERTEX_POINT('',#73114);
#20992=VERTEX_POINT('',#73116);
#20993=VERTEX_POINT('',#73153);
#20994=VERTEX_POINT('',#73154);
#20995=VERTEX_POINT('',#73178);
#20996=VERTEX_POINT('',#73235);
#20997=VERTEX_POINT('',#73237);
#20998=VERTEX_POINT('',#73274);
#20999=VERTEX_POINT('',#73276);
#21000=VERTEX_POINT('',#73280);
#21001=VERTEX_POINT('',#73282);
#21002=VERTEX_POINT('',#73286);
#21003=VERTEX_POINT('',#73288);
#21004=VERTEX_POINT('',#73292);
#21005=VERTEX_POINT('',#73294);
#21006=VERTEX_POINT('',#73298);
#21007=VERTEX_POINT('',#73300);
#21008=VERTEX_POINT('',#73304);
#21009=VERTEX_POINT('',#73306);
#21010=VERTEX_POINT('',#73310);
#21011=VERTEX_POINT('',#73312);
#21012=VERTEX_POINT('',#73316);
#21013=VERTEX_POINT('',#73318);
#21014=VERTEX_POINT('',#73322);
#21015=VERTEX_POINT('',#73324);
#21016=VERTEX_POINT('',#73328);
#21017=VERTEX_POINT('',#73330);
#21018=VERTEX_POINT('',#73334);
#21019=VERTEX_POINT('',#73336);
#21020=VERTEX_POINT('',#73340);
#21021=VERTEX_POINT('',#73342);
#21022=VERTEX_POINT('',#73346);
#21023=VERTEX_POINT('',#73348);
#21024=VERTEX_POINT('',#73352);
#21025=VERTEX_POINT('',#73354);
#21026=VERTEX_POINT('',#73358);
#21027=VERTEX_POINT('',#73360);
#21028=VERTEX_POINT('',#73364);
#21029=VERTEX_POINT('',#73366);
#21030=VERTEX_POINT('',#73370);
#21031=VERTEX_POINT('',#73372);
#21032=VERTEX_POINT('',#73374);
#21033=VERTEX_POINT('',#73400);
#21034=VERTEX_POINT('',#73411);
#21035=VERTEX_POINT('',#73413);
#21036=VERTEX_POINT('',#73417);
#21037=VERTEX_POINT('',#73419);
#21038=VERTEX_POINT('',#73423);
#21039=VERTEX_POINT('',#73425);
#21040=VERTEX_POINT('',#73429);
#21041=VERTEX_POINT('',#73431);
#21042=VERTEX_POINT('',#73435);
#21043=VERTEX_POINT('',#73437);
#21044=VERTEX_POINT('',#73441);
#21045=VERTEX_POINT('',#73443);
#21046=VERTEX_POINT('',#73447);
#21047=VERTEX_POINT('',#73449);
#21048=VERTEX_POINT('',#73453);
#21049=VERTEX_POINT('',#73455);
#21050=VERTEX_POINT('',#73459);
#21051=VERTEX_POINT('',#73461);
#21052=VERTEX_POINT('',#73465);
#21053=VERTEX_POINT('',#73467);
#21054=VERTEX_POINT('',#73471);
#21055=VERTEX_POINT('',#73473);
#21056=VERTEX_POINT('',#73477);
#21057=VERTEX_POINT('',#73479);
#21058=VERTEX_POINT('',#73483);
#21059=VERTEX_POINT('',#73485);
#21060=VERTEX_POINT('',#73489);
#21061=VERTEX_POINT('',#73491);
#21062=VERTEX_POINT('',#73495);
#21063=VERTEX_POINT('',#73497);
#21064=VERTEX_POINT('',#73501);
#21065=VERTEX_POINT('',#73503);
#21066=VERTEX_POINT('',#73507);
#21067=VERTEX_POINT('',#73509);
#21068=VERTEX_POINT('',#73513);
#21069=VERTEX_POINT('',#73515);
#21070=VERTEX_POINT('',#73517);
#21071=VERTEX_POINT('',#73541);
#21072=VERTEX_POINT('',#73554);
#21073=VERTEX_POINT('',#73556);
#21074=VERTEX_POINT('',#73560);
#21075=VERTEX_POINT('',#73562);
#21076=VERTEX_POINT('',#73566);
#21077=VERTEX_POINT('',#73568);
#21078=VERTEX_POINT('',#73572);
#21079=VERTEX_POINT('',#73574);
#21080=VERTEX_POINT('',#73578);
#21081=VERTEX_POINT('',#73580);
#21082=VERTEX_POINT('',#73584);
#21083=VERTEX_POINT('',#73586);
#21084=VERTEX_POINT('',#73590);
#21085=VERTEX_POINT('',#73592);
#21086=VERTEX_POINT('',#73596);
#21087=VERTEX_POINT('',#73598);
#21088=VERTEX_POINT('',#73602);
#21089=VERTEX_POINT('',#73604);
#21090=VERTEX_POINT('',#73608);
#21091=VERTEX_POINT('',#73610);
#21092=VERTEX_POINT('',#73614);
#21093=VERTEX_POINT('',#73616);
#21094=VERTEX_POINT('',#73620);
#21095=VERTEX_POINT('',#73622);
#21096=VERTEX_POINT('',#73626);
#21097=VERTEX_POINT('',#73628);
#21098=VERTEX_POINT('',#73632);
#21099=VERTEX_POINT('',#73634);
#21100=VERTEX_POINT('',#73638);
#21101=VERTEX_POINT('',#73640);
#21102=VERTEX_POINT('',#73644);
#21103=VERTEX_POINT('',#73646);
#21104=VERTEX_POINT('',#73648);
#21105=VERTEX_POINT('',#73672);
#21106=VERTEX_POINT('',#73685);
#21107=VERTEX_POINT('',#73687);
#21108=VERTEX_POINT('',#73691);
#21109=VERTEX_POINT('',#73693);
#21110=VERTEX_POINT('',#73697);
#21111=VERTEX_POINT('',#73699);
#21112=VERTEX_POINT('',#73703);
#21113=VERTEX_POINT('',#73705);
#21114=VERTEX_POINT('',#73709);
#21115=VERTEX_POINT('',#73711);
#21116=VERTEX_POINT('',#73715);
#21117=VERTEX_POINT('',#73717);
#21118=VERTEX_POINT('',#73721);
#21119=VERTEX_POINT('',#73723);
#21120=VERTEX_POINT('',#73727);
#21121=VERTEX_POINT('',#73729);
#21122=VERTEX_POINT('',#73733);
#21123=VERTEX_POINT('',#73735);
#21124=VERTEX_POINT('',#73739);
#21125=VERTEX_POINT('',#73741);
#21126=VERTEX_POINT('',#73745);
#21127=VERTEX_POINT('',#73747);
#21128=VERTEX_POINT('',#73751);
#21129=VERTEX_POINT('',#73753);
#21130=VERTEX_POINT('',#73757);
#21131=VERTEX_POINT('',#73759);
#21132=VERTEX_POINT('',#73763);
#21133=VERTEX_POINT('',#73765);
#21134=VERTEX_POINT('',#73769);
#21135=VERTEX_POINT('',#73771);
#21136=VERTEX_POINT('',#73775);
#21137=VERTEX_POINT('',#73777);
#21138=VERTEX_POINT('',#73781);
#21139=VERTEX_POINT('',#73783);
#21140=VERTEX_POINT('',#73787);
#21141=VERTEX_POINT('',#73789);
#21142=VERTEX_POINT('',#73791);
#21143=VERTEX_POINT('',#73813);
#21144=VERTEX_POINT('',#73828);
#21145=VERTEX_POINT('',#73830);
#21146=VERTEX_POINT('',#73834);
#21147=VERTEX_POINT('',#73836);
#21148=VERTEX_POINT('',#73840);
#21149=VERTEX_POINT('',#73842);
#21150=VERTEX_POINT('',#73846);
#21151=VERTEX_POINT('',#73848);
#21152=VERTEX_POINT('',#73852);
#21153=VERTEX_POINT('',#73854);
#21154=VERTEX_POINT('',#73858);
#21155=VERTEX_POINT('',#73860);
#21156=VERTEX_POINT('',#73864);
#21157=VERTEX_POINT('',#73866);
#21158=VERTEX_POINT('',#73870);
#21159=VERTEX_POINT('',#73872);
#21160=VERTEX_POINT('',#73876);
#21161=VERTEX_POINT('',#73878);
#21162=VERTEX_POINT('',#73882);
#21163=VERTEX_POINT('',#73884);
#21164=VERTEX_POINT('',#73888);
#21165=VERTEX_POINT('',#73890);
#21166=VERTEX_POINT('',#73894);
#21167=VERTEX_POINT('',#73896);
#21168=VERTEX_POINT('',#73900);
#21169=VERTEX_POINT('',#73902);
#21170=VERTEX_POINT('',#73906);
#21171=VERTEX_POINT('',#73908);
#21172=VERTEX_POINT('',#73912);
#21173=VERTEX_POINT('',#73914);
#21174=VERTEX_POINT('',#73918);
#21175=VERTEX_POINT('',#73920);
#21176=VERTEX_POINT('',#73924);
#21177=VERTEX_POINT('',#73926);
#21178=VERTEX_POINT('',#73930);
#21179=VERTEX_POINT('',#73932);
#21180=VERTEX_POINT('',#73934);
#21181=VERTEX_POINT('',#73956);
#21182=VERTEX_POINT('',#73971);
#21183=VERTEX_POINT('',#73973);
#21184=VERTEX_POINT('',#73977);
#21185=VERTEX_POINT('',#73979);
#21186=VERTEX_POINT('',#73983);
#21187=VERTEX_POINT('',#73985);
#21188=VERTEX_POINT('',#73989);
#21189=VERTEX_POINT('',#73991);
#21190=VERTEX_POINT('',#73995);
#21191=VERTEX_POINT('',#73997);
#21192=VERTEX_POINT('',#74001);
#21193=VERTEX_POINT('',#74003);
#21194=VERTEX_POINT('',#74007);
#21195=VERTEX_POINT('',#74009);
#21196=VERTEX_POINT('',#74013);
#21197=VERTEX_POINT('',#74015);
#21198=VERTEX_POINT('',#74019);
#21199=VERTEX_POINT('',#74021);
#21200=VERTEX_POINT('',#74025);
#21201=VERTEX_POINT('',#74027);
#21202=VERTEX_POINT('',#74031);
#21203=VERTEX_POINT('',#74033);
#21204=VERTEX_POINT('',#74037);
#21205=VERTEX_POINT('',#74039);
#21206=VERTEX_POINT('',#74043);
#21207=VERTEX_POINT('',#74045);
#21208=VERTEX_POINT('',#74049);
#21209=VERTEX_POINT('',#74051);
#21210=VERTEX_POINT('',#74055);
#21211=VERTEX_POINT('',#74057);
#21212=VERTEX_POINT('',#74061);
#21213=VERTEX_POINT('',#74063);
#21214=VERTEX_POINT('',#74067);
#21215=VERTEX_POINT('',#74069);
#21216=VERTEX_POINT('',#74073);
#21217=VERTEX_POINT('',#74075);
#21218=VERTEX_POINT('',#74077);
#21219=VERTEX_POINT('',#74097);
#21220=VERTEX_POINT('',#74114);
#21221=VERTEX_POINT('',#74116);
#21222=VERTEX_POINT('',#74120);
#21223=VERTEX_POINT('',#74122);
#21224=VERTEX_POINT('',#74126);
#21225=VERTEX_POINT('',#74128);
#21226=VERTEX_POINT('',#74132);
#21227=VERTEX_POINT('',#74134);
#21228=VERTEX_POINT('',#74138);
#21229=VERTEX_POINT('',#74140);
#21230=VERTEX_POINT('',#74144);
#21231=VERTEX_POINT('',#74146);
#21232=VERTEX_POINT('',#74150);
#21233=VERTEX_POINT('',#74152);
#21234=VERTEX_POINT('',#74156);
#21235=VERTEX_POINT('',#74158);
#21236=VERTEX_POINT('',#74162);
#21237=VERTEX_POINT('',#74164);
#21238=VERTEX_POINT('',#74168);
#21239=VERTEX_POINT('',#74170);
#21240=VERTEX_POINT('',#74174);
#21241=VERTEX_POINT('',#74176);
#21242=VERTEX_POINT('',#74180);
#21243=VERTEX_POINT('',#74182);
#21244=VERTEX_POINT('',#74186);
#21245=VERTEX_POINT('',#74188);
#21246=VERTEX_POINT('',#74192);
#21247=VERTEX_POINT('',#74194);
#21248=VERTEX_POINT('',#74198);
#21249=VERTEX_POINT('',#74200);
#21250=VERTEX_POINT('',#74204);
#21251=VERTEX_POINT('',#74206);
#21252=VERTEX_POINT('',#74210);
#21253=VERTEX_POINT('',#74212);
#21254=VERTEX_POINT('',#74216);
#21255=VERTEX_POINT('',#74218);
#21256=VERTEX_POINT('',#74220);
#21257=VERTEX_POINT('',#74240);
#21258=VERTEX_POINT('',#74257);
#21259=VERTEX_POINT('',#74259);
#21260=VERTEX_POINT('',#74263);
#21261=VERTEX_POINT('',#74265);
#21262=VERTEX_POINT('',#74269);
#21263=VERTEX_POINT('',#74271);
#21264=VERTEX_POINT('',#74275);
#21265=VERTEX_POINT('',#74277);
#21266=VERTEX_POINT('',#74281);
#21267=VERTEX_POINT('',#74283);
#21268=VERTEX_POINT('',#74287);
#21269=VERTEX_POINT('',#74289);
#21270=VERTEX_POINT('',#74293);
#21271=VERTEX_POINT('',#74295);
#21272=VERTEX_POINT('',#74299);
#21273=VERTEX_POINT('',#74301);
#21274=VERTEX_POINT('',#74305);
#21275=VERTEX_POINT('',#74307);
#21276=VERTEX_POINT('',#74311);
#21277=VERTEX_POINT('',#74313);
#21278=VERTEX_POINT('',#74317);
#21279=VERTEX_POINT('',#74319);
#21280=VERTEX_POINT('',#74323);
#21281=VERTEX_POINT('',#74325);
#21282=VERTEX_POINT('',#74329);
#21283=VERTEX_POINT('',#74331);
#21284=VERTEX_POINT('',#74335);
#21285=VERTEX_POINT('',#74337);
#21286=VERTEX_POINT('',#74341);
#21287=VERTEX_POINT('',#74343);
#21288=VERTEX_POINT('',#74347);
#21289=VERTEX_POINT('',#74349);
#21290=VERTEX_POINT('',#74351);
#21291=VERTEX_POINT('',#74366);
#21292=VERTEX_POINT('',#74388);
#21293=VERTEX_POINT('',#74390);
#21294=VERTEX_POINT('',#74394);
#21295=VERTEX_POINT('',#74396);
#21296=VERTEX_POINT('',#74400);
#21297=VERTEX_POINT('',#74402);
#21298=VERTEX_POINT('',#74406);
#21299=VERTEX_POINT('',#74408);
#21300=VERTEX_POINT('',#74412);
#21301=VERTEX_POINT('',#74414);
#21302=VERTEX_POINT('',#74418);
#21303=VERTEX_POINT('',#74420);
#21304=VERTEX_POINT('',#74424);
#21305=VERTEX_POINT('',#74426);
#21306=VERTEX_POINT('',#74430);
#21307=VERTEX_POINT('',#74432);
#21308=VERTEX_POINT('',#74436);
#21309=VERTEX_POINT('',#74438);
#21310=VERTEX_POINT('',#74442);
#21311=VERTEX_POINT('',#74444);
#21312=VERTEX_POINT('',#74448);
#21313=VERTEX_POINT('',#74450);
#21314=VERTEX_POINT('',#74454);
#21315=VERTEX_POINT('',#74456);
#21316=VERTEX_POINT('',#74460);
#21317=VERTEX_POINT('',#74462);
#21318=VERTEX_POINT('',#74466);
#21319=VERTEX_POINT('',#74468);
#21320=VERTEX_POINT('',#74472);
#21321=VERTEX_POINT('',#74474);
#21322=VERTEX_POINT('',#74478);
#21323=VERTEX_POINT('',#74480);
#21324=VERTEX_POINT('',#74484);
#21325=VERTEX_POINT('',#74486);
#21326=VERTEX_POINT('',#74490);
#21327=VERTEX_POINT('',#74492);
#21328=VERTEX_POINT('',#74494);
#21329=VERTEX_POINT('',#74509);
#21330=VERTEX_POINT('',#74531);
#21331=VERTEX_POINT('',#74533);
#21332=VERTEX_POINT('',#74537);
#21333=VERTEX_POINT('',#74539);
#21334=VERTEX_POINT('',#74543);
#21335=VERTEX_POINT('',#74545);
#21336=VERTEX_POINT('',#74549);
#21337=VERTEX_POINT('',#74551);
#21338=VERTEX_POINT('',#74555);
#21339=VERTEX_POINT('',#74557);
#21340=VERTEX_POINT('',#74561);
#21341=VERTEX_POINT('',#74563);
#21342=VERTEX_POINT('',#74567);
#21343=VERTEX_POINT('',#74569);
#21344=VERTEX_POINT('',#74573);
#21345=VERTEX_POINT('',#74575);
#21346=VERTEX_POINT('',#74579);
#21347=VERTEX_POINT('',#74581);
#21348=VERTEX_POINT('',#74585);
#21349=VERTEX_POINT('',#74587);
#21350=VERTEX_POINT('',#74591);
#21351=VERTEX_POINT('',#74593);
#21352=VERTEX_POINT('',#74597);
#21353=VERTEX_POINT('',#74599);
#21354=VERTEX_POINT('',#74603);
#21355=VERTEX_POINT('',#74605);
#21356=VERTEX_POINT('',#74609);
#21357=VERTEX_POINT('',#74611);
#21358=VERTEX_POINT('',#74615);
#21359=VERTEX_POINT('',#74617);
#21360=VERTEX_POINT('',#74621);
#21361=VERTEX_POINT('',#74623);
#21362=VERTEX_POINT('',#74627);
#21363=VERTEX_POINT('',#74629);
#21364=VERTEX_POINT('',#74633);
#21365=VERTEX_POINT('',#74635);
#21366=VERTEX_POINT('',#74637);
#21367=VERTEX_POINT('',#74650);
#21368=VERTEX_POINT('',#74674);
#21369=VERTEX_POINT('',#74676);
#21370=VERTEX_POINT('',#74680);
#21371=VERTEX_POINT('',#74682);
#21372=VERTEX_POINT('',#74686);
#21373=VERTEX_POINT('',#74688);
#21374=VERTEX_POINT('',#74692);
#21375=VERTEX_POINT('',#74694);
#21376=VERTEX_POINT('',#74698);
#21377=VERTEX_POINT('',#74700);
#21378=VERTEX_POINT('',#74704);
#21379=VERTEX_POINT('',#74706);
#21380=VERTEX_POINT('',#74710);
#21381=VERTEX_POINT('',#74712);
#21382=VERTEX_POINT('',#74716);
#21383=VERTEX_POINT('',#74718);
#21384=VERTEX_POINT('',#74722);
#21385=VERTEX_POINT('',#74724);
#21386=VERTEX_POINT('',#74728);
#21387=VERTEX_POINT('',#74730);
#21388=VERTEX_POINT('',#74734);
#21389=VERTEX_POINT('',#74736);
#21390=VERTEX_POINT('',#74740);
#21391=VERTEX_POINT('',#74742);
#21392=VERTEX_POINT('',#74746);
#21393=VERTEX_POINT('',#74748);
#21394=VERTEX_POINT('',#74752);
#21395=VERTEX_POINT('',#74754);
#21396=VERTEX_POINT('',#74758);
#21397=VERTEX_POINT('',#74760);
#21398=VERTEX_POINT('',#74764);
#21399=VERTEX_POINT('',#74766);
#21400=VERTEX_POINT('',#74770);
#21401=VERTEX_POINT('',#74772);
#21402=VERTEX_POINT('',#74776);
#21403=VERTEX_POINT('',#74778);
#21404=VERTEX_POINT('',#74780);
#21405=VERTEX_POINT('',#74793);
#21406=VERTEX_POINT('',#74817);
#21407=VERTEX_POINT('',#74819);
#21408=VERTEX_POINT('',#74823);
#21409=VERTEX_POINT('',#74825);
#21410=VERTEX_POINT('',#74829);
#21411=VERTEX_POINT('',#74831);
#21412=VERTEX_POINT('',#74835);
#21413=VERTEX_POINT('',#74837);
#21414=VERTEX_POINT('',#74841);
#21415=VERTEX_POINT('',#74843);
#21416=VERTEX_POINT('',#74847);
#21417=VERTEX_POINT('',#74849);
#21418=VERTEX_POINT('',#74853);
#21419=VERTEX_POINT('',#74855);
#21420=VERTEX_POINT('',#74859);
#21421=VERTEX_POINT('',#74861);
#21422=VERTEX_POINT('',#74865);
#21423=VERTEX_POINT('',#74867);
#21424=VERTEX_POINT('',#74871);
#21425=VERTEX_POINT('',#74873);
#21426=VERTEX_POINT('',#74877);
#21427=VERTEX_POINT('',#74879);
#21428=VERTEX_POINT('',#74883);
#21429=VERTEX_POINT('',#74885);
#21430=VERTEX_POINT('',#74889);
#21431=VERTEX_POINT('',#74891);
#21432=VERTEX_POINT('',#74895);
#21433=VERTEX_POINT('',#74897);
#21434=VERTEX_POINT('',#74901);
#21435=VERTEX_POINT('',#74903);
#21436=VERTEX_POINT('',#74907);
#21437=VERTEX_POINT('',#74909);
#21438=VERTEX_POINT('',#74913);
#21439=VERTEX_POINT('',#74915);
#21440=VERTEX_POINT('',#74919);
#21441=VERTEX_POINT('',#74921);
#21442=VERTEX_POINT('',#74923);
#21443=VERTEX_POINT('',#74934);
#21444=VERTEX_POINT('',#74960);
#21445=VERTEX_POINT('',#74962);
#21446=VERTEX_POINT('',#74966);
#21447=VERTEX_POINT('',#74968);
#21448=VERTEX_POINT('',#74972);
#21449=VERTEX_POINT('',#74974);
#21450=VERTEX_POINT('',#74978);
#21451=VERTEX_POINT('',#74980);
#21452=VERTEX_POINT('',#74984);
#21453=VERTEX_POINT('',#74986);
#21454=VERTEX_POINT('',#74990);
#21455=VERTEX_POINT('',#74992);
#21456=VERTEX_POINT('',#74996);
#21457=VERTEX_POINT('',#74998);
#21458=VERTEX_POINT('',#75002);
#21459=VERTEX_POINT('',#75004);
#21460=VERTEX_POINT('',#75008);
#21461=VERTEX_POINT('',#75010);
#21462=VERTEX_POINT('',#75014);
#21463=VERTEX_POINT('',#75016);
#21464=VERTEX_POINT('',#75020);
#21465=VERTEX_POINT('',#75022);
#21466=VERTEX_POINT('',#75026);
#21467=VERTEX_POINT('',#75028);
#21468=VERTEX_POINT('',#75032);
#21469=VERTEX_POINT('',#75034);
#21470=VERTEX_POINT('',#75038);
#21471=VERTEX_POINT('',#75040);
#21472=VERTEX_POINT('',#75044);
#21473=VERTEX_POINT('',#75046);
#21474=VERTEX_POINT('',#75050);
#21475=VERTEX_POINT('',#75052);
#21476=VERTEX_POINT('',#75054);
#21477=VERTEX_POINT('',#75065);
#21478=VERTEX_POINT('',#75091);
#21479=VERTEX_POINT('',#75093);
#21480=VERTEX_POINT('',#75097);
#21481=VERTEX_POINT('',#75099);
#21482=VERTEX_POINT('',#75103);
#21483=VERTEX_POINT('',#75105);
#21484=VERTEX_POINT('',#75109);
#21485=VERTEX_POINT('',#75111);
#21486=VERTEX_POINT('',#75115);
#21487=VERTEX_POINT('',#75117);
#21488=VERTEX_POINT('',#75121);
#21489=VERTEX_POINT('',#75123);
#21490=VERTEX_POINT('',#75127);
#21491=VERTEX_POINT('',#75129);
#21492=VERTEX_POINT('',#75133);
#21493=VERTEX_POINT('',#75135);
#21494=VERTEX_POINT('',#75139);
#21495=VERTEX_POINT('',#75141);
#21496=VERTEX_POINT('',#75145);
#21497=VERTEX_POINT('',#75147);
#21498=VERTEX_POINT('',#75151);
#21499=VERTEX_POINT('',#75153);
#21500=VERTEX_POINT('',#75157);
#21501=VERTEX_POINT('',#75159);
#21502=VERTEX_POINT('',#75163);
#21503=VERTEX_POINT('',#75165);
#21504=VERTEX_POINT('',#75169);
#21505=VERTEX_POINT('',#75171);
#21506=VERTEX_POINT('',#75175);
#21507=VERTEX_POINT('',#75177);
#21508=VERTEX_POINT('',#75181);
#21509=VERTEX_POINT('',#75183);
#21510=VERTEX_POINT('',#75187);
#21511=VERTEX_POINT('',#75189);
#21512=VERTEX_POINT('',#75193);
#21513=VERTEX_POINT('',#75195);
#21514=VERTEX_POINT('',#75197);
#21515=VERTEX_POINT('',#75206);
#21516=VERTEX_POINT('',#75234);
#21517=VERTEX_POINT('',#75236);
#21518=VERTEX_POINT('',#75240);
#21519=VERTEX_POINT('',#75242);
#21520=VERTEX_POINT('',#75246);
#21521=VERTEX_POINT('',#75248);
#21522=VERTEX_POINT('',#75252);
#21523=VERTEX_POINT('',#75254);
#21524=VERTEX_POINT('',#75258);
#21525=VERTEX_POINT('',#75260);
#21526=VERTEX_POINT('',#75264);
#21527=VERTEX_POINT('',#75266);
#21528=VERTEX_POINT('',#75270);
#21529=VERTEX_POINT('',#75272);
#21530=VERTEX_POINT('',#75276);
#21531=VERTEX_POINT('',#75278);
#21532=VERTEX_POINT('',#75282);
#21533=VERTEX_POINT('',#75284);
#21534=VERTEX_POINT('',#75288);
#21535=VERTEX_POINT('',#75290);
#21536=VERTEX_POINT('',#75294);
#21537=VERTEX_POINT('',#75296);
#21538=VERTEX_POINT('',#75300);
#21539=VERTEX_POINT('',#75302);
#21540=VERTEX_POINT('',#75306);
#21541=VERTEX_POINT('',#75308);
#21542=VERTEX_POINT('',#75312);
#21543=VERTEX_POINT('',#75314);
#21544=VERTEX_POINT('',#75318);
#21545=VERTEX_POINT('',#75320);
#21546=VERTEX_POINT('',#75324);
#21547=VERTEX_POINT('',#75326);
#21548=VERTEX_POINT('',#75330);
#21549=VERTEX_POINT('',#75332);
#21550=VERTEX_POINT('',#75336);
#21551=VERTEX_POINT('',#75338);
#21552=VERTEX_POINT('',#75340);
#21553=VERTEX_POINT('',#75349);
#21554=VERTEX_POINT('',#75377);
#21555=VERTEX_POINT('',#75379);
#21556=VERTEX_POINT('',#75383);
#21557=VERTEX_POINT('',#75385);
#21558=VERTEX_POINT('',#75389);
#21559=VERTEX_POINT('',#75391);
#21560=VERTEX_POINT('',#75395);
#21561=VERTEX_POINT('',#75397);
#21562=VERTEX_POINT('',#75401);
#21563=VERTEX_POINT('',#75403);
#21564=VERTEX_POINT('',#75407);
#21565=VERTEX_POINT('',#75409);
#21566=VERTEX_POINT('',#75413);
#21567=VERTEX_POINT('',#75415);
#21568=VERTEX_POINT('',#75419);
#21569=VERTEX_POINT('',#75421);
#21570=VERTEX_POINT('',#75425);
#21571=VERTEX_POINT('',#75427);
#21572=VERTEX_POINT('',#75431);
#21573=VERTEX_POINT('',#75433);
#21574=VERTEX_POINT('',#75437);
#21575=VERTEX_POINT('',#75439);
#21576=VERTEX_POINT('',#75443);
#21577=VERTEX_POINT('',#75445);
#21578=VERTEX_POINT('',#75449);
#21579=VERTEX_POINT('',#75451);
#21580=VERTEX_POINT('',#75455);
#21581=VERTEX_POINT('',#75457);
#21582=VERTEX_POINT('',#75461);
#21583=VERTEX_POINT('',#75463);
#21584=VERTEX_POINT('',#75467);
#21585=VERTEX_POINT('',#75469);
#21586=VERTEX_POINT('',#75473);
#21587=VERTEX_POINT('',#75475);
#21588=VERTEX_POINT('',#75479);
#21589=VERTEX_POINT('',#75481);
#21590=VERTEX_POINT('',#75483);
#21591=VERTEX_POINT('',#75490);
#21592=VERTEX_POINT('',#75520);
#21593=VERTEX_POINT('',#75522);
#21594=VERTEX_POINT('',#75526);
#21595=VERTEX_POINT('',#75528);
#21596=VERTEX_POINT('',#75532);
#21597=VERTEX_POINT('',#75534);
#21598=VERTEX_POINT('',#75538);
#21599=VERTEX_POINT('',#75540);
#21600=VERTEX_POINT('',#75544);
#21601=VERTEX_POINT('',#75546);
#21602=VERTEX_POINT('',#75550);
#21603=VERTEX_POINT('',#75552);
#21604=VERTEX_POINT('',#75556);
#21605=VERTEX_POINT('',#75558);
#21606=VERTEX_POINT('',#75562);
#21607=VERTEX_POINT('',#75564);
#21608=VERTEX_POINT('',#75568);
#21609=VERTEX_POINT('',#75570);
#21610=VERTEX_POINT('',#75574);
#21611=VERTEX_POINT('',#75576);
#21612=VERTEX_POINT('',#75580);
#21613=VERTEX_POINT('',#75582);
#21614=VERTEX_POINT('',#75586);
#21615=VERTEX_POINT('',#75588);
#21616=VERTEX_POINT('',#75592);
#21617=VERTEX_POINT('',#75594);
#21618=VERTEX_POINT('',#75598);
#21619=VERTEX_POINT('',#75600);
#21620=VERTEX_POINT('',#75604);
#21621=VERTEX_POINT('',#75606);
#21622=VERTEX_POINT('',#75610);
#21623=VERTEX_POINT('',#75612);
#21624=VERTEX_POINT('',#75616);
#21625=VERTEX_POINT('',#75618);
#21626=VERTEX_POINT('',#75622);
#21627=VERTEX_POINT('',#75624);
#21628=VERTEX_POINT('',#75626);
#21629=VERTEX_POINT('',#75631);
#21630=VERTEX_POINT('',#75663);
#21631=VERTEX_POINT('',#75665);
#21632=VERTEX_POINT('',#75669);
#21633=VERTEX_POINT('',#75671);
#21634=VERTEX_POINT('',#75675);
#21635=VERTEX_POINT('',#75677);
#21636=VERTEX_POINT('',#75681);
#21637=VERTEX_POINT('',#75683);
#21638=VERTEX_POINT('',#75687);
#21639=VERTEX_POINT('',#75689);
#21640=VERTEX_POINT('',#75693);
#21641=VERTEX_POINT('',#75695);
#21642=VERTEX_POINT('',#75699);
#21643=VERTEX_POINT('',#75701);
#21644=VERTEX_POINT('',#75705);
#21645=VERTEX_POINT('',#75707);
#21646=VERTEX_POINT('',#75711);
#21647=VERTEX_POINT('',#75713);
#21648=VERTEX_POINT('',#75717);
#21649=VERTEX_POINT('',#75719);
#21650=VERTEX_POINT('',#75723);
#21651=VERTEX_POINT('',#75725);
#21652=VERTEX_POINT('',#75729);
#21653=VERTEX_POINT('',#75731);
#21654=VERTEX_POINT('',#75735);
#21655=VERTEX_POINT('',#75737);
#21656=VERTEX_POINT('',#75741);
#21657=VERTEX_POINT('',#75743);
#21658=VERTEX_POINT('',#75747);
#21659=VERTEX_POINT('',#75749);
#21660=VERTEX_POINT('',#75753);
#21661=VERTEX_POINT('',#75755);
#21662=VERTEX_POINT('',#75757);
#21663=VERTEX_POINT('',#75762);
#21664=VERTEX_POINT('',#75794);
#21665=VERTEX_POINT('',#75796);
#21666=VERTEX_POINT('',#75800);
#21667=VERTEX_POINT('',#75802);
#21668=VERTEX_POINT('',#75806);
#21669=VERTEX_POINT('',#75808);
#21670=VERTEX_POINT('',#75812);
#21671=VERTEX_POINT('',#75814);
#21672=VERTEX_POINT('',#75818);
#21673=VERTEX_POINT('',#75820);
#21674=VERTEX_POINT('',#75824);
#21675=VERTEX_POINT('',#75826);
#21676=VERTEX_POINT('',#75830);
#21677=VERTEX_POINT('',#75832);
#21678=VERTEX_POINT('',#75836);
#21679=VERTEX_POINT('',#75838);
#21680=VERTEX_POINT('',#75842);
#21681=VERTEX_POINT('',#75844);
#21682=VERTEX_POINT('',#75848);
#21683=VERTEX_POINT('',#75850);
#21684=VERTEX_POINT('',#75854);
#21685=VERTEX_POINT('',#75856);
#21686=VERTEX_POINT('',#75860);
#21687=VERTEX_POINT('',#75862);
#21688=VERTEX_POINT('',#75866);
#21689=VERTEX_POINT('',#75868);
#21690=VERTEX_POINT('',#75872);
#21691=VERTEX_POINT('',#75874);
#21692=VERTEX_POINT('',#75878);
#21693=VERTEX_POINT('',#75880);
#21694=VERTEX_POINT('',#75884);
#21695=VERTEX_POINT('',#75886);
#21696=VERTEX_POINT('',#75890);
#21697=VERTEX_POINT('',#75892);
#21698=VERTEX_POINT('',#75896);
#21699=VERTEX_POINT('',#75898);
#21700=VERTEX_POINT('',#75900);
#21701=VERTEX_POINT('',#75902);
#21702=VERTEX_POINT('',#75934);
#21703=VERTEX_POINT('',#75936);
#21704=VERTEX_POINT('',#75940);
#21705=VERTEX_POINT('',#75942);
#21706=VERTEX_POINT('',#75946);
#21707=VERTEX_POINT('',#75948);
#21708=VERTEX_POINT('',#75952);
#21709=VERTEX_POINT('',#75954);
#21710=VERTEX_POINT('',#75958);
#21711=VERTEX_POINT('',#75960);
#21712=VERTEX_POINT('',#75964);
#21713=VERTEX_POINT('',#75966);
#21714=VERTEX_POINT('',#75970);
#21715=VERTEX_POINT('',#75972);
#21716=VERTEX_POINT('',#75976);
#21717=VERTEX_POINT('',#75978);
#21718=VERTEX_POINT('',#75982);
#21719=VERTEX_POINT('',#75984);
#21720=VERTEX_POINT('',#75988);
#21721=VERTEX_POINT('',#75990);
#21722=VERTEX_POINT('',#75994);
#21723=VERTEX_POINT('',#75996);
#21724=VERTEX_POINT('',#76000);
#21725=VERTEX_POINT('',#76002);
#21726=VERTEX_POINT('',#76006);
#21727=VERTEX_POINT('',#76008);
#21728=VERTEX_POINT('',#76012);
#21729=VERTEX_POINT('',#76014);
#21730=VERTEX_POINT('',#76018);
#21731=VERTEX_POINT('',#76020);
#21732=VERTEX_POINT('',#76024);
#21733=VERTEX_POINT('',#76026);
#21734=VERTEX_POINT('',#76028);
#21735=VERTEX_POINT('',#76030);
#21736=VERTEX_POINT('',#76045);
#21737=VERTEX_POINT('',#76047);
#21738=VERTEX_POINT('',#76051);
#21739=VERTEX_POINT('',#76053);
#21740=VERTEX_POINT('',#76055);
#21741=VERTEX_POINT('',#76057);
#21742=VERTEX_POINT('',#76096);
#21743=VERTEX_POINT('',#76098);
#21744=VERTEX_POINT('',#76102);
#21745=VERTEX_POINT('',#76104);
#21746=VERTEX_POINT('',#76108);
#21747=VERTEX_POINT('',#76110);
#21748=VERTEX_POINT('',#76114);
#21749=VERTEX_POINT('',#76116);
#21750=VERTEX_POINT('',#76120);
#21751=VERTEX_POINT('',#76122);
#21752=VERTEX_POINT('',#76126);
#21753=VERTEX_POINT('',#76128);
#21754=VERTEX_POINT('',#76132);
#21755=VERTEX_POINT('',#76134);
#21756=VERTEX_POINT('',#76138);
#21757=VERTEX_POINT('',#76140);
#21758=VERTEX_POINT('',#76144);
#21759=VERTEX_POINT('',#76146);
#21760=VERTEX_POINT('',#76150);
#21761=VERTEX_POINT('',#76152);
#21762=VERTEX_POINT('',#76156);
#21763=VERTEX_POINT('',#76158);
#21764=VERTEX_POINT('',#76162);
#21765=VERTEX_POINT('',#76164);
#21766=VERTEX_POINT('',#76168);
#21767=VERTEX_POINT('',#76170);
#21768=VERTEX_POINT('',#76174);
#21769=VERTEX_POINT('',#76176);
#21770=VERTEX_POINT('',#76178);
#21771=VERTEX_POINT('',#76180);
#21772=VERTEX_POINT('',#76197);
#21773=VERTEX_POINT('',#76199);
#21774=VERTEX_POINT('',#76203);
#21775=VERTEX_POINT('',#76205);
#21776=VERTEX_POINT('',#76209);
#21777=VERTEX_POINT('',#76211);
#21778=VERTEX_POINT('',#76215);
#21779=VERTEX_POINT('',#76217);
#21780=VERTEX_POINT('',#76221);
#21781=VERTEX_POINT('',#76223);
#21782=VERTEX_POINT('',#76227);
#21783=VERTEX_POINT('',#76229);
#21784=VERTEX_POINT('',#76233);
#21785=VERTEX_POINT('',#76235);
#21786=VERTEX_POINT('',#76239);
#21787=VERTEX_POINT('',#76241);
#21788=VERTEX_POINT('',#76245);
#21789=VERTEX_POINT('',#76247);
#21790=VERTEX_POINT('',#76251);
#21791=VERTEX_POINT('',#76253);
#21792=VERTEX_POINT('',#76257);
#21793=VERTEX_POINT('',#76259);
#21794=VERTEX_POINT('',#76263);
#21795=VERTEX_POINT('',#76265);
#21796=VERTEX_POINT('',#76269);
#21797=VERTEX_POINT('',#76271);
#21798=VERTEX_POINT('',#76275);
#21799=VERTEX_POINT('',#76277);
#21800=VERTEX_POINT('',#76281);
#21801=VERTEX_POINT('',#76283);
#21802=VERTEX_POINT('',#76287);
#21803=VERTEX_POINT('',#76289);
#21804=VERTEX_POINT('',#76293);
#21805=VERTEX_POINT('',#76295);
#21806=VERTEX_POINT('',#76299);
#21807=VERTEX_POINT('',#76301);
#21808=VERTEX_POINT('',#76305);
#21809=VERTEX_POINT('',#76307);
#21810=VERTEX_POINT('',#76311);
#21811=VERTEX_POINT('',#76313);
#21812=VERTEX_POINT('',#76317);
#21813=VERTEX_POINT('',#76319);
#21814=VERTEX_POINT('',#76323);
#21815=VERTEX_POINT('',#76325);
#21816=VERTEX_POINT('',#76329);
#21817=VERTEX_POINT('',#76331);
#21818=VERTEX_POINT('',#76335);
#21819=VERTEX_POINT('',#76337);
#21820=VERTEX_POINT('',#76341);
#21821=VERTEX_POINT('',#76343);
#21822=VERTEX_POINT('',#76347);
#21823=VERTEX_POINT('',#76349);
#21824=VERTEX_POINT('',#76353);
#21825=VERTEX_POINT('',#76355);
#21826=VERTEX_POINT('',#76359);
#21827=VERTEX_POINT('',#76361);
#21828=VERTEX_POINT('',#76363);
#21829=VERTEX_POINT('',#76365);
#21830=VERTEX_POINT('',#76392);
#21831=VERTEX_POINT('',#76394);
#21832=VERTEX_POINT('',#76398);
#21833=VERTEX_POINT('',#76400);
#21834=VERTEX_POINT('',#76404);
#21835=VERTEX_POINT('',#76406);
#21836=VERTEX_POINT('',#76410);
#21837=VERTEX_POINT('',#76412);
#21838=VERTEX_POINT('',#76416);
#21839=VERTEX_POINT('',#76418);
#21840=VERTEX_POINT('',#76422);
#21841=VERTEX_POINT('',#76424);
#21842=VERTEX_POINT('',#76428);
#21843=VERTEX_POINT('',#76430);
#21844=VERTEX_POINT('',#76434);
#21845=VERTEX_POINT('',#76436);
#21846=VERTEX_POINT('',#76440);
#21847=VERTEX_POINT('',#76442);
#21848=VERTEX_POINT('',#76446);
#21849=VERTEX_POINT('',#76448);
#21850=VERTEX_POINT('',#76452);
#21851=VERTEX_POINT('',#76454);
#21852=VERTEX_POINT('',#76458);
#21853=VERTEX_POINT('',#76460);
#21854=VERTEX_POINT('',#76464);
#21855=VERTEX_POINT('',#76466);
#21856=VERTEX_POINT('',#76470);
#21857=VERTEX_POINT('',#76472);
#21858=VERTEX_POINT('',#76476);
#21859=VERTEX_POINT('',#76478);
#21860=VERTEX_POINT('',#76482);
#21861=VERTEX_POINT('',#76484);
#21862=VERTEX_POINT('',#76488);
#21863=VERTEX_POINT('',#76490);
#21864=VERTEX_POINT('',#76494);
#21865=VERTEX_POINT('',#76496);
#21866=VERTEX_POINT('',#76500);
#21867=VERTEX_POINT('',#76502);
#21868=VERTEX_POINT('',#76506);
#21869=VERTEX_POINT('',#76508);
#21870=VERTEX_POINT('',#76512);
#21871=VERTEX_POINT('',#76514);
#21872=VERTEX_POINT('',#76518);
#21873=VERTEX_POINT('',#76520);
#21874=VERTEX_POINT('',#76524);
#21875=VERTEX_POINT('',#76526);
#21876=VERTEX_POINT('',#76530);
#21877=VERTEX_POINT('',#76532);
#21878=VERTEX_POINT('',#76536);
#21879=VERTEX_POINT('',#76538);
#21880=VERTEX_POINT('',#76542);
#21881=VERTEX_POINT('',#76544);
#21882=VERTEX_POINT('',#76548);
#21883=VERTEX_POINT('',#76550);
#21884=VERTEX_POINT('',#76554);
#21885=VERTEX_POINT('',#76556);
#21886=VERTEX_POINT('',#76560);
#21887=VERTEX_POINT('',#76562);
#21888=VERTEX_POINT('',#76566);
#21889=VERTEX_POINT('',#76568);
#21890=VERTEX_POINT('',#76572);
#21891=VERTEX_POINT('',#76574);
#21892=VERTEX_POINT('',#76578);
#21893=VERTEX_POINT('',#76580);
#21894=VERTEX_POINT('',#76584);
#21895=VERTEX_POINT('',#76586);
#21896=VERTEX_POINT('',#76590);
#21897=VERTEX_POINT('',#76592);
#21898=VERTEX_POINT('',#76594);
#21899=VERTEX_POINT('',#76596);
#21900=VERTEX_POINT('',#76607);
#21901=VERTEX_POINT('',#76638);
#21902=VERTEX_POINT('',#76640);
#21903=VERTEX_POINT('',#76644);
#21904=VERTEX_POINT('',#76646);
#21905=VERTEX_POINT('',#76650);
#21906=VERTEX_POINT('',#76652);
#21907=VERTEX_POINT('',#76656);
#21908=VERTEX_POINT('',#76658);
#21909=VERTEX_POINT('',#76662);
#21910=VERTEX_POINT('',#76664);
#21911=VERTEX_POINT('',#76668);
#21912=VERTEX_POINT('',#76670);
#21913=VERTEX_POINT('',#76674);
#21914=VERTEX_POINT('',#76676);
#21915=VERTEX_POINT('',#76680);
#21916=VERTEX_POINT('',#76682);
#21917=VERTEX_POINT('',#76686);
#21918=VERTEX_POINT('',#76688);
#21919=VERTEX_POINT('',#76692);
#21920=VERTEX_POINT('',#76694);
#21921=VERTEX_POINT('',#76698);
#21922=VERTEX_POINT('',#76700);
#21923=VERTEX_POINT('',#76704);
#21924=VERTEX_POINT('',#76706);
#21925=VERTEX_POINT('',#76710);
#21926=VERTEX_POINT('',#76712);
#21927=VERTEX_POINT('',#76716);
#21928=VERTEX_POINT('',#76718);
#21929=VERTEX_POINT('',#76722);
#21930=VERTEX_POINT('',#76724);
#21931=VERTEX_POINT('',#76728);
#21932=VERTEX_POINT('',#76730);
#21933=VERTEX_POINT('',#76734);
#21934=VERTEX_POINT('',#76736);
#21935=VERTEX_POINT('',#76740);
#21936=VERTEX_POINT('',#76742);
#21937=VERTEX_POINT('',#76744);
#21938=VERTEX_POINT('',#76746);
#21939=VERTEX_POINT('',#76778);
#21940=VERTEX_POINT('',#76780);
#21941=VERTEX_POINT('',#76784);
#21942=VERTEX_POINT('',#76786);
#21943=VERTEX_POINT('',#76790);
#21944=VERTEX_POINT('',#76792);
#21945=VERTEX_POINT('',#76796);
#21946=VERTEX_POINT('',#76798);
#21947=VERTEX_POINT('',#76802);
#21948=VERTEX_POINT('',#76804);
#21949=VERTEX_POINT('',#76808);
#21950=VERTEX_POINT('',#76810);
#21951=VERTEX_POINT('',#76814);
#21952=VERTEX_POINT('',#76816);
#21953=VERTEX_POINT('',#76820);
#21954=VERTEX_POINT('',#76822);
#21955=VERTEX_POINT('',#76826);
#21956=VERTEX_POINT('',#76828);
#21957=VERTEX_POINT('',#76832);
#21958=VERTEX_POINT('',#76834);
#21959=VERTEX_POINT('',#76838);
#21960=VERTEX_POINT('',#76840);
#21961=VERTEX_POINT('',#76844);
#21962=VERTEX_POINT('',#76846);
#21963=VERTEX_POINT('',#76850);
#21964=VERTEX_POINT('',#76852);
#21965=VERTEX_POINT('',#76856);
#21966=VERTEX_POINT('',#76858);
#21967=VERTEX_POINT('',#76862);
#21968=VERTEX_POINT('',#76864);
#21969=VERTEX_POINT('',#76868);
#21970=VERTEX_POINT('',#76870);
#21971=VERTEX_POINT('',#76874);
#21972=VERTEX_POINT('',#76876);
#21973=VERTEX_POINT('',#76880);
#21974=VERTEX_POINT('',#76882);
#21975=VERTEX_POINT('',#76884);
#21976=VERTEX_POINT('',#76914);
#21977=VERTEX_POINT('',#76921);
#21978=VERTEX_POINT('',#76923);
#21979=VERTEX_POINT('',#76927);
#21980=VERTEX_POINT('',#76929);
#21981=VERTEX_POINT('',#76933);
#21982=VERTEX_POINT('',#76935);
#21983=VERTEX_POINT('',#76939);
#21984=VERTEX_POINT('',#76941);
#21985=VERTEX_POINT('',#76945);
#21986=VERTEX_POINT('',#76947);
#21987=VERTEX_POINT('',#76951);
#21988=VERTEX_POINT('',#76953);
#21989=VERTEX_POINT('',#76957);
#21990=VERTEX_POINT('',#76959);
#21991=VERTEX_POINT('',#76963);
#21992=VERTEX_POINT('',#76965);
#21993=VERTEX_POINT('',#76969);
#21994=VERTEX_POINT('',#76971);
#21995=VERTEX_POINT('',#76975);
#21996=VERTEX_POINT('',#76977);
#21997=VERTEX_POINT('',#76981);
#21998=VERTEX_POINT('',#76983);
#21999=VERTEX_POINT('',#76987);
#22000=VERTEX_POINT('',#76989);
#22001=VERTEX_POINT('',#76993);
#22002=VERTEX_POINT('',#76995);
#22003=VERTEX_POINT('',#76999);
#22004=VERTEX_POINT('',#77001);
#22005=VERTEX_POINT('',#77005);
#22006=VERTEX_POINT('',#77007);
#22007=VERTEX_POINT('',#77011);
#22008=VERTEX_POINT('',#77013);
#22009=VERTEX_POINT('',#77015);
#22010=VERTEX_POINT('',#77045);
#22011=VERTEX_POINT('',#77052);
#22012=VERTEX_POINT('',#77054);
#22013=VERTEX_POINT('',#77058);
#22014=VERTEX_POINT('',#77060);
#22015=VERTEX_POINT('',#77064);
#22016=VERTEX_POINT('',#77066);
#22017=VERTEX_POINT('',#77070);
#22018=VERTEX_POINT('',#77072);
#22019=VERTEX_POINT('',#77076);
#22020=VERTEX_POINT('',#77078);
#22021=VERTEX_POINT('',#77082);
#22022=VERTEX_POINT('',#77084);
#22023=VERTEX_POINT('',#77088);
#22024=VERTEX_POINT('',#77090);
#22025=VERTEX_POINT('',#77094);
#22026=VERTEX_POINT('',#77096);
#22027=VERTEX_POINT('',#77100);
#22028=VERTEX_POINT('',#77102);
#22029=VERTEX_POINT('',#77106);
#22030=VERTEX_POINT('',#77108);
#22031=VERTEX_POINT('',#77112);
#22032=VERTEX_POINT('',#77114);
#22033=VERTEX_POINT('',#77118);
#22034=VERTEX_POINT('',#77120);
#22035=VERTEX_POINT('',#77124);
#22036=VERTEX_POINT('',#77126);
#22037=VERTEX_POINT('',#77130);
#22038=VERTEX_POINT('',#77132);
#22039=VERTEX_POINT('',#77136);
#22040=VERTEX_POINT('',#77138);
#22041=VERTEX_POINT('',#77142);
#22042=VERTEX_POINT('',#77144);
#22043=VERTEX_POINT('',#77148);
#22044=VERTEX_POINT('',#77150);
#22045=VERTEX_POINT('',#77154);
#22046=VERTEX_POINT('',#77156);
#22047=VERTEX_POINT('',#77158);
#22048=VERTEX_POINT('',#77186);
#22049=VERTEX_POINT('',#77195);
#22050=VERTEX_POINT('',#77197);
#22051=VERTEX_POINT('',#77201);
#22052=VERTEX_POINT('',#77203);
#22053=VERTEX_POINT('',#77207);
#22054=VERTEX_POINT('',#77209);
#22055=VERTEX_POINT('',#77213);
#22056=VERTEX_POINT('',#77215);
#22057=VERTEX_POINT('',#77219);
#22058=VERTEX_POINT('',#77221);
#22059=VERTEX_POINT('',#77225);
#22060=VERTEX_POINT('',#77227);
#22061=VERTEX_POINT('',#77231);
#22062=VERTEX_POINT('',#77233);
#22063=VERTEX_POINT('',#77237);
#22064=VERTEX_POINT('',#77239);
#22065=VERTEX_POINT('',#77243);
#22066=VERTEX_POINT('',#77245);
#22067=VERTEX_POINT('',#77249);
#22068=VERTEX_POINT('',#77251);
#22069=VERTEX_POINT('',#77255);
#22070=VERTEX_POINT('',#77257);
#22071=VERTEX_POINT('',#77261);
#22072=VERTEX_POINT('',#77263);
#22073=VERTEX_POINT('',#77267);
#22074=VERTEX_POINT('',#77269);
#22075=VERTEX_POINT('',#77273);
#22076=VERTEX_POINT('',#77275);
#22077=VERTEX_POINT('',#77279);
#22078=VERTEX_POINT('',#77281);
#22079=VERTEX_POINT('',#77285);
#22080=VERTEX_POINT('',#77287);
#22081=VERTEX_POINT('',#77291);
#22082=VERTEX_POINT('',#77293);
#22083=VERTEX_POINT('',#77297);
#22084=VERTEX_POINT('',#77299);
#22085=VERTEX_POINT('',#77301);
#22086=VERTEX_POINT('',#77327);
#22087=VERTEX_POINT('',#77338);
#22088=VERTEX_POINT('',#77340);
#22089=VERTEX_POINT('',#77370);
#22090=VERTEX_POINT('',#77371);
#22091=VERTEX_POINT('',#77398);
#22092=VERTEX_POINT('',#77401);
#22093=VERTEX_POINT('',#77402);
#22094=VERTEX_POINT('',#77447);
#22095=VERTEX_POINT('',#77448);
#22096=VERTEX_POINT('',#77450);
#22097=VERTEX_POINT('',#77452);
#22098=VERTEX_POINT('',#77457);
#22099=VERTEX_POINT('',#77462);
#22100=VERTEX_POINT('',#77623);
#22101=VERTEX_POINT('',#77784);
#22102=VERTEX_POINT('',#77789);
#22103=VERTEX_POINT('',#77796);
#22104=VERTEX_POINT('',#77797);
#22105=VERTEX_POINT('',#77799);
#22106=VERTEX_POINT('',#77804);
#22107=VERTEX_POINT('',#77808);
#22108=VERTEX_POINT('',#77810);
#22109=VERTEX_POINT('',#77814);
#22110=VERTEX_POINT('',#77815);
#22111=VERTEX_POINT('',#77817);
#22112=VERTEX_POINT('',#77828);
#22113=VERTEX_POINT('',#77841);
#22114=VERTEX_POINT('',#77842);
#22115=VERTEX_POINT('',#77844);
#22116=VERTEX_POINT('',#77846);
#22117=VERTEX_POINT('',#77850);
#22118=VERTEX_POINT('',#77851);
#22119=VERTEX_POINT('',#77853);
#22120=VERTEX_POINT('',#77855);
#22121=VERTEX_POINT('',#77857);
#22122=VERTEX_POINT('',#77894);
#22123=VERTEX_POINT('',#77895);
#22124=VERTEX_POINT('',#77900);
#22125=VERTEX_POINT('',#77904);
#22126=VERTEX_POINT('',#77906);
#22127=VERTEX_POINT('',#77943);
#22128=VERTEX_POINT('',#77944);
#22129=VERTEX_POINT('',#78002);
#22130=VERTEX_POINT('',#78003);
#22131=VERTEX_POINT('',#78005);
#22132=VERTEX_POINT('',#78028);
#22133=VERTEX_POINT('',#78030);
#22134=VERTEX_POINT('',#78039);
#22135=VERTEX_POINT('',#78043);
#22136=VERTEX_POINT('',#78044);
#22137=VERTEX_POINT('',#78046);
#22138=VERTEX_POINT('',#78071);
#22139=VERTEX_POINT('',#78090);
#22140=VERTEX_POINT('',#78094);
#22141=VERTEX_POINT('',#78095);
#22142=VERTEX_POINT('',#78097);
#22143=VERTEX_POINT('',#78100);
#22144=VERTEX_POINT('',#78104);
#22145=VERTEX_POINT('',#78113);
#22146=VERTEX_POINT('',#78114);
#22147=VERTEX_POINT('',#78147);
#22148=VERTEX_POINT('',#78148);
#22149=VERTEX_POINT('',#78150);
#22150=VERTEX_POINT('',#78152);
#22151=VERTEX_POINT('',#78156);
#22152=VERTEX_POINT('',#78157);
#22153=VERTEX_POINT('',#78159);
#22154=VERTEX_POINT('',#78164);
#22155=VERTEX_POINT('',#78165);
#22156=VERTEX_POINT('',#78170);
#22157=VERTEX_POINT('',#78184);
#22158=VERTEX_POINT('',#78186);
#22159=VERTEX_POINT('',#78188);
#22160=VERTEX_POINT('',#78190);
#22161=VERTEX_POINT('',#78354);
#22162=VERTEX_POINT('',#78356);
#22163=VERTEX_POINT('',#78361);
#22164=VERTEX_POINT('',#78559);
#22165=VERTEX_POINT('',#78560);
#22166=VERTEX_POINT('',#78904);
#22167=VERTEX_POINT('',#78931);
#22168=VERTEX_POINT('',#78984);
#22169=VERTEX_POINT('',#79073);
#22170=VERTEX_POINT('',#79075);
#22171=VERTEX_POINT('',#79080);
#22172=VERTEX_POINT('',#79200);
#22173=VERTEX_POINT('',#79201);
#22174=VERTEX_POINT('',#79203);
#22175=VERTEX_POINT('',#79229);
#22176=VERTEX_POINT('',#79513);
#22177=VERTEX_POINT('',#79566);
#22178=VERTEX_POINT('',#79568);
#22179=VERTEX_POINT('',#79587);
#22180=VERTEX_POINT('',#79588);
#22181=VERTEX_POINT('',#79616);
#22182=VERTEX_POINT('',#79617);
#22183=VERTEX_POINT('',#79678);
#22184=VERTEX_POINT('',#79679);
#22185=VERTEX_POINT('',#79766);
#22186=VERTEX_POINT('',#79880);
#22187=VERTEX_POINT('',#79908);
#22188=VERTEX_POINT('',#79915);
#22189=VERTEX_POINT('',#79923);
#22190=VERTEX_POINT('',#79925);
#22191=VERTEX_POINT('',#80014);
#22192=VERTEX_POINT('',#80130);
#22193=VERTEX_POINT('',#80331);
#22194=VERTEX_POINT('',#80450);
#22195=VERTEX_POINT('',#80714);
#22196=VERTEX_POINT('',#81047);
#22197=VERTEX_POINT('',#81090);
#22198=VERTEX_POINT('',#81091);
#22199=VERTEX_POINT('',#81613);
#22200=VERTEX_POINT('',#81618);
#22201=VERTEX_POINT('',#81626);
#22202=VERTEX_POINT('',#81778);
#22203=VERTEX_POINT('',#85005);
#22204=VERTEX_POINT('',#85006);
#22205=VERTEX_POINT('',#85009);
#22206=VERTEX_POINT('',#85013);
#22207=VERTEX_POINT('',#85015);
#22208=VERTEX_POINT('',#85398);
#22209=VERTEX_POINT('',#85399);
#22210=VERTEX_POINT('',#85401);
#22211=VERTEX_POINT('',#85456);
#22212=VERTEX_POINT('',#85513);
#22213=VERTEX_POINT('',#85515);
#22214=VERTEX_POINT('',#85519);
#22215=VERTEX_POINT('',#85908);
#22216=VERTEX_POINT('',#85909);
#22217=VERTEX_POINT('',#85911);
#22218=VERTEX_POINT('',#85913);
#22219=VERTEX_POINT('',#85917);
#22220=VERTEX_POINT('',#85918);
#22221=VERTEX_POINT('',#85923);
#22222=VERTEX_POINT('',#85924);
#22223=VERTEX_POINT('',#85934);
#22224=VERTEX_POINT('',#85935);
#22225=VERTEX_POINT('',#85937);
#22226=VERTEX_POINT('',#85939);
#22227=VERTEX_POINT('',#85943);
#22228=VERTEX_POINT('',#85945);
#22229=VERTEX_POINT('',#85949);
#22230=VERTEX_POINT('',#85953);
#22231=VERTEX_POINT('',#85960);
#22232=VERTEX_POINT('',#85961);
#22233=VERTEX_POINT('',#86017);
#22234=VERTEX_POINT('',#86019);
#22235=VERTEX_POINT('',#86021);
#22236=VERTEX_POINT('',#86080);
#22237=VERTEX_POINT('',#86082);
#22238=VERTEX_POINT('',#86084);
#22239=VERTEX_POINT('',#86086);
#22240=VERTEX_POINT('',#86142);
#22241=VERTEX_POINT('',#86144);
#22242=VERTEX_POINT('',#86146);
#22243=VERTEX_POINT('',#86184);
#22244=VERTEX_POINT('',#86186);
#22245=VERTEX_POINT('',#86189);
#22246=VERTEX_POINT('',#86202);
#22247=VERTEX_POINT('',#86267);
#22248=VERTEX_POINT('',#86274);
#22249=VERTEX_POINT('',#86369);
#22250=VERTEX_POINT('',#86379);
#22251=VERTEX_POINT('',#86383);
#22252=VERTEX_POINT('',#86384);
#22253=VERTEX_POINT('',#86386);
#22254=VERTEX_POINT('',#86388);
#22255=VERTEX_POINT('',#86399);
#22256=VERTEX_POINT('',#86401);
#22257=VERTEX_POINT('',#86414);
#22258=VERTEX_POINT('',#86415);
#22259=VERTEX_POINT('',#86417);
#22260=VERTEX_POINT('',#86419);
#22261=VERTEX_POINT('',#86430);
#22262=VERTEX_POINT('',#86432);
#22263=VERTEX_POINT('',#86445);
#22264=VERTEX_POINT('',#86446);
#22265=VERTEX_POINT('',#86448);
#22266=VERTEX_POINT('',#86450);
#22267=VERTEX_POINT('',#86461);
#22268=VERTEX_POINT('',#86463);
#22269=VERTEX_POINT('',#86476);
#22270=VERTEX_POINT('',#86477);
#22271=VERTEX_POINT('',#86479);
#22272=VERTEX_POINT('',#86481);
#22273=VERTEX_POINT('',#86483);
#22274=VERTEX_POINT('',#86485);
#22275=VERTEX_POINT('',#86535);
#22276=VERTEX_POINT('',#86537);
#22277=VERTEX_POINT('',#86596);
#22278=VERTEX_POINT('',#86601);
#22279=VERTEX_POINT('',#86602);
#22280=VERTEX_POINT('',#86604);
#22281=VERTEX_POINT('',#86606);
#22282=VERTEX_POINT('',#86610);
#22283=VERTEX_POINT('',#86612);
#22284=VERTEX_POINT('',#86616);
#22285=VERTEX_POINT('',#86660);
#22286=VERTEX_POINT('',#86709);
#22287=VERTEX_POINT('',#86711);
#22288=VERTEX_POINT('',#86715);
#22289=VERTEX_POINT('',#86719);
#22290=VERTEX_POINT('',#86720);
#22291=VERTEX_POINT('',#86722);
#22292=VERTEX_POINT('',#86724);
#22293=VERTEX_POINT('',#86726);
#22294=VERTEX_POINT('',#86728);
#22295=VERTEX_POINT('',#86778);
#22296=VERTEX_POINT('',#86780);
#22297=VERTEX_POINT('',#86839);
#22298=VERTEX_POINT('',#86844);
#22299=VERTEX_POINT('',#86845);
#22300=VERTEX_POINT('',#86847);
#22301=VERTEX_POINT('',#86849);
#22302=VERTEX_POINT('',#86853);
#22303=VERTEX_POINT('',#86855);
#22304=VERTEX_POINT('',#86859);
#22305=VERTEX_POINT('',#86903);
#22306=VERTEX_POINT('',#86952);
#22307=VERTEX_POINT('',#86954);
#22308=VERTEX_POINT('',#86958);
#22309=VERTEX_POINT('',#86962);
#22310=VERTEX_POINT('',#86963);
#22311=VERTEX_POINT('',#86965);
#22312=VERTEX_POINT('',#86967);
#22313=VERTEX_POINT('',#86969);
#22314=VERTEX_POINT('',#86971);
#22315=VERTEX_POINT('',#87021);
#22316=VERTEX_POINT('',#87023);
#22317=VERTEX_POINT('',#87082);
#22318=VERTEX_POINT('',#87087);
#22319=VERTEX_POINT('',#87088);
#22320=VERTEX_POINT('',#87090);
#22321=VERTEX_POINT('',#87092);
#22322=VERTEX_POINT('',#87096);
#22323=VERTEX_POINT('',#87098);
#22324=VERTEX_POINT('',#87102);
#22325=VERTEX_POINT('',#87146);
#22326=VERTEX_POINT('',#87195);
#22327=VERTEX_POINT('',#87197);
#22328=VERTEX_POINT('',#87201);
#22329=VERTEX_POINT('',#87205);
#22330=VERTEX_POINT('',#87207);
#22331=VERTEX_POINT('',#87209);
#22332=VERTEX_POINT('',#87211);
#22333=VERTEX_POINT('',#87213);
#22334=VERTEX_POINT('',#87272);
#22335=VERTEX_POINT('',#87274);
#22336=VERTEX_POINT('',#87330);
#22337=VERTEX_POINT('',#87334);
#22338=VERTEX_POINT('',#87384);
#22339=VERTEX_POINT('',#87430);
#22340=VERTEX_POINT('',#87431);
#22341=VERTEX_POINT('',#87433);
#22342=VERTEX_POINT('',#87519);
#22343=VERTEX_POINT('',#87602);
#22344=VERTEX_POINT('',#87604);
#22345=VERTEX_POINT('',#87606);
#22346=VERTEX_POINT('',#87610);
#22347=VERTEX_POINT('',#87611);
#22348=VERTEX_POINT('',#87613);
#22349=VERTEX_POINT('',#87615);
#22350=VERTEX_POINT('',#87626);
#22351=VERTEX_POINT('',#87627);
#22352=VERTEX_POINT('',#88055);
#22353=VERTEX_POINT('',#88056);
#22354=VERTEX_POINT('',#88058);
#22355=VERTEX_POINT('',#88060);
#22356=VERTEX_POINT('',#88497);
#22357=VERTEX_POINT('',#88498);
#22358=VERTEX_POINT('',#88500);
#22359=VERTEX_POINT('',#88502);
#22360=VERTEX_POINT('',#88506);
#22361=VERTEX_POINT('',#88508);
#22362=VERTEX_POINT('',#88512);
#22363=VERTEX_POINT('',#88513);
#22364=VERTEX_POINT('',#88691);
#22365=VERTEX_POINT('',#88692);
#22366=VERTEX_POINT('',#88733);
#22367=VERTEX_POINT('',#88738);
#22368=VERTEX_POINT('',#88757);
#22369=VERTEX_POINT('',#88783);
#22370=VERTEX_POINT('',#88996);
#22371=VERTEX_POINT('',#89267);
#22372=VERTEX_POINT('',#89271);
#22373=VERTEX_POINT('',#89275);
#22374=VERTEX_POINT('',#89276);
#22375=VERTEX_POINT('',#89286);
#22376=VERTEX_POINT('',#89288);
#22377=VERTEX_POINT('',#89299);
#22378=VERTEX_POINT('',#89300);
#22379=VERTEX_POINT('',#89308);
#22380=VERTEX_POINT('',#89310);
#22381=VERTEX_POINT('',#89699);
#22382=VERTEX_POINT('',#89700);
#22383=VERTEX_POINT('',#89702);
#22384=VERTEX_POINT('',#89704);
#22385=VERTEX_POINT('',#89708);
#22386=VERTEX_POINT('',#89709);
#22387=VERTEX_POINT('',#89714);
#22388=VERTEX_POINT('',#89715);
#22389=VERTEX_POINT('',#89723);
#22390=VERTEX_POINT('',#89725);
#22391=VERTEX_POINT('',#89764);
#22392=VERTEX_POINT('',#89845);
#22393=VERTEX_POINT('',#89903);
#22394=VERTEX_POINT('',#89904);
#22395=VERTEX_POINT('',#89909);
#22396=VERTEX_POINT('',#89913);
#22397=VERTEX_POINT('',#89914);
#22398=VERTEX_POINT('',#89919);
#22399=VERTEX_POINT('',#89920);
#22400=VERTEX_POINT('',#89960);
#22401=VERTEX_POINT('',#90041);
#22402=VERTEX_POINT('',#90042);
#22403=VERTEX_POINT('',#90107);
#22404=VERTEX_POINT('',#90108);
#22405=VERTEX_POINT('',#90132);
#22406=VERTEX_POINT('',#90133);
#22407=VERTEX_POINT('',#90138);
#22408=VERTEX_POINT('',#90139);
#22409=VERTEX_POINT('',#90147);
#22410=VERTEX_POINT('',#90149);
#22411=VERTEX_POINT('',#90182);
#22412=VERTEX_POINT('',#90257);
#22413=VERTEX_POINT('',#90300);
#22414=VERTEX_POINT('',#90304);
#22415=VERTEX_POINT('',#90305);
#22416=VERTEX_POINT('',#90310);
#22417=VERTEX_POINT('',#90311);
#22418=VERTEX_POINT('',#90316);
#22419=VERTEX_POINT('',#90349);
#22420=VERTEX_POINT('',#90424);
#22421=VERTEX_POINT('',#90496);
#22422=VERTEX_POINT('',#90497);
#22423=VERTEX_POINT('',#90502);
#22424=VERTEX_POINT('',#90503);
#22425=VERTEX_POINT('',#90511);
#22426=VERTEX_POINT('',#90513);
#22427=VERTEX_POINT('',#90546);
#22428=VERTEX_POINT('',#90621);
#22429=VERTEX_POINT('',#90664);
#22430=VERTEX_POINT('',#90668);
#22431=VERTEX_POINT('',#90669);
#22432=VERTEX_POINT('',#90674);
#22433=VERTEX_POINT('',#90675);
#22434=VERTEX_POINT('',#90680);
#22435=VERTEX_POINT('',#90713);
#22436=VERTEX_POINT('',#90788);
#22437=VERTEX_POINT('',#90860);
#22438=VERTEX_POINT('',#90861);
#22439=VERTEX_POINT('',#90866);
#22440=VERTEX_POINT('',#90867);
#22441=VERTEX_POINT('',#90875);
#22442=VERTEX_POINT('',#90877);
#22443=VERTEX_POINT('',#90910);
#22444=VERTEX_POINT('',#90985);
#22445=VERTEX_POINT('',#91028);
#22446=VERTEX_POINT('',#91032);
#22447=VERTEX_POINT('',#91033);
#22448=VERTEX_POINT('',#91038);
#22449=VERTEX_POINT('',#91039);
#22450=VERTEX_POINT('',#91044);
#22451=VERTEX_POINT('',#91077);
#22452=VERTEX_POINT('',#91152);
#22453=VERTEX_POINT('',#91230);
#22454=VERTEX_POINT('',#91232);
#22455=VERTEX_POINT('',#91236);
#22456=VERTEX_POINT('',#91248);
#22457=VERTEX_POINT('',#91389);
#22458=VERTEX_POINT('',#91396);
#22459=VERTEX_POINT('',#91417);
#22460=VERTEX_POINT('',#91441);
#22461=VERTEX_POINT('',#91462);
#22462=VERTEX_POINT('',#91471);
#22463=VERTEX_POINT('',#91492);
#22464=VERTEX_POINT('',#91508);
#22465=VERTEX_POINT('',#91553);
#22466=VERTEX_POINT('',#91960);
#22467=VERTEX_POINT('',#91962);
#22468=VERTEX_POINT('',#92091);
#22469=VERTEX_POINT('',#92092);
#22470=VERTEX_POINT('',#92444);
#22471=VERTEX_POINT('',#92445);
#22472=VERTEX_POINT('',#92525);
#22473=VERTEX_POINT('',#92530);
#22474=VERTEX_POINT('',#92534);
#22475=VERTEX_POINT('',#92538);
#22476=VERTEX_POINT('',#92539);
#22477=VERTEX_POINT('',#92585);
#22478=VERTEX_POINT('',#92747);
#22479=VERTEX_POINT('',#92748);
#22480=VERTEX_POINT('',#92873);
#22481=VERTEX_POINT('',#92877);
#22482=VERTEX_POINT('',#92919);
#22483=VERTEX_POINT('',#92995);
#22484=VERTEX_POINT('',#92999);
#22485=VERTEX_POINT('',#93003);
#22486=VERTEX_POINT('',#93007);
#22487=VERTEX_POINT('',#93052);
#22488=VERTEX_POINT('',#93092);
#22489=VERTEX_POINT('',#93107);
#22490=VERTEX_POINT('',#93140);
#22491=VERTEX_POINT('',#93394);
#22492=VERTEX_POINT('',#93748);
#22493=VERTEX_POINT('',#93749);
#22494=VERTEX_POINT('',#93751);
#22495=VERTEX_POINT('',#93966);
#22496=VERTEX_POINT('',#94185);
#22497=VERTEX_POINT('',#94186);
#22498=VERTEX_POINT('',#94369);
#22499=VERTEX_POINT('',#94370);
#22500=VERTEX_POINT('',#94422);
#22501=VERTEX_POINT('',#94423);
#22502=VERTEX_POINT('',#94425);
#22503=VERTEX_POINT('',#94508);
#22504=VERTEX_POINT('',#94667);
#22505=VERTEX_POINT('',#94668);
#22506=VERTEX_POINT('',#94758);
#22507=VERTEX_POINT('',#94759);
#22508=VERTEX_POINT('',#94868);
#22509=VERTEX_POINT('',#94870);
#22510=VERTEX_POINT('',#95221);
#22511=VERTEX_POINT('',#96179);
#22512=VERTEX_POINT('',#96264);
#22513=VERTEX_POINT('',#96928);
#22514=VERTEX_POINT('',#96930);
#22515=VERTEX_POINT('',#96934);
#22516=VERTEX_POINT('',#96935);
#22517=VERTEX_POINT('',#96937);
#22518=VERTEX_POINT('',#96939);
#22519=VERTEX_POINT('',#96941);
#22520=VERTEX_POINT('',#96943);
#22521=VERTEX_POINT('',#96945);
#22522=VERTEX_POINT('',#96947);
#22523=VERTEX_POINT('',#96950);
#22524=VERTEX_POINT('',#96951);
#22525=VERTEX_POINT('',#96953);
#22526=VERTEX_POINT('',#96955);
#22527=VERTEX_POINT('',#96957);
#22528=VERTEX_POINT('',#96959);
#22529=VERTEX_POINT('',#96961);
#22530=VERTEX_POINT('',#96963);
#22531=VERTEX_POINT('',#96965);
#22532=VERTEX_POINT('',#96967);
#22533=VERTEX_POINT('',#96969);
#22534=VERTEX_POINT('',#96971);
#22535=VERTEX_POINT('',#96973);
#22536=VERTEX_POINT('',#96975);
#22537=VERTEX_POINT('',#96977);
#22538=VERTEX_POINT('',#96979);
#22539=VERTEX_POINT('',#96983);
#22540=VERTEX_POINT('',#96984);
#22541=VERTEX_POINT('',#96986);
#22542=VERTEX_POINT('',#96988);
#22543=VERTEX_POINT('',#96992);
#22544=VERTEX_POINT('',#96993);
#22545=VERTEX_POINT('',#96995);
#22546=VERTEX_POINT('',#96997);
#22547=VERTEX_POINT('',#97001);
#22548=VERTEX_POINT('',#97002);
#22549=VERTEX_POINT('',#97004);
#22550=VERTEX_POINT('',#97006);
#22551=VERTEX_POINT('',#97010);
#22552=VERTEX_POINT('',#97011);
#22553=VERTEX_POINT('',#97013);
#22554=VERTEX_POINT('',#97015);
#22555=VERTEX_POINT('',#97019);
#22556=VERTEX_POINT('',#97020);
#22557=VERTEX_POINT('',#97022);
#22558=VERTEX_POINT('',#97024);
#22559=VERTEX_POINT('',#97026);
#22560=VERTEX_POINT('',#97028);
#22561=VERTEX_POINT('',#97030);
#22562=VERTEX_POINT('',#97032);
#22563=VERTEX_POINT('',#97036);
#22564=VERTEX_POINT('',#97037);
#22565=VERTEX_POINT('',#97039);
#22566=VERTEX_POINT('',#97041);
#22567=VERTEX_POINT('',#97045);
#22568=VERTEX_POINT('',#97046);
#22569=VERTEX_POINT('',#97048);
#22570=VERTEX_POINT('',#97050);
#22571=VERTEX_POINT('',#97052);
#22572=VERTEX_POINT('',#97054);
#22573=VERTEX_POINT('',#97058);
#22574=VERTEX_POINT('',#97059);
#22575=VERTEX_POINT('',#97061);
#22576=VERTEX_POINT('',#97063);
#22577=VERTEX_POINT('',#97067);
#22578=VERTEX_POINT('',#97068);
#22579=VERTEX_POINT('',#97070);
#22580=VERTEX_POINT('',#97072);
#22581=VERTEX_POINT('',#97074);
#22582=VERTEX_POINT('',#97076);
#22583=VERTEX_POINT('',#97080);
#22584=VERTEX_POINT('',#97081);
#22585=VERTEX_POINT('',#97083);
#22586=VERTEX_POINT('',#97085);
#22587=VERTEX_POINT('',#97107);
#22588=VERTEX_POINT('',#97108);
#22589=VERTEX_POINT('',#97110);
#22590=VERTEX_POINT('',#97112);
#22591=VERTEX_POINT('',#97116);
#22592=VERTEX_POINT('',#97117);
#22593=VERTEX_POINT('',#97122);
#22594=VERTEX_POINT('',#97123);
#22595=VERTEX_POINT('',#97128);
#22596=VERTEX_POINT('',#97129);
#22597=VERTEX_POINT('',#97134);
#22598=VERTEX_POINT('',#97136);
#22599=VERTEX_POINT('',#97140);
#22600=VERTEX_POINT('',#97141);
#22601=VERTEX_POINT('',#97143);
#22602=VERTEX_POINT('',#97145);
#22603=VERTEX_POINT('',#97149);
#22604=VERTEX_POINT('',#97150);
#22605=VERTEX_POINT('',#97155);
#22606=VERTEX_POINT('',#97156);
#22607=VERTEX_POINT('',#97161);
#22608=VERTEX_POINT('',#97162);
#22609=VERTEX_POINT('',#97167);
#22610=VERTEX_POINT('',#97169);
#22611=VERTEX_POINT('',#97282);
#22612=VERTEX_POINT('',#97283);
#22613=VERTEX_POINT('',#97286);
#22614=VERTEX_POINT('',#97290);
#22615=VERTEX_POINT('',#97291);
#22616=VERTEX_POINT('',#97293);
#22617=VERTEX_POINT('',#97295);
#22618=VERTEX_POINT('',#97299);
#22619=VERTEX_POINT('',#97300);
#22620=VERTEX_POINT('',#97302);
#22621=VERTEX_POINT('',#97304);
#22622=VERTEX_POINT('',#97308);
#22623=VERTEX_POINT('',#97309);
#22624=VERTEX_POINT('',#97311);
#22625=VERTEX_POINT('',#97313);
#22626=VERTEX_POINT('',#97315);
#22627=VERTEX_POINT('',#97320);
#22628=VERTEX_POINT('',#97322);
#22629=VERTEX_POINT('',#97360);
#22630=VERTEX_POINT('',#97362);
#22631=VERTEX_POINT('',#97408);
#22632=VERTEX_POINT('',#97410);
#22633=VERTEX_POINT('',#97414);
#22634=VERTEX_POINT('',#97416);
#22635=VERTEX_POINT('',#97601);
#22636=VERTEX_POINT('',#97602);
#22637=VERTEX_POINT('',#97778);
#22638=VERTEX_POINT('',#97780);
#22639=VERTEX_POINT('',#97839);
#22640=VERTEX_POINT('',#98005);
#22641=VERTEX_POINT('',#98006);
#22642=VERTEX_POINT('',#98061);
#22643=VERTEX_POINT('',#98063);
#22644=VERTEX_POINT('',#98287);
#22645=VERTEX_POINT('',#98449);
#22646=VERTEX_POINT('',#98450);
#22647=VERTEX_POINT('',#98665);
#22648=VERTEX_POINT('',#98667);
#22649=VERTEX_POINT('',#98867);
#22650=VERTEX_POINT('',#98871);
#22651=VERTEX_POINT('',#98872);
#22652=VERTEX_POINT('',#98899);
#22653=VERTEX_POINT('',#98981);
#22654=VERTEX_POINT('',#99187);
#22655=VERTEX_POINT('',#99412);
#22656=VERTEX_POINT('',#99413);
#22657=VERTEX_POINT('',#99559);
#22658=VERTEX_POINT('',#99561);
#22659=VERTEX_POINT('',#99746);
#22660=VERTEX_POINT('',#99916);
#22661=VERTEX_POINT('',#99917);
#22662=VERTEX_POINT('',#99972);
#22663=VERTEX_POINT('',#99974);
#22664=VERTEX_POINT('',#100031);
#22665=VERTEX_POINT('',#100208);
#22666=VERTEX_POINT('',#100209);
#22667=VERTEX_POINT('',#100264);
#22668=VERTEX_POINT('',#100266);
#22669=VERTEX_POINT('',#100323);
#22670=VERTEX_POINT('',#100339);
#22671=VERTEX_POINT('',#100343);
#22672=VERTEX_POINT('',#100344);
#22673=VERTEX_POINT('',#100347);
#22674=VERTEX_POINT('',#100351);
#22675=VERTEX_POINT('',#100545);
#22676=VERTEX_POINT('',#100974);
#22677=VERTEX_POINT('',#100975);
#22678=VERTEX_POINT('',#101615);
#22679=VERTEX_POINT('',#101617);
#22680=VERTEX_POINT('',#101793);
#22681=VERTEX_POINT('',#101959);
#22682=VERTEX_POINT('',#101960);
#22683=VERTEX_POINT('',#102184);
#22684=VERTEX_POINT('',#102186);
#22685=VERTEX_POINT('',#102241);
#22686=VERTEX_POINT('',#102403);
#22687=VERTEX_POINT('',#102404);
#22688=VERTEX_POINT('',#102604);
#22689=VERTEX_POINT('',#102606);
#22690=VERTEX_POINT('',#102821);
#22691=VERTEX_POINT('',#102825);
#22692=VERTEX_POINT('',#102876);
#22693=VERTEX_POINT('',#102932);
#22694=VERTEX_POINT('',#102958);
#22695=VERTEX_POINT('',#103279);
#22696=VERTEX_POINT('',#103280);
#22697=VERTEX_POINT('',#103306);
#22698=VERTEX_POINT('',#103308);
#22699=VERTEX_POINT('',#103329);
#22700=VERTEX_POINT('',#105938);
#22701=VERTEX_POINT('',#105939);
#22702=VERTEX_POINT('',#105941);
#22703=VERTEX_POINT('',#105943);
#22704=VERTEX_POINT('',#105947);
#22705=VERTEX_POINT('',#105949);
#22706=VERTEX_POINT('',#105952);
#22707=VERTEX_POINT('',#105954);
#22708=VERTEX_POINT('',#105958);
#22709=VERTEX_POINT('',#105959);
#22710=VERTEX_POINT('',#105962);
#22711=VERTEX_POINT('',#105964);
#22712=VERTEX_POINT('',#105969);
#22713=VERTEX_POINT('',#105970);
#22714=VERTEX_POINT('',#105972);
#22715=VERTEX_POINT('',#105974);
#22716=VERTEX_POINT('',#105981);
#22717=VERTEX_POINT('',#105982);
#22718=VERTEX_POINT('',#105990);
#22719=VERTEX_POINT('',#105991);
#22720=VERTEX_POINT('',#105998);
#22721=VERTEX_POINT('',#106000);
#22722=VERTEX_POINT('',#106002);
#22723=VERTEX_POINT('',#106004);
#22724=VERTEX_POINT('',#106029);
#22725=VERTEX_POINT('',#106030);
#22726=VERTEX_POINT('',#106053);
#22727=VERTEX_POINT('',#106055);
#22728=VERTEX_POINT('',#106057);
#22729=VERTEX_POINT('',#106059);
#22730=VERTEX_POINT('',#106577);
#22731=VERTEX_POINT('',#106579);
#22732=VERTEX_POINT('',#106583);
#22733=VERTEX_POINT('',#106585);
#22734=VERTEX_POINT('',#106604);
#22735=VERTEX_POINT('',#106605);
#22736=VERTEX_POINT('',#106607);
#22737=VERTEX_POINT('',#106611);
#22738=VERTEX_POINT('',#106616);
#22739=VERTEX_POINT('',#106617);
#22740=VERTEX_POINT('',#106679);
#22741=VERTEX_POINT('',#106680);
#22742=VERTEX_POINT('',#106744);
#22743=VERTEX_POINT('',#106745);
#22744=VERTEX_POINT('',#106809);
#22745=VERTEX_POINT('',#106810);
#22746=VERTEX_POINT('',#106872);
#22747=VERTEX_POINT('',#106873);
#22748=VERTEX_POINT('',#106935);
#22749=VERTEX_POINT('',#106936);
#22750=VERTEX_POINT('',#106998);
#22751=VERTEX_POINT('',#106999);
#22752=VERTEX_POINT('',#107061);
#22753=VERTEX_POINT('',#107062);
#22754=VERTEX_POINT('',#107124);
#22755=VERTEX_POINT('',#107125);
#22756=VERTEX_POINT('',#107187);
#22757=VERTEX_POINT('',#107188);
#22758=VERTEX_POINT('',#107250);
#22759=VERTEX_POINT('',#107251);
#22760=VERTEX_POINT('',#107313);
#22761=VERTEX_POINT('',#107314);
#22762=VERTEX_POINT('',#107378);
#22763=VERTEX_POINT('',#107379);
#22764=VERTEX_POINT('',#107443);
#22765=VERTEX_POINT('',#107444);
#22766=VERTEX_POINT('',#107506);
#22767=VERTEX_POINT('',#107507);
#22768=VERTEX_POINT('',#107571);
#22769=VERTEX_POINT('',#107572);
#22770=VERTEX_POINT('',#107636);
#22771=VERTEX_POINT('',#107637);
#22772=VERTEX_POINT('',#107699);
#22773=VERTEX_POINT('',#107700);
#22774=VERTEX_POINT('',#107764);
#22775=VERTEX_POINT('',#107765);
#22776=VERTEX_POINT('',#107829);
#22777=VERTEX_POINT('',#107830);
#22778=VERTEX_POINT('',#107894);
#22779=VERTEX_POINT('',#107895);
#22780=VERTEX_POINT('',#107950);
#22781=VERTEX_POINT('',#107951);
#22782=VERTEX_POINT('',#108011);
#22783=VERTEX_POINT('',#108012);
#22784=VERTEX_POINT('',#108070);
#22785=VERTEX_POINT('',#108071);
#22786=VERTEX_POINT('',#108129);
#22787=VERTEX_POINT('',#108130);
#22788=VERTEX_POINT('',#108192);
#22789=VERTEX_POINT('',#108193);
#22790=VERTEX_POINT('',#108255);
#22791=VERTEX_POINT('',#108256);
#22792=VERTEX_POINT('',#108318);
#22793=VERTEX_POINT('',#108319);
#22794=VERTEX_POINT('',#108381);
#22795=VERTEX_POINT('',#108382);
#22796=VERTEX_POINT('',#108442);
#22797=VERTEX_POINT('',#108443);
#22798=VERTEX_POINT('',#108503);
#22799=VERTEX_POINT('',#108504);
#22800=VERTEX_POINT('',#108561);
#22801=VERTEX_POINT('',#108562);
#22802=VERTEX_POINT('',#108622);
#22803=VERTEX_POINT('',#108623);
#22804=VERTEX_POINT('',#108687);
#22805=VERTEX_POINT('',#108688);
#22806=VERTEX_POINT('',#108752);
#22807=VERTEX_POINT('',#108753);
#22808=VERTEX_POINT('',#108817);
#22809=VERTEX_POINT('',#108818);
#22810=VERTEX_POINT('',#108882);
#22811=VERTEX_POINT('',#108883);
#22812=VERTEX_POINT('',#108941);
#22813=VERTEX_POINT('',#108942);
#22814=VERTEX_POINT('',#108999);
#22815=VERTEX_POINT('',#109000);
#22816=VERTEX_POINT('',#109060);
#22817=VERTEX_POINT('',#109061);
#22818=VERTEX_POINT('',#109119);
#22819=VERTEX_POINT('',#109120);
#22820=VERTEX_POINT('',#109182);
#22821=VERTEX_POINT('',#109183);
#22822=VERTEX_POINT('',#109245);
#22823=VERTEX_POINT('',#109246);
#22824=VERTEX_POINT('',#109310);
#22825=VERTEX_POINT('',#109311);
#22826=VERTEX_POINT('',#109375);
#22827=VERTEX_POINT('',#109376);
#22828=VERTEX_POINT('',#109438);
#22829=VERTEX_POINT('',#109439);
#22830=VERTEX_POINT('',#109501);
#22831=VERTEX_POINT('',#109502);
#22832=VERTEX_POINT('',#109566);
#22833=VERTEX_POINT('',#109567);
#22834=VERTEX_POINT('',#109631);
#22835=VERTEX_POINT('',#109632);
#22836=VERTEX_POINT('',#109696);
#22837=VERTEX_POINT('',#109697);
#22838=VERTEX_POINT('',#109759);
#22839=VERTEX_POINT('',#109760);
#22840=VERTEX_POINT('',#109819);
#22841=VERTEX_POINT('',#109820);
#22842=VERTEX_POINT('',#109880);
#22843=VERTEX_POINT('',#109881);
#22844=VERTEX_POINT('',#109938);
#22845=VERTEX_POINT('',#109939);
#22846=VERTEX_POINT('',#109998);
#22847=VERTEX_POINT('',#109999);
#22848=VERTEX_POINT('',#110061);
#22849=VERTEX_POINT('',#110062);
#22850=VERTEX_POINT('',#110126);
#22851=VERTEX_POINT('',#110127);
#22852=VERTEX_POINT('',#110189);
#22853=VERTEX_POINT('',#110190);
#22854=VERTEX_POINT('',#110252);
#22855=VERTEX_POINT('',#110253);
#22856=VERTEX_POINT('',#110315);
#22857=VERTEX_POINT('',#110316);
#22858=VERTEX_POINT('',#110374);
#22859=VERTEX_POINT('',#110376);
#22860=VERTEX_POINT('',#110380);
#22861=VERTEX_POINT('',#110421);
#22862=VERTEX_POINT('',#110422);
#22863=VERTEX_POINT('',#110446);
#22864=VERTEX_POINT('',#110470);
#22865=VERTEX_POINT('',#110511);
#22866=VERTEX_POINT('',#110512);
#22867=VERTEX_POINT('',#110535);
#22868=VERTEX_POINT('',#110562);
#22869=VERTEX_POINT('',#110603);
#22870=VERTEX_POINT('',#110604);
#22871=VERTEX_POINT('',#110630);
#22872=VERTEX_POINT('',#110654);
#22873=VERTEX_POINT('',#110695);
#22874=VERTEX_POINT('',#110696);
#22875=VERTEX_POINT('',#110719);
#22876=VERTEX_POINT('',#110743);
#22877=VERTEX_POINT('',#110782);
#22878=VERTEX_POINT('',#110783);
#22879=VERTEX_POINT('',#110809);
#22880=VERTEX_POINT('',#110831);
#22881=VERTEX_POINT('',#110872);
#22882=VERTEX_POINT('',#110873);
#22883=VERTEX_POINT('',#110896);
#22884=VERTEX_POINT('',#110923);
#22885=VERTEX_POINT('',#110964);
#22886=VERTEX_POINT('',#110965);
#22887=VERTEX_POINT('',#110988);
#22888=VERTEX_POINT('',#111015);
#22889=VERTEX_POINT('',#111056);
#22890=VERTEX_POINT('',#111057);
#22891=VERTEX_POINT('',#111083);
#22892=VERTEX_POINT('',#111107);
#22893=VERTEX_POINT('',#111146);
#22894=VERTEX_POINT('',#111147);
#22895=VERTEX_POINT('',#111168);
#22896=VERTEX_POINT('',#111193);
#22897=VERTEX_POINT('',#111234);
#22898=VERTEX_POINT('',#111235);
#22899=VERTEX_POINT('',#111258);
#22900=VERTEX_POINT('',#111285);
#22901=VERTEX_POINT('',#111326);
#22902=VERTEX_POINT('',#111327);
#22903=VERTEX_POINT('',#111350);
#22904=VERTEX_POINT('',#111377);
#22905=VERTEX_POINT('',#111418);
#22906=VERTEX_POINT('',#111419);
#22907=VERTEX_POINT('',#111442);
#22908=VERTEX_POINT('',#111466);
#22909=VERTEX_POINT('',#111505);
#22910=VERTEX_POINT('',#111506);
#22911=VERTEX_POINT('',#111530);
#22912=VERTEX_POINT('',#111554);
#22913=VERTEX_POINT('',#111595);
#22914=VERTEX_POINT('',#111596);
#22915=VERTEX_POINT('',#111622);
#22916=VERTEX_POINT('',#111646);
#22917=VERTEX_POINT('',#111687);
#22918=VERTEX_POINT('',#111688);
#22919=VERTEX_POINT('',#111714);
#22920=VERTEX_POINT('',#111738);
#22921=VERTEX_POINT('',#111779);
#22922=VERTEX_POINT('',#111780);
#22923=VERTEX_POINT('',#111801);
#22924=VERTEX_POINT('',#111884);
#22925=VERTEX_POINT('',#111923);
#22926=VERTEX_POINT('',#111924);
#22927=VERTEX_POINT('',#111948);
#22928=VERTEX_POINT('',#111972);
#22929=VERTEX_POINT('',#112013);
#22930=VERTEX_POINT('',#112014);
#22931=VERTEX_POINT('',#112037);
#22932=VERTEX_POINT('',#112064);
#22933=VERTEX_POINT('',#112103);
#22934=VERTEX_POINT('',#112104);
#22935=VERTEX_POINT('',#112127);
#22936=VERTEX_POINT('',#112152);
#22937=VERTEX_POINT('',#112193);
#22938=VERTEX_POINT('',#112194);
#22939=VERTEX_POINT('',#112217);
#22940=VERTEX_POINT('',#112241);
#22941=VERTEX_POINT('',#112280);
#22942=VERTEX_POINT('',#112281);
#22943=VERTEX_POINT('',#112307);
#22944=VERTEX_POINT('',#112331);
#22945=VERTEX_POINT('',#112372);
#22946=VERTEX_POINT('',#112373);
#22947=VERTEX_POINT('',#112396);
#22948=VERTEX_POINT('',#112423);
#22949=VERTEX_POINT('',#112462);
#22950=VERTEX_POINT('',#112463);
#22951=VERTEX_POINT('',#112487);
#22952=VERTEX_POINT('',#112509);
#22953=VERTEX_POINT('',#112548);
#22954=VERTEX_POINT('',#112549);
#22955=VERTEX_POINT('',#112572);
#22956=VERTEX_POINT('',#112599);
#22957=VERTEX_POINT('',#112638);
#22958=VERTEX_POINT('',#112639);
#22959=VERTEX_POINT('',#112665);
#22960=VERTEX_POINT('',#112689);
#22961=VERTEX_POINT('',#112730);
#22962=VERTEX_POINT('',#112731);
#22963=VERTEX_POINT('',#112754);
#22964=VERTEX_POINT('',#112778);
#22965=VERTEX_POINT('',#112819);
#22966=VERTEX_POINT('',#112820);
#22967=VERTEX_POINT('',#112841);
#22968=VERTEX_POINT('',#112865);
#22969=VERTEX_POINT('',#112867);
#22970=VERTEX_POINT('',#113015);
#22971=VERTEX_POINT('',#113016);
#22972=VERTEX_POINT('',#113039);
#22973=VERTEX_POINT('',#113066);
#22974=VERTEX_POINT('',#113105);
#22975=VERTEX_POINT('',#113106);
#22976=VERTEX_POINT('',#113132);
#22977=VERTEX_POINT('',#113156);
#22978=VERTEX_POINT('',#113197);
#22979=VERTEX_POINT('',#113198);
#22980=VERTEX_POINT('',#113221);
#22981=VERTEX_POINT('',#113245);
#22982=VERTEX_POINT('',#113284);
#22983=VERTEX_POINT('',#113285);
#22984=VERTEX_POINT('',#113306);
#22985=VERTEX_POINT('',#113330);
#22986=VERTEX_POINT('',#113383);
#22987=VERTEX_POINT('',#113422);
#22988=VERTEX_POINT('',#113423);
#22989=VERTEX_POINT('',#113446);
#22990=VERTEX_POINT('',#113471);
#22991=VERTEX_POINT('',#113522);
#22992=VERTEX_POINT('',#113563);
#22993=VERTEX_POINT('',#113564);
#22994=VERTEX_POINT('',#113587);
#22995=VERTEX_POINT('',#113611);
#22996=VERTEX_POINT('',#113652);
#22997=VERTEX_POINT('',#113653);
#22998=VERTEX_POINT('',#113676);
#22999=VERTEX_POINT('',#113700);
#23000=VERTEX_POINT('',#113739);
#23001=VERTEX_POINT('',#113740);
#23002=VERTEX_POINT('',#113763);
#23003=VERTEX_POINT('',#113787);
#23004=VERTEX_POINT('',#113840);
#23005=VERTEX_POINT('',#113879);
#23006=VERTEX_POINT('',#113880);
#23007=VERTEX_POINT('',#113901);
#23008=VERTEX_POINT('',#113928);
#23009=VERTEX_POINT('',#113981);
#23010=VERTEX_POINT('',#114022);
#23011=VERTEX_POINT('',#114023);
#23012=VERTEX_POINT('',#114046);
#23013=VERTEX_POINT('',#114070);
#23014=VERTEX_POINT('',#114123);
#23015=VERTEX_POINT('',#114162);
#23016=VERTEX_POINT('',#114163);
#23017=VERTEX_POINT('',#114186);
#23018=VERTEX_POINT('',#114213);
#23019=VERTEX_POINT('',#114264);
#23020=VERTEX_POINT('',#114305);
#23021=VERTEX_POINT('',#114306);
#23022=VERTEX_POINT('',#114329);
#23023=VERTEX_POINT('',#114353);
#23024=VERTEX_POINT('',#114406);
#23025=VERTEX_POINT('',#114443);
#23026=VERTEX_POINT('',#114444);
#23027=VERTEX_POINT('',#114465);
#23028=VERTEX_POINT('',#114492);
#23029=VERTEX_POINT('',#114547);
#23030=VERTEX_POINT('',#114588);
#23031=VERTEX_POINT('',#114589);
#23032=VERTEX_POINT('',#114612);
#23033=VERTEX_POINT('',#114636);
#23034=VERTEX_POINT('',#114691);
#23035=VERTEX_POINT('',#114730);
#23036=VERTEX_POINT('',#114731);
#23037=VERTEX_POINT('',#114754);
#23038=VERTEX_POINT('',#114778);
#23039=VERTEX_POINT('',#114831);
#23040=VERTEX_POINT('',#114872);
#23041=VERTEX_POINT('',#114873);
#23042=VERTEX_POINT('',#114896);
#23043=VERTEX_POINT('',#114920);
#23044=VERTEX_POINT('',#114975);
#23045=VERTEX_POINT('',#115014);
#23046=VERTEX_POINT('',#115015);
#23047=VERTEX_POINT('',#115036);
#23048=VERTEX_POINT('',#115061);
#23049=VERTEX_POINT('',#115116);
#23050=VERTEX_POINT('',#115157);
#23051=VERTEX_POINT('',#115158);
#23052=VERTEX_POINT('',#115181);
#23053=VERTEX_POINT('',#115208);
#23054=VERTEX_POINT('',#115263);
#23055=VERTEX_POINT('',#115302);
#23056=VERTEX_POINT('',#115303);
#23057=VERTEX_POINT('',#115327);
#23058=VERTEX_POINT('',#115349);
#23059=VERTEX_POINT('',#115404);
#23060=VERTEX_POINT('',#115445);
#23061=VERTEX_POINT('',#115446);
#23062=VERTEX_POINT('',#115472);
#23063=VERTEX_POINT('',#115496);
#23064=VERTEX_POINT('',#115553);
#23065=VERTEX_POINT('',#115592);
#23066=VERTEX_POINT('',#115593);
#23067=VERTEX_POINT('',#115612);
#23068=VERTEX_POINT('',#115641);
#23069=VERTEX_POINT('',#115696);
#23070=VERTEX_POINT('',#115737);
#23071=VERTEX_POINT('',#115738);
#23072=VERTEX_POINT('',#115761);
#23073=VERTEX_POINT('',#115785);
#23074=VERTEX_POINT('',#115840);
#23075=VERTEX_POINT('',#115879);
#23076=VERTEX_POINT('',#115880);
#23077=VERTEX_POINT('',#115901);
#23078=VERTEX_POINT('',#115926);
#23079=VERTEX_POINT('',#115983);
#23080=VERTEX_POINT('',#116024);
#23081=VERTEX_POINT('',#116025);
#23082=VERTEX_POINT('',#116048);
#23083=VERTEX_POINT('',#116072);
#23084=VERTEX_POINT('',#116127);
#23085=VERTEX_POINT('',#116166);
#23086=VERTEX_POINT('',#116167);
#23087=VERTEX_POINT('',#116186);
#23088=VERTEX_POINT('',#116215);
#23089=VERTEX_POINT('',#116270);
#23090=VERTEX_POINT('',#116311);
#23091=VERTEX_POINT('',#116312);
#23092=VERTEX_POINT('',#116335);
#23093=VERTEX_POINT('',#116362);
#23094=VERTEX_POINT('',#116419);
#23095=VERTEX_POINT('',#116458);
#23096=VERTEX_POINT('',#116459);
#23097=VERTEX_POINT('',#116480);
#23098=VERTEX_POINT('',#116507);
#23099=VERTEX_POINT('',#116564);
#23100=VERTEX_POINT('',#116605);
#23101=VERTEX_POINT('',#116606);
#23102=VERTEX_POINT('',#116629);
#23103=VERTEX_POINT('',#116656);
#23104=VERTEX_POINT('',#116713);
#23105=VERTEX_POINT('',#116752);
#23106=VERTEX_POINT('',#116753);
#23107=VERTEX_POINT('',#116772);
#23108=VERTEX_POINT('',#116801);
#23109=VERTEX_POINT('',#116858);
#23110=VERTEX_POINT('',#116897);
#23111=VERTEX_POINT('',#116898);
#23112=VERTEX_POINT('',#116919);
#23113=VERTEX_POINT('',#116948);
#23114=VERTEX_POINT('',#117005);
#23115=VERTEX_POINT('',#117044);
#23116=VERTEX_POINT('',#117045);
#23117=VERTEX_POINT('',#117067);
#23118=VERTEX_POINT('',#117093);
#23119=VERTEX_POINT('',#117150);
#23120=VERTEX_POINT('',#117191);
#23121=VERTEX_POINT('',#117192);
#23122=VERTEX_POINT('',#117215);
#23123=VERTEX_POINT('',#117242);
#23124=VERTEX_POINT('',#117297);
#23125=VERTEX_POINT('',#117338);
#23126=VERTEX_POINT('',#117339);
#23127=VERTEX_POINT('',#117360);
#23128=VERTEX_POINT('',#117387);
#23129=VERTEX_POINT('',#117442);
#23130=VERTEX_POINT('',#117481);
#23131=VERTEX_POINT('',#117482);
#23132=VERTEX_POINT('',#117503);
#23133=VERTEX_POINT('',#117532);
#23134=VERTEX_POINT('',#117589);
#23135=VERTEX_POINT('',#117630);
#23136=VERTEX_POINT('',#117631);
#23137=VERTEX_POINT('',#117657);
#23138=VERTEX_POINT('',#117681);
#23139=VERTEX_POINT('',#117738);
#23140=VERTEX_POINT('',#117779);
#23141=VERTEX_POINT('',#117780);
#23142=VERTEX_POINT('',#117801);
#23143=VERTEX_POINT('',#117830);
#23144=VERTEX_POINT('',#117885);
#23145=VERTEX_POINT('',#117887);
#23146=VERTEX_POINT('',#118033);
#23147=VERTEX_POINT('',#118034);
#23148=VERTEX_POINT('',#118057);
#23149=VERTEX_POINT('',#118084);
#23150=VERTEX_POINT('',#118141);
#23151=VERTEX_POINT('',#118180);
#23152=VERTEX_POINT('',#118181);
#23153=VERTEX_POINT('',#118203);
#23154=VERTEX_POINT('',#118229);
#23155=VERTEX_POINT('',#118286);
#23156=VERTEX_POINT('',#118327);
#23157=VERTEX_POINT('',#118328);
#23158=VERTEX_POINT('',#118349);
#23159=VERTEX_POINT('',#118378);
#23160=VERTEX_POINT('',#118435);
#23161=VERTEX_POINT('',#118476);
#23162=VERTEX_POINT('',#118477);
#23163=VERTEX_POINT('',#118501);
#23164=VERTEX_POINT('',#118527);
#23165=VERTEX_POINT('',#118582);
#23166=VERTEX_POINT('',#118584);
#23167=VERTEX_POINT('',#118730);
#23168=VERTEX_POINT('',#118731);
#23169=VERTEX_POINT('',#118752);
#23170=VERTEX_POINT('',#118781);
#23171=VERTEX_POINT('',#118836);
#23172=VERTEX_POINT('',#118873);
#23173=VERTEX_POINT('',#118874);
#23174=VERTEX_POINT('',#118898);
#23175=VERTEX_POINT('',#118922);
#23176=VERTEX_POINT('',#118979);
#23177=VERTEX_POINT('',#119020);
#23178=VERTEX_POINT('',#119021);
#23179=VERTEX_POINT('',#119047);
#23180=VERTEX_POINT('',#119071);
#23181=VERTEX_POINT('',#119128);
#23182=VERTEX_POINT('',#119169);
#23183=VERTEX_POINT('',#119170);
#23184=VERTEX_POINT('',#119194);
#23185=VERTEX_POINT('',#119220);
#23186=VERTEX_POINT('',#119221);
#23187=VERTEX_POINT('',#119252);
#23188=VERTEX_POINT('',#119254);
#23189=VERTEX_POINT('',#119524);
#23190=VERTEX_POINT('',#119525);
#23191=VERTEX_POINT('',#119548);
#23192=VERTEX_POINT('',#119575);
#23193=VERTEX_POINT('',#119630);
#23194=VERTEX_POINT('',#119669);
#23195=VERTEX_POINT('',#119670);
#23196=VERTEX_POINT('',#119691);
#23197=VERTEX_POINT('',#119720);
#23198=VERTEX_POINT('',#119777);
#23199=VERTEX_POINT('',#119818);
#23200=VERTEX_POINT('',#119819);
#23201=VERTEX_POINT('',#119840);
#23202=VERTEX_POINT('',#119869);
#23203=VERTEX_POINT('',#119926);
#23204=VERTEX_POINT('',#119965);
#23205=VERTEX_POINT('',#119966);
#23206=VERTEX_POINT('',#119987);
#23207=VERTEX_POINT('',#120014);
#23208=VERTEX_POINT('',#120069);
#23209=VERTEX_POINT('',#120110);
#23210=VERTEX_POINT('',#120111);
#23211=VERTEX_POINT('',#120132);
#23212=VERTEX_POINT('',#120161);
#23213=VERTEX_POINT('',#120216);
#23214=VERTEX_POINT('',#120255);
#23215=VERTEX_POINT('',#120256);
#23216=VERTEX_POINT('',#120279);
#23217=VERTEX_POINT('',#120304);
#23218=VERTEX_POINT('',#120361);
#23219=VERTEX_POINT('',#120402);
#23220=VERTEX_POINT('',#120403);
#23221=VERTEX_POINT('',#120429);
#23222=VERTEX_POINT('',#120453);
#23223=VERTEX_POINT('',#120510);
#23224=VERTEX_POINT('',#120549);
#23225=VERTEX_POINT('',#120550);
#23226=VERTEX_POINT('',#120574);
#23227=VERTEX_POINT('',#120600);
#23228=VERTEX_POINT('',#120653);
#23229=VERTEX_POINT('',#120694);
#23230=VERTEX_POINT('',#120695);
#23231=VERTEX_POINT('',#120718);
#23232=VERTEX_POINT('',#120745);
#23233=VERTEX_POINT('',#120800);
#23234=VERTEX_POINT('',#120839);
#23235=VERTEX_POINT('',#120840);
#23236=VERTEX_POINT('',#120863);
#23237=VERTEX_POINT('',#120888);
#23238=VERTEX_POINT('',#120943);
#23239=VERTEX_POINT('',#120984);
#23240=VERTEX_POINT('',#120985);
#23241=VERTEX_POINT('',#121011);
#23242=VERTEX_POINT('',#121035);
#23243=VERTEX_POINT('',#121090);
#23244=VERTEX_POINT('',#121127);
#23245=VERTEX_POINT('',#121128);
#23246=VERTEX_POINT('',#121149);
#23247=VERTEX_POINT('',#121176);
#23248=VERTEX_POINT('',#121227);
#23249=VERTEX_POINT('',#121266);
#23250=VERTEX_POINT('',#121267);
#23251=VERTEX_POINT('',#121286);
#23252=VERTEX_POINT('',#121315);
#23253=VERTEX_POINT('',#121368);
#23254=VERTEX_POINT('',#121407);
#23255=VERTEX_POINT('',#121408);
#23256=VERTEX_POINT('',#121431);
#23257=VERTEX_POINT('',#121456);
#23258=VERTEX_POINT('',#121511);
#23259=VERTEX_POINT('',#121552);
#23260=VERTEX_POINT('',#121553);
#23261=VERTEX_POINT('',#121576);
#23262=VERTEX_POINT('',#121600);
#23263=VERTEX_POINT('',#121655);
#23264=VERTEX_POINT('',#121694);
#23265=VERTEX_POINT('',#121695);
#23266=VERTEX_POINT('',#121718);
#23267=VERTEX_POINT('',#121740);
#23268=VERTEX_POINT('',#121791);
#23269=VERTEX_POINT('',#121830);
#23270=VERTEX_POINT('',#121831);
#23271=VERTEX_POINT('',#121852);
#23272=VERTEX_POINT('',#121879);
#23273=VERTEX_POINT('',#121932);
#23274=VERTEX_POINT('',#121973);
#23275=VERTEX_POINT('',#121974);
#23276=VERTEX_POINT('',#121997);
#23277=VERTEX_POINT('',#122021);
#23278=VERTEX_POINT('',#122074);
#23279=VERTEX_POINT('',#122115);
#23280=VERTEX_POINT('',#122116);
#23281=VERTEX_POINT('',#122139);
#23282=VERTEX_POINT('',#122163);
#23283=VERTEX_POINT('',#122218);
#23284=VERTEX_POINT('',#122257);
#23285=VERTEX_POINT('',#122258);
#23286=VERTEX_POINT('',#122281);
#23287=VERTEX_POINT('',#122303);
#23288=VERTEX_POINT('',#122342);
#23289=VERTEX_POINT('',#122343);
#23290=VERTEX_POINT('',#122364);
#23291=VERTEX_POINT('',#122391);
#23292=VERTEX_POINT('',#122432);
#23293=VERTEX_POINT('',#122433);
#23294=VERTEX_POINT('',#122459);
#23295=VERTEX_POINT('',#122483);
#23296=VERTEX_POINT('',#122534);
#23297=VERTEX_POINT('',#122575);
#23298=VERTEX_POINT('',#122576);
#23299=VERTEX_POINT('',#122599);
#23300=VERTEX_POINT('',#122623);
#23301=VERTEX_POINT('',#122676);
#23302=VERTEX_POINT('',#122717);
#23303=VERTEX_POINT('',#122718);
#23304=VERTEX_POINT('',#122741);
#23305=VERTEX_POINT('',#122765);
#23306=VERTEX_POINT('',#122802);
#23307=VERTEX_POINT('',#122803);
#23308=VERTEX_POINT('',#122824);
#23309=VERTEX_POINT('',#122849);
#23310=VERTEX_POINT('',#122890);
#23311=VERTEX_POINT('',#122891);
#23312=VERTEX_POINT('',#122917);
#23313=VERTEX_POINT('',#122941);
#23314=VERTEX_POINT('',#122982);
#23315=VERTEX_POINT('',#122983);
#23316=VERTEX_POINT('',#123006);
#23317=VERTEX_POINT('',#123030);
#23318=VERTEX_POINT('',#123071);
#23319=VERTEX_POINT('',#123072);
#23320=VERTEX_POINT('',#123095);
#23321=VERTEX_POINT('',#123119);
#23322=VERTEX_POINT('',#123156);
#23323=VERTEX_POINT('',#123157);
#23324=VERTEX_POINT('',#123178);
#23325=VERTEX_POINT('',#123203);
#23326=VERTEX_POINT('',#123244);
#23327=VERTEX_POINT('',#123245);
#23328=VERTEX_POINT('',#123268);
#23329=VERTEX_POINT('',#123292);
#23330=VERTEX_POINT('',#123331);
#23331=VERTEX_POINT('',#123332);
#23332=VERTEX_POINT('',#123353);
#23333=VERTEX_POINT('',#123377);
#23334=VERTEX_POINT('',#123418);
#23335=VERTEX_POINT('',#123419);
#23336=VERTEX_POINT('',#123442);
#23337=VERTEX_POINT('',#123466);
#23338=VERTEX_POINT('',#123503);
#23339=VERTEX_POINT('',#123504);
#23340=VERTEX_POINT('',#123525);
#23341=VERTEX_POINT('',#123550);
#23342=VERTEX_POINT('',#123591);
#23343=VERTEX_POINT('',#123592);
#23344=VERTEX_POINT('',#123618);
#23345=VERTEX_POINT('',#123642);
#23346=VERTEX_POINT('',#123681);
#23347=VERTEX_POINT('',#123682);
#23348=VERTEX_POINT('',#123703);
#23349=VERTEX_POINT('',#123730);
#23350=VERTEX_POINT('',#123771);
#23351=VERTEX_POINT('',#123772);
#23352=VERTEX_POINT('',#123795);
#23353=VERTEX_POINT('',#123822);
#23354=VERTEX_POINT('',#123861);
#23355=VERTEX_POINT('',#123862);
#23356=VERTEX_POINT('',#123885);
#23357=VERTEX_POINT('',#123910);
#23358=VERTEX_POINT('',#123951);
#23359=VERTEX_POINT('',#123952);
#23360=VERTEX_POINT('',#123975);
#23361=VERTEX_POINT('',#123999);
#23362=VERTEX_POINT('',#124038);
#23363=VERTEX_POINT('',#124039);
#23364=VERTEX_POINT('',#124065);
#23365=VERTEX_POINT('',#124087);
#23366=VERTEX_POINT('',#124128);
#23367=VERTEX_POINT('',#124129);
#23368=VERTEX_POINT('',#124152);
#23369=VERTEX_POINT('',#124176);
#23370=VERTEX_POINT('',#124215);
#23371=VERTEX_POINT('',#124216);
#23372=VERTEX_POINT('',#124239);
#23373=VERTEX_POINT('',#124264);
#23374=VERTEX_POINT('',#124305);
#23375=VERTEX_POINT('',#124306);
#23376=VERTEX_POINT('',#124332);
#23377=VERTEX_POINT('',#124356);
#23378=VERTEX_POINT('',#124395);
#23379=VERTEX_POINT('',#124396);
#23380=VERTEX_POINT('',#124422);
#23381=VERTEX_POINT('',#124444);
#23382=VERTEX_POINT('',#124485);
#23383=VERTEX_POINT('',#124486);
#23384=VERTEX_POINT('',#124512);
#23385=VERTEX_POINT('',#124536);
#23386=VERTEX_POINT('',#124575);
#23387=VERTEX_POINT('',#124576);
#23388=VERTEX_POINT('',#124599);
#23389=VERTEX_POINT('',#124626);
#23390=VERTEX_POINT('',#124667);
#23391=VERTEX_POINT('',#124668);
#23392=VERTEX_POINT('',#124692);
#23393=VERTEX_POINT('',#124716);
#23394=VERTEX_POINT('',#124757);
#23395=VERTEX_POINT('',#124758);
#23396=VERTEX_POINT('',#124784);
#23397=VERTEX_POINT('',#124808);
#23398=VERTEX_POINT('',#124847);
#23399=VERTEX_POINT('',#124848);
#23400=VERTEX_POINT('',#124871);
#23401=VERTEX_POINT('',#124898);
#23402=VERTEX_POINT('',#124900);
#23403=VERTEX_POINT('',#124904);
#23404=VERTEX_POINT('',#124906);
#23405=VERTEX_POINT('',#124910);
#23406=VERTEX_POINT('',#124912);
#23407=VERTEX_POINT('',#124916);
#23408=VERTEX_POINT('',#124918);
#23409=VERTEX_POINT('',#124922);
#23410=VERTEX_POINT('',#124924);
#23411=VERTEX_POINT('',#124928);
#23412=VERTEX_POINT('',#124930);
#23413=VERTEX_POINT('',#124934);
#23414=VERTEX_POINT('',#124936);
#23415=VERTEX_POINT('',#124940);
#23416=VERTEX_POINT('',#124942);
#23417=VERTEX_POINT('',#124946);
#23418=VERTEX_POINT('',#124948);
#23419=VERTEX_POINT('',#124952);
#23420=VERTEX_POINT('',#124954);
#23421=VERTEX_POINT('',#124958);
#23422=VERTEX_POINT('',#124960);
#23423=VERTEX_POINT('',#124964);
#23424=VERTEX_POINT('',#124966);
#23425=VERTEX_POINT('',#124970);
#23426=VERTEX_POINT('',#124972);
#23427=VERTEX_POINT('',#124976);
#23428=VERTEX_POINT('',#124978);
#23429=VERTEX_POINT('',#124982);
#23430=VERTEX_POINT('',#124984);
#23431=VERTEX_POINT('',#124988);
#23432=VERTEX_POINT('',#124990);
#23433=VERTEX_POINT('',#124994);
#23434=VERTEX_POINT('',#124996);
#23435=VERTEX_POINT('',#125000);
#23436=VERTEX_POINT('',#125002);
#23437=VERTEX_POINT('',#125006);
#23438=VERTEX_POINT('',#125008);
#23439=VERTEX_POINT('',#125012);
#23440=VERTEX_POINT('',#125014);
#23441=VERTEX_POINT('',#125018);
#23442=VERTEX_POINT('',#125020);
#23443=VERTEX_POINT('',#125024);
#23444=VERTEX_POINT('',#125026);
#23445=VERTEX_POINT('',#125030);
#23446=VERTEX_POINT('',#125032);
#23447=VERTEX_POINT('',#125036);
#23448=VERTEX_POINT('',#125038);
#23449=VERTEX_POINT('',#125042);
#23450=VERTEX_POINT('',#125044);
#23451=VERTEX_POINT('',#125048);
#23452=VERTEX_POINT('',#125050);
#23453=VERTEX_POINT('',#125054);
#23454=VERTEX_POINT('',#125056);
#23455=VERTEX_POINT('',#125060);
#23456=VERTEX_POINT('',#125062);
#23457=VERTEX_POINT('',#125066);
#23458=VERTEX_POINT('',#125068);
#23459=VERTEX_POINT('',#125072);
#23460=VERTEX_POINT('',#125074);
#23461=VERTEX_POINT('',#125078);
#23462=VERTEX_POINT('',#125080);
#23463=VERTEX_POINT('',#125084);
#23464=VERTEX_POINT('',#125086);
#23465=VERTEX_POINT('',#125090);
#23466=VERTEX_POINT('',#125092);
#23467=VERTEX_POINT('',#125096);
#23468=VERTEX_POINT('',#125098);
#23469=VERTEX_POINT('',#125102);
#23470=VERTEX_POINT('',#125104);
#23471=VERTEX_POINT('',#125108);
#23472=VERTEX_POINT('',#125110);
#23473=VERTEX_POINT('',#125114);
#23474=VERTEX_POINT('',#125116);
#23475=VERTEX_POINT('',#125120);
#23476=VERTEX_POINT('',#125122);
#23477=VERTEX_POINT('',#125126);
#23478=VERTEX_POINT('',#125128);
#23479=VERTEX_POINT('',#125132);
#23480=VERTEX_POINT('',#125134);
#23481=VERTEX_POINT('',#125138);
#23482=VERTEX_POINT('',#125140);
#23483=VERTEX_POINT('',#125144);
#23484=VERTEX_POINT('',#125146);
#23485=VERTEX_POINT('',#125150);
#23486=VERTEX_POINT('',#125152);
#23487=VERTEX_POINT('',#125156);
#23488=VERTEX_POINT('',#125158);
#23489=VERTEX_POINT('',#125162);
#23490=VERTEX_POINT('',#125164);
#23491=VERTEX_POINT('',#125168);
#23492=VERTEX_POINT('',#125170);
#23493=VERTEX_POINT('',#125174);
#23494=VERTEX_POINT('',#125176);
#23495=VERTEX_POINT('',#125180);
#23496=VERTEX_POINT('',#125182);
#23497=VERTEX_POINT('',#125186);
#23498=VERTEX_POINT('',#125188);
#23499=VERTEX_POINT('',#125192);
#23500=VERTEX_POINT('',#125194);
#23501=VERTEX_POINT('',#125198);
#23502=VERTEX_POINT('',#125200);
#23503=VERTEX_POINT('',#125204);
#23504=VERTEX_POINT('',#125206);
#23505=VERTEX_POINT('',#125210);
#23506=VERTEX_POINT('',#125212);
#23507=VERTEX_POINT('',#125216);
#23508=VERTEX_POINT('',#125218);
#23509=VERTEX_POINT('',#125222);
#23510=VERTEX_POINT('',#125224);
#23511=VERTEX_POINT('',#125228);
#23512=VERTEX_POINT('',#125230);
#23513=VERTEX_POINT('',#125234);
#23514=VERTEX_POINT('',#125236);
#23515=VERTEX_POINT('',#125240);
#23516=VERTEX_POINT('',#125242);
#23517=VERTEX_POINT('',#125246);
#23518=VERTEX_POINT('',#125248);
#23519=VERTEX_POINT('',#125252);
#23520=VERTEX_POINT('',#125254);
#23521=VERTEX_POINT('',#125258);
#23522=VERTEX_POINT('',#125260);
#23523=VERTEX_POINT('',#125264);
#23524=VERTEX_POINT('',#125266);
#23525=VERTEX_POINT('',#125270);
#23526=VERTEX_POINT('',#125272);
#23527=VERTEX_POINT('',#125276);
#23528=VERTEX_POINT('',#125278);
#23529=VERTEX_POINT('',#125282);
#23530=VERTEX_POINT('',#125284);
#23531=VERTEX_POINT('',#125288);
#23532=VERTEX_POINT('',#125290);
#23533=VERTEX_POINT('',#125294);
#23534=VERTEX_POINT('',#125296);
#23535=VERTEX_POINT('',#125300);
#23536=VERTEX_POINT('',#125302);
#23537=VERTEX_POINT('',#125306);
#23538=VERTEX_POINT('',#125308);
#23539=VERTEX_POINT('',#125312);
#23540=VERTEX_POINT('',#125314);
#23541=VERTEX_POINT('',#125318);
#23542=VERTEX_POINT('',#125320);
#23543=VERTEX_POINT('',#125324);
#23544=VERTEX_POINT('',#125326);
#23545=VERTEX_POINT('',#125330);
#23546=VERTEX_POINT('',#125332);
#23547=VERTEX_POINT('',#125336);
#23548=VERTEX_POINT('',#125338);
#23549=VERTEX_POINT('',#125342);
#23550=VERTEX_POINT('',#125344);
#23551=VERTEX_POINT('',#125348);
#23552=VERTEX_POINT('',#125350);
#23553=VERTEX_POINT('',#125354);
#23554=VERTEX_POINT('',#125356);
#23555=VERTEX_POINT('',#125360);
#23556=VERTEX_POINT('',#125362);
#23557=VERTEX_POINT('',#125366);
#23558=VERTEX_POINT('',#125368);
#23559=VERTEX_POINT('',#125372);
#23560=VERTEX_POINT('',#125374);
#23561=VERTEX_POINT('',#125378);
#23562=VERTEX_POINT('',#125380);
#23563=VERTEX_POINT('',#125384);
#23564=VERTEX_POINT('',#125386);
#23565=VERTEX_POINT('',#125390);
#23566=VERTEX_POINT('',#125392);
#23567=VERTEX_POINT('',#125396);
#23568=VERTEX_POINT('',#125398);
#23569=VERTEX_POINT('',#125402);
#23570=VERTEX_POINT('',#125404);
#23571=VERTEX_POINT('',#125408);
#23572=VERTEX_POINT('',#125410);
#23573=VERTEX_POINT('',#125414);
#23574=VERTEX_POINT('',#125416);
#23575=VERTEX_POINT('',#125420);
#23576=VERTEX_POINT('',#125422);
#23577=VERTEX_POINT('',#125426);
#23578=VERTEX_POINT('',#125428);
#23579=VERTEX_POINT('',#125432);
#23580=VERTEX_POINT('',#125434);
#23581=VERTEX_POINT('',#125438);
#23582=VERTEX_POINT('',#125440);
#23583=VERTEX_POINT('',#125444);
#23584=VERTEX_POINT('',#125446);
#23585=VERTEX_POINT('',#125450);
#23586=VERTEX_POINT('',#125452);
#23587=VERTEX_POINT('',#125456);
#23588=VERTEX_POINT('',#125458);
#23589=VERTEX_POINT('',#125462);
#23590=VERTEX_POINT('',#125464);
#23591=VERTEX_POINT('',#125468);
#23592=VERTEX_POINT('',#125470);
#23593=VERTEX_POINT('',#125474);
#23594=VERTEX_POINT('',#125476);
#23595=VERTEX_POINT('',#125480);
#23596=VERTEX_POINT('',#125482);
#23597=VERTEX_POINT('',#125486);
#23598=VERTEX_POINT('',#125488);
#23599=VERTEX_POINT('',#125492);
#23600=VERTEX_POINT('',#125494);
#23601=VERTEX_POINT('',#125498);
#23602=VERTEX_POINT('',#125500);
#23603=VERTEX_POINT('',#125504);
#23604=VERTEX_POINT('',#125506);
#23605=VERTEX_POINT('',#125510);
#23606=VERTEX_POINT('',#125512);
#23607=VERTEX_POINT('',#125516);
#23608=VERTEX_POINT('',#125518);
#23609=VERTEX_POINT('',#125522);
#23610=VERTEX_POINT('',#125524);
#23611=VERTEX_POINT('',#125528);
#23612=VERTEX_POINT('',#125530);
#23613=VERTEX_POINT('',#125534);
#23614=VERTEX_POINT('',#125536);
#23615=VERTEX_POINT('',#125540);
#23616=VERTEX_POINT('',#125542);
#23617=VERTEX_POINT('',#125546);
#23618=VERTEX_POINT('',#125548);
#23619=VERTEX_POINT('',#125552);
#23620=VERTEX_POINT('',#125554);
#23621=VERTEX_POINT('',#125558);
#23622=VERTEX_POINT('',#125560);
#23623=VERTEX_POINT('',#125564);
#23624=VERTEX_POINT('',#125566);
#23625=VERTEX_POINT('',#125570);
#23626=VERTEX_POINT('',#125572);
#23627=VERTEX_POINT('',#125576);
#23628=VERTEX_POINT('',#125578);
#23629=VERTEX_POINT('',#125582);
#23630=VERTEX_POINT('',#125584);
#23631=VERTEX_POINT('',#125588);
#23632=VERTEX_POINT('',#125590);
#23633=VERTEX_POINT('',#125594);
#23634=VERTEX_POINT('',#125596);
#23635=VERTEX_POINT('',#125600);
#23636=VERTEX_POINT('',#125602);
#23637=VERTEX_POINT('',#125606);
#23638=VERTEX_POINT('',#125608);
#23639=VERTEX_POINT('',#125612);
#23640=VERTEX_POINT('',#125614);
#23641=VERTEX_POINT('',#125618);
#23642=VERTEX_POINT('',#125620);
#23643=VERTEX_POINT('',#125624);
#23644=VERTEX_POINT('',#125626);
#23645=VERTEX_POINT('',#125630);
#23646=VERTEX_POINT('',#125632);
#23647=VERTEX_POINT('',#125636);
#23648=VERTEX_POINT('',#125638);
#23649=VERTEX_POINT('',#125642);
#23650=VERTEX_POINT('',#125644);
#23651=VERTEX_POINT('',#125648);
#23652=VERTEX_POINT('',#125650);
#23653=VERTEX_POINT('',#125654);
#23654=VERTEX_POINT('',#125656);
#23655=VERTEX_POINT('',#125660);
#23656=VERTEX_POINT('',#125662);
#23657=VERTEX_POINT('',#125666);
#23658=VERTEX_POINT('',#125668);
#23659=VERTEX_POINT('',#125672);
#23660=VERTEX_POINT('',#125674);
#23661=VERTEX_POINT('',#125678);
#23662=VERTEX_POINT('',#125680);
#23663=VERTEX_POINT('',#125684);
#23664=VERTEX_POINT('',#125686);
#23665=VERTEX_POINT('',#125690);
#23666=VERTEX_POINT('',#125692);
#23667=VERTEX_POINT('',#125696);
#23668=VERTEX_POINT('',#125698);
#23669=VERTEX_POINT('',#125702);
#23670=VERTEX_POINT('',#125704);
#23671=VERTEX_POINT('',#125708);
#23672=VERTEX_POINT('',#125710);
#23673=VERTEX_POINT('',#125714);
#23674=VERTEX_POINT('',#125716);
#23675=VERTEX_POINT('',#125720);
#23676=VERTEX_POINT('',#125722);
#23677=VERTEX_POINT('',#125726);
#23678=VERTEX_POINT('',#125728);
#23679=VERTEX_POINT('',#125732);
#23680=VERTEX_POINT('',#125734);
#23681=VERTEX_POINT('',#125738);
#23682=VERTEX_POINT('',#125740);
#23683=VERTEX_POINT('',#125744);
#23684=VERTEX_POINT('',#125746);
#23685=VERTEX_POINT('',#125750);
#23686=VERTEX_POINT('',#125752);
#23687=VERTEX_POINT('',#125756);
#23688=VERTEX_POINT('',#125758);
#23689=VERTEX_POINT('',#125762);
#23690=VERTEX_POINT('',#125764);
#23691=VERTEX_POINT('',#125768);
#23692=VERTEX_POINT('',#125770);
#23693=VERTEX_POINT('',#125774);
#23694=VERTEX_POINT('',#125776);
#23695=VERTEX_POINT('',#125780);
#23696=VERTEX_POINT('',#125782);
#23697=VERTEX_POINT('',#125786);
#23698=VERTEX_POINT('',#125788);
#23699=VERTEX_POINT('',#125792);
#23700=VERTEX_POINT('',#125794);
#23701=VERTEX_POINT('',#125798);
#23702=VERTEX_POINT('',#125800);
#23703=VERTEX_POINT('',#125804);
#23704=VERTEX_POINT('',#125806);
#23705=VERTEX_POINT('',#125810);
#23706=VERTEX_POINT('',#125812);
#23707=VERTEX_POINT('',#125816);
#23708=VERTEX_POINT('',#125818);
#23709=VERTEX_POINT('',#125822);
#23710=VERTEX_POINT('',#125824);
#23711=VERTEX_POINT('',#125828);
#23712=VERTEX_POINT('',#125830);
#23713=VERTEX_POINT('',#125834);
#23714=VERTEX_POINT('',#125836);
#23715=VERTEX_POINT('',#125840);
#23716=VERTEX_POINT('',#125842);
#23717=VERTEX_POINT('',#125846);
#23718=VERTEX_POINT('',#125848);
#23719=VERTEX_POINT('',#125852);
#23720=VERTEX_POINT('',#125854);
#23721=VERTEX_POINT('',#125858);
#23722=VERTEX_POINT('',#125860);
#23723=VERTEX_POINT('',#125864);
#23724=VERTEX_POINT('',#125866);
#23725=VERTEX_POINT('',#125870);
#23726=VERTEX_POINT('',#125872);
#23727=VERTEX_POINT('',#125876);
#23728=VERTEX_POINT('',#125878);
#23729=VERTEX_POINT('',#125882);
#23730=VERTEX_POINT('',#125884);
#23731=VERTEX_POINT('',#125888);
#23732=VERTEX_POINT('',#125890);
#23733=VERTEX_POINT('',#125894);
#23734=VERTEX_POINT('',#125896);
#23735=VERTEX_POINT('',#125900);
#23736=VERTEX_POINT('',#125902);
#23737=VERTEX_POINT('',#125906);
#23738=VERTEX_POINT('',#125908);
#23739=VERTEX_POINT('',#125912);
#23740=VERTEX_POINT('',#125914);
#23741=VERTEX_POINT('',#125918);
#23742=VERTEX_POINT('',#125920);
#23743=VERTEX_POINT('',#125924);
#23744=VERTEX_POINT('',#125926);
#23745=VERTEX_POINT('',#125930);
#23746=VERTEX_POINT('',#125932);
#23747=VERTEX_POINT('',#125936);
#23748=VERTEX_POINT('',#125938);
#23749=VERTEX_POINT('',#125942);
#23750=VERTEX_POINT('',#125944);
#23751=VERTEX_POINT('',#125948);
#23752=VERTEX_POINT('',#125950);
#23753=VERTEX_POINT('',#125954);
#23754=VERTEX_POINT('',#125956);
#23755=VERTEX_POINT('',#125960);
#23756=VERTEX_POINT('',#125962);
#23757=VERTEX_POINT('',#125966);
#23758=VERTEX_POINT('',#125968);
#23759=VERTEX_POINT('',#125972);
#23760=VERTEX_POINT('',#125974);
#23761=VERTEX_POINT('',#125978);
#23762=VERTEX_POINT('',#125980);
#23763=VERTEX_POINT('',#125984);
#23764=VERTEX_POINT('',#125986);
#23765=VERTEX_POINT('',#125990);
#23766=VERTEX_POINT('',#125992);
#23767=VERTEX_POINT('',#125996);
#23768=VERTEX_POINT('',#125998);
#23769=VERTEX_POINT('',#126002);
#23770=VERTEX_POINT('',#126004);
#23771=VERTEX_POINT('',#126008);
#23772=VERTEX_POINT('',#126010);
#23773=VERTEX_POINT('',#126014);
#23774=VERTEX_POINT('',#126016);
#23775=VERTEX_POINT('',#126020);
#23776=VERTEX_POINT('',#126022);
#23777=VERTEX_POINT('',#126026);
#23778=VERTEX_POINT('',#126028);
#23779=VERTEX_POINT('',#126032);
#23780=VERTEX_POINT('',#126034);
#23781=VERTEX_POINT('',#126038);
#23782=VERTEX_POINT('',#126040);
#23783=VERTEX_POINT('',#126044);
#23784=VERTEX_POINT('',#126046);
#23785=VERTEX_POINT('',#126050);
#23786=VERTEX_POINT('',#126052);
#23787=VERTEX_POINT('',#126056);
#23788=VERTEX_POINT('',#126058);
#23789=VERTEX_POINT('',#126062);
#23790=VERTEX_POINT('',#126064);
#23791=VERTEX_POINT('',#126068);
#23792=VERTEX_POINT('',#126070);
#23793=VERTEX_POINT('',#126074);
#23794=VERTEX_POINT('',#126076);
#23795=VERTEX_POINT('',#126080);
#23796=VERTEX_POINT('',#126082);
#23797=VERTEX_POINT('',#126086);
#23798=VERTEX_POINT('',#126088);
#23799=VERTEX_POINT('',#126092);
#23800=VERTEX_POINT('',#126094);
#23801=VERTEX_POINT('',#126098);
#23802=VERTEX_POINT('',#126100);
#23803=VERTEX_POINT('',#126104);
#23804=VERTEX_POINT('',#126106);
#23805=VERTEX_POINT('',#126110);
#23806=VERTEX_POINT('',#126112);
#23807=VERTEX_POINT('',#126116);
#23808=VERTEX_POINT('',#126118);
#23809=VERTEX_POINT('',#126122);
#23810=VERTEX_POINT('',#126124);
#23811=VERTEX_POINT('',#126128);
#23812=VERTEX_POINT('',#126130);
#23813=VERTEX_POINT('',#126134);
#23814=VERTEX_POINT('',#126136);
#23815=VERTEX_POINT('',#126140);
#23816=VERTEX_POINT('',#126142);
#23817=VERTEX_POINT('',#126146);
#23818=VERTEX_POINT('',#126148);
#23819=VERTEX_POINT('',#126152);
#23820=VERTEX_POINT('',#126154);
#23821=VERTEX_POINT('',#126158);
#23822=VERTEX_POINT('',#126160);
#23823=VERTEX_POINT('',#126164);
#23824=VERTEX_POINT('',#126166);
#23825=VERTEX_POINT('',#126170);
#23826=VERTEX_POINT('',#126172);
#23827=VERTEX_POINT('',#126176);
#23828=VERTEX_POINT('',#126178);
#23829=VERTEX_POINT('',#126182);
#23830=VERTEX_POINT('',#126184);
#23831=VERTEX_POINT('',#126188);
#23832=VERTEX_POINT('',#126190);
#23833=VERTEX_POINT('',#126194);
#23834=VERTEX_POINT('',#126196);
#23835=VERTEX_POINT('',#126200);
#23836=VERTEX_POINT('',#126202);
#23837=VERTEX_POINT('',#126206);
#23838=VERTEX_POINT('',#126208);
#23839=VERTEX_POINT('',#126212);
#23840=VERTEX_POINT('',#126214);
#23841=VERTEX_POINT('',#126218);
#23842=VERTEX_POINT('',#126220);
#23843=VERTEX_POINT('',#126224);
#23844=VERTEX_POINT('',#126226);
#23845=VERTEX_POINT('',#126230);
#23846=VERTEX_POINT('',#126232);
#23847=VERTEX_POINT('',#126236);
#23848=VERTEX_POINT('',#126238);
#23849=VERTEX_POINT('',#126242);
#23850=VERTEX_POINT('',#126244);
#23851=VERTEX_POINT('',#126248);
#23852=VERTEX_POINT('',#126250);
#23853=VERTEX_POINT('',#126254);
#23854=VERTEX_POINT('',#126256);
#23855=VERTEX_POINT('',#126260);
#23856=VERTEX_POINT('',#126262);
#23857=VERTEX_POINT('',#126266);
#23858=VERTEX_POINT('',#126268);
#23859=VERTEX_POINT('',#126272);
#23860=VERTEX_POINT('',#126274);
#23861=VERTEX_POINT('',#126278);
#23862=VERTEX_POINT('',#126280);
#23863=VERTEX_POINT('',#126284);
#23864=VERTEX_POINT('',#126286);
#23865=VERTEX_POINT('',#126290);
#23866=VERTEX_POINT('',#126292);
#23867=VERTEX_POINT('',#126296);
#23868=VERTEX_POINT('',#126298);
#23869=VERTEX_POINT('',#126302);
#23870=VERTEX_POINT('',#126304);
#23871=VERTEX_POINT('',#126308);
#23872=VERTEX_POINT('',#126310);
#23873=VERTEX_POINT('',#126314);
#23874=VERTEX_POINT('',#126316);
#23875=VERTEX_POINT('',#126320);
#23876=VERTEX_POINT('',#126322);
#23877=VERTEX_POINT('',#126326);
#23878=VERTEX_POINT('',#126328);
#23879=VERTEX_POINT('',#126332);
#23880=VERTEX_POINT('',#126334);
#23881=VERTEX_POINT('',#126338);
#23882=VERTEX_POINT('',#126340);
#23883=VERTEX_POINT('',#126344);
#23884=VERTEX_POINT('',#126346);
#23885=VERTEX_POINT('',#126350);
#23886=VERTEX_POINT('',#126352);
#23887=VERTEX_POINT('',#126356);
#23888=VERTEX_POINT('',#126358);
#23889=VERTEX_POINT('',#126362);
#23890=VERTEX_POINT('',#126364);
#23891=VERTEX_POINT('',#126368);
#23892=VERTEX_POINT('',#126370);
#23893=VERTEX_POINT('',#126374);
#23894=VERTEX_POINT('',#126376);
#23895=VERTEX_POINT('',#126380);
#23896=VERTEX_POINT('',#126382);
#23897=VERTEX_POINT('',#126386);
#23898=VERTEX_POINT('',#126388);
#23899=VERTEX_POINT('',#126392);
#23900=VERTEX_POINT('',#126394);
#23901=VERTEX_POINT('',#126398);
#23902=VERTEX_POINT('',#126400);
#23903=VERTEX_POINT('',#126404);
#23904=VERTEX_POINT('',#126406);
#23905=VERTEX_POINT('',#126410);
#23906=VERTEX_POINT('',#126412);
#23907=VERTEX_POINT('',#126416);
#23908=VERTEX_POINT('',#126418);
#23909=VERTEX_POINT('',#126422);
#23910=VERTEX_POINT('',#126424);
#23911=VERTEX_POINT('',#126428);
#23912=VERTEX_POINT('',#126430);
#23913=VERTEX_POINT('',#126434);
#23914=VERTEX_POINT('',#126436);
#23915=VERTEX_POINT('',#126440);
#23916=VERTEX_POINT('',#126442);
#23917=VERTEX_POINT('',#126446);
#23918=VERTEX_POINT('',#126448);
#23919=VERTEX_POINT('',#126452);
#23920=VERTEX_POINT('',#126454);
#23921=VERTEX_POINT('',#126458);
#23922=VERTEX_POINT('',#126460);
#23923=VERTEX_POINT('',#126464);
#23924=VERTEX_POINT('',#126466);
#23925=VERTEX_POINT('',#126470);
#23926=VERTEX_POINT('',#126472);
#23927=VERTEX_POINT('',#126476);
#23928=VERTEX_POINT('',#126478);
#23929=VERTEX_POINT('',#126482);
#23930=VERTEX_POINT('',#126484);
#23931=VERTEX_POINT('',#126488);
#23932=VERTEX_POINT('',#126490);
#23933=VERTEX_POINT('',#126494);
#23934=VERTEX_POINT('',#126496);
#23935=VERTEX_POINT('',#126500);
#23936=VERTEX_POINT('',#126502);
#23937=VERTEX_POINT('',#126506);
#23938=VERTEX_POINT('',#126508);
#23939=VERTEX_POINT('',#126512);
#23940=VERTEX_POINT('',#126514);
#23941=VERTEX_POINT('',#126518);
#23942=VERTEX_POINT('',#126520);
#23943=VERTEX_POINT('',#126524);
#23944=VERTEX_POINT('',#126526);
#23945=VERTEX_POINT('',#126530);
#23946=VERTEX_POINT('',#126532);
#23947=VERTEX_POINT('',#126536);
#23948=VERTEX_POINT('',#126538);
#23949=VERTEX_POINT('',#126542);
#23950=VERTEX_POINT('',#126544);
#23951=VERTEX_POINT('',#126548);
#23952=VERTEX_POINT('',#126550);
#23953=VERTEX_POINT('',#126554);
#23954=VERTEX_POINT('',#126556);
#23955=VERTEX_POINT('',#126560);
#23956=VERTEX_POINT('',#126562);
#23957=VERTEX_POINT('',#126566);
#23958=VERTEX_POINT('',#126568);
#23959=VERTEX_POINT('',#126572);
#23960=VERTEX_POINT('',#126574);
#23961=VERTEX_POINT('',#126578);
#23962=VERTEX_POINT('',#126580);
#23963=VERTEX_POINT('',#126584);
#23964=VERTEX_POINT('',#126586);
#23965=VERTEX_POINT('',#126590);
#23966=VERTEX_POINT('',#126592);
#23967=VERTEX_POINT('',#126596);
#23968=VERTEX_POINT('',#126598);
#23969=VERTEX_POINT('',#126602);
#23970=VERTEX_POINT('',#126604);
#23971=VERTEX_POINT('',#126608);
#23972=VERTEX_POINT('',#126610);
#23973=VERTEX_POINT('',#126614);
#23974=VERTEX_POINT('',#126616);
#23975=VERTEX_POINT('',#126620);
#23976=VERTEX_POINT('',#126622);
#23977=VERTEX_POINT('',#126626);
#23978=VERTEX_POINT('',#126628);
#23979=VERTEX_POINT('',#126632);
#23980=VERTEX_POINT('',#126634);
#23981=VERTEX_POINT('',#126638);
#23982=VERTEX_POINT('',#126640);
#23983=VERTEX_POINT('',#126644);
#23984=VERTEX_POINT('',#126646);
#23985=VERTEX_POINT('',#126650);
#23986=VERTEX_POINT('',#126652);
#23987=VERTEX_POINT('',#126656);
#23988=VERTEX_POINT('',#126658);
#23989=VERTEX_POINT('',#126662);
#23990=VERTEX_POINT('',#126664);
#23991=VERTEX_POINT('',#126668);
#23992=VERTEX_POINT('',#126670);
#23993=VERTEX_POINT('',#126674);
#23994=VERTEX_POINT('',#126676);
#23995=VERTEX_POINT('',#126680);
#23996=VERTEX_POINT('',#126682);
#23997=VERTEX_POINT('',#126686);
#23998=VERTEX_POINT('',#126688);
#23999=VERTEX_POINT('',#126692);
#24000=VERTEX_POINT('',#126694);
#24001=VERTEX_POINT('',#126698);
#24002=VERTEX_POINT('',#126700);
#24003=VERTEX_POINT('',#126704);
#24004=VERTEX_POINT('',#126706);
#24005=VERTEX_POINT('',#126710);
#24006=VERTEX_POINT('',#126712);
#24007=VERTEX_POINT('',#126716);
#24008=VERTEX_POINT('',#126718);
#24009=VERTEX_POINT('',#126722);
#24010=VERTEX_POINT('',#126724);
#24011=VERTEX_POINT('',#126728);
#24012=VERTEX_POINT('',#126730);
#24013=VERTEX_POINT('',#126734);
#24014=VERTEX_POINT('',#126736);
#24015=VERTEX_POINT('',#126740);
#24016=VERTEX_POINT('',#126742);
#24017=VERTEX_POINT('',#126746);
#24018=VERTEX_POINT('',#126748);
#24019=VERTEX_POINT('',#126752);
#24020=VERTEX_POINT('',#126754);
#24021=VERTEX_POINT('',#126758);
#24022=VERTEX_POINT('',#126760);
#24023=VERTEX_POINT('',#126764);
#24024=VERTEX_POINT('',#126766);
#24025=VERTEX_POINT('',#126770);
#24026=VERTEX_POINT('',#126772);
#24027=VERTEX_POINT('',#126776);
#24028=VERTEX_POINT('',#126778);
#24029=VERTEX_POINT('',#126782);
#24030=VERTEX_POINT('',#126784);
#24031=VERTEX_POINT('',#126788);
#24032=VERTEX_POINT('',#126790);
#24033=VERTEX_POINT('',#126794);
#24034=VERTEX_POINT('',#126796);
#24035=VERTEX_POINT('',#126800);
#24036=VERTEX_POINT('',#126802);
#24037=VERTEX_POINT('',#126806);
#24038=VERTEX_POINT('',#126808);
#24039=VERTEX_POINT('',#126812);
#24040=VERTEX_POINT('',#126814);
#24041=VERTEX_POINT('',#126818);
#24042=VERTEX_POINT('',#126820);
#24043=VERTEX_POINT('',#126824);
#24044=VERTEX_POINT('',#126826);
#24045=VERTEX_POINT('',#126830);
#24046=VERTEX_POINT('',#126832);
#24047=VERTEX_POINT('',#126836);
#24048=VERTEX_POINT('',#126838);
#24049=VERTEX_POINT('',#126842);
#24050=VERTEX_POINT('',#126844);
#24051=VERTEX_POINT('',#126848);
#24052=VERTEX_POINT('',#126850);
#24053=VERTEX_POINT('',#126854);
#24054=VERTEX_POINT('',#126856);
#24055=VERTEX_POINT('',#126860);
#24056=VERTEX_POINT('',#126862);
#24057=VERTEX_POINT('',#126866);
#24058=VERTEX_POINT('',#126868);
#24059=VERTEX_POINT('',#126872);
#24060=VERTEX_POINT('',#126874);
#24061=VERTEX_POINT('',#126878);
#24062=VERTEX_POINT('',#126880);
#24063=VERTEX_POINT('',#126884);
#24064=VERTEX_POINT('',#126886);
#24065=VERTEX_POINT('',#126890);
#24066=VERTEX_POINT('',#126892);
#24067=VERTEX_POINT('',#126896);
#24068=VERTEX_POINT('',#126898);
#24069=VERTEX_POINT('',#126902);
#24070=VERTEX_POINT('',#126904);
#24071=VERTEX_POINT('',#126908);
#24072=VERTEX_POINT('',#126910);
#24073=VERTEX_POINT('',#126914);
#24074=VERTEX_POINT('',#126916);
#24075=VERTEX_POINT('',#126920);
#24076=VERTEX_POINT('',#126922);
#24077=VERTEX_POINT('',#126926);
#24078=VERTEX_POINT('',#126928);
#24079=VERTEX_POINT('',#126932);
#24080=VERTEX_POINT('',#126934);
#24081=VERTEX_POINT('',#126938);
#24082=VERTEX_POINT('',#126940);
#24083=VERTEX_POINT('',#126944);
#24084=VERTEX_POINT('',#126946);
#24085=VERTEX_POINT('',#126950);
#24086=VERTEX_POINT('',#126952);
#24087=VERTEX_POINT('',#126956);
#24088=VERTEX_POINT('',#126958);
#24089=VERTEX_POINT('',#126962);
#24090=VERTEX_POINT('',#126964);
#24091=VERTEX_POINT('',#126968);
#24092=VERTEX_POINT('',#126970);
#24093=VERTEX_POINT('',#126974);
#24094=VERTEX_POINT('',#126976);
#24095=VERTEX_POINT('',#126980);
#24096=VERTEX_POINT('',#126982);
#24097=VERTEX_POINT('',#126986);
#24098=VERTEX_POINT('',#126988);
#24099=VERTEX_POINT('',#126992);
#24100=VERTEX_POINT('',#126994);
#24101=VERTEX_POINT('',#126998);
#24102=VERTEX_POINT('',#127000);
#24103=VERTEX_POINT('',#127004);
#24104=VERTEX_POINT('',#127006);
#24105=VERTEX_POINT('',#127010);
#24106=VERTEX_POINT('',#127012);
#24107=VERTEX_POINT('',#127016);
#24108=VERTEX_POINT('',#127018);
#24109=VERTEX_POINT('',#127022);
#24110=VERTEX_POINT('',#127024);
#24111=VERTEX_POINT('',#127028);
#24112=VERTEX_POINT('',#127030);
#24113=VERTEX_POINT('',#127034);
#24114=VERTEX_POINT('',#127036);
#24115=VERTEX_POINT('',#127040);
#24116=VERTEX_POINT('',#127042);
#24117=VERTEX_POINT('',#127046);
#24118=VERTEX_POINT('',#127048);
#24119=VERTEX_POINT('',#127052);
#24120=VERTEX_POINT('',#127054);
#24121=VERTEX_POINT('',#127058);
#24122=VERTEX_POINT('',#127060);
#24123=VERTEX_POINT('',#127064);
#24124=VERTEX_POINT('',#127066);
#24125=VERTEX_POINT('',#127070);
#24126=VERTEX_POINT('',#127072);
#24127=VERTEX_POINT('',#127076);
#24128=VERTEX_POINT('',#127078);
#24129=VERTEX_POINT('',#127082);
#24130=VERTEX_POINT('',#127084);
#24131=VERTEX_POINT('',#127088);
#24132=VERTEX_POINT('',#127090);
#24133=VERTEX_POINT('',#127094);
#24134=VERTEX_POINT('',#127096);
#24135=VERTEX_POINT('',#127100);
#24136=VERTEX_POINT('',#127102);
#24137=VERTEX_POINT('',#127106);
#24138=VERTEX_POINT('',#127108);
#24139=VERTEX_POINT('',#127112);
#24140=VERTEX_POINT('',#127114);
#24141=VERTEX_POINT('',#127118);
#24142=VERTEX_POINT('',#127120);
#24143=VERTEX_POINT('',#127124);
#24144=VERTEX_POINT('',#127126);
#24145=VERTEX_POINT('',#127130);
#24146=VERTEX_POINT('',#127132);
#24147=VERTEX_POINT('',#127136);
#24148=VERTEX_POINT('',#127138);
#24149=VERTEX_POINT('',#127142);
#24150=VERTEX_POINT('',#127144);
#24151=VERTEX_POINT('',#127148);
#24152=VERTEX_POINT('',#127150);
#24153=VERTEX_POINT('',#127154);
#24154=VERTEX_POINT('',#127156);
#24155=VERTEX_POINT('',#127160);
#24156=VERTEX_POINT('',#127162);
#24157=VERTEX_POINT('',#127166);
#24158=VERTEX_POINT('',#127168);
#24159=VERTEX_POINT('',#127172);
#24160=VERTEX_POINT('',#127174);
#24161=VERTEX_POINT('',#127178);
#24162=VERTEX_POINT('',#127180);
#24163=VERTEX_POINT('',#127184);
#24164=VERTEX_POINT('',#127186);
#24165=VERTEX_POINT('',#127190);
#24166=VERTEX_POINT('',#127192);
#24167=VERTEX_POINT('',#127196);
#24168=VERTEX_POINT('',#127198);
#24169=VERTEX_POINT('',#127202);
#24170=VERTEX_POINT('',#127204);
#24171=VERTEX_POINT('',#127208);
#24172=VERTEX_POINT('',#127210);
#24173=VERTEX_POINT('',#127214);
#24174=VERTEX_POINT('',#127216);
#24175=VERTEX_POINT('',#127220);
#24176=VERTEX_POINT('',#127222);
#24177=VERTEX_POINT('',#127226);
#24178=VERTEX_POINT('',#127228);
#24179=VERTEX_POINT('',#127232);
#24180=VERTEX_POINT('',#127234);
#24181=VERTEX_POINT('',#127238);
#24182=VERTEX_POINT('',#127240);
#24183=VERTEX_POINT('',#127244);
#24184=VERTEX_POINT('',#127246);
#24185=VERTEX_POINT('',#127250);
#24186=VERTEX_POINT('',#127252);
#24187=VERTEX_POINT('',#127256);
#24188=VERTEX_POINT('',#127258);
#24189=VERTEX_POINT('',#127262);
#24190=VERTEX_POINT('',#127264);
#24191=VERTEX_POINT('',#127268);
#24192=VERTEX_POINT('',#127270);
#24193=VERTEX_POINT('',#127274);
#24194=VERTEX_POINT('',#127276);
#24195=VERTEX_POINT('',#127280);
#24196=VERTEX_POINT('',#127282);
#24197=VERTEX_POINT('',#127286);
#24198=VERTEX_POINT('',#127288);
#24199=VERTEX_POINT('',#127292);
#24200=VERTEX_POINT('',#127294);
#24201=VERTEX_POINT('',#127298);
#24202=VERTEX_POINT('',#127300);
#24203=VERTEX_POINT('',#127304);
#24204=VERTEX_POINT('',#127306);
#24205=VERTEX_POINT('',#127310);
#24206=VERTEX_POINT('',#127312);
#24207=VERTEX_POINT('',#127316);
#24208=VERTEX_POINT('',#127318);
#24209=VERTEX_POINT('',#127322);
#24210=VERTEX_POINT('',#127324);
#24211=VERTEX_POINT('',#127328);
#24212=VERTEX_POINT('',#127330);
#24213=VERTEX_POINT('',#127334);
#24214=VERTEX_POINT('',#127336);
#24215=VERTEX_POINT('',#127340);
#24216=VERTEX_POINT('',#127342);
#24217=VERTEX_POINT('',#127346);
#24218=VERTEX_POINT('',#127348);
#24219=VERTEX_POINT('',#127352);
#24220=VERTEX_POINT('',#127354);
#24221=VERTEX_POINT('',#127358);
#24222=VERTEX_POINT('',#127360);
#24223=VERTEX_POINT('',#127364);
#24224=VERTEX_POINT('',#127366);
#24225=VERTEX_POINT('',#127370);
#24226=VERTEX_POINT('',#127372);
#24227=VERTEX_POINT('',#127376);
#24228=VERTEX_POINT('',#127378);
#24229=VERTEX_POINT('',#127382);
#24230=VERTEX_POINT('',#127384);
#24231=VERTEX_POINT('',#127388);
#24232=VERTEX_POINT('',#127390);
#24233=VERTEX_POINT('',#127394);
#24234=VERTEX_POINT('',#127396);
#24235=VERTEX_POINT('',#127400);
#24236=VERTEX_POINT('',#127402);
#24237=VERTEX_POINT('',#127406);
#24238=VERTEX_POINT('',#127408);
#24239=VERTEX_POINT('',#127412);
#24240=VERTEX_POINT('',#127414);
#24241=VERTEX_POINT('',#127418);
#24242=VERTEX_POINT('',#127420);
#24243=VERTEX_POINT('',#127424);
#24244=VERTEX_POINT('',#127426);
#24245=VERTEX_POINT('',#127430);
#24246=VERTEX_POINT('',#127432);
#24247=VERTEX_POINT('',#127436);
#24248=VERTEX_POINT('',#127438);
#24249=VERTEX_POINT('',#127442);
#24250=VERTEX_POINT('',#127444);
#24251=VERTEX_POINT('',#127448);
#24252=VERTEX_POINT('',#127450);
#24253=VERTEX_POINT('',#127454);
#24254=VERTEX_POINT('',#127456);
#24255=VERTEX_POINT('',#127460);
#24256=VERTEX_POINT('',#127462);
#24257=VERTEX_POINT('',#127466);
#24258=VERTEX_POINT('',#127468);
#24259=VERTEX_POINT('',#127472);
#24260=VERTEX_POINT('',#127474);
#24261=VERTEX_POINT('',#127478);
#24262=VERTEX_POINT('',#127480);
#24263=VERTEX_POINT('',#127484);
#24264=VERTEX_POINT('',#127486);
#24265=VERTEX_POINT('',#127490);
#24266=VERTEX_POINT('',#127492);
#24267=VERTEX_POINT('',#127496);
#24268=VERTEX_POINT('',#127498);
#24269=VERTEX_POINT('',#127502);
#24270=VERTEX_POINT('',#127504);
#24271=VERTEX_POINT('',#127508);
#24272=VERTEX_POINT('',#127510);
#24273=VERTEX_POINT('',#127514);
#24274=VERTEX_POINT('',#127516);
#24275=VERTEX_POINT('',#127520);
#24276=VERTEX_POINT('',#127522);
#24277=VERTEX_POINT('',#127526);
#24278=VERTEX_POINT('',#127528);
#24279=VERTEX_POINT('',#127532);
#24280=VERTEX_POINT('',#127534);
#24281=VERTEX_POINT('',#127538);
#24282=VERTEX_POINT('',#127540);
#24283=VERTEX_POINT('',#127544);
#24284=VERTEX_POINT('',#127546);
#24285=VERTEX_POINT('',#127550);
#24286=VERTEX_POINT('',#127552);
#24287=VERTEX_POINT('',#127556);
#24288=VERTEX_POINT('',#127558);
#24289=VERTEX_POINT('',#127562);
#24290=VERTEX_POINT('',#127564);
#24291=VERTEX_POINT('',#127568);
#24292=VERTEX_POINT('',#127570);
#24293=VERTEX_POINT('',#127574);
#24294=VERTEX_POINT('',#127576);
#24295=VERTEX_POINT('',#127580);
#24296=VERTEX_POINT('',#127582);
#24297=VERTEX_POINT('',#127586);
#24298=VERTEX_POINT('',#127588);
#24299=VERTEX_POINT('',#127592);
#24300=VERTEX_POINT('',#127594);
#24301=VERTEX_POINT('',#127598);
#24302=VERTEX_POINT('',#127600);
#24303=VERTEX_POINT('',#127604);
#24304=VERTEX_POINT('',#127606);
#24305=VERTEX_POINT('',#127610);
#24306=VERTEX_POINT('',#127612);
#24307=VERTEX_POINT('',#127616);
#24308=VERTEX_POINT('',#127618);
#24309=VERTEX_POINT('',#127622);
#24310=VERTEX_POINT('',#127624);
#24311=VERTEX_POINT('',#127628);
#24312=VERTEX_POINT('',#127630);
#24313=VERTEX_POINT('',#127634);
#24314=VERTEX_POINT('',#127636);
#24315=VERTEX_POINT('',#127640);
#24316=VERTEX_POINT('',#127642);
#24317=VERTEX_POINT('',#127646);
#24318=VERTEX_POINT('',#127648);
#24319=VERTEX_POINT('',#127652);
#24320=VERTEX_POINT('',#127654);
#24321=VERTEX_POINT('',#127658);
#24322=VERTEX_POINT('',#127660);
#24323=VERTEX_POINT('',#127664);
#24324=VERTEX_POINT('',#127666);
#24325=VERTEX_POINT('',#127670);
#24326=VERTEX_POINT('',#127672);
#24327=VERTEX_POINT('',#127676);
#24328=VERTEX_POINT('',#127678);
#24329=VERTEX_POINT('',#127682);
#24330=VERTEX_POINT('',#127684);
#24331=VERTEX_POINT('',#127688);
#24332=VERTEX_POINT('',#127690);
#24333=VERTEX_POINT('',#127694);
#24334=VERTEX_POINT('',#127696);
#24335=VERTEX_POINT('',#127700);
#24336=VERTEX_POINT('',#127702);
#24337=VERTEX_POINT('',#127706);
#24338=VERTEX_POINT('',#127708);
#24339=VERTEX_POINT('',#127712);
#24340=VERTEX_POINT('',#127714);
#24341=VERTEX_POINT('',#127718);
#24342=VERTEX_POINT('',#127720);
#24343=VERTEX_POINT('',#127724);
#24344=VERTEX_POINT('',#127726);
#24345=VERTEX_POINT('',#127730);
#24346=VERTEX_POINT('',#127732);
#24347=VERTEX_POINT('',#127736);
#24348=VERTEX_POINT('',#127738);
#24349=VERTEX_POINT('',#127742);
#24350=VERTEX_POINT('',#127744);
#24351=VERTEX_POINT('',#127748);
#24352=VERTEX_POINT('',#127750);
#24353=VERTEX_POINT('',#127754);
#24354=VERTEX_POINT('',#127756);
#24355=VERTEX_POINT('',#127760);
#24356=VERTEX_POINT('',#127762);
#24357=VERTEX_POINT('',#127766);
#24358=VERTEX_POINT('',#127768);
#24359=VERTEX_POINT('',#127772);
#24360=VERTEX_POINT('',#127774);
#24361=VERTEX_POINT('',#127778);
#24362=VERTEX_POINT('',#127780);
#24363=VERTEX_POINT('',#127784);
#24364=VERTEX_POINT('',#127786);
#24365=VERTEX_POINT('',#127790);
#24366=VERTEX_POINT('',#127792);
#24367=VERTEX_POINT('',#127796);
#24368=VERTEX_POINT('',#127798);
#24369=VERTEX_POINT('',#127802);
#24370=VERTEX_POINT('',#127804);
#24371=VERTEX_POINT('',#127808);
#24372=VERTEX_POINT('',#127810);
#24373=VERTEX_POINT('',#127814);
#24374=VERTEX_POINT('',#127816);
#24375=VERTEX_POINT('',#127820);
#24376=VERTEX_POINT('',#127822);
#24377=VERTEX_POINT('',#127826);
#24378=VERTEX_POINT('',#127828);
#24379=VERTEX_POINT('',#127832);
#24380=VERTEX_POINT('',#127834);
#24381=VERTEX_POINT('',#127838);
#24382=VERTEX_POINT('',#127840);
#24383=VERTEX_POINT('',#127844);
#24384=VERTEX_POINT('',#127846);
#24385=VERTEX_POINT('',#127850);
#24386=VERTEX_POINT('',#127852);
#24387=VERTEX_POINT('',#127856);
#24388=VERTEX_POINT('',#127858);
#24389=VERTEX_POINT('',#127862);
#24390=VERTEX_POINT('',#127864);
#24391=VERTEX_POINT('',#127868);
#24392=VERTEX_POINT('',#127870);
#24393=VERTEX_POINT('',#127874);
#24394=VERTEX_POINT('',#127876);
#24395=VERTEX_POINT('',#127880);
#24396=VERTEX_POINT('',#127882);
#24397=VERTEX_POINT('',#127886);
#24398=VERTEX_POINT('',#127888);
#24399=VERTEX_POINT('',#127892);
#24400=VERTEX_POINT('',#127894);
#24401=VERTEX_POINT('',#127898);
#24402=VERTEX_POINT('',#127900);
#24403=VERTEX_POINT('',#127904);
#24404=VERTEX_POINT('',#127906);
#24405=VERTEX_POINT('',#127910);
#24406=VERTEX_POINT('',#127912);
#24407=VERTEX_POINT('',#127916);
#24408=VERTEX_POINT('',#127918);
#24409=VERTEX_POINT('',#127922);
#24410=VERTEX_POINT('',#127924);
#24411=VERTEX_POINT('',#127928);
#24412=VERTEX_POINT('',#127930);
#24413=VERTEX_POINT('',#127934);
#24414=VERTEX_POINT('',#127936);
#24415=VERTEX_POINT('',#127940);
#24416=VERTEX_POINT('',#127942);
#24417=VERTEX_POINT('',#127946);
#24418=VERTEX_POINT('',#127948);
#24419=VERTEX_POINT('',#127952);
#24420=VERTEX_POINT('',#127954);
#24421=VERTEX_POINT('',#127958);
#24422=VERTEX_POINT('',#127960);
#24423=VERTEX_POINT('',#127964);
#24424=VERTEX_POINT('',#127966);
#24425=VERTEX_POINT('',#127970);
#24426=VERTEX_POINT('',#127972);
#24427=VERTEX_POINT('',#127976);
#24428=VERTEX_POINT('',#127978);
#24429=VERTEX_POINT('',#127982);
#24430=VERTEX_POINT('',#127984);
#24431=VERTEX_POINT('',#127988);
#24432=VERTEX_POINT('',#127990);
#24433=VERTEX_POINT('',#127994);
#24434=VERTEX_POINT('',#127996);
#24435=VERTEX_POINT('',#128000);
#24436=VERTEX_POINT('',#128002);
#24437=VERTEX_POINT('',#128006);
#24438=VERTEX_POINT('',#128008);
#24439=VERTEX_POINT('',#128012);
#24440=VERTEX_POINT('',#128014);
#24441=VERTEX_POINT('',#128018);
#24442=VERTEX_POINT('',#128020);
#24443=VERTEX_POINT('',#128024);
#24444=VERTEX_POINT('',#128026);
#24445=VERTEX_POINT('',#128030);
#24446=VERTEX_POINT('',#128032);
#24447=VERTEX_POINT('',#128036);
#24448=VERTEX_POINT('',#128038);
#24449=VERTEX_POINT('',#128042);
#24450=VERTEX_POINT('',#128044);
#24451=VERTEX_POINT('',#128048);
#24452=VERTEX_POINT('',#128050);
#24453=VERTEX_POINT('',#128054);
#24454=VERTEX_POINT('',#128056);
#24455=VERTEX_POINT('',#128060);
#24456=VERTEX_POINT('',#128062);
#24457=VERTEX_POINT('',#128066);
#24458=VERTEX_POINT('',#128068);
#24459=VERTEX_POINT('',#128072);
#24460=VERTEX_POINT('',#128074);
#24461=VERTEX_POINT('',#128078);
#24462=VERTEX_POINT('',#128080);
#24463=VERTEX_POINT('',#128084);
#24464=VERTEX_POINT('',#128086);
#24465=VERTEX_POINT('',#128090);
#24466=VERTEX_POINT('',#128092);
#24467=VERTEX_POINT('',#128096);
#24468=VERTEX_POINT('',#128098);
#24469=VERTEX_POINT('',#128102);
#24470=VERTEX_POINT('',#128104);
#24471=VERTEX_POINT('',#128108);
#24472=VERTEX_POINT('',#128110);
#24473=VERTEX_POINT('',#128114);
#24474=VERTEX_POINT('',#128116);
#24475=VERTEX_POINT('',#128120);
#24476=VERTEX_POINT('',#128122);
#24477=VERTEX_POINT('',#128126);
#24478=VERTEX_POINT('',#128128);
#24479=VERTEX_POINT('',#128132);
#24480=VERTEX_POINT('',#128134);
#24481=VERTEX_POINT('',#128138);
#24482=VERTEX_POINT('',#128143);
#24483=VERTEX_POINT('',#128147);
#24484=VERTEX_POINT('',#128149);
#24485=VERTEX_POINT('',#128151);
#24486=VERTEX_POINT('',#128155);
#24487=VERTEX_POINT('',#128157);
#24488=VERTEX_POINT('',#128163);
#24489=VERTEX_POINT('',#128166);
#24490=VERTEX_POINT('',#128168);
#24491=VERTEX_POINT('',#128172);
#24492=VERTEX_POINT('',#128174);
#24493=VERTEX_POINT('',#128178);
#24494=VERTEX_POINT('',#128182);
#24495=VERTEX_POINT('',#128186);
#24496=VERTEX_POINT('',#128187);
#24497=VERTEX_POINT('',#128190);
#24498=VERTEX_POINT('',#128196);
#24499=VERTEX_POINT('',#128197);
#24500=VERTEX_POINT('',#128220);
#24501=VERTEX_POINT('',#128244);
#24502=EDGE_CURVE('',#20635,#20635,#17703,.T.);
#24503=EDGE_CURVE('',#20635,#20636,#17704,.T.);
#24504=EDGE_CURVE('',#20636,#20637,#17705,.T.);
#24505=EDGE_CURVE('',#20637,#20636,#17706,.T.);
#24506=EDGE_CURVE('',#20638,#20639,#17707,.T.);
#24507=EDGE_CURVE('',#20638,#20640,#17708,.T.);
#24508=EDGE_CURVE('',#20640,#20640,#17709,.T.);
#24509=EDGE_CURVE('',#20639,#20638,#17710,.T.);
#24510=EDGE_CURVE('',#20641,#20641,#17711,.T.);
#24511=EDGE_CURVE('',#20641,#20635,#4312,.T.);
#24512=EDGE_CURVE('',#20637,#20639,#4313,.T.);
#24513=EDGE_CURVE('',#20640,#20642,#4314,.T.);
#24514=EDGE_CURVE('',#20642,#20642,#17712,.T.);
#24515=EDGE_CURVE('',#20643,#20644,#4315,.T.);
#24516=EDGE_CURVE('',#20643,#20645,#2912,.T.);
#24517=EDGE_CURVE('',#20646,#20645,#4316,.T.);
#24518=EDGE_CURVE('',#20646,#20644,#4317,.T.);
#24519=EDGE_CURVE('',#20646,#20647,#4318,.T.);
#24520=EDGE_CURVE('',#20647,#20648,#17713,.T.);
#24521=EDGE_CURVE('',#20648,#20644,#4319,.T.);
#24522=EDGE_CURVE('',#20643,#20648,#4320,.T.);
#24523=EDGE_CURVE('',#20645,#20647,#4321,.T.);
#24524=EDGE_CURVE('',#20649,#20650,#4322,.T.);
#24525=EDGE_CURVE('',#20649,#20651,#2913,.T.);
#24526=EDGE_CURVE('',#20651,#20652,#4323,.T.);
#24527=EDGE_CURVE('',#20652,#20650,#2914,.T.);
#24528=EDGE_CURVE('',#20651,#20653,#4324,.T.);
#24529=EDGE_CURVE('',#20652,#20653,#4325,.T.);
#24530=EDGE_CURVE('',#20649,#20654,#4326,.T.);
#24531=EDGE_CURVE('',#20654,#20650,#4327,.T.);
#24532=EDGE_CURVE('',#20653,#20654,#17714,.T.);
#24533=EDGE_CURVE('',#20655,#20655,#17715,.T.);
#24534=EDGE_CURVE('',#20655,#20656,#4328,.T.);
#24535=EDGE_CURVE('',#20656,#20656,#17716,.T.);
#24536=EDGE_CURVE('',#20657,#20657,#17717,.T.);
#24537=EDGE_CURVE('',#20657,#20658,#4329,.T.);
#24538=EDGE_CURVE('',#20658,#20658,#17718,.T.);
#24539=EDGE_CURVE('',#20659,#20659,#17719,.T.);
#24540=EDGE_CURVE('',#20659,#20660,#4330,.T.);
#24541=EDGE_CURVE('',#20660,#20660,#17720,.T.);
#24542=EDGE_CURVE('',#20661,#20661,#17721,.T.);
#24543=EDGE_CURVE('',#20661,#20662,#4331,.T.);
#24544=EDGE_CURVE('',#20662,#20662,#17722,.T.);
#24545=EDGE_CURVE('',#20663,#20663,#17723,.T.);
#24546=EDGE_CURVE('',#20663,#20664,#4332,.T.);
#24547=EDGE_CURVE('',#20664,#20664,#17724,.T.);
#24548=EDGE_CURVE('',#20665,#20665,#17725,.T.);
#24549=EDGE_CURVE('',#20665,#20666,#4333,.T.);
#24550=EDGE_CURVE('',#20666,#20666,#17726,.T.);
#24551=EDGE_CURVE('',#20667,#20667,#17727,.T.);
#24552=EDGE_CURVE('',#20667,#20668,#4334,.T.);
#24553=EDGE_CURVE('',#20668,#20668,#17728,.T.);
#24554=EDGE_CURVE('',#20669,#20669,#17729,.T.);
#24555=EDGE_CURVE('',#20669,#20670,#4335,.T.);
#24556=EDGE_CURVE('',#20670,#20670,#17730,.T.);
#24557=EDGE_CURVE('',#20671,#20671,#17731,.T.);
#24558=EDGE_CURVE('',#20671,#20672,#4336,.T.);
#24559=EDGE_CURVE('',#20672,#20672,#17732,.T.);
#24560=EDGE_CURVE('',#20673,#20673,#17733,.T.);
#24561=EDGE_CURVE('',#20673,#20674,#4337,.T.);
#24562=EDGE_CURVE('',#20674,#20674,#17734,.T.);
#24563=EDGE_CURVE('',#20675,#20675,#17735,.T.);
#24564=EDGE_CURVE('',#20675,#20676,#4338,.T.);
#24565=EDGE_CURVE('',#20676,#20676,#17736,.T.);
#24566=EDGE_CURVE('',#20677,#20677,#17737,.T.);
#24567=EDGE_CURVE('',#20677,#20678,#4339,.T.);
#24568=EDGE_CURVE('',#20678,#20678,#17738,.T.);
#24569=EDGE_CURVE('',#20679,#20680,#1808,.T.);
#24570=EDGE_CURVE('',#20680,#20681,#4340,.T.);
#24571=EDGE_CURVE('',#20681,#20681,#1809,.T.);
#24572=EDGE_CURVE('',#20680,#20679,#1810,.T.);
#24573=EDGE_CURVE('',#20682,#20682,#17739,.T.);
#24574=EDGE_CURVE('',#20682,#20683,#4341,.T.);
#24575=EDGE_CURVE('',#20683,#20683,#1811,.T.);
#24576=EDGE_CURVE('',#20684,#20685,#1812,.T.);
#24577=EDGE_CURVE('',#20685,#20686,#4342,.T.);
#24578=EDGE_CURVE('',#20686,#20686,#1813,.T.);
#24579=EDGE_CURVE('',#20685,#20684,#1814,.T.);
#24580=EDGE_CURVE('',#20687,#20687,#17740,.T.);
#24581=EDGE_CURVE('',#20687,#20688,#4343,.T.);
#24582=EDGE_CURVE('',#20688,#20688,#1815,.T.);
#24583=EDGE_CURVE('',#20689,#20690,#1816,.T.);
#24584=EDGE_CURVE('',#20690,#20691,#4344,.T.);
#24585=EDGE_CURVE('',#20691,#20691,#1817,.T.);
#24586=EDGE_CURVE('',#20690,#20689,#1818,.T.);
#24587=EDGE_CURVE('',#20692,#20692,#17741,.T.);
#24588=EDGE_CURVE('',#20692,#20693,#4345,.T.);
#24589=EDGE_CURVE('',#20693,#20693,#1819,.T.);
#24590=EDGE_CURVE('',#20694,#20695,#1820,.T.);
#24591=EDGE_CURVE('',#20695,#20696,#4346,.T.);
#24592=EDGE_CURVE('',#20696,#20696,#1821,.T.);
#24593=EDGE_CURVE('',#20695,#20694,#1822,.T.);
#24594=EDGE_CURVE('',#20697,#20697,#17742,.T.);
#24595=EDGE_CURVE('',#20697,#20698,#4347,.T.);
#24596=EDGE_CURVE('',#20698,#20698,#1823,.T.);
#24597=EDGE_CURVE('',#20699,#20700,#1824,.T.);
#24598=EDGE_CURVE('',#20700,#20701,#4348,.T.);
#24599=EDGE_CURVE('',#20701,#20701,#1825,.T.);
#24600=EDGE_CURVE('',#20700,#20699,#1826,.T.);
#24601=EDGE_CURVE('',#20702,#20702,#17743,.T.);
#24602=EDGE_CURVE('',#20702,#20703,#4349,.T.);
#24603=EDGE_CURVE('',#20703,#20703,#1827,.T.);
#24604=EDGE_CURVE('',#20704,#20705,#1828,.T.);
#24605=EDGE_CURVE('',#20705,#20706,#4350,.T.);
#24606=EDGE_CURVE('',#20706,#20706,#1829,.T.);
#24607=EDGE_CURVE('',#20705,#20704,#1830,.T.);
#24608=EDGE_CURVE('',#20707,#20707,#17744,.T.);
#24609=EDGE_CURVE('',#20707,#20708,#4351,.T.);
#24610=EDGE_CURVE('',#20708,#20708,#1831,.T.);
#24611=EDGE_CURVE('',#20709,#20710,#1832,.T.);
#24612=EDGE_CURVE('',#20710,#20711,#4352,.T.);
#24613=EDGE_CURVE('',#20711,#20711,#1833,.T.);
#24614=EDGE_CURVE('',#20710,#20709,#1834,.T.);
#24615=EDGE_CURVE('',#20712,#20712,#17745,.T.);
#24616=EDGE_CURVE('',#20712,#20713,#4353,.T.);
#24617=EDGE_CURVE('',#20713,#20713,#1835,.T.);
#24618=EDGE_CURVE('',#20714,#20715,#1836,.T.);
#24619=EDGE_CURVE('',#20715,#20716,#4354,.T.);
#24620=EDGE_CURVE('',#20716,#20716,#1837,.T.);
#24621=EDGE_CURVE('',#20715,#20714,#1838,.T.);
#24622=EDGE_CURVE('',#20717,#20717,#17746,.T.);
#24623=EDGE_CURVE('',#20717,#20718,#4355,.T.);
#24624=EDGE_CURVE('',#20718,#20718,#1839,.T.);
#24625=EDGE_CURVE('',#20719,#20720,#1840,.T.);
#24626=EDGE_CURVE('',#20720,#20721,#4356,.T.);
#24627=EDGE_CURVE('',#20721,#20721,#1841,.T.);
#24628=EDGE_CURVE('',#20720,#20719,#1842,.T.);
#24629=EDGE_CURVE('',#20722,#20722,#17747,.T.);
#24630=EDGE_CURVE('',#20722,#20723,#4357,.T.);
#24631=EDGE_CURVE('',#20723,#20723,#1843,.T.);
#24632=EDGE_CURVE('',#20724,#20725,#1844,.T.);
#24633=EDGE_CURVE('',#20725,#20726,#4358,.T.);
#24634=EDGE_CURVE('',#20726,#20726,#1845,.T.);
#24635=EDGE_CURVE('',#20725,#20724,#1846,.T.);
#24636=EDGE_CURVE('',#20727,#20727,#17748,.T.);
#24637=EDGE_CURVE('',#20727,#20728,#4359,.T.);
#24638=EDGE_CURVE('',#20728,#20728,#1847,.T.);
#24639=EDGE_CURVE('',#20729,#20730,#1848,.T.);
#24640=EDGE_CURVE('',#20730,#20731,#4360,.T.);
#24641=EDGE_CURVE('',#20731,#20731,#1849,.T.);
#24642=EDGE_CURVE('',#20730,#20729,#1850,.T.);
#24643=EDGE_CURVE('',#20732,#20732,#17749,.T.);
#24644=EDGE_CURVE('',#20732,#20733,#4361,.T.);
#24645=EDGE_CURVE('',#20733,#20733,#1851,.T.);
#24646=EDGE_CURVE('',#20734,#20735,#1852,.T.);
#24647=EDGE_CURVE('',#20735,#20736,#4362,.T.);
#24648=EDGE_CURVE('',#20736,#20736,#1853,.T.);
#24649=EDGE_CURVE('',#20735,#20734,#1854,.T.);
#24650=EDGE_CURVE('',#20737,#20737,#17750,.T.);
#24651=EDGE_CURVE('',#20737,#20738,#4363,.T.);
#24652=EDGE_CURVE('',#20738,#20738,#1855,.T.);
#24653=EDGE_CURVE('',#20739,#20740,#1856,.T.);
#24654=EDGE_CURVE('',#20740,#20741,#4364,.T.);
#24655=EDGE_CURVE('',#20741,#20741,#1857,.T.);
#24656=EDGE_CURVE('',#20740,#20739,#1858,.T.);
#24657=EDGE_CURVE('',#20742,#20742,#17751,.T.);
#24658=EDGE_CURVE('',#20742,#20743,#4365,.T.);
#24659=EDGE_CURVE('',#20743,#20743,#1859,.T.);
#24660=EDGE_CURVE('',#20744,#20745,#1860,.T.);
#24661=EDGE_CURVE('',#20745,#20746,#4366,.T.);
#24662=EDGE_CURVE('',#20746,#20746,#1861,.T.);
#24663=EDGE_CURVE('',#20745,#20744,#1862,.T.);
#24664=EDGE_CURVE('',#20747,#20747,#17752,.T.);
#24665=EDGE_CURVE('',#20747,#20748,#4367,.T.);
#24666=EDGE_CURVE('',#20748,#20748,#1863,.T.);
#24667=EDGE_CURVE('',#20749,#20750,#1864,.T.);
#24668=EDGE_CURVE('',#20750,#20751,#4368,.T.);
#24669=EDGE_CURVE('',#20751,#20751,#1865,.T.);
#24670=EDGE_CURVE('',#20750,#20749,#1866,.T.);
#24671=EDGE_CURVE('',#20752,#20752,#17753,.T.);
#24672=EDGE_CURVE('',#20752,#20753,#4369,.T.);
#24673=EDGE_CURVE('',#20753,#20753,#1867,.T.);
#24674=EDGE_CURVE('',#20754,#20755,#1868,.T.);
#24675=EDGE_CURVE('',#20755,#20756,#4370,.T.);
#24676=EDGE_CURVE('',#20756,#20756,#1869,.T.);
#24677=EDGE_CURVE('',#20755,#20754,#1870,.T.);
#24678=EDGE_CURVE('',#20757,#20757,#17754,.T.);
#24679=EDGE_CURVE('',#20757,#20758,#4371,.T.);
#24680=EDGE_CURVE('',#20758,#20758,#1871,.T.);
#24681=EDGE_CURVE('',#20759,#20760,#1872,.T.);
#24682=EDGE_CURVE('',#20760,#20761,#4372,.T.);
#24683=EDGE_CURVE('',#20761,#20761,#1873,.T.);
#24684=EDGE_CURVE('',#20760,#20759,#1874,.T.);
#24685=EDGE_CURVE('',#20762,#20762,#17755,.T.);
#24686=EDGE_CURVE('',#20762,#20763,#4373,.T.);
#24687=EDGE_CURVE('',#20763,#20763,#1875,.T.);
#24688=EDGE_CURVE('',#20764,#20765,#1876,.T.);
#24689=EDGE_CURVE('',#20765,#20766,#4374,.T.);
#24690=EDGE_CURVE('',#20766,#20766,#1877,.T.);
#24691=EDGE_CURVE('',#20765,#20764,#1878,.T.);
#24692=EDGE_CURVE('',#20767,#20767,#17756,.T.);
#24693=EDGE_CURVE('',#20767,#20768,#4375,.T.);
#24694=EDGE_CURVE('',#20768,#20768,#1879,.T.);
#24695=EDGE_CURVE('',#20769,#20770,#1880,.T.);
#24696=EDGE_CURVE('',#20770,#20771,#4376,.T.);
#24697=EDGE_CURVE('',#20771,#20771,#1881,.T.);
#24698=EDGE_CURVE('',#20770,#20769,#1882,.T.);
#24699=EDGE_CURVE('',#20772,#20772,#17757,.T.);
#24700=EDGE_CURVE('',#20772,#20773,#4377,.T.);
#24701=EDGE_CURVE('',#20773,#20773,#1883,.T.);
#24702=EDGE_CURVE('',#20774,#20775,#1884,.T.);
#24703=EDGE_CURVE('',#20775,#20776,#4378,.T.);
#24704=EDGE_CURVE('',#20776,#20776,#1885,.T.);
#24705=EDGE_CURVE('',#20775,#20774,#1886,.T.);
#24706=EDGE_CURVE('',#20777,#20777,#17758,.T.);
#24707=EDGE_CURVE('',#20777,#20778,#4379,.T.);
#24708=EDGE_CURVE('',#20778,#20778,#1887,.T.);
#24709=EDGE_CURVE('',#20779,#20780,#1888,.T.);
#24710=EDGE_CURVE('',#20780,#20781,#4380,.T.);
#24711=EDGE_CURVE('',#20781,#20781,#1889,.T.);
#24712=EDGE_CURVE('',#20780,#20779,#1890,.T.);
#24713=EDGE_CURVE('',#20782,#20782,#17759,.T.);
#24714=EDGE_CURVE('',#20782,#20783,#4381,.T.);
#24715=EDGE_CURVE('',#20783,#20783,#1891,.T.);
#24716=EDGE_CURVE('',#20784,#20785,#1892,.T.);
#24717=EDGE_CURVE('',#20785,#20786,#4382,.T.);
#24718=EDGE_CURVE('',#20786,#20786,#1893,.T.);
#24719=EDGE_CURVE('',#20785,#20784,#1894,.T.);
#24720=EDGE_CURVE('',#20787,#20787,#17760,.T.);
#24721=EDGE_CURVE('',#20787,#20788,#4383,.T.);
#24722=EDGE_CURVE('',#20788,#20788,#1895,.T.);
#24723=EDGE_CURVE('',#20789,#20790,#1896,.T.);
#24724=EDGE_CURVE('',#20790,#20791,#4384,.T.);
#24725=EDGE_CURVE('',#20791,#20791,#1897,.T.);
#24726=EDGE_CURVE('',#20790,#20789,#1898,.T.);
#24727=EDGE_CURVE('',#20792,#20792,#17761,.T.);
#24728=EDGE_CURVE('',#20792,#20793,#4385,.T.);
#24729=EDGE_CURVE('',#20793,#20793,#1899,.T.);
#24730=EDGE_CURVE('',#20794,#20795,#1900,.T.);
#24731=EDGE_CURVE('',#20795,#20796,#4386,.T.);
#24732=EDGE_CURVE('',#20796,#20796,#1901,.T.);
#24733=EDGE_CURVE('',#20795,#20794,#1902,.T.);
#24734=EDGE_CURVE('',#20797,#20797,#17762,.T.);
#24735=EDGE_CURVE('',#20797,#20798,#4387,.T.);
#24736=EDGE_CURVE('',#20798,#20798,#1903,.T.);
#24737=EDGE_CURVE('',#20799,#20800,#1904,.T.);
#24738=EDGE_CURVE('',#20800,#20801,#4388,.T.);
#24739=EDGE_CURVE('',#20801,#20801,#1905,.T.);
#24740=EDGE_CURVE('',#20800,#20799,#1906,.T.);
#24741=EDGE_CURVE('',#20802,#20802,#17763,.T.);
#24742=EDGE_CURVE('',#20802,#20803,#4389,.T.);
#24743=EDGE_CURVE('',#20803,#20803,#1907,.T.);
#24744=EDGE_CURVE('',#20804,#20805,#1908,.T.);
#24745=EDGE_CURVE('',#20805,#20806,#4390,.T.);
#24746=EDGE_CURVE('',#20806,#20806,#1909,.T.);
#24747=EDGE_CURVE('',#20805,#20804,#1910,.T.);
#24748=EDGE_CURVE('',#20807,#20807,#17764,.T.);
#24749=EDGE_CURVE('',#20807,#20808,#4391,.T.);
#24750=EDGE_CURVE('',#20808,#20808,#1911,.T.);
#24751=EDGE_CURVE('',#20809,#20810,#1912,.T.);
#24752=EDGE_CURVE('',#20810,#20811,#4392,.T.);
#24753=EDGE_CURVE('',#20811,#20811,#1913,.T.);
#24754=EDGE_CURVE('',#20810,#20809,#1914,.T.);
#24755=EDGE_CURVE('',#20812,#20812,#17765,.T.);
#24756=EDGE_CURVE('',#20812,#20813,#4393,.T.);
#24757=EDGE_CURVE('',#20813,#20813,#1915,.T.);
#24758=EDGE_CURVE('',#20814,#20815,#1916,.T.);
#24759=EDGE_CURVE('',#20815,#20816,#4394,.T.);
#24760=EDGE_CURVE('',#20816,#20816,#1917,.T.);
#24761=EDGE_CURVE('',#20815,#20814,#1918,.T.);
#24762=EDGE_CURVE('',#20817,#20817,#17766,.T.);
#24763=EDGE_CURVE('',#20817,#20818,#4395,.T.);
#24764=EDGE_CURVE('',#20818,#20818,#1919,.T.);
#24765=EDGE_CURVE('',#20819,#20820,#1920,.T.);
#24766=EDGE_CURVE('',#20820,#20821,#4396,.T.);
#24767=EDGE_CURVE('',#20821,#20821,#1921,.T.);
#24768=EDGE_CURVE('',#20820,#20819,#1922,.T.);
#24769=EDGE_CURVE('',#20822,#20822,#17767,.T.);
#24770=EDGE_CURVE('',#20822,#20823,#4397,.T.);
#24771=EDGE_CURVE('',#20823,#20823,#1923,.T.);
#24772=EDGE_CURVE('',#20824,#20825,#1924,.T.);
#24773=EDGE_CURVE('',#20825,#20826,#4398,.T.);
#24774=EDGE_CURVE('',#20826,#20826,#1925,.T.);
#24775=EDGE_CURVE('',#20825,#20824,#1926,.T.);
#24776=EDGE_CURVE('',#20827,#20827,#17768,.T.);
#24777=EDGE_CURVE('',#20827,#20828,#4399,.T.);
#24778=EDGE_CURVE('',#20828,#20828,#1927,.T.);
#24779=EDGE_CURVE('',#20829,#20830,#1928,.T.);
#24780=EDGE_CURVE('',#20830,#20831,#4400,.T.);
#24781=EDGE_CURVE('',#20831,#20831,#1929,.T.);
#24782=EDGE_CURVE('',#20830,#20829,#1930,.T.);
#24783=EDGE_CURVE('',#20832,#20832,#17769,.T.);
#24784=EDGE_CURVE('',#20832,#20833,#4401,.T.);
#24785=EDGE_CURVE('',#20833,#20833,#1931,.T.);
#24786=EDGE_CURVE('',#20834,#20835,#1932,.T.);
#24787=EDGE_CURVE('',#20835,#20836,#4402,.T.);
#24788=EDGE_CURVE('',#20836,#20836,#1933,.T.);
#24789=EDGE_CURVE('',#20835,#20834,#1934,.T.);
#24790=EDGE_CURVE('',#20837,#20837,#17770,.T.);
#24791=EDGE_CURVE('',#20837,#20838,#4403,.T.);
#24792=EDGE_CURVE('',#20838,#20838,#1935,.T.);
#24793=EDGE_CURVE('',#20839,#20840,#1936,.T.);
#24794=EDGE_CURVE('',#20840,#20841,#4404,.T.);
#24795=EDGE_CURVE('',#20841,#20841,#1937,.T.);
#24796=EDGE_CURVE('',#20840,#20839,#1938,.T.);
#24797=EDGE_CURVE('',#20842,#20842,#17771,.T.);
#24798=EDGE_CURVE('',#20842,#20843,#4405,.T.);
#24799=EDGE_CURVE('',#20843,#20843,#1939,.T.);
#24800=EDGE_CURVE('',#20844,#20845,#1940,.T.);
#24801=EDGE_CURVE('',#20845,#20846,#4406,.T.);
#24802=EDGE_CURVE('',#20846,#20846,#1941,.T.);
#24803=EDGE_CURVE('',#20845,#20844,#1942,.T.);
#24804=EDGE_CURVE('',#20847,#20847,#17772,.T.);
#24805=EDGE_CURVE('',#20847,#20848,#4407,.T.);
#24806=EDGE_CURVE('',#20848,#20848,#1943,.T.);
#24807=EDGE_CURVE('',#20849,#20850,#1944,.T.);
#24808=EDGE_CURVE('',#20850,#20851,#4408,.T.);
#24809=EDGE_CURVE('',#20851,#20851,#1945,.T.);
#24810=EDGE_CURVE('',#20850,#20849,#1946,.T.);
#24811=EDGE_CURVE('',#20852,#20852,#17773,.T.);
#24812=EDGE_CURVE('',#20852,#20853,#4409,.T.);
#24813=EDGE_CURVE('',#20853,#20853,#1947,.T.);
#24814=EDGE_CURVE('',#20854,#20855,#1948,.T.);
#24815=EDGE_CURVE('',#20855,#20856,#4410,.T.);
#24816=EDGE_CURVE('',#20856,#20856,#1949,.T.);
#24817=EDGE_CURVE('',#20855,#20854,#1950,.T.);
#24818=EDGE_CURVE('',#20857,#20857,#17774,.T.);
#24819=EDGE_CURVE('',#20857,#20858,#4411,.T.);
#24820=EDGE_CURVE('',#20858,#20858,#1951,.T.);
#24821=EDGE_CURVE('',#20859,#20860,#1952,.T.);
#24822=EDGE_CURVE('',#20860,#20861,#4412,.T.);
#24823=EDGE_CURVE('',#20861,#20861,#1953,.T.);
#24824=EDGE_CURVE('',#20860,#20859,#1954,.T.);
#24825=EDGE_CURVE('',#20862,#20862,#17775,.T.);
#24826=EDGE_CURVE('',#20862,#20863,#4413,.T.);
#24827=EDGE_CURVE('',#20863,#20863,#1955,.T.);
#24828=EDGE_CURVE('',#20864,#20865,#1956,.T.);
#24829=EDGE_CURVE('',#20865,#20866,#4414,.T.);
#24830=EDGE_CURVE('',#20866,#20866,#1957,.T.);
#24831=EDGE_CURVE('',#20865,#20864,#1958,.T.);
#24832=EDGE_CURVE('',#20867,#20867,#17776,.T.);
#24833=EDGE_CURVE('',#20867,#20868,#4415,.T.);
#24834=EDGE_CURVE('',#20868,#20868,#1959,.T.);
#24835=EDGE_CURVE('',#20869,#20870,#1960,.T.);
#24836=EDGE_CURVE('',#20870,#20871,#4416,.T.);
#24837=EDGE_CURVE('',#20871,#20871,#1961,.T.);
#24838=EDGE_CURVE('',#20870,#20869,#1962,.T.);
#24839=EDGE_CURVE('',#20872,#20872,#17777,.T.);
#24840=EDGE_CURVE('',#20872,#20873,#4417,.T.);
#24841=EDGE_CURVE('',#20873,#20873,#1963,.T.);
#24842=EDGE_CURVE('',#20874,#20874,#17778,.T.);
#24843=EDGE_CURVE('',#20874,#20875,#4418,.T.);
#24844=EDGE_CURVE('',#20875,#20875,#1964,.T.);
#24845=EDGE_CURVE('',#20876,#20876,#17779,.T.);
#24846=EDGE_CURVE('',#20876,#20877,#4419,.T.);
#24847=EDGE_CURVE('',#20877,#20877,#17780,.T.);
#24848=EDGE_CURVE('',#20878,#20878,#17781,.T.);
#24849=EDGE_CURVE('',#20878,#20879,#4420,.T.);
#24850=EDGE_CURVE('',#20879,#20879,#1965,.T.);
#24851=EDGE_CURVE('',#20880,#20880,#17782,.T.);
#24852=EDGE_CURVE('',#20880,#20881,#4421,.T.);
#24853=EDGE_CURVE('',#20881,#20881,#17783,.T.);
#24854=EDGE_CURVE('',#20882,#20883,#1966,.T.);
#24855=EDGE_CURVE('',#20883,#20884,#4422,.T.);
#24856=EDGE_CURVE('',#20884,#20884,#1967,.T.);
#24857=EDGE_CURVE('',#20883,#20882,#1968,.T.);
#24858=EDGE_CURVE('',#20885,#20885,#17784,.T.);
#24859=EDGE_CURVE('',#20885,#20886,#4423,.T.);
#24860=EDGE_CURVE('',#20886,#20886,#1969,.T.);
#24861=EDGE_CURVE('',#20887,#20888,#1970,.T.);
#24862=EDGE_CURVE('',#20888,#20889,#4424,.T.);
#24863=EDGE_CURVE('',#20889,#20889,#1971,.T.);
#24864=EDGE_CURVE('',#20888,#20887,#1972,.T.);
#24865=EDGE_CURVE('',#20890,#20890,#17785,.T.);
#24866=EDGE_CURVE('',#20890,#20891,#4425,.T.);
#24867=EDGE_CURVE('',#20891,#20891,#1973,.T.);
#24868=EDGE_CURVE('',#20892,#20892,#17786,.T.);
#24869=EDGE_CURVE('',#20892,#20893,#4426,.T.);
#24870=EDGE_CURVE('',#20893,#20893,#1974,.T.);
#24871=EDGE_CURVE('',#20894,#20894,#17787,.T.);
#24872=EDGE_CURVE('',#20894,#20895,#4427,.T.);
#24873=EDGE_CURVE('',#20895,#20895,#17788,.T.);
#24874=EDGE_CURVE('',#20896,#20896,#17789,.T.);
#24875=EDGE_CURVE('',#20896,#20897,#4428,.T.);
#24876=EDGE_CURVE('',#20897,#20897,#1975,.T.);
#24877=EDGE_CURVE('',#20898,#20898,#17790,.T.);
#24878=EDGE_CURVE('',#20898,#20899,#4429,.T.);
#24879=EDGE_CURVE('',#20899,#20899,#17791,.T.);
#24880=EDGE_CURVE('',#20900,#20901,#1976,.T.);
#24881=EDGE_CURVE('',#20901,#20902,#4430,.T.);
#24882=EDGE_CURVE('',#20902,#20902,#1977,.T.);
#24883=EDGE_CURVE('',#20901,#20900,#1978,.T.);
#24884=EDGE_CURVE('',#20903,#20903,#17792,.T.);
#24885=EDGE_CURVE('',#20903,#20904,#4431,.T.);
#24886=EDGE_CURVE('',#20904,#20904,#1979,.T.);
#24887=EDGE_CURVE('',#20905,#20906,#1980,.T.);
#24888=EDGE_CURVE('',#20906,#20907,#4432,.T.);
#24889=EDGE_CURVE('',#20907,#20907,#1981,.T.);
#24890=EDGE_CURVE('',#20906,#20905,#1982,.T.);
#24891=EDGE_CURVE('',#20908,#20908,#17793,.T.);
#24892=EDGE_CURVE('',#20908,#20909,#4433,.T.);
#24893=EDGE_CURVE('',#20909,#20909,#1983,.T.);
#24894=EDGE_CURVE('',#20910,#20910,#17794,.T.);
#24895=EDGE_CURVE('',#20910,#20911,#4434,.T.);
#24896=EDGE_CURVE('',#20911,#20911,#1984,.T.);
#24897=EDGE_CURVE('',#20912,#20912,#17795,.T.);
#24898=EDGE_CURVE('',#20912,#20913,#4435,.T.);
#24899=EDGE_CURVE('',#20913,#20913,#17796,.T.);
#24900=EDGE_CURVE('',#20914,#20915,#1985,.T.);
#24901=EDGE_CURVE('',#20915,#20916,#4436,.T.);
#24902=EDGE_CURVE('',#20916,#20916,#1986,.T.);
#24903=EDGE_CURVE('',#20915,#20914,#1987,.T.);
#24904=EDGE_CURVE('',#20917,#20917,#17797,.T.);
#24905=EDGE_CURVE('',#20917,#20918,#4437,.T.);
#24906=EDGE_CURVE('',#20918,#20918,#1988,.T.);
#24907=EDGE_CURVE('',#20919,#20920,#1989,.T.);
#24908=EDGE_CURVE('',#20920,#20921,#4438,.T.);
#24909=EDGE_CURVE('',#20921,#20921,#1990,.T.);
#24910=EDGE_CURVE('',#20920,#20919,#1991,.T.);
#24911=EDGE_CURVE('',#20922,#20922,#17798,.T.);
#24912=EDGE_CURVE('',#20922,#20923,#4439,.T.);
#24913=EDGE_CURVE('',#20923,#20923,#1992,.T.);
#24914=EDGE_CURVE('',#20924,#20924,#17799,.T.);
#24915=EDGE_CURVE('',#20924,#20925,#4440,.T.);
#24916=EDGE_CURVE('',#20925,#20925,#1993,.T.);
#24917=EDGE_CURVE('',#20926,#20926,#17800,.T.);
#24918=EDGE_CURVE('',#20926,#20927,#4441,.T.);
#24919=EDGE_CURVE('',#20927,#20927,#17801,.T.);
#24920=EDGE_CURVE('',#20928,#20929,#1994,.T.);
#24921=EDGE_CURVE('',#20929,#20930,#4442,.T.);
#24922=EDGE_CURVE('',#20930,#20930,#1995,.T.);
#24923=EDGE_CURVE('',#20929,#20928,#1996,.T.);
#24924=EDGE_CURVE('',#20931,#20931,#17802,.T.);
#24925=EDGE_CURVE('',#20931,#20932,#4443,.T.);
#24926=EDGE_CURVE('',#20932,#20932,#1997,.T.);
#24927=EDGE_CURVE('',#20933,#20934,#1998,.T.);
#24928=EDGE_CURVE('',#20934,#20935,#4444,.T.);
#24929=EDGE_CURVE('',#20935,#20935,#1999,.T.);
#24930=EDGE_CURVE('',#20934,#20933,#2000,.T.);
#24931=EDGE_CURVE('',#20936,#20936,#17803,.T.);
#24932=EDGE_CURVE('',#20936,#20937,#4445,.T.);
#24933=EDGE_CURVE('',#20937,#20937,#2001,.T.);
#24934=EDGE_CURVE('',#20938,#20939,#2002,.T.);
#24935=EDGE_CURVE('',#20939,#20940,#4446,.T.);
#24936=EDGE_CURVE('',#20940,#20940,#2003,.T.);
#24937=EDGE_CURVE('',#20939,#20938,#2004,.T.);
#24938=EDGE_CURVE('',#20941,#20941,#17804,.T.);
#24939=EDGE_CURVE('',#20941,#20942,#4447,.T.);
#24940=EDGE_CURVE('',#20942,#20942,#2005,.T.);
#24941=EDGE_CURVE('',#20943,#20944,#2006,.T.);
#24942=EDGE_CURVE('',#20944,#20945,#4448,.T.);
#24943=EDGE_CURVE('',#20945,#20945,#2007,.T.);
#24944=EDGE_CURVE('',#20944,#20943,#2008,.T.);
#24945=EDGE_CURVE('',#20946,#20946,#17805,.T.);
#24946=EDGE_CURVE('',#20946,#20947,#4449,.T.);
#24947=EDGE_CURVE('',#20947,#20947,#2009,.T.);
#24948=EDGE_CURVE('',#20948,#20949,#2010,.T.);
#24949=EDGE_CURVE('',#20949,#20950,#4450,.T.);
#24950=EDGE_CURVE('',#20950,#20950,#2011,.T.);
#24951=EDGE_CURVE('',#20949,#20948,#2012,.T.);
#24952=EDGE_CURVE('',#20951,#20951,#17806,.T.);
#24953=EDGE_CURVE('',#20951,#20952,#4451,.T.);
#24954=EDGE_CURVE('',#20952,#20952,#2013,.T.);
#24955=EDGE_CURVE('',#20953,#20954,#2014,.T.);
#24956=EDGE_CURVE('',#20954,#20955,#4452,.T.);
#24957=EDGE_CURVE('',#20955,#20955,#2015,.T.);
#24958=EDGE_CURVE('',#20954,#20953,#2016,.T.);
#24959=EDGE_CURVE('',#20956,#20956,#17807,.T.);
#24960=EDGE_CURVE('',#20956,#20957,#4453,.T.);
#24961=EDGE_CURVE('',#20957,#20957,#2017,.T.);
#24962=EDGE_CURVE('',#20958,#20959,#2018,.T.);
#24963=EDGE_CURVE('',#20959,#20960,#4454,.T.);
#24964=EDGE_CURVE('',#20960,#20960,#2019,.T.);
#24965=EDGE_CURVE('',#20959,#20958,#2020,.T.);
#24966=EDGE_CURVE('',#20961,#20961,#17808,.T.);
#24967=EDGE_CURVE('',#20961,#20962,#4455,.T.);
#24968=EDGE_CURVE('',#20962,#20962,#2021,.T.);
#24969=EDGE_CURVE('',#20963,#20964,#2022,.T.);
#24970=EDGE_CURVE('',#20964,#20965,#4456,.T.);
#24971=EDGE_CURVE('',#20965,#20965,#2023,.T.);
#24972=EDGE_CURVE('',#20964,#20963,#2024,.T.);
#24973=EDGE_CURVE('',#20966,#20966,#17809,.T.);
#24974=EDGE_CURVE('',#20966,#20967,#4457,.T.);
#24975=EDGE_CURVE('',#20967,#20967,#2025,.T.);
#24976=EDGE_CURVE('',#20968,#20969,#2026,.T.);
#24977=EDGE_CURVE('',#20969,#20970,#4458,.T.);
#24978=EDGE_CURVE('',#20970,#20970,#2027,.T.);
#24979=EDGE_CURVE('',#20969,#20968,#2028,.T.);
#24980=EDGE_CURVE('',#20971,#20971,#17810,.T.);
#24981=EDGE_CURVE('',#20971,#20972,#4459,.T.);
#24982=EDGE_CURVE('',#20972,#20972,#2029,.T.);
#24983=EDGE_CURVE('',#20973,#20974,#2030,.T.);
#24984=EDGE_CURVE('',#20974,#20975,#4460,.T.);
#24985=EDGE_CURVE('',#20975,#20975,#2031,.T.);
#24986=EDGE_CURVE('',#20974,#20973,#2032,.T.);
#24987=EDGE_CURVE('',#20976,#20976,#17811,.T.);
#24988=EDGE_CURVE('',#20976,#20977,#4461,.T.);
#24989=EDGE_CURVE('',#20977,#20977,#2033,.T.);
#24990=EDGE_CURVE('',#20978,#20979,#2034,.T.);
#24991=EDGE_CURVE('',#20979,#20980,#4462,.T.);
#24992=EDGE_CURVE('',#20980,#20980,#2035,.T.);
#24993=EDGE_CURVE('',#20979,#20978,#2036,.T.);
#24994=EDGE_CURVE('',#20981,#20981,#17812,.T.);
#24995=EDGE_CURVE('',#20981,#20982,#4463,.T.);
#24996=EDGE_CURVE('',#20982,#20982,#2037,.T.);
#24997=EDGE_CURVE('',#20983,#20984,#2038,.T.);
#24998=EDGE_CURVE('',#20984,#20985,#4464,.T.);
#24999=EDGE_CURVE('',#20985,#20985,#2039,.T.);
#25000=EDGE_CURVE('',#20984,#20983,#2040,.T.);
#25001=EDGE_CURVE('',#20986,#20986,#17813,.T.);
#25002=EDGE_CURVE('',#20986,#20987,#4465,.T.);
#25003=EDGE_CURVE('',#20987,#20987,#2041,.T.);
#25004=EDGE_CURVE('',#20988,#20989,#2042,.T.);
#25005=EDGE_CURVE('',#20989,#20990,#4466,.T.);
#25006=EDGE_CURVE('',#20990,#20990,#2043,.T.);
#25007=EDGE_CURVE('',#20989,#20988,#2044,.T.);
#25008=EDGE_CURVE('',#20991,#20991,#17814,.T.);
#25009=EDGE_CURVE('',#20991,#20992,#4467,.T.);
#25010=EDGE_CURVE('',#20992,#20992,#2045,.T.);
#25011=EDGE_CURVE('',#20993,#20994,#2046,.T.);
#25012=EDGE_CURVE('',#20994,#20995,#4468,.T.);
#25013=EDGE_CURVE('',#20995,#20995,#2047,.T.);
#25014=EDGE_CURVE('',#20994,#20993,#2048,.T.);
#25015=EDGE_CURVE('',#20996,#20996,#17815,.T.);
#25016=EDGE_CURVE('',#20996,#20997,#4469,.T.);
#25017=EDGE_CURVE('',#20997,#20997,#2049,.T.);
#25018=EDGE_CURVE('',#20998,#20998,#17816,.T.);
#25019=EDGE_CURVE('',#20998,#20999,#4470,.T.);
#25020=EDGE_CURVE('',#20999,#20999,#17817,.T.);
#25021=EDGE_CURVE('',#21000,#21000,#17818,.T.);
#25022=EDGE_CURVE('',#21000,#21001,#4471,.T.);
#25023=EDGE_CURVE('',#21001,#21001,#17819,.T.);
#25024=EDGE_CURVE('',#21002,#21002,#17820,.T.);
#25025=EDGE_CURVE('',#21002,#21003,#4472,.T.);
#25026=EDGE_CURVE('',#21003,#21003,#17821,.T.);
#25027=EDGE_CURVE('',#21004,#21004,#17822,.T.);
#25028=EDGE_CURVE('',#21004,#21005,#4473,.T.);
#25029=EDGE_CURVE('',#21005,#21005,#17823,.T.);
#25030=EDGE_CURVE('',#21006,#21006,#17824,.T.);
#25031=EDGE_CURVE('',#21006,#21007,#4474,.T.);
#25032=EDGE_CURVE('',#21007,#21007,#17825,.T.);
#25033=EDGE_CURVE('',#21008,#21008,#17826,.T.);
#25034=EDGE_CURVE('',#21008,#21009,#4475,.T.);
#25035=EDGE_CURVE('',#21009,#21009,#17827,.T.);
#25036=EDGE_CURVE('',#21010,#21010,#17828,.T.);
#25037=EDGE_CURVE('',#21010,#21011,#4476,.T.);
#25038=EDGE_CURVE('',#21011,#21011,#17829,.T.);
#25039=EDGE_CURVE('',#21012,#21012,#17830,.T.);
#25040=EDGE_CURVE('',#21012,#21013,#4477,.T.);
#25041=EDGE_CURVE('',#21013,#21013,#17831,.T.);
#25042=EDGE_CURVE('',#21014,#21014,#17832,.T.);
#25043=EDGE_CURVE('',#21014,#21015,#4478,.T.);
#25044=EDGE_CURVE('',#21015,#21015,#17833,.T.);
#25045=EDGE_CURVE('',#21016,#21016,#17834,.T.);
#25046=EDGE_CURVE('',#21016,#21017,#4479,.T.);
#25047=EDGE_CURVE('',#21017,#21017,#17835,.T.);
#25048=EDGE_CURVE('',#21018,#21018,#17836,.T.);
#25049=EDGE_CURVE('',#21018,#21019,#4480,.T.);
#25050=EDGE_CURVE('',#21019,#21019,#17837,.T.);
#25051=EDGE_CURVE('',#21020,#21020,#17838,.T.);
#25052=EDGE_CURVE('',#21020,#21021,#4481,.T.);
#25053=EDGE_CURVE('',#21021,#21021,#17839,.T.);
#25054=EDGE_CURVE('',#21022,#21022,#17840,.T.);
#25055=EDGE_CURVE('',#21022,#21023,#4482,.T.);
#25056=EDGE_CURVE('',#21023,#21023,#17841,.T.);
#25057=EDGE_CURVE('',#21024,#21024,#17842,.T.);
#25058=EDGE_CURVE('',#21024,#21025,#4483,.T.);
#25059=EDGE_CURVE('',#21025,#21025,#17843,.T.);
#25060=EDGE_CURVE('',#21026,#21026,#17844,.T.);
#25061=EDGE_CURVE('',#21026,#21027,#4484,.T.);
#25062=EDGE_CURVE('',#21027,#21027,#17845,.T.);
#25063=EDGE_CURVE('',#21028,#21028,#17846,.T.);
#25064=EDGE_CURVE('',#21028,#21029,#4485,.T.);
#25065=EDGE_CURVE('',#21029,#21029,#17847,.T.);
#25066=EDGE_CURVE('',#21030,#21030,#17848,.T.);
#25067=EDGE_CURVE('',#21030,#21031,#4486,.T.);
#25068=EDGE_CURVE('',#21032,#21031,#2050,.F.);
#25069=EDGE_CURVE('',#21032,#21033,#17849,.T.);
#25070=EDGE_CURVE('',#21031,#21033,#2051,.F.);
#25071=EDGE_CURVE('',#21034,#21034,#17850,.T.);
#25072=EDGE_CURVE('',#21034,#21035,#4487,.T.);
#25073=EDGE_CURVE('',#21035,#21035,#17851,.T.);
#25074=EDGE_CURVE('',#21036,#21036,#17852,.T.);
#25075=EDGE_CURVE('',#21036,#21037,#4488,.T.);
#25076=EDGE_CURVE('',#21037,#21037,#17853,.T.);
#25077=EDGE_CURVE('',#21038,#21038,#17854,.T.);
#25078=EDGE_CURVE('',#21038,#21039,#4489,.T.);
#25079=EDGE_CURVE('',#21039,#21039,#17855,.T.);
#25080=EDGE_CURVE('',#21040,#21040,#17856,.T.);
#25081=EDGE_CURVE('',#21040,#21041,#4490,.T.);
#25082=EDGE_CURVE('',#21041,#21041,#17857,.T.);
#25083=EDGE_CURVE('',#21042,#21042,#17858,.T.);
#25084=EDGE_CURVE('',#21042,#21043,#4491,.T.);
#25085=EDGE_CURVE('',#21043,#21043,#17859,.T.);
#25086=EDGE_CURVE('',#21044,#21044,#17860,.T.);
#25087=EDGE_CURVE('',#21044,#21045,#4492,.T.);
#25088=EDGE_CURVE('',#21045,#21045,#17861,.T.);
#25089=EDGE_CURVE('',#21046,#21046,#17862,.T.);
#25090=EDGE_CURVE('',#21046,#21047,#4493,.T.);
#25091=EDGE_CURVE('',#21047,#21047,#17863,.T.);
#25092=EDGE_CURVE('',#21048,#21048,#17864,.T.);
#25093=EDGE_CURVE('',#21048,#21049,#4494,.T.);
#25094=EDGE_CURVE('',#21049,#21049,#17865,.T.);
#25095=EDGE_CURVE('',#21050,#21050,#17866,.T.);
#25096=EDGE_CURVE('',#21050,#21051,#4495,.T.);
#25097=EDGE_CURVE('',#21051,#21051,#17867,.T.);
#25098=EDGE_CURVE('',#21052,#21052,#17868,.T.);
#25099=EDGE_CURVE('',#21052,#21053,#4496,.T.);
#25100=EDGE_CURVE('',#21053,#21053,#17869,.T.);
#25101=EDGE_CURVE('',#21054,#21054,#17870,.T.);
#25102=EDGE_CURVE('',#21054,#21055,#4497,.T.);
#25103=EDGE_CURVE('',#21055,#21055,#17871,.T.);
#25104=EDGE_CURVE('',#21056,#21056,#17872,.T.);
#25105=EDGE_CURVE('',#21056,#21057,#4498,.T.);
#25106=EDGE_CURVE('',#21057,#21057,#17873,.T.);
#25107=EDGE_CURVE('',#21058,#21058,#17874,.T.);
#25108=EDGE_CURVE('',#21058,#21059,#4499,.T.);
#25109=EDGE_CURVE('',#21059,#21059,#17875,.T.);
#25110=EDGE_CURVE('',#21060,#21060,#17876,.T.);
#25111=EDGE_CURVE('',#21060,#21061,#4500,.T.);
#25112=EDGE_CURVE('',#21061,#21061,#17877,.T.);
#25113=EDGE_CURVE('',#21062,#21062,#17878,.T.);
#25114=EDGE_CURVE('',#21062,#21063,#4501,.T.);
#25115=EDGE_CURVE('',#21063,#21063,#17879,.T.);
#25116=EDGE_CURVE('',#21064,#21064,#17880,.T.);
#25117=EDGE_CURVE('',#21064,#21065,#4502,.T.);
#25118=EDGE_CURVE('',#21065,#21065,#17881,.T.);
#25119=EDGE_CURVE('',#21066,#21066,#17882,.T.);
#25120=EDGE_CURVE('',#21066,#21067,#4503,.T.);
#25121=EDGE_CURVE('',#21067,#21067,#17883,.T.);
#25122=EDGE_CURVE('',#21068,#21068,#17884,.T.);
#25123=EDGE_CURVE('',#21068,#21069,#4504,.T.);
#25124=EDGE_CURVE('',#21070,#21069,#2052,.F.);
#25125=EDGE_CURVE('',#21070,#21071,#17885,.T.);
#25126=EDGE_CURVE('',#21069,#21071,#2053,.F.);
#25127=EDGE_CURVE('',#21072,#21072,#17886,.T.);
#25128=EDGE_CURVE('',#21072,#21073,#4505,.T.);
#25129=EDGE_CURVE('',#21073,#21073,#17887,.T.);
#25130=EDGE_CURVE('',#21074,#21074,#17888,.T.);
#25131=EDGE_CURVE('',#21074,#21075,#4506,.T.);
#25132=EDGE_CURVE('',#21075,#21075,#17889,.T.);
#25133=EDGE_CURVE('',#21076,#21076,#17890,.T.);
#25134=EDGE_CURVE('',#21076,#21077,#4507,.T.);
#25135=EDGE_CURVE('',#21077,#21077,#17891,.T.);
#25136=EDGE_CURVE('',#21078,#21078,#17892,.T.);
#25137=EDGE_CURVE('',#21078,#21079,#4508,.T.);
#25138=EDGE_CURVE('',#21079,#21079,#17893,.T.);
#25139=EDGE_CURVE('',#21080,#21080,#17894,.T.);
#25140=EDGE_CURVE('',#21080,#21081,#4509,.T.);
#25141=EDGE_CURVE('',#21081,#21081,#17895,.T.);
#25142=EDGE_CURVE('',#21082,#21082,#17896,.T.);
#25143=EDGE_CURVE('',#21082,#21083,#4510,.T.);
#25144=EDGE_CURVE('',#21083,#21083,#17897,.T.);
#25145=EDGE_CURVE('',#21084,#21084,#17898,.T.);
#25146=EDGE_CURVE('',#21084,#21085,#4511,.T.);
#25147=EDGE_CURVE('',#21085,#21085,#17899,.T.);
#25148=EDGE_CURVE('',#21086,#21086,#17900,.T.);
#25149=EDGE_CURVE('',#21086,#21087,#4512,.T.);
#25150=EDGE_CURVE('',#21087,#21087,#17901,.T.);
#25151=EDGE_CURVE('',#21088,#21088,#17902,.T.);
#25152=EDGE_CURVE('',#21088,#21089,#4513,.T.);
#25153=EDGE_CURVE('',#21089,#21089,#17903,.T.);
#25154=EDGE_CURVE('',#21090,#21090,#17904,.T.);
#25155=EDGE_CURVE('',#21090,#21091,#4514,.T.);
#25156=EDGE_CURVE('',#21091,#21091,#17905,.T.);
#25157=EDGE_CURVE('',#21092,#21092,#17906,.T.);
#25158=EDGE_CURVE('',#21092,#21093,#4515,.T.);
#25159=EDGE_CURVE('',#21093,#21093,#17907,.T.);
#25160=EDGE_CURVE('',#21094,#21094,#17908,.T.);
#25161=EDGE_CURVE('',#21094,#21095,#4516,.T.);
#25162=EDGE_CURVE('',#21095,#21095,#17909,.T.);
#25163=EDGE_CURVE('',#21096,#21096,#17910,.T.);
#25164=EDGE_CURVE('',#21096,#21097,#4517,.T.);
#25165=EDGE_CURVE('',#21097,#21097,#17911,.T.);
#25166=EDGE_CURVE('',#21098,#21098,#17912,.T.);
#25167=EDGE_CURVE('',#21098,#21099,#4518,.T.);
#25168=EDGE_CURVE('',#21099,#21099,#17913,.T.);
#25169=EDGE_CURVE('',#21100,#21100,#17914,.T.);
#25170=EDGE_CURVE('',#21100,#21101,#4519,.T.);
#25171=EDGE_CURVE('',#21101,#21101,#17915,.T.);
#25172=EDGE_CURVE('',#21102,#21102,#17916,.T.);
#25173=EDGE_CURVE('',#21102,#21103,#4520,.T.);
#25174=EDGE_CURVE('',#21104,#21103,#2054,.F.);
#25175=EDGE_CURVE('',#21104,#21105,#17917,.T.);
#25176=EDGE_CURVE('',#21103,#21105,#2055,.F.);
#25177=EDGE_CURVE('',#21106,#21106,#17918,.T.);
#25178=EDGE_CURVE('',#21106,#21107,#4521,.T.);
#25179=EDGE_CURVE('',#21107,#21107,#17919,.T.);
#25180=EDGE_CURVE('',#21108,#21108,#17920,.T.);
#25181=EDGE_CURVE('',#21108,#21109,#4522,.T.);
#25182=EDGE_CURVE('',#21109,#21109,#17921,.T.);
#25183=EDGE_CURVE('',#21110,#21110,#17922,.T.);
#25184=EDGE_CURVE('',#21110,#21111,#4523,.T.);
#25185=EDGE_CURVE('',#21111,#21111,#17923,.T.);
#25186=EDGE_CURVE('',#21112,#21112,#17924,.T.);
#25187=EDGE_CURVE('',#21112,#21113,#4524,.T.);
#25188=EDGE_CURVE('',#21113,#21113,#17925,.T.);
#25189=EDGE_CURVE('',#21114,#21114,#17926,.T.);
#25190=EDGE_CURVE('',#21114,#21115,#4525,.T.);
#25191=EDGE_CURVE('',#21115,#21115,#17927,.T.);
#25192=EDGE_CURVE('',#21116,#21116,#17928,.T.);
#25193=EDGE_CURVE('',#21116,#21117,#4526,.T.);
#25194=EDGE_CURVE('',#21117,#21117,#17929,.T.);
#25195=EDGE_CURVE('',#21118,#21118,#17930,.T.);
#25196=EDGE_CURVE('',#21118,#21119,#4527,.T.);
#25197=EDGE_CURVE('',#21119,#21119,#17931,.T.);
#25198=EDGE_CURVE('',#21120,#21120,#17932,.T.);
#25199=EDGE_CURVE('',#21120,#21121,#4528,.T.);
#25200=EDGE_CURVE('',#21121,#21121,#17933,.T.);
#25201=EDGE_CURVE('',#21122,#21122,#17934,.T.);
#25202=EDGE_CURVE('',#21122,#21123,#4529,.T.);
#25203=EDGE_CURVE('',#21123,#21123,#17935,.T.);
#25204=EDGE_CURVE('',#21124,#21124,#17936,.T.);
#25205=EDGE_CURVE('',#21124,#21125,#4530,.T.);
#25206=EDGE_CURVE('',#21125,#21125,#17937,.T.);
#25207=EDGE_CURVE('',#21126,#21126,#17938,.T.);
#25208=EDGE_CURVE('',#21126,#21127,#4531,.T.);
#25209=EDGE_CURVE('',#21127,#21127,#17939,.T.);
#25210=EDGE_CURVE('',#21128,#21128,#17940,.T.);
#25211=EDGE_CURVE('',#21128,#21129,#4532,.T.);
#25212=EDGE_CURVE('',#21129,#21129,#17941,.T.);
#25213=EDGE_CURVE('',#21130,#21130,#17942,.T.);
#25214=EDGE_CURVE('',#21130,#21131,#4533,.T.);
#25215=EDGE_CURVE('',#21131,#21131,#17943,.T.);
#25216=EDGE_CURVE('',#21132,#21132,#17944,.T.);
#25217=EDGE_CURVE('',#21132,#21133,#4534,.T.);
#25218=EDGE_CURVE('',#21133,#21133,#17945,.T.);
#25219=EDGE_CURVE('',#21134,#21134,#17946,.T.);
#25220=EDGE_CURVE('',#21134,#21135,#4535,.T.);
#25221=EDGE_CURVE('',#21135,#21135,#17947,.T.);
#25222=EDGE_CURVE('',#21136,#21136,#17948,.T.);
#25223=EDGE_CURVE('',#21136,#21137,#4536,.T.);
#25224=EDGE_CURVE('',#21137,#21137,#17949,.T.);
#25225=EDGE_CURVE('',#21138,#21138,#17950,.T.);
#25226=EDGE_CURVE('',#21138,#21139,#4537,.T.);
#25227=EDGE_CURVE('',#21139,#21139,#17951,.T.);
#25228=EDGE_CURVE('',#21140,#21140,#17952,.T.);
#25229=EDGE_CURVE('',#21140,#21141,#4538,.T.);
#25230=EDGE_CURVE('',#21142,#21141,#2056,.F.);
#25231=EDGE_CURVE('',#21142,#21143,#17953,.T.);
#25232=EDGE_CURVE('',#21141,#21143,#2057,.F.);
#25233=EDGE_CURVE('',#21144,#21144,#17954,.T.);
#25234=EDGE_CURVE('',#21144,#21145,#4539,.T.);
#25235=EDGE_CURVE('',#21145,#21145,#17955,.T.);
#25236=EDGE_CURVE('',#21146,#21146,#17956,.T.);
#25237=EDGE_CURVE('',#21146,#21147,#4540,.T.);
#25238=EDGE_CURVE('',#21147,#21147,#17957,.T.);
#25239=EDGE_CURVE('',#21148,#21148,#17958,.T.);
#25240=EDGE_CURVE('',#21148,#21149,#4541,.T.);
#25241=EDGE_CURVE('',#21149,#21149,#17959,.T.);
#25242=EDGE_CURVE('',#21150,#21150,#17960,.T.);
#25243=EDGE_CURVE('',#21150,#21151,#4542,.T.);
#25244=EDGE_CURVE('',#21151,#21151,#17961,.T.);
#25245=EDGE_CURVE('',#21152,#21152,#17962,.T.);
#25246=EDGE_CURVE('',#21152,#21153,#4543,.T.);
#25247=EDGE_CURVE('',#21153,#21153,#17963,.T.);
#25248=EDGE_CURVE('',#21154,#21154,#17964,.T.);
#25249=EDGE_CURVE('',#21154,#21155,#4544,.T.);
#25250=EDGE_CURVE('',#21155,#21155,#17965,.T.);
#25251=EDGE_CURVE('',#21156,#21156,#17966,.T.);
#25252=EDGE_CURVE('',#21156,#21157,#4545,.T.);
#25253=EDGE_CURVE('',#21157,#21157,#17967,.T.);
#25254=EDGE_CURVE('',#21158,#21158,#17968,.T.);
#25255=EDGE_CURVE('',#21158,#21159,#4546,.T.);
#25256=EDGE_CURVE('',#21159,#21159,#17969,.T.);
#25257=EDGE_CURVE('',#21160,#21160,#17970,.T.);
#25258=EDGE_CURVE('',#21160,#21161,#4547,.T.);
#25259=EDGE_CURVE('',#21161,#21161,#17971,.T.);
#25260=EDGE_CURVE('',#21162,#21162,#17972,.T.);
#25261=EDGE_CURVE('',#21162,#21163,#4548,.T.);
#25262=EDGE_CURVE('',#21163,#21163,#17973,.T.);
#25263=EDGE_CURVE('',#21164,#21164,#17974,.T.);
#25264=EDGE_CURVE('',#21164,#21165,#4549,.T.);
#25265=EDGE_CURVE('',#21165,#21165,#17975,.T.);
#25266=EDGE_CURVE('',#21166,#21166,#17976,.T.);
#25267=EDGE_CURVE('',#21166,#21167,#4550,.T.);
#25268=EDGE_CURVE('',#21167,#21167,#17977,.T.);
#25269=EDGE_CURVE('',#21168,#21168,#17978,.T.);
#25270=EDGE_CURVE('',#21168,#21169,#4551,.T.);
#25271=EDGE_CURVE('',#21169,#21169,#17979,.T.);
#25272=EDGE_CURVE('',#21170,#21170,#17980,.T.);
#25273=EDGE_CURVE('',#21170,#21171,#4552,.T.);
#25274=EDGE_CURVE('',#21171,#21171,#17981,.T.);
#25275=EDGE_CURVE('',#21172,#21172,#17982,.T.);
#25276=EDGE_CURVE('',#21172,#21173,#4553,.T.);
#25277=EDGE_CURVE('',#21173,#21173,#17983,.T.);
#25278=EDGE_CURVE('',#21174,#21174,#17984,.T.);
#25279=EDGE_CURVE('',#21174,#21175,#4554,.T.);
#25280=EDGE_CURVE('',#21175,#21175,#17985,.T.);
#25281=EDGE_CURVE('',#21176,#21176,#17986,.T.);
#25282=EDGE_CURVE('',#21176,#21177,#4555,.T.);
#25283=EDGE_CURVE('',#21177,#21177,#17987,.T.);
#25284=EDGE_CURVE('',#21178,#21178,#17988,.T.);
#25285=EDGE_CURVE('',#21178,#21179,#4556,.T.);
#25286=EDGE_CURVE('',#21180,#21179,#2058,.F.);
#25287=EDGE_CURVE('',#21180,#21181,#17989,.T.);
#25288=EDGE_CURVE('',#21179,#21181,#2059,.F.);
#25289=EDGE_CURVE('',#21182,#21182,#17990,.T.);
#25290=EDGE_CURVE('',#21182,#21183,#4557,.T.);
#25291=EDGE_CURVE('',#21183,#21183,#17991,.T.);
#25292=EDGE_CURVE('',#21184,#21184,#17992,.T.);
#25293=EDGE_CURVE('',#21184,#21185,#4558,.T.);
#25294=EDGE_CURVE('',#21185,#21185,#17993,.T.);
#25295=EDGE_CURVE('',#21186,#21186,#17994,.T.);
#25296=EDGE_CURVE('',#21186,#21187,#4559,.T.);
#25297=EDGE_CURVE('',#21187,#21187,#17995,.T.);
#25298=EDGE_CURVE('',#21188,#21188,#17996,.T.);
#25299=EDGE_CURVE('',#21188,#21189,#4560,.T.);
#25300=EDGE_CURVE('',#21189,#21189,#17997,.T.);
#25301=EDGE_CURVE('',#21190,#21190,#17998,.T.);
#25302=EDGE_CURVE('',#21190,#21191,#4561,.T.);
#25303=EDGE_CURVE('',#21191,#21191,#17999,.T.);
#25304=EDGE_CURVE('',#21192,#21192,#18000,.T.);
#25305=EDGE_CURVE('',#21192,#21193,#4562,.T.);
#25306=EDGE_CURVE('',#21193,#21193,#18001,.T.);
#25307=EDGE_CURVE('',#21194,#21194,#18002,.T.);
#25308=EDGE_CURVE('',#21194,#21195,#4563,.T.);
#25309=EDGE_CURVE('',#21195,#21195,#18003,.T.);
#25310=EDGE_CURVE('',#21196,#21196,#18004,.T.);
#25311=EDGE_CURVE('',#21196,#21197,#4564,.T.);
#25312=EDGE_CURVE('',#21197,#21197,#18005,.T.);
#25313=EDGE_CURVE('',#21198,#21198,#18006,.T.);
#25314=EDGE_CURVE('',#21198,#21199,#4565,.T.);
#25315=EDGE_CURVE('',#21199,#21199,#18007,.T.);
#25316=EDGE_CURVE('',#21200,#21200,#18008,.T.);
#25317=EDGE_CURVE('',#21200,#21201,#4566,.T.);
#25318=EDGE_CURVE('',#21201,#21201,#18009,.T.);
#25319=EDGE_CURVE('',#21202,#21202,#18010,.T.);
#25320=EDGE_CURVE('',#21202,#21203,#4567,.T.);
#25321=EDGE_CURVE('',#21203,#21203,#18011,.T.);
#25322=EDGE_CURVE('',#21204,#21204,#18012,.T.);
#25323=EDGE_CURVE('',#21204,#21205,#4568,.T.);
#25324=EDGE_CURVE('',#21205,#21205,#18013,.T.);
#25325=EDGE_CURVE('',#21206,#21206,#18014,.T.);
#25326=EDGE_CURVE('',#21206,#21207,#4569,.T.);
#25327=EDGE_CURVE('',#21207,#21207,#18015,.T.);
#25328=EDGE_CURVE('',#21208,#21208,#18016,.T.);
#25329=EDGE_CURVE('',#21208,#21209,#4570,.T.);
#25330=EDGE_CURVE('',#21209,#21209,#18017,.T.);
#25331=EDGE_CURVE('',#21210,#21210,#18018,.T.);
#25332=EDGE_CURVE('',#21210,#21211,#4571,.T.);
#25333=EDGE_CURVE('',#21211,#21211,#18019,.T.);
#25334=EDGE_CURVE('',#21212,#21212,#18020,.T.);
#25335=EDGE_CURVE('',#21212,#21213,#4572,.T.);
#25336=EDGE_CURVE('',#21213,#21213,#18021,.T.);
#25337=EDGE_CURVE('',#21214,#21214,#18022,.T.);
#25338=EDGE_CURVE('',#21214,#21215,#4573,.T.);
#25339=EDGE_CURVE('',#21215,#21215,#18023,.T.);
#25340=EDGE_CURVE('',#21216,#21216,#18024,.T.);
#25341=EDGE_CURVE('',#21216,#21217,#4574,.T.);
#25342=EDGE_CURVE('',#21218,#21217,#2060,.F.);
#25343=EDGE_CURVE('',#21218,#21219,#18025,.T.);
#25344=EDGE_CURVE('',#21217,#21219,#2061,.F.);
#25345=EDGE_CURVE('',#21220,#21220,#18026,.T.);
#25346=EDGE_CURVE('',#21220,#21221,#4575,.T.);
#25347=EDGE_CURVE('',#21221,#21221,#18027,.T.);
#25348=EDGE_CURVE('',#21222,#21222,#18028,.T.);
#25349=EDGE_CURVE('',#21222,#21223,#4576,.T.);
#25350=EDGE_CURVE('',#21223,#21223,#18029,.T.);
#25351=EDGE_CURVE('',#21224,#21224,#18030,.T.);
#25352=EDGE_CURVE('',#21224,#21225,#4577,.T.);
#25353=EDGE_CURVE('',#21225,#21225,#18031,.T.);
#25354=EDGE_CURVE('',#21226,#21226,#18032,.T.);
#25355=EDGE_CURVE('',#21226,#21227,#4578,.T.);
#25356=EDGE_CURVE('',#21227,#21227,#18033,.T.);
#25357=EDGE_CURVE('',#21228,#21228,#18034,.T.);
#25358=EDGE_CURVE('',#21228,#21229,#4579,.T.);
#25359=EDGE_CURVE('',#21229,#21229,#18035,.T.);
#25360=EDGE_CURVE('',#21230,#21230,#18036,.T.);
#25361=EDGE_CURVE('',#21230,#21231,#4580,.T.);
#25362=EDGE_CURVE('',#21231,#21231,#18037,.T.);
#25363=EDGE_CURVE('',#21232,#21232,#18038,.T.);
#25364=EDGE_CURVE('',#21232,#21233,#4581,.T.);
#25365=EDGE_CURVE('',#21233,#21233,#18039,.T.);
#25366=EDGE_CURVE('',#21234,#21234,#18040,.T.);
#25367=EDGE_CURVE('',#21234,#21235,#4582,.T.);
#25368=EDGE_CURVE('',#21235,#21235,#18041,.T.);
#25369=EDGE_CURVE('',#21236,#21236,#18042,.T.);
#25370=EDGE_CURVE('',#21236,#21237,#4583,.T.);
#25371=EDGE_CURVE('',#21237,#21237,#18043,.T.);
#25372=EDGE_CURVE('',#21238,#21238,#18044,.T.);
#25373=EDGE_CURVE('',#21238,#21239,#4584,.T.);
#25374=EDGE_CURVE('',#21239,#21239,#18045,.T.);
#25375=EDGE_CURVE('',#21240,#21240,#18046,.T.);
#25376=EDGE_CURVE('',#21240,#21241,#4585,.T.);
#25377=EDGE_CURVE('',#21241,#21241,#18047,.T.);
#25378=EDGE_CURVE('',#21242,#21242,#18048,.T.);
#25379=EDGE_CURVE('',#21242,#21243,#4586,.T.);
#25380=EDGE_CURVE('',#21243,#21243,#18049,.T.);
#25381=EDGE_CURVE('',#21244,#21244,#18050,.T.);
#25382=EDGE_CURVE('',#21244,#21245,#4587,.T.);
#25383=EDGE_CURVE('',#21245,#21245,#18051,.T.);
#25384=EDGE_CURVE('',#21246,#21246,#18052,.T.);
#25385=EDGE_CURVE('',#21246,#21247,#4588,.T.);
#25386=EDGE_CURVE('',#21247,#21247,#18053,.T.);
#25387=EDGE_CURVE('',#21248,#21248,#18054,.T.);
#25388=EDGE_CURVE('',#21248,#21249,#4589,.T.);
#25389=EDGE_CURVE('',#21249,#21249,#18055,.T.);
#25390=EDGE_CURVE('',#21250,#21250,#18056,.T.);
#25391=EDGE_CURVE('',#21250,#21251,#4590,.T.);
#25392=EDGE_CURVE('',#21251,#21251,#18057,.T.);
#25393=EDGE_CURVE('',#21252,#21252,#18058,.T.);
#25394=EDGE_CURVE('',#21252,#21253,#4591,.T.);
#25395=EDGE_CURVE('',#21253,#21253,#18059,.T.);
#25396=EDGE_CURVE('',#21254,#21254,#18060,.T.);
#25397=EDGE_CURVE('',#21254,#21255,#4592,.T.);
#25398=EDGE_CURVE('',#21256,#21255,#2062,.F.);
#25399=EDGE_CURVE('',#21256,#21257,#18061,.T.);
#25400=EDGE_CURVE('',#21255,#21257,#2063,.F.);
#25401=EDGE_CURVE('',#21258,#21258,#18062,.T.);
#25402=EDGE_CURVE('',#21258,#21259,#4593,.T.);
#25403=EDGE_CURVE('',#21259,#21259,#18063,.T.);
#25404=EDGE_CURVE('',#21260,#21260,#18064,.T.);
#25405=EDGE_CURVE('',#21260,#21261,#4594,.T.);
#25406=EDGE_CURVE('',#21261,#21261,#18065,.T.);
#25407=EDGE_CURVE('',#21262,#21262,#18066,.T.);
#25408=EDGE_CURVE('',#21262,#21263,#4595,.T.);
#25409=EDGE_CURVE('',#21263,#21263,#18067,.T.);
#25410=EDGE_CURVE('',#21264,#21264,#18068,.T.);
#25411=EDGE_CURVE('',#21264,#21265,#4596,.T.);
#25412=EDGE_CURVE('',#21265,#21265,#18069,.T.);
#25413=EDGE_CURVE('',#21266,#21266,#18070,.T.);
#25414=EDGE_CURVE('',#21266,#21267,#4597,.T.);
#25415=EDGE_CURVE('',#21267,#21267,#18071,.T.);
#25416=EDGE_CURVE('',#21268,#21268,#18072,.T.);
#25417=EDGE_CURVE('',#21268,#21269,#4598,.T.);
#25418=EDGE_CURVE('',#21269,#21269,#18073,.T.);
#25419=EDGE_CURVE('',#21270,#21270,#18074,.T.);
#25420=EDGE_CURVE('',#21270,#21271,#4599,.T.);
#25421=EDGE_CURVE('',#21271,#21271,#18075,.T.);
#25422=EDGE_CURVE('',#21272,#21272,#18076,.T.);
#25423=EDGE_CURVE('',#21272,#21273,#4600,.T.);
#25424=EDGE_CURVE('',#21273,#21273,#18077,.T.);
#25425=EDGE_CURVE('',#21274,#21274,#18078,.T.);
#25426=EDGE_CURVE('',#21274,#21275,#4601,.T.);
#25427=EDGE_CURVE('',#21275,#21275,#18079,.T.);
#25428=EDGE_CURVE('',#21276,#21276,#18080,.T.);
#25429=EDGE_CURVE('',#21276,#21277,#4602,.T.);
#25430=EDGE_CURVE('',#21277,#21277,#18081,.T.);
#25431=EDGE_CURVE('',#21278,#21278,#18082,.T.);
#25432=EDGE_CURVE('',#21278,#21279,#4603,.T.);
#25433=EDGE_CURVE('',#21279,#21279,#18083,.T.);
#25434=EDGE_CURVE('',#21280,#21280,#18084,.T.);
#25435=EDGE_CURVE('',#21280,#21281,#4604,.T.);
#25436=EDGE_CURVE('',#21281,#21281,#18085,.T.);
#25437=EDGE_CURVE('',#21282,#21282,#18086,.T.);
#25438=EDGE_CURVE('',#21282,#21283,#4605,.T.);
#25439=EDGE_CURVE('',#21283,#21283,#18087,.T.);
#25440=EDGE_CURVE('',#21284,#21284,#18088,.T.);
#25441=EDGE_CURVE('',#21284,#21285,#4606,.T.);
#25442=EDGE_CURVE('',#21285,#21285,#18089,.T.);
#25443=EDGE_CURVE('',#21286,#21286,#18090,.T.);
#25444=EDGE_CURVE('',#21286,#21287,#4607,.T.);
#25445=EDGE_CURVE('',#21287,#21287,#18091,.T.);
#25446=EDGE_CURVE('',#21288,#21288,#18092,.T.);
#25447=EDGE_CURVE('',#21288,#21289,#4608,.T.);
#25448=EDGE_CURVE('',#21290,#21289,#2064,.F.);
#25449=EDGE_CURVE('',#21290,#21291,#18093,.T.);
#25450=EDGE_CURVE('',#21289,#21291,#2065,.F.);
#25451=EDGE_CURVE('',#21292,#21292,#18094,.T.);
#25452=EDGE_CURVE('',#21292,#21293,#4609,.T.);
#25453=EDGE_CURVE('',#21293,#21293,#18095,.T.);
#25454=EDGE_CURVE('',#21294,#21294,#18096,.T.);
#25455=EDGE_CURVE('',#21294,#21295,#4610,.T.);
#25456=EDGE_CURVE('',#21295,#21295,#18097,.T.);
#25457=EDGE_CURVE('',#21296,#21296,#18098,.T.);
#25458=EDGE_CURVE('',#21296,#21297,#4611,.T.);
#25459=EDGE_CURVE('',#21297,#21297,#18099,.T.);
#25460=EDGE_CURVE('',#21298,#21298,#18100,.T.);
#25461=EDGE_CURVE('',#21298,#21299,#4612,.T.);
#25462=EDGE_CURVE('',#21299,#21299,#18101,.T.);
#25463=EDGE_CURVE('',#21300,#21300,#18102,.T.);
#25464=EDGE_CURVE('',#21300,#21301,#4613,.T.);
#25465=EDGE_CURVE('',#21301,#21301,#18103,.T.);
#25466=EDGE_CURVE('',#21302,#21302,#18104,.T.);
#25467=EDGE_CURVE('',#21302,#21303,#4614,.T.);
#25468=EDGE_CURVE('',#21303,#21303,#18105,.T.);
#25469=EDGE_CURVE('',#21304,#21304,#18106,.T.);
#25470=EDGE_CURVE('',#21304,#21305,#4615,.T.);
#25471=EDGE_CURVE('',#21305,#21305,#18107,.T.);
#25472=EDGE_CURVE('',#21306,#21306,#18108,.T.);
#25473=EDGE_CURVE('',#21306,#21307,#4616,.T.);
#25474=EDGE_CURVE('',#21307,#21307,#18109,.T.);
#25475=EDGE_CURVE('',#21308,#21308,#18110,.T.);
#25476=EDGE_CURVE('',#21308,#21309,#4617,.T.);
#25477=EDGE_CURVE('',#21309,#21309,#18111,.T.);
#25478=EDGE_CURVE('',#21310,#21310,#18112,.T.);
#25479=EDGE_CURVE('',#21310,#21311,#4618,.T.);
#25480=EDGE_CURVE('',#21311,#21311,#18113,.T.);
#25481=EDGE_CURVE('',#21312,#21312,#18114,.T.);
#25482=EDGE_CURVE('',#21312,#21313,#4619,.T.);
#25483=EDGE_CURVE('',#21313,#21313,#18115,.T.);
#25484=EDGE_CURVE('',#21314,#21314,#18116,.T.);
#25485=EDGE_CURVE('',#21314,#21315,#4620,.T.);
#25486=EDGE_CURVE('',#21315,#21315,#18117,.T.);
#25487=EDGE_CURVE('',#21316,#21316,#18118,.T.);
#25488=EDGE_CURVE('',#21316,#21317,#4621,.T.);
#25489=EDGE_CURVE('',#21317,#21317,#18119,.T.);
#25490=EDGE_CURVE('',#21318,#21318,#18120,.T.);
#25491=EDGE_CURVE('',#21318,#21319,#4622,.T.);
#25492=EDGE_CURVE('',#21319,#21319,#18121,.T.);
#25493=EDGE_CURVE('',#21320,#21320,#18122,.T.);
#25494=EDGE_CURVE('',#21320,#21321,#4623,.T.);
#25495=EDGE_CURVE('',#21321,#21321,#18123,.T.);
#25496=EDGE_CURVE('',#21322,#21322,#18124,.T.);
#25497=EDGE_CURVE('',#21322,#21323,#4624,.T.);
#25498=EDGE_CURVE('',#21323,#21323,#18125,.T.);
#25499=EDGE_CURVE('',#21324,#21324,#18126,.T.);
#25500=EDGE_CURVE('',#21324,#21325,#4625,.T.);
#25501=EDGE_CURVE('',#21325,#21325,#18127,.T.);
#25502=EDGE_CURVE('',#21326,#21326,#18128,.T.);
#25503=EDGE_CURVE('',#21326,#21327,#4626,.T.);
#25504=EDGE_CURVE('',#21328,#21327,#2066,.F.);
#25505=EDGE_CURVE('',#21328,#21329,#18129,.T.);
#25506=EDGE_CURVE('',#21327,#21329,#2067,.F.);
#25507=EDGE_CURVE('',#21330,#21330,#18130,.T.);
#25508=EDGE_CURVE('',#21330,#21331,#4627,.T.);
#25509=EDGE_CURVE('',#21331,#21331,#18131,.T.);
#25510=EDGE_CURVE('',#21332,#21332,#18132,.T.);
#25511=EDGE_CURVE('',#21332,#21333,#4628,.T.);
#25512=EDGE_CURVE('',#21333,#21333,#18133,.T.);
#25513=EDGE_CURVE('',#21334,#21334,#18134,.T.);
#25514=EDGE_CURVE('',#21334,#21335,#4629,.T.);
#25515=EDGE_CURVE('',#21335,#21335,#18135,.T.);
#25516=EDGE_CURVE('',#21336,#21336,#18136,.T.);
#25517=EDGE_CURVE('',#21336,#21337,#4630,.T.);
#25518=EDGE_CURVE('',#21337,#21337,#18137,.T.);
#25519=EDGE_CURVE('',#21338,#21338,#18138,.T.);
#25520=EDGE_CURVE('',#21338,#21339,#4631,.T.);
#25521=EDGE_CURVE('',#21339,#21339,#18139,.T.);
#25522=EDGE_CURVE('',#21340,#21340,#18140,.T.);
#25523=EDGE_CURVE('',#21340,#21341,#4632,.T.);
#25524=EDGE_CURVE('',#21341,#21341,#18141,.T.);
#25525=EDGE_CURVE('',#21342,#21342,#18142,.T.);
#25526=EDGE_CURVE('',#21342,#21343,#4633,.T.);
#25527=EDGE_CURVE('',#21343,#21343,#18143,.T.);
#25528=EDGE_CURVE('',#21344,#21344,#18144,.T.);
#25529=EDGE_CURVE('',#21344,#21345,#4634,.T.);
#25530=EDGE_CURVE('',#21345,#21345,#18145,.T.);
#25531=EDGE_CURVE('',#21346,#21346,#18146,.T.);
#25532=EDGE_CURVE('',#21346,#21347,#4635,.T.);
#25533=EDGE_CURVE('',#21347,#21347,#18147,.T.);
#25534=EDGE_CURVE('',#21348,#21348,#18148,.T.);
#25535=EDGE_CURVE('',#21348,#21349,#4636,.T.);
#25536=EDGE_CURVE('',#21349,#21349,#18149,.T.);
#25537=EDGE_CURVE('',#21350,#21350,#18150,.T.);
#25538=EDGE_CURVE('',#21350,#21351,#4637,.T.);
#25539=EDGE_CURVE('',#21351,#21351,#18151,.T.);
#25540=EDGE_CURVE('',#21352,#21352,#18152,.T.);
#25541=EDGE_CURVE('',#21352,#21353,#4638,.T.);
#25542=EDGE_CURVE('',#21353,#21353,#18153,.T.);
#25543=EDGE_CURVE('',#21354,#21354,#18154,.T.);
#25544=EDGE_CURVE('',#21354,#21355,#4639,.T.);
#25545=EDGE_CURVE('',#21355,#21355,#18155,.T.);
#25546=EDGE_CURVE('',#21356,#21356,#18156,.T.);
#25547=EDGE_CURVE('',#21356,#21357,#4640,.T.);
#25548=EDGE_CURVE('',#21357,#21357,#18157,.T.);
#25549=EDGE_CURVE('',#21358,#21358,#18158,.T.);
#25550=EDGE_CURVE('',#21358,#21359,#4641,.T.);
#25551=EDGE_CURVE('',#21359,#21359,#18159,.T.);
#25552=EDGE_CURVE('',#21360,#21360,#18160,.T.);
#25553=EDGE_CURVE('',#21360,#21361,#4642,.T.);
#25554=EDGE_CURVE('',#21361,#21361,#18161,.T.);
#25555=EDGE_CURVE('',#21362,#21362,#18162,.T.);
#25556=EDGE_CURVE('',#21362,#21363,#4643,.T.);
#25557=EDGE_CURVE('',#21363,#21363,#18163,.T.);
#25558=EDGE_CURVE('',#21364,#21364,#18164,.T.);
#25559=EDGE_CURVE('',#21364,#21365,#4644,.T.);
#25560=EDGE_CURVE('',#21366,#21365,#2068,.F.);
#25561=EDGE_CURVE('',#21366,#21367,#18165,.T.);
#25562=EDGE_CURVE('',#21365,#21367,#2069,.F.);
#25563=EDGE_CURVE('',#21368,#21368,#18166,.T.);
#25564=EDGE_CURVE('',#21368,#21369,#4645,.T.);
#25565=EDGE_CURVE('',#21369,#21369,#18167,.T.);
#25566=EDGE_CURVE('',#21370,#21370,#18168,.T.);
#25567=EDGE_CURVE('',#21370,#21371,#4646,.T.);
#25568=EDGE_CURVE('',#21371,#21371,#18169,.T.);
#25569=EDGE_CURVE('',#21372,#21372,#18170,.T.);
#25570=EDGE_CURVE('',#21372,#21373,#4647,.T.);
#25571=EDGE_CURVE('',#21373,#21373,#18171,.T.);
#25572=EDGE_CURVE('',#21374,#21374,#18172,.T.);
#25573=EDGE_CURVE('',#21374,#21375,#4648,.T.);
#25574=EDGE_CURVE('',#21375,#21375,#18173,.T.);
#25575=EDGE_CURVE('',#21376,#21376,#18174,.T.);
#25576=EDGE_CURVE('',#21376,#21377,#4649,.T.);
#25577=EDGE_CURVE('',#21377,#21377,#18175,.T.);
#25578=EDGE_CURVE('',#21378,#21378,#18176,.T.);
#25579=EDGE_CURVE('',#21378,#21379,#4650,.T.);
#25580=EDGE_CURVE('',#21379,#21379,#18177,.T.);
#25581=EDGE_CURVE('',#21380,#21380,#18178,.T.);
#25582=EDGE_CURVE('',#21380,#21381,#4651,.T.);
#25583=EDGE_CURVE('',#21381,#21381,#18179,.T.);
#25584=EDGE_CURVE('',#21382,#21382,#18180,.T.);
#25585=EDGE_CURVE('',#21382,#21383,#4652,.T.);
#25586=EDGE_CURVE('',#21383,#21383,#18181,.T.);
#25587=EDGE_CURVE('',#21384,#21384,#18182,.T.);
#25588=EDGE_CURVE('',#21384,#21385,#4653,.T.);
#25589=EDGE_CURVE('',#21385,#21385,#18183,.T.);
#25590=EDGE_CURVE('',#21386,#21386,#18184,.T.);
#25591=EDGE_CURVE('',#21386,#21387,#4654,.T.);
#25592=EDGE_CURVE('',#21387,#21387,#18185,.T.);
#25593=EDGE_CURVE('',#21388,#21388,#18186,.T.);
#25594=EDGE_CURVE('',#21388,#21389,#4655,.T.);
#25595=EDGE_CURVE('',#21389,#21389,#18187,.T.);
#25596=EDGE_CURVE('',#21390,#21390,#18188,.T.);
#25597=EDGE_CURVE('',#21390,#21391,#4656,.T.);
#25598=EDGE_CURVE('',#21391,#21391,#18189,.T.);
#25599=EDGE_CURVE('',#21392,#21392,#18190,.T.);
#25600=EDGE_CURVE('',#21392,#21393,#4657,.T.);
#25601=EDGE_CURVE('',#21393,#21393,#18191,.T.);
#25602=EDGE_CURVE('',#21394,#21394,#18192,.T.);
#25603=EDGE_CURVE('',#21394,#21395,#4658,.T.);
#25604=EDGE_CURVE('',#21395,#21395,#18193,.T.);
#25605=EDGE_CURVE('',#21396,#21396,#18194,.T.);
#25606=EDGE_CURVE('',#21396,#21397,#4659,.T.);
#25607=EDGE_CURVE('',#21397,#21397,#18195,.T.);
#25608=EDGE_CURVE('',#21398,#21398,#18196,.T.);
#25609=EDGE_CURVE('',#21398,#21399,#4660,.T.);
#25610=EDGE_CURVE('',#21399,#21399,#18197,.T.);
#25611=EDGE_CURVE('',#21400,#21400,#18198,.T.);
#25612=EDGE_CURVE('',#21400,#21401,#4661,.T.);
#25613=EDGE_CURVE('',#21401,#21401,#18199,.T.);
#25614=EDGE_CURVE('',#21402,#21402,#18200,.T.);
#25615=EDGE_CURVE('',#21402,#21403,#4662,.T.);
#25616=EDGE_CURVE('',#21404,#21403,#2070,.F.);
#25617=EDGE_CURVE('',#21404,#21405,#18201,.T.);
#25618=EDGE_CURVE('',#21403,#21405,#2071,.F.);
#25619=EDGE_CURVE('',#21406,#21406,#18202,.T.);
#25620=EDGE_CURVE('',#21406,#21407,#4663,.T.);
#25621=EDGE_CURVE('',#21407,#21407,#18203,.T.);
#25622=EDGE_CURVE('',#21408,#21408,#18204,.T.);
#25623=EDGE_CURVE('',#21408,#21409,#4664,.T.);
#25624=EDGE_CURVE('',#21409,#21409,#18205,.T.);
#25625=EDGE_CURVE('',#21410,#21410,#18206,.T.);
#25626=EDGE_CURVE('',#21410,#21411,#4665,.T.);
#25627=EDGE_CURVE('',#21411,#21411,#18207,.T.);
#25628=EDGE_CURVE('',#21412,#21412,#18208,.T.);
#25629=EDGE_CURVE('',#21412,#21413,#4666,.T.);
#25630=EDGE_CURVE('',#21413,#21413,#18209,.T.);
#25631=EDGE_CURVE('',#21414,#21414,#18210,.T.);
#25632=EDGE_CURVE('',#21414,#21415,#4667,.T.);
#25633=EDGE_CURVE('',#21415,#21415,#18211,.T.);
#25634=EDGE_CURVE('',#21416,#21416,#18212,.T.);
#25635=EDGE_CURVE('',#21416,#21417,#4668,.T.);
#25636=EDGE_CURVE('',#21417,#21417,#18213,.T.);
#25637=EDGE_CURVE('',#21418,#21418,#18214,.T.);
#25638=EDGE_CURVE('',#21418,#21419,#4669,.T.);
#25639=EDGE_CURVE('',#21419,#21419,#18215,.T.);
#25640=EDGE_CURVE('',#21420,#21420,#18216,.T.);
#25641=EDGE_CURVE('',#21420,#21421,#4670,.T.);
#25642=EDGE_CURVE('',#21421,#21421,#18217,.T.);
#25643=EDGE_CURVE('',#21422,#21422,#18218,.T.);
#25644=EDGE_CURVE('',#21422,#21423,#4671,.T.);
#25645=EDGE_CURVE('',#21423,#21423,#18219,.T.);
#25646=EDGE_CURVE('',#21424,#21424,#18220,.T.);
#25647=EDGE_CURVE('',#21424,#21425,#4672,.T.);
#25648=EDGE_CURVE('',#21425,#21425,#18221,.T.);
#25649=EDGE_CURVE('',#21426,#21426,#18222,.T.);
#25650=EDGE_CURVE('',#21426,#21427,#4673,.T.);
#25651=EDGE_CURVE('',#21427,#21427,#18223,.T.);
#25652=EDGE_CURVE('',#21428,#21428,#18224,.T.);
#25653=EDGE_CURVE('',#21428,#21429,#4674,.T.);
#25654=EDGE_CURVE('',#21429,#21429,#18225,.T.);
#25655=EDGE_CURVE('',#21430,#21430,#18226,.T.);
#25656=EDGE_CURVE('',#21430,#21431,#4675,.T.);
#25657=EDGE_CURVE('',#21431,#21431,#18227,.T.);
#25658=EDGE_CURVE('',#21432,#21432,#18228,.T.);
#25659=EDGE_CURVE('',#21432,#21433,#4676,.T.);
#25660=EDGE_CURVE('',#21433,#21433,#18229,.T.);
#25661=EDGE_CURVE('',#21434,#21434,#18230,.T.);
#25662=EDGE_CURVE('',#21434,#21435,#4677,.T.);
#25663=EDGE_CURVE('',#21435,#21435,#18231,.T.);
#25664=EDGE_CURVE('',#21436,#21436,#18232,.T.);
#25665=EDGE_CURVE('',#21436,#21437,#4678,.T.);
#25666=EDGE_CURVE('',#21437,#21437,#18233,.T.);
#25667=EDGE_CURVE('',#21438,#21438,#18234,.T.);
#25668=EDGE_CURVE('',#21438,#21439,#4679,.T.);
#25669=EDGE_CURVE('',#21439,#21439,#18235,.T.);
#25670=EDGE_CURVE('',#21440,#21440,#18236,.T.);
#25671=EDGE_CURVE('',#21440,#21441,#4680,.T.);
#25672=EDGE_CURVE('',#21442,#21441,#2072,.F.);
#25673=EDGE_CURVE('',#21442,#21443,#18237,.T.);
#25674=EDGE_CURVE('',#21441,#21443,#2073,.F.);
#25675=EDGE_CURVE('',#21444,#21444,#18238,.T.);
#25676=EDGE_CURVE('',#21444,#21445,#4681,.T.);
#25677=EDGE_CURVE('',#21445,#21445,#18239,.T.);
#25678=EDGE_CURVE('',#21446,#21446,#18240,.T.);
#25679=EDGE_CURVE('',#21446,#21447,#4682,.T.);
#25680=EDGE_CURVE('',#21447,#21447,#18241,.T.);
#25681=EDGE_CURVE('',#21448,#21448,#18242,.T.);
#25682=EDGE_CURVE('',#21448,#21449,#4683,.T.);
#25683=EDGE_CURVE('',#21449,#21449,#18243,.T.);
#25684=EDGE_CURVE('',#21450,#21450,#18244,.T.);
#25685=EDGE_CURVE('',#21450,#21451,#4684,.T.);
#25686=EDGE_CURVE('',#21451,#21451,#18245,.T.);
#25687=EDGE_CURVE('',#21452,#21452,#18246,.T.);
#25688=EDGE_CURVE('',#21452,#21453,#4685,.T.);
#25689=EDGE_CURVE('',#21453,#21453,#18247,.T.);
#25690=EDGE_CURVE('',#21454,#21454,#18248,.T.);
#25691=EDGE_CURVE('',#21454,#21455,#4686,.T.);
#25692=EDGE_CURVE('',#21455,#21455,#18249,.T.);
#25693=EDGE_CURVE('',#21456,#21456,#18250,.T.);
#25694=EDGE_CURVE('',#21456,#21457,#4687,.T.);
#25695=EDGE_CURVE('',#21457,#21457,#18251,.T.);
#25696=EDGE_CURVE('',#21458,#21458,#18252,.T.);
#25697=EDGE_CURVE('',#21458,#21459,#4688,.T.);
#25698=EDGE_CURVE('',#21459,#21459,#18253,.T.);
#25699=EDGE_CURVE('',#21460,#21460,#18254,.T.);
#25700=EDGE_CURVE('',#21460,#21461,#4689,.T.);
#25701=EDGE_CURVE('',#21461,#21461,#18255,.T.);
#25702=EDGE_CURVE('',#21462,#21462,#18256,.T.);
#25703=EDGE_CURVE('',#21462,#21463,#4690,.T.);
#25704=EDGE_CURVE('',#21463,#21463,#18257,.T.);
#25705=EDGE_CURVE('',#21464,#21464,#18258,.T.);
#25706=EDGE_CURVE('',#21464,#21465,#4691,.T.);
#25707=EDGE_CURVE('',#21465,#21465,#18259,.T.);
#25708=EDGE_CURVE('',#21466,#21466,#18260,.T.);
#25709=EDGE_CURVE('',#21466,#21467,#4692,.T.);
#25710=EDGE_CURVE('',#21467,#21467,#18261,.T.);
#25711=EDGE_CURVE('',#21468,#21468,#18262,.T.);
#25712=EDGE_CURVE('',#21468,#21469,#4693,.T.);
#25713=EDGE_CURVE('',#21469,#21469,#18263,.T.);
#25714=EDGE_CURVE('',#21470,#21470,#18264,.T.);
#25715=EDGE_CURVE('',#21470,#21471,#4694,.T.);
#25716=EDGE_CURVE('',#21471,#21471,#18265,.T.);
#25717=EDGE_CURVE('',#21472,#21472,#18266,.T.);
#25718=EDGE_CURVE('',#21472,#21473,#4695,.T.);
#25719=EDGE_CURVE('',#21473,#21473,#18267,.T.);
#25720=EDGE_CURVE('',#21474,#21474,#18268,.T.);
#25721=EDGE_CURVE('',#21474,#21475,#4696,.T.);
#25722=EDGE_CURVE('',#21476,#21475,#2074,.F.);
#25723=EDGE_CURVE('',#21476,#21477,#18269,.T.);
#25724=EDGE_CURVE('',#21475,#21477,#2075,.F.);
#25725=EDGE_CURVE('',#21478,#21478,#18270,.T.);
#25726=EDGE_CURVE('',#21478,#21479,#4697,.T.);
#25727=EDGE_CURVE('',#21479,#21479,#18271,.T.);
#25728=EDGE_CURVE('',#21480,#21480,#18272,.T.);
#25729=EDGE_CURVE('',#21480,#21481,#4698,.T.);
#25730=EDGE_CURVE('',#21481,#21481,#18273,.T.);
#25731=EDGE_CURVE('',#21482,#21482,#18274,.T.);
#25732=EDGE_CURVE('',#21482,#21483,#4699,.T.);
#25733=EDGE_CURVE('',#21483,#21483,#18275,.T.);
#25734=EDGE_CURVE('',#21484,#21484,#18276,.T.);
#25735=EDGE_CURVE('',#21484,#21485,#4700,.T.);
#25736=EDGE_CURVE('',#21485,#21485,#18277,.T.);
#25737=EDGE_CURVE('',#21486,#21486,#18278,.T.);
#25738=EDGE_CURVE('',#21486,#21487,#4701,.T.);
#25739=EDGE_CURVE('',#21487,#21487,#18279,.T.);
#25740=EDGE_CURVE('',#21488,#21488,#18280,.T.);
#25741=EDGE_CURVE('',#21488,#21489,#4702,.T.);
#25742=EDGE_CURVE('',#21489,#21489,#18281,.T.);
#25743=EDGE_CURVE('',#21490,#21490,#18282,.T.);
#25744=EDGE_CURVE('',#21490,#21491,#4703,.T.);
#25745=EDGE_CURVE('',#21491,#21491,#18283,.T.);
#25746=EDGE_CURVE('',#21492,#21492,#18284,.T.);
#25747=EDGE_CURVE('',#21492,#21493,#4704,.T.);
#25748=EDGE_CURVE('',#21493,#21493,#18285,.T.);
#25749=EDGE_CURVE('',#21494,#21494,#18286,.T.);
#25750=EDGE_CURVE('',#21494,#21495,#4705,.T.);
#25751=EDGE_CURVE('',#21495,#21495,#18287,.T.);
#25752=EDGE_CURVE('',#21496,#21496,#18288,.T.);
#25753=EDGE_CURVE('',#21496,#21497,#4706,.T.);
#25754=EDGE_CURVE('',#21497,#21497,#18289,.T.);
#25755=EDGE_CURVE('',#21498,#21498,#18290,.T.);
#25756=EDGE_CURVE('',#21498,#21499,#4707,.T.);
#25757=EDGE_CURVE('',#21499,#21499,#18291,.T.);
#25758=EDGE_CURVE('',#21500,#21500,#18292,.T.);
#25759=EDGE_CURVE('',#21500,#21501,#4708,.T.);
#25760=EDGE_CURVE('',#21501,#21501,#18293,.T.);
#25761=EDGE_CURVE('',#21502,#21502,#18294,.T.);
#25762=EDGE_CURVE('',#21502,#21503,#4709,.T.);
#25763=EDGE_CURVE('',#21503,#21503,#18295,.T.);
#25764=EDGE_CURVE('',#21504,#21504,#18296,.T.);
#25765=EDGE_CURVE('',#21504,#21505,#4710,.T.);
#25766=EDGE_CURVE('',#21505,#21505,#18297,.T.);
#25767=EDGE_CURVE('',#21506,#21506,#18298,.T.);
#25768=EDGE_CURVE('',#21506,#21507,#4711,.T.);
#25769=EDGE_CURVE('',#21507,#21507,#18299,.T.);
#25770=EDGE_CURVE('',#21508,#21508,#18300,.T.);
#25771=EDGE_CURVE('',#21508,#21509,#4712,.T.);
#25772=EDGE_CURVE('',#21509,#21509,#18301,.T.);
#25773=EDGE_CURVE('',#21510,#21510,#18302,.T.);
#25774=EDGE_CURVE('',#21510,#21511,#4713,.T.);
#25775=EDGE_CURVE('',#21511,#21511,#18303,.T.);
#25776=EDGE_CURVE('',#21512,#21512,#18304,.T.);
#25777=EDGE_CURVE('',#21512,#21513,#4714,.T.);
#25778=EDGE_CURVE('',#21514,#21513,#2076,.F.);
#25779=EDGE_CURVE('',#21514,#21515,#18305,.T.);
#25780=EDGE_CURVE('',#21513,#21515,#2077,.F.);
#25781=EDGE_CURVE('',#21516,#21516,#18306,.T.);
#25782=EDGE_CURVE('',#21516,#21517,#4715,.T.);
#25783=EDGE_CURVE('',#21517,#21517,#18307,.T.);
#25784=EDGE_CURVE('',#21518,#21518,#18308,.T.);
#25785=EDGE_CURVE('',#21518,#21519,#4716,.T.);
#25786=EDGE_CURVE('',#21519,#21519,#18309,.T.);
#25787=EDGE_CURVE('',#21520,#21520,#18310,.T.);
#25788=EDGE_CURVE('',#21520,#21521,#4717,.T.);
#25789=EDGE_CURVE('',#21521,#21521,#18311,.T.);
#25790=EDGE_CURVE('',#21522,#21522,#18312,.T.);
#25791=EDGE_CURVE('',#21522,#21523,#4718,.T.);
#25792=EDGE_CURVE('',#21523,#21523,#18313,.T.);
#25793=EDGE_CURVE('',#21524,#21524,#18314,.T.);
#25794=EDGE_CURVE('',#21524,#21525,#4719,.T.);
#25795=EDGE_CURVE('',#21525,#21525,#18315,.T.);
#25796=EDGE_CURVE('',#21526,#21526,#18316,.T.);
#25797=EDGE_CURVE('',#21526,#21527,#4720,.T.);
#25798=EDGE_CURVE('',#21527,#21527,#18317,.T.);
#25799=EDGE_CURVE('',#21528,#21528,#18318,.T.);
#25800=EDGE_CURVE('',#21528,#21529,#4721,.T.);
#25801=EDGE_CURVE('',#21529,#21529,#18319,.T.);
#25802=EDGE_CURVE('',#21530,#21530,#18320,.T.);
#25803=EDGE_CURVE('',#21530,#21531,#4722,.T.);
#25804=EDGE_CURVE('',#21531,#21531,#18321,.T.);
#25805=EDGE_CURVE('',#21532,#21532,#18322,.T.);
#25806=EDGE_CURVE('',#21532,#21533,#4723,.T.);
#25807=EDGE_CURVE('',#21533,#21533,#18323,.T.);
#25808=EDGE_CURVE('',#21534,#21534,#18324,.T.);
#25809=EDGE_CURVE('',#21534,#21535,#4724,.T.);
#25810=EDGE_CURVE('',#21535,#21535,#18325,.T.);
#25811=EDGE_CURVE('',#21536,#21536,#18326,.T.);
#25812=EDGE_CURVE('',#21536,#21537,#4725,.T.);
#25813=EDGE_CURVE('',#21537,#21537,#18327,.T.);
#25814=EDGE_CURVE('',#21538,#21538,#18328,.T.);
#25815=EDGE_CURVE('',#21538,#21539,#4726,.T.);
#25816=EDGE_CURVE('',#21539,#21539,#18329,.T.);
#25817=EDGE_CURVE('',#21540,#21540,#18330,.T.);
#25818=EDGE_CURVE('',#21540,#21541,#4727,.T.);
#25819=EDGE_CURVE('',#21541,#21541,#18331,.T.);
#25820=EDGE_CURVE('',#21542,#21542,#18332,.T.);
#25821=EDGE_CURVE('',#21542,#21543,#4728,.T.);
#25822=EDGE_CURVE('',#21543,#21543,#18333,.T.);
#25823=EDGE_CURVE('',#21544,#21544,#18334,.T.);
#25824=EDGE_CURVE('',#21544,#21545,#4729,.T.);
#25825=EDGE_CURVE('',#21545,#21545,#18335,.T.);
#25826=EDGE_CURVE('',#21546,#21546,#18336,.T.);
#25827=EDGE_CURVE('',#21546,#21547,#4730,.T.);
#25828=EDGE_CURVE('',#21547,#21547,#18337,.T.);
#25829=EDGE_CURVE('',#21548,#21548,#18338,.T.);
#25830=EDGE_CURVE('',#21548,#21549,#4731,.T.);
#25831=EDGE_CURVE('',#21549,#21549,#18339,.T.);
#25832=EDGE_CURVE('',#21550,#21550,#18340,.T.);
#25833=EDGE_CURVE('',#21550,#21551,#4732,.T.);
#25834=EDGE_CURVE('',#21552,#21551,#2078,.F.);
#25835=EDGE_CURVE('',#21552,#21553,#18341,.T.);
#25836=EDGE_CURVE('',#21551,#21553,#2079,.F.);
#25837=EDGE_CURVE('',#21554,#21554,#18342,.T.);
#25838=EDGE_CURVE('',#21554,#21555,#4733,.T.);
#25839=EDGE_CURVE('',#21555,#21555,#18343,.T.);
#25840=EDGE_CURVE('',#21556,#21556,#18344,.T.);
#25841=EDGE_CURVE('',#21556,#21557,#4734,.T.);
#25842=EDGE_CURVE('',#21557,#21557,#18345,.T.);
#25843=EDGE_CURVE('',#21558,#21558,#18346,.T.);
#25844=EDGE_CURVE('',#21558,#21559,#4735,.T.);
#25845=EDGE_CURVE('',#21559,#21559,#18347,.T.);
#25846=EDGE_CURVE('',#21560,#21560,#18348,.T.);
#25847=EDGE_CURVE('',#21560,#21561,#4736,.T.);
#25848=EDGE_CURVE('',#21561,#21561,#18349,.T.);
#25849=EDGE_CURVE('',#21562,#21562,#18350,.T.);
#25850=EDGE_CURVE('',#21562,#21563,#4737,.T.);
#25851=EDGE_CURVE('',#21563,#21563,#18351,.T.);
#25852=EDGE_CURVE('',#21564,#21564,#18352,.T.);
#25853=EDGE_CURVE('',#21564,#21565,#4738,.T.);
#25854=EDGE_CURVE('',#21565,#21565,#18353,.T.);
#25855=EDGE_CURVE('',#21566,#21566,#18354,.T.);
#25856=EDGE_CURVE('',#21566,#21567,#4739,.T.);
#25857=EDGE_CURVE('',#21567,#21567,#18355,.T.);
#25858=EDGE_CURVE('',#21568,#21568,#18356,.T.);
#25859=EDGE_CURVE('',#21568,#21569,#4740,.T.);
#25860=EDGE_CURVE('',#21569,#21569,#18357,.T.);
#25861=EDGE_CURVE('',#21570,#21570,#18358,.T.);
#25862=EDGE_CURVE('',#21570,#21571,#4741,.T.);
#25863=EDGE_CURVE('',#21571,#21571,#18359,.T.);
#25864=EDGE_CURVE('',#21572,#21572,#18360,.T.);
#25865=EDGE_CURVE('',#21572,#21573,#4742,.T.);
#25866=EDGE_CURVE('',#21573,#21573,#18361,.T.);
#25867=EDGE_CURVE('',#21574,#21574,#18362,.T.);
#25868=EDGE_CURVE('',#21574,#21575,#4743,.T.);
#25869=EDGE_CURVE('',#21575,#21575,#18363,.T.);
#25870=EDGE_CURVE('',#21576,#21576,#18364,.T.);
#25871=EDGE_CURVE('',#21576,#21577,#4744,.T.);
#25872=EDGE_CURVE('',#21577,#21577,#18365,.T.);
#25873=EDGE_CURVE('',#21578,#21578,#18366,.T.);
#25874=EDGE_CURVE('',#21578,#21579,#4745,.T.);
#25875=EDGE_CURVE('',#21579,#21579,#18367,.T.);
#25876=EDGE_CURVE('',#21580,#21580,#18368,.T.);
#25877=EDGE_CURVE('',#21580,#21581,#4746,.T.);
#25878=EDGE_CURVE('',#21581,#21581,#18369,.T.);
#25879=EDGE_CURVE('',#21582,#21582,#18370,.T.);
#25880=EDGE_CURVE('',#21582,#21583,#4747,.T.);
#25881=EDGE_CURVE('',#21583,#21583,#18371,.T.);
#25882=EDGE_CURVE('',#21584,#21584,#18372,.T.);
#25883=EDGE_CURVE('',#21584,#21585,#4748,.T.);
#25884=EDGE_CURVE('',#21585,#21585,#18373,.T.);
#25885=EDGE_CURVE('',#21586,#21586,#18374,.T.);
#25886=EDGE_CURVE('',#21586,#21587,#4749,.T.);
#25887=EDGE_CURVE('',#21587,#21587,#18375,.T.);
#25888=EDGE_CURVE('',#21588,#21588,#18376,.T.);
#25889=EDGE_CURVE('',#21588,#21589,#4750,.T.);
#25890=EDGE_CURVE('',#21590,#21589,#2080,.F.);
#25891=EDGE_CURVE('',#21590,#21591,#18377,.T.);
#25892=EDGE_CURVE('',#21589,#21591,#2081,.F.);
#25893=EDGE_CURVE('',#21592,#21592,#18378,.T.);
#25894=EDGE_CURVE('',#21592,#21593,#4751,.T.);
#25895=EDGE_CURVE('',#21593,#21593,#18379,.T.);
#25896=EDGE_CURVE('',#21594,#21594,#18380,.T.);
#25897=EDGE_CURVE('',#21594,#21595,#4752,.T.);
#25898=EDGE_CURVE('',#21595,#21595,#18381,.T.);
#25899=EDGE_CURVE('',#21596,#21596,#18382,.T.);
#25900=EDGE_CURVE('',#21596,#21597,#4753,.T.);
#25901=EDGE_CURVE('',#21597,#21597,#18383,.T.);
#25902=EDGE_CURVE('',#21598,#21598,#18384,.T.);
#25903=EDGE_CURVE('',#21598,#21599,#4754,.T.);
#25904=EDGE_CURVE('',#21599,#21599,#18385,.T.);
#25905=EDGE_CURVE('',#21600,#21600,#18386,.T.);
#25906=EDGE_CURVE('',#21600,#21601,#4755,.T.);
#25907=EDGE_CURVE('',#21601,#21601,#18387,.T.);
#25908=EDGE_CURVE('',#21602,#21602,#18388,.T.);
#25909=EDGE_CURVE('',#21602,#21603,#4756,.T.);
#25910=EDGE_CURVE('',#21603,#21603,#18389,.T.);
#25911=EDGE_CURVE('',#21604,#21604,#18390,.T.);
#25912=EDGE_CURVE('',#21604,#21605,#4757,.T.);
#25913=EDGE_CURVE('',#21605,#21605,#18391,.T.);
#25914=EDGE_CURVE('',#21606,#21606,#18392,.T.);
#25915=EDGE_CURVE('',#21606,#21607,#4758,.T.);
#25916=EDGE_CURVE('',#21607,#21607,#18393,.T.);
#25917=EDGE_CURVE('',#21608,#21608,#18394,.T.);
#25918=EDGE_CURVE('',#21608,#21609,#4759,.T.);
#25919=EDGE_CURVE('',#21609,#21609,#18395,.T.);
#25920=EDGE_CURVE('',#21610,#21610,#18396,.T.);
#25921=EDGE_CURVE('',#21610,#21611,#4760,.T.);
#25922=EDGE_CURVE('',#21611,#21611,#18397,.T.);
#25923=EDGE_CURVE('',#21612,#21612,#18398,.T.);
#25924=EDGE_CURVE('',#21612,#21613,#4761,.T.);
#25925=EDGE_CURVE('',#21613,#21613,#18399,.T.);
#25926=EDGE_CURVE('',#21614,#21614,#18400,.T.);
#25927=EDGE_CURVE('',#21614,#21615,#4762,.T.);
#25928=EDGE_CURVE('',#21615,#21615,#18401,.T.);
#25929=EDGE_CURVE('',#21616,#21616,#18402,.T.);
#25930=EDGE_CURVE('',#21616,#21617,#4763,.T.);
#25931=EDGE_CURVE('',#21617,#21617,#18403,.T.);
#25932=EDGE_CURVE('',#21618,#21618,#18404,.T.);
#25933=EDGE_CURVE('',#21618,#21619,#4764,.T.);
#25934=EDGE_CURVE('',#21619,#21619,#18405,.T.);
#25935=EDGE_CURVE('',#21620,#21620,#18406,.T.);
#25936=EDGE_CURVE('',#21620,#21621,#4765,.T.);
#25937=EDGE_CURVE('',#21621,#21621,#18407,.T.);
#25938=EDGE_CURVE('',#21622,#21622,#18408,.T.);
#25939=EDGE_CURVE('',#21622,#21623,#4766,.T.);
#25940=EDGE_CURVE('',#21623,#21623,#18409,.T.);
#25941=EDGE_CURVE('',#21624,#21624,#18410,.T.);
#25942=EDGE_CURVE('',#21624,#21625,#4767,.T.);
#25943=EDGE_CURVE('',#21625,#21625,#18411,.T.);
#25944=EDGE_CURVE('',#21626,#21626,#18412,.T.);
#25945=EDGE_CURVE('',#21626,#21627,#4768,.T.);
#25946=EDGE_CURVE('',#21628,#21627,#2082,.F.);
#25947=EDGE_CURVE('',#21628,#21629,#18413,.T.);
#25948=EDGE_CURVE('',#21627,#21629,#2083,.F.);
#25949=EDGE_CURVE('',#21630,#21630,#18414,.T.);
#25950=EDGE_CURVE('',#21630,#21631,#4769,.T.);
#25951=EDGE_CURVE('',#21631,#21631,#18415,.T.);
#25952=EDGE_CURVE('',#21632,#21632,#18416,.T.);
#25953=EDGE_CURVE('',#21632,#21633,#4770,.T.);
#25954=EDGE_CURVE('',#21633,#21633,#18417,.T.);
#25955=EDGE_CURVE('',#21634,#21634,#18418,.T.);
#25956=EDGE_CURVE('',#21634,#21635,#4771,.T.);
#25957=EDGE_CURVE('',#21635,#21635,#18419,.T.);
#25958=EDGE_CURVE('',#21636,#21636,#18420,.T.);
#25959=EDGE_CURVE('',#21636,#21637,#4772,.T.);
#25960=EDGE_CURVE('',#21637,#21637,#18421,.T.);
#25961=EDGE_CURVE('',#21638,#21638,#18422,.T.);
#25962=EDGE_CURVE('',#21638,#21639,#4773,.T.);
#25963=EDGE_CURVE('',#21639,#21639,#18423,.T.);
#25964=EDGE_CURVE('',#21640,#21640,#18424,.T.);
#25965=EDGE_CURVE('',#21640,#21641,#4774,.T.);
#25966=EDGE_CURVE('',#21641,#21641,#18425,.T.);
#25967=EDGE_CURVE('',#21642,#21642,#18426,.T.);
#25968=EDGE_CURVE('',#21642,#21643,#4775,.T.);
#25969=EDGE_CURVE('',#21643,#21643,#18427,.T.);
#25970=EDGE_CURVE('',#21644,#21644,#18428,.T.);
#25971=EDGE_CURVE('',#21644,#21645,#4776,.T.);
#25972=EDGE_CURVE('',#21645,#21645,#18429,.T.);
#25973=EDGE_CURVE('',#21646,#21646,#18430,.T.);
#25974=EDGE_CURVE('',#21646,#21647,#4777,.T.);
#25975=EDGE_CURVE('',#21647,#21647,#18431,.T.);
#25976=EDGE_CURVE('',#21648,#21648,#18432,.T.);
#25977=EDGE_CURVE('',#21648,#21649,#4778,.T.);
#25978=EDGE_CURVE('',#21649,#21649,#18433,.T.);
#25979=EDGE_CURVE('',#21650,#21650,#18434,.T.);
#25980=EDGE_CURVE('',#21650,#21651,#4779,.T.);
#25981=EDGE_CURVE('',#21651,#21651,#18435,.T.);
#25982=EDGE_CURVE('',#21652,#21652,#18436,.T.);
#25983=EDGE_CURVE('',#21652,#21653,#4780,.T.);
#25984=EDGE_CURVE('',#21653,#21653,#18437,.T.);
#25985=EDGE_CURVE('',#21654,#21654,#18438,.T.);
#25986=EDGE_CURVE('',#21654,#21655,#4781,.T.);
#25987=EDGE_CURVE('',#21655,#21655,#18439,.T.);
#25988=EDGE_CURVE('',#21656,#21656,#18440,.T.);
#25989=EDGE_CURVE('',#21656,#21657,#4782,.T.);
#25990=EDGE_CURVE('',#21657,#21657,#18441,.T.);
#25991=EDGE_CURVE('',#21658,#21658,#18442,.T.);
#25992=EDGE_CURVE('',#21658,#21659,#4783,.T.);
#25993=EDGE_CURVE('',#21659,#21659,#18443,.T.);
#25994=EDGE_CURVE('',#21660,#21660,#18444,.T.);
#25995=EDGE_CURVE('',#21660,#21661,#4784,.T.);
#25996=EDGE_CURVE('',#21662,#21661,#2084,.F.);
#25997=EDGE_CURVE('',#21662,#21663,#18445,.T.);
#25998=EDGE_CURVE('',#21661,#21663,#2085,.F.);
#25999=EDGE_CURVE('',#21664,#21664,#18446,.T.);
#26000=EDGE_CURVE('',#21664,#21665,#4785,.T.);
#26001=EDGE_CURVE('',#21665,#21665,#18447,.T.);
#26002=EDGE_CURVE('',#21666,#21666,#18448,.T.);
#26003=EDGE_CURVE('',#21666,#21667,#4786,.T.);
#26004=EDGE_CURVE('',#21667,#21667,#18449,.T.);
#26005=EDGE_CURVE('',#21668,#21668,#18450,.T.);
#26006=EDGE_CURVE('',#21668,#21669,#4787,.T.);
#26007=EDGE_CURVE('',#21669,#21669,#18451,.T.);
#26008=EDGE_CURVE('',#21670,#21670,#18452,.T.);
#26009=EDGE_CURVE('',#21670,#21671,#4788,.T.);
#26010=EDGE_CURVE('',#21671,#21671,#18453,.T.);
#26011=EDGE_CURVE('',#21672,#21672,#18454,.T.);
#26012=EDGE_CURVE('',#21672,#21673,#4789,.T.);
#26013=EDGE_CURVE('',#21673,#21673,#18455,.T.);
#26014=EDGE_CURVE('',#21674,#21674,#18456,.T.);
#26015=EDGE_CURVE('',#21674,#21675,#4790,.T.);
#26016=EDGE_CURVE('',#21675,#21675,#18457,.T.);
#26017=EDGE_CURVE('',#21676,#21676,#18458,.T.);
#26018=EDGE_CURVE('',#21676,#21677,#4791,.T.);
#26019=EDGE_CURVE('',#21677,#21677,#18459,.T.);
#26020=EDGE_CURVE('',#21678,#21678,#18460,.T.);
#26021=EDGE_CURVE('',#21678,#21679,#4792,.T.);
#26022=EDGE_CURVE('',#21679,#21679,#18461,.T.);
#26023=EDGE_CURVE('',#21680,#21680,#18462,.T.);
#26024=EDGE_CURVE('',#21680,#21681,#4793,.T.);
#26025=EDGE_CURVE('',#21681,#21681,#18463,.T.);
#26026=EDGE_CURVE('',#21682,#21682,#18464,.T.);
#26027=EDGE_CURVE('',#21682,#21683,#4794,.T.);
#26028=EDGE_CURVE('',#21683,#21683,#18465,.T.);
#26029=EDGE_CURVE('',#21684,#21684,#18466,.T.);
#26030=EDGE_CURVE('',#21684,#21685,#4795,.T.);
#26031=EDGE_CURVE('',#21685,#21685,#18467,.T.);
#26032=EDGE_CURVE('',#21686,#21686,#18468,.T.);
#26033=EDGE_CURVE('',#21686,#21687,#4796,.T.);
#26034=EDGE_CURVE('',#21687,#21687,#18469,.T.);
#26035=EDGE_CURVE('',#21688,#21688,#18470,.T.);
#26036=EDGE_CURVE('',#21688,#21689,#4797,.T.);
#26037=EDGE_CURVE('',#21689,#21689,#18471,.T.);
#26038=EDGE_CURVE('',#21690,#21690,#18472,.T.);
#26039=EDGE_CURVE('',#21690,#21691,#4798,.T.);
#26040=EDGE_CURVE('',#21691,#21691,#18473,.T.);
#26041=EDGE_CURVE('',#21692,#21692,#18474,.T.);
#26042=EDGE_CURVE('',#21692,#21693,#4799,.T.);
#26043=EDGE_CURVE('',#21693,#21693,#18475,.T.);
#26044=EDGE_CURVE('',#21694,#21694,#18476,.T.);
#26045=EDGE_CURVE('',#21694,#21695,#4800,.T.);
#26046=EDGE_CURVE('',#21695,#21695,#18477,.T.);
#26047=EDGE_CURVE('',#21696,#21696,#18478,.T.);
#26048=EDGE_CURVE('',#21696,#21697,#4801,.T.);
#26049=EDGE_CURVE('',#21697,#21697,#18479,.T.);
#26050=EDGE_CURVE('',#21698,#21698,#18480,.T.);
#26051=EDGE_CURVE('',#21698,#21699,#4802,.T.);
#26052=EDGE_CURVE('',#21699,#21700,#18481,.T.);
#26053=EDGE_CURVE('',#21701,#21700,#2086,.T.);
#26054=EDGE_CURVE('',#21701,#21699,#18482,.T.);
#26055=EDGE_CURVE('',#21702,#21702,#18483,.T.);
#26056=EDGE_CURVE('',#21702,#21703,#4803,.T.);
#26057=EDGE_CURVE('',#21703,#21703,#18484,.T.);
#26058=EDGE_CURVE('',#21704,#21704,#18485,.T.);
#26059=EDGE_CURVE('',#21704,#21705,#4804,.T.);
#26060=EDGE_CURVE('',#21705,#21705,#18486,.T.);
#26061=EDGE_CURVE('',#21706,#21706,#18487,.T.);
#26062=EDGE_CURVE('',#21706,#21707,#4805,.T.);
#26063=EDGE_CURVE('',#21707,#21707,#18488,.T.);
#26064=EDGE_CURVE('',#21708,#21708,#18489,.T.);
#26065=EDGE_CURVE('',#21708,#21709,#4806,.T.);
#26066=EDGE_CURVE('',#21709,#21709,#18490,.T.);
#26067=EDGE_CURVE('',#21710,#21710,#18491,.T.);
#26068=EDGE_CURVE('',#21710,#21711,#4807,.T.);
#26069=EDGE_CURVE('',#21711,#21711,#18492,.T.);
#26070=EDGE_CURVE('',#21712,#21712,#18493,.T.);
#26071=EDGE_CURVE('',#21712,#21713,#4808,.T.);
#26072=EDGE_CURVE('',#21713,#21713,#18494,.T.);
#26073=EDGE_CURVE('',#21714,#21714,#18495,.T.);
#26074=EDGE_CURVE('',#21714,#21715,#4809,.T.);
#26075=EDGE_CURVE('',#21715,#21715,#18496,.T.);
#26076=EDGE_CURVE('',#21716,#21716,#18497,.T.);
#26077=EDGE_CURVE('',#21716,#21717,#4810,.T.);
#26078=EDGE_CURVE('',#21717,#21717,#18498,.T.);
#26079=EDGE_CURVE('',#21718,#21718,#18499,.T.);
#26080=EDGE_CURVE('',#21718,#21719,#4811,.T.);
#26081=EDGE_CURVE('',#21719,#21719,#18500,.T.);
#26082=EDGE_CURVE('',#21720,#21720,#18501,.T.);
#26083=EDGE_CURVE('',#21720,#21721,#4812,.T.);
#26084=EDGE_CURVE('',#21721,#21721,#18502,.T.);
#26085=EDGE_CURVE('',#21722,#21722,#18503,.T.);
#26086=EDGE_CURVE('',#21722,#21723,#4813,.T.);
#26087=EDGE_CURVE('',#21723,#21723,#18504,.T.);
#26088=EDGE_CURVE('',#21724,#21724,#18505,.T.);
#26089=EDGE_CURVE('',#21724,#21725,#4814,.T.);
#26090=EDGE_CURVE('',#21725,#21725,#18506,.T.);
#26091=EDGE_CURVE('',#21726,#21726,#18507,.T.);
#26092=EDGE_CURVE('',#21726,#21727,#4815,.T.);
#26093=EDGE_CURVE('',#21727,#21727,#18508,.T.);
#26094=EDGE_CURVE('',#21728,#21728,#18509,.T.);
#26095=EDGE_CURVE('',#21728,#21729,#4816,.T.);
#26096=EDGE_CURVE('',#21729,#21729,#18510,.T.);
#26097=EDGE_CURVE('',#21730,#21730,#18511,.T.);
#26098=EDGE_CURVE('',#21730,#21731,#4817,.T.);
#26099=EDGE_CURVE('',#21731,#21731,#18512,.T.);
#26100=EDGE_CURVE('',#21732,#21732,#18513,.T.);
#26101=EDGE_CURVE('',#21732,#21733,#4818,.T.);
#26102=EDGE_CURVE('',#21733,#21734,#18514,.T.);
#26103=EDGE_CURVE('',#21735,#21734,#2087,.T.);
#26104=EDGE_CURVE('',#21735,#21733,#18515,.T.);
#26105=EDGE_CURVE('',#21736,#21736,#18516,.T.);
#26106=EDGE_CURVE('',#21736,#21737,#4819,.T.);
#26107=EDGE_CURVE('',#21737,#21737,#18517,.T.);
#26108=EDGE_CURVE('',#21738,#21738,#18518,.T.);
#26109=EDGE_CURVE('',#21738,#21739,#4820,.T.);
#26110=EDGE_CURVE('',#21739,#21740,#18519,.T.);
#26111=EDGE_CURVE('',#21741,#21740,#2088,.T.);
#26112=EDGE_CURVE('',#21741,#21739,#18520,.T.);
#26113=EDGE_CURVE('',#21742,#21742,#18521,.T.);
#26114=EDGE_CURVE('',#21742,#21743,#4821,.T.);
#26115=EDGE_CURVE('',#21743,#21743,#18522,.T.);
#26116=EDGE_CURVE('',#21744,#21744,#18523,.T.);
#26117=EDGE_CURVE('',#21744,#21745,#4822,.T.);
#26118=EDGE_CURVE('',#21745,#21745,#18524,.T.);
#26119=EDGE_CURVE('',#21746,#21746,#18525,.T.);
#26120=EDGE_CURVE('',#21746,#21747,#4823,.T.);
#26121=EDGE_CURVE('',#21747,#21747,#18526,.T.);
#26122=EDGE_CURVE('',#21748,#21748,#18527,.T.);
#26123=EDGE_CURVE('',#21748,#21749,#4824,.T.);
#26124=EDGE_CURVE('',#21749,#21749,#18528,.T.);
#26125=EDGE_CURVE('',#21750,#21750,#18529,.T.);
#26126=EDGE_CURVE('',#21750,#21751,#4825,.T.);
#26127=EDGE_CURVE('',#21751,#21751,#18530,.T.);
#26128=EDGE_CURVE('',#21752,#21752,#18531,.T.);
#26129=EDGE_CURVE('',#21752,#21753,#4826,.T.);
#26130=EDGE_CURVE('',#21753,#21753,#18532,.T.);
#26131=EDGE_CURVE('',#21754,#21754,#18533,.T.);
#26132=EDGE_CURVE('',#21754,#21755,#4827,.T.);
#26133=EDGE_CURVE('',#21755,#21755,#18534,.T.);
#26134=EDGE_CURVE('',#21756,#21756,#18535,.T.);
#26135=EDGE_CURVE('',#21756,#21757,#4828,.T.);
#26136=EDGE_CURVE('',#21757,#21757,#18536,.T.);
#26137=EDGE_CURVE('',#21758,#21758,#18537,.T.);
#26138=EDGE_CURVE('',#21758,#21759,#4829,.T.);
#26139=EDGE_CURVE('',#21759,#21759,#18538,.T.);
#26140=EDGE_CURVE('',#21760,#21760,#18539,.T.);
#26141=EDGE_CURVE('',#21760,#21761,#4830,.T.);
#26142=EDGE_CURVE('',#21761,#21761,#18540,.T.);
#26143=EDGE_CURVE('',#21762,#21762,#18541,.T.);
#26144=EDGE_CURVE('',#21762,#21763,#4831,.T.);
#26145=EDGE_CURVE('',#21763,#21763,#18542,.T.);
#26146=EDGE_CURVE('',#21764,#21764,#18543,.T.);
#26147=EDGE_CURVE('',#21764,#21765,#4832,.T.);
#26148=EDGE_CURVE('',#21765,#21765,#18544,.T.);
#26149=EDGE_CURVE('',#21766,#21766,#18545,.T.);
#26150=EDGE_CURVE('',#21766,#21767,#4833,.T.);
#26151=EDGE_CURVE('',#21767,#21767,#18546,.T.);
#26152=EDGE_CURVE('',#21768,#21768,#18547,.T.);
#26153=EDGE_CURVE('',#21768,#21769,#4834,.T.);
#26154=EDGE_CURVE('',#21769,#21770,#18548,.T.);
#26155=EDGE_CURVE('',#21771,#21770,#2089,.T.);
#26156=EDGE_CURVE('',#21771,#21769,#18549,.T.);
#26157=EDGE_CURVE('',#21772,#21772,#18550,.T.);
#26158=EDGE_CURVE('',#21772,#21773,#4835,.T.);
#26159=EDGE_CURVE('',#21773,#21773,#18551,.T.);
#26160=EDGE_CURVE('',#21774,#21774,#18552,.T.);
#26161=EDGE_CURVE('',#21774,#21775,#4836,.T.);
#26162=EDGE_CURVE('',#21775,#21775,#18553,.T.);
#26163=EDGE_CURVE('',#21776,#21776,#18554,.T.);
#26164=EDGE_CURVE('',#21776,#21777,#4837,.T.);
#26165=EDGE_CURVE('',#21777,#21777,#18555,.T.);
#26166=EDGE_CURVE('',#21778,#21778,#18556,.T.);
#26167=EDGE_CURVE('',#21778,#21779,#4838,.T.);
#26168=EDGE_CURVE('',#21779,#21779,#18557,.T.);
#26169=EDGE_CURVE('',#21780,#21780,#18558,.T.);
#26170=EDGE_CURVE('',#21780,#21781,#4839,.T.);
#26171=EDGE_CURVE('',#21781,#21781,#18559,.T.);
#26172=EDGE_CURVE('',#21782,#21782,#18560,.T.);
#26173=EDGE_CURVE('',#21782,#21783,#4840,.T.);
#26174=EDGE_CURVE('',#21783,#21783,#18561,.T.);
#26175=EDGE_CURVE('',#21784,#21784,#18562,.T.);
#26176=EDGE_CURVE('',#21784,#21785,#4841,.T.);
#26177=EDGE_CURVE('',#21785,#21785,#18563,.T.);
#26178=EDGE_CURVE('',#21786,#21786,#18564,.T.);
#26179=EDGE_CURVE('',#21786,#21787,#4842,.T.);
#26180=EDGE_CURVE('',#21787,#21787,#18565,.T.);
#26181=EDGE_CURVE('',#21788,#21788,#18566,.T.);
#26182=EDGE_CURVE('',#21788,#21789,#4843,.T.);
#26183=EDGE_CURVE('',#21789,#21789,#18567,.T.);
#26184=EDGE_CURVE('',#21790,#21790,#18568,.T.);
#26185=EDGE_CURVE('',#21790,#21791,#4844,.T.);
#26186=EDGE_CURVE('',#21791,#21791,#18569,.T.);
#26187=EDGE_CURVE('',#21792,#21792,#18570,.T.);
#26188=EDGE_CURVE('',#21792,#21793,#4845,.T.);
#26189=EDGE_CURVE('',#21793,#21793,#18571,.T.);
#26190=EDGE_CURVE('',#21794,#21794,#18572,.T.);
#26191=EDGE_CURVE('',#21794,#21795,#4846,.T.);
#26192=EDGE_CURVE('',#21795,#21795,#18573,.T.);
#26193=EDGE_CURVE('',#21796,#21796,#18574,.T.);
#26194=EDGE_CURVE('',#21796,#21797,#4847,.T.);
#26195=EDGE_CURVE('',#21797,#21797,#18575,.T.);
#26196=EDGE_CURVE('',#21798,#21798,#18576,.T.);
#26197=EDGE_CURVE('',#21798,#21799,#4848,.T.);
#26198=EDGE_CURVE('',#21799,#21799,#18577,.T.);
#26199=EDGE_CURVE('',#21800,#21800,#18578,.T.);
#26200=EDGE_CURVE('',#21800,#21801,#4849,.T.);
#26201=EDGE_CURVE('',#21801,#21801,#18579,.T.);
#26202=EDGE_CURVE('',#21802,#21802,#18580,.T.);
#26203=EDGE_CURVE('',#21802,#21803,#4850,.T.);
#26204=EDGE_CURVE('',#21803,#21803,#18581,.T.);
#26205=EDGE_CURVE('',#21804,#21804,#18582,.T.);
#26206=EDGE_CURVE('',#21804,#21805,#4851,.T.);
#26207=EDGE_CURVE('',#21805,#21805,#18583,.T.);
#26208=EDGE_CURVE('',#21806,#21806,#18584,.T.);
#26209=EDGE_CURVE('',#21806,#21807,#4852,.T.);
#26210=EDGE_CURVE('',#21807,#21807,#18585,.T.);
#26211=EDGE_CURVE('',#21808,#21808,#18586,.T.);
#26212=EDGE_CURVE('',#21808,#21809,#4853,.T.);
#26213=EDGE_CURVE('',#21809,#21809,#18587,.T.);
#26214=EDGE_CURVE('',#21810,#21810,#18588,.T.);
#26215=EDGE_CURVE('',#21810,#21811,#4854,.T.);
#26216=EDGE_CURVE('',#21811,#21811,#18589,.T.);
#26217=EDGE_CURVE('',#21812,#21812,#18590,.T.);
#26218=EDGE_CURVE('',#21812,#21813,#4855,.T.);
#26219=EDGE_CURVE('',#21813,#21813,#18591,.T.);
#26220=EDGE_CURVE('',#21814,#21814,#18592,.T.);
#26221=EDGE_CURVE('',#21814,#21815,#4856,.T.);
#26222=EDGE_CURVE('',#21815,#21815,#18593,.T.);
#26223=EDGE_CURVE('',#21816,#21816,#18594,.T.);
#26224=EDGE_CURVE('',#21816,#21817,#4857,.T.);
#26225=EDGE_CURVE('',#21817,#21817,#18595,.T.);
#26226=EDGE_CURVE('',#21818,#21818,#18596,.T.);
#26227=EDGE_CURVE('',#21818,#21819,#4858,.T.);
#26228=EDGE_CURVE('',#21819,#21819,#18597,.T.);
#26229=EDGE_CURVE('',#21820,#21820,#18598,.T.);
#26230=EDGE_CURVE('',#21820,#21821,#4859,.T.);
#26231=EDGE_CURVE('',#21821,#21821,#18599,.T.);
#26232=EDGE_CURVE('',#21822,#21822,#18600,.T.);
#26233=EDGE_CURVE('',#21822,#21823,#4860,.T.);
#26234=EDGE_CURVE('',#21823,#21823,#18601,.T.);
#26235=EDGE_CURVE('',#21824,#21824,#18602,.T.);
#26236=EDGE_CURVE('',#21824,#21825,#4861,.T.);
#26237=EDGE_CURVE('',#21825,#21825,#18603,.T.);
#26238=EDGE_CURVE('',#21826,#21826,#18604,.T.);
#26239=EDGE_CURVE('',#21826,#21827,#4862,.T.);
#26240=EDGE_CURVE('',#21827,#21828,#18605,.T.);
#26241=EDGE_CURVE('',#21829,#21828,#2090,.T.);
#26242=EDGE_CURVE('',#21829,#21827,#18606,.T.);
#26243=EDGE_CURVE('',#21830,#21830,#18607,.T.);
#26244=EDGE_CURVE('',#21830,#21831,#4863,.T.);
#26245=EDGE_CURVE('',#21831,#21831,#18608,.T.);
#26246=EDGE_CURVE('',#21832,#21832,#18609,.T.);
#26247=EDGE_CURVE('',#21832,#21833,#4864,.T.);
#26248=EDGE_CURVE('',#21833,#21833,#18610,.T.);
#26249=EDGE_CURVE('',#21834,#21834,#18611,.T.);
#26250=EDGE_CURVE('',#21834,#21835,#4865,.T.);
#26251=EDGE_CURVE('',#21835,#21835,#18612,.T.);
#26252=EDGE_CURVE('',#21836,#21836,#18613,.T.);
#26253=EDGE_CURVE('',#21836,#21837,#4866,.T.);
#26254=EDGE_CURVE('',#21837,#21837,#18614,.T.);
#26255=EDGE_CURVE('',#21838,#21838,#18615,.T.);
#26256=EDGE_CURVE('',#21838,#21839,#4867,.T.);
#26257=EDGE_CURVE('',#21839,#21839,#18616,.T.);
#26258=EDGE_CURVE('',#21840,#21840,#18617,.T.);
#26259=EDGE_CURVE('',#21840,#21841,#4868,.T.);
#26260=EDGE_CURVE('',#21841,#21841,#18618,.T.);
#26261=EDGE_CURVE('',#21842,#21842,#18619,.T.);
#26262=EDGE_CURVE('',#21842,#21843,#4869,.T.);
#26263=EDGE_CURVE('',#21843,#21843,#18620,.T.);
#26264=EDGE_CURVE('',#21844,#21844,#18621,.T.);
#26265=EDGE_CURVE('',#21844,#21845,#4870,.T.);
#26266=EDGE_CURVE('',#21845,#21845,#18622,.T.);
#26267=EDGE_CURVE('',#21846,#21846,#18623,.T.);
#26268=EDGE_CURVE('',#21846,#21847,#4871,.T.);
#26269=EDGE_CURVE('',#21847,#21847,#18624,.T.);
#26270=EDGE_CURVE('',#21848,#21848,#18625,.T.);
#26271=EDGE_CURVE('',#21848,#21849,#4872,.T.);
#26272=EDGE_CURVE('',#21849,#21849,#18626,.T.);
#26273=EDGE_CURVE('',#21850,#21850,#18627,.T.);
#26274=EDGE_CURVE('',#21850,#21851,#4873,.T.);
#26275=EDGE_CURVE('',#21851,#21851,#18628,.T.);
#26276=EDGE_CURVE('',#21852,#21852,#18629,.T.);
#26277=EDGE_CURVE('',#21852,#21853,#4874,.T.);
#26278=EDGE_CURVE('',#21853,#21853,#18630,.T.);
#26279=EDGE_CURVE('',#21854,#21854,#18631,.T.);
#26280=EDGE_CURVE('',#21854,#21855,#4875,.T.);
#26281=EDGE_CURVE('',#21855,#21855,#18632,.T.);
#26282=EDGE_CURVE('',#21856,#21856,#18633,.T.);
#26283=EDGE_CURVE('',#21856,#21857,#4876,.T.);
#26284=EDGE_CURVE('',#21857,#21857,#18634,.T.);
#26285=EDGE_CURVE('',#21858,#21858,#18635,.T.);
#26286=EDGE_CURVE('',#21858,#21859,#4877,.T.);
#26287=EDGE_CURVE('',#21859,#21859,#18636,.T.);
#26288=EDGE_CURVE('',#21860,#21860,#18637,.T.);
#26289=EDGE_CURVE('',#21860,#21861,#4878,.T.);
#26290=EDGE_CURVE('',#21861,#21861,#18638,.T.);
#26291=EDGE_CURVE('',#21862,#21862,#18639,.T.);
#26292=EDGE_CURVE('',#21862,#21863,#4879,.T.);
#26293=EDGE_CURVE('',#21863,#21863,#18640,.T.);
#26294=EDGE_CURVE('',#21864,#21864,#18641,.T.);
#26295=EDGE_CURVE('',#21864,#21865,#4880,.T.);
#26296=EDGE_CURVE('',#21865,#21865,#18642,.T.);
#26297=EDGE_CURVE('',#21866,#21866,#18643,.T.);
#26298=EDGE_CURVE('',#21866,#21867,#4881,.T.);
#26299=EDGE_CURVE('',#21867,#21867,#18644,.T.);
#26300=EDGE_CURVE('',#21868,#21868,#18645,.T.);
#26301=EDGE_CURVE('',#21868,#21869,#4882,.T.);
#26302=EDGE_CURVE('',#21869,#21869,#18646,.T.);
#26303=EDGE_CURVE('',#21870,#21870,#18647,.T.);
#26304=EDGE_CURVE('',#21870,#21871,#4883,.T.);
#26305=EDGE_CURVE('',#21871,#21871,#18648,.T.);
#26306=EDGE_CURVE('',#21872,#21872,#18649,.T.);
#26307=EDGE_CURVE('',#21872,#21873,#4884,.T.);
#26308=EDGE_CURVE('',#21873,#21873,#18650,.T.);
#26309=EDGE_CURVE('',#21874,#21874,#18651,.T.);
#26310=EDGE_CURVE('',#21874,#21875,#4885,.T.);
#26311=EDGE_CURVE('',#21875,#21875,#18652,.T.);
#26312=EDGE_CURVE('',#21876,#21876,#18653,.T.);
#26313=EDGE_CURVE('',#21876,#21877,#4886,.T.);
#26314=EDGE_CURVE('',#21877,#21877,#18654,.T.);
#26315=EDGE_CURVE('',#21878,#21878,#18655,.T.);
#26316=EDGE_CURVE('',#21878,#21879,#4887,.T.);
#26317=EDGE_CURVE('',#21879,#21879,#18656,.T.);
#26318=EDGE_CURVE('',#21880,#21880,#18657,.T.);
#26319=EDGE_CURVE('',#21880,#21881,#4888,.T.);
#26320=EDGE_CURVE('',#21881,#21881,#18658,.T.);
#26321=EDGE_CURVE('',#21882,#21882,#18659,.T.);
#26322=EDGE_CURVE('',#21882,#21883,#4889,.T.);
#26323=EDGE_CURVE('',#21883,#21883,#18660,.T.);
#26324=EDGE_CURVE('',#21884,#21884,#18661,.T.);
#26325=EDGE_CURVE('',#21884,#21885,#4890,.T.);
#26326=EDGE_CURVE('',#21885,#21885,#18662,.T.);
#26327=EDGE_CURVE('',#21886,#21886,#18663,.T.);
#26328=EDGE_CURVE('',#21886,#21887,#4891,.T.);
#26329=EDGE_CURVE('',#21887,#21887,#18664,.T.);
#26330=EDGE_CURVE('',#21888,#21888,#18665,.T.);
#26331=EDGE_CURVE('',#21888,#21889,#4892,.T.);
#26332=EDGE_CURVE('',#21889,#21889,#18666,.T.);
#26333=EDGE_CURVE('',#21890,#21890,#18667,.T.);
#26334=EDGE_CURVE('',#21890,#21891,#4893,.T.);
#26335=EDGE_CURVE('',#21891,#21891,#18668,.T.);
#26336=EDGE_CURVE('',#21892,#21892,#18669,.T.);
#26337=EDGE_CURVE('',#21892,#21893,#4894,.T.);
#26338=EDGE_CURVE('',#21893,#21893,#18670,.T.);
#26339=EDGE_CURVE('',#21894,#21894,#18671,.T.);
#26340=EDGE_CURVE('',#21894,#21895,#4895,.T.);
#26341=EDGE_CURVE('',#21895,#21895,#18672,.T.);
#26342=EDGE_CURVE('',#21896,#21896,#18673,.T.);
#26343=EDGE_CURVE('',#21896,#21897,#4896,.T.);
#26344=EDGE_CURVE('',#21897,#21898,#18674,.T.);
#26345=EDGE_CURVE('',#21899,#21898,#2091,.T.);
#26346=EDGE_CURVE('',#21900,#21899,#2092,.T.);
#26347=EDGE_CURVE('',#21900,#21897,#18675,.T.);
#26348=EDGE_CURVE('',#21901,#21901,#18676,.T.);
#26349=EDGE_CURVE('',#21901,#21902,#4897,.T.);
#26350=EDGE_CURVE('',#21902,#21902,#18677,.T.);
#26351=EDGE_CURVE('',#21903,#21903,#18678,.T.);
#26352=EDGE_CURVE('',#21903,#21904,#4898,.T.);
#26353=EDGE_CURVE('',#21904,#21904,#18679,.T.);
#26354=EDGE_CURVE('',#21905,#21905,#18680,.T.);
#26355=EDGE_CURVE('',#21905,#21906,#4899,.T.);
#26356=EDGE_CURVE('',#21906,#21906,#18681,.T.);
#26357=EDGE_CURVE('',#21907,#21907,#18682,.T.);
#26358=EDGE_CURVE('',#21907,#21908,#4900,.T.);
#26359=EDGE_CURVE('',#21908,#21908,#18683,.T.);
#26360=EDGE_CURVE('',#21909,#21909,#18684,.T.);
#26361=EDGE_CURVE('',#21909,#21910,#4901,.T.);
#26362=EDGE_CURVE('',#21910,#21910,#18685,.T.);
#26363=EDGE_CURVE('',#21911,#21911,#18686,.T.);
#26364=EDGE_CURVE('',#21911,#21912,#4902,.T.);
#26365=EDGE_CURVE('',#21912,#21912,#18687,.T.);
#26366=EDGE_CURVE('',#21913,#21913,#18688,.T.);
#26367=EDGE_CURVE('',#21913,#21914,#4903,.T.);
#26368=EDGE_CURVE('',#21914,#21914,#18689,.T.);
#26369=EDGE_CURVE('',#21915,#21915,#18690,.T.);
#26370=EDGE_CURVE('',#21915,#21916,#4904,.T.);
#26371=EDGE_CURVE('',#21916,#21916,#18691,.T.);
#26372=EDGE_CURVE('',#21917,#21917,#18692,.T.);
#26373=EDGE_CURVE('',#21917,#21918,#4905,.T.);
#26374=EDGE_CURVE('',#21918,#21918,#18693,.T.);
#26375=EDGE_CURVE('',#21919,#21919,#18694,.T.);
#26376=EDGE_CURVE('',#21919,#21920,#4906,.T.);
#26377=EDGE_CURVE('',#21920,#21920,#18695,.T.);
#26378=EDGE_CURVE('',#21921,#21921,#18696,.T.);
#26379=EDGE_CURVE('',#21921,#21922,#4907,.T.);
#26380=EDGE_CURVE('',#21922,#21922,#18697,.T.);
#26381=EDGE_CURVE('',#21923,#21923,#18698,.T.);
#26382=EDGE_CURVE('',#21923,#21924,#4908,.T.);
#26383=EDGE_CURVE('',#21924,#21924,#18699,.T.);
#26384=EDGE_CURVE('',#21925,#21925,#18700,.T.);
#26385=EDGE_CURVE('',#21925,#21926,#4909,.T.);
#26386=EDGE_CURVE('',#21926,#21926,#18701,.T.);
#26387=EDGE_CURVE('',#21927,#21927,#18702,.T.);
#26388=EDGE_CURVE('',#21927,#21928,#4910,.T.);
#26389=EDGE_CURVE('',#21928,#21928,#18703,.T.);
#26390=EDGE_CURVE('',#21929,#21929,#18704,.T.);
#26391=EDGE_CURVE('',#21929,#21930,#4911,.T.);
#26392=EDGE_CURVE('',#21930,#21930,#18705,.T.);
#26393=EDGE_CURVE('',#21931,#21931,#18706,.T.);
#26394=EDGE_CURVE('',#21931,#21932,#4912,.T.);
#26395=EDGE_CURVE('',#21932,#21932,#18707,.T.);
#26396=EDGE_CURVE('',#21933,#21933,#18708,.T.);
#26397=EDGE_CURVE('',#21933,#21934,#4913,.T.);
#26398=EDGE_CURVE('',#21934,#21934,#18709,.T.);
#26399=EDGE_CURVE('',#21935,#21935,#18710,.T.);
#26400=EDGE_CURVE('',#21935,#21936,#4914,.T.);
#26401=EDGE_CURVE('',#21936,#21937,#18711,.T.);
#26402=EDGE_CURVE('',#21938,#21937,#2093,.T.);
#26403=EDGE_CURVE('',#21938,#21936,#18712,.T.);
#26404=EDGE_CURVE('',#21939,#21939,#18713,.T.);
#26405=EDGE_CURVE('',#21939,#21940,#4915,.T.);
#26406=EDGE_CURVE('',#21940,#21940,#18714,.T.);
#26407=EDGE_CURVE('',#21941,#21941,#18715,.T.);
#26408=EDGE_CURVE('',#21941,#21942,#4916,.T.);
#26409=EDGE_CURVE('',#21942,#21942,#18716,.T.);
#26410=EDGE_CURVE('',#21943,#21943,#18717,.T.);
#26411=EDGE_CURVE('',#21943,#21944,#4917,.T.);
#26412=EDGE_CURVE('',#21944,#21944,#18718,.T.);
#26413=EDGE_CURVE('',#21945,#21945,#18719,.T.);
#26414=EDGE_CURVE('',#21945,#21946,#4918,.T.);
#26415=EDGE_CURVE('',#21946,#21946,#18720,.T.);
#26416=EDGE_CURVE('',#21947,#21947,#18721,.T.);
#26417=EDGE_CURVE('',#21947,#21948,#4919,.T.);
#26418=EDGE_CURVE('',#21948,#21948,#18722,.T.);
#26419=EDGE_CURVE('',#21949,#21949,#18723,.T.);
#26420=EDGE_CURVE('',#21949,#21950,#4920,.T.);
#26421=EDGE_CURVE('',#21950,#21950,#18724,.T.);
#26422=EDGE_CURVE('',#21951,#21951,#18725,.T.);
#26423=EDGE_CURVE('',#21951,#21952,#4921,.T.);
#26424=EDGE_CURVE('',#21952,#21952,#18726,.T.);
#26425=EDGE_CURVE('',#21953,#21953,#18727,.T.);
#26426=EDGE_CURVE('',#21953,#21954,#4922,.T.);
#26427=EDGE_CURVE('',#21954,#21954,#18728,.T.);
#26428=EDGE_CURVE('',#21955,#21955,#18729,.T.);
#26429=EDGE_CURVE('',#21955,#21956,#4923,.T.);
#26430=EDGE_CURVE('',#21956,#21956,#18730,.T.);
#26431=EDGE_CURVE('',#21957,#21957,#18731,.T.);
#26432=EDGE_CURVE('',#21957,#21958,#4924,.T.);
#26433=EDGE_CURVE('',#21958,#21958,#18732,.T.);
#26434=EDGE_CURVE('',#21959,#21959,#18733,.T.);
#26435=EDGE_CURVE('',#21959,#21960,#4925,.T.);
#26436=EDGE_CURVE('',#21960,#21960,#18734,.T.);
#26437=EDGE_CURVE('',#21961,#21961,#18735,.T.);
#26438=EDGE_CURVE('',#21961,#21962,#4926,.T.);
#26439=EDGE_CURVE('',#21962,#21962,#18736,.T.);
#26440=EDGE_CURVE('',#21963,#21963,#18737,.T.);
#26441=EDGE_CURVE('',#21963,#21964,#4927,.T.);
#26442=EDGE_CURVE('',#21964,#21964,#18738,.T.);
#26443=EDGE_CURVE('',#21965,#21965,#18739,.T.);
#26444=EDGE_CURVE('',#21965,#21966,#4928,.T.);
#26445=EDGE_CURVE('',#21966,#21966,#18740,.T.);
#26446=EDGE_CURVE('',#21967,#21967,#18741,.T.);
#26447=EDGE_CURVE('',#21967,#21968,#4929,.T.);
#26448=EDGE_CURVE('',#21968,#21968,#18742,.T.);
#26449=EDGE_CURVE('',#21969,#21969,#18743,.T.);
#26450=EDGE_CURVE('',#21969,#21970,#4930,.T.);
#26451=EDGE_CURVE('',#21970,#21970,#18744,.T.);
#26452=EDGE_CURVE('',#21971,#21971,#18745,.T.);
#26453=EDGE_CURVE('',#21971,#21972,#4931,.T.);
#26454=EDGE_CURVE('',#21972,#21972,#18746,.T.);
#26455=EDGE_CURVE('',#21973,#21973,#18747,.T.);
#26456=EDGE_CURVE('',#21973,#21974,#4932,.T.);
#26457=EDGE_CURVE('',#21975,#21974,#2094,.F.);
#26458=EDGE_CURVE('',#21975,#21976,#18748,.T.);
#26459=EDGE_CURVE('',#21974,#21976,#2095,.F.);
#26460=EDGE_CURVE('',#21977,#21977,#18749,.T.);
#26461=EDGE_CURVE('',#21977,#21978,#4933,.T.);
#26462=EDGE_CURVE('',#21978,#21978,#18750,.T.);
#26463=EDGE_CURVE('',#21979,#21979,#18751,.T.);
#26464=EDGE_CURVE('',#21979,#21980,#4934,.T.);
#26465=EDGE_CURVE('',#21980,#21980,#18752,.T.);
#26466=EDGE_CURVE('',#21981,#21981,#18753,.T.);
#26467=EDGE_CURVE('',#21981,#21982,#4935,.T.);
#26468=EDGE_CURVE('',#21982,#21982,#18754,.T.);
#26469=EDGE_CURVE('',#21983,#21983,#18755,.T.);
#26470=EDGE_CURVE('',#21983,#21984,#4936,.T.);
#26471=EDGE_CURVE('',#21984,#21984,#18756,.T.);
#26472=EDGE_CURVE('',#21985,#21985,#18757,.T.);
#26473=EDGE_CURVE('',#21985,#21986,#4937,.T.);
#26474=EDGE_CURVE('',#21986,#21986,#18758,.T.);
#26475=EDGE_CURVE('',#21987,#21987,#18759,.T.);
#26476=EDGE_CURVE('',#21987,#21988,#4938,.T.);
#26477=EDGE_CURVE('',#21988,#21988,#18760,.T.);
#26478=EDGE_CURVE('',#21989,#21989,#18761,.T.);
#26479=EDGE_CURVE('',#21989,#21990,#4939,.T.);
#26480=EDGE_CURVE('',#21990,#21990,#18762,.T.);
#26481=EDGE_CURVE('',#21991,#21991,#18763,.T.);
#26482=EDGE_CURVE('',#21991,#21992,#4940,.T.);
#26483=EDGE_CURVE('',#21992,#21992,#18764,.T.);
#26484=EDGE_CURVE('',#21993,#21993,#18765,.T.);
#26485=EDGE_CURVE('',#21993,#21994,#4941,.T.);
#26486=EDGE_CURVE('',#21994,#21994,#18766,.T.);
#26487=EDGE_CURVE('',#21995,#21995,#18767,.T.);
#26488=EDGE_CURVE('',#21995,#21996,#4942,.T.);
#26489=EDGE_CURVE('',#21996,#21996,#18768,.T.);
#26490=EDGE_CURVE('',#21997,#21997,#18769,.T.);
#26491=EDGE_CURVE('',#21997,#21998,#4943,.T.);
#26492=EDGE_CURVE('',#21998,#21998,#18770,.T.);
#26493=EDGE_CURVE('',#21999,#21999,#18771,.T.);
#26494=EDGE_CURVE('',#21999,#22000,#4944,.T.);
#26495=EDGE_CURVE('',#22000,#22000,#18772,.T.);
#26496=EDGE_CURVE('',#22001,#22001,#18773,.T.);
#26497=EDGE_CURVE('',#22001,#22002,#4945,.T.);
#26498=EDGE_CURVE('',#22002,#22002,#18774,.T.);
#26499=EDGE_CURVE('',#22003,#22003,#18775,.T.);
#26500=EDGE_CURVE('',#22003,#22004,#4946,.T.);
#26501=EDGE_CURVE('',#22004,#22004,#18776,.T.);
#26502=EDGE_CURVE('',#22005,#22005,#18777,.T.);
#26503=EDGE_CURVE('',#22005,#22006,#4947,.T.);
#26504=EDGE_CURVE('',#22006,#22006,#18778,.T.);
#26505=EDGE_CURVE('',#22007,#22007,#18779,.T.);
#26506=EDGE_CURVE('',#22007,#22008,#4948,.T.);
#26507=EDGE_CURVE('',#22009,#22008,#2096,.F.);
#26508=EDGE_CURVE('',#22009,#22010,#18780,.T.);
#26509=EDGE_CURVE('',#22008,#22010,#2097,.F.);
#26510=EDGE_CURVE('',#22011,#22011,#18781,.T.);
#26511=EDGE_CURVE('',#22011,#22012,#4949,.T.);
#26512=EDGE_CURVE('',#22012,#22012,#18782,.T.);
#26513=EDGE_CURVE('',#22013,#22013,#18783,.T.);
#26514=EDGE_CURVE('',#22013,#22014,#4950,.T.);
#26515=EDGE_CURVE('',#22014,#22014,#18784,.T.);
#26516=EDGE_CURVE('',#22015,#22015,#18785,.T.);
#26517=EDGE_CURVE('',#22015,#22016,#4951,.T.);
#26518=EDGE_CURVE('',#22016,#22016,#18786,.T.);
#26519=EDGE_CURVE('',#22017,#22017,#18787,.T.);
#26520=EDGE_CURVE('',#22017,#22018,#4952,.T.);
#26521=EDGE_CURVE('',#22018,#22018,#18788,.T.);
#26522=EDGE_CURVE('',#22019,#22019,#18789,.T.);
#26523=EDGE_CURVE('',#22019,#22020,#4953,.T.);
#26524=EDGE_CURVE('',#22020,#22020,#18790,.T.);
#26525=EDGE_CURVE('',#22021,#22021,#18791,.T.);
#26526=EDGE_CURVE('',#22021,#22022,#4954,.T.);
#26527=EDGE_CURVE('',#22022,#22022,#18792,.T.);
#26528=EDGE_CURVE('',#22023,#22023,#18793,.T.);
#26529=EDGE_CURVE('',#22023,#22024,#4955,.T.);
#26530=EDGE_CURVE('',#22024,#22024,#18794,.T.);
#26531=EDGE_CURVE('',#22025,#22025,#18795,.T.);
#26532=EDGE_CURVE('',#22025,#22026,#4956,.T.);
#26533=EDGE_CURVE('',#22026,#22026,#18796,.T.);
#26534=EDGE_CURVE('',#22027,#22027,#18797,.T.);
#26535=EDGE_CURVE('',#22027,#22028,#4957,.T.);
#26536=EDGE_CURVE('',#22028,#22028,#18798,.T.);
#26537=EDGE_CURVE('',#22029,#22029,#18799,.T.);
#26538=EDGE_CURVE('',#22029,#22030,#4958,.T.);
#26539=EDGE_CURVE('',#22030,#22030,#18800,.T.);
#26540=EDGE_CURVE('',#22031,#22031,#18801,.T.);
#26541=EDGE_CURVE('',#22031,#22032,#4959,.T.);
#26542=EDGE_CURVE('',#22032,#22032,#18802,.T.);
#26543=EDGE_CURVE('',#22033,#22033,#18803,.T.);
#26544=EDGE_CURVE('',#22033,#22034,#4960,.T.);
#26545=EDGE_CURVE('',#22034,#22034,#18804,.T.);
#26546=EDGE_CURVE('',#22035,#22035,#18805,.T.);
#26547=EDGE_CURVE('',#22035,#22036,#4961,.T.);
#26548=EDGE_CURVE('',#22036,#22036,#18806,.T.);
#26549=EDGE_CURVE('',#22037,#22037,#18807,.T.);
#26550=EDGE_CURVE('',#22037,#22038,#4962,.T.);
#26551=EDGE_CURVE('',#22038,#22038,#18808,.T.);
#26552=EDGE_CURVE('',#22039,#22039,#18809,.T.);
#26553=EDGE_CURVE('',#22039,#22040,#4963,.T.);
#26554=EDGE_CURVE('',#22040,#22040,#18810,.T.);
#26555=EDGE_CURVE('',#22041,#22041,#18811,.T.);
#26556=EDGE_CURVE('',#22041,#22042,#4964,.T.);
#26557=EDGE_CURVE('',#22042,#22042,#18812,.T.);
#26558=EDGE_CURVE('',#22043,#22043,#18813,.T.);
#26559=EDGE_CURVE('',#22043,#22044,#4965,.T.);
#26560=EDGE_CURVE('',#22044,#22044,#18814,.T.);
#26561=EDGE_CURVE('',#22045,#22045,#18815,.T.);
#26562=EDGE_CURVE('',#22045,#22046,#4966,.T.);
#26563=EDGE_CURVE('',#22047,#22046,#2098,.F.);
#26564=EDGE_CURVE('',#22047,#22048,#18816,.T.);
#26565=EDGE_CURVE('',#22046,#22048,#2099,.F.);
#26566=EDGE_CURVE('',#22049,#22049,#18817,.T.);
#26567=EDGE_CURVE('',#22049,#22050,#4967,.T.);
#26568=EDGE_CURVE('',#22050,#22050,#18818,.T.);
#26569=EDGE_CURVE('',#22051,#22051,#18819,.T.);
#26570=EDGE_CURVE('',#22051,#22052,#4968,.T.);
#26571=EDGE_CURVE('',#22052,#22052,#18820,.T.);
#26572=EDGE_CURVE('',#22053,#22053,#18821,.T.);
#26573=EDGE_CURVE('',#22053,#22054,#4969,.T.);
#26574=EDGE_CURVE('',#22054,#22054,#18822,.T.);
#26575=EDGE_CURVE('',#22055,#22055,#18823,.T.);
#26576=EDGE_CURVE('',#22055,#22056,#4970,.T.);
#26577=EDGE_CURVE('',#22056,#22056,#18824,.T.);
#26578=EDGE_CURVE('',#22057,#22057,#18825,.T.);
#26579=EDGE_CURVE('',#22057,#22058,#4971,.T.);
#26580=EDGE_CURVE('',#22058,#22058,#18826,.T.);
#26581=EDGE_CURVE('',#22059,#22059,#18827,.T.);
#26582=EDGE_CURVE('',#22059,#22060,#4972,.T.);
#26583=EDGE_CURVE('',#22060,#22060,#18828,.T.);
#26584=EDGE_CURVE('',#22061,#22061,#18829,.T.);
#26585=EDGE_CURVE('',#22061,#22062,#4973,.T.);
#26586=EDGE_CURVE('',#22062,#22062,#18830,.T.);
#26587=EDGE_CURVE('',#22063,#22063,#18831,.T.);
#26588=EDGE_CURVE('',#22063,#22064,#4974,.T.);
#26589=EDGE_CURVE('',#22064,#22064,#18832,.T.);
#26590=EDGE_CURVE('',#22065,#22065,#18833,.T.);
#26591=EDGE_CURVE('',#22065,#22066,#4975,.T.);
#26592=EDGE_CURVE('',#22066,#22066,#18834,.T.);
#26593=EDGE_CURVE('',#22067,#22067,#18835,.T.);
#26594=EDGE_CURVE('',#22067,#22068,#4976,.T.);
#26595=EDGE_CURVE('',#22068,#22068,#18836,.T.);
#26596=EDGE_CURVE('',#22069,#22069,#18837,.T.);
#26597=EDGE_CURVE('',#22069,#22070,#4977,.T.);
#26598=EDGE_CURVE('',#22070,#22070,#18838,.T.);
#26599=EDGE_CURVE('',#22071,#22071,#18839,.T.);
#26600=EDGE_CURVE('',#22071,#22072,#4978,.T.);
#26601=EDGE_CURVE('',#22072,#22072,#18840,.T.);
#26602=EDGE_CURVE('',#22073,#22073,#18841,.T.);
#26603=EDGE_CURVE('',#22073,#22074,#4979,.T.);
#26604=EDGE_CURVE('',#22074,#22074,#18842,.T.);
#26605=EDGE_CURVE('',#22075,#22075,#18843,.T.);
#26606=EDGE_CURVE('',#22075,#22076,#4980,.T.);
#26607=EDGE_CURVE('',#22076,#22076,#18844,.T.);
#26608=EDGE_CURVE('',#22077,#22077,#18845,.T.);
#26609=EDGE_CURVE('',#22077,#22078,#4981,.T.);
#26610=EDGE_CURVE('',#22078,#22078,#18846,.T.);
#26611=EDGE_CURVE('',#22079,#22079,#18847,.T.);
#26612=EDGE_CURVE('',#22079,#22080,#4982,.T.);
#26613=EDGE_CURVE('',#22080,#22080,#18848,.T.);
#26614=EDGE_CURVE('',#22081,#22081,#18849,.T.);
#26615=EDGE_CURVE('',#22081,#22082,#4983,.T.);
#26616=EDGE_CURVE('',#22082,#22082,#18850,.T.);
#26617=EDGE_CURVE('',#22083,#22083,#18851,.T.);
#26618=EDGE_CURVE('',#22083,#22084,#4984,.T.);
#26619=EDGE_CURVE('',#22085,#22084,#2100,.F.);
#26620=EDGE_CURVE('',#22085,#22086,#18852,.T.);
#26621=EDGE_CURVE('',#22084,#22086,#2101,.F.);
#26622=EDGE_CURVE('',#22087,#22087,#18853,.T.);
#26623=EDGE_CURVE('',#22087,#22088,#4985,.T.);
#26624=EDGE_CURVE('',#22088,#22088,#18854,.T.);
#26625=EDGE_CURVE('',#22089,#22090,#18855,.T.);
#26626=EDGE_CURVE('',#21899,#22089,#18856,.T.);
#26627=EDGE_CURVE('',#21938,#21898,#18857,.T.);
#26628=EDGE_CURVE('',#21975,#21937,#18858,.T.);
#26629=EDGE_CURVE('',#22009,#21976,#18859,.T.);
#26630=EDGE_CURVE('',#22047,#22010,#18860,.T.);
#26631=EDGE_CURVE('',#22085,#22048,#18861,.T.);
#26632=EDGE_CURVE('',#21032,#22086,#18862,.T.);
#26633=EDGE_CURVE('',#21070,#21033,#18863,.T.);
#26634=EDGE_CURVE('',#21104,#21071,#18864,.T.);
#26635=EDGE_CURVE('',#21142,#21105,#18865,.T.);
#26636=EDGE_CURVE('',#21180,#21143,#18866,.T.);
#26637=EDGE_CURVE('',#21218,#21181,#18867,.T.);
#26638=EDGE_CURVE('',#21256,#21219,#18868,.T.);
#26639=EDGE_CURVE('',#21290,#21257,#18869,.T.);
#26640=EDGE_CURVE('',#21328,#21291,#18870,.T.);
#26641=EDGE_CURVE('',#21366,#21329,#18871,.T.);
#26642=EDGE_CURVE('',#21404,#21367,#18872,.T.);
#26643=EDGE_CURVE('',#21442,#21405,#18873,.T.);
#26644=EDGE_CURVE('',#21476,#21443,#18874,.T.);
#26645=EDGE_CURVE('',#21514,#21477,#18875,.T.);
#26646=EDGE_CURVE('',#21552,#21515,#18876,.T.);
#26647=EDGE_CURVE('',#21590,#21553,#18877,.T.);
#26648=EDGE_CURVE('',#21628,#21591,#18878,.T.);
#26649=EDGE_CURVE('',#21662,#21629,#18879,.T.);
#26650=EDGE_CURVE('',#21701,#21663,#18880,.T.);
#26651=EDGE_CURVE('',#22091,#21700,#18881,.T.);
#26652=EDGE_CURVE('',#22090,#22091,#18882,.T.);
#26653=EDGE_CURVE('',#22092,#22093,#2102,.T.);
#26654=EDGE_CURVE('',#22093,#22092,#2103,.T.);
#26655=EDGE_CURVE('',#22094,#22095,#18883,.T.);
#26656=EDGE_CURVE('',#22096,#22094,#18884,.T.);
#26657=EDGE_CURVE('',#22096,#22097,#2104,.T.);
#26658=EDGE_CURVE('',#22097,#22098,#2105,.T.);
#26659=EDGE_CURVE('',#22098,#22099,#2106,.T.);
#26660=EDGE_CURVE('',#22099,#22100,#2107,.T.);
#26661=EDGE_CURVE('',#22100,#22101,#2108,.T.);
#26662=EDGE_CURVE('',#22101,#22102,#2109,.T.);
#26663=EDGE_CURVE('',#22095,#22102,#18885,.T.);
#26664=EDGE_CURVE('',#22103,#22104,#18886,.T.);
#26665=EDGE_CURVE('',#22104,#22105,#4986,.T.);
#26666=EDGE_CURVE('',#22105,#22105,#18887,.T.);
#26667=EDGE_CURVE('',#22104,#22103,#18888,.T.);
#26668=EDGE_CURVE('',#22105,#22106,#18889,.T.);
#26669=EDGE_CURVE('',#22106,#22106,#18890,.T.);
#26670=EDGE_CURVE('',#22103,#22107,#18891,.T.);
#26671=EDGE_CURVE('',#22108,#22107,#18892,.T.);
#26672=EDGE_CURVE('',#22107,#22108,#18893,.T.);
#26673=EDGE_CURVE('',#22109,#22110,#18894,.T.);
#26674=EDGE_CURVE('',#22111,#22110,#2110,.T.);
#26675=EDGE_CURVE('',#22112,#22111,#18895,.T.);
#26676=EDGE_CURVE('',#22112,#22109,#2111,.T.);
#26677=EDGE_CURVE('',#22113,#22114,#18896,.T.);
#26678=EDGE_CURVE('',#22115,#22113,#18897,.T.);
#26679=EDGE_CURVE('',#22116,#22115,#18898,.T.);
#26680=EDGE_CURVE('',#22116,#22114,#18899,.T.);
#26681=EDGE_CURVE('',#22117,#22118,#18900,.T.);
#26682=EDGE_CURVE('',#22118,#22119,#18901,.T.);
#26683=EDGE_CURVE('',#22120,#22119,#4987,.T.);
#26684=EDGE_CURVE('',#22121,#22120,#18902,.T.);
#26685=EDGE_CURVE('',#22117,#22121,#4988,.T.);
#26686=EDGE_CURVE('',#22098,#22110,#2112,.T.);
#26687=EDGE_CURVE('',#22100,#22109,#18903,.T.);
#26688=EDGE_CURVE('',#22122,#22123,#18904,.T.);
#26689=EDGE_CURVE('',#22123,#22108,#4989,.T.);
#26690=EDGE_CURVE('',#22123,#22122,#18905,.T.);
#26691=EDGE_CURVE('',#22122,#22124,#18906,.T.);
#26692=EDGE_CURVE('',#22124,#22124,#18907,.T.);
#26693=EDGE_CURVE('',#22125,#22125,#18908,.T.);
#26694=EDGE_CURVE('',#22125,#22126,#4990,.T.);
#26695=EDGE_CURVE('',#22126,#22126,#2113,.T.);
#26696=EDGE_CURVE('',#22127,#22128,#2114,.T.);
#26697=EDGE_CURVE('',#22128,#22093,#4991,.T.);
#26698=EDGE_CURVE('',#22128,#22127,#2115,.T.);
#26699=EDGE_CURVE('',#22129,#22130,#4992,.T.);
#26700=EDGE_CURVE('',#22130,#22131,#2116,.T.);
#26701=EDGE_CURVE('',#22131,#22132,#4993,.T.);
#26702=EDGE_CURVE('',#22132,#22133,#2117,.T.);
#26703=EDGE_CURVE('',#22134,#22133,#4994,.T.);
#26704=EDGE_CURVE('',#22134,#22129,#4995,.T.);
#26705=EDGE_CURVE('',#22135,#22136,#18909,.T.);
#26706=EDGE_CURVE('',#22136,#22137,#2118,.T.);
#26707=EDGE_CURVE('',#22135,#22137,#4996,.T.);
#26708=EDGE_CURVE('',#22136,#22138,#2119,.T.);
#26709=EDGE_CURVE('',#22139,#22135,#18910,.T.);
#26710=EDGE_CURVE('',#22138,#22139,#18911,.T.);
#26711=EDGE_CURVE('',#22140,#22141,#4997,.T.);
#26712=EDGE_CURVE('',#22141,#22142,#2915,.T.);
#26713=EDGE_CURVE('',#22130,#22142,#4998,.T.);
#26714=EDGE_CURVE('',#22129,#22143,#18912,.T.);
#26715=EDGE_CURVE('',#22143,#22140,#4999,.T.);
#26716=EDGE_CURVE('',#22133,#22144,#2120,.T.);
#26717=EDGE_CURVE('',#22144,#22134,#18913,.T.);
#26718=EDGE_CURVE('',#22145,#22146,#5000,.T.);
#26719=EDGE_CURVE('',#22146,#22140,#2121,.T.);
#26720=EDGE_CURVE('',#22143,#22135,#5001,.T.);
#26721=EDGE_CURVE('',#22137,#22145,#2122,.T.);
#26722=EDGE_CURVE('',#22147,#22148,#5002,.T.);
#26723=EDGE_CURVE('',#22148,#22149,#18914,.T.);
#26724=EDGE_CURVE('',#22149,#22150,#5003,.T.);
#26725=EDGE_CURVE('',#22150,#22147,#18915,.T.);
#26726=EDGE_CURVE('',#22151,#22152,#5004,.T.);
#26727=EDGE_CURVE('',#22151,#22153,#5005,.T.);
#26728=EDGE_CURVE('',#22139,#22153,#5006,.T.);
#26729=EDGE_CURVE('',#22139,#22152,#5007,.T.);
#26730=EDGE_CURVE('',#22154,#22155,#5008,.T.);
#26731=EDGE_CURVE('',#22154,#22151,#18916,.T.);
#26732=EDGE_CURVE('',#22152,#22155,#18917,.T.);
#26733=EDGE_CURVE('',#22138,#22156,#2123,.T.);
#26734=EDGE_CURVE('',#22153,#22157,#18918,.T.);
#26735=EDGE_CURVE('',#22158,#22157,#5009,.T.);
#26736=EDGE_CURVE('',#22158,#22159,#18919,.T.);
#26737=EDGE_CURVE('',#22160,#22159,#2124,.T.);
#26738=EDGE_CURVE('',#22156,#22160,#2125,.T.);
#26739=EDGE_CURVE('',#22157,#22154,#5010,.T.);
#26740=EDGE_CURVE('',#22155,#22158,#5011,.T.);
#26741=EDGE_CURVE('',#22151,#22150,#18920,.T.);
#26742=EDGE_CURVE('',#22147,#22154,#18921,.T.);
#26743=EDGE_CURVE('',#22148,#22157,#18922,.T.);
#26744=EDGE_CURVE('',#22153,#22149,#18923,.T.);
#26745=EDGE_CURVE('',#22159,#22144,#2126,.T.);
#26746=EDGE_CURVE('',#22134,#22158,#18924,.T.);
#26747=EDGE_CURVE('',#22129,#22155,#18925,.T.);
#26748=EDGE_CURVE('',#22152,#22143,#18926,.T.);
#26749=EDGE_CURVE('',#22161,#22131,#18927,.T.);
#26750=EDGE_CURVE('',#22162,#22130,#2127,.T.);
#26751=EDGE_CURVE('',#22162,#22163,#18928,.T.);
#26752=EDGE_CURVE('',#22161,#22163,#2128,.T.);
#26753=EDGE_CURVE('',#22164,#22165,#18929,.T.);
#26754=EDGE_CURVE('',#22163,#22165,#2129,.T.);
#26755=EDGE_CURVE('',#22164,#22162,#2130,.T.);
#26756=EDGE_CURVE('',#22166,#22132,#18930,.T.);
#26757=EDGE_CURVE('',#22166,#22161,#5012,.T.);
#26758=EDGE_CURVE('',#22146,#22167,#18931,.T.);
#26759=EDGE_CURVE('',#22165,#22167,#2131,.T.);
#26760=EDGE_CURVE('',#22140,#22164,#2132,.T.);
#26761=EDGE_CURVE('',#22168,#22145,#18932,.T.);
#26762=EDGE_CURVE('',#22167,#22168,#5013,.T.);
#26763=EDGE_CURVE('',#22160,#22156,#2133,.T.);
#26764=EDGE_CURVE('',#22101,#22169,#18933,.T.);
#26765=EDGE_CURVE('',#22170,#22169,#2134,.T.);
#26766=EDGE_CURVE('',#22170,#22171,#18934,.T.);
#26767=EDGE_CURVE('',#22171,#22102,#2135,.T.);
#26768=EDGE_CURVE('',#22172,#22173,#18935,.T.);
#26769=EDGE_CURVE('',#22174,#22173,#2136,.T.);
#26770=EDGE_CURVE('',#22175,#22174,#2137,.T.);
#26771=EDGE_CURVE('',#22171,#22175,#2138,.T.);
#26772=EDGE_CURVE('',#22172,#22170,#2139,.T.);
#26773=EDGE_CURVE('',#22169,#22109,#2140,.T.);
#26774=EDGE_CURVE('',#22176,#22097,#18936,.T.);
#26775=EDGE_CURVE('',#22096,#22173,#2141,.T.);
#26776=EDGE_CURVE('',#22176,#22172,#2142,.T.);
#26777=EDGE_CURVE('',#22110,#22176,#2143,.T.);
#26778=EDGE_CURVE('',#22177,#22120,#18937,.T.);
#26779=EDGE_CURVE('',#22177,#22178,#18938,.T.);
#26780=EDGE_CURVE('',#22121,#22178,#2144,.T.);
#26781=EDGE_CURVE('',#22179,#22180,#18939,.T.);
#26782=EDGE_CURVE('',#22178,#22180,#18940,.T.);
#26783=EDGE_CURVE('',#22179,#22177,#18941,.T.);
#26784=EDGE_CURVE('',#22181,#22182,#18942,.T.);
#26785=EDGE_CURVE('',#22180,#22182,#2145,.T.);
#26786=EDGE_CURVE('',#22181,#22179,#18943,.T.);
#26787=EDGE_CURVE('',#22119,#22113,#18944,.T.);
#26788=EDGE_CURVE('',#22115,#22117,#2146,.T.);
#26789=EDGE_CURVE('',#22183,#22184,#18945,.T.);
#26790=EDGE_CURVE('',#22182,#22184,#5014,.T.);
#26791=EDGE_CURVE('',#22183,#22181,#5015,.T.);
#26792=EDGE_CURVE('',#22114,#22183,#18946,.T.);
#26793=EDGE_CURVE('',#22184,#22116,#2147,.T.);
#26794=EDGE_CURVE('',#22185,#22169,#2148,.T.);
#26795=EDGE_CURVE('',#22185,#22112,#2149,.T.);
#26796=EDGE_CURVE('',#22186,#22176,#18947,.T.);
#26797=EDGE_CURVE('',#22111,#22186,#2150,.T.);
#26798=EDGE_CURVE('',#22111,#22187,#2151,.T.);
#26799=EDGE_CURVE('',#22187,#22188,#2152,.T.);
#26800=EDGE_CURVE('',#22188,#22189,#18948,.T.);
#26801=EDGE_CURVE('',#22189,#22190,#2153,.T.);
#26802=EDGE_CURVE('',#22190,#22112,#2154,.T.);
#26803=EDGE_CURVE('',#22170,#22191,#2155,.T.);
#26804=EDGE_CURVE('',#22192,#22185,#2156,.T.);
#26805=EDGE_CURVE('',#22192,#22191,#18949,.T.);
#26806=EDGE_CURVE('',#22193,#22172,#2157,.T.);
#26807=EDGE_CURVE('',#22194,#22193,#18950,.T.);
#26808=EDGE_CURVE('',#22186,#22194,#2158,.T.);
#26809=EDGE_CURVE('',#22190,#22195,#2159,.T.);
#26810=EDGE_CURVE('',#22195,#22192,#5016,.T.);
#26811=EDGE_CURVE('',#22196,#22194,#5017,.T.);
#26812=EDGE_CURVE('',#22196,#22187,#2160,.T.);
#26813=EDGE_CURVE('',#22197,#22198,#2161,.T.);
#26814=EDGE_CURVE('',#22198,#22197,#18951,.T.);
#26815=EDGE_CURVE('',#22199,#22198,#2162,.T.);
#26816=EDGE_CURVE('',#22197,#22200,#2163,.T.);
#26817=EDGE_CURVE('',#22200,#22201,#2164,.T.);
#26818=EDGE_CURVE('',#22201,#22202,#2165,.T.);
#26819=EDGE_CURVE('',#22202,#22199,#2166,.T.);
#26820=EDGE_CURVE('',#22198,#22189,#2167,.T.);
#26821=EDGE_CURVE('',#22197,#22188,#18952,.T.);
#26822=EDGE_CURVE('',#22200,#22187,#2168,.T.);
#26823=EDGE_CURVE('',#22201,#22196,#18953,.T.);
#26824=EDGE_CURVE('',#22201,#22113,#2169,.T.);
#26825=EDGE_CURVE('',#22114,#22202,#2170,.T.);
#26826=EDGE_CURVE('',#22202,#22195,#18954,.T.);
#26827=EDGE_CURVE('',#22199,#22190,#2171,.T.);
#26828=EDGE_CURVE('',#22181,#22192,#2172,.T.);
#26829=EDGE_CURVE('',#22191,#22179,#2173,.T.);
#26830=EDGE_CURVE('',#22177,#22193,#2174,.T.);
#26831=EDGE_CURVE('',#22194,#22120,#2175,.T.);
#26832=EDGE_CURVE('',#22119,#22196,#2176,.T.);
#26833=EDGE_CURVE('',#22195,#22183,#2177,.T.);
#26834=EDGE_CURVE('',#22161,#22191,#2916,.T.);
#26835=EDGE_CURVE('',#22193,#22167,#2917,.T.);
#26836=EDGE_CURVE('',#22168,#22166,#2178,.T.);
#26837=EDGE_CURVE('',#22095,#22094,#2179,.T.);
#26838=EDGE_CURVE('',#21771,#21734,#2180,.T.);
#26839=EDGE_CURVE('',#21829,#21770,#2181,.T.);
#26840=EDGE_CURVE('',#21900,#21828,#2182,.T.);
#26841=EDGE_CURVE('',#22089,#22090,#2183,.T.);
#26842=EDGE_CURVE('',#21741,#22091,#2184,.T.);
#26843=EDGE_CURVE('',#21735,#21740,#2185,.T.);
#26844=EDGE_CURVE('',#22090,#22094,#18955,.T.);
#26845=EDGE_CURVE('',#22095,#22089,#18956,.T.);
#26846=EDGE_CURVE('',#22164,#22141,#5018,.T.);
#26847=EDGE_CURVE('',#22162,#22142,#5019,.T.);
#26848=EDGE_CURVE('',#22203,#22204,#18957,.T.);
#26849=EDGE_CURVE('',#22204,#22203,#18958,.T.);
#26850=EDGE_CURVE('',#22204,#22205,#18959,.T.);
#26851=EDGE_CURVE('',#22205,#22205,#18960,.T.);
#26852=EDGE_CURVE('',#22206,#22206,#18961,.T.);
#26853=EDGE_CURVE('',#22206,#22207,#18962,.T.);
#26854=EDGE_CURVE('',#22207,#22207,#18963,.T.);
#26855=EDGE_CURVE('',#22203,#22206,#5020,.T.);
#26856=EDGE_CURVE('',#22208,#22209,#18964,.T.);
#26857=EDGE_CURVE('',#22209,#22210,#2186,.T.);
#26858=EDGE_CURVE('',#22211,#22210,#18965,.T.);
#26859=EDGE_CURVE('',#22208,#22211,#2187,.T.);
#26860=EDGE_CURVE('',#22212,#22212,#18966,.T.);
#26861=EDGE_CURVE('',#22212,#22213,#18967,.T.);
#26862=EDGE_CURVE('',#22213,#22213,#18968,.T.);
#26863=EDGE_CURVE('',#22214,#22214,#18969,.T.);
#26864=EDGE_CURVE('',#22214,#22212,#5021,.T.);
#26865=EDGE_CURVE('',#22209,#22208,#18970,.T.);
#26866=EDGE_CURVE('',#22210,#22211,#18971,.T.);
#26867=EDGE_CURVE('',#22215,#22216,#5022,.T.);
#26868=EDGE_CURVE('',#22216,#22217,#18972,.T.);
#26869=EDGE_CURVE('',#22218,#22217,#5023,.T.);
#26870=EDGE_CURVE('',#22215,#22218,#18973,.T.);
#26871=EDGE_CURVE('',#22219,#22220,#5024,.T.);
#26872=EDGE_CURVE('',#22220,#22216,#5025,.T.);
#26873=EDGE_CURVE('',#22219,#22215,#5026,.T.);
#26874=EDGE_CURVE('',#22221,#22222,#5027,.T.);
#26875=EDGE_CURVE('',#22222,#22220,#18974,.T.);
#26876=EDGE_CURVE('',#22221,#22219,#18975,.T.);
#26877=EDGE_CURVE('',#22217,#22222,#5028,.T.);
#26878=EDGE_CURVE('',#22218,#22221,#5029,.T.);
#26879=EDGE_CURVE('',#22223,#22224,#18976,.T.);
#26880=EDGE_CURVE('',#22224,#22225,#5030,.T.);
#26881=EDGE_CURVE('',#22225,#22226,#18977,.T.);
#26882=EDGE_CURVE('',#22226,#22223,#5031,.T.);
#26883=EDGE_CURVE('',#22224,#22227,#5032,.T.);
#26884=EDGE_CURVE('',#22227,#22228,#5033,.T.);
#26885=EDGE_CURVE('',#22225,#22228,#5034,.T.);
#26886=EDGE_CURVE('',#22228,#22229,#18978,.T.);
#26887=EDGE_CURVE('',#22226,#22229,#5035,.T.);
#26888=EDGE_CURVE('',#22229,#22230,#5036,.T.);
#26889=EDGE_CURVE('',#22223,#22230,#5037,.T.);
#26890=EDGE_CURVE('',#22230,#22227,#18979,.T.);
#26891=EDGE_CURVE('',#22231,#22232,#2188,.T.);
#26892=EDGE_CURVE('',#22232,#22233,#5038,.T.);
#26893=EDGE_CURVE('',#22233,#22234,#18980,.T.);
#26894=EDGE_CURVE('',#22234,#22235,#2189,.T.);
#26895=EDGE_CURVE('',#22235,#22236,#5039,.T.);
#26896=EDGE_CURVE('',#22236,#22237,#18981,.T.);
#26897=EDGE_CURVE('',#22237,#22238,#5040,.T.);
#26898=EDGE_CURVE('',#22238,#22239,#2190,.T.);
#26899=EDGE_CURVE('',#22239,#22240,#18982,.T.);
#26900=EDGE_CURVE('',#22240,#22241,#5041,.T.);
#26901=EDGE_CURVE('',#22241,#22242,#2191,.T.);
#26902=EDGE_CURVE('',#22242,#22243,#18983,.T.);
#26903=EDGE_CURVE('',#22243,#22244,#5042,.T.);
#26904=EDGE_CURVE('',#22244,#22244,#18984,.T.);
#26905=EDGE_CURVE('',#22243,#22245,#2192,.T.);
#26906=EDGE_CURVE('',#22245,#22246,#2193,.T.);
#26907=EDGE_CURVE('',#22246,#22247,#2194,.T.);
#26908=EDGE_CURVE('',#22247,#22248,#2195,.T.);
#26909=EDGE_CURVE('',#22248,#22249,#2196,.T.);
#26910=EDGE_CURVE('',#22249,#22231,#18985,.T.);
#26911=EDGE_CURVE('',#22244,#22250,#18986,.T.);
#26912=EDGE_CURVE('',#22250,#22250,#18987,.T.);
#26913=EDGE_CURVE('',#22251,#22252,#18988,.T.);
#26914=EDGE_CURVE('',#22252,#22253,#5043,.T.);
#26915=EDGE_CURVE('',#22253,#22254,#2197,.T.);
#26916=EDGE_CURVE('',#22255,#22254,#18989,.T.);
#26917=EDGE_CURVE('',#22255,#22256,#2198,.T.);
#26918=EDGE_CURVE('',#22256,#22251,#5044,.T.);
#26919=EDGE_CURVE('',#22257,#22258,#18990,.T.);
#26920=EDGE_CURVE('',#22258,#22259,#5045,.T.);
#26921=EDGE_CURVE('',#22259,#22260,#2199,.T.);
#26922=EDGE_CURVE('',#22261,#22260,#18991,.T.);
#26923=EDGE_CURVE('',#22261,#22262,#2200,.T.);
#26924=EDGE_CURVE('',#22262,#22257,#5046,.T.);
#26925=EDGE_CURVE('',#22263,#22264,#18992,.T.);
#26926=EDGE_CURVE('',#22264,#22265,#5047,.T.);
#26927=EDGE_CURVE('',#22265,#22266,#2201,.T.);
#26928=EDGE_CURVE('',#22267,#22266,#18993,.T.);
#26929=EDGE_CURVE('',#22267,#22268,#2202,.T.);
#26930=EDGE_CURVE('',#22268,#22263,#5048,.T.);
#26931=EDGE_CURVE('',#22269,#22270,#18994,.T.);
#26932=EDGE_CURVE('',#22270,#22271,#5049,.T.);
#26933=EDGE_CURVE('',#22271,#22272,#18995,.T.);
#26934=EDGE_CURVE('',#22272,#22273,#5050,.T.);
#26935=EDGE_CURVE('',#22274,#22273,#2203,.T.);
#26936=EDGE_CURVE('',#22274,#22275,#18996,.T.);
#26937=EDGE_CURVE('',#22276,#22275,#2204,.T.);
#26938=EDGE_CURVE('',#22276,#22277,#5051,.T.);
#26939=EDGE_CURVE('',#22277,#22271,#18997,.T.);
#26940=EDGE_CURVE('',#22270,#22269,#18998,.T.);
#26941=EDGE_CURVE('',#22278,#22279,#18999,.T.);
#26942=EDGE_CURVE('',#22279,#22280,#5052,.T.);
#26943=EDGE_CURVE('',#22280,#22281,#19000,.T.);
#26944=EDGE_CURVE('',#22278,#22281,#5053,.T.);
#26945=EDGE_CURVE('',#22282,#22278,#19001,.T.);
#26946=EDGE_CURVE('',#22283,#22282,#19002,.T.);
#26947=EDGE_CURVE('',#22279,#22283,#19003,.T.);
#26948=EDGE_CURVE('',#22284,#22277,#2205,.T.);
#26949=EDGE_CURVE('',#22285,#22284,#19004,.T.);
#26950=EDGE_CURVE('',#22272,#22285,#2206,.T.);
#26951=EDGE_CURVE('',#22280,#22286,#19005,.T.);
#26952=EDGE_CURVE('',#22287,#22286,#19006,.T.);
#26953=EDGE_CURVE('',#22281,#22287,#19007,.T.);
#26954=EDGE_CURVE('',#22269,#22288,#19008,.T.);
#26955=EDGE_CURVE('',#22288,#22288,#19009,.T.);
#26956=EDGE_CURVE('',#22289,#22290,#19010,.T.);
#26957=EDGE_CURVE('',#22290,#22291,#5054,.T.);
#26958=EDGE_CURVE('',#22291,#22292,#19011,.T.);
#26959=EDGE_CURVE('',#22292,#22293,#5055,.T.);
#26960=EDGE_CURVE('',#22294,#22293,#2207,.T.);
#26961=EDGE_CURVE('',#22294,#22295,#19012,.T.);
#26962=EDGE_CURVE('',#22296,#22295,#2208,.T.);
#26963=EDGE_CURVE('',#22296,#22297,#5056,.T.);
#26964=EDGE_CURVE('',#22297,#22291,#19013,.T.);
#26965=EDGE_CURVE('',#22290,#22289,#19014,.T.);
#26966=EDGE_CURVE('',#22298,#22299,#19015,.T.);
#26967=EDGE_CURVE('',#22299,#22300,#5057,.T.);
#26968=EDGE_CURVE('',#22300,#22301,#19016,.T.);
#26969=EDGE_CURVE('',#22298,#22301,#5058,.T.);
#26970=EDGE_CURVE('',#22302,#22298,#19017,.T.);
#26971=EDGE_CURVE('',#22303,#22302,#19018,.T.);
#26972=EDGE_CURVE('',#22299,#22303,#19019,.T.);
#26973=EDGE_CURVE('',#22304,#22297,#2209,.T.);
#26974=EDGE_CURVE('',#22305,#22304,#19020,.T.);
#26975=EDGE_CURVE('',#22292,#22305,#2210,.T.);
#26976=EDGE_CURVE('',#22300,#22306,#19021,.T.);
#26977=EDGE_CURVE('',#22307,#22306,#19022,.T.);
#26978=EDGE_CURVE('',#22301,#22307,#19023,.T.);
#26979=EDGE_CURVE('',#22289,#22308,#19024,.T.);
#26980=EDGE_CURVE('',#22308,#22308,#19025,.T.);
#26981=EDGE_CURVE('',#22309,#22310,#19026,.T.);
#26982=EDGE_CURVE('',#22310,#22311,#5059,.T.);
#26983=EDGE_CURVE('',#22311,#22312,#19027,.T.);
#26984=EDGE_CURVE('',#22312,#22313,#5060,.T.);
#26985=EDGE_CURVE('',#22314,#22313,#2211,.T.);
#26986=EDGE_CURVE('',#22314,#22315,#19028,.T.);
#26987=EDGE_CURVE('',#22316,#22315,#2212,.T.);
#26988=EDGE_CURVE('',#22316,#22317,#5061,.T.);
#26989=EDGE_CURVE('',#22317,#22311,#19029,.T.);
#26990=EDGE_CURVE('',#22310,#22309,#19030,.T.);
#26991=EDGE_CURVE('',#22318,#22319,#19031,.T.);
#26992=EDGE_CURVE('',#22319,#22320,#5062,.T.);
#26993=EDGE_CURVE('',#22320,#22321,#19032,.T.);
#26994=EDGE_CURVE('',#22318,#22321,#5063,.T.);
#26995=EDGE_CURVE('',#22322,#22318,#19033,.T.);
#26996=EDGE_CURVE('',#22323,#22322,#19034,.T.);
#26997=EDGE_CURVE('',#22319,#22323,#19035,.T.);
#26998=EDGE_CURVE('',#22324,#22317,#2213,.T.);
#26999=EDGE_CURVE('',#22325,#22324,#19036,.T.);
#27000=EDGE_CURVE('',#22312,#22325,#2214,.T.);
#27001=EDGE_CURVE('',#22320,#22326,#19037,.T.);
#27002=EDGE_CURVE('',#22327,#22326,#19038,.T.);
#27003=EDGE_CURVE('',#22321,#22327,#19039,.T.);
#27004=EDGE_CURVE('',#22309,#22328,#19040,.T.);
#27005=EDGE_CURVE('',#22328,#22328,#19041,.T.);
#27006=EDGE_CURVE('',#22329,#22329,#19042,.T.);
#27007=EDGE_CURVE('',#22329,#22330,#5064,.T.);
#27008=EDGE_CURVE('',#22330,#22331,#19043,.T.);
#27009=EDGE_CURVE('',#22331,#22332,#5065,.T.);
#27010=EDGE_CURVE('',#22333,#22332,#2215,.T.);
#27011=EDGE_CURVE('',#22333,#22334,#19044,.T.);
#27012=EDGE_CURVE('',#22335,#22334,#2216,.T.);
#27013=EDGE_CURVE('',#22335,#22336,#5066,.T.);
#27014=EDGE_CURVE('',#22336,#22330,#19045,.T.);
#27015=EDGE_CURVE('',#22336,#22337,#2217,.T.);
#27016=EDGE_CURVE('',#22338,#22337,#19046,.T.);
#27017=EDGE_CURVE('',#22331,#22338,#2218,.T.);
#27018=EDGE_CURVE('',#22339,#22340,#19047,.T.);
#27019=EDGE_CURVE('',#22340,#22341,#2219,.T.);
#27020=EDGE_CURVE('',#22341,#22342,#2220,.T.);
#27021=EDGE_CURVE('',#22342,#22343,#19048,.T.);
#27022=EDGE_CURVE('',#22343,#22344,#5067,.T.);
#27023=EDGE_CURVE('',#22344,#22345,#5068,.T.);
#27024=EDGE_CURVE('',#22345,#22339,#5069,.T.);
#27025=EDGE_CURVE('',#22346,#22347,#5070,.T.);
#27026=EDGE_CURVE('',#22346,#22348,#19049,.T.);
#27027=EDGE_CURVE('',#22349,#22348,#5071,.T.);
#27028=EDGE_CURVE('',#22349,#22347,#19050,.T.);
#27029=EDGE_CURVE('',#22350,#22351,#5072,.T.);
#27030=EDGE_CURVE('',#22351,#22346,#2221,.T.);
#27031=EDGE_CURVE('',#22347,#22350,#2222,.T.);
#27032=EDGE_CURVE('',#22352,#22353,#5073,.T.);
#27033=EDGE_CURVE('',#22352,#22354,#19051,.T.);
#27034=EDGE_CURVE('',#22355,#22354,#5074,.T.);
#27035=EDGE_CURVE('',#22355,#22353,#19052,.T.);
#27036=EDGE_CURVE('',#22354,#22351,#2223,.T.);
#27037=EDGE_CURVE('',#22350,#22355,#2224,.T.);
#27038=EDGE_CURVE('',#22356,#22357,#5075,.T.);
#27039=EDGE_CURVE('',#22357,#22358,#5076,.T.);
#27040=EDGE_CURVE('',#22358,#22359,#5077,.T.);
#27041=EDGE_CURVE('',#22359,#22356,#5078,.T.);
#27042=EDGE_CURVE('',#22348,#22360,#5079,.T.);
#27043=EDGE_CURVE('',#22360,#22361,#5080,.T.);
#27044=EDGE_CURVE('',#22361,#22349,#5081,.T.);
#27045=EDGE_CURVE('',#22362,#22363,#5082,.T.);
#27046=EDGE_CURVE('',#22363,#22352,#5083,.T.);
#27047=EDGE_CURVE('',#22353,#22362,#5084,.T.);
#27048=EDGE_CURVE('',#22364,#22365,#2225,.T.);
#27049=EDGE_CURVE('',#22366,#22364,#2226,.T.);
#27050=EDGE_CURVE('',#22367,#22366,#2227,.T.);
#27051=EDGE_CURVE('',#22368,#22367,#2228,.T.);
#27052=EDGE_CURVE('',#22369,#22368,#2229,.T.);
#27053=EDGE_CURVE('',#22355,#22369,#19053,.T.);
#27054=EDGE_CURVE('',#22365,#22350,#19054,.T.);
#27055=EDGE_CURVE('',#22365,#22370,#2230,.T.);
#27056=EDGE_CURVE('',#22370,#22347,#19055,.T.);
#27057=EDGE_CURVE('',#22371,#22369,#19056,.T.);
#27058=EDGE_CURVE('',#22353,#22371,#19057,.T.);
#27059=EDGE_CURVE('',#22370,#22372,#19058,.T.);
#27060=EDGE_CURVE('',#22372,#22349,#19059,.T.);
#27061=EDGE_CURVE('',#22373,#22374,#2231,.T.);
#27062=EDGE_CURVE('',#22362,#22373,#19060,.T.);
#27063=EDGE_CURVE('',#22374,#22371,#5085,.T.);
#27064=EDGE_CURVE('',#22372,#22375,#5086,.T.);
#27065=EDGE_CURVE('',#22376,#22361,#19061,.T.);
#27066=EDGE_CURVE('',#22375,#22376,#2232,.T.);
#27067=EDGE_CURVE('',#22377,#22378,#2233,.T.);
#27068=EDGE_CURVE('',#22357,#22377,#19062,.T.);
#27069=EDGE_CURVE('',#22379,#22356,#19063,.T.);
#27070=EDGE_CURVE('',#22380,#22379,#2234,.T.);
#27071=EDGE_CURVE('',#22378,#22380,#5087,.T.);
#27072=EDGE_CURVE('',#22379,#22373,#2235,.T.);
#27073=EDGE_CURVE('',#22362,#22356,#19064,.T.);
#27074=EDGE_CURVE('',#22376,#22377,#2236,.T.);
#27075=EDGE_CURVE('',#22357,#22361,#19065,.T.);
#27076=EDGE_CURVE('',#22363,#22359,#19066,.T.);
#27077=EDGE_CURVE('',#22358,#22360,#19067,.T.);
#27078=EDGE_CURVE('',#22359,#22344,#19068,.T.);
#27079=EDGE_CURVE('',#22345,#22358,#19069,.T.);
#27080=EDGE_CURVE('',#22363,#22344,#19070,.T.);
#27081=EDGE_CURVE('',#22345,#22360,#19071,.T.);
#27082=EDGE_CURVE('',#22352,#22343,#19072,.T.);
#27083=EDGE_CURVE('',#22339,#22348,#19073,.T.);
#27084=EDGE_CURVE('',#22354,#22342,#19074,.T.);
#27085=EDGE_CURVE('',#22340,#22346,#19075,.T.);
#27086=EDGE_CURVE('',#22351,#22341,#19076,.T.);
#27087=EDGE_CURVE('',#22381,#22382,#19077,.T.);
#27088=EDGE_CURVE('',#22383,#22382,#19078,.T.);
#27089=EDGE_CURVE('',#22383,#22384,#19079,.T.);
#27090=EDGE_CURVE('',#22381,#22384,#19080,.T.);
#27091=EDGE_CURVE('',#22385,#22386,#19081,.T.);
#27092=EDGE_CURVE('',#22384,#22386,#5088,.T.);
#27093=EDGE_CURVE('',#22385,#22383,#5089,.T.);
#27094=EDGE_CURVE('',#22387,#22388,#19082,.T.);
#27095=EDGE_CURVE('',#22382,#22388,#5090,.T.);
#27096=EDGE_CURVE('',#22387,#22381,#5091,.T.);
#27097=EDGE_CURVE('',#22388,#22385,#19083,.T.);
#27098=EDGE_CURVE('',#22386,#22387,#19084,.T.);
#27099=EDGE_CURVE('',#22331,#22389,#19085,.T.);
#27100=EDGE_CURVE('',#22390,#22389,#5092,.T.);
#27101=EDGE_CURVE('',#22390,#22332,#19086,.T.);
#27102=EDGE_CURVE('',#22391,#22333,#19087,.T.);
#27103=EDGE_CURVE('',#22390,#22391,#2237,.T.);
#27104=EDGE_CURVE('',#22338,#22392,#19088,.T.);
#27105=EDGE_CURVE('',#22392,#22389,#2238,.T.);
#27106=EDGE_CURVE('',#22393,#22394,#19089,.T.);
#27107=EDGE_CURVE('',#22391,#22394,#5093,.T.);
#27108=EDGE_CURVE('',#22393,#22390,#5094,.T.);
#27109=EDGE_CURVE('',#22395,#22334,#19090,.T.);
#27110=EDGE_CURVE('',#22395,#22391,#19091,.T.);
#27111=EDGE_CURVE('',#22396,#22397,#19092,.T.);
#27112=EDGE_CURVE('',#22392,#22397,#5095,.T.);
#27113=EDGE_CURVE('',#22396,#22338,#5096,.T.);
#27114=EDGE_CURVE('',#22398,#22399,#19093,.T.);
#27115=EDGE_CURVE('',#22394,#22399,#19094,.T.);
#27116=EDGE_CURVE('',#22398,#22393,#19095,.T.);
#27117=EDGE_CURVE('',#22400,#22335,#19096,.T.);
#27118=EDGE_CURVE('',#22395,#22400,#2239,.T.);
#27119=EDGE_CURVE('',#22401,#22402,#2240,.T.);
#27120=EDGE_CURVE('',#22402,#22337,#19097,.T.);
#27121=EDGE_CURVE('',#22336,#22401,#19098,.T.);
#27122=EDGE_CURVE('',#22403,#22404,#19099,.T.);
#27123=EDGE_CURVE('',#22397,#22404,#19100,.T.);
#27124=EDGE_CURVE('',#22403,#22396,#19101,.T.);
#27125=EDGE_CURVE('',#22400,#22398,#5097,.T.);
#27126=EDGE_CURVE('',#22399,#22395,#5098,.T.);
#27127=EDGE_CURVE('',#22401,#22400,#5099,.T.);
#27128=EDGE_CURVE('',#22404,#22402,#5100,.T.);
#27129=EDGE_CURVE('',#22337,#22403,#5101,.T.);
#27130=EDGE_CURVE('',#22393,#22388,#5102,.T.);
#27131=EDGE_CURVE('',#22398,#22385,#5103,.T.);
#27132=EDGE_CURVE('',#22404,#22383,#5104,.T.);
#27133=EDGE_CURVE('',#22397,#22382,#5105,.T.);
#27134=EDGE_CURVE('',#22405,#22406,#19102,.T.);
#27135=EDGE_CURVE('',#22321,#22406,#5106,.T.);
#27136=EDGE_CURVE('',#22405,#22327,#5107,.T.);
#27137=EDGE_CURVE('',#22407,#22408,#19103,.T.);
#27138=EDGE_CURVE('',#22406,#22408,#19104,.T.);
#27139=EDGE_CURVE('',#22407,#22405,#19105,.T.);
#27140=EDGE_CURVE('',#22408,#22320,#5108,.T.);
#27141=EDGE_CURVE('',#22326,#22407,#5109,.T.);
#27142=EDGE_CURVE('',#22409,#22315,#19106,.T.);
#27143=EDGE_CURVE('',#22314,#22410,#19107,.T.);
#27144=EDGE_CURVE('',#22409,#22410,#19108,.T.);
#27145=EDGE_CURVE('',#22313,#22411,#19109,.T.);
#27146=EDGE_CURVE('',#22411,#22410,#2241,.T.);
#27147=EDGE_CURVE('',#22412,#22316,#19110,.T.);
#27148=EDGE_CURVE('',#22409,#22412,#2242,.T.);
#27149=EDGE_CURVE('',#22312,#22413,#19111,.T.);
#27150=EDGE_CURVE('',#22411,#22413,#5110,.T.);
#27151=EDGE_CURVE('',#22414,#22415,#19112,.T.);
#27152=EDGE_CURVE('',#22410,#22415,#5111,.T.);
#27153=EDGE_CURVE('',#22414,#22411,#5112,.T.);
#27154=EDGE_CURVE('',#22416,#22417,#19113,.T.);
#27155=EDGE_CURVE('',#22412,#22417,#5113,.T.);
#27156=EDGE_CURVE('',#22416,#22409,#5114,.T.);
#27157=EDGE_CURVE('',#22418,#22317,#19114,.T.);
#27158=EDGE_CURVE('',#22418,#22412,#5115,.T.);
#27159=EDGE_CURVE('',#22325,#22419,#19115,.T.);
#27160=EDGE_CURVE('',#22419,#22413,#2243,.T.);
#27161=EDGE_CURVE('',#22417,#22414,#19116,.T.);
#27162=EDGE_CURVE('',#22415,#22416,#19117,.T.);
#27163=EDGE_CURVE('',#22420,#22324,#19118,.T.);
#27164=EDGE_CURVE('',#22418,#22420,#2244,.T.);
#27165=EDGE_CURVE('',#22419,#22318,#5116,.T.);
#27166=EDGE_CURVE('',#22322,#22325,#5117,.T.);
#27167=EDGE_CURVE('',#22324,#22323,#5118,.T.);
#27168=EDGE_CURVE('',#22319,#22420,#5119,.T.);
#27169=EDGE_CURVE('',#22417,#22408,#5120,.T.);
#27170=EDGE_CURVE('',#22414,#22406,#5121,.T.);
#27171=EDGE_CURVE('',#22421,#22422,#19119,.T.);
#27172=EDGE_CURVE('',#22301,#22422,#5122,.T.);
#27173=EDGE_CURVE('',#22421,#22307,#5123,.T.);
#27174=EDGE_CURVE('',#22423,#22424,#19120,.T.);
#27175=EDGE_CURVE('',#22422,#22424,#19121,.T.);
#27176=EDGE_CURVE('',#22423,#22421,#19122,.T.);
#27177=EDGE_CURVE('',#22424,#22300,#5124,.T.);
#27178=EDGE_CURVE('',#22306,#22423,#5125,.T.);
#27179=EDGE_CURVE('',#22425,#22295,#19123,.T.);
#27180=EDGE_CURVE('',#22294,#22426,#19124,.T.);
#27181=EDGE_CURVE('',#22425,#22426,#19125,.T.);
#27182=EDGE_CURVE('',#22293,#22427,#19126,.T.);
#27183=EDGE_CURVE('',#22427,#22426,#2245,.T.);
#27184=EDGE_CURVE('',#22428,#22296,#19127,.T.);
#27185=EDGE_CURVE('',#22425,#22428,#2246,.T.);
#27186=EDGE_CURVE('',#22292,#22429,#19128,.T.);
#27187=EDGE_CURVE('',#22427,#22429,#5126,.T.);
#27188=EDGE_CURVE('',#22430,#22431,#19129,.T.);
#27189=EDGE_CURVE('',#22426,#22431,#5127,.T.);
#27190=EDGE_CURVE('',#22430,#22427,#5128,.T.);
#27191=EDGE_CURVE('',#22432,#22433,#19130,.T.);
#27192=EDGE_CURVE('',#22428,#22433,#5129,.T.);
#27193=EDGE_CURVE('',#22432,#22425,#5130,.T.);
#27194=EDGE_CURVE('',#22434,#22297,#19131,.T.);
#27195=EDGE_CURVE('',#22434,#22428,#5131,.T.);
#27196=EDGE_CURVE('',#22305,#22435,#19132,.T.);
#27197=EDGE_CURVE('',#22435,#22429,#2247,.T.);
#27198=EDGE_CURVE('',#22433,#22430,#19133,.T.);
#27199=EDGE_CURVE('',#22431,#22432,#19134,.T.);
#27200=EDGE_CURVE('',#22436,#22304,#19135,.T.);
#27201=EDGE_CURVE('',#22434,#22436,#2248,.T.);
#27202=EDGE_CURVE('',#22435,#22298,#5132,.T.);
#27203=EDGE_CURVE('',#22302,#22305,#5133,.T.);
#27204=EDGE_CURVE('',#22304,#22303,#5134,.T.);
#27205=EDGE_CURVE('',#22299,#22436,#5135,.T.);
#27206=EDGE_CURVE('',#22433,#22424,#5136,.T.);
#27207=EDGE_CURVE('',#22430,#22422,#5137,.T.);
#27208=EDGE_CURVE('',#22437,#22438,#19136,.T.);
#27209=EDGE_CURVE('',#22281,#22438,#5138,.T.);
#27210=EDGE_CURVE('',#22437,#22287,#5139,.T.);
#27211=EDGE_CURVE('',#22439,#22440,#19137,.T.);
#27212=EDGE_CURVE('',#22438,#22440,#19138,.T.);
#27213=EDGE_CURVE('',#22439,#22437,#19139,.T.);
#27214=EDGE_CURVE('',#22440,#22280,#5140,.T.);
#27215=EDGE_CURVE('',#22286,#22439,#5141,.T.);
#27216=EDGE_CURVE('',#22441,#22275,#19140,.T.);
#27217=EDGE_CURVE('',#22274,#22442,#19141,.T.);
#27218=EDGE_CURVE('',#22441,#22442,#19142,.T.);
#27219=EDGE_CURVE('',#22273,#22443,#19143,.T.);
#27220=EDGE_CURVE('',#22443,#22442,#2249,.T.);
#27221=EDGE_CURVE('',#22444,#22276,#19144,.T.);
#27222=EDGE_CURVE('',#22441,#22444,#2250,.T.);
#27223=EDGE_CURVE('',#22272,#22445,#19145,.T.);
#27224=EDGE_CURVE('',#22443,#22445,#5142,.T.);
#27225=EDGE_CURVE('',#22446,#22447,#19146,.T.);
#27226=EDGE_CURVE('',#22442,#22447,#5143,.T.);
#27227=EDGE_CURVE('',#22446,#22443,#5144,.T.);
#27228=EDGE_CURVE('',#22448,#22449,#19147,.T.);
#27229=EDGE_CURVE('',#22444,#22449,#5145,.T.);
#27230=EDGE_CURVE('',#22448,#22441,#5146,.T.);
#27231=EDGE_CURVE('',#22450,#22277,#19148,.T.);
#27232=EDGE_CURVE('',#22450,#22444,#5147,.T.);
#27233=EDGE_CURVE('',#22285,#22451,#19149,.T.);
#27234=EDGE_CURVE('',#22451,#22445,#2251,.T.);
#27235=EDGE_CURVE('',#22449,#22446,#19150,.T.);
#27236=EDGE_CURVE('',#22447,#22448,#19151,.T.);
#27237=EDGE_CURVE('',#22452,#22284,#19152,.T.);
#27238=EDGE_CURVE('',#22450,#22452,#2252,.T.);
#27239=EDGE_CURVE('',#22451,#22278,#5148,.T.);
#27240=EDGE_CURVE('',#22282,#22285,#5149,.T.);
#27241=EDGE_CURVE('',#22284,#22283,#5150,.T.);
#27242=EDGE_CURVE('',#22279,#22452,#5151,.T.);
#27243=EDGE_CURVE('',#22449,#22440,#5152,.T.);
#27244=EDGE_CURVE('',#22446,#22438,#5153,.T.);
#27245=EDGE_CURVE('',#22264,#22263,#5154,.T.);
#27246=EDGE_CURVE('',#22258,#22257,#5155,.T.);
#27247=EDGE_CURVE('',#22252,#22251,#5156,.T.);
#27248=EDGE_CURVE('',#22453,#22374,#19153,.T.);
#27249=EDGE_CURVE('',#22371,#22454,#19154,.T.);
#27250=EDGE_CURVE('',#22453,#22454,#5157,.T.);
#27251=EDGE_CURVE('',#22369,#22455,#19155,.T.);
#27252=EDGE_CURVE('',#22454,#22455,#19156,.T.);
#27253=EDGE_CURVE('',#22456,#22453,#19157,.T.);
#27254=EDGE_CURVE('',#22456,#22380,#19158,.T.);
#27255=EDGE_CURVE('',#22368,#22457,#19159,.T.);
#27256=EDGE_CURVE('',#22455,#22457,#2253,.T.);
#27257=EDGE_CURVE('',#22458,#22378,#19160,.T.);
#27258=EDGE_CURVE('',#22458,#22456,#5158,.T.);
#27259=EDGE_CURVE('',#22367,#22459,#19161,.T.);
#27260=EDGE_CURVE('',#22457,#22459,#2254,.T.);
#27261=EDGE_CURVE('',#22460,#22375,#19162,.T.);
#27262=EDGE_CURVE('',#22460,#22458,#19163,.T.);
#27263=EDGE_CURVE('',#22366,#22461,#19164,.T.);
#27264=EDGE_CURVE('',#22459,#22461,#2255,.T.);
#27265=EDGE_CURVE('',#22462,#22372,#19165,.T.);
#27266=EDGE_CURVE('',#22462,#22460,#5159,.T.);
#27267=EDGE_CURVE('',#22364,#22463,#19166,.T.);
#27268=EDGE_CURVE('',#22461,#22463,#2256,.T.);
#27269=EDGE_CURVE('',#22464,#22370,#19167,.T.);
#27270=EDGE_CURVE('',#22464,#22462,#19168,.T.);
#27271=EDGE_CURVE('',#22365,#22465,#19169,.T.);
#27272=EDGE_CURVE('',#22463,#22465,#2257,.T.);
#27273=EDGE_CURVE('',#22465,#22464,#2258,.T.);
#27274=EDGE_CURVE('',#22460,#22466,#5160,.T.);
#27275=EDGE_CURVE('',#22467,#22458,#5161,.T.);
#27276=EDGE_CURVE('',#22467,#22466,#19170,.T.);
#27277=EDGE_CURVE('',#22468,#22469,#19171,.T.);
#27278=EDGE_CURVE('',#22466,#22469,#2259,.T.);
#27279=EDGE_CURVE('',#22468,#22467,#2260,.T.);
#27280=EDGE_CURVE('',#22470,#22471,#19172,.T.);
#27281=EDGE_CURVE('',#22469,#22471,#2261,.T.);
#27282=EDGE_CURVE('',#22470,#22468,#2262,.T.);
#27283=EDGE_CURVE('',#22472,#22236,#19173,.T.);
#27284=EDGE_CURVE('',#22236,#22471,#19174,.T.);
#27285=EDGE_CURVE('',#22470,#22472,#19175,.T.);
#27286=EDGE_CURVE('',#22473,#22237,#19176,.T.);
#27287=EDGE_CURVE('',#22473,#22472,#19177,.T.);
#27288=EDGE_CURVE('',#22235,#22474,#19178,.T.);
#27289=EDGE_CURVE('',#22471,#22474,#5162,.T.);
#27290=EDGE_CURVE('',#22475,#22476,#19179,.T.);
#27291=EDGE_CURVE('',#22476,#22237,#19180,.T.);
#27292=EDGE_CURVE('',#22473,#22475,#19181,.T.);
#27293=EDGE_CURVE('',#22234,#22477,#19182,.T.);
#27294=EDGE_CURVE('',#22474,#22477,#2263,.T.);
#27295=EDGE_CURVE('',#22478,#22479,#19183,.T.);
#27296=EDGE_CURVE('',#22476,#22479,#2264,.T.);
#27297=EDGE_CURVE('',#22478,#22475,#2265,.T.);
#27298=EDGE_CURVE('',#22480,#22238,#19184,.T.);
#27299=EDGE_CURVE('',#22480,#22476,#5163,.T.);
#27300=EDGE_CURVE('',#22233,#22481,#19185,.T.);
#27301=EDGE_CURVE('',#22477,#22481,#19186,.T.);
#27302=EDGE_CURVE('',#22456,#22478,#5164,.T.);
#27303=EDGE_CURVE('',#22479,#22453,#5165,.T.);
#27304=EDGE_CURVE('',#22482,#22239,#19187,.T.);
#27305=EDGE_CURVE('',#22482,#22480,#2266,.T.);
#27306=EDGE_CURVE('',#22233,#22483,#19188,.T.);
#27307=EDGE_CURVE('',#22481,#22483,#19189,.T.);
#27308=EDGE_CURVE('',#22484,#22240,#19190,.T.);
#27309=EDGE_CURVE('',#22484,#22482,#19191,.T.);
#27310=EDGE_CURVE('',#22232,#22485,#19192,.T.);
#27311=EDGE_CURVE('',#22483,#22485,#5166,.T.);
#27312=EDGE_CURVE('',#22486,#22484,#19193,.T.);
#27313=EDGE_CURVE('',#22486,#22240,#19194,.T.);
#27314=EDGE_CURVE('',#22249,#22487,#19195,.T.);
#27315=EDGE_CURVE('',#22485,#22487,#2267,.T.);
#27316=EDGE_CURVE('',#22488,#22241,#19196,.T.);
#27317=EDGE_CURVE('',#22488,#22486,#5167,.T.);
#27318=EDGE_CURVE('',#22248,#22489,#19197,.T.);
#27319=EDGE_CURVE('',#22487,#22489,#2268,.T.);
#27320=EDGE_CURVE('',#22490,#22242,#19198,.T.);
#27321=EDGE_CURVE('',#22490,#22488,#2269,.T.);
#27322=EDGE_CURVE('',#22247,#22461,#19199,.T.);
#27323=EDGE_CURVE('',#22489,#22463,#2270,.T.);
#27324=EDGE_CURVE('',#22491,#22245,#19200,.T.);
#27325=EDGE_CURVE('',#22491,#22490,#2271,.T.);
#27326=EDGE_CURVE('',#22246,#22459,#19201,.T.);
#27327=EDGE_CURVE('',#22457,#22491,#2272,.T.);
#27328=EDGE_CURVE('',#22492,#22493,#19202,.T.);
#27329=EDGE_CURVE('',#22494,#22493,#2273,.T.);
#27330=EDGE_CURVE('',#22494,#22495,#19203,.T.);
#27331=EDGE_CURVE('',#22492,#22495,#2274,.T.);
#27332=EDGE_CURVE('',#22496,#22497,#19204,.T.);
#27333=EDGE_CURVE('',#22497,#22495,#2275,.T.);
#27334=EDGE_CURVE('',#22494,#22496,#2276,.T.);
#27335=EDGE_CURVE('',#22485,#22492,#2277,.T.);
#27336=EDGE_CURVE('',#22493,#22487,#2278,.T.);
#27337=EDGE_CURVE('',#22498,#22499,#19205,.T.);
#27338=EDGE_CURVE('',#22497,#22499,#19206,.T.);
#27339=EDGE_CURVE('',#22498,#22496,#19207,.T.);
#27340=EDGE_CURVE('',#22500,#22501,#19208,.T.);
#27341=EDGE_CURVE('',#22502,#22500,#2279,.T.);
#27342=EDGE_CURVE('',#22502,#22503,#19209,.T.);
#27343=EDGE_CURVE('',#22503,#22501,#2280,.T.);
#27344=EDGE_CURVE('',#22504,#22505,#19210,.T.);
#27345=EDGE_CURVE('',#22499,#22505,#2281,.T.);
#27346=EDGE_CURVE('',#22504,#22498,#2282,.T.);
#27347=EDGE_CURVE('',#22506,#22507,#19211,.T.);
#27348=EDGE_CURVE('',#22503,#22507,#19212,.T.);
#27349=EDGE_CURVE('',#22506,#22502,#19213,.T.);
#27350=EDGE_CURVE('',#22482,#22506,#2283,.T.);
#27351=EDGE_CURVE('',#22507,#22480,#2284,.T.);
#27352=EDGE_CURVE('',#22254,#22267,#5168,.T.);
#27353=EDGE_CURVE('',#22266,#22497,#5169,.T.);
#27354=EDGE_CURVE('',#22505,#22477,#2285,.T.);
#27355=EDGE_CURVE('',#22481,#22261,#5170,.T.);
#27356=EDGE_CURVE('',#22260,#22255,#5171,.T.);
#27357=EDGE_CURVE('',#22464,#22508,#5172,.T.);
#27358=EDGE_CURVE('',#22509,#22462,#5173,.T.);
#27359=EDGE_CURVE('',#22509,#22508,#19214,.T.);
#27360=EDGE_CURVE('',#22493,#22510,#19215,.T.);
#27361=EDGE_CURVE('',#22508,#22510,#2286,.T.);
#27362=EDGE_CURVE('',#22498,#22509,#2287,.T.);
#27363=EDGE_CURVE('',#22491,#22511,#2288,.T.);
#27364=EDGE_CURVE('',#22490,#22501,#2289,.T.);
#27365=EDGE_CURVE('',#22512,#22507,#2290,.T.);
#27366=EDGE_CURVE('',#22512,#22511,#19216,.T.);
#27367=EDGE_CURVE('',#22454,#22512,#5174,.T.);
#27368=EDGE_CURVE('',#22511,#22455,#5175,.T.);
#27369=EDGE_CURVE('',#22510,#22465,#5176,.T.);
#27370=EDGE_CURVE('',#22509,#22466,#5177,.T.);
#27371=EDGE_CURVE('',#22512,#22479,#5178,.T.);
#27372=EDGE_CURVE('',#22504,#22469,#5179,.T.);
#27373=EDGE_CURVE('',#22500,#22488,#2291,.T.);
#27374=EDGE_CURVE('',#22486,#22500,#5180,.T.);
#27375=EDGE_CURVE('',#22502,#22484,#5181,.T.);
#27376=EDGE_CURVE('',#22474,#22504,#2292,.T.);
#27377=EDGE_CURVE('',#22510,#22489,#2293,.T.);
#27378=EDGE_CURVE('',#22256,#22259,#5182,.T.);
#27379=EDGE_CURVE('',#22262,#22483,#5183,.T.);
#27380=EDGE_CURVE('',#22495,#22265,#5184,.T.);
#27381=EDGE_CURVE('',#22268,#22253,#5185,.T.);
#27382=EDGE_CURVE('',#22513,#22513,#19217,.T.);
#27383=EDGE_CURVE('',#22513,#22514,#5186,.T.);
#27384=EDGE_CURVE('',#22514,#22514,#19218,.T.);
#27385=EDGE_CURVE('',#22515,#22516,#19219,.T.);
#27386=EDGE_CURVE('',#22516,#22517,#5187,.T.);
#27387=EDGE_CURVE('',#22517,#22518,#19220,.T.);
#27388=EDGE_CURVE('',#22518,#22519,#5188,.T.);
#27389=EDGE_CURVE('',#22519,#22520,#19221,.T.);
#27390=EDGE_CURVE('',#22520,#22521,#5189,.T.);
#27391=EDGE_CURVE('',#22521,#22522,#19222,.T.);
#27392=EDGE_CURVE('',#22522,#22515,#5190,.T.);
#27393=EDGE_CURVE('',#22523,#22524,#5191,.T.);
#27394=EDGE_CURVE('',#22524,#22525,#19223,.T.);
#27395=EDGE_CURVE('',#22525,#22526,#5192,.T.);
#27396=EDGE_CURVE('',#22526,#22527,#19224,.T.);
#27397=EDGE_CURVE('',#22527,#22528,#5193,.T.);
#27398=EDGE_CURVE('',#22528,#22529,#19225,.T.);
#27399=EDGE_CURVE('',#22529,#22530,#5194,.T.);
#27400=EDGE_CURVE('',#22530,#22531,#19226,.T.);
#27401=EDGE_CURVE('',#22531,#22532,#5195,.T.);
#27402=EDGE_CURVE('',#22532,#22533,#19227,.T.);
#27403=EDGE_CURVE('',#22533,#22534,#5196,.T.);
#27404=EDGE_CURVE('',#22534,#22535,#19228,.T.);
#27405=EDGE_CURVE('',#22535,#22536,#5197,.T.);
#27406=EDGE_CURVE('',#22536,#22537,#19229,.T.);
#27407=EDGE_CURVE('',#22537,#22538,#5198,.T.);
#27408=EDGE_CURVE('',#22538,#22523,#19230,.T.);
#27409=EDGE_CURVE('',#22539,#22540,#5199,.T.);
#27410=EDGE_CURVE('',#22540,#22541,#5200,.T.);
#27411=EDGE_CURVE('',#22541,#22542,#5201,.T.);
#27412=EDGE_CURVE('',#22542,#22539,#5202,.T.);
#27413=EDGE_CURVE('',#22543,#22544,#5203,.T.);
#27414=EDGE_CURVE('',#22544,#22545,#5204,.T.);
#27415=EDGE_CURVE('',#22545,#22546,#5205,.T.);
#27416=EDGE_CURVE('',#22546,#22543,#5206,.T.);
#27417=EDGE_CURVE('',#22547,#22548,#5207,.T.);
#27418=EDGE_CURVE('',#22548,#22549,#5208,.T.);
#27419=EDGE_CURVE('',#22549,#22550,#5209,.T.);
#27420=EDGE_CURVE('',#22550,#22547,#5210,.T.);
#27421=EDGE_CURVE('',#22551,#22552,#5211,.T.);
#27422=EDGE_CURVE('',#22552,#22553,#5212,.T.);
#27423=EDGE_CURVE('',#22553,#22554,#5213,.T.);
#27424=EDGE_CURVE('',#22554,#22551,#5214,.T.);
#27425=EDGE_CURVE('',#22555,#22556,#19231,.T.);
#27426=EDGE_CURVE('',#22556,#22557,#5215,.T.);
#27427=EDGE_CURVE('',#22557,#22558,#19232,.T.);
#27428=EDGE_CURVE('',#22558,#22559,#5216,.T.);
#27429=EDGE_CURVE('',#22559,#22560,#19233,.T.);
#27430=EDGE_CURVE('',#22560,#22561,#5217,.T.);
#27431=EDGE_CURVE('',#22561,#22562,#19234,.T.);
#27432=EDGE_CURVE('',#22562,#22555,#5218,.T.);
#27433=EDGE_CURVE('',#22563,#22564,#5219,.T.);
#27434=EDGE_CURVE('',#22564,#22565,#5220,.T.);
#27435=EDGE_CURVE('',#22565,#22566,#5221,.T.);
#27436=EDGE_CURVE('',#22566,#22563,#5222,.T.);
#27437=EDGE_CURVE('',#22567,#22568,#5223,.T.);
#27438=EDGE_CURVE('',#22568,#22569,#5224,.T.);
#27439=EDGE_CURVE('',#22569,#22570,#5225,.T.);
#27440=EDGE_CURVE('',#22570,#22571,#19235,.T.);
#27441=EDGE_CURVE('',#22571,#22572,#5226,.T.);
#27442=EDGE_CURVE('',#22572,#22567,#19236,.T.);
#27443=EDGE_CURVE('',#22573,#22574,#5227,.T.);
#27444=EDGE_CURVE('',#22574,#22575,#5228,.T.);
#27445=EDGE_CURVE('',#22575,#22576,#5229,.T.);
#27446=EDGE_CURVE('',#22576,#22573,#5230,.T.);
#27447=EDGE_CURVE('',#22577,#22578,#5231,.T.);
#27448=EDGE_CURVE('',#22578,#22579,#5232,.T.);
#27449=EDGE_CURVE('',#22579,#22580,#5233,.T.);
#27450=EDGE_CURVE('',#22580,#22581,#19237,.T.);
#27451=EDGE_CURVE('',#22581,#22582,#5234,.T.);
#27452=EDGE_CURVE('',#22582,#22577,#19238,.T.);
#27453=EDGE_CURVE('',#22583,#22584,#5235,.T.);
#27454=EDGE_CURVE('',#22584,#22585,#5236,.T.);
#27455=EDGE_CURVE('',#22585,#22586,#5237,.T.);
#27456=EDGE_CURVE('',#22586,#22583,#5238,.T.);
#27457=EDGE_CURVE('',#22585,#22573,#19239,.T.);
#27458=EDGE_CURVE('',#22576,#22586,#19240,.T.);
#27459=EDGE_CURVE('',#22566,#22584,#19241,.T.);
#27460=EDGE_CURVE('',#22583,#22563,#19242,.T.);
#27461=EDGE_CURVE('',#22549,#22552,#19243,.T.);
#27462=EDGE_CURVE('',#22551,#22550,#19244,.T.);
#27463=EDGE_CURVE('',#22545,#22548,#19245,.T.);
#27464=EDGE_CURVE('',#22547,#22546,#19246,.T.);
#27465=EDGE_CURVE('',#22541,#22544,#19247,.T.);
#27466=EDGE_CURVE('',#22543,#22542,#19248,.T.);
#27467=EDGE_CURVE('',#22553,#22540,#19249,.T.);
#27468=EDGE_CURVE('',#22539,#22554,#19250,.T.);
#27469=EDGE_CURVE('',#22587,#22588,#5239,.T.);
#27470=EDGE_CURVE('',#22588,#22589,#5240,.T.);
#27471=EDGE_CURVE('',#22589,#22590,#5241,.T.);
#27472=EDGE_CURVE('',#22587,#22590,#5242,.T.);
#27473=EDGE_CURVE('',#22591,#22592,#5243,.T.);
#27474=EDGE_CURVE('',#22591,#22587,#19251,.T.);
#27475=EDGE_CURVE('',#22590,#22592,#19252,.T.);
#27476=EDGE_CURVE('',#22593,#22594,#5244,.T.);
#27477=EDGE_CURVE('',#22593,#22591,#5245,.T.);
#27478=EDGE_CURVE('',#22592,#22594,#5246,.T.);
#27479=EDGE_CURVE('',#22595,#22596,#5247,.T.);
#27480=EDGE_CURVE('',#22595,#22593,#19253,.T.);
#27481=EDGE_CURVE('',#22594,#22596,#19254,.T.);
#27482=EDGE_CURVE('',#22596,#22597,#5248,.T.);
#27483=EDGE_CURVE('',#22597,#22598,#5249,.T.);
#27484=EDGE_CURVE('',#22598,#22595,#5250,.T.);
#27485=EDGE_CURVE('',#22599,#22600,#5251,.T.);
#27486=EDGE_CURVE('',#22600,#22601,#5252,.T.);
#27487=EDGE_CURVE('',#22601,#22602,#5253,.T.);
#27488=EDGE_CURVE('',#22599,#22602,#5254,.T.);
#27489=EDGE_CURVE('',#22603,#22604,#5255,.T.);
#27490=EDGE_CURVE('',#22603,#22599,#19255,.T.);
#27491=EDGE_CURVE('',#22602,#22604,#19256,.T.);
#27492=EDGE_CURVE('',#22605,#22606,#5256,.T.);
#27493=EDGE_CURVE('',#22605,#22603,#5257,.T.);
#27494=EDGE_CURVE('',#22604,#22606,#5258,.T.);
#27495=EDGE_CURVE('',#22607,#22608,#5259,.T.);
#27496=EDGE_CURVE('',#22607,#22605,#19257,.T.);
#27497=EDGE_CURVE('',#22606,#22608,#19258,.T.);
#27498=EDGE_CURVE('',#22608,#22609,#5260,.T.);
#27499=EDGE_CURVE('',#22609,#22610,#5261,.T.);
#27500=EDGE_CURVE('',#22610,#22607,#5262,.T.);
#27501=EDGE_CURVE('',#22549,#22560,#19259,.T.);
#27502=EDGE_CURVE('',#22561,#22548,#19260,.T.);
#27503=EDGE_CURVE('',#22562,#22545,#19261,.T.);
#27504=EDGE_CURVE('',#22552,#22559,#19262,.T.);
#27505=EDGE_CURVE('',#22555,#22544,#19263,.T.);
#27506=EDGE_CURVE('',#22553,#22558,#19264,.T.);
#27507=EDGE_CURVE('',#22556,#22541,#19265,.T.);
#27508=EDGE_CURVE('',#22540,#22557,#19266,.T.);
#27509=EDGE_CURVE('',#22521,#22546,#19267,.T.);
#27510=EDGE_CURVE('',#22543,#22520,#19268,.T.);
#27511=EDGE_CURVE('',#22542,#22519,#19269,.T.);
#27512=EDGE_CURVE('',#22522,#22547,#19270,.T.);
#27513=EDGE_CURVE('',#22539,#22518,#19271,.T.);
#27514=EDGE_CURVE('',#22515,#22550,#19272,.T.);
#27515=EDGE_CURVE('',#22554,#22517,#19273,.T.);
#27516=EDGE_CURVE('',#22516,#22551,#19274,.T.);
#27517=EDGE_CURVE('',#22598,#22574,#19275,.T.);
#27518=EDGE_CURVE('',#22595,#22573,#19276,.T.);
#27519=EDGE_CURVE('',#22593,#22585,#19277,.T.);
#27520=EDGE_CURVE('',#22591,#22584,#19278,.T.);
#27521=EDGE_CURVE('',#22587,#22566,#19279,.T.);
#27522=EDGE_CURVE('',#22565,#22588,#19280,.T.);
#27523=EDGE_CURVE('',#22589,#22568,#19281,.T.);
#27524=EDGE_CURVE('',#22590,#22567,#19282,.T.);
#27525=EDGE_CURVE('',#22592,#22572,#19283,.T.);
#27526=EDGE_CURVE('',#22594,#22571,#19284,.T.);
#27527=EDGE_CURVE('',#22596,#22570,#19285,.T.);
#27528=EDGE_CURVE('',#22569,#22597,#19286,.T.);
#27529=EDGE_CURVE('',#22610,#22578,#19287,.T.);
#27530=EDGE_CURVE('',#22607,#22577,#19288,.T.);
#27531=EDGE_CURVE('',#22605,#22582,#19289,.T.);
#27532=EDGE_CURVE('',#22603,#22581,#19290,.T.);
#27533=EDGE_CURVE('',#22599,#22580,#19291,.T.);
#27534=EDGE_CURVE('',#22579,#22600,#19292,.T.);
#27535=EDGE_CURVE('',#22601,#22564,#19293,.T.);
#27536=EDGE_CURVE('',#22602,#22563,#19294,.T.);
#27537=EDGE_CURVE('',#22604,#22583,#19295,.T.);
#27538=EDGE_CURVE('',#22606,#22586,#19296,.T.);
#27539=EDGE_CURVE('',#22608,#22576,#19297,.T.);
#27540=EDGE_CURVE('',#22575,#22609,#19298,.T.);
#27541=EDGE_CURVE('',#22574,#22532,#19299,.T.);
#27542=EDGE_CURVE('',#22533,#22598,#19300,.T.);
#27543=EDGE_CURVE('',#22534,#22597,#19301,.T.);
#27544=EDGE_CURVE('',#22575,#22531,#19302,.T.);
#27545=EDGE_CURVE('',#22535,#22569,#19303,.T.);
#27546=EDGE_CURVE('',#22609,#22530,#19304,.T.);
#27547=EDGE_CURVE('',#22536,#22568,#19305,.T.);
#27548=EDGE_CURVE('',#22610,#22529,#19306,.T.);
#27549=EDGE_CURVE('',#22537,#22589,#19307,.T.);
#27550=EDGE_CURVE('',#22578,#22528,#19308,.T.);
#27551=EDGE_CURVE('',#22538,#22588,#19309,.T.);
#27552=EDGE_CURVE('',#22579,#22527,#19310,.T.);
#27553=EDGE_CURVE('',#22523,#22565,#19311,.T.);
#27554=EDGE_CURVE('',#22600,#22526,#19312,.T.);
#27555=EDGE_CURVE('',#22524,#22564,#19313,.T.);
#27556=EDGE_CURVE('',#22601,#22525,#19314,.T.);
#27557=EDGE_CURVE('',#22611,#22612,#19315,.T.);
#27558=EDGE_CURVE('',#22612,#22611,#19316,.T.);
#27559=EDGE_CURVE('',#22612,#22613,#19317,.T.);
#27560=EDGE_CURVE('',#22613,#22613,#19318,.T.);
#27561=EDGE_CURVE('',#22614,#22615,#19319,.T.);
#27562=EDGE_CURVE('',#22616,#22614,#19320,.T.);
#27563=EDGE_CURVE('',#22617,#22616,#19321,.T.);
#27564=EDGE_CURVE('',#22617,#22615,#19322,.T.);
#27565=EDGE_CURVE('',#22618,#22619,#19323,.T.);
#27566=EDGE_CURVE('',#22620,#22618,#19324,.T.);
#27567=EDGE_CURVE('',#22621,#22620,#19325,.T.);
#27568=EDGE_CURVE('',#22621,#22619,#19326,.T.);
#27569=EDGE_CURVE('',#22622,#22623,#19327,.T.);
#27570=EDGE_CURVE('',#22622,#22624,#19328,.T.);
#27571=EDGE_CURVE('',#22625,#22624,#19329,.T.);
#27572=EDGE_CURVE('',#22626,#22625,#19330,.T.);
#27573=EDGE_CURVE('',#22623,#22626,#19331,.T.);
#27574=EDGE_CURVE('',#22611,#22623,#5263,.T.);
#27575=EDGE_CURVE('',#22626,#22627,#5264,.T.);
#27576=EDGE_CURVE('',#22627,#22628,#2294,.T.);
#27577=EDGE_CURVE('',#22628,#22629,#19332,.T.);
#27578=EDGE_CURVE('',#22629,#22630,#2295,.T.);
#27579=EDGE_CURVE('',#22622,#22630,#5265,.T.);
#27580=EDGE_CURVE('',#22613,#22631,#19333,.T.);
#27581=EDGE_CURVE('',#22632,#22631,#19334,.T.);
#27582=EDGE_CURVE('',#22631,#22632,#19335,.T.);
#27583=EDGE_CURVE('',#22633,#22633,#19336,.T.);
#27584=EDGE_CURVE('',#22633,#22634,#19337,.T.);
#27585=EDGE_CURVE('',#22634,#22634,#19338,.T.);
#27586=EDGE_CURVE('',#22634,#22632,#5266,.T.);
#27587=EDGE_CURVE('',#22635,#22636,#2296,.T.);
#27588=EDGE_CURVE('',#22636,#22637,#19339,.T.);
#27589=EDGE_CURVE('',#22637,#22638,#2297,.T.);
#27590=EDGE_CURVE('',#22639,#22638,#19340,.T.);
#27591=EDGE_CURVE('',#22639,#22635,#2298,.T.);
#27592=EDGE_CURVE('',#22640,#22641,#2299,.T.);
#27593=EDGE_CURVE('',#22641,#22642,#19341,.T.);
#27594=EDGE_CURVE('',#22642,#22643,#2300,.T.);
#27595=EDGE_CURVE('',#22644,#22643,#19342,.T.);
#27596=EDGE_CURVE('',#22644,#22640,#2301,.T.);
#27597=EDGE_CURVE('',#22645,#22646,#2302,.T.);
#27598=EDGE_CURVE('',#22646,#22647,#19343,.T.);
#27599=EDGE_CURVE('',#22647,#22648,#2303,.T.);
#27600=EDGE_CURVE('',#22649,#22648,#19344,.T.);
#27601=EDGE_CURVE('',#22649,#22645,#19345,.T.);
#27602=EDGE_CURVE('',#22650,#22651,#2304,.T.);
#27603=EDGE_CURVE('',#22651,#22652,#5267,.T.);
#27604=EDGE_CURVE('',#22646,#22652,#19346,.T.);
#27605=EDGE_CURVE('',#22652,#22649,#2305,.T.);
#27606=EDGE_CURVE('',#22651,#22650,#2306,.T.);
#27607=EDGE_CURVE('',#22653,#22644,#2307,.T.);
#27608=EDGE_CURVE('',#22653,#22654,#5268,.T.);
#27609=EDGE_CURVE('',#22636,#22654,#2308,.T.);
#27610=EDGE_CURVE('',#22654,#22639,#2309,.T.);
#27611=EDGE_CURVE('',#22641,#22653,#2310,.T.);
#27612=EDGE_CURVE('',#22655,#22656,#2311,.T.);
#27613=EDGE_CURVE('',#22655,#22657,#19347,.T.);
#27614=EDGE_CURVE('',#22658,#22657,#2312,.T.);
#27615=EDGE_CURVE('',#22659,#22658,#19348,.T.);
#27616=EDGE_CURVE('',#22656,#22659,#2313,.T.);
#27617=EDGE_CURVE('',#22660,#22661,#2314,.T.);
#27618=EDGE_CURVE('',#22660,#22662,#19349,.T.);
#27619=EDGE_CURVE('',#22663,#22662,#2315,.T.);
#27620=EDGE_CURVE('',#22664,#22663,#19350,.T.);
#27621=EDGE_CURVE('',#22661,#22664,#2316,.T.);
#27622=EDGE_CURVE('',#22665,#22666,#2317,.T.);
#27623=EDGE_CURVE('',#22665,#22667,#19351,.T.);
#27624=EDGE_CURVE('',#22668,#22667,#2318,.T.);
#27625=EDGE_CURVE('',#22669,#22668,#19352,.T.);
#27626=EDGE_CURVE('',#22666,#22669,#2319,.T.);
#27627=EDGE_CURVE('',#22670,#22670,#19353,.T.);
#27628=EDGE_CURVE('',#22670,#22633,#19354,.T.);
#27629=EDGE_CURVE('',#22671,#22672,#19355,.T.);
#27630=EDGE_CURVE('',#22672,#22671,#19356,.T.);
#27631=EDGE_CURVE('',#22672,#22673,#19357,.T.);
#27632=EDGE_CURVE('',#22673,#22673,#19358,.T.);
#27633=EDGE_CURVE('',#22664,#22674,#2320,.T.);
#27634=EDGE_CURVE('',#22674,#22675,#5269,.T.);
#27635=EDGE_CURVE('',#22675,#22665,#2321,.T.);
#27636=EDGE_CURVE('',#22669,#22675,#2322,.T.);
#27637=EDGE_CURVE('',#22674,#22660,#2323,.T.);
#27638=EDGE_CURVE('',#22671,#22670,#5270,.T.);
#27639=EDGE_CURVE('',#22638,#22637,#2324,.T.);
#27640=EDGE_CURVE('',#22676,#22677,#2325,.T.);
#27641=EDGE_CURVE('',#22677,#22676,#2326,.T.);
#27642=EDGE_CURVE('',#22657,#22658,#2327,.T.);
#27643=EDGE_CURVE('',#22677,#22678,#19359,.T.);
#27644=EDGE_CURVE('',#22679,#22678,#2328,.T.);
#27645=EDGE_CURVE('',#22680,#22679,#2329,.T.);
#27646=EDGE_CURVE('',#22676,#22680,#19360,.T.);
#27647=EDGE_CURVE('',#22681,#22682,#2330,.T.);
#27648=EDGE_CURVE('',#22681,#22683,#19361,.T.);
#27649=EDGE_CURVE('',#22684,#22683,#2331,.T.);
#27650=EDGE_CURVE('',#22685,#22684,#2332,.T.);
#27651=EDGE_CURVE('',#22682,#22685,#19362,.T.);
#27652=EDGE_CURVE('',#22686,#22687,#2333,.T.);
#27653=EDGE_CURVE('',#22686,#22688,#19363,.T.);
#27654=EDGE_CURVE('',#22689,#22688,#2334,.T.);
#27655=EDGE_CURVE('',#22690,#22689,#19364,.T.);
#27656=EDGE_CURVE('',#22687,#22690,#19365,.T.);
#27657=EDGE_CURVE('',#22691,#22691,#2335,.T.);
#27658=EDGE_CURVE('',#22691,#22692,#5271,.T.);
#27659=EDGE_CURVE('',#22692,#22690,#2336,.T.);
#27660=EDGE_CURVE('',#22688,#22692,#19366,.T.);
#27661=EDGE_CURVE('',#22683,#22693,#2337,.T.);
#27662=EDGE_CURVE('',#22693,#22694,#5272,.T.);
#27663=EDGE_CURVE('',#22694,#22680,#2338,.T.);
#27664=EDGE_CURVE('',#22678,#22694,#2339,.T.);
#27665=EDGE_CURVE('',#22693,#22685,#2340,.T.);
#27666=EDGE_CURVE('',#22695,#22696,#2341,.T.);
#27667=EDGE_CURVE('',#22695,#22697,#19367,.T.);
#27668=EDGE_CURVE('',#22698,#22697,#43,.T.);
#27669=EDGE_CURVE('',#22696,#22698,#19368,.T.);
#27670=EDGE_CURVE('',#22659,#22699,#2342,.T.);
#27671=EDGE_CURVE('',#22699,#22698,#5273,.T.);
#27672=EDGE_CURVE('',#22697,#22698,#44,.T.);
#27673=EDGE_CURVE('',#22699,#22655,#2343,.T.);
#27674=EDGE_CURVE('',#22696,#22695,#2344,.T.);
#27675=EDGE_CURVE('',#22667,#22668,#2345,.T.);
#27676=EDGE_CURVE('',#22682,#22681,#2346,.T.);
#27677=EDGE_CURVE('',#22687,#22686,#2347,.T.);
#27678=EDGE_CURVE('',#22662,#22663,#2348,.T.);
#27679=EDGE_CURVE('',#22643,#22642,#2349,.T.);
#27680=EDGE_CURVE('',#22648,#22647,#2350,.T.);
#27681=EDGE_CURVE('',#22700,#22701,#19369,.T.);
#27682=EDGE_CURVE('',#22701,#22702,#5274,.T.);
#27683=EDGE_CURVE('',#22702,#22703,#19370,.T.);
#27684=EDGE_CURVE('',#22700,#22703,#5275,.T.);
#27685=EDGE_CURVE('',#22616,#22704,#5276,.T.);
#27686=EDGE_CURVE('',#22704,#22705,#19371,.T.);
#27687=EDGE_CURVE('',#22705,#22622,#5277,.T.);
#27688=EDGE_CURVE('',#22630,#22706,#5278,.T.);
#27689=EDGE_CURVE('',#22706,#22707,#19372,.T.);
#27690=EDGE_CURVE('',#22707,#22617,#5279,.T.);
#27691=EDGE_CURVE('',#22708,#22709,#19373,.T.);
#27692=EDGE_CURVE('',#22709,#22618,#5280,.T.);
#27693=EDGE_CURVE('',#22619,#22710,#5281,.T.);
#27694=EDGE_CURVE('',#22710,#22711,#19374,.T.);
#27695=EDGE_CURVE('',#22711,#22627,#5282,.T.);
#27696=EDGE_CURVE('',#22626,#22708,#5283,.T.);
#27697=EDGE_CURVE('',#22712,#22713,#19375,.T.);
#27698=EDGE_CURVE('',#22713,#22714,#5284,.T.);
#27699=EDGE_CURVE('',#22714,#22715,#19376,.T.);
#27700=EDGE_CURVE('',#22712,#22715,#5285,.T.);
#27701=EDGE_CURVE('',#22703,#22625,#5286,.T.);
#27702=EDGE_CURVE('',#22624,#22700,#5287,.T.);
#27703=EDGE_CURVE('',#22716,#22717,#19377,.T.);
#27704=EDGE_CURVE('',#22717,#22712,#5288,.T.);
#27705=EDGE_CURVE('',#22715,#22716,#5289,.T.);
#27706=EDGE_CURVE('',#22615,#22621,#5290,.T.);
#27707=EDGE_CURVE('',#22620,#22614,#5291,.T.);
#27708=EDGE_CURVE('',#22718,#22719,#2351,.T.);
#27709=EDGE_CURVE('',#22719,#22720,#5292,.T.);
#27710=EDGE_CURVE('',#22720,#22721,#5293,.T.);
#27711=EDGE_CURVE('',#22721,#22722,#5294,.T.);
#27712=EDGE_CURVE('',#22722,#22723,#2352,.T.);
#27713=EDGE_CURVE('',#22723,#22718,#5295,.T.);
#27714=EDGE_CURVE('',#22724,#22725,#2353,.T.);
#27715=EDGE_CURVE('',#22725,#22726,#5296,.T.);
#27716=EDGE_CURVE('',#22726,#22727,#5297,.T.);
#27717=EDGE_CURVE('',#22727,#22728,#5298,.T.);
#27718=EDGE_CURVE('',#22728,#22729,#2354,.T.);
#27719=EDGE_CURVE('',#22729,#22724,#5299,.T.);
#27720=EDGE_CURVE('',#22714,#22707,#2355,.T.);
#27721=EDGE_CURVE('',#22715,#22706,#19378,.T.);
#27722=EDGE_CURVE('',#22716,#22630,#2356,.T.);
#27723=EDGE_CURVE('',#22716,#22629,#19379,.T.);
#27724=EDGE_CURVE('',#22717,#22628,#19380,.T.);
#27725=EDGE_CURVE('',#22717,#22627,#2357,.T.);
#27726=EDGE_CURVE('',#22710,#22713,#2358,.T.);
#27727=EDGE_CURVE('',#22711,#22712,#19381,.T.);
#27728=EDGE_CURVE('',#22704,#22701,#2359,.T.);
#27729=EDGE_CURVE('',#22705,#22700,#19382,.T.);
#27730=EDGE_CURVE('',#22708,#22703,#19383,.T.);
#27731=EDGE_CURVE('',#22702,#22709,#2360,.T.);
#27732=EDGE_CURVE('',#22713,#22724,#19384,.T.);
#27733=EDGE_CURVE('',#22725,#22710,#19385,.T.);
#27734=EDGE_CURVE('',#22726,#22619,#19386,.T.);
#27735=EDGE_CURVE('',#22714,#22729,#19387,.T.);
#27736=EDGE_CURVE('',#22726,#22621,#19388,.T.);
#27737=EDGE_CURVE('',#22707,#22728,#19389,.T.);
#27738=EDGE_CURVE('',#22727,#22615,#19390,.T.);
#27739=EDGE_CURVE('',#22617,#22727,#19391,.T.);
#27740=EDGE_CURVE('',#22618,#22721,#19392,.T.);
#27741=EDGE_CURVE('',#22722,#22709,#19393,.T.);
#27742=EDGE_CURVE('',#22620,#22721,#19394,.T.);
#27743=EDGE_CURVE('',#22723,#22702,#19395,.T.);
#27744=EDGE_CURVE('',#22614,#22720,#19396,.T.);
#27745=EDGE_CURVE('',#22718,#22701,#19397,.T.);
#27746=EDGE_CURVE('',#22616,#22720,#19398,.T.);
#27747=EDGE_CURVE('',#22719,#22704,#19399,.T.);
#27748=EDGE_CURVE('',#22730,#22730,#19400,.T.);
#27749=EDGE_CURVE('',#22730,#22731,#5300,.T.);
#27750=EDGE_CURVE('',#22731,#22731,#19401,.T.);
#27751=EDGE_CURVE('',#22732,#22732,#19402,.T.);
#27752=EDGE_CURVE('',#22732,#22733,#5301,.T.);
#27753=EDGE_CURVE('',#22733,#22733,#19403,.T.);
#27754=EDGE_CURVE('',#22734,#22735,#19404,.T.);
#27755=EDGE_CURVE('',#22735,#22736,#2361,.T.);
#27756=EDGE_CURVE('',#22736,#22737,#19405,.T.);
#27757=EDGE_CURVE('',#22734,#22737,#2362,.T.);
#27758=EDGE_CURVE('',#22738,#22739,#2363,.T.);
#27759=EDGE_CURVE('',#22739,#22738,#2364,.T.);
#27760=EDGE_CURVE('',#22740,#22741,#2365,.T.);
#27761=EDGE_CURVE('',#22741,#22740,#2366,.T.);
#27762=EDGE_CURVE('',#22742,#22743,#2367,.T.);
#27763=EDGE_CURVE('',#22743,#22742,#2368,.T.);
#27764=EDGE_CURVE('',#22744,#22745,#2369,.T.);
#27765=EDGE_CURVE('',#22745,#22744,#2370,.T.);
#27766=EDGE_CURVE('',#22746,#22747,#2371,.T.);
#27767=EDGE_CURVE('',#22747,#22746,#2372,.T.);
#27768=EDGE_CURVE('',#22748,#22749,#2373,.T.);
#27769=EDGE_CURVE('',#22749,#22748,#2374,.T.);
#27770=EDGE_CURVE('',#22750,#22751,#2375,.T.);
#27771=EDGE_CURVE('',#22751,#22750,#2376,.T.);
#27772=EDGE_CURVE('',#22752,#22753,#2377,.T.);
#27773=EDGE_CURVE('',#22753,#22752,#2378,.T.);
#27774=EDGE_CURVE('',#22754,#22755,#2379,.T.);
#27775=EDGE_CURVE('',#22755,#22754,#2380,.T.);
#27776=EDGE_CURVE('',#22756,#22757,#2381,.T.);
#27777=EDGE_CURVE('',#22757,#22756,#2382,.T.);
#27778=EDGE_CURVE('',#22758,#22759,#2383,.T.);
#27779=EDGE_CURVE('',#22759,#22758,#2384,.T.);
#27780=EDGE_CURVE('',#22760,#22761,#2385,.T.);
#27781=EDGE_CURVE('',#22761,#22760,#2386,.T.);
#27782=EDGE_CURVE('',#22762,#22763,#2387,.T.);
#27783=EDGE_CURVE('',#22763,#22762,#2388,.T.);
#27784=EDGE_CURVE('',#22764,#22765,#2389,.T.);
#27785=EDGE_CURVE('',#22765,#22764,#2390,.T.);
#27786=EDGE_CURVE('',#22766,#22767,#2391,.T.);
#27787=EDGE_CURVE('',#22767,#22766,#2392,.T.);
#27788=EDGE_CURVE('',#22768,#22769,#2393,.T.);
#27789=EDGE_CURVE('',#22769,#22768,#2394,.T.);
#27790=EDGE_CURVE('',#22770,#22771,#2395,.T.);
#27791=EDGE_CURVE('',#22771,#22770,#2396,.T.);
#27792=EDGE_CURVE('',#22772,#22773,#2397,.T.);
#27793=EDGE_CURVE('',#22773,#22772,#2398,.T.);
#27794=EDGE_CURVE('',#22774,#22775,#2399,.T.);
#27795=EDGE_CURVE('',#22775,#22774,#2400,.T.);
#27796=EDGE_CURVE('',#22776,#22777,#2401,.T.);
#27797=EDGE_CURVE('',#22777,#22776,#2402,.T.);
#27798=EDGE_CURVE('',#22778,#22779,#2403,.T.);
#27799=EDGE_CURVE('',#22779,#22778,#2404,.T.);
#27800=EDGE_CURVE('',#22780,#22781,#2405,.T.);
#27801=EDGE_CURVE('',#22781,#22780,#2406,.T.);
#27802=EDGE_CURVE('',#22782,#22783,#2407,.T.);
#27803=EDGE_CURVE('',#22783,#22782,#2408,.T.);
#27804=EDGE_CURVE('',#22784,#22785,#2409,.T.);
#27805=EDGE_CURVE('',#22785,#22784,#2410,.T.);
#27806=EDGE_CURVE('',#22786,#22787,#2411,.T.);
#27807=EDGE_CURVE('',#22787,#22786,#2412,.T.);
#27808=EDGE_CURVE('',#22788,#22789,#2413,.T.);
#27809=EDGE_CURVE('',#22789,#22788,#2414,.T.);
#27810=EDGE_CURVE('',#22790,#22791,#2415,.T.);
#27811=EDGE_CURVE('',#22791,#22790,#2416,.T.);
#27812=EDGE_CURVE('',#22792,#22793,#2417,.T.);
#27813=EDGE_CURVE('',#22793,#22792,#2418,.T.);
#27814=EDGE_CURVE('',#22794,#22795,#2419,.T.);
#27815=EDGE_CURVE('',#22795,#22794,#2420,.T.);
#27816=EDGE_CURVE('',#22796,#22797,#2421,.T.);
#27817=EDGE_CURVE('',#22797,#22796,#2422,.T.);
#27818=EDGE_CURVE('',#22798,#22799,#2423,.T.);
#27819=EDGE_CURVE('',#22799,#22798,#2424,.T.);
#27820=EDGE_CURVE('',#22800,#22801,#2425,.T.);
#27821=EDGE_CURVE('',#22801,#22800,#2426,.T.);
#27822=EDGE_CURVE('',#22802,#22803,#2427,.T.);
#27823=EDGE_CURVE('',#22803,#22802,#2428,.T.);
#27824=EDGE_CURVE('',#22804,#22805,#2429,.T.);
#27825=EDGE_CURVE('',#22805,#22804,#2430,.T.);
#27826=EDGE_CURVE('',#22806,#22807,#2431,.T.);
#27827=EDGE_CURVE('',#22807,#22806,#2432,.T.);
#27828=EDGE_CURVE('',#22808,#22809,#2433,.T.);
#27829=EDGE_CURVE('',#22809,#22808,#2434,.T.);
#27830=EDGE_CURVE('',#22810,#22811,#2435,.T.);
#27831=EDGE_CURVE('',#22811,#22810,#2436,.T.);
#27832=EDGE_CURVE('',#22812,#22813,#2437,.T.);
#27833=EDGE_CURVE('',#22813,#22812,#2438,.T.);
#27834=EDGE_CURVE('',#22814,#22815,#2439,.T.);
#27835=EDGE_CURVE('',#22815,#22814,#2440,.T.);
#27836=EDGE_CURVE('',#22816,#22817,#2441,.T.);
#27837=EDGE_CURVE('',#22817,#22816,#2442,.T.);
#27838=EDGE_CURVE('',#22818,#22819,#2443,.T.);
#27839=EDGE_CURVE('',#22819,#22818,#2444,.T.);
#27840=EDGE_CURVE('',#22820,#22821,#2445,.T.);
#27841=EDGE_CURVE('',#22821,#22820,#2446,.T.);
#27842=EDGE_CURVE('',#22822,#22823,#2447,.T.);
#27843=EDGE_CURVE('',#22823,#22822,#2448,.T.);
#27844=EDGE_CURVE('',#22824,#22825,#2449,.T.);
#27845=EDGE_CURVE('',#22825,#22824,#2450,.T.);
#27846=EDGE_CURVE('',#22826,#22827,#2451,.T.);
#27847=EDGE_CURVE('',#22827,#22826,#2452,.T.);
#27848=EDGE_CURVE('',#22828,#22829,#2453,.T.);
#27849=EDGE_CURVE('',#22829,#22828,#2454,.T.);
#27850=EDGE_CURVE('',#22830,#22831,#2455,.T.);
#27851=EDGE_CURVE('',#22831,#22830,#2456,.T.);
#27852=EDGE_CURVE('',#22832,#22833,#2457,.T.);
#27853=EDGE_CURVE('',#22833,#22832,#2458,.T.);
#27854=EDGE_CURVE('',#22834,#22835,#2459,.T.);
#27855=EDGE_CURVE('',#22835,#22834,#2460,.T.);
#27856=EDGE_CURVE('',#22836,#22837,#2461,.T.);
#27857=EDGE_CURVE('',#22837,#22836,#2462,.T.);
#27858=EDGE_CURVE('',#22838,#22839,#2463,.T.);
#27859=EDGE_CURVE('',#22839,#22838,#2464,.T.);
#27860=EDGE_CURVE('',#22840,#22841,#2465,.T.);
#27861=EDGE_CURVE('',#22841,#22840,#2466,.T.);
#27862=EDGE_CURVE('',#22842,#22843,#2467,.T.);
#27863=EDGE_CURVE('',#22843,#22842,#2468,.T.);
#27864=EDGE_CURVE('',#22844,#22845,#2469,.T.);
#27865=EDGE_CURVE('',#22845,#22844,#2470,.T.);
#27866=EDGE_CURVE('',#22846,#22847,#2471,.T.);
#27867=EDGE_CURVE('',#22847,#22846,#2472,.T.);
#27868=EDGE_CURVE('',#22848,#22849,#2473,.T.);
#27869=EDGE_CURVE('',#22849,#22848,#2474,.T.);
#27870=EDGE_CURVE('',#22850,#22851,#2475,.T.);
#27871=EDGE_CURVE('',#22851,#22850,#2476,.T.);
#27872=EDGE_CURVE('',#22852,#22853,#2477,.T.);
#27873=EDGE_CURVE('',#22853,#22852,#2478,.T.);
#27874=EDGE_CURVE('',#22854,#22855,#2479,.T.);
#27875=EDGE_CURVE('',#22855,#22854,#2480,.T.);
#27876=EDGE_CURVE('',#22856,#22857,#2481,.T.);
#27877=EDGE_CURVE('',#22857,#22856,#2482,.T.);
#27878=EDGE_CURVE('',#22858,#22858,#19406,.T.);
#27879=EDGE_CURVE('',#22858,#22859,#19407,.T.);
#27880=EDGE_CURVE('',#22859,#22859,#19408,.T.);
#27881=EDGE_CURVE('',#22765,#22860,#5302,.T.);
#27882=EDGE_CURVE('',#22860,#22860,#2483,.T.);
#27883=EDGE_CURVE('',#22861,#22862,#2484,.T.);
#27884=EDGE_CURVE('',#22862,#22863,#5303,.T.);
#27885=EDGE_CURVE('',#22863,#22863,#19409,.T.);
#27886=EDGE_CURVE('',#22862,#22861,#2485,.T.);
#27887=EDGE_CURVE('',#22807,#22864,#5304,.T.);
#27888=EDGE_CURVE('',#22864,#22864,#2486,.T.);
#27889=EDGE_CURVE('',#22865,#22866,#2487,.T.);
#27890=EDGE_CURVE('',#22866,#22867,#5305,.T.);
#27891=EDGE_CURVE('',#22867,#22867,#19410,.T.);
#27892=EDGE_CURVE('',#22866,#22865,#2488,.T.);
#27893=EDGE_CURVE('',#22833,#22868,#5306,.T.);
#27894=EDGE_CURVE('',#22868,#22868,#2489,.T.);
#27895=EDGE_CURVE('',#22869,#22870,#2490,.T.);
#27896=EDGE_CURVE('',#22870,#22871,#5307,.T.);
#27897=EDGE_CURVE('',#22871,#22871,#19411,.T.);
#27898=EDGE_CURVE('',#22870,#22869,#2491,.T.);
#27899=EDGE_CURVE('',#22747,#22872,#5308,.T.);
#27900=EDGE_CURVE('',#22872,#22872,#2492,.T.);
#27901=EDGE_CURVE('',#22873,#22874,#2493,.T.);
#27902=EDGE_CURVE('',#22874,#22875,#5309,.T.);
#27903=EDGE_CURVE('',#22875,#22875,#19412,.T.);
#27904=EDGE_CURVE('',#22874,#22873,#2494,.T.);
#27905=EDGE_CURVE('',#22777,#22876,#5310,.T.);
#27906=EDGE_CURVE('',#22876,#22876,#2495,.T.);
#27907=EDGE_CURVE('',#22877,#22878,#2496,.T.);
#27908=EDGE_CURVE('',#22878,#22879,#5311,.T.);
#27909=EDGE_CURVE('',#22879,#22879,#19413,.T.);
#27910=EDGE_CURVE('',#22878,#22877,#2497,.T.);
#27911=EDGE_CURVE('',#22767,#22880,#5312,.T.);
#27912=EDGE_CURVE('',#22880,#22880,#2498,.T.);
#27913=EDGE_CURVE('',#22881,#22882,#2499,.T.);
#27914=EDGE_CURVE('',#22882,#22883,#5313,.T.);
#27915=EDGE_CURVE('',#22883,#22883,#19414,.T.);
#27916=EDGE_CURVE('',#22882,#22881,#2500,.T.);
#27917=EDGE_CURVE('',#22809,#22884,#5314,.T.);
#27918=EDGE_CURVE('',#22884,#22884,#2501,.T.);
#27919=EDGE_CURVE('',#22885,#22886,#2502,.T.);
#27920=EDGE_CURVE('',#22886,#22887,#5315,.T.);
#27921=EDGE_CURVE('',#22887,#22887,#19415,.T.);
#27922=EDGE_CURVE('',#22886,#22885,#2503,.T.);
#27923=EDGE_CURVE('',#22757,#22888,#5316,.T.);
#27924=EDGE_CURVE('',#22888,#22888,#2504,.T.);
#27925=EDGE_CURVE('',#22889,#22890,#2505,.T.);
#27926=EDGE_CURVE('',#22890,#22891,#5317,.T.);
#27927=EDGE_CURVE('',#22891,#22891,#19416,.T.);
#27928=EDGE_CURVE('',#22890,#22889,#2506,.T.);
#27929=EDGE_CURVE('',#22745,#22892,#5318,.T.);
#27930=EDGE_CURVE('',#22892,#22892,#2507,.T.);
#27931=EDGE_CURVE('',#22893,#22894,#2508,.T.);
#27932=EDGE_CURVE('',#22894,#22895,#5319,.T.);
#27933=EDGE_CURVE('',#22895,#22895,#19417,.T.);
#27934=EDGE_CURVE('',#22894,#22893,#2509,.T.);
#27935=EDGE_CURVE('',#22775,#22896,#5320,.T.);
#27936=EDGE_CURVE('',#22896,#22896,#2510,.T.);
#27937=EDGE_CURVE('',#22897,#22898,#2511,.T.);
#27938=EDGE_CURVE('',#22898,#22899,#5321,.T.);
#27939=EDGE_CURVE('',#22899,#22899,#19418,.T.);
#27940=EDGE_CURVE('',#22898,#22897,#2512,.T.);
#27941=EDGE_CURVE('',#22769,#22900,#5322,.T.);
#27942=EDGE_CURVE('',#22900,#22900,#2513,.T.);
#27943=EDGE_CURVE('',#22901,#22902,#2514,.T.);
#27944=EDGE_CURVE('',#22902,#22903,#5323,.T.);
#27945=EDGE_CURVE('',#22903,#22903,#19419,.T.);
#27946=EDGE_CURVE('',#22902,#22901,#2515,.T.);
#27947=EDGE_CURVE('',#22749,#22904,#5324,.T.);
#27948=EDGE_CURVE('',#22904,#22904,#2516,.T.);
#27949=EDGE_CURVE('',#22905,#22906,#2517,.T.);
#27950=EDGE_CURVE('',#22906,#22907,#5325,.T.);
#27951=EDGE_CURVE('',#22907,#22907,#19420,.T.);
#27952=EDGE_CURVE('',#22906,#22905,#2518,.T.);
#27953=EDGE_CURVE('',#22759,#22908,#5326,.T.);
#27954=EDGE_CURVE('',#22908,#22908,#2519,.T.);
#27955=EDGE_CURVE('',#22909,#22910,#2520,.T.);
#27956=EDGE_CURVE('',#22910,#22911,#5327,.T.);
#27957=EDGE_CURVE('',#22911,#22911,#19421,.T.);
#27958=EDGE_CURVE('',#22910,#22909,#2521,.T.);
#27959=EDGE_CURVE('',#22743,#22912,#5328,.T.);
#27960=EDGE_CURVE('',#22912,#22912,#2522,.T.);
#27961=EDGE_CURVE('',#22913,#22914,#2523,.T.);
#27962=EDGE_CURVE('',#22914,#22915,#5329,.T.);
#27963=EDGE_CURVE('',#22915,#22915,#19422,.T.);
#27964=EDGE_CURVE('',#22914,#22913,#2524,.T.);
#27965=EDGE_CURVE('',#22773,#22916,#5330,.T.);
#27966=EDGE_CURVE('',#22916,#22916,#2525,.T.);
#27967=EDGE_CURVE('',#22917,#22918,#2526,.T.);
#27968=EDGE_CURVE('',#22918,#22919,#5331,.T.);
#27969=EDGE_CURVE('',#22919,#22919,#19423,.T.);
#27970=EDGE_CURVE('',#22918,#22917,#2527,.T.);
#27971=EDGE_CURVE('',#22793,#22920,#5332,.T.);
#27972=EDGE_CURVE('',#22920,#22920,#2528,.T.);
#27973=EDGE_CURVE('',#22921,#22922,#2529,.T.);
#27974=EDGE_CURVE('',#22922,#22923,#5333,.T.);
#27975=EDGE_CURVE('',#22923,#22923,#19424,.T.);
#27976=EDGE_CURVE('',#22922,#22921,#2530,.T.);
#27977=EDGE_CURVE('',#22751,#22924,#5334,.T.);
#27978=EDGE_CURVE('',#22924,#22924,#2531,.T.);
#27979=EDGE_CURVE('',#22925,#22926,#2532,.T.);
#27980=EDGE_CURVE('',#22926,#22927,#5335,.T.);
#27981=EDGE_CURVE('',#22927,#22927,#19425,.T.);
#27982=EDGE_CURVE('',#22926,#22925,#2533,.T.);
#27983=EDGE_CURVE('',#22761,#22928,#5336,.T.);
#27984=EDGE_CURVE('',#22928,#22928,#2534,.T.);
#27985=EDGE_CURVE('',#22929,#22930,#2535,.T.);
#27986=EDGE_CURVE('',#22930,#22931,#5337,.T.);
#27987=EDGE_CURVE('',#22931,#22931,#19426,.T.);
#27988=EDGE_CURVE('',#22930,#22929,#2536,.T.);
#27989=EDGE_CURVE('',#22741,#22932,#5338,.T.);
#27990=EDGE_CURVE('',#22932,#22932,#2537,.T.);
#27991=EDGE_CURVE('',#22933,#22934,#2538,.T.);
#27992=EDGE_CURVE('',#22934,#22935,#5339,.T.);
#27993=EDGE_CURVE('',#22935,#22935,#19427,.T.);
#27994=EDGE_CURVE('',#22934,#22933,#2539,.T.);
#27995=EDGE_CURVE('',#22795,#22936,#5340,.T.);
#27996=EDGE_CURVE('',#22936,#22936,#2540,.T.);
#27997=EDGE_CURVE('',#22937,#22938,#2541,.T.);
#27998=EDGE_CURVE('',#22938,#22939,#5341,.T.);
#27999=EDGE_CURVE('',#22939,#22939,#19428,.T.);
#28000=EDGE_CURVE('',#22938,#22937,#2542,.T.);
#28001=EDGE_CURVE('',#22791,#22940,#5342,.T.);
#28002=EDGE_CURVE('',#22940,#22940,#2543,.T.);
#28003=EDGE_CURVE('',#22941,#22942,#2544,.T.);
#28004=EDGE_CURVE('',#22942,#22943,#5343,.T.);
#28005=EDGE_CURVE('',#22943,#22943,#19429,.T.);
#28006=EDGE_CURVE('',#22942,#22941,#2545,.T.);
#28007=EDGE_CURVE('',#22753,#22944,#5344,.T.);
#28008=EDGE_CURVE('',#22944,#22944,#2546,.T.);
#28009=EDGE_CURVE('',#22945,#22946,#2547,.T.);
#28010=EDGE_CURVE('',#22946,#22947,#5345,.T.);
#28011=EDGE_CURVE('',#22947,#22947,#19430,.T.);
#28012=EDGE_CURVE('',#22946,#22945,#2548,.T.);
#28013=EDGE_CURVE('',#22739,#22948,#5346,.T.);
#28014=EDGE_CURVE('',#22948,#22948,#2549,.T.);
#28015=EDGE_CURVE('',#22949,#22950,#2550,.T.);
#28016=EDGE_CURVE('',#22950,#22951,#5347,.T.);
#28017=EDGE_CURVE('',#22951,#22951,#19431,.T.);
#28018=EDGE_CURVE('',#22950,#22949,#2551,.T.);
#28019=EDGE_CURVE('',#22783,#22952,#5348,.T.);
#28020=EDGE_CURVE('',#22952,#22952,#2552,.T.);
#28021=EDGE_CURVE('',#22953,#22954,#2553,.T.);
#28022=EDGE_CURVE('',#22954,#22955,#5349,.T.);
#28023=EDGE_CURVE('',#22955,#22955,#19432,.T.);
#28024=EDGE_CURVE('',#22954,#22953,#2554,.T.);
#28025=EDGE_CURVE('',#22797,#22956,#5350,.T.);
#28026=EDGE_CURVE('',#22956,#22956,#2555,.T.);
#28027=EDGE_CURVE('',#22957,#22958,#2556,.T.);
#28028=EDGE_CURVE('',#22958,#22959,#5351,.T.);
#28029=EDGE_CURVE('',#22959,#22959,#19433,.T.);
#28030=EDGE_CURVE('',#22958,#22957,#2557,.T.);
#28031=EDGE_CURVE('',#22789,#22960,#5352,.T.);
#28032=EDGE_CURVE('',#22960,#22960,#2558,.T.);
#28033=EDGE_CURVE('',#22961,#22962,#2559,.T.);
#28034=EDGE_CURVE('',#22962,#22963,#5353,.T.);
#28035=EDGE_CURVE('',#22963,#22963,#19434,.T.);
#28036=EDGE_CURVE('',#22962,#22961,#2560,.T.);
#28037=EDGE_CURVE('',#22755,#22964,#5354,.T.);
#28038=EDGE_CURVE('',#22964,#22964,#2561,.T.);
#28039=EDGE_CURVE('',#22965,#22966,#2562,.T.);
#28040=EDGE_CURVE('',#22966,#22967,#5355,.T.);
#28041=EDGE_CURVE('',#22967,#22967,#19435,.T.);
#28042=EDGE_CURVE('',#22966,#22965,#2563,.T.);
#28043=EDGE_CURVE('',#22785,#22968,#5356,.T.);
#28044=EDGE_CURVE('',#22969,#22968,#2564,.T.);
#28045=EDGE_CURVE('',#22968,#22969,#2565,.T.);
#28046=EDGE_CURVE('',#22970,#22971,#2566,.T.);
#28047=EDGE_CURVE('',#22971,#22972,#5357,.T.);
#28048=EDGE_CURVE('',#22972,#22972,#19436,.T.);
#28049=EDGE_CURVE('',#22971,#22970,#2567,.T.);
#28050=EDGE_CURVE('',#22781,#22973,#5358,.T.);
#28051=EDGE_CURVE('',#22973,#22973,#2568,.T.);
#28052=EDGE_CURVE('',#22974,#22975,#2569,.T.);
#28053=EDGE_CURVE('',#22975,#22976,#5359,.T.);
#28054=EDGE_CURVE('',#22976,#22976,#19437,.T.);
#28055=EDGE_CURVE('',#22975,#22974,#2570,.T.);
#28056=EDGE_CURVE('',#22799,#22977,#5360,.T.);
#28057=EDGE_CURVE('',#22977,#22977,#2571,.T.);
#28058=EDGE_CURVE('',#22978,#22979,#2572,.T.);
#28059=EDGE_CURVE('',#22979,#22980,#5361,.T.);
#28060=EDGE_CURVE('',#22980,#22980,#19438,.T.);
#28061=EDGE_CURVE('',#22979,#22978,#2573,.T.);
#28062=EDGE_CURVE('',#22787,#22981,#5362,.T.);
#28063=EDGE_CURVE('',#22981,#22981,#2574,.T.);
#28064=EDGE_CURVE('',#22982,#22983,#2575,.T.);
#28065=EDGE_CURVE('',#22983,#22984,#5363,.T.);
#28066=EDGE_CURVE('',#22984,#22984,#19439,.T.);
#28067=EDGE_CURVE('',#22983,#22982,#2576,.T.);
#28068=EDGE_CURVE('',#22985,#22985,#2577,.T.);
#28069=EDGE_CURVE('',#22985,#22986,#5364,.T.);
#28070=EDGE_CURVE('',#22986,#22986,#2578,.T.);
#28071=EDGE_CURVE('',#22987,#22988,#2579,.T.);
#28072=EDGE_CURVE('',#22988,#22989,#5365,.T.);
#28073=EDGE_CURVE('',#22989,#22989,#19440,.T.);
#28074=EDGE_CURVE('',#22988,#22987,#2580,.T.);
#28075=EDGE_CURVE('',#22990,#22990,#2581,.T.);
#28076=EDGE_CURVE('',#22990,#22991,#5366,.T.);
#28077=EDGE_CURVE('',#22991,#22991,#2582,.T.);
#28078=EDGE_CURVE('',#22992,#22993,#2583,.T.);
#28079=EDGE_CURVE('',#22993,#22994,#5367,.T.);
#28080=EDGE_CURVE('',#22994,#22994,#19441,.T.);
#28081=EDGE_CURVE('',#22993,#22992,#2584,.T.);
#28082=EDGE_CURVE('',#22779,#22995,#5368,.T.);
#28083=EDGE_CURVE('',#22995,#22995,#2585,.T.);
#28084=EDGE_CURVE('',#22996,#22997,#2586,.T.);
#28085=EDGE_CURVE('',#22997,#22998,#5369,.T.);
#28086=EDGE_CURVE('',#22998,#22998,#19442,.T.);
#28087=EDGE_CURVE('',#22997,#22996,#2587,.T.);
#28088=EDGE_CURVE('',#22801,#22999,#5370,.T.);
#28089=EDGE_CURVE('',#22999,#22999,#2588,.T.);
#28090=EDGE_CURVE('',#23000,#23001,#2589,.T.);
#28091=EDGE_CURVE('',#23001,#23002,#5371,.T.);
#28092=EDGE_CURVE('',#23002,#23002,#19443,.T.);
#28093=EDGE_CURVE('',#23001,#23000,#2590,.T.);
#28094=EDGE_CURVE('',#23003,#23003,#2591,.T.);
#28095=EDGE_CURVE('',#23003,#23004,#5372,.T.);
#28096=EDGE_CURVE('',#23004,#23004,#2592,.T.);
#28097=EDGE_CURVE('',#23005,#23006,#2593,.T.);
#28098=EDGE_CURVE('',#23006,#23007,#5373,.T.);
#28099=EDGE_CURVE('',#23007,#23007,#19444,.T.);
#28100=EDGE_CURVE('',#23006,#23005,#2594,.T.);
#28101=EDGE_CURVE('',#23008,#23008,#2595,.T.);
#28102=EDGE_CURVE('',#23008,#23009,#5374,.T.);
#28103=EDGE_CURVE('',#23009,#23009,#2596,.T.);
#28104=EDGE_CURVE('',#23010,#23011,#2597,.T.);
#28105=EDGE_CURVE('',#23011,#23012,#5375,.T.);
#28106=EDGE_CURVE('',#23012,#23012,#19445,.T.);
#28107=EDGE_CURVE('',#23011,#23010,#2598,.T.);
#28108=EDGE_CURVE('',#23013,#23013,#2599,.T.);
#28109=EDGE_CURVE('',#23013,#23014,#5376,.T.);
#28110=EDGE_CURVE('',#23014,#23014,#2600,.T.);
#28111=EDGE_CURVE('',#23015,#23016,#2601,.T.);
#28112=EDGE_CURVE('',#23016,#23017,#5377,.T.);
#28113=EDGE_CURVE('',#23017,#23017,#19446,.T.);
#28114=EDGE_CURVE('',#23016,#23015,#2602,.T.);
#28115=EDGE_CURVE('',#23018,#23018,#2603,.T.);
#28116=EDGE_CURVE('',#23018,#23019,#5378,.T.);
#28117=EDGE_CURVE('',#23019,#23019,#2604,.T.);
#28118=EDGE_CURVE('',#23020,#23021,#2605,.T.);
#28119=EDGE_CURVE('',#23021,#23022,#5379,.T.);
#28120=EDGE_CURVE('',#23022,#23022,#19447,.T.);
#28121=EDGE_CURVE('',#23021,#23020,#2606,.T.);
#28122=EDGE_CURVE('',#23023,#23023,#2607,.T.);
#28123=EDGE_CURVE('',#23023,#23024,#5380,.T.);
#28124=EDGE_CURVE('',#23024,#23024,#2608,.T.);
#28125=EDGE_CURVE('',#23025,#23026,#2609,.T.);
#28126=EDGE_CURVE('',#23026,#23027,#5381,.T.);
#28127=EDGE_CURVE('',#23027,#23027,#19448,.T.);
#28128=EDGE_CURVE('',#23026,#23025,#2610,.T.);
#28129=EDGE_CURVE('',#23028,#23028,#2611,.T.);
#28130=EDGE_CURVE('',#23028,#23029,#5382,.T.);
#28131=EDGE_CURVE('',#23029,#23029,#2612,.T.);
#28132=EDGE_CURVE('',#23030,#23031,#2613,.T.);
#28133=EDGE_CURVE('',#23031,#23032,#5383,.T.);
#28134=EDGE_CURVE('',#23032,#23032,#19449,.T.);
#28135=EDGE_CURVE('',#23031,#23030,#2614,.T.);
#28136=EDGE_CURVE('',#23033,#23033,#2615,.T.);
#28137=EDGE_CURVE('',#23033,#23034,#5384,.T.);
#28138=EDGE_CURVE('',#23034,#23034,#2616,.T.);
#28139=EDGE_CURVE('',#23035,#23036,#2617,.T.);
#28140=EDGE_CURVE('',#23036,#23037,#5385,.T.);
#28141=EDGE_CURVE('',#23037,#23037,#19450,.T.);
#28142=EDGE_CURVE('',#23036,#23035,#2618,.T.);
#28143=EDGE_CURVE('',#23038,#23038,#2619,.T.);
#28144=EDGE_CURVE('',#23038,#23039,#5386,.T.);
#28145=EDGE_CURVE('',#23039,#23039,#2620,.T.);
#28146=EDGE_CURVE('',#23040,#23041,#2621,.T.);
#28147=EDGE_CURVE('',#23041,#23042,#5387,.T.);
#28148=EDGE_CURVE('',#23042,#23042,#19451,.T.);
#28149=EDGE_CURVE('',#23041,#23040,#2622,.T.);
#28150=EDGE_CURVE('',#23043,#23043,#2623,.T.);
#28151=EDGE_CURVE('',#23043,#23044,#5388,.T.);
#28152=EDGE_CURVE('',#23044,#23044,#2624,.T.);
#28153=EDGE_CURVE('',#23045,#23046,#2625,.T.);
#28154=EDGE_CURVE('',#23046,#23047,#5389,.T.);
#28155=EDGE_CURVE('',#23047,#23047,#19452,.T.);
#28156=EDGE_CURVE('',#23046,#23045,#2626,.T.);
#28157=EDGE_CURVE('',#23048,#23048,#2627,.T.);
#28158=EDGE_CURVE('',#23048,#23049,#5390,.T.);
#28159=EDGE_CURVE('',#23049,#23049,#2628,.T.);
#28160=EDGE_CURVE('',#23050,#23051,#2629,.T.);
#28161=EDGE_CURVE('',#23051,#23052,#5391,.T.);
#28162=EDGE_CURVE('',#23052,#23052,#19453,.T.);
#28163=EDGE_CURVE('',#23051,#23050,#2630,.T.);
#28164=EDGE_CURVE('',#23053,#23053,#2631,.T.);
#28165=EDGE_CURVE('',#23053,#23054,#5392,.T.);
#28166=EDGE_CURVE('',#23054,#23054,#2632,.T.);
#28167=EDGE_CURVE('',#23055,#23056,#2633,.T.);
#28168=EDGE_CURVE('',#23056,#23057,#5393,.T.);
#28169=EDGE_CURVE('',#23057,#23057,#19454,.T.);
#28170=EDGE_CURVE('',#23056,#23055,#2634,.T.);
#28171=EDGE_CURVE('',#23058,#23058,#2635,.T.);
#28172=EDGE_CURVE('',#23058,#23059,#5394,.T.);
#28173=EDGE_CURVE('',#23059,#23059,#2636,.T.);
#28174=EDGE_CURVE('',#23060,#23061,#2637,.T.);
#28175=EDGE_CURVE('',#23061,#23062,#5395,.T.);
#28176=EDGE_CURVE('',#23062,#23062,#19455,.T.);
#28177=EDGE_CURVE('',#23061,#23060,#2638,.T.);
#28178=EDGE_CURVE('',#23063,#23063,#2639,.T.);
#28179=EDGE_CURVE('',#23063,#23064,#5396,.T.);
#28180=EDGE_CURVE('',#23064,#23064,#2640,.T.);
#28181=EDGE_CURVE('',#23065,#23066,#2641,.T.);
#28182=EDGE_CURVE('',#23066,#23067,#5397,.T.);
#28183=EDGE_CURVE('',#23067,#23067,#19456,.T.);
#28184=EDGE_CURVE('',#23066,#23065,#2642,.T.);
#28185=EDGE_CURVE('',#23068,#23068,#2643,.T.);
#28186=EDGE_CURVE('',#23068,#23069,#5398,.T.);
#28187=EDGE_CURVE('',#23069,#23069,#2644,.T.);
#28188=EDGE_CURVE('',#23070,#23071,#2645,.T.);
#28189=EDGE_CURVE('',#23071,#23072,#5399,.T.);
#28190=EDGE_CURVE('',#23072,#23072,#19457,.T.);
#28191=EDGE_CURVE('',#23071,#23070,#2646,.T.);
#28192=EDGE_CURVE('',#23073,#23073,#2647,.T.);
#28193=EDGE_CURVE('',#23073,#23074,#5400,.T.);
#28194=EDGE_CURVE('',#23074,#23074,#2648,.T.);
#28195=EDGE_CURVE('',#23075,#23076,#2649,.T.);
#28196=EDGE_CURVE('',#23076,#23077,#5401,.T.);
#28197=EDGE_CURVE('',#23077,#23077,#19458,.T.);
#28198=EDGE_CURVE('',#23076,#23075,#2650,.T.);
#28199=EDGE_CURVE('',#23078,#23078,#2651,.T.);
#28200=EDGE_CURVE('',#23078,#23079,#5402,.T.);
#28201=EDGE_CURVE('',#23079,#23079,#2652,.T.);
#28202=EDGE_CURVE('',#23080,#23081,#2653,.T.);
#28203=EDGE_CURVE('',#23081,#23082,#5403,.T.);
#28204=EDGE_CURVE('',#23082,#23082,#19459,.T.);
#28205=EDGE_CURVE('',#23081,#23080,#2654,.T.);
#28206=EDGE_CURVE('',#23083,#23083,#2655,.T.);
#28207=EDGE_CURVE('',#23083,#23084,#5404,.T.);
#28208=EDGE_CURVE('',#23084,#23084,#2656,.T.);
#28209=EDGE_CURVE('',#23085,#23086,#2657,.T.);
#28210=EDGE_CURVE('',#23086,#23087,#5405,.T.);
#28211=EDGE_CURVE('',#23087,#23087,#19460,.T.);
#28212=EDGE_CURVE('',#23086,#23085,#2658,.T.);
#28213=EDGE_CURVE('',#23088,#23088,#2659,.T.);
#28214=EDGE_CURVE('',#23088,#23089,#5406,.T.);
#28215=EDGE_CURVE('',#23089,#23089,#2660,.T.);
#28216=EDGE_CURVE('',#23090,#23091,#2661,.T.);
#28217=EDGE_CURVE('',#23091,#23092,#5407,.T.);
#28218=EDGE_CURVE('',#23092,#23092,#19461,.T.);
#28219=EDGE_CURVE('',#23091,#23090,#2662,.T.);
#28220=EDGE_CURVE('',#23093,#23093,#2663,.T.);
#28221=EDGE_CURVE('',#23093,#23094,#5408,.T.);
#28222=EDGE_CURVE('',#23094,#23094,#2664,.T.);
#28223=EDGE_CURVE('',#23095,#23096,#2665,.T.);
#28224=EDGE_CURVE('',#23096,#23097,#5409,.T.);
#28225=EDGE_CURVE('',#23097,#23097,#19462,.T.);
#28226=EDGE_CURVE('',#23096,#23095,#2666,.T.);
#28227=EDGE_CURVE('',#23098,#23098,#2667,.T.);
#28228=EDGE_CURVE('',#23098,#23099,#5410,.T.);
#28229=EDGE_CURVE('',#23099,#23099,#2668,.T.);
#28230=EDGE_CURVE('',#23100,#23101,#2669,.T.);
#28231=EDGE_CURVE('',#23101,#23102,#5411,.T.);
#28232=EDGE_CURVE('',#23102,#23102,#19463,.T.);
#28233=EDGE_CURVE('',#23101,#23100,#2670,.T.);
#28234=EDGE_CURVE('',#23103,#23103,#2671,.T.);
#28235=EDGE_CURVE('',#23103,#23104,#5412,.T.);
#28236=EDGE_CURVE('',#23104,#23104,#2672,.T.);
#28237=EDGE_CURVE('',#23105,#23106,#2673,.T.);
#28238=EDGE_CURVE('',#23106,#23107,#5413,.T.);
#28239=EDGE_CURVE('',#23107,#23107,#19464,.T.);
#28240=EDGE_CURVE('',#23106,#23105,#2674,.T.);
#28241=EDGE_CURVE('',#23108,#23108,#2675,.T.);
#28242=EDGE_CURVE('',#23108,#23109,#5414,.T.);
#28243=EDGE_CURVE('',#23109,#23109,#2676,.T.);
#28244=EDGE_CURVE('',#23110,#23111,#2677,.T.);
#28245=EDGE_CURVE('',#23111,#23112,#5415,.T.);
#28246=EDGE_CURVE('',#23112,#23112,#19465,.T.);
#28247=EDGE_CURVE('',#23111,#23110,#2678,.T.);
#28248=EDGE_CURVE('',#23113,#23113,#2679,.T.);
#28249=EDGE_CURVE('',#23113,#23114,#5416,.T.);
#28250=EDGE_CURVE('',#23114,#23114,#2680,.T.);
#28251=EDGE_CURVE('',#23115,#23116,#2681,.T.);
#28252=EDGE_CURVE('',#23116,#23117,#5417,.T.);
#28253=EDGE_CURVE('',#23117,#23117,#19466,.T.);
#28254=EDGE_CURVE('',#23116,#23115,#2682,.T.);
#28255=EDGE_CURVE('',#23118,#23118,#2683,.T.);
#28256=EDGE_CURVE('',#23118,#23119,#5418,.T.);
#28257=EDGE_CURVE('',#23119,#23119,#2684,.T.);
#28258=EDGE_CURVE('',#23120,#23121,#2685,.T.);
#28259=EDGE_CURVE('',#23121,#23122,#5419,.T.);
#28260=EDGE_CURVE('',#23122,#23122,#19467,.T.);
#28261=EDGE_CURVE('',#23121,#23120,#2686,.T.);
#28262=EDGE_CURVE('',#23123,#23123,#2687,.T.);
#28263=EDGE_CURVE('',#23123,#23124,#5420,.T.);
#28264=EDGE_CURVE('',#23124,#23124,#2688,.T.);
#28265=EDGE_CURVE('',#23125,#23126,#2689,.T.);
#28266=EDGE_CURVE('',#23126,#23127,#5421,.T.);
#28267=EDGE_CURVE('',#23127,#23127,#19468,.T.);
#28268=EDGE_CURVE('',#23126,#23125,#2690,.T.);
#28269=EDGE_CURVE('',#23128,#23128,#2691,.T.);
#28270=EDGE_CURVE('',#23128,#23129,#5422,.T.);
#28271=EDGE_CURVE('',#23129,#23129,#2692,.T.);
#28272=EDGE_CURVE('',#23130,#23131,#2693,.T.);
#28273=EDGE_CURVE('',#23131,#23132,#5423,.T.);
#28274=EDGE_CURVE('',#23132,#23132,#19469,.T.);
#28275=EDGE_CURVE('',#23131,#23130,#2694,.T.);
#28276=EDGE_CURVE('',#23133,#23133,#2695,.T.);
#28277=EDGE_CURVE('',#23133,#23134,#5424,.T.);
#28278=EDGE_CURVE('',#23134,#23134,#2696,.T.);
#28279=EDGE_CURVE('',#23135,#23136,#2697,.T.);
#28280=EDGE_CURVE('',#23136,#23137,#5425,.T.);
#28281=EDGE_CURVE('',#23137,#23137,#19470,.T.);
#28282=EDGE_CURVE('',#23136,#23135,#2698,.T.);
#28283=EDGE_CURVE('',#23138,#23138,#2699,.T.);
#28284=EDGE_CURVE('',#23138,#23139,#5426,.T.);
#28285=EDGE_CURVE('',#23139,#23139,#2700,.T.);
#28286=EDGE_CURVE('',#23140,#23141,#2701,.T.);
#28287=EDGE_CURVE('',#23141,#23142,#5427,.T.);
#28288=EDGE_CURVE('',#23142,#23142,#19471,.T.);
#28289=EDGE_CURVE('',#23141,#23140,#2702,.T.);
#28290=EDGE_CURVE('',#23143,#23143,#2703,.T.);
#28291=EDGE_CURVE('',#23143,#23144,#5428,.T.);
#28292=EDGE_CURVE('',#23145,#23144,#2704,.T.);
#28293=EDGE_CURVE('',#23144,#23145,#2705,.T.);
#28294=EDGE_CURVE('',#23146,#23147,#2706,.T.);
#28295=EDGE_CURVE('',#23147,#23148,#5429,.T.);
#28296=EDGE_CURVE('',#23148,#23148,#19472,.T.);
#28297=EDGE_CURVE('',#23147,#23146,#2707,.T.);
#28298=EDGE_CURVE('',#23149,#23149,#2708,.T.);
#28299=EDGE_CURVE('',#23149,#23150,#5430,.T.);
#28300=EDGE_CURVE('',#23150,#23150,#2709,.T.);
#28301=EDGE_CURVE('',#23151,#23152,#2710,.T.);
#28302=EDGE_CURVE('',#23152,#23153,#5431,.T.);
#28303=EDGE_CURVE('',#23153,#23153,#19473,.T.);
#28304=EDGE_CURVE('',#23152,#23151,#2711,.T.);
#28305=EDGE_CURVE('',#23154,#23154,#2712,.T.);
#28306=EDGE_CURVE('',#23154,#23155,#5432,.T.);
#28307=EDGE_CURVE('',#23155,#23155,#2713,.T.);
#28308=EDGE_CURVE('',#23156,#23157,#2714,.T.);
#28309=EDGE_CURVE('',#23157,#23158,#5433,.T.);
#28310=EDGE_CURVE('',#23158,#23158,#19474,.T.);
#28311=EDGE_CURVE('',#23157,#23156,#2715,.T.);
#28312=EDGE_CURVE('',#23159,#23159,#2716,.T.);
#28313=EDGE_CURVE('',#23159,#23160,#5434,.T.);
#28314=EDGE_CURVE('',#23160,#23160,#2717,.T.);
#28315=EDGE_CURVE('',#23161,#23162,#2718,.T.);
#28316=EDGE_CURVE('',#23162,#23163,#5435,.T.);
#28317=EDGE_CURVE('',#23163,#23163,#19475,.T.);
#28318=EDGE_CURVE('',#23162,#23161,#2719,.T.);
#28319=EDGE_CURVE('',#23164,#23164,#2720,.T.);
#28320=EDGE_CURVE('',#23164,#23165,#5436,.T.);
#28321=EDGE_CURVE('',#23166,#23165,#2721,.T.);
#28322=EDGE_CURVE('',#23165,#23166,#2722,.T.);
#28323=EDGE_CURVE('',#23167,#23168,#2723,.T.);
#28324=EDGE_CURVE('',#23168,#23169,#5437,.T.);
#28325=EDGE_CURVE('',#23169,#23169,#19476,.T.);
#28326=EDGE_CURVE('',#23168,#23167,#2724,.T.);
#28327=EDGE_CURVE('',#23170,#23170,#2725,.T.);
#28328=EDGE_CURVE('',#23170,#23171,#5438,.T.);
#28329=EDGE_CURVE('',#23171,#23171,#2726,.T.);
#28330=EDGE_CURVE('',#23172,#23173,#2727,.T.);
#28331=EDGE_CURVE('',#23173,#23174,#5439,.T.);
#28332=EDGE_CURVE('',#23174,#23174,#19477,.T.);
#28333=EDGE_CURVE('',#23173,#23172,#2728,.T.);
#28334=EDGE_CURVE('',#23175,#23175,#2729,.T.);
#28335=EDGE_CURVE('',#23175,#23176,#5440,.T.);
#28336=EDGE_CURVE('',#23176,#23176,#2730,.T.);
#28337=EDGE_CURVE('',#23177,#23178,#2731,.T.);
#28338=EDGE_CURVE('',#23178,#23179,#5441,.T.);
#28339=EDGE_CURVE('',#23179,#23179,#19478,.T.);
#28340=EDGE_CURVE('',#23178,#23177,#2732,.T.);
#28341=EDGE_CURVE('',#23180,#23180,#2733,.T.);
#28342=EDGE_CURVE('',#23180,#23181,#5442,.T.);
#28343=EDGE_CURVE('',#23181,#23181,#2734,.T.);
#28344=EDGE_CURVE('',#23182,#23183,#2735,.T.);
#28345=EDGE_CURVE('',#23183,#23184,#5443,.T.);
#28346=EDGE_CURVE('',#23184,#23184,#19479,.T.);
#28347=EDGE_CURVE('',#23183,#23182,#2736,.T.);
#28348=EDGE_CURVE('',#23185,#23186,#2737,.T.);
#28349=EDGE_CURVE('',#23185,#23187,#5444,.T.);
#28350=EDGE_CURVE('',#23188,#23187,#2738,.T.);
#28351=EDGE_CURVE('',#23187,#23188,#2739,.T.);
#28352=EDGE_CURVE('',#23186,#23185,#2740,.T.);
#28353=EDGE_CURVE('',#23189,#23190,#2741,.T.);
#28354=EDGE_CURVE('',#23190,#23191,#5445,.T.);
#28355=EDGE_CURVE('',#23191,#23191,#19480,.T.);
#28356=EDGE_CURVE('',#23190,#23189,#2742,.T.);
#28357=EDGE_CURVE('',#23192,#23192,#2743,.T.);
#28358=EDGE_CURVE('',#23192,#23193,#5446,.T.);
#28359=EDGE_CURVE('',#23193,#23193,#2744,.T.);
#28360=EDGE_CURVE('',#23194,#23195,#2745,.T.);
#28361=EDGE_CURVE('',#23195,#23196,#5447,.T.);
#28362=EDGE_CURVE('',#23196,#23196,#19481,.T.);
#28363=EDGE_CURVE('',#23195,#23194,#2746,.T.);
#28364=EDGE_CURVE('',#23197,#23197,#2747,.T.);
#28365=EDGE_CURVE('',#23197,#23198,#5448,.T.);
#28366=EDGE_CURVE('',#23198,#23198,#2748,.T.);
#28367=EDGE_CURVE('',#23199,#23200,#2749,.T.);
#28368=EDGE_CURVE('',#23200,#23201,#5449,.T.);
#28369=EDGE_CURVE('',#23201,#23201,#19482,.T.);
#28370=EDGE_CURVE('',#23200,#23199,#2750,.T.);
#28371=EDGE_CURVE('',#23202,#23202,#2751,.T.);
#28372=EDGE_CURVE('',#23202,#23203,#5450,.T.);
#28373=EDGE_CURVE('',#23203,#23203,#2752,.T.);
#28374=EDGE_CURVE('',#23204,#23205,#2753,.T.);
#28375=EDGE_CURVE('',#23205,#23206,#5451,.T.);
#28376=EDGE_CURVE('',#23206,#23206,#19483,.T.);
#28377=EDGE_CURVE('',#23205,#23204,#2754,.T.);
#28378=EDGE_CURVE('',#23207,#23207,#2755,.T.);
#28379=EDGE_CURVE('',#23207,#23208,#5452,.T.);
#28380=EDGE_CURVE('',#23208,#23208,#2756,.T.);
#28381=EDGE_CURVE('',#23209,#23210,#2757,.T.);
#28382=EDGE_CURVE('',#23210,#23211,#5453,.T.);
#28383=EDGE_CURVE('',#23211,#23211,#19484,.T.);
#28384=EDGE_CURVE('',#23210,#23209,#2758,.T.);
#28385=EDGE_CURVE('',#23212,#23212,#2759,.T.);
#28386=EDGE_CURVE('',#23212,#23213,#5454,.T.);
#28387=EDGE_CURVE('',#23213,#23213,#2760,.T.);
#28388=EDGE_CURVE('',#23214,#23215,#2761,.T.);
#28389=EDGE_CURVE('',#23215,#23216,#5455,.T.);
#28390=EDGE_CURVE('',#23216,#23216,#19485,.T.);
#28391=EDGE_CURVE('',#23215,#23214,#2762,.T.);
#28392=EDGE_CURVE('',#23217,#23217,#2763,.T.);
#28393=EDGE_CURVE('',#23217,#23218,#5456,.T.);
#28394=EDGE_CURVE('',#23218,#23218,#2764,.T.);
#28395=EDGE_CURVE('',#23219,#23220,#2765,.T.);
#28396=EDGE_CURVE('',#23220,#23221,#5457,.T.);
#28397=EDGE_CURVE('',#23221,#23221,#19486,.T.);
#28398=EDGE_CURVE('',#23220,#23219,#2766,.T.);
#28399=EDGE_CURVE('',#23222,#23222,#2767,.T.);
#28400=EDGE_CURVE('',#23222,#23223,#5458,.T.);
#28401=EDGE_CURVE('',#23223,#23223,#2768,.T.);
#28402=EDGE_CURVE('',#23224,#23225,#2769,.T.);
#28403=EDGE_CURVE('',#23225,#23226,#5459,.T.);
#28404=EDGE_CURVE('',#23226,#23226,#19487,.T.);
#28405=EDGE_CURVE('',#23225,#23224,#2770,.T.);
#28406=EDGE_CURVE('',#23227,#23227,#2771,.T.);
#28407=EDGE_CURVE('',#23227,#23228,#5460,.T.);
#28408=EDGE_CURVE('',#23228,#23228,#2772,.T.);
#28409=EDGE_CURVE('',#23229,#23230,#2773,.T.);
#28410=EDGE_CURVE('',#23230,#23231,#5461,.T.);
#28411=EDGE_CURVE('',#23231,#23231,#19488,.T.);
#28412=EDGE_CURVE('',#23230,#23229,#2774,.T.);
#28413=EDGE_CURVE('',#23232,#23232,#2775,.T.);
#28414=EDGE_CURVE('',#23232,#23233,#5462,.T.);
#28415=EDGE_CURVE('',#23233,#23233,#2776,.T.);
#28416=EDGE_CURVE('',#23234,#23235,#2777,.T.);
#28417=EDGE_CURVE('',#23235,#23236,#5463,.T.);
#28418=EDGE_CURVE('',#23236,#23236,#19489,.T.);
#28419=EDGE_CURVE('',#23235,#23234,#2778,.T.);
#28420=EDGE_CURVE('',#23237,#23237,#2779,.T.);
#28421=EDGE_CURVE('',#23237,#23238,#5464,.T.);
#28422=EDGE_CURVE('',#23238,#23238,#2780,.T.);
#28423=EDGE_CURVE('',#23239,#23240,#2781,.T.);
#28424=EDGE_CURVE('',#23240,#23241,#5465,.T.);
#28425=EDGE_CURVE('',#23241,#23241,#19490,.T.);
#28426=EDGE_CURVE('',#23240,#23239,#2782,.T.);
#28427=EDGE_CURVE('',#23242,#23242,#2783,.T.);
#28428=EDGE_CURVE('',#23242,#23243,#5466,.T.);
#28429=EDGE_CURVE('',#23243,#23243,#2784,.T.);
#28430=EDGE_CURVE('',#23244,#23245,#2785,.T.);
#28431=EDGE_CURVE('',#23245,#23246,#5467,.T.);
#28432=EDGE_CURVE('',#23246,#23246,#19491,.T.);
#28433=EDGE_CURVE('',#23245,#23244,#2786,.T.);
#28434=EDGE_CURVE('',#23247,#23247,#2787,.T.);
#28435=EDGE_CURVE('',#23247,#23248,#5468,.T.);
#28436=EDGE_CURVE('',#23248,#23248,#2788,.T.);
#28437=EDGE_CURVE('',#23249,#23250,#2789,.T.);
#28438=EDGE_CURVE('',#23250,#23251,#5469,.T.);
#28439=EDGE_CURVE('',#23251,#23251,#19492,.T.);
#28440=EDGE_CURVE('',#23250,#23249,#2790,.T.);
#28441=EDGE_CURVE('',#23252,#23252,#2791,.T.);
#28442=EDGE_CURVE('',#23252,#23253,#5470,.T.);
#28443=EDGE_CURVE('',#23253,#23253,#2792,.T.);
#28444=EDGE_CURVE('',#23254,#23255,#2793,.T.);
#28445=EDGE_CURVE('',#23255,#23256,#5471,.T.);
#28446=EDGE_CURVE('',#23256,#23256,#19493,.T.);
#28447=EDGE_CURVE('',#23255,#23254,#2794,.T.);
#28448=EDGE_CURVE('',#23257,#23257,#2795,.T.);
#28449=EDGE_CURVE('',#23257,#23258,#5472,.T.);
#28450=EDGE_CURVE('',#23258,#23258,#2796,.T.);
#28451=EDGE_CURVE('',#23259,#23260,#2797,.T.);
#28452=EDGE_CURVE('',#23260,#23261,#5473,.T.);
#28453=EDGE_CURVE('',#23261,#23261,#19494,.T.);
#28454=EDGE_CURVE('',#23260,#23259,#2798,.T.);
#28455=EDGE_CURVE('',#23262,#23262,#2799,.T.);
#28456=EDGE_CURVE('',#23262,#23263,#5474,.T.);
#28457=EDGE_CURVE('',#23263,#23263,#2800,.T.);
#28458=EDGE_CURVE('',#23264,#23265,#2801,.T.);
#28459=EDGE_CURVE('',#23265,#23266,#5475,.T.);
#28460=EDGE_CURVE('',#23266,#23266,#19495,.T.);
#28461=EDGE_CURVE('',#23265,#23264,#2802,.T.);
#28462=EDGE_CURVE('',#23267,#23267,#2803,.T.);
#28463=EDGE_CURVE('',#23267,#23268,#5476,.T.);
#28464=EDGE_CURVE('',#23268,#23268,#2804,.T.);
#28465=EDGE_CURVE('',#23269,#23270,#2805,.T.);
#28466=EDGE_CURVE('',#23270,#23271,#5477,.T.);
#28467=EDGE_CURVE('',#23271,#23271,#19496,.T.);
#28468=EDGE_CURVE('',#23270,#23269,#2806,.T.);
#28469=EDGE_CURVE('',#23272,#23272,#2807,.T.);
#28470=EDGE_CURVE('',#23272,#23273,#5478,.T.);
#28471=EDGE_CURVE('',#23273,#23273,#2808,.T.);
#28472=EDGE_CURVE('',#23274,#23275,#2809,.T.);
#28473=EDGE_CURVE('',#23275,#23276,#5479,.T.);
#28474=EDGE_CURVE('',#23276,#23276,#19497,.T.);
#28475=EDGE_CURVE('',#23275,#23274,#2810,.T.);
#28476=EDGE_CURVE('',#23277,#23277,#2811,.T.);
#28477=EDGE_CURVE('',#23277,#23278,#5480,.T.);
#28478=EDGE_CURVE('',#23278,#23278,#2812,.T.);
#28479=EDGE_CURVE('',#23279,#23280,#2813,.T.);
#28480=EDGE_CURVE('',#23280,#23281,#5481,.T.);
#28481=EDGE_CURVE('',#23281,#23281,#19498,.T.);
#28482=EDGE_CURVE('',#23280,#23279,#2814,.T.);
#28483=EDGE_CURVE('',#23282,#23282,#2815,.T.);
#28484=EDGE_CURVE('',#23282,#23283,#5482,.T.);
#28485=EDGE_CURVE('',#23283,#23283,#2816,.T.);
#28486=EDGE_CURVE('',#23284,#23285,#2817,.T.);
#28487=EDGE_CURVE('',#23285,#23286,#5483,.T.);
#28488=EDGE_CURVE('',#23286,#23286,#19499,.T.);
#28489=EDGE_CURVE('',#23285,#23284,#2818,.T.);
#28490=EDGE_CURVE('',#22841,#23287,#5484,.T.);
#28491=EDGE_CURVE('',#23287,#23287,#2819,.T.);
#28492=EDGE_CURVE('',#23288,#23289,#2820,.T.);
#28493=EDGE_CURVE('',#23289,#23290,#5485,.T.);
#28494=EDGE_CURVE('',#23290,#23290,#19500,.T.);
#28495=EDGE_CURVE('',#23289,#23288,#2821,.T.);
#28496=EDGE_CURVE('',#22817,#23291,#5486,.T.);
#28497=EDGE_CURVE('',#23291,#23291,#2822,.T.);
#28498=EDGE_CURVE('',#23292,#23293,#2823,.T.);
#28499=EDGE_CURVE('',#23293,#23294,#5487,.T.);
#28500=EDGE_CURVE('',#23294,#23294,#19501,.T.);
#28501=EDGE_CURVE('',#23293,#23292,#2824,.T.);
#28502=EDGE_CURVE('',#23295,#23295,#2825,.T.);
#28503=EDGE_CURVE('',#23295,#23296,#5488,.T.);
#28504=EDGE_CURVE('',#23296,#23296,#2826,.T.);
#28505=EDGE_CURVE('',#23297,#23298,#2827,.T.);
#28506=EDGE_CURVE('',#23298,#23299,#5489,.T.);
#28507=EDGE_CURVE('',#23299,#23299,#19502,.T.);
#28508=EDGE_CURVE('',#23298,#23297,#2828,.T.);
#28509=EDGE_CURVE('',#23300,#23300,#2829,.T.);
#28510=EDGE_CURVE('',#23300,#23301,#5490,.T.);
#28511=EDGE_CURVE('',#23301,#23301,#2830,.T.);
#28512=EDGE_CURVE('',#23302,#23303,#2831,.T.);
#28513=EDGE_CURVE('',#23303,#23304,#5491,.T.);
#28514=EDGE_CURVE('',#23304,#23304,#19503,.T.);
#28515=EDGE_CURVE('',#23303,#23302,#2832,.T.);
#28516=EDGE_CURVE('',#22857,#23305,#5492,.T.);
#28517=EDGE_CURVE('',#23305,#23305,#2833,.T.);
#28518=EDGE_CURVE('',#23306,#23307,#2834,.T.);
#28519=EDGE_CURVE('',#23307,#23308,#5493,.T.);
#28520=EDGE_CURVE('',#23308,#23308,#19504,.T.);
#28521=EDGE_CURVE('',#23307,#23306,#2835,.T.);
#28522=EDGE_CURVE('',#22843,#23309,#5494,.T.);
#28523=EDGE_CURVE('',#23309,#23309,#2836,.T.);
#28524=EDGE_CURVE('',#23310,#23311,#2837,.T.);
#28525=EDGE_CURVE('',#23311,#23312,#5495,.T.);
#28526=EDGE_CURVE('',#23312,#23312,#19505,.T.);
#28527=EDGE_CURVE('',#23311,#23310,#2838,.T.);
#28528=EDGE_CURVE('',#22815,#23313,#5496,.T.);
#28529=EDGE_CURVE('',#23313,#23313,#2839,.T.);
#28530=EDGE_CURVE('',#23314,#23315,#2840,.T.);
#28531=EDGE_CURVE('',#23315,#23316,#5497,.T.);
#28532=EDGE_CURVE('',#23316,#23316,#19506,.T.);
#28533=EDGE_CURVE('',#23315,#23314,#2841,.T.);
#28534=EDGE_CURVE('',#22811,#23317,#5498,.T.);
#28535=EDGE_CURVE('',#23317,#23317,#2842,.T.);
#28536=EDGE_CURVE('',#23318,#23319,#2843,.T.);
#28537=EDGE_CURVE('',#23319,#23320,#5499,.T.);
#28538=EDGE_CURVE('',#23320,#23320,#19507,.T.);
#28539=EDGE_CURVE('',#23319,#23318,#2844,.T.);
#28540=EDGE_CURVE('',#22855,#23321,#5500,.T.);
#28541=EDGE_CURVE('',#23321,#23321,#2845,.T.);
#28542=EDGE_CURVE('',#23322,#23323,#2846,.T.);
#28543=EDGE_CURVE('',#23323,#23324,#5501,.T.);
#28544=EDGE_CURVE('',#23324,#23324,#19508,.T.);
#28545=EDGE_CURVE('',#23323,#23322,#2847,.T.);
#28546=EDGE_CURVE('',#22839,#23325,#5502,.T.);
#28547=EDGE_CURVE('',#23325,#23325,#2848,.T.);
#28548=EDGE_CURVE('',#23326,#23327,#2849,.T.);
#28549=EDGE_CURVE('',#23327,#23328,#5503,.T.);
#28550=EDGE_CURVE('',#23328,#23328,#19509,.T.);
#28551=EDGE_CURVE('',#23327,#23326,#2850,.T.);
#28552=EDGE_CURVE('',#22845,#23329,#5504,.T.);
#28553=EDGE_CURVE('',#23329,#23329,#2851,.T.);
#28554=EDGE_CURVE('',#23330,#23331,#2852,.T.);
#28555=EDGE_CURVE('',#23331,#23332,#5505,.T.);
#28556=EDGE_CURVE('',#23332,#23332,#19510,.T.);
#28557=EDGE_CURVE('',#23331,#23330,#2853,.T.);
#28558=EDGE_CURVE('',#22813,#23333,#5506,.T.);
#28559=EDGE_CURVE('',#23333,#23333,#2854,.T.);
#28560=EDGE_CURVE('',#23334,#23335,#2855,.T.);
#28561=EDGE_CURVE('',#23335,#23336,#5507,.T.);
#28562=EDGE_CURVE('',#23336,#23336,#19511,.T.);
#28563=EDGE_CURVE('',#23335,#23334,#2856,.T.);
#28564=EDGE_CURVE('',#22819,#23337,#5508,.T.);
#28565=EDGE_CURVE('',#23337,#23337,#2857,.T.);
#28566=EDGE_CURVE('',#23338,#23339,#2858,.T.);
#28567=EDGE_CURVE('',#23339,#23340,#5509,.T.);
#28568=EDGE_CURVE('',#23340,#23340,#19512,.T.);
#28569=EDGE_CURVE('',#23339,#23338,#2859,.T.);
#28570=EDGE_CURVE('',#22853,#23341,#5510,.T.);
#28571=EDGE_CURVE('',#23341,#23341,#2860,.T.);
#28572=EDGE_CURVE('',#23342,#23343,#2861,.T.);
#28573=EDGE_CURVE('',#23343,#23344,#5511,.T.);
#28574=EDGE_CURVE('',#23344,#23344,#19513,.T.);
#28575=EDGE_CURVE('',#23343,#23342,#2862,.T.);
#28576=EDGE_CURVE('',#22837,#23345,#5512,.T.);
#28577=EDGE_CURVE('',#23345,#23345,#2863,.T.);
#28578=EDGE_CURVE('',#23346,#23347,#2864,.T.);
#28579=EDGE_CURVE('',#23347,#23348,#5513,.T.);
#28580=EDGE_CURVE('',#23348,#23348,#19514,.T.);
#28581=EDGE_CURVE('',#23347,#23346,#2865,.T.);
#28582=EDGE_CURVE('',#22847,#23349,#5514,.T.);
#28583=EDGE_CURVE('',#23349,#23349,#2866,.T.);
#28584=EDGE_CURVE('',#23350,#23351,#2867,.T.);
#28585=EDGE_CURVE('',#23351,#23352,#5515,.T.);
#28586=EDGE_CURVE('',#23352,#23352,#19515,.T.);
#28587=EDGE_CURVE('',#23351,#23350,#2868,.T.);
#28588=EDGE_CURVE('',#22827,#23353,#5516,.T.);
#28589=EDGE_CURVE('',#23353,#23353,#2869,.T.);
#28590=EDGE_CURVE('',#23354,#23355,#2870,.T.);
#28591=EDGE_CURVE('',#23355,#23356,#5517,.T.);
#28592=EDGE_CURVE('',#23356,#23356,#19516,.T.);
#28593=EDGE_CURVE('',#23355,#23354,#2871,.T.);
#28594=EDGE_CURVE('',#22821,#23357,#5518,.T.);
#28595=EDGE_CURVE('',#23357,#23357,#2872,.T.);
#28596=EDGE_CURVE('',#23358,#23359,#2873,.T.);
#28597=EDGE_CURVE('',#23359,#23360,#5519,.T.);
#28598=EDGE_CURVE('',#23360,#23360,#19517,.T.);
#28599=EDGE_CURVE('',#23359,#23358,#2874,.T.);
#28600=EDGE_CURVE('',#22851,#23361,#5520,.T.);
#28601=EDGE_CURVE('',#23361,#23361,#2875,.T.);
#28602=EDGE_CURVE('',#23362,#23363,#2876,.T.);
#28603=EDGE_CURVE('',#23363,#23364,#5521,.T.);
#28604=EDGE_CURVE('',#23364,#23364,#19518,.T.);
#28605=EDGE_CURVE('',#23363,#23362,#2877,.T.);
#28606=EDGE_CURVE('',#22835,#23365,#5522,.T.);
#28607=EDGE_CURVE('',#23365,#23365,#2878,.T.);
#28608=EDGE_CURVE('',#23366,#23367,#2879,.T.);
#28609=EDGE_CURVE('',#23367,#23368,#5523,.T.);
#28610=EDGE_CURVE('',#23368,#23368,#19519,.T.);
#28611=EDGE_CURVE('',#23367,#23366,#2880,.T.);
#28612=EDGE_CURVE('',#22803,#23369,#5524,.T.);
#28613=EDGE_CURVE('',#23369,#23369,#2881,.T.);
#28614=EDGE_CURVE('',#23370,#23371,#2882,.T.);
#28615=EDGE_CURVE('',#23371,#23372,#5525,.T.);
#28616=EDGE_CURVE('',#23372,#23372,#19520,.T.);
#28617=EDGE_CURVE('',#23371,#23370,#2883,.T.);
#28618=EDGE_CURVE('',#22829,#23373,#5526,.T.);
#28619=EDGE_CURVE('',#23373,#23373,#2884,.T.);
#28620=EDGE_CURVE('',#23374,#23375,#2885,.T.);
#28621=EDGE_CURVE('',#23375,#23376,#5527,.T.);
#28622=EDGE_CURVE('',#23376,#23376,#19521,.T.);
#28623=EDGE_CURVE('',#23375,#23374,#2886,.T.);
#28624=EDGE_CURVE('',#22823,#23377,#5528,.T.);
#28625=EDGE_CURVE('',#23377,#23377,#2887,.T.);
#28626=EDGE_CURVE('',#23378,#23379,#2888,.T.);
#28627=EDGE_CURVE('',#23379,#23380,#5529,.T.);
#28628=EDGE_CURVE('',#23380,#23380,#19522,.T.);
#28629=EDGE_CURVE('',#23379,#23378,#2889,.T.);
#28630=EDGE_CURVE('',#22849,#23381,#5530,.T.);
#28631=EDGE_CURVE('',#23381,#23381,#2890,.T.);
#28632=EDGE_CURVE('',#23382,#23383,#2891,.T.);
#28633=EDGE_CURVE('',#23383,#23384,#5531,.T.);
#28634=EDGE_CURVE('',#23384,#23384,#19523,.T.);
#28635=EDGE_CURVE('',#23383,#23382,#2892,.T.);
#28636=EDGE_CURVE('',#22763,#23385,#5532,.T.);
#28637=EDGE_CURVE('',#23385,#23385,#2893,.T.);
#28638=EDGE_CURVE('',#23386,#23387,#2894,.T.);
#28639=EDGE_CURVE('',#23387,#23388,#5533,.T.);
#28640=EDGE_CURVE('',#23388,#23388,#19524,.T.);
#28641=EDGE_CURVE('',#23387,#23386,#2895,.T.);
#28642=EDGE_CURVE('',#22805,#23389,#5534,.T.);
#28643=EDGE_CURVE('',#23389,#23389,#2896,.T.);
#28644=EDGE_CURVE('',#23390,#23391,#2897,.T.);
#28645=EDGE_CURVE('',#23391,#23392,#5535,.T.);
#28646=EDGE_CURVE('',#23392,#23392,#19525,.T.);
#28647=EDGE_CURVE('',#23391,#23390,#2898,.T.);
#28648=EDGE_CURVE('',#22825,#23393,#5536,.T.);
#28649=EDGE_CURVE('',#23393,#23393,#2899,.T.);
#28650=EDGE_CURVE('',#23394,#23395,#2900,.T.);
#28651=EDGE_CURVE('',#23395,#23396,#5537,.T.);
#28652=EDGE_CURVE('',#23396,#23396,#19526,.T.);
#28653=EDGE_CURVE('',#23395,#23394,#2901,.T.);
#28654=EDGE_CURVE('',#22831,#23397,#5538,.T.);
#28655=EDGE_CURVE('',#23397,#23397,#2902,.T.);
#28656=EDGE_CURVE('',#23398,#23399,#2903,.T.);
#28657=EDGE_CURVE('',#23399,#23400,#5539,.T.);
#28658=EDGE_CURVE('',#23400,#23400,#19527,.T.);
#28659=EDGE_CURVE('',#23399,#23398,#2904,.T.);
#28660=EDGE_CURVE('',#23401,#23401,#19528,.T.);
#28661=EDGE_CURVE('',#23401,#23402,#5540,.T.);
#28662=EDGE_CURVE('',#23402,#23402,#19529,.T.);
#28663=EDGE_CURVE('',#23403,#23403,#19530,.T.);
#28664=EDGE_CURVE('',#23403,#23404,#5541,.T.);
#28665=EDGE_CURVE('',#23404,#23404,#19531,.T.);
#28666=EDGE_CURVE('',#23405,#23405,#19532,.T.);
#28667=EDGE_CURVE('',#23405,#23406,#5542,.T.);
#28668=EDGE_CURVE('',#23406,#23406,#19533,.T.);
#28669=EDGE_CURVE('',#23407,#23407,#19534,.T.);
#28670=EDGE_CURVE('',#23407,#23408,#5543,.T.);
#28671=EDGE_CURVE('',#23408,#23408,#19535,.T.);
#28672=EDGE_CURVE('',#23409,#23409,#19536,.T.);
#28673=EDGE_CURVE('',#23409,#23410,#5544,.T.);
#28674=EDGE_CURVE('',#23410,#23410,#19537,.T.);
#28675=EDGE_CURVE('',#23411,#23411,#19538,.T.);
#28676=EDGE_CURVE('',#23411,#23412,#5545,.T.);
#28677=EDGE_CURVE('',#23412,#23412,#19539,.T.);
#28678=EDGE_CURVE('',#23413,#23413,#19540,.T.);
#28679=EDGE_CURVE('',#23413,#23414,#5546,.T.);
#28680=EDGE_CURVE('',#23414,#23414,#19541,.T.);
#28681=EDGE_CURVE('',#23415,#23415,#19542,.T.);
#28682=EDGE_CURVE('',#23415,#23416,#5547,.T.);
#28683=EDGE_CURVE('',#23416,#23416,#19543,.T.);
#28684=EDGE_CURVE('',#23417,#23417,#19544,.T.);
#28685=EDGE_CURVE('',#23417,#23418,#5548,.T.);
#28686=EDGE_CURVE('',#23418,#23418,#19545,.T.);
#28687=EDGE_CURVE('',#23419,#23419,#19546,.T.);
#28688=EDGE_CURVE('',#23419,#23420,#5549,.T.);
#28689=EDGE_CURVE('',#23420,#23420,#19547,.T.);
#28690=EDGE_CURVE('',#23421,#23421,#19548,.T.);
#28691=EDGE_CURVE('',#23421,#23422,#5550,.T.);
#28692=EDGE_CURVE('',#23422,#23422,#19549,.T.);
#28693=EDGE_CURVE('',#23423,#23423,#19550,.T.);
#28694=EDGE_CURVE('',#23423,#23424,#5551,.T.);
#28695=EDGE_CURVE('',#23424,#23424,#19551,.T.);
#28696=EDGE_CURVE('',#23425,#23425,#19552,.T.);
#28697=EDGE_CURVE('',#23425,#23426,#5552,.T.);
#28698=EDGE_CURVE('',#23426,#23426,#19553,.T.);
#28699=EDGE_CURVE('',#23427,#23427,#19554,.T.);
#28700=EDGE_CURVE('',#23427,#23428,#5553,.T.);
#28701=EDGE_CURVE('',#23428,#23428,#19555,.T.);
#28702=EDGE_CURVE('',#23429,#23429,#19556,.T.);
#28703=EDGE_CURVE('',#23429,#23430,#5554,.T.);
#28704=EDGE_CURVE('',#23430,#23430,#19557,.T.);
#28705=EDGE_CURVE('',#23431,#23431,#19558,.T.);
#28706=EDGE_CURVE('',#23431,#23432,#5555,.T.);
#28707=EDGE_CURVE('',#23432,#23432,#19559,.T.);
#28708=EDGE_CURVE('',#23433,#23433,#19560,.T.);
#28709=EDGE_CURVE('',#23433,#23434,#5556,.T.);
#28710=EDGE_CURVE('',#23434,#23434,#19561,.T.);
#28711=EDGE_CURVE('',#23435,#23435,#19562,.T.);
#28712=EDGE_CURVE('',#23435,#23436,#5557,.T.);
#28713=EDGE_CURVE('',#23436,#23436,#19563,.T.);
#28714=EDGE_CURVE('',#23437,#23437,#19564,.T.);
#28715=EDGE_CURVE('',#23437,#23438,#5558,.T.);
#28716=EDGE_CURVE('',#23438,#23438,#19565,.T.);
#28717=EDGE_CURVE('',#23439,#23439,#19566,.T.);
#28718=EDGE_CURVE('',#23439,#23440,#5559,.T.);
#28719=EDGE_CURVE('',#23440,#23440,#19567,.T.);
#28720=EDGE_CURVE('',#23441,#23441,#19568,.T.);
#28721=EDGE_CURVE('',#23441,#23442,#5560,.T.);
#28722=EDGE_CURVE('',#23442,#23442,#19569,.T.);
#28723=EDGE_CURVE('',#23443,#23443,#19570,.T.);
#28724=EDGE_CURVE('',#23443,#23444,#5561,.T.);
#28725=EDGE_CURVE('',#23444,#23444,#19571,.T.);
#28726=EDGE_CURVE('',#23445,#23445,#19572,.T.);
#28727=EDGE_CURVE('',#23445,#23446,#5562,.T.);
#28728=EDGE_CURVE('',#23446,#23446,#19573,.T.);
#28729=EDGE_CURVE('',#23447,#23447,#19574,.T.);
#28730=EDGE_CURVE('',#23447,#23448,#5563,.T.);
#28731=EDGE_CURVE('',#23448,#23448,#19575,.T.);
#28732=EDGE_CURVE('',#23449,#23449,#19576,.T.);
#28733=EDGE_CURVE('',#23449,#23450,#5564,.T.);
#28734=EDGE_CURVE('',#23450,#23450,#19577,.T.);
#28735=EDGE_CURVE('',#23451,#23451,#19578,.T.);
#28736=EDGE_CURVE('',#23451,#23452,#5565,.T.);
#28737=EDGE_CURVE('',#23452,#23452,#19579,.T.);
#28738=EDGE_CURVE('',#23453,#23453,#19580,.T.);
#28739=EDGE_CURVE('',#23453,#23454,#5566,.T.);
#28740=EDGE_CURVE('',#23454,#23454,#19581,.T.);
#28741=EDGE_CURVE('',#23455,#23455,#19582,.T.);
#28742=EDGE_CURVE('',#23455,#23456,#5567,.T.);
#28743=EDGE_CURVE('',#23456,#23456,#19583,.T.);
#28744=EDGE_CURVE('',#23457,#23457,#19584,.T.);
#28745=EDGE_CURVE('',#23457,#23458,#5568,.T.);
#28746=EDGE_CURVE('',#23458,#23458,#19585,.T.);
#28747=EDGE_CURVE('',#23459,#23459,#19586,.T.);
#28748=EDGE_CURVE('',#23459,#23460,#5569,.T.);
#28749=EDGE_CURVE('',#23460,#23460,#19587,.T.);
#28750=EDGE_CURVE('',#23461,#23461,#19588,.T.);
#28751=EDGE_CURVE('',#23461,#23462,#5570,.T.);
#28752=EDGE_CURVE('',#23462,#23462,#19589,.T.);
#28753=EDGE_CURVE('',#23463,#23463,#19590,.T.);
#28754=EDGE_CURVE('',#23463,#23464,#5571,.T.);
#28755=EDGE_CURVE('',#23464,#23464,#19591,.T.);
#28756=EDGE_CURVE('',#23465,#23465,#19592,.T.);
#28757=EDGE_CURVE('',#23465,#23466,#5572,.T.);
#28758=EDGE_CURVE('',#23466,#23466,#19593,.T.);
#28759=EDGE_CURVE('',#23467,#23467,#19594,.T.);
#28760=EDGE_CURVE('',#23467,#23468,#5573,.T.);
#28761=EDGE_CURVE('',#23468,#23468,#19595,.T.);
#28762=EDGE_CURVE('',#23469,#23469,#19596,.T.);
#28763=EDGE_CURVE('',#23469,#23470,#5574,.T.);
#28764=EDGE_CURVE('',#23470,#23470,#19597,.T.);
#28765=EDGE_CURVE('',#23471,#23471,#19598,.T.);
#28766=EDGE_CURVE('',#23471,#23472,#5575,.T.);
#28767=EDGE_CURVE('',#23472,#23472,#19599,.T.);
#28768=EDGE_CURVE('',#23473,#23473,#19600,.T.);
#28769=EDGE_CURVE('',#23473,#23474,#5576,.T.);
#28770=EDGE_CURVE('',#23474,#23474,#19601,.T.);
#28771=EDGE_CURVE('',#23475,#23475,#19602,.T.);
#28772=EDGE_CURVE('',#23475,#23476,#5577,.T.);
#28773=EDGE_CURVE('',#23476,#23476,#19603,.T.);
#28774=EDGE_CURVE('',#23477,#23477,#19604,.T.);
#28775=EDGE_CURVE('',#23477,#23478,#5578,.T.);
#28776=EDGE_CURVE('',#23478,#23478,#19605,.T.);
#28777=EDGE_CURVE('',#23479,#23479,#19606,.T.);
#28778=EDGE_CURVE('',#23479,#23480,#5579,.T.);
#28779=EDGE_CURVE('',#23480,#23480,#19607,.T.);
#28780=EDGE_CURVE('',#23481,#23481,#19608,.T.);
#28781=EDGE_CURVE('',#23481,#23482,#5580,.T.);
#28782=EDGE_CURVE('',#23482,#23482,#19609,.T.);
#28783=EDGE_CURVE('',#23483,#23483,#19610,.T.);
#28784=EDGE_CURVE('',#23483,#23484,#5581,.T.);
#28785=EDGE_CURVE('',#23484,#23484,#19611,.T.);
#28786=EDGE_CURVE('',#23485,#23485,#19612,.T.);
#28787=EDGE_CURVE('',#23485,#23486,#5582,.T.);
#28788=EDGE_CURVE('',#23486,#23486,#19613,.T.);
#28789=EDGE_CURVE('',#23487,#23487,#19614,.T.);
#28790=EDGE_CURVE('',#23487,#23488,#5583,.T.);
#28791=EDGE_CURVE('',#23488,#23488,#19615,.T.);
#28792=EDGE_CURVE('',#23489,#23489,#19616,.T.);
#28793=EDGE_CURVE('',#23489,#23490,#5584,.T.);
#28794=EDGE_CURVE('',#23490,#23490,#19617,.T.);
#28795=EDGE_CURVE('',#23491,#23491,#19618,.T.);
#28796=EDGE_CURVE('',#23491,#23492,#5585,.T.);
#28797=EDGE_CURVE('',#23492,#23492,#19619,.T.);
#28798=EDGE_CURVE('',#23493,#23493,#19620,.T.);
#28799=EDGE_CURVE('',#23493,#23494,#5586,.T.);
#28800=EDGE_CURVE('',#23494,#23494,#19621,.T.);
#28801=EDGE_CURVE('',#23495,#23495,#19622,.T.);
#28802=EDGE_CURVE('',#23495,#23496,#5587,.T.);
#28803=EDGE_CURVE('',#23496,#23496,#19623,.T.);
#28804=EDGE_CURVE('',#23497,#23497,#19624,.T.);
#28805=EDGE_CURVE('',#23497,#23498,#5588,.T.);
#28806=EDGE_CURVE('',#23498,#23498,#19625,.T.);
#28807=EDGE_CURVE('',#23499,#23499,#19626,.T.);
#28808=EDGE_CURVE('',#23499,#23500,#5589,.T.);
#28809=EDGE_CURVE('',#23500,#23500,#19627,.T.);
#28810=EDGE_CURVE('',#23501,#23501,#19628,.T.);
#28811=EDGE_CURVE('',#23501,#23502,#5590,.T.);
#28812=EDGE_CURVE('',#23502,#23502,#19629,.T.);
#28813=EDGE_CURVE('',#23503,#23503,#19630,.T.);
#28814=EDGE_CURVE('',#23503,#23504,#5591,.T.);
#28815=EDGE_CURVE('',#23504,#23504,#19631,.T.);
#28816=EDGE_CURVE('',#23505,#23505,#19632,.T.);
#28817=EDGE_CURVE('',#23505,#23506,#5592,.T.);
#28818=EDGE_CURVE('',#23506,#23506,#19633,.T.);
#28819=EDGE_CURVE('',#23507,#23507,#19634,.T.);
#28820=EDGE_CURVE('',#23507,#23508,#5593,.T.);
#28821=EDGE_CURVE('',#23508,#23508,#19635,.T.);
#28822=EDGE_CURVE('',#23509,#23509,#19636,.T.);
#28823=EDGE_CURVE('',#23509,#23510,#5594,.T.);
#28824=EDGE_CURVE('',#23510,#23510,#19637,.T.);
#28825=EDGE_CURVE('',#23511,#23511,#19638,.T.);
#28826=EDGE_CURVE('',#23511,#23512,#5595,.T.);
#28827=EDGE_CURVE('',#23512,#23512,#19639,.T.);
#28828=EDGE_CURVE('',#23513,#23513,#19640,.T.);
#28829=EDGE_CURVE('',#23513,#23514,#5596,.T.);
#28830=EDGE_CURVE('',#23514,#23514,#19641,.T.);
#28831=EDGE_CURVE('',#23515,#23515,#19642,.T.);
#28832=EDGE_CURVE('',#23515,#23516,#5597,.T.);
#28833=EDGE_CURVE('',#23516,#23516,#19643,.T.);
#28834=EDGE_CURVE('',#23517,#23517,#19644,.T.);
#28835=EDGE_CURVE('',#23517,#23518,#5598,.T.);
#28836=EDGE_CURVE('',#23518,#23518,#19645,.T.);
#28837=EDGE_CURVE('',#23519,#23519,#19646,.T.);
#28838=EDGE_CURVE('',#23519,#23520,#5599,.T.);
#28839=EDGE_CURVE('',#23520,#23520,#19647,.T.);
#28840=EDGE_CURVE('',#23521,#23521,#19648,.T.);
#28841=EDGE_CURVE('',#23521,#23522,#5600,.T.);
#28842=EDGE_CURVE('',#23522,#23522,#19649,.T.);
#28843=EDGE_CURVE('',#23523,#23523,#19650,.T.);
#28844=EDGE_CURVE('',#23523,#23524,#5601,.T.);
#28845=EDGE_CURVE('',#23524,#23524,#19651,.T.);
#28846=EDGE_CURVE('',#23525,#23525,#19652,.T.);
#28847=EDGE_CURVE('',#23525,#23526,#5602,.T.);
#28848=EDGE_CURVE('',#23526,#23526,#19653,.T.);
#28849=EDGE_CURVE('',#23527,#23527,#19654,.T.);
#28850=EDGE_CURVE('',#23527,#23528,#5603,.T.);
#28851=EDGE_CURVE('',#23528,#23528,#19655,.T.);
#28852=EDGE_CURVE('',#23529,#23529,#19656,.T.);
#28853=EDGE_CURVE('',#23529,#23530,#5604,.T.);
#28854=EDGE_CURVE('',#23530,#23530,#19657,.T.);
#28855=EDGE_CURVE('',#23531,#23531,#19658,.T.);
#28856=EDGE_CURVE('',#23531,#23532,#5605,.T.);
#28857=EDGE_CURVE('',#23532,#23532,#19659,.T.);
#28858=EDGE_CURVE('',#23533,#23533,#19660,.T.);
#28859=EDGE_CURVE('',#23533,#23534,#5606,.T.);
#28860=EDGE_CURVE('',#23534,#23534,#19661,.T.);
#28861=EDGE_CURVE('',#23535,#23535,#19662,.T.);
#28862=EDGE_CURVE('',#23535,#23536,#5607,.T.);
#28863=EDGE_CURVE('',#23536,#23536,#19663,.T.);
#28864=EDGE_CURVE('',#23537,#23537,#19664,.T.);
#28865=EDGE_CURVE('',#23537,#23538,#5608,.T.);
#28866=EDGE_CURVE('',#23538,#23538,#19665,.T.);
#28867=EDGE_CURVE('',#23539,#23539,#19666,.T.);
#28868=EDGE_CURVE('',#23539,#23540,#5609,.T.);
#28869=EDGE_CURVE('',#23540,#23540,#19667,.T.);
#28870=EDGE_CURVE('',#23541,#23541,#19668,.T.);
#28871=EDGE_CURVE('',#23541,#23542,#5610,.T.);
#28872=EDGE_CURVE('',#23542,#23542,#19669,.T.);
#28873=EDGE_CURVE('',#23543,#23543,#19670,.T.);
#28874=EDGE_CURVE('',#23543,#23544,#5611,.T.);
#28875=EDGE_CURVE('',#23544,#23544,#19671,.T.);
#28876=EDGE_CURVE('',#23545,#23545,#19672,.T.);
#28877=EDGE_CURVE('',#23545,#23546,#5612,.T.);
#28878=EDGE_CURVE('',#23546,#23546,#19673,.T.);
#28879=EDGE_CURVE('',#23547,#23547,#19674,.T.);
#28880=EDGE_CURVE('',#23547,#23548,#5613,.T.);
#28881=EDGE_CURVE('',#23548,#23548,#19675,.T.);
#28882=EDGE_CURVE('',#23549,#23549,#19676,.T.);
#28883=EDGE_CURVE('',#23549,#23550,#5614,.T.);
#28884=EDGE_CURVE('',#23550,#23550,#19677,.T.);
#28885=EDGE_CURVE('',#23551,#23551,#19678,.T.);
#28886=EDGE_CURVE('',#23551,#23552,#5615,.T.);
#28887=EDGE_CURVE('',#23552,#23552,#19679,.T.);
#28888=EDGE_CURVE('',#23553,#23553,#19680,.T.);
#28889=EDGE_CURVE('',#23553,#23554,#5616,.T.);
#28890=EDGE_CURVE('',#23554,#23554,#19681,.T.);
#28891=EDGE_CURVE('',#23555,#23555,#19682,.T.);
#28892=EDGE_CURVE('',#23555,#23556,#5617,.T.);
#28893=EDGE_CURVE('',#23556,#23556,#19683,.T.);
#28894=EDGE_CURVE('',#23557,#23557,#19684,.T.);
#28895=EDGE_CURVE('',#23557,#23558,#5618,.T.);
#28896=EDGE_CURVE('',#23558,#23558,#19685,.T.);
#28897=EDGE_CURVE('',#23559,#23559,#19686,.T.);
#28898=EDGE_CURVE('',#23559,#23560,#5619,.T.);
#28899=EDGE_CURVE('',#23560,#23560,#19687,.T.);
#28900=EDGE_CURVE('',#23561,#23561,#19688,.T.);
#28901=EDGE_CURVE('',#23561,#23562,#5620,.T.);
#28902=EDGE_CURVE('',#23562,#23562,#19689,.T.);
#28903=EDGE_CURVE('',#23563,#23563,#19690,.T.);
#28904=EDGE_CURVE('',#23563,#23564,#5621,.T.);
#28905=EDGE_CURVE('',#23564,#23564,#19691,.T.);
#28906=EDGE_CURVE('',#23565,#23565,#19692,.T.);
#28907=EDGE_CURVE('',#23565,#23566,#5622,.T.);
#28908=EDGE_CURVE('',#23566,#23566,#19693,.T.);
#28909=EDGE_CURVE('',#23567,#23567,#19694,.T.);
#28910=EDGE_CURVE('',#23567,#23568,#5623,.T.);
#28911=EDGE_CURVE('',#23568,#23568,#19695,.T.);
#28912=EDGE_CURVE('',#23569,#23569,#19696,.T.);
#28913=EDGE_CURVE('',#23569,#23570,#5624,.T.);
#28914=EDGE_CURVE('',#23570,#23570,#19697,.T.);
#28915=EDGE_CURVE('',#23571,#23571,#19698,.T.);
#28916=EDGE_CURVE('',#23571,#23572,#5625,.T.);
#28917=EDGE_CURVE('',#23572,#23572,#19699,.T.);
#28918=EDGE_CURVE('',#23573,#23573,#19700,.T.);
#28919=EDGE_CURVE('',#23573,#23574,#5626,.T.);
#28920=EDGE_CURVE('',#23574,#23574,#19701,.T.);
#28921=EDGE_CURVE('',#23575,#23575,#19702,.T.);
#28922=EDGE_CURVE('',#23575,#23576,#5627,.T.);
#28923=EDGE_CURVE('',#23576,#23576,#19703,.T.);
#28924=EDGE_CURVE('',#23577,#23577,#19704,.T.);
#28925=EDGE_CURVE('',#23577,#23578,#5628,.T.);
#28926=EDGE_CURVE('',#23578,#23578,#19705,.T.);
#28927=EDGE_CURVE('',#23579,#23579,#19706,.T.);
#28928=EDGE_CURVE('',#23579,#23580,#5629,.T.);
#28929=EDGE_CURVE('',#23580,#23580,#19707,.T.);
#28930=EDGE_CURVE('',#23581,#23581,#19708,.T.);
#28931=EDGE_CURVE('',#23581,#23582,#5630,.T.);
#28932=EDGE_CURVE('',#23582,#23582,#19709,.T.);
#28933=EDGE_CURVE('',#23583,#23583,#19710,.T.);
#28934=EDGE_CURVE('',#23583,#23584,#5631,.T.);
#28935=EDGE_CURVE('',#23584,#23584,#19711,.T.);
#28936=EDGE_CURVE('',#23585,#23585,#19712,.T.);
#28937=EDGE_CURVE('',#23585,#23586,#5632,.T.);
#28938=EDGE_CURVE('',#23586,#23586,#19713,.T.);
#28939=EDGE_CURVE('',#23587,#23587,#19714,.T.);
#28940=EDGE_CURVE('',#23587,#23588,#5633,.T.);
#28941=EDGE_CURVE('',#23588,#23588,#19715,.T.);
#28942=EDGE_CURVE('',#23589,#23589,#19716,.T.);
#28943=EDGE_CURVE('',#23589,#23590,#5634,.T.);
#28944=EDGE_CURVE('',#23590,#23590,#19717,.T.);
#28945=EDGE_CURVE('',#23591,#23591,#19718,.T.);
#28946=EDGE_CURVE('',#23591,#23592,#5635,.T.);
#28947=EDGE_CURVE('',#23592,#23592,#19719,.T.);
#28948=EDGE_CURVE('',#23593,#23593,#19720,.T.);
#28949=EDGE_CURVE('',#23593,#23594,#5636,.T.);
#28950=EDGE_CURVE('',#23594,#23594,#19721,.T.);
#28951=EDGE_CURVE('',#23595,#23595,#19722,.T.);
#28952=EDGE_CURVE('',#23595,#23596,#5637,.T.);
#28953=EDGE_CURVE('',#23596,#23596,#19723,.T.);
#28954=EDGE_CURVE('',#23597,#23597,#19724,.T.);
#28955=EDGE_CURVE('',#23597,#23598,#5638,.T.);
#28956=EDGE_CURVE('',#23598,#23598,#19725,.T.);
#28957=EDGE_CURVE('',#23599,#23599,#19726,.T.);
#28958=EDGE_CURVE('',#23599,#23600,#5639,.T.);
#28959=EDGE_CURVE('',#23600,#23600,#19727,.T.);
#28960=EDGE_CURVE('',#23601,#23601,#19728,.T.);
#28961=EDGE_CURVE('',#23601,#23602,#5640,.T.);
#28962=EDGE_CURVE('',#23602,#23602,#19729,.T.);
#28963=EDGE_CURVE('',#23603,#23603,#19730,.T.);
#28964=EDGE_CURVE('',#23603,#23604,#5641,.T.);
#28965=EDGE_CURVE('',#23604,#23604,#19731,.T.);
#28966=EDGE_CURVE('',#23605,#23605,#19732,.T.);
#28967=EDGE_CURVE('',#23605,#23606,#5642,.T.);
#28968=EDGE_CURVE('',#23606,#23606,#19733,.T.);
#28969=EDGE_CURVE('',#23607,#23607,#19734,.T.);
#28970=EDGE_CURVE('',#23607,#23608,#5643,.T.);
#28971=EDGE_CURVE('',#23608,#23608,#19735,.T.);
#28972=EDGE_CURVE('',#23609,#23609,#19736,.T.);
#28973=EDGE_CURVE('',#23609,#23610,#5644,.T.);
#28974=EDGE_CURVE('',#23610,#23610,#19737,.T.);
#28975=EDGE_CURVE('',#23611,#23611,#19738,.T.);
#28976=EDGE_CURVE('',#23611,#23612,#5645,.T.);
#28977=EDGE_CURVE('',#23612,#23612,#19739,.T.);
#28978=EDGE_CURVE('',#23613,#23613,#19740,.T.);
#28979=EDGE_CURVE('',#23613,#23614,#5646,.T.);
#28980=EDGE_CURVE('',#23614,#23614,#19741,.T.);
#28981=EDGE_CURVE('',#23615,#23615,#19742,.T.);
#28982=EDGE_CURVE('',#23615,#23616,#5647,.T.);
#28983=EDGE_CURVE('',#23616,#23616,#19743,.T.);
#28984=EDGE_CURVE('',#23617,#23617,#19744,.T.);
#28985=EDGE_CURVE('',#23617,#23618,#5648,.T.);
#28986=EDGE_CURVE('',#23618,#23618,#19745,.T.);
#28987=EDGE_CURVE('',#23619,#23619,#19746,.T.);
#28988=EDGE_CURVE('',#23619,#23620,#5649,.T.);
#28989=EDGE_CURVE('',#23620,#23620,#19747,.T.);
#28990=EDGE_CURVE('',#23621,#23621,#19748,.T.);
#28991=EDGE_CURVE('',#23621,#23622,#5650,.T.);
#28992=EDGE_CURVE('',#23622,#23622,#19749,.T.);
#28993=EDGE_CURVE('',#23623,#23623,#19750,.T.);
#28994=EDGE_CURVE('',#23623,#23624,#5651,.T.);
#28995=EDGE_CURVE('',#23624,#23624,#19751,.T.);
#28996=EDGE_CURVE('',#23625,#23625,#19752,.T.);
#28997=EDGE_CURVE('',#23625,#23626,#5652,.T.);
#28998=EDGE_CURVE('',#23626,#23626,#19753,.T.);
#28999=EDGE_CURVE('',#23627,#23627,#19754,.T.);
#29000=EDGE_CURVE('',#23627,#23628,#5653,.T.);
#29001=EDGE_CURVE('',#23628,#23628,#19755,.T.);
#29002=EDGE_CURVE('',#23629,#23629,#19756,.T.);
#29003=EDGE_CURVE('',#23629,#23630,#5654,.T.);
#29004=EDGE_CURVE('',#23630,#23630,#19757,.T.);
#29005=EDGE_CURVE('',#23631,#23631,#19758,.T.);
#29006=EDGE_CURVE('',#23631,#23632,#5655,.T.);
#29007=EDGE_CURVE('',#23632,#23632,#19759,.T.);
#29008=EDGE_CURVE('',#23633,#23633,#19760,.T.);
#29009=EDGE_CURVE('',#23633,#23634,#5656,.T.);
#29010=EDGE_CURVE('',#23634,#23634,#19761,.T.);
#29011=EDGE_CURVE('',#23635,#23635,#19762,.T.);
#29012=EDGE_CURVE('',#23635,#23636,#5657,.T.);
#29013=EDGE_CURVE('',#23636,#23636,#19763,.T.);
#29014=EDGE_CURVE('',#23637,#23637,#19764,.T.);
#29015=EDGE_CURVE('',#23637,#23638,#5658,.T.);
#29016=EDGE_CURVE('',#23638,#23638,#19765,.T.);
#29017=EDGE_CURVE('',#23639,#23639,#19766,.T.);
#29018=EDGE_CURVE('',#23639,#23640,#5659,.T.);
#29019=EDGE_CURVE('',#23640,#23640,#19767,.T.);
#29020=EDGE_CURVE('',#23641,#23641,#19768,.T.);
#29021=EDGE_CURVE('',#23641,#23642,#5660,.T.);
#29022=EDGE_CURVE('',#23642,#23642,#19769,.T.);
#29023=EDGE_CURVE('',#23643,#23643,#19770,.T.);
#29024=EDGE_CURVE('',#23643,#23644,#5661,.T.);
#29025=EDGE_CURVE('',#23644,#23644,#19771,.T.);
#29026=EDGE_CURVE('',#23645,#23645,#19772,.T.);
#29027=EDGE_CURVE('',#23645,#23646,#5662,.T.);
#29028=EDGE_CURVE('',#23646,#23646,#19773,.T.);
#29029=EDGE_CURVE('',#23647,#23647,#19774,.T.);
#29030=EDGE_CURVE('',#23647,#23648,#5663,.T.);
#29031=EDGE_CURVE('',#23648,#23648,#19775,.T.);
#29032=EDGE_CURVE('',#23649,#23649,#19776,.T.);
#29033=EDGE_CURVE('',#23649,#23650,#5664,.T.);
#29034=EDGE_CURVE('',#23650,#23650,#19777,.T.);
#29035=EDGE_CURVE('',#23651,#23651,#19778,.T.);
#29036=EDGE_CURVE('',#23651,#23652,#5665,.T.);
#29037=EDGE_CURVE('',#23652,#23652,#19779,.T.);
#29038=EDGE_CURVE('',#23653,#23653,#19780,.T.);
#29039=EDGE_CURVE('',#23653,#23654,#5666,.T.);
#29040=EDGE_CURVE('',#23654,#23654,#19781,.T.);
#29041=EDGE_CURVE('',#23655,#23655,#19782,.T.);
#29042=EDGE_CURVE('',#23655,#23656,#5667,.T.);
#29043=EDGE_CURVE('',#23656,#23656,#19783,.T.);
#29044=EDGE_CURVE('',#23657,#23657,#19784,.T.);
#29045=EDGE_CURVE('',#23657,#23658,#5668,.T.);
#29046=EDGE_CURVE('',#23658,#23658,#19785,.T.);
#29047=EDGE_CURVE('',#23659,#23659,#19786,.T.);
#29048=EDGE_CURVE('',#23659,#23660,#5669,.T.);
#29049=EDGE_CURVE('',#23660,#23660,#19787,.T.);
#29050=EDGE_CURVE('',#23661,#23661,#19788,.T.);
#29051=EDGE_CURVE('',#23661,#23662,#5670,.T.);
#29052=EDGE_CURVE('',#23662,#23662,#19789,.T.);
#29053=EDGE_CURVE('',#23663,#23663,#19790,.T.);
#29054=EDGE_CURVE('',#23663,#23664,#5671,.T.);
#29055=EDGE_CURVE('',#23664,#23664,#19791,.T.);
#29056=EDGE_CURVE('',#23665,#23665,#19792,.T.);
#29057=EDGE_CURVE('',#23665,#23666,#5672,.T.);
#29058=EDGE_CURVE('',#23666,#23666,#19793,.T.);
#29059=EDGE_CURVE('',#23667,#23667,#19794,.T.);
#29060=EDGE_CURVE('',#23667,#23668,#5673,.T.);
#29061=EDGE_CURVE('',#23668,#23668,#19795,.T.);
#29062=EDGE_CURVE('',#23669,#23669,#19796,.T.);
#29063=EDGE_CURVE('',#23669,#23670,#5674,.T.);
#29064=EDGE_CURVE('',#23670,#23670,#19797,.T.);
#29065=EDGE_CURVE('',#23671,#23671,#19798,.T.);
#29066=EDGE_CURVE('',#23671,#23672,#5675,.T.);
#29067=EDGE_CURVE('',#23672,#23672,#19799,.T.);
#29068=EDGE_CURVE('',#23673,#23673,#19800,.T.);
#29069=EDGE_CURVE('',#23673,#23674,#5676,.T.);
#29070=EDGE_CURVE('',#23674,#23674,#19801,.T.);
#29071=EDGE_CURVE('',#23675,#23675,#19802,.T.);
#29072=EDGE_CURVE('',#23675,#23676,#5677,.T.);
#29073=EDGE_CURVE('',#23676,#23676,#19803,.T.);
#29074=EDGE_CURVE('',#23677,#23677,#19804,.T.);
#29075=EDGE_CURVE('',#23677,#23678,#5678,.T.);
#29076=EDGE_CURVE('',#23678,#23678,#19805,.T.);
#29077=EDGE_CURVE('',#23679,#23679,#19806,.T.);
#29078=EDGE_CURVE('',#23679,#23680,#5679,.T.);
#29079=EDGE_CURVE('',#23680,#23680,#19807,.T.);
#29080=EDGE_CURVE('',#23681,#23681,#19808,.T.);
#29081=EDGE_CURVE('',#23681,#23682,#5680,.T.);
#29082=EDGE_CURVE('',#23682,#23682,#19809,.T.);
#29083=EDGE_CURVE('',#23683,#23683,#19810,.T.);
#29084=EDGE_CURVE('',#23683,#23684,#5681,.T.);
#29085=EDGE_CURVE('',#23684,#23684,#19811,.T.);
#29086=EDGE_CURVE('',#23685,#23685,#19812,.T.);
#29087=EDGE_CURVE('',#23685,#23686,#5682,.T.);
#29088=EDGE_CURVE('',#23686,#23686,#19813,.T.);
#29089=EDGE_CURVE('',#23687,#23687,#19814,.T.);
#29090=EDGE_CURVE('',#23687,#23688,#5683,.T.);
#29091=EDGE_CURVE('',#23688,#23688,#19815,.T.);
#29092=EDGE_CURVE('',#23689,#23689,#19816,.T.);
#29093=EDGE_CURVE('',#23689,#23690,#5684,.T.);
#29094=EDGE_CURVE('',#23690,#23690,#19817,.T.);
#29095=EDGE_CURVE('',#23691,#23691,#19818,.T.);
#29096=EDGE_CURVE('',#23691,#23692,#5685,.T.);
#29097=EDGE_CURVE('',#23692,#23692,#19819,.T.);
#29098=EDGE_CURVE('',#23693,#23693,#19820,.T.);
#29099=EDGE_CURVE('',#23693,#23694,#5686,.T.);
#29100=EDGE_CURVE('',#23694,#23694,#19821,.T.);
#29101=EDGE_CURVE('',#23695,#23695,#19822,.T.);
#29102=EDGE_CURVE('',#23695,#23696,#5687,.T.);
#29103=EDGE_CURVE('',#23696,#23696,#19823,.T.);
#29104=EDGE_CURVE('',#23697,#23697,#19824,.T.);
#29105=EDGE_CURVE('',#23697,#23698,#5688,.T.);
#29106=EDGE_CURVE('',#23698,#23698,#19825,.T.);
#29107=EDGE_CURVE('',#23699,#23699,#19826,.T.);
#29108=EDGE_CURVE('',#23699,#23700,#5689,.T.);
#29109=EDGE_CURVE('',#23700,#23700,#19827,.T.);
#29110=EDGE_CURVE('',#23701,#23701,#19828,.T.);
#29111=EDGE_CURVE('',#23701,#23702,#5690,.T.);
#29112=EDGE_CURVE('',#23702,#23702,#19829,.T.);
#29113=EDGE_CURVE('',#23703,#23703,#19830,.T.);
#29114=EDGE_CURVE('',#23703,#23704,#5691,.T.);
#29115=EDGE_CURVE('',#23704,#23704,#19831,.T.);
#29116=EDGE_CURVE('',#23705,#23705,#19832,.T.);
#29117=EDGE_CURVE('',#23705,#23706,#5692,.T.);
#29118=EDGE_CURVE('',#23706,#23706,#19833,.T.);
#29119=EDGE_CURVE('',#23707,#23707,#19834,.T.);
#29120=EDGE_CURVE('',#23707,#23708,#5693,.T.);
#29121=EDGE_CURVE('',#23708,#23708,#19835,.T.);
#29122=EDGE_CURVE('',#23709,#23709,#19836,.T.);
#29123=EDGE_CURVE('',#23709,#23710,#5694,.T.);
#29124=EDGE_CURVE('',#23710,#23710,#19837,.T.);
#29125=EDGE_CURVE('',#23711,#23711,#19838,.T.);
#29126=EDGE_CURVE('',#23711,#23712,#5695,.T.);
#29127=EDGE_CURVE('',#23712,#23712,#19839,.T.);
#29128=EDGE_CURVE('',#23713,#23713,#19840,.T.);
#29129=EDGE_CURVE('',#23713,#23714,#5696,.T.);
#29130=EDGE_CURVE('',#23714,#23714,#19841,.T.);
#29131=EDGE_CURVE('',#23715,#23715,#19842,.T.);
#29132=EDGE_CURVE('',#23715,#23716,#5697,.T.);
#29133=EDGE_CURVE('',#23716,#23716,#19843,.T.);
#29134=EDGE_CURVE('',#23717,#23717,#19844,.T.);
#29135=EDGE_CURVE('',#23717,#23718,#5698,.T.);
#29136=EDGE_CURVE('',#23718,#23718,#19845,.T.);
#29137=EDGE_CURVE('',#23719,#23719,#19846,.T.);
#29138=EDGE_CURVE('',#23719,#23720,#5699,.T.);
#29139=EDGE_CURVE('',#23720,#23720,#19847,.T.);
#29140=EDGE_CURVE('',#23721,#23721,#19848,.T.);
#29141=EDGE_CURVE('',#23721,#23722,#5700,.T.);
#29142=EDGE_CURVE('',#23722,#23722,#19849,.T.);
#29143=EDGE_CURVE('',#23723,#23723,#19850,.T.);
#29144=EDGE_CURVE('',#23723,#23724,#5701,.T.);
#29145=EDGE_CURVE('',#23724,#23724,#19851,.T.);
#29146=EDGE_CURVE('',#23725,#23725,#19852,.T.);
#29147=EDGE_CURVE('',#23725,#23726,#5702,.T.);
#29148=EDGE_CURVE('',#23726,#23726,#19853,.T.);
#29149=EDGE_CURVE('',#23727,#23727,#19854,.T.);
#29150=EDGE_CURVE('',#23727,#23728,#5703,.T.);
#29151=EDGE_CURVE('',#23728,#23728,#19855,.T.);
#29152=EDGE_CURVE('',#23729,#23729,#19856,.T.);
#29153=EDGE_CURVE('',#23729,#23730,#5704,.T.);
#29154=EDGE_CURVE('',#23730,#23730,#19857,.T.);
#29155=EDGE_CURVE('',#23731,#23731,#19858,.T.);
#29156=EDGE_CURVE('',#23731,#23732,#5705,.T.);
#29157=EDGE_CURVE('',#23732,#23732,#19859,.T.);
#29158=EDGE_CURVE('',#23733,#23733,#19860,.T.);
#29159=EDGE_CURVE('',#23733,#23734,#5706,.T.);
#29160=EDGE_CURVE('',#23734,#23734,#19861,.T.);
#29161=EDGE_CURVE('',#23735,#23735,#19862,.T.);
#29162=EDGE_CURVE('',#23735,#23736,#5707,.T.);
#29163=EDGE_CURVE('',#23736,#23736,#19863,.T.);
#29164=EDGE_CURVE('',#23737,#23737,#19864,.T.);
#29165=EDGE_CURVE('',#23737,#23738,#5708,.T.);
#29166=EDGE_CURVE('',#23738,#23738,#19865,.T.);
#29167=EDGE_CURVE('',#23739,#23739,#19866,.T.);
#29168=EDGE_CURVE('',#23739,#23740,#5709,.T.);
#29169=EDGE_CURVE('',#23740,#23740,#19867,.T.);
#29170=EDGE_CURVE('',#23741,#23741,#19868,.T.);
#29171=EDGE_CURVE('',#23741,#23742,#5710,.T.);
#29172=EDGE_CURVE('',#23742,#23742,#19869,.T.);
#29173=EDGE_CURVE('',#23743,#23743,#19870,.T.);
#29174=EDGE_CURVE('',#23743,#23744,#5711,.T.);
#29175=EDGE_CURVE('',#23744,#23744,#19871,.T.);
#29176=EDGE_CURVE('',#23745,#23745,#19872,.T.);
#29177=EDGE_CURVE('',#23745,#23746,#5712,.T.);
#29178=EDGE_CURVE('',#23746,#23746,#19873,.T.);
#29179=EDGE_CURVE('',#23747,#23747,#19874,.T.);
#29180=EDGE_CURVE('',#23747,#23748,#5713,.T.);
#29181=EDGE_CURVE('',#23748,#23748,#19875,.T.);
#29182=EDGE_CURVE('',#23749,#23749,#19876,.T.);
#29183=EDGE_CURVE('',#23749,#23750,#5714,.T.);
#29184=EDGE_CURVE('',#23750,#23750,#19877,.T.);
#29185=EDGE_CURVE('',#23751,#23751,#19878,.T.);
#29186=EDGE_CURVE('',#23751,#23752,#5715,.T.);
#29187=EDGE_CURVE('',#23752,#23752,#19879,.T.);
#29188=EDGE_CURVE('',#23753,#23753,#19880,.T.);
#29189=EDGE_CURVE('',#23753,#23754,#5716,.T.);
#29190=EDGE_CURVE('',#23754,#23754,#19881,.T.);
#29191=EDGE_CURVE('',#23755,#23755,#19882,.T.);
#29192=EDGE_CURVE('',#23755,#23756,#5717,.T.);
#29193=EDGE_CURVE('',#23756,#23756,#19883,.T.);
#29194=EDGE_CURVE('',#23757,#23757,#19884,.T.);
#29195=EDGE_CURVE('',#23757,#23758,#5718,.T.);
#29196=EDGE_CURVE('',#23758,#23758,#19885,.T.);
#29197=EDGE_CURVE('',#23759,#23759,#19886,.T.);
#29198=EDGE_CURVE('',#23759,#23760,#5719,.T.);
#29199=EDGE_CURVE('',#23760,#23760,#19887,.T.);
#29200=EDGE_CURVE('',#23761,#23761,#19888,.T.);
#29201=EDGE_CURVE('',#23761,#23762,#5720,.T.);
#29202=EDGE_CURVE('',#23762,#23762,#19889,.T.);
#29203=EDGE_CURVE('',#23763,#23763,#19890,.T.);
#29204=EDGE_CURVE('',#23763,#23764,#5721,.T.);
#29205=EDGE_CURVE('',#23764,#23764,#19891,.T.);
#29206=EDGE_CURVE('',#23765,#23765,#19892,.T.);
#29207=EDGE_CURVE('',#23765,#23766,#5722,.T.);
#29208=EDGE_CURVE('',#23766,#23766,#19893,.T.);
#29209=EDGE_CURVE('',#23767,#23767,#19894,.T.);
#29210=EDGE_CURVE('',#23767,#23768,#5723,.T.);
#29211=EDGE_CURVE('',#23768,#23768,#19895,.T.);
#29212=EDGE_CURVE('',#23769,#23769,#19896,.T.);
#29213=EDGE_CURVE('',#23769,#23770,#5724,.T.);
#29214=EDGE_CURVE('',#23770,#23770,#19897,.T.);
#29215=EDGE_CURVE('',#23771,#23771,#19898,.T.);
#29216=EDGE_CURVE('',#23771,#23772,#5725,.T.);
#29217=EDGE_CURVE('',#23772,#23772,#19899,.T.);
#29218=EDGE_CURVE('',#23773,#23773,#19900,.T.);
#29219=EDGE_CURVE('',#23773,#23774,#5726,.T.);
#29220=EDGE_CURVE('',#23774,#23774,#19901,.T.);
#29221=EDGE_CURVE('',#23775,#23775,#19902,.T.);
#29222=EDGE_CURVE('',#23775,#23776,#5727,.T.);
#29223=EDGE_CURVE('',#23776,#23776,#19903,.T.);
#29224=EDGE_CURVE('',#23777,#23777,#19904,.T.);
#29225=EDGE_CURVE('',#23777,#23778,#5728,.T.);
#29226=EDGE_CURVE('',#23778,#23778,#19905,.T.);
#29227=EDGE_CURVE('',#23779,#23779,#19906,.T.);
#29228=EDGE_CURVE('',#23779,#23780,#5729,.T.);
#29229=EDGE_CURVE('',#23780,#23780,#19907,.T.);
#29230=EDGE_CURVE('',#23781,#23781,#19908,.T.);
#29231=EDGE_CURVE('',#23781,#23782,#5730,.T.);
#29232=EDGE_CURVE('',#23782,#23782,#19909,.T.);
#29233=EDGE_CURVE('',#23783,#23783,#19910,.T.);
#29234=EDGE_CURVE('',#23783,#23784,#5731,.T.);
#29235=EDGE_CURVE('',#23784,#23784,#19911,.T.);
#29236=EDGE_CURVE('',#23785,#23785,#19912,.T.);
#29237=EDGE_CURVE('',#23785,#23786,#5732,.T.);
#29238=EDGE_CURVE('',#23786,#23786,#19913,.T.);
#29239=EDGE_CURVE('',#23787,#23787,#19914,.T.);
#29240=EDGE_CURVE('',#23787,#23788,#5733,.T.);
#29241=EDGE_CURVE('',#23788,#23788,#19915,.T.);
#29242=EDGE_CURVE('',#23789,#23789,#19916,.T.);
#29243=EDGE_CURVE('',#23789,#23790,#5734,.T.);
#29244=EDGE_CURVE('',#23790,#23790,#19917,.T.);
#29245=EDGE_CURVE('',#23791,#23791,#19918,.T.);
#29246=EDGE_CURVE('',#23791,#23792,#5735,.T.);
#29247=EDGE_CURVE('',#23792,#23792,#19919,.T.);
#29248=EDGE_CURVE('',#23793,#23793,#19920,.T.);
#29249=EDGE_CURVE('',#23793,#23794,#5736,.T.);
#29250=EDGE_CURVE('',#23794,#23794,#19921,.T.);
#29251=EDGE_CURVE('',#23795,#23795,#19922,.T.);
#29252=EDGE_CURVE('',#23795,#23796,#5737,.T.);
#29253=EDGE_CURVE('',#23796,#23796,#19923,.T.);
#29254=EDGE_CURVE('',#23797,#23797,#19924,.T.);
#29255=EDGE_CURVE('',#23797,#23798,#5738,.T.);
#29256=EDGE_CURVE('',#23798,#23798,#19925,.T.);
#29257=EDGE_CURVE('',#23799,#23799,#19926,.T.);
#29258=EDGE_CURVE('',#23799,#23800,#5739,.T.);
#29259=EDGE_CURVE('',#23800,#23800,#19927,.T.);
#29260=EDGE_CURVE('',#23801,#23801,#19928,.T.);
#29261=EDGE_CURVE('',#23801,#23802,#5740,.T.);
#29262=EDGE_CURVE('',#23802,#23802,#19929,.T.);
#29263=EDGE_CURVE('',#23803,#23803,#19930,.T.);
#29264=EDGE_CURVE('',#23803,#23804,#5741,.T.);
#29265=EDGE_CURVE('',#23804,#23804,#19931,.T.);
#29266=EDGE_CURVE('',#23805,#23805,#19932,.T.);
#29267=EDGE_CURVE('',#23805,#23806,#5742,.T.);
#29268=EDGE_CURVE('',#23806,#23806,#19933,.T.);
#29269=EDGE_CURVE('',#23807,#23807,#19934,.T.);
#29270=EDGE_CURVE('',#23807,#23808,#5743,.T.);
#29271=EDGE_CURVE('',#23808,#23808,#19935,.T.);
#29272=EDGE_CURVE('',#23809,#23809,#19936,.T.);
#29273=EDGE_CURVE('',#23809,#23810,#5744,.T.);
#29274=EDGE_CURVE('',#23810,#23810,#19937,.T.);
#29275=EDGE_CURVE('',#23811,#23811,#19938,.T.);
#29276=EDGE_CURVE('',#23811,#23812,#5745,.T.);
#29277=EDGE_CURVE('',#23812,#23812,#19939,.T.);
#29278=EDGE_CURVE('',#23813,#23813,#19940,.T.);
#29279=EDGE_CURVE('',#23813,#23814,#5746,.T.);
#29280=EDGE_CURVE('',#23814,#23814,#19941,.T.);
#29281=EDGE_CURVE('',#23815,#23815,#19942,.T.);
#29282=EDGE_CURVE('',#23815,#23816,#5747,.T.);
#29283=EDGE_CURVE('',#23816,#23816,#19943,.T.);
#29284=EDGE_CURVE('',#23817,#23817,#19944,.T.);
#29285=EDGE_CURVE('',#23817,#23818,#5748,.T.);
#29286=EDGE_CURVE('',#23818,#23818,#19945,.T.);
#29287=EDGE_CURVE('',#23819,#23819,#19946,.T.);
#29288=EDGE_CURVE('',#23819,#23820,#5749,.T.);
#29289=EDGE_CURVE('',#23820,#23820,#19947,.T.);
#29290=EDGE_CURVE('',#23821,#23821,#19948,.T.);
#29291=EDGE_CURVE('',#23821,#23822,#5750,.T.);
#29292=EDGE_CURVE('',#23822,#23822,#19949,.T.);
#29293=EDGE_CURVE('',#23823,#23823,#19950,.T.);
#29294=EDGE_CURVE('',#23823,#23824,#5751,.T.);
#29295=EDGE_CURVE('',#23824,#23824,#19951,.T.);
#29296=EDGE_CURVE('',#23825,#23825,#19952,.T.);
#29297=EDGE_CURVE('',#23825,#23826,#5752,.T.);
#29298=EDGE_CURVE('',#23826,#23826,#19953,.T.);
#29299=EDGE_CURVE('',#23827,#23827,#19954,.T.);
#29300=EDGE_CURVE('',#23827,#23828,#5753,.T.);
#29301=EDGE_CURVE('',#23828,#23828,#19955,.T.);
#29302=EDGE_CURVE('',#23829,#23829,#19956,.T.);
#29303=EDGE_CURVE('',#23829,#23830,#5754,.T.);
#29304=EDGE_CURVE('',#23830,#23830,#19957,.T.);
#29305=EDGE_CURVE('',#23831,#23831,#19958,.T.);
#29306=EDGE_CURVE('',#23831,#23832,#5755,.T.);
#29307=EDGE_CURVE('',#23832,#23832,#19959,.T.);
#29308=EDGE_CURVE('',#23833,#23833,#19960,.T.);
#29309=EDGE_CURVE('',#23833,#23834,#5756,.T.);
#29310=EDGE_CURVE('',#23834,#23834,#19961,.T.);
#29311=EDGE_CURVE('',#23835,#23835,#19962,.T.);
#29312=EDGE_CURVE('',#23835,#23836,#5757,.T.);
#29313=EDGE_CURVE('',#23836,#23836,#19963,.T.);
#29314=EDGE_CURVE('',#23837,#23837,#19964,.T.);
#29315=EDGE_CURVE('',#23837,#23838,#5758,.T.);
#29316=EDGE_CURVE('',#23838,#23838,#19965,.T.);
#29317=EDGE_CURVE('',#23839,#23839,#19966,.T.);
#29318=EDGE_CURVE('',#23839,#23840,#5759,.T.);
#29319=EDGE_CURVE('',#23840,#23840,#19967,.T.);
#29320=EDGE_CURVE('',#23841,#23841,#19968,.T.);
#29321=EDGE_CURVE('',#23841,#23842,#5760,.T.);
#29322=EDGE_CURVE('',#23842,#23842,#19969,.T.);
#29323=EDGE_CURVE('',#23843,#23843,#19970,.T.);
#29324=EDGE_CURVE('',#23843,#23844,#5761,.T.);
#29325=EDGE_CURVE('',#23844,#23844,#19971,.T.);
#29326=EDGE_CURVE('',#23845,#23845,#19972,.T.);
#29327=EDGE_CURVE('',#23845,#23846,#5762,.T.);
#29328=EDGE_CURVE('',#23846,#23846,#19973,.T.);
#29329=EDGE_CURVE('',#23847,#23847,#19974,.T.);
#29330=EDGE_CURVE('',#23847,#23848,#5763,.T.);
#29331=EDGE_CURVE('',#23848,#23848,#19975,.T.);
#29332=EDGE_CURVE('',#23849,#23849,#19976,.T.);
#29333=EDGE_CURVE('',#23849,#23850,#5764,.T.);
#29334=EDGE_CURVE('',#23850,#23850,#19977,.T.);
#29335=EDGE_CURVE('',#23851,#23851,#19978,.T.);
#29336=EDGE_CURVE('',#23851,#23852,#5765,.T.);
#29337=EDGE_CURVE('',#23852,#23852,#19979,.T.);
#29338=EDGE_CURVE('',#23853,#23853,#19980,.T.);
#29339=EDGE_CURVE('',#23853,#23854,#5766,.T.);
#29340=EDGE_CURVE('',#23854,#23854,#19981,.T.);
#29341=EDGE_CURVE('',#23855,#23855,#19982,.T.);
#29342=EDGE_CURVE('',#23855,#23856,#5767,.T.);
#29343=EDGE_CURVE('',#23856,#23856,#19983,.T.);
#29344=EDGE_CURVE('',#23857,#23857,#19984,.T.);
#29345=EDGE_CURVE('',#23857,#23858,#5768,.T.);
#29346=EDGE_CURVE('',#23858,#23858,#19985,.T.);
#29347=EDGE_CURVE('',#23859,#23859,#19986,.T.);
#29348=EDGE_CURVE('',#23859,#23860,#5769,.T.);
#29349=EDGE_CURVE('',#23860,#23860,#19987,.T.);
#29350=EDGE_CURVE('',#23861,#23861,#19988,.T.);
#29351=EDGE_CURVE('',#23861,#23862,#5770,.T.);
#29352=EDGE_CURVE('',#23862,#23862,#19989,.T.);
#29353=EDGE_CURVE('',#23863,#23863,#19990,.T.);
#29354=EDGE_CURVE('',#23863,#23864,#5771,.T.);
#29355=EDGE_CURVE('',#23864,#23864,#19991,.T.);
#29356=EDGE_CURVE('',#23865,#23865,#19992,.T.);
#29357=EDGE_CURVE('',#23865,#23866,#5772,.T.);
#29358=EDGE_CURVE('',#23866,#23866,#19993,.T.);
#29359=EDGE_CURVE('',#23867,#23867,#19994,.T.);
#29360=EDGE_CURVE('',#23867,#23868,#5773,.T.);
#29361=EDGE_CURVE('',#23868,#23868,#19995,.T.);
#29362=EDGE_CURVE('',#23869,#23869,#19996,.T.);
#29363=EDGE_CURVE('',#23869,#23870,#5774,.T.);
#29364=EDGE_CURVE('',#23870,#23870,#19997,.T.);
#29365=EDGE_CURVE('',#23871,#23871,#19998,.T.);
#29366=EDGE_CURVE('',#23871,#23872,#5775,.T.);
#29367=EDGE_CURVE('',#23872,#23872,#19999,.T.);
#29368=EDGE_CURVE('',#23873,#23873,#20000,.T.);
#29369=EDGE_CURVE('',#23873,#23874,#5776,.T.);
#29370=EDGE_CURVE('',#23874,#23874,#20001,.T.);
#29371=EDGE_CURVE('',#23875,#23875,#20002,.T.);
#29372=EDGE_CURVE('',#23875,#23876,#5777,.T.);
#29373=EDGE_CURVE('',#23876,#23876,#20003,.T.);
#29374=EDGE_CURVE('',#23877,#23877,#20004,.T.);
#29375=EDGE_CURVE('',#23877,#23878,#5778,.T.);
#29376=EDGE_CURVE('',#23878,#23878,#20005,.T.);
#29377=EDGE_CURVE('',#23879,#23879,#20006,.T.);
#29378=EDGE_CURVE('',#23879,#23880,#5779,.T.);
#29379=EDGE_CURVE('',#23880,#23880,#20007,.T.);
#29380=EDGE_CURVE('',#23881,#23881,#20008,.T.);
#29381=EDGE_CURVE('',#23881,#23882,#5780,.T.);
#29382=EDGE_CURVE('',#23882,#23882,#20009,.T.);
#29383=EDGE_CURVE('',#23883,#23883,#20010,.T.);
#29384=EDGE_CURVE('',#23883,#23884,#5781,.T.);
#29385=EDGE_CURVE('',#23884,#23884,#20011,.T.);
#29386=EDGE_CURVE('',#23885,#23885,#20012,.T.);
#29387=EDGE_CURVE('',#23885,#23886,#5782,.T.);
#29388=EDGE_CURVE('',#23886,#23886,#20013,.T.);
#29389=EDGE_CURVE('',#23887,#23887,#20014,.T.);
#29390=EDGE_CURVE('',#23887,#23888,#5783,.T.);
#29391=EDGE_CURVE('',#23888,#23888,#20015,.T.);
#29392=EDGE_CURVE('',#23889,#23889,#20016,.T.);
#29393=EDGE_CURVE('',#23889,#23890,#5784,.T.);
#29394=EDGE_CURVE('',#23890,#23890,#20017,.T.);
#29395=EDGE_CURVE('',#23891,#23891,#20018,.T.);
#29396=EDGE_CURVE('',#23891,#23892,#5785,.T.);
#29397=EDGE_CURVE('',#23892,#23892,#20019,.T.);
#29398=EDGE_CURVE('',#23893,#23893,#20020,.T.);
#29399=EDGE_CURVE('',#23893,#23894,#5786,.T.);
#29400=EDGE_CURVE('',#23894,#23894,#20021,.T.);
#29401=EDGE_CURVE('',#23895,#23895,#20022,.T.);
#29402=EDGE_CURVE('',#23895,#23896,#5787,.T.);
#29403=EDGE_CURVE('',#23896,#23896,#20023,.T.);
#29404=EDGE_CURVE('',#23897,#23897,#20024,.T.);
#29405=EDGE_CURVE('',#23897,#23898,#5788,.T.);
#29406=EDGE_CURVE('',#23898,#23898,#20025,.T.);
#29407=EDGE_CURVE('',#23899,#23899,#20026,.T.);
#29408=EDGE_CURVE('',#23899,#23900,#5789,.T.);
#29409=EDGE_CURVE('',#23900,#23900,#20027,.T.);
#29410=EDGE_CURVE('',#23901,#23901,#20028,.T.);
#29411=EDGE_CURVE('',#23901,#23902,#5790,.T.);
#29412=EDGE_CURVE('',#23902,#23902,#20029,.T.);
#29413=EDGE_CURVE('',#23903,#23903,#20030,.T.);
#29414=EDGE_CURVE('',#23903,#23904,#5791,.T.);
#29415=EDGE_CURVE('',#23904,#23904,#20031,.T.);
#29416=EDGE_CURVE('',#23905,#23905,#20032,.T.);
#29417=EDGE_CURVE('',#23905,#23906,#5792,.T.);
#29418=EDGE_CURVE('',#23906,#23906,#20033,.T.);
#29419=EDGE_CURVE('',#23907,#23907,#20034,.T.);
#29420=EDGE_CURVE('',#23907,#23908,#5793,.T.);
#29421=EDGE_CURVE('',#23908,#23908,#20035,.T.);
#29422=EDGE_CURVE('',#23909,#23909,#20036,.T.);
#29423=EDGE_CURVE('',#23909,#23910,#5794,.T.);
#29424=EDGE_CURVE('',#23910,#23910,#20037,.T.);
#29425=EDGE_CURVE('',#23911,#23911,#20038,.T.);
#29426=EDGE_CURVE('',#23911,#23912,#5795,.T.);
#29427=EDGE_CURVE('',#23912,#23912,#20039,.T.);
#29428=EDGE_CURVE('',#23913,#23913,#20040,.T.);
#29429=EDGE_CURVE('',#23913,#23914,#5796,.T.);
#29430=EDGE_CURVE('',#23914,#23914,#20041,.T.);
#29431=EDGE_CURVE('',#23915,#23915,#20042,.T.);
#29432=EDGE_CURVE('',#23915,#23916,#5797,.T.);
#29433=EDGE_CURVE('',#23916,#23916,#20043,.T.);
#29434=EDGE_CURVE('',#23917,#23917,#20044,.T.);
#29435=EDGE_CURVE('',#23917,#23918,#5798,.T.);
#29436=EDGE_CURVE('',#23918,#23918,#20045,.T.);
#29437=EDGE_CURVE('',#23919,#23919,#20046,.T.);
#29438=EDGE_CURVE('',#23919,#23920,#5799,.T.);
#29439=EDGE_CURVE('',#23920,#23920,#20047,.T.);
#29440=EDGE_CURVE('',#23921,#23921,#20048,.T.);
#29441=EDGE_CURVE('',#23921,#23922,#5800,.T.);
#29442=EDGE_CURVE('',#23922,#23922,#20049,.T.);
#29443=EDGE_CURVE('',#23923,#23923,#20050,.T.);
#29444=EDGE_CURVE('',#23923,#23924,#5801,.T.);
#29445=EDGE_CURVE('',#23924,#23924,#20051,.T.);
#29446=EDGE_CURVE('',#23925,#23925,#20052,.T.);
#29447=EDGE_CURVE('',#23925,#23926,#5802,.T.);
#29448=EDGE_CURVE('',#23926,#23926,#20053,.T.);
#29449=EDGE_CURVE('',#23927,#23927,#20054,.T.);
#29450=EDGE_CURVE('',#23927,#23928,#5803,.T.);
#29451=EDGE_CURVE('',#23928,#23928,#20055,.T.);
#29452=EDGE_CURVE('',#23929,#23929,#20056,.T.);
#29453=EDGE_CURVE('',#23929,#23930,#5804,.T.);
#29454=EDGE_CURVE('',#23930,#23930,#20057,.T.);
#29455=EDGE_CURVE('',#23931,#23931,#20058,.T.);
#29456=EDGE_CURVE('',#23931,#23932,#5805,.T.);
#29457=EDGE_CURVE('',#23932,#23932,#20059,.T.);
#29458=EDGE_CURVE('',#23933,#23933,#20060,.T.);
#29459=EDGE_CURVE('',#23933,#23934,#5806,.T.);
#29460=EDGE_CURVE('',#23934,#23934,#20061,.T.);
#29461=EDGE_CURVE('',#23935,#23935,#20062,.T.);
#29462=EDGE_CURVE('',#23935,#23936,#5807,.T.);
#29463=EDGE_CURVE('',#23936,#23936,#20063,.T.);
#29464=EDGE_CURVE('',#23937,#23937,#20064,.T.);
#29465=EDGE_CURVE('',#23937,#23938,#5808,.T.);
#29466=EDGE_CURVE('',#23938,#23938,#20065,.T.);
#29467=EDGE_CURVE('',#23939,#23939,#20066,.T.);
#29468=EDGE_CURVE('',#23939,#23940,#5809,.T.);
#29469=EDGE_CURVE('',#23940,#23940,#20067,.T.);
#29470=EDGE_CURVE('',#23941,#23941,#20068,.T.);
#29471=EDGE_CURVE('',#23941,#23942,#5810,.T.);
#29472=EDGE_CURVE('',#23942,#23942,#20069,.T.);
#29473=EDGE_CURVE('',#23943,#23943,#20070,.T.);
#29474=EDGE_CURVE('',#23943,#23944,#5811,.T.);
#29475=EDGE_CURVE('',#23944,#23944,#20071,.T.);
#29476=EDGE_CURVE('',#23945,#23945,#20072,.T.);
#29477=EDGE_CURVE('',#23945,#23946,#5812,.T.);
#29478=EDGE_CURVE('',#23946,#23946,#20073,.T.);
#29479=EDGE_CURVE('',#23947,#23947,#20074,.T.);
#29480=EDGE_CURVE('',#23947,#23948,#5813,.T.);
#29481=EDGE_CURVE('',#23948,#23948,#20075,.T.);
#29482=EDGE_CURVE('',#23949,#23949,#20076,.T.);
#29483=EDGE_CURVE('',#23949,#23950,#5814,.T.);
#29484=EDGE_CURVE('',#23950,#23950,#20077,.T.);
#29485=EDGE_CURVE('',#23951,#23951,#20078,.T.);
#29486=EDGE_CURVE('',#23951,#23952,#5815,.T.);
#29487=EDGE_CURVE('',#23952,#23952,#20079,.T.);
#29488=EDGE_CURVE('',#23953,#23953,#20080,.T.);
#29489=EDGE_CURVE('',#23953,#23954,#5816,.T.);
#29490=EDGE_CURVE('',#23954,#23954,#20081,.T.);
#29491=EDGE_CURVE('',#23955,#23955,#20082,.T.);
#29492=EDGE_CURVE('',#23955,#23956,#5817,.T.);
#29493=EDGE_CURVE('',#23956,#23956,#20083,.T.);
#29494=EDGE_CURVE('',#23957,#23957,#20084,.T.);
#29495=EDGE_CURVE('',#23957,#23958,#5818,.T.);
#29496=EDGE_CURVE('',#23958,#23958,#20085,.T.);
#29497=EDGE_CURVE('',#23959,#23959,#20086,.T.);
#29498=EDGE_CURVE('',#23959,#23960,#5819,.T.);
#29499=EDGE_CURVE('',#23960,#23960,#20087,.T.);
#29500=EDGE_CURVE('',#23961,#23961,#20088,.T.);
#29501=EDGE_CURVE('',#23961,#23962,#5820,.T.);
#29502=EDGE_CURVE('',#23962,#23962,#20089,.T.);
#29503=EDGE_CURVE('',#23963,#23963,#20090,.T.);
#29504=EDGE_CURVE('',#23963,#23964,#5821,.T.);
#29505=EDGE_CURVE('',#23964,#23964,#20091,.T.);
#29506=EDGE_CURVE('',#23965,#23965,#20092,.T.);
#29507=EDGE_CURVE('',#23965,#23966,#5822,.T.);
#29508=EDGE_CURVE('',#23966,#23966,#20093,.T.);
#29509=EDGE_CURVE('',#23967,#23967,#20094,.T.);
#29510=EDGE_CURVE('',#23967,#23968,#5823,.T.);
#29511=EDGE_CURVE('',#23968,#23968,#20095,.T.);
#29512=EDGE_CURVE('',#23969,#23969,#20096,.T.);
#29513=EDGE_CURVE('',#23969,#23970,#5824,.T.);
#29514=EDGE_CURVE('',#23970,#23970,#20097,.T.);
#29515=EDGE_CURVE('',#23971,#23971,#20098,.T.);
#29516=EDGE_CURVE('',#23971,#23972,#5825,.T.);
#29517=EDGE_CURVE('',#23972,#23972,#20099,.T.);
#29518=EDGE_CURVE('',#23973,#23973,#20100,.T.);
#29519=EDGE_CURVE('',#23973,#23974,#5826,.T.);
#29520=EDGE_CURVE('',#23974,#23974,#20101,.T.);
#29521=EDGE_CURVE('',#23975,#23975,#20102,.T.);
#29522=EDGE_CURVE('',#23975,#23976,#5827,.T.);
#29523=EDGE_CURVE('',#23976,#23976,#20103,.T.);
#29524=EDGE_CURVE('',#23977,#23977,#20104,.T.);
#29525=EDGE_CURVE('',#23977,#23978,#5828,.T.);
#29526=EDGE_CURVE('',#23978,#23978,#20105,.T.);
#29527=EDGE_CURVE('',#23979,#23979,#20106,.T.);
#29528=EDGE_CURVE('',#23979,#23980,#5829,.T.);
#29529=EDGE_CURVE('',#23980,#23980,#20107,.T.);
#29530=EDGE_CURVE('',#23981,#23981,#20108,.T.);
#29531=EDGE_CURVE('',#23981,#23982,#5830,.T.);
#29532=EDGE_CURVE('',#23982,#23982,#20109,.T.);
#29533=EDGE_CURVE('',#23983,#23983,#20110,.T.);
#29534=EDGE_CURVE('',#23983,#23984,#5831,.T.);
#29535=EDGE_CURVE('',#23984,#23984,#20111,.T.);
#29536=EDGE_CURVE('',#23985,#23985,#20112,.T.);
#29537=EDGE_CURVE('',#23985,#23986,#5832,.T.);
#29538=EDGE_CURVE('',#23986,#23986,#20113,.T.);
#29539=EDGE_CURVE('',#23987,#23987,#20114,.T.);
#29540=EDGE_CURVE('',#23987,#23988,#5833,.T.);
#29541=EDGE_CURVE('',#23988,#23988,#20115,.T.);
#29542=EDGE_CURVE('',#23989,#23989,#20116,.T.);
#29543=EDGE_CURVE('',#23989,#23990,#5834,.T.);
#29544=EDGE_CURVE('',#23990,#23990,#20117,.T.);
#29545=EDGE_CURVE('',#23991,#23991,#20118,.T.);
#29546=EDGE_CURVE('',#23991,#23992,#5835,.T.);
#29547=EDGE_CURVE('',#23992,#23992,#20119,.T.);
#29548=EDGE_CURVE('',#23993,#23993,#20120,.T.);
#29549=EDGE_CURVE('',#23993,#23994,#5836,.T.);
#29550=EDGE_CURVE('',#23994,#23994,#20121,.T.);
#29551=EDGE_CURVE('',#23995,#23995,#20122,.T.);
#29552=EDGE_CURVE('',#23995,#23996,#5837,.T.);
#29553=EDGE_CURVE('',#23996,#23996,#20123,.T.);
#29554=EDGE_CURVE('',#23997,#23997,#20124,.T.);
#29555=EDGE_CURVE('',#23997,#23998,#5838,.T.);
#29556=EDGE_CURVE('',#23998,#23998,#20125,.T.);
#29557=EDGE_CURVE('',#23999,#23999,#20126,.T.);
#29558=EDGE_CURVE('',#23999,#24000,#5839,.T.);
#29559=EDGE_CURVE('',#24000,#24000,#20127,.T.);
#29560=EDGE_CURVE('',#24001,#24001,#20128,.T.);
#29561=EDGE_CURVE('',#24001,#24002,#5840,.T.);
#29562=EDGE_CURVE('',#24002,#24002,#20129,.T.);
#29563=EDGE_CURVE('',#24003,#24003,#20130,.T.);
#29564=EDGE_CURVE('',#24003,#24004,#5841,.T.);
#29565=EDGE_CURVE('',#24004,#24004,#20131,.T.);
#29566=EDGE_CURVE('',#24005,#24005,#20132,.T.);
#29567=EDGE_CURVE('',#24005,#24006,#5842,.T.);
#29568=EDGE_CURVE('',#24006,#24006,#20133,.T.);
#29569=EDGE_CURVE('',#24007,#24007,#20134,.T.);
#29570=EDGE_CURVE('',#24007,#24008,#5843,.T.);
#29571=EDGE_CURVE('',#24008,#24008,#20135,.T.);
#29572=EDGE_CURVE('',#24009,#24009,#20136,.T.);
#29573=EDGE_CURVE('',#24009,#24010,#5844,.T.);
#29574=EDGE_CURVE('',#24010,#24010,#20137,.T.);
#29575=EDGE_CURVE('',#24011,#24011,#20138,.T.);
#29576=EDGE_CURVE('',#24011,#24012,#5845,.T.);
#29577=EDGE_CURVE('',#24012,#24012,#20139,.T.);
#29578=EDGE_CURVE('',#24013,#24013,#20140,.T.);
#29579=EDGE_CURVE('',#24013,#24014,#5846,.T.);
#29580=EDGE_CURVE('',#24014,#24014,#20141,.T.);
#29581=EDGE_CURVE('',#24015,#24015,#20142,.T.);
#29582=EDGE_CURVE('',#24015,#24016,#5847,.T.);
#29583=EDGE_CURVE('',#24016,#24016,#20143,.T.);
#29584=EDGE_CURVE('',#24017,#24017,#20144,.T.);
#29585=EDGE_CURVE('',#24017,#24018,#5848,.T.);
#29586=EDGE_CURVE('',#24018,#24018,#20145,.T.);
#29587=EDGE_CURVE('',#24019,#24019,#20146,.T.);
#29588=EDGE_CURVE('',#24019,#24020,#5849,.T.);
#29589=EDGE_CURVE('',#24020,#24020,#20147,.T.);
#29590=EDGE_CURVE('',#24021,#24021,#20148,.T.);
#29591=EDGE_CURVE('',#24021,#24022,#5850,.T.);
#29592=EDGE_CURVE('',#24022,#24022,#20149,.T.);
#29593=EDGE_CURVE('',#24023,#24023,#20150,.T.);
#29594=EDGE_CURVE('',#24023,#24024,#5851,.T.);
#29595=EDGE_CURVE('',#24024,#24024,#20151,.T.);
#29596=EDGE_CURVE('',#24025,#24025,#20152,.T.);
#29597=EDGE_CURVE('',#24025,#24026,#5852,.T.);
#29598=EDGE_CURVE('',#24026,#24026,#20153,.T.);
#29599=EDGE_CURVE('',#24027,#24027,#20154,.T.);
#29600=EDGE_CURVE('',#24027,#24028,#5853,.T.);
#29601=EDGE_CURVE('',#24028,#24028,#20155,.T.);
#29602=EDGE_CURVE('',#24029,#24029,#20156,.T.);
#29603=EDGE_CURVE('',#24029,#24030,#5854,.T.);
#29604=EDGE_CURVE('',#24030,#24030,#20157,.T.);
#29605=EDGE_CURVE('',#24031,#24031,#20158,.T.);
#29606=EDGE_CURVE('',#24031,#24032,#5855,.T.);
#29607=EDGE_CURVE('',#24032,#24032,#20159,.T.);
#29608=EDGE_CURVE('',#24033,#24033,#20160,.T.);
#29609=EDGE_CURVE('',#24033,#24034,#5856,.T.);
#29610=EDGE_CURVE('',#24034,#24034,#20161,.T.);
#29611=EDGE_CURVE('',#24035,#24035,#20162,.T.);
#29612=EDGE_CURVE('',#24035,#24036,#5857,.T.);
#29613=EDGE_CURVE('',#24036,#24036,#20163,.T.);
#29614=EDGE_CURVE('',#24037,#24037,#20164,.T.);
#29615=EDGE_CURVE('',#24037,#24038,#5858,.T.);
#29616=EDGE_CURVE('',#24038,#24038,#20165,.T.);
#29617=EDGE_CURVE('',#24039,#24039,#20166,.T.);
#29618=EDGE_CURVE('',#24039,#24040,#5859,.T.);
#29619=EDGE_CURVE('',#24040,#24040,#20167,.T.);
#29620=EDGE_CURVE('',#24041,#24041,#20168,.T.);
#29621=EDGE_CURVE('',#24041,#24042,#5860,.T.);
#29622=EDGE_CURVE('',#24042,#24042,#20169,.T.);
#29623=EDGE_CURVE('',#24043,#24043,#20170,.T.);
#29624=EDGE_CURVE('',#24043,#24044,#5861,.T.);
#29625=EDGE_CURVE('',#24044,#24044,#20171,.T.);
#29626=EDGE_CURVE('',#24045,#24045,#20172,.T.);
#29627=EDGE_CURVE('',#24045,#24046,#5862,.T.);
#29628=EDGE_CURVE('',#24046,#24046,#20173,.T.);
#29629=EDGE_CURVE('',#24047,#24047,#20174,.T.);
#29630=EDGE_CURVE('',#24047,#24048,#5863,.T.);
#29631=EDGE_CURVE('',#24048,#24048,#20175,.T.);
#29632=EDGE_CURVE('',#24049,#24049,#20176,.T.);
#29633=EDGE_CURVE('',#24049,#24050,#5864,.T.);
#29634=EDGE_CURVE('',#24050,#24050,#20177,.T.);
#29635=EDGE_CURVE('',#24051,#24051,#20178,.T.);
#29636=EDGE_CURVE('',#24051,#24052,#5865,.T.);
#29637=EDGE_CURVE('',#24052,#24052,#20179,.T.);
#29638=EDGE_CURVE('',#24053,#24053,#20180,.T.);
#29639=EDGE_CURVE('',#24053,#24054,#5866,.T.);
#29640=EDGE_CURVE('',#24054,#24054,#20181,.T.);
#29641=EDGE_CURVE('',#24055,#24055,#20182,.T.);
#29642=EDGE_CURVE('',#24055,#24056,#5867,.T.);
#29643=EDGE_CURVE('',#24056,#24056,#20183,.T.);
#29644=EDGE_CURVE('',#24057,#24057,#20184,.T.);
#29645=EDGE_CURVE('',#24057,#24058,#5868,.T.);
#29646=EDGE_CURVE('',#24058,#24058,#20185,.T.);
#29647=EDGE_CURVE('',#24059,#24059,#20186,.T.);
#29648=EDGE_CURVE('',#24059,#24060,#5869,.T.);
#29649=EDGE_CURVE('',#24060,#24060,#20187,.T.);
#29650=EDGE_CURVE('',#24061,#24061,#20188,.T.);
#29651=EDGE_CURVE('',#24061,#24062,#5870,.T.);
#29652=EDGE_CURVE('',#24062,#24062,#20189,.T.);
#29653=EDGE_CURVE('',#24063,#24063,#20190,.T.);
#29654=EDGE_CURVE('',#24063,#24064,#5871,.T.);
#29655=EDGE_CURVE('',#24064,#24064,#20191,.T.);
#29656=EDGE_CURVE('',#24065,#24065,#20192,.T.);
#29657=EDGE_CURVE('',#24065,#24066,#5872,.T.);
#29658=EDGE_CURVE('',#24066,#24066,#20193,.T.);
#29659=EDGE_CURVE('',#24067,#24067,#20194,.T.);
#29660=EDGE_CURVE('',#24067,#24068,#5873,.T.);
#29661=EDGE_CURVE('',#24068,#24068,#20195,.T.);
#29662=EDGE_CURVE('',#24069,#24069,#20196,.T.);
#29663=EDGE_CURVE('',#24069,#24070,#5874,.T.);
#29664=EDGE_CURVE('',#24070,#24070,#20197,.T.);
#29665=EDGE_CURVE('',#24071,#24071,#20198,.T.);
#29666=EDGE_CURVE('',#24071,#24072,#5875,.T.);
#29667=EDGE_CURVE('',#24072,#24072,#20199,.T.);
#29668=EDGE_CURVE('',#24073,#24073,#20200,.T.);
#29669=EDGE_CURVE('',#24073,#24074,#5876,.T.);
#29670=EDGE_CURVE('',#24074,#24074,#20201,.T.);
#29671=EDGE_CURVE('',#24075,#24075,#20202,.T.);
#29672=EDGE_CURVE('',#24075,#24076,#5877,.T.);
#29673=EDGE_CURVE('',#24076,#24076,#20203,.T.);
#29674=EDGE_CURVE('',#24077,#24077,#20204,.T.);
#29675=EDGE_CURVE('',#24077,#24078,#5878,.T.);
#29676=EDGE_CURVE('',#24078,#24078,#20205,.T.);
#29677=EDGE_CURVE('',#24079,#24079,#20206,.T.);
#29678=EDGE_CURVE('',#24079,#24080,#5879,.T.);
#29679=EDGE_CURVE('',#24080,#24080,#20207,.T.);
#29680=EDGE_CURVE('',#24081,#24081,#20208,.T.);
#29681=EDGE_CURVE('',#24081,#24082,#5880,.T.);
#29682=EDGE_CURVE('',#24082,#24082,#20209,.T.);
#29683=EDGE_CURVE('',#24083,#24083,#20210,.T.);
#29684=EDGE_CURVE('',#24083,#24084,#5881,.T.);
#29685=EDGE_CURVE('',#24084,#24084,#20211,.T.);
#29686=EDGE_CURVE('',#24085,#24085,#20212,.T.);
#29687=EDGE_CURVE('',#24085,#24086,#5882,.T.);
#29688=EDGE_CURVE('',#24086,#24086,#20213,.T.);
#29689=EDGE_CURVE('',#24087,#24087,#20214,.T.);
#29690=EDGE_CURVE('',#24087,#24088,#5883,.T.);
#29691=EDGE_CURVE('',#24088,#24088,#20215,.T.);
#29692=EDGE_CURVE('',#24089,#24089,#20216,.T.);
#29693=EDGE_CURVE('',#24089,#24090,#5884,.T.);
#29694=EDGE_CURVE('',#24090,#24090,#20217,.T.);
#29695=EDGE_CURVE('',#24091,#24091,#20218,.T.);
#29696=EDGE_CURVE('',#24091,#24092,#5885,.T.);
#29697=EDGE_CURVE('',#24092,#24092,#20219,.T.);
#29698=EDGE_CURVE('',#24093,#24093,#20220,.T.);
#29699=EDGE_CURVE('',#24093,#24094,#5886,.T.);
#29700=EDGE_CURVE('',#24094,#24094,#20221,.T.);
#29701=EDGE_CURVE('',#24095,#24095,#20222,.T.);
#29702=EDGE_CURVE('',#24095,#24096,#5887,.T.);
#29703=EDGE_CURVE('',#24096,#24096,#20223,.T.);
#29704=EDGE_CURVE('',#24097,#24097,#20224,.T.);
#29705=EDGE_CURVE('',#24097,#24098,#5888,.T.);
#29706=EDGE_CURVE('',#24098,#24098,#20225,.T.);
#29707=EDGE_CURVE('',#24099,#24099,#20226,.T.);
#29708=EDGE_CURVE('',#24099,#24100,#5889,.T.);
#29709=EDGE_CURVE('',#24100,#24100,#20227,.T.);
#29710=EDGE_CURVE('',#24101,#24101,#20228,.T.);
#29711=EDGE_CURVE('',#24101,#24102,#5890,.T.);
#29712=EDGE_CURVE('',#24102,#24102,#20229,.T.);
#29713=EDGE_CURVE('',#24103,#24103,#20230,.T.);
#29714=EDGE_CURVE('',#24103,#24104,#5891,.T.);
#29715=EDGE_CURVE('',#24104,#24104,#20231,.T.);
#29716=EDGE_CURVE('',#24105,#24105,#20232,.T.);
#29717=EDGE_CURVE('',#24105,#24106,#5892,.T.);
#29718=EDGE_CURVE('',#24106,#24106,#20233,.T.);
#29719=EDGE_CURVE('',#24107,#24107,#20234,.T.);
#29720=EDGE_CURVE('',#24107,#24108,#5893,.T.);
#29721=EDGE_CURVE('',#24108,#24108,#20235,.T.);
#29722=EDGE_CURVE('',#24109,#24109,#20236,.T.);
#29723=EDGE_CURVE('',#24109,#24110,#5894,.T.);
#29724=EDGE_CURVE('',#24110,#24110,#20237,.T.);
#29725=EDGE_CURVE('',#24111,#24111,#20238,.T.);
#29726=EDGE_CURVE('',#24111,#24112,#5895,.T.);
#29727=EDGE_CURVE('',#24112,#24112,#20239,.T.);
#29728=EDGE_CURVE('',#24113,#24113,#20240,.T.);
#29729=EDGE_CURVE('',#24113,#24114,#5896,.T.);
#29730=EDGE_CURVE('',#24114,#24114,#20241,.T.);
#29731=EDGE_CURVE('',#24115,#24115,#20242,.T.);
#29732=EDGE_CURVE('',#24115,#24116,#5897,.T.);
#29733=EDGE_CURVE('',#24116,#24116,#20243,.T.);
#29734=EDGE_CURVE('',#24117,#24117,#20244,.T.);
#29735=EDGE_CURVE('',#24117,#24118,#5898,.T.);
#29736=EDGE_CURVE('',#24118,#24118,#20245,.T.);
#29737=EDGE_CURVE('',#24119,#24119,#20246,.T.);
#29738=EDGE_CURVE('',#24119,#24120,#5899,.T.);
#29739=EDGE_CURVE('',#24120,#24120,#20247,.T.);
#29740=EDGE_CURVE('',#24121,#24121,#20248,.T.);
#29741=EDGE_CURVE('',#24121,#24122,#5900,.T.);
#29742=EDGE_CURVE('',#24122,#24122,#20249,.T.);
#29743=EDGE_CURVE('',#24123,#24123,#20250,.T.);
#29744=EDGE_CURVE('',#24123,#24124,#5901,.T.);
#29745=EDGE_CURVE('',#24124,#24124,#20251,.T.);
#29746=EDGE_CURVE('',#24125,#24125,#20252,.T.);
#29747=EDGE_CURVE('',#24125,#24126,#5902,.T.);
#29748=EDGE_CURVE('',#24126,#24126,#20253,.T.);
#29749=EDGE_CURVE('',#24127,#24127,#20254,.T.);
#29750=EDGE_CURVE('',#24127,#24128,#5903,.T.);
#29751=EDGE_CURVE('',#24128,#24128,#20255,.T.);
#29752=EDGE_CURVE('',#24129,#24129,#20256,.T.);
#29753=EDGE_CURVE('',#24129,#24130,#5904,.T.);
#29754=EDGE_CURVE('',#24130,#24130,#20257,.T.);
#29755=EDGE_CURVE('',#24131,#24131,#20258,.T.);
#29756=EDGE_CURVE('',#24131,#24132,#5905,.T.);
#29757=EDGE_CURVE('',#24132,#24132,#20259,.T.);
#29758=EDGE_CURVE('',#24133,#24133,#20260,.T.);
#29759=EDGE_CURVE('',#24133,#24134,#5906,.T.);
#29760=EDGE_CURVE('',#24134,#24134,#20261,.T.);
#29761=EDGE_CURVE('',#24135,#24135,#20262,.T.);
#29762=EDGE_CURVE('',#24135,#24136,#5907,.T.);
#29763=EDGE_CURVE('',#24136,#24136,#20263,.T.);
#29764=EDGE_CURVE('',#24137,#24137,#20264,.T.);
#29765=EDGE_CURVE('',#24137,#24138,#5908,.T.);
#29766=EDGE_CURVE('',#24138,#24138,#20265,.T.);
#29767=EDGE_CURVE('',#24139,#24139,#20266,.T.);
#29768=EDGE_CURVE('',#24139,#24140,#5909,.T.);
#29769=EDGE_CURVE('',#24140,#24140,#20267,.T.);
#29770=EDGE_CURVE('',#24141,#24141,#20268,.T.);
#29771=EDGE_CURVE('',#24141,#24142,#5910,.T.);
#29772=EDGE_CURVE('',#24142,#24142,#20269,.T.);
#29773=EDGE_CURVE('',#24143,#24143,#20270,.T.);
#29774=EDGE_CURVE('',#24143,#24144,#5911,.T.);
#29775=EDGE_CURVE('',#24144,#24144,#20271,.T.);
#29776=EDGE_CURVE('',#24145,#24145,#20272,.T.);
#29777=EDGE_CURVE('',#24145,#24146,#5912,.T.);
#29778=EDGE_CURVE('',#24146,#24146,#20273,.T.);
#29779=EDGE_CURVE('',#24147,#24147,#20274,.T.);
#29780=EDGE_CURVE('',#24147,#24148,#5913,.T.);
#29781=EDGE_CURVE('',#24148,#24148,#20275,.T.);
#29782=EDGE_CURVE('',#24149,#24149,#20276,.T.);
#29783=EDGE_CURVE('',#24149,#24150,#5914,.T.);
#29784=EDGE_CURVE('',#24150,#24150,#20277,.T.);
#29785=EDGE_CURVE('',#24151,#24151,#20278,.T.);
#29786=EDGE_CURVE('',#24151,#24152,#5915,.T.);
#29787=EDGE_CURVE('',#24152,#24152,#20279,.T.);
#29788=EDGE_CURVE('',#24153,#24153,#20280,.T.);
#29789=EDGE_CURVE('',#24153,#24154,#5916,.T.);
#29790=EDGE_CURVE('',#24154,#24154,#20281,.T.);
#29791=EDGE_CURVE('',#24155,#24155,#20282,.T.);
#29792=EDGE_CURVE('',#24155,#24156,#5917,.T.);
#29793=EDGE_CURVE('',#24156,#24156,#20283,.T.);
#29794=EDGE_CURVE('',#24157,#24157,#20284,.T.);
#29795=EDGE_CURVE('',#24157,#24158,#5918,.T.);
#29796=EDGE_CURVE('',#24158,#24158,#20285,.T.);
#29797=EDGE_CURVE('',#24159,#24159,#20286,.T.);
#29798=EDGE_CURVE('',#24159,#24160,#5919,.T.);
#29799=EDGE_CURVE('',#24160,#24160,#20287,.T.);
#29800=EDGE_CURVE('',#24161,#24161,#20288,.T.);
#29801=EDGE_CURVE('',#24161,#24162,#5920,.T.);
#29802=EDGE_CURVE('',#24162,#24162,#20289,.T.);
#29803=EDGE_CURVE('',#24163,#24163,#20290,.T.);
#29804=EDGE_CURVE('',#24163,#24164,#5921,.T.);
#29805=EDGE_CURVE('',#24164,#24164,#20291,.T.);
#29806=EDGE_CURVE('',#24165,#24165,#20292,.T.);
#29807=EDGE_CURVE('',#24165,#24166,#5922,.T.);
#29808=EDGE_CURVE('',#24166,#24166,#20293,.T.);
#29809=EDGE_CURVE('',#24167,#24167,#20294,.T.);
#29810=EDGE_CURVE('',#24167,#24168,#5923,.T.);
#29811=EDGE_CURVE('',#24168,#24168,#20295,.T.);
#29812=EDGE_CURVE('',#24169,#24169,#20296,.T.);
#29813=EDGE_CURVE('',#24169,#24170,#5924,.T.);
#29814=EDGE_CURVE('',#24170,#24170,#20297,.T.);
#29815=EDGE_CURVE('',#24171,#24171,#20298,.T.);
#29816=EDGE_CURVE('',#24171,#24172,#5925,.T.);
#29817=EDGE_CURVE('',#24172,#24172,#20299,.T.);
#29818=EDGE_CURVE('',#24173,#24173,#20300,.T.);
#29819=EDGE_CURVE('',#24173,#24174,#5926,.T.);
#29820=EDGE_CURVE('',#24174,#24174,#20301,.T.);
#29821=EDGE_CURVE('',#24175,#24175,#20302,.T.);
#29822=EDGE_CURVE('',#24175,#24176,#5927,.T.);
#29823=EDGE_CURVE('',#24176,#24176,#20303,.T.);
#29824=EDGE_CURVE('',#24177,#24177,#20304,.T.);
#29825=EDGE_CURVE('',#24177,#24178,#5928,.T.);
#29826=EDGE_CURVE('',#24178,#24178,#20305,.T.);
#29827=EDGE_CURVE('',#24179,#24179,#20306,.T.);
#29828=EDGE_CURVE('',#24179,#24180,#5929,.T.);
#29829=EDGE_CURVE('',#24180,#24180,#20307,.T.);
#29830=EDGE_CURVE('',#24181,#24181,#20308,.T.);
#29831=EDGE_CURVE('',#24181,#24182,#5930,.T.);
#29832=EDGE_CURVE('',#24182,#24182,#20309,.T.);
#29833=EDGE_CURVE('',#24183,#24183,#20310,.T.);
#29834=EDGE_CURVE('',#24183,#24184,#5931,.T.);
#29835=EDGE_CURVE('',#24184,#24184,#20311,.T.);
#29836=EDGE_CURVE('',#24185,#24185,#20312,.T.);
#29837=EDGE_CURVE('',#24185,#24186,#5932,.T.);
#29838=EDGE_CURVE('',#24186,#24186,#20313,.T.);
#29839=EDGE_CURVE('',#24187,#24187,#20314,.T.);
#29840=EDGE_CURVE('',#24187,#24188,#5933,.T.);
#29841=EDGE_CURVE('',#24188,#24188,#20315,.T.);
#29842=EDGE_CURVE('',#24189,#24189,#20316,.T.);
#29843=EDGE_CURVE('',#24189,#24190,#5934,.T.);
#29844=EDGE_CURVE('',#24190,#24190,#20317,.T.);
#29845=EDGE_CURVE('',#24191,#24191,#20318,.T.);
#29846=EDGE_CURVE('',#24191,#24192,#5935,.T.);
#29847=EDGE_CURVE('',#24192,#24192,#20319,.T.);
#29848=EDGE_CURVE('',#24193,#24193,#20320,.T.);
#29849=EDGE_CURVE('',#24193,#24194,#5936,.T.);
#29850=EDGE_CURVE('',#24194,#24194,#20321,.T.);
#29851=EDGE_CURVE('',#24195,#24195,#20322,.T.);
#29852=EDGE_CURVE('',#24195,#24196,#5937,.T.);
#29853=EDGE_CURVE('',#24196,#24196,#20323,.T.);
#29854=EDGE_CURVE('',#24197,#24197,#20324,.T.);
#29855=EDGE_CURVE('',#24197,#24198,#5938,.T.);
#29856=EDGE_CURVE('',#24198,#24198,#20325,.T.);
#29857=EDGE_CURVE('',#24199,#24199,#20326,.T.);
#29858=EDGE_CURVE('',#24199,#24200,#5939,.T.);
#29859=EDGE_CURVE('',#24200,#24200,#20327,.T.);
#29860=EDGE_CURVE('',#24201,#24201,#20328,.T.);
#29861=EDGE_CURVE('',#24201,#24202,#5940,.T.);
#29862=EDGE_CURVE('',#24202,#24202,#20329,.T.);
#29863=EDGE_CURVE('',#24203,#24203,#20330,.T.);
#29864=EDGE_CURVE('',#24203,#24204,#5941,.T.);
#29865=EDGE_CURVE('',#24204,#24204,#20331,.T.);
#29866=EDGE_CURVE('',#24205,#24205,#20332,.T.);
#29867=EDGE_CURVE('',#24205,#24206,#5942,.T.);
#29868=EDGE_CURVE('',#24206,#24206,#20333,.T.);
#29869=EDGE_CURVE('',#24207,#24207,#20334,.T.);
#29870=EDGE_CURVE('',#24207,#24208,#5943,.T.);
#29871=EDGE_CURVE('',#24208,#24208,#20335,.T.);
#29872=EDGE_CURVE('',#24209,#24209,#20336,.T.);
#29873=EDGE_CURVE('',#24209,#24210,#5944,.T.);
#29874=EDGE_CURVE('',#24210,#24210,#20337,.T.);
#29875=EDGE_CURVE('',#24211,#24211,#20338,.T.);
#29876=EDGE_CURVE('',#24211,#24212,#5945,.T.);
#29877=EDGE_CURVE('',#24212,#24212,#20339,.T.);
#29878=EDGE_CURVE('',#24213,#24213,#20340,.T.);
#29879=EDGE_CURVE('',#24213,#24214,#5946,.T.);
#29880=EDGE_CURVE('',#24214,#24214,#20341,.T.);
#29881=EDGE_CURVE('',#24215,#24215,#20342,.T.);
#29882=EDGE_CURVE('',#24215,#24216,#5947,.T.);
#29883=EDGE_CURVE('',#24216,#24216,#20343,.T.);
#29884=EDGE_CURVE('',#24217,#24217,#20344,.T.);
#29885=EDGE_CURVE('',#24217,#24218,#5948,.T.);
#29886=EDGE_CURVE('',#24218,#24218,#20345,.T.);
#29887=EDGE_CURVE('',#24219,#24219,#20346,.T.);
#29888=EDGE_CURVE('',#24219,#24220,#5949,.T.);
#29889=EDGE_CURVE('',#24220,#24220,#20347,.T.);
#29890=EDGE_CURVE('',#24221,#24221,#20348,.T.);
#29891=EDGE_CURVE('',#24221,#24222,#5950,.T.);
#29892=EDGE_CURVE('',#24222,#24222,#20349,.T.);
#29893=EDGE_CURVE('',#24223,#24223,#20350,.T.);
#29894=EDGE_CURVE('',#24223,#24224,#5951,.T.);
#29895=EDGE_CURVE('',#24224,#24224,#20351,.T.);
#29896=EDGE_CURVE('',#24225,#24225,#20352,.T.);
#29897=EDGE_CURVE('',#24225,#24226,#5952,.T.);
#29898=EDGE_CURVE('',#24226,#24226,#20353,.T.);
#29899=EDGE_CURVE('',#24227,#24227,#20354,.T.);
#29900=EDGE_CURVE('',#24227,#24228,#5953,.T.);
#29901=EDGE_CURVE('',#24228,#24228,#20355,.T.);
#29902=EDGE_CURVE('',#24229,#24229,#20356,.T.);
#29903=EDGE_CURVE('',#24229,#24230,#5954,.T.);
#29904=EDGE_CURVE('',#24230,#24230,#20357,.T.);
#29905=EDGE_CURVE('',#24231,#24231,#20358,.T.);
#29906=EDGE_CURVE('',#24231,#24232,#5955,.T.);
#29907=EDGE_CURVE('',#24232,#24232,#20359,.T.);
#29908=EDGE_CURVE('',#24233,#24233,#20360,.T.);
#29909=EDGE_CURVE('',#24233,#24234,#5956,.T.);
#29910=EDGE_CURVE('',#24234,#24234,#20361,.T.);
#29911=EDGE_CURVE('',#24235,#24235,#20362,.T.);
#29912=EDGE_CURVE('',#24235,#24236,#5957,.T.);
#29913=EDGE_CURVE('',#24236,#24236,#20363,.T.);
#29914=EDGE_CURVE('',#24237,#24237,#20364,.T.);
#29915=EDGE_CURVE('',#24237,#24238,#5958,.T.);
#29916=EDGE_CURVE('',#24238,#24238,#20365,.T.);
#29917=EDGE_CURVE('',#24239,#24239,#20366,.T.);
#29918=EDGE_CURVE('',#24239,#24240,#5959,.T.);
#29919=EDGE_CURVE('',#24240,#24240,#20367,.T.);
#29920=EDGE_CURVE('',#24241,#24241,#20368,.T.);
#29921=EDGE_CURVE('',#24241,#24242,#5960,.T.);
#29922=EDGE_CURVE('',#24242,#24242,#20369,.T.);
#29923=EDGE_CURVE('',#24243,#24243,#20370,.T.);
#29924=EDGE_CURVE('',#24243,#24244,#5961,.T.);
#29925=EDGE_CURVE('',#24244,#24244,#20371,.T.);
#29926=EDGE_CURVE('',#24245,#24245,#20372,.T.);
#29927=EDGE_CURVE('',#24245,#24246,#5962,.T.);
#29928=EDGE_CURVE('',#24246,#24246,#20373,.T.);
#29929=EDGE_CURVE('',#24247,#24247,#20374,.T.);
#29930=EDGE_CURVE('',#24247,#24248,#5963,.T.);
#29931=EDGE_CURVE('',#24248,#24248,#20375,.T.);
#29932=EDGE_CURVE('',#24249,#24249,#20376,.T.);
#29933=EDGE_CURVE('',#24249,#24250,#5964,.T.);
#29934=EDGE_CURVE('',#24250,#24250,#20377,.T.);
#29935=EDGE_CURVE('',#24251,#24251,#20378,.T.);
#29936=EDGE_CURVE('',#24251,#24252,#5965,.T.);
#29937=EDGE_CURVE('',#24252,#24252,#20379,.T.);
#29938=EDGE_CURVE('',#24253,#24253,#20380,.T.);
#29939=EDGE_CURVE('',#24253,#24254,#5966,.T.);
#29940=EDGE_CURVE('',#24254,#24254,#20381,.T.);
#29941=EDGE_CURVE('',#24255,#24255,#20382,.T.);
#29942=EDGE_CURVE('',#24255,#24256,#5967,.T.);
#29943=EDGE_CURVE('',#24256,#24256,#20383,.T.);
#29944=EDGE_CURVE('',#24257,#24257,#20384,.T.);
#29945=EDGE_CURVE('',#24257,#24258,#5968,.T.);
#29946=EDGE_CURVE('',#24258,#24258,#20385,.T.);
#29947=EDGE_CURVE('',#24259,#24259,#20386,.T.);
#29948=EDGE_CURVE('',#24259,#24260,#5969,.T.);
#29949=EDGE_CURVE('',#24260,#24260,#20387,.T.);
#29950=EDGE_CURVE('',#24261,#24261,#20388,.T.);
#29951=EDGE_CURVE('',#24261,#24262,#5970,.T.);
#29952=EDGE_CURVE('',#24262,#24262,#20389,.T.);
#29953=EDGE_CURVE('',#24263,#24263,#20390,.T.);
#29954=EDGE_CURVE('',#24263,#24264,#5971,.T.);
#29955=EDGE_CURVE('',#24264,#24264,#20391,.T.);
#29956=EDGE_CURVE('',#24265,#24265,#20392,.T.);
#29957=EDGE_CURVE('',#24265,#24266,#5972,.T.);
#29958=EDGE_CURVE('',#24266,#24266,#20393,.T.);
#29959=EDGE_CURVE('',#24267,#24267,#20394,.T.);
#29960=EDGE_CURVE('',#24267,#24268,#5973,.T.);
#29961=EDGE_CURVE('',#24268,#24268,#20395,.T.);
#29962=EDGE_CURVE('',#24269,#24269,#20396,.T.);
#29963=EDGE_CURVE('',#24269,#24270,#5974,.T.);
#29964=EDGE_CURVE('',#24270,#24270,#20397,.T.);
#29965=EDGE_CURVE('',#24271,#24271,#20398,.T.);
#29966=EDGE_CURVE('',#24271,#24272,#5975,.T.);
#29967=EDGE_CURVE('',#24272,#24272,#20399,.T.);
#29968=EDGE_CURVE('',#24273,#24273,#20400,.T.);
#29969=EDGE_CURVE('',#24273,#24274,#5976,.T.);
#29970=EDGE_CURVE('',#24274,#24274,#20401,.T.);
#29971=EDGE_CURVE('',#24275,#24275,#20402,.T.);
#29972=EDGE_CURVE('',#24275,#24276,#5977,.T.);
#29973=EDGE_CURVE('',#24276,#24276,#20403,.T.);
#29974=EDGE_CURVE('',#24277,#24277,#20404,.T.);
#29975=EDGE_CURVE('',#24277,#24278,#5978,.T.);
#29976=EDGE_CURVE('',#24278,#24278,#20405,.T.);
#29977=EDGE_CURVE('',#24279,#24279,#20406,.T.);
#29978=EDGE_CURVE('',#24279,#24280,#5979,.T.);
#29979=EDGE_CURVE('',#24280,#24280,#20407,.T.);
#29980=EDGE_CURVE('',#24281,#24281,#20408,.T.);
#29981=EDGE_CURVE('',#24281,#24282,#5980,.T.);
#29982=EDGE_CURVE('',#24282,#24282,#20409,.T.);
#29983=EDGE_CURVE('',#24283,#24283,#20410,.T.);
#29984=EDGE_CURVE('',#24283,#24284,#5981,.T.);
#29985=EDGE_CURVE('',#24284,#24284,#20411,.T.);
#29986=EDGE_CURVE('',#24285,#24285,#20412,.T.);
#29987=EDGE_CURVE('',#24285,#24286,#5982,.T.);
#29988=EDGE_CURVE('',#24286,#24286,#20413,.T.);
#29989=EDGE_CURVE('',#24287,#24287,#20414,.T.);
#29990=EDGE_CURVE('',#24287,#24288,#5983,.T.);
#29991=EDGE_CURVE('',#24288,#24288,#20415,.T.);
#29992=EDGE_CURVE('',#24289,#24289,#20416,.T.);
#29993=EDGE_CURVE('',#24289,#24290,#5984,.T.);
#29994=EDGE_CURVE('',#24290,#24290,#20417,.T.);
#29995=EDGE_CURVE('',#24291,#24291,#20418,.T.);
#29996=EDGE_CURVE('',#24291,#24292,#5985,.T.);
#29997=EDGE_CURVE('',#24292,#24292,#20419,.T.);
#29998=EDGE_CURVE('',#24293,#24293,#20420,.T.);
#29999=EDGE_CURVE('',#24293,#24294,#5986,.T.);
#30000=EDGE_CURVE('',#24294,#24294,#20421,.T.);
#30001=EDGE_CURVE('',#24295,#24295,#20422,.T.);
#30002=EDGE_CURVE('',#24295,#24296,#5987,.T.);
#30003=EDGE_CURVE('',#24296,#24296,#20423,.T.);
#30004=EDGE_CURVE('',#24297,#24297,#20424,.T.);
#30005=EDGE_CURVE('',#24297,#24298,#5988,.T.);
#30006=EDGE_CURVE('',#24298,#24298,#20425,.T.);
#30007=EDGE_CURVE('',#24299,#24299,#20426,.T.);
#30008=EDGE_CURVE('',#24299,#24300,#5989,.T.);
#30009=EDGE_CURVE('',#24300,#24300,#20427,.T.);
#30010=EDGE_CURVE('',#24301,#24301,#20428,.T.);
#30011=EDGE_CURVE('',#24301,#24302,#5990,.T.);
#30012=EDGE_CURVE('',#24302,#24302,#20429,.T.);
#30013=EDGE_CURVE('',#24303,#24303,#20430,.T.);
#30014=EDGE_CURVE('',#24303,#24304,#5991,.T.);
#30015=EDGE_CURVE('',#24304,#24304,#20431,.T.);
#30016=EDGE_CURVE('',#24305,#24305,#20432,.T.);
#30017=EDGE_CURVE('',#24305,#24306,#5992,.T.);
#30018=EDGE_CURVE('',#24306,#24306,#20433,.T.);
#30019=EDGE_CURVE('',#24307,#24307,#20434,.T.);
#30020=EDGE_CURVE('',#24307,#24308,#5993,.T.);
#30021=EDGE_CURVE('',#24308,#24308,#20435,.T.);
#30022=EDGE_CURVE('',#24309,#24309,#20436,.T.);
#30023=EDGE_CURVE('',#24309,#24310,#5994,.T.);
#30024=EDGE_CURVE('',#24310,#24310,#20437,.T.);
#30025=EDGE_CURVE('',#24311,#24311,#20438,.T.);
#30026=EDGE_CURVE('',#24311,#24312,#5995,.T.);
#30027=EDGE_CURVE('',#24312,#24312,#20439,.T.);
#30028=EDGE_CURVE('',#24313,#24313,#20440,.T.);
#30029=EDGE_CURVE('',#24313,#24314,#5996,.T.);
#30030=EDGE_CURVE('',#24314,#24314,#20441,.T.);
#30031=EDGE_CURVE('',#24315,#24315,#20442,.T.);
#30032=EDGE_CURVE('',#24315,#24316,#5997,.T.);
#30033=EDGE_CURVE('',#24316,#24316,#20443,.T.);
#30034=EDGE_CURVE('',#24317,#24317,#20444,.T.);
#30035=EDGE_CURVE('',#24317,#24318,#5998,.T.);
#30036=EDGE_CURVE('',#24318,#24318,#20445,.T.);
#30037=EDGE_CURVE('',#24319,#24319,#20446,.T.);
#30038=EDGE_CURVE('',#24319,#24320,#5999,.T.);
#30039=EDGE_CURVE('',#24320,#24320,#20447,.T.);
#30040=EDGE_CURVE('',#24321,#24321,#20448,.T.);
#30041=EDGE_CURVE('',#24321,#24322,#6000,.T.);
#30042=EDGE_CURVE('',#24322,#24322,#20449,.T.);
#30043=EDGE_CURVE('',#24323,#24323,#20450,.T.);
#30044=EDGE_CURVE('',#24323,#24324,#6001,.T.);
#30045=EDGE_CURVE('',#24324,#24324,#20451,.T.);
#30046=EDGE_CURVE('',#24325,#24325,#20452,.T.);
#30047=EDGE_CURVE('',#24325,#24326,#6002,.T.);
#30048=EDGE_CURVE('',#24326,#24326,#20453,.T.);
#30049=EDGE_CURVE('',#24327,#24327,#20454,.T.);
#30050=EDGE_CURVE('',#24327,#24328,#6003,.T.);
#30051=EDGE_CURVE('',#24328,#24328,#20455,.T.);
#30052=EDGE_CURVE('',#24329,#24329,#20456,.T.);
#30053=EDGE_CURVE('',#24329,#24330,#6004,.T.);
#30054=EDGE_CURVE('',#24330,#24330,#20457,.T.);
#30055=EDGE_CURVE('',#24331,#24331,#20458,.T.);
#30056=EDGE_CURVE('',#24331,#24332,#6005,.T.);
#30057=EDGE_CURVE('',#24332,#24332,#20459,.T.);
#30058=EDGE_CURVE('',#24333,#24333,#20460,.T.);
#30059=EDGE_CURVE('',#24333,#24334,#6006,.T.);
#30060=EDGE_CURVE('',#24334,#24334,#20461,.T.);
#30061=EDGE_CURVE('',#24335,#24335,#20462,.T.);
#30062=EDGE_CURVE('',#24335,#24336,#6007,.T.);
#30063=EDGE_CURVE('',#24336,#24336,#20463,.T.);
#30064=EDGE_CURVE('',#24337,#24337,#20464,.T.);
#30065=EDGE_CURVE('',#24337,#24338,#6008,.T.);
#30066=EDGE_CURVE('',#24338,#24338,#20465,.T.);
#30067=EDGE_CURVE('',#24339,#24339,#20466,.T.);
#30068=EDGE_CURVE('',#24339,#24340,#6009,.T.);
#30069=EDGE_CURVE('',#24340,#24340,#20467,.T.);
#30070=EDGE_CURVE('',#24341,#24341,#20468,.T.);
#30071=EDGE_CURVE('',#24341,#24342,#6010,.T.);
#30072=EDGE_CURVE('',#24342,#24342,#20469,.T.);
#30073=EDGE_CURVE('',#24343,#24343,#20470,.T.);
#30074=EDGE_CURVE('',#24343,#24344,#6011,.T.);
#30075=EDGE_CURVE('',#24344,#24344,#20471,.T.);
#30076=EDGE_CURVE('',#24345,#24345,#20472,.T.);
#30077=EDGE_CURVE('',#24345,#24346,#6012,.T.);
#30078=EDGE_CURVE('',#24346,#24346,#20473,.T.);
#30079=EDGE_CURVE('',#24347,#24347,#20474,.T.);
#30080=EDGE_CURVE('',#24347,#24348,#6013,.T.);
#30081=EDGE_CURVE('',#24348,#24348,#20475,.T.);
#30082=EDGE_CURVE('',#24349,#24349,#20476,.T.);
#30083=EDGE_CURVE('',#24349,#24350,#6014,.T.);
#30084=EDGE_CURVE('',#24350,#24350,#20477,.T.);
#30085=EDGE_CURVE('',#24351,#24351,#20478,.T.);
#30086=EDGE_CURVE('',#24351,#24352,#6015,.T.);
#30087=EDGE_CURVE('',#24352,#24352,#20479,.T.);
#30088=EDGE_CURVE('',#24353,#24353,#20480,.T.);
#30089=EDGE_CURVE('',#24353,#24354,#6016,.T.);
#30090=EDGE_CURVE('',#24354,#24354,#20481,.T.);
#30091=EDGE_CURVE('',#24355,#24355,#20482,.T.);
#30092=EDGE_CURVE('',#24355,#24356,#6017,.T.);
#30093=EDGE_CURVE('',#24356,#24356,#20483,.T.);
#30094=EDGE_CURVE('',#24357,#24357,#20484,.T.);
#30095=EDGE_CURVE('',#24357,#24358,#6018,.T.);
#30096=EDGE_CURVE('',#24358,#24358,#20485,.T.);
#30097=EDGE_CURVE('',#24359,#24359,#20486,.T.);
#30098=EDGE_CURVE('',#24359,#24360,#6019,.T.);
#30099=EDGE_CURVE('',#24360,#24360,#20487,.T.);
#30100=EDGE_CURVE('',#24361,#24361,#20488,.T.);
#30101=EDGE_CURVE('',#24361,#24362,#6020,.T.);
#30102=EDGE_CURVE('',#24362,#24362,#20489,.T.);
#30103=EDGE_CURVE('',#24363,#24363,#20490,.T.);
#30104=EDGE_CURVE('',#24363,#24364,#6021,.T.);
#30105=EDGE_CURVE('',#24364,#24364,#20491,.T.);
#30106=EDGE_CURVE('',#24365,#24365,#20492,.T.);
#30107=EDGE_CURVE('',#24365,#24366,#6022,.T.);
#30108=EDGE_CURVE('',#24366,#24366,#20493,.T.);
#30109=EDGE_CURVE('',#24367,#24367,#20494,.T.);
#30110=EDGE_CURVE('',#24367,#24368,#6023,.T.);
#30111=EDGE_CURVE('',#24368,#24368,#20495,.T.);
#30112=EDGE_CURVE('',#24369,#24369,#20496,.T.);
#30113=EDGE_CURVE('',#24369,#24370,#6024,.T.);
#30114=EDGE_CURVE('',#24370,#24370,#20497,.T.);
#30115=EDGE_CURVE('',#24371,#24371,#20498,.T.);
#30116=EDGE_CURVE('',#24371,#24372,#6025,.T.);
#30117=EDGE_CURVE('',#24372,#24372,#20499,.T.);
#30118=EDGE_CURVE('',#24373,#24373,#20500,.T.);
#30119=EDGE_CURVE('',#24373,#24374,#6026,.T.);
#30120=EDGE_CURVE('',#24374,#24374,#20501,.T.);
#30121=EDGE_CURVE('',#24375,#24375,#20502,.T.);
#30122=EDGE_CURVE('',#24375,#24376,#6027,.T.);
#30123=EDGE_CURVE('',#24376,#24376,#20503,.T.);
#30124=EDGE_CURVE('',#24377,#24377,#20504,.T.);
#30125=EDGE_CURVE('',#24377,#24378,#6028,.T.);
#30126=EDGE_CURVE('',#24378,#24378,#20505,.T.);
#30127=EDGE_CURVE('',#24379,#24379,#20506,.T.);
#30128=EDGE_CURVE('',#24379,#24380,#6029,.T.);
#30129=EDGE_CURVE('',#24380,#24380,#20507,.T.);
#30130=EDGE_CURVE('',#24381,#24381,#20508,.T.);
#30131=EDGE_CURVE('',#24381,#24382,#6030,.T.);
#30132=EDGE_CURVE('',#24382,#24382,#20509,.T.);
#30133=EDGE_CURVE('',#24383,#24383,#20510,.T.);
#30134=EDGE_CURVE('',#24383,#24384,#6031,.T.);
#30135=EDGE_CURVE('',#24384,#24384,#20511,.T.);
#30136=EDGE_CURVE('',#24385,#24385,#20512,.T.);
#30137=EDGE_CURVE('',#24385,#24386,#6032,.T.);
#30138=EDGE_CURVE('',#24386,#24386,#20513,.T.);
#30139=EDGE_CURVE('',#24387,#24387,#20514,.T.);
#30140=EDGE_CURVE('',#24387,#24388,#6033,.T.);
#30141=EDGE_CURVE('',#24388,#24388,#20515,.T.);
#30142=EDGE_CURVE('',#24389,#24389,#20516,.T.);
#30143=EDGE_CURVE('',#24389,#24390,#6034,.T.);
#30144=EDGE_CURVE('',#24390,#24390,#20517,.T.);
#30145=EDGE_CURVE('',#24391,#24391,#20518,.T.);
#30146=EDGE_CURVE('',#24391,#24392,#6035,.T.);
#30147=EDGE_CURVE('',#24392,#24392,#20519,.T.);
#30148=EDGE_CURVE('',#24393,#24393,#20520,.T.);
#30149=EDGE_CURVE('',#24393,#24394,#6036,.T.);
#30150=EDGE_CURVE('',#24394,#24394,#20521,.T.);
#30151=EDGE_CURVE('',#24395,#24395,#20522,.T.);
#30152=EDGE_CURVE('',#24395,#24396,#6037,.T.);
#30153=EDGE_CURVE('',#24396,#24396,#20523,.T.);
#30154=EDGE_CURVE('',#24397,#24397,#20524,.T.);
#30155=EDGE_CURVE('',#24397,#24398,#6038,.T.);
#30156=EDGE_CURVE('',#24398,#24398,#20525,.T.);
#30157=EDGE_CURVE('',#24399,#24399,#20526,.T.);
#30158=EDGE_CURVE('',#24399,#24400,#6039,.T.);
#30159=EDGE_CURVE('',#24400,#24400,#20527,.T.);
#30160=EDGE_CURVE('',#24401,#24401,#20528,.T.);
#30161=EDGE_CURVE('',#24401,#24402,#6040,.T.);
#30162=EDGE_CURVE('',#24402,#24402,#20529,.T.);
#30163=EDGE_CURVE('',#24403,#24403,#20530,.T.);
#30164=EDGE_CURVE('',#24403,#24404,#6041,.T.);
#30165=EDGE_CURVE('',#24404,#24404,#20531,.T.);
#30166=EDGE_CURVE('',#24405,#24405,#20532,.T.);
#30167=EDGE_CURVE('',#24405,#24406,#6042,.T.);
#30168=EDGE_CURVE('',#24406,#24406,#20533,.T.);
#30169=EDGE_CURVE('',#24407,#24407,#20534,.T.);
#30170=EDGE_CURVE('',#24407,#24408,#6043,.T.);
#30171=EDGE_CURVE('',#24408,#24408,#20535,.T.);
#30172=EDGE_CURVE('',#24409,#24409,#20536,.T.);
#30173=EDGE_CURVE('',#24409,#24410,#6044,.T.);
#30174=EDGE_CURVE('',#24410,#24410,#20537,.T.);
#30175=EDGE_CURVE('',#24411,#24411,#20538,.T.);
#30176=EDGE_CURVE('',#24411,#24412,#6045,.T.);
#30177=EDGE_CURVE('',#24412,#24412,#20539,.T.);
#30178=EDGE_CURVE('',#24413,#24413,#20540,.T.);
#30179=EDGE_CURVE('',#24413,#24414,#6046,.T.);
#30180=EDGE_CURVE('',#24414,#24414,#20541,.T.);
#30181=EDGE_CURVE('',#24415,#24415,#20542,.T.);
#30182=EDGE_CURVE('',#24415,#24416,#6047,.T.);
#30183=EDGE_CURVE('',#24416,#24416,#20543,.T.);
#30184=EDGE_CURVE('',#24417,#24417,#20544,.T.);
#30185=EDGE_CURVE('',#24417,#24418,#6048,.T.);
#30186=EDGE_CURVE('',#24418,#24418,#20545,.T.);
#30187=EDGE_CURVE('',#24419,#24419,#20546,.T.);
#30188=EDGE_CURVE('',#24419,#24420,#6049,.T.);
#30189=EDGE_CURVE('',#24420,#24420,#20547,.T.);
#30190=EDGE_CURVE('',#24421,#24421,#20548,.T.);
#30191=EDGE_CURVE('',#24421,#24422,#6050,.T.);
#30192=EDGE_CURVE('',#24422,#24422,#20549,.T.);
#30193=EDGE_CURVE('',#24423,#24423,#20550,.T.);
#30194=EDGE_CURVE('',#24423,#24424,#6051,.T.);
#30195=EDGE_CURVE('',#24424,#24424,#20551,.T.);
#30196=EDGE_CURVE('',#24425,#24425,#20552,.T.);
#30197=EDGE_CURVE('',#24425,#24426,#6052,.T.);
#30198=EDGE_CURVE('',#24426,#24426,#20553,.T.);
#30199=EDGE_CURVE('',#24427,#24427,#20554,.T.);
#30200=EDGE_CURVE('',#24427,#24428,#6053,.T.);
#30201=EDGE_CURVE('',#24428,#24428,#20555,.T.);
#30202=EDGE_CURVE('',#24429,#24429,#20556,.T.);
#30203=EDGE_CURVE('',#24429,#24430,#6054,.T.);
#30204=EDGE_CURVE('',#24430,#24430,#20557,.T.);
#30205=EDGE_CURVE('',#24431,#24431,#20558,.T.);
#30206=EDGE_CURVE('',#24431,#24432,#6055,.T.);
#30207=EDGE_CURVE('',#24432,#24432,#20559,.T.);
#30208=EDGE_CURVE('',#24433,#24433,#20560,.T.);
#30209=EDGE_CURVE('',#24433,#24434,#6056,.T.);
#30210=EDGE_CURVE('',#24434,#24434,#20561,.T.);
#30211=EDGE_CURVE('',#24435,#24435,#20562,.T.);
#30212=EDGE_CURVE('',#24435,#24436,#6057,.T.);
#30213=EDGE_CURVE('',#24436,#24436,#20563,.T.);
#30214=EDGE_CURVE('',#24437,#24437,#20564,.T.);
#30215=EDGE_CURVE('',#24437,#24438,#6058,.T.);
#30216=EDGE_CURVE('',#24438,#24438,#20565,.T.);
#30217=EDGE_CURVE('',#24439,#24439,#20566,.T.);
#30218=EDGE_CURVE('',#24439,#24440,#6059,.T.);
#30219=EDGE_CURVE('',#24440,#24440,#20567,.T.);
#30220=EDGE_CURVE('',#24441,#24441,#20568,.T.);
#30221=EDGE_CURVE('',#24441,#24442,#6060,.T.);
#30222=EDGE_CURVE('',#24442,#24442,#20569,.T.);
#30223=EDGE_CURVE('',#24443,#24443,#20570,.T.);
#30224=EDGE_CURVE('',#24443,#24444,#6061,.T.);
#30225=EDGE_CURVE('',#24444,#24444,#20571,.T.);
#30226=EDGE_CURVE('',#24445,#24445,#20572,.T.);
#30227=EDGE_CURVE('',#24445,#24446,#6062,.T.);
#30228=EDGE_CURVE('',#24446,#24446,#20573,.T.);
#30229=EDGE_CURVE('',#24447,#24447,#20574,.T.);
#30230=EDGE_CURVE('',#24447,#24448,#6063,.T.);
#30231=EDGE_CURVE('',#24448,#24448,#20575,.T.);
#30232=EDGE_CURVE('',#24449,#24449,#20576,.T.);
#30233=EDGE_CURVE('',#24449,#24450,#6064,.T.);
#30234=EDGE_CURVE('',#24450,#24450,#20577,.T.);
#30235=EDGE_CURVE('',#24451,#24451,#20578,.T.);
#30236=EDGE_CURVE('',#24451,#24452,#6065,.T.);
#30237=EDGE_CURVE('',#24452,#24452,#20579,.T.);
#30238=EDGE_CURVE('',#24453,#24453,#20580,.T.);
#30239=EDGE_CURVE('',#24453,#24454,#6066,.T.);
#30240=EDGE_CURVE('',#24454,#24454,#20581,.T.);
#30241=EDGE_CURVE('',#24455,#24455,#20582,.T.);
#30242=EDGE_CURVE('',#24455,#24456,#6067,.T.);
#30243=EDGE_CURVE('',#24456,#24456,#20583,.T.);
#30244=EDGE_CURVE('',#24457,#24457,#20584,.T.);
#30245=EDGE_CURVE('',#24457,#24458,#6068,.T.);
#30246=EDGE_CURVE('',#24458,#24458,#20585,.T.);
#30247=EDGE_CURVE('',#24459,#24459,#20586,.T.);
#30248=EDGE_CURVE('',#24459,#24460,#6069,.T.);
#30249=EDGE_CURVE('',#24460,#24460,#20587,.T.);
#30250=EDGE_CURVE('',#24461,#24461,#20588,.T.);
#30251=EDGE_CURVE('',#24461,#24462,#6070,.T.);
#30252=EDGE_CURVE('',#24462,#24462,#20589,.T.);
#30253=EDGE_CURVE('',#24463,#24463,#20590,.T.);
#30254=EDGE_CURVE('',#24463,#24464,#6071,.T.);
#30255=EDGE_CURVE('',#24464,#24464,#20591,.T.);
#30256=EDGE_CURVE('',#24465,#24465,#20592,.T.);
#30257=EDGE_CURVE('',#24465,#24466,#6072,.T.);
#30258=EDGE_CURVE('',#24466,#24466,#20593,.T.);
#30259=EDGE_CURVE('',#24467,#24467,#20594,.T.);
#30260=EDGE_CURVE('',#24467,#24468,#6073,.T.);
#30261=EDGE_CURVE('',#24468,#24468,#20595,.T.);
#30262=EDGE_CURVE('',#24469,#24469,#20596,.T.);
#30263=EDGE_CURVE('',#24469,#24470,#6074,.T.);
#30264=EDGE_CURVE('',#24470,#24470,#20597,.T.);
#30265=EDGE_CURVE('',#24471,#24471,#20598,.T.);
#30266=EDGE_CURVE('',#24471,#24472,#6075,.T.);
#30267=EDGE_CURVE('',#24472,#24472,#20599,.T.);
#30268=EDGE_CURVE('',#24473,#24473,#20600,.T.);
#30269=EDGE_CURVE('',#24473,#24474,#6076,.T.);
#30270=EDGE_CURVE('',#24474,#24474,#20601,.T.);
#30271=EDGE_CURVE('',#24475,#24475,#20602,.T.);
#30272=EDGE_CURVE('',#24475,#24476,#6077,.T.);
#30273=EDGE_CURVE('',#24476,#24476,#20603,.T.);
#30274=EDGE_CURVE('',#24477,#24477,#20604,.T.);
#30275=EDGE_CURVE('',#24477,#24478,#6078,.T.);
#30276=EDGE_CURVE('',#24478,#24478,#20605,.T.);
#30277=EDGE_CURVE('',#24479,#24479,#20606,.T.);
#30278=EDGE_CURVE('',#24479,#24480,#6079,.T.);
#30279=EDGE_CURVE('',#24480,#24480,#20607,.T.);
#30280=EDGE_CURVE('',#22736,#24481,#20608,.T.);
#30281=EDGE_CURVE('',#24481,#24481,#20609,.T.);
#30282=EDGE_CURVE('',#22737,#22736,#20610,.T.);
#30283=EDGE_CURVE('',#24481,#24482,#6080,.T.);
#30284=EDGE_CURVE('',#24482,#24482,#20611,.T.);
#30285=EDGE_CURVE('',#24483,#24483,#20612,.T.);
#30286=EDGE_CURVE('',#24483,#24484,#20613,.T.);
#30287=EDGE_CURVE('',#24485,#24484,#20614,.T.);
#30288=EDGE_CURVE('',#24484,#24485,#20615,.T.);
#30289=EDGE_CURVE('',#24486,#24486,#20616,.T.);
#30290=EDGE_CURVE('',#24486,#24487,#20617,.T.);
#30291=EDGE_CURVE('',#24487,#24487,#20618,.T.);
#30292=EDGE_CURVE('',#24487,#24485,#6081,.T.);
#30293=EDGE_CURVE('',#24488,#24488,#20619,.T.);
#30294=EDGE_CURVE('',#24489,#24489,#20620,.T.);
#30295=EDGE_CURVE('',#24489,#24490,#20621,.T.);
#30296=EDGE_CURVE('',#24490,#24490,#20622,.T.);
#30297=EDGE_CURVE('',#24491,#24491,#20623,.T.);
#30298=EDGE_CURVE('',#24491,#24492,#20624,.T.);
#30299=EDGE_CURVE('',#24492,#24492,#20625,.T.);
#30300=EDGE_CURVE('',#24482,#24493,#20626,.T.);
#30301=EDGE_CURVE('',#24493,#24493,#20627,.T.);
#30302=EDGE_CURVE('',#24494,#24494,#20628,.T.);
#30303=EDGE_CURVE('',#24494,#24489,#6082,.T.);
#30304=EDGE_CURVE('',#24495,#24496,#20629,.T.);
#30305=EDGE_CURVE('',#24496,#24495,#20630,.T.);
#30306=EDGE_CURVE('',#24496,#24497,#20631,.T.);
#30307=EDGE_CURVE('',#24497,#24497,#20632,.T.);
#30308=EDGE_CURVE('',#24495,#24491,#6083,.T.);
#30309=EDGE_CURVE('',#24498,#24499,#2905,.T.);
#30310=EDGE_CURVE('',#24499,#24500,#6084,.T.);
#30311=EDGE_CURVE('',#24500,#24500,#20633,.T.);
#30312=EDGE_CURVE('',#24499,#24498,#2906,.T.);
#30313=EDGE_CURVE('',#22771,#24501,#6085,.T.);
#30314=EDGE_CURVE('',#24501,#24501,#2907,.T.);
#30315=EDGE_CURVE('',#22735,#22734,#20634,.T.);
#30316=ORIENTED_EDGE('',*,*,#24502,.F.);
#30317=ORIENTED_EDGE('',*,*,#24503,.T.);
#30318=ORIENTED_EDGE('',*,*,#24504,.T.);
#30319=ORIENTED_EDGE('',*,*,#24505,.T.);
#30320=ORIENTED_EDGE('',*,*,#24503,.F.);
#30321=ORIENTED_EDGE('',*,*,#24506,.F.);
#30322=ORIENTED_EDGE('',*,*,#24507,.T.);
#30323=ORIENTED_EDGE('',*,*,#24508,.T.);
#30324=ORIENTED_EDGE('',*,*,#24507,.F.);
#30325=ORIENTED_EDGE('',*,*,#24509,.F.);
#30326=ORIENTED_EDGE('',*,*,#24510,.T.);
#30327=ORIENTED_EDGE('',*,*,#24511,.T.);
#30328=ORIENTED_EDGE('',*,*,#24502,.T.);
#30329=ORIENTED_EDGE('',*,*,#24511,.F.);
#30330=ORIENTED_EDGE('',*,*,#24504,.F.);
#30331=ORIENTED_EDGE('',*,*,#24505,.F.);
#30332=ORIENTED_EDGE('',*,*,#24512,.T.);
#30333=ORIENTED_EDGE('',*,*,#24509,.T.);
#30334=ORIENTED_EDGE('',*,*,#24506,.T.);
#30335=ORIENTED_EDGE('',*,*,#24512,.F.);
#30336=ORIENTED_EDGE('',*,*,#24508,.F.);
#30337=ORIENTED_EDGE('',*,*,#24513,.T.);
#30338=ORIENTED_EDGE('',*,*,#24514,.T.);
#30339=ORIENTED_EDGE('',*,*,#24513,.F.);
#30340=ORIENTED_EDGE('',*,*,#24510,.F.);
#30341=ORIENTED_EDGE('',*,*,#24514,.F.);
#30342=ORIENTED_EDGE('',*,*,#24515,.F.);
#30343=ORIENTED_EDGE('',*,*,#24516,.T.);
#30344=ORIENTED_EDGE('',*,*,#24517,.F.);
#30345=ORIENTED_EDGE('',*,*,#24518,.T.);
#30346=ORIENTED_EDGE('',*,*,#24518,.F.);
#30347=ORIENTED_EDGE('',*,*,#24519,.T.);
#30348=ORIENTED_EDGE('',*,*,#24520,.T.);
#30349=ORIENTED_EDGE('',*,*,#24521,.T.);
#30350=ORIENTED_EDGE('',*,*,#24516,.F.);
#30351=ORIENTED_EDGE('',*,*,#24522,.T.);
#30352=ORIENTED_EDGE('',*,*,#24520,.F.);
#30353=ORIENTED_EDGE('',*,*,#24523,.F.);
#30354=ORIENTED_EDGE('',*,*,#24519,.F.);
#30355=ORIENTED_EDGE('',*,*,#24517,.T.);
#30356=ORIENTED_EDGE('',*,*,#24523,.T.);
#30357=ORIENTED_EDGE('',*,*,#24522,.F.);
#30358=ORIENTED_EDGE('',*,*,#24515,.T.);
#30359=ORIENTED_EDGE('',*,*,#24521,.F.);
#30360=ORIENTED_EDGE('',*,*,#24524,.F.);
#30361=ORIENTED_EDGE('',*,*,#24525,.T.);
#30362=ORIENTED_EDGE('',*,*,#24526,.T.);
#30363=ORIENTED_EDGE('',*,*,#24527,.T.);
#30364=ORIENTED_EDGE('',*,*,#24526,.F.);
#30365=ORIENTED_EDGE('',*,*,#24528,.T.);
#30366=ORIENTED_EDGE('',*,*,#24529,.F.);
#30367=ORIENTED_EDGE('',*,*,#24530,.F.);
#30368=ORIENTED_EDGE('',*,*,#24524,.T.);
#30369=ORIENTED_EDGE('',*,*,#24531,.F.);
#30370=ORIENTED_EDGE('',*,*,#24527,.F.);
#30371=ORIENTED_EDGE('',*,*,#24529,.T.);
#30372=ORIENTED_EDGE('',*,*,#24532,.T.);
#30373=ORIENTED_EDGE('',*,*,#24531,.T.);
#30374=ORIENTED_EDGE('',*,*,#24525,.F.);
#30375=ORIENTED_EDGE('',*,*,#24530,.T.);
#30376=ORIENTED_EDGE('',*,*,#24532,.F.);
#30377=ORIENTED_EDGE('',*,*,#24528,.F.);
#30378=ORIENTED_EDGE('',*,*,#24533,.T.);
#30379=ORIENTED_EDGE('',*,*,#24534,.T.);
#30380=ORIENTED_EDGE('',*,*,#24535,.F.);
#30381=ORIENTED_EDGE('',*,*,#24534,.F.);
#30382=ORIENTED_EDGE('',*,*,#24536,.T.);
#30383=ORIENTED_EDGE('',*,*,#24537,.T.);
#30384=ORIENTED_EDGE('',*,*,#24538,.F.);
#30385=ORIENTED_EDGE('',*,*,#24537,.F.);
#30386=ORIENTED_EDGE('',*,*,#24539,.T.);
#30387=ORIENTED_EDGE('',*,*,#24540,.T.);
#30388=ORIENTED_EDGE('',*,*,#24541,.F.);
#30389=ORIENTED_EDGE('',*,*,#24540,.F.);
#30390=ORIENTED_EDGE('',*,*,#24542,.T.);
#30391=ORIENTED_EDGE('',*,*,#24543,.T.);
#30392=ORIENTED_EDGE('',*,*,#24544,.F.);
#30393=ORIENTED_EDGE('',*,*,#24543,.F.);
#30394=ORIENTED_EDGE('',*,*,#24545,.T.);
#30395=ORIENTED_EDGE('',*,*,#24546,.T.);
#30396=ORIENTED_EDGE('',*,*,#24547,.F.);
#30397=ORIENTED_EDGE('',*,*,#24546,.F.);
#30398=ORIENTED_EDGE('',*,*,#24548,.T.);
#30399=ORIENTED_EDGE('',*,*,#24549,.T.);
#30400=ORIENTED_EDGE('',*,*,#24550,.F.);
#30401=ORIENTED_EDGE('',*,*,#24549,.F.);
#30402=ORIENTED_EDGE('',*,*,#24551,.T.);
#30403=ORIENTED_EDGE('',*,*,#24552,.T.);
#30404=ORIENTED_EDGE('',*,*,#24553,.F.);
#30405=ORIENTED_EDGE('',*,*,#24552,.F.);
#30406=ORIENTED_EDGE('',*,*,#24554,.T.);
#30407=ORIENTED_EDGE('',*,*,#24555,.T.);
#30408=ORIENTED_EDGE('',*,*,#24556,.F.);
#30409=ORIENTED_EDGE('',*,*,#24555,.F.);
#30410=ORIENTED_EDGE('',*,*,#24557,.T.);
#30411=ORIENTED_EDGE('',*,*,#24558,.T.);
#30412=ORIENTED_EDGE('',*,*,#24559,.F.);
#30413=ORIENTED_EDGE('',*,*,#24558,.F.);
#30414=ORIENTED_EDGE('',*,*,#24560,.T.);
#30415=ORIENTED_EDGE('',*,*,#24561,.T.);
#30416=ORIENTED_EDGE('',*,*,#24562,.F.);
#30417=ORIENTED_EDGE('',*,*,#24561,.F.);
#30418=ORIENTED_EDGE('',*,*,#24563,.T.);
#30419=ORIENTED_EDGE('',*,*,#24564,.T.);
#30420=ORIENTED_EDGE('',*,*,#24565,.F.);
#30421=ORIENTED_EDGE('',*,*,#24564,.F.);
#30422=ORIENTED_EDGE('',*,*,#24566,.T.);
#30423=ORIENTED_EDGE('',*,*,#24567,.T.);
#30424=ORIENTED_EDGE('',*,*,#24568,.F.);
#30425=ORIENTED_EDGE('',*,*,#24567,.F.);
#30426=ORIENTED_EDGE('',*,*,#24569,.T.);
#30427=ORIENTED_EDGE('',*,*,#24570,.T.);
#30428=ORIENTED_EDGE('',*,*,#24571,.F.);
#30429=ORIENTED_EDGE('',*,*,#24570,.F.);
#30430=ORIENTED_EDGE('',*,*,#24572,.T.);
#30431=ORIENTED_EDGE('',*,*,#24573,.T.);
#30432=ORIENTED_EDGE('',*,*,#24574,.T.);
#30433=ORIENTED_EDGE('',*,*,#24575,.F.);
#30434=ORIENTED_EDGE('',*,*,#24574,.F.);
#30435=ORIENTED_EDGE('',*,*,#24576,.T.);
#30436=ORIENTED_EDGE('',*,*,#24577,.T.);
#30437=ORIENTED_EDGE('',*,*,#24578,.F.);
#30438=ORIENTED_EDGE('',*,*,#24577,.F.);
#30439=ORIENTED_EDGE('',*,*,#24579,.T.);
#30440=ORIENTED_EDGE('',*,*,#24580,.T.);
#30441=ORIENTED_EDGE('',*,*,#24581,.T.);
#30442=ORIENTED_EDGE('',*,*,#24582,.F.);
#30443=ORIENTED_EDGE('',*,*,#24581,.F.);
#30444=ORIENTED_EDGE('',*,*,#24583,.T.);
#30445=ORIENTED_EDGE('',*,*,#24584,.T.);
#30446=ORIENTED_EDGE('',*,*,#24585,.F.);
#30447=ORIENTED_EDGE('',*,*,#24584,.F.);
#30448=ORIENTED_EDGE('',*,*,#24586,.T.);
#30449=ORIENTED_EDGE('',*,*,#24587,.T.);
#30450=ORIENTED_EDGE('',*,*,#24588,.T.);
#30451=ORIENTED_EDGE('',*,*,#24589,.F.);
#30452=ORIENTED_EDGE('',*,*,#24588,.F.);
#30453=ORIENTED_EDGE('',*,*,#24590,.T.);
#30454=ORIENTED_EDGE('',*,*,#24591,.T.);
#30455=ORIENTED_EDGE('',*,*,#24592,.F.);
#30456=ORIENTED_EDGE('',*,*,#24591,.F.);
#30457=ORIENTED_EDGE('',*,*,#24593,.T.);
#30458=ORIENTED_EDGE('',*,*,#24594,.T.);
#30459=ORIENTED_EDGE('',*,*,#24595,.T.);
#30460=ORIENTED_EDGE('',*,*,#24596,.F.);
#30461=ORIENTED_EDGE('',*,*,#24595,.F.);
#30462=ORIENTED_EDGE('',*,*,#24597,.T.);
#30463=ORIENTED_EDGE('',*,*,#24598,.T.);
#30464=ORIENTED_EDGE('',*,*,#24599,.F.);
#30465=ORIENTED_EDGE('',*,*,#24598,.F.);
#30466=ORIENTED_EDGE('',*,*,#24600,.T.);
#30467=ORIENTED_EDGE('',*,*,#24601,.T.);
#30468=ORIENTED_EDGE('',*,*,#24602,.T.);
#30469=ORIENTED_EDGE('',*,*,#24603,.F.);
#30470=ORIENTED_EDGE('',*,*,#24602,.F.);
#30471=ORIENTED_EDGE('',*,*,#24604,.T.);
#30472=ORIENTED_EDGE('',*,*,#24605,.T.);
#30473=ORIENTED_EDGE('',*,*,#24606,.F.);
#30474=ORIENTED_EDGE('',*,*,#24605,.F.);
#30475=ORIENTED_EDGE('',*,*,#24607,.T.);
#30476=ORIENTED_EDGE('',*,*,#24608,.T.);
#30477=ORIENTED_EDGE('',*,*,#24609,.T.);
#30478=ORIENTED_EDGE('',*,*,#24610,.F.);
#30479=ORIENTED_EDGE('',*,*,#24609,.F.);
#30480=ORIENTED_EDGE('',*,*,#24611,.T.);
#30481=ORIENTED_EDGE('',*,*,#24612,.T.);
#30482=ORIENTED_EDGE('',*,*,#24613,.F.);
#30483=ORIENTED_EDGE('',*,*,#24612,.F.);
#30484=ORIENTED_EDGE('',*,*,#24614,.T.);
#30485=ORIENTED_EDGE('',*,*,#24615,.T.);
#30486=ORIENTED_EDGE('',*,*,#24616,.T.);
#30487=ORIENTED_EDGE('',*,*,#24617,.F.);
#30488=ORIENTED_EDGE('',*,*,#24616,.F.);
#30489=ORIENTED_EDGE('',*,*,#24618,.T.);
#30490=ORIENTED_EDGE('',*,*,#24619,.T.);
#30491=ORIENTED_EDGE('',*,*,#24620,.F.);
#30492=ORIENTED_EDGE('',*,*,#24619,.F.);
#30493=ORIENTED_EDGE('',*,*,#24621,.T.);
#30494=ORIENTED_EDGE('',*,*,#24622,.T.);
#30495=ORIENTED_EDGE('',*,*,#24623,.T.);
#30496=ORIENTED_EDGE('',*,*,#24624,.F.);
#30497=ORIENTED_EDGE('',*,*,#24623,.F.);
#30498=ORIENTED_EDGE('',*,*,#24625,.T.);
#30499=ORIENTED_EDGE('',*,*,#24626,.T.);
#30500=ORIENTED_EDGE('',*,*,#24627,.F.);
#30501=ORIENTED_EDGE('',*,*,#24626,.F.);
#30502=ORIENTED_EDGE('',*,*,#24628,.T.);
#30503=ORIENTED_EDGE('',*,*,#24629,.T.);
#30504=ORIENTED_EDGE('',*,*,#24630,.T.);
#30505=ORIENTED_EDGE('',*,*,#24631,.F.);
#30506=ORIENTED_EDGE('',*,*,#24630,.F.);
#30507=ORIENTED_EDGE('',*,*,#24632,.T.);
#30508=ORIENTED_EDGE('',*,*,#24633,.T.);
#30509=ORIENTED_EDGE('',*,*,#24634,.F.);
#30510=ORIENTED_EDGE('',*,*,#24633,.F.);
#30511=ORIENTED_EDGE('',*,*,#24635,.T.);
#30512=ORIENTED_EDGE('',*,*,#24636,.T.);
#30513=ORIENTED_EDGE('',*,*,#24637,.T.);
#30514=ORIENTED_EDGE('',*,*,#24638,.F.);
#30515=ORIENTED_EDGE('',*,*,#24637,.F.);
#30516=ORIENTED_EDGE('',*,*,#24639,.T.);
#30517=ORIENTED_EDGE('',*,*,#24640,.T.);
#30518=ORIENTED_EDGE('',*,*,#24641,.F.);
#30519=ORIENTED_EDGE('',*,*,#24640,.F.);
#30520=ORIENTED_EDGE('',*,*,#24642,.T.);
#30521=ORIENTED_EDGE('',*,*,#24643,.T.);
#30522=ORIENTED_EDGE('',*,*,#24644,.T.);
#30523=ORIENTED_EDGE('',*,*,#24645,.F.);
#30524=ORIENTED_EDGE('',*,*,#24644,.F.);
#30525=ORIENTED_EDGE('',*,*,#24646,.T.);
#30526=ORIENTED_EDGE('',*,*,#24647,.T.);
#30527=ORIENTED_EDGE('',*,*,#24648,.F.);
#30528=ORIENTED_EDGE('',*,*,#24647,.F.);
#30529=ORIENTED_EDGE('',*,*,#24649,.T.);
#30530=ORIENTED_EDGE('',*,*,#24650,.T.);
#30531=ORIENTED_EDGE('',*,*,#24651,.T.);
#30532=ORIENTED_EDGE('',*,*,#24652,.F.);
#30533=ORIENTED_EDGE('',*,*,#24651,.F.);
#30534=ORIENTED_EDGE('',*,*,#24653,.T.);
#30535=ORIENTED_EDGE('',*,*,#24654,.T.);
#30536=ORIENTED_EDGE('',*,*,#24655,.F.);
#30537=ORIENTED_EDGE('',*,*,#24654,.F.);
#30538=ORIENTED_EDGE('',*,*,#24656,.T.);
#30539=ORIENTED_EDGE('',*,*,#24657,.T.);
#30540=ORIENTED_EDGE('',*,*,#24658,.T.);
#30541=ORIENTED_EDGE('',*,*,#24659,.F.);
#30542=ORIENTED_EDGE('',*,*,#24658,.F.);
#30543=ORIENTED_EDGE('',*,*,#24660,.T.);
#30544=ORIENTED_EDGE('',*,*,#24661,.T.);
#30545=ORIENTED_EDGE('',*,*,#24662,.F.);
#30546=ORIENTED_EDGE('',*,*,#24661,.F.);
#30547=ORIENTED_EDGE('',*,*,#24663,.T.);
#30548=ORIENTED_EDGE('',*,*,#24664,.T.);
#30549=ORIENTED_EDGE('',*,*,#24665,.T.);
#30550=ORIENTED_EDGE('',*,*,#24666,.F.);
#30551=ORIENTED_EDGE('',*,*,#24665,.F.);
#30552=ORIENTED_EDGE('',*,*,#24667,.T.);
#30553=ORIENTED_EDGE('',*,*,#24668,.T.);
#30554=ORIENTED_EDGE('',*,*,#24669,.F.);
#30555=ORIENTED_EDGE('',*,*,#24668,.F.);
#30556=ORIENTED_EDGE('',*,*,#24670,.T.);
#30557=ORIENTED_EDGE('',*,*,#24671,.T.);
#30558=ORIENTED_EDGE('',*,*,#24672,.T.);
#30559=ORIENTED_EDGE('',*,*,#24673,.F.);
#30560=ORIENTED_EDGE('',*,*,#24672,.F.);
#30561=ORIENTED_EDGE('',*,*,#24674,.T.);
#30562=ORIENTED_EDGE('',*,*,#24675,.T.);
#30563=ORIENTED_EDGE('',*,*,#24676,.F.);
#30564=ORIENTED_EDGE('',*,*,#24675,.F.);
#30565=ORIENTED_EDGE('',*,*,#24677,.T.);
#30566=ORIENTED_EDGE('',*,*,#24678,.T.);
#30567=ORIENTED_EDGE('',*,*,#24679,.T.);
#30568=ORIENTED_EDGE('',*,*,#24680,.F.);
#30569=ORIENTED_EDGE('',*,*,#24679,.F.);
#30570=ORIENTED_EDGE('',*,*,#24681,.T.);
#30571=ORIENTED_EDGE('',*,*,#24682,.T.);
#30572=ORIENTED_EDGE('',*,*,#24683,.F.);
#30573=ORIENTED_EDGE('',*,*,#24682,.F.);
#30574=ORIENTED_EDGE('',*,*,#24684,.T.);
#30575=ORIENTED_EDGE('',*,*,#24685,.T.);
#30576=ORIENTED_EDGE('',*,*,#24686,.T.);
#30577=ORIENTED_EDGE('',*,*,#24687,.F.);
#30578=ORIENTED_EDGE('',*,*,#24686,.F.);
#30579=ORIENTED_EDGE('',*,*,#24688,.T.);
#30580=ORIENTED_EDGE('',*,*,#24689,.T.);
#30581=ORIENTED_EDGE('',*,*,#24690,.F.);
#30582=ORIENTED_EDGE('',*,*,#24689,.F.);
#30583=ORIENTED_EDGE('',*,*,#24691,.T.);
#30584=ORIENTED_EDGE('',*,*,#24692,.T.);
#30585=ORIENTED_EDGE('',*,*,#24693,.T.);
#30586=ORIENTED_EDGE('',*,*,#24694,.F.);
#30587=ORIENTED_EDGE('',*,*,#24693,.F.);
#30588=ORIENTED_EDGE('',*,*,#24695,.T.);
#30589=ORIENTED_EDGE('',*,*,#24696,.T.);
#30590=ORIENTED_EDGE('',*,*,#24697,.F.);
#30591=ORIENTED_EDGE('',*,*,#24696,.F.);
#30592=ORIENTED_EDGE('',*,*,#24698,.T.);
#30593=ORIENTED_EDGE('',*,*,#24699,.T.);
#30594=ORIENTED_EDGE('',*,*,#24700,.T.);
#30595=ORIENTED_EDGE('',*,*,#24701,.F.);
#30596=ORIENTED_EDGE('',*,*,#24700,.F.);
#30597=ORIENTED_EDGE('',*,*,#24702,.T.);
#30598=ORIENTED_EDGE('',*,*,#24703,.T.);
#30599=ORIENTED_EDGE('',*,*,#24704,.F.);
#30600=ORIENTED_EDGE('',*,*,#24703,.F.);
#30601=ORIENTED_EDGE('',*,*,#24705,.T.);
#30602=ORIENTED_EDGE('',*,*,#24706,.T.);
#30603=ORIENTED_EDGE('',*,*,#24707,.T.);
#30604=ORIENTED_EDGE('',*,*,#24708,.F.);
#30605=ORIENTED_EDGE('',*,*,#24707,.F.);
#30606=ORIENTED_EDGE('',*,*,#24709,.T.);
#30607=ORIENTED_EDGE('',*,*,#24710,.T.);
#30608=ORIENTED_EDGE('',*,*,#24711,.F.);
#30609=ORIENTED_EDGE('',*,*,#24710,.F.);
#30610=ORIENTED_EDGE('',*,*,#24712,.T.);
#30611=ORIENTED_EDGE('',*,*,#24713,.T.);
#30612=ORIENTED_EDGE('',*,*,#24714,.T.);
#30613=ORIENTED_EDGE('',*,*,#24715,.F.);
#30614=ORIENTED_EDGE('',*,*,#24714,.F.);
#30615=ORIENTED_EDGE('',*,*,#24716,.T.);
#30616=ORIENTED_EDGE('',*,*,#24717,.T.);
#30617=ORIENTED_EDGE('',*,*,#24718,.F.);
#30618=ORIENTED_EDGE('',*,*,#24717,.F.);
#30619=ORIENTED_EDGE('',*,*,#24719,.T.);
#30620=ORIENTED_EDGE('',*,*,#24720,.T.);
#30621=ORIENTED_EDGE('',*,*,#24721,.T.);
#30622=ORIENTED_EDGE('',*,*,#24722,.F.);
#30623=ORIENTED_EDGE('',*,*,#24721,.F.);
#30624=ORIENTED_EDGE('',*,*,#24723,.T.);
#30625=ORIENTED_EDGE('',*,*,#24724,.T.);
#30626=ORIENTED_EDGE('',*,*,#24725,.F.);
#30627=ORIENTED_EDGE('',*,*,#24724,.F.);
#30628=ORIENTED_EDGE('',*,*,#24726,.T.);
#30629=ORIENTED_EDGE('',*,*,#24727,.T.);
#30630=ORIENTED_EDGE('',*,*,#24728,.T.);
#30631=ORIENTED_EDGE('',*,*,#24729,.F.);
#30632=ORIENTED_EDGE('',*,*,#24728,.F.);
#30633=ORIENTED_EDGE('',*,*,#24730,.T.);
#30634=ORIENTED_EDGE('',*,*,#24731,.T.);
#30635=ORIENTED_EDGE('',*,*,#24732,.F.);
#30636=ORIENTED_EDGE('',*,*,#24731,.F.);
#30637=ORIENTED_EDGE('',*,*,#24733,.T.);
#30638=ORIENTED_EDGE('',*,*,#24734,.T.);
#30639=ORIENTED_EDGE('',*,*,#24735,.T.);
#30640=ORIENTED_EDGE('',*,*,#24736,.F.);
#30641=ORIENTED_EDGE('',*,*,#24735,.F.);
#30642=ORIENTED_EDGE('',*,*,#24737,.T.);
#30643=ORIENTED_EDGE('',*,*,#24738,.T.);
#30644=ORIENTED_EDGE('',*,*,#24739,.F.);
#30645=ORIENTED_EDGE('',*,*,#24738,.F.);
#30646=ORIENTED_EDGE('',*,*,#24740,.T.);
#30647=ORIENTED_EDGE('',*,*,#24741,.T.);
#30648=ORIENTED_EDGE('',*,*,#24742,.T.);
#30649=ORIENTED_EDGE('',*,*,#24743,.F.);
#30650=ORIENTED_EDGE('',*,*,#24742,.F.);
#30651=ORIENTED_EDGE('',*,*,#24744,.T.);
#30652=ORIENTED_EDGE('',*,*,#24745,.T.);
#30653=ORIENTED_EDGE('',*,*,#24746,.F.);
#30654=ORIENTED_EDGE('',*,*,#24745,.F.);
#30655=ORIENTED_EDGE('',*,*,#24747,.T.);
#30656=ORIENTED_EDGE('',*,*,#24748,.T.);
#30657=ORIENTED_EDGE('',*,*,#24749,.T.);
#30658=ORIENTED_EDGE('',*,*,#24750,.F.);
#30659=ORIENTED_EDGE('',*,*,#24749,.F.);
#30660=ORIENTED_EDGE('',*,*,#24751,.T.);
#30661=ORIENTED_EDGE('',*,*,#24752,.T.);
#30662=ORIENTED_EDGE('',*,*,#24753,.F.);
#30663=ORIENTED_EDGE('',*,*,#24752,.F.);
#30664=ORIENTED_EDGE('',*,*,#24754,.T.);
#30665=ORIENTED_EDGE('',*,*,#24755,.T.);
#30666=ORIENTED_EDGE('',*,*,#24756,.T.);
#30667=ORIENTED_EDGE('',*,*,#24757,.F.);
#30668=ORIENTED_EDGE('',*,*,#24756,.F.);
#30669=ORIENTED_EDGE('',*,*,#24758,.T.);
#30670=ORIENTED_EDGE('',*,*,#24759,.T.);
#30671=ORIENTED_EDGE('',*,*,#24760,.F.);
#30672=ORIENTED_EDGE('',*,*,#24759,.F.);
#30673=ORIENTED_EDGE('',*,*,#24761,.T.);
#30674=ORIENTED_EDGE('',*,*,#24762,.T.);
#30675=ORIENTED_EDGE('',*,*,#24763,.T.);
#30676=ORIENTED_EDGE('',*,*,#24764,.F.);
#30677=ORIENTED_EDGE('',*,*,#24763,.F.);
#30678=ORIENTED_EDGE('',*,*,#24765,.T.);
#30679=ORIENTED_EDGE('',*,*,#24766,.T.);
#30680=ORIENTED_EDGE('',*,*,#24767,.F.);
#30681=ORIENTED_EDGE('',*,*,#24766,.F.);
#30682=ORIENTED_EDGE('',*,*,#24768,.T.);
#30683=ORIENTED_EDGE('',*,*,#24769,.T.);
#30684=ORIENTED_EDGE('',*,*,#24770,.T.);
#30685=ORIENTED_EDGE('',*,*,#24771,.F.);
#30686=ORIENTED_EDGE('',*,*,#24770,.F.);
#30687=ORIENTED_EDGE('',*,*,#24772,.T.);
#30688=ORIENTED_EDGE('',*,*,#24773,.T.);
#30689=ORIENTED_EDGE('',*,*,#24774,.F.);
#30690=ORIENTED_EDGE('',*,*,#24773,.F.);
#30691=ORIENTED_EDGE('',*,*,#24775,.T.);
#30692=ORIENTED_EDGE('',*,*,#24776,.T.);
#30693=ORIENTED_EDGE('',*,*,#24777,.T.);
#30694=ORIENTED_EDGE('',*,*,#24778,.F.);
#30695=ORIENTED_EDGE('',*,*,#24777,.F.);
#30696=ORIENTED_EDGE('',*,*,#24779,.T.);
#30697=ORIENTED_EDGE('',*,*,#24780,.T.);
#30698=ORIENTED_EDGE('',*,*,#24781,.F.);
#30699=ORIENTED_EDGE('',*,*,#24780,.F.);
#30700=ORIENTED_EDGE('',*,*,#24782,.T.);
#30701=ORIENTED_EDGE('',*,*,#24783,.T.);
#30702=ORIENTED_EDGE('',*,*,#24784,.T.);
#30703=ORIENTED_EDGE('',*,*,#24785,.F.);
#30704=ORIENTED_EDGE('',*,*,#24784,.F.);
#30705=ORIENTED_EDGE('',*,*,#24786,.T.);
#30706=ORIENTED_EDGE('',*,*,#24787,.T.);
#30707=ORIENTED_EDGE('',*,*,#24788,.F.);
#30708=ORIENTED_EDGE('',*,*,#24787,.F.);
#30709=ORIENTED_EDGE('',*,*,#24789,.T.);
#30710=ORIENTED_EDGE('',*,*,#24790,.T.);
#30711=ORIENTED_EDGE('',*,*,#24791,.T.);
#30712=ORIENTED_EDGE('',*,*,#24792,.F.);
#30713=ORIENTED_EDGE('',*,*,#24791,.F.);
#30714=ORIENTED_EDGE('',*,*,#24793,.T.);
#30715=ORIENTED_EDGE('',*,*,#24794,.T.);
#30716=ORIENTED_EDGE('',*,*,#24795,.F.);
#30717=ORIENTED_EDGE('',*,*,#24794,.F.);
#30718=ORIENTED_EDGE('',*,*,#24796,.T.);
#30719=ORIENTED_EDGE('',*,*,#24797,.T.);
#30720=ORIENTED_EDGE('',*,*,#24798,.T.);
#30721=ORIENTED_EDGE('',*,*,#24799,.F.);
#30722=ORIENTED_EDGE('',*,*,#24798,.F.);
#30723=ORIENTED_EDGE('',*,*,#24800,.T.);
#30724=ORIENTED_EDGE('',*,*,#24801,.T.);
#30725=ORIENTED_EDGE('',*,*,#24802,.F.);
#30726=ORIENTED_EDGE('',*,*,#24801,.F.);
#30727=ORIENTED_EDGE('',*,*,#24803,.T.);
#30728=ORIENTED_EDGE('',*,*,#24804,.T.);
#30729=ORIENTED_EDGE('',*,*,#24805,.T.);
#30730=ORIENTED_EDGE('',*,*,#24806,.F.);
#30731=ORIENTED_EDGE('',*,*,#24805,.F.);
#30732=ORIENTED_EDGE('',*,*,#24807,.T.);
#30733=ORIENTED_EDGE('',*,*,#24808,.T.);
#30734=ORIENTED_EDGE('',*,*,#24809,.F.);
#30735=ORIENTED_EDGE('',*,*,#24808,.F.);
#30736=ORIENTED_EDGE('',*,*,#24810,.T.);
#30737=ORIENTED_EDGE('',*,*,#24811,.T.);
#30738=ORIENTED_EDGE('',*,*,#24812,.T.);
#30739=ORIENTED_EDGE('',*,*,#24813,.F.);
#30740=ORIENTED_EDGE('',*,*,#24812,.F.);
#30741=ORIENTED_EDGE('',*,*,#24814,.T.);
#30742=ORIENTED_EDGE('',*,*,#24815,.T.);
#30743=ORIENTED_EDGE('',*,*,#24816,.F.);
#30744=ORIENTED_EDGE('',*,*,#24815,.F.);
#30745=ORIENTED_EDGE('',*,*,#24817,.T.);
#30746=ORIENTED_EDGE('',*,*,#24818,.T.);
#30747=ORIENTED_EDGE('',*,*,#24819,.T.);
#30748=ORIENTED_EDGE('',*,*,#24820,.F.);
#30749=ORIENTED_EDGE('',*,*,#24819,.F.);
#30750=ORIENTED_EDGE('',*,*,#24821,.T.);
#30751=ORIENTED_EDGE('',*,*,#24822,.T.);
#30752=ORIENTED_EDGE('',*,*,#24823,.F.);
#30753=ORIENTED_EDGE('',*,*,#24822,.F.);
#30754=ORIENTED_EDGE('',*,*,#24824,.T.);
#30755=ORIENTED_EDGE('',*,*,#24825,.T.);
#30756=ORIENTED_EDGE('',*,*,#24826,.T.);
#30757=ORIENTED_EDGE('',*,*,#24827,.F.);
#30758=ORIENTED_EDGE('',*,*,#24826,.F.);
#30759=ORIENTED_EDGE('',*,*,#24828,.T.);
#30760=ORIENTED_EDGE('',*,*,#24829,.T.);
#30761=ORIENTED_EDGE('',*,*,#24830,.F.);
#30762=ORIENTED_EDGE('',*,*,#24829,.F.);
#30763=ORIENTED_EDGE('',*,*,#24831,.T.);
#30764=ORIENTED_EDGE('',*,*,#24832,.T.);
#30765=ORIENTED_EDGE('',*,*,#24833,.T.);
#30766=ORIENTED_EDGE('',*,*,#24834,.F.);
#30767=ORIENTED_EDGE('',*,*,#24833,.F.);
#30768=ORIENTED_EDGE('',*,*,#24835,.T.);
#30769=ORIENTED_EDGE('',*,*,#24836,.T.);
#30770=ORIENTED_EDGE('',*,*,#24837,.F.);
#30771=ORIENTED_EDGE('',*,*,#24836,.F.);
#30772=ORIENTED_EDGE('',*,*,#24838,.T.);
#30773=ORIENTED_EDGE('',*,*,#24839,.T.);
#30774=ORIENTED_EDGE('',*,*,#24840,.T.);
#30775=ORIENTED_EDGE('',*,*,#24841,.F.);
#30776=ORIENTED_EDGE('',*,*,#24840,.F.);
#30777=ORIENTED_EDGE('',*,*,#24842,.T.);
#30778=ORIENTED_EDGE('',*,*,#24843,.T.);
#30779=ORIENTED_EDGE('',*,*,#24844,.F.);
#30780=ORIENTED_EDGE('',*,*,#24843,.F.);
#30781=ORIENTED_EDGE('',*,*,#24845,.T.);
#30782=ORIENTED_EDGE('',*,*,#24846,.T.);
#30783=ORIENTED_EDGE('',*,*,#24847,.F.);
#30784=ORIENTED_EDGE('',*,*,#24846,.F.);
#30785=ORIENTED_EDGE('',*,*,#24848,.T.);
#30786=ORIENTED_EDGE('',*,*,#24849,.T.);
#30787=ORIENTED_EDGE('',*,*,#24850,.F.);
#30788=ORIENTED_EDGE('',*,*,#24849,.F.);
#30789=ORIENTED_EDGE('',*,*,#24851,.T.);
#30790=ORIENTED_EDGE('',*,*,#24852,.T.);
#30791=ORIENTED_EDGE('',*,*,#24853,.F.);
#30792=ORIENTED_EDGE('',*,*,#24852,.F.);
#30793=ORIENTED_EDGE('',*,*,#24854,.T.);
#30794=ORIENTED_EDGE('',*,*,#24855,.T.);
#30795=ORIENTED_EDGE('',*,*,#24856,.F.);
#30796=ORIENTED_EDGE('',*,*,#24855,.F.);
#30797=ORIENTED_EDGE('',*,*,#24857,.T.);
#30798=ORIENTED_EDGE('',*,*,#24858,.T.);
#30799=ORIENTED_EDGE('',*,*,#24859,.T.);
#30800=ORIENTED_EDGE('',*,*,#24860,.F.);
#30801=ORIENTED_EDGE('',*,*,#24859,.F.);
#30802=ORIENTED_EDGE('',*,*,#24861,.T.);
#30803=ORIENTED_EDGE('',*,*,#24862,.T.);
#30804=ORIENTED_EDGE('',*,*,#24863,.F.);
#30805=ORIENTED_EDGE('',*,*,#24862,.F.);
#30806=ORIENTED_EDGE('',*,*,#24864,.T.);
#30807=ORIENTED_EDGE('',*,*,#24865,.T.);
#30808=ORIENTED_EDGE('',*,*,#24866,.T.);
#30809=ORIENTED_EDGE('',*,*,#24867,.F.);
#30810=ORIENTED_EDGE('',*,*,#24866,.F.);
#30811=ORIENTED_EDGE('',*,*,#24868,.T.);
#30812=ORIENTED_EDGE('',*,*,#24869,.T.);
#30813=ORIENTED_EDGE('',*,*,#24870,.F.);
#30814=ORIENTED_EDGE('',*,*,#24869,.F.);
#30815=ORIENTED_EDGE('',*,*,#24871,.T.);
#30816=ORIENTED_EDGE('',*,*,#24872,.T.);
#30817=ORIENTED_EDGE('',*,*,#24873,.F.);
#30818=ORIENTED_EDGE('',*,*,#24872,.F.);
#30819=ORIENTED_EDGE('',*,*,#24874,.T.);
#30820=ORIENTED_EDGE('',*,*,#24875,.T.);
#30821=ORIENTED_EDGE('',*,*,#24876,.F.);
#30822=ORIENTED_EDGE('',*,*,#24875,.F.);
#30823=ORIENTED_EDGE('',*,*,#24877,.T.);
#30824=ORIENTED_EDGE('',*,*,#24878,.T.);
#30825=ORIENTED_EDGE('',*,*,#24879,.F.);
#30826=ORIENTED_EDGE('',*,*,#24878,.F.);
#30827=ORIENTED_EDGE('',*,*,#24880,.T.);
#30828=ORIENTED_EDGE('',*,*,#24881,.T.);
#30829=ORIENTED_EDGE('',*,*,#24882,.F.);
#30830=ORIENTED_EDGE('',*,*,#24881,.F.);
#30831=ORIENTED_EDGE('',*,*,#24883,.T.);
#30832=ORIENTED_EDGE('',*,*,#24884,.T.);
#30833=ORIENTED_EDGE('',*,*,#24885,.T.);
#30834=ORIENTED_EDGE('',*,*,#24886,.F.);
#30835=ORIENTED_EDGE('',*,*,#24885,.F.);
#30836=ORIENTED_EDGE('',*,*,#24887,.T.);
#30837=ORIENTED_EDGE('',*,*,#24888,.T.);
#30838=ORIENTED_EDGE('',*,*,#24889,.F.);
#30839=ORIENTED_EDGE('',*,*,#24888,.F.);
#30840=ORIENTED_EDGE('',*,*,#24890,.T.);
#30841=ORIENTED_EDGE('',*,*,#24891,.T.);
#30842=ORIENTED_EDGE('',*,*,#24892,.T.);
#30843=ORIENTED_EDGE('',*,*,#24893,.F.);
#30844=ORIENTED_EDGE('',*,*,#24892,.F.);
#30845=ORIENTED_EDGE('',*,*,#24894,.T.);
#30846=ORIENTED_EDGE('',*,*,#24895,.T.);
#30847=ORIENTED_EDGE('',*,*,#24896,.F.);
#30848=ORIENTED_EDGE('',*,*,#24895,.F.);
#30849=ORIENTED_EDGE('',*,*,#24897,.T.);
#30850=ORIENTED_EDGE('',*,*,#24898,.T.);
#30851=ORIENTED_EDGE('',*,*,#24899,.F.);
#30852=ORIENTED_EDGE('',*,*,#24898,.F.);
#30853=ORIENTED_EDGE('',*,*,#24900,.T.);
#30854=ORIENTED_EDGE('',*,*,#24901,.T.);
#30855=ORIENTED_EDGE('',*,*,#24902,.F.);
#30856=ORIENTED_EDGE('',*,*,#24901,.F.);
#30857=ORIENTED_EDGE('',*,*,#24903,.T.);
#30858=ORIENTED_EDGE('',*,*,#24904,.T.);
#30859=ORIENTED_EDGE('',*,*,#24905,.T.);
#30860=ORIENTED_EDGE('',*,*,#24906,.F.);
#30861=ORIENTED_EDGE('',*,*,#24905,.F.);
#30862=ORIENTED_EDGE('',*,*,#24907,.T.);
#30863=ORIENTED_EDGE('',*,*,#24908,.T.);
#30864=ORIENTED_EDGE('',*,*,#24909,.F.);
#30865=ORIENTED_EDGE('',*,*,#24908,.F.);
#30866=ORIENTED_EDGE('',*,*,#24910,.T.);
#30867=ORIENTED_EDGE('',*,*,#24911,.T.);
#30868=ORIENTED_EDGE('',*,*,#24912,.T.);
#30869=ORIENTED_EDGE('',*,*,#24913,.F.);
#30870=ORIENTED_EDGE('',*,*,#24912,.F.);
#30871=ORIENTED_EDGE('',*,*,#24914,.T.);
#30872=ORIENTED_EDGE('',*,*,#24915,.T.);
#30873=ORIENTED_EDGE('',*,*,#24916,.F.);
#30874=ORIENTED_EDGE('',*,*,#24915,.F.);
#30875=ORIENTED_EDGE('',*,*,#24917,.T.);
#30876=ORIENTED_EDGE('',*,*,#24918,.T.);
#30877=ORIENTED_EDGE('',*,*,#24919,.F.);
#30878=ORIENTED_EDGE('',*,*,#24918,.F.);
#30879=ORIENTED_EDGE('',*,*,#24920,.T.);
#30880=ORIENTED_EDGE('',*,*,#24921,.T.);
#30881=ORIENTED_EDGE('',*,*,#24922,.F.);
#30882=ORIENTED_EDGE('',*,*,#24921,.F.);
#30883=ORIENTED_EDGE('',*,*,#24923,.T.);
#30884=ORIENTED_EDGE('',*,*,#24924,.T.);
#30885=ORIENTED_EDGE('',*,*,#24925,.T.);
#30886=ORIENTED_EDGE('',*,*,#24926,.F.);
#30887=ORIENTED_EDGE('',*,*,#24925,.F.);
#30888=ORIENTED_EDGE('',*,*,#24927,.T.);
#30889=ORIENTED_EDGE('',*,*,#24928,.T.);
#30890=ORIENTED_EDGE('',*,*,#24929,.F.);
#30891=ORIENTED_EDGE('',*,*,#24928,.F.);
#30892=ORIENTED_EDGE('',*,*,#24930,.T.);
#30893=ORIENTED_EDGE('',*,*,#24931,.T.);
#30894=ORIENTED_EDGE('',*,*,#24932,.T.);
#30895=ORIENTED_EDGE('',*,*,#24933,.F.);
#30896=ORIENTED_EDGE('',*,*,#24932,.F.);
#30897=ORIENTED_EDGE('',*,*,#24934,.T.);
#30898=ORIENTED_EDGE('',*,*,#24935,.T.);
#30899=ORIENTED_EDGE('',*,*,#24936,.F.);
#30900=ORIENTED_EDGE('',*,*,#24935,.F.);
#30901=ORIENTED_EDGE('',*,*,#24937,.T.);
#30902=ORIENTED_EDGE('',*,*,#24938,.T.);
#30903=ORIENTED_EDGE('',*,*,#24939,.T.);
#30904=ORIENTED_EDGE('',*,*,#24940,.F.);
#30905=ORIENTED_EDGE('',*,*,#24939,.F.);
#30906=ORIENTED_EDGE('',*,*,#24941,.T.);
#30907=ORIENTED_EDGE('',*,*,#24942,.T.);
#30908=ORIENTED_EDGE('',*,*,#24943,.F.);
#30909=ORIENTED_EDGE('',*,*,#24942,.F.);
#30910=ORIENTED_EDGE('',*,*,#24944,.T.);
#30911=ORIENTED_EDGE('',*,*,#24945,.T.);
#30912=ORIENTED_EDGE('',*,*,#24946,.T.);
#30913=ORIENTED_EDGE('',*,*,#24947,.F.);
#30914=ORIENTED_EDGE('',*,*,#24946,.F.);
#30915=ORIENTED_EDGE('',*,*,#24948,.T.);
#30916=ORIENTED_EDGE('',*,*,#24949,.T.);
#30917=ORIENTED_EDGE('',*,*,#24950,.F.);
#30918=ORIENTED_EDGE('',*,*,#24949,.F.);
#30919=ORIENTED_EDGE('',*,*,#24951,.T.);
#30920=ORIENTED_EDGE('',*,*,#24952,.T.);
#30921=ORIENTED_EDGE('',*,*,#24953,.T.);
#30922=ORIENTED_EDGE('',*,*,#24954,.F.);
#30923=ORIENTED_EDGE('',*,*,#24953,.F.);
#30924=ORIENTED_EDGE('',*,*,#24955,.T.);
#30925=ORIENTED_EDGE('',*,*,#24956,.T.);
#30926=ORIENTED_EDGE('',*,*,#24957,.F.);
#30927=ORIENTED_EDGE('',*,*,#24956,.F.);
#30928=ORIENTED_EDGE('',*,*,#24958,.T.);
#30929=ORIENTED_EDGE('',*,*,#24959,.T.);
#30930=ORIENTED_EDGE('',*,*,#24960,.T.);
#30931=ORIENTED_EDGE('',*,*,#24961,.F.);
#30932=ORIENTED_EDGE('',*,*,#24960,.F.);
#30933=ORIENTED_EDGE('',*,*,#24962,.T.);
#30934=ORIENTED_EDGE('',*,*,#24963,.T.);
#30935=ORIENTED_EDGE('',*,*,#24964,.F.);
#30936=ORIENTED_EDGE('',*,*,#24963,.F.);
#30937=ORIENTED_EDGE('',*,*,#24965,.T.);
#30938=ORIENTED_EDGE('',*,*,#24966,.T.);
#30939=ORIENTED_EDGE('',*,*,#24967,.T.);
#30940=ORIENTED_EDGE('',*,*,#24968,.F.);
#30941=ORIENTED_EDGE('',*,*,#24967,.F.);
#30942=ORIENTED_EDGE('',*,*,#24969,.T.);
#30943=ORIENTED_EDGE('',*,*,#24970,.T.);
#30944=ORIENTED_EDGE('',*,*,#24971,.F.);
#30945=ORIENTED_EDGE('',*,*,#24970,.F.);
#30946=ORIENTED_EDGE('',*,*,#24972,.T.);
#30947=ORIENTED_EDGE('',*,*,#24973,.T.);
#30948=ORIENTED_EDGE('',*,*,#24974,.T.);
#30949=ORIENTED_EDGE('',*,*,#24975,.F.);
#30950=ORIENTED_EDGE('',*,*,#24974,.F.);
#30951=ORIENTED_EDGE('',*,*,#24976,.T.);
#30952=ORIENTED_EDGE('',*,*,#24977,.T.);
#30953=ORIENTED_EDGE('',*,*,#24978,.F.);
#30954=ORIENTED_EDGE('',*,*,#24977,.F.);
#30955=ORIENTED_EDGE('',*,*,#24979,.T.);
#30956=ORIENTED_EDGE('',*,*,#24980,.T.);
#30957=ORIENTED_EDGE('',*,*,#24981,.T.);
#30958=ORIENTED_EDGE('',*,*,#24982,.F.);
#30959=ORIENTED_EDGE('',*,*,#24981,.F.);
#30960=ORIENTED_EDGE('',*,*,#24983,.T.);
#30961=ORIENTED_EDGE('',*,*,#24984,.T.);
#30962=ORIENTED_EDGE('',*,*,#24985,.F.);
#30963=ORIENTED_EDGE('',*,*,#24984,.F.);
#30964=ORIENTED_EDGE('',*,*,#24986,.T.);
#30965=ORIENTED_EDGE('',*,*,#24987,.T.);
#30966=ORIENTED_EDGE('',*,*,#24988,.T.);
#30967=ORIENTED_EDGE('',*,*,#24989,.F.);
#30968=ORIENTED_EDGE('',*,*,#24988,.F.);
#30969=ORIENTED_EDGE('',*,*,#24990,.T.);
#30970=ORIENTED_EDGE('',*,*,#24991,.T.);
#30971=ORIENTED_EDGE('',*,*,#24992,.F.);
#30972=ORIENTED_EDGE('',*,*,#24991,.F.);
#30973=ORIENTED_EDGE('',*,*,#24993,.T.);
#30974=ORIENTED_EDGE('',*,*,#24994,.T.);
#30975=ORIENTED_EDGE('',*,*,#24995,.T.);
#30976=ORIENTED_EDGE('',*,*,#24996,.F.);
#30977=ORIENTED_EDGE('',*,*,#24995,.F.);
#30978=ORIENTED_EDGE('',*,*,#24997,.T.);
#30979=ORIENTED_EDGE('',*,*,#24998,.T.);
#30980=ORIENTED_EDGE('',*,*,#24999,.F.);
#30981=ORIENTED_EDGE('',*,*,#24998,.F.);
#30982=ORIENTED_EDGE('',*,*,#25000,.T.);
#30983=ORIENTED_EDGE('',*,*,#25001,.T.);
#30984=ORIENTED_EDGE('',*,*,#25002,.T.);
#30985=ORIENTED_EDGE('',*,*,#25003,.F.);
#30986=ORIENTED_EDGE('',*,*,#25002,.F.);
#30987=ORIENTED_EDGE('',*,*,#25004,.T.);
#30988=ORIENTED_EDGE('',*,*,#25005,.T.);
#30989=ORIENTED_EDGE('',*,*,#25006,.F.);
#30990=ORIENTED_EDGE('',*,*,#25005,.F.);
#30991=ORIENTED_EDGE('',*,*,#25007,.T.);
#30992=ORIENTED_EDGE('',*,*,#25008,.T.);
#30993=ORIENTED_EDGE('',*,*,#25009,.T.);
#30994=ORIENTED_EDGE('',*,*,#25010,.F.);
#30995=ORIENTED_EDGE('',*,*,#25009,.F.);
#30996=ORIENTED_EDGE('',*,*,#25011,.T.);
#30997=ORIENTED_EDGE('',*,*,#25012,.T.);
#30998=ORIENTED_EDGE('',*,*,#25013,.F.);
#30999=ORIENTED_EDGE('',*,*,#25012,.F.);
#31000=ORIENTED_EDGE('',*,*,#25014,.T.);
#31001=ORIENTED_EDGE('',*,*,#25015,.T.);
#31002=ORIENTED_EDGE('',*,*,#25016,.T.);
#31003=ORIENTED_EDGE('',*,*,#25017,.F.);
#31004=ORIENTED_EDGE('',*,*,#25016,.F.);
#31005=ORIENTED_EDGE('',*,*,#25018,.T.);
#31006=ORIENTED_EDGE('',*,*,#25019,.T.);
#31007=ORIENTED_EDGE('',*,*,#25020,.F.);
#31008=ORIENTED_EDGE('',*,*,#25019,.F.);
#31009=ORIENTED_EDGE('',*,*,#25021,.T.);
#31010=ORIENTED_EDGE('',*,*,#25022,.T.);
#31011=ORIENTED_EDGE('',*,*,#25023,.F.);
#31012=ORIENTED_EDGE('',*,*,#25022,.F.);
#31013=ORIENTED_EDGE('',*,*,#25024,.T.);
#31014=ORIENTED_EDGE('',*,*,#25025,.T.);
#31015=ORIENTED_EDGE('',*,*,#25026,.F.);
#31016=ORIENTED_EDGE('',*,*,#25025,.F.);
#31017=ORIENTED_EDGE('',*,*,#25027,.T.);
#31018=ORIENTED_EDGE('',*,*,#25028,.T.);
#31019=ORIENTED_EDGE('',*,*,#25029,.F.);
#31020=ORIENTED_EDGE('',*,*,#25028,.F.);
#31021=ORIENTED_EDGE('',*,*,#25030,.T.);
#31022=ORIENTED_EDGE('',*,*,#25031,.T.);
#31023=ORIENTED_EDGE('',*,*,#25032,.F.);
#31024=ORIENTED_EDGE('',*,*,#25031,.F.);
#31025=ORIENTED_EDGE('',*,*,#25033,.T.);
#31026=ORIENTED_EDGE('',*,*,#25034,.T.);
#31027=ORIENTED_EDGE('',*,*,#25035,.F.);
#31028=ORIENTED_EDGE('',*,*,#25034,.F.);
#31029=ORIENTED_EDGE('',*,*,#25036,.T.);
#31030=ORIENTED_EDGE('',*,*,#25037,.T.);
#31031=ORIENTED_EDGE('',*,*,#25038,.F.);
#31032=ORIENTED_EDGE('',*,*,#25037,.F.);
#31033=ORIENTED_EDGE('',*,*,#25039,.T.);
#31034=ORIENTED_EDGE('',*,*,#25040,.T.);
#31035=ORIENTED_EDGE('',*,*,#25041,.F.);
#31036=ORIENTED_EDGE('',*,*,#25040,.F.);
#31037=ORIENTED_EDGE('',*,*,#25042,.T.);
#31038=ORIENTED_EDGE('',*,*,#25043,.T.);
#31039=ORIENTED_EDGE('',*,*,#25044,.F.);
#31040=ORIENTED_EDGE('',*,*,#25043,.F.);
#31041=ORIENTED_EDGE('',*,*,#25045,.T.);
#31042=ORIENTED_EDGE('',*,*,#25046,.T.);
#31043=ORIENTED_EDGE('',*,*,#25047,.F.);
#31044=ORIENTED_EDGE('',*,*,#25046,.F.);
#31045=ORIENTED_EDGE('',*,*,#25048,.T.);
#31046=ORIENTED_EDGE('',*,*,#25049,.T.);
#31047=ORIENTED_EDGE('',*,*,#25050,.F.);
#31048=ORIENTED_EDGE('',*,*,#25049,.F.);
#31049=ORIENTED_EDGE('',*,*,#25051,.T.);
#31050=ORIENTED_EDGE('',*,*,#25052,.T.);
#31051=ORIENTED_EDGE('',*,*,#25053,.F.);
#31052=ORIENTED_EDGE('',*,*,#25052,.F.);
#31053=ORIENTED_EDGE('',*,*,#25054,.T.);
#31054=ORIENTED_EDGE('',*,*,#25055,.T.);
#31055=ORIENTED_EDGE('',*,*,#25056,.F.);
#31056=ORIENTED_EDGE('',*,*,#25055,.F.);
#31057=ORIENTED_EDGE('',*,*,#25057,.T.);
#31058=ORIENTED_EDGE('',*,*,#25058,.T.);
#31059=ORIENTED_EDGE('',*,*,#25059,.F.);
#31060=ORIENTED_EDGE('',*,*,#25058,.F.);
#31061=ORIENTED_EDGE('',*,*,#25060,.T.);
#31062=ORIENTED_EDGE('',*,*,#25061,.T.);
#31063=ORIENTED_EDGE('',*,*,#25062,.F.);
#31064=ORIENTED_EDGE('',*,*,#25061,.F.);
#31065=ORIENTED_EDGE('',*,*,#25063,.T.);
#31066=ORIENTED_EDGE('',*,*,#25064,.T.);
#31067=ORIENTED_EDGE('',*,*,#25065,.F.);
#31068=ORIENTED_EDGE('',*,*,#25064,.F.);
#31069=ORIENTED_EDGE('',*,*,#25066,.T.);
#31070=ORIENTED_EDGE('',*,*,#25067,.T.);
#31071=ORIENTED_EDGE('',*,*,#25068,.F.);
#31072=ORIENTED_EDGE('',*,*,#25069,.T.);
#31073=ORIENTED_EDGE('',*,*,#25070,.F.);
#31074=ORIENTED_EDGE('',*,*,#25067,.F.);
#31075=ORIENTED_EDGE('',*,*,#25071,.T.);
#31076=ORIENTED_EDGE('',*,*,#25072,.T.);
#31077=ORIENTED_EDGE('',*,*,#25073,.F.);
#31078=ORIENTED_EDGE('',*,*,#25072,.F.);
#31079=ORIENTED_EDGE('',*,*,#25074,.T.);
#31080=ORIENTED_EDGE('',*,*,#25075,.T.);
#31081=ORIENTED_EDGE('',*,*,#25076,.F.);
#31082=ORIENTED_EDGE('',*,*,#25075,.F.);
#31083=ORIENTED_EDGE('',*,*,#25077,.T.);
#31084=ORIENTED_EDGE('',*,*,#25078,.T.);
#31085=ORIENTED_EDGE('',*,*,#25079,.F.);
#31086=ORIENTED_EDGE('',*,*,#25078,.F.);
#31087=ORIENTED_EDGE('',*,*,#25080,.T.);
#31088=ORIENTED_EDGE('',*,*,#25081,.T.);
#31089=ORIENTED_EDGE('',*,*,#25082,.F.);
#31090=ORIENTED_EDGE('',*,*,#25081,.F.);
#31091=ORIENTED_EDGE('',*,*,#25083,.T.);
#31092=ORIENTED_EDGE('',*,*,#25084,.T.);
#31093=ORIENTED_EDGE('',*,*,#25085,.F.);
#31094=ORIENTED_EDGE('',*,*,#25084,.F.);
#31095=ORIENTED_EDGE('',*,*,#25086,.T.);
#31096=ORIENTED_EDGE('',*,*,#25087,.T.);
#31097=ORIENTED_EDGE('',*,*,#25088,.F.);
#31098=ORIENTED_EDGE('',*,*,#25087,.F.);
#31099=ORIENTED_EDGE('',*,*,#25089,.T.);
#31100=ORIENTED_EDGE('',*,*,#25090,.T.);
#31101=ORIENTED_EDGE('',*,*,#25091,.F.);
#31102=ORIENTED_EDGE('',*,*,#25090,.F.);
#31103=ORIENTED_EDGE('',*,*,#25092,.T.);
#31104=ORIENTED_EDGE('',*,*,#25093,.T.);
#31105=ORIENTED_EDGE('',*,*,#25094,.F.);
#31106=ORIENTED_EDGE('',*,*,#25093,.F.);
#31107=ORIENTED_EDGE('',*,*,#25095,.T.);
#31108=ORIENTED_EDGE('',*,*,#25096,.T.);
#31109=ORIENTED_EDGE('',*,*,#25097,.F.);
#31110=ORIENTED_EDGE('',*,*,#25096,.F.);
#31111=ORIENTED_EDGE('',*,*,#25098,.T.);
#31112=ORIENTED_EDGE('',*,*,#25099,.T.);
#31113=ORIENTED_EDGE('',*,*,#25100,.F.);
#31114=ORIENTED_EDGE('',*,*,#25099,.F.);
#31115=ORIENTED_EDGE('',*,*,#25101,.T.);
#31116=ORIENTED_EDGE('',*,*,#25102,.T.);
#31117=ORIENTED_EDGE('',*,*,#25103,.F.);
#31118=ORIENTED_EDGE('',*,*,#25102,.F.);
#31119=ORIENTED_EDGE('',*,*,#25104,.T.);
#31120=ORIENTED_EDGE('',*,*,#25105,.T.);
#31121=ORIENTED_EDGE('',*,*,#25106,.F.);
#31122=ORIENTED_EDGE('',*,*,#25105,.F.);
#31123=ORIENTED_EDGE('',*,*,#25107,.T.);
#31124=ORIENTED_EDGE('',*,*,#25108,.T.);
#31125=ORIENTED_EDGE('',*,*,#25109,.F.);
#31126=ORIENTED_EDGE('',*,*,#25108,.F.);
#31127=ORIENTED_EDGE('',*,*,#25110,.T.);
#31128=ORIENTED_EDGE('',*,*,#25111,.T.);
#31129=ORIENTED_EDGE('',*,*,#25112,.F.);
#31130=ORIENTED_EDGE('',*,*,#25111,.F.);
#31131=ORIENTED_EDGE('',*,*,#25113,.T.);
#31132=ORIENTED_EDGE('',*,*,#25114,.T.);
#31133=ORIENTED_EDGE('',*,*,#25115,.F.);
#31134=ORIENTED_EDGE('',*,*,#25114,.F.);
#31135=ORIENTED_EDGE('',*,*,#25116,.T.);
#31136=ORIENTED_EDGE('',*,*,#25117,.T.);
#31137=ORIENTED_EDGE('',*,*,#25118,.F.);
#31138=ORIENTED_EDGE('',*,*,#25117,.F.);
#31139=ORIENTED_EDGE('',*,*,#25119,.T.);
#31140=ORIENTED_EDGE('',*,*,#25120,.T.);
#31141=ORIENTED_EDGE('',*,*,#25121,.F.);
#31142=ORIENTED_EDGE('',*,*,#25120,.F.);
#31143=ORIENTED_EDGE('',*,*,#25122,.T.);
#31144=ORIENTED_EDGE('',*,*,#25123,.T.);
#31145=ORIENTED_EDGE('',*,*,#25124,.F.);
#31146=ORIENTED_EDGE('',*,*,#25125,.T.);
#31147=ORIENTED_EDGE('',*,*,#25126,.F.);
#31148=ORIENTED_EDGE('',*,*,#25123,.F.);
#31149=ORIENTED_EDGE('',*,*,#25127,.T.);
#31150=ORIENTED_EDGE('',*,*,#25128,.T.);
#31151=ORIENTED_EDGE('',*,*,#25129,.F.);
#31152=ORIENTED_EDGE('',*,*,#25128,.F.);
#31153=ORIENTED_EDGE('',*,*,#25130,.T.);
#31154=ORIENTED_EDGE('',*,*,#25131,.T.);
#31155=ORIENTED_EDGE('',*,*,#25132,.F.);
#31156=ORIENTED_EDGE('',*,*,#25131,.F.);
#31157=ORIENTED_EDGE('',*,*,#25133,.T.);
#31158=ORIENTED_EDGE('',*,*,#25134,.T.);
#31159=ORIENTED_EDGE('',*,*,#25135,.F.);
#31160=ORIENTED_EDGE('',*,*,#25134,.F.);
#31161=ORIENTED_EDGE('',*,*,#25136,.T.);
#31162=ORIENTED_EDGE('',*,*,#25137,.T.);
#31163=ORIENTED_EDGE('',*,*,#25138,.F.);
#31164=ORIENTED_EDGE('',*,*,#25137,.F.);
#31165=ORIENTED_EDGE('',*,*,#25139,.T.);
#31166=ORIENTED_EDGE('',*,*,#25140,.T.);
#31167=ORIENTED_EDGE('',*,*,#25141,.F.);
#31168=ORIENTED_EDGE('',*,*,#25140,.F.);
#31169=ORIENTED_EDGE('',*,*,#25142,.T.);
#31170=ORIENTED_EDGE('',*,*,#25143,.T.);
#31171=ORIENTED_EDGE('',*,*,#25144,.F.);
#31172=ORIENTED_EDGE('',*,*,#25143,.F.);
#31173=ORIENTED_EDGE('',*,*,#25145,.T.);
#31174=ORIENTED_EDGE('',*,*,#25146,.T.);
#31175=ORIENTED_EDGE('',*,*,#25147,.F.);
#31176=ORIENTED_EDGE('',*,*,#25146,.F.);
#31177=ORIENTED_EDGE('',*,*,#25148,.T.);
#31178=ORIENTED_EDGE('',*,*,#25149,.T.);
#31179=ORIENTED_EDGE('',*,*,#25150,.F.);
#31180=ORIENTED_EDGE('',*,*,#25149,.F.);
#31181=ORIENTED_EDGE('',*,*,#25151,.T.);
#31182=ORIENTED_EDGE('',*,*,#25152,.T.);
#31183=ORIENTED_EDGE('',*,*,#25153,.F.);
#31184=ORIENTED_EDGE('',*,*,#25152,.F.);
#31185=ORIENTED_EDGE('',*,*,#25154,.T.);
#31186=ORIENTED_EDGE('',*,*,#25155,.T.);
#31187=ORIENTED_EDGE('',*,*,#25156,.F.);
#31188=ORIENTED_EDGE('',*,*,#25155,.F.);
#31189=ORIENTED_EDGE('',*,*,#25157,.T.);
#31190=ORIENTED_EDGE('',*,*,#25158,.T.);
#31191=ORIENTED_EDGE('',*,*,#25159,.F.);
#31192=ORIENTED_EDGE('',*,*,#25158,.F.);
#31193=ORIENTED_EDGE('',*,*,#25160,.T.);
#31194=ORIENTED_EDGE('',*,*,#25161,.T.);
#31195=ORIENTED_EDGE('',*,*,#25162,.F.);
#31196=ORIENTED_EDGE('',*,*,#25161,.F.);
#31197=ORIENTED_EDGE('',*,*,#25163,.T.);
#31198=ORIENTED_EDGE('',*,*,#25164,.T.);
#31199=ORIENTED_EDGE('',*,*,#25165,.F.);
#31200=ORIENTED_EDGE('',*,*,#25164,.F.);
#31201=ORIENTED_EDGE('',*,*,#25166,.T.);
#31202=ORIENTED_EDGE('',*,*,#25167,.T.);
#31203=ORIENTED_EDGE('',*,*,#25168,.F.);
#31204=ORIENTED_EDGE('',*,*,#25167,.F.);
#31205=ORIENTED_EDGE('',*,*,#25169,.T.);
#31206=ORIENTED_EDGE('',*,*,#25170,.T.);
#31207=ORIENTED_EDGE('',*,*,#25171,.F.);
#31208=ORIENTED_EDGE('',*,*,#25170,.F.);
#31209=ORIENTED_EDGE('',*,*,#25172,.T.);
#31210=ORIENTED_EDGE('',*,*,#25173,.T.);
#31211=ORIENTED_EDGE('',*,*,#25174,.F.);
#31212=ORIENTED_EDGE('',*,*,#25175,.T.);
#31213=ORIENTED_EDGE('',*,*,#25176,.F.);
#31214=ORIENTED_EDGE('',*,*,#25173,.F.);
#31215=ORIENTED_EDGE('',*,*,#25177,.T.);
#31216=ORIENTED_EDGE('',*,*,#25178,.T.);
#31217=ORIENTED_EDGE('',*,*,#25179,.F.);
#31218=ORIENTED_EDGE('',*,*,#25178,.F.);
#31219=ORIENTED_EDGE('',*,*,#25180,.T.);
#31220=ORIENTED_EDGE('',*,*,#25181,.T.);
#31221=ORIENTED_EDGE('',*,*,#25182,.F.);
#31222=ORIENTED_EDGE('',*,*,#25181,.F.);
#31223=ORIENTED_EDGE('',*,*,#25183,.T.);
#31224=ORIENTED_EDGE('',*,*,#25184,.T.);
#31225=ORIENTED_EDGE('',*,*,#25185,.F.);
#31226=ORIENTED_EDGE('',*,*,#25184,.F.);
#31227=ORIENTED_EDGE('',*,*,#25186,.T.);
#31228=ORIENTED_EDGE('',*,*,#25187,.T.);
#31229=ORIENTED_EDGE('',*,*,#25188,.F.);
#31230=ORIENTED_EDGE('',*,*,#25187,.F.);
#31231=ORIENTED_EDGE('',*,*,#25189,.T.);
#31232=ORIENTED_EDGE('',*,*,#25190,.T.);
#31233=ORIENTED_EDGE('',*,*,#25191,.F.);
#31234=ORIENTED_EDGE('',*,*,#25190,.F.);
#31235=ORIENTED_EDGE('',*,*,#25192,.T.);
#31236=ORIENTED_EDGE('',*,*,#25193,.T.);
#31237=ORIENTED_EDGE('',*,*,#25194,.F.);
#31238=ORIENTED_EDGE('',*,*,#25193,.F.);
#31239=ORIENTED_EDGE('',*,*,#25195,.T.);
#31240=ORIENTED_EDGE('',*,*,#25196,.T.);
#31241=ORIENTED_EDGE('',*,*,#25197,.F.);
#31242=ORIENTED_EDGE('',*,*,#25196,.F.);
#31243=ORIENTED_EDGE('',*,*,#25198,.T.);
#31244=ORIENTED_EDGE('',*,*,#25199,.T.);
#31245=ORIENTED_EDGE('',*,*,#25200,.F.);
#31246=ORIENTED_EDGE('',*,*,#25199,.F.);
#31247=ORIENTED_EDGE('',*,*,#25201,.T.);
#31248=ORIENTED_EDGE('',*,*,#25202,.T.);
#31249=ORIENTED_EDGE('',*,*,#25203,.F.);
#31250=ORIENTED_EDGE('',*,*,#25202,.F.);
#31251=ORIENTED_EDGE('',*,*,#25204,.T.);
#31252=ORIENTED_EDGE('',*,*,#25205,.T.);
#31253=ORIENTED_EDGE('',*,*,#25206,.F.);
#31254=ORIENTED_EDGE('',*,*,#25205,.F.);
#31255=ORIENTED_EDGE('',*,*,#25207,.T.);
#31256=ORIENTED_EDGE('',*,*,#25208,.T.);
#31257=ORIENTED_EDGE('',*,*,#25209,.F.);
#31258=ORIENTED_EDGE('',*,*,#25208,.F.);
#31259=ORIENTED_EDGE('',*,*,#25210,.T.);
#31260=ORIENTED_EDGE('',*,*,#25211,.T.);
#31261=ORIENTED_EDGE('',*,*,#25212,.F.);
#31262=ORIENTED_EDGE('',*,*,#25211,.F.);
#31263=ORIENTED_EDGE('',*,*,#25213,.T.);
#31264=ORIENTED_EDGE('',*,*,#25214,.T.);
#31265=ORIENTED_EDGE('',*,*,#25215,.F.);
#31266=ORIENTED_EDGE('',*,*,#25214,.F.);
#31267=ORIENTED_EDGE('',*,*,#25216,.T.);
#31268=ORIENTED_EDGE('',*,*,#25217,.T.);
#31269=ORIENTED_EDGE('',*,*,#25218,.F.);
#31270=ORIENTED_EDGE('',*,*,#25217,.F.);
#31271=ORIENTED_EDGE('',*,*,#25219,.T.);
#31272=ORIENTED_EDGE('',*,*,#25220,.T.);
#31273=ORIENTED_EDGE('',*,*,#25221,.F.);
#31274=ORIENTED_EDGE('',*,*,#25220,.F.);
#31275=ORIENTED_EDGE('',*,*,#25222,.T.);
#31276=ORIENTED_EDGE('',*,*,#25223,.T.);
#31277=ORIENTED_EDGE('',*,*,#25224,.F.);
#31278=ORIENTED_EDGE('',*,*,#25223,.F.);
#31279=ORIENTED_EDGE('',*,*,#25225,.T.);
#31280=ORIENTED_EDGE('',*,*,#25226,.T.);
#31281=ORIENTED_EDGE('',*,*,#25227,.F.);
#31282=ORIENTED_EDGE('',*,*,#25226,.F.);
#31283=ORIENTED_EDGE('',*,*,#25228,.T.);
#31284=ORIENTED_EDGE('',*,*,#25229,.T.);
#31285=ORIENTED_EDGE('',*,*,#25230,.F.);
#31286=ORIENTED_EDGE('',*,*,#25231,.T.);
#31287=ORIENTED_EDGE('',*,*,#25232,.F.);
#31288=ORIENTED_EDGE('',*,*,#25229,.F.);
#31289=ORIENTED_EDGE('',*,*,#25233,.T.);
#31290=ORIENTED_EDGE('',*,*,#25234,.T.);
#31291=ORIENTED_EDGE('',*,*,#25235,.F.);
#31292=ORIENTED_EDGE('',*,*,#25234,.F.);
#31293=ORIENTED_EDGE('',*,*,#25236,.T.);
#31294=ORIENTED_EDGE('',*,*,#25237,.T.);
#31295=ORIENTED_EDGE('',*,*,#25238,.F.);
#31296=ORIENTED_EDGE('',*,*,#25237,.F.);
#31297=ORIENTED_EDGE('',*,*,#25239,.T.);
#31298=ORIENTED_EDGE('',*,*,#25240,.T.);
#31299=ORIENTED_EDGE('',*,*,#25241,.F.);
#31300=ORIENTED_EDGE('',*,*,#25240,.F.);
#31301=ORIENTED_EDGE('',*,*,#25242,.T.);
#31302=ORIENTED_EDGE('',*,*,#25243,.T.);
#31303=ORIENTED_EDGE('',*,*,#25244,.F.);
#31304=ORIENTED_EDGE('',*,*,#25243,.F.);
#31305=ORIENTED_EDGE('',*,*,#25245,.T.);
#31306=ORIENTED_EDGE('',*,*,#25246,.T.);
#31307=ORIENTED_EDGE('',*,*,#25247,.F.);
#31308=ORIENTED_EDGE('',*,*,#25246,.F.);
#31309=ORIENTED_EDGE('',*,*,#25248,.T.);
#31310=ORIENTED_EDGE('',*,*,#25249,.T.);
#31311=ORIENTED_EDGE('',*,*,#25250,.F.);
#31312=ORIENTED_EDGE('',*,*,#25249,.F.);
#31313=ORIENTED_EDGE('',*,*,#25251,.T.);
#31314=ORIENTED_EDGE('',*,*,#25252,.T.);
#31315=ORIENTED_EDGE('',*,*,#25253,.F.);
#31316=ORIENTED_EDGE('',*,*,#25252,.F.);
#31317=ORIENTED_EDGE('',*,*,#25254,.T.);
#31318=ORIENTED_EDGE('',*,*,#25255,.T.);
#31319=ORIENTED_EDGE('',*,*,#25256,.F.);
#31320=ORIENTED_EDGE('',*,*,#25255,.F.);
#31321=ORIENTED_EDGE('',*,*,#25257,.T.);
#31322=ORIENTED_EDGE('',*,*,#25258,.T.);
#31323=ORIENTED_EDGE('',*,*,#25259,.F.);
#31324=ORIENTED_EDGE('',*,*,#25258,.F.);
#31325=ORIENTED_EDGE('',*,*,#25260,.T.);
#31326=ORIENTED_EDGE('',*,*,#25261,.T.);
#31327=ORIENTED_EDGE('',*,*,#25262,.F.);
#31328=ORIENTED_EDGE('',*,*,#25261,.F.);
#31329=ORIENTED_EDGE('',*,*,#25263,.T.);
#31330=ORIENTED_EDGE('',*,*,#25264,.T.);
#31331=ORIENTED_EDGE('',*,*,#25265,.F.);
#31332=ORIENTED_EDGE('',*,*,#25264,.F.);
#31333=ORIENTED_EDGE('',*,*,#25266,.T.);
#31334=ORIENTED_EDGE('',*,*,#25267,.T.);
#31335=ORIENTED_EDGE('',*,*,#25268,.F.);
#31336=ORIENTED_EDGE('',*,*,#25267,.F.);
#31337=ORIENTED_EDGE('',*,*,#25269,.T.);
#31338=ORIENTED_EDGE('',*,*,#25270,.T.);
#31339=ORIENTED_EDGE('',*,*,#25271,.F.);
#31340=ORIENTED_EDGE('',*,*,#25270,.F.);
#31341=ORIENTED_EDGE('',*,*,#25272,.T.);
#31342=ORIENTED_EDGE('',*,*,#25273,.T.);
#31343=ORIENTED_EDGE('',*,*,#25274,.F.);
#31344=ORIENTED_EDGE('',*,*,#25273,.F.);
#31345=ORIENTED_EDGE('',*,*,#25275,.T.);
#31346=ORIENTED_EDGE('',*,*,#25276,.T.);
#31347=ORIENTED_EDGE('',*,*,#25277,.F.);
#31348=ORIENTED_EDGE('',*,*,#25276,.F.);
#31349=ORIENTED_EDGE('',*,*,#25278,.T.);
#31350=ORIENTED_EDGE('',*,*,#25279,.T.);
#31351=ORIENTED_EDGE('',*,*,#25280,.F.);
#31352=ORIENTED_EDGE('',*,*,#25279,.F.);
#31353=ORIENTED_EDGE('',*,*,#25281,.T.);
#31354=ORIENTED_EDGE('',*,*,#25282,.T.);
#31355=ORIENTED_EDGE('',*,*,#25283,.F.);
#31356=ORIENTED_EDGE('',*,*,#25282,.F.);
#31357=ORIENTED_EDGE('',*,*,#25284,.T.);
#31358=ORIENTED_EDGE('',*,*,#25285,.T.);
#31359=ORIENTED_EDGE('',*,*,#25286,.F.);
#31360=ORIENTED_EDGE('',*,*,#25287,.T.);
#31361=ORIENTED_EDGE('',*,*,#25288,.F.);
#31362=ORIENTED_EDGE('',*,*,#25285,.F.);
#31363=ORIENTED_EDGE('',*,*,#25289,.T.);
#31364=ORIENTED_EDGE('',*,*,#25290,.T.);
#31365=ORIENTED_EDGE('',*,*,#25291,.F.);
#31366=ORIENTED_EDGE('',*,*,#25290,.F.);
#31367=ORIENTED_EDGE('',*,*,#25292,.T.);
#31368=ORIENTED_EDGE('',*,*,#25293,.T.);
#31369=ORIENTED_EDGE('',*,*,#25294,.F.);
#31370=ORIENTED_EDGE('',*,*,#25293,.F.);
#31371=ORIENTED_EDGE('',*,*,#25295,.T.);
#31372=ORIENTED_EDGE('',*,*,#25296,.T.);
#31373=ORIENTED_EDGE('',*,*,#25297,.F.);
#31374=ORIENTED_EDGE('',*,*,#25296,.F.);
#31375=ORIENTED_EDGE('',*,*,#25298,.T.);
#31376=ORIENTED_EDGE('',*,*,#25299,.T.);
#31377=ORIENTED_EDGE('',*,*,#25300,.F.);
#31378=ORIENTED_EDGE('',*,*,#25299,.F.);
#31379=ORIENTED_EDGE('',*,*,#25301,.T.);
#31380=ORIENTED_EDGE('',*,*,#25302,.T.);
#31381=ORIENTED_EDGE('',*,*,#25303,.F.);
#31382=ORIENTED_EDGE('',*,*,#25302,.F.);
#31383=ORIENTED_EDGE('',*,*,#25304,.T.);
#31384=ORIENTED_EDGE('',*,*,#25305,.T.);
#31385=ORIENTED_EDGE('',*,*,#25306,.F.);
#31386=ORIENTED_EDGE('',*,*,#25305,.F.);
#31387=ORIENTED_EDGE('',*,*,#25307,.T.);
#31388=ORIENTED_EDGE('',*,*,#25308,.T.);
#31389=ORIENTED_EDGE('',*,*,#25309,.F.);
#31390=ORIENTED_EDGE('',*,*,#25308,.F.);
#31391=ORIENTED_EDGE('',*,*,#25310,.T.);
#31392=ORIENTED_EDGE('',*,*,#25311,.T.);
#31393=ORIENTED_EDGE('',*,*,#25312,.F.);
#31394=ORIENTED_EDGE('',*,*,#25311,.F.);
#31395=ORIENTED_EDGE('',*,*,#25313,.T.);
#31396=ORIENTED_EDGE('',*,*,#25314,.T.);
#31397=ORIENTED_EDGE('',*,*,#25315,.F.);
#31398=ORIENTED_EDGE('',*,*,#25314,.F.);
#31399=ORIENTED_EDGE('',*,*,#25316,.T.);
#31400=ORIENTED_EDGE('',*,*,#25317,.T.);
#31401=ORIENTED_EDGE('',*,*,#25318,.F.);
#31402=ORIENTED_EDGE('',*,*,#25317,.F.);
#31403=ORIENTED_EDGE('',*,*,#25319,.T.);
#31404=ORIENTED_EDGE('',*,*,#25320,.T.);
#31405=ORIENTED_EDGE('',*,*,#25321,.F.);
#31406=ORIENTED_EDGE('',*,*,#25320,.F.);
#31407=ORIENTED_EDGE('',*,*,#25322,.T.);
#31408=ORIENTED_EDGE('',*,*,#25323,.T.);
#31409=ORIENTED_EDGE('',*,*,#25324,.F.);
#31410=ORIENTED_EDGE('',*,*,#25323,.F.);
#31411=ORIENTED_EDGE('',*,*,#25325,.T.);
#31412=ORIENTED_EDGE('',*,*,#25326,.T.);
#31413=ORIENTED_EDGE('',*,*,#25327,.F.);
#31414=ORIENTED_EDGE('',*,*,#25326,.F.);
#31415=ORIENTED_EDGE('',*,*,#25328,.T.);
#31416=ORIENTED_EDGE('',*,*,#25329,.T.);
#31417=ORIENTED_EDGE('',*,*,#25330,.F.);
#31418=ORIENTED_EDGE('',*,*,#25329,.F.);
#31419=ORIENTED_EDGE('',*,*,#25331,.T.);
#31420=ORIENTED_EDGE('',*,*,#25332,.T.);
#31421=ORIENTED_EDGE('',*,*,#25333,.F.);
#31422=ORIENTED_EDGE('',*,*,#25332,.F.);
#31423=ORIENTED_EDGE('',*,*,#25334,.T.);
#31424=ORIENTED_EDGE('',*,*,#25335,.T.);
#31425=ORIENTED_EDGE('',*,*,#25336,.F.);
#31426=ORIENTED_EDGE('',*,*,#25335,.F.);
#31427=ORIENTED_EDGE('',*,*,#25337,.T.);
#31428=ORIENTED_EDGE('',*,*,#25338,.T.);
#31429=ORIENTED_EDGE('',*,*,#25339,.F.);
#31430=ORIENTED_EDGE('',*,*,#25338,.F.);
#31431=ORIENTED_EDGE('',*,*,#25340,.T.);
#31432=ORIENTED_EDGE('',*,*,#25341,.T.);
#31433=ORIENTED_EDGE('',*,*,#25342,.F.);
#31434=ORIENTED_EDGE('',*,*,#25343,.T.);
#31435=ORIENTED_EDGE('',*,*,#25344,.F.);
#31436=ORIENTED_EDGE('',*,*,#25341,.F.);
#31437=ORIENTED_EDGE('',*,*,#25345,.T.);
#31438=ORIENTED_EDGE('',*,*,#25346,.T.);
#31439=ORIENTED_EDGE('',*,*,#25347,.F.);
#31440=ORIENTED_EDGE('',*,*,#25346,.F.);
#31441=ORIENTED_EDGE('',*,*,#25348,.T.);
#31442=ORIENTED_EDGE('',*,*,#25349,.T.);
#31443=ORIENTED_EDGE('',*,*,#25350,.F.);
#31444=ORIENTED_EDGE('',*,*,#25349,.F.);
#31445=ORIENTED_EDGE('',*,*,#25351,.T.);
#31446=ORIENTED_EDGE('',*,*,#25352,.T.);
#31447=ORIENTED_EDGE('',*,*,#25353,.F.);
#31448=ORIENTED_EDGE('',*,*,#25352,.F.);
#31449=ORIENTED_EDGE('',*,*,#25354,.T.);
#31450=ORIENTED_EDGE('',*,*,#25355,.T.);
#31451=ORIENTED_EDGE('',*,*,#25356,.F.);
#31452=ORIENTED_EDGE('',*,*,#25355,.F.);
#31453=ORIENTED_EDGE('',*,*,#25357,.T.);
#31454=ORIENTED_EDGE('',*,*,#25358,.T.);
#31455=ORIENTED_EDGE('',*,*,#25359,.F.);
#31456=ORIENTED_EDGE('',*,*,#25358,.F.);
#31457=ORIENTED_EDGE('',*,*,#25360,.T.);
#31458=ORIENTED_EDGE('',*,*,#25361,.T.);
#31459=ORIENTED_EDGE('',*,*,#25362,.F.);
#31460=ORIENTED_EDGE('',*,*,#25361,.F.);
#31461=ORIENTED_EDGE('',*,*,#25363,.T.);
#31462=ORIENTED_EDGE('',*,*,#25364,.T.);
#31463=ORIENTED_EDGE('',*,*,#25365,.F.);
#31464=ORIENTED_EDGE('',*,*,#25364,.F.);
#31465=ORIENTED_EDGE('',*,*,#25366,.T.);
#31466=ORIENTED_EDGE('',*,*,#25367,.T.);
#31467=ORIENTED_EDGE('',*,*,#25368,.F.);
#31468=ORIENTED_EDGE('',*,*,#25367,.F.);
#31469=ORIENTED_EDGE('',*,*,#25369,.T.);
#31470=ORIENTED_EDGE('',*,*,#25370,.T.);
#31471=ORIENTED_EDGE('',*,*,#25371,.F.);
#31472=ORIENTED_EDGE('',*,*,#25370,.F.);
#31473=ORIENTED_EDGE('',*,*,#25372,.T.);
#31474=ORIENTED_EDGE('',*,*,#25373,.T.);
#31475=ORIENTED_EDGE('',*,*,#25374,.F.);
#31476=ORIENTED_EDGE('',*,*,#25373,.F.);
#31477=ORIENTED_EDGE('',*,*,#25375,.T.);
#31478=ORIENTED_EDGE('',*,*,#25376,.T.);
#31479=ORIENTED_EDGE('',*,*,#25377,.F.);
#31480=ORIENTED_EDGE('',*,*,#25376,.F.);
#31481=ORIENTED_EDGE('',*,*,#25378,.T.);
#31482=ORIENTED_EDGE('',*,*,#25379,.T.);
#31483=ORIENTED_EDGE('',*,*,#25380,.F.);
#31484=ORIENTED_EDGE('',*,*,#25379,.F.);
#31485=ORIENTED_EDGE('',*,*,#25381,.T.);
#31486=ORIENTED_EDGE('',*,*,#25382,.T.);
#31487=ORIENTED_EDGE('',*,*,#25383,.F.);
#31488=ORIENTED_EDGE('',*,*,#25382,.F.);
#31489=ORIENTED_EDGE('',*,*,#25384,.T.);
#31490=ORIENTED_EDGE('',*,*,#25385,.T.);
#31491=ORIENTED_EDGE('',*,*,#25386,.F.);
#31492=ORIENTED_EDGE('',*,*,#25385,.F.);
#31493=ORIENTED_EDGE('',*,*,#25387,.T.);
#31494=ORIENTED_EDGE('',*,*,#25388,.T.);
#31495=ORIENTED_EDGE('',*,*,#25389,.F.);
#31496=ORIENTED_EDGE('',*,*,#25388,.F.);
#31497=ORIENTED_EDGE('',*,*,#25390,.T.);
#31498=ORIENTED_EDGE('',*,*,#25391,.T.);
#31499=ORIENTED_EDGE('',*,*,#25392,.F.);
#31500=ORIENTED_EDGE('',*,*,#25391,.F.);
#31501=ORIENTED_EDGE('',*,*,#25393,.T.);
#31502=ORIENTED_EDGE('',*,*,#25394,.T.);
#31503=ORIENTED_EDGE('',*,*,#25395,.F.);
#31504=ORIENTED_EDGE('',*,*,#25394,.F.);
#31505=ORIENTED_EDGE('',*,*,#25396,.T.);
#31506=ORIENTED_EDGE('',*,*,#25397,.T.);
#31507=ORIENTED_EDGE('',*,*,#25398,.F.);
#31508=ORIENTED_EDGE('',*,*,#25399,.T.);
#31509=ORIENTED_EDGE('',*,*,#25400,.F.);
#31510=ORIENTED_EDGE('',*,*,#25397,.F.);
#31511=ORIENTED_EDGE('',*,*,#25401,.T.);
#31512=ORIENTED_EDGE('',*,*,#25402,.T.);
#31513=ORIENTED_EDGE('',*,*,#25403,.F.);
#31514=ORIENTED_EDGE('',*,*,#25402,.F.);
#31515=ORIENTED_EDGE('',*,*,#25404,.T.);
#31516=ORIENTED_EDGE('',*,*,#25405,.T.);
#31517=ORIENTED_EDGE('',*,*,#25406,.F.);
#31518=ORIENTED_EDGE('',*,*,#25405,.F.);
#31519=ORIENTED_EDGE('',*,*,#25407,.T.);
#31520=ORIENTED_EDGE('',*,*,#25408,.T.);
#31521=ORIENTED_EDGE('',*,*,#25409,.F.);
#31522=ORIENTED_EDGE('',*,*,#25408,.F.);
#31523=ORIENTED_EDGE('',*,*,#25410,.T.);
#31524=ORIENTED_EDGE('',*,*,#25411,.T.);
#31525=ORIENTED_EDGE('',*,*,#25412,.F.);
#31526=ORIENTED_EDGE('',*,*,#25411,.F.);
#31527=ORIENTED_EDGE('',*,*,#25413,.T.);
#31528=ORIENTED_EDGE('',*,*,#25414,.T.);
#31529=ORIENTED_EDGE('',*,*,#25415,.F.);
#31530=ORIENTED_EDGE('',*,*,#25414,.F.);
#31531=ORIENTED_EDGE('',*,*,#25416,.T.);
#31532=ORIENTED_EDGE('',*,*,#25417,.T.);
#31533=ORIENTED_EDGE('',*,*,#25418,.F.);
#31534=ORIENTED_EDGE('',*,*,#25417,.F.);
#31535=ORIENTED_EDGE('',*,*,#25419,.T.);
#31536=ORIENTED_EDGE('',*,*,#25420,.T.);
#31537=ORIENTED_EDGE('',*,*,#25421,.F.);
#31538=ORIENTED_EDGE('',*,*,#25420,.F.);
#31539=ORIENTED_EDGE('',*,*,#25422,.T.);
#31540=ORIENTED_EDGE('',*,*,#25423,.T.);
#31541=ORIENTED_EDGE('',*,*,#25424,.F.);
#31542=ORIENTED_EDGE('',*,*,#25423,.F.);
#31543=ORIENTED_EDGE('',*,*,#25425,.T.);
#31544=ORIENTED_EDGE('',*,*,#25426,.T.);
#31545=ORIENTED_EDGE('',*,*,#25427,.F.);
#31546=ORIENTED_EDGE('',*,*,#25426,.F.);
#31547=ORIENTED_EDGE('',*,*,#25428,.T.);
#31548=ORIENTED_EDGE('',*,*,#25429,.T.);
#31549=ORIENTED_EDGE('',*,*,#25430,.F.);
#31550=ORIENTED_EDGE('',*,*,#25429,.F.);
#31551=ORIENTED_EDGE('',*,*,#25431,.T.);
#31552=ORIENTED_EDGE('',*,*,#25432,.T.);
#31553=ORIENTED_EDGE('',*,*,#25433,.F.);
#31554=ORIENTED_EDGE('',*,*,#25432,.F.);
#31555=ORIENTED_EDGE('',*,*,#25434,.T.);
#31556=ORIENTED_EDGE('',*,*,#25435,.T.);
#31557=ORIENTED_EDGE('',*,*,#25436,.F.);
#31558=ORIENTED_EDGE('',*,*,#25435,.F.);
#31559=ORIENTED_EDGE('',*,*,#25437,.T.);
#31560=ORIENTED_EDGE('',*,*,#25438,.T.);
#31561=ORIENTED_EDGE('',*,*,#25439,.F.);
#31562=ORIENTED_EDGE('',*,*,#25438,.F.);
#31563=ORIENTED_EDGE('',*,*,#25440,.T.);
#31564=ORIENTED_EDGE('',*,*,#25441,.T.);
#31565=ORIENTED_EDGE('',*,*,#25442,.F.);
#31566=ORIENTED_EDGE('',*,*,#25441,.F.);
#31567=ORIENTED_EDGE('',*,*,#25443,.T.);
#31568=ORIENTED_EDGE('',*,*,#25444,.T.);
#31569=ORIENTED_EDGE('',*,*,#25445,.F.);
#31570=ORIENTED_EDGE('',*,*,#25444,.F.);
#31571=ORIENTED_EDGE('',*,*,#25446,.T.);
#31572=ORIENTED_EDGE('',*,*,#25447,.T.);
#31573=ORIENTED_EDGE('',*,*,#25448,.F.);
#31574=ORIENTED_EDGE('',*,*,#25449,.T.);
#31575=ORIENTED_EDGE('',*,*,#25450,.F.);
#31576=ORIENTED_EDGE('',*,*,#25447,.F.);
#31577=ORIENTED_EDGE('',*,*,#25451,.T.);
#31578=ORIENTED_EDGE('',*,*,#25452,.T.);
#31579=ORIENTED_EDGE('',*,*,#25453,.F.);
#31580=ORIENTED_EDGE('',*,*,#25452,.F.);
#31581=ORIENTED_EDGE('',*,*,#25454,.T.);
#31582=ORIENTED_EDGE('',*,*,#25455,.T.);
#31583=ORIENTED_EDGE('',*,*,#25456,.F.);
#31584=ORIENTED_EDGE('',*,*,#25455,.F.);
#31585=ORIENTED_EDGE('',*,*,#25457,.T.);
#31586=ORIENTED_EDGE('',*,*,#25458,.T.);
#31587=ORIENTED_EDGE('',*,*,#25459,.F.);
#31588=ORIENTED_EDGE('',*,*,#25458,.F.);
#31589=ORIENTED_EDGE('',*,*,#25460,.T.);
#31590=ORIENTED_EDGE('',*,*,#25461,.T.);
#31591=ORIENTED_EDGE('',*,*,#25462,.F.);
#31592=ORIENTED_EDGE('',*,*,#25461,.F.);
#31593=ORIENTED_EDGE('',*,*,#25463,.T.);
#31594=ORIENTED_EDGE('',*,*,#25464,.T.);
#31595=ORIENTED_EDGE('',*,*,#25465,.F.);
#31596=ORIENTED_EDGE('',*,*,#25464,.F.);
#31597=ORIENTED_EDGE('',*,*,#25466,.T.);
#31598=ORIENTED_EDGE('',*,*,#25467,.T.);
#31599=ORIENTED_EDGE('',*,*,#25468,.F.);
#31600=ORIENTED_EDGE('',*,*,#25467,.F.);
#31601=ORIENTED_EDGE('',*,*,#25469,.T.);
#31602=ORIENTED_EDGE('',*,*,#25470,.T.);
#31603=ORIENTED_EDGE('',*,*,#25471,.F.);
#31604=ORIENTED_EDGE('',*,*,#25470,.F.);
#31605=ORIENTED_EDGE('',*,*,#25472,.T.);
#31606=ORIENTED_EDGE('',*,*,#25473,.T.);
#31607=ORIENTED_EDGE('',*,*,#25474,.F.);
#31608=ORIENTED_EDGE('',*,*,#25473,.F.);
#31609=ORIENTED_EDGE('',*,*,#25475,.T.);
#31610=ORIENTED_EDGE('',*,*,#25476,.T.);
#31611=ORIENTED_EDGE('',*,*,#25477,.F.);
#31612=ORIENTED_EDGE('',*,*,#25476,.F.);
#31613=ORIENTED_EDGE('',*,*,#25478,.T.);
#31614=ORIENTED_EDGE('',*,*,#25479,.T.);
#31615=ORIENTED_EDGE('',*,*,#25480,.F.);
#31616=ORIENTED_EDGE('',*,*,#25479,.F.);
#31617=ORIENTED_EDGE('',*,*,#25481,.T.);
#31618=ORIENTED_EDGE('',*,*,#25482,.T.);
#31619=ORIENTED_EDGE('',*,*,#25483,.F.);
#31620=ORIENTED_EDGE('',*,*,#25482,.F.);
#31621=ORIENTED_EDGE('',*,*,#25484,.T.);
#31622=ORIENTED_EDGE('',*,*,#25485,.T.);
#31623=ORIENTED_EDGE('',*,*,#25486,.F.);
#31624=ORIENTED_EDGE('',*,*,#25485,.F.);
#31625=ORIENTED_EDGE('',*,*,#25487,.T.);
#31626=ORIENTED_EDGE('',*,*,#25488,.T.);
#31627=ORIENTED_EDGE('',*,*,#25489,.F.);
#31628=ORIENTED_EDGE('',*,*,#25488,.F.);
#31629=ORIENTED_EDGE('',*,*,#25490,.T.);
#31630=ORIENTED_EDGE('',*,*,#25491,.T.);
#31631=ORIENTED_EDGE('',*,*,#25492,.F.);
#31632=ORIENTED_EDGE('',*,*,#25491,.F.);
#31633=ORIENTED_EDGE('',*,*,#25493,.T.);
#31634=ORIENTED_EDGE('',*,*,#25494,.T.);
#31635=ORIENTED_EDGE('',*,*,#25495,.F.);
#31636=ORIENTED_EDGE('',*,*,#25494,.F.);
#31637=ORIENTED_EDGE('',*,*,#25496,.T.);
#31638=ORIENTED_EDGE('',*,*,#25497,.T.);
#31639=ORIENTED_EDGE('',*,*,#25498,.F.);
#31640=ORIENTED_EDGE('',*,*,#25497,.F.);
#31641=ORIENTED_EDGE('',*,*,#25499,.T.);
#31642=ORIENTED_EDGE('',*,*,#25500,.T.);
#31643=ORIENTED_EDGE('',*,*,#25501,.F.);
#31644=ORIENTED_EDGE('',*,*,#25500,.F.);
#31645=ORIENTED_EDGE('',*,*,#25502,.T.);
#31646=ORIENTED_EDGE('',*,*,#25503,.T.);
#31647=ORIENTED_EDGE('',*,*,#25504,.F.);
#31648=ORIENTED_EDGE('',*,*,#25505,.T.);
#31649=ORIENTED_EDGE('',*,*,#25506,.F.);
#31650=ORIENTED_EDGE('',*,*,#25503,.F.);
#31651=ORIENTED_EDGE('',*,*,#25507,.T.);
#31652=ORIENTED_EDGE('',*,*,#25508,.T.);
#31653=ORIENTED_EDGE('',*,*,#25509,.F.);
#31654=ORIENTED_EDGE('',*,*,#25508,.F.);
#31655=ORIENTED_EDGE('',*,*,#25510,.T.);
#31656=ORIENTED_EDGE('',*,*,#25511,.T.);
#31657=ORIENTED_EDGE('',*,*,#25512,.F.);
#31658=ORIENTED_EDGE('',*,*,#25511,.F.);
#31659=ORIENTED_EDGE('',*,*,#25513,.T.);
#31660=ORIENTED_EDGE('',*,*,#25514,.T.);
#31661=ORIENTED_EDGE('',*,*,#25515,.F.);
#31662=ORIENTED_EDGE('',*,*,#25514,.F.);
#31663=ORIENTED_EDGE('',*,*,#25516,.T.);
#31664=ORIENTED_EDGE('',*,*,#25517,.T.);
#31665=ORIENTED_EDGE('',*,*,#25518,.F.);
#31666=ORIENTED_EDGE('',*,*,#25517,.F.);
#31667=ORIENTED_EDGE('',*,*,#25519,.T.);
#31668=ORIENTED_EDGE('',*,*,#25520,.T.);
#31669=ORIENTED_EDGE('',*,*,#25521,.F.);
#31670=ORIENTED_EDGE('',*,*,#25520,.F.);
#31671=ORIENTED_EDGE('',*,*,#25522,.T.);
#31672=ORIENTED_EDGE('',*,*,#25523,.T.);
#31673=ORIENTED_EDGE('',*,*,#25524,.F.);
#31674=ORIENTED_EDGE('',*,*,#25523,.F.);
#31675=ORIENTED_EDGE('',*,*,#25525,.T.);
#31676=ORIENTED_EDGE('',*,*,#25526,.T.);
#31677=ORIENTED_EDGE('',*,*,#25527,.F.);
#31678=ORIENTED_EDGE('',*,*,#25526,.F.);
#31679=ORIENTED_EDGE('',*,*,#25528,.T.);
#31680=ORIENTED_EDGE('',*,*,#25529,.T.);
#31681=ORIENTED_EDGE('',*,*,#25530,.F.);
#31682=ORIENTED_EDGE('',*,*,#25529,.F.);
#31683=ORIENTED_EDGE('',*,*,#25531,.T.);
#31684=ORIENTED_EDGE('',*,*,#25532,.T.);
#31685=ORIENTED_EDGE('',*,*,#25533,.F.);
#31686=ORIENTED_EDGE('',*,*,#25532,.F.);
#31687=ORIENTED_EDGE('',*,*,#25534,.T.);
#31688=ORIENTED_EDGE('',*,*,#25535,.T.);
#31689=ORIENTED_EDGE('',*,*,#25536,.F.);
#31690=ORIENTED_EDGE('',*,*,#25535,.F.);
#31691=ORIENTED_EDGE('',*,*,#25537,.T.);
#31692=ORIENTED_EDGE('',*,*,#25538,.T.);
#31693=ORIENTED_EDGE('',*,*,#25539,.F.);
#31694=ORIENTED_EDGE('',*,*,#25538,.F.);
#31695=ORIENTED_EDGE('',*,*,#25540,.T.);
#31696=ORIENTED_EDGE('',*,*,#25541,.T.);
#31697=ORIENTED_EDGE('',*,*,#25542,.F.);
#31698=ORIENTED_EDGE('',*,*,#25541,.F.);
#31699=ORIENTED_EDGE('',*,*,#25543,.T.);
#31700=ORIENTED_EDGE('',*,*,#25544,.T.);
#31701=ORIENTED_EDGE('',*,*,#25545,.F.);
#31702=ORIENTED_EDGE('',*,*,#25544,.F.);
#31703=ORIENTED_EDGE('',*,*,#25546,.T.);
#31704=ORIENTED_EDGE('',*,*,#25547,.T.);
#31705=ORIENTED_EDGE('',*,*,#25548,.F.);
#31706=ORIENTED_EDGE('',*,*,#25547,.F.);
#31707=ORIENTED_EDGE('',*,*,#25549,.T.);
#31708=ORIENTED_EDGE('',*,*,#25550,.T.);
#31709=ORIENTED_EDGE('',*,*,#25551,.F.);
#31710=ORIENTED_EDGE('',*,*,#25550,.F.);
#31711=ORIENTED_EDGE('',*,*,#25552,.T.);
#31712=ORIENTED_EDGE('',*,*,#25553,.T.);
#31713=ORIENTED_EDGE('',*,*,#25554,.F.);
#31714=ORIENTED_EDGE('',*,*,#25553,.F.);
#31715=ORIENTED_EDGE('',*,*,#25555,.T.);
#31716=ORIENTED_EDGE('',*,*,#25556,.T.);
#31717=ORIENTED_EDGE('',*,*,#25557,.F.);
#31718=ORIENTED_EDGE('',*,*,#25556,.F.);
#31719=ORIENTED_EDGE('',*,*,#25558,.T.);
#31720=ORIENTED_EDGE('',*,*,#25559,.T.);
#31721=ORIENTED_EDGE('',*,*,#25560,.F.);
#31722=ORIENTED_EDGE('',*,*,#25561,.T.);
#31723=ORIENTED_EDGE('',*,*,#25562,.F.);
#31724=ORIENTED_EDGE('',*,*,#25559,.F.);
#31725=ORIENTED_EDGE('',*,*,#25563,.T.);
#31726=ORIENTED_EDGE('',*,*,#25564,.T.);
#31727=ORIENTED_EDGE('',*,*,#25565,.F.);
#31728=ORIENTED_EDGE('',*,*,#25564,.F.);
#31729=ORIENTED_EDGE('',*,*,#25566,.T.);
#31730=ORIENTED_EDGE('',*,*,#25567,.T.);
#31731=ORIENTED_EDGE('',*,*,#25568,.F.);
#31732=ORIENTED_EDGE('',*,*,#25567,.F.);
#31733=ORIENTED_EDGE('',*,*,#25569,.T.);
#31734=ORIENTED_EDGE('',*,*,#25570,.T.);
#31735=ORIENTED_EDGE('',*,*,#25571,.F.);
#31736=ORIENTED_EDGE('',*,*,#25570,.F.);
#31737=ORIENTED_EDGE('',*,*,#25572,.T.);
#31738=ORIENTED_EDGE('',*,*,#25573,.T.);
#31739=ORIENTED_EDGE('',*,*,#25574,.F.);
#31740=ORIENTED_EDGE('',*,*,#25573,.F.);
#31741=ORIENTED_EDGE('',*,*,#25575,.T.);
#31742=ORIENTED_EDGE('',*,*,#25576,.T.);
#31743=ORIENTED_EDGE('',*,*,#25577,.F.);
#31744=ORIENTED_EDGE('',*,*,#25576,.F.);
#31745=ORIENTED_EDGE('',*,*,#25578,.T.);
#31746=ORIENTED_EDGE('',*,*,#25579,.T.);
#31747=ORIENTED_EDGE('',*,*,#25580,.F.);
#31748=ORIENTED_EDGE('',*,*,#25579,.F.);
#31749=ORIENTED_EDGE('',*,*,#25581,.T.);
#31750=ORIENTED_EDGE('',*,*,#25582,.T.);
#31751=ORIENTED_EDGE('',*,*,#25583,.F.);
#31752=ORIENTED_EDGE('',*,*,#25582,.F.);
#31753=ORIENTED_EDGE('',*,*,#25584,.T.);
#31754=ORIENTED_EDGE('',*,*,#25585,.T.);
#31755=ORIENTED_EDGE('',*,*,#25586,.F.);
#31756=ORIENTED_EDGE('',*,*,#25585,.F.);
#31757=ORIENTED_EDGE('',*,*,#25587,.T.);
#31758=ORIENTED_EDGE('',*,*,#25588,.T.);
#31759=ORIENTED_EDGE('',*,*,#25589,.F.);
#31760=ORIENTED_EDGE('',*,*,#25588,.F.);
#31761=ORIENTED_EDGE('',*,*,#25590,.T.);
#31762=ORIENTED_EDGE('',*,*,#25591,.T.);
#31763=ORIENTED_EDGE('',*,*,#25592,.F.);
#31764=ORIENTED_EDGE('',*,*,#25591,.F.);
#31765=ORIENTED_EDGE('',*,*,#25593,.T.);
#31766=ORIENTED_EDGE('',*,*,#25594,.T.);
#31767=ORIENTED_EDGE('',*,*,#25595,.F.);
#31768=ORIENTED_EDGE('',*,*,#25594,.F.);
#31769=ORIENTED_EDGE('',*,*,#25596,.T.);
#31770=ORIENTED_EDGE('',*,*,#25597,.T.);
#31771=ORIENTED_EDGE('',*,*,#25598,.F.);
#31772=ORIENTED_EDGE('',*,*,#25597,.F.);
#31773=ORIENTED_EDGE('',*,*,#25599,.T.);
#31774=ORIENTED_EDGE('',*,*,#25600,.T.);
#31775=ORIENTED_EDGE('',*,*,#25601,.F.);
#31776=ORIENTED_EDGE('',*,*,#25600,.F.);
#31777=ORIENTED_EDGE('',*,*,#25602,.T.);
#31778=ORIENTED_EDGE('',*,*,#25603,.T.);
#31779=ORIENTED_EDGE('',*,*,#25604,.F.);
#31780=ORIENTED_EDGE('',*,*,#25603,.F.);
#31781=ORIENTED_EDGE('',*,*,#25605,.T.);
#31782=ORIENTED_EDGE('',*,*,#25606,.T.);
#31783=ORIENTED_EDGE('',*,*,#25607,.F.);
#31784=ORIENTED_EDGE('',*,*,#25606,.F.);
#31785=ORIENTED_EDGE('',*,*,#25608,.T.);
#31786=ORIENTED_EDGE('',*,*,#25609,.T.);
#31787=ORIENTED_EDGE('',*,*,#25610,.F.);
#31788=ORIENTED_EDGE('',*,*,#25609,.F.);
#31789=ORIENTED_EDGE('',*,*,#25611,.T.);
#31790=ORIENTED_EDGE('',*,*,#25612,.T.);
#31791=ORIENTED_EDGE('',*,*,#25613,.F.);
#31792=ORIENTED_EDGE('',*,*,#25612,.F.);
#31793=ORIENTED_EDGE('',*,*,#25614,.T.);
#31794=ORIENTED_EDGE('',*,*,#25615,.T.);
#31795=ORIENTED_EDGE('',*,*,#25616,.F.);
#31796=ORIENTED_EDGE('',*,*,#25617,.T.);
#31797=ORIENTED_EDGE('',*,*,#25618,.F.);
#31798=ORIENTED_EDGE('',*,*,#25615,.F.);
#31799=ORIENTED_EDGE('',*,*,#25619,.T.);
#31800=ORIENTED_EDGE('',*,*,#25620,.T.);
#31801=ORIENTED_EDGE('',*,*,#25621,.F.);
#31802=ORIENTED_EDGE('',*,*,#25620,.F.);
#31803=ORIENTED_EDGE('',*,*,#25622,.T.);
#31804=ORIENTED_EDGE('',*,*,#25623,.T.);
#31805=ORIENTED_EDGE('',*,*,#25624,.F.);
#31806=ORIENTED_EDGE('',*,*,#25623,.F.);
#31807=ORIENTED_EDGE('',*,*,#25625,.T.);
#31808=ORIENTED_EDGE('',*,*,#25626,.T.);
#31809=ORIENTED_EDGE('',*,*,#25627,.F.);
#31810=ORIENTED_EDGE('',*,*,#25626,.F.);
#31811=ORIENTED_EDGE('',*,*,#25628,.T.);
#31812=ORIENTED_EDGE('',*,*,#25629,.T.);
#31813=ORIENTED_EDGE('',*,*,#25630,.F.);
#31814=ORIENTED_EDGE('',*,*,#25629,.F.);
#31815=ORIENTED_EDGE('',*,*,#25631,.T.);
#31816=ORIENTED_EDGE('',*,*,#25632,.T.);
#31817=ORIENTED_EDGE('',*,*,#25633,.F.);
#31818=ORIENTED_EDGE('',*,*,#25632,.F.);
#31819=ORIENTED_EDGE('',*,*,#25634,.T.);
#31820=ORIENTED_EDGE('',*,*,#25635,.T.);
#31821=ORIENTED_EDGE('',*,*,#25636,.F.);
#31822=ORIENTED_EDGE('',*,*,#25635,.F.);
#31823=ORIENTED_EDGE('',*,*,#25637,.T.);
#31824=ORIENTED_EDGE('',*,*,#25638,.T.);
#31825=ORIENTED_EDGE('',*,*,#25639,.F.);
#31826=ORIENTED_EDGE('',*,*,#25638,.F.);
#31827=ORIENTED_EDGE('',*,*,#25640,.T.);
#31828=ORIENTED_EDGE('',*,*,#25641,.T.);
#31829=ORIENTED_EDGE('',*,*,#25642,.F.);
#31830=ORIENTED_EDGE('',*,*,#25641,.F.);
#31831=ORIENTED_EDGE('',*,*,#25643,.T.);
#31832=ORIENTED_EDGE('',*,*,#25644,.T.);
#31833=ORIENTED_EDGE('',*,*,#25645,.F.);
#31834=ORIENTED_EDGE('',*,*,#25644,.F.);
#31835=ORIENTED_EDGE('',*,*,#25646,.T.);
#31836=ORIENTED_EDGE('',*,*,#25647,.T.);
#31837=ORIENTED_EDGE('',*,*,#25648,.F.);
#31838=ORIENTED_EDGE('',*,*,#25647,.F.);
#31839=ORIENTED_EDGE('',*,*,#25649,.T.);
#31840=ORIENTED_EDGE('',*,*,#25650,.T.);
#31841=ORIENTED_EDGE('',*,*,#25651,.F.);
#31842=ORIENTED_EDGE('',*,*,#25650,.F.);
#31843=ORIENTED_EDGE('',*,*,#25652,.T.);
#31844=ORIENTED_EDGE('',*,*,#25653,.T.);
#31845=ORIENTED_EDGE('',*,*,#25654,.F.);
#31846=ORIENTED_EDGE('',*,*,#25653,.F.);
#31847=ORIENTED_EDGE('',*,*,#25655,.T.);
#31848=ORIENTED_EDGE('',*,*,#25656,.T.);
#31849=ORIENTED_EDGE('',*,*,#25657,.F.);
#31850=ORIENTED_EDGE('',*,*,#25656,.F.);
#31851=ORIENTED_EDGE('',*,*,#25658,.T.);
#31852=ORIENTED_EDGE('',*,*,#25659,.T.);
#31853=ORIENTED_EDGE('',*,*,#25660,.F.);
#31854=ORIENTED_EDGE('',*,*,#25659,.F.);
#31855=ORIENTED_EDGE('',*,*,#25661,.T.);
#31856=ORIENTED_EDGE('',*,*,#25662,.T.);
#31857=ORIENTED_EDGE('',*,*,#25663,.F.);
#31858=ORIENTED_EDGE('',*,*,#25662,.F.);
#31859=ORIENTED_EDGE('',*,*,#25664,.T.);
#31860=ORIENTED_EDGE('',*,*,#25665,.T.);
#31861=ORIENTED_EDGE('',*,*,#25666,.F.);
#31862=ORIENTED_EDGE('',*,*,#25665,.F.);
#31863=ORIENTED_EDGE('',*,*,#25667,.T.);
#31864=ORIENTED_EDGE('',*,*,#25668,.T.);
#31865=ORIENTED_EDGE('',*,*,#25669,.F.);
#31866=ORIENTED_EDGE('',*,*,#25668,.F.);
#31867=ORIENTED_EDGE('',*,*,#25670,.T.);
#31868=ORIENTED_EDGE('',*,*,#25671,.T.);
#31869=ORIENTED_EDGE('',*,*,#25672,.F.);
#31870=ORIENTED_EDGE('',*,*,#25673,.T.);
#31871=ORIENTED_EDGE('',*,*,#25674,.F.);
#31872=ORIENTED_EDGE('',*,*,#25671,.F.);
#31873=ORIENTED_EDGE('',*,*,#25675,.T.);
#31874=ORIENTED_EDGE('',*,*,#25676,.T.);
#31875=ORIENTED_EDGE('',*,*,#25677,.F.);
#31876=ORIENTED_EDGE('',*,*,#25676,.F.);
#31877=ORIENTED_EDGE('',*,*,#25678,.T.);
#31878=ORIENTED_EDGE('',*,*,#25679,.T.);
#31879=ORIENTED_EDGE('',*,*,#25680,.F.);
#31880=ORIENTED_EDGE('',*,*,#25679,.F.);
#31881=ORIENTED_EDGE('',*,*,#25681,.T.);
#31882=ORIENTED_EDGE('',*,*,#25682,.T.);
#31883=ORIENTED_EDGE('',*,*,#25683,.F.);
#31884=ORIENTED_EDGE('',*,*,#25682,.F.);
#31885=ORIENTED_EDGE('',*,*,#25684,.T.);
#31886=ORIENTED_EDGE('',*,*,#25685,.T.);
#31887=ORIENTED_EDGE('',*,*,#25686,.F.);
#31888=ORIENTED_EDGE('',*,*,#25685,.F.);
#31889=ORIENTED_EDGE('',*,*,#25687,.T.);
#31890=ORIENTED_EDGE('',*,*,#25688,.T.);
#31891=ORIENTED_EDGE('',*,*,#25689,.F.);
#31892=ORIENTED_EDGE('',*,*,#25688,.F.);
#31893=ORIENTED_EDGE('',*,*,#25690,.T.);
#31894=ORIENTED_EDGE('',*,*,#25691,.T.);
#31895=ORIENTED_EDGE('',*,*,#25692,.F.);
#31896=ORIENTED_EDGE('',*,*,#25691,.F.);
#31897=ORIENTED_EDGE('',*,*,#25693,.T.);
#31898=ORIENTED_EDGE('',*,*,#25694,.T.);
#31899=ORIENTED_EDGE('',*,*,#25695,.F.);
#31900=ORIENTED_EDGE('',*,*,#25694,.F.);
#31901=ORIENTED_EDGE('',*,*,#25696,.T.);
#31902=ORIENTED_EDGE('',*,*,#25697,.T.);
#31903=ORIENTED_EDGE('',*,*,#25698,.F.);
#31904=ORIENTED_EDGE('',*,*,#25697,.F.);
#31905=ORIENTED_EDGE('',*,*,#25699,.T.);
#31906=ORIENTED_EDGE('',*,*,#25700,.T.);
#31907=ORIENTED_EDGE('',*,*,#25701,.F.);
#31908=ORIENTED_EDGE('',*,*,#25700,.F.);
#31909=ORIENTED_EDGE('',*,*,#25702,.T.);
#31910=ORIENTED_EDGE('',*,*,#25703,.T.);
#31911=ORIENTED_EDGE('',*,*,#25704,.F.);
#31912=ORIENTED_EDGE('',*,*,#25703,.F.);
#31913=ORIENTED_EDGE('',*,*,#25705,.T.);
#31914=ORIENTED_EDGE('',*,*,#25706,.T.);
#31915=ORIENTED_EDGE('',*,*,#25707,.F.);
#31916=ORIENTED_EDGE('',*,*,#25706,.F.);
#31917=ORIENTED_EDGE('',*,*,#25708,.T.);
#31918=ORIENTED_EDGE('',*,*,#25709,.T.);
#31919=ORIENTED_EDGE('',*,*,#25710,.F.);
#31920=ORIENTED_EDGE('',*,*,#25709,.F.);
#31921=ORIENTED_EDGE('',*,*,#25711,.T.);
#31922=ORIENTED_EDGE('',*,*,#25712,.T.);
#31923=ORIENTED_EDGE('',*,*,#25713,.F.);
#31924=ORIENTED_EDGE('',*,*,#25712,.F.);
#31925=ORIENTED_EDGE('',*,*,#25714,.T.);
#31926=ORIENTED_EDGE('',*,*,#25715,.T.);
#31927=ORIENTED_EDGE('',*,*,#25716,.F.);
#31928=ORIENTED_EDGE('',*,*,#25715,.F.);
#31929=ORIENTED_EDGE('',*,*,#25717,.T.);
#31930=ORIENTED_EDGE('',*,*,#25718,.T.);
#31931=ORIENTED_EDGE('',*,*,#25719,.F.);
#31932=ORIENTED_EDGE('',*,*,#25718,.F.);
#31933=ORIENTED_EDGE('',*,*,#25720,.T.);
#31934=ORIENTED_EDGE('',*,*,#25721,.T.);
#31935=ORIENTED_EDGE('',*,*,#25722,.F.);
#31936=ORIENTED_EDGE('',*,*,#25723,.T.);
#31937=ORIENTED_EDGE('',*,*,#25724,.F.);
#31938=ORIENTED_EDGE('',*,*,#25721,.F.);
#31939=ORIENTED_EDGE('',*,*,#25725,.T.);
#31940=ORIENTED_EDGE('',*,*,#25726,.T.);
#31941=ORIENTED_EDGE('',*,*,#25727,.F.);
#31942=ORIENTED_EDGE('',*,*,#25726,.F.);
#31943=ORIENTED_EDGE('',*,*,#25728,.T.);
#31944=ORIENTED_EDGE('',*,*,#25729,.T.);
#31945=ORIENTED_EDGE('',*,*,#25730,.F.);
#31946=ORIENTED_EDGE('',*,*,#25729,.F.);
#31947=ORIENTED_EDGE('',*,*,#25731,.T.);
#31948=ORIENTED_EDGE('',*,*,#25732,.T.);
#31949=ORIENTED_EDGE('',*,*,#25733,.F.);
#31950=ORIENTED_EDGE('',*,*,#25732,.F.);
#31951=ORIENTED_EDGE('',*,*,#25734,.T.);
#31952=ORIENTED_EDGE('',*,*,#25735,.T.);
#31953=ORIENTED_EDGE('',*,*,#25736,.F.);
#31954=ORIENTED_EDGE('',*,*,#25735,.F.);
#31955=ORIENTED_EDGE('',*,*,#25737,.T.);
#31956=ORIENTED_EDGE('',*,*,#25738,.T.);
#31957=ORIENTED_EDGE('',*,*,#25739,.F.);
#31958=ORIENTED_EDGE('',*,*,#25738,.F.);
#31959=ORIENTED_EDGE('',*,*,#25740,.T.);
#31960=ORIENTED_EDGE('',*,*,#25741,.T.);
#31961=ORIENTED_EDGE('',*,*,#25742,.F.);
#31962=ORIENTED_EDGE('',*,*,#25741,.F.);
#31963=ORIENTED_EDGE('',*,*,#25743,.T.);
#31964=ORIENTED_EDGE('',*,*,#25744,.T.);
#31965=ORIENTED_EDGE('',*,*,#25745,.F.);
#31966=ORIENTED_EDGE('',*,*,#25744,.F.);
#31967=ORIENTED_EDGE('',*,*,#25746,.T.);
#31968=ORIENTED_EDGE('',*,*,#25747,.T.);
#31969=ORIENTED_EDGE('',*,*,#25748,.F.);
#31970=ORIENTED_EDGE('',*,*,#25747,.F.);
#31971=ORIENTED_EDGE('',*,*,#25749,.T.);
#31972=ORIENTED_EDGE('',*,*,#25750,.T.);
#31973=ORIENTED_EDGE('',*,*,#25751,.F.);
#31974=ORIENTED_EDGE('',*,*,#25750,.F.);
#31975=ORIENTED_EDGE('',*,*,#25752,.T.);
#31976=ORIENTED_EDGE('',*,*,#25753,.T.);
#31977=ORIENTED_EDGE('',*,*,#25754,.F.);
#31978=ORIENTED_EDGE('',*,*,#25753,.F.);
#31979=ORIENTED_EDGE('',*,*,#25755,.T.);
#31980=ORIENTED_EDGE('',*,*,#25756,.T.);
#31981=ORIENTED_EDGE('',*,*,#25757,.F.);
#31982=ORIENTED_EDGE('',*,*,#25756,.F.);
#31983=ORIENTED_EDGE('',*,*,#25758,.T.);
#31984=ORIENTED_EDGE('',*,*,#25759,.T.);
#31985=ORIENTED_EDGE('',*,*,#25760,.F.);
#31986=ORIENTED_EDGE('',*,*,#25759,.F.);
#31987=ORIENTED_EDGE('',*,*,#25761,.T.);
#31988=ORIENTED_EDGE('',*,*,#25762,.T.);
#31989=ORIENTED_EDGE('',*,*,#25763,.F.);
#31990=ORIENTED_EDGE('',*,*,#25762,.F.);
#31991=ORIENTED_EDGE('',*,*,#25764,.T.);
#31992=ORIENTED_EDGE('',*,*,#25765,.T.);
#31993=ORIENTED_EDGE('',*,*,#25766,.F.);
#31994=ORIENTED_EDGE('',*,*,#25765,.F.);
#31995=ORIENTED_EDGE('',*,*,#25767,.T.);
#31996=ORIENTED_EDGE('',*,*,#25768,.T.);
#31997=ORIENTED_EDGE('',*,*,#25769,.F.);
#31998=ORIENTED_EDGE('',*,*,#25768,.F.);
#31999=ORIENTED_EDGE('',*,*,#25770,.T.);
#32000=ORIENTED_EDGE('',*,*,#25771,.T.);
#32001=ORIENTED_EDGE('',*,*,#25772,.F.);
#32002=ORIENTED_EDGE('',*,*,#25771,.F.);
#32003=ORIENTED_EDGE('',*,*,#25773,.T.);
#32004=ORIENTED_EDGE('',*,*,#25774,.T.);
#32005=ORIENTED_EDGE('',*,*,#25775,.F.);
#32006=ORIENTED_EDGE('',*,*,#25774,.F.);
#32007=ORIENTED_EDGE('',*,*,#25776,.T.);
#32008=ORIENTED_EDGE('',*,*,#25777,.T.);
#32009=ORIENTED_EDGE('',*,*,#25778,.F.);
#32010=ORIENTED_EDGE('',*,*,#25779,.T.);
#32011=ORIENTED_EDGE('',*,*,#25780,.F.);
#32012=ORIENTED_EDGE('',*,*,#25777,.F.);
#32013=ORIENTED_EDGE('',*,*,#25781,.T.);
#32014=ORIENTED_EDGE('',*,*,#25782,.T.);
#32015=ORIENTED_EDGE('',*,*,#25783,.F.);
#32016=ORIENTED_EDGE('',*,*,#25782,.F.);
#32017=ORIENTED_EDGE('',*,*,#25784,.T.);
#32018=ORIENTED_EDGE('',*,*,#25785,.T.);
#32019=ORIENTED_EDGE('',*,*,#25786,.F.);
#32020=ORIENTED_EDGE('',*,*,#25785,.F.);
#32021=ORIENTED_EDGE('',*,*,#25787,.T.);
#32022=ORIENTED_EDGE('',*,*,#25788,.T.);
#32023=ORIENTED_EDGE('',*,*,#25789,.F.);
#32024=ORIENTED_EDGE('',*,*,#25788,.F.);
#32025=ORIENTED_EDGE('',*,*,#25790,.T.);
#32026=ORIENTED_EDGE('',*,*,#25791,.T.);
#32027=ORIENTED_EDGE('',*,*,#25792,.F.);
#32028=ORIENTED_EDGE('',*,*,#25791,.F.);
#32029=ORIENTED_EDGE('',*,*,#25793,.T.);
#32030=ORIENTED_EDGE('',*,*,#25794,.T.);
#32031=ORIENTED_EDGE('',*,*,#25795,.F.);
#32032=ORIENTED_EDGE('',*,*,#25794,.F.);
#32033=ORIENTED_EDGE('',*,*,#25796,.T.);
#32034=ORIENTED_EDGE('',*,*,#25797,.T.);
#32035=ORIENTED_EDGE('',*,*,#25798,.F.);
#32036=ORIENTED_EDGE('',*,*,#25797,.F.);
#32037=ORIENTED_EDGE('',*,*,#25799,.T.);
#32038=ORIENTED_EDGE('',*,*,#25800,.T.);
#32039=ORIENTED_EDGE('',*,*,#25801,.F.);
#32040=ORIENTED_EDGE('',*,*,#25800,.F.);
#32041=ORIENTED_EDGE('',*,*,#25802,.T.);
#32042=ORIENTED_EDGE('',*,*,#25803,.T.);
#32043=ORIENTED_EDGE('',*,*,#25804,.F.);
#32044=ORIENTED_EDGE('',*,*,#25803,.F.);
#32045=ORIENTED_EDGE('',*,*,#25805,.T.);
#32046=ORIENTED_EDGE('',*,*,#25806,.T.);
#32047=ORIENTED_EDGE('',*,*,#25807,.F.);
#32048=ORIENTED_EDGE('',*,*,#25806,.F.);
#32049=ORIENTED_EDGE('',*,*,#25808,.T.);
#32050=ORIENTED_EDGE('',*,*,#25809,.T.);
#32051=ORIENTED_EDGE('',*,*,#25810,.F.);
#32052=ORIENTED_EDGE('',*,*,#25809,.F.);
#32053=ORIENTED_EDGE('',*,*,#25811,.T.);
#32054=ORIENTED_EDGE('',*,*,#25812,.T.);
#32055=ORIENTED_EDGE('',*,*,#25813,.F.);
#32056=ORIENTED_EDGE('',*,*,#25812,.F.);
#32057=ORIENTED_EDGE('',*,*,#25814,.T.);
#32058=ORIENTED_EDGE('',*,*,#25815,.T.);
#32059=ORIENTED_EDGE('',*,*,#25816,.F.);
#32060=ORIENTED_EDGE('',*,*,#25815,.F.);
#32061=ORIENTED_EDGE('',*,*,#25817,.T.);
#32062=ORIENTED_EDGE('',*,*,#25818,.T.);
#32063=ORIENTED_EDGE('',*,*,#25819,.F.);
#32064=ORIENTED_EDGE('',*,*,#25818,.F.);
#32065=ORIENTED_EDGE('',*,*,#25820,.T.);
#32066=ORIENTED_EDGE('',*,*,#25821,.T.);
#32067=ORIENTED_EDGE('',*,*,#25822,.F.);
#32068=ORIENTED_EDGE('',*,*,#25821,.F.);
#32069=ORIENTED_EDGE('',*,*,#25823,.T.);
#32070=ORIENTED_EDGE('',*,*,#25824,.T.);
#32071=ORIENTED_EDGE('',*,*,#25825,.F.);
#32072=ORIENTED_EDGE('',*,*,#25824,.F.);
#32073=ORIENTED_EDGE('',*,*,#25826,.T.);
#32074=ORIENTED_EDGE('',*,*,#25827,.T.);
#32075=ORIENTED_EDGE('',*,*,#25828,.F.);
#32076=ORIENTED_EDGE('',*,*,#25827,.F.);
#32077=ORIENTED_EDGE('',*,*,#25829,.T.);
#32078=ORIENTED_EDGE('',*,*,#25830,.T.);
#32079=ORIENTED_EDGE('',*,*,#25831,.F.);
#32080=ORIENTED_EDGE('',*,*,#25830,.F.);
#32081=ORIENTED_EDGE('',*,*,#25832,.T.);
#32082=ORIENTED_EDGE('',*,*,#25833,.T.);
#32083=ORIENTED_EDGE('',*,*,#25834,.F.);
#32084=ORIENTED_EDGE('',*,*,#25835,.T.);
#32085=ORIENTED_EDGE('',*,*,#25836,.F.);
#32086=ORIENTED_EDGE('',*,*,#25833,.F.);
#32087=ORIENTED_EDGE('',*,*,#25837,.T.);
#32088=ORIENTED_EDGE('',*,*,#25838,.T.);
#32089=ORIENTED_EDGE('',*,*,#25839,.F.);
#32090=ORIENTED_EDGE('',*,*,#25838,.F.);
#32091=ORIENTED_EDGE('',*,*,#25840,.T.);
#32092=ORIENTED_EDGE('',*,*,#25841,.T.);
#32093=ORIENTED_EDGE('',*,*,#25842,.F.);
#32094=ORIENTED_EDGE('',*,*,#25841,.F.);
#32095=ORIENTED_EDGE('',*,*,#25843,.T.);
#32096=ORIENTED_EDGE('',*,*,#25844,.T.);
#32097=ORIENTED_EDGE('',*,*,#25845,.F.);
#32098=ORIENTED_EDGE('',*,*,#25844,.F.);
#32099=ORIENTED_EDGE('',*,*,#25846,.T.);
#32100=ORIENTED_EDGE('',*,*,#25847,.T.);
#32101=ORIENTED_EDGE('',*,*,#25848,.F.);
#32102=ORIENTED_EDGE('',*,*,#25847,.F.);
#32103=ORIENTED_EDGE('',*,*,#25849,.T.);
#32104=ORIENTED_EDGE('',*,*,#25850,.T.);
#32105=ORIENTED_EDGE('',*,*,#25851,.F.);
#32106=ORIENTED_EDGE('',*,*,#25850,.F.);
#32107=ORIENTED_EDGE('',*,*,#25852,.T.);
#32108=ORIENTED_EDGE('',*,*,#25853,.T.);
#32109=ORIENTED_EDGE('',*,*,#25854,.F.);
#32110=ORIENTED_EDGE('',*,*,#25853,.F.);
#32111=ORIENTED_EDGE('',*,*,#25855,.T.);
#32112=ORIENTED_EDGE('',*,*,#25856,.T.);
#32113=ORIENTED_EDGE('',*,*,#25857,.F.);
#32114=ORIENTED_EDGE('',*,*,#25856,.F.);
#32115=ORIENTED_EDGE('',*,*,#25858,.T.);
#32116=ORIENTED_EDGE('',*,*,#25859,.T.);
#32117=ORIENTED_EDGE('',*,*,#25860,.F.);
#32118=ORIENTED_EDGE('',*,*,#25859,.F.);
#32119=ORIENTED_EDGE('',*,*,#25861,.T.);
#32120=ORIENTED_EDGE('',*,*,#25862,.T.);
#32121=ORIENTED_EDGE('',*,*,#25863,.F.);
#32122=ORIENTED_EDGE('',*,*,#25862,.F.);
#32123=ORIENTED_EDGE('',*,*,#25864,.T.);
#32124=ORIENTED_EDGE('',*,*,#25865,.T.);
#32125=ORIENTED_EDGE('',*,*,#25866,.F.);
#32126=ORIENTED_EDGE('',*,*,#25865,.F.);
#32127=ORIENTED_EDGE('',*,*,#25867,.T.);
#32128=ORIENTED_EDGE('',*,*,#25868,.T.);
#32129=ORIENTED_EDGE('',*,*,#25869,.F.);
#32130=ORIENTED_EDGE('',*,*,#25868,.F.);
#32131=ORIENTED_EDGE('',*,*,#25870,.T.);
#32132=ORIENTED_EDGE('',*,*,#25871,.T.);
#32133=ORIENTED_EDGE('',*,*,#25872,.F.);
#32134=ORIENTED_EDGE('',*,*,#25871,.F.);
#32135=ORIENTED_EDGE('',*,*,#25873,.T.);
#32136=ORIENTED_EDGE('',*,*,#25874,.T.);
#32137=ORIENTED_EDGE('',*,*,#25875,.F.);
#32138=ORIENTED_EDGE('',*,*,#25874,.F.);
#32139=ORIENTED_EDGE('',*,*,#25876,.T.);
#32140=ORIENTED_EDGE('',*,*,#25877,.T.);
#32141=ORIENTED_EDGE('',*,*,#25878,.F.);
#32142=ORIENTED_EDGE('',*,*,#25877,.F.);
#32143=ORIENTED_EDGE('',*,*,#25879,.T.);
#32144=ORIENTED_EDGE('',*,*,#25880,.T.);
#32145=ORIENTED_EDGE('',*,*,#25881,.F.);
#32146=ORIENTED_EDGE('',*,*,#25880,.F.);
#32147=ORIENTED_EDGE('',*,*,#25882,.T.);
#32148=ORIENTED_EDGE('',*,*,#25883,.T.);
#32149=ORIENTED_EDGE('',*,*,#25884,.F.);
#32150=ORIENTED_EDGE('',*,*,#25883,.F.);
#32151=ORIENTED_EDGE('',*,*,#25885,.T.);
#32152=ORIENTED_EDGE('',*,*,#25886,.T.);
#32153=ORIENTED_EDGE('',*,*,#25887,.F.);
#32154=ORIENTED_EDGE('',*,*,#25886,.F.);
#32155=ORIENTED_EDGE('',*,*,#25888,.T.);
#32156=ORIENTED_EDGE('',*,*,#25889,.T.);
#32157=ORIENTED_EDGE('',*,*,#25890,.F.);
#32158=ORIENTED_EDGE('',*,*,#25891,.T.);
#32159=ORIENTED_EDGE('',*,*,#25892,.F.);
#32160=ORIENTED_EDGE('',*,*,#25889,.F.);
#32161=ORIENTED_EDGE('',*,*,#25893,.T.);
#32162=ORIENTED_EDGE('',*,*,#25894,.T.);
#32163=ORIENTED_EDGE('',*,*,#25895,.F.);
#32164=ORIENTED_EDGE('',*,*,#25894,.F.);
#32165=ORIENTED_EDGE('',*,*,#25896,.T.);
#32166=ORIENTED_EDGE('',*,*,#25897,.T.);
#32167=ORIENTED_EDGE('',*,*,#25898,.F.);
#32168=ORIENTED_EDGE('',*,*,#25897,.F.);
#32169=ORIENTED_EDGE('',*,*,#25899,.T.);
#32170=ORIENTED_EDGE('',*,*,#25900,.T.);
#32171=ORIENTED_EDGE('',*,*,#25901,.F.);
#32172=ORIENTED_EDGE('',*,*,#25900,.F.);
#32173=ORIENTED_EDGE('',*,*,#25902,.T.);
#32174=ORIENTED_EDGE('',*,*,#25903,.T.);
#32175=ORIENTED_EDGE('',*,*,#25904,.F.);
#32176=ORIENTED_EDGE('',*,*,#25903,.F.);
#32177=ORIENTED_EDGE('',*,*,#25905,.T.);
#32178=ORIENTED_EDGE('',*,*,#25906,.T.);
#32179=ORIENTED_EDGE('',*,*,#25907,.F.);
#32180=ORIENTED_EDGE('',*,*,#25906,.F.);
#32181=ORIENTED_EDGE('',*,*,#25908,.T.);
#32182=ORIENTED_EDGE('',*,*,#25909,.T.);
#32183=ORIENTED_EDGE('',*,*,#25910,.F.);
#32184=ORIENTED_EDGE('',*,*,#25909,.F.);
#32185=ORIENTED_EDGE('',*,*,#25911,.T.);
#32186=ORIENTED_EDGE('',*,*,#25912,.T.);
#32187=ORIENTED_EDGE('',*,*,#25913,.F.);
#32188=ORIENTED_EDGE('',*,*,#25912,.F.);
#32189=ORIENTED_EDGE('',*,*,#25914,.T.);
#32190=ORIENTED_EDGE('',*,*,#25915,.T.);
#32191=ORIENTED_EDGE('',*,*,#25916,.F.);
#32192=ORIENTED_EDGE('',*,*,#25915,.F.);
#32193=ORIENTED_EDGE('',*,*,#25917,.T.);
#32194=ORIENTED_EDGE('',*,*,#25918,.T.);
#32195=ORIENTED_EDGE('',*,*,#25919,.F.);
#32196=ORIENTED_EDGE('',*,*,#25918,.F.);
#32197=ORIENTED_EDGE('',*,*,#25920,.T.);
#32198=ORIENTED_EDGE('',*,*,#25921,.T.);
#32199=ORIENTED_EDGE('',*,*,#25922,.F.);
#32200=ORIENTED_EDGE('',*,*,#25921,.F.);
#32201=ORIENTED_EDGE('',*,*,#25923,.T.);
#32202=ORIENTED_EDGE('',*,*,#25924,.T.);
#32203=ORIENTED_EDGE('',*,*,#25925,.F.);
#32204=ORIENTED_EDGE('',*,*,#25924,.F.);
#32205=ORIENTED_EDGE('',*,*,#25926,.T.);
#32206=ORIENTED_EDGE('',*,*,#25927,.T.);
#32207=ORIENTED_EDGE('',*,*,#25928,.F.);
#32208=ORIENTED_EDGE('',*,*,#25927,.F.);
#32209=ORIENTED_EDGE('',*,*,#25929,.T.);
#32210=ORIENTED_EDGE('',*,*,#25930,.T.);
#32211=ORIENTED_EDGE('',*,*,#25931,.F.);
#32212=ORIENTED_EDGE('',*,*,#25930,.F.);
#32213=ORIENTED_EDGE('',*,*,#25932,.T.);
#32214=ORIENTED_EDGE('',*,*,#25933,.T.);
#32215=ORIENTED_EDGE('',*,*,#25934,.F.);
#32216=ORIENTED_EDGE('',*,*,#25933,.F.);
#32217=ORIENTED_EDGE('',*,*,#25935,.T.);
#32218=ORIENTED_EDGE('',*,*,#25936,.T.);
#32219=ORIENTED_EDGE('',*,*,#25937,.F.);
#32220=ORIENTED_EDGE('',*,*,#25936,.F.);
#32221=ORIENTED_EDGE('',*,*,#25938,.T.);
#32222=ORIENTED_EDGE('',*,*,#25939,.T.);
#32223=ORIENTED_EDGE('',*,*,#25940,.F.);
#32224=ORIENTED_EDGE('',*,*,#25939,.F.);
#32225=ORIENTED_EDGE('',*,*,#25941,.T.);
#32226=ORIENTED_EDGE('',*,*,#25942,.T.);
#32227=ORIENTED_EDGE('',*,*,#25943,.F.);
#32228=ORIENTED_EDGE('',*,*,#25942,.F.);
#32229=ORIENTED_EDGE('',*,*,#25944,.T.);
#32230=ORIENTED_EDGE('',*,*,#25945,.T.);
#32231=ORIENTED_EDGE('',*,*,#25946,.F.);
#32232=ORIENTED_EDGE('',*,*,#25947,.T.);
#32233=ORIENTED_EDGE('',*,*,#25948,.F.);
#32234=ORIENTED_EDGE('',*,*,#25945,.F.);
#32235=ORIENTED_EDGE('',*,*,#25949,.T.);
#32236=ORIENTED_EDGE('',*,*,#25950,.T.);
#32237=ORIENTED_EDGE('',*,*,#25951,.F.);
#32238=ORIENTED_EDGE('',*,*,#25950,.F.);
#32239=ORIENTED_EDGE('',*,*,#25952,.T.);
#32240=ORIENTED_EDGE('',*,*,#25953,.T.);
#32241=ORIENTED_EDGE('',*,*,#25954,.F.);
#32242=ORIENTED_EDGE('',*,*,#25953,.F.);
#32243=ORIENTED_EDGE('',*,*,#25955,.T.);
#32244=ORIENTED_EDGE('',*,*,#25956,.T.);
#32245=ORIENTED_EDGE('',*,*,#25957,.F.);
#32246=ORIENTED_EDGE('',*,*,#25956,.F.);
#32247=ORIENTED_EDGE('',*,*,#25958,.T.);
#32248=ORIENTED_EDGE('',*,*,#25959,.T.);
#32249=ORIENTED_EDGE('',*,*,#25960,.F.);
#32250=ORIENTED_EDGE('',*,*,#25959,.F.);
#32251=ORIENTED_EDGE('',*,*,#25961,.T.);
#32252=ORIENTED_EDGE('',*,*,#25962,.T.);
#32253=ORIENTED_EDGE('',*,*,#25963,.F.);
#32254=ORIENTED_EDGE('',*,*,#25962,.F.);
#32255=ORIENTED_EDGE('',*,*,#25964,.T.);
#32256=ORIENTED_EDGE('',*,*,#25965,.T.);
#32257=ORIENTED_EDGE('',*,*,#25966,.F.);
#32258=ORIENTED_EDGE('',*,*,#25965,.F.);
#32259=ORIENTED_EDGE('',*,*,#25967,.T.);
#32260=ORIENTED_EDGE('',*,*,#25968,.T.);
#32261=ORIENTED_EDGE('',*,*,#25969,.F.);
#32262=ORIENTED_EDGE('',*,*,#25968,.F.);
#32263=ORIENTED_EDGE('',*,*,#25970,.T.);
#32264=ORIENTED_EDGE('',*,*,#25971,.T.);
#32265=ORIENTED_EDGE('',*,*,#25972,.F.);
#32266=ORIENTED_EDGE('',*,*,#25971,.F.);
#32267=ORIENTED_EDGE('',*,*,#25973,.T.);
#32268=ORIENTED_EDGE('',*,*,#25974,.T.);
#32269=ORIENTED_EDGE('',*,*,#25975,.F.);
#32270=ORIENTED_EDGE('',*,*,#25974,.F.);
#32271=ORIENTED_EDGE('',*,*,#25976,.T.);
#32272=ORIENTED_EDGE('',*,*,#25977,.T.);
#32273=ORIENTED_EDGE('',*,*,#25978,.F.);
#32274=ORIENTED_EDGE('',*,*,#25977,.F.);
#32275=ORIENTED_EDGE('',*,*,#25979,.T.);
#32276=ORIENTED_EDGE('',*,*,#25980,.T.);
#32277=ORIENTED_EDGE('',*,*,#25981,.F.);
#32278=ORIENTED_EDGE('',*,*,#25980,.F.);
#32279=ORIENTED_EDGE('',*,*,#25982,.T.);
#32280=ORIENTED_EDGE('',*,*,#25983,.T.);
#32281=ORIENTED_EDGE('',*,*,#25984,.F.);
#32282=ORIENTED_EDGE('',*,*,#25983,.F.);
#32283=ORIENTED_EDGE('',*,*,#25985,.T.);
#32284=ORIENTED_EDGE('',*,*,#25986,.T.);
#32285=ORIENTED_EDGE('',*,*,#25987,.F.);
#32286=ORIENTED_EDGE('',*,*,#25986,.F.);
#32287=ORIENTED_EDGE('',*,*,#25988,.T.);
#32288=ORIENTED_EDGE('',*,*,#25989,.T.);
#32289=ORIENTED_EDGE('',*,*,#25990,.F.);
#32290=ORIENTED_EDGE('',*,*,#25989,.F.);
#32291=ORIENTED_EDGE('',*,*,#25991,.T.);
#32292=ORIENTED_EDGE('',*,*,#25992,.T.);
#32293=ORIENTED_EDGE('',*,*,#25993,.F.);
#32294=ORIENTED_EDGE('',*,*,#25992,.F.);
#32295=ORIENTED_EDGE('',*,*,#25994,.T.);
#32296=ORIENTED_EDGE('',*,*,#25995,.T.);
#32297=ORIENTED_EDGE('',*,*,#25996,.F.);
#32298=ORIENTED_EDGE('',*,*,#25997,.T.);
#32299=ORIENTED_EDGE('',*,*,#25998,.F.);
#32300=ORIENTED_EDGE('',*,*,#25995,.F.);
#32301=ORIENTED_EDGE('',*,*,#25999,.T.);
#32302=ORIENTED_EDGE('',*,*,#26000,.T.);
#32303=ORIENTED_EDGE('',*,*,#26001,.F.);
#32304=ORIENTED_EDGE('',*,*,#26000,.F.);
#32305=ORIENTED_EDGE('',*,*,#26002,.T.);
#32306=ORIENTED_EDGE('',*,*,#26003,.T.);
#32307=ORIENTED_EDGE('',*,*,#26004,.F.);
#32308=ORIENTED_EDGE('',*,*,#26003,.F.);
#32309=ORIENTED_EDGE('',*,*,#26005,.T.);
#32310=ORIENTED_EDGE('',*,*,#26006,.T.);
#32311=ORIENTED_EDGE('',*,*,#26007,.F.);
#32312=ORIENTED_EDGE('',*,*,#26006,.F.);
#32313=ORIENTED_EDGE('',*,*,#26008,.T.);
#32314=ORIENTED_EDGE('',*,*,#26009,.T.);
#32315=ORIENTED_EDGE('',*,*,#26010,.F.);
#32316=ORIENTED_EDGE('',*,*,#26009,.F.);
#32317=ORIENTED_EDGE('',*,*,#26011,.T.);
#32318=ORIENTED_EDGE('',*,*,#26012,.T.);
#32319=ORIENTED_EDGE('',*,*,#26013,.F.);
#32320=ORIENTED_EDGE('',*,*,#26012,.F.);
#32321=ORIENTED_EDGE('',*,*,#26014,.T.);
#32322=ORIENTED_EDGE('',*,*,#26015,.T.);
#32323=ORIENTED_EDGE('',*,*,#26016,.F.);
#32324=ORIENTED_EDGE('',*,*,#26015,.F.);
#32325=ORIENTED_EDGE('',*,*,#26017,.T.);
#32326=ORIENTED_EDGE('',*,*,#26018,.T.);
#32327=ORIENTED_EDGE('',*,*,#26019,.F.);
#32328=ORIENTED_EDGE('',*,*,#26018,.F.);
#32329=ORIENTED_EDGE('',*,*,#26020,.T.);
#32330=ORIENTED_EDGE('',*,*,#26021,.T.);
#32331=ORIENTED_EDGE('',*,*,#26022,.F.);
#32332=ORIENTED_EDGE('',*,*,#26021,.F.);
#32333=ORIENTED_EDGE('',*,*,#26023,.T.);
#32334=ORIENTED_EDGE('',*,*,#26024,.T.);
#32335=ORIENTED_EDGE('',*,*,#26025,.F.);
#32336=ORIENTED_EDGE('',*,*,#26024,.F.);
#32337=ORIENTED_EDGE('',*,*,#26026,.T.);
#32338=ORIENTED_EDGE('',*,*,#26027,.T.);
#32339=ORIENTED_EDGE('',*,*,#26028,.F.);
#32340=ORIENTED_EDGE('',*,*,#26027,.F.);
#32341=ORIENTED_EDGE('',*,*,#26029,.T.);
#32342=ORIENTED_EDGE('',*,*,#26030,.T.);
#32343=ORIENTED_EDGE('',*,*,#26031,.F.);
#32344=ORIENTED_EDGE('',*,*,#26030,.F.);
#32345=ORIENTED_EDGE('',*,*,#26032,.T.);
#32346=ORIENTED_EDGE('',*,*,#26033,.T.);
#32347=ORIENTED_EDGE('',*,*,#26034,.F.);
#32348=ORIENTED_EDGE('',*,*,#26033,.F.);
#32349=ORIENTED_EDGE('',*,*,#26035,.T.);
#32350=ORIENTED_EDGE('',*,*,#26036,.T.);
#32351=ORIENTED_EDGE('',*,*,#26037,.F.);
#32352=ORIENTED_EDGE('',*,*,#26036,.F.);
#32353=ORIENTED_EDGE('',*,*,#26038,.T.);
#32354=ORIENTED_EDGE('',*,*,#26039,.T.);
#32355=ORIENTED_EDGE('',*,*,#26040,.F.);
#32356=ORIENTED_EDGE('',*,*,#26039,.F.);
#32357=ORIENTED_EDGE('',*,*,#26041,.T.);
#32358=ORIENTED_EDGE('',*,*,#26042,.T.);
#32359=ORIENTED_EDGE('',*,*,#26043,.F.);
#32360=ORIENTED_EDGE('',*,*,#26042,.F.);
#32361=ORIENTED_EDGE('',*,*,#26044,.T.);
#32362=ORIENTED_EDGE('',*,*,#26045,.T.);
#32363=ORIENTED_EDGE('',*,*,#26046,.F.);
#32364=ORIENTED_EDGE('',*,*,#26045,.F.);
#32365=ORIENTED_EDGE('',*,*,#26047,.T.);
#32366=ORIENTED_EDGE('',*,*,#26048,.T.);
#32367=ORIENTED_EDGE('',*,*,#26049,.F.);
#32368=ORIENTED_EDGE('',*,*,#26048,.F.);
#32369=ORIENTED_EDGE('',*,*,#26050,.T.);
#32370=ORIENTED_EDGE('',*,*,#26051,.T.);
#32371=ORIENTED_EDGE('',*,*,#26052,.T.);
#32372=ORIENTED_EDGE('',*,*,#26053,.F.);
#32373=ORIENTED_EDGE('',*,*,#26054,.T.);
#32374=ORIENTED_EDGE('',*,*,#26051,.F.);
#32375=ORIENTED_EDGE('',*,*,#26055,.T.);
#32376=ORIENTED_EDGE('',*,*,#26056,.T.);
#32377=ORIENTED_EDGE('',*,*,#26057,.F.);
#32378=ORIENTED_EDGE('',*,*,#26056,.F.);
#32379=ORIENTED_EDGE('',*,*,#26058,.T.);
#32380=ORIENTED_EDGE('',*,*,#26059,.T.);
#32381=ORIENTED_EDGE('',*,*,#26060,.F.);
#32382=ORIENTED_EDGE('',*,*,#26059,.F.);
#32383=ORIENTED_EDGE('',*,*,#26061,.T.);
#32384=ORIENTED_EDGE('',*,*,#26062,.T.);
#32385=ORIENTED_EDGE('',*,*,#26063,.F.);
#32386=ORIENTED_EDGE('',*,*,#26062,.F.);
#32387=ORIENTED_EDGE('',*,*,#26064,.T.);
#32388=ORIENTED_EDGE('',*,*,#26065,.T.);
#32389=ORIENTED_EDGE('',*,*,#26066,.F.);
#32390=ORIENTED_EDGE('',*,*,#26065,.F.);
#32391=ORIENTED_EDGE('',*,*,#26067,.T.);
#32392=ORIENTED_EDGE('',*,*,#26068,.T.);
#32393=ORIENTED_EDGE('',*,*,#26069,.F.);
#32394=ORIENTED_EDGE('',*,*,#26068,.F.);
#32395=ORIENTED_EDGE('',*,*,#26070,.T.);
#32396=ORIENTED_EDGE('',*,*,#26071,.T.);
#32397=ORIENTED_EDGE('',*,*,#26072,.F.);
#32398=ORIENTED_EDGE('',*,*,#26071,.F.);
#32399=ORIENTED_EDGE('',*,*,#26073,.T.);
#32400=ORIENTED_EDGE('',*,*,#26074,.T.);
#32401=ORIENTED_EDGE('',*,*,#26075,.F.);
#32402=ORIENTED_EDGE('',*,*,#26074,.F.);
#32403=ORIENTED_EDGE('',*,*,#26076,.T.);
#32404=ORIENTED_EDGE('',*,*,#26077,.T.);
#32405=ORIENTED_EDGE('',*,*,#26078,.F.);
#32406=ORIENTED_EDGE('',*,*,#26077,.F.);
#32407=ORIENTED_EDGE('',*,*,#26079,.T.);
#32408=ORIENTED_EDGE('',*,*,#26080,.T.);
#32409=ORIENTED_EDGE('',*,*,#26081,.F.);
#32410=ORIENTED_EDGE('',*,*,#26080,.F.);
#32411=ORIENTED_EDGE('',*,*,#26082,.T.);
#32412=ORIENTED_EDGE('',*,*,#26083,.T.);
#32413=ORIENTED_EDGE('',*,*,#26084,.F.);
#32414=ORIENTED_EDGE('',*,*,#26083,.F.);
#32415=ORIENTED_EDGE('',*,*,#26085,.T.);
#32416=ORIENTED_EDGE('',*,*,#26086,.T.);
#32417=ORIENTED_EDGE('',*,*,#26087,.F.);
#32418=ORIENTED_EDGE('',*,*,#26086,.F.);
#32419=ORIENTED_EDGE('',*,*,#26088,.T.);
#32420=ORIENTED_EDGE('',*,*,#26089,.T.);
#32421=ORIENTED_EDGE('',*,*,#26090,.F.);
#32422=ORIENTED_EDGE('',*,*,#26089,.F.);
#32423=ORIENTED_EDGE('',*,*,#26091,.T.);
#32424=ORIENTED_EDGE('',*,*,#26092,.T.);
#32425=ORIENTED_EDGE('',*,*,#26093,.F.);
#32426=ORIENTED_EDGE('',*,*,#26092,.F.);
#32427=ORIENTED_EDGE('',*,*,#26094,.T.);
#32428=ORIENTED_EDGE('',*,*,#26095,.T.);
#32429=ORIENTED_EDGE('',*,*,#26096,.F.);
#32430=ORIENTED_EDGE('',*,*,#26095,.F.);
#32431=ORIENTED_EDGE('',*,*,#26097,.T.);
#32432=ORIENTED_EDGE('',*,*,#26098,.T.);
#32433=ORIENTED_EDGE('',*,*,#26099,.F.);
#32434=ORIENTED_EDGE('',*,*,#26098,.F.);
#32435=ORIENTED_EDGE('',*,*,#26100,.T.);
#32436=ORIENTED_EDGE('',*,*,#26101,.T.);
#32437=ORIENTED_EDGE('',*,*,#26102,.T.);
#32438=ORIENTED_EDGE('',*,*,#26103,.F.);
#32439=ORIENTED_EDGE('',*,*,#26104,.T.);
#32440=ORIENTED_EDGE('',*,*,#26101,.F.);
#32441=ORIENTED_EDGE('',*,*,#26105,.T.);
#32442=ORIENTED_EDGE('',*,*,#26106,.T.);
#32443=ORIENTED_EDGE('',*,*,#26107,.F.);
#32444=ORIENTED_EDGE('',*,*,#26106,.F.);
#32445=ORIENTED_EDGE('',*,*,#26108,.T.);
#32446=ORIENTED_EDGE('',*,*,#26109,.T.);
#32447=ORIENTED_EDGE('',*,*,#26110,.T.);
#32448=ORIENTED_EDGE('',*,*,#26111,.F.);
#32449=ORIENTED_EDGE('',*,*,#26112,.T.);
#32450=ORIENTED_EDGE('',*,*,#26109,.F.);
#32451=ORIENTED_EDGE('',*,*,#26113,.T.);
#32452=ORIENTED_EDGE('',*,*,#26114,.T.);
#32453=ORIENTED_EDGE('',*,*,#26115,.F.);
#32454=ORIENTED_EDGE('',*,*,#26114,.F.);
#32455=ORIENTED_EDGE('',*,*,#26116,.T.);
#32456=ORIENTED_EDGE('',*,*,#26117,.T.);
#32457=ORIENTED_EDGE('',*,*,#26118,.F.);
#32458=ORIENTED_EDGE('',*,*,#26117,.F.);
#32459=ORIENTED_EDGE('',*,*,#26119,.T.);
#32460=ORIENTED_EDGE('',*,*,#26120,.T.);
#32461=ORIENTED_EDGE('',*,*,#26121,.F.);
#32462=ORIENTED_EDGE('',*,*,#26120,.F.);
#32463=ORIENTED_EDGE('',*,*,#26122,.T.);
#32464=ORIENTED_EDGE('',*,*,#26123,.T.);
#32465=ORIENTED_EDGE('',*,*,#26124,.F.);
#32466=ORIENTED_EDGE('',*,*,#26123,.F.);
#32467=ORIENTED_EDGE('',*,*,#26125,.T.);
#32468=ORIENTED_EDGE('',*,*,#26126,.T.);
#32469=ORIENTED_EDGE('',*,*,#26127,.F.);
#32470=ORIENTED_EDGE('',*,*,#26126,.F.);
#32471=ORIENTED_EDGE('',*,*,#26128,.T.);
#32472=ORIENTED_EDGE('',*,*,#26129,.T.);
#32473=ORIENTED_EDGE('',*,*,#26130,.F.);
#32474=ORIENTED_EDGE('',*,*,#26129,.F.);
#32475=ORIENTED_EDGE('',*,*,#26131,.T.);
#32476=ORIENTED_EDGE('',*,*,#26132,.T.);
#32477=ORIENTED_EDGE('',*,*,#26133,.F.);
#32478=ORIENTED_EDGE('',*,*,#26132,.F.);
#32479=ORIENTED_EDGE('',*,*,#26134,.T.);
#32480=ORIENTED_EDGE('',*,*,#26135,.T.);
#32481=ORIENTED_EDGE('',*,*,#26136,.F.);
#32482=ORIENTED_EDGE('',*,*,#26135,.F.);
#32483=ORIENTED_EDGE('',*,*,#26137,.T.);
#32484=ORIENTED_EDGE('',*,*,#26138,.T.);
#32485=ORIENTED_EDGE('',*,*,#26139,.F.);
#32486=ORIENTED_EDGE('',*,*,#26138,.F.);
#32487=ORIENTED_EDGE('',*,*,#26140,.T.);
#32488=ORIENTED_EDGE('',*,*,#26141,.T.);
#32489=ORIENTED_EDGE('',*,*,#26142,.F.);
#32490=ORIENTED_EDGE('',*,*,#26141,.F.);
#32491=ORIENTED_EDGE('',*,*,#26143,.T.);
#32492=ORIENTED_EDGE('',*,*,#26144,.T.);
#32493=ORIENTED_EDGE('',*,*,#26145,.F.);
#32494=ORIENTED_EDGE('',*,*,#26144,.F.);
#32495=ORIENTED_EDGE('',*,*,#26146,.T.);
#32496=ORIENTED_EDGE('',*,*,#26147,.T.);
#32497=ORIENTED_EDGE('',*,*,#26148,.F.);
#32498=ORIENTED_EDGE('',*,*,#26147,.F.);
#32499=ORIENTED_EDGE('',*,*,#26149,.T.);
#32500=ORIENTED_EDGE('',*,*,#26150,.T.);
#32501=ORIENTED_EDGE('',*,*,#26151,.F.);
#32502=ORIENTED_EDGE('',*,*,#26150,.F.);
#32503=ORIENTED_EDGE('',*,*,#26152,.T.);
#32504=ORIENTED_EDGE('',*,*,#26153,.T.);
#32505=ORIENTED_EDGE('',*,*,#26154,.T.);
#32506=ORIENTED_EDGE('',*,*,#26155,.F.);
#32507=ORIENTED_EDGE('',*,*,#26156,.T.);
#32508=ORIENTED_EDGE('',*,*,#26153,.F.);
#32509=ORIENTED_EDGE('',*,*,#26157,.T.);
#32510=ORIENTED_EDGE('',*,*,#26158,.T.);
#32511=ORIENTED_EDGE('',*,*,#26159,.F.);
#32512=ORIENTED_EDGE('',*,*,#26158,.F.);
#32513=ORIENTED_EDGE('',*,*,#26160,.T.);
#32514=ORIENTED_EDGE('',*,*,#26161,.T.);
#32515=ORIENTED_EDGE('',*,*,#26162,.F.);
#32516=ORIENTED_EDGE('',*,*,#26161,.F.);
#32517=ORIENTED_EDGE('',*,*,#26163,.T.);
#32518=ORIENTED_EDGE('',*,*,#26164,.T.);
#32519=ORIENTED_EDGE('',*,*,#26165,.F.);
#32520=ORIENTED_EDGE('',*,*,#26164,.F.);
#32521=ORIENTED_EDGE('',*,*,#26166,.T.);
#32522=ORIENTED_EDGE('',*,*,#26167,.T.);
#32523=ORIENTED_EDGE('',*,*,#26168,.F.);
#32524=ORIENTED_EDGE('',*,*,#26167,.F.);
#32525=ORIENTED_EDGE('',*,*,#26169,.T.);
#32526=ORIENTED_EDGE('',*,*,#26170,.T.);
#32527=ORIENTED_EDGE('',*,*,#26171,.F.);
#32528=ORIENTED_EDGE('',*,*,#26170,.F.);
#32529=ORIENTED_EDGE('',*,*,#26172,.T.);
#32530=ORIENTED_EDGE('',*,*,#26173,.T.);
#32531=ORIENTED_EDGE('',*,*,#26174,.F.);
#32532=ORIENTED_EDGE('',*,*,#26173,.F.);
#32533=ORIENTED_EDGE('',*,*,#26175,.T.);
#32534=ORIENTED_EDGE('',*,*,#26176,.T.);
#32535=ORIENTED_EDGE('',*,*,#26177,.F.);
#32536=ORIENTED_EDGE('',*,*,#26176,.F.);
#32537=ORIENTED_EDGE('',*,*,#26178,.T.);
#32538=ORIENTED_EDGE('',*,*,#26179,.T.);
#32539=ORIENTED_EDGE('',*,*,#26180,.F.);
#32540=ORIENTED_EDGE('',*,*,#26179,.F.);
#32541=ORIENTED_EDGE('',*,*,#26181,.T.);
#32542=ORIENTED_EDGE('',*,*,#26182,.T.);
#32543=ORIENTED_EDGE('',*,*,#26183,.F.);
#32544=ORIENTED_EDGE('',*,*,#26182,.F.);
#32545=ORIENTED_EDGE('',*,*,#26184,.T.);
#32546=ORIENTED_EDGE('',*,*,#26185,.T.);
#32547=ORIENTED_EDGE('',*,*,#26186,.F.);
#32548=ORIENTED_EDGE('',*,*,#26185,.F.);
#32549=ORIENTED_EDGE('',*,*,#26187,.T.);
#32550=ORIENTED_EDGE('',*,*,#26188,.T.);
#32551=ORIENTED_EDGE('',*,*,#26189,.F.);
#32552=ORIENTED_EDGE('',*,*,#26188,.F.);
#32553=ORIENTED_EDGE('',*,*,#26190,.T.);
#32554=ORIENTED_EDGE('',*,*,#26191,.T.);
#32555=ORIENTED_EDGE('',*,*,#26192,.F.);
#32556=ORIENTED_EDGE('',*,*,#26191,.F.);
#32557=ORIENTED_EDGE('',*,*,#26193,.T.);
#32558=ORIENTED_EDGE('',*,*,#26194,.T.);
#32559=ORIENTED_EDGE('',*,*,#26195,.F.);
#32560=ORIENTED_EDGE('',*,*,#26194,.F.);
#32561=ORIENTED_EDGE('',*,*,#26196,.T.);
#32562=ORIENTED_EDGE('',*,*,#26197,.T.);
#32563=ORIENTED_EDGE('',*,*,#26198,.F.);
#32564=ORIENTED_EDGE('',*,*,#26197,.F.);
#32565=ORIENTED_EDGE('',*,*,#26199,.T.);
#32566=ORIENTED_EDGE('',*,*,#26200,.T.);
#32567=ORIENTED_EDGE('',*,*,#26201,.F.);
#32568=ORIENTED_EDGE('',*,*,#26200,.F.);
#32569=ORIENTED_EDGE('',*,*,#26202,.T.);
#32570=ORIENTED_EDGE('',*,*,#26203,.T.);
#32571=ORIENTED_EDGE('',*,*,#26204,.F.);
#32572=ORIENTED_EDGE('',*,*,#26203,.F.);
#32573=ORIENTED_EDGE('',*,*,#26205,.T.);
#32574=ORIENTED_EDGE('',*,*,#26206,.T.);
#32575=ORIENTED_EDGE('',*,*,#26207,.F.);
#32576=ORIENTED_EDGE('',*,*,#26206,.F.);
#32577=ORIENTED_EDGE('',*,*,#26208,.T.);
#32578=ORIENTED_EDGE('',*,*,#26209,.T.);
#32579=ORIENTED_EDGE('',*,*,#26210,.F.);
#32580=ORIENTED_EDGE('',*,*,#26209,.F.);
#32581=ORIENTED_EDGE('',*,*,#26211,.T.);
#32582=ORIENTED_EDGE('',*,*,#26212,.T.);
#32583=ORIENTED_EDGE('',*,*,#26213,.F.);
#32584=ORIENTED_EDGE('',*,*,#26212,.F.);
#32585=ORIENTED_EDGE('',*,*,#26214,.T.);
#32586=ORIENTED_EDGE('',*,*,#26215,.T.);
#32587=ORIENTED_EDGE('',*,*,#26216,.F.);
#32588=ORIENTED_EDGE('',*,*,#26215,.F.);
#32589=ORIENTED_EDGE('',*,*,#26217,.T.);
#32590=ORIENTED_EDGE('',*,*,#26218,.T.);
#32591=ORIENTED_EDGE('',*,*,#26219,.F.);
#32592=ORIENTED_EDGE('',*,*,#26218,.F.);
#32593=ORIENTED_EDGE('',*,*,#26220,.T.);
#32594=ORIENTED_EDGE('',*,*,#26221,.T.);
#32595=ORIENTED_EDGE('',*,*,#26222,.F.);
#32596=ORIENTED_EDGE('',*,*,#26221,.F.);
#32597=ORIENTED_EDGE('',*,*,#26223,.T.);
#32598=ORIENTED_EDGE('',*,*,#26224,.T.);
#32599=ORIENTED_EDGE('',*,*,#26225,.F.);
#32600=ORIENTED_EDGE('',*,*,#26224,.F.);
#32601=ORIENTED_EDGE('',*,*,#26226,.T.);
#32602=ORIENTED_EDGE('',*,*,#26227,.T.);
#32603=ORIENTED_EDGE('',*,*,#26228,.F.);
#32604=ORIENTED_EDGE('',*,*,#26227,.F.);
#32605=ORIENTED_EDGE('',*,*,#26229,.T.);
#32606=ORIENTED_EDGE('',*,*,#26230,.T.);
#32607=ORIENTED_EDGE('',*,*,#26231,.F.);
#32608=ORIENTED_EDGE('',*,*,#26230,.F.);
#32609=ORIENTED_EDGE('',*,*,#26232,.T.);
#32610=ORIENTED_EDGE('',*,*,#26233,.T.);
#32611=ORIENTED_EDGE('',*,*,#26234,.F.);
#32612=ORIENTED_EDGE('',*,*,#26233,.F.);
#32613=ORIENTED_EDGE('',*,*,#26235,.T.);
#32614=ORIENTED_EDGE('',*,*,#26236,.T.);
#32615=ORIENTED_EDGE('',*,*,#26237,.F.);
#32616=ORIENTED_EDGE('',*,*,#26236,.F.);
#32617=ORIENTED_EDGE('',*,*,#26238,.T.);
#32618=ORIENTED_EDGE('',*,*,#26239,.T.);
#32619=ORIENTED_EDGE('',*,*,#26240,.T.);
#32620=ORIENTED_EDGE('',*,*,#26241,.F.);
#32621=ORIENTED_EDGE('',*,*,#26242,.T.);
#32622=ORIENTED_EDGE('',*,*,#26239,.F.);
#32623=ORIENTED_EDGE('',*,*,#26243,.T.);
#32624=ORIENTED_EDGE('',*,*,#26244,.T.);
#32625=ORIENTED_EDGE('',*,*,#26245,.F.);
#32626=ORIENTED_EDGE('',*,*,#26244,.F.);
#32627=ORIENTED_EDGE('',*,*,#26246,.T.);
#32628=ORIENTED_EDGE('',*,*,#26247,.T.);
#32629=ORIENTED_EDGE('',*,*,#26248,.F.);
#32630=ORIENTED_EDGE('',*,*,#26247,.F.);
#32631=ORIENTED_EDGE('',*,*,#26249,.T.);
#32632=ORIENTED_EDGE('',*,*,#26250,.T.);
#32633=ORIENTED_EDGE('',*,*,#26251,.F.);
#32634=ORIENTED_EDGE('',*,*,#26250,.F.);
#32635=ORIENTED_EDGE('',*,*,#26252,.T.);
#32636=ORIENTED_EDGE('',*,*,#26253,.T.);
#32637=ORIENTED_EDGE('',*,*,#26254,.F.);
#32638=ORIENTED_EDGE('',*,*,#26253,.F.);
#32639=ORIENTED_EDGE('',*,*,#26255,.T.);
#32640=ORIENTED_EDGE('',*,*,#26256,.T.);
#32641=ORIENTED_EDGE('',*,*,#26257,.F.);
#32642=ORIENTED_EDGE('',*,*,#26256,.F.);
#32643=ORIENTED_EDGE('',*,*,#26258,.T.);
#32644=ORIENTED_EDGE('',*,*,#26259,.T.);
#32645=ORIENTED_EDGE('',*,*,#26260,.F.);
#32646=ORIENTED_EDGE('',*,*,#26259,.F.);
#32647=ORIENTED_EDGE('',*,*,#26261,.T.);
#32648=ORIENTED_EDGE('',*,*,#26262,.T.);
#32649=ORIENTED_EDGE('',*,*,#26263,.F.);
#32650=ORIENTED_EDGE('',*,*,#26262,.F.);
#32651=ORIENTED_EDGE('',*,*,#26264,.T.);
#32652=ORIENTED_EDGE('',*,*,#26265,.T.);
#32653=ORIENTED_EDGE('',*,*,#26266,.F.);
#32654=ORIENTED_EDGE('',*,*,#26265,.F.);
#32655=ORIENTED_EDGE('',*,*,#26267,.T.);
#32656=ORIENTED_EDGE('',*,*,#26268,.T.);
#32657=ORIENTED_EDGE('',*,*,#26269,.F.);
#32658=ORIENTED_EDGE('',*,*,#26268,.F.);
#32659=ORIENTED_EDGE('',*,*,#26270,.T.);
#32660=ORIENTED_EDGE('',*,*,#26271,.T.);
#32661=ORIENTED_EDGE('',*,*,#26272,.F.);
#32662=ORIENTED_EDGE('',*,*,#26271,.F.);
#32663=ORIENTED_EDGE('',*,*,#26273,.T.);
#32664=ORIENTED_EDGE('',*,*,#26274,.T.);
#32665=ORIENTED_EDGE('',*,*,#26275,.F.);
#32666=ORIENTED_EDGE('',*,*,#26274,.F.);
#32667=ORIENTED_EDGE('',*,*,#26276,.T.);
#32668=ORIENTED_EDGE('',*,*,#26277,.T.);
#32669=ORIENTED_EDGE('',*,*,#26278,.F.);
#32670=ORIENTED_EDGE('',*,*,#26277,.F.);
#32671=ORIENTED_EDGE('',*,*,#26279,.T.);
#32672=ORIENTED_EDGE('',*,*,#26280,.T.);
#32673=ORIENTED_EDGE('',*,*,#26281,.F.);
#32674=ORIENTED_EDGE('',*,*,#26280,.F.);
#32675=ORIENTED_EDGE('',*,*,#26282,.T.);
#32676=ORIENTED_EDGE('',*,*,#26283,.T.);
#32677=ORIENTED_EDGE('',*,*,#26284,.F.);
#32678=ORIENTED_EDGE('',*,*,#26283,.F.);
#32679=ORIENTED_EDGE('',*,*,#26285,.T.);
#32680=ORIENTED_EDGE('',*,*,#26286,.T.);
#32681=ORIENTED_EDGE('',*,*,#26287,.F.);
#32682=ORIENTED_EDGE('',*,*,#26286,.F.);
#32683=ORIENTED_EDGE('',*,*,#26288,.T.);
#32684=ORIENTED_EDGE('',*,*,#26289,.T.);
#32685=ORIENTED_EDGE('',*,*,#26290,.F.);
#32686=ORIENTED_EDGE('',*,*,#26289,.F.);
#32687=ORIENTED_EDGE('',*,*,#26291,.T.);
#32688=ORIENTED_EDGE('',*,*,#26292,.T.);
#32689=ORIENTED_EDGE('',*,*,#26293,.F.);
#32690=ORIENTED_EDGE('',*,*,#26292,.F.);
#32691=ORIENTED_EDGE('',*,*,#26294,.T.);
#32692=ORIENTED_EDGE('',*,*,#26295,.T.);
#32693=ORIENTED_EDGE('',*,*,#26296,.F.);
#32694=ORIENTED_EDGE('',*,*,#26295,.F.);
#32695=ORIENTED_EDGE('',*,*,#26297,.T.);
#32696=ORIENTED_EDGE('',*,*,#26298,.T.);
#32697=ORIENTED_EDGE('',*,*,#26299,.F.);
#32698=ORIENTED_EDGE('',*,*,#26298,.F.);
#32699=ORIENTED_EDGE('',*,*,#26300,.T.);
#32700=ORIENTED_EDGE('',*,*,#26301,.T.);
#32701=ORIENTED_EDGE('',*,*,#26302,.F.);
#32702=ORIENTED_EDGE('',*,*,#26301,.F.);
#32703=ORIENTED_EDGE('',*,*,#26303,.T.);
#32704=ORIENTED_EDGE('',*,*,#26304,.T.);
#32705=ORIENTED_EDGE('',*,*,#26305,.F.);
#32706=ORIENTED_EDGE('',*,*,#26304,.F.);
#32707=ORIENTED_EDGE('',*,*,#26306,.T.);
#32708=ORIENTED_EDGE('',*,*,#26307,.T.);
#32709=ORIENTED_EDGE('',*,*,#26308,.F.);
#32710=ORIENTED_EDGE('',*,*,#26307,.F.);
#32711=ORIENTED_EDGE('',*,*,#26309,.T.);
#32712=ORIENTED_EDGE('',*,*,#26310,.T.);
#32713=ORIENTED_EDGE('',*,*,#26311,.F.);
#32714=ORIENTED_EDGE('',*,*,#26310,.F.);
#32715=ORIENTED_EDGE('',*,*,#26312,.T.);
#32716=ORIENTED_EDGE('',*,*,#26313,.T.);
#32717=ORIENTED_EDGE('',*,*,#26314,.F.);
#32718=ORIENTED_EDGE('',*,*,#26313,.F.);
#32719=ORIENTED_EDGE('',*,*,#26315,.T.);
#32720=ORIENTED_EDGE('',*,*,#26316,.T.);
#32721=ORIENTED_EDGE('',*,*,#26317,.F.);
#32722=ORIENTED_EDGE('',*,*,#26316,.F.);
#32723=ORIENTED_EDGE('',*,*,#26318,.T.);
#32724=ORIENTED_EDGE('',*,*,#26319,.T.);
#32725=ORIENTED_EDGE('',*,*,#26320,.F.);
#32726=ORIENTED_EDGE('',*,*,#26319,.F.);
#32727=ORIENTED_EDGE('',*,*,#26321,.T.);
#32728=ORIENTED_EDGE('',*,*,#26322,.T.);
#32729=ORIENTED_EDGE('',*,*,#26323,.F.);
#32730=ORIENTED_EDGE('',*,*,#26322,.F.);
#32731=ORIENTED_EDGE('',*,*,#26324,.T.);
#32732=ORIENTED_EDGE('',*,*,#26325,.T.);
#32733=ORIENTED_EDGE('',*,*,#26326,.F.);
#32734=ORIENTED_EDGE('',*,*,#26325,.F.);
#32735=ORIENTED_EDGE('',*,*,#26327,.T.);
#32736=ORIENTED_EDGE('',*,*,#26328,.T.);
#32737=ORIENTED_EDGE('',*,*,#26329,.F.);
#32738=ORIENTED_EDGE('',*,*,#26328,.F.);
#32739=ORIENTED_EDGE('',*,*,#26330,.T.);
#32740=ORIENTED_EDGE('',*,*,#26331,.T.);
#32741=ORIENTED_EDGE('',*,*,#26332,.F.);
#32742=ORIENTED_EDGE('',*,*,#26331,.F.);
#32743=ORIENTED_EDGE('',*,*,#26333,.T.);
#32744=ORIENTED_EDGE('',*,*,#26334,.T.);
#32745=ORIENTED_EDGE('',*,*,#26335,.F.);
#32746=ORIENTED_EDGE('',*,*,#26334,.F.);
#32747=ORIENTED_EDGE('',*,*,#26336,.T.);
#32748=ORIENTED_EDGE('',*,*,#26337,.T.);
#32749=ORIENTED_EDGE('',*,*,#26338,.F.);
#32750=ORIENTED_EDGE('',*,*,#26337,.F.);
#32751=ORIENTED_EDGE('',*,*,#26339,.T.);
#32752=ORIENTED_EDGE('',*,*,#26340,.T.);
#32753=ORIENTED_EDGE('',*,*,#26341,.F.);
#32754=ORIENTED_EDGE('',*,*,#26340,.F.);
#32755=ORIENTED_EDGE('',*,*,#26342,.T.);
#32756=ORIENTED_EDGE('',*,*,#26343,.T.);
#32757=ORIENTED_EDGE('',*,*,#26344,.T.);
#32758=ORIENTED_EDGE('',*,*,#26345,.F.);
#32759=ORIENTED_EDGE('',*,*,#26346,.F.);
#32760=ORIENTED_EDGE('',*,*,#26347,.T.);
#32761=ORIENTED_EDGE('',*,*,#26343,.F.);
#32762=ORIENTED_EDGE('',*,*,#26348,.T.);
#32763=ORIENTED_EDGE('',*,*,#26349,.T.);
#32764=ORIENTED_EDGE('',*,*,#26350,.F.);
#32765=ORIENTED_EDGE('',*,*,#26349,.F.);
#32766=ORIENTED_EDGE('',*,*,#26351,.T.);
#32767=ORIENTED_EDGE('',*,*,#26352,.T.);
#32768=ORIENTED_EDGE('',*,*,#26353,.F.);
#32769=ORIENTED_EDGE('',*,*,#26352,.F.);
#32770=ORIENTED_EDGE('',*,*,#26354,.T.);
#32771=ORIENTED_EDGE('',*,*,#26355,.T.);
#32772=ORIENTED_EDGE('',*,*,#26356,.F.);
#32773=ORIENTED_EDGE('',*,*,#26355,.F.);
#32774=ORIENTED_EDGE('',*,*,#26357,.T.);
#32775=ORIENTED_EDGE('',*,*,#26358,.T.);
#32776=ORIENTED_EDGE('',*,*,#26359,.F.);
#32777=ORIENTED_EDGE('',*,*,#26358,.F.);
#32778=ORIENTED_EDGE('',*,*,#26360,.T.);
#32779=ORIENTED_EDGE('',*,*,#26361,.T.);
#32780=ORIENTED_EDGE('',*,*,#26362,.F.);
#32781=ORIENTED_EDGE('',*,*,#26361,.F.);
#32782=ORIENTED_EDGE('',*,*,#26363,.T.);
#32783=ORIENTED_EDGE('',*,*,#26364,.T.);
#32784=ORIENTED_EDGE('',*,*,#26365,.F.);
#32785=ORIENTED_EDGE('',*,*,#26364,.F.);
#32786=ORIENTED_EDGE('',*,*,#26366,.T.);
#32787=ORIENTED_EDGE('',*,*,#26367,.T.);
#32788=ORIENTED_EDGE('',*,*,#26368,.F.);
#32789=ORIENTED_EDGE('',*,*,#26367,.F.);
#32790=ORIENTED_EDGE('',*,*,#26369,.T.);
#32791=ORIENTED_EDGE('',*,*,#26370,.T.);
#32792=ORIENTED_EDGE('',*,*,#26371,.F.);
#32793=ORIENTED_EDGE('',*,*,#26370,.F.);
#32794=ORIENTED_EDGE('',*,*,#26372,.T.);
#32795=ORIENTED_EDGE('',*,*,#26373,.T.);
#32796=ORIENTED_EDGE('',*,*,#26374,.F.);
#32797=ORIENTED_EDGE('',*,*,#26373,.F.);
#32798=ORIENTED_EDGE('',*,*,#26375,.T.);
#32799=ORIENTED_EDGE('',*,*,#26376,.T.);
#32800=ORIENTED_EDGE('',*,*,#26377,.F.);
#32801=ORIENTED_EDGE('',*,*,#26376,.F.);
#32802=ORIENTED_EDGE('',*,*,#26378,.T.);
#32803=ORIENTED_EDGE('',*,*,#26379,.T.);
#32804=ORIENTED_EDGE('',*,*,#26380,.F.);
#32805=ORIENTED_EDGE('',*,*,#26379,.F.);
#32806=ORIENTED_EDGE('',*,*,#26381,.T.);
#32807=ORIENTED_EDGE('',*,*,#26382,.T.);
#32808=ORIENTED_EDGE('',*,*,#26383,.F.);
#32809=ORIENTED_EDGE('',*,*,#26382,.F.);
#32810=ORIENTED_EDGE('',*,*,#26384,.T.);
#32811=ORIENTED_EDGE('',*,*,#26385,.T.);
#32812=ORIENTED_EDGE('',*,*,#26386,.F.);
#32813=ORIENTED_EDGE('',*,*,#26385,.F.);
#32814=ORIENTED_EDGE('',*,*,#26387,.T.);
#32815=ORIENTED_EDGE('',*,*,#26388,.T.);
#32816=ORIENTED_EDGE('',*,*,#26389,.F.);
#32817=ORIENTED_EDGE('',*,*,#26388,.F.);
#32818=ORIENTED_EDGE('',*,*,#26390,.T.);
#32819=ORIENTED_EDGE('',*,*,#26391,.T.);
#32820=ORIENTED_EDGE('',*,*,#26392,.F.);
#32821=ORIENTED_EDGE('',*,*,#26391,.F.);
#32822=ORIENTED_EDGE('',*,*,#26393,.T.);
#32823=ORIENTED_EDGE('',*,*,#26394,.T.);
#32824=ORIENTED_EDGE('',*,*,#26395,.F.);
#32825=ORIENTED_EDGE('',*,*,#26394,.F.);
#32826=ORIENTED_EDGE('',*,*,#26396,.T.);
#32827=ORIENTED_EDGE('',*,*,#26397,.T.);
#32828=ORIENTED_EDGE('',*,*,#26398,.F.);
#32829=ORIENTED_EDGE('',*,*,#26397,.F.);
#32830=ORIENTED_EDGE('',*,*,#26399,.T.);
#32831=ORIENTED_EDGE('',*,*,#26400,.T.);
#32832=ORIENTED_EDGE('',*,*,#26401,.T.);
#32833=ORIENTED_EDGE('',*,*,#26402,.F.);
#32834=ORIENTED_EDGE('',*,*,#26403,.T.);
#32835=ORIENTED_EDGE('',*,*,#26400,.F.);
#32836=ORIENTED_EDGE('',*,*,#26404,.T.);
#32837=ORIENTED_EDGE('',*,*,#26405,.T.);
#32838=ORIENTED_EDGE('',*,*,#26406,.F.);
#32839=ORIENTED_EDGE('',*,*,#26405,.F.);
#32840=ORIENTED_EDGE('',*,*,#26407,.T.);
#32841=ORIENTED_EDGE('',*,*,#26408,.T.);
#32842=ORIENTED_EDGE('',*,*,#26409,.F.);
#32843=ORIENTED_EDGE('',*,*,#26408,.F.);
#32844=ORIENTED_EDGE('',*,*,#26410,.T.);
#32845=ORIENTED_EDGE('',*,*,#26411,.T.);
#32846=ORIENTED_EDGE('',*,*,#26412,.F.);
#32847=ORIENTED_EDGE('',*,*,#26411,.F.);
#32848=ORIENTED_EDGE('',*,*,#26413,.T.);
#32849=ORIENTED_EDGE('',*,*,#26414,.T.);
#32850=ORIENTED_EDGE('',*,*,#26415,.F.);
#32851=ORIENTED_EDGE('',*,*,#26414,.F.);
#32852=ORIENTED_EDGE('',*,*,#26416,.T.);
#32853=ORIENTED_EDGE('',*,*,#26417,.T.);
#32854=ORIENTED_EDGE('',*,*,#26418,.F.);
#32855=ORIENTED_EDGE('',*,*,#26417,.F.);
#32856=ORIENTED_EDGE('',*,*,#26419,.T.);
#32857=ORIENTED_EDGE('',*,*,#26420,.T.);
#32858=ORIENTED_EDGE('',*,*,#26421,.F.);
#32859=ORIENTED_EDGE('',*,*,#26420,.F.);
#32860=ORIENTED_EDGE('',*,*,#26422,.T.);
#32861=ORIENTED_EDGE('',*,*,#26423,.T.);
#32862=ORIENTED_EDGE('',*,*,#26424,.F.);
#32863=ORIENTED_EDGE('',*,*,#26423,.F.);
#32864=ORIENTED_EDGE('',*,*,#26425,.T.);
#32865=ORIENTED_EDGE('',*,*,#26426,.T.);
#32866=ORIENTED_EDGE('',*,*,#26427,.F.);
#32867=ORIENTED_EDGE('',*,*,#26426,.F.);
#32868=ORIENTED_EDGE('',*,*,#26428,.T.);
#32869=ORIENTED_EDGE('',*,*,#26429,.T.);
#32870=ORIENTED_EDGE('',*,*,#26430,.F.);
#32871=ORIENTED_EDGE('',*,*,#26429,.F.);
#32872=ORIENTED_EDGE('',*,*,#26431,.T.);
#32873=ORIENTED_EDGE('',*,*,#26432,.T.);
#32874=ORIENTED_EDGE('',*,*,#26433,.F.);
#32875=ORIENTED_EDGE('',*,*,#26432,.F.);
#32876=ORIENTED_EDGE('',*,*,#26434,.T.);
#32877=ORIENTED_EDGE('',*,*,#26435,.T.);
#32878=ORIENTED_EDGE('',*,*,#26436,.F.);
#32879=ORIENTED_EDGE('',*,*,#26435,.F.);
#32880=ORIENTED_EDGE('',*,*,#26437,.T.);
#32881=ORIENTED_EDGE('',*,*,#26438,.T.);
#32882=ORIENTED_EDGE('',*,*,#26439,.F.);
#32883=ORIENTED_EDGE('',*,*,#26438,.F.);
#32884=ORIENTED_EDGE('',*,*,#26440,.T.);
#32885=ORIENTED_EDGE('',*,*,#26441,.T.);
#32886=ORIENTED_EDGE('',*,*,#26442,.F.);
#32887=ORIENTED_EDGE('',*,*,#26441,.F.);
#32888=ORIENTED_EDGE('',*,*,#26443,.T.);
#32889=ORIENTED_EDGE('',*,*,#26444,.T.);
#32890=ORIENTED_EDGE('',*,*,#26445,.F.);
#32891=ORIENTED_EDGE('',*,*,#26444,.F.);
#32892=ORIENTED_EDGE('',*,*,#26446,.T.);
#32893=ORIENTED_EDGE('',*,*,#26447,.T.);
#32894=ORIENTED_EDGE('',*,*,#26448,.F.);
#32895=ORIENTED_EDGE('',*,*,#26447,.F.);
#32896=ORIENTED_EDGE('',*,*,#26449,.T.);
#32897=ORIENTED_EDGE('',*,*,#26450,.T.);
#32898=ORIENTED_EDGE('',*,*,#26451,.F.);
#32899=ORIENTED_EDGE('',*,*,#26450,.F.);
#32900=ORIENTED_EDGE('',*,*,#26452,.T.);
#32901=ORIENTED_EDGE('',*,*,#26453,.T.);
#32902=ORIENTED_EDGE('',*,*,#26454,.F.);
#32903=ORIENTED_EDGE('',*,*,#26453,.F.);
#32904=ORIENTED_EDGE('',*,*,#26455,.T.);
#32905=ORIENTED_EDGE('',*,*,#26456,.T.);
#32906=ORIENTED_EDGE('',*,*,#26457,.F.);
#32907=ORIENTED_EDGE('',*,*,#26458,.T.);
#32908=ORIENTED_EDGE('',*,*,#26459,.F.);
#32909=ORIENTED_EDGE('',*,*,#26456,.F.);
#32910=ORIENTED_EDGE('',*,*,#26460,.T.);
#32911=ORIENTED_EDGE('',*,*,#26461,.T.);
#32912=ORIENTED_EDGE('',*,*,#26462,.F.);
#32913=ORIENTED_EDGE('',*,*,#26461,.F.);
#32914=ORIENTED_EDGE('',*,*,#26463,.T.);
#32915=ORIENTED_EDGE('',*,*,#26464,.T.);
#32916=ORIENTED_EDGE('',*,*,#26465,.F.);
#32917=ORIENTED_EDGE('',*,*,#26464,.F.);
#32918=ORIENTED_EDGE('',*,*,#26466,.T.);
#32919=ORIENTED_EDGE('',*,*,#26467,.T.);
#32920=ORIENTED_EDGE('',*,*,#26468,.F.);
#32921=ORIENTED_EDGE('',*,*,#26467,.F.);
#32922=ORIENTED_EDGE('',*,*,#26469,.T.);
#32923=ORIENTED_EDGE('',*,*,#26470,.T.);
#32924=ORIENTED_EDGE('',*,*,#26471,.F.);
#32925=ORIENTED_EDGE('',*,*,#26470,.F.);
#32926=ORIENTED_EDGE('',*,*,#26472,.T.);
#32927=ORIENTED_EDGE('',*,*,#26473,.T.);
#32928=ORIENTED_EDGE('',*,*,#26474,.F.);
#32929=ORIENTED_EDGE('',*,*,#26473,.F.);
#32930=ORIENTED_EDGE('',*,*,#26475,.T.);
#32931=ORIENTED_EDGE('',*,*,#26476,.T.);
#32932=ORIENTED_EDGE('',*,*,#26477,.F.);
#32933=ORIENTED_EDGE('',*,*,#26476,.F.);
#32934=ORIENTED_EDGE('',*,*,#26478,.T.);
#32935=ORIENTED_EDGE('',*,*,#26479,.T.);
#32936=ORIENTED_EDGE('',*,*,#26480,.F.);
#32937=ORIENTED_EDGE('',*,*,#26479,.F.);
#32938=ORIENTED_EDGE('',*,*,#26481,.T.);
#32939=ORIENTED_EDGE('',*,*,#26482,.T.);
#32940=ORIENTED_EDGE('',*,*,#26483,.F.);
#32941=ORIENTED_EDGE('',*,*,#26482,.F.);
#32942=ORIENTED_EDGE('',*,*,#26484,.T.);
#32943=ORIENTED_EDGE('',*,*,#26485,.T.);
#32944=ORIENTED_EDGE('',*,*,#26486,.F.);
#32945=ORIENTED_EDGE('',*,*,#26485,.F.);
#32946=ORIENTED_EDGE('',*,*,#26487,.T.);
#32947=ORIENTED_EDGE('',*,*,#26488,.T.);
#32948=ORIENTED_EDGE('',*,*,#26489,.F.);
#32949=ORIENTED_EDGE('',*,*,#26488,.F.);
#32950=ORIENTED_EDGE('',*,*,#26490,.T.);
#32951=ORIENTED_EDGE('',*,*,#26491,.T.);
#32952=ORIENTED_EDGE('',*,*,#26492,.F.);
#32953=ORIENTED_EDGE('',*,*,#26491,.F.);
#32954=ORIENTED_EDGE('',*,*,#26493,.T.);
#32955=ORIENTED_EDGE('',*,*,#26494,.T.);
#32956=ORIENTED_EDGE('',*,*,#26495,.F.);
#32957=ORIENTED_EDGE('',*,*,#26494,.F.);
#32958=ORIENTED_EDGE('',*,*,#26496,.T.);
#32959=ORIENTED_EDGE('',*,*,#26497,.T.);
#32960=ORIENTED_EDGE('',*,*,#26498,.F.);
#32961=ORIENTED_EDGE('',*,*,#26497,.F.);
#32962=ORIENTED_EDGE('',*,*,#26499,.T.);
#32963=ORIENTED_EDGE('',*,*,#26500,.T.);
#32964=ORIENTED_EDGE('',*,*,#26501,.F.);
#32965=ORIENTED_EDGE('',*,*,#26500,.F.);
#32966=ORIENTED_EDGE('',*,*,#26502,.T.);
#32967=ORIENTED_EDGE('',*,*,#26503,.T.);
#32968=ORIENTED_EDGE('',*,*,#26504,.F.);
#32969=ORIENTED_EDGE('',*,*,#26503,.F.);
#32970=ORIENTED_EDGE('',*,*,#26505,.T.);
#32971=ORIENTED_EDGE('',*,*,#26506,.T.);
#32972=ORIENTED_EDGE('',*,*,#26507,.F.);
#32973=ORIENTED_EDGE('',*,*,#26508,.T.);
#32974=ORIENTED_EDGE('',*,*,#26509,.F.);
#32975=ORIENTED_EDGE('',*,*,#26506,.F.);
#32976=ORIENTED_EDGE('',*,*,#26510,.T.);
#32977=ORIENTED_EDGE('',*,*,#26511,.T.);
#32978=ORIENTED_EDGE('',*,*,#26512,.F.);
#32979=ORIENTED_EDGE('',*,*,#26511,.F.);
#32980=ORIENTED_EDGE('',*,*,#26513,.T.);
#32981=ORIENTED_EDGE('',*,*,#26514,.T.);
#32982=ORIENTED_EDGE('',*,*,#26515,.F.);
#32983=ORIENTED_EDGE('',*,*,#26514,.F.);
#32984=ORIENTED_EDGE('',*,*,#26516,.T.);
#32985=ORIENTED_EDGE('',*,*,#26517,.T.);
#32986=ORIENTED_EDGE('',*,*,#26518,.F.);
#32987=ORIENTED_EDGE('',*,*,#26517,.F.);
#32988=ORIENTED_EDGE('',*,*,#26519,.T.);
#32989=ORIENTED_EDGE('',*,*,#26520,.T.);
#32990=ORIENTED_EDGE('',*,*,#26521,.F.);
#32991=ORIENTED_EDGE('',*,*,#26520,.F.);
#32992=ORIENTED_EDGE('',*,*,#26522,.T.);
#32993=ORIENTED_EDGE('',*,*,#26523,.T.);
#32994=ORIENTED_EDGE('',*,*,#26524,.F.);
#32995=ORIENTED_EDGE('',*,*,#26523,.F.);
#32996=ORIENTED_EDGE('',*,*,#26525,.T.);
#32997=ORIENTED_EDGE('',*,*,#26526,.T.);
#32998=ORIENTED_EDGE('',*,*,#26527,.F.);
#32999=ORIENTED_EDGE('',*,*,#26526,.F.);
#33000=ORIENTED_EDGE('',*,*,#26528,.T.);
#33001=ORIENTED_EDGE('',*,*,#26529,.T.);
#33002=ORIENTED_EDGE('',*,*,#26530,.F.);
#33003=ORIENTED_EDGE('',*,*,#26529,.F.);
#33004=ORIENTED_EDGE('',*,*,#26531,.T.);
#33005=ORIENTED_EDGE('',*,*,#26532,.T.);
#33006=ORIENTED_EDGE('',*,*,#26533,.F.);
#33007=ORIENTED_EDGE('',*,*,#26532,.F.);
#33008=ORIENTED_EDGE('',*,*,#26534,.T.);
#33009=ORIENTED_EDGE('',*,*,#26535,.T.);
#33010=ORIENTED_EDGE('',*,*,#26536,.F.);
#33011=ORIENTED_EDGE('',*,*,#26535,.F.);
#33012=ORIENTED_EDGE('',*,*,#26537,.T.);
#33013=ORIENTED_EDGE('',*,*,#26538,.T.);
#33014=ORIENTED_EDGE('',*,*,#26539,.F.);
#33015=ORIENTED_EDGE('',*,*,#26538,.F.);
#33016=ORIENTED_EDGE('',*,*,#26540,.T.);
#33017=ORIENTED_EDGE('',*,*,#26541,.T.);
#33018=ORIENTED_EDGE('',*,*,#26542,.F.);
#33019=ORIENTED_EDGE('',*,*,#26541,.F.);
#33020=ORIENTED_EDGE('',*,*,#26543,.T.);
#33021=ORIENTED_EDGE('',*,*,#26544,.T.);
#33022=ORIENTED_EDGE('',*,*,#26545,.F.);
#33023=ORIENTED_EDGE('',*,*,#26544,.F.);
#33024=ORIENTED_EDGE('',*,*,#26546,.T.);
#33025=ORIENTED_EDGE('',*,*,#26547,.T.);
#33026=ORIENTED_EDGE('',*,*,#26548,.F.);
#33027=ORIENTED_EDGE('',*,*,#26547,.F.);
#33028=ORIENTED_EDGE('',*,*,#26549,.T.);
#33029=ORIENTED_EDGE('',*,*,#26550,.T.);
#33030=ORIENTED_EDGE('',*,*,#26551,.F.);
#33031=ORIENTED_EDGE('',*,*,#26550,.F.);
#33032=ORIENTED_EDGE('',*,*,#26552,.T.);
#33033=ORIENTED_EDGE('',*,*,#26553,.T.);
#33034=ORIENTED_EDGE('',*,*,#26554,.F.);
#33035=ORIENTED_EDGE('',*,*,#26553,.F.);
#33036=ORIENTED_EDGE('',*,*,#26555,.T.);
#33037=ORIENTED_EDGE('',*,*,#26556,.T.);
#33038=ORIENTED_EDGE('',*,*,#26557,.F.);
#33039=ORIENTED_EDGE('',*,*,#26556,.F.);
#33040=ORIENTED_EDGE('',*,*,#26558,.T.);
#33041=ORIENTED_EDGE('',*,*,#26559,.T.);
#33042=ORIENTED_EDGE('',*,*,#26560,.F.);
#33043=ORIENTED_EDGE('',*,*,#26559,.F.);
#33044=ORIENTED_EDGE('',*,*,#26561,.T.);
#33045=ORIENTED_EDGE('',*,*,#26562,.T.);
#33046=ORIENTED_EDGE('',*,*,#26563,.F.);
#33047=ORIENTED_EDGE('',*,*,#26564,.T.);
#33048=ORIENTED_EDGE('',*,*,#26565,.F.);
#33049=ORIENTED_EDGE('',*,*,#26562,.F.);
#33050=ORIENTED_EDGE('',*,*,#26566,.T.);
#33051=ORIENTED_EDGE('',*,*,#26567,.T.);
#33052=ORIENTED_EDGE('',*,*,#26568,.F.);
#33053=ORIENTED_EDGE('',*,*,#26567,.F.);
#33054=ORIENTED_EDGE('',*,*,#26569,.T.);
#33055=ORIENTED_EDGE('',*,*,#26570,.T.);
#33056=ORIENTED_EDGE('',*,*,#26571,.F.);
#33057=ORIENTED_EDGE('',*,*,#26570,.F.);
#33058=ORIENTED_EDGE('',*,*,#26572,.T.);
#33059=ORIENTED_EDGE('',*,*,#26573,.T.);
#33060=ORIENTED_EDGE('',*,*,#26574,.F.);
#33061=ORIENTED_EDGE('',*,*,#26573,.F.);
#33062=ORIENTED_EDGE('',*,*,#26575,.T.);
#33063=ORIENTED_EDGE('',*,*,#26576,.T.);
#33064=ORIENTED_EDGE('',*,*,#26577,.F.);
#33065=ORIENTED_EDGE('',*,*,#26576,.F.);
#33066=ORIENTED_EDGE('',*,*,#26578,.T.);
#33067=ORIENTED_EDGE('',*,*,#26579,.T.);
#33068=ORIENTED_EDGE('',*,*,#26580,.F.);
#33069=ORIENTED_EDGE('',*,*,#26579,.F.);
#33070=ORIENTED_EDGE('',*,*,#26581,.T.);
#33071=ORIENTED_EDGE('',*,*,#26582,.T.);
#33072=ORIENTED_EDGE('',*,*,#26583,.F.);
#33073=ORIENTED_EDGE('',*,*,#26582,.F.);
#33074=ORIENTED_EDGE('',*,*,#26584,.T.);
#33075=ORIENTED_EDGE('',*,*,#26585,.T.);
#33076=ORIENTED_EDGE('',*,*,#26586,.F.);
#33077=ORIENTED_EDGE('',*,*,#26585,.F.);
#33078=ORIENTED_EDGE('',*,*,#26587,.T.);
#33079=ORIENTED_EDGE('',*,*,#26588,.T.);
#33080=ORIENTED_EDGE('',*,*,#26589,.F.);
#33081=ORIENTED_EDGE('',*,*,#26588,.F.);
#33082=ORIENTED_EDGE('',*,*,#26590,.T.);
#33083=ORIENTED_EDGE('',*,*,#26591,.T.);
#33084=ORIENTED_EDGE('',*,*,#26592,.F.);
#33085=ORIENTED_EDGE('',*,*,#26591,.F.);
#33086=ORIENTED_EDGE('',*,*,#26593,.T.);
#33087=ORIENTED_EDGE('',*,*,#26594,.T.);
#33088=ORIENTED_EDGE('',*,*,#26595,.F.);
#33089=ORIENTED_EDGE('',*,*,#26594,.F.);
#33090=ORIENTED_EDGE('',*,*,#26596,.T.);
#33091=ORIENTED_EDGE('',*,*,#26597,.T.);
#33092=ORIENTED_EDGE('',*,*,#26598,.F.);
#33093=ORIENTED_EDGE('',*,*,#26597,.F.);
#33094=ORIENTED_EDGE('',*,*,#26599,.T.);
#33095=ORIENTED_EDGE('',*,*,#26600,.T.);
#33096=ORIENTED_EDGE('',*,*,#26601,.F.);
#33097=ORIENTED_EDGE('',*,*,#26600,.F.);
#33098=ORIENTED_EDGE('',*,*,#26602,.T.);
#33099=ORIENTED_EDGE('',*,*,#26603,.T.);
#33100=ORIENTED_EDGE('',*,*,#26604,.F.);
#33101=ORIENTED_EDGE('',*,*,#26603,.F.);
#33102=ORIENTED_EDGE('',*,*,#26605,.T.);
#33103=ORIENTED_EDGE('',*,*,#26606,.T.);
#33104=ORIENTED_EDGE('',*,*,#26607,.F.);
#33105=ORIENTED_EDGE('',*,*,#26606,.F.);
#33106=ORIENTED_EDGE('',*,*,#26608,.T.);
#33107=ORIENTED_EDGE('',*,*,#26609,.T.);
#33108=ORIENTED_EDGE('',*,*,#26610,.F.);
#33109=ORIENTED_EDGE('',*,*,#26609,.F.);
#33110=ORIENTED_EDGE('',*,*,#26611,.T.);
#33111=ORIENTED_EDGE('',*,*,#26612,.T.);
#33112=ORIENTED_EDGE('',*,*,#26613,.F.);
#33113=ORIENTED_EDGE('',*,*,#26612,.F.);
#33114=ORIENTED_EDGE('',*,*,#26614,.T.);
#33115=ORIENTED_EDGE('',*,*,#26615,.T.);
#33116=ORIENTED_EDGE('',*,*,#26616,.F.);
#33117=ORIENTED_EDGE('',*,*,#26615,.F.);
#33118=ORIENTED_EDGE('',*,*,#26617,.T.);
#33119=ORIENTED_EDGE('',*,*,#26618,.T.);
#33120=ORIENTED_EDGE('',*,*,#26619,.F.);
#33121=ORIENTED_EDGE('',*,*,#26620,.T.);
#33122=ORIENTED_EDGE('',*,*,#26621,.F.);
#33123=ORIENTED_EDGE('',*,*,#26618,.F.);
#33124=ORIENTED_EDGE('',*,*,#26622,.T.);
#33125=ORIENTED_EDGE('',*,*,#26623,.T.);
#33126=ORIENTED_EDGE('',*,*,#26624,.F.);
#33127=ORIENTED_EDGE('',*,*,#26623,.F.);
#33128=ORIENTED_EDGE('',*,*,#26625,.F.);
#33129=ORIENTED_EDGE('',*,*,#26626,.F.);
#33130=ORIENTED_EDGE('',*,*,#26345,.T.);
#33131=ORIENTED_EDGE('',*,*,#26627,.F.);
#33132=ORIENTED_EDGE('',*,*,#26402,.T.);
#33133=ORIENTED_EDGE('',*,*,#26628,.F.);
#33134=ORIENTED_EDGE('',*,*,#26457,.T.);
#33135=ORIENTED_EDGE('',*,*,#26459,.T.);
#33136=ORIENTED_EDGE('',*,*,#26629,.F.);
#33137=ORIENTED_EDGE('',*,*,#26507,.T.);
#33138=ORIENTED_EDGE('',*,*,#26509,.T.);
#33139=ORIENTED_EDGE('',*,*,#26630,.F.);
#33140=ORIENTED_EDGE('',*,*,#26563,.T.);
#33141=ORIENTED_EDGE('',*,*,#26565,.T.);
#33142=ORIENTED_EDGE('',*,*,#26631,.F.);
#33143=ORIENTED_EDGE('',*,*,#26619,.T.);
#33144=ORIENTED_EDGE('',*,*,#26621,.T.);
#33145=ORIENTED_EDGE('',*,*,#26632,.F.);
#33146=ORIENTED_EDGE('',*,*,#25068,.T.);
#33147=ORIENTED_EDGE('',*,*,#25070,.T.);
#33148=ORIENTED_EDGE('',*,*,#26633,.F.);
#33149=ORIENTED_EDGE('',*,*,#25124,.T.);
#33150=ORIENTED_EDGE('',*,*,#25126,.T.);
#33151=ORIENTED_EDGE('',*,*,#26634,.F.);
#33152=ORIENTED_EDGE('',*,*,#25174,.T.);
#33153=ORIENTED_EDGE('',*,*,#25176,.T.);
#33154=ORIENTED_EDGE('',*,*,#26635,.F.);
#33155=ORIENTED_EDGE('',*,*,#25230,.T.);
#33156=ORIENTED_EDGE('',*,*,#25232,.T.);
#33157=ORIENTED_EDGE('',*,*,#26636,.F.);
#33158=ORIENTED_EDGE('',*,*,#25286,.T.);
#33159=ORIENTED_EDGE('',*,*,#25288,.T.);
#33160=ORIENTED_EDGE('',*,*,#26637,.F.);
#33161=ORIENTED_EDGE('',*,*,#25342,.T.);
#33162=ORIENTED_EDGE('',*,*,#25344,.T.);
#33163=ORIENTED_EDGE('',*,*,#26638,.F.);
#33164=ORIENTED_EDGE('',*,*,#25398,.T.);
#33165=ORIENTED_EDGE('',*,*,#25400,.T.);
#33166=ORIENTED_EDGE('',*,*,#26639,.F.);
#33167=ORIENTED_EDGE('',*,*,#25448,.T.);
#33168=ORIENTED_EDGE('',*,*,#25450,.T.);
#33169=ORIENTED_EDGE('',*,*,#26640,.F.);
#33170=ORIENTED_EDGE('',*,*,#25504,.T.);
#33171=ORIENTED_EDGE('',*,*,#25506,.T.);
#33172=ORIENTED_EDGE('',*,*,#26641,.F.);
#33173=ORIENTED_EDGE('',*,*,#25560,.T.);
#33174=ORIENTED_EDGE('',*,*,#25562,.T.);
#33175=ORIENTED_EDGE('',*,*,#26642,.F.);
#33176=ORIENTED_EDGE('',*,*,#25616,.T.);
#33177=ORIENTED_EDGE('',*,*,#25618,.T.);
#33178=ORIENTED_EDGE('',*,*,#26643,.F.);
#33179=ORIENTED_EDGE('',*,*,#25672,.T.);
#33180=ORIENTED_EDGE('',*,*,#25674,.T.);
#33181=ORIENTED_EDGE('',*,*,#26644,.F.);
#33182=ORIENTED_EDGE('',*,*,#25722,.T.);
#33183=ORIENTED_EDGE('',*,*,#25724,.T.);
#33184=ORIENTED_EDGE('',*,*,#26645,.F.);
#33185=ORIENTED_EDGE('',*,*,#25778,.T.);
#33186=ORIENTED_EDGE('',*,*,#25780,.T.);
#33187=ORIENTED_EDGE('',*,*,#26646,.F.);
#33188=ORIENTED_EDGE('',*,*,#25834,.T.);
#33189=ORIENTED_EDGE('',*,*,#25836,.T.);
#33190=ORIENTED_EDGE('',*,*,#26647,.F.);
#33191=ORIENTED_EDGE('',*,*,#25890,.T.);
#33192=ORIENTED_EDGE('',*,*,#25892,.T.);
#33193=ORIENTED_EDGE('',*,*,#26648,.F.);
#33194=ORIENTED_EDGE('',*,*,#25946,.T.);
#33195=ORIENTED_EDGE('',*,*,#25948,.T.);
#33196=ORIENTED_EDGE('',*,*,#26649,.F.);
#33197=ORIENTED_EDGE('',*,*,#25996,.T.);
#33198=ORIENTED_EDGE('',*,*,#25998,.T.);
#33199=ORIENTED_EDGE('',*,*,#26650,.F.);
#33200=ORIENTED_EDGE('',*,*,#26053,.T.);
#33201=ORIENTED_EDGE('',*,*,#26651,.F.);
#33202=ORIENTED_EDGE('',*,*,#26652,.F.);
#33203=ORIENTED_EDGE('',*,*,#24992,.T.);
#33204=ORIENTED_EDGE('',*,*,#24999,.T.);
#33205=ORIENTED_EDGE('',*,*,#24971,.T.);
#33206=ORIENTED_EDGE('',*,*,#24985,.T.);
#33207=ORIENTED_EDGE('',*,*,#24978,.T.);
#33208=ORIENTED_EDGE('',*,*,#24578,.T.);
#33209=ORIENTED_EDGE('',*,*,#24585,.T.);
#33210=ORIENTED_EDGE('',*,*,#25013,.T.);
#33211=ORIENTED_EDGE('',*,*,#25006,.T.);
#33212=ORIENTED_EDGE('',*,*,#26653,.T.);
#33213=ORIENTED_EDGE('',*,*,#26654,.T.);
#33214=ORIENTED_EDGE('',*,*,#24571,.T.);
#33215=ORIENTED_EDGE('',*,*,#24950,.T.);
#33216=ORIENTED_EDGE('',*,*,#24964,.T.);
#33217=ORIENTED_EDGE('',*,*,#24592,.T.);
#33218=ORIENTED_EDGE('',*,*,#24599,.T.);
#33219=ORIENTED_EDGE('',*,*,#24606,.T.);
#33220=ORIENTED_EDGE('',*,*,#24613,.T.);
#33221=ORIENTED_EDGE('',*,*,#24620,.T.);
#33222=ORIENTED_EDGE('',*,*,#24669,.T.);
#33223=ORIENTED_EDGE('',*,*,#24634,.T.);
#33224=ORIENTED_EDGE('',*,*,#24641,.T.);
#33225=ORIENTED_EDGE('',*,*,#24627,.T.);
#33226=ORIENTED_EDGE('',*,*,#24655,.T.);
#33227=ORIENTED_EDGE('',*,*,#24648,.T.);
#33228=ORIENTED_EDGE('',*,*,#24753,.T.);
#33229=ORIENTED_EDGE('',*,*,#24746,.T.);
#33230=ORIENTED_EDGE('',*,*,#24774,.T.);
#33231=ORIENTED_EDGE('',*,*,#24760,.T.);
#33232=ORIENTED_EDGE('',*,*,#24767,.T.);
#33233=ORIENTED_EDGE('',*,*,#24704,.T.);
#33234=ORIENTED_EDGE('',*,*,#24711,.T.);
#33235=ORIENTED_EDGE('',*,*,#24732,.T.);
#33236=ORIENTED_EDGE('',*,*,#24739,.T.);
#33237=ORIENTED_EDGE('',*,*,#24718,.T.);
#33238=ORIENTED_EDGE('',*,*,#24725,.T.);
#33239=ORIENTED_EDGE('',*,*,#24837,.T.);
#33240=ORIENTED_EDGE('',*,*,#24823,.T.);
#33241=ORIENTED_EDGE('',*,*,#24816,.T.);
#33242=ORIENTED_EDGE('',*,*,#24788,.T.);
#33243=ORIENTED_EDGE('',*,*,#24795,.T.);
#33244=ORIENTED_EDGE('',*,*,#24781,.T.);
#33245=ORIENTED_EDGE('',*,*,#24809,.T.);
#33246=ORIENTED_EDGE('',*,*,#24802,.T.);
#33247=ORIENTED_EDGE('',*,*,#24683,.T.);
#33248=ORIENTED_EDGE('',*,*,#24676,.T.);
#33249=ORIENTED_EDGE('',*,*,#24662,.T.);
#33250=ORIENTED_EDGE('',*,*,#24697,.T.);
#33251=ORIENTED_EDGE('',*,*,#24690,.T.);
#33252=ORIENTED_EDGE('',*,*,#26655,.F.);
#33253=ORIENTED_EDGE('',*,*,#26656,.F.);
#33254=ORIENTED_EDGE('',*,*,#26657,.T.);
#33255=ORIENTED_EDGE('',*,*,#26658,.T.);
#33256=ORIENTED_EDGE('',*,*,#26659,.T.);
#33257=ORIENTED_EDGE('',*,*,#26660,.T.);
#33258=ORIENTED_EDGE('',*,*,#26661,.T.);
#33259=ORIENTED_EDGE('',*,*,#26662,.T.);
#33260=ORIENTED_EDGE('',*,*,#26663,.F.);
#33261=ORIENTED_EDGE('',*,*,#26664,.T.);
#33262=ORIENTED_EDGE('',*,*,#26665,.T.);
#33263=ORIENTED_EDGE('',*,*,#26666,.T.);
#33264=ORIENTED_EDGE('',*,*,#26665,.F.);
#33265=ORIENTED_EDGE('',*,*,#26667,.T.);
#33266=ORIENTED_EDGE('',*,*,#26666,.F.);
#33267=ORIENTED_EDGE('',*,*,#26668,.T.);
#33268=ORIENTED_EDGE('',*,*,#26669,.F.);
#33269=ORIENTED_EDGE('',*,*,#26668,.F.);
#33270=ORIENTED_EDGE('',*,*,#26664,.F.);
#33271=ORIENTED_EDGE('',*,*,#26670,.T.);
#33272=ORIENTED_EDGE('',*,*,#26671,.F.);
#33273=ORIENTED_EDGE('',*,*,#26672,.F.);
#33274=ORIENTED_EDGE('',*,*,#26670,.F.);
#33275=ORIENTED_EDGE('',*,*,#26667,.F.);
#33276=ORIENTED_EDGE('',*,*,#26673,.T.);
#33277=ORIENTED_EDGE('',*,*,#26674,.F.);
#33278=ORIENTED_EDGE('',*,*,#26675,.F.);
#33279=ORIENTED_EDGE('',*,*,#26676,.T.);
#33280=ORIENTED_EDGE('',*,*,#26677,.F.);
#33281=ORIENTED_EDGE('',*,*,#26678,.F.);
#33282=ORIENTED_EDGE('',*,*,#26679,.F.);
#33283=ORIENTED_EDGE('',*,*,#26680,.T.);
#33284=ORIENTED_EDGE('',*,*,#26681,.T.);
#33285=ORIENTED_EDGE('',*,*,#26682,.T.);
#33286=ORIENTED_EDGE('',*,*,#26683,.F.);
#33287=ORIENTED_EDGE('',*,*,#26684,.F.);
#33288=ORIENTED_EDGE('',*,*,#26685,.F.);
#33289=ORIENTED_EDGE('',*,*,#26660,.F.);
#33290=ORIENTED_EDGE('',*,*,#26659,.F.);
#33291=ORIENTED_EDGE('',*,*,#26686,.T.);
#33292=ORIENTED_EDGE('',*,*,#26673,.F.);
#33293=ORIENTED_EDGE('',*,*,#26687,.F.);
#33294=ORIENTED_EDGE('',*,*,#26688,.T.);
#33295=ORIENTED_EDGE('',*,*,#26689,.T.);
#33296=ORIENTED_EDGE('',*,*,#26671,.T.);
#33297=ORIENTED_EDGE('',*,*,#26672,.T.);
#33298=ORIENTED_EDGE('',*,*,#26689,.F.);
#33299=ORIENTED_EDGE('',*,*,#26690,.T.);
#33300=ORIENTED_EDGE('',*,*,#26688,.F.);
#33301=ORIENTED_EDGE('',*,*,#26691,.T.);
#33302=ORIENTED_EDGE('',*,*,#26692,.F.);
#33303=ORIENTED_EDGE('',*,*,#26691,.F.);
#33304=ORIENTED_EDGE('',*,*,#26690,.F.);
#33305=ORIENTED_EDGE('',*,*,#26693,.T.);
#33306=ORIENTED_EDGE('',*,*,#26694,.T.);
#33307=ORIENTED_EDGE('',*,*,#26695,.F.);
#33308=ORIENTED_EDGE('',*,*,#26694,.F.);
#33309=ORIENTED_EDGE('',*,*,#26696,.T.);
#33310=ORIENTED_EDGE('',*,*,#26697,.T.);
#33311=ORIENTED_EDGE('',*,*,#26653,.F.);
#33312=ORIENTED_EDGE('',*,*,#26654,.F.);
#33313=ORIENTED_EDGE('',*,*,#26697,.F.);
#33314=ORIENTED_EDGE('',*,*,#26698,.T.);
#33315=ORIENTED_EDGE('',*,*,#26696,.F.);
#33316=ORIENTED_EDGE('',*,*,#26698,.F.);
#33317=ORIENTED_EDGE('',*,*,#26695,.T.);
#33318=ORIENTED_EDGE('',*,*,#26693,.F.);
#33319=ORIENTED_EDGE('',*,*,#26692,.T.);
#33320=ORIENTED_EDGE('',*,*,#26699,.T.);
#33321=ORIENTED_EDGE('',*,*,#26700,.T.);
#33322=ORIENTED_EDGE('',*,*,#26701,.T.);
#33323=ORIENTED_EDGE('',*,*,#26702,.T.);
#33324=ORIENTED_EDGE('',*,*,#26703,.F.);
#33325=ORIENTED_EDGE('',*,*,#26704,.T.);
#33326=ORIENTED_EDGE('',*,*,#26705,.T.);
#33327=ORIENTED_EDGE('',*,*,#26706,.T.);
#33328=ORIENTED_EDGE('',*,*,#26707,.F.);
#33329=ORIENTED_EDGE('',*,*,#26708,.F.);
#33330=ORIENTED_EDGE('',*,*,#26705,.F.);
#33331=ORIENTED_EDGE('',*,*,#26709,.F.);
#33332=ORIENTED_EDGE('',*,*,#26710,.F.);
#33333=ORIENTED_EDGE('',*,*,#26711,.T.);
#33334=ORIENTED_EDGE('',*,*,#26712,.T.);
#33335=ORIENTED_EDGE('',*,*,#26713,.F.);
#33336=ORIENTED_EDGE('',*,*,#26699,.F.);
#33337=ORIENTED_EDGE('',*,*,#26714,.T.);
#33338=ORIENTED_EDGE('',*,*,#26715,.T.);
#33339=ORIENTED_EDGE('',*,*,#26703,.T.);
#33340=ORIENTED_EDGE('',*,*,#26716,.T.);
#33341=ORIENTED_EDGE('',*,*,#26717,.T.);
#33342=ORIENTED_EDGE('',*,*,#26718,.T.);
#33343=ORIENTED_EDGE('',*,*,#26719,.T.);
#33344=ORIENTED_EDGE('',*,*,#26715,.F.);
#33345=ORIENTED_EDGE('',*,*,#26720,.T.);
#33346=ORIENTED_EDGE('',*,*,#26707,.T.);
#33347=ORIENTED_EDGE('',*,*,#26721,.T.);
#33348=ORIENTED_EDGE('',*,*,#26722,.T.);
#33349=ORIENTED_EDGE('',*,*,#26723,.T.);
#33350=ORIENTED_EDGE('',*,*,#26724,.T.);
#33351=ORIENTED_EDGE('',*,*,#26725,.T.);
#33352=ORIENTED_EDGE('',*,*,#26726,.F.);
#33353=ORIENTED_EDGE('',*,*,#26727,.T.);
#33354=ORIENTED_EDGE('',*,*,#26728,.F.);
#33355=ORIENTED_EDGE('',*,*,#26729,.T.);
#33356=ORIENTED_EDGE('',*,*,#26730,.F.);
#33357=ORIENTED_EDGE('',*,*,#26731,.T.);
#33358=ORIENTED_EDGE('',*,*,#26726,.T.);
#33359=ORIENTED_EDGE('',*,*,#26732,.T.);
#33360=ORIENTED_EDGE('',*,*,#26733,.F.);
#33361=ORIENTED_EDGE('',*,*,#26710,.T.);
#33362=ORIENTED_EDGE('',*,*,#26728,.T.);
#33363=ORIENTED_EDGE('',*,*,#26734,.T.);
#33364=ORIENTED_EDGE('',*,*,#26735,.F.);
#33365=ORIENTED_EDGE('',*,*,#26736,.T.);
#33366=ORIENTED_EDGE('',*,*,#26737,.F.);
#33367=ORIENTED_EDGE('',*,*,#26738,.F.);
#33368=ORIENTED_EDGE('',*,*,#26735,.T.);
#33369=ORIENTED_EDGE('',*,*,#26739,.T.);
#33370=ORIENTED_EDGE('',*,*,#26730,.T.);
#33371=ORIENTED_EDGE('',*,*,#26740,.T.);
#33372=ORIENTED_EDGE('',*,*,#26741,.F.);
#33373=ORIENTED_EDGE('',*,*,#26731,.F.);
#33374=ORIENTED_EDGE('',*,*,#26742,.F.);
#33375=ORIENTED_EDGE('',*,*,#26725,.F.);
#33376=ORIENTED_EDGE('',*,*,#26742,.T.);
#33377=ORIENTED_EDGE('',*,*,#26739,.F.);
#33378=ORIENTED_EDGE('',*,*,#26743,.F.);
#33379=ORIENTED_EDGE('',*,*,#26722,.F.);
#33380=ORIENTED_EDGE('',*,*,#26741,.T.);
#33381=ORIENTED_EDGE('',*,*,#26724,.F.);
#33382=ORIENTED_EDGE('',*,*,#26744,.F.);
#33383=ORIENTED_EDGE('',*,*,#26727,.F.);
#33384=ORIENTED_EDGE('',*,*,#26743,.T.);
#33385=ORIENTED_EDGE('',*,*,#26734,.F.);
#33386=ORIENTED_EDGE('',*,*,#26744,.T.);
#33387=ORIENTED_EDGE('',*,*,#26723,.F.);
#33388=ORIENTED_EDGE('',*,*,#26745,.F.);
#33389=ORIENTED_EDGE('',*,*,#26736,.F.);
#33390=ORIENTED_EDGE('',*,*,#26746,.F.);
#33391=ORIENTED_EDGE('',*,*,#26717,.F.);
#33392=ORIENTED_EDGE('',*,*,#26746,.T.);
#33393=ORIENTED_EDGE('',*,*,#26740,.F.);
#33394=ORIENTED_EDGE('',*,*,#26747,.F.);
#33395=ORIENTED_EDGE('',*,*,#26704,.F.);
#33396=ORIENTED_EDGE('',*,*,#26709,.T.);
#33397=ORIENTED_EDGE('',*,*,#26720,.F.);
#33398=ORIENTED_EDGE('',*,*,#26748,.F.);
#33399=ORIENTED_EDGE('',*,*,#26729,.F.);
#33400=ORIENTED_EDGE('',*,*,#26747,.T.);
#33401=ORIENTED_EDGE('',*,*,#26732,.F.);
#33402=ORIENTED_EDGE('',*,*,#26748,.T.);
#33403=ORIENTED_EDGE('',*,*,#26714,.F.);
#33404=ORIENTED_EDGE('',*,*,#26749,.T.);
#33405=ORIENTED_EDGE('',*,*,#26700,.F.);
#33406=ORIENTED_EDGE('',*,*,#26750,.F.);
#33407=ORIENTED_EDGE('',*,*,#26751,.T.);
#33408=ORIENTED_EDGE('',*,*,#26752,.F.);
#33409=ORIENTED_EDGE('',*,*,#26753,.T.);
#33410=ORIENTED_EDGE('',*,*,#26754,.F.);
#33411=ORIENTED_EDGE('',*,*,#26751,.F.);
#33412=ORIENTED_EDGE('',*,*,#26755,.F.);
#33413=ORIENTED_EDGE('',*,*,#26756,.T.);
#33414=ORIENTED_EDGE('',*,*,#26701,.F.);
#33415=ORIENTED_EDGE('',*,*,#26749,.F.);
#33416=ORIENTED_EDGE('',*,*,#26757,.F.);
#33417=ORIENTED_EDGE('',*,*,#26758,.T.);
#33418=ORIENTED_EDGE('',*,*,#26759,.F.);
#33419=ORIENTED_EDGE('',*,*,#26753,.F.);
#33420=ORIENTED_EDGE('',*,*,#26760,.F.);
#33421=ORIENTED_EDGE('',*,*,#26719,.F.);
#33422=ORIENTED_EDGE('',*,*,#26758,.F.);
#33423=ORIENTED_EDGE('',*,*,#26718,.F.);
#33424=ORIENTED_EDGE('',*,*,#26761,.F.);
#33425=ORIENTED_EDGE('',*,*,#26762,.F.);
#33426=ORIENTED_EDGE('',*,*,#26763,.T.);
#33427=ORIENTED_EDGE('',*,*,#26738,.T.);
#33428=ORIENTED_EDGE('',*,*,#26764,.T.);
#33429=ORIENTED_EDGE('',*,*,#26765,.F.);
#33430=ORIENTED_EDGE('',*,*,#26766,.T.);
#33431=ORIENTED_EDGE('',*,*,#26767,.T.);
#33432=ORIENTED_EDGE('',*,*,#26662,.F.);
#33433=ORIENTED_EDGE('',*,*,#26768,.T.);
#33434=ORIENTED_EDGE('',*,*,#26769,.F.);
#33435=ORIENTED_EDGE('',*,*,#26770,.F.);
#33436=ORIENTED_EDGE('',*,*,#26771,.F.);
#33437=ORIENTED_EDGE('',*,*,#26766,.F.);
#33438=ORIENTED_EDGE('',*,*,#26772,.F.);
#33439=ORIENTED_EDGE('',*,*,#26687,.T.);
#33440=ORIENTED_EDGE('',*,*,#26773,.F.);
#33441=ORIENTED_EDGE('',*,*,#26764,.F.);
#33442=ORIENTED_EDGE('',*,*,#26661,.F.);
#33443=ORIENTED_EDGE('',*,*,#26774,.T.);
#33444=ORIENTED_EDGE('',*,*,#26657,.F.);
#33445=ORIENTED_EDGE('',*,*,#26775,.T.);
#33446=ORIENTED_EDGE('',*,*,#26768,.F.);
#33447=ORIENTED_EDGE('',*,*,#26776,.F.);
#33448=ORIENTED_EDGE('',*,*,#26774,.F.);
#33449=ORIENTED_EDGE('',*,*,#26777,.F.);
#33450=ORIENTED_EDGE('',*,*,#26686,.F.);
#33451=ORIENTED_EDGE('',*,*,#26658,.F.);
#33452=ORIENTED_EDGE('',*,*,#26684,.T.);
#33453=ORIENTED_EDGE('',*,*,#26778,.F.);
#33454=ORIENTED_EDGE('',*,*,#26779,.T.);
#33455=ORIENTED_EDGE('',*,*,#26780,.F.);
#33456=ORIENTED_EDGE('',*,*,#26781,.T.);
#33457=ORIENTED_EDGE('',*,*,#26782,.F.);
#33458=ORIENTED_EDGE('',*,*,#26779,.F.);
#33459=ORIENTED_EDGE('',*,*,#26783,.F.);
#33460=ORIENTED_EDGE('',*,*,#26784,.T.);
#33461=ORIENTED_EDGE('',*,*,#26785,.F.);
#33462=ORIENTED_EDGE('',*,*,#26781,.F.);
#33463=ORIENTED_EDGE('',*,*,#26786,.F.);
#33464=ORIENTED_EDGE('',*,*,#26678,.T.);
#33465=ORIENTED_EDGE('',*,*,#26787,.F.);
#33466=ORIENTED_EDGE('',*,*,#26682,.F.);
#33467=ORIENTED_EDGE('',*,*,#26681,.F.);
#33468=ORIENTED_EDGE('',*,*,#26788,.F.);
#33469=ORIENTED_EDGE('',*,*,#26789,.T.);
#33470=ORIENTED_EDGE('',*,*,#26790,.F.);
#33471=ORIENTED_EDGE('',*,*,#26784,.F.);
#33472=ORIENTED_EDGE('',*,*,#26791,.F.);
#33473=ORIENTED_EDGE('',*,*,#26789,.F.);
#33474=ORIENTED_EDGE('',*,*,#26792,.F.);
#33475=ORIENTED_EDGE('',*,*,#26680,.F.);
#33476=ORIENTED_EDGE('',*,*,#26793,.F.);
#33477=ORIENTED_EDGE('',*,*,#26794,.T.);
#33478=ORIENTED_EDGE('',*,*,#26773,.T.);
#33479=ORIENTED_EDGE('',*,*,#26676,.F.);
#33480=ORIENTED_EDGE('',*,*,#26795,.F.);
#33481=ORIENTED_EDGE('',*,*,#26674,.T.);
#33482=ORIENTED_EDGE('',*,*,#26777,.T.);
#33483=ORIENTED_EDGE('',*,*,#26796,.F.);
#33484=ORIENTED_EDGE('',*,*,#26797,.F.);
#33485=ORIENTED_EDGE('',*,*,#26798,.T.);
#33486=ORIENTED_EDGE('',*,*,#26799,.T.);
#33487=ORIENTED_EDGE('',*,*,#26800,.T.);
#33488=ORIENTED_EDGE('',*,*,#26801,.T.);
#33489=ORIENTED_EDGE('',*,*,#26802,.T.);
#33490=ORIENTED_EDGE('',*,*,#26675,.T.);
#33491=ORIENTED_EDGE('',*,*,#26803,.F.);
#33492=ORIENTED_EDGE('',*,*,#26765,.T.);
#33493=ORIENTED_EDGE('',*,*,#26794,.F.);
#33494=ORIENTED_EDGE('',*,*,#26804,.F.);
#33495=ORIENTED_EDGE('',*,*,#26805,.T.);
#33496=ORIENTED_EDGE('',*,*,#26796,.T.);
#33497=ORIENTED_EDGE('',*,*,#26776,.T.);
#33498=ORIENTED_EDGE('',*,*,#26806,.F.);
#33499=ORIENTED_EDGE('',*,*,#26807,.F.);
#33500=ORIENTED_EDGE('',*,*,#26808,.F.);
#33501=ORIENTED_EDGE('',*,*,#26802,.F.);
#33502=ORIENTED_EDGE('',*,*,#26809,.T.);
#33503=ORIENTED_EDGE('',*,*,#26810,.T.);
#33504=ORIENTED_EDGE('',*,*,#26804,.T.);
#33505=ORIENTED_EDGE('',*,*,#26795,.T.);
#33506=ORIENTED_EDGE('',*,*,#26811,.F.);
#33507=ORIENTED_EDGE('',*,*,#26812,.T.);
#33508=ORIENTED_EDGE('',*,*,#26798,.F.);
#33509=ORIENTED_EDGE('',*,*,#26797,.T.);
#33510=ORIENTED_EDGE('',*,*,#26808,.T.);
#33511=ORIENTED_EDGE('',*,*,#26813,.T.);
#33512=ORIENTED_EDGE('',*,*,#26814,.T.);
#33513=ORIENTED_EDGE('',*,*,#26815,.T.);
#33514=ORIENTED_EDGE('',*,*,#26813,.F.);
#33515=ORIENTED_EDGE('',*,*,#26816,.T.);
#33516=ORIENTED_EDGE('',*,*,#26817,.T.);
#33517=ORIENTED_EDGE('',*,*,#26818,.T.);
#33518=ORIENTED_EDGE('',*,*,#26819,.T.);
#33519=ORIENTED_EDGE('',*,*,#26820,.T.);
#33520=ORIENTED_EDGE('',*,*,#26800,.F.);
#33521=ORIENTED_EDGE('',*,*,#26821,.F.);
#33522=ORIENTED_EDGE('',*,*,#26814,.F.);
#33523=ORIENTED_EDGE('',*,*,#26821,.T.);
#33524=ORIENTED_EDGE('',*,*,#26799,.F.);
#33525=ORIENTED_EDGE('',*,*,#26822,.F.);
#33526=ORIENTED_EDGE('',*,*,#26816,.F.);
#33527=ORIENTED_EDGE('',*,*,#26822,.T.);
#33528=ORIENTED_EDGE('',*,*,#26812,.F.);
#33529=ORIENTED_EDGE('',*,*,#26823,.F.);
#33530=ORIENTED_EDGE('',*,*,#26817,.F.);
#33531=ORIENTED_EDGE('',*,*,#26824,.T.);
#33532=ORIENTED_EDGE('',*,*,#26677,.T.);
#33533=ORIENTED_EDGE('',*,*,#26825,.T.);
#33534=ORIENTED_EDGE('',*,*,#26818,.F.);
#33535=ORIENTED_EDGE('',*,*,#26826,.T.);
#33536=ORIENTED_EDGE('',*,*,#26809,.F.);
#33537=ORIENTED_EDGE('',*,*,#26827,.F.);
#33538=ORIENTED_EDGE('',*,*,#26819,.F.);
#33539=ORIENTED_EDGE('',*,*,#26827,.T.);
#33540=ORIENTED_EDGE('',*,*,#26801,.F.);
#33541=ORIENTED_EDGE('',*,*,#26820,.F.);
#33542=ORIENTED_EDGE('',*,*,#26815,.F.);
#33543=ORIENTED_EDGE('',*,*,#26828,.F.);
#33544=ORIENTED_EDGE('',*,*,#26786,.T.);
#33545=ORIENTED_EDGE('',*,*,#26829,.F.);
#33546=ORIENTED_EDGE('',*,*,#26805,.F.);
#33547=ORIENTED_EDGE('',*,*,#26685,.T.);
#33548=ORIENTED_EDGE('',*,*,#26780,.T.);
#33549=ORIENTED_EDGE('',*,*,#26782,.T.);
#33550=ORIENTED_EDGE('',*,*,#26785,.T.);
#33551=ORIENTED_EDGE('',*,*,#26790,.T.);
#33552=ORIENTED_EDGE('',*,*,#26793,.T.);
#33553=ORIENTED_EDGE('',*,*,#26679,.T.);
#33554=ORIENTED_EDGE('',*,*,#26788,.T.);
#33555=ORIENTED_EDGE('',*,*,#26830,.F.);
#33556=ORIENTED_EDGE('',*,*,#26778,.T.);
#33557=ORIENTED_EDGE('',*,*,#26831,.F.);
#33558=ORIENTED_EDGE('',*,*,#26807,.T.);
#33559=ORIENTED_EDGE('',*,*,#26832,.F.);
#33560=ORIENTED_EDGE('',*,*,#26787,.T.);
#33561=ORIENTED_EDGE('',*,*,#26824,.F.);
#33562=ORIENTED_EDGE('',*,*,#26823,.T.);
#33563=ORIENTED_EDGE('',*,*,#26825,.F.);
#33564=ORIENTED_EDGE('',*,*,#26792,.T.);
#33565=ORIENTED_EDGE('',*,*,#26833,.F.);
#33566=ORIENTED_EDGE('',*,*,#26826,.F.);
#33567=ORIENTED_EDGE('',*,*,#26833,.T.);
#33568=ORIENTED_EDGE('',*,*,#26791,.T.);
#33569=ORIENTED_EDGE('',*,*,#26828,.T.);
#33570=ORIENTED_EDGE('',*,*,#26810,.F.);
#33571=ORIENTED_EDGE('',*,*,#26831,.T.);
#33572=ORIENTED_EDGE('',*,*,#26683,.T.);
#33573=ORIENTED_EDGE('',*,*,#26832,.T.);
#33574=ORIENTED_EDGE('',*,*,#26811,.T.);
#33575=ORIENTED_EDGE('',*,*,#26834,.F.);
#33576=ORIENTED_EDGE('',*,*,#26752,.T.);
#33577=ORIENTED_EDGE('',*,*,#26754,.T.);
#33578=ORIENTED_EDGE('',*,*,#26759,.T.);
#33579=ORIENTED_EDGE('',*,*,#26835,.F.);
#33580=ORIENTED_EDGE('',*,*,#26806,.T.);
#33581=ORIENTED_EDGE('',*,*,#26772,.T.);
#33582=ORIENTED_EDGE('',*,*,#26803,.T.);
#33583=ORIENTED_EDGE('',*,*,#26836,.T.);
#33584=ORIENTED_EDGE('',*,*,#26757,.T.);
#33585=ORIENTED_EDGE('',*,*,#26834,.T.);
#33586=ORIENTED_EDGE('',*,*,#26829,.T.);
#33587=ORIENTED_EDGE('',*,*,#26783,.T.);
#33588=ORIENTED_EDGE('',*,*,#26830,.T.);
#33589=ORIENTED_EDGE('',*,*,#26835,.T.);
#33590=ORIENTED_EDGE('',*,*,#26762,.T.);
#33591=ORIENTED_EDGE('',*,*,#26663,.T.);
#33592=ORIENTED_EDGE('',*,*,#26767,.F.);
#33593=ORIENTED_EDGE('',*,*,#26771,.T.);
#33594=ORIENTED_EDGE('',*,*,#26770,.T.);
#33595=ORIENTED_EDGE('',*,*,#26769,.T.);
#33596=ORIENTED_EDGE('',*,*,#26775,.F.);
#33597=ORIENTED_EDGE('',*,*,#26656,.T.);
#33598=ORIENTED_EDGE('',*,*,#26837,.F.);
#33599=ORIENTED_EDGE('',*,*,#26838,.F.);
#33600=ORIENTED_EDGE('',*,*,#26155,.T.);
#33601=ORIENTED_EDGE('',*,*,#26839,.F.);
#33602=ORIENTED_EDGE('',*,*,#26241,.T.);
#33603=ORIENTED_EDGE('',*,*,#26840,.F.);
#33604=ORIENTED_EDGE('',*,*,#26346,.T.);
#33605=ORIENTED_EDGE('',*,*,#26626,.T.);
#33606=ORIENTED_EDGE('',*,*,#26841,.T.);
#33607=ORIENTED_EDGE('',*,*,#26652,.T.);
#33608=ORIENTED_EDGE('',*,*,#26842,.F.);
#33609=ORIENTED_EDGE('',*,*,#26111,.T.);
#33610=ORIENTED_EDGE('',*,*,#26843,.F.);
#33611=ORIENTED_EDGE('',*,*,#26103,.T.);
#33612=ORIENTED_EDGE('',*,*,#24844,.T.);
#33613=ORIENTED_EDGE('',*,*,#24850,.T.);
#33614=ORIENTED_EDGE('',*,*,#24856,.T.);
#33615=ORIENTED_EDGE('',*,*,#24863,.T.);
#33616=ORIENTED_EDGE('',*,*,#24830,.T.);
#33617=ORIENTED_EDGE('',*,*,#24943,.T.);
#33618=ORIENTED_EDGE('',*,*,#24936,.T.);
#33619=ORIENTED_EDGE('',*,*,#24957,.T.);
#33620=ORIENTED_EDGE('',*,*,#24902,.T.);
#33621=ORIENTED_EDGE('',*,*,#24896,.T.);
#33622=ORIENTED_EDGE('',*,*,#24889,.T.);
#33623=ORIENTED_EDGE('',*,*,#24882,.T.);
#33624=ORIENTED_EDGE('',*,*,#24876,.T.);
#33625=ORIENTED_EDGE('',*,*,#24870,.T.);
#33626=ORIENTED_EDGE('',*,*,#24916,.T.);
#33627=ORIENTED_EDGE('',*,*,#24922,.T.);
#33628=ORIENTED_EDGE('',*,*,#24929,.T.);
#33629=ORIENTED_EDGE('',*,*,#24909,.T.);
#33630=ORIENTED_EDGE('',*,*,#25399,.F.);
#33631=ORIENTED_EDGE('',*,*,#26638,.T.);
#33632=ORIENTED_EDGE('',*,*,#25343,.F.);
#33633=ORIENTED_EDGE('',*,*,#26637,.T.);
#33634=ORIENTED_EDGE('',*,*,#25287,.F.);
#33635=ORIENTED_EDGE('',*,*,#26636,.T.);
#33636=ORIENTED_EDGE('',*,*,#25231,.F.);
#33637=ORIENTED_EDGE('',*,*,#26635,.T.);
#33638=ORIENTED_EDGE('',*,*,#25175,.F.);
#33639=ORIENTED_EDGE('',*,*,#26634,.T.);
#33640=ORIENTED_EDGE('',*,*,#25125,.F.);
#33641=ORIENTED_EDGE('',*,*,#26633,.T.);
#33642=ORIENTED_EDGE('',*,*,#25069,.F.);
#33643=ORIENTED_EDGE('',*,*,#26632,.T.);
#33644=ORIENTED_EDGE('',*,*,#26620,.F.);
#33645=ORIENTED_EDGE('',*,*,#26631,.T.);
#33646=ORIENTED_EDGE('',*,*,#26564,.F.);
#33647=ORIENTED_EDGE('',*,*,#26630,.T.);
#33648=ORIENTED_EDGE('',*,*,#26508,.F.);
#33649=ORIENTED_EDGE('',*,*,#26629,.T.);
#33650=ORIENTED_EDGE('',*,*,#26458,.F.);
#33651=ORIENTED_EDGE('',*,*,#26628,.T.);
#33652=ORIENTED_EDGE('',*,*,#26401,.F.);
#33653=ORIENTED_EDGE('',*,*,#26403,.F.);
#33654=ORIENTED_EDGE('',*,*,#26627,.T.);
#33655=ORIENTED_EDGE('',*,*,#26344,.F.);
#33656=ORIENTED_EDGE('',*,*,#26347,.F.);
#33657=ORIENTED_EDGE('',*,*,#26840,.T.);
#33658=ORIENTED_EDGE('',*,*,#26240,.F.);
#33659=ORIENTED_EDGE('',*,*,#26242,.F.);
#33660=ORIENTED_EDGE('',*,*,#26839,.T.);
#33661=ORIENTED_EDGE('',*,*,#26154,.F.);
#33662=ORIENTED_EDGE('',*,*,#26156,.F.);
#33663=ORIENTED_EDGE('',*,*,#26838,.T.);
#33664=ORIENTED_EDGE('',*,*,#26102,.F.);
#33665=ORIENTED_EDGE('',*,*,#26104,.F.);
#33666=ORIENTED_EDGE('',*,*,#26843,.T.);
#33667=ORIENTED_EDGE('',*,*,#26110,.F.);
#33668=ORIENTED_EDGE('',*,*,#26112,.F.);
#33669=ORIENTED_EDGE('',*,*,#26842,.T.);
#33670=ORIENTED_EDGE('',*,*,#26651,.T.);
#33671=ORIENTED_EDGE('',*,*,#26052,.F.);
#33672=ORIENTED_EDGE('',*,*,#26054,.F.);
#33673=ORIENTED_EDGE('',*,*,#26650,.T.);
#33674=ORIENTED_EDGE('',*,*,#25997,.F.);
#33675=ORIENTED_EDGE('',*,*,#26649,.T.);
#33676=ORIENTED_EDGE('',*,*,#25947,.F.);
#33677=ORIENTED_EDGE('',*,*,#26648,.T.);
#33678=ORIENTED_EDGE('',*,*,#25891,.F.);
#33679=ORIENTED_EDGE('',*,*,#26647,.T.);
#33680=ORIENTED_EDGE('',*,*,#25835,.F.);
#33681=ORIENTED_EDGE('',*,*,#26646,.T.);
#33682=ORIENTED_EDGE('',*,*,#25779,.F.);
#33683=ORIENTED_EDGE('',*,*,#26645,.T.);
#33684=ORIENTED_EDGE('',*,*,#25723,.F.);
#33685=ORIENTED_EDGE('',*,*,#26644,.T.);
#33686=ORIENTED_EDGE('',*,*,#25673,.F.);
#33687=ORIENTED_EDGE('',*,*,#26643,.T.);
#33688=ORIENTED_EDGE('',*,*,#25617,.F.);
#33689=ORIENTED_EDGE('',*,*,#26642,.T.);
#33690=ORIENTED_EDGE('',*,*,#25561,.F.);
#33691=ORIENTED_EDGE('',*,*,#26641,.T.);
#33692=ORIENTED_EDGE('',*,*,#25505,.F.);
#33693=ORIENTED_EDGE('',*,*,#26640,.T.);
#33694=ORIENTED_EDGE('',*,*,#25449,.F.);
#33695=ORIENTED_EDGE('',*,*,#26639,.T.);
#33696=ORIENTED_EDGE('',*,*,#25442,.T.);
#33697=ORIENTED_EDGE('',*,*,#25436,.T.);
#33698=ORIENTED_EDGE('',*,*,#25336,.T.);
#33699=ORIENTED_EDGE('',*,*,#25330,.T.);
#33700=ORIENTED_EDGE('',*,*,#25324,.T.);
#33701=ORIENTED_EDGE('',*,*,#25380,.T.);
#33702=ORIENTED_EDGE('',*,*,#25554,.T.);
#33703=ORIENTED_EDGE('',*,*,#25542,.T.);
#33704=ORIENTED_EDGE('',*,*,#25548,.T.);
#33705=ORIENTED_EDGE('',*,*,#25604,.T.);
#33706=ORIENTED_EDGE('',*,*,#25598,.T.);
#33707=ORIENTED_EDGE('',*,*,#25492,.T.);
#33708=ORIENTED_EDGE('',*,*,#25486,.T.);
#33709=ORIENTED_EDGE('',*,*,#25498,.T.);
#33710=ORIENTED_EDGE('',*,*,#26433,.T.);
#33711=ORIENTED_EDGE('',*,*,#26427,.T.);
#33712=ORIENTED_EDGE('',*,*,#26421,.T.);
#33713=ORIENTED_EDGE('',*,*,#26377,.T.);
#33714=ORIENTED_EDGE('',*,*,#26527,.T.);
#33715=ORIENTED_EDGE('',*,*,#26489,.T.);
#33716=ORIENTED_EDGE('',*,*,#26483,.T.);
#33717=ORIENTED_EDGE('',*,*,#26477,.T.);
#33718=ORIENTED_EDGE('',*,*,#26308,.T.);
#33719=ORIENTED_EDGE('',*,*,#26272,.T.);
#33720=ORIENTED_EDGE('',*,*,#26260,.T.);
#33721=ORIENTED_EDGE('',*,*,#26266,.T.);
#33722=ORIENTED_EDGE('',*,*,#26365,.T.);
#33723=ORIENTED_EDGE('',*,*,#26371,.T.);
#33724=ORIENTED_EDGE('',*,*,#26314,.T.);
#33725=ORIENTED_EDGE('',*,*,#26320,.T.);
#33726=ORIENTED_EDGE('',*,*,#25268,.T.);
#33727=ORIENTED_EDGE('',*,*,#25100,.T.);
#33728=ORIENTED_EDGE('',*,*,#25094,.T.);
#33729=ORIENTED_EDGE('',*,*,#25088,.T.);
#33730=ORIENTED_EDGE('',*,*,#25274,.T.);
#33731=ORIENTED_EDGE('',*,*,#25280,.T.);
#33732=ORIENTED_EDGE('',*,*,#26589,.T.);
#33733=ORIENTED_EDGE('',*,*,#26583,.T.);
#33734=ORIENTED_EDGE('',*,*,#26539,.T.);
#33735=ORIENTED_EDGE('',*,*,#26533,.T.);
#33736=ORIENTED_EDGE('',*,*,#25044,.T.);
#33737=ORIENTED_EDGE('',*,*,#25038,.T.);
#33738=ORIENTED_EDGE('',*,*,#25032,.T.);
#33739=ORIENTED_EDGE('',*,*,#26595,.T.);
#33740=ORIENTED_EDGE('',*,*,#25990,.T.);
#33741=ORIENTED_EDGE('',*,*,#26034,.T.);
#33742=ORIENTED_EDGE('',*,*,#26040,.T.);
#33743=ORIENTED_EDGE('',*,*,#26046,.T.);
#33744=ORIENTED_EDGE('',*,*,#25940,.T.);
#33745=ORIENTED_EDGE('',*,*,#25934,.T.);
#33746=ORIENTED_EDGE('',*,*,#25928,.T.);
#33747=ORIENTED_EDGE('',*,*,#25984,.T.);
#33748=ORIENTED_EDGE('',*,*,#26148,.T.);
#33749=ORIENTED_EDGE('',*,*,#26198,.T.);
#33750=ORIENTED_EDGE('',*,*,#26192,.T.);
#33751=ORIENTED_EDGE('',*,*,#26090,.T.);
#33752=ORIENTED_EDGE('',*,*,#26096,.T.);
#33753=ORIENTED_EDGE('',*,*,#25716,.T.);
#33754=ORIENTED_EDGE('',*,*,#25710,.T.);
#33755=ORIENTED_EDGE('',*,*,#25760,.T.);
#33756=ORIENTED_EDGE('',*,*,#25610,.T.);
#33757=ORIENTED_EDGE('',*,*,#25666,.T.);
#33758=ORIENTED_EDGE('',*,*,#25654,.T.);
#33759=ORIENTED_EDGE('',*,*,#25660,.T.);
#33760=ORIENTED_EDGE('',*,*,#25872,.T.);
#33761=ORIENTED_EDGE('',*,*,#25878,.T.);
#33762=ORIENTED_EDGE('',*,*,#25884,.T.);
#33763=ORIENTED_EDGE('',*,*,#25766,.T.);
#33764=ORIENTED_EDGE('',*,*,#25772,.T.);
#33765=ORIENTED_EDGE('',*,*,#25828,.T.);
#33766=ORIENTED_EDGE('',*,*,#25822,.T.);
#33767=ORIENTED_EDGE('',*,*,#25816,.T.);
#33768=ORIENTED_EDGE('',*,*,#25188,.T.);
#33769=ORIENTED_EDGE('',*,*,#25076,.T.);
#33770=ORIENTED_EDGE('',*,*,#25020,.T.);
#33771=ORIENTED_EDGE('',*,*,#26571,.T.);
#33772=ORIENTED_EDGE('',*,*,#26409,.T.);
#33773=ORIENTED_EDGE('',*,*,#26353,.T.);
#33774=ORIENTED_EDGE('',*,*,#26515,.T.);
#33775=ORIENTED_EDGE('',*,*,#26465,.T.);
#33776=ORIENTED_EDGE('',*,*,#25518,.T.);
#33777=ORIENTED_EDGE('',*,*,#25462,.T.);
#33778=ORIENTED_EDGE('',*,*,#25630,.T.);
#33779=ORIENTED_EDGE('',*,*,#25574,.T.);
#33780=ORIENTED_EDGE('',*,*,#25412,.T.);
#33781=ORIENTED_EDGE('',*,*,#25356,.T.);
#33782=ORIENTED_EDGE('',*,*,#25300,.T.);
#33783=ORIENTED_EDGE('',*,*,#25244,.T.);
#33784=ORIENTED_EDGE('',*,*,#25848,.T.);
#33785=ORIENTED_EDGE('',*,*,#25792,.T.);
#33786=ORIENTED_EDGE('',*,*,#25686,.T.);
#33787=ORIENTED_EDGE('',*,*,#25736,.T.);
#33788=ORIENTED_EDGE('',*,*,#25904,.T.);
#33789=ORIENTED_EDGE('',*,*,#25960,.T.);
#33790=ORIENTED_EDGE('',*,*,#26010,.T.);
#33791=ORIENTED_EDGE('',*,*,#26066,.T.);
#33792=ORIENTED_EDGE('',*,*,#26359,.T.);
#33793=ORIENTED_EDGE('',*,*,#26302,.T.);
#33794=ORIENTED_EDGE('',*,*,#26471,.T.);
#33795=ORIENTED_EDGE('',*,*,#26415,.T.);
#33796=ORIENTED_EDGE('',*,*,#26210,.T.);
#33797=ORIENTED_EDGE('',*,*,#26254,.T.);
#33798=ORIENTED_EDGE('',*,*,#26168,.T.);
#33799=ORIENTED_EDGE('',*,*,#26124,.T.);
#33800=ORIENTED_EDGE('',*,*,#25294,.T.);
#33801=ORIENTED_EDGE('',*,*,#25350,.T.);
#33802=ORIENTED_EDGE('',*,*,#25456,.T.);
#33803=ORIENTED_EDGE('',*,*,#25406,.T.);
#33804=ORIENTED_EDGE('',*,*,#25238,.T.);
#33805=ORIENTED_EDGE('',*,*,#25182,.T.);
#33806=ORIENTED_EDGE('',*,*,#25144,.T.);
#33807=ORIENTED_EDGE('',*,*,#25138,.T.);
#33808=ORIENTED_EDGE('',*,*,#25150,.T.);
#33809=ORIENTED_EDGE('',*,*,#25156,.T.);
#33810=ORIENTED_EDGE('',*,*,#25212,.T.);
#33811=ORIENTED_EDGE('',*,*,#25218,.T.);
#33812=ORIENTED_EDGE('',*,*,#25224,.T.);
#33813=ORIENTED_EDGE('',*,*,#25898,.T.);
#33814=ORIENTED_EDGE('',*,*,#25842,.T.);
#33815=ORIENTED_EDGE('',*,*,#25730,.T.);
#33816=ORIENTED_EDGE('',*,*,#25786,.T.);
#33817=ORIENTED_EDGE('',*,*,#25568,.T.);
#33818=ORIENTED_EDGE('',*,*,#25512,.T.);
#33819=ORIENTED_EDGE('',*,*,#25680,.T.);
#33820=ORIENTED_EDGE('',*,*,#25624,.T.);
#33821=ORIENTED_EDGE('',*,*,#25954,.T.);
#33822=ORIENTED_EDGE('',*,*,#26004,.T.);
#33823=ORIENTED_EDGE('',*,*,#26060,.T.);
#33824=ORIENTED_EDGE('',*,*,#26118,.T.);
#33825=ORIENTED_EDGE('',*,*,#26248,.T.);
#33826=ORIENTED_EDGE('',*,*,#26296,.T.);
#33827=ORIENTED_EDGE('',*,*,#26162,.T.);
#33828=ORIENTED_EDGE('',*,*,#26204,.T.);
#33829=ORIENTED_EDGE('',*,*,#25910,.T.);
#33830=ORIENTED_EDGE('',*,*,#25866,.T.);
#33831=ORIENTED_EDGE('',*,*,#25860,.T.);
#33832=ORIENTED_EDGE('',*,*,#25854,.T.);
#33833=ORIENTED_EDGE('',*,*,#25916,.T.);
#33834=ORIENTED_EDGE('',*,*,#25922,.T.);
#33835=ORIENTED_EDGE('',*,*,#25966,.T.);
#33836=ORIENTED_EDGE('',*,*,#25972,.T.);
#33837=ORIENTED_EDGE('',*,*,#25748,.T.);
#33838=ORIENTED_EDGE('',*,*,#25742,.T.);
#33839=ORIENTED_EDGE('',*,*,#25704,.T.);
#33840=ORIENTED_EDGE('',*,*,#25698,.T.);
#33841=ORIENTED_EDGE('',*,*,#25810,.T.);
#33842=ORIENTED_EDGE('',*,*,#25804,.T.);
#33843=ORIENTED_EDGE('',*,*,#25798,.T.);
#33844=ORIENTED_EDGE('',*,*,#25754,.T.);
#33845=ORIENTED_EDGE('',*,*,#26142,.T.);
#33846=ORIENTED_EDGE('',*,*,#26136,.T.);
#33847=ORIENTED_EDGE('',*,*,#26180,.T.);
#33848=ORIENTED_EDGE('',*,*,#26174,.T.);
#33849=ORIENTED_EDGE('',*,*,#26222,.T.);
#33850=ORIENTED_EDGE('',*,*,#26228,.T.);
#33851=ORIENTED_EDGE('',*,*,#26216,.T.);
#33852=ORIENTED_EDGE('',*,*,#26186,.T.);
#33853=ORIENTED_EDGE('',*,*,#26022,.T.);
#33854=ORIENTED_EDGE('',*,*,#26028,.T.);
#33855=ORIENTED_EDGE('',*,*,#26016,.T.);
#33856=ORIENTED_EDGE('',*,*,#25978,.T.);
#33857=ORIENTED_EDGE('',*,*,#26130,.T.);
#33858=ORIENTED_EDGE('',*,*,#26084,.T.);
#33859=ORIENTED_EDGE('',*,*,#26072,.T.);
#33860=ORIENTED_EDGE('',*,*,#26078,.T.);
#33861=ORIENTED_EDGE('',*,*,#25480,.T.);
#33862=ORIENTED_EDGE('',*,*,#25474,.T.);
#33863=ORIENTED_EDGE('',*,*,#25530,.T.);
#33864=ORIENTED_EDGE('',*,*,#25524,.T.);
#33865=ORIENTED_EDGE('',*,*,#25424,.T.);
#33866=ORIENTED_EDGE('',*,*,#25418,.T.);
#33867=ORIENTED_EDGE('',*,*,#25430,.T.);
#33868=ORIENTED_EDGE('',*,*,#25468,.T.);
#33869=ORIENTED_EDGE('',*,*,#25636,.T.);
#33870=ORIENTED_EDGE('',*,*,#25642,.T.);
#33871=ORIENTED_EDGE('',*,*,#25648,.T.);
#33872=ORIENTED_EDGE('',*,*,#25692,.T.);
#33873=ORIENTED_EDGE('',*,*,#25536,.T.);
#33874=ORIENTED_EDGE('',*,*,#25580,.T.);
#33875=ORIENTED_EDGE('',*,*,#25592,.T.);
#33876=ORIENTED_EDGE('',*,*,#25586,.T.);
#33877=ORIENTED_EDGE('',*,*,#25200,.T.);
#33878=ORIENTED_EDGE('',*,*,#25194,.T.);
#33879=ORIENTED_EDGE('',*,*,#25206,.T.);
#33880=ORIENTED_EDGE('',*,*,#25250,.T.);
#33881=ORIENTED_EDGE('',*,*,#25082,.T.);
#33882=ORIENTED_EDGE('',*,*,#25026,.T.);
#33883=ORIENTED_EDGE('',*,*,#26521,.T.);
#33884=ORIENTED_EDGE('',*,*,#26577,.T.);
#33885=ORIENTED_EDGE('',*,*,#25318,.T.);
#33886=ORIENTED_EDGE('',*,*,#25362,.T.);
#33887=ORIENTED_EDGE('',*,*,#25374,.T.);
#33888=ORIENTED_EDGE('',*,*,#25368,.T.);
#33889=ORIENTED_EDGE('',*,*,#25306,.T.);
#33890=ORIENTED_EDGE('',*,*,#25312,.T.);
#33891=ORIENTED_EDGE('',*,*,#25256,.T.);
#33892=ORIENTED_EDGE('',*,*,#25262,.T.);
#33893=ORIENTED_EDGE('',*,*,#26383,.T.);
#33894=ORIENTED_EDGE('',*,*,#26395,.T.);
#33895=ORIENTED_EDGE('',*,*,#26389,.T.);
#33896=ORIENTED_EDGE('',*,*,#26338,.T.);
#33897=ORIENTED_EDGE('',*,*,#26332,.T.);
#33898=ORIENTED_EDGE('',*,*,#26451,.T.);
#33899=ORIENTED_EDGE('',*,*,#26445,.T.);
#33900=ORIENTED_EDGE('',*,*,#26439,.T.);
#33901=ORIENTED_EDGE('',*,*,#26234,.T.);
#33902=ORIENTED_EDGE('',*,*,#26326,.T.);
#33903=ORIENTED_EDGE('',*,*,#26278,.T.);
#33904=ORIENTED_EDGE('',*,*,#26290,.T.);
#33905=ORIENTED_EDGE('',*,*,#26284,.T.);
#33906=ORIENTED_EDGE('',*,*,#25062,.T.);
#33907=ORIENTED_EDGE('',*,*,#25056,.T.);
#33908=ORIENTED_EDGE('',*,*,#25050,.T.);
#33909=ORIENTED_EDGE('',*,*,#25168,.T.);
#33910=ORIENTED_EDGE('',*,*,#25162,.T.);
#33911=ORIENTED_EDGE('',*,*,#25118,.T.);
#33912=ORIENTED_EDGE('',*,*,#25112,.T.);
#33913=ORIENTED_EDGE('',*,*,#25106,.T.);
#33914=ORIENTED_EDGE('',*,*,#26551,.T.);
#33915=ORIENTED_EDGE('',*,*,#26545,.T.);
#33916=ORIENTED_EDGE('',*,*,#26495,.T.);
#33917=ORIENTED_EDGE('',*,*,#26501,.T.);
#33918=ORIENTED_EDGE('',*,*,#26613,.T.);
#33919=ORIENTED_EDGE('',*,*,#26607,.T.);
#33920=ORIENTED_EDGE('',*,*,#26601,.T.);
#33921=ORIENTED_EDGE('',*,*,#26557,.T.);
#33922=ORIENTED_EDGE('',*,*,#25132,.T.);
#33923=ORIENTED_EDGE('',*,*,#24568,.T.);
#33924=ORIENTED_EDGE('',*,*,#24562,.T.);
#33925=ORIENTED_EDGE('',*,*,#24556,.T.);
#33926=ORIENTED_EDGE('',*,*,#24550,.T.);
#33927=ORIENTED_EDGE('',*,*,#24544,.T.);
#33928=ORIENTED_EDGE('',*,*,#24538,.T.);
#33929=ORIENTED_EDGE('',*,*,#26669,.T.);
#33930=ORIENTED_EDGE('',*,*,#25386,.T.);
#33931=ORIENTED_EDGE('',*,*,#25392,.T.);
#33932=ORIENTED_EDGE('',*,*,#26844,.T.);
#33933=ORIENTED_EDGE('',*,*,#26655,.T.);
#33934=ORIENTED_EDGE('',*,*,#26845,.T.);
#33935=ORIENTED_EDGE('',*,*,#26625,.T.);
#33936=ORIENTED_EDGE('',*,*,#26845,.F.);
#33937=ORIENTED_EDGE('',*,*,#26837,.T.);
#33938=ORIENTED_EDGE('',*,*,#26844,.F.);
#33939=ORIENTED_EDGE('',*,*,#26841,.F.);
#33940=ORIENTED_EDGE('',*,*,#26721,.F.);
#33941=ORIENTED_EDGE('',*,*,#26706,.F.);
#33942=ORIENTED_EDGE('',*,*,#26708,.T.);
#33943=ORIENTED_EDGE('',*,*,#26733,.T.);
#33944=ORIENTED_EDGE('',*,*,#26763,.F.);
#33945=ORIENTED_EDGE('',*,*,#26737,.T.);
#33946=ORIENTED_EDGE('',*,*,#26745,.T.);
#33947=ORIENTED_EDGE('',*,*,#26716,.F.);
#33948=ORIENTED_EDGE('',*,*,#26702,.F.);
#33949=ORIENTED_EDGE('',*,*,#26756,.F.);
#33950=ORIENTED_EDGE('',*,*,#26836,.F.);
#33951=ORIENTED_EDGE('',*,*,#26761,.T.);
#33952=ORIENTED_EDGE('',*,*,#26711,.F.);
#33953=ORIENTED_EDGE('',*,*,#26760,.T.);
#33954=ORIENTED_EDGE('',*,*,#26846,.T.);
#33955=ORIENTED_EDGE('',*,*,#26750,.T.);
#33956=ORIENTED_EDGE('',*,*,#26713,.T.);
#33957=ORIENTED_EDGE('',*,*,#26847,.F.);
#33958=ORIENTED_EDGE('',*,*,#26712,.F.);
#33959=ORIENTED_EDGE('',*,*,#26846,.F.);
#33960=ORIENTED_EDGE('',*,*,#26755,.T.);
#33961=ORIENTED_EDGE('',*,*,#26847,.T.);
#33962=ORIENTED_EDGE('',*,*,#26622,.F.);
#33963=ORIENTED_EDGE('',*,*,#26617,.F.);
#33964=ORIENTED_EDGE('',*,*,#26624,.T.);
#33965=ORIENTED_EDGE('',*,*,#26614,.F.);
#33966=ORIENTED_EDGE('',*,*,#26611,.F.);
#33967=ORIENTED_EDGE('',*,*,#26616,.T.);
#33968=ORIENTED_EDGE('',*,*,#26608,.F.);
#33969=ORIENTED_EDGE('',*,*,#26605,.F.);
#33970=ORIENTED_EDGE('',*,*,#26610,.T.);
#33971=ORIENTED_EDGE('',*,*,#26602,.F.);
#33972=ORIENTED_EDGE('',*,*,#26599,.F.);
#33973=ORIENTED_EDGE('',*,*,#26604,.T.);
#33974=ORIENTED_EDGE('',*,*,#26596,.F.);
#33975=ORIENTED_EDGE('',*,*,#26593,.F.);
#33976=ORIENTED_EDGE('',*,*,#26598,.T.);
#33977=ORIENTED_EDGE('',*,*,#26590,.F.);
#33978=ORIENTED_EDGE('',*,*,#26587,.F.);
#33979=ORIENTED_EDGE('',*,*,#26592,.T.);
#33980=ORIENTED_EDGE('',*,*,#26584,.F.);
#33981=ORIENTED_EDGE('',*,*,#26581,.F.);
#33982=ORIENTED_EDGE('',*,*,#26586,.T.);
#33983=ORIENTED_EDGE('',*,*,#26578,.F.);
#33984=ORIENTED_EDGE('',*,*,#26575,.F.);
#33985=ORIENTED_EDGE('',*,*,#26580,.T.);
#33986=ORIENTED_EDGE('',*,*,#26572,.F.);
#33987=ORIENTED_EDGE('',*,*,#26569,.F.);
#33988=ORIENTED_EDGE('',*,*,#26574,.T.);
#33989=ORIENTED_EDGE('',*,*,#26566,.F.);
#33990=ORIENTED_EDGE('',*,*,#26561,.F.);
#33991=ORIENTED_EDGE('',*,*,#26568,.T.);
#33992=ORIENTED_EDGE('',*,*,#26558,.F.);
#33993=ORIENTED_EDGE('',*,*,#26555,.F.);
#33994=ORIENTED_EDGE('',*,*,#26560,.T.);
#33995=ORIENTED_EDGE('',*,*,#26552,.F.);
#33996=ORIENTED_EDGE('',*,*,#26549,.F.);
#33997=ORIENTED_EDGE('',*,*,#26554,.T.);
#33998=ORIENTED_EDGE('',*,*,#26546,.F.);
#33999=ORIENTED_EDGE('',*,*,#26543,.F.);
#34000=ORIENTED_EDGE('',*,*,#26548,.T.);
#34001=ORIENTED_EDGE('',*,*,#26540,.F.);
#34002=ORIENTED_EDGE('',*,*,#26537,.F.);
#34003=ORIENTED_EDGE('',*,*,#26542,.T.);
#34004=ORIENTED_EDGE('',*,*,#26534,.F.);
#34005=ORIENTED_EDGE('',*,*,#26531,.F.);
#34006=ORIENTED_EDGE('',*,*,#26536,.T.);
#34007=ORIENTED_EDGE('',*,*,#26528,.F.);
#34008=ORIENTED_EDGE('',*,*,#26525,.F.);
#34009=ORIENTED_EDGE('',*,*,#26530,.T.);
#34010=ORIENTED_EDGE('',*,*,#26522,.F.);
#34011=ORIENTED_EDGE('',*,*,#26519,.F.);
#34012=ORIENTED_EDGE('',*,*,#26524,.T.);
#34013=ORIENTED_EDGE('',*,*,#26516,.F.);
#34014=ORIENTED_EDGE('',*,*,#26513,.F.);
#34015=ORIENTED_EDGE('',*,*,#26518,.T.);
#34016=ORIENTED_EDGE('',*,*,#26510,.F.);
#34017=ORIENTED_EDGE('',*,*,#26505,.F.);
#34018=ORIENTED_EDGE('',*,*,#26512,.T.);
#34019=ORIENTED_EDGE('',*,*,#26502,.F.);
#34020=ORIENTED_EDGE('',*,*,#26499,.F.);
#34021=ORIENTED_EDGE('',*,*,#26504,.T.);
#34022=ORIENTED_EDGE('',*,*,#26496,.F.);
#34023=ORIENTED_EDGE('',*,*,#26493,.F.);
#34024=ORIENTED_EDGE('',*,*,#26498,.T.);
#34025=ORIENTED_EDGE('',*,*,#26490,.F.);
#34026=ORIENTED_EDGE('',*,*,#26487,.F.);
#34027=ORIENTED_EDGE('',*,*,#26492,.T.);
#34028=ORIENTED_EDGE('',*,*,#26484,.F.);
#34029=ORIENTED_EDGE('',*,*,#26481,.F.);
#34030=ORIENTED_EDGE('',*,*,#26486,.T.);
#34031=ORIENTED_EDGE('',*,*,#26478,.F.);
#34032=ORIENTED_EDGE('',*,*,#26475,.F.);
#34033=ORIENTED_EDGE('',*,*,#26480,.T.);
#34034=ORIENTED_EDGE('',*,*,#26472,.F.);
#34035=ORIENTED_EDGE('',*,*,#26469,.F.);
#34036=ORIENTED_EDGE('',*,*,#26474,.T.);
#34037=ORIENTED_EDGE('',*,*,#26466,.F.);
#34038=ORIENTED_EDGE('',*,*,#26463,.F.);
#34039=ORIENTED_EDGE('',*,*,#26468,.T.);
#34040=ORIENTED_EDGE('',*,*,#26460,.F.);
#34041=ORIENTED_EDGE('',*,*,#26455,.F.);
#34042=ORIENTED_EDGE('',*,*,#26462,.T.);
#34043=ORIENTED_EDGE('',*,*,#26452,.F.);
#34044=ORIENTED_EDGE('',*,*,#26449,.F.);
#34045=ORIENTED_EDGE('',*,*,#26454,.T.);
#34046=ORIENTED_EDGE('',*,*,#26446,.F.);
#34047=ORIENTED_EDGE('',*,*,#26443,.F.);
#34048=ORIENTED_EDGE('',*,*,#26448,.T.);
#34049=ORIENTED_EDGE('',*,*,#26440,.F.);
#34050=ORIENTED_EDGE('',*,*,#26437,.F.);
#34051=ORIENTED_EDGE('',*,*,#26442,.T.);
#34052=ORIENTED_EDGE('',*,*,#26434,.F.);
#34053=ORIENTED_EDGE('',*,*,#26431,.F.);
#34054=ORIENTED_EDGE('',*,*,#26436,.T.);
#34055=ORIENTED_EDGE('',*,*,#26428,.F.);
#34056=ORIENTED_EDGE('',*,*,#26425,.F.);
#34057=ORIENTED_EDGE('',*,*,#26430,.T.);
#34058=ORIENTED_EDGE('',*,*,#26422,.F.);
#34059=ORIENTED_EDGE('',*,*,#26419,.F.);
#34060=ORIENTED_EDGE('',*,*,#26424,.T.);
#34061=ORIENTED_EDGE('',*,*,#26416,.F.);
#34062=ORIENTED_EDGE('',*,*,#26413,.F.);
#34063=ORIENTED_EDGE('',*,*,#26418,.T.);
#34064=ORIENTED_EDGE('',*,*,#26410,.F.);
#34065=ORIENTED_EDGE('',*,*,#26407,.F.);
#34066=ORIENTED_EDGE('',*,*,#26412,.T.);
#34067=ORIENTED_EDGE('',*,*,#26404,.F.);
#34068=ORIENTED_EDGE('',*,*,#26399,.F.);
#34069=ORIENTED_EDGE('',*,*,#26406,.T.);
#34070=ORIENTED_EDGE('',*,*,#26396,.F.);
#34071=ORIENTED_EDGE('',*,*,#26393,.F.);
#34072=ORIENTED_EDGE('',*,*,#26398,.T.);
#34073=ORIENTED_EDGE('',*,*,#26390,.F.);
#34074=ORIENTED_EDGE('',*,*,#26387,.F.);
#34075=ORIENTED_EDGE('',*,*,#26392,.T.);
#34076=ORIENTED_EDGE('',*,*,#26384,.F.);
#34077=ORIENTED_EDGE('',*,*,#26381,.F.);
#34078=ORIENTED_EDGE('',*,*,#26386,.T.);
#34079=ORIENTED_EDGE('',*,*,#26378,.F.);
#34080=ORIENTED_EDGE('',*,*,#26375,.F.);
#34081=ORIENTED_EDGE('',*,*,#26380,.T.);
#34082=ORIENTED_EDGE('',*,*,#26372,.F.);
#34083=ORIENTED_EDGE('',*,*,#26369,.F.);
#34084=ORIENTED_EDGE('',*,*,#26374,.T.);
#34085=ORIENTED_EDGE('',*,*,#26366,.F.);
#34086=ORIENTED_EDGE('',*,*,#26363,.F.);
#34087=ORIENTED_EDGE('',*,*,#26368,.T.);
#34088=ORIENTED_EDGE('',*,*,#26360,.F.);
#34089=ORIENTED_EDGE('',*,*,#26357,.F.);
#34090=ORIENTED_EDGE('',*,*,#26362,.T.);
#34091=ORIENTED_EDGE('',*,*,#26354,.F.);
#34092=ORIENTED_EDGE('',*,*,#26351,.F.);
#34093=ORIENTED_EDGE('',*,*,#26356,.T.);
#34094=ORIENTED_EDGE('',*,*,#26348,.F.);
#34095=ORIENTED_EDGE('',*,*,#26342,.F.);
#34096=ORIENTED_EDGE('',*,*,#26350,.T.);
#34097=ORIENTED_EDGE('',*,*,#26339,.F.);
#34098=ORIENTED_EDGE('',*,*,#26336,.F.);
#34099=ORIENTED_EDGE('',*,*,#26341,.T.);
#34100=ORIENTED_EDGE('',*,*,#26333,.F.);
#34101=ORIENTED_EDGE('',*,*,#26330,.F.);
#34102=ORIENTED_EDGE('',*,*,#26335,.T.);
#34103=ORIENTED_EDGE('',*,*,#26327,.F.);
#34104=ORIENTED_EDGE('',*,*,#26324,.F.);
#34105=ORIENTED_EDGE('',*,*,#26329,.T.);
#34106=ORIENTED_EDGE('',*,*,#26321,.F.);
#34107=ORIENTED_EDGE('',*,*,#26318,.F.);
#34108=ORIENTED_EDGE('',*,*,#26323,.T.);
#34109=ORIENTED_EDGE('',*,*,#26315,.F.);
#34110=ORIENTED_EDGE('',*,*,#26312,.F.);
#34111=ORIENTED_EDGE('',*,*,#26317,.T.);
#34112=ORIENTED_EDGE('',*,*,#26309,.F.);
#34113=ORIENTED_EDGE('',*,*,#26306,.F.);
#34114=ORIENTED_EDGE('',*,*,#26311,.T.);
#34115=ORIENTED_EDGE('',*,*,#26303,.F.);
#34116=ORIENTED_EDGE('',*,*,#26300,.F.);
#34117=ORIENTED_EDGE('',*,*,#26305,.T.);
#34118=ORIENTED_EDGE('',*,*,#26297,.F.);
#34119=ORIENTED_EDGE('',*,*,#26294,.F.);
#34120=ORIENTED_EDGE('',*,*,#26299,.T.);
#34121=ORIENTED_EDGE('',*,*,#26291,.F.);
#34122=ORIENTED_EDGE('',*,*,#26288,.F.);
#34123=ORIENTED_EDGE('',*,*,#26293,.T.);
#34124=ORIENTED_EDGE('',*,*,#26285,.F.);
#34125=ORIENTED_EDGE('',*,*,#26282,.F.);
#34126=ORIENTED_EDGE('',*,*,#26287,.T.);
#34127=ORIENTED_EDGE('',*,*,#26279,.F.);
#34128=ORIENTED_EDGE('',*,*,#26276,.F.);
#34129=ORIENTED_EDGE('',*,*,#26281,.T.);
#34130=ORIENTED_EDGE('',*,*,#26273,.F.);
#34131=ORIENTED_EDGE('',*,*,#26270,.F.);
#34132=ORIENTED_EDGE('',*,*,#26275,.T.);
#34133=ORIENTED_EDGE('',*,*,#26267,.F.);
#34134=ORIENTED_EDGE('',*,*,#26264,.F.);
#34135=ORIENTED_EDGE('',*,*,#26269,.T.);
#34136=ORIENTED_EDGE('',*,*,#26261,.F.);
#34137=ORIENTED_EDGE('',*,*,#26258,.F.);
#34138=ORIENTED_EDGE('',*,*,#26263,.T.);
#34139=ORIENTED_EDGE('',*,*,#26255,.F.);
#34140=ORIENTED_EDGE('',*,*,#26252,.F.);
#34141=ORIENTED_EDGE('',*,*,#26257,.T.);
#34142=ORIENTED_EDGE('',*,*,#26249,.F.);
#34143=ORIENTED_EDGE('',*,*,#26246,.F.);
#34144=ORIENTED_EDGE('',*,*,#26251,.T.);
#34145=ORIENTED_EDGE('',*,*,#26243,.F.);
#34146=ORIENTED_EDGE('',*,*,#26238,.F.);
#34147=ORIENTED_EDGE('',*,*,#26245,.T.);
#34148=ORIENTED_EDGE('',*,*,#26235,.F.);
#34149=ORIENTED_EDGE('',*,*,#26232,.F.);
#34150=ORIENTED_EDGE('',*,*,#26237,.T.);
#34151=ORIENTED_EDGE('',*,*,#26229,.F.);
#34152=ORIENTED_EDGE('',*,*,#26226,.F.);
#34153=ORIENTED_EDGE('',*,*,#26231,.T.);
#34154=ORIENTED_EDGE('',*,*,#26223,.F.);
#34155=ORIENTED_EDGE('',*,*,#26220,.F.);
#34156=ORIENTED_EDGE('',*,*,#26225,.T.);
#34157=ORIENTED_EDGE('',*,*,#26217,.F.);
#34158=ORIENTED_EDGE('',*,*,#26214,.F.);
#34159=ORIENTED_EDGE('',*,*,#26219,.T.);
#34160=ORIENTED_EDGE('',*,*,#26211,.F.);
#34161=ORIENTED_EDGE('',*,*,#26208,.F.);
#34162=ORIENTED_EDGE('',*,*,#26213,.T.);
#34163=ORIENTED_EDGE('',*,*,#26205,.F.);
#34164=ORIENTED_EDGE('',*,*,#26202,.F.);
#34165=ORIENTED_EDGE('',*,*,#26207,.T.);
#34166=ORIENTED_EDGE('',*,*,#26199,.F.);
#34167=ORIENTED_EDGE('',*,*,#26196,.F.);
#34168=ORIENTED_EDGE('',*,*,#26201,.T.);
#34169=ORIENTED_EDGE('',*,*,#26193,.F.);
#34170=ORIENTED_EDGE('',*,*,#26190,.F.);
#34171=ORIENTED_EDGE('',*,*,#26195,.T.);
#34172=ORIENTED_EDGE('',*,*,#26187,.F.);
#34173=ORIENTED_EDGE('',*,*,#26184,.F.);
#34174=ORIENTED_EDGE('',*,*,#26189,.T.);
#34175=ORIENTED_EDGE('',*,*,#26181,.F.);
#34176=ORIENTED_EDGE('',*,*,#26178,.F.);
#34177=ORIENTED_EDGE('',*,*,#26183,.T.);
#34178=ORIENTED_EDGE('',*,*,#26175,.F.);
#34179=ORIENTED_EDGE('',*,*,#26172,.F.);
#34180=ORIENTED_EDGE('',*,*,#26177,.T.);
#34181=ORIENTED_EDGE('',*,*,#26169,.F.);
#34182=ORIENTED_EDGE('',*,*,#26166,.F.);
#34183=ORIENTED_EDGE('',*,*,#26171,.T.);
#34184=ORIENTED_EDGE('',*,*,#26163,.F.);
#34185=ORIENTED_EDGE('',*,*,#26160,.F.);
#34186=ORIENTED_EDGE('',*,*,#26165,.T.);
#34187=ORIENTED_EDGE('',*,*,#26157,.F.);
#34188=ORIENTED_EDGE('',*,*,#26152,.F.);
#34189=ORIENTED_EDGE('',*,*,#26159,.T.);
#34190=ORIENTED_EDGE('',*,*,#26149,.F.);
#34191=ORIENTED_EDGE('',*,*,#26146,.F.);
#34192=ORIENTED_EDGE('',*,*,#26151,.T.);
#34193=ORIENTED_EDGE('',*,*,#26143,.F.);
#34194=ORIENTED_EDGE('',*,*,#26140,.F.);
#34195=ORIENTED_EDGE('',*,*,#26145,.T.);
#34196=ORIENTED_EDGE('',*,*,#26137,.F.);
#34197=ORIENTED_EDGE('',*,*,#26134,.F.);
#34198=ORIENTED_EDGE('',*,*,#26139,.T.);
#34199=ORIENTED_EDGE('',*,*,#26131,.F.);
#34200=ORIENTED_EDGE('',*,*,#26128,.F.);
#34201=ORIENTED_EDGE('',*,*,#26133,.T.);
#34202=ORIENTED_EDGE('',*,*,#26125,.F.);
#34203=ORIENTED_EDGE('',*,*,#26122,.F.);
#34204=ORIENTED_EDGE('',*,*,#26127,.T.);
#34205=ORIENTED_EDGE('',*,*,#26119,.F.);
#34206=ORIENTED_EDGE('',*,*,#26116,.F.);
#34207=ORIENTED_EDGE('',*,*,#26121,.T.);
#34208=ORIENTED_EDGE('',*,*,#26113,.F.);
#34209=ORIENTED_EDGE('',*,*,#26108,.F.);
#34210=ORIENTED_EDGE('',*,*,#26115,.T.);
#34211=ORIENTED_EDGE('',*,*,#26105,.F.);
#34212=ORIENTED_EDGE('',*,*,#26100,.F.);
#34213=ORIENTED_EDGE('',*,*,#26107,.T.);
#34214=ORIENTED_EDGE('',*,*,#26097,.F.);
#34215=ORIENTED_EDGE('',*,*,#26094,.F.);
#34216=ORIENTED_EDGE('',*,*,#26099,.T.);
#34217=ORIENTED_EDGE('',*,*,#26091,.F.);
#34218=ORIENTED_EDGE('',*,*,#26088,.F.);
#34219=ORIENTED_EDGE('',*,*,#26093,.T.);
#34220=ORIENTED_EDGE('',*,*,#26085,.F.);
#34221=ORIENTED_EDGE('',*,*,#26082,.F.);
#34222=ORIENTED_EDGE('',*,*,#26087,.T.);
#34223=ORIENTED_EDGE('',*,*,#26079,.F.);
#34224=ORIENTED_EDGE('',*,*,#26076,.F.);
#34225=ORIENTED_EDGE('',*,*,#26081,.T.);
#34226=ORIENTED_EDGE('',*,*,#26073,.F.);
#34227=ORIENTED_EDGE('',*,*,#26070,.F.);
#34228=ORIENTED_EDGE('',*,*,#26075,.T.);
#34229=ORIENTED_EDGE('',*,*,#26067,.F.);
#34230=ORIENTED_EDGE('',*,*,#26064,.F.);
#34231=ORIENTED_EDGE('',*,*,#26069,.T.);
#34232=ORIENTED_EDGE('',*,*,#26061,.F.);
#34233=ORIENTED_EDGE('',*,*,#26058,.F.);
#34234=ORIENTED_EDGE('',*,*,#26063,.T.);
#34235=ORIENTED_EDGE('',*,*,#26055,.F.);
#34236=ORIENTED_EDGE('',*,*,#26050,.F.);
#34237=ORIENTED_EDGE('',*,*,#26057,.T.);
#34238=ORIENTED_EDGE('',*,*,#26047,.F.);
#34239=ORIENTED_EDGE('',*,*,#26044,.F.);
#34240=ORIENTED_EDGE('',*,*,#26049,.T.);
#34241=ORIENTED_EDGE('',*,*,#26041,.F.);
#34242=ORIENTED_EDGE('',*,*,#26038,.F.);
#34243=ORIENTED_EDGE('',*,*,#26043,.T.);
#34244=ORIENTED_EDGE('',*,*,#26035,.F.);
#34245=ORIENTED_EDGE('',*,*,#26032,.F.);
#34246=ORIENTED_EDGE('',*,*,#26037,.T.);
#34247=ORIENTED_EDGE('',*,*,#26029,.F.);
#34248=ORIENTED_EDGE('',*,*,#26026,.F.);
#34249=ORIENTED_EDGE('',*,*,#26031,.T.);
#34250=ORIENTED_EDGE('',*,*,#26023,.F.);
#34251=ORIENTED_EDGE('',*,*,#26020,.F.);
#34252=ORIENTED_EDGE('',*,*,#26025,.T.);
#34253=ORIENTED_EDGE('',*,*,#26017,.F.);
#34254=ORIENTED_EDGE('',*,*,#26014,.F.);
#34255=ORIENTED_EDGE('',*,*,#26019,.T.);
#34256=ORIENTED_EDGE('',*,*,#26011,.F.);
#34257=ORIENTED_EDGE('',*,*,#26008,.F.);
#34258=ORIENTED_EDGE('',*,*,#26013,.T.);
#34259=ORIENTED_EDGE('',*,*,#26005,.F.);
#34260=ORIENTED_EDGE('',*,*,#26002,.F.);
#34261=ORIENTED_EDGE('',*,*,#26007,.T.);
#34262=ORIENTED_EDGE('',*,*,#25999,.F.);
#34263=ORIENTED_EDGE('',*,*,#25994,.F.);
#34264=ORIENTED_EDGE('',*,*,#26001,.T.);
#34265=ORIENTED_EDGE('',*,*,#25991,.F.);
#34266=ORIENTED_EDGE('',*,*,#25988,.F.);
#34267=ORIENTED_EDGE('',*,*,#25993,.T.);
#34268=ORIENTED_EDGE('',*,*,#25985,.F.);
#34269=ORIENTED_EDGE('',*,*,#25982,.F.);
#34270=ORIENTED_EDGE('',*,*,#25987,.T.);
#34271=ORIENTED_EDGE('',*,*,#25979,.F.);
#34272=ORIENTED_EDGE('',*,*,#25976,.F.);
#34273=ORIENTED_EDGE('',*,*,#25981,.T.);
#34274=ORIENTED_EDGE('',*,*,#25973,.F.);
#34275=ORIENTED_EDGE('',*,*,#25970,.F.);
#34276=ORIENTED_EDGE('',*,*,#25975,.T.);
#34277=ORIENTED_EDGE('',*,*,#25967,.F.);
#34278=ORIENTED_EDGE('',*,*,#25964,.F.);
#34279=ORIENTED_EDGE('',*,*,#25969,.T.);
#34280=ORIENTED_EDGE('',*,*,#25961,.F.);
#34281=ORIENTED_EDGE('',*,*,#25958,.F.);
#34282=ORIENTED_EDGE('',*,*,#25963,.T.);
#34283=ORIENTED_EDGE('',*,*,#25955,.F.);
#34284=ORIENTED_EDGE('',*,*,#25952,.F.);
#34285=ORIENTED_EDGE('',*,*,#25957,.T.);
#34286=ORIENTED_EDGE('',*,*,#25949,.F.);
#34287=ORIENTED_EDGE('',*,*,#25944,.F.);
#34288=ORIENTED_EDGE('',*,*,#25951,.T.);
#34289=ORIENTED_EDGE('',*,*,#25941,.F.);
#34290=ORIENTED_EDGE('',*,*,#25938,.F.);
#34291=ORIENTED_EDGE('',*,*,#25943,.T.);
#34292=ORIENTED_EDGE('',*,*,#25935,.F.);
#34293=ORIENTED_EDGE('',*,*,#25932,.F.);
#34294=ORIENTED_EDGE('',*,*,#25937,.T.);
#34295=ORIENTED_EDGE('',*,*,#25929,.F.);
#34296=ORIENTED_EDGE('',*,*,#25926,.F.);
#34297=ORIENTED_EDGE('',*,*,#25931,.T.);
#34298=ORIENTED_EDGE('',*,*,#25923,.F.);
#34299=ORIENTED_EDGE('',*,*,#25920,.F.);
#34300=ORIENTED_EDGE('',*,*,#25925,.T.);
#34301=ORIENTED_EDGE('',*,*,#25917,.F.);
#34302=ORIENTED_EDGE('',*,*,#25914,.F.);
#34303=ORIENTED_EDGE('',*,*,#25919,.T.);
#34304=ORIENTED_EDGE('',*,*,#25911,.F.);
#34305=ORIENTED_EDGE('',*,*,#25908,.F.);
#34306=ORIENTED_EDGE('',*,*,#25913,.T.);
#34307=ORIENTED_EDGE('',*,*,#25905,.F.);
#34308=ORIENTED_EDGE('',*,*,#25902,.F.);
#34309=ORIENTED_EDGE('',*,*,#25907,.T.);
#34310=ORIENTED_EDGE('',*,*,#25899,.F.);
#34311=ORIENTED_EDGE('',*,*,#25896,.F.);
#34312=ORIENTED_EDGE('',*,*,#25901,.T.);
#34313=ORIENTED_EDGE('',*,*,#25893,.F.);
#34314=ORIENTED_EDGE('',*,*,#25888,.F.);
#34315=ORIENTED_EDGE('',*,*,#25895,.T.);
#34316=ORIENTED_EDGE('',*,*,#25885,.F.);
#34317=ORIENTED_EDGE('',*,*,#25882,.F.);
#34318=ORIENTED_EDGE('',*,*,#25887,.T.);
#34319=ORIENTED_EDGE('',*,*,#25879,.F.);
#34320=ORIENTED_EDGE('',*,*,#25876,.F.);
#34321=ORIENTED_EDGE('',*,*,#25881,.T.);
#34322=ORIENTED_EDGE('',*,*,#25873,.F.);
#34323=ORIENTED_EDGE('',*,*,#25870,.F.);
#34324=ORIENTED_EDGE('',*,*,#25875,.T.);
#34325=ORIENTED_EDGE('',*,*,#25867,.F.);
#34326=ORIENTED_EDGE('',*,*,#25864,.F.);
#34327=ORIENTED_EDGE('',*,*,#25869,.T.);
#34328=ORIENTED_EDGE('',*,*,#25861,.F.);
#34329=ORIENTED_EDGE('',*,*,#25858,.F.);
#34330=ORIENTED_EDGE('',*,*,#25863,.T.);
#34331=ORIENTED_EDGE('',*,*,#25855,.F.);
#34332=ORIENTED_EDGE('',*,*,#25852,.F.);
#34333=ORIENTED_EDGE('',*,*,#25857,.T.);
#34334=ORIENTED_EDGE('',*,*,#25849,.F.);
#34335=ORIENTED_EDGE('',*,*,#25846,.F.);
#34336=ORIENTED_EDGE('',*,*,#25851,.T.);
#34337=ORIENTED_EDGE('',*,*,#25843,.F.);
#34338=ORIENTED_EDGE('',*,*,#25840,.F.);
#34339=ORIENTED_EDGE('',*,*,#25845,.T.);
#34340=ORIENTED_EDGE('',*,*,#25837,.F.);
#34341=ORIENTED_EDGE('',*,*,#25832,.F.);
#34342=ORIENTED_EDGE('',*,*,#25839,.T.);
#34343=ORIENTED_EDGE('',*,*,#25829,.F.);
#34344=ORIENTED_EDGE('',*,*,#25826,.F.);
#34345=ORIENTED_EDGE('',*,*,#25831,.T.);
#34346=ORIENTED_EDGE('',*,*,#25823,.F.);
#34347=ORIENTED_EDGE('',*,*,#25820,.F.);
#34348=ORIENTED_EDGE('',*,*,#25825,.T.);
#34349=ORIENTED_EDGE('',*,*,#25817,.F.);
#34350=ORIENTED_EDGE('',*,*,#25814,.F.);
#34351=ORIENTED_EDGE('',*,*,#25819,.T.);
#34352=ORIENTED_EDGE('',*,*,#25811,.F.);
#34353=ORIENTED_EDGE('',*,*,#25808,.F.);
#34354=ORIENTED_EDGE('',*,*,#25813,.T.);
#34355=ORIENTED_EDGE('',*,*,#25805,.F.);
#34356=ORIENTED_EDGE('',*,*,#25802,.F.);
#34357=ORIENTED_EDGE('',*,*,#25807,.T.);
#34358=ORIENTED_EDGE('',*,*,#25799,.F.);
#34359=ORIENTED_EDGE('',*,*,#25796,.F.);
#34360=ORIENTED_EDGE('',*,*,#25801,.T.);
#34361=ORIENTED_EDGE('',*,*,#25793,.F.);
#34362=ORIENTED_EDGE('',*,*,#25790,.F.);
#34363=ORIENTED_EDGE('',*,*,#25795,.T.);
#34364=ORIENTED_EDGE('',*,*,#25787,.F.);
#34365=ORIENTED_EDGE('',*,*,#25784,.F.);
#34366=ORIENTED_EDGE('',*,*,#25789,.T.);
#34367=ORIENTED_EDGE('',*,*,#25781,.F.);
#34368=ORIENTED_EDGE('',*,*,#25776,.F.);
#34369=ORIENTED_EDGE('',*,*,#25783,.T.);
#34370=ORIENTED_EDGE('',*,*,#25773,.F.);
#34371=ORIENTED_EDGE('',*,*,#25770,.F.);
#34372=ORIENTED_EDGE('',*,*,#25775,.T.);
#34373=ORIENTED_EDGE('',*,*,#25767,.F.);
#34374=ORIENTED_EDGE('',*,*,#25764,.F.);
#34375=ORIENTED_EDGE('',*,*,#25769,.T.);
#34376=ORIENTED_EDGE('',*,*,#25761,.F.);
#34377=ORIENTED_EDGE('',*,*,#25758,.F.);
#34378=ORIENTED_EDGE('',*,*,#25763,.T.);
#34379=ORIENTED_EDGE('',*,*,#25755,.F.);
#34380=ORIENTED_EDGE('',*,*,#25752,.F.);
#34381=ORIENTED_EDGE('',*,*,#25757,.T.);
#34382=ORIENTED_EDGE('',*,*,#25749,.F.);
#34383=ORIENTED_EDGE('',*,*,#25746,.F.);
#34384=ORIENTED_EDGE('',*,*,#25751,.T.);
#34385=ORIENTED_EDGE('',*,*,#25743,.F.);
#34386=ORIENTED_EDGE('',*,*,#25740,.F.);
#34387=ORIENTED_EDGE('',*,*,#25745,.T.);
#34388=ORIENTED_EDGE('',*,*,#25737,.F.);
#34389=ORIENTED_EDGE('',*,*,#25734,.F.);
#34390=ORIENTED_EDGE('',*,*,#25739,.T.);
#34391=ORIENTED_EDGE('',*,*,#25731,.F.);
#34392=ORIENTED_EDGE('',*,*,#25728,.F.);
#34393=ORIENTED_EDGE('',*,*,#25733,.T.);
#34394=ORIENTED_EDGE('',*,*,#25725,.F.);
#34395=ORIENTED_EDGE('',*,*,#25720,.F.);
#34396=ORIENTED_EDGE('',*,*,#25727,.T.);
#34397=ORIENTED_EDGE('',*,*,#25717,.F.);
#34398=ORIENTED_EDGE('',*,*,#25714,.F.);
#34399=ORIENTED_EDGE('',*,*,#25719,.T.);
#34400=ORIENTED_EDGE('',*,*,#25711,.F.);
#34401=ORIENTED_EDGE('',*,*,#25708,.F.);
#34402=ORIENTED_EDGE('',*,*,#25713,.T.);
#34403=ORIENTED_EDGE('',*,*,#25705,.F.);
#34404=ORIENTED_EDGE('',*,*,#25702,.F.);
#34405=ORIENTED_EDGE('',*,*,#25707,.T.);
#34406=ORIENTED_EDGE('',*,*,#25699,.F.);
#34407=ORIENTED_EDGE('',*,*,#25696,.F.);
#34408=ORIENTED_EDGE('',*,*,#25701,.T.);
#34409=ORIENTED_EDGE('',*,*,#25693,.F.);
#34410=ORIENTED_EDGE('',*,*,#25690,.F.);
#34411=ORIENTED_EDGE('',*,*,#25695,.T.);
#34412=ORIENTED_EDGE('',*,*,#25687,.F.);
#34413=ORIENTED_EDGE('',*,*,#25684,.F.);
#34414=ORIENTED_EDGE('',*,*,#25689,.T.);
#34415=ORIENTED_EDGE('',*,*,#25681,.F.);
#34416=ORIENTED_EDGE('',*,*,#25678,.F.);
#34417=ORIENTED_EDGE('',*,*,#25683,.T.);
#34418=ORIENTED_EDGE('',*,*,#25675,.F.);
#34419=ORIENTED_EDGE('',*,*,#25670,.F.);
#34420=ORIENTED_EDGE('',*,*,#25677,.T.);
#34421=ORIENTED_EDGE('',*,*,#25667,.F.);
#34422=ORIENTED_EDGE('',*,*,#25664,.F.);
#34423=ORIENTED_EDGE('',*,*,#25669,.T.);
#34424=ORIENTED_EDGE('',*,*,#25661,.F.);
#34425=ORIENTED_EDGE('',*,*,#25658,.F.);
#34426=ORIENTED_EDGE('',*,*,#25663,.T.);
#34427=ORIENTED_EDGE('',*,*,#25655,.F.);
#34428=ORIENTED_EDGE('',*,*,#25652,.F.);
#34429=ORIENTED_EDGE('',*,*,#25657,.T.);
#34430=ORIENTED_EDGE('',*,*,#25649,.F.);
#34431=ORIENTED_EDGE('',*,*,#25646,.F.);
#34432=ORIENTED_EDGE('',*,*,#25651,.T.);
#34433=ORIENTED_EDGE('',*,*,#25643,.F.);
#34434=ORIENTED_EDGE('',*,*,#25640,.F.);
#34435=ORIENTED_EDGE('',*,*,#25645,.T.);
#34436=ORIENTED_EDGE('',*,*,#25637,.F.);
#34437=ORIENTED_EDGE('',*,*,#25634,.F.);
#34438=ORIENTED_EDGE('',*,*,#25639,.T.);
#34439=ORIENTED_EDGE('',*,*,#25631,.F.);
#34440=ORIENTED_EDGE('',*,*,#25628,.F.);
#34441=ORIENTED_EDGE('',*,*,#25633,.T.);
#34442=ORIENTED_EDGE('',*,*,#25625,.F.);
#34443=ORIENTED_EDGE('',*,*,#25622,.F.);
#34444=ORIENTED_EDGE('',*,*,#25627,.T.);
#34445=ORIENTED_EDGE('',*,*,#25619,.F.);
#34446=ORIENTED_EDGE('',*,*,#25614,.F.);
#34447=ORIENTED_EDGE('',*,*,#25621,.T.);
#34448=ORIENTED_EDGE('',*,*,#25611,.F.);
#34449=ORIENTED_EDGE('',*,*,#25608,.F.);
#34450=ORIENTED_EDGE('',*,*,#25613,.T.);
#34451=ORIENTED_EDGE('',*,*,#25605,.F.);
#34452=ORIENTED_EDGE('',*,*,#25602,.F.);
#34453=ORIENTED_EDGE('',*,*,#25607,.T.);
#34454=ORIENTED_EDGE('',*,*,#25599,.F.);
#34455=ORIENTED_EDGE('',*,*,#25596,.F.);
#34456=ORIENTED_EDGE('',*,*,#25601,.T.);
#34457=ORIENTED_EDGE('',*,*,#25593,.F.);
#34458=ORIENTED_EDGE('',*,*,#25590,.F.);
#34459=ORIENTED_EDGE('',*,*,#25595,.T.);
#34460=ORIENTED_EDGE('',*,*,#25587,.F.);
#34461=ORIENTED_EDGE('',*,*,#25584,.F.);
#34462=ORIENTED_EDGE('',*,*,#25589,.T.);
#34463=ORIENTED_EDGE('',*,*,#25581,.F.);
#34464=ORIENTED_EDGE('',*,*,#25578,.F.);
#34465=ORIENTED_EDGE('',*,*,#25583,.T.);
#34466=ORIENTED_EDGE('',*,*,#25575,.F.);
#34467=ORIENTED_EDGE('',*,*,#25572,.F.);
#34468=ORIENTED_EDGE('',*,*,#25577,.T.);
#34469=ORIENTED_EDGE('',*,*,#25569,.F.);
#34470=ORIENTED_EDGE('',*,*,#25566,.F.);
#34471=ORIENTED_EDGE('',*,*,#25571,.T.);
#34472=ORIENTED_EDGE('',*,*,#25563,.F.);
#34473=ORIENTED_EDGE('',*,*,#25558,.F.);
#34474=ORIENTED_EDGE('',*,*,#25565,.T.);
#34475=ORIENTED_EDGE('',*,*,#25555,.F.);
#34476=ORIENTED_EDGE('',*,*,#25552,.F.);
#34477=ORIENTED_EDGE('',*,*,#25557,.T.);
#34478=ORIENTED_EDGE('',*,*,#25549,.F.);
#34479=ORIENTED_EDGE('',*,*,#25546,.F.);
#34480=ORIENTED_EDGE('',*,*,#25551,.T.);
#34481=ORIENTED_EDGE('',*,*,#25543,.F.);
#34482=ORIENTED_EDGE('',*,*,#25540,.F.);
#34483=ORIENTED_EDGE('',*,*,#25545,.T.);
#34484=ORIENTED_EDGE('',*,*,#25537,.F.);
#34485=ORIENTED_EDGE('',*,*,#25534,.F.);
#34486=ORIENTED_EDGE('',*,*,#25539,.T.);
#34487=ORIENTED_EDGE('',*,*,#25531,.F.);
#34488=ORIENTED_EDGE('',*,*,#25528,.F.);
#34489=ORIENTED_EDGE('',*,*,#25533,.T.);
#34490=ORIENTED_EDGE('',*,*,#25525,.F.);
#34491=ORIENTED_EDGE('',*,*,#25522,.F.);
#34492=ORIENTED_EDGE('',*,*,#25527,.T.);
#34493=ORIENTED_EDGE('',*,*,#25519,.F.);
#34494=ORIENTED_EDGE('',*,*,#25516,.F.);
#34495=ORIENTED_EDGE('',*,*,#25521,.T.);
#34496=ORIENTED_EDGE('',*,*,#25513,.F.);
#34497=ORIENTED_EDGE('',*,*,#25510,.F.);
#34498=ORIENTED_EDGE('',*,*,#25515,.T.);
#34499=ORIENTED_EDGE('',*,*,#25507,.F.);
#34500=ORIENTED_EDGE('',*,*,#25502,.F.);
#34501=ORIENTED_EDGE('',*,*,#25509,.T.);
#34502=ORIENTED_EDGE('',*,*,#25499,.F.);
#34503=ORIENTED_EDGE('',*,*,#25496,.F.);
#34504=ORIENTED_EDGE('',*,*,#25501,.T.);
#34505=ORIENTED_EDGE('',*,*,#25493,.F.);
#34506=ORIENTED_EDGE('',*,*,#25490,.F.);
#34507=ORIENTED_EDGE('',*,*,#25495,.T.);
#34508=ORIENTED_EDGE('',*,*,#25487,.F.);
#34509=ORIENTED_EDGE('',*,*,#25484,.F.);
#34510=ORIENTED_EDGE('',*,*,#25489,.T.);
#34511=ORIENTED_EDGE('',*,*,#25481,.F.);
#34512=ORIENTED_EDGE('',*,*,#25478,.F.);
#34513=ORIENTED_EDGE('',*,*,#25483,.T.);
#34514=ORIENTED_EDGE('',*,*,#25475,.F.);
#34515=ORIENTED_EDGE('',*,*,#25472,.F.);
#34516=ORIENTED_EDGE('',*,*,#25477,.T.);
#34517=ORIENTED_EDGE('',*,*,#25469,.F.);
#34518=ORIENTED_EDGE('',*,*,#25466,.F.);
#34519=ORIENTED_EDGE('',*,*,#25471,.T.);
#34520=ORIENTED_EDGE('',*,*,#25463,.F.);
#34521=ORIENTED_EDGE('',*,*,#25460,.F.);
#34522=ORIENTED_EDGE('',*,*,#25465,.T.);
#34523=ORIENTED_EDGE('',*,*,#25457,.F.);
#34524=ORIENTED_EDGE('',*,*,#25454,.F.);
#34525=ORIENTED_EDGE('',*,*,#25459,.T.);
#34526=ORIENTED_EDGE('',*,*,#25451,.F.);
#34527=ORIENTED_EDGE('',*,*,#25446,.F.);
#34528=ORIENTED_EDGE('',*,*,#25453,.T.);
#34529=ORIENTED_EDGE('',*,*,#25443,.F.);
#34530=ORIENTED_EDGE('',*,*,#25440,.F.);
#34531=ORIENTED_EDGE('',*,*,#25445,.T.);
#34532=ORIENTED_EDGE('',*,*,#25437,.F.);
#34533=ORIENTED_EDGE('',*,*,#25434,.F.);
#34534=ORIENTED_EDGE('',*,*,#25439,.T.);
#34535=ORIENTED_EDGE('',*,*,#25431,.F.);
#34536=ORIENTED_EDGE('',*,*,#25428,.F.);
#34537=ORIENTED_EDGE('',*,*,#25433,.T.);
#34538=ORIENTED_EDGE('',*,*,#25425,.F.);
#34539=ORIENTED_EDGE('',*,*,#25422,.F.);
#34540=ORIENTED_EDGE('',*,*,#25427,.T.);
#34541=ORIENTED_EDGE('',*,*,#25419,.F.);
#34542=ORIENTED_EDGE('',*,*,#25416,.F.);
#34543=ORIENTED_EDGE('',*,*,#25421,.T.);
#34544=ORIENTED_EDGE('',*,*,#25413,.F.);
#34545=ORIENTED_EDGE('',*,*,#25410,.F.);
#34546=ORIENTED_EDGE('',*,*,#25415,.T.);
#34547=ORIENTED_EDGE('',*,*,#25407,.F.);
#34548=ORIENTED_EDGE('',*,*,#25404,.F.);
#34549=ORIENTED_EDGE('',*,*,#25409,.T.);
#34550=ORIENTED_EDGE('',*,*,#25401,.F.);
#34551=ORIENTED_EDGE('',*,*,#25396,.F.);
#34552=ORIENTED_EDGE('',*,*,#25403,.T.);
#34553=ORIENTED_EDGE('',*,*,#25393,.F.);
#34554=ORIENTED_EDGE('',*,*,#25390,.F.);
#34555=ORIENTED_EDGE('',*,*,#25395,.T.);
#34556=ORIENTED_EDGE('',*,*,#25387,.F.);
#34557=ORIENTED_EDGE('',*,*,#25384,.F.);
#34558=ORIENTED_EDGE('',*,*,#25389,.T.);
#34559=ORIENTED_EDGE('',*,*,#25381,.F.);
#34560=ORIENTED_EDGE('',*,*,#25378,.F.);
#34561=ORIENTED_EDGE('',*,*,#25383,.T.);
#34562=ORIENTED_EDGE('',*,*,#25375,.F.);
#34563=ORIENTED_EDGE('',*,*,#25372,.F.);
#34564=ORIENTED_EDGE('',*,*,#25377,.T.);
#34565=ORIENTED_EDGE('',*,*,#25369,.F.);
#34566=ORIENTED_EDGE('',*,*,#25366,.F.);
#34567=ORIENTED_EDGE('',*,*,#25371,.T.);
#34568=ORIENTED_EDGE('',*,*,#25363,.F.);
#34569=ORIENTED_EDGE('',*,*,#25360,.F.);
#34570=ORIENTED_EDGE('',*,*,#25365,.T.);
#34571=ORIENTED_EDGE('',*,*,#25357,.F.);
#34572=ORIENTED_EDGE('',*,*,#25354,.F.);
#34573=ORIENTED_EDGE('',*,*,#25359,.T.);
#34574=ORIENTED_EDGE('',*,*,#25351,.F.);
#34575=ORIENTED_EDGE('',*,*,#25348,.F.);
#34576=ORIENTED_EDGE('',*,*,#25353,.T.);
#34577=ORIENTED_EDGE('',*,*,#25345,.F.);
#34578=ORIENTED_EDGE('',*,*,#25340,.F.);
#34579=ORIENTED_EDGE('',*,*,#25347,.T.);
#34580=ORIENTED_EDGE('',*,*,#25337,.F.);
#34581=ORIENTED_EDGE('',*,*,#25334,.F.);
#34582=ORIENTED_EDGE('',*,*,#25339,.T.);
#34583=ORIENTED_EDGE('',*,*,#25331,.F.);
#34584=ORIENTED_EDGE('',*,*,#25328,.F.);
#34585=ORIENTED_EDGE('',*,*,#25333,.T.);
#34586=ORIENTED_EDGE('',*,*,#25325,.F.);
#34587=ORIENTED_EDGE('',*,*,#25322,.F.);
#34588=ORIENTED_EDGE('',*,*,#25327,.T.);
#34589=ORIENTED_EDGE('',*,*,#25319,.F.);
#34590=ORIENTED_EDGE('',*,*,#25316,.F.);
#34591=ORIENTED_EDGE('',*,*,#25321,.T.);
#34592=ORIENTED_EDGE('',*,*,#25313,.F.);
#34593=ORIENTED_EDGE('',*,*,#25310,.F.);
#34594=ORIENTED_EDGE('',*,*,#25315,.T.);
#34595=ORIENTED_EDGE('',*,*,#25307,.F.);
#34596=ORIENTED_EDGE('',*,*,#25304,.F.);
#34597=ORIENTED_EDGE('',*,*,#25309,.T.);
#34598=ORIENTED_EDGE('',*,*,#25301,.F.);
#34599=ORIENTED_EDGE('',*,*,#25298,.F.);
#34600=ORIENTED_EDGE('',*,*,#25303,.T.);
#34601=ORIENTED_EDGE('',*,*,#25295,.F.);
#34602=ORIENTED_EDGE('',*,*,#25292,.F.);
#34603=ORIENTED_EDGE('',*,*,#25297,.T.);
#34604=ORIENTED_EDGE('',*,*,#25289,.F.);
#34605=ORIENTED_EDGE('',*,*,#25284,.F.);
#34606=ORIENTED_EDGE('',*,*,#25291,.T.);
#34607=ORIENTED_EDGE('',*,*,#25281,.F.);
#34608=ORIENTED_EDGE('',*,*,#25278,.F.);
#34609=ORIENTED_EDGE('',*,*,#25283,.T.);
#34610=ORIENTED_EDGE('',*,*,#25275,.F.);
#34611=ORIENTED_EDGE('',*,*,#25272,.F.);
#34612=ORIENTED_EDGE('',*,*,#25277,.T.);
#34613=ORIENTED_EDGE('',*,*,#25269,.F.);
#34614=ORIENTED_EDGE('',*,*,#25266,.F.);
#34615=ORIENTED_EDGE('',*,*,#25271,.T.);
#34616=ORIENTED_EDGE('',*,*,#25263,.F.);
#34617=ORIENTED_EDGE('',*,*,#25260,.F.);
#34618=ORIENTED_EDGE('',*,*,#25265,.T.);
#34619=ORIENTED_EDGE('',*,*,#25257,.F.);
#34620=ORIENTED_EDGE('',*,*,#25254,.F.);
#34621=ORIENTED_EDGE('',*,*,#25259,.T.);
#34622=ORIENTED_EDGE('',*,*,#25251,.F.);
#34623=ORIENTED_EDGE('',*,*,#25248,.F.);
#34624=ORIENTED_EDGE('',*,*,#25253,.T.);
#34625=ORIENTED_EDGE('',*,*,#25245,.F.);
#34626=ORIENTED_EDGE('',*,*,#25242,.F.);
#34627=ORIENTED_EDGE('',*,*,#25247,.T.);
#34628=ORIENTED_EDGE('',*,*,#25239,.F.);
#34629=ORIENTED_EDGE('',*,*,#25236,.F.);
#34630=ORIENTED_EDGE('',*,*,#25241,.T.);
#34631=ORIENTED_EDGE('',*,*,#25233,.F.);
#34632=ORIENTED_EDGE('',*,*,#25228,.F.);
#34633=ORIENTED_EDGE('',*,*,#25235,.T.);
#34634=ORIENTED_EDGE('',*,*,#25225,.F.);
#34635=ORIENTED_EDGE('',*,*,#25222,.F.);
#34636=ORIENTED_EDGE('',*,*,#25227,.T.);
#34637=ORIENTED_EDGE('',*,*,#25219,.F.);
#34638=ORIENTED_EDGE('',*,*,#25216,.F.);
#34639=ORIENTED_EDGE('',*,*,#25221,.T.);
#34640=ORIENTED_EDGE('',*,*,#25213,.F.);
#34641=ORIENTED_EDGE('',*,*,#25210,.F.);
#34642=ORIENTED_EDGE('',*,*,#25215,.T.);
#34643=ORIENTED_EDGE('',*,*,#25207,.F.);
#34644=ORIENTED_EDGE('',*,*,#25204,.F.);
#34645=ORIENTED_EDGE('',*,*,#25209,.T.);
#34646=ORIENTED_EDGE('',*,*,#25201,.F.);
#34647=ORIENTED_EDGE('',*,*,#25198,.F.);
#34648=ORIENTED_EDGE('',*,*,#25203,.T.);
#34649=ORIENTED_EDGE('',*,*,#25195,.F.);
#34650=ORIENTED_EDGE('',*,*,#25192,.F.);
#34651=ORIENTED_EDGE('',*,*,#25197,.T.);
#34652=ORIENTED_EDGE('',*,*,#25189,.F.);
#34653=ORIENTED_EDGE('',*,*,#25186,.F.);
#34654=ORIENTED_EDGE('',*,*,#25191,.T.);
#34655=ORIENTED_EDGE('',*,*,#25183,.F.);
#34656=ORIENTED_EDGE('',*,*,#25180,.F.);
#34657=ORIENTED_EDGE('',*,*,#25185,.T.);
#34658=ORIENTED_EDGE('',*,*,#25177,.F.);
#34659=ORIENTED_EDGE('',*,*,#25172,.F.);
#34660=ORIENTED_EDGE('',*,*,#25179,.T.);
#34661=ORIENTED_EDGE('',*,*,#25169,.F.);
#34662=ORIENTED_EDGE('',*,*,#25166,.F.);
#34663=ORIENTED_EDGE('',*,*,#25171,.T.);
#34664=ORIENTED_EDGE('',*,*,#25163,.F.);
#34665=ORIENTED_EDGE('',*,*,#25160,.F.);
#34666=ORIENTED_EDGE('',*,*,#25165,.T.);
#34667=ORIENTED_EDGE('',*,*,#25157,.F.);
#34668=ORIENTED_EDGE('',*,*,#25154,.F.);
#34669=ORIENTED_EDGE('',*,*,#25159,.T.);
#34670=ORIENTED_EDGE('',*,*,#25151,.F.);
#34671=ORIENTED_EDGE('',*,*,#25148,.F.);
#34672=ORIENTED_EDGE('',*,*,#25153,.T.);
#34673=ORIENTED_EDGE('',*,*,#25145,.F.);
#34674=ORIENTED_EDGE('',*,*,#25142,.F.);
#34675=ORIENTED_EDGE('',*,*,#25147,.T.);
#34676=ORIENTED_EDGE('',*,*,#25139,.F.);
#34677=ORIENTED_EDGE('',*,*,#25136,.F.);
#34678=ORIENTED_EDGE('',*,*,#25141,.T.);
#34679=ORIENTED_EDGE('',*,*,#25133,.F.);
#34680=ORIENTED_EDGE('',*,*,#25130,.F.);
#34681=ORIENTED_EDGE('',*,*,#25135,.T.);
#34682=ORIENTED_EDGE('',*,*,#25127,.F.);
#34683=ORIENTED_EDGE('',*,*,#25122,.F.);
#34684=ORIENTED_EDGE('',*,*,#25129,.T.);
#34685=ORIENTED_EDGE('',*,*,#25119,.F.);
#34686=ORIENTED_EDGE('',*,*,#25116,.F.);
#34687=ORIENTED_EDGE('',*,*,#25121,.T.);
#34688=ORIENTED_EDGE('',*,*,#25113,.F.);
#34689=ORIENTED_EDGE('',*,*,#25110,.F.);
#34690=ORIENTED_EDGE('',*,*,#25115,.T.);
#34691=ORIENTED_EDGE('',*,*,#25107,.F.);
#34692=ORIENTED_EDGE('',*,*,#25104,.F.);
#34693=ORIENTED_EDGE('',*,*,#25109,.T.);
#34694=ORIENTED_EDGE('',*,*,#25101,.F.);
#34695=ORIENTED_EDGE('',*,*,#25098,.F.);
#34696=ORIENTED_EDGE('',*,*,#25103,.T.);
#34697=ORIENTED_EDGE('',*,*,#25095,.F.);
#34698=ORIENTED_EDGE('',*,*,#25092,.F.);
#34699=ORIENTED_EDGE('',*,*,#25097,.T.);
#34700=ORIENTED_EDGE('',*,*,#25089,.F.);
#34701=ORIENTED_EDGE('',*,*,#25086,.F.);
#34702=ORIENTED_EDGE('',*,*,#25091,.T.);
#34703=ORIENTED_EDGE('',*,*,#25083,.F.);
#34704=ORIENTED_EDGE('',*,*,#25080,.F.);
#34705=ORIENTED_EDGE('',*,*,#25085,.T.);
#34706=ORIENTED_EDGE('',*,*,#25077,.F.);
#34707=ORIENTED_EDGE('',*,*,#25074,.F.);
#34708=ORIENTED_EDGE('',*,*,#25079,.T.);
#34709=ORIENTED_EDGE('',*,*,#25071,.F.);
#34710=ORIENTED_EDGE('',*,*,#25066,.F.);
#34711=ORIENTED_EDGE('',*,*,#25073,.T.);
#34712=ORIENTED_EDGE('',*,*,#25063,.F.);
#34713=ORIENTED_EDGE('',*,*,#25060,.F.);
#34714=ORIENTED_EDGE('',*,*,#25065,.T.);
#34715=ORIENTED_EDGE('',*,*,#25057,.F.);
#34716=ORIENTED_EDGE('',*,*,#25054,.F.);
#34717=ORIENTED_EDGE('',*,*,#25059,.T.);
#34718=ORIENTED_EDGE('',*,*,#25051,.F.);
#34719=ORIENTED_EDGE('',*,*,#25048,.F.);
#34720=ORIENTED_EDGE('',*,*,#25053,.T.);
#34721=ORIENTED_EDGE('',*,*,#25045,.F.);
#34722=ORIENTED_EDGE('',*,*,#25042,.F.);
#34723=ORIENTED_EDGE('',*,*,#25047,.T.);
#34724=ORIENTED_EDGE('',*,*,#25039,.F.);
#34725=ORIENTED_EDGE('',*,*,#25036,.F.);
#34726=ORIENTED_EDGE('',*,*,#25041,.T.);
#34727=ORIENTED_EDGE('',*,*,#25033,.F.);
#34728=ORIENTED_EDGE('',*,*,#25030,.F.);
#34729=ORIENTED_EDGE('',*,*,#25035,.T.);
#34730=ORIENTED_EDGE('',*,*,#25027,.F.);
#34731=ORIENTED_EDGE('',*,*,#25024,.F.);
#34732=ORIENTED_EDGE('',*,*,#25029,.T.);
#34733=ORIENTED_EDGE('',*,*,#25021,.F.);
#34734=ORIENTED_EDGE('',*,*,#25018,.F.);
#34735=ORIENTED_EDGE('',*,*,#25023,.T.);
#34736=ORIENTED_EDGE('',*,*,#25015,.F.);
#34737=ORIENTED_EDGE('',*,*,#25011,.F.);
#34738=ORIENTED_EDGE('',*,*,#25014,.F.);
#34739=ORIENTED_EDGE('',*,*,#25017,.T.);
#34740=ORIENTED_EDGE('',*,*,#25008,.F.);
#34741=ORIENTED_EDGE('',*,*,#25004,.F.);
#34742=ORIENTED_EDGE('',*,*,#25007,.F.);
#34743=ORIENTED_EDGE('',*,*,#25010,.T.);
#34744=ORIENTED_EDGE('',*,*,#25001,.F.);
#34745=ORIENTED_EDGE('',*,*,#24997,.F.);
#34746=ORIENTED_EDGE('',*,*,#25000,.F.);
#34747=ORIENTED_EDGE('',*,*,#25003,.T.);
#34748=ORIENTED_EDGE('',*,*,#24994,.F.);
#34749=ORIENTED_EDGE('',*,*,#24990,.F.);
#34750=ORIENTED_EDGE('',*,*,#24993,.F.);
#34751=ORIENTED_EDGE('',*,*,#24996,.T.);
#34752=ORIENTED_EDGE('',*,*,#24987,.F.);
#34753=ORIENTED_EDGE('',*,*,#24983,.F.);
#34754=ORIENTED_EDGE('',*,*,#24986,.F.);
#34755=ORIENTED_EDGE('',*,*,#24989,.T.);
#34756=ORIENTED_EDGE('',*,*,#24980,.F.);
#34757=ORIENTED_EDGE('',*,*,#24976,.F.);
#34758=ORIENTED_EDGE('',*,*,#24979,.F.);
#34759=ORIENTED_EDGE('',*,*,#24982,.T.);
#34760=ORIENTED_EDGE('',*,*,#24973,.F.);
#34761=ORIENTED_EDGE('',*,*,#24969,.F.);
#34762=ORIENTED_EDGE('',*,*,#24972,.F.);
#34763=ORIENTED_EDGE('',*,*,#24975,.T.);
#34764=ORIENTED_EDGE('',*,*,#24966,.F.);
#34765=ORIENTED_EDGE('',*,*,#24962,.F.);
#34766=ORIENTED_EDGE('',*,*,#24965,.F.);
#34767=ORIENTED_EDGE('',*,*,#24968,.T.);
#34768=ORIENTED_EDGE('',*,*,#24959,.F.);
#34769=ORIENTED_EDGE('',*,*,#24955,.F.);
#34770=ORIENTED_EDGE('',*,*,#24958,.F.);
#34771=ORIENTED_EDGE('',*,*,#24961,.T.);
#34772=ORIENTED_EDGE('',*,*,#24952,.F.);
#34773=ORIENTED_EDGE('',*,*,#24948,.F.);
#34774=ORIENTED_EDGE('',*,*,#24951,.F.);
#34775=ORIENTED_EDGE('',*,*,#24954,.T.);
#34776=ORIENTED_EDGE('',*,*,#24945,.F.);
#34777=ORIENTED_EDGE('',*,*,#24941,.F.);
#34778=ORIENTED_EDGE('',*,*,#24944,.F.);
#34779=ORIENTED_EDGE('',*,*,#24947,.T.);
#34780=ORIENTED_EDGE('',*,*,#24938,.F.);
#34781=ORIENTED_EDGE('',*,*,#24934,.F.);
#34782=ORIENTED_EDGE('',*,*,#24937,.F.);
#34783=ORIENTED_EDGE('',*,*,#24940,.T.);
#34784=ORIENTED_EDGE('',*,*,#24931,.F.);
#34785=ORIENTED_EDGE('',*,*,#24927,.F.);
#34786=ORIENTED_EDGE('',*,*,#24930,.F.);
#34787=ORIENTED_EDGE('',*,*,#24933,.T.);
#34788=ORIENTED_EDGE('',*,*,#24924,.F.);
#34789=ORIENTED_EDGE('',*,*,#24920,.F.);
#34790=ORIENTED_EDGE('',*,*,#24923,.F.);
#34791=ORIENTED_EDGE('',*,*,#24926,.T.);
#34792=ORIENTED_EDGE('',*,*,#24917,.F.);
#34793=ORIENTED_EDGE('',*,*,#24914,.F.);
#34794=ORIENTED_EDGE('',*,*,#24919,.T.);
#34795=ORIENTED_EDGE('',*,*,#24911,.F.);
#34796=ORIENTED_EDGE('',*,*,#24907,.F.);
#34797=ORIENTED_EDGE('',*,*,#24910,.F.);
#34798=ORIENTED_EDGE('',*,*,#24913,.T.);
#34799=ORIENTED_EDGE('',*,*,#24904,.F.);
#34800=ORIENTED_EDGE('',*,*,#24900,.F.);
#34801=ORIENTED_EDGE('',*,*,#24903,.F.);
#34802=ORIENTED_EDGE('',*,*,#24906,.T.);
#34803=ORIENTED_EDGE('',*,*,#24897,.F.);
#34804=ORIENTED_EDGE('',*,*,#24894,.F.);
#34805=ORIENTED_EDGE('',*,*,#24899,.T.);
#34806=ORIENTED_EDGE('',*,*,#24891,.F.);
#34807=ORIENTED_EDGE('',*,*,#24887,.F.);
#34808=ORIENTED_EDGE('',*,*,#24890,.F.);
#34809=ORIENTED_EDGE('',*,*,#24893,.T.);
#34810=ORIENTED_EDGE('',*,*,#24884,.F.);
#34811=ORIENTED_EDGE('',*,*,#24880,.F.);
#34812=ORIENTED_EDGE('',*,*,#24883,.F.);
#34813=ORIENTED_EDGE('',*,*,#24886,.T.);
#34814=ORIENTED_EDGE('',*,*,#24877,.F.);
#34815=ORIENTED_EDGE('',*,*,#24874,.F.);
#34816=ORIENTED_EDGE('',*,*,#24879,.T.);
#34817=ORIENTED_EDGE('',*,*,#24871,.F.);
#34818=ORIENTED_EDGE('',*,*,#24868,.F.);
#34819=ORIENTED_EDGE('',*,*,#24873,.T.);
#34820=ORIENTED_EDGE('',*,*,#24865,.F.);
#34821=ORIENTED_EDGE('',*,*,#24861,.F.);
#34822=ORIENTED_EDGE('',*,*,#24864,.F.);
#34823=ORIENTED_EDGE('',*,*,#24867,.T.);
#34824=ORIENTED_EDGE('',*,*,#24858,.F.);
#34825=ORIENTED_EDGE('',*,*,#24854,.F.);
#34826=ORIENTED_EDGE('',*,*,#24857,.F.);
#34827=ORIENTED_EDGE('',*,*,#24860,.T.);
#34828=ORIENTED_EDGE('',*,*,#24851,.F.);
#34829=ORIENTED_EDGE('',*,*,#24848,.F.);
#34830=ORIENTED_EDGE('',*,*,#24853,.T.);
#34831=ORIENTED_EDGE('',*,*,#24845,.F.);
#34832=ORIENTED_EDGE('',*,*,#24842,.F.);
#34833=ORIENTED_EDGE('',*,*,#24847,.T.);
#34834=ORIENTED_EDGE('',*,*,#24839,.F.);
#34835=ORIENTED_EDGE('',*,*,#24835,.F.);
#34836=ORIENTED_EDGE('',*,*,#24838,.F.);
#34837=ORIENTED_EDGE('',*,*,#24841,.T.);
#34838=ORIENTED_EDGE('',*,*,#24832,.F.);
#34839=ORIENTED_EDGE('',*,*,#24828,.F.);
#34840=ORIENTED_EDGE('',*,*,#24831,.F.);
#34841=ORIENTED_EDGE('',*,*,#24834,.T.);
#34842=ORIENTED_EDGE('',*,*,#24825,.F.);
#34843=ORIENTED_EDGE('',*,*,#24821,.F.);
#34844=ORIENTED_EDGE('',*,*,#24824,.F.);
#34845=ORIENTED_EDGE('',*,*,#24827,.T.);
#34846=ORIENTED_EDGE('',*,*,#24818,.F.);
#34847=ORIENTED_EDGE('',*,*,#24814,.F.);
#34848=ORIENTED_EDGE('',*,*,#24817,.F.);
#34849=ORIENTED_EDGE('',*,*,#24820,.T.);
#34850=ORIENTED_EDGE('',*,*,#24811,.F.);
#34851=ORIENTED_EDGE('',*,*,#24807,.F.);
#34852=ORIENTED_EDGE('',*,*,#24810,.F.);
#34853=ORIENTED_EDGE('',*,*,#24813,.T.);
#34854=ORIENTED_EDGE('',*,*,#24804,.F.);
#34855=ORIENTED_EDGE('',*,*,#24800,.F.);
#34856=ORIENTED_EDGE('',*,*,#24803,.F.);
#34857=ORIENTED_EDGE('',*,*,#24806,.T.);
#34858=ORIENTED_EDGE('',*,*,#24797,.F.);
#34859=ORIENTED_EDGE('',*,*,#24793,.F.);
#34860=ORIENTED_EDGE('',*,*,#24796,.F.);
#34861=ORIENTED_EDGE('',*,*,#24799,.T.);
#34862=ORIENTED_EDGE('',*,*,#24790,.F.);
#34863=ORIENTED_EDGE('',*,*,#24786,.F.);
#34864=ORIENTED_EDGE('',*,*,#24789,.F.);
#34865=ORIENTED_EDGE('',*,*,#24792,.T.);
#34866=ORIENTED_EDGE('',*,*,#24783,.F.);
#34867=ORIENTED_EDGE('',*,*,#24779,.F.);
#34868=ORIENTED_EDGE('',*,*,#24782,.F.);
#34869=ORIENTED_EDGE('',*,*,#24785,.T.);
#34870=ORIENTED_EDGE('',*,*,#24776,.F.);
#34871=ORIENTED_EDGE('',*,*,#24772,.F.);
#34872=ORIENTED_EDGE('',*,*,#24775,.F.);
#34873=ORIENTED_EDGE('',*,*,#24778,.T.);
#34874=ORIENTED_EDGE('',*,*,#24769,.F.);
#34875=ORIENTED_EDGE('',*,*,#24765,.F.);
#34876=ORIENTED_EDGE('',*,*,#24768,.F.);
#34877=ORIENTED_EDGE('',*,*,#24771,.T.);
#34878=ORIENTED_EDGE('',*,*,#24762,.F.);
#34879=ORIENTED_EDGE('',*,*,#24758,.F.);
#34880=ORIENTED_EDGE('',*,*,#24761,.F.);
#34881=ORIENTED_EDGE('',*,*,#24764,.T.);
#34882=ORIENTED_EDGE('',*,*,#24755,.F.);
#34883=ORIENTED_EDGE('',*,*,#24751,.F.);
#34884=ORIENTED_EDGE('',*,*,#24754,.F.);
#34885=ORIENTED_EDGE('',*,*,#24757,.T.);
#34886=ORIENTED_EDGE('',*,*,#24748,.F.);
#34887=ORIENTED_EDGE('',*,*,#24744,.F.);
#34888=ORIENTED_EDGE('',*,*,#24747,.F.);
#34889=ORIENTED_EDGE('',*,*,#24750,.T.);
#34890=ORIENTED_EDGE('',*,*,#24741,.F.);
#34891=ORIENTED_EDGE('',*,*,#24737,.F.);
#34892=ORIENTED_EDGE('',*,*,#24740,.F.);
#34893=ORIENTED_EDGE('',*,*,#24743,.T.);
#34894=ORIENTED_EDGE('',*,*,#24734,.F.);
#34895=ORIENTED_EDGE('',*,*,#24730,.F.);
#34896=ORIENTED_EDGE('',*,*,#24733,.F.);
#34897=ORIENTED_EDGE('',*,*,#24736,.T.);
#34898=ORIENTED_EDGE('',*,*,#24727,.F.);
#34899=ORIENTED_EDGE('',*,*,#24723,.F.);
#34900=ORIENTED_EDGE('',*,*,#24726,.F.);
#34901=ORIENTED_EDGE('',*,*,#24729,.T.);
#34902=ORIENTED_EDGE('',*,*,#24720,.F.);
#34903=ORIENTED_EDGE('',*,*,#24716,.F.);
#34904=ORIENTED_EDGE('',*,*,#24719,.F.);
#34905=ORIENTED_EDGE('',*,*,#24722,.T.);
#34906=ORIENTED_EDGE('',*,*,#24713,.F.);
#34907=ORIENTED_EDGE('',*,*,#24709,.F.);
#34908=ORIENTED_EDGE('',*,*,#24712,.F.);
#34909=ORIENTED_EDGE('',*,*,#24715,.T.);
#34910=ORIENTED_EDGE('',*,*,#24706,.F.);
#34911=ORIENTED_EDGE('',*,*,#24702,.F.);
#34912=ORIENTED_EDGE('',*,*,#24705,.F.);
#34913=ORIENTED_EDGE('',*,*,#24708,.T.);
#34914=ORIENTED_EDGE('',*,*,#24699,.F.);
#34915=ORIENTED_EDGE('',*,*,#24695,.F.);
#34916=ORIENTED_EDGE('',*,*,#24698,.F.);
#34917=ORIENTED_EDGE('',*,*,#24701,.T.);
#34918=ORIENTED_EDGE('',*,*,#24692,.F.);
#34919=ORIENTED_EDGE('',*,*,#24688,.F.);
#34920=ORIENTED_EDGE('',*,*,#24691,.F.);
#34921=ORIENTED_EDGE('',*,*,#24694,.T.);
#34922=ORIENTED_EDGE('',*,*,#24685,.F.);
#34923=ORIENTED_EDGE('',*,*,#24681,.F.);
#34924=ORIENTED_EDGE('',*,*,#24684,.F.);
#34925=ORIENTED_EDGE('',*,*,#24687,.T.);
#34926=ORIENTED_EDGE('',*,*,#24678,.F.);
#34927=ORIENTED_EDGE('',*,*,#24674,.F.);
#34928=ORIENTED_EDGE('',*,*,#24677,.F.);
#34929=ORIENTED_EDGE('',*,*,#24680,.T.);
#34930=ORIENTED_EDGE('',*,*,#24671,.F.);
#34931=ORIENTED_EDGE('',*,*,#24667,.F.);
#34932=ORIENTED_EDGE('',*,*,#24670,.F.);
#34933=ORIENTED_EDGE('',*,*,#24673,.T.);
#34934=ORIENTED_EDGE('',*,*,#24664,.F.);
#34935=ORIENTED_EDGE('',*,*,#24660,.F.);
#34936=ORIENTED_EDGE('',*,*,#24663,.F.);
#34937=ORIENTED_EDGE('',*,*,#24666,.T.);
#34938=ORIENTED_EDGE('',*,*,#24657,.F.);
#34939=ORIENTED_EDGE('',*,*,#24653,.F.);
#34940=ORIENTED_EDGE('',*,*,#24656,.F.);
#34941=ORIENTED_EDGE('',*,*,#24659,.T.);
#34942=ORIENTED_EDGE('',*,*,#24650,.F.);
#34943=ORIENTED_EDGE('',*,*,#24646,.F.);
#34944=ORIENTED_EDGE('',*,*,#24649,.F.);
#34945=ORIENTED_EDGE('',*,*,#24652,.T.);
#34946=ORIENTED_EDGE('',*,*,#24643,.F.);
#34947=ORIENTED_EDGE('',*,*,#24639,.F.);
#34948=ORIENTED_EDGE('',*,*,#24642,.F.);
#34949=ORIENTED_EDGE('',*,*,#24645,.T.);
#34950=ORIENTED_EDGE('',*,*,#24636,.F.);
#34951=ORIENTED_EDGE('',*,*,#24632,.F.);
#34952=ORIENTED_EDGE('',*,*,#24635,.F.);
#34953=ORIENTED_EDGE('',*,*,#24638,.T.);
#34954=ORIENTED_EDGE('',*,*,#24629,.F.);
#34955=ORIENTED_EDGE('',*,*,#24625,.F.);
#34956=ORIENTED_EDGE('',*,*,#24628,.F.);
#34957=ORIENTED_EDGE('',*,*,#24631,.T.);
#34958=ORIENTED_EDGE('',*,*,#24622,.F.);
#34959=ORIENTED_EDGE('',*,*,#24618,.F.);
#34960=ORIENTED_EDGE('',*,*,#24621,.F.);
#34961=ORIENTED_EDGE('',*,*,#24624,.T.);
#34962=ORIENTED_EDGE('',*,*,#24615,.F.);
#34963=ORIENTED_EDGE('',*,*,#24611,.F.);
#34964=ORIENTED_EDGE('',*,*,#24614,.F.);
#34965=ORIENTED_EDGE('',*,*,#24617,.T.);
#34966=ORIENTED_EDGE('',*,*,#24608,.F.);
#34967=ORIENTED_EDGE('',*,*,#24604,.F.);
#34968=ORIENTED_EDGE('',*,*,#24607,.F.);
#34969=ORIENTED_EDGE('',*,*,#24610,.T.);
#34970=ORIENTED_EDGE('',*,*,#24601,.F.);
#34971=ORIENTED_EDGE('',*,*,#24597,.F.);
#34972=ORIENTED_EDGE('',*,*,#24600,.F.);
#34973=ORIENTED_EDGE('',*,*,#24603,.T.);
#34974=ORIENTED_EDGE('',*,*,#24594,.F.);
#34975=ORIENTED_EDGE('',*,*,#24590,.F.);
#34976=ORIENTED_EDGE('',*,*,#24593,.F.);
#34977=ORIENTED_EDGE('',*,*,#24596,.T.);
#34978=ORIENTED_EDGE('',*,*,#24587,.F.);
#34979=ORIENTED_EDGE('',*,*,#24583,.F.);
#34980=ORIENTED_EDGE('',*,*,#24586,.F.);
#34981=ORIENTED_EDGE('',*,*,#24589,.T.);
#34982=ORIENTED_EDGE('',*,*,#24580,.F.);
#34983=ORIENTED_EDGE('',*,*,#24576,.F.);
#34984=ORIENTED_EDGE('',*,*,#24579,.F.);
#34985=ORIENTED_EDGE('',*,*,#24582,.T.);
#34986=ORIENTED_EDGE('',*,*,#24573,.F.);
#34987=ORIENTED_EDGE('',*,*,#24569,.F.);
#34988=ORIENTED_EDGE('',*,*,#24572,.F.);
#34989=ORIENTED_EDGE('',*,*,#24575,.T.);
#34990=ORIENTED_EDGE('',*,*,#24566,.F.);
#34991=ORIENTED_EDGE('',*,*,#24565,.T.);
#34992=ORIENTED_EDGE('',*,*,#24563,.F.);
#34993=ORIENTED_EDGE('',*,*,#24560,.F.);
#34994=ORIENTED_EDGE('',*,*,#24559,.T.);
#34995=ORIENTED_EDGE('',*,*,#24557,.F.);
#34996=ORIENTED_EDGE('',*,*,#24554,.F.);
#34997=ORIENTED_EDGE('',*,*,#24553,.T.);
#34998=ORIENTED_EDGE('',*,*,#24551,.F.);
#34999=ORIENTED_EDGE('',*,*,#24548,.F.);
#35000=ORIENTED_EDGE('',*,*,#24547,.T.);
#35001=ORIENTED_EDGE('',*,*,#24545,.F.);
#35002=ORIENTED_EDGE('',*,*,#24542,.F.);
#35003=ORIENTED_EDGE('',*,*,#24541,.T.);
#35004=ORIENTED_EDGE('',*,*,#24539,.F.);
#35005=ORIENTED_EDGE('',*,*,#24536,.F.);
#35006=ORIENTED_EDGE('',*,*,#24535,.T.);
#35007=ORIENTED_EDGE('',*,*,#24533,.F.);
#35008=ORIENTED_EDGE('',*,*,#26848,.F.);
#35009=ORIENTED_EDGE('',*,*,#26849,.F.);
#35010=ORIENTED_EDGE('',*,*,#26850,.T.);
#35011=ORIENTED_EDGE('',*,*,#26851,.F.);
#35012=ORIENTED_EDGE('',*,*,#26850,.F.);
#35013=ORIENTED_EDGE('',*,*,#26852,.F.);
#35014=ORIENTED_EDGE('',*,*,#26853,.T.);
#35015=ORIENTED_EDGE('',*,*,#26854,.F.);
#35016=ORIENTED_EDGE('',*,*,#26853,.F.);
#35017=ORIENTED_EDGE('',*,*,#26848,.T.);
#35018=ORIENTED_EDGE('',*,*,#26849,.T.);
#35019=ORIENTED_EDGE('',*,*,#26855,.T.);
#35020=ORIENTED_EDGE('',*,*,#26852,.T.);
#35021=ORIENTED_EDGE('',*,*,#26855,.F.);
#35022=ORIENTED_EDGE('',*,*,#26856,.T.);
#35023=ORIENTED_EDGE('',*,*,#26857,.T.);
#35024=ORIENTED_EDGE('',*,*,#26858,.F.);
#35025=ORIENTED_EDGE('',*,*,#26859,.F.);
#35026=ORIENTED_EDGE('',*,*,#26860,.F.);
#35027=ORIENTED_EDGE('',*,*,#26861,.T.);
#35028=ORIENTED_EDGE('',*,*,#26862,.F.);
#35029=ORIENTED_EDGE('',*,*,#26861,.F.);
#35030=ORIENTED_EDGE('',*,*,#26863,.F.);
#35031=ORIENTED_EDGE('',*,*,#26864,.T.);
#35032=ORIENTED_EDGE('',*,*,#26860,.T.);
#35033=ORIENTED_EDGE('',*,*,#26864,.F.);
#35034=ORIENTED_EDGE('',*,*,#26863,.T.);
#35035=ORIENTED_EDGE('',*,*,#26862,.T.);
#35036=ORIENTED_EDGE('',*,*,#26856,.F.);
#35037=ORIENTED_EDGE('',*,*,#26865,.F.);
#35038=ORIENTED_EDGE('',*,*,#26857,.F.);
#35039=ORIENTED_EDGE('',*,*,#26865,.T.);
#35040=ORIENTED_EDGE('',*,*,#26859,.T.);
#35041=ORIENTED_EDGE('',*,*,#26866,.F.);
#35042=ORIENTED_EDGE('',*,*,#26851,.T.);
#35043=ORIENTED_EDGE('',*,*,#26854,.T.);
#35044=ORIENTED_EDGE('',*,*,#26858,.T.);
#35045=ORIENTED_EDGE('',*,*,#26866,.T.);
#35046=ORIENTED_EDGE('',*,*,#26867,.T.);
#35047=ORIENTED_EDGE('',*,*,#26868,.T.);
#35048=ORIENTED_EDGE('',*,*,#26869,.F.);
#35049=ORIENTED_EDGE('',*,*,#26870,.F.);
#35050=ORIENTED_EDGE('',*,*,#26871,.T.);
#35051=ORIENTED_EDGE('',*,*,#26872,.T.);
#35052=ORIENTED_EDGE('',*,*,#26867,.F.);
#35053=ORIENTED_EDGE('',*,*,#26873,.F.);
#35054=ORIENTED_EDGE('',*,*,#26874,.T.);
#35055=ORIENTED_EDGE('',*,*,#26875,.T.);
#35056=ORIENTED_EDGE('',*,*,#26871,.F.);
#35057=ORIENTED_EDGE('',*,*,#26876,.F.);
#35058=ORIENTED_EDGE('',*,*,#26869,.T.);
#35059=ORIENTED_EDGE('',*,*,#26877,.T.);
#35060=ORIENTED_EDGE('',*,*,#26874,.F.);
#35061=ORIENTED_EDGE('',*,*,#26878,.F.);
#35062=ORIENTED_EDGE('',*,*,#26870,.T.);
#35063=ORIENTED_EDGE('',*,*,#26878,.T.);
#35064=ORIENTED_EDGE('',*,*,#26876,.T.);
#35065=ORIENTED_EDGE('',*,*,#26873,.T.);
#35066=ORIENTED_EDGE('',*,*,#26868,.F.);
#35067=ORIENTED_EDGE('',*,*,#26872,.F.);
#35068=ORIENTED_EDGE('',*,*,#26875,.F.);
#35069=ORIENTED_EDGE('',*,*,#26877,.F.);
#35070=ORIENTED_EDGE('',*,*,#26879,.T.);
#35071=ORIENTED_EDGE('',*,*,#26880,.T.);
#35072=ORIENTED_EDGE('',*,*,#26881,.T.);
#35073=ORIENTED_EDGE('',*,*,#26882,.T.);
#35074=ORIENTED_EDGE('',*,*,#26883,.T.);
#35075=ORIENTED_EDGE('',*,*,#26884,.T.);
#35076=ORIENTED_EDGE('',*,*,#26885,.F.);
#35077=ORIENTED_EDGE('',*,*,#26880,.F.);
#35078=ORIENTED_EDGE('',*,*,#26885,.T.);
#35079=ORIENTED_EDGE('',*,*,#26886,.T.);
#35080=ORIENTED_EDGE('',*,*,#26887,.F.);
#35081=ORIENTED_EDGE('',*,*,#26881,.F.);
#35082=ORIENTED_EDGE('',*,*,#26887,.T.);
#35083=ORIENTED_EDGE('',*,*,#26888,.T.);
#35084=ORIENTED_EDGE('',*,*,#26889,.F.);
#35085=ORIENTED_EDGE('',*,*,#26882,.F.);
#35086=ORIENTED_EDGE('',*,*,#26889,.T.);
#35087=ORIENTED_EDGE('',*,*,#26890,.T.);
#35088=ORIENTED_EDGE('',*,*,#26883,.F.);
#35089=ORIENTED_EDGE('',*,*,#26879,.F.);
#35090=ORIENTED_EDGE('',*,*,#26890,.F.);
#35091=ORIENTED_EDGE('',*,*,#26888,.F.);
#35092=ORIENTED_EDGE('',*,*,#26886,.F.);
#35093=ORIENTED_EDGE('',*,*,#26884,.F.);
#35094=ORIENTED_EDGE('',*,*,#26891,.T.);
#35095=ORIENTED_EDGE('',*,*,#26892,.T.);
#35096=ORIENTED_EDGE('',*,*,#26893,.T.);
#35097=ORIENTED_EDGE('',*,*,#26894,.T.);
#35098=ORIENTED_EDGE('',*,*,#26895,.T.);
#35099=ORIENTED_EDGE('',*,*,#26896,.T.);
#35100=ORIENTED_EDGE('',*,*,#26897,.T.);
#35101=ORIENTED_EDGE('',*,*,#26898,.T.);
#35102=ORIENTED_EDGE('',*,*,#26899,.T.);
#35103=ORIENTED_EDGE('',*,*,#26900,.T.);
#35104=ORIENTED_EDGE('',*,*,#26901,.T.);
#35105=ORIENTED_EDGE('',*,*,#26902,.T.);
#35106=ORIENTED_EDGE('',*,*,#26903,.T.);
#35107=ORIENTED_EDGE('',*,*,#26904,.T.);
#35108=ORIENTED_EDGE('',*,*,#26903,.F.);
#35109=ORIENTED_EDGE('',*,*,#26905,.T.);
#35110=ORIENTED_EDGE('',*,*,#26906,.T.);
#35111=ORIENTED_EDGE('',*,*,#26907,.T.);
#35112=ORIENTED_EDGE('',*,*,#26908,.T.);
#35113=ORIENTED_EDGE('',*,*,#26909,.T.);
#35114=ORIENTED_EDGE('',*,*,#26910,.T.);
#35115=ORIENTED_EDGE('',*,*,#26904,.F.);
#35116=ORIENTED_EDGE('',*,*,#26911,.T.);
#35117=ORIENTED_EDGE('',*,*,#26912,.F.);
#35118=ORIENTED_EDGE('',*,*,#26911,.F.);
#35119=ORIENTED_EDGE('',*,*,#26913,.T.);
#35120=ORIENTED_EDGE('',*,*,#26914,.T.);
#35121=ORIENTED_EDGE('',*,*,#26915,.T.);
#35122=ORIENTED_EDGE('',*,*,#26916,.F.);
#35123=ORIENTED_EDGE('',*,*,#26917,.T.);
#35124=ORIENTED_EDGE('',*,*,#26918,.T.);
#35125=ORIENTED_EDGE('',*,*,#26919,.T.);
#35126=ORIENTED_EDGE('',*,*,#26920,.T.);
#35127=ORIENTED_EDGE('',*,*,#26921,.T.);
#35128=ORIENTED_EDGE('',*,*,#26922,.F.);
#35129=ORIENTED_EDGE('',*,*,#26923,.T.);
#35130=ORIENTED_EDGE('',*,*,#26924,.T.);
#35131=ORIENTED_EDGE('',*,*,#26925,.T.);
#35132=ORIENTED_EDGE('',*,*,#26926,.T.);
#35133=ORIENTED_EDGE('',*,*,#26927,.T.);
#35134=ORIENTED_EDGE('',*,*,#26928,.F.);
#35135=ORIENTED_EDGE('',*,*,#26929,.T.);
#35136=ORIENTED_EDGE('',*,*,#26930,.T.);
#35137=ORIENTED_EDGE('',*,*,#26931,.T.);
#35138=ORIENTED_EDGE('',*,*,#26932,.T.);
#35139=ORIENTED_EDGE('',*,*,#26933,.T.);
#35140=ORIENTED_EDGE('',*,*,#26934,.T.);
#35141=ORIENTED_EDGE('',*,*,#26935,.F.);
#35142=ORIENTED_EDGE('',*,*,#26936,.T.);
#35143=ORIENTED_EDGE('',*,*,#26937,.F.);
#35144=ORIENTED_EDGE('',*,*,#26938,.T.);
#35145=ORIENTED_EDGE('',*,*,#26939,.T.);
#35146=ORIENTED_EDGE('',*,*,#26932,.F.);
#35147=ORIENTED_EDGE('',*,*,#26940,.T.);
#35148=ORIENTED_EDGE('',*,*,#26941,.T.);
#35149=ORIENTED_EDGE('',*,*,#26942,.T.);
#35150=ORIENTED_EDGE('',*,*,#26943,.T.);
#35151=ORIENTED_EDGE('',*,*,#26944,.F.);
#35152=ORIENTED_EDGE('',*,*,#26941,.F.);
#35153=ORIENTED_EDGE('',*,*,#26945,.F.);
#35154=ORIENTED_EDGE('',*,*,#26946,.F.);
#35155=ORIENTED_EDGE('',*,*,#26947,.F.);
#35156=ORIENTED_EDGE('',*,*,#26939,.F.);
#35157=ORIENTED_EDGE('',*,*,#26948,.F.);
#35158=ORIENTED_EDGE('',*,*,#26949,.F.);
#35159=ORIENTED_EDGE('',*,*,#26950,.F.);
#35160=ORIENTED_EDGE('',*,*,#26933,.F.);
#35161=ORIENTED_EDGE('',*,*,#26943,.F.);
#35162=ORIENTED_EDGE('',*,*,#26951,.T.);
#35163=ORIENTED_EDGE('',*,*,#26952,.F.);
#35164=ORIENTED_EDGE('',*,*,#26953,.F.);
#35165=ORIENTED_EDGE('',*,*,#26931,.F.);
#35166=ORIENTED_EDGE('',*,*,#26954,.T.);
#35167=ORIENTED_EDGE('',*,*,#26955,.T.);
#35168=ORIENTED_EDGE('',*,*,#26954,.F.);
#35169=ORIENTED_EDGE('',*,*,#26940,.F.);
#35170=ORIENTED_EDGE('',*,*,#26956,.T.);
#35171=ORIENTED_EDGE('',*,*,#26957,.T.);
#35172=ORIENTED_EDGE('',*,*,#26958,.T.);
#35173=ORIENTED_EDGE('',*,*,#26959,.T.);
#35174=ORIENTED_EDGE('',*,*,#26960,.F.);
#35175=ORIENTED_EDGE('',*,*,#26961,.T.);
#35176=ORIENTED_EDGE('',*,*,#26962,.F.);
#35177=ORIENTED_EDGE('',*,*,#26963,.T.);
#35178=ORIENTED_EDGE('',*,*,#26964,.T.);
#35179=ORIENTED_EDGE('',*,*,#26957,.F.);
#35180=ORIENTED_EDGE('',*,*,#26965,.T.);
#35181=ORIENTED_EDGE('',*,*,#26966,.T.);
#35182=ORIENTED_EDGE('',*,*,#26967,.T.);
#35183=ORIENTED_EDGE('',*,*,#26968,.T.);
#35184=ORIENTED_EDGE('',*,*,#26969,.F.);
#35185=ORIENTED_EDGE('',*,*,#26966,.F.);
#35186=ORIENTED_EDGE('',*,*,#26970,.F.);
#35187=ORIENTED_EDGE('',*,*,#26971,.F.);
#35188=ORIENTED_EDGE('',*,*,#26972,.F.);
#35189=ORIENTED_EDGE('',*,*,#26964,.F.);
#35190=ORIENTED_EDGE('',*,*,#26973,.F.);
#35191=ORIENTED_EDGE('',*,*,#26974,.F.);
#35192=ORIENTED_EDGE('',*,*,#26975,.F.);
#35193=ORIENTED_EDGE('',*,*,#26958,.F.);
#35194=ORIENTED_EDGE('',*,*,#26968,.F.);
#35195=ORIENTED_EDGE('',*,*,#26976,.T.);
#35196=ORIENTED_EDGE('',*,*,#26977,.F.);
#35197=ORIENTED_EDGE('',*,*,#26978,.F.);
#35198=ORIENTED_EDGE('',*,*,#26956,.F.);
#35199=ORIENTED_EDGE('',*,*,#26979,.T.);
#35200=ORIENTED_EDGE('',*,*,#26980,.T.);
#35201=ORIENTED_EDGE('',*,*,#26979,.F.);
#35202=ORIENTED_EDGE('',*,*,#26965,.F.);
#35203=ORIENTED_EDGE('',*,*,#26981,.T.);
#35204=ORIENTED_EDGE('',*,*,#26982,.T.);
#35205=ORIENTED_EDGE('',*,*,#26983,.T.);
#35206=ORIENTED_EDGE('',*,*,#26984,.T.);
#35207=ORIENTED_EDGE('',*,*,#26985,.F.);
#35208=ORIENTED_EDGE('',*,*,#26986,.T.);
#35209=ORIENTED_EDGE('',*,*,#26987,.F.);
#35210=ORIENTED_EDGE('',*,*,#26988,.T.);
#35211=ORIENTED_EDGE('',*,*,#26989,.T.);
#35212=ORIENTED_EDGE('',*,*,#26982,.F.);
#35213=ORIENTED_EDGE('',*,*,#26990,.T.);
#35214=ORIENTED_EDGE('',*,*,#26991,.T.);
#35215=ORIENTED_EDGE('',*,*,#26992,.T.);
#35216=ORIENTED_EDGE('',*,*,#26993,.T.);
#35217=ORIENTED_EDGE('',*,*,#26994,.F.);
#35218=ORIENTED_EDGE('',*,*,#26991,.F.);
#35219=ORIENTED_EDGE('',*,*,#26995,.F.);
#35220=ORIENTED_EDGE('',*,*,#26996,.F.);
#35221=ORIENTED_EDGE('',*,*,#26997,.F.);
#35222=ORIENTED_EDGE('',*,*,#26989,.F.);
#35223=ORIENTED_EDGE('',*,*,#26998,.F.);
#35224=ORIENTED_EDGE('',*,*,#26999,.F.);
#35225=ORIENTED_EDGE('',*,*,#27000,.F.);
#35226=ORIENTED_EDGE('',*,*,#26983,.F.);
#35227=ORIENTED_EDGE('',*,*,#26993,.F.);
#35228=ORIENTED_EDGE('',*,*,#27001,.T.);
#35229=ORIENTED_EDGE('',*,*,#27002,.F.);
#35230=ORIENTED_EDGE('',*,*,#27003,.F.);
#35231=ORIENTED_EDGE('',*,*,#26981,.F.);
#35232=ORIENTED_EDGE('',*,*,#27004,.T.);
#35233=ORIENTED_EDGE('',*,*,#27005,.T.);
#35234=ORIENTED_EDGE('',*,*,#27004,.F.);
#35235=ORIENTED_EDGE('',*,*,#26990,.F.);
#35236=ORIENTED_EDGE('',*,*,#27006,.T.);
#35237=ORIENTED_EDGE('',*,*,#27007,.T.);
#35238=ORIENTED_EDGE('',*,*,#27008,.T.);
#35239=ORIENTED_EDGE('',*,*,#27009,.T.);
#35240=ORIENTED_EDGE('',*,*,#27010,.F.);
#35241=ORIENTED_EDGE('',*,*,#27011,.T.);
#35242=ORIENTED_EDGE('',*,*,#27012,.F.);
#35243=ORIENTED_EDGE('',*,*,#27013,.T.);
#35244=ORIENTED_EDGE('',*,*,#27014,.T.);
#35245=ORIENTED_EDGE('',*,*,#27007,.F.);
#35246=ORIENTED_EDGE('',*,*,#27014,.F.);
#35247=ORIENTED_EDGE('',*,*,#27015,.T.);
#35248=ORIENTED_EDGE('',*,*,#27016,.F.);
#35249=ORIENTED_EDGE('',*,*,#27017,.F.);
#35250=ORIENTED_EDGE('',*,*,#27008,.F.);
#35251=ORIENTED_EDGE('',*,*,#27018,.T.);
#35252=ORIENTED_EDGE('',*,*,#27019,.T.);
#35253=ORIENTED_EDGE('',*,*,#27020,.T.);
#35254=ORIENTED_EDGE('',*,*,#27021,.T.);
#35255=ORIENTED_EDGE('',*,*,#27022,.T.);
#35256=ORIENTED_EDGE('',*,*,#27023,.T.);
#35257=ORIENTED_EDGE('',*,*,#27024,.T.);
#35258=ORIENTED_EDGE('',*,*,#27025,.F.);
#35259=ORIENTED_EDGE('',*,*,#27026,.T.);
#35260=ORIENTED_EDGE('',*,*,#27027,.F.);
#35261=ORIENTED_EDGE('',*,*,#27028,.T.);
#35262=ORIENTED_EDGE('',*,*,#27029,.T.);
#35263=ORIENTED_EDGE('',*,*,#27030,.T.);
#35264=ORIENTED_EDGE('',*,*,#27025,.T.);
#35265=ORIENTED_EDGE('',*,*,#27031,.T.);
#35266=ORIENTED_EDGE('',*,*,#27032,.F.);
#35267=ORIENTED_EDGE('',*,*,#27033,.T.);
#35268=ORIENTED_EDGE('',*,*,#27034,.F.);
#35269=ORIENTED_EDGE('',*,*,#27035,.T.);
#35270=ORIENTED_EDGE('',*,*,#27034,.T.);
#35271=ORIENTED_EDGE('',*,*,#27036,.T.);
#35272=ORIENTED_EDGE('',*,*,#27029,.F.);
#35273=ORIENTED_EDGE('',*,*,#27037,.T.);
#35274=ORIENTED_EDGE('',*,*,#27038,.T.);
#35275=ORIENTED_EDGE('',*,*,#27039,.T.);
#35276=ORIENTED_EDGE('',*,*,#27040,.T.);
#35277=ORIENTED_EDGE('',*,*,#27041,.T.);
#35278=ORIENTED_EDGE('',*,*,#27027,.T.);
#35279=ORIENTED_EDGE('',*,*,#27042,.T.);
#35280=ORIENTED_EDGE('',*,*,#27043,.T.);
#35281=ORIENTED_EDGE('',*,*,#27044,.T.);
#35282=ORIENTED_EDGE('',*,*,#27045,.T.);
#35283=ORIENTED_EDGE('',*,*,#27046,.T.);
#35284=ORIENTED_EDGE('',*,*,#27032,.T.);
#35285=ORIENTED_EDGE('',*,*,#27047,.T.);
#35286=ORIENTED_EDGE('',*,*,#27048,.F.);
#35287=ORIENTED_EDGE('',*,*,#27049,.F.);
#35288=ORIENTED_EDGE('',*,*,#27050,.F.);
#35289=ORIENTED_EDGE('',*,*,#27051,.F.);
#35290=ORIENTED_EDGE('',*,*,#27052,.F.);
#35291=ORIENTED_EDGE('',*,*,#27053,.F.);
#35292=ORIENTED_EDGE('',*,*,#27037,.F.);
#35293=ORIENTED_EDGE('',*,*,#27054,.F.);
#35294=ORIENTED_EDGE('',*,*,#27055,.F.);
#35295=ORIENTED_EDGE('',*,*,#27054,.T.);
#35296=ORIENTED_EDGE('',*,*,#27031,.F.);
#35297=ORIENTED_EDGE('',*,*,#27056,.F.);
#35298=ORIENTED_EDGE('',*,*,#27057,.F.);
#35299=ORIENTED_EDGE('',*,*,#27058,.F.);
#35300=ORIENTED_EDGE('',*,*,#27035,.F.);
#35301=ORIENTED_EDGE('',*,*,#27053,.T.);
#35302=ORIENTED_EDGE('',*,*,#27059,.F.);
#35303=ORIENTED_EDGE('',*,*,#27056,.T.);
#35304=ORIENTED_EDGE('',*,*,#27028,.F.);
#35305=ORIENTED_EDGE('',*,*,#27060,.F.);
#35306=ORIENTED_EDGE('',*,*,#27061,.F.);
#35307=ORIENTED_EDGE('',*,*,#27062,.F.);
#35308=ORIENTED_EDGE('',*,*,#27047,.F.);
#35309=ORIENTED_EDGE('',*,*,#27058,.T.);
#35310=ORIENTED_EDGE('',*,*,#27063,.F.);
#35311=ORIENTED_EDGE('',*,*,#27064,.F.);
#35312=ORIENTED_EDGE('',*,*,#27060,.T.);
#35313=ORIENTED_EDGE('',*,*,#27044,.F.);
#35314=ORIENTED_EDGE('',*,*,#27065,.F.);
#35315=ORIENTED_EDGE('',*,*,#27066,.F.);
#35316=ORIENTED_EDGE('',*,*,#27067,.F.);
#35317=ORIENTED_EDGE('',*,*,#27068,.F.);
#35318=ORIENTED_EDGE('',*,*,#27038,.F.);
#35319=ORIENTED_EDGE('',*,*,#27069,.F.);
#35320=ORIENTED_EDGE('',*,*,#27070,.F.);
#35321=ORIENTED_EDGE('',*,*,#27071,.F.);
#35322=ORIENTED_EDGE('',*,*,#27072,.F.);
#35323=ORIENTED_EDGE('',*,*,#27069,.T.);
#35324=ORIENTED_EDGE('',*,*,#27073,.F.);
#35325=ORIENTED_EDGE('',*,*,#27062,.T.);
#35326=ORIENTED_EDGE('',*,*,#27074,.F.);
#35327=ORIENTED_EDGE('',*,*,#27065,.T.);
#35328=ORIENTED_EDGE('',*,*,#27075,.F.);
#35329=ORIENTED_EDGE('',*,*,#27068,.T.);
#35330=ORIENTED_EDGE('',*,*,#27073,.T.);
#35331=ORIENTED_EDGE('',*,*,#27041,.F.);
#35332=ORIENTED_EDGE('',*,*,#27076,.F.);
#35333=ORIENTED_EDGE('',*,*,#27045,.F.);
#35334=ORIENTED_EDGE('',*,*,#27075,.T.);
#35335=ORIENTED_EDGE('',*,*,#27043,.F.);
#35336=ORIENTED_EDGE('',*,*,#27077,.F.);
#35337=ORIENTED_EDGE('',*,*,#27039,.F.);
#35338=ORIENTED_EDGE('',*,*,#27078,.F.);
#35339=ORIENTED_EDGE('',*,*,#27040,.F.);
#35340=ORIENTED_EDGE('',*,*,#27079,.F.);
#35341=ORIENTED_EDGE('',*,*,#27023,.F.);
#35342=ORIENTED_EDGE('',*,*,#27076,.T.);
#35343=ORIENTED_EDGE('',*,*,#27078,.T.);
#35344=ORIENTED_EDGE('',*,*,#27080,.F.);
#35345=ORIENTED_EDGE('',*,*,#27079,.T.);
#35346=ORIENTED_EDGE('',*,*,#27077,.T.);
#35347=ORIENTED_EDGE('',*,*,#27081,.F.);
#35348=ORIENTED_EDGE('',*,*,#27080,.T.);
#35349=ORIENTED_EDGE('',*,*,#27022,.F.);
#35350=ORIENTED_EDGE('',*,*,#27082,.F.);
#35351=ORIENTED_EDGE('',*,*,#27046,.F.);
#35352=ORIENTED_EDGE('',*,*,#27081,.T.);
#35353=ORIENTED_EDGE('',*,*,#27042,.F.);
#35354=ORIENTED_EDGE('',*,*,#27083,.F.);
#35355=ORIENTED_EDGE('',*,*,#27024,.F.);
#35356=ORIENTED_EDGE('',*,*,#27082,.T.);
#35357=ORIENTED_EDGE('',*,*,#27021,.F.);
#35358=ORIENTED_EDGE('',*,*,#27084,.F.);
#35359=ORIENTED_EDGE('',*,*,#27033,.F.);
#35360=ORIENTED_EDGE('',*,*,#27083,.T.);
#35361=ORIENTED_EDGE('',*,*,#27026,.F.);
#35362=ORIENTED_EDGE('',*,*,#27085,.F.);
#35363=ORIENTED_EDGE('',*,*,#27018,.F.);
#35364=ORIENTED_EDGE('',*,*,#27084,.T.);
#35365=ORIENTED_EDGE('',*,*,#27020,.F.);
#35366=ORIENTED_EDGE('',*,*,#27086,.F.);
#35367=ORIENTED_EDGE('',*,*,#27036,.F.);
#35368=ORIENTED_EDGE('',*,*,#27085,.T.);
#35369=ORIENTED_EDGE('',*,*,#27030,.F.);
#35370=ORIENTED_EDGE('',*,*,#27086,.T.);
#35371=ORIENTED_EDGE('',*,*,#27019,.F.);
#35372=ORIENTED_EDGE('',*,*,#27087,.T.);
#35373=ORIENTED_EDGE('',*,*,#27088,.F.);
#35374=ORIENTED_EDGE('',*,*,#27089,.T.);
#35375=ORIENTED_EDGE('',*,*,#27090,.F.);
#35376=ORIENTED_EDGE('',*,*,#27091,.T.);
#35377=ORIENTED_EDGE('',*,*,#27092,.F.);
#35378=ORIENTED_EDGE('',*,*,#27089,.F.);
#35379=ORIENTED_EDGE('',*,*,#27093,.F.);
#35380=ORIENTED_EDGE('',*,*,#27094,.T.);
#35381=ORIENTED_EDGE('',*,*,#27095,.F.);
#35382=ORIENTED_EDGE('',*,*,#27087,.F.);
#35383=ORIENTED_EDGE('',*,*,#27096,.F.);
#35384=ORIENTED_EDGE('',*,*,#27091,.F.);
#35385=ORIENTED_EDGE('',*,*,#27097,.F.);
#35386=ORIENTED_EDGE('',*,*,#27094,.F.);
#35387=ORIENTED_EDGE('',*,*,#27098,.F.);
#35388=ORIENTED_EDGE('',*,*,#27099,.T.);
#35389=ORIENTED_EDGE('',*,*,#27100,.F.);
#35390=ORIENTED_EDGE('',*,*,#27101,.T.);
#35391=ORIENTED_EDGE('',*,*,#27009,.F.);
#35392=ORIENTED_EDGE('',*,*,#27102,.T.);
#35393=ORIENTED_EDGE('',*,*,#27010,.T.);
#35394=ORIENTED_EDGE('',*,*,#27101,.F.);
#35395=ORIENTED_EDGE('',*,*,#27103,.T.);
#35396=ORIENTED_EDGE('',*,*,#27104,.T.);
#35397=ORIENTED_EDGE('',*,*,#27105,.T.);
#35398=ORIENTED_EDGE('',*,*,#27099,.F.);
#35399=ORIENTED_EDGE('',*,*,#27017,.T.);
#35400=ORIENTED_EDGE('',*,*,#27106,.T.);
#35401=ORIENTED_EDGE('',*,*,#27107,.F.);
#35402=ORIENTED_EDGE('',*,*,#27103,.F.);
#35403=ORIENTED_EDGE('',*,*,#27108,.F.);
#35404=ORIENTED_EDGE('',*,*,#27109,.T.);
#35405=ORIENTED_EDGE('',*,*,#27011,.F.);
#35406=ORIENTED_EDGE('',*,*,#27102,.F.);
#35407=ORIENTED_EDGE('',*,*,#27110,.F.);
#35408=ORIENTED_EDGE('',*,*,#27111,.T.);
#35409=ORIENTED_EDGE('',*,*,#27112,.F.);
#35410=ORIENTED_EDGE('',*,*,#27104,.F.);
#35411=ORIENTED_EDGE('',*,*,#27113,.F.);
#35412=ORIENTED_EDGE('',*,*,#27114,.T.);
#35413=ORIENTED_EDGE('',*,*,#27115,.F.);
#35414=ORIENTED_EDGE('',*,*,#27106,.F.);
#35415=ORIENTED_EDGE('',*,*,#27116,.F.);
#35416=ORIENTED_EDGE('',*,*,#27117,.T.);
#35417=ORIENTED_EDGE('',*,*,#27012,.T.);
#35418=ORIENTED_EDGE('',*,*,#27109,.F.);
#35419=ORIENTED_EDGE('',*,*,#27118,.T.);
#35420=ORIENTED_EDGE('',*,*,#27119,.T.);
#35421=ORIENTED_EDGE('',*,*,#27120,.T.);
#35422=ORIENTED_EDGE('',*,*,#27015,.F.);
#35423=ORIENTED_EDGE('',*,*,#27121,.T.);
#35424=ORIENTED_EDGE('',*,*,#27122,.T.);
#35425=ORIENTED_EDGE('',*,*,#27123,.F.);
#35426=ORIENTED_EDGE('',*,*,#27111,.F.);
#35427=ORIENTED_EDGE('',*,*,#27124,.F.);
#35428=ORIENTED_EDGE('',*,*,#27114,.F.);
#35429=ORIENTED_EDGE('',*,*,#27125,.F.);
#35430=ORIENTED_EDGE('',*,*,#27118,.F.);
#35431=ORIENTED_EDGE('',*,*,#27126,.F.);
#35432=ORIENTED_EDGE('',*,*,#27117,.F.);
#35433=ORIENTED_EDGE('',*,*,#27127,.F.);
#35434=ORIENTED_EDGE('',*,*,#27121,.F.);
#35435=ORIENTED_EDGE('',*,*,#27013,.F.);
#35436=ORIENTED_EDGE('',*,*,#27120,.F.);
#35437=ORIENTED_EDGE('',*,*,#27128,.F.);
#35438=ORIENTED_EDGE('',*,*,#27122,.F.);
#35439=ORIENTED_EDGE('',*,*,#27129,.F.);
#35440=ORIENTED_EDGE('',*,*,#27096,.T.);
#35441=ORIENTED_EDGE('',*,*,#27090,.T.);
#35442=ORIENTED_EDGE('',*,*,#27092,.T.);
#35443=ORIENTED_EDGE('',*,*,#27098,.T.);
#35444=ORIENTED_EDGE('',*,*,#27126,.T.);
#35445=ORIENTED_EDGE('',*,*,#27110,.T.);
#35446=ORIENTED_EDGE('',*,*,#27107,.T.);
#35447=ORIENTED_EDGE('',*,*,#27115,.T.);
#35448=ORIENTED_EDGE('',*,*,#27130,.T.);
#35449=ORIENTED_EDGE('',*,*,#27097,.T.);
#35450=ORIENTED_EDGE('',*,*,#27131,.F.);
#35451=ORIENTED_EDGE('',*,*,#27116,.T.);
#35452=ORIENTED_EDGE('',*,*,#27132,.T.);
#35453=ORIENTED_EDGE('',*,*,#27088,.T.);
#35454=ORIENTED_EDGE('',*,*,#27133,.F.);
#35455=ORIENTED_EDGE('',*,*,#27123,.T.);
#35456=ORIENTED_EDGE('',*,*,#27131,.T.);
#35457=ORIENTED_EDGE('',*,*,#27093,.T.);
#35458=ORIENTED_EDGE('',*,*,#27132,.F.);
#35459=ORIENTED_EDGE('',*,*,#27128,.T.);
#35460=ORIENTED_EDGE('',*,*,#27119,.F.);
#35461=ORIENTED_EDGE('',*,*,#27127,.T.);
#35462=ORIENTED_EDGE('',*,*,#27125,.T.);
#35463=ORIENTED_EDGE('',*,*,#27133,.T.);
#35464=ORIENTED_EDGE('',*,*,#27095,.T.);
#35465=ORIENTED_EDGE('',*,*,#27130,.F.);
#35466=ORIENTED_EDGE('',*,*,#27108,.T.);
#35467=ORIENTED_EDGE('',*,*,#27100,.T.);
#35468=ORIENTED_EDGE('',*,*,#27105,.F.);
#35469=ORIENTED_EDGE('',*,*,#27112,.T.);
#35470=ORIENTED_EDGE('',*,*,#27124,.T.);
#35471=ORIENTED_EDGE('',*,*,#27113,.T.);
#35472=ORIENTED_EDGE('',*,*,#27016,.T.);
#35473=ORIENTED_EDGE('',*,*,#27129,.T.);
#35474=ORIENTED_EDGE('',*,*,#27134,.T.);
#35475=ORIENTED_EDGE('',*,*,#27135,.F.);
#35476=ORIENTED_EDGE('',*,*,#27003,.T.);
#35477=ORIENTED_EDGE('',*,*,#27136,.F.);
#35478=ORIENTED_EDGE('',*,*,#27137,.T.);
#35479=ORIENTED_EDGE('',*,*,#27138,.F.);
#35480=ORIENTED_EDGE('',*,*,#27134,.F.);
#35481=ORIENTED_EDGE('',*,*,#27139,.F.);
#35482=ORIENTED_EDGE('',*,*,#27001,.F.);
#35483=ORIENTED_EDGE('',*,*,#27140,.F.);
#35484=ORIENTED_EDGE('',*,*,#27137,.F.);
#35485=ORIENTED_EDGE('',*,*,#27141,.F.);
#35486=ORIENTED_EDGE('',*,*,#27142,.T.);
#35487=ORIENTED_EDGE('',*,*,#26986,.F.);
#35488=ORIENTED_EDGE('',*,*,#27143,.T.);
#35489=ORIENTED_EDGE('',*,*,#27144,.F.);
#35490=ORIENTED_EDGE('',*,*,#27145,.T.);
#35491=ORIENTED_EDGE('',*,*,#27146,.T.);
#35492=ORIENTED_EDGE('',*,*,#27143,.F.);
#35493=ORIENTED_EDGE('',*,*,#26985,.T.);
#35494=ORIENTED_EDGE('',*,*,#27147,.T.);
#35495=ORIENTED_EDGE('',*,*,#26987,.T.);
#35496=ORIENTED_EDGE('',*,*,#27142,.F.);
#35497=ORIENTED_EDGE('',*,*,#27148,.T.);
#35498=ORIENTED_EDGE('',*,*,#27149,.T.);
#35499=ORIENTED_EDGE('',*,*,#27150,.F.);
#35500=ORIENTED_EDGE('',*,*,#27145,.F.);
#35501=ORIENTED_EDGE('',*,*,#26984,.F.);
#35502=ORIENTED_EDGE('',*,*,#27151,.T.);
#35503=ORIENTED_EDGE('',*,*,#27152,.F.);
#35504=ORIENTED_EDGE('',*,*,#27146,.F.);
#35505=ORIENTED_EDGE('',*,*,#27153,.F.);
#35506=ORIENTED_EDGE('',*,*,#27154,.T.);
#35507=ORIENTED_EDGE('',*,*,#27155,.F.);
#35508=ORIENTED_EDGE('',*,*,#27148,.F.);
#35509=ORIENTED_EDGE('',*,*,#27156,.F.);
#35510=ORIENTED_EDGE('',*,*,#27157,.T.);
#35511=ORIENTED_EDGE('',*,*,#26988,.F.);
#35512=ORIENTED_EDGE('',*,*,#27147,.F.);
#35513=ORIENTED_EDGE('',*,*,#27158,.F.);
#35514=ORIENTED_EDGE('',*,*,#27159,.T.);
#35515=ORIENTED_EDGE('',*,*,#27160,.T.);
#35516=ORIENTED_EDGE('',*,*,#27149,.F.);
#35517=ORIENTED_EDGE('',*,*,#27000,.T.);
#35518=ORIENTED_EDGE('',*,*,#27151,.F.);
#35519=ORIENTED_EDGE('',*,*,#27161,.F.);
#35520=ORIENTED_EDGE('',*,*,#27154,.F.);
#35521=ORIENTED_EDGE('',*,*,#27162,.F.);
#35522=ORIENTED_EDGE('',*,*,#27163,.T.);
#35523=ORIENTED_EDGE('',*,*,#26998,.T.);
#35524=ORIENTED_EDGE('',*,*,#27157,.F.);
#35525=ORIENTED_EDGE('',*,*,#27164,.T.);
#35526=ORIENTED_EDGE('',*,*,#26995,.T.);
#35527=ORIENTED_EDGE('',*,*,#27165,.F.);
#35528=ORIENTED_EDGE('',*,*,#27159,.F.);
#35529=ORIENTED_EDGE('',*,*,#27166,.F.);
#35530=ORIENTED_EDGE('',*,*,#26997,.T.);
#35531=ORIENTED_EDGE('',*,*,#27167,.F.);
#35532=ORIENTED_EDGE('',*,*,#27163,.F.);
#35533=ORIENTED_EDGE('',*,*,#27168,.F.);
#35534=ORIENTED_EDGE('',*,*,#27139,.T.);
#35535=ORIENTED_EDGE('',*,*,#27136,.T.);
#35536=ORIENTED_EDGE('',*,*,#27002,.T.);
#35537=ORIENTED_EDGE('',*,*,#27141,.T.);
#35538=ORIENTED_EDGE('',*,*,#27156,.T.);
#35539=ORIENTED_EDGE('',*,*,#27144,.T.);
#35540=ORIENTED_EDGE('',*,*,#27152,.T.);
#35541=ORIENTED_EDGE('',*,*,#27162,.T.);
#35542=ORIENTED_EDGE('',*,*,#27169,.F.);
#35543=ORIENTED_EDGE('',*,*,#27161,.T.);
#35544=ORIENTED_EDGE('',*,*,#27170,.T.);
#35545=ORIENTED_EDGE('',*,*,#27138,.T.);
#35546=ORIENTED_EDGE('',*,*,#27169,.T.);
#35547=ORIENTED_EDGE('',*,*,#27140,.T.);
#35548=ORIENTED_EDGE('',*,*,#26992,.F.);
#35549=ORIENTED_EDGE('',*,*,#27168,.T.);
#35550=ORIENTED_EDGE('',*,*,#27164,.F.);
#35551=ORIENTED_EDGE('',*,*,#27158,.T.);
#35552=ORIENTED_EDGE('',*,*,#27155,.T.);
#35553=ORIENTED_EDGE('',*,*,#26994,.T.);
#35554=ORIENTED_EDGE('',*,*,#27135,.T.);
#35555=ORIENTED_EDGE('',*,*,#27170,.F.);
#35556=ORIENTED_EDGE('',*,*,#27153,.T.);
#35557=ORIENTED_EDGE('',*,*,#27150,.T.);
#35558=ORIENTED_EDGE('',*,*,#27160,.F.);
#35559=ORIENTED_EDGE('',*,*,#27165,.T.);
#35560=ORIENTED_EDGE('',*,*,#27167,.T.);
#35561=ORIENTED_EDGE('',*,*,#26996,.T.);
#35562=ORIENTED_EDGE('',*,*,#27166,.T.);
#35563=ORIENTED_EDGE('',*,*,#26999,.T.);
#35564=ORIENTED_EDGE('',*,*,#27171,.T.);
#35565=ORIENTED_EDGE('',*,*,#27172,.F.);
#35566=ORIENTED_EDGE('',*,*,#26978,.T.);
#35567=ORIENTED_EDGE('',*,*,#27173,.F.);
#35568=ORIENTED_EDGE('',*,*,#27174,.T.);
#35569=ORIENTED_EDGE('',*,*,#27175,.F.);
#35570=ORIENTED_EDGE('',*,*,#27171,.F.);
#35571=ORIENTED_EDGE('',*,*,#27176,.F.);
#35572=ORIENTED_EDGE('',*,*,#26976,.F.);
#35573=ORIENTED_EDGE('',*,*,#27177,.F.);
#35574=ORIENTED_EDGE('',*,*,#27174,.F.);
#35575=ORIENTED_EDGE('',*,*,#27178,.F.);
#35576=ORIENTED_EDGE('',*,*,#27179,.T.);
#35577=ORIENTED_EDGE('',*,*,#26961,.F.);
#35578=ORIENTED_EDGE('',*,*,#27180,.T.);
#35579=ORIENTED_EDGE('',*,*,#27181,.F.);
#35580=ORIENTED_EDGE('',*,*,#27182,.T.);
#35581=ORIENTED_EDGE('',*,*,#27183,.T.);
#35582=ORIENTED_EDGE('',*,*,#27180,.F.);
#35583=ORIENTED_EDGE('',*,*,#26960,.T.);
#35584=ORIENTED_EDGE('',*,*,#27184,.T.);
#35585=ORIENTED_EDGE('',*,*,#26962,.T.);
#35586=ORIENTED_EDGE('',*,*,#27179,.F.);
#35587=ORIENTED_EDGE('',*,*,#27185,.T.);
#35588=ORIENTED_EDGE('',*,*,#27186,.T.);
#35589=ORIENTED_EDGE('',*,*,#27187,.F.);
#35590=ORIENTED_EDGE('',*,*,#27182,.F.);
#35591=ORIENTED_EDGE('',*,*,#26959,.F.);
#35592=ORIENTED_EDGE('',*,*,#27188,.T.);
#35593=ORIENTED_EDGE('',*,*,#27189,.F.);
#35594=ORIENTED_EDGE('',*,*,#27183,.F.);
#35595=ORIENTED_EDGE('',*,*,#27190,.F.);
#35596=ORIENTED_EDGE('',*,*,#27191,.T.);
#35597=ORIENTED_EDGE('',*,*,#27192,.F.);
#35598=ORIENTED_EDGE('',*,*,#27185,.F.);
#35599=ORIENTED_EDGE('',*,*,#27193,.F.);
#35600=ORIENTED_EDGE('',*,*,#27194,.T.);
#35601=ORIENTED_EDGE('',*,*,#26963,.F.);
#35602=ORIENTED_EDGE('',*,*,#27184,.F.);
#35603=ORIENTED_EDGE('',*,*,#27195,.F.);
#35604=ORIENTED_EDGE('',*,*,#27196,.T.);
#35605=ORIENTED_EDGE('',*,*,#27197,.T.);
#35606=ORIENTED_EDGE('',*,*,#27186,.F.);
#35607=ORIENTED_EDGE('',*,*,#26975,.T.);
#35608=ORIENTED_EDGE('',*,*,#27188,.F.);
#35609=ORIENTED_EDGE('',*,*,#27198,.F.);
#35610=ORIENTED_EDGE('',*,*,#27191,.F.);
#35611=ORIENTED_EDGE('',*,*,#27199,.F.);
#35612=ORIENTED_EDGE('',*,*,#27200,.T.);
#35613=ORIENTED_EDGE('',*,*,#26973,.T.);
#35614=ORIENTED_EDGE('',*,*,#27194,.F.);
#35615=ORIENTED_EDGE('',*,*,#27201,.T.);
#35616=ORIENTED_EDGE('',*,*,#26970,.T.);
#35617=ORIENTED_EDGE('',*,*,#27202,.F.);
#35618=ORIENTED_EDGE('',*,*,#27196,.F.);
#35619=ORIENTED_EDGE('',*,*,#27203,.F.);
#35620=ORIENTED_EDGE('',*,*,#26972,.T.);
#35621=ORIENTED_EDGE('',*,*,#27204,.F.);
#35622=ORIENTED_EDGE('',*,*,#27200,.F.);
#35623=ORIENTED_EDGE('',*,*,#27205,.F.);
#35624=ORIENTED_EDGE('',*,*,#27176,.T.);
#35625=ORIENTED_EDGE('',*,*,#27173,.T.);
#35626=ORIENTED_EDGE('',*,*,#26977,.T.);
#35627=ORIENTED_EDGE('',*,*,#27178,.T.);
#35628=ORIENTED_EDGE('',*,*,#27193,.T.);
#35629=ORIENTED_EDGE('',*,*,#27181,.T.);
#35630=ORIENTED_EDGE('',*,*,#27189,.T.);
#35631=ORIENTED_EDGE('',*,*,#27199,.T.);
#35632=ORIENTED_EDGE('',*,*,#27206,.F.);
#35633=ORIENTED_EDGE('',*,*,#27198,.T.);
#35634=ORIENTED_EDGE('',*,*,#27207,.T.);
#35635=ORIENTED_EDGE('',*,*,#27175,.T.);
#35636=ORIENTED_EDGE('',*,*,#27206,.T.);
#35637=ORIENTED_EDGE('',*,*,#27177,.T.);
#35638=ORIENTED_EDGE('',*,*,#26967,.F.);
#35639=ORIENTED_EDGE('',*,*,#27205,.T.);
#35640=ORIENTED_EDGE('',*,*,#27201,.F.);
#35641=ORIENTED_EDGE('',*,*,#27195,.T.);
#35642=ORIENTED_EDGE('',*,*,#27192,.T.);
#35643=ORIENTED_EDGE('',*,*,#26969,.T.);
#35644=ORIENTED_EDGE('',*,*,#27172,.T.);
#35645=ORIENTED_EDGE('',*,*,#27207,.F.);
#35646=ORIENTED_EDGE('',*,*,#27190,.T.);
#35647=ORIENTED_EDGE('',*,*,#27187,.T.);
#35648=ORIENTED_EDGE('',*,*,#27197,.F.);
#35649=ORIENTED_EDGE('',*,*,#27202,.T.);
#35650=ORIENTED_EDGE('',*,*,#27204,.T.);
#35651=ORIENTED_EDGE('',*,*,#26971,.T.);
#35652=ORIENTED_EDGE('',*,*,#27203,.T.);
#35653=ORIENTED_EDGE('',*,*,#26974,.T.);
#35654=ORIENTED_EDGE('',*,*,#27208,.T.);
#35655=ORIENTED_EDGE('',*,*,#27209,.F.);
#35656=ORIENTED_EDGE('',*,*,#26953,.T.);
#35657=ORIENTED_EDGE('',*,*,#27210,.F.);
#35658=ORIENTED_EDGE('',*,*,#27211,.T.);
#35659=ORIENTED_EDGE('',*,*,#27212,.F.);
#35660=ORIENTED_EDGE('',*,*,#27208,.F.);
#35661=ORIENTED_EDGE('',*,*,#27213,.F.);
#35662=ORIENTED_EDGE('',*,*,#26951,.F.);
#35663=ORIENTED_EDGE('',*,*,#27214,.F.);
#35664=ORIENTED_EDGE('',*,*,#27211,.F.);
#35665=ORIENTED_EDGE('',*,*,#27215,.F.);
#35666=ORIENTED_EDGE('',*,*,#27216,.T.);
#35667=ORIENTED_EDGE('',*,*,#26936,.F.);
#35668=ORIENTED_EDGE('',*,*,#27217,.T.);
#35669=ORIENTED_EDGE('',*,*,#27218,.F.);
#35670=ORIENTED_EDGE('',*,*,#27219,.T.);
#35671=ORIENTED_EDGE('',*,*,#27220,.T.);
#35672=ORIENTED_EDGE('',*,*,#27217,.F.);
#35673=ORIENTED_EDGE('',*,*,#26935,.T.);
#35674=ORIENTED_EDGE('',*,*,#27221,.T.);
#35675=ORIENTED_EDGE('',*,*,#26937,.T.);
#35676=ORIENTED_EDGE('',*,*,#27216,.F.);
#35677=ORIENTED_EDGE('',*,*,#27222,.T.);
#35678=ORIENTED_EDGE('',*,*,#27223,.T.);
#35679=ORIENTED_EDGE('',*,*,#27224,.F.);
#35680=ORIENTED_EDGE('',*,*,#27219,.F.);
#35681=ORIENTED_EDGE('',*,*,#26934,.F.);
#35682=ORIENTED_EDGE('',*,*,#27225,.T.);
#35683=ORIENTED_EDGE('',*,*,#27226,.F.);
#35684=ORIENTED_EDGE('',*,*,#27220,.F.);
#35685=ORIENTED_EDGE('',*,*,#27227,.F.);
#35686=ORIENTED_EDGE('',*,*,#27228,.T.);
#35687=ORIENTED_EDGE('',*,*,#27229,.F.);
#35688=ORIENTED_EDGE('',*,*,#27222,.F.);
#35689=ORIENTED_EDGE('',*,*,#27230,.F.);
#35690=ORIENTED_EDGE('',*,*,#27231,.T.);
#35691=ORIENTED_EDGE('',*,*,#26938,.F.);
#35692=ORIENTED_EDGE('',*,*,#27221,.F.);
#35693=ORIENTED_EDGE('',*,*,#27232,.F.);
#35694=ORIENTED_EDGE('',*,*,#27233,.T.);
#35695=ORIENTED_EDGE('',*,*,#27234,.T.);
#35696=ORIENTED_EDGE('',*,*,#27223,.F.);
#35697=ORIENTED_EDGE('',*,*,#26950,.T.);
#35698=ORIENTED_EDGE('',*,*,#27225,.F.);
#35699=ORIENTED_EDGE('',*,*,#27235,.F.);
#35700=ORIENTED_EDGE('',*,*,#27228,.F.);
#35701=ORIENTED_EDGE('',*,*,#27236,.F.);
#35702=ORIENTED_EDGE('',*,*,#27237,.T.);
#35703=ORIENTED_EDGE('',*,*,#26948,.T.);
#35704=ORIENTED_EDGE('',*,*,#27231,.F.);
#35705=ORIENTED_EDGE('',*,*,#27238,.T.);
#35706=ORIENTED_EDGE('',*,*,#26945,.T.);
#35707=ORIENTED_EDGE('',*,*,#27239,.F.);
#35708=ORIENTED_EDGE('',*,*,#27233,.F.);
#35709=ORIENTED_EDGE('',*,*,#27240,.F.);
#35710=ORIENTED_EDGE('',*,*,#26947,.T.);
#35711=ORIENTED_EDGE('',*,*,#27241,.F.);
#35712=ORIENTED_EDGE('',*,*,#27237,.F.);
#35713=ORIENTED_EDGE('',*,*,#27242,.F.);
#35714=ORIENTED_EDGE('',*,*,#27213,.T.);
#35715=ORIENTED_EDGE('',*,*,#27210,.T.);
#35716=ORIENTED_EDGE('',*,*,#26952,.T.);
#35717=ORIENTED_EDGE('',*,*,#27215,.T.);
#35718=ORIENTED_EDGE('',*,*,#27230,.T.);
#35719=ORIENTED_EDGE('',*,*,#27218,.T.);
#35720=ORIENTED_EDGE('',*,*,#27226,.T.);
#35721=ORIENTED_EDGE('',*,*,#27236,.T.);
#35722=ORIENTED_EDGE('',*,*,#27243,.F.);
#35723=ORIENTED_EDGE('',*,*,#27235,.T.);
#35724=ORIENTED_EDGE('',*,*,#27244,.T.);
#35725=ORIENTED_EDGE('',*,*,#27212,.T.);
#35726=ORIENTED_EDGE('',*,*,#27243,.T.);
#35727=ORIENTED_EDGE('',*,*,#27214,.T.);
#35728=ORIENTED_EDGE('',*,*,#26942,.F.);
#35729=ORIENTED_EDGE('',*,*,#27242,.T.);
#35730=ORIENTED_EDGE('',*,*,#27238,.F.);
#35731=ORIENTED_EDGE('',*,*,#27232,.T.);
#35732=ORIENTED_EDGE('',*,*,#27229,.T.);
#35733=ORIENTED_EDGE('',*,*,#26944,.T.);
#35734=ORIENTED_EDGE('',*,*,#27209,.T.);
#35735=ORIENTED_EDGE('',*,*,#27244,.F.);
#35736=ORIENTED_EDGE('',*,*,#27227,.T.);
#35737=ORIENTED_EDGE('',*,*,#27224,.T.);
#35738=ORIENTED_EDGE('',*,*,#27234,.F.);
#35739=ORIENTED_EDGE('',*,*,#27239,.T.);
#35740=ORIENTED_EDGE('',*,*,#27241,.T.);
#35741=ORIENTED_EDGE('',*,*,#26946,.T.);
#35742=ORIENTED_EDGE('',*,*,#27240,.T.);
#35743=ORIENTED_EDGE('',*,*,#26949,.T.);
#35744=ORIENTED_EDGE('',*,*,#26925,.F.);
#35745=ORIENTED_EDGE('',*,*,#27245,.F.);
#35746=ORIENTED_EDGE('',*,*,#26919,.F.);
#35747=ORIENTED_EDGE('',*,*,#27246,.F.);
#35748=ORIENTED_EDGE('',*,*,#26913,.F.);
#35749=ORIENTED_EDGE('',*,*,#27247,.F.);
#35750=ORIENTED_EDGE('',*,*,#27248,.T.);
#35751=ORIENTED_EDGE('',*,*,#27063,.T.);
#35752=ORIENTED_EDGE('',*,*,#27249,.T.);
#35753=ORIENTED_EDGE('',*,*,#27250,.F.);
#35754=ORIENTED_EDGE('',*,*,#27249,.F.);
#35755=ORIENTED_EDGE('',*,*,#27057,.T.);
#35756=ORIENTED_EDGE('',*,*,#27251,.T.);
#35757=ORIENTED_EDGE('',*,*,#27252,.F.);
#35758=ORIENTED_EDGE('',*,*,#27072,.T.);
#35759=ORIENTED_EDGE('',*,*,#27061,.T.);
#35760=ORIENTED_EDGE('',*,*,#27248,.F.);
#35761=ORIENTED_EDGE('',*,*,#27253,.F.);
#35762=ORIENTED_EDGE('',*,*,#27254,.T.);
#35763=ORIENTED_EDGE('',*,*,#27070,.T.);
#35764=ORIENTED_EDGE('',*,*,#27251,.F.);
#35765=ORIENTED_EDGE('',*,*,#27052,.T.);
#35766=ORIENTED_EDGE('',*,*,#27255,.T.);
#35767=ORIENTED_EDGE('',*,*,#27256,.F.);
#35768=ORIENTED_EDGE('',*,*,#27257,.T.);
#35769=ORIENTED_EDGE('',*,*,#27071,.T.);
#35770=ORIENTED_EDGE('',*,*,#27254,.F.);
#35771=ORIENTED_EDGE('',*,*,#27258,.F.);
#35772=ORIENTED_EDGE('',*,*,#27255,.F.);
#35773=ORIENTED_EDGE('',*,*,#27051,.T.);
#35774=ORIENTED_EDGE('',*,*,#27259,.T.);
#35775=ORIENTED_EDGE('',*,*,#27260,.F.);
#35776=ORIENTED_EDGE('',*,*,#27261,.T.);
#35777=ORIENTED_EDGE('',*,*,#27066,.T.);
#35778=ORIENTED_EDGE('',*,*,#27074,.T.);
#35779=ORIENTED_EDGE('',*,*,#27067,.T.);
#35780=ORIENTED_EDGE('',*,*,#27257,.F.);
#35781=ORIENTED_EDGE('',*,*,#27262,.F.);
#35782=ORIENTED_EDGE('',*,*,#27259,.F.);
#35783=ORIENTED_EDGE('',*,*,#27050,.T.);
#35784=ORIENTED_EDGE('',*,*,#27263,.T.);
#35785=ORIENTED_EDGE('',*,*,#27264,.F.);
#35786=ORIENTED_EDGE('',*,*,#27265,.T.);
#35787=ORIENTED_EDGE('',*,*,#27064,.T.);
#35788=ORIENTED_EDGE('',*,*,#27261,.F.);
#35789=ORIENTED_EDGE('',*,*,#27266,.F.);
#35790=ORIENTED_EDGE('',*,*,#27263,.F.);
#35791=ORIENTED_EDGE('',*,*,#27049,.T.);
#35792=ORIENTED_EDGE('',*,*,#27267,.T.);
#35793=ORIENTED_EDGE('',*,*,#27268,.F.);
#35794=ORIENTED_EDGE('',*,*,#27269,.T.);
#35795=ORIENTED_EDGE('',*,*,#27059,.T.);
#35796=ORIENTED_EDGE('',*,*,#27265,.F.);
#35797=ORIENTED_EDGE('',*,*,#27270,.F.);
#35798=ORIENTED_EDGE('',*,*,#27267,.F.);
#35799=ORIENTED_EDGE('',*,*,#27048,.T.);
#35800=ORIENTED_EDGE('',*,*,#27271,.T.);
#35801=ORIENTED_EDGE('',*,*,#27272,.F.);
#35802=ORIENTED_EDGE('',*,*,#27271,.F.);
#35803=ORIENTED_EDGE('',*,*,#27055,.T.);
#35804=ORIENTED_EDGE('',*,*,#27269,.F.);
#35805=ORIENTED_EDGE('',*,*,#27273,.F.);
#35806=ORIENTED_EDGE('',*,*,#27274,.F.);
#35807=ORIENTED_EDGE('',*,*,#27262,.T.);
#35808=ORIENTED_EDGE('',*,*,#27275,.F.);
#35809=ORIENTED_EDGE('',*,*,#27276,.T.);
#35810=ORIENTED_EDGE('',*,*,#27277,.T.);
#35811=ORIENTED_EDGE('',*,*,#27278,.F.);
#35812=ORIENTED_EDGE('',*,*,#27276,.F.);
#35813=ORIENTED_EDGE('',*,*,#27279,.F.);
#35814=ORIENTED_EDGE('',*,*,#27280,.T.);
#35815=ORIENTED_EDGE('',*,*,#27281,.F.);
#35816=ORIENTED_EDGE('',*,*,#27277,.F.);
#35817=ORIENTED_EDGE('',*,*,#27282,.F.);
#35818=ORIENTED_EDGE('',*,*,#27283,.T.);
#35819=ORIENTED_EDGE('',*,*,#27284,.T.);
#35820=ORIENTED_EDGE('',*,*,#27280,.F.);
#35821=ORIENTED_EDGE('',*,*,#27285,.T.);
#35822=ORIENTED_EDGE('',*,*,#27286,.T.);
#35823=ORIENTED_EDGE('',*,*,#26896,.F.);
#35824=ORIENTED_EDGE('',*,*,#27283,.F.);
#35825=ORIENTED_EDGE('',*,*,#27287,.F.);
#35826=ORIENTED_EDGE('',*,*,#27288,.T.);
#35827=ORIENTED_EDGE('',*,*,#27289,.F.);
#35828=ORIENTED_EDGE('',*,*,#27284,.F.);
#35829=ORIENTED_EDGE('',*,*,#26895,.F.);
#35830=ORIENTED_EDGE('',*,*,#27290,.T.);
#35831=ORIENTED_EDGE('',*,*,#27291,.T.);
#35832=ORIENTED_EDGE('',*,*,#27286,.F.);
#35833=ORIENTED_EDGE('',*,*,#27292,.T.);
#35834=ORIENTED_EDGE('',*,*,#27293,.T.);
#35835=ORIENTED_EDGE('',*,*,#27294,.F.);
#35836=ORIENTED_EDGE('',*,*,#27288,.F.);
#35837=ORIENTED_EDGE('',*,*,#26894,.F.);
#35838=ORIENTED_EDGE('',*,*,#27295,.T.);
#35839=ORIENTED_EDGE('',*,*,#27296,.F.);
#35840=ORIENTED_EDGE('',*,*,#27290,.F.);
#35841=ORIENTED_EDGE('',*,*,#27297,.F.);
#35842=ORIENTED_EDGE('',*,*,#27298,.T.);
#35843=ORIENTED_EDGE('',*,*,#26897,.F.);
#35844=ORIENTED_EDGE('',*,*,#27291,.F.);
#35845=ORIENTED_EDGE('',*,*,#27299,.F.);
#35846=ORIENTED_EDGE('',*,*,#27300,.T.);
#35847=ORIENTED_EDGE('',*,*,#27301,.F.);
#35848=ORIENTED_EDGE('',*,*,#27293,.F.);
#35849=ORIENTED_EDGE('',*,*,#26893,.F.);
#35850=ORIENTED_EDGE('',*,*,#27302,.F.);
#35851=ORIENTED_EDGE('',*,*,#27253,.T.);
#35852=ORIENTED_EDGE('',*,*,#27303,.F.);
#35853=ORIENTED_EDGE('',*,*,#27295,.F.);
#35854=ORIENTED_EDGE('',*,*,#27304,.T.);
#35855=ORIENTED_EDGE('',*,*,#26898,.F.);
#35856=ORIENTED_EDGE('',*,*,#27298,.F.);
#35857=ORIENTED_EDGE('',*,*,#27305,.F.);
#35858=ORIENTED_EDGE('',*,*,#27306,.T.);
#35859=ORIENTED_EDGE('',*,*,#27307,.F.);
#35860=ORIENTED_EDGE('',*,*,#27300,.F.);
#35861=ORIENTED_EDGE('',*,*,#27308,.T.);
#35862=ORIENTED_EDGE('',*,*,#26899,.F.);
#35863=ORIENTED_EDGE('',*,*,#27304,.F.);
#35864=ORIENTED_EDGE('',*,*,#27309,.F.);
#35865=ORIENTED_EDGE('',*,*,#27310,.T.);
#35866=ORIENTED_EDGE('',*,*,#27311,.F.);
#35867=ORIENTED_EDGE('',*,*,#27306,.F.);
#35868=ORIENTED_EDGE('',*,*,#26892,.F.);
#35869=ORIENTED_EDGE('',*,*,#27312,.F.);
#35870=ORIENTED_EDGE('',*,*,#27313,.T.);
#35871=ORIENTED_EDGE('',*,*,#27308,.F.);
#35872=ORIENTED_EDGE('',*,*,#27314,.T.);
#35873=ORIENTED_EDGE('',*,*,#27315,.F.);
#35874=ORIENTED_EDGE('',*,*,#27310,.F.);
#35875=ORIENTED_EDGE('',*,*,#26891,.F.);
#35876=ORIENTED_EDGE('',*,*,#26910,.F.);
#35877=ORIENTED_EDGE('',*,*,#27316,.T.);
#35878=ORIENTED_EDGE('',*,*,#26900,.F.);
#35879=ORIENTED_EDGE('',*,*,#27313,.F.);
#35880=ORIENTED_EDGE('',*,*,#27317,.F.);
#35881=ORIENTED_EDGE('',*,*,#27318,.T.);
#35882=ORIENTED_EDGE('',*,*,#27319,.F.);
#35883=ORIENTED_EDGE('',*,*,#27314,.F.);
#35884=ORIENTED_EDGE('',*,*,#26909,.F.);
#35885=ORIENTED_EDGE('',*,*,#27320,.T.);
#35886=ORIENTED_EDGE('',*,*,#26901,.F.);
#35887=ORIENTED_EDGE('',*,*,#27316,.F.);
#35888=ORIENTED_EDGE('',*,*,#27321,.F.);
#35889=ORIENTED_EDGE('',*,*,#27322,.T.);
#35890=ORIENTED_EDGE('',*,*,#27268,.T.);
#35891=ORIENTED_EDGE('',*,*,#27323,.F.);
#35892=ORIENTED_EDGE('',*,*,#27318,.F.);
#35893=ORIENTED_EDGE('',*,*,#26908,.F.);
#35894=ORIENTED_EDGE('',*,*,#27324,.T.);
#35895=ORIENTED_EDGE('',*,*,#26905,.F.);
#35896=ORIENTED_EDGE('',*,*,#26902,.F.);
#35897=ORIENTED_EDGE('',*,*,#27320,.F.);
#35898=ORIENTED_EDGE('',*,*,#27325,.F.);
#35899=ORIENTED_EDGE('',*,*,#27326,.T.);
#35900=ORIENTED_EDGE('',*,*,#27264,.T.);
#35901=ORIENTED_EDGE('',*,*,#27322,.F.);
#35902=ORIENTED_EDGE('',*,*,#26907,.F.);
#35903=ORIENTED_EDGE('',*,*,#27327,.F.);
#35904=ORIENTED_EDGE('',*,*,#27260,.T.);
#35905=ORIENTED_EDGE('',*,*,#27326,.F.);
#35906=ORIENTED_EDGE('',*,*,#26906,.F.);
#35907=ORIENTED_EDGE('',*,*,#27324,.F.);
#35908=ORIENTED_EDGE('',*,*,#26912,.T.);
#35909=ORIENTED_EDGE('',*,*,#27006,.F.);
#35910=ORIENTED_EDGE('',*,*,#27328,.T.);
#35911=ORIENTED_EDGE('',*,*,#27329,.F.);
#35912=ORIENTED_EDGE('',*,*,#27330,.T.);
#35913=ORIENTED_EDGE('',*,*,#27331,.F.);
#35914=ORIENTED_EDGE('',*,*,#27332,.T.);
#35915=ORIENTED_EDGE('',*,*,#27333,.T.);
#35916=ORIENTED_EDGE('',*,*,#27330,.F.);
#35917=ORIENTED_EDGE('',*,*,#27334,.T.);
#35918=ORIENTED_EDGE('',*,*,#27335,.F.);
#35919=ORIENTED_EDGE('',*,*,#27315,.T.);
#35920=ORIENTED_EDGE('',*,*,#27336,.F.);
#35921=ORIENTED_EDGE('',*,*,#27328,.F.);
#35922=ORIENTED_EDGE('',*,*,#27337,.T.);
#35923=ORIENTED_EDGE('',*,*,#27338,.F.);
#35924=ORIENTED_EDGE('',*,*,#27332,.F.);
#35925=ORIENTED_EDGE('',*,*,#27339,.F.);
#35926=ORIENTED_EDGE('',*,*,#27340,.F.);
#35927=ORIENTED_EDGE('',*,*,#27341,.F.);
#35928=ORIENTED_EDGE('',*,*,#27342,.T.);
#35929=ORIENTED_EDGE('',*,*,#27343,.T.);
#35930=ORIENTED_EDGE('',*,*,#27344,.T.);
#35931=ORIENTED_EDGE('',*,*,#27345,.F.);
#35932=ORIENTED_EDGE('',*,*,#27337,.F.);
#35933=ORIENTED_EDGE('',*,*,#27346,.F.);
#35934=ORIENTED_EDGE('',*,*,#27347,.T.);
#35935=ORIENTED_EDGE('',*,*,#27348,.F.);
#35936=ORIENTED_EDGE('',*,*,#27342,.F.);
#35937=ORIENTED_EDGE('',*,*,#27349,.F.);
#35938=ORIENTED_EDGE('',*,*,#27350,.F.);
#35939=ORIENTED_EDGE('',*,*,#27305,.T.);
#35940=ORIENTED_EDGE('',*,*,#27351,.F.);
#35941=ORIENTED_EDGE('',*,*,#27347,.F.);
#35942=ORIENTED_EDGE('',*,*,#27352,.T.);
#35943=ORIENTED_EDGE('',*,*,#26928,.T.);
#35944=ORIENTED_EDGE('',*,*,#27353,.T.);
#35945=ORIENTED_EDGE('',*,*,#27338,.T.);
#35946=ORIENTED_EDGE('',*,*,#27345,.T.);
#35947=ORIENTED_EDGE('',*,*,#27354,.T.);
#35948=ORIENTED_EDGE('',*,*,#27301,.T.);
#35949=ORIENTED_EDGE('',*,*,#27355,.T.);
#35950=ORIENTED_EDGE('',*,*,#26922,.T.);
#35951=ORIENTED_EDGE('',*,*,#27356,.T.);
#35952=ORIENTED_EDGE('',*,*,#26916,.T.);
#35953=ORIENTED_EDGE('',*,*,#27005,.F.);
#35954=ORIENTED_EDGE('',*,*,#26980,.F.);
#35955=ORIENTED_EDGE('',*,*,#26955,.F.);
#35956=ORIENTED_EDGE('',*,*,#27357,.F.);
#35957=ORIENTED_EDGE('',*,*,#27270,.T.);
#35958=ORIENTED_EDGE('',*,*,#27358,.F.);
#35959=ORIENTED_EDGE('',*,*,#27359,.T.);
#35960=ORIENTED_EDGE('',*,*,#27334,.F.);
#35961=ORIENTED_EDGE('',*,*,#27329,.T.);
#35962=ORIENTED_EDGE('',*,*,#27360,.T.);
#35963=ORIENTED_EDGE('',*,*,#27361,.F.);
#35964=ORIENTED_EDGE('',*,*,#27359,.F.);
#35965=ORIENTED_EDGE('',*,*,#27362,.F.);
#35966=ORIENTED_EDGE('',*,*,#27339,.T.);
#35967=ORIENTED_EDGE('',*,*,#27363,.F.);
#35968=ORIENTED_EDGE('',*,*,#27325,.T.);
#35969=ORIENTED_EDGE('',*,*,#27364,.T.);
#35970=ORIENTED_EDGE('',*,*,#27343,.F.);
#35971=ORIENTED_EDGE('',*,*,#27348,.T.);
#35972=ORIENTED_EDGE('',*,*,#27365,.F.);
#35973=ORIENTED_EDGE('',*,*,#27366,.T.);
#35974=ORIENTED_EDGE('',*,*,#27367,.F.);
#35975=ORIENTED_EDGE('',*,*,#27252,.T.);
#35976=ORIENTED_EDGE('',*,*,#27368,.F.);
#35977=ORIENTED_EDGE('',*,*,#27366,.F.);
#35978=ORIENTED_EDGE('',*,*,#27369,.T.);
#35979=ORIENTED_EDGE('',*,*,#27273,.T.);
#35980=ORIENTED_EDGE('',*,*,#27357,.T.);
#35981=ORIENTED_EDGE('',*,*,#27361,.T.);
#35982=ORIENTED_EDGE('',*,*,#27368,.T.);
#35983=ORIENTED_EDGE('',*,*,#27256,.T.);
#35984=ORIENTED_EDGE('',*,*,#27327,.T.);
#35985=ORIENTED_EDGE('',*,*,#27363,.T.);
#35986=ORIENTED_EDGE('',*,*,#27275,.T.);
#35987=ORIENTED_EDGE('',*,*,#27258,.T.);
#35988=ORIENTED_EDGE('',*,*,#27302,.T.);
#35989=ORIENTED_EDGE('',*,*,#27297,.T.);
#35990=ORIENTED_EDGE('',*,*,#27292,.F.);
#35991=ORIENTED_EDGE('',*,*,#27287,.T.);
#35992=ORIENTED_EDGE('',*,*,#27285,.F.);
#35993=ORIENTED_EDGE('',*,*,#27282,.T.);
#35994=ORIENTED_EDGE('',*,*,#27279,.T.);
#35995=ORIENTED_EDGE('',*,*,#27358,.T.);
#35996=ORIENTED_EDGE('',*,*,#27266,.T.);
#35997=ORIENTED_EDGE('',*,*,#27274,.T.);
#35998=ORIENTED_EDGE('',*,*,#27370,.F.);
#35999=ORIENTED_EDGE('',*,*,#27303,.T.);
#36000=ORIENTED_EDGE('',*,*,#27250,.T.);
#36001=ORIENTED_EDGE('',*,*,#27367,.T.);
#36002=ORIENTED_EDGE('',*,*,#27371,.T.);
#36003=ORIENTED_EDGE('',*,*,#27299,.T.);
#36004=ORIENTED_EDGE('',*,*,#27296,.T.);
#36005=ORIENTED_EDGE('',*,*,#27371,.F.);
#36006=ORIENTED_EDGE('',*,*,#27365,.T.);
#36007=ORIENTED_EDGE('',*,*,#27351,.T.);
#36008=ORIENTED_EDGE('',*,*,#27370,.T.);
#36009=ORIENTED_EDGE('',*,*,#27278,.T.);
#36010=ORIENTED_EDGE('',*,*,#27372,.F.);
#36011=ORIENTED_EDGE('',*,*,#27346,.T.);
#36012=ORIENTED_EDGE('',*,*,#27362,.T.);
#36013=ORIENTED_EDGE('',*,*,#27364,.F.);
#36014=ORIENTED_EDGE('',*,*,#27321,.T.);
#36015=ORIENTED_EDGE('',*,*,#27373,.F.);
#36016=ORIENTED_EDGE('',*,*,#27340,.T.);
#36017=ORIENTED_EDGE('',*,*,#27374,.F.);
#36018=ORIENTED_EDGE('',*,*,#27312,.T.);
#36019=ORIENTED_EDGE('',*,*,#27375,.F.);
#36020=ORIENTED_EDGE('',*,*,#27341,.T.);
#36021=ORIENTED_EDGE('',*,*,#27376,.F.);
#36022=ORIENTED_EDGE('',*,*,#27294,.T.);
#36023=ORIENTED_EDGE('',*,*,#27354,.F.);
#36024=ORIENTED_EDGE('',*,*,#27344,.F.);
#36025=ORIENTED_EDGE('',*,*,#27375,.T.);
#36026=ORIENTED_EDGE('',*,*,#27309,.T.);
#36027=ORIENTED_EDGE('',*,*,#27350,.T.);
#36028=ORIENTED_EDGE('',*,*,#27349,.T.);
#36029=ORIENTED_EDGE('',*,*,#27373,.T.);
#36030=ORIENTED_EDGE('',*,*,#27317,.T.);
#36031=ORIENTED_EDGE('',*,*,#27374,.T.);
#36032=ORIENTED_EDGE('',*,*,#27336,.T.);
#36033=ORIENTED_EDGE('',*,*,#27319,.T.);
#36034=ORIENTED_EDGE('',*,*,#27377,.F.);
#36035=ORIENTED_EDGE('',*,*,#27360,.F.);
#36036=ORIENTED_EDGE('',*,*,#27372,.T.);
#36037=ORIENTED_EDGE('',*,*,#27281,.T.);
#36038=ORIENTED_EDGE('',*,*,#27289,.T.);
#36039=ORIENTED_EDGE('',*,*,#27376,.T.);
#36040=ORIENTED_EDGE('',*,*,#27323,.T.);
#36041=ORIENTED_EDGE('',*,*,#27272,.T.);
#36042=ORIENTED_EDGE('',*,*,#27369,.F.);
#36043=ORIENTED_EDGE('',*,*,#27377,.T.);
#36044=ORIENTED_EDGE('',*,*,#26921,.F.);
#36045=ORIENTED_EDGE('',*,*,#27378,.F.);
#36046=ORIENTED_EDGE('',*,*,#26917,.F.);
#36047=ORIENTED_EDGE('',*,*,#27356,.F.);
#36048=ORIENTED_EDGE('',*,*,#26923,.F.);
#36049=ORIENTED_EDGE('',*,*,#27355,.F.);
#36050=ORIENTED_EDGE('',*,*,#27307,.T.);
#36051=ORIENTED_EDGE('',*,*,#27379,.F.);
#36052=ORIENTED_EDGE('',*,*,#26927,.F.);
#36053=ORIENTED_EDGE('',*,*,#27380,.F.);
#36054=ORIENTED_EDGE('',*,*,#27333,.F.);
#36055=ORIENTED_EDGE('',*,*,#27353,.F.);
#36056=ORIENTED_EDGE('',*,*,#26929,.F.);
#36057=ORIENTED_EDGE('',*,*,#27352,.F.);
#36058=ORIENTED_EDGE('',*,*,#26915,.F.);
#36059=ORIENTED_EDGE('',*,*,#27381,.F.);
#36060=ORIENTED_EDGE('',*,*,#26930,.F.);
#36061=ORIENTED_EDGE('',*,*,#27381,.T.);
#36062=ORIENTED_EDGE('',*,*,#26914,.F.);
#36063=ORIENTED_EDGE('',*,*,#27247,.T.);
#36064=ORIENTED_EDGE('',*,*,#26918,.F.);
#36065=ORIENTED_EDGE('',*,*,#27378,.T.);
#36066=ORIENTED_EDGE('',*,*,#26920,.F.);
#36067=ORIENTED_EDGE('',*,*,#27246,.T.);
#36068=ORIENTED_EDGE('',*,*,#26924,.F.);
#36069=ORIENTED_EDGE('',*,*,#27379,.T.);
#36070=ORIENTED_EDGE('',*,*,#27311,.T.);
#36071=ORIENTED_EDGE('',*,*,#27335,.T.);
#36072=ORIENTED_EDGE('',*,*,#27331,.T.);
#36073=ORIENTED_EDGE('',*,*,#27380,.T.);
#36074=ORIENTED_EDGE('',*,*,#26926,.F.);
#36075=ORIENTED_EDGE('',*,*,#27245,.T.);
#36076=ORIENTED_EDGE('',*,*,#27382,.F.);
#36077=ORIENTED_EDGE('',*,*,#27383,.T.);
#36078=ORIENTED_EDGE('',*,*,#27384,.T.);
#36079=ORIENTED_EDGE('',*,*,#27383,.F.);
#36080=ORIENTED_EDGE('',*,*,#27385,.T.);
#36081=ORIENTED_EDGE('',*,*,#27386,.T.);
#36082=ORIENTED_EDGE('',*,*,#27387,.T.);
#36083=ORIENTED_EDGE('',*,*,#27388,.T.);
#36084=ORIENTED_EDGE('',*,*,#27389,.T.);
#36085=ORIENTED_EDGE('',*,*,#27390,.T.);
#36086=ORIENTED_EDGE('',*,*,#27391,.T.);
#36087=ORIENTED_EDGE('',*,*,#27392,.T.);
#36088=ORIENTED_EDGE('',*,*,#27393,.T.);
#36089=ORIENTED_EDGE('',*,*,#27394,.T.);
#36090=ORIENTED_EDGE('',*,*,#27395,.T.);
#36091=ORIENTED_EDGE('',*,*,#27396,.T.);
#36092=ORIENTED_EDGE('',*,*,#27397,.T.);
#36093=ORIENTED_EDGE('',*,*,#27398,.T.);
#36094=ORIENTED_EDGE('',*,*,#27399,.T.);
#36095=ORIENTED_EDGE('',*,*,#27400,.T.);
#36096=ORIENTED_EDGE('',*,*,#27401,.T.);
#36097=ORIENTED_EDGE('',*,*,#27402,.T.);
#36098=ORIENTED_EDGE('',*,*,#27403,.T.);
#36099=ORIENTED_EDGE('',*,*,#27404,.T.);
#36100=ORIENTED_EDGE('',*,*,#27405,.T.);
#36101=ORIENTED_EDGE('',*,*,#27406,.T.);
#36102=ORIENTED_EDGE('',*,*,#27407,.T.);
#36103=ORIENTED_EDGE('',*,*,#27408,.T.);
#36104=ORIENTED_EDGE('',*,*,#27409,.T.);
#36105=ORIENTED_EDGE('',*,*,#27410,.T.);
#36106=ORIENTED_EDGE('',*,*,#27411,.T.);
#36107=ORIENTED_EDGE('',*,*,#27412,.T.);
#36108=ORIENTED_EDGE('',*,*,#27413,.T.);
#36109=ORIENTED_EDGE('',*,*,#27414,.T.);
#36110=ORIENTED_EDGE('',*,*,#27415,.T.);
#36111=ORIENTED_EDGE('',*,*,#27416,.T.);
#36112=ORIENTED_EDGE('',*,*,#27417,.T.);
#36113=ORIENTED_EDGE('',*,*,#27418,.T.);
#36114=ORIENTED_EDGE('',*,*,#27419,.T.);
#36115=ORIENTED_EDGE('',*,*,#27420,.T.);
#36116=ORIENTED_EDGE('',*,*,#27421,.T.);
#36117=ORIENTED_EDGE('',*,*,#27422,.T.);
#36118=ORIENTED_EDGE('',*,*,#27423,.T.);
#36119=ORIENTED_EDGE('',*,*,#27424,.T.);
#36120=ORIENTED_EDGE('',*,*,#27425,.T.);
#36121=ORIENTED_EDGE('',*,*,#27426,.T.);
#36122=ORIENTED_EDGE('',*,*,#27427,.T.);
#36123=ORIENTED_EDGE('',*,*,#27428,.T.);
#36124=ORIENTED_EDGE('',*,*,#27429,.T.);
#36125=ORIENTED_EDGE('',*,*,#27430,.T.);
#36126=ORIENTED_EDGE('',*,*,#27431,.T.);
#36127=ORIENTED_EDGE('',*,*,#27432,.T.);
#36128=ORIENTED_EDGE('',*,*,#27433,.T.);
#36129=ORIENTED_EDGE('',*,*,#27434,.T.);
#36130=ORIENTED_EDGE('',*,*,#27435,.T.);
#36131=ORIENTED_EDGE('',*,*,#27436,.T.);
#36132=ORIENTED_EDGE('',*,*,#27437,.T.);
#36133=ORIENTED_EDGE('',*,*,#27438,.T.);
#36134=ORIENTED_EDGE('',*,*,#27439,.T.);
#36135=ORIENTED_EDGE('',*,*,#27440,.T.);
#36136=ORIENTED_EDGE('',*,*,#27441,.T.);
#36137=ORIENTED_EDGE('',*,*,#27442,.T.);
#36138=ORIENTED_EDGE('',*,*,#27382,.T.);
#36139=ORIENTED_EDGE('',*,*,#27443,.T.);
#36140=ORIENTED_EDGE('',*,*,#27444,.T.);
#36141=ORIENTED_EDGE('',*,*,#27445,.T.);
#36142=ORIENTED_EDGE('',*,*,#27446,.T.);
#36143=ORIENTED_EDGE('',*,*,#27447,.T.);
#36144=ORIENTED_EDGE('',*,*,#27448,.T.);
#36145=ORIENTED_EDGE('',*,*,#27449,.T.);
#36146=ORIENTED_EDGE('',*,*,#27450,.T.);
#36147=ORIENTED_EDGE('',*,*,#27451,.T.);
#36148=ORIENTED_EDGE('',*,*,#27452,.T.);
#36149=ORIENTED_EDGE('',*,*,#27384,.F.);
#36150=ORIENTED_EDGE('',*,*,#27453,.T.);
#36151=ORIENTED_EDGE('',*,*,#27454,.T.);
#36152=ORIENTED_EDGE('',*,*,#27455,.T.);
#36153=ORIENTED_EDGE('',*,*,#27456,.T.);
#36154=ORIENTED_EDGE('',*,*,#27455,.F.);
#36155=ORIENTED_EDGE('',*,*,#27457,.T.);
#36156=ORIENTED_EDGE('',*,*,#27446,.F.);
#36157=ORIENTED_EDGE('',*,*,#27458,.T.);
#36158=ORIENTED_EDGE('',*,*,#27436,.F.);
#36159=ORIENTED_EDGE('',*,*,#27459,.T.);
#36160=ORIENTED_EDGE('',*,*,#27453,.F.);
#36161=ORIENTED_EDGE('',*,*,#27460,.T.);
#36162=ORIENTED_EDGE('',*,*,#27419,.F.);
#36163=ORIENTED_EDGE('',*,*,#27461,.T.);
#36164=ORIENTED_EDGE('',*,*,#27421,.F.);
#36165=ORIENTED_EDGE('',*,*,#27462,.T.);
#36166=ORIENTED_EDGE('',*,*,#27415,.F.);
#36167=ORIENTED_EDGE('',*,*,#27463,.T.);
#36168=ORIENTED_EDGE('',*,*,#27417,.F.);
#36169=ORIENTED_EDGE('',*,*,#27464,.T.);
#36170=ORIENTED_EDGE('',*,*,#27411,.F.);
#36171=ORIENTED_EDGE('',*,*,#27465,.T.);
#36172=ORIENTED_EDGE('',*,*,#27413,.F.);
#36173=ORIENTED_EDGE('',*,*,#27466,.T.);
#36174=ORIENTED_EDGE('',*,*,#27423,.F.);
#36175=ORIENTED_EDGE('',*,*,#27467,.T.);
#36176=ORIENTED_EDGE('',*,*,#27409,.F.);
#36177=ORIENTED_EDGE('',*,*,#27468,.T.);
#36178=ORIENTED_EDGE('',*,*,#27469,.T.);
#36179=ORIENTED_EDGE('',*,*,#27470,.T.);
#36180=ORIENTED_EDGE('',*,*,#27471,.T.);
#36181=ORIENTED_EDGE('',*,*,#27472,.F.);
#36182=ORIENTED_EDGE('',*,*,#27473,.F.);
#36183=ORIENTED_EDGE('',*,*,#27474,.T.);
#36184=ORIENTED_EDGE('',*,*,#27472,.T.);
#36185=ORIENTED_EDGE('',*,*,#27475,.T.);
#36186=ORIENTED_EDGE('',*,*,#27476,.F.);
#36187=ORIENTED_EDGE('',*,*,#27477,.T.);
#36188=ORIENTED_EDGE('',*,*,#27473,.T.);
#36189=ORIENTED_EDGE('',*,*,#27478,.T.);
#36190=ORIENTED_EDGE('',*,*,#27479,.F.);
#36191=ORIENTED_EDGE('',*,*,#27480,.T.);
#36192=ORIENTED_EDGE('',*,*,#27476,.T.);
#36193=ORIENTED_EDGE('',*,*,#27481,.T.);
#36194=ORIENTED_EDGE('',*,*,#27482,.T.);
#36195=ORIENTED_EDGE('',*,*,#27483,.T.);
#36196=ORIENTED_EDGE('',*,*,#27484,.T.);
#36197=ORIENTED_EDGE('',*,*,#27479,.T.);
#36198=ORIENTED_EDGE('',*,*,#27485,.T.);
#36199=ORIENTED_EDGE('',*,*,#27486,.T.);
#36200=ORIENTED_EDGE('',*,*,#27487,.T.);
#36201=ORIENTED_EDGE('',*,*,#27488,.F.);
#36202=ORIENTED_EDGE('',*,*,#27489,.F.);
#36203=ORIENTED_EDGE('',*,*,#27490,.T.);
#36204=ORIENTED_EDGE('',*,*,#27488,.T.);
#36205=ORIENTED_EDGE('',*,*,#27491,.T.);
#36206=ORIENTED_EDGE('',*,*,#27492,.F.);
#36207=ORIENTED_EDGE('',*,*,#27493,.T.);
#36208=ORIENTED_EDGE('',*,*,#27489,.T.);
#36209=ORIENTED_EDGE('',*,*,#27494,.T.);
#36210=ORIENTED_EDGE('',*,*,#27495,.F.);
#36211=ORIENTED_EDGE('',*,*,#27496,.T.);
#36212=ORIENTED_EDGE('',*,*,#27492,.T.);
#36213=ORIENTED_EDGE('',*,*,#27497,.T.);
#36214=ORIENTED_EDGE('',*,*,#27498,.T.);
#36215=ORIENTED_EDGE('',*,*,#27499,.T.);
#36216=ORIENTED_EDGE('',*,*,#27500,.T.);
#36217=ORIENTED_EDGE('',*,*,#27495,.T.);
#36218=ORIENTED_EDGE('',*,*,#27501,.F.);
#36219=ORIENTED_EDGE('',*,*,#27418,.F.);
#36220=ORIENTED_EDGE('',*,*,#27502,.F.);
#36221=ORIENTED_EDGE('',*,*,#27430,.F.);
#36222=ORIENTED_EDGE('',*,*,#27502,.T.);
#36223=ORIENTED_EDGE('',*,*,#27463,.F.);
#36224=ORIENTED_EDGE('',*,*,#27503,.F.);
#36225=ORIENTED_EDGE('',*,*,#27431,.F.);
#36226=ORIENTED_EDGE('',*,*,#27501,.T.);
#36227=ORIENTED_EDGE('',*,*,#27429,.F.);
#36228=ORIENTED_EDGE('',*,*,#27504,.F.);
#36229=ORIENTED_EDGE('',*,*,#27461,.F.);
#36230=ORIENTED_EDGE('',*,*,#27503,.T.);
#36231=ORIENTED_EDGE('',*,*,#27414,.F.);
#36232=ORIENTED_EDGE('',*,*,#27505,.F.);
#36233=ORIENTED_EDGE('',*,*,#27432,.F.);
#36234=ORIENTED_EDGE('',*,*,#27504,.T.);
#36235=ORIENTED_EDGE('',*,*,#27428,.F.);
#36236=ORIENTED_EDGE('',*,*,#27506,.F.);
#36237=ORIENTED_EDGE('',*,*,#27422,.F.);
#36238=ORIENTED_EDGE('',*,*,#27505,.T.);
#36239=ORIENTED_EDGE('',*,*,#27465,.F.);
#36240=ORIENTED_EDGE('',*,*,#27507,.F.);
#36241=ORIENTED_EDGE('',*,*,#27425,.F.);
#36242=ORIENTED_EDGE('',*,*,#27506,.T.);
#36243=ORIENTED_EDGE('',*,*,#27427,.F.);
#36244=ORIENTED_EDGE('',*,*,#27508,.F.);
#36245=ORIENTED_EDGE('',*,*,#27467,.F.);
#36246=ORIENTED_EDGE('',*,*,#27507,.T.);
#36247=ORIENTED_EDGE('',*,*,#27410,.F.);
#36248=ORIENTED_EDGE('',*,*,#27508,.T.);
#36249=ORIENTED_EDGE('',*,*,#27426,.F.);
#36250=ORIENTED_EDGE('',*,*,#27509,.F.);
#36251=ORIENTED_EDGE('',*,*,#27390,.F.);
#36252=ORIENTED_EDGE('',*,*,#27510,.F.);
#36253=ORIENTED_EDGE('',*,*,#27416,.F.);
#36254=ORIENTED_EDGE('',*,*,#27510,.T.);
#36255=ORIENTED_EDGE('',*,*,#27389,.F.);
#36256=ORIENTED_EDGE('',*,*,#27511,.F.);
#36257=ORIENTED_EDGE('',*,*,#27466,.F.);
#36258=ORIENTED_EDGE('',*,*,#27509,.T.);
#36259=ORIENTED_EDGE('',*,*,#27464,.F.);
#36260=ORIENTED_EDGE('',*,*,#27512,.F.);
#36261=ORIENTED_EDGE('',*,*,#27391,.F.);
#36262=ORIENTED_EDGE('',*,*,#27511,.T.);
#36263=ORIENTED_EDGE('',*,*,#27388,.F.);
#36264=ORIENTED_EDGE('',*,*,#27513,.F.);
#36265=ORIENTED_EDGE('',*,*,#27412,.F.);
#36266=ORIENTED_EDGE('',*,*,#27512,.T.);
#36267=ORIENTED_EDGE('',*,*,#27420,.F.);
#36268=ORIENTED_EDGE('',*,*,#27514,.F.);
#36269=ORIENTED_EDGE('',*,*,#27392,.F.);
#36270=ORIENTED_EDGE('',*,*,#27513,.T.);
#36271=ORIENTED_EDGE('',*,*,#27387,.F.);
#36272=ORIENTED_EDGE('',*,*,#27515,.F.);
#36273=ORIENTED_EDGE('',*,*,#27468,.F.);
#36274=ORIENTED_EDGE('',*,*,#27514,.T.);
#36275=ORIENTED_EDGE('',*,*,#27462,.F.);
#36276=ORIENTED_EDGE('',*,*,#27516,.F.);
#36277=ORIENTED_EDGE('',*,*,#27385,.F.);
#36278=ORIENTED_EDGE('',*,*,#27515,.T.);
#36279=ORIENTED_EDGE('',*,*,#27386,.F.);
#36280=ORIENTED_EDGE('',*,*,#27516,.T.);
#36281=ORIENTED_EDGE('',*,*,#27424,.F.);
#36282=ORIENTED_EDGE('',*,*,#27484,.F.);
#36283=ORIENTED_EDGE('',*,*,#27517,.T.);
#36284=ORIENTED_EDGE('',*,*,#27443,.F.);
#36285=ORIENTED_EDGE('',*,*,#27518,.F.);
#36286=ORIENTED_EDGE('',*,*,#27518,.T.);
#36287=ORIENTED_EDGE('',*,*,#27457,.F.);
#36288=ORIENTED_EDGE('',*,*,#27519,.F.);
#36289=ORIENTED_EDGE('',*,*,#27480,.F.);
#36290=ORIENTED_EDGE('',*,*,#27519,.T.);
#36291=ORIENTED_EDGE('',*,*,#27454,.F.);
#36292=ORIENTED_EDGE('',*,*,#27520,.F.);
#36293=ORIENTED_EDGE('',*,*,#27477,.F.);
#36294=ORIENTED_EDGE('',*,*,#27520,.T.);
#36295=ORIENTED_EDGE('',*,*,#27459,.F.);
#36296=ORIENTED_EDGE('',*,*,#27521,.F.);
#36297=ORIENTED_EDGE('',*,*,#27474,.F.);
#36298=ORIENTED_EDGE('',*,*,#27435,.F.);
#36299=ORIENTED_EDGE('',*,*,#27522,.T.);
#36300=ORIENTED_EDGE('',*,*,#27469,.F.);
#36301=ORIENTED_EDGE('',*,*,#27521,.T.);
#36302=ORIENTED_EDGE('',*,*,#27471,.F.);
#36303=ORIENTED_EDGE('',*,*,#27523,.T.);
#36304=ORIENTED_EDGE('',*,*,#27437,.F.);
#36305=ORIENTED_EDGE('',*,*,#27524,.F.);
#36306=ORIENTED_EDGE('',*,*,#27524,.T.);
#36307=ORIENTED_EDGE('',*,*,#27442,.F.);
#36308=ORIENTED_EDGE('',*,*,#27525,.F.);
#36309=ORIENTED_EDGE('',*,*,#27475,.F.);
#36310=ORIENTED_EDGE('',*,*,#27525,.T.);
#36311=ORIENTED_EDGE('',*,*,#27441,.F.);
#36312=ORIENTED_EDGE('',*,*,#27526,.F.);
#36313=ORIENTED_EDGE('',*,*,#27478,.F.);
#36314=ORIENTED_EDGE('',*,*,#27526,.T.);
#36315=ORIENTED_EDGE('',*,*,#27440,.F.);
#36316=ORIENTED_EDGE('',*,*,#27527,.F.);
#36317=ORIENTED_EDGE('',*,*,#27481,.F.);
#36318=ORIENTED_EDGE('',*,*,#27439,.F.);
#36319=ORIENTED_EDGE('',*,*,#27528,.T.);
#36320=ORIENTED_EDGE('',*,*,#27482,.F.);
#36321=ORIENTED_EDGE('',*,*,#27527,.T.);
#36322=ORIENTED_EDGE('',*,*,#27500,.F.);
#36323=ORIENTED_EDGE('',*,*,#27529,.T.);
#36324=ORIENTED_EDGE('',*,*,#27447,.F.);
#36325=ORIENTED_EDGE('',*,*,#27530,.F.);
#36326=ORIENTED_EDGE('',*,*,#27530,.T.);
#36327=ORIENTED_EDGE('',*,*,#27452,.F.);
#36328=ORIENTED_EDGE('',*,*,#27531,.F.);
#36329=ORIENTED_EDGE('',*,*,#27496,.F.);
#36330=ORIENTED_EDGE('',*,*,#27531,.T.);
#36331=ORIENTED_EDGE('',*,*,#27451,.F.);
#36332=ORIENTED_EDGE('',*,*,#27532,.F.);
#36333=ORIENTED_EDGE('',*,*,#27493,.F.);
#36334=ORIENTED_EDGE('',*,*,#27532,.T.);
#36335=ORIENTED_EDGE('',*,*,#27450,.F.);
#36336=ORIENTED_EDGE('',*,*,#27533,.F.);
#36337=ORIENTED_EDGE('',*,*,#27490,.F.);
#36338=ORIENTED_EDGE('',*,*,#27449,.F.);
#36339=ORIENTED_EDGE('',*,*,#27534,.T.);
#36340=ORIENTED_EDGE('',*,*,#27485,.F.);
#36341=ORIENTED_EDGE('',*,*,#27533,.T.);
#36342=ORIENTED_EDGE('',*,*,#27487,.F.);
#36343=ORIENTED_EDGE('',*,*,#27535,.T.);
#36344=ORIENTED_EDGE('',*,*,#27433,.F.);
#36345=ORIENTED_EDGE('',*,*,#27536,.F.);
#36346=ORIENTED_EDGE('',*,*,#27536,.T.);
#36347=ORIENTED_EDGE('',*,*,#27460,.F.);
#36348=ORIENTED_EDGE('',*,*,#27537,.F.);
#36349=ORIENTED_EDGE('',*,*,#27491,.F.);
#36350=ORIENTED_EDGE('',*,*,#27537,.T.);
#36351=ORIENTED_EDGE('',*,*,#27456,.F.);
#36352=ORIENTED_EDGE('',*,*,#27538,.F.);
#36353=ORIENTED_EDGE('',*,*,#27494,.F.);
#36354=ORIENTED_EDGE('',*,*,#27538,.T.);
#36355=ORIENTED_EDGE('',*,*,#27458,.F.);
#36356=ORIENTED_EDGE('',*,*,#27539,.F.);
#36357=ORIENTED_EDGE('',*,*,#27497,.F.);
#36358=ORIENTED_EDGE('',*,*,#27445,.F.);
#36359=ORIENTED_EDGE('',*,*,#27540,.T.);
#36360=ORIENTED_EDGE('',*,*,#27498,.F.);
#36361=ORIENTED_EDGE('',*,*,#27539,.T.);
#36362=ORIENTED_EDGE('',*,*,#27541,.F.);
#36363=ORIENTED_EDGE('',*,*,#27517,.F.);
#36364=ORIENTED_EDGE('',*,*,#27542,.F.);
#36365=ORIENTED_EDGE('',*,*,#27402,.F.);
#36366=ORIENTED_EDGE('',*,*,#27542,.T.);
#36367=ORIENTED_EDGE('',*,*,#27483,.F.);
#36368=ORIENTED_EDGE('',*,*,#27543,.F.);
#36369=ORIENTED_EDGE('',*,*,#27403,.F.);
#36370=ORIENTED_EDGE('',*,*,#27541,.T.);
#36371=ORIENTED_EDGE('',*,*,#27401,.F.);
#36372=ORIENTED_EDGE('',*,*,#27544,.F.);
#36373=ORIENTED_EDGE('',*,*,#27444,.F.);
#36374=ORIENTED_EDGE('',*,*,#27543,.T.);
#36375=ORIENTED_EDGE('',*,*,#27528,.F.);
#36376=ORIENTED_EDGE('',*,*,#27545,.F.);
#36377=ORIENTED_EDGE('',*,*,#27404,.F.);
#36378=ORIENTED_EDGE('',*,*,#27544,.T.);
#36379=ORIENTED_EDGE('',*,*,#27400,.F.);
#36380=ORIENTED_EDGE('',*,*,#27546,.F.);
#36381=ORIENTED_EDGE('',*,*,#27540,.F.);
#36382=ORIENTED_EDGE('',*,*,#27545,.T.);
#36383=ORIENTED_EDGE('',*,*,#27438,.F.);
#36384=ORIENTED_EDGE('',*,*,#27547,.F.);
#36385=ORIENTED_EDGE('',*,*,#27405,.F.);
#36386=ORIENTED_EDGE('',*,*,#27546,.T.);
#36387=ORIENTED_EDGE('',*,*,#27399,.F.);
#36388=ORIENTED_EDGE('',*,*,#27548,.F.);
#36389=ORIENTED_EDGE('',*,*,#27499,.F.);
#36390=ORIENTED_EDGE('',*,*,#27547,.T.);
#36391=ORIENTED_EDGE('',*,*,#27523,.F.);
#36392=ORIENTED_EDGE('',*,*,#27549,.F.);
#36393=ORIENTED_EDGE('',*,*,#27406,.F.);
#36394=ORIENTED_EDGE('',*,*,#27548,.T.);
#36395=ORIENTED_EDGE('',*,*,#27398,.F.);
#36396=ORIENTED_EDGE('',*,*,#27550,.F.);
#36397=ORIENTED_EDGE('',*,*,#27529,.F.);
#36398=ORIENTED_EDGE('',*,*,#27549,.T.);
#36399=ORIENTED_EDGE('',*,*,#27470,.F.);
#36400=ORIENTED_EDGE('',*,*,#27551,.F.);
#36401=ORIENTED_EDGE('',*,*,#27407,.F.);
#36402=ORIENTED_EDGE('',*,*,#27550,.T.);
#36403=ORIENTED_EDGE('',*,*,#27397,.F.);
#36404=ORIENTED_EDGE('',*,*,#27552,.F.);
#36405=ORIENTED_EDGE('',*,*,#27448,.F.);
#36406=ORIENTED_EDGE('',*,*,#27551,.T.);
#36407=ORIENTED_EDGE('',*,*,#27522,.F.);
#36408=ORIENTED_EDGE('',*,*,#27553,.F.);
#36409=ORIENTED_EDGE('',*,*,#27408,.F.);
#36410=ORIENTED_EDGE('',*,*,#27552,.T.);
#36411=ORIENTED_EDGE('',*,*,#27396,.F.);
#36412=ORIENTED_EDGE('',*,*,#27554,.F.);
#36413=ORIENTED_EDGE('',*,*,#27534,.F.);
#36414=ORIENTED_EDGE('',*,*,#27553,.T.);
#36415=ORIENTED_EDGE('',*,*,#27434,.F.);
#36416=ORIENTED_EDGE('',*,*,#27555,.F.);
#36417=ORIENTED_EDGE('',*,*,#27393,.F.);
#36418=ORIENTED_EDGE('',*,*,#27554,.T.);
#36419=ORIENTED_EDGE('',*,*,#27395,.F.);
#36420=ORIENTED_EDGE('',*,*,#27556,.F.);
#36421=ORIENTED_EDGE('',*,*,#27486,.F.);
#36422=ORIENTED_EDGE('',*,*,#27555,.T.);
#36423=ORIENTED_EDGE('',*,*,#27535,.F.);
#36424=ORIENTED_EDGE('',*,*,#27556,.T.);
#36425=ORIENTED_EDGE('',*,*,#27394,.F.);
#36426=ORIENTED_EDGE('',*,*,#27557,.F.);
#36427=ORIENTED_EDGE('',*,*,#27558,.F.);
#36428=ORIENTED_EDGE('',*,*,#27559,.T.);
#36429=ORIENTED_EDGE('',*,*,#27560,.T.);
#36430=ORIENTED_EDGE('',*,*,#27559,.F.);
#36431=ORIENTED_EDGE('',*,*,#27561,.F.);
#36432=ORIENTED_EDGE('',*,*,#27562,.F.);
#36433=ORIENTED_EDGE('',*,*,#27563,.F.);
#36434=ORIENTED_EDGE('',*,*,#27564,.T.);
#36435=ORIENTED_EDGE('',*,*,#27565,.F.);
#36436=ORIENTED_EDGE('',*,*,#27566,.F.);
#36437=ORIENTED_EDGE('',*,*,#27567,.F.);
#36438=ORIENTED_EDGE('',*,*,#27568,.T.);
#36439=ORIENTED_EDGE('',*,*,#27569,.F.);
#36440=ORIENTED_EDGE('',*,*,#27570,.T.);
#36441=ORIENTED_EDGE('',*,*,#27571,.F.);
#36442=ORIENTED_EDGE('',*,*,#27572,.F.);
#36443=ORIENTED_EDGE('',*,*,#27573,.F.);
#36444=ORIENTED_EDGE('',*,*,#27557,.T.);
#36445=ORIENTED_EDGE('',*,*,#27558,.T.);
#36446=ORIENTED_EDGE('',*,*,#27574,.T.);
#36447=ORIENTED_EDGE('',*,*,#27573,.T.);
#36448=ORIENTED_EDGE('',*,*,#27575,.T.);
#36449=ORIENTED_EDGE('',*,*,#27576,.T.);
#36450=ORIENTED_EDGE('',*,*,#27577,.T.);
#36451=ORIENTED_EDGE('',*,*,#27578,.T.);
#36452=ORIENTED_EDGE('',*,*,#27579,.F.);
#36453=ORIENTED_EDGE('',*,*,#27569,.T.);
#36454=ORIENTED_EDGE('',*,*,#27574,.F.);
#36455=ORIENTED_EDGE('',*,*,#27560,.F.);
#36456=ORIENTED_EDGE('',*,*,#27580,.T.);
#36457=ORIENTED_EDGE('',*,*,#27581,.F.);
#36458=ORIENTED_EDGE('',*,*,#27582,.F.);
#36459=ORIENTED_EDGE('',*,*,#27580,.F.);
#36460=ORIENTED_EDGE('',*,*,#27583,.T.);
#36461=ORIENTED_EDGE('',*,*,#27584,.T.);
#36462=ORIENTED_EDGE('',*,*,#27585,.F.);
#36463=ORIENTED_EDGE('',*,*,#27584,.F.);
#36464=ORIENTED_EDGE('',*,*,#27585,.T.);
#36465=ORIENTED_EDGE('',*,*,#27586,.T.);
#36466=ORIENTED_EDGE('',*,*,#27581,.T.);
#36467=ORIENTED_EDGE('',*,*,#27582,.T.);
#36468=ORIENTED_EDGE('',*,*,#27586,.F.);
#36469=ORIENTED_EDGE('',*,*,#27587,.T.);
#36470=ORIENTED_EDGE('',*,*,#27588,.T.);
#36471=ORIENTED_EDGE('',*,*,#27589,.T.);
#36472=ORIENTED_EDGE('',*,*,#27590,.F.);
#36473=ORIENTED_EDGE('',*,*,#27591,.T.);
#36474=ORIENTED_EDGE('',*,*,#27592,.T.);
#36475=ORIENTED_EDGE('',*,*,#27593,.T.);
#36476=ORIENTED_EDGE('',*,*,#27594,.T.);
#36477=ORIENTED_EDGE('',*,*,#27595,.F.);
#36478=ORIENTED_EDGE('',*,*,#27596,.T.);
#36479=ORIENTED_EDGE('',*,*,#27597,.T.);
#36480=ORIENTED_EDGE('',*,*,#27598,.T.);
#36481=ORIENTED_EDGE('',*,*,#27599,.T.);
#36482=ORIENTED_EDGE('',*,*,#27600,.F.);
#36483=ORIENTED_EDGE('',*,*,#27601,.T.);
#36484=ORIENTED_EDGE('',*,*,#27602,.T.);
#36485=ORIENTED_EDGE('',*,*,#27603,.T.);
#36486=ORIENTED_EDGE('',*,*,#27604,.F.);
#36487=ORIENTED_EDGE('',*,*,#27597,.F.);
#36488=ORIENTED_EDGE('',*,*,#27601,.F.);
#36489=ORIENTED_EDGE('',*,*,#27605,.F.);
#36490=ORIENTED_EDGE('',*,*,#27603,.F.);
#36491=ORIENTED_EDGE('',*,*,#27606,.T.);
#36492=ORIENTED_EDGE('',*,*,#27596,.F.);
#36493=ORIENTED_EDGE('',*,*,#27607,.F.);
#36494=ORIENTED_EDGE('',*,*,#27608,.T.);
#36495=ORIENTED_EDGE('',*,*,#27609,.F.);
#36496=ORIENTED_EDGE('',*,*,#27587,.F.);
#36497=ORIENTED_EDGE('',*,*,#27591,.F.);
#36498=ORIENTED_EDGE('',*,*,#27610,.F.);
#36499=ORIENTED_EDGE('',*,*,#27608,.F.);
#36500=ORIENTED_EDGE('',*,*,#27611,.F.);
#36501=ORIENTED_EDGE('',*,*,#27592,.F.);
#36502=ORIENTED_EDGE('',*,*,#27612,.F.);
#36503=ORIENTED_EDGE('',*,*,#27613,.T.);
#36504=ORIENTED_EDGE('',*,*,#27614,.F.);
#36505=ORIENTED_EDGE('',*,*,#27615,.F.);
#36506=ORIENTED_EDGE('',*,*,#27616,.F.);
#36507=ORIENTED_EDGE('',*,*,#27617,.F.);
#36508=ORIENTED_EDGE('',*,*,#27618,.T.);
#36509=ORIENTED_EDGE('',*,*,#27619,.F.);
#36510=ORIENTED_EDGE('',*,*,#27620,.F.);
#36511=ORIENTED_EDGE('',*,*,#27621,.F.);
#36512=ORIENTED_EDGE('',*,*,#27622,.F.);
#36513=ORIENTED_EDGE('',*,*,#27623,.T.);
#36514=ORIENTED_EDGE('',*,*,#27624,.F.);
#36515=ORIENTED_EDGE('',*,*,#27625,.F.);
#36516=ORIENTED_EDGE('',*,*,#27626,.F.);
#36517=ORIENTED_EDGE('',*,*,#27627,.F.);
#36518=ORIENTED_EDGE('',*,*,#27628,.T.);
#36519=ORIENTED_EDGE('',*,*,#27583,.F.);
#36520=ORIENTED_EDGE('',*,*,#27628,.F.);
#36521=ORIENTED_EDGE('',*,*,#27629,.F.);
#36522=ORIENTED_EDGE('',*,*,#27630,.F.);
#36523=ORIENTED_EDGE('',*,*,#27631,.T.);
#36524=ORIENTED_EDGE('',*,*,#27632,.F.);
#36525=ORIENTED_EDGE('',*,*,#27631,.F.);
#36526=ORIENTED_EDGE('',*,*,#27621,.T.);
#36527=ORIENTED_EDGE('',*,*,#27633,.T.);
#36528=ORIENTED_EDGE('',*,*,#27634,.T.);
#36529=ORIENTED_EDGE('',*,*,#27635,.T.);
#36530=ORIENTED_EDGE('',*,*,#27622,.T.);
#36531=ORIENTED_EDGE('',*,*,#27626,.T.);
#36532=ORIENTED_EDGE('',*,*,#27636,.T.);
#36533=ORIENTED_EDGE('',*,*,#27634,.F.);
#36534=ORIENTED_EDGE('',*,*,#27637,.T.);
#36535=ORIENTED_EDGE('',*,*,#27617,.T.);
#36536=ORIENTED_EDGE('',*,*,#27629,.T.);
#36537=ORIENTED_EDGE('',*,*,#27630,.T.);
#36538=ORIENTED_EDGE('',*,*,#27638,.T.);
#36539=ORIENTED_EDGE('',*,*,#27627,.T.);
#36540=ORIENTED_EDGE('',*,*,#27638,.F.);
#36541=ORIENTED_EDGE('',*,*,#27639,.F.);
#36542=ORIENTED_EDGE('',*,*,#27589,.F.);
#36543=ORIENTED_EDGE('',*,*,#27640,.T.);
#36544=ORIENTED_EDGE('',*,*,#27641,.T.);
#36545=ORIENTED_EDGE('',*,*,#27614,.T.);
#36546=ORIENTED_EDGE('',*,*,#27642,.T.);
#36547=ORIENTED_EDGE('',*,*,#27641,.F.);
#36548=ORIENTED_EDGE('',*,*,#27643,.T.);
#36549=ORIENTED_EDGE('',*,*,#27644,.F.);
#36550=ORIENTED_EDGE('',*,*,#27645,.F.);
#36551=ORIENTED_EDGE('',*,*,#27646,.F.);
#36552=ORIENTED_EDGE('',*,*,#27647,.F.);
#36553=ORIENTED_EDGE('',*,*,#27648,.T.);
#36554=ORIENTED_EDGE('',*,*,#27649,.F.);
#36555=ORIENTED_EDGE('',*,*,#27650,.F.);
#36556=ORIENTED_EDGE('',*,*,#27651,.F.);
#36557=ORIENTED_EDGE('',*,*,#27652,.F.);
#36558=ORIENTED_EDGE('',*,*,#27653,.T.);
#36559=ORIENTED_EDGE('',*,*,#27654,.F.);
#36560=ORIENTED_EDGE('',*,*,#27655,.F.);
#36561=ORIENTED_EDGE('',*,*,#27656,.F.);
#36562=ORIENTED_EDGE('',*,*,#27657,.F.);
#36563=ORIENTED_EDGE('',*,*,#27658,.T.);
#36564=ORIENTED_EDGE('',*,*,#27659,.T.);
#36565=ORIENTED_EDGE('',*,*,#27655,.T.);
#36566=ORIENTED_EDGE('',*,*,#27654,.T.);
#36567=ORIENTED_EDGE('',*,*,#27660,.T.);
#36568=ORIENTED_EDGE('',*,*,#27658,.F.);
#36569=ORIENTED_EDGE('',*,*,#27649,.T.);
#36570=ORIENTED_EDGE('',*,*,#27661,.T.);
#36571=ORIENTED_EDGE('',*,*,#27662,.T.);
#36572=ORIENTED_EDGE('',*,*,#27663,.T.);
#36573=ORIENTED_EDGE('',*,*,#27645,.T.);
#36574=ORIENTED_EDGE('',*,*,#27644,.T.);
#36575=ORIENTED_EDGE('',*,*,#27664,.T.);
#36576=ORIENTED_EDGE('',*,*,#27662,.F.);
#36577=ORIENTED_EDGE('',*,*,#27665,.T.);
#36578=ORIENTED_EDGE('',*,*,#27650,.T.);
#36579=ORIENTED_EDGE('',*,*,#27666,.F.);
#36580=ORIENTED_EDGE('',*,*,#27667,.T.);
#36581=ORIENTED_EDGE('',*,*,#27668,.F.);
#36582=ORIENTED_EDGE('',*,*,#27669,.F.);
#36583=ORIENTED_EDGE('',*,*,#27616,.T.);
#36584=ORIENTED_EDGE('',*,*,#27670,.T.);
#36585=ORIENTED_EDGE('',*,*,#27671,.T.);
#36586=ORIENTED_EDGE('',*,*,#27668,.T.);
#36587=ORIENTED_EDGE('',*,*,#27672,.T.);
#36588=ORIENTED_EDGE('',*,*,#27671,.F.);
#36589=ORIENTED_EDGE('',*,*,#27673,.T.);
#36590=ORIENTED_EDGE('',*,*,#27612,.T.);
#36591=ORIENTED_EDGE('',*,*,#27674,.T.);
#36592=ORIENTED_EDGE('',*,*,#27666,.T.);
#36593=ORIENTED_EDGE('',*,*,#27667,.F.);
#36594=ORIENTED_EDGE('',*,*,#27674,.F.);
#36595=ORIENTED_EDGE('',*,*,#27669,.T.);
#36596=ORIENTED_EDGE('',*,*,#27672,.F.);
#36597=ORIENTED_EDGE('',*,*,#27624,.T.);
#36598=ORIENTED_EDGE('',*,*,#27675,.T.);
#36599=ORIENTED_EDGE('',*,*,#27657,.T.);
#36600=ORIENTED_EDGE('',*,*,#27676,.T.);
#36601=ORIENTED_EDGE('',*,*,#27647,.T.);
#36602=ORIENTED_EDGE('',*,*,#27677,.T.);
#36603=ORIENTED_EDGE('',*,*,#27652,.T.);
#36604=ORIENTED_EDGE('',*,*,#27653,.F.);
#36605=ORIENTED_EDGE('',*,*,#27677,.F.);
#36606=ORIENTED_EDGE('',*,*,#27656,.T.);
#36607=ORIENTED_EDGE('',*,*,#27659,.F.);
#36608=ORIENTED_EDGE('',*,*,#27660,.F.);
#36609=ORIENTED_EDGE('',*,*,#27648,.F.);
#36610=ORIENTED_EDGE('',*,*,#27676,.F.);
#36611=ORIENTED_EDGE('',*,*,#27651,.T.);
#36612=ORIENTED_EDGE('',*,*,#27665,.F.);
#36613=ORIENTED_EDGE('',*,*,#27661,.F.);
#36614=ORIENTED_EDGE('',*,*,#27643,.F.);
#36615=ORIENTED_EDGE('',*,*,#27640,.F.);
#36616=ORIENTED_EDGE('',*,*,#27646,.T.);
#36617=ORIENTED_EDGE('',*,*,#27663,.F.);
#36618=ORIENTED_EDGE('',*,*,#27664,.F.);
#36619=ORIENTED_EDGE('',*,*,#27632,.T.);
#36620=ORIENTED_EDGE('',*,*,#27623,.F.);
#36621=ORIENTED_EDGE('',*,*,#27635,.F.);
#36622=ORIENTED_EDGE('',*,*,#27636,.F.);
#36623=ORIENTED_EDGE('',*,*,#27625,.T.);
#36624=ORIENTED_EDGE('',*,*,#27675,.F.);
#36625=ORIENTED_EDGE('',*,*,#27618,.F.);
#36626=ORIENTED_EDGE('',*,*,#27637,.F.);
#36627=ORIENTED_EDGE('',*,*,#27633,.F.);
#36628=ORIENTED_EDGE('',*,*,#27620,.T.);
#36629=ORIENTED_EDGE('',*,*,#27678,.F.);
#36630=ORIENTED_EDGE('',*,*,#27613,.F.);
#36631=ORIENTED_EDGE('',*,*,#27673,.F.);
#36632=ORIENTED_EDGE('',*,*,#27670,.F.);
#36633=ORIENTED_EDGE('',*,*,#27615,.T.);
#36634=ORIENTED_EDGE('',*,*,#27642,.F.);
#36635=ORIENTED_EDGE('',*,*,#27619,.T.);
#36636=ORIENTED_EDGE('',*,*,#27678,.T.);
#36637=ORIENTED_EDGE('',*,*,#27602,.F.);
#36638=ORIENTED_EDGE('',*,*,#27606,.F.);
#36639=ORIENTED_EDGE('',*,*,#27679,.F.);
#36640=ORIENTED_EDGE('',*,*,#27594,.F.);
#36641=ORIENTED_EDGE('',*,*,#27680,.F.);
#36642=ORIENTED_EDGE('',*,*,#27599,.F.);
#36643=ORIENTED_EDGE('',*,*,#27598,.F.);
#36644=ORIENTED_EDGE('',*,*,#27604,.T.);
#36645=ORIENTED_EDGE('',*,*,#27605,.T.);
#36646=ORIENTED_EDGE('',*,*,#27600,.T.);
#36647=ORIENTED_EDGE('',*,*,#27680,.T.);
#36648=ORIENTED_EDGE('',*,*,#27593,.F.);
#36649=ORIENTED_EDGE('',*,*,#27611,.T.);
#36650=ORIENTED_EDGE('',*,*,#27607,.T.);
#36651=ORIENTED_EDGE('',*,*,#27595,.T.);
#36652=ORIENTED_EDGE('',*,*,#27679,.T.);
#36653=ORIENTED_EDGE('',*,*,#27588,.F.);
#36654=ORIENTED_EDGE('',*,*,#27609,.T.);
#36655=ORIENTED_EDGE('',*,*,#27610,.T.);
#36656=ORIENTED_EDGE('',*,*,#27590,.T.);
#36657=ORIENTED_EDGE('',*,*,#27639,.T.);
#36658=ORIENTED_EDGE('',*,*,#27681,.T.);
#36659=ORIENTED_EDGE('',*,*,#27682,.T.);
#36660=ORIENTED_EDGE('',*,*,#27683,.T.);
#36661=ORIENTED_EDGE('',*,*,#27684,.F.);
#36662=ORIENTED_EDGE('',*,*,#27563,.T.);
#36663=ORIENTED_EDGE('',*,*,#27685,.T.);
#36664=ORIENTED_EDGE('',*,*,#27686,.T.);
#36665=ORIENTED_EDGE('',*,*,#27687,.T.);
#36666=ORIENTED_EDGE('',*,*,#27579,.T.);
#36667=ORIENTED_EDGE('',*,*,#27688,.T.);
#36668=ORIENTED_EDGE('',*,*,#27689,.T.);
#36669=ORIENTED_EDGE('',*,*,#27690,.T.);
#36670=ORIENTED_EDGE('',*,*,#27691,.T.);
#36671=ORIENTED_EDGE('',*,*,#27692,.T.);
#36672=ORIENTED_EDGE('',*,*,#27565,.T.);
#36673=ORIENTED_EDGE('',*,*,#27693,.T.);
#36674=ORIENTED_EDGE('',*,*,#27694,.T.);
#36675=ORIENTED_EDGE('',*,*,#27695,.T.);
#36676=ORIENTED_EDGE('',*,*,#27575,.F.);
#36677=ORIENTED_EDGE('',*,*,#27696,.T.);
#36678=ORIENTED_EDGE('',*,*,#27697,.T.);
#36679=ORIENTED_EDGE('',*,*,#27698,.T.);
#36680=ORIENTED_EDGE('',*,*,#27699,.T.);
#36681=ORIENTED_EDGE('',*,*,#27700,.F.);
#36682=ORIENTED_EDGE('',*,*,#27684,.T.);
#36683=ORIENTED_EDGE('',*,*,#27701,.T.);
#36684=ORIENTED_EDGE('',*,*,#27571,.T.);
#36685=ORIENTED_EDGE('',*,*,#27702,.T.);
#36686=ORIENTED_EDGE('',*,*,#27703,.T.);
#36687=ORIENTED_EDGE('',*,*,#27704,.T.);
#36688=ORIENTED_EDGE('',*,*,#27700,.T.);
#36689=ORIENTED_EDGE('',*,*,#27705,.T.);
#36690=ORIENTED_EDGE('',*,*,#27561,.T.);
#36691=ORIENTED_EDGE('',*,*,#27706,.T.);
#36692=ORIENTED_EDGE('',*,*,#27567,.T.);
#36693=ORIENTED_EDGE('',*,*,#27707,.T.);
#36694=ORIENTED_EDGE('',*,*,#27708,.T.);
#36695=ORIENTED_EDGE('',*,*,#27709,.T.);
#36696=ORIENTED_EDGE('',*,*,#27710,.T.);
#36697=ORIENTED_EDGE('',*,*,#27711,.T.);
#36698=ORIENTED_EDGE('',*,*,#27712,.T.);
#36699=ORIENTED_EDGE('',*,*,#27713,.T.);
#36700=ORIENTED_EDGE('',*,*,#27714,.T.);
#36701=ORIENTED_EDGE('',*,*,#27715,.T.);
#36702=ORIENTED_EDGE('',*,*,#27716,.T.);
#36703=ORIENTED_EDGE('',*,*,#27717,.T.);
#36704=ORIENTED_EDGE('',*,*,#27718,.T.);
#36705=ORIENTED_EDGE('',*,*,#27719,.T.);
#36706=ORIENTED_EDGE('',*,*,#27699,.F.);
#36707=ORIENTED_EDGE('',*,*,#27720,.T.);
#36708=ORIENTED_EDGE('',*,*,#27689,.F.);
#36709=ORIENTED_EDGE('',*,*,#27721,.F.);
#36710=ORIENTED_EDGE('',*,*,#27721,.T.);
#36711=ORIENTED_EDGE('',*,*,#27688,.F.);
#36712=ORIENTED_EDGE('',*,*,#27722,.F.);
#36713=ORIENTED_EDGE('',*,*,#27705,.F.);
#36714=ORIENTED_EDGE('',*,*,#27722,.T.);
#36715=ORIENTED_EDGE('',*,*,#27578,.F.);
#36716=ORIENTED_EDGE('',*,*,#27723,.F.);
#36717=ORIENTED_EDGE('',*,*,#27723,.T.);
#36718=ORIENTED_EDGE('',*,*,#27577,.F.);
#36719=ORIENTED_EDGE('',*,*,#27724,.F.);
#36720=ORIENTED_EDGE('',*,*,#27703,.F.);
#36721=ORIENTED_EDGE('',*,*,#27724,.T.);
#36722=ORIENTED_EDGE('',*,*,#27576,.F.);
#36723=ORIENTED_EDGE('',*,*,#27725,.F.);
#36724=ORIENTED_EDGE('',*,*,#27694,.F.);
#36725=ORIENTED_EDGE('',*,*,#27726,.T.);
#36726=ORIENTED_EDGE('',*,*,#27697,.F.);
#36727=ORIENTED_EDGE('',*,*,#27727,.F.);
#36728=ORIENTED_EDGE('',*,*,#27725,.T.);
#36729=ORIENTED_EDGE('',*,*,#27695,.F.);
#36730=ORIENTED_EDGE('',*,*,#27727,.T.);
#36731=ORIENTED_EDGE('',*,*,#27704,.F.);
#36732=ORIENTED_EDGE('',*,*,#27686,.F.);
#36733=ORIENTED_EDGE('',*,*,#27728,.T.);
#36734=ORIENTED_EDGE('',*,*,#27681,.F.);
#36735=ORIENTED_EDGE('',*,*,#27729,.F.);
#36736=ORIENTED_EDGE('',*,*,#27729,.T.);
#36737=ORIENTED_EDGE('',*,*,#27702,.F.);
#36738=ORIENTED_EDGE('',*,*,#27570,.F.);
#36739=ORIENTED_EDGE('',*,*,#27687,.F.);
#36740=ORIENTED_EDGE('',*,*,#27572,.T.);
#36741=ORIENTED_EDGE('',*,*,#27701,.F.);
#36742=ORIENTED_EDGE('',*,*,#27730,.F.);
#36743=ORIENTED_EDGE('',*,*,#27696,.F.);
#36744=ORIENTED_EDGE('',*,*,#27683,.F.);
#36745=ORIENTED_EDGE('',*,*,#27731,.T.);
#36746=ORIENTED_EDGE('',*,*,#27691,.F.);
#36747=ORIENTED_EDGE('',*,*,#27730,.T.);
#36748=ORIENTED_EDGE('',*,*,#27732,.F.);
#36749=ORIENTED_EDGE('',*,*,#27726,.F.);
#36750=ORIENTED_EDGE('',*,*,#27733,.F.);
#36751=ORIENTED_EDGE('',*,*,#27714,.F.);
#36752=ORIENTED_EDGE('',*,*,#27733,.T.);
#36753=ORIENTED_EDGE('',*,*,#27693,.F.);
#36754=ORIENTED_EDGE('',*,*,#27734,.F.);
#36755=ORIENTED_EDGE('',*,*,#27715,.F.);
#36756=ORIENTED_EDGE('',*,*,#27732,.T.);
#36757=ORIENTED_EDGE('',*,*,#27719,.F.);
#36758=ORIENTED_EDGE('',*,*,#27735,.F.);
#36759=ORIENTED_EDGE('',*,*,#27698,.F.);
#36760=ORIENTED_EDGE('',*,*,#27736,.F.);
#36761=ORIENTED_EDGE('',*,*,#27734,.T.);
#36762=ORIENTED_EDGE('',*,*,#27568,.F.);
#36763=ORIENTED_EDGE('',*,*,#27735,.T.);
#36764=ORIENTED_EDGE('',*,*,#27718,.F.);
#36765=ORIENTED_EDGE('',*,*,#27737,.F.);
#36766=ORIENTED_EDGE('',*,*,#27720,.F.);
#36767=ORIENTED_EDGE('',*,*,#27736,.T.);
#36768=ORIENTED_EDGE('',*,*,#27706,.F.);
#36769=ORIENTED_EDGE('',*,*,#27738,.F.);
#36770=ORIENTED_EDGE('',*,*,#27716,.F.);
#36771=ORIENTED_EDGE('',*,*,#27737,.T.);
#36772=ORIENTED_EDGE('',*,*,#27717,.F.);
#36773=ORIENTED_EDGE('',*,*,#27739,.F.);
#36774=ORIENTED_EDGE('',*,*,#27690,.F.);
#36775=ORIENTED_EDGE('',*,*,#27740,.F.);
#36776=ORIENTED_EDGE('',*,*,#27692,.F.);
#36777=ORIENTED_EDGE('',*,*,#27741,.F.);
#36778=ORIENTED_EDGE('',*,*,#27711,.F.);
#36779=ORIENTED_EDGE('',*,*,#27566,.T.);
#36780=ORIENTED_EDGE('',*,*,#27740,.T.);
#36781=ORIENTED_EDGE('',*,*,#27742,.F.);
#36782=ORIENTED_EDGE('',*,*,#27739,.T.);
#36783=ORIENTED_EDGE('',*,*,#27738,.T.);
#36784=ORIENTED_EDGE('',*,*,#27564,.F.);
#36785=ORIENTED_EDGE('',*,*,#27741,.T.);
#36786=ORIENTED_EDGE('',*,*,#27731,.F.);
#36787=ORIENTED_EDGE('',*,*,#27743,.F.);
#36788=ORIENTED_EDGE('',*,*,#27712,.F.);
#36789=ORIENTED_EDGE('',*,*,#27742,.T.);
#36790=ORIENTED_EDGE('',*,*,#27710,.F.);
#36791=ORIENTED_EDGE('',*,*,#27744,.F.);
#36792=ORIENTED_EDGE('',*,*,#27707,.F.);
#36793=ORIENTED_EDGE('',*,*,#27743,.T.);
#36794=ORIENTED_EDGE('',*,*,#27682,.F.);
#36795=ORIENTED_EDGE('',*,*,#27745,.F.);
#36796=ORIENTED_EDGE('',*,*,#27713,.F.);
#36797=ORIENTED_EDGE('',*,*,#27562,.T.);
#36798=ORIENTED_EDGE('',*,*,#27744,.T.);
#36799=ORIENTED_EDGE('',*,*,#27746,.F.);
#36800=ORIENTED_EDGE('',*,*,#27745,.T.);
#36801=ORIENTED_EDGE('',*,*,#27728,.F.);
#36802=ORIENTED_EDGE('',*,*,#27747,.F.);
#36803=ORIENTED_EDGE('',*,*,#27708,.F.);
#36804=ORIENTED_EDGE('',*,*,#27746,.T.);
#36805=ORIENTED_EDGE('',*,*,#27709,.F.);
#36806=ORIENTED_EDGE('',*,*,#27747,.T.);
#36807=ORIENTED_EDGE('',*,*,#27685,.F.);
#36808=ORIENTED_EDGE('',*,*,#27748,.F.);
#36809=ORIENTED_EDGE('',*,*,#27749,.T.);
#36810=ORIENTED_EDGE('',*,*,#27750,.T.);
#36811=ORIENTED_EDGE('',*,*,#27749,.F.);
#36812=ORIENTED_EDGE('',*,*,#27751,.F.);
#36813=ORIENTED_EDGE('',*,*,#27752,.T.);
#36814=ORIENTED_EDGE('',*,*,#27753,.T.);
#36815=ORIENTED_EDGE('',*,*,#27752,.F.);
#36816=ORIENTED_EDGE('',*,*,#27753,.F.);
#36817=ORIENTED_EDGE('',*,*,#27751,.T.);
#36818=ORIENTED_EDGE('',*,*,#27750,.F.);
#36819=ORIENTED_EDGE('',*,*,#27748,.T.);
#36820=ORIENTED_EDGE('',*,*,#27754,.T.);
#36821=ORIENTED_EDGE('',*,*,#27755,.T.);
#36822=ORIENTED_EDGE('',*,*,#27756,.T.);
#36823=ORIENTED_EDGE('',*,*,#27757,.F.);
#36824=ORIENTED_EDGE('',*,*,#27758,.T.);
#36825=ORIENTED_EDGE('',*,*,#27759,.T.);
#36826=ORIENTED_EDGE('',*,*,#27760,.T.);
#36827=ORIENTED_EDGE('',*,*,#27761,.T.);
#36828=ORIENTED_EDGE('',*,*,#27762,.T.);
#36829=ORIENTED_EDGE('',*,*,#27763,.T.);
#36830=ORIENTED_EDGE('',*,*,#27764,.T.);
#36831=ORIENTED_EDGE('',*,*,#27765,.T.);
#36832=ORIENTED_EDGE('',*,*,#27766,.T.);
#36833=ORIENTED_EDGE('',*,*,#27767,.T.);
#36834=ORIENTED_EDGE('',*,*,#27768,.T.);
#36835=ORIENTED_EDGE('',*,*,#27769,.T.);
#36836=ORIENTED_EDGE('',*,*,#27770,.T.);
#36837=ORIENTED_EDGE('',*,*,#27771,.T.);
#36838=ORIENTED_EDGE('',*,*,#27772,.T.);
#36839=ORIENTED_EDGE('',*,*,#27773,.T.);
#36840=ORIENTED_EDGE('',*,*,#27774,.T.);
#36841=ORIENTED_EDGE('',*,*,#27775,.T.);
#36842=ORIENTED_EDGE('',*,*,#27776,.T.);
#36843=ORIENTED_EDGE('',*,*,#27777,.T.);
#36844=ORIENTED_EDGE('',*,*,#27778,.T.);
#36845=ORIENTED_EDGE('',*,*,#27779,.T.);
#36846=ORIENTED_EDGE('',*,*,#27780,.T.);
#36847=ORIENTED_EDGE('',*,*,#27781,.T.);
#36848=ORIENTED_EDGE('',*,*,#27782,.T.);
#36849=ORIENTED_EDGE('',*,*,#27783,.T.);
#36850=ORIENTED_EDGE('',*,*,#27784,.T.);
#36851=ORIENTED_EDGE('',*,*,#27785,.T.);
#36852=ORIENTED_EDGE('',*,*,#27786,.T.);
#36853=ORIENTED_EDGE('',*,*,#27787,.T.);
#36854=ORIENTED_EDGE('',*,*,#27788,.T.);
#36855=ORIENTED_EDGE('',*,*,#27789,.T.);
#36856=ORIENTED_EDGE('',*,*,#27790,.T.);
#36857=ORIENTED_EDGE('',*,*,#27791,.T.);
#36858=ORIENTED_EDGE('',*,*,#27792,.T.);
#36859=ORIENTED_EDGE('',*,*,#27793,.T.);
#36860=ORIENTED_EDGE('',*,*,#27794,.T.);
#36861=ORIENTED_EDGE('',*,*,#27795,.T.);
#36862=ORIENTED_EDGE('',*,*,#27796,.T.);
#36863=ORIENTED_EDGE('',*,*,#27797,.T.);
#36864=ORIENTED_EDGE('',*,*,#27798,.T.);
#36865=ORIENTED_EDGE('',*,*,#27799,.T.);
#36866=ORIENTED_EDGE('',*,*,#27800,.T.);
#36867=ORIENTED_EDGE('',*,*,#27801,.T.);
#36868=ORIENTED_EDGE('',*,*,#27802,.T.);
#36869=ORIENTED_EDGE('',*,*,#27803,.T.);
#36870=ORIENTED_EDGE('',*,*,#27804,.T.);
#36871=ORIENTED_EDGE('',*,*,#27805,.T.);
#36872=ORIENTED_EDGE('',*,*,#27806,.T.);
#36873=ORIENTED_EDGE('',*,*,#27807,.T.);
#36874=ORIENTED_EDGE('',*,*,#27808,.T.);
#36875=ORIENTED_EDGE('',*,*,#27809,.T.);
#36876=ORIENTED_EDGE('',*,*,#27810,.T.);
#36877=ORIENTED_EDGE('',*,*,#27811,.T.);
#36878=ORIENTED_EDGE('',*,*,#27812,.T.);
#36879=ORIENTED_EDGE('',*,*,#27813,.T.);
#36880=ORIENTED_EDGE('',*,*,#27814,.T.);
#36881=ORIENTED_EDGE('',*,*,#27815,.T.);
#36882=ORIENTED_EDGE('',*,*,#27816,.T.);
#36883=ORIENTED_EDGE('',*,*,#27817,.T.);
#36884=ORIENTED_EDGE('',*,*,#27818,.T.);
#36885=ORIENTED_EDGE('',*,*,#27819,.T.);
#36886=ORIENTED_EDGE('',*,*,#27820,.T.);
#36887=ORIENTED_EDGE('',*,*,#27821,.T.);
#36888=ORIENTED_EDGE('',*,*,#27822,.T.);
#36889=ORIENTED_EDGE('',*,*,#27823,.T.);
#36890=ORIENTED_EDGE('',*,*,#27824,.T.);
#36891=ORIENTED_EDGE('',*,*,#27825,.T.);
#36892=ORIENTED_EDGE('',*,*,#27826,.T.);
#36893=ORIENTED_EDGE('',*,*,#27827,.T.);
#36894=ORIENTED_EDGE('',*,*,#27828,.T.);
#36895=ORIENTED_EDGE('',*,*,#27829,.T.);
#36896=ORIENTED_EDGE('',*,*,#27830,.T.);
#36897=ORIENTED_EDGE('',*,*,#27831,.T.);
#36898=ORIENTED_EDGE('',*,*,#27832,.T.);
#36899=ORIENTED_EDGE('',*,*,#27833,.T.);
#36900=ORIENTED_EDGE('',*,*,#27834,.T.);
#36901=ORIENTED_EDGE('',*,*,#27835,.T.);
#36902=ORIENTED_EDGE('',*,*,#27836,.T.);
#36903=ORIENTED_EDGE('',*,*,#27837,.T.);
#36904=ORIENTED_EDGE('',*,*,#27838,.T.);
#36905=ORIENTED_EDGE('',*,*,#27839,.T.);
#36906=ORIENTED_EDGE('',*,*,#27840,.T.);
#36907=ORIENTED_EDGE('',*,*,#27841,.T.);
#36908=ORIENTED_EDGE('',*,*,#27842,.T.);
#36909=ORIENTED_EDGE('',*,*,#27843,.T.);
#36910=ORIENTED_EDGE('',*,*,#27844,.T.);
#36911=ORIENTED_EDGE('',*,*,#27845,.T.);
#36912=ORIENTED_EDGE('',*,*,#27846,.T.);
#36913=ORIENTED_EDGE('',*,*,#27847,.T.);
#36914=ORIENTED_EDGE('',*,*,#27848,.T.);
#36915=ORIENTED_EDGE('',*,*,#27849,.T.);
#36916=ORIENTED_EDGE('',*,*,#27850,.T.);
#36917=ORIENTED_EDGE('',*,*,#27851,.T.);
#36918=ORIENTED_EDGE('',*,*,#27852,.T.);
#36919=ORIENTED_EDGE('',*,*,#27853,.T.);
#36920=ORIENTED_EDGE('',*,*,#27854,.T.);
#36921=ORIENTED_EDGE('',*,*,#27855,.T.);
#36922=ORIENTED_EDGE('',*,*,#27856,.T.);
#36923=ORIENTED_EDGE('',*,*,#27857,.T.);
#36924=ORIENTED_EDGE('',*,*,#27858,.T.);
#36925=ORIENTED_EDGE('',*,*,#27859,.T.);
#36926=ORIENTED_EDGE('',*,*,#27860,.T.);
#36927=ORIENTED_EDGE('',*,*,#27861,.T.);
#36928=ORIENTED_EDGE('',*,*,#27862,.T.);
#36929=ORIENTED_EDGE('',*,*,#27863,.T.);
#36930=ORIENTED_EDGE('',*,*,#27864,.T.);
#36931=ORIENTED_EDGE('',*,*,#27865,.T.);
#36932=ORIENTED_EDGE('',*,*,#27866,.T.);
#36933=ORIENTED_EDGE('',*,*,#27867,.T.);
#36934=ORIENTED_EDGE('',*,*,#27868,.T.);
#36935=ORIENTED_EDGE('',*,*,#27869,.T.);
#36936=ORIENTED_EDGE('',*,*,#27870,.T.);
#36937=ORIENTED_EDGE('',*,*,#27871,.T.);
#36938=ORIENTED_EDGE('',*,*,#27872,.T.);
#36939=ORIENTED_EDGE('',*,*,#27873,.T.);
#36940=ORIENTED_EDGE('',*,*,#27874,.T.);
#36941=ORIENTED_EDGE('',*,*,#27875,.T.);
#36942=ORIENTED_EDGE('',*,*,#27876,.T.);
#36943=ORIENTED_EDGE('',*,*,#27877,.T.);
#36944=ORIENTED_EDGE('',*,*,#27878,.F.);
#36945=ORIENTED_EDGE('',*,*,#27879,.T.);
#36946=ORIENTED_EDGE('',*,*,#27880,.F.);
#36947=ORIENTED_EDGE('',*,*,#27879,.F.);
#36948=ORIENTED_EDGE('',*,*,#27784,.F.);
#36949=ORIENTED_EDGE('',*,*,#27785,.F.);
#36950=ORIENTED_EDGE('',*,*,#27881,.T.);
#36951=ORIENTED_EDGE('',*,*,#27882,.F.);
#36952=ORIENTED_EDGE('',*,*,#27881,.F.);
#36953=ORIENTED_EDGE('',*,*,#27883,.T.);
#36954=ORIENTED_EDGE('',*,*,#27884,.T.);
#36955=ORIENTED_EDGE('',*,*,#27885,.F.);
#36956=ORIENTED_EDGE('',*,*,#27884,.F.);
#36957=ORIENTED_EDGE('',*,*,#27886,.T.);
#36958=ORIENTED_EDGE('',*,*,#27826,.F.);
#36959=ORIENTED_EDGE('',*,*,#27827,.F.);
#36960=ORIENTED_EDGE('',*,*,#27887,.T.);
#36961=ORIENTED_EDGE('',*,*,#27888,.F.);
#36962=ORIENTED_EDGE('',*,*,#27887,.F.);
#36963=ORIENTED_EDGE('',*,*,#27889,.T.);
#36964=ORIENTED_EDGE('',*,*,#27890,.T.);
#36965=ORIENTED_EDGE('',*,*,#27891,.F.);
#36966=ORIENTED_EDGE('',*,*,#27890,.F.);
#36967=ORIENTED_EDGE('',*,*,#27892,.T.);
#36968=ORIENTED_EDGE('',*,*,#27852,.F.);
#36969=ORIENTED_EDGE('',*,*,#27853,.F.);
#36970=ORIENTED_EDGE('',*,*,#27893,.T.);
#36971=ORIENTED_EDGE('',*,*,#27894,.F.);
#36972=ORIENTED_EDGE('',*,*,#27893,.F.);
#36973=ORIENTED_EDGE('',*,*,#27895,.T.);
#36974=ORIENTED_EDGE('',*,*,#27896,.T.);
#36975=ORIENTED_EDGE('',*,*,#27897,.F.);
#36976=ORIENTED_EDGE('',*,*,#27896,.F.);
#36977=ORIENTED_EDGE('',*,*,#27898,.T.);
#36978=ORIENTED_EDGE('',*,*,#27766,.F.);
#36979=ORIENTED_EDGE('',*,*,#27767,.F.);
#36980=ORIENTED_EDGE('',*,*,#27899,.T.);
#36981=ORIENTED_EDGE('',*,*,#27900,.F.);
#36982=ORIENTED_EDGE('',*,*,#27899,.F.);
#36983=ORIENTED_EDGE('',*,*,#27901,.T.);
#36984=ORIENTED_EDGE('',*,*,#27902,.T.);
#36985=ORIENTED_EDGE('',*,*,#27903,.F.);
#36986=ORIENTED_EDGE('',*,*,#27902,.F.);
#36987=ORIENTED_EDGE('',*,*,#27904,.T.);
#36988=ORIENTED_EDGE('',*,*,#27796,.F.);
#36989=ORIENTED_EDGE('',*,*,#27797,.F.);
#36990=ORIENTED_EDGE('',*,*,#27905,.T.);
#36991=ORIENTED_EDGE('',*,*,#27906,.F.);
#36992=ORIENTED_EDGE('',*,*,#27905,.F.);
#36993=ORIENTED_EDGE('',*,*,#27907,.T.);
#36994=ORIENTED_EDGE('',*,*,#27908,.T.);
#36995=ORIENTED_EDGE('',*,*,#27909,.F.);
#36996=ORIENTED_EDGE('',*,*,#27908,.F.);
#36997=ORIENTED_EDGE('',*,*,#27910,.T.);
#36998=ORIENTED_EDGE('',*,*,#27786,.F.);
#36999=ORIENTED_EDGE('',*,*,#27787,.F.);
#37000=ORIENTED_EDGE('',*,*,#27911,.T.);
#37001=ORIENTED_EDGE('',*,*,#27912,.F.);
#37002=ORIENTED_EDGE('',*,*,#27911,.F.);
#37003=ORIENTED_EDGE('',*,*,#27913,.T.);
#37004=ORIENTED_EDGE('',*,*,#27914,.T.);
#37005=ORIENTED_EDGE('',*,*,#27915,.F.);
#37006=ORIENTED_EDGE('',*,*,#27914,.F.);
#37007=ORIENTED_EDGE('',*,*,#27916,.T.);
#37008=ORIENTED_EDGE('',*,*,#27828,.F.);
#37009=ORIENTED_EDGE('',*,*,#27829,.F.);
#37010=ORIENTED_EDGE('',*,*,#27917,.T.);
#37011=ORIENTED_EDGE('',*,*,#27918,.F.);
#37012=ORIENTED_EDGE('',*,*,#27917,.F.);
#37013=ORIENTED_EDGE('',*,*,#27919,.T.);
#37014=ORIENTED_EDGE('',*,*,#27920,.T.);
#37015=ORIENTED_EDGE('',*,*,#27921,.F.);
#37016=ORIENTED_EDGE('',*,*,#27920,.F.);
#37017=ORIENTED_EDGE('',*,*,#27922,.T.);
#37018=ORIENTED_EDGE('',*,*,#27776,.F.);
#37019=ORIENTED_EDGE('',*,*,#27777,.F.);
#37020=ORIENTED_EDGE('',*,*,#27923,.T.);
#37021=ORIENTED_EDGE('',*,*,#27924,.F.);
#37022=ORIENTED_EDGE('',*,*,#27923,.F.);
#37023=ORIENTED_EDGE('',*,*,#27925,.T.);
#37024=ORIENTED_EDGE('',*,*,#27926,.T.);
#37025=ORIENTED_EDGE('',*,*,#27927,.F.);
#37026=ORIENTED_EDGE('',*,*,#27926,.F.);
#37027=ORIENTED_EDGE('',*,*,#27928,.T.);
#37028=ORIENTED_EDGE('',*,*,#27764,.F.);
#37029=ORIENTED_EDGE('',*,*,#27765,.F.);
#37030=ORIENTED_EDGE('',*,*,#27929,.T.);
#37031=ORIENTED_EDGE('',*,*,#27930,.F.);
#37032=ORIENTED_EDGE('',*,*,#27929,.F.);
#37033=ORIENTED_EDGE('',*,*,#27931,.T.);
#37034=ORIENTED_EDGE('',*,*,#27932,.T.);
#37035=ORIENTED_EDGE('',*,*,#27933,.F.);
#37036=ORIENTED_EDGE('',*,*,#27932,.F.);
#37037=ORIENTED_EDGE('',*,*,#27934,.T.);
#37038=ORIENTED_EDGE('',*,*,#27794,.F.);
#37039=ORIENTED_EDGE('',*,*,#27795,.F.);
#37040=ORIENTED_EDGE('',*,*,#27935,.T.);
#37041=ORIENTED_EDGE('',*,*,#27936,.F.);
#37042=ORIENTED_EDGE('',*,*,#27935,.F.);
#37043=ORIENTED_EDGE('',*,*,#27937,.T.);
#37044=ORIENTED_EDGE('',*,*,#27938,.T.);
#37045=ORIENTED_EDGE('',*,*,#27939,.F.);
#37046=ORIENTED_EDGE('',*,*,#27938,.F.);
#37047=ORIENTED_EDGE('',*,*,#27940,.T.);
#37048=ORIENTED_EDGE('',*,*,#27788,.F.);
#37049=ORIENTED_EDGE('',*,*,#27789,.F.);
#37050=ORIENTED_EDGE('',*,*,#27941,.T.);
#37051=ORIENTED_EDGE('',*,*,#27942,.F.);
#37052=ORIENTED_EDGE('',*,*,#27941,.F.);
#37053=ORIENTED_EDGE('',*,*,#27943,.T.);
#37054=ORIENTED_EDGE('',*,*,#27944,.T.);
#37055=ORIENTED_EDGE('',*,*,#27945,.F.);
#37056=ORIENTED_EDGE('',*,*,#27944,.F.);
#37057=ORIENTED_EDGE('',*,*,#27946,.T.);
#37058=ORIENTED_EDGE('',*,*,#27768,.F.);
#37059=ORIENTED_EDGE('',*,*,#27769,.F.);
#37060=ORIENTED_EDGE('',*,*,#27947,.T.);
#37061=ORIENTED_EDGE('',*,*,#27948,.F.);
#37062=ORIENTED_EDGE('',*,*,#27947,.F.);
#37063=ORIENTED_EDGE('',*,*,#27949,.T.);
#37064=ORIENTED_EDGE('',*,*,#27950,.T.);
#37065=ORIENTED_EDGE('',*,*,#27951,.F.);
#37066=ORIENTED_EDGE('',*,*,#27950,.F.);
#37067=ORIENTED_EDGE('',*,*,#27952,.T.);
#37068=ORIENTED_EDGE('',*,*,#27778,.F.);
#37069=ORIENTED_EDGE('',*,*,#27779,.F.);
#37070=ORIENTED_EDGE('',*,*,#27953,.T.);
#37071=ORIENTED_EDGE('',*,*,#27954,.F.);
#37072=ORIENTED_EDGE('',*,*,#27953,.F.);
#37073=ORIENTED_EDGE('',*,*,#27955,.T.);
#37074=ORIENTED_EDGE('',*,*,#27956,.T.);
#37075=ORIENTED_EDGE('',*,*,#27957,.F.);
#37076=ORIENTED_EDGE('',*,*,#27956,.F.);
#37077=ORIENTED_EDGE('',*,*,#27958,.T.);
#37078=ORIENTED_EDGE('',*,*,#27762,.F.);
#37079=ORIENTED_EDGE('',*,*,#27763,.F.);
#37080=ORIENTED_EDGE('',*,*,#27959,.T.);
#37081=ORIENTED_EDGE('',*,*,#27960,.F.);
#37082=ORIENTED_EDGE('',*,*,#27959,.F.);
#37083=ORIENTED_EDGE('',*,*,#27961,.T.);
#37084=ORIENTED_EDGE('',*,*,#27962,.T.);
#37085=ORIENTED_EDGE('',*,*,#27963,.F.);
#37086=ORIENTED_EDGE('',*,*,#27962,.F.);
#37087=ORIENTED_EDGE('',*,*,#27964,.T.);
#37088=ORIENTED_EDGE('',*,*,#27792,.F.);
#37089=ORIENTED_EDGE('',*,*,#27793,.F.);
#37090=ORIENTED_EDGE('',*,*,#27965,.T.);
#37091=ORIENTED_EDGE('',*,*,#27966,.F.);
#37092=ORIENTED_EDGE('',*,*,#27965,.F.);
#37093=ORIENTED_EDGE('',*,*,#27967,.T.);
#37094=ORIENTED_EDGE('',*,*,#27968,.T.);
#37095=ORIENTED_EDGE('',*,*,#27969,.F.);
#37096=ORIENTED_EDGE('',*,*,#27968,.F.);
#37097=ORIENTED_EDGE('',*,*,#27970,.T.);
#37098=ORIENTED_EDGE('',*,*,#27812,.F.);
#37099=ORIENTED_EDGE('',*,*,#27813,.F.);
#37100=ORIENTED_EDGE('',*,*,#27971,.T.);
#37101=ORIENTED_EDGE('',*,*,#27972,.F.);
#37102=ORIENTED_EDGE('',*,*,#27971,.F.);
#37103=ORIENTED_EDGE('',*,*,#27973,.T.);
#37104=ORIENTED_EDGE('',*,*,#27974,.T.);
#37105=ORIENTED_EDGE('',*,*,#27975,.F.);
#37106=ORIENTED_EDGE('',*,*,#27974,.F.);
#37107=ORIENTED_EDGE('',*,*,#27976,.T.);
#37108=ORIENTED_EDGE('',*,*,#27770,.F.);
#37109=ORIENTED_EDGE('',*,*,#27771,.F.);
#37110=ORIENTED_EDGE('',*,*,#27977,.T.);
#37111=ORIENTED_EDGE('',*,*,#27978,.F.);
#37112=ORIENTED_EDGE('',*,*,#27977,.F.);
#37113=ORIENTED_EDGE('',*,*,#27979,.T.);
#37114=ORIENTED_EDGE('',*,*,#27980,.T.);
#37115=ORIENTED_EDGE('',*,*,#27981,.F.);
#37116=ORIENTED_EDGE('',*,*,#27980,.F.);
#37117=ORIENTED_EDGE('',*,*,#27982,.T.);
#37118=ORIENTED_EDGE('',*,*,#27780,.F.);
#37119=ORIENTED_EDGE('',*,*,#27781,.F.);
#37120=ORIENTED_EDGE('',*,*,#27983,.T.);
#37121=ORIENTED_EDGE('',*,*,#27984,.F.);
#37122=ORIENTED_EDGE('',*,*,#27983,.F.);
#37123=ORIENTED_EDGE('',*,*,#27985,.T.);
#37124=ORIENTED_EDGE('',*,*,#27986,.T.);
#37125=ORIENTED_EDGE('',*,*,#27987,.F.);
#37126=ORIENTED_EDGE('',*,*,#27986,.F.);
#37127=ORIENTED_EDGE('',*,*,#27988,.T.);
#37128=ORIENTED_EDGE('',*,*,#27760,.F.);
#37129=ORIENTED_EDGE('',*,*,#27761,.F.);
#37130=ORIENTED_EDGE('',*,*,#27989,.T.);
#37131=ORIENTED_EDGE('',*,*,#27990,.F.);
#37132=ORIENTED_EDGE('',*,*,#27989,.F.);
#37133=ORIENTED_EDGE('',*,*,#27991,.T.);
#37134=ORIENTED_EDGE('',*,*,#27992,.T.);
#37135=ORIENTED_EDGE('',*,*,#27993,.F.);
#37136=ORIENTED_EDGE('',*,*,#27992,.F.);
#37137=ORIENTED_EDGE('',*,*,#27994,.T.);
#37138=ORIENTED_EDGE('',*,*,#27814,.F.);
#37139=ORIENTED_EDGE('',*,*,#27815,.F.);
#37140=ORIENTED_EDGE('',*,*,#27995,.T.);
#37141=ORIENTED_EDGE('',*,*,#27996,.F.);
#37142=ORIENTED_EDGE('',*,*,#27995,.F.);
#37143=ORIENTED_EDGE('',*,*,#27997,.T.);
#37144=ORIENTED_EDGE('',*,*,#27998,.T.);
#37145=ORIENTED_EDGE('',*,*,#27999,.F.);
#37146=ORIENTED_EDGE('',*,*,#27998,.F.);
#37147=ORIENTED_EDGE('',*,*,#28000,.T.);
#37148=ORIENTED_EDGE('',*,*,#27810,.F.);
#37149=ORIENTED_EDGE('',*,*,#27811,.F.);
#37150=ORIENTED_EDGE('',*,*,#28001,.T.);
#37151=ORIENTED_EDGE('',*,*,#28002,.F.);
#37152=ORIENTED_EDGE('',*,*,#28001,.F.);
#37153=ORIENTED_EDGE('',*,*,#28003,.T.);
#37154=ORIENTED_EDGE('',*,*,#28004,.T.);
#37155=ORIENTED_EDGE('',*,*,#28005,.F.);
#37156=ORIENTED_EDGE('',*,*,#28004,.F.);
#37157=ORIENTED_EDGE('',*,*,#28006,.T.);
#37158=ORIENTED_EDGE('',*,*,#27772,.F.);
#37159=ORIENTED_EDGE('',*,*,#27773,.F.);
#37160=ORIENTED_EDGE('',*,*,#28007,.T.);
#37161=ORIENTED_EDGE('',*,*,#28008,.F.);
#37162=ORIENTED_EDGE('',*,*,#28007,.F.);
#37163=ORIENTED_EDGE('',*,*,#28009,.T.);
#37164=ORIENTED_EDGE('',*,*,#28010,.T.);
#37165=ORIENTED_EDGE('',*,*,#28011,.F.);
#37166=ORIENTED_EDGE('',*,*,#28010,.F.);
#37167=ORIENTED_EDGE('',*,*,#28012,.T.);
#37168=ORIENTED_EDGE('',*,*,#27758,.F.);
#37169=ORIENTED_EDGE('',*,*,#27759,.F.);
#37170=ORIENTED_EDGE('',*,*,#28013,.T.);
#37171=ORIENTED_EDGE('',*,*,#28014,.F.);
#37172=ORIENTED_EDGE('',*,*,#28013,.F.);
#37173=ORIENTED_EDGE('',*,*,#28015,.T.);
#37174=ORIENTED_EDGE('',*,*,#28016,.T.);
#37175=ORIENTED_EDGE('',*,*,#28017,.F.);
#37176=ORIENTED_EDGE('',*,*,#28016,.F.);
#37177=ORIENTED_EDGE('',*,*,#28018,.T.);
#37178=ORIENTED_EDGE('',*,*,#27802,.F.);
#37179=ORIENTED_EDGE('',*,*,#27803,.F.);
#37180=ORIENTED_EDGE('',*,*,#28019,.T.);
#37181=ORIENTED_EDGE('',*,*,#28020,.F.);
#37182=ORIENTED_EDGE('',*,*,#28019,.F.);
#37183=ORIENTED_EDGE('',*,*,#28021,.T.);
#37184=ORIENTED_EDGE('',*,*,#28022,.T.);
#37185=ORIENTED_EDGE('',*,*,#28023,.F.);
#37186=ORIENTED_EDGE('',*,*,#28022,.F.);
#37187=ORIENTED_EDGE('',*,*,#28024,.T.);
#37188=ORIENTED_EDGE('',*,*,#27816,.F.);
#37189=ORIENTED_EDGE('',*,*,#27817,.F.);
#37190=ORIENTED_EDGE('',*,*,#28025,.T.);
#37191=ORIENTED_EDGE('',*,*,#28026,.F.);
#37192=ORIENTED_EDGE('',*,*,#28025,.F.);
#37193=ORIENTED_EDGE('',*,*,#28027,.T.);
#37194=ORIENTED_EDGE('',*,*,#28028,.T.);
#37195=ORIENTED_EDGE('',*,*,#28029,.F.);
#37196=ORIENTED_EDGE('',*,*,#28028,.F.);
#37197=ORIENTED_EDGE('',*,*,#28030,.T.);
#37198=ORIENTED_EDGE('',*,*,#27808,.F.);
#37199=ORIENTED_EDGE('',*,*,#27809,.F.);
#37200=ORIENTED_EDGE('',*,*,#28031,.T.);
#37201=ORIENTED_EDGE('',*,*,#28032,.F.);
#37202=ORIENTED_EDGE('',*,*,#28031,.F.);
#37203=ORIENTED_EDGE('',*,*,#28033,.T.);
#37204=ORIENTED_EDGE('',*,*,#28034,.T.);
#37205=ORIENTED_EDGE('',*,*,#28035,.F.);
#37206=ORIENTED_EDGE('',*,*,#28034,.F.);
#37207=ORIENTED_EDGE('',*,*,#28036,.T.);
#37208=ORIENTED_EDGE('',*,*,#27774,.F.);
#37209=ORIENTED_EDGE('',*,*,#27775,.F.);
#37210=ORIENTED_EDGE('',*,*,#28037,.T.);
#37211=ORIENTED_EDGE('',*,*,#28038,.F.);
#37212=ORIENTED_EDGE('',*,*,#28037,.F.);
#37213=ORIENTED_EDGE('',*,*,#28039,.T.);
#37214=ORIENTED_EDGE('',*,*,#28040,.T.);
#37215=ORIENTED_EDGE('',*,*,#28041,.F.);
#37216=ORIENTED_EDGE('',*,*,#28040,.F.);
#37217=ORIENTED_EDGE('',*,*,#28042,.T.);
#37218=ORIENTED_EDGE('',*,*,#27804,.F.);
#37219=ORIENTED_EDGE('',*,*,#27805,.F.);
#37220=ORIENTED_EDGE('',*,*,#28043,.T.);
#37221=ORIENTED_EDGE('',*,*,#28044,.F.);
#37222=ORIENTED_EDGE('',*,*,#28045,.F.);
#37223=ORIENTED_EDGE('',*,*,#28043,.F.);
#37224=ORIENTED_EDGE('',*,*,#28046,.T.);
#37225=ORIENTED_EDGE('',*,*,#28047,.T.);
#37226=ORIENTED_EDGE('',*,*,#28048,.F.);
#37227=ORIENTED_EDGE('',*,*,#28047,.F.);
#37228=ORIENTED_EDGE('',*,*,#28049,.T.);
#37229=ORIENTED_EDGE('',*,*,#27800,.F.);
#37230=ORIENTED_EDGE('',*,*,#27801,.F.);
#37231=ORIENTED_EDGE('',*,*,#28050,.T.);
#37232=ORIENTED_EDGE('',*,*,#28051,.F.);
#37233=ORIENTED_EDGE('',*,*,#28050,.F.);
#37234=ORIENTED_EDGE('',*,*,#28052,.T.);
#37235=ORIENTED_EDGE('',*,*,#28053,.T.);
#37236=ORIENTED_EDGE('',*,*,#28054,.F.);
#37237=ORIENTED_EDGE('',*,*,#28053,.F.);
#37238=ORIENTED_EDGE('',*,*,#28055,.T.);
#37239=ORIENTED_EDGE('',*,*,#27818,.F.);
#37240=ORIENTED_EDGE('',*,*,#27819,.F.);
#37241=ORIENTED_EDGE('',*,*,#28056,.T.);
#37242=ORIENTED_EDGE('',*,*,#28057,.F.);
#37243=ORIENTED_EDGE('',*,*,#28056,.F.);
#37244=ORIENTED_EDGE('',*,*,#28058,.T.);
#37245=ORIENTED_EDGE('',*,*,#28059,.T.);
#37246=ORIENTED_EDGE('',*,*,#28060,.F.);
#37247=ORIENTED_EDGE('',*,*,#28059,.F.);
#37248=ORIENTED_EDGE('',*,*,#28061,.T.);
#37249=ORIENTED_EDGE('',*,*,#27806,.F.);
#37250=ORIENTED_EDGE('',*,*,#27807,.F.);
#37251=ORIENTED_EDGE('',*,*,#28062,.T.);
#37252=ORIENTED_EDGE('',*,*,#28063,.F.);
#37253=ORIENTED_EDGE('',*,*,#28062,.F.);
#37254=ORIENTED_EDGE('',*,*,#28064,.T.);
#37255=ORIENTED_EDGE('',*,*,#28065,.T.);
#37256=ORIENTED_EDGE('',*,*,#28066,.F.);
#37257=ORIENTED_EDGE('',*,*,#28065,.F.);
#37258=ORIENTED_EDGE('',*,*,#28067,.T.);
#37259=ORIENTED_EDGE('',*,*,#28068,.F.);
#37260=ORIENTED_EDGE('',*,*,#28069,.T.);
#37261=ORIENTED_EDGE('',*,*,#28070,.F.);
#37262=ORIENTED_EDGE('',*,*,#28069,.F.);
#37263=ORIENTED_EDGE('',*,*,#28071,.T.);
#37264=ORIENTED_EDGE('',*,*,#28072,.T.);
#37265=ORIENTED_EDGE('',*,*,#28073,.F.);
#37266=ORIENTED_EDGE('',*,*,#28072,.F.);
#37267=ORIENTED_EDGE('',*,*,#28074,.T.);
#37268=ORIENTED_EDGE('',*,*,#28075,.F.);
#37269=ORIENTED_EDGE('',*,*,#28076,.T.);
#37270=ORIENTED_EDGE('',*,*,#28077,.F.);
#37271=ORIENTED_EDGE('',*,*,#28076,.F.);
#37272=ORIENTED_EDGE('',*,*,#28078,.T.);
#37273=ORIENTED_EDGE('',*,*,#28079,.T.);
#37274=ORIENTED_EDGE('',*,*,#28080,.F.);
#37275=ORIENTED_EDGE('',*,*,#28079,.F.);
#37276=ORIENTED_EDGE('',*,*,#28081,.T.);
#37277=ORIENTED_EDGE('',*,*,#27798,.F.);
#37278=ORIENTED_EDGE('',*,*,#27799,.F.);
#37279=ORIENTED_EDGE('',*,*,#28082,.T.);
#37280=ORIENTED_EDGE('',*,*,#28083,.F.);
#37281=ORIENTED_EDGE('',*,*,#28082,.F.);
#37282=ORIENTED_EDGE('',*,*,#28084,.T.);
#37283=ORIENTED_EDGE('',*,*,#28085,.T.);
#37284=ORIENTED_EDGE('',*,*,#28086,.F.);
#37285=ORIENTED_EDGE('',*,*,#28085,.F.);
#37286=ORIENTED_EDGE('',*,*,#28087,.T.);
#37287=ORIENTED_EDGE('',*,*,#27820,.F.);
#37288=ORIENTED_EDGE('',*,*,#27821,.F.);
#37289=ORIENTED_EDGE('',*,*,#28088,.T.);
#37290=ORIENTED_EDGE('',*,*,#28089,.F.);
#37291=ORIENTED_EDGE('',*,*,#28088,.F.);
#37292=ORIENTED_EDGE('',*,*,#28090,.T.);
#37293=ORIENTED_EDGE('',*,*,#28091,.T.);
#37294=ORIENTED_EDGE('',*,*,#28092,.F.);
#37295=ORIENTED_EDGE('',*,*,#28091,.F.);
#37296=ORIENTED_EDGE('',*,*,#28093,.T.);
#37297=ORIENTED_EDGE('',*,*,#28094,.F.);
#37298=ORIENTED_EDGE('',*,*,#28095,.T.);
#37299=ORIENTED_EDGE('',*,*,#28096,.F.);
#37300=ORIENTED_EDGE('',*,*,#28095,.F.);
#37301=ORIENTED_EDGE('',*,*,#28097,.T.);
#37302=ORIENTED_EDGE('',*,*,#28098,.T.);
#37303=ORIENTED_EDGE('',*,*,#28099,.F.);
#37304=ORIENTED_EDGE('',*,*,#28098,.F.);
#37305=ORIENTED_EDGE('',*,*,#28100,.T.);
#37306=ORIENTED_EDGE('',*,*,#28101,.F.);
#37307=ORIENTED_EDGE('',*,*,#28102,.T.);
#37308=ORIENTED_EDGE('',*,*,#28103,.F.);
#37309=ORIENTED_EDGE('',*,*,#28102,.F.);
#37310=ORIENTED_EDGE('',*,*,#28104,.T.);
#37311=ORIENTED_EDGE('',*,*,#28105,.T.);
#37312=ORIENTED_EDGE('',*,*,#28106,.F.);
#37313=ORIENTED_EDGE('',*,*,#28105,.F.);
#37314=ORIENTED_EDGE('',*,*,#28107,.T.);
#37315=ORIENTED_EDGE('',*,*,#28108,.F.);
#37316=ORIENTED_EDGE('',*,*,#28109,.T.);
#37317=ORIENTED_EDGE('',*,*,#28110,.F.);
#37318=ORIENTED_EDGE('',*,*,#28109,.F.);
#37319=ORIENTED_EDGE('',*,*,#28111,.T.);
#37320=ORIENTED_EDGE('',*,*,#28112,.T.);
#37321=ORIENTED_EDGE('',*,*,#28113,.F.);
#37322=ORIENTED_EDGE('',*,*,#28112,.F.);
#37323=ORIENTED_EDGE('',*,*,#28114,.T.);
#37324=ORIENTED_EDGE('',*,*,#28115,.F.);
#37325=ORIENTED_EDGE('',*,*,#28116,.T.);
#37326=ORIENTED_EDGE('',*,*,#28117,.F.);
#37327=ORIENTED_EDGE('',*,*,#28116,.F.);
#37328=ORIENTED_EDGE('',*,*,#28118,.T.);
#37329=ORIENTED_EDGE('',*,*,#28119,.T.);
#37330=ORIENTED_EDGE('',*,*,#28120,.F.);
#37331=ORIENTED_EDGE('',*,*,#28119,.F.);
#37332=ORIENTED_EDGE('',*,*,#28121,.T.);
#37333=ORIENTED_EDGE('',*,*,#28122,.F.);
#37334=ORIENTED_EDGE('',*,*,#28123,.T.);
#37335=ORIENTED_EDGE('',*,*,#28124,.F.);
#37336=ORIENTED_EDGE('',*,*,#28123,.F.);
#37337=ORIENTED_EDGE('',*,*,#28125,.T.);
#37338=ORIENTED_EDGE('',*,*,#28126,.T.);
#37339=ORIENTED_EDGE('',*,*,#28127,.F.);
#37340=ORIENTED_EDGE('',*,*,#28126,.F.);
#37341=ORIENTED_EDGE('',*,*,#28128,.T.);
#37342=ORIENTED_EDGE('',*,*,#28129,.F.);
#37343=ORIENTED_EDGE('',*,*,#28130,.T.);
#37344=ORIENTED_EDGE('',*,*,#28131,.F.);
#37345=ORIENTED_EDGE('',*,*,#28130,.F.);
#37346=ORIENTED_EDGE('',*,*,#28132,.T.);
#37347=ORIENTED_EDGE('',*,*,#28133,.T.);
#37348=ORIENTED_EDGE('',*,*,#28134,.F.);
#37349=ORIENTED_EDGE('',*,*,#28133,.F.);
#37350=ORIENTED_EDGE('',*,*,#28135,.T.);
#37351=ORIENTED_EDGE('',*,*,#28136,.F.);
#37352=ORIENTED_EDGE('',*,*,#28137,.T.);
#37353=ORIENTED_EDGE('',*,*,#28138,.F.);
#37354=ORIENTED_EDGE('',*,*,#28137,.F.);
#37355=ORIENTED_EDGE('',*,*,#28139,.T.);
#37356=ORIENTED_EDGE('',*,*,#28140,.T.);
#37357=ORIENTED_EDGE('',*,*,#28141,.F.);
#37358=ORIENTED_EDGE('',*,*,#28140,.F.);
#37359=ORIENTED_EDGE('',*,*,#28142,.T.);
#37360=ORIENTED_EDGE('',*,*,#28143,.F.);
#37361=ORIENTED_EDGE('',*,*,#28144,.T.);
#37362=ORIENTED_EDGE('',*,*,#28145,.F.);
#37363=ORIENTED_EDGE('',*,*,#28144,.F.);
#37364=ORIENTED_EDGE('',*,*,#28146,.T.);
#37365=ORIENTED_EDGE('',*,*,#28147,.T.);
#37366=ORIENTED_EDGE('',*,*,#28148,.F.);
#37367=ORIENTED_EDGE('',*,*,#28147,.F.);
#37368=ORIENTED_EDGE('',*,*,#28149,.T.);
#37369=ORIENTED_EDGE('',*,*,#28150,.F.);
#37370=ORIENTED_EDGE('',*,*,#28151,.T.);
#37371=ORIENTED_EDGE('',*,*,#28152,.F.);
#37372=ORIENTED_EDGE('',*,*,#28151,.F.);
#37373=ORIENTED_EDGE('',*,*,#28153,.T.);
#37374=ORIENTED_EDGE('',*,*,#28154,.T.);
#37375=ORIENTED_EDGE('',*,*,#28155,.F.);
#37376=ORIENTED_EDGE('',*,*,#28154,.F.);
#37377=ORIENTED_EDGE('',*,*,#28156,.T.);
#37378=ORIENTED_EDGE('',*,*,#28157,.F.);
#37379=ORIENTED_EDGE('',*,*,#28158,.T.);
#37380=ORIENTED_EDGE('',*,*,#28159,.F.);
#37381=ORIENTED_EDGE('',*,*,#28158,.F.);
#37382=ORIENTED_EDGE('',*,*,#28160,.T.);
#37383=ORIENTED_EDGE('',*,*,#28161,.T.);
#37384=ORIENTED_EDGE('',*,*,#28162,.F.);
#37385=ORIENTED_EDGE('',*,*,#28161,.F.);
#37386=ORIENTED_EDGE('',*,*,#28163,.T.);
#37387=ORIENTED_EDGE('',*,*,#28164,.F.);
#37388=ORIENTED_EDGE('',*,*,#28165,.T.);
#37389=ORIENTED_EDGE('',*,*,#28166,.F.);
#37390=ORIENTED_EDGE('',*,*,#28165,.F.);
#37391=ORIENTED_EDGE('',*,*,#28167,.T.);
#37392=ORIENTED_EDGE('',*,*,#28168,.T.);
#37393=ORIENTED_EDGE('',*,*,#28169,.F.);
#37394=ORIENTED_EDGE('',*,*,#28168,.F.);
#37395=ORIENTED_EDGE('',*,*,#28170,.T.);
#37396=ORIENTED_EDGE('',*,*,#28171,.F.);
#37397=ORIENTED_EDGE('',*,*,#28172,.T.);
#37398=ORIENTED_EDGE('',*,*,#28173,.F.);
#37399=ORIENTED_EDGE('',*,*,#28172,.F.);
#37400=ORIENTED_EDGE('',*,*,#28174,.T.);
#37401=ORIENTED_EDGE('',*,*,#28175,.T.);
#37402=ORIENTED_EDGE('',*,*,#28176,.F.);
#37403=ORIENTED_EDGE('',*,*,#28175,.F.);
#37404=ORIENTED_EDGE('',*,*,#28177,.T.);
#37405=ORIENTED_EDGE('',*,*,#28178,.F.);
#37406=ORIENTED_EDGE('',*,*,#28179,.T.);
#37407=ORIENTED_EDGE('',*,*,#28180,.F.);
#37408=ORIENTED_EDGE('',*,*,#28179,.F.);
#37409=ORIENTED_EDGE('',*,*,#28181,.T.);
#37410=ORIENTED_EDGE('',*,*,#28182,.T.);
#37411=ORIENTED_EDGE('',*,*,#28183,.F.);
#37412=ORIENTED_EDGE('',*,*,#28182,.F.);
#37413=ORIENTED_EDGE('',*,*,#28184,.T.);
#37414=ORIENTED_EDGE('',*,*,#28185,.F.);
#37415=ORIENTED_EDGE('',*,*,#28186,.T.);
#37416=ORIENTED_EDGE('',*,*,#28187,.F.);
#37417=ORIENTED_EDGE('',*,*,#28186,.F.);
#37418=ORIENTED_EDGE('',*,*,#28188,.T.);
#37419=ORIENTED_EDGE('',*,*,#28189,.T.);
#37420=ORIENTED_EDGE('',*,*,#28190,.F.);
#37421=ORIENTED_EDGE('',*,*,#28189,.F.);
#37422=ORIENTED_EDGE('',*,*,#28191,.T.);
#37423=ORIENTED_EDGE('',*,*,#28192,.F.);
#37424=ORIENTED_EDGE('',*,*,#28193,.T.);
#37425=ORIENTED_EDGE('',*,*,#28194,.F.);
#37426=ORIENTED_EDGE('',*,*,#28193,.F.);
#37427=ORIENTED_EDGE('',*,*,#28195,.T.);
#37428=ORIENTED_EDGE('',*,*,#28196,.T.);
#37429=ORIENTED_EDGE('',*,*,#28197,.F.);
#37430=ORIENTED_EDGE('',*,*,#28196,.F.);
#37431=ORIENTED_EDGE('',*,*,#28198,.T.);
#37432=ORIENTED_EDGE('',*,*,#28199,.F.);
#37433=ORIENTED_EDGE('',*,*,#28200,.T.);
#37434=ORIENTED_EDGE('',*,*,#28201,.F.);
#37435=ORIENTED_EDGE('',*,*,#28200,.F.);
#37436=ORIENTED_EDGE('',*,*,#28202,.T.);
#37437=ORIENTED_EDGE('',*,*,#28203,.T.);
#37438=ORIENTED_EDGE('',*,*,#28204,.F.);
#37439=ORIENTED_EDGE('',*,*,#28203,.F.);
#37440=ORIENTED_EDGE('',*,*,#28205,.T.);
#37441=ORIENTED_EDGE('',*,*,#28206,.F.);
#37442=ORIENTED_EDGE('',*,*,#28207,.T.);
#37443=ORIENTED_EDGE('',*,*,#28208,.F.);
#37444=ORIENTED_EDGE('',*,*,#28207,.F.);
#37445=ORIENTED_EDGE('',*,*,#28209,.T.);
#37446=ORIENTED_EDGE('',*,*,#28210,.T.);
#37447=ORIENTED_EDGE('',*,*,#28211,.F.);
#37448=ORIENTED_EDGE('',*,*,#28210,.F.);
#37449=ORIENTED_EDGE('',*,*,#28212,.T.);
#37450=ORIENTED_EDGE('',*,*,#28213,.F.);
#37451=ORIENTED_EDGE('',*,*,#28214,.T.);
#37452=ORIENTED_EDGE('',*,*,#28215,.F.);
#37453=ORIENTED_EDGE('',*,*,#28214,.F.);
#37454=ORIENTED_EDGE('',*,*,#28216,.T.);
#37455=ORIENTED_EDGE('',*,*,#28217,.T.);
#37456=ORIENTED_EDGE('',*,*,#28218,.F.);
#37457=ORIENTED_EDGE('',*,*,#28217,.F.);
#37458=ORIENTED_EDGE('',*,*,#28219,.T.);
#37459=ORIENTED_EDGE('',*,*,#28220,.F.);
#37460=ORIENTED_EDGE('',*,*,#28221,.T.);
#37461=ORIENTED_EDGE('',*,*,#28222,.F.);
#37462=ORIENTED_EDGE('',*,*,#28221,.F.);
#37463=ORIENTED_EDGE('',*,*,#28223,.T.);
#37464=ORIENTED_EDGE('',*,*,#28224,.T.);
#37465=ORIENTED_EDGE('',*,*,#28225,.F.);
#37466=ORIENTED_EDGE('',*,*,#28224,.F.);
#37467=ORIENTED_EDGE('',*,*,#28226,.T.);
#37468=ORIENTED_EDGE('',*,*,#28227,.F.);
#37469=ORIENTED_EDGE('',*,*,#28228,.T.);
#37470=ORIENTED_EDGE('',*,*,#28229,.F.);
#37471=ORIENTED_EDGE('',*,*,#28228,.F.);
#37472=ORIENTED_EDGE('',*,*,#28230,.T.);
#37473=ORIENTED_EDGE('',*,*,#28231,.T.);
#37474=ORIENTED_EDGE('',*,*,#28232,.F.);
#37475=ORIENTED_EDGE('',*,*,#28231,.F.);
#37476=ORIENTED_EDGE('',*,*,#28233,.T.);
#37477=ORIENTED_EDGE('',*,*,#28234,.F.);
#37478=ORIENTED_EDGE('',*,*,#28235,.T.);
#37479=ORIENTED_EDGE('',*,*,#28236,.F.);
#37480=ORIENTED_EDGE('',*,*,#28235,.F.);
#37481=ORIENTED_EDGE('',*,*,#28237,.T.);
#37482=ORIENTED_EDGE('',*,*,#28238,.T.);
#37483=ORIENTED_EDGE('',*,*,#28239,.F.);
#37484=ORIENTED_EDGE('',*,*,#28238,.F.);
#37485=ORIENTED_EDGE('',*,*,#28240,.T.);
#37486=ORIENTED_EDGE('',*,*,#28241,.F.);
#37487=ORIENTED_EDGE('',*,*,#28242,.T.);
#37488=ORIENTED_EDGE('',*,*,#28243,.F.);
#37489=ORIENTED_EDGE('',*,*,#28242,.F.);
#37490=ORIENTED_EDGE('',*,*,#28244,.T.);
#37491=ORIENTED_EDGE('',*,*,#28245,.T.);
#37492=ORIENTED_EDGE('',*,*,#28246,.F.);
#37493=ORIENTED_EDGE('',*,*,#28245,.F.);
#37494=ORIENTED_EDGE('',*,*,#28247,.T.);
#37495=ORIENTED_EDGE('',*,*,#28248,.F.);
#37496=ORIENTED_EDGE('',*,*,#28249,.T.);
#37497=ORIENTED_EDGE('',*,*,#28250,.F.);
#37498=ORIENTED_EDGE('',*,*,#28249,.F.);
#37499=ORIENTED_EDGE('',*,*,#28251,.T.);
#37500=ORIENTED_EDGE('',*,*,#28252,.T.);
#37501=ORIENTED_EDGE('',*,*,#28253,.F.);
#37502=ORIENTED_EDGE('',*,*,#28252,.F.);
#37503=ORIENTED_EDGE('',*,*,#28254,.T.);
#37504=ORIENTED_EDGE('',*,*,#28255,.F.);
#37505=ORIENTED_EDGE('',*,*,#28256,.T.);
#37506=ORIENTED_EDGE('',*,*,#28257,.F.);
#37507=ORIENTED_EDGE('',*,*,#28256,.F.);
#37508=ORIENTED_EDGE('',*,*,#28258,.T.);
#37509=ORIENTED_EDGE('',*,*,#28259,.T.);
#37510=ORIENTED_EDGE('',*,*,#28260,.F.);
#37511=ORIENTED_EDGE('',*,*,#28259,.F.);
#37512=ORIENTED_EDGE('',*,*,#28261,.T.);
#37513=ORIENTED_EDGE('',*,*,#28262,.F.);
#37514=ORIENTED_EDGE('',*,*,#28263,.T.);
#37515=ORIENTED_EDGE('',*,*,#28264,.F.);
#37516=ORIENTED_EDGE('',*,*,#28263,.F.);
#37517=ORIENTED_EDGE('',*,*,#28265,.T.);
#37518=ORIENTED_EDGE('',*,*,#28266,.T.);
#37519=ORIENTED_EDGE('',*,*,#28267,.F.);
#37520=ORIENTED_EDGE('',*,*,#28266,.F.);
#37521=ORIENTED_EDGE('',*,*,#28268,.T.);
#37522=ORIENTED_EDGE('',*,*,#28269,.F.);
#37523=ORIENTED_EDGE('',*,*,#28270,.T.);
#37524=ORIENTED_EDGE('',*,*,#28271,.F.);
#37525=ORIENTED_EDGE('',*,*,#28270,.F.);
#37526=ORIENTED_EDGE('',*,*,#28272,.T.);
#37527=ORIENTED_EDGE('',*,*,#28273,.T.);
#37528=ORIENTED_EDGE('',*,*,#28274,.F.);
#37529=ORIENTED_EDGE('',*,*,#28273,.F.);
#37530=ORIENTED_EDGE('',*,*,#28275,.T.);
#37531=ORIENTED_EDGE('',*,*,#28276,.F.);
#37532=ORIENTED_EDGE('',*,*,#28277,.T.);
#37533=ORIENTED_EDGE('',*,*,#28278,.F.);
#37534=ORIENTED_EDGE('',*,*,#28277,.F.);
#37535=ORIENTED_EDGE('',*,*,#28279,.T.);
#37536=ORIENTED_EDGE('',*,*,#28280,.T.);
#37537=ORIENTED_EDGE('',*,*,#28281,.F.);
#37538=ORIENTED_EDGE('',*,*,#28280,.F.);
#37539=ORIENTED_EDGE('',*,*,#28282,.T.);
#37540=ORIENTED_EDGE('',*,*,#28283,.F.);
#37541=ORIENTED_EDGE('',*,*,#28284,.T.);
#37542=ORIENTED_EDGE('',*,*,#28285,.F.);
#37543=ORIENTED_EDGE('',*,*,#28284,.F.);
#37544=ORIENTED_EDGE('',*,*,#28286,.T.);
#37545=ORIENTED_EDGE('',*,*,#28287,.T.);
#37546=ORIENTED_EDGE('',*,*,#28288,.F.);
#37547=ORIENTED_EDGE('',*,*,#28287,.F.);
#37548=ORIENTED_EDGE('',*,*,#28289,.T.);
#37549=ORIENTED_EDGE('',*,*,#28290,.F.);
#37550=ORIENTED_EDGE('',*,*,#28291,.T.);
#37551=ORIENTED_EDGE('',*,*,#28292,.F.);
#37552=ORIENTED_EDGE('',*,*,#28293,.F.);
#37553=ORIENTED_EDGE('',*,*,#28291,.F.);
#37554=ORIENTED_EDGE('',*,*,#28294,.T.);
#37555=ORIENTED_EDGE('',*,*,#28295,.T.);
#37556=ORIENTED_EDGE('',*,*,#28296,.F.);
#37557=ORIENTED_EDGE('',*,*,#28295,.F.);
#37558=ORIENTED_EDGE('',*,*,#28297,.T.);
#37559=ORIENTED_EDGE('',*,*,#28298,.F.);
#37560=ORIENTED_EDGE('',*,*,#28299,.T.);
#37561=ORIENTED_EDGE('',*,*,#28300,.F.);
#37562=ORIENTED_EDGE('',*,*,#28299,.F.);
#37563=ORIENTED_EDGE('',*,*,#28301,.T.);
#37564=ORIENTED_EDGE('',*,*,#28302,.T.);
#37565=ORIENTED_EDGE('',*,*,#28303,.F.);
#37566=ORIENTED_EDGE('',*,*,#28302,.F.);
#37567=ORIENTED_EDGE('',*,*,#28304,.T.);
#37568=ORIENTED_EDGE('',*,*,#28305,.F.);
#37569=ORIENTED_EDGE('',*,*,#28306,.T.);
#37570=ORIENTED_EDGE('',*,*,#28307,.F.);
#37571=ORIENTED_EDGE('',*,*,#28306,.F.);
#37572=ORIENTED_EDGE('',*,*,#28308,.T.);
#37573=ORIENTED_EDGE('',*,*,#28309,.T.);
#37574=ORIENTED_EDGE('',*,*,#28310,.F.);
#37575=ORIENTED_EDGE('',*,*,#28309,.F.);
#37576=ORIENTED_EDGE('',*,*,#28311,.T.);
#37577=ORIENTED_EDGE('',*,*,#28312,.F.);
#37578=ORIENTED_EDGE('',*,*,#28313,.T.);
#37579=ORIENTED_EDGE('',*,*,#28314,.F.);
#37580=ORIENTED_EDGE('',*,*,#28313,.F.);
#37581=ORIENTED_EDGE('',*,*,#28315,.T.);
#37582=ORIENTED_EDGE('',*,*,#28316,.T.);
#37583=ORIENTED_EDGE('',*,*,#28317,.F.);
#37584=ORIENTED_EDGE('',*,*,#28316,.F.);
#37585=ORIENTED_EDGE('',*,*,#28318,.T.);
#37586=ORIENTED_EDGE('',*,*,#28319,.F.);
#37587=ORIENTED_EDGE('',*,*,#28320,.T.);
#37588=ORIENTED_EDGE('',*,*,#28321,.F.);
#37589=ORIENTED_EDGE('',*,*,#28322,.F.);
#37590=ORIENTED_EDGE('',*,*,#28320,.F.);
#37591=ORIENTED_EDGE('',*,*,#28323,.T.);
#37592=ORIENTED_EDGE('',*,*,#28324,.T.);
#37593=ORIENTED_EDGE('',*,*,#28325,.F.);
#37594=ORIENTED_EDGE('',*,*,#28324,.F.);
#37595=ORIENTED_EDGE('',*,*,#28326,.T.);
#37596=ORIENTED_EDGE('',*,*,#28327,.F.);
#37597=ORIENTED_EDGE('',*,*,#28328,.T.);
#37598=ORIENTED_EDGE('',*,*,#28329,.F.);
#37599=ORIENTED_EDGE('',*,*,#28328,.F.);
#37600=ORIENTED_EDGE('',*,*,#28330,.T.);
#37601=ORIENTED_EDGE('',*,*,#28331,.T.);
#37602=ORIENTED_EDGE('',*,*,#28332,.F.);
#37603=ORIENTED_EDGE('',*,*,#28331,.F.);
#37604=ORIENTED_EDGE('',*,*,#28333,.T.);
#37605=ORIENTED_EDGE('',*,*,#28334,.F.);
#37606=ORIENTED_EDGE('',*,*,#28335,.T.);
#37607=ORIENTED_EDGE('',*,*,#28336,.F.);
#37608=ORIENTED_EDGE('',*,*,#28335,.F.);
#37609=ORIENTED_EDGE('',*,*,#28337,.T.);
#37610=ORIENTED_EDGE('',*,*,#28338,.T.);
#37611=ORIENTED_EDGE('',*,*,#28339,.F.);
#37612=ORIENTED_EDGE('',*,*,#28338,.F.);
#37613=ORIENTED_EDGE('',*,*,#28340,.T.);
#37614=ORIENTED_EDGE('',*,*,#28341,.F.);
#37615=ORIENTED_EDGE('',*,*,#28342,.T.);
#37616=ORIENTED_EDGE('',*,*,#28343,.F.);
#37617=ORIENTED_EDGE('',*,*,#28342,.F.);
#37618=ORIENTED_EDGE('',*,*,#28344,.T.);
#37619=ORIENTED_EDGE('',*,*,#28345,.T.);
#37620=ORIENTED_EDGE('',*,*,#28346,.F.);
#37621=ORIENTED_EDGE('',*,*,#28345,.F.);
#37622=ORIENTED_EDGE('',*,*,#28347,.T.);
#37623=ORIENTED_EDGE('',*,*,#28348,.F.);
#37624=ORIENTED_EDGE('',*,*,#28349,.T.);
#37625=ORIENTED_EDGE('',*,*,#28350,.F.);
#37626=ORIENTED_EDGE('',*,*,#28351,.F.);
#37627=ORIENTED_EDGE('',*,*,#28349,.F.);
#37628=ORIENTED_EDGE('',*,*,#28352,.F.);
#37629=ORIENTED_EDGE('',*,*,#28353,.T.);
#37630=ORIENTED_EDGE('',*,*,#28354,.T.);
#37631=ORIENTED_EDGE('',*,*,#28355,.F.);
#37632=ORIENTED_EDGE('',*,*,#28354,.F.);
#37633=ORIENTED_EDGE('',*,*,#28356,.T.);
#37634=ORIENTED_EDGE('',*,*,#28357,.F.);
#37635=ORIENTED_EDGE('',*,*,#28358,.T.);
#37636=ORIENTED_EDGE('',*,*,#28359,.F.);
#37637=ORIENTED_EDGE('',*,*,#28358,.F.);
#37638=ORIENTED_EDGE('',*,*,#28360,.T.);
#37639=ORIENTED_EDGE('',*,*,#28361,.T.);
#37640=ORIENTED_EDGE('',*,*,#28362,.F.);
#37641=ORIENTED_EDGE('',*,*,#28361,.F.);
#37642=ORIENTED_EDGE('',*,*,#28363,.T.);
#37643=ORIENTED_EDGE('',*,*,#28364,.F.);
#37644=ORIENTED_EDGE('',*,*,#28365,.T.);
#37645=ORIENTED_EDGE('',*,*,#28366,.F.);
#37646=ORIENTED_EDGE('',*,*,#28365,.F.);
#37647=ORIENTED_EDGE('',*,*,#28367,.T.);
#37648=ORIENTED_EDGE('',*,*,#28368,.T.);
#37649=ORIENTED_EDGE('',*,*,#28369,.F.);
#37650=ORIENTED_EDGE('',*,*,#28368,.F.);
#37651=ORIENTED_EDGE('',*,*,#28370,.T.);
#37652=ORIENTED_EDGE('',*,*,#28371,.F.);
#37653=ORIENTED_EDGE('',*,*,#28372,.T.);
#37654=ORIENTED_EDGE('',*,*,#28373,.F.);
#37655=ORIENTED_EDGE('',*,*,#28372,.F.);
#37656=ORIENTED_EDGE('',*,*,#28374,.T.);
#37657=ORIENTED_EDGE('',*,*,#28375,.T.);
#37658=ORIENTED_EDGE('',*,*,#28376,.F.);
#37659=ORIENTED_EDGE('',*,*,#28375,.F.);
#37660=ORIENTED_EDGE('',*,*,#28377,.T.);
#37661=ORIENTED_EDGE('',*,*,#28378,.F.);
#37662=ORIENTED_EDGE('',*,*,#28379,.T.);
#37663=ORIENTED_EDGE('',*,*,#28380,.F.);
#37664=ORIENTED_EDGE('',*,*,#28379,.F.);
#37665=ORIENTED_EDGE('',*,*,#28381,.T.);
#37666=ORIENTED_EDGE('',*,*,#28382,.T.);
#37667=ORIENTED_EDGE('',*,*,#28383,.F.);
#37668=ORIENTED_EDGE('',*,*,#28382,.F.);
#37669=ORIENTED_EDGE('',*,*,#28384,.T.);
#37670=ORIENTED_EDGE('',*,*,#28385,.F.);
#37671=ORIENTED_EDGE('',*,*,#28386,.T.);
#37672=ORIENTED_EDGE('',*,*,#28387,.F.);
#37673=ORIENTED_EDGE('',*,*,#28386,.F.);
#37674=ORIENTED_EDGE('',*,*,#28388,.T.);
#37675=ORIENTED_EDGE('',*,*,#28389,.T.);
#37676=ORIENTED_EDGE('',*,*,#28390,.F.);
#37677=ORIENTED_EDGE('',*,*,#28389,.F.);
#37678=ORIENTED_EDGE('',*,*,#28391,.T.);
#37679=ORIENTED_EDGE('',*,*,#28392,.F.);
#37680=ORIENTED_EDGE('',*,*,#28393,.T.);
#37681=ORIENTED_EDGE('',*,*,#28394,.F.);
#37682=ORIENTED_EDGE('',*,*,#28393,.F.);
#37683=ORIENTED_EDGE('',*,*,#28395,.T.);
#37684=ORIENTED_EDGE('',*,*,#28396,.T.);
#37685=ORIENTED_EDGE('',*,*,#28397,.F.);
#37686=ORIENTED_EDGE('',*,*,#28396,.F.);
#37687=ORIENTED_EDGE('',*,*,#28398,.T.);
#37688=ORIENTED_EDGE('',*,*,#28399,.F.);
#37689=ORIENTED_EDGE('',*,*,#28400,.T.);
#37690=ORIENTED_EDGE('',*,*,#28401,.F.);
#37691=ORIENTED_EDGE('',*,*,#28400,.F.);
#37692=ORIENTED_EDGE('',*,*,#28402,.T.);
#37693=ORIENTED_EDGE('',*,*,#28403,.T.);
#37694=ORIENTED_EDGE('',*,*,#28404,.F.);
#37695=ORIENTED_EDGE('',*,*,#28403,.F.);
#37696=ORIENTED_EDGE('',*,*,#28405,.T.);
#37697=ORIENTED_EDGE('',*,*,#28406,.F.);
#37698=ORIENTED_EDGE('',*,*,#28407,.T.);
#37699=ORIENTED_EDGE('',*,*,#28408,.F.);
#37700=ORIENTED_EDGE('',*,*,#28407,.F.);
#37701=ORIENTED_EDGE('',*,*,#28409,.T.);
#37702=ORIENTED_EDGE('',*,*,#28410,.T.);
#37703=ORIENTED_EDGE('',*,*,#28411,.F.);
#37704=ORIENTED_EDGE('',*,*,#28410,.F.);
#37705=ORIENTED_EDGE('',*,*,#28412,.T.);
#37706=ORIENTED_EDGE('',*,*,#28413,.F.);
#37707=ORIENTED_EDGE('',*,*,#28414,.T.);
#37708=ORIENTED_EDGE('',*,*,#28415,.F.);
#37709=ORIENTED_EDGE('',*,*,#28414,.F.);
#37710=ORIENTED_EDGE('',*,*,#28416,.T.);
#37711=ORIENTED_EDGE('',*,*,#28417,.T.);
#37712=ORIENTED_EDGE('',*,*,#28418,.F.);
#37713=ORIENTED_EDGE('',*,*,#28417,.F.);
#37714=ORIENTED_EDGE('',*,*,#28419,.T.);
#37715=ORIENTED_EDGE('',*,*,#28420,.F.);
#37716=ORIENTED_EDGE('',*,*,#28421,.T.);
#37717=ORIENTED_EDGE('',*,*,#28422,.F.);
#37718=ORIENTED_EDGE('',*,*,#28421,.F.);
#37719=ORIENTED_EDGE('',*,*,#28423,.T.);
#37720=ORIENTED_EDGE('',*,*,#28424,.T.);
#37721=ORIENTED_EDGE('',*,*,#28425,.F.);
#37722=ORIENTED_EDGE('',*,*,#28424,.F.);
#37723=ORIENTED_EDGE('',*,*,#28426,.T.);
#37724=ORIENTED_EDGE('',*,*,#28427,.F.);
#37725=ORIENTED_EDGE('',*,*,#28428,.T.);
#37726=ORIENTED_EDGE('',*,*,#28429,.F.);
#37727=ORIENTED_EDGE('',*,*,#28428,.F.);
#37728=ORIENTED_EDGE('',*,*,#28430,.T.);
#37729=ORIENTED_EDGE('',*,*,#28431,.T.);
#37730=ORIENTED_EDGE('',*,*,#28432,.F.);
#37731=ORIENTED_EDGE('',*,*,#28431,.F.);
#37732=ORIENTED_EDGE('',*,*,#28433,.T.);
#37733=ORIENTED_EDGE('',*,*,#28434,.F.);
#37734=ORIENTED_EDGE('',*,*,#28435,.T.);
#37735=ORIENTED_EDGE('',*,*,#28436,.F.);
#37736=ORIENTED_EDGE('',*,*,#28435,.F.);
#37737=ORIENTED_EDGE('',*,*,#28437,.T.);
#37738=ORIENTED_EDGE('',*,*,#28438,.T.);
#37739=ORIENTED_EDGE('',*,*,#28439,.F.);
#37740=ORIENTED_EDGE('',*,*,#28438,.F.);
#37741=ORIENTED_EDGE('',*,*,#28440,.T.);
#37742=ORIENTED_EDGE('',*,*,#28441,.F.);
#37743=ORIENTED_EDGE('',*,*,#28442,.T.);
#37744=ORIENTED_EDGE('',*,*,#28443,.F.);
#37745=ORIENTED_EDGE('',*,*,#28442,.F.);
#37746=ORIENTED_EDGE('',*,*,#28444,.T.);
#37747=ORIENTED_EDGE('',*,*,#28445,.T.);
#37748=ORIENTED_EDGE('',*,*,#28446,.F.);
#37749=ORIENTED_EDGE('',*,*,#28445,.F.);
#37750=ORIENTED_EDGE('',*,*,#28447,.T.);
#37751=ORIENTED_EDGE('',*,*,#28448,.F.);
#37752=ORIENTED_EDGE('',*,*,#28449,.T.);
#37753=ORIENTED_EDGE('',*,*,#28450,.F.);
#37754=ORIENTED_EDGE('',*,*,#28449,.F.);
#37755=ORIENTED_EDGE('',*,*,#28451,.T.);
#37756=ORIENTED_EDGE('',*,*,#28452,.T.);
#37757=ORIENTED_EDGE('',*,*,#28453,.F.);
#37758=ORIENTED_EDGE('',*,*,#28452,.F.);
#37759=ORIENTED_EDGE('',*,*,#28454,.T.);
#37760=ORIENTED_EDGE('',*,*,#28455,.F.);
#37761=ORIENTED_EDGE('',*,*,#28456,.T.);
#37762=ORIENTED_EDGE('',*,*,#28457,.F.);
#37763=ORIENTED_EDGE('',*,*,#28456,.F.);
#37764=ORIENTED_EDGE('',*,*,#28458,.T.);
#37765=ORIENTED_EDGE('',*,*,#28459,.T.);
#37766=ORIENTED_EDGE('',*,*,#28460,.F.);
#37767=ORIENTED_EDGE('',*,*,#28459,.F.);
#37768=ORIENTED_EDGE('',*,*,#28461,.T.);
#37769=ORIENTED_EDGE('',*,*,#28462,.F.);
#37770=ORIENTED_EDGE('',*,*,#28463,.T.);
#37771=ORIENTED_EDGE('',*,*,#28464,.F.);
#37772=ORIENTED_EDGE('',*,*,#28463,.F.);
#37773=ORIENTED_EDGE('',*,*,#28465,.T.);
#37774=ORIENTED_EDGE('',*,*,#28466,.T.);
#37775=ORIENTED_EDGE('',*,*,#28467,.F.);
#37776=ORIENTED_EDGE('',*,*,#28466,.F.);
#37777=ORIENTED_EDGE('',*,*,#28468,.T.);
#37778=ORIENTED_EDGE('',*,*,#28469,.F.);
#37779=ORIENTED_EDGE('',*,*,#28470,.T.);
#37780=ORIENTED_EDGE('',*,*,#28471,.F.);
#37781=ORIENTED_EDGE('',*,*,#28470,.F.);
#37782=ORIENTED_EDGE('',*,*,#28472,.T.);
#37783=ORIENTED_EDGE('',*,*,#28473,.T.);
#37784=ORIENTED_EDGE('',*,*,#28474,.F.);
#37785=ORIENTED_EDGE('',*,*,#28473,.F.);
#37786=ORIENTED_EDGE('',*,*,#28475,.T.);
#37787=ORIENTED_EDGE('',*,*,#28476,.F.);
#37788=ORIENTED_EDGE('',*,*,#28477,.T.);
#37789=ORIENTED_EDGE('',*,*,#28478,.F.);
#37790=ORIENTED_EDGE('',*,*,#28477,.F.);
#37791=ORIENTED_EDGE('',*,*,#28479,.T.);
#37792=ORIENTED_EDGE('',*,*,#28480,.T.);
#37793=ORIENTED_EDGE('',*,*,#28481,.F.);
#37794=ORIENTED_EDGE('',*,*,#28480,.F.);
#37795=ORIENTED_EDGE('',*,*,#28482,.T.);
#37796=ORIENTED_EDGE('',*,*,#28483,.F.);
#37797=ORIENTED_EDGE('',*,*,#28484,.T.);
#37798=ORIENTED_EDGE('',*,*,#28485,.F.);
#37799=ORIENTED_EDGE('',*,*,#28484,.F.);
#37800=ORIENTED_EDGE('',*,*,#28486,.T.);
#37801=ORIENTED_EDGE('',*,*,#28487,.T.);
#37802=ORIENTED_EDGE('',*,*,#28488,.F.);
#37803=ORIENTED_EDGE('',*,*,#28487,.F.);
#37804=ORIENTED_EDGE('',*,*,#28489,.T.);
#37805=ORIENTED_EDGE('',*,*,#27860,.F.);
#37806=ORIENTED_EDGE('',*,*,#27861,.F.);
#37807=ORIENTED_EDGE('',*,*,#28490,.T.);
#37808=ORIENTED_EDGE('',*,*,#28491,.F.);
#37809=ORIENTED_EDGE('',*,*,#28490,.F.);
#37810=ORIENTED_EDGE('',*,*,#28492,.T.);
#37811=ORIENTED_EDGE('',*,*,#28493,.T.);
#37812=ORIENTED_EDGE('',*,*,#28494,.F.);
#37813=ORIENTED_EDGE('',*,*,#28493,.F.);
#37814=ORIENTED_EDGE('',*,*,#28495,.T.);
#37815=ORIENTED_EDGE('',*,*,#27836,.F.);
#37816=ORIENTED_EDGE('',*,*,#27837,.F.);
#37817=ORIENTED_EDGE('',*,*,#28496,.T.);
#37818=ORIENTED_EDGE('',*,*,#28497,.F.);
#37819=ORIENTED_EDGE('',*,*,#28496,.F.);
#37820=ORIENTED_EDGE('',*,*,#28498,.T.);
#37821=ORIENTED_EDGE('',*,*,#28499,.T.);
#37822=ORIENTED_EDGE('',*,*,#28500,.F.);
#37823=ORIENTED_EDGE('',*,*,#28499,.F.);
#37824=ORIENTED_EDGE('',*,*,#28501,.T.);
#37825=ORIENTED_EDGE('',*,*,#28502,.F.);
#37826=ORIENTED_EDGE('',*,*,#28503,.T.);
#37827=ORIENTED_EDGE('',*,*,#28504,.F.);
#37828=ORIENTED_EDGE('',*,*,#28503,.F.);
#37829=ORIENTED_EDGE('',*,*,#28505,.T.);
#37830=ORIENTED_EDGE('',*,*,#28506,.T.);
#37831=ORIENTED_EDGE('',*,*,#28507,.F.);
#37832=ORIENTED_EDGE('',*,*,#28506,.F.);
#37833=ORIENTED_EDGE('',*,*,#28508,.T.);
#37834=ORIENTED_EDGE('',*,*,#28509,.F.);
#37835=ORIENTED_EDGE('',*,*,#28510,.T.);
#37836=ORIENTED_EDGE('',*,*,#28511,.F.);
#37837=ORIENTED_EDGE('',*,*,#28510,.F.);
#37838=ORIENTED_EDGE('',*,*,#28512,.T.);
#37839=ORIENTED_EDGE('',*,*,#28513,.T.);
#37840=ORIENTED_EDGE('',*,*,#28514,.F.);
#37841=ORIENTED_EDGE('',*,*,#28513,.F.);
#37842=ORIENTED_EDGE('',*,*,#28515,.T.);
#37843=ORIENTED_EDGE('',*,*,#27876,.F.);
#37844=ORIENTED_EDGE('',*,*,#27877,.F.);
#37845=ORIENTED_EDGE('',*,*,#28516,.T.);
#37846=ORIENTED_EDGE('',*,*,#28517,.F.);
#37847=ORIENTED_EDGE('',*,*,#28516,.F.);
#37848=ORIENTED_EDGE('',*,*,#28518,.T.);
#37849=ORIENTED_EDGE('',*,*,#28519,.T.);
#37850=ORIENTED_EDGE('',*,*,#28520,.F.);
#37851=ORIENTED_EDGE('',*,*,#28519,.F.);
#37852=ORIENTED_EDGE('',*,*,#28521,.T.);
#37853=ORIENTED_EDGE('',*,*,#27862,.F.);
#37854=ORIENTED_EDGE('',*,*,#27863,.F.);
#37855=ORIENTED_EDGE('',*,*,#28522,.T.);
#37856=ORIENTED_EDGE('',*,*,#28523,.F.);
#37857=ORIENTED_EDGE('',*,*,#28522,.F.);
#37858=ORIENTED_EDGE('',*,*,#28524,.T.);
#37859=ORIENTED_EDGE('',*,*,#28525,.T.);
#37860=ORIENTED_EDGE('',*,*,#28526,.F.);
#37861=ORIENTED_EDGE('',*,*,#28525,.F.);
#37862=ORIENTED_EDGE('',*,*,#28527,.T.);
#37863=ORIENTED_EDGE('',*,*,#27834,.F.);
#37864=ORIENTED_EDGE('',*,*,#27835,.F.);
#37865=ORIENTED_EDGE('',*,*,#28528,.T.);
#37866=ORIENTED_EDGE('',*,*,#28529,.F.);
#37867=ORIENTED_EDGE('',*,*,#28528,.F.);
#37868=ORIENTED_EDGE('',*,*,#28530,.T.);
#37869=ORIENTED_EDGE('',*,*,#28531,.T.);
#37870=ORIENTED_EDGE('',*,*,#28532,.F.);
#37871=ORIENTED_EDGE('',*,*,#28531,.F.);
#37872=ORIENTED_EDGE('',*,*,#28533,.T.);
#37873=ORIENTED_EDGE('',*,*,#27830,.F.);
#37874=ORIENTED_EDGE('',*,*,#27831,.F.);
#37875=ORIENTED_EDGE('',*,*,#28534,.T.);
#37876=ORIENTED_EDGE('',*,*,#28535,.F.);
#37877=ORIENTED_EDGE('',*,*,#28534,.F.);
#37878=ORIENTED_EDGE('',*,*,#28536,.T.);
#37879=ORIENTED_EDGE('',*,*,#28537,.T.);
#37880=ORIENTED_EDGE('',*,*,#28538,.F.);
#37881=ORIENTED_EDGE('',*,*,#28537,.F.);
#37882=ORIENTED_EDGE('',*,*,#28539,.T.);
#37883=ORIENTED_EDGE('',*,*,#27874,.F.);
#37884=ORIENTED_EDGE('',*,*,#27875,.F.);
#37885=ORIENTED_EDGE('',*,*,#28540,.T.);
#37886=ORIENTED_EDGE('',*,*,#28541,.F.);
#37887=ORIENTED_EDGE('',*,*,#28540,.F.);
#37888=ORIENTED_EDGE('',*,*,#28542,.T.);
#37889=ORIENTED_EDGE('',*,*,#28543,.T.);
#37890=ORIENTED_EDGE('',*,*,#28544,.F.);
#37891=ORIENTED_EDGE('',*,*,#28543,.F.);
#37892=ORIENTED_EDGE('',*,*,#28545,.T.);
#37893=ORIENTED_EDGE('',*,*,#27858,.F.);
#37894=ORIENTED_EDGE('',*,*,#27859,.F.);
#37895=ORIENTED_EDGE('',*,*,#28546,.T.);
#37896=ORIENTED_EDGE('',*,*,#28547,.F.);
#37897=ORIENTED_EDGE('',*,*,#28546,.F.);
#37898=ORIENTED_EDGE('',*,*,#28548,.T.);
#37899=ORIENTED_EDGE('',*,*,#28549,.T.);
#37900=ORIENTED_EDGE('',*,*,#28550,.F.);
#37901=ORIENTED_EDGE('',*,*,#28549,.F.);
#37902=ORIENTED_EDGE('',*,*,#28551,.T.);
#37903=ORIENTED_EDGE('',*,*,#27864,.F.);
#37904=ORIENTED_EDGE('',*,*,#27865,.F.);
#37905=ORIENTED_EDGE('',*,*,#28552,.T.);
#37906=ORIENTED_EDGE('',*,*,#28553,.F.);
#37907=ORIENTED_EDGE('',*,*,#28552,.F.);
#37908=ORIENTED_EDGE('',*,*,#28554,.T.);
#37909=ORIENTED_EDGE('',*,*,#28555,.T.);
#37910=ORIENTED_EDGE('',*,*,#28556,.F.);
#37911=ORIENTED_EDGE('',*,*,#28555,.F.);
#37912=ORIENTED_EDGE('',*,*,#28557,.T.);
#37913=ORIENTED_EDGE('',*,*,#27832,.F.);
#37914=ORIENTED_EDGE('',*,*,#27833,.F.);
#37915=ORIENTED_EDGE('',*,*,#28558,.T.);
#37916=ORIENTED_EDGE('',*,*,#28559,.F.);
#37917=ORIENTED_EDGE('',*,*,#28558,.F.);
#37918=ORIENTED_EDGE('',*,*,#28560,.T.);
#37919=ORIENTED_EDGE('',*,*,#28561,.T.);
#37920=ORIENTED_EDGE('',*,*,#28562,.F.);
#37921=ORIENTED_EDGE('',*,*,#28561,.F.);
#37922=ORIENTED_EDGE('',*,*,#28563,.T.);
#37923=ORIENTED_EDGE('',*,*,#27838,.F.);
#37924=ORIENTED_EDGE('',*,*,#27839,.F.);
#37925=ORIENTED_EDGE('',*,*,#28564,.T.);
#37926=ORIENTED_EDGE('',*,*,#28565,.F.);
#37927=ORIENTED_EDGE('',*,*,#28564,.F.);
#37928=ORIENTED_EDGE('',*,*,#28566,.T.);
#37929=ORIENTED_EDGE('',*,*,#28567,.T.);
#37930=ORIENTED_EDGE('',*,*,#28568,.F.);
#37931=ORIENTED_EDGE('',*,*,#28567,.F.);
#37932=ORIENTED_EDGE('',*,*,#28569,.T.);
#37933=ORIENTED_EDGE('',*,*,#27872,.F.);
#37934=ORIENTED_EDGE('',*,*,#27873,.F.);
#37935=ORIENTED_EDGE('',*,*,#28570,.T.);
#37936=ORIENTED_EDGE('',*,*,#28571,.F.);
#37937=ORIENTED_EDGE('',*,*,#28570,.F.);
#37938=ORIENTED_EDGE('',*,*,#28572,.T.);
#37939=ORIENTED_EDGE('',*,*,#28573,.T.);
#37940=ORIENTED_EDGE('',*,*,#28574,.F.);
#37941=ORIENTED_EDGE('',*,*,#28573,.F.);
#37942=ORIENTED_EDGE('',*,*,#28575,.T.);
#37943=ORIENTED_EDGE('',*,*,#27856,.F.);
#37944=ORIENTED_EDGE('',*,*,#27857,.F.);
#37945=ORIENTED_EDGE('',*,*,#28576,.T.);
#37946=ORIENTED_EDGE('',*,*,#28577,.F.);
#37947=ORIENTED_EDGE('',*,*,#28576,.F.);
#37948=ORIENTED_EDGE('',*,*,#28578,.T.);
#37949=ORIENTED_EDGE('',*,*,#28579,.T.);
#37950=ORIENTED_EDGE('',*,*,#28580,.F.);
#37951=ORIENTED_EDGE('',*,*,#28579,.F.);
#37952=ORIENTED_EDGE('',*,*,#28581,.T.);
#37953=ORIENTED_EDGE('',*,*,#27866,.F.);
#37954=ORIENTED_EDGE('',*,*,#27867,.F.);
#37955=ORIENTED_EDGE('',*,*,#28582,.T.);
#37956=ORIENTED_EDGE('',*,*,#28583,.F.);
#37957=ORIENTED_EDGE('',*,*,#28582,.F.);
#37958=ORIENTED_EDGE('',*,*,#28584,.T.);
#37959=ORIENTED_EDGE('',*,*,#28585,.T.);
#37960=ORIENTED_EDGE('',*,*,#28586,.F.);
#37961=ORIENTED_EDGE('',*,*,#28585,.F.);
#37962=ORIENTED_EDGE('',*,*,#28587,.T.);
#37963=ORIENTED_EDGE('',*,*,#27846,.F.);
#37964=ORIENTED_EDGE('',*,*,#27847,.F.);
#37965=ORIENTED_EDGE('',*,*,#28588,.T.);
#37966=ORIENTED_EDGE('',*,*,#28589,.F.);
#37967=ORIENTED_EDGE('',*,*,#28588,.F.);
#37968=ORIENTED_EDGE('',*,*,#28590,.T.);
#37969=ORIENTED_EDGE('',*,*,#28591,.T.);
#37970=ORIENTED_EDGE('',*,*,#28592,.F.);
#37971=ORIENTED_EDGE('',*,*,#28591,.F.);
#37972=ORIENTED_EDGE('',*,*,#28593,.T.);
#37973=ORIENTED_EDGE('',*,*,#27840,.F.);
#37974=ORIENTED_EDGE('',*,*,#27841,.F.);
#37975=ORIENTED_EDGE('',*,*,#28594,.T.);
#37976=ORIENTED_EDGE('',*,*,#28595,.F.);
#37977=ORIENTED_EDGE('',*,*,#28594,.F.);
#37978=ORIENTED_EDGE('',*,*,#28596,.T.);
#37979=ORIENTED_EDGE('',*,*,#28597,.T.);
#37980=ORIENTED_EDGE('',*,*,#28598,.F.);
#37981=ORIENTED_EDGE('',*,*,#28597,.F.);
#37982=ORIENTED_EDGE('',*,*,#28599,.T.);
#37983=ORIENTED_EDGE('',*,*,#27870,.F.);
#37984=ORIENTED_EDGE('',*,*,#27871,.F.);
#37985=ORIENTED_EDGE('',*,*,#28600,.T.);
#37986=ORIENTED_EDGE('',*,*,#28601,.F.);
#37987=ORIENTED_EDGE('',*,*,#28600,.F.);
#37988=ORIENTED_EDGE('',*,*,#28602,.T.);
#37989=ORIENTED_EDGE('',*,*,#28603,.T.);
#37990=ORIENTED_EDGE('',*,*,#28604,.F.);
#37991=ORIENTED_EDGE('',*,*,#28603,.F.);
#37992=ORIENTED_EDGE('',*,*,#28605,.T.);
#37993=ORIENTED_EDGE('',*,*,#27854,.F.);
#37994=ORIENTED_EDGE('',*,*,#27855,.F.);
#37995=ORIENTED_EDGE('',*,*,#28606,.T.);
#37996=ORIENTED_EDGE('',*,*,#28607,.F.);
#37997=ORIENTED_EDGE('',*,*,#28606,.F.);
#37998=ORIENTED_EDGE('',*,*,#28608,.T.);
#37999=ORIENTED_EDGE('',*,*,#28609,.T.);
#38000=ORIENTED_EDGE('',*,*,#28610,.F.);
#38001=ORIENTED_EDGE('',*,*,#28609,.F.);
#38002=ORIENTED_EDGE('',*,*,#28611,.T.);
#38003=ORIENTED_EDGE('',*,*,#27822,.F.);
#38004=ORIENTED_EDGE('',*,*,#27823,.F.);
#38005=ORIENTED_EDGE('',*,*,#28612,.T.);
#38006=ORIENTED_EDGE('',*,*,#28613,.F.);
#38007=ORIENTED_EDGE('',*,*,#28612,.F.);
#38008=ORIENTED_EDGE('',*,*,#28614,.T.);
#38009=ORIENTED_EDGE('',*,*,#28615,.T.);
#38010=ORIENTED_EDGE('',*,*,#28616,.F.);
#38011=ORIENTED_EDGE('',*,*,#28615,.F.);
#38012=ORIENTED_EDGE('',*,*,#28617,.T.);
#38013=ORIENTED_EDGE('',*,*,#27848,.F.);
#38014=ORIENTED_EDGE('',*,*,#27849,.F.);
#38015=ORIENTED_EDGE('',*,*,#28618,.T.);
#38016=ORIENTED_EDGE('',*,*,#28619,.F.);
#38017=ORIENTED_EDGE('',*,*,#28618,.F.);
#38018=ORIENTED_EDGE('',*,*,#28620,.T.);
#38019=ORIENTED_EDGE('',*,*,#28621,.T.);
#38020=ORIENTED_EDGE('',*,*,#28622,.F.);
#38021=ORIENTED_EDGE('',*,*,#28621,.F.);
#38022=ORIENTED_EDGE('',*,*,#28623,.T.);
#38023=ORIENTED_EDGE('',*,*,#27842,.F.);
#38024=ORIENTED_EDGE('',*,*,#27843,.F.);
#38025=ORIENTED_EDGE('',*,*,#28624,.T.);
#38026=ORIENTED_EDGE('',*,*,#28625,.F.);
#38027=ORIENTED_EDGE('',*,*,#28624,.F.);
#38028=ORIENTED_EDGE('',*,*,#28626,.T.);
#38029=ORIENTED_EDGE('',*,*,#28627,.T.);
#38030=ORIENTED_EDGE('',*,*,#28628,.F.);
#38031=ORIENTED_EDGE('',*,*,#28627,.F.);
#38032=ORIENTED_EDGE('',*,*,#28629,.T.);
#38033=ORIENTED_EDGE('',*,*,#27868,.F.);
#38034=ORIENTED_EDGE('',*,*,#27869,.F.);
#38035=ORIENTED_EDGE('',*,*,#28630,.T.);
#38036=ORIENTED_EDGE('',*,*,#28631,.F.);
#38037=ORIENTED_EDGE('',*,*,#28630,.F.);
#38038=ORIENTED_EDGE('',*,*,#28632,.T.);
#38039=ORIENTED_EDGE('',*,*,#28633,.T.);
#38040=ORIENTED_EDGE('',*,*,#28634,.F.);
#38041=ORIENTED_EDGE('',*,*,#28633,.F.);
#38042=ORIENTED_EDGE('',*,*,#28635,.T.);
#38043=ORIENTED_EDGE('',*,*,#27782,.F.);
#38044=ORIENTED_EDGE('',*,*,#27783,.F.);
#38045=ORIENTED_EDGE('',*,*,#28636,.T.);
#38046=ORIENTED_EDGE('',*,*,#28637,.F.);
#38047=ORIENTED_EDGE('',*,*,#28636,.F.);
#38048=ORIENTED_EDGE('',*,*,#28638,.T.);
#38049=ORIENTED_EDGE('',*,*,#28639,.T.);
#38050=ORIENTED_EDGE('',*,*,#28640,.F.);
#38051=ORIENTED_EDGE('',*,*,#28639,.F.);
#38052=ORIENTED_EDGE('',*,*,#28641,.T.);
#38053=ORIENTED_EDGE('',*,*,#27824,.F.);
#38054=ORIENTED_EDGE('',*,*,#27825,.F.);
#38055=ORIENTED_EDGE('',*,*,#28642,.T.);
#38056=ORIENTED_EDGE('',*,*,#28643,.F.);
#38057=ORIENTED_EDGE('',*,*,#28642,.F.);
#38058=ORIENTED_EDGE('',*,*,#28644,.T.);
#38059=ORIENTED_EDGE('',*,*,#28645,.T.);
#38060=ORIENTED_EDGE('',*,*,#28646,.F.);
#38061=ORIENTED_EDGE('',*,*,#28645,.F.);
#38062=ORIENTED_EDGE('',*,*,#28647,.T.);
#38063=ORIENTED_EDGE('',*,*,#27844,.F.);
#38064=ORIENTED_EDGE('',*,*,#27845,.F.);
#38065=ORIENTED_EDGE('',*,*,#28648,.T.);
#38066=ORIENTED_EDGE('',*,*,#28649,.F.);
#38067=ORIENTED_EDGE('',*,*,#28648,.F.);
#38068=ORIENTED_EDGE('',*,*,#28650,.T.);
#38069=ORIENTED_EDGE('',*,*,#28651,.T.);
#38070=ORIENTED_EDGE('',*,*,#28652,.F.);
#38071=ORIENTED_EDGE('',*,*,#28651,.F.);
#38072=ORIENTED_EDGE('',*,*,#28653,.T.);
#38073=ORIENTED_EDGE('',*,*,#27850,.F.);
#38074=ORIENTED_EDGE('',*,*,#27851,.F.);
#38075=ORIENTED_EDGE('',*,*,#28654,.T.);
#38076=ORIENTED_EDGE('',*,*,#28655,.F.);
#38077=ORIENTED_EDGE('',*,*,#28654,.F.);
#38078=ORIENTED_EDGE('',*,*,#28656,.T.);
#38079=ORIENTED_EDGE('',*,*,#28657,.T.);
#38080=ORIENTED_EDGE('',*,*,#28658,.F.);
#38081=ORIENTED_EDGE('',*,*,#28657,.F.);
#38082=ORIENTED_EDGE('',*,*,#28659,.T.);
#38083=ORIENTED_EDGE('',*,*,#28660,.F.);
#38084=ORIENTED_EDGE('',*,*,#28661,.T.);
#38085=ORIENTED_EDGE('',*,*,#28662,.F.);
#38086=ORIENTED_EDGE('',*,*,#28661,.F.);
#38087=ORIENTED_EDGE('',*,*,#28663,.T.);
#38088=ORIENTED_EDGE('',*,*,#28664,.T.);
#38089=ORIENTED_EDGE('',*,*,#28665,.F.);
#38090=ORIENTED_EDGE('',*,*,#28664,.F.);
#38091=ORIENTED_EDGE('',*,*,#28666,.F.);
#38092=ORIENTED_EDGE('',*,*,#28667,.T.);
#38093=ORIENTED_EDGE('',*,*,#28668,.F.);
#38094=ORIENTED_EDGE('',*,*,#28667,.F.);
#38095=ORIENTED_EDGE('',*,*,#28669,.T.);
#38096=ORIENTED_EDGE('',*,*,#28670,.T.);
#38097=ORIENTED_EDGE('',*,*,#28671,.F.);
#38098=ORIENTED_EDGE('',*,*,#28670,.F.);
#38099=ORIENTED_EDGE('',*,*,#28672,.F.);
#38100=ORIENTED_EDGE('',*,*,#28673,.T.);
#38101=ORIENTED_EDGE('',*,*,#28674,.F.);
#38102=ORIENTED_EDGE('',*,*,#28673,.F.);
#38103=ORIENTED_EDGE('',*,*,#28675,.T.);
#38104=ORIENTED_EDGE('',*,*,#28676,.T.);
#38105=ORIENTED_EDGE('',*,*,#28677,.F.);
#38106=ORIENTED_EDGE('',*,*,#28676,.F.);
#38107=ORIENTED_EDGE('',*,*,#28678,.F.);
#38108=ORIENTED_EDGE('',*,*,#28679,.T.);
#38109=ORIENTED_EDGE('',*,*,#28680,.F.);
#38110=ORIENTED_EDGE('',*,*,#28679,.F.);
#38111=ORIENTED_EDGE('',*,*,#28681,.T.);
#38112=ORIENTED_EDGE('',*,*,#28682,.T.);
#38113=ORIENTED_EDGE('',*,*,#28683,.F.);
#38114=ORIENTED_EDGE('',*,*,#28682,.F.);
#38115=ORIENTED_EDGE('',*,*,#28684,.F.);
#38116=ORIENTED_EDGE('',*,*,#28685,.T.);
#38117=ORIENTED_EDGE('',*,*,#28686,.F.);
#38118=ORIENTED_EDGE('',*,*,#28685,.F.);
#38119=ORIENTED_EDGE('',*,*,#28687,.T.);
#38120=ORIENTED_EDGE('',*,*,#28688,.T.);
#38121=ORIENTED_EDGE('',*,*,#28689,.F.);
#38122=ORIENTED_EDGE('',*,*,#28688,.F.);
#38123=ORIENTED_EDGE('',*,*,#28690,.F.);
#38124=ORIENTED_EDGE('',*,*,#28691,.T.);
#38125=ORIENTED_EDGE('',*,*,#28692,.F.);
#38126=ORIENTED_EDGE('',*,*,#28691,.F.);
#38127=ORIENTED_EDGE('',*,*,#28693,.T.);
#38128=ORIENTED_EDGE('',*,*,#28694,.T.);
#38129=ORIENTED_EDGE('',*,*,#28695,.F.);
#38130=ORIENTED_EDGE('',*,*,#28694,.F.);
#38131=ORIENTED_EDGE('',*,*,#28696,.F.);
#38132=ORIENTED_EDGE('',*,*,#28697,.T.);
#38133=ORIENTED_EDGE('',*,*,#28698,.F.);
#38134=ORIENTED_EDGE('',*,*,#28697,.F.);
#38135=ORIENTED_EDGE('',*,*,#28699,.T.);
#38136=ORIENTED_EDGE('',*,*,#28700,.T.);
#38137=ORIENTED_EDGE('',*,*,#28701,.F.);
#38138=ORIENTED_EDGE('',*,*,#28700,.F.);
#38139=ORIENTED_EDGE('',*,*,#28702,.F.);
#38140=ORIENTED_EDGE('',*,*,#28703,.T.);
#38141=ORIENTED_EDGE('',*,*,#28704,.F.);
#38142=ORIENTED_EDGE('',*,*,#28703,.F.);
#38143=ORIENTED_EDGE('',*,*,#28705,.T.);
#38144=ORIENTED_EDGE('',*,*,#28706,.T.);
#38145=ORIENTED_EDGE('',*,*,#28707,.F.);
#38146=ORIENTED_EDGE('',*,*,#28706,.F.);
#38147=ORIENTED_EDGE('',*,*,#28708,.F.);
#38148=ORIENTED_EDGE('',*,*,#28709,.T.);
#38149=ORIENTED_EDGE('',*,*,#28710,.F.);
#38150=ORIENTED_EDGE('',*,*,#28709,.F.);
#38151=ORIENTED_EDGE('',*,*,#28711,.T.);
#38152=ORIENTED_EDGE('',*,*,#28712,.T.);
#38153=ORIENTED_EDGE('',*,*,#28713,.F.);
#38154=ORIENTED_EDGE('',*,*,#28712,.F.);
#38155=ORIENTED_EDGE('',*,*,#28714,.F.);
#38156=ORIENTED_EDGE('',*,*,#28715,.T.);
#38157=ORIENTED_EDGE('',*,*,#28716,.F.);
#38158=ORIENTED_EDGE('',*,*,#28715,.F.);
#38159=ORIENTED_EDGE('',*,*,#28717,.T.);
#38160=ORIENTED_EDGE('',*,*,#28718,.T.);
#38161=ORIENTED_EDGE('',*,*,#28719,.F.);
#38162=ORIENTED_EDGE('',*,*,#28718,.F.);
#38163=ORIENTED_EDGE('',*,*,#28720,.F.);
#38164=ORIENTED_EDGE('',*,*,#28721,.T.);
#38165=ORIENTED_EDGE('',*,*,#28722,.F.);
#38166=ORIENTED_EDGE('',*,*,#28721,.F.);
#38167=ORIENTED_EDGE('',*,*,#28723,.T.);
#38168=ORIENTED_EDGE('',*,*,#28724,.T.);
#38169=ORIENTED_EDGE('',*,*,#28725,.F.);
#38170=ORIENTED_EDGE('',*,*,#28724,.F.);
#38171=ORIENTED_EDGE('',*,*,#28726,.F.);
#38172=ORIENTED_EDGE('',*,*,#28727,.T.);
#38173=ORIENTED_EDGE('',*,*,#28728,.F.);
#38174=ORIENTED_EDGE('',*,*,#28727,.F.);
#38175=ORIENTED_EDGE('',*,*,#28729,.T.);
#38176=ORIENTED_EDGE('',*,*,#28730,.T.);
#38177=ORIENTED_EDGE('',*,*,#28731,.F.);
#38178=ORIENTED_EDGE('',*,*,#28730,.F.);
#38179=ORIENTED_EDGE('',*,*,#28732,.F.);
#38180=ORIENTED_EDGE('',*,*,#28733,.T.);
#38181=ORIENTED_EDGE('',*,*,#28734,.F.);
#38182=ORIENTED_EDGE('',*,*,#28733,.F.);
#38183=ORIENTED_EDGE('',*,*,#28735,.T.);
#38184=ORIENTED_EDGE('',*,*,#28736,.T.);
#38185=ORIENTED_EDGE('',*,*,#28737,.F.);
#38186=ORIENTED_EDGE('',*,*,#28736,.F.);
#38187=ORIENTED_EDGE('',*,*,#28738,.F.);
#38188=ORIENTED_EDGE('',*,*,#28739,.T.);
#38189=ORIENTED_EDGE('',*,*,#28740,.F.);
#38190=ORIENTED_EDGE('',*,*,#28739,.F.);
#38191=ORIENTED_EDGE('',*,*,#28741,.T.);
#38192=ORIENTED_EDGE('',*,*,#28742,.T.);
#38193=ORIENTED_EDGE('',*,*,#28743,.F.);
#38194=ORIENTED_EDGE('',*,*,#28742,.F.);
#38195=ORIENTED_EDGE('',*,*,#28744,.F.);
#38196=ORIENTED_EDGE('',*,*,#28745,.T.);
#38197=ORIENTED_EDGE('',*,*,#28746,.F.);
#38198=ORIENTED_EDGE('',*,*,#28745,.F.);
#38199=ORIENTED_EDGE('',*,*,#28747,.T.);
#38200=ORIENTED_EDGE('',*,*,#28748,.T.);
#38201=ORIENTED_EDGE('',*,*,#28749,.F.);
#38202=ORIENTED_EDGE('',*,*,#28748,.F.);
#38203=ORIENTED_EDGE('',*,*,#28750,.F.);
#38204=ORIENTED_EDGE('',*,*,#28751,.T.);
#38205=ORIENTED_EDGE('',*,*,#28752,.F.);
#38206=ORIENTED_EDGE('',*,*,#28751,.F.);
#38207=ORIENTED_EDGE('',*,*,#28753,.T.);
#38208=ORIENTED_EDGE('',*,*,#28754,.T.);
#38209=ORIENTED_EDGE('',*,*,#28755,.F.);
#38210=ORIENTED_EDGE('',*,*,#28754,.F.);
#38211=ORIENTED_EDGE('',*,*,#28756,.F.);
#38212=ORIENTED_EDGE('',*,*,#28757,.T.);
#38213=ORIENTED_EDGE('',*,*,#28758,.F.);
#38214=ORIENTED_EDGE('',*,*,#28757,.F.);
#38215=ORIENTED_EDGE('',*,*,#28759,.T.);
#38216=ORIENTED_EDGE('',*,*,#28760,.T.);
#38217=ORIENTED_EDGE('',*,*,#28761,.F.);
#38218=ORIENTED_EDGE('',*,*,#28760,.F.);
#38219=ORIENTED_EDGE('',*,*,#28762,.F.);
#38220=ORIENTED_EDGE('',*,*,#28763,.T.);
#38221=ORIENTED_EDGE('',*,*,#28764,.F.);
#38222=ORIENTED_EDGE('',*,*,#28763,.F.);
#38223=ORIENTED_EDGE('',*,*,#28765,.T.);
#38224=ORIENTED_EDGE('',*,*,#28766,.T.);
#38225=ORIENTED_EDGE('',*,*,#28767,.F.);
#38226=ORIENTED_EDGE('',*,*,#28766,.F.);
#38227=ORIENTED_EDGE('',*,*,#28768,.F.);
#38228=ORIENTED_EDGE('',*,*,#28769,.T.);
#38229=ORIENTED_EDGE('',*,*,#28770,.F.);
#38230=ORIENTED_EDGE('',*,*,#28769,.F.);
#38231=ORIENTED_EDGE('',*,*,#28771,.T.);
#38232=ORIENTED_EDGE('',*,*,#28772,.T.);
#38233=ORIENTED_EDGE('',*,*,#28773,.F.);
#38234=ORIENTED_EDGE('',*,*,#28772,.F.);
#38235=ORIENTED_EDGE('',*,*,#28774,.F.);
#38236=ORIENTED_EDGE('',*,*,#28775,.T.);
#38237=ORIENTED_EDGE('',*,*,#28776,.F.);
#38238=ORIENTED_EDGE('',*,*,#28775,.F.);
#38239=ORIENTED_EDGE('',*,*,#28777,.T.);
#38240=ORIENTED_EDGE('',*,*,#28778,.T.);
#38241=ORIENTED_EDGE('',*,*,#28779,.F.);
#38242=ORIENTED_EDGE('',*,*,#28778,.F.);
#38243=ORIENTED_EDGE('',*,*,#28780,.F.);
#38244=ORIENTED_EDGE('',*,*,#28781,.T.);
#38245=ORIENTED_EDGE('',*,*,#28782,.F.);
#38246=ORIENTED_EDGE('',*,*,#28781,.F.);
#38247=ORIENTED_EDGE('',*,*,#28783,.T.);
#38248=ORIENTED_EDGE('',*,*,#28784,.T.);
#38249=ORIENTED_EDGE('',*,*,#28785,.F.);
#38250=ORIENTED_EDGE('',*,*,#28784,.F.);
#38251=ORIENTED_EDGE('',*,*,#28786,.F.);
#38252=ORIENTED_EDGE('',*,*,#28787,.T.);
#38253=ORIENTED_EDGE('',*,*,#28788,.F.);
#38254=ORIENTED_EDGE('',*,*,#28787,.F.);
#38255=ORIENTED_EDGE('',*,*,#28789,.T.);
#38256=ORIENTED_EDGE('',*,*,#28790,.T.);
#38257=ORIENTED_EDGE('',*,*,#28791,.F.);
#38258=ORIENTED_EDGE('',*,*,#28790,.F.);
#38259=ORIENTED_EDGE('',*,*,#28792,.F.);
#38260=ORIENTED_EDGE('',*,*,#28793,.T.);
#38261=ORIENTED_EDGE('',*,*,#28794,.F.);
#38262=ORIENTED_EDGE('',*,*,#28793,.F.);
#38263=ORIENTED_EDGE('',*,*,#28795,.T.);
#38264=ORIENTED_EDGE('',*,*,#28796,.T.);
#38265=ORIENTED_EDGE('',*,*,#28797,.F.);
#38266=ORIENTED_EDGE('',*,*,#28796,.F.);
#38267=ORIENTED_EDGE('',*,*,#28798,.F.);
#38268=ORIENTED_EDGE('',*,*,#28799,.T.);
#38269=ORIENTED_EDGE('',*,*,#28800,.F.);
#38270=ORIENTED_EDGE('',*,*,#28799,.F.);
#38271=ORIENTED_EDGE('',*,*,#28801,.T.);
#38272=ORIENTED_EDGE('',*,*,#28802,.T.);
#38273=ORIENTED_EDGE('',*,*,#28803,.F.);
#38274=ORIENTED_EDGE('',*,*,#28802,.F.);
#38275=ORIENTED_EDGE('',*,*,#28804,.F.);
#38276=ORIENTED_EDGE('',*,*,#28805,.T.);
#38277=ORIENTED_EDGE('',*,*,#28806,.F.);
#38278=ORIENTED_EDGE('',*,*,#28805,.F.);
#38279=ORIENTED_EDGE('',*,*,#28807,.T.);
#38280=ORIENTED_EDGE('',*,*,#28808,.T.);
#38281=ORIENTED_EDGE('',*,*,#28809,.F.);
#38282=ORIENTED_EDGE('',*,*,#28808,.F.);
#38283=ORIENTED_EDGE('',*,*,#28810,.F.);
#38284=ORIENTED_EDGE('',*,*,#28811,.T.);
#38285=ORIENTED_EDGE('',*,*,#28812,.F.);
#38286=ORIENTED_EDGE('',*,*,#28811,.F.);
#38287=ORIENTED_EDGE('',*,*,#28813,.T.);
#38288=ORIENTED_EDGE('',*,*,#28814,.T.);
#38289=ORIENTED_EDGE('',*,*,#28815,.F.);
#38290=ORIENTED_EDGE('',*,*,#28814,.F.);
#38291=ORIENTED_EDGE('',*,*,#28816,.F.);
#38292=ORIENTED_EDGE('',*,*,#28817,.T.);
#38293=ORIENTED_EDGE('',*,*,#28818,.F.);
#38294=ORIENTED_EDGE('',*,*,#28817,.F.);
#38295=ORIENTED_EDGE('',*,*,#28819,.T.);
#38296=ORIENTED_EDGE('',*,*,#28820,.T.);
#38297=ORIENTED_EDGE('',*,*,#28821,.F.);
#38298=ORIENTED_EDGE('',*,*,#28820,.F.);
#38299=ORIENTED_EDGE('',*,*,#28822,.F.);
#38300=ORIENTED_EDGE('',*,*,#28823,.T.);
#38301=ORIENTED_EDGE('',*,*,#28824,.F.);
#38302=ORIENTED_EDGE('',*,*,#28823,.F.);
#38303=ORIENTED_EDGE('',*,*,#28825,.T.);
#38304=ORIENTED_EDGE('',*,*,#28826,.T.);
#38305=ORIENTED_EDGE('',*,*,#28827,.F.);
#38306=ORIENTED_EDGE('',*,*,#28826,.F.);
#38307=ORIENTED_EDGE('',*,*,#28828,.F.);
#38308=ORIENTED_EDGE('',*,*,#28829,.T.);
#38309=ORIENTED_EDGE('',*,*,#28830,.F.);
#38310=ORIENTED_EDGE('',*,*,#28829,.F.);
#38311=ORIENTED_EDGE('',*,*,#28831,.T.);
#38312=ORIENTED_EDGE('',*,*,#28832,.T.);
#38313=ORIENTED_EDGE('',*,*,#28833,.F.);
#38314=ORIENTED_EDGE('',*,*,#28832,.F.);
#38315=ORIENTED_EDGE('',*,*,#28834,.F.);
#38316=ORIENTED_EDGE('',*,*,#28835,.T.);
#38317=ORIENTED_EDGE('',*,*,#28836,.F.);
#38318=ORIENTED_EDGE('',*,*,#28835,.F.);
#38319=ORIENTED_EDGE('',*,*,#28837,.T.);
#38320=ORIENTED_EDGE('',*,*,#28838,.T.);
#38321=ORIENTED_EDGE('',*,*,#28839,.F.);
#38322=ORIENTED_EDGE('',*,*,#28838,.F.);
#38323=ORIENTED_EDGE('',*,*,#28840,.F.);
#38324=ORIENTED_EDGE('',*,*,#28841,.T.);
#38325=ORIENTED_EDGE('',*,*,#28842,.F.);
#38326=ORIENTED_EDGE('',*,*,#28841,.F.);
#38327=ORIENTED_EDGE('',*,*,#28843,.T.);
#38328=ORIENTED_EDGE('',*,*,#28844,.T.);
#38329=ORIENTED_EDGE('',*,*,#28845,.F.);
#38330=ORIENTED_EDGE('',*,*,#28844,.F.);
#38331=ORIENTED_EDGE('',*,*,#28846,.F.);
#38332=ORIENTED_EDGE('',*,*,#28847,.T.);
#38333=ORIENTED_EDGE('',*,*,#28848,.F.);
#38334=ORIENTED_EDGE('',*,*,#28847,.F.);
#38335=ORIENTED_EDGE('',*,*,#28849,.T.);
#38336=ORIENTED_EDGE('',*,*,#28850,.T.);
#38337=ORIENTED_EDGE('',*,*,#28851,.F.);
#38338=ORIENTED_EDGE('',*,*,#28850,.F.);
#38339=ORIENTED_EDGE('',*,*,#28852,.F.);
#38340=ORIENTED_EDGE('',*,*,#28853,.T.);
#38341=ORIENTED_EDGE('',*,*,#28854,.F.);
#38342=ORIENTED_EDGE('',*,*,#28853,.F.);
#38343=ORIENTED_EDGE('',*,*,#28855,.T.);
#38344=ORIENTED_EDGE('',*,*,#28856,.T.);
#38345=ORIENTED_EDGE('',*,*,#28857,.F.);
#38346=ORIENTED_EDGE('',*,*,#28856,.F.);
#38347=ORIENTED_EDGE('',*,*,#28858,.F.);
#38348=ORIENTED_EDGE('',*,*,#28859,.T.);
#38349=ORIENTED_EDGE('',*,*,#28860,.F.);
#38350=ORIENTED_EDGE('',*,*,#28859,.F.);
#38351=ORIENTED_EDGE('',*,*,#28861,.T.);
#38352=ORIENTED_EDGE('',*,*,#28862,.T.);
#38353=ORIENTED_EDGE('',*,*,#28863,.F.);
#38354=ORIENTED_EDGE('',*,*,#28862,.F.);
#38355=ORIENTED_EDGE('',*,*,#28864,.F.);
#38356=ORIENTED_EDGE('',*,*,#28865,.T.);
#38357=ORIENTED_EDGE('',*,*,#28866,.F.);
#38358=ORIENTED_EDGE('',*,*,#28865,.F.);
#38359=ORIENTED_EDGE('',*,*,#28867,.T.);
#38360=ORIENTED_EDGE('',*,*,#28868,.T.);
#38361=ORIENTED_EDGE('',*,*,#28869,.F.);
#38362=ORIENTED_EDGE('',*,*,#28868,.F.);
#38363=ORIENTED_EDGE('',*,*,#28870,.F.);
#38364=ORIENTED_EDGE('',*,*,#28871,.T.);
#38365=ORIENTED_EDGE('',*,*,#28872,.F.);
#38366=ORIENTED_EDGE('',*,*,#28871,.F.);
#38367=ORIENTED_EDGE('',*,*,#28873,.T.);
#38368=ORIENTED_EDGE('',*,*,#28874,.T.);
#38369=ORIENTED_EDGE('',*,*,#28875,.F.);
#38370=ORIENTED_EDGE('',*,*,#28874,.F.);
#38371=ORIENTED_EDGE('',*,*,#28876,.F.);
#38372=ORIENTED_EDGE('',*,*,#28877,.T.);
#38373=ORIENTED_EDGE('',*,*,#28878,.F.);
#38374=ORIENTED_EDGE('',*,*,#28877,.F.);
#38375=ORIENTED_EDGE('',*,*,#28879,.T.);
#38376=ORIENTED_EDGE('',*,*,#28880,.T.);
#38377=ORIENTED_EDGE('',*,*,#28881,.F.);
#38378=ORIENTED_EDGE('',*,*,#28880,.F.);
#38379=ORIENTED_EDGE('',*,*,#28882,.F.);
#38380=ORIENTED_EDGE('',*,*,#28883,.T.);
#38381=ORIENTED_EDGE('',*,*,#28884,.F.);
#38382=ORIENTED_EDGE('',*,*,#28883,.F.);
#38383=ORIENTED_EDGE('',*,*,#28885,.T.);
#38384=ORIENTED_EDGE('',*,*,#28886,.T.);
#38385=ORIENTED_EDGE('',*,*,#28887,.F.);
#38386=ORIENTED_EDGE('',*,*,#28886,.F.);
#38387=ORIENTED_EDGE('',*,*,#28888,.F.);
#38388=ORIENTED_EDGE('',*,*,#28889,.T.);
#38389=ORIENTED_EDGE('',*,*,#28890,.F.);
#38390=ORIENTED_EDGE('',*,*,#28889,.F.);
#38391=ORIENTED_EDGE('',*,*,#28891,.T.);
#38392=ORIENTED_EDGE('',*,*,#28892,.T.);
#38393=ORIENTED_EDGE('',*,*,#28893,.F.);
#38394=ORIENTED_EDGE('',*,*,#28892,.F.);
#38395=ORIENTED_EDGE('',*,*,#28894,.F.);
#38396=ORIENTED_EDGE('',*,*,#28895,.T.);
#38397=ORIENTED_EDGE('',*,*,#28896,.F.);
#38398=ORIENTED_EDGE('',*,*,#28895,.F.);
#38399=ORIENTED_EDGE('',*,*,#28897,.T.);
#38400=ORIENTED_EDGE('',*,*,#28898,.T.);
#38401=ORIENTED_EDGE('',*,*,#28899,.F.);
#38402=ORIENTED_EDGE('',*,*,#28898,.F.);
#38403=ORIENTED_EDGE('',*,*,#28900,.F.);
#38404=ORIENTED_EDGE('',*,*,#28901,.T.);
#38405=ORIENTED_EDGE('',*,*,#28902,.F.);
#38406=ORIENTED_EDGE('',*,*,#28901,.F.);
#38407=ORIENTED_EDGE('',*,*,#28903,.T.);
#38408=ORIENTED_EDGE('',*,*,#28904,.T.);
#38409=ORIENTED_EDGE('',*,*,#28905,.F.);
#38410=ORIENTED_EDGE('',*,*,#28904,.F.);
#38411=ORIENTED_EDGE('',*,*,#28906,.F.);
#38412=ORIENTED_EDGE('',*,*,#28907,.T.);
#38413=ORIENTED_EDGE('',*,*,#28908,.F.);
#38414=ORIENTED_EDGE('',*,*,#28907,.F.);
#38415=ORIENTED_EDGE('',*,*,#28909,.T.);
#38416=ORIENTED_EDGE('',*,*,#28910,.T.);
#38417=ORIENTED_EDGE('',*,*,#28911,.F.);
#38418=ORIENTED_EDGE('',*,*,#28910,.F.);
#38419=ORIENTED_EDGE('',*,*,#28912,.F.);
#38420=ORIENTED_EDGE('',*,*,#28913,.T.);
#38421=ORIENTED_EDGE('',*,*,#28914,.F.);
#38422=ORIENTED_EDGE('',*,*,#28913,.F.);
#38423=ORIENTED_EDGE('',*,*,#28915,.T.);
#38424=ORIENTED_EDGE('',*,*,#28916,.T.);
#38425=ORIENTED_EDGE('',*,*,#28917,.F.);
#38426=ORIENTED_EDGE('',*,*,#28916,.F.);
#38427=ORIENTED_EDGE('',*,*,#28918,.F.);
#38428=ORIENTED_EDGE('',*,*,#28919,.T.);
#38429=ORIENTED_EDGE('',*,*,#28920,.F.);
#38430=ORIENTED_EDGE('',*,*,#28919,.F.);
#38431=ORIENTED_EDGE('',*,*,#28921,.T.);
#38432=ORIENTED_EDGE('',*,*,#28922,.T.);
#38433=ORIENTED_EDGE('',*,*,#28923,.F.);
#38434=ORIENTED_EDGE('',*,*,#28922,.F.);
#38435=ORIENTED_EDGE('',*,*,#28924,.F.);
#38436=ORIENTED_EDGE('',*,*,#28925,.T.);
#38437=ORIENTED_EDGE('',*,*,#28926,.F.);
#38438=ORIENTED_EDGE('',*,*,#28925,.F.);
#38439=ORIENTED_EDGE('',*,*,#28927,.T.);
#38440=ORIENTED_EDGE('',*,*,#28928,.T.);
#38441=ORIENTED_EDGE('',*,*,#28929,.F.);
#38442=ORIENTED_EDGE('',*,*,#28928,.F.);
#38443=ORIENTED_EDGE('',*,*,#28930,.F.);
#38444=ORIENTED_EDGE('',*,*,#28931,.T.);
#38445=ORIENTED_EDGE('',*,*,#28932,.F.);
#38446=ORIENTED_EDGE('',*,*,#28931,.F.);
#38447=ORIENTED_EDGE('',*,*,#28933,.T.);
#38448=ORIENTED_EDGE('',*,*,#28934,.T.);
#38449=ORIENTED_EDGE('',*,*,#28935,.F.);
#38450=ORIENTED_EDGE('',*,*,#28934,.F.);
#38451=ORIENTED_EDGE('',*,*,#28936,.F.);
#38452=ORIENTED_EDGE('',*,*,#28937,.T.);
#38453=ORIENTED_EDGE('',*,*,#28938,.F.);
#38454=ORIENTED_EDGE('',*,*,#28937,.F.);
#38455=ORIENTED_EDGE('',*,*,#28939,.T.);
#38456=ORIENTED_EDGE('',*,*,#28940,.T.);
#38457=ORIENTED_EDGE('',*,*,#28941,.F.);
#38458=ORIENTED_EDGE('',*,*,#28940,.F.);
#38459=ORIENTED_EDGE('',*,*,#28942,.F.);
#38460=ORIENTED_EDGE('',*,*,#28943,.T.);
#38461=ORIENTED_EDGE('',*,*,#28944,.F.);
#38462=ORIENTED_EDGE('',*,*,#28943,.F.);
#38463=ORIENTED_EDGE('',*,*,#28945,.T.);
#38464=ORIENTED_EDGE('',*,*,#28946,.T.);
#38465=ORIENTED_EDGE('',*,*,#28947,.F.);
#38466=ORIENTED_EDGE('',*,*,#28946,.F.);
#38467=ORIENTED_EDGE('',*,*,#28948,.F.);
#38468=ORIENTED_EDGE('',*,*,#28949,.T.);
#38469=ORIENTED_EDGE('',*,*,#28950,.F.);
#38470=ORIENTED_EDGE('',*,*,#28949,.F.);
#38471=ORIENTED_EDGE('',*,*,#28951,.T.);
#38472=ORIENTED_EDGE('',*,*,#28952,.T.);
#38473=ORIENTED_EDGE('',*,*,#28953,.F.);
#38474=ORIENTED_EDGE('',*,*,#28952,.F.);
#38475=ORIENTED_EDGE('',*,*,#28954,.F.);
#38476=ORIENTED_EDGE('',*,*,#28955,.T.);
#38477=ORIENTED_EDGE('',*,*,#28956,.F.);
#38478=ORIENTED_EDGE('',*,*,#28955,.F.);
#38479=ORIENTED_EDGE('',*,*,#28957,.T.);
#38480=ORIENTED_EDGE('',*,*,#28958,.T.);
#38481=ORIENTED_EDGE('',*,*,#28959,.F.);
#38482=ORIENTED_EDGE('',*,*,#28958,.F.);
#38483=ORIENTED_EDGE('',*,*,#28960,.F.);
#38484=ORIENTED_EDGE('',*,*,#28961,.T.);
#38485=ORIENTED_EDGE('',*,*,#28962,.F.);
#38486=ORIENTED_EDGE('',*,*,#28961,.F.);
#38487=ORIENTED_EDGE('',*,*,#28963,.T.);
#38488=ORIENTED_EDGE('',*,*,#28964,.T.);
#38489=ORIENTED_EDGE('',*,*,#28965,.F.);
#38490=ORIENTED_EDGE('',*,*,#28964,.F.);
#38491=ORIENTED_EDGE('',*,*,#28966,.F.);
#38492=ORIENTED_EDGE('',*,*,#28967,.T.);
#38493=ORIENTED_EDGE('',*,*,#28968,.F.);
#38494=ORIENTED_EDGE('',*,*,#28967,.F.);
#38495=ORIENTED_EDGE('',*,*,#28969,.T.);
#38496=ORIENTED_EDGE('',*,*,#28970,.T.);
#38497=ORIENTED_EDGE('',*,*,#28971,.F.);
#38498=ORIENTED_EDGE('',*,*,#28970,.F.);
#38499=ORIENTED_EDGE('',*,*,#28972,.F.);
#38500=ORIENTED_EDGE('',*,*,#28973,.T.);
#38501=ORIENTED_EDGE('',*,*,#28974,.F.);
#38502=ORIENTED_EDGE('',*,*,#28973,.F.);
#38503=ORIENTED_EDGE('',*,*,#28975,.T.);
#38504=ORIENTED_EDGE('',*,*,#28976,.T.);
#38505=ORIENTED_EDGE('',*,*,#28977,.F.);
#38506=ORIENTED_EDGE('',*,*,#28976,.F.);
#38507=ORIENTED_EDGE('',*,*,#28978,.F.);
#38508=ORIENTED_EDGE('',*,*,#28979,.T.);
#38509=ORIENTED_EDGE('',*,*,#28980,.F.);
#38510=ORIENTED_EDGE('',*,*,#28979,.F.);
#38511=ORIENTED_EDGE('',*,*,#28981,.T.);
#38512=ORIENTED_EDGE('',*,*,#28982,.T.);
#38513=ORIENTED_EDGE('',*,*,#28983,.F.);
#38514=ORIENTED_EDGE('',*,*,#28982,.F.);
#38515=ORIENTED_EDGE('',*,*,#28984,.F.);
#38516=ORIENTED_EDGE('',*,*,#28985,.T.);
#38517=ORIENTED_EDGE('',*,*,#28986,.F.);
#38518=ORIENTED_EDGE('',*,*,#28985,.F.);
#38519=ORIENTED_EDGE('',*,*,#28987,.T.);
#38520=ORIENTED_EDGE('',*,*,#28988,.T.);
#38521=ORIENTED_EDGE('',*,*,#28989,.F.);
#38522=ORIENTED_EDGE('',*,*,#28988,.F.);
#38523=ORIENTED_EDGE('',*,*,#28990,.F.);
#38524=ORIENTED_EDGE('',*,*,#28991,.T.);
#38525=ORIENTED_EDGE('',*,*,#28992,.F.);
#38526=ORIENTED_EDGE('',*,*,#28991,.F.);
#38527=ORIENTED_EDGE('',*,*,#28993,.T.);
#38528=ORIENTED_EDGE('',*,*,#28994,.T.);
#38529=ORIENTED_EDGE('',*,*,#28995,.F.);
#38530=ORIENTED_EDGE('',*,*,#28994,.F.);
#38531=ORIENTED_EDGE('',*,*,#28996,.F.);
#38532=ORIENTED_EDGE('',*,*,#28997,.T.);
#38533=ORIENTED_EDGE('',*,*,#28998,.F.);
#38534=ORIENTED_EDGE('',*,*,#28997,.F.);
#38535=ORIENTED_EDGE('',*,*,#28999,.T.);
#38536=ORIENTED_EDGE('',*,*,#29000,.T.);
#38537=ORIENTED_EDGE('',*,*,#29001,.F.);
#38538=ORIENTED_EDGE('',*,*,#29000,.F.);
#38539=ORIENTED_EDGE('',*,*,#29002,.F.);
#38540=ORIENTED_EDGE('',*,*,#29003,.T.);
#38541=ORIENTED_EDGE('',*,*,#29004,.F.);
#38542=ORIENTED_EDGE('',*,*,#29003,.F.);
#38543=ORIENTED_EDGE('',*,*,#29005,.T.);
#38544=ORIENTED_EDGE('',*,*,#29006,.T.);
#38545=ORIENTED_EDGE('',*,*,#29007,.F.);
#38546=ORIENTED_EDGE('',*,*,#29006,.F.);
#38547=ORIENTED_EDGE('',*,*,#29008,.F.);
#38548=ORIENTED_EDGE('',*,*,#29009,.T.);
#38549=ORIENTED_EDGE('',*,*,#29010,.F.);
#38550=ORIENTED_EDGE('',*,*,#29009,.F.);
#38551=ORIENTED_EDGE('',*,*,#29011,.T.);
#38552=ORIENTED_EDGE('',*,*,#29012,.T.);
#38553=ORIENTED_EDGE('',*,*,#29013,.F.);
#38554=ORIENTED_EDGE('',*,*,#29012,.F.);
#38555=ORIENTED_EDGE('',*,*,#29014,.F.);
#38556=ORIENTED_EDGE('',*,*,#29015,.T.);
#38557=ORIENTED_EDGE('',*,*,#29016,.F.);
#38558=ORIENTED_EDGE('',*,*,#29015,.F.);
#38559=ORIENTED_EDGE('',*,*,#29017,.T.);
#38560=ORIENTED_EDGE('',*,*,#29018,.T.);
#38561=ORIENTED_EDGE('',*,*,#29019,.F.);
#38562=ORIENTED_EDGE('',*,*,#29018,.F.);
#38563=ORIENTED_EDGE('',*,*,#29020,.F.);
#38564=ORIENTED_EDGE('',*,*,#29021,.T.);
#38565=ORIENTED_EDGE('',*,*,#29022,.F.);
#38566=ORIENTED_EDGE('',*,*,#29021,.F.);
#38567=ORIENTED_EDGE('',*,*,#29023,.T.);
#38568=ORIENTED_EDGE('',*,*,#29024,.T.);
#38569=ORIENTED_EDGE('',*,*,#29025,.F.);
#38570=ORIENTED_EDGE('',*,*,#29024,.F.);
#38571=ORIENTED_EDGE('',*,*,#29026,.F.);
#38572=ORIENTED_EDGE('',*,*,#29027,.T.);
#38573=ORIENTED_EDGE('',*,*,#29028,.F.);
#38574=ORIENTED_EDGE('',*,*,#29027,.F.);
#38575=ORIENTED_EDGE('',*,*,#29029,.T.);
#38576=ORIENTED_EDGE('',*,*,#29030,.T.);
#38577=ORIENTED_EDGE('',*,*,#29031,.F.);
#38578=ORIENTED_EDGE('',*,*,#29030,.F.);
#38579=ORIENTED_EDGE('',*,*,#29032,.F.);
#38580=ORIENTED_EDGE('',*,*,#29033,.T.);
#38581=ORIENTED_EDGE('',*,*,#29034,.F.);
#38582=ORIENTED_EDGE('',*,*,#29033,.F.);
#38583=ORIENTED_EDGE('',*,*,#29035,.T.);
#38584=ORIENTED_EDGE('',*,*,#29036,.T.);
#38585=ORIENTED_EDGE('',*,*,#29037,.F.);
#38586=ORIENTED_EDGE('',*,*,#29036,.F.);
#38587=ORIENTED_EDGE('',*,*,#29038,.F.);
#38588=ORIENTED_EDGE('',*,*,#29039,.T.);
#38589=ORIENTED_EDGE('',*,*,#29040,.F.);
#38590=ORIENTED_EDGE('',*,*,#29039,.F.);
#38591=ORIENTED_EDGE('',*,*,#29041,.T.);
#38592=ORIENTED_EDGE('',*,*,#29042,.T.);
#38593=ORIENTED_EDGE('',*,*,#29043,.F.);
#38594=ORIENTED_EDGE('',*,*,#29042,.F.);
#38595=ORIENTED_EDGE('',*,*,#29044,.F.);
#38596=ORIENTED_EDGE('',*,*,#29045,.T.);
#38597=ORIENTED_EDGE('',*,*,#29046,.F.);
#38598=ORIENTED_EDGE('',*,*,#29045,.F.);
#38599=ORIENTED_EDGE('',*,*,#29047,.T.);
#38600=ORIENTED_EDGE('',*,*,#29048,.T.);
#38601=ORIENTED_EDGE('',*,*,#29049,.F.);
#38602=ORIENTED_EDGE('',*,*,#29048,.F.);
#38603=ORIENTED_EDGE('',*,*,#29050,.F.);
#38604=ORIENTED_EDGE('',*,*,#29051,.T.);
#38605=ORIENTED_EDGE('',*,*,#29052,.F.);
#38606=ORIENTED_EDGE('',*,*,#29051,.F.);
#38607=ORIENTED_EDGE('',*,*,#29053,.T.);
#38608=ORIENTED_EDGE('',*,*,#29054,.T.);
#38609=ORIENTED_EDGE('',*,*,#29055,.F.);
#38610=ORIENTED_EDGE('',*,*,#29054,.F.);
#38611=ORIENTED_EDGE('',*,*,#29056,.F.);
#38612=ORIENTED_EDGE('',*,*,#29057,.T.);
#38613=ORIENTED_EDGE('',*,*,#29058,.F.);
#38614=ORIENTED_EDGE('',*,*,#29057,.F.);
#38615=ORIENTED_EDGE('',*,*,#29059,.T.);
#38616=ORIENTED_EDGE('',*,*,#29060,.T.);
#38617=ORIENTED_EDGE('',*,*,#29061,.F.);
#38618=ORIENTED_EDGE('',*,*,#29060,.F.);
#38619=ORIENTED_EDGE('',*,*,#29062,.F.);
#38620=ORIENTED_EDGE('',*,*,#29063,.T.);
#38621=ORIENTED_EDGE('',*,*,#29064,.F.);
#38622=ORIENTED_EDGE('',*,*,#29063,.F.);
#38623=ORIENTED_EDGE('',*,*,#29065,.T.);
#38624=ORIENTED_EDGE('',*,*,#29066,.T.);
#38625=ORIENTED_EDGE('',*,*,#29067,.F.);
#38626=ORIENTED_EDGE('',*,*,#29066,.F.);
#38627=ORIENTED_EDGE('',*,*,#29068,.F.);
#38628=ORIENTED_EDGE('',*,*,#29069,.T.);
#38629=ORIENTED_EDGE('',*,*,#29070,.F.);
#38630=ORIENTED_EDGE('',*,*,#29069,.F.);
#38631=ORIENTED_EDGE('',*,*,#29071,.T.);
#38632=ORIENTED_EDGE('',*,*,#29072,.T.);
#38633=ORIENTED_EDGE('',*,*,#29073,.F.);
#38634=ORIENTED_EDGE('',*,*,#29072,.F.);
#38635=ORIENTED_EDGE('',*,*,#29074,.F.);
#38636=ORIENTED_EDGE('',*,*,#29075,.T.);
#38637=ORIENTED_EDGE('',*,*,#29076,.F.);
#38638=ORIENTED_EDGE('',*,*,#29075,.F.);
#38639=ORIENTED_EDGE('',*,*,#29077,.T.);
#38640=ORIENTED_EDGE('',*,*,#29078,.T.);
#38641=ORIENTED_EDGE('',*,*,#29079,.F.);
#38642=ORIENTED_EDGE('',*,*,#29078,.F.);
#38643=ORIENTED_EDGE('',*,*,#29080,.F.);
#38644=ORIENTED_EDGE('',*,*,#29081,.T.);
#38645=ORIENTED_EDGE('',*,*,#29082,.F.);
#38646=ORIENTED_EDGE('',*,*,#29081,.F.);
#38647=ORIENTED_EDGE('',*,*,#29083,.T.);
#38648=ORIENTED_EDGE('',*,*,#29084,.T.);
#38649=ORIENTED_EDGE('',*,*,#29085,.F.);
#38650=ORIENTED_EDGE('',*,*,#29084,.F.);
#38651=ORIENTED_EDGE('',*,*,#29086,.F.);
#38652=ORIENTED_EDGE('',*,*,#29087,.T.);
#38653=ORIENTED_EDGE('',*,*,#29088,.F.);
#38654=ORIENTED_EDGE('',*,*,#29087,.F.);
#38655=ORIENTED_EDGE('',*,*,#29089,.T.);
#38656=ORIENTED_EDGE('',*,*,#29090,.T.);
#38657=ORIENTED_EDGE('',*,*,#29091,.F.);
#38658=ORIENTED_EDGE('',*,*,#29090,.F.);
#38659=ORIENTED_EDGE('',*,*,#29092,.F.);
#38660=ORIENTED_EDGE('',*,*,#29093,.T.);
#38661=ORIENTED_EDGE('',*,*,#29094,.F.);
#38662=ORIENTED_EDGE('',*,*,#29093,.F.);
#38663=ORIENTED_EDGE('',*,*,#29095,.T.);
#38664=ORIENTED_EDGE('',*,*,#29096,.T.);
#38665=ORIENTED_EDGE('',*,*,#29097,.F.);
#38666=ORIENTED_EDGE('',*,*,#29096,.F.);
#38667=ORIENTED_EDGE('',*,*,#29098,.F.);
#38668=ORIENTED_EDGE('',*,*,#29099,.T.);
#38669=ORIENTED_EDGE('',*,*,#29100,.F.);
#38670=ORIENTED_EDGE('',*,*,#29099,.F.);
#38671=ORIENTED_EDGE('',*,*,#29101,.T.);
#38672=ORIENTED_EDGE('',*,*,#29102,.T.);
#38673=ORIENTED_EDGE('',*,*,#29103,.F.);
#38674=ORIENTED_EDGE('',*,*,#29102,.F.);
#38675=ORIENTED_EDGE('',*,*,#29104,.F.);
#38676=ORIENTED_EDGE('',*,*,#29105,.T.);
#38677=ORIENTED_EDGE('',*,*,#29106,.F.);
#38678=ORIENTED_EDGE('',*,*,#29105,.F.);
#38679=ORIENTED_EDGE('',*,*,#29107,.T.);
#38680=ORIENTED_EDGE('',*,*,#29108,.T.);
#38681=ORIENTED_EDGE('',*,*,#29109,.F.);
#38682=ORIENTED_EDGE('',*,*,#29108,.F.);
#38683=ORIENTED_EDGE('',*,*,#29110,.F.);
#38684=ORIENTED_EDGE('',*,*,#29111,.T.);
#38685=ORIENTED_EDGE('',*,*,#29112,.F.);
#38686=ORIENTED_EDGE('',*,*,#29111,.F.);
#38687=ORIENTED_EDGE('',*,*,#29113,.T.);
#38688=ORIENTED_EDGE('',*,*,#29114,.T.);
#38689=ORIENTED_EDGE('',*,*,#29115,.F.);
#38690=ORIENTED_EDGE('',*,*,#29114,.F.);
#38691=ORIENTED_EDGE('',*,*,#29116,.F.);
#38692=ORIENTED_EDGE('',*,*,#29117,.T.);
#38693=ORIENTED_EDGE('',*,*,#29118,.F.);
#38694=ORIENTED_EDGE('',*,*,#29117,.F.);
#38695=ORIENTED_EDGE('',*,*,#29119,.T.);
#38696=ORIENTED_EDGE('',*,*,#29120,.T.);
#38697=ORIENTED_EDGE('',*,*,#29121,.F.);
#38698=ORIENTED_EDGE('',*,*,#29120,.F.);
#38699=ORIENTED_EDGE('',*,*,#29122,.F.);
#38700=ORIENTED_EDGE('',*,*,#29123,.T.);
#38701=ORIENTED_EDGE('',*,*,#29124,.F.);
#38702=ORIENTED_EDGE('',*,*,#29123,.F.);
#38703=ORIENTED_EDGE('',*,*,#29125,.T.);
#38704=ORIENTED_EDGE('',*,*,#29126,.T.);
#38705=ORIENTED_EDGE('',*,*,#29127,.F.);
#38706=ORIENTED_EDGE('',*,*,#29126,.F.);
#38707=ORIENTED_EDGE('',*,*,#29128,.F.);
#38708=ORIENTED_EDGE('',*,*,#29129,.T.);
#38709=ORIENTED_EDGE('',*,*,#29130,.F.);
#38710=ORIENTED_EDGE('',*,*,#29129,.F.);
#38711=ORIENTED_EDGE('',*,*,#29131,.T.);
#38712=ORIENTED_EDGE('',*,*,#29132,.T.);
#38713=ORIENTED_EDGE('',*,*,#29133,.F.);
#38714=ORIENTED_EDGE('',*,*,#29132,.F.);
#38715=ORIENTED_EDGE('',*,*,#29134,.F.);
#38716=ORIENTED_EDGE('',*,*,#29135,.T.);
#38717=ORIENTED_EDGE('',*,*,#29136,.F.);
#38718=ORIENTED_EDGE('',*,*,#29135,.F.);
#38719=ORIENTED_EDGE('',*,*,#29137,.T.);
#38720=ORIENTED_EDGE('',*,*,#29138,.T.);
#38721=ORIENTED_EDGE('',*,*,#29139,.F.);
#38722=ORIENTED_EDGE('',*,*,#29138,.F.);
#38723=ORIENTED_EDGE('',*,*,#29140,.F.);
#38724=ORIENTED_EDGE('',*,*,#29141,.T.);
#38725=ORIENTED_EDGE('',*,*,#29142,.F.);
#38726=ORIENTED_EDGE('',*,*,#29141,.F.);
#38727=ORIENTED_EDGE('',*,*,#29143,.T.);
#38728=ORIENTED_EDGE('',*,*,#29144,.T.);
#38729=ORIENTED_EDGE('',*,*,#29145,.F.);
#38730=ORIENTED_EDGE('',*,*,#29144,.F.);
#38731=ORIENTED_EDGE('',*,*,#29146,.F.);
#38732=ORIENTED_EDGE('',*,*,#29147,.T.);
#38733=ORIENTED_EDGE('',*,*,#29148,.F.);
#38734=ORIENTED_EDGE('',*,*,#29147,.F.);
#38735=ORIENTED_EDGE('',*,*,#29149,.T.);
#38736=ORIENTED_EDGE('',*,*,#29150,.T.);
#38737=ORIENTED_EDGE('',*,*,#29151,.F.);
#38738=ORIENTED_EDGE('',*,*,#29150,.F.);
#38739=ORIENTED_EDGE('',*,*,#29152,.F.);
#38740=ORIENTED_EDGE('',*,*,#29153,.T.);
#38741=ORIENTED_EDGE('',*,*,#29154,.F.);
#38742=ORIENTED_EDGE('',*,*,#29153,.F.);
#38743=ORIENTED_EDGE('',*,*,#29155,.T.);
#38744=ORIENTED_EDGE('',*,*,#29156,.T.);
#38745=ORIENTED_EDGE('',*,*,#29157,.F.);
#38746=ORIENTED_EDGE('',*,*,#29156,.F.);
#38747=ORIENTED_EDGE('',*,*,#29158,.F.);
#38748=ORIENTED_EDGE('',*,*,#29159,.T.);
#38749=ORIENTED_EDGE('',*,*,#29160,.F.);
#38750=ORIENTED_EDGE('',*,*,#29159,.F.);
#38751=ORIENTED_EDGE('',*,*,#29161,.T.);
#38752=ORIENTED_EDGE('',*,*,#29162,.T.);
#38753=ORIENTED_EDGE('',*,*,#29163,.F.);
#38754=ORIENTED_EDGE('',*,*,#29162,.F.);
#38755=ORIENTED_EDGE('',*,*,#29164,.F.);
#38756=ORIENTED_EDGE('',*,*,#29165,.T.);
#38757=ORIENTED_EDGE('',*,*,#29166,.F.);
#38758=ORIENTED_EDGE('',*,*,#29165,.F.);
#38759=ORIENTED_EDGE('',*,*,#29167,.T.);
#38760=ORIENTED_EDGE('',*,*,#29168,.T.);
#38761=ORIENTED_EDGE('',*,*,#29169,.F.);
#38762=ORIENTED_EDGE('',*,*,#29168,.F.);
#38763=ORIENTED_EDGE('',*,*,#29170,.F.);
#38764=ORIENTED_EDGE('',*,*,#29171,.T.);
#38765=ORIENTED_EDGE('',*,*,#29172,.F.);
#38766=ORIENTED_EDGE('',*,*,#29171,.F.);
#38767=ORIENTED_EDGE('',*,*,#29173,.T.);
#38768=ORIENTED_EDGE('',*,*,#29174,.T.);
#38769=ORIENTED_EDGE('',*,*,#29175,.F.);
#38770=ORIENTED_EDGE('',*,*,#29174,.F.);
#38771=ORIENTED_EDGE('',*,*,#29176,.F.);
#38772=ORIENTED_EDGE('',*,*,#29177,.T.);
#38773=ORIENTED_EDGE('',*,*,#29178,.F.);
#38774=ORIENTED_EDGE('',*,*,#29177,.F.);
#38775=ORIENTED_EDGE('',*,*,#29179,.T.);
#38776=ORIENTED_EDGE('',*,*,#29180,.T.);
#38777=ORIENTED_EDGE('',*,*,#29181,.F.);
#38778=ORIENTED_EDGE('',*,*,#29180,.F.);
#38779=ORIENTED_EDGE('',*,*,#29182,.F.);
#38780=ORIENTED_EDGE('',*,*,#29183,.T.);
#38781=ORIENTED_EDGE('',*,*,#29184,.F.);
#38782=ORIENTED_EDGE('',*,*,#29183,.F.);
#38783=ORIENTED_EDGE('',*,*,#29185,.T.);
#38784=ORIENTED_EDGE('',*,*,#29186,.T.);
#38785=ORIENTED_EDGE('',*,*,#29187,.F.);
#38786=ORIENTED_EDGE('',*,*,#29186,.F.);
#38787=ORIENTED_EDGE('',*,*,#29188,.F.);
#38788=ORIENTED_EDGE('',*,*,#29189,.T.);
#38789=ORIENTED_EDGE('',*,*,#29190,.F.);
#38790=ORIENTED_EDGE('',*,*,#29189,.F.);
#38791=ORIENTED_EDGE('',*,*,#29191,.T.);
#38792=ORIENTED_EDGE('',*,*,#29192,.T.);
#38793=ORIENTED_EDGE('',*,*,#29193,.F.);
#38794=ORIENTED_EDGE('',*,*,#29192,.F.);
#38795=ORIENTED_EDGE('',*,*,#29194,.F.);
#38796=ORIENTED_EDGE('',*,*,#29195,.T.);
#38797=ORIENTED_EDGE('',*,*,#29196,.F.);
#38798=ORIENTED_EDGE('',*,*,#29195,.F.);
#38799=ORIENTED_EDGE('',*,*,#29197,.T.);
#38800=ORIENTED_EDGE('',*,*,#29198,.T.);
#38801=ORIENTED_EDGE('',*,*,#29199,.F.);
#38802=ORIENTED_EDGE('',*,*,#29198,.F.);
#38803=ORIENTED_EDGE('',*,*,#29200,.F.);
#38804=ORIENTED_EDGE('',*,*,#29201,.T.);
#38805=ORIENTED_EDGE('',*,*,#29202,.F.);
#38806=ORIENTED_EDGE('',*,*,#29201,.F.);
#38807=ORIENTED_EDGE('',*,*,#29203,.T.);
#38808=ORIENTED_EDGE('',*,*,#29204,.T.);
#38809=ORIENTED_EDGE('',*,*,#29205,.F.);
#38810=ORIENTED_EDGE('',*,*,#29204,.F.);
#38811=ORIENTED_EDGE('',*,*,#29206,.F.);
#38812=ORIENTED_EDGE('',*,*,#29207,.T.);
#38813=ORIENTED_EDGE('',*,*,#29208,.F.);
#38814=ORIENTED_EDGE('',*,*,#29207,.F.);
#38815=ORIENTED_EDGE('',*,*,#29209,.T.);
#38816=ORIENTED_EDGE('',*,*,#29210,.T.);
#38817=ORIENTED_EDGE('',*,*,#29211,.F.);
#38818=ORIENTED_EDGE('',*,*,#29210,.F.);
#38819=ORIENTED_EDGE('',*,*,#29212,.F.);
#38820=ORIENTED_EDGE('',*,*,#29213,.T.);
#38821=ORIENTED_EDGE('',*,*,#29214,.F.);
#38822=ORIENTED_EDGE('',*,*,#29213,.F.);
#38823=ORIENTED_EDGE('',*,*,#29215,.T.);
#38824=ORIENTED_EDGE('',*,*,#29216,.T.);
#38825=ORIENTED_EDGE('',*,*,#29217,.F.);
#38826=ORIENTED_EDGE('',*,*,#29216,.F.);
#38827=ORIENTED_EDGE('',*,*,#29218,.F.);
#38828=ORIENTED_EDGE('',*,*,#29219,.T.);
#38829=ORIENTED_EDGE('',*,*,#29220,.F.);
#38830=ORIENTED_EDGE('',*,*,#29219,.F.);
#38831=ORIENTED_EDGE('',*,*,#29221,.T.);
#38832=ORIENTED_EDGE('',*,*,#29222,.T.);
#38833=ORIENTED_EDGE('',*,*,#29223,.F.);
#38834=ORIENTED_EDGE('',*,*,#29222,.F.);
#38835=ORIENTED_EDGE('',*,*,#29224,.F.);
#38836=ORIENTED_EDGE('',*,*,#29225,.T.);
#38837=ORIENTED_EDGE('',*,*,#29226,.F.);
#38838=ORIENTED_EDGE('',*,*,#29225,.F.);
#38839=ORIENTED_EDGE('',*,*,#29227,.T.);
#38840=ORIENTED_EDGE('',*,*,#29228,.T.);
#38841=ORIENTED_EDGE('',*,*,#29229,.F.);
#38842=ORIENTED_EDGE('',*,*,#29228,.F.);
#38843=ORIENTED_EDGE('',*,*,#29230,.F.);
#38844=ORIENTED_EDGE('',*,*,#29231,.T.);
#38845=ORIENTED_EDGE('',*,*,#29232,.F.);
#38846=ORIENTED_EDGE('',*,*,#29231,.F.);
#38847=ORIENTED_EDGE('',*,*,#29233,.T.);
#38848=ORIENTED_EDGE('',*,*,#29234,.T.);
#38849=ORIENTED_EDGE('',*,*,#29235,.F.);
#38850=ORIENTED_EDGE('',*,*,#29234,.F.);
#38851=ORIENTED_EDGE('',*,*,#29236,.F.);
#38852=ORIENTED_EDGE('',*,*,#29237,.T.);
#38853=ORIENTED_EDGE('',*,*,#29238,.F.);
#38854=ORIENTED_EDGE('',*,*,#29237,.F.);
#38855=ORIENTED_EDGE('',*,*,#29239,.T.);
#38856=ORIENTED_EDGE('',*,*,#29240,.T.);
#38857=ORIENTED_EDGE('',*,*,#29241,.F.);
#38858=ORIENTED_EDGE('',*,*,#29240,.F.);
#38859=ORIENTED_EDGE('',*,*,#29242,.F.);
#38860=ORIENTED_EDGE('',*,*,#29243,.T.);
#38861=ORIENTED_EDGE('',*,*,#29244,.F.);
#38862=ORIENTED_EDGE('',*,*,#29243,.F.);
#38863=ORIENTED_EDGE('',*,*,#29245,.T.);
#38864=ORIENTED_EDGE('',*,*,#29246,.T.);
#38865=ORIENTED_EDGE('',*,*,#29247,.F.);
#38866=ORIENTED_EDGE('',*,*,#29246,.F.);
#38867=ORIENTED_EDGE('',*,*,#29248,.F.);
#38868=ORIENTED_EDGE('',*,*,#29249,.T.);
#38869=ORIENTED_EDGE('',*,*,#29250,.F.);
#38870=ORIENTED_EDGE('',*,*,#29249,.F.);
#38871=ORIENTED_EDGE('',*,*,#29251,.T.);
#38872=ORIENTED_EDGE('',*,*,#29252,.T.);
#38873=ORIENTED_EDGE('',*,*,#29253,.F.);
#38874=ORIENTED_EDGE('',*,*,#29252,.F.);
#38875=ORIENTED_EDGE('',*,*,#29254,.F.);
#38876=ORIENTED_EDGE('',*,*,#29255,.T.);
#38877=ORIENTED_EDGE('',*,*,#29256,.F.);
#38878=ORIENTED_EDGE('',*,*,#29255,.F.);
#38879=ORIENTED_EDGE('',*,*,#29257,.T.);
#38880=ORIENTED_EDGE('',*,*,#29258,.T.);
#38881=ORIENTED_EDGE('',*,*,#29259,.F.);
#38882=ORIENTED_EDGE('',*,*,#29258,.F.);
#38883=ORIENTED_EDGE('',*,*,#29260,.F.);
#38884=ORIENTED_EDGE('',*,*,#29261,.T.);
#38885=ORIENTED_EDGE('',*,*,#29262,.F.);
#38886=ORIENTED_EDGE('',*,*,#29261,.F.);
#38887=ORIENTED_EDGE('',*,*,#29263,.T.);
#38888=ORIENTED_EDGE('',*,*,#29264,.T.);
#38889=ORIENTED_EDGE('',*,*,#29265,.F.);
#38890=ORIENTED_EDGE('',*,*,#29264,.F.);
#38891=ORIENTED_EDGE('',*,*,#29266,.F.);
#38892=ORIENTED_EDGE('',*,*,#29267,.T.);
#38893=ORIENTED_EDGE('',*,*,#29268,.F.);
#38894=ORIENTED_EDGE('',*,*,#29267,.F.);
#38895=ORIENTED_EDGE('',*,*,#29269,.T.);
#38896=ORIENTED_EDGE('',*,*,#29270,.T.);
#38897=ORIENTED_EDGE('',*,*,#29271,.F.);
#38898=ORIENTED_EDGE('',*,*,#29270,.F.);
#38899=ORIENTED_EDGE('',*,*,#29272,.F.);
#38900=ORIENTED_EDGE('',*,*,#29273,.T.);
#38901=ORIENTED_EDGE('',*,*,#29274,.F.);
#38902=ORIENTED_EDGE('',*,*,#29273,.F.);
#38903=ORIENTED_EDGE('',*,*,#29275,.T.);
#38904=ORIENTED_EDGE('',*,*,#29276,.T.);
#38905=ORIENTED_EDGE('',*,*,#29277,.F.);
#38906=ORIENTED_EDGE('',*,*,#29276,.F.);
#38907=ORIENTED_EDGE('',*,*,#29278,.F.);
#38908=ORIENTED_EDGE('',*,*,#29279,.T.);
#38909=ORIENTED_EDGE('',*,*,#29280,.F.);
#38910=ORIENTED_EDGE('',*,*,#29279,.F.);
#38911=ORIENTED_EDGE('',*,*,#29281,.T.);
#38912=ORIENTED_EDGE('',*,*,#29282,.T.);
#38913=ORIENTED_EDGE('',*,*,#29283,.F.);
#38914=ORIENTED_EDGE('',*,*,#29282,.F.);
#38915=ORIENTED_EDGE('',*,*,#29284,.F.);
#38916=ORIENTED_EDGE('',*,*,#29285,.T.);
#38917=ORIENTED_EDGE('',*,*,#29286,.F.);
#38918=ORIENTED_EDGE('',*,*,#29285,.F.);
#38919=ORIENTED_EDGE('',*,*,#29287,.T.);
#38920=ORIENTED_EDGE('',*,*,#29288,.T.);
#38921=ORIENTED_EDGE('',*,*,#29289,.F.);
#38922=ORIENTED_EDGE('',*,*,#29288,.F.);
#38923=ORIENTED_EDGE('',*,*,#29290,.F.);
#38924=ORIENTED_EDGE('',*,*,#29291,.T.);
#38925=ORIENTED_EDGE('',*,*,#29292,.F.);
#38926=ORIENTED_EDGE('',*,*,#29291,.F.);
#38927=ORIENTED_EDGE('',*,*,#29293,.T.);
#38928=ORIENTED_EDGE('',*,*,#29294,.T.);
#38929=ORIENTED_EDGE('',*,*,#29295,.F.);
#38930=ORIENTED_EDGE('',*,*,#29294,.F.);
#38931=ORIENTED_EDGE('',*,*,#29296,.F.);
#38932=ORIENTED_EDGE('',*,*,#29297,.T.);
#38933=ORIENTED_EDGE('',*,*,#29298,.F.);
#38934=ORIENTED_EDGE('',*,*,#29297,.F.);
#38935=ORIENTED_EDGE('',*,*,#29299,.T.);
#38936=ORIENTED_EDGE('',*,*,#29300,.T.);
#38937=ORIENTED_EDGE('',*,*,#29301,.F.);
#38938=ORIENTED_EDGE('',*,*,#29300,.F.);
#38939=ORIENTED_EDGE('',*,*,#29302,.F.);
#38940=ORIENTED_EDGE('',*,*,#29303,.T.);
#38941=ORIENTED_EDGE('',*,*,#29304,.F.);
#38942=ORIENTED_EDGE('',*,*,#29303,.F.);
#38943=ORIENTED_EDGE('',*,*,#29305,.T.);
#38944=ORIENTED_EDGE('',*,*,#29306,.T.);
#38945=ORIENTED_EDGE('',*,*,#29307,.F.);
#38946=ORIENTED_EDGE('',*,*,#29306,.F.);
#38947=ORIENTED_EDGE('',*,*,#29308,.F.);
#38948=ORIENTED_EDGE('',*,*,#29309,.T.);
#38949=ORIENTED_EDGE('',*,*,#29310,.F.);
#38950=ORIENTED_EDGE('',*,*,#29309,.F.);
#38951=ORIENTED_EDGE('',*,*,#29311,.T.);
#38952=ORIENTED_EDGE('',*,*,#29312,.T.);
#38953=ORIENTED_EDGE('',*,*,#29313,.F.);
#38954=ORIENTED_EDGE('',*,*,#29312,.F.);
#38955=ORIENTED_EDGE('',*,*,#29314,.F.);
#38956=ORIENTED_EDGE('',*,*,#29315,.T.);
#38957=ORIENTED_EDGE('',*,*,#29316,.F.);
#38958=ORIENTED_EDGE('',*,*,#29315,.F.);
#38959=ORIENTED_EDGE('',*,*,#29317,.T.);
#38960=ORIENTED_EDGE('',*,*,#29318,.T.);
#38961=ORIENTED_EDGE('',*,*,#29319,.F.);
#38962=ORIENTED_EDGE('',*,*,#29318,.F.);
#38963=ORIENTED_EDGE('',*,*,#29320,.F.);
#38964=ORIENTED_EDGE('',*,*,#29321,.T.);
#38965=ORIENTED_EDGE('',*,*,#29322,.F.);
#38966=ORIENTED_EDGE('',*,*,#29321,.F.);
#38967=ORIENTED_EDGE('',*,*,#29323,.T.);
#38968=ORIENTED_EDGE('',*,*,#29324,.T.);
#38969=ORIENTED_EDGE('',*,*,#29325,.F.);
#38970=ORIENTED_EDGE('',*,*,#29324,.F.);
#38971=ORIENTED_EDGE('',*,*,#29326,.F.);
#38972=ORIENTED_EDGE('',*,*,#29327,.T.);
#38973=ORIENTED_EDGE('',*,*,#29328,.F.);
#38974=ORIENTED_EDGE('',*,*,#29327,.F.);
#38975=ORIENTED_EDGE('',*,*,#29329,.T.);
#38976=ORIENTED_EDGE('',*,*,#29330,.T.);
#38977=ORIENTED_EDGE('',*,*,#29331,.F.);
#38978=ORIENTED_EDGE('',*,*,#29330,.F.);
#38979=ORIENTED_EDGE('',*,*,#29332,.F.);
#38980=ORIENTED_EDGE('',*,*,#29333,.T.);
#38981=ORIENTED_EDGE('',*,*,#29334,.F.);
#38982=ORIENTED_EDGE('',*,*,#29333,.F.);
#38983=ORIENTED_EDGE('',*,*,#29335,.T.);
#38984=ORIENTED_EDGE('',*,*,#29336,.T.);
#38985=ORIENTED_EDGE('',*,*,#29337,.F.);
#38986=ORIENTED_EDGE('',*,*,#29336,.F.);
#38987=ORIENTED_EDGE('',*,*,#29338,.F.);
#38988=ORIENTED_EDGE('',*,*,#29339,.T.);
#38989=ORIENTED_EDGE('',*,*,#29340,.F.);
#38990=ORIENTED_EDGE('',*,*,#29339,.F.);
#38991=ORIENTED_EDGE('',*,*,#29341,.T.);
#38992=ORIENTED_EDGE('',*,*,#29342,.T.);
#38993=ORIENTED_EDGE('',*,*,#29343,.F.);
#38994=ORIENTED_EDGE('',*,*,#29342,.F.);
#38995=ORIENTED_EDGE('',*,*,#29344,.F.);
#38996=ORIENTED_EDGE('',*,*,#29345,.T.);
#38997=ORIENTED_EDGE('',*,*,#29346,.F.);
#38998=ORIENTED_EDGE('',*,*,#29345,.F.);
#38999=ORIENTED_EDGE('',*,*,#29347,.T.);
#39000=ORIENTED_EDGE('',*,*,#29348,.T.);
#39001=ORIENTED_EDGE('',*,*,#29349,.F.);
#39002=ORIENTED_EDGE('',*,*,#29348,.F.);
#39003=ORIENTED_EDGE('',*,*,#29350,.F.);
#39004=ORIENTED_EDGE('',*,*,#29351,.T.);
#39005=ORIENTED_EDGE('',*,*,#29352,.F.);
#39006=ORIENTED_EDGE('',*,*,#29351,.F.);
#39007=ORIENTED_EDGE('',*,*,#29353,.T.);
#39008=ORIENTED_EDGE('',*,*,#29354,.T.);
#39009=ORIENTED_EDGE('',*,*,#29355,.F.);
#39010=ORIENTED_EDGE('',*,*,#29354,.F.);
#39011=ORIENTED_EDGE('',*,*,#29356,.F.);
#39012=ORIENTED_EDGE('',*,*,#29357,.T.);
#39013=ORIENTED_EDGE('',*,*,#29358,.F.);
#39014=ORIENTED_EDGE('',*,*,#29357,.F.);
#39015=ORIENTED_EDGE('',*,*,#29359,.T.);
#39016=ORIENTED_EDGE('',*,*,#29360,.T.);
#39017=ORIENTED_EDGE('',*,*,#29361,.F.);
#39018=ORIENTED_EDGE('',*,*,#29360,.F.);
#39019=ORIENTED_EDGE('',*,*,#29362,.F.);
#39020=ORIENTED_EDGE('',*,*,#29363,.T.);
#39021=ORIENTED_EDGE('',*,*,#29364,.F.);
#39022=ORIENTED_EDGE('',*,*,#29363,.F.);
#39023=ORIENTED_EDGE('',*,*,#29365,.T.);
#39024=ORIENTED_EDGE('',*,*,#29366,.T.);
#39025=ORIENTED_EDGE('',*,*,#29367,.F.);
#39026=ORIENTED_EDGE('',*,*,#29366,.F.);
#39027=ORIENTED_EDGE('',*,*,#29368,.F.);
#39028=ORIENTED_EDGE('',*,*,#29369,.T.);
#39029=ORIENTED_EDGE('',*,*,#29370,.F.);
#39030=ORIENTED_EDGE('',*,*,#29369,.F.);
#39031=ORIENTED_EDGE('',*,*,#29371,.T.);
#39032=ORIENTED_EDGE('',*,*,#29372,.T.);
#39033=ORIENTED_EDGE('',*,*,#29373,.F.);
#39034=ORIENTED_EDGE('',*,*,#29372,.F.);
#39035=ORIENTED_EDGE('',*,*,#29374,.F.);
#39036=ORIENTED_EDGE('',*,*,#29375,.T.);
#39037=ORIENTED_EDGE('',*,*,#29376,.F.);
#39038=ORIENTED_EDGE('',*,*,#29375,.F.);
#39039=ORIENTED_EDGE('',*,*,#29377,.T.);
#39040=ORIENTED_EDGE('',*,*,#29378,.T.);
#39041=ORIENTED_EDGE('',*,*,#29379,.F.);
#39042=ORIENTED_EDGE('',*,*,#29378,.F.);
#39043=ORIENTED_EDGE('',*,*,#29380,.F.);
#39044=ORIENTED_EDGE('',*,*,#29381,.T.);
#39045=ORIENTED_EDGE('',*,*,#29382,.F.);
#39046=ORIENTED_EDGE('',*,*,#29381,.F.);
#39047=ORIENTED_EDGE('',*,*,#29383,.T.);
#39048=ORIENTED_EDGE('',*,*,#29384,.T.);
#39049=ORIENTED_EDGE('',*,*,#29385,.F.);
#39050=ORIENTED_EDGE('',*,*,#29384,.F.);
#39051=ORIENTED_EDGE('',*,*,#29386,.F.);
#39052=ORIENTED_EDGE('',*,*,#29387,.T.);
#39053=ORIENTED_EDGE('',*,*,#29388,.F.);
#39054=ORIENTED_EDGE('',*,*,#29387,.F.);
#39055=ORIENTED_EDGE('',*,*,#29389,.T.);
#39056=ORIENTED_EDGE('',*,*,#29390,.T.);
#39057=ORIENTED_EDGE('',*,*,#29391,.F.);
#39058=ORIENTED_EDGE('',*,*,#29390,.F.);
#39059=ORIENTED_EDGE('',*,*,#29392,.F.);
#39060=ORIENTED_EDGE('',*,*,#29393,.T.);
#39061=ORIENTED_EDGE('',*,*,#29394,.F.);
#39062=ORIENTED_EDGE('',*,*,#29393,.F.);
#39063=ORIENTED_EDGE('',*,*,#29395,.T.);
#39064=ORIENTED_EDGE('',*,*,#29396,.T.);
#39065=ORIENTED_EDGE('',*,*,#29397,.F.);
#39066=ORIENTED_EDGE('',*,*,#29396,.F.);
#39067=ORIENTED_EDGE('',*,*,#29398,.F.);
#39068=ORIENTED_EDGE('',*,*,#29399,.T.);
#39069=ORIENTED_EDGE('',*,*,#29400,.F.);
#39070=ORIENTED_EDGE('',*,*,#29399,.F.);
#39071=ORIENTED_EDGE('',*,*,#29401,.T.);
#39072=ORIENTED_EDGE('',*,*,#29402,.T.);
#39073=ORIENTED_EDGE('',*,*,#29403,.F.);
#39074=ORIENTED_EDGE('',*,*,#29402,.F.);
#39075=ORIENTED_EDGE('',*,*,#29404,.F.);
#39076=ORIENTED_EDGE('',*,*,#29405,.T.);
#39077=ORIENTED_EDGE('',*,*,#29406,.F.);
#39078=ORIENTED_EDGE('',*,*,#29405,.F.);
#39079=ORIENTED_EDGE('',*,*,#29407,.T.);
#39080=ORIENTED_EDGE('',*,*,#29408,.T.);
#39081=ORIENTED_EDGE('',*,*,#29409,.F.);
#39082=ORIENTED_EDGE('',*,*,#29408,.F.);
#39083=ORIENTED_EDGE('',*,*,#29410,.F.);
#39084=ORIENTED_EDGE('',*,*,#29411,.T.);
#39085=ORIENTED_EDGE('',*,*,#29412,.F.);
#39086=ORIENTED_EDGE('',*,*,#29411,.F.);
#39087=ORIENTED_EDGE('',*,*,#29413,.T.);
#39088=ORIENTED_EDGE('',*,*,#29414,.T.);
#39089=ORIENTED_EDGE('',*,*,#29415,.F.);
#39090=ORIENTED_EDGE('',*,*,#29414,.F.);
#39091=ORIENTED_EDGE('',*,*,#29416,.F.);
#39092=ORIENTED_EDGE('',*,*,#29417,.T.);
#39093=ORIENTED_EDGE('',*,*,#29418,.F.);
#39094=ORIENTED_EDGE('',*,*,#29417,.F.);
#39095=ORIENTED_EDGE('',*,*,#29419,.T.);
#39096=ORIENTED_EDGE('',*,*,#29420,.T.);
#39097=ORIENTED_EDGE('',*,*,#29421,.F.);
#39098=ORIENTED_EDGE('',*,*,#29420,.F.);
#39099=ORIENTED_EDGE('',*,*,#29422,.F.);
#39100=ORIENTED_EDGE('',*,*,#29423,.T.);
#39101=ORIENTED_EDGE('',*,*,#29424,.F.);
#39102=ORIENTED_EDGE('',*,*,#29423,.F.);
#39103=ORIENTED_EDGE('',*,*,#29425,.T.);
#39104=ORIENTED_EDGE('',*,*,#29426,.T.);
#39105=ORIENTED_EDGE('',*,*,#29427,.F.);
#39106=ORIENTED_EDGE('',*,*,#29426,.F.);
#39107=ORIENTED_EDGE('',*,*,#29428,.F.);
#39108=ORIENTED_EDGE('',*,*,#29429,.T.);
#39109=ORIENTED_EDGE('',*,*,#29430,.F.);
#39110=ORIENTED_EDGE('',*,*,#29429,.F.);
#39111=ORIENTED_EDGE('',*,*,#29431,.T.);
#39112=ORIENTED_EDGE('',*,*,#29432,.T.);
#39113=ORIENTED_EDGE('',*,*,#29433,.F.);
#39114=ORIENTED_EDGE('',*,*,#29432,.F.);
#39115=ORIENTED_EDGE('',*,*,#29434,.F.);
#39116=ORIENTED_EDGE('',*,*,#29435,.T.);
#39117=ORIENTED_EDGE('',*,*,#29436,.F.);
#39118=ORIENTED_EDGE('',*,*,#29435,.F.);
#39119=ORIENTED_EDGE('',*,*,#29437,.T.);
#39120=ORIENTED_EDGE('',*,*,#29438,.T.);
#39121=ORIENTED_EDGE('',*,*,#29439,.F.);
#39122=ORIENTED_EDGE('',*,*,#29438,.F.);
#39123=ORIENTED_EDGE('',*,*,#29440,.F.);
#39124=ORIENTED_EDGE('',*,*,#29441,.T.);
#39125=ORIENTED_EDGE('',*,*,#29442,.F.);
#39126=ORIENTED_EDGE('',*,*,#29441,.F.);
#39127=ORIENTED_EDGE('',*,*,#29443,.T.);
#39128=ORIENTED_EDGE('',*,*,#29444,.T.);
#39129=ORIENTED_EDGE('',*,*,#29445,.F.);
#39130=ORIENTED_EDGE('',*,*,#29444,.F.);
#39131=ORIENTED_EDGE('',*,*,#29446,.F.);
#39132=ORIENTED_EDGE('',*,*,#29447,.T.);
#39133=ORIENTED_EDGE('',*,*,#29448,.F.);
#39134=ORIENTED_EDGE('',*,*,#29447,.F.);
#39135=ORIENTED_EDGE('',*,*,#29449,.T.);
#39136=ORIENTED_EDGE('',*,*,#29450,.T.);
#39137=ORIENTED_EDGE('',*,*,#29451,.F.);
#39138=ORIENTED_EDGE('',*,*,#29450,.F.);
#39139=ORIENTED_EDGE('',*,*,#29452,.F.);
#39140=ORIENTED_EDGE('',*,*,#29453,.T.);
#39141=ORIENTED_EDGE('',*,*,#29454,.F.);
#39142=ORIENTED_EDGE('',*,*,#29453,.F.);
#39143=ORIENTED_EDGE('',*,*,#29455,.T.);
#39144=ORIENTED_EDGE('',*,*,#29456,.T.);
#39145=ORIENTED_EDGE('',*,*,#29457,.F.);
#39146=ORIENTED_EDGE('',*,*,#29456,.F.);
#39147=ORIENTED_EDGE('',*,*,#29458,.F.);
#39148=ORIENTED_EDGE('',*,*,#29459,.T.);
#39149=ORIENTED_EDGE('',*,*,#29460,.F.);
#39150=ORIENTED_EDGE('',*,*,#29459,.F.);
#39151=ORIENTED_EDGE('',*,*,#29461,.T.);
#39152=ORIENTED_EDGE('',*,*,#29462,.T.);
#39153=ORIENTED_EDGE('',*,*,#29463,.F.);
#39154=ORIENTED_EDGE('',*,*,#29462,.F.);
#39155=ORIENTED_EDGE('',*,*,#29464,.F.);
#39156=ORIENTED_EDGE('',*,*,#29465,.T.);
#39157=ORIENTED_EDGE('',*,*,#29466,.F.);
#39158=ORIENTED_EDGE('',*,*,#29465,.F.);
#39159=ORIENTED_EDGE('',*,*,#29467,.T.);
#39160=ORIENTED_EDGE('',*,*,#29468,.T.);
#39161=ORIENTED_EDGE('',*,*,#29469,.F.);
#39162=ORIENTED_EDGE('',*,*,#29468,.F.);
#39163=ORIENTED_EDGE('',*,*,#29470,.F.);
#39164=ORIENTED_EDGE('',*,*,#29471,.T.);
#39165=ORIENTED_EDGE('',*,*,#29472,.F.);
#39166=ORIENTED_EDGE('',*,*,#29471,.F.);
#39167=ORIENTED_EDGE('',*,*,#29473,.T.);
#39168=ORIENTED_EDGE('',*,*,#29474,.T.);
#39169=ORIENTED_EDGE('',*,*,#29475,.F.);
#39170=ORIENTED_EDGE('',*,*,#29474,.F.);
#39171=ORIENTED_EDGE('',*,*,#29476,.F.);
#39172=ORIENTED_EDGE('',*,*,#29477,.T.);
#39173=ORIENTED_EDGE('',*,*,#29478,.F.);
#39174=ORIENTED_EDGE('',*,*,#29477,.F.);
#39175=ORIENTED_EDGE('',*,*,#29479,.T.);
#39176=ORIENTED_EDGE('',*,*,#29480,.T.);
#39177=ORIENTED_EDGE('',*,*,#29481,.F.);
#39178=ORIENTED_EDGE('',*,*,#29480,.F.);
#39179=ORIENTED_EDGE('',*,*,#29482,.F.);
#39180=ORIENTED_EDGE('',*,*,#29483,.T.);
#39181=ORIENTED_EDGE('',*,*,#29484,.F.);
#39182=ORIENTED_EDGE('',*,*,#29483,.F.);
#39183=ORIENTED_EDGE('',*,*,#29485,.T.);
#39184=ORIENTED_EDGE('',*,*,#29486,.T.);
#39185=ORIENTED_EDGE('',*,*,#29487,.F.);
#39186=ORIENTED_EDGE('',*,*,#29486,.F.);
#39187=ORIENTED_EDGE('',*,*,#29488,.F.);
#39188=ORIENTED_EDGE('',*,*,#29489,.T.);
#39189=ORIENTED_EDGE('',*,*,#29490,.F.);
#39190=ORIENTED_EDGE('',*,*,#29489,.F.);
#39191=ORIENTED_EDGE('',*,*,#29491,.T.);
#39192=ORIENTED_EDGE('',*,*,#29492,.T.);
#39193=ORIENTED_EDGE('',*,*,#29493,.F.);
#39194=ORIENTED_EDGE('',*,*,#29492,.F.);
#39195=ORIENTED_EDGE('',*,*,#29494,.F.);
#39196=ORIENTED_EDGE('',*,*,#29495,.T.);
#39197=ORIENTED_EDGE('',*,*,#29496,.F.);
#39198=ORIENTED_EDGE('',*,*,#29495,.F.);
#39199=ORIENTED_EDGE('',*,*,#29497,.T.);
#39200=ORIENTED_EDGE('',*,*,#29498,.T.);
#39201=ORIENTED_EDGE('',*,*,#29499,.F.);
#39202=ORIENTED_EDGE('',*,*,#29498,.F.);
#39203=ORIENTED_EDGE('',*,*,#29500,.F.);
#39204=ORIENTED_EDGE('',*,*,#29501,.T.);
#39205=ORIENTED_EDGE('',*,*,#29502,.F.);
#39206=ORIENTED_EDGE('',*,*,#29501,.F.);
#39207=ORIENTED_EDGE('',*,*,#29503,.T.);
#39208=ORIENTED_EDGE('',*,*,#29504,.T.);
#39209=ORIENTED_EDGE('',*,*,#29505,.F.);
#39210=ORIENTED_EDGE('',*,*,#29504,.F.);
#39211=ORIENTED_EDGE('',*,*,#29506,.F.);
#39212=ORIENTED_EDGE('',*,*,#29507,.T.);
#39213=ORIENTED_EDGE('',*,*,#29508,.F.);
#39214=ORIENTED_EDGE('',*,*,#29507,.F.);
#39215=ORIENTED_EDGE('',*,*,#29509,.T.);
#39216=ORIENTED_EDGE('',*,*,#29510,.T.);
#39217=ORIENTED_EDGE('',*,*,#29511,.F.);
#39218=ORIENTED_EDGE('',*,*,#29510,.F.);
#39219=ORIENTED_EDGE('',*,*,#29512,.F.);
#39220=ORIENTED_EDGE('',*,*,#29513,.T.);
#39221=ORIENTED_EDGE('',*,*,#29514,.F.);
#39222=ORIENTED_EDGE('',*,*,#29513,.F.);
#39223=ORIENTED_EDGE('',*,*,#29515,.T.);
#39224=ORIENTED_EDGE('',*,*,#29516,.T.);
#39225=ORIENTED_EDGE('',*,*,#29517,.F.);
#39226=ORIENTED_EDGE('',*,*,#29516,.F.);
#39227=ORIENTED_EDGE('',*,*,#29518,.F.);
#39228=ORIENTED_EDGE('',*,*,#29519,.T.);
#39229=ORIENTED_EDGE('',*,*,#29520,.F.);
#39230=ORIENTED_EDGE('',*,*,#29519,.F.);
#39231=ORIENTED_EDGE('',*,*,#29521,.T.);
#39232=ORIENTED_EDGE('',*,*,#29522,.T.);
#39233=ORIENTED_EDGE('',*,*,#29523,.F.);
#39234=ORIENTED_EDGE('',*,*,#29522,.F.);
#39235=ORIENTED_EDGE('',*,*,#29524,.F.);
#39236=ORIENTED_EDGE('',*,*,#29525,.T.);
#39237=ORIENTED_EDGE('',*,*,#29526,.F.);
#39238=ORIENTED_EDGE('',*,*,#29525,.F.);
#39239=ORIENTED_EDGE('',*,*,#29527,.T.);
#39240=ORIENTED_EDGE('',*,*,#29528,.T.);
#39241=ORIENTED_EDGE('',*,*,#29529,.F.);
#39242=ORIENTED_EDGE('',*,*,#29528,.F.);
#39243=ORIENTED_EDGE('',*,*,#29530,.F.);
#39244=ORIENTED_EDGE('',*,*,#29531,.T.);
#39245=ORIENTED_EDGE('',*,*,#29532,.F.);
#39246=ORIENTED_EDGE('',*,*,#29531,.F.);
#39247=ORIENTED_EDGE('',*,*,#29533,.T.);
#39248=ORIENTED_EDGE('',*,*,#29534,.T.);
#39249=ORIENTED_EDGE('',*,*,#29535,.F.);
#39250=ORIENTED_EDGE('',*,*,#29534,.F.);
#39251=ORIENTED_EDGE('',*,*,#29536,.F.);
#39252=ORIENTED_EDGE('',*,*,#29537,.T.);
#39253=ORIENTED_EDGE('',*,*,#29538,.F.);
#39254=ORIENTED_EDGE('',*,*,#29537,.F.);
#39255=ORIENTED_EDGE('',*,*,#29539,.T.);
#39256=ORIENTED_EDGE('',*,*,#29540,.T.);
#39257=ORIENTED_EDGE('',*,*,#29541,.F.);
#39258=ORIENTED_EDGE('',*,*,#29540,.F.);
#39259=ORIENTED_EDGE('',*,*,#29542,.F.);
#39260=ORIENTED_EDGE('',*,*,#29543,.T.);
#39261=ORIENTED_EDGE('',*,*,#29544,.F.);
#39262=ORIENTED_EDGE('',*,*,#29543,.F.);
#39263=ORIENTED_EDGE('',*,*,#29545,.T.);
#39264=ORIENTED_EDGE('',*,*,#29546,.T.);
#39265=ORIENTED_EDGE('',*,*,#29547,.F.);
#39266=ORIENTED_EDGE('',*,*,#29546,.F.);
#39267=ORIENTED_EDGE('',*,*,#29548,.F.);
#39268=ORIENTED_EDGE('',*,*,#29549,.T.);
#39269=ORIENTED_EDGE('',*,*,#29550,.F.);
#39270=ORIENTED_EDGE('',*,*,#29549,.F.);
#39271=ORIENTED_EDGE('',*,*,#29551,.T.);
#39272=ORIENTED_EDGE('',*,*,#29552,.T.);
#39273=ORIENTED_EDGE('',*,*,#29553,.F.);
#39274=ORIENTED_EDGE('',*,*,#29552,.F.);
#39275=ORIENTED_EDGE('',*,*,#29554,.F.);
#39276=ORIENTED_EDGE('',*,*,#29555,.T.);
#39277=ORIENTED_EDGE('',*,*,#29556,.F.);
#39278=ORIENTED_EDGE('',*,*,#29555,.F.);
#39279=ORIENTED_EDGE('',*,*,#29557,.T.);
#39280=ORIENTED_EDGE('',*,*,#29558,.T.);
#39281=ORIENTED_EDGE('',*,*,#29559,.F.);
#39282=ORIENTED_EDGE('',*,*,#29558,.F.);
#39283=ORIENTED_EDGE('',*,*,#29560,.F.);
#39284=ORIENTED_EDGE('',*,*,#29561,.T.);
#39285=ORIENTED_EDGE('',*,*,#29562,.F.);
#39286=ORIENTED_EDGE('',*,*,#29561,.F.);
#39287=ORIENTED_EDGE('',*,*,#29563,.T.);
#39288=ORIENTED_EDGE('',*,*,#29564,.T.);
#39289=ORIENTED_EDGE('',*,*,#29565,.F.);
#39290=ORIENTED_EDGE('',*,*,#29564,.F.);
#39291=ORIENTED_EDGE('',*,*,#29566,.F.);
#39292=ORIENTED_EDGE('',*,*,#29567,.T.);
#39293=ORIENTED_EDGE('',*,*,#29568,.F.);
#39294=ORIENTED_EDGE('',*,*,#29567,.F.);
#39295=ORIENTED_EDGE('',*,*,#29569,.T.);
#39296=ORIENTED_EDGE('',*,*,#29570,.T.);
#39297=ORIENTED_EDGE('',*,*,#29571,.F.);
#39298=ORIENTED_EDGE('',*,*,#29570,.F.);
#39299=ORIENTED_EDGE('',*,*,#29572,.F.);
#39300=ORIENTED_EDGE('',*,*,#29573,.T.);
#39301=ORIENTED_EDGE('',*,*,#29574,.F.);
#39302=ORIENTED_EDGE('',*,*,#29573,.F.);
#39303=ORIENTED_EDGE('',*,*,#29575,.T.);
#39304=ORIENTED_EDGE('',*,*,#29576,.T.);
#39305=ORIENTED_EDGE('',*,*,#29577,.F.);
#39306=ORIENTED_EDGE('',*,*,#29576,.F.);
#39307=ORIENTED_EDGE('',*,*,#29578,.F.);
#39308=ORIENTED_EDGE('',*,*,#29579,.T.);
#39309=ORIENTED_EDGE('',*,*,#29580,.F.);
#39310=ORIENTED_EDGE('',*,*,#29579,.F.);
#39311=ORIENTED_EDGE('',*,*,#29581,.T.);
#39312=ORIENTED_EDGE('',*,*,#29582,.T.);
#39313=ORIENTED_EDGE('',*,*,#29583,.F.);
#39314=ORIENTED_EDGE('',*,*,#29582,.F.);
#39315=ORIENTED_EDGE('',*,*,#29584,.F.);
#39316=ORIENTED_EDGE('',*,*,#29585,.T.);
#39317=ORIENTED_EDGE('',*,*,#29586,.F.);
#39318=ORIENTED_EDGE('',*,*,#29585,.F.);
#39319=ORIENTED_EDGE('',*,*,#29587,.T.);
#39320=ORIENTED_EDGE('',*,*,#29588,.T.);
#39321=ORIENTED_EDGE('',*,*,#29589,.F.);
#39322=ORIENTED_EDGE('',*,*,#29588,.F.);
#39323=ORIENTED_EDGE('',*,*,#29590,.F.);
#39324=ORIENTED_EDGE('',*,*,#29591,.T.);
#39325=ORIENTED_EDGE('',*,*,#29592,.F.);
#39326=ORIENTED_EDGE('',*,*,#29591,.F.);
#39327=ORIENTED_EDGE('',*,*,#29593,.T.);
#39328=ORIENTED_EDGE('',*,*,#29594,.T.);
#39329=ORIENTED_EDGE('',*,*,#29595,.F.);
#39330=ORIENTED_EDGE('',*,*,#29594,.F.);
#39331=ORIENTED_EDGE('',*,*,#29596,.F.);
#39332=ORIENTED_EDGE('',*,*,#29597,.T.);
#39333=ORIENTED_EDGE('',*,*,#29598,.F.);
#39334=ORIENTED_EDGE('',*,*,#29597,.F.);
#39335=ORIENTED_EDGE('',*,*,#29599,.T.);
#39336=ORIENTED_EDGE('',*,*,#29600,.T.);
#39337=ORIENTED_EDGE('',*,*,#29601,.F.);
#39338=ORIENTED_EDGE('',*,*,#29600,.F.);
#39339=ORIENTED_EDGE('',*,*,#29602,.F.);
#39340=ORIENTED_EDGE('',*,*,#29603,.T.);
#39341=ORIENTED_EDGE('',*,*,#29604,.F.);
#39342=ORIENTED_EDGE('',*,*,#29603,.F.);
#39343=ORIENTED_EDGE('',*,*,#29605,.T.);
#39344=ORIENTED_EDGE('',*,*,#29606,.T.);
#39345=ORIENTED_EDGE('',*,*,#29607,.F.);
#39346=ORIENTED_EDGE('',*,*,#29606,.F.);
#39347=ORIENTED_EDGE('',*,*,#29608,.F.);
#39348=ORIENTED_EDGE('',*,*,#29609,.T.);
#39349=ORIENTED_EDGE('',*,*,#29610,.F.);
#39350=ORIENTED_EDGE('',*,*,#29609,.F.);
#39351=ORIENTED_EDGE('',*,*,#29611,.T.);
#39352=ORIENTED_EDGE('',*,*,#29612,.T.);
#39353=ORIENTED_EDGE('',*,*,#29613,.F.);
#39354=ORIENTED_EDGE('',*,*,#29612,.F.);
#39355=ORIENTED_EDGE('',*,*,#29614,.F.);
#39356=ORIENTED_EDGE('',*,*,#29615,.T.);
#39357=ORIENTED_EDGE('',*,*,#29616,.F.);
#39358=ORIENTED_EDGE('',*,*,#29615,.F.);
#39359=ORIENTED_EDGE('',*,*,#29617,.T.);
#39360=ORIENTED_EDGE('',*,*,#29618,.T.);
#39361=ORIENTED_EDGE('',*,*,#29619,.F.);
#39362=ORIENTED_EDGE('',*,*,#29618,.F.);
#39363=ORIENTED_EDGE('',*,*,#29620,.F.);
#39364=ORIENTED_EDGE('',*,*,#29621,.T.);
#39365=ORIENTED_EDGE('',*,*,#29622,.F.);
#39366=ORIENTED_EDGE('',*,*,#29621,.F.);
#39367=ORIENTED_EDGE('',*,*,#29623,.T.);
#39368=ORIENTED_EDGE('',*,*,#29624,.T.);
#39369=ORIENTED_EDGE('',*,*,#29625,.F.);
#39370=ORIENTED_EDGE('',*,*,#29624,.F.);
#39371=ORIENTED_EDGE('',*,*,#29626,.F.);
#39372=ORIENTED_EDGE('',*,*,#29627,.T.);
#39373=ORIENTED_EDGE('',*,*,#29628,.F.);
#39374=ORIENTED_EDGE('',*,*,#29627,.F.);
#39375=ORIENTED_EDGE('',*,*,#29629,.T.);
#39376=ORIENTED_EDGE('',*,*,#29630,.T.);
#39377=ORIENTED_EDGE('',*,*,#29631,.F.);
#39378=ORIENTED_EDGE('',*,*,#29630,.F.);
#39379=ORIENTED_EDGE('',*,*,#29632,.F.);
#39380=ORIENTED_EDGE('',*,*,#29633,.T.);
#39381=ORIENTED_EDGE('',*,*,#29634,.F.);
#39382=ORIENTED_EDGE('',*,*,#29633,.F.);
#39383=ORIENTED_EDGE('',*,*,#29635,.T.);
#39384=ORIENTED_EDGE('',*,*,#29636,.T.);
#39385=ORIENTED_EDGE('',*,*,#29637,.F.);
#39386=ORIENTED_EDGE('',*,*,#29636,.F.);
#39387=ORIENTED_EDGE('',*,*,#29638,.F.);
#39388=ORIENTED_EDGE('',*,*,#29639,.T.);
#39389=ORIENTED_EDGE('',*,*,#29640,.F.);
#39390=ORIENTED_EDGE('',*,*,#29639,.F.);
#39391=ORIENTED_EDGE('',*,*,#29641,.T.);
#39392=ORIENTED_EDGE('',*,*,#29642,.T.);
#39393=ORIENTED_EDGE('',*,*,#29643,.F.);
#39394=ORIENTED_EDGE('',*,*,#29642,.F.);
#39395=ORIENTED_EDGE('',*,*,#29644,.F.);
#39396=ORIENTED_EDGE('',*,*,#29645,.T.);
#39397=ORIENTED_EDGE('',*,*,#29646,.F.);
#39398=ORIENTED_EDGE('',*,*,#29645,.F.);
#39399=ORIENTED_EDGE('',*,*,#29647,.T.);
#39400=ORIENTED_EDGE('',*,*,#29648,.T.);
#39401=ORIENTED_EDGE('',*,*,#29649,.F.);
#39402=ORIENTED_EDGE('',*,*,#29648,.F.);
#39403=ORIENTED_EDGE('',*,*,#29650,.F.);
#39404=ORIENTED_EDGE('',*,*,#29651,.T.);
#39405=ORIENTED_EDGE('',*,*,#29652,.F.);
#39406=ORIENTED_EDGE('',*,*,#29651,.F.);
#39407=ORIENTED_EDGE('',*,*,#29653,.T.);
#39408=ORIENTED_EDGE('',*,*,#29654,.T.);
#39409=ORIENTED_EDGE('',*,*,#29655,.F.);
#39410=ORIENTED_EDGE('',*,*,#29654,.F.);
#39411=ORIENTED_EDGE('',*,*,#29656,.F.);
#39412=ORIENTED_EDGE('',*,*,#29657,.T.);
#39413=ORIENTED_EDGE('',*,*,#29658,.F.);
#39414=ORIENTED_EDGE('',*,*,#29657,.F.);
#39415=ORIENTED_EDGE('',*,*,#29659,.T.);
#39416=ORIENTED_EDGE('',*,*,#29660,.T.);
#39417=ORIENTED_EDGE('',*,*,#29661,.F.);
#39418=ORIENTED_EDGE('',*,*,#29660,.F.);
#39419=ORIENTED_EDGE('',*,*,#29662,.F.);
#39420=ORIENTED_EDGE('',*,*,#29663,.T.);
#39421=ORIENTED_EDGE('',*,*,#29664,.F.);
#39422=ORIENTED_EDGE('',*,*,#29663,.F.);
#39423=ORIENTED_EDGE('',*,*,#29665,.T.);
#39424=ORIENTED_EDGE('',*,*,#29666,.T.);
#39425=ORIENTED_EDGE('',*,*,#29667,.F.);
#39426=ORIENTED_EDGE('',*,*,#29666,.F.);
#39427=ORIENTED_EDGE('',*,*,#29668,.F.);
#39428=ORIENTED_EDGE('',*,*,#29669,.T.);
#39429=ORIENTED_EDGE('',*,*,#29670,.F.);
#39430=ORIENTED_EDGE('',*,*,#29669,.F.);
#39431=ORIENTED_EDGE('',*,*,#29671,.T.);
#39432=ORIENTED_EDGE('',*,*,#29672,.T.);
#39433=ORIENTED_EDGE('',*,*,#29673,.F.);
#39434=ORIENTED_EDGE('',*,*,#29672,.F.);
#39435=ORIENTED_EDGE('',*,*,#29674,.F.);
#39436=ORIENTED_EDGE('',*,*,#29675,.T.);
#39437=ORIENTED_EDGE('',*,*,#29676,.F.);
#39438=ORIENTED_EDGE('',*,*,#29675,.F.);
#39439=ORIENTED_EDGE('',*,*,#29677,.T.);
#39440=ORIENTED_EDGE('',*,*,#29678,.T.);
#39441=ORIENTED_EDGE('',*,*,#29679,.F.);
#39442=ORIENTED_EDGE('',*,*,#29678,.F.);
#39443=ORIENTED_EDGE('',*,*,#29680,.F.);
#39444=ORIENTED_EDGE('',*,*,#29681,.T.);
#39445=ORIENTED_EDGE('',*,*,#29682,.F.);
#39446=ORIENTED_EDGE('',*,*,#29681,.F.);
#39447=ORIENTED_EDGE('',*,*,#29683,.T.);
#39448=ORIENTED_EDGE('',*,*,#29684,.T.);
#39449=ORIENTED_EDGE('',*,*,#29685,.F.);
#39450=ORIENTED_EDGE('',*,*,#29684,.F.);
#39451=ORIENTED_EDGE('',*,*,#29686,.F.);
#39452=ORIENTED_EDGE('',*,*,#29687,.T.);
#39453=ORIENTED_EDGE('',*,*,#29688,.F.);
#39454=ORIENTED_EDGE('',*,*,#29687,.F.);
#39455=ORIENTED_EDGE('',*,*,#29689,.T.);
#39456=ORIENTED_EDGE('',*,*,#29690,.T.);
#39457=ORIENTED_EDGE('',*,*,#29691,.F.);
#39458=ORIENTED_EDGE('',*,*,#29690,.F.);
#39459=ORIENTED_EDGE('',*,*,#29692,.F.);
#39460=ORIENTED_EDGE('',*,*,#29693,.T.);
#39461=ORIENTED_EDGE('',*,*,#29694,.F.);
#39462=ORIENTED_EDGE('',*,*,#29693,.F.);
#39463=ORIENTED_EDGE('',*,*,#29695,.T.);
#39464=ORIENTED_EDGE('',*,*,#29696,.T.);
#39465=ORIENTED_EDGE('',*,*,#29697,.F.);
#39466=ORIENTED_EDGE('',*,*,#29696,.F.);
#39467=ORIENTED_EDGE('',*,*,#29698,.F.);
#39468=ORIENTED_EDGE('',*,*,#29699,.T.);
#39469=ORIENTED_EDGE('',*,*,#29700,.F.);
#39470=ORIENTED_EDGE('',*,*,#29699,.F.);
#39471=ORIENTED_EDGE('',*,*,#29701,.T.);
#39472=ORIENTED_EDGE('',*,*,#29702,.T.);
#39473=ORIENTED_EDGE('',*,*,#29703,.F.);
#39474=ORIENTED_EDGE('',*,*,#29702,.F.);
#39475=ORIENTED_EDGE('',*,*,#29704,.F.);
#39476=ORIENTED_EDGE('',*,*,#29705,.T.);
#39477=ORIENTED_EDGE('',*,*,#29706,.F.);
#39478=ORIENTED_EDGE('',*,*,#29705,.F.);
#39479=ORIENTED_EDGE('',*,*,#29707,.T.);
#39480=ORIENTED_EDGE('',*,*,#29708,.T.);
#39481=ORIENTED_EDGE('',*,*,#29709,.F.);
#39482=ORIENTED_EDGE('',*,*,#29708,.F.);
#39483=ORIENTED_EDGE('',*,*,#29710,.F.);
#39484=ORIENTED_EDGE('',*,*,#29711,.T.);
#39485=ORIENTED_EDGE('',*,*,#29712,.F.);
#39486=ORIENTED_EDGE('',*,*,#29711,.F.);
#39487=ORIENTED_EDGE('',*,*,#29713,.T.);
#39488=ORIENTED_EDGE('',*,*,#29714,.T.);
#39489=ORIENTED_EDGE('',*,*,#29715,.F.);
#39490=ORIENTED_EDGE('',*,*,#29714,.F.);
#39491=ORIENTED_EDGE('',*,*,#29716,.F.);
#39492=ORIENTED_EDGE('',*,*,#29717,.T.);
#39493=ORIENTED_EDGE('',*,*,#29718,.F.);
#39494=ORIENTED_EDGE('',*,*,#29717,.F.);
#39495=ORIENTED_EDGE('',*,*,#29719,.T.);
#39496=ORIENTED_EDGE('',*,*,#29720,.T.);
#39497=ORIENTED_EDGE('',*,*,#29721,.F.);
#39498=ORIENTED_EDGE('',*,*,#29720,.F.);
#39499=ORIENTED_EDGE('',*,*,#29722,.F.);
#39500=ORIENTED_EDGE('',*,*,#29723,.T.);
#39501=ORIENTED_EDGE('',*,*,#29724,.F.);
#39502=ORIENTED_EDGE('',*,*,#29723,.F.);
#39503=ORIENTED_EDGE('',*,*,#29725,.T.);
#39504=ORIENTED_EDGE('',*,*,#29726,.T.);
#39505=ORIENTED_EDGE('',*,*,#29727,.F.);
#39506=ORIENTED_EDGE('',*,*,#29726,.F.);
#39507=ORIENTED_EDGE('',*,*,#29728,.F.);
#39508=ORIENTED_EDGE('',*,*,#29729,.T.);
#39509=ORIENTED_EDGE('',*,*,#29730,.F.);
#39510=ORIENTED_EDGE('',*,*,#29729,.F.);
#39511=ORIENTED_EDGE('',*,*,#29731,.T.);
#39512=ORIENTED_EDGE('',*,*,#29732,.T.);
#39513=ORIENTED_EDGE('',*,*,#29733,.F.);
#39514=ORIENTED_EDGE('',*,*,#29732,.F.);
#39515=ORIENTED_EDGE('',*,*,#29734,.F.);
#39516=ORIENTED_EDGE('',*,*,#29735,.T.);
#39517=ORIENTED_EDGE('',*,*,#29736,.F.);
#39518=ORIENTED_EDGE('',*,*,#29735,.F.);
#39519=ORIENTED_EDGE('',*,*,#29737,.T.);
#39520=ORIENTED_EDGE('',*,*,#29738,.T.);
#39521=ORIENTED_EDGE('',*,*,#29739,.F.);
#39522=ORIENTED_EDGE('',*,*,#29738,.F.);
#39523=ORIENTED_EDGE('',*,*,#29740,.F.);
#39524=ORIENTED_EDGE('',*,*,#29741,.T.);
#39525=ORIENTED_EDGE('',*,*,#29742,.F.);
#39526=ORIENTED_EDGE('',*,*,#29741,.F.);
#39527=ORIENTED_EDGE('',*,*,#29743,.T.);
#39528=ORIENTED_EDGE('',*,*,#29744,.T.);
#39529=ORIENTED_EDGE('',*,*,#29745,.F.);
#39530=ORIENTED_EDGE('',*,*,#29744,.F.);
#39531=ORIENTED_EDGE('',*,*,#29746,.F.);
#39532=ORIENTED_EDGE('',*,*,#29747,.T.);
#39533=ORIENTED_EDGE('',*,*,#29748,.F.);
#39534=ORIENTED_EDGE('',*,*,#29747,.F.);
#39535=ORIENTED_EDGE('',*,*,#29749,.T.);
#39536=ORIENTED_EDGE('',*,*,#29750,.T.);
#39537=ORIENTED_EDGE('',*,*,#29751,.F.);
#39538=ORIENTED_EDGE('',*,*,#29750,.F.);
#39539=ORIENTED_EDGE('',*,*,#29752,.F.);
#39540=ORIENTED_EDGE('',*,*,#29753,.T.);
#39541=ORIENTED_EDGE('',*,*,#29754,.F.);
#39542=ORIENTED_EDGE('',*,*,#29753,.F.);
#39543=ORIENTED_EDGE('',*,*,#29755,.T.);
#39544=ORIENTED_EDGE('',*,*,#29756,.T.);
#39545=ORIENTED_EDGE('',*,*,#29757,.F.);
#39546=ORIENTED_EDGE('',*,*,#29756,.F.);
#39547=ORIENTED_EDGE('',*,*,#29758,.F.);
#39548=ORIENTED_EDGE('',*,*,#29759,.T.);
#39549=ORIENTED_EDGE('',*,*,#29760,.F.);
#39550=ORIENTED_EDGE('',*,*,#29759,.F.);
#39551=ORIENTED_EDGE('',*,*,#29761,.T.);
#39552=ORIENTED_EDGE('',*,*,#29762,.T.);
#39553=ORIENTED_EDGE('',*,*,#29763,.F.);
#39554=ORIENTED_EDGE('',*,*,#29762,.F.);
#39555=ORIENTED_EDGE('',*,*,#29764,.F.);
#39556=ORIENTED_EDGE('',*,*,#29765,.T.);
#39557=ORIENTED_EDGE('',*,*,#29766,.F.);
#39558=ORIENTED_EDGE('',*,*,#29765,.F.);
#39559=ORIENTED_EDGE('',*,*,#29767,.T.);
#39560=ORIENTED_EDGE('',*,*,#29768,.T.);
#39561=ORIENTED_EDGE('',*,*,#29769,.F.);
#39562=ORIENTED_EDGE('',*,*,#29768,.F.);
#39563=ORIENTED_EDGE('',*,*,#29770,.F.);
#39564=ORIENTED_EDGE('',*,*,#29771,.T.);
#39565=ORIENTED_EDGE('',*,*,#29772,.F.);
#39566=ORIENTED_EDGE('',*,*,#29771,.F.);
#39567=ORIENTED_EDGE('',*,*,#29773,.T.);
#39568=ORIENTED_EDGE('',*,*,#29774,.T.);
#39569=ORIENTED_EDGE('',*,*,#29775,.F.);
#39570=ORIENTED_EDGE('',*,*,#29774,.F.);
#39571=ORIENTED_EDGE('',*,*,#29776,.F.);
#39572=ORIENTED_EDGE('',*,*,#29777,.T.);
#39573=ORIENTED_EDGE('',*,*,#29778,.F.);
#39574=ORIENTED_EDGE('',*,*,#29777,.F.);
#39575=ORIENTED_EDGE('',*,*,#29779,.T.);
#39576=ORIENTED_EDGE('',*,*,#29780,.T.);
#39577=ORIENTED_EDGE('',*,*,#29781,.F.);
#39578=ORIENTED_EDGE('',*,*,#29780,.F.);
#39579=ORIENTED_EDGE('',*,*,#29782,.F.);
#39580=ORIENTED_EDGE('',*,*,#29783,.T.);
#39581=ORIENTED_EDGE('',*,*,#29784,.F.);
#39582=ORIENTED_EDGE('',*,*,#29783,.F.);
#39583=ORIENTED_EDGE('',*,*,#29785,.T.);
#39584=ORIENTED_EDGE('',*,*,#29786,.T.);
#39585=ORIENTED_EDGE('',*,*,#29787,.F.);
#39586=ORIENTED_EDGE('',*,*,#29786,.F.);
#39587=ORIENTED_EDGE('',*,*,#29788,.F.);
#39588=ORIENTED_EDGE('',*,*,#29789,.T.);
#39589=ORIENTED_EDGE('',*,*,#29790,.F.);
#39590=ORIENTED_EDGE('',*,*,#29789,.F.);
#39591=ORIENTED_EDGE('',*,*,#29791,.T.);
#39592=ORIENTED_EDGE('',*,*,#29792,.T.);
#39593=ORIENTED_EDGE('',*,*,#29793,.F.);
#39594=ORIENTED_EDGE('',*,*,#29792,.F.);
#39595=ORIENTED_EDGE('',*,*,#29794,.F.);
#39596=ORIENTED_EDGE('',*,*,#29795,.T.);
#39597=ORIENTED_EDGE('',*,*,#29796,.F.);
#39598=ORIENTED_EDGE('',*,*,#29795,.F.);
#39599=ORIENTED_EDGE('',*,*,#29797,.T.);
#39600=ORIENTED_EDGE('',*,*,#29798,.T.);
#39601=ORIENTED_EDGE('',*,*,#29799,.F.);
#39602=ORIENTED_EDGE('',*,*,#29798,.F.);
#39603=ORIENTED_EDGE('',*,*,#29800,.F.);
#39604=ORIENTED_EDGE('',*,*,#29801,.T.);
#39605=ORIENTED_EDGE('',*,*,#29802,.F.);
#39606=ORIENTED_EDGE('',*,*,#29801,.F.);
#39607=ORIENTED_EDGE('',*,*,#29803,.T.);
#39608=ORIENTED_EDGE('',*,*,#29804,.T.);
#39609=ORIENTED_EDGE('',*,*,#29805,.F.);
#39610=ORIENTED_EDGE('',*,*,#29804,.F.);
#39611=ORIENTED_EDGE('',*,*,#29806,.F.);
#39612=ORIENTED_EDGE('',*,*,#29807,.T.);
#39613=ORIENTED_EDGE('',*,*,#29808,.F.);
#39614=ORIENTED_EDGE('',*,*,#29807,.F.);
#39615=ORIENTED_EDGE('',*,*,#29809,.T.);
#39616=ORIENTED_EDGE('',*,*,#29810,.T.);
#39617=ORIENTED_EDGE('',*,*,#29811,.F.);
#39618=ORIENTED_EDGE('',*,*,#29810,.F.);
#39619=ORIENTED_EDGE('',*,*,#29812,.F.);
#39620=ORIENTED_EDGE('',*,*,#29813,.T.);
#39621=ORIENTED_EDGE('',*,*,#29814,.F.);
#39622=ORIENTED_EDGE('',*,*,#29813,.F.);
#39623=ORIENTED_EDGE('',*,*,#29815,.T.);
#39624=ORIENTED_EDGE('',*,*,#29816,.T.);
#39625=ORIENTED_EDGE('',*,*,#29817,.F.);
#39626=ORIENTED_EDGE('',*,*,#29816,.F.);
#39627=ORIENTED_EDGE('',*,*,#29818,.F.);
#39628=ORIENTED_EDGE('',*,*,#29819,.T.);
#39629=ORIENTED_EDGE('',*,*,#29820,.F.);
#39630=ORIENTED_EDGE('',*,*,#29819,.F.);
#39631=ORIENTED_EDGE('',*,*,#29821,.T.);
#39632=ORIENTED_EDGE('',*,*,#29822,.T.);
#39633=ORIENTED_EDGE('',*,*,#29823,.F.);
#39634=ORIENTED_EDGE('',*,*,#29822,.F.);
#39635=ORIENTED_EDGE('',*,*,#29824,.F.);
#39636=ORIENTED_EDGE('',*,*,#29825,.T.);
#39637=ORIENTED_EDGE('',*,*,#29826,.F.);
#39638=ORIENTED_EDGE('',*,*,#29825,.F.);
#39639=ORIENTED_EDGE('',*,*,#29827,.T.);
#39640=ORIENTED_EDGE('',*,*,#29828,.T.);
#39641=ORIENTED_EDGE('',*,*,#29829,.F.);
#39642=ORIENTED_EDGE('',*,*,#29828,.F.);
#39643=ORIENTED_EDGE('',*,*,#29830,.F.);
#39644=ORIENTED_EDGE('',*,*,#29831,.T.);
#39645=ORIENTED_EDGE('',*,*,#29832,.F.);
#39646=ORIENTED_EDGE('',*,*,#29831,.F.);
#39647=ORIENTED_EDGE('',*,*,#29833,.T.);
#39648=ORIENTED_EDGE('',*,*,#29834,.T.);
#39649=ORIENTED_EDGE('',*,*,#29835,.F.);
#39650=ORIENTED_EDGE('',*,*,#29834,.F.);
#39651=ORIENTED_EDGE('',*,*,#29836,.F.);
#39652=ORIENTED_EDGE('',*,*,#29837,.T.);
#39653=ORIENTED_EDGE('',*,*,#29838,.F.);
#39654=ORIENTED_EDGE('',*,*,#29837,.F.);
#39655=ORIENTED_EDGE('',*,*,#29839,.T.);
#39656=ORIENTED_EDGE('',*,*,#29840,.T.);
#39657=ORIENTED_EDGE('',*,*,#29841,.F.);
#39658=ORIENTED_EDGE('',*,*,#29840,.F.);
#39659=ORIENTED_EDGE('',*,*,#29842,.F.);
#39660=ORIENTED_EDGE('',*,*,#29843,.T.);
#39661=ORIENTED_EDGE('',*,*,#29844,.F.);
#39662=ORIENTED_EDGE('',*,*,#29843,.F.);
#39663=ORIENTED_EDGE('',*,*,#29845,.T.);
#39664=ORIENTED_EDGE('',*,*,#29846,.T.);
#39665=ORIENTED_EDGE('',*,*,#29847,.F.);
#39666=ORIENTED_EDGE('',*,*,#29846,.F.);
#39667=ORIENTED_EDGE('',*,*,#29848,.F.);
#39668=ORIENTED_EDGE('',*,*,#29849,.T.);
#39669=ORIENTED_EDGE('',*,*,#29850,.F.);
#39670=ORIENTED_EDGE('',*,*,#29849,.F.);
#39671=ORIENTED_EDGE('',*,*,#29851,.T.);
#39672=ORIENTED_EDGE('',*,*,#29852,.T.);
#39673=ORIENTED_EDGE('',*,*,#29853,.F.);
#39674=ORIENTED_EDGE('',*,*,#29852,.F.);
#39675=ORIENTED_EDGE('',*,*,#29854,.F.);
#39676=ORIENTED_EDGE('',*,*,#29855,.T.);
#39677=ORIENTED_EDGE('',*,*,#29856,.F.);
#39678=ORIENTED_EDGE('',*,*,#29855,.F.);
#39679=ORIENTED_EDGE('',*,*,#29857,.T.);
#39680=ORIENTED_EDGE('',*,*,#29858,.T.);
#39681=ORIENTED_EDGE('',*,*,#29859,.F.);
#39682=ORIENTED_EDGE('',*,*,#29858,.F.);
#39683=ORIENTED_EDGE('',*,*,#29860,.F.);
#39684=ORIENTED_EDGE('',*,*,#29861,.T.);
#39685=ORIENTED_EDGE('',*,*,#29862,.F.);
#39686=ORIENTED_EDGE('',*,*,#29861,.F.);
#39687=ORIENTED_EDGE('',*,*,#29863,.T.);
#39688=ORIENTED_EDGE('',*,*,#29864,.T.);
#39689=ORIENTED_EDGE('',*,*,#29865,.F.);
#39690=ORIENTED_EDGE('',*,*,#29864,.F.);
#39691=ORIENTED_EDGE('',*,*,#29866,.F.);
#39692=ORIENTED_EDGE('',*,*,#29867,.T.);
#39693=ORIENTED_EDGE('',*,*,#29868,.F.);
#39694=ORIENTED_EDGE('',*,*,#29867,.F.);
#39695=ORIENTED_EDGE('',*,*,#29869,.T.);
#39696=ORIENTED_EDGE('',*,*,#29870,.T.);
#39697=ORIENTED_EDGE('',*,*,#29871,.F.);
#39698=ORIENTED_EDGE('',*,*,#29870,.F.);
#39699=ORIENTED_EDGE('',*,*,#29872,.F.);
#39700=ORIENTED_EDGE('',*,*,#29873,.T.);
#39701=ORIENTED_EDGE('',*,*,#29874,.F.);
#39702=ORIENTED_EDGE('',*,*,#29873,.F.);
#39703=ORIENTED_EDGE('',*,*,#29875,.T.);
#39704=ORIENTED_EDGE('',*,*,#29876,.T.);
#39705=ORIENTED_EDGE('',*,*,#29877,.F.);
#39706=ORIENTED_EDGE('',*,*,#29876,.F.);
#39707=ORIENTED_EDGE('',*,*,#29878,.F.);
#39708=ORIENTED_EDGE('',*,*,#29879,.T.);
#39709=ORIENTED_EDGE('',*,*,#29880,.F.);
#39710=ORIENTED_EDGE('',*,*,#29879,.F.);
#39711=ORIENTED_EDGE('',*,*,#29881,.T.);
#39712=ORIENTED_EDGE('',*,*,#29882,.T.);
#39713=ORIENTED_EDGE('',*,*,#29883,.F.);
#39714=ORIENTED_EDGE('',*,*,#29882,.F.);
#39715=ORIENTED_EDGE('',*,*,#29884,.F.);
#39716=ORIENTED_EDGE('',*,*,#29885,.T.);
#39717=ORIENTED_EDGE('',*,*,#29886,.F.);
#39718=ORIENTED_EDGE('',*,*,#29885,.F.);
#39719=ORIENTED_EDGE('',*,*,#29887,.T.);
#39720=ORIENTED_EDGE('',*,*,#29888,.T.);
#39721=ORIENTED_EDGE('',*,*,#29889,.F.);
#39722=ORIENTED_EDGE('',*,*,#29888,.F.);
#39723=ORIENTED_EDGE('',*,*,#29890,.F.);
#39724=ORIENTED_EDGE('',*,*,#29891,.T.);
#39725=ORIENTED_EDGE('',*,*,#29892,.F.);
#39726=ORIENTED_EDGE('',*,*,#29891,.F.);
#39727=ORIENTED_EDGE('',*,*,#29893,.T.);
#39728=ORIENTED_EDGE('',*,*,#29894,.T.);
#39729=ORIENTED_EDGE('',*,*,#29895,.F.);
#39730=ORIENTED_EDGE('',*,*,#29894,.F.);
#39731=ORIENTED_EDGE('',*,*,#29896,.F.);
#39732=ORIENTED_EDGE('',*,*,#29897,.T.);
#39733=ORIENTED_EDGE('',*,*,#29898,.F.);
#39734=ORIENTED_EDGE('',*,*,#29897,.F.);
#39735=ORIENTED_EDGE('',*,*,#29899,.T.);
#39736=ORIENTED_EDGE('',*,*,#29900,.T.);
#39737=ORIENTED_EDGE('',*,*,#29901,.F.);
#39738=ORIENTED_EDGE('',*,*,#29900,.F.);
#39739=ORIENTED_EDGE('',*,*,#29902,.F.);
#39740=ORIENTED_EDGE('',*,*,#29903,.T.);
#39741=ORIENTED_EDGE('',*,*,#29904,.F.);
#39742=ORIENTED_EDGE('',*,*,#29903,.F.);
#39743=ORIENTED_EDGE('',*,*,#29905,.T.);
#39744=ORIENTED_EDGE('',*,*,#29906,.T.);
#39745=ORIENTED_EDGE('',*,*,#29907,.F.);
#39746=ORIENTED_EDGE('',*,*,#29906,.F.);
#39747=ORIENTED_EDGE('',*,*,#29908,.F.);
#39748=ORIENTED_EDGE('',*,*,#29909,.T.);
#39749=ORIENTED_EDGE('',*,*,#29910,.F.);
#39750=ORIENTED_EDGE('',*,*,#29909,.F.);
#39751=ORIENTED_EDGE('',*,*,#29911,.T.);
#39752=ORIENTED_EDGE('',*,*,#29912,.T.);
#39753=ORIENTED_EDGE('',*,*,#29913,.F.);
#39754=ORIENTED_EDGE('',*,*,#29912,.F.);
#39755=ORIENTED_EDGE('',*,*,#29914,.F.);
#39756=ORIENTED_EDGE('',*,*,#29915,.T.);
#39757=ORIENTED_EDGE('',*,*,#29916,.F.);
#39758=ORIENTED_EDGE('',*,*,#29915,.F.);
#39759=ORIENTED_EDGE('',*,*,#29917,.T.);
#39760=ORIENTED_EDGE('',*,*,#29918,.T.);
#39761=ORIENTED_EDGE('',*,*,#29919,.F.);
#39762=ORIENTED_EDGE('',*,*,#29918,.F.);
#39763=ORIENTED_EDGE('',*,*,#29920,.F.);
#39764=ORIENTED_EDGE('',*,*,#29921,.T.);
#39765=ORIENTED_EDGE('',*,*,#29922,.F.);
#39766=ORIENTED_EDGE('',*,*,#29921,.F.);
#39767=ORIENTED_EDGE('',*,*,#29923,.T.);
#39768=ORIENTED_EDGE('',*,*,#29924,.T.);
#39769=ORIENTED_EDGE('',*,*,#29925,.F.);
#39770=ORIENTED_EDGE('',*,*,#29924,.F.);
#39771=ORIENTED_EDGE('',*,*,#29926,.F.);
#39772=ORIENTED_EDGE('',*,*,#29927,.T.);
#39773=ORIENTED_EDGE('',*,*,#29928,.F.);
#39774=ORIENTED_EDGE('',*,*,#29927,.F.);
#39775=ORIENTED_EDGE('',*,*,#29929,.T.);
#39776=ORIENTED_EDGE('',*,*,#29930,.T.);
#39777=ORIENTED_EDGE('',*,*,#29931,.F.);
#39778=ORIENTED_EDGE('',*,*,#29930,.F.);
#39779=ORIENTED_EDGE('',*,*,#29932,.F.);
#39780=ORIENTED_EDGE('',*,*,#29933,.T.);
#39781=ORIENTED_EDGE('',*,*,#29934,.F.);
#39782=ORIENTED_EDGE('',*,*,#29933,.F.);
#39783=ORIENTED_EDGE('',*,*,#29935,.T.);
#39784=ORIENTED_EDGE('',*,*,#29936,.T.);
#39785=ORIENTED_EDGE('',*,*,#29937,.F.);
#39786=ORIENTED_EDGE('',*,*,#29936,.F.);
#39787=ORIENTED_EDGE('',*,*,#29938,.F.);
#39788=ORIENTED_EDGE('',*,*,#29939,.T.);
#39789=ORIENTED_EDGE('',*,*,#29940,.F.);
#39790=ORIENTED_EDGE('',*,*,#29939,.F.);
#39791=ORIENTED_EDGE('',*,*,#29941,.T.);
#39792=ORIENTED_EDGE('',*,*,#29942,.T.);
#39793=ORIENTED_EDGE('',*,*,#29943,.F.);
#39794=ORIENTED_EDGE('',*,*,#29942,.F.);
#39795=ORIENTED_EDGE('',*,*,#29944,.F.);
#39796=ORIENTED_EDGE('',*,*,#29945,.T.);
#39797=ORIENTED_EDGE('',*,*,#29946,.F.);
#39798=ORIENTED_EDGE('',*,*,#29945,.F.);
#39799=ORIENTED_EDGE('',*,*,#29947,.T.);
#39800=ORIENTED_EDGE('',*,*,#29948,.T.);
#39801=ORIENTED_EDGE('',*,*,#29949,.F.);
#39802=ORIENTED_EDGE('',*,*,#29948,.F.);
#39803=ORIENTED_EDGE('',*,*,#29950,.F.);
#39804=ORIENTED_EDGE('',*,*,#29951,.T.);
#39805=ORIENTED_EDGE('',*,*,#29952,.F.);
#39806=ORIENTED_EDGE('',*,*,#29951,.F.);
#39807=ORIENTED_EDGE('',*,*,#29953,.T.);
#39808=ORIENTED_EDGE('',*,*,#29954,.T.);
#39809=ORIENTED_EDGE('',*,*,#29955,.F.);
#39810=ORIENTED_EDGE('',*,*,#29954,.F.);
#39811=ORIENTED_EDGE('',*,*,#29956,.F.);
#39812=ORIENTED_EDGE('',*,*,#29957,.T.);
#39813=ORIENTED_EDGE('',*,*,#29958,.F.);
#39814=ORIENTED_EDGE('',*,*,#29957,.F.);
#39815=ORIENTED_EDGE('',*,*,#29959,.T.);
#39816=ORIENTED_EDGE('',*,*,#29960,.T.);
#39817=ORIENTED_EDGE('',*,*,#29961,.F.);
#39818=ORIENTED_EDGE('',*,*,#29960,.F.);
#39819=ORIENTED_EDGE('',*,*,#29962,.F.);
#39820=ORIENTED_EDGE('',*,*,#29963,.T.);
#39821=ORIENTED_EDGE('',*,*,#29964,.F.);
#39822=ORIENTED_EDGE('',*,*,#29963,.F.);
#39823=ORIENTED_EDGE('',*,*,#29965,.T.);
#39824=ORIENTED_EDGE('',*,*,#29966,.T.);
#39825=ORIENTED_EDGE('',*,*,#29967,.F.);
#39826=ORIENTED_EDGE('',*,*,#29966,.F.);
#39827=ORIENTED_EDGE('',*,*,#29968,.F.);
#39828=ORIENTED_EDGE('',*,*,#29969,.T.);
#39829=ORIENTED_EDGE('',*,*,#29970,.F.);
#39830=ORIENTED_EDGE('',*,*,#29969,.F.);
#39831=ORIENTED_EDGE('',*,*,#29971,.T.);
#39832=ORIENTED_EDGE('',*,*,#29972,.T.);
#39833=ORIENTED_EDGE('',*,*,#29973,.F.);
#39834=ORIENTED_EDGE('',*,*,#29972,.F.);
#39835=ORIENTED_EDGE('',*,*,#29974,.F.);
#39836=ORIENTED_EDGE('',*,*,#29975,.T.);
#39837=ORIENTED_EDGE('',*,*,#29976,.F.);
#39838=ORIENTED_EDGE('',*,*,#29975,.F.);
#39839=ORIENTED_EDGE('',*,*,#29977,.T.);
#39840=ORIENTED_EDGE('',*,*,#29978,.T.);
#39841=ORIENTED_EDGE('',*,*,#29979,.F.);
#39842=ORIENTED_EDGE('',*,*,#29978,.F.);
#39843=ORIENTED_EDGE('',*,*,#29980,.F.);
#39844=ORIENTED_EDGE('',*,*,#29981,.T.);
#39845=ORIENTED_EDGE('',*,*,#29982,.F.);
#39846=ORIENTED_EDGE('',*,*,#29981,.F.);
#39847=ORIENTED_EDGE('',*,*,#29983,.T.);
#39848=ORIENTED_EDGE('',*,*,#29984,.T.);
#39849=ORIENTED_EDGE('',*,*,#29985,.F.);
#39850=ORIENTED_EDGE('',*,*,#29984,.F.);
#39851=ORIENTED_EDGE('',*,*,#29986,.F.);
#39852=ORIENTED_EDGE('',*,*,#29987,.T.);
#39853=ORIENTED_EDGE('',*,*,#29988,.F.);
#39854=ORIENTED_EDGE('',*,*,#29987,.F.);
#39855=ORIENTED_EDGE('',*,*,#29989,.T.);
#39856=ORIENTED_EDGE('',*,*,#29990,.T.);
#39857=ORIENTED_EDGE('',*,*,#29991,.F.);
#39858=ORIENTED_EDGE('',*,*,#29990,.F.);
#39859=ORIENTED_EDGE('',*,*,#29992,.F.);
#39860=ORIENTED_EDGE('',*,*,#29993,.T.);
#39861=ORIENTED_EDGE('',*,*,#29994,.F.);
#39862=ORIENTED_EDGE('',*,*,#29993,.F.);
#39863=ORIENTED_EDGE('',*,*,#29995,.T.);
#39864=ORIENTED_EDGE('',*,*,#29996,.T.);
#39865=ORIENTED_EDGE('',*,*,#29997,.F.);
#39866=ORIENTED_EDGE('',*,*,#29996,.F.);
#39867=ORIENTED_EDGE('',*,*,#29998,.F.);
#39868=ORIENTED_EDGE('',*,*,#29999,.T.);
#39869=ORIENTED_EDGE('',*,*,#30000,.F.);
#39870=ORIENTED_EDGE('',*,*,#29999,.F.);
#39871=ORIENTED_EDGE('',*,*,#30001,.T.);
#39872=ORIENTED_EDGE('',*,*,#30002,.T.);
#39873=ORIENTED_EDGE('',*,*,#30003,.F.);
#39874=ORIENTED_EDGE('',*,*,#30002,.F.);
#39875=ORIENTED_EDGE('',*,*,#30004,.F.);
#39876=ORIENTED_EDGE('',*,*,#30005,.T.);
#39877=ORIENTED_EDGE('',*,*,#30006,.F.);
#39878=ORIENTED_EDGE('',*,*,#30005,.F.);
#39879=ORIENTED_EDGE('',*,*,#30007,.T.);
#39880=ORIENTED_EDGE('',*,*,#30008,.T.);
#39881=ORIENTED_EDGE('',*,*,#30009,.F.);
#39882=ORIENTED_EDGE('',*,*,#30008,.F.);
#39883=ORIENTED_EDGE('',*,*,#30010,.F.);
#39884=ORIENTED_EDGE('',*,*,#30011,.T.);
#39885=ORIENTED_EDGE('',*,*,#30012,.F.);
#39886=ORIENTED_EDGE('',*,*,#30011,.F.);
#39887=ORIENTED_EDGE('',*,*,#30013,.T.);
#39888=ORIENTED_EDGE('',*,*,#30014,.T.);
#39889=ORIENTED_EDGE('',*,*,#30015,.F.);
#39890=ORIENTED_EDGE('',*,*,#30014,.F.);
#39891=ORIENTED_EDGE('',*,*,#30016,.F.);
#39892=ORIENTED_EDGE('',*,*,#30017,.T.);
#39893=ORIENTED_EDGE('',*,*,#30018,.F.);
#39894=ORIENTED_EDGE('',*,*,#30017,.F.);
#39895=ORIENTED_EDGE('',*,*,#30019,.T.);
#39896=ORIENTED_EDGE('',*,*,#30020,.T.);
#39897=ORIENTED_EDGE('',*,*,#30021,.F.);
#39898=ORIENTED_EDGE('',*,*,#30020,.F.);
#39899=ORIENTED_EDGE('',*,*,#30022,.F.);
#39900=ORIENTED_EDGE('',*,*,#30023,.T.);
#39901=ORIENTED_EDGE('',*,*,#30024,.F.);
#39902=ORIENTED_EDGE('',*,*,#30023,.F.);
#39903=ORIENTED_EDGE('',*,*,#30025,.T.);
#39904=ORIENTED_EDGE('',*,*,#30026,.T.);
#39905=ORIENTED_EDGE('',*,*,#30027,.F.);
#39906=ORIENTED_EDGE('',*,*,#30026,.F.);
#39907=ORIENTED_EDGE('',*,*,#30028,.F.);
#39908=ORIENTED_EDGE('',*,*,#30029,.T.);
#39909=ORIENTED_EDGE('',*,*,#30030,.F.);
#39910=ORIENTED_EDGE('',*,*,#30029,.F.);
#39911=ORIENTED_EDGE('',*,*,#30031,.T.);
#39912=ORIENTED_EDGE('',*,*,#30032,.T.);
#39913=ORIENTED_EDGE('',*,*,#30033,.F.);
#39914=ORIENTED_EDGE('',*,*,#30032,.F.);
#39915=ORIENTED_EDGE('',*,*,#30034,.F.);
#39916=ORIENTED_EDGE('',*,*,#30035,.T.);
#39917=ORIENTED_EDGE('',*,*,#30036,.F.);
#39918=ORIENTED_EDGE('',*,*,#30035,.F.);
#39919=ORIENTED_EDGE('',*,*,#30037,.T.);
#39920=ORIENTED_EDGE('',*,*,#30038,.T.);
#39921=ORIENTED_EDGE('',*,*,#30039,.F.);
#39922=ORIENTED_EDGE('',*,*,#30038,.F.);
#39923=ORIENTED_EDGE('',*,*,#30040,.F.);
#39924=ORIENTED_EDGE('',*,*,#30041,.T.);
#39925=ORIENTED_EDGE('',*,*,#30042,.F.);
#39926=ORIENTED_EDGE('',*,*,#30041,.F.);
#39927=ORIENTED_EDGE('',*,*,#30043,.T.);
#39928=ORIENTED_EDGE('',*,*,#30044,.T.);
#39929=ORIENTED_EDGE('',*,*,#30045,.F.);
#39930=ORIENTED_EDGE('',*,*,#30044,.F.);
#39931=ORIENTED_EDGE('',*,*,#30046,.F.);
#39932=ORIENTED_EDGE('',*,*,#30047,.T.);
#39933=ORIENTED_EDGE('',*,*,#30048,.F.);
#39934=ORIENTED_EDGE('',*,*,#30047,.F.);
#39935=ORIENTED_EDGE('',*,*,#30049,.T.);
#39936=ORIENTED_EDGE('',*,*,#30050,.T.);
#39937=ORIENTED_EDGE('',*,*,#30051,.F.);
#39938=ORIENTED_EDGE('',*,*,#30050,.F.);
#39939=ORIENTED_EDGE('',*,*,#30052,.F.);
#39940=ORIENTED_EDGE('',*,*,#30053,.T.);
#39941=ORIENTED_EDGE('',*,*,#30054,.F.);
#39942=ORIENTED_EDGE('',*,*,#30053,.F.);
#39943=ORIENTED_EDGE('',*,*,#30055,.T.);
#39944=ORIENTED_EDGE('',*,*,#30056,.T.);
#39945=ORIENTED_EDGE('',*,*,#30057,.F.);
#39946=ORIENTED_EDGE('',*,*,#30056,.F.);
#39947=ORIENTED_EDGE('',*,*,#30058,.F.);
#39948=ORIENTED_EDGE('',*,*,#30059,.T.);
#39949=ORIENTED_EDGE('',*,*,#30060,.F.);
#39950=ORIENTED_EDGE('',*,*,#30059,.F.);
#39951=ORIENTED_EDGE('',*,*,#30061,.T.);
#39952=ORIENTED_EDGE('',*,*,#30062,.T.);
#39953=ORIENTED_EDGE('',*,*,#30063,.F.);
#39954=ORIENTED_EDGE('',*,*,#30062,.F.);
#39955=ORIENTED_EDGE('',*,*,#30064,.F.);
#39956=ORIENTED_EDGE('',*,*,#30065,.T.);
#39957=ORIENTED_EDGE('',*,*,#30066,.F.);
#39958=ORIENTED_EDGE('',*,*,#30065,.F.);
#39959=ORIENTED_EDGE('',*,*,#30067,.T.);
#39960=ORIENTED_EDGE('',*,*,#30068,.T.);
#39961=ORIENTED_EDGE('',*,*,#30069,.F.);
#39962=ORIENTED_EDGE('',*,*,#30068,.F.);
#39963=ORIENTED_EDGE('',*,*,#30070,.F.);
#39964=ORIENTED_EDGE('',*,*,#30071,.T.);
#39965=ORIENTED_EDGE('',*,*,#30072,.F.);
#39966=ORIENTED_EDGE('',*,*,#30071,.F.);
#39967=ORIENTED_EDGE('',*,*,#30073,.T.);
#39968=ORIENTED_EDGE('',*,*,#30074,.T.);
#39969=ORIENTED_EDGE('',*,*,#30075,.F.);
#39970=ORIENTED_EDGE('',*,*,#30074,.F.);
#39971=ORIENTED_EDGE('',*,*,#30076,.F.);
#39972=ORIENTED_EDGE('',*,*,#30077,.T.);
#39973=ORIENTED_EDGE('',*,*,#30078,.F.);
#39974=ORIENTED_EDGE('',*,*,#30077,.F.);
#39975=ORIENTED_EDGE('',*,*,#30079,.T.);
#39976=ORIENTED_EDGE('',*,*,#30080,.T.);
#39977=ORIENTED_EDGE('',*,*,#30081,.F.);
#39978=ORIENTED_EDGE('',*,*,#30080,.F.);
#39979=ORIENTED_EDGE('',*,*,#30082,.F.);
#39980=ORIENTED_EDGE('',*,*,#30083,.T.);
#39981=ORIENTED_EDGE('',*,*,#30084,.F.);
#39982=ORIENTED_EDGE('',*,*,#30083,.F.);
#39983=ORIENTED_EDGE('',*,*,#30085,.T.);
#39984=ORIENTED_EDGE('',*,*,#30086,.T.);
#39985=ORIENTED_EDGE('',*,*,#30087,.F.);
#39986=ORIENTED_EDGE('',*,*,#30086,.F.);
#39987=ORIENTED_EDGE('',*,*,#30088,.F.);
#39988=ORIENTED_EDGE('',*,*,#30089,.T.);
#39989=ORIENTED_EDGE('',*,*,#30090,.F.);
#39990=ORIENTED_EDGE('',*,*,#30089,.F.);
#39991=ORIENTED_EDGE('',*,*,#30091,.T.);
#39992=ORIENTED_EDGE('',*,*,#30092,.T.);
#39993=ORIENTED_EDGE('',*,*,#30093,.F.);
#39994=ORIENTED_EDGE('',*,*,#30092,.F.);
#39995=ORIENTED_EDGE('',*,*,#30094,.F.);
#39996=ORIENTED_EDGE('',*,*,#30095,.T.);
#39997=ORIENTED_EDGE('',*,*,#30096,.F.);
#39998=ORIENTED_EDGE('',*,*,#30095,.F.);
#39999=ORIENTED_EDGE('',*,*,#30097,.T.);
#40000=ORIENTED_EDGE('',*,*,#30098,.T.);
#40001=ORIENTED_EDGE('',*,*,#30099,.F.);
#40002=ORIENTED_EDGE('',*,*,#30098,.F.);
#40003=ORIENTED_EDGE('',*,*,#30100,.F.);
#40004=ORIENTED_EDGE('',*,*,#30101,.T.);
#40005=ORIENTED_EDGE('',*,*,#30102,.F.);
#40006=ORIENTED_EDGE('',*,*,#30101,.F.);
#40007=ORIENTED_EDGE('',*,*,#30103,.T.);
#40008=ORIENTED_EDGE('',*,*,#30104,.T.);
#40009=ORIENTED_EDGE('',*,*,#30105,.F.);
#40010=ORIENTED_EDGE('',*,*,#30104,.F.);
#40011=ORIENTED_EDGE('',*,*,#30106,.F.);
#40012=ORIENTED_EDGE('',*,*,#30107,.T.);
#40013=ORIENTED_EDGE('',*,*,#30108,.F.);
#40014=ORIENTED_EDGE('',*,*,#30107,.F.);
#40015=ORIENTED_EDGE('',*,*,#30109,.T.);
#40016=ORIENTED_EDGE('',*,*,#30110,.T.);
#40017=ORIENTED_EDGE('',*,*,#30111,.F.);
#40018=ORIENTED_EDGE('',*,*,#30110,.F.);
#40019=ORIENTED_EDGE('',*,*,#30112,.F.);
#40020=ORIENTED_EDGE('',*,*,#30113,.T.);
#40021=ORIENTED_EDGE('',*,*,#30114,.F.);
#40022=ORIENTED_EDGE('',*,*,#30113,.F.);
#40023=ORIENTED_EDGE('',*,*,#30115,.T.);
#40024=ORIENTED_EDGE('',*,*,#30116,.T.);
#40025=ORIENTED_EDGE('',*,*,#30117,.F.);
#40026=ORIENTED_EDGE('',*,*,#30116,.F.);
#40027=ORIENTED_EDGE('',*,*,#30118,.F.);
#40028=ORIENTED_EDGE('',*,*,#30119,.T.);
#40029=ORIENTED_EDGE('',*,*,#30120,.F.);
#40030=ORIENTED_EDGE('',*,*,#30119,.F.);
#40031=ORIENTED_EDGE('',*,*,#30121,.T.);
#40032=ORIENTED_EDGE('',*,*,#30122,.T.);
#40033=ORIENTED_EDGE('',*,*,#30123,.F.);
#40034=ORIENTED_EDGE('',*,*,#30122,.F.);
#40035=ORIENTED_EDGE('',*,*,#30124,.F.);
#40036=ORIENTED_EDGE('',*,*,#30125,.T.);
#40037=ORIENTED_EDGE('',*,*,#30126,.F.);
#40038=ORIENTED_EDGE('',*,*,#30125,.F.);
#40039=ORIENTED_EDGE('',*,*,#30127,.T.);
#40040=ORIENTED_EDGE('',*,*,#30128,.T.);
#40041=ORIENTED_EDGE('',*,*,#30129,.F.);
#40042=ORIENTED_EDGE('',*,*,#30128,.F.);
#40043=ORIENTED_EDGE('',*,*,#30130,.F.);
#40044=ORIENTED_EDGE('',*,*,#30131,.T.);
#40045=ORIENTED_EDGE('',*,*,#30132,.F.);
#40046=ORIENTED_EDGE('',*,*,#30131,.F.);
#40047=ORIENTED_EDGE('',*,*,#30133,.T.);
#40048=ORIENTED_EDGE('',*,*,#30134,.T.);
#40049=ORIENTED_EDGE('',*,*,#30135,.F.);
#40050=ORIENTED_EDGE('',*,*,#30134,.F.);
#40051=ORIENTED_EDGE('',*,*,#30136,.F.);
#40052=ORIENTED_EDGE('',*,*,#30137,.T.);
#40053=ORIENTED_EDGE('',*,*,#30138,.F.);
#40054=ORIENTED_EDGE('',*,*,#30137,.F.);
#40055=ORIENTED_EDGE('',*,*,#30139,.T.);
#40056=ORIENTED_EDGE('',*,*,#30140,.T.);
#40057=ORIENTED_EDGE('',*,*,#30141,.F.);
#40058=ORIENTED_EDGE('',*,*,#30140,.F.);
#40059=ORIENTED_EDGE('',*,*,#30142,.F.);
#40060=ORIENTED_EDGE('',*,*,#30143,.T.);
#40061=ORIENTED_EDGE('',*,*,#30144,.F.);
#40062=ORIENTED_EDGE('',*,*,#30143,.F.);
#40063=ORIENTED_EDGE('',*,*,#30145,.T.);
#40064=ORIENTED_EDGE('',*,*,#30146,.T.);
#40065=ORIENTED_EDGE('',*,*,#30147,.F.);
#40066=ORIENTED_EDGE('',*,*,#30146,.F.);
#40067=ORIENTED_EDGE('',*,*,#30148,.F.);
#40068=ORIENTED_EDGE('',*,*,#30149,.T.);
#40069=ORIENTED_EDGE('',*,*,#30150,.F.);
#40070=ORIENTED_EDGE('',*,*,#30149,.F.);
#40071=ORIENTED_EDGE('',*,*,#30151,.T.);
#40072=ORIENTED_EDGE('',*,*,#30152,.T.);
#40073=ORIENTED_EDGE('',*,*,#30153,.F.);
#40074=ORIENTED_EDGE('',*,*,#30152,.F.);
#40075=ORIENTED_EDGE('',*,*,#30154,.F.);
#40076=ORIENTED_EDGE('',*,*,#30155,.T.);
#40077=ORIENTED_EDGE('',*,*,#30156,.F.);
#40078=ORIENTED_EDGE('',*,*,#30155,.F.);
#40079=ORIENTED_EDGE('',*,*,#30157,.T.);
#40080=ORIENTED_EDGE('',*,*,#30158,.T.);
#40081=ORIENTED_EDGE('',*,*,#30159,.F.);
#40082=ORIENTED_EDGE('',*,*,#30158,.F.);
#40083=ORIENTED_EDGE('',*,*,#30160,.F.);
#40084=ORIENTED_EDGE('',*,*,#30161,.T.);
#40085=ORIENTED_EDGE('',*,*,#30162,.F.);
#40086=ORIENTED_EDGE('',*,*,#30161,.F.);
#40087=ORIENTED_EDGE('',*,*,#30163,.T.);
#40088=ORIENTED_EDGE('',*,*,#30164,.T.);
#40089=ORIENTED_EDGE('',*,*,#30165,.F.);
#40090=ORIENTED_EDGE('',*,*,#30164,.F.);
#40091=ORIENTED_EDGE('',*,*,#30166,.F.);
#40092=ORIENTED_EDGE('',*,*,#30167,.T.);
#40093=ORIENTED_EDGE('',*,*,#30168,.F.);
#40094=ORIENTED_EDGE('',*,*,#30167,.F.);
#40095=ORIENTED_EDGE('',*,*,#30169,.T.);
#40096=ORIENTED_EDGE('',*,*,#30170,.T.);
#40097=ORIENTED_EDGE('',*,*,#30171,.F.);
#40098=ORIENTED_EDGE('',*,*,#30170,.F.);
#40099=ORIENTED_EDGE('',*,*,#30172,.F.);
#40100=ORIENTED_EDGE('',*,*,#30173,.T.);
#40101=ORIENTED_EDGE('',*,*,#30174,.F.);
#40102=ORIENTED_EDGE('',*,*,#30173,.F.);
#40103=ORIENTED_EDGE('',*,*,#30175,.T.);
#40104=ORIENTED_EDGE('',*,*,#30176,.T.);
#40105=ORIENTED_EDGE('',*,*,#30177,.F.);
#40106=ORIENTED_EDGE('',*,*,#30176,.F.);
#40107=ORIENTED_EDGE('',*,*,#30178,.F.);
#40108=ORIENTED_EDGE('',*,*,#30179,.T.);
#40109=ORIENTED_EDGE('',*,*,#30180,.F.);
#40110=ORIENTED_EDGE('',*,*,#30179,.F.);
#40111=ORIENTED_EDGE('',*,*,#30181,.T.);
#40112=ORIENTED_EDGE('',*,*,#30182,.T.);
#40113=ORIENTED_EDGE('',*,*,#30183,.F.);
#40114=ORIENTED_EDGE('',*,*,#30182,.F.);
#40115=ORIENTED_EDGE('',*,*,#30184,.F.);
#40116=ORIENTED_EDGE('',*,*,#30185,.T.);
#40117=ORIENTED_EDGE('',*,*,#30186,.F.);
#40118=ORIENTED_EDGE('',*,*,#30185,.F.);
#40119=ORIENTED_EDGE('',*,*,#30187,.T.);
#40120=ORIENTED_EDGE('',*,*,#30188,.T.);
#40121=ORIENTED_EDGE('',*,*,#30189,.F.);
#40122=ORIENTED_EDGE('',*,*,#30188,.F.);
#40123=ORIENTED_EDGE('',*,*,#30190,.F.);
#40124=ORIENTED_EDGE('',*,*,#30191,.T.);
#40125=ORIENTED_EDGE('',*,*,#30192,.F.);
#40126=ORIENTED_EDGE('',*,*,#30191,.F.);
#40127=ORIENTED_EDGE('',*,*,#30193,.T.);
#40128=ORIENTED_EDGE('',*,*,#30194,.T.);
#40129=ORIENTED_EDGE('',*,*,#30195,.F.);
#40130=ORIENTED_EDGE('',*,*,#30194,.F.);
#40131=ORIENTED_EDGE('',*,*,#30196,.F.);
#40132=ORIENTED_EDGE('',*,*,#30197,.T.);
#40133=ORIENTED_EDGE('',*,*,#30198,.F.);
#40134=ORIENTED_EDGE('',*,*,#30197,.F.);
#40135=ORIENTED_EDGE('',*,*,#30199,.T.);
#40136=ORIENTED_EDGE('',*,*,#30200,.T.);
#40137=ORIENTED_EDGE('',*,*,#30201,.F.);
#40138=ORIENTED_EDGE('',*,*,#30200,.F.);
#40139=ORIENTED_EDGE('',*,*,#30202,.F.);
#40140=ORIENTED_EDGE('',*,*,#30203,.T.);
#40141=ORIENTED_EDGE('',*,*,#30204,.F.);
#40142=ORIENTED_EDGE('',*,*,#30203,.F.);
#40143=ORIENTED_EDGE('',*,*,#30205,.T.);
#40144=ORIENTED_EDGE('',*,*,#30206,.T.);
#40145=ORIENTED_EDGE('',*,*,#30207,.F.);
#40146=ORIENTED_EDGE('',*,*,#30206,.F.);
#40147=ORIENTED_EDGE('',*,*,#30208,.F.);
#40148=ORIENTED_EDGE('',*,*,#30209,.T.);
#40149=ORIENTED_EDGE('',*,*,#30210,.F.);
#40150=ORIENTED_EDGE('',*,*,#30209,.F.);
#40151=ORIENTED_EDGE('',*,*,#30211,.T.);
#40152=ORIENTED_EDGE('',*,*,#30212,.T.);
#40153=ORIENTED_EDGE('',*,*,#30213,.F.);
#40154=ORIENTED_EDGE('',*,*,#30212,.F.);
#40155=ORIENTED_EDGE('',*,*,#30214,.F.);
#40156=ORIENTED_EDGE('',*,*,#30215,.T.);
#40157=ORIENTED_EDGE('',*,*,#30216,.F.);
#40158=ORIENTED_EDGE('',*,*,#30215,.F.);
#40159=ORIENTED_EDGE('',*,*,#30217,.T.);
#40160=ORIENTED_EDGE('',*,*,#30218,.T.);
#40161=ORIENTED_EDGE('',*,*,#30219,.F.);
#40162=ORIENTED_EDGE('',*,*,#30218,.F.);
#40163=ORIENTED_EDGE('',*,*,#30220,.F.);
#40164=ORIENTED_EDGE('',*,*,#30221,.T.);
#40165=ORIENTED_EDGE('',*,*,#30222,.F.);
#40166=ORIENTED_EDGE('',*,*,#30221,.F.);
#40167=ORIENTED_EDGE('',*,*,#30223,.T.);
#40168=ORIENTED_EDGE('',*,*,#30224,.T.);
#40169=ORIENTED_EDGE('',*,*,#30225,.F.);
#40170=ORIENTED_EDGE('',*,*,#30224,.F.);
#40171=ORIENTED_EDGE('',*,*,#30226,.F.);
#40172=ORIENTED_EDGE('',*,*,#30227,.T.);
#40173=ORIENTED_EDGE('',*,*,#30228,.F.);
#40174=ORIENTED_EDGE('',*,*,#30227,.F.);
#40175=ORIENTED_EDGE('',*,*,#30229,.T.);
#40176=ORIENTED_EDGE('',*,*,#30230,.T.);
#40177=ORIENTED_EDGE('',*,*,#30231,.F.);
#40178=ORIENTED_EDGE('',*,*,#30230,.F.);
#40179=ORIENTED_EDGE('',*,*,#30232,.F.);
#40180=ORIENTED_EDGE('',*,*,#30233,.T.);
#40181=ORIENTED_EDGE('',*,*,#30234,.F.);
#40182=ORIENTED_EDGE('',*,*,#30233,.F.);
#40183=ORIENTED_EDGE('',*,*,#30235,.T.);
#40184=ORIENTED_EDGE('',*,*,#30236,.T.);
#40185=ORIENTED_EDGE('',*,*,#30237,.F.);
#40186=ORIENTED_EDGE('',*,*,#30236,.F.);
#40187=ORIENTED_EDGE('',*,*,#30238,.F.);
#40188=ORIENTED_EDGE('',*,*,#30239,.T.);
#40189=ORIENTED_EDGE('',*,*,#30240,.F.);
#40190=ORIENTED_EDGE('',*,*,#30239,.F.);
#40191=ORIENTED_EDGE('',*,*,#30241,.T.);
#40192=ORIENTED_EDGE('',*,*,#30242,.T.);
#40193=ORIENTED_EDGE('',*,*,#30243,.F.);
#40194=ORIENTED_EDGE('',*,*,#30242,.F.);
#40195=ORIENTED_EDGE('',*,*,#30244,.F.);
#40196=ORIENTED_EDGE('',*,*,#30245,.T.);
#40197=ORIENTED_EDGE('',*,*,#30246,.F.);
#40198=ORIENTED_EDGE('',*,*,#30245,.F.);
#40199=ORIENTED_EDGE('',*,*,#30247,.T.);
#40200=ORIENTED_EDGE('',*,*,#30248,.T.);
#40201=ORIENTED_EDGE('',*,*,#30249,.F.);
#40202=ORIENTED_EDGE('',*,*,#30248,.F.);
#40203=ORIENTED_EDGE('',*,*,#30250,.F.);
#40204=ORIENTED_EDGE('',*,*,#30251,.T.);
#40205=ORIENTED_EDGE('',*,*,#30252,.F.);
#40206=ORIENTED_EDGE('',*,*,#30251,.F.);
#40207=ORIENTED_EDGE('',*,*,#30253,.T.);
#40208=ORIENTED_EDGE('',*,*,#30254,.T.);
#40209=ORIENTED_EDGE('',*,*,#30255,.F.);
#40210=ORIENTED_EDGE('',*,*,#30254,.F.);
#40211=ORIENTED_EDGE('',*,*,#30256,.F.);
#40212=ORIENTED_EDGE('',*,*,#30257,.T.);
#40213=ORIENTED_EDGE('',*,*,#30258,.F.);
#40214=ORIENTED_EDGE('',*,*,#30257,.F.);
#40215=ORIENTED_EDGE('',*,*,#30259,.T.);
#40216=ORIENTED_EDGE('',*,*,#30260,.T.);
#40217=ORIENTED_EDGE('',*,*,#30261,.F.);
#40218=ORIENTED_EDGE('',*,*,#30260,.F.);
#40219=ORIENTED_EDGE('',*,*,#30262,.F.);
#40220=ORIENTED_EDGE('',*,*,#30263,.T.);
#40221=ORIENTED_EDGE('',*,*,#30264,.F.);
#40222=ORIENTED_EDGE('',*,*,#30263,.F.);
#40223=ORIENTED_EDGE('',*,*,#30265,.T.);
#40224=ORIENTED_EDGE('',*,*,#30266,.T.);
#40225=ORIENTED_EDGE('',*,*,#30267,.F.);
#40226=ORIENTED_EDGE('',*,*,#30266,.F.);
#40227=ORIENTED_EDGE('',*,*,#30268,.F.);
#40228=ORIENTED_EDGE('',*,*,#30269,.T.);
#40229=ORIENTED_EDGE('',*,*,#30270,.F.);
#40230=ORIENTED_EDGE('',*,*,#30269,.F.);
#40231=ORIENTED_EDGE('',*,*,#30271,.T.);
#40232=ORIENTED_EDGE('',*,*,#30272,.T.);
#40233=ORIENTED_EDGE('',*,*,#30273,.F.);
#40234=ORIENTED_EDGE('',*,*,#30272,.F.);
#40235=ORIENTED_EDGE('',*,*,#30274,.F.);
#40236=ORIENTED_EDGE('',*,*,#30275,.T.);
#40237=ORIENTED_EDGE('',*,*,#30276,.F.);
#40238=ORIENTED_EDGE('',*,*,#30275,.F.);
#40239=ORIENTED_EDGE('',*,*,#30277,.T.);
#40240=ORIENTED_EDGE('',*,*,#30278,.T.);
#40241=ORIENTED_EDGE('',*,*,#30279,.F.);
#40242=ORIENTED_EDGE('',*,*,#30278,.F.);
#40243=ORIENTED_EDGE('',*,*,#27756,.F.);
#40244=ORIENTED_EDGE('',*,*,#30280,.T.);
#40245=ORIENTED_EDGE('',*,*,#30281,.F.);
#40246=ORIENTED_EDGE('',*,*,#30280,.F.);
#40247=ORIENTED_EDGE('',*,*,#30282,.F.);
#40248=ORIENTED_EDGE('',*,*,#30281,.T.);
#40249=ORIENTED_EDGE('',*,*,#30283,.T.);
#40250=ORIENTED_EDGE('',*,*,#30284,.T.);
#40251=ORIENTED_EDGE('',*,*,#30283,.F.);
#40252=ORIENTED_EDGE('',*,*,#30285,.F.);
#40253=ORIENTED_EDGE('',*,*,#30286,.T.);
#40254=ORIENTED_EDGE('',*,*,#30287,.F.);
#40255=ORIENTED_EDGE('',*,*,#30288,.F.);
#40256=ORIENTED_EDGE('',*,*,#30286,.F.);
#40257=ORIENTED_EDGE('',*,*,#30289,.F.);
#40258=ORIENTED_EDGE('',*,*,#30290,.T.);
#40259=ORIENTED_EDGE('',*,*,#30291,.F.);
#40260=ORIENTED_EDGE('',*,*,#30290,.F.);
#40261=ORIENTED_EDGE('',*,*,#30291,.T.);
#40262=ORIENTED_EDGE('',*,*,#30292,.T.);
#40263=ORIENTED_EDGE('',*,*,#30287,.T.);
#40264=ORIENTED_EDGE('',*,*,#30288,.T.);
#40265=ORIENTED_EDGE('',*,*,#30292,.F.);
#40266=ORIENTED_EDGE('',*,*,#30293,.F.);
#40267=ORIENTED_EDGE('',*,*,#27878,.T.);
#40268=ORIENTED_EDGE('',*,*,#30294,.F.);
#40269=ORIENTED_EDGE('',*,*,#30295,.T.);
#40270=ORIENTED_EDGE('',*,*,#30296,.F.);
#40271=ORIENTED_EDGE('',*,*,#30295,.F.);
#40272=ORIENTED_EDGE('',*,*,#30297,.F.);
#40273=ORIENTED_EDGE('',*,*,#30298,.T.);
#40274=ORIENTED_EDGE('',*,*,#30299,.F.);
#40275=ORIENTED_EDGE('',*,*,#30298,.F.);
#40276=ORIENTED_EDGE('',*,*,#30284,.F.);
#40277=ORIENTED_EDGE('',*,*,#30300,.T.);
#40278=ORIENTED_EDGE('',*,*,#30301,.F.);
#40279=ORIENTED_EDGE('',*,*,#30300,.F.);
#40280=ORIENTED_EDGE('',*,*,#30302,.T.);
#40281=ORIENTED_EDGE('',*,*,#30303,.T.);
#40282=ORIENTED_EDGE('',*,*,#30294,.T.);
#40283=ORIENTED_EDGE('',*,*,#30303,.F.);
#40284=ORIENTED_EDGE('',*,*,#30304,.F.);
#40285=ORIENTED_EDGE('',*,*,#30305,.F.);
#40286=ORIENTED_EDGE('',*,*,#30306,.T.);
#40287=ORIENTED_EDGE('',*,*,#30307,.F.);
#40288=ORIENTED_EDGE('',*,*,#30306,.F.);
#40289=ORIENTED_EDGE('',*,*,#30304,.T.);
#40290=ORIENTED_EDGE('',*,*,#30305,.T.);
#40291=ORIENTED_EDGE('',*,*,#30308,.T.);
#40292=ORIENTED_EDGE('',*,*,#30297,.T.);
#40293=ORIENTED_EDGE('',*,*,#30308,.F.);
#40294=ORIENTED_EDGE('',*,*,#30309,.T.);
#40295=ORIENTED_EDGE('',*,*,#30310,.T.);
#40296=ORIENTED_EDGE('',*,*,#30311,.F.);
#40297=ORIENTED_EDGE('',*,*,#30310,.F.);
#40298=ORIENTED_EDGE('',*,*,#30312,.T.);
#40299=ORIENTED_EDGE('',*,*,#27790,.F.);
#40300=ORIENTED_EDGE('',*,*,#27791,.F.);
#40301=ORIENTED_EDGE('',*,*,#30313,.T.);
#40302=ORIENTED_EDGE('',*,*,#30314,.F.);
#40303=ORIENTED_EDGE('',*,*,#30313,.F.);
#40304=ORIENTED_EDGE('',*,*,#30314,.T.);
#40305=ORIENTED_EDGE('',*,*,#30309,.F.);
#40306=ORIENTED_EDGE('',*,*,#30312,.F.);
#40307=ORIENTED_EDGE('',*,*,#30311,.T.);
#40308=ORIENTED_EDGE('',*,*,#30299,.T.);
#40309=ORIENTED_EDGE('',*,*,#30301,.T.);
#40310=ORIENTED_EDGE('',*,*,#30307,.T.);
#40311=ORIENTED_EDGE('',*,*,#30302,.F.);
#40312=ORIENTED_EDGE('',*,*,#30296,.T.);
#40313=ORIENTED_EDGE('',*,*,#30293,.T.);
#40314=ORIENTED_EDGE('',*,*,#30289,.T.);
#40315=ORIENTED_EDGE('',*,*,#30285,.T.);
#40316=ORIENTED_EDGE('',*,*,#27880,.T.);
#40317=ORIENTED_EDGE('',*,*,#27754,.F.);
#40318=ORIENTED_EDGE('',*,*,#30315,.F.);
#40319=ORIENTED_EDGE('',*,*,#29350,.T.);
#40320=ORIENTED_EDGE('',*,*,#29290,.T.);
#40321=ORIENTED_EDGE('',*,*,#29230,.T.);
#40322=ORIENTED_EDGE('',*,*,#29170,.T.);
#40323=ORIENTED_EDGE('',*,*,#29110,.T.);
#40324=ORIENTED_EDGE('',*,*,#29050,.T.);
#40325=ORIENTED_EDGE('',*,*,#28990,.T.);
#40326=ORIENTED_EDGE('',*,*,#28930,.T.);
#40327=ORIENTED_EDGE('',*,*,#29464,.T.);
#40328=ORIENTED_EDGE('',*,*,#29404,.T.);
#40329=ORIENTED_EDGE('',*,*,#29344,.T.);
#40330=ORIENTED_EDGE('',*,*,#29284,.T.);
#40331=ORIENTED_EDGE('',*,*,#29356,.T.);
#40332=ORIENTED_EDGE('',*,*,#29296,.T.);
#40333=ORIENTED_EDGE('',*,*,#29236,.T.);
#40334=ORIENTED_EDGE('',*,*,#29176,.T.);
#40335=ORIENTED_EDGE('',*,*,#29116,.T.);
#40336=ORIENTED_EDGE('',*,*,#29056,.T.);
#40337=ORIENTED_EDGE('',*,*,#29410,.T.);
#40338=ORIENTED_EDGE('',*,*,#28876,.T.);
#40339=ORIENTED_EDGE('',*,*,#28936,.T.);
#40340=ORIENTED_EDGE('',*,*,#28996,.T.);
#40341=ORIENTED_EDGE('',*,*,#29512,.T.);
#40342=ORIENTED_EDGE('',*,*,#29572,.T.);
#40343=ORIENTED_EDGE('',*,*,#29038,.T.);
#40344=ORIENTED_EDGE('',*,*,#29098,.T.);
#40345=ORIENTED_EDGE('',*,*,#29212,.T.);
#40346=ORIENTED_EDGE('',*,*,#29152,.T.);
#40347=ORIENTED_EDGE('',*,*,#29092,.T.);
#40348=ORIENTED_EDGE('',*,*,#29272,.T.);
#40349=ORIENTED_EDGE('',*,*,#29332,.T.);
#40350=ORIENTED_EDGE('',*,*,#29392,.T.);
#40351=ORIENTED_EDGE('',*,*,#29452,.T.);
#40352=ORIENTED_EDGE('',*,*,#29224,.T.);
#40353=ORIENTED_EDGE('',*,*,#29164,.T.);
#40354=ORIENTED_EDGE('',*,*,#29104,.T.);
#40355=ORIENTED_EDGE('',*,*,#29044,.T.);
#40356=ORIENTED_EDGE('',*,*,#28984,.T.);
#40357=ORIENTED_EDGE('',*,*,#29518,.T.);
#40358=ORIENTED_EDGE('',*,*,#29458,.T.);
#40359=ORIENTED_EDGE('',*,*,#29398,.T.);
#40360=ORIENTED_EDGE('',*,*,#29338,.T.);
#40361=ORIENTED_EDGE('',*,*,#29278,.T.);
#40362=ORIENTED_EDGE('',*,*,#29218,.T.);
#40363=ORIENTED_EDGE('',*,*,#29158,.T.);
#40364=ORIENTED_EDGE('',*,*,#28780,.T.);
#40365=ORIENTED_EDGE('',*,*,#28720,.T.);
#40366=ORIENTED_EDGE('',*,*,#28660,.T.);
#40367=ORIENTED_EDGE('',*,*,#28840,.T.);
#40368=ORIENTED_EDGE('',*,*,#28900,.T.);
#40369=ORIENTED_EDGE('',*,*,#28960,.T.);
#40370=ORIENTED_EDGE('',*,*,#29020,.T.);
#40371=ORIENTED_EDGE('',*,*,#29194,.T.);
#40372=ORIENTED_EDGE('',*,*,#29134,.T.);
#40373=ORIENTED_EDGE('',*,*,#29074,.T.);
#40374=ORIENTED_EDGE('',*,*,#29014,.T.);
#40375=ORIENTED_EDGE('',*,*,#28954,.T.);
#40376=ORIENTED_EDGE('',*,*,#29086,.T.);
#40377=ORIENTED_EDGE('',*,*,#29026,.T.);
#40378=ORIENTED_EDGE('',*,*,#28966,.T.);
#40379=ORIENTED_EDGE('',*,*,#28906,.T.);
#40380=ORIENTED_EDGE('',*,*,#28846,.T.);
#40381=ORIENTED_EDGE('',*,*,#28786,.T.);
#40382=ORIENTED_EDGE('',*,*,#28726,.T.);
#40383=ORIENTED_EDGE('',*,*,#29080,.T.);
#40384=ORIENTED_EDGE('',*,*,#29140,.T.);
#40385=ORIENTED_EDGE('',*,*,#30226,.T.);
#40386=ORIENTED_EDGE('',*,*,#28666,.T.);
#40387=ORIENTED_EDGE('',*,*,#28768,.T.);
#40388=ORIENTED_EDGE('',*,*,#29302,.T.);
#40389=ORIENTED_EDGE('',*,*,#29242,.T.);
#40390=ORIENTED_EDGE('',*,*,#29182,.T.);
#40391=ORIENTED_EDGE('',*,*,#29122,.T.);
#40392=ORIENTED_EDGE('',*,*,#29062,.T.);
#40393=ORIENTED_EDGE('',*,*,#29002,.T.);
#40394=ORIENTED_EDGE('',*,*,#28942,.T.);
#40395=ORIENTED_EDGE('',*,*,#28882,.T.);
#40396=ORIENTED_EDGE('',*,*,#28822,.T.);
#40397=ORIENTED_EDGE('',*,*,#28894,.T.);
#40398=ORIENTED_EDGE('',*,*,#28834,.T.);
#40399=ORIENTED_EDGE('',*,*,#28774,.T.);
#40400=ORIENTED_EDGE('',*,*,#28714,.T.);
#40401=ORIENTED_EDGE('',*,*,#29248,.T.);
#40402=ORIENTED_EDGE('',*,*,#29188,.T.);
#40403=ORIENTED_EDGE('',*,*,#29128,.T.);
#40404=ORIENTED_EDGE('',*,*,#29068,.T.);
#40405=ORIENTED_EDGE('',*,*,#29008,.T.);
#40406=ORIENTED_EDGE('',*,*,#28948,.T.);
#40407=ORIENTED_EDGE('',*,*,#28888,.T.);
#40408=ORIENTED_EDGE('',*,*,#28828,.T.);
#40409=ORIENTED_EDGE('',*,*,#29950,.T.);
#40410=ORIENTED_EDGE('',*,*,#29890,.T.);
#40411=ORIENTED_EDGE('',*,*,#29830,.T.);
#40412=ORIENTED_EDGE('',*,*,#29770,.T.);
#40413=ORIENTED_EDGE('',*,*,#29710,.T.);
#40414=ORIENTED_EDGE('',*,*,#29650,.T.);
#40415=ORIENTED_EDGE('',*,*,#29590,.T.);
#40416=ORIENTED_EDGE('',*,*,#29944,.T.);
#40417=ORIENTED_EDGE('',*,*,#30004,.T.);
#40418=ORIENTED_EDGE('',*,*,#29470,.T.);
#40419=ORIENTED_EDGE('',*,*,#29530,.T.);
#40420=ORIENTED_EDGE('',*,*,#29896,.T.);
#40421=ORIENTED_EDGE('',*,*,#29836,.T.);
#40422=ORIENTED_EDGE('',*,*,#29776,.T.);
#40423=ORIENTED_EDGE('',*,*,#29716,.T.);
#40424=ORIENTED_EDGE('',*,*,#29656,.T.);
#40425=ORIENTED_EDGE('',*,*,#29596,.T.);
#40426=ORIENTED_EDGE('',*,*,#29536,.T.);
#40427=ORIENTED_EDGE('',*,*,#29476,.T.);
#40428=ORIENTED_EDGE('',*,*,#29416,.T.);
#40429=ORIENTED_EDGE('',*,*,#29758,.T.);
#40430=ORIENTED_EDGE('',*,*,#29698,.T.);
#40431=ORIENTED_EDGE('',*,*,#29638,.T.);
#40432=ORIENTED_EDGE('',*,*,#29578,.T.);
#40433=ORIENTED_EDGE('',*,*,#30112,.T.);
#40434=ORIENTED_EDGE('',*,*,#30052,.T.);
#40435=ORIENTED_EDGE('',*,*,#29992,.T.);
#40436=ORIENTED_EDGE('',*,*,#29932,.T.);
#40437=ORIENTED_EDGE('',*,*,#29872,.T.);
#40438=ORIENTED_EDGE('',*,*,#29812,.T.);
#40439=ORIENTED_EDGE('',*,*,#29752,.T.);
#40440=ORIENTED_EDGE('',*,*,#29692,.T.);
#40441=ORIENTED_EDGE('',*,*,#29644,.T.);
#40442=ORIENTED_EDGE('',*,*,#29584,.T.);
#40443=ORIENTED_EDGE('',*,*,#29524,.T.);
#40444=ORIENTED_EDGE('',*,*,#29704,.T.);
#40445=ORIENTED_EDGE('',*,*,#29764,.T.);
#40446=ORIENTED_EDGE('',*,*,#29824,.T.);
#40447=ORIENTED_EDGE('',*,*,#29884,.T.);
#40448=ORIENTED_EDGE('',*,*,#30058,.T.);
#40449=ORIENTED_EDGE('',*,*,#29998,.T.);
#40450=ORIENTED_EDGE('',*,*,#29938,.T.);
#40451=ORIENTED_EDGE('',*,*,#29878,.T.);
#40452=ORIENTED_EDGE('',*,*,#29818,.T.);
#40453=ORIENTED_EDGE('',*,*,#29680,.T.);
#40454=ORIENTED_EDGE('',*,*,#29620,.T.);
#40455=ORIENTED_EDGE('',*,*,#29560,.T.);
#40456=ORIENTED_EDGE('',*,*,#29500,.T.);
#40457=ORIENTED_EDGE('',*,*,#29440,.T.);
#40458=ORIENTED_EDGE('',*,*,#29380,.T.);
#40459=ORIENTED_EDGE('',*,*,#29320,.T.);
#40460=ORIENTED_EDGE('',*,*,#29260,.T.);
#40461=ORIENTED_EDGE('',*,*,#29200,.T.);
#40462=ORIENTED_EDGE('',*,*,#29734,.T.);
#40463=ORIENTED_EDGE('',*,*,#29674,.T.);
#40464=ORIENTED_EDGE('',*,*,#29614,.T.);
#40465=ORIENTED_EDGE('',*,*,#29626,.T.);
#40466=ORIENTED_EDGE('',*,*,#29566,.T.);
#40467=ORIENTED_EDGE('',*,*,#29506,.T.);
#40468=ORIENTED_EDGE('',*,*,#29446,.T.);
#40469=ORIENTED_EDGE('',*,*,#29386,.T.);
#40470=ORIENTED_EDGE('',*,*,#29326,.T.);
#40471=ORIENTED_EDGE('',*,*,#29266,.T.);
#40472=ORIENTED_EDGE('',*,*,#29206,.T.);
#40473=ORIENTED_EDGE('',*,*,#29146,.T.);
#40474=ORIENTED_EDGE('',*,*,#29842,.T.);
#40475=ORIENTED_EDGE('',*,*,#29308,.T.);
#40476=ORIENTED_EDGE('',*,*,#29368,.T.);
#40477=ORIENTED_EDGE('',*,*,#29428,.T.);
#40478=ORIENTED_EDGE('',*,*,#29782,.T.);
#40479=ORIENTED_EDGE('',*,*,#29722,.T.);
#40480=ORIENTED_EDGE('',*,*,#29662,.T.);
#40481=ORIENTED_EDGE('',*,*,#29602,.T.);
#40482=ORIENTED_EDGE('',*,*,#29542,.T.);
#40483=ORIENTED_EDGE('',*,*,#29482,.T.);
#40484=ORIENTED_EDGE('',*,*,#29422,.T.);
#40485=ORIENTED_EDGE('',*,*,#29362,.T.);
#40486=ORIENTED_EDGE('',*,*,#29554,.T.);
#40487=ORIENTED_EDGE('',*,*,#29494,.T.);
#40488=ORIENTED_EDGE('',*,*,#29434,.T.);
#40489=ORIENTED_EDGE('',*,*,#29374,.T.);
#40490=ORIENTED_EDGE('',*,*,#29314,.T.);
#40491=ORIENTED_EDGE('',*,*,#29254,.T.);
#40492=ORIENTED_EDGE('',*,*,#29788,.T.);
#40493=ORIENTED_EDGE('',*,*,#29728,.T.);
#40494=ORIENTED_EDGE('',*,*,#29668,.T.);
#40495=ORIENTED_EDGE('',*,*,#29608,.T.);
#40496=ORIENTED_EDGE('',*,*,#29548,.T.);
#40497=ORIENTED_EDGE('',*,*,#29488,.T.);
#40498=ORIENTED_EDGE('',*,*,#30166,.T.);
#40499=ORIENTED_EDGE('',*,*,#28690,.T.);
#40500=ORIENTED_EDGE('',*,*,#30250,.T.);
#40501=ORIENTED_EDGE('',*,*,#30190,.T.);
#40502=ORIENTED_EDGE('',*,*,#30130,.T.);
#40503=ORIENTED_EDGE('',*,*,#30070,.T.);
#40504=ORIENTED_EDGE('',*,*,#30010,.T.);
#40505=ORIENTED_EDGE('',*,*,#28924,.T.);
#40506=ORIENTED_EDGE('',*,*,#28864,.T.);
#40507=ORIENTED_EDGE('',*,*,#28804,.T.);
#40508=ORIENTED_EDGE('',*,*,#28744,.T.);
#40509=ORIENTED_EDGE('',*,*,#28684,.T.);
#40510=ORIENTED_EDGE('',*,*,#30244,.T.);
#40511=ORIENTED_EDGE('',*,*,#28816,.T.);
#40512=ORIENTED_EDGE('',*,*,#28756,.T.);
#40513=ORIENTED_EDGE('',*,*,#28696,.T.);
#40514=ORIENTED_EDGE('',*,*,#30256,.T.);
#40515=ORIENTED_EDGE('',*,*,#30196,.T.);
#40516=ORIENTED_EDGE('',*,*,#30136,.T.);
#40517=ORIENTED_EDGE('',*,*,#30076,.T.);
#40518=ORIENTED_EDGE('',*,*,#30016,.T.);
#40519=ORIENTED_EDGE('',*,*,#28750,.T.);
#40520=ORIENTED_EDGE('',*,*,#28810,.T.);
#40521=ORIENTED_EDGE('',*,*,#28870,.T.);
#40522=ORIENTED_EDGE('',*,*,#29956,.T.);
#40523=ORIENTED_EDGE('',*,*,#29032,.T.);
#40524=ORIENTED_EDGE('',*,*,#28972,.T.);
#40525=ORIENTED_EDGE('',*,*,#28912,.T.);
#40526=ORIENTED_EDGE('',*,*,#28852,.T.);
#40527=ORIENTED_EDGE('',*,*,#28792,.T.);
#40528=ORIENTED_EDGE('',*,*,#28732,.T.);
#40529=ORIENTED_EDGE('',*,*,#28672,.T.);
#40530=ORIENTED_EDGE('',*,*,#30232,.T.);
#40531=ORIENTED_EDGE('',*,*,#30172,.T.);
#40532=ORIENTED_EDGE('',*,*,#28978,.T.);
#40533=ORIENTED_EDGE('',*,*,#30064,.T.);
#40534=ORIENTED_EDGE('',*,*,#30124,.T.);
#40535=ORIENTED_EDGE('',*,*,#30184,.T.);
#40536=ORIENTED_EDGE('',*,*,#28918,.T.);
#40537=ORIENTED_EDGE('',*,*,#28858,.T.);
#40538=ORIENTED_EDGE('',*,*,#28798,.T.);
#40539=ORIENTED_EDGE('',*,*,#28738,.T.);
#40540=ORIENTED_EDGE('',*,*,#28678,.T.);
#40541=ORIENTED_EDGE('',*,*,#30238,.T.);
#40542=ORIENTED_EDGE('',*,*,#30178,.T.);
#40543=ORIENTED_EDGE('',*,*,#30118,.T.);
#40544=ORIENTED_EDGE('',*,*,#29980,.T.);
#40545=ORIENTED_EDGE('',*,*,#29920,.T.);
#40546=ORIENTED_EDGE('',*,*,#29860,.T.);
#40547=ORIENTED_EDGE('',*,*,#29800,.T.);
#40548=ORIENTED_EDGE('',*,*,#29740,.T.);
#40549=ORIENTED_EDGE('',*,*,#30274,.T.);
#40550=ORIENTED_EDGE('',*,*,#30214,.T.);
#40551=ORIENTED_EDGE('',*,*,#30154,.T.);
#40552=ORIENTED_EDGE('',*,*,#30094,.T.);
#40553=ORIENTED_EDGE('',*,*,#30034,.T.);
#40554=ORIENTED_EDGE('',*,*,#29974,.T.);
#40555=ORIENTED_EDGE('',*,*,#29914,.T.);
#40556=ORIENTED_EDGE('',*,*,#30106,.T.);
#40557=ORIENTED_EDGE('',*,*,#30046,.T.);
#40558=ORIENTED_EDGE('',*,*,#29986,.T.);
#40559=ORIENTED_EDGE('',*,*,#29926,.T.);
#40560=ORIENTED_EDGE('',*,*,#29866,.T.);
#40561=ORIENTED_EDGE('',*,*,#29806,.T.);
#40562=ORIENTED_EDGE('',*,*,#29746,.T.);
#40563=ORIENTED_EDGE('',*,*,#29686,.T.);
#40564=ORIENTED_EDGE('',*,*,#30220,.T.);
#40565=ORIENTED_EDGE('',*,*,#30160,.T.);
#40566=ORIENTED_EDGE('',*,*,#30100,.T.);
#40567=ORIENTED_EDGE('',*,*,#30040,.T.);
#40568=ORIENTED_EDGE('',*,*,#28762,.T.);
#40569=ORIENTED_EDGE('',*,*,#28702,.T.);
#40570=ORIENTED_EDGE('',*,*,#30262,.T.);
#40571=ORIENTED_EDGE('',*,*,#30202,.T.);
#40572=ORIENTED_EDGE('',*,*,#30142,.T.);
#40573=ORIENTED_EDGE('',*,*,#30082,.T.);
#40574=ORIENTED_EDGE('',*,*,#30022,.T.);
#40575=ORIENTED_EDGE('',*,*,#29962,.T.);
#40576=ORIENTED_EDGE('',*,*,#29902,.T.);
#40577=ORIENTED_EDGE('',*,*,#30268,.T.);
#40578=ORIENTED_EDGE('',*,*,#28708,.T.);
#40579=ORIENTED_EDGE('',*,*,#29794,.T.);
#40580=ORIENTED_EDGE('',*,*,#29854,.T.);
#40581=ORIENTED_EDGE('',*,*,#29848,.T.);
#40582=ORIENTED_EDGE('',*,*,#29908,.T.);
#40583=ORIENTED_EDGE('',*,*,#29968,.T.);
#40584=ORIENTED_EDGE('',*,*,#30028,.T.);
#40585=ORIENTED_EDGE('',*,*,#30088,.T.);
#40586=ORIENTED_EDGE('',*,*,#30148,.T.);
#40587=ORIENTED_EDGE('',*,*,#30208,.T.);
#40588=ORIENTED_EDGE('',*,*,#29632,.T.);
#40589=ORIENTED_EDGE('',*,*,#27755,.F.);
#40590=ORIENTED_EDGE('',*,*,#30315,.T.);
#40591=ORIENTED_EDGE('',*,*,#27757,.T.);
#40592=ORIENTED_EDGE('',*,*,#30282,.T.);
#40593=ORIENTED_EDGE('',*,*,#28371,.T.);
#40594=ORIENTED_EDGE('',*,*,#28334,.T.);
#40595=ORIENTED_EDGE('',*,*,#28298,.T.);
#40596=ORIENTED_EDGE('',*,*,#28262,.T.);
#40597=ORIENTED_EDGE('',*,*,#28241,.T.);
#40598=ORIENTED_EDGE('',*,*,#28206,.T.);
#40599=ORIENTED_EDGE('',*,*,#28234,.T.);
#40600=ORIENTED_EDGE('',*,*,#28269,.T.);
#40601=ORIENTED_EDGE('',*,*,#28305,.T.);
#40602=ORIENTED_EDGE('',*,*,#28341,.T.);
#40603=ORIENTED_EDGE('',*,*,#28319,.T.);
#40604=ORIENTED_EDGE('',*,*,#28357,.T.);
#40605=ORIENTED_EDGE('',*,*,#28392,.T.);
#40606=ORIENTED_EDGE('',*,*,#28427,.T.);
#40607=ORIENTED_EDGE('',*,*,#28455,.T.);
#40608=ORIENTED_EDGE('',*,*,#28327,.T.);
#40609=ORIENTED_EDGE('',*,*,#28364,.T.);
#40610=ORIENTED_EDGE('',*,*,#28399,.T.);
#40611=ORIENTED_EDGE('',*,*,#28290,.T.);
#40612=ORIENTED_EDGE('',*,*,#28227,.T.);
#40613=ORIENTED_EDGE('',*,*,#28192,.T.);
#40614=ORIENTED_EDGE('',*,*,#28157,.T.);
#40615=ORIENTED_EDGE('',*,*,#28122,.T.);
#40616=ORIENTED_EDGE('',*,*,#28068,.T.);
#40617=ORIENTED_EDGE('',*,*,#28094,.T.);
#40618=ORIENTED_EDGE('',*,*,#28129,.T.);
#40619=ORIENTED_EDGE('',*,*,#28164,.T.);
#40620=ORIENTED_EDGE('',*,*,#28199,.T.);
#40621=ORIENTED_EDGE('',*,*,#28283,.T.);
#40622=ORIENTED_EDGE('',*,*,#28248,.T.);
#40623=ORIENTED_EDGE('',*,*,#28213,.T.);
#40624=ORIENTED_EDGE('',*,*,#28178,.T.);
#40625=ORIENTED_EDGE('',*,*,#28312,.T.);
#40626=ORIENTED_EDGE('',*,*,#28276,.T.);
#40627=ORIENTED_EDGE('',*,*,#28255,.T.);
#40628=ORIENTED_EDGE('',*,*,#28220,.T.);
#40629=ORIENTED_EDGE('',*,*,#28185,.T.);
#40630=ORIENTED_EDGE('',*,*,#28150,.T.);
#40631=ORIENTED_EDGE('',*,*,#28509,.T.);
#40632=ORIENTED_EDGE('',*,*,#28476,.T.);
#40633=ORIENTED_EDGE('',*,*,#28441,.T.);
#40634=ORIENTED_EDGE('',*,*,#28406,.T.);
#40635=ORIENTED_EDGE('',*,*,#28420,.T.);
#40636=ORIENTED_EDGE('',*,*,#28385,.T.);
#40637=ORIENTED_EDGE('',*,*,#28352,.T.);
#40638=ORIENTED_EDGE('',*,*,#28348,.T.);
#40639=ORIENTED_EDGE('',*,*,#28483,.T.);
#40640=ORIENTED_EDGE('',*,*,#28448,.T.);
#40641=ORIENTED_EDGE('',*,*,#28413,.T.);
#40642=ORIENTED_EDGE('',*,*,#28378,.T.);
#40643=ORIENTED_EDGE('',*,*,#28462,.T.);
#40644=ORIENTED_EDGE('',*,*,#28502,.T.);
#40645=ORIENTED_EDGE('',*,*,#28469,.T.);
#40646=ORIENTED_EDGE('',*,*,#28434,.T.);
#40647=ORIENTED_EDGE('',*,*,#28143,.T.);
#40648=ORIENTED_EDGE('',*,*,#28108,.T.);
#40649=ORIENTED_EDGE('',*,*,#28075,.T.);
#40650=ORIENTED_EDGE('',*,*,#28101,.T.);
#40651=ORIENTED_EDGE('',*,*,#28136,.T.);
#40652=ORIENTED_EDGE('',*,*,#28171,.T.);
#40653=ORIENTED_EDGE('',*,*,#28115,.T.);
#40654=ORIENTED_EDGE('',*,*,#30279,.T.);
#40655=ORIENTED_EDGE('',*,*,#30276,.T.);
#40656=ORIENTED_EDGE('',*,*,#30277,.F.);
#40657=ORIENTED_EDGE('',*,*,#30273,.T.);
#40658=ORIENTED_EDGE('',*,*,#30270,.T.);
#40659=ORIENTED_EDGE('',*,*,#30271,.F.);
#40660=ORIENTED_EDGE('',*,*,#30267,.T.);
#40661=ORIENTED_EDGE('',*,*,#30264,.T.);
#40662=ORIENTED_EDGE('',*,*,#30265,.F.);
#40663=ORIENTED_EDGE('',*,*,#30261,.T.);
#40664=ORIENTED_EDGE('',*,*,#30258,.T.);
#40665=ORIENTED_EDGE('',*,*,#30259,.F.);
#40666=ORIENTED_EDGE('',*,*,#30255,.T.);
#40667=ORIENTED_EDGE('',*,*,#30252,.T.);
#40668=ORIENTED_EDGE('',*,*,#30253,.F.);
#40669=ORIENTED_EDGE('',*,*,#30249,.T.);
#40670=ORIENTED_EDGE('',*,*,#30246,.T.);
#40671=ORIENTED_EDGE('',*,*,#30247,.F.);
#40672=ORIENTED_EDGE('',*,*,#30243,.T.);
#40673=ORIENTED_EDGE('',*,*,#30240,.T.);
#40674=ORIENTED_EDGE('',*,*,#30241,.F.);
#40675=ORIENTED_EDGE('',*,*,#30237,.T.);
#40676=ORIENTED_EDGE('',*,*,#30234,.T.);
#40677=ORIENTED_EDGE('',*,*,#30235,.F.);
#40678=ORIENTED_EDGE('',*,*,#30231,.T.);
#40679=ORIENTED_EDGE('',*,*,#30228,.T.);
#40680=ORIENTED_EDGE('',*,*,#30229,.F.);
#40681=ORIENTED_EDGE('',*,*,#30225,.T.);
#40682=ORIENTED_EDGE('',*,*,#30222,.T.);
#40683=ORIENTED_EDGE('',*,*,#30223,.F.);
#40684=ORIENTED_EDGE('',*,*,#30219,.T.);
#40685=ORIENTED_EDGE('',*,*,#30216,.T.);
#40686=ORIENTED_EDGE('',*,*,#30217,.F.);
#40687=ORIENTED_EDGE('',*,*,#30213,.T.);
#40688=ORIENTED_EDGE('',*,*,#30210,.T.);
#40689=ORIENTED_EDGE('',*,*,#30211,.F.);
#40690=ORIENTED_EDGE('',*,*,#30207,.T.);
#40691=ORIENTED_EDGE('',*,*,#30204,.T.);
#40692=ORIENTED_EDGE('',*,*,#30205,.F.);
#40693=ORIENTED_EDGE('',*,*,#30201,.T.);
#40694=ORIENTED_EDGE('',*,*,#30198,.T.);
#40695=ORIENTED_EDGE('',*,*,#30199,.F.);
#40696=ORIENTED_EDGE('',*,*,#30195,.T.);
#40697=ORIENTED_EDGE('',*,*,#30192,.T.);
#40698=ORIENTED_EDGE('',*,*,#30193,.F.);
#40699=ORIENTED_EDGE('',*,*,#30189,.T.);
#40700=ORIENTED_EDGE('',*,*,#30186,.T.);
#40701=ORIENTED_EDGE('',*,*,#30187,.F.);
#40702=ORIENTED_EDGE('',*,*,#30183,.T.);
#40703=ORIENTED_EDGE('',*,*,#30180,.T.);
#40704=ORIENTED_EDGE('',*,*,#30181,.F.);
#40705=ORIENTED_EDGE('',*,*,#30177,.T.);
#40706=ORIENTED_EDGE('',*,*,#30174,.T.);
#40707=ORIENTED_EDGE('',*,*,#30175,.F.);
#40708=ORIENTED_EDGE('',*,*,#30171,.T.);
#40709=ORIENTED_EDGE('',*,*,#30168,.T.);
#40710=ORIENTED_EDGE('',*,*,#30169,.F.);
#40711=ORIENTED_EDGE('',*,*,#30165,.T.);
#40712=ORIENTED_EDGE('',*,*,#30162,.T.);
#40713=ORIENTED_EDGE('',*,*,#30163,.F.);
#40714=ORIENTED_EDGE('',*,*,#30159,.T.);
#40715=ORIENTED_EDGE('',*,*,#30156,.T.);
#40716=ORIENTED_EDGE('',*,*,#30157,.F.);
#40717=ORIENTED_EDGE('',*,*,#30153,.T.);
#40718=ORIENTED_EDGE('',*,*,#30150,.T.);
#40719=ORIENTED_EDGE('',*,*,#30151,.F.);
#40720=ORIENTED_EDGE('',*,*,#30147,.T.);
#40721=ORIENTED_EDGE('',*,*,#30144,.T.);
#40722=ORIENTED_EDGE('',*,*,#30145,.F.);
#40723=ORIENTED_EDGE('',*,*,#30141,.T.);
#40724=ORIENTED_EDGE('',*,*,#30138,.T.);
#40725=ORIENTED_EDGE('',*,*,#30139,.F.);
#40726=ORIENTED_EDGE('',*,*,#30135,.T.);
#40727=ORIENTED_EDGE('',*,*,#30132,.T.);
#40728=ORIENTED_EDGE('',*,*,#30133,.F.);
#40729=ORIENTED_EDGE('',*,*,#30129,.T.);
#40730=ORIENTED_EDGE('',*,*,#30126,.T.);
#40731=ORIENTED_EDGE('',*,*,#30127,.F.);
#40732=ORIENTED_EDGE('',*,*,#30123,.T.);
#40733=ORIENTED_EDGE('',*,*,#30120,.T.);
#40734=ORIENTED_EDGE('',*,*,#30121,.F.);
#40735=ORIENTED_EDGE('',*,*,#30117,.T.);
#40736=ORIENTED_EDGE('',*,*,#30114,.T.);
#40737=ORIENTED_EDGE('',*,*,#30115,.F.);
#40738=ORIENTED_EDGE('',*,*,#30111,.T.);
#40739=ORIENTED_EDGE('',*,*,#30108,.T.);
#40740=ORIENTED_EDGE('',*,*,#30109,.F.);
#40741=ORIENTED_EDGE('',*,*,#30105,.T.);
#40742=ORIENTED_EDGE('',*,*,#30102,.T.);
#40743=ORIENTED_EDGE('',*,*,#30103,.F.);
#40744=ORIENTED_EDGE('',*,*,#30099,.T.);
#40745=ORIENTED_EDGE('',*,*,#30096,.T.);
#40746=ORIENTED_EDGE('',*,*,#30097,.F.);
#40747=ORIENTED_EDGE('',*,*,#30093,.T.);
#40748=ORIENTED_EDGE('',*,*,#30090,.T.);
#40749=ORIENTED_EDGE('',*,*,#30091,.F.);
#40750=ORIENTED_EDGE('',*,*,#30087,.T.);
#40751=ORIENTED_EDGE('',*,*,#30084,.T.);
#40752=ORIENTED_EDGE('',*,*,#30085,.F.);
#40753=ORIENTED_EDGE('',*,*,#30081,.T.);
#40754=ORIENTED_EDGE('',*,*,#30078,.T.);
#40755=ORIENTED_EDGE('',*,*,#30079,.F.);
#40756=ORIENTED_EDGE('',*,*,#30075,.T.);
#40757=ORIENTED_EDGE('',*,*,#30072,.T.);
#40758=ORIENTED_EDGE('',*,*,#30073,.F.);
#40759=ORIENTED_EDGE('',*,*,#30069,.T.);
#40760=ORIENTED_EDGE('',*,*,#30066,.T.);
#40761=ORIENTED_EDGE('',*,*,#30067,.F.);
#40762=ORIENTED_EDGE('',*,*,#30063,.T.);
#40763=ORIENTED_EDGE('',*,*,#30060,.T.);
#40764=ORIENTED_EDGE('',*,*,#30061,.F.);
#40765=ORIENTED_EDGE('',*,*,#30057,.T.);
#40766=ORIENTED_EDGE('',*,*,#30054,.T.);
#40767=ORIENTED_EDGE('',*,*,#30055,.F.);
#40768=ORIENTED_EDGE('',*,*,#30051,.T.);
#40769=ORIENTED_EDGE('',*,*,#30048,.T.);
#40770=ORIENTED_EDGE('',*,*,#30049,.F.);
#40771=ORIENTED_EDGE('',*,*,#30045,.T.);
#40772=ORIENTED_EDGE('',*,*,#30042,.T.);
#40773=ORIENTED_EDGE('',*,*,#30043,.F.);
#40774=ORIENTED_EDGE('',*,*,#30039,.T.);
#40775=ORIENTED_EDGE('',*,*,#30036,.T.);
#40776=ORIENTED_EDGE('',*,*,#30037,.F.);
#40777=ORIENTED_EDGE('',*,*,#30033,.T.);
#40778=ORIENTED_EDGE('',*,*,#30030,.T.);
#40779=ORIENTED_EDGE('',*,*,#30031,.F.);
#40780=ORIENTED_EDGE('',*,*,#30027,.T.);
#40781=ORIENTED_EDGE('',*,*,#30024,.T.);
#40782=ORIENTED_EDGE('',*,*,#30025,.F.);
#40783=ORIENTED_EDGE('',*,*,#30021,.T.);
#40784=ORIENTED_EDGE('',*,*,#30018,.T.);
#40785=ORIENTED_EDGE('',*,*,#30019,.F.);
#40786=ORIENTED_EDGE('',*,*,#30015,.T.);
#40787=ORIENTED_EDGE('',*,*,#30012,.T.);
#40788=ORIENTED_EDGE('',*,*,#30013,.F.);
#40789=ORIENTED_EDGE('',*,*,#30009,.T.);
#40790=ORIENTED_EDGE('',*,*,#30006,.T.);
#40791=ORIENTED_EDGE('',*,*,#30007,.F.);
#40792=ORIENTED_EDGE('',*,*,#30003,.T.);
#40793=ORIENTED_EDGE('',*,*,#30000,.T.);
#40794=ORIENTED_EDGE('',*,*,#30001,.F.);
#40795=ORIENTED_EDGE('',*,*,#29997,.T.);
#40796=ORIENTED_EDGE('',*,*,#29994,.T.);
#40797=ORIENTED_EDGE('',*,*,#29995,.F.);
#40798=ORIENTED_EDGE('',*,*,#29991,.T.);
#40799=ORIENTED_EDGE('',*,*,#29988,.T.);
#40800=ORIENTED_EDGE('',*,*,#29989,.F.);
#40801=ORIENTED_EDGE('',*,*,#29985,.T.);
#40802=ORIENTED_EDGE('',*,*,#29982,.T.);
#40803=ORIENTED_EDGE('',*,*,#29983,.F.);
#40804=ORIENTED_EDGE('',*,*,#29979,.T.);
#40805=ORIENTED_EDGE('',*,*,#29976,.T.);
#40806=ORIENTED_EDGE('',*,*,#29977,.F.);
#40807=ORIENTED_EDGE('',*,*,#29973,.T.);
#40808=ORIENTED_EDGE('',*,*,#29970,.T.);
#40809=ORIENTED_EDGE('',*,*,#29971,.F.);
#40810=ORIENTED_EDGE('',*,*,#29967,.T.);
#40811=ORIENTED_EDGE('',*,*,#29964,.T.);
#40812=ORIENTED_EDGE('',*,*,#29965,.F.);
#40813=ORIENTED_EDGE('',*,*,#29961,.T.);
#40814=ORIENTED_EDGE('',*,*,#29958,.T.);
#40815=ORIENTED_EDGE('',*,*,#29959,.F.);
#40816=ORIENTED_EDGE('',*,*,#29955,.T.);
#40817=ORIENTED_EDGE('',*,*,#29952,.T.);
#40818=ORIENTED_EDGE('',*,*,#29953,.F.);
#40819=ORIENTED_EDGE('',*,*,#29949,.T.);
#40820=ORIENTED_EDGE('',*,*,#29946,.T.);
#40821=ORIENTED_EDGE('',*,*,#29947,.F.);
#40822=ORIENTED_EDGE('',*,*,#29943,.T.);
#40823=ORIENTED_EDGE('',*,*,#29940,.T.);
#40824=ORIENTED_EDGE('',*,*,#29941,.F.);
#40825=ORIENTED_EDGE('',*,*,#29937,.T.);
#40826=ORIENTED_EDGE('',*,*,#29934,.T.);
#40827=ORIENTED_EDGE('',*,*,#29935,.F.);
#40828=ORIENTED_EDGE('',*,*,#29931,.T.);
#40829=ORIENTED_EDGE('',*,*,#29928,.T.);
#40830=ORIENTED_EDGE('',*,*,#29929,.F.);
#40831=ORIENTED_EDGE('',*,*,#29925,.T.);
#40832=ORIENTED_EDGE('',*,*,#29922,.T.);
#40833=ORIENTED_EDGE('',*,*,#29923,.F.);
#40834=ORIENTED_EDGE('',*,*,#29919,.T.);
#40835=ORIENTED_EDGE('',*,*,#29916,.T.);
#40836=ORIENTED_EDGE('',*,*,#29917,.F.);
#40837=ORIENTED_EDGE('',*,*,#29913,.T.);
#40838=ORIENTED_EDGE('',*,*,#29910,.T.);
#40839=ORIENTED_EDGE('',*,*,#29911,.F.);
#40840=ORIENTED_EDGE('',*,*,#29907,.T.);
#40841=ORIENTED_EDGE('',*,*,#29904,.T.);
#40842=ORIENTED_EDGE('',*,*,#29905,.F.);
#40843=ORIENTED_EDGE('',*,*,#29901,.T.);
#40844=ORIENTED_EDGE('',*,*,#29898,.T.);
#40845=ORIENTED_EDGE('',*,*,#29899,.F.);
#40846=ORIENTED_EDGE('',*,*,#29895,.T.);
#40847=ORIENTED_EDGE('',*,*,#29892,.T.);
#40848=ORIENTED_EDGE('',*,*,#29893,.F.);
#40849=ORIENTED_EDGE('',*,*,#29889,.T.);
#40850=ORIENTED_EDGE('',*,*,#29886,.T.);
#40851=ORIENTED_EDGE('',*,*,#29887,.F.);
#40852=ORIENTED_EDGE('',*,*,#29883,.T.);
#40853=ORIENTED_EDGE('',*,*,#29880,.T.);
#40854=ORIENTED_EDGE('',*,*,#29881,.F.);
#40855=ORIENTED_EDGE('',*,*,#29877,.T.);
#40856=ORIENTED_EDGE('',*,*,#29874,.T.);
#40857=ORIENTED_EDGE('',*,*,#29875,.F.);
#40858=ORIENTED_EDGE('',*,*,#29871,.T.);
#40859=ORIENTED_EDGE('',*,*,#29868,.T.);
#40860=ORIENTED_EDGE('',*,*,#29869,.F.);
#40861=ORIENTED_EDGE('',*,*,#29865,.T.);
#40862=ORIENTED_EDGE('',*,*,#29862,.T.);
#40863=ORIENTED_EDGE('',*,*,#29863,.F.);
#40864=ORIENTED_EDGE('',*,*,#29859,.T.);
#40865=ORIENTED_EDGE('',*,*,#29856,.T.);
#40866=ORIENTED_EDGE('',*,*,#29857,.F.);
#40867=ORIENTED_EDGE('',*,*,#29853,.T.);
#40868=ORIENTED_EDGE('',*,*,#29850,.T.);
#40869=ORIENTED_EDGE('',*,*,#29851,.F.);
#40870=ORIENTED_EDGE('',*,*,#29847,.T.);
#40871=ORIENTED_EDGE('',*,*,#29844,.T.);
#40872=ORIENTED_EDGE('',*,*,#29845,.F.);
#40873=ORIENTED_EDGE('',*,*,#29841,.T.);
#40874=ORIENTED_EDGE('',*,*,#29838,.T.);
#40875=ORIENTED_EDGE('',*,*,#29839,.F.);
#40876=ORIENTED_EDGE('',*,*,#29835,.T.);
#40877=ORIENTED_EDGE('',*,*,#29832,.T.);
#40878=ORIENTED_EDGE('',*,*,#29833,.F.);
#40879=ORIENTED_EDGE('',*,*,#29829,.T.);
#40880=ORIENTED_EDGE('',*,*,#29826,.T.);
#40881=ORIENTED_EDGE('',*,*,#29827,.F.);
#40882=ORIENTED_EDGE('',*,*,#29823,.T.);
#40883=ORIENTED_EDGE('',*,*,#29820,.T.);
#40884=ORIENTED_EDGE('',*,*,#29821,.F.);
#40885=ORIENTED_EDGE('',*,*,#29817,.T.);
#40886=ORIENTED_EDGE('',*,*,#29814,.T.);
#40887=ORIENTED_EDGE('',*,*,#29815,.F.);
#40888=ORIENTED_EDGE('',*,*,#29811,.T.);
#40889=ORIENTED_EDGE('',*,*,#29808,.T.);
#40890=ORIENTED_EDGE('',*,*,#29809,.F.);
#40891=ORIENTED_EDGE('',*,*,#29805,.T.);
#40892=ORIENTED_EDGE('',*,*,#29802,.T.);
#40893=ORIENTED_EDGE('',*,*,#29803,.F.);
#40894=ORIENTED_EDGE('',*,*,#29799,.T.);
#40895=ORIENTED_EDGE('',*,*,#29796,.T.);
#40896=ORIENTED_EDGE('',*,*,#29797,.F.);
#40897=ORIENTED_EDGE('',*,*,#29793,.T.);
#40898=ORIENTED_EDGE('',*,*,#29790,.T.);
#40899=ORIENTED_EDGE('',*,*,#29791,.F.);
#40900=ORIENTED_EDGE('',*,*,#29787,.T.);
#40901=ORIENTED_EDGE('',*,*,#29784,.T.);
#40902=ORIENTED_EDGE('',*,*,#29785,.F.);
#40903=ORIENTED_EDGE('',*,*,#29781,.T.);
#40904=ORIENTED_EDGE('',*,*,#29778,.T.);
#40905=ORIENTED_EDGE('',*,*,#29779,.F.);
#40906=ORIENTED_EDGE('',*,*,#29775,.T.);
#40907=ORIENTED_EDGE('',*,*,#29772,.T.);
#40908=ORIENTED_EDGE('',*,*,#29773,.F.);
#40909=ORIENTED_EDGE('',*,*,#29769,.T.);
#40910=ORIENTED_EDGE('',*,*,#29766,.T.);
#40911=ORIENTED_EDGE('',*,*,#29767,.F.);
#40912=ORIENTED_EDGE('',*,*,#29763,.T.);
#40913=ORIENTED_EDGE('',*,*,#29760,.T.);
#40914=ORIENTED_EDGE('',*,*,#29761,.F.);
#40915=ORIENTED_EDGE('',*,*,#29757,.T.);
#40916=ORIENTED_EDGE('',*,*,#29754,.T.);
#40917=ORIENTED_EDGE('',*,*,#29755,.F.);
#40918=ORIENTED_EDGE('',*,*,#29751,.T.);
#40919=ORIENTED_EDGE('',*,*,#29748,.T.);
#40920=ORIENTED_EDGE('',*,*,#29749,.F.);
#40921=ORIENTED_EDGE('',*,*,#29745,.T.);
#40922=ORIENTED_EDGE('',*,*,#29742,.T.);
#40923=ORIENTED_EDGE('',*,*,#29743,.F.);
#40924=ORIENTED_EDGE('',*,*,#29739,.T.);
#40925=ORIENTED_EDGE('',*,*,#29736,.T.);
#40926=ORIENTED_EDGE('',*,*,#29737,.F.);
#40927=ORIENTED_EDGE('',*,*,#29733,.T.);
#40928=ORIENTED_EDGE('',*,*,#29730,.T.);
#40929=ORIENTED_EDGE('',*,*,#29731,.F.);
#40930=ORIENTED_EDGE('',*,*,#29727,.T.);
#40931=ORIENTED_EDGE('',*,*,#29724,.T.);
#40932=ORIENTED_EDGE('',*,*,#29725,.F.);
#40933=ORIENTED_EDGE('',*,*,#29721,.T.);
#40934=ORIENTED_EDGE('',*,*,#29718,.T.);
#40935=ORIENTED_EDGE('',*,*,#29719,.F.);
#40936=ORIENTED_EDGE('',*,*,#29715,.T.);
#40937=ORIENTED_EDGE('',*,*,#29712,.T.);
#40938=ORIENTED_EDGE('',*,*,#29713,.F.);
#40939=ORIENTED_EDGE('',*,*,#29709,.T.);
#40940=ORIENTED_EDGE('',*,*,#29706,.T.);
#40941=ORIENTED_EDGE('',*,*,#29707,.F.);
#40942=ORIENTED_EDGE('',*,*,#29703,.T.);
#40943=ORIENTED_EDGE('',*,*,#29700,.T.);
#40944=ORIENTED_EDGE('',*,*,#29701,.F.);
#40945=ORIENTED_EDGE('',*,*,#29697,.T.);
#40946=ORIENTED_EDGE('',*,*,#29694,.T.);
#40947=ORIENTED_EDGE('',*,*,#29695,.F.);
#40948=ORIENTED_EDGE('',*,*,#29691,.T.);
#40949=ORIENTED_EDGE('',*,*,#29688,.T.);
#40950=ORIENTED_EDGE('',*,*,#29689,.F.);
#40951=ORIENTED_EDGE('',*,*,#29685,.T.);
#40952=ORIENTED_EDGE('',*,*,#29682,.T.);
#40953=ORIENTED_EDGE('',*,*,#29683,.F.);
#40954=ORIENTED_EDGE('',*,*,#29679,.T.);
#40955=ORIENTED_EDGE('',*,*,#29676,.T.);
#40956=ORIENTED_EDGE('',*,*,#29677,.F.);
#40957=ORIENTED_EDGE('',*,*,#29673,.T.);
#40958=ORIENTED_EDGE('',*,*,#29670,.T.);
#40959=ORIENTED_EDGE('',*,*,#29671,.F.);
#40960=ORIENTED_EDGE('',*,*,#29667,.T.);
#40961=ORIENTED_EDGE('',*,*,#29664,.T.);
#40962=ORIENTED_EDGE('',*,*,#29665,.F.);
#40963=ORIENTED_EDGE('',*,*,#29661,.T.);
#40964=ORIENTED_EDGE('',*,*,#29658,.T.);
#40965=ORIENTED_EDGE('',*,*,#29659,.F.);
#40966=ORIENTED_EDGE('',*,*,#29655,.T.);
#40967=ORIENTED_EDGE('',*,*,#29652,.T.);
#40968=ORIENTED_EDGE('',*,*,#29653,.F.);
#40969=ORIENTED_EDGE('',*,*,#29649,.T.);
#40970=ORIENTED_EDGE('',*,*,#29646,.T.);
#40971=ORIENTED_EDGE('',*,*,#29647,.F.);
#40972=ORIENTED_EDGE('',*,*,#29643,.T.);
#40973=ORIENTED_EDGE('',*,*,#29640,.T.);
#40974=ORIENTED_EDGE('',*,*,#29641,.F.);
#40975=ORIENTED_EDGE('',*,*,#29637,.T.);
#40976=ORIENTED_EDGE('',*,*,#29634,.T.);
#40977=ORIENTED_EDGE('',*,*,#29635,.F.);
#40978=ORIENTED_EDGE('',*,*,#29631,.T.);
#40979=ORIENTED_EDGE('',*,*,#29628,.T.);
#40980=ORIENTED_EDGE('',*,*,#29629,.F.);
#40981=ORIENTED_EDGE('',*,*,#29625,.T.);
#40982=ORIENTED_EDGE('',*,*,#29622,.T.);
#40983=ORIENTED_EDGE('',*,*,#29623,.F.);
#40984=ORIENTED_EDGE('',*,*,#29619,.T.);
#40985=ORIENTED_EDGE('',*,*,#29616,.T.);
#40986=ORIENTED_EDGE('',*,*,#29617,.F.);
#40987=ORIENTED_EDGE('',*,*,#29613,.T.);
#40988=ORIENTED_EDGE('',*,*,#29610,.T.);
#40989=ORIENTED_EDGE('',*,*,#29611,.F.);
#40990=ORIENTED_EDGE('',*,*,#29607,.T.);
#40991=ORIENTED_EDGE('',*,*,#29604,.T.);
#40992=ORIENTED_EDGE('',*,*,#29605,.F.);
#40993=ORIENTED_EDGE('',*,*,#29601,.T.);
#40994=ORIENTED_EDGE('',*,*,#29598,.T.);
#40995=ORIENTED_EDGE('',*,*,#29599,.F.);
#40996=ORIENTED_EDGE('',*,*,#29595,.T.);
#40997=ORIENTED_EDGE('',*,*,#29592,.T.);
#40998=ORIENTED_EDGE('',*,*,#29593,.F.);
#40999=ORIENTED_EDGE('',*,*,#29589,.T.);
#41000=ORIENTED_EDGE('',*,*,#29586,.T.);
#41001=ORIENTED_EDGE('',*,*,#29587,.F.);
#41002=ORIENTED_EDGE('',*,*,#29583,.T.);
#41003=ORIENTED_EDGE('',*,*,#29580,.T.);
#41004=ORIENTED_EDGE('',*,*,#29581,.F.);
#41005=ORIENTED_EDGE('',*,*,#29577,.T.);
#41006=ORIENTED_EDGE('',*,*,#29574,.T.);
#41007=ORIENTED_EDGE('',*,*,#29575,.F.);
#41008=ORIENTED_EDGE('',*,*,#29571,.T.);
#41009=ORIENTED_EDGE('',*,*,#29568,.T.);
#41010=ORIENTED_EDGE('',*,*,#29569,.F.);
#41011=ORIENTED_EDGE('',*,*,#29565,.T.);
#41012=ORIENTED_EDGE('',*,*,#29562,.T.);
#41013=ORIENTED_EDGE('',*,*,#29563,.F.);
#41014=ORIENTED_EDGE('',*,*,#29559,.T.);
#41015=ORIENTED_EDGE('',*,*,#29556,.T.);
#41016=ORIENTED_EDGE('',*,*,#29557,.F.);
#41017=ORIENTED_EDGE('',*,*,#29553,.T.);
#41018=ORIENTED_EDGE('',*,*,#29550,.T.);
#41019=ORIENTED_EDGE('',*,*,#29551,.F.);
#41020=ORIENTED_EDGE('',*,*,#29547,.T.);
#41021=ORIENTED_EDGE('',*,*,#29544,.T.);
#41022=ORIENTED_EDGE('',*,*,#29545,.F.);
#41023=ORIENTED_EDGE('',*,*,#29541,.T.);
#41024=ORIENTED_EDGE('',*,*,#29538,.T.);
#41025=ORIENTED_EDGE('',*,*,#29539,.F.);
#41026=ORIENTED_EDGE('',*,*,#29535,.T.);
#41027=ORIENTED_EDGE('',*,*,#29532,.T.);
#41028=ORIENTED_EDGE('',*,*,#29533,.F.);
#41029=ORIENTED_EDGE('',*,*,#29529,.T.);
#41030=ORIENTED_EDGE('',*,*,#29526,.T.);
#41031=ORIENTED_EDGE('',*,*,#29527,.F.);
#41032=ORIENTED_EDGE('',*,*,#29523,.T.);
#41033=ORIENTED_EDGE('',*,*,#29520,.T.);
#41034=ORIENTED_EDGE('',*,*,#29521,.F.);
#41035=ORIENTED_EDGE('',*,*,#29517,.T.);
#41036=ORIENTED_EDGE('',*,*,#29514,.T.);
#41037=ORIENTED_EDGE('',*,*,#29515,.F.);
#41038=ORIENTED_EDGE('',*,*,#29511,.T.);
#41039=ORIENTED_EDGE('',*,*,#29508,.T.);
#41040=ORIENTED_EDGE('',*,*,#29509,.F.);
#41041=ORIENTED_EDGE('',*,*,#29505,.T.);
#41042=ORIENTED_EDGE('',*,*,#29502,.T.);
#41043=ORIENTED_EDGE('',*,*,#29503,.F.);
#41044=ORIENTED_EDGE('',*,*,#29499,.T.);
#41045=ORIENTED_EDGE('',*,*,#29496,.T.);
#41046=ORIENTED_EDGE('',*,*,#29497,.F.);
#41047=ORIENTED_EDGE('',*,*,#29493,.T.);
#41048=ORIENTED_EDGE('',*,*,#29490,.T.);
#41049=ORIENTED_EDGE('',*,*,#29491,.F.);
#41050=ORIENTED_EDGE('',*,*,#29487,.T.);
#41051=ORIENTED_EDGE('',*,*,#29484,.T.);
#41052=ORIENTED_EDGE('',*,*,#29485,.F.);
#41053=ORIENTED_EDGE('',*,*,#29481,.T.);
#41054=ORIENTED_EDGE('',*,*,#29478,.T.);
#41055=ORIENTED_EDGE('',*,*,#29479,.F.);
#41056=ORIENTED_EDGE('',*,*,#29475,.T.);
#41057=ORIENTED_EDGE('',*,*,#29472,.T.);
#41058=ORIENTED_EDGE('',*,*,#29473,.F.);
#41059=ORIENTED_EDGE('',*,*,#29469,.T.);
#41060=ORIENTED_EDGE('',*,*,#29466,.T.);
#41061=ORIENTED_EDGE('',*,*,#29467,.F.);
#41062=ORIENTED_EDGE('',*,*,#29463,.T.);
#41063=ORIENTED_EDGE('',*,*,#29460,.T.);
#41064=ORIENTED_EDGE('',*,*,#29461,.F.);
#41065=ORIENTED_EDGE('',*,*,#29457,.T.);
#41066=ORIENTED_EDGE('',*,*,#29454,.T.);
#41067=ORIENTED_EDGE('',*,*,#29455,.F.);
#41068=ORIENTED_EDGE('',*,*,#29451,.T.);
#41069=ORIENTED_EDGE('',*,*,#29448,.T.);
#41070=ORIENTED_EDGE('',*,*,#29449,.F.);
#41071=ORIENTED_EDGE('',*,*,#29445,.T.);
#41072=ORIENTED_EDGE('',*,*,#29442,.T.);
#41073=ORIENTED_EDGE('',*,*,#29443,.F.);
#41074=ORIENTED_EDGE('',*,*,#29439,.T.);
#41075=ORIENTED_EDGE('',*,*,#29436,.T.);
#41076=ORIENTED_EDGE('',*,*,#29437,.F.);
#41077=ORIENTED_EDGE('',*,*,#29433,.T.);
#41078=ORIENTED_EDGE('',*,*,#29430,.T.);
#41079=ORIENTED_EDGE('',*,*,#29431,.F.);
#41080=ORIENTED_EDGE('',*,*,#29427,.T.);
#41081=ORIENTED_EDGE('',*,*,#29424,.T.);
#41082=ORIENTED_EDGE('',*,*,#29425,.F.);
#41083=ORIENTED_EDGE('',*,*,#29421,.T.);
#41084=ORIENTED_EDGE('',*,*,#29418,.T.);
#41085=ORIENTED_EDGE('',*,*,#29419,.F.);
#41086=ORIENTED_EDGE('',*,*,#29415,.T.);
#41087=ORIENTED_EDGE('',*,*,#29412,.T.);
#41088=ORIENTED_EDGE('',*,*,#29413,.F.);
#41089=ORIENTED_EDGE('',*,*,#29409,.T.);
#41090=ORIENTED_EDGE('',*,*,#29406,.T.);
#41091=ORIENTED_EDGE('',*,*,#29407,.F.);
#41092=ORIENTED_EDGE('',*,*,#29403,.T.);
#41093=ORIENTED_EDGE('',*,*,#29400,.T.);
#41094=ORIENTED_EDGE('',*,*,#29401,.F.);
#41095=ORIENTED_EDGE('',*,*,#29397,.T.);
#41096=ORIENTED_EDGE('',*,*,#29394,.T.);
#41097=ORIENTED_EDGE('',*,*,#29395,.F.);
#41098=ORIENTED_EDGE('',*,*,#29391,.T.);
#41099=ORIENTED_EDGE('',*,*,#29388,.T.);
#41100=ORIENTED_EDGE('',*,*,#29389,.F.);
#41101=ORIENTED_EDGE('',*,*,#29385,.T.);
#41102=ORIENTED_EDGE('',*,*,#29382,.T.);
#41103=ORIENTED_EDGE('',*,*,#29383,.F.);
#41104=ORIENTED_EDGE('',*,*,#29379,.T.);
#41105=ORIENTED_EDGE('',*,*,#29376,.T.);
#41106=ORIENTED_EDGE('',*,*,#29377,.F.);
#41107=ORIENTED_EDGE('',*,*,#29373,.T.);
#41108=ORIENTED_EDGE('',*,*,#29370,.T.);
#41109=ORIENTED_EDGE('',*,*,#29371,.F.);
#41110=ORIENTED_EDGE('',*,*,#29367,.T.);
#41111=ORIENTED_EDGE('',*,*,#29364,.T.);
#41112=ORIENTED_EDGE('',*,*,#29365,.F.);
#41113=ORIENTED_EDGE('',*,*,#29361,.T.);
#41114=ORIENTED_EDGE('',*,*,#29358,.T.);
#41115=ORIENTED_EDGE('',*,*,#29359,.F.);
#41116=ORIENTED_EDGE('',*,*,#29355,.T.);
#41117=ORIENTED_EDGE('',*,*,#29352,.T.);
#41118=ORIENTED_EDGE('',*,*,#29353,.F.);
#41119=ORIENTED_EDGE('',*,*,#29349,.T.);
#41120=ORIENTED_EDGE('',*,*,#29346,.T.);
#41121=ORIENTED_EDGE('',*,*,#29347,.F.);
#41122=ORIENTED_EDGE('',*,*,#29343,.T.);
#41123=ORIENTED_EDGE('',*,*,#29340,.T.);
#41124=ORIENTED_EDGE('',*,*,#29341,.F.);
#41125=ORIENTED_EDGE('',*,*,#29337,.T.);
#41126=ORIENTED_EDGE('',*,*,#29334,.T.);
#41127=ORIENTED_EDGE('',*,*,#29335,.F.);
#41128=ORIENTED_EDGE('',*,*,#29331,.T.);
#41129=ORIENTED_EDGE('',*,*,#29328,.T.);
#41130=ORIENTED_EDGE('',*,*,#29329,.F.);
#41131=ORIENTED_EDGE('',*,*,#29325,.T.);
#41132=ORIENTED_EDGE('',*,*,#29322,.T.);
#41133=ORIENTED_EDGE('',*,*,#29323,.F.);
#41134=ORIENTED_EDGE('',*,*,#29319,.T.);
#41135=ORIENTED_EDGE('',*,*,#29316,.T.);
#41136=ORIENTED_EDGE('',*,*,#29317,.F.);
#41137=ORIENTED_EDGE('',*,*,#29313,.T.);
#41138=ORIENTED_EDGE('',*,*,#29310,.T.);
#41139=ORIENTED_EDGE('',*,*,#29311,.F.);
#41140=ORIENTED_EDGE('',*,*,#29307,.T.);
#41141=ORIENTED_EDGE('',*,*,#29304,.T.);
#41142=ORIENTED_EDGE('',*,*,#29305,.F.);
#41143=ORIENTED_EDGE('',*,*,#29301,.T.);
#41144=ORIENTED_EDGE('',*,*,#29298,.T.);
#41145=ORIENTED_EDGE('',*,*,#29299,.F.);
#41146=ORIENTED_EDGE('',*,*,#29295,.T.);
#41147=ORIENTED_EDGE('',*,*,#29292,.T.);
#41148=ORIENTED_EDGE('',*,*,#29293,.F.);
#41149=ORIENTED_EDGE('',*,*,#29289,.T.);
#41150=ORIENTED_EDGE('',*,*,#29286,.T.);
#41151=ORIENTED_EDGE('',*,*,#29287,.F.);
#41152=ORIENTED_EDGE('',*,*,#29283,.T.);
#41153=ORIENTED_EDGE('',*,*,#29280,.T.);
#41154=ORIENTED_EDGE('',*,*,#29281,.F.);
#41155=ORIENTED_EDGE('',*,*,#29277,.T.);
#41156=ORIENTED_EDGE('',*,*,#29274,.T.);
#41157=ORIENTED_EDGE('',*,*,#29275,.F.);
#41158=ORIENTED_EDGE('',*,*,#29271,.T.);
#41159=ORIENTED_EDGE('',*,*,#29268,.T.);
#41160=ORIENTED_EDGE('',*,*,#29269,.F.);
#41161=ORIENTED_EDGE('',*,*,#29265,.T.);
#41162=ORIENTED_EDGE('',*,*,#29262,.T.);
#41163=ORIENTED_EDGE('',*,*,#29263,.F.);
#41164=ORIENTED_EDGE('',*,*,#29259,.T.);
#41165=ORIENTED_EDGE('',*,*,#29256,.T.);
#41166=ORIENTED_EDGE('',*,*,#29257,.F.);
#41167=ORIENTED_EDGE('',*,*,#29253,.T.);
#41168=ORIENTED_EDGE('',*,*,#29250,.T.);
#41169=ORIENTED_EDGE('',*,*,#29251,.F.);
#41170=ORIENTED_EDGE('',*,*,#29247,.T.);
#41171=ORIENTED_EDGE('',*,*,#29244,.T.);
#41172=ORIENTED_EDGE('',*,*,#29245,.F.);
#41173=ORIENTED_EDGE('',*,*,#29241,.T.);
#41174=ORIENTED_EDGE('',*,*,#29238,.T.);
#41175=ORIENTED_EDGE('',*,*,#29239,.F.);
#41176=ORIENTED_EDGE('',*,*,#29235,.T.);
#41177=ORIENTED_EDGE('',*,*,#29232,.T.);
#41178=ORIENTED_EDGE('',*,*,#29233,.F.);
#41179=ORIENTED_EDGE('',*,*,#29229,.T.);
#41180=ORIENTED_EDGE('',*,*,#29226,.T.);
#41181=ORIENTED_EDGE('',*,*,#29227,.F.);
#41182=ORIENTED_EDGE('',*,*,#29223,.T.);
#41183=ORIENTED_EDGE('',*,*,#29220,.T.);
#41184=ORIENTED_EDGE('',*,*,#29221,.F.);
#41185=ORIENTED_EDGE('',*,*,#29217,.T.);
#41186=ORIENTED_EDGE('',*,*,#29214,.T.);
#41187=ORIENTED_EDGE('',*,*,#29215,.F.);
#41188=ORIENTED_EDGE('',*,*,#29211,.T.);
#41189=ORIENTED_EDGE('',*,*,#29208,.T.);
#41190=ORIENTED_EDGE('',*,*,#29209,.F.);
#41191=ORIENTED_EDGE('',*,*,#29205,.T.);
#41192=ORIENTED_EDGE('',*,*,#29202,.T.);
#41193=ORIENTED_EDGE('',*,*,#29203,.F.);
#41194=ORIENTED_EDGE('',*,*,#29199,.T.);
#41195=ORIENTED_EDGE('',*,*,#29196,.T.);
#41196=ORIENTED_EDGE('',*,*,#29197,.F.);
#41197=ORIENTED_EDGE('',*,*,#29193,.T.);
#41198=ORIENTED_EDGE('',*,*,#29190,.T.);
#41199=ORIENTED_EDGE('',*,*,#29191,.F.);
#41200=ORIENTED_EDGE('',*,*,#29187,.T.);
#41201=ORIENTED_EDGE('',*,*,#29184,.T.);
#41202=ORIENTED_EDGE('',*,*,#29185,.F.);
#41203=ORIENTED_EDGE('',*,*,#29181,.T.);
#41204=ORIENTED_EDGE('',*,*,#29178,.T.);
#41205=ORIENTED_EDGE('',*,*,#29179,.F.);
#41206=ORIENTED_EDGE('',*,*,#29175,.T.);
#41207=ORIENTED_EDGE('',*,*,#29172,.T.);
#41208=ORIENTED_EDGE('',*,*,#29173,.F.);
#41209=ORIENTED_EDGE('',*,*,#29169,.T.);
#41210=ORIENTED_EDGE('',*,*,#29166,.T.);
#41211=ORIENTED_EDGE('',*,*,#29167,.F.);
#41212=ORIENTED_EDGE('',*,*,#29163,.T.);
#41213=ORIENTED_EDGE('',*,*,#29160,.T.);
#41214=ORIENTED_EDGE('',*,*,#29161,.F.);
#41215=ORIENTED_EDGE('',*,*,#29157,.T.);
#41216=ORIENTED_EDGE('',*,*,#29154,.T.);
#41217=ORIENTED_EDGE('',*,*,#29155,.F.);
#41218=ORIENTED_EDGE('',*,*,#29151,.T.);
#41219=ORIENTED_EDGE('',*,*,#29148,.T.);
#41220=ORIENTED_EDGE('',*,*,#29149,.F.);
#41221=ORIENTED_EDGE('',*,*,#29145,.T.);
#41222=ORIENTED_EDGE('',*,*,#29142,.T.);
#41223=ORIENTED_EDGE('',*,*,#29143,.F.);
#41224=ORIENTED_EDGE('',*,*,#29139,.T.);
#41225=ORIENTED_EDGE('',*,*,#29136,.T.);
#41226=ORIENTED_EDGE('',*,*,#29137,.F.);
#41227=ORIENTED_EDGE('',*,*,#29133,.T.);
#41228=ORIENTED_EDGE('',*,*,#29130,.T.);
#41229=ORIENTED_EDGE('',*,*,#29131,.F.);
#41230=ORIENTED_EDGE('',*,*,#29127,.T.);
#41231=ORIENTED_EDGE('',*,*,#29124,.T.);
#41232=ORIENTED_EDGE('',*,*,#29125,.F.);
#41233=ORIENTED_EDGE('',*,*,#29121,.T.);
#41234=ORIENTED_EDGE('',*,*,#29118,.T.);
#41235=ORIENTED_EDGE('',*,*,#29119,.F.);
#41236=ORIENTED_EDGE('',*,*,#29115,.T.);
#41237=ORIENTED_EDGE('',*,*,#29112,.T.);
#41238=ORIENTED_EDGE('',*,*,#29113,.F.);
#41239=ORIENTED_EDGE('',*,*,#29109,.T.);
#41240=ORIENTED_EDGE('',*,*,#29106,.T.);
#41241=ORIENTED_EDGE('',*,*,#29107,.F.);
#41242=ORIENTED_EDGE('',*,*,#29103,.T.);
#41243=ORIENTED_EDGE('',*,*,#29100,.T.);
#41244=ORIENTED_EDGE('',*,*,#29101,.F.);
#41245=ORIENTED_EDGE('',*,*,#29097,.T.);
#41246=ORIENTED_EDGE('',*,*,#29094,.T.);
#41247=ORIENTED_EDGE('',*,*,#29095,.F.);
#41248=ORIENTED_EDGE('',*,*,#29091,.T.);
#41249=ORIENTED_EDGE('',*,*,#29088,.T.);
#41250=ORIENTED_EDGE('',*,*,#29089,.F.);
#41251=ORIENTED_EDGE('',*,*,#29085,.T.);
#41252=ORIENTED_EDGE('',*,*,#29082,.T.);
#41253=ORIENTED_EDGE('',*,*,#29083,.F.);
#41254=ORIENTED_EDGE('',*,*,#29079,.T.);
#41255=ORIENTED_EDGE('',*,*,#29076,.T.);
#41256=ORIENTED_EDGE('',*,*,#29077,.F.);
#41257=ORIENTED_EDGE('',*,*,#29073,.T.);
#41258=ORIENTED_EDGE('',*,*,#29070,.T.);
#41259=ORIENTED_EDGE('',*,*,#29071,.F.);
#41260=ORIENTED_EDGE('',*,*,#29067,.T.);
#41261=ORIENTED_EDGE('',*,*,#29064,.T.);
#41262=ORIENTED_EDGE('',*,*,#29065,.F.);
#41263=ORIENTED_EDGE('',*,*,#29061,.T.);
#41264=ORIENTED_EDGE('',*,*,#29058,.T.);
#41265=ORIENTED_EDGE('',*,*,#29059,.F.);
#41266=ORIENTED_EDGE('',*,*,#29055,.T.);
#41267=ORIENTED_EDGE('',*,*,#29052,.T.);
#41268=ORIENTED_EDGE('',*,*,#29053,.F.);
#41269=ORIENTED_EDGE('',*,*,#29049,.T.);
#41270=ORIENTED_EDGE('',*,*,#29046,.T.);
#41271=ORIENTED_EDGE('',*,*,#29047,.F.);
#41272=ORIENTED_EDGE('',*,*,#29043,.T.);
#41273=ORIENTED_EDGE('',*,*,#29040,.T.);
#41274=ORIENTED_EDGE('',*,*,#29041,.F.);
#41275=ORIENTED_EDGE('',*,*,#29037,.T.);
#41276=ORIENTED_EDGE('',*,*,#29034,.T.);
#41277=ORIENTED_EDGE('',*,*,#29035,.F.);
#41278=ORIENTED_EDGE('',*,*,#29031,.T.);
#41279=ORIENTED_EDGE('',*,*,#29028,.T.);
#41280=ORIENTED_EDGE('',*,*,#29029,.F.);
#41281=ORIENTED_EDGE('',*,*,#29025,.T.);
#41282=ORIENTED_EDGE('',*,*,#29022,.T.);
#41283=ORIENTED_EDGE('',*,*,#29023,.F.);
#41284=ORIENTED_EDGE('',*,*,#29019,.T.);
#41285=ORIENTED_EDGE('',*,*,#29016,.T.);
#41286=ORIENTED_EDGE('',*,*,#29017,.F.);
#41287=ORIENTED_EDGE('',*,*,#29013,.T.);
#41288=ORIENTED_EDGE('',*,*,#29010,.T.);
#41289=ORIENTED_EDGE('',*,*,#29011,.F.);
#41290=ORIENTED_EDGE('',*,*,#29007,.T.);
#41291=ORIENTED_EDGE('',*,*,#29004,.T.);
#41292=ORIENTED_EDGE('',*,*,#29005,.F.);
#41293=ORIENTED_EDGE('',*,*,#29001,.T.);
#41294=ORIENTED_EDGE('',*,*,#28998,.T.);
#41295=ORIENTED_EDGE('',*,*,#28999,.F.);
#41296=ORIENTED_EDGE('',*,*,#28995,.T.);
#41297=ORIENTED_EDGE('',*,*,#28992,.T.);
#41298=ORIENTED_EDGE('',*,*,#28993,.F.);
#41299=ORIENTED_EDGE('',*,*,#28989,.T.);
#41300=ORIENTED_EDGE('',*,*,#28986,.T.);
#41301=ORIENTED_EDGE('',*,*,#28987,.F.);
#41302=ORIENTED_EDGE('',*,*,#28983,.T.);
#41303=ORIENTED_EDGE('',*,*,#28980,.T.);
#41304=ORIENTED_EDGE('',*,*,#28981,.F.);
#41305=ORIENTED_EDGE('',*,*,#28977,.T.);
#41306=ORIENTED_EDGE('',*,*,#28974,.T.);
#41307=ORIENTED_EDGE('',*,*,#28975,.F.);
#41308=ORIENTED_EDGE('',*,*,#28971,.T.);
#41309=ORIENTED_EDGE('',*,*,#28968,.T.);
#41310=ORIENTED_EDGE('',*,*,#28969,.F.);
#41311=ORIENTED_EDGE('',*,*,#28965,.T.);
#41312=ORIENTED_EDGE('',*,*,#28962,.T.);
#41313=ORIENTED_EDGE('',*,*,#28963,.F.);
#41314=ORIENTED_EDGE('',*,*,#28959,.T.);
#41315=ORIENTED_EDGE('',*,*,#28956,.T.);
#41316=ORIENTED_EDGE('',*,*,#28957,.F.);
#41317=ORIENTED_EDGE('',*,*,#28953,.T.);
#41318=ORIENTED_EDGE('',*,*,#28950,.T.);
#41319=ORIENTED_EDGE('',*,*,#28951,.F.);
#41320=ORIENTED_EDGE('',*,*,#28947,.T.);
#41321=ORIENTED_EDGE('',*,*,#28944,.T.);
#41322=ORIENTED_EDGE('',*,*,#28945,.F.);
#41323=ORIENTED_EDGE('',*,*,#28941,.T.);
#41324=ORIENTED_EDGE('',*,*,#28938,.T.);
#41325=ORIENTED_EDGE('',*,*,#28939,.F.);
#41326=ORIENTED_EDGE('',*,*,#28935,.T.);
#41327=ORIENTED_EDGE('',*,*,#28932,.T.);
#41328=ORIENTED_EDGE('',*,*,#28933,.F.);
#41329=ORIENTED_EDGE('',*,*,#28929,.T.);
#41330=ORIENTED_EDGE('',*,*,#28926,.T.);
#41331=ORIENTED_EDGE('',*,*,#28927,.F.);
#41332=ORIENTED_EDGE('',*,*,#28923,.T.);
#41333=ORIENTED_EDGE('',*,*,#28920,.T.);
#41334=ORIENTED_EDGE('',*,*,#28921,.F.);
#41335=ORIENTED_EDGE('',*,*,#28917,.T.);
#41336=ORIENTED_EDGE('',*,*,#28914,.T.);
#41337=ORIENTED_EDGE('',*,*,#28915,.F.);
#41338=ORIENTED_EDGE('',*,*,#28911,.T.);
#41339=ORIENTED_EDGE('',*,*,#28908,.T.);
#41340=ORIENTED_EDGE('',*,*,#28909,.F.);
#41341=ORIENTED_EDGE('',*,*,#28905,.T.);
#41342=ORIENTED_EDGE('',*,*,#28902,.T.);
#41343=ORIENTED_EDGE('',*,*,#28903,.F.);
#41344=ORIENTED_EDGE('',*,*,#28899,.T.);
#41345=ORIENTED_EDGE('',*,*,#28896,.T.);
#41346=ORIENTED_EDGE('',*,*,#28897,.F.);
#41347=ORIENTED_EDGE('',*,*,#28893,.T.);
#41348=ORIENTED_EDGE('',*,*,#28890,.T.);
#41349=ORIENTED_EDGE('',*,*,#28891,.F.);
#41350=ORIENTED_EDGE('',*,*,#28887,.T.);
#41351=ORIENTED_EDGE('',*,*,#28884,.T.);
#41352=ORIENTED_EDGE('',*,*,#28885,.F.);
#41353=ORIENTED_EDGE('',*,*,#28881,.T.);
#41354=ORIENTED_EDGE('',*,*,#28878,.T.);
#41355=ORIENTED_EDGE('',*,*,#28879,.F.);
#41356=ORIENTED_EDGE('',*,*,#28875,.T.);
#41357=ORIENTED_EDGE('',*,*,#28872,.T.);
#41358=ORIENTED_EDGE('',*,*,#28873,.F.);
#41359=ORIENTED_EDGE('',*,*,#28869,.T.);
#41360=ORIENTED_EDGE('',*,*,#28866,.T.);
#41361=ORIENTED_EDGE('',*,*,#28867,.F.);
#41362=ORIENTED_EDGE('',*,*,#28863,.T.);
#41363=ORIENTED_EDGE('',*,*,#28860,.T.);
#41364=ORIENTED_EDGE('',*,*,#28861,.F.);
#41365=ORIENTED_EDGE('',*,*,#28857,.T.);
#41366=ORIENTED_EDGE('',*,*,#28854,.T.);
#41367=ORIENTED_EDGE('',*,*,#28855,.F.);
#41368=ORIENTED_EDGE('',*,*,#28851,.T.);
#41369=ORIENTED_EDGE('',*,*,#28848,.T.);
#41370=ORIENTED_EDGE('',*,*,#28849,.F.);
#41371=ORIENTED_EDGE('',*,*,#28845,.T.);
#41372=ORIENTED_EDGE('',*,*,#28842,.T.);
#41373=ORIENTED_EDGE('',*,*,#28843,.F.);
#41374=ORIENTED_EDGE('',*,*,#28839,.T.);
#41375=ORIENTED_EDGE('',*,*,#28836,.T.);
#41376=ORIENTED_EDGE('',*,*,#28837,.F.);
#41377=ORIENTED_EDGE('',*,*,#28833,.T.);
#41378=ORIENTED_EDGE('',*,*,#28830,.T.);
#41379=ORIENTED_EDGE('',*,*,#28831,.F.);
#41380=ORIENTED_EDGE('',*,*,#28827,.T.);
#41381=ORIENTED_EDGE('',*,*,#28824,.T.);
#41382=ORIENTED_EDGE('',*,*,#28825,.F.);
#41383=ORIENTED_EDGE('',*,*,#28821,.T.);
#41384=ORIENTED_EDGE('',*,*,#28818,.T.);
#41385=ORIENTED_EDGE('',*,*,#28819,.F.);
#41386=ORIENTED_EDGE('',*,*,#28815,.T.);
#41387=ORIENTED_EDGE('',*,*,#28812,.T.);
#41388=ORIENTED_EDGE('',*,*,#28813,.F.);
#41389=ORIENTED_EDGE('',*,*,#28809,.T.);
#41390=ORIENTED_EDGE('',*,*,#28806,.T.);
#41391=ORIENTED_EDGE('',*,*,#28807,.F.);
#41392=ORIENTED_EDGE('',*,*,#28803,.T.);
#41393=ORIENTED_EDGE('',*,*,#28800,.T.);
#41394=ORIENTED_EDGE('',*,*,#28801,.F.);
#41395=ORIENTED_EDGE('',*,*,#28797,.T.);
#41396=ORIENTED_EDGE('',*,*,#28794,.T.);
#41397=ORIENTED_EDGE('',*,*,#28795,.F.);
#41398=ORIENTED_EDGE('',*,*,#28791,.T.);
#41399=ORIENTED_EDGE('',*,*,#28788,.T.);
#41400=ORIENTED_EDGE('',*,*,#28789,.F.);
#41401=ORIENTED_EDGE('',*,*,#28785,.T.);
#41402=ORIENTED_EDGE('',*,*,#28782,.T.);
#41403=ORIENTED_EDGE('',*,*,#28783,.F.);
#41404=ORIENTED_EDGE('',*,*,#28779,.T.);
#41405=ORIENTED_EDGE('',*,*,#28776,.T.);
#41406=ORIENTED_EDGE('',*,*,#28777,.F.);
#41407=ORIENTED_EDGE('',*,*,#28773,.T.);
#41408=ORIENTED_EDGE('',*,*,#28770,.T.);
#41409=ORIENTED_EDGE('',*,*,#28771,.F.);
#41410=ORIENTED_EDGE('',*,*,#28767,.T.);
#41411=ORIENTED_EDGE('',*,*,#28764,.T.);
#41412=ORIENTED_EDGE('',*,*,#28765,.F.);
#41413=ORIENTED_EDGE('',*,*,#28761,.T.);
#41414=ORIENTED_EDGE('',*,*,#28758,.T.);
#41415=ORIENTED_EDGE('',*,*,#28759,.F.);
#41416=ORIENTED_EDGE('',*,*,#28755,.T.);
#41417=ORIENTED_EDGE('',*,*,#28752,.T.);
#41418=ORIENTED_EDGE('',*,*,#28753,.F.);
#41419=ORIENTED_EDGE('',*,*,#28749,.T.);
#41420=ORIENTED_EDGE('',*,*,#28746,.T.);
#41421=ORIENTED_EDGE('',*,*,#28747,.F.);
#41422=ORIENTED_EDGE('',*,*,#28743,.T.);
#41423=ORIENTED_EDGE('',*,*,#28740,.T.);
#41424=ORIENTED_EDGE('',*,*,#28741,.F.);
#41425=ORIENTED_EDGE('',*,*,#28737,.T.);
#41426=ORIENTED_EDGE('',*,*,#28734,.T.);
#41427=ORIENTED_EDGE('',*,*,#28735,.F.);
#41428=ORIENTED_EDGE('',*,*,#28731,.T.);
#41429=ORIENTED_EDGE('',*,*,#28728,.T.);
#41430=ORIENTED_EDGE('',*,*,#28729,.F.);
#41431=ORIENTED_EDGE('',*,*,#28725,.T.);
#41432=ORIENTED_EDGE('',*,*,#28722,.T.);
#41433=ORIENTED_EDGE('',*,*,#28723,.F.);
#41434=ORIENTED_EDGE('',*,*,#28719,.T.);
#41435=ORIENTED_EDGE('',*,*,#28716,.T.);
#41436=ORIENTED_EDGE('',*,*,#28717,.F.);
#41437=ORIENTED_EDGE('',*,*,#28713,.T.);
#41438=ORIENTED_EDGE('',*,*,#28710,.T.);
#41439=ORIENTED_EDGE('',*,*,#28711,.F.);
#41440=ORIENTED_EDGE('',*,*,#28707,.T.);
#41441=ORIENTED_EDGE('',*,*,#28704,.T.);
#41442=ORIENTED_EDGE('',*,*,#28705,.F.);
#41443=ORIENTED_EDGE('',*,*,#28701,.T.);
#41444=ORIENTED_EDGE('',*,*,#28698,.T.);
#41445=ORIENTED_EDGE('',*,*,#28699,.F.);
#41446=ORIENTED_EDGE('',*,*,#28695,.T.);
#41447=ORIENTED_EDGE('',*,*,#28692,.T.);
#41448=ORIENTED_EDGE('',*,*,#28693,.F.);
#41449=ORIENTED_EDGE('',*,*,#28689,.T.);
#41450=ORIENTED_EDGE('',*,*,#28686,.T.);
#41451=ORIENTED_EDGE('',*,*,#28687,.F.);
#41452=ORIENTED_EDGE('',*,*,#28683,.T.);
#41453=ORIENTED_EDGE('',*,*,#28680,.T.);
#41454=ORIENTED_EDGE('',*,*,#28681,.F.);
#41455=ORIENTED_EDGE('',*,*,#28677,.T.);
#41456=ORIENTED_EDGE('',*,*,#28674,.T.);
#41457=ORIENTED_EDGE('',*,*,#28675,.F.);
#41458=ORIENTED_EDGE('',*,*,#28671,.T.);
#41459=ORIENTED_EDGE('',*,*,#28668,.T.);
#41460=ORIENTED_EDGE('',*,*,#28669,.F.);
#41461=ORIENTED_EDGE('',*,*,#28665,.T.);
#41462=ORIENTED_EDGE('',*,*,#28662,.T.);
#41463=ORIENTED_EDGE('',*,*,#28663,.F.);
#41464=ORIENTED_EDGE('',*,*,#28658,.T.);
#41465=ORIENTED_EDGE('',*,*,#28655,.T.);
#41466=ORIENTED_EDGE('',*,*,#28656,.F.);
#41467=ORIENTED_EDGE('',*,*,#28659,.F.);
#41468=ORIENTED_EDGE('',*,*,#28652,.T.);
#41469=ORIENTED_EDGE('',*,*,#28649,.T.);
#41470=ORIENTED_EDGE('',*,*,#28650,.F.);
#41471=ORIENTED_EDGE('',*,*,#28653,.F.);
#41472=ORIENTED_EDGE('',*,*,#28646,.T.);
#41473=ORIENTED_EDGE('',*,*,#28643,.T.);
#41474=ORIENTED_EDGE('',*,*,#28644,.F.);
#41475=ORIENTED_EDGE('',*,*,#28647,.F.);
#41476=ORIENTED_EDGE('',*,*,#28640,.T.);
#41477=ORIENTED_EDGE('',*,*,#28637,.T.);
#41478=ORIENTED_EDGE('',*,*,#28638,.F.);
#41479=ORIENTED_EDGE('',*,*,#28641,.F.);
#41480=ORIENTED_EDGE('',*,*,#28634,.T.);
#41481=ORIENTED_EDGE('',*,*,#28631,.T.);
#41482=ORIENTED_EDGE('',*,*,#28632,.F.);
#41483=ORIENTED_EDGE('',*,*,#28635,.F.);
#41484=ORIENTED_EDGE('',*,*,#28628,.T.);
#41485=ORIENTED_EDGE('',*,*,#28625,.T.);
#41486=ORIENTED_EDGE('',*,*,#28626,.F.);
#41487=ORIENTED_EDGE('',*,*,#28629,.F.);
#41488=ORIENTED_EDGE('',*,*,#28622,.T.);
#41489=ORIENTED_EDGE('',*,*,#28619,.T.);
#41490=ORIENTED_EDGE('',*,*,#28620,.F.);
#41491=ORIENTED_EDGE('',*,*,#28623,.F.);
#41492=ORIENTED_EDGE('',*,*,#28616,.T.);
#41493=ORIENTED_EDGE('',*,*,#28613,.T.);
#41494=ORIENTED_EDGE('',*,*,#28614,.F.);
#41495=ORIENTED_EDGE('',*,*,#28617,.F.);
#41496=ORIENTED_EDGE('',*,*,#28610,.T.);
#41497=ORIENTED_EDGE('',*,*,#28607,.T.);
#41498=ORIENTED_EDGE('',*,*,#28608,.F.);
#41499=ORIENTED_EDGE('',*,*,#28611,.F.);
#41500=ORIENTED_EDGE('',*,*,#28604,.T.);
#41501=ORIENTED_EDGE('',*,*,#28601,.T.);
#41502=ORIENTED_EDGE('',*,*,#28602,.F.);
#41503=ORIENTED_EDGE('',*,*,#28605,.F.);
#41504=ORIENTED_EDGE('',*,*,#28598,.T.);
#41505=ORIENTED_EDGE('',*,*,#28595,.T.);
#41506=ORIENTED_EDGE('',*,*,#28596,.F.);
#41507=ORIENTED_EDGE('',*,*,#28599,.F.);
#41508=ORIENTED_EDGE('',*,*,#28592,.T.);
#41509=ORIENTED_EDGE('',*,*,#28589,.T.);
#41510=ORIENTED_EDGE('',*,*,#28590,.F.);
#41511=ORIENTED_EDGE('',*,*,#28593,.F.);
#41512=ORIENTED_EDGE('',*,*,#28586,.T.);
#41513=ORIENTED_EDGE('',*,*,#28583,.T.);
#41514=ORIENTED_EDGE('',*,*,#28584,.F.);
#41515=ORIENTED_EDGE('',*,*,#28587,.F.);
#41516=ORIENTED_EDGE('',*,*,#28580,.T.);
#41517=ORIENTED_EDGE('',*,*,#28577,.T.);
#41518=ORIENTED_EDGE('',*,*,#28578,.F.);
#41519=ORIENTED_EDGE('',*,*,#28581,.F.);
#41520=ORIENTED_EDGE('',*,*,#28574,.T.);
#41521=ORIENTED_EDGE('',*,*,#28571,.T.);
#41522=ORIENTED_EDGE('',*,*,#28572,.F.);
#41523=ORIENTED_EDGE('',*,*,#28575,.F.);
#41524=ORIENTED_EDGE('',*,*,#28568,.T.);
#41525=ORIENTED_EDGE('',*,*,#28565,.T.);
#41526=ORIENTED_EDGE('',*,*,#28566,.F.);
#41527=ORIENTED_EDGE('',*,*,#28569,.F.);
#41528=ORIENTED_EDGE('',*,*,#28562,.T.);
#41529=ORIENTED_EDGE('',*,*,#28559,.T.);
#41530=ORIENTED_EDGE('',*,*,#28560,.F.);
#41531=ORIENTED_EDGE('',*,*,#28563,.F.);
#41532=ORIENTED_EDGE('',*,*,#28556,.T.);
#41533=ORIENTED_EDGE('',*,*,#28553,.T.);
#41534=ORIENTED_EDGE('',*,*,#28554,.F.);
#41535=ORIENTED_EDGE('',*,*,#28557,.F.);
#41536=ORIENTED_EDGE('',*,*,#28550,.T.);
#41537=ORIENTED_EDGE('',*,*,#28547,.T.);
#41538=ORIENTED_EDGE('',*,*,#28548,.F.);
#41539=ORIENTED_EDGE('',*,*,#28551,.F.);
#41540=ORIENTED_EDGE('',*,*,#28544,.T.);
#41541=ORIENTED_EDGE('',*,*,#28541,.T.);
#41542=ORIENTED_EDGE('',*,*,#28542,.F.);
#41543=ORIENTED_EDGE('',*,*,#28545,.F.);
#41544=ORIENTED_EDGE('',*,*,#28538,.T.);
#41545=ORIENTED_EDGE('',*,*,#28535,.T.);
#41546=ORIENTED_EDGE('',*,*,#28536,.F.);
#41547=ORIENTED_EDGE('',*,*,#28539,.F.);
#41548=ORIENTED_EDGE('',*,*,#28532,.T.);
#41549=ORIENTED_EDGE('',*,*,#28529,.T.);
#41550=ORIENTED_EDGE('',*,*,#28530,.F.);
#41551=ORIENTED_EDGE('',*,*,#28533,.F.);
#41552=ORIENTED_EDGE('',*,*,#28526,.T.);
#41553=ORIENTED_EDGE('',*,*,#28523,.T.);
#41554=ORIENTED_EDGE('',*,*,#28524,.F.);
#41555=ORIENTED_EDGE('',*,*,#28527,.F.);
#41556=ORIENTED_EDGE('',*,*,#28520,.T.);
#41557=ORIENTED_EDGE('',*,*,#28517,.T.);
#41558=ORIENTED_EDGE('',*,*,#28518,.F.);
#41559=ORIENTED_EDGE('',*,*,#28521,.F.);
#41560=ORIENTED_EDGE('',*,*,#28514,.T.);
#41561=ORIENTED_EDGE('',*,*,#28511,.T.);
#41562=ORIENTED_EDGE('',*,*,#28512,.F.);
#41563=ORIENTED_EDGE('',*,*,#28515,.F.);
#41564=ORIENTED_EDGE('',*,*,#28507,.T.);
#41565=ORIENTED_EDGE('',*,*,#28504,.T.);
#41566=ORIENTED_EDGE('',*,*,#28505,.F.);
#41567=ORIENTED_EDGE('',*,*,#28508,.F.);
#41568=ORIENTED_EDGE('',*,*,#28500,.T.);
#41569=ORIENTED_EDGE('',*,*,#28497,.T.);
#41570=ORIENTED_EDGE('',*,*,#28498,.F.);
#41571=ORIENTED_EDGE('',*,*,#28501,.F.);
#41572=ORIENTED_EDGE('',*,*,#28494,.T.);
#41573=ORIENTED_EDGE('',*,*,#28491,.T.);
#41574=ORIENTED_EDGE('',*,*,#28492,.F.);
#41575=ORIENTED_EDGE('',*,*,#28495,.F.);
#41576=ORIENTED_EDGE('',*,*,#28488,.T.);
#41577=ORIENTED_EDGE('',*,*,#28485,.T.);
#41578=ORIENTED_EDGE('',*,*,#28486,.F.);
#41579=ORIENTED_EDGE('',*,*,#28489,.F.);
#41580=ORIENTED_EDGE('',*,*,#28481,.T.);
#41581=ORIENTED_EDGE('',*,*,#28478,.T.);
#41582=ORIENTED_EDGE('',*,*,#28479,.F.);
#41583=ORIENTED_EDGE('',*,*,#28482,.F.);
#41584=ORIENTED_EDGE('',*,*,#28474,.T.);
#41585=ORIENTED_EDGE('',*,*,#28471,.T.);
#41586=ORIENTED_EDGE('',*,*,#28472,.F.);
#41587=ORIENTED_EDGE('',*,*,#28475,.F.);
#41588=ORIENTED_EDGE('',*,*,#28467,.T.);
#41589=ORIENTED_EDGE('',*,*,#28464,.T.);
#41590=ORIENTED_EDGE('',*,*,#28465,.F.);
#41591=ORIENTED_EDGE('',*,*,#28468,.F.);
#41592=ORIENTED_EDGE('',*,*,#28460,.T.);
#41593=ORIENTED_EDGE('',*,*,#28457,.T.);
#41594=ORIENTED_EDGE('',*,*,#28458,.F.);
#41595=ORIENTED_EDGE('',*,*,#28461,.F.);
#41596=ORIENTED_EDGE('',*,*,#28453,.T.);
#41597=ORIENTED_EDGE('',*,*,#28450,.T.);
#41598=ORIENTED_EDGE('',*,*,#28451,.F.);
#41599=ORIENTED_EDGE('',*,*,#28454,.F.);
#41600=ORIENTED_EDGE('',*,*,#28446,.T.);
#41601=ORIENTED_EDGE('',*,*,#28443,.T.);
#41602=ORIENTED_EDGE('',*,*,#28444,.F.);
#41603=ORIENTED_EDGE('',*,*,#28447,.F.);
#41604=ORIENTED_EDGE('',*,*,#28439,.T.);
#41605=ORIENTED_EDGE('',*,*,#28436,.T.);
#41606=ORIENTED_EDGE('',*,*,#28437,.F.);
#41607=ORIENTED_EDGE('',*,*,#28440,.F.);
#41608=ORIENTED_EDGE('',*,*,#28432,.T.);
#41609=ORIENTED_EDGE('',*,*,#28429,.T.);
#41610=ORIENTED_EDGE('',*,*,#28430,.F.);
#41611=ORIENTED_EDGE('',*,*,#28433,.F.);
#41612=ORIENTED_EDGE('',*,*,#28425,.T.);
#41613=ORIENTED_EDGE('',*,*,#28422,.T.);
#41614=ORIENTED_EDGE('',*,*,#28423,.F.);
#41615=ORIENTED_EDGE('',*,*,#28426,.F.);
#41616=ORIENTED_EDGE('',*,*,#28418,.T.);
#41617=ORIENTED_EDGE('',*,*,#28415,.T.);
#41618=ORIENTED_EDGE('',*,*,#28416,.F.);
#41619=ORIENTED_EDGE('',*,*,#28419,.F.);
#41620=ORIENTED_EDGE('',*,*,#28411,.T.);
#41621=ORIENTED_EDGE('',*,*,#28408,.T.);
#41622=ORIENTED_EDGE('',*,*,#28409,.F.);
#41623=ORIENTED_EDGE('',*,*,#28412,.F.);
#41624=ORIENTED_EDGE('',*,*,#28404,.T.);
#41625=ORIENTED_EDGE('',*,*,#28401,.T.);
#41626=ORIENTED_EDGE('',*,*,#28402,.F.);
#41627=ORIENTED_EDGE('',*,*,#28405,.F.);
#41628=ORIENTED_EDGE('',*,*,#28397,.T.);
#41629=ORIENTED_EDGE('',*,*,#28394,.T.);
#41630=ORIENTED_EDGE('',*,*,#28395,.F.);
#41631=ORIENTED_EDGE('',*,*,#28398,.F.);
#41632=ORIENTED_EDGE('',*,*,#28390,.T.);
#41633=ORIENTED_EDGE('',*,*,#28387,.T.);
#41634=ORIENTED_EDGE('',*,*,#28388,.F.);
#41635=ORIENTED_EDGE('',*,*,#28391,.F.);
#41636=ORIENTED_EDGE('',*,*,#28383,.T.);
#41637=ORIENTED_EDGE('',*,*,#28380,.T.);
#41638=ORIENTED_EDGE('',*,*,#28381,.F.);
#41639=ORIENTED_EDGE('',*,*,#28384,.F.);
#41640=ORIENTED_EDGE('',*,*,#28376,.T.);
#41641=ORIENTED_EDGE('',*,*,#28373,.T.);
#41642=ORIENTED_EDGE('',*,*,#28374,.F.);
#41643=ORIENTED_EDGE('',*,*,#28377,.F.);
#41644=ORIENTED_EDGE('',*,*,#28369,.T.);
#41645=ORIENTED_EDGE('',*,*,#28366,.T.);
#41646=ORIENTED_EDGE('',*,*,#28367,.F.);
#41647=ORIENTED_EDGE('',*,*,#28370,.F.);
#41648=ORIENTED_EDGE('',*,*,#28362,.T.);
#41649=ORIENTED_EDGE('',*,*,#28359,.T.);
#41650=ORIENTED_EDGE('',*,*,#28360,.F.);
#41651=ORIENTED_EDGE('',*,*,#28363,.F.);
#41652=ORIENTED_EDGE('',*,*,#28355,.T.);
#41653=ORIENTED_EDGE('',*,*,#28350,.T.);
#41654=ORIENTED_EDGE('',*,*,#28351,.T.);
#41655=ORIENTED_EDGE('',*,*,#28353,.F.);
#41656=ORIENTED_EDGE('',*,*,#28356,.F.);
#41657=ORIENTED_EDGE('',*,*,#28346,.T.);
#41658=ORIENTED_EDGE('',*,*,#28343,.T.);
#41659=ORIENTED_EDGE('',*,*,#28344,.F.);
#41660=ORIENTED_EDGE('',*,*,#28347,.F.);
#41661=ORIENTED_EDGE('',*,*,#28339,.T.);
#41662=ORIENTED_EDGE('',*,*,#28336,.T.);
#41663=ORIENTED_EDGE('',*,*,#28337,.F.);
#41664=ORIENTED_EDGE('',*,*,#28340,.F.);
#41665=ORIENTED_EDGE('',*,*,#28332,.T.);
#41666=ORIENTED_EDGE('',*,*,#28329,.T.);
#41667=ORIENTED_EDGE('',*,*,#28330,.F.);
#41668=ORIENTED_EDGE('',*,*,#28333,.F.);
#41669=ORIENTED_EDGE('',*,*,#28325,.T.);
#41670=ORIENTED_EDGE('',*,*,#28321,.T.);
#41671=ORIENTED_EDGE('',*,*,#28322,.T.);
#41672=ORIENTED_EDGE('',*,*,#28323,.F.);
#41673=ORIENTED_EDGE('',*,*,#28326,.F.);
#41674=ORIENTED_EDGE('',*,*,#28317,.T.);
#41675=ORIENTED_EDGE('',*,*,#28314,.T.);
#41676=ORIENTED_EDGE('',*,*,#28315,.F.);
#41677=ORIENTED_EDGE('',*,*,#28318,.F.);
#41678=ORIENTED_EDGE('',*,*,#28310,.T.);
#41679=ORIENTED_EDGE('',*,*,#28307,.T.);
#41680=ORIENTED_EDGE('',*,*,#28308,.F.);
#41681=ORIENTED_EDGE('',*,*,#28311,.F.);
#41682=ORIENTED_EDGE('',*,*,#28303,.T.);
#41683=ORIENTED_EDGE('',*,*,#28300,.T.);
#41684=ORIENTED_EDGE('',*,*,#28301,.F.);
#41685=ORIENTED_EDGE('',*,*,#28304,.F.);
#41686=ORIENTED_EDGE('',*,*,#28296,.T.);
#41687=ORIENTED_EDGE('',*,*,#28292,.T.);
#41688=ORIENTED_EDGE('',*,*,#28293,.T.);
#41689=ORIENTED_EDGE('',*,*,#28294,.F.);
#41690=ORIENTED_EDGE('',*,*,#28297,.F.);
#41691=ORIENTED_EDGE('',*,*,#28288,.T.);
#41692=ORIENTED_EDGE('',*,*,#28285,.T.);
#41693=ORIENTED_EDGE('',*,*,#28286,.F.);
#41694=ORIENTED_EDGE('',*,*,#28289,.F.);
#41695=ORIENTED_EDGE('',*,*,#28281,.T.);
#41696=ORIENTED_EDGE('',*,*,#28278,.T.);
#41697=ORIENTED_EDGE('',*,*,#28279,.F.);
#41698=ORIENTED_EDGE('',*,*,#28282,.F.);
#41699=ORIENTED_EDGE('',*,*,#28274,.T.);
#41700=ORIENTED_EDGE('',*,*,#28271,.T.);
#41701=ORIENTED_EDGE('',*,*,#28272,.F.);
#41702=ORIENTED_EDGE('',*,*,#28275,.F.);
#41703=ORIENTED_EDGE('',*,*,#28267,.T.);
#41704=ORIENTED_EDGE('',*,*,#28264,.T.);
#41705=ORIENTED_EDGE('',*,*,#28265,.F.);
#41706=ORIENTED_EDGE('',*,*,#28268,.F.);
#41707=ORIENTED_EDGE('',*,*,#28260,.T.);
#41708=ORIENTED_EDGE('',*,*,#28257,.T.);
#41709=ORIENTED_EDGE('',*,*,#28258,.F.);
#41710=ORIENTED_EDGE('',*,*,#28261,.F.);
#41711=ORIENTED_EDGE('',*,*,#28253,.T.);
#41712=ORIENTED_EDGE('',*,*,#28250,.T.);
#41713=ORIENTED_EDGE('',*,*,#28251,.F.);
#41714=ORIENTED_EDGE('',*,*,#28254,.F.);
#41715=ORIENTED_EDGE('',*,*,#28246,.T.);
#41716=ORIENTED_EDGE('',*,*,#28243,.T.);
#41717=ORIENTED_EDGE('',*,*,#28244,.F.);
#41718=ORIENTED_EDGE('',*,*,#28247,.F.);
#41719=ORIENTED_EDGE('',*,*,#28239,.T.);
#41720=ORIENTED_EDGE('',*,*,#28236,.T.);
#41721=ORIENTED_EDGE('',*,*,#28237,.F.);
#41722=ORIENTED_EDGE('',*,*,#28240,.F.);
#41723=ORIENTED_EDGE('',*,*,#28232,.T.);
#41724=ORIENTED_EDGE('',*,*,#28229,.T.);
#41725=ORIENTED_EDGE('',*,*,#28230,.F.);
#41726=ORIENTED_EDGE('',*,*,#28233,.F.);
#41727=ORIENTED_EDGE('',*,*,#28225,.T.);
#41728=ORIENTED_EDGE('',*,*,#28222,.T.);
#41729=ORIENTED_EDGE('',*,*,#28223,.F.);
#41730=ORIENTED_EDGE('',*,*,#28226,.F.);
#41731=ORIENTED_EDGE('',*,*,#28218,.T.);
#41732=ORIENTED_EDGE('',*,*,#28215,.T.);
#41733=ORIENTED_EDGE('',*,*,#28216,.F.);
#41734=ORIENTED_EDGE('',*,*,#28219,.F.);
#41735=ORIENTED_EDGE('',*,*,#28211,.T.);
#41736=ORIENTED_EDGE('',*,*,#28208,.T.);
#41737=ORIENTED_EDGE('',*,*,#28209,.F.);
#41738=ORIENTED_EDGE('',*,*,#28212,.F.);
#41739=ORIENTED_EDGE('',*,*,#28204,.T.);
#41740=ORIENTED_EDGE('',*,*,#28201,.T.);
#41741=ORIENTED_EDGE('',*,*,#28202,.F.);
#41742=ORIENTED_EDGE('',*,*,#28205,.F.);
#41743=ORIENTED_EDGE('',*,*,#28197,.T.);
#41744=ORIENTED_EDGE('',*,*,#28194,.T.);
#41745=ORIENTED_EDGE('',*,*,#28195,.F.);
#41746=ORIENTED_EDGE('',*,*,#28198,.F.);
#41747=ORIENTED_EDGE('',*,*,#28190,.T.);
#41748=ORIENTED_EDGE('',*,*,#28187,.T.);
#41749=ORIENTED_EDGE('',*,*,#28188,.F.);
#41750=ORIENTED_EDGE('',*,*,#28191,.F.);
#41751=ORIENTED_EDGE('',*,*,#28183,.T.);
#41752=ORIENTED_EDGE('',*,*,#28180,.T.);
#41753=ORIENTED_EDGE('',*,*,#28181,.F.);
#41754=ORIENTED_EDGE('',*,*,#28184,.F.);
#41755=ORIENTED_EDGE('',*,*,#28176,.T.);
#41756=ORIENTED_EDGE('',*,*,#28173,.T.);
#41757=ORIENTED_EDGE('',*,*,#28174,.F.);
#41758=ORIENTED_EDGE('',*,*,#28177,.F.);
#41759=ORIENTED_EDGE('',*,*,#28169,.T.);
#41760=ORIENTED_EDGE('',*,*,#28166,.T.);
#41761=ORIENTED_EDGE('',*,*,#28167,.F.);
#41762=ORIENTED_EDGE('',*,*,#28170,.F.);
#41763=ORIENTED_EDGE('',*,*,#28162,.T.);
#41764=ORIENTED_EDGE('',*,*,#28159,.T.);
#41765=ORIENTED_EDGE('',*,*,#28160,.F.);
#41766=ORIENTED_EDGE('',*,*,#28163,.F.);
#41767=ORIENTED_EDGE('',*,*,#28155,.T.);
#41768=ORIENTED_EDGE('',*,*,#28152,.T.);
#41769=ORIENTED_EDGE('',*,*,#28153,.F.);
#41770=ORIENTED_EDGE('',*,*,#28156,.F.);
#41771=ORIENTED_EDGE('',*,*,#28148,.T.);
#41772=ORIENTED_EDGE('',*,*,#28145,.T.);
#41773=ORIENTED_EDGE('',*,*,#28146,.F.);
#41774=ORIENTED_EDGE('',*,*,#28149,.F.);
#41775=ORIENTED_EDGE('',*,*,#28141,.T.);
#41776=ORIENTED_EDGE('',*,*,#28138,.T.);
#41777=ORIENTED_EDGE('',*,*,#28139,.F.);
#41778=ORIENTED_EDGE('',*,*,#28142,.F.);
#41779=ORIENTED_EDGE('',*,*,#28134,.T.);
#41780=ORIENTED_EDGE('',*,*,#28131,.T.);
#41781=ORIENTED_EDGE('',*,*,#28132,.F.);
#41782=ORIENTED_EDGE('',*,*,#28135,.F.);
#41783=ORIENTED_EDGE('',*,*,#28127,.T.);
#41784=ORIENTED_EDGE('',*,*,#28124,.T.);
#41785=ORIENTED_EDGE('',*,*,#28125,.F.);
#41786=ORIENTED_EDGE('',*,*,#28128,.F.);
#41787=ORIENTED_EDGE('',*,*,#28120,.T.);
#41788=ORIENTED_EDGE('',*,*,#28117,.T.);
#41789=ORIENTED_EDGE('',*,*,#28118,.F.);
#41790=ORIENTED_EDGE('',*,*,#28121,.F.);
#41791=ORIENTED_EDGE('',*,*,#28113,.T.);
#41792=ORIENTED_EDGE('',*,*,#28110,.T.);
#41793=ORIENTED_EDGE('',*,*,#28111,.F.);
#41794=ORIENTED_EDGE('',*,*,#28114,.F.);
#41795=ORIENTED_EDGE('',*,*,#28106,.T.);
#41796=ORIENTED_EDGE('',*,*,#28103,.T.);
#41797=ORIENTED_EDGE('',*,*,#28104,.F.);
#41798=ORIENTED_EDGE('',*,*,#28107,.F.);
#41799=ORIENTED_EDGE('',*,*,#28099,.T.);
#41800=ORIENTED_EDGE('',*,*,#28096,.T.);
#41801=ORIENTED_EDGE('',*,*,#28097,.F.);
#41802=ORIENTED_EDGE('',*,*,#28100,.F.);
#41803=ORIENTED_EDGE('',*,*,#28092,.T.);
#41804=ORIENTED_EDGE('',*,*,#28089,.T.);
#41805=ORIENTED_EDGE('',*,*,#28090,.F.);
#41806=ORIENTED_EDGE('',*,*,#28093,.F.);
#41807=ORIENTED_EDGE('',*,*,#28086,.T.);
#41808=ORIENTED_EDGE('',*,*,#28083,.T.);
#41809=ORIENTED_EDGE('',*,*,#28084,.F.);
#41810=ORIENTED_EDGE('',*,*,#28087,.F.);
#41811=ORIENTED_EDGE('',*,*,#28080,.T.);
#41812=ORIENTED_EDGE('',*,*,#28077,.T.);
#41813=ORIENTED_EDGE('',*,*,#28078,.F.);
#41814=ORIENTED_EDGE('',*,*,#28081,.F.);
#41815=ORIENTED_EDGE('',*,*,#28073,.T.);
#41816=ORIENTED_EDGE('',*,*,#28070,.T.);
#41817=ORIENTED_EDGE('',*,*,#28071,.F.);
#41818=ORIENTED_EDGE('',*,*,#28074,.F.);
#41819=ORIENTED_EDGE('',*,*,#28066,.T.);
#41820=ORIENTED_EDGE('',*,*,#28063,.T.);
#41821=ORIENTED_EDGE('',*,*,#28064,.F.);
#41822=ORIENTED_EDGE('',*,*,#28067,.F.);
#41823=ORIENTED_EDGE('',*,*,#28060,.T.);
#41824=ORIENTED_EDGE('',*,*,#28057,.T.);
#41825=ORIENTED_EDGE('',*,*,#28058,.F.);
#41826=ORIENTED_EDGE('',*,*,#28061,.F.);
#41827=ORIENTED_EDGE('',*,*,#28054,.T.);
#41828=ORIENTED_EDGE('',*,*,#28051,.T.);
#41829=ORIENTED_EDGE('',*,*,#28052,.F.);
#41830=ORIENTED_EDGE('',*,*,#28055,.F.);
#41831=ORIENTED_EDGE('',*,*,#28048,.T.);
#41832=ORIENTED_EDGE('',*,*,#28044,.T.);
#41833=ORIENTED_EDGE('',*,*,#28045,.T.);
#41834=ORIENTED_EDGE('',*,*,#28046,.F.);
#41835=ORIENTED_EDGE('',*,*,#28049,.F.);
#41836=ORIENTED_EDGE('',*,*,#28041,.T.);
#41837=ORIENTED_EDGE('',*,*,#28038,.T.);
#41838=ORIENTED_EDGE('',*,*,#28039,.F.);
#41839=ORIENTED_EDGE('',*,*,#28042,.F.);
#41840=ORIENTED_EDGE('',*,*,#28035,.T.);
#41841=ORIENTED_EDGE('',*,*,#28032,.T.);
#41842=ORIENTED_EDGE('',*,*,#28033,.F.);
#41843=ORIENTED_EDGE('',*,*,#28036,.F.);
#41844=ORIENTED_EDGE('',*,*,#28029,.T.);
#41845=ORIENTED_EDGE('',*,*,#28026,.T.);
#41846=ORIENTED_EDGE('',*,*,#28027,.F.);
#41847=ORIENTED_EDGE('',*,*,#28030,.F.);
#41848=ORIENTED_EDGE('',*,*,#28023,.T.);
#41849=ORIENTED_EDGE('',*,*,#28020,.T.);
#41850=ORIENTED_EDGE('',*,*,#28021,.F.);
#41851=ORIENTED_EDGE('',*,*,#28024,.F.);
#41852=ORIENTED_EDGE('',*,*,#28017,.T.);
#41853=ORIENTED_EDGE('',*,*,#28014,.T.);
#41854=ORIENTED_EDGE('',*,*,#28015,.F.);
#41855=ORIENTED_EDGE('',*,*,#28018,.F.);
#41856=ORIENTED_EDGE('',*,*,#28011,.T.);
#41857=ORIENTED_EDGE('',*,*,#28008,.T.);
#41858=ORIENTED_EDGE('',*,*,#28009,.F.);
#41859=ORIENTED_EDGE('',*,*,#28012,.F.);
#41860=ORIENTED_EDGE('',*,*,#28005,.T.);
#41861=ORIENTED_EDGE('',*,*,#28002,.T.);
#41862=ORIENTED_EDGE('',*,*,#28003,.F.);
#41863=ORIENTED_EDGE('',*,*,#28006,.F.);
#41864=ORIENTED_EDGE('',*,*,#27999,.T.);
#41865=ORIENTED_EDGE('',*,*,#27996,.T.);
#41866=ORIENTED_EDGE('',*,*,#27997,.F.);
#41867=ORIENTED_EDGE('',*,*,#28000,.F.);
#41868=ORIENTED_EDGE('',*,*,#27993,.T.);
#41869=ORIENTED_EDGE('',*,*,#27990,.T.);
#41870=ORIENTED_EDGE('',*,*,#27991,.F.);
#41871=ORIENTED_EDGE('',*,*,#27994,.F.);
#41872=ORIENTED_EDGE('',*,*,#27987,.T.);
#41873=ORIENTED_EDGE('',*,*,#27984,.T.);
#41874=ORIENTED_EDGE('',*,*,#27985,.F.);
#41875=ORIENTED_EDGE('',*,*,#27988,.F.);
#41876=ORIENTED_EDGE('',*,*,#27981,.T.);
#41877=ORIENTED_EDGE('',*,*,#27978,.T.);
#41878=ORIENTED_EDGE('',*,*,#27979,.F.);
#41879=ORIENTED_EDGE('',*,*,#27982,.F.);
#41880=ORIENTED_EDGE('',*,*,#27975,.T.);
#41881=ORIENTED_EDGE('',*,*,#27972,.T.);
#41882=ORIENTED_EDGE('',*,*,#27973,.F.);
#41883=ORIENTED_EDGE('',*,*,#27976,.F.);
#41884=ORIENTED_EDGE('',*,*,#27969,.T.);
#41885=ORIENTED_EDGE('',*,*,#27966,.T.);
#41886=ORIENTED_EDGE('',*,*,#27967,.F.);
#41887=ORIENTED_EDGE('',*,*,#27970,.F.);
#41888=ORIENTED_EDGE('',*,*,#27963,.T.);
#41889=ORIENTED_EDGE('',*,*,#27960,.T.);
#41890=ORIENTED_EDGE('',*,*,#27961,.F.);
#41891=ORIENTED_EDGE('',*,*,#27964,.F.);
#41892=ORIENTED_EDGE('',*,*,#27957,.T.);
#41893=ORIENTED_EDGE('',*,*,#27954,.T.);
#41894=ORIENTED_EDGE('',*,*,#27955,.F.);
#41895=ORIENTED_EDGE('',*,*,#27958,.F.);
#41896=ORIENTED_EDGE('',*,*,#27951,.T.);
#41897=ORIENTED_EDGE('',*,*,#27948,.T.);
#41898=ORIENTED_EDGE('',*,*,#27949,.F.);
#41899=ORIENTED_EDGE('',*,*,#27952,.F.);
#41900=ORIENTED_EDGE('',*,*,#27945,.T.);
#41901=ORIENTED_EDGE('',*,*,#27942,.T.);
#41902=ORIENTED_EDGE('',*,*,#27943,.F.);
#41903=ORIENTED_EDGE('',*,*,#27946,.F.);
#41904=ORIENTED_EDGE('',*,*,#27939,.T.);
#41905=ORIENTED_EDGE('',*,*,#27936,.T.);
#41906=ORIENTED_EDGE('',*,*,#27937,.F.);
#41907=ORIENTED_EDGE('',*,*,#27940,.F.);
#41908=ORIENTED_EDGE('',*,*,#27933,.T.);
#41909=ORIENTED_EDGE('',*,*,#27930,.T.);
#41910=ORIENTED_EDGE('',*,*,#27931,.F.);
#41911=ORIENTED_EDGE('',*,*,#27934,.F.);
#41912=ORIENTED_EDGE('',*,*,#27927,.T.);
#41913=ORIENTED_EDGE('',*,*,#27924,.T.);
#41914=ORIENTED_EDGE('',*,*,#27925,.F.);
#41915=ORIENTED_EDGE('',*,*,#27928,.F.);
#41916=ORIENTED_EDGE('',*,*,#27921,.T.);
#41917=ORIENTED_EDGE('',*,*,#27918,.T.);
#41918=ORIENTED_EDGE('',*,*,#27919,.F.);
#41919=ORIENTED_EDGE('',*,*,#27922,.F.);
#41920=ORIENTED_EDGE('',*,*,#27915,.T.);
#41921=ORIENTED_EDGE('',*,*,#27912,.T.);
#41922=ORIENTED_EDGE('',*,*,#27913,.F.);
#41923=ORIENTED_EDGE('',*,*,#27916,.F.);
#41924=ORIENTED_EDGE('',*,*,#27909,.T.);
#41925=ORIENTED_EDGE('',*,*,#27906,.T.);
#41926=ORIENTED_EDGE('',*,*,#27907,.F.);
#41927=ORIENTED_EDGE('',*,*,#27910,.F.);
#41928=ORIENTED_EDGE('',*,*,#27903,.T.);
#41929=ORIENTED_EDGE('',*,*,#27900,.T.);
#41930=ORIENTED_EDGE('',*,*,#27901,.F.);
#41931=ORIENTED_EDGE('',*,*,#27904,.F.);
#41932=ORIENTED_EDGE('',*,*,#27897,.T.);
#41933=ORIENTED_EDGE('',*,*,#27894,.T.);
#41934=ORIENTED_EDGE('',*,*,#27895,.F.);
#41935=ORIENTED_EDGE('',*,*,#27898,.F.);
#41936=ORIENTED_EDGE('',*,*,#27891,.T.);
#41937=ORIENTED_EDGE('',*,*,#27888,.T.);
#41938=ORIENTED_EDGE('',*,*,#27889,.F.);
#41939=ORIENTED_EDGE('',*,*,#27892,.F.);
#41940=ORIENTED_EDGE('',*,*,#27885,.T.);
#41941=ORIENTED_EDGE('',*,*,#27882,.T.);
#41942=ORIENTED_EDGE('',*,*,#27883,.F.);
#41943=ORIENTED_EDGE('',*,*,#27886,.F.);
#41944=TOROIDAL_SURFACE('',#45551,30.,11.5);
#41945=TOROIDAL_SURFACE('',#45556,29.9999999999957,11.5);
#41946=TOROIDAL_SURFACE('',#47410,62.7000000000001,0.3);
#41947=TOROIDAL_SURFACE('',#47418,10.9885950377664,1.);
#41948=TOROIDAL_SURFACE('',#47421,9.19091713639506,0.2);
#41949=TOROIDAL_SURFACE('',#47425,63.,2.);
#41950=TOROIDAL_SURFACE('',#47428,22.4734498738832,0.5);
#41951=TOROIDAL_SURFACE('',#47437,63.2999999999999,0.3);
#41952=TOROIDAL_SURFACE('',#47442,8.79091713639511,0.2);
#41953=TOROIDAL_SURFACE('',#47453,7.3031389659941,1.);
#41954=TOROIDAL_SURFACE('',#47473,5.888925403621,1.);
#41955=TOROIDAL_SURFACE('',#47480,5.888925403621,1.);
#41956=TOROIDAL_SURFACE('',#47481,7.3031389659941,1.);
#41957=TOROIDAL_SURFACE('',#47487,7.3031389659941,1.);
#41958=TOROIDAL_SURFACE('',#47503,22.4734498738832,0.5);
#41959=TOROIDAL_SURFACE('',#47520,63.,2.);
#41960=TOROIDAL_SURFACE('',#48138,10.4786337076502,0.5);
#41961=TOROIDAL_SURFACE('',#48143,8.99369514600215,0.5);
#41962=TOROIDAL_SURFACE('',#48150,7.98801213467717,1.);
#41963=TOROIDAL_SURFACE('',#48190,27.5226030790361,1.);
#41964=TOROIDAL_SURFACE('',#48211,4.46802221877416,0.5);
#41965=TOROIDAL_SURFACE('',#48215,15.5,0.5);
#41966=TOROIDAL_SURFACE('',#48217,3.46802221877416,0.5);
#41967=TOROIDAL_SURFACE('',#48221,15.5,0.5);
#41968=TOROIDAL_SURFACE('',#48233,4.46802221877416,0.5);
#41969=TOROIDAL_SURFACE('',#48237,15.5,0.5);
#41970=TOROIDAL_SURFACE('',#48239,3.46802221877416,0.5);
#41971=TOROIDAL_SURFACE('',#48243,15.5,0.5);
#41972=TOROIDAL_SURFACE('',#48255,4.46802221877416,0.5);
#41973=TOROIDAL_SURFACE('',#48259,15.5,0.5);
#41974=TOROIDAL_SURFACE('',#48261,3.46802221877416,0.5);
#41975=TOROIDAL_SURFACE('',#48265,15.5,0.5);
#41976=TOROIDAL_SURFACE('',#48273,25.3226030790361,0.7);
#41977=TOROIDAL_SURFACE('',#48290,29.5,0.5);
#41978=TOROIDAL_SURFACE('',#48293,29.5,0.5);
#41979=TOROIDAL_SURFACE('',#48322,29.5,0.5);
#41980=TOROIDAL_SURFACE('',#48324,29.5,0.5);
#41981=TOROIDAL_SURFACE('',#48327,4.05563473233925,0.7);
#41982=TOROIDAL_SURFACE('',#48336,4.05563473233925,0.7);
#41983=TOROIDAL_SURFACE('',#48346,26.7226030790361,0.7);
#41984=TOROIDAL_SURFACE('',#48351,4.05563473233925,0.7);
#41985=TOROIDAL_SURFACE('',#48358,5.45563473233925,0.7);
#41986=TOROIDAL_SURFACE('',#48374,3.46802221877416,0.5);
#41987=TOROIDAL_SURFACE('',#48379,16.5,0.5);
#41988=TOROIDAL_SURFACE('',#48394,3.46802221877416,0.5);
#41989=TOROIDAL_SURFACE('',#48408,3.46802221877416,0.5);
#41990=TOROIDAL_SURFACE('',#48413,16.5,0.5);
#41991=TOROIDAL_SURFACE('',#48428,3.46802221877416,0.5);
#41992=TOROIDAL_SURFACE('',#48442,3.46802221877416,0.5);
#41993=TOROIDAL_SURFACE('',#48447,16.5,0.5);
#41994=TOROIDAL_SURFACE('',#48462,3.46802221877416,0.5);
#41995=TOROIDAL_SURFACE('',#48480,29.5,0.5);
#41996=TOROIDAL_SURFACE('',#48495,29.5,0.5);
#41997=TOROIDAL_SURFACE('',#48503,2.,1.);
#41998=TOROIDAL_SURFACE('',#48507,27.5226030790361,1.);
#41999=TOROIDAL_SURFACE('',#48512,2.,1.);
#42000=TOROIDAL_SURFACE('',#48520,29.5226030790361,1.);
#42001=TOROIDAL_SURFACE('',#48528,29.5226030790361,1.);
#42002=TOROIDAL_SURFACE('',#48648,7.,1.);
#42003=TOROIDAL_SURFACE('',#48650,7.,1.);
#42004=TOROIDAL_SURFACE('',#48656,7.,1.);
#42005=TOROIDAL_SURFACE('',#48658,7.,1.);
#42006=TOROIDAL_SURFACE('',#48664,7.,1.);
#42007=TOROIDAL_SURFACE('',#48666,7.,1.);
#42008=TOROIDAL_SURFACE('',#48672,7.,1.);
#42009=TOROIDAL_SURFACE('',#48674,7.,1.);
#42010=TOROIDAL_SURFACE('',#48680,7.00000000000001,1.);
#42011=TOROIDAL_SURFACE('',#48684,7.,1.);
#42012=TOROIDAL_SURFACE('',#48691,2.58578643762686,1.);
#42013=TOROIDAL_SURFACE('',#48695,2.58578643762686,1.);
#42014=TOROIDAL_SURFACE('',#48702,2.58578643762695,1.);
#42015=TOROIDAL_SURFACE('',#48706,2.58578643762694,1.);
#42016=TOROIDAL_SURFACE('',#48713,7.00000000000001,1.);
#42017=TOROIDAL_SURFACE('',#48717,7.,1.);
#42018=TOROIDAL_SURFACE('',#48721,3.,2.);
#42019=TOROIDAL_SURFACE('',#48728,3.,2.);
#42020=TOROIDAL_SURFACE('',#48730,3.,2.);
#42021=TOROIDAL_SURFACE('',#48736,3.,2.);
#42022=TOROIDAL_SURFACE('',#48738,3.,2.);
#42023=TOROIDAL_SURFACE('',#48744,3.,2.);
#42024=TOROIDAL_SURFACE('',#48746,3.,2.);
#42025=TOROIDAL_SURFACE('',#48752,3.,2.);
#42026=TOROIDAL_SURFACE('',#48754,18.9499999999999,0.5);
#42027=TOROIDAL_SURFACE('',#48759,12.7099993856753,0.5);
#42028=TOROIDAL_SURFACE('',#48764,12.7099993856753,0.5);
#42029=TOROIDAL_SURFACE('',#48769,18.4499999999999,1.);
#42030=TOROIDAL_SURFACE('',#48777,18.95,0.5);
#42031=TOROIDAL_SURFACE('',#48781,18.95,0.5);
#42032=TOROIDAL_SURFACE('',#48802,18.95,0.5);
#42033=TOROIDAL_SURFACE('',#48805,18.45,1.);
#42034=TOROIDAL_SURFACE('',#48849,17.122381608453,1.);
#42035=TOROIDAL_SURFACE('',#48853,20.4499999999999,1.);
#42036=TOROIDAL_SURFACE('',#48855,17.122381608453,1.);
#42037=TOROIDAL_SURFACE('',#48858,17.122381608453,1.);
#42038=TOROIDAL_SURFACE('',#48863,17.122381608453,1.);
#42039=TOROIDAL_SURFACE('',#48905,8.81821463020445,0.5);
#42040=TOROIDAL_SURFACE('',#50886,126.91606204049,0.5);
#42041=TOROIDAL_SURFACE('',#50892,11.8670707361131,0.5);
#42042=TOROIDAL_SURFACE('',#50897,11.8670707361131,0.5);
#42043=TOROIDAL_SURFACE('',#50904,16.1492953136408,0.5);
#42044=TOROIDAL_SURFACE('',#50908,129.,1.);
#42045=TOROIDAL_SURFACE('',#50912,128.41606204049,1.);
#42046=TOROIDAL_SURFACE('',#50917,129.,1.);
#42047=ADVANCED_FACE('',(#9467),#41944,.T.);
#42048=ADVANCED_FACE('',(#9468),#41945,.T.);
#42049=ADVANCED_FACE('',(#9469),#7860,.T.);
#42050=ADVANCED_FACE('',(#9470),#7861,.T.);
#42051=ADVANCED_FACE('',(#9471),#7862,.T.);
#42052=ADVANCED_FACE('',(#9472),#2950,.F.);
#42053=ADVANCED_FACE('',(#9473),#2951,.F.);
#42054=ADVANCED_FACE('',(#9474),#2952,.F.);
#42055=ADVANCED_FACE('',(#9475),#2953,.T.);
#42056=ADVANCED_FACE('',(#9476),#7863,.F.);
#42057=ADVANCED_FACE('',(#9477),#2954,.T.);
#42058=ADVANCED_FACE('',(#9478),#2955,.T.);
#42059=ADVANCED_FACE('',(#9479),#7864,.T.);
#42060=ADVANCED_FACE('',(#9480),#2956,.T.);
#42061=ADVANCED_FACE('',(#9481),#2957,.T.);
#42062=ADVANCED_FACE('',(#9482),#2958,.T.);
#42063=ADVANCED_FACE('',(#9483),#7865,.F.);
#42064=ADVANCED_FACE('',(#9484),#7866,.F.);
#42065=ADVANCED_FACE('',(#9485),#7867,.T.);
#42066=ADVANCED_FACE('',(#9486),#7868,.F.);
#42067=ADVANCED_FACE('',(#9487),#7869,.T.);
#42068=ADVANCED_FACE('',(#9488),#7870,.F.);
#42069=ADVANCED_FACE('',(#9489),#7871,.T.);
#42070=ADVANCED_FACE('',(#9490),#7872,.F.);
#42071=ADVANCED_FACE('',(#9491),#7873,.T.);
#42072=ADVANCED_FACE('',(#9492),#7874,.F.);
#42073=ADVANCED_FACE('',(#9493),#7875,.T.);
#42074=ADVANCED_FACE('',(#9494),#7876,.F.);
#42075=ADVANCED_FACE('',(#9495),#7877,.T.);
#42076=ADVANCED_FACE('',(#9496),#7878,.T.);
#42077=ADVANCED_FACE('',(#9497),#7879,.F.);
#42078=ADVANCED_FACE('',(#9498),#7880,.T.);
#42079=ADVANCED_FACE('',(#9499),#7881,.F.);
#42080=ADVANCED_FACE('',(#9500),#7882,.T.);
#42081=ADVANCED_FACE('',(#9501),#7883,.F.);
#42082=ADVANCED_FACE('',(#9502),#7884,.T.);
#42083=ADVANCED_FACE('',(#9503),#7885,.F.);
#42084=ADVANCED_FACE('',(#9504),#7886,.T.);
#42085=ADVANCED_FACE('',(#9505),#7887,.F.);
#42086=ADVANCED_FACE('',(#9506),#7888,.T.);
#42087=ADVANCED_FACE('',(#9507),#7889,.F.);
#42088=ADVANCED_FACE('',(#9508),#7890,.T.);
#42089=ADVANCED_FACE('',(#9509),#7891,.F.);
#42090=ADVANCED_FACE('',(#9510),#7892,.T.);
#42091=ADVANCED_FACE('',(#9511),#7893,.F.);
#42092=ADVANCED_FACE('',(#9512),#7894,.T.);
#42093=ADVANCED_FACE('',(#9513),#7895,.F.);
#42094=ADVANCED_FACE('',(#9514),#7896,.T.);
#42095=ADVANCED_FACE('',(#9515),#7897,.F.);
#42096=ADVANCED_FACE('',(#9516),#7898,.T.);
#42097=ADVANCED_FACE('',(#9517),#7899,.F.);
#42098=ADVANCED_FACE('',(#9518),#7900,.T.);
#42099=ADVANCED_FACE('',(#9519),#7901,.F.);
#42100=ADVANCED_FACE('',(#9520),#7902,.T.);
#42101=ADVANCED_FACE('',(#9521),#7903,.F.);
#42102=ADVANCED_FACE('',(#9522),#7904,.T.);
#42103=ADVANCED_FACE('',(#9523),#7905,.F.);
#42104=ADVANCED_FACE('',(#9524),#7906,.T.);
#42105=ADVANCED_FACE('',(#9525),#7907,.F.);
#42106=ADVANCED_FACE('',(#9526),#7908,.T.);
#42107=ADVANCED_FACE('',(#9527),#7909,.F.);
#42108=ADVANCED_FACE('',(#9528),#7910,.T.);
#42109=ADVANCED_FACE('',(#9529),#7911,.F.);
#42110=ADVANCED_FACE('',(#9530),#7912,.T.);
#42111=ADVANCED_FACE('',(#9531),#7913,.F.);
#42112=ADVANCED_FACE('',(#9532),#7914,.T.);
#42113=ADVANCED_FACE('',(#9533),#7915,.F.);
#42114=ADVANCED_FACE('',(#9534),#7916,.T.);
#42115=ADVANCED_FACE('',(#9535),#7917,.F.);
#42116=ADVANCED_FACE('',(#9536),#7918,.T.);
#42117=ADVANCED_FACE('',(#9537),#7919,.F.);
#42118=ADVANCED_FACE('',(#9538),#7920,.T.);
#42119=ADVANCED_FACE('',(#9539),#7921,.F.);
#42120=ADVANCED_FACE('',(#9540),#7922,.T.);
#42121=ADVANCED_FACE('',(#9541),#7923,.F.);
#42122=ADVANCED_FACE('',(#9542),#7924,.T.);
#42123=ADVANCED_FACE('',(#9543),#7925,.F.);
#42124=ADVANCED_FACE('',(#9544),#7926,.T.);
#42125=ADVANCED_FACE('',(#9545),#7927,.F.);
#42126=ADVANCED_FACE('',(#9546),#7928,.T.);
#42127=ADVANCED_FACE('',(#9547),#7929,.F.);
#42128=ADVANCED_FACE('',(#9548),#7930,.T.);
#42129=ADVANCED_FACE('',(#9549),#7931,.F.);
#42130=ADVANCED_FACE('',(#9550),#7932,.T.);
#42131=ADVANCED_FACE('',(#9551),#7933,.F.);
#42132=ADVANCED_FACE('',(#9552),#7934,.T.);
#42133=ADVANCED_FACE('',(#9553),#7935,.F.);
#42134=ADVANCED_FACE('',(#9554),#7936,.T.);
#42135=ADVANCED_FACE('',(#9555),#7937,.F.);
#42136=ADVANCED_FACE('',(#9556),#7938,.T.);
#42137=ADVANCED_FACE('',(#9557),#7939,.F.);
#42138=ADVANCED_FACE('',(#9558),#7940,.T.);
#42139=ADVANCED_FACE('',(#9559),#7941,.F.);
#42140=ADVANCED_FACE('',(#9560),#7942,.T.);
#42141=ADVANCED_FACE('',(#9561),#7943,.F.);
#42142=ADVANCED_FACE('',(#9562),#7944,.T.);
#42143=ADVANCED_FACE('',(#9563),#7945,.F.);
#42144=ADVANCED_FACE('',(#9564),#7946,.T.);
#42145=ADVANCED_FACE('',(#9565),#7947,.F.);
#42146=ADVANCED_FACE('',(#9566),#7948,.T.);
#42147=ADVANCED_FACE('',(#9567),#7949,.F.);
#42148=ADVANCED_FACE('',(#9568),#7950,.T.);
#42149=ADVANCED_FACE('',(#9569),#7951,.F.);
#42150=ADVANCED_FACE('',(#9570),#7952,.T.);
#42151=ADVANCED_FACE('',(#9571),#7953,.F.);
#42152=ADVANCED_FACE('',(#9572),#7954,.T.);
#42153=ADVANCED_FACE('',(#9573),#7955,.F.);
#42154=ADVANCED_FACE('',(#9574),#7956,.T.);
#42155=ADVANCED_FACE('',(#9575),#7957,.F.);
#42156=ADVANCED_FACE('',(#9576),#7958,.T.);
#42157=ADVANCED_FACE('',(#9577),#7959,.F.);
#42158=ADVANCED_FACE('',(#9578),#7960,.T.);
#42159=ADVANCED_FACE('',(#9579),#7961,.F.);
#42160=ADVANCED_FACE('',(#9580),#7962,.T.);
#42161=ADVANCED_FACE('',(#9581),#7963,.F.);
#42162=ADVANCED_FACE('',(#9582),#7964,.T.);
#42163=ADVANCED_FACE('',(#9583),#7965,.F.);
#42164=ADVANCED_FACE('',(#9584),#7966,.T.);
#42165=ADVANCED_FACE('',(#9585),#7967,.F.);
#42166=ADVANCED_FACE('',(#9586),#7968,.T.);
#42167=ADVANCED_FACE('',(#9587),#7969,.F.);
#42168=ADVANCED_FACE('',(#9588),#7970,.T.);
#42169=ADVANCED_FACE('',(#9589),#7971,.F.);
#42170=ADVANCED_FACE('',(#9590),#7972,.T.);
#42171=ADVANCED_FACE('',(#9591),#7973,.F.);
#42172=ADVANCED_FACE('',(#9592),#7974,.T.);
#42173=ADVANCED_FACE('',(#9593),#7975,.F.);
#42174=ADVANCED_FACE('',(#9594),#7976,.T.);
#42175=ADVANCED_FACE('',(#9595),#7977,.F.);
#42176=ADVANCED_FACE('',(#9596),#7978,.T.);
#42177=ADVANCED_FACE('',(#9597),#7979,.F.);
#42178=ADVANCED_FACE('',(#9598),#7980,.T.);
#42179=ADVANCED_FACE('',(#9599),#7981,.F.);
#42180=ADVANCED_FACE('',(#9600),#7982,.T.);
#42181=ADVANCED_FACE('',(#9601),#7983,.F.);
#42182=ADVANCED_FACE('',(#9602),#7984,.T.);
#42183=ADVANCED_FACE('',(#9603),#7985,.F.);
#42184=ADVANCED_FACE('',(#9604),#7986,.T.);
#42185=ADVANCED_FACE('',(#9605),#7987,.F.);
#42186=ADVANCED_FACE('',(#9606),#7988,.T.);
#42187=ADVANCED_FACE('',(#9607),#7989,.F.);
#42188=ADVANCED_FACE('',(#9608),#7990,.T.);
#42189=ADVANCED_FACE('',(#9609),#7991,.F.);
#42190=ADVANCED_FACE('',(#9610),#7992,.T.);
#42191=ADVANCED_FACE('',(#9611),#7993,.F.);
#42192=ADVANCED_FACE('',(#9612),#7994,.T.);
#42193=ADVANCED_FACE('',(#9613),#7995,.F.);
#42194=ADVANCED_FACE('',(#9614),#7996,.T.);
#42195=ADVANCED_FACE('',(#9615),#7997,.F.);
#42196=ADVANCED_FACE('',(#9616),#7998,.T.);
#42197=ADVANCED_FACE('',(#9617),#7999,.F.);
#42198=ADVANCED_FACE('',(#9618),#8000,.T.);
#42199=ADVANCED_FACE('',(#9619),#8001,.F.);
#42200=ADVANCED_FACE('',(#9620),#8002,.T.);
#42201=ADVANCED_FACE('',(#9621),#8003,.F.);
#42202=ADVANCED_FACE('',(#9622),#8004,.T.);
#42203=ADVANCED_FACE('',(#9623),#8005,.F.);
#42204=ADVANCED_FACE('',(#9624),#8006,.T.);
#42205=ADVANCED_FACE('',(#9625),#8007,.F.);
#42206=ADVANCED_FACE('',(#9626),#8008,.T.);
#42207=ADVANCED_FACE('',(#9627),#8009,.F.);
#42208=ADVANCED_FACE('',(#9628),#8010,.T.);
#42209=ADVANCED_FACE('',(#9629),#8011,.F.);
#42210=ADVANCED_FACE('',(#9630),#8012,.T.);
#42211=ADVANCED_FACE('',(#9631),#8013,.F.);
#42212=ADVANCED_FACE('',(#9632),#8014,.T.);
#42213=ADVANCED_FACE('',(#9633),#8015,.F.);
#42214=ADVANCED_FACE('',(#9634),#8016,.T.);
#42215=ADVANCED_FACE('',(#9635),#8017,.F.);
#42216=ADVANCED_FACE('',(#9636),#8018,.T.);
#42217=ADVANCED_FACE('',(#9637),#8019,.F.);
#42218=ADVANCED_FACE('',(#9638),#8020,.T.);
#42219=ADVANCED_FACE('',(#9639),#8021,.F.);
#42220=ADVANCED_FACE('',(#9640),#8022,.T.);
#42221=ADVANCED_FACE('',(#9641),#8023,.F.);
#42222=ADVANCED_FACE('',(#9642),#8024,.T.);
#42223=ADVANCED_FACE('',(#9643),#8025,.F.);
#42224=ADVANCED_FACE('',(#9644),#8026,.T.);
#42225=ADVANCED_FACE('',(#9645),#8027,.F.);
#42226=ADVANCED_FACE('',(#9646),#8028,.T.);
#42227=ADVANCED_FACE('',(#9647),#8029,.F.);
#42228=ADVANCED_FACE('',(#9648),#8030,.T.);
#42229=ADVANCED_FACE('',(#9649),#8031,.F.);
#42230=ADVANCED_FACE('',(#9650),#8032,.T.);
#42231=ADVANCED_FACE('',(#9651),#8033,.F.);
#42232=ADVANCED_FACE('',(#9652),#8034,.T.);
#42233=ADVANCED_FACE('',(#9653),#8035,.F.);
#42234=ADVANCED_FACE('',(#9654),#8036,.T.);
#42235=ADVANCED_FACE('',(#9655),#8037,.F.);
#42236=ADVANCED_FACE('',(#9656),#8038,.T.);
#42237=ADVANCED_FACE('',(#9657),#8039,.F.);
#42238=ADVANCED_FACE('',(#9658),#8040,.T.);
#42239=ADVANCED_FACE('',(#9659),#8041,.F.);
#42240=ADVANCED_FACE('',(#9660),#8042,.T.);
#42241=ADVANCED_FACE('',(#9661),#8043,.F.);
#42242=ADVANCED_FACE('',(#9662),#8044,.T.);
#42243=ADVANCED_FACE('',(#9663),#8045,.F.);
#42244=ADVANCED_FACE('',(#9664),#8046,.T.);
#42245=ADVANCED_FACE('',(#9665),#8047,.F.);
#42246=ADVANCED_FACE('',(#9666),#8048,.T.);
#42247=ADVANCED_FACE('',(#9667),#8049,.F.);
#42248=ADVANCED_FACE('',(#9668),#8050,.T.);
#42249=ADVANCED_FACE('',(#9669),#8051,.F.);
#42250=ADVANCED_FACE('',(#9670),#8052,.T.);
#42251=ADVANCED_FACE('',(#9671),#8053,.F.);
#42252=ADVANCED_FACE('',(#9672),#8054,.T.);
#42253=ADVANCED_FACE('',(#9673),#8055,.F.);
#42254=ADVANCED_FACE('',(#9674),#8056,.T.);
#42255=ADVANCED_FACE('',(#9675),#8057,.F.);
#42256=ADVANCED_FACE('',(#9676),#8058,.T.);
#42257=ADVANCED_FACE('',(#9677),#8059,.F.);
#42258=ADVANCED_FACE('',(#9678),#8060,.T.);
#42259=ADVANCED_FACE('',(#9679),#8061,.F.);
#42260=ADVANCED_FACE('',(#9680),#8062,.T.);
#42261=ADVANCED_FACE('',(#9681),#8063,.F.);
#42262=ADVANCED_FACE('',(#9682),#8064,.T.);
#42263=ADVANCED_FACE('',(#9683),#8065,.F.);
#42264=ADVANCED_FACE('',(#9684),#8066,.T.);
#42265=ADVANCED_FACE('',(#9685),#8067,.F.);
#42266=ADVANCED_FACE('',(#9686),#8068,.T.);
#42267=ADVANCED_FACE('',(#9687),#8069,.F.);
#42268=ADVANCED_FACE('',(#9688),#8070,.T.);
#42269=ADVANCED_FACE('',(#9689),#8071,.F.);
#42270=ADVANCED_FACE('',(#9690),#8072,.T.);
#42271=ADVANCED_FACE('',(#9691),#8073,.F.);
#42272=ADVANCED_FACE('',(#9692),#8074,.T.);
#42273=ADVANCED_FACE('',(#9693),#8075,.F.);
#42274=ADVANCED_FACE('',(#9694),#8076,.T.);
#42275=ADVANCED_FACE('',(#9695),#8077,.F.);
#42276=ADVANCED_FACE('',(#9696),#8078,.T.);
#42277=ADVANCED_FACE('',(#9697),#8079,.F.);
#42278=ADVANCED_FACE('',(#9698),#8080,.T.);
#42279=ADVANCED_FACE('',(#9699),#8081,.F.);
#42280=ADVANCED_FACE('',(#9700),#8082,.T.);
#42281=ADVANCED_FACE('',(#9701),#8083,.F.);
#42282=ADVANCED_FACE('',(#9702),#8084,.T.);
#42283=ADVANCED_FACE('',(#9703),#8085,.F.);
#42284=ADVANCED_FACE('',(#9704),#8086,.T.);
#42285=ADVANCED_FACE('',(#9705),#8087,.F.);
#42286=ADVANCED_FACE('',(#9706),#8088,.T.);
#42287=ADVANCED_FACE('',(#9707),#8089,.F.);
#42288=ADVANCED_FACE('',(#9708),#8090,.T.);
#42289=ADVANCED_FACE('',(#9709),#8091,.F.);
#42290=ADVANCED_FACE('',(#9710),#8092,.T.);
#42291=ADVANCED_FACE('',(#9711),#8093,.F.);
#42292=ADVANCED_FACE('',(#9712),#8094,.T.);
#42293=ADVANCED_FACE('',(#9713),#8095,.F.);
#42294=ADVANCED_FACE('',(#9714),#8096,.T.);
#42295=ADVANCED_FACE('',(#9715),#8097,.F.);
#42296=ADVANCED_FACE('',(#9716),#8098,.T.);
#42297=ADVANCED_FACE('',(#9717),#8099,.F.);
#42298=ADVANCED_FACE('',(#9718),#8100,.T.);
#42299=ADVANCED_FACE('',(#9719),#8101,.F.);
#42300=ADVANCED_FACE('',(#9720),#8102,.T.);
#42301=ADVANCED_FACE('',(#9721),#8103,.F.);
#42302=ADVANCED_FACE('',(#9722),#8104,.T.);
#42303=ADVANCED_FACE('',(#9723),#8105,.F.);
#42304=ADVANCED_FACE('',(#9724),#8106,.T.);
#42305=ADVANCED_FACE('',(#9725),#8107,.F.);
#42306=ADVANCED_FACE('',(#9726),#8108,.T.);
#42307=ADVANCED_FACE('',(#9727),#8109,.F.);
#42308=ADVANCED_FACE('',(#9728),#8110,.T.);
#42309=ADVANCED_FACE('',(#9729),#8111,.F.);
#42310=ADVANCED_FACE('',(#9730),#8112,.T.);
#42311=ADVANCED_FACE('',(#9731),#8113,.F.);
#42312=ADVANCED_FACE('',(#9732),#8114,.T.);
#42313=ADVANCED_FACE('',(#9733),#8115,.F.);
#42314=ADVANCED_FACE('',(#9734),#8116,.T.);
#42315=ADVANCED_FACE('',(#9735),#8117,.F.);
#42316=ADVANCED_FACE('',(#9736),#8118,.T.);
#42317=ADVANCED_FACE('',(#9737),#8119,.F.);
#42318=ADVANCED_FACE('',(#9738),#8120,.T.);
#42319=ADVANCED_FACE('',(#9739),#8121,.F.);
#42320=ADVANCED_FACE('',(#9740),#8122,.T.);
#42321=ADVANCED_FACE('',(#9741),#8123,.F.);
#42322=ADVANCED_FACE('',(#9742),#8124,.T.);
#42323=ADVANCED_FACE('',(#9743),#8125,.F.);
#42324=ADVANCED_FACE('',(#9744),#8126,.T.);
#42325=ADVANCED_FACE('',(#9745),#8127,.F.);
#42326=ADVANCED_FACE('',(#9746),#8128,.T.);
#42327=ADVANCED_FACE('',(#9747),#8129,.F.);
#42328=ADVANCED_FACE('',(#9748),#8130,.T.);
#42329=ADVANCED_FACE('',(#9749),#8131,.F.);
#42330=ADVANCED_FACE('',(#9750),#8132,.T.);
#42331=ADVANCED_FACE('',(#9751),#8133,.F.);
#42332=ADVANCED_FACE('',(#9752),#8134,.T.);
#42333=ADVANCED_FACE('',(#9753),#8135,.F.);
#42334=ADVANCED_FACE('',(#9754),#8136,.T.);
#42335=ADVANCED_FACE('',(#9755),#8137,.F.);
#42336=ADVANCED_FACE('',(#9756),#8138,.T.);
#42337=ADVANCED_FACE('',(#9757),#8139,.F.);
#42338=ADVANCED_FACE('',(#9758),#8140,.T.);
#42339=ADVANCED_FACE('',(#9759),#8141,.F.);
#42340=ADVANCED_FACE('',(#9760),#8142,.T.);
#42341=ADVANCED_FACE('',(#9761),#8143,.F.);
#42342=ADVANCED_FACE('',(#9762),#8144,.T.);
#42343=ADVANCED_FACE('',(#9763),#8145,.F.);
#42344=ADVANCED_FACE('',(#9764),#8146,.T.);
#42345=ADVANCED_FACE('',(#9765),#8147,.F.);
#42346=ADVANCED_FACE('',(#9766),#8148,.T.);
#42347=ADVANCED_FACE('',(#9767),#8149,.F.);
#42348=ADVANCED_FACE('',(#9768),#8150,.T.);
#42349=ADVANCED_FACE('',(#9769),#8151,.F.);
#42350=ADVANCED_FACE('',(#9770),#8152,.T.);
#42351=ADVANCED_FACE('',(#9771),#8153,.F.);
#42352=ADVANCED_FACE('',(#9772),#8154,.T.);
#42353=ADVANCED_FACE('',(#9773),#8155,.F.);
#42354=ADVANCED_FACE('',(#9774),#8156,.T.);
#42355=ADVANCED_FACE('',(#9775),#8157,.F.);
#42356=ADVANCED_FACE('',(#9776),#8158,.T.);
#42357=ADVANCED_FACE('',(#9777),#8159,.F.);
#42358=ADVANCED_FACE('',(#9778),#8160,.T.);
#42359=ADVANCED_FACE('',(#9779),#8161,.F.);
#42360=ADVANCED_FACE('',(#9780),#8162,.T.);
#42361=ADVANCED_FACE('',(#9781),#8163,.F.);
#42362=ADVANCED_FACE('',(#9782),#8164,.T.);
#42363=ADVANCED_FACE('',(#9783),#8165,.F.);
#42364=ADVANCED_FACE('',(#9784),#8166,.T.);
#42365=ADVANCED_FACE('',(#9785),#8167,.F.);
#42366=ADVANCED_FACE('',(#9786),#8168,.T.);
#42367=ADVANCED_FACE('',(#9787),#8169,.F.);
#42368=ADVANCED_FACE('',(#9788),#8170,.T.);
#42369=ADVANCED_FACE('',(#9789),#8171,.F.);
#42370=ADVANCED_FACE('',(#9790),#8172,.T.);
#42371=ADVANCED_FACE('',(#9791),#8173,.F.);
#42372=ADVANCED_FACE('',(#9792),#8174,.T.);
#42373=ADVANCED_FACE('',(#9793),#8175,.F.);
#42374=ADVANCED_FACE('',(#9794),#8176,.T.);
#42375=ADVANCED_FACE('',(#9795),#8177,.F.);
#42376=ADVANCED_FACE('',(#9796),#8178,.T.);
#42377=ADVANCED_FACE('',(#9797),#8179,.F.);
#42378=ADVANCED_FACE('',(#9798),#8180,.T.);
#42379=ADVANCED_FACE('',(#9799),#8181,.F.);
#42380=ADVANCED_FACE('',(#9800),#8182,.T.);
#42381=ADVANCED_FACE('',(#9801),#8183,.F.);
#42382=ADVANCED_FACE('',(#9802),#8184,.T.);
#42383=ADVANCED_FACE('',(#9803),#8185,.F.);
#42384=ADVANCED_FACE('',(#9804),#8186,.T.);
#42385=ADVANCED_FACE('',(#9805),#8187,.F.);
#42386=ADVANCED_FACE('',(#9806),#8188,.T.);
#42387=ADVANCED_FACE('',(#9807),#8189,.F.);
#42388=ADVANCED_FACE('',(#9808),#8190,.T.);
#42389=ADVANCED_FACE('',(#9809),#8191,.F.);
#42390=ADVANCED_FACE('',(#9810),#8192,.T.);
#42391=ADVANCED_FACE('',(#9811),#8193,.F.);
#42392=ADVANCED_FACE('',(#9812),#8194,.T.);
#42393=ADVANCED_FACE('',(#9813),#8195,.F.);
#42394=ADVANCED_FACE('',(#9814),#8196,.T.);
#42395=ADVANCED_FACE('',(#9815),#8197,.F.);
#42396=ADVANCED_FACE('',(#9816),#8198,.T.);
#42397=ADVANCED_FACE('',(#9817),#8199,.F.);
#42398=ADVANCED_FACE('',(#9818),#8200,.T.);
#42399=ADVANCED_FACE('',(#9819),#8201,.F.);
#42400=ADVANCED_FACE('',(#9820),#8202,.T.);
#42401=ADVANCED_FACE('',(#9821),#8203,.F.);
#42402=ADVANCED_FACE('',(#9822),#8204,.T.);
#42403=ADVANCED_FACE('',(#9823),#8205,.F.);
#42404=ADVANCED_FACE('',(#9824),#8206,.T.);
#42405=ADVANCED_FACE('',(#9825),#8207,.F.);
#42406=ADVANCED_FACE('',(#9826),#8208,.T.);
#42407=ADVANCED_FACE('',(#9827),#8209,.F.);
#42408=ADVANCED_FACE('',(#9828),#8210,.T.);
#42409=ADVANCED_FACE('',(#9829),#8211,.F.);
#42410=ADVANCED_FACE('',(#9830),#8212,.T.);
#42411=ADVANCED_FACE('',(#9831),#8213,.F.);
#42412=ADVANCED_FACE('',(#9832),#8214,.T.);
#42413=ADVANCED_FACE('',(#9833),#8215,.F.);
#42414=ADVANCED_FACE('',(#9834),#8216,.T.);
#42415=ADVANCED_FACE('',(#9835),#8217,.F.);
#42416=ADVANCED_FACE('',(#9836),#8218,.T.);
#42417=ADVANCED_FACE('',(#9837),#8219,.F.);
#42418=ADVANCED_FACE('',(#9838),#8220,.T.);
#42419=ADVANCED_FACE('',(#9839),#8221,.F.);
#42420=ADVANCED_FACE('',(#9840),#8222,.T.);
#42421=ADVANCED_FACE('',(#9841),#8223,.F.);
#42422=ADVANCED_FACE('',(#9842),#8224,.T.);
#42423=ADVANCED_FACE('',(#9843),#8225,.F.);
#42424=ADVANCED_FACE('',(#9844),#8226,.T.);
#42425=ADVANCED_FACE('',(#9845),#8227,.F.);
#42426=ADVANCED_FACE('',(#9846),#8228,.T.);
#42427=ADVANCED_FACE('',(#9847),#8229,.F.);
#42428=ADVANCED_FACE('',(#9848),#8230,.T.);
#42429=ADVANCED_FACE('',(#9849),#8231,.F.);
#42430=ADVANCED_FACE('',(#9850),#8232,.T.);
#42431=ADVANCED_FACE('',(#9851),#8233,.F.);
#42432=ADVANCED_FACE('',(#9852),#8234,.T.);
#42433=ADVANCED_FACE('',(#9853),#8235,.F.);
#42434=ADVANCED_FACE('',(#9854),#8236,.T.);
#42435=ADVANCED_FACE('',(#9855),#8237,.F.);
#42436=ADVANCED_FACE('',(#9856),#8238,.T.);
#42437=ADVANCED_FACE('',(#9857),#8239,.F.);
#42438=ADVANCED_FACE('',(#9858),#8240,.T.);
#42439=ADVANCED_FACE('',(#9859),#8241,.F.);
#42440=ADVANCED_FACE('',(#9860),#8242,.T.);
#42441=ADVANCED_FACE('',(#9861),#8243,.F.);
#42442=ADVANCED_FACE('',(#9862),#8244,.T.);
#42443=ADVANCED_FACE('',(#9863),#8245,.F.);
#42444=ADVANCED_FACE('',(#9864),#8246,.T.);
#42445=ADVANCED_FACE('',(#9865),#8247,.F.);
#42446=ADVANCED_FACE('',(#9866),#8248,.T.);
#42447=ADVANCED_FACE('',(#9867),#8249,.F.);
#42448=ADVANCED_FACE('',(#9868),#8250,.T.);
#42449=ADVANCED_FACE('',(#9869),#8251,.F.);
#42450=ADVANCED_FACE('',(#9870),#8252,.T.);
#42451=ADVANCED_FACE('',(#9871),#8253,.F.);
#42452=ADVANCED_FACE('',(#9872),#8254,.T.);
#42453=ADVANCED_FACE('',(#9873),#8255,.F.);
#42454=ADVANCED_FACE('',(#9874),#8256,.T.);
#42455=ADVANCED_FACE('',(#9875),#8257,.F.);
#42456=ADVANCED_FACE('',(#9876),#8258,.T.);
#42457=ADVANCED_FACE('',(#9877),#8259,.F.);
#42458=ADVANCED_FACE('',(#9878),#8260,.T.);
#42459=ADVANCED_FACE('',(#9879),#8261,.F.);
#42460=ADVANCED_FACE('',(#9880),#8262,.T.);
#42461=ADVANCED_FACE('',(#9881),#8263,.F.);
#42462=ADVANCED_FACE('',(#9882),#8264,.T.);
#42463=ADVANCED_FACE('',(#9883),#8265,.F.);
#42464=ADVANCED_FACE('',(#9884),#8266,.T.);
#42465=ADVANCED_FACE('',(#9885),#8267,.F.);
#42466=ADVANCED_FACE('',(#9886),#8268,.T.);
#42467=ADVANCED_FACE('',(#9887),#8269,.F.);
#42468=ADVANCED_FACE('',(#9888),#8270,.T.);
#42469=ADVANCED_FACE('',(#9889),#8271,.F.);
#42470=ADVANCED_FACE('',(#9890),#8272,.T.);
#42471=ADVANCED_FACE('',(#9891),#8273,.F.);
#42472=ADVANCED_FACE('',(#9892),#8274,.T.);
#42473=ADVANCED_FACE('',(#9893),#8275,.F.);
#42474=ADVANCED_FACE('',(#9894),#8276,.T.);
#42475=ADVANCED_FACE('',(#9895),#8277,.F.);
#42476=ADVANCED_FACE('',(#9896),#8278,.T.);
#42477=ADVANCED_FACE('',(#9897),#8279,.F.);
#42478=ADVANCED_FACE('',(#9898),#8280,.T.);
#42479=ADVANCED_FACE('',(#9899),#8281,.F.);
#42480=ADVANCED_FACE('',(#9900),#8282,.T.);
#42481=ADVANCED_FACE('',(#9901),#8283,.F.);
#42482=ADVANCED_FACE('',(#9902),#8284,.T.);
#42483=ADVANCED_FACE('',(#9903),#8285,.F.);
#42484=ADVANCED_FACE('',(#9904),#8286,.T.);
#42485=ADVANCED_FACE('',(#9905),#8287,.F.);
#42486=ADVANCED_FACE('',(#9906),#8288,.T.);
#42487=ADVANCED_FACE('',(#9907),#8289,.F.);
#42488=ADVANCED_FACE('',(#9908),#8290,.T.);
#42489=ADVANCED_FACE('',(#9909),#8291,.F.);
#42490=ADVANCED_FACE('',(#9910),#8292,.T.);
#42491=ADVANCED_FACE('',(#9911),#8293,.F.);
#42492=ADVANCED_FACE('',(#9912),#8294,.T.);
#42493=ADVANCED_FACE('',(#9913),#8295,.F.);
#42494=ADVANCED_FACE('',(#9914),#8296,.T.);
#42495=ADVANCED_FACE('',(#9915),#8297,.F.);
#42496=ADVANCED_FACE('',(#9916),#8298,.T.);
#42497=ADVANCED_FACE('',(#9917),#8299,.F.);
#42498=ADVANCED_FACE('',(#9918),#8300,.T.);
#42499=ADVANCED_FACE('',(#9919),#8301,.F.);
#42500=ADVANCED_FACE('',(#9920),#8302,.T.);
#42501=ADVANCED_FACE('',(#9921),#8303,.F.);
#42502=ADVANCED_FACE('',(#9922),#8304,.T.);
#42503=ADVANCED_FACE('',(#9923),#8305,.F.);
#42504=ADVANCED_FACE('',(#9924),#8306,.T.);
#42505=ADVANCED_FACE('',(#9925),#8307,.F.);
#42506=ADVANCED_FACE('',(#9926),#8308,.T.);
#42507=ADVANCED_FACE('',(#9927),#8309,.F.);
#42508=ADVANCED_FACE('',(#9928),#8310,.T.);
#42509=ADVANCED_FACE('',(#9929),#8311,.F.);
#42510=ADVANCED_FACE('',(#9930),#8312,.T.);
#42511=ADVANCED_FACE('',(#9931),#8313,.F.);
#42512=ADVANCED_FACE('',(#9932),#8314,.T.);
#42513=ADVANCED_FACE('',(#9933),#8315,.F.);
#42514=ADVANCED_FACE('',(#9934),#8316,.T.);
#42515=ADVANCED_FACE('',(#9935),#8317,.F.);
#42516=ADVANCED_FACE('',(#9936),#8318,.T.);
#42517=ADVANCED_FACE('',(#9937),#8319,.F.);
#42518=ADVANCED_FACE('',(#9938),#8320,.T.);
#42519=ADVANCED_FACE('',(#9939),#8321,.F.);
#42520=ADVANCED_FACE('',(#9940),#8322,.T.);
#42521=ADVANCED_FACE('',(#9941),#8323,.F.);
#42522=ADVANCED_FACE('',(#9942),#8324,.T.);
#42523=ADVANCED_FACE('',(#9943),#8325,.F.);
#42524=ADVANCED_FACE('',(#9944),#8326,.T.);
#42525=ADVANCED_FACE('',(#9945),#8327,.F.);
#42526=ADVANCED_FACE('',(#9946),#8328,.T.);
#42527=ADVANCED_FACE('',(#9947),#8329,.F.);
#42528=ADVANCED_FACE('',(#9948),#8330,.T.);
#42529=ADVANCED_FACE('',(#9949),#8331,.F.);
#42530=ADVANCED_FACE('',(#9950),#8332,.T.);
#42531=ADVANCED_FACE('',(#9951),#8333,.F.);
#42532=ADVANCED_FACE('',(#9952),#8334,.T.);
#42533=ADVANCED_FACE('',(#9953),#8335,.F.);
#42534=ADVANCED_FACE('',(#9954),#8336,.T.);
#42535=ADVANCED_FACE('',(#9955),#8337,.F.);
#42536=ADVANCED_FACE('',(#9956),#8338,.T.);
#42537=ADVANCED_FACE('',(#9957),#8339,.F.);
#42538=ADVANCED_FACE('',(#9958),#8340,.T.);
#42539=ADVANCED_FACE('',(#9959),#8341,.F.);
#42540=ADVANCED_FACE('',(#9960),#8342,.T.);
#42541=ADVANCED_FACE('',(#9961),#8343,.F.);
#42542=ADVANCED_FACE('',(#9962),#8344,.T.);
#42543=ADVANCED_FACE('',(#9963),#8345,.F.);
#42544=ADVANCED_FACE('',(#9964),#8346,.T.);
#42545=ADVANCED_FACE('',(#9965),#8347,.F.);
#42546=ADVANCED_FACE('',(#9966),#8348,.T.);
#42547=ADVANCED_FACE('',(#9967),#8349,.F.);
#42548=ADVANCED_FACE('',(#9968),#8350,.T.);
#42549=ADVANCED_FACE('',(#9969),#8351,.F.);
#42550=ADVANCED_FACE('',(#9970),#8352,.T.);
#42551=ADVANCED_FACE('',(#9971),#8353,.F.);
#42552=ADVANCED_FACE('',(#9972),#8354,.T.);
#42553=ADVANCED_FACE('',(#9973),#8355,.F.);
#42554=ADVANCED_FACE('',(#9974),#8356,.T.);
#42555=ADVANCED_FACE('',(#9975),#8357,.F.);
#42556=ADVANCED_FACE('',(#9976),#8358,.T.);
#42557=ADVANCED_FACE('',(#9977),#8359,.F.);
#42558=ADVANCED_FACE('',(#9978),#8360,.T.);
#42559=ADVANCED_FACE('',(#9979),#8361,.F.);
#42560=ADVANCED_FACE('',(#9980),#8362,.T.);
#42561=ADVANCED_FACE('',(#9981),#8363,.F.);
#42562=ADVANCED_FACE('',(#9982),#8364,.T.);
#42563=ADVANCED_FACE('',(#9983),#8365,.F.);
#42564=ADVANCED_FACE('',(#9984),#8366,.T.);
#42565=ADVANCED_FACE('',(#9985),#8367,.F.);
#42566=ADVANCED_FACE('',(#9986),#8368,.T.);
#42567=ADVANCED_FACE('',(#9987),#8369,.F.);
#42568=ADVANCED_FACE('',(#9988),#8370,.T.);
#42569=ADVANCED_FACE('',(#9989),#8371,.F.);
#42570=ADVANCED_FACE('',(#9990),#8372,.T.);
#42571=ADVANCED_FACE('',(#9991),#8373,.F.);
#42572=ADVANCED_FACE('',(#9992),#8374,.T.);
#42573=ADVANCED_FACE('',(#9993),#8375,.F.);
#42574=ADVANCED_FACE('',(#9994),#8376,.T.);
#42575=ADVANCED_FACE('',(#9995),#8377,.F.);
#42576=ADVANCED_FACE('',(#9996),#8378,.T.);
#42577=ADVANCED_FACE('',(#9997),#8379,.F.);
#42578=ADVANCED_FACE('',(#9998),#8380,.T.);
#42579=ADVANCED_FACE('',(#9999),#8381,.F.);
#42580=ADVANCED_FACE('',(#10000),#8382,.T.);
#42581=ADVANCED_FACE('',(#10001),#8383,.F.);
#42582=ADVANCED_FACE('',(#10002),#8384,.T.);
#42583=ADVANCED_FACE('',(#10003),#8385,.F.);
#42584=ADVANCED_FACE('',(#10004),#8386,.T.);
#42585=ADVANCED_FACE('',(#10005),#8387,.F.);
#42586=ADVANCED_FACE('',(#10006),#8388,.T.);
#42587=ADVANCED_FACE('',(#10007),#8389,.F.);
#42588=ADVANCED_FACE('',(#10008),#8390,.T.);
#42589=ADVANCED_FACE('',(#10009),#8391,.F.);
#42590=ADVANCED_FACE('',(#10010),#8392,.T.);
#42591=ADVANCED_FACE('',(#10011),#8393,.F.);
#42592=ADVANCED_FACE('',(#10012),#8394,.T.);
#42593=ADVANCED_FACE('',(#10013),#8395,.F.);
#42594=ADVANCED_FACE('',(#10014),#8396,.T.);
#42595=ADVANCED_FACE('',(#10015),#8397,.F.);
#42596=ADVANCED_FACE('',(#10016),#8398,.T.);
#42597=ADVANCED_FACE('',(#10017),#8399,.F.);
#42598=ADVANCED_FACE('',(#10018),#8400,.T.);
#42599=ADVANCED_FACE('',(#10019),#8401,.F.);
#42600=ADVANCED_FACE('',(#10020),#8402,.T.);
#42601=ADVANCED_FACE('',(#10021),#8403,.F.);
#42602=ADVANCED_FACE('',(#10022),#8404,.T.);
#42603=ADVANCED_FACE('',(#10023),#8405,.F.);
#42604=ADVANCED_FACE('',(#10024),#8406,.T.);
#42605=ADVANCED_FACE('',(#10025),#8407,.F.);
#42606=ADVANCED_FACE('',(#10026),#8408,.T.);
#42607=ADVANCED_FACE('',(#10027),#8409,.F.);
#42608=ADVANCED_FACE('',(#10028),#8410,.T.);
#42609=ADVANCED_FACE('',(#10029),#8411,.F.);
#42610=ADVANCED_FACE('',(#10030),#8412,.T.);
#42611=ADVANCED_FACE('',(#10031),#8413,.F.);
#42612=ADVANCED_FACE('',(#10032),#8414,.T.);
#42613=ADVANCED_FACE('',(#10033),#8415,.F.);
#42614=ADVANCED_FACE('',(#10034),#8416,.T.);
#42615=ADVANCED_FACE('',(#10035),#8417,.F.);
#42616=ADVANCED_FACE('',(#10036),#8418,.T.);
#42617=ADVANCED_FACE('',(#10037),#8419,.F.);
#42618=ADVANCED_FACE('',(#10038),#8420,.T.);
#42619=ADVANCED_FACE('',(#10039),#8421,.F.);
#42620=ADVANCED_FACE('',(#10040),#8422,.T.);
#42621=ADVANCED_FACE('',(#10041),#8423,.F.);
#42622=ADVANCED_FACE('',(#10042),#8424,.T.);
#42623=ADVANCED_FACE('',(#10043),#8425,.F.);
#42624=ADVANCED_FACE('',(#10044),#8426,.T.);
#42625=ADVANCED_FACE('',(#10045),#8427,.F.);
#42626=ADVANCED_FACE('',(#10046),#8428,.T.);
#42627=ADVANCED_FACE('',(#10047),#8429,.F.);
#42628=ADVANCED_FACE('',(#10048),#8430,.T.);
#42629=ADVANCED_FACE('',(#10049),#8431,.F.);
#42630=ADVANCED_FACE('',(#10050),#8432,.T.);
#42631=ADVANCED_FACE('',(#10051),#8433,.F.);
#42632=ADVANCED_FACE('',(#10052),#8434,.T.);
#42633=ADVANCED_FACE('',(#10053),#8435,.F.);
#42634=ADVANCED_FACE('',(#10054),#8436,.T.);
#42635=ADVANCED_FACE('',(#10055),#8437,.F.);
#42636=ADVANCED_FACE('',(#10056),#8438,.T.);
#42637=ADVANCED_FACE('',(#10057),#8439,.F.);
#42638=ADVANCED_FACE('',(#10058),#8440,.T.);
#42639=ADVANCED_FACE('',(#10059),#8441,.F.);
#42640=ADVANCED_FACE('',(#10060),#8442,.T.);
#42641=ADVANCED_FACE('',(#10061),#8443,.F.);
#42642=ADVANCED_FACE('',(#10062),#8444,.T.);
#42643=ADVANCED_FACE('',(#10063),#8445,.F.);
#42644=ADVANCED_FACE('',(#10064),#8446,.T.);
#42645=ADVANCED_FACE('',(#10065),#8447,.F.);
#42646=ADVANCED_FACE('',(#10066),#8448,.T.);
#42647=ADVANCED_FACE('',(#10067),#8449,.F.);
#42648=ADVANCED_FACE('',(#10068),#8450,.T.);
#42649=ADVANCED_FACE('',(#10069),#8451,.F.);
#42650=ADVANCED_FACE('',(#10070),#8452,.T.);
#42651=ADVANCED_FACE('',(#10071),#8453,.F.);
#42652=ADVANCED_FACE('',(#10072),#8454,.T.);
#42653=ADVANCED_FACE('',(#10073),#8455,.F.);
#42654=ADVANCED_FACE('',(#10074),#8456,.T.);
#42655=ADVANCED_FACE('',(#10075),#8457,.F.);
#42656=ADVANCED_FACE('',(#10076),#8458,.T.);
#42657=ADVANCED_FACE('',(#10077),#8459,.F.);
#42658=ADVANCED_FACE('',(#10078),#8460,.T.);
#42659=ADVANCED_FACE('',(#10079),#8461,.F.);
#42660=ADVANCED_FACE('',(#10080),#8462,.T.);
#42661=ADVANCED_FACE('',(#10081),#8463,.F.);
#42662=ADVANCED_FACE('',(#10082),#8464,.T.);
#42663=ADVANCED_FACE('',(#10083),#8465,.F.);
#42664=ADVANCED_FACE('',(#10084),#8466,.T.);
#42665=ADVANCED_FACE('',(#10085),#8467,.F.);
#42666=ADVANCED_FACE('',(#10086),#8468,.T.);
#42667=ADVANCED_FACE('',(#10087),#8469,.F.);
#42668=ADVANCED_FACE('',(#10088),#8470,.T.);
#42669=ADVANCED_FACE('',(#10089),#8471,.F.);
#42670=ADVANCED_FACE('',(#10090),#8472,.T.);
#42671=ADVANCED_FACE('',(#10091),#8473,.F.);
#42672=ADVANCED_FACE('',(#10092),#8474,.T.);
#42673=ADVANCED_FACE('',(#10093),#8475,.F.);
#42674=ADVANCED_FACE('',(#10094),#8476,.T.);
#42675=ADVANCED_FACE('',(#10095),#8477,.F.);
#42676=ADVANCED_FACE('',(#10096),#8478,.T.);
#42677=ADVANCED_FACE('',(#10097),#8479,.F.);
#42678=ADVANCED_FACE('',(#10098),#8480,.T.);
#42679=ADVANCED_FACE('',(#10099),#8481,.F.);
#42680=ADVANCED_FACE('',(#10100),#8482,.T.);
#42681=ADVANCED_FACE('',(#10101),#8483,.F.);
#42682=ADVANCED_FACE('',(#10102),#8484,.T.);
#42683=ADVANCED_FACE('',(#10103),#8485,.F.);
#42684=ADVANCED_FACE('',(#10104),#8486,.T.);
#42685=ADVANCED_FACE('',(#10105),#8487,.F.);
#42686=ADVANCED_FACE('',(#10106),#8488,.T.);
#42687=ADVANCED_FACE('',(#10107),#8489,.F.);
#42688=ADVANCED_FACE('',(#10108),#8490,.T.);
#42689=ADVANCED_FACE('',(#10109),#8491,.F.);
#42690=ADVANCED_FACE('',(#10110),#8492,.T.);
#42691=ADVANCED_FACE('',(#10111),#8493,.F.);
#42692=ADVANCED_FACE('',(#10112),#8494,.T.);
#42693=ADVANCED_FACE('',(#10113),#8495,.F.);
#42694=ADVANCED_FACE('',(#10114),#8496,.T.);
#42695=ADVANCED_FACE('',(#10115),#8497,.F.);
#42696=ADVANCED_FACE('',(#10116),#8498,.T.);
#42697=ADVANCED_FACE('',(#10117),#8499,.F.);
#42698=ADVANCED_FACE('',(#10118),#8500,.T.);
#42699=ADVANCED_FACE('',(#10119),#8501,.F.);
#42700=ADVANCED_FACE('',(#10120),#8502,.T.);
#42701=ADVANCED_FACE('',(#10121),#8503,.F.);
#42702=ADVANCED_FACE('',(#10122),#8504,.T.);
#42703=ADVANCED_FACE('',(#10123),#8505,.F.);
#42704=ADVANCED_FACE('',(#10124),#8506,.T.);
#42705=ADVANCED_FACE('',(#10125),#8507,.F.);
#42706=ADVANCED_FACE('',(#10126),#8508,.T.);
#42707=ADVANCED_FACE('',(#10127),#8509,.F.);
#42708=ADVANCED_FACE('',(#10128),#8510,.T.);
#42709=ADVANCED_FACE('',(#10129),#8511,.F.);
#42710=ADVANCED_FACE('',(#10130),#8512,.T.);
#42711=ADVANCED_FACE('',(#10131),#8513,.F.);
#42712=ADVANCED_FACE('',(#10132),#8514,.T.);
#42713=ADVANCED_FACE('',(#10133),#8515,.F.);
#42714=ADVANCED_FACE('',(#10134),#8516,.T.);
#42715=ADVANCED_FACE('',(#10135),#8517,.F.);
#42716=ADVANCED_FACE('',(#10136),#8518,.T.);
#42717=ADVANCED_FACE('',(#10137),#8519,.F.);
#42718=ADVANCED_FACE('',(#10138),#8520,.T.);
#42719=ADVANCED_FACE('',(#10139),#8521,.F.);
#42720=ADVANCED_FACE('',(#10140),#8522,.T.);
#42721=ADVANCED_FACE('',(#10141),#8523,.F.);
#42722=ADVANCED_FACE('',(#10142,#83,#84,#85,#86,#87,#88,#89,#90,#91,#92,
#93,#94,#95,#96,#97,#98,#99,#100,#101,#102,#103,#104,#105,#106,#107,#108,
#109,#110,#111,#112,#113,#114,#115,#116,#117,#118,#119,#120,#121,#122,#123,
#124,#125,#126,#127,#128,#129,#130),#1517,.T.);
#42723=ADVANCED_FACE('',(#10143),#41946,.T.);
#42724=ADVANCED_FACE('',(#10144),#71,.F.);
#42725=ADVANCED_FACE('',(#10145),#41947,.T.);
#42726=ADVANCED_FACE('',(#10146),#41948,.T.);
#42727=ADVANCED_FACE('',(#10147),#41949,.T.);
#42728=ADVANCED_FACE('',(#10148),#41950,.T.);
#42729=ADVANCED_FACE('',(#10149),#8524,.T.);
#42730=ADVANCED_FACE('',(#10150),#41951,.T.);
#42731=ADVANCED_FACE('',(#10151),#8525,.F.);
#42732=ADVANCED_FACE('',(#10152),#41952,.T.);
#42733=ADVANCED_FACE('',(#10153),#8526,.F.);
#42734=ADVANCED_FACE('',(#10154),#8527,.T.);
#42735=ADVANCED_FACE('',(#10155,#131),#1518,.T.);
#42736=ADVANCED_FACE('',(#10156),#2959,.F.);
#42737=ADVANCED_FACE('',(#10157),#58,.T.);
#42738=ADVANCED_FACE('',(#10158),#2960,.F.);
#42739=ADVANCED_FACE('',(#10159),#8528,.T.);
#42740=ADVANCED_FACE('',(#10160),#41953,.T.);
#42741=ADVANCED_FACE('',(#10161),#8529,.T.);
#42742=ADVANCED_FACE('',(#10162),#8530,.T.);
#42743=ADVANCED_FACE('',(#10163),#2961,.F.);
#42744=ADVANCED_FACE('',(#10164),#2962,.T.);
#42745=ADVANCED_FACE('',(#10165),#2963,.T.);
#42746=ADVANCED_FACE('',(#10166),#72,.T.);
#42747=ADVANCED_FACE('',(#10167),#73,.T.);
#42748=ADVANCED_FACE('',(#10168),#2964,.T.);
#42749=ADVANCED_FACE('',(#10169),#41954,.T.);
#42750=ADVANCED_FACE('',(#10170),#8531,.T.);
#42751=ADVANCED_FACE('',(#10171),#8532,.T.);
#42752=ADVANCED_FACE('',(#10172),#41955,.T.);
#42753=ADVANCED_FACE('',(#10173),#41956,.T.);
#42754=ADVANCED_FACE('',(#10174),#8533,.T.);
#42755=ADVANCED_FACE('',(#10175),#8534,.T.);
#42756=ADVANCED_FACE('',(#10176),#41957,.T.);
#42757=ADVANCED_FACE('',(#10177),#1519,.T.);
#42758=ADVANCED_FACE('',(#10178),#1520,.T.);
#42759=ADVANCED_FACE('',(#10179),#8535,.T.);
#42760=ADVANCED_FACE('',(#10180),#1521,.T.);
#42761=ADVANCED_FACE('',(#10181),#8536,.T.);
#42762=ADVANCED_FACE('',(#10182),#8537,.F.);
#42763=ADVANCED_FACE('',(#10183),#1522,.T.);
#42764=ADVANCED_FACE('',(#10184),#1523,.T.);
#42765=ADVANCED_FACE('',(#10185),#1524,.T.);
#42766=ADVANCED_FACE('',(#10186),#1525,.T.);
#42767=ADVANCED_FACE('',(#10187),#1526,.T.);
#42768=ADVANCED_FACE('',(#10188),#1527,.T.);
#42769=ADVANCED_FACE('',(#10189),#41958,.T.);
#42770=ADVANCED_FACE('',(#10190),#1528,.T.);
#42771=ADVANCED_FACE('',(#10191),#1529,.T.);
#42772=ADVANCED_FACE('',(#10192),#8538,.T.);
#42773=ADVANCED_FACE('',(#10193),#1530,.T.);
#42774=ADVANCED_FACE('',(#10194),#1531,.T.);
#42775=ADVANCED_FACE('',(#10195),#1532,.T.);
#42776=ADVANCED_FACE('',(#10196),#8539,.T.);
#42777=ADVANCED_FACE('',(#10197),#1533,.T.);
#42778=ADVANCED_FACE('',(#10198),#1534,.T.);
#42779=ADVANCED_FACE('',(#10199),#45,.T.);
#42780=ADVANCED_FACE('',(#10200),#46,.T.);
#42781=ADVANCED_FACE('',(#10201),#59,.T.);
#42782=ADVANCED_FACE('',(#10202),#47,.T.);
#42783=ADVANCED_FACE('',(#10203),#41959,.T.);
#42784=ADVANCED_FACE('',(#10204),#1535,.T.);
#42785=ADVANCED_FACE('',(#10205),#1536,.T.);
#42786=ADVANCED_FACE('',(#10206),#74,.T.);
#42787=ADVANCED_FACE('',(#10207),#1537,.T.);
#42788=ADVANCED_FACE('',(#10208),#1538,.T.);
#42789=ADVANCED_FACE('',(#10209),#1539,.T.);
#42790=ADVANCED_FACE('',(#10210),#2965,.T.);
#42791=ADVANCED_FACE('',(#10211),#1540,.T.);
#42792=ADVANCED_FACE('',(#10212),#1541,.T.);
#42793=ADVANCED_FACE('',(#10213),#1542,.T.);
#42794=ADVANCED_FACE('',(#10214),#2966,.T.);
#42795=ADVANCED_FACE('',(#10215),#2967,.T.);
#42796=ADVANCED_FACE('',(#10216),#48,.T.);
#42797=ADVANCED_FACE('',(#10217),#75,.T.);
#42798=ADVANCED_FACE('',(#10218),#1543,.T.);
#42799=ADVANCED_FACE('',(#10219,#132,#133,#134,#135,#136,#137,#138,#139,
#140,#141,#142,#143,#144,#145,#146,#147,#148,#149),#1544,.F.);
#42800=ADVANCED_FACE('',(#10220,#150,#151,#152,#153,#154,#155,#156,#157,
#158,#159,#160,#161,#162,#163,#164,#165,#166,#167,#168,#169,#170,#171,#172,
#173,#174,#175,#176,#177,#178,#179,#180,#181,#182,#183,#184,#185,#186,#187,
#188,#189,#190,#191,#192,#193,#194,#195,#196,#197,#198,#199,#200,#201,#202,
#203,#204,#205,#206,#207,#208,#209,#210,#211,#212,#213,#214,#215,#216,#217,
#218,#219,#220,#221,#222,#223,#224,#225,#226,#227,#228,#229,#230,#231,#232,
#233,#234,#235,#236,#237,#238,#239,#240,#241,#242,#243,#244,#245,#246,#247,
#248,#249,#250,#251,#252,#253,#254,#255,#256,#257,#258,#259,#260,#261,#262,
#263,#264,#265,#266,#267,#268,#269,#270,#271,#272,#273,#274,#275,#276,#277,
#278,#279,#280,#281,#282,#283,#284,#285,#286,#287,#288,#289,#290,#291,#292,
#293,#294,#295,#296,#297,#298,#299,#300,#301,#302,#303,#304,#305,#306,#307,
#308,#309,#310,#311,#312,#313,#314,#315,#316,#317,#318,#319,#320,#321,#322,
#323,#324,#325,#326,#327,#328,#329,#330,#331,#332,#333,#334,#335,#336,#337,
#338,#339,#340,#341,#342,#343,#344,#345,#346,#347,#348,#349,#350,#351,#352,
#353,#354,#355,#356,#357,#358,#359,#360,#361,#362,#363,#364,#365,#366,#367,
#368,#369,#370,#371,#372,#373,#374,#375,#376,#377,#378,#379,#380,#381,#382,
#383,#384,#385),#2968,.T.);
#42801=ADVANCED_FACE('',(#10221),#2969,.F.);
#42802=ADVANCED_FACE('',(#10222),#49,.T.);
#42803=ADVANCED_FACE('',(#10223),#1545,.T.);
#42804=ADVANCED_FACE('',(#10224),#2970,.T.);
#42805=ADVANCED_FACE('',(#10225),#2971,.T.);
#42806=ADVANCED_FACE('',(#10226),#8540,.F.);
#42807=ADVANCED_FACE('',(#10227),#2972,.F.);
#42808=ADVANCED_FACE('',(#10228,#386),#2973,.T.);
#42809=ADVANCED_FACE('',(#10229),#2974,.F.);
#42810=ADVANCED_FACE('',(#10230,#387),#2975,.T.);
#42811=ADVANCED_FACE('',(#10231),#2976,.F.);
#42812=ADVANCED_FACE('',(#10232,#388),#2977,.T.);
#42813=ADVANCED_FACE('',(#10233),#2978,.F.);
#42814=ADVANCED_FACE('',(#10234,#389),#2979,.T.);
#42815=ADVANCED_FACE('',(#10235),#2980,.F.);
#42816=ADVANCED_FACE('',(#10236,#390),#2981,.T.);
#42817=ADVANCED_FACE('',(#10237),#2982,.F.);
#42818=ADVANCED_FACE('',(#10238,#391),#2983,.T.);
#42819=ADVANCED_FACE('',(#10239),#2984,.F.);
#42820=ADVANCED_FACE('',(#10240,#392),#2985,.T.);
#42821=ADVANCED_FACE('',(#10241),#2986,.F.);
#42822=ADVANCED_FACE('',(#10242,#393),#2987,.T.);
#42823=ADVANCED_FACE('',(#10243),#2988,.F.);
#42824=ADVANCED_FACE('',(#10244,#394),#2989,.T.);
#42825=ADVANCED_FACE('',(#10245),#2990,.F.);
#42826=ADVANCED_FACE('',(#10246,#395),#2991,.T.);
#42827=ADVANCED_FACE('',(#10247),#2992,.F.);
#42828=ADVANCED_FACE('',(#10248,#396),#2993,.T.);
#42829=ADVANCED_FACE('',(#10249),#2994,.F.);
#42830=ADVANCED_FACE('',(#10250,#397),#2995,.T.);
#42831=ADVANCED_FACE('',(#10251),#2996,.F.);
#42832=ADVANCED_FACE('',(#10252,#398),#2997,.T.);
#42833=ADVANCED_FACE('',(#10253),#2998,.F.);
#42834=ADVANCED_FACE('',(#10254,#399),#2999,.T.);
#42835=ADVANCED_FACE('',(#10255),#3000,.F.);
#42836=ADVANCED_FACE('',(#10256,#400),#3001,.T.);
#42837=ADVANCED_FACE('',(#10257),#3002,.F.);
#42838=ADVANCED_FACE('',(#10258,#401),#3003,.T.);
#42839=ADVANCED_FACE('',(#10259),#3004,.F.);
#42840=ADVANCED_FACE('',(#10260,#402),#3005,.T.);
#42841=ADVANCED_FACE('',(#10261),#3006,.F.);
#42842=ADVANCED_FACE('',(#10262,#403),#3007,.T.);
#42843=ADVANCED_FACE('',(#10263),#3008,.F.);
#42844=ADVANCED_FACE('',(#10264,#404),#3009,.T.);
#42845=ADVANCED_FACE('',(#10265),#3010,.F.);
#42846=ADVANCED_FACE('',(#10266,#405),#3011,.T.);
#42847=ADVANCED_FACE('',(#10267),#3012,.F.);
#42848=ADVANCED_FACE('',(#10268,#406),#3013,.T.);
#42849=ADVANCED_FACE('',(#10269),#3014,.F.);
#42850=ADVANCED_FACE('',(#10270,#407),#3015,.T.);
#42851=ADVANCED_FACE('',(#10271),#3016,.F.);
#42852=ADVANCED_FACE('',(#10272,#408),#3017,.T.);
#42853=ADVANCED_FACE('',(#10273),#3018,.F.);
#42854=ADVANCED_FACE('',(#10274,#409),#3019,.T.);
#42855=ADVANCED_FACE('',(#10275),#3020,.F.);
#42856=ADVANCED_FACE('',(#10276,#410),#3021,.T.);
#42857=ADVANCED_FACE('',(#10277),#3022,.F.);
#42858=ADVANCED_FACE('',(#10278,#411),#3023,.T.);
#42859=ADVANCED_FACE('',(#10279),#3024,.F.);
#42860=ADVANCED_FACE('',(#10280,#412),#3025,.T.);
#42861=ADVANCED_FACE('',(#10281),#3026,.F.);
#42862=ADVANCED_FACE('',(#10282,#413),#3027,.T.);
#42863=ADVANCED_FACE('',(#10283),#3028,.F.);
#42864=ADVANCED_FACE('',(#10284,#414),#3029,.T.);
#42865=ADVANCED_FACE('',(#10285),#3030,.F.);
#42866=ADVANCED_FACE('',(#10286,#415),#3031,.T.);
#42867=ADVANCED_FACE('',(#10287),#3032,.F.);
#42868=ADVANCED_FACE('',(#10288,#416),#3033,.T.);
#42869=ADVANCED_FACE('',(#10289),#3034,.F.);
#42870=ADVANCED_FACE('',(#10290,#417),#3035,.T.);
#42871=ADVANCED_FACE('',(#10291),#3036,.F.);
#42872=ADVANCED_FACE('',(#10292,#418),#3037,.T.);
#42873=ADVANCED_FACE('',(#10293),#3038,.F.);
#42874=ADVANCED_FACE('',(#10294,#419),#3039,.T.);
#42875=ADVANCED_FACE('',(#10295),#3040,.F.);
#42876=ADVANCED_FACE('',(#10296,#420),#3041,.T.);
#42877=ADVANCED_FACE('',(#10297),#3042,.F.);
#42878=ADVANCED_FACE('',(#10298,#421),#3043,.T.);
#42879=ADVANCED_FACE('',(#10299),#3044,.F.);
#42880=ADVANCED_FACE('',(#10300,#422),#3045,.T.);
#42881=ADVANCED_FACE('',(#10301),#3046,.F.);
#42882=ADVANCED_FACE('',(#10302,#423),#3047,.T.);
#42883=ADVANCED_FACE('',(#10303),#3048,.F.);
#42884=ADVANCED_FACE('',(#10304,#424),#3049,.T.);
#42885=ADVANCED_FACE('',(#10305),#3050,.F.);
#42886=ADVANCED_FACE('',(#10306,#425),#3051,.T.);
#42887=ADVANCED_FACE('',(#10307),#3052,.F.);
#42888=ADVANCED_FACE('',(#10308,#426),#3053,.T.);
#42889=ADVANCED_FACE('',(#10309),#3054,.F.);
#42890=ADVANCED_FACE('',(#10310,#427),#3055,.T.);
#42891=ADVANCED_FACE('',(#10311),#3056,.F.);
#42892=ADVANCED_FACE('',(#10312,#428),#3057,.T.);
#42893=ADVANCED_FACE('',(#10313),#3058,.F.);
#42894=ADVANCED_FACE('',(#10314,#429),#3059,.T.);
#42895=ADVANCED_FACE('',(#10315),#3060,.F.);
#42896=ADVANCED_FACE('',(#10316,#430),#3061,.T.);
#42897=ADVANCED_FACE('',(#10317),#3062,.F.);
#42898=ADVANCED_FACE('',(#10318,#431),#3063,.T.);
#42899=ADVANCED_FACE('',(#10319),#3064,.F.);
#42900=ADVANCED_FACE('',(#10320,#432),#3065,.T.);
#42901=ADVANCED_FACE('',(#10321),#3066,.F.);
#42902=ADVANCED_FACE('',(#10322,#433),#3067,.T.);
#42903=ADVANCED_FACE('',(#10323),#3068,.F.);
#42904=ADVANCED_FACE('',(#10324,#434),#3069,.T.);
#42905=ADVANCED_FACE('',(#10325),#3070,.F.);
#42906=ADVANCED_FACE('',(#10326,#435),#3071,.T.);
#42907=ADVANCED_FACE('',(#10327),#3072,.F.);
#42908=ADVANCED_FACE('',(#10328,#436),#3073,.T.);
#42909=ADVANCED_FACE('',(#10329),#3074,.F.);
#42910=ADVANCED_FACE('',(#10330,#437),#3075,.T.);
#42911=ADVANCED_FACE('',(#10331),#3076,.F.);
#42912=ADVANCED_FACE('',(#10332,#438),#3077,.T.);
#42913=ADVANCED_FACE('',(#10333),#3078,.F.);
#42914=ADVANCED_FACE('',(#10334,#439),#3079,.T.);
#42915=ADVANCED_FACE('',(#10335),#3080,.F.);
#42916=ADVANCED_FACE('',(#10336,#440),#3081,.T.);
#42917=ADVANCED_FACE('',(#10337),#3082,.F.);
#42918=ADVANCED_FACE('',(#10338,#441),#3083,.T.);
#42919=ADVANCED_FACE('',(#10339),#3084,.F.);
#42920=ADVANCED_FACE('',(#10340,#442),#3085,.T.);
#42921=ADVANCED_FACE('',(#10341),#3086,.F.);
#42922=ADVANCED_FACE('',(#10342,#443),#3087,.T.);
#42923=ADVANCED_FACE('',(#10343),#3088,.F.);
#42924=ADVANCED_FACE('',(#10344,#444),#3089,.T.);
#42925=ADVANCED_FACE('',(#10345),#3090,.F.);
#42926=ADVANCED_FACE('',(#10346,#445),#3091,.T.);
#42927=ADVANCED_FACE('',(#10347),#3092,.F.);
#42928=ADVANCED_FACE('',(#10348,#446),#3093,.T.);
#42929=ADVANCED_FACE('',(#10349),#3094,.F.);
#42930=ADVANCED_FACE('',(#10350,#447),#3095,.T.);
#42931=ADVANCED_FACE('',(#10351),#3096,.F.);
#42932=ADVANCED_FACE('',(#10352,#448),#3097,.T.);
#42933=ADVANCED_FACE('',(#10353),#3098,.F.);
#42934=ADVANCED_FACE('',(#10354,#449),#3099,.T.);
#42935=ADVANCED_FACE('',(#10355),#3100,.F.);
#42936=ADVANCED_FACE('',(#10356,#450),#3101,.T.);
#42937=ADVANCED_FACE('',(#10357),#3102,.F.);
#42938=ADVANCED_FACE('',(#10358,#451),#3103,.T.);
#42939=ADVANCED_FACE('',(#10359),#3104,.F.);
#42940=ADVANCED_FACE('',(#10360,#452),#3105,.T.);
#42941=ADVANCED_FACE('',(#10361),#3106,.F.);
#42942=ADVANCED_FACE('',(#10362,#453),#3107,.T.);
#42943=ADVANCED_FACE('',(#10363),#3108,.F.);
#42944=ADVANCED_FACE('',(#10364,#454),#3109,.T.);
#42945=ADVANCED_FACE('',(#10365),#3110,.F.);
#42946=ADVANCED_FACE('',(#10366,#455),#3111,.T.);
#42947=ADVANCED_FACE('',(#10367),#3112,.F.);
#42948=ADVANCED_FACE('',(#10368,#456),#3113,.T.);
#42949=ADVANCED_FACE('',(#10369),#3114,.F.);
#42950=ADVANCED_FACE('',(#10370,#457),#3115,.T.);
#42951=ADVANCED_FACE('',(#10371),#3116,.F.);
#42952=ADVANCED_FACE('',(#10372,#458),#3117,.T.);
#42953=ADVANCED_FACE('',(#10373),#3118,.F.);
#42954=ADVANCED_FACE('',(#10374,#459),#3119,.T.);
#42955=ADVANCED_FACE('',(#10375),#3120,.F.);
#42956=ADVANCED_FACE('',(#10376,#460),#3121,.T.);
#42957=ADVANCED_FACE('',(#10377),#3122,.F.);
#42958=ADVANCED_FACE('',(#10378,#461),#3123,.T.);
#42959=ADVANCED_FACE('',(#10379),#3124,.F.);
#42960=ADVANCED_FACE('',(#10380,#462),#3125,.T.);
#42961=ADVANCED_FACE('',(#10381),#3126,.F.);
#42962=ADVANCED_FACE('',(#10382,#463),#3127,.T.);
#42963=ADVANCED_FACE('',(#10383),#3128,.F.);
#42964=ADVANCED_FACE('',(#10384,#464),#3129,.T.);
#42965=ADVANCED_FACE('',(#10385),#3130,.F.);
#42966=ADVANCED_FACE('',(#10386,#465),#3131,.T.);
#42967=ADVANCED_FACE('',(#10387),#3132,.F.);
#42968=ADVANCED_FACE('',(#10388,#466),#3133,.T.);
#42969=ADVANCED_FACE('',(#10389),#3134,.F.);
#42970=ADVANCED_FACE('',(#10390,#467),#3135,.T.);
#42971=ADVANCED_FACE('',(#10391),#3136,.F.);
#42972=ADVANCED_FACE('',(#10392,#468),#3137,.T.);
#42973=ADVANCED_FACE('',(#10393),#3138,.F.);
#42974=ADVANCED_FACE('',(#10394,#469),#3139,.T.);
#42975=ADVANCED_FACE('',(#10395),#3140,.F.);
#42976=ADVANCED_FACE('',(#10396,#470),#3141,.T.);
#42977=ADVANCED_FACE('',(#10397),#3142,.F.);
#42978=ADVANCED_FACE('',(#10398,#471),#3143,.T.);
#42979=ADVANCED_FACE('',(#10399),#3144,.F.);
#42980=ADVANCED_FACE('',(#10400,#472),#3145,.T.);
#42981=ADVANCED_FACE('',(#10401),#3146,.F.);
#42982=ADVANCED_FACE('',(#10402,#473),#3147,.T.);
#42983=ADVANCED_FACE('',(#10403),#3148,.F.);
#42984=ADVANCED_FACE('',(#10404,#474),#3149,.T.);
#42985=ADVANCED_FACE('',(#10405),#3150,.F.);
#42986=ADVANCED_FACE('',(#10406,#475),#3151,.T.);
#42987=ADVANCED_FACE('',(#10407),#3152,.F.);
#42988=ADVANCED_FACE('',(#10408,#476),#3153,.T.);
#42989=ADVANCED_FACE('',(#10409),#3154,.F.);
#42990=ADVANCED_FACE('',(#10410,#477),#3155,.T.);
#42991=ADVANCED_FACE('',(#10411),#3156,.F.);
#42992=ADVANCED_FACE('',(#10412,#478),#3157,.T.);
#42993=ADVANCED_FACE('',(#10413),#3158,.F.);
#42994=ADVANCED_FACE('',(#10414,#479),#3159,.T.);
#42995=ADVANCED_FACE('',(#10415),#3160,.F.);
#42996=ADVANCED_FACE('',(#10416,#480),#3161,.T.);
#42997=ADVANCED_FACE('',(#10417),#3162,.F.);
#42998=ADVANCED_FACE('',(#10418,#481),#3163,.T.);
#42999=ADVANCED_FACE('',(#10419),#3164,.F.);
#43000=ADVANCED_FACE('',(#10420,#482),#3165,.T.);
#43001=ADVANCED_FACE('',(#10421),#3166,.F.);
#43002=ADVANCED_FACE('',(#10422,#483),#3167,.T.);
#43003=ADVANCED_FACE('',(#10423),#3168,.F.);
#43004=ADVANCED_FACE('',(#10424,#484),#3169,.T.);
#43005=ADVANCED_FACE('',(#10425),#3170,.F.);
#43006=ADVANCED_FACE('',(#10426,#485),#3171,.T.);
#43007=ADVANCED_FACE('',(#10427),#3172,.F.);
#43008=ADVANCED_FACE('',(#10428,#486),#3173,.T.);
#43009=ADVANCED_FACE('',(#10429),#3174,.F.);
#43010=ADVANCED_FACE('',(#10430,#487),#3175,.T.);
#43011=ADVANCED_FACE('',(#10431),#3176,.F.);
#43012=ADVANCED_FACE('',(#10432,#488),#3177,.T.);
#43013=ADVANCED_FACE('',(#10433),#3178,.F.);
#43014=ADVANCED_FACE('',(#10434,#489),#3179,.T.);
#43015=ADVANCED_FACE('',(#10435),#3180,.F.);
#43016=ADVANCED_FACE('',(#10436,#490),#3181,.T.);
#43017=ADVANCED_FACE('',(#10437),#3182,.F.);
#43018=ADVANCED_FACE('',(#10438,#491),#3183,.T.);
#43019=ADVANCED_FACE('',(#10439),#3184,.F.);
#43020=ADVANCED_FACE('',(#10440,#492),#3185,.T.);
#43021=ADVANCED_FACE('',(#10441),#3186,.F.);
#43022=ADVANCED_FACE('',(#10442,#493),#3187,.T.);
#43023=ADVANCED_FACE('',(#10443),#3188,.F.);
#43024=ADVANCED_FACE('',(#10444,#494),#3189,.T.);
#43025=ADVANCED_FACE('',(#10445),#3190,.F.);
#43026=ADVANCED_FACE('',(#10446,#495),#3191,.T.);
#43027=ADVANCED_FACE('',(#10447),#3192,.F.);
#43028=ADVANCED_FACE('',(#10448,#496),#3193,.T.);
#43029=ADVANCED_FACE('',(#10449),#3194,.F.);
#43030=ADVANCED_FACE('',(#10450,#497),#3195,.T.);
#43031=ADVANCED_FACE('',(#10451),#3196,.F.);
#43032=ADVANCED_FACE('',(#10452,#498),#3197,.T.);
#43033=ADVANCED_FACE('',(#10453),#3198,.F.);
#43034=ADVANCED_FACE('',(#10454,#499),#3199,.T.);
#43035=ADVANCED_FACE('',(#10455),#3200,.F.);
#43036=ADVANCED_FACE('',(#10456,#500),#3201,.T.);
#43037=ADVANCED_FACE('',(#10457),#3202,.F.);
#43038=ADVANCED_FACE('',(#10458,#501),#3203,.T.);
#43039=ADVANCED_FACE('',(#10459),#3204,.F.);
#43040=ADVANCED_FACE('',(#10460,#502),#3205,.T.);
#43041=ADVANCED_FACE('',(#10461),#3206,.F.);
#43042=ADVANCED_FACE('',(#10462,#503),#3207,.T.);
#43043=ADVANCED_FACE('',(#10463),#3208,.F.);
#43044=ADVANCED_FACE('',(#10464,#504),#3209,.T.);
#43045=ADVANCED_FACE('',(#10465),#3210,.F.);
#43046=ADVANCED_FACE('',(#10466,#505),#3211,.T.);
#43047=ADVANCED_FACE('',(#10467),#3212,.F.);
#43048=ADVANCED_FACE('',(#10468,#506),#3213,.T.);
#43049=ADVANCED_FACE('',(#10469),#3214,.F.);
#43050=ADVANCED_FACE('',(#10470,#507),#3215,.T.);
#43051=ADVANCED_FACE('',(#10471),#3216,.F.);
#43052=ADVANCED_FACE('',(#10472,#508),#3217,.T.);
#43053=ADVANCED_FACE('',(#10473),#3218,.F.);
#43054=ADVANCED_FACE('',(#10474,#509),#3219,.T.);
#43055=ADVANCED_FACE('',(#10475),#3220,.F.);
#43056=ADVANCED_FACE('',(#10476,#510),#3221,.T.);
#43057=ADVANCED_FACE('',(#10477),#3222,.F.);
#43058=ADVANCED_FACE('',(#10478,#511),#3223,.T.);
#43059=ADVANCED_FACE('',(#10479),#3224,.F.);
#43060=ADVANCED_FACE('',(#10480,#512),#3225,.T.);
#43061=ADVANCED_FACE('',(#10481),#3226,.F.);
#43062=ADVANCED_FACE('',(#10482,#513),#3227,.T.);
#43063=ADVANCED_FACE('',(#10483),#3228,.F.);
#43064=ADVANCED_FACE('',(#10484,#514),#3229,.T.);
#43065=ADVANCED_FACE('',(#10485),#3230,.F.);
#43066=ADVANCED_FACE('',(#10486,#515),#3231,.T.);
#43067=ADVANCED_FACE('',(#10487),#3232,.F.);
#43068=ADVANCED_FACE('',(#10488,#516),#3233,.T.);
#43069=ADVANCED_FACE('',(#10489),#3234,.F.);
#43070=ADVANCED_FACE('',(#10490,#517),#3235,.T.);
#43071=ADVANCED_FACE('',(#10491),#3236,.F.);
#43072=ADVANCED_FACE('',(#10492,#518),#3237,.T.);
#43073=ADVANCED_FACE('',(#10493),#3238,.F.);
#43074=ADVANCED_FACE('',(#10494,#519),#3239,.T.);
#43075=ADVANCED_FACE('',(#10495),#3240,.F.);
#43076=ADVANCED_FACE('',(#10496,#520),#3241,.T.);
#43077=ADVANCED_FACE('',(#10497),#3242,.F.);
#43078=ADVANCED_FACE('',(#10498,#521),#3243,.T.);
#43079=ADVANCED_FACE('',(#10499),#3244,.F.);
#43080=ADVANCED_FACE('',(#10500,#522),#3245,.T.);
#43081=ADVANCED_FACE('',(#10501),#3246,.F.);
#43082=ADVANCED_FACE('',(#10502,#523),#3247,.T.);
#43083=ADVANCED_FACE('',(#10503),#3248,.F.);
#43084=ADVANCED_FACE('',(#10504,#524),#3249,.T.);
#43085=ADVANCED_FACE('',(#10505),#3250,.F.);
#43086=ADVANCED_FACE('',(#10506,#525),#3251,.T.);
#43087=ADVANCED_FACE('',(#10507),#3252,.F.);
#43088=ADVANCED_FACE('',(#10508,#526),#3253,.T.);
#43089=ADVANCED_FACE('',(#10509),#3254,.F.);
#43090=ADVANCED_FACE('',(#10510,#527),#3255,.T.);
#43091=ADVANCED_FACE('',(#10511),#3256,.F.);
#43092=ADVANCED_FACE('',(#10512,#528),#3257,.T.);
#43093=ADVANCED_FACE('',(#10513),#3258,.F.);
#43094=ADVANCED_FACE('',(#10514,#529),#3259,.T.);
#43095=ADVANCED_FACE('',(#10515),#3260,.F.);
#43096=ADVANCED_FACE('',(#10516,#530),#3261,.T.);
#43097=ADVANCED_FACE('',(#10517),#3262,.F.);
#43098=ADVANCED_FACE('',(#10518,#531),#3263,.T.);
#43099=ADVANCED_FACE('',(#10519),#3264,.F.);
#43100=ADVANCED_FACE('',(#10520,#532),#3265,.T.);
#43101=ADVANCED_FACE('',(#10521),#3266,.F.);
#43102=ADVANCED_FACE('',(#10522,#533),#3267,.T.);
#43103=ADVANCED_FACE('',(#10523),#3268,.F.);
#43104=ADVANCED_FACE('',(#10524,#534),#3269,.T.);
#43105=ADVANCED_FACE('',(#10525),#3270,.F.);
#43106=ADVANCED_FACE('',(#10526,#535),#3271,.T.);
#43107=ADVANCED_FACE('',(#10527),#3272,.F.);
#43108=ADVANCED_FACE('',(#10528,#536),#3273,.T.);
#43109=ADVANCED_FACE('',(#10529),#3274,.F.);
#43110=ADVANCED_FACE('',(#10530,#537),#3275,.T.);
#43111=ADVANCED_FACE('',(#10531),#3276,.F.);
#43112=ADVANCED_FACE('',(#10532,#538),#3277,.T.);
#43113=ADVANCED_FACE('',(#10533),#3278,.F.);
#43114=ADVANCED_FACE('',(#10534,#539),#3279,.T.);
#43115=ADVANCED_FACE('',(#10535),#3280,.F.);
#43116=ADVANCED_FACE('',(#10536,#540),#3281,.T.);
#43117=ADVANCED_FACE('',(#10537),#3282,.F.);
#43118=ADVANCED_FACE('',(#10538,#541),#3283,.T.);
#43119=ADVANCED_FACE('',(#10539),#3284,.F.);
#43120=ADVANCED_FACE('',(#10540,#542),#3285,.T.);
#43121=ADVANCED_FACE('',(#10541),#3286,.F.);
#43122=ADVANCED_FACE('',(#10542,#543),#3287,.T.);
#43123=ADVANCED_FACE('',(#10543),#3288,.F.);
#43124=ADVANCED_FACE('',(#10544,#544),#3289,.T.);
#43125=ADVANCED_FACE('',(#10545),#3290,.F.);
#43126=ADVANCED_FACE('',(#10546,#545),#3291,.T.);
#43127=ADVANCED_FACE('',(#10547),#3292,.F.);
#43128=ADVANCED_FACE('',(#10548,#546),#3293,.T.);
#43129=ADVANCED_FACE('',(#10549),#3294,.F.);
#43130=ADVANCED_FACE('',(#10550,#547),#3295,.T.);
#43131=ADVANCED_FACE('',(#10551),#3296,.F.);
#43132=ADVANCED_FACE('',(#10552,#548),#3297,.T.);
#43133=ADVANCED_FACE('',(#10553),#3298,.F.);
#43134=ADVANCED_FACE('',(#10554,#549),#3299,.T.);
#43135=ADVANCED_FACE('',(#10555),#3300,.F.);
#43136=ADVANCED_FACE('',(#10556,#550),#3301,.T.);
#43137=ADVANCED_FACE('',(#10557),#3302,.F.);
#43138=ADVANCED_FACE('',(#10558,#551),#3303,.T.);
#43139=ADVANCED_FACE('',(#10559),#3304,.F.);
#43140=ADVANCED_FACE('',(#10560,#552),#3305,.T.);
#43141=ADVANCED_FACE('',(#10561),#3306,.F.);
#43142=ADVANCED_FACE('',(#10562,#553),#3307,.T.);
#43143=ADVANCED_FACE('',(#10563),#3308,.F.);
#43144=ADVANCED_FACE('',(#10564,#554),#3309,.T.);
#43145=ADVANCED_FACE('',(#10565),#3310,.F.);
#43146=ADVANCED_FACE('',(#10566,#555),#3311,.T.);
#43147=ADVANCED_FACE('',(#10567),#3312,.F.);
#43148=ADVANCED_FACE('',(#10568,#556),#3313,.T.);
#43149=ADVANCED_FACE('',(#10569),#3314,.F.);
#43150=ADVANCED_FACE('',(#10570,#557),#3315,.T.);
#43151=ADVANCED_FACE('',(#10571),#3316,.F.);
#43152=ADVANCED_FACE('',(#10572,#558),#3317,.T.);
#43153=ADVANCED_FACE('',(#10573),#3318,.F.);
#43154=ADVANCED_FACE('',(#10574,#559),#3319,.T.);
#43155=ADVANCED_FACE('',(#10575),#3320,.F.);
#43156=ADVANCED_FACE('',(#10576,#560),#3321,.T.);
#43157=ADVANCED_FACE('',(#10577),#3322,.F.);
#43158=ADVANCED_FACE('',(#10578,#561),#3323,.T.);
#43159=ADVANCED_FACE('',(#10579),#3324,.F.);
#43160=ADVANCED_FACE('',(#10580,#562),#3325,.T.);
#43161=ADVANCED_FACE('',(#10581),#3326,.F.);
#43162=ADVANCED_FACE('',(#10582,#563),#3327,.T.);
#43163=ADVANCED_FACE('',(#10583),#3328,.F.);
#43164=ADVANCED_FACE('',(#10584,#564),#3329,.T.);
#43165=ADVANCED_FACE('',(#10585),#3330,.F.);
#43166=ADVANCED_FACE('',(#10586,#565),#3331,.T.);
#43167=ADVANCED_FACE('',(#10587),#3332,.F.);
#43168=ADVANCED_FACE('',(#10588,#566),#3333,.T.);
#43169=ADVANCED_FACE('',(#10589),#3334,.F.);
#43170=ADVANCED_FACE('',(#10590,#567),#3335,.T.);
#43171=ADVANCED_FACE('',(#10591),#3336,.F.);
#43172=ADVANCED_FACE('',(#10592,#568),#3337,.T.);
#43173=ADVANCED_FACE('',(#10593),#3338,.F.);
#43174=ADVANCED_FACE('',(#10594,#569),#3339,.T.);
#43175=ADVANCED_FACE('',(#10595),#3340,.F.);
#43176=ADVANCED_FACE('',(#10596,#570),#3341,.T.);
#43177=ADVANCED_FACE('',(#10597),#3342,.F.);
#43178=ADVANCED_FACE('',(#10598,#571),#3343,.T.);
#43179=ADVANCED_FACE('',(#10599),#3344,.F.);
#43180=ADVANCED_FACE('',(#10600,#572),#3345,.T.);
#43181=ADVANCED_FACE('',(#10601),#3346,.F.);
#43182=ADVANCED_FACE('',(#10602,#573),#3347,.T.);
#43183=ADVANCED_FACE('',(#10603),#3348,.F.);
#43184=ADVANCED_FACE('',(#10604,#574),#3349,.T.);
#43185=ADVANCED_FACE('',(#10605),#3350,.F.);
#43186=ADVANCED_FACE('',(#10606,#575),#3351,.T.);
#43187=ADVANCED_FACE('',(#10607),#3352,.F.);
#43188=ADVANCED_FACE('',(#10608,#576),#3353,.T.);
#43189=ADVANCED_FACE('',(#10609),#3354,.F.);
#43190=ADVANCED_FACE('',(#10610,#577),#3355,.T.);
#43191=ADVANCED_FACE('',(#10611),#3356,.F.);
#43192=ADVANCED_FACE('',(#10612,#578),#3357,.T.);
#43193=ADVANCED_FACE('',(#10613),#3358,.F.);
#43194=ADVANCED_FACE('',(#10614,#579),#3359,.T.);
#43195=ADVANCED_FACE('',(#10615),#3360,.F.);
#43196=ADVANCED_FACE('',(#10616,#580),#3361,.T.);
#43197=ADVANCED_FACE('',(#10617),#3362,.F.);
#43198=ADVANCED_FACE('',(#10618,#581),#3363,.T.);
#43199=ADVANCED_FACE('',(#10619),#3364,.F.);
#43200=ADVANCED_FACE('',(#10620,#582),#3365,.T.);
#43201=ADVANCED_FACE('',(#10621),#3366,.F.);
#43202=ADVANCED_FACE('',(#10622,#583),#3367,.T.);
#43203=ADVANCED_FACE('',(#10623),#3368,.F.);
#43204=ADVANCED_FACE('',(#10624,#584),#3369,.T.);
#43205=ADVANCED_FACE('',(#10625),#3370,.F.);
#43206=ADVANCED_FACE('',(#10626,#585),#3371,.T.);
#43207=ADVANCED_FACE('',(#10627),#3372,.F.);
#43208=ADVANCED_FACE('',(#10628,#586),#3373,.T.);
#43209=ADVANCED_FACE('',(#10629),#3374,.F.);
#43210=ADVANCED_FACE('',(#10630,#587),#3375,.T.);
#43211=ADVANCED_FACE('',(#10631),#3376,.F.);
#43212=ADVANCED_FACE('',(#10632,#588),#3377,.T.);
#43213=ADVANCED_FACE('',(#10633),#3378,.F.);
#43214=ADVANCED_FACE('',(#10634,#589),#3379,.T.);
#43215=ADVANCED_FACE('',(#10635),#3380,.F.);
#43216=ADVANCED_FACE('',(#10636,#590),#3381,.T.);
#43217=ADVANCED_FACE('',(#10637),#3382,.F.);
#43218=ADVANCED_FACE('',(#10638,#591),#3383,.T.);
#43219=ADVANCED_FACE('',(#10639),#3384,.F.);
#43220=ADVANCED_FACE('',(#10640,#592),#3385,.T.);
#43221=ADVANCED_FACE('',(#10641),#3386,.F.);
#43222=ADVANCED_FACE('',(#10642,#593),#3387,.T.);
#43223=ADVANCED_FACE('',(#10643),#3388,.F.);
#43224=ADVANCED_FACE('',(#10644,#594),#3389,.T.);
#43225=ADVANCED_FACE('',(#10645),#3390,.F.);
#43226=ADVANCED_FACE('',(#10646,#595),#3391,.T.);
#43227=ADVANCED_FACE('',(#10647),#3392,.F.);
#43228=ADVANCED_FACE('',(#10648,#596),#3393,.T.);
#43229=ADVANCED_FACE('',(#10649),#3394,.F.);
#43230=ADVANCED_FACE('',(#10650,#597),#3395,.T.);
#43231=ADVANCED_FACE('',(#10651),#3396,.F.);
#43232=ADVANCED_FACE('',(#10652,#598),#3397,.T.);
#43233=ADVANCED_FACE('',(#10653),#3398,.F.);
#43234=ADVANCED_FACE('',(#10654,#599),#3399,.T.);
#43235=ADVANCED_FACE('',(#10655),#3400,.F.);
#43236=ADVANCED_FACE('',(#10656,#600),#3401,.T.);
#43237=ADVANCED_FACE('',(#10657),#3402,.F.);
#43238=ADVANCED_FACE('',(#10658,#601),#3403,.T.);
#43239=ADVANCED_FACE('',(#10659),#3404,.F.);
#43240=ADVANCED_FACE('',(#10660,#602),#3405,.T.);
#43241=ADVANCED_FACE('',(#10661),#3406,.F.);
#43242=ADVANCED_FACE('',(#10662,#603),#3407,.T.);
#43243=ADVANCED_FACE('',(#10663),#3408,.F.);
#43244=ADVANCED_FACE('',(#10664,#604),#3409,.T.);
#43245=ADVANCED_FACE('',(#10665),#3410,.F.);
#43246=ADVANCED_FACE('',(#10666,#605),#3411,.T.);
#43247=ADVANCED_FACE('',(#10667),#3412,.F.);
#43248=ADVANCED_FACE('',(#10668,#606),#3413,.T.);
#43249=ADVANCED_FACE('',(#10669),#3414,.F.);
#43250=ADVANCED_FACE('',(#10670,#607),#3415,.T.);
#43251=ADVANCED_FACE('',(#10671),#3416,.F.);
#43252=ADVANCED_FACE('',(#10672,#608),#3417,.T.);
#43253=ADVANCED_FACE('',(#10673),#3418,.F.);
#43254=ADVANCED_FACE('',(#10674,#609),#3419,.T.);
#43255=ADVANCED_FACE('',(#10675),#3420,.F.);
#43256=ADVANCED_FACE('',(#10676,#610),#3421,.T.);
#43257=ADVANCED_FACE('',(#10677),#3422,.F.);
#43258=ADVANCED_FACE('',(#10678,#611),#3423,.T.);
#43259=ADVANCED_FACE('',(#10679),#3424,.F.);
#43260=ADVANCED_FACE('',(#10680,#612),#3425,.T.);
#43261=ADVANCED_FACE('',(#10681),#3426,.F.);
#43262=ADVANCED_FACE('',(#10682,#613),#3427,.T.);
#43263=ADVANCED_FACE('',(#10683),#3428,.F.);
#43264=ADVANCED_FACE('',(#10684,#614),#3429,.T.);
#43265=ADVANCED_FACE('',(#10685),#3430,.F.);
#43266=ADVANCED_FACE('',(#10686,#615),#3431,.T.);
#43267=ADVANCED_FACE('',(#10687),#3432,.F.);
#43268=ADVANCED_FACE('',(#10688,#616),#3433,.T.);
#43269=ADVANCED_FACE('',(#10689),#3434,.F.);
#43270=ADVANCED_FACE('',(#10690,#617),#3435,.T.);
#43271=ADVANCED_FACE('',(#10691),#3436,.F.);
#43272=ADVANCED_FACE('',(#10692,#618),#3437,.T.);
#43273=ADVANCED_FACE('',(#10693),#3438,.F.);
#43274=ADVANCED_FACE('',(#10694,#619),#3439,.T.);
#43275=ADVANCED_FACE('',(#10695),#3440,.F.);
#43276=ADVANCED_FACE('',(#10696,#620),#3441,.T.);
#43277=ADVANCED_FACE('',(#10697),#3442,.F.);
#43278=ADVANCED_FACE('',(#10698,#621),#3443,.T.);
#43279=ADVANCED_FACE('',(#10699),#3444,.F.);
#43280=ADVANCED_FACE('',(#10700,#622),#3445,.T.);
#43281=ADVANCED_FACE('',(#10701),#3446,.F.);
#43282=ADVANCED_FACE('',(#10702,#623),#3447,.T.);
#43283=ADVANCED_FACE('',(#10703),#3448,.F.);
#43284=ADVANCED_FACE('',(#10704,#624),#3449,.T.);
#43285=ADVANCED_FACE('',(#10705),#3450,.F.);
#43286=ADVANCED_FACE('',(#10706,#625),#3451,.T.);
#43287=ADVANCED_FACE('',(#10707),#3452,.F.);
#43288=ADVANCED_FACE('',(#10708,#626),#3453,.T.);
#43289=ADVANCED_FACE('',(#10709),#3454,.F.);
#43290=ADVANCED_FACE('',(#10710,#627),#3455,.T.);
#43291=ADVANCED_FACE('',(#10711),#3456,.F.);
#43292=ADVANCED_FACE('',(#10712,#628),#3457,.T.);
#43293=ADVANCED_FACE('',(#10713),#3458,.F.);
#43294=ADVANCED_FACE('',(#10714,#629),#3459,.T.);
#43295=ADVANCED_FACE('',(#10715),#3460,.F.);
#43296=ADVANCED_FACE('',(#10716,#630),#3461,.T.);
#43297=ADVANCED_FACE('',(#10717),#3462,.F.);
#43298=ADVANCED_FACE('',(#10718,#631),#3463,.T.);
#43299=ADVANCED_FACE('',(#10719),#3464,.F.);
#43300=ADVANCED_FACE('',(#10720,#632),#3465,.T.);
#43301=ADVANCED_FACE('',(#10721),#3466,.F.);
#43302=ADVANCED_FACE('',(#10722,#633),#3467,.T.);
#43303=ADVANCED_FACE('',(#10723),#3468,.F.);
#43304=ADVANCED_FACE('',(#10724,#634),#3469,.T.);
#43305=ADVANCED_FACE('',(#10725),#3470,.F.);
#43306=ADVANCED_FACE('',(#10726,#635),#3471,.T.);
#43307=ADVANCED_FACE('',(#10727),#3472,.F.);
#43308=ADVANCED_FACE('',(#10728,#636),#3473,.T.);
#43309=ADVANCED_FACE('',(#10729),#3474,.F.);
#43310=ADVANCED_FACE('',(#10730,#637),#3475,.T.);
#43311=ADVANCED_FACE('',(#10731),#3476,.F.);
#43312=ADVANCED_FACE('',(#10732,#638),#3477,.T.);
#43313=ADVANCED_FACE('',(#10733),#3478,.F.);
#43314=ADVANCED_FACE('',(#10734,#639),#3479,.T.);
#43315=ADVANCED_FACE('',(#10735),#3480,.F.);
#43316=ADVANCED_FACE('',(#10736,#640),#3481,.T.);
#43317=ADVANCED_FACE('',(#10737),#3482,.F.);
#43318=ADVANCED_FACE('',(#10738,#641),#3483,.T.);
#43319=ADVANCED_FACE('',(#10739),#3484,.F.);
#43320=ADVANCED_FACE('',(#10740,#642),#3485,.T.);
#43321=ADVANCED_FACE('',(#10741),#3486,.F.);
#43322=ADVANCED_FACE('',(#10742,#643),#3487,.T.);
#43323=ADVANCED_FACE('',(#10743),#3488,.F.);
#43324=ADVANCED_FACE('',(#10744,#644),#1546,.T.);
#43325=ADVANCED_FACE('',(#10745),#3489,.F.);
#43326=ADVANCED_FACE('',(#10746,#645),#1547,.T.);
#43327=ADVANCED_FACE('',(#10747),#3490,.F.);
#43328=ADVANCED_FACE('',(#10748,#646),#1548,.T.);
#43329=ADVANCED_FACE('',(#10749),#3491,.F.);
#43330=ADVANCED_FACE('',(#10750,#647),#1549,.T.);
#43331=ADVANCED_FACE('',(#10751),#3492,.F.);
#43332=ADVANCED_FACE('',(#10752,#648),#1550,.T.);
#43333=ADVANCED_FACE('',(#10753),#3493,.F.);
#43334=ADVANCED_FACE('',(#10754,#649),#1551,.T.);
#43335=ADVANCED_FACE('',(#10755),#3494,.F.);
#43336=ADVANCED_FACE('',(#10756,#650),#1552,.T.);
#43337=ADVANCED_FACE('',(#10757),#3495,.F.);
#43338=ADVANCED_FACE('',(#10758,#651),#1553,.T.);
#43339=ADVANCED_FACE('',(#10759),#3496,.F.);
#43340=ADVANCED_FACE('',(#10760,#652),#1554,.T.);
#43341=ADVANCED_FACE('',(#10761),#3497,.F.);
#43342=ADVANCED_FACE('',(#10762,#653),#1555,.T.);
#43343=ADVANCED_FACE('',(#10763),#3498,.F.);
#43344=ADVANCED_FACE('',(#10764,#654),#1556,.T.);
#43345=ADVANCED_FACE('',(#10765),#3499,.F.);
#43346=ADVANCED_FACE('',(#10766,#655),#1557,.T.);
#43347=ADVANCED_FACE('',(#10767),#3500,.F.);
#43348=ADVANCED_FACE('',(#10768,#656),#1558,.T.);
#43349=ADVANCED_FACE('',(#10769),#3501,.F.);
#43350=ADVANCED_FACE('',(#10770,#657),#1559,.T.);
#43351=ADVANCED_FACE('',(#10771),#3502,.F.);
#43352=ADVANCED_FACE('',(#10772,#658),#3503,.T.);
#43353=ADVANCED_FACE('',(#10773),#3504,.F.);
#43354=ADVANCED_FACE('',(#10774,#659),#1560,.T.);
#43355=ADVANCED_FACE('',(#10775),#3505,.F.);
#43356=ADVANCED_FACE('',(#10776,#660),#1561,.T.);
#43357=ADVANCED_FACE('',(#10777),#3506,.F.);
#43358=ADVANCED_FACE('',(#10778,#661),#3507,.T.);
#43359=ADVANCED_FACE('',(#10779),#3508,.F.);
#43360=ADVANCED_FACE('',(#10780,#662),#1562,.T.);
#43361=ADVANCED_FACE('',(#10781),#3509,.F.);
#43362=ADVANCED_FACE('',(#10782,#663),#1563,.T.);
#43363=ADVANCED_FACE('',(#10783),#3510,.F.);
#43364=ADVANCED_FACE('',(#10784,#664),#3511,.T.);
#43365=ADVANCED_FACE('',(#10785),#3512,.F.);
#43366=ADVANCED_FACE('',(#10786,#665),#3513,.T.);
#43367=ADVANCED_FACE('',(#10787),#3514,.F.);
#43368=ADVANCED_FACE('',(#10788,#666),#1564,.T.);
#43369=ADVANCED_FACE('',(#10789),#3515,.F.);
#43370=ADVANCED_FACE('',(#10790,#667),#1565,.T.);
#43371=ADVANCED_FACE('',(#10791),#3516,.F.);
#43372=ADVANCED_FACE('',(#10792,#668),#3517,.T.);
#43373=ADVANCED_FACE('',(#10793),#3518,.F.);
#43374=ADVANCED_FACE('',(#10794,#669),#3519,.T.);
#43375=ADVANCED_FACE('',(#10795),#3520,.F.);
#43376=ADVANCED_FACE('',(#10796,#670),#1566,.T.);
#43377=ADVANCED_FACE('',(#10797),#3521,.F.);
#43378=ADVANCED_FACE('',(#10798,#671),#1567,.T.);
#43379=ADVANCED_FACE('',(#10799),#3522,.F.);
#43380=ADVANCED_FACE('',(#10800,#672),#1568,.T.);
#43381=ADVANCED_FACE('',(#10801),#3523,.F.);
#43382=ADVANCED_FACE('',(#10802,#673),#1569,.T.);
#43383=ADVANCED_FACE('',(#10803),#3524,.F.);
#43384=ADVANCED_FACE('',(#10804,#674),#1570,.T.);
#43385=ADVANCED_FACE('',(#10805),#3525,.F.);
#43386=ADVANCED_FACE('',(#10806,#675),#1571,.T.);
#43387=ADVANCED_FACE('',(#10807),#3526,.F.);
#43388=ADVANCED_FACE('',(#10808,#676),#1572,.T.);
#43389=ADVANCED_FACE('',(#10809),#3527,.F.);
#43390=ADVANCED_FACE('',(#10810,#677),#1573,.T.);
#43391=ADVANCED_FACE('',(#10811),#3528,.F.);
#43392=ADVANCED_FACE('',(#10812,#678),#1574,.T.);
#43393=ADVANCED_FACE('',(#10813),#3529,.F.);
#43394=ADVANCED_FACE('',(#10814,#679),#1575,.T.);
#43395=ADVANCED_FACE('',(#10815),#3530,.F.);
#43396=ADVANCED_FACE('',(#10816,#680),#1576,.T.);
#43397=ADVANCED_FACE('',(#10817),#3531,.F.);
#43398=ADVANCED_FACE('',(#10818,#681),#1577,.T.);
#43399=ADVANCED_FACE('',(#10819),#3532,.F.);
#43400=ADVANCED_FACE('',(#10820,#682),#1578,.T.);
#43401=ADVANCED_FACE('',(#10821),#3533,.F.);
#43402=ADVANCED_FACE('',(#10822,#683),#1579,.T.);
#43403=ADVANCED_FACE('',(#10823),#3534,.F.);
#43404=ADVANCED_FACE('',(#10824,#684),#1580,.T.);
#43405=ADVANCED_FACE('',(#10825),#3535,.F.);
#43406=ADVANCED_FACE('',(#10826,#685),#1581,.T.);
#43407=ADVANCED_FACE('',(#10827),#3536,.F.);
#43408=ADVANCED_FACE('',(#10828,#686),#1582,.T.);
#43409=ADVANCED_FACE('',(#10829),#3537,.F.);
#43410=ADVANCED_FACE('',(#10830,#687),#1583,.T.);
#43411=ADVANCED_FACE('',(#10831),#3538,.F.);
#43412=ADVANCED_FACE('',(#10832,#688),#1584,.T.);
#43413=ADVANCED_FACE('',(#10833),#3539,.F.);
#43414=ADVANCED_FACE('',(#10834,#689),#1585,.T.);
#43415=ADVANCED_FACE('',(#10835),#3540,.F.);
#43416=ADVANCED_FACE('',(#10836,#690),#1586,.T.);
#43417=ADVANCED_FACE('',(#10837),#3541,.F.);
#43418=ADVANCED_FACE('',(#10838,#691),#1587,.T.);
#43419=ADVANCED_FACE('',(#10839),#3542,.F.);
#43420=ADVANCED_FACE('',(#10840,#692),#1588,.T.);
#43421=ADVANCED_FACE('',(#10841),#3543,.F.);
#43422=ADVANCED_FACE('',(#10842,#693),#1589,.T.);
#43423=ADVANCED_FACE('',(#10843),#3544,.F.);
#43424=ADVANCED_FACE('',(#10844,#694),#1590,.T.);
#43425=ADVANCED_FACE('',(#10845),#3545,.F.);
#43426=ADVANCED_FACE('',(#10846,#695),#1591,.T.);
#43427=ADVANCED_FACE('',(#10847),#3546,.F.);
#43428=ADVANCED_FACE('',(#10848,#696),#1592,.T.);
#43429=ADVANCED_FACE('',(#10849),#3547,.F.);
#43430=ADVANCED_FACE('',(#10850,#697),#1593,.T.);
#43431=ADVANCED_FACE('',(#10851),#3548,.F.);
#43432=ADVANCED_FACE('',(#10852,#698),#1594,.T.);
#43433=ADVANCED_FACE('',(#10853),#3549,.F.);
#43434=ADVANCED_FACE('',(#10854,#699),#1595,.T.);
#43435=ADVANCED_FACE('',(#10855),#3550,.F.);
#43436=ADVANCED_FACE('',(#10856,#700),#1596,.T.);
#43437=ADVANCED_FACE('',(#10857),#3551,.F.);
#43438=ADVANCED_FACE('',(#10858,#701),#1597,.T.);
#43439=ADVANCED_FACE('',(#10859),#3552,.F.);
#43440=ADVANCED_FACE('',(#10860,#702),#1598,.T.);
#43441=ADVANCED_FACE('',(#10861),#3553,.F.);
#43442=ADVANCED_FACE('',(#10862,#703),#1599,.T.);
#43443=ADVANCED_FACE('',(#10863),#3554,.F.);
#43444=ADVANCED_FACE('',(#10864,#704),#1600,.T.);
#43445=ADVANCED_FACE('',(#10865),#3555,.F.);
#43446=ADVANCED_FACE('',(#10866,#705),#1601,.T.);
#43447=ADVANCED_FACE('',(#10867),#3556,.F.);
#43448=ADVANCED_FACE('',(#10868,#706),#1602,.T.);
#43449=ADVANCED_FACE('',(#10869),#3557,.F.);
#43450=ADVANCED_FACE('',(#10870,#707),#1603,.T.);
#43451=ADVANCED_FACE('',(#10871),#3558,.F.);
#43452=ADVANCED_FACE('',(#10872,#708),#1604,.T.);
#43453=ADVANCED_FACE('',(#10873,#709),#3559,.T.);
#43454=ADVANCED_FACE('',(#10874),#3560,.T.);
#43455=ADVANCED_FACE('',(#10875,#710),#3561,.T.);
#43456=ADVANCED_FACE('',(#10876),#3562,.T.);
#43457=ADVANCED_FACE('',(#10877,#711),#3563,.T.);
#43458=ADVANCED_FACE('',(#10878),#3564,.T.);
#43459=ADVANCED_FACE('',(#10879,#712),#3565,.T.);
#43460=ADVANCED_FACE('',(#10880),#3566,.T.);
#43461=ADVANCED_FACE('',(#10881,#713),#3567,.T.);
#43462=ADVANCED_FACE('',(#10882),#3568,.T.);
#43463=ADVANCED_FACE('',(#10883,#714),#3569,.T.);
#43464=ADVANCED_FACE('',(#10884),#3570,.T.);
#43465=ADVANCED_FACE('',(#10885),#41960,.T.);
#43466=ADVANCED_FACE('',(#10886),#41961,.T.);
#43467=ADVANCED_FACE('',(#10887),#76,.T.);
#43468=ADVANCED_FACE('',(#10888),#1605,.T.);
#43469=ADVANCED_FACE('',(#10889),#41962,.T.);
#43470=ADVANCED_FACE('',(#10890),#77,.T.);
#43471=ADVANCED_FACE('',(#10891),#3571,.F.);
#43472=ADVANCED_FACE('',(#10892,#715),#3572,.F.);
#43473=ADVANCED_FACE('',(#10893),#1606,.T.);
#43474=ADVANCED_FACE('',(#10894),#3573,.F.);
#43475=ADVANCED_FACE('',(#10895,#716),#3574,.F.);
#43476=ADVANCED_FACE('',(#10896),#8541,.F.);
#43477=ADVANCED_FACE('',(#10897),#3575,.F.);
#43478=ADVANCED_FACE('',(#10898),#8542,.F.);
#43479=ADVANCED_FACE('',(#10899),#3576,.F.);
#43480=ADVANCED_FACE('',(#10900),#3577,.F.);
#43481=ADVANCED_FACE('',(#10901),#3578,.F.);
#43482=ADVANCED_FACE('',(#10902),#3579,.T.);
#43483=ADVANCED_FACE('',(#10903),#3580,.F.);
#43484=ADVANCED_FACE('',(#10904),#8543,.F.);
#43485=ADVANCED_FACE('',(#10905),#3581,.F.);
#43486=ADVANCED_FACE('',(#10906),#8544,.F.);
#43487=ADVANCED_FACE('',(#10907),#3582,.F.);
#43488=ADVANCED_FACE('',(#10908),#8545,.T.);
#43489=ADVANCED_FACE('',(#10909),#41963,.T.);
#43490=ADVANCED_FACE('',(#10910),#8546,.F.);
#43491=ADVANCED_FACE('',(#10911),#8547,.F.);
#43492=ADVANCED_FACE('',(#10912),#8548,.F.);
#43493=ADVANCED_FACE('',(#10913),#8549,.T.);
#43494=ADVANCED_FACE('',(#10914),#8550,.T.);
#43495=ADVANCED_FACE('',(#10915),#41964,.F.);
#43496=ADVANCED_FACE('',(#10916),#41965,.T.);
#43497=ADVANCED_FACE('',(#10917),#41966,.T.);
#43498=ADVANCED_FACE('',(#10918),#41967,.T.);
#43499=ADVANCED_FACE('',(#10919),#8551,.T.);
#43500=ADVANCED_FACE('',(#10920),#8552,.T.);
#43501=ADVANCED_FACE('',(#10921),#41968,.F.);
#43502=ADVANCED_FACE('',(#10922),#41969,.T.);
#43503=ADVANCED_FACE('',(#10923),#41970,.T.);
#43504=ADVANCED_FACE('',(#10924),#41971,.T.);
#43505=ADVANCED_FACE('',(#10925),#8553,.T.);
#43506=ADVANCED_FACE('',(#10926),#8554,.T.);
#43507=ADVANCED_FACE('',(#10927),#41972,.F.);
#43508=ADVANCED_FACE('',(#10928),#41973,.T.);
#43509=ADVANCED_FACE('',(#10929),#41974,.T.);
#43510=ADVANCED_FACE('',(#10930),#41975,.T.);
#43511=ADVANCED_FACE('',(#10931),#8555,.T.);
#43512=ADVANCED_FACE('',(#10932),#41976,.T.);
#43513=ADVANCED_FACE('',(#10933),#3583,.F.);
#43514=ADVANCED_FACE('',(#10934),#8556,.T.);
#43515=ADVANCED_FACE('',(#10935),#50,.T.);
#43516=ADVANCED_FACE('',(#10936),#8557,.T.);
#43517=ADVANCED_FACE('',(#10937),#51,.T.);
#43518=ADVANCED_FACE('',(#10938),#3584,.T.);
#43519=ADVANCED_FACE('',(#10939),#3585,.F.);
#43520=ADVANCED_FACE('',(#10940),#3586,.F.);
#43521=ADVANCED_FACE('',(#10941),#1607,.T.);
#43522=ADVANCED_FACE('',(#10942),#1608,.T.);
#43523=ADVANCED_FACE('',(#10943),#41977,.T.);
#43524=ADVANCED_FACE('',(#10944),#41978,.T.);
#43525=ADVANCED_FACE('',(#10945),#8558,.T.);
#43526=ADVANCED_FACE('',(#10946),#8559,.T.);
#43527=ADVANCED_FACE('',(#10947),#8560,.T.);
#43528=ADVANCED_FACE('',(#10948),#60,.T.);
#43529=ADVANCED_FACE('',(#10949),#61,.T.);
#43530=ADVANCED_FACE('',(#10950),#8561,.T.);
#43531=ADVANCED_FACE('',(#10951),#8562,.T.);
#43532=ADVANCED_FACE('',(#10952),#8563,.T.);
#43533=ADVANCED_FACE('',(#10953),#62,.T.);
#43534=ADVANCED_FACE('',(#10954),#63,.T.);
#43535=ADVANCED_FACE('',(#10955),#8564,.T.);
#43536=ADVANCED_FACE('',(#10956),#8565,.T.);
#43537=ADVANCED_FACE('',(#10957),#41979,.T.);
#43538=ADVANCED_FACE('',(#10958),#41980,.T.);
#43539=ADVANCED_FACE('',(#10959),#1609,.T.);
#43540=ADVANCED_FACE('',(#10960),#1610,.T.);
#43541=ADVANCED_FACE('',(#10961),#41981,.T.);
#43542=ADVANCED_FACE('',(#10962),#8566,.T.);
#43543=ADVANCED_FACE('',(#10963),#8567,.T.);
#43544=ADVANCED_FACE('',(#10964),#41982,.T.);
#43545=ADVANCED_FACE('',(#10965),#8568,.F.);
#43546=ADVANCED_FACE('',(#10966),#1611,.F.);
#43547=ADVANCED_FACE('',(#10967),#1612,.F.);
#43548=ADVANCED_FACE('',(#10968),#8569,.T.);
#43549=ADVANCED_FACE('',(#10969),#41983,.F.);
#43550=ADVANCED_FACE('',(#10970),#8570,.F.);
#43551=ADVANCED_FACE('',(#10971),#41984,.T.);
#43552=ADVANCED_FACE('',(#10972),#1613,.F.);
#43553=ADVANCED_FACE('',(#10973),#1614,.F.);
#43554=ADVANCED_FACE('',(#10974),#41985,.F.);
#43555=ADVANCED_FACE('',(#10975),#8571,.T.);
#43556=ADVANCED_FACE('',(#10976),#8572,.F.);
#43557=ADVANCED_FACE('',(#10977),#8573,.F.);
#43558=ADVANCED_FACE('',(#10978),#3587,.T.);
#43559=ADVANCED_FACE('',(#10979),#3588,.F.);
#43560=ADVANCED_FACE('',(#10980),#8574,.T.);
#43561=ADVANCED_FACE('',(#10981),#8575,.T.);
#43562=ADVANCED_FACE('',(#10982),#3589,.T.);
#43563=ADVANCED_FACE('',(#10983),#3590,.T.);
#43564=ADVANCED_FACE('',(#10984),#3591,.T.);
#43565=ADVANCED_FACE('',(#10985),#8576,.T.);
#43566=ADVANCED_FACE('',(#10986),#41986,.T.);
#43567=ADVANCED_FACE('',(#10987),#8577,.T.);
#43568=ADVANCED_FACE('',(#10988),#41987,.F.);
#43569=ADVANCED_FACE('',(#10989),#1615,.F.);
#43570=ADVANCED_FACE('',(#10990),#1616,.F.);
#43571=ADVANCED_FACE('',(#10991),#8578,.F.);
#43572=ADVANCED_FACE('',(#10992),#8579,.T.);
#43573=ADVANCED_FACE('',(#10993),#8580,.T.);
#43574=ADVANCED_FACE('',(#10994),#8581,.F.);
#43575=ADVANCED_FACE('',(#10995),#1617,.F.);
#43576=ADVANCED_FACE('',(#10996),#41988,.T.);
#43577=ADVANCED_FACE('',(#10997),#1618,.F.);
#43578=ADVANCED_FACE('',(#10998),#8582,.F.);
#43579=ADVANCED_FACE('',(#10999),#8583,.F.);
#43580=ADVANCED_FACE('',(#11000),#3592,.T.);
#43581=ADVANCED_FACE('',(#11001),#3593,.F.);
#43582=ADVANCED_FACE('',(#11002),#8584,.T.);
#43583=ADVANCED_FACE('',(#11003),#3594,.T.);
#43584=ADVANCED_FACE('',(#11004),#3595,.T.);
#43585=ADVANCED_FACE('',(#11005),#3596,.T.);
#43586=ADVANCED_FACE('',(#11006),#8585,.T.);
#43587=ADVANCED_FACE('',(#11007),#41989,.T.);
#43588=ADVANCED_FACE('',(#11008),#8586,.T.);
#43589=ADVANCED_FACE('',(#11009),#41990,.F.);
#43590=ADVANCED_FACE('',(#11010),#1619,.F.);
#43591=ADVANCED_FACE('',(#11011),#1620,.F.);
#43592=ADVANCED_FACE('',(#11012),#8587,.F.);
#43593=ADVANCED_FACE('',(#11013),#8588,.T.);
#43594=ADVANCED_FACE('',(#11014),#8589,.T.);
#43595=ADVANCED_FACE('',(#11015),#8590,.F.);
#43596=ADVANCED_FACE('',(#11016),#1621,.F.);
#43597=ADVANCED_FACE('',(#11017),#41991,.T.);
#43598=ADVANCED_FACE('',(#11018),#1622,.F.);
#43599=ADVANCED_FACE('',(#11019),#8591,.F.);
#43600=ADVANCED_FACE('',(#11020),#8592,.F.);
#43601=ADVANCED_FACE('',(#11021),#3597,.T.);
#43602=ADVANCED_FACE('',(#11022),#3598,.F.);
#43603=ADVANCED_FACE('',(#11023),#8593,.T.);
#43604=ADVANCED_FACE('',(#11024),#3599,.T.);
#43605=ADVANCED_FACE('',(#11025),#3600,.T.);
#43606=ADVANCED_FACE('',(#11026),#3601,.T.);
#43607=ADVANCED_FACE('',(#11027),#8594,.T.);
#43608=ADVANCED_FACE('',(#11028),#41992,.T.);
#43609=ADVANCED_FACE('',(#11029),#8595,.T.);
#43610=ADVANCED_FACE('',(#11030),#41993,.F.);
#43611=ADVANCED_FACE('',(#11031),#1623,.F.);
#43612=ADVANCED_FACE('',(#11032),#1624,.F.);
#43613=ADVANCED_FACE('',(#11033),#8596,.F.);
#43614=ADVANCED_FACE('',(#11034),#8597,.T.);
#43615=ADVANCED_FACE('',(#11035),#8598,.T.);
#43616=ADVANCED_FACE('',(#11036),#8599,.F.);
#43617=ADVANCED_FACE('',(#11037),#1625,.F.);
#43618=ADVANCED_FACE('',(#11038),#41994,.T.);
#43619=ADVANCED_FACE('',(#11039),#1626,.F.);
#43620=ADVANCED_FACE('',(#11040),#8600,.F.);
#43621=ADVANCED_FACE('',(#11041),#8601,.F.);
#43622=ADVANCED_FACE('',(#11042),#3602,.T.);
#43623=ADVANCED_FACE('',(#11043),#3603,.F.);
#43624=ADVANCED_FACE('',(#11044),#8602,.T.);
#43625=ADVANCED_FACE('',(#11045),#3604,.T.);
#43626=ADVANCED_FACE('',(#11046),#3605,.T.);
#43627=ADVANCED_FACE('',(#11047),#3606,.T.);
#43628=ADVANCED_FACE('',(#11048),#3607,.F.);
#43629=ADVANCED_FACE('',(#11049),#3608,.F.);
#43630=ADVANCED_FACE('',(#11050),#3609,.F.);
#43631=ADVANCED_FACE('',(#11051),#8603,.T.);
#43632=ADVANCED_FACE('',(#11052),#41995,.T.);
#43633=ADVANCED_FACE('',(#11053),#1627,.F.);
#43634=ADVANCED_FACE('',(#11054),#1628,.T.);
#43635=ADVANCED_FACE('',(#11055),#8604,.T.);
#43636=ADVANCED_FACE('',(#11056),#1629,.T.);
#43637=ADVANCED_FACE('',(#11057),#1630,.F.);
#43638=ADVANCED_FACE('',(#11058),#1631,.T.);
#43639=ADVANCED_FACE('',(#11059),#8605,.T.);
#43640=ADVANCED_FACE('',(#11060),#1632,.T.);
#43641=ADVANCED_FACE('',(#11061),#41996,.T.);
#43642=ADVANCED_FACE('',(#11062),#1633,.T.);
#43643=ADVANCED_FACE('',(#11063),#1634,.T.);
#43644=ADVANCED_FACE('',(#11064),#8606,.T.);
#43645=ADVANCED_FACE('',(#11065),#1635,.T.);
#43646=ADVANCED_FACE('',(#11066),#1636,.T.);
#43647=ADVANCED_FACE('',(#11067),#41997,.T.);
#43648=ADVANCED_FACE('',(#11068),#41998,.T.);
#43649=ADVANCED_FACE('',(#11069),#8607,.F.);
#43650=ADVANCED_FACE('',(#11070),#41999,.T.);
#43651=ADVANCED_FACE('',(#11071),#1637,.F.);
#43652=ADVANCED_FACE('',(#11072),#1638,.T.);
#43653=ADVANCED_FACE('',(#11073),#8608,.F.);
#43654=ADVANCED_FACE('',(#11074),#42000,.F.);
#43655=ADVANCED_FACE('',(#11075),#8609,.T.);
#43656=ADVANCED_FACE('',(#11076),#1639,.F.);
#43657=ADVANCED_FACE('',(#11077),#64,.F.);
#43658=ADVANCED_FACE('',(#11078),#42001,.F.);
#43659=ADVANCED_FACE('',(#11079),#8610,.F.);
#43660=ADVANCED_FACE('',(#11080),#65,.F.);
#43661=ADVANCED_FACE('',(#11081),#1640,.F.);
#43662=ADVANCED_FACE('',(#11082),#8611,.F.);
#43663=ADVANCED_FACE('',(#11083),#1641,.F.);
#43664=ADVANCED_FACE('',(#11084),#1642,.F.);
#43665=ADVANCED_FACE('',(#11085),#1643,.F.);
#43666=ADVANCED_FACE('',(#11086),#1644,.F.);
#43667=ADVANCED_FACE('',(#11087),#1645,.F.);
#43668=ADVANCED_FACE('',(#11088),#1646,.F.);
#43669=ADVANCED_FACE('',(#11089,#717),#3610,.F.);
#43670=ADVANCED_FACE('',(#11090),#1647,.T.);
#43671=ADVANCED_FACE('',(#11091),#1648,.T.);
#43672=ADVANCED_FACE('',(#11092),#1649,.T.);
#43673=ADVANCED_FACE('',(#11093),#1650,.T.);
#43674=ADVANCED_FACE('',(#11094),#1651,.T.);
#43675=ADVANCED_FACE('',(#11095),#1652,.T.);
#43676=ADVANCED_FACE('',(#11096),#1653,.T.);
#43677=ADVANCED_FACE('',(#11097),#1654,.T.);
#43678=ADVANCED_FACE('',(#11098,#718,#719,#720),#3611,.F.);
#43679=ADVANCED_FACE('',(#11099),#8612,.T.);
#43680=ADVANCED_FACE('',(#11100),#1655,.T.);
#43681=ADVANCED_FACE('',(#11101),#1656,.T.);
#43682=ADVANCED_FACE('',(#11102),#8613,.T.);
#43683=ADVANCED_FACE('',(#11103),#52,.T.);
#43684=ADVANCED_FACE('',(#11104),#53,.T.);
#43685=ADVANCED_FACE('',(#11105),#3612,.T.);
#43686=ADVANCED_FACE('',(#11106),#3613,.F.);
#43687=ADVANCED_FACE('',(#11107),#3614,.F.);
#43688=ADVANCED_FACE('',(#11108),#54,.F.);
#43689=ADVANCED_FACE('',(#11109),#55,.F.);
#43690=ADVANCED_FACE('',(#11110),#1657,.T.);
#43691=ADVANCED_FACE('',(#11111),#8614,.F.);
#43692=ADVANCED_FACE('',(#11112),#1658,.T.);
#43693=ADVANCED_FACE('',(#11113),#3615,.F.);
#43694=ADVANCED_FACE('',(#11114),#3616,.F.);
#43695=ADVANCED_FACE('',(#11115),#1659,.T.);
#43696=ADVANCED_FACE('',(#11116),#56,.F.);
#43697=ADVANCED_FACE('',(#11117),#57,.T.);
#43698=ADVANCED_FACE('',(#11118),#8615,.F.);
#43699=ADVANCED_FACE('',(#11119),#8616,.F.);
#43700=ADVANCED_FACE('',(#11120),#8617,.F.);
#43701=ADVANCED_FACE('',(#11121),#8618,.F.);
#43702=ADVANCED_FACE('',(#11122),#3617,.F.);
#43703=ADVANCED_FACE('',(#11123),#8619,.F.);
#43704=ADVANCED_FACE('',(#11124,#721),#3618,.F.);
#43705=ADVANCED_FACE('',(#11125),#3619,.T.);
#43706=ADVANCED_FACE('',(#11126),#3620,.T.);
#43707=ADVANCED_FACE('',(#11127),#3621,.T.);
#43708=ADVANCED_FACE('',(#11128),#3622,.T.);
#43709=ADVANCED_FACE('',(#11129),#3623,.T.);
#43710=ADVANCED_FACE('',(#11130),#3624,.F.);
#43711=ADVANCED_FACE('',(#11131,#722),#3625,.F.);
#43712=ADVANCED_FACE('',(#11132),#3626,.F.);
#43713=ADVANCED_FACE('',(#11133,#723),#3627,.F.);
#43714=ADVANCED_FACE('',(#11134),#3628,.F.);
#43715=ADVANCED_FACE('',(#11135),#8620,.T.);
#43716=ADVANCED_FACE('',(#11136),#8621,.T.);
#43717=ADVANCED_FACE('',(#11137),#8622,.T.);
#43718=ADVANCED_FACE('',(#11138),#8623,.T.);
#43719=ADVANCED_FACE('',(#11139),#8624,.T.);
#43720=ADVANCED_FACE('',(#11140),#8625,.T.);
#43721=ADVANCED_FACE('',(#11141),#3629,.F.);
#43722=ADVANCED_FACE('',(#11142),#78,.T.);
#43723=ADVANCED_FACE('',(#11143),#3630,.F.);
#43724=ADVANCED_FACE('',(#11144),#79,.T.);
#43725=ADVANCED_FACE('',(#11145),#3631,.F.);
#43726=ADVANCED_FACE('',(#11146),#3632,.F.);
#43727=ADVANCED_FACE('',(#11147),#80,.T.);
#43728=ADVANCED_FACE('',(#11148),#3633,.F.);
#43729=ADVANCED_FACE('',(#11149),#81,.T.);
#43730=ADVANCED_FACE('',(#11150),#3634,.F.);
#43731=ADVANCED_FACE('',(#11151),#8626,.T.);
#43732=ADVANCED_FACE('',(#11152),#42002,.T.);
#43733=ADVANCED_FACE('',(#11153),#42003,.T.);
#43734=ADVANCED_FACE('',(#11154),#8627,.T.);
#43735=ADVANCED_FACE('',(#11155),#8628,.T.);
#43736=ADVANCED_FACE('',(#11156),#42004,.T.);
#43737=ADVANCED_FACE('',(#11157),#42005,.T.);
#43738=ADVANCED_FACE('',(#11158),#8629,.T.);
#43739=ADVANCED_FACE('',(#11159),#8630,.T.);
#43740=ADVANCED_FACE('',(#11160),#42006,.T.);
#43741=ADVANCED_FACE('',(#11161),#42007,.T.);
#43742=ADVANCED_FACE('',(#11162),#8631,.T.);
#43743=ADVANCED_FACE('',(#11163),#8632,.T.);
#43744=ADVANCED_FACE('',(#11164),#42008,.T.);
#43745=ADVANCED_FACE('',(#11165),#42009,.T.);
#43746=ADVANCED_FACE('',(#11166),#8633,.T.);
#43747=ADVANCED_FACE('',(#11167),#8634,.T.);
#43748=ADVANCED_FACE('',(#11168),#42010,.T.);
#43749=ADVANCED_FACE('',(#11169),#8635,.T.);
#43750=ADVANCED_FACE('',(#11170),#42011,.T.);
#43751=ADVANCED_FACE('',(#11171),#8636,.T.);
#43752=ADVANCED_FACE('',(#11172),#8637,.T.);
#43753=ADVANCED_FACE('',(#11173),#42012,.T.);
#43754=ADVANCED_FACE('',(#11174),#8638,.T.);
#43755=ADVANCED_FACE('',(#11175),#42013,.T.);
#43756=ADVANCED_FACE('',(#11176),#8639,.T.);
#43757=ADVANCED_FACE('',(#11177),#8640,.T.);
#43758=ADVANCED_FACE('',(#11178),#42014,.T.);
#43759=ADVANCED_FACE('',(#11179),#8641,.T.);
#43760=ADVANCED_FACE('',(#11180),#42015,.T.);
#43761=ADVANCED_FACE('',(#11181),#8642,.T.);
#43762=ADVANCED_FACE('',(#11182),#8643,.T.);
#43763=ADVANCED_FACE('',(#11183),#42016,.T.);
#43764=ADVANCED_FACE('',(#11184),#8644,.T.);
#43765=ADVANCED_FACE('',(#11185),#42017,.T.);
#43766=ADVANCED_FACE('',(#11186),#8645,.T.);
#43767=ADVANCED_FACE('',(#11187),#42018,.F.);
#43768=ADVANCED_FACE('',(#11188),#8646,.F.);
#43769=ADVANCED_FACE('',(#11189),#8647,.F.);
#43770=ADVANCED_FACE('',(#11190),#42019,.F.);
#43771=ADVANCED_FACE('',(#11191),#42020,.F.);
#43772=ADVANCED_FACE('',(#11192),#8648,.F.);
#43773=ADVANCED_FACE('',(#11193),#8649,.F.);
#43774=ADVANCED_FACE('',(#11194),#42021,.F.);
#43775=ADVANCED_FACE('',(#11195),#42022,.F.);
#43776=ADVANCED_FACE('',(#11196),#8650,.F.);
#43777=ADVANCED_FACE('',(#11197),#8651,.F.);
#43778=ADVANCED_FACE('',(#11198),#42023,.F.);
#43779=ADVANCED_FACE('',(#11199),#42024,.F.);
#43780=ADVANCED_FACE('',(#11200),#8652,.F.);
#43781=ADVANCED_FACE('',(#11201),#8653,.F.);
#43782=ADVANCED_FACE('',(#11202),#42025,.F.);
#43783=ADVANCED_FACE('',(#11203),#42026,.T.);
#43784=ADVANCED_FACE('',(#11204),#42027,.T.);
#43785=ADVANCED_FACE('',(#11205),#42028,.T.);
#43786=ADVANCED_FACE('',(#11206),#42029,.T.);
#43787=ADVANCED_FACE('',(#11207),#8654,.T.);
#43788=ADVANCED_FACE('',(#11208),#42030,.T.);
#43789=ADVANCED_FACE('',(#11209),#42031,.T.);
#43790=ADVANCED_FACE('',(#11210),#8655,.T.);
#43791=ADVANCED_FACE('',(#11211),#1660,.T.);
#43792=ADVANCED_FACE('',(#11212),#1661,.T.);
#43793=ADVANCED_FACE('',(#11213),#1662,.T.);
#43794=ADVANCED_FACE('',(#11214),#8656,.F.);
#43795=ADVANCED_FACE('',(#11215),#8657,.T.);
#43796=ADVANCED_FACE('',(#11216),#1663,.T.);
#43797=ADVANCED_FACE('',(#11217),#1664,.T.);
#43798=ADVANCED_FACE('',(#11218),#1665,.T.);
#43799=ADVANCED_FACE('',(#11219),#42032,.T.);
#43800=ADVANCED_FACE('',(#11220),#42033,.T.);
#43801=ADVANCED_FACE('',(#11221),#8658,.F.);
#43802=ADVANCED_FACE('',(#11222,#724,#725,#726),#8659,.T.);
#43803=ADVANCED_FACE('',(#11223),#1666,.T.);
#43804=ADVANCED_FACE('',(#11224),#1667,.T.);
#43805=ADVANCED_FACE('',(#11225),#1668,.T.);
#43806=ADVANCED_FACE('',(#11226),#8660,.F.);
#43807=ADVANCED_FACE('',(#11227),#8661,.T.);
#43808=ADVANCED_FACE('',(#11228),#1669,.T.);
#43809=ADVANCED_FACE('',(#11229),#8662,.T.);
#43810=ADVANCED_FACE('',(#11230),#3635,.F.);
#43811=ADVANCED_FACE('',(#11231),#1670,.T.);
#43812=ADVANCED_FACE('',(#11232,#727),#8663,.F.);
#43813=ADVANCED_FACE('',(#11233,#728),#8664,.T.);
#43814=ADVANCED_FACE('',(#11234),#1671,.T.);
#43815=ADVANCED_FACE('',(#11235),#1672,.T.);
#43816=ADVANCED_FACE('',(#11236),#1673,.T.);
#43817=ADVANCED_FACE('',(#11237),#3636,.F.);
#43818=ADVANCED_FACE('',(#11238),#1674,.T.);
#43819=ADVANCED_FACE('',(#11239),#1675,.T.);
#43820=ADVANCED_FACE('',(#11240),#1676,.T.);
#43821=ADVANCED_FACE('',(#11241,#729),#8665,.F.);
#43822=ADVANCED_FACE('',(#11242,#730),#8666,.T.);
#43823=ADVANCED_FACE('',(#11243),#1677,.T.);
#43824=ADVANCED_FACE('',(#11244),#1678,.T.);
#43825=ADVANCED_FACE('',(#11245),#1679,.T.);
#43826=ADVANCED_FACE('',(#11246),#8667,.T.);
#43827=ADVANCED_FACE('',(#11247),#3637,.F.);
#43828=ADVANCED_FACE('',(#11248),#3638,.T.);
#43829=ADVANCED_FACE('',(#11249),#8668,.T.);
#43830=ADVANCED_FACE('',(#11250),#3639,.T.);
#43831=ADVANCED_FACE('',(#11251),#3640,.F.);
#43832=ADVANCED_FACE('',(#11252),#8669,.F.);
#43833=ADVANCED_FACE('',(#11253),#3641,.T.);
#43834=ADVANCED_FACE('',(#11254),#3642,.F.);
#43835=ADVANCED_FACE('',(#11255),#42034,.T.);
#43836=ADVANCED_FACE('',(#11256),#8670,.T.);
#43837=ADVANCED_FACE('',(#11257),#1680,.F.);
#43838=ADVANCED_FACE('',(#11258),#42035,.F.);
#43839=ADVANCED_FACE('',(#11259),#1681,.F.);
#43840=ADVANCED_FACE('',(#11260),#42036,.T.);
#43841=ADVANCED_FACE('',(#11261),#8671,.T.);
#43842=ADVANCED_FACE('',(#11262),#42037,.T.);
#43843=ADVANCED_FACE('',(#11263),#8672,.T.);
#43844=ADVANCED_FACE('',(#11264),#8673,.T.);
#43845=ADVANCED_FACE('',(#11265),#42038,.T.);
#43846=ADVANCED_FACE('',(#11266),#1682,.T.);
#43847=ADVANCED_FACE('',(#11267),#8674,.T.);
#43848=ADVANCED_FACE('',(#11268),#8675,.T.);
#43849=ADVANCED_FACE('',(#11269),#66,.T.);
#43850=ADVANCED_FACE('',(#11270),#1683,.T.);
#43851=ADVANCED_FACE('',(#11271),#8676,.T.);
#43852=ADVANCED_FACE('',(#11272),#8677,.T.);
#43853=ADVANCED_FACE('',(#11273),#8678,.T.);
#43854=ADVANCED_FACE('',(#11274),#67,.T.);
#43855=ADVANCED_FACE('',(#11275),#68,.T.);
#43856=ADVANCED_FACE('',(#11276),#1684,.T.);
#43857=ADVANCED_FACE('',(#11277),#8679,.T.);
#43858=ADVANCED_FACE('',(#11278),#8680,.T.);
#43859=ADVANCED_FACE('',(#11279),#69,.T.);
#43860=ADVANCED_FACE('',(#11280),#1685,.T.);
#43861=ADVANCED_FACE('',(#11281),#8681,.T.);
#43862=ADVANCED_FACE('',(#11282),#8682,.F.);
#43863=ADVANCED_FACE('',(#11283),#8683,.T.);
#43864=ADVANCED_FACE('',(#11284),#3643,.F.);
#43865=ADVANCED_FACE('',(#11285,#731),#3644,.T.);
#43866=ADVANCED_FACE('',(#11286),#3645,.T.);
#43867=ADVANCED_FACE('',(#11287,#732,#733,#734,#735,#736,#737,#738,#739,
#740,#741,#742,#743,#744,#745,#746,#747,#748,#749,#750,#751,#752,#753,#754,
#755,#756,#757,#758,#759,#760,#761,#762,#763,#764,#765,#766,#767,#768,#769,
#770,#771,#772,#773,#774,#775,#776,#777,#778,#779,#780,#781,#782,#783,#784,
#785,#786,#787,#788,#789,#790,#791),#1686,.F.);
#43868=ADVANCED_FACE('',(#11288),#42039,.F.);
#43869=ADVANCED_FACE('',(#11289),#8684,.T.);
#43870=ADVANCED_FACE('',(#11290),#8685,.F.);
#43871=ADVANCED_FACE('',(#11291),#8686,.T.);
#43872=ADVANCED_FACE('',(#11292),#8687,.F.);
#43873=ADVANCED_FACE('',(#11293),#8688,.T.);
#43874=ADVANCED_FACE('',(#11294),#8689,.F.);
#43875=ADVANCED_FACE('',(#11295),#8690,.T.);
#43876=ADVANCED_FACE('',(#11296),#8691,.F.);
#43877=ADVANCED_FACE('',(#11297),#8692,.T.);
#43878=ADVANCED_FACE('',(#11298),#8693,.F.);
#43879=ADVANCED_FACE('',(#11299),#8694,.T.);
#43880=ADVANCED_FACE('',(#11300),#8695,.F.);
#43881=ADVANCED_FACE('',(#11301),#8696,.T.);
#43882=ADVANCED_FACE('',(#11302),#8697,.F.);
#43883=ADVANCED_FACE('',(#11303),#8698,.T.);
#43884=ADVANCED_FACE('',(#11304),#8699,.F.);
#43885=ADVANCED_FACE('',(#11305),#8700,.T.);
#43886=ADVANCED_FACE('',(#11306),#8701,.F.);
#43887=ADVANCED_FACE('',(#11307),#8702,.T.);
#43888=ADVANCED_FACE('',(#11308),#8703,.F.);
#43889=ADVANCED_FACE('',(#11309),#8704,.T.);
#43890=ADVANCED_FACE('',(#11310),#8705,.F.);
#43891=ADVANCED_FACE('',(#11311),#8706,.T.);
#43892=ADVANCED_FACE('',(#11312),#8707,.F.);
#43893=ADVANCED_FACE('',(#11313),#8708,.T.);
#43894=ADVANCED_FACE('',(#11314),#8709,.F.);
#43895=ADVANCED_FACE('',(#11315),#8710,.T.);
#43896=ADVANCED_FACE('',(#11316),#8711,.F.);
#43897=ADVANCED_FACE('',(#11317),#8712,.T.);
#43898=ADVANCED_FACE('',(#11318),#8713,.F.);
#43899=ADVANCED_FACE('',(#11319),#8714,.T.);
#43900=ADVANCED_FACE('',(#11320),#8715,.F.);
#43901=ADVANCED_FACE('',(#11321),#8716,.T.);
#43902=ADVANCED_FACE('',(#11322),#8717,.F.);
#43903=ADVANCED_FACE('',(#11323),#8718,.T.);
#43904=ADVANCED_FACE('',(#11324),#8719,.F.);
#43905=ADVANCED_FACE('',(#11325),#8720,.T.);
#43906=ADVANCED_FACE('',(#11326),#8721,.F.);
#43907=ADVANCED_FACE('',(#11327),#8722,.T.);
#43908=ADVANCED_FACE('',(#11328),#8723,.F.);
#43909=ADVANCED_FACE('',(#11329),#8724,.T.);
#43910=ADVANCED_FACE('',(#11330),#8725,.F.);
#43911=ADVANCED_FACE('',(#11331),#8726,.T.);
#43912=ADVANCED_FACE('',(#11332),#8727,.F.);
#43913=ADVANCED_FACE('',(#11333),#8728,.T.);
#43914=ADVANCED_FACE('',(#11334),#8729,.F.);
#43915=ADVANCED_FACE('',(#11335),#8730,.T.);
#43916=ADVANCED_FACE('',(#11336),#8731,.F.);
#43917=ADVANCED_FACE('',(#11337),#8732,.T.);
#43918=ADVANCED_FACE('',(#11338),#8733,.F.);
#43919=ADVANCED_FACE('',(#11339),#8734,.T.);
#43920=ADVANCED_FACE('',(#11340),#8735,.F.);
#43921=ADVANCED_FACE('',(#11341),#8736,.T.);
#43922=ADVANCED_FACE('',(#11342),#8737,.F.);
#43923=ADVANCED_FACE('',(#11343),#8738,.T.);
#43924=ADVANCED_FACE('',(#11344),#8739,.F.);
#43925=ADVANCED_FACE('',(#11345),#8740,.T.);
#43926=ADVANCED_FACE('',(#11346),#8741,.F.);
#43927=ADVANCED_FACE('',(#11347),#8742,.T.);
#43928=ADVANCED_FACE('',(#11348),#8743,.F.);
#43929=ADVANCED_FACE('',(#11349),#8744,.T.);
#43930=ADVANCED_FACE('',(#11350),#8745,.F.);
#43931=ADVANCED_FACE('',(#11351),#8746,.T.);
#43932=ADVANCED_FACE('',(#11352),#8747,.F.);
#43933=ADVANCED_FACE('',(#11353),#8748,.T.);
#43934=ADVANCED_FACE('',(#11354),#8749,.F.);
#43935=ADVANCED_FACE('',(#11355),#8750,.T.);
#43936=ADVANCED_FACE('',(#11356),#8751,.F.);
#43937=ADVANCED_FACE('',(#11357),#8752,.T.);
#43938=ADVANCED_FACE('',(#11358),#8753,.F.);
#43939=ADVANCED_FACE('',(#11359),#8754,.T.);
#43940=ADVANCED_FACE('',(#11360),#8755,.F.);
#43941=ADVANCED_FACE('',(#11361),#8756,.T.);
#43942=ADVANCED_FACE('',(#11362),#8757,.F.);
#43943=ADVANCED_FACE('',(#11363),#8758,.T.);
#43944=ADVANCED_FACE('',(#11364),#8759,.F.);
#43945=ADVANCED_FACE('',(#11365),#8760,.T.);
#43946=ADVANCED_FACE('',(#11366),#8761,.F.);
#43947=ADVANCED_FACE('',(#11367),#8762,.T.);
#43948=ADVANCED_FACE('',(#11368),#8763,.F.);
#43949=ADVANCED_FACE('',(#11369),#8764,.T.);
#43950=ADVANCED_FACE('',(#11370),#8765,.F.);
#43951=ADVANCED_FACE('',(#11371),#8766,.T.);
#43952=ADVANCED_FACE('',(#11372),#8767,.F.);
#43953=ADVANCED_FACE('',(#11373),#8768,.T.);
#43954=ADVANCED_FACE('',(#11374),#8769,.F.);
#43955=ADVANCED_FACE('',(#11375),#8770,.T.);
#43956=ADVANCED_FACE('',(#11376),#8771,.F.);
#43957=ADVANCED_FACE('',(#11377),#8772,.T.);
#43958=ADVANCED_FACE('',(#11378),#8773,.F.);
#43959=ADVANCED_FACE('',(#11379),#8774,.T.);
#43960=ADVANCED_FACE('',(#11380),#8775,.F.);
#43961=ADVANCED_FACE('',(#11381),#8776,.T.);
#43962=ADVANCED_FACE('',(#11382),#8777,.F.);
#43963=ADVANCED_FACE('',(#11383),#8778,.T.);
#43964=ADVANCED_FACE('',(#11384),#8779,.F.);
#43965=ADVANCED_FACE('',(#11385),#8780,.T.);
#43966=ADVANCED_FACE('',(#11386),#8781,.F.);
#43967=ADVANCED_FACE('',(#11387),#8782,.T.);
#43968=ADVANCED_FACE('',(#11388),#8783,.F.);
#43969=ADVANCED_FACE('',(#11389),#8784,.T.);
#43970=ADVANCED_FACE('',(#11390),#8785,.F.);
#43971=ADVANCED_FACE('',(#11391),#8786,.T.);
#43972=ADVANCED_FACE('',(#11392),#8787,.F.);
#43973=ADVANCED_FACE('',(#11393),#8788,.T.);
#43974=ADVANCED_FACE('',(#11394),#8789,.F.);
#43975=ADVANCED_FACE('',(#11395),#8790,.T.);
#43976=ADVANCED_FACE('',(#11396),#8791,.F.);
#43977=ADVANCED_FACE('',(#11397),#8792,.T.);
#43978=ADVANCED_FACE('',(#11398),#8793,.F.);
#43979=ADVANCED_FACE('',(#11399),#8794,.T.);
#43980=ADVANCED_FACE('',(#11400),#8795,.F.);
#43981=ADVANCED_FACE('',(#11401),#8796,.T.);
#43982=ADVANCED_FACE('',(#11402),#8797,.F.);
#43983=ADVANCED_FACE('',(#11403),#8798,.T.);
#43984=ADVANCED_FACE('',(#11404),#8799,.F.);
#43985=ADVANCED_FACE('',(#11405),#8800,.T.);
#43986=ADVANCED_FACE('',(#11406),#8801,.F.);
#43987=ADVANCED_FACE('',(#11407),#8802,.T.);
#43988=ADVANCED_FACE('',(#11408),#8803,.F.);
#43989=ADVANCED_FACE('',(#11409),#8804,.T.);
#43990=ADVANCED_FACE('',(#11410),#8805,.F.);
#43991=ADVANCED_FACE('',(#11411),#8806,.T.);
#43992=ADVANCED_FACE('',(#11412),#8807,.F.);
#43993=ADVANCED_FACE('',(#11413),#8808,.T.);
#43994=ADVANCED_FACE('',(#11414),#8809,.F.);
#43995=ADVANCED_FACE('',(#11415),#8810,.T.);
#43996=ADVANCED_FACE('',(#11416),#8811,.F.);
#43997=ADVANCED_FACE('',(#11417),#8812,.T.);
#43998=ADVANCED_FACE('',(#11418),#8813,.F.);
#43999=ADVANCED_FACE('',(#11419),#8814,.T.);
#44000=ADVANCED_FACE('',(#11420),#8815,.F.);
#44001=ADVANCED_FACE('',(#11421),#8816,.T.);
#44002=ADVANCED_FACE('',(#11422),#8817,.F.);
#44003=ADVANCED_FACE('',(#11423),#8818,.T.);
#44004=ADVANCED_FACE('',(#11424),#8819,.F.);
#44005=ADVANCED_FACE('',(#11425),#8820,.T.);
#44006=ADVANCED_FACE('',(#11426),#8821,.F.);
#44007=ADVANCED_FACE('',(#11427),#8822,.T.);
#44008=ADVANCED_FACE('',(#11428),#8823,.F.);
#44009=ADVANCED_FACE('',(#11429),#8824,.T.);
#44010=ADVANCED_FACE('',(#11430),#8825,.F.);
#44011=ADVANCED_FACE('',(#11431),#8826,.T.);
#44012=ADVANCED_FACE('',(#11432),#8827,.F.);
#44013=ADVANCED_FACE('',(#11433),#8828,.T.);
#44014=ADVANCED_FACE('',(#11434),#8829,.F.);
#44015=ADVANCED_FACE('',(#11435),#8830,.T.);
#44016=ADVANCED_FACE('',(#11436),#8831,.F.);
#44017=ADVANCED_FACE('',(#11437),#8832,.T.);
#44018=ADVANCED_FACE('',(#11438),#8833,.F.);
#44019=ADVANCED_FACE('',(#11439),#8834,.T.);
#44020=ADVANCED_FACE('',(#11440),#8835,.F.);
#44021=ADVANCED_FACE('',(#11441),#8836,.T.);
#44022=ADVANCED_FACE('',(#11442),#8837,.F.);
#44023=ADVANCED_FACE('',(#11443),#8838,.T.);
#44024=ADVANCED_FACE('',(#11444),#8839,.F.);
#44025=ADVANCED_FACE('',(#11445),#8840,.T.);
#44026=ADVANCED_FACE('',(#11446),#8841,.F.);
#44027=ADVANCED_FACE('',(#11447),#8842,.T.);
#44028=ADVANCED_FACE('',(#11448),#8843,.F.);
#44029=ADVANCED_FACE('',(#11449),#8844,.T.);
#44030=ADVANCED_FACE('',(#11450),#8845,.F.);
#44031=ADVANCED_FACE('',(#11451),#8846,.T.);
#44032=ADVANCED_FACE('',(#11452),#8847,.F.);
#44033=ADVANCED_FACE('',(#11453),#8848,.T.);
#44034=ADVANCED_FACE('',(#11454),#8849,.F.);
#44035=ADVANCED_FACE('',(#11455),#8850,.T.);
#44036=ADVANCED_FACE('',(#11456),#8851,.F.);
#44037=ADVANCED_FACE('',(#11457),#8852,.T.);
#44038=ADVANCED_FACE('',(#11458),#8853,.F.);
#44039=ADVANCED_FACE('',(#11459),#8854,.T.);
#44040=ADVANCED_FACE('',(#11460),#8855,.F.);
#44041=ADVANCED_FACE('',(#11461),#8856,.T.);
#44042=ADVANCED_FACE('',(#11462),#8857,.F.);
#44043=ADVANCED_FACE('',(#11463),#8858,.T.);
#44044=ADVANCED_FACE('',(#11464),#8859,.F.);
#44045=ADVANCED_FACE('',(#11465),#8860,.T.);
#44046=ADVANCED_FACE('',(#11466),#8861,.F.);
#44047=ADVANCED_FACE('',(#11467),#8862,.T.);
#44048=ADVANCED_FACE('',(#11468),#8863,.F.);
#44049=ADVANCED_FACE('',(#11469),#8864,.T.);
#44050=ADVANCED_FACE('',(#11470),#8865,.F.);
#44051=ADVANCED_FACE('',(#11471),#8866,.T.);
#44052=ADVANCED_FACE('',(#11472),#8867,.F.);
#44053=ADVANCED_FACE('',(#11473),#8868,.T.);
#44054=ADVANCED_FACE('',(#11474),#8869,.F.);
#44055=ADVANCED_FACE('',(#11475),#8870,.T.);
#44056=ADVANCED_FACE('',(#11476),#8871,.F.);
#44057=ADVANCED_FACE('',(#11477),#8872,.T.);
#44058=ADVANCED_FACE('',(#11478),#8873,.F.);
#44059=ADVANCED_FACE('',(#11479),#8874,.T.);
#44060=ADVANCED_FACE('',(#11480),#8875,.F.);
#44061=ADVANCED_FACE('',(#11481),#8876,.T.);
#44062=ADVANCED_FACE('',(#11482),#8877,.F.);
#44063=ADVANCED_FACE('',(#11483),#8878,.T.);
#44064=ADVANCED_FACE('',(#11484),#8879,.F.);
#44065=ADVANCED_FACE('',(#11485),#8880,.T.);
#44066=ADVANCED_FACE('',(#11486),#8881,.F.);
#44067=ADVANCED_FACE('',(#11487),#8882,.T.);
#44068=ADVANCED_FACE('',(#11488),#8883,.F.);
#44069=ADVANCED_FACE('',(#11489),#8884,.T.);
#44070=ADVANCED_FACE('',(#11490),#8885,.F.);
#44071=ADVANCED_FACE('',(#11491),#8886,.T.);
#44072=ADVANCED_FACE('',(#11492),#8887,.F.);
#44073=ADVANCED_FACE('',(#11493),#8888,.T.);
#44074=ADVANCED_FACE('',(#11494),#8889,.F.);
#44075=ADVANCED_FACE('',(#11495),#8890,.T.);
#44076=ADVANCED_FACE('',(#11496),#8891,.F.);
#44077=ADVANCED_FACE('',(#11497),#8892,.T.);
#44078=ADVANCED_FACE('',(#11498),#8893,.F.);
#44079=ADVANCED_FACE('',(#11499),#8894,.T.);
#44080=ADVANCED_FACE('',(#11500),#8895,.F.);
#44081=ADVANCED_FACE('',(#11501),#8896,.T.);
#44082=ADVANCED_FACE('',(#11502),#8897,.F.);
#44083=ADVANCED_FACE('',(#11503),#8898,.T.);
#44084=ADVANCED_FACE('',(#11504),#8899,.F.);
#44085=ADVANCED_FACE('',(#11505),#8900,.T.);
#44086=ADVANCED_FACE('',(#11506),#8901,.F.);
#44087=ADVANCED_FACE('',(#11507),#8902,.T.);
#44088=ADVANCED_FACE('',(#11508),#8903,.F.);
#44089=ADVANCED_FACE('',(#11509),#8904,.T.);
#44090=ADVANCED_FACE('',(#11510),#8905,.F.);
#44091=ADVANCED_FACE('',(#11511),#8906,.T.);
#44092=ADVANCED_FACE('',(#11512),#8907,.F.);
#44093=ADVANCED_FACE('',(#11513),#8908,.T.);
#44094=ADVANCED_FACE('',(#11514),#8909,.F.);
#44095=ADVANCED_FACE('',(#11515),#8910,.T.);
#44096=ADVANCED_FACE('',(#11516),#8911,.F.);
#44097=ADVANCED_FACE('',(#11517),#8912,.T.);
#44098=ADVANCED_FACE('',(#11518),#8913,.F.);
#44099=ADVANCED_FACE('',(#11519),#8914,.T.);
#44100=ADVANCED_FACE('',(#11520),#8915,.F.);
#44101=ADVANCED_FACE('',(#11521),#8916,.T.);
#44102=ADVANCED_FACE('',(#11522),#8917,.F.);
#44103=ADVANCED_FACE('',(#11523),#8918,.T.);
#44104=ADVANCED_FACE('',(#11524),#8919,.F.);
#44105=ADVANCED_FACE('',(#11525),#8920,.T.);
#44106=ADVANCED_FACE('',(#11526),#8921,.F.);
#44107=ADVANCED_FACE('',(#11527),#8922,.T.);
#44108=ADVANCED_FACE('',(#11528),#8923,.F.);
#44109=ADVANCED_FACE('',(#11529),#8924,.T.);
#44110=ADVANCED_FACE('',(#11530),#8925,.F.);
#44111=ADVANCED_FACE('',(#11531),#8926,.T.);
#44112=ADVANCED_FACE('',(#11532),#8927,.F.);
#44113=ADVANCED_FACE('',(#11533),#8928,.T.);
#44114=ADVANCED_FACE('',(#11534),#8929,.F.);
#44115=ADVANCED_FACE('',(#11535),#8930,.T.);
#44116=ADVANCED_FACE('',(#11536),#8931,.F.);
#44117=ADVANCED_FACE('',(#11537),#8932,.T.);
#44118=ADVANCED_FACE('',(#11538),#8933,.F.);
#44119=ADVANCED_FACE('',(#11539),#8934,.T.);
#44120=ADVANCED_FACE('',(#11540),#8935,.F.);
#44121=ADVANCED_FACE('',(#11541),#8936,.T.);
#44122=ADVANCED_FACE('',(#11542),#8937,.F.);
#44123=ADVANCED_FACE('',(#11543),#8938,.T.);
#44124=ADVANCED_FACE('',(#11544),#8939,.F.);
#44125=ADVANCED_FACE('',(#11545),#8940,.T.);
#44126=ADVANCED_FACE('',(#11546),#8941,.F.);
#44127=ADVANCED_FACE('',(#11547),#8942,.T.);
#44128=ADVANCED_FACE('',(#11548),#8943,.F.);
#44129=ADVANCED_FACE('',(#11549),#8944,.T.);
#44130=ADVANCED_FACE('',(#11550),#8945,.F.);
#44131=ADVANCED_FACE('',(#11551),#8946,.T.);
#44132=ADVANCED_FACE('',(#11552),#8947,.F.);
#44133=ADVANCED_FACE('',(#11553),#8948,.T.);
#44134=ADVANCED_FACE('',(#11554),#8949,.F.);
#44135=ADVANCED_FACE('',(#11555),#8950,.T.);
#44136=ADVANCED_FACE('',(#11556),#8951,.F.);
#44137=ADVANCED_FACE('',(#11557),#8952,.T.);
#44138=ADVANCED_FACE('',(#11558),#8953,.F.);
#44139=ADVANCED_FACE('',(#11559),#8954,.T.);
#44140=ADVANCED_FACE('',(#11560),#8955,.F.);
#44141=ADVANCED_FACE('',(#11561),#8956,.T.);
#44142=ADVANCED_FACE('',(#11562),#8957,.F.);
#44143=ADVANCED_FACE('',(#11563),#8958,.T.);
#44144=ADVANCED_FACE('',(#11564),#8959,.F.);
#44145=ADVANCED_FACE('',(#11565),#8960,.T.);
#44146=ADVANCED_FACE('',(#11566),#8961,.F.);
#44147=ADVANCED_FACE('',(#11567),#8962,.T.);
#44148=ADVANCED_FACE('',(#11568),#8963,.F.);
#44149=ADVANCED_FACE('',(#11569),#8964,.T.);
#44150=ADVANCED_FACE('',(#11570),#8965,.F.);
#44151=ADVANCED_FACE('',(#11571),#8966,.T.);
#44152=ADVANCED_FACE('',(#11572),#8967,.F.);
#44153=ADVANCED_FACE('',(#11573),#8968,.T.);
#44154=ADVANCED_FACE('',(#11574),#8969,.F.);
#44155=ADVANCED_FACE('',(#11575),#8970,.T.);
#44156=ADVANCED_FACE('',(#11576),#8971,.F.);
#44157=ADVANCED_FACE('',(#11577),#8972,.T.);
#44158=ADVANCED_FACE('',(#11578),#8973,.F.);
#44159=ADVANCED_FACE('',(#11579),#8974,.T.);
#44160=ADVANCED_FACE('',(#11580),#8975,.F.);
#44161=ADVANCED_FACE('',(#11581),#8976,.T.);
#44162=ADVANCED_FACE('',(#11582),#8977,.F.);
#44163=ADVANCED_FACE('',(#11583),#8978,.T.);
#44164=ADVANCED_FACE('',(#11584),#8979,.F.);
#44165=ADVANCED_FACE('',(#11585),#8980,.T.);
#44166=ADVANCED_FACE('',(#11586),#8981,.F.);
#44167=ADVANCED_FACE('',(#11587),#8982,.T.);
#44168=ADVANCED_FACE('',(#11588),#8983,.F.);
#44169=ADVANCED_FACE('',(#11589),#8984,.T.);
#44170=ADVANCED_FACE('',(#11590),#8985,.F.);
#44171=ADVANCED_FACE('',(#11591),#8986,.T.);
#44172=ADVANCED_FACE('',(#11592),#8987,.F.);
#44173=ADVANCED_FACE('',(#11593),#8988,.T.);
#44174=ADVANCED_FACE('',(#11594),#8989,.F.);
#44175=ADVANCED_FACE('',(#11595),#8990,.T.);
#44176=ADVANCED_FACE('',(#11596),#8991,.F.);
#44177=ADVANCED_FACE('',(#11597),#8992,.T.);
#44178=ADVANCED_FACE('',(#11598),#8993,.F.);
#44179=ADVANCED_FACE('',(#11599),#8994,.T.);
#44180=ADVANCED_FACE('',(#11600),#8995,.F.);
#44181=ADVANCED_FACE('',(#11601),#8996,.T.);
#44182=ADVANCED_FACE('',(#11602),#8997,.F.);
#44183=ADVANCED_FACE('',(#11603),#8998,.T.);
#44184=ADVANCED_FACE('',(#11604),#8999,.F.);
#44185=ADVANCED_FACE('',(#11605),#9000,.T.);
#44186=ADVANCED_FACE('',(#11606),#9001,.F.);
#44187=ADVANCED_FACE('',(#11607),#9002,.T.);
#44188=ADVANCED_FACE('',(#11608),#9003,.F.);
#44189=ADVANCED_FACE('',(#11609),#9004,.T.);
#44190=ADVANCED_FACE('',(#11610),#9005,.F.);
#44191=ADVANCED_FACE('',(#11611),#9006,.T.);
#44192=ADVANCED_FACE('',(#11612),#9007,.F.);
#44193=ADVANCED_FACE('',(#11613),#9008,.T.);
#44194=ADVANCED_FACE('',(#11614),#9009,.F.);
#44195=ADVANCED_FACE('',(#11615),#9010,.T.);
#44196=ADVANCED_FACE('',(#11616),#9011,.F.);
#44197=ADVANCED_FACE('',(#11617),#9012,.T.);
#44198=ADVANCED_FACE('',(#11618),#9013,.F.);
#44199=ADVANCED_FACE('',(#11619),#9014,.T.);
#44200=ADVANCED_FACE('',(#11620),#9015,.F.);
#44201=ADVANCED_FACE('',(#11621),#9016,.T.);
#44202=ADVANCED_FACE('',(#11622),#9017,.F.);
#44203=ADVANCED_FACE('',(#11623),#9018,.T.);
#44204=ADVANCED_FACE('',(#11624),#9019,.F.);
#44205=ADVANCED_FACE('',(#11625),#9020,.T.);
#44206=ADVANCED_FACE('',(#11626),#9021,.F.);
#44207=ADVANCED_FACE('',(#11627),#9022,.T.);
#44208=ADVANCED_FACE('',(#11628),#9023,.F.);
#44209=ADVANCED_FACE('',(#11629),#9024,.T.);
#44210=ADVANCED_FACE('',(#11630),#9025,.F.);
#44211=ADVANCED_FACE('',(#11631),#9026,.T.);
#44212=ADVANCED_FACE('',(#11632),#9027,.F.);
#44213=ADVANCED_FACE('',(#11633),#9028,.T.);
#44214=ADVANCED_FACE('',(#11634),#9029,.F.);
#44215=ADVANCED_FACE('',(#11635),#9030,.T.);
#44216=ADVANCED_FACE('',(#11636),#9031,.F.);
#44217=ADVANCED_FACE('',(#11637),#9032,.T.);
#44218=ADVANCED_FACE('',(#11638),#9033,.F.);
#44219=ADVANCED_FACE('',(#11639),#9034,.T.);
#44220=ADVANCED_FACE('',(#11640),#9035,.F.);
#44221=ADVANCED_FACE('',(#11641),#9036,.T.);
#44222=ADVANCED_FACE('',(#11642),#9037,.F.);
#44223=ADVANCED_FACE('',(#11643),#9038,.T.);
#44224=ADVANCED_FACE('',(#11644),#9039,.F.);
#44225=ADVANCED_FACE('',(#11645),#9040,.T.);
#44226=ADVANCED_FACE('',(#11646),#9041,.F.);
#44227=ADVANCED_FACE('',(#11647),#9042,.T.);
#44228=ADVANCED_FACE('',(#11648),#9043,.F.);
#44229=ADVANCED_FACE('',(#11649),#9044,.T.);
#44230=ADVANCED_FACE('',(#11650),#9045,.F.);
#44231=ADVANCED_FACE('',(#11651),#9046,.T.);
#44232=ADVANCED_FACE('',(#11652),#9047,.F.);
#44233=ADVANCED_FACE('',(#11653),#9048,.T.);
#44234=ADVANCED_FACE('',(#11654),#9049,.F.);
#44235=ADVANCED_FACE('',(#11655),#9050,.T.);
#44236=ADVANCED_FACE('',(#11656),#9051,.F.);
#44237=ADVANCED_FACE('',(#11657),#9052,.T.);
#44238=ADVANCED_FACE('',(#11658),#9053,.F.);
#44239=ADVANCED_FACE('',(#11659),#9054,.T.);
#44240=ADVANCED_FACE('',(#11660),#9055,.F.);
#44241=ADVANCED_FACE('',(#11661),#9056,.T.);
#44242=ADVANCED_FACE('',(#11662),#9057,.F.);
#44243=ADVANCED_FACE('',(#11663),#9058,.T.);
#44244=ADVANCED_FACE('',(#11664),#9059,.F.);
#44245=ADVANCED_FACE('',(#11665),#9060,.T.);
#44246=ADVANCED_FACE('',(#11666),#9061,.F.);
#44247=ADVANCED_FACE('',(#11667),#9062,.T.);
#44248=ADVANCED_FACE('',(#11668),#9063,.F.);
#44249=ADVANCED_FACE('',(#11669),#9064,.T.);
#44250=ADVANCED_FACE('',(#11670),#9065,.F.);
#44251=ADVANCED_FACE('',(#11671),#9066,.T.);
#44252=ADVANCED_FACE('',(#11672),#9067,.F.);
#44253=ADVANCED_FACE('',(#11673),#9068,.T.);
#44254=ADVANCED_FACE('',(#11674),#9069,.F.);
#44255=ADVANCED_FACE('',(#11675),#9070,.T.);
#44256=ADVANCED_FACE('',(#11676),#9071,.F.);
#44257=ADVANCED_FACE('',(#11677),#9072,.T.);
#44258=ADVANCED_FACE('',(#11678),#9073,.F.);
#44259=ADVANCED_FACE('',(#11679),#9074,.T.);
#44260=ADVANCED_FACE('',(#11680),#9075,.F.);
#44261=ADVANCED_FACE('',(#11681),#9076,.T.);
#44262=ADVANCED_FACE('',(#11682),#9077,.F.);
#44263=ADVANCED_FACE('',(#11683),#9078,.T.);
#44264=ADVANCED_FACE('',(#11684),#9079,.F.);
#44265=ADVANCED_FACE('',(#11685),#9080,.T.);
#44266=ADVANCED_FACE('',(#11686),#9081,.F.);
#44267=ADVANCED_FACE('',(#11687),#9082,.T.);
#44268=ADVANCED_FACE('',(#11688),#9083,.F.);
#44269=ADVANCED_FACE('',(#11689),#9084,.T.);
#44270=ADVANCED_FACE('',(#11690),#9085,.F.);
#44271=ADVANCED_FACE('',(#11691),#9086,.T.);
#44272=ADVANCED_FACE('',(#11692),#9087,.F.);
#44273=ADVANCED_FACE('',(#11693),#9088,.T.);
#44274=ADVANCED_FACE('',(#11694),#9089,.F.);
#44275=ADVANCED_FACE('',(#11695),#9090,.T.);
#44276=ADVANCED_FACE('',(#11696),#9091,.F.);
#44277=ADVANCED_FACE('',(#11697),#9092,.T.);
#44278=ADVANCED_FACE('',(#11698),#9093,.F.);
#44279=ADVANCED_FACE('',(#11699),#9094,.T.);
#44280=ADVANCED_FACE('',(#11700),#9095,.F.);
#44281=ADVANCED_FACE('',(#11701),#9096,.T.);
#44282=ADVANCED_FACE('',(#11702),#9097,.F.);
#44283=ADVANCED_FACE('',(#11703),#9098,.T.);
#44284=ADVANCED_FACE('',(#11704),#9099,.F.);
#44285=ADVANCED_FACE('',(#11705),#9100,.T.);
#44286=ADVANCED_FACE('',(#11706),#9101,.F.);
#44287=ADVANCED_FACE('',(#11707),#9102,.T.);
#44288=ADVANCED_FACE('',(#11708),#9103,.F.);
#44289=ADVANCED_FACE('',(#11709),#9104,.T.);
#44290=ADVANCED_FACE('',(#11710),#9105,.F.);
#44291=ADVANCED_FACE('',(#11711),#9106,.T.);
#44292=ADVANCED_FACE('',(#11712),#9107,.F.);
#44293=ADVANCED_FACE('',(#11713),#9108,.T.);
#44294=ADVANCED_FACE('',(#11714),#9109,.F.);
#44295=ADVANCED_FACE('',(#11715),#9110,.T.);
#44296=ADVANCED_FACE('',(#11716),#9111,.F.);
#44297=ADVANCED_FACE('',(#11717),#9112,.T.);
#44298=ADVANCED_FACE('',(#11718),#9113,.F.);
#44299=ADVANCED_FACE('',(#11719),#9114,.T.);
#44300=ADVANCED_FACE('',(#11720),#9115,.F.);
#44301=ADVANCED_FACE('',(#11721),#9116,.T.);
#44302=ADVANCED_FACE('',(#11722),#9117,.F.);
#44303=ADVANCED_FACE('',(#11723),#9118,.T.);
#44304=ADVANCED_FACE('',(#11724),#9119,.F.);
#44305=ADVANCED_FACE('',(#11725),#9120,.T.);
#44306=ADVANCED_FACE('',(#11726),#9121,.F.);
#44307=ADVANCED_FACE('',(#11727),#9122,.T.);
#44308=ADVANCED_FACE('',(#11728),#9123,.F.);
#44309=ADVANCED_FACE('',(#11729),#9124,.T.);
#44310=ADVANCED_FACE('',(#11730),#9125,.F.);
#44311=ADVANCED_FACE('',(#11731),#9126,.T.);
#44312=ADVANCED_FACE('',(#11732),#9127,.F.);
#44313=ADVANCED_FACE('',(#11733),#9128,.T.);
#44314=ADVANCED_FACE('',(#11734),#9129,.F.);
#44315=ADVANCED_FACE('',(#11735),#9130,.T.);
#44316=ADVANCED_FACE('',(#11736),#9131,.F.);
#44317=ADVANCED_FACE('',(#11737),#9132,.T.);
#44318=ADVANCED_FACE('',(#11738),#9133,.F.);
#44319=ADVANCED_FACE('',(#11739),#9134,.T.);
#44320=ADVANCED_FACE('',(#11740),#9135,.F.);
#44321=ADVANCED_FACE('',(#11741),#9136,.T.);
#44322=ADVANCED_FACE('',(#11742),#9137,.F.);
#44323=ADVANCED_FACE('',(#11743),#9138,.T.);
#44324=ADVANCED_FACE('',(#11744),#9139,.F.);
#44325=ADVANCED_FACE('',(#11745),#9140,.T.);
#44326=ADVANCED_FACE('',(#11746),#9141,.F.);
#44327=ADVANCED_FACE('',(#11747),#9142,.T.);
#44328=ADVANCED_FACE('',(#11748),#9143,.F.);
#44329=ADVANCED_FACE('',(#11749),#9144,.T.);
#44330=ADVANCED_FACE('',(#11750),#9145,.F.);
#44331=ADVANCED_FACE('',(#11751),#9146,.T.);
#44332=ADVANCED_FACE('',(#11752),#9147,.F.);
#44333=ADVANCED_FACE('',(#11753),#9148,.T.);
#44334=ADVANCED_FACE('',(#11754),#9149,.F.);
#44335=ADVANCED_FACE('',(#11755),#9150,.T.);
#44336=ADVANCED_FACE('',(#11756),#9151,.F.);
#44337=ADVANCED_FACE('',(#11757),#9152,.T.);
#44338=ADVANCED_FACE('',(#11758),#9153,.F.);
#44339=ADVANCED_FACE('',(#11759),#9154,.T.);
#44340=ADVANCED_FACE('',(#11760),#9155,.F.);
#44341=ADVANCED_FACE('',(#11761),#9156,.T.);
#44342=ADVANCED_FACE('',(#11762),#9157,.F.);
#44343=ADVANCED_FACE('',(#11763),#9158,.T.);
#44344=ADVANCED_FACE('',(#11764),#9159,.F.);
#44345=ADVANCED_FACE('',(#11765),#9160,.T.);
#44346=ADVANCED_FACE('',(#11766),#9161,.F.);
#44347=ADVANCED_FACE('',(#11767),#9162,.T.);
#44348=ADVANCED_FACE('',(#11768),#9163,.F.);
#44349=ADVANCED_FACE('',(#11769),#9164,.T.);
#44350=ADVANCED_FACE('',(#11770),#9165,.F.);
#44351=ADVANCED_FACE('',(#11771),#9166,.T.);
#44352=ADVANCED_FACE('',(#11772),#9167,.F.);
#44353=ADVANCED_FACE('',(#11773),#9168,.T.);
#44354=ADVANCED_FACE('',(#11774),#9169,.F.);
#44355=ADVANCED_FACE('',(#11775),#9170,.T.);
#44356=ADVANCED_FACE('',(#11776),#9171,.F.);
#44357=ADVANCED_FACE('',(#11777),#9172,.T.);
#44358=ADVANCED_FACE('',(#11778),#9173,.F.);
#44359=ADVANCED_FACE('',(#11779),#9174,.T.);
#44360=ADVANCED_FACE('',(#11780),#9175,.F.);
#44361=ADVANCED_FACE('',(#11781),#9176,.T.);
#44362=ADVANCED_FACE('',(#11782),#9177,.F.);
#44363=ADVANCED_FACE('',(#11783),#9178,.T.);
#44364=ADVANCED_FACE('',(#11784),#9179,.F.);
#44365=ADVANCED_FACE('',(#11785),#9180,.T.);
#44366=ADVANCED_FACE('',(#11786),#9181,.F.);
#44367=ADVANCED_FACE('',(#11787),#9182,.T.);
#44368=ADVANCED_FACE('',(#11788),#9183,.F.);
#44369=ADVANCED_FACE('',(#11789),#9184,.T.);
#44370=ADVANCED_FACE('',(#11790),#9185,.F.);
#44371=ADVANCED_FACE('',(#11791),#9186,.T.);
#44372=ADVANCED_FACE('',(#11792),#9187,.F.);
#44373=ADVANCED_FACE('',(#11793),#9188,.T.);
#44374=ADVANCED_FACE('',(#11794),#9189,.F.);
#44375=ADVANCED_FACE('',(#11795),#9190,.T.);
#44376=ADVANCED_FACE('',(#11796),#9191,.F.);
#44377=ADVANCED_FACE('',(#11797),#9192,.T.);
#44378=ADVANCED_FACE('',(#11798),#9193,.F.);
#44379=ADVANCED_FACE('',(#11799),#9194,.T.);
#44380=ADVANCED_FACE('',(#11800),#9195,.F.);
#44381=ADVANCED_FACE('',(#11801),#9196,.T.);
#44382=ADVANCED_FACE('',(#11802),#9197,.F.);
#44383=ADVANCED_FACE('',(#11803),#9198,.T.);
#44384=ADVANCED_FACE('',(#11804),#9199,.F.);
#44385=ADVANCED_FACE('',(#11805),#9200,.T.);
#44386=ADVANCED_FACE('',(#11806),#9201,.F.);
#44387=ADVANCED_FACE('',(#11807),#9202,.T.);
#44388=ADVANCED_FACE('',(#11808),#9203,.F.);
#44389=ADVANCED_FACE('',(#11809),#9204,.T.);
#44390=ADVANCED_FACE('',(#11810),#9205,.F.);
#44391=ADVANCED_FACE('',(#11811),#9206,.T.);
#44392=ADVANCED_FACE('',(#11812),#9207,.F.);
#44393=ADVANCED_FACE('',(#11813),#9208,.T.);
#44394=ADVANCED_FACE('',(#11814),#9209,.F.);
#44395=ADVANCED_FACE('',(#11815),#9210,.T.);
#44396=ADVANCED_FACE('',(#11816),#9211,.F.);
#44397=ADVANCED_FACE('',(#11817),#9212,.T.);
#44398=ADVANCED_FACE('',(#11818),#9213,.F.);
#44399=ADVANCED_FACE('',(#11819),#9214,.T.);
#44400=ADVANCED_FACE('',(#11820),#9215,.F.);
#44401=ADVANCED_FACE('',(#11821),#9216,.T.);
#44402=ADVANCED_FACE('',(#11822),#9217,.F.);
#44403=ADVANCED_FACE('',(#11823),#9218,.T.);
#44404=ADVANCED_FACE('',(#11824),#9219,.F.);
#44405=ADVANCED_FACE('',(#11825),#9220,.T.);
#44406=ADVANCED_FACE('',(#11826),#9221,.F.);
#44407=ADVANCED_FACE('',(#11827),#9222,.T.);
#44408=ADVANCED_FACE('',(#11828),#9223,.F.);
#44409=ADVANCED_FACE('',(#11829),#9224,.T.);
#44410=ADVANCED_FACE('',(#11830),#9225,.F.);
#44411=ADVANCED_FACE('',(#11831),#9226,.T.);
#44412=ADVANCED_FACE('',(#11832),#9227,.F.);
#44413=ADVANCED_FACE('',(#11833),#9228,.T.);
#44414=ADVANCED_FACE('',(#11834),#9229,.F.);
#44415=ADVANCED_FACE('',(#11835),#9230,.T.);
#44416=ADVANCED_FACE('',(#11836),#9231,.F.);
#44417=ADVANCED_FACE('',(#11837),#9232,.T.);
#44418=ADVANCED_FACE('',(#11838),#9233,.F.);
#44419=ADVANCED_FACE('',(#11839),#9234,.T.);
#44420=ADVANCED_FACE('',(#11840),#9235,.F.);
#44421=ADVANCED_FACE('',(#11841),#9236,.T.);
#44422=ADVANCED_FACE('',(#11842),#9237,.F.);
#44423=ADVANCED_FACE('',(#11843),#9238,.T.);
#44424=ADVANCED_FACE('',(#11844),#9239,.F.);
#44425=ADVANCED_FACE('',(#11845),#9240,.T.);
#44426=ADVANCED_FACE('',(#11846),#9241,.F.);
#44427=ADVANCED_FACE('',(#11847),#9242,.T.);
#44428=ADVANCED_FACE('',(#11848),#9243,.F.);
#44429=ADVANCED_FACE('',(#11849),#9244,.T.);
#44430=ADVANCED_FACE('',(#11850),#9245,.F.);
#44431=ADVANCED_FACE('',(#11851),#9246,.T.);
#44432=ADVANCED_FACE('',(#11852),#9247,.F.);
#44433=ADVANCED_FACE('',(#11853),#9248,.T.);
#44434=ADVANCED_FACE('',(#11854),#9249,.F.);
#44435=ADVANCED_FACE('',(#11855),#9250,.T.);
#44436=ADVANCED_FACE('',(#11856),#9251,.F.);
#44437=ADVANCED_FACE('',(#11857),#9252,.T.);
#44438=ADVANCED_FACE('',(#11858),#9253,.F.);
#44439=ADVANCED_FACE('',(#11859),#9254,.T.);
#44440=ADVANCED_FACE('',(#11860),#9255,.F.);
#44441=ADVANCED_FACE('',(#11861),#9256,.T.);
#44442=ADVANCED_FACE('',(#11862),#9257,.F.);
#44443=ADVANCED_FACE('',(#11863),#9258,.T.);
#44444=ADVANCED_FACE('',(#11864),#9259,.F.);
#44445=ADVANCED_FACE('',(#11865),#9260,.T.);
#44446=ADVANCED_FACE('',(#11866),#9261,.F.);
#44447=ADVANCED_FACE('',(#11867),#9262,.T.);
#44448=ADVANCED_FACE('',(#11868),#9263,.F.);
#44449=ADVANCED_FACE('',(#11869),#9264,.T.);
#44450=ADVANCED_FACE('',(#11870),#9265,.F.);
#44451=ADVANCED_FACE('',(#11871),#9266,.T.);
#44452=ADVANCED_FACE('',(#11872),#9267,.F.);
#44453=ADVANCED_FACE('',(#11873),#9268,.T.);
#44454=ADVANCED_FACE('',(#11874),#9269,.F.);
#44455=ADVANCED_FACE('',(#11875),#9270,.T.);
#44456=ADVANCED_FACE('',(#11876),#9271,.F.);
#44457=ADVANCED_FACE('',(#11877),#9272,.T.);
#44458=ADVANCED_FACE('',(#11878),#9273,.F.);
#44459=ADVANCED_FACE('',(#11879),#9274,.T.);
#44460=ADVANCED_FACE('',(#11880),#9275,.F.);
#44461=ADVANCED_FACE('',(#11881),#9276,.T.);
#44462=ADVANCED_FACE('',(#11882),#9277,.F.);
#44463=ADVANCED_FACE('',(#11883),#9278,.T.);
#44464=ADVANCED_FACE('',(#11884),#9279,.F.);
#44465=ADVANCED_FACE('',(#11885),#9280,.T.);
#44466=ADVANCED_FACE('',(#11886),#9281,.F.);
#44467=ADVANCED_FACE('',(#11887),#9282,.T.);
#44468=ADVANCED_FACE('',(#11888),#9283,.F.);
#44469=ADVANCED_FACE('',(#11889),#9284,.T.);
#44470=ADVANCED_FACE('',(#11890),#9285,.F.);
#44471=ADVANCED_FACE('',(#11891),#9286,.T.);
#44472=ADVANCED_FACE('',(#11892),#9287,.F.);
#44473=ADVANCED_FACE('',(#11893),#9288,.T.);
#44474=ADVANCED_FACE('',(#11894),#9289,.F.);
#44475=ADVANCED_FACE('',(#11895),#9290,.T.);
#44476=ADVANCED_FACE('',(#11896),#9291,.F.);
#44477=ADVANCED_FACE('',(#11897),#9292,.T.);
#44478=ADVANCED_FACE('',(#11898),#9293,.F.);
#44479=ADVANCED_FACE('',(#11899),#9294,.T.);
#44480=ADVANCED_FACE('',(#11900),#9295,.F.);
#44481=ADVANCED_FACE('',(#11901),#9296,.T.);
#44482=ADVANCED_FACE('',(#11902),#9297,.F.);
#44483=ADVANCED_FACE('',(#11903),#9298,.T.);
#44484=ADVANCED_FACE('',(#11904),#9299,.F.);
#44485=ADVANCED_FACE('',(#11905),#9300,.T.);
#44486=ADVANCED_FACE('',(#11906),#9301,.F.);
#44487=ADVANCED_FACE('',(#11907),#9302,.T.);
#44488=ADVANCED_FACE('',(#11908),#9303,.F.);
#44489=ADVANCED_FACE('',(#11909),#9304,.T.);
#44490=ADVANCED_FACE('',(#11910),#9305,.F.);
#44491=ADVANCED_FACE('',(#11911),#9306,.T.);
#44492=ADVANCED_FACE('',(#11912),#9307,.F.);
#44493=ADVANCED_FACE('',(#11913),#9308,.T.);
#44494=ADVANCED_FACE('',(#11914),#9309,.F.);
#44495=ADVANCED_FACE('',(#11915),#9310,.T.);
#44496=ADVANCED_FACE('',(#11916),#9311,.F.);
#44497=ADVANCED_FACE('',(#11917),#9312,.T.);
#44498=ADVANCED_FACE('',(#11918),#9313,.F.);
#44499=ADVANCED_FACE('',(#11919),#9314,.T.);
#44500=ADVANCED_FACE('',(#11920),#9315,.F.);
#44501=ADVANCED_FACE('',(#11921),#9316,.T.);
#44502=ADVANCED_FACE('',(#11922),#9317,.F.);
#44503=ADVANCED_FACE('',(#11923),#9318,.T.);
#44504=ADVANCED_FACE('',(#11924),#9319,.F.);
#44505=ADVANCED_FACE('',(#11925),#9320,.T.);
#44506=ADVANCED_FACE('',(#11926),#9321,.F.);
#44507=ADVANCED_FACE('',(#11927),#9322,.T.);
#44508=ADVANCED_FACE('',(#11928),#9323,.F.);
#44509=ADVANCED_FACE('',(#11929),#9324,.T.);
#44510=ADVANCED_FACE('',(#11930),#9325,.F.);
#44511=ADVANCED_FACE('',(#11931),#9326,.T.);
#44512=ADVANCED_FACE('',(#11932),#9327,.F.);
#44513=ADVANCED_FACE('',(#11933),#9328,.T.);
#44514=ADVANCED_FACE('',(#11934),#9329,.F.);
#44515=ADVANCED_FACE('',(#11935),#9330,.T.);
#44516=ADVANCED_FACE('',(#11936),#9331,.F.);
#44517=ADVANCED_FACE('',(#11937),#9332,.T.);
#44518=ADVANCED_FACE('',(#11938),#9333,.F.);
#44519=ADVANCED_FACE('',(#11939),#9334,.T.);
#44520=ADVANCED_FACE('',(#11940),#9335,.F.);
#44521=ADVANCED_FACE('',(#11941),#9336,.T.);
#44522=ADVANCED_FACE('',(#11942),#9337,.F.);
#44523=ADVANCED_FACE('',(#11943),#9338,.T.);
#44524=ADVANCED_FACE('',(#11944),#9339,.F.);
#44525=ADVANCED_FACE('',(#11945),#9340,.T.);
#44526=ADVANCED_FACE('',(#11946),#9341,.F.);
#44527=ADVANCED_FACE('',(#11947),#9342,.T.);
#44528=ADVANCED_FACE('',(#11948),#9343,.F.);
#44529=ADVANCED_FACE('',(#11949),#9344,.T.);
#44530=ADVANCED_FACE('',(#11950),#9345,.F.);
#44531=ADVANCED_FACE('',(#11951),#9346,.T.);
#44532=ADVANCED_FACE('',(#11952),#9347,.F.);
#44533=ADVANCED_FACE('',(#11953),#9348,.T.);
#44534=ADVANCED_FACE('',(#11954),#9349,.F.);
#44535=ADVANCED_FACE('',(#11955),#9350,.T.);
#44536=ADVANCED_FACE('',(#11956),#9351,.F.);
#44537=ADVANCED_FACE('',(#11957),#9352,.T.);
#44538=ADVANCED_FACE('',(#11958),#9353,.F.);
#44539=ADVANCED_FACE('',(#11959),#9354,.T.);
#44540=ADVANCED_FACE('',(#11960),#9355,.F.);
#44541=ADVANCED_FACE('',(#11961),#9356,.T.);
#44542=ADVANCED_FACE('',(#11962),#9357,.F.);
#44543=ADVANCED_FACE('',(#11963),#9358,.T.);
#44544=ADVANCED_FACE('',(#11964),#9359,.F.);
#44545=ADVANCED_FACE('',(#11965),#9360,.T.);
#44546=ADVANCED_FACE('',(#11966),#9361,.F.);
#44547=ADVANCED_FACE('',(#11967),#9362,.T.);
#44548=ADVANCED_FACE('',(#11968),#9363,.F.);
#44549=ADVANCED_FACE('',(#11969),#9364,.T.);
#44550=ADVANCED_FACE('',(#11970),#9365,.F.);
#44551=ADVANCED_FACE('',(#11971),#9366,.T.);
#44552=ADVANCED_FACE('',(#11972),#9367,.F.);
#44553=ADVANCED_FACE('',(#11973),#9368,.T.);
#44554=ADVANCED_FACE('',(#11974),#9369,.F.);
#44555=ADVANCED_FACE('',(#11975),#9370,.T.);
#44556=ADVANCED_FACE('',(#11976),#9371,.F.);
#44557=ADVANCED_FACE('',(#11977),#9372,.T.);
#44558=ADVANCED_FACE('',(#11978),#9373,.F.);
#44559=ADVANCED_FACE('',(#11979),#9374,.T.);
#44560=ADVANCED_FACE('',(#11980),#9375,.F.);
#44561=ADVANCED_FACE('',(#11981),#9376,.T.);
#44562=ADVANCED_FACE('',(#11982),#9377,.F.);
#44563=ADVANCED_FACE('',(#11983),#9378,.T.);
#44564=ADVANCED_FACE('',(#11984),#9379,.F.);
#44565=ADVANCED_FACE('',(#11985),#9380,.T.);
#44566=ADVANCED_FACE('',(#11986),#9381,.F.);
#44567=ADVANCED_FACE('',(#11987),#9382,.T.);
#44568=ADVANCED_FACE('',(#11988),#9383,.F.);
#44569=ADVANCED_FACE('',(#11989),#9384,.T.);
#44570=ADVANCED_FACE('',(#11990),#9385,.F.);
#44571=ADVANCED_FACE('',(#11991),#9386,.T.);
#44572=ADVANCED_FACE('',(#11992),#9387,.F.);
#44573=ADVANCED_FACE('',(#11993),#9388,.T.);
#44574=ADVANCED_FACE('',(#11994),#9389,.F.);
#44575=ADVANCED_FACE('',(#11995),#9390,.T.);
#44576=ADVANCED_FACE('',(#11996),#9391,.F.);
#44577=ADVANCED_FACE('',(#11997),#9392,.T.);
#44578=ADVANCED_FACE('',(#11998),#9393,.F.);
#44579=ADVANCED_FACE('',(#11999),#9394,.T.);
#44580=ADVANCED_FACE('',(#12000),#9395,.F.);
#44581=ADVANCED_FACE('',(#12001),#9396,.T.);
#44582=ADVANCED_FACE('',(#12002),#9397,.F.);
#44583=ADVANCED_FACE('',(#12003),#9398,.T.);
#44584=ADVANCED_FACE('',(#12004),#9399,.F.);
#44585=ADVANCED_FACE('',(#12005),#9400,.T.);
#44586=ADVANCED_FACE('',(#12006),#9401,.F.);
#44587=ADVANCED_FACE('',(#12007),#9402,.T.);
#44588=ADVANCED_FACE('',(#12008),#9403,.F.);
#44589=ADVANCED_FACE('',(#12009),#9404,.T.);
#44590=ADVANCED_FACE('',(#12010),#9405,.F.);
#44591=ADVANCED_FACE('',(#12011),#9406,.T.);
#44592=ADVANCED_FACE('',(#12012),#9407,.F.);
#44593=ADVANCED_FACE('',(#12013),#9408,.T.);
#44594=ADVANCED_FACE('',(#12014),#9409,.F.);
#44595=ADVANCED_FACE('',(#12015),#9410,.T.);
#44596=ADVANCED_FACE('',(#12016),#9411,.F.);
#44597=ADVANCED_FACE('',(#12017),#9412,.T.);
#44598=ADVANCED_FACE('',(#12018),#9413,.F.);
#44599=ADVANCED_FACE('',(#12019),#9414,.T.);
#44600=ADVANCED_FACE('',(#12020),#9415,.F.);
#44601=ADVANCED_FACE('',(#12021),#9416,.T.);
#44602=ADVANCED_FACE('',(#12022),#9417,.F.);
#44603=ADVANCED_FACE('',(#12023),#9418,.T.);
#44604=ADVANCED_FACE('',(#12024),#9419,.F.);
#44605=ADVANCED_FACE('',(#12025),#9420,.T.);
#44606=ADVANCED_FACE('',(#12026),#9421,.F.);
#44607=ADVANCED_FACE('',(#12027),#9422,.T.);
#44608=ADVANCED_FACE('',(#12028),#9423,.F.);
#44609=ADVANCED_FACE('',(#12029),#9424,.T.);
#44610=ADVANCED_FACE('',(#12030),#9425,.F.);
#44611=ADVANCED_FACE('',(#12031),#9426,.T.);
#44612=ADVANCED_FACE('',(#12032),#9427,.F.);
#44613=ADVANCED_FACE('',(#12033),#9428,.T.);
#44614=ADVANCED_FACE('',(#12034),#9429,.F.);
#44615=ADVANCED_FACE('',(#12035),#9430,.T.);
#44616=ADVANCED_FACE('',(#12036),#9431,.F.);
#44617=ADVANCED_FACE('',(#12037),#9432,.T.);
#44618=ADVANCED_FACE('',(#12038),#9433,.F.);
#44619=ADVANCED_FACE('',(#12039),#9434,.T.);
#44620=ADVANCED_FACE('',(#12040),#9435,.F.);
#44621=ADVANCED_FACE('',(#12041),#9436,.T.);
#44622=ADVANCED_FACE('',(#12042),#9437,.F.);
#44623=ADVANCED_FACE('',(#12043),#9438,.T.);
#44624=ADVANCED_FACE('',(#12044),#9439,.F.);
#44625=ADVANCED_FACE('',(#12045),#9440,.T.);
#44626=ADVANCED_FACE('',(#12046),#9441,.F.);
#44627=ADVANCED_FACE('',(#12047),#9442,.T.);
#44628=ADVANCED_FACE('',(#12048),#9443,.F.);
#44629=ADVANCED_FACE('',(#12049),#9444,.T.);
#44630=ADVANCED_FACE('',(#12050),#9445,.F.);
#44631=ADVANCED_FACE('',(#12051),#9446,.T.);
#44632=ADVANCED_FACE('',(#12052),#9447,.F.);
#44633=ADVANCED_FACE('',(#12053),#9448,.T.);
#44634=ADVANCED_FACE('',(#12054),#9449,.F.);
#44635=ADVANCED_FACE('',(#12055),#9450,.T.);
#44636=ADVANCED_FACE('',(#12056),#9451,.F.);
#44637=ADVANCED_FACE('',(#12057),#9452,.T.);
#44638=ADVANCED_FACE('',(#12058),#9453,.F.);
#44639=ADVANCED_FACE('',(#12059),#9454,.T.);
#44640=ADVANCED_FACE('',(#12060),#9455,.F.);
#44641=ADVANCED_FACE('',(#12061),#9456,.T.);
#44642=ADVANCED_FACE('',(#12062),#9457,.F.);
#44643=ADVANCED_FACE('',(#12063),#9458,.T.);
#44644=ADVANCED_FACE('',(#12064),#9459,.F.);
#44645=ADVANCED_FACE('',(#12065),#9460,.T.);
#44646=ADVANCED_FACE('',(#12066),#9461,.F.);
#44647=ADVANCED_FACE('',(#12067),#42040,.T.);
#44648=ADVANCED_FACE('',(#12068),#9462,.T.);
#44649=ADVANCED_FACE('',(#12069),#42041,.T.);
#44650=ADVANCED_FACE('',(#12070),#42042,.T.);
#44651=ADVANCED_FACE('',(#12071),#9463,.T.);
#44652=ADVANCED_FACE('',(#12072,#792),#70,.T.);
#44653=ADVANCED_FACE('',(#12073),#42043,.T.);
#44654=ADVANCED_FACE('',(#12074),#42044,.T.);
#44655=ADVANCED_FACE('',(#12075),#42045,.T.);
#44656=ADVANCED_FACE('',(#12076),#82,.T.);
#44657=ADVANCED_FACE('',(#12077),#42046,.T.);
#44658=ADVANCED_FACE('',(#12078),#9464,.T.);
#44659=ADVANCED_FACE('',(#12079),#9465,.F.);
#44660=ADVANCED_FACE('',(#12080),#9466,.T.);
#44661=ADVANCED_FACE('',(#12081,#793),#1687,.T.);
#44662=ADVANCED_FACE('',(#12082),#3646,.F.);
#44663=ADVANCED_FACE('',(#12083,#794),#3647,.F.);
#44664=ADVANCED_FACE('',(#12084,#795),#3648,.F.);
#44665=ADVANCED_FACE('',(#12085,#796),#3649,.F.);
#44666=ADVANCED_FACE('',(#12086),#3650,.T.);
#44667=ADVANCED_FACE('',(#12087,#797),#3651,.T.);
#44668=ADVANCED_FACE('',(#12088,#798,#799,#800,#801,#802,#803,#804,#805,
#806,#807,#808,#809,#810,#811,#812,#813,#814,#815,#816,#817,#818,#819,#820,
#821,#822,#823,#824,#825,#826,#827,#828,#829,#830,#831,#832,#833,#834,#835,
#836,#837,#838,#839,#840,#841,#842,#843,#844,#845,#846,#847,#848,#849,#850,
#851,#852,#853,#854,#855,#856,#857,#858,#859,#860,#861,#862,#863,#864,#865,
#866,#867,#868,#869,#870,#871,#872,#873,#874,#875,#876,#877,#878,#879,#880,
#881,#882,#883,#884,#885,#886,#887,#888,#889,#890,#891,#892,#893,#894,#895,
#896,#897,#898,#899,#900,#901,#902,#903,#904,#905,#906,#907,#908,#909,#910,
#911,#912,#913,#914,#915,#916,#917,#918,#919,#920,#921,#922,#923,#924,#925,
#926,#927,#928,#929,#930,#931,#932,#933,#934,#935,#936,#937,#938,#939,#940,
#941,#942,#943,#944,#945,#946,#947,#948,#949,#950,#951,#952,#953,#954,#955,
#956,#957,#958,#959,#960,#961,#962,#963,#964,#965,#966,#967,#968,#969,#970,
#971,#972,#973,#974,#975,#976,#977,#978,#979,#980,#981,#982,#983,#984,#985,
#986,#987,#988,#989,#990,#991,#992,#993,#994,#995,#996,#997,#998,#999,#1000,
#1001,#1002,#1003,#1004,#1005,#1006,#1007,#1008,#1009,#1010,#1011,#1012,
#1013,#1014,#1015,#1016,#1017,#1018,#1019,#1020,#1021,#1022,#1023,#1024,
#1025,#1026,#1027,#1028,#1029,#1030,#1031,#1032,#1033,#1034,#1035,#1036,
#1037,#1038,#1039,#1040,#1041,#1042,#1043,#1044,#1045,#1046,#1047,#1048,
#1049,#1050,#1051,#1052,#1053,#1054,#1055,#1056,#1057,#1058,#1059,#1060,
#1061,#1062,#1063,#1064,#1065,#1066,#1067),#3652,.F.);
#44669=ADVANCED_FACE('',(#12089,#1068,#1069,#1070,#1071,#1072,#1073,#1074,
#1075,#1076,#1077,#1078,#1079,#1080,#1081,#1082,#1083,#1084,#1085,#1086,
#1087,#1088,#1089,#1090,#1091,#1092,#1093,#1094,#1095,#1096,#1097,#1098,
#1099,#1100,#1101,#1102,#1103,#1104,#1105,#1106,#1107,#1108,#1109,#1110,
#1111,#1112,#1113,#1114,#1115,#1116,#1117,#1118,#1119,#1120,#1121,#1122,
#1123,#1124,#1125,#1126,#1127),#1688,.F.);
#44670=ADVANCED_FACE('',(#12090),#3653,.F.);
#44671=ADVANCED_FACE('',(#12091,#1128),#3654,.T.);
#44672=ADVANCED_FACE('',(#12092),#3655,.F.);
#44673=ADVANCED_FACE('',(#12093,#1129),#3656,.T.);
#44674=ADVANCED_FACE('',(#12094),#3657,.F.);
#44675=ADVANCED_FACE('',(#12095,#1130),#3658,.T.);
#44676=ADVANCED_FACE('',(#12096),#3659,.F.);
#44677=ADVANCED_FACE('',(#12097,#1131),#3660,.T.);
#44678=ADVANCED_FACE('',(#12098),#3661,.F.);
#44679=ADVANCED_FACE('',(#12099,#1132),#3662,.T.);
#44680=ADVANCED_FACE('',(#12100),#3663,.F.);
#44681=ADVANCED_FACE('',(#12101,#1133),#3664,.T.);
#44682=ADVANCED_FACE('',(#12102),#3665,.F.);
#44683=ADVANCED_FACE('',(#12103,#1134),#3666,.T.);
#44684=ADVANCED_FACE('',(#12104),#3667,.F.);
#44685=ADVANCED_FACE('',(#12105,#1135),#3668,.T.);
#44686=ADVANCED_FACE('',(#12106),#3669,.F.);
#44687=ADVANCED_FACE('',(#12107,#1136),#3670,.T.);
#44688=ADVANCED_FACE('',(#12108),#3671,.F.);
#44689=ADVANCED_FACE('',(#12109,#1137),#3672,.T.);
#44690=ADVANCED_FACE('',(#12110),#3673,.F.);
#44691=ADVANCED_FACE('',(#12111,#1138),#3674,.T.);
#44692=ADVANCED_FACE('',(#12112),#3675,.F.);
#44693=ADVANCED_FACE('',(#12113,#1139),#3676,.T.);
#44694=ADVANCED_FACE('',(#12114),#3677,.F.);
#44695=ADVANCED_FACE('',(#12115,#1140),#3678,.T.);
#44696=ADVANCED_FACE('',(#12116),#3679,.F.);
#44697=ADVANCED_FACE('',(#12117,#1141),#3680,.T.);
#44698=ADVANCED_FACE('',(#12118),#3681,.F.);
#44699=ADVANCED_FACE('',(#12119,#1142),#3682,.T.);
#44700=ADVANCED_FACE('',(#12120),#3683,.F.);
#44701=ADVANCED_FACE('',(#12121,#1143),#3684,.T.);
#44702=ADVANCED_FACE('',(#12122),#3685,.F.);
#44703=ADVANCED_FACE('',(#12123,#1144),#3686,.T.);
#44704=ADVANCED_FACE('',(#12124),#3687,.F.);
#44705=ADVANCED_FACE('',(#12125,#1145),#3688,.T.);
#44706=ADVANCED_FACE('',(#12126),#3689,.F.);
#44707=ADVANCED_FACE('',(#12127,#1146),#3690,.T.);
#44708=ADVANCED_FACE('',(#12128),#3691,.F.);
#44709=ADVANCED_FACE('',(#12129,#1147),#3692,.T.);
#44710=ADVANCED_FACE('',(#12130),#3693,.F.);
#44711=ADVANCED_FACE('',(#12131,#1148),#3694,.T.);
#44712=ADVANCED_FACE('',(#12132),#3695,.F.);
#44713=ADVANCED_FACE('',(#12133,#1149),#3696,.T.);
#44714=ADVANCED_FACE('',(#12134),#3697,.F.);
#44715=ADVANCED_FACE('',(#12135,#1150),#3698,.T.);
#44716=ADVANCED_FACE('',(#12136),#3699,.F.);
#44717=ADVANCED_FACE('',(#12137,#1151),#3700,.T.);
#44718=ADVANCED_FACE('',(#12138),#3701,.F.);
#44719=ADVANCED_FACE('',(#12139,#1152),#3702,.T.);
#44720=ADVANCED_FACE('',(#12140),#3703,.F.);
#44721=ADVANCED_FACE('',(#12141,#1153),#3704,.T.);
#44722=ADVANCED_FACE('',(#12142),#3705,.F.);
#44723=ADVANCED_FACE('',(#12143,#1154),#3706,.T.);
#44724=ADVANCED_FACE('',(#12144),#3707,.F.);
#44725=ADVANCED_FACE('',(#12145,#1155),#3708,.T.);
#44726=ADVANCED_FACE('',(#12146),#3709,.F.);
#44727=ADVANCED_FACE('',(#12147,#1156),#3710,.T.);
#44728=ADVANCED_FACE('',(#12148),#3711,.F.);
#44729=ADVANCED_FACE('',(#12149,#1157),#3712,.T.);
#44730=ADVANCED_FACE('',(#12150),#3713,.F.);
#44731=ADVANCED_FACE('',(#12151,#1158),#3714,.T.);
#44732=ADVANCED_FACE('',(#12152),#3715,.F.);
#44733=ADVANCED_FACE('',(#12153,#1159),#3716,.T.);
#44734=ADVANCED_FACE('',(#12154),#3717,.F.);
#44735=ADVANCED_FACE('',(#12155,#1160),#3718,.T.);
#44736=ADVANCED_FACE('',(#12156),#3719,.F.);
#44737=ADVANCED_FACE('',(#12157,#1161),#3720,.T.);
#44738=ADVANCED_FACE('',(#12158),#3721,.F.);
#44739=ADVANCED_FACE('',(#12159,#1162),#3722,.T.);
#44740=ADVANCED_FACE('',(#12160),#3723,.F.);
#44741=ADVANCED_FACE('',(#12161,#1163),#3724,.T.);
#44742=ADVANCED_FACE('',(#12162),#3725,.F.);
#44743=ADVANCED_FACE('',(#12163,#1164),#3726,.T.);
#44744=ADVANCED_FACE('',(#12164),#3727,.F.);
#44745=ADVANCED_FACE('',(#12165,#1165),#3728,.T.);
#44746=ADVANCED_FACE('',(#12166),#3729,.F.);
#44747=ADVANCED_FACE('',(#12167,#1166),#3730,.T.);
#44748=ADVANCED_FACE('',(#12168),#3731,.F.);
#44749=ADVANCED_FACE('',(#12169,#1167),#3732,.T.);
#44750=ADVANCED_FACE('',(#12170),#3733,.F.);
#44751=ADVANCED_FACE('',(#12171,#1168),#3734,.T.);
#44752=ADVANCED_FACE('',(#12172),#3735,.F.);
#44753=ADVANCED_FACE('',(#12173,#1169),#3736,.T.);
#44754=ADVANCED_FACE('',(#12174),#3737,.F.);
#44755=ADVANCED_FACE('',(#12175,#1170),#3738,.T.);
#44756=ADVANCED_FACE('',(#12176),#3739,.F.);
#44757=ADVANCED_FACE('',(#12177,#1171),#3740,.T.);
#44758=ADVANCED_FACE('',(#12178),#3741,.F.);
#44759=ADVANCED_FACE('',(#12179,#1172),#3742,.T.);
#44760=ADVANCED_FACE('',(#12180),#3743,.F.);
#44761=ADVANCED_FACE('',(#12181,#1173),#3744,.T.);
#44762=ADVANCED_FACE('',(#12182),#3745,.F.);
#44763=ADVANCED_FACE('',(#12183,#1174),#3746,.T.);
#44764=ADVANCED_FACE('',(#12184),#3747,.F.);
#44765=ADVANCED_FACE('',(#12185,#1175),#3748,.T.);
#44766=ADVANCED_FACE('',(#12186),#3749,.F.);
#44767=ADVANCED_FACE('',(#12187,#1176),#3750,.T.);
#44768=ADVANCED_FACE('',(#12188),#3751,.F.);
#44769=ADVANCED_FACE('',(#12189,#1177),#3752,.T.);
#44770=ADVANCED_FACE('',(#12190),#3753,.F.);
#44771=ADVANCED_FACE('',(#12191,#1178),#3754,.T.);
#44772=ADVANCED_FACE('',(#12192),#3755,.F.);
#44773=ADVANCED_FACE('',(#12193,#1179),#3756,.T.);
#44774=ADVANCED_FACE('',(#12194),#3757,.F.);
#44775=ADVANCED_FACE('',(#12195,#1180),#3758,.T.);
#44776=ADVANCED_FACE('',(#12196),#3759,.F.);
#44777=ADVANCED_FACE('',(#12197,#1181),#3760,.T.);
#44778=ADVANCED_FACE('',(#12198),#3761,.F.);
#44779=ADVANCED_FACE('',(#12199,#1182),#3762,.T.);
#44780=ADVANCED_FACE('',(#12200),#3763,.F.);
#44781=ADVANCED_FACE('',(#12201,#1183),#3764,.T.);
#44782=ADVANCED_FACE('',(#12202),#3765,.F.);
#44783=ADVANCED_FACE('',(#12203,#1184),#3766,.T.);
#44784=ADVANCED_FACE('',(#12204),#3767,.F.);
#44785=ADVANCED_FACE('',(#12205,#1185),#3768,.T.);
#44786=ADVANCED_FACE('',(#12206),#3769,.F.);
#44787=ADVANCED_FACE('',(#12207,#1186),#3770,.T.);
#44788=ADVANCED_FACE('',(#12208),#3771,.F.);
#44789=ADVANCED_FACE('',(#12209,#1187),#3772,.T.);
#44790=ADVANCED_FACE('',(#12210),#3773,.F.);
#44791=ADVANCED_FACE('',(#12211,#1188),#3774,.T.);
#44792=ADVANCED_FACE('',(#12212),#3775,.F.);
#44793=ADVANCED_FACE('',(#12213,#1189),#3776,.T.);
#44794=ADVANCED_FACE('',(#12214),#3777,.F.);
#44795=ADVANCED_FACE('',(#12215,#1190),#3778,.T.);
#44796=ADVANCED_FACE('',(#12216),#3779,.F.);
#44797=ADVANCED_FACE('',(#12217,#1191),#3780,.T.);
#44798=ADVANCED_FACE('',(#12218),#3781,.F.);
#44799=ADVANCED_FACE('',(#12219,#1192),#3782,.T.);
#44800=ADVANCED_FACE('',(#12220),#3783,.F.);
#44801=ADVANCED_FACE('',(#12221,#1193),#3784,.T.);
#44802=ADVANCED_FACE('',(#12222),#3785,.F.);
#44803=ADVANCED_FACE('',(#12223,#1194),#3786,.T.);
#44804=ADVANCED_FACE('',(#12224),#3787,.F.);
#44805=ADVANCED_FACE('',(#12225,#1195),#3788,.T.);
#44806=ADVANCED_FACE('',(#12226),#3789,.F.);
#44807=ADVANCED_FACE('',(#12227,#1196),#3790,.T.);
#44808=ADVANCED_FACE('',(#12228),#3791,.F.);
#44809=ADVANCED_FACE('',(#12229,#1197),#3792,.T.);
#44810=ADVANCED_FACE('',(#12230),#3793,.F.);
#44811=ADVANCED_FACE('',(#12231,#1198),#3794,.T.);
#44812=ADVANCED_FACE('',(#12232),#3795,.F.);
#44813=ADVANCED_FACE('',(#12233,#1199),#3796,.T.);
#44814=ADVANCED_FACE('',(#12234),#3797,.F.);
#44815=ADVANCED_FACE('',(#12235,#1200),#3798,.T.);
#44816=ADVANCED_FACE('',(#12236),#3799,.F.);
#44817=ADVANCED_FACE('',(#12237,#1201),#3800,.T.);
#44818=ADVANCED_FACE('',(#12238),#3801,.F.);
#44819=ADVANCED_FACE('',(#12239,#1202),#3802,.T.);
#44820=ADVANCED_FACE('',(#12240),#3803,.F.);
#44821=ADVANCED_FACE('',(#12241,#1203),#3804,.T.);
#44822=ADVANCED_FACE('',(#12242),#3805,.F.);
#44823=ADVANCED_FACE('',(#12243,#1204),#3806,.T.);
#44824=ADVANCED_FACE('',(#12244),#3807,.F.);
#44825=ADVANCED_FACE('',(#12245,#1205),#3808,.T.);
#44826=ADVANCED_FACE('',(#12246),#3809,.F.);
#44827=ADVANCED_FACE('',(#12247,#1206),#3810,.T.);
#44828=ADVANCED_FACE('',(#12248),#3811,.F.);
#44829=ADVANCED_FACE('',(#12249,#1207),#3812,.T.);
#44830=ADVANCED_FACE('',(#12250),#3813,.F.);
#44831=ADVANCED_FACE('',(#12251,#1208),#3814,.T.);
#44832=ADVANCED_FACE('',(#12252),#3815,.F.);
#44833=ADVANCED_FACE('',(#12253,#1209),#3816,.T.);
#44834=ADVANCED_FACE('',(#12254),#3817,.F.);
#44835=ADVANCED_FACE('',(#12255,#1210),#3818,.T.);
#44836=ADVANCED_FACE('',(#12256),#3819,.F.);
#44837=ADVANCED_FACE('',(#12257,#1211),#3820,.T.);
#44838=ADVANCED_FACE('',(#12258),#3821,.F.);
#44839=ADVANCED_FACE('',(#12259,#1212),#3822,.T.);
#44840=ADVANCED_FACE('',(#12260),#3823,.F.);
#44841=ADVANCED_FACE('',(#12261,#1213),#3824,.T.);
#44842=ADVANCED_FACE('',(#12262),#3825,.F.);
#44843=ADVANCED_FACE('',(#12263,#1214),#3826,.T.);
#44844=ADVANCED_FACE('',(#12264),#3827,.F.);
#44845=ADVANCED_FACE('',(#12265,#1215),#3828,.T.);
#44846=ADVANCED_FACE('',(#12266),#3829,.F.);
#44847=ADVANCED_FACE('',(#12267,#1216),#3830,.T.);
#44848=ADVANCED_FACE('',(#12268),#3831,.F.);
#44849=ADVANCED_FACE('',(#12269,#1217),#3832,.T.);
#44850=ADVANCED_FACE('',(#12270),#3833,.F.);
#44851=ADVANCED_FACE('',(#12271,#1218),#3834,.T.);
#44852=ADVANCED_FACE('',(#12272),#3835,.F.);
#44853=ADVANCED_FACE('',(#12273,#1219),#3836,.T.);
#44854=ADVANCED_FACE('',(#12274),#3837,.F.);
#44855=ADVANCED_FACE('',(#12275,#1220),#3838,.T.);
#44856=ADVANCED_FACE('',(#12276),#3839,.F.);
#44857=ADVANCED_FACE('',(#12277,#1221),#3840,.T.);
#44858=ADVANCED_FACE('',(#12278),#3841,.F.);
#44859=ADVANCED_FACE('',(#12279,#1222),#3842,.T.);
#44860=ADVANCED_FACE('',(#12280),#3843,.F.);
#44861=ADVANCED_FACE('',(#12281,#1223),#3844,.T.);
#44862=ADVANCED_FACE('',(#12282),#3845,.F.);
#44863=ADVANCED_FACE('',(#12283,#1224),#3846,.T.);
#44864=ADVANCED_FACE('',(#12284),#3847,.F.);
#44865=ADVANCED_FACE('',(#12285,#1225),#3848,.T.);
#44866=ADVANCED_FACE('',(#12286),#3849,.F.);
#44867=ADVANCED_FACE('',(#12287,#1226),#3850,.T.);
#44868=ADVANCED_FACE('',(#12288),#3851,.F.);
#44869=ADVANCED_FACE('',(#12289,#1227),#3852,.T.);
#44870=ADVANCED_FACE('',(#12290),#3853,.F.);
#44871=ADVANCED_FACE('',(#12291,#1228),#3854,.T.);
#44872=ADVANCED_FACE('',(#12292),#3855,.F.);
#44873=ADVANCED_FACE('',(#12293,#1229),#3856,.T.);
#44874=ADVANCED_FACE('',(#12294),#3857,.F.);
#44875=ADVANCED_FACE('',(#12295,#1230),#3858,.T.);
#44876=ADVANCED_FACE('',(#12296),#3859,.F.);
#44877=ADVANCED_FACE('',(#12297,#1231),#3860,.T.);
#44878=ADVANCED_FACE('',(#12298),#3861,.F.);
#44879=ADVANCED_FACE('',(#12299,#1232),#3862,.T.);
#44880=ADVANCED_FACE('',(#12300),#3863,.F.);
#44881=ADVANCED_FACE('',(#12301,#1233),#3864,.T.);
#44882=ADVANCED_FACE('',(#12302),#3865,.F.);
#44883=ADVANCED_FACE('',(#12303,#1234),#3866,.T.);
#44884=ADVANCED_FACE('',(#12304),#3867,.F.);
#44885=ADVANCED_FACE('',(#12305,#1235),#3868,.T.);
#44886=ADVANCED_FACE('',(#12306),#3869,.F.);
#44887=ADVANCED_FACE('',(#12307,#1236),#3870,.T.);
#44888=ADVANCED_FACE('',(#12308),#3871,.F.);
#44889=ADVANCED_FACE('',(#12309,#1237),#3872,.T.);
#44890=ADVANCED_FACE('',(#12310),#3873,.F.);
#44891=ADVANCED_FACE('',(#12311,#1238),#3874,.T.);
#44892=ADVANCED_FACE('',(#12312),#3875,.F.);
#44893=ADVANCED_FACE('',(#12313,#1239),#3876,.T.);
#44894=ADVANCED_FACE('',(#12314),#3877,.F.);
#44895=ADVANCED_FACE('',(#12315,#1240),#3878,.T.);
#44896=ADVANCED_FACE('',(#12316),#3879,.F.);
#44897=ADVANCED_FACE('',(#12317,#1241),#3880,.T.);
#44898=ADVANCED_FACE('',(#12318),#3881,.F.);
#44899=ADVANCED_FACE('',(#12319,#1242),#3882,.T.);
#44900=ADVANCED_FACE('',(#12320),#3883,.F.);
#44901=ADVANCED_FACE('',(#12321,#1243),#3884,.T.);
#44902=ADVANCED_FACE('',(#12322),#3885,.F.);
#44903=ADVANCED_FACE('',(#12323,#1244),#3886,.T.);
#44904=ADVANCED_FACE('',(#12324),#3887,.F.);
#44905=ADVANCED_FACE('',(#12325,#1245),#3888,.T.);
#44906=ADVANCED_FACE('',(#12326),#3889,.F.);
#44907=ADVANCED_FACE('',(#12327,#1246),#3890,.T.);
#44908=ADVANCED_FACE('',(#12328),#3891,.F.);
#44909=ADVANCED_FACE('',(#12329,#1247),#3892,.T.);
#44910=ADVANCED_FACE('',(#12330),#3893,.F.);
#44911=ADVANCED_FACE('',(#12331,#1248),#3894,.T.);
#44912=ADVANCED_FACE('',(#12332),#3895,.F.);
#44913=ADVANCED_FACE('',(#12333,#1249),#3896,.T.);
#44914=ADVANCED_FACE('',(#12334),#3897,.F.);
#44915=ADVANCED_FACE('',(#12335,#1250),#3898,.T.);
#44916=ADVANCED_FACE('',(#12336),#3899,.F.);
#44917=ADVANCED_FACE('',(#12337,#1251),#3900,.T.);
#44918=ADVANCED_FACE('',(#12338),#3901,.F.);
#44919=ADVANCED_FACE('',(#12339,#1252),#3902,.T.);
#44920=ADVANCED_FACE('',(#12340),#3903,.F.);
#44921=ADVANCED_FACE('',(#12341,#1253),#3904,.T.);
#44922=ADVANCED_FACE('',(#12342),#3905,.F.);
#44923=ADVANCED_FACE('',(#12343,#1254),#3906,.T.);
#44924=ADVANCED_FACE('',(#12344),#3907,.F.);
#44925=ADVANCED_FACE('',(#12345,#1255),#3908,.T.);
#44926=ADVANCED_FACE('',(#12346),#3909,.F.);
#44927=ADVANCED_FACE('',(#12347,#1256),#3910,.T.);
#44928=ADVANCED_FACE('',(#12348),#3911,.F.);
#44929=ADVANCED_FACE('',(#12349,#1257),#3912,.T.);
#44930=ADVANCED_FACE('',(#12350),#3913,.F.);
#44931=ADVANCED_FACE('',(#12351,#1258),#3914,.T.);
#44932=ADVANCED_FACE('',(#12352),#3915,.F.);
#44933=ADVANCED_FACE('',(#12353,#1259),#3916,.T.);
#44934=ADVANCED_FACE('',(#12354),#3917,.F.);
#44935=ADVANCED_FACE('',(#12355,#1260),#3918,.T.);
#44936=ADVANCED_FACE('',(#12356),#3919,.F.);
#44937=ADVANCED_FACE('',(#12357,#1261),#3920,.T.);
#44938=ADVANCED_FACE('',(#12358),#3921,.F.);
#44939=ADVANCED_FACE('',(#12359,#1262),#3922,.T.);
#44940=ADVANCED_FACE('',(#12360),#3923,.F.);
#44941=ADVANCED_FACE('',(#12361,#1263),#3924,.T.);
#44942=ADVANCED_FACE('',(#12362),#3925,.F.);
#44943=ADVANCED_FACE('',(#12363,#1264),#3926,.T.);
#44944=ADVANCED_FACE('',(#12364),#3927,.F.);
#44945=ADVANCED_FACE('',(#12365,#1265),#3928,.T.);
#44946=ADVANCED_FACE('',(#12366),#3929,.F.);
#44947=ADVANCED_FACE('',(#12367,#1266),#3930,.T.);
#44948=ADVANCED_FACE('',(#12368),#3931,.F.);
#44949=ADVANCED_FACE('',(#12369,#1267),#3932,.T.);
#44950=ADVANCED_FACE('',(#12370),#3933,.F.);
#44951=ADVANCED_FACE('',(#12371,#1268),#3934,.T.);
#44952=ADVANCED_FACE('',(#12372),#3935,.F.);
#44953=ADVANCED_FACE('',(#12373,#1269),#3936,.T.);
#44954=ADVANCED_FACE('',(#12374),#3937,.F.);
#44955=ADVANCED_FACE('',(#12375,#1270),#3938,.T.);
#44956=ADVANCED_FACE('',(#12376),#3939,.F.);
#44957=ADVANCED_FACE('',(#12377,#1271),#3940,.T.);
#44958=ADVANCED_FACE('',(#12378),#3941,.F.);
#44959=ADVANCED_FACE('',(#12379,#1272),#3942,.T.);
#44960=ADVANCED_FACE('',(#12380),#3943,.F.);
#44961=ADVANCED_FACE('',(#12381,#1273),#3944,.T.);
#44962=ADVANCED_FACE('',(#12382),#3945,.F.);
#44963=ADVANCED_FACE('',(#12383,#1274),#3946,.T.);
#44964=ADVANCED_FACE('',(#12384),#3947,.F.);
#44965=ADVANCED_FACE('',(#12385,#1275),#3948,.T.);
#44966=ADVANCED_FACE('',(#12386),#3949,.F.);
#44967=ADVANCED_FACE('',(#12387,#1276),#3950,.T.);
#44968=ADVANCED_FACE('',(#12388),#3951,.F.);
#44969=ADVANCED_FACE('',(#12389,#1277),#3952,.T.);
#44970=ADVANCED_FACE('',(#12390),#3953,.F.);
#44971=ADVANCED_FACE('',(#12391,#1278),#3954,.T.);
#44972=ADVANCED_FACE('',(#12392),#3955,.F.);
#44973=ADVANCED_FACE('',(#12393,#1279),#3956,.T.);
#44974=ADVANCED_FACE('',(#12394),#3957,.F.);
#44975=ADVANCED_FACE('',(#12395,#1280),#3958,.T.);
#44976=ADVANCED_FACE('',(#12396),#3959,.F.);
#44977=ADVANCED_FACE('',(#12397,#1281),#3960,.T.);
#44978=ADVANCED_FACE('',(#12398),#3961,.F.);
#44979=ADVANCED_FACE('',(#12399,#1282),#3962,.T.);
#44980=ADVANCED_FACE('',(#12400),#3963,.F.);
#44981=ADVANCED_FACE('',(#12401,#1283),#3964,.T.);
#44982=ADVANCED_FACE('',(#12402),#3965,.F.);
#44983=ADVANCED_FACE('',(#12403,#1284),#3966,.T.);
#44984=ADVANCED_FACE('',(#12404),#3967,.F.);
#44985=ADVANCED_FACE('',(#12405,#1285),#3968,.T.);
#44986=ADVANCED_FACE('',(#12406),#3969,.F.);
#44987=ADVANCED_FACE('',(#12407,#1286),#3970,.T.);
#44988=ADVANCED_FACE('',(#12408),#3971,.F.);
#44989=ADVANCED_FACE('',(#12409,#1287),#3972,.T.);
#44990=ADVANCED_FACE('',(#12410),#3973,.F.);
#44991=ADVANCED_FACE('',(#12411,#1288),#3974,.T.);
#44992=ADVANCED_FACE('',(#12412),#3975,.F.);
#44993=ADVANCED_FACE('',(#12413,#1289),#3976,.T.);
#44994=ADVANCED_FACE('',(#12414),#3977,.F.);
#44995=ADVANCED_FACE('',(#12415,#1290),#3978,.T.);
#44996=ADVANCED_FACE('',(#12416),#3979,.F.);
#44997=ADVANCED_FACE('',(#12417,#1291),#3980,.T.);
#44998=ADVANCED_FACE('',(#12418),#3981,.F.);
#44999=ADVANCED_FACE('',(#12419,#1292),#3982,.T.);
#45000=ADVANCED_FACE('',(#12420),#3983,.F.);
#45001=ADVANCED_FACE('',(#12421,#1293),#3984,.T.);
#45002=ADVANCED_FACE('',(#12422),#3985,.F.);
#45003=ADVANCED_FACE('',(#12423,#1294),#3986,.T.);
#45004=ADVANCED_FACE('',(#12424),#3987,.F.);
#45005=ADVANCED_FACE('',(#12425,#1295),#3988,.T.);
#45006=ADVANCED_FACE('',(#12426),#3989,.F.);
#45007=ADVANCED_FACE('',(#12427,#1296),#3990,.T.);
#45008=ADVANCED_FACE('',(#12428),#3991,.F.);
#45009=ADVANCED_FACE('',(#12429,#1297),#3992,.T.);
#45010=ADVANCED_FACE('',(#12430),#3993,.F.);
#45011=ADVANCED_FACE('',(#12431,#1298),#3994,.T.);
#45012=ADVANCED_FACE('',(#12432),#3995,.F.);
#45013=ADVANCED_FACE('',(#12433,#1299),#3996,.T.);
#45014=ADVANCED_FACE('',(#12434),#3997,.F.);
#45015=ADVANCED_FACE('',(#12435,#1300),#3998,.T.);
#45016=ADVANCED_FACE('',(#12436),#3999,.F.);
#45017=ADVANCED_FACE('',(#12437,#1301),#4000,.T.);
#45018=ADVANCED_FACE('',(#12438),#4001,.F.);
#45019=ADVANCED_FACE('',(#12439,#1302),#4002,.T.);
#45020=ADVANCED_FACE('',(#12440),#4003,.F.);
#45021=ADVANCED_FACE('',(#12441,#1303),#4004,.T.);
#45022=ADVANCED_FACE('',(#12442),#4005,.F.);
#45023=ADVANCED_FACE('',(#12443,#1304),#4006,.T.);
#45024=ADVANCED_FACE('',(#12444),#4007,.F.);
#45025=ADVANCED_FACE('',(#12445,#1305),#4008,.T.);
#45026=ADVANCED_FACE('',(#12446),#4009,.F.);
#45027=ADVANCED_FACE('',(#12447,#1306),#4010,.T.);
#45028=ADVANCED_FACE('',(#12448),#4011,.F.);
#45029=ADVANCED_FACE('',(#12449,#1307),#4012,.T.);
#45030=ADVANCED_FACE('',(#12450),#4013,.F.);
#45031=ADVANCED_FACE('',(#12451,#1308),#4014,.T.);
#45032=ADVANCED_FACE('',(#12452),#4015,.F.);
#45033=ADVANCED_FACE('',(#12453,#1309),#4016,.T.);
#45034=ADVANCED_FACE('',(#12454),#4017,.F.);
#45035=ADVANCED_FACE('',(#12455,#1310),#4018,.T.);
#45036=ADVANCED_FACE('',(#12456),#4019,.F.);
#45037=ADVANCED_FACE('',(#12457,#1311),#4020,.T.);
#45038=ADVANCED_FACE('',(#12458),#4021,.F.);
#45039=ADVANCED_FACE('',(#12459,#1312),#4022,.T.);
#45040=ADVANCED_FACE('',(#12460),#4023,.F.);
#45041=ADVANCED_FACE('',(#12461,#1313),#4024,.T.);
#45042=ADVANCED_FACE('',(#12462),#4025,.F.);
#45043=ADVANCED_FACE('',(#12463,#1314),#4026,.T.);
#45044=ADVANCED_FACE('',(#12464),#4027,.F.);
#45045=ADVANCED_FACE('',(#12465,#1315),#4028,.T.);
#45046=ADVANCED_FACE('',(#12466),#4029,.F.);
#45047=ADVANCED_FACE('',(#12467,#1316),#4030,.T.);
#45048=ADVANCED_FACE('',(#12468),#4031,.F.);
#45049=ADVANCED_FACE('',(#12469,#1317),#4032,.T.);
#45050=ADVANCED_FACE('',(#12470),#4033,.F.);
#45051=ADVANCED_FACE('',(#12471,#1318),#4034,.T.);
#45052=ADVANCED_FACE('',(#12472),#4035,.F.);
#45053=ADVANCED_FACE('',(#12473,#1319),#4036,.T.);
#45054=ADVANCED_FACE('',(#12474),#4037,.F.);
#45055=ADVANCED_FACE('',(#12475,#1320),#4038,.T.);
#45056=ADVANCED_FACE('',(#12476),#4039,.F.);
#45057=ADVANCED_FACE('',(#12477,#1321),#4040,.T.);
#45058=ADVANCED_FACE('',(#12478),#4041,.F.);
#45059=ADVANCED_FACE('',(#12479,#1322),#4042,.T.);
#45060=ADVANCED_FACE('',(#12480),#4043,.F.);
#45061=ADVANCED_FACE('',(#12481,#1323),#4044,.T.);
#45062=ADVANCED_FACE('',(#12482),#4045,.F.);
#45063=ADVANCED_FACE('',(#12483,#1324),#4046,.T.);
#45064=ADVANCED_FACE('',(#12484),#4047,.F.);
#45065=ADVANCED_FACE('',(#12485,#1325),#4048,.T.);
#45066=ADVANCED_FACE('',(#12486),#4049,.F.);
#45067=ADVANCED_FACE('',(#12487,#1326),#4050,.T.);
#45068=ADVANCED_FACE('',(#12488),#4051,.F.);
#45069=ADVANCED_FACE('',(#12489,#1327),#4052,.T.);
#45070=ADVANCED_FACE('',(#12490),#4053,.F.);
#45071=ADVANCED_FACE('',(#12491,#1328),#4054,.T.);
#45072=ADVANCED_FACE('',(#12492),#4055,.F.);
#45073=ADVANCED_FACE('',(#12493,#1329),#4056,.T.);
#45074=ADVANCED_FACE('',(#12494),#4057,.F.);
#45075=ADVANCED_FACE('',(#12495,#1330),#4058,.T.);
#45076=ADVANCED_FACE('',(#12496),#4059,.F.);
#45077=ADVANCED_FACE('',(#12497,#1331),#4060,.T.);
#45078=ADVANCED_FACE('',(#12498),#4061,.F.);
#45079=ADVANCED_FACE('',(#12499,#1332),#4062,.T.);
#45080=ADVANCED_FACE('',(#12500),#4063,.F.);
#45081=ADVANCED_FACE('',(#12501,#1333),#4064,.T.);
#45082=ADVANCED_FACE('',(#12502),#4065,.F.);
#45083=ADVANCED_FACE('',(#12503,#1334),#4066,.T.);
#45084=ADVANCED_FACE('',(#12504),#4067,.F.);
#45085=ADVANCED_FACE('',(#12505,#1335),#4068,.T.);
#45086=ADVANCED_FACE('',(#12506),#4069,.F.);
#45087=ADVANCED_FACE('',(#12507,#1336),#4070,.T.);
#45088=ADVANCED_FACE('',(#12508),#4071,.F.);
#45089=ADVANCED_FACE('',(#12509,#1337),#4072,.T.);
#45090=ADVANCED_FACE('',(#12510),#4073,.F.);
#45091=ADVANCED_FACE('',(#12511,#1338),#4074,.T.);
#45092=ADVANCED_FACE('',(#12512),#4075,.F.);
#45093=ADVANCED_FACE('',(#12513,#1339),#4076,.T.);
#45094=ADVANCED_FACE('',(#12514),#4077,.F.);
#45095=ADVANCED_FACE('',(#12515,#1340),#4078,.T.);
#45096=ADVANCED_FACE('',(#12516),#4079,.F.);
#45097=ADVANCED_FACE('',(#12517,#1341),#4080,.T.);
#45098=ADVANCED_FACE('',(#12518),#4081,.F.);
#45099=ADVANCED_FACE('',(#12519,#1342),#4082,.T.);
#45100=ADVANCED_FACE('',(#12520),#4083,.F.);
#45101=ADVANCED_FACE('',(#12521,#1343),#4084,.T.);
#45102=ADVANCED_FACE('',(#12522),#4085,.F.);
#45103=ADVANCED_FACE('',(#12523,#1344),#4086,.T.);
#45104=ADVANCED_FACE('',(#12524),#4087,.F.);
#45105=ADVANCED_FACE('',(#12525,#1345),#4088,.T.);
#45106=ADVANCED_FACE('',(#12526),#4089,.F.);
#45107=ADVANCED_FACE('',(#12527,#1346),#4090,.T.);
#45108=ADVANCED_FACE('',(#12528),#4091,.F.);
#45109=ADVANCED_FACE('',(#12529,#1347),#4092,.T.);
#45110=ADVANCED_FACE('',(#12530),#4093,.F.);
#45111=ADVANCED_FACE('',(#12531,#1348),#4094,.T.);
#45112=ADVANCED_FACE('',(#12532),#4095,.F.);
#45113=ADVANCED_FACE('',(#12533,#1349),#4096,.T.);
#45114=ADVANCED_FACE('',(#12534),#4097,.F.);
#45115=ADVANCED_FACE('',(#12535,#1350),#4098,.T.);
#45116=ADVANCED_FACE('',(#12536),#4099,.F.);
#45117=ADVANCED_FACE('',(#12537,#1351),#4100,.T.);
#45118=ADVANCED_FACE('',(#12538),#4101,.F.);
#45119=ADVANCED_FACE('',(#12539,#1352),#4102,.T.);
#45120=ADVANCED_FACE('',(#12540),#4103,.F.);
#45121=ADVANCED_FACE('',(#12541,#1353),#4104,.T.);
#45122=ADVANCED_FACE('',(#12542),#4105,.F.);
#45123=ADVANCED_FACE('',(#12543,#1354),#4106,.T.);
#45124=ADVANCED_FACE('',(#12544),#4107,.F.);
#45125=ADVANCED_FACE('',(#12545,#1355),#4108,.T.);
#45126=ADVANCED_FACE('',(#12546),#4109,.F.);
#45127=ADVANCED_FACE('',(#12547,#1356),#4110,.T.);
#45128=ADVANCED_FACE('',(#12548),#4111,.F.);
#45129=ADVANCED_FACE('',(#12549,#1357),#4112,.T.);
#45130=ADVANCED_FACE('',(#12550),#4113,.F.);
#45131=ADVANCED_FACE('',(#12551,#1358),#4114,.T.);
#45132=ADVANCED_FACE('',(#12552),#4115,.F.);
#45133=ADVANCED_FACE('',(#12553,#1359),#4116,.T.);
#45134=ADVANCED_FACE('',(#12554),#4117,.F.);
#45135=ADVANCED_FACE('',(#12555,#1360),#4118,.T.);
#45136=ADVANCED_FACE('',(#12556),#4119,.F.);
#45137=ADVANCED_FACE('',(#12557,#1361),#4120,.T.);
#45138=ADVANCED_FACE('',(#12558),#4121,.F.);
#45139=ADVANCED_FACE('',(#12559,#1362),#4122,.T.);
#45140=ADVANCED_FACE('',(#12560),#4123,.F.);
#45141=ADVANCED_FACE('',(#12561,#1363),#4124,.T.);
#45142=ADVANCED_FACE('',(#12562),#4125,.F.);
#45143=ADVANCED_FACE('',(#12563,#1364),#4126,.T.);
#45144=ADVANCED_FACE('',(#12564),#4127,.F.);
#45145=ADVANCED_FACE('',(#12565,#1365),#4128,.T.);
#45146=ADVANCED_FACE('',(#12566),#4129,.F.);
#45147=ADVANCED_FACE('',(#12567,#1366),#4130,.T.);
#45148=ADVANCED_FACE('',(#12568),#4131,.F.);
#45149=ADVANCED_FACE('',(#12569,#1367),#4132,.T.);
#45150=ADVANCED_FACE('',(#12570),#4133,.F.);
#45151=ADVANCED_FACE('',(#12571,#1368),#4134,.T.);
#45152=ADVANCED_FACE('',(#12572),#4135,.F.);
#45153=ADVANCED_FACE('',(#12573,#1369),#4136,.T.);
#45154=ADVANCED_FACE('',(#12574),#4137,.F.);
#45155=ADVANCED_FACE('',(#12575,#1370),#4138,.T.);
#45156=ADVANCED_FACE('',(#12576),#4139,.F.);
#45157=ADVANCED_FACE('',(#12577,#1371),#4140,.T.);
#45158=ADVANCED_FACE('',(#12578),#4141,.F.);
#45159=ADVANCED_FACE('',(#12579,#1372),#4142,.T.);
#45160=ADVANCED_FACE('',(#12580),#4143,.F.);
#45161=ADVANCED_FACE('',(#12581,#1373),#4144,.T.);
#45162=ADVANCED_FACE('',(#12582),#4145,.F.);
#45163=ADVANCED_FACE('',(#12583,#1374),#4146,.T.);
#45164=ADVANCED_FACE('',(#12584),#4147,.F.);
#45165=ADVANCED_FACE('',(#12585,#1375),#4148,.T.);
#45166=ADVANCED_FACE('',(#12586),#4149,.F.);
#45167=ADVANCED_FACE('',(#12587,#1376),#4150,.T.);
#45168=ADVANCED_FACE('',(#12588),#4151,.F.);
#45169=ADVANCED_FACE('',(#12589,#1377),#4152,.T.);
#45170=ADVANCED_FACE('',(#12590),#4153,.F.);
#45171=ADVANCED_FACE('',(#12591,#1378),#4154,.T.);
#45172=ADVANCED_FACE('',(#12592),#4155,.F.);
#45173=ADVANCED_FACE('',(#12593,#1379),#4156,.T.);
#45174=ADVANCED_FACE('',(#12594),#4157,.F.);
#45175=ADVANCED_FACE('',(#12595,#1380),#4158,.T.);
#45176=ADVANCED_FACE('',(#12596),#4159,.F.);
#45177=ADVANCED_FACE('',(#12597,#1381),#4160,.T.);
#45178=ADVANCED_FACE('',(#12598),#4161,.F.);
#45179=ADVANCED_FACE('',(#12599,#1382),#4162,.T.);
#45180=ADVANCED_FACE('',(#12600),#4163,.F.);
#45181=ADVANCED_FACE('',(#12601,#1383),#4164,.T.);
#45182=ADVANCED_FACE('',(#12602),#4165,.F.);
#45183=ADVANCED_FACE('',(#12603,#1384),#4166,.T.);
#45184=ADVANCED_FACE('',(#12604),#4167,.F.);
#45185=ADVANCED_FACE('',(#12605,#1385),#4168,.T.);
#45186=ADVANCED_FACE('',(#12606),#4169,.F.);
#45187=ADVANCED_FACE('',(#12607,#1386),#4170,.T.);
#45188=ADVANCED_FACE('',(#12608),#4171,.F.);
#45189=ADVANCED_FACE('',(#12609,#1387),#4172,.T.);
#45190=ADVANCED_FACE('',(#12610),#4173,.F.);
#45191=ADVANCED_FACE('',(#12611,#1388),#4174,.T.);
#45192=ADVANCED_FACE('',(#12612),#4175,.F.);
#45193=ADVANCED_FACE('',(#12613,#1389),#4176,.T.);
#45194=ADVANCED_FACE('',(#12614),#4177,.F.);
#45195=ADVANCED_FACE('',(#12615,#1390),#4178,.T.);
#45196=ADVANCED_FACE('',(#12616),#4179,.F.);
#45197=ADVANCED_FACE('',(#12617,#1391),#4180,.T.);
#45198=ADVANCED_FACE('',(#12618),#4181,.F.);
#45199=ADVANCED_FACE('',(#12619,#1392),#4182,.T.);
#45200=ADVANCED_FACE('',(#12620),#4183,.F.);
#45201=ADVANCED_FACE('',(#12621,#1393),#4184,.T.);
#45202=ADVANCED_FACE('',(#12622),#4185,.F.);
#45203=ADVANCED_FACE('',(#12623,#1394),#4186,.T.);
#45204=ADVANCED_FACE('',(#12624),#4187,.F.);
#45205=ADVANCED_FACE('',(#12625,#1395),#4188,.T.);
#45206=ADVANCED_FACE('',(#12626),#4189,.F.);
#45207=ADVANCED_FACE('',(#12627,#1396),#4190,.T.);
#45208=ADVANCED_FACE('',(#12628),#4191,.F.);
#45209=ADVANCED_FACE('',(#12629,#1397),#4192,.T.);
#45210=ADVANCED_FACE('',(#12630),#4193,.F.);
#45211=ADVANCED_FACE('',(#12631,#1398),#1689,.T.);
#45212=ADVANCED_FACE('',(#12632),#4194,.F.);
#45213=ADVANCED_FACE('',(#12633,#1399),#1690,.T.);
#45214=ADVANCED_FACE('',(#12634),#4195,.F.);
#45215=ADVANCED_FACE('',(#12635,#1400),#1691,.T.);
#45216=ADVANCED_FACE('',(#12636),#4196,.F.);
#45217=ADVANCED_FACE('',(#12637,#1401),#1692,.T.);
#45218=ADVANCED_FACE('',(#12638),#4197,.F.);
#45219=ADVANCED_FACE('',(#12639,#1402),#1693,.T.);
#45220=ADVANCED_FACE('',(#12640),#4198,.F.);
#45221=ADVANCED_FACE('',(#12641,#1403),#1694,.T.);
#45222=ADVANCED_FACE('',(#12642),#4199,.F.);
#45223=ADVANCED_FACE('',(#12643,#1404),#1695,.T.);
#45224=ADVANCED_FACE('',(#12644),#4200,.F.);
#45225=ADVANCED_FACE('',(#12645,#1405),#1696,.T.);
#45226=ADVANCED_FACE('',(#12646),#4201,.F.);
#45227=ADVANCED_FACE('',(#12647,#1406),#1697,.T.);
#45228=ADVANCED_FACE('',(#12648),#4202,.F.);
#45229=ADVANCED_FACE('',(#12649,#1407),#1698,.T.);
#45230=ADVANCED_FACE('',(#12650),#4203,.F.);
#45231=ADVANCED_FACE('',(#12651,#1408),#1699,.T.);
#45232=ADVANCED_FACE('',(#12652),#4204,.F.);
#45233=ADVANCED_FACE('',(#12653,#1409),#1700,.T.);
#45234=ADVANCED_FACE('',(#12654),#4205,.F.);
#45235=ADVANCED_FACE('',(#12655,#1410),#1701,.T.);
#45236=ADVANCED_FACE('',(#12656),#4206,.F.);
#45237=ADVANCED_FACE('',(#12657,#1411),#1702,.T.);
#45238=ADVANCED_FACE('',(#12658),#4207,.F.);
#45239=ADVANCED_FACE('',(#12659,#1412),#1703,.T.);
#45240=ADVANCED_FACE('',(#12660),#4208,.F.);
#45241=ADVANCED_FACE('',(#12661,#1413),#1704,.T.);
#45242=ADVANCED_FACE('',(#12662),#4209,.F.);
#45243=ADVANCED_FACE('',(#12663,#1414),#1705,.T.);
#45244=ADVANCED_FACE('',(#12664),#4210,.F.);
#45245=ADVANCED_FACE('',(#12665,#1415),#1706,.T.);
#45246=ADVANCED_FACE('',(#12666),#4211,.F.);
#45247=ADVANCED_FACE('',(#12667,#1416),#1707,.T.);
#45248=ADVANCED_FACE('',(#12668),#4212,.F.);
#45249=ADVANCED_FACE('',(#12669,#1417),#1708,.T.);
#45250=ADVANCED_FACE('',(#12670),#4213,.F.);
#45251=ADVANCED_FACE('',(#12671,#1418),#1709,.T.);
#45252=ADVANCED_FACE('',(#12672),#4214,.F.);
#45253=ADVANCED_FACE('',(#12673,#1419),#1710,.T.);
#45254=ADVANCED_FACE('',(#12674),#4215,.F.);
#45255=ADVANCED_FACE('',(#12675,#1420),#1711,.T.);
#45256=ADVANCED_FACE('',(#12676),#4216,.F.);
#45257=ADVANCED_FACE('',(#12677,#1421),#1712,.T.);
#45258=ADVANCED_FACE('',(#12678),#4217,.F.);
#45259=ADVANCED_FACE('',(#12679,#1422),#1713,.T.);
#45260=ADVANCED_FACE('',(#12680),#4218,.F.);
#45261=ADVANCED_FACE('',(#12681,#1423),#1714,.T.);
#45262=ADVANCED_FACE('',(#12682),#4219,.F.);
#45263=ADVANCED_FACE('',(#12683,#1424),#1715,.T.);
#45264=ADVANCED_FACE('',(#12684),#4220,.F.);
#45265=ADVANCED_FACE('',(#12685,#1425),#1716,.T.);
#45266=ADVANCED_FACE('',(#12686),#4221,.F.);
#45267=ADVANCED_FACE('',(#12687,#1426),#1717,.T.);
#45268=ADVANCED_FACE('',(#12688),#4222,.F.);
#45269=ADVANCED_FACE('',(#12689,#1427),#1718,.T.);
#45270=ADVANCED_FACE('',(#12690),#4223,.F.);
#45271=ADVANCED_FACE('',(#12691,#1428),#1719,.T.);
#45272=ADVANCED_FACE('',(#12692),#4224,.F.);
#45273=ADVANCED_FACE('',(#12693,#1429),#1720,.T.);
#45274=ADVANCED_FACE('',(#12694),#4225,.F.);
#45275=ADVANCED_FACE('',(#12695,#1430),#1721,.T.);
#45276=ADVANCED_FACE('',(#12696),#4226,.F.);
#45277=ADVANCED_FACE('',(#12697,#1431),#1722,.T.);
#45278=ADVANCED_FACE('',(#12698),#4227,.F.);
#45279=ADVANCED_FACE('',(#12699,#1432),#1723,.T.);
#45280=ADVANCED_FACE('',(#12700),#4228,.F.);
#45281=ADVANCED_FACE('',(#12701,#1433),#1724,.T.);
#45282=ADVANCED_FACE('',(#12702),#4229,.F.);
#45283=ADVANCED_FACE('',(#12703,#1434),#1725,.T.);
#45284=ADVANCED_FACE('',(#12704),#4230,.F.);
#45285=ADVANCED_FACE('',(#12705,#1435),#1726,.T.);
#45286=ADVANCED_FACE('',(#12706),#4231,.F.);
#45287=ADVANCED_FACE('',(#12707,#1436),#1727,.T.);
#45288=ADVANCED_FACE('',(#12708),#4232,.F.);
#45289=ADVANCED_FACE('',(#12709,#1437),#1728,.T.);
#45290=ADVANCED_FACE('',(#12710),#4233,.F.);
#45291=ADVANCED_FACE('',(#12711,#1438),#1729,.T.);
#45292=ADVANCED_FACE('',(#12712),#4234,.F.);
#45293=ADVANCED_FACE('',(#12713,#1439),#1730,.T.);
#45294=ADVANCED_FACE('',(#12714),#4235,.F.);
#45295=ADVANCED_FACE('',(#12715,#1440),#1731,.T.);
#45296=ADVANCED_FACE('',(#12716),#4236,.F.);
#45297=ADVANCED_FACE('',(#12717,#1441),#1732,.T.);
#45298=ADVANCED_FACE('',(#12718),#4237,.F.);
#45299=ADVANCED_FACE('',(#12719,#1442),#1733,.T.);
#45300=ADVANCED_FACE('',(#12720),#4238,.F.);
#45301=ADVANCED_FACE('',(#12721,#1443),#1734,.T.);
#45302=ADVANCED_FACE('',(#12722),#4239,.F.);
#45303=ADVANCED_FACE('',(#12723,#1444),#1735,.T.);
#45304=ADVANCED_FACE('',(#12724),#4240,.F.);
#45305=ADVANCED_FACE('',(#12725,#1445),#1736,.T.);
#45306=ADVANCED_FACE('',(#12726),#4241,.F.);
#45307=ADVANCED_FACE('',(#12727,#1446),#1737,.T.);
#45308=ADVANCED_FACE('',(#12728),#4242,.F.);
#45309=ADVANCED_FACE('',(#12729,#1447),#1738,.T.);
#45310=ADVANCED_FACE('',(#12730),#4243,.F.);
#45311=ADVANCED_FACE('',(#12731,#1448),#1739,.T.);
#45312=ADVANCED_FACE('',(#12732),#4244,.F.);
#45313=ADVANCED_FACE('',(#12733,#1449),#1740,.T.);
#45314=ADVANCED_FACE('',(#12734),#4245,.F.);
#45315=ADVANCED_FACE('',(#12735,#1450),#1741,.T.);
#45316=ADVANCED_FACE('',(#12736),#4246,.F.);
#45317=ADVANCED_FACE('',(#12737,#1451),#1742,.T.);
#45318=ADVANCED_FACE('',(#12738),#4247,.F.);
#45319=ADVANCED_FACE('',(#12739,#1452),#1743,.T.);
#45320=ADVANCED_FACE('',(#12740),#4248,.F.);
#45321=ADVANCED_FACE('',(#12741,#1453),#1744,.T.);
#45322=ADVANCED_FACE('',(#12742),#4249,.F.);
#45323=ADVANCED_FACE('',(#12743,#1454),#1745,.T.);
#45324=ADVANCED_FACE('',(#12744),#4250,.F.);
#45325=ADVANCED_FACE('',(#12745,#1455),#1746,.T.);
#45326=ADVANCED_FACE('',(#12746),#4251,.F.);
#45327=ADVANCED_FACE('',(#12747,#1456),#1747,.T.);
#45328=ADVANCED_FACE('',(#12748),#4252,.F.);
#45329=ADVANCED_FACE('',(#12749,#1457),#1748,.T.);
#45330=ADVANCED_FACE('',(#12750),#4253,.F.);
#45331=ADVANCED_FACE('',(#12751,#1458),#1749,.T.);
#45332=ADVANCED_FACE('',(#12752),#4254,.F.);
#45333=ADVANCED_FACE('',(#12753,#1459),#1750,.T.);
#45334=ADVANCED_FACE('',(#12754),#4255,.F.);
#45335=ADVANCED_FACE('',(#12755,#1460),#1751,.T.);
#45336=ADVANCED_FACE('',(#12756),#4256,.F.);
#45337=ADVANCED_FACE('',(#12757,#1461),#1752,.T.);
#45338=ADVANCED_FACE('',(#12758),#4257,.F.);
#45339=ADVANCED_FACE('',(#12759,#1462),#1753,.T.);
#45340=ADVANCED_FACE('',(#12760),#4258,.F.);
#45341=ADVANCED_FACE('',(#12761,#1463),#1754,.T.);
#45342=ADVANCED_FACE('',(#12762),#4259,.F.);
#45343=ADVANCED_FACE('',(#12763,#1464),#1755,.T.);
#45344=ADVANCED_FACE('',(#12764),#4260,.F.);
#45345=ADVANCED_FACE('',(#12765,#1465),#1756,.T.);
#45346=ADVANCED_FACE('',(#12766),#4261,.F.);
#45347=ADVANCED_FACE('',(#12767,#1466),#1757,.T.);
#45348=ADVANCED_FACE('',(#12768),#4262,.F.);
#45349=ADVANCED_FACE('',(#12769,#1467),#1758,.T.);
#45350=ADVANCED_FACE('',(#12770),#4263,.F.);
#45351=ADVANCED_FACE('',(#12771,#1468),#1759,.T.);
#45352=ADVANCED_FACE('',(#12772),#4264,.F.);
#45353=ADVANCED_FACE('',(#12773,#1469),#1760,.T.);
#45354=ADVANCED_FACE('',(#12774),#4265,.F.);
#45355=ADVANCED_FACE('',(#12775,#1470),#1761,.T.);
#45356=ADVANCED_FACE('',(#12776),#4266,.F.);
#45357=ADVANCED_FACE('',(#12777,#1471),#1762,.T.);
#45358=ADVANCED_FACE('',(#12778),#4267,.F.);
#45359=ADVANCED_FACE('',(#12779,#1472),#1763,.T.);
#45360=ADVANCED_FACE('',(#12780),#4268,.F.);
#45361=ADVANCED_FACE('',(#12781,#1473),#1764,.T.);
#45362=ADVANCED_FACE('',(#12782),#4269,.F.);
#45363=ADVANCED_FACE('',(#12783,#1474),#1765,.T.);
#45364=ADVANCED_FACE('',(#12784),#4270,.F.);
#45365=ADVANCED_FACE('',(#12785,#1475),#1766,.T.);
#45366=ADVANCED_FACE('',(#12786),#4271,.F.);
#45367=ADVANCED_FACE('',(#12787,#1476),#1767,.T.);
#45368=ADVANCED_FACE('',(#12788),#4272,.F.);
#45369=ADVANCED_FACE('',(#12789,#1477),#1768,.T.);
#45370=ADVANCED_FACE('',(#12790),#4273,.F.);
#45371=ADVANCED_FACE('',(#12791,#1478),#1769,.T.);
#45372=ADVANCED_FACE('',(#12792),#4274,.F.);
#45373=ADVANCED_FACE('',(#12793,#1479),#1770,.T.);
#45374=ADVANCED_FACE('',(#12794),#4275,.F.);
#45375=ADVANCED_FACE('',(#12795,#1480),#1771,.T.);
#45376=ADVANCED_FACE('',(#12796),#4276,.F.);
#45377=ADVANCED_FACE('',(#12797,#1481),#1772,.T.);
#45378=ADVANCED_FACE('',(#12798),#4277,.F.);
#45379=ADVANCED_FACE('',(#12799,#1482),#1773,.T.);
#45380=ADVANCED_FACE('',(#12800),#4278,.F.);
#45381=ADVANCED_FACE('',(#12801,#1483),#1774,.T.);
#45382=ADVANCED_FACE('',(#12802),#4279,.F.);
#45383=ADVANCED_FACE('',(#12803,#1484),#1775,.T.);
#45384=ADVANCED_FACE('',(#12804),#4280,.F.);
#45385=ADVANCED_FACE('',(#12805,#1485),#1776,.T.);
#45386=ADVANCED_FACE('',(#12806),#4281,.F.);
#45387=ADVANCED_FACE('',(#12807,#1486),#1777,.T.);
#45388=ADVANCED_FACE('',(#12808),#4282,.F.);
#45389=ADVANCED_FACE('',(#12809,#1487),#1778,.T.);
#45390=ADVANCED_FACE('',(#12810),#4283,.F.);
#45391=ADVANCED_FACE('',(#12811,#1488),#1779,.T.);
#45392=ADVANCED_FACE('',(#12812),#4284,.F.);
#45393=ADVANCED_FACE('',(#12813,#1489),#1780,.T.);
#45394=ADVANCED_FACE('',(#12814),#4285,.F.);
#45395=ADVANCED_FACE('',(#12815,#1490),#1781,.T.);
#45396=ADVANCED_FACE('',(#12816),#4286,.F.);
#45397=ADVANCED_FACE('',(#12817,#1491),#1782,.T.);
#45398=ADVANCED_FACE('',(#12818),#4287,.F.);
#45399=ADVANCED_FACE('',(#12819,#1492),#1783,.T.);
#45400=ADVANCED_FACE('',(#12820),#4288,.F.);
#45401=ADVANCED_FACE('',(#12821,#1493),#1784,.T.);
#45402=ADVANCED_FACE('',(#12822),#4289,.F.);
#45403=ADVANCED_FACE('',(#12823,#1494),#1785,.T.);
#45404=ADVANCED_FACE('',(#12824),#4290,.F.);
#45405=ADVANCED_FACE('',(#12825,#1495),#1786,.T.);
#45406=ADVANCED_FACE('',(#12826),#4291,.F.);
#45407=ADVANCED_FACE('',(#12827,#1496),#1787,.T.);
#45408=ADVANCED_FACE('',(#12828),#4292,.F.);
#45409=ADVANCED_FACE('',(#12829,#1497),#1788,.T.);
#45410=ADVANCED_FACE('',(#12830),#4293,.F.);
#45411=ADVANCED_FACE('',(#12831,#1498),#1789,.T.);
#45412=ADVANCED_FACE('',(#12832),#4294,.F.);
#45413=ADVANCED_FACE('',(#12833,#1499),#1790,.T.);
#45414=ADVANCED_FACE('',(#12834),#4295,.F.);
#45415=ADVANCED_FACE('',(#12835,#1500),#1791,.T.);
#45416=ADVANCED_FACE('',(#12836),#4296,.F.);
#45417=ADVANCED_FACE('',(#12837,#1501),#1792,.T.);
#45418=ADVANCED_FACE('',(#12838),#4297,.F.);
#45419=ADVANCED_FACE('',(#12839,#1502),#1793,.T.);
#45420=ADVANCED_FACE('',(#12840),#4298,.F.);
#45421=ADVANCED_FACE('',(#12841,#1503),#1794,.T.);
#45422=ADVANCED_FACE('',(#12842),#4299,.F.);
#45423=ADVANCED_FACE('',(#12843,#1504),#1795,.T.);
#45424=ADVANCED_FACE('',(#12844),#4300,.F.);
#45425=ADVANCED_FACE('',(#12845,#1505),#1796,.T.);
#45426=ADVANCED_FACE('',(#12846),#4301,.F.);
#45427=ADVANCED_FACE('',(#12847,#1506),#1797,.T.);
#45428=ADVANCED_FACE('',(#12848),#4302,.F.);
#45429=ADVANCED_FACE('',(#12849,#1507),#1798,.T.);
#45430=ADVANCED_FACE('',(#12850),#4303,.F.);
#45431=ADVANCED_FACE('',(#12851,#1508),#1799,.T.);
#45432=ADVANCED_FACE('',(#12852),#4304,.F.);
#45433=ADVANCED_FACE('',(#12853,#1509),#1800,.T.);
#45434=ADVANCED_FACE('',(#12854),#4305,.F.);
#45435=ADVANCED_FACE('',(#12855,#1510),#1801,.T.);
#45436=ADVANCED_FACE('',(#12856),#4306,.F.);
#45437=ADVANCED_FACE('',(#12857,#1511),#1802,.T.);
#45438=ADVANCED_FACE('',(#12858),#4307,.F.);
#45439=ADVANCED_FACE('',(#12859,#1512),#1803,.T.);
#45440=ADVANCED_FACE('',(#12860),#4308,.F.);
#45441=ADVANCED_FACE('',(#12861,#1513),#1804,.T.);
#45442=ADVANCED_FACE('',(#12862),#4309,.F.);
#45443=ADVANCED_FACE('',(#12863,#1514),#1805,.T.);
#45444=ADVANCED_FACE('',(#12864),#4310,.F.);
#45445=ADVANCED_FACE('',(#12865,#1515),#1806,.T.);
#45446=ADVANCED_FACE('',(#12866),#4311,.F.);
#45447=ADVANCED_FACE('',(#12867,#1516),#1807,.T.);
#45448=CLOSED_SHELL('',(#42047,#42048,#42049,#42050,#42051,#42052,#42053));
#45449=CLOSED_SHELL('',(#42054,#42055,#42056,#42057,#42058));
#45450=CLOSED_SHELL('',(#42059,#42060,#42061,#42062,#42063));
#45451=CLOSED_SHELL('',(#42064,#42065,#42066,#42067,#42068,#42069,#42070,
#42071,#42072,#42073,#42074,#42075,#42076,#42077,#42078,#42079,#42080,#42081,
#42082,#42083,#42084,#42085,#42086,#42087,#42088,#42089,#42090,#42091,#42092,
#42093,#42094,#42095,#42096,#42097,#42098,#42099,#42100,#42101,#42102,#42103,
#42104,#42105,#42106,#42107,#42108,#42109,#42110,#42111,#42112,#42113,#42114,
#42115,#42116,#42117,#42118,#42119,#42120,#42121,#42122,#42123,#42124,#42125,
#42126,#42127,#42128,#42129,#42130,#42131,#42132,#42133,#42134,#42135,#42136,
#42137,#42138,#42139,#42140,#42141,#42142,#42143,#42144,#42145,#42146,#42147,
#42148,#42149,#42150,#42151,#42152,#42153,#42154,#42155,#42156,#42157,#42158,
#42159,#42160,#42161,#42162,#42163,#42164,#42165,#42166,#42167,#42168,#42169,
#42170,#42171,#42172,#42173,#42174,#42175,#42176,#42177,#42178,#42179,#42180,
#42181,#42182,#42183,#42184,#42185,#42186,#42187,#42188,#42189,#42190,#42191,
#42192,#42193,#42194,#42195,#42196,#42197,#42198,#42199,#42200,#42201,#42202,
#42203,#42204,#42205,#42206,#42207,#42208,#42209,#42210,#42211,#42212,#42213,
#42214,#42215,#42216,#42217,#42218,#42219,#42220,#42221,#42222,#42223,#42224,
#42225,#42226,#42227,#42228,#42229,#42230,#42231,#42232,#42233,#42234,#42235,
#42236,#42237,#42238,#42239,#42240,#42241,#42242,#42243,#42244,#42245,#42246,
#42247,#42248,#42249,#42250,#42251,#42252,#42253,#42254,#42255,#42256,#42257,
#42258,#42259,#42260,#42261,#42262,#42263,#42264,#42265,#42266,#42267,#42268,
#42269,#42270,#42271,#42272,#42273,#42274,#42275,#42276,#42277,#42278,#42279,
#42280,#42281,#42282,#42283,#42284,#42285,#42286,#42287,#42288,#42289,#42290,
#42291,#42292,#42293,#42294,#42295,#42296,#42297,#42298,#42299,#42300,#42301,
#42302,#42303,#42304,#42305,#42306,#42307,#42308,#42309,#42310,#42311,#42312,
#42313,#42314,#42315,#42316,#42317,#42318,#42319,#42320,#42321,#42322,#42323,
#42324,#42325,#42326,#42327,#42328,#42329,#42330,#42331,#42332,#42333,#42334,
#42335,#42336,#42337,#42338,#42339,#42340,#42341,#42342,#42343,#42344,#42345,
#42346,#42347,#42348,#42349,#42350,#42351,#42352,#42353,#42354,#42355,#42356,
#42357,#42358,#42359,#42360,#42361,#42362,#42363,#42364,#42365,#42366,#42367,
#42368,#42369,#42370,#42371,#42372,#42373,#42374,#42375,#42376,#42377,#42378,
#42379,#42380,#42381,#42382,#42383,#42384,#42385,#42386,#42387,#42388,#42389,
#42390,#42391,#42392,#42393,#42394,#42395,#42396,#42397,#42398,#42399,#42400,
#42401,#42402,#42403,#42404,#42405,#42406,#42407,#42408,#42409,#42410,#42411,
#42412,#42413,#42414,#42415,#42416,#42417,#42418,#42419,#42420,#42421,#42422,
#42423,#42424,#42425,#42426,#42427,#42428,#42429,#42430,#42431,#42432,#42433,
#42434,#42435,#42436,#42437,#42438,#42439,#42440,#42441,#42442,#42443,#42444,
#42445,#42446,#42447,#42448,#42449,#42450,#42451,#42452,#42453,#42454,#42455,
#42456,#42457,#42458,#42459,#42460,#42461,#42462,#42463,#42464,#42465,#42466,
#42467,#42468,#42469,#42470,#42471,#42472,#42473,#42474,#42475,#42476,#42477,
#42478,#42479,#42480,#42481,#42482,#42483,#42484,#42485,#42486,#42487,#42488,
#42489,#42490,#42491,#42492,#42493,#42494,#42495,#42496,#42497,#42498,#42499,
#42500,#42501,#42502,#42503,#42504,#42505,#42506,#42507,#42508,#42509,#42510,
#42511,#42512,#42513,#42514,#42515,#42516,#42517,#42518,#42519,#42520,#42521,
#42522,#42523,#42524,#42525,#42526,#42527,#42528,#42529,#42530,#42531,#42532,
#42533,#42534,#42535,#42536,#42537,#42538,#42539,#42540,#42541,#42542,#42543,
#42544,#42545,#42546,#42547,#42548,#42549,#42550,#42551,#42552,#42553,#42554,
#42555,#42556,#42557,#42558,#42559,#42560,#42561,#42562,#42563,#42564,#42565,
#42566,#42567,#42568,#42569,#42570,#42571,#42572,#42573,#42574,#42575,#42576,
#42577,#42578,#42579,#42580,#42581,#42582,#42583,#42584,#42585,#42586,#42587,
#42588,#42589,#42590,#42591,#42592,#42593,#42594,#42595,#42596,#42597,#42598,
#42599,#42600,#42601,#42602,#42603,#42604,#42605,#42606,#42607,#42608,#42609,
#42610,#42611,#42612,#42613,#42614,#42615,#42616,#42617,#42618,#42619,#42620,
#42621,#42622,#42623,#42624,#42625,#42626,#42627,#42628,#42629,#42630,#42631,
#42632,#42633,#42634,#42635,#42636,#42637,#42638,#42639,#42640,#42641,#42642,
#42643,#42644,#42645,#42646,#42647,#42648,#42649,#42650,#42651,#42652,#42653,
#42654,#42655,#42656,#42657,#42658,#42659,#42660,#42661,#42662,#42663,#42664,
#42665,#42666,#42667,#42668,#42669,#42670,#42671,#42672,#42673,#42674,#42675,
#42676,#42677,#42678,#42679,#42680,#42681,#42682,#42683,#42684,#42685,#42686,
#42687,#42688,#42689,#42690,#42691,#42692,#42693,#42694,#42695,#42696,#42697,
#42698,#42699,#42700,#42701,#42702,#42703,#42704,#42705,#42706,#42707,#42708,
#42709,#42710,#42711,#42712,#42713,#42714,#42715,#42716,#42717,#42718,#42719,
#42720,#42721,#42722,#42723,#42724,#42725,#42726,#42727,#42728,#42729,#42730,
#42731,#42732,#42733,#42734,#42735,#42736,#42737,#42738,#42739,#42740,#42741,
#42742,#42743,#42744,#42745,#42746,#42747,#42748,#42749,#42750,#42751,#42752,
#42753,#42754,#42755,#42756,#42757,#42758,#42759,#42760,#42761,#42762,#42763,
#42764,#42765,#42766,#42767,#42768,#42769,#42770,#42771,#42772,#42773,#42774,
#42775,#42776,#42777,#42778,#42779,#42780,#42781,#42782,#42783,#42784,#42785,
#42786,#42787,#42788,#42789,#42790,#42791,#42792,#42793,#42794,#42795,#42796,
#42797,#42798,#42799,#42800,#42801,#42802,#42803,#42804,#42805,#42806,#42807,
#42808,#42809,#42810,#42811,#42812,#42813,#42814,#42815,#42816,#42817,#42818,
#42819,#42820,#42821,#42822,#42823,#42824,#42825,#42826,#42827,#42828,#42829,
#42830,#42831,#42832,#42833,#42834,#42835,#42836,#42837,#42838,#42839,#42840,
#42841,#42842,#42843,#42844,#42845,#42846,#42847,#42848,#42849,#42850,#42851,
#42852,#42853,#42854,#42855,#42856,#42857,#42858,#42859,#42860,#42861,#42862,
#42863,#42864,#42865,#42866,#42867,#42868,#42869,#42870,#42871,#42872,#42873,
#42874,#42875,#42876,#42877,#42878,#42879,#42880,#42881,#42882,#42883,#42884,
#42885,#42886,#42887,#42888,#42889,#42890,#42891,#42892,#42893,#42894,#42895,
#42896,#42897,#42898,#42899,#42900,#42901,#42902,#42903,#42904,#42905,#42906,
#42907,#42908,#42909,#42910,#42911,#42912,#42913,#42914,#42915,#42916,#42917,
#42918,#42919,#42920,#42921,#42922,#42923,#42924,#42925,#42926,#42927,#42928,
#42929,#42930,#42931,#42932,#42933,#42934,#42935,#42936,#42937,#42938,#42939,
#42940,#42941,#42942,#42943,#42944,#42945,#42946,#42947,#42948,#42949,#42950,
#42951,#42952,#42953,#42954,#42955,#42956,#42957,#42958,#42959,#42960,#42961,
#42962,#42963,#42964,#42965,#42966,#42967,#42968,#42969,#42970,#42971,#42972,
#42973,#42974,#42975,#42976,#42977,#42978,#42979,#42980,#42981,#42982,#42983,
#42984,#42985,#42986,#42987,#42988,#42989,#42990,#42991,#42992,#42993,#42994,
#42995,#42996,#42997,#42998,#42999,#43000,#43001,#43002,#43003,#43004,#43005,
#43006,#43007,#43008,#43009,#43010,#43011,#43012,#43013,#43014,#43015,#43016,
#43017,#43018,#43019,#43020,#43021,#43022,#43023,#43024,#43025,#43026,#43027,
#43028,#43029,#43030,#43031,#43032,#43033,#43034,#43035,#43036,#43037,#43038,
#43039,#43040,#43041,#43042,#43043,#43044,#43045,#43046,#43047,#43048,#43049,
#43050,#43051,#43052,#43053,#43054,#43055,#43056,#43057,#43058,#43059,#43060,
#43061,#43062,#43063,#43064,#43065,#43066,#43067,#43068,#43069,#43070,#43071,
#43072,#43073,#43074,#43075,#43076,#43077,#43078,#43079,#43080,#43081,#43082,
#43083,#43084,#43085,#43086,#43087,#43088,#43089,#43090,#43091,#43092,#43093,
#43094,#43095,#43096,#43097,#43098,#43099,#43100,#43101,#43102,#43103,#43104,
#43105,#43106,#43107,#43108,#43109,#43110,#43111,#43112,#43113,#43114,#43115,
#43116,#43117,#43118,#43119,#43120,#43121,#43122,#43123,#43124,#43125,#43126,
#43127,#43128,#43129,#43130,#43131,#43132,#43133,#43134,#43135,#43136,#43137,
#43138,#43139,#43140,#43141,#43142,#43143,#43144,#43145,#43146,#43147,#43148,
#43149,#43150,#43151,#43152,#43153,#43154,#43155,#43156,#43157,#43158,#43159,
#43160,#43161,#43162,#43163,#43164,#43165,#43166,#43167,#43168,#43169,#43170,
#43171,#43172,#43173,#43174,#43175,#43176,#43177,#43178,#43179,#43180,#43181,
#43182,#43183,#43184,#43185,#43186,#43187,#43188,#43189,#43190,#43191,#43192,
#43193,#43194,#43195,#43196,#43197,#43198,#43199,#43200,#43201,#43202,#43203,
#43204,#43205,#43206,#43207,#43208,#43209,#43210,#43211,#43212,#43213,#43214,
#43215,#43216,#43217,#43218,#43219,#43220,#43221,#43222,#43223,#43224,#43225,
#43226,#43227,#43228,#43229,#43230,#43231,#43232,#43233,#43234,#43235,#43236,
#43237,#43238,#43239,#43240,#43241,#43242,#43243,#43244,#43245,#43246,#43247,
#43248,#43249,#43250,#43251,#43252,#43253,#43254,#43255,#43256,#43257,#43258,
#43259,#43260,#43261,#43262,#43263,#43264,#43265,#43266,#43267,#43268,#43269,
#43270,#43271,#43272,#43273,#43274,#43275,#43276,#43277,#43278,#43279,#43280,
#43281,#43282,#43283,#43284,#43285,#43286,#43287,#43288,#43289,#43290,#43291,
#43292,#43293,#43294,#43295,#43296,#43297,#43298,#43299,#43300,#43301,#43302,
#43303,#43304,#43305,#43306,#43307,#43308,#43309,#43310,#43311,#43312,#43313,
#43314,#43315,#43316,#43317,#43318,#43319,#43320,#43321,#43322,#43323,#43324,
#43325,#43326,#43327,#43328,#43329,#43330,#43331,#43332,#43333,#43334,#43335,
#43336,#43337,#43338,#43339,#43340,#43341,#43342,#43343,#43344,#43345,#43346,
#43347,#43348,#43349,#43350,#43351,#43352,#43353,#43354,#43355,#43356,#43357,
#43358,#43359,#43360,#43361,#43362,#43363,#43364,#43365,#43366,#43367,#43368,
#43369,#43370,#43371,#43372,#43373,#43374,#43375,#43376,#43377,#43378,#43379,
#43380,#43381,#43382,#43383,#43384,#43385,#43386,#43387,#43388,#43389,#43390,
#43391,#43392,#43393,#43394,#43395,#43396,#43397,#43398,#43399,#43400,#43401,
#43402,#43403,#43404,#43405,#43406,#43407,#43408,#43409,#43410,#43411,#43412,
#43413,#43414,#43415,#43416,#43417,#43418,#43419,#43420,#43421,#43422,#43423,
#43424,#43425,#43426,#43427,#43428,#43429,#43430,#43431,#43432,#43433,#43434,
#43435,#43436,#43437,#43438,#43439,#43440,#43441,#43442,#43443,#43444,#43445,
#43446,#43447,#43448,#43449,#43450,#43451,#43452,#43453,#43454,#43455,#43456,
#43457,#43458,#43459,#43460,#43461,#43462,#43463,#43464));
#45452=CLOSED_SHELL('',(#43465,#43466,#43467,#43468,#43469,#43470,#43471,
#43472,#43473,#43474,#43475));
#45453=CLOSED_SHELL('',(#43476,#43477,#43478,#43479,#43480,#43481));
#45454=CLOSED_SHELL('',(#43482,#43483,#43484,#43485,#43486,#43487));
#45455=CLOSED_SHELL('',(#43488,#43489,#43490,#43491,#43492,#43493,#43494,
#43495,#43496,#43497,#43498,#43499,#43500,#43501,#43502,#43503,#43504,#43505,
#43506,#43507,#43508,#43509,#43510,#43511,#43512,#43513,#43514,#43515,#43516,
#43517,#43518,#43519,#43520,#43521,#43522,#43523,#43524,#43525,#43526,#43527,
#43528,#43529,#43530,#43531,#43532,#43533,#43534,#43535,#43536,#43537,#43538,
#43539,#43540,#43541,#43542,#43543,#43544,#43545,#43546,#43547,#43548,#43549,
#43550,#43551,#43552,#43553,#43554,#43555,#43556,#43557,#43558,#43559,#43560,
#43561,#43562,#43563,#43564,#43565,#43566,#43567,#43568,#43569,#43570,#43571,
#43572,#43573,#43574,#43575,#43576,#43577,#43578,#43579,#43580,#43581,#43582,
#43583,#43584,#43585,#43586,#43587,#43588,#43589,#43590,#43591,#43592,#43593,
#43594,#43595,#43596,#43597,#43598,#43599,#43600,#43601,#43602,#43603,#43604,
#43605,#43606,#43607,#43608,#43609,#43610,#43611,#43612,#43613,#43614,#43615,
#43616,#43617,#43618,#43619,#43620,#43621,#43622,#43623,#43624,#43625,#43626,
#43627,#43628,#43629,#43630,#43631,#43632,#43633,#43634,#43635,#43636,#43637,
#43638,#43639,#43640,#43641,#43642,#43643,#43644,#43645,#43646,#43647,#43648,
#43649,#43650,#43651,#43652,#43653,#43654,#43655,#43656,#43657,#43658,#43659,
#43660,#43661,#43662,#43663,#43664,#43665,#43666,#43667,#43668,#43669,#43670,
#43671,#43672,#43673,#43674,#43675,#43676,#43677,#43678,#43679,#43680,#43681,
#43682,#43683,#43684,#43685,#43686,#43687,#43688,#43689,#43690,#43691,#43692,
#43693,#43694,#43695,#43696,#43697,#43698,#43699,#43700,#43701,#43702));
#45456=CLOSED_SHELL('',(#43703,#43704,#43705,#43706,#43707,#43708,#43709,
#43710,#43711,#43712,#43713,#43714,#43715,#43716,#43717,#43718,#43719,#43720,
#43721,#43722,#43723,#43724,#43725,#43726,#43727,#43728,#43729,#43730,#43731,
#43732,#43733,#43734,#43735,#43736,#43737,#43738,#43739,#43740,#43741,#43742,
#43743,#43744,#43745,#43746,#43747,#43748,#43749,#43750,#43751,#43752,#43753,
#43754,#43755,#43756,#43757,#43758,#43759,#43760,#43761,#43762,#43763,#43764,
#43765,#43766,#43767,#43768,#43769,#43770,#43771,#43772,#43773,#43774,#43775,
#43776,#43777,#43778,#43779,#43780,#43781,#43782));
#45457=CLOSED_SHELL('',(#43783,#43784,#43785,#43786,#43787,#43788,#43789,
#43790,#43791,#43792,#43793,#43794,#43795,#43796,#43797,#43798,#43799,#43800,
#43801,#43802,#43803,#43804,#43805,#43806,#43807,#43808,#43809,#43810,#43811,
#43812,#43813,#43814,#43815,#43816,#43817,#43818,#43819,#43820,#43821,#43822,
#43823,#43824,#43825,#43826,#43827,#43828,#43829,#43830,#43831,#43832,#43833,
#43834,#43835,#43836,#43837,#43838,#43839,#43840,#43841,#43842,#43843,#43844,
#43845,#43846,#43847,#43848,#43849,#43850,#43851,#43852,#43853,#43854,#43855,
#43856,#43857,#43858,#43859,#43860,#43861));
#45458=CLOSED_SHELL('',(#43862,#43863,#43864,#43865,#43866));
#45459=CLOSED_SHELL('',(#43867,#43868,#43869,#43870,#43871,#43872,#43873,
#43874,#43875,#43876,#43877,#43878,#43879,#43880,#43881,#43882,#43883,#43884,
#43885,#43886,#43887,#43888,#43889,#43890,#43891,#43892,#43893,#43894,#43895,
#43896,#43897,#43898,#43899,#43900,#43901,#43902,#43903,#43904,#43905,#43906,
#43907,#43908,#43909,#43910,#43911,#43912,#43913,#43914,#43915,#43916,#43917,
#43918,#43919,#43920,#43921,#43922,#43923,#43924,#43925,#43926,#43927,#43928,
#43929,#43930,#43931,#43932,#43933,#43934,#43935,#43936,#43937,#43938,#43939,
#43940,#43941,#43942,#43943,#43944,#43945,#43946,#43947,#43948,#43949,#43950,
#43951,#43952,#43953,#43954,#43955,#43956,#43957,#43958,#43959,#43960,#43961,
#43962,#43963,#43964,#43965,#43966,#43967,#43968,#43969,#43970,#43971,#43972,
#43973,#43974,#43975,#43976,#43977,#43978,#43979,#43980,#43981,#43982,#43983,
#43984,#43985,#43986,#43987,#43988,#43989,#43990,#43991,#43992,#43993,#43994,
#43995,#43996,#43997,#43998,#43999,#44000,#44001,#44002,#44003,#44004,#44005,
#44006,#44007,#44008,#44009,#44010,#44011,#44012,#44013,#44014,#44015,#44016,
#44017,#44018,#44019,#44020,#44021,#44022,#44023,#44024,#44025,#44026,#44027,
#44028,#44029,#44030,#44031,#44032,#44033,#44034,#44035,#44036,#44037,#44038,
#44039,#44040,#44041,#44042,#44043,#44044,#44045,#44046,#44047,#44048,#44049,
#44050,#44051,#44052,#44053,#44054,#44055,#44056,#44057,#44058,#44059,#44060,
#44061,#44062,#44063,#44064,#44065,#44066,#44067,#44068,#44069,#44070,#44071,
#44072,#44073,#44074,#44075,#44076,#44077,#44078,#44079,#44080,#44081,#44082,
#44083,#44084,#44085,#44086,#44087,#44088,#44089,#44090,#44091,#44092,#44093,
#44094,#44095,#44096,#44097,#44098,#44099,#44100,#44101,#44102,#44103,#44104,
#44105,#44106,#44107,#44108,#44109,#44110,#44111,#44112,#44113,#44114,#44115,
#44116,#44117,#44118,#44119,#44120,#44121,#44122,#44123,#44124,#44125,#44126,
#44127,#44128,#44129,#44130,#44131,#44132,#44133,#44134,#44135,#44136,#44137,
#44138,#44139,#44140,#44141,#44142,#44143,#44144,#44145,#44146,#44147,#44148,
#44149,#44150,#44151,#44152,#44153,#44154,#44155,#44156,#44157,#44158,#44159,
#44160,#44161,#44162,#44163,#44164,#44165,#44166,#44167,#44168,#44169,#44170,
#44171,#44172,#44173,#44174,#44175,#44176,#44177,#44178,#44179,#44180,#44181,
#44182,#44183,#44184,#44185,#44186,#44187,#44188,#44189,#44190,#44191,#44192,
#44193,#44194,#44195,#44196,#44197,#44198,#44199,#44200,#44201,#44202,#44203,
#44204,#44205,#44206,#44207,#44208,#44209,#44210,#44211,#44212,#44213,#44214,
#44215,#44216,#44217,#44218,#44219,#44220,#44221,#44222,#44223,#44224,#44225,
#44226,#44227,#44228,#44229,#44230,#44231,#44232,#44233,#44234,#44235,#44236,
#44237,#44238,#44239,#44240,#44241,#44242,#44243,#44244,#44245,#44246,#44247,
#44248,#44249,#44250,#44251,#44252,#44253,#44254,#44255,#44256,#44257,#44258,
#44259,#44260,#44261,#44262,#44263,#44264,#44265,#44266,#44267,#44268,#44269,
#44270,#44271,#44272,#44273,#44274,#44275,#44276,#44277,#44278,#44279,#44280,
#44281,#44282,#44283,#44284,#44285,#44286,#44287,#44288,#44289,#44290,#44291,
#44292,#44293,#44294,#44295,#44296,#44297,#44298,#44299,#44300,#44301,#44302,
#44303,#44304,#44305,#44306,#44307,#44308,#44309,#44310,#44311,#44312,#44313,
#44314,#44315,#44316,#44317,#44318,#44319,#44320,#44321,#44322,#44323,#44324,
#44325,#44326,#44327,#44328,#44329,#44330,#44331,#44332,#44333,#44334,#44335,
#44336,#44337,#44338,#44339,#44340,#44341,#44342,#44343,#44344,#44345,#44346,
#44347,#44348,#44349,#44350,#44351,#44352,#44353,#44354,#44355,#44356,#44357,
#44358,#44359,#44360,#44361,#44362,#44363,#44364,#44365,#44366,#44367,#44368,
#44369,#44370,#44371,#44372,#44373,#44374,#44375,#44376,#44377,#44378,#44379,
#44380,#44381,#44382,#44383,#44384,#44385,#44386,#44387,#44388,#44389,#44390,
#44391,#44392,#44393,#44394,#44395,#44396,#44397,#44398,#44399,#44400,#44401,
#44402,#44403,#44404,#44405,#44406,#44407,#44408,#44409,#44410,#44411,#44412,
#44413,#44414,#44415,#44416,#44417,#44418,#44419,#44420,#44421,#44422,#44423,
#44424,#44425,#44426,#44427,#44428,#44429,#44430,#44431,#44432,#44433,#44434,
#44435,#44436,#44437,#44438,#44439,#44440,#44441,#44442,#44443,#44444,#44445,
#44446,#44447,#44448,#44449,#44450,#44451,#44452,#44453,#44454,#44455,#44456,
#44457,#44458,#44459,#44460,#44461,#44462,#44463,#44464,#44465,#44466,#44467,
#44468,#44469,#44470,#44471,#44472,#44473,#44474,#44475,#44476,#44477,#44478,
#44479,#44480,#44481,#44482,#44483,#44484,#44485,#44486,#44487,#44488,#44489,
#44490,#44491,#44492,#44493,#44494,#44495,#44496,#44497,#44498,#44499,#44500,
#44501,#44502,#44503,#44504,#44505,#44506,#44507,#44508,#44509,#44510,#44511,
#44512,#44513,#44514,#44515,#44516,#44517,#44518,#44519,#44520,#44521,#44522,
#44523,#44524,#44525,#44526,#44527,#44528,#44529,#44530,#44531,#44532,#44533,
#44534,#44535,#44536,#44537,#44538,#44539,#44540,#44541,#44542,#44543,#44544,
#44545,#44546,#44547,#44548,#44549,#44550,#44551,#44552,#44553,#44554,#44555,
#44556,#44557,#44558,#44559,#44560,#44561,#44562,#44563,#44564,#44565,#44566,
#44567,#44568,#44569,#44570,#44571,#44572,#44573,#44574,#44575,#44576,#44577,
#44578,#44579,#44580,#44581,#44582,#44583,#44584,#44585,#44586,#44587,#44588,
#44589,#44590,#44591,#44592,#44593,#44594,#44595,#44596,#44597,#44598,#44599,
#44600,#44601,#44602,#44603,#44604,#44605,#44606,#44607,#44608,#44609,#44610,
#44611,#44612,#44613,#44614,#44615,#44616,#44617,#44618,#44619,#44620,#44621,
#44622,#44623,#44624,#44625,#44626,#44627,#44628,#44629,#44630,#44631,#44632,
#44633,#44634,#44635,#44636,#44637,#44638,#44639,#44640,#44641,#44642,#44643,
#44644,#44645,#44646,#44647,#44648,#44649,#44650,#44651,#44652,#44653,#44654,
#44655,#44656,#44657,#44658,#44659,#44660,#44661,#44662,#44663,#44664,#44665,
#44666,#44667,#44668,#44669,#44670,#44671,#44672,#44673,#44674,#44675,#44676,
#44677,#44678,#44679,#44680,#44681,#44682,#44683,#44684,#44685,#44686,#44687,
#44688,#44689,#44690,#44691,#44692,#44693,#44694,#44695,#44696,#44697,#44698,
#44699,#44700,#44701,#44702,#44703,#44704,#44705,#44706,#44707,#44708,#44709,
#44710,#44711,#44712,#44713,#44714,#44715,#44716,#44717,#44718,#44719,#44720,
#44721,#44722,#44723,#44724,#44725,#44726,#44727,#44728,#44729,#44730,#44731,
#44732,#44733,#44734,#44735,#44736,#44737,#44738,#44739,#44740,#44741,#44742,
#44743,#44744,#44745,#44746,#44747,#44748,#44749,#44750,#44751,#44752,#44753,
#44754,#44755,#44756,#44757,#44758,#44759,#44760,#44761,#44762,#44763,#44764,
#44765,#44766,#44767,#44768,#44769,#44770,#44771,#44772,#44773,#44774,#44775,
#44776,#44777,#44778,#44779,#44780,#44781,#44782,#44783,#44784,#44785,#44786,
#44787,#44788,#44789,#44790,#44791,#44792,#44793,#44794,#44795,#44796,#44797,
#44798,#44799,#44800,#44801,#44802,#44803,#44804,#44805,#44806,#44807,#44808,
#44809,#44810,#44811,#44812,#44813,#44814,#44815,#44816,#44817,#44818,#44819,
#44820,#44821,#44822,#44823,#44824,#44825,#44826,#44827,#44828,#44829,#44830,
#44831,#44832,#44833,#44834,#44835,#44836,#44837,#44838,#44839,#44840,#44841,
#44842,#44843,#44844,#44845,#44846,#44847,#44848,#44849,#44850,#44851,#44852,
#44853,#44854,#44855,#44856,#44857,#44858,#44859,#44860,#44861,#44862,#44863,
#44864,#44865,#44866,#44867,#44868,#44869,#44870,#44871,#44872,#44873,#44874,
#44875,#44876,#44877,#44878,#44879,#44880,#44881,#44882,#44883,#44884,#44885,
#44886,#44887,#44888,#44889,#44890,#44891,#44892,#44893,#44894,#44895,#44896,
#44897,#44898,#44899,#44900,#44901,#44902,#44903,#44904,#44905,#44906,#44907,
#44908,#44909,#44910,#44911,#44912,#44913,#44914,#44915,#44916,#44917,#44918,
#44919,#44920,#44921,#44922,#44923,#44924,#44925,#44926,#44927,#44928,#44929,
#44930,#44931,#44932,#44933,#44934,#44935,#44936,#44937,#44938,#44939,#44940,
#44941,#44942,#44943,#44944,#44945,#44946,#44947,#44948,#44949,#44950,#44951,
#44952,#44953,#44954,#44955,#44956,#44957,#44958,#44959,#44960,#44961,#44962,
#44963,#44964,#44965,#44966,#44967,#44968,#44969,#44970,#44971,#44972,#44973,
#44974,#44975,#44976,#44977,#44978,#44979,#44980,#44981,#44982,#44983,#44984,
#44985,#44986,#44987,#44988,#44989,#44990,#44991,#44992,#44993,#44994,#44995,
#44996,#44997,#44998,#44999,#45000,#45001,#45002,#45003,#45004,#45005,#45006,
#45007,#45008,#45009,#45010,#45011,#45012,#45013,#45014,#45015,#45016,#45017,
#45018,#45019,#45020,#45021,#45022,#45023,#45024,#45025,#45026,#45027,#45028,
#45029,#45030,#45031,#45032,#45033,#45034,#45035,#45036,#45037,#45038,#45039,
#45040,#45041,#45042,#45043,#45044,#45045,#45046,#45047,#45048,#45049,#45050,
#45051,#45052,#45053,#45054,#45055,#45056,#45057,#45058,#45059,#45060,#45061,
#45062,#45063,#45064,#45065,#45066,#45067,#45068,#45069,#45070,#45071,#45072,
#45073,#45074,#45075,#45076,#45077,#45078,#45079,#45080,#45081,#45082,#45083,
#45084,#45085,#45086,#45087,#45088,#45089,#45090,#45091,#45092,#45093,#45094,
#45095,#45096,#45097,#45098,#45099,#45100,#45101,#45102,#45103,#45104,#45105,
#45106,#45107,#45108,#45109,#45110,#45111,#45112,#45113,#45114,#45115,#45116,
#45117,#45118,#45119,#45120,#45121,#45122,#45123,#45124,#45125,#45126,#45127,
#45128,#45129,#45130,#45131,#45132,#45133,#45134,#45135,#45136,#45137,#45138,
#45139,#45140,#45141,#45142,#45143,#45144,#45145,#45146,#45147,#45148,#45149,
#45150,#45151,#45152,#45153,#45154,#45155,#45156,#45157,#45158,#45159,#45160,
#45161,#45162,#45163,#45164,#45165,#45166,#45167,#45168,#45169,#45170,#45171,
#45172,#45173,#45174,#45175,#45176,#45177,#45178,#45179,#45180,#45181,#45182,
#45183,#45184,#45185,#45186,#45187,#45188,#45189,#45190,#45191,#45192,#45193,
#45194,#45195,#45196,#45197,#45198,#45199,#45200,#45201,#45202,#45203,#45204,
#45205,#45206,#45207,#45208,#45209,#45210,#45211,#45212,#45213,#45214,#45215,
#45216,#45217,#45218,#45219,#45220,#45221,#45222,#45223,#45224,#45225,#45226,
#45227,#45228,#45229,#45230,#45231,#45232,#45233,#45234,#45235,#45236,#45237,
#45238,#45239,#45240,#45241,#45242,#45243,#45244,#45245,#45246,#45247,#45248,
#45249,#45250,#45251,#45252,#45253,#45254,#45255,#45256,#45257,#45258,#45259,
#45260,#45261,#45262,#45263,#45264,#45265,#45266,#45267,#45268,#45269,#45270,
#45271,#45272,#45273,#45274,#45275,#45276,#45277,#45278,#45279,#45280,#45281,
#45282,#45283,#45284,#45285,#45286,#45287,#45288,#45289,#45290,#45291,#45292,
#45293,#45294,#45295,#45296,#45297,#45298,#45299,#45300,#45301,#45302,#45303,
#45304,#45305,#45306,#45307,#45308,#45309,#45310,#45311,#45312,#45313,#45314,
#45315,#45316,#45317,#45318,#45319,#45320,#45321,#45322,#45323,#45324,#45325,
#45326,#45327,#45328,#45329,#45330,#45331,#45332,#45333,#45334,#45335,#45336,
#45337,#45338,#45339,#45340,#45341,#45342,#45343,#45344,#45345,#45346,#45347,
#45348,#45349,#45350,#45351,#45352,#45353,#45354,#45355,#45356,#45357,#45358,
#45359,#45360,#45361,#45362,#45363,#45364,#45365,#45366,#45367,#45368,#45369,
#45370,#45371,#45372,#45373,#45374,#45375,#45376,#45377,#45378,#45379,#45380,
#45381,#45382,#45383,#45384,#45385,#45386,#45387,#45388,#45389,#45390,#45391,
#45392,#45393,#45394,#45395,#45396,#45397,#45398,#45399,#45400,#45401,#45402,
#45403,#45404,#45405,#45406,#45407,#45408,#45409,#45410,#45411,#45412,#45413,
#45414,#45415,#45416,#45417,#45418,#45419,#45420,#45421,#45422,#45423,#45424,
#45425,#45426,#45427,#45428,#45429,#45430,#45431,#45432,#45433,#45434,#45435,
#45436,#45437,#45438,#45439,#45440,#45441,#45442,#45443,#45444,#45445,#45446,
#45447));
#45460=DERIVED_UNIT_ELEMENT(#45476,1.);
#45461=DERIVED_UNIT_ELEMENT(#130912,-3.);
#45462=DERIVED_UNIT_ELEMENT(#45476,1.);
#45463=DERIVED_UNIT_ELEMENT(#130912,-3.);
#45464=DERIVED_UNIT_ELEMENT(#45476,1.);
#45465=DERIVED_UNIT_ELEMENT(#130912,-3.);
#45466=DERIVED_UNIT_ELEMENT(#45476,1.);
#45467=DERIVED_UNIT_ELEMENT(#130912,-3.);
#45468=DERIVED_UNIT_ELEMENT(#45476,1.);
#45469=DERIVED_UNIT_ELEMENT(#130912,-3.);
#45470=DERIVED_UNIT_ELEMENT(#45476,1.);
#45471=DERIVED_UNIT_ELEMENT(#130912,-3.);
#45472=DERIVED_UNIT_ELEMENT(#45476,1.);
#45473=DERIVED_UNIT_ELEMENT(#130912,-3.);
#45474=DERIVED_UNIT_ELEMENT(#45476,1.);
#45475=DERIVED_UNIT_ELEMENT(#130912,-3.);
#45476=(
MASS_UNIT()
NAMED_UNIT(*)
SI_UNIT(.KILO.,.GRAM.)
);
#45477=DERIVED_UNIT((#45460,#45461));
#45478=DERIVED_UNIT((#45462,#45463));
#45479=DERIVED_UNIT((#45464,#45465));
#45480=DERIVED_UNIT((#45466,#45467));
#45481=DERIVED_UNIT((#45468,#45469));
#45482=DERIVED_UNIT((#45470,#45471));
#45483=DERIVED_UNIT((#45472,#45473));
#45484=DERIVED_UNIT((#45474,#45475));
#45485=MEASURE_REPRESENTATION_ITEM('density measure',
POSITIVE_RATIO_MEASURE(7850.),#45477);
#45486=MEASURE_REPRESENTATION_ITEM('density measure',
POSITIVE_RATIO_MEASURE(7850.),#45478);
#45487=MEASURE_REPRESENTATION_ITEM('density measure',
POSITIVE_RATIO_MEASURE(7850.),#45479);
#45488=MEASURE_REPRESENTATION_ITEM('density measure',
POSITIVE_RATIO_MEASURE(7850.),#45480);
#45489=MEASURE_REPRESENTATION_ITEM('density measure',
POSITIVE_RATIO_MEASURE(7850.),#45481);
#45490=MEASURE_REPRESENTATION_ITEM('density measure',
POSITIVE_RATIO_MEASURE(7850.),#45482);
#45491=MEASURE_REPRESENTATION_ITEM('density measure',
POSITIVE_RATIO_MEASURE(7850.),#45483);
#45492=MEASURE_REPRESENTATION_ITEM('density measure',
POSITIVE_RATIO_MEASURE(7850.),#45484);
#45493=PROPERTY_DEFINITION_REPRESENTATION(#45533,#45509);
#45494=PROPERTY_DEFINITION_REPRESENTATION(#45534,#45510);
#45495=PROPERTY_DEFINITION_REPRESENTATION(#45535,#45511);
#45496=PROPERTY_DEFINITION_REPRESENTATION(#45536,#45512);
#45497=PROPERTY_DEFINITION_REPRESENTATION(#45537,#45513);
#45498=PROPERTY_DEFINITION_REPRESENTATION(#45538,#45514);
#45499=PROPERTY_DEFINITION_REPRESENTATION(#45539,#45515);
#45500=PROPERTY_DEFINITION_REPRESENTATION(#45540,#45516);
#45501=PROPERTY_DEFINITION_REPRESENTATION(#45541,#45517);
#45502=PROPERTY_DEFINITION_REPRESENTATION(#45542,#45518);
#45503=PROPERTY_DEFINITION_REPRESENTATION(#45543,#45519);
#45504=PROPERTY_DEFINITION_REPRESENTATION(#45544,#45520);
#45505=PROPERTY_DEFINITION_REPRESENTATION(#45545,#45521);
#45506=PROPERTY_DEFINITION_REPRESENTATION(#45546,#45522);
#45507=PROPERTY_DEFINITION_REPRESENTATION(#45547,#45523);
#45508=PROPERTY_DEFINITION_REPRESENTATION(#45548,#45524);
#45509=REPRESENTATION('material name',(#45525),#130902);
#45510=REPRESENTATION('density',(#45485),#130902);
#45511=REPRESENTATION('material name',(#45526),#130903);
#45512=REPRESENTATION('density',(#45486),#130903);
#45513=REPRESENTATION('material name',(#45527),#130904);
#45514=REPRESENTATION('density',(#45487),#130904);
#45515=REPRESENTATION('material name',(#45528),#130905);
#45516=REPRESENTATION('density',(#45488),#130905);
#45517=REPRESENTATION('material name',(#45529),#130906);
#45518=REPRESENTATION('density',(#45489),#130906);
#45519=REPRESENTATION('material name',(#45530),#130907);
#45520=REPRESENTATION('density',(#45490),#130907);
#45521=REPRESENTATION('material name',(#45531),#130908);
#45522=REPRESENTATION('density',(#45491),#130908);
#45523=REPRESENTATION('material name',(#45532),#130909);
#45524=REPRESENTATION('density',(#45492),#130909);
#45525=DESCRIPTIVE_REPRESENTATION_ITEM('Steel','Steel');
#45526=DESCRIPTIVE_REPRESENTATION_ITEM('Steel','Steel');
#45527=DESCRIPTIVE_REPRESENTATION_ITEM('Steel','Steel');
#45528=DESCRIPTIVE_REPRESENTATION_ITEM('Steel','Steel');
#45529=DESCRIPTIVE_REPRESENTATION_ITEM('Steel','Steel');
#45530=DESCRIPTIVE_REPRESENTATION_ITEM('Steel','Steel');
#45531=DESCRIPTIVE_REPRESENTATION_ITEM('Steel','Steel');
#45532=DESCRIPTIVE_REPRESENTATION_ITEM('Steel','Steel');
#45533=PROPERTY_DEFINITION('material property','material name',#130952);
#45534=PROPERTY_DEFINITION('material property','density of part',#130952);
#45535=PROPERTY_DEFINITION('material property','material name',#130953);
#45536=PROPERTY_DEFINITION('material property','density of part',#130953);
#45537=PROPERTY_DEFINITION('material property','material name',#130954);
#45538=PROPERTY_DEFINITION('material property','density of part',#130954);
#45539=PROPERTY_DEFINITION('material property','material name',#130955);
#45540=PROPERTY_DEFINITION('material property','density of part',#130955);
#45541=PROPERTY_DEFINITION('material property','material name',#130956);
#45542=PROPERTY_DEFINITION('material property','density of part',#130956);
#45543=PROPERTY_DEFINITION('material property','material name',#130957);
#45544=PROPERTY_DEFINITION('material property','density of part',#130957);
#45545=PROPERTY_DEFINITION('material property','material name',#130958);
#45546=PROPERTY_DEFINITION('material property','density of part',#130958);
#45547=PROPERTY_DEFINITION('material property','material name',#130959);
#45548=PROPERTY_DEFINITION('material property','density of part',#130959);
#45549=AXIS2_PLACEMENT_3D('',#65479,#51601,#51602);
#45550=AXIS2_PLACEMENT_3D('',#65480,#51603,#51604);
#45551=AXIS2_PLACEMENT_3D('',#65481,#51605,#51606);
#45552=AXIS2_PLACEMENT_3D('',#65483,#51607,#51608);
#45553=AXIS2_PLACEMENT_3D('',#65485,#51609,#51610);
#45554=AXIS2_PLACEMENT_3D('',#65487,#51611,#51612);
#45555=AXIS2_PLACEMENT_3D('',#65488,#51613,#51614);
#45556=AXIS2_PLACEMENT_3D('',#65489,#51615,#51616);
#45557=AXIS2_PLACEMENT_3D('',#65492,#51617,#51618);
#45558=AXIS2_PLACEMENT_3D('',#65494,#51619,#51620);
#45559=AXIS2_PLACEMENT_3D('',#65495,#51621,#51622);
#45560=AXIS2_PLACEMENT_3D('',#65496,#51623,#51624);
#45561=AXIS2_PLACEMENT_3D('',#65497,#51625,#51626);
#45562=AXIS2_PLACEMENT_3D('',#65499,#51627,#51628);
#45563=AXIS2_PLACEMENT_3D('',#65501,#51630,#51631);
#45564=AXIS2_PLACEMENT_3D('',#65503,#51633,#51634);
#45565=AXIS2_PLACEMENT_3D('',#65506,#51636,#51637);
#45566=AXIS2_PLACEMENT_3D('',#65507,#51638,#51639);
#45567=AXIS2_PLACEMENT_3D('',#65508,#51640,#51641);
#45568=AXIS2_PLACEMENT_3D('',#65509,#51642,#51643);
#45569=AXIS2_PLACEMENT_3D('',#65510,#51644,#51645);
#45570=AXIS2_PLACEMENT_3D('',#65515,#51647,#51648);
#45571=AXIS2_PLACEMENT_3D('',#65519,#51651,#51652);
#45572=AXIS2_PLACEMENT_3D('',#65523,#51654,#51655);
#45573=AXIS2_PLACEMENT_3D('',#65525,#51657,#51658);
#45574=AXIS2_PLACEMENT_3D('',#65528,#51661,#51662);
#45575=AXIS2_PLACEMENT_3D('',#65529,#51663,#51664);
#45576=AXIS2_PLACEMENT_3D('',#65530,#51665,#51666);
#45577=AXIS2_PLACEMENT_3D('',#65535,#51668,#51669);
#45578=AXIS2_PLACEMENT_3D('',#65538,#51671,#51672);
#45579=AXIS2_PLACEMENT_3D('',#65539,#51673,#51674);
#45580=AXIS2_PLACEMENT_3D('',#65543,#51677,#51678);
#45581=AXIS2_PLACEMENT_3D('',#65547,#51681,#51682);
#45582=AXIS2_PLACEMENT_3D('',#65548,#51683,#51684);
#45583=AXIS2_PLACEMENT_3D('',#65549,#51685,#51686);
#45584=AXIS2_PLACEMENT_3D('',#65550,#51687,#51688);
#45585=AXIS2_PLACEMENT_3D('',#65552,#51689,#51690);
#45586=AXIS2_PLACEMENT_3D('',#65555,#51692,#51693);
#45587=AXIS2_PLACEMENT_3D('',#65556,#51694,#51695);
#45588=AXIS2_PLACEMENT_3D('',#65558,#51696,#51697);
#45589=AXIS2_PLACEMENT_3D('',#65561,#51699,#51700);
#45590=AXIS2_PLACEMENT_3D('',#65562,#51701,#51702);
#45591=AXIS2_PLACEMENT_3D('',#65564,#51703,#51704);
#45592=AXIS2_PLACEMENT_3D('',#65567,#51706,#51707);
#45593=AXIS2_PLACEMENT_3D('',#65568,#51708,#51709);
#45594=AXIS2_PLACEMENT_3D('',#65570,#51710,#51711);
#45595=AXIS2_PLACEMENT_3D('',#65573,#51713,#51714);
#45596=AXIS2_PLACEMENT_3D('',#65574,#51715,#51716);
#45597=AXIS2_PLACEMENT_3D('',#65576,#51717,#51718);
#45598=AXIS2_PLACEMENT_3D('',#65579,#51720,#51721);
#45599=AXIS2_PLACEMENT_3D('',#65580,#51722,#51723);
#45600=AXIS2_PLACEMENT_3D('',#65582,#51724,#51725);
#45601=AXIS2_PLACEMENT_3D('',#65585,#51727,#51728);
#45602=AXIS2_PLACEMENT_3D('',#65586,#51729,#51730);
#45603=AXIS2_PLACEMENT_3D('',#65588,#51731,#51732);
#45604=AXIS2_PLACEMENT_3D('',#65591,#51734,#51735);
#45605=AXIS2_PLACEMENT_3D('',#65592,#51736,#51737);
#45606=AXIS2_PLACEMENT_3D('',#65594,#51738,#51739);
#45607=AXIS2_PLACEMENT_3D('',#65597,#51741,#51742);
#45608=AXIS2_PLACEMENT_3D('',#65598,#51743,#51744);
#45609=AXIS2_PLACEMENT_3D('',#65600,#51745,#51746);
#45610=AXIS2_PLACEMENT_3D('',#65603,#51748,#51749);
#45611=AXIS2_PLACEMENT_3D('',#65604,#51750,#51751);
#45612=AXIS2_PLACEMENT_3D('',#65606,#51752,#51753);
#45613=AXIS2_PLACEMENT_3D('',#65609,#51755,#51756);
#45614=AXIS2_PLACEMENT_3D('',#65610,#51757,#51758);
#45615=AXIS2_PLACEMENT_3D('',#65612,#51759,#51760);
#45616=AXIS2_PLACEMENT_3D('',#65615,#51762,#51763);
#45617=AXIS2_PLACEMENT_3D('',#65616,#51764,#51765);
#45618=AXIS2_PLACEMENT_3D('',#65618,#51766,#51767);
#45619=AXIS2_PLACEMENT_3D('',#65621,#51769,#51770);
#45620=AXIS2_PLACEMENT_3D('',#65622,#51771,#51772);
#45621=AXIS2_PLACEMENT_3D('',#65704,#51774,#51775);
#45622=AXIS2_PLACEMENT_3D('',#65706,#51776,#51777);
#45623=AXIS2_PLACEMENT_3D('',#65743,#51779,#51780);
#45624=AXIS2_PLACEMENT_3D('',#65825,#51782,#51783);
#45625=AXIS2_PLACEMENT_3D('',#65827,#51784,#51785);
#45626=AXIS2_PLACEMENT_3D('',#65864,#51787,#51788);
#45627=AXIS2_PLACEMENT_3D('',#65946,#51790,#51791);
#45628=AXIS2_PLACEMENT_3D('',#65948,#51792,#51793);
#45629=AXIS2_PLACEMENT_3D('',#65985,#51795,#51796);
#45630=AXIS2_PLACEMENT_3D('',#66067,#51798,#51799);
#45631=AXIS2_PLACEMENT_3D('',#66069,#51800,#51801);
#45632=AXIS2_PLACEMENT_3D('',#66106,#51803,#51804);
#45633=AXIS2_PLACEMENT_3D('',#66188,#51806,#51807);
#45634=AXIS2_PLACEMENT_3D('',#66190,#51808,#51809);
#45635=AXIS2_PLACEMENT_3D('',#66227,#51811,#51812);
#45636=AXIS2_PLACEMENT_3D('',#66309,#51814,#51815);
#45637=AXIS2_PLACEMENT_3D('',#66311,#51816,#51817);
#45638=AXIS2_PLACEMENT_3D('',#66348,#51819,#51820);
#45639=AXIS2_PLACEMENT_3D('',#66430,#51822,#51823);
#45640=AXIS2_PLACEMENT_3D('',#66432,#51824,#51825);
#45641=AXIS2_PLACEMENT_3D('',#66469,#51827,#51828);
#45642=AXIS2_PLACEMENT_3D('',#66551,#51830,#51831);
#45643=AXIS2_PLACEMENT_3D('',#66553,#51832,#51833);
#45644=AXIS2_PLACEMENT_3D('',#66590,#51835,#51836);
#45645=AXIS2_PLACEMENT_3D('',#66672,#51838,#51839);
#45646=AXIS2_PLACEMENT_3D('',#66674,#51840,#51841);
#45647=AXIS2_PLACEMENT_3D('',#66711,#51843,#51844);
#45648=AXIS2_PLACEMENT_3D('',#66793,#51846,#51847);
#45649=AXIS2_PLACEMENT_3D('',#66795,#51848,#51849);
#45650=AXIS2_PLACEMENT_3D('',#66832,#51851,#51852);
#45651=AXIS2_PLACEMENT_3D('',#66914,#51854,#51855);
#45652=AXIS2_PLACEMENT_3D('',#66916,#51856,#51857);
#45653=AXIS2_PLACEMENT_3D('',#66953,#51859,#51860);
#45654=AXIS2_PLACEMENT_3D('',#67035,#51862,#51863);
#45655=AXIS2_PLACEMENT_3D('',#67037,#51864,#51865);
#45656=AXIS2_PLACEMENT_3D('',#67074,#51867,#51868);
#45657=AXIS2_PLACEMENT_3D('',#67156,#51870,#51871);
#45658=AXIS2_PLACEMENT_3D('',#67158,#51872,#51873);
#45659=AXIS2_PLACEMENT_3D('',#67195,#51875,#51876);
#45660=AXIS2_PLACEMENT_3D('',#67277,#51878,#51879);
#45661=AXIS2_PLACEMENT_3D('',#67279,#51880,#51881);
#45662=AXIS2_PLACEMENT_3D('',#67316,#51883,#51884);
#45663=AXIS2_PLACEMENT_3D('',#67398,#51886,#51887);
#45664=AXIS2_PLACEMENT_3D('',#67400,#51888,#51889);
#45665=AXIS2_PLACEMENT_3D('',#67437,#51891,#51892);
#45666=AXIS2_PLACEMENT_3D('',#67519,#51894,#51895);
#45667=AXIS2_PLACEMENT_3D('',#67521,#51896,#51897);
#45668=AXIS2_PLACEMENT_3D('',#67558,#51899,#51900);
#45669=AXIS2_PLACEMENT_3D('',#67640,#51902,#51903);
#45670=AXIS2_PLACEMENT_3D('',#67642,#51904,#51905);
#45671=AXIS2_PLACEMENT_3D('',#67679,#51907,#51908);
#45672=AXIS2_PLACEMENT_3D('',#67761,#51910,#51911);
#45673=AXIS2_PLACEMENT_3D('',#67763,#51912,#51913);
#45674=AXIS2_PLACEMENT_3D('',#67800,#51915,#51916);
#45675=AXIS2_PLACEMENT_3D('',#67882,#51918,#51919);
#45676=AXIS2_PLACEMENT_3D('',#67884,#51920,#51921);
#45677=AXIS2_PLACEMENT_3D('',#67921,#51923,#51924);
#45678=AXIS2_PLACEMENT_3D('',#68003,#51926,#51927);
#45679=AXIS2_PLACEMENT_3D('',#68005,#51928,#51929);
#45680=AXIS2_PLACEMENT_3D('',#68042,#51931,#51932);
#45681=AXIS2_PLACEMENT_3D('',#68124,#51934,#51935);
#45682=AXIS2_PLACEMENT_3D('',#68126,#51936,#51937);
#45683=AXIS2_PLACEMENT_3D('',#68163,#51939,#51940);
#45684=AXIS2_PLACEMENT_3D('',#68245,#51942,#51943);
#45685=AXIS2_PLACEMENT_3D('',#68247,#51944,#51945);
#45686=AXIS2_PLACEMENT_3D('',#68284,#51947,#51948);
#45687=AXIS2_PLACEMENT_3D('',#68366,#51950,#51951);
#45688=AXIS2_PLACEMENT_3D('',#68368,#51952,#51953);
#45689=AXIS2_PLACEMENT_3D('',#68405,#51955,#51956);
#45690=AXIS2_PLACEMENT_3D('',#68487,#51958,#51959);
#45691=AXIS2_PLACEMENT_3D('',#68489,#51960,#51961);
#45692=AXIS2_PLACEMENT_3D('',#68526,#51963,#51964);
#45693=AXIS2_PLACEMENT_3D('',#68608,#51966,#51967);
#45694=AXIS2_PLACEMENT_3D('',#68610,#51968,#51969);
#45695=AXIS2_PLACEMENT_3D('',#68647,#51971,#51972);
#45696=AXIS2_PLACEMENT_3D('',#68729,#51974,#51975);
#45697=AXIS2_PLACEMENT_3D('',#68731,#51976,#51977);
#45698=AXIS2_PLACEMENT_3D('',#68768,#51979,#51980);
#45699=AXIS2_PLACEMENT_3D('',#68850,#51982,#51983);
#45700=AXIS2_PLACEMENT_3D('',#68852,#51984,#51985);
#45701=AXIS2_PLACEMENT_3D('',#68889,#51987,#51988);
#45702=AXIS2_PLACEMENT_3D('',#68971,#51990,#51991);
#45703=AXIS2_PLACEMENT_3D('',#68973,#51992,#51993);
#45704=AXIS2_PLACEMENT_3D('',#69010,#51995,#51996);
#45705=AXIS2_PLACEMENT_3D('',#69092,#51998,#51999);
#45706=AXIS2_PLACEMENT_3D('',#69094,#52000,#52001);
#45707=AXIS2_PLACEMENT_3D('',#69131,#52003,#52004);
#45708=AXIS2_PLACEMENT_3D('',#69213,#52006,#52007);
#45709=AXIS2_PLACEMENT_3D('',#69215,#52008,#52009);
#45710=AXIS2_PLACEMENT_3D('',#69252,#52011,#52012);
#45711=AXIS2_PLACEMENT_3D('',#69334,#52014,#52015);
#45712=AXIS2_PLACEMENT_3D('',#69336,#52016,#52017);
#45713=AXIS2_PLACEMENT_3D('',#69373,#52019,#52020);
#45714=AXIS2_PLACEMENT_3D('',#69455,#52022,#52023);
#45715=AXIS2_PLACEMENT_3D('',#69457,#52024,#52025);
#45716=AXIS2_PLACEMENT_3D('',#69494,#52027,#52028);
#45717=AXIS2_PLACEMENT_3D('',#69578,#52030,#52031);
#45718=AXIS2_PLACEMENT_3D('',#69580,#52032,#52033);
#45719=AXIS2_PLACEMENT_3D('',#69617,#52035,#52036);
#45720=AXIS2_PLACEMENT_3D('',#69699,#52038,#52039);
#45721=AXIS2_PLACEMENT_3D('',#69701,#52040,#52041);
#45722=AXIS2_PLACEMENT_3D('',#69738,#52043,#52044);
#45723=AXIS2_PLACEMENT_3D('',#69820,#52046,#52047);
#45724=AXIS2_PLACEMENT_3D('',#69822,#52048,#52049);
#45725=AXIS2_PLACEMENT_3D('',#69859,#52051,#52052);
#45726=AXIS2_PLACEMENT_3D('',#69941,#52054,#52055);
#45727=AXIS2_PLACEMENT_3D('',#69943,#52056,#52057);
#45728=AXIS2_PLACEMENT_3D('',#69980,#52059,#52060);
#45729=AXIS2_PLACEMENT_3D('',#70062,#52062,#52063);
#45730=AXIS2_PLACEMENT_3D('',#70064,#52064,#52065);
#45731=AXIS2_PLACEMENT_3D('',#70101,#52067,#52068);
#45732=AXIS2_PLACEMENT_3D('',#70195,#52070,#52071);
#45733=AXIS2_PLACEMENT_3D('',#70197,#52072,#52073);
#45734=AXIS2_PLACEMENT_3D('',#70234,#52075,#52076);
#45735=AXIS2_PLACEMENT_3D('',#70316,#52078,#52079);
#45736=AXIS2_PLACEMENT_3D('',#70318,#52080,#52081);
#45737=AXIS2_PLACEMENT_3D('',#70355,#52083,#52084);
#45738=AXIS2_PLACEMENT_3D('',#70357,#52085,#52086);
#45739=AXIS2_PLACEMENT_3D('',#70404,#52088,#52089);
#45740=AXIS2_PLACEMENT_3D('',#70406,#52090,#52091);
#45741=AXIS2_PLACEMENT_3D('',#70409,#52093,#52094);
#45742=AXIS2_PLACEMENT_3D('',#70410,#52095,#52096);
#45743=AXIS2_PLACEMENT_3D('',#70412,#52097,#52098);
#45744=AXIS2_PLACEMENT_3D('',#70461,#52100,#52101);
#45745=AXIS2_PLACEMENT_3D('',#70463,#52102,#52103);
#45746=AXIS2_PLACEMENT_3D('',#70466,#52105,#52106);
#45747=AXIS2_PLACEMENT_3D('',#70467,#52107,#52108);
#45748=AXIS2_PLACEMENT_3D('',#70565,#52110,#52111);
#45749=AXIS2_PLACEMENT_3D('',#70567,#52112,#52113);
#45750=AXIS2_PLACEMENT_3D('',#70604,#52115,#52116);
#45751=AXIS2_PLACEMENT_3D('',#70704,#52118,#52119);
#45752=AXIS2_PLACEMENT_3D('',#70706,#52120,#52121);
#45753=AXIS2_PLACEMENT_3D('',#70743,#52123,#52124);
#45754=AXIS2_PLACEMENT_3D('',#70745,#52125,#52126);
#45755=AXIS2_PLACEMENT_3D('',#70796,#52128,#52129);
#45756=AXIS2_PLACEMENT_3D('',#70798,#52130,#52131);
#45757=AXIS2_PLACEMENT_3D('',#70801,#52133,#52134);
#45758=AXIS2_PLACEMENT_3D('',#70802,#52135,#52136);
#45759=AXIS2_PLACEMENT_3D('',#70804,#52137,#52138);
#45760=AXIS2_PLACEMENT_3D('',#70853,#52140,#52141);
#45761=AXIS2_PLACEMENT_3D('',#70855,#52142,#52143);
#45762=AXIS2_PLACEMENT_3D('',#70858,#52145,#52146);
#45763=AXIS2_PLACEMENT_3D('',#70859,#52147,#52148);
#45764=AXIS2_PLACEMENT_3D('',#70951,#52150,#52151);
#45765=AXIS2_PLACEMENT_3D('',#70953,#52152,#52153);
#45766=AXIS2_PLACEMENT_3D('',#70990,#52155,#52156);
#45767=AXIS2_PLACEMENT_3D('',#71086,#52158,#52159);
#45768=AXIS2_PLACEMENT_3D('',#71088,#52160,#52161);
#45769=AXIS2_PLACEMENT_3D('',#71125,#52163,#52164);
#45770=AXIS2_PLACEMENT_3D('',#71127,#52165,#52166);
#45771=AXIS2_PLACEMENT_3D('',#71178,#52168,#52169);
#45772=AXIS2_PLACEMENT_3D('',#71180,#52170,#52171);
#45773=AXIS2_PLACEMENT_3D('',#71183,#52173,#52174);
#45774=AXIS2_PLACEMENT_3D('',#71184,#52175,#52176);
#45775=AXIS2_PLACEMENT_3D('',#71276,#52178,#52179);
#45776=AXIS2_PLACEMENT_3D('',#71278,#52180,#52181);
#45777=AXIS2_PLACEMENT_3D('',#71315,#52183,#52184);
#45778=AXIS2_PLACEMENT_3D('',#71405,#52186,#52187);
#45779=AXIS2_PLACEMENT_3D('',#71407,#52188,#52189);
#45780=AXIS2_PLACEMENT_3D('',#71444,#52191,#52192);
#45781=AXIS2_PLACEMENT_3D('',#71446,#52193,#52194);
#45782=AXIS2_PLACEMENT_3D('',#71499,#52196,#52197);
#45783=AXIS2_PLACEMENT_3D('',#71501,#52198,#52199);
#45784=AXIS2_PLACEMENT_3D('',#71504,#52201,#52202);
#45785=AXIS2_PLACEMENT_3D('',#71505,#52203,#52204);
#45786=AXIS2_PLACEMENT_3D('',#71599,#52206,#52207);
#45787=AXIS2_PLACEMENT_3D('',#71601,#52208,#52209);
#45788=AXIS2_PLACEMENT_3D('',#71638,#52211,#52212);
#45789=AXIS2_PLACEMENT_3D('',#71730,#52214,#52215);
#45790=AXIS2_PLACEMENT_3D('',#71732,#52216,#52217);
#45791=AXIS2_PLACEMENT_3D('',#71769,#52219,#52220);
#45792=AXIS2_PLACEMENT_3D('',#71867,#52222,#52223);
#45793=AXIS2_PLACEMENT_3D('',#71869,#52224,#52225);
#45794=AXIS2_PLACEMENT_3D('',#71906,#52227,#52228);
#45795=AXIS2_PLACEMENT_3D('',#72008,#52230,#52231);
#45796=AXIS2_PLACEMENT_3D('',#72010,#52232,#52233);
#45797=AXIS2_PLACEMENT_3D('',#72047,#52235,#52236);
#45798=AXIS2_PLACEMENT_3D('',#72129,#52238,#52239);
#45799=AXIS2_PLACEMENT_3D('',#72131,#52240,#52241);
#45800=AXIS2_PLACEMENT_3D('',#72168,#52243,#52244);
#45801=AXIS2_PLACEMENT_3D('',#72264,#52246,#52247);
#45802=AXIS2_PLACEMENT_3D('',#72266,#52248,#52249);
#45803=AXIS2_PLACEMENT_3D('',#72303,#52251,#52252);
#45804=AXIS2_PLACEMENT_3D('',#72385,#52254,#52255);
#45805=AXIS2_PLACEMENT_3D('',#72387,#52256,#52257);
#45806=AXIS2_PLACEMENT_3D('',#72424,#52259,#52260);
#45807=AXIS2_PLACEMENT_3D('',#72506,#52262,#52263);
#45808=AXIS2_PLACEMENT_3D('',#72508,#52264,#52265);
#45809=AXIS2_PLACEMENT_3D('',#72545,#52267,#52268);
#45810=AXIS2_PLACEMENT_3D('',#72627,#52270,#52271);
#45811=AXIS2_PLACEMENT_3D('',#72629,#52272,#52273);
#45812=AXIS2_PLACEMENT_3D('',#72666,#52275,#52276);
#45813=AXIS2_PLACEMENT_3D('',#72748,#52278,#52279);
#45814=AXIS2_PLACEMENT_3D('',#72750,#52280,#52281);
#45815=AXIS2_PLACEMENT_3D('',#72787,#52283,#52284);
#45816=AXIS2_PLACEMENT_3D('',#72869,#52286,#52287);
#45817=AXIS2_PLACEMENT_3D('',#72871,#52288,#52289);
#45818=AXIS2_PLACEMENT_3D('',#72908,#52291,#52292);
#45819=AXIS2_PLACEMENT_3D('',#72990,#52294,#52295);
#45820=AXIS2_PLACEMENT_3D('',#72992,#52296,#52297);
#45821=AXIS2_PLACEMENT_3D('',#73029,#52299,#52300);
#45822=AXIS2_PLACEMENT_3D('',#73113,#52302,#52303);
#45823=AXIS2_PLACEMENT_3D('',#73115,#52304,#52305);
#45824=AXIS2_PLACEMENT_3D('',#73152,#52307,#52308);
#45825=AXIS2_PLACEMENT_3D('',#73234,#52310,#52311);
#45826=AXIS2_PLACEMENT_3D('',#73236,#52312,#52313);
#45827=AXIS2_PLACEMENT_3D('',#73273,#52315,#52316);
#45828=AXIS2_PLACEMENT_3D('',#73275,#52317,#52318);
#45829=AXIS2_PLACEMENT_3D('',#73278,#52320,#52321);
#45830=AXIS2_PLACEMENT_3D('',#73279,#52322,#52323);
#45831=AXIS2_PLACEMENT_3D('',#73281,#52324,#52325);
#45832=AXIS2_PLACEMENT_3D('',#73284,#52327,#52328);
#45833=AXIS2_PLACEMENT_3D('',#73285,#52329,#52330);
#45834=AXIS2_PLACEMENT_3D('',#73287,#52331,#52332);
#45835=AXIS2_PLACEMENT_3D('',#73290,#52334,#52335);
#45836=AXIS2_PLACEMENT_3D('',#73291,#52336,#52337);
#45837=AXIS2_PLACEMENT_3D('',#73293,#52338,#52339);
#45838=AXIS2_PLACEMENT_3D('',#73296,#52341,#52342);
#45839=AXIS2_PLACEMENT_3D('',#73297,#52343,#52344);
#45840=AXIS2_PLACEMENT_3D('',#73299,#52345,#52346);
#45841=AXIS2_PLACEMENT_3D('',#73302,#52348,#52349);
#45842=AXIS2_PLACEMENT_3D('',#73303,#52350,#52351);
#45843=AXIS2_PLACEMENT_3D('',#73305,#52352,#52353);
#45844=AXIS2_PLACEMENT_3D('',#73308,#52355,#52356);
#45845=AXIS2_PLACEMENT_3D('',#73309,#52357,#52358);
#45846=AXIS2_PLACEMENT_3D('',#73311,#52359,#52360);
#45847=AXIS2_PLACEMENT_3D('',#73314,#52362,#52363);
#45848=AXIS2_PLACEMENT_3D('',#73315,#52364,#52365);
#45849=AXIS2_PLACEMENT_3D('',#73317,#52366,#52367);
#45850=AXIS2_PLACEMENT_3D('',#73320,#52369,#52370);
#45851=AXIS2_PLACEMENT_3D('',#73321,#52371,#52372);
#45852=AXIS2_PLACEMENT_3D('',#73323,#52373,#52374);
#45853=AXIS2_PLACEMENT_3D('',#73326,#52376,#52377);
#45854=AXIS2_PLACEMENT_3D('',#73327,#52378,#52379);
#45855=AXIS2_PLACEMENT_3D('',#73329,#52380,#52381);
#45856=AXIS2_PLACEMENT_3D('',#73332,#52383,#52384);
#45857=AXIS2_PLACEMENT_3D('',#73333,#52385,#52386);
#45858=AXIS2_PLACEMENT_3D('',#73335,#52387,#52388);
#45859=AXIS2_PLACEMENT_3D('',#73338,#52390,#52391);
#45860=AXIS2_PLACEMENT_3D('',#73339,#52392,#52393);
#45861=AXIS2_PLACEMENT_3D('',#73341,#52394,#52395);
#45862=AXIS2_PLACEMENT_3D('',#73344,#52397,#52398);
#45863=AXIS2_PLACEMENT_3D('',#73345,#52399,#52400);
#45864=AXIS2_PLACEMENT_3D('',#73347,#52401,#52402);
#45865=AXIS2_PLACEMENT_3D('',#73350,#52404,#52405);
#45866=AXIS2_PLACEMENT_3D('',#73351,#52406,#52407);
#45867=AXIS2_PLACEMENT_3D('',#73353,#52408,#52409);
#45868=AXIS2_PLACEMENT_3D('',#73356,#52411,#52412);
#45869=AXIS2_PLACEMENT_3D('',#73357,#52413,#52414);
#45870=AXIS2_PLACEMENT_3D('',#73359,#52415,#52416);
#45871=AXIS2_PLACEMENT_3D('',#73362,#52418,#52419);
#45872=AXIS2_PLACEMENT_3D('',#73363,#52420,#52421);
#45873=AXIS2_PLACEMENT_3D('',#73365,#52422,#52423);
#45874=AXIS2_PLACEMENT_3D('',#73368,#52425,#52426);
#45875=AXIS2_PLACEMENT_3D('',#73369,#52427,#52428);
#45876=AXIS2_PLACEMENT_3D('',#73371,#52429,#52430);
#45877=AXIS2_PLACEMENT_3D('',#73401,#52432,#52433);
#45878=AXIS2_PLACEMENT_3D('',#73410,#52434,#52435);
#45879=AXIS2_PLACEMENT_3D('',#73412,#52436,#52437);
#45880=AXIS2_PLACEMENT_3D('',#73415,#52439,#52440);
#45881=AXIS2_PLACEMENT_3D('',#73416,#52441,#52442);
#45882=AXIS2_PLACEMENT_3D('',#73418,#52443,#52444);
#45883=AXIS2_PLACEMENT_3D('',#73421,#52446,#52447);
#45884=AXIS2_PLACEMENT_3D('',#73422,#52448,#52449);
#45885=AXIS2_PLACEMENT_3D('',#73424,#52450,#52451);
#45886=AXIS2_PLACEMENT_3D('',#73427,#52453,#52454);
#45887=AXIS2_PLACEMENT_3D('',#73428,#52455,#52456);
#45888=AXIS2_PLACEMENT_3D('',#73430,#52457,#52458);
#45889=AXIS2_PLACEMENT_3D('',#73433,#52460,#52461);
#45890=AXIS2_PLACEMENT_3D('',#73434,#52462,#52463);
#45891=AXIS2_PLACEMENT_3D('',#73436,#52464,#52465);
#45892=AXIS2_PLACEMENT_3D('',#73439,#52467,#52468);
#45893=AXIS2_PLACEMENT_3D('',#73440,#52469,#52470);
#45894=AXIS2_PLACEMENT_3D('',#73442,#52471,#52472);
#45895=AXIS2_PLACEMENT_3D('',#73445,#52474,#52475);
#45896=AXIS2_PLACEMENT_3D('',#73446,#52476,#52477);
#45897=AXIS2_PLACEMENT_3D('',#73448,#52478,#52479);
#45898=AXIS2_PLACEMENT_3D('',#73451,#52481,#52482);
#45899=AXIS2_PLACEMENT_3D('',#73452,#52483,#52484);
#45900=AXIS2_PLACEMENT_3D('',#73454,#52485,#52486);
#45901=AXIS2_PLACEMENT_3D('',#73457,#52488,#52489);
#45902=AXIS2_PLACEMENT_3D('',#73458,#52490,#52491);
#45903=AXIS2_PLACEMENT_3D('',#73460,#52492,#52493);
#45904=AXIS2_PLACEMENT_3D('',#73463,#52495,#52496);
#45905=AXIS2_PLACEMENT_3D('',#73464,#52497,#52498);
#45906=AXIS2_PLACEMENT_3D('',#73466,#52499,#52500);
#45907=AXIS2_PLACEMENT_3D('',#73469,#52502,#52503);
#45908=AXIS2_PLACEMENT_3D('',#73470,#52504,#52505);
#45909=AXIS2_PLACEMENT_3D('',#73472,#52506,#52507);
#45910=AXIS2_PLACEMENT_3D('',#73475,#52509,#52510);
#45911=AXIS2_PLACEMENT_3D('',#73476,#52511,#52512);
#45912=AXIS2_PLACEMENT_3D('',#73478,#52513,#52514);
#45913=AXIS2_PLACEMENT_3D('',#73481,#52516,#52517);
#45914=AXIS2_PLACEMENT_3D('',#73482,#52518,#52519);
#45915=AXIS2_PLACEMENT_3D('',#73484,#52520,#52521);
#45916=AXIS2_PLACEMENT_3D('',#73487,#52523,#52524);
#45917=AXIS2_PLACEMENT_3D('',#73488,#52525,#52526);
#45918=AXIS2_PLACEMENT_3D('',#73490,#52527,#52528);
#45919=AXIS2_PLACEMENT_3D('',#73493,#52530,#52531);
#45920=AXIS2_PLACEMENT_3D('',#73494,#52532,#52533);
#45921=AXIS2_PLACEMENT_3D('',#73496,#52534,#52535);
#45922=AXIS2_PLACEMENT_3D('',#73499,#52537,#52538);
#45923=AXIS2_PLACEMENT_3D('',#73500,#52539,#52540);
#45924=AXIS2_PLACEMENT_3D('',#73502,#52541,#52542);
#45925=AXIS2_PLACEMENT_3D('',#73505,#52544,#52545);
#45926=AXIS2_PLACEMENT_3D('',#73506,#52546,#52547);
#45927=AXIS2_PLACEMENT_3D('',#73508,#52548,#52549);
#45928=AXIS2_PLACEMENT_3D('',#73511,#52551,#52552);
#45929=AXIS2_PLACEMENT_3D('',#73512,#52553,#52554);
#45930=AXIS2_PLACEMENT_3D('',#73514,#52555,#52556);
#45931=AXIS2_PLACEMENT_3D('',#73542,#52558,#52559);
#45932=AXIS2_PLACEMENT_3D('',#73553,#52560,#52561);
#45933=AXIS2_PLACEMENT_3D('',#73555,#52562,#52563);
#45934=AXIS2_PLACEMENT_3D('',#73558,#52565,#52566);
#45935=AXIS2_PLACEMENT_3D('',#73559,#52567,#52568);
#45936=AXIS2_PLACEMENT_3D('',#73561,#52569,#52570);
#45937=AXIS2_PLACEMENT_3D('',#73564,#52572,#52573);
#45938=AXIS2_PLACEMENT_3D('',#73565,#52574,#52575);
#45939=AXIS2_PLACEMENT_3D('',#73567,#52576,#52577);
#45940=AXIS2_PLACEMENT_3D('',#73570,#52579,#52580);
#45941=AXIS2_PLACEMENT_3D('',#73571,#52581,#52582);
#45942=AXIS2_PLACEMENT_3D('',#73573,#52583,#52584);
#45943=AXIS2_PLACEMENT_3D('',#73576,#52586,#52587);
#45944=AXIS2_PLACEMENT_3D('',#73577,#52588,#52589);
#45945=AXIS2_PLACEMENT_3D('',#73579,#52590,#52591);
#45946=AXIS2_PLACEMENT_3D('',#73582,#52593,#52594);
#45947=AXIS2_PLACEMENT_3D('',#73583,#52595,#52596);
#45948=AXIS2_PLACEMENT_3D('',#73585,#52597,#52598);
#45949=AXIS2_PLACEMENT_3D('',#73588,#52600,#52601);
#45950=AXIS2_PLACEMENT_3D('',#73589,#52602,#52603);
#45951=AXIS2_PLACEMENT_3D('',#73591,#52604,#52605);
#45952=AXIS2_PLACEMENT_3D('',#73594,#52607,#52608);
#45953=AXIS2_PLACEMENT_3D('',#73595,#52609,#52610);
#45954=AXIS2_PLACEMENT_3D('',#73597,#52611,#52612);
#45955=AXIS2_PLACEMENT_3D('',#73600,#52614,#52615);
#45956=AXIS2_PLACEMENT_3D('',#73601,#52616,#52617);
#45957=AXIS2_PLACEMENT_3D('',#73603,#52618,#52619);
#45958=AXIS2_PLACEMENT_3D('',#73606,#52621,#52622);
#45959=AXIS2_PLACEMENT_3D('',#73607,#52623,#52624);
#45960=AXIS2_PLACEMENT_3D('',#73609,#52625,#52626);
#45961=AXIS2_PLACEMENT_3D('',#73612,#52628,#52629);
#45962=AXIS2_PLACEMENT_3D('',#73613,#52630,#52631);
#45963=AXIS2_PLACEMENT_3D('',#73615,#52632,#52633);
#45964=AXIS2_PLACEMENT_3D('',#73618,#52635,#52636);
#45965=AXIS2_PLACEMENT_3D('',#73619,#52637,#52638);
#45966=AXIS2_PLACEMENT_3D('',#73621,#52639,#52640);
#45967=AXIS2_PLACEMENT_3D('',#73624,#52642,#52643);
#45968=AXIS2_PLACEMENT_3D('',#73625,#52644,#52645);
#45969=AXIS2_PLACEMENT_3D('',#73627,#52646,#52647);
#45970=AXIS2_PLACEMENT_3D('',#73630,#52649,#52650);
#45971=AXIS2_PLACEMENT_3D('',#73631,#52651,#52652);
#45972=AXIS2_PLACEMENT_3D('',#73633,#52653,#52654);
#45973=AXIS2_PLACEMENT_3D('',#73636,#52656,#52657);
#45974=AXIS2_PLACEMENT_3D('',#73637,#52658,#52659);
#45975=AXIS2_PLACEMENT_3D('',#73639,#52660,#52661);
#45976=AXIS2_PLACEMENT_3D('',#73642,#52663,#52664);
#45977=AXIS2_PLACEMENT_3D('',#73643,#52665,#52666);
#45978=AXIS2_PLACEMENT_3D('',#73645,#52667,#52668);
#45979=AXIS2_PLACEMENT_3D('',#73673,#52670,#52671);
#45980=AXIS2_PLACEMENT_3D('',#73684,#52672,#52673);
#45981=AXIS2_PLACEMENT_3D('',#73686,#52674,#52675);
#45982=AXIS2_PLACEMENT_3D('',#73689,#52677,#52678);
#45983=AXIS2_PLACEMENT_3D('',#73690,#52679,#52680);
#45984=AXIS2_PLACEMENT_3D('',#73692,#52681,#52682);
#45985=AXIS2_PLACEMENT_3D('',#73695,#52684,#52685);
#45986=AXIS2_PLACEMENT_3D('',#73696,#52686,#52687);
#45987=AXIS2_PLACEMENT_3D('',#73698,#52688,#52689);
#45988=AXIS2_PLACEMENT_3D('',#73701,#52691,#52692);
#45989=AXIS2_PLACEMENT_3D('',#73702,#52693,#52694);
#45990=AXIS2_PLACEMENT_3D('',#73704,#52695,#52696);
#45991=AXIS2_PLACEMENT_3D('',#73707,#52698,#52699);
#45992=AXIS2_PLACEMENT_3D('',#73708,#52700,#52701);
#45993=AXIS2_PLACEMENT_3D('',#73710,#52702,#52703);
#45994=AXIS2_PLACEMENT_3D('',#73713,#52705,#52706);
#45995=AXIS2_PLACEMENT_3D('',#73714,#52707,#52708);
#45996=AXIS2_PLACEMENT_3D('',#73716,#52709,#52710);
#45997=AXIS2_PLACEMENT_3D('',#73719,#52712,#52713);
#45998=AXIS2_PLACEMENT_3D('',#73720,#52714,#52715);
#45999=AXIS2_PLACEMENT_3D('',#73722,#52716,#52717);
#46000=AXIS2_PLACEMENT_3D('',#73725,#52719,#52720);
#46001=AXIS2_PLACEMENT_3D('',#73726,#52721,#52722);
#46002=AXIS2_PLACEMENT_3D('',#73728,#52723,#52724);
#46003=AXIS2_PLACEMENT_3D('',#73731,#52726,#52727);
#46004=AXIS2_PLACEMENT_3D('',#73732,#52728,#52729);
#46005=AXIS2_PLACEMENT_3D('',#73734,#52730,#52731);
#46006=AXIS2_PLACEMENT_3D('',#73737,#52733,#52734);
#46007=AXIS2_PLACEMENT_3D('',#73738,#52735,#52736);
#46008=AXIS2_PLACEMENT_3D('',#73740,#52737,#52738);
#46009=AXIS2_PLACEMENT_3D('',#73743,#52740,#52741);
#46010=AXIS2_PLACEMENT_3D('',#73744,#52742,#52743);
#46011=AXIS2_PLACEMENT_3D('',#73746,#52744,#52745);
#46012=AXIS2_PLACEMENT_3D('',#73749,#52747,#52748);
#46013=AXIS2_PLACEMENT_3D('',#73750,#52749,#52750);
#46014=AXIS2_PLACEMENT_3D('',#73752,#52751,#52752);
#46015=AXIS2_PLACEMENT_3D('',#73755,#52754,#52755);
#46016=AXIS2_PLACEMENT_3D('',#73756,#52756,#52757);
#46017=AXIS2_PLACEMENT_3D('',#73758,#52758,#52759);
#46018=AXIS2_PLACEMENT_3D('',#73761,#52761,#52762);
#46019=AXIS2_PLACEMENT_3D('',#73762,#52763,#52764);
#46020=AXIS2_PLACEMENT_3D('',#73764,#52765,#52766);
#46021=AXIS2_PLACEMENT_3D('',#73767,#52768,#52769);
#46022=AXIS2_PLACEMENT_3D('',#73768,#52770,#52771);
#46023=AXIS2_PLACEMENT_3D('',#73770,#52772,#52773);
#46024=AXIS2_PLACEMENT_3D('',#73773,#52775,#52776);
#46025=AXIS2_PLACEMENT_3D('',#73774,#52777,#52778);
#46026=AXIS2_PLACEMENT_3D('',#73776,#52779,#52780);
#46027=AXIS2_PLACEMENT_3D('',#73779,#52782,#52783);
#46028=AXIS2_PLACEMENT_3D('',#73780,#52784,#52785);
#46029=AXIS2_PLACEMENT_3D('',#73782,#52786,#52787);
#46030=AXIS2_PLACEMENT_3D('',#73785,#52789,#52790);
#46031=AXIS2_PLACEMENT_3D('',#73786,#52791,#52792);
#46032=AXIS2_PLACEMENT_3D('',#73788,#52793,#52794);
#46033=AXIS2_PLACEMENT_3D('',#73814,#52796,#52797);
#46034=AXIS2_PLACEMENT_3D('',#73827,#52798,#52799);
#46035=AXIS2_PLACEMENT_3D('',#73829,#52800,#52801);
#46036=AXIS2_PLACEMENT_3D('',#73832,#52803,#52804);
#46037=AXIS2_PLACEMENT_3D('',#73833,#52805,#52806);
#46038=AXIS2_PLACEMENT_3D('',#73835,#52807,#52808);
#46039=AXIS2_PLACEMENT_3D('',#73838,#52810,#52811);
#46040=AXIS2_PLACEMENT_3D('',#73839,#52812,#52813);
#46041=AXIS2_PLACEMENT_3D('',#73841,#52814,#52815);
#46042=AXIS2_PLACEMENT_3D('',#73844,#52817,#52818);
#46043=AXIS2_PLACEMENT_3D('',#73845,#52819,#52820);
#46044=AXIS2_PLACEMENT_3D('',#73847,#52821,#52822);
#46045=AXIS2_PLACEMENT_3D('',#73850,#52824,#52825);
#46046=AXIS2_PLACEMENT_3D('',#73851,#52826,#52827);
#46047=AXIS2_PLACEMENT_3D('',#73853,#52828,#52829);
#46048=AXIS2_PLACEMENT_3D('',#73856,#52831,#52832);
#46049=AXIS2_PLACEMENT_3D('',#73857,#52833,#52834);
#46050=AXIS2_PLACEMENT_3D('',#73859,#52835,#52836);
#46051=AXIS2_PLACEMENT_3D('',#73862,#52838,#52839);
#46052=AXIS2_PLACEMENT_3D('',#73863,#52840,#52841);
#46053=AXIS2_PLACEMENT_3D('',#73865,#52842,#52843);
#46054=AXIS2_PLACEMENT_3D('',#73868,#52845,#52846);
#46055=AXIS2_PLACEMENT_3D('',#73869,#52847,#52848);
#46056=AXIS2_PLACEMENT_3D('',#73871,#52849,#52850);
#46057=AXIS2_PLACEMENT_3D('',#73874,#52852,#52853);
#46058=AXIS2_PLACEMENT_3D('',#73875,#52854,#52855);
#46059=AXIS2_PLACEMENT_3D('',#73877,#52856,#52857);
#46060=AXIS2_PLACEMENT_3D('',#73880,#52859,#52860);
#46061=AXIS2_PLACEMENT_3D('',#73881,#52861,#52862);
#46062=AXIS2_PLACEMENT_3D('',#73883,#52863,#52864);
#46063=AXIS2_PLACEMENT_3D('',#73886,#52866,#52867);
#46064=AXIS2_PLACEMENT_3D('',#73887,#52868,#52869);
#46065=AXIS2_PLACEMENT_3D('',#73889,#52870,#52871);
#46066=AXIS2_PLACEMENT_3D('',#73892,#52873,#52874);
#46067=AXIS2_PLACEMENT_3D('',#73893,#52875,#52876);
#46068=AXIS2_PLACEMENT_3D('',#73895,#52877,#52878);
#46069=AXIS2_PLACEMENT_3D('',#73898,#52880,#52881);
#46070=AXIS2_PLACEMENT_3D('',#73899,#52882,#52883);
#46071=AXIS2_PLACEMENT_3D('',#73901,#52884,#52885);
#46072=AXIS2_PLACEMENT_3D('',#73904,#52887,#52888);
#46073=AXIS2_PLACEMENT_3D('',#73905,#52889,#52890);
#46074=AXIS2_PLACEMENT_3D('',#73907,#52891,#52892);
#46075=AXIS2_PLACEMENT_3D('',#73910,#52894,#52895);
#46076=AXIS2_PLACEMENT_3D('',#73911,#52896,#52897);
#46077=AXIS2_PLACEMENT_3D('',#73913,#52898,#52899);
#46078=AXIS2_PLACEMENT_3D('',#73916,#52901,#52902);
#46079=AXIS2_PLACEMENT_3D('',#73917,#52903,#52904);
#46080=AXIS2_PLACEMENT_3D('',#73919,#52905,#52906);
#46081=AXIS2_PLACEMENT_3D('',#73922,#52908,#52909);
#46082=AXIS2_PLACEMENT_3D('',#73923,#52910,#52911);
#46083=AXIS2_PLACEMENT_3D('',#73925,#52912,#52913);
#46084=AXIS2_PLACEMENT_3D('',#73928,#52915,#52916);
#46085=AXIS2_PLACEMENT_3D('',#73929,#52917,#52918);
#46086=AXIS2_PLACEMENT_3D('',#73931,#52919,#52920);
#46087=AXIS2_PLACEMENT_3D('',#73957,#52922,#52923);
#46088=AXIS2_PLACEMENT_3D('',#73970,#52924,#52925);
#46089=AXIS2_PLACEMENT_3D('',#73972,#52926,#52927);
#46090=AXIS2_PLACEMENT_3D('',#73975,#52929,#52930);
#46091=AXIS2_PLACEMENT_3D('',#73976,#52931,#52932);
#46092=AXIS2_PLACEMENT_3D('',#73978,#52933,#52934);
#46093=AXIS2_PLACEMENT_3D('',#73981,#52936,#52937);
#46094=AXIS2_PLACEMENT_3D('',#73982,#52938,#52939);
#46095=AXIS2_PLACEMENT_3D('',#73984,#52940,#52941);
#46096=AXIS2_PLACEMENT_3D('',#73987,#52943,#52944);
#46097=AXIS2_PLACEMENT_3D('',#73988,#52945,#52946);
#46098=AXIS2_PLACEMENT_3D('',#73990,#52947,#52948);
#46099=AXIS2_PLACEMENT_3D('',#73993,#52950,#52951);
#46100=AXIS2_PLACEMENT_3D('',#73994,#52952,#52953);
#46101=AXIS2_PLACEMENT_3D('',#73996,#52954,#52955);
#46102=AXIS2_PLACEMENT_3D('',#73999,#52957,#52958);
#46103=AXIS2_PLACEMENT_3D('',#74000,#52959,#52960);
#46104=AXIS2_PLACEMENT_3D('',#74002,#52961,#52962);
#46105=AXIS2_PLACEMENT_3D('',#74005,#52964,#52965);
#46106=AXIS2_PLACEMENT_3D('',#74006,#52966,#52967);
#46107=AXIS2_PLACEMENT_3D('',#74008,#52968,#52969);
#46108=AXIS2_PLACEMENT_3D('',#74011,#52971,#52972);
#46109=AXIS2_PLACEMENT_3D('',#74012,#52973,#52974);
#46110=AXIS2_PLACEMENT_3D('',#74014,#52975,#52976);
#46111=AXIS2_PLACEMENT_3D('',#74017,#52978,#52979);
#46112=AXIS2_PLACEMENT_3D('',#74018,#52980,#52981);
#46113=AXIS2_PLACEMENT_3D('',#74020,#52982,#52983);
#46114=AXIS2_PLACEMENT_3D('',#74023,#52985,#52986);
#46115=AXIS2_PLACEMENT_3D('',#74024,#52987,#52988);
#46116=AXIS2_PLACEMENT_3D('',#74026,#52989,#52990);
#46117=AXIS2_PLACEMENT_3D('',#74029,#52992,#52993);
#46118=AXIS2_PLACEMENT_3D('',#74030,#52994,#52995);
#46119=AXIS2_PLACEMENT_3D('',#74032,#52996,#52997);
#46120=AXIS2_PLACEMENT_3D('',#74035,#52999,#53000);
#46121=AXIS2_PLACEMENT_3D('',#74036,#53001,#53002);
#46122=AXIS2_PLACEMENT_3D('',#74038,#53003,#53004);
#46123=AXIS2_PLACEMENT_3D('',#74041,#53006,#53007);
#46124=AXIS2_PLACEMENT_3D('',#74042,#53008,#53009);
#46125=AXIS2_PLACEMENT_3D('',#74044,#53010,#53011);
#46126=AXIS2_PLACEMENT_3D('',#74047,#53013,#53014);
#46127=AXIS2_PLACEMENT_3D('',#74048,#53015,#53016);
#46128=AXIS2_PLACEMENT_3D('',#74050,#53017,#53018);
#46129=AXIS2_PLACEMENT_3D('',#74053,#53020,#53021);
#46130=AXIS2_PLACEMENT_3D('',#74054,#53022,#53023);
#46131=AXIS2_PLACEMENT_3D('',#74056,#53024,#53025);
#46132=AXIS2_PLACEMENT_3D('',#74059,#53027,#53028);
#46133=AXIS2_PLACEMENT_3D('',#74060,#53029,#53030);
#46134=AXIS2_PLACEMENT_3D('',#74062,#53031,#53032);
#46135=AXIS2_PLACEMENT_3D('',#74065,#53034,#53035);
#46136=AXIS2_PLACEMENT_3D('',#74066,#53036,#53037);
#46137=AXIS2_PLACEMENT_3D('',#74068,#53038,#53039);
#46138=AXIS2_PLACEMENT_3D('',#74071,#53041,#53042);
#46139=AXIS2_PLACEMENT_3D('',#74072,#53043,#53044);
#46140=AXIS2_PLACEMENT_3D('',#74074,#53045,#53046);
#46141=AXIS2_PLACEMENT_3D('',#74098,#53048,#53049);
#46142=AXIS2_PLACEMENT_3D('',#74113,#53050,#53051);
#46143=AXIS2_PLACEMENT_3D('',#74115,#53052,#53053);
#46144=AXIS2_PLACEMENT_3D('',#74118,#53055,#53056);
#46145=AXIS2_PLACEMENT_3D('',#74119,#53057,#53058);
#46146=AXIS2_PLACEMENT_3D('',#74121,#53059,#53060);
#46147=AXIS2_PLACEMENT_3D('',#74124,#53062,#53063);
#46148=AXIS2_PLACEMENT_3D('',#74125,#53064,#53065);
#46149=AXIS2_PLACEMENT_3D('',#74127,#53066,#53067);
#46150=AXIS2_PLACEMENT_3D('',#74130,#53069,#53070);
#46151=AXIS2_PLACEMENT_3D('',#74131,#53071,#53072);
#46152=AXIS2_PLACEMENT_3D('',#74133,#53073,#53074);
#46153=AXIS2_PLACEMENT_3D('',#74136,#53076,#53077);
#46154=AXIS2_PLACEMENT_3D('',#74137,#53078,#53079);
#46155=AXIS2_PLACEMENT_3D('',#74139,#53080,#53081);
#46156=AXIS2_PLACEMENT_3D('',#74142,#53083,#53084);
#46157=AXIS2_PLACEMENT_3D('',#74143,#53085,#53086);
#46158=AXIS2_PLACEMENT_3D('',#74145,#53087,#53088);
#46159=AXIS2_PLACEMENT_3D('',#74148,#53090,#53091);
#46160=AXIS2_PLACEMENT_3D('',#74149,#53092,#53093);
#46161=AXIS2_PLACEMENT_3D('',#74151,#53094,#53095);
#46162=AXIS2_PLACEMENT_3D('',#74154,#53097,#53098);
#46163=AXIS2_PLACEMENT_3D('',#74155,#53099,#53100);
#46164=AXIS2_PLACEMENT_3D('',#74157,#53101,#53102);
#46165=AXIS2_PLACEMENT_3D('',#74160,#53104,#53105);
#46166=AXIS2_PLACEMENT_3D('',#74161,#53106,#53107);
#46167=AXIS2_PLACEMENT_3D('',#74163,#53108,#53109);
#46168=AXIS2_PLACEMENT_3D('',#74166,#53111,#53112);
#46169=AXIS2_PLACEMENT_3D('',#74167,#53113,#53114);
#46170=AXIS2_PLACEMENT_3D('',#74169,#53115,#53116);
#46171=AXIS2_PLACEMENT_3D('',#74172,#53118,#53119);
#46172=AXIS2_PLACEMENT_3D('',#74173,#53120,#53121);
#46173=AXIS2_PLACEMENT_3D('',#74175,#53122,#53123);
#46174=AXIS2_PLACEMENT_3D('',#74178,#53125,#53126);
#46175=AXIS2_PLACEMENT_3D('',#74179,#53127,#53128);
#46176=AXIS2_PLACEMENT_3D('',#74181,#53129,#53130);
#46177=AXIS2_PLACEMENT_3D('',#74184,#53132,#53133);
#46178=AXIS2_PLACEMENT_3D('',#74185,#53134,#53135);
#46179=AXIS2_PLACEMENT_3D('',#74187,#53136,#53137);
#46180=AXIS2_PLACEMENT_3D('',#74190,#53139,#53140);
#46181=AXIS2_PLACEMENT_3D('',#74191,#53141,#53142);
#46182=AXIS2_PLACEMENT_3D('',#74193,#53143,#53144);
#46183=AXIS2_PLACEMENT_3D('',#74196,#53146,#53147);
#46184=AXIS2_PLACEMENT_3D('',#74197,#53148,#53149);
#46185=AXIS2_PLACEMENT_3D('',#74199,#53150,#53151);
#46186=AXIS2_PLACEMENT_3D('',#74202,#53153,#53154);
#46187=AXIS2_PLACEMENT_3D('',#74203,#53155,#53156);
#46188=AXIS2_PLACEMENT_3D('',#74205,#53157,#53158);
#46189=AXIS2_PLACEMENT_3D('',#74208,#53160,#53161);
#46190=AXIS2_PLACEMENT_3D('',#74209,#53162,#53163);
#46191=AXIS2_PLACEMENT_3D('',#74211,#53164,#53165);
#46192=AXIS2_PLACEMENT_3D('',#74214,#53167,#53168);
#46193=AXIS2_PLACEMENT_3D('',#74215,#53169,#53170);
#46194=AXIS2_PLACEMENT_3D('',#74217,#53171,#53172);
#46195=AXIS2_PLACEMENT_3D('',#74241,#53174,#53175);
#46196=AXIS2_PLACEMENT_3D('',#74256,#53176,#53177);
#46197=AXIS2_PLACEMENT_3D('',#74258,#53178,#53179);
#46198=AXIS2_PLACEMENT_3D('',#74261,#53181,#53182);
#46199=AXIS2_PLACEMENT_3D('',#74262,#53183,#53184);
#46200=AXIS2_PLACEMENT_3D('',#74264,#53185,#53186);
#46201=AXIS2_PLACEMENT_3D('',#74267,#53188,#53189);
#46202=AXIS2_PLACEMENT_3D('',#74268,#53190,#53191);
#46203=AXIS2_PLACEMENT_3D('',#74270,#53192,#53193);
#46204=AXIS2_PLACEMENT_3D('',#74273,#53195,#53196);
#46205=AXIS2_PLACEMENT_3D('',#74274,#53197,#53198);
#46206=AXIS2_PLACEMENT_3D('',#74276,#53199,#53200);
#46207=AXIS2_PLACEMENT_3D('',#74279,#53202,#53203);
#46208=AXIS2_PLACEMENT_3D('',#74280,#53204,#53205);
#46209=AXIS2_PLACEMENT_3D('',#74282,#53206,#53207);
#46210=AXIS2_PLACEMENT_3D('',#74285,#53209,#53210);
#46211=AXIS2_PLACEMENT_3D('',#74286,#53211,#53212);
#46212=AXIS2_PLACEMENT_3D('',#74288,#53213,#53214);
#46213=AXIS2_PLACEMENT_3D('',#74291,#53216,#53217);
#46214=AXIS2_PLACEMENT_3D('',#74292,#53218,#53219);
#46215=AXIS2_PLACEMENT_3D('',#74294,#53220,#53221);
#46216=AXIS2_PLACEMENT_3D('',#74297,#53223,#53224);
#46217=AXIS2_PLACEMENT_3D('',#74298,#53225,#53226);
#46218=AXIS2_PLACEMENT_3D('',#74300,#53227,#53228);
#46219=AXIS2_PLACEMENT_3D('',#74303,#53230,#53231);
#46220=AXIS2_PLACEMENT_3D('',#74304,#53232,#53233);
#46221=AXIS2_PLACEMENT_3D('',#74306,#53234,#53235);
#46222=AXIS2_PLACEMENT_3D('',#74309,#53237,#53238);
#46223=AXIS2_PLACEMENT_3D('',#74310,#53239,#53240);
#46224=AXIS2_PLACEMENT_3D('',#74312,#53241,#53242);
#46225=AXIS2_PLACEMENT_3D('',#74315,#53244,#53245);
#46226=AXIS2_PLACEMENT_3D('',#74316,#53246,#53247);
#46227=AXIS2_PLACEMENT_3D('',#74318,#53248,#53249);
#46228=AXIS2_PLACEMENT_3D('',#74321,#53251,#53252);
#46229=AXIS2_PLACEMENT_3D('',#74322,#53253,#53254);
#46230=AXIS2_PLACEMENT_3D('',#74324,#53255,#53256);
#46231=AXIS2_PLACEMENT_3D('',#74327,#53258,#53259);
#46232=AXIS2_PLACEMENT_3D('',#74328,#53260,#53261);
#46233=AXIS2_PLACEMENT_3D('',#74330,#53262,#53263);
#46234=AXIS2_PLACEMENT_3D('',#74333,#53265,#53266);
#46235=AXIS2_PLACEMENT_3D('',#74334,#53267,#53268);
#46236=AXIS2_PLACEMENT_3D('',#74336,#53269,#53270);
#46237=AXIS2_PLACEMENT_3D('',#74339,#53272,#53273);
#46238=AXIS2_PLACEMENT_3D('',#74340,#53274,#53275);
#46239=AXIS2_PLACEMENT_3D('',#74342,#53276,#53277);
#46240=AXIS2_PLACEMENT_3D('',#74345,#53279,#53280);
#46241=AXIS2_PLACEMENT_3D('',#74346,#53281,#53282);
#46242=AXIS2_PLACEMENT_3D('',#74348,#53283,#53284);
#46243=AXIS2_PLACEMENT_3D('',#74367,#53286,#53287);
#46244=AXIS2_PLACEMENT_3D('',#74387,#53288,#53289);
#46245=AXIS2_PLACEMENT_3D('',#74389,#53290,#53291);
#46246=AXIS2_PLACEMENT_3D('',#74392,#53293,#53294);
#46247=AXIS2_PLACEMENT_3D('',#74393,#53295,#53296);
#46248=AXIS2_PLACEMENT_3D('',#74395,#53297,#53298);
#46249=AXIS2_PLACEMENT_3D('',#74398,#53300,#53301);
#46250=AXIS2_PLACEMENT_3D('',#74399,#53302,#53303);
#46251=AXIS2_PLACEMENT_3D('',#74401,#53304,#53305);
#46252=AXIS2_PLACEMENT_3D('',#74404,#53307,#53308);
#46253=AXIS2_PLACEMENT_3D('',#74405,#53309,#53310);
#46254=AXIS2_PLACEMENT_3D('',#74407,#53311,#53312);
#46255=AXIS2_PLACEMENT_3D('',#74410,#53314,#53315);
#46256=AXIS2_PLACEMENT_3D('',#74411,#53316,#53317);
#46257=AXIS2_PLACEMENT_3D('',#74413,#53318,#53319);
#46258=AXIS2_PLACEMENT_3D('',#74416,#53321,#53322);
#46259=AXIS2_PLACEMENT_3D('',#74417,#53323,#53324);
#46260=AXIS2_PLACEMENT_3D('',#74419,#53325,#53326);
#46261=AXIS2_PLACEMENT_3D('',#74422,#53328,#53329);
#46262=AXIS2_PLACEMENT_3D('',#74423,#53330,#53331);
#46263=AXIS2_PLACEMENT_3D('',#74425,#53332,#53333);
#46264=AXIS2_PLACEMENT_3D('',#74428,#53335,#53336);
#46265=AXIS2_PLACEMENT_3D('',#74429,#53337,#53338);
#46266=AXIS2_PLACEMENT_3D('',#74431,#53339,#53340);
#46267=AXIS2_PLACEMENT_3D('',#74434,#53342,#53343);
#46268=AXIS2_PLACEMENT_3D('',#74435,#53344,#53345);
#46269=AXIS2_PLACEMENT_3D('',#74437,#53346,#53347);
#46270=AXIS2_PLACEMENT_3D('',#74440,#53349,#53350);
#46271=AXIS2_PLACEMENT_3D('',#74441,#53351,#53352);
#46272=AXIS2_PLACEMENT_3D('',#74443,#53353,#53354);
#46273=AXIS2_PLACEMENT_3D('',#74446,#53356,#53357);
#46274=AXIS2_PLACEMENT_3D('',#74447,#53358,#53359);
#46275=AXIS2_PLACEMENT_3D('',#74449,#53360,#53361);
#46276=AXIS2_PLACEMENT_3D('',#74452,#53363,#53364);
#46277=AXIS2_PLACEMENT_3D('',#74453,#53365,#53366);
#46278=AXIS2_PLACEMENT_3D('',#74455,#53367,#53368);
#46279=AXIS2_PLACEMENT_3D('',#74458,#53370,#53371);
#46280=AXIS2_PLACEMENT_3D('',#74459,#53372,#53373);
#46281=AXIS2_PLACEMENT_3D('',#74461,#53374,#53375);
#46282=AXIS2_PLACEMENT_3D('',#74464,#53377,#53378);
#46283=AXIS2_PLACEMENT_3D('',#74465,#53379,#53380);
#46284=AXIS2_PLACEMENT_3D('',#74467,#53381,#53382);
#46285=AXIS2_PLACEMENT_3D('',#74470,#53384,#53385);
#46286=AXIS2_PLACEMENT_3D('',#74471,#53386,#53387);
#46287=AXIS2_PLACEMENT_3D('',#74473,#53388,#53389);
#46288=AXIS2_PLACEMENT_3D('',#74476,#53391,#53392);
#46289=AXIS2_PLACEMENT_3D('',#74477,#53393,#53394);
#46290=AXIS2_PLACEMENT_3D('',#74479,#53395,#53396);
#46291=AXIS2_PLACEMENT_3D('',#74482,#53398,#53399);
#46292=AXIS2_PLACEMENT_3D('',#74483,#53400,#53401);
#46293=AXIS2_PLACEMENT_3D('',#74485,#53402,#53403);
#46294=AXIS2_PLACEMENT_3D('',#74488,#53405,#53406);
#46295=AXIS2_PLACEMENT_3D('',#74489,#53407,#53408);
#46296=AXIS2_PLACEMENT_3D('',#74491,#53409,#53410);
#46297=AXIS2_PLACEMENT_3D('',#74510,#53412,#53413);
#46298=AXIS2_PLACEMENT_3D('',#74530,#53414,#53415);
#46299=AXIS2_PLACEMENT_3D('',#74532,#53416,#53417);
#46300=AXIS2_PLACEMENT_3D('',#74535,#53419,#53420);
#46301=AXIS2_PLACEMENT_3D('',#74536,#53421,#53422);
#46302=AXIS2_PLACEMENT_3D('',#74538,#53423,#53424);
#46303=AXIS2_PLACEMENT_3D('',#74541,#53426,#53427);
#46304=AXIS2_PLACEMENT_3D('',#74542,#53428,#53429);
#46305=AXIS2_PLACEMENT_3D('',#74544,#53430,#53431);
#46306=AXIS2_PLACEMENT_3D('',#74547,#53433,#53434);
#46307=AXIS2_PLACEMENT_3D('',#74548,#53435,#53436);
#46308=AXIS2_PLACEMENT_3D('',#74550,#53437,#53438);
#46309=AXIS2_PLACEMENT_3D('',#74553,#53440,#53441);
#46310=AXIS2_PLACEMENT_3D('',#74554,#53442,#53443);
#46311=AXIS2_PLACEMENT_3D('',#74556,#53444,#53445);
#46312=AXIS2_PLACEMENT_3D('',#74559,#53447,#53448);
#46313=AXIS2_PLACEMENT_3D('',#74560,#53449,#53450);
#46314=AXIS2_PLACEMENT_3D('',#74562,#53451,#53452);
#46315=AXIS2_PLACEMENT_3D('',#74565,#53454,#53455);
#46316=AXIS2_PLACEMENT_3D('',#74566,#53456,#53457);
#46317=AXIS2_PLACEMENT_3D('',#74568,#53458,#53459);
#46318=AXIS2_PLACEMENT_3D('',#74571,#53461,#53462);
#46319=AXIS2_PLACEMENT_3D('',#74572,#53463,#53464);
#46320=AXIS2_PLACEMENT_3D('',#74574,#53465,#53466);
#46321=AXIS2_PLACEMENT_3D('',#74577,#53468,#53469);
#46322=AXIS2_PLACEMENT_3D('',#74578,#53470,#53471);
#46323=AXIS2_PLACEMENT_3D('',#74580,#53472,#53473);
#46324=AXIS2_PLACEMENT_3D('',#74583,#53475,#53476);
#46325=AXIS2_PLACEMENT_3D('',#74584,#53477,#53478);
#46326=AXIS2_PLACEMENT_3D('',#74586,#53479,#53480);
#46327=AXIS2_PLACEMENT_3D('',#74589,#53482,#53483);
#46328=AXIS2_PLACEMENT_3D('',#74590,#53484,#53485);
#46329=AXIS2_PLACEMENT_3D('',#74592,#53486,#53487);
#46330=AXIS2_PLACEMENT_3D('',#74595,#53489,#53490);
#46331=AXIS2_PLACEMENT_3D('',#74596,#53491,#53492);
#46332=AXIS2_PLACEMENT_3D('',#74598,#53493,#53494);
#46333=AXIS2_PLACEMENT_3D('',#74601,#53496,#53497);
#46334=AXIS2_PLACEMENT_3D('',#74602,#53498,#53499);
#46335=AXIS2_PLACEMENT_3D('',#74604,#53500,#53501);
#46336=AXIS2_PLACEMENT_3D('',#74607,#53503,#53504);
#46337=AXIS2_PLACEMENT_3D('',#74608,#53505,#53506);
#46338=AXIS2_PLACEMENT_3D('',#74610,#53507,#53508);
#46339=AXIS2_PLACEMENT_3D('',#74613,#53510,#53511);
#46340=AXIS2_PLACEMENT_3D('',#74614,#53512,#53513);
#46341=AXIS2_PLACEMENT_3D('',#74616,#53514,#53515);
#46342=AXIS2_PLACEMENT_3D('',#74619,#53517,#53518);
#46343=AXIS2_PLACEMENT_3D('',#74620,#53519,#53520);
#46344=AXIS2_PLACEMENT_3D('',#74622,#53521,#53522);
#46345=AXIS2_PLACEMENT_3D('',#74625,#53524,#53525);
#46346=AXIS2_PLACEMENT_3D('',#74626,#53526,#53527);
#46347=AXIS2_PLACEMENT_3D('',#74628,#53528,#53529);
#46348=AXIS2_PLACEMENT_3D('',#74631,#53531,#53532);
#46349=AXIS2_PLACEMENT_3D('',#74632,#53533,#53534);
#46350=AXIS2_PLACEMENT_3D('',#74634,#53535,#53536);
#46351=AXIS2_PLACEMENT_3D('',#74651,#53538,#53539);
#46352=AXIS2_PLACEMENT_3D('',#74673,#53540,#53541);
#46353=AXIS2_PLACEMENT_3D('',#74675,#53542,#53543);
#46354=AXIS2_PLACEMENT_3D('',#74678,#53545,#53546);
#46355=AXIS2_PLACEMENT_3D('',#74679,#53547,#53548);
#46356=AXIS2_PLACEMENT_3D('',#74681,#53549,#53550);
#46357=AXIS2_PLACEMENT_3D('',#74684,#53552,#53553);
#46358=AXIS2_PLACEMENT_3D('',#74685,#53554,#53555);
#46359=AXIS2_PLACEMENT_3D('',#74687,#53556,#53557);
#46360=AXIS2_PLACEMENT_3D('',#74690,#53559,#53560);
#46361=AXIS2_PLACEMENT_3D('',#74691,#53561,#53562);
#46362=AXIS2_PLACEMENT_3D('',#74693,#53563,#53564);
#46363=AXIS2_PLACEMENT_3D('',#74696,#53566,#53567);
#46364=AXIS2_PLACEMENT_3D('',#74697,#53568,#53569);
#46365=AXIS2_PLACEMENT_3D('',#74699,#53570,#53571);
#46366=AXIS2_PLACEMENT_3D('',#74702,#53573,#53574);
#46367=AXIS2_PLACEMENT_3D('',#74703,#53575,#53576);
#46368=AXIS2_PLACEMENT_3D('',#74705,#53577,#53578);
#46369=AXIS2_PLACEMENT_3D('',#74708,#53580,#53581);
#46370=AXIS2_PLACEMENT_3D('',#74709,#53582,#53583);
#46371=AXIS2_PLACEMENT_3D('',#74711,#53584,#53585);
#46372=AXIS2_PLACEMENT_3D('',#74714,#53587,#53588);
#46373=AXIS2_PLACEMENT_3D('',#74715,#53589,#53590);
#46374=AXIS2_PLACEMENT_3D('',#74717,#53591,#53592);
#46375=AXIS2_PLACEMENT_3D('',#74720,#53594,#53595);
#46376=AXIS2_PLACEMENT_3D('',#74721,#53596,#53597);
#46377=AXIS2_PLACEMENT_3D('',#74723,#53598,#53599);
#46378=AXIS2_PLACEMENT_3D('',#74726,#53601,#53602);
#46379=AXIS2_PLACEMENT_3D('',#74727,#53603,#53604);
#46380=AXIS2_PLACEMENT_3D('',#74729,#53605,#53606);
#46381=AXIS2_PLACEMENT_3D('',#74732,#53608,#53609);
#46382=AXIS2_PLACEMENT_3D('',#74733,#53610,#53611);
#46383=AXIS2_PLACEMENT_3D('',#74735,#53612,#53613);
#46384=AXIS2_PLACEMENT_3D('',#74738,#53615,#53616);
#46385=AXIS2_PLACEMENT_3D('',#74739,#53617,#53618);
#46386=AXIS2_PLACEMENT_3D('',#74741,#53619,#53620);
#46387=AXIS2_PLACEMENT_3D('',#74744,#53622,#53623);
#46388=AXIS2_PLACEMENT_3D('',#74745,#53624,#53625);
#46389=AXIS2_PLACEMENT_3D('',#74747,#53626,#53627);
#46390=AXIS2_PLACEMENT_3D('',#74750,#53629,#53630);
#46391=AXIS2_PLACEMENT_3D('',#74751,#53631,#53632);
#46392=AXIS2_PLACEMENT_3D('',#74753,#53633,#53634);
#46393=AXIS2_PLACEMENT_3D('',#74756,#53636,#53637);
#46394=AXIS2_PLACEMENT_3D('',#74757,#53638,#53639);
#46395=AXIS2_PLACEMENT_3D('',#74759,#53640,#53641);
#46396=AXIS2_PLACEMENT_3D('',#74762,#53643,#53644);
#46397=AXIS2_PLACEMENT_3D('',#74763,#53645,#53646);
#46398=AXIS2_PLACEMENT_3D('',#74765,#53647,#53648);
#46399=AXIS2_PLACEMENT_3D('',#74768,#53650,#53651);
#46400=AXIS2_PLACEMENT_3D('',#74769,#53652,#53653);
#46401=AXIS2_PLACEMENT_3D('',#74771,#53654,#53655);
#46402=AXIS2_PLACEMENT_3D('',#74774,#53657,#53658);
#46403=AXIS2_PLACEMENT_3D('',#74775,#53659,#53660);
#46404=AXIS2_PLACEMENT_3D('',#74777,#53661,#53662);
#46405=AXIS2_PLACEMENT_3D('',#74794,#53664,#53665);
#46406=AXIS2_PLACEMENT_3D('',#74816,#53666,#53667);
#46407=AXIS2_PLACEMENT_3D('',#74818,#53668,#53669);
#46408=AXIS2_PLACEMENT_3D('',#74821,#53671,#53672);
#46409=AXIS2_PLACEMENT_3D('',#74822,#53673,#53674);
#46410=AXIS2_PLACEMENT_3D('',#74824,#53675,#53676);
#46411=AXIS2_PLACEMENT_3D('',#74827,#53678,#53679);
#46412=AXIS2_PLACEMENT_3D('',#74828,#53680,#53681);
#46413=AXIS2_PLACEMENT_3D('',#74830,#53682,#53683);
#46414=AXIS2_PLACEMENT_3D('',#74833,#53685,#53686);
#46415=AXIS2_PLACEMENT_3D('',#74834,#53687,#53688);
#46416=AXIS2_PLACEMENT_3D('',#74836,#53689,#53690);
#46417=AXIS2_PLACEMENT_3D('',#74839,#53692,#53693);
#46418=AXIS2_PLACEMENT_3D('',#74840,#53694,#53695);
#46419=AXIS2_PLACEMENT_3D('',#74842,#53696,#53697);
#46420=AXIS2_PLACEMENT_3D('',#74845,#53699,#53700);
#46421=AXIS2_PLACEMENT_3D('',#74846,#53701,#53702);
#46422=AXIS2_PLACEMENT_3D('',#74848,#53703,#53704);
#46423=AXIS2_PLACEMENT_3D('',#74851,#53706,#53707);
#46424=AXIS2_PLACEMENT_3D('',#74852,#53708,#53709);
#46425=AXIS2_PLACEMENT_3D('',#74854,#53710,#53711);
#46426=AXIS2_PLACEMENT_3D('',#74857,#53713,#53714);
#46427=AXIS2_PLACEMENT_3D('',#74858,#53715,#53716);
#46428=AXIS2_PLACEMENT_3D('',#74860,#53717,#53718);
#46429=AXIS2_PLACEMENT_3D('',#74863,#53720,#53721);
#46430=AXIS2_PLACEMENT_3D('',#74864,#53722,#53723);
#46431=AXIS2_PLACEMENT_3D('',#74866,#53724,#53725);
#46432=AXIS2_PLACEMENT_3D('',#74869,#53727,#53728);
#46433=AXIS2_PLACEMENT_3D('',#74870,#53729,#53730);
#46434=AXIS2_PLACEMENT_3D('',#74872,#53731,#53732);
#46435=AXIS2_PLACEMENT_3D('',#74875,#53734,#53735);
#46436=AXIS2_PLACEMENT_3D('',#74876,#53736,#53737);
#46437=AXIS2_PLACEMENT_3D('',#74878,#53738,#53739);
#46438=AXIS2_PLACEMENT_3D('',#74881,#53741,#53742);
#46439=AXIS2_PLACEMENT_3D('',#74882,#53743,#53744);
#46440=AXIS2_PLACEMENT_3D('',#74884,#53745,#53746);
#46441=AXIS2_PLACEMENT_3D('',#74887,#53748,#53749);
#46442=AXIS2_PLACEMENT_3D('',#74888,#53750,#53751);
#46443=AXIS2_PLACEMENT_3D('',#74890,#53752,#53753);
#46444=AXIS2_PLACEMENT_3D('',#74893,#53755,#53756);
#46445=AXIS2_PLACEMENT_3D('',#74894,#53757,#53758);
#46446=AXIS2_PLACEMENT_3D('',#74896,#53759,#53760);
#46447=AXIS2_PLACEMENT_3D('',#74899,#53762,#53763);
#46448=AXIS2_PLACEMENT_3D('',#74900,#53764,#53765);
#46449=AXIS2_PLACEMENT_3D('',#74902,#53766,#53767);
#46450=AXIS2_PLACEMENT_3D('',#74905,#53769,#53770);
#46451=AXIS2_PLACEMENT_3D('',#74906,#53771,#53772);
#46452=AXIS2_PLACEMENT_3D('',#74908,#53773,#53774);
#46453=AXIS2_PLACEMENT_3D('',#74911,#53776,#53777);
#46454=AXIS2_PLACEMENT_3D('',#74912,#53778,#53779);
#46455=AXIS2_PLACEMENT_3D('',#74914,#53780,#53781);
#46456=AXIS2_PLACEMENT_3D('',#74917,#53783,#53784);
#46457=AXIS2_PLACEMENT_3D('',#74918,#53785,#53786);
#46458=AXIS2_PLACEMENT_3D('',#74920,#53787,#53788);
#46459=AXIS2_PLACEMENT_3D('',#74935,#53790,#53791);
#46460=AXIS2_PLACEMENT_3D('',#74959,#53792,#53793);
#46461=AXIS2_PLACEMENT_3D('',#74961,#53794,#53795);
#46462=AXIS2_PLACEMENT_3D('',#74964,#53797,#53798);
#46463=AXIS2_PLACEMENT_3D('',#74965,#53799,#53800);
#46464=AXIS2_PLACEMENT_3D('',#74967,#53801,#53802);
#46465=AXIS2_PLACEMENT_3D('',#74970,#53804,#53805);
#46466=AXIS2_PLACEMENT_3D('',#74971,#53806,#53807);
#46467=AXIS2_PLACEMENT_3D('',#74973,#53808,#53809);
#46468=AXIS2_PLACEMENT_3D('',#74976,#53811,#53812);
#46469=AXIS2_PLACEMENT_3D('',#74977,#53813,#53814);
#46470=AXIS2_PLACEMENT_3D('',#74979,#53815,#53816);
#46471=AXIS2_PLACEMENT_3D('',#74982,#53818,#53819);
#46472=AXIS2_PLACEMENT_3D('',#74983,#53820,#53821);
#46473=AXIS2_PLACEMENT_3D('',#74985,#53822,#53823);
#46474=AXIS2_PLACEMENT_3D('',#74988,#53825,#53826);
#46475=AXIS2_PLACEMENT_3D('',#74989,#53827,#53828);
#46476=AXIS2_PLACEMENT_3D('',#74991,#53829,#53830);
#46477=AXIS2_PLACEMENT_3D('',#74994,#53832,#53833);
#46478=AXIS2_PLACEMENT_3D('',#74995,#53834,#53835);
#46479=AXIS2_PLACEMENT_3D('',#74997,#53836,#53837);
#46480=AXIS2_PLACEMENT_3D('',#75000,#53839,#53840);
#46481=AXIS2_PLACEMENT_3D('',#75001,#53841,#53842);
#46482=AXIS2_PLACEMENT_3D('',#75003,#53843,#53844);
#46483=AXIS2_PLACEMENT_3D('',#75006,#53846,#53847);
#46484=AXIS2_PLACEMENT_3D('',#75007,#53848,#53849);
#46485=AXIS2_PLACEMENT_3D('',#75009,#53850,#53851);
#46486=AXIS2_PLACEMENT_3D('',#75012,#53853,#53854);
#46487=AXIS2_PLACEMENT_3D('',#75013,#53855,#53856);
#46488=AXIS2_PLACEMENT_3D('',#75015,#53857,#53858);
#46489=AXIS2_PLACEMENT_3D('',#75018,#53860,#53861);
#46490=AXIS2_PLACEMENT_3D('',#75019,#53862,#53863);
#46491=AXIS2_PLACEMENT_3D('',#75021,#53864,#53865);
#46492=AXIS2_PLACEMENT_3D('',#75024,#53867,#53868);
#46493=AXIS2_PLACEMENT_3D('',#75025,#53869,#53870);
#46494=AXIS2_PLACEMENT_3D('',#75027,#53871,#53872);
#46495=AXIS2_PLACEMENT_3D('',#75030,#53874,#53875);
#46496=AXIS2_PLACEMENT_3D('',#75031,#53876,#53877);
#46497=AXIS2_PLACEMENT_3D('',#75033,#53878,#53879);
#46498=AXIS2_PLACEMENT_3D('',#75036,#53881,#53882);
#46499=AXIS2_PLACEMENT_3D('',#75037,#53883,#53884);
#46500=AXIS2_PLACEMENT_3D('',#75039,#53885,#53886);
#46501=AXIS2_PLACEMENT_3D('',#75042,#53888,#53889);
#46502=AXIS2_PLACEMENT_3D('',#75043,#53890,#53891);
#46503=AXIS2_PLACEMENT_3D('',#75045,#53892,#53893);
#46504=AXIS2_PLACEMENT_3D('',#75048,#53895,#53896);
#46505=AXIS2_PLACEMENT_3D('',#75049,#53897,#53898);
#46506=AXIS2_PLACEMENT_3D('',#75051,#53899,#53900);
#46507=AXIS2_PLACEMENT_3D('',#75066,#53902,#53903);
#46508=AXIS2_PLACEMENT_3D('',#75090,#53904,#53905);
#46509=AXIS2_PLACEMENT_3D('',#75092,#53906,#53907);
#46510=AXIS2_PLACEMENT_3D('',#75095,#53909,#53910);
#46511=AXIS2_PLACEMENT_3D('',#75096,#53911,#53912);
#46512=AXIS2_PLACEMENT_3D('',#75098,#53913,#53914);
#46513=AXIS2_PLACEMENT_3D('',#75101,#53916,#53917);
#46514=AXIS2_PLACEMENT_3D('',#75102,#53918,#53919);
#46515=AXIS2_PLACEMENT_3D('',#75104,#53920,#53921);
#46516=AXIS2_PLACEMENT_3D('',#75107,#53923,#53924);
#46517=AXIS2_PLACEMENT_3D('',#75108,#53925,#53926);
#46518=AXIS2_PLACEMENT_3D('',#75110,#53927,#53928);
#46519=AXIS2_PLACEMENT_3D('',#75113,#53930,#53931);
#46520=AXIS2_PLACEMENT_3D('',#75114,#53932,#53933);
#46521=AXIS2_PLACEMENT_3D('',#75116,#53934,#53935);
#46522=AXIS2_PLACEMENT_3D('',#75119,#53937,#53938);
#46523=AXIS2_PLACEMENT_3D('',#75120,#53939,#53940);
#46524=AXIS2_PLACEMENT_3D('',#75122,#53941,#53942);
#46525=AXIS2_PLACEMENT_3D('',#75125,#53944,#53945);
#46526=AXIS2_PLACEMENT_3D('',#75126,#53946,#53947);
#46527=AXIS2_PLACEMENT_3D('',#75128,#53948,#53949);
#46528=AXIS2_PLACEMENT_3D('',#75131,#53951,#53952);
#46529=AXIS2_PLACEMENT_3D('',#75132,#53953,#53954);
#46530=AXIS2_PLACEMENT_3D('',#75134,#53955,#53956);
#46531=AXIS2_PLACEMENT_3D('',#75137,#53958,#53959);
#46532=AXIS2_PLACEMENT_3D('',#75138,#53960,#53961);
#46533=AXIS2_PLACEMENT_3D('',#75140,#53962,#53963);
#46534=AXIS2_PLACEMENT_3D('',#75143,#53965,#53966);
#46535=AXIS2_PLACEMENT_3D('',#75144,#53967,#53968);
#46536=AXIS2_PLACEMENT_3D('',#75146,#53969,#53970);
#46537=AXIS2_PLACEMENT_3D('',#75149,#53972,#53973);
#46538=AXIS2_PLACEMENT_3D('',#75150,#53974,#53975);
#46539=AXIS2_PLACEMENT_3D('',#75152,#53976,#53977);
#46540=AXIS2_PLACEMENT_3D('',#75155,#53979,#53980);
#46541=AXIS2_PLACEMENT_3D('',#75156,#53981,#53982);
#46542=AXIS2_PLACEMENT_3D('',#75158,#53983,#53984);
#46543=AXIS2_PLACEMENT_3D('',#75161,#53986,#53987);
#46544=AXIS2_PLACEMENT_3D('',#75162,#53988,#53989);
#46545=AXIS2_PLACEMENT_3D('',#75164,#53990,#53991);
#46546=AXIS2_PLACEMENT_3D('',#75167,#53993,#53994);
#46547=AXIS2_PLACEMENT_3D('',#75168,#53995,#53996);
#46548=AXIS2_PLACEMENT_3D('',#75170,#53997,#53998);
#46549=AXIS2_PLACEMENT_3D('',#75173,#54000,#54001);
#46550=AXIS2_PLACEMENT_3D('',#75174,#54002,#54003);
#46551=AXIS2_PLACEMENT_3D('',#75176,#54004,#54005);
#46552=AXIS2_PLACEMENT_3D('',#75179,#54007,#54008);
#46553=AXIS2_PLACEMENT_3D('',#75180,#54009,#54010);
#46554=AXIS2_PLACEMENT_3D('',#75182,#54011,#54012);
#46555=AXIS2_PLACEMENT_3D('',#75185,#54014,#54015);
#46556=AXIS2_PLACEMENT_3D('',#75186,#54016,#54017);
#46557=AXIS2_PLACEMENT_3D('',#75188,#54018,#54019);
#46558=AXIS2_PLACEMENT_3D('',#75191,#54021,#54022);
#46559=AXIS2_PLACEMENT_3D('',#75192,#54023,#54024);
#46560=AXIS2_PLACEMENT_3D('',#75194,#54025,#54026);
#46561=AXIS2_PLACEMENT_3D('',#75207,#54028,#54029);
#46562=AXIS2_PLACEMENT_3D('',#75233,#54030,#54031);
#46563=AXIS2_PLACEMENT_3D('',#75235,#54032,#54033);
#46564=AXIS2_PLACEMENT_3D('',#75238,#54035,#54036);
#46565=AXIS2_PLACEMENT_3D('',#75239,#54037,#54038);
#46566=AXIS2_PLACEMENT_3D('',#75241,#54039,#54040);
#46567=AXIS2_PLACEMENT_3D('',#75244,#54042,#54043);
#46568=AXIS2_PLACEMENT_3D('',#75245,#54044,#54045);
#46569=AXIS2_PLACEMENT_3D('',#75247,#54046,#54047);
#46570=AXIS2_PLACEMENT_3D('',#75250,#54049,#54050);
#46571=AXIS2_PLACEMENT_3D('',#75251,#54051,#54052);
#46572=AXIS2_PLACEMENT_3D('',#75253,#54053,#54054);
#46573=AXIS2_PLACEMENT_3D('',#75256,#54056,#54057);
#46574=AXIS2_PLACEMENT_3D('',#75257,#54058,#54059);
#46575=AXIS2_PLACEMENT_3D('',#75259,#54060,#54061);
#46576=AXIS2_PLACEMENT_3D('',#75262,#54063,#54064);
#46577=AXIS2_PLACEMENT_3D('',#75263,#54065,#54066);
#46578=AXIS2_PLACEMENT_3D('',#75265,#54067,#54068);
#46579=AXIS2_PLACEMENT_3D('',#75268,#54070,#54071);
#46580=AXIS2_PLACEMENT_3D('',#75269,#54072,#54073);
#46581=AXIS2_PLACEMENT_3D('',#75271,#54074,#54075);
#46582=AXIS2_PLACEMENT_3D('',#75274,#54077,#54078);
#46583=AXIS2_PLACEMENT_3D('',#75275,#54079,#54080);
#46584=AXIS2_PLACEMENT_3D('',#75277,#54081,#54082);
#46585=AXIS2_PLACEMENT_3D('',#75280,#54084,#54085);
#46586=AXIS2_PLACEMENT_3D('',#75281,#54086,#54087);
#46587=AXIS2_PLACEMENT_3D('',#75283,#54088,#54089);
#46588=AXIS2_PLACEMENT_3D('',#75286,#54091,#54092);
#46589=AXIS2_PLACEMENT_3D('',#75287,#54093,#54094);
#46590=AXIS2_PLACEMENT_3D('',#75289,#54095,#54096);
#46591=AXIS2_PLACEMENT_3D('',#75292,#54098,#54099);
#46592=AXIS2_PLACEMENT_3D('',#75293,#54100,#54101);
#46593=AXIS2_PLACEMENT_3D('',#75295,#54102,#54103);
#46594=AXIS2_PLACEMENT_3D('',#75298,#54105,#54106);
#46595=AXIS2_PLACEMENT_3D('',#75299,#54107,#54108);
#46596=AXIS2_PLACEMENT_3D('',#75301,#54109,#54110);
#46597=AXIS2_PLACEMENT_3D('',#75304,#54112,#54113);
#46598=AXIS2_PLACEMENT_3D('',#75305,#54114,#54115);
#46599=AXIS2_PLACEMENT_3D('',#75307,#54116,#54117);
#46600=AXIS2_PLACEMENT_3D('',#75310,#54119,#54120);
#46601=AXIS2_PLACEMENT_3D('',#75311,#54121,#54122);
#46602=AXIS2_PLACEMENT_3D('',#75313,#54123,#54124);
#46603=AXIS2_PLACEMENT_3D('',#75316,#54126,#54127);
#46604=AXIS2_PLACEMENT_3D('',#75317,#54128,#54129);
#46605=AXIS2_PLACEMENT_3D('',#75319,#54130,#54131);
#46606=AXIS2_PLACEMENT_3D('',#75322,#54133,#54134);
#46607=AXIS2_PLACEMENT_3D('',#75323,#54135,#54136);
#46608=AXIS2_PLACEMENT_3D('',#75325,#54137,#54138);
#46609=AXIS2_PLACEMENT_3D('',#75328,#54140,#54141);
#46610=AXIS2_PLACEMENT_3D('',#75329,#54142,#54143);
#46611=AXIS2_PLACEMENT_3D('',#75331,#54144,#54145);
#46612=AXIS2_PLACEMENT_3D('',#75334,#54147,#54148);
#46613=AXIS2_PLACEMENT_3D('',#75335,#54149,#54150);
#46614=AXIS2_PLACEMENT_3D('',#75337,#54151,#54152);
#46615=AXIS2_PLACEMENT_3D('',#75350,#54154,#54155);
#46616=AXIS2_PLACEMENT_3D('',#75376,#54156,#54157);
#46617=AXIS2_PLACEMENT_3D('',#75378,#54158,#54159);
#46618=AXIS2_PLACEMENT_3D('',#75381,#54161,#54162);
#46619=AXIS2_PLACEMENT_3D('',#75382,#54163,#54164);
#46620=AXIS2_PLACEMENT_3D('',#75384,#54165,#54166);
#46621=AXIS2_PLACEMENT_3D('',#75387,#54168,#54169);
#46622=AXIS2_PLACEMENT_3D('',#75388,#54170,#54171);
#46623=AXIS2_PLACEMENT_3D('',#75390,#54172,#54173);
#46624=AXIS2_PLACEMENT_3D('',#75393,#54175,#54176);
#46625=AXIS2_PLACEMENT_3D('',#75394,#54177,#54178);
#46626=AXIS2_PLACEMENT_3D('',#75396,#54179,#54180);
#46627=AXIS2_PLACEMENT_3D('',#75399,#54182,#54183);
#46628=AXIS2_PLACEMENT_3D('',#75400,#54184,#54185);
#46629=AXIS2_PLACEMENT_3D('',#75402,#54186,#54187);
#46630=AXIS2_PLACEMENT_3D('',#75405,#54189,#54190);
#46631=AXIS2_PLACEMENT_3D('',#75406,#54191,#54192);
#46632=AXIS2_PLACEMENT_3D('',#75408,#54193,#54194);
#46633=AXIS2_PLACEMENT_3D('',#75411,#54196,#54197);
#46634=AXIS2_PLACEMENT_3D('',#75412,#54198,#54199);
#46635=AXIS2_PLACEMENT_3D('',#75414,#54200,#54201);
#46636=AXIS2_PLACEMENT_3D('',#75417,#54203,#54204);
#46637=AXIS2_PLACEMENT_3D('',#75418,#54205,#54206);
#46638=AXIS2_PLACEMENT_3D('',#75420,#54207,#54208);
#46639=AXIS2_PLACEMENT_3D('',#75423,#54210,#54211);
#46640=AXIS2_PLACEMENT_3D('',#75424,#54212,#54213);
#46641=AXIS2_PLACEMENT_3D('',#75426,#54214,#54215);
#46642=AXIS2_PLACEMENT_3D('',#75429,#54217,#54218);
#46643=AXIS2_PLACEMENT_3D('',#75430,#54219,#54220);
#46644=AXIS2_PLACEMENT_3D('',#75432,#54221,#54222);
#46645=AXIS2_PLACEMENT_3D('',#75435,#54224,#54225);
#46646=AXIS2_PLACEMENT_3D('',#75436,#54226,#54227);
#46647=AXIS2_PLACEMENT_3D('',#75438,#54228,#54229);
#46648=AXIS2_PLACEMENT_3D('',#75441,#54231,#54232);
#46649=AXIS2_PLACEMENT_3D('',#75442,#54233,#54234);
#46650=AXIS2_PLACEMENT_3D('',#75444,#54235,#54236);
#46651=AXIS2_PLACEMENT_3D('',#75447,#54238,#54239);
#46652=AXIS2_PLACEMENT_3D('',#75448,#54240,#54241);
#46653=AXIS2_PLACEMENT_3D('',#75450,#54242,#54243);
#46654=AXIS2_PLACEMENT_3D('',#75453,#54245,#54246);
#46655=AXIS2_PLACEMENT_3D('',#75454,#54247,#54248);
#46656=AXIS2_PLACEMENT_3D('',#75456,#54249,#54250);
#46657=AXIS2_PLACEMENT_3D('',#75459,#54252,#54253);
#46658=AXIS2_PLACEMENT_3D('',#75460,#54254,#54255);
#46659=AXIS2_PLACEMENT_3D('',#75462,#54256,#54257);
#46660=AXIS2_PLACEMENT_3D('',#75465,#54259,#54260);
#46661=AXIS2_PLACEMENT_3D('',#75466,#54261,#54262);
#46662=AXIS2_PLACEMENT_3D('',#75468,#54263,#54264);
#46663=AXIS2_PLACEMENT_3D('',#75471,#54266,#54267);
#46664=AXIS2_PLACEMENT_3D('',#75472,#54268,#54269);
#46665=AXIS2_PLACEMENT_3D('',#75474,#54270,#54271);
#46666=AXIS2_PLACEMENT_3D('',#75477,#54273,#54274);
#46667=AXIS2_PLACEMENT_3D('',#75478,#54275,#54276);
#46668=AXIS2_PLACEMENT_3D('',#75480,#54277,#54278);
#46669=AXIS2_PLACEMENT_3D('',#75491,#54280,#54281);
#46670=AXIS2_PLACEMENT_3D('',#75519,#54282,#54283);
#46671=AXIS2_PLACEMENT_3D('',#75521,#54284,#54285);
#46672=AXIS2_PLACEMENT_3D('',#75524,#54287,#54288);
#46673=AXIS2_PLACEMENT_3D('',#75525,#54289,#54290);
#46674=AXIS2_PLACEMENT_3D('',#75527,#54291,#54292);
#46675=AXIS2_PLACEMENT_3D('',#75530,#54294,#54295);
#46676=AXIS2_PLACEMENT_3D('',#75531,#54296,#54297);
#46677=AXIS2_PLACEMENT_3D('',#75533,#54298,#54299);
#46678=AXIS2_PLACEMENT_3D('',#75536,#54301,#54302);
#46679=AXIS2_PLACEMENT_3D('',#75537,#54303,#54304);
#46680=AXIS2_PLACEMENT_3D('',#75539,#54305,#54306);
#46681=AXIS2_PLACEMENT_3D('',#75542,#54308,#54309);
#46682=AXIS2_PLACEMENT_3D('',#75543,#54310,#54311);
#46683=AXIS2_PLACEMENT_3D('',#75545,#54312,#54313);
#46684=AXIS2_PLACEMENT_3D('',#75548,#54315,#54316);
#46685=AXIS2_PLACEMENT_3D('',#75549,#54317,#54318);
#46686=AXIS2_PLACEMENT_3D('',#75551,#54319,#54320);
#46687=AXIS2_PLACEMENT_3D('',#75554,#54322,#54323);
#46688=AXIS2_PLACEMENT_3D('',#75555,#54324,#54325);
#46689=AXIS2_PLACEMENT_3D('',#75557,#54326,#54327);
#46690=AXIS2_PLACEMENT_3D('',#75560,#54329,#54330);
#46691=AXIS2_PLACEMENT_3D('',#75561,#54331,#54332);
#46692=AXIS2_PLACEMENT_3D('',#75563,#54333,#54334);
#46693=AXIS2_PLACEMENT_3D('',#75566,#54336,#54337);
#46694=AXIS2_PLACEMENT_3D('',#75567,#54338,#54339);
#46695=AXIS2_PLACEMENT_3D('',#75569,#54340,#54341);
#46696=AXIS2_PLACEMENT_3D('',#75572,#54343,#54344);
#46697=AXIS2_PLACEMENT_3D('',#75573,#54345,#54346);
#46698=AXIS2_PLACEMENT_3D('',#75575,#54347,#54348);
#46699=AXIS2_PLACEMENT_3D('',#75578,#54350,#54351);
#46700=AXIS2_PLACEMENT_3D('',#75579,#54352,#54353);
#46701=AXIS2_PLACEMENT_3D('',#75581,#54354,#54355);
#46702=AXIS2_PLACEMENT_3D('',#75584,#54357,#54358);
#46703=AXIS2_PLACEMENT_3D('',#75585,#54359,#54360);
#46704=AXIS2_PLACEMENT_3D('',#75587,#54361,#54362);
#46705=AXIS2_PLACEMENT_3D('',#75590,#54364,#54365);
#46706=AXIS2_PLACEMENT_3D('',#75591,#54366,#54367);
#46707=AXIS2_PLACEMENT_3D('',#75593,#54368,#54369);
#46708=AXIS2_PLACEMENT_3D('',#75596,#54371,#54372);
#46709=AXIS2_PLACEMENT_3D('',#75597,#54373,#54374);
#46710=AXIS2_PLACEMENT_3D('',#75599,#54375,#54376);
#46711=AXIS2_PLACEMENT_3D('',#75602,#54378,#54379);
#46712=AXIS2_PLACEMENT_3D('',#75603,#54380,#54381);
#46713=AXIS2_PLACEMENT_3D('',#75605,#54382,#54383);
#46714=AXIS2_PLACEMENT_3D('',#75608,#54385,#54386);
#46715=AXIS2_PLACEMENT_3D('',#75609,#54387,#54388);
#46716=AXIS2_PLACEMENT_3D('',#75611,#54389,#54390);
#46717=AXIS2_PLACEMENT_3D('',#75614,#54392,#54393);
#46718=AXIS2_PLACEMENT_3D('',#75615,#54394,#54395);
#46719=AXIS2_PLACEMENT_3D('',#75617,#54396,#54397);
#46720=AXIS2_PLACEMENT_3D('',#75620,#54399,#54400);
#46721=AXIS2_PLACEMENT_3D('',#75621,#54401,#54402);
#46722=AXIS2_PLACEMENT_3D('',#75623,#54403,#54404);
#46723=AXIS2_PLACEMENT_3D('',#75632,#54406,#54407);
#46724=AXIS2_PLACEMENT_3D('',#75662,#54408,#54409);
#46725=AXIS2_PLACEMENT_3D('',#75664,#54410,#54411);
#46726=AXIS2_PLACEMENT_3D('',#75667,#54413,#54414);
#46727=AXIS2_PLACEMENT_3D('',#75668,#54415,#54416);
#46728=AXIS2_PLACEMENT_3D('',#75670,#54417,#54418);
#46729=AXIS2_PLACEMENT_3D('',#75673,#54420,#54421);
#46730=AXIS2_PLACEMENT_3D('',#75674,#54422,#54423);
#46731=AXIS2_PLACEMENT_3D('',#75676,#54424,#54425);
#46732=AXIS2_PLACEMENT_3D('',#75679,#54427,#54428);
#46733=AXIS2_PLACEMENT_3D('',#75680,#54429,#54430);
#46734=AXIS2_PLACEMENT_3D('',#75682,#54431,#54432);
#46735=AXIS2_PLACEMENT_3D('',#75685,#54434,#54435);
#46736=AXIS2_PLACEMENT_3D('',#75686,#54436,#54437);
#46737=AXIS2_PLACEMENT_3D('',#75688,#54438,#54439);
#46738=AXIS2_PLACEMENT_3D('',#75691,#54441,#54442);
#46739=AXIS2_PLACEMENT_3D('',#75692,#54443,#54444);
#46740=AXIS2_PLACEMENT_3D('',#75694,#54445,#54446);
#46741=AXIS2_PLACEMENT_3D('',#75697,#54448,#54449);
#46742=AXIS2_PLACEMENT_3D('',#75698,#54450,#54451);
#46743=AXIS2_PLACEMENT_3D('',#75700,#54452,#54453);
#46744=AXIS2_PLACEMENT_3D('',#75703,#54455,#54456);
#46745=AXIS2_PLACEMENT_3D('',#75704,#54457,#54458);
#46746=AXIS2_PLACEMENT_3D('',#75706,#54459,#54460);
#46747=AXIS2_PLACEMENT_3D('',#75709,#54462,#54463);
#46748=AXIS2_PLACEMENT_3D('',#75710,#54464,#54465);
#46749=AXIS2_PLACEMENT_3D('',#75712,#54466,#54467);
#46750=AXIS2_PLACEMENT_3D('',#75715,#54469,#54470);
#46751=AXIS2_PLACEMENT_3D('',#75716,#54471,#54472);
#46752=AXIS2_PLACEMENT_3D('',#75718,#54473,#54474);
#46753=AXIS2_PLACEMENT_3D('',#75721,#54476,#54477);
#46754=AXIS2_PLACEMENT_3D('',#75722,#54478,#54479);
#46755=AXIS2_PLACEMENT_3D('',#75724,#54480,#54481);
#46756=AXIS2_PLACEMENT_3D('',#75727,#54483,#54484);
#46757=AXIS2_PLACEMENT_3D('',#75728,#54485,#54486);
#46758=AXIS2_PLACEMENT_3D('',#75730,#54487,#54488);
#46759=AXIS2_PLACEMENT_3D('',#75733,#54490,#54491);
#46760=AXIS2_PLACEMENT_3D('',#75734,#54492,#54493);
#46761=AXIS2_PLACEMENT_3D('',#75736,#54494,#54495);
#46762=AXIS2_PLACEMENT_3D('',#75739,#54497,#54498);
#46763=AXIS2_PLACEMENT_3D('',#75740,#54499,#54500);
#46764=AXIS2_PLACEMENT_3D('',#75742,#54501,#54502);
#46765=AXIS2_PLACEMENT_3D('',#75745,#54504,#54505);
#46766=AXIS2_PLACEMENT_3D('',#75746,#54506,#54507);
#46767=AXIS2_PLACEMENT_3D('',#75748,#54508,#54509);
#46768=AXIS2_PLACEMENT_3D('',#75751,#54511,#54512);
#46769=AXIS2_PLACEMENT_3D('',#75752,#54513,#54514);
#46770=AXIS2_PLACEMENT_3D('',#75754,#54515,#54516);
#46771=AXIS2_PLACEMENT_3D('',#75763,#54518,#54519);
#46772=AXIS2_PLACEMENT_3D('',#75793,#54520,#54521);
#46773=AXIS2_PLACEMENT_3D('',#75795,#54522,#54523);
#46774=AXIS2_PLACEMENT_3D('',#75798,#54525,#54526);
#46775=AXIS2_PLACEMENT_3D('',#75799,#54527,#54528);
#46776=AXIS2_PLACEMENT_3D('',#75801,#54529,#54530);
#46777=AXIS2_PLACEMENT_3D('',#75804,#54532,#54533);
#46778=AXIS2_PLACEMENT_3D('',#75805,#54534,#54535);
#46779=AXIS2_PLACEMENT_3D('',#75807,#54536,#54537);
#46780=AXIS2_PLACEMENT_3D('',#75810,#54539,#54540);
#46781=AXIS2_PLACEMENT_3D('',#75811,#54541,#54542);
#46782=AXIS2_PLACEMENT_3D('',#75813,#54543,#54544);
#46783=AXIS2_PLACEMENT_3D('',#75816,#54546,#54547);
#46784=AXIS2_PLACEMENT_3D('',#75817,#54548,#54549);
#46785=AXIS2_PLACEMENT_3D('',#75819,#54550,#54551);
#46786=AXIS2_PLACEMENT_3D('',#75822,#54553,#54554);
#46787=AXIS2_PLACEMENT_3D('',#75823,#54555,#54556);
#46788=AXIS2_PLACEMENT_3D('',#75825,#54557,#54558);
#46789=AXIS2_PLACEMENT_3D('',#75828,#54560,#54561);
#46790=AXIS2_PLACEMENT_3D('',#75829,#54562,#54563);
#46791=AXIS2_PLACEMENT_3D('',#75831,#54564,#54565);
#46792=AXIS2_PLACEMENT_3D('',#75834,#54567,#54568);
#46793=AXIS2_PLACEMENT_3D('',#75835,#54569,#54570);
#46794=AXIS2_PLACEMENT_3D('',#75837,#54571,#54572);
#46795=AXIS2_PLACEMENT_3D('',#75840,#54574,#54575);
#46796=AXIS2_PLACEMENT_3D('',#75841,#54576,#54577);
#46797=AXIS2_PLACEMENT_3D('',#75843,#54578,#54579);
#46798=AXIS2_PLACEMENT_3D('',#75846,#54581,#54582);
#46799=AXIS2_PLACEMENT_3D('',#75847,#54583,#54584);
#46800=AXIS2_PLACEMENT_3D('',#75849,#54585,#54586);
#46801=AXIS2_PLACEMENT_3D('',#75852,#54588,#54589);
#46802=AXIS2_PLACEMENT_3D('',#75853,#54590,#54591);
#46803=AXIS2_PLACEMENT_3D('',#75855,#54592,#54593);
#46804=AXIS2_PLACEMENT_3D('',#75858,#54595,#54596);
#46805=AXIS2_PLACEMENT_3D('',#75859,#54597,#54598);
#46806=AXIS2_PLACEMENT_3D('',#75861,#54599,#54600);
#46807=AXIS2_PLACEMENT_3D('',#75864,#54602,#54603);
#46808=AXIS2_PLACEMENT_3D('',#75865,#54604,#54605);
#46809=AXIS2_PLACEMENT_3D('',#75867,#54606,#54607);
#46810=AXIS2_PLACEMENT_3D('',#75870,#54609,#54610);
#46811=AXIS2_PLACEMENT_3D('',#75871,#54611,#54612);
#46812=AXIS2_PLACEMENT_3D('',#75873,#54613,#54614);
#46813=AXIS2_PLACEMENT_3D('',#75876,#54616,#54617);
#46814=AXIS2_PLACEMENT_3D('',#75877,#54618,#54619);
#46815=AXIS2_PLACEMENT_3D('',#75879,#54620,#54621);
#46816=AXIS2_PLACEMENT_3D('',#75882,#54623,#54624);
#46817=AXIS2_PLACEMENT_3D('',#75883,#54625,#54626);
#46818=AXIS2_PLACEMENT_3D('',#75885,#54627,#54628);
#46819=AXIS2_PLACEMENT_3D('',#75888,#54630,#54631);
#46820=AXIS2_PLACEMENT_3D('',#75889,#54632,#54633);
#46821=AXIS2_PLACEMENT_3D('',#75891,#54634,#54635);
#46822=AXIS2_PLACEMENT_3D('',#75894,#54637,#54638);
#46823=AXIS2_PLACEMENT_3D('',#75895,#54639,#54640);
#46824=AXIS2_PLACEMENT_3D('',#75897,#54641,#54642);
#46825=AXIS2_PLACEMENT_3D('',#75901,#54644,#54645);
#46826=AXIS2_PLACEMENT_3D('',#75932,#54646,#54647);
#46827=AXIS2_PLACEMENT_3D('',#75933,#54648,#54649);
#46828=AXIS2_PLACEMENT_3D('',#75935,#54650,#54651);
#46829=AXIS2_PLACEMENT_3D('',#75938,#54653,#54654);
#46830=AXIS2_PLACEMENT_3D('',#75939,#54655,#54656);
#46831=AXIS2_PLACEMENT_3D('',#75941,#54657,#54658);
#46832=AXIS2_PLACEMENT_3D('',#75944,#54660,#54661);
#46833=AXIS2_PLACEMENT_3D('',#75945,#54662,#54663);
#46834=AXIS2_PLACEMENT_3D('',#75947,#54664,#54665);
#46835=AXIS2_PLACEMENT_3D('',#75950,#54667,#54668);
#46836=AXIS2_PLACEMENT_3D('',#75951,#54669,#54670);
#46837=AXIS2_PLACEMENT_3D('',#75953,#54671,#54672);
#46838=AXIS2_PLACEMENT_3D('',#75956,#54674,#54675);
#46839=AXIS2_PLACEMENT_3D('',#75957,#54676,#54677);
#46840=AXIS2_PLACEMENT_3D('',#75959,#54678,#54679);
#46841=AXIS2_PLACEMENT_3D('',#75962,#54681,#54682);
#46842=AXIS2_PLACEMENT_3D('',#75963,#54683,#54684);
#46843=AXIS2_PLACEMENT_3D('',#75965,#54685,#54686);
#46844=AXIS2_PLACEMENT_3D('',#75968,#54688,#54689);
#46845=AXIS2_PLACEMENT_3D('',#75969,#54690,#54691);
#46846=AXIS2_PLACEMENT_3D('',#75971,#54692,#54693);
#46847=AXIS2_PLACEMENT_3D('',#75974,#54695,#54696);
#46848=AXIS2_PLACEMENT_3D('',#75975,#54697,#54698);
#46849=AXIS2_PLACEMENT_3D('',#75977,#54699,#54700);
#46850=AXIS2_PLACEMENT_3D('',#75980,#54702,#54703);
#46851=AXIS2_PLACEMENT_3D('',#75981,#54704,#54705);
#46852=AXIS2_PLACEMENT_3D('',#75983,#54706,#54707);
#46853=AXIS2_PLACEMENT_3D('',#75986,#54709,#54710);
#46854=AXIS2_PLACEMENT_3D('',#75987,#54711,#54712);
#46855=AXIS2_PLACEMENT_3D('',#75989,#54713,#54714);
#46856=AXIS2_PLACEMENT_3D('',#75992,#54716,#54717);
#46857=AXIS2_PLACEMENT_3D('',#75993,#54718,#54719);
#46858=AXIS2_PLACEMENT_3D('',#75995,#54720,#54721);
#46859=AXIS2_PLACEMENT_3D('',#75998,#54723,#54724);
#46860=AXIS2_PLACEMENT_3D('',#75999,#54725,#54726);
#46861=AXIS2_PLACEMENT_3D('',#76001,#54727,#54728);
#46862=AXIS2_PLACEMENT_3D('',#76004,#54730,#54731);
#46863=AXIS2_PLACEMENT_3D('',#76005,#54732,#54733);
#46864=AXIS2_PLACEMENT_3D('',#76007,#54734,#54735);
#46865=AXIS2_PLACEMENT_3D('',#76010,#54737,#54738);
#46866=AXIS2_PLACEMENT_3D('',#76011,#54739,#54740);
#46867=AXIS2_PLACEMENT_3D('',#76013,#54741,#54742);
#46868=AXIS2_PLACEMENT_3D('',#76016,#54744,#54745);
#46869=AXIS2_PLACEMENT_3D('',#76017,#54746,#54747);
#46870=AXIS2_PLACEMENT_3D('',#76019,#54748,#54749);
#46871=AXIS2_PLACEMENT_3D('',#76022,#54751,#54752);
#46872=AXIS2_PLACEMENT_3D('',#76023,#54753,#54754);
#46873=AXIS2_PLACEMENT_3D('',#76025,#54755,#54756);
#46874=AXIS2_PLACEMENT_3D('',#76029,#54758,#54759);
#46875=AXIS2_PLACEMENT_3D('',#76043,#54760,#54761);
#46876=AXIS2_PLACEMENT_3D('',#76044,#54762,#54763);
#46877=AXIS2_PLACEMENT_3D('',#76046,#54764,#54765);
#46878=AXIS2_PLACEMENT_3D('',#76049,#54767,#54768);
#46879=AXIS2_PLACEMENT_3D('',#76050,#54769,#54770);
#46880=AXIS2_PLACEMENT_3D('',#76052,#54771,#54772);
#46881=AXIS2_PLACEMENT_3D('',#76056,#54774,#54775);
#46882=AXIS2_PLACEMENT_3D('',#76094,#54776,#54777);
#46883=AXIS2_PLACEMENT_3D('',#76095,#54778,#54779);
#46884=AXIS2_PLACEMENT_3D('',#76097,#54780,#54781);
#46885=AXIS2_PLACEMENT_3D('',#76100,#54783,#54784);
#46886=AXIS2_PLACEMENT_3D('',#76101,#54785,#54786);
#46887=AXIS2_PLACEMENT_3D('',#76103,#54787,#54788);
#46888=AXIS2_PLACEMENT_3D('',#76106,#54790,#54791);
#46889=AXIS2_PLACEMENT_3D('',#76107,#54792,#54793);
#46890=AXIS2_PLACEMENT_3D('',#76109,#54794,#54795);
#46891=AXIS2_PLACEMENT_3D('',#76112,#54797,#54798);
#46892=AXIS2_PLACEMENT_3D('',#76113,#54799,#54800);
#46893=AXIS2_PLACEMENT_3D('',#76115,#54801,#54802);
#46894=AXIS2_PLACEMENT_3D('',#76118,#54804,#54805);
#46895=AXIS2_PLACEMENT_3D('',#76119,#54806,#54807);
#46896=AXIS2_PLACEMENT_3D('',#76121,#54808,#54809);
#46897=AXIS2_PLACEMENT_3D('',#76124,#54811,#54812);
#46898=AXIS2_PLACEMENT_3D('',#76125,#54813,#54814);
#46899=AXIS2_PLACEMENT_3D('',#76127,#54815,#54816);
#46900=AXIS2_PLACEMENT_3D('',#76130,#54818,#54819);
#46901=AXIS2_PLACEMENT_3D('',#76131,#54820,#54821);
#46902=AXIS2_PLACEMENT_3D('',#76133,#54822,#54823);
#46903=AXIS2_PLACEMENT_3D('',#76136,#54825,#54826);
#46904=AXIS2_PLACEMENT_3D('',#76137,#54827,#54828);
#46905=AXIS2_PLACEMENT_3D('',#76139,#54829,#54830);
#46906=AXIS2_PLACEMENT_3D('',#76142,#54832,#54833);
#46907=AXIS2_PLACEMENT_3D('',#76143,#54834,#54835);
#46908=AXIS2_PLACEMENT_3D('',#76145,#54836,#54837);
#46909=AXIS2_PLACEMENT_3D('',#76148,#54839,#54840);
#46910=AXIS2_PLACEMENT_3D('',#76149,#54841,#54842);
#46911=AXIS2_PLACEMENT_3D('',#76151,#54843,#54844);
#46912=AXIS2_PLACEMENT_3D('',#76154,#54846,#54847);
#46913=AXIS2_PLACEMENT_3D('',#76155,#54848,#54849);
#46914=AXIS2_PLACEMENT_3D('',#76157,#54850,#54851);
#46915=AXIS2_PLACEMENT_3D('',#76160,#54853,#54854);
#46916=AXIS2_PLACEMENT_3D('',#76161,#54855,#54856);
#46917=AXIS2_PLACEMENT_3D('',#76163,#54857,#54858);
#46918=AXIS2_PLACEMENT_3D('',#76166,#54860,#54861);
#46919=AXIS2_PLACEMENT_3D('',#76167,#54862,#54863);
#46920=AXIS2_PLACEMENT_3D('',#76169,#54864,#54865);
#46921=AXIS2_PLACEMENT_3D('',#76172,#54867,#54868);
#46922=AXIS2_PLACEMENT_3D('',#76173,#54869,#54870);
#46923=AXIS2_PLACEMENT_3D('',#76175,#54871,#54872);
#46924=AXIS2_PLACEMENT_3D('',#76179,#54874,#54875);
#46925=AXIS2_PLACEMENT_3D('',#76195,#54876,#54877);
#46926=AXIS2_PLACEMENT_3D('',#76196,#54878,#54879);
#46927=AXIS2_PLACEMENT_3D('',#76198,#54880,#54881);
#46928=AXIS2_PLACEMENT_3D('',#76201,#54883,#54884);
#46929=AXIS2_PLACEMENT_3D('',#76202,#54885,#54886);
#46930=AXIS2_PLACEMENT_3D('',#76204,#54887,#54888);
#46931=AXIS2_PLACEMENT_3D('',#76207,#54890,#54891);
#46932=AXIS2_PLACEMENT_3D('',#76208,#54892,#54893);
#46933=AXIS2_PLACEMENT_3D('',#76210,#54894,#54895);
#46934=AXIS2_PLACEMENT_3D('',#76213,#54897,#54898);
#46935=AXIS2_PLACEMENT_3D('',#76214,#54899,#54900);
#46936=AXIS2_PLACEMENT_3D('',#76216,#54901,#54902);
#46937=AXIS2_PLACEMENT_3D('',#76219,#54904,#54905);
#46938=AXIS2_PLACEMENT_3D('',#76220,#54906,#54907);
#46939=AXIS2_PLACEMENT_3D('',#76222,#54908,#54909);
#46940=AXIS2_PLACEMENT_3D('',#76225,#54911,#54912);
#46941=AXIS2_PLACEMENT_3D('',#76226,#54913,#54914);
#46942=AXIS2_PLACEMENT_3D('',#76228,#54915,#54916);
#46943=AXIS2_PLACEMENT_3D('',#76231,#54918,#54919);
#46944=AXIS2_PLACEMENT_3D('',#76232,#54920,#54921);
#46945=AXIS2_PLACEMENT_3D('',#76234,#54922,#54923);
#46946=AXIS2_PLACEMENT_3D('',#76237,#54925,#54926);
#46947=AXIS2_PLACEMENT_3D('',#76238,#54927,#54928);
#46948=AXIS2_PLACEMENT_3D('',#76240,#54929,#54930);
#46949=AXIS2_PLACEMENT_3D('',#76243,#54932,#54933);
#46950=AXIS2_PLACEMENT_3D('',#76244,#54934,#54935);
#46951=AXIS2_PLACEMENT_3D('',#76246,#54936,#54937);
#46952=AXIS2_PLACEMENT_3D('',#76249,#54939,#54940);
#46953=AXIS2_PLACEMENT_3D('',#76250,#54941,#54942);
#46954=AXIS2_PLACEMENT_3D('',#76252,#54943,#54944);
#46955=AXIS2_PLACEMENT_3D('',#76255,#54946,#54947);
#46956=AXIS2_PLACEMENT_3D('',#76256,#54948,#54949);
#46957=AXIS2_PLACEMENT_3D('',#76258,#54950,#54951);
#46958=AXIS2_PLACEMENT_3D('',#76261,#54953,#54954);
#46959=AXIS2_PLACEMENT_3D('',#76262,#54955,#54956);
#46960=AXIS2_PLACEMENT_3D('',#76264,#54957,#54958);
#46961=AXIS2_PLACEMENT_3D('',#76267,#54960,#54961);
#46962=AXIS2_PLACEMENT_3D('',#76268,#54962,#54963);
#46963=AXIS2_PLACEMENT_3D('',#76270,#54964,#54965);
#46964=AXIS2_PLACEMENT_3D('',#76273,#54967,#54968);
#46965=AXIS2_PLACEMENT_3D('',#76274,#54969,#54970);
#46966=AXIS2_PLACEMENT_3D('',#76276,#54971,#54972);
#46967=AXIS2_PLACEMENT_3D('',#76279,#54974,#54975);
#46968=AXIS2_PLACEMENT_3D('',#76280,#54976,#54977);
#46969=AXIS2_PLACEMENT_3D('',#76282,#54978,#54979);
#46970=AXIS2_PLACEMENT_3D('',#76285,#54981,#54982);
#46971=AXIS2_PLACEMENT_3D('',#76286,#54983,#54984);
#46972=AXIS2_PLACEMENT_3D('',#76288,#54985,#54986);
#46973=AXIS2_PLACEMENT_3D('',#76291,#54988,#54989);
#46974=AXIS2_PLACEMENT_3D('',#76292,#54990,#54991);
#46975=AXIS2_PLACEMENT_3D('',#76294,#54992,#54993);
#46976=AXIS2_PLACEMENT_3D('',#76297,#54995,#54996);
#46977=AXIS2_PLACEMENT_3D('',#76298,#54997,#54998);
#46978=AXIS2_PLACEMENT_3D('',#76300,#54999,#55000);
#46979=AXIS2_PLACEMENT_3D('',#76303,#55002,#55003);
#46980=AXIS2_PLACEMENT_3D('',#76304,#55004,#55005);
#46981=AXIS2_PLACEMENT_3D('',#76306,#55006,#55007);
#46982=AXIS2_PLACEMENT_3D('',#76309,#55009,#55010);
#46983=AXIS2_PLACEMENT_3D('',#76310,#55011,#55012);
#46984=AXIS2_PLACEMENT_3D('',#76312,#55013,#55014);
#46985=AXIS2_PLACEMENT_3D('',#76315,#55016,#55017);
#46986=AXIS2_PLACEMENT_3D('',#76316,#55018,#55019);
#46987=AXIS2_PLACEMENT_3D('',#76318,#55020,#55021);
#46988=AXIS2_PLACEMENT_3D('',#76321,#55023,#55024);
#46989=AXIS2_PLACEMENT_3D('',#76322,#55025,#55026);
#46990=AXIS2_PLACEMENT_3D('',#76324,#55027,#55028);
#46991=AXIS2_PLACEMENT_3D('',#76327,#55030,#55031);
#46992=AXIS2_PLACEMENT_3D('',#76328,#55032,#55033);
#46993=AXIS2_PLACEMENT_3D('',#76330,#55034,#55035);
#46994=AXIS2_PLACEMENT_3D('',#76333,#55037,#55038);
#46995=AXIS2_PLACEMENT_3D('',#76334,#55039,#55040);
#46996=AXIS2_PLACEMENT_3D('',#76336,#55041,#55042);
#46997=AXIS2_PLACEMENT_3D('',#76339,#55044,#55045);
#46998=AXIS2_PLACEMENT_3D('',#76340,#55046,#55047);
#46999=AXIS2_PLACEMENT_3D('',#76342,#55048,#55049);
#47000=AXIS2_PLACEMENT_3D('',#76345,#55051,#55052);
#47001=AXIS2_PLACEMENT_3D('',#76346,#55053,#55054);
#47002=AXIS2_PLACEMENT_3D('',#76348,#55055,#55056);
#47003=AXIS2_PLACEMENT_3D('',#76351,#55058,#55059);
#47004=AXIS2_PLACEMENT_3D('',#76352,#55060,#55061);
#47005=AXIS2_PLACEMENT_3D('',#76354,#55062,#55063);
#47006=AXIS2_PLACEMENT_3D('',#76357,#55065,#55066);
#47007=AXIS2_PLACEMENT_3D('',#76358,#55067,#55068);
#47008=AXIS2_PLACEMENT_3D('',#76360,#55069,#55070);
#47009=AXIS2_PLACEMENT_3D('',#76364,#55072,#55073);
#47010=AXIS2_PLACEMENT_3D('',#76390,#55074,#55075);
#47011=AXIS2_PLACEMENT_3D('',#76391,#55076,#55077);
#47012=AXIS2_PLACEMENT_3D('',#76393,#55078,#55079);
#47013=AXIS2_PLACEMENT_3D('',#76396,#55081,#55082);
#47014=AXIS2_PLACEMENT_3D('',#76397,#55083,#55084);
#47015=AXIS2_PLACEMENT_3D('',#76399,#55085,#55086);
#47016=AXIS2_PLACEMENT_3D('',#76402,#55088,#55089);
#47017=AXIS2_PLACEMENT_3D('',#76403,#55090,#55091);
#47018=AXIS2_PLACEMENT_3D('',#76405,#55092,#55093);
#47019=AXIS2_PLACEMENT_3D('',#76408,#55095,#55096);
#47020=AXIS2_PLACEMENT_3D('',#76409,#55097,#55098);
#47021=AXIS2_PLACEMENT_3D('',#76411,#55099,#55100);
#47022=AXIS2_PLACEMENT_3D('',#76414,#55102,#55103);
#47023=AXIS2_PLACEMENT_3D('',#76415,#55104,#55105);
#47024=AXIS2_PLACEMENT_3D('',#76417,#55106,#55107);
#47025=AXIS2_PLACEMENT_3D('',#76420,#55109,#55110);
#47026=AXIS2_PLACEMENT_3D('',#76421,#55111,#55112);
#47027=AXIS2_PLACEMENT_3D('',#76423,#55113,#55114);
#47028=AXIS2_PLACEMENT_3D('',#76426,#55116,#55117);
#47029=AXIS2_PLACEMENT_3D('',#76427,#55118,#55119);
#47030=AXIS2_PLACEMENT_3D('',#76429,#55120,#55121);
#47031=AXIS2_PLACEMENT_3D('',#76432,#55123,#55124);
#47032=AXIS2_PLACEMENT_3D('',#76433,#55125,#55126);
#47033=AXIS2_PLACEMENT_3D('',#76435,#55127,#55128);
#47034=AXIS2_PLACEMENT_3D('',#76438,#55130,#55131);
#47035=AXIS2_PLACEMENT_3D('',#76439,#55132,#55133);
#47036=AXIS2_PLACEMENT_3D('',#76441,#55134,#55135);
#47037=AXIS2_PLACEMENT_3D('',#76444,#55137,#55138);
#47038=AXIS2_PLACEMENT_3D('',#76445,#55139,#55140);
#47039=AXIS2_PLACEMENT_3D('',#76447,#55141,#55142);
#47040=AXIS2_PLACEMENT_3D('',#76450,#55144,#55145);
#47041=AXIS2_PLACEMENT_3D('',#76451,#55146,#55147);
#47042=AXIS2_PLACEMENT_3D('',#76453,#55148,#55149);
#47043=AXIS2_PLACEMENT_3D('',#76456,#55151,#55152);
#47044=AXIS2_PLACEMENT_3D('',#76457,#55153,#55154);
#47045=AXIS2_PLACEMENT_3D('',#76459,#55155,#55156);
#47046=AXIS2_PLACEMENT_3D('',#76462,#55158,#55159);
#47047=AXIS2_PLACEMENT_3D('',#76463,#55160,#55161);
#47048=AXIS2_PLACEMENT_3D('',#76465,#55162,#55163);
#47049=AXIS2_PLACEMENT_3D('',#76468,#55165,#55166);
#47050=AXIS2_PLACEMENT_3D('',#76469,#55167,#55168);
#47051=AXIS2_PLACEMENT_3D('',#76471,#55169,#55170);
#47052=AXIS2_PLACEMENT_3D('',#76474,#55172,#55173);
#47053=AXIS2_PLACEMENT_3D('',#76475,#55174,#55175);
#47054=AXIS2_PLACEMENT_3D('',#76477,#55176,#55177);
#47055=AXIS2_PLACEMENT_3D('',#76480,#55179,#55180);
#47056=AXIS2_PLACEMENT_3D('',#76481,#55181,#55182);
#47057=AXIS2_PLACEMENT_3D('',#76483,#55183,#55184);
#47058=AXIS2_PLACEMENT_3D('',#76486,#55186,#55187);
#47059=AXIS2_PLACEMENT_3D('',#76487,#55188,#55189);
#47060=AXIS2_PLACEMENT_3D('',#76489,#55190,#55191);
#47061=AXIS2_PLACEMENT_3D('',#76492,#55193,#55194);
#47062=AXIS2_PLACEMENT_3D('',#76493,#55195,#55196);
#47063=AXIS2_PLACEMENT_3D('',#76495,#55197,#55198);
#47064=AXIS2_PLACEMENT_3D('',#76498,#55200,#55201);
#47065=AXIS2_PLACEMENT_3D('',#76499,#55202,#55203);
#47066=AXIS2_PLACEMENT_3D('',#76501,#55204,#55205);
#47067=AXIS2_PLACEMENT_3D('',#76504,#55207,#55208);
#47068=AXIS2_PLACEMENT_3D('',#76505,#55209,#55210);
#47069=AXIS2_PLACEMENT_3D('',#76507,#55211,#55212);
#47070=AXIS2_PLACEMENT_3D('',#76510,#55214,#55215);
#47071=AXIS2_PLACEMENT_3D('',#76511,#55216,#55217);
#47072=AXIS2_PLACEMENT_3D('',#76513,#55218,#55219);
#47073=AXIS2_PLACEMENT_3D('',#76516,#55221,#55222);
#47074=AXIS2_PLACEMENT_3D('',#76517,#55223,#55224);
#47075=AXIS2_PLACEMENT_3D('',#76519,#55225,#55226);
#47076=AXIS2_PLACEMENT_3D('',#76522,#55228,#55229);
#47077=AXIS2_PLACEMENT_3D('',#76523,#55230,#55231);
#47078=AXIS2_PLACEMENT_3D('',#76525,#55232,#55233);
#47079=AXIS2_PLACEMENT_3D('',#76528,#55235,#55236);
#47080=AXIS2_PLACEMENT_3D('',#76529,#55237,#55238);
#47081=AXIS2_PLACEMENT_3D('',#76531,#55239,#55240);
#47082=AXIS2_PLACEMENT_3D('',#76534,#55242,#55243);
#47083=AXIS2_PLACEMENT_3D('',#76535,#55244,#55245);
#47084=AXIS2_PLACEMENT_3D('',#76537,#55246,#55247);
#47085=AXIS2_PLACEMENT_3D('',#76540,#55249,#55250);
#47086=AXIS2_PLACEMENT_3D('',#76541,#55251,#55252);
#47087=AXIS2_PLACEMENT_3D('',#76543,#55253,#55254);
#47088=AXIS2_PLACEMENT_3D('',#76546,#55256,#55257);
#47089=AXIS2_PLACEMENT_3D('',#76547,#55258,#55259);
#47090=AXIS2_PLACEMENT_3D('',#76549,#55260,#55261);
#47091=AXIS2_PLACEMENT_3D('',#76552,#55263,#55264);
#47092=AXIS2_PLACEMENT_3D('',#76553,#55265,#55266);
#47093=AXIS2_PLACEMENT_3D('',#76555,#55267,#55268);
#47094=AXIS2_PLACEMENT_3D('',#76558,#55270,#55271);
#47095=AXIS2_PLACEMENT_3D('',#76559,#55272,#55273);
#47096=AXIS2_PLACEMENT_3D('',#76561,#55274,#55275);
#47097=AXIS2_PLACEMENT_3D('',#76564,#55277,#55278);
#47098=AXIS2_PLACEMENT_3D('',#76565,#55279,#55280);
#47099=AXIS2_PLACEMENT_3D('',#76567,#55281,#55282);
#47100=AXIS2_PLACEMENT_3D('',#76570,#55284,#55285);
#47101=AXIS2_PLACEMENT_3D('',#76571,#55286,#55287);
#47102=AXIS2_PLACEMENT_3D('',#76573,#55288,#55289);
#47103=AXIS2_PLACEMENT_3D('',#76576,#55291,#55292);
#47104=AXIS2_PLACEMENT_3D('',#76577,#55293,#55294);
#47105=AXIS2_PLACEMENT_3D('',#76579,#55295,#55296);
#47106=AXIS2_PLACEMENT_3D('',#76582,#55298,#55299);
#47107=AXIS2_PLACEMENT_3D('',#76583,#55300,#55301);
#47108=AXIS2_PLACEMENT_3D('',#76585,#55302,#55303);
#47109=AXIS2_PLACEMENT_3D('',#76588,#55305,#55306);
#47110=AXIS2_PLACEMENT_3D('',#76589,#55307,#55308);
#47111=AXIS2_PLACEMENT_3D('',#76591,#55309,#55310);
#47112=AXIS2_PLACEMENT_3D('',#76595,#55312,#55313);
#47113=AXIS2_PLACEMENT_3D('',#76636,#55314,#55315);
#47114=AXIS2_PLACEMENT_3D('',#76637,#55316,#55317);
#47115=AXIS2_PLACEMENT_3D('',#76639,#55318,#55319);
#47116=AXIS2_PLACEMENT_3D('',#76642,#55321,#55322);
#47117=AXIS2_PLACEMENT_3D('',#76643,#55323,#55324);
#47118=AXIS2_PLACEMENT_3D('',#76645,#55325,#55326);
#47119=AXIS2_PLACEMENT_3D('',#76648,#55328,#55329);
#47120=AXIS2_PLACEMENT_3D('',#76649,#55330,#55331);
#47121=AXIS2_PLACEMENT_3D('',#76651,#55332,#55333);
#47122=AXIS2_PLACEMENT_3D('',#76654,#55335,#55336);
#47123=AXIS2_PLACEMENT_3D('',#76655,#55337,#55338);
#47124=AXIS2_PLACEMENT_3D('',#76657,#55339,#55340);
#47125=AXIS2_PLACEMENT_3D('',#76660,#55342,#55343);
#47126=AXIS2_PLACEMENT_3D('',#76661,#55344,#55345);
#47127=AXIS2_PLACEMENT_3D('',#76663,#55346,#55347);
#47128=AXIS2_PLACEMENT_3D('',#76666,#55349,#55350);
#47129=AXIS2_PLACEMENT_3D('',#76667,#55351,#55352);
#47130=AXIS2_PLACEMENT_3D('',#76669,#55353,#55354);
#47131=AXIS2_PLACEMENT_3D('',#76672,#55356,#55357);
#47132=AXIS2_PLACEMENT_3D('',#76673,#55358,#55359);
#47133=AXIS2_PLACEMENT_3D('',#76675,#55360,#55361);
#47134=AXIS2_PLACEMENT_3D('',#76678,#55363,#55364);
#47135=AXIS2_PLACEMENT_3D('',#76679,#55365,#55366);
#47136=AXIS2_PLACEMENT_3D('',#76681,#55367,#55368);
#47137=AXIS2_PLACEMENT_3D('',#76684,#55370,#55371);
#47138=AXIS2_PLACEMENT_3D('',#76685,#55372,#55373);
#47139=AXIS2_PLACEMENT_3D('',#76687,#55374,#55375);
#47140=AXIS2_PLACEMENT_3D('',#76690,#55377,#55378);
#47141=AXIS2_PLACEMENT_3D('',#76691,#55379,#55380);
#47142=AXIS2_PLACEMENT_3D('',#76693,#55381,#55382);
#47143=AXIS2_PLACEMENT_3D('',#76696,#55384,#55385);
#47144=AXIS2_PLACEMENT_3D('',#76697,#55386,#55387);
#47145=AXIS2_PLACEMENT_3D('',#76699,#55388,#55389);
#47146=AXIS2_PLACEMENT_3D('',#76702,#55391,#55392);
#47147=AXIS2_PLACEMENT_3D('',#76703,#55393,#55394);
#47148=AXIS2_PLACEMENT_3D('',#76705,#55395,#55396);
#47149=AXIS2_PLACEMENT_3D('',#76708,#55398,#55399);
#47150=AXIS2_PLACEMENT_3D('',#76709,#55400,#55401);
#47151=AXIS2_PLACEMENT_3D('',#76711,#55402,#55403);
#47152=AXIS2_PLACEMENT_3D('',#76714,#55405,#55406);
#47153=AXIS2_PLACEMENT_3D('',#76715,#55407,#55408);
#47154=AXIS2_PLACEMENT_3D('',#76717,#55409,#55410);
#47155=AXIS2_PLACEMENT_3D('',#76720,#55412,#55413);
#47156=AXIS2_PLACEMENT_3D('',#76721,#55414,#55415);
#47157=AXIS2_PLACEMENT_3D('',#76723,#55416,#55417);
#47158=AXIS2_PLACEMENT_3D('',#76726,#55419,#55420);
#47159=AXIS2_PLACEMENT_3D('',#76727,#55421,#55422);
#47160=AXIS2_PLACEMENT_3D('',#76729,#55423,#55424);
#47161=AXIS2_PLACEMENT_3D('',#76732,#55426,#55427);
#47162=AXIS2_PLACEMENT_3D('',#76733,#55428,#55429);
#47163=AXIS2_PLACEMENT_3D('',#76735,#55430,#55431);
#47164=AXIS2_PLACEMENT_3D('',#76738,#55433,#55434);
#47165=AXIS2_PLACEMENT_3D('',#76739,#55435,#55436);
#47166=AXIS2_PLACEMENT_3D('',#76741,#55437,#55438);
#47167=AXIS2_PLACEMENT_3D('',#76745,#55440,#55441);
#47168=AXIS2_PLACEMENT_3D('',#76776,#55442,#55443);
#47169=AXIS2_PLACEMENT_3D('',#76777,#55444,#55445);
#47170=AXIS2_PLACEMENT_3D('',#76779,#55446,#55447);
#47171=AXIS2_PLACEMENT_3D('',#76782,#55449,#55450);
#47172=AXIS2_PLACEMENT_3D('',#76783,#55451,#55452);
#47173=AXIS2_PLACEMENT_3D('',#76785,#55453,#55454);
#47174=AXIS2_PLACEMENT_3D('',#76788,#55456,#55457);
#47175=AXIS2_PLACEMENT_3D('',#76789,#55458,#55459);
#47176=AXIS2_PLACEMENT_3D('',#76791,#55460,#55461);
#47177=AXIS2_PLACEMENT_3D('',#76794,#55463,#55464);
#47178=AXIS2_PLACEMENT_3D('',#76795,#55465,#55466);
#47179=AXIS2_PLACEMENT_3D('',#76797,#55467,#55468);
#47180=AXIS2_PLACEMENT_3D('',#76800,#55470,#55471);
#47181=AXIS2_PLACEMENT_3D('',#76801,#55472,#55473);
#47182=AXIS2_PLACEMENT_3D('',#76803,#55474,#55475);
#47183=AXIS2_PLACEMENT_3D('',#76806,#55477,#55478);
#47184=AXIS2_PLACEMENT_3D('',#76807,#55479,#55480);
#47185=AXIS2_PLACEMENT_3D('',#76809,#55481,#55482);
#47186=AXIS2_PLACEMENT_3D('',#76812,#55484,#55485);
#47187=AXIS2_PLACEMENT_3D('',#76813,#55486,#55487);
#47188=AXIS2_PLACEMENT_3D('',#76815,#55488,#55489);
#47189=AXIS2_PLACEMENT_3D('',#76818,#55491,#55492);
#47190=AXIS2_PLACEMENT_3D('',#76819,#55493,#55494);
#47191=AXIS2_PLACEMENT_3D('',#76821,#55495,#55496);
#47192=AXIS2_PLACEMENT_3D('',#76824,#55498,#55499);
#47193=AXIS2_PLACEMENT_3D('',#76825,#55500,#55501);
#47194=AXIS2_PLACEMENT_3D('',#76827,#55502,#55503);
#47195=AXIS2_PLACEMENT_3D('',#76830,#55505,#55506);
#47196=AXIS2_PLACEMENT_3D('',#76831,#55507,#55508);
#47197=AXIS2_PLACEMENT_3D('',#76833,#55509,#55510);
#47198=AXIS2_PLACEMENT_3D('',#76836,#55512,#55513);
#47199=AXIS2_PLACEMENT_3D('',#76837,#55514,#55515);
#47200=AXIS2_PLACEMENT_3D('',#76839,#55516,#55517);
#47201=AXIS2_PLACEMENT_3D('',#76842,#55519,#55520);
#47202=AXIS2_PLACEMENT_3D('',#76843,#55521,#55522);
#47203=AXIS2_PLACEMENT_3D('',#76845,#55523,#55524);
#47204=AXIS2_PLACEMENT_3D('',#76848,#55526,#55527);
#47205=AXIS2_PLACEMENT_3D('',#76849,#55528,#55529);
#47206=AXIS2_PLACEMENT_3D('',#76851,#55530,#55531);
#47207=AXIS2_PLACEMENT_3D('',#76854,#55533,#55534);
#47208=AXIS2_PLACEMENT_3D('',#76855,#55535,#55536);
#47209=AXIS2_PLACEMENT_3D('',#76857,#55537,#55538);
#47210=AXIS2_PLACEMENT_3D('',#76860,#55540,#55541);
#47211=AXIS2_PLACEMENT_3D('',#76861,#55542,#55543);
#47212=AXIS2_PLACEMENT_3D('',#76863,#55544,#55545);
#47213=AXIS2_PLACEMENT_3D('',#76866,#55547,#55548);
#47214=AXIS2_PLACEMENT_3D('',#76867,#55549,#55550);
#47215=AXIS2_PLACEMENT_3D('',#76869,#55551,#55552);
#47216=AXIS2_PLACEMENT_3D('',#76872,#55554,#55555);
#47217=AXIS2_PLACEMENT_3D('',#76873,#55556,#55557);
#47218=AXIS2_PLACEMENT_3D('',#76875,#55558,#55559);
#47219=AXIS2_PLACEMENT_3D('',#76878,#55561,#55562);
#47220=AXIS2_PLACEMENT_3D('',#76879,#55563,#55564);
#47221=AXIS2_PLACEMENT_3D('',#76881,#55565,#55566);
#47222=AXIS2_PLACEMENT_3D('',#76915,#55568,#55569);
#47223=AXIS2_PLACEMENT_3D('',#76920,#55570,#55571);
#47224=AXIS2_PLACEMENT_3D('',#76922,#55572,#55573);
#47225=AXIS2_PLACEMENT_3D('',#76925,#55575,#55576);
#47226=AXIS2_PLACEMENT_3D('',#76926,#55577,#55578);
#47227=AXIS2_PLACEMENT_3D('',#76928,#55579,#55580);
#47228=AXIS2_PLACEMENT_3D('',#76931,#55582,#55583);
#47229=AXIS2_PLACEMENT_3D('',#76932,#55584,#55585);
#47230=AXIS2_PLACEMENT_3D('',#76934,#55586,#55587);
#47231=AXIS2_PLACEMENT_3D('',#76937,#55589,#55590);
#47232=AXIS2_PLACEMENT_3D('',#76938,#55591,#55592);
#47233=AXIS2_PLACEMENT_3D('',#76940,#55593,#55594);
#47234=AXIS2_PLACEMENT_3D('',#76943,#55596,#55597);
#47235=AXIS2_PLACEMENT_3D('',#76944,#55598,#55599);
#47236=AXIS2_PLACEMENT_3D('',#76946,#55600,#55601);
#47237=AXIS2_PLACEMENT_3D('',#76949,#55603,#55604);
#47238=AXIS2_PLACEMENT_3D('',#76950,#55605,#55606);
#47239=AXIS2_PLACEMENT_3D('',#76952,#55607,#55608);
#47240=AXIS2_PLACEMENT_3D('',#76955,#55610,#55611);
#47241=AXIS2_PLACEMENT_3D('',#76956,#55612,#55613);
#47242=AXIS2_PLACEMENT_3D('',#76958,#55614,#55615);
#47243=AXIS2_PLACEMENT_3D('',#76961,#55617,#55618);
#47244=AXIS2_PLACEMENT_3D('',#76962,#55619,#55620);
#47245=AXIS2_PLACEMENT_3D('',#76964,#55621,#55622);
#47246=AXIS2_PLACEMENT_3D('',#76967,#55624,#55625);
#47247=AXIS2_PLACEMENT_3D('',#76968,#55626,#55627);
#47248=AXIS2_PLACEMENT_3D('',#76970,#55628,#55629);
#47249=AXIS2_PLACEMENT_3D('',#76973,#55631,#55632);
#47250=AXIS2_PLACEMENT_3D('',#76974,#55633,#55634);
#47251=AXIS2_PLACEMENT_3D('',#76976,#55635,#55636);
#47252=AXIS2_PLACEMENT_3D('',#76979,#55638,#55639);
#47253=AXIS2_PLACEMENT_3D('',#76980,#55640,#55641);
#47254=AXIS2_PLACEMENT_3D('',#76982,#55642,#55643);
#47255=AXIS2_PLACEMENT_3D('',#76985,#55645,#55646);
#47256=AXIS2_PLACEMENT_3D('',#76986,#55647,#55648);
#47257=AXIS2_PLACEMENT_3D('',#76988,#55649,#55650);
#47258=AXIS2_PLACEMENT_3D('',#76991,#55652,#55653);
#47259=AXIS2_PLACEMENT_3D('',#76992,#55654,#55655);
#47260=AXIS2_PLACEMENT_3D('',#76994,#55656,#55657);
#47261=AXIS2_PLACEMENT_3D('',#76997,#55659,#55660);
#47262=AXIS2_PLACEMENT_3D('',#76998,#55661,#55662);
#47263=AXIS2_PLACEMENT_3D('',#77000,#55663,#55664);
#47264=AXIS2_PLACEMENT_3D('',#77003,#55666,#55667);
#47265=AXIS2_PLACEMENT_3D('',#77004,#55668,#55669);
#47266=AXIS2_PLACEMENT_3D('',#77006,#55670,#55671);
#47267=AXIS2_PLACEMENT_3D('',#77009,#55673,#55674);
#47268=AXIS2_PLACEMENT_3D('',#77010,#55675,#55676);
#47269=AXIS2_PLACEMENT_3D('',#77012,#55677,#55678);
#47270=AXIS2_PLACEMENT_3D('',#77046,#55680,#55681);
#47271=AXIS2_PLACEMENT_3D('',#77051,#55682,#55683);
#47272=AXIS2_PLACEMENT_3D('',#77053,#55684,#55685);
#47273=AXIS2_PLACEMENT_3D('',#77056,#55687,#55688);
#47274=AXIS2_PLACEMENT_3D('',#77057,#55689,#55690);
#47275=AXIS2_PLACEMENT_3D('',#77059,#55691,#55692);
#47276=AXIS2_PLACEMENT_3D('',#77062,#55694,#55695);
#47277=AXIS2_PLACEMENT_3D('',#77063,#55696,#55697);
#47278=AXIS2_PLACEMENT_3D('',#77065,#55698,#55699);
#47279=AXIS2_PLACEMENT_3D('',#77068,#55701,#55702);
#47280=AXIS2_PLACEMENT_3D('',#77069,#55703,#55704);
#47281=AXIS2_PLACEMENT_3D('',#77071,#55705,#55706);
#47282=AXIS2_PLACEMENT_3D('',#77074,#55708,#55709);
#47283=AXIS2_PLACEMENT_3D('',#77075,#55710,#55711);
#47284=AXIS2_PLACEMENT_3D('',#77077,#55712,#55713);
#47285=AXIS2_PLACEMENT_3D('',#77080,#55715,#55716);
#47286=AXIS2_PLACEMENT_3D('',#77081,#55717,#55718);
#47287=AXIS2_PLACEMENT_3D('',#77083,#55719,#55720);
#47288=AXIS2_PLACEMENT_3D('',#77086,#55722,#55723);
#47289=AXIS2_PLACEMENT_3D('',#77087,#55724,#55725);
#47290=AXIS2_PLACEMENT_3D('',#77089,#55726,#55727);
#47291=AXIS2_PLACEMENT_3D('',#77092,#55729,#55730);
#47292=AXIS2_PLACEMENT_3D('',#77093,#55731,#55732);
#47293=AXIS2_PLACEMENT_3D('',#77095,#55733,#55734);
#47294=AXIS2_PLACEMENT_3D('',#77098,#55736,#55737);
#47295=AXIS2_PLACEMENT_3D('',#77099,#55738,#55739);
#47296=AXIS2_PLACEMENT_3D('',#77101,#55740,#55741);
#47297=AXIS2_PLACEMENT_3D('',#77104,#55743,#55744);
#47298=AXIS2_PLACEMENT_3D('',#77105,#55745,#55746);
#47299=AXIS2_PLACEMENT_3D('',#77107,#55747,#55748);
#47300=AXIS2_PLACEMENT_3D('',#77110,#55750,#55751);
#47301=AXIS2_PLACEMENT_3D('',#77111,#55752,#55753);
#47302=AXIS2_PLACEMENT_3D('',#77113,#55754,#55755);
#47303=AXIS2_PLACEMENT_3D('',#77116,#55757,#55758);
#47304=AXIS2_PLACEMENT_3D('',#77117,#55759,#55760);
#47305=AXIS2_PLACEMENT_3D('',#77119,#55761,#55762);
#47306=AXIS2_PLACEMENT_3D('',#77122,#55764,#55765);
#47307=AXIS2_PLACEMENT_3D('',#77123,#55766,#55767);
#47308=AXIS2_PLACEMENT_3D('',#77125,#55768,#55769);
#47309=AXIS2_PLACEMENT_3D('',#77128,#55771,#55772);
#47310=AXIS2_PLACEMENT_3D('',#77129,#55773,#55774);
#47311=AXIS2_PLACEMENT_3D('',#77131,#55775,#55776);
#47312=AXIS2_PLACEMENT_3D('',#77134,#55778,#55779);
#47313=AXIS2_PLACEMENT_3D('',#77135,#55780,#55781);
#47314=AXIS2_PLACEMENT_3D('',#77137,#55782,#55783);
#47315=AXIS2_PLACEMENT_3D('',#77140,#55785,#55786);
#47316=AXIS2_PLACEMENT_3D('',#77141,#55787,#55788);
#47317=AXIS2_PLACEMENT_3D('',#77143,#55789,#55790);
#47318=AXIS2_PLACEMENT_3D('',#77146,#55792,#55793);
#47319=AXIS2_PLACEMENT_3D('',#77147,#55794,#55795);
#47320=AXIS2_PLACEMENT_3D('',#77149,#55796,#55797);
#47321=AXIS2_PLACEMENT_3D('',#77152,#55799,#55800);
#47322=AXIS2_PLACEMENT_3D('',#77153,#55801,#55802);
#47323=AXIS2_PLACEMENT_3D('',#77155,#55803,#55804);
#47324=AXIS2_PLACEMENT_3D('',#77187,#55806,#55807);
#47325=AXIS2_PLACEMENT_3D('',#77194,#55808,#55809);
#47326=AXIS2_PLACEMENT_3D('',#77196,#55810,#55811);
#47327=AXIS2_PLACEMENT_3D('',#77199,#55813,#55814);
#47328=AXIS2_PLACEMENT_3D('',#77200,#55815,#55816);
#47329=AXIS2_PLACEMENT_3D('',#77202,#55817,#55818);
#47330=AXIS2_PLACEMENT_3D('',#77205,#55820,#55821);
#47331=AXIS2_PLACEMENT_3D('',#77206,#55822,#55823);
#47332=AXIS2_PLACEMENT_3D('',#77208,#55824,#55825);
#47333=AXIS2_PLACEMENT_3D('',#77211,#55827,#55828);
#47334=AXIS2_PLACEMENT_3D('',#77212,#55829,#55830);
#47335=AXIS2_PLACEMENT_3D('',#77214,#55831,#55832);
#47336=AXIS2_PLACEMENT_3D('',#77217,#55834,#55835);
#47337=AXIS2_PLACEMENT_3D('',#77218,#55836,#55837);
#47338=AXIS2_PLACEMENT_3D('',#77220,#55838,#55839);
#47339=AXIS2_PLACEMENT_3D('',#77223,#55841,#55842);
#47340=AXIS2_PLACEMENT_3D('',#77224,#55843,#55844);
#47341=AXIS2_PLACEMENT_3D('',#77226,#55845,#55846);
#47342=AXIS2_PLACEMENT_3D('',#77229,#55848,#55849);
#47343=AXIS2_PLACEMENT_3D('',#77230,#55850,#55851);
#47344=AXIS2_PLACEMENT_3D('',#77232,#55852,#55853);
#47345=AXIS2_PLACEMENT_3D('',#77235,#55855,#55856);
#47346=AXIS2_PLACEMENT_3D('',#77236,#55857,#55858);
#47347=AXIS2_PLACEMENT_3D('',#77238,#55859,#55860);
#47348=AXIS2_PLACEMENT_3D('',#77241,#55862,#55863);
#47349=AXIS2_PLACEMENT_3D('',#77242,#55864,#55865);
#47350=AXIS2_PLACEMENT_3D('',#77244,#55866,#55867);
#47351=AXIS2_PLACEMENT_3D('',#77247,#55869,#55870);
#47352=AXIS2_PLACEMENT_3D('',#77248,#55871,#55872);
#47353=AXIS2_PLACEMENT_3D('',#77250,#55873,#55874);
#47354=AXIS2_PLACEMENT_3D('',#77253,#55876,#55877);
#47355=AXIS2_PLACEMENT_3D('',#77254,#55878,#55879);
#47356=AXIS2_PLACEMENT_3D('',#77256,#55880,#55881);
#47357=AXIS2_PLACEMENT_3D('',#77259,#55883,#55884);
#47358=AXIS2_PLACEMENT_3D('',#77260,#55885,#55886);
#47359=AXIS2_PLACEMENT_3D('',#77262,#55887,#55888);
#47360=AXIS2_PLACEMENT_3D('',#77265,#55890,#55891);
#47361=AXIS2_PLACEMENT_3D('',#77266,#55892,#55893);
#47362=AXIS2_PLACEMENT_3D('',#77268,#55894,#55895);
#47363=AXIS2_PLACEMENT_3D('',#77271,#55897,#55898);
#47364=AXIS2_PLACEMENT_3D('',#77272,#55899,#55900);
#47365=AXIS2_PLACEMENT_3D('',#77274,#55901,#55902);
#47366=AXIS2_PLACEMENT_3D('',#77277,#55904,#55905);
#47367=AXIS2_PLACEMENT_3D('',#77278,#55906,#55907);
#47368=AXIS2_PLACEMENT_3D('',#77280,#55908,#55909);
#47369=AXIS2_PLACEMENT_3D('',#77283,#55911,#55912);
#47370=AXIS2_PLACEMENT_3D('',#77284,#55913,#55914);
#47371=AXIS2_PLACEMENT_3D('',#77286,#55915,#55916);
#47372=AXIS2_PLACEMENT_3D('',#77289,#55918,#55919);
#47373=AXIS2_PLACEMENT_3D('',#77290,#55920,#55921);
#47374=AXIS2_PLACEMENT_3D('',#77292,#55922,#55923);
#47375=AXIS2_PLACEMENT_3D('',#77295,#55925,#55926);
#47376=AXIS2_PLACEMENT_3D('',#77296,#55927,#55928);
#47377=AXIS2_PLACEMENT_3D('',#77298,#55929,#55930);
#47378=AXIS2_PLACEMENT_3D('',#77328,#55932,#55933);
#47379=AXIS2_PLACEMENT_3D('',#77337,#55934,#55935);
#47380=AXIS2_PLACEMENT_3D('',#77339,#55936,#55937);
#47381=AXIS2_PLACEMENT_3D('',#77342,#55939,#55940);
#47382=AXIS2_PLACEMENT_3D('',#77372,#55941,#55942);
#47383=AXIS2_PLACEMENT_3D('',#77373,#55943,#55944);
#47384=AXIS2_PLACEMENT_3D('',#77374,#55945,#55946);
#47385=AXIS2_PLACEMENT_3D('',#77375,#55947,#55948);
#47386=AXIS2_PLACEMENT_3D('',#77376,#55949,#55950);
#47387=AXIS2_PLACEMENT_3D('',#77377,#55951,#55952);
#47388=AXIS2_PLACEMENT_3D('',#77378,#55953,#55954);
#47389=AXIS2_PLACEMENT_3D('',#77379,#55955,#55956);
#47390=AXIS2_PLACEMENT_3D('',#77380,#55957,#55958);
#47391=AXIS2_PLACEMENT_3D('',#77381,#55959,#55960);
#47392=AXIS2_PLACEMENT_3D('',#77382,#55961,#55962);
#47393=AXIS2_PLACEMENT_3D('',#77383,#55963,#55964);
#47394=AXIS2_PLACEMENT_3D('',#77384,#55965,#55966);
#47395=AXIS2_PLACEMENT_3D('',#77385,#55967,#55968);
#47396=AXIS2_PLACEMENT_3D('',#77386,#55969,#55970);
#47397=AXIS2_PLACEMENT_3D('',#77387,#55971,#55972);
#47398=AXIS2_PLACEMENT_3D('',#77388,#55973,#55974);
#47399=AXIS2_PLACEMENT_3D('',#77389,#55975,#55976);
#47400=AXIS2_PLACEMENT_3D('',#77390,#55977,#55978);
#47401=AXIS2_PLACEMENT_3D('',#77391,#55979,#55980);
#47402=AXIS2_PLACEMENT_3D('',#77392,#55981,#55982);
#47403=AXIS2_PLACEMENT_3D('',#77393,#55983,#55984);
#47404=AXIS2_PLACEMENT_3D('',#77394,#55985,#55986);
#47405=AXIS2_PLACEMENT_3D('',#77395,#55987,#55988);
#47406=AXIS2_PLACEMENT_3D('',#77396,#55989,#55990);
#47407=AXIS2_PLACEMENT_3D('',#77397,#55991,#55992);
#47408=AXIS2_PLACEMENT_3D('',#77399,#55993,#55994);
#47409=AXIS2_PLACEMENT_3D('',#77400,#55995,#55996);
#47410=AXIS2_PLACEMENT_3D('',#77446,#55997,#55998);
#47411=AXIS2_PLACEMENT_3D('',#77449,#55999,#56000);
#47412=AXIS2_PLACEMENT_3D('',#77451,#56001,#56002);
#47413=AXIS2_PLACEMENT_3D('',#77794,#56003,#56004);
#47414=AXIS2_PLACEMENT_3D('',#77795,#56005,#56006);
#47415=AXIS2_PLACEMENT_3D('',#77798,#56007,#56008);
#47416=AXIS2_PLACEMENT_3D('',#77801,#56010,#56011);
#47417=AXIS2_PLACEMENT_3D('',#77802,#56012,#56013);
#47418=AXIS2_PLACEMENT_3D('',#77803,#56014,#56015);
#47419=AXIS2_PLACEMENT_3D('',#77805,#56016,#56017);
#47420=AXIS2_PLACEMENT_3D('',#77806,#56018,#56019);
#47421=AXIS2_PLACEMENT_3D('',#77807,#56020,#56021);
#47422=AXIS2_PLACEMENT_3D('',#77809,#56022,#56023);
#47423=AXIS2_PLACEMENT_3D('',#77811,#56024,#56025);
#47424=AXIS2_PLACEMENT_3D('',#77812,#56026,#56027);
#47425=AXIS2_PLACEMENT_3D('',#77813,#56028,#56029);
#47426=AXIS2_PLACEMENT_3D('',#77816,#56030,#56031);
#47427=AXIS2_PLACEMENT_3D('',#77829,#56032,#56033);
#47428=AXIS2_PLACEMENT_3D('',#77840,#56034,#56035);
#47429=AXIS2_PLACEMENT_3D('',#77843,#56036,#56037);
#47430=AXIS2_PLACEMENT_3D('',#77845,#56038,#56039);
#47431=AXIS2_PLACEMENT_3D('',#77847,#56040,#56041);
#47432=AXIS2_PLACEMENT_3D('',#77848,#56042,#56043);
#47433=AXIS2_PLACEMENT_3D('',#77849,#56044,#56045);
#47434=AXIS2_PLACEMENT_3D('',#77852,#56046,#56047);
#47435=AXIS2_PLACEMENT_3D('',#77854,#56048,#56049);
#47436=AXIS2_PLACEMENT_3D('',#77858,#56051,#56052);
#47437=AXIS2_PLACEMENT_3D('',#77860,#56054,#56055);
#47438=AXIS2_PLACEMENT_3D('',#77892,#56056,#56057);
#47439=AXIS2_PLACEMENT_3D('',#77893,#56058,#56059);
#47440=AXIS2_PLACEMENT_3D('',#77896,#56060,#56061);
#47441=AXIS2_PLACEMENT_3D('',#77898,#56063,#56064);
#47442=AXIS2_PLACEMENT_3D('',#77899,#56065,#56066);
#47443=AXIS2_PLACEMENT_3D('',#77901,#56067,#56068);
#47444=AXIS2_PLACEMENT_3D('',#77902,#56069,#56070);
#47445=AXIS2_PLACEMENT_3D('',#77903,#56071,#56072);
#47446=AXIS2_PLACEMENT_3D('',#77905,#56073,#56074);
#47447=AXIS2_PLACEMENT_3D('',#77942,#56076,#56077);
#47448=AXIS2_PLACEMENT_3D('',#77999,#56079,#56080);
#47449=AXIS2_PLACEMENT_3D('',#78000,#56081,#56082);
#47450=AXIS2_PLACEMENT_3D('',#78001,#56083,#56084);
#47451=AXIS2_PLACEMENT_3D('',#78042,#56089,#56090);
#47452=AXIS2_PLACEMENT_3D('',#78045,#56091,#56092);
#47453=AXIS2_PLACEMENT_3D('',#78070,#56094,#56095);
#47454=AXIS2_PLACEMENT_3D('',#78091,#56096,#56097);
#47455=AXIS2_PLACEMENT_3D('',#78092,#56098,#56099);
#47456=AXIS2_PLACEMENT_3D('',#78093,#56100,#56101);
#47457=AXIS2_PLACEMENT_3D('',#78098,#56103,#56104);
#47458=AXIS2_PLACEMENT_3D('',#78101,#56106,#56107);
#47459=AXIS2_PLACEMENT_3D('',#78103,#56109,#56110);
#47460=AXIS2_PLACEMENT_3D('',#78111,#56111,#56112);
#47461=AXIS2_PLACEMENT_3D('',#78112,#56113,#56114);
#47462=AXIS2_PLACEMENT_3D('',#78146,#56117,#56118);
#47463=AXIS2_PLACEMENT_3D('',#78151,#56120,#56121);
#47464=AXIS2_PLACEMENT_3D('',#78154,#56123,#56124);
#47465=AXIS2_PLACEMENT_3D('',#78155,#56125,#56126);
#47466=AXIS2_PLACEMENT_3D('',#78163,#56131,#56132);
#47467=AXIS2_PLACEMENT_3D('',#78167,#56134,#56135);
#47468=AXIS2_PLACEMENT_3D('',#78168,#56136,#56137);
#47469=AXIS2_PLACEMENT_3D('',#78169,#56138,#56139);
#47470=AXIS2_PLACEMENT_3D('',#78185,#56140,#56141);
#47471=AXIS2_PLACEMENT_3D('',#78189,#56143,#56144);
#47472=AXIS2_PLACEMENT_3D('',#78294,#56145,#56146);
#47473=AXIS2_PLACEMENT_3D('',#78297,#56149,#56150);
#47474=AXIS2_PLACEMENT_3D('',#78298,#56151,#56152);
#47475=AXIS2_PLACEMENT_3D('',#78299,#56153,#56154);
#47476=AXIS2_PLACEMENT_3D('',#78300,#56155,#56156);
#47477=AXIS2_PLACEMENT_3D('',#78301,#56157,#56158);
#47478=AXIS2_PLACEMENT_3D('',#78302,#56159,#56160);
#47479=AXIS2_PLACEMENT_3D('',#78303,#56161,#56162);
#47480=AXIS2_PLACEMENT_3D('',#78304,#56163,#56164);
#47481=AXIS2_PLACEMENT_3D('',#78305,#56165,#56166);
#47482=AXIS2_PLACEMENT_3D('',#78324,#56167,#56168);
#47483=AXIS2_PLACEMENT_3D('',#78325,#56169,#56170);
#47484=AXIS2_PLACEMENT_3D('',#78326,#56171,#56172);
#47485=AXIS2_PLACEMENT_3D('',#78327,#56173,#56174);
#47486=AXIS2_PLACEMENT_3D('',#78328,#56175,#56176);
#47487=AXIS2_PLACEMENT_3D('',#78329,#56177,#56178);
#47488=AXIS2_PLACEMENT_3D('',#78355,#56179,#56180);
#47489=AXIS2_PLACEMENT_3D('',#78362,#56181,#56182);
#47490=AXIS2_PLACEMENT_3D('',#78561,#56183,#56184);
#47491=AXIS2_PLACEMENT_3D('',#78903,#56185,#56186);
#47492=AXIS2_PLACEMENT_3D('',#78905,#56187,#56188);
#47493=AXIS2_PLACEMENT_3D('',#78932,#56190,#56191);
#47494=AXIS2_PLACEMENT_3D('',#78983,#56192,#56193);
#47495=AXIS2_PLACEMENT_3D('',#78985,#56194,#56195);
#47496=AXIS2_PLACEMENT_3D('',#78987,#56197,#56198);
#47497=AXIS2_PLACEMENT_3D('',#79074,#56199,#56200);
#47498=AXIS2_PLACEMENT_3D('',#79081,#56201,#56202);
#47499=AXIS2_PLACEMENT_3D('',#79202,#56203,#56204);
#47500=AXIS2_PLACEMENT_3D('',#79514,#56205,#56206);
#47501=AXIS2_PLACEMENT_3D('',#79567,#56207,#56208);
#47502=AXIS2_PLACEMENT_3D('',#79569,#56209,#56210);
#47503=AXIS2_PLACEMENT_3D('',#79586,#56211,#56212);
#47504=AXIS2_PLACEMENT_3D('',#79589,#56213,#56214);
#47505=AXIS2_PLACEMENT_3D('',#79590,#56215,#56216);
#47506=AXIS2_PLACEMENT_3D('',#79591,#56217,#56218);
#47507=AXIS2_PLACEMENT_3D('',#79618,#56219,#56220);
#47508=AXIS2_PLACEMENT_3D('',#79635,#56221,#56222);
#47509=AXIS2_PLACEMENT_3D('',#79660,#56223,#56224);
#47510=AXIS2_PLACEMENT_3D('',#79677,#56225,#56226);
#47511=AXIS2_PLACEMENT_3D('',#79680,#56227,#56228);
#47512=AXIS2_PLACEMENT_3D('',#79707,#56231,#56232);
#47513=AXIS2_PLACEMENT_3D('',#79881,#56233,#56234);
#47514=AXIS2_PLACEMENT_3D('',#79907,#56235,#56236);
#47515=AXIS2_PLACEMENT_3D('',#79924,#56237,#56238);
#47516=AXIS2_PLACEMENT_3D('',#80258,#56239,#56240);
#47517=AXIS2_PLACEMENT_3D('',#80451,#56241,#56242);
#47518=AXIS2_PLACEMENT_3D('',#81089,#56245,#56246);
#47519=AXIS2_PLACEMENT_3D('',#81336,#56247,#56248);
#47520=AXIS2_PLACEMENT_3D('',#81961,#56249,#56250);
#47521=AXIS2_PLACEMENT_3D('',#81999,#56251,#56252);
#47522=AXIS2_PLACEMENT_3D('',#82145,#56253,#56254);
#47523=AXIS2_PLACEMENT_3D('',#82146,#56255,#56256);
#47524=AXIS2_PLACEMENT_3D('',#82284,#56257,#56258);
#47525=AXIS2_PLACEMENT_3D('',#82357,#56259,#56260);
#47526=AXIS2_PLACEMENT_3D('',#82410,#56261,#56262);
#47527=AXIS2_PLACEMENT_3D('',#82411,#56263,#56264);
#47528=AXIS2_PLACEMENT_3D('',#82472,#56265,#56266);
#47529=AXIS2_PLACEMENT_3D('',#82473,#56267,#56268);
#47530=AXIS2_PLACEMENT_3D('',#82474,#56269,#56270);
#47531=AXIS2_PLACEMENT_3D('',#83489,#56271,#56272);
#47532=AXIS2_PLACEMENT_3D('',#83490,#56273,#56274);
#47533=AXIS2_PLACEMENT_3D('',#83491,#56275,#56276);
#47534=AXIS2_PLACEMENT_3D('',#83492,#56277,#56278);
#47535=AXIS2_PLACEMENT_3D('',#83691,#56279,#56280);
#47536=AXIS2_PLACEMENT_3D('',#83693,#56282,#56283);
#47537=AXIS2_PLACEMENT_3D('',#83695,#56285,#56286);
#47538=AXIS2_PLACEMENT_3D('',#83696,#56287,#56288);
#47539=AXIS2_PLACEMENT_3D('',#83697,#56289,#56290);
#47540=AXIS2_PLACEMENT_3D('',#83698,#56291,#56292);
#47541=AXIS2_PLACEMENT_3D('',#83699,#56293,#56294);
#47542=AXIS2_PLACEMENT_3D('',#83700,#56295,#56296);
#47543=AXIS2_PLACEMENT_3D('',#83701,#56297,#56298);
#47544=AXIS2_PLACEMENT_3D('',#83702,#56299,#56300);
#47545=AXIS2_PLACEMENT_3D('',#83703,#56301,#56302);
#47546=AXIS2_PLACEMENT_3D('',#83704,#56303,#56304);
#47547=AXIS2_PLACEMENT_3D('',#83705,#56305,#56306);
#47548=AXIS2_PLACEMENT_3D('',#83706,#56307,#56308);
#47549=AXIS2_PLACEMENT_3D('',#83707,#56309,#56310);
#47550=AXIS2_PLACEMENT_3D('',#83708,#56311,#56312);
#47551=AXIS2_PLACEMENT_3D('',#83709,#56313,#56314);
#47552=AXIS2_PLACEMENT_3D('',#83710,#56315,#56316);
#47553=AXIS2_PLACEMENT_3D('',#83711,#56317,#56318);
#47554=AXIS2_PLACEMENT_3D('',#83712,#56319,#56320);
#47555=AXIS2_PLACEMENT_3D('',#83713,#56321,#56322);
#47556=AXIS2_PLACEMENT_3D('',#83714,#56323,#56324);
#47557=AXIS2_PLACEMENT_3D('',#83715,#56325,#56326);
#47558=AXIS2_PLACEMENT_3D('',#83716,#56327,#56328);
#47559=AXIS2_PLACEMENT_3D('',#83717,#56329,#56330);
#47560=AXIS2_PLACEMENT_3D('',#83718,#56331,#56332);
#47561=AXIS2_PLACEMENT_3D('',#83719,#56333,#56334);
#47562=AXIS2_PLACEMENT_3D('',#83720,#56335,#56336);
#47563=AXIS2_PLACEMENT_3D('',#83721,#56337,#56338);
#47564=AXIS2_PLACEMENT_3D('',#83722,#56339,#56340);
#47565=AXIS2_PLACEMENT_3D('',#83723,#56341,#56342);
#47566=AXIS2_PLACEMENT_3D('',#83724,#56343,#56344);
#47567=AXIS2_PLACEMENT_3D('',#83725,#56345,#56346);
#47568=AXIS2_PLACEMENT_3D('',#83726,#56347,#56348);
#47569=AXIS2_PLACEMENT_3D('',#83727,#56349,#56350);
#47570=AXIS2_PLACEMENT_3D('',#83728,#56351,#56352);
#47571=AXIS2_PLACEMENT_3D('',#83729,#56353,#56354);
#47572=AXIS2_PLACEMENT_3D('',#83730,#56355,#56356);
#47573=AXIS2_PLACEMENT_3D('',#83731,#56357,#56358);
#47574=AXIS2_PLACEMENT_3D('',#83732,#56359,#56360);
#47575=AXIS2_PLACEMENT_3D('',#83733,#56361,#56362);
#47576=AXIS2_PLACEMENT_3D('',#83734,#56363,#56364);
#47577=AXIS2_PLACEMENT_3D('',#83735,#56365,#56366);
#47578=AXIS2_PLACEMENT_3D('',#83736,#56367,#56368);
#47579=AXIS2_PLACEMENT_3D('',#83737,#56369,#56370);
#47580=AXIS2_PLACEMENT_3D('',#83738,#56371,#56372);
#47581=AXIS2_PLACEMENT_3D('',#83739,#56373,#56374);
#47582=AXIS2_PLACEMENT_3D('',#83740,#56375,#56376);
#47583=AXIS2_PLACEMENT_3D('',#83741,#56377,#56378);
#47584=AXIS2_PLACEMENT_3D('',#83742,#56379,#56380);
#47585=AXIS2_PLACEMENT_3D('',#83743,#56381,#56382);
#47586=AXIS2_PLACEMENT_3D('',#83744,#56383,#56384);
#47587=AXIS2_PLACEMENT_3D('',#83745,#56385,#56386);
#47588=AXIS2_PLACEMENT_3D('',#83746,#56387,#56388);
#47589=AXIS2_PLACEMENT_3D('',#83747,#56389,#56390);
#47590=AXIS2_PLACEMENT_3D('',#83748,#56391,#56392);
#47591=AXIS2_PLACEMENT_3D('',#83749,#56393,#56394);
#47592=AXIS2_PLACEMENT_3D('',#83750,#56395,#56396);
#47593=AXIS2_PLACEMENT_3D('',#83751,#56397,#56398);
#47594=AXIS2_PLACEMENT_3D('',#83752,#56399,#56400);
#47595=AXIS2_PLACEMENT_3D('',#83753,#56401,#56402);
#47596=AXIS2_PLACEMENT_3D('',#83754,#56403,#56404);
#47597=AXIS2_PLACEMENT_3D('',#83755,#56405,#56406);
#47598=AXIS2_PLACEMENT_3D('',#83756,#56407,#56408);
#47599=AXIS2_PLACEMENT_3D('',#83757,#56409,#56410);
#47600=AXIS2_PLACEMENT_3D('',#83758,#56411,#56412);
#47601=AXIS2_PLACEMENT_3D('',#83759,#56413,#56414);
#47602=AXIS2_PLACEMENT_3D('',#83760,#56415,#56416);
#47603=AXIS2_PLACEMENT_3D('',#83761,#56417,#56418);
#47604=AXIS2_PLACEMENT_3D('',#83762,#56419,#56420);
#47605=AXIS2_PLACEMENT_3D('',#83763,#56421,#56422);
#47606=AXIS2_PLACEMENT_3D('',#83764,#56423,#56424);
#47607=AXIS2_PLACEMENT_3D('',#83765,#56425,#56426);
#47608=AXIS2_PLACEMENT_3D('',#83766,#56427,#56428);
#47609=AXIS2_PLACEMENT_3D('',#83767,#56429,#56430);
#47610=AXIS2_PLACEMENT_3D('',#83768,#56431,#56432);
#47611=AXIS2_PLACEMENT_3D('',#83769,#56433,#56434);
#47612=AXIS2_PLACEMENT_3D('',#83770,#56435,#56436);
#47613=AXIS2_PLACEMENT_3D('',#83771,#56437,#56438);
#47614=AXIS2_PLACEMENT_3D('',#83772,#56439,#56440);
#47615=AXIS2_PLACEMENT_3D('',#83773,#56441,#56442);
#47616=AXIS2_PLACEMENT_3D('',#83774,#56443,#56444);
#47617=AXIS2_PLACEMENT_3D('',#83775,#56445,#56446);
#47618=AXIS2_PLACEMENT_3D('',#83776,#56447,#56448);
#47619=AXIS2_PLACEMENT_3D('',#83777,#56449,#56450);
#47620=AXIS2_PLACEMENT_3D('',#83778,#56451,#56452);
#47621=AXIS2_PLACEMENT_3D('',#83779,#56453,#56454);
#47622=AXIS2_PLACEMENT_3D('',#83780,#56455,#56456);
#47623=AXIS2_PLACEMENT_3D('',#83781,#56457,#56458);
#47624=AXIS2_PLACEMENT_3D('',#83782,#56459,#56460);
#47625=AXIS2_PLACEMENT_3D('',#83783,#56461,#56462);
#47626=AXIS2_PLACEMENT_3D('',#83784,#56463,#56464);
#47627=AXIS2_PLACEMENT_3D('',#83785,#56465,#56466);
#47628=AXIS2_PLACEMENT_3D('',#83786,#56467,#56468);
#47629=AXIS2_PLACEMENT_3D('',#83787,#56469,#56470);
#47630=AXIS2_PLACEMENT_3D('',#83788,#56471,#56472);
#47631=AXIS2_PLACEMENT_3D('',#83789,#56473,#56474);
#47632=AXIS2_PLACEMENT_3D('',#83790,#56475,#56476);
#47633=AXIS2_PLACEMENT_3D('',#83791,#56477,#56478);
#47634=AXIS2_PLACEMENT_3D('',#83792,#56479,#56480);
#47635=AXIS2_PLACEMENT_3D('',#83793,#56481,#56482);
#47636=AXIS2_PLACEMENT_3D('',#83794,#56483,#56484);
#47637=AXIS2_PLACEMENT_3D('',#83795,#56485,#56486);
#47638=AXIS2_PLACEMENT_3D('',#83796,#56487,#56488);
#47639=AXIS2_PLACEMENT_3D('',#83797,#56489,#56490);
#47640=AXIS2_PLACEMENT_3D('',#83798,#56491,#56492);
#47641=AXIS2_PLACEMENT_3D('',#83799,#56493,#56494);
#47642=AXIS2_PLACEMENT_3D('',#83800,#56495,#56496);
#47643=AXIS2_PLACEMENT_3D('',#83801,#56497,#56498);
#47644=AXIS2_PLACEMENT_3D('',#83802,#56499,#56500);
#47645=AXIS2_PLACEMENT_3D('',#83803,#56501,#56502);
#47646=AXIS2_PLACEMENT_3D('',#83804,#56503,#56504);
#47647=AXIS2_PLACEMENT_3D('',#83805,#56505,#56506);
#47648=AXIS2_PLACEMENT_3D('',#83806,#56507,#56508);
#47649=AXIS2_PLACEMENT_3D('',#83807,#56509,#56510);
#47650=AXIS2_PLACEMENT_3D('',#83808,#56511,#56512);
#47651=AXIS2_PLACEMENT_3D('',#83809,#56513,#56514);
#47652=AXIS2_PLACEMENT_3D('',#83810,#56515,#56516);
#47653=AXIS2_PLACEMENT_3D('',#83811,#56517,#56518);
#47654=AXIS2_PLACEMENT_3D('',#83812,#56519,#56520);
#47655=AXIS2_PLACEMENT_3D('',#83813,#56521,#56522);
#47656=AXIS2_PLACEMENT_3D('',#83814,#56523,#56524);
#47657=AXIS2_PLACEMENT_3D('',#83815,#56525,#56526);
#47658=AXIS2_PLACEMENT_3D('',#83816,#56527,#56528);
#47659=AXIS2_PLACEMENT_3D('',#83817,#56529,#56530);
#47660=AXIS2_PLACEMENT_3D('',#83818,#56531,#56532);
#47661=AXIS2_PLACEMENT_3D('',#83819,#56533,#56534);
#47662=AXIS2_PLACEMENT_3D('',#83820,#56535,#56536);
#47663=AXIS2_PLACEMENT_3D('',#83821,#56537,#56538);
#47664=AXIS2_PLACEMENT_3D('',#83822,#56539,#56540);
#47665=AXIS2_PLACEMENT_3D('',#83823,#56541,#56542);
#47666=AXIS2_PLACEMENT_3D('',#83824,#56543,#56544);
#47667=AXIS2_PLACEMENT_3D('',#83825,#56545,#56546);
#47668=AXIS2_PLACEMENT_3D('',#83826,#56547,#56548);
#47669=AXIS2_PLACEMENT_3D('',#83827,#56549,#56550);
#47670=AXIS2_PLACEMENT_3D('',#83828,#56551,#56552);
#47671=AXIS2_PLACEMENT_3D('',#83829,#56553,#56554);
#47672=AXIS2_PLACEMENT_3D('',#83830,#56555,#56556);
#47673=AXIS2_PLACEMENT_3D('',#83831,#56557,#56558);
#47674=AXIS2_PLACEMENT_3D('',#83832,#56559,#56560);
#47675=AXIS2_PLACEMENT_3D('',#83833,#56561,#56562);
#47676=AXIS2_PLACEMENT_3D('',#83834,#56563,#56564);
#47677=AXIS2_PLACEMENT_3D('',#83835,#56565,#56566);
#47678=AXIS2_PLACEMENT_3D('',#83836,#56567,#56568);
#47679=AXIS2_PLACEMENT_3D('',#83837,#56569,#56570);
#47680=AXIS2_PLACEMENT_3D('',#83838,#56571,#56572);
#47681=AXIS2_PLACEMENT_3D('',#83839,#56573,#56574);
#47682=AXIS2_PLACEMENT_3D('',#83840,#56575,#56576);
#47683=AXIS2_PLACEMENT_3D('',#83841,#56577,#56578);
#47684=AXIS2_PLACEMENT_3D('',#83842,#56579,#56580);
#47685=AXIS2_PLACEMENT_3D('',#83843,#56581,#56582);
#47686=AXIS2_PLACEMENT_3D('',#83844,#56583,#56584);
#47687=AXIS2_PLACEMENT_3D('',#83845,#56585,#56586);
#47688=AXIS2_PLACEMENT_3D('',#83846,#56587,#56588);
#47689=AXIS2_PLACEMENT_3D('',#83847,#56589,#56590);
#47690=AXIS2_PLACEMENT_3D('',#83848,#56591,#56592);
#47691=AXIS2_PLACEMENT_3D('',#83849,#56593,#56594);
#47692=AXIS2_PLACEMENT_3D('',#83850,#56595,#56596);
#47693=AXIS2_PLACEMENT_3D('',#83851,#56597,#56598);
#47694=AXIS2_PLACEMENT_3D('',#83852,#56599,#56600);
#47695=AXIS2_PLACEMENT_3D('',#83853,#56601,#56602);
#47696=AXIS2_PLACEMENT_3D('',#83854,#56603,#56604);
#47697=AXIS2_PLACEMENT_3D('',#83855,#56605,#56606);
#47698=AXIS2_PLACEMENT_3D('',#83856,#56607,#56608);
#47699=AXIS2_PLACEMENT_3D('',#83857,#56609,#56610);
#47700=AXIS2_PLACEMENT_3D('',#83858,#56611,#56612);
#47701=AXIS2_PLACEMENT_3D('',#83859,#56613,#56614);
#47702=AXIS2_PLACEMENT_3D('',#83860,#56615,#56616);
#47703=AXIS2_PLACEMENT_3D('',#83861,#56617,#56618);
#47704=AXIS2_PLACEMENT_3D('',#83862,#56619,#56620);
#47705=AXIS2_PLACEMENT_3D('',#83863,#56621,#56622);
#47706=AXIS2_PLACEMENT_3D('',#83864,#56623,#56624);
#47707=AXIS2_PLACEMENT_3D('',#83865,#56625,#56626);
#47708=AXIS2_PLACEMENT_3D('',#83866,#56627,#56628);
#47709=AXIS2_PLACEMENT_3D('',#83867,#56629,#56630);
#47710=AXIS2_PLACEMENT_3D('',#83868,#56631,#56632);
#47711=AXIS2_PLACEMENT_3D('',#83869,#56633,#56634);
#47712=AXIS2_PLACEMENT_3D('',#83870,#56635,#56636);
#47713=AXIS2_PLACEMENT_3D('',#83871,#56637,#56638);
#47714=AXIS2_PLACEMENT_3D('',#83872,#56639,#56640);
#47715=AXIS2_PLACEMENT_3D('',#83873,#56641,#56642);
#47716=AXIS2_PLACEMENT_3D('',#83874,#56643,#56644);
#47717=AXIS2_PLACEMENT_3D('',#83875,#56645,#56646);
#47718=AXIS2_PLACEMENT_3D('',#83876,#56647,#56648);
#47719=AXIS2_PLACEMENT_3D('',#83877,#56649,#56650);
#47720=AXIS2_PLACEMENT_3D('',#83878,#56651,#56652);
#47721=AXIS2_PLACEMENT_3D('',#83879,#56653,#56654);
#47722=AXIS2_PLACEMENT_3D('',#83880,#56655,#56656);
#47723=AXIS2_PLACEMENT_3D('',#83881,#56657,#56658);
#47724=AXIS2_PLACEMENT_3D('',#83882,#56659,#56660);
#47725=AXIS2_PLACEMENT_3D('',#83883,#56661,#56662);
#47726=AXIS2_PLACEMENT_3D('',#83884,#56663,#56664);
#47727=AXIS2_PLACEMENT_3D('',#83885,#56665,#56666);
#47728=AXIS2_PLACEMENT_3D('',#83886,#56667,#56668);
#47729=AXIS2_PLACEMENT_3D('',#83887,#56669,#56670);
#47730=AXIS2_PLACEMENT_3D('',#83888,#56671,#56672);
#47731=AXIS2_PLACEMENT_3D('',#83889,#56673,#56674);
#47732=AXIS2_PLACEMENT_3D('',#83890,#56675,#56676);
#47733=AXIS2_PLACEMENT_3D('',#83891,#56677,#56678);
#47734=AXIS2_PLACEMENT_3D('',#83892,#56679,#56680);
#47735=AXIS2_PLACEMENT_3D('',#83893,#56681,#56682);
#47736=AXIS2_PLACEMENT_3D('',#83894,#56683,#56684);
#47737=AXIS2_PLACEMENT_3D('',#83895,#56685,#56686);
#47738=AXIS2_PLACEMENT_3D('',#83896,#56687,#56688);
#47739=AXIS2_PLACEMENT_3D('',#83897,#56689,#56690);
#47740=AXIS2_PLACEMENT_3D('',#83898,#56691,#56692);
#47741=AXIS2_PLACEMENT_3D('',#83899,#56693,#56694);
#47742=AXIS2_PLACEMENT_3D('',#83900,#56695,#56696);
#47743=AXIS2_PLACEMENT_3D('',#83901,#56697,#56698);
#47744=AXIS2_PLACEMENT_3D('',#83902,#56699,#56700);
#47745=AXIS2_PLACEMENT_3D('',#83903,#56701,#56702);
#47746=AXIS2_PLACEMENT_3D('',#83904,#56703,#56704);
#47747=AXIS2_PLACEMENT_3D('',#83905,#56705,#56706);
#47748=AXIS2_PLACEMENT_3D('',#83906,#56707,#56708);
#47749=AXIS2_PLACEMENT_3D('',#83907,#56709,#56710);
#47750=AXIS2_PLACEMENT_3D('',#83908,#56711,#56712);
#47751=AXIS2_PLACEMENT_3D('',#83909,#56713,#56714);
#47752=AXIS2_PLACEMENT_3D('',#83910,#56715,#56716);
#47753=AXIS2_PLACEMENT_3D('',#83911,#56717,#56718);
#47754=AXIS2_PLACEMENT_3D('',#83912,#56719,#56720);
#47755=AXIS2_PLACEMENT_3D('',#83913,#56721,#56722);
#47756=AXIS2_PLACEMENT_3D('',#83914,#56723,#56724);
#47757=AXIS2_PLACEMENT_3D('',#83915,#56725,#56726);
#47758=AXIS2_PLACEMENT_3D('',#83916,#56727,#56728);
#47759=AXIS2_PLACEMENT_3D('',#83917,#56729,#56730);
#47760=AXIS2_PLACEMENT_3D('',#83918,#56731,#56732);
#47761=AXIS2_PLACEMENT_3D('',#83919,#56733,#56734);
#47762=AXIS2_PLACEMENT_3D('',#83920,#56735,#56736);
#47763=AXIS2_PLACEMENT_3D('',#83921,#56737,#56738);
#47764=AXIS2_PLACEMENT_3D('',#83922,#56739,#56740);
#47765=AXIS2_PLACEMENT_3D('',#83923,#56741,#56742);
#47766=AXIS2_PLACEMENT_3D('',#83924,#56743,#56744);
#47767=AXIS2_PLACEMENT_3D('',#83925,#56745,#56746);
#47768=AXIS2_PLACEMENT_3D('',#83926,#56747,#56748);
#47769=AXIS2_PLACEMENT_3D('',#83927,#56749,#56750);
#47770=AXIS2_PLACEMENT_3D('',#83928,#56751,#56752);
#47771=AXIS2_PLACEMENT_3D('',#83929,#56753,#56754);
#47772=AXIS2_PLACEMENT_3D('',#83930,#56755,#56756);
#47773=AXIS2_PLACEMENT_3D('',#83931,#56757,#56758);
#47774=AXIS2_PLACEMENT_3D('',#83932,#56759,#56760);
#47775=AXIS2_PLACEMENT_3D('',#83933,#56761,#56762);
#47776=AXIS2_PLACEMENT_3D('',#83934,#56763,#56764);
#47777=AXIS2_PLACEMENT_3D('',#83935,#56765,#56766);
#47778=AXIS2_PLACEMENT_3D('',#83936,#56767,#56768);
#47779=AXIS2_PLACEMENT_3D('',#83937,#56769,#56770);
#47780=AXIS2_PLACEMENT_3D('',#83938,#56771,#56772);
#47781=AXIS2_PLACEMENT_3D('',#83939,#56773,#56774);
#47782=AXIS2_PLACEMENT_3D('',#83940,#56775,#56776);
#47783=AXIS2_PLACEMENT_3D('',#83941,#56777,#56778);
#47784=AXIS2_PLACEMENT_3D('',#83942,#56779,#56780);
#47785=AXIS2_PLACEMENT_3D('',#83943,#56781,#56782);
#47786=AXIS2_PLACEMENT_3D('',#83944,#56783,#56784);
#47787=AXIS2_PLACEMENT_3D('',#83945,#56785,#56786);
#47788=AXIS2_PLACEMENT_3D('',#83946,#56787,#56788);
#47789=AXIS2_PLACEMENT_3D('',#83947,#56789,#56790);
#47790=AXIS2_PLACEMENT_3D('',#83948,#56791,#56792);
#47791=AXIS2_PLACEMENT_3D('',#83949,#56793,#56794);
#47792=AXIS2_PLACEMENT_3D('',#83950,#56795,#56796);
#47793=AXIS2_PLACEMENT_3D('',#83951,#56797,#56798);
#47794=AXIS2_PLACEMENT_3D('',#83952,#56799,#56800);
#47795=AXIS2_PLACEMENT_3D('',#83953,#56801,#56802);
#47796=AXIS2_PLACEMENT_3D('',#83954,#56803,#56804);
#47797=AXIS2_PLACEMENT_3D('',#83955,#56805,#56806);
#47798=AXIS2_PLACEMENT_3D('',#83956,#56807,#56808);
#47799=AXIS2_PLACEMENT_3D('',#83957,#56809,#56810);
#47800=AXIS2_PLACEMENT_3D('',#83958,#56811,#56812);
#47801=AXIS2_PLACEMENT_3D('',#83959,#56813,#56814);
#47802=AXIS2_PLACEMENT_3D('',#83960,#56815,#56816);
#47803=AXIS2_PLACEMENT_3D('',#83961,#56817,#56818);
#47804=AXIS2_PLACEMENT_3D('',#83962,#56819,#56820);
#47805=AXIS2_PLACEMENT_3D('',#83963,#56821,#56822);
#47806=AXIS2_PLACEMENT_3D('',#83964,#56823,#56824);
#47807=AXIS2_PLACEMENT_3D('',#83965,#56825,#56826);
#47808=AXIS2_PLACEMENT_3D('',#83966,#56827,#56828);
#47809=AXIS2_PLACEMENT_3D('',#83967,#56829,#56830);
#47810=AXIS2_PLACEMENT_3D('',#83968,#56831,#56832);
#47811=AXIS2_PLACEMENT_3D('',#83969,#56833,#56834);
#47812=AXIS2_PLACEMENT_3D('',#83970,#56835,#56836);
#47813=AXIS2_PLACEMENT_3D('',#83971,#56837,#56838);
#47814=AXIS2_PLACEMENT_3D('',#83972,#56839,#56840);
#47815=AXIS2_PLACEMENT_3D('',#83973,#56841,#56842);
#47816=AXIS2_PLACEMENT_3D('',#83974,#56843,#56844);
#47817=AXIS2_PLACEMENT_3D('',#83975,#56845,#56846);
#47818=AXIS2_PLACEMENT_3D('',#83976,#56847,#56848);
#47819=AXIS2_PLACEMENT_3D('',#83977,#56849,#56850);
#47820=AXIS2_PLACEMENT_3D('',#83978,#56851,#56852);
#47821=AXIS2_PLACEMENT_3D('',#83979,#56853,#56854);
#47822=AXIS2_PLACEMENT_3D('',#83980,#56855,#56856);
#47823=AXIS2_PLACEMENT_3D('',#83981,#56857,#56858);
#47824=AXIS2_PLACEMENT_3D('',#83982,#56859,#56860);
#47825=AXIS2_PLACEMENT_3D('',#83983,#56861,#56862);
#47826=AXIS2_PLACEMENT_3D('',#83984,#56863,#56864);
#47827=AXIS2_PLACEMENT_3D('',#83985,#56865,#56866);
#47828=AXIS2_PLACEMENT_3D('',#83986,#56867,#56868);
#47829=AXIS2_PLACEMENT_3D('',#83987,#56869,#56870);
#47830=AXIS2_PLACEMENT_3D('',#83988,#56871,#56872);
#47831=AXIS2_PLACEMENT_3D('',#83989,#56873,#56874);
#47832=AXIS2_PLACEMENT_3D('',#83990,#56875,#56876);
#47833=AXIS2_PLACEMENT_3D('',#83991,#56877,#56878);
#47834=AXIS2_PLACEMENT_3D('',#83992,#56879,#56880);
#47835=AXIS2_PLACEMENT_3D('',#83993,#56881,#56882);
#47836=AXIS2_PLACEMENT_3D('',#83994,#56883,#56884);
#47837=AXIS2_PLACEMENT_3D('',#83995,#56885,#56886);
#47838=AXIS2_PLACEMENT_3D('',#83996,#56887,#56888);
#47839=AXIS2_PLACEMENT_3D('',#83997,#56889,#56890);
#47840=AXIS2_PLACEMENT_3D('',#83998,#56891,#56892);
#47841=AXIS2_PLACEMENT_3D('',#83999,#56893,#56894);
#47842=AXIS2_PLACEMENT_3D('',#84000,#56895,#56896);
#47843=AXIS2_PLACEMENT_3D('',#84001,#56897,#56898);
#47844=AXIS2_PLACEMENT_3D('',#84002,#56899,#56900);
#47845=AXIS2_PLACEMENT_3D('',#84003,#56901,#56902);
#47846=AXIS2_PLACEMENT_3D('',#84004,#56903,#56904);
#47847=AXIS2_PLACEMENT_3D('',#84005,#56905,#56906);
#47848=AXIS2_PLACEMENT_3D('',#84006,#56907,#56908);
#47849=AXIS2_PLACEMENT_3D('',#84007,#56909,#56910);
#47850=AXIS2_PLACEMENT_3D('',#84008,#56911,#56912);
#47851=AXIS2_PLACEMENT_3D('',#84009,#56913,#56914);
#47852=AXIS2_PLACEMENT_3D('',#84010,#56915,#56916);
#47853=AXIS2_PLACEMENT_3D('',#84011,#56917,#56918);
#47854=AXIS2_PLACEMENT_3D('',#84012,#56919,#56920);
#47855=AXIS2_PLACEMENT_3D('',#84013,#56921,#56922);
#47856=AXIS2_PLACEMENT_3D('',#84014,#56923,#56924);
#47857=AXIS2_PLACEMENT_3D('',#84015,#56925,#56926);
#47858=AXIS2_PLACEMENT_3D('',#84016,#56927,#56928);
#47859=AXIS2_PLACEMENT_3D('',#84017,#56929,#56930);
#47860=AXIS2_PLACEMENT_3D('',#84018,#56931,#56932);
#47861=AXIS2_PLACEMENT_3D('',#84019,#56933,#56934);
#47862=AXIS2_PLACEMENT_3D('',#84020,#56935,#56936);
#47863=AXIS2_PLACEMENT_3D('',#84021,#56937,#56938);
#47864=AXIS2_PLACEMENT_3D('',#84022,#56939,#56940);
#47865=AXIS2_PLACEMENT_3D('',#84023,#56941,#56942);
#47866=AXIS2_PLACEMENT_3D('',#84024,#56943,#56944);
#47867=AXIS2_PLACEMENT_3D('',#84025,#56945,#56946);
#47868=AXIS2_PLACEMENT_3D('',#84026,#56947,#56948);
#47869=AXIS2_PLACEMENT_3D('',#84027,#56949,#56950);
#47870=AXIS2_PLACEMENT_3D('',#84028,#56951,#56952);
#47871=AXIS2_PLACEMENT_3D('',#84029,#56953,#56954);
#47872=AXIS2_PLACEMENT_3D('',#84030,#56955,#56956);
#47873=AXIS2_PLACEMENT_3D('',#84031,#56957,#56958);
#47874=AXIS2_PLACEMENT_3D('',#84032,#56959,#56960);
#47875=AXIS2_PLACEMENT_3D('',#84033,#56961,#56962);
#47876=AXIS2_PLACEMENT_3D('',#84034,#56963,#56964);
#47877=AXIS2_PLACEMENT_3D('',#84035,#56965,#56966);
#47878=AXIS2_PLACEMENT_3D('',#84036,#56967,#56968);
#47879=AXIS2_PLACEMENT_3D('',#84037,#56969,#56970);
#47880=AXIS2_PLACEMENT_3D('',#84038,#56971,#56972);
#47881=AXIS2_PLACEMENT_3D('',#84039,#56973,#56974);
#47882=AXIS2_PLACEMENT_3D('',#84040,#56975,#56976);
#47883=AXIS2_PLACEMENT_3D('',#84041,#56977,#56978);
#47884=AXIS2_PLACEMENT_3D('',#84042,#56979,#56980);
#47885=AXIS2_PLACEMENT_3D('',#84043,#56981,#56982);
#47886=AXIS2_PLACEMENT_3D('',#84044,#56983,#56984);
#47887=AXIS2_PLACEMENT_3D('',#84045,#56985,#56986);
#47888=AXIS2_PLACEMENT_3D('',#84046,#56987,#56988);
#47889=AXIS2_PLACEMENT_3D('',#84047,#56989,#56990);
#47890=AXIS2_PLACEMENT_3D('',#84048,#56991,#56992);
#47891=AXIS2_PLACEMENT_3D('',#84049,#56993,#56994);
#47892=AXIS2_PLACEMENT_3D('',#84050,#56995,#56996);
#47893=AXIS2_PLACEMENT_3D('',#84051,#56997,#56998);
#47894=AXIS2_PLACEMENT_3D('',#84052,#56999,#57000);
#47895=AXIS2_PLACEMENT_3D('',#84053,#57001,#57002);
#47896=AXIS2_PLACEMENT_3D('',#84054,#57003,#57004);
#47897=AXIS2_PLACEMENT_3D('',#84055,#57005,#57006);
#47898=AXIS2_PLACEMENT_3D('',#84056,#57007,#57008);
#47899=AXIS2_PLACEMENT_3D('',#84057,#57009,#57010);
#47900=AXIS2_PLACEMENT_3D('',#84058,#57011,#57012);
#47901=AXIS2_PLACEMENT_3D('',#84059,#57013,#57014);
#47902=AXIS2_PLACEMENT_3D('',#84060,#57015,#57016);
#47903=AXIS2_PLACEMENT_3D('',#84061,#57017,#57018);
#47904=AXIS2_PLACEMENT_3D('',#84062,#57019,#57020);
#47905=AXIS2_PLACEMENT_3D('',#84063,#57021,#57022);
#47906=AXIS2_PLACEMENT_3D('',#84064,#57023,#57024);
#47907=AXIS2_PLACEMENT_3D('',#84065,#57025,#57026);
#47908=AXIS2_PLACEMENT_3D('',#84066,#57027,#57028);
#47909=AXIS2_PLACEMENT_3D('',#84067,#57029,#57030);
#47910=AXIS2_PLACEMENT_3D('',#84068,#57031,#57032);
#47911=AXIS2_PLACEMENT_3D('',#84069,#57033,#57034);
#47912=AXIS2_PLACEMENT_3D('',#84070,#57035,#57036);
#47913=AXIS2_PLACEMENT_3D('',#84071,#57037,#57038);
#47914=AXIS2_PLACEMENT_3D('',#84072,#57039,#57040);
#47915=AXIS2_PLACEMENT_3D('',#84073,#57041,#57042);
#47916=AXIS2_PLACEMENT_3D('',#84074,#57043,#57044);
#47917=AXIS2_PLACEMENT_3D('',#84075,#57045,#57046);
#47918=AXIS2_PLACEMENT_3D('',#84076,#57047,#57048);
#47919=AXIS2_PLACEMENT_3D('',#84077,#57049,#57050);
#47920=AXIS2_PLACEMENT_3D('',#84078,#57051,#57052);
#47921=AXIS2_PLACEMENT_3D('',#84079,#57053,#57054);
#47922=AXIS2_PLACEMENT_3D('',#84080,#57055,#57056);
#47923=AXIS2_PLACEMENT_3D('',#84081,#57057,#57058);
#47924=AXIS2_PLACEMENT_3D('',#84082,#57059,#57060);
#47925=AXIS2_PLACEMENT_3D('',#84083,#57061,#57062);
#47926=AXIS2_PLACEMENT_3D('',#84084,#57063,#57064);
#47927=AXIS2_PLACEMENT_3D('',#84085,#57065,#57066);
#47928=AXIS2_PLACEMENT_3D('',#84086,#57067,#57068);
#47929=AXIS2_PLACEMENT_3D('',#84087,#57069,#57070);
#47930=AXIS2_PLACEMENT_3D('',#84088,#57071,#57072);
#47931=AXIS2_PLACEMENT_3D('',#84089,#57073,#57074);
#47932=AXIS2_PLACEMENT_3D('',#84090,#57075,#57076);
#47933=AXIS2_PLACEMENT_3D('',#84091,#57077,#57078);
#47934=AXIS2_PLACEMENT_3D('',#84092,#57079,#57080);
#47935=AXIS2_PLACEMENT_3D('',#84093,#57081,#57082);
#47936=AXIS2_PLACEMENT_3D('',#84094,#57083,#57084);
#47937=AXIS2_PLACEMENT_3D('',#84095,#57085,#57086);
#47938=AXIS2_PLACEMENT_3D('',#84096,#57087,#57088);
#47939=AXIS2_PLACEMENT_3D('',#84097,#57089,#57090);
#47940=AXIS2_PLACEMENT_3D('',#84098,#57091,#57092);
#47941=AXIS2_PLACEMENT_3D('',#84099,#57093,#57094);
#47942=AXIS2_PLACEMENT_3D('',#84100,#57095,#57096);
#47943=AXIS2_PLACEMENT_3D('',#84101,#57097,#57098);
#47944=AXIS2_PLACEMENT_3D('',#84102,#57099,#57100);
#47945=AXIS2_PLACEMENT_3D('',#84103,#57101,#57102);
#47946=AXIS2_PLACEMENT_3D('',#84104,#57103,#57104);
#47947=AXIS2_PLACEMENT_3D('',#84105,#57105,#57106);
#47948=AXIS2_PLACEMENT_3D('',#84106,#57107,#57108);
#47949=AXIS2_PLACEMENT_3D('',#84107,#57109,#57110);
#47950=AXIS2_PLACEMENT_3D('',#84108,#57111,#57112);
#47951=AXIS2_PLACEMENT_3D('',#84109,#57113,#57114);
#47952=AXIS2_PLACEMENT_3D('',#84110,#57115,#57116);
#47953=AXIS2_PLACEMENT_3D('',#84111,#57117,#57118);
#47954=AXIS2_PLACEMENT_3D('',#84112,#57119,#57120);
#47955=AXIS2_PLACEMENT_3D('',#84113,#57121,#57122);
#47956=AXIS2_PLACEMENT_3D('',#84114,#57123,#57124);
#47957=AXIS2_PLACEMENT_3D('',#84115,#57125,#57126);
#47958=AXIS2_PLACEMENT_3D('',#84116,#57127,#57128);
#47959=AXIS2_PLACEMENT_3D('',#84117,#57129,#57130);
#47960=AXIS2_PLACEMENT_3D('',#84118,#57131,#57132);
#47961=AXIS2_PLACEMENT_3D('',#84119,#57133,#57134);
#47962=AXIS2_PLACEMENT_3D('',#84120,#57135,#57136);
#47963=AXIS2_PLACEMENT_3D('',#84121,#57137,#57138);
#47964=AXIS2_PLACEMENT_3D('',#84122,#57139,#57140);
#47965=AXIS2_PLACEMENT_3D('',#84123,#57141,#57142);
#47966=AXIS2_PLACEMENT_3D('',#84124,#57143,#57144);
#47967=AXIS2_PLACEMENT_3D('',#84125,#57145,#57146);
#47968=AXIS2_PLACEMENT_3D('',#84126,#57147,#57148);
#47969=AXIS2_PLACEMENT_3D('',#84127,#57149,#57150);
#47970=AXIS2_PLACEMENT_3D('',#84128,#57151,#57152);
#47971=AXIS2_PLACEMENT_3D('',#84129,#57153,#57154);
#47972=AXIS2_PLACEMENT_3D('',#84130,#57155,#57156);
#47973=AXIS2_PLACEMENT_3D('',#84131,#57157,#57158);
#47974=AXIS2_PLACEMENT_3D('',#84132,#57159,#57160);
#47975=AXIS2_PLACEMENT_3D('',#84133,#57161,#57162);
#47976=AXIS2_PLACEMENT_3D('',#84134,#57163,#57164);
#47977=AXIS2_PLACEMENT_3D('',#84135,#57165,#57166);
#47978=AXIS2_PLACEMENT_3D('',#84136,#57167,#57168);
#47979=AXIS2_PLACEMENT_3D('',#84137,#57169,#57170);
#47980=AXIS2_PLACEMENT_3D('',#84138,#57171,#57172);
#47981=AXIS2_PLACEMENT_3D('',#84139,#57173,#57174);
#47982=AXIS2_PLACEMENT_3D('',#84140,#57175,#57176);
#47983=AXIS2_PLACEMENT_3D('',#84141,#57177,#57178);
#47984=AXIS2_PLACEMENT_3D('',#84142,#57179,#57180);
#47985=AXIS2_PLACEMENT_3D('',#84143,#57181,#57182);
#47986=AXIS2_PLACEMENT_3D('',#84144,#57183,#57184);
#47987=AXIS2_PLACEMENT_3D('',#84145,#57185,#57186);
#47988=AXIS2_PLACEMENT_3D('',#84146,#57187,#57188);
#47989=AXIS2_PLACEMENT_3D('',#84147,#57189,#57190);
#47990=AXIS2_PLACEMENT_3D('',#84148,#57191,#57192);
#47991=AXIS2_PLACEMENT_3D('',#84149,#57193,#57194);
#47992=AXIS2_PLACEMENT_3D('',#84150,#57195,#57196);
#47993=AXIS2_PLACEMENT_3D('',#84151,#57197,#57198);
#47994=AXIS2_PLACEMENT_3D('',#84152,#57199,#57200);
#47995=AXIS2_PLACEMENT_3D('',#84153,#57201,#57202);
#47996=AXIS2_PLACEMENT_3D('',#84154,#57203,#57204);
#47997=AXIS2_PLACEMENT_3D('',#84155,#57205,#57206);
#47998=AXIS2_PLACEMENT_3D('',#84156,#57207,#57208);
#47999=AXIS2_PLACEMENT_3D('',#84157,#57209,#57210);
#48000=AXIS2_PLACEMENT_3D('',#84158,#57211,#57212);
#48001=AXIS2_PLACEMENT_3D('',#84159,#57213,#57214);
#48002=AXIS2_PLACEMENT_3D('',#84160,#57215,#57216);
#48003=AXIS2_PLACEMENT_3D('',#84161,#57217,#57218);
#48004=AXIS2_PLACEMENT_3D('',#84162,#57219,#57220);
#48005=AXIS2_PLACEMENT_3D('',#84163,#57221,#57222);
#48006=AXIS2_PLACEMENT_3D('',#84164,#57223,#57224);
#48007=AXIS2_PLACEMENT_3D('',#84165,#57225,#57226);
#48008=AXIS2_PLACEMENT_3D('',#84166,#57227,#57228);
#48009=AXIS2_PLACEMENT_3D('',#84167,#57229,#57230);
#48010=AXIS2_PLACEMENT_3D('',#84168,#57231,#57232);
#48011=AXIS2_PLACEMENT_3D('',#84169,#57233,#57234);
#48012=AXIS2_PLACEMENT_3D('',#84170,#57235,#57236);
#48013=AXIS2_PLACEMENT_3D('',#84171,#57237,#57238);
#48014=AXIS2_PLACEMENT_3D('',#84172,#57239,#57240);
#48015=AXIS2_PLACEMENT_3D('',#84173,#57241,#57242);
#48016=AXIS2_PLACEMENT_3D('',#84174,#57243,#57244);
#48017=AXIS2_PLACEMENT_3D('',#84175,#57245,#57246);
#48018=AXIS2_PLACEMENT_3D('',#84176,#57247,#57248);
#48019=AXIS2_PLACEMENT_3D('',#84177,#57249,#57250);
#48020=AXIS2_PLACEMENT_3D('',#84178,#57251,#57252);
#48021=AXIS2_PLACEMENT_3D('',#84179,#57253,#57254);
#48022=AXIS2_PLACEMENT_3D('',#84180,#57255,#57256);
#48023=AXIS2_PLACEMENT_3D('',#84181,#57257,#57258);
#48024=AXIS2_PLACEMENT_3D('',#84182,#57259,#57260);
#48025=AXIS2_PLACEMENT_3D('',#84183,#57261,#57262);
#48026=AXIS2_PLACEMENT_3D('',#84184,#57263,#57264);
#48027=AXIS2_PLACEMENT_3D('',#84185,#57265,#57266);
#48028=AXIS2_PLACEMENT_3D('',#84186,#57267,#57268);
#48029=AXIS2_PLACEMENT_3D('',#84187,#57269,#57270);
#48030=AXIS2_PLACEMENT_3D('',#84188,#57271,#57272);
#48031=AXIS2_PLACEMENT_3D('',#84189,#57273,#57274);
#48032=AXIS2_PLACEMENT_3D('',#84190,#57275,#57276);
#48033=AXIS2_PLACEMENT_3D('',#84191,#57277,#57278);
#48034=AXIS2_PLACEMENT_3D('',#84192,#57279,#57280);
#48035=AXIS2_PLACEMENT_3D('',#84193,#57281,#57282);
#48036=AXIS2_PLACEMENT_3D('',#84194,#57283,#57284);
#48037=AXIS2_PLACEMENT_3D('',#84195,#57285,#57286);
#48038=AXIS2_PLACEMENT_3D('',#84196,#57287,#57288);
#48039=AXIS2_PLACEMENT_3D('',#84197,#57289,#57290);
#48040=AXIS2_PLACEMENT_3D('',#84198,#57291,#57292);
#48041=AXIS2_PLACEMENT_3D('',#84199,#57293,#57294);
#48042=AXIS2_PLACEMENT_3D('',#84200,#57295,#57296);
#48043=AXIS2_PLACEMENT_3D('',#84201,#57297,#57298);
#48044=AXIS2_PLACEMENT_3D('',#84202,#57299,#57300);
#48045=AXIS2_PLACEMENT_3D('',#84203,#57301,#57302);
#48046=AXIS2_PLACEMENT_3D('',#84204,#57303,#57304);
#48047=AXIS2_PLACEMENT_3D('',#84205,#57305,#57306);
#48048=AXIS2_PLACEMENT_3D('',#84206,#57307,#57308);
#48049=AXIS2_PLACEMENT_3D('',#84207,#57309,#57310);
#48050=AXIS2_PLACEMENT_3D('',#84208,#57311,#57312);
#48051=AXIS2_PLACEMENT_3D('',#84209,#57313,#57314);
#48052=AXIS2_PLACEMENT_3D('',#84210,#57315,#57316);
#48053=AXIS2_PLACEMENT_3D('',#84211,#57317,#57318);
#48054=AXIS2_PLACEMENT_3D('',#84212,#57319,#57320);
#48055=AXIS2_PLACEMENT_3D('',#84225,#57321,#57322);
#48056=AXIS2_PLACEMENT_3D('',#84238,#57323,#57324);
#48057=AXIS2_PLACEMENT_3D('',#84251,#57325,#57326);
#48058=AXIS2_PLACEMENT_3D('',#84264,#57327,#57328);
#48059=AXIS2_PLACEMENT_3D('',#84277,#57329,#57330);
#48060=AXIS2_PLACEMENT_3D('',#84290,#57331,#57332);
#48061=AXIS2_PLACEMENT_3D('',#84303,#57333,#57334);
#48062=AXIS2_PLACEMENT_3D('',#84316,#57335,#57336);
#48063=AXIS2_PLACEMENT_3D('',#84329,#57337,#57338);
#48064=AXIS2_PLACEMENT_3D('',#84342,#57339,#57340);
#48065=AXIS2_PLACEMENT_3D('',#84355,#57341,#57342);
#48066=AXIS2_PLACEMENT_3D('',#84368,#57343,#57344);
#48067=AXIS2_PLACEMENT_3D('',#84381,#57345,#57346);
#48068=AXIS2_PLACEMENT_3D('',#84394,#57347,#57348);
#48069=AXIS2_PLACEMENT_3D('',#84395,#57349,#57350);
#48070=AXIS2_PLACEMENT_3D('',#84396,#57351,#57352);
#48071=AXIS2_PLACEMENT_3D('',#84409,#57353,#57354);
#48072=AXIS2_PLACEMENT_3D('',#84422,#57355,#57356);
#48073=AXIS2_PLACEMENT_3D('',#84423,#57357,#57358);
#48074=AXIS2_PLACEMENT_3D('',#84424,#57359,#57360);
#48075=AXIS2_PLACEMENT_3D('',#84437,#57361,#57362);
#48076=AXIS2_PLACEMENT_3D('',#84450,#57363,#57364);
#48077=AXIS2_PLACEMENT_3D('',#84451,#57365,#57366);
#48078=AXIS2_PLACEMENT_3D('',#84452,#57367,#57368);
#48079=AXIS2_PLACEMENT_3D('',#84453,#57369,#57370);
#48080=AXIS2_PLACEMENT_3D('',#84454,#57371,#57372);
#48081=AXIS2_PLACEMENT_3D('',#84467,#57373,#57374);
#48082=AXIS2_PLACEMENT_3D('',#84480,#57375,#57376);
#48083=AXIS2_PLACEMENT_3D('',#84481,#57377,#57378);
#48084=AXIS2_PLACEMENT_3D('',#84482,#57379,#57380);
#48085=AXIS2_PLACEMENT_3D('',#84483,#57381,#57382);
#48086=AXIS2_PLACEMENT_3D('',#84484,#57383,#57384);
#48087=AXIS2_PLACEMENT_3D('',#84497,#57385,#57386);
#48088=AXIS2_PLACEMENT_3D('',#84510,#57387,#57388);
#48089=AXIS2_PLACEMENT_3D('',#84523,#57389,#57390);
#48090=AXIS2_PLACEMENT_3D('',#84536,#57391,#57392);
#48091=AXIS2_PLACEMENT_3D('',#84549,#57393,#57394);
#48092=AXIS2_PLACEMENT_3D('',#84562,#57395,#57396);
#48093=AXIS2_PLACEMENT_3D('',#84575,#57397,#57398);
#48094=AXIS2_PLACEMENT_3D('',#84588,#57399,#57400);
#48095=AXIS2_PLACEMENT_3D('',#84601,#57401,#57402);
#48096=AXIS2_PLACEMENT_3D('',#84614,#57403,#57404);
#48097=AXIS2_PLACEMENT_3D('',#84627,#57405,#57406);
#48098=AXIS2_PLACEMENT_3D('',#84640,#57407,#57408);
#48099=AXIS2_PLACEMENT_3D('',#84653,#57409,#57410);
#48100=AXIS2_PLACEMENT_3D('',#84666,#57411,#57412);
#48101=AXIS2_PLACEMENT_3D('',#84679,#57413,#57414);
#48102=AXIS2_PLACEMENT_3D('',#84692,#57415,#57416);
#48103=AXIS2_PLACEMENT_3D('',#84705,#57417,#57418);
#48104=AXIS2_PLACEMENT_3D('',#84718,#57419,#57420);
#48105=AXIS2_PLACEMENT_3D('',#84731,#57421,#57422);
#48106=AXIS2_PLACEMENT_3D('',#84744,#57423,#57424);
#48107=AXIS2_PLACEMENT_3D('',#84757,#57425,#57426);
#48108=AXIS2_PLACEMENT_3D('',#84770,#57427,#57428);
#48109=AXIS2_PLACEMENT_3D('',#84783,#57429,#57430);
#48110=AXIS2_PLACEMENT_3D('',#84796,#57431,#57432);
#48111=AXIS2_PLACEMENT_3D('',#84809,#57433,#57434);
#48112=AXIS2_PLACEMENT_3D('',#84822,#57435,#57436);
#48113=AXIS2_PLACEMENT_3D('',#84835,#57437,#57438);
#48114=AXIS2_PLACEMENT_3D('',#84848,#57439,#57440);
#48115=AXIS2_PLACEMENT_3D('',#84861,#57441,#57442);
#48116=AXIS2_PLACEMENT_3D('',#84874,#57443,#57444);
#48117=AXIS2_PLACEMENT_3D('',#84887,#57445,#57446);
#48118=AXIS2_PLACEMENT_3D('',#84900,#57447,#57448);
#48119=AXIS2_PLACEMENT_3D('',#84913,#57449,#57450);
#48120=AXIS2_PLACEMENT_3D('',#84926,#57451,#57452);
#48121=AXIS2_PLACEMENT_3D('',#84939,#57453,#57454);
#48122=AXIS2_PLACEMENT_3D('',#84952,#57455,#57456);
#48123=AXIS2_PLACEMENT_3D('',#84965,#57457,#57458);
#48124=AXIS2_PLACEMENT_3D('',#84978,#57459,#57460);
#48125=AXIS2_PLACEMENT_3D('',#84991,#57461,#57462);
#48126=AXIS2_PLACEMENT_3D('',#84992,#57463,#57464);
#48127=AXIS2_PLACEMENT_3D('',#84993,#57465,#57466);
#48128=AXIS2_PLACEMENT_3D('',#84994,#57467,#57468);
#48129=AXIS2_PLACEMENT_3D('',#84995,#57469,#57470);
#48130=AXIS2_PLACEMENT_3D('',#84996,#57471,#57472);
#48131=AXIS2_PLACEMENT_3D('',#84997,#57473,#57474);
#48132=AXIS2_PLACEMENT_3D('',#84998,#57475,#57476);
#48133=AXIS2_PLACEMENT_3D('',#84999,#57477,#57478);
#48134=AXIS2_PLACEMENT_3D('',#85000,#57479,#57480);
#48135=AXIS2_PLACEMENT_3D('',#85001,#57481,#57482);
#48136=AXIS2_PLACEMENT_3D('',#85002,#57483,#57484);
#48137=AXIS2_PLACEMENT_3D('',#85003,#57485,#57486);
#48138=AXIS2_PLACEMENT_3D('',#85004,#57487,#57488);
#48139=AXIS2_PLACEMENT_3D('',#85007,#57489,#57490);
#48140=AXIS2_PLACEMENT_3D('',#85008,#57491,#57492);
#48141=AXIS2_PLACEMENT_3D('',#85010,#57493,#57494);
#48142=AXIS2_PLACEMENT_3D('',#85011,#57495,#57496);
#48143=AXIS2_PLACEMENT_3D('',#85012,#57497,#57498);
#48144=AXIS2_PLACEMENT_3D('',#85014,#57499,#57500);
#48145=AXIS2_PLACEMENT_3D('',#85016,#57501,#57502);
#48146=AXIS2_PLACEMENT_3D('',#85017,#57503,#57504);
#48147=AXIS2_PLACEMENT_3D('',#85018,#57505,#57506);
#48148=AXIS2_PLACEMENT_3D('',#85400,#57508,#57509);
#48149=AXIS2_PLACEMENT_3D('',#85457,#57510,#57511);
#48150=AXIS2_PLACEMENT_3D('',#85512,#57512,#57513);
#48151=AXIS2_PLACEMENT_3D('',#85514,#57514,#57515);
#48152=AXIS2_PLACEMENT_3D('',#85516,#57516,#57517);
#48153=AXIS2_PLACEMENT_3D('',#85517,#57518,#57519);
#48154=AXIS2_PLACEMENT_3D('',#85518,#57520,#57521);
#48155=AXIS2_PLACEMENT_3D('',#85520,#57522,#57523);
#48156=AXIS2_PLACEMENT_3D('',#85522,#57525,#57526);
#48157=AXIS2_PLACEMENT_3D('',#85523,#57527,#57528);
#48158=AXIS2_PLACEMENT_3D('',#85524,#57529,#57530);
#48159=AXIS2_PLACEMENT_3D('',#85903,#57531,#57532);
#48160=AXIS2_PLACEMENT_3D('',#85904,#57533,#57534);
#48161=AXIS2_PLACEMENT_3D('',#85905,#57535,#57536);
#48162=AXIS2_PLACEMENT_3D('',#85906,#57537,#57538);
#48163=AXIS2_PLACEMENT_3D('',#85907,#57539,#57540);
#48164=AXIS2_PLACEMENT_3D('',#85912,#57542,#57543);
#48165=AXIS2_PLACEMENT_3D('',#85915,#57545,#57546);
#48166=AXIS2_PLACEMENT_3D('',#85916,#57547,#57548);
#48167=AXIS2_PLACEMENT_3D('',#85922,#57552,#57553);
#48168=AXIS2_PLACEMENT_3D('',#85926,#57555,#57556);
#48169=AXIS2_PLACEMENT_3D('',#85927,#57557,#57558);
#48170=AXIS2_PLACEMENT_3D('',#85928,#57559,#57560);
#48171=AXIS2_PLACEMENT_3D('',#85931,#57563,#57564);
#48172=AXIS2_PLACEMENT_3D('',#85932,#57565,#57566);
#48173=AXIS2_PLACEMENT_3D('',#85933,#57567,#57568);
#48174=AXIS2_PLACEMENT_3D('',#85936,#57569,#57570);
#48175=AXIS2_PLACEMENT_3D('',#85940,#57572,#57573);
#48176=AXIS2_PLACEMENT_3D('',#85942,#57575,#57576);
#48177=AXIS2_PLACEMENT_3D('',#85948,#57580,#57581);
#48178=AXIS2_PLACEMENT_3D('',#85950,#57582,#57583);
#48179=AXIS2_PLACEMENT_3D('',#85952,#57585,#57586);
#48180=AXIS2_PLACEMENT_3D('',#85956,#57589,#57590);
#48181=AXIS2_PLACEMENT_3D('',#85957,#57591,#57592);
#48182=AXIS2_PLACEMENT_3D('',#85958,#57593,#57594);
#48183=AXIS2_PLACEMENT_3D('',#85959,#57595,#57596);
#48184=AXIS2_PLACEMENT_3D('',#86020,#57598,#57599);
#48185=AXIS2_PLACEMENT_3D('',#86083,#57601,#57602);
#48186=AXIS2_PLACEMENT_3D('',#86143,#57604,#57605);
#48187=AXIS2_PLACEMENT_3D('',#86185,#57607,#57608);
#48188=AXIS2_PLACEMENT_3D('',#86188,#57610,#57611);
#48189=AXIS2_PLACEMENT_3D('',#86377,#57612,#57613);
#48190=AXIS2_PLACEMENT_3D('',#86378,#57614,#57615);
#48191=AXIS2_PLACEMENT_3D('',#86380,#57616,#57617);
#48192=AXIS2_PLACEMENT_3D('',#86381,#57618,#57619);
#48193=AXIS2_PLACEMENT_3D('',#86382,#57620,#57621);
#48194=AXIS2_PLACEMENT_3D('',#86385,#57622,#57623);
#48195=AXIS2_PLACEMENT_3D('',#86400,#57625,#57626);
#48196=AXIS2_PLACEMENT_3D('',#86413,#57628,#57629);
#48197=AXIS2_PLACEMENT_3D('',#86416,#57630,#57631);
#48198=AXIS2_PLACEMENT_3D('',#86431,#57633,#57634);
#48199=AXIS2_PLACEMENT_3D('',#86444,#57636,#57637);
#48200=AXIS2_PLACEMENT_3D('',#86447,#57638,#57639);
#48201=AXIS2_PLACEMENT_3D('',#86462,#57641,#57642);
#48202=AXIS2_PLACEMENT_3D('',#86475,#57644,#57645);
#48203=AXIS2_PLACEMENT_3D('',#86478,#57646,#57647);
#48204=AXIS2_PLACEMENT_3D('',#86482,#57649,#57650);
#48205=AXIS2_PLACEMENT_3D('',#86536,#57652,#57653);
#48206=AXIS2_PLACEMENT_3D('',#86598,#57655,#57656);
#48207=AXIS2_PLACEMENT_3D('',#86599,#57657,#57658);
#48208=AXIS2_PLACEMENT_3D('',#86600,#57659,#57660);
#48209=AXIS2_PLACEMENT_3D('',#86603,#57661,#57662);
#48210=AXIS2_PLACEMENT_3D('',#86607,#57664,#57665);
#48211=AXIS2_PLACEMENT_3D('',#86609,#57667,#57668);
#48212=AXIS2_PLACEMENT_3D('',#86611,#57669,#57670);
#48213=AXIS2_PLACEMENT_3D('',#86613,#57671,#57672);
#48214=AXIS2_PLACEMENT_3D('',#86614,#57673,#57674);
#48215=AXIS2_PLACEMENT_3D('',#86615,#57675,#57676);
#48216=AXIS2_PLACEMENT_3D('',#86661,#57677,#57678);
#48217=AXIS2_PLACEMENT_3D('',#86708,#57679,#57680);
#48218=AXIS2_PLACEMENT_3D('',#86710,#57681,#57682);
#48219=AXIS2_PLACEMENT_3D('',#86712,#57683,#57684);
#48220=AXIS2_PLACEMENT_3D('',#86713,#57685,#57686);
#48221=AXIS2_PLACEMENT_3D('',#86714,#57687,#57688);
#48222=AXIS2_PLACEMENT_3D('',#86716,#57689,#57690);
#48223=AXIS2_PLACEMENT_3D('',#86717,#57691,#57692);
#48224=AXIS2_PLACEMENT_3D('',#86718,#57693,#57694);
#48225=AXIS2_PLACEMENT_3D('',#86721,#57695,#57696);
#48226=AXIS2_PLACEMENT_3D('',#86725,#57698,#57699);
#48227=AXIS2_PLACEMENT_3D('',#86779,#57701,#57702);
#48228=AXIS2_PLACEMENT_3D('',#86841,#57704,#57705);
#48229=AXIS2_PLACEMENT_3D('',#86842,#57706,#57707);
#48230=AXIS2_PLACEMENT_3D('',#86843,#57708,#57709);
#48231=AXIS2_PLACEMENT_3D('',#86846,#57710,#57711);
#48232=AXIS2_PLACEMENT_3D('',#86850,#57713,#57714);
#48233=AXIS2_PLACEMENT_3D('',#86852,#57716,#57717);
#48234=AXIS2_PLACEMENT_3D('',#86854,#57718,#57719);
#48235=AXIS2_PLACEMENT_3D('',#86856,#57720,#57721);
#48236=AXIS2_PLACEMENT_3D('',#86857,#57722,#57723);
#48237=AXIS2_PLACEMENT_3D('',#86858,#57724,#57725);
#48238=AXIS2_PLACEMENT_3D('',#86904,#57726,#57727);
#48239=AXIS2_PLACEMENT_3D('',#86951,#57728,#57729);
#48240=AXIS2_PLACEMENT_3D('',#86953,#57730,#57731);
#48241=AXIS2_PLACEMENT_3D('',#86955,#57732,#57733);
#48242=AXIS2_PLACEMENT_3D('',#86956,#57734,#57735);
#48243=AXIS2_PLACEMENT_3D('',#86957,#57736,#57737);
#48244=AXIS2_PLACEMENT_3D('',#86959,#57738,#57739);
#48245=AXIS2_PLACEMENT_3D('',#86960,#57740,#57741);
#48246=AXIS2_PLACEMENT_3D('',#86961,#57742,#57743);
#48247=AXIS2_PLACEMENT_3D('',#86964,#57744,#57745);
#48248=AXIS2_PLACEMENT_3D('',#86968,#57747,#57748);
#48249=AXIS2_PLACEMENT_3D('',#87022,#57750,#57751);
#48250=AXIS2_PLACEMENT_3D('',#87084,#57753,#57754);
#48251=AXIS2_PLACEMENT_3D('',#87085,#57755,#57756);
#48252=AXIS2_PLACEMENT_3D('',#87086,#57757,#57758);
#48253=AXIS2_PLACEMENT_3D('',#87089,#57759,#57760);
#48254=AXIS2_PLACEMENT_3D('',#87093,#57762,#57763);
#48255=AXIS2_PLACEMENT_3D('',#87095,#57765,#57766);
#48256=AXIS2_PLACEMENT_3D('',#87097,#57767,#57768);
#48257=AXIS2_PLACEMENT_3D('',#87099,#57769,#57770);
#48258=AXIS2_PLACEMENT_3D('',#87100,#57771,#57772);
#48259=AXIS2_PLACEMENT_3D('',#87101,#57773,#57774);
#48260=AXIS2_PLACEMENT_3D('',#87147,#57775,#57776);
#48261=AXIS2_PLACEMENT_3D('',#87194,#57777,#57778);
#48262=AXIS2_PLACEMENT_3D('',#87196,#57779,#57780);
#48263=AXIS2_PLACEMENT_3D('',#87198,#57781,#57782);
#48264=AXIS2_PLACEMENT_3D('',#87199,#57783,#57784);
#48265=AXIS2_PLACEMENT_3D('',#87200,#57785,#57786);
#48266=AXIS2_PLACEMENT_3D('',#87202,#57787,#57788);
#48267=AXIS2_PLACEMENT_3D('',#87203,#57789,#57790);
#48268=AXIS2_PLACEMENT_3D('',#87204,#57791,#57792);
#48269=AXIS2_PLACEMENT_3D('',#87206,#57793,#57794);
#48270=AXIS2_PLACEMENT_3D('',#87210,#57796,#57797);
#48271=AXIS2_PLACEMENT_3D('',#87273,#57799,#57800);
#48272=AXIS2_PLACEMENT_3D('',#87332,#57802,#57803);
#48273=AXIS2_PLACEMENT_3D('',#87333,#57804,#57805);
#48274=AXIS2_PLACEMENT_3D('',#87385,#57806,#57807);
#48275=AXIS2_PLACEMENT_3D('',#87429,#57808,#57809);
#48276=AXIS2_PLACEMENT_3D('',#87432,#57810,#57811);
#48277=AXIS2_PLACEMENT_3D('',#87603,#57812,#57813);
#48278=AXIS2_PLACEMENT_3D('',#87609,#57817,#57818);
#48279=AXIS2_PLACEMENT_3D('',#87614,#57820,#57821);
#48280=AXIS2_PLACEMENT_3D('',#87617,#57823,#57824);
#48281=AXIS2_PLACEMENT_3D('',#88054,#57826,#57827);
#48282=AXIS2_PLACEMENT_3D('',#88059,#57829,#57830);
#48283=AXIS2_PLACEMENT_3D('',#88062,#57832,#57833);
#48284=AXIS2_PLACEMENT_3D('',#88496,#57834,#57835);
#48285=AXIS2_PLACEMENT_3D('',#88505,#57840,#57841);
#48286=AXIS2_PLACEMENT_3D('',#88511,#57845,#57846);
#48287=AXIS2_PLACEMENT_3D('',#88826,#57850,#57851);
#48288=AXIS2_PLACEMENT_3D('',#88827,#57852,#57853);
#48289=AXIS2_PLACEMENT_3D('',#89265,#57854,#57855);
#48290=AXIS2_PLACEMENT_3D('',#89266,#57856,#57857);
#48291=AXIS2_PLACEMENT_3D('',#89268,#57858,#57859);
#48292=AXIS2_PLACEMENT_3D('',#89269,#57860,#57861);
#48293=AXIS2_PLACEMENT_3D('',#89270,#57862,#57863);
#48294=AXIS2_PLACEMENT_3D('',#89272,#57864,#57865);
#48295=AXIS2_PLACEMENT_3D('',#89273,#57866,#57867);
#48296=AXIS2_PLACEMENT_3D('',#89274,#57868,#57869);
#48297=AXIS2_PLACEMENT_3D('',#89283,#57870,#57871);
#48298=AXIS2_PLACEMENT_3D('',#89285,#57873,#57874);
#48299=AXIS2_PLACEMENT_3D('',#89289,#57876,#57877);
#48300=AXIS2_PLACEMENT_3D('',#89298,#57878,#57879);
#48301=AXIS2_PLACEMENT_3D('',#89307,#57880,#57881);
#48302=AXIS2_PLACEMENT_3D('',#89309,#57882,#57883);
#48303=AXIS2_PLACEMENT_3D('',#89320,#57885,#57886);
#48304=AXIS2_PLACEMENT_3D('',#89327,#57887,#57888);
#48305=AXIS2_PLACEMENT_3D('',#89328,#57889,#57890);
#48306=AXIS2_PLACEMENT_3D('',#89335,#57891,#57892);
#48307=AXIS2_PLACEMENT_3D('',#89336,#57893,#57894);
#48308=AXIS2_PLACEMENT_3D('',#89337,#57895,#57896);
#48309=AXIS2_PLACEMENT_3D('',#89338,#57897,#57898);
#48310=AXIS2_PLACEMENT_3D('',#89339,#57899,#57900);
#48311=AXIS2_PLACEMENT_3D('',#89340,#57901,#57902);
#48312=AXIS2_PLACEMENT_3D('',#89341,#57903,#57904);
#48313=AXIS2_PLACEMENT_3D('',#89342,#57905,#57906);
#48314=AXIS2_PLACEMENT_3D('',#89343,#57907,#57908);
#48315=AXIS2_PLACEMENT_3D('',#89344,#57909,#57910);
#48316=AXIS2_PLACEMENT_3D('',#89345,#57911,#57912);
#48317=AXIS2_PLACEMENT_3D('',#89346,#57913,#57914);
#48318=AXIS2_PLACEMENT_3D('',#89347,#57915,#57916);
#48319=AXIS2_PLACEMENT_3D('',#89348,#57917,#57918);
#48320=AXIS2_PLACEMENT_3D('',#89349,#57919,#57920);
#48321=AXIS2_PLACEMENT_3D('',#89350,#57921,#57922);
#48322=AXIS2_PLACEMENT_3D('',#89351,#57923,#57924);
#48323=AXIS2_PLACEMENT_3D('',#89352,#57925,#57926);
#48324=AXIS2_PLACEMENT_3D('',#89353,#57927,#57928);
#48325=AXIS2_PLACEMENT_3D('',#89354,#57929,#57930);
#48326=AXIS2_PLACEMENT_3D('',#89523,#57931,#57932);
#48327=AXIS2_PLACEMENT_3D('',#89698,#57933,#57934);
#48328=AXIS2_PLACEMENT_3D('',#89701,#57935,#57936);
#48329=AXIS2_PLACEMENT_3D('',#89703,#57937,#57938);
#48330=AXIS2_PLACEMENT_3D('',#89705,#57939,#57940);
#48331=AXIS2_PLACEMENT_3D('',#89706,#57941,#57942);
#48332=AXIS2_PLACEMENT_3D('',#89707,#57943,#57944);
#48333=AXIS2_PLACEMENT_3D('',#89710,#57945,#57946);
#48334=AXIS2_PLACEMENT_3D('',#89713,#57949,#57950);
#48335=AXIS2_PLACEMENT_3D('',#89716,#57951,#57952);
#48336=AXIS2_PLACEMENT_3D('',#89719,#57955,#57956);
#48337=AXIS2_PLACEMENT_3D('',#89720,#57957,#57958);
#48338=AXIS2_PLACEMENT_3D('',#89721,#57959,#57960);
#48339=AXIS2_PLACEMENT_3D('',#89722,#57961,#57962);
#48340=AXIS2_PLACEMENT_3D('',#89724,#57963,#57964);
#48341=AXIS2_PLACEMENT_3D('',#89727,#57966,#57967);
#48342=AXIS2_PLACEMENT_3D('',#89765,#57968,#57969);
#48343=AXIS2_PLACEMENT_3D('',#89846,#57970,#57971);
#48344=AXIS2_PLACEMENT_3D('',#89902,#57972,#57973);
#48345=AXIS2_PLACEMENT_3D('',#89905,#57974,#57975);
#48346=AXIS2_PLACEMENT_3D('',#89908,#57978,#57979);
#48347=AXIS2_PLACEMENT_3D('',#89910,#57980,#57981);
#48348=AXIS2_PLACEMENT_3D('',#89911,#57982,#57983);
#48349=AXIS2_PLACEMENT_3D('',#89912,#57984,#57985);
#48350=AXIS2_PLACEMENT_3D('',#89915,#57986,#57987);
#48351=AXIS2_PLACEMENT_3D('',#89918,#57990,#57991);
#48352=AXIS2_PLACEMENT_3D('',#89921,#57992,#57993);
#48353=AXIS2_PLACEMENT_3D('',#89922,#57994,#57995);
#48354=AXIS2_PLACEMENT_3D('',#89923,#57996,#57997);
#48355=AXIS2_PLACEMENT_3D('',#89961,#57998,#57999);
#48356=AXIS2_PLACEMENT_3D('',#90104,#58000,#58001);
#48357=AXIS2_PLACEMENT_3D('',#90105,#58002,#58003);
#48358=AXIS2_PLACEMENT_3D('',#90106,#58004,#58005);
#48359=AXIS2_PLACEMENT_3D('',#90109,#58006,#58007);
#48360=AXIS2_PLACEMENT_3D('',#90110,#58008,#58009);
#48361=AXIS2_PLACEMENT_3D('',#90111,#58010,#58011);
#48362=AXIS2_PLACEMENT_3D('',#90112,#58012,#58013);
#48363=AXIS2_PLACEMENT_3D('',#90115,#58016,#58017);
#48364=AXIS2_PLACEMENT_3D('',#90117,#58019,#58020);
#48365=AXIS2_PLACEMENT_3D('',#90120,#58023,#58024);
#48366=AXIS2_PLACEMENT_3D('',#90121,#58025,#58026);
#48367=AXIS2_PLACEMENT_3D('',#90122,#58027,#58028);
#48368=AXIS2_PLACEMENT_3D('',#90125,#58031,#58032);
#48369=AXIS2_PLACEMENT_3D('',#90128,#58035,#58036);
#48370=AXIS2_PLACEMENT_3D('',#90129,#58037,#58038);
#48371=AXIS2_PLACEMENT_3D('',#90130,#58039,#58040);
#48372=AXIS2_PLACEMENT_3D('',#90131,#58041,#58042);
#48373=AXIS2_PLACEMENT_3D('',#90134,#58043,#58044);
#48374=AXIS2_PLACEMENT_3D('',#90137,#58047,#58048);
#48375=AXIS2_PLACEMENT_3D('',#90140,#58049,#58050);
#48376=AXIS2_PLACEMENT_3D('',#90141,#58051,#58052);
#48377=AXIS2_PLACEMENT_3D('',#90142,#58053,#58054);
#48378=AXIS2_PLACEMENT_3D('',#90143,#58055,#58056);
#48379=AXIS2_PLACEMENT_3D('',#90146,#58059,#58060);
#48380=AXIS2_PLACEMENT_3D('',#90148,#58061,#58062);
#48381=AXIS2_PLACEMENT_3D('',#90150,#58063,#58064);
#48382=AXIS2_PLACEMENT_3D('',#90151,#58065,#58066);
#48383=AXIS2_PLACEMENT_3D('',#90183,#58067,#58068);
#48384=AXIS2_PLACEMENT_3D('',#90258,#58069,#58070);
#48385=AXIS2_PLACEMENT_3D('',#90299,#58071,#58072);
#48386=AXIS2_PLACEMENT_3D('',#90301,#58073,#58074);
#48387=AXIS2_PLACEMENT_3D('',#90303,#58076,#58077);
#48388=AXIS2_PLACEMENT_3D('',#90306,#58078,#58079);
#48389=AXIS2_PLACEMENT_3D('',#90309,#58082,#58083);
#48390=AXIS2_PLACEMENT_3D('',#90312,#58084,#58085);
#48391=AXIS2_PLACEMENT_3D('',#90315,#58088,#58089);
#48392=AXIS2_PLACEMENT_3D('',#90317,#58090,#58091);
#48393=AXIS2_PLACEMENT_3D('',#90350,#58093,#58094);
#48394=AXIS2_PLACEMENT_3D('',#90391,#58095,#58096);
#48395=AXIS2_PLACEMENT_3D('',#90392,#58097,#58098);
#48396=AXIS2_PLACEMENT_3D('',#90393,#58099,#58100);
#48397=AXIS2_PLACEMENT_3D('',#90425,#58101,#58102);
#48398=AXIS2_PLACEMENT_3D('',#90481,#58103,#58104);
#48399=AXIS2_PLACEMENT_3D('',#90484,#58107,#58108);
#48400=AXIS2_PLACEMENT_3D('',#90487,#58111,#58112);
#48401=AXIS2_PLACEMENT_3D('',#90488,#58113,#58114);
#48402=AXIS2_PLACEMENT_3D('',#90489,#58115,#58116);
#48403=AXIS2_PLACEMENT_3D('',#90492,#58119,#58120);
#48404=AXIS2_PLACEMENT_3D('',#90493,#58121,#58122);
#48405=AXIS2_PLACEMENT_3D('',#90494,#58123,#58124);
#48406=AXIS2_PLACEMENT_3D('',#90495,#58125,#58126);
#48407=AXIS2_PLACEMENT_3D('',#90498,#58127,#58128);
#48408=AXIS2_PLACEMENT_3D('',#90501,#58131,#58132);
#48409=AXIS2_PLACEMENT_3D('',#90504,#58133,#58134);
#48410=AXIS2_PLACEMENT_3D('',#90505,#58135,#58136);
#48411=AXIS2_PLACEMENT_3D('',#90506,#58137,#58138);
#48412=AXIS2_PLACEMENT_3D('',#90507,#58139,#58140);
#48413=AXIS2_PLACEMENT_3D('',#90510,#58143,#58144);
#48414=AXIS2_PLACEMENT_3D('',#90512,#58145,#58146);
#48415=AXIS2_PLACEMENT_3D('',#90514,#58147,#58148);
#48416=AXIS2_PLACEMENT_3D('',#90515,#58149,#58150);
#48417=AXIS2_PLACEMENT_3D('',#90547,#58151,#58152);
#48418=AXIS2_PLACEMENT_3D('',#90622,#58153,#58154);
#48419=AXIS2_PLACEMENT_3D('',#90663,#58155,#58156);
#48420=AXIS2_PLACEMENT_3D('',#90665,#58157,#58158);
#48421=AXIS2_PLACEMENT_3D('',#90667,#58160,#58161);
#48422=AXIS2_PLACEMENT_3D('',#90670,#58162,#58163);
#48423=AXIS2_PLACEMENT_3D('',#90673,#58166,#58167);
#48424=AXIS2_PLACEMENT_3D('',#90676,#58168,#58169);
#48425=AXIS2_PLACEMENT_3D('',#90679,#58172,#58173);
#48426=AXIS2_PLACEMENT_3D('',#90681,#58174,#58175);
#48427=AXIS2_PLACEMENT_3D('',#90714,#58177,#58178);
#48428=AXIS2_PLACEMENT_3D('',#90755,#58179,#58180);
#48429=AXIS2_PLACEMENT_3D('',#90756,#58181,#58182);
#48430=AXIS2_PLACEMENT_3D('',#90757,#58183,#58184);
#48431=AXIS2_PLACEMENT_3D('',#90789,#58185,#58186);
#48432=AXIS2_PLACEMENT_3D('',#90845,#58187,#58188);
#48433=AXIS2_PLACEMENT_3D('',#90848,#58191,#58192);
#48434=AXIS2_PLACEMENT_3D('',#90851,#58195,#58196);
#48435=AXIS2_PLACEMENT_3D('',#90852,#58197,#58198);
#48436=AXIS2_PLACEMENT_3D('',#90853,#58199,#58200);
#48437=AXIS2_PLACEMENT_3D('',#90856,#58203,#58204);
#48438=AXIS2_PLACEMENT_3D('',#90857,#58205,#58206);
#48439=AXIS2_PLACEMENT_3D('',#90858,#58207,#58208);
#48440=AXIS2_PLACEMENT_3D('',#90859,#58209,#58210);
#48441=AXIS2_PLACEMENT_3D('',#90862,#58211,#58212);
#48442=AXIS2_PLACEMENT_3D('',#90865,#58215,#58216);
#48443=AXIS2_PLACEMENT_3D('',#90868,#58217,#58218);
#48444=AXIS2_PLACEMENT_3D('',#90869,#58219,#58220);
#48445=AXIS2_PLACEMENT_3D('',#90870,#58221,#58222);
#48446=AXIS2_PLACEMENT_3D('',#90871,#58223,#58224);
#48447=AXIS2_PLACEMENT_3D('',#90874,#58227,#58228);
#48448=AXIS2_PLACEMENT_3D('',#90876,#58229,#58230);
#48449=AXIS2_PLACEMENT_3D('',#90878,#58231,#58232);
#48450=AXIS2_PLACEMENT_3D('',#90879,#58233,#58234);
#48451=AXIS2_PLACEMENT_3D('',#90911,#58235,#58236);
#48452=AXIS2_PLACEMENT_3D('',#90986,#58237,#58238);
#48453=AXIS2_PLACEMENT_3D('',#91027,#58239,#58240);
#48454=AXIS2_PLACEMENT_3D('',#91029,#58241,#58242);
#48455=AXIS2_PLACEMENT_3D('',#91031,#58244,#58245);
#48456=AXIS2_PLACEMENT_3D('',#91034,#58246,#58247);
#48457=AXIS2_PLACEMENT_3D('',#91037,#58250,#58251);
#48458=AXIS2_PLACEMENT_3D('',#91040,#58252,#58253);
#48459=AXIS2_PLACEMENT_3D('',#91043,#58256,#58257);
#48460=AXIS2_PLACEMENT_3D('',#91045,#58258,#58259);
#48461=AXIS2_PLACEMENT_3D('',#91078,#58261,#58262);
#48462=AXIS2_PLACEMENT_3D('',#91119,#58263,#58264);
#48463=AXIS2_PLACEMENT_3D('',#91120,#58265,#58266);
#48464=AXIS2_PLACEMENT_3D('',#91121,#58267,#58268);
#48465=AXIS2_PLACEMENT_3D('',#91153,#58269,#58270);
#48466=AXIS2_PLACEMENT_3D('',#91209,#58271,#58272);
#48467=AXIS2_PLACEMENT_3D('',#91212,#58275,#58276);
#48468=AXIS2_PLACEMENT_3D('',#91215,#58279,#58280);
#48469=AXIS2_PLACEMENT_3D('',#91216,#58281,#58282);
#48470=AXIS2_PLACEMENT_3D('',#91217,#58283,#58284);
#48471=AXIS2_PLACEMENT_3D('',#91220,#58287,#58288);
#48472=AXIS2_PLACEMENT_3D('',#91221,#58289,#58290);
#48473=AXIS2_PLACEMENT_3D('',#91222,#58291,#58292);
#48474=AXIS2_PLACEMENT_3D('',#91223,#58293,#58294);
#48475=AXIS2_PLACEMENT_3D('',#91225,#58296,#58297);
#48476=AXIS2_PLACEMENT_3D('',#91227,#58299,#58300);
#48477=AXIS2_PLACEMENT_3D('',#91229,#58302,#58303);
#48478=AXIS2_PLACEMENT_3D('',#91231,#58304,#58305);
#48479=AXIS2_PLACEMENT_3D('',#91233,#58306,#58307);
#48480=AXIS2_PLACEMENT_3D('',#91235,#58309,#58310);
#48481=AXIS2_PLACEMENT_3D('',#91237,#58311,#58312);
#48482=AXIS2_PLACEMENT_3D('',#91238,#58313,#58314);
#48483=AXIS2_PLACEMENT_3D('',#91249,#58315,#58316);
#48484=AXIS2_PLACEMENT_3D('',#91250,#58317,#58318);
#48485=AXIS2_PLACEMENT_3D('',#91390,#58319,#58320);
#48486=AXIS2_PLACEMENT_3D('',#91395,#58321,#58322);
#48487=AXIS2_PLACEMENT_3D('',#91397,#58323,#58324);
#48488=AXIS2_PLACEMENT_3D('',#91418,#58326,#58327);
#48489=AXIS2_PLACEMENT_3D('',#91442,#58328,#58329);
#48490=AXIS2_PLACEMENT_3D('',#91443,#58330,#58331);
#48491=AXIS2_PLACEMENT_3D('',#91463,#58332,#58333);
#48492=AXIS2_PLACEMENT_3D('',#91470,#58334,#58335);
#48493=AXIS2_PLACEMENT_3D('',#91472,#58336,#58337);
#48494=AXIS2_PLACEMENT_3D('',#91493,#58339,#58340);
#48495=AXIS2_PLACEMENT_3D('',#91507,#58341,#58342);
#48496=AXIS2_PLACEMENT_3D('',#91509,#58343,#58344);
#48497=AXIS2_PLACEMENT_3D('',#91510,#58345,#58346);
#48498=AXIS2_PLACEMENT_3D('',#91554,#58347,#58348);
#48499=AXIS2_PLACEMENT_3D('',#91959,#58349,#58350);
#48500=AXIS2_PLACEMENT_3D('',#91964,#58353,#58354);
#48501=AXIS2_PLACEMENT_3D('',#92093,#58355,#58356);
#48502=AXIS2_PLACEMENT_3D('',#92446,#58357,#58358);
#48503=AXIS2_PLACEMENT_3D('',#92524,#58359,#58360);
#48504=AXIS2_PLACEMENT_3D('',#92526,#58361,#58362);
#48505=AXIS2_PLACEMENT_3D('',#92527,#58363,#58364);
#48506=AXIS2_PLACEMENT_3D('',#92528,#58365,#58366);
#48507=AXIS2_PLACEMENT_3D('',#92529,#58367,#58368);
#48508=AXIS2_PLACEMENT_3D('',#92531,#58369,#58370);
#48509=AXIS2_PLACEMENT_3D('',#92532,#58371,#58372);
#48510=AXIS2_PLACEMENT_3D('',#92533,#58373,#58374);
#48511=AXIS2_PLACEMENT_3D('',#92535,#58375,#58376);
#48512=AXIS2_PLACEMENT_3D('',#92537,#58378,#58379);
#48513=AXIS2_PLACEMENT_3D('',#92540,#58380,#58381);
#48514=AXIS2_PLACEMENT_3D('',#92541,#58382,#58383);
#48515=AXIS2_PLACEMENT_3D('',#92542,#58384,#58385);
#48516=AXIS2_PLACEMENT_3D('',#92586,#58386,#58387);
#48517=AXIS2_PLACEMENT_3D('',#92749,#58388,#58389);
#48518=AXIS2_PLACEMENT_3D('',#92872,#58390,#58391);
#48519=AXIS2_PLACEMENT_3D('',#92874,#58392,#58393);
#48520=AXIS2_PLACEMENT_3D('',#92876,#58395,#58396);
#48521=AXIS2_PLACEMENT_3D('',#92878,#58397,#58398);
#48522=AXIS2_PLACEMENT_3D('',#92879,#58399,#58400);
#48523=AXIS2_PLACEMENT_3D('',#92880,#58401,#58402);
#48524=AXIS2_PLACEMENT_3D('',#92920,#58405,#58406);
#48525=AXIS2_PLACEMENT_3D('',#92994,#58407,#58408);
#48526=AXIS2_PLACEMENT_3D('',#92996,#58409,#58410);
#48527=AXIS2_PLACEMENT_3D('',#92997,#58411,#58412);
#48528=AXIS2_PLACEMENT_3D('',#92998,#58413,#58414);
#48529=AXIS2_PLACEMENT_3D('',#93000,#58415,#58416);
#48530=AXIS2_PLACEMENT_3D('',#93001,#58417,#58418);
#48531=AXIS2_PLACEMENT_3D('',#93002,#58419,#58420);
#48532=AXIS2_PLACEMENT_3D('',#93004,#58421,#58422);
#48533=AXIS2_PLACEMENT_3D('',#93006,#58424,#58425);
#48534=AXIS2_PLACEMENT_3D('',#93008,#58426,#58427);
#48535=AXIS2_PLACEMENT_3D('',#93009,#58428,#58429);
#48536=AXIS2_PLACEMENT_3D('',#93053,#58430,#58431);
#48537=AXIS2_PLACEMENT_3D('',#93091,#58432,#58433);
#48538=AXIS2_PLACEMENT_3D('',#93093,#58434,#58435);
#48539=AXIS2_PLACEMENT_3D('',#93108,#58437,#58438);
#48540=AXIS2_PLACEMENT_3D('',#93141,#58439,#58440);
#48541=AXIS2_PLACEMENT_3D('',#93272,#58441,#58442);
#48542=AXIS2_PLACEMENT_3D('',#93395,#58443,#58444);
#48543=AXIS2_PLACEMENT_3D('',#93445,#58445,#58446);
#48544=AXIS2_PLACEMENT_3D('',#93591,#58447,#58448);
#48545=AXIS2_PLACEMENT_3D('',#93750,#58449,#58450);
#48546=AXIS2_PLACEMENT_3D('',#93967,#58451,#58452);
#48547=AXIS2_PLACEMENT_3D('',#94187,#58453,#58454);
#48548=AXIS2_PLACEMENT_3D('',#94371,#58455,#58456);
#48549=AXIS2_PLACEMENT_3D('',#94372,#58457,#58458);
#48550=AXIS2_PLACEMENT_3D('',#94373,#58459,#58460);
#48551=AXIS2_PLACEMENT_3D('',#94424,#58461,#58462);
#48552=AXIS2_PLACEMENT_3D('',#94509,#58463,#58464);
#48553=AXIS2_PLACEMENT_3D('',#94669,#58465,#58466);
#48554=AXIS2_PLACEMENT_3D('',#94760,#58467,#58468);
#48555=AXIS2_PLACEMENT_3D('',#94761,#58469,#58470);
#48556=AXIS2_PLACEMENT_3D('',#94762,#58471,#58472);
#48557=AXIS2_PLACEMENT_3D('',#94831,#58473,#58474);
#48558=AXIS2_PLACEMENT_3D('',#94867,#58479,#58480);
#48559=AXIS2_PLACEMENT_3D('',#94872,#58483,#58484);
#48560=AXIS2_PLACEMENT_3D('',#95222,#58485,#58486);
#48561=AXIS2_PLACEMENT_3D('',#96545,#58487,#58488);
#48562=AXIS2_PLACEMENT_3D('',#96546,#58489,#58490);
#48563=AXIS2_PLACEMENT_3D('',#96566,#58494,#58495);
#48564=AXIS2_PLACEMENT_3D('',#96567,#58496,#58497);
#48565=AXIS2_PLACEMENT_3D('',#96569,#58499,#58500);
#48566=AXIS2_PLACEMENT_3D('',#96748,#58503,#58504);
#48567=AXIS2_PLACEMENT_3D('',#96799,#58507,#58508);
#48568=AXIS2_PLACEMENT_3D('',#96800,#58509,#58510);
#48569=AXIS2_PLACEMENT_3D('',#96917,#58511,#58512);
#48570=AXIS2_PLACEMENT_3D('',#96919,#58514,#58515);
#48571=AXIS2_PLACEMENT_3D('',#96921,#58517,#58518);
#48572=AXIS2_PLACEMENT_3D('',#96923,#58520,#58521);
#48573=AXIS2_PLACEMENT_3D('',#96925,#58523,#58524);
#48574=AXIS2_PLACEMENT_3D('',#96926,#58525,#58526);
#48575=AXIS2_PLACEMENT_3D('',#96927,#58527,#58528);
#48576=AXIS2_PLACEMENT_3D('',#96929,#58529,#58530);
#48577=AXIS2_PLACEMENT_3D('',#96932,#58532,#58533);
#48578=AXIS2_PLACEMENT_3D('',#96933,#58534,#58535);
#48579=AXIS2_PLACEMENT_3D('',#96936,#58536,#58537);
#48580=AXIS2_PLACEMENT_3D('',#96940,#58539,#58540);
#48581=AXIS2_PLACEMENT_3D('',#96944,#58542,#58543);
#48582=AXIS2_PLACEMENT_3D('',#96948,#58545,#58546);
#48583=AXIS2_PLACEMENT_3D('',#96954,#58549,#58550);
#48584=AXIS2_PLACEMENT_3D('',#96958,#58552,#58553);
#48585=AXIS2_PLACEMENT_3D('',#96962,#58555,#58556);
#48586=AXIS2_PLACEMENT_3D('',#96966,#58558,#58559);
#48587=AXIS2_PLACEMENT_3D('',#96970,#58561,#58562);
#48588=AXIS2_PLACEMENT_3D('',#96974,#58564,#58565);
#48589=AXIS2_PLACEMENT_3D('',#96978,#58567,#58568);
#48590=AXIS2_PLACEMENT_3D('',#96981,#58570,#58571);
#48591=AXIS2_PLACEMENT_3D('',#96982,#58572,#58573);
#48592=AXIS2_PLACEMENT_3D('',#96991,#58578,#58579);
#48593=AXIS2_PLACEMENT_3D('',#97000,#58584,#58585);
#48594=AXIS2_PLACEMENT_3D('',#97009,#58590,#58591);
#48595=AXIS2_PLACEMENT_3D('',#97018,#58596,#58597);
#48596=AXIS2_PLACEMENT_3D('',#97021,#58598,#58599);
#48597=AXIS2_PLACEMENT_3D('',#97025,#58601,#58602);
#48598=AXIS2_PLACEMENT_3D('',#97029,#58604,#58605);
#48599=AXIS2_PLACEMENT_3D('',#97033,#58607,#58608);
#48600=AXIS2_PLACEMENT_3D('',#97035,#58610,#58611);
#48601=AXIS2_PLACEMENT_3D('',#97044,#58616,#58617);
#48602=AXIS2_PLACEMENT_3D('',#97053,#58621,#58622);
#48603=AXIS2_PLACEMENT_3D('',#97056,#58624,#58625);
#48604=AXIS2_PLACEMENT_3D('',#97057,#58626,#58627);
#48605=AXIS2_PLACEMENT_3D('',#97066,#58632,#58633);
#48606=AXIS2_PLACEMENT_3D('',#97075,#58637,#58638);
#48607=AXIS2_PLACEMENT_3D('',#97078,#58640,#58641);
#48608=AXIS2_PLACEMENT_3D('',#97079,#58642,#58643);
#48609=AXIS2_PLACEMENT_3D('',#97088,#58648,#58649);
#48610=AXIS2_PLACEMENT_3D('',#97089,#58650,#58651);
#48611=AXIS2_PLACEMENT_3D('',#97090,#58652,#58653);
#48612=AXIS2_PLACEMENT_3D('',#97091,#58654,#58655);
#48613=AXIS2_PLACEMENT_3D('',#97092,#58656,#58657);
#48614=AXIS2_PLACEMENT_3D('',#97093,#58658,#58659);
#48615=AXIS2_PLACEMENT_3D('',#97094,#58660,#58661);
#48616=AXIS2_PLACEMENT_3D('',#97095,#58662,#58663);
#48617=AXIS2_PLACEMENT_3D('',#97096,#58664,#58665);
#48618=AXIS2_PLACEMENT_3D('',#97097,#58666,#58667);
#48619=AXIS2_PLACEMENT_3D('',#97098,#58668,#58669);
#48620=AXIS2_PLACEMENT_3D('',#97099,#58670,#58671);
#48621=AXIS2_PLACEMENT_3D('',#97100,#58672,#58673);
#48622=AXIS2_PLACEMENT_3D('',#97101,#58674,#58675);
#48623=AXIS2_PLACEMENT_3D('',#97102,#58676,#58677);
#48624=AXIS2_PLACEMENT_3D('',#97103,#58678,#58679);
#48625=AXIS2_PLACEMENT_3D('',#97104,#58680,#58681);
#48626=AXIS2_PLACEMENT_3D('',#97105,#58682,#58683);
#48627=AXIS2_PLACEMENT_3D('',#97106,#58684,#58685);
#48628=AXIS2_PLACEMENT_3D('',#97115,#58690,#58691);
#48629=AXIS2_PLACEMENT_3D('',#97119,#58693,#58694);
#48630=AXIS2_PLACEMENT_3D('',#97120,#58695,#58696);
#48631=AXIS2_PLACEMENT_3D('',#97121,#58697,#58698);
#48632=AXIS2_PLACEMENT_3D('',#97127,#58702,#58703);
#48633=AXIS2_PLACEMENT_3D('',#97131,#58705,#58706);
#48634=AXIS2_PLACEMENT_3D('',#97132,#58707,#58708);
#48635=AXIS2_PLACEMENT_3D('',#97133,#58709,#58710);
#48636=AXIS2_PLACEMENT_3D('',#97139,#58714,#58715);
#48637=AXIS2_PLACEMENT_3D('',#97148,#58720,#58721);
#48638=AXIS2_PLACEMENT_3D('',#97152,#58723,#58724);
#48639=AXIS2_PLACEMENT_3D('',#97153,#58725,#58726);
#48640=AXIS2_PLACEMENT_3D('',#97154,#58727,#58728);
#48641=AXIS2_PLACEMENT_3D('',#97160,#58732,#58733);
#48642=AXIS2_PLACEMENT_3D('',#97164,#58735,#58736);
#48643=AXIS2_PLACEMENT_3D('',#97165,#58737,#58738);
#48644=AXIS2_PLACEMENT_3D('',#97166,#58739,#58740);
#48645=AXIS2_PLACEMENT_3D('',#97172,#58744,#58745);
#48646=AXIS2_PLACEMENT_3D('',#97173,#58746,#58747);
#48647=AXIS2_PLACEMENT_3D('',#97174,#58748,#58749);
#48648=AXIS2_PLACEMENT_3D('',#97175,#58750,#58751);
#48649=AXIS2_PLACEMENT_3D('',#97176,#58752,#58753);
#48650=AXIS2_PLACEMENT_3D('',#97177,#58754,#58755);
#48651=AXIS2_PLACEMENT_3D('',#97178,#58756,#58757);
#48652=AXIS2_PLACEMENT_3D('',#97179,#58758,#58759);
#48653=AXIS2_PLACEMENT_3D('',#97180,#58760,#58761);
#48654=AXIS2_PLACEMENT_3D('',#97181,#58762,#58763);
#48655=AXIS2_PLACEMENT_3D('',#97182,#58764,#58765);
#48656=AXIS2_PLACEMENT_3D('',#97183,#58766,#58767);
#48657=AXIS2_PLACEMENT_3D('',#97184,#58768,#58769);
#48658=AXIS2_PLACEMENT_3D('',#97185,#58770,#58771);
#48659=AXIS2_PLACEMENT_3D('',#97186,#58772,#58773);
#48660=AXIS2_PLACEMENT_3D('',#97187,#58774,#58775);
#48661=AXIS2_PLACEMENT_3D('',#97188,#58776,#58777);
#48662=AXIS2_PLACEMENT_3D('',#97189,#58778,#58779);
#48663=AXIS2_PLACEMENT_3D('',#97190,#58780,#58781);
#48664=AXIS2_PLACEMENT_3D('',#97191,#58782,#58783);
#48665=AXIS2_PLACEMENT_3D('',#97192,#58784,#58785);
#48666=AXIS2_PLACEMENT_3D('',#97193,#58786,#58787);
#48667=AXIS2_PLACEMENT_3D('',#97194,#58788,#58789);
#48668=AXIS2_PLACEMENT_3D('',#97195,#58790,#58791);
#48669=AXIS2_PLACEMENT_3D('',#97196,#58792,#58793);
#48670=AXIS2_PLACEMENT_3D('',#97197,#58794,#58795);
#48671=AXIS2_PLACEMENT_3D('',#97198,#58796,#58797);
#48672=AXIS2_PLACEMENT_3D('',#97199,#58798,#58799);
#48673=AXIS2_PLACEMENT_3D('',#97200,#58800,#58801);
#48674=AXIS2_PLACEMENT_3D('',#97201,#58802,#58803);
#48675=AXIS2_PLACEMENT_3D('',#97202,#58804,#58805);
#48676=AXIS2_PLACEMENT_3D('',#97203,#58806,#58807);
#48677=AXIS2_PLACEMENT_3D('',#97204,#58808,#58809);
#48678=AXIS2_PLACEMENT_3D('',#97205,#58810,#58811);
#48679=AXIS2_PLACEMENT_3D('',#97206,#58812,#58813);
#48680=AXIS2_PLACEMENT_3D('',#97207,#58814,#58815);
#48681=AXIS2_PLACEMENT_3D('',#97208,#58816,#58817);
#48682=AXIS2_PLACEMENT_3D('',#97209,#58818,#58819);
#48683=AXIS2_PLACEMENT_3D('',#97210,#58820,#58821);
#48684=AXIS2_PLACEMENT_3D('',#97211,#58822,#58823);
#48685=AXIS2_PLACEMENT_3D('',#97212,#58824,#58825);
#48686=AXIS2_PLACEMENT_3D('',#97213,#58826,#58827);
#48687=AXIS2_PLACEMENT_3D('',#97214,#58828,#58829);
#48688=AXIS2_PLACEMENT_3D('',#97215,#58830,#58831);
#48689=AXIS2_PLACEMENT_3D('',#97216,#58832,#58833);
#48690=AXIS2_PLACEMENT_3D('',#97217,#58834,#58835);
#48691=AXIS2_PLACEMENT_3D('',#97218,#58836,#58837);
#48692=AXIS2_PLACEMENT_3D('',#97219,#58838,#58839);
#48693=AXIS2_PLACEMENT_3D('',#97220,#58840,#58841);
#48694=AXIS2_PLACEMENT_3D('',#97221,#58842,#58843);
#48695=AXIS2_PLACEMENT_3D('',#97222,#58844,#58845);
#48696=AXIS2_PLACEMENT_3D('',#97223,#58846,#58847);
#48697=AXIS2_PLACEMENT_3D('',#97224,#58848,#58849);
#48698=AXIS2_PLACEMENT_3D('',#97225,#58850,#58851);
#48699=AXIS2_PLACEMENT_3D('',#97226,#58852,#58853);
#48700=AXIS2_PLACEMENT_3D('',#97227,#58854,#58855);
#48701=AXIS2_PLACEMENT_3D('',#97228,#58856,#58857);
#48702=AXIS2_PLACEMENT_3D('',#97229,#58858,#58859);
#48703=AXIS2_PLACEMENT_3D('',#97230,#58860,#58861);
#48704=AXIS2_PLACEMENT_3D('',#97231,#58862,#58863);
#48705=AXIS2_PLACEMENT_3D('',#97232,#58864,#58865);
#48706=AXIS2_PLACEMENT_3D('',#97233,#58866,#58867);
#48707=AXIS2_PLACEMENT_3D('',#97234,#58868,#58869);
#48708=AXIS2_PLACEMENT_3D('',#97235,#58870,#58871);
#48709=AXIS2_PLACEMENT_3D('',#97236,#58872,#58873);
#48710=AXIS2_PLACEMENT_3D('',#97237,#58874,#58875);
#48711=AXIS2_PLACEMENT_3D('',#97238,#58876,#58877);
#48712=AXIS2_PLACEMENT_3D('',#97239,#58878,#58879);
#48713=AXIS2_PLACEMENT_3D('',#97240,#58880,#58881);
#48714=AXIS2_PLACEMENT_3D('',#97241,#58882,#58883);
#48715=AXIS2_PLACEMENT_3D('',#97242,#58884,#58885);
#48716=AXIS2_PLACEMENT_3D('',#97243,#58886,#58887);
#48717=AXIS2_PLACEMENT_3D('',#97244,#58888,#58889);
#48718=AXIS2_PLACEMENT_3D('',#97245,#58890,#58891);
#48719=AXIS2_PLACEMENT_3D('',#97246,#58892,#58893);
#48720=AXIS2_PLACEMENT_3D('',#97247,#58894,#58895);
#48721=AXIS2_PLACEMENT_3D('',#97248,#58896,#58897);
#48722=AXIS2_PLACEMENT_3D('',#97249,#58898,#58899);
#48723=AXIS2_PLACEMENT_3D('',#97250,#58900,#58901);
#48724=AXIS2_PLACEMENT_3D('',#97251,#58902,#58903);
#48725=AXIS2_PLACEMENT_3D('',#97252,#58904,#58905);
#48726=AXIS2_PLACEMENT_3D('',#97253,#58906,#58907);
#48727=AXIS2_PLACEMENT_3D('',#97254,#58908,#58909);
#48728=AXIS2_PLACEMENT_3D('',#97255,#58910,#58911);
#48729=AXIS2_PLACEMENT_3D('',#97256,#58912,#58913);
#48730=AXIS2_PLACEMENT_3D('',#97257,#58914,#58915);
#48731=AXIS2_PLACEMENT_3D('',#97258,#58916,#58917);
#48732=AXIS2_PLACEMENT_3D('',#97259,#58918,#58919);
#48733=AXIS2_PLACEMENT_3D('',#97260,#58920,#58921);
#48734=AXIS2_PLACEMENT_3D('',#97261,#58922,#58923);
#48735=AXIS2_PLACEMENT_3D('',#97262,#58924,#58925);
#48736=AXIS2_PLACEMENT_3D('',#97263,#58926,#58927);
#48737=AXIS2_PLACEMENT_3D('',#97264,#58928,#58929);
#48738=AXIS2_PLACEMENT_3D('',#97265,#58930,#58931);
#48739=AXIS2_PLACEMENT_3D('',#97266,#58932,#58933);
#48740=AXIS2_PLACEMENT_3D('',#97267,#58934,#58935);
#48741=AXIS2_PLACEMENT_3D('',#97268,#58936,#58937);
#48742=AXIS2_PLACEMENT_3D('',#97269,#58938,#58939);
#48743=AXIS2_PLACEMENT_3D('',#97270,#58940,#58941);
#48744=AXIS2_PLACEMENT_3D('',#97271,#58942,#58943);
#48745=AXIS2_PLACEMENT_3D('',#97272,#58944,#58945);
#48746=AXIS2_PLACEMENT_3D('',#97273,#58946,#58947);
#48747=AXIS2_PLACEMENT_3D('',#97274,#58948,#58949);
#48748=AXIS2_PLACEMENT_3D('',#97275,#58950,#58951);
#48749=AXIS2_PLACEMENT_3D('',#97276,#58952,#58953);
#48750=AXIS2_PLACEMENT_3D('',#97277,#58954,#58955);
#48751=AXIS2_PLACEMENT_3D('',#97278,#58956,#58957);
#48752=AXIS2_PLACEMENT_3D('',#97279,#58958,#58959);
#48753=AXIS2_PLACEMENT_3D('',#97280,#58960,#58961);
#48754=AXIS2_PLACEMENT_3D('',#97281,#58962,#58963);
#48755=AXIS2_PLACEMENT_3D('',#97284,#58964,#58965);
#48756=AXIS2_PLACEMENT_3D('',#97285,#58966,#58967);
#48757=AXIS2_PLACEMENT_3D('',#97287,#58968,#58969);
#48758=AXIS2_PLACEMENT_3D('',#97288,#58970,#58971);
#48759=AXIS2_PLACEMENT_3D('',#97289,#58972,#58973);
#48760=AXIS2_PLACEMENT_3D('',#97292,#58974,#58975);
#48761=AXIS2_PLACEMENT_3D('',#97294,#58976,#58977);
#48762=AXIS2_PLACEMENT_3D('',#97296,#58978,#58979);
#48763=AXIS2_PLACEMENT_3D('',#97297,#58980,#58981);
#48764=AXIS2_PLACEMENT_3D('',#97298,#58982,#58983);
#48765=AXIS2_PLACEMENT_3D('',#97301,#58984,#58985);
#48766=AXIS2_PLACEMENT_3D('',#97303,#58986,#58987);
#48767=AXIS2_PLACEMENT_3D('',#97305,#58988,#58989);
#48768=AXIS2_PLACEMENT_3D('',#97306,#58990,#58991);
#48769=AXIS2_PLACEMENT_3D('',#97307,#58992,#58993);
#48770=AXIS2_PLACEMENT_3D('',#97310,#58994,#58995);
#48771=AXIS2_PLACEMENT_3D('',#97312,#58996,#58997);
#48772=AXIS2_PLACEMENT_3D('',#97314,#58998,#58999);
#48773=AXIS2_PLACEMENT_3D('',#97316,#59000,#59001);
#48774=AXIS2_PLACEMENT_3D('',#97317,#59002,#59003);
#48775=AXIS2_PLACEMENT_3D('',#97318,#59004,#59005);
#48776=AXIS2_PLACEMENT_3D('',#97361,#59008,#59009);
#48777=AXIS2_PLACEMENT_3D('',#97407,#59011,#59012);
#48778=AXIS2_PLACEMENT_3D('',#97409,#59013,#59014);
#48779=AXIS2_PLACEMENT_3D('',#97411,#59015,#59016);
#48780=AXIS2_PLACEMENT_3D('',#97412,#59017,#59018);
#48781=AXIS2_PLACEMENT_3D('',#97413,#59019,#59020);
#48782=AXIS2_PLACEMENT_3D('',#97415,#59021,#59022);
#48783=AXIS2_PLACEMENT_3D('',#97417,#59023,#59024);
#48784=AXIS2_PLACEMENT_3D('',#97418,#59025,#59026);
#48785=AXIS2_PLACEMENT_3D('',#97419,#59027,#59028);
#48786=AXIS2_PLACEMENT_3D('',#97779,#59030,#59031);
#48787=AXIS2_PLACEMENT_3D('',#97840,#59032,#59033);
#48788=AXIS2_PLACEMENT_3D('',#98062,#59034,#59035);
#48789=AXIS2_PLACEMENT_3D('',#98288,#59036,#59037);
#48790=AXIS2_PLACEMENT_3D('',#98666,#59038,#59039);
#48791=AXIS2_PLACEMENT_3D('',#98868,#59040,#59041);
#48792=AXIS2_PLACEMENT_3D('',#98869,#59042,#59043);
#48793=AXIS2_PLACEMENT_3D('',#98870,#59044,#59045);
#48794=AXIS2_PLACEMENT_3D('',#98901,#59047,#59048);
#48795=AXIS2_PLACEMENT_3D('',#98980,#59049,#59050);
#48796=AXIS2_PLACEMENT_3D('',#99560,#59052,#59053);
#48797=AXIS2_PLACEMENT_3D('',#99747,#59054,#59055);
#48798=AXIS2_PLACEMENT_3D('',#99973,#59056,#59057);
#48799=AXIS2_PLACEMENT_3D('',#100032,#59058,#59059);
#48800=AXIS2_PLACEMENT_3D('',#100265,#59060,#59061);
#48801=AXIS2_PLACEMENT_3D('',#100324,#59062,#59063);
#48802=AXIS2_PLACEMENT_3D('',#100338,#59064,#59065);
#48803=AXIS2_PLACEMENT_3D('',#100340,#59066,#59067);
#48804=AXIS2_PLACEMENT_3D('',#100341,#59068,#59069);
#48805=AXIS2_PLACEMENT_3D('',#100342,#59070,#59071);
#48806=AXIS2_PLACEMENT_3D('',#100345,#59072,#59073);
#48807=AXIS2_PLACEMENT_3D('',#100346,#59074,#59075);
#48808=AXIS2_PLACEMENT_3D('',#100348,#59076,#59077);
#48809=AXIS2_PLACEMENT_3D('',#100349,#59078,#59079);
#48810=AXIS2_PLACEMENT_3D('',#100350,#59080,#59081);
#48811=AXIS2_PLACEMENT_3D('',#100752,#59083,#59084);
#48812=AXIS2_PLACEMENT_3D('',#101616,#59086,#59087);
#48813=AXIS2_PLACEMENT_3D('',#101802,#59088,#59089);
#48814=AXIS2_PLACEMENT_3D('',#102185,#59090,#59091);
#48815=AXIS2_PLACEMENT_3D('',#102252,#59092,#59093);
#48816=AXIS2_PLACEMENT_3D('',#102605,#59094,#59095);
#48817=AXIS2_PLACEMENT_3D('',#102822,#59096,#59097);
#48818=AXIS2_PLACEMENT_3D('',#102823,#59098,#59099);
#48819=AXIS2_PLACEMENT_3D('',#102824,#59100,#59101);
#48820=AXIS2_PLACEMENT_3D('',#102930,#59103,#59104);
#48821=AXIS2_PLACEMENT_3D('',#102931,#59105,#59106);
#48822=AXIS2_PLACEMENT_3D('',#103307,#59108,#59109);
#48823=AXIS2_PLACEMENT_3D('',#103327,#59110,#59111);
#48824=AXIS2_PLACEMENT_3D('',#103328,#59112,#59113);
#48825=AXIS2_PLACEMENT_3D('',#103500,#59115,#59116);
#48826=AXIS2_PLACEMENT_3D('',#103580,#59117,#59118);
#48827=AXIS2_PLACEMENT_3D('',#103792,#59119,#59120);
#48828=AXIS2_PLACEMENT_3D('',#104545,#59121,#59122);
#48829=AXIS2_PLACEMENT_3D('',#105183,#59123,#59124);
#48830=AXIS2_PLACEMENT_3D('',#105184,#59125,#59126);
#48831=AXIS2_PLACEMENT_3D('',#105937,#59127,#59128);
#48832=AXIS2_PLACEMENT_3D('',#105940,#59129,#59130);
#48833=AXIS2_PLACEMENT_3D('',#105944,#59132,#59133);
#48834=AXIS2_PLACEMENT_3D('',#105946,#59135,#59136);
#48835=AXIS2_PLACEMENT_3D('',#105950,#59138,#59139);
#48836=AXIS2_PLACEMENT_3D('',#105955,#59142,#59143);
#48837=AXIS2_PLACEMENT_3D('',#105957,#59145,#59146);
#48838=AXIS2_PLACEMENT_3D('',#105960,#59147,#59148);
#48839=AXIS2_PLACEMENT_3D('',#105965,#59151,#59152);
#48840=AXIS2_PLACEMENT_3D('',#105968,#59155,#59156);
#48841=AXIS2_PLACEMENT_3D('',#105971,#59157,#59158);
#48842=AXIS2_PLACEMENT_3D('',#105975,#59160,#59161);
#48843=AXIS2_PLACEMENT_3D('',#105977,#59163,#59164);
#48844=AXIS2_PLACEMENT_3D('',#105980,#59167,#59168);
#48845=AXIS2_PLACEMENT_3D('',#105983,#59169,#59170);
#48846=AXIS2_PLACEMENT_3D('',#105986,#59173,#59174);
#48847=AXIS2_PLACEMENT_3D('',#105989,#59177,#59178);
#48848=AXIS2_PLACEMENT_3D('',#106028,#59183,#59184);
#48849=AXIS2_PLACEMENT_3D('',#106067,#59189,#59190);
#48850=AXIS2_PLACEMENT_3D('',#106117,#59191,#59192);
#48851=AXIS2_PLACEMENT_3D('',#106118,#59193,#59194);
#48852=AXIS2_PLACEMENT_3D('',#106198,#59195,#59196);
#48853=AXIS2_PLACEMENT_3D('',#106199,#59197,#59198);
#48854=AXIS2_PLACEMENT_3D('',#106200,#59199,#59200);
#48855=AXIS2_PLACEMENT_3D('',#106280,#59201,#59202);
#48856=AXIS2_PLACEMENT_3D('',#106336,#59203,#59204);
#48857=AXIS2_PLACEMENT_3D('',#106337,#59205,#59206);
#48858=AXIS2_PLACEMENT_3D('',#106338,#59207,#59208);
#48859=AXIS2_PLACEMENT_3D('',#106388,#59209,#59210);
#48860=AXIS2_PLACEMENT_3D('',#106389,#59211,#59212);
#48861=AXIS2_PLACEMENT_3D('',#106390,#59213,#59214);
#48862=AXIS2_PLACEMENT_3D('',#106391,#59215,#59216);
#48863=AXIS2_PLACEMENT_3D('',#106392,#59217,#59218);
#48864=AXIS2_PLACEMENT_3D('',#106433,#59219,#59220);
#48865=AXIS2_PLACEMENT_3D('',#106434,#59221,#59222);
#48866=AXIS2_PLACEMENT_3D('',#106435,#59223,#59224);
#48867=AXIS2_PLACEMENT_3D('',#106436,#59225,#59226);
#48868=AXIS2_PLACEMENT_3D('',#106437,#59227,#59228);
#48869=AXIS2_PLACEMENT_3D('',#106438,#59229,#59230);
#48870=AXIS2_PLACEMENT_3D('',#106439,#59231,#59232);
#48871=AXIS2_PLACEMENT_3D('',#106440,#59233,#59234);
#48872=AXIS2_PLACEMENT_3D('',#106483,#59235,#59236);
#48873=AXIS2_PLACEMENT_3D('',#106484,#59237,#59238);
#48874=AXIS2_PLACEMENT_3D('',#106485,#59239,#59240);
#48875=AXIS2_PLACEMENT_3D('',#106486,#59241,#59242);
#48876=AXIS2_PLACEMENT_3D('',#106487,#59243,#59244);
#48877=AXIS2_PLACEMENT_3D('',#106488,#59245,#59246);
#48878=AXIS2_PLACEMENT_3D('',#106489,#59247,#59248);
#48879=AXIS2_PLACEMENT_3D('',#106490,#59249,#59250);
#48880=AXIS2_PLACEMENT_3D('',#106491,#59251,#59252);
#48881=AXIS2_PLACEMENT_3D('',#106492,#59253,#59254);
#48882=AXIS2_PLACEMENT_3D('',#106493,#59255,#59256);
#48883=AXIS2_PLACEMENT_3D('',#106524,#59257,#59258);
#48884=AXIS2_PLACEMENT_3D('',#106525,#59259,#59260);
#48885=AXIS2_PLACEMENT_3D('',#106526,#59261,#59262);
#48886=AXIS2_PLACEMENT_3D('',#106527,#59263,#59264);
#48887=AXIS2_PLACEMENT_3D('',#106528,#59265,#59266);
#48888=AXIS2_PLACEMENT_3D('',#106529,#59267,#59268);
#48889=AXIS2_PLACEMENT_3D('',#106530,#59269,#59270);
#48890=AXIS2_PLACEMENT_3D('',#106573,#59271,#59272);
#48891=AXIS2_PLACEMENT_3D('',#106574,#59273,#59274);
#48892=AXIS2_PLACEMENT_3D('',#106575,#59275,#59276);
#48893=AXIS2_PLACEMENT_3D('',#106576,#59277,#59278);
#48894=AXIS2_PLACEMENT_3D('',#106578,#59279,#59280);
#48895=AXIS2_PLACEMENT_3D('',#106581,#59282,#59283);
#48896=AXIS2_PLACEMENT_3D('',#106582,#59284,#59285);
#48897=AXIS2_PLACEMENT_3D('',#106584,#59286,#59287);
#48898=AXIS2_PLACEMENT_3D('',#106587,#59289,#59290);
#48899=AXIS2_PLACEMENT_3D('',#106588,#59291,#59292);
#48900=AXIS2_PLACEMENT_3D('',#106589,#59293,#59294);
#48901=AXIS2_PLACEMENT_3D('',#106590,#59295,#59296);
#48902=AXIS2_PLACEMENT_3D('',#106591,#59297,#59298);
#48903=AXIS2_PLACEMENT_3D('',#106606,#59299,#59300);
#48904=AXIS2_PLACEMENT_3D('',#106612,#59301,#59302);
#48905=AXIS2_PLACEMENT_3D('',#110373,#59303,#59304);
#48906=AXIS2_PLACEMENT_3D('',#110375,#59305,#59306);
#48907=AXIS2_PLACEMENT_3D('',#110377,#59307,#59308);
#48908=AXIS2_PLACEMENT_3D('',#110378,#59309,#59310);
#48909=AXIS2_PLACEMENT_3D('',#110379,#59311,#59312);
#48910=AXIS2_PLACEMENT_3D('',#110420,#59314,#59315);
#48911=AXIS2_PLACEMENT_3D('',#110448,#59317,#59318);
#48912=AXIS2_PLACEMENT_3D('',#110469,#59319,#59320);
#48913=AXIS2_PLACEMENT_3D('',#110510,#59322,#59323);
#48914=AXIS2_PLACEMENT_3D('',#110537,#59325,#59326);
#48915=AXIS2_PLACEMENT_3D('',#110561,#59327,#59328);
#48916=AXIS2_PLACEMENT_3D('',#110602,#59330,#59331);
#48917=AXIS2_PLACEMENT_3D('',#110632,#59333,#59334);
#48918=AXIS2_PLACEMENT_3D('',#110653,#59335,#59336);
#48919=AXIS2_PLACEMENT_3D('',#110694,#59338,#59339);
#48920=AXIS2_PLACEMENT_3D('',#110721,#59341,#59342);
#48921=AXIS2_PLACEMENT_3D('',#110742,#59343,#59344);
#48922=AXIS2_PLACEMENT_3D('',#110781,#59346,#59347);
#48923=AXIS2_PLACEMENT_3D('',#110811,#59349,#59350);
#48924=AXIS2_PLACEMENT_3D('',#110830,#59351,#59352);
#48925=AXIS2_PLACEMENT_3D('',#110871,#59354,#59355);
#48926=AXIS2_PLACEMENT_3D('',#110898,#59357,#59358);
#48927=AXIS2_PLACEMENT_3D('',#110922,#59359,#59360);
#48928=AXIS2_PLACEMENT_3D('',#110963,#59362,#59363);
#48929=AXIS2_PLACEMENT_3D('',#110990,#59365,#59366);
#48930=AXIS2_PLACEMENT_3D('',#111014,#59367,#59368);
#48931=AXIS2_PLACEMENT_3D('',#111055,#59370,#59371);
#48932=AXIS2_PLACEMENT_3D('',#111085,#59373,#59374);
#48933=AXIS2_PLACEMENT_3D('',#111106,#59375,#59376);
#48934=AXIS2_PLACEMENT_3D('',#111145,#59378,#59379);
#48935=AXIS2_PLACEMENT_3D('',#111170,#59381,#59382);
#48936=AXIS2_PLACEMENT_3D('',#111192,#59383,#59384);
#48937=AXIS2_PLACEMENT_3D('',#111233,#59386,#59387);
#48938=AXIS2_PLACEMENT_3D('',#111260,#59389,#59390);
#48939=AXIS2_PLACEMENT_3D('',#111284,#59391,#59392);
#48940=AXIS2_PLACEMENT_3D('',#111325,#59394,#59395);
#48941=AXIS2_PLACEMENT_3D('',#111352,#59397,#59398);
#48942=AXIS2_PLACEMENT_3D('',#111376,#59399,#59400);
#48943=AXIS2_PLACEMENT_3D('',#111417,#59402,#59403);
#48944=AXIS2_PLACEMENT_3D('',#111444,#59405,#59406);
#48945=AXIS2_PLACEMENT_3D('',#111465,#59407,#59408);
#48946=AXIS2_PLACEMENT_3D('',#111504,#59410,#59411);
#48947=AXIS2_PLACEMENT_3D('',#111532,#59413,#59414);
#48948=AXIS2_PLACEMENT_3D('',#111553,#59415,#59416);
#48949=AXIS2_PLACEMENT_3D('',#111594,#59418,#59419);
#48950=AXIS2_PLACEMENT_3D('',#111624,#59421,#59422);
#48951=AXIS2_PLACEMENT_3D('',#111645,#59423,#59424);
#48952=AXIS2_PLACEMENT_3D('',#111686,#59426,#59427);
#48953=AXIS2_PLACEMENT_3D('',#111716,#59429,#59430);
#48954=AXIS2_PLACEMENT_3D('',#111737,#59431,#59432);
#48955=AXIS2_PLACEMENT_3D('',#111778,#59434,#59435);
#48956=AXIS2_PLACEMENT_3D('',#111803,#59437,#59438);
#48957=AXIS2_PLACEMENT_3D('',#111883,#59439,#59440);
#48958=AXIS2_PLACEMENT_3D('',#111922,#59442,#59443);
#48959=AXIS2_PLACEMENT_3D('',#111950,#59445,#59446);
#48960=AXIS2_PLACEMENT_3D('',#111971,#59447,#59448);
#48961=AXIS2_PLACEMENT_3D('',#112012,#59450,#59451);
#48962=AXIS2_PLACEMENT_3D('',#112039,#59453,#59454);
#48963=AXIS2_PLACEMENT_3D('',#112063,#59455,#59456);
#48964=AXIS2_PLACEMENT_3D('',#112102,#59458,#59459);
#48965=AXIS2_PLACEMENT_3D('',#112129,#59461,#59462);
#48966=AXIS2_PLACEMENT_3D('',#112151,#59463,#59464);
#48967=AXIS2_PLACEMENT_3D('',#112192,#59466,#59467);
#48968=AXIS2_PLACEMENT_3D('',#112219,#59469,#59470);
#48969=AXIS2_PLACEMENT_3D('',#112240,#59471,#59472);
#48970=AXIS2_PLACEMENT_3D('',#112279,#59474,#59475);
#48971=AXIS2_PLACEMENT_3D('',#112309,#59477,#59478);
#48972=AXIS2_PLACEMENT_3D('',#112330,#59479,#59480);
#48973=AXIS2_PLACEMENT_3D('',#112371,#59482,#59483);
#48974=AXIS2_PLACEMENT_3D('',#112398,#59485,#59486);
#48975=AXIS2_PLACEMENT_3D('',#112422,#59487,#59488);
#48976=AXIS2_PLACEMENT_3D('',#112461,#59490,#59491);
#48977=AXIS2_PLACEMENT_3D('',#112489,#59493,#59494);
#48978=AXIS2_PLACEMENT_3D('',#112508,#59495,#59496);
#48979=AXIS2_PLACEMENT_3D('',#112547,#59498,#59499);
#48980=AXIS2_PLACEMENT_3D('',#112574,#59501,#59502);
#48981=AXIS2_PLACEMENT_3D('',#112598,#59503,#59504);
#48982=AXIS2_PLACEMENT_3D('',#112637,#59506,#59507);
#48983=AXIS2_PLACEMENT_3D('',#112667,#59509,#59510);
#48984=AXIS2_PLACEMENT_3D('',#112688,#59511,#59512);
#48985=AXIS2_PLACEMENT_3D('',#112729,#59514,#59515);
#48986=AXIS2_PLACEMENT_3D('',#112756,#59517,#59518);
#48987=AXIS2_PLACEMENT_3D('',#112777,#59519,#59520);
#48988=AXIS2_PLACEMENT_3D('',#112818,#59522,#59523);
#48989=AXIS2_PLACEMENT_3D('',#112843,#59525,#59526);
#48990=AXIS2_PLACEMENT_3D('',#112864,#59527,#59528);
#48991=AXIS2_PLACEMENT_3D('',#113014,#59530,#59531);
#48992=AXIS2_PLACEMENT_3D('',#113041,#59533,#59534);
#48993=AXIS2_PLACEMENT_3D('',#113065,#59535,#59536);
#48994=AXIS2_PLACEMENT_3D('',#113104,#59538,#59539);
#48995=AXIS2_PLACEMENT_3D('',#113134,#59541,#59542);
#48996=AXIS2_PLACEMENT_3D('',#113155,#59543,#59544);
#48997=AXIS2_PLACEMENT_3D('',#113196,#59546,#59547);
#48998=AXIS2_PLACEMENT_3D('',#113223,#59549,#59550);
#48999=AXIS2_PLACEMENT_3D('',#113244,#59551,#59552);
#49000=AXIS2_PLACEMENT_3D('',#113283,#59554,#59555);
#49001=AXIS2_PLACEMENT_3D('',#113308,#59557,#59558);
#49002=AXIS2_PLACEMENT_3D('',#113329,#59559,#59560);
#49003=AXIS2_PLACEMENT_3D('',#113421,#59562,#59563);
#49004=AXIS2_PLACEMENT_3D('',#113448,#59565,#59566);
#49005=AXIS2_PLACEMENT_3D('',#113470,#59567,#59568);
#49006=AXIS2_PLACEMENT_3D('',#113562,#59570,#59571);
#49007=AXIS2_PLACEMENT_3D('',#113589,#59573,#59574);
#49008=AXIS2_PLACEMENT_3D('',#113610,#59575,#59576);
#49009=AXIS2_PLACEMENT_3D('',#113651,#59578,#59579);
#49010=AXIS2_PLACEMENT_3D('',#113678,#59581,#59582);
#49011=AXIS2_PLACEMENT_3D('',#113699,#59583,#59584);
#49012=AXIS2_PLACEMENT_3D('',#113738,#59586,#59587);
#49013=AXIS2_PLACEMENT_3D('',#113765,#59589,#59590);
#49014=AXIS2_PLACEMENT_3D('',#113786,#59591,#59592);
#49015=AXIS2_PLACEMENT_3D('',#113878,#59594,#59595);
#49016=AXIS2_PLACEMENT_3D('',#113903,#59597,#59598);
#49017=AXIS2_PLACEMENT_3D('',#113927,#59599,#59600);
#49018=AXIS2_PLACEMENT_3D('',#114021,#59602,#59603);
#49019=AXIS2_PLACEMENT_3D('',#114048,#59605,#59606);
#49020=AXIS2_PLACEMENT_3D('',#114069,#59607,#59608);
#49021=AXIS2_PLACEMENT_3D('',#114161,#59610,#59611);
#49022=AXIS2_PLACEMENT_3D('',#114188,#59613,#59614);
#49023=AXIS2_PLACEMENT_3D('',#114212,#59615,#59616);
#49024=AXIS2_PLACEMENT_3D('',#114304,#59618,#59619);
#49025=AXIS2_PLACEMENT_3D('',#114331,#59621,#59622);
#49026=AXIS2_PLACEMENT_3D('',#114352,#59623,#59624);
#49027=AXIS2_PLACEMENT_3D('',#114442,#59626,#59627);
#49028=AXIS2_PLACEMENT_3D('',#114467,#59629,#59630);
#49029=AXIS2_PLACEMENT_3D('',#114491,#59631,#59632);
#49030=AXIS2_PLACEMENT_3D('',#114587,#59634,#59635);
#49031=AXIS2_PLACEMENT_3D('',#114614,#59637,#59638);
#49032=AXIS2_PLACEMENT_3D('',#114635,#59639,#59640);
#49033=AXIS2_PLACEMENT_3D('',#114729,#59642,#59643);
#49034=AXIS2_PLACEMENT_3D('',#114756,#59645,#59646);
#49035=AXIS2_PLACEMENT_3D('',#114777,#59647,#59648);
#49036=AXIS2_PLACEMENT_3D('',#114871,#59650,#59651);
#49037=AXIS2_PLACEMENT_3D('',#114898,#59653,#59654);
#49038=AXIS2_PLACEMENT_3D('',#114919,#59655,#59656);
#49039=AXIS2_PLACEMENT_3D('',#115013,#59658,#59659);
#49040=AXIS2_PLACEMENT_3D('',#115038,#59661,#59662);
#49041=AXIS2_PLACEMENT_3D('',#115060,#59663,#59664);
#49042=AXIS2_PLACEMENT_3D('',#115156,#59666,#59667);
#49043=AXIS2_PLACEMENT_3D('',#115183,#59669,#59670);
#49044=AXIS2_PLACEMENT_3D('',#115207,#59671,#59672);
#49045=AXIS2_PLACEMENT_3D('',#115301,#59674,#59675);
#49046=AXIS2_PLACEMENT_3D('',#115329,#59677,#59678);
#49047=AXIS2_PLACEMENT_3D('',#115348,#59679,#59680);
#49048=AXIS2_PLACEMENT_3D('',#115444,#59682,#59683);
#49049=AXIS2_PLACEMENT_3D('',#115474,#59685,#59686);
#49050=AXIS2_PLACEMENT_3D('',#115495,#59687,#59688);
#49051=AXIS2_PLACEMENT_3D('',#115591,#59690,#59691);
#49052=AXIS2_PLACEMENT_3D('',#115614,#59693,#59694);
#49053=AXIS2_PLACEMENT_3D('',#115640,#59695,#59696);
#49054=AXIS2_PLACEMENT_3D('',#115736,#59698,#59699);
#49055=AXIS2_PLACEMENT_3D('',#115763,#59701,#59702);
#49056=AXIS2_PLACEMENT_3D('',#115784,#59703,#59704);
#49057=AXIS2_PLACEMENT_3D('',#115878,#59706,#59707);
#49058=AXIS2_PLACEMENT_3D('',#115903,#59709,#59710);
#49059=AXIS2_PLACEMENT_3D('',#115925,#59711,#59712);
#49060=AXIS2_PLACEMENT_3D('',#116023,#59714,#59715);
#49061=AXIS2_PLACEMENT_3D('',#116050,#59717,#59718);
#49062=AXIS2_PLACEMENT_3D('',#116071,#59719,#59720);
#49063=AXIS2_PLACEMENT_3D('',#116165,#59722,#59723);
#49064=AXIS2_PLACEMENT_3D('',#116188,#59725,#59726);
#49065=AXIS2_PLACEMENT_3D('',#116214,#59727,#59728);
#49066=AXIS2_PLACEMENT_3D('',#116310,#59730,#59731);
#49067=AXIS2_PLACEMENT_3D('',#116337,#59733,#59734);
#49068=AXIS2_PLACEMENT_3D('',#116361,#59735,#59736);
#49069=AXIS2_PLACEMENT_3D('',#116457,#59738,#59739);
#49070=AXIS2_PLACEMENT_3D('',#116482,#59741,#59742);
#49071=AXIS2_PLACEMENT_3D('',#116506,#59743,#59744);
#49072=AXIS2_PLACEMENT_3D('',#116604,#59746,#59747);
#49073=AXIS2_PLACEMENT_3D('',#116631,#59749,#59750);
#49074=AXIS2_PLACEMENT_3D('',#116655,#59751,#59752);
#49075=AXIS2_PLACEMENT_3D('',#116751,#59754,#59755);
#49076=AXIS2_PLACEMENT_3D('',#116774,#59757,#59758);
#49077=AXIS2_PLACEMENT_3D('',#116800,#59759,#59760);
#49078=AXIS2_PLACEMENT_3D('',#116896,#59762,#59763);
#49079=AXIS2_PLACEMENT_3D('',#116921,#59765,#59766);
#49080=AXIS2_PLACEMENT_3D('',#116947,#59767,#59768);
#49081=AXIS2_PLACEMENT_3D('',#117043,#59770,#59771);
#49082=AXIS2_PLACEMENT_3D('',#117069,#59773,#59774);
#49083=AXIS2_PLACEMENT_3D('',#117092,#59775,#59776);
#49084=AXIS2_PLACEMENT_3D('',#117190,#59778,#59779);
#49085=AXIS2_PLACEMENT_3D('',#117217,#59781,#59782);
#49086=AXIS2_PLACEMENT_3D('',#117241,#59783,#59784);
#49087=AXIS2_PLACEMENT_3D('',#117337,#59786,#59787);
#49088=AXIS2_PLACEMENT_3D('',#117362,#59789,#59790);
#49089=AXIS2_PLACEMENT_3D('',#117386,#59791,#59792);
#49090=AXIS2_PLACEMENT_3D('',#117480,#59794,#59795);
#49091=AXIS2_PLACEMENT_3D('',#117505,#59797,#59798);
#49092=AXIS2_PLACEMENT_3D('',#117531,#59799,#59800);
#49093=AXIS2_PLACEMENT_3D('',#117629,#59802,#59803);
#49094=AXIS2_PLACEMENT_3D('',#117659,#59805,#59806);
#49095=AXIS2_PLACEMENT_3D('',#117680,#59807,#59808);
#49096=AXIS2_PLACEMENT_3D('',#117778,#59810,#59811);
#49097=AXIS2_PLACEMENT_3D('',#117803,#59813,#59814);
#49098=AXIS2_PLACEMENT_3D('',#117829,#59815,#59816);
#49099=AXIS2_PLACEMENT_3D('',#118032,#59818,#59819);
#49100=AXIS2_PLACEMENT_3D('',#118059,#59821,#59822);
#49101=AXIS2_PLACEMENT_3D('',#118083,#59823,#59824);
#49102=AXIS2_PLACEMENT_3D('',#118179,#59826,#59827);
#49103=AXIS2_PLACEMENT_3D('',#118205,#59829,#59830);
#49104=AXIS2_PLACEMENT_3D('',#118228,#59831,#59832);
#49105=AXIS2_PLACEMENT_3D('',#118326,#59834,#59835);
#49106=AXIS2_PLACEMENT_3D('',#118351,#59837,#59838);
#49107=AXIS2_PLACEMENT_3D('',#118377,#59839,#59840);
#49108=AXIS2_PLACEMENT_3D('',#118475,#59842,#59843);
#49109=AXIS2_PLACEMENT_3D('',#118503,#59845,#59846);
#49110=AXIS2_PLACEMENT_3D('',#118526,#59847,#59848);
#49111=AXIS2_PLACEMENT_3D('',#118729,#59850,#59851);
#49112=AXIS2_PLACEMENT_3D('',#118754,#59853,#59854);
#49113=AXIS2_PLACEMENT_3D('',#118780,#59855,#59856);
#49114=AXIS2_PLACEMENT_3D('',#118872,#59858,#59859);
#49115=AXIS2_PLACEMENT_3D('',#118900,#59861,#59862);
#49116=AXIS2_PLACEMENT_3D('',#118921,#59863,#59864);
#49117=AXIS2_PLACEMENT_3D('',#119019,#59866,#59867);
#49118=AXIS2_PLACEMENT_3D('',#119049,#59869,#59870);
#49119=AXIS2_PLACEMENT_3D('',#119070,#59871,#59872);
#49120=AXIS2_PLACEMENT_3D('',#119168,#59874,#59875);
#49121=AXIS2_PLACEMENT_3D('',#119196,#59877,#59878);
#49122=AXIS2_PLACEMENT_3D('',#119219,#59879,#59880);
#49123=AXIS2_PLACEMENT_3D('',#119523,#59882,#59883);
#49124=AXIS2_PLACEMENT_3D('',#119550,#59885,#59886);
#49125=AXIS2_PLACEMENT_3D('',#119574,#59887,#59888);
#49126=AXIS2_PLACEMENT_3D('',#119668,#59890,#59891);
#49127=AXIS2_PLACEMENT_3D('',#119693,#59893,#59894);
#49128=AXIS2_PLACEMENT_3D('',#119719,#59895,#59896);
#49129=AXIS2_PLACEMENT_3D('',#119817,#59898,#59899);
#49130=AXIS2_PLACEMENT_3D('',#119842,#59901,#59902);
#49131=AXIS2_PLACEMENT_3D('',#119868,#59903,#59904);
#49132=AXIS2_PLACEMENT_3D('',#119964,#59906,#59907);
#49133=AXIS2_PLACEMENT_3D('',#119989,#59909,#59910);
#49134=AXIS2_PLACEMENT_3D('',#120013,#59911,#59912);
#49135=AXIS2_PLACEMENT_3D('',#120109,#59914,#59915);
#49136=AXIS2_PLACEMENT_3D('',#120134,#59917,#59918);
#49137=AXIS2_PLACEMENT_3D('',#120160,#59919,#59920);
#49138=AXIS2_PLACEMENT_3D('',#120254,#59922,#59923);
#49139=AXIS2_PLACEMENT_3D('',#120281,#59925,#59926);
#49140=AXIS2_PLACEMENT_3D('',#120303,#59927,#59928);
#49141=AXIS2_PLACEMENT_3D('',#120401,#59930,#59931);
#49142=AXIS2_PLACEMENT_3D('',#120431,#59933,#59934);
#49143=AXIS2_PLACEMENT_3D('',#120452,#59935,#59936);
#49144=AXIS2_PLACEMENT_3D('',#120548,#59938,#59939);
#49145=AXIS2_PLACEMENT_3D('',#120576,#59941,#59942);
#49146=AXIS2_PLACEMENT_3D('',#120599,#59943,#59944);
#49147=AXIS2_PLACEMENT_3D('',#120693,#59946,#59947);
#49148=AXIS2_PLACEMENT_3D('',#120720,#59949,#59950);
#49149=AXIS2_PLACEMENT_3D('',#120744,#59951,#59952);
#49150=AXIS2_PLACEMENT_3D('',#120838,#59954,#59955);
#49151=AXIS2_PLACEMENT_3D('',#120865,#59957,#59958);
#49152=AXIS2_PLACEMENT_3D('',#120887,#59959,#59960);
#49153=AXIS2_PLACEMENT_3D('',#120983,#59962,#59963);
#49154=AXIS2_PLACEMENT_3D('',#121013,#59965,#59966);
#49155=AXIS2_PLACEMENT_3D('',#121034,#59967,#59968);
#49156=AXIS2_PLACEMENT_3D('',#121126,#59970,#59971);
#49157=AXIS2_PLACEMENT_3D('',#121151,#59973,#59974);
#49158=AXIS2_PLACEMENT_3D('',#121175,#59975,#59976);
#49159=AXIS2_PLACEMENT_3D('',#121265,#59978,#59979);
#49160=AXIS2_PLACEMENT_3D('',#121288,#59981,#59982);
#49161=AXIS2_PLACEMENT_3D('',#121314,#59983,#59984);
#49162=AXIS2_PLACEMENT_3D('',#121406,#59986,#59987);
#49163=AXIS2_PLACEMENT_3D('',#121433,#59989,#59990);
#49164=AXIS2_PLACEMENT_3D('',#121455,#59991,#59992);
#49165=AXIS2_PLACEMENT_3D('',#121551,#59994,#59995);
#49166=AXIS2_PLACEMENT_3D('',#121578,#59997,#59998);
#49167=AXIS2_PLACEMENT_3D('',#121599,#59999,#60000);
#49168=AXIS2_PLACEMENT_3D('',#121693,#60002,#60003);
#49169=AXIS2_PLACEMENT_3D('',#121720,#60005,#60006);
#49170=AXIS2_PLACEMENT_3D('',#121739,#60007,#60008);
#49171=AXIS2_PLACEMENT_3D('',#121829,#60010,#60011);
#49172=AXIS2_PLACEMENT_3D('',#121854,#60013,#60014);
#49173=AXIS2_PLACEMENT_3D('',#121878,#60015,#60016);
#49174=AXIS2_PLACEMENT_3D('',#121972,#60018,#60019);
#49175=AXIS2_PLACEMENT_3D('',#121999,#60021,#60022);
#49176=AXIS2_PLACEMENT_3D('',#122020,#60023,#60024);
#49177=AXIS2_PLACEMENT_3D('',#122114,#60026,#60027);
#49178=AXIS2_PLACEMENT_3D('',#122141,#60029,#60030);
#49179=AXIS2_PLACEMENT_3D('',#122162,#60031,#60032);
#49180=AXIS2_PLACEMENT_3D('',#122256,#60034,#60035);
#49181=AXIS2_PLACEMENT_3D('',#122283,#60037,#60038);
#49182=AXIS2_PLACEMENT_3D('',#122302,#60039,#60040);
#49183=AXIS2_PLACEMENT_3D('',#122341,#60042,#60043);
#49184=AXIS2_PLACEMENT_3D('',#122366,#60045,#60046);
#49185=AXIS2_PLACEMENT_3D('',#122390,#60047,#60048);
#49186=AXIS2_PLACEMENT_3D('',#122431,#60050,#60051);
#49187=AXIS2_PLACEMENT_3D('',#122461,#60053,#60054);
#49188=AXIS2_PLACEMENT_3D('',#122482,#60055,#60056);
#49189=AXIS2_PLACEMENT_3D('',#122574,#60058,#60059);
#49190=AXIS2_PLACEMENT_3D('',#122601,#60061,#60062);
#49191=AXIS2_PLACEMENT_3D('',#122622,#60063,#60064);
#49192=AXIS2_PLACEMENT_3D('',#122716,#60066,#60067);
#49193=AXIS2_PLACEMENT_3D('',#122743,#60069,#60070);
#49194=AXIS2_PLACEMENT_3D('',#122764,#60071,#60072);
#49195=AXIS2_PLACEMENT_3D('',#122801,#60074,#60075);
#49196=AXIS2_PLACEMENT_3D('',#122826,#60077,#60078);
#49197=AXIS2_PLACEMENT_3D('',#122848,#60079,#60080);
#49198=AXIS2_PLACEMENT_3D('',#122889,#60082,#60083);
#49199=AXIS2_PLACEMENT_3D('',#122919,#60085,#60086);
#49200=AXIS2_PLACEMENT_3D('',#122940,#60087,#60088);
#49201=AXIS2_PLACEMENT_3D('',#122981,#60090,#60091);
#49202=AXIS2_PLACEMENT_3D('',#123008,#60093,#60094);
#49203=AXIS2_PLACEMENT_3D('',#123029,#60095,#60096);
#49204=AXIS2_PLACEMENT_3D('',#123070,#60098,#60099);
#49205=AXIS2_PLACEMENT_3D('',#123097,#60101,#60102);
#49206=AXIS2_PLACEMENT_3D('',#123118,#60103,#60104);
#49207=AXIS2_PLACEMENT_3D('',#123155,#60106,#60107);
#49208=AXIS2_PLACEMENT_3D('',#123180,#60109,#60110);
#49209=AXIS2_PLACEMENT_3D('',#123202,#60111,#60112);
#49210=AXIS2_PLACEMENT_3D('',#123243,#60114,#60115);
#49211=AXIS2_PLACEMENT_3D('',#123270,#60117,#60118);
#49212=AXIS2_PLACEMENT_3D('',#123291,#60119,#60120);
#49213=AXIS2_PLACEMENT_3D('',#123330,#60122,#60123);
#49214=AXIS2_PLACEMENT_3D('',#123355,#60125,#60126);
#49215=AXIS2_PLACEMENT_3D('',#123376,#60127,#60128);
#49216=AXIS2_PLACEMENT_3D('',#123417,#60130,#60131);
#49217=AXIS2_PLACEMENT_3D('',#123444,#60133,#60134);
#49218=AXIS2_PLACEMENT_3D('',#123465,#60135,#60136);
#49219=AXIS2_PLACEMENT_3D('',#123502,#60138,#60139);
#49220=AXIS2_PLACEMENT_3D('',#123527,#60141,#60142);
#49221=AXIS2_PLACEMENT_3D('',#123549,#60143,#60144);
#49222=AXIS2_PLACEMENT_3D('',#123590,#60146,#60147);
#49223=AXIS2_PLACEMENT_3D('',#123620,#60149,#60150);
#49224=AXIS2_PLACEMENT_3D('',#123641,#60151,#60152);
#49225=AXIS2_PLACEMENT_3D('',#123680,#60154,#60155);
#49226=AXIS2_PLACEMENT_3D('',#123705,#60157,#60158);
#49227=AXIS2_PLACEMENT_3D('',#123729,#60159,#60160);
#49228=AXIS2_PLACEMENT_3D('',#123770,#60162,#60163);
#49229=AXIS2_PLACEMENT_3D('',#123797,#60165,#60166);
#49230=AXIS2_PLACEMENT_3D('',#123821,#60167,#60168);
#49231=AXIS2_PLACEMENT_3D('',#123860,#60170,#60171);
#49232=AXIS2_PLACEMENT_3D('',#123887,#60173,#60174);
#49233=AXIS2_PLACEMENT_3D('',#123909,#60175,#60176);
#49234=AXIS2_PLACEMENT_3D('',#123950,#60178,#60179);
#49235=AXIS2_PLACEMENT_3D('',#123977,#60181,#60182);
#49236=AXIS2_PLACEMENT_3D('',#123998,#60183,#60184);
#49237=AXIS2_PLACEMENT_3D('',#124037,#60186,#60187);
#49238=AXIS2_PLACEMENT_3D('',#124067,#60189,#60190);
#49239=AXIS2_PLACEMENT_3D('',#124086,#60191,#60192);
#49240=AXIS2_PLACEMENT_3D('',#124127,#60194,#60195);
#49241=AXIS2_PLACEMENT_3D('',#124154,#60197,#60198);
#49242=AXIS2_PLACEMENT_3D('',#124175,#60199,#60200);
#49243=AXIS2_PLACEMENT_3D('',#124214,#60202,#60203);
#49244=AXIS2_PLACEMENT_3D('',#124241,#60205,#60206);
#49245=AXIS2_PLACEMENT_3D('',#124263,#60207,#60208);
#49246=AXIS2_PLACEMENT_3D('',#124304,#60210,#60211);
#49247=AXIS2_PLACEMENT_3D('',#124334,#60213,#60214);
#49248=AXIS2_PLACEMENT_3D('',#124355,#60215,#60216);
#49249=AXIS2_PLACEMENT_3D('',#124394,#60218,#60219);
#49250=AXIS2_PLACEMENT_3D('',#124424,#60221,#60222);
#49251=AXIS2_PLACEMENT_3D('',#124443,#60223,#60224);
#49252=AXIS2_PLACEMENT_3D('',#124484,#60226,#60227);
#49253=AXIS2_PLACEMENT_3D('',#124514,#60229,#60230);
#49254=AXIS2_PLACEMENT_3D('',#124535,#60231,#60232);
#49255=AXIS2_PLACEMENT_3D('',#124574,#60234,#60235);
#49256=AXIS2_PLACEMENT_3D('',#124601,#60237,#60238);
#49257=AXIS2_PLACEMENT_3D('',#124625,#60239,#60240);
#49258=AXIS2_PLACEMENT_3D('',#124666,#60242,#60243);
#49259=AXIS2_PLACEMENT_3D('',#124694,#60245,#60246);
#49260=AXIS2_PLACEMENT_3D('',#124715,#60247,#60248);
#49261=AXIS2_PLACEMENT_3D('',#124756,#60250,#60251);
#49262=AXIS2_PLACEMENT_3D('',#124786,#60253,#60254);
#49263=AXIS2_PLACEMENT_3D('',#124807,#60255,#60256);
#49264=AXIS2_PLACEMENT_3D('',#124846,#60258,#60259);
#49265=AXIS2_PLACEMENT_3D('',#124873,#60261,#60262);
#49266=AXIS2_PLACEMENT_3D('',#124897,#60263,#60264);
#49267=AXIS2_PLACEMENT_3D('',#124899,#60265,#60266);
#49268=AXIS2_PLACEMENT_3D('',#124902,#60268,#60269);
#49269=AXIS2_PLACEMENT_3D('',#124903,#60270,#60271);
#49270=AXIS2_PLACEMENT_3D('',#124905,#60272,#60273);
#49271=AXIS2_PLACEMENT_3D('',#124908,#60275,#60276);
#49272=AXIS2_PLACEMENT_3D('',#124909,#60277,#60278);
#49273=AXIS2_PLACEMENT_3D('',#124911,#60279,#60280);
#49274=AXIS2_PLACEMENT_3D('',#124914,#60282,#60283);
#49275=AXIS2_PLACEMENT_3D('',#124915,#60284,#60285);
#49276=AXIS2_PLACEMENT_3D('',#124917,#60286,#60287);
#49277=AXIS2_PLACEMENT_3D('',#124920,#60289,#60290);
#49278=AXIS2_PLACEMENT_3D('',#124921,#60291,#60292);
#49279=AXIS2_PLACEMENT_3D('',#124923,#60293,#60294);
#49280=AXIS2_PLACEMENT_3D('',#124926,#60296,#60297);
#49281=AXIS2_PLACEMENT_3D('',#124927,#60298,#60299);
#49282=AXIS2_PLACEMENT_3D('',#124929,#60300,#60301);
#49283=AXIS2_PLACEMENT_3D('',#124932,#60303,#60304);
#49284=AXIS2_PLACEMENT_3D('',#124933,#60305,#60306);
#49285=AXIS2_PLACEMENT_3D('',#124935,#60307,#60308);
#49286=AXIS2_PLACEMENT_3D('',#124938,#60310,#60311);
#49287=AXIS2_PLACEMENT_3D('',#124939,#60312,#60313);
#49288=AXIS2_PLACEMENT_3D('',#124941,#60314,#60315);
#49289=AXIS2_PLACEMENT_3D('',#124944,#60317,#60318);
#49290=AXIS2_PLACEMENT_3D('',#124945,#60319,#60320);
#49291=AXIS2_PLACEMENT_3D('',#124947,#60321,#60322);
#49292=AXIS2_PLACEMENT_3D('',#124950,#60324,#60325);
#49293=AXIS2_PLACEMENT_3D('',#124951,#60326,#60327);
#49294=AXIS2_PLACEMENT_3D('',#124953,#60328,#60329);
#49295=AXIS2_PLACEMENT_3D('',#124956,#60331,#60332);
#49296=AXIS2_PLACEMENT_3D('',#124957,#60333,#60334);
#49297=AXIS2_PLACEMENT_3D('',#124959,#60335,#60336);
#49298=AXIS2_PLACEMENT_3D('',#124962,#60338,#60339);
#49299=AXIS2_PLACEMENT_3D('',#124963,#60340,#60341);
#49300=AXIS2_PLACEMENT_3D('',#124965,#60342,#60343);
#49301=AXIS2_PLACEMENT_3D('',#124968,#60345,#60346);
#49302=AXIS2_PLACEMENT_3D('',#124969,#60347,#60348);
#49303=AXIS2_PLACEMENT_3D('',#124971,#60349,#60350);
#49304=AXIS2_PLACEMENT_3D('',#124974,#60352,#60353);
#49305=AXIS2_PLACEMENT_3D('',#124975,#60354,#60355);
#49306=AXIS2_PLACEMENT_3D('',#124977,#60356,#60357);
#49307=AXIS2_PLACEMENT_3D('',#124980,#60359,#60360);
#49308=AXIS2_PLACEMENT_3D('',#124981,#60361,#60362);
#49309=AXIS2_PLACEMENT_3D('',#124983,#60363,#60364);
#49310=AXIS2_PLACEMENT_3D('',#124986,#60366,#60367);
#49311=AXIS2_PLACEMENT_3D('',#124987,#60368,#60369);
#49312=AXIS2_PLACEMENT_3D('',#124989,#60370,#60371);
#49313=AXIS2_PLACEMENT_3D('',#124992,#60373,#60374);
#49314=AXIS2_PLACEMENT_3D('',#124993,#60375,#60376);
#49315=AXIS2_PLACEMENT_3D('',#124995,#60377,#60378);
#49316=AXIS2_PLACEMENT_3D('',#124998,#60380,#60381);
#49317=AXIS2_PLACEMENT_3D('',#124999,#60382,#60383);
#49318=AXIS2_PLACEMENT_3D('',#125001,#60384,#60385);
#49319=AXIS2_PLACEMENT_3D('',#125004,#60387,#60388);
#49320=AXIS2_PLACEMENT_3D('',#125005,#60389,#60390);
#49321=AXIS2_PLACEMENT_3D('',#125007,#60391,#60392);
#49322=AXIS2_PLACEMENT_3D('',#125010,#60394,#60395);
#49323=AXIS2_PLACEMENT_3D('',#125011,#60396,#60397);
#49324=AXIS2_PLACEMENT_3D('',#125013,#60398,#60399);
#49325=AXIS2_PLACEMENT_3D('',#125016,#60401,#60402);
#49326=AXIS2_PLACEMENT_3D('',#125017,#60403,#60404);
#49327=AXIS2_PLACEMENT_3D('',#125019,#60405,#60406);
#49328=AXIS2_PLACEMENT_3D('',#125022,#60408,#60409);
#49329=AXIS2_PLACEMENT_3D('',#125023,#60410,#60411);
#49330=AXIS2_PLACEMENT_3D('',#125025,#60412,#60413);
#49331=AXIS2_PLACEMENT_3D('',#125028,#60415,#60416);
#49332=AXIS2_PLACEMENT_3D('',#125029,#60417,#60418);
#49333=AXIS2_PLACEMENT_3D('',#125031,#60419,#60420);
#49334=AXIS2_PLACEMENT_3D('',#125034,#60422,#60423);
#49335=AXIS2_PLACEMENT_3D('',#125035,#60424,#60425);
#49336=AXIS2_PLACEMENT_3D('',#125037,#60426,#60427);
#49337=AXIS2_PLACEMENT_3D('',#125040,#60429,#60430);
#49338=AXIS2_PLACEMENT_3D('',#125041,#60431,#60432);
#49339=AXIS2_PLACEMENT_3D('',#125043,#60433,#60434);
#49340=AXIS2_PLACEMENT_3D('',#125046,#60436,#60437);
#49341=AXIS2_PLACEMENT_3D('',#125047,#60438,#60439);
#49342=AXIS2_PLACEMENT_3D('',#125049,#60440,#60441);
#49343=AXIS2_PLACEMENT_3D('',#125052,#60443,#60444);
#49344=AXIS2_PLACEMENT_3D('',#125053,#60445,#60446);
#49345=AXIS2_PLACEMENT_3D('',#125055,#60447,#60448);
#49346=AXIS2_PLACEMENT_3D('',#125058,#60450,#60451);
#49347=AXIS2_PLACEMENT_3D('',#125059,#60452,#60453);
#49348=AXIS2_PLACEMENT_3D('',#125061,#60454,#60455);
#49349=AXIS2_PLACEMENT_3D('',#125064,#60457,#60458);
#49350=AXIS2_PLACEMENT_3D('',#125065,#60459,#60460);
#49351=AXIS2_PLACEMENT_3D('',#125067,#60461,#60462);
#49352=AXIS2_PLACEMENT_3D('',#125070,#60464,#60465);
#49353=AXIS2_PLACEMENT_3D('',#125071,#60466,#60467);
#49354=AXIS2_PLACEMENT_3D('',#125073,#60468,#60469);
#49355=AXIS2_PLACEMENT_3D('',#125076,#60471,#60472);
#49356=AXIS2_PLACEMENT_3D('',#125077,#60473,#60474);
#49357=AXIS2_PLACEMENT_3D('',#125079,#60475,#60476);
#49358=AXIS2_PLACEMENT_3D('',#125082,#60478,#60479);
#49359=AXIS2_PLACEMENT_3D('',#125083,#60480,#60481);
#49360=AXIS2_PLACEMENT_3D('',#125085,#60482,#60483);
#49361=AXIS2_PLACEMENT_3D('',#125088,#60485,#60486);
#49362=AXIS2_PLACEMENT_3D('',#125089,#60487,#60488);
#49363=AXIS2_PLACEMENT_3D('',#125091,#60489,#60490);
#49364=AXIS2_PLACEMENT_3D('',#125094,#60492,#60493);
#49365=AXIS2_PLACEMENT_3D('',#125095,#60494,#60495);
#49366=AXIS2_PLACEMENT_3D('',#125097,#60496,#60497);
#49367=AXIS2_PLACEMENT_3D('',#125100,#60499,#60500);
#49368=AXIS2_PLACEMENT_3D('',#125101,#60501,#60502);
#49369=AXIS2_PLACEMENT_3D('',#125103,#60503,#60504);
#49370=AXIS2_PLACEMENT_3D('',#125106,#60506,#60507);
#49371=AXIS2_PLACEMENT_3D('',#125107,#60508,#60509);
#49372=AXIS2_PLACEMENT_3D('',#125109,#60510,#60511);
#49373=AXIS2_PLACEMENT_3D('',#125112,#60513,#60514);
#49374=AXIS2_PLACEMENT_3D('',#125113,#60515,#60516);
#49375=AXIS2_PLACEMENT_3D('',#125115,#60517,#60518);
#49376=AXIS2_PLACEMENT_3D('',#125118,#60520,#60521);
#49377=AXIS2_PLACEMENT_3D('',#125119,#60522,#60523);
#49378=AXIS2_PLACEMENT_3D('',#125121,#60524,#60525);
#49379=AXIS2_PLACEMENT_3D('',#125124,#60527,#60528);
#49380=AXIS2_PLACEMENT_3D('',#125125,#60529,#60530);
#49381=AXIS2_PLACEMENT_3D('',#125127,#60531,#60532);
#49382=AXIS2_PLACEMENT_3D('',#125130,#60534,#60535);
#49383=AXIS2_PLACEMENT_3D('',#125131,#60536,#60537);
#49384=AXIS2_PLACEMENT_3D('',#125133,#60538,#60539);
#49385=AXIS2_PLACEMENT_3D('',#125136,#60541,#60542);
#49386=AXIS2_PLACEMENT_3D('',#125137,#60543,#60544);
#49387=AXIS2_PLACEMENT_3D('',#125139,#60545,#60546);
#49388=AXIS2_PLACEMENT_3D('',#125142,#60548,#60549);
#49389=AXIS2_PLACEMENT_3D('',#125143,#60550,#60551);
#49390=AXIS2_PLACEMENT_3D('',#125145,#60552,#60553);
#49391=AXIS2_PLACEMENT_3D('',#125148,#60555,#60556);
#49392=AXIS2_PLACEMENT_3D('',#125149,#60557,#60558);
#49393=AXIS2_PLACEMENT_3D('',#125151,#60559,#60560);
#49394=AXIS2_PLACEMENT_3D('',#125154,#60562,#60563);
#49395=AXIS2_PLACEMENT_3D('',#125155,#60564,#60565);
#49396=AXIS2_PLACEMENT_3D('',#125157,#60566,#60567);
#49397=AXIS2_PLACEMENT_3D('',#125160,#60569,#60570);
#49398=AXIS2_PLACEMENT_3D('',#125161,#60571,#60572);
#49399=AXIS2_PLACEMENT_3D('',#125163,#60573,#60574);
#49400=AXIS2_PLACEMENT_3D('',#125166,#60576,#60577);
#49401=AXIS2_PLACEMENT_3D('',#125167,#60578,#60579);
#49402=AXIS2_PLACEMENT_3D('',#125169,#60580,#60581);
#49403=AXIS2_PLACEMENT_3D('',#125172,#60583,#60584);
#49404=AXIS2_PLACEMENT_3D('',#125173,#60585,#60586);
#49405=AXIS2_PLACEMENT_3D('',#125175,#60587,#60588);
#49406=AXIS2_PLACEMENT_3D('',#125178,#60590,#60591);
#49407=AXIS2_PLACEMENT_3D('',#125179,#60592,#60593);
#49408=AXIS2_PLACEMENT_3D('',#125181,#60594,#60595);
#49409=AXIS2_PLACEMENT_3D('',#125184,#60597,#60598);
#49410=AXIS2_PLACEMENT_3D('',#125185,#60599,#60600);
#49411=AXIS2_PLACEMENT_3D('',#125187,#60601,#60602);
#49412=AXIS2_PLACEMENT_3D('',#125190,#60604,#60605);
#49413=AXIS2_PLACEMENT_3D('',#125191,#60606,#60607);
#49414=AXIS2_PLACEMENT_3D('',#125193,#60608,#60609);
#49415=AXIS2_PLACEMENT_3D('',#125196,#60611,#60612);
#49416=AXIS2_PLACEMENT_3D('',#125197,#60613,#60614);
#49417=AXIS2_PLACEMENT_3D('',#125199,#60615,#60616);
#49418=AXIS2_PLACEMENT_3D('',#125202,#60618,#60619);
#49419=AXIS2_PLACEMENT_3D('',#125203,#60620,#60621);
#49420=AXIS2_PLACEMENT_3D('',#125205,#60622,#60623);
#49421=AXIS2_PLACEMENT_3D('',#125208,#60625,#60626);
#49422=AXIS2_PLACEMENT_3D('',#125209,#60627,#60628);
#49423=AXIS2_PLACEMENT_3D('',#125211,#60629,#60630);
#49424=AXIS2_PLACEMENT_3D('',#125214,#60632,#60633);
#49425=AXIS2_PLACEMENT_3D('',#125215,#60634,#60635);
#49426=AXIS2_PLACEMENT_3D('',#125217,#60636,#60637);
#49427=AXIS2_PLACEMENT_3D('',#125220,#60639,#60640);
#49428=AXIS2_PLACEMENT_3D('',#125221,#60641,#60642);
#49429=AXIS2_PLACEMENT_3D('',#125223,#60643,#60644);
#49430=AXIS2_PLACEMENT_3D('',#125226,#60646,#60647);
#49431=AXIS2_PLACEMENT_3D('',#125227,#60648,#60649);
#49432=AXIS2_PLACEMENT_3D('',#125229,#60650,#60651);
#49433=AXIS2_PLACEMENT_3D('',#125232,#60653,#60654);
#49434=AXIS2_PLACEMENT_3D('',#125233,#60655,#60656);
#49435=AXIS2_PLACEMENT_3D('',#125235,#60657,#60658);
#49436=AXIS2_PLACEMENT_3D('',#125238,#60660,#60661);
#49437=AXIS2_PLACEMENT_3D('',#125239,#60662,#60663);
#49438=AXIS2_PLACEMENT_3D('',#125241,#60664,#60665);
#49439=AXIS2_PLACEMENT_3D('',#125244,#60667,#60668);
#49440=AXIS2_PLACEMENT_3D('',#125245,#60669,#60670);
#49441=AXIS2_PLACEMENT_3D('',#125247,#60671,#60672);
#49442=AXIS2_PLACEMENT_3D('',#125250,#60674,#60675);
#49443=AXIS2_PLACEMENT_3D('',#125251,#60676,#60677);
#49444=AXIS2_PLACEMENT_3D('',#125253,#60678,#60679);
#49445=AXIS2_PLACEMENT_3D('',#125256,#60681,#60682);
#49446=AXIS2_PLACEMENT_3D('',#125257,#60683,#60684);
#49447=AXIS2_PLACEMENT_3D('',#125259,#60685,#60686);
#49448=AXIS2_PLACEMENT_3D('',#125262,#60688,#60689);
#49449=AXIS2_PLACEMENT_3D('',#125263,#60690,#60691);
#49450=AXIS2_PLACEMENT_3D('',#125265,#60692,#60693);
#49451=AXIS2_PLACEMENT_3D('',#125268,#60695,#60696);
#49452=AXIS2_PLACEMENT_3D('',#125269,#60697,#60698);
#49453=AXIS2_PLACEMENT_3D('',#125271,#60699,#60700);
#49454=AXIS2_PLACEMENT_3D('',#125274,#60702,#60703);
#49455=AXIS2_PLACEMENT_3D('',#125275,#60704,#60705);
#49456=AXIS2_PLACEMENT_3D('',#125277,#60706,#60707);
#49457=AXIS2_PLACEMENT_3D('',#125280,#60709,#60710);
#49458=AXIS2_PLACEMENT_3D('',#125281,#60711,#60712);
#49459=AXIS2_PLACEMENT_3D('',#125283,#60713,#60714);
#49460=AXIS2_PLACEMENT_3D('',#125286,#60716,#60717);
#49461=AXIS2_PLACEMENT_3D('',#125287,#60718,#60719);
#49462=AXIS2_PLACEMENT_3D('',#125289,#60720,#60721);
#49463=AXIS2_PLACEMENT_3D('',#125292,#60723,#60724);
#49464=AXIS2_PLACEMENT_3D('',#125293,#60725,#60726);
#49465=AXIS2_PLACEMENT_3D('',#125295,#60727,#60728);
#49466=AXIS2_PLACEMENT_3D('',#125298,#60730,#60731);
#49467=AXIS2_PLACEMENT_3D('',#125299,#60732,#60733);
#49468=AXIS2_PLACEMENT_3D('',#125301,#60734,#60735);
#49469=AXIS2_PLACEMENT_3D('',#125304,#60737,#60738);
#49470=AXIS2_PLACEMENT_3D('',#125305,#60739,#60740);
#49471=AXIS2_PLACEMENT_3D('',#125307,#60741,#60742);
#49472=AXIS2_PLACEMENT_3D('',#125310,#60744,#60745);
#49473=AXIS2_PLACEMENT_3D('',#125311,#60746,#60747);
#49474=AXIS2_PLACEMENT_3D('',#125313,#60748,#60749);
#49475=AXIS2_PLACEMENT_3D('',#125316,#60751,#60752);
#49476=AXIS2_PLACEMENT_3D('',#125317,#60753,#60754);
#49477=AXIS2_PLACEMENT_3D('',#125319,#60755,#60756);
#49478=AXIS2_PLACEMENT_3D('',#125322,#60758,#60759);
#49479=AXIS2_PLACEMENT_3D('',#125323,#60760,#60761);
#49480=AXIS2_PLACEMENT_3D('',#125325,#60762,#60763);
#49481=AXIS2_PLACEMENT_3D('',#125328,#60765,#60766);
#49482=AXIS2_PLACEMENT_3D('',#125329,#60767,#60768);
#49483=AXIS2_PLACEMENT_3D('',#125331,#60769,#60770);
#49484=AXIS2_PLACEMENT_3D('',#125334,#60772,#60773);
#49485=AXIS2_PLACEMENT_3D('',#125335,#60774,#60775);
#49486=AXIS2_PLACEMENT_3D('',#125337,#60776,#60777);
#49487=AXIS2_PLACEMENT_3D('',#125340,#60779,#60780);
#49488=AXIS2_PLACEMENT_3D('',#125341,#60781,#60782);
#49489=AXIS2_PLACEMENT_3D('',#125343,#60783,#60784);
#49490=AXIS2_PLACEMENT_3D('',#125346,#60786,#60787);
#49491=AXIS2_PLACEMENT_3D('',#125347,#60788,#60789);
#49492=AXIS2_PLACEMENT_3D('',#125349,#60790,#60791);
#49493=AXIS2_PLACEMENT_3D('',#125352,#60793,#60794);
#49494=AXIS2_PLACEMENT_3D('',#125353,#60795,#60796);
#49495=AXIS2_PLACEMENT_3D('',#125355,#60797,#60798);
#49496=AXIS2_PLACEMENT_3D('',#125358,#60800,#60801);
#49497=AXIS2_PLACEMENT_3D('',#125359,#60802,#60803);
#49498=AXIS2_PLACEMENT_3D('',#125361,#60804,#60805);
#49499=AXIS2_PLACEMENT_3D('',#125364,#60807,#60808);
#49500=AXIS2_PLACEMENT_3D('',#125365,#60809,#60810);
#49501=AXIS2_PLACEMENT_3D('',#125367,#60811,#60812);
#49502=AXIS2_PLACEMENT_3D('',#125370,#60814,#60815);
#49503=AXIS2_PLACEMENT_3D('',#125371,#60816,#60817);
#49504=AXIS2_PLACEMENT_3D('',#125373,#60818,#60819);
#49505=AXIS2_PLACEMENT_3D('',#125376,#60821,#60822);
#49506=AXIS2_PLACEMENT_3D('',#125377,#60823,#60824);
#49507=AXIS2_PLACEMENT_3D('',#125379,#60825,#60826);
#49508=AXIS2_PLACEMENT_3D('',#125382,#60828,#60829);
#49509=AXIS2_PLACEMENT_3D('',#125383,#60830,#60831);
#49510=AXIS2_PLACEMENT_3D('',#125385,#60832,#60833);
#49511=AXIS2_PLACEMENT_3D('',#125388,#60835,#60836);
#49512=AXIS2_PLACEMENT_3D('',#125389,#60837,#60838);
#49513=AXIS2_PLACEMENT_3D('',#125391,#60839,#60840);
#49514=AXIS2_PLACEMENT_3D('',#125394,#60842,#60843);
#49515=AXIS2_PLACEMENT_3D('',#125395,#60844,#60845);
#49516=AXIS2_PLACEMENT_3D('',#125397,#60846,#60847);
#49517=AXIS2_PLACEMENT_3D('',#125400,#60849,#60850);
#49518=AXIS2_PLACEMENT_3D('',#125401,#60851,#60852);
#49519=AXIS2_PLACEMENT_3D('',#125403,#60853,#60854);
#49520=AXIS2_PLACEMENT_3D('',#125406,#60856,#60857);
#49521=AXIS2_PLACEMENT_3D('',#125407,#60858,#60859);
#49522=AXIS2_PLACEMENT_3D('',#125409,#60860,#60861);
#49523=AXIS2_PLACEMENT_3D('',#125412,#60863,#60864);
#49524=AXIS2_PLACEMENT_3D('',#125413,#60865,#60866);
#49525=AXIS2_PLACEMENT_3D('',#125415,#60867,#60868);
#49526=AXIS2_PLACEMENT_3D('',#125418,#60870,#60871);
#49527=AXIS2_PLACEMENT_3D('',#125419,#60872,#60873);
#49528=AXIS2_PLACEMENT_3D('',#125421,#60874,#60875);
#49529=AXIS2_PLACEMENT_3D('',#125424,#60877,#60878);
#49530=AXIS2_PLACEMENT_3D('',#125425,#60879,#60880);
#49531=AXIS2_PLACEMENT_3D('',#125427,#60881,#60882);
#49532=AXIS2_PLACEMENT_3D('',#125430,#60884,#60885);
#49533=AXIS2_PLACEMENT_3D('',#125431,#60886,#60887);
#49534=AXIS2_PLACEMENT_3D('',#125433,#60888,#60889);
#49535=AXIS2_PLACEMENT_3D('',#125436,#60891,#60892);
#49536=AXIS2_PLACEMENT_3D('',#125437,#60893,#60894);
#49537=AXIS2_PLACEMENT_3D('',#125439,#60895,#60896);
#49538=AXIS2_PLACEMENT_3D('',#125442,#60898,#60899);
#49539=AXIS2_PLACEMENT_3D('',#125443,#60900,#60901);
#49540=AXIS2_PLACEMENT_3D('',#125445,#60902,#60903);
#49541=AXIS2_PLACEMENT_3D('',#125448,#60905,#60906);
#49542=AXIS2_PLACEMENT_3D('',#125449,#60907,#60908);
#49543=AXIS2_PLACEMENT_3D('',#125451,#60909,#60910);
#49544=AXIS2_PLACEMENT_3D('',#125454,#60912,#60913);
#49545=AXIS2_PLACEMENT_3D('',#125455,#60914,#60915);
#49546=AXIS2_PLACEMENT_3D('',#125457,#60916,#60917);
#49547=AXIS2_PLACEMENT_3D('',#125460,#60919,#60920);
#49548=AXIS2_PLACEMENT_3D('',#125461,#60921,#60922);
#49549=AXIS2_PLACEMENT_3D('',#125463,#60923,#60924);
#49550=AXIS2_PLACEMENT_3D('',#125466,#60926,#60927);
#49551=AXIS2_PLACEMENT_3D('',#125467,#60928,#60929);
#49552=AXIS2_PLACEMENT_3D('',#125469,#60930,#60931);
#49553=AXIS2_PLACEMENT_3D('',#125472,#60933,#60934);
#49554=AXIS2_PLACEMENT_3D('',#125473,#60935,#60936);
#49555=AXIS2_PLACEMENT_3D('',#125475,#60937,#60938);
#49556=AXIS2_PLACEMENT_3D('',#125478,#60940,#60941);
#49557=AXIS2_PLACEMENT_3D('',#125479,#60942,#60943);
#49558=AXIS2_PLACEMENT_3D('',#125481,#60944,#60945);
#49559=AXIS2_PLACEMENT_3D('',#125484,#60947,#60948);
#49560=AXIS2_PLACEMENT_3D('',#125485,#60949,#60950);
#49561=AXIS2_PLACEMENT_3D('',#125487,#60951,#60952);
#49562=AXIS2_PLACEMENT_3D('',#125490,#60954,#60955);
#49563=AXIS2_PLACEMENT_3D('',#125491,#60956,#60957);
#49564=AXIS2_PLACEMENT_3D('',#125493,#60958,#60959);
#49565=AXIS2_PLACEMENT_3D('',#125496,#60961,#60962);
#49566=AXIS2_PLACEMENT_3D('',#125497,#60963,#60964);
#49567=AXIS2_PLACEMENT_3D('',#125499,#60965,#60966);
#49568=AXIS2_PLACEMENT_3D('',#125502,#60968,#60969);
#49569=AXIS2_PLACEMENT_3D('',#125503,#60970,#60971);
#49570=AXIS2_PLACEMENT_3D('',#125505,#60972,#60973);
#49571=AXIS2_PLACEMENT_3D('',#125508,#60975,#60976);
#49572=AXIS2_PLACEMENT_3D('',#125509,#60977,#60978);
#49573=AXIS2_PLACEMENT_3D('',#125511,#60979,#60980);
#49574=AXIS2_PLACEMENT_3D('',#125514,#60982,#60983);
#49575=AXIS2_PLACEMENT_3D('',#125515,#60984,#60985);
#49576=AXIS2_PLACEMENT_3D('',#125517,#60986,#60987);
#49577=AXIS2_PLACEMENT_3D('',#125520,#60989,#60990);
#49578=AXIS2_PLACEMENT_3D('',#125521,#60991,#60992);
#49579=AXIS2_PLACEMENT_3D('',#125523,#60993,#60994);
#49580=AXIS2_PLACEMENT_3D('',#125526,#60996,#60997);
#49581=AXIS2_PLACEMENT_3D('',#125527,#60998,#60999);
#49582=AXIS2_PLACEMENT_3D('',#125529,#61000,#61001);
#49583=AXIS2_PLACEMENT_3D('',#125532,#61003,#61004);
#49584=AXIS2_PLACEMENT_3D('',#125533,#61005,#61006);
#49585=AXIS2_PLACEMENT_3D('',#125535,#61007,#61008);
#49586=AXIS2_PLACEMENT_3D('',#125538,#61010,#61011);
#49587=AXIS2_PLACEMENT_3D('',#125539,#61012,#61013);
#49588=AXIS2_PLACEMENT_3D('',#125541,#61014,#61015);
#49589=AXIS2_PLACEMENT_3D('',#125544,#61017,#61018);
#49590=AXIS2_PLACEMENT_3D('',#125545,#61019,#61020);
#49591=AXIS2_PLACEMENT_3D('',#125547,#61021,#61022);
#49592=AXIS2_PLACEMENT_3D('',#125550,#61024,#61025);
#49593=AXIS2_PLACEMENT_3D('',#125551,#61026,#61027);
#49594=AXIS2_PLACEMENT_3D('',#125553,#61028,#61029);
#49595=AXIS2_PLACEMENT_3D('',#125556,#61031,#61032);
#49596=AXIS2_PLACEMENT_3D('',#125557,#61033,#61034);
#49597=AXIS2_PLACEMENT_3D('',#125559,#61035,#61036);
#49598=AXIS2_PLACEMENT_3D('',#125562,#61038,#61039);
#49599=AXIS2_PLACEMENT_3D('',#125563,#61040,#61041);
#49600=AXIS2_PLACEMENT_3D('',#125565,#61042,#61043);
#49601=AXIS2_PLACEMENT_3D('',#125568,#61045,#61046);
#49602=AXIS2_PLACEMENT_3D('',#125569,#61047,#61048);
#49603=AXIS2_PLACEMENT_3D('',#125571,#61049,#61050);
#49604=AXIS2_PLACEMENT_3D('',#125574,#61052,#61053);
#49605=AXIS2_PLACEMENT_3D('',#125575,#61054,#61055);
#49606=AXIS2_PLACEMENT_3D('',#125577,#61056,#61057);
#49607=AXIS2_PLACEMENT_3D('',#125580,#61059,#61060);
#49608=AXIS2_PLACEMENT_3D('',#125581,#61061,#61062);
#49609=AXIS2_PLACEMENT_3D('',#125583,#61063,#61064);
#49610=AXIS2_PLACEMENT_3D('',#125586,#61066,#61067);
#49611=AXIS2_PLACEMENT_3D('',#125587,#61068,#61069);
#49612=AXIS2_PLACEMENT_3D('',#125589,#61070,#61071);
#49613=AXIS2_PLACEMENT_3D('',#125592,#61073,#61074);
#49614=AXIS2_PLACEMENT_3D('',#125593,#61075,#61076);
#49615=AXIS2_PLACEMENT_3D('',#125595,#61077,#61078);
#49616=AXIS2_PLACEMENT_3D('',#125598,#61080,#61081);
#49617=AXIS2_PLACEMENT_3D('',#125599,#61082,#61083);
#49618=AXIS2_PLACEMENT_3D('',#125601,#61084,#61085);
#49619=AXIS2_PLACEMENT_3D('',#125604,#61087,#61088);
#49620=AXIS2_PLACEMENT_3D('',#125605,#61089,#61090);
#49621=AXIS2_PLACEMENT_3D('',#125607,#61091,#61092);
#49622=AXIS2_PLACEMENT_3D('',#125610,#61094,#61095);
#49623=AXIS2_PLACEMENT_3D('',#125611,#61096,#61097);
#49624=AXIS2_PLACEMENT_3D('',#125613,#61098,#61099);
#49625=AXIS2_PLACEMENT_3D('',#125616,#61101,#61102);
#49626=AXIS2_PLACEMENT_3D('',#125617,#61103,#61104);
#49627=AXIS2_PLACEMENT_3D('',#125619,#61105,#61106);
#49628=AXIS2_PLACEMENT_3D('',#125622,#61108,#61109);
#49629=AXIS2_PLACEMENT_3D('',#125623,#61110,#61111);
#49630=AXIS2_PLACEMENT_3D('',#125625,#61112,#61113);
#49631=AXIS2_PLACEMENT_3D('',#125628,#61115,#61116);
#49632=AXIS2_PLACEMENT_3D('',#125629,#61117,#61118);
#49633=AXIS2_PLACEMENT_3D('',#125631,#61119,#61120);
#49634=AXIS2_PLACEMENT_3D('',#125634,#61122,#61123);
#49635=AXIS2_PLACEMENT_3D('',#125635,#61124,#61125);
#49636=AXIS2_PLACEMENT_3D('',#125637,#61126,#61127);
#49637=AXIS2_PLACEMENT_3D('',#125640,#61129,#61130);
#49638=AXIS2_PLACEMENT_3D('',#125641,#61131,#61132);
#49639=AXIS2_PLACEMENT_3D('',#125643,#61133,#61134);
#49640=AXIS2_PLACEMENT_3D('',#125646,#61136,#61137);
#49641=AXIS2_PLACEMENT_3D('',#125647,#61138,#61139);
#49642=AXIS2_PLACEMENT_3D('',#125649,#61140,#61141);
#49643=AXIS2_PLACEMENT_3D('',#125652,#61143,#61144);
#49644=AXIS2_PLACEMENT_3D('',#125653,#61145,#61146);
#49645=AXIS2_PLACEMENT_3D('',#125655,#61147,#61148);
#49646=AXIS2_PLACEMENT_3D('',#125658,#61150,#61151);
#49647=AXIS2_PLACEMENT_3D('',#125659,#61152,#61153);
#49648=AXIS2_PLACEMENT_3D('',#125661,#61154,#61155);
#49649=AXIS2_PLACEMENT_3D('',#125664,#61157,#61158);
#49650=AXIS2_PLACEMENT_3D('',#125665,#61159,#61160);
#49651=AXIS2_PLACEMENT_3D('',#125667,#61161,#61162);
#49652=AXIS2_PLACEMENT_3D('',#125670,#61164,#61165);
#49653=AXIS2_PLACEMENT_3D('',#125671,#61166,#61167);
#49654=AXIS2_PLACEMENT_3D('',#125673,#61168,#61169);
#49655=AXIS2_PLACEMENT_3D('',#125676,#61171,#61172);
#49656=AXIS2_PLACEMENT_3D('',#125677,#61173,#61174);
#49657=AXIS2_PLACEMENT_3D('',#125679,#61175,#61176);
#49658=AXIS2_PLACEMENT_3D('',#125682,#61178,#61179);
#49659=AXIS2_PLACEMENT_3D('',#125683,#61180,#61181);
#49660=AXIS2_PLACEMENT_3D('',#125685,#61182,#61183);
#49661=AXIS2_PLACEMENT_3D('',#125688,#61185,#61186);
#49662=AXIS2_PLACEMENT_3D('',#125689,#61187,#61188);
#49663=AXIS2_PLACEMENT_3D('',#125691,#61189,#61190);
#49664=AXIS2_PLACEMENT_3D('',#125694,#61192,#61193);
#49665=AXIS2_PLACEMENT_3D('',#125695,#61194,#61195);
#49666=AXIS2_PLACEMENT_3D('',#125697,#61196,#61197);
#49667=AXIS2_PLACEMENT_3D('',#125700,#61199,#61200);
#49668=AXIS2_PLACEMENT_3D('',#125701,#61201,#61202);
#49669=AXIS2_PLACEMENT_3D('',#125703,#61203,#61204);
#49670=AXIS2_PLACEMENT_3D('',#125706,#61206,#61207);
#49671=AXIS2_PLACEMENT_3D('',#125707,#61208,#61209);
#49672=AXIS2_PLACEMENT_3D('',#125709,#61210,#61211);
#49673=AXIS2_PLACEMENT_3D('',#125712,#61213,#61214);
#49674=AXIS2_PLACEMENT_3D('',#125713,#61215,#61216);
#49675=AXIS2_PLACEMENT_3D('',#125715,#61217,#61218);
#49676=AXIS2_PLACEMENT_3D('',#125718,#61220,#61221);
#49677=AXIS2_PLACEMENT_3D('',#125719,#61222,#61223);
#49678=AXIS2_PLACEMENT_3D('',#125721,#61224,#61225);
#49679=AXIS2_PLACEMENT_3D('',#125724,#61227,#61228);
#49680=AXIS2_PLACEMENT_3D('',#125725,#61229,#61230);
#49681=AXIS2_PLACEMENT_3D('',#125727,#61231,#61232);
#49682=AXIS2_PLACEMENT_3D('',#125730,#61234,#61235);
#49683=AXIS2_PLACEMENT_3D('',#125731,#61236,#61237);
#49684=AXIS2_PLACEMENT_3D('',#125733,#61238,#61239);
#49685=AXIS2_PLACEMENT_3D('',#125736,#61241,#61242);
#49686=AXIS2_PLACEMENT_3D('',#125737,#61243,#61244);
#49687=AXIS2_PLACEMENT_3D('',#125739,#61245,#61246);
#49688=AXIS2_PLACEMENT_3D('',#125742,#61248,#61249);
#49689=AXIS2_PLACEMENT_3D('',#125743,#61250,#61251);
#49690=AXIS2_PLACEMENT_3D('',#125745,#61252,#61253);
#49691=AXIS2_PLACEMENT_3D('',#125748,#61255,#61256);
#49692=AXIS2_PLACEMENT_3D('',#125749,#61257,#61258);
#49693=AXIS2_PLACEMENT_3D('',#125751,#61259,#61260);
#49694=AXIS2_PLACEMENT_3D('',#125754,#61262,#61263);
#49695=AXIS2_PLACEMENT_3D('',#125755,#61264,#61265);
#49696=AXIS2_PLACEMENT_3D('',#125757,#61266,#61267);
#49697=AXIS2_PLACEMENT_3D('',#125760,#61269,#61270);
#49698=AXIS2_PLACEMENT_3D('',#125761,#61271,#61272);
#49699=AXIS2_PLACEMENT_3D('',#125763,#61273,#61274);
#49700=AXIS2_PLACEMENT_3D('',#125766,#61276,#61277);
#49701=AXIS2_PLACEMENT_3D('',#125767,#61278,#61279);
#49702=AXIS2_PLACEMENT_3D('',#125769,#61280,#61281);
#49703=AXIS2_PLACEMENT_3D('',#125772,#61283,#61284);
#49704=AXIS2_PLACEMENT_3D('',#125773,#61285,#61286);
#49705=AXIS2_PLACEMENT_3D('',#125775,#61287,#61288);
#49706=AXIS2_PLACEMENT_3D('',#125778,#61290,#61291);
#49707=AXIS2_PLACEMENT_3D('',#125779,#61292,#61293);
#49708=AXIS2_PLACEMENT_3D('',#125781,#61294,#61295);
#49709=AXIS2_PLACEMENT_3D('',#125784,#61297,#61298);
#49710=AXIS2_PLACEMENT_3D('',#125785,#61299,#61300);
#49711=AXIS2_PLACEMENT_3D('',#125787,#61301,#61302);
#49712=AXIS2_PLACEMENT_3D('',#125790,#61304,#61305);
#49713=AXIS2_PLACEMENT_3D('',#125791,#61306,#61307);
#49714=AXIS2_PLACEMENT_3D('',#125793,#61308,#61309);
#49715=AXIS2_PLACEMENT_3D('',#125796,#61311,#61312);
#49716=AXIS2_PLACEMENT_3D('',#125797,#61313,#61314);
#49717=AXIS2_PLACEMENT_3D('',#125799,#61315,#61316);
#49718=AXIS2_PLACEMENT_3D('',#125802,#61318,#61319);
#49719=AXIS2_PLACEMENT_3D('',#125803,#61320,#61321);
#49720=AXIS2_PLACEMENT_3D('',#125805,#61322,#61323);
#49721=AXIS2_PLACEMENT_3D('',#125808,#61325,#61326);
#49722=AXIS2_PLACEMENT_3D('',#125809,#61327,#61328);
#49723=AXIS2_PLACEMENT_3D('',#125811,#61329,#61330);
#49724=AXIS2_PLACEMENT_3D('',#125814,#61332,#61333);
#49725=AXIS2_PLACEMENT_3D('',#125815,#61334,#61335);
#49726=AXIS2_PLACEMENT_3D('',#125817,#61336,#61337);
#49727=AXIS2_PLACEMENT_3D('',#125820,#61339,#61340);
#49728=AXIS2_PLACEMENT_3D('',#125821,#61341,#61342);
#49729=AXIS2_PLACEMENT_3D('',#125823,#61343,#61344);
#49730=AXIS2_PLACEMENT_3D('',#125826,#61346,#61347);
#49731=AXIS2_PLACEMENT_3D('',#125827,#61348,#61349);
#49732=AXIS2_PLACEMENT_3D('',#125829,#61350,#61351);
#49733=AXIS2_PLACEMENT_3D('',#125832,#61353,#61354);
#49734=AXIS2_PLACEMENT_3D('',#125833,#61355,#61356);
#49735=AXIS2_PLACEMENT_3D('',#125835,#61357,#61358);
#49736=AXIS2_PLACEMENT_3D('',#125838,#61360,#61361);
#49737=AXIS2_PLACEMENT_3D('',#125839,#61362,#61363);
#49738=AXIS2_PLACEMENT_3D('',#125841,#61364,#61365);
#49739=AXIS2_PLACEMENT_3D('',#125844,#61367,#61368);
#49740=AXIS2_PLACEMENT_3D('',#125845,#61369,#61370);
#49741=AXIS2_PLACEMENT_3D('',#125847,#61371,#61372);
#49742=AXIS2_PLACEMENT_3D('',#125850,#61374,#61375);
#49743=AXIS2_PLACEMENT_3D('',#125851,#61376,#61377);
#49744=AXIS2_PLACEMENT_3D('',#125853,#61378,#61379);
#49745=AXIS2_PLACEMENT_3D('',#125856,#61381,#61382);
#49746=AXIS2_PLACEMENT_3D('',#125857,#61383,#61384);
#49747=AXIS2_PLACEMENT_3D('',#125859,#61385,#61386);
#49748=AXIS2_PLACEMENT_3D('',#125862,#61388,#61389);
#49749=AXIS2_PLACEMENT_3D('',#125863,#61390,#61391);
#49750=AXIS2_PLACEMENT_3D('',#125865,#61392,#61393);
#49751=AXIS2_PLACEMENT_3D('',#125868,#61395,#61396);
#49752=AXIS2_PLACEMENT_3D('',#125869,#61397,#61398);
#49753=AXIS2_PLACEMENT_3D('',#125871,#61399,#61400);
#49754=AXIS2_PLACEMENT_3D('',#125874,#61402,#61403);
#49755=AXIS2_PLACEMENT_3D('',#125875,#61404,#61405);
#49756=AXIS2_PLACEMENT_3D('',#125877,#61406,#61407);
#49757=AXIS2_PLACEMENT_3D('',#125880,#61409,#61410);
#49758=AXIS2_PLACEMENT_3D('',#125881,#61411,#61412);
#49759=AXIS2_PLACEMENT_3D('',#125883,#61413,#61414);
#49760=AXIS2_PLACEMENT_3D('',#125886,#61416,#61417);
#49761=AXIS2_PLACEMENT_3D('',#125887,#61418,#61419);
#49762=AXIS2_PLACEMENT_3D('',#125889,#61420,#61421);
#49763=AXIS2_PLACEMENT_3D('',#125892,#61423,#61424);
#49764=AXIS2_PLACEMENT_3D('',#125893,#61425,#61426);
#49765=AXIS2_PLACEMENT_3D('',#125895,#61427,#61428);
#49766=AXIS2_PLACEMENT_3D('',#125898,#61430,#61431);
#49767=AXIS2_PLACEMENT_3D('',#125899,#61432,#61433);
#49768=AXIS2_PLACEMENT_3D('',#125901,#61434,#61435);
#49769=AXIS2_PLACEMENT_3D('',#125904,#61437,#61438);
#49770=AXIS2_PLACEMENT_3D('',#125905,#61439,#61440);
#49771=AXIS2_PLACEMENT_3D('',#125907,#61441,#61442);
#49772=AXIS2_PLACEMENT_3D('',#125910,#61444,#61445);
#49773=AXIS2_PLACEMENT_3D('',#125911,#61446,#61447);
#49774=AXIS2_PLACEMENT_3D('',#125913,#61448,#61449);
#49775=AXIS2_PLACEMENT_3D('',#125916,#61451,#61452);
#49776=AXIS2_PLACEMENT_3D('',#125917,#61453,#61454);
#49777=AXIS2_PLACEMENT_3D('',#125919,#61455,#61456);
#49778=AXIS2_PLACEMENT_3D('',#125922,#61458,#61459);
#49779=AXIS2_PLACEMENT_3D('',#125923,#61460,#61461);
#49780=AXIS2_PLACEMENT_3D('',#125925,#61462,#61463);
#49781=AXIS2_PLACEMENT_3D('',#125928,#61465,#61466);
#49782=AXIS2_PLACEMENT_3D('',#125929,#61467,#61468);
#49783=AXIS2_PLACEMENT_3D('',#125931,#61469,#61470);
#49784=AXIS2_PLACEMENT_3D('',#125934,#61472,#61473);
#49785=AXIS2_PLACEMENT_3D('',#125935,#61474,#61475);
#49786=AXIS2_PLACEMENT_3D('',#125937,#61476,#61477);
#49787=AXIS2_PLACEMENT_3D('',#125940,#61479,#61480);
#49788=AXIS2_PLACEMENT_3D('',#125941,#61481,#61482);
#49789=AXIS2_PLACEMENT_3D('',#125943,#61483,#61484);
#49790=AXIS2_PLACEMENT_3D('',#125946,#61486,#61487);
#49791=AXIS2_PLACEMENT_3D('',#125947,#61488,#61489);
#49792=AXIS2_PLACEMENT_3D('',#125949,#61490,#61491);
#49793=AXIS2_PLACEMENT_3D('',#125952,#61493,#61494);
#49794=AXIS2_PLACEMENT_3D('',#125953,#61495,#61496);
#49795=AXIS2_PLACEMENT_3D('',#125955,#61497,#61498);
#49796=AXIS2_PLACEMENT_3D('',#125958,#61500,#61501);
#49797=AXIS2_PLACEMENT_3D('',#125959,#61502,#61503);
#49798=AXIS2_PLACEMENT_3D('',#125961,#61504,#61505);
#49799=AXIS2_PLACEMENT_3D('',#125964,#61507,#61508);
#49800=AXIS2_PLACEMENT_3D('',#125965,#61509,#61510);
#49801=AXIS2_PLACEMENT_3D('',#125967,#61511,#61512);
#49802=AXIS2_PLACEMENT_3D('',#125970,#61514,#61515);
#49803=AXIS2_PLACEMENT_3D('',#125971,#61516,#61517);
#49804=AXIS2_PLACEMENT_3D('',#125973,#61518,#61519);
#49805=AXIS2_PLACEMENT_3D('',#125976,#61521,#61522);
#49806=AXIS2_PLACEMENT_3D('',#125977,#61523,#61524);
#49807=AXIS2_PLACEMENT_3D('',#125979,#61525,#61526);
#49808=AXIS2_PLACEMENT_3D('',#125982,#61528,#61529);
#49809=AXIS2_PLACEMENT_3D('',#125983,#61530,#61531);
#49810=AXIS2_PLACEMENT_3D('',#125985,#61532,#61533);
#49811=AXIS2_PLACEMENT_3D('',#125988,#61535,#61536);
#49812=AXIS2_PLACEMENT_3D('',#125989,#61537,#61538);
#49813=AXIS2_PLACEMENT_3D('',#125991,#61539,#61540);
#49814=AXIS2_PLACEMENT_3D('',#125994,#61542,#61543);
#49815=AXIS2_PLACEMENT_3D('',#125995,#61544,#61545);
#49816=AXIS2_PLACEMENT_3D('',#125997,#61546,#61547);
#49817=AXIS2_PLACEMENT_3D('',#126000,#61549,#61550);
#49818=AXIS2_PLACEMENT_3D('',#126001,#61551,#61552);
#49819=AXIS2_PLACEMENT_3D('',#126003,#61553,#61554);
#49820=AXIS2_PLACEMENT_3D('',#126006,#61556,#61557);
#49821=AXIS2_PLACEMENT_3D('',#126007,#61558,#61559);
#49822=AXIS2_PLACEMENT_3D('',#126009,#61560,#61561);
#49823=AXIS2_PLACEMENT_3D('',#126012,#61563,#61564);
#49824=AXIS2_PLACEMENT_3D('',#126013,#61565,#61566);
#49825=AXIS2_PLACEMENT_3D('',#126015,#61567,#61568);
#49826=AXIS2_PLACEMENT_3D('',#126018,#61570,#61571);
#49827=AXIS2_PLACEMENT_3D('',#126019,#61572,#61573);
#49828=AXIS2_PLACEMENT_3D('',#126021,#61574,#61575);
#49829=AXIS2_PLACEMENT_3D('',#126024,#61577,#61578);
#49830=AXIS2_PLACEMENT_3D('',#126025,#61579,#61580);
#49831=AXIS2_PLACEMENT_3D('',#126027,#61581,#61582);
#49832=AXIS2_PLACEMENT_3D('',#126030,#61584,#61585);
#49833=AXIS2_PLACEMENT_3D('',#126031,#61586,#61587);
#49834=AXIS2_PLACEMENT_3D('',#126033,#61588,#61589);
#49835=AXIS2_PLACEMENT_3D('',#126036,#61591,#61592);
#49836=AXIS2_PLACEMENT_3D('',#126037,#61593,#61594);
#49837=AXIS2_PLACEMENT_3D('',#126039,#61595,#61596);
#49838=AXIS2_PLACEMENT_3D('',#126042,#61598,#61599);
#49839=AXIS2_PLACEMENT_3D('',#126043,#61600,#61601);
#49840=AXIS2_PLACEMENT_3D('',#126045,#61602,#61603);
#49841=AXIS2_PLACEMENT_3D('',#126048,#61605,#61606);
#49842=AXIS2_PLACEMENT_3D('',#126049,#61607,#61608);
#49843=AXIS2_PLACEMENT_3D('',#126051,#61609,#61610);
#49844=AXIS2_PLACEMENT_3D('',#126054,#61612,#61613);
#49845=AXIS2_PLACEMENT_3D('',#126055,#61614,#61615);
#49846=AXIS2_PLACEMENT_3D('',#126057,#61616,#61617);
#49847=AXIS2_PLACEMENT_3D('',#126060,#61619,#61620);
#49848=AXIS2_PLACEMENT_3D('',#126061,#61621,#61622);
#49849=AXIS2_PLACEMENT_3D('',#126063,#61623,#61624);
#49850=AXIS2_PLACEMENT_3D('',#126066,#61626,#61627);
#49851=AXIS2_PLACEMENT_3D('',#126067,#61628,#61629);
#49852=AXIS2_PLACEMENT_3D('',#126069,#61630,#61631);
#49853=AXIS2_PLACEMENT_3D('',#126072,#61633,#61634);
#49854=AXIS2_PLACEMENT_3D('',#126073,#61635,#61636);
#49855=AXIS2_PLACEMENT_3D('',#126075,#61637,#61638);
#49856=AXIS2_PLACEMENT_3D('',#126078,#61640,#61641);
#49857=AXIS2_PLACEMENT_3D('',#126079,#61642,#61643);
#49858=AXIS2_PLACEMENT_3D('',#126081,#61644,#61645);
#49859=AXIS2_PLACEMENT_3D('',#126084,#61647,#61648);
#49860=AXIS2_PLACEMENT_3D('',#126085,#61649,#61650);
#49861=AXIS2_PLACEMENT_3D('',#126087,#61651,#61652);
#49862=AXIS2_PLACEMENT_3D('',#126090,#61654,#61655);
#49863=AXIS2_PLACEMENT_3D('',#126091,#61656,#61657);
#49864=AXIS2_PLACEMENT_3D('',#126093,#61658,#61659);
#49865=AXIS2_PLACEMENT_3D('',#126096,#61661,#61662);
#49866=AXIS2_PLACEMENT_3D('',#126097,#61663,#61664);
#49867=AXIS2_PLACEMENT_3D('',#126099,#61665,#61666);
#49868=AXIS2_PLACEMENT_3D('',#126102,#61668,#61669);
#49869=AXIS2_PLACEMENT_3D('',#126103,#61670,#61671);
#49870=AXIS2_PLACEMENT_3D('',#126105,#61672,#61673);
#49871=AXIS2_PLACEMENT_3D('',#126108,#61675,#61676);
#49872=AXIS2_PLACEMENT_3D('',#126109,#61677,#61678);
#49873=AXIS2_PLACEMENT_3D('',#126111,#61679,#61680);
#49874=AXIS2_PLACEMENT_3D('',#126114,#61682,#61683);
#49875=AXIS2_PLACEMENT_3D('',#126115,#61684,#61685);
#49876=AXIS2_PLACEMENT_3D('',#126117,#61686,#61687);
#49877=AXIS2_PLACEMENT_3D('',#126120,#61689,#61690);
#49878=AXIS2_PLACEMENT_3D('',#126121,#61691,#61692);
#49879=AXIS2_PLACEMENT_3D('',#126123,#61693,#61694);
#49880=AXIS2_PLACEMENT_3D('',#126126,#61696,#61697);
#49881=AXIS2_PLACEMENT_3D('',#126127,#61698,#61699);
#49882=AXIS2_PLACEMENT_3D('',#126129,#61700,#61701);
#49883=AXIS2_PLACEMENT_3D('',#126132,#61703,#61704);
#49884=AXIS2_PLACEMENT_3D('',#126133,#61705,#61706);
#49885=AXIS2_PLACEMENT_3D('',#126135,#61707,#61708);
#49886=AXIS2_PLACEMENT_3D('',#126138,#61710,#61711);
#49887=AXIS2_PLACEMENT_3D('',#126139,#61712,#61713);
#49888=AXIS2_PLACEMENT_3D('',#126141,#61714,#61715);
#49889=AXIS2_PLACEMENT_3D('',#126144,#61717,#61718);
#49890=AXIS2_PLACEMENT_3D('',#126145,#61719,#61720);
#49891=AXIS2_PLACEMENT_3D('',#126147,#61721,#61722);
#49892=AXIS2_PLACEMENT_3D('',#126150,#61724,#61725);
#49893=AXIS2_PLACEMENT_3D('',#126151,#61726,#61727);
#49894=AXIS2_PLACEMENT_3D('',#126153,#61728,#61729);
#49895=AXIS2_PLACEMENT_3D('',#126156,#61731,#61732);
#49896=AXIS2_PLACEMENT_3D('',#126157,#61733,#61734);
#49897=AXIS2_PLACEMENT_3D('',#126159,#61735,#61736);
#49898=AXIS2_PLACEMENT_3D('',#126162,#61738,#61739);
#49899=AXIS2_PLACEMENT_3D('',#126163,#61740,#61741);
#49900=AXIS2_PLACEMENT_3D('',#126165,#61742,#61743);
#49901=AXIS2_PLACEMENT_3D('',#126168,#61745,#61746);
#49902=AXIS2_PLACEMENT_3D('',#126169,#61747,#61748);
#49903=AXIS2_PLACEMENT_3D('',#126171,#61749,#61750);
#49904=AXIS2_PLACEMENT_3D('',#126174,#61752,#61753);
#49905=AXIS2_PLACEMENT_3D('',#126175,#61754,#61755);
#49906=AXIS2_PLACEMENT_3D('',#126177,#61756,#61757);
#49907=AXIS2_PLACEMENT_3D('',#126180,#61759,#61760);
#49908=AXIS2_PLACEMENT_3D('',#126181,#61761,#61762);
#49909=AXIS2_PLACEMENT_3D('',#126183,#61763,#61764);
#49910=AXIS2_PLACEMENT_3D('',#126186,#61766,#61767);
#49911=AXIS2_PLACEMENT_3D('',#126187,#61768,#61769);
#49912=AXIS2_PLACEMENT_3D('',#126189,#61770,#61771);
#49913=AXIS2_PLACEMENT_3D('',#126192,#61773,#61774);
#49914=AXIS2_PLACEMENT_3D('',#126193,#61775,#61776);
#49915=AXIS2_PLACEMENT_3D('',#126195,#61777,#61778);
#49916=AXIS2_PLACEMENT_3D('',#126198,#61780,#61781);
#49917=AXIS2_PLACEMENT_3D('',#126199,#61782,#61783);
#49918=AXIS2_PLACEMENT_3D('',#126201,#61784,#61785);
#49919=AXIS2_PLACEMENT_3D('',#126204,#61787,#61788);
#49920=AXIS2_PLACEMENT_3D('',#126205,#61789,#61790);
#49921=AXIS2_PLACEMENT_3D('',#126207,#61791,#61792);
#49922=AXIS2_PLACEMENT_3D('',#126210,#61794,#61795);
#49923=AXIS2_PLACEMENT_3D('',#126211,#61796,#61797);
#49924=AXIS2_PLACEMENT_3D('',#126213,#61798,#61799);
#49925=AXIS2_PLACEMENT_3D('',#126216,#61801,#61802);
#49926=AXIS2_PLACEMENT_3D('',#126217,#61803,#61804);
#49927=AXIS2_PLACEMENT_3D('',#126219,#61805,#61806);
#49928=AXIS2_PLACEMENT_3D('',#126222,#61808,#61809);
#49929=AXIS2_PLACEMENT_3D('',#126223,#61810,#61811);
#49930=AXIS2_PLACEMENT_3D('',#126225,#61812,#61813);
#49931=AXIS2_PLACEMENT_3D('',#126228,#61815,#61816);
#49932=AXIS2_PLACEMENT_3D('',#126229,#61817,#61818);
#49933=AXIS2_PLACEMENT_3D('',#126231,#61819,#61820);
#49934=AXIS2_PLACEMENT_3D('',#126234,#61822,#61823);
#49935=AXIS2_PLACEMENT_3D('',#126235,#61824,#61825);
#49936=AXIS2_PLACEMENT_3D('',#126237,#61826,#61827);
#49937=AXIS2_PLACEMENT_3D('',#126240,#61829,#61830);
#49938=AXIS2_PLACEMENT_3D('',#126241,#61831,#61832);
#49939=AXIS2_PLACEMENT_3D('',#126243,#61833,#61834);
#49940=AXIS2_PLACEMENT_3D('',#126246,#61836,#61837);
#49941=AXIS2_PLACEMENT_3D('',#126247,#61838,#61839);
#49942=AXIS2_PLACEMENT_3D('',#126249,#61840,#61841);
#49943=AXIS2_PLACEMENT_3D('',#126252,#61843,#61844);
#49944=AXIS2_PLACEMENT_3D('',#126253,#61845,#61846);
#49945=AXIS2_PLACEMENT_3D('',#126255,#61847,#61848);
#49946=AXIS2_PLACEMENT_3D('',#126258,#61850,#61851);
#49947=AXIS2_PLACEMENT_3D('',#126259,#61852,#61853);
#49948=AXIS2_PLACEMENT_3D('',#126261,#61854,#61855);
#49949=AXIS2_PLACEMENT_3D('',#126264,#61857,#61858);
#49950=AXIS2_PLACEMENT_3D('',#126265,#61859,#61860);
#49951=AXIS2_PLACEMENT_3D('',#126267,#61861,#61862);
#49952=AXIS2_PLACEMENT_3D('',#126270,#61864,#61865);
#49953=AXIS2_PLACEMENT_3D('',#126271,#61866,#61867);
#49954=AXIS2_PLACEMENT_3D('',#126273,#61868,#61869);
#49955=AXIS2_PLACEMENT_3D('',#126276,#61871,#61872);
#49956=AXIS2_PLACEMENT_3D('',#126277,#61873,#61874);
#49957=AXIS2_PLACEMENT_3D('',#126279,#61875,#61876);
#49958=AXIS2_PLACEMENT_3D('',#126282,#61878,#61879);
#49959=AXIS2_PLACEMENT_3D('',#126283,#61880,#61881);
#49960=AXIS2_PLACEMENT_3D('',#126285,#61882,#61883);
#49961=AXIS2_PLACEMENT_3D('',#126288,#61885,#61886);
#49962=AXIS2_PLACEMENT_3D('',#126289,#61887,#61888);
#49963=AXIS2_PLACEMENT_3D('',#126291,#61889,#61890);
#49964=AXIS2_PLACEMENT_3D('',#126294,#61892,#61893);
#49965=AXIS2_PLACEMENT_3D('',#126295,#61894,#61895);
#49966=AXIS2_PLACEMENT_3D('',#126297,#61896,#61897);
#49967=AXIS2_PLACEMENT_3D('',#126300,#61899,#61900);
#49968=AXIS2_PLACEMENT_3D('',#126301,#61901,#61902);
#49969=AXIS2_PLACEMENT_3D('',#126303,#61903,#61904);
#49970=AXIS2_PLACEMENT_3D('',#126306,#61906,#61907);
#49971=AXIS2_PLACEMENT_3D('',#126307,#61908,#61909);
#49972=AXIS2_PLACEMENT_3D('',#126309,#61910,#61911);
#49973=AXIS2_PLACEMENT_3D('',#126312,#61913,#61914);
#49974=AXIS2_PLACEMENT_3D('',#126313,#61915,#61916);
#49975=AXIS2_PLACEMENT_3D('',#126315,#61917,#61918);
#49976=AXIS2_PLACEMENT_3D('',#126318,#61920,#61921);
#49977=AXIS2_PLACEMENT_3D('',#126319,#61922,#61923);
#49978=AXIS2_PLACEMENT_3D('',#126321,#61924,#61925);
#49979=AXIS2_PLACEMENT_3D('',#126324,#61927,#61928);
#49980=AXIS2_PLACEMENT_3D('',#126325,#61929,#61930);
#49981=AXIS2_PLACEMENT_3D('',#126327,#61931,#61932);
#49982=AXIS2_PLACEMENT_3D('',#126330,#61934,#61935);
#49983=AXIS2_PLACEMENT_3D('',#126331,#61936,#61937);
#49984=AXIS2_PLACEMENT_3D('',#126333,#61938,#61939);
#49985=AXIS2_PLACEMENT_3D('',#126336,#61941,#61942);
#49986=AXIS2_PLACEMENT_3D('',#126337,#61943,#61944);
#49987=AXIS2_PLACEMENT_3D('',#126339,#61945,#61946);
#49988=AXIS2_PLACEMENT_3D('',#126342,#61948,#61949);
#49989=AXIS2_PLACEMENT_3D('',#126343,#61950,#61951);
#49990=AXIS2_PLACEMENT_3D('',#126345,#61952,#61953);
#49991=AXIS2_PLACEMENT_3D('',#126348,#61955,#61956);
#49992=AXIS2_PLACEMENT_3D('',#126349,#61957,#61958);
#49993=AXIS2_PLACEMENT_3D('',#126351,#61959,#61960);
#49994=AXIS2_PLACEMENT_3D('',#126354,#61962,#61963);
#49995=AXIS2_PLACEMENT_3D('',#126355,#61964,#61965);
#49996=AXIS2_PLACEMENT_3D('',#126357,#61966,#61967);
#49997=AXIS2_PLACEMENT_3D('',#126360,#61969,#61970);
#49998=AXIS2_PLACEMENT_3D('',#126361,#61971,#61972);
#49999=AXIS2_PLACEMENT_3D('',#126363,#61973,#61974);
#50000=AXIS2_PLACEMENT_3D('',#126366,#61976,#61977);
#50001=AXIS2_PLACEMENT_3D('',#126367,#61978,#61979);
#50002=AXIS2_PLACEMENT_3D('',#126369,#61980,#61981);
#50003=AXIS2_PLACEMENT_3D('',#126372,#61983,#61984);
#50004=AXIS2_PLACEMENT_3D('',#126373,#61985,#61986);
#50005=AXIS2_PLACEMENT_3D('',#126375,#61987,#61988);
#50006=AXIS2_PLACEMENT_3D('',#126378,#61990,#61991);
#50007=AXIS2_PLACEMENT_3D('',#126379,#61992,#61993);
#50008=AXIS2_PLACEMENT_3D('',#126381,#61994,#61995);
#50009=AXIS2_PLACEMENT_3D('',#126384,#61997,#61998);
#50010=AXIS2_PLACEMENT_3D('',#126385,#61999,#62000);
#50011=AXIS2_PLACEMENT_3D('',#126387,#62001,#62002);
#50012=AXIS2_PLACEMENT_3D('',#126390,#62004,#62005);
#50013=AXIS2_PLACEMENT_3D('',#126391,#62006,#62007);
#50014=AXIS2_PLACEMENT_3D('',#126393,#62008,#62009);
#50015=AXIS2_PLACEMENT_3D('',#126396,#62011,#62012);
#50016=AXIS2_PLACEMENT_3D('',#126397,#62013,#62014);
#50017=AXIS2_PLACEMENT_3D('',#126399,#62015,#62016);
#50018=AXIS2_PLACEMENT_3D('',#126402,#62018,#62019);
#50019=AXIS2_PLACEMENT_3D('',#126403,#62020,#62021);
#50020=AXIS2_PLACEMENT_3D('',#126405,#62022,#62023);
#50021=AXIS2_PLACEMENT_3D('',#126408,#62025,#62026);
#50022=AXIS2_PLACEMENT_3D('',#126409,#62027,#62028);
#50023=AXIS2_PLACEMENT_3D('',#126411,#62029,#62030);
#50024=AXIS2_PLACEMENT_3D('',#126414,#62032,#62033);
#50025=AXIS2_PLACEMENT_3D('',#126415,#62034,#62035);
#50026=AXIS2_PLACEMENT_3D('',#126417,#62036,#62037);
#50027=AXIS2_PLACEMENT_3D('',#126420,#62039,#62040);
#50028=AXIS2_PLACEMENT_3D('',#126421,#62041,#62042);
#50029=AXIS2_PLACEMENT_3D('',#126423,#62043,#62044);
#50030=AXIS2_PLACEMENT_3D('',#126426,#62046,#62047);
#50031=AXIS2_PLACEMENT_3D('',#126427,#62048,#62049);
#50032=AXIS2_PLACEMENT_3D('',#126429,#62050,#62051);
#50033=AXIS2_PLACEMENT_3D('',#126432,#62053,#62054);
#50034=AXIS2_PLACEMENT_3D('',#126433,#62055,#62056);
#50035=AXIS2_PLACEMENT_3D('',#126435,#62057,#62058);
#50036=AXIS2_PLACEMENT_3D('',#126438,#62060,#62061);
#50037=AXIS2_PLACEMENT_3D('',#126439,#62062,#62063);
#50038=AXIS2_PLACEMENT_3D('',#126441,#62064,#62065);
#50039=AXIS2_PLACEMENT_3D('',#126444,#62067,#62068);
#50040=AXIS2_PLACEMENT_3D('',#126445,#62069,#62070);
#50041=AXIS2_PLACEMENT_3D('',#126447,#62071,#62072);
#50042=AXIS2_PLACEMENT_3D('',#126450,#62074,#62075);
#50043=AXIS2_PLACEMENT_3D('',#126451,#62076,#62077);
#50044=AXIS2_PLACEMENT_3D('',#126453,#62078,#62079);
#50045=AXIS2_PLACEMENT_3D('',#126456,#62081,#62082);
#50046=AXIS2_PLACEMENT_3D('',#126457,#62083,#62084);
#50047=AXIS2_PLACEMENT_3D('',#126459,#62085,#62086);
#50048=AXIS2_PLACEMENT_3D('',#126462,#62088,#62089);
#50049=AXIS2_PLACEMENT_3D('',#126463,#62090,#62091);
#50050=AXIS2_PLACEMENT_3D('',#126465,#62092,#62093);
#50051=AXIS2_PLACEMENT_3D('',#126468,#62095,#62096);
#50052=AXIS2_PLACEMENT_3D('',#126469,#62097,#62098);
#50053=AXIS2_PLACEMENT_3D('',#126471,#62099,#62100);
#50054=AXIS2_PLACEMENT_3D('',#126474,#62102,#62103);
#50055=AXIS2_PLACEMENT_3D('',#126475,#62104,#62105);
#50056=AXIS2_PLACEMENT_3D('',#126477,#62106,#62107);
#50057=AXIS2_PLACEMENT_3D('',#126480,#62109,#62110);
#50058=AXIS2_PLACEMENT_3D('',#126481,#62111,#62112);
#50059=AXIS2_PLACEMENT_3D('',#126483,#62113,#62114);
#50060=AXIS2_PLACEMENT_3D('',#126486,#62116,#62117);
#50061=AXIS2_PLACEMENT_3D('',#126487,#62118,#62119);
#50062=AXIS2_PLACEMENT_3D('',#126489,#62120,#62121);
#50063=AXIS2_PLACEMENT_3D('',#126492,#62123,#62124);
#50064=AXIS2_PLACEMENT_3D('',#126493,#62125,#62126);
#50065=AXIS2_PLACEMENT_3D('',#126495,#62127,#62128);
#50066=AXIS2_PLACEMENT_3D('',#126498,#62130,#62131);
#50067=AXIS2_PLACEMENT_3D('',#126499,#62132,#62133);
#50068=AXIS2_PLACEMENT_3D('',#126501,#62134,#62135);
#50069=AXIS2_PLACEMENT_3D('',#126504,#62137,#62138);
#50070=AXIS2_PLACEMENT_3D('',#126505,#62139,#62140);
#50071=AXIS2_PLACEMENT_3D('',#126507,#62141,#62142);
#50072=AXIS2_PLACEMENT_3D('',#126510,#62144,#62145);
#50073=AXIS2_PLACEMENT_3D('',#126511,#62146,#62147);
#50074=AXIS2_PLACEMENT_3D('',#126513,#62148,#62149);
#50075=AXIS2_PLACEMENT_3D('',#126516,#62151,#62152);
#50076=AXIS2_PLACEMENT_3D('',#126517,#62153,#62154);
#50077=AXIS2_PLACEMENT_3D('',#126519,#62155,#62156);
#50078=AXIS2_PLACEMENT_3D('',#126522,#62158,#62159);
#50079=AXIS2_PLACEMENT_3D('',#126523,#62160,#62161);
#50080=AXIS2_PLACEMENT_3D('',#126525,#62162,#62163);
#50081=AXIS2_PLACEMENT_3D('',#126528,#62165,#62166);
#50082=AXIS2_PLACEMENT_3D('',#126529,#62167,#62168);
#50083=AXIS2_PLACEMENT_3D('',#126531,#62169,#62170);
#50084=AXIS2_PLACEMENT_3D('',#126534,#62172,#62173);
#50085=AXIS2_PLACEMENT_3D('',#126535,#62174,#62175);
#50086=AXIS2_PLACEMENT_3D('',#126537,#62176,#62177);
#50087=AXIS2_PLACEMENT_3D('',#126540,#62179,#62180);
#50088=AXIS2_PLACEMENT_3D('',#126541,#62181,#62182);
#50089=AXIS2_PLACEMENT_3D('',#126543,#62183,#62184);
#50090=AXIS2_PLACEMENT_3D('',#126546,#62186,#62187);
#50091=AXIS2_PLACEMENT_3D('',#126547,#62188,#62189);
#50092=AXIS2_PLACEMENT_3D('',#126549,#62190,#62191);
#50093=AXIS2_PLACEMENT_3D('',#126552,#62193,#62194);
#50094=AXIS2_PLACEMENT_3D('',#126553,#62195,#62196);
#50095=AXIS2_PLACEMENT_3D('',#126555,#62197,#62198);
#50096=AXIS2_PLACEMENT_3D('',#126558,#62200,#62201);
#50097=AXIS2_PLACEMENT_3D('',#126559,#62202,#62203);
#50098=AXIS2_PLACEMENT_3D('',#126561,#62204,#62205);
#50099=AXIS2_PLACEMENT_3D('',#126564,#62207,#62208);
#50100=AXIS2_PLACEMENT_3D('',#126565,#62209,#62210);
#50101=AXIS2_PLACEMENT_3D('',#126567,#62211,#62212);
#50102=AXIS2_PLACEMENT_3D('',#126570,#62214,#62215);
#50103=AXIS2_PLACEMENT_3D('',#126571,#62216,#62217);
#50104=AXIS2_PLACEMENT_3D('',#126573,#62218,#62219);
#50105=AXIS2_PLACEMENT_3D('',#126576,#62221,#62222);
#50106=AXIS2_PLACEMENT_3D('',#126577,#62223,#62224);
#50107=AXIS2_PLACEMENT_3D('',#126579,#62225,#62226);
#50108=AXIS2_PLACEMENT_3D('',#126582,#62228,#62229);
#50109=AXIS2_PLACEMENT_3D('',#126583,#62230,#62231);
#50110=AXIS2_PLACEMENT_3D('',#126585,#62232,#62233);
#50111=AXIS2_PLACEMENT_3D('',#126588,#62235,#62236);
#50112=AXIS2_PLACEMENT_3D('',#126589,#62237,#62238);
#50113=AXIS2_PLACEMENT_3D('',#126591,#62239,#62240);
#50114=AXIS2_PLACEMENT_3D('',#126594,#62242,#62243);
#50115=AXIS2_PLACEMENT_3D('',#126595,#62244,#62245);
#50116=AXIS2_PLACEMENT_3D('',#126597,#62246,#62247);
#50117=AXIS2_PLACEMENT_3D('',#126600,#62249,#62250);
#50118=AXIS2_PLACEMENT_3D('',#126601,#62251,#62252);
#50119=AXIS2_PLACEMENT_3D('',#126603,#62253,#62254);
#50120=AXIS2_PLACEMENT_3D('',#126606,#62256,#62257);
#50121=AXIS2_PLACEMENT_3D('',#126607,#62258,#62259);
#50122=AXIS2_PLACEMENT_3D('',#126609,#62260,#62261);
#50123=AXIS2_PLACEMENT_3D('',#126612,#62263,#62264);
#50124=AXIS2_PLACEMENT_3D('',#126613,#62265,#62266);
#50125=AXIS2_PLACEMENT_3D('',#126615,#62267,#62268);
#50126=AXIS2_PLACEMENT_3D('',#126618,#62270,#62271);
#50127=AXIS2_PLACEMENT_3D('',#126619,#62272,#62273);
#50128=AXIS2_PLACEMENT_3D('',#126621,#62274,#62275);
#50129=AXIS2_PLACEMENT_3D('',#126624,#62277,#62278);
#50130=AXIS2_PLACEMENT_3D('',#126625,#62279,#62280);
#50131=AXIS2_PLACEMENT_3D('',#126627,#62281,#62282);
#50132=AXIS2_PLACEMENT_3D('',#126630,#62284,#62285);
#50133=AXIS2_PLACEMENT_3D('',#126631,#62286,#62287);
#50134=AXIS2_PLACEMENT_3D('',#126633,#62288,#62289);
#50135=AXIS2_PLACEMENT_3D('',#126636,#62291,#62292);
#50136=AXIS2_PLACEMENT_3D('',#126637,#62293,#62294);
#50137=AXIS2_PLACEMENT_3D('',#126639,#62295,#62296);
#50138=AXIS2_PLACEMENT_3D('',#126642,#62298,#62299);
#50139=AXIS2_PLACEMENT_3D('',#126643,#62300,#62301);
#50140=AXIS2_PLACEMENT_3D('',#126645,#62302,#62303);
#50141=AXIS2_PLACEMENT_3D('',#126648,#62305,#62306);
#50142=AXIS2_PLACEMENT_3D('',#126649,#62307,#62308);
#50143=AXIS2_PLACEMENT_3D('',#126651,#62309,#62310);
#50144=AXIS2_PLACEMENT_3D('',#126654,#62312,#62313);
#50145=AXIS2_PLACEMENT_3D('',#126655,#62314,#62315);
#50146=AXIS2_PLACEMENT_3D('',#126657,#62316,#62317);
#50147=AXIS2_PLACEMENT_3D('',#126660,#62319,#62320);
#50148=AXIS2_PLACEMENT_3D('',#126661,#62321,#62322);
#50149=AXIS2_PLACEMENT_3D('',#126663,#62323,#62324);
#50150=AXIS2_PLACEMENT_3D('',#126666,#62326,#62327);
#50151=AXIS2_PLACEMENT_3D('',#126667,#62328,#62329);
#50152=AXIS2_PLACEMENT_3D('',#126669,#62330,#62331);
#50153=AXIS2_PLACEMENT_3D('',#126672,#62333,#62334);
#50154=AXIS2_PLACEMENT_3D('',#126673,#62335,#62336);
#50155=AXIS2_PLACEMENT_3D('',#126675,#62337,#62338);
#50156=AXIS2_PLACEMENT_3D('',#126678,#62340,#62341);
#50157=AXIS2_PLACEMENT_3D('',#126679,#62342,#62343);
#50158=AXIS2_PLACEMENT_3D('',#126681,#62344,#62345);
#50159=AXIS2_PLACEMENT_3D('',#126684,#62347,#62348);
#50160=AXIS2_PLACEMENT_3D('',#126685,#62349,#62350);
#50161=AXIS2_PLACEMENT_3D('',#126687,#62351,#62352);
#50162=AXIS2_PLACEMENT_3D('',#126690,#62354,#62355);
#50163=AXIS2_PLACEMENT_3D('',#126691,#62356,#62357);
#50164=AXIS2_PLACEMENT_3D('',#126693,#62358,#62359);
#50165=AXIS2_PLACEMENT_3D('',#126696,#62361,#62362);
#50166=AXIS2_PLACEMENT_3D('',#126697,#62363,#62364);
#50167=AXIS2_PLACEMENT_3D('',#126699,#62365,#62366);
#50168=AXIS2_PLACEMENT_3D('',#126702,#62368,#62369);
#50169=AXIS2_PLACEMENT_3D('',#126703,#62370,#62371);
#50170=AXIS2_PLACEMENT_3D('',#126705,#62372,#62373);
#50171=AXIS2_PLACEMENT_3D('',#126708,#62375,#62376);
#50172=AXIS2_PLACEMENT_3D('',#126709,#62377,#62378);
#50173=AXIS2_PLACEMENT_3D('',#126711,#62379,#62380);
#50174=AXIS2_PLACEMENT_3D('',#126714,#62382,#62383);
#50175=AXIS2_PLACEMENT_3D('',#126715,#62384,#62385);
#50176=AXIS2_PLACEMENT_3D('',#126717,#62386,#62387);
#50177=AXIS2_PLACEMENT_3D('',#126720,#62389,#62390);
#50178=AXIS2_PLACEMENT_3D('',#126721,#62391,#62392);
#50179=AXIS2_PLACEMENT_3D('',#126723,#62393,#62394);
#50180=AXIS2_PLACEMENT_3D('',#126726,#62396,#62397);
#50181=AXIS2_PLACEMENT_3D('',#126727,#62398,#62399);
#50182=AXIS2_PLACEMENT_3D('',#126729,#62400,#62401);
#50183=AXIS2_PLACEMENT_3D('',#126732,#62403,#62404);
#50184=AXIS2_PLACEMENT_3D('',#126733,#62405,#62406);
#50185=AXIS2_PLACEMENT_3D('',#126735,#62407,#62408);
#50186=AXIS2_PLACEMENT_3D('',#126738,#62410,#62411);
#50187=AXIS2_PLACEMENT_3D('',#126739,#62412,#62413);
#50188=AXIS2_PLACEMENT_3D('',#126741,#62414,#62415);
#50189=AXIS2_PLACEMENT_3D('',#126744,#62417,#62418);
#50190=AXIS2_PLACEMENT_3D('',#126745,#62419,#62420);
#50191=AXIS2_PLACEMENT_3D('',#126747,#62421,#62422);
#50192=AXIS2_PLACEMENT_3D('',#126750,#62424,#62425);
#50193=AXIS2_PLACEMENT_3D('',#126751,#62426,#62427);
#50194=AXIS2_PLACEMENT_3D('',#126753,#62428,#62429);
#50195=AXIS2_PLACEMENT_3D('',#126756,#62431,#62432);
#50196=AXIS2_PLACEMENT_3D('',#126757,#62433,#62434);
#50197=AXIS2_PLACEMENT_3D('',#126759,#62435,#62436);
#50198=AXIS2_PLACEMENT_3D('',#126762,#62438,#62439);
#50199=AXIS2_PLACEMENT_3D('',#126763,#62440,#62441);
#50200=AXIS2_PLACEMENT_3D('',#126765,#62442,#62443);
#50201=AXIS2_PLACEMENT_3D('',#126768,#62445,#62446);
#50202=AXIS2_PLACEMENT_3D('',#126769,#62447,#62448);
#50203=AXIS2_PLACEMENT_3D('',#126771,#62449,#62450);
#50204=AXIS2_PLACEMENT_3D('',#126774,#62452,#62453);
#50205=AXIS2_PLACEMENT_3D('',#126775,#62454,#62455);
#50206=AXIS2_PLACEMENT_3D('',#126777,#62456,#62457);
#50207=AXIS2_PLACEMENT_3D('',#126780,#62459,#62460);
#50208=AXIS2_PLACEMENT_3D('',#126781,#62461,#62462);
#50209=AXIS2_PLACEMENT_3D('',#126783,#62463,#62464);
#50210=AXIS2_PLACEMENT_3D('',#126786,#62466,#62467);
#50211=AXIS2_PLACEMENT_3D('',#126787,#62468,#62469);
#50212=AXIS2_PLACEMENT_3D('',#126789,#62470,#62471);
#50213=AXIS2_PLACEMENT_3D('',#126792,#62473,#62474);
#50214=AXIS2_PLACEMENT_3D('',#126793,#62475,#62476);
#50215=AXIS2_PLACEMENT_3D('',#126795,#62477,#62478);
#50216=AXIS2_PLACEMENT_3D('',#126798,#62480,#62481);
#50217=AXIS2_PLACEMENT_3D('',#126799,#62482,#62483);
#50218=AXIS2_PLACEMENT_3D('',#126801,#62484,#62485);
#50219=AXIS2_PLACEMENT_3D('',#126804,#62487,#62488);
#50220=AXIS2_PLACEMENT_3D('',#126805,#62489,#62490);
#50221=AXIS2_PLACEMENT_3D('',#126807,#62491,#62492);
#50222=AXIS2_PLACEMENT_3D('',#126810,#62494,#62495);
#50223=AXIS2_PLACEMENT_3D('',#126811,#62496,#62497);
#50224=AXIS2_PLACEMENT_3D('',#126813,#62498,#62499);
#50225=AXIS2_PLACEMENT_3D('',#126816,#62501,#62502);
#50226=AXIS2_PLACEMENT_3D('',#126817,#62503,#62504);
#50227=AXIS2_PLACEMENT_3D('',#126819,#62505,#62506);
#50228=AXIS2_PLACEMENT_3D('',#126822,#62508,#62509);
#50229=AXIS2_PLACEMENT_3D('',#126823,#62510,#62511);
#50230=AXIS2_PLACEMENT_3D('',#126825,#62512,#62513);
#50231=AXIS2_PLACEMENT_3D('',#126828,#62515,#62516);
#50232=AXIS2_PLACEMENT_3D('',#126829,#62517,#62518);
#50233=AXIS2_PLACEMENT_3D('',#126831,#62519,#62520);
#50234=AXIS2_PLACEMENT_3D('',#126834,#62522,#62523);
#50235=AXIS2_PLACEMENT_3D('',#126835,#62524,#62525);
#50236=AXIS2_PLACEMENT_3D('',#126837,#62526,#62527);
#50237=AXIS2_PLACEMENT_3D('',#126840,#62529,#62530);
#50238=AXIS2_PLACEMENT_3D('',#126841,#62531,#62532);
#50239=AXIS2_PLACEMENT_3D('',#126843,#62533,#62534);
#50240=AXIS2_PLACEMENT_3D('',#126846,#62536,#62537);
#50241=AXIS2_PLACEMENT_3D('',#126847,#62538,#62539);
#50242=AXIS2_PLACEMENT_3D('',#126849,#62540,#62541);
#50243=AXIS2_PLACEMENT_3D('',#126852,#62543,#62544);
#50244=AXIS2_PLACEMENT_3D('',#126853,#62545,#62546);
#50245=AXIS2_PLACEMENT_3D('',#126855,#62547,#62548);
#50246=AXIS2_PLACEMENT_3D('',#126858,#62550,#62551);
#50247=AXIS2_PLACEMENT_3D('',#126859,#62552,#62553);
#50248=AXIS2_PLACEMENT_3D('',#126861,#62554,#62555);
#50249=AXIS2_PLACEMENT_3D('',#126864,#62557,#62558);
#50250=AXIS2_PLACEMENT_3D('',#126865,#62559,#62560);
#50251=AXIS2_PLACEMENT_3D('',#126867,#62561,#62562);
#50252=AXIS2_PLACEMENT_3D('',#126870,#62564,#62565);
#50253=AXIS2_PLACEMENT_3D('',#126871,#62566,#62567);
#50254=AXIS2_PLACEMENT_3D('',#126873,#62568,#62569);
#50255=AXIS2_PLACEMENT_3D('',#126876,#62571,#62572);
#50256=AXIS2_PLACEMENT_3D('',#126877,#62573,#62574);
#50257=AXIS2_PLACEMENT_3D('',#126879,#62575,#62576);
#50258=AXIS2_PLACEMENT_3D('',#126882,#62578,#62579);
#50259=AXIS2_PLACEMENT_3D('',#126883,#62580,#62581);
#50260=AXIS2_PLACEMENT_3D('',#126885,#62582,#62583);
#50261=AXIS2_PLACEMENT_3D('',#126888,#62585,#62586);
#50262=AXIS2_PLACEMENT_3D('',#126889,#62587,#62588);
#50263=AXIS2_PLACEMENT_3D('',#126891,#62589,#62590);
#50264=AXIS2_PLACEMENT_3D('',#126894,#62592,#62593);
#50265=AXIS2_PLACEMENT_3D('',#126895,#62594,#62595);
#50266=AXIS2_PLACEMENT_3D('',#126897,#62596,#62597);
#50267=AXIS2_PLACEMENT_3D('',#126900,#62599,#62600);
#50268=AXIS2_PLACEMENT_3D('',#126901,#62601,#62602);
#50269=AXIS2_PLACEMENT_3D('',#126903,#62603,#62604);
#50270=AXIS2_PLACEMENT_3D('',#126906,#62606,#62607);
#50271=AXIS2_PLACEMENT_3D('',#126907,#62608,#62609);
#50272=AXIS2_PLACEMENT_3D('',#126909,#62610,#62611);
#50273=AXIS2_PLACEMENT_3D('',#126912,#62613,#62614);
#50274=AXIS2_PLACEMENT_3D('',#126913,#62615,#62616);
#50275=AXIS2_PLACEMENT_3D('',#126915,#62617,#62618);
#50276=AXIS2_PLACEMENT_3D('',#126918,#62620,#62621);
#50277=AXIS2_PLACEMENT_3D('',#126919,#62622,#62623);
#50278=AXIS2_PLACEMENT_3D('',#126921,#62624,#62625);
#50279=AXIS2_PLACEMENT_3D('',#126924,#62627,#62628);
#50280=AXIS2_PLACEMENT_3D('',#126925,#62629,#62630);
#50281=AXIS2_PLACEMENT_3D('',#126927,#62631,#62632);
#50282=AXIS2_PLACEMENT_3D('',#126930,#62634,#62635);
#50283=AXIS2_PLACEMENT_3D('',#126931,#62636,#62637);
#50284=AXIS2_PLACEMENT_3D('',#126933,#62638,#62639);
#50285=AXIS2_PLACEMENT_3D('',#126936,#62641,#62642);
#50286=AXIS2_PLACEMENT_3D('',#126937,#62643,#62644);
#50287=AXIS2_PLACEMENT_3D('',#126939,#62645,#62646);
#50288=AXIS2_PLACEMENT_3D('',#126942,#62648,#62649);
#50289=AXIS2_PLACEMENT_3D('',#126943,#62650,#62651);
#50290=AXIS2_PLACEMENT_3D('',#126945,#62652,#62653);
#50291=AXIS2_PLACEMENT_3D('',#126948,#62655,#62656);
#50292=AXIS2_PLACEMENT_3D('',#126949,#62657,#62658);
#50293=AXIS2_PLACEMENT_3D('',#126951,#62659,#62660);
#50294=AXIS2_PLACEMENT_3D('',#126954,#62662,#62663);
#50295=AXIS2_PLACEMENT_3D('',#126955,#62664,#62665);
#50296=AXIS2_PLACEMENT_3D('',#126957,#62666,#62667);
#50297=AXIS2_PLACEMENT_3D('',#126960,#62669,#62670);
#50298=AXIS2_PLACEMENT_3D('',#126961,#62671,#62672);
#50299=AXIS2_PLACEMENT_3D('',#126963,#62673,#62674);
#50300=AXIS2_PLACEMENT_3D('',#126966,#62676,#62677);
#50301=AXIS2_PLACEMENT_3D('',#126967,#62678,#62679);
#50302=AXIS2_PLACEMENT_3D('',#126969,#62680,#62681);
#50303=AXIS2_PLACEMENT_3D('',#126972,#62683,#62684);
#50304=AXIS2_PLACEMENT_3D('',#126973,#62685,#62686);
#50305=AXIS2_PLACEMENT_3D('',#126975,#62687,#62688);
#50306=AXIS2_PLACEMENT_3D('',#126978,#62690,#62691);
#50307=AXIS2_PLACEMENT_3D('',#126979,#62692,#62693);
#50308=AXIS2_PLACEMENT_3D('',#126981,#62694,#62695);
#50309=AXIS2_PLACEMENT_3D('',#126984,#62697,#62698);
#50310=AXIS2_PLACEMENT_3D('',#126985,#62699,#62700);
#50311=AXIS2_PLACEMENT_3D('',#126987,#62701,#62702);
#50312=AXIS2_PLACEMENT_3D('',#126990,#62704,#62705);
#50313=AXIS2_PLACEMENT_3D('',#126991,#62706,#62707);
#50314=AXIS2_PLACEMENT_3D('',#126993,#62708,#62709);
#50315=AXIS2_PLACEMENT_3D('',#126996,#62711,#62712);
#50316=AXIS2_PLACEMENT_3D('',#126997,#62713,#62714);
#50317=AXIS2_PLACEMENT_3D('',#126999,#62715,#62716);
#50318=AXIS2_PLACEMENT_3D('',#127002,#62718,#62719);
#50319=AXIS2_PLACEMENT_3D('',#127003,#62720,#62721);
#50320=AXIS2_PLACEMENT_3D('',#127005,#62722,#62723);
#50321=AXIS2_PLACEMENT_3D('',#127008,#62725,#62726);
#50322=AXIS2_PLACEMENT_3D('',#127009,#62727,#62728);
#50323=AXIS2_PLACEMENT_3D('',#127011,#62729,#62730);
#50324=AXIS2_PLACEMENT_3D('',#127014,#62732,#62733);
#50325=AXIS2_PLACEMENT_3D('',#127015,#62734,#62735);
#50326=AXIS2_PLACEMENT_3D('',#127017,#62736,#62737);
#50327=AXIS2_PLACEMENT_3D('',#127020,#62739,#62740);
#50328=AXIS2_PLACEMENT_3D('',#127021,#62741,#62742);
#50329=AXIS2_PLACEMENT_3D('',#127023,#62743,#62744);
#50330=AXIS2_PLACEMENT_3D('',#127026,#62746,#62747);
#50331=AXIS2_PLACEMENT_3D('',#127027,#62748,#62749);
#50332=AXIS2_PLACEMENT_3D('',#127029,#62750,#62751);
#50333=AXIS2_PLACEMENT_3D('',#127032,#62753,#62754);
#50334=AXIS2_PLACEMENT_3D('',#127033,#62755,#62756);
#50335=AXIS2_PLACEMENT_3D('',#127035,#62757,#62758);
#50336=AXIS2_PLACEMENT_3D('',#127038,#62760,#62761);
#50337=AXIS2_PLACEMENT_3D('',#127039,#62762,#62763);
#50338=AXIS2_PLACEMENT_3D('',#127041,#62764,#62765);
#50339=AXIS2_PLACEMENT_3D('',#127044,#62767,#62768);
#50340=AXIS2_PLACEMENT_3D('',#127045,#62769,#62770);
#50341=AXIS2_PLACEMENT_3D('',#127047,#62771,#62772);
#50342=AXIS2_PLACEMENT_3D('',#127050,#62774,#62775);
#50343=AXIS2_PLACEMENT_3D('',#127051,#62776,#62777);
#50344=AXIS2_PLACEMENT_3D('',#127053,#62778,#62779);
#50345=AXIS2_PLACEMENT_3D('',#127056,#62781,#62782);
#50346=AXIS2_PLACEMENT_3D('',#127057,#62783,#62784);
#50347=AXIS2_PLACEMENT_3D('',#127059,#62785,#62786);
#50348=AXIS2_PLACEMENT_3D('',#127062,#62788,#62789);
#50349=AXIS2_PLACEMENT_3D('',#127063,#62790,#62791);
#50350=AXIS2_PLACEMENT_3D('',#127065,#62792,#62793);
#50351=AXIS2_PLACEMENT_3D('',#127068,#62795,#62796);
#50352=AXIS2_PLACEMENT_3D('',#127069,#62797,#62798);
#50353=AXIS2_PLACEMENT_3D('',#127071,#62799,#62800);
#50354=AXIS2_PLACEMENT_3D('',#127074,#62802,#62803);
#50355=AXIS2_PLACEMENT_3D('',#127075,#62804,#62805);
#50356=AXIS2_PLACEMENT_3D('',#127077,#62806,#62807);
#50357=AXIS2_PLACEMENT_3D('',#127080,#62809,#62810);
#50358=AXIS2_PLACEMENT_3D('',#127081,#62811,#62812);
#50359=AXIS2_PLACEMENT_3D('',#127083,#62813,#62814);
#50360=AXIS2_PLACEMENT_3D('',#127086,#62816,#62817);
#50361=AXIS2_PLACEMENT_3D('',#127087,#62818,#62819);
#50362=AXIS2_PLACEMENT_3D('',#127089,#62820,#62821);
#50363=AXIS2_PLACEMENT_3D('',#127092,#62823,#62824);
#50364=AXIS2_PLACEMENT_3D('',#127093,#62825,#62826);
#50365=AXIS2_PLACEMENT_3D('',#127095,#62827,#62828);
#50366=AXIS2_PLACEMENT_3D('',#127098,#62830,#62831);
#50367=AXIS2_PLACEMENT_3D('',#127099,#62832,#62833);
#50368=AXIS2_PLACEMENT_3D('',#127101,#62834,#62835);
#50369=AXIS2_PLACEMENT_3D('',#127104,#62837,#62838);
#50370=AXIS2_PLACEMENT_3D('',#127105,#62839,#62840);
#50371=AXIS2_PLACEMENT_3D('',#127107,#62841,#62842);
#50372=AXIS2_PLACEMENT_3D('',#127110,#62844,#62845);
#50373=AXIS2_PLACEMENT_3D('',#127111,#62846,#62847);
#50374=AXIS2_PLACEMENT_3D('',#127113,#62848,#62849);
#50375=AXIS2_PLACEMENT_3D('',#127116,#62851,#62852);
#50376=AXIS2_PLACEMENT_3D('',#127117,#62853,#62854);
#50377=AXIS2_PLACEMENT_3D('',#127119,#62855,#62856);
#50378=AXIS2_PLACEMENT_3D('',#127122,#62858,#62859);
#50379=AXIS2_PLACEMENT_3D('',#127123,#62860,#62861);
#50380=AXIS2_PLACEMENT_3D('',#127125,#62862,#62863);
#50381=AXIS2_PLACEMENT_3D('',#127128,#62865,#62866);
#50382=AXIS2_PLACEMENT_3D('',#127129,#62867,#62868);
#50383=AXIS2_PLACEMENT_3D('',#127131,#62869,#62870);
#50384=AXIS2_PLACEMENT_3D('',#127134,#62872,#62873);
#50385=AXIS2_PLACEMENT_3D('',#127135,#62874,#62875);
#50386=AXIS2_PLACEMENT_3D('',#127137,#62876,#62877);
#50387=AXIS2_PLACEMENT_3D('',#127140,#62879,#62880);
#50388=AXIS2_PLACEMENT_3D('',#127141,#62881,#62882);
#50389=AXIS2_PLACEMENT_3D('',#127143,#62883,#62884);
#50390=AXIS2_PLACEMENT_3D('',#127146,#62886,#62887);
#50391=AXIS2_PLACEMENT_3D('',#127147,#62888,#62889);
#50392=AXIS2_PLACEMENT_3D('',#127149,#62890,#62891);
#50393=AXIS2_PLACEMENT_3D('',#127152,#62893,#62894);
#50394=AXIS2_PLACEMENT_3D('',#127153,#62895,#62896);
#50395=AXIS2_PLACEMENT_3D('',#127155,#62897,#62898);
#50396=AXIS2_PLACEMENT_3D('',#127158,#62900,#62901);
#50397=AXIS2_PLACEMENT_3D('',#127159,#62902,#62903);
#50398=AXIS2_PLACEMENT_3D('',#127161,#62904,#62905);
#50399=AXIS2_PLACEMENT_3D('',#127164,#62907,#62908);
#50400=AXIS2_PLACEMENT_3D('',#127165,#62909,#62910);
#50401=AXIS2_PLACEMENT_3D('',#127167,#62911,#62912);
#50402=AXIS2_PLACEMENT_3D('',#127170,#62914,#62915);
#50403=AXIS2_PLACEMENT_3D('',#127171,#62916,#62917);
#50404=AXIS2_PLACEMENT_3D('',#127173,#62918,#62919);
#50405=AXIS2_PLACEMENT_3D('',#127176,#62921,#62922);
#50406=AXIS2_PLACEMENT_3D('',#127177,#62923,#62924);
#50407=AXIS2_PLACEMENT_3D('',#127179,#62925,#62926);
#50408=AXIS2_PLACEMENT_3D('',#127182,#62928,#62929);
#50409=AXIS2_PLACEMENT_3D('',#127183,#62930,#62931);
#50410=AXIS2_PLACEMENT_3D('',#127185,#62932,#62933);
#50411=AXIS2_PLACEMENT_3D('',#127188,#62935,#62936);
#50412=AXIS2_PLACEMENT_3D('',#127189,#62937,#62938);
#50413=AXIS2_PLACEMENT_3D('',#127191,#62939,#62940);
#50414=AXIS2_PLACEMENT_3D('',#127194,#62942,#62943);
#50415=AXIS2_PLACEMENT_3D('',#127195,#62944,#62945);
#50416=AXIS2_PLACEMENT_3D('',#127197,#62946,#62947);
#50417=AXIS2_PLACEMENT_3D('',#127200,#62949,#62950);
#50418=AXIS2_PLACEMENT_3D('',#127201,#62951,#62952);
#50419=AXIS2_PLACEMENT_3D('',#127203,#62953,#62954);
#50420=AXIS2_PLACEMENT_3D('',#127206,#62956,#62957);
#50421=AXIS2_PLACEMENT_3D('',#127207,#62958,#62959);
#50422=AXIS2_PLACEMENT_3D('',#127209,#62960,#62961);
#50423=AXIS2_PLACEMENT_3D('',#127212,#62963,#62964);
#50424=AXIS2_PLACEMENT_3D('',#127213,#62965,#62966);
#50425=AXIS2_PLACEMENT_3D('',#127215,#62967,#62968);
#50426=AXIS2_PLACEMENT_3D('',#127218,#62970,#62971);
#50427=AXIS2_PLACEMENT_3D('',#127219,#62972,#62973);
#50428=AXIS2_PLACEMENT_3D('',#127221,#62974,#62975);
#50429=AXIS2_PLACEMENT_3D('',#127224,#62977,#62978);
#50430=AXIS2_PLACEMENT_3D('',#127225,#62979,#62980);
#50431=AXIS2_PLACEMENT_3D('',#127227,#62981,#62982);
#50432=AXIS2_PLACEMENT_3D('',#127230,#62984,#62985);
#50433=AXIS2_PLACEMENT_3D('',#127231,#62986,#62987);
#50434=AXIS2_PLACEMENT_3D('',#127233,#62988,#62989);
#50435=AXIS2_PLACEMENT_3D('',#127236,#62991,#62992);
#50436=AXIS2_PLACEMENT_3D('',#127237,#62993,#62994);
#50437=AXIS2_PLACEMENT_3D('',#127239,#62995,#62996);
#50438=AXIS2_PLACEMENT_3D('',#127242,#62998,#62999);
#50439=AXIS2_PLACEMENT_3D('',#127243,#63000,#63001);
#50440=AXIS2_PLACEMENT_3D('',#127245,#63002,#63003);
#50441=AXIS2_PLACEMENT_3D('',#127248,#63005,#63006);
#50442=AXIS2_PLACEMENT_3D('',#127249,#63007,#63008);
#50443=AXIS2_PLACEMENT_3D('',#127251,#63009,#63010);
#50444=AXIS2_PLACEMENT_3D('',#127254,#63012,#63013);
#50445=AXIS2_PLACEMENT_3D('',#127255,#63014,#63015);
#50446=AXIS2_PLACEMENT_3D('',#127257,#63016,#63017);
#50447=AXIS2_PLACEMENT_3D('',#127260,#63019,#63020);
#50448=AXIS2_PLACEMENT_3D('',#127261,#63021,#63022);
#50449=AXIS2_PLACEMENT_3D('',#127263,#63023,#63024);
#50450=AXIS2_PLACEMENT_3D('',#127266,#63026,#63027);
#50451=AXIS2_PLACEMENT_3D('',#127267,#63028,#63029);
#50452=AXIS2_PLACEMENT_3D('',#127269,#63030,#63031);
#50453=AXIS2_PLACEMENT_3D('',#127272,#63033,#63034);
#50454=AXIS2_PLACEMENT_3D('',#127273,#63035,#63036);
#50455=AXIS2_PLACEMENT_3D('',#127275,#63037,#63038);
#50456=AXIS2_PLACEMENT_3D('',#127278,#63040,#63041);
#50457=AXIS2_PLACEMENT_3D('',#127279,#63042,#63043);
#50458=AXIS2_PLACEMENT_3D('',#127281,#63044,#63045);
#50459=AXIS2_PLACEMENT_3D('',#127284,#63047,#63048);
#50460=AXIS2_PLACEMENT_3D('',#127285,#63049,#63050);
#50461=AXIS2_PLACEMENT_3D('',#127287,#63051,#63052);
#50462=AXIS2_PLACEMENT_3D('',#127290,#63054,#63055);
#50463=AXIS2_PLACEMENT_3D('',#127291,#63056,#63057);
#50464=AXIS2_PLACEMENT_3D('',#127293,#63058,#63059);
#50465=AXIS2_PLACEMENT_3D('',#127296,#63061,#63062);
#50466=AXIS2_PLACEMENT_3D('',#127297,#63063,#63064);
#50467=AXIS2_PLACEMENT_3D('',#127299,#63065,#63066);
#50468=AXIS2_PLACEMENT_3D('',#127302,#63068,#63069);
#50469=AXIS2_PLACEMENT_3D('',#127303,#63070,#63071);
#50470=AXIS2_PLACEMENT_3D('',#127305,#63072,#63073);
#50471=AXIS2_PLACEMENT_3D('',#127308,#63075,#63076);
#50472=AXIS2_PLACEMENT_3D('',#127309,#63077,#63078);
#50473=AXIS2_PLACEMENT_3D('',#127311,#63079,#63080);
#50474=AXIS2_PLACEMENT_3D('',#127314,#63082,#63083);
#50475=AXIS2_PLACEMENT_3D('',#127315,#63084,#63085);
#50476=AXIS2_PLACEMENT_3D('',#127317,#63086,#63087);
#50477=AXIS2_PLACEMENT_3D('',#127320,#63089,#63090);
#50478=AXIS2_PLACEMENT_3D('',#127321,#63091,#63092);
#50479=AXIS2_PLACEMENT_3D('',#127323,#63093,#63094);
#50480=AXIS2_PLACEMENT_3D('',#127326,#63096,#63097);
#50481=AXIS2_PLACEMENT_3D('',#127327,#63098,#63099);
#50482=AXIS2_PLACEMENT_3D('',#127329,#63100,#63101);
#50483=AXIS2_PLACEMENT_3D('',#127332,#63103,#63104);
#50484=AXIS2_PLACEMENT_3D('',#127333,#63105,#63106);
#50485=AXIS2_PLACEMENT_3D('',#127335,#63107,#63108);
#50486=AXIS2_PLACEMENT_3D('',#127338,#63110,#63111);
#50487=AXIS2_PLACEMENT_3D('',#127339,#63112,#63113);
#50488=AXIS2_PLACEMENT_3D('',#127341,#63114,#63115);
#50489=AXIS2_PLACEMENT_3D('',#127344,#63117,#63118);
#50490=AXIS2_PLACEMENT_3D('',#127345,#63119,#63120);
#50491=AXIS2_PLACEMENT_3D('',#127347,#63121,#63122);
#50492=AXIS2_PLACEMENT_3D('',#127350,#63124,#63125);
#50493=AXIS2_PLACEMENT_3D('',#127351,#63126,#63127);
#50494=AXIS2_PLACEMENT_3D('',#127353,#63128,#63129);
#50495=AXIS2_PLACEMENT_3D('',#127356,#63131,#63132);
#50496=AXIS2_PLACEMENT_3D('',#127357,#63133,#63134);
#50497=AXIS2_PLACEMENT_3D('',#127359,#63135,#63136);
#50498=AXIS2_PLACEMENT_3D('',#127362,#63138,#63139);
#50499=AXIS2_PLACEMENT_3D('',#127363,#63140,#63141);
#50500=AXIS2_PLACEMENT_3D('',#127365,#63142,#63143);
#50501=AXIS2_PLACEMENT_3D('',#127368,#63145,#63146);
#50502=AXIS2_PLACEMENT_3D('',#127369,#63147,#63148);
#50503=AXIS2_PLACEMENT_3D('',#127371,#63149,#63150);
#50504=AXIS2_PLACEMENT_3D('',#127374,#63152,#63153);
#50505=AXIS2_PLACEMENT_3D('',#127375,#63154,#63155);
#50506=AXIS2_PLACEMENT_3D('',#127377,#63156,#63157);
#50507=AXIS2_PLACEMENT_3D('',#127380,#63159,#63160);
#50508=AXIS2_PLACEMENT_3D('',#127381,#63161,#63162);
#50509=AXIS2_PLACEMENT_3D('',#127383,#63163,#63164);
#50510=AXIS2_PLACEMENT_3D('',#127386,#63166,#63167);
#50511=AXIS2_PLACEMENT_3D('',#127387,#63168,#63169);
#50512=AXIS2_PLACEMENT_3D('',#127389,#63170,#63171);
#50513=AXIS2_PLACEMENT_3D('',#127392,#63173,#63174);
#50514=AXIS2_PLACEMENT_3D('',#127393,#63175,#63176);
#50515=AXIS2_PLACEMENT_3D('',#127395,#63177,#63178);
#50516=AXIS2_PLACEMENT_3D('',#127398,#63180,#63181);
#50517=AXIS2_PLACEMENT_3D('',#127399,#63182,#63183);
#50518=AXIS2_PLACEMENT_3D('',#127401,#63184,#63185);
#50519=AXIS2_PLACEMENT_3D('',#127404,#63187,#63188);
#50520=AXIS2_PLACEMENT_3D('',#127405,#63189,#63190);
#50521=AXIS2_PLACEMENT_3D('',#127407,#63191,#63192);
#50522=AXIS2_PLACEMENT_3D('',#127410,#63194,#63195);
#50523=AXIS2_PLACEMENT_3D('',#127411,#63196,#63197);
#50524=AXIS2_PLACEMENT_3D('',#127413,#63198,#63199);
#50525=AXIS2_PLACEMENT_3D('',#127416,#63201,#63202);
#50526=AXIS2_PLACEMENT_3D('',#127417,#63203,#63204);
#50527=AXIS2_PLACEMENT_3D('',#127419,#63205,#63206);
#50528=AXIS2_PLACEMENT_3D('',#127422,#63208,#63209);
#50529=AXIS2_PLACEMENT_3D('',#127423,#63210,#63211);
#50530=AXIS2_PLACEMENT_3D('',#127425,#63212,#63213);
#50531=AXIS2_PLACEMENT_3D('',#127428,#63215,#63216);
#50532=AXIS2_PLACEMENT_3D('',#127429,#63217,#63218);
#50533=AXIS2_PLACEMENT_3D('',#127431,#63219,#63220);
#50534=AXIS2_PLACEMENT_3D('',#127434,#63222,#63223);
#50535=AXIS2_PLACEMENT_3D('',#127435,#63224,#63225);
#50536=AXIS2_PLACEMENT_3D('',#127437,#63226,#63227);
#50537=AXIS2_PLACEMENT_3D('',#127440,#63229,#63230);
#50538=AXIS2_PLACEMENT_3D('',#127441,#63231,#63232);
#50539=AXIS2_PLACEMENT_3D('',#127443,#63233,#63234);
#50540=AXIS2_PLACEMENT_3D('',#127446,#63236,#63237);
#50541=AXIS2_PLACEMENT_3D('',#127447,#63238,#63239);
#50542=AXIS2_PLACEMENT_3D('',#127449,#63240,#63241);
#50543=AXIS2_PLACEMENT_3D('',#127452,#63243,#63244);
#50544=AXIS2_PLACEMENT_3D('',#127453,#63245,#63246);
#50545=AXIS2_PLACEMENT_3D('',#127455,#63247,#63248);
#50546=AXIS2_PLACEMENT_3D('',#127458,#63250,#63251);
#50547=AXIS2_PLACEMENT_3D('',#127459,#63252,#63253);
#50548=AXIS2_PLACEMENT_3D('',#127461,#63254,#63255);
#50549=AXIS2_PLACEMENT_3D('',#127464,#63257,#63258);
#50550=AXIS2_PLACEMENT_3D('',#127465,#63259,#63260);
#50551=AXIS2_PLACEMENT_3D('',#127467,#63261,#63262);
#50552=AXIS2_PLACEMENT_3D('',#127470,#63264,#63265);
#50553=AXIS2_PLACEMENT_3D('',#127471,#63266,#63267);
#50554=AXIS2_PLACEMENT_3D('',#127473,#63268,#63269);
#50555=AXIS2_PLACEMENT_3D('',#127476,#63271,#63272);
#50556=AXIS2_PLACEMENT_3D('',#127477,#63273,#63274);
#50557=AXIS2_PLACEMENT_3D('',#127479,#63275,#63276);
#50558=AXIS2_PLACEMENT_3D('',#127482,#63278,#63279);
#50559=AXIS2_PLACEMENT_3D('',#127483,#63280,#63281);
#50560=AXIS2_PLACEMENT_3D('',#127485,#63282,#63283);
#50561=AXIS2_PLACEMENT_3D('',#127488,#63285,#63286);
#50562=AXIS2_PLACEMENT_3D('',#127489,#63287,#63288);
#50563=AXIS2_PLACEMENT_3D('',#127491,#63289,#63290);
#50564=AXIS2_PLACEMENT_3D('',#127494,#63292,#63293);
#50565=AXIS2_PLACEMENT_3D('',#127495,#63294,#63295);
#50566=AXIS2_PLACEMENT_3D('',#127497,#63296,#63297);
#50567=AXIS2_PLACEMENT_3D('',#127500,#63299,#63300);
#50568=AXIS2_PLACEMENT_3D('',#127501,#63301,#63302);
#50569=AXIS2_PLACEMENT_3D('',#127503,#63303,#63304);
#50570=AXIS2_PLACEMENT_3D('',#127506,#63306,#63307);
#50571=AXIS2_PLACEMENT_3D('',#127507,#63308,#63309);
#50572=AXIS2_PLACEMENT_3D('',#127509,#63310,#63311);
#50573=AXIS2_PLACEMENT_3D('',#127512,#63313,#63314);
#50574=AXIS2_PLACEMENT_3D('',#127513,#63315,#63316);
#50575=AXIS2_PLACEMENT_3D('',#127515,#63317,#63318);
#50576=AXIS2_PLACEMENT_3D('',#127518,#63320,#63321);
#50577=AXIS2_PLACEMENT_3D('',#127519,#63322,#63323);
#50578=AXIS2_PLACEMENT_3D('',#127521,#63324,#63325);
#50579=AXIS2_PLACEMENT_3D('',#127524,#63327,#63328);
#50580=AXIS2_PLACEMENT_3D('',#127525,#63329,#63330);
#50581=AXIS2_PLACEMENT_3D('',#127527,#63331,#63332);
#50582=AXIS2_PLACEMENT_3D('',#127530,#63334,#63335);
#50583=AXIS2_PLACEMENT_3D('',#127531,#63336,#63337);
#50584=AXIS2_PLACEMENT_3D('',#127533,#63338,#63339);
#50585=AXIS2_PLACEMENT_3D('',#127536,#63341,#63342);
#50586=AXIS2_PLACEMENT_3D('',#127537,#63343,#63344);
#50587=AXIS2_PLACEMENT_3D('',#127539,#63345,#63346);
#50588=AXIS2_PLACEMENT_3D('',#127542,#63348,#63349);
#50589=AXIS2_PLACEMENT_3D('',#127543,#63350,#63351);
#50590=AXIS2_PLACEMENT_3D('',#127545,#63352,#63353);
#50591=AXIS2_PLACEMENT_3D('',#127548,#63355,#63356);
#50592=AXIS2_PLACEMENT_3D('',#127549,#63357,#63358);
#50593=AXIS2_PLACEMENT_3D('',#127551,#63359,#63360);
#50594=AXIS2_PLACEMENT_3D('',#127554,#63362,#63363);
#50595=AXIS2_PLACEMENT_3D('',#127555,#63364,#63365);
#50596=AXIS2_PLACEMENT_3D('',#127557,#63366,#63367);
#50597=AXIS2_PLACEMENT_3D('',#127560,#63369,#63370);
#50598=AXIS2_PLACEMENT_3D('',#127561,#63371,#63372);
#50599=AXIS2_PLACEMENT_3D('',#127563,#63373,#63374);
#50600=AXIS2_PLACEMENT_3D('',#127566,#63376,#63377);
#50601=AXIS2_PLACEMENT_3D('',#127567,#63378,#63379);
#50602=AXIS2_PLACEMENT_3D('',#127569,#63380,#63381);
#50603=AXIS2_PLACEMENT_3D('',#127572,#63383,#63384);
#50604=AXIS2_PLACEMENT_3D('',#127573,#63385,#63386);
#50605=AXIS2_PLACEMENT_3D('',#127575,#63387,#63388);
#50606=AXIS2_PLACEMENT_3D('',#127578,#63390,#63391);
#50607=AXIS2_PLACEMENT_3D('',#127579,#63392,#63393);
#50608=AXIS2_PLACEMENT_3D('',#127581,#63394,#63395);
#50609=AXIS2_PLACEMENT_3D('',#127584,#63397,#63398);
#50610=AXIS2_PLACEMENT_3D('',#127585,#63399,#63400);
#50611=AXIS2_PLACEMENT_3D('',#127587,#63401,#63402);
#50612=AXIS2_PLACEMENT_3D('',#127590,#63404,#63405);
#50613=AXIS2_PLACEMENT_3D('',#127591,#63406,#63407);
#50614=AXIS2_PLACEMENT_3D('',#127593,#63408,#63409);
#50615=AXIS2_PLACEMENT_3D('',#127596,#63411,#63412);
#50616=AXIS2_PLACEMENT_3D('',#127597,#63413,#63414);
#50617=AXIS2_PLACEMENT_3D('',#127599,#63415,#63416);
#50618=AXIS2_PLACEMENT_3D('',#127602,#63418,#63419);
#50619=AXIS2_PLACEMENT_3D('',#127603,#63420,#63421);
#50620=AXIS2_PLACEMENT_3D('',#127605,#63422,#63423);
#50621=AXIS2_PLACEMENT_3D('',#127608,#63425,#63426);
#50622=AXIS2_PLACEMENT_3D('',#127609,#63427,#63428);
#50623=AXIS2_PLACEMENT_3D('',#127611,#63429,#63430);
#50624=AXIS2_PLACEMENT_3D('',#127614,#63432,#63433);
#50625=AXIS2_PLACEMENT_3D('',#127615,#63434,#63435);
#50626=AXIS2_PLACEMENT_3D('',#127617,#63436,#63437);
#50627=AXIS2_PLACEMENT_3D('',#127620,#63439,#63440);
#50628=AXIS2_PLACEMENT_3D('',#127621,#63441,#63442);
#50629=AXIS2_PLACEMENT_3D('',#127623,#63443,#63444);
#50630=AXIS2_PLACEMENT_3D('',#127626,#63446,#63447);
#50631=AXIS2_PLACEMENT_3D('',#127627,#63448,#63449);
#50632=AXIS2_PLACEMENT_3D('',#127629,#63450,#63451);
#50633=AXIS2_PLACEMENT_3D('',#127632,#63453,#63454);
#50634=AXIS2_PLACEMENT_3D('',#127633,#63455,#63456);
#50635=AXIS2_PLACEMENT_3D('',#127635,#63457,#63458);
#50636=AXIS2_PLACEMENT_3D('',#127638,#63460,#63461);
#50637=AXIS2_PLACEMENT_3D('',#127639,#63462,#63463);
#50638=AXIS2_PLACEMENT_3D('',#127641,#63464,#63465);
#50639=AXIS2_PLACEMENT_3D('',#127644,#63467,#63468);
#50640=AXIS2_PLACEMENT_3D('',#127645,#63469,#63470);
#50641=AXIS2_PLACEMENT_3D('',#127647,#63471,#63472);
#50642=AXIS2_PLACEMENT_3D('',#127650,#63474,#63475);
#50643=AXIS2_PLACEMENT_3D('',#127651,#63476,#63477);
#50644=AXIS2_PLACEMENT_3D('',#127653,#63478,#63479);
#50645=AXIS2_PLACEMENT_3D('',#127656,#63481,#63482);
#50646=AXIS2_PLACEMENT_3D('',#127657,#63483,#63484);
#50647=AXIS2_PLACEMENT_3D('',#127659,#63485,#63486);
#50648=AXIS2_PLACEMENT_3D('',#127662,#63488,#63489);
#50649=AXIS2_PLACEMENT_3D('',#127663,#63490,#63491);
#50650=AXIS2_PLACEMENT_3D('',#127665,#63492,#63493);
#50651=AXIS2_PLACEMENT_3D('',#127668,#63495,#63496);
#50652=AXIS2_PLACEMENT_3D('',#127669,#63497,#63498);
#50653=AXIS2_PLACEMENT_3D('',#127671,#63499,#63500);
#50654=AXIS2_PLACEMENT_3D('',#127674,#63502,#63503);
#50655=AXIS2_PLACEMENT_3D('',#127675,#63504,#63505);
#50656=AXIS2_PLACEMENT_3D('',#127677,#63506,#63507);
#50657=AXIS2_PLACEMENT_3D('',#127680,#63509,#63510);
#50658=AXIS2_PLACEMENT_3D('',#127681,#63511,#63512);
#50659=AXIS2_PLACEMENT_3D('',#127683,#63513,#63514);
#50660=AXIS2_PLACEMENT_3D('',#127686,#63516,#63517);
#50661=AXIS2_PLACEMENT_3D('',#127687,#63518,#63519);
#50662=AXIS2_PLACEMENT_3D('',#127689,#63520,#63521);
#50663=AXIS2_PLACEMENT_3D('',#127692,#63523,#63524);
#50664=AXIS2_PLACEMENT_3D('',#127693,#63525,#63526);
#50665=AXIS2_PLACEMENT_3D('',#127695,#63527,#63528);
#50666=AXIS2_PLACEMENT_3D('',#127698,#63530,#63531);
#50667=AXIS2_PLACEMENT_3D('',#127699,#63532,#63533);
#50668=AXIS2_PLACEMENT_3D('',#127701,#63534,#63535);
#50669=AXIS2_PLACEMENT_3D('',#127704,#63537,#63538);
#50670=AXIS2_PLACEMENT_3D('',#127705,#63539,#63540);
#50671=AXIS2_PLACEMENT_3D('',#127707,#63541,#63542);
#50672=AXIS2_PLACEMENT_3D('',#127710,#63544,#63545);
#50673=AXIS2_PLACEMENT_3D('',#127711,#63546,#63547);
#50674=AXIS2_PLACEMENT_3D('',#127713,#63548,#63549);
#50675=AXIS2_PLACEMENT_3D('',#127716,#63551,#63552);
#50676=AXIS2_PLACEMENT_3D('',#127717,#63553,#63554);
#50677=AXIS2_PLACEMENT_3D('',#127719,#63555,#63556);
#50678=AXIS2_PLACEMENT_3D('',#127722,#63558,#63559);
#50679=AXIS2_PLACEMENT_3D('',#127723,#63560,#63561);
#50680=AXIS2_PLACEMENT_3D('',#127725,#63562,#63563);
#50681=AXIS2_PLACEMENT_3D('',#127728,#63565,#63566);
#50682=AXIS2_PLACEMENT_3D('',#127729,#63567,#63568);
#50683=AXIS2_PLACEMENT_3D('',#127731,#63569,#63570);
#50684=AXIS2_PLACEMENT_3D('',#127734,#63572,#63573);
#50685=AXIS2_PLACEMENT_3D('',#127735,#63574,#63575);
#50686=AXIS2_PLACEMENT_3D('',#127737,#63576,#63577);
#50687=AXIS2_PLACEMENT_3D('',#127740,#63579,#63580);
#50688=AXIS2_PLACEMENT_3D('',#127741,#63581,#63582);
#50689=AXIS2_PLACEMENT_3D('',#127743,#63583,#63584);
#50690=AXIS2_PLACEMENT_3D('',#127746,#63586,#63587);
#50691=AXIS2_PLACEMENT_3D('',#127747,#63588,#63589);
#50692=AXIS2_PLACEMENT_3D('',#127749,#63590,#63591);
#50693=AXIS2_PLACEMENT_3D('',#127752,#63593,#63594);
#50694=AXIS2_PLACEMENT_3D('',#127753,#63595,#63596);
#50695=AXIS2_PLACEMENT_3D('',#127755,#63597,#63598);
#50696=AXIS2_PLACEMENT_3D('',#127758,#63600,#63601);
#50697=AXIS2_PLACEMENT_3D('',#127759,#63602,#63603);
#50698=AXIS2_PLACEMENT_3D('',#127761,#63604,#63605);
#50699=AXIS2_PLACEMENT_3D('',#127764,#63607,#63608);
#50700=AXIS2_PLACEMENT_3D('',#127765,#63609,#63610);
#50701=AXIS2_PLACEMENT_3D('',#127767,#63611,#63612);
#50702=AXIS2_PLACEMENT_3D('',#127770,#63614,#63615);
#50703=AXIS2_PLACEMENT_3D('',#127771,#63616,#63617);
#50704=AXIS2_PLACEMENT_3D('',#127773,#63618,#63619);
#50705=AXIS2_PLACEMENT_3D('',#127776,#63621,#63622);
#50706=AXIS2_PLACEMENT_3D('',#127777,#63623,#63624);
#50707=AXIS2_PLACEMENT_3D('',#127779,#63625,#63626);
#50708=AXIS2_PLACEMENT_3D('',#127782,#63628,#63629);
#50709=AXIS2_PLACEMENT_3D('',#127783,#63630,#63631);
#50710=AXIS2_PLACEMENT_3D('',#127785,#63632,#63633);
#50711=AXIS2_PLACEMENT_3D('',#127788,#63635,#63636);
#50712=AXIS2_PLACEMENT_3D('',#127789,#63637,#63638);
#50713=AXIS2_PLACEMENT_3D('',#127791,#63639,#63640);
#50714=AXIS2_PLACEMENT_3D('',#127794,#63642,#63643);
#50715=AXIS2_PLACEMENT_3D('',#127795,#63644,#63645);
#50716=AXIS2_PLACEMENT_3D('',#127797,#63646,#63647);
#50717=AXIS2_PLACEMENT_3D('',#127800,#63649,#63650);
#50718=AXIS2_PLACEMENT_3D('',#127801,#63651,#63652);
#50719=AXIS2_PLACEMENT_3D('',#127803,#63653,#63654);
#50720=AXIS2_PLACEMENT_3D('',#127806,#63656,#63657);
#50721=AXIS2_PLACEMENT_3D('',#127807,#63658,#63659);
#50722=AXIS2_PLACEMENT_3D('',#127809,#63660,#63661);
#50723=AXIS2_PLACEMENT_3D('',#127812,#63663,#63664);
#50724=AXIS2_PLACEMENT_3D('',#127813,#63665,#63666);
#50725=AXIS2_PLACEMENT_3D('',#127815,#63667,#63668);
#50726=AXIS2_PLACEMENT_3D('',#127818,#63670,#63671);
#50727=AXIS2_PLACEMENT_3D('',#127819,#63672,#63673);
#50728=AXIS2_PLACEMENT_3D('',#127821,#63674,#63675);
#50729=AXIS2_PLACEMENT_3D('',#127824,#63677,#63678);
#50730=AXIS2_PLACEMENT_3D('',#127825,#63679,#63680);
#50731=AXIS2_PLACEMENT_3D('',#127827,#63681,#63682);
#50732=AXIS2_PLACEMENT_3D('',#127830,#63684,#63685);
#50733=AXIS2_PLACEMENT_3D('',#127831,#63686,#63687);
#50734=AXIS2_PLACEMENT_3D('',#127833,#63688,#63689);
#50735=AXIS2_PLACEMENT_3D('',#127836,#63691,#63692);
#50736=AXIS2_PLACEMENT_3D('',#127837,#63693,#63694);
#50737=AXIS2_PLACEMENT_3D('',#127839,#63695,#63696);
#50738=AXIS2_PLACEMENT_3D('',#127842,#63698,#63699);
#50739=AXIS2_PLACEMENT_3D('',#127843,#63700,#63701);
#50740=AXIS2_PLACEMENT_3D('',#127845,#63702,#63703);
#50741=AXIS2_PLACEMENT_3D('',#127848,#63705,#63706);
#50742=AXIS2_PLACEMENT_3D('',#127849,#63707,#63708);
#50743=AXIS2_PLACEMENT_3D('',#127851,#63709,#63710);
#50744=AXIS2_PLACEMENT_3D('',#127854,#63712,#63713);
#50745=AXIS2_PLACEMENT_3D('',#127855,#63714,#63715);
#50746=AXIS2_PLACEMENT_3D('',#127857,#63716,#63717);
#50747=AXIS2_PLACEMENT_3D('',#127860,#63719,#63720);
#50748=AXIS2_PLACEMENT_3D('',#127861,#63721,#63722);
#50749=AXIS2_PLACEMENT_3D('',#127863,#63723,#63724);
#50750=AXIS2_PLACEMENT_3D('',#127866,#63726,#63727);
#50751=AXIS2_PLACEMENT_3D('',#127867,#63728,#63729);
#50752=AXIS2_PLACEMENT_3D('',#127869,#63730,#63731);
#50753=AXIS2_PLACEMENT_3D('',#127872,#63733,#63734);
#50754=AXIS2_PLACEMENT_3D('',#127873,#63735,#63736);
#50755=AXIS2_PLACEMENT_3D('',#127875,#63737,#63738);
#50756=AXIS2_PLACEMENT_3D('',#127878,#63740,#63741);
#50757=AXIS2_PLACEMENT_3D('',#127879,#63742,#63743);
#50758=AXIS2_PLACEMENT_3D('',#127881,#63744,#63745);
#50759=AXIS2_PLACEMENT_3D('',#127884,#63747,#63748);
#50760=AXIS2_PLACEMENT_3D('',#127885,#63749,#63750);
#50761=AXIS2_PLACEMENT_3D('',#127887,#63751,#63752);
#50762=AXIS2_PLACEMENT_3D('',#127890,#63754,#63755);
#50763=AXIS2_PLACEMENT_3D('',#127891,#63756,#63757);
#50764=AXIS2_PLACEMENT_3D('',#127893,#63758,#63759);
#50765=AXIS2_PLACEMENT_3D('',#127896,#63761,#63762);
#50766=AXIS2_PLACEMENT_3D('',#127897,#63763,#63764);
#50767=AXIS2_PLACEMENT_3D('',#127899,#63765,#63766);
#50768=AXIS2_PLACEMENT_3D('',#127902,#63768,#63769);
#50769=AXIS2_PLACEMENT_3D('',#127903,#63770,#63771);
#50770=AXIS2_PLACEMENT_3D('',#127905,#63772,#63773);
#50771=AXIS2_PLACEMENT_3D('',#127908,#63775,#63776);
#50772=AXIS2_PLACEMENT_3D('',#127909,#63777,#63778);
#50773=AXIS2_PLACEMENT_3D('',#127911,#63779,#63780);
#50774=AXIS2_PLACEMENT_3D('',#127914,#63782,#63783);
#50775=AXIS2_PLACEMENT_3D('',#127915,#63784,#63785);
#50776=AXIS2_PLACEMENT_3D('',#127917,#63786,#63787);
#50777=AXIS2_PLACEMENT_3D('',#127920,#63789,#63790);
#50778=AXIS2_PLACEMENT_3D('',#127921,#63791,#63792);
#50779=AXIS2_PLACEMENT_3D('',#127923,#63793,#63794);
#50780=AXIS2_PLACEMENT_3D('',#127926,#63796,#63797);
#50781=AXIS2_PLACEMENT_3D('',#127927,#63798,#63799);
#50782=AXIS2_PLACEMENT_3D('',#127929,#63800,#63801);
#50783=AXIS2_PLACEMENT_3D('',#127932,#63803,#63804);
#50784=AXIS2_PLACEMENT_3D('',#127933,#63805,#63806);
#50785=AXIS2_PLACEMENT_3D('',#127935,#63807,#63808);
#50786=AXIS2_PLACEMENT_3D('',#127938,#63810,#63811);
#50787=AXIS2_PLACEMENT_3D('',#127939,#63812,#63813);
#50788=AXIS2_PLACEMENT_3D('',#127941,#63814,#63815);
#50789=AXIS2_PLACEMENT_3D('',#127944,#63817,#63818);
#50790=AXIS2_PLACEMENT_3D('',#127945,#63819,#63820);
#50791=AXIS2_PLACEMENT_3D('',#127947,#63821,#63822);
#50792=AXIS2_PLACEMENT_3D('',#127950,#63824,#63825);
#50793=AXIS2_PLACEMENT_3D('',#127951,#63826,#63827);
#50794=AXIS2_PLACEMENT_3D('',#127953,#63828,#63829);
#50795=AXIS2_PLACEMENT_3D('',#127956,#63831,#63832);
#50796=AXIS2_PLACEMENT_3D('',#127957,#63833,#63834);
#50797=AXIS2_PLACEMENT_3D('',#127959,#63835,#63836);
#50798=AXIS2_PLACEMENT_3D('',#127962,#63838,#63839);
#50799=AXIS2_PLACEMENT_3D('',#127963,#63840,#63841);
#50800=AXIS2_PLACEMENT_3D('',#127965,#63842,#63843);
#50801=AXIS2_PLACEMENT_3D('',#127968,#63845,#63846);
#50802=AXIS2_PLACEMENT_3D('',#127969,#63847,#63848);
#50803=AXIS2_PLACEMENT_3D('',#127971,#63849,#63850);
#50804=AXIS2_PLACEMENT_3D('',#127974,#63852,#63853);
#50805=AXIS2_PLACEMENT_3D('',#127975,#63854,#63855);
#50806=AXIS2_PLACEMENT_3D('',#127977,#63856,#63857);
#50807=AXIS2_PLACEMENT_3D('',#127980,#63859,#63860);
#50808=AXIS2_PLACEMENT_3D('',#127981,#63861,#63862);
#50809=AXIS2_PLACEMENT_3D('',#127983,#63863,#63864);
#50810=AXIS2_PLACEMENT_3D('',#127986,#63866,#63867);
#50811=AXIS2_PLACEMENT_3D('',#127987,#63868,#63869);
#50812=AXIS2_PLACEMENT_3D('',#127989,#63870,#63871);
#50813=AXIS2_PLACEMENT_3D('',#127992,#63873,#63874);
#50814=AXIS2_PLACEMENT_3D('',#127993,#63875,#63876);
#50815=AXIS2_PLACEMENT_3D('',#127995,#63877,#63878);
#50816=AXIS2_PLACEMENT_3D('',#127998,#63880,#63881);
#50817=AXIS2_PLACEMENT_3D('',#127999,#63882,#63883);
#50818=AXIS2_PLACEMENT_3D('',#128001,#63884,#63885);
#50819=AXIS2_PLACEMENT_3D('',#128004,#63887,#63888);
#50820=AXIS2_PLACEMENT_3D('',#128005,#63889,#63890);
#50821=AXIS2_PLACEMENT_3D('',#128007,#63891,#63892);
#50822=AXIS2_PLACEMENT_3D('',#128010,#63894,#63895);
#50823=AXIS2_PLACEMENT_3D('',#128011,#63896,#63897);
#50824=AXIS2_PLACEMENT_3D('',#128013,#63898,#63899);
#50825=AXIS2_PLACEMENT_3D('',#128016,#63901,#63902);
#50826=AXIS2_PLACEMENT_3D('',#128017,#63903,#63904);
#50827=AXIS2_PLACEMENT_3D('',#128019,#63905,#63906);
#50828=AXIS2_PLACEMENT_3D('',#128022,#63908,#63909);
#50829=AXIS2_PLACEMENT_3D('',#128023,#63910,#63911);
#50830=AXIS2_PLACEMENT_3D('',#128025,#63912,#63913);
#50831=AXIS2_PLACEMENT_3D('',#128028,#63915,#63916);
#50832=AXIS2_PLACEMENT_3D('',#128029,#63917,#63918);
#50833=AXIS2_PLACEMENT_3D('',#128031,#63919,#63920);
#50834=AXIS2_PLACEMENT_3D('',#128034,#63922,#63923);
#50835=AXIS2_PLACEMENT_3D('',#128035,#63924,#63925);
#50836=AXIS2_PLACEMENT_3D('',#128037,#63926,#63927);
#50837=AXIS2_PLACEMENT_3D('',#128040,#63929,#63930);
#50838=AXIS2_PLACEMENT_3D('',#128041,#63931,#63932);
#50839=AXIS2_PLACEMENT_3D('',#128043,#63933,#63934);
#50840=AXIS2_PLACEMENT_3D('',#128046,#63936,#63937);
#50841=AXIS2_PLACEMENT_3D('',#128047,#63938,#63939);
#50842=AXIS2_PLACEMENT_3D('',#128049,#63940,#63941);
#50843=AXIS2_PLACEMENT_3D('',#128052,#63943,#63944);
#50844=AXIS2_PLACEMENT_3D('',#128053,#63945,#63946);
#50845=AXIS2_PLACEMENT_3D('',#128055,#63947,#63948);
#50846=AXIS2_PLACEMENT_3D('',#128058,#63950,#63951);
#50847=AXIS2_PLACEMENT_3D('',#128059,#63952,#63953);
#50848=AXIS2_PLACEMENT_3D('',#128061,#63954,#63955);
#50849=AXIS2_PLACEMENT_3D('',#128064,#63957,#63958);
#50850=AXIS2_PLACEMENT_3D('',#128065,#63959,#63960);
#50851=AXIS2_PLACEMENT_3D('',#128067,#63961,#63962);
#50852=AXIS2_PLACEMENT_3D('',#128070,#63964,#63965);
#50853=AXIS2_PLACEMENT_3D('',#128071,#63966,#63967);
#50854=AXIS2_PLACEMENT_3D('',#128073,#63968,#63969);
#50855=AXIS2_PLACEMENT_3D('',#128076,#63971,#63972);
#50856=AXIS2_PLACEMENT_3D('',#128077,#63973,#63974);
#50857=AXIS2_PLACEMENT_3D('',#128079,#63975,#63976);
#50858=AXIS2_PLACEMENT_3D('',#128082,#63978,#63979);
#50859=AXIS2_PLACEMENT_3D('',#128083,#63980,#63981);
#50860=AXIS2_PLACEMENT_3D('',#128085,#63982,#63983);
#50861=AXIS2_PLACEMENT_3D('',#128088,#63985,#63986);
#50862=AXIS2_PLACEMENT_3D('',#128089,#63987,#63988);
#50863=AXIS2_PLACEMENT_3D('',#128091,#63989,#63990);
#50864=AXIS2_PLACEMENT_3D('',#128094,#63992,#63993);
#50865=AXIS2_PLACEMENT_3D('',#128095,#63994,#63995);
#50866=AXIS2_PLACEMENT_3D('',#128097,#63996,#63997);
#50867=AXIS2_PLACEMENT_3D('',#128100,#63999,#64000);
#50868=AXIS2_PLACEMENT_3D('',#128101,#64001,#64002);
#50869=AXIS2_PLACEMENT_3D('',#128103,#64003,#64004);
#50870=AXIS2_PLACEMENT_3D('',#128106,#64006,#64007);
#50871=AXIS2_PLACEMENT_3D('',#128107,#64008,#64009);
#50872=AXIS2_PLACEMENT_3D('',#128109,#64010,#64011);
#50873=AXIS2_PLACEMENT_3D('',#128112,#64013,#64014);
#50874=AXIS2_PLACEMENT_3D('',#128113,#64015,#64016);
#50875=AXIS2_PLACEMENT_3D('',#128115,#64017,#64018);
#50876=AXIS2_PLACEMENT_3D('',#128118,#64020,#64021);
#50877=AXIS2_PLACEMENT_3D('',#128119,#64022,#64023);
#50878=AXIS2_PLACEMENT_3D('',#128121,#64024,#64025);
#50879=AXIS2_PLACEMENT_3D('',#128124,#64027,#64028);
#50880=AXIS2_PLACEMENT_3D('',#128125,#64029,#64030);
#50881=AXIS2_PLACEMENT_3D('',#128127,#64031,#64032);
#50882=AXIS2_PLACEMENT_3D('',#128130,#64034,#64035);
#50883=AXIS2_PLACEMENT_3D('',#128131,#64036,#64037);
#50884=AXIS2_PLACEMENT_3D('',#128133,#64038,#64039);
#50885=AXIS2_PLACEMENT_3D('',#128136,#64041,#64042);
#50886=AXIS2_PLACEMENT_3D('',#128137,#64043,#64044);
#50887=AXIS2_PLACEMENT_3D('',#128139,#64045,#64046);
#50888=AXIS2_PLACEMENT_3D('',#128140,#64047,#64048);
#50889=AXIS2_PLACEMENT_3D('',#128141,#64049,#64050);
#50890=AXIS2_PLACEMENT_3D('',#128142,#64051,#64052);
#50891=AXIS2_PLACEMENT_3D('',#128145,#64054,#64055);
#50892=AXIS2_PLACEMENT_3D('',#128146,#64056,#64057);
#50893=AXIS2_PLACEMENT_3D('',#128148,#64058,#64059);
#50894=AXIS2_PLACEMENT_3D('',#128150,#64060,#64061);
#50895=AXIS2_PLACEMENT_3D('',#128152,#64062,#64063);
#50896=AXIS2_PLACEMENT_3D('',#128153,#64064,#64065);
#50897=AXIS2_PLACEMENT_3D('',#128154,#64066,#64067);
#50898=AXIS2_PLACEMENT_3D('',#128156,#64068,#64069);
#50899=AXIS2_PLACEMENT_3D('',#128158,#64070,#64071);
#50900=AXIS2_PLACEMENT_3D('',#128159,#64072,#64073);
#50901=AXIS2_PLACEMENT_3D('',#128160,#64074,#64075);
#50902=AXIS2_PLACEMENT_3D('',#128162,#64077,#64078);
#50903=AXIS2_PLACEMENT_3D('',#128164,#64079,#64080);
#50904=AXIS2_PLACEMENT_3D('',#128165,#64081,#64082);
#50905=AXIS2_PLACEMENT_3D('',#128167,#64083,#64084);
#50906=AXIS2_PLACEMENT_3D('',#128169,#64085,#64086);
#50907=AXIS2_PLACEMENT_3D('',#128170,#64087,#64088);
#50908=AXIS2_PLACEMENT_3D('',#128171,#64089,#64090);
#50909=AXIS2_PLACEMENT_3D('',#128173,#64091,#64092);
#50910=AXIS2_PLACEMENT_3D('',#128175,#64093,#64094);
#50911=AXIS2_PLACEMENT_3D('',#128176,#64095,#64096);
#50912=AXIS2_PLACEMENT_3D('',#128177,#64097,#64098);
#50913=AXIS2_PLACEMENT_3D('',#128179,#64099,#64100);
#50914=AXIS2_PLACEMENT_3D('',#128180,#64101,#64102);
#50915=AXIS2_PLACEMENT_3D('',#128181,#64103,#64104);
#50916=AXIS2_PLACEMENT_3D('',#128183,#64105,#64106);
#50917=AXIS2_PLACEMENT_3D('',#128185,#64108,#64109);
#50918=AXIS2_PLACEMENT_3D('',#128188,#64110,#64111);
#50919=AXIS2_PLACEMENT_3D('',#128189,#64112,#64113);
#50920=AXIS2_PLACEMENT_3D('',#128191,#64114,#64115);
#50921=AXIS2_PLACEMENT_3D('',#128192,#64116,#64117);
#50922=AXIS2_PLACEMENT_3D('',#128193,#64118,#64119);
#50923=AXIS2_PLACEMENT_3D('',#128195,#64121,#64122);
#50924=AXIS2_PLACEMENT_3D('',#128222,#64124,#64125);
#50925=AXIS2_PLACEMENT_3D('',#128243,#64126,#64127);
#50926=AXIS2_PLACEMENT_3D('',#128300,#64129,#64130);
#50927=AXIS2_PLACEMENT_3D('',#128301,#64131,#64132);
#50928=AXIS2_PLACEMENT_3D('',#128302,#64133,#64134);
#50929=AXIS2_PLACEMENT_3D('',#128303,#64135,#64136);
#50930=AXIS2_PLACEMENT_3D('',#128304,#64137,#64138);
#50931=AXIS2_PLACEMENT_3D('',#128305,#64139,#64140);
#50932=AXIS2_PLACEMENT_3D('',#128306,#64141,#64142);
#50933=AXIS2_PLACEMENT_3D('',#128307,#64143,#64144);
#50934=AXIS2_PLACEMENT_3D('',#128320,#64145,#64146);
#50935=AXIS2_PLACEMENT_3D('',#128321,#64147,#64148);
#50936=AXIS2_PLACEMENT_3D('',#128322,#64149,#64150);
#50937=AXIS2_PLACEMENT_3D('',#128323,#64151,#64152);
#50938=AXIS2_PLACEMENT_3D('',#128324,#64153,#64154);
#50939=AXIS2_PLACEMENT_3D('',#128325,#64155,#64156);
#50940=AXIS2_PLACEMENT_3D('',#128326,#64157,#64158);
#50941=AXIS2_PLACEMENT_3D('',#128327,#64159,#64160);
#50942=AXIS2_PLACEMENT_3D('',#128328,#64161,#64162);
#50943=AXIS2_PLACEMENT_3D('',#128329,#64163,#64164);
#50944=AXIS2_PLACEMENT_3D('',#128330,#64165,#64166);
#50945=AXIS2_PLACEMENT_3D('',#128331,#64167,#64168);
#50946=AXIS2_PLACEMENT_3D('',#128332,#64169,#64170);
#50947=AXIS2_PLACEMENT_3D('',#128333,#64171,#64172);
#50948=AXIS2_PLACEMENT_3D('',#128334,#64173,#64174);
#50949=AXIS2_PLACEMENT_3D('',#128335,#64175,#64176);
#50950=AXIS2_PLACEMENT_3D('',#128336,#64177,#64178);
#50951=AXIS2_PLACEMENT_3D('',#128337,#64179,#64180);
#50952=AXIS2_PLACEMENT_3D('',#128338,#64181,#64182);
#50953=AXIS2_PLACEMENT_3D('',#128339,#64183,#64184);
#50954=AXIS2_PLACEMENT_3D('',#128340,#64185,#64186);
#50955=AXIS2_PLACEMENT_3D('',#128341,#64187,#64188);
#50956=AXIS2_PLACEMENT_3D('',#128342,#64189,#64190);
#50957=AXIS2_PLACEMENT_3D('',#128343,#64191,#64192);
#50958=AXIS2_PLACEMENT_3D('',#128344,#64193,#64194);
#50959=AXIS2_PLACEMENT_3D('',#128345,#64195,#64196);
#50960=AXIS2_PLACEMENT_3D('',#128346,#64197,#64198);
#50961=AXIS2_PLACEMENT_3D('',#128347,#64199,#64200);
#50962=AXIS2_PLACEMENT_3D('',#128348,#64201,#64202);
#50963=AXIS2_PLACEMENT_3D('',#128349,#64203,#64204);
#50964=AXIS2_PLACEMENT_3D('',#128350,#64205,#64206);
#50965=AXIS2_PLACEMENT_3D('',#128351,#64207,#64208);
#50966=AXIS2_PLACEMENT_3D('',#128352,#64209,#64210);
#50967=AXIS2_PLACEMENT_3D('',#128353,#64211,#64212);
#50968=AXIS2_PLACEMENT_3D('',#128354,#64213,#64214);
#50969=AXIS2_PLACEMENT_3D('',#128355,#64215,#64216);
#50970=AXIS2_PLACEMENT_3D('',#128356,#64217,#64218);
#50971=AXIS2_PLACEMENT_3D('',#128357,#64219,#64220);
#50972=AXIS2_PLACEMENT_3D('',#128358,#64221,#64222);
#50973=AXIS2_PLACEMENT_3D('',#128359,#64223,#64224);
#50974=AXIS2_PLACEMENT_3D('',#128360,#64225,#64226);
#50975=AXIS2_PLACEMENT_3D('',#128361,#64227,#64228);
#50976=AXIS2_PLACEMENT_3D('',#128362,#64229,#64230);
#50977=AXIS2_PLACEMENT_3D('',#128363,#64231,#64232);
#50978=AXIS2_PLACEMENT_3D('',#128364,#64233,#64234);
#50979=AXIS2_PLACEMENT_3D('',#128365,#64235,#64236);
#50980=AXIS2_PLACEMENT_3D('',#128366,#64237,#64238);
#50981=AXIS2_PLACEMENT_3D('',#128367,#64239,#64240);
#50982=AXIS2_PLACEMENT_3D('',#128368,#64241,#64242);
#50983=AXIS2_PLACEMENT_3D('',#128369,#64243,#64244);
#50984=AXIS2_PLACEMENT_3D('',#128370,#64245,#64246);
#50985=AXIS2_PLACEMENT_3D('',#128371,#64247,#64248);
#50986=AXIS2_PLACEMENT_3D('',#128372,#64249,#64250);
#50987=AXIS2_PLACEMENT_3D('',#128373,#64251,#64252);
#50988=AXIS2_PLACEMENT_3D('',#128374,#64253,#64254);
#50989=AXIS2_PLACEMENT_3D('',#128375,#64255,#64256);
#50990=AXIS2_PLACEMENT_3D('',#128376,#64257,#64258);
#50991=AXIS2_PLACEMENT_3D('',#128377,#64259,#64260);
#50992=AXIS2_PLACEMENT_3D('',#128378,#64261,#64262);
#50993=AXIS2_PLACEMENT_3D('',#128379,#64263,#64264);
#50994=AXIS2_PLACEMENT_3D('',#128380,#64265,#64266);
#50995=AXIS2_PLACEMENT_3D('',#128381,#64267,#64268);
#50996=AXIS2_PLACEMENT_3D('',#128382,#64269,#64270);
#50997=AXIS2_PLACEMENT_3D('',#128383,#64271,#64272);
#50998=AXIS2_PLACEMENT_3D('',#128384,#64273,#64274);
#50999=AXIS2_PLACEMENT_3D('',#128385,#64275,#64276);
#51000=AXIS2_PLACEMENT_3D('',#128386,#64277,#64278);
#51001=AXIS2_PLACEMENT_3D('',#128387,#64279,#64280);
#51002=AXIS2_PLACEMENT_3D('',#128388,#64281,#64282);
#51003=AXIS2_PLACEMENT_3D('',#128389,#64283,#64284);
#51004=AXIS2_PLACEMENT_3D('',#128390,#64285,#64286);
#51005=AXIS2_PLACEMENT_3D('',#128391,#64287,#64288);
#51006=AXIS2_PLACEMENT_3D('',#128392,#64289,#64290);
#51007=AXIS2_PLACEMENT_3D('',#128393,#64291,#64292);
#51008=AXIS2_PLACEMENT_3D('',#128394,#64293,#64294);
#51009=AXIS2_PLACEMENT_3D('',#128395,#64295,#64296);
#51010=AXIS2_PLACEMENT_3D('',#128396,#64297,#64298);
#51011=AXIS2_PLACEMENT_3D('',#128397,#64299,#64300);
#51012=AXIS2_PLACEMENT_3D('',#128398,#64301,#64302);
#51013=AXIS2_PLACEMENT_3D('',#128399,#64303,#64304);
#51014=AXIS2_PLACEMENT_3D('',#128400,#64305,#64306);
#51015=AXIS2_PLACEMENT_3D('',#128401,#64307,#64308);
#51016=AXIS2_PLACEMENT_3D('',#128402,#64309,#64310);
#51017=AXIS2_PLACEMENT_3D('',#128403,#64311,#64312);
#51018=AXIS2_PLACEMENT_3D('',#128404,#64313,#64314);
#51019=AXIS2_PLACEMENT_3D('',#128405,#64315,#64316);
#51020=AXIS2_PLACEMENT_3D('',#128406,#64317,#64318);
#51021=AXIS2_PLACEMENT_3D('',#128407,#64319,#64320);
#51022=AXIS2_PLACEMENT_3D('',#128408,#64321,#64322);
#51023=AXIS2_PLACEMENT_3D('',#128409,#64323,#64324);
#51024=AXIS2_PLACEMENT_3D('',#128410,#64325,#64326);
#51025=AXIS2_PLACEMENT_3D('',#128411,#64327,#64328);
#51026=AXIS2_PLACEMENT_3D('',#128412,#64329,#64330);
#51027=AXIS2_PLACEMENT_3D('',#128413,#64331,#64332);
#51028=AXIS2_PLACEMENT_3D('',#128414,#64333,#64334);
#51029=AXIS2_PLACEMENT_3D('',#128415,#64335,#64336);
#51030=AXIS2_PLACEMENT_3D('',#128416,#64337,#64338);
#51031=AXIS2_PLACEMENT_3D('',#128417,#64339,#64340);
#51032=AXIS2_PLACEMENT_3D('',#128418,#64341,#64342);
#51033=AXIS2_PLACEMENT_3D('',#128419,#64343,#64344);
#51034=AXIS2_PLACEMENT_3D('',#128420,#64345,#64346);
#51035=AXIS2_PLACEMENT_3D('',#128421,#64347,#64348);
#51036=AXIS2_PLACEMENT_3D('',#128422,#64349,#64350);
#51037=AXIS2_PLACEMENT_3D('',#128423,#64351,#64352);
#51038=AXIS2_PLACEMENT_3D('',#128424,#64353,#64354);
#51039=AXIS2_PLACEMENT_3D('',#128425,#64355,#64356);
#51040=AXIS2_PLACEMENT_3D('',#128426,#64357,#64358);
#51041=AXIS2_PLACEMENT_3D('',#128427,#64359,#64360);
#51042=AXIS2_PLACEMENT_3D('',#128428,#64361,#64362);
#51043=AXIS2_PLACEMENT_3D('',#128429,#64363,#64364);
#51044=AXIS2_PLACEMENT_3D('',#128430,#64365,#64366);
#51045=AXIS2_PLACEMENT_3D('',#128431,#64367,#64368);
#51046=AXIS2_PLACEMENT_3D('',#128432,#64369,#64370);
#51047=AXIS2_PLACEMENT_3D('',#128433,#64371,#64372);
#51048=AXIS2_PLACEMENT_3D('',#128434,#64373,#64374);
#51049=AXIS2_PLACEMENT_3D('',#128435,#64375,#64376);
#51050=AXIS2_PLACEMENT_3D('',#128436,#64377,#64378);
#51051=AXIS2_PLACEMENT_3D('',#128437,#64379,#64380);
#51052=AXIS2_PLACEMENT_3D('',#128438,#64381,#64382);
#51053=AXIS2_PLACEMENT_3D('',#128439,#64383,#64384);
#51054=AXIS2_PLACEMENT_3D('',#128440,#64385,#64386);
#51055=AXIS2_PLACEMENT_3D('',#128441,#64387,#64388);
#51056=AXIS2_PLACEMENT_3D('',#128442,#64389,#64390);
#51057=AXIS2_PLACEMENT_3D('',#128443,#64391,#64392);
#51058=AXIS2_PLACEMENT_3D('',#128444,#64393,#64394);
#51059=AXIS2_PLACEMENT_3D('',#128445,#64395,#64396);
#51060=AXIS2_PLACEMENT_3D('',#128446,#64397,#64398);
#51061=AXIS2_PLACEMENT_3D('',#128447,#64399,#64400);
#51062=AXIS2_PLACEMENT_3D('',#128448,#64401,#64402);
#51063=AXIS2_PLACEMENT_3D('',#128449,#64403,#64404);
#51064=AXIS2_PLACEMENT_3D('',#128450,#64405,#64406);
#51065=AXIS2_PLACEMENT_3D('',#128451,#64407,#64408);
#51066=AXIS2_PLACEMENT_3D('',#128452,#64409,#64410);
#51067=AXIS2_PLACEMENT_3D('',#128453,#64411,#64412);
#51068=AXIS2_PLACEMENT_3D('',#128454,#64413,#64414);
#51069=AXIS2_PLACEMENT_3D('',#128455,#64415,#64416);
#51070=AXIS2_PLACEMENT_3D('',#128456,#64417,#64418);
#51071=AXIS2_PLACEMENT_3D('',#128457,#64419,#64420);
#51072=AXIS2_PLACEMENT_3D('',#128458,#64421,#64422);
#51073=AXIS2_PLACEMENT_3D('',#128459,#64423,#64424);
#51074=AXIS2_PLACEMENT_3D('',#128460,#64425,#64426);
#51075=AXIS2_PLACEMENT_3D('',#128461,#64427,#64428);
#51076=AXIS2_PLACEMENT_3D('',#128462,#64429,#64430);
#51077=AXIS2_PLACEMENT_3D('',#128463,#64431,#64432);
#51078=AXIS2_PLACEMENT_3D('',#128464,#64433,#64434);
#51079=AXIS2_PLACEMENT_3D('',#128465,#64435,#64436);
#51080=AXIS2_PLACEMENT_3D('',#128466,#64437,#64438);
#51081=AXIS2_PLACEMENT_3D('',#128467,#64439,#64440);
#51082=AXIS2_PLACEMENT_3D('',#128468,#64441,#64442);
#51083=AXIS2_PLACEMENT_3D('',#128469,#64443,#64444);
#51084=AXIS2_PLACEMENT_3D('',#128470,#64445,#64446);
#51085=AXIS2_PLACEMENT_3D('',#128471,#64447,#64448);
#51086=AXIS2_PLACEMENT_3D('',#128472,#64449,#64450);
#51087=AXIS2_PLACEMENT_3D('',#128473,#64451,#64452);
#51088=AXIS2_PLACEMENT_3D('',#128474,#64453,#64454);
#51089=AXIS2_PLACEMENT_3D('',#128475,#64455,#64456);
#51090=AXIS2_PLACEMENT_3D('',#128476,#64457,#64458);
#51091=AXIS2_PLACEMENT_3D('',#128477,#64459,#64460);
#51092=AXIS2_PLACEMENT_3D('',#128478,#64461,#64462);
#51093=AXIS2_PLACEMENT_3D('',#128479,#64463,#64464);
#51094=AXIS2_PLACEMENT_3D('',#128480,#64465,#64466);
#51095=AXIS2_PLACEMENT_3D('',#128481,#64467,#64468);
#51096=AXIS2_PLACEMENT_3D('',#128482,#64469,#64470);
#51097=AXIS2_PLACEMENT_3D('',#128483,#64471,#64472);
#51098=AXIS2_PLACEMENT_3D('',#128484,#64473,#64474);
#51099=AXIS2_PLACEMENT_3D('',#128485,#64475,#64476);
#51100=AXIS2_PLACEMENT_3D('',#128486,#64477,#64478);
#51101=AXIS2_PLACEMENT_3D('',#128487,#64479,#64480);
#51102=AXIS2_PLACEMENT_3D('',#128488,#64481,#64482);
#51103=AXIS2_PLACEMENT_3D('',#128489,#64483,#64484);
#51104=AXIS2_PLACEMENT_3D('',#128490,#64485,#64486);
#51105=AXIS2_PLACEMENT_3D('',#128491,#64487,#64488);
#51106=AXIS2_PLACEMENT_3D('',#128492,#64489,#64490);
#51107=AXIS2_PLACEMENT_3D('',#128493,#64491,#64492);
#51108=AXIS2_PLACEMENT_3D('',#128494,#64493,#64494);
#51109=AXIS2_PLACEMENT_3D('',#128495,#64495,#64496);
#51110=AXIS2_PLACEMENT_3D('',#128496,#64497,#64498);
#51111=AXIS2_PLACEMENT_3D('',#128497,#64499,#64500);
#51112=AXIS2_PLACEMENT_3D('',#128498,#64501,#64502);
#51113=AXIS2_PLACEMENT_3D('',#128499,#64503,#64504);
#51114=AXIS2_PLACEMENT_3D('',#128500,#64505,#64506);
#51115=AXIS2_PLACEMENT_3D('',#128501,#64507,#64508);
#51116=AXIS2_PLACEMENT_3D('',#128502,#64509,#64510);
#51117=AXIS2_PLACEMENT_3D('',#128503,#64511,#64512);
#51118=AXIS2_PLACEMENT_3D('',#128504,#64513,#64514);
#51119=AXIS2_PLACEMENT_3D('',#128505,#64515,#64516);
#51120=AXIS2_PLACEMENT_3D('',#128506,#64517,#64518);
#51121=AXIS2_PLACEMENT_3D('',#128507,#64519,#64520);
#51122=AXIS2_PLACEMENT_3D('',#128508,#64521,#64522);
#51123=AXIS2_PLACEMENT_3D('',#128509,#64523,#64524);
#51124=AXIS2_PLACEMENT_3D('',#128510,#64525,#64526);
#51125=AXIS2_PLACEMENT_3D('',#128511,#64527,#64528);
#51126=AXIS2_PLACEMENT_3D('',#128512,#64529,#64530);
#51127=AXIS2_PLACEMENT_3D('',#128513,#64531,#64532);
#51128=AXIS2_PLACEMENT_3D('',#128514,#64533,#64534);
#51129=AXIS2_PLACEMENT_3D('',#128515,#64535,#64536);
#51130=AXIS2_PLACEMENT_3D('',#128516,#64537,#64538);
#51131=AXIS2_PLACEMENT_3D('',#128517,#64539,#64540);
#51132=AXIS2_PLACEMENT_3D('',#128518,#64541,#64542);
#51133=AXIS2_PLACEMENT_3D('',#128519,#64543,#64544);
#51134=AXIS2_PLACEMENT_3D('',#128520,#64545,#64546);
#51135=AXIS2_PLACEMENT_3D('',#128521,#64547,#64548);
#51136=AXIS2_PLACEMENT_3D('',#128522,#64549,#64550);
#51137=AXIS2_PLACEMENT_3D('',#128523,#64551,#64552);
#51138=AXIS2_PLACEMENT_3D('',#128524,#64553,#64554);
#51139=AXIS2_PLACEMENT_3D('',#128525,#64555,#64556);
#51140=AXIS2_PLACEMENT_3D('',#128526,#64557,#64558);
#51141=AXIS2_PLACEMENT_3D('',#128527,#64559,#64560);
#51142=AXIS2_PLACEMENT_3D('',#128528,#64561,#64562);
#51143=AXIS2_PLACEMENT_3D('',#128529,#64563,#64564);
#51144=AXIS2_PLACEMENT_3D('',#128530,#64565,#64566);
#51145=AXIS2_PLACEMENT_3D('',#128531,#64567,#64568);
#51146=AXIS2_PLACEMENT_3D('',#128532,#64569,#64570);
#51147=AXIS2_PLACEMENT_3D('',#128533,#64571,#64572);
#51148=AXIS2_PLACEMENT_3D('',#128534,#64573,#64574);
#51149=AXIS2_PLACEMENT_3D('',#128535,#64575,#64576);
#51150=AXIS2_PLACEMENT_3D('',#128536,#64577,#64578);
#51151=AXIS2_PLACEMENT_3D('',#128537,#64579,#64580);
#51152=AXIS2_PLACEMENT_3D('',#128538,#64581,#64582);
#51153=AXIS2_PLACEMENT_3D('',#128539,#64583,#64584);
#51154=AXIS2_PLACEMENT_3D('',#128540,#64585,#64586);
#51155=AXIS2_PLACEMENT_3D('',#128541,#64587,#64588);
#51156=AXIS2_PLACEMENT_3D('',#128542,#64589,#64590);
#51157=AXIS2_PLACEMENT_3D('',#128543,#64591,#64592);
#51158=AXIS2_PLACEMENT_3D('',#128544,#64593,#64594);
#51159=AXIS2_PLACEMENT_3D('',#128545,#64595,#64596);
#51160=AXIS2_PLACEMENT_3D('',#128546,#64597,#64598);
#51161=AXIS2_PLACEMENT_3D('',#128547,#64599,#64600);
#51162=AXIS2_PLACEMENT_3D('',#128548,#64601,#64602);
#51163=AXIS2_PLACEMENT_3D('',#128549,#64603,#64604);
#51164=AXIS2_PLACEMENT_3D('',#128550,#64605,#64606);
#51165=AXIS2_PLACEMENT_3D('',#128551,#64607,#64608);
#51166=AXIS2_PLACEMENT_3D('',#128552,#64609,#64610);
#51167=AXIS2_PLACEMENT_3D('',#128553,#64611,#64612);
#51168=AXIS2_PLACEMENT_3D('',#128554,#64613,#64614);
#51169=AXIS2_PLACEMENT_3D('',#128555,#64615,#64616);
#51170=AXIS2_PLACEMENT_3D('',#128556,#64617,#64618);
#51171=AXIS2_PLACEMENT_3D('',#128557,#64619,#64620);
#51172=AXIS2_PLACEMENT_3D('',#128558,#64621,#64622);
#51173=AXIS2_PLACEMENT_3D('',#128559,#64623,#64624);
#51174=AXIS2_PLACEMENT_3D('',#128560,#64625,#64626);
#51175=AXIS2_PLACEMENT_3D('',#128561,#64627,#64628);
#51176=AXIS2_PLACEMENT_3D('',#128562,#64629,#64630);
#51177=AXIS2_PLACEMENT_3D('',#128563,#64631,#64632);
#51178=AXIS2_PLACEMENT_3D('',#128564,#64633,#64634);
#51179=AXIS2_PLACEMENT_3D('',#128565,#64635,#64636);
#51180=AXIS2_PLACEMENT_3D('',#128566,#64637,#64638);
#51181=AXIS2_PLACEMENT_3D('',#128567,#64639,#64640);
#51182=AXIS2_PLACEMENT_3D('',#128568,#64641,#64642);
#51183=AXIS2_PLACEMENT_3D('',#128569,#64643,#64644);
#51184=AXIS2_PLACEMENT_3D('',#128570,#64645,#64646);
#51185=AXIS2_PLACEMENT_3D('',#128571,#64647,#64648);
#51186=AXIS2_PLACEMENT_3D('',#128572,#64649,#64650);
#51187=AXIS2_PLACEMENT_3D('',#128573,#64651,#64652);
#51188=AXIS2_PLACEMENT_3D('',#128574,#64653,#64654);
#51189=AXIS2_PLACEMENT_3D('',#128575,#64655,#64656);
#51190=AXIS2_PLACEMENT_3D('',#128576,#64657,#64658);
#51191=AXIS2_PLACEMENT_3D('',#128577,#64659,#64660);
#51192=AXIS2_PLACEMENT_3D('',#128578,#64661,#64662);
#51193=AXIS2_PLACEMENT_3D('',#128579,#64663,#64664);
#51194=AXIS2_PLACEMENT_3D('',#128580,#64665,#64666);
#51195=AXIS2_PLACEMENT_3D('',#128581,#64667,#64668);
#51196=AXIS2_PLACEMENT_3D('',#128582,#64669,#64670);
#51197=AXIS2_PLACEMENT_3D('',#128583,#64671,#64672);
#51198=AXIS2_PLACEMENT_3D('',#128584,#64673,#64674);
#51199=AXIS2_PLACEMENT_3D('',#128585,#64675,#64676);
#51200=AXIS2_PLACEMENT_3D('',#128586,#64677,#64678);
#51201=AXIS2_PLACEMENT_3D('',#128587,#64679,#64680);
#51202=AXIS2_PLACEMENT_3D('',#128588,#64681,#64682);
#51203=AXIS2_PLACEMENT_3D('',#128589,#64683,#64684);
#51204=AXIS2_PLACEMENT_3D('',#128590,#64685,#64686);
#51205=AXIS2_PLACEMENT_3D('',#128591,#64687,#64688);
#51206=AXIS2_PLACEMENT_3D('',#128592,#64689,#64690);
#51207=AXIS2_PLACEMENT_3D('',#128593,#64691,#64692);
#51208=AXIS2_PLACEMENT_3D('',#128594,#64693,#64694);
#51209=AXIS2_PLACEMENT_3D('',#128595,#64695,#64696);
#51210=AXIS2_PLACEMENT_3D('',#128596,#64697,#64698);
#51211=AXIS2_PLACEMENT_3D('',#128597,#64699,#64700);
#51212=AXIS2_PLACEMENT_3D('',#128598,#64701,#64702);
#51213=AXIS2_PLACEMENT_3D('',#128599,#64703,#64704);
#51214=AXIS2_PLACEMENT_3D('',#128600,#64705,#64706);
#51215=AXIS2_PLACEMENT_3D('',#128601,#64707,#64708);
#51216=AXIS2_PLACEMENT_3D('',#128602,#64709,#64710);
#51217=AXIS2_PLACEMENT_3D('',#128603,#64711,#64712);
#51218=AXIS2_PLACEMENT_3D('',#128604,#64713,#64714);
#51219=AXIS2_PLACEMENT_3D('',#128605,#64715,#64716);
#51220=AXIS2_PLACEMENT_3D('',#128606,#64717,#64718);
#51221=AXIS2_PLACEMENT_3D('',#128607,#64719,#64720);
#51222=AXIS2_PLACEMENT_3D('',#128608,#64721,#64722);
#51223=AXIS2_PLACEMENT_3D('',#128609,#64723,#64724);
#51224=AXIS2_PLACEMENT_3D('',#128610,#64725,#64726);
#51225=AXIS2_PLACEMENT_3D('',#128611,#64727,#64728);
#51226=AXIS2_PLACEMENT_3D('',#128612,#64729,#64730);
#51227=AXIS2_PLACEMENT_3D('',#128613,#64731,#64732);
#51228=AXIS2_PLACEMENT_3D('',#128614,#64733,#64734);
#51229=AXIS2_PLACEMENT_3D('',#128615,#64735,#64736);
#51230=AXIS2_PLACEMENT_3D('',#128616,#64737,#64738);
#51231=AXIS2_PLACEMENT_3D('',#128617,#64739,#64740);
#51232=AXIS2_PLACEMENT_3D('',#128618,#64741,#64742);
#51233=AXIS2_PLACEMENT_3D('',#128619,#64743,#64744);
#51234=AXIS2_PLACEMENT_3D('',#128620,#64745,#64746);
#51235=AXIS2_PLACEMENT_3D('',#128621,#64747,#64748);
#51236=AXIS2_PLACEMENT_3D('',#128622,#64749,#64750);
#51237=AXIS2_PLACEMENT_3D('',#128623,#64751,#64752);
#51238=AXIS2_PLACEMENT_3D('',#128624,#64753,#64754);
#51239=AXIS2_PLACEMENT_3D('',#128625,#64755,#64756);
#51240=AXIS2_PLACEMENT_3D('',#128626,#64757,#64758);
#51241=AXIS2_PLACEMENT_3D('',#128627,#64759,#64760);
#51242=AXIS2_PLACEMENT_3D('',#128628,#64761,#64762);
#51243=AXIS2_PLACEMENT_3D('',#128629,#64763,#64764);
#51244=AXIS2_PLACEMENT_3D('',#128630,#64765,#64766);
#51245=AXIS2_PLACEMENT_3D('',#128631,#64767,#64768);
#51246=AXIS2_PLACEMENT_3D('',#128632,#64769,#64770);
#51247=AXIS2_PLACEMENT_3D('',#128633,#64771,#64772);
#51248=AXIS2_PLACEMENT_3D('',#128634,#64773,#64774);
#51249=AXIS2_PLACEMENT_3D('',#128635,#64775,#64776);
#51250=AXIS2_PLACEMENT_3D('',#128636,#64777,#64778);
#51251=AXIS2_PLACEMENT_3D('',#128637,#64779,#64780);
#51252=AXIS2_PLACEMENT_3D('',#128638,#64781,#64782);
#51253=AXIS2_PLACEMENT_3D('',#128639,#64783,#64784);
#51254=AXIS2_PLACEMENT_3D('',#128640,#64785,#64786);
#51255=AXIS2_PLACEMENT_3D('',#128641,#64787,#64788);
#51256=AXIS2_PLACEMENT_3D('',#128642,#64789,#64790);
#51257=AXIS2_PLACEMENT_3D('',#128643,#64791,#64792);
#51258=AXIS2_PLACEMENT_3D('',#128644,#64793,#64794);
#51259=AXIS2_PLACEMENT_3D('',#128645,#64795,#64796);
#51260=AXIS2_PLACEMENT_3D('',#128646,#64797,#64798);
#51261=AXIS2_PLACEMENT_3D('',#128647,#64799,#64800);
#51262=AXIS2_PLACEMENT_3D('',#128648,#64801,#64802);
#51263=AXIS2_PLACEMENT_3D('',#128649,#64803,#64804);
#51264=AXIS2_PLACEMENT_3D('',#128650,#64805,#64806);
#51265=AXIS2_PLACEMENT_3D('',#128651,#64807,#64808);
#51266=AXIS2_PLACEMENT_3D('',#128652,#64809,#64810);
#51267=AXIS2_PLACEMENT_3D('',#128653,#64811,#64812);
#51268=AXIS2_PLACEMENT_3D('',#128654,#64813,#64814);
#51269=AXIS2_PLACEMENT_3D('',#128655,#64815,#64816);
#51270=AXIS2_PLACEMENT_3D('',#128656,#64817,#64818);
#51271=AXIS2_PLACEMENT_3D('',#128657,#64819,#64820);
#51272=AXIS2_PLACEMENT_3D('',#128658,#64821,#64822);
#51273=AXIS2_PLACEMENT_3D('',#128659,#64823,#64824);
#51274=AXIS2_PLACEMENT_3D('',#128660,#64825,#64826);
#51275=AXIS2_PLACEMENT_3D('',#128661,#64827,#64828);
#51276=AXIS2_PLACEMENT_3D('',#128662,#64829,#64830);
#51277=AXIS2_PLACEMENT_3D('',#128663,#64831,#64832);
#51278=AXIS2_PLACEMENT_3D('',#128664,#64833,#64834);
#51279=AXIS2_PLACEMENT_3D('',#128665,#64835,#64836);
#51280=AXIS2_PLACEMENT_3D('',#128666,#64837,#64838);
#51281=AXIS2_PLACEMENT_3D('',#128667,#64839,#64840);
#51282=AXIS2_PLACEMENT_3D('',#128668,#64841,#64842);
#51283=AXIS2_PLACEMENT_3D('',#128669,#64843,#64844);
#51284=AXIS2_PLACEMENT_3D('',#128670,#64845,#64846);
#51285=AXIS2_PLACEMENT_3D('',#128671,#64847,#64848);
#51286=AXIS2_PLACEMENT_3D('',#128672,#64849,#64850);
#51287=AXIS2_PLACEMENT_3D('',#128673,#64851,#64852);
#51288=AXIS2_PLACEMENT_3D('',#128674,#64853,#64854);
#51289=AXIS2_PLACEMENT_3D('',#128675,#64855,#64856);
#51290=AXIS2_PLACEMENT_3D('',#128676,#64857,#64858);
#51291=AXIS2_PLACEMENT_3D('',#128677,#64859,#64860);
#51292=AXIS2_PLACEMENT_3D('',#128678,#64861,#64862);
#51293=AXIS2_PLACEMENT_3D('',#128679,#64863,#64864);
#51294=AXIS2_PLACEMENT_3D('',#128680,#64865,#64866);
#51295=AXIS2_PLACEMENT_3D('',#128681,#64867,#64868);
#51296=AXIS2_PLACEMENT_3D('',#128682,#64869,#64870);
#51297=AXIS2_PLACEMENT_3D('',#128683,#64871,#64872);
#51298=AXIS2_PLACEMENT_3D('',#128684,#64873,#64874);
#51299=AXIS2_PLACEMENT_3D('',#128685,#64875,#64876);
#51300=AXIS2_PLACEMENT_3D('',#128686,#64877,#64878);
#51301=AXIS2_PLACEMENT_3D('',#128687,#64879,#64880);
#51302=AXIS2_PLACEMENT_3D('',#128688,#64881,#64882);
#51303=AXIS2_PLACEMENT_3D('',#128689,#64883,#64884);
#51304=AXIS2_PLACEMENT_3D('',#128690,#64885,#64886);
#51305=AXIS2_PLACEMENT_3D('',#128691,#64887,#64888);
#51306=AXIS2_PLACEMENT_3D('',#128692,#64889,#64890);
#51307=AXIS2_PLACEMENT_3D('',#128693,#64891,#64892);
#51308=AXIS2_PLACEMENT_3D('',#128694,#64893,#64894);
#51309=AXIS2_PLACEMENT_3D('',#128695,#64895,#64896);
#51310=AXIS2_PLACEMENT_3D('',#128696,#64897,#64898);
#51311=AXIS2_PLACEMENT_3D('',#128697,#64899,#64900);
#51312=AXIS2_PLACEMENT_3D('',#128698,#64901,#64902);
#51313=AXIS2_PLACEMENT_3D('',#128699,#64903,#64904);
#51314=AXIS2_PLACEMENT_3D('',#128700,#64905,#64906);
#51315=AXIS2_PLACEMENT_3D('',#128701,#64907,#64908);
#51316=AXIS2_PLACEMENT_3D('',#128702,#64909,#64910);
#51317=AXIS2_PLACEMENT_3D('',#128703,#64911,#64912);
#51318=AXIS2_PLACEMENT_3D('',#128704,#64913,#64914);
#51319=AXIS2_PLACEMENT_3D('',#128705,#64915,#64916);
#51320=AXIS2_PLACEMENT_3D('',#128706,#64917,#64918);
#51321=AXIS2_PLACEMENT_3D('',#128707,#64919,#64920);
#51322=AXIS2_PLACEMENT_3D('',#128708,#64921,#64922);
#51323=AXIS2_PLACEMENT_3D('',#128709,#64923,#64924);
#51324=AXIS2_PLACEMENT_3D('',#128710,#64925,#64926);
#51325=AXIS2_PLACEMENT_3D('',#128711,#64927,#64928);
#51326=AXIS2_PLACEMENT_3D('',#128712,#64929,#64930);
#51327=AXIS2_PLACEMENT_3D('',#128713,#64931,#64932);
#51328=AXIS2_PLACEMENT_3D('',#128714,#64933,#64934);
#51329=AXIS2_PLACEMENT_3D('',#128715,#64935,#64936);
#51330=AXIS2_PLACEMENT_3D('',#128716,#64937,#64938);
#51331=AXIS2_PLACEMENT_3D('',#128717,#64939,#64940);
#51332=AXIS2_PLACEMENT_3D('',#128718,#64941,#64942);
#51333=AXIS2_PLACEMENT_3D('',#128719,#64943,#64944);
#51334=AXIS2_PLACEMENT_3D('',#128720,#64945,#64946);
#51335=AXIS2_PLACEMENT_3D('',#128721,#64947,#64948);
#51336=AXIS2_PLACEMENT_3D('',#128722,#64949,#64950);
#51337=AXIS2_PLACEMENT_3D('',#128723,#64951,#64952);
#51338=AXIS2_PLACEMENT_3D('',#128724,#64953,#64954);
#51339=AXIS2_PLACEMENT_3D('',#128725,#64955,#64956);
#51340=AXIS2_PLACEMENT_3D('',#128726,#64957,#64958);
#51341=AXIS2_PLACEMENT_3D('',#128727,#64959,#64960);
#51342=AXIS2_PLACEMENT_3D('',#128728,#64961,#64962);
#51343=AXIS2_PLACEMENT_3D('',#128729,#64963,#64964);
#51344=AXIS2_PLACEMENT_3D('',#128730,#64965,#64966);
#51345=AXIS2_PLACEMENT_3D('',#128731,#64967,#64968);
#51346=AXIS2_PLACEMENT_3D('',#128732,#64969,#64970);
#51347=AXIS2_PLACEMENT_3D('',#128733,#64971,#64972);
#51348=AXIS2_PLACEMENT_3D('',#128734,#64973,#64974);
#51349=AXIS2_PLACEMENT_3D('',#128735,#64975,#64976);
#51350=AXIS2_PLACEMENT_3D('',#128736,#64977,#64978);
#51351=AXIS2_PLACEMENT_3D('',#128737,#64979,#64980);
#51352=AXIS2_PLACEMENT_3D('',#128738,#64981,#64982);
#51353=AXIS2_PLACEMENT_3D('',#128739,#64983,#64984);
#51354=AXIS2_PLACEMENT_3D('',#128740,#64985,#64986);
#51355=AXIS2_PLACEMENT_3D('',#128741,#64987,#64988);
#51356=AXIS2_PLACEMENT_3D('',#128742,#64989,#64990);
#51357=AXIS2_PLACEMENT_3D('',#128743,#64991,#64992);
#51358=AXIS2_PLACEMENT_3D('',#128744,#64993,#64994);
#51359=AXIS2_PLACEMENT_3D('',#128745,#64995,#64996);
#51360=AXIS2_PLACEMENT_3D('',#128746,#64997,#64998);
#51361=AXIS2_PLACEMENT_3D('',#128747,#64999,#65000);
#51362=AXIS2_PLACEMENT_3D('',#128748,#65001,#65002);
#51363=AXIS2_PLACEMENT_3D('',#128749,#65003,#65004);
#51364=AXIS2_PLACEMENT_3D('',#128750,#65005,#65006);
#51365=AXIS2_PLACEMENT_3D('',#128751,#65007,#65008);
#51366=AXIS2_PLACEMENT_3D('',#128752,#65009,#65010);
#51367=AXIS2_PLACEMENT_3D('',#128753,#65011,#65012);
#51368=AXIS2_PLACEMENT_3D('',#128754,#65013,#65014);
#51369=AXIS2_PLACEMENT_3D('',#128755,#65015,#65016);
#51370=AXIS2_PLACEMENT_3D('',#128756,#65017,#65018);
#51371=AXIS2_PLACEMENT_3D('',#128757,#65019,#65020);
#51372=AXIS2_PLACEMENT_3D('',#128758,#65021,#65022);
#51373=AXIS2_PLACEMENT_3D('',#128759,#65023,#65024);
#51374=AXIS2_PLACEMENT_3D('',#128760,#65025,#65026);
#51375=AXIS2_PLACEMENT_3D('',#128761,#65027,#65028);
#51376=AXIS2_PLACEMENT_3D('',#128762,#65029,#65030);
#51377=AXIS2_PLACEMENT_3D('',#128763,#65031,#65032);
#51378=AXIS2_PLACEMENT_3D('',#128764,#65033,#65034);
#51379=AXIS2_PLACEMENT_3D('',#128765,#65035,#65036);
#51380=AXIS2_PLACEMENT_3D('',#128766,#65037,#65038);
#51381=AXIS2_PLACEMENT_3D('',#128767,#65039,#65040);
#51382=AXIS2_PLACEMENT_3D('',#128768,#65041,#65042);
#51383=AXIS2_PLACEMENT_3D('',#128769,#65043,#65044);
#51384=AXIS2_PLACEMENT_3D('',#128770,#65045,#65046);
#51385=AXIS2_PLACEMENT_3D('',#128771,#65047,#65048);
#51386=AXIS2_PLACEMENT_3D('',#128772,#65049,#65050);
#51387=AXIS2_PLACEMENT_3D('',#128773,#65051,#65052);
#51388=AXIS2_PLACEMENT_3D('',#128774,#65053,#65054);
#51389=AXIS2_PLACEMENT_3D('',#128775,#65055,#65056);
#51390=AXIS2_PLACEMENT_3D('',#128776,#65057,#65058);
#51391=AXIS2_PLACEMENT_3D('',#128777,#65059,#65060);
#51392=AXIS2_PLACEMENT_3D('',#128778,#65061,#65062);
#51393=AXIS2_PLACEMENT_3D('',#128779,#65063,#65064);
#51394=AXIS2_PLACEMENT_3D('',#128780,#65065,#65066);
#51395=AXIS2_PLACEMENT_3D('',#128781,#65067,#65068);
#51396=AXIS2_PLACEMENT_3D('',#128782,#65069,#65070);
#51397=AXIS2_PLACEMENT_3D('',#128783,#65071,#65072);
#51398=AXIS2_PLACEMENT_3D('',#128784,#65073,#65074);
#51399=AXIS2_PLACEMENT_3D('',#128785,#65075,#65076);
#51400=AXIS2_PLACEMENT_3D('',#128786,#65077,#65078);
#51401=AXIS2_PLACEMENT_3D('',#128787,#65079,#65080);
#51402=AXIS2_PLACEMENT_3D('',#128788,#65081,#65082);
#51403=AXIS2_PLACEMENT_3D('',#128789,#65083,#65084);
#51404=AXIS2_PLACEMENT_3D('',#128790,#65085,#65086);
#51405=AXIS2_PLACEMENT_3D('',#128791,#65087,#65088);
#51406=AXIS2_PLACEMENT_3D('',#128792,#65089,#65090);
#51407=AXIS2_PLACEMENT_3D('',#128793,#65091,#65092);
#51408=AXIS2_PLACEMENT_3D('',#128794,#65093,#65094);
#51409=AXIS2_PLACEMENT_3D('',#128795,#65095,#65096);
#51410=AXIS2_PLACEMENT_3D('',#128796,#65097,#65098);
#51411=AXIS2_PLACEMENT_3D('',#128797,#65099,#65100);
#51412=AXIS2_PLACEMENT_3D('',#128798,#65101,#65102);
#51413=AXIS2_PLACEMENT_3D('',#128799,#65103,#65104);
#51414=AXIS2_PLACEMENT_3D('',#128800,#65105,#65106);
#51415=AXIS2_PLACEMENT_3D('',#128801,#65107,#65108);
#51416=AXIS2_PLACEMENT_3D('',#128802,#65109,#65110);
#51417=AXIS2_PLACEMENT_3D('',#128803,#65111,#65112);
#51418=AXIS2_PLACEMENT_3D('',#128804,#65113,#65114);
#51419=AXIS2_PLACEMENT_3D('',#128805,#65115,#65116);
#51420=AXIS2_PLACEMENT_3D('',#128806,#65117,#65118);
#51421=AXIS2_PLACEMENT_3D('',#128807,#65119,#65120);
#51422=AXIS2_PLACEMENT_3D('',#128808,#65121,#65122);
#51423=AXIS2_PLACEMENT_3D('',#128809,#65123,#65124);
#51424=AXIS2_PLACEMENT_3D('',#128810,#65125,#65126);
#51425=AXIS2_PLACEMENT_3D('',#128811,#65127,#65128);
#51426=AXIS2_PLACEMENT_3D('',#128812,#65129,#65130);
#51427=AXIS2_PLACEMENT_3D('',#128813,#65131,#65132);
#51428=AXIS2_PLACEMENT_3D('',#128814,#65133,#65134);
#51429=AXIS2_PLACEMENT_3D('',#128815,#65135,#65136);
#51430=AXIS2_PLACEMENT_3D('',#128816,#65137,#65138);
#51431=AXIS2_PLACEMENT_3D('',#128817,#65139,#65140);
#51432=AXIS2_PLACEMENT_3D('',#128818,#65141,#65142);
#51433=AXIS2_PLACEMENT_3D('',#128819,#65143,#65144);
#51434=AXIS2_PLACEMENT_3D('',#128820,#65145,#65146);
#51435=AXIS2_PLACEMENT_3D('',#128821,#65147,#65148);
#51436=AXIS2_PLACEMENT_3D('',#128822,#65149,#65150);
#51437=AXIS2_PLACEMENT_3D('',#128823,#65151,#65152);
#51438=AXIS2_PLACEMENT_3D('',#128824,#65153,#65154);
#51439=AXIS2_PLACEMENT_3D('',#128825,#65155,#65156);
#51440=AXIS2_PLACEMENT_3D('',#128826,#65157,#65158);
#51441=AXIS2_PLACEMENT_3D('',#128827,#65159,#65160);
#51442=AXIS2_PLACEMENT_3D('',#128828,#65161,#65162);
#51443=AXIS2_PLACEMENT_3D('',#128829,#65163,#65164);
#51444=AXIS2_PLACEMENT_3D('',#128830,#65165,#65166);
#51445=AXIS2_PLACEMENT_3D('',#128831,#65167,#65168);
#51446=AXIS2_PLACEMENT_3D('',#128832,#65169,#65170);
#51447=AXIS2_PLACEMENT_3D('',#128833,#65171,#65172);
#51448=AXIS2_PLACEMENT_3D('',#128834,#65173,#65174);
#51449=AXIS2_PLACEMENT_3D('',#128835,#65175,#65176);
#51450=AXIS2_PLACEMENT_3D('',#128836,#65177,#65178);
#51451=AXIS2_PLACEMENT_3D('',#128837,#65179,#65180);
#51452=AXIS2_PLACEMENT_3D('',#128838,#65181,#65182);
#51453=AXIS2_PLACEMENT_3D('',#128839,#65183,#65184);
#51454=AXIS2_PLACEMENT_3D('',#128840,#65185,#65186);
#51455=AXIS2_PLACEMENT_3D('',#128841,#65187,#65188);
#51456=AXIS2_PLACEMENT_3D('',#128842,#65189,#65190);
#51457=AXIS2_PLACEMENT_3D('',#128843,#65191,#65192);
#51458=AXIS2_PLACEMENT_3D('',#128844,#65193,#65194);
#51459=AXIS2_PLACEMENT_3D('',#128845,#65195,#65196);
#51460=AXIS2_PLACEMENT_3D('',#128846,#65197,#65198);
#51461=AXIS2_PLACEMENT_3D('',#128847,#65199,#65200);
#51462=AXIS2_PLACEMENT_3D('',#128848,#65201,#65202);
#51463=AXIS2_PLACEMENT_3D('',#128849,#65203,#65204);
#51464=AXIS2_PLACEMENT_3D('',#128850,#65205,#65206);
#51465=AXIS2_PLACEMENT_3D('',#128851,#65207,#65208);
#51466=AXIS2_PLACEMENT_3D('',#128852,#65209,#65210);
#51467=AXIS2_PLACEMENT_3D('',#128853,#65211,#65212);
#51468=AXIS2_PLACEMENT_3D('',#128854,#65213,#65214);
#51469=AXIS2_PLACEMENT_3D('',#128855,#65215,#65216);
#51470=AXIS2_PLACEMENT_3D('',#128856,#65217,#65218);
#51471=AXIS2_PLACEMENT_3D('',#128857,#65219,#65220);
#51472=AXIS2_PLACEMENT_3D('',#128858,#65221,#65222);
#51473=AXIS2_PLACEMENT_3D('',#128859,#65223,#65224);
#51474=AXIS2_PLACEMENT_3D('',#128860,#65225,#65226);
#51475=AXIS2_PLACEMENT_3D('',#128877,#65227,#65228);
#51476=AXIS2_PLACEMENT_3D('',#128894,#65229,#65230);
#51477=AXIS2_PLACEMENT_3D('',#128911,#65231,#65232);
#51478=AXIS2_PLACEMENT_3D('',#128928,#65233,#65234);
#51479=AXIS2_PLACEMENT_3D('',#128945,#65235,#65236);
#51480=AXIS2_PLACEMENT_3D('',#128962,#65237,#65238);
#51481=AXIS2_PLACEMENT_3D('',#128979,#65239,#65240);
#51482=AXIS2_PLACEMENT_3D('',#128996,#65241,#65242);
#51483=AXIS2_PLACEMENT_3D('',#129013,#65243,#65244);
#51484=AXIS2_PLACEMENT_3D('',#129030,#65245,#65246);
#51485=AXIS2_PLACEMENT_3D('',#129047,#65247,#65248);
#51486=AXIS2_PLACEMENT_3D('',#129064,#65249,#65250);
#51487=AXIS2_PLACEMENT_3D('',#129081,#65251,#65252);
#51488=AXIS2_PLACEMENT_3D('',#129098,#65253,#65254);
#51489=AXIS2_PLACEMENT_3D('',#129115,#65255,#65256);
#51490=AXIS2_PLACEMENT_3D('',#129132,#65257,#65258);
#51491=AXIS2_PLACEMENT_3D('',#129149,#65259,#65260);
#51492=AXIS2_PLACEMENT_3D('',#129166,#65261,#65262);
#51493=AXIS2_PLACEMENT_3D('',#129183,#65263,#65264);
#51494=AXIS2_PLACEMENT_3D('',#129200,#65265,#65266);
#51495=AXIS2_PLACEMENT_3D('',#129217,#65267,#65268);
#51496=AXIS2_PLACEMENT_3D('',#129234,#65269,#65270);
#51497=AXIS2_PLACEMENT_3D('',#129251,#65271,#65272);
#51498=AXIS2_PLACEMENT_3D('',#129268,#65273,#65274);
#51499=AXIS2_PLACEMENT_3D('',#129285,#65275,#65276);
#51500=AXIS2_PLACEMENT_3D('',#129302,#65277,#65278);
#51501=AXIS2_PLACEMENT_3D('',#129319,#65279,#65280);
#51502=AXIS2_PLACEMENT_3D('',#129336,#65281,#65282);
#51503=AXIS2_PLACEMENT_3D('',#129353,#65283,#65284);
#51504=AXIS2_PLACEMENT_3D('',#129370,#65285,#65286);
#51505=AXIS2_PLACEMENT_3D('',#129387,#65287,#65288);
#51506=AXIS2_PLACEMENT_3D('',#129404,#65289,#65290);
#51507=AXIS2_PLACEMENT_3D('',#129421,#65291,#65292);
#51508=AXIS2_PLACEMENT_3D('',#129438,#65293,#65294);
#51509=AXIS2_PLACEMENT_3D('',#129455,#65295,#65296);
#51510=AXIS2_PLACEMENT_3D('',#129472,#65297,#65298);
#51511=AXIS2_PLACEMENT_3D('',#129489,#65299,#65300);
#51512=AXIS2_PLACEMENT_3D('',#129506,#65301,#65302);
#51513=AXIS2_PLACEMENT_3D('',#129523,#65303,#65304);
#51514=AXIS2_PLACEMENT_3D('',#129540,#65305,#65306);
#51515=AXIS2_PLACEMENT_3D('',#129557,#65307,#65308);
#51516=AXIS2_PLACEMENT_3D('',#129574,#65309,#65310);
#51517=AXIS2_PLACEMENT_3D('',#129591,#65311,#65312);
#51518=AXIS2_PLACEMENT_3D('',#129608,#65313,#65314);
#51519=AXIS2_PLACEMENT_3D('',#129625,#65315,#65316);
#51520=AXIS2_PLACEMENT_3D('',#129642,#65317,#65318);
#51521=AXIS2_PLACEMENT_3D('',#129659,#65319,#65320);
#51522=AXIS2_PLACEMENT_3D('',#129676,#65321,#65322);
#51523=AXIS2_PLACEMENT_3D('',#129693,#65323,#65324);
#51524=AXIS2_PLACEMENT_3D('',#129710,#65325,#65326);
#51525=AXIS2_PLACEMENT_3D('',#129727,#65327,#65328);
#51526=AXIS2_PLACEMENT_3D('',#129744,#65329,#65330);
#51527=AXIS2_PLACEMENT_3D('',#129761,#65331,#65332);
#51528=AXIS2_PLACEMENT_3D('',#129778,#65333,#65334);
#51529=AXIS2_PLACEMENT_3D('',#129795,#65335,#65336);
#51530=AXIS2_PLACEMENT_3D('',#129812,#65337,#65338);
#51531=AXIS2_PLACEMENT_3D('',#129829,#65339,#65340);
#51532=AXIS2_PLACEMENT_3D('',#129846,#65341,#65342);
#51533=AXIS2_PLACEMENT_3D('',#129863,#65343,#65344);
#51534=AXIS2_PLACEMENT_3D('',#129880,#65345,#65346);
#51535=AXIS2_PLACEMENT_3D('',#129897,#65347,#65348);
#51536=AXIS2_PLACEMENT_3D('',#129914,#65349,#65350);
#51537=AXIS2_PLACEMENT_3D('',#129931,#65351,#65352);
#51538=AXIS2_PLACEMENT_3D('',#129948,#65353,#65354);
#51539=AXIS2_PLACEMENT_3D('',#129965,#65355,#65356);
#51540=AXIS2_PLACEMENT_3D('',#129982,#65357,#65358);
#51541=AXIS2_PLACEMENT_3D('',#129999,#65359,#65360);
#51542=AXIS2_PLACEMENT_3D('',#130016,#65361,#65362);
#51543=AXIS2_PLACEMENT_3D('',#130033,#65363,#65364);
#51544=AXIS2_PLACEMENT_3D('',#130050,#65365,#65366);
#51545=AXIS2_PLACEMENT_3D('',#130067,#65367,#65368);
#51546=AXIS2_PLACEMENT_3D('',#130084,#65369,#65370);
#51547=AXIS2_PLACEMENT_3D('',#130101,#65371,#65372);
#51548=AXIS2_PLACEMENT_3D('',#130118,#65373,#65374);
#51549=AXIS2_PLACEMENT_3D('',#130135,#65375,#65376);
#51550=AXIS2_PLACEMENT_3D('',#130152,#65377,#65378);
#51551=AXIS2_PLACEMENT_3D('',#130169,#65379,#65380);
#51552=AXIS2_PLACEMENT_3D('',#130186,#65381,#65382);
#51553=AXIS2_PLACEMENT_3D('',#130203,#65383,#65384);
#51554=AXIS2_PLACEMENT_3D('',#130220,#65385,#65386);
#51555=AXIS2_PLACEMENT_3D('',#130237,#65387,#65388);
#51556=AXIS2_PLACEMENT_3D('',#130254,#65389,#65390);
#51557=AXIS2_PLACEMENT_3D('',#130271,#65391,#65392);
#51558=AXIS2_PLACEMENT_3D('',#130288,#65393,#65394);
#51559=AXIS2_PLACEMENT_3D('',#130305,#65395,#65396);
#51560=AXIS2_PLACEMENT_3D('',#130322,#65397,#65398);
#51561=AXIS2_PLACEMENT_3D('',#130339,#65399,#65400);
#51562=AXIS2_PLACEMENT_3D('',#130356,#65401,#65402);
#51563=AXIS2_PLACEMENT_3D('',#130373,#65403,#65404);
#51564=AXIS2_PLACEMENT_3D('',#130390,#65405,#65406);
#51565=AXIS2_PLACEMENT_3D('',#130407,#65407,#65408);
#51566=AXIS2_PLACEMENT_3D('',#130424,#65409,#65410);
#51567=AXIS2_PLACEMENT_3D('',#130441,#65411,#65412);
#51568=AXIS2_PLACEMENT_3D('',#130458,#65413,#65414);
#51569=AXIS2_PLACEMENT_3D('',#130475,#65415,#65416);
#51570=AXIS2_PLACEMENT_3D('',#130492,#65417,#65418);
#51571=AXIS2_PLACEMENT_3D('',#130509,#65419,#65420);
#51572=AXIS2_PLACEMENT_3D('',#130526,#65421,#65422);
#51573=AXIS2_PLACEMENT_3D('',#130543,#65423,#65424);
#51574=AXIS2_PLACEMENT_3D('',#130560,#65425,#65426);
#51575=AXIS2_PLACEMENT_3D('',#130577,#65427,#65428);
#51576=AXIS2_PLACEMENT_3D('',#130594,#65429,#65430);
#51577=AXIS2_PLACEMENT_3D('',#130611,#65431,#65432);
#51578=AXIS2_PLACEMENT_3D('',#130628,#65433,#65434);
#51579=AXIS2_PLACEMENT_3D('',#130645,#65435,#65436);
#51580=AXIS2_PLACEMENT_3D('',#130662,#65437,#65438);
#51581=AXIS2_PLACEMENT_3D('',#130679,#65439,#65440);
#51582=AXIS2_PLACEMENT_3D('',#130696,#65441,#65442);
#51583=AXIS2_PLACEMENT_3D('',#130713,#65443,#65444);
#51584=AXIS2_PLACEMENT_3D('',#130730,#65445,#65446);
#51585=AXIS2_PLACEMENT_3D('',#130747,#65447,#65448);
#51586=AXIS2_PLACEMENT_3D('',#130764,#65449,#65450);
#51587=AXIS2_PLACEMENT_3D('',#130781,#65451,#65452);
#51588=AXIS2_PLACEMENT_3D('',#130798,#65453,#65454);
#51589=AXIS2_PLACEMENT_3D('',#130815,#65455,#65456);
#51590=AXIS2_PLACEMENT_3D('',#130832,#65457,#65458);
#51591=AXIS2_PLACEMENT_3D('',#130849,#65459,#65460);
#51592=AXIS2_PLACEMENT_3D('',#130866,#65461,#65462);
#51593=AXIS2_PLACEMENT_3D('',#130883,#65463,#65464);
#51594=AXIS2_PLACEMENT_3D('',#130884,#65465,#65466);
#51595=AXIS2_PLACEMENT_3D('',#130885,#65467,#65468);
#51596=AXIS2_PLACEMENT_3D('',#130886,#65469,#65470);
#51597=AXIS2_PLACEMENT_3D('',#130887,#65471,#65472);
#51598=AXIS2_PLACEMENT_3D('',#130888,#65473,#65474);
#51599=AXIS2_PLACEMENT_3D('',#130889,#65475,#65476);
#51600=AXIS2_PLACEMENT_3D('',#130890,#65477,#65478);
#51601=DIRECTION('axis',(0.,0.,1.));
#51602=DIRECTION('refdir',(1.,0.,0.));
#51603=DIRECTION('axis',(0.,0.,1.));
#51604=DIRECTION('refdir',(1.,0.,0.));
#51605=DIRECTION('center_axis',(-1.,0.,0.));
#51606=DIRECTION('ref_axis',(0.,0.,1.));
#51607=DIRECTION('center_axis',(0.,-1.,-3.7789907496129E-15));
#51608=DIRECTION('ref_axis',(0.,3.7789907496129E-15,-1.));
#51609=DIRECTION('center_axis',(1.,0.,0.));
#51610=DIRECTION('ref_axis',(0.,0.,1.));
#51611=DIRECTION('center_axis',(0.,3.7789907496129E-15,-1.));
#51612=DIRECTION('ref_axis',(0.,1.,3.7789907496129E-15));
#51613=DIRECTION('center_axis',(0.,3.7789907496129E-15,-1.));
#51614=DIRECTION('ref_axis',(0.,1.,3.7789907496129E-15));
#51615=DIRECTION('center_axis',(-1.,0.,0.));
#51616=DIRECTION('ref_axis',(0.,0.,1.));
#51617=DIRECTION('center_axis',(0.,3.7789907496129E-15,-1.));
#51618=DIRECTION('ref_axis',(0.,1.,3.7789907496129E-15));
#51619=DIRECTION('center_axis',(1.,0.,0.));
#51620=DIRECTION('ref_axis',(0.,0.,1.));
#51621=DIRECTION('center_axis',(0.,1.,0.));
#51622=DIRECTION('ref_axis',(0.,0.,1.));
#51623=DIRECTION('center_axis',(0.,3.7789907496129E-15,-1.));
#51624=DIRECTION('ref_axis',(0.,1.,3.7789907496129E-15));
#51625=DIRECTION('center_axis',(0.,-1.,0.));
#51626=DIRECTION('ref_axis',(0.,0.,-1.));
#51627=DIRECTION('center_axis',(0.,1.,0.));
#51628=DIRECTION('ref_axis',(0.,0.,1.));
#51629=DIRECTION('',(0.,1.,0.));
#51630=DIRECTION('center_axis',(0.,0.,-1.));
#51631=DIRECTION('ref_axis',(-1.,0.,0.));
#51632=DIRECTION('',(0.,0.,1.));
#51633=DIRECTION('center_axis',(0.,1.,-3.7789907496129E-15));
#51634=DIRECTION('ref_axis',(0.,3.7789907496129E-15,1.));
#51635=DIRECTION('',(0.,-1.,3.7789907496129E-15));
#51636=DIRECTION('center_axis',(0.,1.,0.));
#51637=DIRECTION('ref_axis',(0.,0.,1.));
#51638=DIRECTION('center_axis',(0.,1.,0.));
#51639=DIRECTION('ref_axis',(0.,0.,1.));
#51640=DIRECTION('center_axis',(0.,1.,0.));
#51641=DIRECTION('ref_axis',(0.,0.,1.));
#51642=DIRECTION('axis',(0.,0.,1.));
#51643=DIRECTION('refdir',(1.,0.,0.));
#51644=DIRECTION('center_axis',(0.,-0.0958457525203355,0.995396198367168));
#51645=DIRECTION('ref_axis',(1.,0.,0.));
#51646=DIRECTION('',(0.,-0.995396198367168,-0.0958457525203355));
#51647=DIRECTION('center_axis',(0.,0.0958457525203352,-0.995396198367168));
#51648=DIRECTION('ref_axis',(-9.08813207382089E-14,0.995396198367168,0.0958457525203352));
#51649=DIRECTION('',(0.,0.995396198367168,0.0958457525203355));
#51650=DIRECTION('',(-1.,0.,0.));
#51651=DIRECTION('center_axis',(0.,0.,1.));
#51652=DIRECTION('ref_axis',(1.,0.,0.));
#51653=DIRECTION('',(0.,1.,0.));
#51654=DIRECTION('center_axis',(0.,0.,1.));
#51655=DIRECTION('ref_axis',(1.,0.,0.));
#51656=DIRECTION('',(0.,-1.,0.));
#51657=DIRECTION('center_axis',(0.,0.,-1.));
#51658=DIRECTION('ref_axis',(-1.,0.,0.));
#51659=DIRECTION('',(0.,0.,-1.));
#51660=DIRECTION('',(0.,0.,-1.));
#51661=DIRECTION('center_axis',(-1.,0.,0.));
#51662=DIRECTION('ref_axis',(0.,0.,1.));
#51663=DIRECTION('center_axis',(1.,0.,0.));
#51664=DIRECTION('ref_axis',(0.,0.,-1.));
#51665=DIRECTION('center_axis',(0.,0.0958457525203355,-0.995396198367168));
#51666=DIRECTION('ref_axis',(-1.,0.,0.));
#51667=DIRECTION('',(0.,0.0958457525203355,-0.995396198367168));
#51668=DIRECTION('center_axis',(0.,0.0479781285213982,-0.998848386484948));
#51669=DIRECTION('ref_axis',(0.,0.998848386484948,0.0479781285213982));
#51670=DIRECTION('',(0.,0.0958457525203355,-0.995396198367168));
#51671=DIRECTION('center_axis',(0.,2.12953059333849E-15,1.));
#51672=DIRECTION('ref_axis',(0.,-1.,2.12953059333849E-15));
#51673=DIRECTION('center_axis',(1.,0.,0.));
#51674=DIRECTION('ref_axis',(0.,0.,-1.));
#51675=DIRECTION('',(0.,0.,-1.));
#51676=DIRECTION('',(0.,-1.,0.));
#51677=DIRECTION('center_axis',(-1.,0.,0.));
#51678=DIRECTION('ref_axis',(0.,0.,1.));
#51679=DIRECTION('',(0.,0.,-1.));
#51680=DIRECTION('',(0.,1.,0.));
#51681=DIRECTION('center_axis',(0.,0.,1.));
#51682=DIRECTION('ref_axis',(1.,0.,0.));
#51683=DIRECTION('center_axis',(0.,0.,1.));
#51684=DIRECTION('ref_axis',(1.,0.,0.));
#51685=DIRECTION('center_axis',(0.,0.,-1.));
#51686=DIRECTION('ref_axis',(-1.,0.,0.));
#51687=DIRECTION('center_axis',(0.,-0.333233134534162,0.94284446121751));
#51688=DIRECTION('ref_axis',(0.,-0.94284446121751,-0.333233134534162));
#51689=DIRECTION('center_axis',(0.,0.333233134534162,-0.94284446121751));
#51690=DIRECTION('ref_axis',(0.,-0.94284446121751,-0.333233134534162));
#51691=DIRECTION('',(0.,-0.333233134534162,0.94284446121751));
#51692=DIRECTION('center_axis',(0.,0.333233134534159,-0.942844461217511));
#51693=DIRECTION('ref_axis',(0.,-0.942844461217511,-0.333233134534159));
#51694=DIRECTION('center_axis',(0.,-0.333233134534162,0.94284446121751));
#51695=DIRECTION('ref_axis',(0.,-0.94284446121751,-0.333233134534162));
#51696=DIRECTION('center_axis',(0.,0.333233134534159,-0.942844461217511));
#51697=DIRECTION('ref_axis',(0.,-0.942844461217511,-0.333233134534159));
#51698=DIRECTION('',(0.,0.333233134534162,-0.94284446121751));
#51699=DIRECTION('center_axis',(0.,0.333233134534162,-0.94284446121751));
#51700=DIRECTION('ref_axis',(0.,-0.94284446121751,-0.333233134534162));
#51701=DIRECTION('center_axis',(0.,-0.333233134534162,0.94284446121751));
#51702=DIRECTION('ref_axis',(0.,-0.94284446121751,-0.333233134534162));
#51703=DIRECTION('center_axis',(0.,0.333233134534162,-0.94284446121751));
#51704=DIRECTION('ref_axis',(0.,-0.94284446121751,-0.333233134534162));
#51705=DIRECTION('',(0.,-0.333233134534162,0.94284446121751));
#51706=DIRECTION('center_axis',(0.,0.333233134534159,-0.942844461217511));
#51707=DIRECTION('ref_axis',(0.,-0.942844461217511,-0.333233134534159));
#51708=DIRECTION('center_axis',(0.,-0.333233134534162,0.94284446121751));
#51709=DIRECTION('ref_axis',(0.,-0.94284446121751,-0.333233134534162));
#51710=DIRECTION('center_axis',(0.,0.333233134534159,-0.942844461217511));
#51711=DIRECTION('ref_axis',(0.,-0.942844461217511,-0.333233134534159));
#51712=DIRECTION('',(0.,0.333233134534162,-0.94284446121751));
#51713=DIRECTION('center_axis',(0.,0.333233134534162,-0.94284446121751));
#51714=DIRECTION('ref_axis',(0.,-0.94284446121751,-0.333233134534162));
#51715=DIRECTION('center_axis',(0.,-0.333233134534162,0.94284446121751));
#51716=DIRECTION('ref_axis',(0.,-0.94284446121751,-0.333233134534162));
#51717=DIRECTION('center_axis',(0.,0.333233134534162,-0.94284446121751));
#51718=DIRECTION('ref_axis',(0.,-0.94284446121751,-0.333233134534162));
#51719=DIRECTION('',(0.,-0.333233134534162,0.94284446121751));
#51720=DIRECTION('center_axis',(0.,0.333233134534159,-0.942844461217511));
#51721=DIRECTION('ref_axis',(0.,-0.942844461217511,-0.333233134534159));
#51722=DIRECTION('center_axis',(0.,-0.333233134534162,0.94284446121751));
#51723=DIRECTION('ref_axis',(0.,-0.94284446121751,-0.333233134534162));
#51724=DIRECTION('center_axis',(0.,0.333233134534159,-0.942844461217511));
#51725=DIRECTION('ref_axis',(0.,-0.942844461217511,-0.333233134534159));
#51726=DIRECTION('',(0.,0.333233134534162,-0.94284446121751));
#51727=DIRECTION('center_axis',(0.,0.333233134534162,-0.94284446121751));
#51728=DIRECTION('ref_axis',(0.,-0.94284446121751,-0.333233134534162));
#51729=DIRECTION('center_axis',(0.,-0.333233134534162,0.94284446121751));
#51730=DIRECTION('ref_axis',(0.,-0.94284446121751,-0.333233134534162));
#51731=DIRECTION('center_axis',(0.,0.333233134534162,-0.94284446121751));
#51732=DIRECTION('ref_axis',(0.,-0.94284446121751,-0.333233134534162));
#51733=DIRECTION('',(0.,-0.333233134534162,0.94284446121751));
#51734=DIRECTION('center_axis',(0.,0.333233134534159,-0.942844461217511));
#51735=DIRECTION('ref_axis',(0.,-0.942844461217511,-0.333233134534159));
#51736=DIRECTION('center_axis',(0.,-0.333233134534162,0.94284446121751));
#51737=DIRECTION('ref_axis',(0.,-0.94284446121751,-0.333233134534162));
#51738=DIRECTION('center_axis',(0.,0.333233134534159,-0.942844461217511));
#51739=DIRECTION('ref_axis',(0.,-0.942844461217511,-0.333233134534159));
#51740=DIRECTION('',(0.,0.333233134534162,-0.94284446121751));
#51741=DIRECTION('center_axis',(0.,0.333233134534162,-0.94284446121751));
#51742=DIRECTION('ref_axis',(0.,-0.94284446121751,-0.333233134534162));
#51743=DIRECTION('center_axis',(0.,-0.333233134534162,0.94284446121751));
#51744=DIRECTION('ref_axis',(0.,-0.94284446121751,-0.333233134534162));
#51745=DIRECTION('center_axis',(0.,0.333233134534162,-0.94284446121751));
#51746=DIRECTION('ref_axis',(0.,-0.94284446121751,-0.333233134534162));
#51747=DIRECTION('',(0.,-0.333233134534162,0.94284446121751));
#51748=DIRECTION('center_axis',(0.,0.333233134534159,-0.942844461217511));
#51749=DIRECTION('ref_axis',(0.,-0.942844461217511,-0.333233134534159));
#51750=DIRECTION('center_axis',(0.,-0.333233134534162,0.94284446121751));
#51751=DIRECTION('ref_axis',(0.,-0.94284446121751,-0.333233134534162));
#51752=DIRECTION('center_axis',(0.,0.333233134534159,-0.942844461217511));
#51753=DIRECTION('ref_axis',(0.,-0.942844461217511,-0.333233134534159));
#51754=DIRECTION('',(0.,0.333233134534162,-0.94284446121751));
#51755=DIRECTION('center_axis',(0.,0.333233134534162,-0.94284446121751));
#51756=DIRECTION('ref_axis',(0.,-0.94284446121751,-0.333233134534162));
#51757=DIRECTION('center_axis',(0.,-0.333233134534162,0.94284446121751));
#51758=DIRECTION('ref_axis',(0.,-0.94284446121751,-0.333233134534162));
#51759=DIRECTION('center_axis',(0.,0.333233134534162,-0.94284446121751));
#51760=DIRECTION('ref_axis',(0.,-0.94284446121751,-0.333233134534162));
#51761=DIRECTION('',(0.,-0.333233134534162,0.94284446121751));
#51762=DIRECTION('center_axis',(0.,0.333233134534159,-0.942844461217511));
#51763=DIRECTION('ref_axis',(0.,-0.942844461217511,-0.333233134534159));
#51764=DIRECTION('center_axis',(0.,-0.333233134534162,0.94284446121751));
#51765=DIRECTION('ref_axis',(0.,-0.94284446121751,-0.333233134534162));
#51766=DIRECTION('center_axis',(0.,0.333233134534159,-0.942844461217511));
#51767=DIRECTION('ref_axis',(0.,-0.942844461217511,-0.333233134534159));
#51768=DIRECTION('',(0.,0.333233134534162,-0.94284446121751));
#51769=DIRECTION('center_axis',(0.,0.333233134534162,-0.94284446121751));
#51770=DIRECTION('ref_axis',(0.,-0.94284446121751,-0.333233134534162));
#51771=DIRECTION('center_axis',(0.,-0.333233134534162,0.94284446121751));
#51772=DIRECTION('ref_axis',(0.,-0.94284446121751,-0.333233134534161));
#51773=DIRECTION('',(0.,0.333233134534162,-0.94284446121751));
#51774=DIRECTION('center_axis',(0.,-0.333233134534162,0.94284446121751));
#51775=DIRECTION('ref_axis',(0.,-0.94284446121751,-0.333233134534162));
#51776=DIRECTION('center_axis',(0.,0.333233134534162,-0.94284446121751));
#51777=DIRECTION('ref_axis',(0.,0.94284446121751,0.333233134534162));
#51778=DIRECTION('',(0.,-0.333233134534162,0.94284446121751));
#51779=DIRECTION('center_axis',(0.,-0.333233134534162,0.94284446121751));
#51780=DIRECTION('ref_axis',(0.,-0.94284446121751,-0.333233134534162));
#51781=DIRECTION('',(0.,0.333233134534162,-0.94284446121751));
#51782=DIRECTION('center_axis',(0.,-0.333233134534162,0.94284446121751));
#51783=DIRECTION('ref_axis',(0.,-0.94284446121751,-0.333233134534162));
#51784=DIRECTION('center_axis',(0.,0.333233134534162,-0.94284446121751));
#51785=DIRECTION('ref_axis',(0.,0.94284446121751,0.333233134534162));
#51786=DIRECTION('',(0.,-0.333233134534162,0.94284446121751));
#51787=DIRECTION('center_axis',(0.,-0.333233134534162,0.94284446121751));
#51788=DIRECTION('ref_axis',(0.,-0.94284446121751,-0.333233134534162));
#51789=DIRECTION('',(0.,0.333233134534162,-0.94284446121751));
#51790=DIRECTION('center_axis',(0.,-0.333233134534162,0.94284446121751));
#51791=DIRECTION('ref_axis',(0.,-0.94284446121751,-0.333233134534162));
#51792=DIRECTION('center_axis',(0.,0.333233134534162,-0.94284446121751));
#51793=DIRECTION('ref_axis',(0.,0.94284446121751,0.333233134534162));
#51794=DIRECTION('',(0.,-0.333233134534162,0.94284446121751));
#51795=DIRECTION('center_axis',(0.,-0.333233134534162,0.94284446121751));
#51796=DIRECTION('ref_axis',(0.,-0.94284446121751,-0.333233134534162));
#51797=DIRECTION('',(0.,0.333233134534162,-0.94284446121751));
#51798=DIRECTION('center_axis',(0.,-0.333233134534162,0.94284446121751));
#51799=DIRECTION('ref_axis',(0.,-0.94284446121751,-0.333233134534162));
#51800=DIRECTION('center_axis',(0.,0.333233134534162,-0.94284446121751));
#51801=DIRECTION('ref_axis',(0.,0.94284446121751,0.333233134534162));
#51802=DIRECTION('',(0.,-0.333233134534162,0.94284446121751));
#51803=DIRECTION('center_axis',(0.,-0.333233134534162,0.94284446121751));
#51804=DIRECTION('ref_axis',(0.,-0.94284446121751,-0.333233134534162));
#51805=DIRECTION('',(0.,0.333233134534162,-0.94284446121751));
#51806=DIRECTION('center_axis',(0.,-0.333233134534162,0.94284446121751));
#51807=DIRECTION('ref_axis',(0.,-0.94284446121751,-0.333233134534162));
#51808=DIRECTION('center_axis',(0.,0.333233134534162,-0.94284446121751));
#51809=DIRECTION('ref_axis',(0.,0.94284446121751,0.333233134534162));
#51810=DIRECTION('',(0.,-0.333233134534162,0.94284446121751));
#51811=DIRECTION('center_axis',(0.,-0.333233134534162,0.94284446121751));
#51812=DIRECTION('ref_axis',(0.,-0.94284446121751,-0.333233134534162));
#51813=DIRECTION('',(0.,0.333233134534162,-0.94284446121751));
#51814=DIRECTION('center_axis',(0.,-0.333233134534162,0.94284446121751));
#51815=DIRECTION('ref_axis',(0.,-0.94284446121751,-0.333233134534162));
#51816=DIRECTION('center_axis',(0.,0.333233134534162,-0.94284446121751));
#51817=DIRECTION('ref_axis',(0.,0.94284446121751,0.333233134534162));
#51818=DIRECTION('',(0.,-0.333233134534162,0.94284446121751));
#51819=DIRECTION('center_axis',(0.,-0.333233134534162,0.94284446121751));
#51820=DIRECTION('ref_axis',(0.,-0.94284446121751,-0.333233134534161));
#51821=DIRECTION('',(0.,0.333233134534162,-0.94284446121751));
#51822=DIRECTION('center_axis',(0.,-0.333233134534162,0.94284446121751));
#51823=DIRECTION('ref_axis',(0.,-0.94284446121751,-0.333233134534162));
#51824=DIRECTION('center_axis',(0.,0.333233134534162,-0.94284446121751));
#51825=DIRECTION('ref_axis',(0.,0.94284446121751,0.333233134534162));
#51826=DIRECTION('',(0.,-0.333233134534162,0.94284446121751));
#51827=DIRECTION('center_axis',(0.,-0.333233134534162,0.94284446121751));
#51828=DIRECTION('ref_axis',(0.,-0.94284446121751,-0.333233134534162));
#51829=DIRECTION('',(0.,0.333233134534162,-0.94284446121751));
#51830=DIRECTION('center_axis',(0.,-0.333233134534162,0.94284446121751));
#51831=DIRECTION('ref_axis',(0.,-0.94284446121751,-0.333233134534162));
#51832=DIRECTION('center_axis',(0.,0.333233134534162,-0.94284446121751));
#51833=DIRECTION('ref_axis',(0.,0.94284446121751,0.333233134534162));
#51834=DIRECTION('',(0.,-0.333233134534162,0.94284446121751));
#51835=DIRECTION('center_axis',(0.,-0.333233134534162,0.94284446121751));
#51836=DIRECTION('ref_axis',(0.,-0.94284446121751,-0.333233134534161));
#51837=DIRECTION('',(0.,0.333233134534162,-0.94284446121751));
#51838=DIRECTION('center_axis',(0.,-0.333233134534162,0.94284446121751));
#51839=DIRECTION('ref_axis',(0.,-0.94284446121751,-0.333233134534162));
#51840=DIRECTION('center_axis',(0.,0.333233134534162,-0.94284446121751));
#51841=DIRECTION('ref_axis',(0.,0.94284446121751,0.333233134534162));
#51842=DIRECTION('',(0.,-0.333233134534162,0.94284446121751));
#51843=DIRECTION('center_axis',(0.,-0.333233134534162,0.94284446121751));
#51844=DIRECTION('ref_axis',(0.,-0.94284446121751,-0.333233134534162));
#51845=DIRECTION('',(0.,0.333233134534162,-0.94284446121751));
#51846=DIRECTION('center_axis',(0.,-0.333233134534162,0.94284446121751));
#51847=DIRECTION('ref_axis',(0.,-0.94284446121751,-0.333233134534162));
#51848=DIRECTION('center_axis',(0.,0.333233134534162,-0.94284446121751));
#51849=DIRECTION('ref_axis',(0.,0.94284446121751,0.333233134534162));
#51850=DIRECTION('',(0.,-0.333233134534162,0.94284446121751));
#51851=DIRECTION('center_axis',(0.,-0.333233134534162,0.94284446121751));
#51852=DIRECTION('ref_axis',(0.,-0.94284446121751,-0.333233134534161));
#51853=DIRECTION('',(0.,0.333233134534162,-0.94284446121751));
#51854=DIRECTION('center_axis',(0.,-0.333233134534162,0.94284446121751));
#51855=DIRECTION('ref_axis',(0.,-0.94284446121751,-0.333233134534162));
#51856=DIRECTION('center_axis',(0.,0.333233134534162,-0.94284446121751));
#51857=DIRECTION('ref_axis',(0.,0.94284446121751,0.333233134534162));
#51858=DIRECTION('',(0.,-0.333233134534162,0.94284446121751));
#51859=DIRECTION('center_axis',(0.,-0.333233134534162,0.94284446121751));
#51860=DIRECTION('ref_axis',(0.,-0.94284446121751,-0.333233134534162));
#51861=DIRECTION('',(0.,0.333233134534162,-0.94284446121751));
#51862=DIRECTION('center_axis',(0.,-0.333233134534162,0.94284446121751));
#51863=DIRECTION('ref_axis',(0.,-0.94284446121751,-0.333233134534162));
#51864=DIRECTION('center_axis',(0.,0.333233134534162,-0.94284446121751));
#51865=DIRECTION('ref_axis',(0.,0.94284446121751,0.333233134534162));
#51866=DIRECTION('',(0.,-0.333233134534162,0.94284446121751));
#51867=DIRECTION('center_axis',(0.,-0.333233134534162,0.94284446121751));
#51868=DIRECTION('ref_axis',(0.,-0.94284446121751,-0.333233134534161));
#51869=DIRECTION('',(0.,0.333233134534162,-0.94284446121751));
#51870=DIRECTION('center_axis',(0.,-0.333233134534162,0.94284446121751));
#51871=DIRECTION('ref_axis',(0.,-0.94284446121751,-0.333233134534162));
#51872=DIRECTION('center_axis',(0.,0.333233134534162,-0.94284446121751));
#51873=DIRECTION('ref_axis',(0.,0.94284446121751,0.333233134534162));
#51874=DIRECTION('',(0.,-0.333233134534162,0.94284446121751));
#51875=DIRECTION('center_axis',(0.,-0.333233134534162,0.94284446121751));
#51876=DIRECTION('ref_axis',(0.,-0.94284446121751,-0.333233134534162));
#51877=DIRECTION('',(0.,0.333233134534162,-0.94284446121751));
#51878=DIRECTION('center_axis',(0.,-0.333233134534162,0.94284446121751));
#51879=DIRECTION('ref_axis',(0.,-0.94284446121751,-0.333233134534162));
#51880=DIRECTION('center_axis',(0.,0.333233134534162,-0.94284446121751));
#51881=DIRECTION('ref_axis',(0.,0.94284446121751,0.333233134534162));
#51882=DIRECTION('',(0.,-0.333233134534162,0.94284446121751));
#51883=DIRECTION('center_axis',(0.,-0.333233134534162,0.94284446121751));
#51884=DIRECTION('ref_axis',(0.,-0.94284446121751,-0.333233134534162));
#51885=DIRECTION('',(0.,0.333233134534162,-0.94284446121751));
#51886=DIRECTION('center_axis',(0.,-0.333233134534162,0.94284446121751));
#51887=DIRECTION('ref_axis',(0.,-0.94284446121751,-0.333233134534162));
#51888=DIRECTION('center_axis',(0.,0.333233134534162,-0.94284446121751));
#51889=DIRECTION('ref_axis',(0.,0.94284446121751,0.333233134534162));
#51890=DIRECTION('',(0.,-0.333233134534162,0.94284446121751));
#51891=DIRECTION('center_axis',(0.,-0.333233134534162,0.94284446121751));
#51892=DIRECTION('ref_axis',(0.,-0.94284446121751,-0.333233134534162));
#51893=DIRECTION('',(0.,0.333233134534162,-0.94284446121751));
#51894=DIRECTION('center_axis',(0.,-0.333233134534162,0.94284446121751));
#51895=DIRECTION('ref_axis',(0.,-0.94284446121751,-0.333233134534162));
#51896=DIRECTION('center_axis',(0.,0.333233134534162,-0.94284446121751));
#51897=DIRECTION('ref_axis',(0.,0.94284446121751,0.333233134534162));
#51898=DIRECTION('',(0.,-0.333233134534162,0.94284446121751));
#51899=DIRECTION('center_axis',(0.,-0.333233134534162,0.94284446121751));
#51900=DIRECTION('ref_axis',(0.,-0.94284446121751,-0.333233134534161));
#51901=DIRECTION('',(0.,0.333233134534162,-0.94284446121751));
#51902=DIRECTION('center_axis',(0.,-0.333233134534162,0.94284446121751));
#51903=DIRECTION('ref_axis',(0.,-0.94284446121751,-0.333233134534162));
#51904=DIRECTION('center_axis',(0.,0.333233134534162,-0.94284446121751));
#51905=DIRECTION('ref_axis',(0.,0.94284446121751,0.333233134534162));
#51906=DIRECTION('',(0.,-0.333233134534162,0.94284446121751));
#51907=DIRECTION('center_axis',(0.,-0.333233134534162,0.94284446121751));
#51908=DIRECTION('ref_axis',(0.,-0.94284446121751,-0.333233134534162));
#51909=DIRECTION('',(0.,0.333233134534162,-0.94284446121751));
#51910=DIRECTION('center_axis',(0.,-0.333233134534162,0.94284446121751));
#51911=DIRECTION('ref_axis',(0.,-0.94284446121751,-0.333233134534162));
#51912=DIRECTION('center_axis',(0.,0.333233134534162,-0.94284446121751));
#51913=DIRECTION('ref_axis',(0.,0.94284446121751,0.333233134534162));
#51914=DIRECTION('',(0.,-0.333233134534162,0.94284446121751));
#51915=DIRECTION('center_axis',(0.,-0.333233134534162,0.94284446121751));
#51916=DIRECTION('ref_axis',(0.,-0.94284446121751,-0.333233134534162));
#51917=DIRECTION('',(0.,0.333233134534162,-0.94284446121751));
#51918=DIRECTION('center_axis',(0.,-0.333233134534162,0.94284446121751));
#51919=DIRECTION('ref_axis',(0.,-0.94284446121751,-0.333233134534162));
#51920=DIRECTION('center_axis',(0.,0.333233134534162,-0.94284446121751));
#51921=DIRECTION('ref_axis',(0.,0.94284446121751,0.333233134534162));
#51922=DIRECTION('',(0.,-0.333233134534162,0.94284446121751));
#51923=DIRECTION('center_axis',(0.,-0.333233134534162,0.94284446121751));
#51924=DIRECTION('ref_axis',(0.,-0.94284446121751,-0.333233134534162));
#51925=DIRECTION('',(0.,0.333233134534162,-0.94284446121751));
#51926=DIRECTION('center_axis',(0.,-0.333233134534162,0.94284446121751));
#51927=DIRECTION('ref_axis',(0.,-0.94284446121751,-0.333233134534162));
#51928=DIRECTION('center_axis',(0.,0.333233134534162,-0.94284446121751));
#51929=DIRECTION('ref_axis',(0.,0.94284446121751,0.333233134534162));
#51930=DIRECTION('',(0.,-0.333233134534162,0.94284446121751));
#51931=DIRECTION('center_axis',(0.,-0.333233134534162,0.94284446121751));
#51932=DIRECTION('ref_axis',(0.,-0.94284446121751,-0.333233134534162));
#51933=DIRECTION('',(0.,0.333233134534162,-0.94284446121751));
#51934=DIRECTION('center_axis',(0.,-0.333233134534162,0.94284446121751));
#51935=DIRECTION('ref_axis',(0.,-0.94284446121751,-0.333233134534162));
#51936=DIRECTION('center_axis',(0.,0.333233134534162,-0.94284446121751));
#51937=DIRECTION('ref_axis',(0.,0.94284446121751,0.333233134534162));
#51938=DIRECTION('',(0.,-0.333233134534162,0.94284446121751));
#51939=DIRECTION('center_axis',(0.,-0.333233134534162,0.94284446121751));
#51940=DIRECTION('ref_axis',(0.,-0.94284446121751,-0.333233134534162));
#51941=DIRECTION('',(0.,0.333233134534162,-0.94284446121751));
#51942=DIRECTION('center_axis',(0.,-0.333233134534162,0.94284446121751));
#51943=DIRECTION('ref_axis',(0.,-0.94284446121751,-0.333233134534162));
#51944=DIRECTION('center_axis',(0.,0.333233134534162,-0.94284446121751));
#51945=DIRECTION('ref_axis',(0.,0.94284446121751,0.333233134534162));
#51946=DIRECTION('',(0.,-0.333233134534162,0.94284446121751));
#51947=DIRECTION('center_axis',(0.,-0.333233134534162,0.94284446121751));
#51948=DIRECTION('ref_axis',(0.,-0.94284446121751,-0.333233134534161));
#51949=DIRECTION('',(0.,0.333233134534162,-0.94284446121751));
#51950=DIRECTION('center_axis',(0.,-0.333233134534162,0.94284446121751));
#51951=DIRECTION('ref_axis',(0.,-0.94284446121751,-0.333233134534162));
#51952=DIRECTION('center_axis',(0.,0.333233134534162,-0.94284446121751));
#51953=DIRECTION('ref_axis',(0.,0.94284446121751,0.333233134534162));
#51954=DIRECTION('',(0.,-0.333233134534162,0.94284446121751));
#51955=DIRECTION('center_axis',(0.,-0.333233134534162,0.94284446121751));
#51956=DIRECTION('ref_axis',(0.,-0.94284446121751,-0.333233134534162));
#51957=DIRECTION('',(0.,0.333233134534162,-0.94284446121751));
#51958=DIRECTION('center_axis',(0.,-0.333233134534162,0.94284446121751));
#51959=DIRECTION('ref_axis',(0.,-0.94284446121751,-0.333233134534162));
#51960=DIRECTION('center_axis',(0.,0.333233134534162,-0.94284446121751));
#51961=DIRECTION('ref_axis',(0.,0.94284446121751,0.333233134534162));
#51962=DIRECTION('',(0.,-0.333233134534162,0.94284446121751));
#51963=DIRECTION('center_axis',(0.,-0.333233134534162,0.94284446121751));
#51964=DIRECTION('ref_axis',(0.,-0.94284446121751,-0.333233134534161));
#51965=DIRECTION('',(0.,0.333233134534162,-0.94284446121751));
#51966=DIRECTION('center_axis',(0.,-0.333233134534162,0.94284446121751));
#51967=DIRECTION('ref_axis',(0.,-0.94284446121751,-0.333233134534162));
#51968=DIRECTION('center_axis',(0.,0.333233134534162,-0.94284446121751));
#51969=DIRECTION('ref_axis',(0.,0.94284446121751,0.333233134534162));
#51970=DIRECTION('',(0.,-0.333233134534162,0.94284446121751));
#51971=DIRECTION('center_axis',(0.,-0.333233134534162,0.94284446121751));
#51972=DIRECTION('ref_axis',(0.,-0.94284446121751,-0.333233134534162));
#51973=DIRECTION('',(0.,0.333233134534162,-0.94284446121751));
#51974=DIRECTION('center_axis',(0.,-0.333233134534162,0.94284446121751));
#51975=DIRECTION('ref_axis',(0.,-0.94284446121751,-0.333233134534162));
#51976=DIRECTION('center_axis',(0.,0.333233134534162,-0.94284446121751));
#51977=DIRECTION('ref_axis',(0.,0.94284446121751,0.333233134534162));
#51978=DIRECTION('',(0.,-0.333233134534162,0.94284446121751));
#51979=DIRECTION('center_axis',(0.,-0.333233134534162,0.94284446121751));
#51980=DIRECTION('ref_axis',(0.,-0.94284446121751,-0.333233134534162));
#51981=DIRECTION('',(0.,0.333233134534162,-0.94284446121751));
#51982=DIRECTION('center_axis',(0.,-0.333233134534162,0.94284446121751));
#51983=DIRECTION('ref_axis',(0.,-0.94284446121751,-0.333233134534162));
#51984=DIRECTION('center_axis',(0.,0.333233134534162,-0.94284446121751));
#51985=DIRECTION('ref_axis',(0.,0.94284446121751,0.333233134534162));
#51986=DIRECTION('',(0.,-0.333233134534162,0.94284446121751));
#51987=DIRECTION('center_axis',(0.,-0.333233134534162,0.94284446121751));
#51988=DIRECTION('ref_axis',(0.,-0.94284446121751,-0.333233134534162));
#51989=DIRECTION('',(0.,0.333233134534162,-0.94284446121751));
#51990=DIRECTION('center_axis',(0.,-0.333233134534162,0.94284446121751));
#51991=DIRECTION('ref_axis',(0.,-0.94284446121751,-0.333233134534162));
#51992=DIRECTION('center_axis',(0.,0.333233134534162,-0.94284446121751));
#51993=DIRECTION('ref_axis',(0.,0.94284446121751,0.333233134534162));
#51994=DIRECTION('',(0.,-0.333233134534162,0.94284446121751));
#51995=DIRECTION('center_axis',(0.,-0.333233134534162,0.94284446121751));
#51996=DIRECTION('ref_axis',(0.,-0.94284446121751,-0.333233134534161));
#51997=DIRECTION('',(0.,0.333233134534162,-0.94284446121751));
#51998=DIRECTION('center_axis',(0.,-0.333233134534162,0.94284446121751));
#51999=DIRECTION('ref_axis',(0.,-0.94284446121751,-0.333233134534162));
#52000=DIRECTION('center_axis',(0.,0.333233134534162,-0.94284446121751));
#52001=DIRECTION('ref_axis',(0.,0.94284446121751,0.333233134534162));
#52002=DIRECTION('',(0.,-0.333233134534162,0.94284446121751));
#52003=DIRECTION('center_axis',(0.,-0.333233134534162,0.94284446121751));
#52004=DIRECTION('ref_axis',(0.,-0.94284446121751,-0.333233134534162));
#52005=DIRECTION('',(0.,0.333233134534162,-0.94284446121751));
#52006=DIRECTION('center_axis',(0.,-0.333233134534162,0.94284446121751));
#52007=DIRECTION('ref_axis',(0.,-0.94284446121751,-0.333233134534162));
#52008=DIRECTION('center_axis',(0.,0.333233134534162,-0.94284446121751));
#52009=DIRECTION('ref_axis',(0.,0.94284446121751,0.333233134534162));
#52010=DIRECTION('',(0.,-0.333233134534162,0.94284446121751));
#52011=DIRECTION('center_axis',(0.,-0.333233134534162,0.94284446121751));
#52012=DIRECTION('ref_axis',(0.,-0.94284446121751,-0.333233134534162));
#52013=DIRECTION('',(0.,0.333233134534162,-0.94284446121751));
#52014=DIRECTION('center_axis',(0.,-0.333233134534162,0.94284446121751));
#52015=DIRECTION('ref_axis',(0.,-0.94284446121751,-0.333233134534162));
#52016=DIRECTION('center_axis',(0.,0.333233134534162,-0.94284446121751));
#52017=DIRECTION('ref_axis',(0.,0.94284446121751,0.333233134534162));
#52018=DIRECTION('',(0.,-0.333233134534162,0.94284446121751));
#52019=DIRECTION('center_axis',(0.,-0.333233134534162,0.94284446121751));
#52020=DIRECTION('ref_axis',(0.,-0.94284446121751,-0.333233134534162));
#52021=DIRECTION('',(0.,0.333233134534162,-0.94284446121751));
#52022=DIRECTION('center_axis',(0.,-0.333233134534162,0.94284446121751));
#52023=DIRECTION('ref_axis',(0.,-0.94284446121751,-0.333233134534162));
#52024=DIRECTION('center_axis',(0.,0.333233134534162,-0.94284446121751));
#52025=DIRECTION('ref_axis',(0.,0.94284446121751,0.333233134534162));
#52026=DIRECTION('',(0.,-0.333233134534162,0.94284446121751));
#52027=DIRECTION('center_axis',(0.,-0.333233134534162,0.94284446121751));
#52028=DIRECTION('ref_axis',(0.,-0.94284446121751,-0.333233134534162));
#52029=DIRECTION('',(0.,0.333233134534162,-0.94284446121751));
#52030=DIRECTION('center_axis',(0.,-0.333233134534162,0.94284446121751));
#52031=DIRECTION('ref_axis',(0.,-0.94284446121751,-0.333233134534162));
#52032=DIRECTION('center_axis',(0.,0.333233134534162,-0.94284446121751));
#52033=DIRECTION('ref_axis',(0.,0.94284446121751,0.333233134534162));
#52034=DIRECTION('',(0.,-0.333233134534162,0.94284446121751));
#52035=DIRECTION('center_axis',(0.,-0.333233134534162,0.94284446121751));
#52036=DIRECTION('ref_axis',(0.,-0.94284446121751,-0.333233134534162));
#52037=DIRECTION('',(0.,0.333233134534162,-0.94284446121751));
#52038=DIRECTION('center_axis',(0.,-0.333233134534162,0.94284446121751));
#52039=DIRECTION('ref_axis',(0.,-0.94284446121751,-0.333233134534162));
#52040=DIRECTION('center_axis',(0.,0.333233134534162,-0.94284446121751));
#52041=DIRECTION('ref_axis',(0.,0.94284446121751,0.333233134534162));
#52042=DIRECTION('',(0.,-0.333233134534162,0.94284446121751));
#52043=DIRECTION('center_axis',(0.,-0.333233134534162,0.94284446121751));
#52044=DIRECTION('ref_axis',(0.,-0.94284446121751,-0.333233134534162));
#52045=DIRECTION('',(0.,0.333233134534162,-0.94284446121751));
#52046=DIRECTION('center_axis',(0.,-0.333233134534162,0.94284446121751));
#52047=DIRECTION('ref_axis',(0.,-0.94284446121751,-0.333233134534162));
#52048=DIRECTION('center_axis',(0.,0.333233134534162,-0.94284446121751));
#52049=DIRECTION('ref_axis',(0.,0.94284446121751,0.333233134534162));
#52050=DIRECTION('',(0.,-0.333233134534162,0.94284446121751));
#52051=DIRECTION('center_axis',(0.,-0.333233134534162,0.94284446121751));
#52052=DIRECTION('ref_axis',(0.,-0.94284446121751,-0.333233134534162));
#52053=DIRECTION('',(0.,0.333233134534162,-0.94284446121751));
#52054=DIRECTION('center_axis',(0.,-0.333233134534162,0.94284446121751));
#52055=DIRECTION('ref_axis',(0.,-0.94284446121751,-0.333233134534162));
#52056=DIRECTION('center_axis',(0.,0.333233134534162,-0.94284446121751));
#52057=DIRECTION('ref_axis',(0.,0.94284446121751,0.333233134534162));
#52058=DIRECTION('',(0.,-0.333233134534162,0.94284446121751));
#52059=DIRECTION('center_axis',(0.,-0.333233134534162,0.94284446121751));
#52060=DIRECTION('ref_axis',(0.,-0.94284446121751,-0.333233134534161));
#52061=DIRECTION('',(0.,0.333233134534162,-0.94284446121751));
#52062=DIRECTION('center_axis',(0.,-0.333233134534162,0.94284446121751));
#52063=DIRECTION('ref_axis',(0.,-0.94284446121751,-0.333233134534162));
#52064=DIRECTION('center_axis',(0.,0.333233134534162,-0.94284446121751));
#52065=DIRECTION('ref_axis',(0.,0.94284446121751,0.333233134534162));
#52066=DIRECTION('',(0.,-0.333233134534162,0.94284446121751));
#52067=DIRECTION('center_axis',(0.,-0.333233134534162,0.94284446121751));
#52068=DIRECTION('ref_axis',(0.,-0.94284446121751,-0.333233134534162));
#52069=DIRECTION('',(0.,0.333233134534162,-0.94284446121751));
#52070=DIRECTION('center_axis',(0.,-0.333233134534162,0.94284446121751));
#52071=DIRECTION('ref_axis',(0.,-0.94284446121751,-0.333233134534162));
#52072=DIRECTION('center_axis',(0.,0.333233134534162,-0.94284446121751));
#52073=DIRECTION('ref_axis',(0.,0.94284446121751,0.333233134534162));
#52074=DIRECTION('',(0.,-0.333233134534162,0.94284446121751));
#52075=DIRECTION('center_axis',(0.,-0.333233134534162,0.94284446121751));
#52076=DIRECTION('ref_axis',(0.,-0.94284446121751,-0.333233134534162));
#52077=DIRECTION('',(0.,0.333233134534162,-0.94284446121751));
#52078=DIRECTION('center_axis',(0.,-0.333233134534162,0.94284446121751));
#52079=DIRECTION('ref_axis',(0.,-0.94284446121751,-0.333233134534162));
#52080=DIRECTION('center_axis',(0.,0.333233134534162,-0.94284446121751));
#52081=DIRECTION('ref_axis',(0.,0.94284446121751,0.333233134534162));
#52082=DIRECTION('',(0.,-0.333233134534162,0.94284446121751));
#52083=DIRECTION('center_axis',(0.,-0.333233134534162,0.94284446121751));
#52084=DIRECTION('ref_axis',(0.,-0.94284446121751,-0.333233134534162));
#52085=DIRECTION('center_axis',(0.,0.333233134534159,-0.942844461217511));
#52086=DIRECTION('ref_axis',(0.,-0.942844461217511,-0.333233134534159));
#52087=DIRECTION('',(0.,0.333233134534162,-0.94284446121751));
#52088=DIRECTION('center_axis',(0.,-0.333233134534162,0.94284446121751));
#52089=DIRECTION('ref_axis',(0.,-0.94284446121751,-0.333233134534162));
#52090=DIRECTION('center_axis',(0.,0.333233134534162,-0.94284446121751));
#52091=DIRECTION('ref_axis',(0.,0.94284446121751,0.333233134534162));
#52092=DIRECTION('',(0.,-0.333233134534162,0.94284446121751));
#52093=DIRECTION('center_axis',(0.,0.333233134534159,-0.942844461217511));
#52094=DIRECTION('ref_axis',(0.,-0.942844461217511,-0.333233134534159));
#52095=DIRECTION('center_axis',(0.,-0.333233134534162,0.94284446121751));
#52096=DIRECTION('ref_axis',(0.,-0.94284446121751,-0.333233134534162));
#52097=DIRECTION('center_axis',(0.,0.333233134534159,-0.942844461217511));
#52098=DIRECTION('ref_axis',(0.,-0.942844461217511,-0.333233134534159));
#52099=DIRECTION('',(0.,0.333233134534162,-0.94284446121751));
#52100=DIRECTION('center_axis',(0.,-0.333233134534162,0.94284446121751));
#52101=DIRECTION('ref_axis',(0.,-0.94284446121751,-0.333233134534162));
#52102=DIRECTION('center_axis',(0.,0.333233134534162,-0.94284446121751));
#52103=DIRECTION('ref_axis',(0.,0.94284446121751,0.333233134534162));
#52104=DIRECTION('',(0.,-0.333233134534162,0.94284446121751));
#52105=DIRECTION('center_axis',(0.,0.333233134534159,-0.942844461217511));
#52106=DIRECTION('ref_axis',(0.,-0.942844461217511,-0.333233134534159));
#52107=DIRECTION('center_axis',(0.,-0.333233134534162,0.94284446121751));
#52108=DIRECTION('ref_axis',(0.,-0.94284446121751,-0.333233134534162));
#52109=DIRECTION('',(0.,0.333233134534162,-0.94284446121751));
#52110=DIRECTION('center_axis',(0.,-0.333233134534162,0.94284446121751));
#52111=DIRECTION('ref_axis',(0.,-0.94284446121751,-0.333233134534162));
#52112=DIRECTION('center_axis',(0.,0.333233134534162,-0.94284446121751));
#52113=DIRECTION('ref_axis',(0.,0.94284446121751,0.333233134534162));
#52114=DIRECTION('',(0.,-0.333233134534162,0.94284446121751));
#52115=DIRECTION('center_axis',(0.,-0.333233134534162,0.94284446121751));
#52116=DIRECTION('ref_axis',(0.,-0.94284446121751,-0.333233134534162));
#52117=DIRECTION('',(0.,0.333233134534162,-0.94284446121751));
#52118=DIRECTION('center_axis',(0.,-0.333233134534162,0.94284446121751));
#52119=DIRECTION('ref_axis',(0.,-0.94284446121751,-0.333233134534162));
#52120=DIRECTION('center_axis',(0.,0.333233134534162,-0.94284446121751));
#52121=DIRECTION('ref_axis',(0.,0.94284446121751,0.333233134534162));
#52122=DIRECTION('',(0.,-0.333233134534162,0.94284446121751));
#52123=DIRECTION('center_axis',(0.,-0.333233134534162,0.94284446121751));
#52124=DIRECTION('ref_axis',(0.,-0.94284446121751,-0.333233134534162));
#52125=DIRECTION('center_axis',(0.,0.333233134534159,-0.942844461217511));
#52126=DIRECTION('ref_axis',(0.,-0.942844461217511,-0.333233134534159));
#52127=DIRECTION('',(0.,0.333233134534162,-0.94284446121751));
#52128=DIRECTION('center_axis',(0.,-0.333233134534162,0.94284446121751));
#52129=DIRECTION('ref_axis',(0.,-0.94284446121751,-0.333233134534162));
#52130=DIRECTION('center_axis',(0.,0.333233134534162,-0.94284446121751));
#52131=DIRECTION('ref_axis',(0.,0.94284446121751,0.333233134534162));
#52132=DIRECTION('',(0.,-0.333233134534162,0.94284446121751));
#52133=DIRECTION('center_axis',(0.,0.333233134534159,-0.942844461217511));
#52134=DIRECTION('ref_axis',(0.,-0.942844461217511,-0.333233134534159));
#52135=DIRECTION('center_axis',(0.,-0.333233134534162,0.94284446121751));
#52136=DIRECTION('ref_axis',(0.,-0.94284446121751,-0.333233134534162));
#52137=DIRECTION('center_axis',(0.,0.333233134534159,-0.942844461217511));
#52138=DIRECTION('ref_axis',(0.,-0.942844461217511,-0.333233134534159));
#52139=DIRECTION('',(0.,0.333233134534162,-0.94284446121751));
#52140=DIRECTION('center_axis',(0.,-0.333233134534162,0.94284446121751));
#52141=DIRECTION('ref_axis',(0.,-0.94284446121751,-0.333233134534162));
#52142=DIRECTION('center_axis',(0.,0.333233134534162,-0.94284446121751));
#52143=DIRECTION('ref_axis',(0.,0.94284446121751,0.333233134534162));
#52144=DIRECTION('',(0.,-0.333233134534162,0.94284446121751));
#52145=DIRECTION('center_axis',(0.,0.333233134534159,-0.942844461217511));
#52146=DIRECTION('ref_axis',(0.,-0.942844461217511,-0.333233134534159));
#52147=DIRECTION('center_axis',(0.,-0.333233134534162,0.94284446121751));
#52148=DIRECTION('ref_axis',(0.,-0.94284446121751,-0.333233134534162));
#52149=DIRECTION('',(0.,0.333233134534162,-0.94284446121751));
#52150=DIRECTION('center_axis',(0.,-0.333233134534162,0.94284446121751));
#52151=DIRECTION('ref_axis',(0.,-0.94284446121751,-0.333233134534162));
#52152=DIRECTION('center_axis',(0.,0.333233134534162,-0.94284446121751));
#52153=DIRECTION('ref_axis',(0.,0.94284446121751,0.333233134534162));
#52154=DIRECTION('',(0.,-0.333233134534162,0.94284446121751));
#52155=DIRECTION('center_axis',(0.,-0.333233134534162,0.94284446121751));
#52156=DIRECTION('ref_axis',(0.,-0.94284446121751,-0.333233134534162));
#52157=DIRECTION('',(0.,0.333233134534162,-0.94284446121751));
#52158=DIRECTION('center_axis',(0.,-0.333233134534162,0.94284446121751));
#52159=DIRECTION('ref_axis',(0.,-0.94284446121751,-0.333233134534162));
#52160=DIRECTION('center_axis',(0.,0.333233134534162,-0.94284446121751));
#52161=DIRECTION('ref_axis',(0.,0.94284446121751,0.333233134534162));
#52162=DIRECTION('',(0.,-0.333233134534162,0.94284446121751));
#52163=DIRECTION('center_axis',(0.,-0.333233134534162,0.94284446121751));
#52164=DIRECTION('ref_axis',(0.,-0.94284446121751,-0.333233134534162));
#52165=DIRECTION('center_axis',(0.,0.333233134534159,-0.942844461217511));
#52166=DIRECTION('ref_axis',(0.,-0.942844461217511,-0.333233134534159));
#52167=DIRECTION('',(0.,0.333233134534162,-0.94284446121751));
#52168=DIRECTION('center_axis',(0.,-0.333233134534162,0.94284446121751));
#52169=DIRECTION('ref_axis',(0.,-0.94284446121751,-0.333233134534162));
#52170=DIRECTION('center_axis',(0.,0.333233134534162,-0.94284446121751));
#52171=DIRECTION('ref_axis',(0.,0.94284446121751,0.333233134534162));
#52172=DIRECTION('',(0.,-0.333233134534162,0.94284446121751));
#52173=DIRECTION('center_axis',(0.,0.333233134534159,-0.942844461217511));
#52174=DIRECTION('ref_axis',(0.,-0.942844461217511,-0.333233134534159));
#52175=DIRECTION('center_axis',(0.,-0.333233134534162,0.94284446121751));
#52176=DIRECTION('ref_axis',(0.,-0.94284446121751,-0.333233134534162));
#52177=DIRECTION('',(0.,0.333233134534162,-0.94284446121751));
#52178=DIRECTION('center_axis',(0.,-0.333233134534162,0.94284446121751));
#52179=DIRECTION('ref_axis',(0.,-0.94284446121751,-0.333233134534162));
#52180=DIRECTION('center_axis',(0.,0.333233134534162,-0.94284446121751));
#52181=DIRECTION('ref_axis',(0.,0.94284446121751,0.333233134534162));
#52182=DIRECTION('',(0.,-0.333233134534162,0.94284446121751));
#52183=DIRECTION('center_axis',(0.,-0.333233134534162,0.94284446121751));
#52184=DIRECTION('ref_axis',(0.,-0.94284446121751,-0.333233134534162));
#52185=DIRECTION('',(0.,0.333233134534162,-0.94284446121751));
#52186=DIRECTION('center_axis',(0.,-0.333233134534162,0.94284446121751));
#52187=DIRECTION('ref_axis',(0.,-0.94284446121751,-0.333233134534162));
#52188=DIRECTION('center_axis',(0.,0.333233134534162,-0.94284446121751));
#52189=DIRECTION('ref_axis',(0.,0.94284446121751,0.333233134534162));
#52190=DIRECTION('',(0.,-0.333233134534162,0.94284446121751));
#52191=DIRECTION('center_axis',(0.,-0.333233134534162,0.94284446121751));
#52192=DIRECTION('ref_axis',(0.,-0.94284446121751,-0.333233134534162));
#52193=DIRECTION('center_axis',(0.,0.333233134534159,-0.942844461217511));
#52194=DIRECTION('ref_axis',(0.,-0.942844461217511,-0.333233134534159));
#52195=DIRECTION('',(0.,0.333233134534162,-0.94284446121751));
#52196=DIRECTION('center_axis',(0.,-0.333233134534162,0.94284446121751));
#52197=DIRECTION('ref_axis',(0.,-0.94284446121751,-0.333233134534162));
#52198=DIRECTION('center_axis',(0.,0.333233134534162,-0.94284446121751));
#52199=DIRECTION('ref_axis',(0.,0.94284446121751,0.333233134534162));
#52200=DIRECTION('',(0.,-0.333233134534162,0.94284446121751));
#52201=DIRECTION('center_axis',(0.,0.333233134534159,-0.942844461217511));
#52202=DIRECTION('ref_axis',(0.,-0.942844461217511,-0.333233134534159));
#52203=DIRECTION('center_axis',(0.,-0.333233134534162,0.94284446121751));
#52204=DIRECTION('ref_axis',(0.,-0.94284446121751,-0.333233134534162));
#52205=DIRECTION('',(0.,0.333233134534162,-0.94284446121751));
#52206=DIRECTION('center_axis',(0.,-0.333233134534162,0.94284446121751));
#52207=DIRECTION('ref_axis',(0.,-0.94284446121751,-0.333233134534162));
#52208=DIRECTION('center_axis',(0.,0.333233134534162,-0.94284446121751));
#52209=DIRECTION('ref_axis',(0.,0.94284446121751,0.333233134534162));
#52210=DIRECTION('',(0.,-0.333233134534162,0.94284446121751));
#52211=DIRECTION('center_axis',(0.,-0.333233134534162,0.94284446121751));
#52212=DIRECTION('ref_axis',(0.,-0.94284446121751,-0.333233134534161));
#52213=DIRECTION('',(0.,0.333233134534162,-0.94284446121751));
#52214=DIRECTION('center_axis',(0.,-0.333233134534162,0.94284446121751));
#52215=DIRECTION('ref_axis',(0.,-0.94284446121751,-0.333233134534162));
#52216=DIRECTION('center_axis',(0.,0.333233134534162,-0.94284446121751));
#52217=DIRECTION('ref_axis',(0.,0.94284446121751,0.333233134534162));
#52218=DIRECTION('',(0.,-0.333233134534162,0.94284446121751));
#52219=DIRECTION('center_axis',(0.,-0.333233134534162,0.94284446121751));
#52220=DIRECTION('ref_axis',(0.,-0.94284446121751,-0.333233134534162));
#52221=DIRECTION('',(0.,0.333233134534162,-0.94284446121751));
#52222=DIRECTION('center_axis',(0.,-0.333233134534162,0.94284446121751));
#52223=DIRECTION('ref_axis',(0.,-0.94284446121751,-0.333233134534162));
#52224=DIRECTION('center_axis',(0.,0.333233134534162,-0.94284446121751));
#52225=DIRECTION('ref_axis',(0.,0.94284446121751,0.333233134534162));
#52226=DIRECTION('',(0.,-0.333233134534162,0.94284446121751));
#52227=DIRECTION('center_axis',(0.,-0.333233134534162,0.94284446121751));
#52228=DIRECTION('ref_axis',(0.,-0.94284446121751,-0.333233134534162));
#52229=DIRECTION('',(0.,0.333233134534162,-0.94284446121751));
#52230=DIRECTION('center_axis',(0.,-0.333233134534162,0.94284446121751));
#52231=DIRECTION('ref_axis',(0.,-0.94284446121751,-0.333233134534162));
#52232=DIRECTION('center_axis',(0.,0.333233134534162,-0.94284446121751));
#52233=DIRECTION('ref_axis',(0.,0.94284446121751,0.333233134534162));
#52234=DIRECTION('',(0.,-0.333233134534162,0.94284446121751));
#52235=DIRECTION('center_axis',(0.,-0.333233134534162,0.94284446121751));
#52236=DIRECTION('ref_axis',(0.,-0.94284446121751,-0.333233134534162));
#52237=DIRECTION('',(0.,0.333233134534162,-0.94284446121751));
#52238=DIRECTION('center_axis',(0.,-0.333233134534162,0.94284446121751));
#52239=DIRECTION('ref_axis',(0.,-0.94284446121751,-0.333233134534162));
#52240=DIRECTION('center_axis',(0.,0.333233134534162,-0.94284446121751));
#52241=DIRECTION('ref_axis',(0.,0.94284446121751,0.333233134534162));
#52242=DIRECTION('',(0.,-0.333233134534162,0.94284446121751));
#52243=DIRECTION('center_axis',(0.,-0.333233134534162,0.94284446121751));
#52244=DIRECTION('ref_axis',(0.,-0.94284446121751,-0.333233134534161));
#52245=DIRECTION('',(0.,0.333233134534162,-0.94284446121751));
#52246=DIRECTION('center_axis',(0.,-0.333233134534162,0.94284446121751));
#52247=DIRECTION('ref_axis',(0.,-0.94284446121751,-0.333233134534162));
#52248=DIRECTION('center_axis',(0.,0.333233134534162,-0.94284446121751));
#52249=DIRECTION('ref_axis',(0.,0.94284446121751,0.333233134534162));
#52250=DIRECTION('',(0.,-0.333233134534162,0.94284446121751));
#52251=DIRECTION('center_axis',(0.,-0.333233134534162,0.94284446121751));
#52252=DIRECTION('ref_axis',(0.,-0.94284446121751,-0.333233134534162));
#52253=DIRECTION('',(0.,0.333233134534162,-0.94284446121751));
#52254=DIRECTION('center_axis',(0.,-0.333233134534162,0.94284446121751));
#52255=DIRECTION('ref_axis',(0.,-0.94284446121751,-0.333233134534162));
#52256=DIRECTION('center_axis',(0.,0.333233134534162,-0.94284446121751));
#52257=DIRECTION('ref_axis',(0.,0.94284446121751,0.333233134534162));
#52258=DIRECTION('',(0.,-0.333233134534162,0.94284446121751));
#52259=DIRECTION('center_axis',(0.,-0.333233134534162,0.94284446121751));
#52260=DIRECTION('ref_axis',(0.,-0.94284446121751,-0.333233134534162));
#52261=DIRECTION('',(0.,0.333233134534162,-0.94284446121751));
#52262=DIRECTION('center_axis',(0.,-0.333233134534162,0.94284446121751));
#52263=DIRECTION('ref_axis',(0.,-0.94284446121751,-0.333233134534162));
#52264=DIRECTION('center_axis',(0.,0.333233134534162,-0.94284446121751));
#52265=DIRECTION('ref_axis',(0.,0.94284446121751,0.333233134534162));
#52266=DIRECTION('',(0.,-0.333233134534162,0.94284446121751));
#52267=DIRECTION('center_axis',(0.,-0.333233134534162,0.94284446121751));
#52268=DIRECTION('ref_axis',(0.,-0.94284446121751,-0.333233134534162));
#52269=DIRECTION('',(0.,0.333233134534162,-0.94284446121751));
#52270=DIRECTION('center_axis',(0.,-0.333233134534162,0.94284446121751));
#52271=DIRECTION('ref_axis',(0.,-0.94284446121751,-0.333233134534162));
#52272=DIRECTION('center_axis',(0.,0.333233134534162,-0.94284446121751));
#52273=DIRECTION('ref_axis',(0.,0.94284446121751,0.333233134534162));
#52274=DIRECTION('',(0.,-0.333233134534162,0.94284446121751));
#52275=DIRECTION('center_axis',(0.,-0.333233134534162,0.94284446121751));
#52276=DIRECTION('ref_axis',(0.,-0.94284446121751,-0.333233134534161));
#52277=DIRECTION('',(0.,0.333233134534162,-0.94284446121751));
#52278=DIRECTION('center_axis',(0.,-0.333233134534162,0.94284446121751));
#52279=DIRECTION('ref_axis',(0.,-0.94284446121751,-0.333233134534162));
#52280=DIRECTION('center_axis',(0.,0.333233134534162,-0.94284446121751));
#52281=DIRECTION('ref_axis',(0.,0.94284446121751,0.333233134534162));
#52282=DIRECTION('',(0.,-0.333233134534162,0.94284446121751));
#52283=DIRECTION('center_axis',(0.,-0.333233134534162,0.94284446121751));
#52284=DIRECTION('ref_axis',(0.,-0.94284446121751,-0.333233134534162));
#52285=DIRECTION('',(0.,0.333233134534162,-0.94284446121751));
#52286=DIRECTION('center_axis',(0.,-0.333233134534162,0.94284446121751));
#52287=DIRECTION('ref_axis',(0.,-0.94284446121751,-0.333233134534162));
#52288=DIRECTION('center_axis',(0.,0.333233134534162,-0.94284446121751));
#52289=DIRECTION('ref_axis',(0.,0.94284446121751,0.333233134534162));
#52290=DIRECTION('',(0.,-0.333233134534162,0.94284446121751));
#52291=DIRECTION('center_axis',(0.,-0.333233134534162,0.94284446121751));
#52292=DIRECTION('ref_axis',(0.,-0.94284446121751,-0.333233134534162));
#52293=DIRECTION('',(0.,0.333233134534162,-0.94284446121751));
#52294=DIRECTION('center_axis',(0.,-0.333233134534162,0.94284446121751));
#52295=DIRECTION('ref_axis',(0.,-0.94284446121751,-0.333233134534162));
#52296=DIRECTION('center_axis',(0.,0.333233134534162,-0.94284446121751));
#52297=DIRECTION('ref_axis',(0.,0.94284446121751,0.333233134534162));
#52298=DIRECTION('',(0.,-0.333233134534162,0.94284446121751));
#52299=DIRECTION('center_axis',(0.,-0.333233134534162,0.94284446121751));
#52300=DIRECTION('ref_axis',(0.,-0.94284446121751,-0.333233134534161));
#52301=DIRECTION('',(0.,0.333233134534162,-0.94284446121751));
#52302=DIRECTION('center_axis',(0.,-0.333233134534162,0.94284446121751));
#52303=DIRECTION('ref_axis',(0.,-0.94284446121751,-0.333233134534162));
#52304=DIRECTION('center_axis',(0.,0.333233134534162,-0.94284446121751));
#52305=DIRECTION('ref_axis',(0.,0.94284446121751,0.333233134534162));
#52306=DIRECTION('',(0.,-0.333233134534162,0.94284446121751));
#52307=DIRECTION('center_axis',(0.,-0.333233134534162,0.94284446121751));
#52308=DIRECTION('ref_axis',(0.,-0.94284446121751,-0.333233134534162));
#52309=DIRECTION('',(0.,0.333233134534162,-0.94284446121751));
#52310=DIRECTION('center_axis',(0.,-0.333233134534162,0.94284446121751));
#52311=DIRECTION('ref_axis',(0.,-0.94284446121751,-0.333233134534162));
#52312=DIRECTION('center_axis',(0.,0.333233134534162,-0.94284446121751));
#52313=DIRECTION('ref_axis',(0.,0.94284446121751,0.333233134534162));
#52314=DIRECTION('',(0.,-0.333233134534162,0.94284446121751));
#52315=DIRECTION('center_axis',(0.,-0.333233134534162,0.94284446121751));
#52316=DIRECTION('ref_axis',(0.,-0.94284446121751,-0.333233134534161));
#52317=DIRECTION('center_axis',(0.,0.333233134534159,-0.942844461217511));
#52318=DIRECTION('ref_axis',(0.,-0.942844461217511,-0.333233134534159));
#52319=DIRECTION('',(0.,0.333233134534162,-0.94284446121751));
#52320=DIRECTION('center_axis',(0.,0.333233134534162,-0.94284446121751));
#52321=DIRECTION('ref_axis',(0.,-0.94284446121751,-0.333233134534162));
#52322=DIRECTION('center_axis',(0.,-0.333233134534162,0.94284446121751));
#52323=DIRECTION('ref_axis',(0.,-0.94284446121751,-0.333233134534162));
#52324=DIRECTION('center_axis',(0.,0.333233134534162,-0.94284446121751));
#52325=DIRECTION('ref_axis',(0.,0.94284446121751,0.333233134534162));
#52326=DIRECTION('',(0.,-0.333233134534162,0.94284446121751));
#52327=DIRECTION('center_axis',(0.,0.333233134534159,-0.942844461217511));
#52328=DIRECTION('ref_axis',(0.,-0.942844461217511,-0.333233134534159));
#52329=DIRECTION('center_axis',(0.,-0.333233134534162,0.94284446121751));
#52330=DIRECTION('ref_axis',(0.,-0.94284446121751,-0.333233134534162));
#52331=DIRECTION('center_axis',(0.,0.333233134534159,-0.942844461217511));
#52332=DIRECTION('ref_axis',(0.,-0.942844461217511,-0.333233134534159));
#52333=DIRECTION('',(0.,0.333233134534162,-0.94284446121751));
#52334=DIRECTION('center_axis',(0.,0.333233134534162,-0.94284446121751));
#52335=DIRECTION('ref_axis',(0.,-0.94284446121751,-0.333233134534162));
#52336=DIRECTION('center_axis',(0.,-0.333233134534162,0.94284446121751));
#52337=DIRECTION('ref_axis',(0.,-0.94284446121751,-0.333233134534162));
#52338=DIRECTION('center_axis',(0.,0.333233134534162,-0.94284446121751));
#52339=DIRECTION('ref_axis',(0.,0.94284446121751,0.333233134534162));
#52340=DIRECTION('',(0.,-0.333233134534162,0.94284446121751));
#52341=DIRECTION('center_axis',(0.,0.333233134534159,-0.942844461217511));
#52342=DIRECTION('ref_axis',(0.,-0.942844461217511,-0.333233134534159));
#52343=DIRECTION('center_axis',(0.,-0.333233134534162,0.94284446121751));
#52344=DIRECTION('ref_axis',(0.,-0.94284446121751,-0.333233134534162));
#52345=DIRECTION('center_axis',(0.,0.333233134534159,-0.942844461217511));
#52346=DIRECTION('ref_axis',(0.,-0.942844461217511,-0.333233134534159));
#52347=DIRECTION('',(0.,0.333233134534162,-0.94284446121751));
#52348=DIRECTION('center_axis',(0.,0.333233134534162,-0.94284446121751));
#52349=DIRECTION('ref_axis',(0.,-0.94284446121751,-0.333233134534162));
#52350=DIRECTION('center_axis',(0.,-0.333233134534162,0.94284446121751));
#52351=DIRECTION('ref_axis',(0.,-0.94284446121751,-0.333233134534162));
#52352=DIRECTION('center_axis',(0.,0.333233134534162,-0.94284446121751));
#52353=DIRECTION('ref_axis',(0.,0.94284446121751,0.333233134534162));
#52354=DIRECTION('',(0.,-0.333233134534162,0.94284446121751));
#52355=DIRECTION('center_axis',(0.,0.333233134534159,-0.942844461217511));
#52356=DIRECTION('ref_axis',(0.,-0.942844461217511,-0.333233134534159));
#52357=DIRECTION('center_axis',(0.,-0.333233134534162,0.94284446121751));
#52358=DIRECTION('ref_axis',(0.,-0.94284446121751,-0.333233134534162));
#52359=DIRECTION('center_axis',(0.,0.333233134534159,-0.942844461217511));
#52360=DIRECTION('ref_axis',(0.,-0.942844461217511,-0.333233134534159));
#52361=DIRECTION('',(0.,0.333233134534162,-0.94284446121751));
#52362=DIRECTION('center_axis',(0.,0.333233134534162,-0.94284446121751));
#52363=DIRECTION('ref_axis',(0.,-0.94284446121751,-0.333233134534162));
#52364=DIRECTION('center_axis',(0.,-0.333233134534162,0.94284446121751));
#52365=DIRECTION('ref_axis',(0.,-0.94284446121751,-0.333233134534162));
#52366=DIRECTION('center_axis',(0.,0.333233134534162,-0.94284446121751));
#52367=DIRECTION('ref_axis',(0.,0.94284446121751,0.333233134534162));
#52368=DIRECTION('',(0.,-0.333233134534162,0.94284446121751));
#52369=DIRECTION('center_axis',(0.,0.333233134534159,-0.942844461217511));
#52370=DIRECTION('ref_axis',(0.,-0.942844461217511,-0.333233134534159));
#52371=DIRECTION('center_axis',(0.,-0.333233134534162,0.94284446121751));
#52372=DIRECTION('ref_axis',(0.,-0.94284446121751,-0.333233134534162));
#52373=DIRECTION('center_axis',(0.,0.333233134534159,-0.942844461217511));
#52374=DIRECTION('ref_axis',(0.,-0.942844461217511,-0.333233134534159));
#52375=DIRECTION('',(0.,0.333233134534162,-0.94284446121751));
#52376=DIRECTION('center_axis',(0.,0.333233134534162,-0.94284446121751));
#52377=DIRECTION('ref_axis',(0.,-0.94284446121751,-0.333233134534162));
#52378=DIRECTION('center_axis',(0.,-0.333233134534162,0.94284446121751));
#52379=DIRECTION('ref_axis',(0.,-0.94284446121751,-0.333233134534162));
#52380=DIRECTION('center_axis',(0.,0.333233134534162,-0.94284446121751));
#52381=DIRECTION('ref_axis',(0.,0.94284446121751,0.333233134534162));
#52382=DIRECTION('',(0.,-0.333233134534162,0.94284446121751));
#52383=DIRECTION('center_axis',(0.,0.333233134534159,-0.942844461217511));
#52384=DIRECTION('ref_axis',(0.,-0.942844461217511,-0.333233134534159));
#52385=DIRECTION('center_axis',(0.,-0.333233134534162,0.94284446121751));
#52386=DIRECTION('ref_axis',(0.,-0.94284446121751,-0.333233134534162));
#52387=DIRECTION('center_axis',(0.,0.333233134534159,-0.942844461217511));
#52388=DIRECTION('ref_axis',(0.,-0.942844461217511,-0.333233134534159));
#52389=DIRECTION('',(0.,0.333233134534162,-0.94284446121751));
#52390=DIRECTION('center_axis',(0.,0.333233134534162,-0.94284446121751));
#52391=DIRECTION('ref_axis',(0.,-0.94284446121751,-0.333233134534162));
#52392=DIRECTION('center_axis',(0.,-0.333233134534162,0.94284446121751));
#52393=DIRECTION('ref_axis',(0.,-0.94284446121751,-0.333233134534162));
#52394=DIRECTION('center_axis',(0.,0.333233134534162,-0.94284446121751));
#52395=DIRECTION('ref_axis',(0.,0.94284446121751,0.333233134534162));
#52396=DIRECTION('',(0.,-0.333233134534162,0.94284446121751));
#52397=DIRECTION('center_axis',(0.,0.333233134534159,-0.942844461217511));
#52398=DIRECTION('ref_axis',(0.,-0.942844461217511,-0.333233134534159));
#52399=DIRECTION('center_axis',(0.,-0.333233134534162,0.94284446121751));
#52400=DIRECTION('ref_axis',(0.,-0.94284446121751,-0.333233134534162));
#52401=DIRECTION('center_axis',(0.,0.333233134534159,-0.942844461217511));
#52402=DIRECTION('ref_axis',(0.,-0.942844461217511,-0.333233134534159));
#52403=DIRECTION('',(0.,0.333233134534162,-0.94284446121751));
#52404=DIRECTION('center_axis',(0.,0.333233134534162,-0.94284446121751));
#52405=DIRECTION('ref_axis',(0.,-0.94284446121751,-0.333233134534162));
#52406=DIRECTION('center_axis',(0.,-0.333233134534162,0.94284446121751));
#52407=DIRECTION('ref_axis',(0.,-0.94284446121751,-0.333233134534162));
#52408=DIRECTION('center_axis',(0.,0.333233134534162,-0.94284446121751));
#52409=DIRECTION('ref_axis',(0.,0.94284446121751,0.333233134534162));
#52410=DIRECTION('',(0.,-0.333233134534162,0.94284446121751));
#52411=DIRECTION('center_axis',(0.,0.333233134534159,-0.942844461217511));
#52412=DIRECTION('ref_axis',(0.,-0.942844461217511,-0.333233134534159));
#52413=DIRECTION('center_axis',(0.,-0.333233134534162,0.94284446121751));
#52414=DIRECTION('ref_axis',(0.,-0.94284446121751,-0.333233134534162));
#52415=DIRECTION('center_axis',(0.,0.333233134534159,-0.942844461217511));
#52416=DIRECTION('ref_axis',(0.,-0.942844461217511,-0.333233134534159));
#52417=DIRECTION('',(0.,0.333233134534162,-0.94284446121751));
#52418=DIRECTION('center_axis',(0.,0.333233134534162,-0.94284446121751));
#52419=DIRECTION('ref_axis',(0.,-0.94284446121751,-0.333233134534162));
#52420=DIRECTION('center_axis',(0.,-0.333233134534162,0.94284446121751));
#52421=DIRECTION('ref_axis',(0.,-0.94284446121751,-0.333233134534162));
#52422=DIRECTION('center_axis',(0.,0.333233134534162,-0.94284446121751));
#52423=DIRECTION('ref_axis',(0.,0.94284446121751,0.333233134534162));
#52424=DIRECTION('',(0.,-0.333233134534162,0.94284446121751));
#52425=DIRECTION('center_axis',(0.,0.333233134534159,-0.942844461217511));
#52426=DIRECTION('ref_axis',(0.,-0.942844461217511,-0.333233134534159));
#52427=DIRECTION('center_axis',(0.,-0.333233134534162,0.94284446121751));
#52428=DIRECTION('ref_axis',(0.,-0.94284446121751,-0.333233134534162));
#52429=DIRECTION('center_axis',(0.,0.333233134534159,-0.942844461217511));
#52430=DIRECTION('ref_axis',(0.,-0.942844461217511,-0.333233134534159));
#52431=DIRECTION('',(0.,0.333233134534162,-0.94284446121751));
#52432=DIRECTION('center_axis',(0.,-0.333233134534162,0.94284446121751));
#52433=DIRECTION('ref_axis',(0.,-0.94284446121751,-0.333233134534162));
#52434=DIRECTION('center_axis',(0.,-0.333233134534162,0.94284446121751));
#52435=DIRECTION('ref_axis',(0.,-0.94284446121751,-0.333233134534162));
#52436=DIRECTION('center_axis',(0.,0.333233134534162,-0.94284446121751));
#52437=DIRECTION('ref_axis',(0.,0.94284446121751,0.333233134534162));
#52438=DIRECTION('',(0.,-0.333233134534162,0.94284446121751));
#52439=DIRECTION('center_axis',(0.,0.333233134534159,-0.942844461217511));
#52440=DIRECTION('ref_axis',(0.,-0.942844461217511,-0.333233134534159));
#52441=DIRECTION('center_axis',(0.,-0.333233134534162,0.94284446121751));
#52442=DIRECTION('ref_axis',(0.,-0.94284446121751,-0.333233134534161));
#52443=DIRECTION('center_axis',(0.,0.333233134534159,-0.942844461217511));
#52444=DIRECTION('ref_axis',(0.,-0.942844461217511,-0.333233134534159));
#52445=DIRECTION('',(0.,0.333233134534162,-0.94284446121751));
#52446=DIRECTION('center_axis',(0.,0.333233134534162,-0.94284446121751));
#52447=DIRECTION('ref_axis',(0.,-0.94284446121751,-0.333233134534162));
#52448=DIRECTION('center_axis',(0.,-0.333233134534162,0.94284446121751));
#52449=DIRECTION('ref_axis',(0.,-0.94284446121751,-0.333233134534162));
#52450=DIRECTION('center_axis',(0.,0.333233134534162,-0.94284446121751));
#52451=DIRECTION('ref_axis',(0.,0.94284446121751,0.333233134534162));
#52452=DIRECTION('',(0.,-0.333233134534162,0.94284446121751));
#52453=DIRECTION('center_axis',(0.,0.333233134534159,-0.942844461217511));
#52454=DIRECTION('ref_axis',(0.,-0.942844461217511,-0.333233134534159));
#52455=DIRECTION('center_axis',(0.,-0.333233134534162,0.94284446121751));
#52456=DIRECTION('ref_axis',(0.,-0.94284446121751,-0.333233134534162));
#52457=DIRECTION('center_axis',(0.,0.333233134534159,-0.942844461217511));
#52458=DIRECTION('ref_axis',(0.,-0.942844461217511,-0.333233134534159));
#52459=DIRECTION('',(0.,0.333233134534162,-0.94284446121751));
#52460=DIRECTION('center_axis',(0.,0.333233134534162,-0.94284446121751));
#52461=DIRECTION('ref_axis',(0.,-0.94284446121751,-0.333233134534162));
#52462=DIRECTION('center_axis',(0.,-0.333233134534162,0.94284446121751));
#52463=DIRECTION('ref_axis',(0.,-0.94284446121751,-0.333233134534162));
#52464=DIRECTION('center_axis',(0.,0.333233134534162,-0.94284446121751));
#52465=DIRECTION('ref_axis',(0.,0.94284446121751,0.333233134534162));
#52466=DIRECTION('',(0.,-0.333233134534162,0.94284446121751));
#52467=DIRECTION('center_axis',(0.,0.333233134534159,-0.942844461217511));
#52468=DIRECTION('ref_axis',(0.,-0.942844461217511,-0.333233134534159));
#52469=DIRECTION('center_axis',(0.,-0.333233134534162,0.94284446121751));
#52470=DIRECTION('ref_axis',(0.,-0.94284446121751,-0.333233134534162));
#52471=DIRECTION('center_axis',(0.,0.333233134534159,-0.942844461217511));
#52472=DIRECTION('ref_axis',(0.,-0.942844461217511,-0.333233134534159));
#52473=DIRECTION('',(0.,0.333233134534162,-0.94284446121751));
#52474=DIRECTION('center_axis',(0.,0.333233134534162,-0.94284446121751));
#52475=DIRECTION('ref_axis',(0.,-0.94284446121751,-0.333233134534162));
#52476=DIRECTION('center_axis',(0.,-0.333233134534162,0.94284446121751));
#52477=DIRECTION('ref_axis',(0.,-0.94284446121751,-0.333233134534162));
#52478=DIRECTION('center_axis',(0.,0.333233134534162,-0.94284446121751));
#52479=DIRECTION('ref_axis',(0.,0.94284446121751,0.333233134534162));
#52480=DIRECTION('',(0.,-0.333233134534162,0.94284446121751));
#52481=DIRECTION('center_axis',(0.,0.333233134534159,-0.942844461217511));
#52482=DIRECTION('ref_axis',(0.,-0.942844461217511,-0.333233134534159));
#52483=DIRECTION('center_axis',(0.,-0.333233134534162,0.94284446121751));
#52484=DIRECTION('ref_axis',(0.,-0.94284446121751,-0.333233134534162));
#52485=DIRECTION('center_axis',(0.,0.333233134534159,-0.942844461217511));
#52486=DIRECTION('ref_axis',(0.,-0.942844461217511,-0.333233134534159));
#52487=DIRECTION('',(0.,0.333233134534162,-0.94284446121751));
#52488=DIRECTION('center_axis',(0.,0.333233134534162,-0.94284446121751));
#52489=DIRECTION('ref_axis',(0.,-0.94284446121751,-0.333233134534162));
#52490=DIRECTION('center_axis',(0.,-0.333233134534162,0.94284446121751));
#52491=DIRECTION('ref_axis',(0.,-0.94284446121751,-0.333233134534162));
#52492=DIRECTION('center_axis',(0.,0.333233134534162,-0.94284446121751));
#52493=DIRECTION('ref_axis',(0.,0.94284446121751,0.333233134534162));
#52494=DIRECTION('',(0.,-0.333233134534162,0.94284446121751));
#52495=DIRECTION('center_axis',(0.,0.333233134534159,-0.942844461217511));
#52496=DIRECTION('ref_axis',(0.,-0.942844461217511,-0.333233134534159));
#52497=DIRECTION('center_axis',(0.,-0.333233134534162,0.94284446121751));
#52498=DIRECTION('ref_axis',(0.,-0.94284446121751,-0.333233134534162));
#52499=DIRECTION('center_axis',(0.,0.333233134534159,-0.942844461217511));
#52500=DIRECTION('ref_axis',(0.,-0.942844461217511,-0.333233134534159));
#52501=DIRECTION('',(0.,0.333233134534162,-0.94284446121751));
#52502=DIRECTION('center_axis',(0.,0.333233134534162,-0.94284446121751));
#52503=DIRECTION('ref_axis',(0.,-0.94284446121751,-0.333233134534162));
#52504=DIRECTION('center_axis',(0.,-0.333233134534162,0.94284446121751));
#52505=DIRECTION('ref_axis',(0.,-0.94284446121751,-0.333233134534162));
#52506=DIRECTION('center_axis',(0.,0.333233134534162,-0.94284446121751));
#52507=DIRECTION('ref_axis',(0.,0.94284446121751,0.333233134534162));
#52508=DIRECTION('',(0.,-0.333233134534162,0.94284446121751));
#52509=DIRECTION('center_axis',(0.,0.333233134534159,-0.942844461217511));
#52510=DIRECTION('ref_axis',(0.,-0.942844461217511,-0.333233134534159));
#52511=DIRECTION('center_axis',(0.,-0.333233134534162,0.94284446121751));
#52512=DIRECTION('ref_axis',(0.,-0.94284446121751,-0.333233134534162));
#52513=DIRECTION('center_axis',(0.,0.333233134534159,-0.942844461217511));
#52514=DIRECTION('ref_axis',(0.,-0.942844461217511,-0.333233134534159));
#52515=DIRECTION('',(0.,0.333233134534162,-0.94284446121751));
#52516=DIRECTION('center_axis',(0.,0.333233134534162,-0.94284446121751));
#52517=DIRECTION('ref_axis',(0.,-0.94284446121751,-0.333233134534162));
#52518=DIRECTION('center_axis',(0.,-0.333233134534162,0.94284446121751));
#52519=DIRECTION('ref_axis',(0.,-0.94284446121751,-0.333233134534162));
#52520=DIRECTION('center_axis',(0.,0.333233134534162,-0.94284446121751));
#52521=DIRECTION('ref_axis',(0.,0.94284446121751,0.333233134534162));
#52522=DIRECTION('',(0.,-0.333233134534162,0.94284446121751));
#52523=DIRECTION('center_axis',(0.,0.333233134534159,-0.942844461217511));
#52524=DIRECTION('ref_axis',(0.,-0.942844461217511,-0.333233134534159));
#52525=DIRECTION('center_axis',(0.,-0.333233134534162,0.94284446121751));
#52526=DIRECTION('ref_axis',(0.,-0.94284446121751,-0.333233134534162));
#52527=DIRECTION('center_axis',(0.,0.333233134534159,-0.942844461217511));
#52528=DIRECTION('ref_axis',(0.,-0.942844461217511,-0.333233134534159));
#52529=DIRECTION('',(0.,0.333233134534162,-0.94284446121751));
#52530=DIRECTION('center_axis',(0.,0.333233134534162,-0.94284446121751));
#52531=DIRECTION('ref_axis',(0.,-0.94284446121751,-0.333233134534162));
#52532=DIRECTION('center_axis',(0.,-0.333233134534162,0.94284446121751));
#52533=DIRECTION('ref_axis',(0.,-0.94284446121751,-0.333233134534162));
#52534=DIRECTION('center_axis',(0.,0.333233134534162,-0.94284446121751));
#52535=DIRECTION('ref_axis',(0.,0.94284446121751,0.333233134534162));
#52536=DIRECTION('',(0.,-0.333233134534162,0.94284446121751));
#52537=DIRECTION('center_axis',(0.,0.333233134534159,-0.942844461217511));
#52538=DIRECTION('ref_axis',(0.,-0.942844461217511,-0.333233134534159));
#52539=DIRECTION('center_axis',(0.,-0.333233134534162,0.94284446121751));
#52540=DIRECTION('ref_axis',(0.,-0.94284446121751,-0.333233134534162));
#52541=DIRECTION('center_axis',(0.,0.333233134534159,-0.942844461217511));
#52542=DIRECTION('ref_axis',(0.,-0.942844461217511,-0.333233134534159));
#52543=DIRECTION('',(0.,0.333233134534162,-0.94284446121751));
#52544=DIRECTION('center_axis',(0.,0.333233134534162,-0.94284446121751));
#52545=DIRECTION('ref_axis',(0.,-0.94284446121751,-0.333233134534162));
#52546=DIRECTION('center_axis',(0.,-0.333233134534162,0.94284446121751));
#52547=DIRECTION('ref_axis',(0.,-0.94284446121751,-0.333233134534162));
#52548=DIRECTION('center_axis',(0.,0.333233134534162,-0.94284446121751));
#52549=DIRECTION('ref_axis',(0.,0.94284446121751,0.333233134534162));
#52550=DIRECTION('',(0.,-0.333233134534162,0.94284446121751));
#52551=DIRECTION('center_axis',(0.,0.333233134534159,-0.942844461217511));
#52552=DIRECTION('ref_axis',(0.,-0.942844461217511,-0.333233134534159));
#52553=DIRECTION('center_axis',(0.,-0.333233134534162,0.94284446121751));
#52554=DIRECTION('ref_axis',(0.,-0.94284446121751,-0.333233134534162));
#52555=DIRECTION('center_axis',(0.,0.333233134534159,-0.942844461217511));
#52556=DIRECTION('ref_axis',(0.,-0.942844461217511,-0.333233134534159));
#52557=DIRECTION('',(0.,0.333233134534162,-0.94284446121751));
#52558=DIRECTION('center_axis',(0.,-0.333233134534162,0.94284446121751));
#52559=DIRECTION('ref_axis',(0.,-0.94284446121751,-0.333233134534162));
#52560=DIRECTION('center_axis',(0.,-0.333233134534162,0.94284446121751));
#52561=DIRECTION('ref_axis',(0.,-0.94284446121751,-0.333233134534162));
#52562=DIRECTION('center_axis',(0.,0.333233134534162,-0.94284446121751));
#52563=DIRECTION('ref_axis',(0.,0.94284446121751,0.333233134534162));
#52564=DIRECTION('',(0.,-0.333233134534162,0.94284446121751));
#52565=DIRECTION('center_axis',(0.,0.333233134534159,-0.942844461217511));
#52566=DIRECTION('ref_axis',(0.,-0.942844461217511,-0.333233134534159));
#52567=DIRECTION('center_axis',(0.,-0.333233134534162,0.94284446121751));
#52568=DIRECTION('ref_axis',(0.,-0.94284446121751,-0.333233134534161));
#52569=DIRECTION('center_axis',(0.,0.333233134534159,-0.942844461217511));
#52570=DIRECTION('ref_axis',(0.,-0.942844461217511,-0.333233134534159));
#52571=DIRECTION('',(0.,0.333233134534162,-0.94284446121751));
#52572=DIRECTION('center_axis',(0.,0.333233134534162,-0.94284446121751));
#52573=DIRECTION('ref_axis',(0.,-0.94284446121751,-0.333233134534162));
#52574=DIRECTION('center_axis',(0.,-0.333233134534162,0.94284446121751));
#52575=DIRECTION('ref_axis',(0.,-0.94284446121751,-0.333233134534162));
#52576=DIRECTION('center_axis',(0.,0.333233134534162,-0.94284446121751));
#52577=DIRECTION('ref_axis',(0.,0.94284446121751,0.333233134534162));
#52578=DIRECTION('',(0.,-0.333233134534162,0.94284446121751));
#52579=DIRECTION('center_axis',(0.,0.333233134534159,-0.942844461217511));
#52580=DIRECTION('ref_axis',(0.,-0.942844461217511,-0.333233134534159));
#52581=DIRECTION('center_axis',(0.,-0.333233134534162,0.94284446121751));
#52582=DIRECTION('ref_axis',(0.,-0.94284446121751,-0.333233134534162));
#52583=DIRECTION('center_axis',(0.,0.333233134534159,-0.942844461217511));
#52584=DIRECTION('ref_axis',(0.,-0.942844461217511,-0.333233134534159));
#52585=DIRECTION('',(0.,0.333233134534162,-0.94284446121751));
#52586=DIRECTION('center_axis',(0.,0.333233134534162,-0.94284446121751));
#52587=DIRECTION('ref_axis',(0.,-0.94284446121751,-0.333233134534162));
#52588=DIRECTION('center_axis',(0.,-0.333233134534162,0.94284446121751));
#52589=DIRECTION('ref_axis',(0.,-0.94284446121751,-0.333233134534162));
#52590=DIRECTION('center_axis',(0.,0.333233134534162,-0.94284446121751));
#52591=DIRECTION('ref_axis',(0.,0.94284446121751,0.333233134534162));
#52592=DIRECTION('',(0.,-0.333233134534162,0.94284446121751));
#52593=DIRECTION('center_axis',(0.,0.333233134534159,-0.942844461217511));
#52594=DIRECTION('ref_axis',(0.,-0.942844461217511,-0.333233134534159));
#52595=DIRECTION('center_axis',(0.,-0.333233134534162,0.94284446121751));
#52596=DIRECTION('ref_axis',(0.,-0.94284446121751,-0.333233134534162));
#52597=DIRECTION('center_axis',(0.,0.333233134534159,-0.942844461217511));
#52598=DIRECTION('ref_axis',(0.,-0.942844461217511,-0.333233134534159));
#52599=DIRECTION('',(0.,0.333233134534162,-0.94284446121751));
#52600=DIRECTION('center_axis',(0.,0.333233134534162,-0.94284446121751));
#52601=DIRECTION('ref_axis',(0.,-0.94284446121751,-0.333233134534162));
#52602=DIRECTION('center_axis',(0.,-0.333233134534162,0.94284446121751));
#52603=DIRECTION('ref_axis',(0.,-0.94284446121751,-0.333233134534162));
#52604=DIRECTION('center_axis',(0.,0.333233134534162,-0.94284446121751));
#52605=DIRECTION('ref_axis',(0.,0.94284446121751,0.333233134534162));
#52606=DIRECTION('',(0.,-0.333233134534162,0.94284446121751));
#52607=DIRECTION('center_axis',(0.,0.333233134534159,-0.942844461217511));
#52608=DIRECTION('ref_axis',(0.,-0.942844461217511,-0.333233134534159));
#52609=DIRECTION('center_axis',(0.,-0.333233134534162,0.94284446121751));
#52610=DIRECTION('ref_axis',(0.,-0.94284446121751,-0.333233134534162));
#52611=DIRECTION('center_axis',(0.,0.333233134534159,-0.942844461217511));
#52612=DIRECTION('ref_axis',(0.,-0.942844461217511,-0.333233134534159));
#52613=DIRECTION('',(0.,0.333233134534162,-0.94284446121751));
#52614=DIRECTION('center_axis',(0.,0.333233134534162,-0.94284446121751));
#52615=DIRECTION('ref_axis',(0.,-0.94284446121751,-0.333233134534162));
#52616=DIRECTION('center_axis',(0.,-0.333233134534162,0.94284446121751));
#52617=DIRECTION('ref_axis',(0.,-0.94284446121751,-0.333233134534162));
#52618=DIRECTION('center_axis',(0.,0.333233134534162,-0.94284446121751));
#52619=DIRECTION('ref_axis',(0.,0.94284446121751,0.333233134534162));
#52620=DIRECTION('',(0.,-0.333233134534162,0.94284446121751));
#52621=DIRECTION('center_axis',(0.,0.333233134534159,-0.942844461217511));
#52622=DIRECTION('ref_axis',(0.,-0.942844461217511,-0.333233134534159));
#52623=DIRECTION('center_axis',(0.,-0.333233134534162,0.94284446121751));
#52624=DIRECTION('ref_axis',(0.,-0.94284446121751,-0.333233134534162));
#52625=DIRECTION('center_axis',(0.,0.333233134534159,-0.942844461217511));
#52626=DIRECTION('ref_axis',(0.,-0.942844461217511,-0.333233134534159));
#52627=DIRECTION('',(0.,0.333233134534162,-0.94284446121751));
#52628=DIRECTION('center_axis',(0.,0.333233134534162,-0.94284446121751));
#52629=DIRECTION('ref_axis',(0.,-0.94284446121751,-0.333233134534162));
#52630=DIRECTION('center_axis',(0.,-0.333233134534162,0.94284446121751));
#52631=DIRECTION('ref_axis',(0.,-0.94284446121751,-0.333233134534162));
#52632=DIRECTION('center_axis',(0.,0.333233134534162,-0.94284446121751));
#52633=DIRECTION('ref_axis',(0.,0.94284446121751,0.333233134534162));
#52634=DIRECTION('',(0.,-0.333233134534162,0.94284446121751));
#52635=DIRECTION('center_axis',(0.,0.333233134534159,-0.942844461217511));
#52636=DIRECTION('ref_axis',(0.,-0.942844461217511,-0.333233134534159));
#52637=DIRECTION('center_axis',(0.,-0.333233134534162,0.94284446121751));
#52638=DIRECTION('ref_axis',(0.,-0.94284446121751,-0.333233134534162));
#52639=DIRECTION('center_axis',(0.,0.333233134534159,-0.942844461217511));
#52640=DIRECTION('ref_axis',(0.,-0.942844461217511,-0.333233134534159));
#52641=DIRECTION('',(0.,0.333233134534162,-0.94284446121751));
#52642=DIRECTION('center_axis',(0.,0.333233134534162,-0.94284446121751));
#52643=DIRECTION('ref_axis',(0.,-0.94284446121751,-0.333233134534162));
#52644=DIRECTION('center_axis',(0.,-0.333233134534162,0.94284446121751));
#52645=DIRECTION('ref_axis',(0.,-0.94284446121751,-0.333233134534162));
#52646=DIRECTION('center_axis',(0.,0.333233134534162,-0.94284446121751));
#52647=DIRECTION('ref_axis',(0.,0.94284446121751,0.333233134534162));
#52648=DIRECTION('',(0.,-0.333233134534162,0.94284446121751));
#52649=DIRECTION('center_axis',(0.,0.333233134534159,-0.942844461217511));
#52650=DIRECTION('ref_axis',(0.,-0.942844461217511,-0.333233134534159));
#52651=DIRECTION('center_axis',(0.,-0.333233134534162,0.94284446121751));
#52652=DIRECTION('ref_axis',(0.,-0.94284446121751,-0.333233134534162));
#52653=DIRECTION('center_axis',(0.,0.333233134534159,-0.942844461217511));
#52654=DIRECTION('ref_axis',(0.,-0.942844461217511,-0.333233134534159));
#52655=DIRECTION('',(0.,0.333233134534162,-0.94284446121751));
#52656=DIRECTION('center_axis',(0.,0.333233134534162,-0.94284446121751));
#52657=DIRECTION('ref_axis',(0.,-0.94284446121751,-0.333233134534162));
#52658=DIRECTION('center_axis',(0.,-0.333233134534162,0.94284446121751));
#52659=DIRECTION('ref_axis',(0.,-0.94284446121751,-0.333233134534162));
#52660=DIRECTION('center_axis',(0.,0.333233134534162,-0.94284446121751));
#52661=DIRECTION('ref_axis',(0.,0.94284446121751,0.333233134534162));
#52662=DIRECTION('',(0.,-0.333233134534162,0.94284446121751));
#52663=DIRECTION('center_axis',(0.,0.333233134534159,-0.942844461217511));
#52664=DIRECTION('ref_axis',(0.,-0.942844461217511,-0.333233134534159));
#52665=DIRECTION('center_axis',(0.,-0.333233134534162,0.94284446121751));
#52666=DIRECTION('ref_axis',(0.,-0.94284446121751,-0.333233134534162));
#52667=DIRECTION('center_axis',(0.,0.333233134534159,-0.942844461217511));
#52668=DIRECTION('ref_axis',(0.,-0.942844461217511,-0.333233134534159));
#52669=DIRECTION('',(0.,0.333233134534162,-0.94284446121751));
#52670=DIRECTION('center_axis',(0.,-0.333233134534162,0.94284446121751));
#52671=DIRECTION('ref_axis',(0.,-0.94284446121751,-0.333233134534162));
#52672=DIRECTION('center_axis',(0.,-0.333233134534162,0.94284446121751));
#52673=DIRECTION('ref_axis',(0.,-0.94284446121751,-0.333233134534162));
#52674=DIRECTION('center_axis',(0.,0.333233134534162,-0.94284446121751));
#52675=DIRECTION('ref_axis',(0.,0.94284446121751,0.333233134534162));
#52676=DIRECTION('',(0.,-0.333233134534162,0.94284446121751));
#52677=DIRECTION('center_axis',(0.,0.333233134534159,-0.942844461217511));
#52678=DIRECTION('ref_axis',(0.,-0.942844461217511,-0.333233134534159));
#52679=DIRECTION('center_axis',(0.,-0.333233134534162,0.94284446121751));
#52680=DIRECTION('ref_axis',(0.,-0.94284446121751,-0.333233134534162));
#52681=DIRECTION('center_axis',(0.,0.333233134534159,-0.942844461217511));
#52682=DIRECTION('ref_axis',(0.,-0.942844461217511,-0.333233134534159));
#52683=DIRECTION('',(0.,0.333233134534162,-0.94284446121751));
#52684=DIRECTION('center_axis',(0.,0.333233134534162,-0.94284446121751));
#52685=DIRECTION('ref_axis',(0.,-0.94284446121751,-0.333233134534162));
#52686=DIRECTION('center_axis',(0.,-0.333233134534162,0.94284446121751));
#52687=DIRECTION('ref_axis',(0.,-0.94284446121751,-0.333233134534162));
#52688=DIRECTION('center_axis',(0.,0.333233134534162,-0.94284446121751));
#52689=DIRECTION('ref_axis',(0.,0.94284446121751,0.333233134534162));
#52690=DIRECTION('',(0.,-0.333233134534162,0.94284446121751));
#52691=DIRECTION('center_axis',(0.,0.333233134534159,-0.942844461217511));
#52692=DIRECTION('ref_axis',(0.,-0.942844461217511,-0.333233134534159));
#52693=DIRECTION('center_axis',(0.,-0.333233134534162,0.94284446121751));
#52694=DIRECTION('ref_axis',(0.,-0.94284446121751,-0.333233134534162));
#52695=DIRECTION('center_axis',(0.,0.333233134534159,-0.942844461217511));
#52696=DIRECTION('ref_axis',(0.,-0.942844461217511,-0.333233134534159));
#52697=DIRECTION('',(0.,0.333233134534162,-0.94284446121751));
#52698=DIRECTION('center_axis',(0.,0.333233134534162,-0.94284446121751));
#52699=DIRECTION('ref_axis',(0.,-0.94284446121751,-0.333233134534162));
#52700=DIRECTION('center_axis',(0.,-0.333233134534162,0.94284446121751));
#52701=DIRECTION('ref_axis',(0.,-0.94284446121751,-0.333233134534161));
#52702=DIRECTION('center_axis',(0.,0.333233134534162,-0.94284446121751));
#52703=DIRECTION('ref_axis',(0.,0.94284446121751,0.333233134534162));
#52704=DIRECTION('',(0.,-0.333233134534162,0.94284446121751));
#52705=DIRECTION('center_axis',(0.,0.333233134534159,-0.942844461217511));
#52706=DIRECTION('ref_axis',(0.,-0.942844461217511,-0.333233134534159));
#52707=DIRECTION('center_axis',(0.,-0.333233134534162,0.94284446121751));
#52708=DIRECTION('ref_axis',(0.,-0.94284446121751,-0.333233134534162));
#52709=DIRECTION('center_axis',(0.,0.333233134534159,-0.942844461217511));
#52710=DIRECTION('ref_axis',(0.,-0.942844461217511,-0.333233134534159));
#52711=DIRECTION('',(0.,0.333233134534162,-0.94284446121751));
#52712=DIRECTION('center_axis',(0.,0.333233134534162,-0.94284446121751));
#52713=DIRECTION('ref_axis',(0.,-0.94284446121751,-0.333233134534162));
#52714=DIRECTION('center_axis',(0.,-0.333233134534162,0.94284446121751));
#52715=DIRECTION('ref_axis',(0.,-0.94284446121751,-0.333233134534162));
#52716=DIRECTION('center_axis',(0.,0.333233134534162,-0.94284446121751));
#52717=DIRECTION('ref_axis',(0.,0.94284446121751,0.333233134534162));
#52718=DIRECTION('',(0.,-0.333233134534162,0.94284446121751));
#52719=DIRECTION('center_axis',(0.,0.333233134534159,-0.942844461217511));
#52720=DIRECTION('ref_axis',(0.,-0.942844461217511,-0.333233134534159));
#52721=DIRECTION('center_axis',(0.,-0.333233134534162,0.94284446121751));
#52722=DIRECTION('ref_axis',(0.,-0.94284446121751,-0.333233134534162));
#52723=DIRECTION('center_axis',(0.,0.333233134534159,-0.942844461217511));
#52724=DIRECTION('ref_axis',(0.,-0.942844461217511,-0.333233134534159));
#52725=DIRECTION('',(0.,0.333233134534162,-0.94284446121751));
#52726=DIRECTION('center_axis',(0.,0.333233134534162,-0.94284446121751));
#52727=DIRECTION('ref_axis',(0.,-0.94284446121751,-0.333233134534162));
#52728=DIRECTION('center_axis',(0.,-0.333233134534162,0.94284446121751));
#52729=DIRECTION('ref_axis',(0.,-0.94284446121751,-0.333233134534162));
#52730=DIRECTION('center_axis',(0.,0.333233134534162,-0.94284446121751));
#52731=DIRECTION('ref_axis',(0.,0.94284446121751,0.333233134534162));
#52732=DIRECTION('',(0.,-0.333233134534162,0.94284446121751));
#52733=DIRECTION('center_axis',(0.,0.333233134534159,-0.942844461217511));
#52734=DIRECTION('ref_axis',(0.,-0.942844461217511,-0.333233134534159));
#52735=DIRECTION('center_axis',(0.,-0.333233134534162,0.94284446121751));
#52736=DIRECTION('ref_axis',(0.,-0.94284446121751,-0.333233134534162));
#52737=DIRECTION('center_axis',(0.,0.333233134534159,-0.942844461217511));
#52738=DIRECTION('ref_axis',(0.,-0.942844461217511,-0.333233134534159));
#52739=DIRECTION('',(0.,0.333233134534161,-0.94284446121751));
#52740=DIRECTION('center_axis',(0.,0.333233134534162,-0.94284446121751));
#52741=DIRECTION('ref_axis',(0.,-0.94284446121751,-0.333233134534162));
#52742=DIRECTION('center_axis',(0.,-0.333233134534162,0.94284446121751));
#52743=DIRECTION('ref_axis',(0.,-0.94284446121751,-0.333233134534162));
#52744=DIRECTION('center_axis',(0.,0.333233134534162,-0.94284446121751));
#52745=DIRECTION('ref_axis',(0.,0.94284446121751,0.333233134534162));
#52746=DIRECTION('',(0.,-0.333233134534162,0.94284446121751));
#52747=DIRECTION('center_axis',(0.,0.333233134534159,-0.942844461217511));
#52748=DIRECTION('ref_axis',(0.,-0.942844461217511,-0.333233134534159));
#52749=DIRECTION('center_axis',(0.,-0.333233134534162,0.94284446121751));
#52750=DIRECTION('ref_axis',(0.,-0.94284446121751,-0.333233134534162));
#52751=DIRECTION('center_axis',(0.,0.333233134534159,-0.942844461217511));
#52752=DIRECTION('ref_axis',(0.,-0.942844461217511,-0.333233134534159));
#52753=DIRECTION('',(0.,0.333233134534162,-0.94284446121751));
#52754=DIRECTION('center_axis',(0.,0.333233134534162,-0.94284446121751));
#52755=DIRECTION('ref_axis',(0.,-0.94284446121751,-0.333233134534162));
#52756=DIRECTION('center_axis',(0.,-0.333233134534162,0.94284446121751));
#52757=DIRECTION('ref_axis',(0.,-0.94284446121751,-0.333233134534162));
#52758=DIRECTION('center_axis',(0.,0.333233134534162,-0.94284446121751));
#52759=DIRECTION('ref_axis',(0.,0.94284446121751,0.333233134534162));
#52760=DIRECTION('',(0.,-0.333233134534162,0.94284446121751));
#52761=DIRECTION('center_axis',(0.,0.333233134534159,-0.942844461217511));
#52762=DIRECTION('ref_axis',(0.,-0.942844461217511,-0.333233134534159));
#52763=DIRECTION('center_axis',(0.,-0.333233134534162,0.94284446121751));
#52764=DIRECTION('ref_axis',(0.,-0.94284446121751,-0.333233134534162));
#52765=DIRECTION('center_axis',(0.,0.333233134534159,-0.942844461217511));
#52766=DIRECTION('ref_axis',(0.,-0.942844461217511,-0.333233134534159));
#52767=DIRECTION('',(0.,0.333233134534162,-0.94284446121751));
#52768=DIRECTION('center_axis',(0.,0.333233134534162,-0.94284446121751));
#52769=DIRECTION('ref_axis',(0.,-0.94284446121751,-0.333233134534162));
#52770=DIRECTION('center_axis',(0.,-0.333233134534162,0.94284446121751));
#52771=DIRECTION('ref_axis',(0.,-0.94284446121751,-0.333233134534162));
#52772=DIRECTION('center_axis',(0.,0.333233134534162,-0.94284446121751));
#52773=DIRECTION('ref_axis',(0.,0.94284446121751,0.333233134534162));
#52774=DIRECTION('',(0.,-0.333233134534162,0.94284446121751));
#52775=DIRECTION('center_axis',(0.,0.333233134534159,-0.942844461217511));
#52776=DIRECTION('ref_axis',(0.,-0.942844461217511,-0.333233134534159));
#52777=DIRECTION('center_axis',(0.,-0.333233134534162,0.94284446121751));
#52778=DIRECTION('ref_axis',(0.,-0.94284446121751,-0.333233134534162));
#52779=DIRECTION('center_axis',(0.,0.333233134534159,-0.942844461217511));
#52780=DIRECTION('ref_axis',(0.,-0.942844461217511,-0.333233134534159));
#52781=DIRECTION('',(0.,0.333233134534162,-0.94284446121751));
#52782=DIRECTION('center_axis',(0.,0.333233134534162,-0.94284446121751));
#52783=DIRECTION('ref_axis',(0.,-0.94284446121751,-0.333233134534162));
#52784=DIRECTION('center_axis',(0.,-0.333233134534162,0.94284446121751));
#52785=DIRECTION('ref_axis',(0.,-0.94284446121751,-0.333233134534162));
#52786=DIRECTION('center_axis',(0.,0.333233134534162,-0.94284446121751));
#52787=DIRECTION('ref_axis',(0.,0.94284446121751,0.333233134534162));
#52788=DIRECTION('',(0.,-0.333233134534162,0.94284446121751));
#52789=DIRECTION('center_axis',(0.,0.333233134534159,-0.942844461217511));
#52790=DIRECTION('ref_axis',(0.,-0.942844461217511,-0.333233134534159));
#52791=DIRECTION('center_axis',(0.,-0.333233134534162,0.94284446121751));
#52792=DIRECTION('ref_axis',(0.,-0.94284446121751,-0.333233134534162));
#52793=DIRECTION('center_axis',(0.,0.333233134534159,-0.942844461217511));
#52794=DIRECTION('ref_axis',(0.,-0.942844461217511,-0.333233134534159));
#52795=DIRECTION('',(0.,0.333233134534162,-0.94284446121751));
#52796=DIRECTION('center_axis',(0.,-0.333233134534162,0.94284446121751));
#52797=DIRECTION('ref_axis',(0.,-0.94284446121751,-0.333233134534162));
#52798=DIRECTION('center_axis',(0.,-0.333233134534162,0.94284446121751));
#52799=DIRECTION('ref_axis',(0.,-0.94284446121751,-0.333233134534162));
#52800=DIRECTION('center_axis',(0.,0.333233134534162,-0.94284446121751));
#52801=DIRECTION('ref_axis',(0.,0.94284446121751,0.333233134534162));
#52802=DIRECTION('',(0.,-0.333233134534162,0.94284446121751));
#52803=DIRECTION('center_axis',(0.,0.333233134534159,-0.942844461217511));
#52804=DIRECTION('ref_axis',(0.,-0.942844461217511,-0.333233134534159));
#52805=DIRECTION('center_axis',(0.,-0.333233134534162,0.94284446121751));
#52806=DIRECTION('ref_axis',(0.,-0.94284446121751,-0.333233134534162));
#52807=DIRECTION('center_axis',(0.,0.333233134534159,-0.942844461217511));
#52808=DIRECTION('ref_axis',(0.,-0.942844461217511,-0.333233134534159));
#52809=DIRECTION('',(0.,0.333233134534162,-0.94284446121751));
#52810=DIRECTION('center_axis',(0.,0.333233134534162,-0.94284446121751));
#52811=DIRECTION('ref_axis',(0.,-0.94284446121751,-0.333233134534162));
#52812=DIRECTION('center_axis',(0.,-0.333233134534162,0.94284446121751));
#52813=DIRECTION('ref_axis',(0.,-0.94284446121751,-0.333233134534162));
#52814=DIRECTION('center_axis',(0.,0.333233134534162,-0.94284446121751));
#52815=DIRECTION('ref_axis',(0.,0.94284446121751,0.333233134534162));
#52816=DIRECTION('',(0.,-0.333233134534162,0.94284446121751));
#52817=DIRECTION('center_axis',(0.,0.333233134534159,-0.942844461217511));
#52818=DIRECTION('ref_axis',(0.,-0.942844461217511,-0.333233134534159));
#52819=DIRECTION('center_axis',(0.,-0.333233134534162,0.94284446121751));
#52820=DIRECTION('ref_axis',(0.,-0.94284446121751,-0.333233134534162));
#52821=DIRECTION('center_axis',(0.,0.333233134534159,-0.942844461217511));
#52822=DIRECTION('ref_axis',(0.,-0.942844461217511,-0.333233134534159));
#52823=DIRECTION('',(0.,0.333233134534162,-0.94284446121751));
#52824=DIRECTION('center_axis',(0.,0.333233134534162,-0.94284446121751));
#52825=DIRECTION('ref_axis',(0.,-0.94284446121751,-0.333233134534162));
#52826=DIRECTION('center_axis',(0.,-0.333233134534162,0.94284446121751));
#52827=DIRECTION('ref_axis',(0.,-0.94284446121751,-0.333233134534162));
#52828=DIRECTION('center_axis',(0.,0.333233134534162,-0.94284446121751));
#52829=DIRECTION('ref_axis',(0.,0.94284446121751,0.333233134534162));
#52830=DIRECTION('',(0.,-0.333233134534162,0.942844461217511));
#52831=DIRECTION('center_axis',(0.,0.333233134534159,-0.942844461217511));
#52832=DIRECTION('ref_axis',(0.,-0.942844461217511,-0.333233134534159));
#52833=DIRECTION('center_axis',(0.,-0.333233134534162,0.94284446121751));
#52834=DIRECTION('ref_axis',(0.,-0.94284446121751,-0.333233134534162));
#52835=DIRECTION('center_axis',(0.,0.333233134534159,-0.942844461217511));
#52836=DIRECTION('ref_axis',(0.,-0.942844461217511,-0.333233134534159));
#52837=DIRECTION('',(0.,0.333233134534162,-0.94284446121751));
#52838=DIRECTION('center_axis',(0.,0.333233134534162,-0.94284446121751));
#52839=DIRECTION('ref_axis',(0.,-0.94284446121751,-0.333233134534162));
#52840=DIRECTION('center_axis',(0.,-0.333233134534162,0.94284446121751));
#52841=DIRECTION('ref_axis',(0.,-0.94284446121751,-0.333233134534162));
#52842=DIRECTION('center_axis',(0.,0.333233134534162,-0.94284446121751));
#52843=DIRECTION('ref_axis',(0.,0.94284446121751,0.333233134534162));
#52844=DIRECTION('',(0.,-0.333233134534162,0.94284446121751));
#52845=DIRECTION('center_axis',(0.,0.333233134534159,-0.942844461217511));
#52846=DIRECTION('ref_axis',(0.,-0.942844461217511,-0.333233134534159));
#52847=DIRECTION('center_axis',(0.,-0.333233134534162,0.94284446121751));
#52848=DIRECTION('ref_axis',(0.,-0.94284446121751,-0.333233134534162));
#52849=DIRECTION('center_axis',(0.,0.333233134534159,-0.942844461217511));
#52850=DIRECTION('ref_axis',(0.,-0.942844461217511,-0.333233134534159));
#52851=DIRECTION('',(0.,0.333233134534162,-0.94284446121751));
#52852=DIRECTION('center_axis',(0.,0.333233134534162,-0.94284446121751));
#52853=DIRECTION('ref_axis',(0.,-0.94284446121751,-0.333233134534162));
#52854=DIRECTION('center_axis',(0.,-0.333233134534162,0.94284446121751));
#52855=DIRECTION('ref_axis',(0.,-0.94284446121751,-0.333233134534162));
#52856=DIRECTION('center_axis',(0.,0.333233134534162,-0.94284446121751));
#52857=DIRECTION('ref_axis',(0.,0.94284446121751,0.333233134534162));
#52858=DIRECTION('',(0.,-0.333233134534162,0.94284446121751));
#52859=DIRECTION('center_axis',(0.,0.333233134534159,-0.942844461217511));
#52860=DIRECTION('ref_axis',(0.,-0.942844461217511,-0.333233134534159));
#52861=DIRECTION('center_axis',(0.,-0.333233134534162,0.94284446121751));
#52862=DIRECTION('ref_axis',(0.,-0.94284446121751,-0.333233134534162));
#52863=DIRECTION('center_axis',(0.,0.333233134534159,-0.942844461217511));
#52864=DIRECTION('ref_axis',(0.,-0.942844461217511,-0.333233134534159));
#52865=DIRECTION('',(0.,0.333233134534162,-0.94284446121751));
#52866=DIRECTION('center_axis',(0.,0.333233134534162,-0.94284446121751));
#52867=DIRECTION('ref_axis',(0.,-0.94284446121751,-0.333233134534162));
#52868=DIRECTION('center_axis',(0.,-0.333233134534162,0.94284446121751));
#52869=DIRECTION('ref_axis',(0.,-0.94284446121751,-0.333233134534162));
#52870=DIRECTION('center_axis',(0.,0.333233134534162,-0.94284446121751));
#52871=DIRECTION('ref_axis',(0.,0.94284446121751,0.333233134534162));
#52872=DIRECTION('',(0.,-0.333233134534162,0.94284446121751));
#52873=DIRECTION('center_axis',(0.,0.333233134534159,-0.942844461217511));
#52874=DIRECTION('ref_axis',(0.,-0.942844461217511,-0.333233134534159));
#52875=DIRECTION('center_axis',(0.,-0.333233134534162,0.94284446121751));
#52876=DIRECTION('ref_axis',(0.,-0.94284446121751,-0.333233134534162));
#52877=DIRECTION('center_axis',(0.,0.333233134534159,-0.942844461217511));
#52878=DIRECTION('ref_axis',(0.,-0.942844461217511,-0.333233134534159));
#52879=DIRECTION('',(0.,0.333233134534162,-0.94284446121751));
#52880=DIRECTION('center_axis',(0.,0.333233134534162,-0.94284446121751));
#52881=DIRECTION('ref_axis',(0.,-0.94284446121751,-0.333233134534162));
#52882=DIRECTION('center_axis',(0.,-0.333233134534162,0.94284446121751));
#52883=DIRECTION('ref_axis',(0.,-0.94284446121751,-0.333233134534162));
#52884=DIRECTION('center_axis',(0.,0.333233134534162,-0.94284446121751));
#52885=DIRECTION('ref_axis',(0.,0.94284446121751,0.333233134534162));
#52886=DIRECTION('',(0.,-0.333233134534162,0.94284446121751));
#52887=DIRECTION('center_axis',(0.,0.333233134534159,-0.942844461217511));
#52888=DIRECTION('ref_axis',(0.,-0.942844461217511,-0.333233134534159));
#52889=DIRECTION('center_axis',(0.,-0.333233134534162,0.94284446121751));
#52890=DIRECTION('ref_axis',(0.,-0.94284446121751,-0.333233134534162));
#52891=DIRECTION('center_axis',(0.,0.333233134534159,-0.942844461217511));
#52892=DIRECTION('ref_axis',(0.,-0.942844461217511,-0.333233134534159));
#52893=DIRECTION('',(0.,0.333233134534162,-0.94284446121751));
#52894=DIRECTION('center_axis',(0.,0.333233134534162,-0.94284446121751));
#52895=DIRECTION('ref_axis',(0.,-0.94284446121751,-0.333233134534162));
#52896=DIRECTION('center_axis',(0.,-0.333233134534162,0.94284446121751));
#52897=DIRECTION('ref_axis',(0.,-0.94284446121751,-0.333233134534162));
#52898=DIRECTION('center_axis',(0.,0.333233134534162,-0.94284446121751));
#52899=DIRECTION('ref_axis',(0.,0.94284446121751,0.333233134534162));
#52900=DIRECTION('',(0.,-0.333233134534162,0.94284446121751));
#52901=DIRECTION('center_axis',(0.,0.333233134534159,-0.942844461217511));
#52902=DIRECTION('ref_axis',(0.,-0.942844461217511,-0.333233134534159));
#52903=DIRECTION('center_axis',(0.,-0.333233134534162,0.94284446121751));
#52904=DIRECTION('ref_axis',(0.,-0.94284446121751,-0.333233134534162));
#52905=DIRECTION('center_axis',(0.,0.333233134534159,-0.942844461217511));
#52906=DIRECTION('ref_axis',(0.,-0.942844461217511,-0.333233134534159));
#52907=DIRECTION('',(0.,0.333233134534162,-0.94284446121751));
#52908=DIRECTION('center_axis',(0.,0.333233134534162,-0.94284446121751));
#52909=DIRECTION('ref_axis',(0.,-0.94284446121751,-0.333233134534162));
#52910=DIRECTION('center_axis',(0.,-0.333233134534162,0.94284446121751));
#52911=DIRECTION('ref_axis',(0.,-0.94284446121751,-0.333233134534162));
#52912=DIRECTION('center_axis',(0.,0.333233134534162,-0.94284446121751));
#52913=DIRECTION('ref_axis',(0.,0.94284446121751,0.333233134534162));
#52914=DIRECTION('',(0.,-0.333233134534162,0.94284446121751));
#52915=DIRECTION('center_axis',(0.,0.333233134534159,-0.942844461217511));
#52916=DIRECTION('ref_axis',(0.,-0.942844461217511,-0.333233134534159));
#52917=DIRECTION('center_axis',(0.,-0.333233134534162,0.94284446121751));
#52918=DIRECTION('ref_axis',(0.,-0.94284446121751,-0.333233134534162));
#52919=DIRECTION('center_axis',(0.,0.333233134534159,-0.942844461217511));
#52920=DIRECTION('ref_axis',(0.,-0.942844461217511,-0.333233134534159));
#52921=DIRECTION('',(0.,0.333233134534162,-0.94284446121751));
#52922=DIRECTION('center_axis',(0.,-0.333233134534162,0.94284446121751));
#52923=DIRECTION('ref_axis',(0.,-0.94284446121751,-0.333233134534162));
#52924=DIRECTION('center_axis',(0.,-0.333233134534162,0.94284446121751));
#52925=DIRECTION('ref_axis',(0.,-0.94284446121751,-0.333233134534162));
#52926=DIRECTION('center_axis',(0.,0.333233134534162,-0.94284446121751));
#52927=DIRECTION('ref_axis',(0.,0.94284446121751,0.333233134534162));
#52928=DIRECTION('',(0.,-0.333233134534162,0.94284446121751));
#52929=DIRECTION('center_axis',(0.,0.333233134534159,-0.942844461217511));
#52930=DIRECTION('ref_axis',(0.,-0.942844461217511,-0.333233134534159));
#52931=DIRECTION('center_axis',(0.,-0.333233134534162,0.94284446121751));
#52932=DIRECTION('ref_axis',(0.,-0.94284446121751,-0.333233134534162));
#52933=DIRECTION('center_axis',(0.,0.333233134534159,-0.942844461217511));
#52934=DIRECTION('ref_axis',(0.,-0.942844461217511,-0.333233134534159));
#52935=DIRECTION('',(0.,0.333233134534162,-0.94284446121751));
#52936=DIRECTION('center_axis',(0.,0.333233134534162,-0.94284446121751));
#52937=DIRECTION('ref_axis',(0.,-0.94284446121751,-0.333233134534162));
#52938=DIRECTION('center_axis',(0.,-0.333233134534162,0.94284446121751));
#52939=DIRECTION('ref_axis',(0.,-0.94284446121751,-0.333233134534162));
#52940=DIRECTION('center_axis',(0.,0.333233134534162,-0.94284446121751));
#52941=DIRECTION('ref_axis',(0.,0.94284446121751,0.333233134534162));
#52942=DIRECTION('',(0.,-0.333233134534162,0.94284446121751));
#52943=DIRECTION('center_axis',(0.,0.333233134534159,-0.942844461217511));
#52944=DIRECTION('ref_axis',(0.,-0.942844461217511,-0.333233134534159));
#52945=DIRECTION('center_axis',(0.,-0.333233134534162,0.94284446121751));
#52946=DIRECTION('ref_axis',(0.,-0.94284446121751,-0.333233134534162));
#52947=DIRECTION('center_axis',(0.,0.333233134534159,-0.942844461217511));
#52948=DIRECTION('ref_axis',(0.,-0.942844461217511,-0.333233134534159));
#52949=DIRECTION('',(0.,0.333233134534162,-0.94284446121751));
#52950=DIRECTION('center_axis',(0.,0.333233134534162,-0.94284446121751));
#52951=DIRECTION('ref_axis',(0.,-0.94284446121751,-0.333233134534162));
#52952=DIRECTION('center_axis',(0.,-0.333233134534162,0.94284446121751));
#52953=DIRECTION('ref_axis',(0.,-0.94284446121751,-0.333233134534162));
#52954=DIRECTION('center_axis',(0.,0.333233134534162,-0.94284446121751));
#52955=DIRECTION('ref_axis',(0.,0.94284446121751,0.333233134534162));
#52956=DIRECTION('',(0.,-0.333233134534162,0.94284446121751));
#52957=DIRECTION('center_axis',(0.,0.333233134534159,-0.942844461217511));
#52958=DIRECTION('ref_axis',(0.,-0.942844461217511,-0.333233134534159));
#52959=DIRECTION('center_axis',(0.,-0.333233134534162,0.94284446121751));
#52960=DIRECTION('ref_axis',(0.,-0.94284446121751,-0.333233134534162));
#52961=DIRECTION('center_axis',(0.,0.333233134534159,-0.942844461217511));
#52962=DIRECTION('ref_axis',(0.,-0.942844461217511,-0.333233134534159));
#52963=DIRECTION('',(0.,0.333233134534162,-0.94284446121751));
#52964=DIRECTION('center_axis',(0.,0.333233134534162,-0.94284446121751));
#52965=DIRECTION('ref_axis',(0.,-0.94284446121751,-0.333233134534162));
#52966=DIRECTION('center_axis',(0.,-0.333233134534162,0.94284446121751));
#52967=DIRECTION('ref_axis',(0.,-0.94284446121751,-0.333233134534162));
#52968=DIRECTION('center_axis',(0.,0.333233134534162,-0.94284446121751));
#52969=DIRECTION('ref_axis',(0.,0.94284446121751,0.333233134534162));
#52970=DIRECTION('',(0.,-0.333233134534162,0.94284446121751));
#52971=DIRECTION('center_axis',(0.,0.333233134534159,-0.942844461217511));
#52972=DIRECTION('ref_axis',(0.,-0.942844461217511,-0.333233134534159));
#52973=DIRECTION('center_axis',(0.,-0.333233134534162,0.94284446121751));
#52974=DIRECTION('ref_axis',(0.,-0.94284446121751,-0.333233134534162));
#52975=DIRECTION('center_axis',(0.,0.333233134534159,-0.942844461217511));
#52976=DIRECTION('ref_axis',(0.,-0.942844461217511,-0.333233134534159));
#52977=DIRECTION('',(0.,0.333233134534162,-0.94284446121751));
#52978=DIRECTION('center_axis',(0.,0.333233134534162,-0.94284446121751));
#52979=DIRECTION('ref_axis',(0.,-0.94284446121751,-0.333233134534162));
#52980=DIRECTION('center_axis',(0.,-0.333233134534162,0.94284446121751));
#52981=DIRECTION('ref_axis',(0.,-0.94284446121751,-0.333233134534162));
#52982=DIRECTION('center_axis',(0.,0.333233134534162,-0.94284446121751));
#52983=DIRECTION('ref_axis',(0.,0.94284446121751,0.333233134534162));
#52984=DIRECTION('',(0.,-0.333233134534162,0.94284446121751));
#52985=DIRECTION('center_axis',(0.,0.333233134534159,-0.942844461217511));
#52986=DIRECTION('ref_axis',(0.,-0.942844461217511,-0.333233134534159));
#52987=DIRECTION('center_axis',(0.,-0.333233134534162,0.94284446121751));
#52988=DIRECTION('ref_axis',(0.,-0.94284446121751,-0.333233134534162));
#52989=DIRECTION('center_axis',(0.,0.333233134534159,-0.942844461217511));
#52990=DIRECTION('ref_axis',(0.,-0.942844461217511,-0.333233134534159));
#52991=DIRECTION('',(0.,0.333233134534162,-0.94284446121751));
#52992=DIRECTION('center_axis',(0.,0.333233134534162,-0.94284446121751));
#52993=DIRECTION('ref_axis',(0.,-0.94284446121751,-0.333233134534162));
#52994=DIRECTION('center_axis',(0.,-0.333233134534162,0.94284446121751));
#52995=DIRECTION('ref_axis',(0.,-0.94284446121751,-0.333233134534162));
#52996=DIRECTION('center_axis',(0.,0.333233134534162,-0.94284446121751));
#52997=DIRECTION('ref_axis',(0.,0.94284446121751,0.333233134534162));
#52998=DIRECTION('',(0.,-0.333233134534162,0.94284446121751));
#52999=DIRECTION('center_axis',(0.,0.333233134534159,-0.942844461217511));
#53000=DIRECTION('ref_axis',(0.,-0.942844461217511,-0.333233134534159));
#53001=DIRECTION('center_axis',(0.,-0.333233134534162,0.94284446121751));
#53002=DIRECTION('ref_axis',(0.,-0.94284446121751,-0.333233134534162));
#53003=DIRECTION('center_axis',(0.,0.333233134534159,-0.942844461217511));
#53004=DIRECTION('ref_axis',(0.,-0.942844461217511,-0.333233134534159));
#53005=DIRECTION('',(0.,0.333233134534162,-0.94284446121751));
#53006=DIRECTION('center_axis',(0.,0.333233134534162,-0.94284446121751));
#53007=DIRECTION('ref_axis',(0.,-0.94284446121751,-0.333233134534162));
#53008=DIRECTION('center_axis',(0.,-0.333233134534162,0.94284446121751));
#53009=DIRECTION('ref_axis',(0.,-0.94284446121751,-0.333233134534162));
#53010=DIRECTION('center_axis',(0.,0.333233134534162,-0.94284446121751));
#53011=DIRECTION('ref_axis',(0.,0.94284446121751,0.333233134534162));
#53012=DIRECTION('',(0.,-0.333233134534162,0.94284446121751));
#53013=DIRECTION('center_axis',(0.,0.333233134534159,-0.942844461217511));
#53014=DIRECTION('ref_axis',(0.,-0.942844461217511,-0.333233134534159));
#53015=DIRECTION('center_axis',(0.,-0.333233134534162,0.94284446121751));
#53016=DIRECTION('ref_axis',(0.,-0.94284446121751,-0.333233134534162));
#53017=DIRECTION('center_axis',(0.,0.333233134534159,-0.942844461217511));
#53018=DIRECTION('ref_axis',(0.,-0.942844461217511,-0.333233134534159));
#53019=DIRECTION('',(0.,0.333233134534162,-0.94284446121751));
#53020=DIRECTION('center_axis',(0.,0.333233134534162,-0.94284446121751));
#53021=DIRECTION('ref_axis',(0.,-0.94284446121751,-0.333233134534162));
#53022=DIRECTION('center_axis',(0.,-0.333233134534162,0.94284446121751));
#53023=DIRECTION('ref_axis',(0.,-0.94284446121751,-0.333233134534162));
#53024=DIRECTION('center_axis',(0.,0.333233134534162,-0.94284446121751));
#53025=DIRECTION('ref_axis',(0.,0.94284446121751,0.333233134534162));
#53026=DIRECTION('',(0.,-0.333233134534162,0.94284446121751));
#53027=DIRECTION('center_axis',(0.,0.333233134534159,-0.942844461217511));
#53028=DIRECTION('ref_axis',(0.,-0.942844461217511,-0.333233134534159));
#53029=DIRECTION('center_axis',(0.,-0.333233134534162,0.94284446121751));
#53030=DIRECTION('ref_axis',(0.,-0.94284446121751,-0.333233134534162));
#53031=DIRECTION('center_axis',(0.,0.333233134534159,-0.942844461217511));
#53032=DIRECTION('ref_axis',(0.,-0.942844461217511,-0.333233134534159));
#53033=DIRECTION('',(0.,0.333233134534162,-0.94284446121751));
#53034=DIRECTION('center_axis',(0.,0.333233134534162,-0.94284446121751));
#53035=DIRECTION('ref_axis',(0.,-0.94284446121751,-0.333233134534162));
#53036=DIRECTION('center_axis',(0.,-0.333233134534162,0.94284446121751));
#53037=DIRECTION('ref_axis',(0.,-0.94284446121751,-0.333233134534162));
#53038=DIRECTION('center_axis',(0.,0.333233134534162,-0.94284446121751));
#53039=DIRECTION('ref_axis',(0.,0.94284446121751,0.333233134534162));
#53040=DIRECTION('',(0.,-0.333233134534162,0.94284446121751));
#53041=DIRECTION('center_axis',(0.,0.333233134534159,-0.942844461217511));
#53042=DIRECTION('ref_axis',(0.,-0.942844461217511,-0.333233134534159));
#53043=DIRECTION('center_axis',(0.,-0.333233134534162,0.94284446121751));
#53044=DIRECTION('ref_axis',(0.,-0.94284446121751,-0.333233134534162));
#53045=DIRECTION('center_axis',(0.,0.333233134534159,-0.942844461217511));
#53046=DIRECTION('ref_axis',(0.,-0.942844461217511,-0.333233134534159));
#53047=DIRECTION('',(0.,0.333233134534162,-0.94284446121751));
#53048=DIRECTION('center_axis',(0.,-0.333233134534162,0.94284446121751));
#53049=DIRECTION('ref_axis',(0.,-0.94284446121751,-0.333233134534162));
#53050=DIRECTION('center_axis',(0.,-0.333233134534162,0.94284446121751));
#53051=DIRECTION('ref_axis',(0.,-0.94284446121751,-0.333233134534162));
#53052=DIRECTION('center_axis',(0.,0.333233134534162,-0.94284446121751));
#53053=DIRECTION('ref_axis',(0.,0.94284446121751,0.333233134534162));
#53054=DIRECTION('',(0.,-0.333233134534162,0.94284446121751));
#53055=DIRECTION('center_axis',(0.,0.333233134534159,-0.942844461217511));
#53056=DIRECTION('ref_axis',(0.,-0.942844461217511,-0.333233134534159));
#53057=DIRECTION('center_axis',(0.,-0.333233134534162,0.94284446121751));
#53058=DIRECTION('ref_axis',(0.,-0.94284446121751,-0.333233134534161));
#53059=DIRECTION('center_axis',(0.,0.333233134534159,-0.942844461217511));
#53060=DIRECTION('ref_axis',(0.,-0.942844461217511,-0.333233134534159));
#53061=DIRECTION('',(0.,0.333233134534162,-0.94284446121751));
#53062=DIRECTION('center_axis',(0.,0.333233134534162,-0.94284446121751));
#53063=DIRECTION('ref_axis',(0.,-0.94284446121751,-0.333233134534162));
#53064=DIRECTION('center_axis',(0.,-0.333233134534162,0.94284446121751));
#53065=DIRECTION('ref_axis',(0.,-0.94284446121751,-0.333233134534162));
#53066=DIRECTION('center_axis',(0.,0.333233134534162,-0.94284446121751));
#53067=DIRECTION('ref_axis',(0.,0.94284446121751,0.333233134534162));
#53068=DIRECTION('',(0.,-0.333233134534162,0.94284446121751));
#53069=DIRECTION('center_axis',(0.,0.333233134534159,-0.942844461217511));
#53070=DIRECTION('ref_axis',(0.,-0.942844461217511,-0.333233134534159));
#53071=DIRECTION('center_axis',(0.,-0.333233134534162,0.94284446121751));
#53072=DIRECTION('ref_axis',(0.,-0.94284446121751,-0.333233134534162));
#53073=DIRECTION('center_axis',(0.,0.333233134534159,-0.942844461217511));
#53074=DIRECTION('ref_axis',(0.,-0.942844461217511,-0.333233134534159));
#53075=DIRECTION('',(0.,0.333233134534162,-0.94284446121751));
#53076=DIRECTION('center_axis',(0.,0.333233134534162,-0.94284446121751));
#53077=DIRECTION('ref_axis',(0.,-0.94284446121751,-0.333233134534162));
#53078=DIRECTION('center_axis',(0.,-0.333233134534162,0.94284446121751));
#53079=DIRECTION('ref_axis',(0.,-0.94284446121751,-0.333233134534162));
#53080=DIRECTION('center_axis',(0.,0.333233134534162,-0.94284446121751));
#53081=DIRECTION('ref_axis',(0.,0.94284446121751,0.333233134534162));
#53082=DIRECTION('',(0.,-0.333233134534162,0.94284446121751));
#53083=DIRECTION('center_axis',(0.,0.333233134534159,-0.942844461217511));
#53084=DIRECTION('ref_axis',(0.,-0.942844461217511,-0.333233134534159));
#53085=DIRECTION('center_axis',(0.,-0.333233134534162,0.94284446121751));
#53086=DIRECTION('ref_axis',(0.,-0.94284446121751,-0.333233134534162));
#53087=DIRECTION('center_axis',(0.,0.333233134534159,-0.942844461217511));
#53088=DIRECTION('ref_axis',(0.,-0.942844461217511,-0.333233134534159));
#53089=DIRECTION('',(0.,0.333233134534162,-0.94284446121751));
#53090=DIRECTION('center_axis',(0.,0.333233134534162,-0.94284446121751));
#53091=DIRECTION('ref_axis',(0.,-0.94284446121751,-0.333233134534162));
#53092=DIRECTION('center_axis',(0.,-0.333233134534162,0.94284446121751));
#53093=DIRECTION('ref_axis',(0.,-0.94284446121751,-0.333233134534162));
#53094=DIRECTION('center_axis',(0.,0.333233134534162,-0.94284446121751));
#53095=DIRECTION('ref_axis',(0.,0.94284446121751,0.333233134534162));
#53096=DIRECTION('',(0.,-0.333233134534162,0.94284446121751));
#53097=DIRECTION('center_axis',(0.,0.333233134534159,-0.942844461217511));
#53098=DIRECTION('ref_axis',(0.,-0.942844461217511,-0.333233134534159));
#53099=DIRECTION('center_axis',(0.,-0.333233134534162,0.94284446121751));
#53100=DIRECTION('ref_axis',(0.,-0.94284446121751,-0.333233134534162));
#53101=DIRECTION('center_axis',(0.,0.333233134534159,-0.942844461217511));
#53102=DIRECTION('ref_axis',(0.,-0.942844461217511,-0.333233134534159));
#53103=DIRECTION('',(0.,0.333233134534162,-0.94284446121751));
#53104=DIRECTION('center_axis',(0.,0.333233134534162,-0.94284446121751));
#53105=DIRECTION('ref_axis',(0.,-0.94284446121751,-0.333233134534162));
#53106=DIRECTION('center_axis',(0.,-0.333233134534162,0.94284446121751));
#53107=DIRECTION('ref_axis',(0.,-0.94284446121751,-0.333233134534162));
#53108=DIRECTION('center_axis',(0.,0.333233134534162,-0.94284446121751));
#53109=DIRECTION('ref_axis',(0.,0.94284446121751,0.333233134534162));
#53110=DIRECTION('',(0.,-0.333233134534162,0.94284446121751));
#53111=DIRECTION('center_axis',(0.,0.333233134534159,-0.942844461217511));
#53112=DIRECTION('ref_axis',(0.,-0.942844461217511,-0.333233134534159));
#53113=DIRECTION('center_axis',(0.,-0.333233134534162,0.94284446121751));
#53114=DIRECTION('ref_axis',(0.,-0.94284446121751,-0.333233134534162));
#53115=DIRECTION('center_axis',(0.,0.333233134534159,-0.942844461217511));
#53116=DIRECTION('ref_axis',(0.,-0.942844461217511,-0.333233134534159));
#53117=DIRECTION('',(0.,0.333233134534162,-0.94284446121751));
#53118=DIRECTION('center_axis',(0.,0.333233134534162,-0.94284446121751));
#53119=DIRECTION('ref_axis',(0.,-0.94284446121751,-0.333233134534162));
#53120=DIRECTION('center_axis',(0.,-0.333233134534162,0.94284446121751));
#53121=DIRECTION('ref_axis',(0.,-0.94284446121751,-0.333233134534162));
#53122=DIRECTION('center_axis',(0.,0.333233134534162,-0.94284446121751));
#53123=DIRECTION('ref_axis',(0.,0.94284446121751,0.333233134534162));
#53124=DIRECTION('',(0.,-0.333233134534162,0.94284446121751));
#53125=DIRECTION('center_axis',(0.,0.333233134534159,-0.942844461217511));
#53126=DIRECTION('ref_axis',(0.,-0.942844461217511,-0.333233134534159));
#53127=DIRECTION('center_axis',(0.,-0.333233134534162,0.94284446121751));
#53128=DIRECTION('ref_axis',(0.,-0.94284446121751,-0.333233134534162));
#53129=DIRECTION('center_axis',(0.,0.333233134534159,-0.942844461217511));
#53130=DIRECTION('ref_axis',(0.,-0.942844461217511,-0.333233134534159));
#53131=DIRECTION('',(0.,0.333233134534162,-0.94284446121751));
#53132=DIRECTION('center_axis',(0.,0.333233134534162,-0.94284446121751));
#53133=DIRECTION('ref_axis',(0.,-0.94284446121751,-0.333233134534162));
#53134=DIRECTION('center_axis',(0.,-0.333233134534162,0.94284446121751));
#53135=DIRECTION('ref_axis',(0.,-0.94284446121751,-0.333233134534162));
#53136=DIRECTION('center_axis',(0.,0.333233134534162,-0.94284446121751));
#53137=DIRECTION('ref_axis',(0.,0.94284446121751,0.333233134534162));
#53138=DIRECTION('',(0.,-0.333233134534162,0.94284446121751));
#53139=DIRECTION('center_axis',(0.,0.333233134534159,-0.942844461217511));
#53140=DIRECTION('ref_axis',(0.,-0.942844461217511,-0.333233134534159));
#53141=DIRECTION('center_axis',(0.,-0.333233134534162,0.94284446121751));
#53142=DIRECTION('ref_axis',(0.,-0.94284446121751,-0.333233134534162));
#53143=DIRECTION('center_axis',(0.,0.333233134534159,-0.942844461217511));
#53144=DIRECTION('ref_axis',(0.,-0.942844461217511,-0.333233134534159));
#53145=DIRECTION('',(0.,0.333233134534162,-0.94284446121751));
#53146=DIRECTION('center_axis',(0.,0.333233134534162,-0.94284446121751));
#53147=DIRECTION('ref_axis',(0.,-0.94284446121751,-0.333233134534162));
#53148=DIRECTION('center_axis',(0.,-0.333233134534162,0.94284446121751));
#53149=DIRECTION('ref_axis',(0.,-0.94284446121751,-0.333233134534162));
#53150=DIRECTION('center_axis',(0.,0.333233134534162,-0.94284446121751));
#53151=DIRECTION('ref_axis',(0.,0.94284446121751,0.333233134534162));
#53152=DIRECTION('',(0.,-0.333233134534162,0.94284446121751));
#53153=DIRECTION('center_axis',(0.,0.333233134534159,-0.942844461217511));
#53154=DIRECTION('ref_axis',(0.,-0.942844461217511,-0.333233134534159));
#53155=DIRECTION('center_axis',(0.,-0.333233134534162,0.94284446121751));
#53156=DIRECTION('ref_axis',(0.,-0.94284446121751,-0.333233134534162));
#53157=DIRECTION('center_axis',(0.,0.333233134534159,-0.942844461217511));
#53158=DIRECTION('ref_axis',(0.,-0.942844461217511,-0.333233134534159));
#53159=DIRECTION('',(0.,0.333233134534161,-0.94284446121751));
#53160=DIRECTION('center_axis',(0.,0.333233134534162,-0.94284446121751));
#53161=DIRECTION('ref_axis',(0.,-0.94284446121751,-0.333233134534162));
#53162=DIRECTION('center_axis',(0.,-0.333233134534162,0.94284446121751));
#53163=DIRECTION('ref_axis',(0.,-0.94284446121751,-0.333233134534162));
#53164=DIRECTION('center_axis',(0.,0.333233134534162,-0.94284446121751));
#53165=DIRECTION('ref_axis',(0.,0.94284446121751,0.333233134534162));
#53166=DIRECTION('',(0.,-0.333233134534162,0.94284446121751));
#53167=DIRECTION('center_axis',(0.,0.333233134534159,-0.942844461217511));
#53168=DIRECTION('ref_axis',(0.,-0.942844461217511,-0.333233134534159));
#53169=DIRECTION('center_axis',(0.,-0.333233134534162,0.94284446121751));
#53170=DIRECTION('ref_axis',(0.,-0.94284446121751,-0.333233134534162));
#53171=DIRECTION('center_axis',(0.,0.333233134534159,-0.942844461217511));
#53172=DIRECTION('ref_axis',(0.,-0.942844461217511,-0.333233134534159));
#53173=DIRECTION('',(0.,0.333233134534162,-0.94284446121751));
#53174=DIRECTION('center_axis',(0.,-0.333233134534162,0.94284446121751));
#53175=DIRECTION('ref_axis',(0.,-0.94284446121751,-0.333233134534162));
#53176=DIRECTION('center_axis',(0.,-0.333233134534162,0.94284446121751));
#53177=DIRECTION('ref_axis',(0.,-0.94284446121751,-0.333233134534162));
#53178=DIRECTION('center_axis',(0.,0.333233134534162,-0.94284446121751));
#53179=DIRECTION('ref_axis',(0.,0.94284446121751,0.333233134534162));
#53180=DIRECTION('',(0.,-0.333233134534162,0.94284446121751));
#53181=DIRECTION('center_axis',(0.,0.333233134534159,-0.942844461217511));
#53182=DIRECTION('ref_axis',(0.,-0.942844461217511,-0.333233134534159));
#53183=DIRECTION('center_axis',(0.,-0.333233134534162,0.94284446121751));
#53184=DIRECTION('ref_axis',(0.,-0.94284446121751,-0.333233134534161));
#53185=DIRECTION('center_axis',(0.,0.333233134534159,-0.942844461217511));
#53186=DIRECTION('ref_axis',(0.,-0.942844461217511,-0.333233134534159));
#53187=DIRECTION('',(0.,0.333233134534162,-0.94284446121751));
#53188=DIRECTION('center_axis',(0.,0.333233134534162,-0.94284446121751));
#53189=DIRECTION('ref_axis',(0.,-0.94284446121751,-0.333233134534162));
#53190=DIRECTION('center_axis',(0.,-0.333233134534162,0.94284446121751));
#53191=DIRECTION('ref_axis',(0.,-0.94284446121751,-0.333233134534162));
#53192=DIRECTION('center_axis',(0.,0.333233134534162,-0.94284446121751));
#53193=DIRECTION('ref_axis',(0.,0.94284446121751,0.333233134534162));
#53194=DIRECTION('',(0.,-0.333233134534162,0.94284446121751));
#53195=DIRECTION('center_axis',(0.,0.333233134534159,-0.942844461217511));
#53196=DIRECTION('ref_axis',(0.,-0.942844461217511,-0.333233134534159));
#53197=DIRECTION('center_axis',(0.,-0.333233134534162,0.94284446121751));
#53198=DIRECTION('ref_axis',(0.,-0.94284446121751,-0.333233134534162));
#53199=DIRECTION('center_axis',(0.,0.333233134534159,-0.942844461217511));
#53200=DIRECTION('ref_axis',(0.,-0.942844461217511,-0.333233134534159));
#53201=DIRECTION('',(0.,0.333233134534162,-0.94284446121751));
#53202=DIRECTION('center_axis',(0.,0.333233134534162,-0.94284446121751));
#53203=DIRECTION('ref_axis',(0.,-0.94284446121751,-0.333233134534162));
#53204=DIRECTION('center_axis',(0.,-0.333233134534162,0.94284446121751));
#53205=DIRECTION('ref_axis',(0.,-0.94284446121751,-0.333233134534162));
#53206=DIRECTION('center_axis',(0.,0.333233134534162,-0.94284446121751));
#53207=DIRECTION('ref_axis',(0.,0.94284446121751,0.333233134534162));
#53208=DIRECTION('',(0.,-0.333233134534162,0.94284446121751));
#53209=DIRECTION('center_axis',(0.,0.333233134534159,-0.942844461217511));
#53210=DIRECTION('ref_axis',(0.,-0.942844461217511,-0.333233134534159));
#53211=DIRECTION('center_axis',(0.,-0.333233134534162,0.94284446121751));
#53212=DIRECTION('ref_axis',(0.,-0.94284446121751,-0.333233134534162));
#53213=DIRECTION('center_axis',(0.,0.333233134534159,-0.942844461217511));
#53214=DIRECTION('ref_axis',(0.,-0.942844461217511,-0.333233134534159));
#53215=DIRECTION('',(0.,0.333233134534162,-0.94284446121751));
#53216=DIRECTION('center_axis',(0.,0.333233134534162,-0.94284446121751));
#53217=DIRECTION('ref_axis',(0.,-0.94284446121751,-0.333233134534162));
#53218=DIRECTION('center_axis',(0.,-0.333233134534162,0.94284446121751));
#53219=DIRECTION('ref_axis',(0.,-0.94284446121751,-0.333233134534162));
#53220=DIRECTION('center_axis',(0.,0.333233134534162,-0.94284446121751));
#53221=DIRECTION('ref_axis',(0.,0.94284446121751,0.333233134534162));
#53222=DIRECTION('',(0.,-0.333233134534162,0.94284446121751));
#53223=DIRECTION('center_axis',(0.,0.333233134534159,-0.942844461217511));
#53224=DIRECTION('ref_axis',(0.,-0.942844461217511,-0.333233134534159));
#53225=DIRECTION('center_axis',(0.,-0.333233134534162,0.94284446121751));
#53226=DIRECTION('ref_axis',(0.,-0.94284446121751,-0.333233134534162));
#53227=DIRECTION('center_axis',(0.,0.333233134534159,-0.942844461217511));
#53228=DIRECTION('ref_axis',(0.,-0.942844461217511,-0.333233134534159));
#53229=DIRECTION('',(0.,0.333233134534162,-0.94284446121751));
#53230=DIRECTION('center_axis',(0.,0.333233134534162,-0.94284446121751));
#53231=DIRECTION('ref_axis',(0.,-0.94284446121751,-0.333233134534162));
#53232=DIRECTION('center_axis',(0.,-0.333233134534162,0.94284446121751));
#53233=DIRECTION('ref_axis',(0.,-0.94284446121751,-0.333233134534162));
#53234=DIRECTION('center_axis',(0.,0.333233134534162,-0.94284446121751));
#53235=DIRECTION('ref_axis',(0.,0.94284446121751,0.333233134534162));
#53236=DIRECTION('',(0.,-0.333233134534162,0.94284446121751));
#53237=DIRECTION('center_axis',(0.,0.333233134534159,-0.942844461217511));
#53238=DIRECTION('ref_axis',(0.,-0.942844461217511,-0.333233134534159));
#53239=DIRECTION('center_axis',(0.,-0.333233134534162,0.94284446121751));
#53240=DIRECTION('ref_axis',(0.,-0.94284446121751,-0.333233134534162));
#53241=DIRECTION('center_axis',(0.,0.333233134534159,-0.942844461217511));
#53242=DIRECTION('ref_axis',(0.,-0.942844461217511,-0.333233134534159));
#53243=DIRECTION('',(0.,0.333233134534162,-0.94284446121751));
#53244=DIRECTION('center_axis',(0.,0.333233134534162,-0.94284446121751));
#53245=DIRECTION('ref_axis',(0.,-0.94284446121751,-0.333233134534162));
#53246=DIRECTION('center_axis',(0.,-0.333233134534162,0.94284446121751));
#53247=DIRECTION('ref_axis',(0.,-0.94284446121751,-0.333233134534162));
#53248=DIRECTION('center_axis',(0.,0.333233134534162,-0.94284446121751));
#53249=DIRECTION('ref_axis',(0.,0.94284446121751,0.333233134534162));
#53250=DIRECTION('',(0.,-0.333233134534162,0.94284446121751));
#53251=DIRECTION('center_axis',(0.,0.333233134534159,-0.942844461217511));
#53252=DIRECTION('ref_axis',(0.,-0.942844461217511,-0.333233134534159));
#53253=DIRECTION('center_axis',(0.,-0.333233134534162,0.94284446121751));
#53254=DIRECTION('ref_axis',(0.,-0.94284446121751,-0.333233134534161));
#53255=DIRECTION('center_axis',(0.,0.333233134534159,-0.942844461217511));
#53256=DIRECTION('ref_axis',(0.,-0.942844461217511,-0.333233134534159));
#53257=DIRECTION('',(0.,0.333233134534162,-0.94284446121751));
#53258=DIRECTION('center_axis',(0.,0.333233134534162,-0.94284446121751));
#53259=DIRECTION('ref_axis',(0.,-0.94284446121751,-0.333233134534162));
#53260=DIRECTION('center_axis',(0.,-0.333233134534162,0.94284446121751));
#53261=DIRECTION('ref_axis',(0.,-0.94284446121751,-0.333233134534162));
#53262=DIRECTION('center_axis',(0.,0.333233134534162,-0.94284446121751));
#53263=DIRECTION('ref_axis',(0.,0.94284446121751,0.333233134534162));
#53264=DIRECTION('',(0.,-0.333233134534162,0.94284446121751));
#53265=DIRECTION('center_axis',(0.,0.333233134534159,-0.942844461217511));
#53266=DIRECTION('ref_axis',(0.,-0.942844461217511,-0.333233134534159));
#53267=DIRECTION('center_axis',(0.,-0.333233134534162,0.94284446121751));
#53268=DIRECTION('ref_axis',(0.,-0.94284446121751,-0.333233134534162));
#53269=DIRECTION('center_axis',(0.,0.333233134534159,-0.942844461217511));
#53270=DIRECTION('ref_axis',(0.,-0.942844461217511,-0.333233134534159));
#53271=DIRECTION('',(0.,0.333233134534162,-0.94284446121751));
#53272=DIRECTION('center_axis',(0.,0.333233134534162,-0.94284446121751));
#53273=DIRECTION('ref_axis',(0.,-0.94284446121751,-0.333233134534162));
#53274=DIRECTION('center_axis',(0.,-0.333233134534162,0.94284446121751));
#53275=DIRECTION('ref_axis',(0.,-0.94284446121751,-0.333233134534162));
#53276=DIRECTION('center_axis',(0.,0.333233134534162,-0.94284446121751));
#53277=DIRECTION('ref_axis',(0.,0.94284446121751,0.333233134534162));
#53278=DIRECTION('',(0.,-0.333233134534162,0.94284446121751));
#53279=DIRECTION('center_axis',(0.,0.333233134534159,-0.942844461217511));
#53280=DIRECTION('ref_axis',(0.,-0.942844461217511,-0.333233134534159));
#53281=DIRECTION('center_axis',(0.,-0.333233134534162,0.94284446121751));
#53282=DIRECTION('ref_axis',(0.,-0.94284446121751,-0.333233134534162));
#53283=DIRECTION('center_axis',(0.,0.333233134534159,-0.942844461217511));
#53284=DIRECTION('ref_axis',(0.,-0.942844461217511,-0.333233134534159));
#53285=DIRECTION('',(0.,0.333233134534162,-0.94284446121751));
#53286=DIRECTION('center_axis',(0.,-0.333233134534162,0.94284446121751));
#53287=DIRECTION('ref_axis',(0.,-0.94284446121751,-0.333233134534162));
#53288=DIRECTION('center_axis',(0.,-0.333233134534162,0.94284446121751));
#53289=DIRECTION('ref_axis',(0.,-0.94284446121751,-0.333233134534162));
#53290=DIRECTION('center_axis',(0.,0.333233134534162,-0.94284446121751));
#53291=DIRECTION('ref_axis',(0.,0.94284446121751,0.333233134534162));
#53292=DIRECTION('',(0.,-0.333233134534162,0.94284446121751));
#53293=DIRECTION('center_axis',(0.,0.333233134534159,-0.942844461217511));
#53294=DIRECTION('ref_axis',(0.,-0.942844461217511,-0.333233134534159));
#53295=DIRECTION('center_axis',(0.,-0.333233134534162,0.94284446121751));
#53296=DIRECTION('ref_axis',(0.,-0.94284446121751,-0.333233134534162));
#53297=DIRECTION('center_axis',(0.,0.333233134534159,-0.942844461217511));
#53298=DIRECTION('ref_axis',(0.,-0.942844461217511,-0.333233134534159));
#53299=DIRECTION('',(0.,0.333233134534162,-0.94284446121751));
#53300=DIRECTION('center_axis',(0.,0.333233134534162,-0.94284446121751));
#53301=DIRECTION('ref_axis',(0.,-0.94284446121751,-0.333233134534162));
#53302=DIRECTION('center_axis',(0.,-0.333233134534162,0.94284446121751));
#53303=DIRECTION('ref_axis',(0.,-0.94284446121751,-0.333233134534162));
#53304=DIRECTION('center_axis',(0.,0.333233134534162,-0.94284446121751));
#53305=DIRECTION('ref_axis',(0.,0.94284446121751,0.333233134534162));
#53306=DIRECTION('',(0.,-0.333233134534162,0.94284446121751));
#53307=DIRECTION('center_axis',(0.,0.333233134534159,-0.942844461217511));
#53308=DIRECTION('ref_axis',(0.,-0.942844461217511,-0.333233134534159));
#53309=DIRECTION('center_axis',(0.,-0.333233134534162,0.94284446121751));
#53310=DIRECTION('ref_axis',(0.,-0.94284446121751,-0.333233134534162));
#53311=DIRECTION('center_axis',(0.,0.333233134534159,-0.942844461217511));
#53312=DIRECTION('ref_axis',(0.,-0.942844461217511,-0.333233134534159));
#53313=DIRECTION('',(0.,0.333233134534162,-0.94284446121751));
#53314=DIRECTION('center_axis',(0.,0.333233134534162,-0.94284446121751));
#53315=DIRECTION('ref_axis',(0.,-0.94284446121751,-0.333233134534162));
#53316=DIRECTION('center_axis',(0.,-0.333233134534162,0.94284446121751));
#53317=DIRECTION('ref_axis',(0.,-0.94284446121751,-0.333233134534162));
#53318=DIRECTION('center_axis',(0.,0.333233134534162,-0.94284446121751));
#53319=DIRECTION('ref_axis',(0.,0.94284446121751,0.333233134534162));
#53320=DIRECTION('',(0.,-0.333233134534162,0.94284446121751));
#53321=DIRECTION('center_axis',(0.,0.333233134534159,-0.942844461217511));
#53322=DIRECTION('ref_axis',(0.,-0.942844461217511,-0.333233134534159));
#53323=DIRECTION('center_axis',(0.,-0.333233134534162,0.94284446121751));
#53324=DIRECTION('ref_axis',(0.,-0.94284446121751,-0.333233134534162));
#53325=DIRECTION('center_axis',(0.,0.333233134534159,-0.942844461217511));
#53326=DIRECTION('ref_axis',(0.,-0.942844461217511,-0.333233134534159));
#53327=DIRECTION('',(0.,0.333233134534162,-0.94284446121751));
#53328=DIRECTION('center_axis',(0.,0.333233134534162,-0.94284446121751));
#53329=DIRECTION('ref_axis',(0.,-0.94284446121751,-0.333233134534162));
#53330=DIRECTION('center_axis',(0.,-0.333233134534162,0.94284446121751));
#53331=DIRECTION('ref_axis',(0.,-0.94284446121751,-0.333233134534162));
#53332=DIRECTION('center_axis',(0.,0.333233134534162,-0.94284446121751));
#53333=DIRECTION('ref_axis',(0.,0.94284446121751,0.333233134534162));
#53334=DIRECTION('',(0.,-0.333233134534162,0.94284446121751));
#53335=DIRECTION('center_axis',(0.,0.333233134534159,-0.942844461217511));
#53336=DIRECTION('ref_axis',(0.,-0.942844461217511,-0.333233134534159));
#53337=DIRECTION('center_axis',(0.,-0.333233134534162,0.94284446121751));
#53338=DIRECTION('ref_axis',(0.,-0.94284446121751,-0.333233134534162));
#53339=DIRECTION('center_axis',(0.,0.333233134534159,-0.942844461217511));
#53340=DIRECTION('ref_axis',(0.,-0.942844461217511,-0.333233134534159));
#53341=DIRECTION('',(0.,0.333233134534162,-0.94284446121751));
#53342=DIRECTION('center_axis',(0.,0.333233134534162,-0.94284446121751));
#53343=DIRECTION('ref_axis',(0.,-0.94284446121751,-0.333233134534162));
#53344=DIRECTION('center_axis',(0.,-0.333233134534162,0.94284446121751));
#53345=DIRECTION('ref_axis',(0.,-0.94284446121751,-0.333233134534162));
#53346=DIRECTION('center_axis',(0.,0.333233134534162,-0.94284446121751));
#53347=DIRECTION('ref_axis',(0.,0.94284446121751,0.333233134534162));
#53348=DIRECTION('',(0.,-0.333233134534162,0.94284446121751));
#53349=DIRECTION('center_axis',(0.,0.333233134534159,-0.942844461217511));
#53350=DIRECTION('ref_axis',(0.,-0.942844461217511,-0.333233134534159));
#53351=DIRECTION('center_axis',(0.,-0.333233134534162,0.94284446121751));
#53352=DIRECTION('ref_axis',(0.,-0.94284446121751,-0.333233134534162));
#53353=DIRECTION('center_axis',(0.,0.333233134534159,-0.942844461217511));
#53354=DIRECTION('ref_axis',(0.,-0.942844461217511,-0.333233134534159));
#53355=DIRECTION('',(0.,0.333233134534162,-0.94284446121751));
#53356=DIRECTION('center_axis',(0.,0.333233134534162,-0.94284446121751));
#53357=DIRECTION('ref_axis',(0.,-0.94284446121751,-0.333233134534162));
#53358=DIRECTION('center_axis',(0.,-0.333233134534162,0.94284446121751));
#53359=DIRECTION('ref_axis',(0.,-0.94284446121751,-0.333233134534162));
#53360=DIRECTION('center_axis',(0.,0.333233134534162,-0.94284446121751));
#53361=DIRECTION('ref_axis',(0.,0.94284446121751,0.333233134534162));
#53362=DIRECTION('',(0.,-0.333233134534162,0.94284446121751));
#53363=DIRECTION('center_axis',(0.,0.333233134534159,-0.942844461217511));
#53364=DIRECTION('ref_axis',(0.,-0.942844461217511,-0.333233134534159));
#53365=DIRECTION('center_axis',(0.,-0.333233134534162,0.94284446121751));
#53366=DIRECTION('ref_axis',(0.,-0.94284446121751,-0.333233134534162));
#53367=DIRECTION('center_axis',(0.,0.333233134534159,-0.942844461217511));
#53368=DIRECTION('ref_axis',(0.,-0.942844461217511,-0.333233134534159));
#53369=DIRECTION('',(0.,0.333233134534162,-0.94284446121751));
#53370=DIRECTION('center_axis',(0.,0.333233134534162,-0.94284446121751));
#53371=DIRECTION('ref_axis',(0.,-0.94284446121751,-0.333233134534162));
#53372=DIRECTION('center_axis',(0.,-0.333233134534162,0.94284446121751));
#53373=DIRECTION('ref_axis',(0.,-0.94284446121751,-0.333233134534162));
#53374=DIRECTION('center_axis',(0.,0.333233134534162,-0.94284446121751));
#53375=DIRECTION('ref_axis',(0.,0.94284446121751,0.333233134534162));
#53376=DIRECTION('',(0.,-0.333233134534162,0.94284446121751));
#53377=DIRECTION('center_axis',(0.,0.333233134534159,-0.942844461217511));
#53378=DIRECTION('ref_axis',(0.,-0.942844461217511,-0.333233134534159));
#53379=DIRECTION('center_axis',(0.,-0.333233134534162,0.94284446121751));
#53380=DIRECTION('ref_axis',(0.,-0.94284446121751,-0.333233134534162));
#53381=DIRECTION('center_axis',(0.,0.333233134534159,-0.942844461217511));
#53382=DIRECTION('ref_axis',(0.,-0.942844461217511,-0.333233134534159));
#53383=DIRECTION('',(0.,0.333233134534162,-0.94284446121751));
#53384=DIRECTION('center_axis',(0.,0.333233134534162,-0.94284446121751));
#53385=DIRECTION('ref_axis',(0.,-0.94284446121751,-0.333233134534162));
#53386=DIRECTION('center_axis',(0.,-0.333233134534162,0.94284446121751));
#53387=DIRECTION('ref_axis',(0.,-0.94284446121751,-0.333233134534162));
#53388=DIRECTION('center_axis',(0.,0.333233134534162,-0.94284446121751));
#53389=DIRECTION('ref_axis',(0.,0.94284446121751,0.333233134534162));
#53390=DIRECTION('',(0.,-0.333233134534162,0.94284446121751));
#53391=DIRECTION('center_axis',(0.,0.333233134534159,-0.942844461217511));
#53392=DIRECTION('ref_axis',(0.,-0.942844461217511,-0.333233134534159));
#53393=DIRECTION('center_axis',(0.,-0.333233134534162,0.94284446121751));
#53394=DIRECTION('ref_axis',(0.,-0.94284446121751,-0.333233134534162));
#53395=DIRECTION('center_axis',(0.,0.333233134534159,-0.942844461217511));
#53396=DIRECTION('ref_axis',(0.,-0.942844461217511,-0.333233134534159));
#53397=DIRECTION('',(0.,0.333233134534162,-0.94284446121751));
#53398=DIRECTION('center_axis',(0.,0.333233134534162,-0.94284446121751));
#53399=DIRECTION('ref_axis',(0.,-0.94284446121751,-0.333233134534162));
#53400=DIRECTION('center_axis',(0.,-0.333233134534162,0.94284446121751));
#53401=DIRECTION('ref_axis',(0.,-0.94284446121751,-0.333233134534162));
#53402=DIRECTION('center_axis',(0.,0.333233134534162,-0.94284446121751));
#53403=DIRECTION('ref_axis',(0.,0.94284446121751,0.333233134534162));
#53404=DIRECTION('',(0.,-0.333233134534162,0.94284446121751));
#53405=DIRECTION('center_axis',(0.,0.333233134534159,-0.942844461217511));
#53406=DIRECTION('ref_axis',(0.,-0.942844461217511,-0.333233134534159));
#53407=DIRECTION('center_axis',(0.,-0.333233134534162,0.94284446121751));
#53408=DIRECTION('ref_axis',(0.,-0.94284446121751,-0.333233134534162));
#53409=DIRECTION('center_axis',(0.,0.333233134534159,-0.942844461217511));
#53410=DIRECTION('ref_axis',(0.,-0.942844461217511,-0.333233134534159));
#53411=DIRECTION('',(0.,0.333233134534162,-0.94284446121751));
#53412=DIRECTION('center_axis',(0.,-0.333233134534162,0.94284446121751));
#53413=DIRECTION('ref_axis',(0.,-0.94284446121751,-0.333233134534162));
#53414=DIRECTION('center_axis',(0.,-0.333233134534162,0.94284446121751));
#53415=DIRECTION('ref_axis',(0.,-0.94284446121751,-0.333233134534162));
#53416=DIRECTION('center_axis',(0.,0.333233134534162,-0.94284446121751));
#53417=DIRECTION('ref_axis',(0.,0.94284446121751,0.333233134534162));
#53418=DIRECTION('',(0.,-0.333233134534162,0.94284446121751));
#53419=DIRECTION('center_axis',(0.,0.333233134534159,-0.942844461217511));
#53420=DIRECTION('ref_axis',(0.,-0.942844461217511,-0.333233134534159));
#53421=DIRECTION('center_axis',(0.,-0.333233134534162,0.94284446121751));
#53422=DIRECTION('ref_axis',(0.,-0.94284446121751,-0.333233134534162));
#53423=DIRECTION('center_axis',(0.,0.333233134534159,-0.942844461217511));
#53424=DIRECTION('ref_axis',(0.,-0.942844461217511,-0.333233134534159));
#53425=DIRECTION('',(0.,0.333233134534162,-0.94284446121751));
#53426=DIRECTION('center_axis',(0.,0.333233134534162,-0.94284446121751));
#53427=DIRECTION('ref_axis',(0.,-0.94284446121751,-0.333233134534162));
#53428=DIRECTION('center_axis',(0.,-0.333233134534162,0.94284446121751));
#53429=DIRECTION('ref_axis',(0.,-0.94284446121751,-0.333233134534162));
#53430=DIRECTION('center_axis',(0.,0.333233134534162,-0.94284446121751));
#53431=DIRECTION('ref_axis',(0.,0.94284446121751,0.333233134534162));
#53432=DIRECTION('',(0.,-0.333233134534162,0.94284446121751));
#53433=DIRECTION('center_axis',(0.,0.333233134534159,-0.942844461217511));
#53434=DIRECTION('ref_axis',(0.,-0.942844461217511,-0.333233134534159));
#53435=DIRECTION('center_axis',(0.,-0.333233134534162,0.94284446121751));
#53436=DIRECTION('ref_axis',(0.,-0.94284446121751,-0.333233134534162));
#53437=DIRECTION('center_axis',(0.,0.333233134534159,-0.942844461217511));
#53438=DIRECTION('ref_axis',(0.,-0.942844461217511,-0.333233134534159));
#53439=DIRECTION('',(0.,0.333233134534162,-0.94284446121751));
#53440=DIRECTION('center_axis',(0.,0.333233134534162,-0.94284446121751));
#53441=DIRECTION('ref_axis',(0.,-0.94284446121751,-0.333233134534162));
#53442=DIRECTION('center_axis',(0.,-0.333233134534162,0.94284446121751));
#53443=DIRECTION('ref_axis',(0.,-0.94284446121751,-0.333233134534162));
#53444=DIRECTION('center_axis',(0.,0.333233134534162,-0.94284446121751));
#53445=DIRECTION('ref_axis',(0.,0.94284446121751,0.333233134534162));
#53446=DIRECTION('',(0.,-0.333233134534162,0.94284446121751));
#53447=DIRECTION('center_axis',(0.,0.333233134534159,-0.942844461217511));
#53448=DIRECTION('ref_axis',(0.,-0.942844461217511,-0.333233134534159));
#53449=DIRECTION('center_axis',(0.,-0.333233134534162,0.94284446121751));
#53450=DIRECTION('ref_axis',(0.,-0.94284446121751,-0.333233134534162));
#53451=DIRECTION('center_axis',(0.,0.333233134534159,-0.942844461217511));
#53452=DIRECTION('ref_axis',(0.,-0.942844461217511,-0.333233134534159));
#53453=DIRECTION('',(0.,0.333233134534162,-0.94284446121751));
#53454=DIRECTION('center_axis',(0.,0.333233134534162,-0.94284446121751));
#53455=DIRECTION('ref_axis',(0.,-0.94284446121751,-0.333233134534162));
#53456=DIRECTION('center_axis',(0.,-0.333233134534162,0.94284446121751));
#53457=DIRECTION('ref_axis',(0.,-0.94284446121751,-0.333233134534162));
#53458=DIRECTION('center_axis',(0.,0.333233134534162,-0.94284446121751));
#53459=DIRECTION('ref_axis',(0.,0.94284446121751,0.333233134534162));
#53460=DIRECTION('',(0.,-0.333233134534162,0.94284446121751));
#53461=DIRECTION('center_axis',(0.,0.333233134534159,-0.942844461217511));
#53462=DIRECTION('ref_axis',(0.,-0.942844461217511,-0.333233134534159));
#53463=DIRECTION('center_axis',(0.,-0.333233134534162,0.94284446121751));
#53464=DIRECTION('ref_axis',(0.,-0.94284446121751,-0.333233134534162));
#53465=DIRECTION('center_axis',(0.,0.333233134534159,-0.942844461217511));
#53466=DIRECTION('ref_axis',(0.,-0.942844461217511,-0.333233134534159));
#53467=DIRECTION('',(0.,0.333233134534162,-0.94284446121751));
#53468=DIRECTION('center_axis',(0.,0.333233134534162,-0.94284446121751));
#53469=DIRECTION('ref_axis',(0.,-0.94284446121751,-0.333233134534162));
#53470=DIRECTION('center_axis',(0.,-0.333233134534162,0.94284446121751));
#53471=DIRECTION('ref_axis',(0.,-0.94284446121751,-0.333233134534162));
#53472=DIRECTION('center_axis',(0.,0.333233134534162,-0.94284446121751));
#53473=DIRECTION('ref_axis',(0.,0.94284446121751,0.333233134534162));
#53474=DIRECTION('',(0.,-0.333233134534162,0.94284446121751));
#53475=DIRECTION('center_axis',(0.,0.333233134534159,-0.942844461217511));
#53476=DIRECTION('ref_axis',(0.,-0.942844461217511,-0.333233134534159));
#53477=DIRECTION('center_axis',(0.,-0.333233134534162,0.94284446121751));
#53478=DIRECTION('ref_axis',(0.,-0.94284446121751,-0.333233134534162));
#53479=DIRECTION('center_axis',(0.,0.333233134534159,-0.942844461217511));
#53480=DIRECTION('ref_axis',(0.,-0.942844461217511,-0.333233134534159));
#53481=DIRECTION('',(0.,0.333233134534162,-0.94284446121751));
#53482=DIRECTION('center_axis',(0.,0.333233134534162,-0.94284446121751));
#53483=DIRECTION('ref_axis',(0.,-0.94284446121751,-0.333233134534162));
#53484=DIRECTION('center_axis',(0.,-0.333233134534162,0.94284446121751));
#53485=DIRECTION('ref_axis',(0.,-0.94284446121751,-0.333233134534162));
#53486=DIRECTION('center_axis',(0.,0.333233134534162,-0.94284446121751));
#53487=DIRECTION('ref_axis',(0.,0.94284446121751,0.333233134534162));
#53488=DIRECTION('',(0.,-0.333233134534162,0.94284446121751));
#53489=DIRECTION('center_axis',(0.,0.333233134534159,-0.942844461217511));
#53490=DIRECTION('ref_axis',(0.,-0.942844461217511,-0.333233134534159));
#53491=DIRECTION('center_axis',(0.,-0.333233134534162,0.94284446121751));
#53492=DIRECTION('ref_axis',(0.,-0.94284446121751,-0.333233134534162));
#53493=DIRECTION('center_axis',(0.,0.333233134534159,-0.942844461217511));
#53494=DIRECTION('ref_axis',(0.,-0.942844461217511,-0.333233134534159));
#53495=DIRECTION('',(0.,0.333233134534162,-0.94284446121751));
#53496=DIRECTION('center_axis',(0.,0.333233134534162,-0.94284446121751));
#53497=DIRECTION('ref_axis',(0.,-0.94284446121751,-0.333233134534162));
#53498=DIRECTION('center_axis',(0.,-0.333233134534162,0.94284446121751));
#53499=DIRECTION('ref_axis',(0.,-0.94284446121751,-0.333233134534162));
#53500=DIRECTION('center_axis',(0.,0.333233134534162,-0.94284446121751));
#53501=DIRECTION('ref_axis',(0.,0.94284446121751,0.333233134534162));
#53502=DIRECTION('',(0.,-0.333233134534162,0.94284446121751));
#53503=DIRECTION('center_axis',(0.,0.333233134534159,-0.942844461217511));
#53504=DIRECTION('ref_axis',(0.,-0.942844461217511,-0.333233134534159));
#53505=DIRECTION('center_axis',(0.,-0.333233134534162,0.94284446121751));
#53506=DIRECTION('ref_axis',(0.,-0.94284446121751,-0.333233134534162));
#53507=DIRECTION('center_axis',(0.,0.333233134534159,-0.942844461217511));
#53508=DIRECTION('ref_axis',(0.,-0.942844461217511,-0.333233134534159));
#53509=DIRECTION('',(0.,0.333233134534162,-0.94284446121751));
#53510=DIRECTION('center_axis',(0.,0.333233134534162,-0.94284446121751));
#53511=DIRECTION('ref_axis',(0.,-0.94284446121751,-0.333233134534162));
#53512=DIRECTION('center_axis',(0.,-0.333233134534162,0.94284446121751));
#53513=DIRECTION('ref_axis',(0.,-0.94284446121751,-0.333233134534162));
#53514=DIRECTION('center_axis',(0.,0.333233134534162,-0.94284446121751));
#53515=DIRECTION('ref_axis',(0.,0.94284446121751,0.333233134534162));
#53516=DIRECTION('',(0.,-0.333233134534162,0.94284446121751));
#53517=DIRECTION('center_axis',(0.,0.333233134534159,-0.942844461217511));
#53518=DIRECTION('ref_axis',(0.,-0.942844461217511,-0.333233134534159));
#53519=DIRECTION('center_axis',(0.,-0.333233134534162,0.94284446121751));
#53520=DIRECTION('ref_axis',(0.,-0.94284446121751,-0.333233134534162));
#53521=DIRECTION('center_axis',(0.,0.333233134534159,-0.942844461217511));
#53522=DIRECTION('ref_axis',(0.,-0.942844461217511,-0.333233134534159));
#53523=DIRECTION('',(0.,0.333233134534161,-0.94284446121751));
#53524=DIRECTION('center_axis',(0.,0.333233134534162,-0.94284446121751));
#53525=DIRECTION('ref_axis',(0.,-0.94284446121751,-0.333233134534162));
#53526=DIRECTION('center_axis',(0.,-0.333233134534162,0.94284446121751));
#53527=DIRECTION('ref_axis',(0.,-0.94284446121751,-0.333233134534162));
#53528=DIRECTION('center_axis',(0.,0.333233134534162,-0.94284446121751));
#53529=DIRECTION('ref_axis',(0.,0.94284446121751,0.333233134534162));
#53530=DIRECTION('',(0.,-0.333233134534162,0.94284446121751));
#53531=DIRECTION('center_axis',(0.,0.333233134534159,-0.942844461217511));
#53532=DIRECTION('ref_axis',(0.,-0.942844461217511,-0.333233134534159));
#53533=DIRECTION('center_axis',(0.,-0.333233134534162,0.94284446121751));
#53534=DIRECTION('ref_axis',(0.,-0.94284446121751,-0.333233134534162));
#53535=DIRECTION('center_axis',(0.,0.333233134534159,-0.942844461217511));
#53536=DIRECTION('ref_axis',(0.,-0.942844461217511,-0.333233134534159));
#53537=DIRECTION('',(0.,0.333233134534162,-0.94284446121751));
#53538=DIRECTION('center_axis',(0.,-0.333233134534162,0.94284446121751));
#53539=DIRECTION('ref_axis',(0.,-0.94284446121751,-0.333233134534162));
#53540=DIRECTION('center_axis',(0.,-0.333233134534162,0.94284446121751));
#53541=DIRECTION('ref_axis',(0.,-0.94284446121751,-0.333233134534162));
#53542=DIRECTION('center_axis',(0.,0.333233134534162,-0.94284446121751));
#53543=DIRECTION('ref_axis',(0.,0.94284446121751,0.333233134534162));
#53544=DIRECTION('',(0.,-0.333233134534162,0.94284446121751));
#53545=DIRECTION('center_axis',(0.,0.333233134534159,-0.942844461217511));
#53546=DIRECTION('ref_axis',(0.,-0.942844461217511,-0.333233134534159));
#53547=DIRECTION('center_axis',(0.,-0.333233134534162,0.94284446121751));
#53548=DIRECTION('ref_axis',(0.,-0.94284446121751,-0.333233134534162));
#53549=DIRECTION('center_axis',(0.,0.333233134534159,-0.942844461217511));
#53550=DIRECTION('ref_axis',(0.,-0.942844461217511,-0.333233134534159));
#53551=DIRECTION('',(0.,0.333233134534162,-0.94284446121751));
#53552=DIRECTION('center_axis',(0.,0.333233134534162,-0.94284446121751));
#53553=DIRECTION('ref_axis',(0.,-0.94284446121751,-0.333233134534162));
#53554=DIRECTION('center_axis',(0.,-0.333233134534162,0.94284446121751));
#53555=DIRECTION('ref_axis',(0.,-0.94284446121751,-0.333233134534162));
#53556=DIRECTION('center_axis',(0.,0.333233134534162,-0.94284446121751));
#53557=DIRECTION('ref_axis',(0.,0.94284446121751,0.333233134534162));
#53558=DIRECTION('',(0.,-0.333233134534162,0.94284446121751));
#53559=DIRECTION('center_axis',(0.,0.333233134534159,-0.942844461217511));
#53560=DIRECTION('ref_axis',(0.,-0.942844461217511,-0.333233134534159));
#53561=DIRECTION('center_axis',(0.,-0.333233134534162,0.94284446121751));
#53562=DIRECTION('ref_axis',(0.,-0.94284446121751,-0.333233134534162));
#53563=DIRECTION('center_axis',(0.,0.333233134534159,-0.942844461217511));
#53564=DIRECTION('ref_axis',(0.,-0.942844461217511,-0.333233134534159));
#53565=DIRECTION('',(0.,0.333233134534162,-0.94284446121751));
#53566=DIRECTION('center_axis',(0.,0.333233134534162,-0.94284446121751));
#53567=DIRECTION('ref_axis',(0.,-0.94284446121751,-0.333233134534162));
#53568=DIRECTION('center_axis',(0.,-0.333233134534162,0.94284446121751));
#53569=DIRECTION('ref_axis',(0.,-0.94284446121751,-0.333233134534162));
#53570=DIRECTION('center_axis',(0.,0.333233134534162,-0.94284446121751));
#53571=DIRECTION('ref_axis',(0.,0.94284446121751,0.333233134534162));
#53572=DIRECTION('',(0.,-0.333233134534162,0.94284446121751));
#53573=DIRECTION('center_axis',(0.,0.333233134534159,-0.942844461217511));
#53574=DIRECTION('ref_axis',(0.,-0.942844461217511,-0.333233134534159));
#53575=DIRECTION('center_axis',(0.,-0.333233134534162,0.94284446121751));
#53576=DIRECTION('ref_axis',(0.,-0.94284446121751,-0.333233134534162));
#53577=DIRECTION('center_axis',(0.,0.333233134534159,-0.942844461217511));
#53578=DIRECTION('ref_axis',(0.,-0.942844461217511,-0.333233134534159));
#53579=DIRECTION('',(0.,0.333233134534162,-0.94284446121751));
#53580=DIRECTION('center_axis',(0.,0.333233134534162,-0.94284446121751));
#53581=DIRECTION('ref_axis',(0.,-0.94284446121751,-0.333233134534162));
#53582=DIRECTION('center_axis',(0.,-0.333233134534162,0.94284446121751));
#53583=DIRECTION('ref_axis',(0.,-0.94284446121751,-0.333233134534162));
#53584=DIRECTION('center_axis',(0.,0.333233134534162,-0.94284446121751));
#53585=DIRECTION('ref_axis',(0.,0.94284446121751,0.333233134534162));
#53586=DIRECTION('',(0.,-0.333233134534162,0.94284446121751));
#53587=DIRECTION('center_axis',(0.,0.333233134534159,-0.942844461217511));
#53588=DIRECTION('ref_axis',(0.,-0.942844461217511,-0.333233134534159));
#53589=DIRECTION('center_axis',(0.,-0.333233134534162,0.94284446121751));
#53590=DIRECTION('ref_axis',(0.,-0.94284446121751,-0.333233134534162));
#53591=DIRECTION('center_axis',(0.,0.333233134534159,-0.942844461217511));
#53592=DIRECTION('ref_axis',(0.,-0.942844461217511,-0.333233134534159));
#53593=DIRECTION('',(0.,0.333233134534162,-0.94284446121751));
#53594=DIRECTION('center_axis',(0.,0.333233134534162,-0.94284446121751));
#53595=DIRECTION('ref_axis',(0.,-0.94284446121751,-0.333233134534162));
#53596=DIRECTION('center_axis',(0.,-0.333233134534162,0.94284446121751));
#53597=DIRECTION('ref_axis',(0.,-0.94284446121751,-0.333233134534162));
#53598=DIRECTION('center_axis',(0.,0.333233134534162,-0.94284446121751));
#53599=DIRECTION('ref_axis',(0.,0.94284446121751,0.333233134534162));
#53600=DIRECTION('',(0.,-0.333233134534162,0.94284446121751));
#53601=DIRECTION('center_axis',(0.,0.333233134534159,-0.942844461217511));
#53602=DIRECTION('ref_axis',(0.,-0.942844461217511,-0.333233134534159));
#53603=DIRECTION('center_axis',(0.,-0.333233134534162,0.94284446121751));
#53604=DIRECTION('ref_axis',(0.,-0.94284446121751,-0.333233134534162));
#53605=DIRECTION('center_axis',(0.,0.333233134534159,-0.942844461217511));
#53606=DIRECTION('ref_axis',(0.,-0.942844461217511,-0.333233134534159));
#53607=DIRECTION('',(0.,0.333233134534162,-0.94284446121751));
#53608=DIRECTION('center_axis',(0.,0.333233134534162,-0.94284446121751));
#53609=DIRECTION('ref_axis',(0.,-0.94284446121751,-0.333233134534162));
#53610=DIRECTION('center_axis',(0.,-0.333233134534162,0.94284446121751));
#53611=DIRECTION('ref_axis',(0.,-0.94284446121751,-0.333233134534162));
#53612=DIRECTION('center_axis',(0.,0.333233134534162,-0.94284446121751));
#53613=DIRECTION('ref_axis',(0.,0.94284446121751,0.333233134534162));
#53614=DIRECTION('',(0.,-0.333233134534162,0.94284446121751));
#53615=DIRECTION('center_axis',(0.,0.333233134534159,-0.942844461217511));
#53616=DIRECTION('ref_axis',(0.,-0.942844461217511,-0.333233134534159));
#53617=DIRECTION('center_axis',(0.,-0.333233134534162,0.94284446121751));
#53618=DIRECTION('ref_axis',(0.,-0.94284446121751,-0.333233134534162));
#53619=DIRECTION('center_axis',(0.,0.333233134534159,-0.942844461217511));
#53620=DIRECTION('ref_axis',(0.,-0.942844461217511,-0.333233134534159));
#53621=DIRECTION('',(0.,0.333233134534162,-0.94284446121751));
#53622=DIRECTION('center_axis',(0.,0.333233134534162,-0.94284446121751));
#53623=DIRECTION('ref_axis',(0.,-0.94284446121751,-0.333233134534162));
#53624=DIRECTION('center_axis',(0.,-0.333233134534162,0.94284446121751));
#53625=DIRECTION('ref_axis',(0.,-0.94284446121751,-0.333233134534162));
#53626=DIRECTION('center_axis',(0.,0.333233134534162,-0.94284446121751));
#53627=DIRECTION('ref_axis',(0.,0.94284446121751,0.333233134534162));
#53628=DIRECTION('',(0.,-0.333233134534162,0.94284446121751));
#53629=DIRECTION('center_axis',(0.,0.333233134534159,-0.942844461217511));
#53630=DIRECTION('ref_axis',(0.,-0.942844461217511,-0.333233134534159));
#53631=DIRECTION('center_axis',(0.,-0.333233134534162,0.94284446121751));
#53632=DIRECTION('ref_axis',(0.,-0.94284446121751,-0.333233134534162));
#53633=DIRECTION('center_axis',(0.,0.333233134534159,-0.942844461217511));
#53634=DIRECTION('ref_axis',(0.,-0.942844461217511,-0.333233134534159));
#53635=DIRECTION('',(0.,0.333233134534162,-0.94284446121751));
#53636=DIRECTION('center_axis',(0.,0.333233134534162,-0.94284446121751));
#53637=DIRECTION('ref_axis',(0.,-0.94284446121751,-0.333233134534162));
#53638=DIRECTION('center_axis',(0.,-0.333233134534162,0.94284446121751));
#53639=DIRECTION('ref_axis',(0.,-0.94284446121751,-0.333233134534162));
#53640=DIRECTION('center_axis',(0.,0.333233134534162,-0.94284446121751));
#53641=DIRECTION('ref_axis',(0.,0.94284446121751,0.333233134534162));
#53642=DIRECTION('',(0.,-0.333233134534162,0.94284446121751));
#53643=DIRECTION('center_axis',(0.,0.333233134534159,-0.942844461217511));
#53644=DIRECTION('ref_axis',(0.,-0.942844461217511,-0.333233134534159));
#53645=DIRECTION('center_axis',(0.,-0.333233134534162,0.94284446121751));
#53646=DIRECTION('ref_axis',(0.,-0.94284446121751,-0.333233134534162));
#53647=DIRECTION('center_axis',(0.,0.333233134534159,-0.942844461217511));
#53648=DIRECTION('ref_axis',(0.,-0.942844461217511,-0.333233134534159));
#53649=DIRECTION('',(0.,0.333233134534162,-0.94284446121751));
#53650=DIRECTION('center_axis',(0.,0.333233134534162,-0.94284446121751));
#53651=DIRECTION('ref_axis',(0.,-0.94284446121751,-0.333233134534162));
#53652=DIRECTION('center_axis',(0.,-0.333233134534162,0.94284446121751));
#53653=DIRECTION('ref_axis',(0.,-0.94284446121751,-0.333233134534162));
#53654=DIRECTION('center_axis',(0.,0.333233134534162,-0.94284446121751));
#53655=DIRECTION('ref_axis',(0.,0.94284446121751,0.333233134534162));
#53656=DIRECTION('',(0.,-0.333233134534162,0.94284446121751));
#53657=DIRECTION('center_axis',(0.,0.333233134534159,-0.942844461217511));
#53658=DIRECTION('ref_axis',(0.,-0.942844461217511,-0.333233134534159));
#53659=DIRECTION('center_axis',(0.,-0.333233134534162,0.94284446121751));
#53660=DIRECTION('ref_axis',(0.,-0.94284446121751,-0.333233134534162));
#53661=DIRECTION('center_axis',(0.,0.333233134534159,-0.942844461217511));
#53662=DIRECTION('ref_axis',(0.,-0.942844461217511,-0.333233134534159));
#53663=DIRECTION('',(0.,0.333233134534162,-0.94284446121751));
#53664=DIRECTION('center_axis',(0.,-0.333233134534162,0.94284446121751));
#53665=DIRECTION('ref_axis',(0.,-0.94284446121751,-0.333233134534162));
#53666=DIRECTION('center_axis',(0.,-0.333233134534162,0.94284446121751));
#53667=DIRECTION('ref_axis',(0.,-0.94284446121751,-0.333233134534162));
#53668=DIRECTION('center_axis',(0.,0.333233134534162,-0.94284446121751));
#53669=DIRECTION('ref_axis',(0.,0.94284446121751,0.333233134534162));
#53670=DIRECTION('',(0.,-0.333233134534162,0.94284446121751));
#53671=DIRECTION('center_axis',(0.,0.333233134534159,-0.942844461217511));
#53672=DIRECTION('ref_axis',(0.,-0.942844461217511,-0.333233134534159));
#53673=DIRECTION('center_axis',(0.,-0.333233134534162,0.94284446121751));
#53674=DIRECTION('ref_axis',(0.,-0.94284446121751,-0.333233134534161));
#53675=DIRECTION('center_axis',(0.,0.333233134534159,-0.942844461217511));
#53676=DIRECTION('ref_axis',(0.,-0.942844461217511,-0.333233134534159));
#53677=DIRECTION('',(0.,0.333233134534162,-0.94284446121751));
#53678=DIRECTION('center_axis',(0.,0.333233134534162,-0.94284446121751));
#53679=DIRECTION('ref_axis',(0.,-0.94284446121751,-0.333233134534162));
#53680=DIRECTION('center_axis',(0.,-0.333233134534162,0.94284446121751));
#53681=DIRECTION('ref_axis',(0.,-0.94284446121751,-0.333233134534162));
#53682=DIRECTION('center_axis',(0.,0.333233134534162,-0.94284446121751));
#53683=DIRECTION('ref_axis',(0.,0.94284446121751,0.333233134534162));
#53684=DIRECTION('',(0.,-0.333233134534162,0.94284446121751));
#53685=DIRECTION('center_axis',(0.,0.333233134534159,-0.942844461217511));
#53686=DIRECTION('ref_axis',(0.,-0.942844461217511,-0.333233134534159));
#53687=DIRECTION('center_axis',(0.,-0.333233134534162,0.94284446121751));
#53688=DIRECTION('ref_axis',(0.,-0.94284446121751,-0.333233134534162));
#53689=DIRECTION('center_axis',(0.,0.333233134534159,-0.942844461217511));
#53690=DIRECTION('ref_axis',(0.,-0.942844461217511,-0.333233134534159));
#53691=DIRECTION('',(0.,0.333233134534162,-0.94284446121751));
#53692=DIRECTION('center_axis',(0.,0.333233134534162,-0.94284446121751));
#53693=DIRECTION('ref_axis',(0.,-0.94284446121751,-0.333233134534162));
#53694=DIRECTION('center_axis',(0.,-0.333233134534162,0.94284446121751));
#53695=DIRECTION('ref_axis',(0.,-0.94284446121751,-0.333233134534162));
#53696=DIRECTION('center_axis',(0.,0.333233134534162,-0.94284446121751));
#53697=DIRECTION('ref_axis',(0.,0.94284446121751,0.333233134534162));
#53698=DIRECTION('',(0.,-0.333233134534162,0.94284446121751));
#53699=DIRECTION('center_axis',(0.,0.333233134534159,-0.942844461217511));
#53700=DIRECTION('ref_axis',(0.,-0.942844461217511,-0.333233134534159));
#53701=DIRECTION('center_axis',(0.,-0.333233134534162,0.94284446121751));
#53702=DIRECTION('ref_axis',(0.,-0.94284446121751,-0.333233134534162));
#53703=DIRECTION('center_axis',(0.,0.333233134534159,-0.942844461217511));
#53704=DIRECTION('ref_axis',(0.,-0.942844461217511,-0.333233134534159));
#53705=DIRECTION('',(0.,0.333233134534162,-0.94284446121751));
#53706=DIRECTION('center_axis',(0.,0.333233134534162,-0.94284446121751));
#53707=DIRECTION('ref_axis',(0.,-0.94284446121751,-0.333233134534162));
#53708=DIRECTION('center_axis',(0.,-0.333233134534162,0.94284446121751));
#53709=DIRECTION('ref_axis',(0.,-0.94284446121751,-0.333233134534162));
#53710=DIRECTION('center_axis',(0.,0.333233134534162,-0.94284446121751));
#53711=DIRECTION('ref_axis',(0.,0.94284446121751,0.333233134534162));
#53712=DIRECTION('',(0.,-0.333233134534162,0.94284446121751));
#53713=DIRECTION('center_axis',(0.,0.333233134534159,-0.942844461217511));
#53714=DIRECTION('ref_axis',(0.,-0.942844461217511,-0.333233134534159));
#53715=DIRECTION('center_axis',(0.,-0.333233134534162,0.94284446121751));
#53716=DIRECTION('ref_axis',(0.,-0.94284446121751,-0.333233134534162));
#53717=DIRECTION('center_axis',(0.,0.333233134534159,-0.942844461217511));
#53718=DIRECTION('ref_axis',(0.,-0.942844461217511,-0.333233134534159));
#53719=DIRECTION('',(0.,0.333233134534162,-0.94284446121751));
#53720=DIRECTION('center_axis',(0.,0.333233134534162,-0.94284446121751));
#53721=DIRECTION('ref_axis',(0.,-0.94284446121751,-0.333233134534162));
#53722=DIRECTION('center_axis',(0.,-0.333233134534162,0.94284446121751));
#53723=DIRECTION('ref_axis',(0.,-0.94284446121751,-0.333233134534162));
#53724=DIRECTION('center_axis',(0.,0.333233134534162,-0.94284446121751));
#53725=DIRECTION('ref_axis',(0.,0.94284446121751,0.333233134534162));
#53726=DIRECTION('',(0.,-0.333233134534162,0.94284446121751));
#53727=DIRECTION('center_axis',(0.,0.333233134534159,-0.942844461217511));
#53728=DIRECTION('ref_axis',(0.,-0.942844461217511,-0.333233134534159));
#53729=DIRECTION('center_axis',(0.,-0.333233134534162,0.94284446121751));
#53730=DIRECTION('ref_axis',(0.,-0.94284446121751,-0.333233134534162));
#53731=DIRECTION('center_axis',(0.,0.333233134534159,-0.942844461217511));
#53732=DIRECTION('ref_axis',(0.,-0.942844461217511,-0.333233134534159));
#53733=DIRECTION('',(0.,0.333233134534162,-0.94284446121751));
#53734=DIRECTION('center_axis',(0.,0.333233134534162,-0.94284446121751));
#53735=DIRECTION('ref_axis',(0.,-0.94284446121751,-0.333233134534162));
#53736=DIRECTION('center_axis',(0.,-0.333233134534162,0.94284446121751));
#53737=DIRECTION('ref_axis',(0.,-0.94284446121751,-0.333233134534162));
#53738=DIRECTION('center_axis',(0.,0.333233134534162,-0.94284446121751));
#53739=DIRECTION('ref_axis',(0.,0.94284446121751,0.333233134534162));
#53740=DIRECTION('',(0.,-0.333233134534162,0.94284446121751));
#53741=DIRECTION('center_axis',(0.,0.333233134534159,-0.942844461217511));
#53742=DIRECTION('ref_axis',(0.,-0.942844461217511,-0.333233134534159));
#53743=DIRECTION('center_axis',(0.,-0.333233134534162,0.94284446121751));
#53744=DIRECTION('ref_axis',(0.,-0.94284446121751,-0.333233134534162));
#53745=DIRECTION('center_axis',(0.,0.333233134534159,-0.942844461217511));
#53746=DIRECTION('ref_axis',(0.,-0.942844461217511,-0.333233134534159));
#53747=DIRECTION('',(0.,0.333233134534162,-0.94284446121751));
#53748=DIRECTION('center_axis',(0.,0.333233134534162,-0.94284446121751));
#53749=DIRECTION('ref_axis',(0.,-0.94284446121751,-0.333233134534162));
#53750=DIRECTION('center_axis',(0.,-0.333233134534162,0.94284446121751));
#53751=DIRECTION('ref_axis',(0.,-0.94284446121751,-0.333233134534162));
#53752=DIRECTION('center_axis',(0.,0.333233134534162,-0.94284446121751));
#53753=DIRECTION('ref_axis',(0.,0.94284446121751,0.333233134534162));
#53754=DIRECTION('',(0.,-0.333233134534162,0.94284446121751));
#53755=DIRECTION('center_axis',(0.,0.333233134534159,-0.942844461217511));
#53756=DIRECTION('ref_axis',(0.,-0.942844461217511,-0.333233134534159));
#53757=DIRECTION('center_axis',(0.,-0.333233134534162,0.94284446121751));
#53758=DIRECTION('ref_axis',(0.,-0.94284446121751,-0.333233134534162));
#53759=DIRECTION('center_axis',(0.,0.333233134534159,-0.942844461217511));
#53760=DIRECTION('ref_axis',(0.,-0.942844461217511,-0.333233134534159));
#53761=DIRECTION('',(0.,0.333233134534162,-0.94284446121751));
#53762=DIRECTION('center_axis',(0.,0.333233134534162,-0.94284446121751));
#53763=DIRECTION('ref_axis',(0.,-0.94284446121751,-0.333233134534162));
#53764=DIRECTION('center_axis',(0.,-0.333233134534162,0.94284446121751));
#53765=DIRECTION('ref_axis',(0.,-0.94284446121751,-0.333233134534162));
#53766=DIRECTION('center_axis',(0.,0.333233134534162,-0.94284446121751));
#53767=DIRECTION('ref_axis',(0.,0.94284446121751,0.333233134534162));
#53768=DIRECTION('',(0.,-0.333233134534162,0.94284446121751));
#53769=DIRECTION('center_axis',(0.,0.333233134534159,-0.942844461217511));
#53770=DIRECTION('ref_axis',(0.,-0.942844461217511,-0.333233134534159));
#53771=DIRECTION('center_axis',(0.,-0.333233134534162,0.94284446121751));
#53772=DIRECTION('ref_axis',(0.,-0.94284446121751,-0.333233134534162));
#53773=DIRECTION('center_axis',(0.,0.333233134534159,-0.942844461217511));
#53774=DIRECTION('ref_axis',(0.,-0.942844461217511,-0.333233134534159));
#53775=DIRECTION('',(0.,0.333233134534162,-0.94284446121751));
#53776=DIRECTION('center_axis',(0.,0.333233134534162,-0.94284446121751));
#53777=DIRECTION('ref_axis',(0.,-0.94284446121751,-0.333233134534162));
#53778=DIRECTION('center_axis',(0.,-0.333233134534162,0.94284446121751));
#53779=DIRECTION('ref_axis',(0.,-0.94284446121751,-0.333233134534162));
#53780=DIRECTION('center_axis',(0.,0.333233134534162,-0.94284446121751));
#53781=DIRECTION('ref_axis',(0.,0.94284446121751,0.333233134534162));
#53782=DIRECTION('',(0.,-0.333233134534162,0.94284446121751));
#53783=DIRECTION('center_axis',(0.,0.333233134534159,-0.942844461217511));
#53784=DIRECTION('ref_axis',(0.,-0.942844461217511,-0.333233134534159));
#53785=DIRECTION('center_axis',(0.,-0.333233134534162,0.94284446121751));
#53786=DIRECTION('ref_axis',(0.,-0.94284446121751,-0.333233134534162));
#53787=DIRECTION('center_axis',(0.,0.333233134534159,-0.942844461217511));
#53788=DIRECTION('ref_axis',(0.,-0.942844461217511,-0.333233134534159));
#53789=DIRECTION('',(0.,0.333233134534162,-0.94284446121751));
#53790=DIRECTION('center_axis',(0.,-0.333233134534162,0.94284446121751));
#53791=DIRECTION('ref_axis',(0.,-0.94284446121751,-0.333233134534162));
#53792=DIRECTION('center_axis',(0.,-0.333233134534162,0.94284446121751));
#53793=DIRECTION('ref_axis',(0.,-0.94284446121751,-0.333233134534162));
#53794=DIRECTION('center_axis',(0.,0.333233134534162,-0.94284446121751));
#53795=DIRECTION('ref_axis',(0.,0.94284446121751,0.333233134534162));
#53796=DIRECTION('',(0.,-0.333233134534162,0.94284446121751));
#53797=DIRECTION('center_axis',(0.,0.333233134534159,-0.942844461217511));
#53798=DIRECTION('ref_axis',(0.,-0.942844461217511,-0.333233134534159));
#53799=DIRECTION('center_axis',(0.,-0.333233134534162,0.94284446121751));
#53800=DIRECTION('ref_axis',(0.,-0.94284446121751,-0.333233134534161));
#53801=DIRECTION('center_axis',(0.,0.333233134534159,-0.942844461217511));
#53802=DIRECTION('ref_axis',(0.,-0.942844461217511,-0.333233134534159));
#53803=DIRECTION('',(0.,0.333233134534162,-0.94284446121751));
#53804=DIRECTION('center_axis',(0.,0.333233134534162,-0.94284446121751));
#53805=DIRECTION('ref_axis',(0.,-0.94284446121751,-0.333233134534162));
#53806=DIRECTION('center_axis',(0.,-0.333233134534162,0.94284446121751));
#53807=DIRECTION('ref_axis',(0.,-0.94284446121751,-0.333233134534162));
#53808=DIRECTION('center_axis',(0.,0.333233134534162,-0.94284446121751));
#53809=DIRECTION('ref_axis',(0.,0.94284446121751,0.333233134534162));
#53810=DIRECTION('',(0.,-0.333233134534162,0.94284446121751));
#53811=DIRECTION('center_axis',(0.,0.333233134534159,-0.942844461217511));
#53812=DIRECTION('ref_axis',(0.,-0.942844461217511,-0.333233134534159));
#53813=DIRECTION('center_axis',(0.,-0.333233134534162,0.94284446121751));
#53814=DIRECTION('ref_axis',(0.,-0.94284446121751,-0.333233134534162));
#53815=DIRECTION('center_axis',(0.,0.333233134534159,-0.942844461217511));
#53816=DIRECTION('ref_axis',(0.,-0.942844461217511,-0.333233134534159));
#53817=DIRECTION('',(0.,0.333233134534162,-0.94284446121751));
#53818=DIRECTION('center_axis',(0.,0.333233134534162,-0.94284446121751));
#53819=DIRECTION('ref_axis',(0.,-0.94284446121751,-0.333233134534162));
#53820=DIRECTION('center_axis',(0.,-0.333233134534162,0.94284446121751));
#53821=DIRECTION('ref_axis',(0.,-0.94284446121751,-0.333233134534161));
#53822=DIRECTION('center_axis',(0.,0.333233134534162,-0.94284446121751));
#53823=DIRECTION('ref_axis',(0.,0.94284446121751,0.333233134534162));
#53824=DIRECTION('',(0.,-0.333233134534162,0.94284446121751));
#53825=DIRECTION('center_axis',(0.,0.333233134534159,-0.942844461217511));
#53826=DIRECTION('ref_axis',(0.,-0.942844461217511,-0.333233134534159));
#53827=DIRECTION('center_axis',(0.,-0.333233134534162,0.94284446121751));
#53828=DIRECTION('ref_axis',(0.,-0.94284446121751,-0.333233134534162));
#53829=DIRECTION('center_axis',(0.,0.333233134534159,-0.942844461217511));
#53830=DIRECTION('ref_axis',(0.,-0.942844461217511,-0.333233134534159));
#53831=DIRECTION('',(0.,0.333233134534162,-0.94284446121751));
#53832=DIRECTION('center_axis',(0.,0.333233134534162,-0.94284446121751));
#53833=DIRECTION('ref_axis',(0.,-0.94284446121751,-0.333233134534162));
#53834=DIRECTION('center_axis',(0.,-0.333233134534162,0.94284446121751));
#53835=DIRECTION('ref_axis',(0.,-0.94284446121751,-0.333233134534162));
#53836=DIRECTION('center_axis',(0.,0.333233134534162,-0.94284446121751));
#53837=DIRECTION('ref_axis',(0.,0.94284446121751,0.333233134534162));
#53838=DIRECTION('',(0.,-0.333233134534162,0.94284446121751));
#53839=DIRECTION('center_axis',(0.,0.333233134534159,-0.942844461217511));
#53840=DIRECTION('ref_axis',(0.,-0.942844461217511,-0.333233134534159));
#53841=DIRECTION('center_axis',(0.,-0.333233134534162,0.94284446121751));
#53842=DIRECTION('ref_axis',(0.,-0.94284446121751,-0.333233134534162));
#53843=DIRECTION('center_axis',(0.,0.333233134534159,-0.942844461217511));
#53844=DIRECTION('ref_axis',(0.,-0.942844461217511,-0.333233134534159));
#53845=DIRECTION('',(0.,0.333233134534162,-0.94284446121751));
#53846=DIRECTION('center_axis',(0.,0.333233134534162,-0.94284446121751));
#53847=DIRECTION('ref_axis',(0.,-0.94284446121751,-0.333233134534162));
#53848=DIRECTION('center_axis',(0.,-0.333233134534162,0.94284446121751));
#53849=DIRECTION('ref_axis',(0.,-0.94284446121751,-0.333233134534162));
#53850=DIRECTION('center_axis',(0.,0.333233134534162,-0.94284446121751));
#53851=DIRECTION('ref_axis',(0.,0.94284446121751,0.333233134534162));
#53852=DIRECTION('',(0.,-0.333233134534162,0.94284446121751));
#53853=DIRECTION('center_axis',(0.,0.333233134534159,-0.942844461217511));
#53854=DIRECTION('ref_axis',(0.,-0.942844461217511,-0.333233134534159));
#53855=DIRECTION('center_axis',(0.,-0.333233134534162,0.94284446121751));
#53856=DIRECTION('ref_axis',(0.,-0.94284446121751,-0.333233134534162));
#53857=DIRECTION('center_axis',(0.,0.333233134534159,-0.942844461217511));
#53858=DIRECTION('ref_axis',(0.,-0.942844461217511,-0.333233134534159));
#53859=DIRECTION('',(0.,0.333233134534162,-0.94284446121751));
#53860=DIRECTION('center_axis',(0.,0.333233134534162,-0.94284446121751));
#53861=DIRECTION('ref_axis',(0.,-0.94284446121751,-0.333233134534162));
#53862=DIRECTION('center_axis',(0.,-0.333233134534162,0.94284446121751));
#53863=DIRECTION('ref_axis',(0.,-0.94284446121751,-0.333233134534162));
#53864=DIRECTION('center_axis',(0.,0.333233134534162,-0.94284446121751));
#53865=DIRECTION('ref_axis',(0.,0.94284446121751,0.333233134534162));
#53866=DIRECTION('',(0.,-0.333233134534162,0.94284446121751));
#53867=DIRECTION('center_axis',(0.,0.333233134534159,-0.942844461217511));
#53868=DIRECTION('ref_axis',(0.,-0.942844461217511,-0.333233134534159));
#53869=DIRECTION('center_axis',(0.,-0.333233134534162,0.94284446121751));
#53870=DIRECTION('ref_axis',(0.,-0.94284446121751,-0.333233134534162));
#53871=DIRECTION('center_axis',(0.,0.333233134534159,-0.942844461217511));
#53872=DIRECTION('ref_axis',(0.,-0.942844461217511,-0.333233134534159));
#53873=DIRECTION('',(0.,0.333233134534162,-0.94284446121751));
#53874=DIRECTION('center_axis',(0.,0.333233134534162,-0.94284446121751));
#53875=DIRECTION('ref_axis',(0.,-0.94284446121751,-0.333233134534162));
#53876=DIRECTION('center_axis',(0.,-0.333233134534162,0.94284446121751));
#53877=DIRECTION('ref_axis',(0.,-0.94284446121751,-0.333233134534162));
#53878=DIRECTION('center_axis',(0.,0.333233134534162,-0.94284446121751));
#53879=DIRECTION('ref_axis',(0.,0.94284446121751,0.333233134534162));
#53880=DIRECTION('',(0.,-0.333233134534162,0.94284446121751));
#53881=DIRECTION('center_axis',(0.,0.333233134534159,-0.942844461217511));
#53882=DIRECTION('ref_axis',(0.,-0.942844461217511,-0.333233134534159));
#53883=DIRECTION('center_axis',(0.,-0.333233134534162,0.94284446121751));
#53884=DIRECTION('ref_axis',(0.,-0.94284446121751,-0.333233134534162));
#53885=DIRECTION('center_axis',(0.,0.333233134534159,-0.942844461217511));
#53886=DIRECTION('ref_axis',(0.,-0.942844461217511,-0.333233134534159));
#53887=DIRECTION('',(0.,0.333233134534162,-0.94284446121751));
#53888=DIRECTION('center_axis',(0.,0.333233134534162,-0.94284446121751));
#53889=DIRECTION('ref_axis',(0.,-0.94284446121751,-0.333233134534162));
#53890=DIRECTION('center_axis',(0.,-0.333233134534162,0.94284446121751));
#53891=DIRECTION('ref_axis',(0.,-0.94284446121751,-0.333233134534162));
#53892=DIRECTION('center_axis',(0.,0.333233134534162,-0.94284446121751));
#53893=DIRECTION('ref_axis',(0.,0.94284446121751,0.333233134534162));
#53894=DIRECTION('',(0.,-0.333233134534162,0.94284446121751));
#53895=DIRECTION('center_axis',(0.,0.333233134534159,-0.942844461217511));
#53896=DIRECTION('ref_axis',(0.,-0.942844461217511,-0.333233134534159));
#53897=DIRECTION('center_axis',(0.,-0.333233134534162,0.94284446121751));
#53898=DIRECTION('ref_axis',(0.,-0.94284446121751,-0.333233134534162));
#53899=DIRECTION('center_axis',(0.,0.333233134534159,-0.942844461217511));
#53900=DIRECTION('ref_axis',(0.,-0.942844461217511,-0.333233134534159));
#53901=DIRECTION('',(0.,0.333233134534162,-0.94284446121751));
#53902=DIRECTION('center_axis',(0.,-0.333233134534162,0.94284446121751));
#53903=DIRECTION('ref_axis',(0.,-0.94284446121751,-0.333233134534162));
#53904=DIRECTION('center_axis',(0.,-0.333233134534162,0.94284446121751));
#53905=DIRECTION('ref_axis',(0.,-0.94284446121751,-0.333233134534162));
#53906=DIRECTION('center_axis',(0.,0.333233134534162,-0.94284446121751));
#53907=DIRECTION('ref_axis',(0.,0.94284446121751,0.333233134534162));
#53908=DIRECTION('',(0.,-0.333233134534162,0.94284446121751));
#53909=DIRECTION('center_axis',(0.,0.333233134534159,-0.942844461217511));
#53910=DIRECTION('ref_axis',(0.,-0.942844461217511,-0.333233134534159));
#53911=DIRECTION('center_axis',(0.,-0.333233134534162,0.94284446121751));
#53912=DIRECTION('ref_axis',(0.,-0.94284446121751,-0.333233134534162));
#53913=DIRECTION('center_axis',(0.,0.333233134534159,-0.942844461217511));
#53914=DIRECTION('ref_axis',(0.,-0.942844461217511,-0.333233134534159));
#53915=DIRECTION('',(0.,0.333233134534162,-0.94284446121751));
#53916=DIRECTION('center_axis',(0.,0.333233134534162,-0.94284446121751));
#53917=DIRECTION('ref_axis',(0.,-0.94284446121751,-0.333233134534162));
#53918=DIRECTION('center_axis',(0.,-0.333233134534162,0.94284446121751));
#53919=DIRECTION('ref_axis',(0.,-0.94284446121751,-0.333233134534162));
#53920=DIRECTION('center_axis',(0.,0.333233134534162,-0.94284446121751));
#53921=DIRECTION('ref_axis',(0.,0.94284446121751,0.333233134534162));
#53922=DIRECTION('',(0.,-0.333233134534162,0.94284446121751));
#53923=DIRECTION('center_axis',(0.,0.333233134534159,-0.942844461217511));
#53924=DIRECTION('ref_axis',(0.,-0.942844461217511,-0.333233134534159));
#53925=DIRECTION('center_axis',(0.,-0.333233134534162,0.94284446121751));
#53926=DIRECTION('ref_axis',(0.,-0.94284446121751,-0.333233134534162));
#53927=DIRECTION('center_axis',(0.,0.333233134534159,-0.942844461217511));
#53928=DIRECTION('ref_axis',(0.,-0.942844461217511,-0.333233134534159));
#53929=DIRECTION('',(0.,0.333233134534162,-0.94284446121751));
#53930=DIRECTION('center_axis',(0.,0.333233134534162,-0.94284446121751));
#53931=DIRECTION('ref_axis',(0.,-0.94284446121751,-0.333233134534162));
#53932=DIRECTION('center_axis',(0.,-0.333233134534162,0.94284446121751));
#53933=DIRECTION('ref_axis',(0.,-0.94284446121751,-0.333233134534162));
#53934=DIRECTION('center_axis',(0.,0.333233134534162,-0.94284446121751));
#53935=DIRECTION('ref_axis',(0.,0.94284446121751,0.333233134534162));
#53936=DIRECTION('',(0.,-0.333233134534162,0.94284446121751));
#53937=DIRECTION('center_axis',(0.,0.333233134534159,-0.942844461217511));
#53938=DIRECTION('ref_axis',(0.,-0.942844461217511,-0.333233134534159));
#53939=DIRECTION('center_axis',(0.,-0.333233134534162,0.94284446121751));
#53940=DIRECTION('ref_axis',(0.,-0.94284446121751,-0.333233134534162));
#53941=DIRECTION('center_axis',(0.,0.333233134534159,-0.942844461217511));
#53942=DIRECTION('ref_axis',(0.,-0.942844461217511,-0.333233134534159));
#53943=DIRECTION('',(0.,0.333233134534162,-0.94284446121751));
#53944=DIRECTION('center_axis',(0.,0.333233134534162,-0.94284446121751));
#53945=DIRECTION('ref_axis',(0.,-0.94284446121751,-0.333233134534162));
#53946=DIRECTION('center_axis',(0.,-0.333233134534162,0.94284446121751));
#53947=DIRECTION('ref_axis',(0.,-0.94284446121751,-0.333233134534162));
#53948=DIRECTION('center_axis',(0.,0.333233134534162,-0.94284446121751));
#53949=DIRECTION('ref_axis',(0.,0.94284446121751,0.333233134534162));
#53950=DIRECTION('',(0.,-0.333233134534162,0.94284446121751));
#53951=DIRECTION('center_axis',(0.,0.333233134534159,-0.942844461217511));
#53952=DIRECTION('ref_axis',(0.,-0.942844461217511,-0.333233134534159));
#53953=DIRECTION('center_axis',(0.,-0.333233134534162,0.94284446121751));
#53954=DIRECTION('ref_axis',(0.,-0.94284446121751,-0.333233134534162));
#53955=DIRECTION('center_axis',(0.,0.333233134534159,-0.942844461217511));
#53956=DIRECTION('ref_axis',(0.,-0.942844461217511,-0.333233134534159));
#53957=DIRECTION('',(0.,0.333233134534162,-0.94284446121751));
#53958=DIRECTION('center_axis',(0.,0.333233134534162,-0.94284446121751));
#53959=DIRECTION('ref_axis',(0.,-0.94284446121751,-0.333233134534162));
#53960=DIRECTION('center_axis',(0.,-0.333233134534162,0.94284446121751));
#53961=DIRECTION('ref_axis',(0.,-0.94284446121751,-0.333233134534162));
#53962=DIRECTION('center_axis',(0.,0.333233134534162,-0.94284446121751));
#53963=DIRECTION('ref_axis',(0.,0.94284446121751,0.333233134534162));
#53964=DIRECTION('',(0.,-0.333233134534162,0.94284446121751));
#53965=DIRECTION('center_axis',(0.,0.333233134534159,-0.942844461217511));
#53966=DIRECTION('ref_axis',(0.,-0.942844461217511,-0.333233134534159));
#53967=DIRECTION('center_axis',(0.,-0.333233134534162,0.94284446121751));
#53968=DIRECTION('ref_axis',(0.,-0.94284446121751,-0.333233134534162));
#53969=DIRECTION('center_axis',(0.,0.333233134534159,-0.942844461217511));
#53970=DIRECTION('ref_axis',(0.,-0.942844461217511,-0.333233134534159));
#53971=DIRECTION('',(0.,0.333233134534162,-0.94284446121751));
#53972=DIRECTION('center_axis',(0.,0.333233134534162,-0.94284446121751));
#53973=DIRECTION('ref_axis',(0.,-0.94284446121751,-0.333233134534162));
#53974=DIRECTION('center_axis',(0.,-0.333233134534162,0.94284446121751));
#53975=DIRECTION('ref_axis',(0.,-0.94284446121751,-0.333233134534162));
#53976=DIRECTION('center_axis',(0.,0.333233134534162,-0.94284446121751));
#53977=DIRECTION('ref_axis',(0.,0.94284446121751,0.333233134534162));
#53978=DIRECTION('',(0.,-0.333233134534162,0.94284446121751));
#53979=DIRECTION('center_axis',(0.,0.333233134534159,-0.942844461217511));
#53980=DIRECTION('ref_axis',(0.,-0.942844461217511,-0.333233134534159));
#53981=DIRECTION('center_axis',(0.,-0.333233134534162,0.94284446121751));
#53982=DIRECTION('ref_axis',(0.,-0.94284446121751,-0.333233134534162));
#53983=DIRECTION('center_axis',(0.,0.333233134534159,-0.942844461217511));
#53984=DIRECTION('ref_axis',(0.,-0.942844461217511,-0.333233134534159));
#53985=DIRECTION('',(0.,0.333233134534162,-0.94284446121751));
#53986=DIRECTION('center_axis',(0.,0.333233134534162,-0.94284446121751));
#53987=DIRECTION('ref_axis',(0.,-0.94284446121751,-0.333233134534162));
#53988=DIRECTION('center_axis',(0.,-0.333233134534162,0.94284446121751));
#53989=DIRECTION('ref_axis',(0.,-0.94284446121751,-0.333233134534162));
#53990=DIRECTION('center_axis',(0.,0.333233134534162,-0.94284446121751));
#53991=DIRECTION('ref_axis',(0.,0.94284446121751,0.333233134534162));
#53992=DIRECTION('',(0.,-0.333233134534162,0.94284446121751));
#53993=DIRECTION('center_axis',(0.,0.333233134534159,-0.942844461217511));
#53994=DIRECTION('ref_axis',(0.,-0.942844461217511,-0.333233134534159));
#53995=DIRECTION('center_axis',(0.,-0.333233134534162,0.94284446121751));
#53996=DIRECTION('ref_axis',(0.,-0.94284446121751,-0.333233134534161));
#53997=DIRECTION('center_axis',(0.,0.333233134534159,-0.942844461217511));
#53998=DIRECTION('ref_axis',(0.,-0.942844461217511,-0.333233134534159));
#53999=DIRECTION('',(0.,0.333233134534162,-0.94284446121751));
#54000=DIRECTION('center_axis',(0.,0.333233134534162,-0.94284446121751));
#54001=DIRECTION('ref_axis',(0.,-0.94284446121751,-0.333233134534162));
#54002=DIRECTION('center_axis',(0.,-0.333233134534162,0.94284446121751));
#54003=DIRECTION('ref_axis',(0.,-0.94284446121751,-0.333233134534162));
#54004=DIRECTION('center_axis',(0.,0.333233134534162,-0.94284446121751));
#54005=DIRECTION('ref_axis',(0.,0.94284446121751,0.333233134534162));
#54006=DIRECTION('',(0.,-0.333233134534162,0.94284446121751));
#54007=DIRECTION('center_axis',(0.,0.333233134534159,-0.942844461217511));
#54008=DIRECTION('ref_axis',(0.,-0.942844461217511,-0.333233134534159));
#54009=DIRECTION('center_axis',(0.,-0.333233134534162,0.94284446121751));
#54010=DIRECTION('ref_axis',(0.,-0.94284446121751,-0.333233134534162));
#54011=DIRECTION('center_axis',(0.,0.333233134534159,-0.942844461217511));
#54012=DIRECTION('ref_axis',(0.,-0.942844461217511,-0.333233134534159));
#54013=DIRECTION('',(0.,0.333233134534162,-0.94284446121751));
#54014=DIRECTION('center_axis',(0.,0.333233134534162,-0.94284446121751));
#54015=DIRECTION('ref_axis',(0.,-0.94284446121751,-0.333233134534162));
#54016=DIRECTION('center_axis',(0.,-0.333233134534162,0.94284446121751));
#54017=DIRECTION('ref_axis',(0.,-0.94284446121751,-0.333233134534162));
#54018=DIRECTION('center_axis',(0.,0.333233134534162,-0.94284446121751));
#54019=DIRECTION('ref_axis',(0.,0.94284446121751,0.333233134534162));
#54020=DIRECTION('',(0.,-0.333233134534162,0.94284446121751));
#54021=DIRECTION('center_axis',(0.,0.333233134534159,-0.942844461217511));
#54022=DIRECTION('ref_axis',(0.,-0.942844461217511,-0.333233134534159));
#54023=DIRECTION('center_axis',(0.,-0.333233134534162,0.94284446121751));
#54024=DIRECTION('ref_axis',(0.,-0.94284446121751,-0.333233134534162));
#54025=DIRECTION('center_axis',(0.,0.333233134534159,-0.942844461217511));
#54026=DIRECTION('ref_axis',(0.,-0.942844461217511,-0.333233134534159));
#54027=DIRECTION('',(0.,0.333233134534162,-0.94284446121751));
#54028=DIRECTION('center_axis',(0.,-0.333233134534162,0.94284446121751));
#54029=DIRECTION('ref_axis',(0.,-0.94284446121751,-0.333233134534162));
#54030=DIRECTION('center_axis',(0.,-0.333233134534162,0.94284446121751));
#54031=DIRECTION('ref_axis',(0.,-0.94284446121751,-0.333233134534162));
#54032=DIRECTION('center_axis',(0.,0.333233134534162,-0.94284446121751));
#54033=DIRECTION('ref_axis',(0.,0.94284446121751,0.333233134534162));
#54034=DIRECTION('',(0.,-0.333233134534162,0.94284446121751));
#54035=DIRECTION('center_axis',(0.,0.333233134534159,-0.942844461217511));
#54036=DIRECTION('ref_axis',(0.,-0.942844461217511,-0.333233134534159));
#54037=DIRECTION('center_axis',(0.,-0.333233134534162,0.94284446121751));
#54038=DIRECTION('ref_axis',(0.,-0.94284446121751,-0.333233134534161));
#54039=DIRECTION('center_axis',(0.,0.333233134534159,-0.942844461217511));
#54040=DIRECTION('ref_axis',(0.,-0.942844461217511,-0.333233134534159));
#54041=DIRECTION('',(0.,0.333233134534162,-0.94284446121751));
#54042=DIRECTION('center_axis',(0.,0.333233134534162,-0.94284446121751));
#54043=DIRECTION('ref_axis',(0.,-0.94284446121751,-0.333233134534162));
#54044=DIRECTION('center_axis',(0.,-0.333233134534162,0.94284446121751));
#54045=DIRECTION('ref_axis',(0.,-0.94284446121751,-0.333233134534162));
#54046=DIRECTION('center_axis',(0.,0.333233134534162,-0.94284446121751));
#54047=DIRECTION('ref_axis',(0.,0.94284446121751,0.333233134534162));
#54048=DIRECTION('',(0.,-0.333233134534162,0.94284446121751));
#54049=DIRECTION('center_axis',(0.,0.333233134534159,-0.942844461217511));
#54050=DIRECTION('ref_axis',(0.,-0.942844461217511,-0.333233134534159));
#54051=DIRECTION('center_axis',(0.,-0.333233134534162,0.94284446121751));
#54052=DIRECTION('ref_axis',(0.,-0.94284446121751,-0.333233134534162));
#54053=DIRECTION('center_axis',(0.,0.333233134534159,-0.942844461217511));
#54054=DIRECTION('ref_axis',(0.,-0.942844461217511,-0.333233134534159));
#54055=DIRECTION('',(0.,0.333233134534162,-0.94284446121751));
#54056=DIRECTION('center_axis',(0.,0.333233134534162,-0.94284446121751));
#54057=DIRECTION('ref_axis',(0.,-0.94284446121751,-0.333233134534162));
#54058=DIRECTION('center_axis',(0.,-0.333233134534162,0.94284446121751));
#54059=DIRECTION('ref_axis',(0.,-0.94284446121751,-0.333233134534162));
#54060=DIRECTION('center_axis',(0.,0.333233134534162,-0.94284446121751));
#54061=DIRECTION('ref_axis',(0.,0.94284446121751,0.333233134534162));
#54062=DIRECTION('',(0.,-0.333233134534162,0.94284446121751));
#54063=DIRECTION('center_axis',(0.,0.333233134534159,-0.942844461217511));
#54064=DIRECTION('ref_axis',(0.,-0.942844461217511,-0.333233134534159));
#54065=DIRECTION('center_axis',(0.,-0.333233134534162,0.94284446121751));
#54066=DIRECTION('ref_axis',(0.,-0.94284446121751,-0.333233134534161));
#54067=DIRECTION('center_axis',(0.,0.333233134534159,-0.942844461217511));
#54068=DIRECTION('ref_axis',(0.,-0.942844461217511,-0.333233134534159));
#54069=DIRECTION('',(0.,0.333233134534162,-0.94284446121751));
#54070=DIRECTION('center_axis',(0.,0.333233134534162,-0.94284446121751));
#54071=DIRECTION('ref_axis',(0.,-0.94284446121751,-0.333233134534162));
#54072=DIRECTION('center_axis',(0.,-0.333233134534162,0.94284446121751));
#54073=DIRECTION('ref_axis',(0.,-0.94284446121751,-0.333233134534162));
#54074=DIRECTION('center_axis',(0.,0.333233134534162,-0.94284446121751));
#54075=DIRECTION('ref_axis',(0.,0.94284446121751,0.333233134534162));
#54076=DIRECTION('',(0.,-0.333233134534162,0.94284446121751));
#54077=DIRECTION('center_axis',(0.,0.333233134534159,-0.942844461217511));
#54078=DIRECTION('ref_axis',(0.,-0.942844461217511,-0.333233134534159));
#54079=DIRECTION('center_axis',(0.,-0.333233134534162,0.94284446121751));
#54080=DIRECTION('ref_axis',(0.,-0.94284446121751,-0.333233134534162));
#54081=DIRECTION('center_axis',(0.,0.333233134534159,-0.942844461217511));
#54082=DIRECTION('ref_axis',(0.,-0.942844461217511,-0.333233134534159));
#54083=DIRECTION('',(0.,0.333233134534162,-0.94284446121751));
#54084=DIRECTION('center_axis',(0.,0.333233134534162,-0.94284446121751));
#54085=DIRECTION('ref_axis',(0.,-0.94284446121751,-0.333233134534162));
#54086=DIRECTION('center_axis',(0.,-0.333233134534162,0.94284446121751));
#54087=DIRECTION('ref_axis',(0.,-0.94284446121751,-0.333233134534162));
#54088=DIRECTION('center_axis',(0.,0.333233134534162,-0.94284446121751));
#54089=DIRECTION('ref_axis',(0.,0.94284446121751,0.333233134534162));
#54090=DIRECTION('',(0.,-0.333233134534162,0.94284446121751));
#54091=DIRECTION('center_axis',(0.,0.333233134534159,-0.942844461217511));
#54092=DIRECTION('ref_axis',(0.,-0.942844461217511,-0.333233134534159));
#54093=DIRECTION('center_axis',(0.,-0.333233134534162,0.94284446121751));
#54094=DIRECTION('ref_axis',(0.,-0.94284446121751,-0.333233134534162));
#54095=DIRECTION('center_axis',(0.,0.333233134534159,-0.942844461217511));
#54096=DIRECTION('ref_axis',(0.,-0.942844461217511,-0.333233134534159));
#54097=DIRECTION('',(0.,0.333233134534162,-0.94284446121751));
#54098=DIRECTION('center_axis',(0.,0.333233134534162,-0.94284446121751));
#54099=DIRECTION('ref_axis',(0.,-0.94284446121751,-0.333233134534162));
#54100=DIRECTION('center_axis',(0.,-0.333233134534162,0.94284446121751));
#54101=DIRECTION('ref_axis',(0.,-0.94284446121751,-0.333233134534162));
#54102=DIRECTION('center_axis',(0.,0.333233134534162,-0.94284446121751));
#54103=DIRECTION('ref_axis',(0.,0.94284446121751,0.333233134534162));
#54104=DIRECTION('',(0.,-0.333233134534162,0.94284446121751));
#54105=DIRECTION('center_axis',(0.,0.333233134534159,-0.942844461217511));
#54106=DIRECTION('ref_axis',(0.,-0.942844461217511,-0.333233134534159));
#54107=DIRECTION('center_axis',(0.,-0.333233134534162,0.94284446121751));
#54108=DIRECTION('ref_axis',(0.,-0.94284446121751,-0.333233134534162));
#54109=DIRECTION('center_axis',(0.,0.333233134534159,-0.942844461217511));
#54110=DIRECTION('ref_axis',(0.,-0.942844461217511,-0.333233134534159));
#54111=DIRECTION('',(0.,0.333233134534162,-0.94284446121751));
#54112=DIRECTION('center_axis',(0.,0.333233134534162,-0.94284446121751));
#54113=DIRECTION('ref_axis',(0.,-0.94284446121751,-0.333233134534162));
#54114=DIRECTION('center_axis',(0.,-0.333233134534162,0.94284446121751));
#54115=DIRECTION('ref_axis',(0.,-0.94284446121751,-0.333233134534162));
#54116=DIRECTION('center_axis',(0.,0.333233134534162,-0.94284446121751));
#54117=DIRECTION('ref_axis',(0.,0.94284446121751,0.333233134534162));
#54118=DIRECTION('',(0.,-0.333233134534162,0.94284446121751));
#54119=DIRECTION('center_axis',(0.,0.333233134534159,-0.942844461217511));
#54120=DIRECTION('ref_axis',(0.,-0.942844461217511,-0.333233134534159));
#54121=DIRECTION('center_axis',(0.,-0.333233134534162,0.94284446121751));
#54122=DIRECTION('ref_axis',(0.,-0.94284446121751,-0.333233134534162));
#54123=DIRECTION('center_axis',(0.,0.333233134534159,-0.942844461217511));
#54124=DIRECTION('ref_axis',(0.,-0.942844461217511,-0.333233134534159));
#54125=DIRECTION('',(0.,0.333233134534162,-0.94284446121751));
#54126=DIRECTION('center_axis',(0.,0.333233134534162,-0.94284446121751));
#54127=DIRECTION('ref_axis',(0.,-0.94284446121751,-0.333233134534162));
#54128=DIRECTION('center_axis',(0.,-0.333233134534162,0.94284446121751));
#54129=DIRECTION('ref_axis',(0.,-0.94284446121751,-0.333233134534162));
#54130=DIRECTION('center_axis',(0.,0.333233134534162,-0.94284446121751));
#54131=DIRECTION('ref_axis',(0.,0.94284446121751,0.333233134534162));
#54132=DIRECTION('',(0.,-0.333233134534162,0.94284446121751));
#54133=DIRECTION('center_axis',(0.,0.333233134534159,-0.942844461217511));
#54134=DIRECTION('ref_axis',(0.,-0.942844461217511,-0.333233134534159));
#54135=DIRECTION('center_axis',(0.,-0.333233134534162,0.94284446121751));
#54136=DIRECTION('ref_axis',(0.,-0.94284446121751,-0.333233134534162));
#54137=DIRECTION('center_axis',(0.,0.333233134534159,-0.942844461217511));
#54138=DIRECTION('ref_axis',(0.,-0.942844461217511,-0.333233134534159));
#54139=DIRECTION('',(0.,0.333233134534162,-0.94284446121751));
#54140=DIRECTION('center_axis',(0.,0.333233134534162,-0.94284446121751));
#54141=DIRECTION('ref_axis',(0.,-0.94284446121751,-0.333233134534162));
#54142=DIRECTION('center_axis',(0.,-0.333233134534162,0.94284446121751));
#54143=DIRECTION('ref_axis',(0.,-0.94284446121751,-0.333233134534162));
#54144=DIRECTION('center_axis',(0.,0.333233134534162,-0.94284446121751));
#54145=DIRECTION('ref_axis',(0.,0.94284446121751,0.333233134534162));
#54146=DIRECTION('',(0.,-0.333233134534162,0.94284446121751));
#54147=DIRECTION('center_axis',(0.,0.333233134534159,-0.942844461217511));
#54148=DIRECTION('ref_axis',(0.,-0.942844461217511,-0.333233134534159));
#54149=DIRECTION('center_axis',(0.,-0.333233134534162,0.94284446121751));
#54150=DIRECTION('ref_axis',(0.,-0.94284446121751,-0.333233134534162));
#54151=DIRECTION('center_axis',(0.,0.333233134534159,-0.942844461217511));
#54152=DIRECTION('ref_axis',(0.,-0.942844461217511,-0.333233134534159));
#54153=DIRECTION('',(0.,0.333233134534162,-0.94284446121751));
#54154=DIRECTION('center_axis',(0.,-0.333233134534162,0.94284446121751));
#54155=DIRECTION('ref_axis',(0.,-0.94284446121751,-0.333233134534162));
#54156=DIRECTION('center_axis',(0.,-0.333233134534162,0.94284446121751));
#54157=DIRECTION('ref_axis',(0.,-0.94284446121751,-0.333233134534162));
#54158=DIRECTION('center_axis',(0.,0.333233134534162,-0.94284446121751));
#54159=DIRECTION('ref_axis',(0.,0.94284446121751,0.333233134534162));
#54160=DIRECTION('',(0.,-0.333233134534162,0.94284446121751));
#54161=DIRECTION('center_axis',(0.,0.333233134534159,-0.942844461217511));
#54162=DIRECTION('ref_axis',(0.,-0.942844461217511,-0.333233134534159));
#54163=DIRECTION('center_axis',(0.,-0.333233134534162,0.94284446121751));
#54164=DIRECTION('ref_axis',(0.,-0.94284446121751,-0.333233134534161));
#54165=DIRECTION('center_axis',(0.,0.333233134534159,-0.942844461217511));
#54166=DIRECTION('ref_axis',(0.,-0.942844461217511,-0.333233134534159));
#54167=DIRECTION('',(0.,0.333233134534162,-0.94284446121751));
#54168=DIRECTION('center_axis',(0.,0.333233134534162,-0.94284446121751));
#54169=DIRECTION('ref_axis',(0.,-0.94284446121751,-0.333233134534162));
#54170=DIRECTION('center_axis',(0.,-0.333233134534162,0.94284446121751));
#54171=DIRECTION('ref_axis',(0.,-0.94284446121751,-0.333233134534162));
#54172=DIRECTION('center_axis',(0.,0.333233134534162,-0.94284446121751));
#54173=DIRECTION('ref_axis',(0.,0.94284446121751,0.333233134534162));
#54174=DIRECTION('',(0.,-0.333233134534162,0.94284446121751));
#54175=DIRECTION('center_axis',(0.,0.333233134534159,-0.942844461217511));
#54176=DIRECTION('ref_axis',(0.,-0.942844461217511,-0.333233134534159));
#54177=DIRECTION('center_axis',(0.,-0.333233134534162,0.94284446121751));
#54178=DIRECTION('ref_axis',(0.,-0.94284446121751,-0.333233134534162));
#54179=DIRECTION('center_axis',(0.,0.333233134534159,-0.942844461217511));
#54180=DIRECTION('ref_axis',(0.,-0.942844461217511,-0.333233134534159));
#54181=DIRECTION('',(0.,0.333233134534162,-0.94284446121751));
#54182=DIRECTION('center_axis',(0.,0.333233134534162,-0.94284446121751));
#54183=DIRECTION('ref_axis',(0.,-0.94284446121751,-0.333233134534162));
#54184=DIRECTION('center_axis',(0.,-0.333233134534162,0.94284446121751));
#54185=DIRECTION('ref_axis',(0.,-0.94284446121751,-0.333233134534162));
#54186=DIRECTION('center_axis',(0.,0.333233134534162,-0.94284446121751));
#54187=DIRECTION('ref_axis',(0.,0.94284446121751,0.333233134534162));
#54188=DIRECTION('',(0.,-0.333233134534162,0.94284446121751));
#54189=DIRECTION('center_axis',(0.,0.333233134534159,-0.942844461217511));
#54190=DIRECTION('ref_axis',(0.,-0.942844461217511,-0.333233134534159));
#54191=DIRECTION('center_axis',(0.,-0.333233134534162,0.94284446121751));
#54192=DIRECTION('ref_axis',(0.,-0.94284446121751,-0.333233134534162));
#54193=DIRECTION('center_axis',(0.,0.333233134534159,-0.942844461217511));
#54194=DIRECTION('ref_axis',(0.,-0.942844461217511,-0.333233134534159));
#54195=DIRECTION('',(0.,0.333233134534162,-0.94284446121751));
#54196=DIRECTION('center_axis',(0.,0.333233134534162,-0.94284446121751));
#54197=DIRECTION('ref_axis',(0.,-0.94284446121751,-0.333233134534162));
#54198=DIRECTION('center_axis',(0.,-0.333233134534162,0.94284446121751));
#54199=DIRECTION('ref_axis',(0.,-0.94284446121751,-0.333233134534162));
#54200=DIRECTION('center_axis',(0.,0.333233134534162,-0.94284446121751));
#54201=DIRECTION('ref_axis',(0.,0.94284446121751,0.333233134534162));
#54202=DIRECTION('',(0.,-0.333233134534162,0.94284446121751));
#54203=DIRECTION('center_axis',(0.,0.333233134534159,-0.942844461217511));
#54204=DIRECTION('ref_axis',(0.,-0.942844461217511,-0.333233134534159));
#54205=DIRECTION('center_axis',(0.,-0.333233134534162,0.94284446121751));
#54206=DIRECTION('ref_axis',(0.,-0.94284446121751,-0.333233134534162));
#54207=DIRECTION('center_axis',(0.,0.333233134534159,-0.942844461217511));
#54208=DIRECTION('ref_axis',(0.,-0.942844461217511,-0.333233134534159));
#54209=DIRECTION('',(0.,0.333233134534162,-0.94284446121751));
#54210=DIRECTION('center_axis',(0.,0.333233134534162,-0.94284446121751));
#54211=DIRECTION('ref_axis',(0.,-0.94284446121751,-0.333233134534162));
#54212=DIRECTION('center_axis',(0.,-0.333233134534162,0.94284446121751));
#54213=DIRECTION('ref_axis',(0.,-0.94284446121751,-0.333233134534162));
#54214=DIRECTION('center_axis',(0.,0.333233134534162,-0.94284446121751));
#54215=DIRECTION('ref_axis',(0.,0.94284446121751,0.333233134534162));
#54216=DIRECTION('',(0.,-0.333233134534162,0.94284446121751));
#54217=DIRECTION('center_axis',(0.,0.333233134534159,-0.942844461217511));
#54218=DIRECTION('ref_axis',(0.,-0.942844461217511,-0.333233134534159));
#54219=DIRECTION('center_axis',(0.,-0.333233134534162,0.94284446121751));
#54220=DIRECTION('ref_axis',(0.,-0.94284446121751,-0.333233134534162));
#54221=DIRECTION('center_axis',(0.,0.333233134534159,-0.942844461217511));
#54222=DIRECTION('ref_axis',(0.,-0.942844461217511,-0.333233134534159));
#54223=DIRECTION('',(0.,0.333233134534162,-0.94284446121751));
#54224=DIRECTION('center_axis',(0.,0.333233134534162,-0.94284446121751));
#54225=DIRECTION('ref_axis',(0.,-0.94284446121751,-0.333233134534162));
#54226=DIRECTION('center_axis',(0.,-0.333233134534162,0.94284446121751));
#54227=DIRECTION('ref_axis',(0.,-0.94284446121751,-0.333233134534162));
#54228=DIRECTION('center_axis',(0.,0.333233134534162,-0.94284446121751));
#54229=DIRECTION('ref_axis',(0.,0.94284446121751,0.333233134534162));
#54230=DIRECTION('',(0.,-0.333233134534162,0.94284446121751));
#54231=DIRECTION('center_axis',(0.,0.333233134534159,-0.942844461217511));
#54232=DIRECTION('ref_axis',(0.,-0.942844461217511,-0.333233134534159));
#54233=DIRECTION('center_axis',(0.,-0.333233134534162,0.94284446121751));
#54234=DIRECTION('ref_axis',(0.,-0.94284446121751,-0.333233134534162));
#54235=DIRECTION('center_axis',(0.,0.333233134534159,-0.942844461217511));
#54236=DIRECTION('ref_axis',(0.,-0.942844461217511,-0.333233134534159));
#54237=DIRECTION('',(0.,0.333233134534162,-0.94284446121751));
#54238=DIRECTION('center_axis',(0.,0.333233134534162,-0.94284446121751));
#54239=DIRECTION('ref_axis',(0.,-0.94284446121751,-0.333233134534162));
#54240=DIRECTION('center_axis',(0.,-0.333233134534162,0.94284446121751));
#54241=DIRECTION('ref_axis',(0.,-0.94284446121751,-0.333233134534162));
#54242=DIRECTION('center_axis',(0.,0.333233134534162,-0.94284446121751));
#54243=DIRECTION('ref_axis',(0.,0.94284446121751,0.333233134534162));
#54244=DIRECTION('',(0.,-0.333233134534162,0.94284446121751));
#54245=DIRECTION('center_axis',(0.,0.333233134534159,-0.942844461217511));
#54246=DIRECTION('ref_axis',(0.,-0.942844461217511,-0.333233134534159));
#54247=DIRECTION('center_axis',(0.,-0.333233134534162,0.94284446121751));
#54248=DIRECTION('ref_axis',(0.,-0.94284446121751,-0.333233134534162));
#54249=DIRECTION('center_axis',(0.,0.333233134534159,-0.942844461217511));
#54250=DIRECTION('ref_axis',(0.,-0.942844461217511,-0.333233134534159));
#54251=DIRECTION('',(0.,0.333233134534162,-0.94284446121751));
#54252=DIRECTION('center_axis',(0.,0.333233134534162,-0.94284446121751));
#54253=DIRECTION('ref_axis',(0.,-0.94284446121751,-0.333233134534162));
#54254=DIRECTION('center_axis',(0.,-0.333233134534162,0.94284446121751));
#54255=DIRECTION('ref_axis',(0.,-0.94284446121751,-0.333233134534162));
#54256=DIRECTION('center_axis',(0.,0.333233134534162,-0.94284446121751));
#54257=DIRECTION('ref_axis',(0.,0.94284446121751,0.333233134534162));
#54258=DIRECTION('',(0.,-0.333233134534162,0.94284446121751));
#54259=DIRECTION('center_axis',(0.,0.333233134534159,-0.942844461217511));
#54260=DIRECTION('ref_axis',(0.,-0.942844461217511,-0.333233134534159));
#54261=DIRECTION('center_axis',(0.,-0.333233134534162,0.94284446121751));
#54262=DIRECTION('ref_axis',(0.,-0.94284446121751,-0.333233134534162));
#54263=DIRECTION('center_axis',(0.,0.333233134534159,-0.942844461217511));
#54264=DIRECTION('ref_axis',(0.,-0.942844461217511,-0.333233134534159));
#54265=DIRECTION('',(0.,0.333233134534162,-0.94284446121751));
#54266=DIRECTION('center_axis',(0.,0.333233134534162,-0.94284446121751));
#54267=DIRECTION('ref_axis',(0.,-0.94284446121751,-0.333233134534162));
#54268=DIRECTION('center_axis',(0.,-0.333233134534162,0.94284446121751));
#54269=DIRECTION('ref_axis',(0.,-0.94284446121751,-0.333233134534162));
#54270=DIRECTION('center_axis',(0.,0.333233134534162,-0.94284446121751));
#54271=DIRECTION('ref_axis',(0.,0.94284446121751,0.333233134534162));
#54272=DIRECTION('',(0.,-0.333233134534162,0.94284446121751));
#54273=DIRECTION('center_axis',(0.,0.333233134534159,-0.942844461217511));
#54274=DIRECTION('ref_axis',(0.,-0.942844461217511,-0.333233134534159));
#54275=DIRECTION('center_axis',(0.,-0.333233134534162,0.94284446121751));
#54276=DIRECTION('ref_axis',(0.,-0.94284446121751,-0.333233134534162));
#54277=DIRECTION('center_axis',(0.,0.333233134534159,-0.942844461217511));
#54278=DIRECTION('ref_axis',(0.,-0.942844461217511,-0.333233134534159));
#54279=DIRECTION('',(0.,0.333233134534162,-0.94284446121751));
#54280=DIRECTION('center_axis',(0.,-0.333233134534162,0.94284446121751));
#54281=DIRECTION('ref_axis',(0.,-0.94284446121751,-0.333233134534162));
#54282=DIRECTION('center_axis',(0.,-0.333233134534162,0.94284446121751));
#54283=DIRECTION('ref_axis',(0.,-0.94284446121751,-0.333233134534162));
#54284=DIRECTION('center_axis',(0.,0.333233134534162,-0.94284446121751));
#54285=DIRECTION('ref_axis',(0.,0.94284446121751,0.333233134534162));
#54286=DIRECTION('',(0.,-0.333233134534162,0.94284446121751));
#54287=DIRECTION('center_axis',(0.,0.333233134534159,-0.942844461217511));
#54288=DIRECTION('ref_axis',(0.,-0.942844461217511,-0.333233134534159));
#54289=DIRECTION('center_axis',(0.,-0.333233134534162,0.94284446121751));
#54290=DIRECTION('ref_axis',(0.,-0.94284446121751,-0.333233134534162));
#54291=DIRECTION('center_axis',(0.,0.333233134534159,-0.942844461217511));
#54292=DIRECTION('ref_axis',(0.,-0.942844461217511,-0.333233134534159));
#54293=DIRECTION('',(0.,0.333233134534162,-0.94284446121751));
#54294=DIRECTION('center_axis',(0.,0.333233134534162,-0.94284446121751));
#54295=DIRECTION('ref_axis',(0.,-0.94284446121751,-0.333233134534162));
#54296=DIRECTION('center_axis',(0.,-0.333233134534162,0.94284446121751));
#54297=DIRECTION('ref_axis',(0.,-0.94284446121751,-0.333233134534162));
#54298=DIRECTION('center_axis',(0.,0.333233134534162,-0.94284446121751));
#54299=DIRECTION('ref_axis',(0.,0.94284446121751,0.333233134534162));
#54300=DIRECTION('',(0.,-0.333233134534162,0.94284446121751));
#54301=DIRECTION('center_axis',(0.,0.333233134534159,-0.942844461217511));
#54302=DIRECTION('ref_axis',(0.,-0.942844461217511,-0.333233134534159));
#54303=DIRECTION('center_axis',(0.,-0.333233134534162,0.94284446121751));
#54304=DIRECTION('ref_axis',(0.,-0.94284446121751,-0.333233134534162));
#54305=DIRECTION('center_axis',(0.,0.333233134534159,-0.942844461217511));
#54306=DIRECTION('ref_axis',(0.,-0.942844461217511,-0.333233134534159));
#54307=DIRECTION('',(0.,0.333233134534162,-0.94284446121751));
#54308=DIRECTION('center_axis',(0.,0.333233134534162,-0.94284446121751));
#54309=DIRECTION('ref_axis',(0.,-0.94284446121751,-0.333233134534162));
#54310=DIRECTION('center_axis',(0.,-0.333233134534162,0.94284446121751));
#54311=DIRECTION('ref_axis',(0.,-0.94284446121751,-0.333233134534162));
#54312=DIRECTION('center_axis',(0.,0.333233134534162,-0.94284446121751));
#54313=DIRECTION('ref_axis',(0.,0.94284446121751,0.333233134534162));
#54314=DIRECTION('',(0.,-0.333233134534162,0.94284446121751));
#54315=DIRECTION('center_axis',(0.,0.333233134534159,-0.942844461217511));
#54316=DIRECTION('ref_axis',(0.,-0.942844461217511,-0.333233134534159));
#54317=DIRECTION('center_axis',(0.,-0.333233134534162,0.94284446121751));
#54318=DIRECTION('ref_axis',(0.,-0.94284446121751,-0.333233134534162));
#54319=DIRECTION('center_axis',(0.,0.333233134534159,-0.942844461217511));
#54320=DIRECTION('ref_axis',(0.,-0.942844461217511,-0.333233134534159));
#54321=DIRECTION('',(0.,0.333233134534162,-0.94284446121751));
#54322=DIRECTION('center_axis',(0.,0.333233134534162,-0.94284446121751));
#54323=DIRECTION('ref_axis',(0.,-0.94284446121751,-0.333233134534162));
#54324=DIRECTION('center_axis',(0.,-0.333233134534162,0.94284446121751));
#54325=DIRECTION('ref_axis',(0.,-0.94284446121751,-0.333233134534162));
#54326=DIRECTION('center_axis',(0.,0.333233134534162,-0.94284446121751));
#54327=DIRECTION('ref_axis',(0.,0.94284446121751,0.333233134534162));
#54328=DIRECTION('',(0.,-0.333233134534162,0.94284446121751));
#54329=DIRECTION('center_axis',(0.,0.333233134534159,-0.942844461217511));
#54330=DIRECTION('ref_axis',(0.,-0.942844461217511,-0.333233134534159));
#54331=DIRECTION('center_axis',(0.,-0.333233134534162,0.94284446121751));
#54332=DIRECTION('ref_axis',(0.,-0.94284446121751,-0.333233134534162));
#54333=DIRECTION('center_axis',(0.,0.333233134534159,-0.942844461217511));
#54334=DIRECTION('ref_axis',(0.,-0.942844461217511,-0.333233134534159));
#54335=DIRECTION('',(0.,0.333233134534162,-0.94284446121751));
#54336=DIRECTION('center_axis',(0.,0.333233134534162,-0.94284446121751));
#54337=DIRECTION('ref_axis',(0.,-0.94284446121751,-0.333233134534162));
#54338=DIRECTION('center_axis',(0.,-0.333233134534162,0.94284446121751));
#54339=DIRECTION('ref_axis',(0.,-0.94284446121751,-0.333233134534162));
#54340=DIRECTION('center_axis',(0.,0.333233134534162,-0.94284446121751));
#54341=DIRECTION('ref_axis',(0.,0.94284446121751,0.333233134534162));
#54342=DIRECTION('',(0.,-0.333233134534162,0.94284446121751));
#54343=DIRECTION('center_axis',(0.,0.333233134534159,-0.942844461217511));
#54344=DIRECTION('ref_axis',(0.,-0.942844461217511,-0.333233134534159));
#54345=DIRECTION('center_axis',(0.,-0.333233134534162,0.94284446121751));
#54346=DIRECTION('ref_axis',(0.,-0.94284446121751,-0.333233134534162));
#54347=DIRECTION('center_axis',(0.,0.333233134534159,-0.942844461217511));
#54348=DIRECTION('ref_axis',(0.,-0.942844461217511,-0.333233134534159));
#54349=DIRECTION('',(0.,0.333233134534162,-0.94284446121751));
#54350=DIRECTION('center_axis',(0.,0.333233134534162,-0.94284446121751));
#54351=DIRECTION('ref_axis',(0.,-0.94284446121751,-0.333233134534162));
#54352=DIRECTION('center_axis',(0.,-0.333233134534162,0.94284446121751));
#54353=DIRECTION('ref_axis',(0.,-0.94284446121751,-0.333233134534162));
#54354=DIRECTION('center_axis',(0.,0.333233134534162,-0.94284446121751));
#54355=DIRECTION('ref_axis',(0.,0.94284446121751,0.333233134534162));
#54356=DIRECTION('',(0.,-0.333233134534162,0.94284446121751));
#54357=DIRECTION('center_axis',(0.,0.333233134534159,-0.942844461217511));
#54358=DIRECTION('ref_axis',(0.,-0.942844461217511,-0.333233134534159));
#54359=DIRECTION('center_axis',(0.,-0.333233134534162,0.94284446121751));
#54360=DIRECTION('ref_axis',(0.,-0.94284446121751,-0.333233134534162));
#54361=DIRECTION('center_axis',(0.,0.333233134534159,-0.942844461217511));
#54362=DIRECTION('ref_axis',(0.,-0.942844461217511,-0.333233134534159));
#54363=DIRECTION('',(0.,0.333233134534162,-0.94284446121751));
#54364=DIRECTION('center_axis',(0.,0.333233134534162,-0.94284446121751));
#54365=DIRECTION('ref_axis',(0.,-0.94284446121751,-0.333233134534162));
#54366=DIRECTION('center_axis',(0.,-0.333233134534162,0.94284446121751));
#54367=DIRECTION('ref_axis',(0.,-0.94284446121751,-0.333233134534162));
#54368=DIRECTION('center_axis',(0.,0.333233134534162,-0.94284446121751));
#54369=DIRECTION('ref_axis',(0.,0.94284446121751,0.333233134534162));
#54370=DIRECTION('',(0.,-0.333233134534162,0.94284446121751));
#54371=DIRECTION('center_axis',(0.,0.333233134534159,-0.942844461217511));
#54372=DIRECTION('ref_axis',(0.,-0.942844461217511,-0.333233134534159));
#54373=DIRECTION('center_axis',(0.,-0.333233134534162,0.94284446121751));
#54374=DIRECTION('ref_axis',(0.,-0.94284446121751,-0.333233134534162));
#54375=DIRECTION('center_axis',(0.,0.333233134534159,-0.942844461217511));
#54376=DIRECTION('ref_axis',(0.,-0.942844461217511,-0.333233134534159));
#54377=DIRECTION('',(0.,0.333233134534162,-0.94284446121751));
#54378=DIRECTION('center_axis',(0.,0.333233134534162,-0.94284446121751));
#54379=DIRECTION('ref_axis',(0.,-0.94284446121751,-0.333233134534162));
#54380=DIRECTION('center_axis',(0.,-0.333233134534162,0.94284446121751));
#54381=DIRECTION('ref_axis',(0.,-0.94284446121751,-0.333233134534162));
#54382=DIRECTION('center_axis',(0.,0.333233134534162,-0.94284446121751));
#54383=DIRECTION('ref_axis',(0.,0.94284446121751,0.333233134534162));
#54384=DIRECTION('',(0.,-0.333233134534162,0.94284446121751));
#54385=DIRECTION('center_axis',(0.,0.333233134534159,-0.942844461217511));
#54386=DIRECTION('ref_axis',(0.,-0.942844461217511,-0.333233134534159));
#54387=DIRECTION('center_axis',(0.,-0.333233134534162,0.94284446121751));
#54388=DIRECTION('ref_axis',(0.,-0.94284446121751,-0.333233134534162));
#54389=DIRECTION('center_axis',(0.,0.333233134534159,-0.942844461217511));
#54390=DIRECTION('ref_axis',(0.,-0.942844461217511,-0.333233134534159));
#54391=DIRECTION('',(0.,0.333233134534162,-0.94284446121751));
#54392=DIRECTION('center_axis',(0.,0.333233134534162,-0.94284446121751));
#54393=DIRECTION('ref_axis',(0.,-0.94284446121751,-0.333233134534162));
#54394=DIRECTION('center_axis',(0.,-0.333233134534162,0.94284446121751));
#54395=DIRECTION('ref_axis',(0.,-0.94284446121751,-0.333233134534162));
#54396=DIRECTION('center_axis',(0.,0.333233134534162,-0.94284446121751));
#54397=DIRECTION('ref_axis',(0.,0.94284446121751,0.333233134534162));
#54398=DIRECTION('',(0.,-0.333233134534162,0.94284446121751));
#54399=DIRECTION('center_axis',(0.,0.333233134534159,-0.942844461217511));
#54400=DIRECTION('ref_axis',(0.,-0.942844461217511,-0.333233134534159));
#54401=DIRECTION('center_axis',(0.,-0.333233134534162,0.94284446121751));
#54402=DIRECTION('ref_axis',(0.,-0.94284446121751,-0.333233134534162));
#54403=DIRECTION('center_axis',(0.,0.333233134534159,-0.942844461217511));
#54404=DIRECTION('ref_axis',(0.,-0.942844461217511,-0.333233134534159));
#54405=DIRECTION('',(0.,0.333233134534162,-0.94284446121751));
#54406=DIRECTION('center_axis',(0.,-0.333233134534162,0.94284446121751));
#54407=DIRECTION('ref_axis',(0.,-0.94284446121751,-0.333233134534162));
#54408=DIRECTION('center_axis',(0.,-0.333233134534162,0.94284446121751));
#54409=DIRECTION('ref_axis',(0.,-0.94284446121751,-0.333233134534162));
#54410=DIRECTION('center_axis',(0.,0.333233134534162,-0.94284446121751));
#54411=DIRECTION('ref_axis',(0.,0.94284446121751,0.333233134534162));
#54412=DIRECTION('',(0.,-0.333233134534162,0.94284446121751));
#54413=DIRECTION('center_axis',(0.,0.333233134534159,-0.942844461217511));
#54414=DIRECTION('ref_axis',(0.,-0.942844461217511,-0.333233134534159));
#54415=DIRECTION('center_axis',(0.,-0.333233134534162,0.94284446121751));
#54416=DIRECTION('ref_axis',(0.,-0.94284446121751,-0.333233134534162));
#54417=DIRECTION('center_axis',(0.,0.333233134534159,-0.942844461217511));
#54418=DIRECTION('ref_axis',(0.,-0.942844461217511,-0.333233134534159));
#54419=DIRECTION('',(0.,0.333233134534162,-0.94284446121751));
#54420=DIRECTION('center_axis',(0.,0.333233134534162,-0.94284446121751));
#54421=DIRECTION('ref_axis',(0.,-0.94284446121751,-0.333233134534162));
#54422=DIRECTION('center_axis',(0.,-0.333233134534162,0.94284446121751));
#54423=DIRECTION('ref_axis',(0.,-0.94284446121751,-0.333233134534162));
#54424=DIRECTION('center_axis',(0.,0.333233134534162,-0.94284446121751));
#54425=DIRECTION('ref_axis',(0.,0.94284446121751,0.333233134534162));
#54426=DIRECTION('',(0.,-0.333233134534162,0.94284446121751));
#54427=DIRECTION('center_axis',(0.,0.333233134534159,-0.942844461217511));
#54428=DIRECTION('ref_axis',(0.,-0.942844461217511,-0.333233134534159));
#54429=DIRECTION('center_axis',(0.,-0.333233134534162,0.94284446121751));
#54430=DIRECTION('ref_axis',(0.,-0.94284446121751,-0.333233134534162));
#54431=DIRECTION('center_axis',(0.,0.333233134534159,-0.942844461217511));
#54432=DIRECTION('ref_axis',(0.,-0.942844461217511,-0.333233134534159));
#54433=DIRECTION('',(0.,0.333233134534162,-0.94284446121751));
#54434=DIRECTION('center_axis',(0.,0.333233134534162,-0.94284446121751));
#54435=DIRECTION('ref_axis',(0.,-0.94284446121751,-0.333233134534162));
#54436=DIRECTION('center_axis',(0.,-0.333233134534162,0.94284446121751));
#54437=DIRECTION('ref_axis',(0.,-0.94284446121751,-0.333233134534162));
#54438=DIRECTION('center_axis',(0.,0.333233134534162,-0.94284446121751));
#54439=DIRECTION('ref_axis',(0.,0.94284446121751,0.333233134534162));
#54440=DIRECTION('',(0.,-0.333233134534162,0.94284446121751));
#54441=DIRECTION('center_axis',(0.,0.333233134534159,-0.942844461217511));
#54442=DIRECTION('ref_axis',(0.,-0.942844461217511,-0.333233134534159));
#54443=DIRECTION('center_axis',(0.,-0.333233134534162,0.94284446121751));
#54444=DIRECTION('ref_axis',(0.,-0.94284446121751,-0.333233134534162));
#54445=DIRECTION('center_axis',(0.,0.333233134534159,-0.942844461217511));
#54446=DIRECTION('ref_axis',(0.,-0.942844461217511,-0.333233134534159));
#54447=DIRECTION('',(0.,0.333233134534162,-0.94284446121751));
#54448=DIRECTION('center_axis',(0.,0.333233134534162,-0.94284446121751));
#54449=DIRECTION('ref_axis',(0.,-0.94284446121751,-0.333233134534162));
#54450=DIRECTION('center_axis',(0.,-0.333233134534162,0.94284446121751));
#54451=DIRECTION('ref_axis',(0.,-0.94284446121751,-0.333233134534162));
#54452=DIRECTION('center_axis',(0.,0.333233134534162,-0.94284446121751));
#54453=DIRECTION('ref_axis',(0.,0.94284446121751,0.333233134534162));
#54454=DIRECTION('',(0.,-0.333233134534162,0.94284446121751));
#54455=DIRECTION('center_axis',(0.,0.333233134534159,-0.942844461217511));
#54456=DIRECTION('ref_axis',(0.,-0.942844461217511,-0.333233134534159));
#54457=DIRECTION('center_axis',(0.,-0.333233134534162,0.94284446121751));
#54458=DIRECTION('ref_axis',(0.,-0.94284446121751,-0.333233134534162));
#54459=DIRECTION('center_axis',(0.,0.333233134534159,-0.942844461217511));
#54460=DIRECTION('ref_axis',(0.,-0.942844461217511,-0.333233134534159));
#54461=DIRECTION('',(0.,0.333233134534162,-0.94284446121751));
#54462=DIRECTION('center_axis',(0.,0.333233134534162,-0.94284446121751));
#54463=DIRECTION('ref_axis',(0.,-0.94284446121751,-0.333233134534162));
#54464=DIRECTION('center_axis',(0.,-0.333233134534162,0.94284446121751));
#54465=DIRECTION('ref_axis',(0.,-0.94284446121751,-0.333233134534162));
#54466=DIRECTION('center_axis',(0.,0.333233134534162,-0.94284446121751));
#54467=DIRECTION('ref_axis',(0.,0.94284446121751,0.333233134534162));
#54468=DIRECTION('',(0.,-0.333233134534162,0.94284446121751));
#54469=DIRECTION('center_axis',(0.,0.333233134534159,-0.942844461217511));
#54470=DIRECTION('ref_axis',(0.,-0.942844461217511,-0.333233134534159));
#54471=DIRECTION('center_axis',(0.,-0.333233134534162,0.94284446121751));
#54472=DIRECTION('ref_axis',(0.,-0.94284446121751,-0.333233134534162));
#54473=DIRECTION('center_axis',(0.,0.333233134534159,-0.942844461217511));
#54474=DIRECTION('ref_axis',(0.,-0.942844461217511,-0.333233134534159));
#54475=DIRECTION('',(0.,0.333233134534162,-0.94284446121751));
#54476=DIRECTION('center_axis',(0.,0.333233134534162,-0.94284446121751));
#54477=DIRECTION('ref_axis',(0.,-0.94284446121751,-0.333233134534162));
#54478=DIRECTION('center_axis',(0.,-0.333233134534162,0.94284446121751));
#54479=DIRECTION('ref_axis',(0.,-0.94284446121751,-0.333233134534162));
#54480=DIRECTION('center_axis',(0.,0.333233134534162,-0.94284446121751));
#54481=DIRECTION('ref_axis',(0.,0.94284446121751,0.333233134534162));
#54482=DIRECTION('',(0.,-0.333233134534162,0.94284446121751));
#54483=DIRECTION('center_axis',(0.,0.333233134534159,-0.942844461217511));
#54484=DIRECTION('ref_axis',(0.,-0.942844461217511,-0.333233134534159));
#54485=DIRECTION('center_axis',(0.,-0.333233134534162,0.94284446121751));
#54486=DIRECTION('ref_axis',(0.,-0.94284446121751,-0.333233134534162));
#54487=DIRECTION('center_axis',(0.,0.333233134534159,-0.942844461217511));
#54488=DIRECTION('ref_axis',(0.,-0.942844461217511,-0.333233134534159));
#54489=DIRECTION('',(0.,0.333233134534162,-0.94284446121751));
#54490=DIRECTION('center_axis',(0.,0.333233134534162,-0.94284446121751));
#54491=DIRECTION('ref_axis',(0.,-0.94284446121751,-0.333233134534162));
#54492=DIRECTION('center_axis',(0.,-0.333233134534162,0.94284446121751));
#54493=DIRECTION('ref_axis',(0.,-0.94284446121751,-0.333233134534162));
#54494=DIRECTION('center_axis',(0.,0.333233134534162,-0.94284446121751));
#54495=DIRECTION('ref_axis',(0.,0.94284446121751,0.333233134534162));
#54496=DIRECTION('',(0.,-0.333233134534162,0.94284446121751));
#54497=DIRECTION('center_axis',(0.,0.333233134534159,-0.942844461217511));
#54498=DIRECTION('ref_axis',(0.,-0.942844461217511,-0.333233134534159));
#54499=DIRECTION('center_axis',(0.,-0.333233134534162,0.94284446121751));
#54500=DIRECTION('ref_axis',(0.,-0.94284446121751,-0.333233134534162));
#54501=DIRECTION('center_axis',(0.,0.333233134534159,-0.942844461217511));
#54502=DIRECTION('ref_axis',(0.,-0.942844461217511,-0.333233134534159));
#54503=DIRECTION('',(0.,0.333233134534162,-0.94284446121751));
#54504=DIRECTION('center_axis',(0.,0.333233134534162,-0.94284446121751));
#54505=DIRECTION('ref_axis',(0.,-0.94284446121751,-0.333233134534162));
#54506=DIRECTION('center_axis',(0.,-0.333233134534162,0.94284446121751));
#54507=DIRECTION('ref_axis',(0.,-0.94284446121751,-0.333233134534162));
#54508=DIRECTION('center_axis',(0.,0.333233134534162,-0.94284446121751));
#54509=DIRECTION('ref_axis',(0.,0.94284446121751,0.333233134534162));
#54510=DIRECTION('',(0.,-0.333233134534162,0.94284446121751));
#54511=DIRECTION('center_axis',(0.,0.333233134534159,-0.942844461217511));
#54512=DIRECTION('ref_axis',(0.,-0.942844461217511,-0.333233134534159));
#54513=DIRECTION('center_axis',(0.,-0.333233134534162,0.94284446121751));
#54514=DIRECTION('ref_axis',(0.,-0.94284446121751,-0.333233134534162));
#54515=DIRECTION('center_axis',(0.,0.333233134534159,-0.942844461217511));
#54516=DIRECTION('ref_axis',(0.,-0.942844461217511,-0.333233134534159));
#54517=DIRECTION('',(0.,0.333233134534162,-0.94284446121751));
#54518=DIRECTION('center_axis',(0.,-0.333233134534162,0.94284446121751));
#54519=DIRECTION('ref_axis',(0.,-0.94284446121751,-0.333233134534162));
#54520=DIRECTION('center_axis',(0.,-0.333233134534162,0.94284446121751));
#54521=DIRECTION('ref_axis',(0.,-0.94284446121751,-0.333233134534162));
#54522=DIRECTION('center_axis',(0.,0.333233134534162,-0.94284446121751));
#54523=DIRECTION('ref_axis',(0.,0.94284446121751,0.333233134534162));
#54524=DIRECTION('',(0.,-0.333233134534162,0.94284446121751));
#54525=DIRECTION('center_axis',(0.,0.333233134534159,-0.942844461217511));
#54526=DIRECTION('ref_axis',(0.,-0.942844461217511,-0.333233134534159));
#54527=DIRECTION('center_axis',(0.,-0.333233134534162,0.94284446121751));
#54528=DIRECTION('ref_axis',(0.,-0.94284446121751,-0.333233134534162));
#54529=DIRECTION('center_axis',(0.,0.333233134534159,-0.942844461217511));
#54530=DIRECTION('ref_axis',(0.,-0.942844461217511,-0.333233134534159));
#54531=DIRECTION('',(0.,0.333233134534162,-0.94284446121751));
#54532=DIRECTION('center_axis',(0.,0.333233134534162,-0.94284446121751));
#54533=DIRECTION('ref_axis',(0.,-0.94284446121751,-0.333233134534162));
#54534=DIRECTION('center_axis',(0.,-0.333233134534162,0.94284446121751));
#54535=DIRECTION('ref_axis',(0.,-0.94284446121751,-0.333233134534162));
#54536=DIRECTION('center_axis',(0.,0.333233134534162,-0.94284446121751));
#54537=DIRECTION('ref_axis',(0.,0.94284446121751,0.333233134534162));
#54538=DIRECTION('',(0.,-0.333233134534162,0.94284446121751));
#54539=DIRECTION('center_axis',(0.,0.333233134534159,-0.942844461217511));
#54540=DIRECTION('ref_axis',(0.,-0.942844461217511,-0.333233134534159));
#54541=DIRECTION('center_axis',(0.,-0.333233134534162,0.94284446121751));
#54542=DIRECTION('ref_axis',(0.,-0.94284446121751,-0.333233134534162));
#54543=DIRECTION('center_axis',(0.,0.333233134534159,-0.942844461217511));
#54544=DIRECTION('ref_axis',(0.,-0.942844461217511,-0.333233134534159));
#54545=DIRECTION('',(0.,0.333233134534162,-0.94284446121751));
#54546=DIRECTION('center_axis',(0.,0.333233134534162,-0.94284446121751));
#54547=DIRECTION('ref_axis',(0.,-0.94284446121751,-0.333233134534162));
#54548=DIRECTION('center_axis',(0.,-0.333233134534162,0.94284446121751));
#54549=DIRECTION('ref_axis',(0.,-0.94284446121751,-0.333233134534162));
#54550=DIRECTION('center_axis',(0.,0.333233134534162,-0.94284446121751));
#54551=DIRECTION('ref_axis',(0.,0.94284446121751,0.333233134534162));
#54552=DIRECTION('',(0.,-0.333233134534162,0.94284446121751));
#54553=DIRECTION('center_axis',(0.,0.333233134534159,-0.942844461217511));
#54554=DIRECTION('ref_axis',(0.,-0.942844461217511,-0.333233134534159));
#54555=DIRECTION('center_axis',(0.,-0.333233134534162,0.94284446121751));
#54556=DIRECTION('ref_axis',(0.,-0.94284446121751,-0.333233134534162));
#54557=DIRECTION('center_axis',(0.,0.333233134534159,-0.942844461217511));
#54558=DIRECTION('ref_axis',(0.,-0.942844461217511,-0.333233134534159));
#54559=DIRECTION('',(0.,0.333233134534162,-0.94284446121751));
#54560=DIRECTION('center_axis',(0.,0.333233134534162,-0.94284446121751));
#54561=DIRECTION('ref_axis',(0.,-0.94284446121751,-0.333233134534162));
#54562=DIRECTION('center_axis',(0.,-0.333233134534162,0.94284446121751));
#54563=DIRECTION('ref_axis',(0.,-0.94284446121751,-0.333233134534162));
#54564=DIRECTION('center_axis',(0.,0.333233134534162,-0.94284446121751));
#54565=DIRECTION('ref_axis',(0.,0.94284446121751,0.333233134534162));
#54566=DIRECTION('',(0.,-0.333233134534162,0.94284446121751));
#54567=DIRECTION('center_axis',(0.,0.333233134534159,-0.942844461217511));
#54568=DIRECTION('ref_axis',(0.,-0.942844461217511,-0.333233134534159));
#54569=DIRECTION('center_axis',(0.,-0.333233134534162,0.94284446121751));
#54570=DIRECTION('ref_axis',(0.,-0.94284446121751,-0.333233134534162));
#54571=DIRECTION('center_axis',(0.,0.333233134534159,-0.942844461217511));
#54572=DIRECTION('ref_axis',(0.,-0.942844461217511,-0.333233134534159));
#54573=DIRECTION('',(0.,0.333233134534162,-0.94284446121751));
#54574=DIRECTION('center_axis',(0.,0.333233134534162,-0.94284446121751));
#54575=DIRECTION('ref_axis',(0.,-0.94284446121751,-0.333233134534162));
#54576=DIRECTION('center_axis',(0.,-0.333233134534162,0.94284446121751));
#54577=DIRECTION('ref_axis',(0.,-0.94284446121751,-0.333233134534162));
#54578=DIRECTION('center_axis',(0.,0.333233134534162,-0.94284446121751));
#54579=DIRECTION('ref_axis',(0.,0.94284446121751,0.333233134534162));
#54580=DIRECTION('',(0.,-0.333233134534162,0.94284446121751));
#54581=DIRECTION('center_axis',(0.,0.333233134534159,-0.942844461217511));
#54582=DIRECTION('ref_axis',(0.,-0.942844461217511,-0.333233134534159));
#54583=DIRECTION('center_axis',(0.,-0.333233134534162,0.94284446121751));
#54584=DIRECTION('ref_axis',(0.,-0.94284446121751,-0.333233134534162));
#54585=DIRECTION('center_axis',(0.,0.333233134534159,-0.942844461217511));
#54586=DIRECTION('ref_axis',(0.,-0.942844461217511,-0.333233134534159));
#54587=DIRECTION('',(0.,0.333233134534162,-0.94284446121751));
#54588=DIRECTION('center_axis',(0.,0.333233134534162,-0.94284446121751));
#54589=DIRECTION('ref_axis',(0.,-0.94284446121751,-0.333233134534162));
#54590=DIRECTION('center_axis',(0.,-0.333233134534162,0.94284446121751));
#54591=DIRECTION('ref_axis',(0.,-0.94284446121751,-0.333233134534162));
#54592=DIRECTION('center_axis',(0.,0.333233134534162,-0.94284446121751));
#54593=DIRECTION('ref_axis',(0.,0.94284446121751,0.333233134534162));
#54594=DIRECTION('',(0.,-0.333233134534162,0.94284446121751));
#54595=DIRECTION('center_axis',(0.,0.333233134534159,-0.942844461217511));
#54596=DIRECTION('ref_axis',(0.,-0.942844461217511,-0.333233134534159));
#54597=DIRECTION('center_axis',(0.,-0.333233134534162,0.94284446121751));
#54598=DIRECTION('ref_axis',(0.,-0.94284446121751,-0.333233134534162));
#54599=DIRECTION('center_axis',(0.,0.333233134534159,-0.942844461217511));
#54600=DIRECTION('ref_axis',(0.,-0.942844461217511,-0.333233134534159));
#54601=DIRECTION('',(0.,0.333233134534162,-0.94284446121751));
#54602=DIRECTION('center_axis',(0.,0.333233134534162,-0.94284446121751));
#54603=DIRECTION('ref_axis',(0.,-0.94284446121751,-0.333233134534162));
#54604=DIRECTION('center_axis',(0.,-0.333233134534162,0.94284446121751));
#54605=DIRECTION('ref_axis',(0.,-0.94284446121751,-0.333233134534162));
#54606=DIRECTION('center_axis',(0.,0.333233134534162,-0.94284446121751));
#54607=DIRECTION('ref_axis',(0.,0.94284446121751,0.333233134534162));
#54608=DIRECTION('',(0.,-0.333233134534162,0.94284446121751));
#54609=DIRECTION('center_axis',(0.,0.333233134534159,-0.942844461217511));
#54610=DIRECTION('ref_axis',(0.,-0.942844461217511,-0.333233134534159));
#54611=DIRECTION('center_axis',(0.,-0.333233134534162,0.94284446121751));
#54612=DIRECTION('ref_axis',(0.,-0.94284446121751,-0.333233134534162));
#54613=DIRECTION('center_axis',(0.,0.333233134534159,-0.942844461217511));
#54614=DIRECTION('ref_axis',(0.,-0.942844461217511,-0.333233134534159));
#54615=DIRECTION('',(0.,0.333233134534162,-0.94284446121751));
#54616=DIRECTION('center_axis',(0.,0.333233134534162,-0.94284446121751));
#54617=DIRECTION('ref_axis',(0.,-0.94284446121751,-0.333233134534162));
#54618=DIRECTION('center_axis',(0.,-0.333233134534162,0.94284446121751));
#54619=DIRECTION('ref_axis',(0.,-0.94284446121751,-0.333233134534161));
#54620=DIRECTION('center_axis',(0.,0.333233134534162,-0.94284446121751));
#54621=DIRECTION('ref_axis',(0.,0.94284446121751,0.333233134534162));
#54622=DIRECTION('',(0.,-0.333233134534162,0.94284446121751));
#54623=DIRECTION('center_axis',(0.,0.333233134534159,-0.942844461217511));
#54624=DIRECTION('ref_axis',(0.,-0.942844461217511,-0.333233134534159));
#54625=DIRECTION('center_axis',(0.,-0.333233134534162,0.94284446121751));
#54626=DIRECTION('ref_axis',(0.,-0.94284446121751,-0.333233134534162));
#54627=DIRECTION('center_axis',(0.,0.333233134534159,-0.942844461217511));
#54628=DIRECTION('ref_axis',(0.,-0.942844461217511,-0.333233134534159));
#54629=DIRECTION('',(0.,0.333233134534162,-0.94284446121751));
#54630=DIRECTION('center_axis',(0.,0.333233134534162,-0.94284446121751));
#54631=DIRECTION('ref_axis',(0.,-0.94284446121751,-0.333233134534162));
#54632=DIRECTION('center_axis',(0.,-0.333233134534162,0.94284446121751));
#54633=DIRECTION('ref_axis',(0.,-0.94284446121751,-0.333233134534162));
#54634=DIRECTION('center_axis',(0.,0.333233134534162,-0.94284446121751));
#54635=DIRECTION('ref_axis',(0.,0.94284446121751,0.333233134534162));
#54636=DIRECTION('',(0.,-0.333233134534162,0.94284446121751));
#54637=DIRECTION('center_axis',(0.,0.333233134534159,-0.942844461217511));
#54638=DIRECTION('ref_axis',(0.,-0.942844461217511,-0.333233134534159));
#54639=DIRECTION('center_axis',(0.,-0.333233134534162,0.94284446121751));
#54640=DIRECTION('ref_axis',(0.,-0.94284446121751,-0.333233134534162));
#54641=DIRECTION('center_axis',(0.,0.333233134534159,-0.942844461217511));
#54642=DIRECTION('ref_axis',(0.,-0.942844461217511,-0.333233134534159));
#54643=DIRECTION('',(0.,0.333233134534162,-0.94284446121751));
#54644=DIRECTION('center_axis',(0.,-0.333233134534162,0.94284446121751));
#54645=DIRECTION('ref_axis',(0.,-0.94284446121751,-0.333233134534162));
#54646=DIRECTION('center_axis',(0.,-0.333233134534162,0.94284446121751));
#54647=DIRECTION('ref_axis',(0.,-0.94284446121751,-0.333233134534162));
#54648=DIRECTION('center_axis',(0.,-0.333233134534162,0.94284446121751));
#54649=DIRECTION('ref_axis',(0.,-0.94284446121751,-0.333233134534162));
#54650=DIRECTION('center_axis',(0.,0.333233134534162,-0.94284446121751));
#54651=DIRECTION('ref_axis',(0.,0.94284446121751,0.333233134534162));
#54652=DIRECTION('',(0.,-0.333233134534162,0.94284446121751));
#54653=DIRECTION('center_axis',(0.,0.333233134534159,-0.942844461217511));
#54654=DIRECTION('ref_axis',(0.,-0.942844461217511,-0.333233134534159));
#54655=DIRECTION('center_axis',(0.,-0.333233134534162,0.94284446121751));
#54656=DIRECTION('ref_axis',(0.,-0.94284446121751,-0.333233134534161));
#54657=DIRECTION('center_axis',(0.,0.333233134534159,-0.942844461217511));
#54658=DIRECTION('ref_axis',(0.,-0.942844461217511,-0.333233134534159));
#54659=DIRECTION('',(0.,0.333233134534162,-0.94284446121751));
#54660=DIRECTION('center_axis',(0.,0.333233134534162,-0.94284446121751));
#54661=DIRECTION('ref_axis',(0.,-0.94284446121751,-0.333233134534162));
#54662=DIRECTION('center_axis',(0.,-0.333233134534162,0.94284446121751));
#54663=DIRECTION('ref_axis',(0.,-0.94284446121751,-0.333233134534162));
#54664=DIRECTION('center_axis',(0.,0.333233134534162,-0.94284446121751));
#54665=DIRECTION('ref_axis',(0.,0.94284446121751,0.333233134534162));
#54666=DIRECTION('',(0.,-0.333233134534162,0.94284446121751));
#54667=DIRECTION('center_axis',(0.,0.333233134534159,-0.942844461217511));
#54668=DIRECTION('ref_axis',(0.,-0.942844461217511,-0.333233134534159));
#54669=DIRECTION('center_axis',(0.,-0.333233134534162,0.94284446121751));
#54670=DIRECTION('ref_axis',(0.,-0.94284446121751,-0.333233134534162));
#54671=DIRECTION('center_axis',(0.,0.333233134534159,-0.942844461217511));
#54672=DIRECTION('ref_axis',(0.,-0.942844461217511,-0.333233134534159));
#54673=DIRECTION('',(0.,0.333233134534162,-0.94284446121751));
#54674=DIRECTION('center_axis',(0.,0.333233134534162,-0.94284446121751));
#54675=DIRECTION('ref_axis',(0.,-0.94284446121751,-0.333233134534162));
#54676=DIRECTION('center_axis',(0.,-0.333233134534162,0.94284446121751));
#54677=DIRECTION('ref_axis',(0.,-0.94284446121751,-0.333233134534162));
#54678=DIRECTION('center_axis',(0.,0.333233134534162,-0.94284446121751));
#54679=DIRECTION('ref_axis',(0.,0.94284446121751,0.333233134534162));
#54680=DIRECTION('',(0.,-0.333233134534162,0.94284446121751));
#54681=DIRECTION('center_axis',(0.,0.333233134534159,-0.942844461217511));
#54682=DIRECTION('ref_axis',(0.,-0.942844461217511,-0.333233134534159));
#54683=DIRECTION('center_axis',(0.,-0.333233134534162,0.94284446121751));
#54684=DIRECTION('ref_axis',(0.,-0.94284446121751,-0.333233134534162));
#54685=DIRECTION('center_axis',(0.,0.333233134534159,-0.942844461217511));
#54686=DIRECTION('ref_axis',(0.,-0.942844461217511,-0.333233134534159));
#54687=DIRECTION('',(0.,0.333233134534161,-0.94284446121751));
#54688=DIRECTION('center_axis',(0.,0.333233134534162,-0.94284446121751));
#54689=DIRECTION('ref_axis',(0.,-0.94284446121751,-0.333233134534162));
#54690=DIRECTION('center_axis',(0.,-0.333233134534162,0.94284446121751));
#54691=DIRECTION('ref_axis',(0.,-0.94284446121751,-0.333233134534162));
#54692=DIRECTION('center_axis',(0.,0.333233134534162,-0.94284446121751));
#54693=DIRECTION('ref_axis',(0.,0.94284446121751,0.333233134534162));
#54694=DIRECTION('',(0.,-0.333233134534162,0.94284446121751));
#54695=DIRECTION('center_axis',(0.,0.333233134534159,-0.942844461217511));
#54696=DIRECTION('ref_axis',(0.,-0.942844461217511,-0.333233134534159));
#54697=DIRECTION('center_axis',(0.,-0.333233134534162,0.94284446121751));
#54698=DIRECTION('ref_axis',(0.,-0.94284446121751,-0.333233134534162));
#54699=DIRECTION('center_axis',(0.,0.333233134534159,-0.942844461217511));
#54700=DIRECTION('ref_axis',(0.,-0.942844461217511,-0.333233134534159));
#54701=DIRECTION('',(0.,0.333233134534162,-0.94284446121751));
#54702=DIRECTION('center_axis',(0.,0.333233134534162,-0.94284446121751));
#54703=DIRECTION('ref_axis',(0.,-0.94284446121751,-0.333233134534162));
#54704=DIRECTION('center_axis',(0.,-0.333233134534162,0.94284446121751));
#54705=DIRECTION('ref_axis',(0.,-0.94284446121751,-0.333233134534162));
#54706=DIRECTION('center_axis',(0.,0.333233134534162,-0.94284446121751));
#54707=DIRECTION('ref_axis',(0.,0.94284446121751,0.333233134534162));
#54708=DIRECTION('',(0.,-0.333233134534162,0.94284446121751));
#54709=DIRECTION('center_axis',(0.,0.333233134534159,-0.942844461217511));
#54710=DIRECTION('ref_axis',(0.,-0.942844461217511,-0.333233134534159));
#54711=DIRECTION('center_axis',(0.,-0.333233134534162,0.94284446121751));
#54712=DIRECTION('ref_axis',(0.,-0.94284446121751,-0.333233134534162));
#54713=DIRECTION('center_axis',(0.,0.333233134534159,-0.942844461217511));
#54714=DIRECTION('ref_axis',(0.,-0.942844461217511,-0.333233134534159));
#54715=DIRECTION('',(0.,0.333233134534162,-0.94284446121751));
#54716=DIRECTION('center_axis',(0.,0.333233134534162,-0.94284446121751));
#54717=DIRECTION('ref_axis',(0.,-0.94284446121751,-0.333233134534162));
#54718=DIRECTION('center_axis',(0.,-0.333233134534162,0.94284446121751));
#54719=DIRECTION('ref_axis',(0.,-0.94284446121751,-0.333233134534162));
#54720=DIRECTION('center_axis',(0.,0.333233134534162,-0.94284446121751));
#54721=DIRECTION('ref_axis',(0.,0.94284446121751,0.333233134534162));
#54722=DIRECTION('',(0.,-0.333233134534162,0.94284446121751));
#54723=DIRECTION('center_axis',(0.,0.333233134534159,-0.942844461217511));
#54724=DIRECTION('ref_axis',(0.,-0.942844461217511,-0.333233134534159));
#54725=DIRECTION('center_axis',(0.,-0.333233134534162,0.94284446121751));
#54726=DIRECTION('ref_axis',(0.,-0.94284446121751,-0.333233134534162));
#54727=DIRECTION('center_axis',(0.,0.333233134534159,-0.942844461217511));
#54728=DIRECTION('ref_axis',(0.,-0.942844461217511,-0.333233134534159));
#54729=DIRECTION('',(0.,0.333233134534162,-0.94284446121751));
#54730=DIRECTION('center_axis',(0.,0.333233134534162,-0.94284446121751));
#54731=DIRECTION('ref_axis',(0.,-0.94284446121751,-0.333233134534162));
#54732=DIRECTION('center_axis',(0.,-0.333233134534162,0.94284446121751));
#54733=DIRECTION('ref_axis',(0.,-0.94284446121751,-0.333233134534162));
#54734=DIRECTION('center_axis',(0.,0.333233134534162,-0.94284446121751));
#54735=DIRECTION('ref_axis',(0.,0.94284446121751,0.333233134534162));
#54736=DIRECTION('',(0.,-0.333233134534162,0.94284446121751));
#54737=DIRECTION('center_axis',(0.,0.333233134534159,-0.942844461217511));
#54738=DIRECTION('ref_axis',(0.,-0.942844461217511,-0.333233134534159));
#54739=DIRECTION('center_axis',(0.,-0.333233134534162,0.94284446121751));
#54740=DIRECTION('ref_axis',(0.,-0.94284446121751,-0.333233134534162));
#54741=DIRECTION('center_axis',(0.,0.333233134534159,-0.942844461217511));
#54742=DIRECTION('ref_axis',(0.,-0.942844461217511,-0.333233134534159));
#54743=DIRECTION('',(0.,0.333233134534162,-0.94284446121751));
#54744=DIRECTION('center_axis',(0.,0.333233134534162,-0.94284446121751));
#54745=DIRECTION('ref_axis',(0.,-0.94284446121751,-0.333233134534162));
#54746=DIRECTION('center_axis',(0.,-0.333233134534162,0.94284446121751));
#54747=DIRECTION('ref_axis',(0.,-0.94284446121751,-0.333233134534162));
#54748=DIRECTION('center_axis',(0.,0.333233134534162,-0.94284446121751));
#54749=DIRECTION('ref_axis',(0.,0.94284446121751,0.333233134534162));
#54750=DIRECTION('',(0.,-0.333233134534162,0.94284446121751));
#54751=DIRECTION('center_axis',(0.,0.333233134534159,-0.942844461217511));
#54752=DIRECTION('ref_axis',(0.,-0.942844461217511,-0.333233134534159));
#54753=DIRECTION('center_axis',(0.,-0.333233134534162,0.94284446121751));
#54754=DIRECTION('ref_axis',(0.,-0.94284446121751,-0.333233134534162));
#54755=DIRECTION('center_axis',(0.,0.333233134534159,-0.942844461217511));
#54756=DIRECTION('ref_axis',(0.,-0.942844461217511,-0.333233134534159));
#54757=DIRECTION('',(0.,0.333233134534162,-0.94284446121751));
#54758=DIRECTION('center_axis',(0.,-0.333233134534162,0.94284446121751));
#54759=DIRECTION('ref_axis',(0.,-0.94284446121751,-0.333233134534162));
#54760=DIRECTION('center_axis',(0.,-0.333233134534162,0.94284446121751));
#54761=DIRECTION('ref_axis',(0.,-0.94284446121751,-0.333233134534162));
#54762=DIRECTION('center_axis',(0.,-0.333233134534162,0.94284446121751));
#54763=DIRECTION('ref_axis',(0.,-0.94284446121751,-0.333233134534162));
#54764=DIRECTION('center_axis',(0.,0.333233134534162,-0.94284446121751));
#54765=DIRECTION('ref_axis',(0.,0.94284446121751,0.333233134534162));
#54766=DIRECTION('',(0.,-0.333233134534162,0.94284446121751));
#54767=DIRECTION('center_axis',(0.,0.333233134534159,-0.942844461217511));
#54768=DIRECTION('ref_axis',(0.,-0.942844461217511,-0.333233134534159));
#54769=DIRECTION('center_axis',(0.,-0.333233134534162,0.94284446121751));
#54770=DIRECTION('ref_axis',(0.,-0.94284446121751,-0.333233134534162));
#54771=DIRECTION('center_axis',(0.,0.333233134534159,-0.942844461217511));
#54772=DIRECTION('ref_axis',(0.,-0.942844461217511,-0.333233134534159));
#54773=DIRECTION('',(0.,0.333233134534162,-0.94284446121751));
#54774=DIRECTION('center_axis',(0.,-0.333233134534162,0.94284446121751));
#54775=DIRECTION('ref_axis',(0.,-0.94284446121751,-0.333233134534162));
#54776=DIRECTION('center_axis',(0.,-0.333233134534162,0.94284446121751));
#54777=DIRECTION('ref_axis',(0.,-0.94284446121751,-0.333233134534162));
#54778=DIRECTION('center_axis',(0.,-0.333233134534162,0.94284446121751));
#54779=DIRECTION('ref_axis',(0.,-0.94284446121751,-0.333233134534162));
#54780=DIRECTION('center_axis',(0.,0.333233134534162,-0.94284446121751));
#54781=DIRECTION('ref_axis',(0.,0.94284446121751,0.333233134534162));
#54782=DIRECTION('',(0.,-0.333233134534162,0.94284446121751));
#54783=DIRECTION('center_axis',(0.,0.333233134534159,-0.942844461217511));
#54784=DIRECTION('ref_axis',(0.,-0.942844461217511,-0.333233134534159));
#54785=DIRECTION('center_axis',(0.,-0.333233134534162,0.94284446121751));
#54786=DIRECTION('ref_axis',(0.,-0.94284446121751,-0.333233134534162));
#54787=DIRECTION('center_axis',(0.,0.333233134534159,-0.942844461217511));
#54788=DIRECTION('ref_axis',(0.,-0.942844461217511,-0.333233134534159));
#54789=DIRECTION('',(0.,0.333233134534162,-0.94284446121751));
#54790=DIRECTION('center_axis',(0.,0.333233134534162,-0.94284446121751));
#54791=DIRECTION('ref_axis',(0.,-0.94284446121751,-0.333233134534162));
#54792=DIRECTION('center_axis',(0.,-0.333233134534162,0.94284446121751));
#54793=DIRECTION('ref_axis',(0.,-0.94284446121751,-0.333233134534162));
#54794=DIRECTION('center_axis',(0.,0.333233134534162,-0.94284446121751));
#54795=DIRECTION('ref_axis',(0.,0.94284446121751,0.333233134534162));
#54796=DIRECTION('',(0.,-0.333233134534162,0.94284446121751));
#54797=DIRECTION('center_axis',(0.,0.333233134534159,-0.942844461217511));
#54798=DIRECTION('ref_axis',(0.,-0.942844461217511,-0.333233134534159));
#54799=DIRECTION('center_axis',(0.,-0.333233134534162,0.94284446121751));
#54800=DIRECTION('ref_axis',(0.,-0.94284446121751,-0.333233134534162));
#54801=DIRECTION('center_axis',(0.,0.333233134534159,-0.942844461217511));
#54802=DIRECTION('ref_axis',(0.,-0.942844461217511,-0.333233134534159));
#54803=DIRECTION('',(0.,0.333233134534162,-0.94284446121751));
#54804=DIRECTION('center_axis',(0.,0.333233134534162,-0.94284446121751));
#54805=DIRECTION('ref_axis',(0.,-0.94284446121751,-0.333233134534162));
#54806=DIRECTION('center_axis',(0.,-0.333233134534162,0.94284446121751));
#54807=DIRECTION('ref_axis',(0.,-0.94284446121751,-0.333233134534162));
#54808=DIRECTION('center_axis',(0.,0.333233134534162,-0.94284446121751));
#54809=DIRECTION('ref_axis',(0.,0.94284446121751,0.333233134534162));
#54810=DIRECTION('',(0.,-0.333233134534162,0.94284446121751));
#54811=DIRECTION('center_axis',(0.,0.333233134534159,-0.942844461217511));
#54812=DIRECTION('ref_axis',(0.,-0.942844461217511,-0.333233134534159));
#54813=DIRECTION('center_axis',(0.,-0.333233134534162,0.94284446121751));
#54814=DIRECTION('ref_axis',(0.,-0.94284446121751,-0.333233134534162));
#54815=DIRECTION('center_axis',(0.,0.333233134534159,-0.942844461217511));
#54816=DIRECTION('ref_axis',(0.,-0.942844461217511,-0.333233134534159));
#54817=DIRECTION('',(0.,0.333233134534162,-0.94284446121751));
#54818=DIRECTION('center_axis',(0.,0.333233134534162,-0.94284446121751));
#54819=DIRECTION('ref_axis',(0.,-0.94284446121751,-0.333233134534162));
#54820=DIRECTION('center_axis',(0.,-0.333233134534162,0.94284446121751));
#54821=DIRECTION('ref_axis',(0.,-0.94284446121751,-0.333233134534162));
#54822=DIRECTION('center_axis',(0.,0.333233134534162,-0.94284446121751));
#54823=DIRECTION('ref_axis',(0.,0.94284446121751,0.333233134534162));
#54824=DIRECTION('',(0.,-0.333233134534162,0.94284446121751));
#54825=DIRECTION('center_axis',(0.,0.333233134534159,-0.942844461217511));
#54826=DIRECTION('ref_axis',(0.,-0.942844461217511,-0.333233134534159));
#54827=DIRECTION('center_axis',(0.,-0.333233134534162,0.94284446121751));
#54828=DIRECTION('ref_axis',(0.,-0.94284446121751,-0.333233134534162));
#54829=DIRECTION('center_axis',(0.,0.333233134534159,-0.942844461217511));
#54830=DIRECTION('ref_axis',(0.,-0.942844461217511,-0.333233134534159));
#54831=DIRECTION('',(0.,0.333233134534162,-0.94284446121751));
#54832=DIRECTION('center_axis',(0.,0.333233134534162,-0.94284446121751));
#54833=DIRECTION('ref_axis',(0.,-0.94284446121751,-0.333233134534162));
#54834=DIRECTION('center_axis',(0.,-0.333233134534162,0.94284446121751));
#54835=DIRECTION('ref_axis',(0.,-0.94284446121751,-0.333233134534162));
#54836=DIRECTION('center_axis',(0.,0.333233134534162,-0.94284446121751));
#54837=DIRECTION('ref_axis',(0.,0.94284446121751,0.333233134534162));
#54838=DIRECTION('',(0.,-0.333233134534162,0.94284446121751));
#54839=DIRECTION('center_axis',(0.,0.333233134534159,-0.942844461217511));
#54840=DIRECTION('ref_axis',(0.,-0.942844461217511,-0.333233134534159));
#54841=DIRECTION('center_axis',(0.,-0.333233134534162,0.94284446121751));
#54842=DIRECTION('ref_axis',(0.,-0.94284446121751,-0.333233134534162));
#54843=DIRECTION('center_axis',(0.,0.333233134534159,-0.942844461217511));
#54844=DIRECTION('ref_axis',(0.,-0.942844461217511,-0.333233134534159));
#54845=DIRECTION('',(0.,0.333233134534162,-0.94284446121751));
#54846=DIRECTION('center_axis',(0.,0.333233134534162,-0.94284446121751));
#54847=DIRECTION('ref_axis',(0.,-0.94284446121751,-0.333233134534162));
#54848=DIRECTION('center_axis',(0.,-0.333233134534162,0.94284446121751));
#54849=DIRECTION('ref_axis',(0.,-0.94284446121751,-0.333233134534162));
#54850=DIRECTION('center_axis',(0.,0.333233134534162,-0.94284446121751));
#54851=DIRECTION('ref_axis',(0.,0.94284446121751,0.333233134534162));
#54852=DIRECTION('',(0.,-0.333233134534162,0.94284446121751));
#54853=DIRECTION('center_axis',(0.,0.333233134534159,-0.942844461217511));
#54854=DIRECTION('ref_axis',(0.,-0.942844461217511,-0.333233134534159));
#54855=DIRECTION('center_axis',(0.,-0.333233134534162,0.94284446121751));
#54856=DIRECTION('ref_axis',(0.,-0.94284446121751,-0.333233134534162));
#54857=DIRECTION('center_axis',(0.,0.333233134534159,-0.942844461217511));
#54858=DIRECTION('ref_axis',(0.,-0.942844461217511,-0.333233134534159));
#54859=DIRECTION('',(0.,0.333233134534162,-0.94284446121751));
#54860=DIRECTION('center_axis',(0.,0.333233134534162,-0.94284446121751));
#54861=DIRECTION('ref_axis',(0.,-0.94284446121751,-0.333233134534162));
#54862=DIRECTION('center_axis',(0.,-0.333233134534162,0.94284446121751));
#54863=DIRECTION('ref_axis',(0.,-0.94284446121751,-0.333233134534162));
#54864=DIRECTION('center_axis',(0.,0.333233134534162,-0.94284446121751));
#54865=DIRECTION('ref_axis',(0.,0.94284446121751,0.333233134534162));
#54866=DIRECTION('',(0.,-0.333233134534162,0.94284446121751));
#54867=DIRECTION('center_axis',(0.,0.333233134534159,-0.942844461217511));
#54868=DIRECTION('ref_axis',(0.,-0.942844461217511,-0.333233134534159));
#54869=DIRECTION('center_axis',(0.,-0.333233134534162,0.94284446121751));
#54870=DIRECTION('ref_axis',(0.,-0.94284446121751,-0.333233134534162));
#54871=DIRECTION('center_axis',(0.,0.333233134534159,-0.942844461217511));
#54872=DIRECTION('ref_axis',(0.,-0.942844461217511,-0.333233134534159));
#54873=DIRECTION('',(0.,0.333233134534162,-0.94284446121751));
#54874=DIRECTION('center_axis',(0.,-0.333233134534162,0.94284446121751));
#54875=DIRECTION('ref_axis',(0.,-0.94284446121751,-0.333233134534162));
#54876=DIRECTION('center_axis',(0.,-0.333233134534162,0.94284446121751));
#54877=DIRECTION('ref_axis',(0.,-0.94284446121751,-0.333233134534162));
#54878=DIRECTION('center_axis',(0.,-0.333233134534162,0.94284446121751));
#54879=DIRECTION('ref_axis',(0.,-0.94284446121751,-0.333233134534162));
#54880=DIRECTION('center_axis',(0.,0.333233134534162,-0.94284446121751));
#54881=DIRECTION('ref_axis',(0.,0.94284446121751,0.333233134534162));
#54882=DIRECTION('',(0.,-0.333233134534162,0.94284446121751));
#54883=DIRECTION('center_axis',(0.,0.333233134534159,-0.942844461217511));
#54884=DIRECTION('ref_axis',(0.,-0.942844461217511,-0.333233134534159));
#54885=DIRECTION('center_axis',(0.,-0.333233134534162,0.94284446121751));
#54886=DIRECTION('ref_axis',(0.,-0.94284446121751,-0.333233134534161));
#54887=DIRECTION('center_axis',(0.,0.333233134534159,-0.942844461217511));
#54888=DIRECTION('ref_axis',(0.,-0.942844461217511,-0.333233134534159));
#54889=DIRECTION('',(0.,0.333233134534162,-0.94284446121751));
#54890=DIRECTION('center_axis',(0.,0.333233134534162,-0.94284446121751));
#54891=DIRECTION('ref_axis',(0.,-0.94284446121751,-0.333233134534162));
#54892=DIRECTION('center_axis',(0.,-0.333233134534162,0.94284446121751));
#54893=DIRECTION('ref_axis',(0.,-0.94284446121751,-0.333233134534162));
#54894=DIRECTION('center_axis',(0.,0.333233134534162,-0.94284446121751));
#54895=DIRECTION('ref_axis',(0.,0.94284446121751,0.333233134534162));
#54896=DIRECTION('',(0.,-0.333233134534162,0.94284446121751));
#54897=DIRECTION('center_axis',(0.,0.333233134534159,-0.942844461217511));
#54898=DIRECTION('ref_axis',(0.,-0.942844461217511,-0.333233134534159));
#54899=DIRECTION('center_axis',(0.,-0.333233134534162,0.94284446121751));
#54900=DIRECTION('ref_axis',(0.,-0.94284446121751,-0.333233134534162));
#54901=DIRECTION('center_axis',(0.,0.333233134534159,-0.942844461217511));
#54902=DIRECTION('ref_axis',(0.,-0.942844461217511,-0.333233134534159));
#54903=DIRECTION('',(0.,0.333233134534162,-0.94284446121751));
#54904=DIRECTION('center_axis',(0.,0.333233134534162,-0.94284446121751));
#54905=DIRECTION('ref_axis',(0.,-0.94284446121751,-0.333233134534162));
#54906=DIRECTION('center_axis',(0.,-0.333233134534162,0.94284446121751));
#54907=DIRECTION('ref_axis',(0.,-0.94284446121751,-0.333233134534162));
#54908=DIRECTION('center_axis',(0.,0.333233134534162,-0.94284446121751));
#54909=DIRECTION('ref_axis',(0.,0.94284446121751,0.333233134534162));
#54910=DIRECTION('',(0.,-0.333233134534162,0.94284446121751));
#54911=DIRECTION('center_axis',(0.,0.333233134534159,-0.942844461217511));
#54912=DIRECTION('ref_axis',(0.,-0.942844461217511,-0.333233134534159));
#54913=DIRECTION('center_axis',(0.,-0.333233134534162,0.94284446121751));
#54914=DIRECTION('ref_axis',(0.,-0.94284446121751,-0.333233134534161));
#54915=DIRECTION('center_axis',(0.,0.333233134534159,-0.942844461217511));
#54916=DIRECTION('ref_axis',(0.,-0.942844461217511,-0.333233134534159));
#54917=DIRECTION('',(0.,0.333233134534162,-0.94284446121751));
#54918=DIRECTION('center_axis',(0.,0.333233134534162,-0.94284446121751));
#54919=DIRECTION('ref_axis',(0.,-0.94284446121751,-0.333233134534162));
#54920=DIRECTION('center_axis',(0.,-0.333233134534162,0.94284446121751));
#54921=DIRECTION('ref_axis',(0.,-0.94284446121751,-0.333233134534162));
#54922=DIRECTION('center_axis',(0.,0.333233134534162,-0.94284446121751));
#54923=DIRECTION('ref_axis',(0.,0.94284446121751,0.333233134534162));
#54924=DIRECTION('',(0.,-0.333233134534162,0.94284446121751));
#54925=DIRECTION('center_axis',(0.,0.333233134534159,-0.942844461217511));
#54926=DIRECTION('ref_axis',(0.,-0.942844461217511,-0.333233134534159));
#54927=DIRECTION('center_axis',(0.,-0.333233134534162,0.94284446121751));
#54928=DIRECTION('ref_axis',(0.,-0.94284446121751,-0.333233134534162));
#54929=DIRECTION('center_axis',(0.,0.333233134534159,-0.942844461217511));
#54930=DIRECTION('ref_axis',(0.,-0.942844461217511,-0.333233134534159));
#54931=DIRECTION('',(0.,0.333233134534162,-0.94284446121751));
#54932=DIRECTION('center_axis',(0.,0.333233134534162,-0.94284446121751));
#54933=DIRECTION('ref_axis',(0.,-0.94284446121751,-0.333233134534162));
#54934=DIRECTION('center_axis',(0.,-0.333233134534162,0.94284446121751));
#54935=DIRECTION('ref_axis',(0.,-0.94284446121751,-0.333233134534162));
#54936=DIRECTION('center_axis',(0.,0.333233134534162,-0.94284446121751));
#54937=DIRECTION('ref_axis',(0.,0.94284446121751,0.333233134534162));
#54938=DIRECTION('',(0.,-0.333233134534162,0.94284446121751));
#54939=DIRECTION('center_axis',(0.,0.333233134534159,-0.942844461217511));
#54940=DIRECTION('ref_axis',(0.,-0.942844461217511,-0.333233134534159));
#54941=DIRECTION('center_axis',(0.,-0.333233134534162,0.94284446121751));
#54942=DIRECTION('ref_axis',(0.,-0.94284446121751,-0.333233134534162));
#54943=DIRECTION('center_axis',(0.,0.333233134534159,-0.942844461217511));
#54944=DIRECTION('ref_axis',(0.,-0.942844461217511,-0.333233134534159));
#54945=DIRECTION('',(0.,0.333233134534162,-0.94284446121751));
#54946=DIRECTION('center_axis',(0.,0.333233134534162,-0.94284446121751));
#54947=DIRECTION('ref_axis',(0.,-0.94284446121751,-0.333233134534162));
#54948=DIRECTION('center_axis',(0.,-0.333233134534162,0.94284446121751));
#54949=DIRECTION('ref_axis',(0.,-0.94284446121751,-0.333233134534162));
#54950=DIRECTION('center_axis',(0.,0.333233134534162,-0.94284446121751));
#54951=DIRECTION('ref_axis',(0.,0.94284446121751,0.333233134534162));
#54952=DIRECTION('',(0.,-0.333233134534162,0.94284446121751));
#54953=DIRECTION('center_axis',(0.,0.333233134534159,-0.942844461217511));
#54954=DIRECTION('ref_axis',(0.,-0.942844461217511,-0.333233134534159));
#54955=DIRECTION('center_axis',(0.,-0.333233134534162,0.94284446121751));
#54956=DIRECTION('ref_axis',(0.,-0.94284446121751,-0.333233134534162));
#54957=DIRECTION('center_axis',(0.,0.333233134534159,-0.942844461217511));
#54958=DIRECTION('ref_axis',(0.,-0.942844461217511,-0.333233134534159));
#54959=DIRECTION('',(0.,0.333233134534162,-0.94284446121751));
#54960=DIRECTION('center_axis',(0.,0.333233134534162,-0.94284446121751));
#54961=DIRECTION('ref_axis',(0.,-0.94284446121751,-0.333233134534162));
#54962=DIRECTION('center_axis',(0.,-0.333233134534162,0.94284446121751));
#54963=DIRECTION('ref_axis',(0.,-0.94284446121751,-0.333233134534162));
#54964=DIRECTION('center_axis',(0.,0.333233134534162,-0.94284446121751));
#54965=DIRECTION('ref_axis',(0.,0.94284446121751,0.333233134534162));
#54966=DIRECTION('',(0.,-0.333233134534162,0.94284446121751));
#54967=DIRECTION('center_axis',(0.,0.333233134534159,-0.942844461217511));
#54968=DIRECTION('ref_axis',(0.,-0.942844461217511,-0.333233134534159));
#54969=DIRECTION('center_axis',(0.,-0.333233134534162,0.94284446121751));
#54970=DIRECTION('ref_axis',(0.,-0.94284446121751,-0.333233134534162));
#54971=DIRECTION('center_axis',(0.,0.333233134534159,-0.942844461217511));
#54972=DIRECTION('ref_axis',(0.,-0.942844461217511,-0.333233134534159));
#54973=DIRECTION('',(0.,0.333233134534162,-0.94284446121751));
#54974=DIRECTION('center_axis',(0.,0.333233134534162,-0.94284446121751));
#54975=DIRECTION('ref_axis',(0.,-0.94284446121751,-0.333233134534162));
#54976=DIRECTION('center_axis',(0.,-0.333233134534162,0.94284446121751));
#54977=DIRECTION('ref_axis',(0.,-0.94284446121751,-0.333233134534162));
#54978=DIRECTION('center_axis',(0.,0.333233134534162,-0.94284446121751));
#54979=DIRECTION('ref_axis',(0.,0.94284446121751,0.333233134534162));
#54980=DIRECTION('',(0.,-0.333233134534162,0.94284446121751));
#54981=DIRECTION('center_axis',(0.,0.333233134534159,-0.942844461217511));
#54982=DIRECTION('ref_axis',(0.,-0.942844461217511,-0.333233134534159));
#54983=DIRECTION('center_axis',(0.,-0.333233134534162,0.94284446121751));
#54984=DIRECTION('ref_axis',(0.,-0.94284446121751,-0.333233134534161));
#54985=DIRECTION('center_axis',(0.,0.333233134534159,-0.942844461217511));
#54986=DIRECTION('ref_axis',(0.,-0.942844461217511,-0.333233134534159));
#54987=DIRECTION('',(0.,0.333233134534162,-0.94284446121751));
#54988=DIRECTION('center_axis',(0.,0.333233134534162,-0.94284446121751));
#54989=DIRECTION('ref_axis',(0.,-0.94284446121751,-0.333233134534162));
#54990=DIRECTION('center_axis',(0.,-0.333233134534162,0.94284446121751));
#54991=DIRECTION('ref_axis',(0.,-0.94284446121751,-0.333233134534162));
#54992=DIRECTION('center_axis',(0.,0.333233134534162,-0.94284446121751));
#54993=DIRECTION('ref_axis',(0.,0.94284446121751,0.333233134534162));
#54994=DIRECTION('',(0.,-0.333233134534162,0.94284446121751));
#54995=DIRECTION('center_axis',(0.,0.333233134534159,-0.942844461217511));
#54996=DIRECTION('ref_axis',(0.,-0.942844461217511,-0.333233134534159));
#54997=DIRECTION('center_axis',(0.,-0.333233134534162,0.94284446121751));
#54998=DIRECTION('ref_axis',(0.,-0.94284446121751,-0.333233134534162));
#54999=DIRECTION('center_axis',(0.,0.333233134534159,-0.942844461217511));
#55000=DIRECTION('ref_axis',(0.,-0.942844461217511,-0.333233134534159));
#55001=DIRECTION('',(0.,0.333233134534162,-0.94284446121751));
#55002=DIRECTION('center_axis',(0.,0.333233134534162,-0.94284446121751));
#55003=DIRECTION('ref_axis',(0.,-0.94284446121751,-0.333233134534162));
#55004=DIRECTION('center_axis',(0.,-0.333233134534162,0.94284446121751));
#55005=DIRECTION('ref_axis',(0.,-0.94284446121751,-0.333233134534162));
#55006=DIRECTION('center_axis',(0.,0.333233134534162,-0.94284446121751));
#55007=DIRECTION('ref_axis',(0.,0.94284446121751,0.333233134534162));
#55008=DIRECTION('',(0.,-0.333233134534162,0.94284446121751));
#55009=DIRECTION('center_axis',(0.,0.333233134534159,-0.942844461217511));
#55010=DIRECTION('ref_axis',(0.,-0.942844461217511,-0.333233134534159));
#55011=DIRECTION('center_axis',(0.,-0.333233134534162,0.94284446121751));
#55012=DIRECTION('ref_axis',(0.,-0.94284446121751,-0.333233134534162));
#55013=DIRECTION('center_axis',(0.,0.333233134534159,-0.942844461217511));
#55014=DIRECTION('ref_axis',(0.,-0.942844461217511,-0.333233134534159));
#55015=DIRECTION('',(0.,0.333233134534162,-0.94284446121751));
#55016=DIRECTION('center_axis',(0.,0.333233134534162,-0.94284446121751));
#55017=DIRECTION('ref_axis',(0.,-0.94284446121751,-0.333233134534162));
#55018=DIRECTION('center_axis',(0.,-0.333233134534162,0.94284446121751));
#55019=DIRECTION('ref_axis',(0.,-0.94284446121751,-0.333233134534162));
#55020=DIRECTION('center_axis',(0.,0.333233134534162,-0.94284446121751));
#55021=DIRECTION('ref_axis',(0.,0.94284446121751,0.333233134534162));
#55022=DIRECTION('',(0.,-0.333233134534162,0.94284446121751));
#55023=DIRECTION('center_axis',(0.,0.333233134534159,-0.942844461217511));
#55024=DIRECTION('ref_axis',(0.,-0.942844461217511,-0.333233134534159));
#55025=DIRECTION('center_axis',(0.,-0.333233134534162,0.94284446121751));
#55026=DIRECTION('ref_axis',(0.,-0.94284446121751,-0.333233134534162));
#55027=DIRECTION('center_axis',(0.,0.333233134534159,-0.942844461217511));
#55028=DIRECTION('ref_axis',(0.,-0.942844461217511,-0.333233134534159));
#55029=DIRECTION('',(0.,0.333233134534162,-0.94284446121751));
#55030=DIRECTION('center_axis',(0.,0.333233134534162,-0.94284446121751));
#55031=DIRECTION('ref_axis',(0.,-0.94284446121751,-0.333233134534162));
#55032=DIRECTION('center_axis',(0.,-0.333233134534162,0.94284446121751));
#55033=DIRECTION('ref_axis',(0.,-0.94284446121751,-0.333233134534162));
#55034=DIRECTION('center_axis',(0.,0.333233134534162,-0.94284446121751));
#55035=DIRECTION('ref_axis',(0.,0.94284446121751,0.333233134534162));
#55036=DIRECTION('',(0.,-0.333233134534162,0.94284446121751));
#55037=DIRECTION('center_axis',(0.,0.333233134534159,-0.942844461217511));
#55038=DIRECTION('ref_axis',(0.,-0.942844461217511,-0.333233134534159));
#55039=DIRECTION('center_axis',(0.,-0.333233134534162,0.94284446121751));
#55040=DIRECTION('ref_axis',(0.,-0.94284446121751,-0.333233134534162));
#55041=DIRECTION('center_axis',(0.,0.333233134534159,-0.942844461217511));
#55042=DIRECTION('ref_axis',(0.,-0.942844461217511,-0.333233134534159));
#55043=DIRECTION('',(0.,0.333233134534162,-0.94284446121751));
#55044=DIRECTION('center_axis',(0.,0.333233134534162,-0.94284446121751));
#55045=DIRECTION('ref_axis',(0.,-0.94284446121751,-0.333233134534162));
#55046=DIRECTION('center_axis',(0.,-0.333233134534162,0.94284446121751));
#55047=DIRECTION('ref_axis',(0.,-0.94284446121751,-0.333233134534162));
#55048=DIRECTION('center_axis',(0.,0.333233134534162,-0.94284446121751));
#55049=DIRECTION('ref_axis',(0.,0.94284446121751,0.333233134534162));
#55050=DIRECTION('',(0.,-0.333233134534162,0.94284446121751));
#55051=DIRECTION('center_axis',(0.,0.333233134534159,-0.942844461217511));
#55052=DIRECTION('ref_axis',(0.,-0.942844461217511,-0.333233134534159));
#55053=DIRECTION('center_axis',(0.,-0.333233134534162,0.94284446121751));
#55054=DIRECTION('ref_axis',(0.,-0.94284446121751,-0.333233134534162));
#55055=DIRECTION('center_axis',(0.,0.333233134534159,-0.942844461217511));
#55056=DIRECTION('ref_axis',(0.,-0.942844461217511,-0.333233134534159));
#55057=DIRECTION('',(0.,0.333233134534162,-0.94284446121751));
#55058=DIRECTION('center_axis',(0.,0.333233134534162,-0.94284446121751));
#55059=DIRECTION('ref_axis',(0.,-0.94284446121751,-0.333233134534162));
#55060=DIRECTION('center_axis',(0.,-0.333233134534162,0.94284446121751));
#55061=DIRECTION('ref_axis',(0.,-0.94284446121751,-0.333233134534162));
#55062=DIRECTION('center_axis',(0.,0.333233134534162,-0.94284446121751));
#55063=DIRECTION('ref_axis',(0.,0.94284446121751,0.333233134534162));
#55064=DIRECTION('',(0.,-0.333233134534162,0.94284446121751));
#55065=DIRECTION('center_axis',(0.,0.333233134534159,-0.942844461217511));
#55066=DIRECTION('ref_axis',(0.,-0.942844461217511,-0.333233134534159));
#55067=DIRECTION('center_axis',(0.,-0.333233134534162,0.94284446121751));
#55068=DIRECTION('ref_axis',(0.,-0.94284446121751,-0.333233134534162));
#55069=DIRECTION('center_axis',(0.,0.333233134534159,-0.942844461217511));
#55070=DIRECTION('ref_axis',(0.,-0.942844461217511,-0.333233134534159));
#55071=DIRECTION('',(0.,0.333233134534162,-0.94284446121751));
#55072=DIRECTION('center_axis',(0.,-0.333233134534162,0.94284446121751));
#55073=DIRECTION('ref_axis',(0.,-0.94284446121751,-0.333233134534162));
#55074=DIRECTION('center_axis',(0.,-0.333233134534162,0.94284446121751));
#55075=DIRECTION('ref_axis',(0.,-0.94284446121751,-0.333233134534162));
#55076=DIRECTION('center_axis',(0.,-0.333233134534162,0.94284446121751));
#55077=DIRECTION('ref_axis',(0.,-0.94284446121751,-0.333233134534162));
#55078=DIRECTION('center_axis',(0.,0.333233134534162,-0.94284446121751));
#55079=DIRECTION('ref_axis',(0.,0.94284446121751,0.333233134534162));
#55080=DIRECTION('',(0.,-0.333233134534162,0.94284446121751));
#55081=DIRECTION('center_axis',(0.,0.333233134534159,-0.942844461217511));
#55082=DIRECTION('ref_axis',(0.,-0.942844461217511,-0.333233134534159));
#55083=DIRECTION('center_axis',(0.,-0.333233134534162,0.94284446121751));
#55084=DIRECTION('ref_axis',(0.,-0.94284446121751,-0.333233134534162));
#55085=DIRECTION('center_axis',(0.,0.333233134534159,-0.942844461217511));
#55086=DIRECTION('ref_axis',(0.,-0.942844461217511,-0.333233134534159));
#55087=DIRECTION('',(0.,0.333233134534162,-0.94284446121751));
#55088=DIRECTION('center_axis',(0.,0.333233134534162,-0.94284446121751));
#55089=DIRECTION('ref_axis',(0.,-0.94284446121751,-0.333233134534162));
#55090=DIRECTION('center_axis',(0.,-0.333233134534162,0.94284446121751));
#55091=DIRECTION('ref_axis',(0.,-0.94284446121751,-0.333233134534162));
#55092=DIRECTION('center_axis',(0.,0.333233134534162,-0.94284446121751));
#55093=DIRECTION('ref_axis',(0.,0.94284446121751,0.333233134534162));
#55094=DIRECTION('',(0.,-0.333233134534162,0.94284446121751));
#55095=DIRECTION('center_axis',(0.,0.333233134534159,-0.942844461217511));
#55096=DIRECTION('ref_axis',(0.,-0.942844461217511,-0.333233134534159));
#55097=DIRECTION('center_axis',(0.,-0.333233134534162,0.94284446121751));
#55098=DIRECTION('ref_axis',(0.,-0.94284446121751,-0.333233134534162));
#55099=DIRECTION('center_axis',(0.,0.333233134534159,-0.942844461217511));
#55100=DIRECTION('ref_axis',(0.,-0.942844461217511,-0.333233134534159));
#55101=DIRECTION('',(0.,0.333233134534162,-0.94284446121751));
#55102=DIRECTION('center_axis',(0.,0.333233134534162,-0.94284446121751));
#55103=DIRECTION('ref_axis',(0.,-0.94284446121751,-0.333233134534162));
#55104=DIRECTION('center_axis',(0.,-0.333233134534162,0.94284446121751));
#55105=DIRECTION('ref_axis',(0.,-0.94284446121751,-0.333233134534162));
#55106=DIRECTION('center_axis',(0.,0.333233134534162,-0.94284446121751));
#55107=DIRECTION('ref_axis',(0.,0.94284446121751,0.333233134534162));
#55108=DIRECTION('',(0.,-0.333233134534162,0.94284446121751));
#55109=DIRECTION('center_axis',(0.,0.333233134534159,-0.942844461217511));
#55110=DIRECTION('ref_axis',(0.,-0.942844461217511,-0.333233134534159));
#55111=DIRECTION('center_axis',(0.,-0.333233134534162,0.94284446121751));
#55112=DIRECTION('ref_axis',(0.,-0.94284446121751,-0.333233134534161));
#55113=DIRECTION('center_axis',(0.,0.333233134534159,-0.942844461217511));
#55114=DIRECTION('ref_axis',(0.,-0.942844461217511,-0.333233134534159));
#55115=DIRECTION('',(0.,0.333233134534162,-0.94284446121751));
#55116=DIRECTION('center_axis',(0.,0.333233134534162,-0.94284446121751));
#55117=DIRECTION('ref_axis',(0.,-0.94284446121751,-0.333233134534162));
#55118=DIRECTION('center_axis',(0.,-0.333233134534162,0.94284446121751));
#55119=DIRECTION('ref_axis',(0.,-0.94284446121751,-0.333233134534162));
#55120=DIRECTION('center_axis',(0.,0.333233134534162,-0.94284446121751));
#55121=DIRECTION('ref_axis',(0.,0.94284446121751,0.333233134534162));
#55122=DIRECTION('',(0.,-0.333233134534162,0.94284446121751));
#55123=DIRECTION('center_axis',(0.,0.333233134534159,-0.942844461217511));
#55124=DIRECTION('ref_axis',(0.,-0.942844461217511,-0.333233134534159));
#55125=DIRECTION('center_axis',(0.,-0.333233134534162,0.94284446121751));
#55126=DIRECTION('ref_axis',(0.,-0.94284446121751,-0.333233134534162));
#55127=DIRECTION('center_axis',(0.,0.333233134534159,-0.942844461217511));
#55128=DIRECTION('ref_axis',(0.,-0.942844461217511,-0.333233134534159));
#55129=DIRECTION('',(0.,0.333233134534162,-0.94284446121751));
#55130=DIRECTION('center_axis',(0.,0.333233134534162,-0.94284446121751));
#55131=DIRECTION('ref_axis',(0.,-0.94284446121751,-0.333233134534162));
#55132=DIRECTION('center_axis',(0.,-0.333233134534162,0.94284446121751));
#55133=DIRECTION('ref_axis',(0.,-0.94284446121751,-0.333233134534162));
#55134=DIRECTION('center_axis',(0.,0.333233134534162,-0.94284446121751));
#55135=DIRECTION('ref_axis',(0.,0.94284446121751,0.333233134534162));
#55136=DIRECTION('',(0.,-0.333233134534162,0.94284446121751));
#55137=DIRECTION('center_axis',(0.,0.333233134534159,-0.942844461217511));
#55138=DIRECTION('ref_axis',(0.,-0.942844461217511,-0.333233134534159));
#55139=DIRECTION('center_axis',(0.,-0.333233134534162,0.94284446121751));
#55140=DIRECTION('ref_axis',(0.,-0.94284446121751,-0.333233134534162));
#55141=DIRECTION('center_axis',(0.,0.333233134534159,-0.942844461217511));
#55142=DIRECTION('ref_axis',(0.,-0.942844461217511,-0.333233134534159));
#55143=DIRECTION('',(0.,0.333233134534162,-0.94284446121751));
#55144=DIRECTION('center_axis',(0.,0.333233134534162,-0.94284446121751));
#55145=DIRECTION('ref_axis',(0.,-0.94284446121751,-0.333233134534162));
#55146=DIRECTION('center_axis',(0.,-0.333233134534162,0.94284446121751));
#55147=DIRECTION('ref_axis',(0.,-0.94284446121751,-0.333233134534162));
#55148=DIRECTION('center_axis',(0.,0.333233134534162,-0.94284446121751));
#55149=DIRECTION('ref_axis',(0.,0.94284446121751,0.333233134534162));
#55150=DIRECTION('',(0.,-0.333233134534162,0.94284446121751));
#55151=DIRECTION('center_axis',(0.,0.333233134534159,-0.942844461217511));
#55152=DIRECTION('ref_axis',(0.,-0.942844461217511,-0.333233134534159));
#55153=DIRECTION('center_axis',(0.,-0.333233134534162,0.94284446121751));
#55154=DIRECTION('ref_axis',(0.,-0.94284446121751,-0.333233134534162));
#55155=DIRECTION('center_axis',(0.,0.333233134534159,-0.942844461217511));
#55156=DIRECTION('ref_axis',(0.,-0.942844461217511,-0.333233134534159));
#55157=DIRECTION('',(0.,0.333233134534162,-0.94284446121751));
#55158=DIRECTION('center_axis',(0.,0.333233134534162,-0.94284446121751));
#55159=DIRECTION('ref_axis',(0.,-0.94284446121751,-0.333233134534162));
#55160=DIRECTION('center_axis',(0.,-0.333233134534162,0.94284446121751));
#55161=DIRECTION('ref_axis',(0.,-0.94284446121751,-0.333233134534162));
#55162=DIRECTION('center_axis',(0.,0.333233134534162,-0.94284446121751));
#55163=DIRECTION('ref_axis',(0.,0.94284446121751,0.333233134534162));
#55164=DIRECTION('',(0.,-0.333233134534162,0.94284446121751));
#55165=DIRECTION('center_axis',(0.,0.333233134534159,-0.942844461217511));
#55166=DIRECTION('ref_axis',(0.,-0.942844461217511,-0.333233134534159));
#55167=DIRECTION('center_axis',(0.,-0.333233134534162,0.94284446121751));
#55168=DIRECTION('ref_axis',(0.,-0.94284446121751,-0.333233134534162));
#55169=DIRECTION('center_axis',(0.,0.333233134534159,-0.942844461217511));
#55170=DIRECTION('ref_axis',(0.,-0.942844461217511,-0.333233134534159));
#55171=DIRECTION('',(0.,0.333233134534162,-0.94284446121751));
#55172=DIRECTION('center_axis',(0.,0.333233134534162,-0.94284446121751));
#55173=DIRECTION('ref_axis',(0.,-0.94284446121751,-0.333233134534162));
#55174=DIRECTION('center_axis',(0.,-0.333233134534162,0.94284446121751));
#55175=DIRECTION('ref_axis',(0.,-0.94284446121751,-0.333233134534162));
#55176=DIRECTION('center_axis',(0.,0.333233134534162,-0.94284446121751));
#55177=DIRECTION('ref_axis',(0.,0.94284446121751,0.333233134534162));
#55178=DIRECTION('',(0.,-0.333233134534162,0.94284446121751));
#55179=DIRECTION('center_axis',(0.,0.333233134534159,-0.942844461217511));
#55180=DIRECTION('ref_axis',(0.,-0.942844461217511,-0.333233134534159));
#55181=DIRECTION('center_axis',(0.,-0.333233134534162,0.94284446121751));
#55182=DIRECTION('ref_axis',(0.,-0.94284446121751,-0.333233134534162));
#55183=DIRECTION('center_axis',(0.,0.333233134534159,-0.942844461217511));
#55184=DIRECTION('ref_axis',(0.,-0.942844461217511,-0.333233134534159));
#55185=DIRECTION('',(0.,0.333233134534162,-0.94284446121751));
#55186=DIRECTION('center_axis',(0.,0.333233134534162,-0.94284446121751));
#55187=DIRECTION('ref_axis',(0.,-0.94284446121751,-0.333233134534162));
#55188=DIRECTION('center_axis',(0.,-0.333233134534162,0.94284446121751));
#55189=DIRECTION('ref_axis',(0.,-0.94284446121751,-0.333233134534162));
#55190=DIRECTION('center_axis',(0.,0.333233134534162,-0.94284446121751));
#55191=DIRECTION('ref_axis',(0.,0.94284446121751,0.333233134534162));
#55192=DIRECTION('',(0.,-0.333233134534162,0.94284446121751));
#55193=DIRECTION('center_axis',(0.,0.333233134534159,-0.942844461217511));
#55194=DIRECTION('ref_axis',(0.,-0.942844461217511,-0.333233134534159));
#55195=DIRECTION('center_axis',(0.,-0.333233134534162,0.94284446121751));
#55196=DIRECTION('ref_axis',(0.,-0.94284446121751,-0.333233134534162));
#55197=DIRECTION('center_axis',(0.,0.333233134534159,-0.942844461217511));
#55198=DIRECTION('ref_axis',(0.,-0.942844461217511,-0.333233134534159));
#55199=DIRECTION('',(0.,0.333233134534162,-0.94284446121751));
#55200=DIRECTION('center_axis',(0.,0.333233134534162,-0.94284446121751));
#55201=DIRECTION('ref_axis',(0.,-0.94284446121751,-0.333233134534162));
#55202=DIRECTION('center_axis',(0.,-0.333233134534162,0.94284446121751));
#55203=DIRECTION('ref_axis',(0.,-0.94284446121751,-0.333233134534162));
#55204=DIRECTION('center_axis',(0.,0.333233134534162,-0.94284446121751));
#55205=DIRECTION('ref_axis',(0.,0.94284446121751,0.333233134534162));
#55206=DIRECTION('',(0.,-0.333233134534162,0.94284446121751));
#55207=DIRECTION('center_axis',(0.,0.333233134534159,-0.942844461217511));
#55208=DIRECTION('ref_axis',(0.,-0.942844461217511,-0.333233134534159));
#55209=DIRECTION('center_axis',(0.,-0.333233134534162,0.94284446121751));
#55210=DIRECTION('ref_axis',(0.,-0.94284446121751,-0.333233134534162));
#55211=DIRECTION('center_axis',(0.,0.333233134534159,-0.942844461217511));
#55212=DIRECTION('ref_axis',(0.,-0.942844461217511,-0.333233134534159));
#55213=DIRECTION('',(0.,0.333233134534162,-0.94284446121751));
#55214=DIRECTION('center_axis',(0.,0.333233134534162,-0.94284446121751));
#55215=DIRECTION('ref_axis',(0.,-0.94284446121751,-0.333233134534162));
#55216=DIRECTION('center_axis',(0.,-0.333233134534162,0.94284446121751));
#55217=DIRECTION('ref_axis',(0.,-0.94284446121751,-0.333233134534162));
#55218=DIRECTION('center_axis',(0.,0.333233134534162,-0.94284446121751));
#55219=DIRECTION('ref_axis',(0.,0.94284446121751,0.333233134534162));
#55220=DIRECTION('',(0.,-0.333233134534162,0.94284446121751));
#55221=DIRECTION('center_axis',(0.,0.333233134534159,-0.942844461217511));
#55222=DIRECTION('ref_axis',(0.,-0.942844461217511,-0.333233134534159));
#55223=DIRECTION('center_axis',(0.,-0.333233134534162,0.94284446121751));
#55224=DIRECTION('ref_axis',(0.,-0.94284446121751,-0.333233134534162));
#55225=DIRECTION('center_axis',(0.,0.333233134534159,-0.942844461217511));
#55226=DIRECTION('ref_axis',(0.,-0.942844461217511,-0.333233134534159));
#55227=DIRECTION('',(0.,0.333233134534162,-0.94284446121751));
#55228=DIRECTION('center_axis',(0.,0.333233134534162,-0.94284446121751));
#55229=DIRECTION('ref_axis',(0.,-0.94284446121751,-0.333233134534162));
#55230=DIRECTION('center_axis',(0.,-0.333233134534162,0.94284446121751));
#55231=DIRECTION('ref_axis',(0.,-0.94284446121751,-0.333233134534162));
#55232=DIRECTION('center_axis',(0.,0.333233134534162,-0.94284446121751));
#55233=DIRECTION('ref_axis',(0.,0.94284446121751,0.333233134534162));
#55234=DIRECTION('',(0.,-0.333233134534162,0.94284446121751));
#55235=DIRECTION('center_axis',(0.,0.333233134534159,-0.942844461217511));
#55236=DIRECTION('ref_axis',(0.,-0.942844461217511,-0.333233134534159));
#55237=DIRECTION('center_axis',(0.,-0.333233134534162,0.94284446121751));
#55238=DIRECTION('ref_axis',(0.,-0.94284446121751,-0.333233134534162));
#55239=DIRECTION('center_axis',(0.,0.333233134534159,-0.942844461217511));
#55240=DIRECTION('ref_axis',(0.,-0.942844461217511,-0.333233134534159));
#55241=DIRECTION('',(0.,0.333233134534162,-0.94284446121751));
#55242=DIRECTION('center_axis',(0.,0.333233134534162,-0.94284446121751));
#55243=DIRECTION('ref_axis',(0.,-0.94284446121751,-0.333233134534162));
#55244=DIRECTION('center_axis',(0.,-0.333233134534162,0.94284446121751));
#55245=DIRECTION('ref_axis',(0.,-0.94284446121751,-0.333233134534162));
#55246=DIRECTION('center_axis',(0.,0.333233134534162,-0.94284446121751));
#55247=DIRECTION('ref_axis',(0.,0.94284446121751,0.333233134534162));
#55248=DIRECTION('',(0.,-0.333233134534162,0.94284446121751));
#55249=DIRECTION('center_axis',(0.,0.333233134534159,-0.942844461217511));
#55250=DIRECTION('ref_axis',(0.,-0.942844461217511,-0.333233134534159));
#55251=DIRECTION('center_axis',(0.,-0.333233134534162,0.94284446121751));
#55252=DIRECTION('ref_axis',(0.,-0.94284446121751,-0.333233134534162));
#55253=DIRECTION('center_axis',(0.,0.333233134534159,-0.942844461217511));
#55254=DIRECTION('ref_axis',(0.,-0.942844461217511,-0.333233134534159));
#55255=DIRECTION('',(0.,0.333233134534162,-0.94284446121751));
#55256=DIRECTION('center_axis',(0.,0.333233134534162,-0.94284446121751));
#55257=DIRECTION('ref_axis',(0.,-0.94284446121751,-0.333233134534162));
#55258=DIRECTION('center_axis',(0.,-0.333233134534162,0.94284446121751));
#55259=DIRECTION('ref_axis',(0.,-0.94284446121751,-0.333233134534162));
#55260=DIRECTION('center_axis',(0.,0.333233134534162,-0.94284446121751));
#55261=DIRECTION('ref_axis',(0.,0.94284446121751,0.333233134534162));
#55262=DIRECTION('',(0.,-0.333233134534162,0.94284446121751));
#55263=DIRECTION('center_axis',(0.,0.333233134534159,-0.942844461217511));
#55264=DIRECTION('ref_axis',(0.,-0.942844461217511,-0.333233134534159));
#55265=DIRECTION('center_axis',(0.,-0.333233134534162,0.94284446121751));
#55266=DIRECTION('ref_axis',(0.,-0.94284446121751,-0.333233134534162));
#55267=DIRECTION('center_axis',(0.,0.333233134534159,-0.942844461217511));
#55268=DIRECTION('ref_axis',(0.,-0.942844461217511,-0.333233134534159));
#55269=DIRECTION('',(0.,0.333233134534162,-0.94284446121751));
#55270=DIRECTION('center_axis',(0.,0.333233134534162,-0.94284446121751));
#55271=DIRECTION('ref_axis',(0.,-0.94284446121751,-0.333233134534162));
#55272=DIRECTION('center_axis',(0.,-0.333233134534162,0.94284446121751));
#55273=DIRECTION('ref_axis',(0.,-0.94284446121751,-0.333233134534162));
#55274=DIRECTION('center_axis',(0.,0.333233134534162,-0.94284446121751));
#55275=DIRECTION('ref_axis',(0.,0.94284446121751,0.333233134534162));
#55276=DIRECTION('',(0.,-0.333233134534162,0.94284446121751));
#55277=DIRECTION('center_axis',(0.,0.333233134534159,-0.942844461217511));
#55278=DIRECTION('ref_axis',(0.,-0.942844461217511,-0.333233134534159));
#55279=DIRECTION('center_axis',(0.,-0.333233134534162,0.94284446121751));
#55280=DIRECTION('ref_axis',(0.,-0.94284446121751,-0.333233134534162));
#55281=DIRECTION('center_axis',(0.,0.333233134534159,-0.942844461217511));
#55282=DIRECTION('ref_axis',(0.,-0.942844461217511,-0.333233134534159));
#55283=DIRECTION('',(0.,0.333233134534162,-0.94284446121751));
#55284=DIRECTION('center_axis',(0.,0.333233134534162,-0.94284446121751));
#55285=DIRECTION('ref_axis',(0.,-0.94284446121751,-0.333233134534162));
#55286=DIRECTION('center_axis',(0.,-0.333233134534162,0.94284446121751));
#55287=DIRECTION('ref_axis',(0.,-0.94284446121751,-0.333233134534162));
#55288=DIRECTION('center_axis',(0.,0.333233134534162,-0.94284446121751));
#55289=DIRECTION('ref_axis',(0.,0.94284446121751,0.333233134534162));
#55290=DIRECTION('',(0.,-0.333233134534162,0.94284446121751));
#55291=DIRECTION('center_axis',(0.,0.333233134534159,-0.942844461217511));
#55292=DIRECTION('ref_axis',(0.,-0.942844461217511,-0.333233134534159));
#55293=DIRECTION('center_axis',(0.,-0.333233134534162,0.94284446121751));
#55294=DIRECTION('ref_axis',(0.,-0.94284446121751,-0.333233134534162));
#55295=DIRECTION('center_axis',(0.,0.333233134534159,-0.942844461217511));
#55296=DIRECTION('ref_axis',(0.,-0.942844461217511,-0.333233134534159));
#55297=DIRECTION('',(0.,0.333233134534162,-0.94284446121751));
#55298=DIRECTION('center_axis',(0.,0.333233134534162,-0.94284446121751));
#55299=DIRECTION('ref_axis',(0.,-0.94284446121751,-0.333233134534162));
#55300=DIRECTION('center_axis',(0.,-0.333233134534162,0.94284446121751));
#55301=DIRECTION('ref_axis',(0.,-0.94284446121751,-0.333233134534162));
#55302=DIRECTION('center_axis',(0.,0.333233134534162,-0.94284446121751));
#55303=DIRECTION('ref_axis',(0.,0.94284446121751,0.333233134534162));
#55304=DIRECTION('',(0.,-0.333233134534162,0.94284446121751));
#55305=DIRECTION('center_axis',(0.,0.333233134534159,-0.942844461217511));
#55306=DIRECTION('ref_axis',(0.,-0.942844461217511,-0.333233134534159));
#55307=DIRECTION('center_axis',(0.,-0.333233134534162,0.94284446121751));
#55308=DIRECTION('ref_axis',(0.,-0.94284446121751,-0.333233134534162));
#55309=DIRECTION('center_axis',(0.,0.333233134534159,-0.942844461217511));
#55310=DIRECTION('ref_axis',(0.,-0.942844461217511,-0.333233134534159));
#55311=DIRECTION('',(0.,0.333233134534162,-0.94284446121751));
#55312=DIRECTION('center_axis',(0.,-0.333233134534162,0.94284446121751));
#55313=DIRECTION('ref_axis',(0.,-0.94284446121751,-0.333233134534162));
#55314=DIRECTION('center_axis',(0.,-0.333233134534162,0.94284446121751));
#55315=DIRECTION('ref_axis',(0.,-0.94284446121751,-0.333233134534162));
#55316=DIRECTION('center_axis',(0.,-0.333233134534162,0.94284446121751));
#55317=DIRECTION('ref_axis',(0.,-0.94284446121751,-0.333233134534162));
#55318=DIRECTION('center_axis',(0.,0.333233134534162,-0.94284446121751));
#55319=DIRECTION('ref_axis',(0.,0.94284446121751,0.333233134534162));
#55320=DIRECTION('',(0.,-0.333233134534162,0.94284446121751));
#55321=DIRECTION('center_axis',(0.,0.333233134534159,-0.942844461217511));
#55322=DIRECTION('ref_axis',(0.,-0.942844461217511,-0.333233134534159));
#55323=DIRECTION('center_axis',(0.,-0.333233134534162,0.94284446121751));
#55324=DIRECTION('ref_axis',(0.,-0.94284446121751,-0.333233134534162));
#55325=DIRECTION('center_axis',(0.,0.333233134534159,-0.942844461217511));
#55326=DIRECTION('ref_axis',(0.,-0.942844461217511,-0.333233134534159));
#55327=DIRECTION('',(0.,0.333233134534162,-0.94284446121751));
#55328=DIRECTION('center_axis',(0.,0.333233134534162,-0.94284446121751));
#55329=DIRECTION('ref_axis',(0.,-0.94284446121751,-0.333233134534162));
#55330=DIRECTION('center_axis',(0.,-0.333233134534162,0.94284446121751));
#55331=DIRECTION('ref_axis',(0.,-0.94284446121751,-0.333233134534162));
#55332=DIRECTION('center_axis',(0.,0.333233134534162,-0.94284446121751));
#55333=DIRECTION('ref_axis',(0.,0.94284446121751,0.333233134534162));
#55334=DIRECTION('',(0.,-0.333233134534162,0.94284446121751));
#55335=DIRECTION('center_axis',(0.,0.333233134534159,-0.942844461217511));
#55336=DIRECTION('ref_axis',(0.,-0.942844461217511,-0.333233134534159));
#55337=DIRECTION('center_axis',(0.,-0.333233134534162,0.94284446121751));
#55338=DIRECTION('ref_axis',(0.,-0.94284446121751,-0.333233134534162));
#55339=DIRECTION('center_axis',(0.,0.333233134534159,-0.942844461217511));
#55340=DIRECTION('ref_axis',(0.,-0.942844461217511,-0.333233134534159));
#55341=DIRECTION('',(0.,0.333233134534162,-0.94284446121751));
#55342=DIRECTION('center_axis',(0.,0.333233134534162,-0.94284446121751));
#55343=DIRECTION('ref_axis',(0.,-0.94284446121751,-0.333233134534162));
#55344=DIRECTION('center_axis',(0.,-0.333233134534162,0.94284446121751));
#55345=DIRECTION('ref_axis',(0.,-0.94284446121751,-0.333233134534162));
#55346=DIRECTION('center_axis',(0.,0.333233134534162,-0.94284446121751));
#55347=DIRECTION('ref_axis',(0.,0.94284446121751,0.333233134534162));
#55348=DIRECTION('',(0.,-0.333233134534162,0.94284446121751));
#55349=DIRECTION('center_axis',(0.,0.333233134534159,-0.942844461217511));
#55350=DIRECTION('ref_axis',(0.,-0.942844461217511,-0.333233134534159));
#55351=DIRECTION('center_axis',(0.,-0.333233134534162,0.94284446121751));
#55352=DIRECTION('ref_axis',(0.,-0.94284446121751,-0.333233134534161));
#55353=DIRECTION('center_axis',(0.,0.333233134534159,-0.942844461217511));
#55354=DIRECTION('ref_axis',(0.,-0.942844461217511,-0.333233134534159));
#55355=DIRECTION('',(0.,0.333233134534162,-0.94284446121751));
#55356=DIRECTION('center_axis',(0.,0.333233134534162,-0.94284446121751));
#55357=DIRECTION('ref_axis',(0.,-0.94284446121751,-0.333233134534162));
#55358=DIRECTION('center_axis',(0.,-0.333233134534162,0.94284446121751));
#55359=DIRECTION('ref_axis',(0.,-0.94284446121751,-0.333233134534162));
#55360=DIRECTION('center_axis',(0.,0.333233134534162,-0.94284446121751));
#55361=DIRECTION('ref_axis',(0.,0.94284446121751,0.333233134534162));
#55362=DIRECTION('',(0.,-0.333233134534162,0.94284446121751));
#55363=DIRECTION('center_axis',(0.,0.333233134534159,-0.942844461217511));
#55364=DIRECTION('ref_axis',(0.,-0.942844461217511,-0.333233134534159));
#55365=DIRECTION('center_axis',(0.,-0.333233134534162,0.94284446121751));
#55366=DIRECTION('ref_axis',(0.,-0.94284446121751,-0.333233134534162));
#55367=DIRECTION('center_axis',(0.,0.333233134534159,-0.942844461217511));
#55368=DIRECTION('ref_axis',(0.,-0.942844461217511,-0.333233134534159));
#55369=DIRECTION('',(0.,0.333233134534162,-0.94284446121751));
#55370=DIRECTION('center_axis',(0.,0.333233134534162,-0.94284446121751));
#55371=DIRECTION('ref_axis',(0.,-0.94284446121751,-0.333233134534162));
#55372=DIRECTION('center_axis',(0.,-0.333233134534162,0.94284446121751));
#55373=DIRECTION('ref_axis',(0.,-0.94284446121751,-0.333233134534162));
#55374=DIRECTION('center_axis',(0.,0.333233134534162,-0.94284446121751));
#55375=DIRECTION('ref_axis',(0.,0.94284446121751,0.333233134534162));
#55376=DIRECTION('',(0.,-0.333233134534162,0.94284446121751));
#55377=DIRECTION('center_axis',(0.,0.333233134534159,-0.942844461217511));
#55378=DIRECTION('ref_axis',(0.,-0.942844461217511,-0.333233134534159));
#55379=DIRECTION('center_axis',(0.,-0.333233134534162,0.94284446121751));
#55380=DIRECTION('ref_axis',(0.,-0.94284446121751,-0.333233134534162));
#55381=DIRECTION('center_axis',(0.,0.333233134534159,-0.942844461217511));
#55382=DIRECTION('ref_axis',(0.,-0.942844461217511,-0.333233134534159));
#55383=DIRECTION('',(0.,0.333233134534162,-0.94284446121751));
#55384=DIRECTION('center_axis',(0.,0.333233134534162,-0.94284446121751));
#55385=DIRECTION('ref_axis',(0.,-0.94284446121751,-0.333233134534162));
#55386=DIRECTION('center_axis',(0.,-0.333233134534162,0.94284446121751));
#55387=DIRECTION('ref_axis',(0.,-0.94284446121751,-0.333233134534162));
#55388=DIRECTION('center_axis',(0.,0.333233134534162,-0.94284446121751));
#55389=DIRECTION('ref_axis',(0.,0.94284446121751,0.333233134534162));
#55390=DIRECTION('',(0.,-0.333233134534162,0.94284446121751));
#55391=DIRECTION('center_axis',(0.,0.333233134534159,-0.942844461217511));
#55392=DIRECTION('ref_axis',(0.,-0.942844461217511,-0.333233134534159));
#55393=DIRECTION('center_axis',(0.,-0.333233134534162,0.94284446121751));
#55394=DIRECTION('ref_axis',(0.,-0.94284446121751,-0.333233134534162));
#55395=DIRECTION('center_axis',(0.,0.333233134534159,-0.942844461217511));
#55396=DIRECTION('ref_axis',(0.,-0.942844461217511,-0.333233134534159));
#55397=DIRECTION('',(0.,0.333233134534162,-0.94284446121751));
#55398=DIRECTION('center_axis',(0.,0.333233134534162,-0.94284446121751));
#55399=DIRECTION('ref_axis',(0.,-0.94284446121751,-0.333233134534162));
#55400=DIRECTION('center_axis',(0.,-0.333233134534162,0.94284446121751));
#55401=DIRECTION('ref_axis',(0.,-0.94284446121751,-0.333233134534162));
#55402=DIRECTION('center_axis',(0.,0.333233134534162,-0.94284446121751));
#55403=DIRECTION('ref_axis',(0.,0.94284446121751,0.333233134534162));
#55404=DIRECTION('',(0.,-0.333233134534162,0.94284446121751));
#55405=DIRECTION('center_axis',(0.,0.333233134534159,-0.942844461217511));
#55406=DIRECTION('ref_axis',(0.,-0.942844461217511,-0.333233134534159));
#55407=DIRECTION('center_axis',(0.,-0.333233134534162,0.94284446121751));
#55408=DIRECTION('ref_axis',(0.,-0.94284446121751,-0.333233134534162));
#55409=DIRECTION('center_axis',(0.,0.333233134534159,-0.942844461217511));
#55410=DIRECTION('ref_axis',(0.,-0.942844461217511,-0.333233134534159));
#55411=DIRECTION('',(0.,0.333233134534162,-0.94284446121751));
#55412=DIRECTION('center_axis',(0.,0.333233134534162,-0.94284446121751));
#55413=DIRECTION('ref_axis',(0.,-0.94284446121751,-0.333233134534162));
#55414=DIRECTION('center_axis',(0.,-0.333233134534162,0.94284446121751));
#55415=DIRECTION('ref_axis',(0.,-0.94284446121751,-0.333233134534162));
#55416=DIRECTION('center_axis',(0.,0.333233134534162,-0.94284446121751));
#55417=DIRECTION('ref_axis',(0.,0.94284446121751,0.333233134534162));
#55418=DIRECTION('',(0.,-0.333233134534162,0.94284446121751));
#55419=DIRECTION('center_axis',(0.,0.333233134534159,-0.942844461217511));
#55420=DIRECTION('ref_axis',(0.,-0.942844461217511,-0.333233134534159));
#55421=DIRECTION('center_axis',(0.,-0.333233134534162,0.94284446121751));
#55422=DIRECTION('ref_axis',(0.,-0.94284446121751,-0.333233134534162));
#55423=DIRECTION('center_axis',(0.,0.333233134534159,-0.942844461217511));
#55424=DIRECTION('ref_axis',(0.,-0.942844461217511,-0.333233134534159));
#55425=DIRECTION('',(0.,0.333233134534162,-0.94284446121751));
#55426=DIRECTION('center_axis',(0.,0.333233134534162,-0.94284446121751));
#55427=DIRECTION('ref_axis',(0.,-0.94284446121751,-0.333233134534162));
#55428=DIRECTION('center_axis',(0.,-0.333233134534162,0.94284446121751));
#55429=DIRECTION('ref_axis',(0.,-0.94284446121751,-0.333233134534162));
#55430=DIRECTION('center_axis',(0.,0.333233134534162,-0.94284446121751));
#55431=DIRECTION('ref_axis',(0.,0.94284446121751,0.333233134534162));
#55432=DIRECTION('',(0.,-0.333233134534162,0.94284446121751));
#55433=DIRECTION('center_axis',(0.,0.333233134534159,-0.942844461217511));
#55434=DIRECTION('ref_axis',(0.,-0.942844461217511,-0.333233134534159));
#55435=DIRECTION('center_axis',(0.,-0.333233134534162,0.94284446121751));
#55436=DIRECTION('ref_axis',(0.,-0.94284446121751,-0.333233134534162));
#55437=DIRECTION('center_axis',(0.,0.333233134534159,-0.942844461217511));
#55438=DIRECTION('ref_axis',(0.,-0.942844461217511,-0.333233134534159));
#55439=DIRECTION('',(0.,0.333233134534162,-0.94284446121751));
#55440=DIRECTION('center_axis',(0.,-0.333233134534162,0.94284446121751));
#55441=DIRECTION('ref_axis',(0.,-0.94284446121751,-0.333233134534162));
#55442=DIRECTION('center_axis',(0.,-0.333233134534162,0.94284446121751));
#55443=DIRECTION('ref_axis',(0.,-0.94284446121751,-0.333233134534162));
#55444=DIRECTION('center_axis',(0.,-0.333233134534162,0.94284446121751));
#55445=DIRECTION('ref_axis',(0.,-0.94284446121751,-0.333233134534162));
#55446=DIRECTION('center_axis',(0.,0.333233134534162,-0.94284446121751));
#55447=DIRECTION('ref_axis',(0.,0.94284446121751,0.333233134534162));
#55448=DIRECTION('',(0.,-0.333233134534162,0.94284446121751));
#55449=DIRECTION('center_axis',(0.,0.333233134534159,-0.942844461217511));
#55450=DIRECTION('ref_axis',(0.,-0.942844461217511,-0.333233134534159));
#55451=DIRECTION('center_axis',(0.,-0.333233134534162,0.94284446121751));
#55452=DIRECTION('ref_axis',(0.,-0.94284446121751,-0.333233134534161));
#55453=DIRECTION('center_axis',(0.,0.333233134534159,-0.942844461217511));
#55454=DIRECTION('ref_axis',(0.,-0.942844461217511,-0.333233134534159));
#55455=DIRECTION('',(0.,0.333233134534162,-0.94284446121751));
#55456=DIRECTION('center_axis',(0.,0.333233134534162,-0.94284446121751));
#55457=DIRECTION('ref_axis',(0.,-0.94284446121751,-0.333233134534162));
#55458=DIRECTION('center_axis',(0.,-0.333233134534162,0.94284446121751));
#55459=DIRECTION('ref_axis',(0.,-0.94284446121751,-0.333233134534162));
#55460=DIRECTION('center_axis',(0.,0.333233134534162,-0.94284446121751));
#55461=DIRECTION('ref_axis',(0.,0.94284446121751,0.333233134534162));
#55462=DIRECTION('',(0.,-0.333233134534162,0.94284446121751));
#55463=DIRECTION('center_axis',(0.,0.333233134534159,-0.942844461217511));
#55464=DIRECTION('ref_axis',(0.,-0.942844461217511,-0.333233134534159));
#55465=DIRECTION('center_axis',(0.,-0.333233134534162,0.94284446121751));
#55466=DIRECTION('ref_axis',(0.,-0.94284446121751,-0.333233134534162));
#55467=DIRECTION('center_axis',(0.,0.333233134534159,-0.942844461217511));
#55468=DIRECTION('ref_axis',(0.,-0.942844461217511,-0.333233134534159));
#55469=DIRECTION('',(0.,0.333233134534162,-0.94284446121751));
#55470=DIRECTION('center_axis',(0.,0.333233134534162,-0.94284446121751));
#55471=DIRECTION('ref_axis',(0.,-0.94284446121751,-0.333233134534162));
#55472=DIRECTION('center_axis',(0.,-0.333233134534162,0.94284446121751));
#55473=DIRECTION('ref_axis',(0.,-0.94284446121751,-0.333233134534162));
#55474=DIRECTION('center_axis',(0.,0.333233134534162,-0.94284446121751));
#55475=DIRECTION('ref_axis',(0.,0.94284446121751,0.333233134534162));
#55476=DIRECTION('',(0.,-0.333233134534162,0.942844461217511));
#55477=DIRECTION('center_axis',(0.,0.333233134534159,-0.942844461217511));
#55478=DIRECTION('ref_axis',(0.,-0.942844461217511,-0.333233134534159));
#55479=DIRECTION('center_axis',(0.,-0.333233134534162,0.94284446121751));
#55480=DIRECTION('ref_axis',(0.,-0.94284446121751,-0.333233134534162));
#55481=DIRECTION('center_axis',(0.,0.333233134534159,-0.942844461217511));
#55482=DIRECTION('ref_axis',(0.,-0.942844461217511,-0.333233134534159));
#55483=DIRECTION('',(0.,0.333233134534162,-0.94284446121751));
#55484=DIRECTION('center_axis',(0.,0.333233134534162,-0.94284446121751));
#55485=DIRECTION('ref_axis',(0.,-0.94284446121751,-0.333233134534162));
#55486=DIRECTION('center_axis',(0.,-0.333233134534162,0.94284446121751));
#55487=DIRECTION('ref_axis',(0.,-0.94284446121751,-0.333233134534162));
#55488=DIRECTION('center_axis',(0.,0.333233134534162,-0.94284446121751));
#55489=DIRECTION('ref_axis',(0.,0.94284446121751,0.333233134534162));
#55490=DIRECTION('',(0.,-0.333233134534162,0.94284446121751));
#55491=DIRECTION('center_axis',(0.,0.333233134534159,-0.942844461217511));
#55492=DIRECTION('ref_axis',(0.,-0.942844461217511,-0.333233134534159));
#55493=DIRECTION('center_axis',(0.,-0.333233134534162,0.94284446121751));
#55494=DIRECTION('ref_axis',(0.,-0.94284446121751,-0.333233134534162));
#55495=DIRECTION('center_axis',(0.,0.333233134534159,-0.942844461217511));
#55496=DIRECTION('ref_axis',(0.,-0.942844461217511,-0.333233134534159));
#55497=DIRECTION('',(0.,0.333233134534162,-0.94284446121751));
#55498=DIRECTION('center_axis',(0.,0.333233134534162,-0.94284446121751));
#55499=DIRECTION('ref_axis',(0.,-0.94284446121751,-0.333233134534162));
#55500=DIRECTION('center_axis',(0.,-0.333233134534162,0.94284446121751));
#55501=DIRECTION('ref_axis',(0.,-0.94284446121751,-0.333233134534162));
#55502=DIRECTION('center_axis',(0.,0.333233134534162,-0.94284446121751));
#55503=DIRECTION('ref_axis',(0.,0.94284446121751,0.333233134534162));
#55504=DIRECTION('',(0.,-0.333233134534162,0.94284446121751));
#55505=DIRECTION('center_axis',(0.,0.333233134534159,-0.942844461217511));
#55506=DIRECTION('ref_axis',(0.,-0.942844461217511,-0.333233134534159));
#55507=DIRECTION('center_axis',(0.,-0.333233134534162,0.94284446121751));
#55508=DIRECTION('ref_axis',(0.,-0.94284446121751,-0.333233134534162));
#55509=DIRECTION('center_axis',(0.,0.333233134534159,-0.942844461217511));
#55510=DIRECTION('ref_axis',(0.,-0.942844461217511,-0.333233134534159));
#55511=DIRECTION('',(0.,0.333233134534162,-0.94284446121751));
#55512=DIRECTION('center_axis',(0.,0.333233134534162,-0.94284446121751));
#55513=DIRECTION('ref_axis',(0.,-0.94284446121751,-0.333233134534162));
#55514=DIRECTION('center_axis',(0.,-0.333233134534162,0.94284446121751));
#55515=DIRECTION('ref_axis',(0.,-0.94284446121751,-0.333233134534162));
#55516=DIRECTION('center_axis',(0.,0.333233134534162,-0.94284446121751));
#55517=DIRECTION('ref_axis',(0.,0.94284446121751,0.333233134534162));
#55518=DIRECTION('',(0.,-0.333233134534162,0.94284446121751));
#55519=DIRECTION('center_axis',(0.,0.333233134534159,-0.942844461217511));
#55520=DIRECTION('ref_axis',(0.,-0.942844461217511,-0.333233134534159));
#55521=DIRECTION('center_axis',(0.,-0.333233134534162,0.94284446121751));
#55522=DIRECTION('ref_axis',(0.,-0.94284446121751,-0.333233134534162));
#55523=DIRECTION('center_axis',(0.,0.333233134534159,-0.942844461217511));
#55524=DIRECTION('ref_axis',(0.,-0.942844461217511,-0.333233134534159));
#55525=DIRECTION('',(0.,0.333233134534162,-0.94284446121751));
#55526=DIRECTION('center_axis',(0.,0.333233134534162,-0.94284446121751));
#55527=DIRECTION('ref_axis',(0.,-0.94284446121751,-0.333233134534162));
#55528=DIRECTION('center_axis',(0.,-0.333233134534162,0.94284446121751));
#55529=DIRECTION('ref_axis',(0.,-0.94284446121751,-0.333233134534162));
#55530=DIRECTION('center_axis',(0.,0.333233134534162,-0.94284446121751));
#55531=DIRECTION('ref_axis',(0.,0.94284446121751,0.333233134534162));
#55532=DIRECTION('',(0.,-0.333233134534162,0.94284446121751));
#55533=DIRECTION('center_axis',(0.,0.333233134534159,-0.942844461217511));
#55534=DIRECTION('ref_axis',(0.,-0.942844461217511,-0.333233134534159));
#55535=DIRECTION('center_axis',(0.,-0.333233134534162,0.94284446121751));
#55536=DIRECTION('ref_axis',(0.,-0.94284446121751,-0.333233134534162));
#55537=DIRECTION('center_axis',(0.,0.333233134534159,-0.942844461217511));
#55538=DIRECTION('ref_axis',(0.,-0.942844461217511,-0.333233134534159));
#55539=DIRECTION('',(0.,0.333233134534162,-0.94284446121751));
#55540=DIRECTION('center_axis',(0.,0.333233134534162,-0.94284446121751));
#55541=DIRECTION('ref_axis',(0.,-0.94284446121751,-0.333233134534162));
#55542=DIRECTION('center_axis',(0.,-0.333233134534162,0.94284446121751));
#55543=DIRECTION('ref_axis',(0.,-0.94284446121751,-0.333233134534162));
#55544=DIRECTION('center_axis',(0.,0.333233134534162,-0.94284446121751));
#55545=DIRECTION('ref_axis',(0.,0.94284446121751,0.333233134534162));
#55546=DIRECTION('',(0.,-0.333233134534162,0.94284446121751));
#55547=DIRECTION('center_axis',(0.,0.333233134534159,-0.942844461217511));
#55548=DIRECTION('ref_axis',(0.,-0.942844461217511,-0.333233134534159));
#55549=DIRECTION('center_axis',(0.,-0.333233134534162,0.94284446121751));
#55550=DIRECTION('ref_axis',(0.,-0.94284446121751,-0.333233134534162));
#55551=DIRECTION('center_axis',(0.,0.333233134534159,-0.942844461217511));
#55552=DIRECTION('ref_axis',(0.,-0.942844461217511,-0.333233134534159));
#55553=DIRECTION('',(0.,0.333233134534162,-0.94284446121751));
#55554=DIRECTION('center_axis',(0.,0.333233134534162,-0.94284446121751));
#55555=DIRECTION('ref_axis',(0.,-0.94284446121751,-0.333233134534162));
#55556=DIRECTION('center_axis',(0.,-0.333233134534162,0.94284446121751));
#55557=DIRECTION('ref_axis',(0.,-0.94284446121751,-0.333233134534162));
#55558=DIRECTION('center_axis',(0.,0.333233134534162,-0.94284446121751));
#55559=DIRECTION('ref_axis',(0.,0.94284446121751,0.333233134534162));
#55560=DIRECTION('',(0.,-0.333233134534162,0.94284446121751));
#55561=DIRECTION('center_axis',(0.,0.333233134534159,-0.942844461217511));
#55562=DIRECTION('ref_axis',(0.,-0.942844461217511,-0.333233134534159));
#55563=DIRECTION('center_axis',(0.,-0.333233134534162,0.94284446121751));
#55564=DIRECTION('ref_axis',(0.,-0.94284446121751,-0.333233134534162));
#55565=DIRECTION('center_axis',(0.,0.333233134534159,-0.942844461217511));
#55566=DIRECTION('ref_axis',(0.,-0.942844461217511,-0.333233134534159));
#55567=DIRECTION('',(0.,0.333233134534162,-0.94284446121751));
#55568=DIRECTION('center_axis',(0.,-0.333233134534162,0.94284446121751));
#55569=DIRECTION('ref_axis',(0.,-0.94284446121751,-0.333233134534162));
#55570=DIRECTION('center_axis',(0.,-0.333233134534162,0.94284446121751));
#55571=DIRECTION('ref_axis',(0.,-0.94284446121751,-0.333233134534162));
#55572=DIRECTION('center_axis',(0.,0.333233134534162,-0.94284446121751));
#55573=DIRECTION('ref_axis',(0.,0.94284446121751,0.333233134534162));
#55574=DIRECTION('',(0.,-0.333233134534162,0.94284446121751));
#55575=DIRECTION('center_axis',(0.,0.333233134534159,-0.942844461217511));
#55576=DIRECTION('ref_axis',(0.,-0.942844461217511,-0.333233134534159));
#55577=DIRECTION('center_axis',(0.,-0.333233134534162,0.94284446121751));
#55578=DIRECTION('ref_axis',(0.,-0.94284446121751,-0.333233134534162));
#55579=DIRECTION('center_axis',(0.,0.333233134534159,-0.942844461217511));
#55580=DIRECTION('ref_axis',(0.,-0.942844461217511,-0.333233134534159));
#55581=DIRECTION('',(0.,0.333233134534162,-0.94284446121751));
#55582=DIRECTION('center_axis',(0.,0.333233134534162,-0.94284446121751));
#55583=DIRECTION('ref_axis',(0.,-0.94284446121751,-0.333233134534162));
#55584=DIRECTION('center_axis',(0.,-0.333233134534162,0.94284446121751));
#55585=DIRECTION('ref_axis',(0.,-0.94284446121751,-0.333233134534162));
#55586=DIRECTION('center_axis',(0.,0.333233134534162,-0.94284446121751));
#55587=DIRECTION('ref_axis',(0.,0.94284446121751,0.333233134534162));
#55588=DIRECTION('',(0.,-0.333233134534162,0.94284446121751));
#55589=DIRECTION('center_axis',(0.,0.333233134534159,-0.942844461217511));
#55590=DIRECTION('ref_axis',(0.,-0.942844461217511,-0.333233134534159));
#55591=DIRECTION('center_axis',(0.,-0.333233134534162,0.94284446121751));
#55592=DIRECTION('ref_axis',(0.,-0.94284446121751,-0.333233134534162));
#55593=DIRECTION('center_axis',(0.,0.333233134534159,-0.942844461217511));
#55594=DIRECTION('ref_axis',(0.,-0.942844461217511,-0.333233134534159));
#55595=DIRECTION('',(0.,0.333233134534162,-0.94284446121751));
#55596=DIRECTION('center_axis',(0.,0.333233134534162,-0.94284446121751));
#55597=DIRECTION('ref_axis',(0.,-0.94284446121751,-0.333233134534162));
#55598=DIRECTION('center_axis',(0.,-0.333233134534162,0.94284446121751));
#55599=DIRECTION('ref_axis',(0.,-0.94284446121751,-0.333233134534162));
#55600=DIRECTION('center_axis',(0.,0.333233134534162,-0.94284446121751));
#55601=DIRECTION('ref_axis',(0.,0.94284446121751,0.333233134534162));
#55602=DIRECTION('',(0.,-0.333233134534162,0.94284446121751));
#55603=DIRECTION('center_axis',(0.,0.333233134534159,-0.942844461217511));
#55604=DIRECTION('ref_axis',(0.,-0.942844461217511,-0.333233134534159));
#55605=DIRECTION('center_axis',(0.,-0.333233134534162,0.94284446121751));
#55606=DIRECTION('ref_axis',(0.,-0.94284446121751,-0.333233134534161));
#55607=DIRECTION('center_axis',(0.,0.333233134534159,-0.942844461217511));
#55608=DIRECTION('ref_axis',(0.,-0.942844461217511,-0.333233134534159));
#55609=DIRECTION('',(0.,0.333233134534162,-0.94284446121751));
#55610=DIRECTION('center_axis',(0.,0.333233134534162,-0.94284446121751));
#55611=DIRECTION('ref_axis',(0.,-0.94284446121751,-0.333233134534162));
#55612=DIRECTION('center_axis',(0.,-0.333233134534162,0.94284446121751));
#55613=DIRECTION('ref_axis',(0.,-0.94284446121751,-0.333233134534162));
#55614=DIRECTION('center_axis',(0.,0.333233134534162,-0.94284446121751));
#55615=DIRECTION('ref_axis',(0.,0.94284446121751,0.333233134534162));
#55616=DIRECTION('',(0.,-0.333233134534162,0.94284446121751));
#55617=DIRECTION('center_axis',(0.,0.333233134534159,-0.942844461217511));
#55618=DIRECTION('ref_axis',(0.,-0.942844461217511,-0.333233134534159));
#55619=DIRECTION('center_axis',(0.,-0.333233134534162,0.94284446121751));
#55620=DIRECTION('ref_axis',(0.,-0.94284446121751,-0.333233134534162));
#55621=DIRECTION('center_axis',(0.,0.333233134534159,-0.942844461217511));
#55622=DIRECTION('ref_axis',(0.,-0.942844461217511,-0.333233134534159));
#55623=DIRECTION('',(0.,0.333233134534162,-0.94284446121751));
#55624=DIRECTION('center_axis',(0.,0.333233134534162,-0.94284446121751));
#55625=DIRECTION('ref_axis',(0.,-0.94284446121751,-0.333233134534162));
#55626=DIRECTION('center_axis',(0.,-0.333233134534162,0.94284446121751));
#55627=DIRECTION('ref_axis',(0.,-0.94284446121751,-0.333233134534162));
#55628=DIRECTION('center_axis',(0.,0.333233134534162,-0.94284446121751));
#55629=DIRECTION('ref_axis',(0.,0.94284446121751,0.333233134534162));
#55630=DIRECTION('',(0.,-0.333233134534162,0.94284446121751));
#55631=DIRECTION('center_axis',(0.,0.333233134534159,-0.942844461217511));
#55632=DIRECTION('ref_axis',(0.,-0.942844461217511,-0.333233134534159));
#55633=DIRECTION('center_axis',(0.,-0.333233134534162,0.94284446121751));
#55634=DIRECTION('ref_axis',(0.,-0.94284446121751,-0.333233134534162));
#55635=DIRECTION('center_axis',(0.,0.333233134534159,-0.942844461217511));
#55636=DIRECTION('ref_axis',(0.,-0.942844461217511,-0.333233134534159));
#55637=DIRECTION('',(0.,0.333233134534162,-0.94284446121751));
#55638=DIRECTION('center_axis',(0.,0.333233134534162,-0.94284446121751));
#55639=DIRECTION('ref_axis',(0.,-0.94284446121751,-0.333233134534162));
#55640=DIRECTION('center_axis',(0.,-0.333233134534162,0.94284446121751));
#55641=DIRECTION('ref_axis',(0.,-0.94284446121751,-0.333233134534162));
#55642=DIRECTION('center_axis',(0.,0.333233134534162,-0.94284446121751));
#55643=DIRECTION('ref_axis',(0.,0.94284446121751,0.333233134534162));
#55644=DIRECTION('',(0.,-0.333233134534162,0.94284446121751));
#55645=DIRECTION('center_axis',(0.,0.333233134534159,-0.942844461217511));
#55646=DIRECTION('ref_axis',(0.,-0.942844461217511,-0.333233134534159));
#55647=DIRECTION('center_axis',(0.,-0.333233134534162,0.94284446121751));
#55648=DIRECTION('ref_axis',(0.,-0.94284446121751,-0.333233134534162));
#55649=DIRECTION('center_axis',(0.,0.333233134534159,-0.942844461217511));
#55650=DIRECTION('ref_axis',(0.,-0.942844461217511,-0.333233134534159));
#55651=DIRECTION('',(0.,0.333233134534162,-0.94284446121751));
#55652=DIRECTION('center_axis',(0.,0.333233134534162,-0.94284446121751));
#55653=DIRECTION('ref_axis',(0.,-0.94284446121751,-0.333233134534162));
#55654=DIRECTION('center_axis',(0.,-0.333233134534162,0.94284446121751));
#55655=DIRECTION('ref_axis',(0.,-0.94284446121751,-0.333233134534162));
#55656=DIRECTION('center_axis',(0.,0.333233134534162,-0.94284446121751));
#55657=DIRECTION('ref_axis',(0.,0.94284446121751,0.333233134534162));
#55658=DIRECTION('',(0.,-0.333233134534162,0.94284446121751));
#55659=DIRECTION('center_axis',(0.,0.333233134534159,-0.942844461217511));
#55660=DIRECTION('ref_axis',(0.,-0.942844461217511,-0.333233134534159));
#55661=DIRECTION('center_axis',(0.,-0.333233134534162,0.94284446121751));
#55662=DIRECTION('ref_axis',(0.,-0.94284446121751,-0.333233134534162));
#55663=DIRECTION('center_axis',(0.,0.333233134534159,-0.942844461217511));
#55664=DIRECTION('ref_axis',(0.,-0.942844461217511,-0.333233134534159));
#55665=DIRECTION('',(0.,0.333233134534162,-0.94284446121751));
#55666=DIRECTION('center_axis',(0.,0.333233134534162,-0.94284446121751));
#55667=DIRECTION('ref_axis',(0.,-0.94284446121751,-0.333233134534162));
#55668=DIRECTION('center_axis',(0.,-0.333233134534162,0.94284446121751));
#55669=DIRECTION('ref_axis',(0.,-0.94284446121751,-0.333233134534162));
#55670=DIRECTION('center_axis',(0.,0.333233134534162,-0.94284446121751));
#55671=DIRECTION('ref_axis',(0.,0.94284446121751,0.333233134534162));
#55672=DIRECTION('',(0.,-0.333233134534162,0.94284446121751));
#55673=DIRECTION('center_axis',(0.,0.333233134534159,-0.942844461217511));
#55674=DIRECTION('ref_axis',(0.,-0.942844461217511,-0.333233134534159));
#55675=DIRECTION('center_axis',(0.,-0.333233134534162,0.94284446121751));
#55676=DIRECTION('ref_axis',(0.,-0.94284446121751,-0.333233134534162));
#55677=DIRECTION('center_axis',(0.,0.333233134534159,-0.942844461217511));
#55678=DIRECTION('ref_axis',(0.,-0.942844461217511,-0.333233134534159));
#55679=DIRECTION('',(0.,0.333233134534162,-0.94284446121751));
#55680=DIRECTION('center_axis',(0.,-0.333233134534162,0.94284446121751));
#55681=DIRECTION('ref_axis',(0.,-0.94284446121751,-0.333233134534162));
#55682=DIRECTION('center_axis',(0.,-0.333233134534162,0.94284446121751));
#55683=DIRECTION('ref_axis',(0.,-0.94284446121751,-0.333233134534162));
#55684=DIRECTION('center_axis',(0.,0.333233134534162,-0.94284446121751));
#55685=DIRECTION('ref_axis',(0.,0.94284446121751,0.333233134534162));
#55686=DIRECTION('',(0.,-0.333233134534162,0.94284446121751));
#55687=DIRECTION('center_axis',(0.,0.333233134534159,-0.942844461217511));
#55688=DIRECTION('ref_axis',(0.,-0.942844461217511,-0.333233134534159));
#55689=DIRECTION('center_axis',(0.,-0.333233134534162,0.94284446121751));
#55690=DIRECTION('ref_axis',(0.,-0.94284446121751,-0.333233134534162));
#55691=DIRECTION('center_axis',(0.,0.333233134534159,-0.942844461217511));
#55692=DIRECTION('ref_axis',(0.,-0.942844461217511,-0.333233134534159));
#55693=DIRECTION('',(0.,0.333233134534162,-0.94284446121751));
#55694=DIRECTION('center_axis',(0.,0.333233134534162,-0.94284446121751));
#55695=DIRECTION('ref_axis',(0.,-0.94284446121751,-0.333233134534162));
#55696=DIRECTION('center_axis',(0.,-0.333233134534162,0.94284446121751));
#55697=DIRECTION('ref_axis',(0.,-0.94284446121751,-0.333233134534162));
#55698=DIRECTION('center_axis',(0.,0.333233134534162,-0.94284446121751));
#55699=DIRECTION('ref_axis',(0.,0.94284446121751,0.333233134534162));
#55700=DIRECTION('',(0.,-0.333233134534162,0.94284446121751));
#55701=DIRECTION('center_axis',(0.,0.333233134534159,-0.942844461217511));
#55702=DIRECTION('ref_axis',(0.,-0.942844461217511,-0.333233134534159));
#55703=DIRECTION('center_axis',(0.,-0.333233134534162,0.94284446121751));
#55704=DIRECTION('ref_axis',(0.,-0.94284446121751,-0.333233134534162));
#55705=DIRECTION('center_axis',(0.,0.333233134534159,-0.942844461217511));
#55706=DIRECTION('ref_axis',(0.,-0.942844461217511,-0.333233134534159));
#55707=DIRECTION('',(0.,0.333233134534162,-0.94284446121751));
#55708=DIRECTION('center_axis',(0.,0.333233134534162,-0.94284446121751));
#55709=DIRECTION('ref_axis',(0.,-0.94284446121751,-0.333233134534162));
#55710=DIRECTION('center_axis',(0.,-0.333233134534162,0.94284446121751));
#55711=DIRECTION('ref_axis',(0.,-0.94284446121751,-0.333233134534162));
#55712=DIRECTION('center_axis',(0.,0.333233134534162,-0.94284446121751));
#55713=DIRECTION('ref_axis',(0.,0.94284446121751,0.333233134534162));
#55714=DIRECTION('',(0.,-0.333233134534162,0.94284446121751));
#55715=DIRECTION('center_axis',(0.,0.333233134534159,-0.942844461217511));
#55716=DIRECTION('ref_axis',(0.,-0.942844461217511,-0.333233134534159));
#55717=DIRECTION('center_axis',(0.,-0.333233134534162,0.94284446121751));
#55718=DIRECTION('ref_axis',(0.,-0.94284446121751,-0.333233134534162));
#55719=DIRECTION('center_axis',(0.,0.333233134534159,-0.942844461217511));
#55720=DIRECTION('ref_axis',(0.,-0.942844461217511,-0.333233134534159));
#55721=DIRECTION('',(0.,0.333233134534162,-0.94284446121751));
#55722=DIRECTION('center_axis',(0.,0.333233134534162,-0.94284446121751));
#55723=DIRECTION('ref_axis',(0.,-0.94284446121751,-0.333233134534162));
#55724=DIRECTION('center_axis',(0.,-0.333233134534162,0.94284446121751));
#55725=DIRECTION('ref_axis',(0.,-0.94284446121751,-0.333233134534162));
#55726=DIRECTION('center_axis',(0.,0.333233134534162,-0.94284446121751));
#55727=DIRECTION('ref_axis',(0.,0.94284446121751,0.333233134534162));
#55728=DIRECTION('',(0.,-0.333233134534162,0.94284446121751));
#55729=DIRECTION('center_axis',(0.,0.333233134534159,-0.942844461217511));
#55730=DIRECTION('ref_axis',(0.,-0.942844461217511,-0.333233134534159));
#55731=DIRECTION('center_axis',(0.,-0.333233134534162,0.94284446121751));
#55732=DIRECTION('ref_axis',(0.,-0.94284446121751,-0.333233134534162));
#55733=DIRECTION('center_axis',(0.,0.333233134534159,-0.942844461217511));
#55734=DIRECTION('ref_axis',(0.,-0.942844461217511,-0.333233134534159));
#55735=DIRECTION('',(0.,0.333233134534162,-0.94284446121751));
#55736=DIRECTION('center_axis',(0.,0.333233134534162,-0.94284446121751));
#55737=DIRECTION('ref_axis',(0.,-0.94284446121751,-0.333233134534162));
#55738=DIRECTION('center_axis',(0.,-0.333233134534162,0.94284446121751));
#55739=DIRECTION('ref_axis',(0.,-0.94284446121751,-0.333233134534162));
#55740=DIRECTION('center_axis',(0.,0.333233134534162,-0.94284446121751));
#55741=DIRECTION('ref_axis',(0.,0.94284446121751,0.333233134534162));
#55742=DIRECTION('',(0.,-0.333233134534162,0.94284446121751));
#55743=DIRECTION('center_axis',(0.,0.333233134534159,-0.942844461217511));
#55744=DIRECTION('ref_axis',(0.,-0.942844461217511,-0.333233134534159));
#55745=DIRECTION('center_axis',(0.,-0.333233134534162,0.94284446121751));
#55746=DIRECTION('ref_axis',(0.,-0.94284446121751,-0.333233134534162));
#55747=DIRECTION('center_axis',(0.,0.333233134534159,-0.942844461217511));
#55748=DIRECTION('ref_axis',(0.,-0.942844461217511,-0.333233134534159));
#55749=DIRECTION('',(0.,0.333233134534162,-0.94284446121751));
#55750=DIRECTION('center_axis',(0.,0.333233134534162,-0.94284446121751));
#55751=DIRECTION('ref_axis',(0.,-0.94284446121751,-0.333233134534162));
#55752=DIRECTION('center_axis',(0.,-0.333233134534162,0.94284446121751));
#55753=DIRECTION('ref_axis',(0.,-0.94284446121751,-0.333233134534162));
#55754=DIRECTION('center_axis',(0.,0.333233134534162,-0.94284446121751));
#55755=DIRECTION('ref_axis',(0.,0.94284446121751,0.333233134534162));
#55756=DIRECTION('',(0.,-0.333233134534162,0.94284446121751));
#55757=DIRECTION('center_axis',(0.,0.333233134534159,-0.942844461217511));
#55758=DIRECTION('ref_axis',(0.,-0.942844461217511,-0.333233134534159));
#55759=DIRECTION('center_axis',(0.,-0.333233134534162,0.94284446121751));
#55760=DIRECTION('ref_axis',(0.,-0.94284446121751,-0.333233134534162));
#55761=DIRECTION('center_axis',(0.,0.333233134534159,-0.942844461217511));
#55762=DIRECTION('ref_axis',(0.,-0.942844461217511,-0.333233134534159));
#55763=DIRECTION('',(0.,0.333233134534161,-0.94284446121751));
#55764=DIRECTION('center_axis',(0.,0.333233134534162,-0.94284446121751));
#55765=DIRECTION('ref_axis',(0.,-0.94284446121751,-0.333233134534162));
#55766=DIRECTION('center_axis',(0.,-0.333233134534162,0.94284446121751));
#55767=DIRECTION('ref_axis',(0.,-0.94284446121751,-0.333233134534162));
#55768=DIRECTION('center_axis',(0.,0.333233134534162,-0.94284446121751));
#55769=DIRECTION('ref_axis',(0.,0.94284446121751,0.333233134534162));
#55770=DIRECTION('',(0.,-0.333233134534162,0.94284446121751));
#55771=DIRECTION('center_axis',(0.,0.333233134534159,-0.942844461217511));
#55772=DIRECTION('ref_axis',(0.,-0.942844461217511,-0.333233134534159));
#55773=DIRECTION('center_axis',(0.,-0.333233134534162,0.94284446121751));
#55774=DIRECTION('ref_axis',(0.,-0.94284446121751,-0.333233134534162));
#55775=DIRECTION('center_axis',(0.,0.333233134534159,-0.942844461217511));
#55776=DIRECTION('ref_axis',(0.,-0.942844461217511,-0.333233134534159));
#55777=DIRECTION('',(0.,0.333233134534162,-0.94284446121751));
#55778=DIRECTION('center_axis',(0.,0.333233134534162,-0.94284446121751));
#55779=DIRECTION('ref_axis',(0.,-0.94284446121751,-0.333233134534162));
#55780=DIRECTION('center_axis',(0.,-0.333233134534162,0.94284446121751));
#55781=DIRECTION('ref_axis',(0.,-0.94284446121751,-0.333233134534162));
#55782=DIRECTION('center_axis',(0.,0.333233134534162,-0.94284446121751));
#55783=DIRECTION('ref_axis',(0.,0.94284446121751,0.333233134534162));
#55784=DIRECTION('',(0.,-0.333233134534162,0.94284446121751));
#55785=DIRECTION('center_axis',(0.,0.333233134534159,-0.942844461217511));
#55786=DIRECTION('ref_axis',(0.,-0.942844461217511,-0.333233134534159));
#55787=DIRECTION('center_axis',(0.,-0.333233134534162,0.94284446121751));
#55788=DIRECTION('ref_axis',(0.,-0.94284446121751,-0.333233134534162));
#55789=DIRECTION('center_axis',(0.,0.333233134534159,-0.942844461217511));
#55790=DIRECTION('ref_axis',(0.,-0.942844461217511,-0.333233134534159));
#55791=DIRECTION('',(0.,0.333233134534162,-0.94284446121751));
#55792=DIRECTION('center_axis',(0.,0.333233134534162,-0.94284446121751));
#55793=DIRECTION('ref_axis',(0.,-0.94284446121751,-0.333233134534162));
#55794=DIRECTION('center_axis',(0.,-0.333233134534162,0.94284446121751));
#55795=DIRECTION('ref_axis',(0.,-0.94284446121751,-0.333233134534162));
#55796=DIRECTION('center_axis',(0.,0.333233134534162,-0.94284446121751));
#55797=DIRECTION('ref_axis',(0.,0.94284446121751,0.333233134534162));
#55798=DIRECTION('',(0.,-0.333233134534162,0.94284446121751));
#55799=DIRECTION('center_axis',(0.,0.333233134534159,-0.942844461217511));
#55800=DIRECTION('ref_axis',(0.,-0.942844461217511,-0.333233134534159));
#55801=DIRECTION('center_axis',(0.,-0.333233134534162,0.94284446121751));
#55802=DIRECTION('ref_axis',(0.,-0.94284446121751,-0.333233134534162));
#55803=DIRECTION('center_axis',(0.,0.333233134534159,-0.942844461217511));
#55804=DIRECTION('ref_axis',(0.,-0.942844461217511,-0.333233134534159));
#55805=DIRECTION('',(0.,0.333233134534162,-0.94284446121751));
#55806=DIRECTION('center_axis',(0.,-0.333233134534162,0.94284446121751));
#55807=DIRECTION('ref_axis',(0.,-0.94284446121751,-0.333233134534162));
#55808=DIRECTION('center_axis',(0.,-0.333233134534162,0.94284446121751));
#55809=DIRECTION('ref_axis',(0.,-0.94284446121751,-0.333233134534162));
#55810=DIRECTION('center_axis',(0.,0.333233134534162,-0.94284446121751));
#55811=DIRECTION('ref_axis',(0.,0.94284446121751,0.333233134534162));
#55812=DIRECTION('',(0.,-0.333233134534162,0.94284446121751));
#55813=DIRECTION('center_axis',(0.,0.333233134534159,-0.942844461217511));
#55814=DIRECTION('ref_axis',(0.,-0.942844461217511,-0.333233134534159));
#55815=DIRECTION('center_axis',(0.,-0.333233134534162,0.94284446121751));
#55816=DIRECTION('ref_axis',(0.,-0.94284446121751,-0.333233134534161));
#55817=DIRECTION('center_axis',(0.,0.333233134534159,-0.942844461217511));
#55818=DIRECTION('ref_axis',(0.,-0.942844461217511,-0.333233134534159));
#55819=DIRECTION('',(0.,0.333233134534162,-0.94284446121751));
#55820=DIRECTION('center_axis',(0.,0.333233134534162,-0.94284446121751));
#55821=DIRECTION('ref_axis',(0.,-0.94284446121751,-0.333233134534162));
#55822=DIRECTION('center_axis',(0.,-0.333233134534162,0.94284446121751));
#55823=DIRECTION('ref_axis',(0.,-0.94284446121751,-0.333233134534162));
#55824=DIRECTION('center_axis',(0.,0.333233134534162,-0.94284446121751));
#55825=DIRECTION('ref_axis',(0.,0.94284446121751,0.333233134534162));
#55826=DIRECTION('',(0.,-0.333233134534162,0.94284446121751));
#55827=DIRECTION('center_axis',(0.,0.333233134534159,-0.942844461217511));
#55828=DIRECTION('ref_axis',(0.,-0.942844461217511,-0.333233134534159));
#55829=DIRECTION('center_axis',(0.,-0.333233134534162,0.94284446121751));
#55830=DIRECTION('ref_axis',(0.,-0.94284446121751,-0.333233134534162));
#55831=DIRECTION('center_axis',(0.,0.333233134534159,-0.942844461217511));
#55832=DIRECTION('ref_axis',(0.,-0.942844461217511,-0.333233134534159));
#55833=DIRECTION('',(0.,0.333233134534162,-0.94284446121751));
#55834=DIRECTION('center_axis',(0.,0.333233134534162,-0.94284446121751));
#55835=DIRECTION('ref_axis',(0.,-0.94284446121751,-0.333233134534162));
#55836=DIRECTION('center_axis',(0.,-0.333233134534162,0.94284446121751));
#55837=DIRECTION('ref_axis',(0.,-0.94284446121751,-0.333233134534162));
#55838=DIRECTION('center_axis',(0.,0.333233134534162,-0.94284446121751));
#55839=DIRECTION('ref_axis',(0.,0.94284446121751,0.333233134534162));
#55840=DIRECTION('',(0.,-0.333233134534162,0.94284446121751));
#55841=DIRECTION('center_axis',(0.,0.333233134534159,-0.942844461217511));
#55842=DIRECTION('ref_axis',(0.,-0.942844461217511,-0.333233134534159));
#55843=DIRECTION('center_axis',(0.,-0.333233134534162,0.94284446121751));
#55844=DIRECTION('ref_axis',(0.,-0.94284446121751,-0.333233134534162));
#55845=DIRECTION('center_axis',(0.,0.333233134534159,-0.942844461217511));
#55846=DIRECTION('ref_axis',(0.,-0.942844461217511,-0.333233134534159));
#55847=DIRECTION('',(0.,0.333233134534162,-0.94284446121751));
#55848=DIRECTION('center_axis',(0.,0.333233134534162,-0.94284446121751));
#55849=DIRECTION('ref_axis',(0.,-0.94284446121751,-0.333233134534162));
#55850=DIRECTION('center_axis',(0.,-0.333233134534162,0.94284446121751));
#55851=DIRECTION('ref_axis',(0.,-0.94284446121751,-0.333233134534162));
#55852=DIRECTION('center_axis',(0.,0.333233134534162,-0.94284446121751));
#55853=DIRECTION('ref_axis',(0.,0.94284446121751,0.333233134534162));
#55854=DIRECTION('',(0.,-0.333233134534162,0.94284446121751));
#55855=DIRECTION('center_axis',(0.,0.333233134534159,-0.942844461217511));
#55856=DIRECTION('ref_axis',(0.,-0.942844461217511,-0.333233134534159));
#55857=DIRECTION('center_axis',(0.,-0.333233134534162,0.94284446121751));
#55858=DIRECTION('ref_axis',(0.,-0.94284446121751,-0.333233134534162));
#55859=DIRECTION('center_axis',(0.,0.333233134534159,-0.942844461217511));
#55860=DIRECTION('ref_axis',(0.,-0.942844461217511,-0.333233134534159));
#55861=DIRECTION('',(0.,0.333233134534162,-0.94284446121751));
#55862=DIRECTION('center_axis',(0.,0.333233134534162,-0.94284446121751));
#55863=DIRECTION('ref_axis',(0.,-0.94284446121751,-0.333233134534162));
#55864=DIRECTION('center_axis',(0.,-0.333233134534162,0.94284446121751));
#55865=DIRECTION('ref_axis',(0.,-0.94284446121751,-0.333233134534162));
#55866=DIRECTION('center_axis',(0.,0.333233134534162,-0.94284446121751));
#55867=DIRECTION('ref_axis',(0.,0.94284446121751,0.333233134534162));
#55868=DIRECTION('',(0.,-0.333233134534162,0.94284446121751));
#55869=DIRECTION('center_axis',(0.,0.333233134534159,-0.942844461217511));
#55870=DIRECTION('ref_axis',(0.,-0.942844461217511,-0.333233134534159));
#55871=DIRECTION('center_axis',(0.,-0.333233134534162,0.94284446121751));
#55872=DIRECTION('ref_axis',(0.,-0.94284446121751,-0.333233134534162));
#55873=DIRECTION('center_axis',(0.,0.333233134534159,-0.942844461217511));
#55874=DIRECTION('ref_axis',(0.,-0.942844461217511,-0.333233134534159));
#55875=DIRECTION('',(0.,0.333233134534162,-0.94284446121751));
#55876=DIRECTION('center_axis',(0.,0.333233134534162,-0.94284446121751));
#55877=DIRECTION('ref_axis',(0.,-0.94284446121751,-0.333233134534162));
#55878=DIRECTION('center_axis',(0.,-0.333233134534162,0.94284446121751));
#55879=DIRECTION('ref_axis',(0.,-0.94284446121751,-0.333233134534161));
#55880=DIRECTION('center_axis',(0.,0.333233134534162,-0.94284446121751));
#55881=DIRECTION('ref_axis',(0.,0.94284446121751,0.333233134534162));
#55882=DIRECTION('',(0.,-0.333233134534162,0.94284446121751));
#55883=DIRECTION('center_axis',(0.,0.333233134534159,-0.942844461217511));
#55884=DIRECTION('ref_axis',(0.,-0.942844461217511,-0.333233134534159));
#55885=DIRECTION('center_axis',(0.,-0.333233134534162,0.94284446121751));
#55886=DIRECTION('ref_axis',(0.,-0.94284446121751,-0.333233134534162));
#55887=DIRECTION('center_axis',(0.,0.333233134534159,-0.942844461217511));
#55888=DIRECTION('ref_axis',(0.,-0.942844461217511,-0.333233134534159));
#55889=DIRECTION('',(0.,0.333233134534162,-0.94284446121751));
#55890=DIRECTION('center_axis',(0.,0.333233134534162,-0.94284446121751));
#55891=DIRECTION('ref_axis',(0.,-0.94284446121751,-0.333233134534162));
#55892=DIRECTION('center_axis',(0.,-0.333233134534162,0.94284446121751));
#55893=DIRECTION('ref_axis',(0.,-0.94284446121751,-0.333233134534162));
#55894=DIRECTION('center_axis',(0.,0.333233134534162,-0.94284446121751));
#55895=DIRECTION('ref_axis',(0.,0.94284446121751,0.333233134534162));
#55896=DIRECTION('',(0.,-0.333233134534162,0.94284446121751));
#55897=DIRECTION('center_axis',(0.,0.333233134534159,-0.942844461217511));
#55898=DIRECTION('ref_axis',(0.,-0.942844461217511,-0.333233134534159));
#55899=DIRECTION('center_axis',(0.,-0.333233134534162,0.94284446121751));
#55900=DIRECTION('ref_axis',(0.,-0.94284446121751,-0.333233134534162));
#55901=DIRECTION('center_axis',(0.,0.333233134534159,-0.942844461217511));
#55902=DIRECTION('ref_axis',(0.,-0.942844461217511,-0.333233134534159));
#55903=DIRECTION('',(0.,0.333233134534162,-0.94284446121751));
#55904=DIRECTION('center_axis',(0.,0.333233134534162,-0.94284446121751));
#55905=DIRECTION('ref_axis',(0.,-0.94284446121751,-0.333233134534162));
#55906=DIRECTION('center_axis',(0.,-0.333233134534162,0.94284446121751));
#55907=DIRECTION('ref_axis',(0.,-0.94284446121751,-0.333233134534162));
#55908=DIRECTION('center_axis',(0.,0.333233134534162,-0.94284446121751));
#55909=DIRECTION('ref_axis',(0.,0.94284446121751,0.333233134534162));
#55910=DIRECTION('',(0.,-0.333233134534162,0.94284446121751));
#55911=DIRECTION('center_axis',(0.,0.333233134534159,-0.942844461217511));
#55912=DIRECTION('ref_axis',(0.,-0.942844461217511,-0.333233134534159));
#55913=DIRECTION('center_axis',(0.,-0.333233134534162,0.94284446121751));
#55914=DIRECTION('ref_axis',(0.,-0.94284446121751,-0.333233134534162));
#55915=DIRECTION('center_axis',(0.,0.333233134534159,-0.942844461217511));
#55916=DIRECTION('ref_axis',(0.,-0.942844461217511,-0.333233134534159));
#55917=DIRECTION('',(0.,0.333233134534162,-0.94284446121751));
#55918=DIRECTION('center_axis',(0.,0.333233134534162,-0.94284446121751));
#55919=DIRECTION('ref_axis',(0.,-0.94284446121751,-0.333233134534162));
#55920=DIRECTION('center_axis',(0.,-0.333233134534162,0.94284446121751));
#55921=DIRECTION('ref_axis',(0.,-0.94284446121751,-0.333233134534162));
#55922=DIRECTION('center_axis',(0.,0.333233134534162,-0.94284446121751));
#55923=DIRECTION('ref_axis',(0.,0.94284446121751,0.333233134534162));
#55924=DIRECTION('',(0.,-0.333233134534162,0.94284446121751));
#55925=DIRECTION('center_axis',(0.,0.333233134534159,-0.942844461217511));
#55926=DIRECTION('ref_axis',(0.,-0.942844461217511,-0.333233134534159));
#55927=DIRECTION('center_axis',(0.,-0.333233134534162,0.94284446121751));
#55928=DIRECTION('ref_axis',(0.,-0.94284446121751,-0.333233134534162));
#55929=DIRECTION('center_axis',(0.,0.333233134534159,-0.942844461217511));
#55930=DIRECTION('ref_axis',(0.,-0.942844461217511,-0.333233134534159));
#55931=DIRECTION('',(0.,0.333233134534162,-0.94284446121751));
#55932=DIRECTION('center_axis',(0.,-0.333233134534162,0.94284446121751));
#55933=DIRECTION('ref_axis',(0.,-0.94284446121751,-0.333233134534162));
#55934=DIRECTION('center_axis',(0.,-0.333233134534162,0.94284446121751));
#55935=DIRECTION('ref_axis',(0.,-0.94284446121751,-0.333233134534162));
#55936=DIRECTION('center_axis',(0.,0.333233134534162,-0.94284446121751));
#55937=DIRECTION('ref_axis',(0.,0.94284446121751,0.333233134534162));
#55938=DIRECTION('',(0.,-0.333233134534162,0.94284446121751));
#55939=DIRECTION('center_axis',(0.,0.333233134534159,-0.942844461217511));
#55940=DIRECTION('ref_axis',(0.,-0.942844461217511,-0.333233134534159));
#55941=DIRECTION('center_axis',(0.,0.333233134534162,-0.94284446121751));
#55942=DIRECTION('ref_axis',(0.,0.94284446121751,0.333233134534162));
#55943=DIRECTION('center_axis',(-0.816874943384427,0.543798202596429,0.192350829796967));
#55944=DIRECTION('ref_axis',(-0.137012003453352,0.140999089472445,-0.980483027735636));
#55945=DIRECTION('center_axis',(0.,-0.333233134534162,0.94284446121751));
#55946=DIRECTION('ref_axis',(0.,-0.94284446121751,-0.333233134534162));
#55947=DIRECTION('center_axis',(0.,-0.333233134534162,0.94284446121751));
#55948=DIRECTION('ref_axis',(0.,-0.94284446121751,-0.333233134534162));
#55949=DIRECTION('center_axis',(0.,-0.333233134534162,0.94284446121751));
#55950=DIRECTION('ref_axis',(0.,-0.94284446121751,-0.333233134534162));
#55951=DIRECTION('center_axis',(0.,-0.333233134534162,0.94284446121751));
#55952=DIRECTION('ref_axis',(0.,-0.94284446121751,-0.333233134534162));
#55953=DIRECTION('center_axis',(0.,-0.333233134534162,0.94284446121751));
#55954=DIRECTION('ref_axis',(0.,-0.94284446121751,-0.333233134534162));
#55955=DIRECTION('center_axis',(0.,-0.333233134534162,0.94284446121751));
#55956=DIRECTION('ref_axis',(0.,-0.94284446121751,-0.333233134534162));
#55957=DIRECTION('center_axis',(0.,-0.333233134534162,0.94284446121751));
#55958=DIRECTION('ref_axis',(0.,-0.94284446121751,-0.333233134534162));
#55959=DIRECTION('center_axis',(0.,-0.333233134534162,0.94284446121751));
#55960=DIRECTION('ref_axis',(0.,-0.94284446121751,-0.333233134534162));
#55961=DIRECTION('center_axis',(0.,-0.333233134534162,0.94284446121751));
#55962=DIRECTION('ref_axis',(0.,-0.94284446121751,-0.333233134534162));
#55963=DIRECTION('center_axis',(0.,-0.333233134534162,0.94284446121751));
#55964=DIRECTION('ref_axis',(0.,-0.94284446121751,-0.333233134534162));
#55965=DIRECTION('center_axis',(0.,-0.333233134534162,0.94284446121751));
#55966=DIRECTION('ref_axis',(0.,-0.94284446121751,-0.333233134534162));
#55967=DIRECTION('center_axis',(0.,-0.333233134534162,0.94284446121751));
#55968=DIRECTION('ref_axis',(0.,-0.94284446121751,-0.333233134534162));
#55969=DIRECTION('center_axis',(0.,-0.333233134534162,0.94284446121751));
#55970=DIRECTION('ref_axis',(0.,-0.94284446121751,-0.333233134534162));
#55971=DIRECTION('center_axis',(0.,-0.333233134534162,0.94284446121751));
#55972=DIRECTION('ref_axis',(0.,-0.94284446121751,-0.333233134534162));
#55973=DIRECTION('center_axis',(0.,-0.333233134534162,0.94284446121751));
#55974=DIRECTION('ref_axis',(0.,-0.94284446121751,-0.333233134534162));
#55975=DIRECTION('center_axis',(0.,-0.333233134534162,0.94284446121751));
#55976=DIRECTION('ref_axis',(0.,-0.94284446121751,-0.333233134534162));
#55977=DIRECTION('center_axis',(0.,-0.333233134534162,0.94284446121751));
#55978=DIRECTION('ref_axis',(0.,-0.94284446121751,-0.333233134534162));
#55979=DIRECTION('center_axis',(0.,-0.333233134534162,0.94284446121751));
#55980=DIRECTION('ref_axis',(0.,-0.94284446121751,-0.333233134534162));
#55981=DIRECTION('center_axis',(0.,-0.333233134534162,0.94284446121751));
#55982=DIRECTION('ref_axis',(0.,-0.94284446121751,-0.333233134534162));
#55983=DIRECTION('center_axis',(0.,-0.333233134534162,0.94284446121751));
#55984=DIRECTION('ref_axis',(0.,-0.94284446121751,-0.333233134534162));
#55985=DIRECTION('center_axis',(0.,-0.333233134534162,0.94284446121751));
#55986=DIRECTION('ref_axis',(0.,-0.94284446121751,-0.333233134534162));
#55987=DIRECTION('center_axis',(0.,-0.333233134534162,0.94284446121751));
#55988=DIRECTION('ref_axis',(0.,-0.94284446121751,-0.333233134534162));
#55989=DIRECTION('center_axis',(0.,-0.333233134534162,0.94284446121751));
#55990=DIRECTION('ref_axis',(0.,-0.94284446121751,-0.333233134534162));
#55991=DIRECTION('center_axis',(0.,-0.333233134534162,0.94284446121751));
#55992=DIRECTION('ref_axis',(0.,-0.94284446121751,-0.333233134534162));
#55993=DIRECTION('center_axis',(0.,-0.333233134534162,0.94284446121751));
#55994=DIRECTION('ref_axis',(0.,-0.94284446121751,-0.333233134534162));
#55995=DIRECTION('center_axis',(0.816885842678963,0.543832096794536,0.192208664026204));
#55996=DIRECTION('ref_axis',(-1.43377373465901E-14,0.33323313453417,-0.942844461217507));
#55997=DIRECTION('center_axis',(0.,0.333233134534162,-0.94284446121751));
#55998=DIRECTION('ref_axis',(0.,0.94284446121751,0.333233134534162));
#55999=DIRECTION('center_axis',(0.,-0.333233134534162,0.94284446121751));
#56000=DIRECTION('ref_axis',(0.,0.94284446121751,0.333233134534162));
#56001=DIRECTION('center_axis',(-0.809731323701899,-0.553327332132966,-0.195356205252313));
#56002=DIRECTION('ref_axis',(0.000159129308641561,-0.333124458135407,0.942882850660598));
#56003=DIRECTION('center_axis',(0.809731322759568,-0.553327335018826,-0.195356200984262));
#56004=DIRECTION('ref_axis',(-0.58680078359079,-0.763450698364046,-0.269829337813154));
#56005=DIRECTION('center_axis',(0.,-0.333233134534242,0.942844461217482));
#56006=DIRECTION('ref_axis',(0.,-0.942844461217482,-0.333233134534242));
#56007=DIRECTION('center_axis',(0.,0.333233134534242,-0.942844461217482));
#56008=DIRECTION('ref_axis',(0.,-0.942844461217482,-0.333233134534242));
#56009=DIRECTION('',(-1.18291797137864E-16,0.824470733586849,0.565904593954461));
#56010=DIRECTION('center_axis',(0.,-0.333233134534162,0.94284446121751));
#56011=DIRECTION('ref_axis',(0.,0.94284446121751,0.333233134534162));
#56012=DIRECTION('center_axis',(0.,0.333233134534242,-0.942844461217482));
#56013=DIRECTION('ref_axis',(0.,-0.942844461217482,-0.333233134534242));
#56014=DIRECTION('center_axis',(0.,-0.333233134534162,0.94284446121751));
#56015=DIRECTION('ref_axis',(0.,-0.94284446121751,-0.333233134534163));
#56016=DIRECTION('center_axis',(-1.,0.,0.));
#56017=DIRECTION('ref_axis',(0.,0.94284446121751,0.333233134534162));
#56018=DIRECTION('center_axis',(0.,0.333233134534162,-0.94284446121751));
#56019=DIRECTION('ref_axis',(0.,-0.94284446121751,-0.333233134534162));
#56020=DIRECTION('center_axis',(0.,0.333233134534202,-0.942844461217496));
#56021=DIRECTION('ref_axis',(0.,0.942844461217497,0.333233134534199));
#56022=DIRECTION('center_axis',(-1.,0.,0.));
#56023=DIRECTION('ref_axis',(0.,-0.942844461217496,-0.333233134534202));
#56024=DIRECTION('center_axis',(0.,-0.333233134534202,0.942844461217496));
#56025=DIRECTION('ref_axis',(0.,0.942844461217496,0.333233134534202));
#56026=DIRECTION('center_axis',(0.,-0.333233134534202,0.942844461217496));
#56027=DIRECTION('ref_axis',(0.,0.942844461217496,0.333233134534202));
#56028=DIRECTION('center_axis',(0.,0.333233134534162,-0.94284446121751));
#56029=DIRECTION('ref_axis',(0.,0.94284446121751,0.333233134534161));
#56030=DIRECTION('center_axis',(0.,0.333233134534162,-0.94284446121751));
#56031=DIRECTION('ref_axis',(0.,0.94284446121751,0.333233134534162));
#56032=DIRECTION('center_axis',(0.,0.333233134534162,-0.94284446121751));
#56033=DIRECTION('ref_axis',(0.,0.94284446121751,0.333233134534162));
#56034=DIRECTION('center_axis',(0.,-1.,0.));
#56035=DIRECTION('ref_axis',(0.,0.,-1.));
#56036=DIRECTION('center_axis',(0.,1.,0.));
#56037=DIRECTION('ref_axis',(0.,0.,-1.));
#56038=DIRECTION('center_axis',(0.747684665568337,0.,0.664053944249987));
#56039=DIRECTION('ref_axis',(0.664053944249987,0.,-0.747684665568336));
#56040=DIRECTION('center_axis',(0.,-1.,0.));
#56041=DIRECTION('ref_axis',(0.,0.,-1.));
#56042=DIRECTION('center_axis',(0.747684665568331,0.,-0.664053944249993));
#56043=DIRECTION('ref_axis',(-0.664053944249993,0.,-0.747684665568331));
#56044=DIRECTION('center_axis',(0.,0.,1.));
#56045=DIRECTION('ref_axis',(1.,0.,0.));
#56046=DIRECTION('center_axis',(0.,0.,1.));
#56047=DIRECTION('ref_axis',(1.,0.,0.));
#56048=DIRECTION('center_axis',(0.,0.,1.));
#56049=DIRECTION('ref_axis',(1.,0.,0.));
#56050=DIRECTION('',(0.,0.,-1.));
#56051=DIRECTION('center_axis',(0.,0.,1.));
#56052=DIRECTION('ref_axis',(1.,0.,0.));
#56053=DIRECTION('',(0.,0.,1.));
#56054=DIRECTION('center_axis',(0.,0.333233134534162,-0.94284446121751));
#56055=DIRECTION('ref_axis',(0.,0.94284446121751,0.333233134534162));
#56056=DIRECTION('center_axis',(0.762076920749875,-0.61044884773581,-0.215849417785665));
#56057=DIRECTION('ref_axis',(-0.113718860840941,-0.454371624364075,0.883523880640354));
#56058=DIRECTION('center_axis',(0.,-0.333233134534162,0.94284446121751));
#56059=DIRECTION('ref_axis',(0.,-0.94284446121751,-0.333233134534162));
#56060=DIRECTION('center_axis',(0.,0.33323313453416,-0.942844461217511));
#56061=DIRECTION('ref_axis',(0.,0.942844461217511,0.333233134534161));
#56062=DIRECTION('',(0.,-0.333233134534162,0.94284446121751));
#56063=DIRECTION('center_axis',(0.,0.33323313453416,-0.942844461217511));
#56064=DIRECTION('ref_axis',(0.,0.942844461217511,0.333233134534161));
#56065=DIRECTION('center_axis',(0.,0.33323313453416,-0.942844461217511));
#56066=DIRECTION('ref_axis',(0.,0.942844461217512,0.333233134534158));
#56067=DIRECTION('center_axis',(-1.,0.,0.));
#56068=DIRECTION('ref_axis',(0.,-0.94284446121751,-0.333233134534163));
#56069=DIRECTION('center_axis',(0.,-0.33323313453416,0.942844461217511));
#56070=DIRECTION('ref_axis',(0.,0.942844461217511,0.33323313453416));
#56071=DIRECTION('center_axis',(0.,-0.333233134534162,0.94284446121751));
#56072=DIRECTION('ref_axis',(0.,-0.94284446121751,-0.333233134534162));
#56073=DIRECTION('center_axis',(0.,0.333233134534162,-0.94284446121751));
#56074=DIRECTION('ref_axis',(0.,0.94284446121751,0.333233134534162));
#56075=DIRECTION('',(0.,-0.333233134534162,0.94284446121751));
#56076=DIRECTION('center_axis',(0.,-0.333233134534162,0.94284446121751));
#56077=DIRECTION('ref_axis',(0.,-0.94284446121751,-0.333233134534162));
#56078=DIRECTION('',(0.,0.333233134534162,-0.94284446121751));
#56079=DIRECTION('center_axis',(0.,0.333233134534162,-0.94284446121751));
#56080=DIRECTION('ref_axis',(0.,0.94284446121751,0.333233134534162));
#56081=DIRECTION('center_axis',(0.,1.,0.));
#56082=DIRECTION('ref_axis',(1.,0.,0.));
#56083=DIRECTION('center_axis',(1.,0.,0.));
#56084=DIRECTION('ref_axis',(0.,0.0958457525203355,-0.995396198367168));
#56085=DIRECTION('',(0.,0.0958457525203355,-0.995396198367168));
#56086=DIRECTION('',(0.,-0.999992762491362,0.00380459786244685));
#56087=DIRECTION('',(0.,0.0958457525203355,-0.995396198367168));
#56088=DIRECTION('',(0.,0.995396198367168,0.0958457525203355));
#56089=DIRECTION('center_axis',(0.,0.0958457525203355,-0.995396198367168));
#56090=DIRECTION('ref_axis',(-1.,0.,0.));
#56091=DIRECTION('center_axis',(0.,0.0958457525203355,-0.995396198367168));
#56092=DIRECTION('ref_axis',(1.,-1.34077497793431E-14,-1.29101946472523E-15));
#56093=DIRECTION('',(0.,0.0958457525203355,-0.995396198367168));
#56094=DIRECTION('center_axis',(0.,-0.0958457525203355,0.995396198367168));
#56095=DIRECTION('ref_axis',(1.,0.,0.));
#56096=DIRECTION('center_axis',(0.,0.995396198367168,0.0958457525203355));
#56097=DIRECTION('ref_axis',(0.,-0.0958457525203355,0.995396198367168));
#56098=DIRECTION('center_axis',(0.,-0.0958457525203355,0.995396198367168));
#56099=DIRECTION('ref_axis',(-1.,-1.38980017783282E-14,-1.33822536308449E-15));
#56100=DIRECTION('center_axis',(0.,0.0958457525203355,-0.995396198367168));
#56101=DIRECTION('ref_axis',(-1.,0.,0.));
#56102=DIRECTION('',(0.,0.0958457525203355,-0.995396198367168));
#56103=DIRECTION('center_axis',(0.,-0.0479781285213995,0.998848386484948));
#56104=DIRECTION('ref_axis',(-1.81973168778901E-14,-0.998848386484948,-0.0479781285213995));
#56105=DIRECTION('',(0.,0.0958457525203355,-0.995396198367168));
#56106=DIRECTION('center_axis',(0.,0.0958457525203355,-0.995396198367168));
#56107=DIRECTION('ref_axis',(1.,1.34077497793431E-14,1.29101946472523E-15));
#56108=DIRECTION('',(0.,0.0958457525203355,-0.995396198367168));
#56109=DIRECTION('center_axis',(0.,0.0958457525203355,-0.995396198367168));
#56110=DIRECTION('ref_axis',(-1.,0.,0.));
#56111=DIRECTION('center_axis',(0.,0.0958457525203355,-0.995396198367168));
#56112=DIRECTION('ref_axis',(1.,2.68154995586863E-14,2.58203892945045E-15));
#56113=DIRECTION('center_axis',(-1.,0.,0.));
#56114=DIRECTION('ref_axis',(0.,-0.0958457525203355,0.995396198367168));
#56115=DIRECTION('',(0.,0.999992762491366,-0.00380459786137058));
#56116=DIRECTION('',(0.,-0.995396198367168,-0.0958457525203355));
#56117=DIRECTION('center_axis',(0.,-0.0958457525203355,0.995396198367168));
#56118=DIRECTION('ref_axis',(1.,0.,0.));
#56119=DIRECTION('',(0.,-0.995396198367168,-0.0958457525203355));
#56120=DIRECTION('center_axis',(0.,-0.0958457525203355,0.995396198367168));
#56121=DIRECTION('ref_axis',(1.,0.,0.));
#56122=DIRECTION('',(0.,0.995396198367168,0.0958457525203355));
#56123=DIRECTION('center_axis',(0.,-0.0958457525203355,0.995396198367168));
#56124=DIRECTION('ref_axis',(1.,0.,0.));
#56125=DIRECTION('center_axis',(0.70710678118655,-0.0677731815550566,0.703851401832732));
#56126=DIRECTION('ref_axis',(-8.71684762352402E-19,-0.995396198367168,-0.0958457525203355));
#56127=DIRECTION('',(0.707106781186545,0.0677731815550571,-0.703851401832737));
#56128=DIRECTION('',(0.,-0.995396198367168,-0.0958457525203355));
#56129=DIRECTION('',(-0.707106781186545,-0.0677731815550571,0.703851401832737));
#56130=DIRECTION('',(0.,0.995396198367168,0.0958457525203355));
#56131=DIRECTION('center_axis',(0.,0.0958457525203355,-0.995396198367168));
#56132=DIRECTION('ref_axis',(-1.,0.,0.));
#56133=DIRECTION('',(-0.707106781186545,0.0677731815550571,-0.703851401832737));
#56134=DIRECTION('center_axis',(0.,0.0958457525203355,-0.995396198367168));
#56135=DIRECTION('ref_axis',(1.,0.,0.));
#56136=DIRECTION('center_axis',(0.,-0.0958457525203355,0.995396198367168));
#56137=DIRECTION('ref_axis',(-1.,0.,0.));
#56138=DIRECTION('center_axis',(0.,0.0958457525203355,-0.995396198367168));
#56139=DIRECTION('ref_axis',(-1.,0.,0.));
#56140=DIRECTION('center_axis',(0.,0.0958457525203355,-0.995396198367168));
#56141=DIRECTION('ref_axis',(1.,0.,0.));
#56142=DIRECTION('',(0.707106781186545,-0.0677731815550571,0.703851401832737));
#56143=DIRECTION('center_axis',(0.,-0.0958457525203355,0.995396198367168));
#56144=DIRECTION('ref_axis',(-1.,0.,0.));
#56145=DIRECTION('center_axis',(-0.70710678118655,-0.0677731815550566,0.703851401832732));
#56146=DIRECTION('ref_axis',(-8.71684762352402E-19,0.995396198367168,0.0958457525203355));
#56147=DIRECTION('',(0.,0.995396198367168,0.0958457525203355));
#56148=DIRECTION('',(0.,-0.995396198367168,-0.0958457525203355));
#56149=DIRECTION('center_axis',(0.,-0.0958457525203355,0.995396198367168));
#56150=DIRECTION('ref_axis',(1.,0.,0.));
#56151=DIRECTION('center_axis',(0.,-0.995396198367168,-0.0958457525203355));
#56152=DIRECTION('ref_axis',(0.,0.0958457525203355,-0.995396198367168));
#56153=DIRECTION('center_axis',(0.,-0.995396198367168,-0.0958457525203355));
#56154=DIRECTION('ref_axis',(0.,0.0958457525203355,-0.995396198367168));
#56155=DIRECTION('center_axis',(0.,-0.995396198367168,-0.0958457525203355));
#56156=DIRECTION('ref_axis',(0.,0.0958457525203355,-0.995396198367168));
#56157=DIRECTION('center_axis',(0.,-0.995396198367168,-0.0958457525203355));
#56158=DIRECTION('ref_axis',(0.,0.0958457525203355,-0.995396198367168));
#56159=DIRECTION('center_axis',(0.,0.995396198367168,0.0958457525203355));
#56160=DIRECTION('ref_axis',(0.,-0.0958457525203355,0.995396198367168));
#56161=DIRECTION('center_axis',(0.,-0.995396198367168,-0.0958457525203355));
#56162=DIRECTION('ref_axis',(0.,0.0958457525203355,-0.995396198367168));
#56163=DIRECTION('center_axis',(0.,-0.0958457525203355,0.995396198367168));
#56164=DIRECTION('ref_axis',(1.,0.,0.));
#56165=DIRECTION('center_axis',(0.,-0.0958457525203355,0.995396198367168));
#56166=DIRECTION('ref_axis',(1.,0.,0.));
#56167=DIRECTION('center_axis',(0.,0.995396198367168,0.0958457525203355));
#56168=DIRECTION('ref_axis',(0.,-0.0958457525203355,0.995396198367168));
#56169=DIRECTION('center_axis',(0.,-0.995396198367168,-0.0958457525203355));
#56170=DIRECTION('ref_axis',(0.,0.0958457525203355,-0.995396198367168));
#56171=DIRECTION('center_axis',(0.,0.995396198367168,0.0958457525203355));
#56172=DIRECTION('ref_axis',(0.,-0.0958457525203355,0.995396198367168));
#56173=DIRECTION('center_axis',(0.,0.995396198367168,0.0958457525203355));
#56174=DIRECTION('ref_axis',(0.,-0.0958457525203355,0.995396198367168));
#56175=DIRECTION('center_axis',(0.,0.995396198367168,0.0958457525203355));
#56176=DIRECTION('ref_axis',(0.,-0.0958457525203355,0.995396198367168));
#56177=DIRECTION('center_axis',(0.,-0.0958457525203355,0.995396198367168));
#56178=DIRECTION('ref_axis',(1.,0.,0.));
#56179=DIRECTION('center_axis',(2.27199593986439E-14,0.999992816774261,
-0.00379030340206436));
#56180=DIRECTION('ref_axis',(0.999989540168118,1.7336051598704E-5,0.00457375707892275));
#56181=DIRECTION('center_axis',(0.,-0.993714552529049,-0.111943682680141));
#56182=DIRECTION('ref_axis',(0.,0.111943682680141,-0.993714552529049));
#56183=DIRECTION('center_axis',(0.,0.993714513001089,0.111944033565922));
#56184=DIRECTION('ref_axis',(0.,-0.111944033565922,0.993714513001089));
#56185=DIRECTION('center_axis',(-4.72985282513324E-19,-0.999992762691407,
0.00380454528272082));
#56186=DIRECTION('ref_axis',(1.,0.,-8.9883652947822E-12));
#56187=DIRECTION('center_axis',(1.05594678446211E-16,0.999992763056819,
-0.00380444923602132));
#56188=DIRECTION('ref_axis',(-7.13779962151542E-30,0.00380444923602132,
0.999992763056819));
#56189=DIRECTION('',(-3.137034099265E-5,0.999992710161712,-0.00381819844128151));
#56190=DIRECTION('center_axis',(-7.48214981472191E-6,0.999992732962714,
-0.00381234386965002));
#56191=DIRECTION('ref_axis',(0.396180495354598,0.00350335413362759,0.918165966266666));
#56192=DIRECTION('center_axis',(-2.39349104903811E-19,0.999992762286848,
-0.00380465161595737));
#56193=DIRECTION('ref_axis',(-1.,0.,4.51194621314849E-12));
#56194=DIRECTION('center_axis',(1.05594678446211E-16,-0.999992763056819,
0.00380444923602132));
#56195=DIRECTION('ref_axis',(-7.13779962151542E-30,-0.00380444923602132,
-0.999992763056819));
#56196=DIRECTION('',(-3.13703409353662E-5,-0.999992710161712,0.00381819844125435));
#56197=DIRECTION('center_axis',(0.,0.,-1.));
#56198=DIRECTION('ref_axis',(-1.,0.,0.));
#56199=DIRECTION('center_axis',(0.806909120659315,-0.558829829394105,-0.191329278408108));
#56200=DIRECTION('ref_axis',(-0.0849118339894143,-0.430294016492482,0.898686285540912));
#56201=DIRECTION('center_axis',(-0.835086390772497,0.517595659589867,0.186347667332585));
#56202=DIRECTION('ref_axis',(-0.526823571888351,-0.849974660859252,-1.43332569245731E-15));
#56203=DIRECTION('center_axis',(-0.835086381169178,-0.517595614917961,-0.186347834448014));
#56204=DIRECTION('ref_axis',(0.526823543416339,-0.849974678506515,9.57696623692639E-15));
#56205=DIRECTION('center_axis',(-0.806910218572417,-0.558828457766669,-0.191328654292922));
#56206=DIRECTION('ref_axis',(-0.590327175091889,0.751857820045504,0.293638629584822));
#56207=DIRECTION('center_axis',(-0.000872658099433895,0.999999542363192,
-0.0003920985191296));
#56208=DIRECTION('ref_axis',(0.999999619233104,0.000872658510876435,8.78244352734673E-7));
#56209=DIRECTION('center_axis',(0.747684665568336,3.91836177343196E-14,
-0.664053944249987));
#56210=DIRECTION('ref_axis',(-0.664053944249987,-4.89999445230472E-28,-0.747684665568336));
#56211=DIRECTION('center_axis',(0.,-1.,0.));
#56212=DIRECTION('ref_axis',(6.1857730524649E-16,0.,1.));
#56213=DIRECTION('center_axis',(0.747684665568342,2.64861897890156E-14,
0.664053944249981));
#56214=DIRECTION('ref_axis',(0.664053944249981,1.07359285114335E-28,-0.747684665568342));
#56215=DIRECTION('center_axis',(0.,-1.,0.));
#56216=DIRECTION('ref_axis',(0.,0.,-1.));
#56217=DIRECTION('center_axis',(0.,1.,0.));
#56218=DIRECTION('ref_axis',(0.,0.,1.));
#56219=DIRECTION('center_axis',(0.,0.,1.));
#56220=DIRECTION('ref_axis',(1.,0.,0.));
#56221=DIRECTION('center_axis',(0.000872658094508672,0.9999995423632,-0.000392098510262023));
#56222=DIRECTION('ref_axis',(-0.664054348043085,0.000872658504590579,0.747683797679344));
#56223=DIRECTION('center_axis',(-0.000872658095697528,0.999999542363198,
0.000392098510701838));
#56224=DIRECTION('ref_axis',(0.664054348059308,0.000872658505683059,-0.747683797664936));
#56225=DIRECTION('center_axis',(0.,0.,1.));
#56226=DIRECTION('ref_axis',(-0.708339837726479,-0.705871570676724,0.));
#56227=DIRECTION('center_axis',(-2.7852630342689E-14,-2.77555756158361E-14,
1.));
#56228=DIRECTION('ref_axis',(1.,-2.69380981579098E-30,2.7852630342689E-14));
#56229=DIRECTION('',(0.,0.,-1.));
#56230=DIRECTION('',(0.,0.,1.));
#56231=DIRECTION('center_axis',(0.000872658101303331,0.99999954236319,0.000392098519876546));
#56232=DIRECTION('ref_axis',(-0.999999619233102,0.000872658512739778,-8.78240000660092E-7));
#56233=DIRECTION('center_axis',(-0.781122637833718,-0.588690990414065,-0.208063313606701));
#56234=DIRECTION('ref_axis',(0.084909986182804,-0.430291959918125,0.898687444819529));
#56235=DIRECTION('center_axis',(0.,-0.333233134534162,0.94284446121751));
#56236=DIRECTION('ref_axis',(1.21997367885991E-7,0.942844461217503,0.333233134534159));
#56237=DIRECTION('center_axis',(0.,-0.333233134534161,0.942844461217511));
#56238=DIRECTION('ref_axis',(0.,-0.94284446121751,-0.333233134534161));
#56239=DIRECTION('center_axis',(0.00349620323913664,0.999992628662834,-0.00158719340524177));
#56240=DIRECTION('ref_axis',(-0.658393043656588,0.00349652845883053,0.752666177234869));
#56241=DIRECTION('center_axis',(0.00349064703388849,-0.999992652747851,
0.00158424543605274));
#56242=DIRECTION('ref_axis',(0.65839306424128,0.0034906514143529,0.75266618650746));
#56243=DIRECTION('',(0.,0.,1.));
#56244=DIRECTION('',(0.,0.,1.));
#56245=DIRECTION('center_axis',(6.57149350991999E-17,1.,0.));
#56246=DIRECTION('ref_axis',(1.,0.,0.));
#56247=DIRECTION('center_axis',(0.,0.333233134534161,-0.942844461217511));
#56248=DIRECTION('ref_axis',(0.,-0.94284446121751,-0.333233134534161));
#56249=DIRECTION('center_axis',(0.,-0.333233134534161,0.942844461217511));
#56250=DIRECTION('ref_axis',(-4.36200015704239E-7,0.942844461217421,0.33323313453413));
#56251=DIRECTION('center_axis',(-0.465249795635371,-0.834587947184017,-0.294967093209419));
#56252=DIRECTION('ref_axis',(0.885179432457581,-0.438657466759802,-0.15503870229703));
#56253=DIRECTION('center_axis',(0.0034906470338884,-0.999992652747851,-0.00158424543605272));
#56254=DIRECTION('ref_axis',(0.999993907657794,0.00349065141435304,8.88178419700162E-15));
#56255=DIRECTION('center_axis',(0.,-1.,0.));
#56256=DIRECTION('ref_axis',(2.09732571729144E-13,0.,-1.));
#56257=DIRECTION('center_axis',(0.00348618203660982,0.999992670981315,0.0015825670488381));
#56258=DIRECTION('ref_axis',(-0.999993923233682,0.00348618641343271,-7.06608105368013E-9));
#56259=DIRECTION('center_axis',(0.,-1.,0.));
#56260=DIRECTION('ref_axis',(0.,0.,-1.));
#56261=DIRECTION('center_axis',(-0.99999390765779,0.00349065141522374,0.));
#56262=DIRECTION('ref_axis',(-0.00349065141522374,-0.99999390765779,0.));
#56263=DIRECTION('center_axis',(0.99999390765779,0.00349065141522374,0.));
#56264=DIRECTION('ref_axis',(-0.00349065141522374,0.99999390765779,0.));
#56265=DIRECTION('center_axis',(0.,-1.,0.));
#56266=DIRECTION('ref_axis',(0.835314349256296,0.,0.549772623842377));
#56267=DIRECTION('center_axis',(-4.38167354516293E-13,-1.,-6.55088140642138E-13));
#56268=DIRECTION('ref_axis',(0.835314349256533,-5.8579526746184E-15,-0.549772623842016));
#56269=DIRECTION('center_axis',(0.,-1.,0.));
#56270=DIRECTION('ref_axis',(-7.6571373978539E-16,0.,1.));
#56271=DIRECTION('center_axis',(0.,-0.333233134534162,0.94284446121751));
#56272=DIRECTION('ref_axis',(0.,-0.94284446121751,-0.333233134534162));
#56273=DIRECTION('center_axis',(0.,0.333233134534162,-0.94284446121751));
#56274=DIRECTION('ref_axis',(0.,0.94284446121751,0.333233134534162));
#56275=DIRECTION('center_axis',(-4.48634137349537E-12,0.333233134518338,
-0.942844461223103));
#56276=DIRECTION('ref_axis',(0.26200914408981,0.909906558382195,0.321591765171923));
#56277=DIRECTION('center_axis',(1.18843000706592E-12,0.333233134529897,
-0.942844461219018));
#56278=DIRECTION('ref_axis',(-0.254118622727095,0.911893761488375,0.322294110001823));
#56279=DIRECTION('center_axis',(-1.,0.,0.));
#56280=DIRECTION('ref_axis',(0.,0.,1.));
#56281=DIRECTION('',(0.,0.,-1.));
#56282=DIRECTION('center_axis',(1.,0.,0.));
#56283=DIRECTION('ref_axis',(0.,0.,-1.));
#56284=DIRECTION('',(0.,0.,-1.));
#56285=DIRECTION('center_axis',(0.,0.,-1.));
#56286=DIRECTION('ref_axis',(-1.,0.,0.));
#56287=DIRECTION('center_axis',(0.,0.333233134534162,-0.94284446121751));
#56288=DIRECTION('ref_axis',(0.,0.94284446121751,0.333233134534162));
#56289=DIRECTION('center_axis',(0.,-0.333233134534159,0.942844461217511));
#56290=DIRECTION('ref_axis',(0.,-0.942844461217511,-0.333233134534159));
#56291=DIRECTION('center_axis',(0.,0.333233134534162,-0.94284446121751));
#56292=DIRECTION('ref_axis',(0.,0.94284446121751,0.333233134534162));
#56293=DIRECTION('center_axis',(0.,-0.333233134534159,0.942844461217511));
#56294=DIRECTION('ref_axis',(0.,-0.942844461217511,-0.333233134534159));
#56295=DIRECTION('center_axis',(0.,0.333233134534162,-0.94284446121751));
#56296=DIRECTION('ref_axis',(0.,0.94284446121751,0.333233134534162));
#56297=DIRECTION('center_axis',(0.,-0.333233134534159,0.942844461217511));
#56298=DIRECTION('ref_axis',(0.,-0.942844461217511,-0.333233134534159));
#56299=DIRECTION('center_axis',(0.,0.333233134534162,-0.94284446121751));
#56300=DIRECTION('ref_axis',(0.,0.94284446121751,0.333233134534162));
#56301=DIRECTION('center_axis',(0.,-0.333233134534159,0.942844461217511));
#56302=DIRECTION('ref_axis',(0.,-0.942844461217511,-0.333233134534159));
#56303=DIRECTION('center_axis',(0.,0.333233134534162,-0.94284446121751));
#56304=DIRECTION('ref_axis',(0.,0.94284446121751,0.333233134534162));
#56305=DIRECTION('center_axis',(0.,-0.333233134534159,0.942844461217511));
#56306=DIRECTION('ref_axis',(0.,-0.942844461217511,-0.333233134534159));
#56307=DIRECTION('center_axis',(0.,0.333233134534162,-0.94284446121751));
#56308=DIRECTION('ref_axis',(0.,0.94284446121751,0.333233134534162));
#56309=DIRECTION('center_axis',(0.,-0.333233134534159,0.942844461217511));
#56310=DIRECTION('ref_axis',(0.,-0.942844461217511,-0.333233134534159));
#56311=DIRECTION('center_axis',(0.,0.333233134534162,-0.94284446121751));
#56312=DIRECTION('ref_axis',(0.,0.94284446121751,0.333233134534162));
#56313=DIRECTION('center_axis',(0.,-0.333233134534159,0.942844461217511));
#56314=DIRECTION('ref_axis',(0.,-0.942844461217511,-0.333233134534159));
#56315=DIRECTION('center_axis',(0.,0.333233134534162,-0.94284446121751));
#56316=DIRECTION('ref_axis',(0.,0.94284446121751,0.333233134534162));
#56317=DIRECTION('center_axis',(0.,-0.333233134534159,0.942844461217511));
#56318=DIRECTION('ref_axis',(0.,-0.942844461217511,-0.333233134534159));
#56319=DIRECTION('center_axis',(0.,0.333233134534162,-0.94284446121751));
#56320=DIRECTION('ref_axis',(0.,0.94284446121751,0.333233134534162));
#56321=DIRECTION('center_axis',(0.,-0.333233134534159,0.942844461217511));
#56322=DIRECTION('ref_axis',(0.,-0.942844461217511,-0.333233134534159));
#56323=DIRECTION('center_axis',(0.,0.333233134534162,-0.94284446121751));
#56324=DIRECTION('ref_axis',(0.,0.94284446121751,0.333233134534162));
#56325=DIRECTION('center_axis',(0.,-0.333233134534159,0.942844461217511));
#56326=DIRECTION('ref_axis',(0.,-0.942844461217511,-0.333233134534159));
#56327=DIRECTION('center_axis',(0.,0.333233134534162,-0.94284446121751));
#56328=DIRECTION('ref_axis',(0.,0.94284446121751,0.333233134534162));
#56329=DIRECTION('center_axis',(0.,-0.333233134534159,0.942844461217511));
#56330=DIRECTION('ref_axis',(0.,-0.942844461217511,-0.333233134534159));
#56331=DIRECTION('center_axis',(0.,0.333233134534162,-0.94284446121751));
#56332=DIRECTION('ref_axis',(0.,0.94284446121751,0.333233134534162));
#56333=DIRECTION('center_axis',(0.,-0.333233134534159,0.942844461217511));
#56334=DIRECTION('ref_axis',(0.,-0.942844461217511,-0.333233134534159));
#56335=DIRECTION('center_axis',(0.,0.333233134534162,-0.94284446121751));
#56336=DIRECTION('ref_axis',(0.,0.94284446121751,0.333233134534162));
#56337=DIRECTION('center_axis',(0.,-0.333233134534159,0.942844461217511));
#56338=DIRECTION('ref_axis',(0.,-0.942844461217511,-0.333233134534159));
#56339=DIRECTION('center_axis',(0.,0.333233134534162,-0.94284446121751));
#56340=DIRECTION('ref_axis',(0.,0.94284446121751,0.333233134534162));
#56341=DIRECTION('center_axis',(0.,-0.333233134534159,0.942844461217511));
#56342=DIRECTION('ref_axis',(0.,-0.942844461217511,-0.333233134534159));
#56343=DIRECTION('center_axis',(0.,0.333233134534162,-0.94284446121751));
#56344=DIRECTION('ref_axis',(0.,0.94284446121751,0.333233134534162));
#56345=DIRECTION('center_axis',(0.,-0.333233134534159,0.942844461217511));
#56346=DIRECTION('ref_axis',(0.,-0.942844461217511,-0.333233134534159));
#56347=DIRECTION('center_axis',(0.,0.333233134534162,-0.94284446121751));
#56348=DIRECTION('ref_axis',(0.,0.94284446121751,0.333233134534162));
#56349=DIRECTION('center_axis',(0.,-0.333233134534159,0.942844461217511));
#56350=DIRECTION('ref_axis',(0.,-0.942844461217511,-0.333233134534159));
#56351=DIRECTION('center_axis',(0.,0.333233134534162,-0.94284446121751));
#56352=DIRECTION('ref_axis',(0.,0.94284446121751,0.333233134534162));
#56353=DIRECTION('center_axis',(0.,-0.333233134534159,0.942844461217511));
#56354=DIRECTION('ref_axis',(0.,-0.942844461217511,-0.333233134534159));
#56355=DIRECTION('center_axis',(0.,0.333233134534162,-0.94284446121751));
#56356=DIRECTION('ref_axis',(0.,0.94284446121751,0.333233134534162));
#56357=DIRECTION('center_axis',(0.,-0.333233134534159,0.942844461217511));
#56358=DIRECTION('ref_axis',(0.,-0.942844461217511,-0.333233134534159));
#56359=DIRECTION('center_axis',(0.,0.333233134534162,-0.94284446121751));
#56360=DIRECTION('ref_axis',(0.,0.94284446121751,0.333233134534162));
#56361=DIRECTION('center_axis',(0.,-0.333233134534159,0.942844461217511));
#56362=DIRECTION('ref_axis',(0.,-0.942844461217511,-0.333233134534159));
#56363=DIRECTION('center_axis',(0.,0.333233134534162,-0.94284446121751));
#56364=DIRECTION('ref_axis',(0.,0.94284446121751,0.333233134534162));
#56365=DIRECTION('center_axis',(0.,-0.333233134534159,0.942844461217511));
#56366=DIRECTION('ref_axis',(0.,-0.942844461217511,-0.333233134534159));
#56367=DIRECTION('center_axis',(0.,0.333233134534162,-0.94284446121751));
#56368=DIRECTION('ref_axis',(0.,0.94284446121751,0.333233134534162));
#56369=DIRECTION('center_axis',(0.,-0.333233134534159,0.942844461217511));
#56370=DIRECTION('ref_axis',(0.,-0.942844461217511,-0.333233134534159));
#56371=DIRECTION('center_axis',(0.,0.333233134534162,-0.94284446121751));
#56372=DIRECTION('ref_axis',(0.,0.94284446121751,0.333233134534162));
#56373=DIRECTION('center_axis',(0.,-0.333233134534159,0.942844461217511));
#56374=DIRECTION('ref_axis',(0.,-0.942844461217511,-0.333233134534159));
#56375=DIRECTION('center_axis',(0.,0.333233134534162,-0.94284446121751));
#56376=DIRECTION('ref_axis',(0.,0.94284446121751,0.333233134534162));
#56377=DIRECTION('center_axis',(0.,-0.333233134534159,0.942844461217511));
#56378=DIRECTION('ref_axis',(0.,-0.942844461217511,-0.333233134534159));
#56379=DIRECTION('center_axis',(0.,0.333233134534162,-0.94284446121751));
#56380=DIRECTION('ref_axis',(0.,0.94284446121751,0.333233134534162));
#56381=DIRECTION('center_axis',(0.,-0.333233134534159,0.942844461217511));
#56382=DIRECTION('ref_axis',(0.,-0.942844461217511,-0.333233134534159));
#56383=DIRECTION('center_axis',(0.,0.333233134534162,-0.94284446121751));
#56384=DIRECTION('ref_axis',(0.,0.94284446121751,0.333233134534162));
#56385=DIRECTION('center_axis',(0.,-0.333233134534159,0.942844461217511));
#56386=DIRECTION('ref_axis',(0.,-0.942844461217511,-0.333233134534159));
#56387=DIRECTION('center_axis',(0.,0.333233134534162,-0.94284446121751));
#56388=DIRECTION('ref_axis',(0.,0.94284446121751,0.333233134534162));
#56389=DIRECTION('center_axis',(0.,-0.333233134534159,0.942844461217511));
#56390=DIRECTION('ref_axis',(0.,-0.942844461217511,-0.333233134534159));
#56391=DIRECTION('center_axis',(0.,0.333233134534162,-0.94284446121751));
#56392=DIRECTION('ref_axis',(0.,0.94284446121751,0.333233134534162));
#56393=DIRECTION('center_axis',(0.,-0.333233134534159,0.942844461217511));
#56394=DIRECTION('ref_axis',(0.,-0.942844461217511,-0.333233134534159));
#56395=DIRECTION('center_axis',(0.,0.333233134534162,-0.94284446121751));
#56396=DIRECTION('ref_axis',(0.,0.94284446121751,0.333233134534162));
#56397=DIRECTION('center_axis',(0.,-0.333233134534159,0.942844461217511));
#56398=DIRECTION('ref_axis',(0.,-0.942844461217511,-0.333233134534159));
#56399=DIRECTION('center_axis',(0.,0.333233134534162,-0.94284446121751));
#56400=DIRECTION('ref_axis',(0.,0.94284446121751,0.333233134534162));
#56401=DIRECTION('center_axis',(0.,-0.333233134534159,0.942844461217511));
#56402=DIRECTION('ref_axis',(0.,-0.942844461217511,-0.333233134534159));
#56403=DIRECTION('center_axis',(0.,0.333233134534162,-0.94284446121751));
#56404=DIRECTION('ref_axis',(0.,0.94284446121751,0.333233134534162));
#56405=DIRECTION('center_axis',(0.,-0.333233134534159,0.942844461217511));
#56406=DIRECTION('ref_axis',(0.,-0.942844461217511,-0.333233134534159));
#56407=DIRECTION('center_axis',(0.,0.333233134534162,-0.94284446121751));
#56408=DIRECTION('ref_axis',(0.,0.94284446121751,0.333233134534162));
#56409=DIRECTION('center_axis',(0.,-0.333233134534159,0.942844461217511));
#56410=DIRECTION('ref_axis',(0.,-0.942844461217511,-0.333233134534159));
#56411=DIRECTION('center_axis',(0.,0.333233134534162,-0.94284446121751));
#56412=DIRECTION('ref_axis',(0.,0.94284446121751,0.333233134534162));
#56413=DIRECTION('center_axis',(0.,-0.333233134534159,0.942844461217511));
#56414=DIRECTION('ref_axis',(0.,-0.942844461217511,-0.333233134534159));
#56415=DIRECTION('center_axis',(0.,0.333233134534162,-0.94284446121751));
#56416=DIRECTION('ref_axis',(0.,0.94284446121751,0.333233134534162));
#56417=DIRECTION('center_axis',(0.,-0.333233134534159,0.942844461217511));
#56418=DIRECTION('ref_axis',(0.,-0.942844461217511,-0.333233134534159));
#56419=DIRECTION('center_axis',(0.,0.333233134534162,-0.94284446121751));
#56420=DIRECTION('ref_axis',(0.,0.94284446121751,0.333233134534162));
#56421=DIRECTION('center_axis',(0.,-0.333233134534159,0.942844461217511));
#56422=DIRECTION('ref_axis',(0.,-0.942844461217511,-0.333233134534159));
#56423=DIRECTION('center_axis',(0.,0.333233134534162,-0.94284446121751));
#56424=DIRECTION('ref_axis',(0.,0.94284446121751,0.333233134534162));
#56425=DIRECTION('center_axis',(0.,-0.333233134534159,0.942844461217511));
#56426=DIRECTION('ref_axis',(0.,-0.942844461217511,-0.333233134534159));
#56427=DIRECTION('center_axis',(0.,0.333233134534162,-0.94284446121751));
#56428=DIRECTION('ref_axis',(0.,0.94284446121751,0.333233134534162));
#56429=DIRECTION('center_axis',(0.,-0.333233134534159,0.942844461217511));
#56430=DIRECTION('ref_axis',(0.,-0.942844461217511,-0.333233134534159));
#56431=DIRECTION('center_axis',(0.,0.333233134534162,-0.94284446121751));
#56432=DIRECTION('ref_axis',(0.,0.94284446121751,0.333233134534162));
#56433=DIRECTION('center_axis',(0.,-0.333233134534159,0.942844461217511));
#56434=DIRECTION('ref_axis',(0.,-0.942844461217511,-0.333233134534159));
#56435=DIRECTION('center_axis',(0.,0.333233134534162,-0.94284446121751));
#56436=DIRECTION('ref_axis',(0.,0.94284446121751,0.333233134534162));
#56437=DIRECTION('center_axis',(0.,-0.333233134534159,0.942844461217511));
#56438=DIRECTION('ref_axis',(0.,-0.942844461217511,-0.333233134534159));
#56439=DIRECTION('center_axis',(0.,0.333233134534162,-0.94284446121751));
#56440=DIRECTION('ref_axis',(0.,0.94284446121751,0.333233134534162));
#56441=DIRECTION('center_axis',(0.,-0.333233134534159,0.942844461217511));
#56442=DIRECTION('ref_axis',(0.,-0.942844461217511,-0.333233134534159));
#56443=DIRECTION('center_axis',(0.,0.333233134534162,-0.94284446121751));
#56444=DIRECTION('ref_axis',(0.,0.94284446121751,0.333233134534162));
#56445=DIRECTION('center_axis',(0.,-0.333233134534159,0.942844461217511));
#56446=DIRECTION('ref_axis',(0.,-0.942844461217511,-0.333233134534159));
#56447=DIRECTION('center_axis',(0.,0.333233134534162,-0.94284446121751));
#56448=DIRECTION('ref_axis',(0.,0.94284446121751,0.333233134534162));
#56449=DIRECTION('center_axis',(0.,-0.333233134534159,0.942844461217511));
#56450=DIRECTION('ref_axis',(0.,-0.942844461217511,-0.333233134534159));
#56451=DIRECTION('center_axis',(0.,0.333233134534162,-0.94284446121751));
#56452=DIRECTION('ref_axis',(0.,0.94284446121751,0.333233134534162));
#56453=DIRECTION('center_axis',(0.,-0.333233134534159,0.942844461217511));
#56454=DIRECTION('ref_axis',(0.,-0.942844461217511,-0.333233134534159));
#56455=DIRECTION('center_axis',(0.,0.333233134534162,-0.94284446121751));
#56456=DIRECTION('ref_axis',(0.,0.94284446121751,0.333233134534162));
#56457=DIRECTION('center_axis',(0.,-0.333233134534159,0.942844461217511));
#56458=DIRECTION('ref_axis',(0.,-0.942844461217511,-0.333233134534159));
#56459=DIRECTION('center_axis',(0.,0.333233134534162,-0.94284446121751));
#56460=DIRECTION('ref_axis',(0.,0.94284446121751,0.333233134534162));
#56461=DIRECTION('center_axis',(0.,-0.333233134534159,0.942844461217511));
#56462=DIRECTION('ref_axis',(0.,-0.942844461217511,-0.333233134534159));
#56463=DIRECTION('center_axis',(0.,0.333233134534162,-0.94284446121751));
#56464=DIRECTION('ref_axis',(0.,0.94284446121751,0.333233134534162));
#56465=DIRECTION('center_axis',(0.,-0.333233134534159,0.942844461217511));
#56466=DIRECTION('ref_axis',(0.,-0.942844461217511,-0.333233134534159));
#56467=DIRECTION('center_axis',(0.,0.333233134534162,-0.94284446121751));
#56468=DIRECTION('ref_axis',(0.,0.94284446121751,0.333233134534162));
#56469=DIRECTION('center_axis',(0.,-0.333233134534159,0.942844461217511));
#56470=DIRECTION('ref_axis',(0.,-0.942844461217511,-0.333233134534159));
#56471=DIRECTION('center_axis',(0.,0.333233134534162,-0.94284446121751));
#56472=DIRECTION('ref_axis',(0.,0.94284446121751,0.333233134534162));
#56473=DIRECTION('center_axis',(0.,-0.333233134534159,0.942844461217511));
#56474=DIRECTION('ref_axis',(0.,-0.942844461217511,-0.333233134534159));
#56475=DIRECTION('center_axis',(0.,0.333233134534162,-0.94284446121751));
#56476=DIRECTION('ref_axis',(0.,0.94284446121751,0.333233134534162));
#56477=DIRECTION('center_axis',(0.,-0.333233134534159,0.942844461217511));
#56478=DIRECTION('ref_axis',(0.,-0.942844461217511,-0.333233134534159));
#56479=DIRECTION('center_axis',(0.,0.333233134534162,-0.94284446121751));
#56480=DIRECTION('ref_axis',(0.,0.94284446121751,0.333233134534162));
#56481=DIRECTION('center_axis',(0.,-0.333233134534159,0.942844461217511));
#56482=DIRECTION('ref_axis',(0.,-0.942844461217511,-0.333233134534159));
#56483=DIRECTION('center_axis',(0.,0.333233134534162,-0.94284446121751));
#56484=DIRECTION('ref_axis',(0.,0.94284446121751,0.333233134534162));
#56485=DIRECTION('center_axis',(0.,-0.333233134534159,0.942844461217511));
#56486=DIRECTION('ref_axis',(0.,-0.942844461217511,-0.333233134534159));
#56487=DIRECTION('center_axis',(0.,0.333233134534162,-0.94284446121751));
#56488=DIRECTION('ref_axis',(0.,0.94284446121751,0.333233134534162));
#56489=DIRECTION('center_axis',(0.,-0.333233134534159,0.942844461217511));
#56490=DIRECTION('ref_axis',(0.,-0.942844461217511,-0.333233134534159));
#56491=DIRECTION('center_axis',(0.,0.333233134534162,-0.94284446121751));
#56492=DIRECTION('ref_axis',(0.,0.94284446121751,0.333233134534162));
#56493=DIRECTION('center_axis',(0.,-0.333233134534159,0.942844461217511));
#56494=DIRECTION('ref_axis',(0.,-0.942844461217511,-0.333233134534159));
#56495=DIRECTION('center_axis',(0.,0.333233134534162,-0.94284446121751));
#56496=DIRECTION('ref_axis',(0.,0.94284446121751,0.333233134534162));
#56497=DIRECTION('center_axis',(0.,-0.333233134534159,0.942844461217511));
#56498=DIRECTION('ref_axis',(0.,-0.942844461217511,-0.333233134534159));
#56499=DIRECTION('center_axis',(0.,0.333233134534162,-0.94284446121751));
#56500=DIRECTION('ref_axis',(0.,0.94284446121751,0.333233134534162));
#56501=DIRECTION('center_axis',(0.,-0.333233134534159,0.942844461217511));
#56502=DIRECTION('ref_axis',(0.,-0.942844461217511,-0.333233134534159));
#56503=DIRECTION('center_axis',(0.,0.333233134534162,-0.94284446121751));
#56504=DIRECTION('ref_axis',(0.,0.94284446121751,0.333233134534162));
#56505=DIRECTION('center_axis',(0.,-0.333233134534159,0.942844461217511));
#56506=DIRECTION('ref_axis',(0.,-0.942844461217511,-0.333233134534159));
#56507=DIRECTION('center_axis',(0.,0.333233134534162,-0.94284446121751));
#56508=DIRECTION('ref_axis',(0.,0.94284446121751,0.333233134534162));
#56509=DIRECTION('center_axis',(0.,-0.333233134534159,0.942844461217511));
#56510=DIRECTION('ref_axis',(0.,-0.942844461217511,-0.333233134534159));
#56511=DIRECTION('center_axis',(0.,0.333233134534162,-0.94284446121751));
#56512=DIRECTION('ref_axis',(0.,0.94284446121751,0.333233134534162));
#56513=DIRECTION('center_axis',(0.,-0.333233134534159,0.942844461217511));
#56514=DIRECTION('ref_axis',(0.,-0.942844461217511,-0.333233134534159));
#56515=DIRECTION('center_axis',(0.,0.333233134534162,-0.94284446121751));
#56516=DIRECTION('ref_axis',(0.,0.94284446121751,0.333233134534162));
#56517=DIRECTION('center_axis',(0.,-0.333233134534159,0.942844461217511));
#56518=DIRECTION('ref_axis',(0.,-0.942844461217511,-0.333233134534159));
#56519=DIRECTION('center_axis',(0.,0.333233134534162,-0.94284446121751));
#56520=DIRECTION('ref_axis',(0.,0.94284446121751,0.333233134534162));
#56521=DIRECTION('center_axis',(0.,-0.333233134534159,0.942844461217511));
#56522=DIRECTION('ref_axis',(0.,-0.942844461217511,-0.333233134534159));
#56523=DIRECTION('center_axis',(0.,0.333233134534162,-0.94284446121751));
#56524=DIRECTION('ref_axis',(0.,0.94284446121751,0.333233134534162));
#56525=DIRECTION('center_axis',(0.,-0.333233134534159,0.942844461217511));
#56526=DIRECTION('ref_axis',(0.,-0.942844461217511,-0.333233134534159));
#56527=DIRECTION('center_axis',(0.,0.333233134534162,-0.94284446121751));
#56528=DIRECTION('ref_axis',(0.,0.94284446121751,0.333233134534162));
#56529=DIRECTION('center_axis',(0.,-0.333233134534159,0.942844461217511));
#56530=DIRECTION('ref_axis',(0.,-0.942844461217511,-0.333233134534159));
#56531=DIRECTION('center_axis',(0.,0.333233134534162,-0.94284446121751));
#56532=DIRECTION('ref_axis',(0.,0.94284446121751,0.333233134534162));
#56533=DIRECTION('center_axis',(0.,-0.333233134534159,0.942844461217511));
#56534=DIRECTION('ref_axis',(0.,-0.942844461217511,-0.333233134534159));
#56535=DIRECTION('center_axis',(0.,0.333233134534162,-0.94284446121751));
#56536=DIRECTION('ref_axis',(0.,0.94284446121751,0.333233134534162));
#56537=DIRECTION('center_axis',(0.,-0.333233134534159,0.942844461217511));
#56538=DIRECTION('ref_axis',(0.,-0.942844461217511,-0.333233134534159));
#56539=DIRECTION('center_axis',(0.,0.333233134534162,-0.94284446121751));
#56540=DIRECTION('ref_axis',(0.,0.94284446121751,0.333233134534162));
#56541=DIRECTION('center_axis',(0.,-0.333233134534159,0.942844461217511));
#56542=DIRECTION('ref_axis',(0.,-0.942844461217511,-0.333233134534159));
#56543=DIRECTION('center_axis',(0.,0.333233134534162,-0.94284446121751));
#56544=DIRECTION('ref_axis',(0.,0.94284446121751,0.333233134534162));
#56545=DIRECTION('center_axis',(0.,-0.333233134534159,0.942844461217511));
#56546=DIRECTION('ref_axis',(0.,-0.942844461217511,-0.333233134534159));
#56547=DIRECTION('center_axis',(0.,0.333233134534162,-0.94284446121751));
#56548=DIRECTION('ref_axis',(0.,0.94284446121751,0.333233134534162));
#56549=DIRECTION('center_axis',(0.,-0.333233134534159,0.942844461217511));
#56550=DIRECTION('ref_axis',(0.,-0.942844461217511,-0.333233134534159));
#56551=DIRECTION('center_axis',(0.,0.333233134534162,-0.94284446121751));
#56552=DIRECTION('ref_axis',(0.,0.94284446121751,0.333233134534162));
#56553=DIRECTION('center_axis',(0.,-0.333233134534159,0.942844461217511));
#56554=DIRECTION('ref_axis',(0.,-0.942844461217511,-0.333233134534159));
#56555=DIRECTION('center_axis',(0.,0.333233134534162,-0.94284446121751));
#56556=DIRECTION('ref_axis',(0.,0.94284446121751,0.333233134534162));
#56557=DIRECTION('center_axis',(0.,-0.333233134534159,0.942844461217511));
#56558=DIRECTION('ref_axis',(0.,-0.942844461217511,-0.333233134534159));
#56559=DIRECTION('center_axis',(0.,0.333233134534162,-0.94284446121751));
#56560=DIRECTION('ref_axis',(0.,0.94284446121751,0.333233134534162));
#56561=DIRECTION('center_axis',(0.,-0.333233134534159,0.942844461217511));
#56562=DIRECTION('ref_axis',(0.,-0.942844461217511,-0.333233134534159));
#56563=DIRECTION('center_axis',(0.,0.333233134534162,-0.94284446121751));
#56564=DIRECTION('ref_axis',(0.,0.94284446121751,0.333233134534162));
#56565=DIRECTION('center_axis',(0.,-0.333233134534159,0.942844461217511));
#56566=DIRECTION('ref_axis',(0.,-0.942844461217511,-0.333233134534159));
#56567=DIRECTION('center_axis',(0.,0.333233134534162,-0.94284446121751));
#56568=DIRECTION('ref_axis',(0.,0.94284446121751,0.333233134534162));
#56569=DIRECTION('center_axis',(0.,-0.333233134534159,0.942844461217511));
#56570=DIRECTION('ref_axis',(0.,-0.942844461217511,-0.333233134534159));
#56571=DIRECTION('center_axis',(0.,0.333233134534162,-0.94284446121751));
#56572=DIRECTION('ref_axis',(0.,0.94284446121751,0.333233134534162));
#56573=DIRECTION('center_axis',(0.,-0.333233134534159,0.942844461217511));
#56574=DIRECTION('ref_axis',(0.,-0.942844461217511,-0.333233134534159));
#56575=DIRECTION('center_axis',(0.,0.333233134534162,-0.94284446121751));
#56576=DIRECTION('ref_axis',(0.,0.94284446121751,0.333233134534162));
#56577=DIRECTION('center_axis',(0.,-0.333233134534159,0.942844461217511));
#56578=DIRECTION('ref_axis',(0.,-0.942844461217511,-0.333233134534159));
#56579=DIRECTION('center_axis',(0.,0.333233134534162,-0.94284446121751));
#56580=DIRECTION('ref_axis',(0.,0.94284446121751,0.333233134534162));
#56581=DIRECTION('center_axis',(0.,-0.333233134534159,0.942844461217511));
#56582=DIRECTION('ref_axis',(0.,-0.942844461217511,-0.333233134534159));
#56583=DIRECTION('center_axis',(0.,0.333233134534162,-0.94284446121751));
#56584=DIRECTION('ref_axis',(0.,0.94284446121751,0.333233134534162));
#56585=DIRECTION('center_axis',(0.,-0.333233134534159,0.942844461217511));
#56586=DIRECTION('ref_axis',(0.,-0.942844461217511,-0.333233134534159));
#56587=DIRECTION('center_axis',(0.,0.333233134534162,-0.94284446121751));
#56588=DIRECTION('ref_axis',(0.,0.94284446121751,0.333233134534162));
#56589=DIRECTION('center_axis',(0.,-0.333233134534159,0.942844461217511));
#56590=DIRECTION('ref_axis',(0.,-0.942844461217511,-0.333233134534159));
#56591=DIRECTION('center_axis',(0.,0.333233134534162,-0.94284446121751));
#56592=DIRECTION('ref_axis',(0.,0.94284446121751,0.333233134534162));
#56593=DIRECTION('center_axis',(0.,-0.333233134534159,0.942844461217511));
#56594=DIRECTION('ref_axis',(0.,-0.942844461217511,-0.333233134534159));
#56595=DIRECTION('center_axis',(0.,0.333233134534162,-0.94284446121751));
#56596=DIRECTION('ref_axis',(0.,0.94284446121751,0.333233134534162));
#56597=DIRECTION('center_axis',(0.,-0.333233134534159,0.942844461217511));
#56598=DIRECTION('ref_axis',(0.,-0.942844461217511,-0.333233134534159));
#56599=DIRECTION('center_axis',(0.,0.333233134534162,-0.94284446121751));
#56600=DIRECTION('ref_axis',(0.,0.94284446121751,0.333233134534162));
#56601=DIRECTION('center_axis',(0.,-0.333233134534159,0.942844461217511));
#56602=DIRECTION('ref_axis',(0.,-0.942844461217511,-0.333233134534159));
#56603=DIRECTION('center_axis',(0.,0.333233134534162,-0.94284446121751));
#56604=DIRECTION('ref_axis',(0.,0.94284446121751,0.333233134534162));
#56605=DIRECTION('center_axis',(0.,-0.333233134534159,0.942844461217511));
#56606=DIRECTION('ref_axis',(0.,-0.942844461217511,-0.333233134534159));
#56607=DIRECTION('center_axis',(0.,0.333233134534162,-0.94284446121751));
#56608=DIRECTION('ref_axis',(0.,0.94284446121751,0.333233134534162));
#56609=DIRECTION('center_axis',(0.,-0.333233134534159,0.942844461217511));
#56610=DIRECTION('ref_axis',(0.,-0.942844461217511,-0.333233134534159));
#56611=DIRECTION('center_axis',(0.,0.333233134534162,-0.94284446121751));
#56612=DIRECTION('ref_axis',(0.,0.94284446121751,0.333233134534162));
#56613=DIRECTION('center_axis',(0.,-0.333233134534159,0.942844461217511));
#56614=DIRECTION('ref_axis',(0.,-0.942844461217511,-0.333233134534159));
#56615=DIRECTION('center_axis',(0.,0.333233134534162,-0.94284446121751));
#56616=DIRECTION('ref_axis',(0.,0.94284446121751,0.333233134534162));
#56617=DIRECTION('center_axis',(0.,-0.333233134534159,0.942844461217511));
#56618=DIRECTION('ref_axis',(0.,-0.942844461217511,-0.333233134534159));
#56619=DIRECTION('center_axis',(0.,0.333233134534162,-0.94284446121751));
#56620=DIRECTION('ref_axis',(0.,0.94284446121751,0.333233134534162));
#56621=DIRECTION('center_axis',(0.,-0.333233134534159,0.942844461217511));
#56622=DIRECTION('ref_axis',(0.,-0.942844461217511,-0.333233134534159));
#56623=DIRECTION('center_axis',(0.,0.333233134534162,-0.94284446121751));
#56624=DIRECTION('ref_axis',(0.,0.94284446121751,0.333233134534162));
#56625=DIRECTION('center_axis',(0.,-0.333233134534159,0.942844461217511));
#56626=DIRECTION('ref_axis',(0.,-0.942844461217511,-0.333233134534159));
#56627=DIRECTION('center_axis',(0.,0.333233134534162,-0.94284446121751));
#56628=DIRECTION('ref_axis',(0.,0.94284446121751,0.333233134534162));
#56629=DIRECTION('center_axis',(0.,-0.333233134534159,0.942844461217511));
#56630=DIRECTION('ref_axis',(0.,-0.942844461217511,-0.333233134534159));
#56631=DIRECTION('center_axis',(0.,0.333233134534162,-0.94284446121751));
#56632=DIRECTION('ref_axis',(0.,0.94284446121751,0.333233134534162));
#56633=DIRECTION('center_axis',(0.,-0.333233134534159,0.942844461217511));
#56634=DIRECTION('ref_axis',(0.,-0.942844461217511,-0.333233134534159));
#56635=DIRECTION('center_axis',(0.,0.333233134534162,-0.94284446121751));
#56636=DIRECTION('ref_axis',(0.,0.94284446121751,0.333233134534162));
#56637=DIRECTION('center_axis',(0.,-0.333233134534159,0.942844461217511));
#56638=DIRECTION('ref_axis',(0.,-0.942844461217511,-0.333233134534159));
#56639=DIRECTION('center_axis',(0.,0.333233134534162,-0.94284446121751));
#56640=DIRECTION('ref_axis',(0.,0.94284446121751,0.333233134534162));
#56641=DIRECTION('center_axis',(0.,-0.333233134534159,0.942844461217511));
#56642=DIRECTION('ref_axis',(0.,-0.942844461217511,-0.333233134534159));
#56643=DIRECTION('center_axis',(0.,0.333233134534162,-0.94284446121751));
#56644=DIRECTION('ref_axis',(0.,0.94284446121751,0.333233134534162));
#56645=DIRECTION('center_axis',(0.,-0.333233134534159,0.942844461217511));
#56646=DIRECTION('ref_axis',(0.,-0.942844461217511,-0.333233134534159));
#56647=DIRECTION('center_axis',(0.,0.333233134534162,-0.94284446121751));
#56648=DIRECTION('ref_axis',(0.,0.94284446121751,0.333233134534162));
#56649=DIRECTION('center_axis',(0.,-0.333233134534159,0.942844461217511));
#56650=DIRECTION('ref_axis',(0.,-0.942844461217511,-0.333233134534159));
#56651=DIRECTION('center_axis',(0.,0.333233134534162,-0.94284446121751));
#56652=DIRECTION('ref_axis',(0.,0.94284446121751,0.333233134534162));
#56653=DIRECTION('center_axis',(0.,-0.333233134534159,0.942844461217511));
#56654=DIRECTION('ref_axis',(0.,-0.942844461217511,-0.333233134534159));
#56655=DIRECTION('center_axis',(0.,0.333233134534162,-0.94284446121751));
#56656=DIRECTION('ref_axis',(0.,0.94284446121751,0.333233134534162));
#56657=DIRECTION('center_axis',(0.,-0.333233134534159,0.942844461217511));
#56658=DIRECTION('ref_axis',(0.,-0.942844461217511,-0.333233134534159));
#56659=DIRECTION('center_axis',(0.,0.333233134534162,-0.94284446121751));
#56660=DIRECTION('ref_axis',(0.,0.94284446121751,0.333233134534162));
#56661=DIRECTION('center_axis',(0.,-0.333233134534159,0.942844461217511));
#56662=DIRECTION('ref_axis',(0.,-0.942844461217511,-0.333233134534159));
#56663=DIRECTION('center_axis',(0.,0.333233134534162,-0.94284446121751));
#56664=DIRECTION('ref_axis',(0.,0.94284446121751,0.333233134534162));
#56665=DIRECTION('center_axis',(0.,-0.333233134534159,0.942844461217511));
#56666=DIRECTION('ref_axis',(0.,-0.942844461217511,-0.333233134534159));
#56667=DIRECTION('center_axis',(0.,0.333233134534162,-0.94284446121751));
#56668=DIRECTION('ref_axis',(0.,0.94284446121751,0.333233134534162));
#56669=DIRECTION('center_axis',(0.,-0.333233134534159,0.942844461217511));
#56670=DIRECTION('ref_axis',(0.,-0.942844461217511,-0.333233134534159));
#56671=DIRECTION('center_axis',(0.,0.333233134534162,-0.94284446121751));
#56672=DIRECTION('ref_axis',(0.,0.94284446121751,0.333233134534162));
#56673=DIRECTION('center_axis',(0.,-0.333233134534159,0.942844461217511));
#56674=DIRECTION('ref_axis',(0.,-0.942844461217511,-0.333233134534159));
#56675=DIRECTION('center_axis',(0.,0.333233134534162,-0.94284446121751));
#56676=DIRECTION('ref_axis',(0.,0.94284446121751,0.333233134534162));
#56677=DIRECTION('center_axis',(0.,-0.333233134534159,0.942844461217511));
#56678=DIRECTION('ref_axis',(0.,-0.942844461217511,-0.333233134534159));
#56679=DIRECTION('center_axis',(0.,0.333233134534162,-0.94284446121751));
#56680=DIRECTION('ref_axis',(0.,0.94284446121751,0.333233134534162));
#56681=DIRECTION('center_axis',(0.,-0.333233134534159,0.942844461217511));
#56682=DIRECTION('ref_axis',(0.,-0.942844461217511,-0.333233134534159));
#56683=DIRECTION('center_axis',(0.,0.333233134534162,-0.94284446121751));
#56684=DIRECTION('ref_axis',(0.,0.94284446121751,0.333233134534162));
#56685=DIRECTION('center_axis',(0.,-0.333233134534159,0.942844461217511));
#56686=DIRECTION('ref_axis',(0.,-0.942844461217511,-0.333233134534159));
#56687=DIRECTION('center_axis',(0.,0.333233134534162,-0.94284446121751));
#56688=DIRECTION('ref_axis',(0.,0.94284446121751,0.333233134534162));
#56689=DIRECTION('center_axis',(0.,-0.333233134534159,0.942844461217511));
#56690=DIRECTION('ref_axis',(0.,-0.942844461217511,-0.333233134534159));
#56691=DIRECTION('center_axis',(0.,0.333233134534162,-0.94284446121751));
#56692=DIRECTION('ref_axis',(0.,0.94284446121751,0.333233134534162));
#56693=DIRECTION('center_axis',(0.,-0.333233134534159,0.942844461217511));
#56694=DIRECTION('ref_axis',(0.,-0.942844461217511,-0.333233134534159));
#56695=DIRECTION('center_axis',(0.,0.333233134534162,-0.94284446121751));
#56696=DIRECTION('ref_axis',(0.,0.94284446121751,0.333233134534162));
#56697=DIRECTION('center_axis',(0.,-0.333233134534159,0.942844461217511));
#56698=DIRECTION('ref_axis',(0.,-0.942844461217511,-0.333233134534159));
#56699=DIRECTION('center_axis',(0.,0.333233134534162,-0.94284446121751));
#56700=DIRECTION('ref_axis',(0.,0.94284446121751,0.333233134534162));
#56701=DIRECTION('center_axis',(0.,-0.333233134534159,0.942844461217511));
#56702=DIRECTION('ref_axis',(0.,-0.942844461217511,-0.333233134534159));
#56703=DIRECTION('center_axis',(0.,0.333233134534162,-0.94284446121751));
#56704=DIRECTION('ref_axis',(0.,0.94284446121751,0.333233134534162));
#56705=DIRECTION('center_axis',(0.,-0.333233134534159,0.942844461217511));
#56706=DIRECTION('ref_axis',(0.,-0.942844461217511,-0.333233134534159));
#56707=DIRECTION('center_axis',(0.,0.333233134534162,-0.94284446121751));
#56708=DIRECTION('ref_axis',(0.,0.94284446121751,0.333233134534162));
#56709=DIRECTION('center_axis',(0.,-0.333233134534159,0.942844461217511));
#56710=DIRECTION('ref_axis',(0.,-0.942844461217511,-0.333233134534159));
#56711=DIRECTION('center_axis',(0.,0.333233134534162,-0.94284446121751));
#56712=DIRECTION('ref_axis',(0.,0.94284446121751,0.333233134534162));
#56713=DIRECTION('center_axis',(0.,-0.333233134534159,0.942844461217511));
#56714=DIRECTION('ref_axis',(0.,-0.942844461217511,-0.333233134534159));
#56715=DIRECTION('center_axis',(0.,0.333233134534162,-0.94284446121751));
#56716=DIRECTION('ref_axis',(0.,0.94284446121751,0.333233134534162));
#56717=DIRECTION('center_axis',(0.,-0.333233134534159,0.942844461217511));
#56718=DIRECTION('ref_axis',(0.,-0.942844461217511,-0.333233134534159));
#56719=DIRECTION('center_axis',(0.,0.333233134534162,-0.94284446121751));
#56720=DIRECTION('ref_axis',(0.,0.94284446121751,0.333233134534162));
#56721=DIRECTION('center_axis',(0.,-0.333233134534159,0.942844461217511));
#56722=DIRECTION('ref_axis',(0.,-0.942844461217511,-0.333233134534159));
#56723=DIRECTION('center_axis',(0.,0.333233134534162,-0.94284446121751));
#56724=DIRECTION('ref_axis',(0.,0.94284446121751,0.333233134534162));
#56725=DIRECTION('center_axis',(0.,-0.333233134534159,0.942844461217511));
#56726=DIRECTION('ref_axis',(0.,-0.942844461217511,-0.333233134534159));
#56727=DIRECTION('center_axis',(0.,0.333233134534162,-0.94284446121751));
#56728=DIRECTION('ref_axis',(0.,0.94284446121751,0.333233134534162));
#56729=DIRECTION('center_axis',(0.,-0.333233134534159,0.942844461217511));
#56730=DIRECTION('ref_axis',(0.,-0.942844461217511,-0.333233134534159));
#56731=DIRECTION('center_axis',(0.,0.333233134534162,-0.94284446121751));
#56732=DIRECTION('ref_axis',(0.,0.94284446121751,0.333233134534162));
#56733=DIRECTION('center_axis',(0.,-0.333233134534159,0.942844461217511));
#56734=DIRECTION('ref_axis',(0.,-0.942844461217511,-0.333233134534159));
#56735=DIRECTION('center_axis',(0.,0.333233134534162,-0.94284446121751));
#56736=DIRECTION('ref_axis',(0.,0.94284446121751,0.333233134534162));
#56737=DIRECTION('center_axis',(0.,-0.333233134534159,0.942844461217511));
#56738=DIRECTION('ref_axis',(0.,-0.942844461217511,-0.333233134534159));
#56739=DIRECTION('center_axis',(0.,0.333233134534162,-0.94284446121751));
#56740=DIRECTION('ref_axis',(0.,0.94284446121751,0.333233134534162));
#56741=DIRECTION('center_axis',(0.,-0.333233134534159,0.942844461217511));
#56742=DIRECTION('ref_axis',(0.,-0.942844461217511,-0.333233134534159));
#56743=DIRECTION('center_axis',(0.,0.333233134534162,-0.94284446121751));
#56744=DIRECTION('ref_axis',(0.,0.94284446121751,0.333233134534162));
#56745=DIRECTION('center_axis',(0.,-0.333233134534159,0.942844461217511));
#56746=DIRECTION('ref_axis',(0.,-0.942844461217511,-0.333233134534159));
#56747=DIRECTION('center_axis',(0.,0.333233134534162,-0.94284446121751));
#56748=DIRECTION('ref_axis',(0.,0.94284446121751,0.333233134534162));
#56749=DIRECTION('center_axis',(0.,-0.333233134534159,0.942844461217511));
#56750=DIRECTION('ref_axis',(0.,-0.942844461217511,-0.333233134534159));
#56751=DIRECTION('center_axis',(0.,0.333233134534162,-0.94284446121751));
#56752=DIRECTION('ref_axis',(0.,0.94284446121751,0.333233134534162));
#56753=DIRECTION('center_axis',(0.,-0.333233134534159,0.942844461217511));
#56754=DIRECTION('ref_axis',(0.,-0.942844461217511,-0.333233134534159));
#56755=DIRECTION('center_axis',(0.,0.333233134534162,-0.94284446121751));
#56756=DIRECTION('ref_axis',(0.,0.94284446121751,0.333233134534162));
#56757=DIRECTION('center_axis',(0.,-0.333233134534159,0.942844461217511));
#56758=DIRECTION('ref_axis',(0.,-0.942844461217511,-0.333233134534159));
#56759=DIRECTION('center_axis',(0.,0.333233134534162,-0.94284446121751));
#56760=DIRECTION('ref_axis',(0.,0.94284446121751,0.333233134534162));
#56761=DIRECTION('center_axis',(0.,-0.333233134534159,0.942844461217511));
#56762=DIRECTION('ref_axis',(0.,-0.942844461217511,-0.333233134534159));
#56763=DIRECTION('center_axis',(0.,0.333233134534162,-0.94284446121751));
#56764=DIRECTION('ref_axis',(0.,0.94284446121751,0.333233134534162));
#56765=DIRECTION('center_axis',(0.,-0.333233134534159,0.942844461217511));
#56766=DIRECTION('ref_axis',(0.,-0.942844461217511,-0.333233134534159));
#56767=DIRECTION('center_axis',(0.,0.333233134534162,-0.94284446121751));
#56768=DIRECTION('ref_axis',(0.,0.94284446121751,0.333233134534162));
#56769=DIRECTION('center_axis',(0.,-0.333233134534159,0.942844461217511));
#56770=DIRECTION('ref_axis',(0.,-0.942844461217511,-0.333233134534159));
#56771=DIRECTION('center_axis',(0.,0.333233134534162,-0.94284446121751));
#56772=DIRECTION('ref_axis',(0.,0.94284446121751,0.333233134534162));
#56773=DIRECTION('center_axis',(0.,-0.333233134534159,0.942844461217511));
#56774=DIRECTION('ref_axis',(0.,-0.942844461217511,-0.333233134534159));
#56775=DIRECTION('center_axis',(0.,0.333233134534162,-0.94284446121751));
#56776=DIRECTION('ref_axis',(0.,0.94284446121751,0.333233134534162));
#56777=DIRECTION('center_axis',(0.,-0.333233134534159,0.942844461217511));
#56778=DIRECTION('ref_axis',(0.,-0.942844461217511,-0.333233134534159));
#56779=DIRECTION('center_axis',(0.,0.333233134534162,-0.94284446121751));
#56780=DIRECTION('ref_axis',(0.,0.94284446121751,0.333233134534162));
#56781=DIRECTION('center_axis',(0.,-0.333233134534159,0.942844461217511));
#56782=DIRECTION('ref_axis',(0.,-0.942844461217511,-0.333233134534159));
#56783=DIRECTION('center_axis',(0.,0.333233134534162,-0.94284446121751));
#56784=DIRECTION('ref_axis',(0.,0.94284446121751,0.333233134534162));
#56785=DIRECTION('center_axis',(0.,-0.333233134534159,0.942844461217511));
#56786=DIRECTION('ref_axis',(0.,-0.942844461217511,-0.333233134534159));
#56787=DIRECTION('center_axis',(0.,0.333233134534162,-0.94284446121751));
#56788=DIRECTION('ref_axis',(0.,0.94284446121751,0.333233134534162));
#56789=DIRECTION('center_axis',(0.,-0.333233134534159,0.942844461217511));
#56790=DIRECTION('ref_axis',(0.,-0.942844461217511,-0.333233134534159));
#56791=DIRECTION('center_axis',(0.,0.333233134534162,-0.94284446121751));
#56792=DIRECTION('ref_axis',(0.,0.94284446121751,0.333233134534162));
#56793=DIRECTION('center_axis',(0.,-0.333233134534159,0.942844461217511));
#56794=DIRECTION('ref_axis',(0.,-0.942844461217511,-0.333233134534159));
#56795=DIRECTION('center_axis',(0.,0.333233134534162,-0.94284446121751));
#56796=DIRECTION('ref_axis',(0.,0.94284446121751,0.333233134534162));
#56797=DIRECTION('center_axis',(0.,-0.333233134534159,0.942844461217511));
#56798=DIRECTION('ref_axis',(0.,-0.942844461217511,-0.333233134534159));
#56799=DIRECTION('center_axis',(0.,0.333233134534162,-0.94284446121751));
#56800=DIRECTION('ref_axis',(0.,0.94284446121751,0.333233134534162));
#56801=DIRECTION('center_axis',(0.,-0.333233134534159,0.942844461217511));
#56802=DIRECTION('ref_axis',(0.,-0.942844461217511,-0.333233134534159));
#56803=DIRECTION('center_axis',(0.,0.333233134534162,-0.94284446121751));
#56804=DIRECTION('ref_axis',(0.,0.94284446121751,0.333233134534162));
#56805=DIRECTION('center_axis',(0.,-0.333233134534159,0.942844461217511));
#56806=DIRECTION('ref_axis',(0.,-0.942844461217511,-0.333233134534159));
#56807=DIRECTION('center_axis',(0.,0.333233134534162,-0.94284446121751));
#56808=DIRECTION('ref_axis',(0.,0.94284446121751,0.333233134534162));
#56809=DIRECTION('center_axis',(0.,-0.333233134534159,0.942844461217511));
#56810=DIRECTION('ref_axis',(0.,-0.942844461217511,-0.333233134534159));
#56811=DIRECTION('center_axis',(0.,0.333233134534162,-0.94284446121751));
#56812=DIRECTION('ref_axis',(0.,0.94284446121751,0.333233134534162));
#56813=DIRECTION('center_axis',(0.,-0.333233134534159,0.942844461217511));
#56814=DIRECTION('ref_axis',(0.,-0.942844461217511,-0.333233134534159));
#56815=DIRECTION('center_axis',(0.,0.333233134534162,-0.94284446121751));
#56816=DIRECTION('ref_axis',(0.,0.94284446121751,0.333233134534162));
#56817=DIRECTION('center_axis',(0.,-0.333233134534159,0.942844461217511));
#56818=DIRECTION('ref_axis',(0.,-0.942844461217511,-0.333233134534159));
#56819=DIRECTION('center_axis',(0.,0.333233134534162,-0.94284446121751));
#56820=DIRECTION('ref_axis',(0.,0.94284446121751,0.333233134534162));
#56821=DIRECTION('center_axis',(0.,-0.333233134534159,0.942844461217511));
#56822=DIRECTION('ref_axis',(0.,-0.942844461217511,-0.333233134534159));
#56823=DIRECTION('center_axis',(0.,0.333233134534162,-0.94284446121751));
#56824=DIRECTION('ref_axis',(0.,0.94284446121751,0.333233134534162));
#56825=DIRECTION('center_axis',(0.,-0.333233134534159,0.942844461217511));
#56826=DIRECTION('ref_axis',(0.,-0.942844461217511,-0.333233134534159));
#56827=DIRECTION('center_axis',(0.,0.333233134534162,-0.94284446121751));
#56828=DIRECTION('ref_axis',(0.,0.94284446121751,0.333233134534162));
#56829=DIRECTION('center_axis',(0.,-0.333233134534159,0.942844461217511));
#56830=DIRECTION('ref_axis',(0.,-0.942844461217511,-0.333233134534159));
#56831=DIRECTION('center_axis',(0.,0.333233134534162,-0.94284446121751));
#56832=DIRECTION('ref_axis',(0.,0.94284446121751,0.333233134534162));
#56833=DIRECTION('center_axis',(0.,-0.333233134534159,0.942844461217511));
#56834=DIRECTION('ref_axis',(0.,-0.942844461217511,-0.333233134534159));
#56835=DIRECTION('center_axis',(0.,0.333233134534162,-0.94284446121751));
#56836=DIRECTION('ref_axis',(0.,0.94284446121751,0.333233134534162));
#56837=DIRECTION('center_axis',(0.,-0.333233134534159,0.942844461217511));
#56838=DIRECTION('ref_axis',(0.,-0.942844461217511,-0.333233134534159));
#56839=DIRECTION('center_axis',(0.,0.333233134534162,-0.94284446121751));
#56840=DIRECTION('ref_axis',(0.,0.94284446121751,0.333233134534162));
#56841=DIRECTION('center_axis',(0.,-0.333233134534159,0.942844461217511));
#56842=DIRECTION('ref_axis',(0.,-0.942844461217511,-0.333233134534159));
#56843=DIRECTION('center_axis',(0.,0.333233134534162,-0.94284446121751));
#56844=DIRECTION('ref_axis',(0.,0.94284446121751,0.333233134534162));
#56845=DIRECTION('center_axis',(0.,-0.333233134534159,0.942844461217511));
#56846=DIRECTION('ref_axis',(0.,-0.942844461217511,-0.333233134534159));
#56847=DIRECTION('center_axis',(0.,0.333233134534162,-0.94284446121751));
#56848=DIRECTION('ref_axis',(0.,0.94284446121751,0.333233134534162));
#56849=DIRECTION('center_axis',(0.,-0.333233134534159,0.942844461217511));
#56850=DIRECTION('ref_axis',(0.,-0.942844461217511,-0.333233134534159));
#56851=DIRECTION('center_axis',(0.,0.333233134534162,-0.94284446121751));
#56852=DIRECTION('ref_axis',(0.,0.94284446121751,0.333233134534162));
#56853=DIRECTION('center_axis',(0.,-0.333233134534159,0.942844461217511));
#56854=DIRECTION('ref_axis',(0.,-0.942844461217511,-0.333233134534159));
#56855=DIRECTION('center_axis',(0.,0.333233134534162,-0.94284446121751));
#56856=DIRECTION('ref_axis',(0.,0.94284446121751,0.333233134534162));
#56857=DIRECTION('center_axis',(0.,-0.333233134534159,0.942844461217511));
#56858=DIRECTION('ref_axis',(0.,-0.942844461217511,-0.333233134534159));
#56859=DIRECTION('center_axis',(0.,0.333233134534162,-0.94284446121751));
#56860=DIRECTION('ref_axis',(0.,0.94284446121751,0.333233134534162));
#56861=DIRECTION('center_axis',(0.,-0.333233134534159,0.942844461217511));
#56862=DIRECTION('ref_axis',(0.,-0.942844461217511,-0.333233134534159));
#56863=DIRECTION('center_axis',(0.,0.333233134534162,-0.94284446121751));
#56864=DIRECTION('ref_axis',(0.,0.94284446121751,0.333233134534162));
#56865=DIRECTION('center_axis',(0.,-0.333233134534159,0.942844461217511));
#56866=DIRECTION('ref_axis',(0.,-0.942844461217511,-0.333233134534159));
#56867=DIRECTION('center_axis',(0.,0.333233134534162,-0.94284446121751));
#56868=DIRECTION('ref_axis',(0.,0.94284446121751,0.333233134534162));
#56869=DIRECTION('center_axis',(0.,-0.333233134534159,0.942844461217511));
#56870=DIRECTION('ref_axis',(0.,-0.942844461217511,-0.333233134534159));
#56871=DIRECTION('center_axis',(0.,0.333233134534162,-0.94284446121751));
#56872=DIRECTION('ref_axis',(0.,0.94284446121751,0.333233134534162));
#56873=DIRECTION('center_axis',(0.,-0.333233134534159,0.942844461217511));
#56874=DIRECTION('ref_axis',(0.,-0.942844461217511,-0.333233134534159));
#56875=DIRECTION('center_axis',(0.,0.333233134534162,-0.94284446121751));
#56876=DIRECTION('ref_axis',(0.,0.94284446121751,0.333233134534162));
#56877=DIRECTION('center_axis',(0.,-0.333233134534159,0.942844461217511));
#56878=DIRECTION('ref_axis',(0.,-0.942844461217511,-0.333233134534159));
#56879=DIRECTION('center_axis',(0.,0.333233134534162,-0.94284446121751));
#56880=DIRECTION('ref_axis',(0.,0.94284446121751,0.333233134534162));
#56881=DIRECTION('center_axis',(0.,-0.333233134534159,0.942844461217511));
#56882=DIRECTION('ref_axis',(0.,-0.942844461217511,-0.333233134534159));
#56883=DIRECTION('center_axis',(0.,0.333233134534162,-0.94284446121751));
#56884=DIRECTION('ref_axis',(0.,0.94284446121751,0.333233134534162));
#56885=DIRECTION('center_axis',(0.,-0.333233134534159,0.942844461217511));
#56886=DIRECTION('ref_axis',(0.,-0.942844461217511,-0.333233134534159));
#56887=DIRECTION('center_axis',(0.,0.333233134534162,-0.94284446121751));
#56888=DIRECTION('ref_axis',(0.,0.94284446121751,0.333233134534162));
#56889=DIRECTION('center_axis',(0.,-0.333233134534159,0.942844461217511));
#56890=DIRECTION('ref_axis',(0.,-0.942844461217511,-0.333233134534159));
#56891=DIRECTION('center_axis',(0.,0.333233134534162,-0.94284446121751));
#56892=DIRECTION('ref_axis',(0.,0.94284446121751,0.333233134534162));
#56893=DIRECTION('center_axis',(0.,-0.333233134534159,0.942844461217511));
#56894=DIRECTION('ref_axis',(0.,-0.942844461217511,-0.333233134534159));
#56895=DIRECTION('center_axis',(0.,0.333233134534162,-0.94284446121751));
#56896=DIRECTION('ref_axis',(0.,0.94284446121751,0.333233134534162));
#56897=DIRECTION('center_axis',(0.,-0.333233134534159,0.942844461217511));
#56898=DIRECTION('ref_axis',(0.,-0.942844461217511,-0.333233134534159));
#56899=DIRECTION('center_axis',(0.,0.333233134534162,-0.94284446121751));
#56900=DIRECTION('ref_axis',(0.,0.94284446121751,0.333233134534162));
#56901=DIRECTION('center_axis',(0.,-0.333233134534159,0.942844461217511));
#56902=DIRECTION('ref_axis',(0.,-0.942844461217511,-0.333233134534159));
#56903=DIRECTION('center_axis',(0.,0.333233134534162,-0.94284446121751));
#56904=DIRECTION('ref_axis',(0.,0.94284446121751,0.333233134534162));
#56905=DIRECTION('center_axis',(0.,-0.333233134534159,0.942844461217511));
#56906=DIRECTION('ref_axis',(0.,-0.942844461217511,-0.333233134534159));
#56907=DIRECTION('center_axis',(0.,0.333233134534162,-0.94284446121751));
#56908=DIRECTION('ref_axis',(0.,0.94284446121751,0.333233134534162));
#56909=DIRECTION('center_axis',(0.,-0.333233134534159,0.942844461217511));
#56910=DIRECTION('ref_axis',(0.,-0.942844461217511,-0.333233134534159));
#56911=DIRECTION('center_axis',(0.,0.333233134534162,-0.94284446121751));
#56912=DIRECTION('ref_axis',(0.,0.94284446121751,0.333233134534162));
#56913=DIRECTION('center_axis',(0.,-0.333233134534159,0.942844461217511));
#56914=DIRECTION('ref_axis',(0.,-0.942844461217511,-0.333233134534159));
#56915=DIRECTION('center_axis',(0.,0.333233134534162,-0.94284446121751));
#56916=DIRECTION('ref_axis',(0.,0.94284446121751,0.333233134534162));
#56917=DIRECTION('center_axis',(0.,-0.333233134534159,0.942844461217511));
#56918=DIRECTION('ref_axis',(0.,-0.942844461217511,-0.333233134534159));
#56919=DIRECTION('center_axis',(0.,0.333233134534162,-0.94284446121751));
#56920=DIRECTION('ref_axis',(0.,0.94284446121751,0.333233134534162));
#56921=DIRECTION('center_axis',(0.,-0.333233134534159,0.942844461217511));
#56922=DIRECTION('ref_axis',(0.,-0.942844461217511,-0.333233134534159));
#56923=DIRECTION('center_axis',(0.,0.333233134534162,-0.94284446121751));
#56924=DIRECTION('ref_axis',(0.,0.94284446121751,0.333233134534162));
#56925=DIRECTION('center_axis',(0.,-0.333233134534159,0.942844461217511));
#56926=DIRECTION('ref_axis',(0.,-0.942844461217511,-0.333233134534159));
#56927=DIRECTION('center_axis',(0.,0.333233134534162,-0.94284446121751));
#56928=DIRECTION('ref_axis',(0.,0.94284446121751,0.333233134534162));
#56929=DIRECTION('center_axis',(0.,-0.333233134534159,0.942844461217511));
#56930=DIRECTION('ref_axis',(0.,-0.942844461217511,-0.333233134534159));
#56931=DIRECTION('center_axis',(0.,0.333233134534162,-0.94284446121751));
#56932=DIRECTION('ref_axis',(0.,0.94284446121751,0.333233134534162));
#56933=DIRECTION('center_axis',(0.,-0.333233134534159,0.942844461217511));
#56934=DIRECTION('ref_axis',(0.,-0.942844461217511,-0.333233134534159));
#56935=DIRECTION('center_axis',(0.,0.333233134534162,-0.94284446121751));
#56936=DIRECTION('ref_axis',(0.,0.94284446121751,0.333233134534162));
#56937=DIRECTION('center_axis',(0.,-0.333233134534159,0.942844461217511));
#56938=DIRECTION('ref_axis',(0.,-0.942844461217511,-0.333233134534159));
#56939=DIRECTION('center_axis',(0.,0.333233134534162,-0.94284446121751));
#56940=DIRECTION('ref_axis',(0.,0.94284446121751,0.333233134534162));
#56941=DIRECTION('center_axis',(0.,-0.333233134534159,0.942844461217511));
#56942=DIRECTION('ref_axis',(0.,-0.942844461217511,-0.333233134534159));
#56943=DIRECTION('center_axis',(0.,0.333233134534162,-0.94284446121751));
#56944=DIRECTION('ref_axis',(0.,0.94284446121751,0.333233134534162));
#56945=DIRECTION('center_axis',(0.,-0.333233134534159,0.942844461217511));
#56946=DIRECTION('ref_axis',(0.,-0.942844461217511,-0.333233134534159));
#56947=DIRECTION('center_axis',(0.,0.333233134534162,-0.94284446121751));
#56948=DIRECTION('ref_axis',(0.,0.94284446121751,0.333233134534162));
#56949=DIRECTION('center_axis',(0.,-0.333233134534159,0.942844461217511));
#56950=DIRECTION('ref_axis',(0.,-0.942844461217511,-0.333233134534159));
#56951=DIRECTION('center_axis',(0.,0.333233134534162,-0.94284446121751));
#56952=DIRECTION('ref_axis',(0.,0.94284446121751,0.333233134534162));
#56953=DIRECTION('center_axis',(0.,-0.333233134534159,0.942844461217511));
#56954=DIRECTION('ref_axis',(0.,-0.942844461217511,-0.333233134534159));
#56955=DIRECTION('center_axis',(0.,0.333233134534162,-0.94284446121751));
#56956=DIRECTION('ref_axis',(0.,0.94284446121751,0.333233134534162));
#56957=DIRECTION('center_axis',(0.,-0.333233134534159,0.942844461217511));
#56958=DIRECTION('ref_axis',(0.,-0.942844461217511,-0.333233134534159));
#56959=DIRECTION('center_axis',(0.,0.333233134534162,-0.94284446121751));
#56960=DIRECTION('ref_axis',(0.,0.94284446121751,0.333233134534162));
#56961=DIRECTION('center_axis',(0.,-0.333233134534159,0.942844461217511));
#56962=DIRECTION('ref_axis',(0.,-0.942844461217511,-0.333233134534159));
#56963=DIRECTION('center_axis',(0.,0.333233134534162,-0.94284446121751));
#56964=DIRECTION('ref_axis',(0.,0.94284446121751,0.333233134534162));
#56965=DIRECTION('center_axis',(0.,-0.333233134534159,0.942844461217511));
#56966=DIRECTION('ref_axis',(0.,-0.942844461217511,-0.333233134534159));
#56967=DIRECTION('center_axis',(0.,0.333233134534162,-0.94284446121751));
#56968=DIRECTION('ref_axis',(0.,0.94284446121751,0.333233134534162));
#56969=DIRECTION('center_axis',(0.,-0.333233134534159,0.942844461217511));
#56970=DIRECTION('ref_axis',(0.,-0.942844461217511,-0.333233134534159));
#56971=DIRECTION('center_axis',(0.,0.333233134534162,-0.94284446121751));
#56972=DIRECTION('ref_axis',(0.,0.94284446121751,0.333233134534162));
#56973=DIRECTION('center_axis',(0.,-0.333233134534159,0.942844461217511));
#56974=DIRECTION('ref_axis',(0.,-0.942844461217511,-0.333233134534159));
#56975=DIRECTION('center_axis',(0.,0.333233134534162,-0.94284446121751));
#56976=DIRECTION('ref_axis',(0.,0.94284446121751,0.333233134534162));
#56977=DIRECTION('center_axis',(0.,-0.333233134534159,0.942844461217511));
#56978=DIRECTION('ref_axis',(0.,-0.942844461217511,-0.333233134534159));
#56979=DIRECTION('center_axis',(0.,0.333233134534162,-0.94284446121751));
#56980=DIRECTION('ref_axis',(0.,0.94284446121751,0.333233134534162));
#56981=DIRECTION('center_axis',(0.,-0.333233134534159,0.942844461217511));
#56982=DIRECTION('ref_axis',(0.,-0.942844461217511,-0.333233134534159));
#56983=DIRECTION('center_axis',(0.,0.333233134534162,-0.94284446121751));
#56984=DIRECTION('ref_axis',(0.,0.94284446121751,0.333233134534162));
#56985=DIRECTION('center_axis',(0.,-0.333233134534159,0.942844461217511));
#56986=DIRECTION('ref_axis',(0.,-0.942844461217511,-0.333233134534159));
#56987=DIRECTION('center_axis',(0.,0.333233134534162,-0.94284446121751));
#56988=DIRECTION('ref_axis',(0.,0.94284446121751,0.333233134534162));
#56989=DIRECTION('center_axis',(0.,-0.333233134534159,0.942844461217511));
#56990=DIRECTION('ref_axis',(0.,-0.942844461217511,-0.333233134534159));
#56991=DIRECTION('center_axis',(0.,0.333233134534162,-0.94284446121751));
#56992=DIRECTION('ref_axis',(0.,0.94284446121751,0.333233134534162));
#56993=DIRECTION('center_axis',(0.,-0.333233134534159,0.942844461217511));
#56994=DIRECTION('ref_axis',(0.,-0.942844461217511,-0.333233134534159));
#56995=DIRECTION('center_axis',(0.,0.333233134534162,-0.94284446121751));
#56996=DIRECTION('ref_axis',(0.,0.94284446121751,0.333233134534162));
#56997=DIRECTION('center_axis',(0.,-0.333233134534159,0.942844461217511));
#56998=DIRECTION('ref_axis',(0.,-0.942844461217511,-0.333233134534159));
#56999=DIRECTION('center_axis',(0.,0.333233134534162,-0.94284446121751));
#57000=DIRECTION('ref_axis',(0.,0.94284446121751,0.333233134534162));
#57001=DIRECTION('center_axis',(0.,-0.333233134534159,0.942844461217511));
#57002=DIRECTION('ref_axis',(0.,-0.942844461217511,-0.333233134534159));
#57003=DIRECTION('center_axis',(0.,0.333233134534162,-0.94284446121751));
#57004=DIRECTION('ref_axis',(0.,0.94284446121751,0.333233134534162));
#57005=DIRECTION('center_axis',(0.,-0.333233134534159,0.942844461217511));
#57006=DIRECTION('ref_axis',(0.,-0.942844461217511,-0.333233134534159));
#57007=DIRECTION('center_axis',(0.,0.333233134534162,-0.94284446121751));
#57008=DIRECTION('ref_axis',(0.,0.94284446121751,0.333233134534162));
#57009=DIRECTION('center_axis',(0.,-0.333233134534159,0.942844461217511));
#57010=DIRECTION('ref_axis',(0.,-0.942844461217511,-0.333233134534159));
#57011=DIRECTION('center_axis',(0.,0.333233134534162,-0.94284446121751));
#57012=DIRECTION('ref_axis',(0.,0.94284446121751,0.333233134534162));
#57013=DIRECTION('center_axis',(0.,-0.333233134534159,0.942844461217511));
#57014=DIRECTION('ref_axis',(0.,-0.942844461217511,-0.333233134534159));
#57015=DIRECTION('center_axis',(0.,0.333233134534162,-0.94284446121751));
#57016=DIRECTION('ref_axis',(0.,0.94284446121751,0.333233134534162));
#57017=DIRECTION('center_axis',(0.,-0.333233134534159,0.942844461217511));
#57018=DIRECTION('ref_axis',(0.,-0.942844461217511,-0.333233134534159));
#57019=DIRECTION('center_axis',(0.,0.333233134534162,-0.94284446121751));
#57020=DIRECTION('ref_axis',(0.,0.94284446121751,0.333233134534162));
#57021=DIRECTION('center_axis',(0.,-0.333233134534159,0.942844461217511));
#57022=DIRECTION('ref_axis',(0.,-0.942844461217511,-0.333233134534159));
#57023=DIRECTION('center_axis',(0.,0.333233134534162,-0.94284446121751));
#57024=DIRECTION('ref_axis',(0.,0.94284446121751,0.333233134534162));
#57025=DIRECTION('center_axis',(0.,-0.333233134534159,0.942844461217511));
#57026=DIRECTION('ref_axis',(0.,-0.942844461217511,-0.333233134534159));
#57027=DIRECTION('center_axis',(0.,0.333233134534162,-0.94284446121751));
#57028=DIRECTION('ref_axis',(0.,0.94284446121751,0.333233134534162));
#57029=DIRECTION('center_axis',(0.,-0.333233134534159,0.942844461217511));
#57030=DIRECTION('ref_axis',(0.,-0.942844461217511,-0.333233134534159));
#57031=DIRECTION('center_axis',(0.,0.333233134534162,-0.94284446121751));
#57032=DIRECTION('ref_axis',(0.,0.94284446121751,0.333233134534162));
#57033=DIRECTION('center_axis',(0.,-0.333233134534159,0.942844461217511));
#57034=DIRECTION('ref_axis',(0.,-0.942844461217511,-0.333233134534159));
#57035=DIRECTION('center_axis',(0.,0.333233134534162,-0.94284446121751));
#57036=DIRECTION('ref_axis',(0.,0.94284446121751,0.333233134534162));
#57037=DIRECTION('center_axis',(0.,-0.333233134534159,0.942844461217511));
#57038=DIRECTION('ref_axis',(0.,-0.942844461217511,-0.333233134534159));
#57039=DIRECTION('center_axis',(0.,0.333233134534162,-0.94284446121751));
#57040=DIRECTION('ref_axis',(0.,0.94284446121751,0.333233134534162));
#57041=DIRECTION('center_axis',(0.,-0.333233134534159,0.942844461217511));
#57042=DIRECTION('ref_axis',(0.,-0.942844461217511,-0.333233134534159));
#57043=DIRECTION('center_axis',(0.,0.333233134534162,-0.94284446121751));
#57044=DIRECTION('ref_axis',(0.,0.94284446121751,0.333233134534162));
#57045=DIRECTION('center_axis',(0.,-0.333233134534159,0.942844461217511));
#57046=DIRECTION('ref_axis',(0.,-0.942844461217511,-0.333233134534159));
#57047=DIRECTION('center_axis',(0.,0.333233134534162,-0.94284446121751));
#57048=DIRECTION('ref_axis',(0.,0.94284446121751,0.333233134534162));
#57049=DIRECTION('center_axis',(0.,-0.333233134534159,0.942844461217511));
#57050=DIRECTION('ref_axis',(0.,-0.942844461217511,-0.333233134534159));
#57051=DIRECTION('center_axis',(0.,0.333233134534162,-0.94284446121751));
#57052=DIRECTION('ref_axis',(0.,0.94284446121751,0.333233134534162));
#57053=DIRECTION('center_axis',(0.,-0.333233134534159,0.942844461217511));
#57054=DIRECTION('ref_axis',(0.,-0.942844461217511,-0.333233134534159));
#57055=DIRECTION('center_axis',(0.,0.333233134534162,-0.94284446121751));
#57056=DIRECTION('ref_axis',(0.,0.94284446121751,0.333233134534162));
#57057=DIRECTION('center_axis',(0.,-0.333233134534159,0.942844461217511));
#57058=DIRECTION('ref_axis',(0.,-0.942844461217511,-0.333233134534159));
#57059=DIRECTION('center_axis',(0.,0.333233134534162,-0.94284446121751));
#57060=DIRECTION('ref_axis',(0.,0.94284446121751,0.333233134534162));
#57061=DIRECTION('center_axis',(0.,-0.333233134534159,0.942844461217511));
#57062=DIRECTION('ref_axis',(0.,-0.942844461217511,-0.333233134534159));
#57063=DIRECTION('center_axis',(0.,0.333233134534162,-0.94284446121751));
#57064=DIRECTION('ref_axis',(0.,0.94284446121751,0.333233134534162));
#57065=DIRECTION('center_axis',(0.,-0.333233134534159,0.942844461217511));
#57066=DIRECTION('ref_axis',(0.,-0.942844461217511,-0.333233134534159));
#57067=DIRECTION('center_axis',(0.,0.333233134534162,-0.94284446121751));
#57068=DIRECTION('ref_axis',(0.,0.94284446121751,0.333233134534162));
#57069=DIRECTION('center_axis',(0.,-0.333233134534159,0.942844461217511));
#57070=DIRECTION('ref_axis',(0.,-0.942844461217511,-0.333233134534159));
#57071=DIRECTION('center_axis',(0.,0.333233134534162,-0.94284446121751));
#57072=DIRECTION('ref_axis',(0.,0.94284446121751,0.333233134534162));
#57073=DIRECTION('center_axis',(0.,-0.333233134534159,0.942844461217511));
#57074=DIRECTION('ref_axis',(0.,-0.942844461217511,-0.333233134534159));
#57075=DIRECTION('center_axis',(0.,0.333233134534162,-0.94284446121751));
#57076=DIRECTION('ref_axis',(0.,0.94284446121751,0.333233134534162));
#57077=DIRECTION('center_axis',(0.,-0.333233134534159,0.942844461217511));
#57078=DIRECTION('ref_axis',(0.,-0.942844461217511,-0.333233134534159));
#57079=DIRECTION('center_axis',(0.,0.333233134534162,-0.94284446121751));
#57080=DIRECTION('ref_axis',(0.,0.94284446121751,0.333233134534162));
#57081=DIRECTION('center_axis',(0.,-0.333233134534159,0.942844461217511));
#57082=DIRECTION('ref_axis',(0.,-0.942844461217511,-0.333233134534159));
#57083=DIRECTION('center_axis',(0.,0.333233134534162,-0.94284446121751));
#57084=DIRECTION('ref_axis',(0.,0.94284446121751,0.333233134534162));
#57085=DIRECTION('center_axis',(0.,-0.333233134534159,0.942844461217511));
#57086=DIRECTION('ref_axis',(0.,-0.942844461217511,-0.333233134534159));
#57087=DIRECTION('center_axis',(0.,0.333233134534162,-0.94284446121751));
#57088=DIRECTION('ref_axis',(0.,0.94284446121751,0.333233134534162));
#57089=DIRECTION('center_axis',(0.,-0.333233134534159,0.942844461217511));
#57090=DIRECTION('ref_axis',(0.,-0.942844461217511,-0.333233134534159));
#57091=DIRECTION('center_axis',(0.,0.333233134534162,-0.94284446121751));
#57092=DIRECTION('ref_axis',(0.,0.94284446121751,0.333233134534162));
#57093=DIRECTION('center_axis',(0.,-0.333233134534159,0.942844461217511));
#57094=DIRECTION('ref_axis',(0.,-0.942844461217511,-0.333233134534159));
#57095=DIRECTION('center_axis',(0.,0.333233134534162,-0.94284446121751));
#57096=DIRECTION('ref_axis',(0.,0.94284446121751,0.333233134534162));
#57097=DIRECTION('center_axis',(0.,-0.333233134534159,0.942844461217511));
#57098=DIRECTION('ref_axis',(0.,-0.942844461217511,-0.333233134534159));
#57099=DIRECTION('center_axis',(0.,0.333233134534162,-0.94284446121751));
#57100=DIRECTION('ref_axis',(0.,0.94284446121751,0.333233134534162));
#57101=DIRECTION('center_axis',(0.,-0.333233134534159,0.942844461217511));
#57102=DIRECTION('ref_axis',(0.,-0.942844461217511,-0.333233134534159));
#57103=DIRECTION('center_axis',(0.,0.333233134534162,-0.94284446121751));
#57104=DIRECTION('ref_axis',(0.,0.94284446121751,0.333233134534162));
#57105=DIRECTION('center_axis',(0.,-0.333233134534159,0.942844461217511));
#57106=DIRECTION('ref_axis',(0.,-0.942844461217511,-0.333233134534159));
#57107=DIRECTION('center_axis',(0.,0.333233134534162,-0.94284446121751));
#57108=DIRECTION('ref_axis',(0.,0.94284446121751,0.333233134534162));
#57109=DIRECTION('center_axis',(0.,-0.333233134534159,0.942844461217511));
#57110=DIRECTION('ref_axis',(0.,-0.942844461217511,-0.333233134534159));
#57111=DIRECTION('center_axis',(0.,0.333233134534162,-0.94284446121751));
#57112=DIRECTION('ref_axis',(0.,0.94284446121751,0.333233134534162));
#57113=DIRECTION('center_axis',(0.,-0.333233134534159,0.942844461217511));
#57114=DIRECTION('ref_axis',(0.,-0.942844461217511,-0.333233134534159));
#57115=DIRECTION('center_axis',(0.,0.333233134534162,-0.94284446121751));
#57116=DIRECTION('ref_axis',(0.,0.94284446121751,0.333233134534162));
#57117=DIRECTION('center_axis',(0.,-0.333233134534159,0.942844461217511));
#57118=DIRECTION('ref_axis',(0.,-0.942844461217511,-0.333233134534159));
#57119=DIRECTION('center_axis',(0.,0.333233134534162,-0.94284446121751));
#57120=DIRECTION('ref_axis',(0.,0.94284446121751,0.333233134534162));
#57121=DIRECTION('center_axis',(0.,-0.333233134534159,0.942844461217511));
#57122=DIRECTION('ref_axis',(0.,-0.942844461217511,-0.333233134534159));
#57123=DIRECTION('center_axis',(0.,0.333233134534162,-0.94284446121751));
#57124=DIRECTION('ref_axis',(0.,0.94284446121751,0.333233134534162));
#57125=DIRECTION('center_axis',(0.,-0.333233134534159,0.942844461217511));
#57126=DIRECTION('ref_axis',(0.,-0.942844461217511,-0.333233134534159));
#57127=DIRECTION('center_axis',(0.,0.333233134534162,-0.94284446121751));
#57128=DIRECTION('ref_axis',(0.,0.94284446121751,0.333233134534162));
#57129=DIRECTION('center_axis',(0.,-0.333233134534159,0.942844461217511));
#57130=DIRECTION('ref_axis',(0.,-0.942844461217511,-0.333233134534159));
#57131=DIRECTION('center_axis',(0.,0.333233134534162,-0.94284446121751));
#57132=DIRECTION('ref_axis',(0.,0.94284446121751,0.333233134534162));
#57133=DIRECTION('center_axis',(0.,-0.333233134534159,0.942844461217511));
#57134=DIRECTION('ref_axis',(0.,-0.942844461217511,-0.333233134534159));
#57135=DIRECTION('center_axis',(0.,0.333233134534162,-0.94284446121751));
#57136=DIRECTION('ref_axis',(0.,0.94284446121751,0.333233134534162));
#57137=DIRECTION('center_axis',(0.,-0.333233134534159,0.942844461217511));
#57138=DIRECTION('ref_axis',(0.,-0.942844461217511,-0.333233134534159));
#57139=DIRECTION('center_axis',(0.,0.333233134534162,-0.94284446121751));
#57140=DIRECTION('ref_axis',(0.,0.94284446121751,0.333233134534162));
#57141=DIRECTION('center_axis',(0.,-0.333233134534159,0.942844461217511));
#57142=DIRECTION('ref_axis',(0.,-0.942844461217511,-0.333233134534159));
#57143=DIRECTION('center_axis',(0.,0.333233134534162,-0.94284446121751));
#57144=DIRECTION('ref_axis',(0.,0.94284446121751,0.333233134534162));
#57145=DIRECTION('center_axis',(0.,-0.333233134534159,0.942844461217511));
#57146=DIRECTION('ref_axis',(0.,-0.942844461217511,-0.333233134534159));
#57147=DIRECTION('center_axis',(0.,0.333233134534162,-0.94284446121751));
#57148=DIRECTION('ref_axis',(0.,0.94284446121751,0.333233134534162));
#57149=DIRECTION('center_axis',(0.,-0.333233134534159,0.942844461217511));
#57150=DIRECTION('ref_axis',(0.,-0.942844461217511,-0.333233134534159));
#57151=DIRECTION('center_axis',(0.,0.333233134534162,-0.94284446121751));
#57152=DIRECTION('ref_axis',(0.,0.94284446121751,0.333233134534162));
#57153=DIRECTION('center_axis',(0.,-0.333233134534159,0.942844461217511));
#57154=DIRECTION('ref_axis',(0.,-0.942844461217511,-0.333233134534159));
#57155=DIRECTION('center_axis',(0.,0.333233134534162,-0.94284446121751));
#57156=DIRECTION('ref_axis',(0.,0.94284446121751,0.333233134534162));
#57157=DIRECTION('center_axis',(0.,-0.333233134534159,0.942844461217511));
#57158=DIRECTION('ref_axis',(0.,-0.942844461217511,-0.333233134534159));
#57159=DIRECTION('center_axis',(0.,0.333233134534162,-0.94284446121751));
#57160=DIRECTION('ref_axis',(0.,0.94284446121751,0.333233134534162));
#57161=DIRECTION('center_axis',(0.,-0.333233134534159,0.942844461217511));
#57162=DIRECTION('ref_axis',(0.,-0.942844461217511,-0.333233134534159));
#57163=DIRECTION('center_axis',(0.,0.333233134534162,-0.94284446121751));
#57164=DIRECTION('ref_axis',(0.,0.94284446121751,0.333233134534162));
#57165=DIRECTION('center_axis',(0.,-0.333233134534159,0.942844461217511));
#57166=DIRECTION('ref_axis',(0.,-0.942844461217511,-0.333233134534159));
#57167=DIRECTION('center_axis',(0.,0.333233134534162,-0.94284446121751));
#57168=DIRECTION('ref_axis',(0.,0.94284446121751,0.333233134534162));
#57169=DIRECTION('center_axis',(0.,-0.333233134534159,0.942844461217511));
#57170=DIRECTION('ref_axis',(0.,-0.942844461217511,-0.333233134534159));
#57171=DIRECTION('center_axis',(0.,0.333233134534162,-0.94284446121751));
#57172=DIRECTION('ref_axis',(0.,0.94284446121751,0.333233134534162));
#57173=DIRECTION('center_axis',(0.,-0.333233134534159,0.942844461217511));
#57174=DIRECTION('ref_axis',(0.,-0.942844461217511,-0.333233134534159));
#57175=DIRECTION('center_axis',(0.,0.333233134534162,-0.94284446121751));
#57176=DIRECTION('ref_axis',(0.,0.94284446121751,0.333233134534162));
#57177=DIRECTION('center_axis',(0.,-0.333233134534159,0.942844461217511));
#57178=DIRECTION('ref_axis',(0.,-0.942844461217511,-0.333233134534159));
#57179=DIRECTION('center_axis',(0.,0.333233134534162,-0.94284446121751));
#57180=DIRECTION('ref_axis',(0.,0.94284446121751,0.333233134534162));
#57181=DIRECTION('center_axis',(0.,-0.333233134534159,0.942844461217511));
#57182=DIRECTION('ref_axis',(0.,-0.942844461217511,-0.333233134534159));
#57183=DIRECTION('center_axis',(0.,0.333233134534162,-0.94284446121751));
#57184=DIRECTION('ref_axis',(0.,0.94284446121751,0.333233134534162));
#57185=DIRECTION('center_axis',(0.,-0.333233134534159,0.942844461217511));
#57186=DIRECTION('ref_axis',(0.,-0.942844461217511,-0.333233134534159));
#57187=DIRECTION('center_axis',(0.,0.333233134534162,-0.94284446121751));
#57188=DIRECTION('ref_axis',(0.,0.94284446121751,0.333233134534162));
#57189=DIRECTION('center_axis',(0.,-0.333233134534159,0.942844461217511));
#57190=DIRECTION('ref_axis',(0.,-0.942844461217511,-0.333233134534159));
#57191=DIRECTION('center_axis',(0.,0.333233134534162,-0.94284446121751));
#57192=DIRECTION('ref_axis',(0.,0.94284446121751,0.333233134534162));
#57193=DIRECTION('center_axis',(0.,-0.333233134534159,0.942844461217511));
#57194=DIRECTION('ref_axis',(0.,-0.942844461217511,-0.333233134534159));
#57195=DIRECTION('center_axis',(0.,0.333233134534162,-0.94284446121751));
#57196=DIRECTION('ref_axis',(0.,0.94284446121751,0.333233134534162));
#57197=DIRECTION('center_axis',(0.,-0.333233134534159,0.942844461217511));
#57198=DIRECTION('ref_axis',(0.,-0.942844461217511,-0.333233134534159));
#57199=DIRECTION('center_axis',(0.,0.333233134534162,-0.94284446121751));
#57200=DIRECTION('ref_axis',(0.,0.94284446121751,0.333233134534162));
#57201=DIRECTION('center_axis',(0.,-0.333233134534159,0.942844461217511));
#57202=DIRECTION('ref_axis',(0.,-0.942844461217511,-0.333233134534159));
#57203=DIRECTION('center_axis',(0.,0.333233134534162,-0.94284446121751));
#57204=DIRECTION('ref_axis',(0.,0.94284446121751,0.333233134534162));
#57205=DIRECTION('center_axis',(0.,-0.333233134534159,0.942844461217511));
#57206=DIRECTION('ref_axis',(0.,-0.942844461217511,-0.333233134534159));
#57207=DIRECTION('center_axis',(0.,0.333233134534162,-0.94284446121751));
#57208=DIRECTION('ref_axis',(0.,0.94284446121751,0.333233134534162));
#57209=DIRECTION('center_axis',(0.,-0.333233134534159,0.942844461217511));
#57210=DIRECTION('ref_axis',(0.,-0.942844461217511,-0.333233134534159));
#57211=DIRECTION('center_axis',(0.,0.333233134534162,-0.94284446121751));
#57212=DIRECTION('ref_axis',(0.,0.94284446121751,0.333233134534162));
#57213=DIRECTION('center_axis',(0.,-0.333233134534159,0.942844461217511));
#57214=DIRECTION('ref_axis',(0.,-0.942844461217511,-0.333233134534159));
#57215=DIRECTION('center_axis',(0.,0.333233134534162,-0.94284446121751));
#57216=DIRECTION('ref_axis',(0.,0.94284446121751,0.333233134534162));
#57217=DIRECTION('center_axis',(0.,-0.333233134534159,0.942844461217511));
#57218=DIRECTION('ref_axis',(0.,-0.942844461217511,-0.333233134534159));
#57219=DIRECTION('center_axis',(0.,0.333233134534162,-0.94284446121751));
#57220=DIRECTION('ref_axis',(0.,0.94284446121751,0.333233134534162));
#57221=DIRECTION('center_axis',(0.,-0.333233134534159,0.942844461217511));
#57222=DIRECTION('ref_axis',(0.,-0.942844461217511,-0.333233134534159));
#57223=DIRECTION('center_axis',(0.,0.333233134534162,-0.94284446121751));
#57224=DIRECTION('ref_axis',(0.,0.94284446121751,0.333233134534162));
#57225=DIRECTION('center_axis',(0.,-0.333233134534159,0.942844461217511));
#57226=DIRECTION('ref_axis',(0.,-0.942844461217511,-0.333233134534159));
#57227=DIRECTION('center_axis',(0.,0.333233134534162,-0.94284446121751));
#57228=DIRECTION('ref_axis',(0.,0.94284446121751,0.333233134534162));
#57229=DIRECTION('center_axis',(0.,-0.333233134534159,0.942844461217511));
#57230=DIRECTION('ref_axis',(0.,-0.942844461217511,-0.333233134534159));
#57231=DIRECTION('center_axis',(0.,0.333233134534162,-0.94284446121751));
#57232=DIRECTION('ref_axis',(0.,0.94284446121751,0.333233134534162));
#57233=DIRECTION('center_axis',(0.,-0.333233134534159,0.942844461217511));
#57234=DIRECTION('ref_axis',(0.,-0.942844461217511,-0.333233134534159));
#57235=DIRECTION('center_axis',(0.,0.333233134534162,-0.94284446121751));
#57236=DIRECTION('ref_axis',(0.,0.94284446121751,0.333233134534162));
#57237=DIRECTION('center_axis',(0.,-0.333233134534159,0.942844461217511));
#57238=DIRECTION('ref_axis',(0.,-0.942844461217511,-0.333233134534159));
#57239=DIRECTION('center_axis',(0.,0.333233134534162,-0.94284446121751));
#57240=DIRECTION('ref_axis',(0.,0.94284446121751,0.333233134534162));
#57241=DIRECTION('center_axis',(0.,-0.333233134534159,0.942844461217511));
#57242=DIRECTION('ref_axis',(0.,-0.942844461217511,-0.333233134534159));
#57243=DIRECTION('center_axis',(0.,0.333233134534162,-0.94284446121751));
#57244=DIRECTION('ref_axis',(0.,0.94284446121751,0.333233134534162));
#57245=DIRECTION('center_axis',(0.,-0.333233134534159,0.942844461217511));
#57246=DIRECTION('ref_axis',(0.,-0.942844461217511,-0.333233134534159));
#57247=DIRECTION('center_axis',(0.,0.333233134534162,-0.94284446121751));
#57248=DIRECTION('ref_axis',(0.,0.94284446121751,0.333233134534162));
#57249=DIRECTION('center_axis',(0.,-0.333233134534159,0.942844461217511));
#57250=DIRECTION('ref_axis',(0.,-0.942844461217511,-0.333233134534159));
#57251=DIRECTION('center_axis',(0.,0.333233134534162,-0.94284446121751));
#57252=DIRECTION('ref_axis',(0.,0.94284446121751,0.333233134534162));
#57253=DIRECTION('center_axis',(0.,-0.333233134534159,0.942844461217511));
#57254=DIRECTION('ref_axis',(0.,-0.942844461217511,-0.333233134534159));
#57255=DIRECTION('center_axis',(0.,0.333233134534162,-0.94284446121751));
#57256=DIRECTION('ref_axis',(0.,0.94284446121751,0.333233134534162));
#57257=DIRECTION('center_axis',(0.,-0.333233134534159,0.942844461217511));
#57258=DIRECTION('ref_axis',(0.,-0.942844461217511,-0.333233134534159));
#57259=DIRECTION('center_axis',(0.,0.333233134534162,-0.94284446121751));
#57260=DIRECTION('ref_axis',(0.,0.94284446121751,0.333233134534162));
#57261=DIRECTION('center_axis',(0.,-0.333233134534159,0.942844461217511));
#57262=DIRECTION('ref_axis',(0.,-0.942844461217511,-0.333233134534159));
#57263=DIRECTION('center_axis',(0.,0.333233134534162,-0.94284446121751));
#57264=DIRECTION('ref_axis',(0.,0.94284446121751,0.333233134534162));
#57265=DIRECTION('center_axis',(0.,-0.333233134534159,0.942844461217511));
#57266=DIRECTION('ref_axis',(0.,-0.942844461217511,-0.333233134534159));
#57267=DIRECTION('center_axis',(0.,0.333233134534162,-0.94284446121751));
#57268=DIRECTION('ref_axis',(0.,0.94284446121751,0.333233134534162));
#57269=DIRECTION('center_axis',(0.,-0.333233134534159,0.942844461217511));
#57270=DIRECTION('ref_axis',(0.,-0.942844461217511,-0.333233134534159));
#57271=DIRECTION('center_axis',(0.,0.333233134534162,-0.94284446121751));
#57272=DIRECTION('ref_axis',(0.,0.94284446121751,0.333233134534162));
#57273=DIRECTION('center_axis',(0.,-0.333233134534159,0.942844461217511));
#57274=DIRECTION('ref_axis',(0.,-0.942844461217511,-0.333233134534159));
#57275=DIRECTION('center_axis',(0.,0.333233134534162,-0.94284446121751));
#57276=DIRECTION('ref_axis',(0.,0.94284446121751,0.333233134534162));
#57277=DIRECTION('center_axis',(0.,-0.333233134534159,0.942844461217511));
#57278=DIRECTION('ref_axis',(0.,-0.942844461217511,-0.333233134534159));
#57279=DIRECTION('center_axis',(0.,0.333233134534162,-0.94284446121751));
#57280=DIRECTION('ref_axis',(0.,0.94284446121751,0.333233134534162));
#57281=DIRECTION('center_axis',(0.,-0.333233134534159,0.942844461217511));
#57282=DIRECTION('ref_axis',(0.,-0.942844461217511,-0.333233134534159));
#57283=DIRECTION('center_axis',(0.,0.333233134534162,-0.94284446121751));
#57284=DIRECTION('ref_axis',(0.,0.94284446121751,0.333233134534162));
#57285=DIRECTION('center_axis',(0.,-0.333233134534159,0.942844461217511));
#57286=DIRECTION('ref_axis',(0.,-0.942844461217511,-0.333233134534159));
#57287=DIRECTION('center_axis',(0.,0.333233134534162,-0.94284446121751));
#57288=DIRECTION('ref_axis',(0.,0.94284446121751,0.333233134534162));
#57289=DIRECTION('center_axis',(0.,-0.333233134534159,0.942844461217511));
#57290=DIRECTION('ref_axis',(0.,-0.942844461217511,-0.333233134534159));
#57291=DIRECTION('center_axis',(0.,0.333233134534162,-0.94284446121751));
#57292=DIRECTION('ref_axis',(0.,0.94284446121751,0.333233134534162));
#57293=DIRECTION('center_axis',(0.,-0.333233134534159,0.942844461217511));
#57294=DIRECTION('ref_axis',(0.,-0.942844461217511,-0.333233134534159));
#57295=DIRECTION('center_axis',(0.,0.333233134534162,-0.94284446121751));
#57296=DIRECTION('ref_axis',(0.,0.94284446121751,0.333233134534162));
#57297=DIRECTION('center_axis',(0.,-0.333233134534159,0.942844461217511));
#57298=DIRECTION('ref_axis',(0.,-0.942844461217511,-0.333233134534159));
#57299=DIRECTION('center_axis',(0.,0.333233134534162,-0.94284446121751));
#57300=DIRECTION('ref_axis',(0.,0.94284446121751,0.333233134534162));
#57301=DIRECTION('center_axis',(0.,-0.333233134534159,0.942844461217511));
#57302=DIRECTION('ref_axis',(0.,-0.942844461217511,-0.333233134534159));
#57303=DIRECTION('center_axis',(0.,0.333233134534162,-0.94284446121751));
#57304=DIRECTION('ref_axis',(0.,0.94284446121751,0.333233134534162));
#57305=DIRECTION('center_axis',(0.,-0.333233134534159,0.942844461217511));
#57306=DIRECTION('ref_axis',(0.,-0.942844461217511,-0.333233134534159));
#57307=DIRECTION('center_axis',(0.,0.333233134534162,-0.94284446121751));
#57308=DIRECTION('ref_axis',(0.,0.94284446121751,0.333233134534162));
#57309=DIRECTION('center_axis',(0.,-0.333233134534159,0.942844461217511));
#57310=DIRECTION('ref_axis',(0.,-0.942844461217511,-0.333233134534159));
#57311=DIRECTION('center_axis',(0.,0.333233134534162,-0.94284446121751));
#57312=DIRECTION('ref_axis',(0.,0.94284446121751,0.333233134534162));
#57313=DIRECTION('center_axis',(0.,-0.333233134534159,0.942844461217511));
#57314=DIRECTION('ref_axis',(0.,-0.942844461217511,-0.333233134534159));
#57315=DIRECTION('center_axis',(0.,0.333233134534162,-0.94284446121751));
#57316=DIRECTION('ref_axis',(0.,0.94284446121751,0.333233134534162));
#57317=DIRECTION('center_axis',(0.,-0.333233134534159,0.942844461217511));
#57318=DIRECTION('ref_axis',(0.,-0.942844461217511,-0.333233134534159));
#57319=DIRECTION('center_axis',(0.,0.333233134534162,-0.94284446121751));
#57320=DIRECTION('ref_axis',(0.,0.94284446121751,0.333233134534162));
#57321=DIRECTION('center_axis',(0.,0.333233134534162,-0.94284446121751));
#57322=DIRECTION('ref_axis',(0.,0.94284446121751,0.333233134534162));
#57323=DIRECTION('center_axis',(0.,0.333233134534162,-0.94284446121751));
#57324=DIRECTION('ref_axis',(0.,0.94284446121751,0.333233134534162));
#57325=DIRECTION('center_axis',(0.,0.333233134534162,-0.94284446121751));
#57326=DIRECTION('ref_axis',(0.,0.94284446121751,0.333233134534162));
#57327=DIRECTION('center_axis',(0.,0.333233134534162,-0.94284446121751));
#57328=DIRECTION('ref_axis',(0.,0.94284446121751,0.333233134534162));
#57329=DIRECTION('center_axis',(0.,0.333233134534162,-0.94284446121751));
#57330=DIRECTION('ref_axis',(0.,0.94284446121751,0.333233134534162));
#57331=DIRECTION('center_axis',(0.,0.333233134534162,-0.94284446121751));
#57332=DIRECTION('ref_axis',(0.,0.94284446121751,0.333233134534162));
#57333=DIRECTION('center_axis',(0.,0.333233134534162,-0.94284446121751));
#57334=DIRECTION('ref_axis',(0.,0.94284446121751,0.333233134534162));
#57335=DIRECTION('center_axis',(0.,0.333233134534162,-0.94284446121751));
#57336=DIRECTION('ref_axis',(0.,0.94284446121751,0.333233134534162));
#57337=DIRECTION('center_axis',(0.,0.333233134534162,-0.94284446121751));
#57338=DIRECTION('ref_axis',(0.,0.94284446121751,0.333233134534162));
#57339=DIRECTION('center_axis',(0.,0.333233134534162,-0.94284446121751));
#57340=DIRECTION('ref_axis',(0.,0.94284446121751,0.333233134534162));
#57341=DIRECTION('center_axis',(0.,0.333233134534162,-0.94284446121751));
#57342=DIRECTION('ref_axis',(0.,0.94284446121751,0.333233134534162));
#57343=DIRECTION('center_axis',(0.,0.333233134534162,-0.94284446121751));
#57344=DIRECTION('ref_axis',(0.,0.94284446121751,0.333233134534162));
#57345=DIRECTION('center_axis',(0.,0.333233134534162,-0.94284446121751));
#57346=DIRECTION('ref_axis',(0.,0.94284446121751,0.333233134534162));
#57347=DIRECTION('center_axis',(0.,0.333233134534162,-0.94284446121751));
#57348=DIRECTION('ref_axis',(0.,0.94284446121751,0.333233134534162));
#57349=DIRECTION('center_axis',(0.,-0.333233134534159,0.942844461217511));
#57350=DIRECTION('ref_axis',(0.,-0.942844461217511,-0.333233134534159));
#57351=DIRECTION('center_axis',(0.,0.333233134534162,-0.94284446121751));
#57352=DIRECTION('ref_axis',(0.,0.94284446121751,0.333233134534162));
#57353=DIRECTION('center_axis',(0.,0.333233134534162,-0.94284446121751));
#57354=DIRECTION('ref_axis',(0.,0.94284446121751,0.333233134534162));
#57355=DIRECTION('center_axis',(0.,0.333233134534162,-0.94284446121751));
#57356=DIRECTION('ref_axis',(0.,0.94284446121751,0.333233134534162));
#57357=DIRECTION('center_axis',(0.,-0.333233134534159,0.942844461217511));
#57358=DIRECTION('ref_axis',(0.,-0.942844461217511,-0.333233134534159));
#57359=DIRECTION('center_axis',(0.,0.333233134534162,-0.94284446121751));
#57360=DIRECTION('ref_axis',(0.,0.94284446121751,0.333233134534162));
#57361=DIRECTION('center_axis',(0.,0.333233134534162,-0.94284446121751));
#57362=DIRECTION('ref_axis',(0.,0.94284446121751,0.333233134534162));
#57363=DIRECTION('center_axis',(0.,0.333233134534162,-0.94284446121751));
#57364=DIRECTION('ref_axis',(0.,0.94284446121751,0.333233134534162));
#57365=DIRECTION('center_axis',(0.,-0.333233134534159,0.942844461217511));
#57366=DIRECTION('ref_axis',(0.,-0.942844461217511,-0.333233134534159));
#57367=DIRECTION('center_axis',(0.,0.333233134534162,-0.94284446121751));
#57368=DIRECTION('ref_axis',(0.,0.94284446121751,0.333233134534162));
#57369=DIRECTION('center_axis',(0.,-0.333233134534159,0.942844461217511));
#57370=DIRECTION('ref_axis',(0.,-0.942844461217511,-0.333233134534159));
#57371=DIRECTION('center_axis',(0.,0.333233134534162,-0.94284446121751));
#57372=DIRECTION('ref_axis',(0.,0.94284446121751,0.333233134534162));
#57373=DIRECTION('center_axis',(0.,0.333233134534162,-0.94284446121751));
#57374=DIRECTION('ref_axis',(0.,0.94284446121751,0.333233134534162));
#57375=DIRECTION('center_axis',(0.,0.333233134534162,-0.94284446121751));
#57376=DIRECTION('ref_axis',(0.,0.94284446121751,0.333233134534162));
#57377=DIRECTION('center_axis',(0.,-0.333233134534159,0.942844461217511));
#57378=DIRECTION('ref_axis',(0.,-0.942844461217511,-0.333233134534159));
#57379=DIRECTION('center_axis',(0.,0.333233134534162,-0.94284446121751));
#57380=DIRECTION('ref_axis',(0.,0.94284446121751,0.333233134534162));
#57381=DIRECTION('center_axis',(0.,-0.333233134534159,0.942844461217511));
#57382=DIRECTION('ref_axis',(0.,-0.942844461217511,-0.333233134534159));
#57383=DIRECTION('center_axis',(0.,0.333233134534162,-0.94284446121751));
#57384=DIRECTION('ref_axis',(0.,0.94284446121751,0.333233134534162));
#57385=DIRECTION('center_axis',(0.,0.333233134534162,-0.94284446121751));
#57386=DIRECTION('ref_axis',(0.,0.94284446121751,0.333233134534162));
#57387=DIRECTION('center_axis',(0.,0.333233134534162,-0.94284446121751));
#57388=DIRECTION('ref_axis',(0.,0.94284446121751,0.333233134534162));
#57389=DIRECTION('center_axis',(0.,0.333233134534162,-0.94284446121751));
#57390=DIRECTION('ref_axis',(0.,0.94284446121751,0.333233134534162));
#57391=DIRECTION('center_axis',(0.,0.333233134534162,-0.94284446121751));
#57392=DIRECTION('ref_axis',(0.,0.94284446121751,0.333233134534162));
#57393=DIRECTION('center_axis',(0.,0.333233134534162,-0.94284446121751));
#57394=DIRECTION('ref_axis',(0.,0.94284446121751,0.333233134534162));
#57395=DIRECTION('center_axis',(0.,0.333233134534162,-0.94284446121751));
#57396=DIRECTION('ref_axis',(0.,0.94284446121751,0.333233134534162));
#57397=DIRECTION('center_axis',(0.,0.333233134534162,-0.94284446121751));
#57398=DIRECTION('ref_axis',(0.,0.94284446121751,0.333233134534162));
#57399=DIRECTION('center_axis',(0.,0.333233134534162,-0.94284446121751));
#57400=DIRECTION('ref_axis',(0.,0.94284446121751,0.333233134534162));
#57401=DIRECTION('center_axis',(0.,0.333233134534162,-0.94284446121751));
#57402=DIRECTION('ref_axis',(0.,0.94284446121751,0.333233134534162));
#57403=DIRECTION('center_axis',(0.,0.333233134534162,-0.94284446121751));
#57404=DIRECTION('ref_axis',(0.,0.94284446121751,0.333233134534162));
#57405=DIRECTION('center_axis',(0.,0.333233134534162,-0.94284446121751));
#57406=DIRECTION('ref_axis',(0.,0.94284446121751,0.333233134534162));
#57407=DIRECTION('center_axis',(0.,0.333233134534162,-0.94284446121751));
#57408=DIRECTION('ref_axis',(0.,0.94284446121751,0.333233134534162));
#57409=DIRECTION('center_axis',(0.,0.333233134534162,-0.94284446121751));
#57410=DIRECTION('ref_axis',(0.,0.94284446121751,0.333233134534162));
#57411=DIRECTION('center_axis',(0.,0.333233134534162,-0.94284446121751));
#57412=DIRECTION('ref_axis',(0.,0.94284446121751,0.333233134534162));
#57413=DIRECTION('center_axis',(0.,0.333233134534162,-0.94284446121751));
#57414=DIRECTION('ref_axis',(0.,0.94284446121751,0.333233134534162));
#57415=DIRECTION('center_axis',(0.,0.333233134534162,-0.94284446121751));
#57416=DIRECTION('ref_axis',(0.,0.94284446121751,0.333233134534162));
#57417=DIRECTION('center_axis',(0.,0.333233134534162,-0.94284446121751));
#57418=DIRECTION('ref_axis',(0.,0.94284446121751,0.333233134534162));
#57419=DIRECTION('center_axis',(0.,0.333233134534162,-0.94284446121751));
#57420=DIRECTION('ref_axis',(0.,0.94284446121751,0.333233134534162));
#57421=DIRECTION('center_axis',(0.,0.333233134534162,-0.94284446121751));
#57422=DIRECTION('ref_axis',(0.,0.94284446121751,0.333233134534162));
#57423=DIRECTION('center_axis',(0.,0.333233134534162,-0.94284446121751));
#57424=DIRECTION('ref_axis',(0.,0.94284446121751,0.333233134534162));
#57425=DIRECTION('center_axis',(0.,0.333233134534162,-0.94284446121751));
#57426=DIRECTION('ref_axis',(0.,0.94284446121751,0.333233134534162));
#57427=DIRECTION('center_axis',(0.,0.333233134534162,-0.94284446121751));
#57428=DIRECTION('ref_axis',(0.,0.94284446121751,0.333233134534162));
#57429=DIRECTION('center_axis',(0.,0.333233134534162,-0.94284446121751));
#57430=DIRECTION('ref_axis',(0.,0.94284446121751,0.333233134534162));
#57431=DIRECTION('center_axis',(0.,0.333233134534162,-0.94284446121751));
#57432=DIRECTION('ref_axis',(0.,0.94284446121751,0.333233134534162));
#57433=DIRECTION('center_axis',(0.,0.333233134534162,-0.94284446121751));
#57434=DIRECTION('ref_axis',(0.,0.94284446121751,0.333233134534162));
#57435=DIRECTION('center_axis',(0.,0.333233134534162,-0.94284446121751));
#57436=DIRECTION('ref_axis',(0.,0.94284446121751,0.333233134534162));
#57437=DIRECTION('center_axis',(0.,0.333233134534162,-0.94284446121751));
#57438=DIRECTION('ref_axis',(0.,0.94284446121751,0.333233134534162));
#57439=DIRECTION('center_axis',(0.,0.333233134534162,-0.94284446121751));
#57440=DIRECTION('ref_axis',(0.,0.94284446121751,0.333233134534162));
#57441=DIRECTION('center_axis',(0.,0.333233134534162,-0.94284446121751));
#57442=DIRECTION('ref_axis',(0.,0.94284446121751,0.333233134534162));
#57443=DIRECTION('center_axis',(0.,0.333233134534162,-0.94284446121751));
#57444=DIRECTION('ref_axis',(0.,0.94284446121751,0.333233134534162));
#57445=DIRECTION('center_axis',(0.,0.333233134534162,-0.94284446121751));
#57446=DIRECTION('ref_axis',(0.,0.94284446121751,0.333233134534162));
#57447=DIRECTION('center_axis',(0.,0.333233134534162,-0.94284446121751));
#57448=DIRECTION('ref_axis',(0.,0.94284446121751,0.333233134534162));
#57449=DIRECTION('center_axis',(0.,0.333233134534162,-0.94284446121751));
#57450=DIRECTION('ref_axis',(0.,0.94284446121751,0.333233134534162));
#57451=DIRECTION('center_axis',(0.,0.333233134534162,-0.94284446121751));
#57452=DIRECTION('ref_axis',(0.,0.94284446121751,0.333233134534162));
#57453=DIRECTION('center_axis',(0.,0.333233134534162,-0.94284446121751));
#57454=DIRECTION('ref_axis',(0.,0.94284446121751,0.333233134534162));
#57455=DIRECTION('center_axis',(0.,0.333233134534162,-0.94284446121751));
#57456=DIRECTION('ref_axis',(0.,0.94284446121751,0.333233134534162));
#57457=DIRECTION('center_axis',(0.,0.333233134534162,-0.94284446121751));
#57458=DIRECTION('ref_axis',(0.,0.94284446121751,0.333233134534162));
#57459=DIRECTION('center_axis',(0.,0.333233134534162,-0.94284446121751));
#57460=DIRECTION('ref_axis',(0.,0.94284446121751,0.333233134534162));
#57461=DIRECTION('center_axis',(0.,-0.333233134534159,0.942844461217511));
#57462=DIRECTION('ref_axis',(0.,-0.942844461217511,-0.333233134534159));
#57463=DIRECTION('center_axis',(0.,-0.333233134534162,0.94284446121751));
#57464=DIRECTION('ref_axis',(0.,-0.94284446121751,-0.333233134534162));
#57465=DIRECTION('center_axis',(0.,-0.333233134534159,0.942844461217511));
#57466=DIRECTION('ref_axis',(0.,-0.942844461217511,-0.333233134534159));
#57467=DIRECTION('center_axis',(0.,-0.333233134534162,0.94284446121751));
#57468=DIRECTION('ref_axis',(0.,-0.94284446121751,-0.333233134534162));
#57469=DIRECTION('center_axis',(0.,-0.333233134534159,0.942844461217511));
#57470=DIRECTION('ref_axis',(0.,-0.942844461217511,-0.333233134534159));
#57471=DIRECTION('center_axis',(0.,-0.333233134534162,0.94284446121751));
#57472=DIRECTION('ref_axis',(0.,-0.94284446121751,-0.333233134534162));
#57473=DIRECTION('center_axis',(0.,-0.333233134534159,0.942844461217511));
#57474=DIRECTION('ref_axis',(0.,-0.942844461217511,-0.333233134534159));
#57475=DIRECTION('center_axis',(0.,-0.333233134534162,0.94284446121751));
#57476=DIRECTION('ref_axis',(0.,-0.94284446121751,-0.333233134534162));
#57477=DIRECTION('center_axis',(0.,-0.333233134534159,0.942844461217511));
#57478=DIRECTION('ref_axis',(0.,-0.942844461217511,-0.333233134534159));
#57479=DIRECTION('center_axis',(0.,-0.333233134534162,0.94284446121751));
#57480=DIRECTION('ref_axis',(0.,-0.94284446121751,-0.333233134534162));
#57481=DIRECTION('center_axis',(0.,-0.333233134534159,0.942844461217511));
#57482=DIRECTION('ref_axis',(0.,-0.942844461217511,-0.333233134534159));
#57483=DIRECTION('center_axis',(0.,-0.333233134534162,0.94284446121751));
#57484=DIRECTION('ref_axis',(0.,-0.94284446121751,-0.333233134534162));
#57485=DIRECTION('axis',(0.,0.,1.));
#57486=DIRECTION('refdir',(1.,0.,0.));
#57487=DIRECTION('center_axis',(0.,-1.,0.));
#57488=DIRECTION('ref_axis',(0.,0.,-1.));
#57489=DIRECTION('center_axis',(0.,-1.,0.));
#57490=DIRECTION('ref_axis',(0.,0.,-1.));
#57491=DIRECTION('center_axis',(0.,-1.,0.));
#57492=DIRECTION('ref_axis',(0.,0.,-1.));
#57493=DIRECTION('center_axis',(-1.,0.,0.));
#57494=DIRECTION('ref_axis',(0.,0.,1.));
#57495=DIRECTION('center_axis',(0.,1.,0.));
#57496=DIRECTION('ref_axis',(0.,0.,-1.));
#57497=DIRECTION('center_axis',(0.,1.,0.));
#57498=DIRECTION('ref_axis',(0.,0.,1.));
#57499=DIRECTION('center_axis',(0.,1.,0.));
#57500=DIRECTION('ref_axis',(0.,0.,-1.));
#57501=DIRECTION('center_axis',(-1.,0.,0.));
#57502=DIRECTION('ref_axis',(0.,0.,-1.));
#57503=DIRECTION('center_axis',(0.,-1.,0.));
#57504=DIRECTION('ref_axis',(0.,0.,1.));
#57505=DIRECTION('center_axis',(0.,1.,0.));
#57506=DIRECTION('ref_axis',(0.,0.,1.));
#57507=DIRECTION('',(5.12151535729607E-18,-0.999125146621934,0.041820346575534));
#57508=DIRECTION('center_axis',(0.,-1.,0.));
#57509=DIRECTION('ref_axis',(0.,0.,-1.));
#57510=DIRECTION('center_axis',(8.61122783338974E-15,1.,9.154793709916E-16));
#57511=DIRECTION('ref_axis',(0.161066048973386,-4.83449910768251E-16,-0.986943629529115));
#57512=DIRECTION('center_axis',(0.,1.,0.));
#57513=DIRECTION('ref_axis',(0.,0.,1.));
#57514=DIRECTION('center_axis',(0.,1.,0.));
#57515=DIRECTION('ref_axis',(0.,0.,-1.));
#57516=DIRECTION('center_axis',(-1.,0.,0.));
#57517=DIRECTION('ref_axis',(0.,0.,-1.));
#57518=DIRECTION('center_axis',(0.,-1.,0.));
#57519=DIRECTION('ref_axis',(0.,0.,1.));
#57520=DIRECTION('center_axis',(0.,1.,0.));
#57521=DIRECTION('ref_axis',(0.,0.,1.));
#57522=DIRECTION('center_axis',(0.,1.,0.));
#57523=DIRECTION('ref_axis',(0.,0.,1.));
#57524=DIRECTION('',(4.99439982873439E-18,-0.999168053100577,0.0407823695143096));
#57525=DIRECTION('center_axis',(0.,-1.,0.));
#57526=DIRECTION('ref_axis',(0.,0.,-1.));
#57527=DIRECTION('center_axis',(0.,1.,0.));
#57528=DIRECTION('ref_axis',(0.,0.,1.));
#57529=DIRECTION('center_axis',(0.,-1.,0.));
#57530=DIRECTION('ref_axis',(0.,0.,-1.));
#57531=DIRECTION('center_axis',(8.61122783338974E-15,1.,9.154793709916E-16));
#57532=DIRECTION('ref_axis',(0.161066048973386,-4.83449910768251E-16,-0.986943629529115));
#57533=DIRECTION('center_axis',(0.,-1.,0.));
#57534=DIRECTION('ref_axis',(0.,0.,-1.));
#57535=DIRECTION('center_axis',(0.,1.,0.));
#57536=DIRECTION('ref_axis',(0.,0.,1.));
#57537=DIRECTION('axis',(0.,0.,1.));
#57538=DIRECTION('refdir',(1.,0.,0.));
#57539=DIRECTION('center_axis',(0.,1.,0.));
#57540=DIRECTION('ref_axis',(0.,0.,1.));
#57541=DIRECTION('',(0.,1.,0.));
#57542=DIRECTION('center_axis',(0.,1.,0.));
#57543=DIRECTION('ref_axis',(0.,0.,1.));
#57544=DIRECTION('',(0.,1.,0.));
#57545=DIRECTION('center_axis',(0.,1.,0.));
#57546=DIRECTION('ref_axis',(0.,0.,-1.));
#57547=DIRECTION('center_axis',(-3.75424127281594E-15,0.,1.));
#57548=DIRECTION('ref_axis',(1.,0.,3.75424127281594E-15));
#57549=DIRECTION('',(0.,1.,0.));
#57550=DIRECTION('',(1.,0.,3.75424127281594E-15));
#57551=DIRECTION('',(1.,0.,3.75424127281594E-15));
#57552=DIRECTION('center_axis',(0.,1.,0.));
#57553=DIRECTION('ref_axis',(0.,0.,1.));
#57554=DIRECTION('',(0.,1.,0.));
#57555=DIRECTION('center_axis',(0.,1.,0.));
#57556=DIRECTION('ref_axis',(0.,0.,1.));
#57557=DIRECTION('center_axis',(0.,1.,0.));
#57558=DIRECTION('ref_axis',(0.,0.,-1.));
#57559=DIRECTION('center_axis',(-3.75424127281594E-15,0.,-1.));
#57560=DIRECTION('ref_axis',(-1.,0.,3.75424127281594E-15));
#57561=DIRECTION('',(-1.,0.,3.75424127281594E-15));
#57562=DIRECTION('',(-1.,0.,3.75424127281594E-15));
#57563=DIRECTION('center_axis',(0.,-1.,0.));
#57564=DIRECTION('ref_axis',(0.,0.,-1.));
#57565=DIRECTION('center_axis',(0.,1.,0.));
#57566=DIRECTION('ref_axis',(0.,0.,1.));
#57567=DIRECTION('center_axis',(0.,1.,0.));
#57568=DIRECTION('ref_axis',(0.,0.,1.));
#57569=DIRECTION('center_axis',(0.,1.,0.));
#57570=DIRECTION('ref_axis',(0.,0.,1.));
#57571=DIRECTION('',(1.,0.,-3.75424127281594E-15));
#57572=DIRECTION('center_axis',(0.,1.,0.));
#57573=DIRECTION('ref_axis',(0.,0.,1.));
#57574=DIRECTION('',(-1.,0.,-3.75424127281594E-15));
#57575=DIRECTION('center_axis',(3.75424127281594E-15,0.,1.));
#57576=DIRECTION('ref_axis',(1.,0.,-3.75424127281594E-15));
#57577=DIRECTION('',(0.,1.,0.));
#57578=DIRECTION('',(1.,0.,-3.75424127281594E-15));
#57579=DIRECTION('',(0.,1.,0.));
#57580=DIRECTION('center_axis',(0.,1.,0.));
#57581=DIRECTION('ref_axis',(0.,0.,1.));
#57582=DIRECTION('center_axis',(0.,1.,0.));
#57583=DIRECTION('ref_axis',(0.,0.,1.));
#57584=DIRECTION('',(0.,1.,0.));
#57585=DIRECTION('center_axis',(3.75424127281594E-15,0.,-1.));
#57586=DIRECTION('ref_axis',(-1.,0.,-3.75424127281594E-15));
#57587=DIRECTION('',(-1.,0.,-3.75424127281594E-15));
#57588=DIRECTION('',(0.,1.,0.));
#57589=DIRECTION('center_axis',(0.,1.,0.));
#57590=DIRECTION('ref_axis',(0.,0.,1.));
#57591=DIRECTION('center_axis',(0.,1.,0.));
#57592=DIRECTION('ref_axis',(0.,0.,1.));
#57593=DIRECTION('center_axis',(0.,1.,0.));
#57594=DIRECTION('ref_axis',(0.,0.,1.));
#57595=DIRECTION('center_axis',(0.,0.,-1.));
#57596=DIRECTION('ref_axis',(-1.,0.,0.));
#57597=DIRECTION('',(0.,0.,-1.));
#57598=DIRECTION('center_axis',(0.,0.,1.));
#57599=DIRECTION('ref_axis',(-1.,0.,0.));
#57600=DIRECTION('',(0.,0.,-1.));
#57601=DIRECTION('center_axis',(0.,0.,1.));
#57602=DIRECTION('ref_axis',(-1.,0.,0.));
#57603=DIRECTION('',(0.,0.,1.));
#57604=DIRECTION('center_axis',(0.,0.,1.));
#57605=DIRECTION('ref_axis',(-1.,-2.6760472293316E-15,0.));
#57606=DIRECTION('',(0.,0.,1.));
#57607=DIRECTION('center_axis',(-0.674290861195454,-0.353082477337477,0.648586616193645));
#57608=DIRECTION('ref_axis',(0.738465865105631,-0.322427194837445,0.592206779852315));
#57609=DIRECTION('',(0.,0.,1.));
#57610=DIRECTION('center_axis',(0.,0.,-1.));
#57611=DIRECTION('ref_axis',(-1.,0.,0.));
#57612=DIRECTION('center_axis',(0.997947005577613,-0.0140531647494822,0.0624842589713604));
#57613=DIRECTION('ref_axis',(-0.0640450849043188,-0.219494029111198,0.973509423829133));
#57614=DIRECTION('center_axis',(0.,0.,-1.));
#57615=DIRECTION('ref_axis',(-1.,0.,0.));
#57616=DIRECTION('center_axis',(-1.55697293342929E-16,-1.,0.));
#57617=DIRECTION('ref_axis',(1.,-1.55697293342929E-16,0.));
#57618=DIRECTION('center_axis',(0.,0.,1.));
#57619=DIRECTION('ref_axis',(-1.,0.,0.));
#57620=DIRECTION('center_axis',(0.,0.,-1.));
#57621=DIRECTION('ref_axis',(-6.12323399573677E-17,1.,0.));
#57622=DIRECTION('center_axis',(0.,0.,1.));
#57623=DIRECTION('ref_axis',(1.,0.,0.));
#57624=DIRECTION('',(0.,0.,-1.));
#57625=DIRECTION('center_axis',(0.,0.,1.));
#57626=DIRECTION('ref_axis',(1.,0.,0.));
#57627=DIRECTION('',(0.,0.,1.));
#57628=DIRECTION('center_axis',(0.,0.,-1.));
#57629=DIRECTION('ref_axis',(-2.83276944882399E-16,1.,0.));
#57630=DIRECTION('center_axis',(0.,0.,1.));
#57631=DIRECTION('ref_axis',(1.,0.,0.));
#57632=DIRECTION('',(0.,0.,-1.));
#57633=DIRECTION('center_axis',(0.,0.,1.));
#57634=DIRECTION('ref_axis',(1.,0.,0.));
#57635=DIRECTION('',(0.,0.,1.));
#57636=DIRECTION('center_axis',(0.,0.,-1.));
#57637=DIRECTION('ref_axis',(-6.12323399573677E-17,1.,0.));
#57638=DIRECTION('center_axis',(0.,0.,1.));
#57639=DIRECTION('ref_axis',(1.,0.,0.));
#57640=DIRECTION('',(0.,0.,-1.));
#57641=DIRECTION('center_axis',(0.,0.,1.));
#57642=DIRECTION('ref_axis',(1.,0.,0.));
#57643=DIRECTION('',(0.,0.,1.));
#57644=DIRECTION('center_axis',(0.,0.,-1.));
#57645=DIRECTION('ref_axis',(-1.,0.,0.));
#57646=DIRECTION('center_axis',(0.,0.,1.));
#57647=DIRECTION('ref_axis',(1.,0.,0.));
#57648=DIRECTION('',(0.,0.,1.));
#57649=DIRECTION('center_axis',(0.,0.,-1.));
#57650=DIRECTION('ref_axis',(1.,0.,0.));
#57651=DIRECTION('',(0.,0.,-1.));
#57652=DIRECTION('center_axis',(0.,0.,-1.));
#57653=DIRECTION('ref_axis',(1.,-1.73472347597681E-15,0.));
#57654=DIRECTION('',(0.,0.,1.));
#57655=DIRECTION('center_axis',(0.,0.,-1.));
#57656=DIRECTION('ref_axis',(1.,0.,0.));
#57657=DIRECTION('center_axis',(0.,0.,1.));
#57658=DIRECTION('ref_axis',(1.,0.,0.));
#57659=DIRECTION('center_axis',(0.,0.,1.));
#57660=DIRECTION('ref_axis',(1.,0.,0.));
#57661=DIRECTION('center_axis',(0.,0.,1.));
#57662=DIRECTION('ref_axis',(1.,0.,0.));
#57663=DIRECTION('',(0.,0.,1.));
#57664=DIRECTION('center_axis',(0.,0.,-1.));
#57665=DIRECTION('ref_axis',(1.,0.,0.));
#57666=DIRECTION('',(0.,0.,1.));
#57667=DIRECTION('center_axis',(0.,0.,1.));
#57668=DIRECTION('ref_axis',(1.,0.,0.));
#57669=DIRECTION('center_axis',(0.710660584319699,0.703535026771507,0.));
#57670=DIRECTION('ref_axis',(-0.703535026771507,0.710660584319699,0.));
#57671=DIRECTION('center_axis',(0.,0.,-1.));
#57672=DIRECTION('ref_axis',(1.,-7.7650619940415E-16,0.));
#57673=DIRECTION('center_axis',(0.710660584319702,0.703535026771503,-4.88175490844999E-15));
#57674=DIRECTION('ref_axis',(-0.703535026771503,0.710660584319702,-2.41028291557853E-29));
#57675=DIRECTION('center_axis',(0.,0.,1.));
#57676=DIRECTION('ref_axis',(0.710660584319704,0.703535026771501,0.));
#57677=DIRECTION('center_axis',(0.,0.,1.));
#57678=DIRECTION('ref_axis',(1.,0.,0.));
#57679=DIRECTION('center_axis',(0.,0.,1.));
#57680=DIRECTION('ref_axis',(1.,0.,0.));
#57681=DIRECTION('center_axis',(0.710660584319702,0.703535026771503,4.88175490844999E-15));
#57682=DIRECTION('ref_axis',(-0.703535026771503,0.710660584319702,2.41028291557853E-29));
#57683=DIRECTION('center_axis',(0.,0.,1.));
#57684=DIRECTION('ref_axis',(1.,0.,0.));
#57685=DIRECTION('center_axis',(-0.710660584319702,-0.703535026771503,0.));
#57686=DIRECTION('ref_axis',(0.703535026771503,-0.710660584319702,0.));
#57687=DIRECTION('center_axis',(0.,0.,1.));
#57688=DIRECTION('ref_axis',(1.,0.,0.));
#57689=DIRECTION('center_axis',(0.,-1.,0.));
#57690=DIRECTION('ref_axis',(-1.,0.,0.));
#57691=DIRECTION('center_axis',(0.,0.,1.));
#57692=DIRECTION('ref_axis',(1.,0.,0.));
#57693=DIRECTION('center_axis',(0.,0.,-1.));
#57694=DIRECTION('ref_axis',(-1.,0.,0.));
#57695=DIRECTION('center_axis',(0.,0.,1.));
#57696=DIRECTION('ref_axis',(1.,0.,0.));
#57697=DIRECTION('',(0.,0.,1.));
#57698=DIRECTION('center_axis',(0.,0.,-1.));
#57699=DIRECTION('ref_axis',(1.,0.,0.));
#57700=DIRECTION('',(0.,0.,-1.));
#57701=DIRECTION('center_axis',(0.,0.,-1.));
#57702=DIRECTION('ref_axis',(1.,-1.73472347597681E-15,0.));
#57703=DIRECTION('',(0.,0.,1.));
#57704=DIRECTION('center_axis',(0.,0.,-1.));
#57705=DIRECTION('ref_axis',(1.,0.,0.));
#57706=DIRECTION('center_axis',(0.,0.,1.));
#57707=DIRECTION('ref_axis',(1.,0.,0.));
#57708=DIRECTION('center_axis',(0.,0.,1.));
#57709=DIRECTION('ref_axis',(1.,0.,0.));
#57710=DIRECTION('center_axis',(0.,0.,1.));
#57711=DIRECTION('ref_axis',(1.,0.,0.));
#57712=DIRECTION('',(0.,0.,1.));
#57713=DIRECTION('center_axis',(0.,0.,-1.));
#57714=DIRECTION('ref_axis',(1.,0.,0.));
#57715=DIRECTION('',(0.,0.,1.));
#57716=DIRECTION('center_axis',(0.,0.,1.));
#57717=DIRECTION('ref_axis',(1.,0.,0.));
#57718=DIRECTION('center_axis',(0.710660584319699,0.703535026771507,0.));
#57719=DIRECTION('ref_axis',(-0.703535026771507,0.710660584319699,0.));
#57720=DIRECTION('center_axis',(0.,0.,-1.));
#57721=DIRECTION('ref_axis',(1.,-2.32951859821245E-15,0.));
#57722=DIRECTION('center_axis',(0.710660584319702,0.703535026771503,-4.88175490844999E-15));
#57723=DIRECTION('ref_axis',(-0.703535026771503,0.710660584319702,-2.41028291557853E-29));
#57724=DIRECTION('center_axis',(0.,0.,1.));
#57725=DIRECTION('ref_axis',(0.710660584319704,0.703535026771501,0.));
#57726=DIRECTION('center_axis',(0.,0.,1.));
#57727=DIRECTION('ref_axis',(1.,0.,0.));
#57728=DIRECTION('center_axis',(0.,0.,1.));
#57729=DIRECTION('ref_axis',(1.,0.,0.));
#57730=DIRECTION('center_axis',(0.710660584319702,0.703535026771503,4.88175490844999E-15));
#57731=DIRECTION('ref_axis',(-0.703535026771503,0.710660584319702,2.41028291557853E-29));
#57732=DIRECTION('center_axis',(0.,0.,1.));
#57733=DIRECTION('ref_axis',(1.,0.,0.));
#57734=DIRECTION('center_axis',(-0.710660584319702,-0.703535026771503,0.));
#57735=DIRECTION('ref_axis',(0.703535026771503,-0.710660584319702,0.));
#57736=DIRECTION('center_axis',(0.,0.,1.));
#57737=DIRECTION('ref_axis',(1.,0.,0.));
#57738=DIRECTION('center_axis',(0.,-1.,0.));
#57739=DIRECTION('ref_axis',(-1.,0.,0.));
#57740=DIRECTION('center_axis',(0.,0.,1.));
#57741=DIRECTION('ref_axis',(1.,0.,0.));
#57742=DIRECTION('center_axis',(0.,0.,-1.));
#57743=DIRECTION('ref_axis',(-1.,0.,0.));
#57744=DIRECTION('center_axis',(0.,0.,1.));
#57745=DIRECTION('ref_axis',(1.,0.,0.));
#57746=DIRECTION('',(0.,0.,1.));
#57747=DIRECTION('center_axis',(0.,0.,-1.));
#57748=DIRECTION('ref_axis',(1.,0.,0.));
#57749=DIRECTION('',(0.,0.,-1.));
#57750=DIRECTION('center_axis',(0.,0.,-1.));
#57751=DIRECTION('ref_axis',(1.,0.,0.));
#57752=DIRECTION('',(0.,0.,1.));
#57753=DIRECTION('center_axis',(0.,0.,-1.));
#57754=DIRECTION('ref_axis',(1.,0.,0.));
#57755=DIRECTION('center_axis',(0.,0.,1.));
#57756=DIRECTION('ref_axis',(1.,0.,0.));
#57757=DIRECTION('center_axis',(0.,0.,1.));
#57758=DIRECTION('ref_axis',(1.,0.,0.));
#57759=DIRECTION('center_axis',(0.,0.,1.));
#57760=DIRECTION('ref_axis',(1.,0.,0.));
#57761=DIRECTION('',(0.,0.,1.));
#57762=DIRECTION('center_axis',(0.,0.,-1.));
#57763=DIRECTION('ref_axis',(1.,0.,0.));
#57764=DIRECTION('',(0.,0.,1.));
#57765=DIRECTION('center_axis',(0.,0.,1.));
#57766=DIRECTION('ref_axis',(1.,0.,0.));
#57767=DIRECTION('center_axis',(0.710660584319699,0.703535026771507,0.));
#57768=DIRECTION('ref_axis',(-0.703535026771507,0.710660584319699,0.));
#57769=DIRECTION('center_axis',(0.,0.,-1.));
#57770=DIRECTION('ref_axis',(1.,-2.32951859821245E-15,0.));
#57771=DIRECTION('center_axis',(0.710660584319702,0.703535026771503,-4.88175490844999E-15));
#57772=DIRECTION('ref_axis',(-0.703535026771503,0.710660584319702,-2.41028291557853E-29));
#57773=DIRECTION('center_axis',(0.,0.,1.));
#57774=DIRECTION('ref_axis',(0.710660584319704,0.703535026771501,0.));
#57775=DIRECTION('center_axis',(0.,0.,1.));
#57776=DIRECTION('ref_axis',(1.,0.,0.));
#57777=DIRECTION('center_axis',(0.,0.,1.));
#57778=DIRECTION('ref_axis',(1.,0.,0.));
#57779=DIRECTION('center_axis',(0.710660584319702,0.703535026771503,4.88175490844999E-15));
#57780=DIRECTION('ref_axis',(-0.703535026771503,0.710660584319702,2.41028291557853E-29));
#57781=DIRECTION('center_axis',(0.,0.,1.));
#57782=DIRECTION('ref_axis',(1.,0.,0.));
#57783=DIRECTION('center_axis',(-0.710660584319702,-0.703535026771503,0.));
#57784=DIRECTION('ref_axis',(0.703535026771503,-0.710660584319702,0.));
#57785=DIRECTION('center_axis',(0.,0.,1.));
#57786=DIRECTION('ref_axis',(1.,0.,0.));
#57787=DIRECTION('center_axis',(0.,-1.,0.));
#57788=DIRECTION('ref_axis',(-1.,0.,0.));
#57789=DIRECTION('center_axis',(0.,0.,1.));
#57790=DIRECTION('ref_axis',(1.,0.,0.));
#57791=DIRECTION('center_axis',(0.,0.,-1.));
#57792=DIRECTION('ref_axis',(-1.,0.,0.));
#57793=DIRECTION('center_axis',(0.,0.,1.));
#57794=DIRECTION('ref_axis',(-1.,0.,0.));
#57795=DIRECTION('',(0.,0.,1.));
#57796=DIRECTION('center_axis',(0.,0.,-1.));
#57797=DIRECTION('ref_axis',(1.,-1.73321670543144E-15,0.));
#57798=DIRECTION('',(0.,0.,-1.));
#57799=DIRECTION('center_axis',(0.,0.,-1.));
#57800=DIRECTION('ref_axis',(1.,-3.59975777281914E-15,0.));
#57801=DIRECTION('',(0.,0.,1.));
#57802=DIRECTION('center_axis',(0.,0.,-1.));
#57803=DIRECTION('ref_axis',(1.,-1.73321670543144E-15,0.));
#57804=DIRECTION('center_axis',(0.,0.,1.));
#57805=DIRECTION('ref_axis',(0.,-1.,0.));
#57806=DIRECTION('center_axis',(0.,0.,1.));
#57807=DIRECTION('ref_axis',(1.,0.,0.));
#57808=DIRECTION('center_axis',(1.27486239704332E-16,-1.,0.));
#57809=DIRECTION('ref_axis',(1.,1.27486239704332E-16,0.));
#57810=DIRECTION('center_axis',(-1.27486239704332E-16,1.,0.));
#57811=DIRECTION('ref_axis',(1.,1.27486239704332E-16,0.));
#57812=DIRECTION('center_axis',(-1.27486239704332E-16,1.,0.));
#57813=DIRECTION('ref_axis',(1.,1.27486239704332E-16,-1.88173394004264E-13));
#57814=DIRECTION('',(0.,0.,-1.));
#57815=DIRECTION('',(-1.,-1.27486239704332E-16,0.));
#57816=DIRECTION('',(0.,0.,1.));
#57817=DIRECTION('center_axis',(-1.27486239704332E-16,1.,0.));
#57818=DIRECTION('ref_axis',(-1.,-1.27486239704332E-16,0.));
#57819=DIRECTION('',(1.27486239704332E-16,-1.,0.));
#57820=DIRECTION('center_axis',(1.27486239704332E-16,-1.,0.));
#57821=DIRECTION('ref_axis',(1.,1.27486239704332E-16,0.));
#57822=DIRECTION('',(0.,1.,0.));
#57823=DIRECTION('center_axis',(0.,1.,0.));
#57824=DIRECTION('ref_axis',(0.,0.,1.));
#57825=DIRECTION('',(-1.27486239704332E-16,1.,0.));
#57826=DIRECTION('center_axis',(-1.27486239704332E-16,1.,0.));
#57827=DIRECTION('ref_axis',(-1.,-1.27486239704332E-16,0.));
#57828=DIRECTION('',(0.,-1.,0.));
#57829=DIRECTION('center_axis',(1.27486239704332E-16,-1.,0.));
#57830=DIRECTION('ref_axis',(1.,1.27486239704332E-16,0.));
#57831=DIRECTION('',(-1.27486239704332E-16,1.,0.));
#57832=DIRECTION('center_axis',(0.,1.,0.));
#57833=DIRECTION('ref_axis',(0.,0.,1.));
#57834=DIRECTION('center_axis',(0.,0.,-1.));
#57835=DIRECTION('ref_axis',(-1.,0.,0.));
#57836=DIRECTION('',(-1.,0.,0.));
#57837=DIRECTION('',(0.,1.,0.));
#57838=DIRECTION('',(1.,1.27486239704332E-16,0.));
#57839=DIRECTION('',(0.,-1.,0.));
#57840=DIRECTION('center_axis',(1.,0.,0.));
#57841=DIRECTION('ref_axis',(0.,0.,-1.));
#57842=DIRECTION('',(0.,0.,-1.));
#57843=DIRECTION('',(0.,-1.,0.));
#57844=DIRECTION('',(0.,0.,1.));
#57845=DIRECTION('center_axis',(-1.,0.,0.));
#57846=DIRECTION('ref_axis',(0.,0.,1.));
#57847=DIRECTION('',(0.,1.,0.));
#57848=DIRECTION('',(0.,0.,1.));
#57849=DIRECTION('',(0.,0.,-1.));
#57850=DIRECTION('center_axis',(0.00367439112755605,0.,-0.999993249402136));
#57851=DIRECTION('ref_axis',(-0.999993249402136,0.,-0.00367439112755605));
#57852=DIRECTION('center_axis',(-1.,0.,-1.23259516440783E-29));
#57853=DIRECTION('ref_axis',(-1.23259516440783E-29,0.,1.));
#57854=DIRECTION('center_axis',(-0.0036743911275285,0.,-0.999993249402136));
#57855=DIRECTION('ref_axis',(-0.999993249402136,0.,0.0036743911275285));
#57856=DIRECTION('center_axis',(0.,1.,0.));
#57857=DIRECTION('ref_axis',(0.,0.,1.));
#57858=DIRECTION('center_axis',(0.,-1.,0.));
#57859=DIRECTION('ref_axis',(0.,0.,-1.));
#57860=DIRECTION('center_axis',(0.,0.,-1.));
#57861=DIRECTION('ref_axis',(-1.,0.,0.));
#57862=DIRECTION('center_axis',(0.,1.,0.));
#57863=DIRECTION('ref_axis',(0.,0.,1.));
#57864=DIRECTION('center_axis',(0.,-1.,0.));
#57865=DIRECTION('ref_axis',(0.,0.,-1.));
#57866=DIRECTION('center_axis',(0.,0.,-1.));
#57867=DIRECTION('ref_axis',(-1.,0.,0.));
#57868=DIRECTION('center_axis',(0.,0.,-1.));
#57869=DIRECTION('ref_axis',(-1.,0.,0.));
#57870=DIRECTION('center_axis',(0.,0.,-1.));
#57871=DIRECTION('ref_axis',(-1.,0.,0.));
#57872=DIRECTION('',(0.,0.,1.));
#57873=DIRECTION('center_axis',(0.,0.,1.));
#57874=DIRECTION('ref_axis',(1.,0.,0.));
#57875=DIRECTION('',(0.,0.,-1.));
#57876=DIRECTION('center_axis',(0.,0.,-1.));
#57877=DIRECTION('ref_axis',(-1.,0.,0.));
#57878=DIRECTION('center_axis',(-1.,0.,0.));
#57879=DIRECTION('ref_axis',(0.,0.,1.));
#57880=DIRECTION('center_axis',(-1.,0.,0.));
#57881=DIRECTION('ref_axis',(0.,0.,1.));
#57882=DIRECTION('center_axis',(1.,0.,0.));
#57883=DIRECTION('ref_axis',(0.,0.,-1.));
#57884=DIRECTION('',(1.,0.,0.));
#57885=DIRECTION('center_axis',(0.,1.,0.));
#57886=DIRECTION('ref_axis',(1.,0.,0.));
#57887=DIRECTION('center_axis',(0.,1.,0.));
#57888=DIRECTION('ref_axis',(0.,0.,-1.));
#57889=DIRECTION('center_axis',(0.,1.,0.));
#57890=DIRECTION('ref_axis',(1.,0.,0.));
#57891=DIRECTION('center_axis',(0.,1.,0.));
#57892=DIRECTION('ref_axis',(0.,0.,-1.));
#57893=DIRECTION('center_axis',(0.,-1.,0.));
#57894=DIRECTION('ref_axis',(0.,0.,-1.));
#57895=DIRECTION('center_axis',(0.,1.,0.));
#57896=DIRECTION('ref_axis',(0.,0.,1.));
#57897=DIRECTION('center_axis',(0.,1.,0.));
#57898=DIRECTION('ref_axis',(0.,0.,1.));
#57899=DIRECTION('center_axis',(0.,1.,0.));
#57900=DIRECTION('ref_axis',(0.,0.,1.));
#57901=DIRECTION('center_axis',(1.,1.27486239704332E-16,0.));
#57902=DIRECTION('ref_axis',(-1.27486239704332E-16,1.,0.));
#57903=DIRECTION('center_axis',(1.,0.,0.));
#57904=DIRECTION('ref_axis',(0.,0.,-1.));
#57905=DIRECTION('center_axis',(-1.,0.,0.));
#57906=DIRECTION('ref_axis',(0.,0.,1.));
#57907=DIRECTION('center_axis',(0.,1.,0.));
#57908=DIRECTION('ref_axis',(1.,0.,0.));
#57909=DIRECTION('center_axis',(0.,0.,1.));
#57910=DIRECTION('ref_axis',(-1.,0.,0.));
#57911=DIRECTION('center_axis',(0.,1.,0.));
#57912=DIRECTION('ref_axis',(1.,0.,0.));
#57913=DIRECTION('center_axis',(0.,0.,1.));
#57914=DIRECTION('ref_axis',(-1.,0.,0.));
#57915=DIRECTION('center_axis',(0.,0.,-1.));
#57916=DIRECTION('ref_axis',(-1.,0.,0.));
#57917=DIRECTION('center_axis',(0.,0.,1.));
#57918=DIRECTION('ref_axis',(1.,0.,0.));
#57919=DIRECTION('center_axis',(0.,0.,-1.));
#57920=DIRECTION('ref_axis',(-1.,0.,0.));
#57921=DIRECTION('center_axis',(0.,0.,1.));
#57922=DIRECTION('ref_axis',(1.,0.,0.));
#57923=DIRECTION('center_axis',(1.27486239704332E-16,-1.,0.));
#57924=DIRECTION('ref_axis',(1.,2.368475785867E-16,0.));
#57925=DIRECTION('center_axis',(-0.00367439112755605,2.03969681564559E-16,
0.999993249402136));
#57926=DIRECTION('ref_axis',(0.999993249402136,6.24671789190351E-35,0.00367439112755605));
#57927=DIRECTION('center_axis',(1.27486239704332E-16,-1.,0.));
#57928=DIRECTION('ref_axis',(1.,2.368475785867E-16,0.));
#57929=DIRECTION('center_axis',(0.0036743911275283,0.,0.999993249402136));
#57930=DIRECTION('ref_axis',(0.999993249402136,0.,-0.0036743911275283));
#57931=DIRECTION('center_axis',(-1.,1.56267011062633E-16,2.83753250766951E-16));
#57932=DIRECTION('ref_axis',(2.83753250766951E-16,1.09476442525376E-47,
1.));
#57933=DIRECTION('center_axis',(0.,0.,1.));
#57934=DIRECTION('ref_axis',(1.,0.,0.));
#57935=DIRECTION('center_axis',(0.,-1.,0.));
#57936=DIRECTION('ref_axis',(0.,0.,-1.));
#57937=DIRECTION('center_axis',(0.,0.,-1.));
#57938=DIRECTION('ref_axis',(1.,0.,0.));
#57939=DIRECTION('center_axis',(0.,-1.,0.));
#57940=DIRECTION('ref_axis',(0.,0.,-1.));
#57941=DIRECTION('center_axis',(0.,0.,1.));
#57942=DIRECTION('ref_axis',(1.,0.,0.));
#57943=DIRECTION('center_axis',(0.,1.,0.));
#57944=DIRECTION('ref_axis',(0.,0.,1.));
#57945=DIRECTION('center_axis',(0.,-1.,0.));
#57946=DIRECTION('ref_axis',(0.,0.,-1.));
#57947=DIRECTION('',(0.,1.,0.));
#57948=DIRECTION('',(0.,-1.,0.));
#57949=DIRECTION('center_axis',(0.,-1.,0.));
#57950=DIRECTION('ref_axis',(0.,0.,-1.));
#57951=DIRECTION('center_axis',(0.,-1.,0.));
#57952=DIRECTION('ref_axis',(0.,0.,-1.));
#57953=DIRECTION('',(0.,1.,0.));
#57954=DIRECTION('',(0.,-1.,0.));
#57955=DIRECTION('center_axis',(0.,0.,1.));
#57956=DIRECTION('ref_axis',(1.,0.,0.));
#57957=DIRECTION('center_axis',(0.,0.,-1.));
#57958=DIRECTION('ref_axis',(1.,0.,0.));
#57959=DIRECTION('center_axis',(0.,0.,1.));
#57960=DIRECTION('ref_axis',(1.,0.,0.));
#57961=DIRECTION('center_axis',(0.,0.,-1.));
#57962=DIRECTION('ref_axis',(-1.,0.,0.));
#57963=DIRECTION('center_axis',(0.,0.,1.));
#57964=DIRECTION('ref_axis',(-1.,9.91270557701024E-15,0.));
#57965=DIRECTION('',(0.,0.,1.));
#57966=DIRECTION('center_axis',(0.,0.,-1.));
#57967=DIRECTION('ref_axis',(1.,0.,0.));
#57968=DIRECTION('center_axis',(0.988416151653142,0.151767951660399,0.));
#57969=DIRECTION('ref_axis',(-0.151767951660399,0.988416151653142,0.));
#57970=DIRECTION('center_axis',(0.,-1.,0.));
#57971=DIRECTION('ref_axis',(0.,0.,-1.));
#57972=DIRECTION('center_axis',(0.,1.,0.));
#57973=DIRECTION('ref_axis',(0.,0.,1.));
#57974=DIRECTION('center_axis',(0.,-1.,0.));
#57975=DIRECTION('ref_axis',(0.,0.,-1.));
#57976=DIRECTION('',(0.,1.,0.));
#57977=DIRECTION('',(0.,-1.,0.));
#57978=DIRECTION('center_axis',(0.,0.,1.));
#57979=DIRECTION('ref_axis',(1.,0.,0.));
#57980=DIRECTION('center_axis',(0.988416151653139,-0.151767951660418,0.));
#57981=DIRECTION('ref_axis',(-0.151767951660418,-0.988416151653139,0.));
#57982=DIRECTION('center_axis',(0.,0.,1.));
#57983=DIRECTION('ref_axis',(1.,0.,0.));
#57984=DIRECTION('center_axis',(0.,1.,0.));
#57985=DIRECTION('ref_axis',(0.,0.,1.));
#57986=DIRECTION('center_axis',(0.,-1.,0.));
#57987=DIRECTION('ref_axis',(0.,0.,-1.));
#57988=DIRECTION('',(0.,-1.,0.));
#57989=DIRECTION('',(0.,1.,0.));
#57990=DIRECTION('center_axis',(0.,0.,1.));
#57991=DIRECTION('ref_axis',(1.,0.,0.));
#57992=DIRECTION('center_axis',(0.,1.,0.));
#57993=DIRECTION('ref_axis',(0.,0.,1.));
#57994=DIRECTION('center_axis',(0.,0.,-1.));
#57995=DIRECTION('ref_axis',(1.,0.,0.));
#57996=DIRECTION('center_axis',(0.,0.,1.));
#57997=DIRECTION('ref_axis',(1.,0.,0.));
#57998=DIRECTION('center_axis',(0.,0.,1.));
#57999=DIRECTION('ref_axis',(1.,0.,0.));
#58000=DIRECTION('center_axis',(0.,-1.,0.));
#58001=DIRECTION('ref_axis',(0.,0.,-1.));
#58002=DIRECTION('center_axis',(0.,0.,-1.));
#58003=DIRECTION('ref_axis',(-1.,0.,0.));
#58004=DIRECTION('center_axis',(0.,0.,1.));
#58005=DIRECTION('ref_axis',(1.,0.,0.));
#58006=DIRECTION('center_axis',(0.,1.,0.));
#58007=DIRECTION('ref_axis',(0.,0.,1.));
#58008=DIRECTION('center_axis',(0.,0.,1.));
#58009=DIRECTION('ref_axis',(1.,0.,0.));
#58010=DIRECTION('center_axis',(0.,0.,-1.));
#58011=DIRECTION('ref_axis',(1.,0.,0.));
#58012=DIRECTION('center_axis',(0.,-1.,0.));
#58013=DIRECTION('ref_axis',(0.,0.,-1.));
#58014=DIRECTION('',(0.,1.,0.));
#58015=DIRECTION('',(0.,-1.,0.));
#58016=DIRECTION('center_axis',(0.,0.,-1.));
#58017=DIRECTION('ref_axis',(-1.,0.,0.));
#58018=DIRECTION('',(0.,0.,-1.));
#58019=DIRECTION('center_axis',(0.,-1.,0.));
#58020=DIRECTION('ref_axis',(0.,0.,-1.));
#58021=DIRECTION('',(0.,1.,0.));
#58022=DIRECTION('',(0.,-1.,0.));
#58023=DIRECTION('center_axis',(0.,0.,1.));
#58024=DIRECTION('ref_axis',(1.,0.,0.));
#58025=DIRECTION('center_axis',(0.,0.,1.));
#58026=DIRECTION('ref_axis',(1.,0.,0.));
#58027=DIRECTION('center_axis',(0.,0.,1.));
#58028=DIRECTION('ref_axis',(1.,0.,0.));
#58029=DIRECTION('',(0.,0.,1.));
#58030=DIRECTION('',(0.,0.,1.));
#58031=DIRECTION('center_axis',(0.,0.,1.));
#58032=DIRECTION('ref_axis',(1.,0.,0.));
#58033=DIRECTION('',(0.,0.,1.));
#58034=DIRECTION('',(0.,0.,1.));
#58035=DIRECTION('center_axis',(1.,0.,0.));
#58036=DIRECTION('ref_axis',(0.,0.,-1.));
#58037=DIRECTION('center_axis',(-1.,0.,0.));
#58038=DIRECTION('ref_axis',(0.,0.,1.));
#58039=DIRECTION('center_axis',(0.,0.,1.));
#58040=DIRECTION('ref_axis',(1.,0.,0.));
#58041=DIRECTION('center_axis',(0.710660584319708,0.703535026771498,0.));
#58042=DIRECTION('ref_axis',(-0.703535026771498,0.710660584319708,0.));
#58043=DIRECTION('center_axis',(0.710660584319702,0.703535026771503,0.));
#58044=DIRECTION('ref_axis',(-0.703535026771503,0.710660584319702,0.));
#58045=DIRECTION('',(-0.710660584319708,-0.703535026771497,0.));
#58046=DIRECTION('',(0.710660584319708,0.703535026771497,0.));
#58047=DIRECTION('center_axis',(0.,0.,1.));
#58048=DIRECTION('ref_axis',(-0.710660584319708,-0.703535026771497,0.));
#58049=DIRECTION('center_axis',(-0.710660584319705,-0.7035350267715,0.));
#58050=DIRECTION('ref_axis',(0.7035350267715,-0.710660584319705,0.));
#58051=DIRECTION('center_axis',(0.,0.,-1.));
#58052=DIRECTION('ref_axis',(1.,0.,0.));
#58053=DIRECTION('center_axis',(0.,0.,1.));
#58054=DIRECTION('ref_axis',(1.,0.,0.));
#58055=DIRECTION('center_axis',(-0.710660584319708,-0.703535026771498,0.));
#58056=DIRECTION('ref_axis',(0.703535026771498,-0.710660584319708,0.));
#58057=DIRECTION('',(0.710660584319708,0.703535026771497,0.));
#58058=DIRECTION('',(-0.710660584319708,-0.703535026771497,0.));
#58059=DIRECTION('center_axis',(0.,0.,1.));
#58060=DIRECTION('ref_axis',(1.,0.,0.));
#58061=DIRECTION('center_axis',(-0.538450589001472,0.842657085179949,1.16942162228788E-14));
#58062=DIRECTION('ref_axis',(0.842657085179949,0.538450589001472,-2.58948405569131E-29));
#58063=DIRECTION('center_axis',(0.837188370386661,-0.546914648267284,0.));
#58064=DIRECTION('ref_axis',(-0.546914648267284,-0.837188370386661,0.));
#58065=DIRECTION('center_axis',(0.,0.,1.));
#58066=DIRECTION('ref_axis',(1.,0.,0.));
#58067=DIRECTION('center_axis',(0.,0.,1.));
#58068=DIRECTION('ref_axis',(1.,0.,0.));
#58069=DIRECTION('center_axis',(0.,0.,1.));
#58070=DIRECTION('ref_axis',(1.,0.,0.));
#58071=DIRECTION('center_axis',(0.,0.,-1.));
#58072=DIRECTION('ref_axis',(-1.,0.,0.));
#58073=DIRECTION('center_axis',(0.,0.,1.));
#58074=DIRECTION('ref_axis',(-1.,-6.93889390390722E-15,0.));
#58075=DIRECTION('',(0.,0.,1.));
#58076=DIRECTION('center_axis',(-0.710660584319708,-0.703535026771498,0.));
#58077=DIRECTION('ref_axis',(0.703535026771498,-0.710660584319708,0.));
#58078=DIRECTION('center_axis',(0.710660584319703,0.703535026771502,-3.66131618133748E-15));
#58079=DIRECTION('ref_axis',(-0.703535026771502,0.710660584319703,4.48656828425865E-30));
#58080=DIRECTION('',(-0.710660584319708,-0.703535026771497,0.));
#58081=DIRECTION('',(0.710660584319708,0.703535026771497,0.));
#58082=DIRECTION('center_axis',(0.710660584319708,0.703535026771498,0.));
#58083=DIRECTION('ref_axis',(-0.703535026771498,0.710660584319708,0.));
#58084=DIRECTION('center_axis',(0.7106605843197,0.703535026771505,0.));
#58085=DIRECTION('ref_axis',(-0.703535026771505,0.7106605843197,0.));
#58086=DIRECTION('',(-0.710660584319708,-0.703535026771497,0.));
#58087=DIRECTION('',(0.710660584319708,0.703535026771497,0.));
#58088=DIRECTION('center_axis',(0.,0.,-1.));
#58089=DIRECTION('ref_axis',(0.989914405816618,-0.141666753886477,0.));
#58090=DIRECTION('center_axis',(0.,0.,1.));
#58091=DIRECTION('ref_axis',(-1.,6.93889390390722E-15,0.));
#58092=DIRECTION('',(0.,0.,-1.));
#58093=DIRECTION('center_axis',(0.710660584319718,0.703535026771487,0.));
#58094=DIRECTION('ref_axis',(-0.703535026771487,0.710660584319718,0.));
#58095=DIRECTION('center_axis',(0.,0.,1.));
#58096=DIRECTION('ref_axis',(-0.710660584319708,-0.703535026771497,0.));
#58097=DIRECTION('center_axis',(0.,0.,1.));
#58098=DIRECTION('ref_axis',(1.,0.,0.));
#58099=DIRECTION('center_axis',(0.,0.,-1.));
#58100=DIRECTION('ref_axis',(1.,0.,0.));
#58101=DIRECTION('center_axis',(0.710660584319702,0.703535026771503,9.76350981689998E-15));
#58102=DIRECTION('ref_axis',(-0.703535026771503,0.710660584319702,-1.13654707447903E-31));
#58103=DIRECTION('center_axis',(-0.710660584319708,-0.703535026771498,0.));
#58104=DIRECTION('ref_axis',(0.703535026771498,-0.710660584319708,0.));
#58105=DIRECTION('',(0.710660584319708,0.703535026771497,0.));
#58106=DIRECTION('',(-0.710660584319708,-0.703535026771497,0.));
#58107=DIRECTION('center_axis',(0.710660584319708,0.703535026771498,0.));
#58108=DIRECTION('ref_axis',(-0.703535026771498,0.710660584319708,0.));
#58109=DIRECTION('',(0.710660584319708,0.703535026771497,0.));
#58110=DIRECTION('',(-0.710660584319708,-0.703535026771497,0.));
#58111=DIRECTION('center_axis',(0.,0.,1.));
#58112=DIRECTION('ref_axis',(1.,0.,0.));
#58113=DIRECTION('center_axis',(0.,0.,1.));
#58114=DIRECTION('ref_axis',(1.,0.,0.));
#58115=DIRECTION('center_axis',(0.,0.,1.));
#58116=DIRECTION('ref_axis',(-0.710660584319707,-0.703535026771498,0.));
#58117=DIRECTION('',(0.,0.,1.));
#58118=DIRECTION('',(0.,0.,1.));
#58119=DIRECTION('center_axis',(-0.703535026771498,0.710660584319708,0.));
#58120=DIRECTION('ref_axis',(-0.710660584319708,-0.703535026771498,0.));
#58121=DIRECTION('center_axis',(0.703535026771498,-0.710660584319708,0.));
#58122=DIRECTION('ref_axis',(0.710660584319708,0.703535026771498,0.));
#58123=DIRECTION('center_axis',(0.,0.,1.));
#58124=DIRECTION('ref_axis',(1.,0.,0.));
#58125=DIRECTION('center_axis',(0.710660584319708,0.703535026771498,0.));
#58126=DIRECTION('ref_axis',(-0.703535026771498,0.710660584319708,0.));
#58127=DIRECTION('center_axis',(0.710660584319702,0.703535026771503,0.));
#58128=DIRECTION('ref_axis',(-0.703535026771503,0.710660584319702,0.));
#58129=DIRECTION('',(-0.710660584319708,-0.703535026771497,0.));
#58130=DIRECTION('',(0.710660584319708,0.703535026771497,0.));
#58131=DIRECTION('center_axis',(0.,0.,1.));
#58132=DIRECTION('ref_axis',(-0.710660584319708,-0.703535026771497,0.));
#58133=DIRECTION('center_axis',(-0.710660584319705,-0.7035350267715,0.));
#58134=DIRECTION('ref_axis',(0.7035350267715,-0.710660584319705,0.));
#58135=DIRECTION('center_axis',(0.,0.,-1.));
#58136=DIRECTION('ref_axis',(1.,0.,0.));
#58137=DIRECTION('center_axis',(0.,0.,1.));
#58138=DIRECTION('ref_axis',(1.,0.,0.));
#58139=DIRECTION('center_axis',(-0.710660584319708,-0.703535026771498,0.));
#58140=DIRECTION('ref_axis',(0.703535026771498,-0.710660584319708,0.));
#58141=DIRECTION('',(0.710660584319708,0.703535026771497,0.));
#58142=DIRECTION('',(-0.710660584319708,-0.703535026771497,0.));
#58143=DIRECTION('center_axis',(0.,0.,1.));
#58144=DIRECTION('ref_axis',(1.,0.,0.));
#58145=DIRECTION('center_axis',(-0.538450589001472,0.842657085179949,1.16942162228788E-14));
#58146=DIRECTION('ref_axis',(0.842657085179949,0.538450589001472,-6.90946196667231E-29));
#58147=DIRECTION('center_axis',(0.837188370386661,-0.546914648267284,0.));
#58148=DIRECTION('ref_axis',(-0.546914648267284,-0.837188370386661,0.));
#58149=DIRECTION('center_axis',(0.,0.,1.));
#58150=DIRECTION('ref_axis',(1.,0.,0.));
#58151=DIRECTION('center_axis',(0.,0.,1.));
#58152=DIRECTION('ref_axis',(1.,0.,0.));
#58153=DIRECTION('center_axis',(0.,0.,1.));
#58154=DIRECTION('ref_axis',(1.,0.,0.));
#58155=DIRECTION('center_axis',(0.,0.,-1.));
#58156=DIRECTION('ref_axis',(-1.,0.,0.));
#58157=DIRECTION('center_axis',(0.,0.,1.));
#58158=DIRECTION('ref_axis',(-1.,-2.77555756156289E-14,0.));
#58159=DIRECTION('',(0.,0.,1.));
#58160=DIRECTION('center_axis',(-0.710660584319708,-0.703535026771498,0.));
#58161=DIRECTION('ref_axis',(0.703535026771498,-0.710660584319708,0.));
#58162=DIRECTION('center_axis',(0.710660584319703,0.703535026771502,-3.66131618133748E-15));
#58163=DIRECTION('ref_axis',(-0.703535026771502,0.710660584319703,-1.3070762122351E-29));
#58164=DIRECTION('',(-0.710660584319708,-0.703535026771497,0.));
#58165=DIRECTION('',(0.710660584319708,0.703535026771497,0.));
#58166=DIRECTION('center_axis',(0.710660584319708,0.703535026771498,0.));
#58167=DIRECTION('ref_axis',(-0.703535026771498,0.710660584319708,0.));
#58168=DIRECTION('center_axis',(0.7106605843197,0.703535026771505,0.));
#58169=DIRECTION('ref_axis',(-0.703535026771505,0.7106605843197,0.));
#58170=DIRECTION('',(-0.710660584319708,-0.703535026771497,0.));
#58171=DIRECTION('',(0.710660584319708,0.703535026771497,0.));
#58172=DIRECTION('center_axis',(0.,0.,-1.));
#58173=DIRECTION('ref_axis',(0.989914405816619,-0.141666753886473,0.));
#58174=DIRECTION('center_axis',(0.,0.,1.));
#58175=DIRECTION('ref_axis',(-1.,2.77555756156289E-14,0.));
#58176=DIRECTION('',(0.,0.,-1.));
#58177=DIRECTION('center_axis',(0.710660584319718,0.703535026771487,0.));
#58178=DIRECTION('ref_axis',(-0.703535026771488,0.710660584319718,0.));
#58179=DIRECTION('center_axis',(0.,0.,1.));
#58180=DIRECTION('ref_axis',(-0.710660584319709,-0.703535026771496,0.));
#58181=DIRECTION('center_axis',(0.,0.,1.));
#58182=DIRECTION('ref_axis',(1.,0.,0.));
#58183=DIRECTION('center_axis',(0.,0.,-1.));
#58184=DIRECTION('ref_axis',(1.,0.,0.));
#58185=DIRECTION('center_axis',(0.710660584319702,0.703535026771503,9.76350981689998E-15));
#58186=DIRECTION('ref_axis',(-0.703535026771503,0.710660584319702,4.82056583115707E-29));
#58187=DIRECTION('center_axis',(-0.710660584319708,-0.703535026771498,0.));
#58188=DIRECTION('ref_axis',(0.703535026771498,-0.710660584319708,0.));
#58189=DIRECTION('',(0.710660584319708,0.703535026771497,0.));
#58190=DIRECTION('',(-0.710660584319708,-0.703535026771497,0.));
#58191=DIRECTION('center_axis',(0.710660584319708,0.703535026771498,0.));
#58192=DIRECTION('ref_axis',(-0.703535026771498,0.710660584319708,0.));
#58193=DIRECTION('',(0.710660584319708,0.703535026771497,0.));
#58194=DIRECTION('',(-0.710660584319708,-0.703535026771497,0.));
#58195=DIRECTION('center_axis',(0.,0.,1.));
#58196=DIRECTION('ref_axis',(1.,0.,0.));
#58197=DIRECTION('center_axis',(0.,0.,1.));
#58198=DIRECTION('ref_axis',(1.,0.,0.));
#58199=DIRECTION('center_axis',(0.,0.,1.));
#58200=DIRECTION('ref_axis',(-0.710660584319709,-0.703535026771496,0.));
#58201=DIRECTION('',(0.,0.,1.));
#58202=DIRECTION('',(0.,0.,1.));
#58203=DIRECTION('center_axis',(-0.703535026771498,0.710660584319708,0.));
#58204=DIRECTION('ref_axis',(-0.710660584319708,-0.703535026771498,0.));
#58205=DIRECTION('center_axis',(0.703535026771498,-0.710660584319708,0.));
#58206=DIRECTION('ref_axis',(0.710660584319708,0.703535026771498,0.));
#58207=DIRECTION('center_axis',(0.,0.,1.));
#58208=DIRECTION('ref_axis',(1.,0.,0.));
#58209=DIRECTION('center_axis',(0.710660584319708,0.703535026771498,0.));
#58210=DIRECTION('ref_axis',(-0.703535026771498,0.710660584319708,0.));
#58211=DIRECTION('center_axis',(0.710660584319702,0.703535026771503,0.));
#58212=DIRECTION('ref_axis',(-0.703535026771503,0.710660584319702,0.));
#58213=DIRECTION('',(-0.710660584319708,-0.703535026771497,0.));
#58214=DIRECTION('',(0.710660584319708,0.703535026771497,0.));
#58215=DIRECTION('center_axis',(0.,0.,1.));
#58216=DIRECTION('ref_axis',(-0.710660584319709,-0.703535026771496,0.));
#58217=DIRECTION('center_axis',(-0.710660584319705,-0.7035350267715,0.));
#58218=DIRECTION('ref_axis',(0.7035350267715,-0.710660584319705,0.));
#58219=DIRECTION('center_axis',(0.,0.,-1.));
#58220=DIRECTION('ref_axis',(1.,0.,0.));
#58221=DIRECTION('center_axis',(0.,0.,1.));
#58222=DIRECTION('ref_axis',(1.,0.,0.));
#58223=DIRECTION('center_axis',(-0.710660584319708,-0.703535026771498,0.));
#58224=DIRECTION('ref_axis',(0.703535026771498,-0.710660584319708,0.));
#58225=DIRECTION('',(0.710660584319708,0.703535026771497,0.));
#58226=DIRECTION('',(-0.710660584319708,-0.703535026771497,0.));
#58227=DIRECTION('center_axis',(0.,0.,1.));
#58228=DIRECTION('ref_axis',(1.,0.,0.));
#58229=DIRECTION('center_axis',(-0.538450589001472,0.842657085179949,1.16942162228788E-14));
#58230=DIRECTION('ref_axis',(0.842657085179949,0.538450589001472,-6.90946196667231E-29));
#58231=DIRECTION('center_axis',(0.837188370386661,-0.546914648267284,0.));
#58232=DIRECTION('ref_axis',(-0.546914648267284,-0.837188370386661,0.));
#58233=DIRECTION('center_axis',(0.,0.,1.));
#58234=DIRECTION('ref_axis',(1.,0.,0.));
#58235=DIRECTION('center_axis',(0.,0.,1.));
#58236=DIRECTION('ref_axis',(1.,0.,0.));
#58237=DIRECTION('center_axis',(0.,0.,1.));
#58238=DIRECTION('ref_axis',(1.,0.,0.));
#58239=DIRECTION('center_axis',(0.,0.,-1.));
#58240=DIRECTION('ref_axis',(-1.,0.,0.));
#58241=DIRECTION('center_axis',(0.,0.,1.));
#58242=DIRECTION('ref_axis',(-1.,-2.77555756156289E-14,0.));
#58243=DIRECTION('',(0.,0.,1.));
#58244=DIRECTION('center_axis',(-0.710660584319708,-0.703535026771498,0.));
#58245=DIRECTION('ref_axis',(0.703535026771498,-0.710660584319708,0.));
#58246=DIRECTION('center_axis',(0.710660584319703,0.703535026771502,-3.66131618133748E-15));
#58247=DIRECTION('ref_axis',(-0.703535026771502,0.710660584319703,-1.3070762122351E-29));
#58248=DIRECTION('',(-0.710660584319708,-0.703535026771497,0.));
#58249=DIRECTION('',(0.710660584319708,0.703535026771497,0.));
#58250=DIRECTION('center_axis',(0.710660584319708,0.703535026771498,0.));
#58251=DIRECTION('ref_axis',(-0.703535026771498,0.710660584319708,0.));
#58252=DIRECTION('center_axis',(0.7106605843197,0.703535026771505,0.));
#58253=DIRECTION('ref_axis',(-0.703535026771505,0.7106605843197,0.));
#58254=DIRECTION('',(-0.710660584319708,-0.703535026771497,0.));
#58255=DIRECTION('',(0.710660584319708,0.703535026771497,0.));
#58256=DIRECTION('center_axis',(0.,0.,-1.));
#58257=DIRECTION('ref_axis',(0.989914405816618,-0.141666753886482,0.));
#58258=DIRECTION('center_axis',(0.,0.,1.));
#58259=DIRECTION('ref_axis',(-1.,4.85722573273506E-14,0.));
#58260=DIRECTION('',(0.,0.,-1.));
#58261=DIRECTION('center_axis',(0.710660584319718,0.703535026771487,0.));
#58262=DIRECTION('ref_axis',(-0.703535026771487,0.710660584319718,0.));
#58263=DIRECTION('center_axis',(0.,0.,1.));
#58264=DIRECTION('ref_axis',(-0.710660584319709,-0.703535026771496,0.));
#58265=DIRECTION('center_axis',(0.,0.,1.));
#58266=DIRECTION('ref_axis',(1.,0.,0.));
#58267=DIRECTION('center_axis',(0.,0.,-1.));
#58268=DIRECTION('ref_axis',(1.,0.,0.));
#58269=DIRECTION('center_axis',(0.710660584319702,0.703535026771503,9.76350981689998E-15));
#58270=DIRECTION('ref_axis',(-0.703535026771503,0.710660584319702,4.82056583115707E-29));
#58271=DIRECTION('center_axis',(-0.710660584319708,-0.703535026771498,0.));
#58272=DIRECTION('ref_axis',(0.703535026771498,-0.710660584319708,0.));
#58273=DIRECTION('',(0.710660584319708,0.703535026771497,0.));
#58274=DIRECTION('',(-0.710660584319708,-0.703535026771497,0.));
#58275=DIRECTION('center_axis',(0.710660584319708,0.703535026771498,0.));
#58276=DIRECTION('ref_axis',(-0.703535026771498,0.710660584319708,0.));
#58277=DIRECTION('',(0.710660584319708,0.703535026771497,0.));
#58278=DIRECTION('',(-0.710660584319708,-0.703535026771497,0.));
#58279=DIRECTION('center_axis',(0.,0.,1.));
#58280=DIRECTION('ref_axis',(1.,0.,0.));
#58281=DIRECTION('center_axis',(0.,0.,1.));
#58282=DIRECTION('ref_axis',(1.,0.,0.));
#58283=DIRECTION('center_axis',(0.,0.,1.));
#58284=DIRECTION('ref_axis',(-0.710660584319707,-0.703535026771498,0.));
#58285=DIRECTION('',(0.,0.,1.));
#58286=DIRECTION('',(0.,0.,1.));
#58287=DIRECTION('center_axis',(-0.703535026771498,0.710660584319708,0.));
#58288=DIRECTION('ref_axis',(-0.710660584319708,-0.703535026771498,0.));
#58289=DIRECTION('center_axis',(0.703535026771498,-0.710660584319708,0.));
#58290=DIRECTION('ref_axis',(0.710660584319708,0.703535026771498,0.));
#58291=DIRECTION('center_axis',(0.,0.,1.));
#58292=DIRECTION('ref_axis',(1.,0.,0.));
#58293=DIRECTION('center_axis',(0.,0.,1.));
#58294=DIRECTION('ref_axis',(1.,0.,0.));
#58295=DIRECTION('',(1.,0.,0.));
#58296=DIRECTION('center_axis',(0.,0.,1.));
#58297=DIRECTION('ref_axis',(1.,0.,0.));
#58298=DIRECTION('',(1.,0.,0.));
#58299=DIRECTION('center_axis',(0.,0.,1.));
#58300=DIRECTION('ref_axis',(1.,0.,0.));
#58301=DIRECTION('',(1.,0.,0.));
#58302=DIRECTION('center_axis',(0.,0.,1.));
#58303=DIRECTION('ref_axis',(1.,0.,0.));
#58304=DIRECTION('center_axis',(0.,0.,1.));
#58305=DIRECTION('ref_axis',(1.,0.,0.));
#58306=DIRECTION('center_axis',(0.,0.,-1.));
#58307=DIRECTION('ref_axis',(-1.,0.,0.));
#58308=DIRECTION('',(0.,0.,1.));
#58309=DIRECTION('center_axis',(0.,-1.,0.));
#58310=DIRECTION('ref_axis',(0.,0.,-1.));
#58311=DIRECTION('center_axis',(0.00367439112755605,0.,-0.999993249402136));
#58312=DIRECTION('ref_axis',(-0.999993249402136,0.,-0.00367439112755605));
#58313=DIRECTION('center_axis',(0.,-1.,0.));
#58314=DIRECTION('ref_axis',(0.,0.,-1.));
#58315=DIRECTION('center_axis',(0.,-1.,0.));
#58316=DIRECTION('ref_axis',(0.,0.,-1.));
#58317=DIRECTION('center_axis',(1.,0.,0.));
#58318=DIRECTION('ref_axis',(0.,0.,-1.));
#58319=DIRECTION('center_axis',(0.993664622325388,0.,-0.112386023770502));
#58320=DIRECTION('ref_axis',(-0.112386023770502,0.,-0.993664622325388));
#58321=DIRECTION('center_axis',(1.,0.,0.));
#58322=DIRECTION('ref_axis',(0.,0.,-1.));
#58323=DIRECTION('center_axis',(1.,0.,0.));
#58324=DIRECTION('ref_axis',(0.,0.,-1.));
#58325=DIRECTION('',(1.,0.,0.));
#58326=DIRECTION('center_axis',(0.992466262760427,0.,-0.12251823244869));
#58327=DIRECTION('ref_axis',(-0.12251823244869,0.,-0.992466262760427));
#58328=DIRECTION('center_axis',(0.,0.,-1.));
#58329=DIRECTION('ref_axis',(-1.,0.,0.));
#58330=DIRECTION('center_axis',(0.,-1.,0.));
#58331=DIRECTION('ref_axis',(0.,0.,-1.));
#58332=DIRECTION('center_axis',(0.998253744921096,0.,-0.0590716577641654));
#58333=DIRECTION('ref_axis',(-0.0590716577641654,0.,-0.998253744921096));
#58334=DIRECTION('center_axis',(0.,0.,-1.));
#58335=DIRECTION('ref_axis',(-1.,0.,0.));
#58336=DIRECTION('center_axis',(0.,0.,-1.));
#58337=DIRECTION('ref_axis',(-1.,0.,0.));
#58338=DIRECTION('',(0.,0.,-1.));
#58339=DIRECTION('center_axis',(0.997326999817373,0.,-0.073067471800225));
#58340=DIRECTION('ref_axis',(-0.073067471800225,0.,-0.997326999817374));
#58341=DIRECTION('center_axis',(0.,-1.,0.));
#58342=DIRECTION('ref_axis',(0.,0.,-1.));
#58343=DIRECTION('center_axis',(-0.00367439112755605,2.77553882489006E-14,
-0.999993249402136));
#58344=DIRECTION('ref_axis',(-0.999993249402136,2.07077330159731E-32,0.00367439112755605));
#58345=DIRECTION('center_axis',(0.,-1.,0.));
#58346=DIRECTION('ref_axis',(0.,0.,-1.));
#58347=DIRECTION('center_axis',(1.,0.,-2.83753250766945E-16));
#58348=DIRECTION('ref_axis',(-2.83753250766945E-16,0.,-1.));
#58349=DIRECTION('center_axis',(0.,1.,0.));
#58350=DIRECTION('ref_axis',(0.,0.,1.));
#58351=DIRECTION('',(0.,-1.,0.));
#58352=DIRECTION('',(0.,1.,0.));
#58353=DIRECTION('center_axis',(4.16333634234433E-14,1.,0.));
#58354=DIRECTION('ref_axis',(-1.,4.16333634234433E-14,0.));
#58355=DIRECTION('center_axis',(-1.,-1.30289899094001E-16,0.));
#58356=DIRECTION('ref_axis',(1.30289899094001E-16,-1.,0.));
#58357=DIRECTION('center_axis',(-0.99083605930949,-0.135069995084183,-4.3932954632363E-16));
#58358=DIRECTION('ref_axis',(-0.135069995084183,0.99083605930949,-1.6477538710012E-33));
#58359=DIRECTION('center_axis',(0.,0.,-1.));
#58360=DIRECTION('ref_axis',(-1.,0.,0.));
#58361=DIRECTION('center_axis',(-0.870187309198622,0.492721064000376,0.));
#58362=DIRECTION('ref_axis',(-0.492721064000376,-0.870187309198622,0.));
#58363=DIRECTION('center_axis',(0.,0.,1.));
#58364=DIRECTION('ref_axis',(-1.,2.13045726893401E-14,0.));
#58365=DIRECTION('center_axis',(0.,0.,-1.));
#58366=DIRECTION('ref_axis',(-1.,0.,0.));
#58367=DIRECTION('center_axis',(0.,0.,-1.));
#58368=DIRECTION('ref_axis',(-1.,0.,0.));
#58369=DIRECTION('center_axis',(-0.589792031258401,-0.807555174501464,0.));
#58370=DIRECTION('ref_axis',(-0.807555174501464,0.589792031258401,0.));
#58371=DIRECTION('center_axis',(0.,0.,-1.));
#58372=DIRECTION('ref_axis',(-1.,0.,0.));
#58373=DIRECTION('center_axis',(0.,0.,-1.));
#58374=DIRECTION('ref_axis',(-1.,0.,0.));
#58375=DIRECTION('center_axis',(0.,0.,1.));
#58376=DIRECTION('ref_axis',(1.,0.,0.));
#58377=DIRECTION('',(0.,0.,1.));
#58378=DIRECTION('center_axis',(0.,0.,-1.));
#58379=DIRECTION('ref_axis',(-1.,0.,0.));
#58380=DIRECTION('center_axis',(-0.950587351628009,-0.310457222375076,0.));
#58381=DIRECTION('ref_axis',(0.310457222375076,-0.950587351628009,0.));
#58382=DIRECTION('center_axis',(0.,0.,1.));
#58383=DIRECTION('ref_axis',(-1.,-2.42861286636753E-14,0.));
#58384=DIRECTION('center_axis',(0.,0.,-1.));
#58385=DIRECTION('ref_axis',(-1.,0.,0.));
#58386=DIRECTION('center_axis',(-0.813624755504625,0.581390365615083,-1.49473109573578E-14));
#58387=DIRECTION('ref_axis',(-0.581390365615083,-0.813624755504625,-2.20695383221015E-29));
#58388=DIRECTION('center_axis',(0.,-1.,0.));
#58389=DIRECTION('ref_axis',(0.,0.,-1.));
#58390=DIRECTION('center_axis',(0.,0.,-1.));
#58391=DIRECTION('ref_axis',(-1.,0.,0.));
#58392=DIRECTION('center_axis',(-1.40023216580064E-13,-1.91722619337689E-13,
1.));
#58393=DIRECTION('ref_axis',(-3.59356979302414E-28,-1.,-1.91722619337689E-13));
#58394=DIRECTION('',(0.,0.,-1.));
#58395=DIRECTION('center_axis',(0.,0.,-1.));
#58396=DIRECTION('ref_axis',(-1.,0.,0.));
#58397=DIRECTION('center_axis',(-0.0533420240673326,0.998576300774458,-2.72423821176928E-15));
#58398=DIRECTION('ref_axis',(-0.998576300774458,-0.0533420240673326,-4.56897457660181E-33));
#58399=DIRECTION('center_axis',(0.,0.,-1.));
#58400=DIRECTION('ref_axis',(-1.,0.,0.));
#58401=DIRECTION('center_axis',(0.,-1.,0.));
#58402=DIRECTION('ref_axis',(0.,0.,-1.));
#58403=DIRECTION('',(0.,-1.,0.));
#58404=DIRECTION('',(0.,1.,0.));
#58405=DIRECTION('center_axis',(0.498280113808025,0.867016106069237,0.));
#58406=DIRECTION('ref_axis',(-0.867016106069237,0.498280113808025,0.));
#58407=DIRECTION('center_axis',(0.,0.,1.));
#58408=DIRECTION('ref_axis',(0.0533420240673336,-0.998576300774458,0.));
#58409=DIRECTION('center_axis',(0.,0.,1.));
#58410=DIRECTION('ref_axis',(1.,0.,0.));
#58411=DIRECTION('center_axis',(1.,0.,0.));
#58412=DIRECTION('ref_axis',(0.,0.,1.));
#58413=DIRECTION('center_axis',(0.,0.,-1.));
#58414=DIRECTION('ref_axis',(-1.,0.,0.));
#58415=DIRECTION('center_axis',(0.0533420240673341,0.998576300774458,0.));
#58416=DIRECTION('ref_axis',(-0.998576300774458,0.0533420240673341,0.));
#58417=DIRECTION('center_axis',(0.,0.,-1.));
#58418=DIRECTION('ref_axis',(-1.,0.,0.));
#58419=DIRECTION('center_axis',(0.,0.,-1.));
#58420=DIRECTION('ref_axis',(-1.,0.,0.));
#58421=DIRECTION('center_axis',(0.,0.,1.));
#58422=DIRECTION('ref_axis',(1.,0.,0.));
#58423=DIRECTION('',(0.,0.,1.));
#58424=DIRECTION('center_axis',(0.,0.,1.));
#58425=DIRECTION('ref_axis',(0.0533420240673479,0.998576300774457,0.));
#58426=DIRECTION('center_axis',(-1.,0.,0.));
#58427=DIRECTION('ref_axis',(0.,0.,1.));
#58428=DIRECTION('center_axis',(0.,0.,1.));
#58429=DIRECTION('ref_axis',(1.,0.,0.));
#58430=DIRECTION('center_axis',(0.00693238621491237,0.993966797804128,0.109462079664029));
#58431=DIRECTION('ref_axis',(-1.22354345465345E-17,-0.109464710021979,0.993990682682591));
#58432=DIRECTION('center_axis',(0.,0.,-1.));
#58433=DIRECTION('ref_axis',(-1.,0.,0.));
#58434=DIRECTION('center_axis',(2.96529885867188E-15,5.55111512312578E-14,
1.));
#58435=DIRECTION('ref_axis',(0.,-1.,5.55111512312578E-14));
#58436=DIRECTION('',(0.,0.,-1.));
#58437=DIRECTION('center_axis',(0.124001141217911,0.992275239756939,-0.00368314294652425));
#58438=DIRECTION('ref_axis',(-0.992281970201119,0.12400198229781,6.2356654373776E-21));
#58439=DIRECTION('center_axis',(0.0139772935711188,0.879101978084599,0.47642874324727));
#58440=DIRECTION('ref_axis',(2.72212200690293E-17,-0.476475288755116,0.879187863431775));
#58441=DIRECTION('center_axis',(0.994025548953269,0.0701103237587535,-0.0836525584222893));
#58442=DIRECTION('ref_axis',(0.0838589147843666,1.84650881221684E-17,0.996477637687464));
#58443=DIRECTION('center_axis',(-0.456401891282935,0.882037283977672,0.117079218081824));
#58444=DIRECTION('ref_axis',(-0.888145434138644,-0.459562496096754,1.03214570261012E-16));
#58445=DIRECTION('center_axis',(0.992758434166036,-0.0700209519858698,-0.0976102334552734));
#58446=DIRECTION('ref_axis',(-0.0978504052290823,-1.24014805477136E-16,
-0.995201134543417));
#58447=DIRECTION('center_axis',(0.,0.,-1.));
#58448=DIRECTION('ref_axis',(-1.,0.,0.));
#58449=DIRECTION('center_axis',(-1.,0.,4.00096335390287E-16));
#58450=DIRECTION('ref_axis',(4.00096335390287E-16,0.,1.));
#58451=DIRECTION('center_axis',(0.0764633074491056,0.,0.997072395874013));
#58452=DIRECTION('ref_axis',(-0.997072395874013,-2.08166817117216E-14,0.0764633074491056));
#58453=DIRECTION('center_axis',(-0.763137786294476,0.64623580768135,-4.48416170640668E-15));
#58454=DIRECTION('ref_axis',(-0.64623580768135,-0.763137786294476,3.55662332953577E-29));
#58455=DIRECTION('center_axis',(-0.780043230375354,0.625725625770259,1.2139561508471E-13));
#58456=DIRECTION('ref_axis',(-0.625725625770259,-0.780043230375354,-2.63473956355127E-28));
#58457=DIRECTION('center_axis',(5.89460815835388E-12,7.1840930855476E-12,
1.));
#58458=DIRECTION('ref_axis',(-0.625713604765022,-0.780052873087435,9.29240284524464E-12));
#58459=DIRECTION('center_axis',(-0.0132304380228111,-0.00122043043743016,
-0.999911729133763));
#58460=DIRECTION('ref_axis',(-0.646190117710228,-0.763117574189617,0.00948154716257832));
#58461=DIRECTION('center_axis',(-0.0764633074494057,-3.38289393019627E-13,
0.99707239587399));
#58462=DIRECTION('ref_axis',(-0.99707239587399,3.46944695195615E-15,-0.0764633074494057));
#58463=DIRECTION('center_axis',(0.76313778629449,0.646235807681333,0.));
#58464=DIRECTION('ref_axis',(-0.646235807681333,0.76313778629449,0.));
#58465=DIRECTION('center_axis',(-1.,-1.18445362812728E-16,0.));
#58466=DIRECTION('ref_axis',(1.18445362812728E-16,-1.,0.));
#58467=DIRECTION('center_axis',(0.780043230375353,0.625725625770261,0.));
#58468=DIRECTION('ref_axis',(-0.62572562577026,0.780043230375353,0.));
#58469=DIRECTION('center_axis',(0.0135861973191934,-0.00164484670762636,
-0.99990635047574));
#58470=DIRECTION('ref_axis',(0.625603637149145,-0.780079720485556,0.00978360224753608));
#58471=DIRECTION('center_axis',(-7.88065731198386E-12,9.56133411252272E-12,
1.));
#58472=DIRECTION('ref_axis',(0.646224932541722,-0.763146995382572,1.23893231864011E-11));
#58473=DIRECTION('center_axis',(0.,0.,-1.));
#58474=DIRECTION('ref_axis',(-1.,0.,0.));
#58475=DIRECTION('',(-1.,0.,0.));
#58476=DIRECTION('',(-1.,0.,0.));
#58477=DIRECTION('',(-1.,0.,0.));
#58478=DIRECTION('',(-1.,0.,0.));
#58479=DIRECTION('center_axis',(-1.27486239704332E-16,1.,0.));
#58480=DIRECTION('ref_axis',(-1.,-1.27486239704332E-16,0.));
#58481=DIRECTION('',(1.27486239704332E-16,-1.,0.));
#58482=DIRECTION('',(0.,1.,0.));
#58483=DIRECTION('center_axis',(4.62592926927149E-16,1.,3.77688604714562E-13));
#58484=DIRECTION('ref_axis',(8.56727719098818E-33,-3.77688604714562E-13,
1.));
#58485=DIRECTION('center_axis',(-1.,-1.18445362812727E-16,3.8759154073836E-16));
#58486=DIRECTION('ref_axis',(3.8759154073836E-16,5.47382212626882E-48,1.));
#58487=DIRECTION('center_axis',(0.,-1.,1.88844727276056E-13));
#58488=DIRECTION('ref_axis',(0.,-1.88844727276056E-13,-1.));
#58489=DIRECTION('center_axis',(-1.27486239704332E-16,1.,0.));
#58490=DIRECTION('ref_axis',(-1.,-1.27486239704332E-16,0.));
#58491=DIRECTION('',(0.,-1.,0.));
#58492=DIRECTION('',(-1.27486239704332E-16,1.,0.));
#58493=DIRECTION('',(-1.27486239704332E-16,1.,0.));
#58494=DIRECTION('center_axis',(0.,0.,-1.));
#58495=DIRECTION('ref_axis',(-1.,0.,0.));
#58496=DIRECTION('center_axis',(1.,0.,0.));
#58497=DIRECTION('ref_axis',(0.,0.,-1.));
#58498=DIRECTION('',(0.,0.,-1.));
#58499=DIRECTION('center_axis',(-1.,0.,0.));
#58500=DIRECTION('ref_axis',(0.,0.,1.));
#58501=DIRECTION('',(0.,0.,-1.));
#58502=DIRECTION('',(0.,0.,-1.));
#58503=DIRECTION('center_axis',(-1.,0.,0.));
#58504=DIRECTION('ref_axis',(0.,0.,1.));
#58505=DIRECTION('',(1.,0.,0.));
#58506=DIRECTION('',(-1.,0.,0.));
#58507=DIRECTION('center_axis',(0.,0.,-1.));
#58508=DIRECTION('ref_axis',(-1.,0.,0.));
#58509=DIRECTION('center_axis',(0.,1.,0.));
#58510=DIRECTION('ref_axis',(0.,0.,1.));
#58511=DIRECTION('center_axis',(-1.,0.,0.));
#58512=DIRECTION('ref_axis',(0.,0.,1.));
#58513=DIRECTION('',(1.,0.,0.));
#58514=DIRECTION('center_axis',(-1.,0.,0.));
#58515=DIRECTION('ref_axis',(0.,0.,1.));
#58516=DIRECTION('',(1.,0.,0.));
#58517=DIRECTION('center_axis',(-1.,0.,0.));
#58518=DIRECTION('ref_axis',(0.,0.,1.));
#58519=DIRECTION('',(1.,0.,0.));
#58520=DIRECTION('center_axis',(-1.,0.,0.));
#58521=DIRECTION('ref_axis',(0.,0.,1.));
#58522=DIRECTION('',(1.,0.,0.));
#58523=DIRECTION('center_axis',(0.,1.,0.));
#58524=DIRECTION('ref_axis',(0.,0.,1.));
#58525=DIRECTION('axis',(0.,0.,1.));
#58526=DIRECTION('refdir',(1.,0.,0.));
#58527=DIRECTION('center_axis',(0.,1.,0.));
#58528=DIRECTION('ref_axis',(0.,0.,1.));
#58529=DIRECTION('center_axis',(0.,1.,0.));
#58530=DIRECTION('ref_axis',(0.,0.,1.));
#58531=DIRECTION('',(0.,1.,0.));
#58532=DIRECTION('center_axis',(0.,1.,0.));
#58533=DIRECTION('ref_axis',(0.,0.,1.));
#58534=DIRECTION('center_axis',(0.,0.,-1.));
#58535=DIRECTION('ref_axis',(-1.,0.,0.));
#58536=DIRECTION('center_axis',(0.,0.,1.));
#58537=DIRECTION('ref_axis',(-1.,0.,0.));
#58538=DIRECTION('',(-1.,0.,0.));
#58539=DIRECTION('center_axis',(0.,0.,1.));
#58540=DIRECTION('ref_axis',(-1.,0.,0.));
#58541=DIRECTION('',(0.,-1.,0.));
#58542=DIRECTION('center_axis',(0.,0.,1.));
#58543=DIRECTION('ref_axis',(-1.,0.,0.));
#58544=DIRECTION('',(1.,0.,0.));
#58545=DIRECTION('center_axis',(0.,0.,1.));
#58546=DIRECTION('ref_axis',(-1.,0.,0.));
#58547=DIRECTION('',(0.,1.,0.));
#58548=DIRECTION('',(0.,1.,0.));
#58549=DIRECTION('center_axis',(0.,0.,-1.));
#58550=DIRECTION('ref_axis',(-1.,0.,0.));
#58551=DIRECTION('',(0.70710678118655,0.707106781186544,0.));
#58552=DIRECTION('center_axis',(0.,0.,-1.));
#58553=DIRECTION('ref_axis',(-1.,0.,0.));
#58554=DIRECTION('',(1.,0.,0.));
#58555=DIRECTION('center_axis',(0.,0.,-1.));
#58556=DIRECTION('ref_axis',(-1.,0.,0.));
#58557=DIRECTION('',(0.707106781186551,-0.707106781186544,0.));
#58558=DIRECTION('center_axis',(0.,0.,-1.));
#58559=DIRECTION('ref_axis',(-1.,0.,0.));
#58560=DIRECTION('',(0.,-1.,0.));
#58561=DIRECTION('center_axis',(0.,0.,-1.));
#58562=DIRECTION('ref_axis',(-1.,0.,0.));
#58563=DIRECTION('',(-0.707106781186548,-0.707106781186546,0.));
#58564=DIRECTION('center_axis',(0.,0.,-1.));
#58565=DIRECTION('ref_axis',(-1.,0.,0.));
#58566=DIRECTION('',(-1.,0.,0.));
#58567=DIRECTION('center_axis',(0.,0.,-1.));
#58568=DIRECTION('ref_axis',(-1.,0.,0.));
#58569=DIRECTION('',(-0.707106781186548,0.707106781186546,0.));
#58570=DIRECTION('center_axis',(0.,0.,-1.));
#58571=DIRECTION('ref_axis',(-1.,0.,0.));
#58572=DIRECTION('center_axis',(-1.,0.,0.));
#58573=DIRECTION('ref_axis',(0.,0.,1.));
#58574=DIRECTION('',(0.,0.,-1.));
#58575=DIRECTION('',(0.,-1.,0.));
#58576=DIRECTION('',(0.,0.,1.));
#58577=DIRECTION('',(0.,1.,0.));
#58578=DIRECTION('center_axis',(0.,-1.,0.));
#58579=DIRECTION('ref_axis',(0.,0.,-1.));
#58580=DIRECTION('',(0.,0.,-1.));
#58581=DIRECTION('',(1.,0.,0.));
#58582=DIRECTION('',(0.,0.,1.));
#58583=DIRECTION('',(-1.,0.,0.));
#58584=DIRECTION('center_axis',(1.,0.,0.));
#58585=DIRECTION('ref_axis',(0.,0.,-1.));
#58586=DIRECTION('',(0.,0.,-1.));
#58587=DIRECTION('',(0.,1.,0.));
#58588=DIRECTION('',(0.,0.,1.));
#58589=DIRECTION('',(0.,-1.,0.));
#58590=DIRECTION('center_axis',(0.,1.,0.));
#58591=DIRECTION('ref_axis',(0.,0.,1.));
#58592=DIRECTION('',(0.,0.,-1.));
#58593=DIRECTION('',(-1.,0.,0.));
#58594=DIRECTION('',(0.,0.,1.));
#58595=DIRECTION('',(1.,0.,0.));
#58596=DIRECTION('center_axis',(0.,0.,-1.));
#58597=DIRECTION('ref_axis',(-1.,0.,0.));
#58598=DIRECTION('center_axis',(0.,0.,-1.));
#58599=DIRECTION('ref_axis',(-1.,0.,0.));
#58600=DIRECTION('',(0.,1.,0.));
#58601=DIRECTION('center_axis',(0.,0.,-1.));
#58602=DIRECTION('ref_axis',(-1.,0.,0.));
#58603=DIRECTION('',(1.,0.,0.));
#58604=DIRECTION('center_axis',(0.,0.,-1.));
#58605=DIRECTION('ref_axis',(-1.,0.,0.));
#58606=DIRECTION('',(0.,-1.,0.));
#58607=DIRECTION('center_axis',(0.,0.,-1.));
#58608=DIRECTION('ref_axis',(-1.,0.,0.));
#58609=DIRECTION('',(-1.,0.,0.));
#58610=DIRECTION('center_axis',(1.,0.,0.));
#58611=DIRECTION('ref_axis',(0.,0.,-1.));
#58612=DIRECTION('',(0.,0.,-1.));
#58613=DIRECTION('',(0.,-1.,0.));
#58614=DIRECTION('',(0.,0.,1.));
#58615=DIRECTION('',(0.,1.,0.));
#58616=DIRECTION('center_axis',(0.,1.,0.));
#58617=DIRECTION('ref_axis',(0.,0.,1.));
#58618=DIRECTION('',(0.,0.,-1.));
#58619=DIRECTION('',(1.,0.,0.));
#58620=DIRECTION('',(0.,0.,1.));
#58621=DIRECTION('center_axis',(0.,-1.,0.));
#58622=DIRECTION('ref_axis',(0.,0.,1.));
#58623=DIRECTION('',(-1.,0.,0.));
#58624=DIRECTION('center_axis',(0.,-1.,0.));
#58625=DIRECTION('ref_axis',(0.,0.,1.));
#58626=DIRECTION('center_axis',(-1.,0.,0.));
#58627=DIRECTION('ref_axis',(0.,0.,1.));
#58628=DIRECTION('',(0.,0.,-1.));
#58629=DIRECTION('',(0.,1.,0.));
#58630=DIRECTION('',(0.,0.,1.));
#58631=DIRECTION('',(0.,-1.,0.));
#58632=DIRECTION('center_axis',(0.,-1.,0.));
#58633=DIRECTION('ref_axis',(0.,0.,-1.));
#58634=DIRECTION('',(0.,0.,-1.));
#58635=DIRECTION('',(-1.,0.,0.));
#58636=DIRECTION('',(0.,0.,1.));
#58637=DIRECTION('center_axis',(0.,1.,0.));
#58638=DIRECTION('ref_axis',(0.,0.,-1.));
#58639=DIRECTION('',(1.,0.,0.));
#58640=DIRECTION('center_axis',(0.,1.,0.));
#58641=DIRECTION('ref_axis',(0.,0.,-1.));
#58642=DIRECTION('center_axis',(0.,0.,-1.));
#58643=DIRECTION('ref_axis',(-1.,0.,0.));
#58644=DIRECTION('',(0.,-1.,0.));
#58645=DIRECTION('',(1.,0.,0.));
#58646=DIRECTION('',(0.,1.,0.));
#58647=DIRECTION('',(-1.,0.,0.));
#58648=DIRECTION('center_axis',(0.,1.,0.));
#58649=DIRECTION('ref_axis',(0.,0.,1.));
#58650=DIRECTION('center_axis',(0.,1.,0.));
#58651=DIRECTION('ref_axis',(0.,0.,-1.));
#58652=DIRECTION('center_axis',(0.,-1.,0.));
#58653=DIRECTION('ref_axis',(0.,0.,1.));
#58654=DIRECTION('center_axis',(0.,-1.,0.));
#58655=DIRECTION('ref_axis',(0.,0.,-1.));
#58656=DIRECTION('center_axis',(0.,1.,0.));
#58657=DIRECTION('ref_axis',(0.,0.,-1.));
#58658=DIRECTION('center_axis',(0.,-1.,0.));
#58659=DIRECTION('ref_axis',(0.,0.,1.));
#58660=DIRECTION('center_axis',(0.,0.,-1.));
#58661=DIRECTION('ref_axis',(-1.,0.,0.));
#58662=DIRECTION('center_axis',(0.,0.,1.));
#58663=DIRECTION('ref_axis',(-1.,0.,0.));
#58664=DIRECTION('center_axis',(0.,0.,-1.));
#58665=DIRECTION('ref_axis',(-1.,0.,0.));
#58666=DIRECTION('center_axis',(0.,0.,-1.));
#58667=DIRECTION('ref_axis',(-1.,0.,0.));
#58668=DIRECTION('center_axis',(0.,0.,1.));
#58669=DIRECTION('ref_axis',(-1.,0.,0.));
#58670=DIRECTION('center_axis',(0.,0.,-1.));
#58671=DIRECTION('ref_axis',(-1.,0.,0.));
#58672=DIRECTION('center_axis',(0.,0.,-1.));
#58673=DIRECTION('ref_axis',(-1.,0.,0.));
#58674=DIRECTION('center_axis',(0.,0.,1.));
#58675=DIRECTION('ref_axis',(-1.,0.,0.));
#58676=DIRECTION('center_axis',(0.,0.,-1.));
#58677=DIRECTION('ref_axis',(-1.,0.,0.));
#58678=DIRECTION('center_axis',(0.,0.,-1.));
#58679=DIRECTION('ref_axis',(-1.,0.,0.));
#58680=DIRECTION('center_axis',(0.,0.,1.));
#58681=DIRECTION('ref_axis',(-1.,0.,0.));
#58682=DIRECTION('center_axis',(0.,0.,-1.));
#58683=DIRECTION('ref_axis',(-1.,0.,0.));
#58684=DIRECTION('center_axis',(0.707106781186547,0.707106781186549,0.));
#58685=DIRECTION('ref_axis',(0.,0.,-1.));
#58686=DIRECTION('',(0.,0.,-1.));
#58687=DIRECTION('',(0.707106781186549,-0.707106781186546,0.));
#58688=DIRECTION('',(0.,0.,1.));
#58689=DIRECTION('',(0.707106781186548,-0.707106781186546,0.));
#58690=DIRECTION('center_axis',(0.,1.,0.));
#58691=DIRECTION('ref_axis',(0.,0.,1.));
#58692=DIRECTION('',(0.,-0.707106781186546,-0.707106781186548));
#58693=DIRECTION('center_axis',(0.,-1.,0.));
#58694=DIRECTION('ref_axis',(0.,0.,-1.));
#58695=DIRECTION('center_axis',(0.,1.,0.));
#58696=DIRECTION('ref_axis',(0.,0.,1.));
#58697=DIRECTION('center_axis',(0.,0.707106781186549,-0.707106781186547));
#58698=DIRECTION('ref_axis',(1.,0.,0.));
#58699=DIRECTION('',(0.,-0.707106781186546,-0.707106781186548));
#58700=DIRECTION('',(-1.,0.,0.));
#58701=DIRECTION('',(1.,0.,0.));
#58702=DIRECTION('center_axis',(0.,1.,0.));
#58703=DIRECTION('ref_axis',(0.,0.,1.));
#58704=DIRECTION('',(-0.707106781186549,-0.707106781186546,0.));
#58705=DIRECTION('center_axis',(0.,-1.,0.));
#58706=DIRECTION('ref_axis',(0.,0.,-1.));
#58707=DIRECTION('center_axis',(0.,1.,0.));
#58708=DIRECTION('ref_axis',(0.,0.,1.));
#58709=DIRECTION('center_axis',(-0.707106781186547,0.707106781186549,0.));
#58710=DIRECTION('ref_axis',(0.,0.,-1.));
#58711=DIRECTION('',(0.,0.,-1.));
#58712=DIRECTION('',(0.707106781186549,0.707106781186547,0.));
#58713=DIRECTION('',(0.,0.,1.));
#58714=DIRECTION('center_axis',(0.707106781186545,-0.707106781186551,0.));
#58715=DIRECTION('ref_axis',(0.,0.,-1.));
#58716=DIRECTION('',(0.,0.,-1.));
#58717=DIRECTION('',(-0.70710678118655,-0.707106781186544,0.));
#58718=DIRECTION('',(0.,0.,1.));
#58719=DIRECTION('',(-0.70710678118655,-0.707106781186544,0.));
#58720=DIRECTION('center_axis',(0.,-1.,0.));
#58721=DIRECTION('ref_axis',(0.,0.,-1.));
#58722=DIRECTION('',(0.,-0.707106781186544,0.70710678118655));
#58723=DIRECTION('center_axis',(0.,-1.,0.));
#58724=DIRECTION('ref_axis',(0.,0.,-1.));
#58725=DIRECTION('center_axis',(0.,1.,0.));
#58726=DIRECTION('ref_axis',(0.,0.,1.));
#58727=DIRECTION('center_axis',(0.,-0.707106781186551,-0.707106781186545));
#58728=DIRECTION('ref_axis',(-1.,0.,0.));
#58729=DIRECTION('',(0.,-0.707106781186544,0.70710678118655));
#58730=DIRECTION('',(-1.,0.,0.));
#58731=DIRECTION('',(1.,0.,0.));
#58732=DIRECTION('center_axis',(0.,-1.,0.));
#58733=DIRECTION('ref_axis',(0.,0.,-1.));
#58734=DIRECTION('',(0.707106781186551,-0.707106781186544,0.));
#58735=DIRECTION('center_axis',(0.,-1.,0.));
#58736=DIRECTION('ref_axis',(0.,0.,-1.));
#58737=DIRECTION('center_axis',(0.,1.,0.));
#58738=DIRECTION('ref_axis',(0.,0.,1.));
#58739=DIRECTION('center_axis',(-0.707106781186544,-0.707106781186551,0.));
#58740=DIRECTION('ref_axis',(0.,0.,-1.));
#58741=DIRECTION('',(0.,0.,-1.));
#58742=DIRECTION('',(-0.707106781186551,0.707106781186544,0.));
#58743=DIRECTION('',(0.,0.,1.));
#58744=DIRECTION('center_axis',(0.,-1.,0.));
#58745=DIRECTION('ref_axis',(0.,0.,-1.));
#58746=DIRECTION('center_axis',(0.,1.,0.));
#58747=DIRECTION('ref_axis',(0.,0.,1.));
#58748=DIRECTION('center_axis',(0.,-1.,0.));
#58749=DIRECTION('ref_axis',(0.,0.,-1.));
#58750=DIRECTION('center_axis',(0.,0.,-1.));
#58751=DIRECTION('ref_axis',(-1.,0.,0.));
#58752=DIRECTION('center_axis',(-1.,0.,0.));
#58753=DIRECTION('ref_axis',(0.,0.,1.));
#58754=DIRECTION('center_axis',(0.,0.,-1.));
#58755=DIRECTION('ref_axis',(-1.,0.,0.));
#58756=DIRECTION('center_axis',(-1.,0.,0.));
#58757=DIRECTION('ref_axis',(0.,0.,1.));
#58758=DIRECTION('center_axis',(-1.,0.,0.));
#58759=DIRECTION('ref_axis',(0.,0.,1.));
#58760=DIRECTION('center_axis',(-1.,0.,0.));
#58761=DIRECTION('ref_axis',(0.,0.,1.));
#58762=DIRECTION('center_axis',(1.,0.,0.));
#58763=DIRECTION('ref_axis',(0.,0.,-1.));
#58764=DIRECTION('center_axis',(-1.,0.,0.));
#58765=DIRECTION('ref_axis',(0.,0.,1.));
#58766=DIRECTION('center_axis',(0.,0.,-1.));
#58767=DIRECTION('ref_axis',(-1.,0.,0.));
#58768=DIRECTION('center_axis',(0.,1.,0.));
#58769=DIRECTION('ref_axis',(0.,0.,1.));
#58770=DIRECTION('center_axis',(0.,0.,-1.));
#58771=DIRECTION('ref_axis',(-1.,0.,0.));
#58772=DIRECTION('center_axis',(0.,-1.,0.));
#58773=DIRECTION('ref_axis',(0.,0.,-1.));
#58774=DIRECTION('center_axis',(0.,1.,0.));
#58775=DIRECTION('ref_axis',(0.,0.,1.));
#58776=DIRECTION('center_axis',(1.,0.,0.));
#58777=DIRECTION('ref_axis',(0.,0.,-1.));
#58778=DIRECTION('center_axis',(1.,0.,0.));
#58779=DIRECTION('ref_axis',(0.,0.,-1.));
#58780=DIRECTION('center_axis',(-1.,0.,0.));
#58781=DIRECTION('ref_axis',(0.,0.,1.));
#58782=DIRECTION('center_axis',(0.,0.,-1.));
#58783=DIRECTION('ref_axis',(-1.,0.,0.));
#58784=DIRECTION('center_axis',(0.,1.,0.));
#58785=DIRECTION('ref_axis',(0.,0.,1.));
#58786=DIRECTION('center_axis',(0.,0.,-1.));
#58787=DIRECTION('ref_axis',(-1.,0.,0.));
#58788=DIRECTION('center_axis',(0.,1.,0.));
#58789=DIRECTION('ref_axis',(0.,0.,1.));
#58790=DIRECTION('center_axis',(0.,-1.,0.));
#58791=DIRECTION('ref_axis',(0.,0.,-1.));
#58792=DIRECTION('center_axis',(0.,1.,0.));
#58793=DIRECTION('ref_axis',(0.,0.,1.));
#58794=DIRECTION('center_axis',(0.,1.,0.));
#58795=DIRECTION('ref_axis',(0.,0.,1.));
#58796=DIRECTION('center_axis',(0.,1.,0.));
#58797=DIRECTION('ref_axis',(0.,0.,1.));
#58798=DIRECTION('center_axis',(0.,0.,-1.));
#58799=DIRECTION('ref_axis',(-1.,0.,0.));
#58800=DIRECTION('center_axis',(1.,0.,0.));
#58801=DIRECTION('ref_axis',(0.,0.,-1.));
#58802=DIRECTION('center_axis',(0.,0.,-1.));
#58803=DIRECTION('ref_axis',(-1.,0.,0.));
#58804=DIRECTION('center_axis',(-1.,0.,0.));
#58805=DIRECTION('ref_axis',(0.,0.,1.));
#58806=DIRECTION('center_axis',(-1.,0.,0.));
#58807=DIRECTION('ref_axis',(0.,0.,1.));
#58808=DIRECTION('center_axis',(0.,0.,-1.));
#58809=DIRECTION('ref_axis',(-1.,0.,0.));
#58810=DIRECTION('center_axis',(0.,0.,1.));
#58811=DIRECTION('ref_axis',(-1.,-1.11022302462516E-13,0.));
#58812=DIRECTION('center_axis',(0.,0.,1.));
#58813=DIRECTION('ref_axis',(1.,0.,0.));
#58814=DIRECTION('center_axis',(0.,-1.,0.));
#58815=DIRECTION('ref_axis',(0.,0.,-1.));
#58816=DIRECTION('center_axis',(-1.,0.,0.));
#58817=DIRECTION('ref_axis',(0.,0.,1.));
#58818=DIRECTION('center_axis',(1.,0.,0.));
#58819=DIRECTION('ref_axis',(0.,0.,-1.));
#58820=DIRECTION('center_axis',(-1.,0.,0.));
#58821=DIRECTION('ref_axis',(0.,0.,1.));
#58822=DIRECTION('center_axis',(0.,-1.,0.));
#58823=DIRECTION('ref_axis',(0.,0.,-1.));
#58824=DIRECTION('center_axis',(0.,0.,-1.));
#58825=DIRECTION('ref_axis',(-1.,0.,0.));
#58826=DIRECTION('center_axis',(0.,0.,1.));
#58827=DIRECTION('ref_axis',(1.,0.,0.));
#58828=DIRECTION('center_axis',(0.,0.,1.));
#58829=DIRECTION('ref_axis',(-1.,0.,0.));
#58830=DIRECTION('center_axis',(0.,0.,-1.));
#58831=DIRECTION('ref_axis',(-1.,0.,0.));
#58832=DIRECTION('center_axis',(0.,0.,1.));
#58833=DIRECTION('ref_axis',(-1.,0.,0.));
#58834=DIRECTION('center_axis',(0.,0.,1.));
#58835=DIRECTION('ref_axis',(1.,0.,0.));
#58836=DIRECTION('center_axis',(0.,1.,0.));
#58837=DIRECTION('ref_axis',(0.,0.,1.));
#58838=DIRECTION('center_axis',(1.,0.,0.));
#58839=DIRECTION('ref_axis',(0.,0.,-1.));
#58840=DIRECTION('center_axis',(-1.,0.,0.));
#58841=DIRECTION('ref_axis',(0.,0.,1.));
#58842=DIRECTION('center_axis',(1.,0.,0.));
#58843=DIRECTION('ref_axis',(0.,0.,-1.));
#58844=DIRECTION('center_axis',(0.,1.,0.));
#58845=DIRECTION('ref_axis',(0.,0.,1.));
#58846=DIRECTION('center_axis',(0.,0.,-1.));
#58847=DIRECTION('ref_axis',(-1.,0.,0.));
#58848=DIRECTION('center_axis',(0.,0.,1.));
#58849=DIRECTION('ref_axis',(1.,0.,0.));
#58850=DIRECTION('center_axis',(0.,0.,1.));
#58851=DIRECTION('ref_axis',(-1.,0.,0.));
#58852=DIRECTION('center_axis',(0.,0.,-1.));
#58853=DIRECTION('ref_axis',(-1.,0.,0.));
#58854=DIRECTION('center_axis',(0.,0.,1.));
#58855=DIRECTION('ref_axis',(-1.,1.11022302462516E-13,0.));
#58856=DIRECTION('center_axis',(0.,0.,1.));
#58857=DIRECTION('ref_axis',(1.,0.,0.));
#58858=DIRECTION('center_axis',(0.,-1.,0.));
#58859=DIRECTION('ref_axis',(0.,0.,-1.));
#58860=DIRECTION('center_axis',(-1.,0.,0.));
#58861=DIRECTION('ref_axis',(0.,0.,1.));
#58862=DIRECTION('center_axis',(1.,0.,0.));
#58863=DIRECTION('ref_axis',(0.,0.,-1.));
#58864=DIRECTION('center_axis',(-1.,0.,0.));
#58865=DIRECTION('ref_axis',(0.,0.,1.));
#58866=DIRECTION('center_axis',(0.,-1.,0.));
#58867=DIRECTION('ref_axis',(0.,0.,-1.));
#58868=DIRECTION('center_axis',(0.,0.,-1.));
#58869=DIRECTION('ref_axis',(-1.,0.,0.));
#58870=DIRECTION('center_axis',(0.,0.,1.));
#58871=DIRECTION('ref_axis',(1.,0.,0.));
#58872=DIRECTION('center_axis',(0.,0.,1.));
#58873=DIRECTION('ref_axis',(-1.,1.11022302462516E-13,0.));
#58874=DIRECTION('center_axis',(0.,0.,-1.));
#58875=DIRECTION('ref_axis',(-1.,0.,0.));
#58876=DIRECTION('center_axis',(0.,0.,1.));
#58877=DIRECTION('ref_axis',(-1.,-2.22044604925031E-13,0.));
#58878=DIRECTION('center_axis',(0.,0.,1.));
#58879=DIRECTION('ref_axis',(1.,0.,0.));
#58880=DIRECTION('center_axis',(0.,1.,0.));
#58881=DIRECTION('ref_axis',(0.,0.,1.));
#58882=DIRECTION('center_axis',(1.,0.,0.));
#58883=DIRECTION('ref_axis',(0.,0.,-1.));
#58884=DIRECTION('center_axis',(-1.,0.,0.));
#58885=DIRECTION('ref_axis',(0.,0.,1.));
#58886=DIRECTION('center_axis',(1.,0.,0.));
#58887=DIRECTION('ref_axis',(0.,0.,-1.));
#58888=DIRECTION('center_axis',(0.,1.,0.));
#58889=DIRECTION('ref_axis',(0.,0.,1.));
#58890=DIRECTION('center_axis',(0.,0.,-1.));
#58891=DIRECTION('ref_axis',(-1.,0.,0.));
#58892=DIRECTION('center_axis',(0.,0.,1.));
#58893=DIRECTION('ref_axis',(1.,0.,0.));
#58894=DIRECTION('center_axis',(0.,0.,1.));
#58895=DIRECTION('ref_axis',(-1.,-1.11022302462516E-13,0.));
#58896=DIRECTION('center_axis',(0.,0.,-1.));
#58897=DIRECTION('ref_axis',(-1.,0.,0.));
#58898=DIRECTION('center_axis',(0.,-1.,0.));
#58899=DIRECTION('ref_axis',(0.,0.,-1.));
#58900=DIRECTION('center_axis',(0.707106781186535,0.70710678118656,0.));
#58901=DIRECTION('ref_axis',(-0.70710678118656,0.707106781186535,0.));
#58902=DIRECTION('center_axis',(0.707106781186549,0.707106781186547,0.));
#58903=DIRECTION('ref_axis',(-0.707106781186547,0.707106781186549,0.));
#58904=DIRECTION('center_axis',(0.707106781186561,0.707106781186534,0.));
#58905=DIRECTION('ref_axis',(-0.707106781186534,0.707106781186561,0.));
#58906=DIRECTION('center_axis',(0.,-1.,0.));
#58907=DIRECTION('ref_axis',(0.,0.,-1.));
#58908=DIRECTION('center_axis',(0.,-1.,0.));
#58909=DIRECTION('ref_axis',(0.,0.,-1.));
#58910=DIRECTION('center_axis',(0.,0.,-1.));
#58911=DIRECTION('ref_axis',(-1.,0.,0.));
#58912=DIRECTION('center_axis',(1.,0.,0.));
#58913=DIRECTION('ref_axis',(0.,0.,-1.));
#58914=DIRECTION('center_axis',(0.,0.,-1.));
#58915=DIRECTION('ref_axis',(-1.,0.,0.));
#58916=DIRECTION('center_axis',(0.707106781186567,-0.707106781186528,0.));
#58917=DIRECTION('ref_axis',(0.707106781186528,0.707106781186567,0.));
#58918=DIRECTION('center_axis',(-1.,0.,0.));
#58919=DIRECTION('ref_axis',(0.,0.,1.));
#58920=DIRECTION('center_axis',(1.,0.,0.));
#58921=DIRECTION('ref_axis',(0.,0.,-1.));
#58922=DIRECTION('center_axis',(-0.707106781186551,0.707106781186544,0.));
#58923=DIRECTION('ref_axis',(-0.707106781186544,-0.707106781186551,0.));
#58924=DIRECTION('center_axis',(0.707106781186561,-0.707106781186534,1.59462515335074E-14));
#58925=DIRECTION('ref_axis',(0.707106781186534,0.707106781186561,1.36377391314472E-28));
#58926=DIRECTION('center_axis',(0.,0.,-1.));
#58927=DIRECTION('ref_axis',(-1.,0.,0.));
#58928=DIRECTION('center_axis',(0.707106781186565,-0.70710678118653,0.));
#58929=DIRECTION('ref_axis',(0.70710678118653,0.707106781186565,0.));
#58930=DIRECTION('center_axis',(0.,0.,-1.));
#58931=DIRECTION('ref_axis',(-1.,0.,0.));
#58932=DIRECTION('center_axis',(1.,0.,0.));
#58933=DIRECTION('ref_axis',(0.,0.,-1.));
#58934=DIRECTION('center_axis',(0.707106781186549,-0.707106781186547,0.));
#58935=DIRECTION('ref_axis',(0.707106781186547,0.707106781186549,0.));
#58936=DIRECTION('center_axis',(0.70710678118656,-0.707106781186535,0.));
#58937=DIRECTION('ref_axis',(0.707106781186535,0.70710678118656,0.));
#58938=DIRECTION('center_axis',(1.,0.,0.));
#58939=DIRECTION('ref_axis',(0.,0.,-1.));
#58940=DIRECTION('center_axis',(1.,0.,0.));
#58941=DIRECTION('ref_axis',(0.,0.,-1.));
#58942=DIRECTION('center_axis',(0.,0.,-1.));
#58943=DIRECTION('ref_axis',(-1.,0.,0.));
#58944=DIRECTION('center_axis',(0.,-1.,0.));
#58945=DIRECTION('ref_axis',(0.,0.,-1.));
#58946=DIRECTION('center_axis',(0.,0.,-1.));
#58947=DIRECTION('ref_axis',(-1.,0.,0.));
#58948=DIRECTION('center_axis',(0.707106781186568,0.707106781186527,0.));
#58949=DIRECTION('ref_axis',(-0.707106781186527,0.707106781186568,0.));
#58950=DIRECTION('center_axis',(0.,1.,0.));
#58951=DIRECTION('ref_axis',(0.,0.,1.));
#58952=DIRECTION('center_axis',(0.,-1.,0.));
#58953=DIRECTION('ref_axis',(0.,0.,-1.));
#58954=DIRECTION('center_axis',(-0.70710678118655,-0.707106781186545,0.));
#58955=DIRECTION('ref_axis',(0.707106781186545,-0.707106781186551,0.));
#58956=DIRECTION('center_axis',(0.707106781186561,0.707106781186534,2.45326946669344E-15));
#58957=DIRECTION('ref_axis',(-0.707106781186534,0.707106781186561,-1.81613594474679E-29));
#58958=DIRECTION('center_axis',(0.,0.,-1.));
#58959=DIRECTION('ref_axis',(-1.,0.,0.));
#58960=DIRECTION('axis',(0.,0.,1.));
#58961=DIRECTION('refdir',(1.,0.,0.));
#58962=DIRECTION('center_axis',(1.,0.,0.));
#58963=DIRECTION('ref_axis',(0.,0.,-1.));
#58964=DIRECTION('center_axis',(1.,0.,0.));
#58965=DIRECTION('ref_axis',(0.,0.,-1.));
#58966=DIRECTION('center_axis',(1.,0.,0.));
#58967=DIRECTION('ref_axis',(0.,0.,-1.));
#58968=DIRECTION('center_axis',(0.,-1.,0.));
#58969=DIRECTION('ref_axis',(0.,0.,1.));
#58970=DIRECTION('center_axis',(1.,0.,0.));
#58971=DIRECTION('ref_axis',(0.,0.,-1.));
#58972=DIRECTION('center_axis',(0.,-1.,0.));
#58973=DIRECTION('ref_axis',(0.,0.,-1.));
#58974=DIRECTION('center_axis',(0.,1.,0.));
#58975=DIRECTION('ref_axis',(0.,0.,-1.));
#58976=DIRECTION('center_axis',(-0.666555993111408,0.,0.745454967149099));
#58977=DIRECTION('ref_axis',(0.745454967149099,0.,0.666555993111408));
#58978=DIRECTION('center_axis',(0.,-1.,0.));
#58979=DIRECTION('ref_axis',(0.,0.,-1.));
#58980=DIRECTION('center_axis',(-0.666555993111408,0.,-0.745454967149099));
#58981=DIRECTION('ref_axis',(0.745454967149099,0.,-0.666555993111408));
#58982=DIRECTION('center_axis',(0.,-1.,0.));
#58983=DIRECTION('ref_axis',(0.,0.,-1.));
#58984=DIRECTION('center_axis',(0.,1.,0.));
#58985=DIRECTION('ref_axis',(0.,0.,-1.));
#58986=DIRECTION('center_axis',(-0.666555993111408,0.,0.745454967149099));
#58987=DIRECTION('ref_axis',(0.745454967149099,0.,0.666555993111408));
#58988=DIRECTION('center_axis',(0.,-1.,0.));
#58989=DIRECTION('ref_axis',(0.,0.,-1.));
#58990=DIRECTION('center_axis',(-0.666555993111408,0.,-0.745454967149099));
#58991=DIRECTION('ref_axis',(0.745454967149099,0.,-0.666555993111408));
#58992=DIRECTION('center_axis',(1.,0.,0.));
#58993=DIRECTION('ref_axis',(0.,0.,-1.));
#58994=DIRECTION('center_axis',(-1.,0.,0.));
#58995=DIRECTION('ref_axis',(0.,0.,-1.));
#58996=DIRECTION('center_axis',(0.,0.,-1.));
#58997=DIRECTION('ref_axis',(-1.,0.,0.));
#58998=DIRECTION('center_axis',(1.,0.,0.));
#58999=DIRECTION('ref_axis',(0.,0.,-1.));
#59000=DIRECTION('center_axis',(0.,0.,1.));
#59001=DIRECTION('ref_axis',(1.,0.,0.));
#59002=DIRECTION('center_axis',(-1.,0.,0.));
#59003=DIRECTION('ref_axis',(0.,0.,-1.));
#59004=DIRECTION('center_axis',(-1.,0.,0.));
#59005=DIRECTION('ref_axis',(0.,0.,1.));
#59006=DIRECTION('',(1.,0.,0.));
#59007=DIRECTION('',(-1.,0.,0.));
#59008=DIRECTION('center_axis',(-1.,0.,1.56170177914177E-16));
#59009=DIRECTION('ref_axis',(-1.56170177914177E-16,0.,-1.));
#59010=DIRECTION('',(-1.,0.,0.));
#59011=DIRECTION('center_axis',(1.,0.,0.));
#59012=DIRECTION('ref_axis',(0.,0.,-1.));
#59013=DIRECTION('center_axis',(0.,-1.,0.));
#59014=DIRECTION('ref_axis',(0.,0.,1.));
#59015=DIRECTION('center_axis',(-1.,0.,0.));
#59016=DIRECTION('ref_axis',(0.,0.,-1.));
#59017=DIRECTION('center_axis',(-1.,0.,0.));
#59018=DIRECTION('ref_axis',(0.,0.,-1.));
#59019=DIRECTION('center_axis',(-1.,0.,0.));
#59020=DIRECTION('ref_axis',(0.,0.,1.));
#59021=DIRECTION('center_axis',(1.,0.,0.));
#59022=DIRECTION('ref_axis',(0.,0.,1.));
#59023=DIRECTION('center_axis',(0.,-1.,0.));
#59024=DIRECTION('ref_axis',(0.,0.,-1.));
#59025=DIRECTION('center_axis',(1.,0.,0.));
#59026=DIRECTION('ref_axis',(0.,0.,1.));
#59027=DIRECTION('center_axis',(-1.,0.,0.));
#59028=DIRECTION('ref_axis',(0.,0.,1.));
#59029=DIRECTION('',(1.,0.,0.));
#59030=DIRECTION('center_axis',(0.928966301520812,-0.281372335152031,0.240522804843608));
#59031=DIRECTION('ref_axis',(0.289882267482667,0.957062313017866,5.63993829393187E-15));
#59032=DIRECTION('center_axis',(-0.929823364809375,-0.279861066194094,-0.238969232084962));
#59033=DIRECTION('ref_axis',(0.2882113740593,-0.957566814307414,1.1677602810686E-14));
#59034=DIRECTION('center_axis',(-0.983705916475484,-0.132945851001502,0.121029213798216));
#59035=DIRECTION('ref_axis',(0.133930380500437,-0.990990743235782,1.03475023686325E-15));
#59036=DIRECTION('center_axis',(0.984136564099166,-0.131218424609742,-0.119402463316403));
#59037=DIRECTION('ref_axis',(0.132163933909845,0.991227872173434,-1.63884198414844E-15));
#59038=DIRECTION('center_axis',(0.999634880550771,-0.016329642943714,0.0215278505098936));
#59039=DIRECTION('ref_axis',(0.0215307213626423,4.0425685051786E-18,-0.999768187150204));
#59040=DIRECTION('center_axis',(-0.999680792908394,-0.01526908890116,-0.0201287658382933));
#59041=DIRECTION('ref_axis',(-0.0201311127099917,7.84436696756394E-18,0.999797348616737));
#59042=DIRECTION('center_axis',(0.000137653858420446,0.78765469274787,-0.616116925626681));
#59043=DIRECTION('ref_axis',(-0.000104683403461457,0.616116939438223,0.787654687016247));
#59044=DIRECTION('center_axis',(0.,-1.,0.));
#59045=DIRECTION('ref_axis',(0.,0.,1.));
#59046=DIRECTION('',(0.,-1.,0.));
#59047=DIRECTION('center_axis',(-0.000142617395615587,0.787779221568786,
0.615957691505477));
#59048=DIRECTION('ref_axis',(0.000106417131381098,0.615957706238014,-0.787779215771398));
#59049=DIRECTION('center_axis',(0.,-1.,0.));
#59050=DIRECTION('ref_axis',(0.,0.,1.));
#59051=DIRECTION('',(0.,1.,0.));
#59052=DIRECTION('center_axis',(0.285542519778965,-0.0955884964586558,0.953587074546972));
#59053=DIRECTION('ref_axis',(0.957973697650931,-3.97542076374563E-16,-0.28685605206968));
#59054=DIRECTION('center_axis',(-0.314704251896522,-0.0942607213325078,
-0.944497829670416));
#59055=DIRECTION('ref_axis',(-0.948721970571128,-5.65830961415102E-16,0.316111724799374));
#59056=DIRECTION('center_axis',(0.971123571857389,-0.158256544871534,0.178532557782247));
#59057=DIRECTION('ref_axis',(0.180811134609775,-8.5786423277988E-17,-0.983517835934421));
#59058=DIRECTION('center_axis',(-0.972285724910778,-0.155194176083419,-0.174857761750832));
#59059=DIRECTION('ref_axis',(-0.177002324580309,2.03190884905465E-16,0.984210433338911));
#59060=DIRECTION('center_axis',(-0.971123571857389,0.158256544871534,0.178532557782247));
#59061=DIRECTION('ref_axis',(0.180811134609775,-8.5786423277988E-17,0.983517835934421));
#59062=DIRECTION('center_axis',(0.972285724910778,0.155194176083419,-0.174857761750832));
#59063=DIRECTION('ref_axis',(-0.177002324580309,2.03190884905465E-16,-0.984210433338911));
#59064=DIRECTION('center_axis',(-1.,0.,0.));
#59065=DIRECTION('ref_axis',(0.,0.,1.));
#59066=DIRECTION('center_axis',(-1.,0.,0.));
#59067=DIRECTION('ref_axis',(0.,0.,1.));
#59068=DIRECTION('center_axis',(0.,-1.,0.));
#59069=DIRECTION('ref_axis',(0.,0.,-1.));
#59070=DIRECTION('center_axis',(1.,0.,0.));
#59071=DIRECTION('ref_axis',(0.,0.,-1.));
#59072=DIRECTION('center_axis',(1.,0.,0.));
#59073=DIRECTION('ref_axis',(0.,0.,-1.));
#59074=DIRECTION('center_axis',(1.,0.,0.));
#59075=DIRECTION('ref_axis',(0.,0.,-1.));
#59076=DIRECTION('center_axis',(0.,-1.,0.));
#59077=DIRECTION('ref_axis',(0.,0.,1.));
#59078=DIRECTION('center_axis',(-1.,0.,0.));
#59079=DIRECTION('ref_axis',(0.,0.,-1.));
#59080=DIRECTION('center_axis',(0.,1.,0.));
#59081=DIRECTION('ref_axis',(0.,0.,1.));
#59082=DIRECTION('',(0.,1.,0.));
#59083=DIRECTION('center_axis',(-1.,0.,0.));
#59084=DIRECTION('ref_axis',(0.,0.,1.));
#59085=DIRECTION('',(1.,0.,0.));
#59086=DIRECTION('center_axis',(0.928966301520812,0.281372335152031,0.240522804843608));
#59087=DIRECTION('ref_axis',(-0.289882267482667,0.957062313017866,-6.01031194250061E-15));
#59088=DIRECTION('center_axis',(-0.929823364809375,0.279861066194094,-0.238969232084962));
#59089=DIRECTION('ref_axis',(-0.2882113740593,-0.957566814307414,-1.12718317199366E-14));
#59090=DIRECTION('center_axis',(-0.983705916475484,0.132945851001502,0.121029213798216));
#59091=DIRECTION('ref_axis',(-0.133930380500437,-0.990990743235782,-1.03475023686325E-15));
#59092=DIRECTION('center_axis',(0.984136564099166,0.131218424609742,-0.119402463316403));
#59093=DIRECTION('ref_axis',(-0.132163933909845,0.991227872173434,1.63884198414844E-15));
#59094=DIRECTION('center_axis',(0.999634880550771,0.016329642943714,0.0215278505098936));
#59095=DIRECTION('ref_axis',(0.0215307213626423,-4.0425685051786E-18,-0.999768187150204));
#59096=DIRECTION('center_axis',(-0.000137653858420442,0.787654692747871,
0.616116925626681));
#59097=DIRECTION('ref_axis',(-0.000104683403375652,-0.616116939438222,0.787654687016248));
#59098=DIRECTION('center_axis',(-0.999680792908394,0.01526908890116,-0.0201287658382933));
#59099=DIRECTION('ref_axis',(-0.0201311127099917,-7.84436696756394E-18,
0.999797348616737));
#59100=DIRECTION('center_axis',(0.,1.,0.));
#59101=DIRECTION('ref_axis',(0.,0.,1.));
#59102=DIRECTION('',(0.,1.,0.));
#59103=DIRECTION('center_axis',(0.000142617394872601,0.787779221593475,
-0.615957691473901));
#59104=DIRECTION('ref_axis',(0.000106417135254732,-0.615957706206436,-0.787779215796088));
#59105=DIRECTION('center_axis',(0.,1.,0.));
#59106=DIRECTION('ref_axis',(0.,0.,1.));
#59107=DIRECTION('',(0.,-1.,0.));
#59108=DIRECTION('center_axis',(-1.24353895001492E-16,0.,-1.));
#59109=DIRECTION('ref_axis',(-1.,0.,1.24353895001492E-16));
#59110=DIRECTION('center_axis',(0.,0.,1.));
#59111=DIRECTION('ref_axis',(1.,0.,0.));
#59112=DIRECTION('center_axis',(-0.173648177666927,-0.984807753012209,0.));
#59113=DIRECTION('ref_axis',(0.984807753012209,-0.173648177666927,0.));
#59114=DIRECTION('',(0.173648177666927,0.984807753012209,0.));
#59115=DIRECTION('center_axis',(0.,-1.,0.));
#59116=DIRECTION('ref_axis',(0.,0.,-1.));
#59117=DIRECTION('center_axis',(-1.,0.,0.));
#59118=DIRECTION('ref_axis',(0.,0.,1.));
#59119=DIRECTION('center_axis',(-1.,0.,0.));
#59120=DIRECTION('ref_axis',(0.,0.,1.));
#59121=DIRECTION('center_axis',(1.,0.,0.));
#59122=DIRECTION('ref_axis',(0.,0.,-1.));
#59123=DIRECTION('center_axis',(-1.,0.,0.));
#59124=DIRECTION('ref_axis',(0.,0.,1.));
#59125=DIRECTION('center_axis',(-1.,0.,0.));
#59126=DIRECTION('ref_axis',(0.,0.,1.));
#59127=DIRECTION('center_axis',(0.,-1.,0.));
#59128=DIRECTION('ref_axis',(0.,0.,-1.));
#59129=DIRECTION('center_axis',(0.,-1.,0.));
#59130=DIRECTION('ref_axis',(0.,0.,-1.));
#59131=DIRECTION('',(0.,-1.,0.));
#59132=DIRECTION('center_axis',(0.,1.,0.));
#59133=DIRECTION('ref_axis',(0.,0.,-1.));
#59134=DIRECTION('',(0.,-1.,0.));
#59135=DIRECTION('center_axis',(0.,-1.,0.));
#59136=DIRECTION('ref_axis',(0.,0.,-1.));
#59137=DIRECTION('',(0.,0.,1.));
#59138=DIRECTION('center_axis',(0.,1.,0.));
#59139=DIRECTION('ref_axis',(0.,0.,-1.));
#59140=DIRECTION('',(0.,0.,-1.));
#59141=DIRECTION('',(1.56170177914177E-16,0.,1.));
#59142=DIRECTION('center_axis',(0.,1.,0.));
#59143=DIRECTION('ref_axis',(-8.10505695128492E-16,0.,-1.));
#59144=DIRECTION('',(0.,0.,-1.));
#59145=DIRECTION('center_axis',(0.,-1.,0.));
#59146=DIRECTION('ref_axis',(0.,0.,-1.));
#59147=DIRECTION('center_axis',(0.,-1.,0.));
#59148=DIRECTION('ref_axis',(0.,0.,-1.));
#59149=DIRECTION('',(0.,0.,-1.));
#59150=DIRECTION('',(0.,0.,1.));
#59151=DIRECTION('center_axis',(0.,-1.,0.));
#59152=DIRECTION('ref_axis',(0.,0.,-1.));
#59153=DIRECTION('',(-1.56170177914177E-16,0.,-1.));
#59154=DIRECTION('',(0.,0.,1.));
#59155=DIRECTION('center_axis',(0.,-1.,0.));
#59156=DIRECTION('ref_axis',(0.,0.,-1.));
#59157=DIRECTION('center_axis',(0.,1.,0.));
#59158=DIRECTION('ref_axis',(-7.65781678570401E-16,0.,-1.));
#59159=DIRECTION('',(0.,1.,0.));
#59160=DIRECTION('center_axis',(0.,-1.,0.));
#59161=DIRECTION('ref_axis',(0.,0.,-1.));
#59162=DIRECTION('',(0.,1.,0.));
#59163=DIRECTION('center_axis',(1.,0.,0.));
#59164=DIRECTION('ref_axis',(0.,0.,-1.));
#59165=DIRECTION('',(0.,0.,-1.));
#59166=DIRECTION('',(0.,0.,1.));
#59167=DIRECTION('center_axis',(1.,0.,-1.56170177914177E-16));
#59168=DIRECTION('ref_axis',(-1.56170177914177E-16,0.,-1.));
#59169=DIRECTION('center_axis',(1.,0.,-1.56170177914177E-16));
#59170=DIRECTION('ref_axis',(-1.56170177914177E-16,0.,-1.));
#59171=DIRECTION('',(1.56170177914177E-16,0.,1.));
#59172=DIRECTION('',(-1.56170177914177E-16,0.,-1.));
#59173=DIRECTION('center_axis',(0.,1.,0.));
#59174=DIRECTION('ref_axis',(1.22464679914735E-16,0.,-1.));
#59175=DIRECTION('',(0.,-1.,0.));
#59176=DIRECTION('',(0.,1.,0.));
#59177=DIRECTION('center_axis',(-1.,0.,0.));
#59178=DIRECTION('ref_axis',(0.,0.,1.));
#59179=DIRECTION('',(0.,0.,-1.));
#59180=DIRECTION('',(0.,-1.,0.));
#59181=DIRECTION('',(0.,0.,1.));
#59182=DIRECTION('',(0.,1.,0.));
#59183=DIRECTION('center_axis',(-1.,0.,0.));
#59184=DIRECTION('ref_axis',(0.,0.,1.));
#59185=DIRECTION('',(0.,0.,-1.));
#59186=DIRECTION('',(0.,1.,0.));
#59187=DIRECTION('',(0.,0.,1.));
#59188=DIRECTION('',(0.,-1.,0.));
#59189=DIRECTION('center_axis',(0.,-1.,0.));
#59190=DIRECTION('ref_axis',(0.,0.,-1.));
#59191=DIRECTION('center_axis',(0.,0.,-1.));
#59192=DIRECTION('ref_axis',(-1.,0.,0.));
#59193=DIRECTION('center_axis',(1.56170177914177E-16,0.,1.));
#59194=DIRECTION('ref_axis',(1.,0.,-1.56170177914177E-16));
#59195=DIRECTION('center_axis',(0.,0.431316910928101,-0.902200488997562));
#59196=DIRECTION('ref_axis',(0.,0.902200488997562,0.431316910928101));
#59197=DIRECTION('center_axis',(1.,0.,-1.56170177914177E-16));
#59198=DIRECTION('ref_axis',(0.,1.06001713493349E-14,1.));
#59199=DIRECTION('center_axis',(0.,0.431316910928101,0.902200488997562));
#59200=DIRECTION('ref_axis',(0.,-0.902200488997562,0.431316910928101));
#59201=DIRECTION('center_axis',(0.,-1.,0.));
#59202=DIRECTION('ref_axis',(0.,0.,-1.));
#59203=DIRECTION('center_axis',(0.,0.,-1.));
#59204=DIRECTION('ref_axis',(-1.,0.,0.));
#59205=DIRECTION('center_axis',(-1.56170177914177E-16,0.,-1.));
#59206=DIRECTION('ref_axis',(-1.,0.,1.56170177914177E-16));
#59207=DIRECTION('center_axis',(0.,-1.,0.));
#59208=DIRECTION('ref_axis',(0.,0.,-1.));
#59209=DIRECTION('center_axis',(0.,0.,-1.));
#59210=DIRECTION('ref_axis',(-1.,0.,0.));
#59211=DIRECTION('center_axis',(0.,0.,1.));
#59212=DIRECTION('ref_axis',(1.,0.,0.));
#59213=DIRECTION('center_axis',(0.,0.,-1.));
#59214=DIRECTION('ref_axis',(-1.,0.,0.));
#59215=DIRECTION('center_axis',(0.,0.,1.));
#59216=DIRECTION('ref_axis',(1.,0.,0.));
#59217=DIRECTION('center_axis',(0.,-1.,0.));
#59218=DIRECTION('ref_axis',(0.,0.,-1.));
#59219=DIRECTION('center_axis',(0.,1.,0.));
#59220=DIRECTION('ref_axis',(0.,0.,1.));
#59221=DIRECTION('center_axis',(0.,0.,-1.));
#59222=DIRECTION('ref_axis',(-1.,0.,0.));
#59223=DIRECTION('center_axis',(0.,0.,1.));
#59224=DIRECTION('ref_axis',(1.,0.,0.));
#59225=DIRECTION('center_axis',(0.,0.,-1.));
#59226=DIRECTION('ref_axis',(-1.,0.,0.));
#59227=DIRECTION('center_axis',(0.,-1.,0.));
#59228=DIRECTION('ref_axis',(0.480804881866777,0.,0.876827614513295));
#59229=DIRECTION('center_axis',(0.,1.,0.));
#59230=DIRECTION('ref_axis',(0.,0.,1.));
#59231=DIRECTION('center_axis',(0.,1.,0.));
#59232=DIRECTION('ref_axis',(1.,0.,0.));
#59233=DIRECTION('center_axis',(0.,1.,0.));
#59234=DIRECTION('ref_axis',(0.,0.,-1.));
#59235=DIRECTION('center_axis',(0.,0.,-1.));
#59236=DIRECTION('ref_axis',(-1.,0.,0.));
#59237=DIRECTION('center_axis',(0.,1.,0.));
#59238=DIRECTION('ref_axis',(0.,0.,1.));
#59239=DIRECTION('center_axis',(0.,1.,0.));
#59240=DIRECTION('ref_axis',(0.,0.,1.));
#59241=DIRECTION('center_axis',(0.,0.,1.));
#59242=DIRECTION('ref_axis',(1.,0.,0.));
#59243=DIRECTION('center_axis',(0.,0.,-1.));
#59244=DIRECTION('ref_axis',(-1.,0.,0.));
#59245=DIRECTION('center_axis',(0.,0.,-1.));
#59246=DIRECTION('ref_axis',(-1.,0.,0.));
#59247=DIRECTION('center_axis',(0.,0.,-1.));
#59248=DIRECTION('ref_axis',(-1.,0.,0.));
#59249=DIRECTION('center_axis',(0.,0.,1.));
#59250=DIRECTION('ref_axis',(1.,0.,0.));
#59251=DIRECTION('center_axis',(0.,1.,0.));
#59252=DIRECTION('ref_axis',(1.,0.,0.));
#59253=DIRECTION('center_axis',(0.,1.,0.));
#59254=DIRECTION('ref_axis',(0.,0.,-1.));
#59255=DIRECTION('center_axis',(0.,1.,0.));
#59256=DIRECTION('ref_axis',(1.,0.,0.));
#59257=DIRECTION('center_axis',(0.,1.,0.));
#59258=DIRECTION('ref_axis',(0.,0.,1.));
#59259=DIRECTION('center_axis',(0.,1.,0.));
#59260=DIRECTION('ref_axis',(0.,0.,1.));
#59261=DIRECTION('center_axis',(0.,1.,0.));
#59262=DIRECTION('ref_axis',(0.,0.,1.));
#59263=DIRECTION('center_axis',(0.,-1.,0.));
#59264=DIRECTION('ref_axis',(-0.48080488186677,0.,0.876827614513298));
#59265=DIRECTION('center_axis',(0.,1.,0.));
#59266=DIRECTION('ref_axis',(0.,0.,1.));
#59267=DIRECTION('center_axis',(0.,1.,0.));
#59268=DIRECTION('ref_axis',(1.,0.,0.));
#59269=DIRECTION('center_axis',(0.,0.,1.));
#59270=DIRECTION('ref_axis',(-1.,0.,0.));
#59271=DIRECTION('center_axis',(0.,0.,-1.));
#59272=DIRECTION('ref_axis',(-1.,0.,0.));
#59273=DIRECTION('center_axis',(0.,0.,-1.));
#59274=DIRECTION('ref_axis',(-1.,0.,0.));
#59275=DIRECTION('axis',(0.,0.,1.));
#59276=DIRECTION('refdir',(1.,0.,0.));
#59277=DIRECTION('center_axis',(0.,1.,0.));
#59278=DIRECTION('ref_axis',(0.,0.,1.));
#59279=DIRECTION('center_axis',(0.,1.,0.));
#59280=DIRECTION('ref_axis',(0.,0.,1.));
#59281=DIRECTION('',(0.,1.,0.));
#59282=DIRECTION('center_axis',(0.,1.,0.));
#59283=DIRECTION('ref_axis',(0.,0.,1.));
#59284=DIRECTION('center_axis',(0.,1.,0.));
#59285=DIRECTION('ref_axis',(0.,0.,1.));
#59286=DIRECTION('center_axis',(0.,1.,0.));
#59287=DIRECTION('ref_axis',(0.,0.,1.));
#59288=DIRECTION('',(0.,-1.,0.));
#59289=DIRECTION('center_axis',(0.,1.,0.));
#59290=DIRECTION('ref_axis',(0.,0.,1.));
#59291=DIRECTION('center_axis',(0.,1.,0.));
#59292=DIRECTION('ref_axis',(0.,0.,1.));
#59293=DIRECTION('center_axis',(0.,1.,0.));
#59294=DIRECTION('ref_axis',(0.,0.,1.));
#59295=DIRECTION('center_axis',(0.,1.,0.));
#59296=DIRECTION('ref_axis',(0.,0.,1.));
#59297=DIRECTION('axis',(0.,0.,1.));
#59298=DIRECTION('refdir',(1.,0.,0.));
#59299=DIRECTION('center_axis',(0.,1.,0.));
#59300=DIRECTION('ref_axis',(0.,0.,1.));
#59301=DIRECTION('center_axis',(0.,-1.,0.));
#59302=DIRECTION('ref_axis',(0.,0.,1.));
#59303=DIRECTION('center_axis',(0.,-1.,2.84598943930249E-15));
#59304=DIRECTION('ref_axis',(0.,0.,-1.));
#59305=DIRECTION('center_axis',(0.,-1.,2.84598943930249E-15));
#59306=DIRECTION('ref_axis',(0.,-2.84598943930249E-15,-1.));
#59307=DIRECTION('center_axis',(1.,3.48533185724896E-31,1.22464679914735E-16));
#59308=DIRECTION('ref_axis',(-1.22464679914735E-16,0.,1.));
#59309=DIRECTION('center_axis',(0.,1.,-2.84598943930249E-15));
#59310=DIRECTION('ref_axis',(0.,-2.84598943930249E-15,-1.));
#59311=DIRECTION('center_axis',(0.,1.,0.));
#59312=DIRECTION('ref_axis',(0.,0.,1.));
#59313=DIRECTION('',(0.,-1.,0.));
#59314=DIRECTION('center_axis',(0.,1.,0.));
#59315=DIRECTION('ref_axis',(0.,0.,1.));
#59316=DIRECTION('',(0.,1.,0.));
#59317=DIRECTION('center_axis',(0.,-1.,0.));
#59318=DIRECTION('ref_axis',(0.,0.,-1.));
#59319=DIRECTION('center_axis',(0.,1.,0.));
#59320=DIRECTION('ref_axis',(0.,0.,1.));
#59321=DIRECTION('',(0.,-1.,0.));
#59322=DIRECTION('center_axis',(0.,1.,0.));
#59323=DIRECTION('ref_axis',(0.,0.,1.));
#59324=DIRECTION('',(0.,1.,0.));
#59325=DIRECTION('center_axis',(0.,-1.,0.));
#59326=DIRECTION('ref_axis',(0.,0.,-1.));
#59327=DIRECTION('center_axis',(0.,1.,0.));
#59328=DIRECTION('ref_axis',(0.,0.,1.));
#59329=DIRECTION('',(0.,-1.,0.));
#59330=DIRECTION('center_axis',(0.,1.,0.));
#59331=DIRECTION('ref_axis',(0.,0.,1.));
#59332=DIRECTION('',(0.,1.,0.));
#59333=DIRECTION('center_axis',(0.,-1.,0.));
#59334=DIRECTION('ref_axis',(0.,0.,-1.));
#59335=DIRECTION('center_axis',(0.,1.,0.));
#59336=DIRECTION('ref_axis',(0.,0.,1.));
#59337=DIRECTION('',(0.,-1.,0.));
#59338=DIRECTION('center_axis',(0.,1.,0.));
#59339=DIRECTION('ref_axis',(0.,0.,1.));
#59340=DIRECTION('',(0.,1.,0.));
#59341=DIRECTION('center_axis',(0.,-1.,0.));
#59342=DIRECTION('ref_axis',(0.,0.,-1.));
#59343=DIRECTION('center_axis',(0.,1.,0.));
#59344=DIRECTION('ref_axis',(0.,0.,1.));
#59345=DIRECTION('',(0.,-1.,0.));
#59346=DIRECTION('center_axis',(0.,1.,0.));
#59347=DIRECTION('ref_axis',(0.,0.,1.));
#59348=DIRECTION('',(0.,1.,0.));
#59349=DIRECTION('center_axis',(0.,-1.,0.));
#59350=DIRECTION('ref_axis',(0.,0.,-1.));
#59351=DIRECTION('center_axis',(0.,1.,0.));
#59352=DIRECTION('ref_axis',(0.,0.,1.));
#59353=DIRECTION('',(0.,-1.,0.));
#59354=DIRECTION('center_axis',(0.,1.,0.));
#59355=DIRECTION('ref_axis',(0.,0.,1.));
#59356=DIRECTION('',(0.,1.,0.));
#59357=DIRECTION('center_axis',(0.,-1.,0.));
#59358=DIRECTION('ref_axis',(0.,0.,-1.));
#59359=DIRECTION('center_axis',(0.,1.,0.));
#59360=DIRECTION('ref_axis',(0.,0.,1.));
#59361=DIRECTION('',(0.,-1.,0.));
#59362=DIRECTION('center_axis',(0.,1.,0.));
#59363=DIRECTION('ref_axis',(0.,0.,1.));
#59364=DIRECTION('',(0.,1.,0.));
#59365=DIRECTION('center_axis',(0.,-1.,0.));
#59366=DIRECTION('ref_axis',(0.,0.,-1.));
#59367=DIRECTION('center_axis',(0.,1.,0.));
#59368=DIRECTION('ref_axis',(0.,0.,1.));
#59369=DIRECTION('',(0.,-1.,0.));
#59370=DIRECTION('center_axis',(0.,1.,0.));
#59371=DIRECTION('ref_axis',(0.,0.,1.));
#59372=DIRECTION('',(0.,1.,0.));
#59373=DIRECTION('center_axis',(0.,-1.,0.));
#59374=DIRECTION('ref_axis',(0.,0.,-1.));
#59375=DIRECTION('center_axis',(0.,1.,0.));
#59376=DIRECTION('ref_axis',(0.,0.,1.));
#59377=DIRECTION('',(0.,-1.,0.));
#59378=DIRECTION('center_axis',(0.,1.,0.));
#59379=DIRECTION('ref_axis',(0.,0.,1.));
#59380=DIRECTION('',(0.,1.,0.));
#59381=DIRECTION('center_axis',(0.,-1.,0.));
#59382=DIRECTION('ref_axis',(0.,0.,-1.));
#59383=DIRECTION('center_axis',(0.,1.,0.));
#59384=DIRECTION('ref_axis',(0.,0.,1.));
#59385=DIRECTION('',(0.,-1.,0.));
#59386=DIRECTION('center_axis',(0.,1.,0.));
#59387=DIRECTION('ref_axis',(0.,0.,1.));
#59388=DIRECTION('',(0.,1.,0.));
#59389=DIRECTION('center_axis',(0.,-1.,0.));
#59390=DIRECTION('ref_axis',(0.,0.,-1.));
#59391=DIRECTION('center_axis',(0.,1.,0.));
#59392=DIRECTION('ref_axis',(0.,0.,1.));
#59393=DIRECTION('',(0.,-1.,0.));
#59394=DIRECTION('center_axis',(0.,1.,0.));
#59395=DIRECTION('ref_axis',(0.,0.,1.));
#59396=DIRECTION('',(0.,1.,0.));
#59397=DIRECTION('center_axis',(0.,-1.,0.));
#59398=DIRECTION('ref_axis',(0.,0.,-1.));
#59399=DIRECTION('center_axis',(0.,1.,0.));
#59400=DIRECTION('ref_axis',(0.,0.,1.));
#59401=DIRECTION('',(0.,-1.,0.));
#59402=DIRECTION('center_axis',(0.,1.,0.));
#59403=DIRECTION('ref_axis',(0.,0.,1.));
#59404=DIRECTION('',(0.,1.,0.));
#59405=DIRECTION('center_axis',(0.,-1.,0.));
#59406=DIRECTION('ref_axis',(0.,0.,-1.));
#59407=DIRECTION('center_axis',(0.,1.,0.));
#59408=DIRECTION('ref_axis',(0.,0.,1.));
#59409=DIRECTION('',(0.,-1.,0.));
#59410=DIRECTION('center_axis',(0.,1.,0.));
#59411=DIRECTION('ref_axis',(0.,0.,1.));
#59412=DIRECTION('',(0.,1.,0.));
#59413=DIRECTION('center_axis',(0.,-1.,0.));
#59414=DIRECTION('ref_axis',(0.,0.,-1.));
#59415=DIRECTION('center_axis',(0.,1.,0.));
#59416=DIRECTION('ref_axis',(0.,0.,1.));
#59417=DIRECTION('',(0.,-1.,0.));
#59418=DIRECTION('center_axis',(0.,1.,0.));
#59419=DIRECTION('ref_axis',(0.,0.,1.));
#59420=DIRECTION('',(0.,1.,0.));
#59421=DIRECTION('center_axis',(0.,-1.,0.));
#59422=DIRECTION('ref_axis',(0.,0.,-1.));
#59423=DIRECTION('center_axis',(0.,1.,0.));
#59424=DIRECTION('ref_axis',(0.,0.,1.));
#59425=DIRECTION('',(0.,-1.,0.));
#59426=DIRECTION('center_axis',(0.,1.,0.));
#59427=DIRECTION('ref_axis',(0.,0.,1.));
#59428=DIRECTION('',(0.,1.,0.));
#59429=DIRECTION('center_axis',(0.,-1.,0.));
#59430=DIRECTION('ref_axis',(0.,0.,-1.));
#59431=DIRECTION('center_axis',(0.,1.,0.));
#59432=DIRECTION('ref_axis',(0.,0.,1.));
#59433=DIRECTION('',(0.,-1.,0.));
#59434=DIRECTION('center_axis',(0.,1.,0.));
#59435=DIRECTION('ref_axis',(0.,0.,1.));
#59436=DIRECTION('',(0.,1.,0.));
#59437=DIRECTION('center_axis',(0.,-1.,0.));
#59438=DIRECTION('ref_axis',(0.,0.,-1.));
#59439=DIRECTION('center_axis',(0.,1.,0.));
#59440=DIRECTION('ref_axis',(0.,0.,1.));
#59441=DIRECTION('',(0.,-1.,0.));
#59442=DIRECTION('center_axis',(0.,1.,0.));
#59443=DIRECTION('ref_axis',(0.,0.,1.));
#59444=DIRECTION('',(0.,1.,0.));
#59445=DIRECTION('center_axis',(0.,-1.,0.));
#59446=DIRECTION('ref_axis',(0.,0.,-1.));
#59447=DIRECTION('center_axis',(0.,1.,0.));
#59448=DIRECTION('ref_axis',(0.,0.,1.));
#59449=DIRECTION('',(0.,-1.,0.));
#59450=DIRECTION('center_axis',(0.,1.,0.));
#59451=DIRECTION('ref_axis',(0.,0.,1.));
#59452=DIRECTION('',(0.,1.,0.));
#59453=DIRECTION('center_axis',(0.,-1.,0.));
#59454=DIRECTION('ref_axis',(0.,0.,-1.));
#59455=DIRECTION('center_axis',(0.,1.,0.));
#59456=DIRECTION('ref_axis',(0.,0.,1.));
#59457=DIRECTION('',(0.,-1.,0.));
#59458=DIRECTION('center_axis',(0.,1.,0.));
#59459=DIRECTION('ref_axis',(0.,0.,1.));
#59460=DIRECTION('',(0.,1.,0.));
#59461=DIRECTION('center_axis',(0.,-1.,0.));
#59462=DIRECTION('ref_axis',(0.,0.,-1.));
#59463=DIRECTION('center_axis',(0.,1.,0.));
#59464=DIRECTION('ref_axis',(0.,0.,1.));
#59465=DIRECTION('',(0.,-1.,0.));
#59466=DIRECTION('center_axis',(0.,1.,0.));
#59467=DIRECTION('ref_axis',(0.,0.,1.));
#59468=DIRECTION('',(0.,1.,0.));
#59469=DIRECTION('center_axis',(0.,-1.,0.));
#59470=DIRECTION('ref_axis',(0.,0.,-1.));
#59471=DIRECTION('center_axis',(0.,1.,0.));
#59472=DIRECTION('ref_axis',(0.,0.,1.));
#59473=DIRECTION('',(0.,-1.,0.));
#59474=DIRECTION('center_axis',(0.,1.,0.));
#59475=DIRECTION('ref_axis',(0.,0.,1.));
#59476=DIRECTION('',(0.,1.,0.));
#59477=DIRECTION('center_axis',(0.,-1.,0.));
#59478=DIRECTION('ref_axis',(0.,0.,-1.));
#59479=DIRECTION('center_axis',(0.,1.,0.));
#59480=DIRECTION('ref_axis',(0.,0.,1.));
#59481=DIRECTION('',(0.,-1.,0.));
#59482=DIRECTION('center_axis',(0.,1.,0.));
#59483=DIRECTION('ref_axis',(0.,0.,1.));
#59484=DIRECTION('',(0.,1.,0.));
#59485=DIRECTION('center_axis',(0.,-1.,0.));
#59486=DIRECTION('ref_axis',(0.,0.,-1.));
#59487=DIRECTION('center_axis',(0.,1.,0.));
#59488=DIRECTION('ref_axis',(0.,0.,1.));
#59489=DIRECTION('',(0.,-1.,0.));
#59490=DIRECTION('center_axis',(0.,1.,0.));
#59491=DIRECTION('ref_axis',(0.,0.,1.));
#59492=DIRECTION('',(0.,1.,0.));
#59493=DIRECTION('center_axis',(0.,-1.,0.));
#59494=DIRECTION('ref_axis',(0.,0.,-1.));
#59495=DIRECTION('center_axis',(0.,1.,0.));
#59496=DIRECTION('ref_axis',(0.,0.,1.));
#59497=DIRECTION('',(0.,-1.,0.));
#59498=DIRECTION('center_axis',(0.,1.,0.));
#59499=DIRECTION('ref_axis',(0.,0.,1.));
#59500=DIRECTION('',(0.,1.,0.));
#59501=DIRECTION('center_axis',(0.,-1.,0.));
#59502=DIRECTION('ref_axis',(0.,0.,-1.));
#59503=DIRECTION('center_axis',(0.,1.,0.));
#59504=DIRECTION('ref_axis',(0.,0.,1.));
#59505=DIRECTION('',(0.,-1.,0.));
#59506=DIRECTION('center_axis',(0.,1.,0.));
#59507=DIRECTION('ref_axis',(0.,0.,1.));
#59508=DIRECTION('',(0.,1.,0.));
#59509=DIRECTION('center_axis',(0.,-1.,0.));
#59510=DIRECTION('ref_axis',(0.,0.,-1.));
#59511=DIRECTION('center_axis',(0.,1.,0.));
#59512=DIRECTION('ref_axis',(0.,0.,1.));
#59513=DIRECTION('',(0.,-1.,0.));
#59514=DIRECTION('center_axis',(0.,1.,0.));
#59515=DIRECTION('ref_axis',(0.,0.,1.));
#59516=DIRECTION('',(0.,1.,0.));
#59517=DIRECTION('center_axis',(0.,-1.,0.));
#59518=DIRECTION('ref_axis',(0.,0.,-1.));
#59519=DIRECTION('center_axis',(0.,1.,0.));
#59520=DIRECTION('ref_axis',(0.,0.,1.));
#59521=DIRECTION('',(0.,-1.,0.));
#59522=DIRECTION('center_axis',(0.,1.,0.));
#59523=DIRECTION('ref_axis',(0.,0.,1.));
#59524=DIRECTION('',(0.,1.,0.));
#59525=DIRECTION('center_axis',(0.,-1.,0.));
#59526=DIRECTION('ref_axis',(0.,0.,-1.));
#59527=DIRECTION('center_axis',(0.,1.,0.));
#59528=DIRECTION('ref_axis',(0.,0.,1.));
#59529=DIRECTION('',(0.,-1.,0.));
#59530=DIRECTION('center_axis',(0.,1.,0.));
#59531=DIRECTION('ref_axis',(0.,0.,1.));
#59532=DIRECTION('',(0.,1.,0.));
#59533=DIRECTION('center_axis',(0.,-1.,0.));
#59534=DIRECTION('ref_axis',(0.,0.,-1.));
#59535=DIRECTION('center_axis',(0.,1.,0.));
#59536=DIRECTION('ref_axis',(0.,0.,1.));
#59537=DIRECTION('',(0.,-1.,0.));
#59538=DIRECTION('center_axis',(0.,1.,0.));
#59539=DIRECTION('ref_axis',(0.,0.,1.));
#59540=DIRECTION('',(0.,1.,0.));
#59541=DIRECTION('center_axis',(0.,-1.,0.));
#59542=DIRECTION('ref_axis',(0.,0.,-1.));
#59543=DIRECTION('center_axis',(0.,1.,0.));
#59544=DIRECTION('ref_axis',(0.,0.,1.));
#59545=DIRECTION('',(0.,-1.,0.));
#59546=DIRECTION('center_axis',(0.,1.,0.));
#59547=DIRECTION('ref_axis',(0.,0.,1.));
#59548=DIRECTION('',(0.,1.,0.));
#59549=DIRECTION('center_axis',(0.,-1.,0.));
#59550=DIRECTION('ref_axis',(0.,0.,-1.));
#59551=DIRECTION('center_axis',(0.,1.,0.));
#59552=DIRECTION('ref_axis',(0.,0.,1.));
#59553=DIRECTION('',(0.,-1.,0.));
#59554=DIRECTION('center_axis',(0.,1.,0.));
#59555=DIRECTION('ref_axis',(0.,0.,1.));
#59556=DIRECTION('',(0.,1.,0.));
#59557=DIRECTION('center_axis',(0.,-1.,0.));
#59558=DIRECTION('ref_axis',(0.,0.,-1.));
#59559=DIRECTION('center_axis',(0.,1.,0.));
#59560=DIRECTION('ref_axis',(0.,0.,1.));
#59561=DIRECTION('',(0.,-1.,0.));
#59562=DIRECTION('center_axis',(0.,1.,0.));
#59563=DIRECTION('ref_axis',(0.,0.,1.));
#59564=DIRECTION('',(0.,1.,0.));
#59565=DIRECTION('center_axis',(0.,-1.,0.));
#59566=DIRECTION('ref_axis',(0.,0.,-1.));
#59567=DIRECTION('center_axis',(0.,1.,0.));
#59568=DIRECTION('ref_axis',(0.,0.,1.));
#59569=DIRECTION('',(0.,-1.,0.));
#59570=DIRECTION('center_axis',(0.,1.,0.));
#59571=DIRECTION('ref_axis',(0.,0.,1.));
#59572=DIRECTION('',(0.,1.,0.));
#59573=DIRECTION('center_axis',(0.,-1.,0.));
#59574=DIRECTION('ref_axis',(0.,0.,-1.));
#59575=DIRECTION('center_axis',(0.,1.,0.));
#59576=DIRECTION('ref_axis',(0.,0.,1.));
#59577=DIRECTION('',(0.,-1.,0.));
#59578=DIRECTION('center_axis',(0.,1.,0.));
#59579=DIRECTION('ref_axis',(0.,0.,1.));
#59580=DIRECTION('',(0.,1.,0.));
#59581=DIRECTION('center_axis',(0.,-1.,0.));
#59582=DIRECTION('ref_axis',(0.,0.,-1.));
#59583=DIRECTION('center_axis',(0.,1.,0.));
#59584=DIRECTION('ref_axis',(0.,0.,1.));
#59585=DIRECTION('',(0.,-1.,0.));
#59586=DIRECTION('center_axis',(0.,1.,0.));
#59587=DIRECTION('ref_axis',(0.,0.,1.));
#59588=DIRECTION('',(0.,1.,0.));
#59589=DIRECTION('center_axis',(0.,-1.,0.));
#59590=DIRECTION('ref_axis',(0.,0.,-1.));
#59591=DIRECTION('center_axis',(0.,1.,0.));
#59592=DIRECTION('ref_axis',(0.,0.,1.));
#59593=DIRECTION('',(0.,-1.,0.));
#59594=DIRECTION('center_axis',(0.,1.,0.));
#59595=DIRECTION('ref_axis',(0.,0.,1.));
#59596=DIRECTION('',(0.,1.,0.));
#59597=DIRECTION('center_axis',(0.,-1.,0.));
#59598=DIRECTION('ref_axis',(0.,0.,-1.));
#59599=DIRECTION('center_axis',(0.,1.,0.));
#59600=DIRECTION('ref_axis',(0.,0.,1.));
#59601=DIRECTION('',(0.,-1.,0.));
#59602=DIRECTION('center_axis',(0.,1.,0.));
#59603=DIRECTION('ref_axis',(0.,0.,1.));
#59604=DIRECTION('',(0.,1.,0.));
#59605=DIRECTION('center_axis',(0.,-1.,0.));
#59606=DIRECTION('ref_axis',(0.,0.,-1.));
#59607=DIRECTION('center_axis',(0.,1.,0.));
#59608=DIRECTION('ref_axis',(0.,0.,1.));
#59609=DIRECTION('',(0.,-1.,0.));
#59610=DIRECTION('center_axis',(0.,1.,0.));
#59611=DIRECTION('ref_axis',(0.,0.,1.));
#59612=DIRECTION('',(0.,1.,0.));
#59613=DIRECTION('center_axis',(0.,-1.,0.));
#59614=DIRECTION('ref_axis',(0.,0.,-1.));
#59615=DIRECTION('center_axis',(0.,1.,0.));
#59616=DIRECTION('ref_axis',(0.,0.,1.));
#59617=DIRECTION('',(0.,-1.,0.));
#59618=DIRECTION('center_axis',(0.,1.,0.));
#59619=DIRECTION('ref_axis',(0.,0.,1.));
#59620=DIRECTION('',(0.,1.,0.));
#59621=DIRECTION('center_axis',(0.,-1.,0.));
#59622=DIRECTION('ref_axis',(0.,0.,-1.));
#59623=DIRECTION('center_axis',(0.,1.,0.));
#59624=DIRECTION('ref_axis',(0.,0.,1.));
#59625=DIRECTION('',(0.,-1.,0.));
#59626=DIRECTION('center_axis',(0.,1.,0.));
#59627=DIRECTION('ref_axis',(0.,0.,1.));
#59628=DIRECTION('',(0.,1.,0.));
#59629=DIRECTION('center_axis',(0.,-1.,0.));
#59630=DIRECTION('ref_axis',(0.,0.,-1.));
#59631=DIRECTION('center_axis',(0.,1.,0.));
#59632=DIRECTION('ref_axis',(0.,0.,1.));
#59633=DIRECTION('',(0.,-1.,0.));
#59634=DIRECTION('center_axis',(0.,1.,0.));
#59635=DIRECTION('ref_axis',(0.,0.,1.));
#59636=DIRECTION('',(0.,1.,0.));
#59637=DIRECTION('center_axis',(0.,-1.,0.));
#59638=DIRECTION('ref_axis',(0.,0.,-1.));
#59639=DIRECTION('center_axis',(0.,1.,0.));
#59640=DIRECTION('ref_axis',(0.,0.,1.));
#59641=DIRECTION('',(0.,-1.,0.));
#59642=DIRECTION('center_axis',(0.,1.,0.));
#59643=DIRECTION('ref_axis',(0.,0.,1.));
#59644=DIRECTION('',(0.,1.,0.));
#59645=DIRECTION('center_axis',(0.,-1.,0.));
#59646=DIRECTION('ref_axis',(0.,0.,-1.));
#59647=DIRECTION('center_axis',(0.,1.,0.));
#59648=DIRECTION('ref_axis',(0.,0.,1.));
#59649=DIRECTION('',(0.,-1.,0.));
#59650=DIRECTION('center_axis',(0.,1.,0.));
#59651=DIRECTION('ref_axis',(0.,0.,1.));
#59652=DIRECTION('',(0.,1.,0.));
#59653=DIRECTION('center_axis',(0.,-1.,0.));
#59654=DIRECTION('ref_axis',(0.,0.,-1.));
#59655=DIRECTION('center_axis',(0.,1.,0.));
#59656=DIRECTION('ref_axis',(0.,0.,1.));
#59657=DIRECTION('',(0.,-1.,0.));
#59658=DIRECTION('center_axis',(0.,1.,0.));
#59659=DIRECTION('ref_axis',(0.,0.,1.));
#59660=DIRECTION('',(0.,1.,0.));
#59661=DIRECTION('center_axis',(0.,-1.,0.));
#59662=DIRECTION('ref_axis',(0.,0.,-1.));
#59663=DIRECTION('center_axis',(0.,1.,0.));
#59664=DIRECTION('ref_axis',(0.,0.,1.));
#59665=DIRECTION('',(0.,-1.,0.));
#59666=DIRECTION('center_axis',(0.,1.,0.));
#59667=DIRECTION('ref_axis',(0.,0.,1.));
#59668=DIRECTION('',(0.,1.,0.));
#59669=DIRECTION('center_axis',(0.,-1.,0.));
#59670=DIRECTION('ref_axis',(0.,0.,-1.));
#59671=DIRECTION('center_axis',(0.,1.,0.));
#59672=DIRECTION('ref_axis',(0.,0.,1.));
#59673=DIRECTION('',(0.,-1.,0.));
#59674=DIRECTION('center_axis',(0.,1.,0.));
#59675=DIRECTION('ref_axis',(0.,0.,1.));
#59676=DIRECTION('',(0.,1.,0.));
#59677=DIRECTION('center_axis',(0.,-1.,0.));
#59678=DIRECTION('ref_axis',(0.,0.,-1.));
#59679=DIRECTION('center_axis',(0.,1.,0.));
#59680=DIRECTION('ref_axis',(0.,0.,1.));
#59681=DIRECTION('',(0.,-1.,0.));
#59682=DIRECTION('center_axis',(0.,1.,0.));
#59683=DIRECTION('ref_axis',(0.,0.,1.));
#59684=DIRECTION('',(0.,1.,0.));
#59685=DIRECTION('center_axis',(0.,-1.,0.));
#59686=DIRECTION('ref_axis',(0.,0.,-1.));
#59687=DIRECTION('center_axis',(0.,1.,0.));
#59688=DIRECTION('ref_axis',(0.,0.,1.));
#59689=DIRECTION('',(0.,-1.,0.));
#59690=DIRECTION('center_axis',(0.,1.,0.));
#59691=DIRECTION('ref_axis',(0.,0.,1.));
#59692=DIRECTION('',(0.,1.,0.));
#59693=DIRECTION('center_axis',(0.,-1.,0.));
#59694=DIRECTION('ref_axis',(0.,0.,-1.));
#59695=DIRECTION('center_axis',(0.,1.,0.));
#59696=DIRECTION('ref_axis',(0.,0.,1.));
#59697=DIRECTION('',(0.,-1.,0.));
#59698=DIRECTION('center_axis',(0.,1.,0.));
#59699=DIRECTION('ref_axis',(0.,0.,1.));
#59700=DIRECTION('',(0.,1.,0.));
#59701=DIRECTION('center_axis',(0.,-1.,0.));
#59702=DIRECTION('ref_axis',(0.,0.,-1.));
#59703=DIRECTION('center_axis',(0.,1.,0.));
#59704=DIRECTION('ref_axis',(0.,0.,1.));
#59705=DIRECTION('',(0.,-1.,0.));
#59706=DIRECTION('center_axis',(0.,1.,0.));
#59707=DIRECTION('ref_axis',(0.,0.,1.));
#59708=DIRECTION('',(0.,1.,0.));
#59709=DIRECTION('center_axis',(0.,-1.,0.));
#59710=DIRECTION('ref_axis',(0.,0.,-1.));
#59711=DIRECTION('center_axis',(0.,1.,0.));
#59712=DIRECTION('ref_axis',(0.,0.,1.));
#59713=DIRECTION('',(0.,-1.,0.));
#59714=DIRECTION('center_axis',(0.,1.,0.));
#59715=DIRECTION('ref_axis',(0.,0.,1.));
#59716=DIRECTION('',(0.,1.,0.));
#59717=DIRECTION('center_axis',(0.,-1.,0.));
#59718=DIRECTION('ref_axis',(0.,0.,-1.));
#59719=DIRECTION('center_axis',(0.,1.,0.));
#59720=DIRECTION('ref_axis',(0.,0.,1.));
#59721=DIRECTION('',(0.,-1.,0.));
#59722=DIRECTION('center_axis',(0.,1.,0.));
#59723=DIRECTION('ref_axis',(0.,0.,1.));
#59724=DIRECTION('',(0.,1.,0.));
#59725=DIRECTION('center_axis',(0.,-1.,0.));
#59726=DIRECTION('ref_axis',(0.,0.,-1.));
#59727=DIRECTION('center_axis',(0.,1.,0.));
#59728=DIRECTION('ref_axis',(0.,0.,1.));
#59729=DIRECTION('',(0.,-1.,0.));
#59730=DIRECTION('center_axis',(0.,1.,0.));
#59731=DIRECTION('ref_axis',(0.,0.,1.));
#59732=DIRECTION('',(0.,1.,0.));
#59733=DIRECTION('center_axis',(0.,-1.,0.));
#59734=DIRECTION('ref_axis',(0.,0.,-1.));
#59735=DIRECTION('center_axis',(0.,1.,0.));
#59736=DIRECTION('ref_axis',(0.,0.,1.));
#59737=DIRECTION('',(0.,-1.,0.));
#59738=DIRECTION('center_axis',(0.,1.,0.));
#59739=DIRECTION('ref_axis',(0.,0.,1.));
#59740=DIRECTION('',(0.,1.,0.));
#59741=DIRECTION('center_axis',(0.,-1.,0.));
#59742=DIRECTION('ref_axis',(0.,0.,-1.));
#59743=DIRECTION('center_axis',(0.,1.,0.));
#59744=DIRECTION('ref_axis',(0.,0.,1.));
#59745=DIRECTION('',(0.,-1.,0.));
#59746=DIRECTION('center_axis',(0.,1.,0.));
#59747=DIRECTION('ref_axis',(0.,0.,1.));
#59748=DIRECTION('',(0.,1.,0.));
#59749=DIRECTION('center_axis',(0.,-1.,0.));
#59750=DIRECTION('ref_axis',(0.,0.,-1.));
#59751=DIRECTION('center_axis',(0.,1.,0.));
#59752=DIRECTION('ref_axis',(0.,0.,1.));
#59753=DIRECTION('',(0.,-1.,0.));
#59754=DIRECTION('center_axis',(0.,1.,0.));
#59755=DIRECTION('ref_axis',(0.,0.,1.));
#59756=DIRECTION('',(0.,1.,0.));
#59757=DIRECTION('center_axis',(0.,-1.,0.));
#59758=DIRECTION('ref_axis',(0.,0.,-1.));
#59759=DIRECTION('center_axis',(0.,1.,0.));
#59760=DIRECTION('ref_axis',(0.,0.,1.));
#59761=DIRECTION('',(0.,-1.,0.));
#59762=DIRECTION('center_axis',(0.,1.,0.));
#59763=DIRECTION('ref_axis',(0.,0.,1.));
#59764=DIRECTION('',(0.,1.,0.));
#59765=DIRECTION('center_axis',(0.,-1.,0.));
#59766=DIRECTION('ref_axis',(0.,0.,-1.));
#59767=DIRECTION('center_axis',(0.,1.,0.));
#59768=DIRECTION('ref_axis',(0.,0.,1.));
#59769=DIRECTION('',(0.,-1.,0.));
#59770=DIRECTION('center_axis',(0.,1.,0.));
#59771=DIRECTION('ref_axis',(0.,0.,1.));
#59772=DIRECTION('',(0.,1.,0.));
#59773=DIRECTION('center_axis',(0.,-1.,0.));
#59774=DIRECTION('ref_axis',(0.,0.,-1.));
#59775=DIRECTION('center_axis',(0.,1.,0.));
#59776=DIRECTION('ref_axis',(0.,0.,1.));
#59777=DIRECTION('',(0.,-1.,0.));
#59778=DIRECTION('center_axis',(0.,1.,0.));
#59779=DIRECTION('ref_axis',(0.,0.,1.));
#59780=DIRECTION('',(0.,1.,0.));
#59781=DIRECTION('center_axis',(0.,-1.,0.));
#59782=DIRECTION('ref_axis',(0.,0.,-1.));
#59783=DIRECTION('center_axis',(0.,1.,0.));
#59784=DIRECTION('ref_axis',(0.,0.,1.));
#59785=DIRECTION('',(0.,-1.,0.));
#59786=DIRECTION('center_axis',(0.,1.,0.));
#59787=DIRECTION('ref_axis',(0.,0.,1.));
#59788=DIRECTION('',(0.,1.,0.));
#59789=DIRECTION('center_axis',(0.,-1.,0.));
#59790=DIRECTION('ref_axis',(0.,0.,-1.));
#59791=DIRECTION('center_axis',(0.,1.,0.));
#59792=DIRECTION('ref_axis',(0.,0.,1.));
#59793=DIRECTION('',(0.,-1.,0.));
#59794=DIRECTION('center_axis',(0.,1.,0.));
#59795=DIRECTION('ref_axis',(0.,0.,1.));
#59796=DIRECTION('',(0.,1.,0.));
#59797=DIRECTION('center_axis',(0.,-1.,0.));
#59798=DIRECTION('ref_axis',(0.,0.,-1.));
#59799=DIRECTION('center_axis',(0.,1.,0.));
#59800=DIRECTION('ref_axis',(0.,0.,1.));
#59801=DIRECTION('',(0.,-1.,0.));
#59802=DIRECTION('center_axis',(0.,1.,0.));
#59803=DIRECTION('ref_axis',(0.,0.,1.));
#59804=DIRECTION('',(0.,1.,0.));
#59805=DIRECTION('center_axis',(0.,-1.,0.));
#59806=DIRECTION('ref_axis',(0.,0.,-1.));
#59807=DIRECTION('center_axis',(0.,1.,0.));
#59808=DIRECTION('ref_axis',(0.,0.,1.));
#59809=DIRECTION('',(0.,-1.,0.));
#59810=DIRECTION('center_axis',(0.,1.,0.));
#59811=DIRECTION('ref_axis',(0.,0.,1.));
#59812=DIRECTION('',(0.,1.,0.));
#59813=DIRECTION('center_axis',(0.,-1.,0.));
#59814=DIRECTION('ref_axis',(0.,0.,-1.));
#59815=DIRECTION('center_axis',(0.,1.,0.));
#59816=DIRECTION('ref_axis',(0.,0.,1.));
#59817=DIRECTION('',(0.,-1.,0.));
#59818=DIRECTION('center_axis',(0.,1.,0.));
#59819=DIRECTION('ref_axis',(0.,0.,1.));
#59820=DIRECTION('',(0.,1.,0.));
#59821=DIRECTION('center_axis',(0.,-1.,0.));
#59822=DIRECTION('ref_axis',(0.,0.,-1.));
#59823=DIRECTION('center_axis',(0.,1.,0.));
#59824=DIRECTION('ref_axis',(0.,0.,1.));
#59825=DIRECTION('',(0.,-1.,0.));
#59826=DIRECTION('center_axis',(0.,1.,0.));
#59827=DIRECTION('ref_axis',(0.,0.,1.));
#59828=DIRECTION('',(0.,1.,0.));
#59829=DIRECTION('center_axis',(0.,-1.,0.));
#59830=DIRECTION('ref_axis',(0.,0.,-1.));
#59831=DIRECTION('center_axis',(0.,1.,0.));
#59832=DIRECTION('ref_axis',(0.,0.,1.));
#59833=DIRECTION('',(0.,-1.,0.));
#59834=DIRECTION('center_axis',(0.,1.,0.));
#59835=DIRECTION('ref_axis',(0.,0.,1.));
#59836=DIRECTION('',(0.,1.,0.));
#59837=DIRECTION('center_axis',(0.,-1.,0.));
#59838=DIRECTION('ref_axis',(0.,0.,-1.));
#59839=DIRECTION('center_axis',(0.,1.,0.));
#59840=DIRECTION('ref_axis',(0.,0.,1.));
#59841=DIRECTION('',(0.,-1.,0.));
#59842=DIRECTION('center_axis',(0.,1.,0.));
#59843=DIRECTION('ref_axis',(0.,0.,1.));
#59844=DIRECTION('',(0.,1.,0.));
#59845=DIRECTION('center_axis',(0.,-1.,0.));
#59846=DIRECTION('ref_axis',(0.,0.,-1.));
#59847=DIRECTION('center_axis',(0.,1.,0.));
#59848=DIRECTION('ref_axis',(0.,0.,1.));
#59849=DIRECTION('',(0.,-1.,0.));
#59850=DIRECTION('center_axis',(0.,1.,0.));
#59851=DIRECTION('ref_axis',(0.,0.,1.));
#59852=DIRECTION('',(0.,1.,0.));
#59853=DIRECTION('center_axis',(0.,-1.,0.));
#59854=DIRECTION('ref_axis',(0.,0.,-1.));
#59855=DIRECTION('center_axis',(0.,1.,0.));
#59856=DIRECTION('ref_axis',(0.,0.,1.));
#59857=DIRECTION('',(0.,-1.,0.));
#59858=DIRECTION('center_axis',(0.,1.,0.));
#59859=DIRECTION('ref_axis',(0.,0.,1.));
#59860=DIRECTION('',(0.,1.,0.));
#59861=DIRECTION('center_axis',(0.,-1.,0.));
#59862=DIRECTION('ref_axis',(0.,0.,-1.));
#59863=DIRECTION('center_axis',(0.,1.,0.));
#59864=DIRECTION('ref_axis',(0.,0.,1.));
#59865=DIRECTION('',(0.,-1.,0.));
#59866=DIRECTION('center_axis',(0.,1.,0.));
#59867=DIRECTION('ref_axis',(0.,0.,1.));
#59868=DIRECTION('',(0.,1.,0.));
#59869=DIRECTION('center_axis',(0.,-1.,0.));
#59870=DIRECTION('ref_axis',(0.,0.,-1.));
#59871=DIRECTION('center_axis',(0.,1.,0.));
#59872=DIRECTION('ref_axis',(0.,0.,1.));
#59873=DIRECTION('',(0.,-1.,0.));
#59874=DIRECTION('center_axis',(0.,1.,0.));
#59875=DIRECTION('ref_axis',(0.,0.,1.));
#59876=DIRECTION('',(0.,1.,0.));
#59877=DIRECTION('center_axis',(0.,-1.,0.));
#59878=DIRECTION('ref_axis',(0.,0.,-1.));
#59879=DIRECTION('center_axis',(0.,1.,0.));
#59880=DIRECTION('ref_axis',(0.,0.,1.));
#59881=DIRECTION('',(0.,-1.,0.));
#59882=DIRECTION('center_axis',(0.,1.,0.));
#59883=DIRECTION('ref_axis',(0.,0.,1.));
#59884=DIRECTION('',(0.,1.,0.));
#59885=DIRECTION('center_axis',(0.,-1.,0.));
#59886=DIRECTION('ref_axis',(0.,0.,-1.));
#59887=DIRECTION('center_axis',(0.,1.,0.));
#59888=DIRECTION('ref_axis',(0.,0.,1.));
#59889=DIRECTION('',(0.,-1.,0.));
#59890=DIRECTION('center_axis',(0.,1.,0.));
#59891=DIRECTION('ref_axis',(0.,0.,1.));
#59892=DIRECTION('',(0.,1.,0.));
#59893=DIRECTION('center_axis',(0.,-1.,0.));
#59894=DIRECTION('ref_axis',(0.,0.,-1.));
#59895=DIRECTION('center_axis',(0.,1.,0.));
#59896=DIRECTION('ref_axis',(0.,0.,1.));
#59897=DIRECTION('',(0.,-1.,0.));
#59898=DIRECTION('center_axis',(0.,1.,0.));
#59899=DIRECTION('ref_axis',(0.,0.,1.));
#59900=DIRECTION('',(0.,1.,0.));
#59901=DIRECTION('center_axis',(0.,-1.,0.));
#59902=DIRECTION('ref_axis',(0.,0.,-1.));
#59903=DIRECTION('center_axis',(0.,1.,0.));
#59904=DIRECTION('ref_axis',(0.,0.,1.));
#59905=DIRECTION('',(0.,-1.,0.));
#59906=DIRECTION('center_axis',(0.,1.,0.));
#59907=DIRECTION('ref_axis',(0.,0.,1.));
#59908=DIRECTION('',(0.,1.,0.));
#59909=DIRECTION('center_axis',(0.,-1.,0.));
#59910=DIRECTION('ref_axis',(0.,0.,-1.));
#59911=DIRECTION('center_axis',(0.,1.,0.));
#59912=DIRECTION('ref_axis',(0.,0.,1.));
#59913=DIRECTION('',(0.,-1.,0.));
#59914=DIRECTION('center_axis',(0.,1.,0.));
#59915=DIRECTION('ref_axis',(0.,0.,1.));
#59916=DIRECTION('',(0.,1.,0.));
#59917=DIRECTION('center_axis',(0.,-1.,0.));
#59918=DIRECTION('ref_axis',(0.,0.,-1.));
#59919=DIRECTION('center_axis',(0.,1.,0.));
#59920=DIRECTION('ref_axis',(0.,0.,1.));
#59921=DIRECTION('',(0.,-1.,0.));
#59922=DIRECTION('center_axis',(0.,1.,0.));
#59923=DIRECTION('ref_axis',(0.,0.,1.));
#59924=DIRECTION('',(0.,1.,0.));
#59925=DIRECTION('center_axis',(0.,-1.,0.));
#59926=DIRECTION('ref_axis',(0.,0.,-1.));
#59927=DIRECTION('center_axis',(0.,1.,0.));
#59928=DIRECTION('ref_axis',(0.,0.,1.));
#59929=DIRECTION('',(0.,-1.,0.));
#59930=DIRECTION('center_axis',(0.,1.,0.));
#59931=DIRECTION('ref_axis',(0.,0.,1.));
#59932=DIRECTION('',(0.,1.,0.));
#59933=DIRECTION('center_axis',(0.,-1.,0.));
#59934=DIRECTION('ref_axis',(0.,0.,-1.));
#59935=DIRECTION('center_axis',(0.,1.,0.));
#59936=DIRECTION('ref_axis',(0.,0.,1.));
#59937=DIRECTION('',(0.,-1.,0.));
#59938=DIRECTION('center_axis',(0.,1.,0.));
#59939=DIRECTION('ref_axis',(0.,0.,1.));
#59940=DIRECTION('',(0.,1.,0.));
#59941=DIRECTION('center_axis',(0.,-1.,0.));
#59942=DIRECTION('ref_axis',(0.,0.,-1.));
#59943=DIRECTION('center_axis',(0.,1.,0.));
#59944=DIRECTION('ref_axis',(0.,0.,1.));
#59945=DIRECTION('',(0.,-1.,0.));
#59946=DIRECTION('center_axis',(0.,1.,0.));
#59947=DIRECTION('ref_axis',(0.,0.,1.));
#59948=DIRECTION('',(0.,1.,0.));
#59949=DIRECTION('center_axis',(0.,-1.,0.));
#59950=DIRECTION('ref_axis',(0.,0.,-1.));
#59951=DIRECTION('center_axis',(0.,1.,0.));
#59952=DIRECTION('ref_axis',(0.,0.,1.));
#59953=DIRECTION('',(0.,-1.,0.));
#59954=DIRECTION('center_axis',(0.,1.,0.));
#59955=DIRECTION('ref_axis',(0.,0.,1.));
#59956=DIRECTION('',(0.,1.,0.));
#59957=DIRECTION('center_axis',(0.,-1.,0.));
#59958=DIRECTION('ref_axis',(0.,0.,-1.));
#59959=DIRECTION('center_axis',(0.,1.,0.));
#59960=DIRECTION('ref_axis',(0.,0.,1.));
#59961=DIRECTION('',(0.,-1.,0.));
#59962=DIRECTION('center_axis',(0.,1.,0.));
#59963=DIRECTION('ref_axis',(0.,0.,1.));
#59964=DIRECTION('',(0.,1.,0.));
#59965=DIRECTION('center_axis',(0.,-1.,0.));
#59966=DIRECTION('ref_axis',(0.,0.,-1.));
#59967=DIRECTION('center_axis',(0.,1.,0.));
#59968=DIRECTION('ref_axis',(0.,0.,1.));
#59969=DIRECTION('',(0.,-1.,0.));
#59970=DIRECTION('center_axis',(0.,1.,0.));
#59971=DIRECTION('ref_axis',(0.,0.,1.));
#59972=DIRECTION('',(0.,1.,0.));
#59973=DIRECTION('center_axis',(0.,-1.,0.));
#59974=DIRECTION('ref_axis',(0.,0.,-1.));
#59975=DIRECTION('center_axis',(0.,1.,0.));
#59976=DIRECTION('ref_axis',(0.,0.,1.));
#59977=DIRECTION('',(0.,-1.,0.));
#59978=DIRECTION('center_axis',(0.,1.,0.));
#59979=DIRECTION('ref_axis',(0.,0.,1.));
#59980=DIRECTION('',(0.,1.,0.));
#59981=DIRECTION('center_axis',(0.,-1.,0.));
#59982=DIRECTION('ref_axis',(0.,0.,-1.));
#59983=DIRECTION('center_axis',(0.,1.,0.));
#59984=DIRECTION('ref_axis',(0.,0.,1.));
#59985=DIRECTION('',(0.,-1.,0.));
#59986=DIRECTION('center_axis',(0.,1.,0.));
#59987=DIRECTION('ref_axis',(0.,0.,1.));
#59988=DIRECTION('',(0.,1.,0.));
#59989=DIRECTION('center_axis',(0.,-1.,0.));
#59990=DIRECTION('ref_axis',(0.,0.,-1.));
#59991=DIRECTION('center_axis',(0.,1.,0.));
#59992=DIRECTION('ref_axis',(0.,0.,1.));
#59993=DIRECTION('',(0.,-1.,0.));
#59994=DIRECTION('center_axis',(0.,1.,0.));
#59995=DIRECTION('ref_axis',(0.,0.,1.));
#59996=DIRECTION('',(0.,1.,0.));
#59997=DIRECTION('center_axis',(0.,-1.,0.));
#59998=DIRECTION('ref_axis',(0.,0.,-1.));
#59999=DIRECTION('center_axis',(0.,1.,0.));
#60000=DIRECTION('ref_axis',(0.,0.,1.));
#60001=DIRECTION('',(0.,-1.,0.));
#60002=DIRECTION('center_axis',(0.,1.,0.));
#60003=DIRECTION('ref_axis',(0.,0.,1.));
#60004=DIRECTION('',(0.,1.,0.));
#60005=DIRECTION('center_axis',(0.,-1.,0.));
#60006=DIRECTION('ref_axis',(0.,0.,-1.));
#60007=DIRECTION('center_axis',(0.,1.,0.));
#60008=DIRECTION('ref_axis',(0.,0.,1.));
#60009=DIRECTION('',(0.,-1.,0.));
#60010=DIRECTION('center_axis',(0.,1.,0.));
#60011=DIRECTION('ref_axis',(0.,0.,1.));
#60012=DIRECTION('',(0.,1.,0.));
#60013=DIRECTION('center_axis',(0.,-1.,0.));
#60014=DIRECTION('ref_axis',(0.,0.,-1.));
#60015=DIRECTION('center_axis',(0.,1.,0.));
#60016=DIRECTION('ref_axis',(0.,0.,1.));
#60017=DIRECTION('',(0.,-1.,0.));
#60018=DIRECTION('center_axis',(0.,1.,0.));
#60019=DIRECTION('ref_axis',(0.,0.,1.));
#60020=DIRECTION('',(0.,1.,0.));
#60021=DIRECTION('center_axis',(0.,-1.,0.));
#60022=DIRECTION('ref_axis',(0.,0.,-1.));
#60023=DIRECTION('center_axis',(0.,1.,0.));
#60024=DIRECTION('ref_axis',(0.,0.,1.));
#60025=DIRECTION('',(0.,-1.,0.));
#60026=DIRECTION('center_axis',(0.,1.,0.));
#60027=DIRECTION('ref_axis',(0.,0.,1.));
#60028=DIRECTION('',(0.,1.,0.));
#60029=DIRECTION('center_axis',(0.,-1.,0.));
#60030=DIRECTION('ref_axis',(0.,0.,-1.));
#60031=DIRECTION('center_axis',(0.,1.,0.));
#60032=DIRECTION('ref_axis',(0.,0.,1.));
#60033=DIRECTION('',(0.,-1.,0.));
#60034=DIRECTION('center_axis',(0.,1.,0.));
#60035=DIRECTION('ref_axis',(0.,0.,1.));
#60036=DIRECTION('',(0.,1.,0.));
#60037=DIRECTION('center_axis',(0.,-1.,0.));
#60038=DIRECTION('ref_axis',(0.,0.,-1.));
#60039=DIRECTION('center_axis',(0.,1.,0.));
#60040=DIRECTION('ref_axis',(0.,0.,1.));
#60041=DIRECTION('',(0.,-1.,0.));
#60042=DIRECTION('center_axis',(0.,1.,0.));
#60043=DIRECTION('ref_axis',(0.,0.,1.));
#60044=DIRECTION('',(0.,1.,0.));
#60045=DIRECTION('center_axis',(0.,-1.,0.));
#60046=DIRECTION('ref_axis',(0.,0.,-1.));
#60047=DIRECTION('center_axis',(0.,1.,0.));
#60048=DIRECTION('ref_axis',(0.,0.,1.));
#60049=DIRECTION('',(0.,-1.,0.));
#60050=DIRECTION('center_axis',(0.,1.,0.));
#60051=DIRECTION('ref_axis',(0.,0.,1.));
#60052=DIRECTION('',(0.,1.,0.));
#60053=DIRECTION('center_axis',(0.,-1.,0.));
#60054=DIRECTION('ref_axis',(0.,0.,-1.));
#60055=DIRECTION('center_axis',(0.,1.,0.));
#60056=DIRECTION('ref_axis',(0.,0.,1.));
#60057=DIRECTION('',(0.,-1.,0.));
#60058=DIRECTION('center_axis',(0.,1.,0.));
#60059=DIRECTION('ref_axis',(0.,0.,1.));
#60060=DIRECTION('',(0.,1.,0.));
#60061=DIRECTION('center_axis',(0.,-1.,0.));
#60062=DIRECTION('ref_axis',(0.,0.,-1.));
#60063=DIRECTION('center_axis',(0.,1.,0.));
#60064=DIRECTION('ref_axis',(0.,0.,1.));
#60065=DIRECTION('',(0.,-1.,0.));
#60066=DIRECTION('center_axis',(0.,1.,0.));
#60067=DIRECTION('ref_axis',(0.,0.,1.));
#60068=DIRECTION('',(0.,1.,0.));
#60069=DIRECTION('center_axis',(0.,-1.,0.));
#60070=DIRECTION('ref_axis',(0.,0.,-1.));
#60071=DIRECTION('center_axis',(0.,1.,0.));
#60072=DIRECTION('ref_axis',(0.,0.,1.));
#60073=DIRECTION('',(0.,-1.,0.));
#60074=DIRECTION('center_axis',(0.,1.,0.));
#60075=DIRECTION('ref_axis',(0.,0.,1.));
#60076=DIRECTION('',(0.,1.,0.));
#60077=DIRECTION('center_axis',(0.,-1.,0.));
#60078=DIRECTION('ref_axis',(0.,0.,-1.));
#60079=DIRECTION('center_axis',(0.,1.,0.));
#60080=DIRECTION('ref_axis',(0.,0.,1.));
#60081=DIRECTION('',(0.,-1.,0.));
#60082=DIRECTION('center_axis',(0.,1.,0.));
#60083=DIRECTION('ref_axis',(0.,0.,1.));
#60084=DIRECTION('',(0.,1.,0.));
#60085=DIRECTION('center_axis',(0.,-1.,0.));
#60086=DIRECTION('ref_axis',(0.,0.,-1.));
#60087=DIRECTION('center_axis',(0.,1.,0.));
#60088=DIRECTION('ref_axis',(0.,0.,1.));
#60089=DIRECTION('',(0.,-1.,0.));
#60090=DIRECTION('center_axis',(0.,1.,0.));
#60091=DIRECTION('ref_axis',(0.,0.,1.));
#60092=DIRECTION('',(0.,1.,0.));
#60093=DIRECTION('center_axis',(0.,-1.,0.));
#60094=DIRECTION('ref_axis',(0.,0.,-1.));
#60095=DIRECTION('center_axis',(0.,1.,0.));
#60096=DIRECTION('ref_axis',(0.,0.,1.));
#60097=DIRECTION('',(0.,-1.,0.));
#60098=DIRECTION('center_axis',(0.,1.,0.));
#60099=DIRECTION('ref_axis',(0.,0.,1.));
#60100=DIRECTION('',(0.,1.,0.));
#60101=DIRECTION('center_axis',(0.,-1.,0.));
#60102=DIRECTION('ref_axis',(0.,0.,-1.));
#60103=DIRECTION('center_axis',(0.,1.,0.));
#60104=DIRECTION('ref_axis',(0.,0.,1.));
#60105=DIRECTION('',(0.,-1.,0.));
#60106=DIRECTION('center_axis',(0.,1.,0.));
#60107=DIRECTION('ref_axis',(0.,0.,1.));
#60108=DIRECTION('',(0.,1.,0.));
#60109=DIRECTION('center_axis',(0.,-1.,0.));
#60110=DIRECTION('ref_axis',(0.,0.,-1.));
#60111=DIRECTION('center_axis',(0.,1.,0.));
#60112=DIRECTION('ref_axis',(0.,0.,1.));
#60113=DIRECTION('',(0.,-1.,0.));
#60114=DIRECTION('center_axis',(0.,1.,0.));
#60115=DIRECTION('ref_axis',(0.,0.,1.));
#60116=DIRECTION('',(0.,1.,0.));
#60117=DIRECTION('center_axis',(0.,-1.,0.));
#60118=DIRECTION('ref_axis',(0.,0.,-1.));
#60119=DIRECTION('center_axis',(0.,1.,0.));
#60120=DIRECTION('ref_axis',(0.,0.,1.));
#60121=DIRECTION('',(0.,-1.,0.));
#60122=DIRECTION('center_axis',(0.,1.,0.));
#60123=DIRECTION('ref_axis',(0.,0.,1.));
#60124=DIRECTION('',(0.,1.,0.));
#60125=DIRECTION('center_axis',(0.,-1.,0.));
#60126=DIRECTION('ref_axis',(0.,0.,-1.));
#60127=DIRECTION('center_axis',(0.,1.,0.));
#60128=DIRECTION('ref_axis',(0.,0.,1.));
#60129=DIRECTION('',(0.,-1.,0.));
#60130=DIRECTION('center_axis',(0.,1.,0.));
#60131=DIRECTION('ref_axis',(0.,0.,1.));
#60132=DIRECTION('',(0.,1.,0.));
#60133=DIRECTION('center_axis',(0.,-1.,0.));
#60134=DIRECTION('ref_axis',(0.,0.,-1.));
#60135=DIRECTION('center_axis',(0.,1.,0.));
#60136=DIRECTION('ref_axis',(0.,0.,1.));
#60137=DIRECTION('',(0.,-1.,0.));
#60138=DIRECTION('center_axis',(0.,1.,0.));
#60139=DIRECTION('ref_axis',(0.,0.,1.));
#60140=DIRECTION('',(0.,1.,0.));
#60141=DIRECTION('center_axis',(0.,-1.,0.));
#60142=DIRECTION('ref_axis',(0.,0.,-1.));
#60143=DIRECTION('center_axis',(0.,1.,0.));
#60144=DIRECTION('ref_axis',(0.,0.,1.));
#60145=DIRECTION('',(0.,-1.,0.));
#60146=DIRECTION('center_axis',(0.,1.,0.));
#60147=DIRECTION('ref_axis',(0.,0.,1.));
#60148=DIRECTION('',(0.,1.,0.));
#60149=DIRECTION('center_axis',(0.,-1.,0.));
#60150=DIRECTION('ref_axis',(0.,0.,-1.));
#60151=DIRECTION('center_axis',(0.,1.,0.));
#60152=DIRECTION('ref_axis',(0.,0.,1.));
#60153=DIRECTION('',(0.,-1.,0.));
#60154=DIRECTION('center_axis',(0.,1.,0.));
#60155=DIRECTION('ref_axis',(0.,0.,1.));
#60156=DIRECTION('',(0.,1.,0.));
#60157=DIRECTION('center_axis',(0.,-1.,0.));
#60158=DIRECTION('ref_axis',(0.,0.,-1.));
#60159=DIRECTION('center_axis',(0.,1.,0.));
#60160=DIRECTION('ref_axis',(0.,0.,1.));
#60161=DIRECTION('',(0.,-1.,0.));
#60162=DIRECTION('center_axis',(0.,1.,0.));
#60163=DIRECTION('ref_axis',(0.,0.,1.));
#60164=DIRECTION('',(0.,1.,0.));
#60165=DIRECTION('center_axis',(0.,-1.,0.));
#60166=DIRECTION('ref_axis',(0.,0.,-1.));
#60167=DIRECTION('center_axis',(0.,1.,0.));
#60168=DIRECTION('ref_axis',(0.,0.,1.));
#60169=DIRECTION('',(0.,-1.,0.));
#60170=DIRECTION('center_axis',(0.,1.,0.));
#60171=DIRECTION('ref_axis',(0.,0.,1.));
#60172=DIRECTION('',(0.,1.,0.));
#60173=DIRECTION('center_axis',(0.,-1.,0.));
#60174=DIRECTION('ref_axis',(0.,0.,-1.));
#60175=DIRECTION('center_axis',(0.,1.,0.));
#60176=DIRECTION('ref_axis',(0.,0.,1.));
#60177=DIRECTION('',(0.,-1.,0.));
#60178=DIRECTION('center_axis',(0.,1.,0.));
#60179=DIRECTION('ref_axis',(0.,0.,1.));
#60180=DIRECTION('',(0.,1.,0.));
#60181=DIRECTION('center_axis',(0.,-1.,0.));
#60182=DIRECTION('ref_axis',(0.,0.,-1.));
#60183=DIRECTION('center_axis',(0.,1.,0.));
#60184=DIRECTION('ref_axis',(0.,0.,1.));
#60185=DIRECTION('',(0.,-1.,0.));
#60186=DIRECTION('center_axis',(0.,1.,0.));
#60187=DIRECTION('ref_axis',(0.,0.,1.));
#60188=DIRECTION('',(0.,1.,0.));
#60189=DIRECTION('center_axis',(0.,-1.,0.));
#60190=DIRECTION('ref_axis',(0.,0.,-1.));
#60191=DIRECTION('center_axis',(0.,1.,0.));
#60192=DIRECTION('ref_axis',(0.,0.,1.));
#60193=DIRECTION('',(0.,-1.,0.));
#60194=DIRECTION('center_axis',(0.,1.,0.));
#60195=DIRECTION('ref_axis',(0.,0.,1.));
#60196=DIRECTION('',(0.,1.,0.));
#60197=DIRECTION('center_axis',(0.,-1.,0.));
#60198=DIRECTION('ref_axis',(0.,0.,-1.));
#60199=DIRECTION('center_axis',(0.,1.,0.));
#60200=DIRECTION('ref_axis',(0.,0.,1.));
#60201=DIRECTION('',(0.,-1.,0.));
#60202=DIRECTION('center_axis',(0.,1.,0.));
#60203=DIRECTION('ref_axis',(0.,0.,1.));
#60204=DIRECTION('',(0.,1.,0.));
#60205=DIRECTION('center_axis',(0.,-1.,0.));
#60206=DIRECTION('ref_axis',(0.,0.,-1.));
#60207=DIRECTION('center_axis',(0.,1.,0.));
#60208=DIRECTION('ref_axis',(0.,0.,1.));
#60209=DIRECTION('',(0.,-1.,0.));
#60210=DIRECTION('center_axis',(0.,1.,0.));
#60211=DIRECTION('ref_axis',(0.,0.,1.));
#60212=DIRECTION('',(0.,1.,0.));
#60213=DIRECTION('center_axis',(0.,-1.,0.));
#60214=DIRECTION('ref_axis',(0.,0.,-1.));
#60215=DIRECTION('center_axis',(0.,1.,0.));
#60216=DIRECTION('ref_axis',(0.,0.,1.));
#60217=DIRECTION('',(0.,-1.,0.));
#60218=DIRECTION('center_axis',(0.,1.,0.));
#60219=DIRECTION('ref_axis',(0.,0.,1.));
#60220=DIRECTION('',(0.,1.,0.));
#60221=DIRECTION('center_axis',(0.,-1.,0.));
#60222=DIRECTION('ref_axis',(0.,0.,-1.));
#60223=DIRECTION('center_axis',(0.,1.,0.));
#60224=DIRECTION('ref_axis',(0.,0.,1.));
#60225=DIRECTION('',(0.,-1.,0.));
#60226=DIRECTION('center_axis',(0.,1.,0.));
#60227=DIRECTION('ref_axis',(0.,0.,1.));
#60228=DIRECTION('',(0.,1.,0.));
#60229=DIRECTION('center_axis',(0.,-1.,0.));
#60230=DIRECTION('ref_axis',(0.,0.,-1.));
#60231=DIRECTION('center_axis',(0.,1.,0.));
#60232=DIRECTION('ref_axis',(0.,0.,1.));
#60233=DIRECTION('',(0.,-1.,0.));
#60234=DIRECTION('center_axis',(0.,1.,0.));
#60235=DIRECTION('ref_axis',(0.,0.,1.));
#60236=DIRECTION('',(0.,1.,0.));
#60237=DIRECTION('center_axis',(0.,-1.,0.));
#60238=DIRECTION('ref_axis',(0.,0.,-1.));
#60239=DIRECTION('center_axis',(0.,1.,0.));
#60240=DIRECTION('ref_axis',(0.,0.,1.));
#60241=DIRECTION('',(0.,-1.,0.));
#60242=DIRECTION('center_axis',(0.,1.,0.));
#60243=DIRECTION('ref_axis',(0.,0.,1.));
#60244=DIRECTION('',(0.,1.,0.));
#60245=DIRECTION('center_axis',(0.,-1.,0.));
#60246=DIRECTION('ref_axis',(0.,0.,-1.));
#60247=DIRECTION('center_axis',(0.,1.,0.));
#60248=DIRECTION('ref_axis',(0.,0.,1.));
#60249=DIRECTION('',(0.,-1.,0.));
#60250=DIRECTION('center_axis',(0.,1.,0.));
#60251=DIRECTION('ref_axis',(0.,0.,1.));
#60252=DIRECTION('',(0.,1.,0.));
#60253=DIRECTION('center_axis',(0.,-1.,0.));
#60254=DIRECTION('ref_axis',(0.,0.,-1.));
#60255=DIRECTION('center_axis',(0.,1.,0.));
#60256=DIRECTION('ref_axis',(0.,0.,1.));
#60257=DIRECTION('',(0.,-1.,0.));
#60258=DIRECTION('center_axis',(0.,1.,0.));
#60259=DIRECTION('ref_axis',(0.,0.,1.));
#60260=DIRECTION('',(0.,1.,0.));
#60261=DIRECTION('center_axis',(0.,-1.,0.));
#60262=DIRECTION('ref_axis',(0.,0.,-1.));
#60263=DIRECTION('center_axis',(0.,1.,0.));
#60264=DIRECTION('ref_axis',(0.,0.,1.));
#60265=DIRECTION('center_axis',(0.,1.,0.));
#60266=DIRECTION('ref_axis',(0.,0.,1.));
#60267=DIRECTION('',(0.,-1.,0.));
#60268=DIRECTION('center_axis',(0.,-1.,0.));
#60269=DIRECTION('ref_axis',(0.,0.,-1.));
#60270=DIRECTION('center_axis',(0.,1.,0.));
#60271=DIRECTION('ref_axis',(0.,0.,1.));
#60272=DIRECTION('center_axis',(0.,-1.,0.));
#60273=DIRECTION('ref_axis',(0.,0.,-1.));
#60274=DIRECTION('',(0.,1.,0.));
#60275=DIRECTION('center_axis',(0.,-1.,0.));
#60276=DIRECTION('ref_axis',(0.,0.,-1.));
#60277=DIRECTION('center_axis',(0.,1.,0.));
#60278=DIRECTION('ref_axis',(0.,0.,1.));
#60279=DIRECTION('center_axis',(0.,1.,0.));
#60280=DIRECTION('ref_axis',(0.,0.,1.));
#60281=DIRECTION('',(0.,-1.,0.));
#60282=DIRECTION('center_axis',(0.,-1.,0.));
#60283=DIRECTION('ref_axis',(0.,0.,-1.));
#60284=DIRECTION('center_axis',(0.,1.,0.));
#60285=DIRECTION('ref_axis',(0.,0.,1.));
#60286=DIRECTION('center_axis',(0.,-1.,0.));
#60287=DIRECTION('ref_axis',(0.,0.,-1.));
#60288=DIRECTION('',(0.,1.,0.));
#60289=DIRECTION('center_axis',(0.,-1.,0.));
#60290=DIRECTION('ref_axis',(0.,0.,-1.));
#60291=DIRECTION('center_axis',(0.,1.,0.));
#60292=DIRECTION('ref_axis',(0.,0.,1.));
#60293=DIRECTION('center_axis',(0.,1.,0.));
#60294=DIRECTION('ref_axis',(0.,0.,1.));
#60295=DIRECTION('',(0.,-1.,0.));
#60296=DIRECTION('center_axis',(0.,-1.,0.));
#60297=DIRECTION('ref_axis',(0.,0.,-1.));
#60298=DIRECTION('center_axis',(0.,1.,0.));
#60299=DIRECTION('ref_axis',(0.,0.,1.));
#60300=DIRECTION('center_axis',(0.,-1.,0.));
#60301=DIRECTION('ref_axis',(0.,0.,-1.));
#60302=DIRECTION('',(0.,1.,0.));
#60303=DIRECTION('center_axis',(0.,-1.,0.));
#60304=DIRECTION('ref_axis',(0.,0.,-1.));
#60305=DIRECTION('center_axis',(0.,1.,0.));
#60306=DIRECTION('ref_axis',(0.,0.,1.));
#60307=DIRECTION('center_axis',(0.,1.,0.));
#60308=DIRECTION('ref_axis',(0.,0.,1.));
#60309=DIRECTION('',(0.,-1.,0.));
#60310=DIRECTION('center_axis',(0.,-1.,0.));
#60311=DIRECTION('ref_axis',(0.,0.,-1.));
#60312=DIRECTION('center_axis',(0.,1.,0.));
#60313=DIRECTION('ref_axis',(0.,0.,1.));
#60314=DIRECTION('center_axis',(0.,-1.,0.));
#60315=DIRECTION('ref_axis',(0.,0.,-1.));
#60316=DIRECTION('',(0.,1.,0.));
#60317=DIRECTION('center_axis',(0.,-1.,0.));
#60318=DIRECTION('ref_axis',(0.,0.,-1.));
#60319=DIRECTION('center_axis',(0.,1.,0.));
#60320=DIRECTION('ref_axis',(0.,0.,1.));
#60321=DIRECTION('center_axis',(0.,1.,0.));
#60322=DIRECTION('ref_axis',(0.,0.,1.));
#60323=DIRECTION('',(0.,-1.,0.));
#60324=DIRECTION('center_axis',(0.,-1.,0.));
#60325=DIRECTION('ref_axis',(0.,0.,-1.));
#60326=DIRECTION('center_axis',(0.,1.,0.));
#60327=DIRECTION('ref_axis',(0.,0.,1.));
#60328=DIRECTION('center_axis',(0.,-1.,0.));
#60329=DIRECTION('ref_axis',(0.,0.,-1.));
#60330=DIRECTION('',(0.,1.,0.));
#60331=DIRECTION('center_axis',(0.,-1.,0.));
#60332=DIRECTION('ref_axis',(0.,0.,-1.));
#60333=DIRECTION('center_axis',(0.,1.,0.));
#60334=DIRECTION('ref_axis',(0.,0.,1.));
#60335=DIRECTION('center_axis',(0.,1.,0.));
#60336=DIRECTION('ref_axis',(0.,0.,1.));
#60337=DIRECTION('',(0.,-1.,0.));
#60338=DIRECTION('center_axis',(0.,-1.,0.));
#60339=DIRECTION('ref_axis',(0.,0.,-1.));
#60340=DIRECTION('center_axis',(0.,1.,0.));
#60341=DIRECTION('ref_axis',(0.,0.,1.));
#60342=DIRECTION('center_axis',(0.,-1.,0.));
#60343=DIRECTION('ref_axis',(0.,0.,-1.));
#60344=DIRECTION('',(0.,1.,0.));
#60345=DIRECTION('center_axis',(0.,-1.,0.));
#60346=DIRECTION('ref_axis',(0.,0.,-1.));
#60347=DIRECTION('center_axis',(0.,1.,0.));
#60348=DIRECTION('ref_axis',(0.,0.,1.));
#60349=DIRECTION('center_axis',(0.,1.,0.));
#60350=DIRECTION('ref_axis',(0.,0.,1.));
#60351=DIRECTION('',(0.,-1.,0.));
#60352=DIRECTION('center_axis',(0.,-1.,0.));
#60353=DIRECTION('ref_axis',(0.,0.,-1.));
#60354=DIRECTION('center_axis',(0.,1.,0.));
#60355=DIRECTION('ref_axis',(0.,0.,1.));
#60356=DIRECTION('center_axis',(0.,-1.,0.));
#60357=DIRECTION('ref_axis',(0.,0.,-1.));
#60358=DIRECTION('',(0.,1.,0.));
#60359=DIRECTION('center_axis',(0.,-1.,0.));
#60360=DIRECTION('ref_axis',(0.,0.,-1.));
#60361=DIRECTION('center_axis',(0.,1.,0.));
#60362=DIRECTION('ref_axis',(0.,0.,1.));
#60363=DIRECTION('center_axis',(0.,1.,0.));
#60364=DIRECTION('ref_axis',(0.,0.,1.));
#60365=DIRECTION('',(0.,-1.,0.));
#60366=DIRECTION('center_axis',(0.,-1.,0.));
#60367=DIRECTION('ref_axis',(0.,0.,-1.));
#60368=DIRECTION('center_axis',(0.,1.,0.));
#60369=DIRECTION('ref_axis',(0.,0.,1.));
#60370=DIRECTION('center_axis',(0.,-1.,0.));
#60371=DIRECTION('ref_axis',(0.,0.,-1.));
#60372=DIRECTION('',(0.,1.,0.));
#60373=DIRECTION('center_axis',(0.,-1.,0.));
#60374=DIRECTION('ref_axis',(0.,0.,-1.));
#60375=DIRECTION('center_axis',(0.,1.,0.));
#60376=DIRECTION('ref_axis',(0.,0.,1.));
#60377=DIRECTION('center_axis',(0.,1.,0.));
#60378=DIRECTION('ref_axis',(0.,0.,1.));
#60379=DIRECTION('',(0.,-1.,0.));
#60380=DIRECTION('center_axis',(0.,-1.,0.));
#60381=DIRECTION('ref_axis',(0.,0.,-1.));
#60382=DIRECTION('center_axis',(0.,1.,0.));
#60383=DIRECTION('ref_axis',(0.,0.,1.));
#60384=DIRECTION('center_axis',(0.,-1.,0.));
#60385=DIRECTION('ref_axis',(0.,0.,-1.));
#60386=DIRECTION('',(0.,1.,0.));
#60387=DIRECTION('center_axis',(0.,-1.,0.));
#60388=DIRECTION('ref_axis',(0.,0.,-1.));
#60389=DIRECTION('center_axis',(0.,1.,0.));
#60390=DIRECTION('ref_axis',(0.,0.,1.));
#60391=DIRECTION('center_axis',(0.,1.,0.));
#60392=DIRECTION('ref_axis',(0.,0.,1.));
#60393=DIRECTION('',(0.,-1.,0.));
#60394=DIRECTION('center_axis',(0.,-1.,0.));
#60395=DIRECTION('ref_axis',(0.,0.,-1.));
#60396=DIRECTION('center_axis',(0.,1.,0.));
#60397=DIRECTION('ref_axis',(0.,0.,1.));
#60398=DIRECTION('center_axis',(0.,-1.,0.));
#60399=DIRECTION('ref_axis',(0.,0.,-1.));
#60400=DIRECTION('',(0.,1.,0.));
#60401=DIRECTION('center_axis',(0.,-1.,0.));
#60402=DIRECTION('ref_axis',(0.,0.,-1.));
#60403=DIRECTION('center_axis',(0.,1.,0.));
#60404=DIRECTION('ref_axis',(0.,0.,1.));
#60405=DIRECTION('center_axis',(0.,1.,0.));
#60406=DIRECTION('ref_axis',(0.,0.,1.));
#60407=DIRECTION('',(0.,-1.,0.));
#60408=DIRECTION('center_axis',(0.,-1.,0.));
#60409=DIRECTION('ref_axis',(0.,0.,-1.));
#60410=DIRECTION('center_axis',(0.,1.,0.));
#60411=DIRECTION('ref_axis',(0.,0.,1.));
#60412=DIRECTION('center_axis',(0.,-1.,0.));
#60413=DIRECTION('ref_axis',(0.,0.,-1.));
#60414=DIRECTION('',(0.,1.,0.));
#60415=DIRECTION('center_axis',(0.,-1.,0.));
#60416=DIRECTION('ref_axis',(0.,0.,-1.));
#60417=DIRECTION('center_axis',(0.,1.,0.));
#60418=DIRECTION('ref_axis',(0.,0.,1.));
#60419=DIRECTION('center_axis',(0.,1.,0.));
#60420=DIRECTION('ref_axis',(0.,0.,1.));
#60421=DIRECTION('',(0.,-1.,0.));
#60422=DIRECTION('center_axis',(0.,-1.,0.));
#60423=DIRECTION('ref_axis',(0.,0.,-1.));
#60424=DIRECTION('center_axis',(0.,1.,0.));
#60425=DIRECTION('ref_axis',(0.,0.,1.));
#60426=DIRECTION('center_axis',(0.,-1.,0.));
#60427=DIRECTION('ref_axis',(0.,0.,-1.));
#60428=DIRECTION('',(0.,1.,0.));
#60429=DIRECTION('center_axis',(0.,-1.,0.));
#60430=DIRECTION('ref_axis',(0.,0.,-1.));
#60431=DIRECTION('center_axis',(0.,1.,0.));
#60432=DIRECTION('ref_axis',(0.,0.,1.));
#60433=DIRECTION('center_axis',(0.,1.,0.));
#60434=DIRECTION('ref_axis',(0.,0.,1.));
#60435=DIRECTION('',(0.,-1.,0.));
#60436=DIRECTION('center_axis',(0.,-1.,0.));
#60437=DIRECTION('ref_axis',(0.,0.,-1.));
#60438=DIRECTION('center_axis',(0.,1.,0.));
#60439=DIRECTION('ref_axis',(0.,0.,1.));
#60440=DIRECTION('center_axis',(0.,-1.,0.));
#60441=DIRECTION('ref_axis',(0.,0.,-1.));
#60442=DIRECTION('',(0.,1.,0.));
#60443=DIRECTION('center_axis',(0.,-1.,0.));
#60444=DIRECTION('ref_axis',(0.,0.,-1.));
#60445=DIRECTION('center_axis',(0.,1.,0.));
#60446=DIRECTION('ref_axis',(0.,0.,1.));
#60447=DIRECTION('center_axis',(0.,1.,0.));
#60448=DIRECTION('ref_axis',(0.,0.,1.));
#60449=DIRECTION('',(0.,-1.,0.));
#60450=DIRECTION('center_axis',(0.,-1.,0.));
#60451=DIRECTION('ref_axis',(0.,0.,-1.));
#60452=DIRECTION('center_axis',(0.,1.,0.));
#60453=DIRECTION('ref_axis',(0.,0.,1.));
#60454=DIRECTION('center_axis',(0.,-1.,0.));
#60455=DIRECTION('ref_axis',(0.,0.,-1.));
#60456=DIRECTION('',(0.,1.,0.));
#60457=DIRECTION('center_axis',(0.,-1.,0.));
#60458=DIRECTION('ref_axis',(0.,0.,-1.));
#60459=DIRECTION('center_axis',(0.,1.,0.));
#60460=DIRECTION('ref_axis',(0.,0.,1.));
#60461=DIRECTION('center_axis',(0.,1.,0.));
#60462=DIRECTION('ref_axis',(0.,0.,1.));
#60463=DIRECTION('',(0.,-1.,0.));
#60464=DIRECTION('center_axis',(0.,-1.,0.));
#60465=DIRECTION('ref_axis',(0.,0.,-1.));
#60466=DIRECTION('center_axis',(0.,1.,0.));
#60467=DIRECTION('ref_axis',(0.,0.,1.));
#60468=DIRECTION('center_axis',(0.,-1.,0.));
#60469=DIRECTION('ref_axis',(0.,0.,-1.));
#60470=DIRECTION('',(0.,1.,0.));
#60471=DIRECTION('center_axis',(0.,-1.,0.));
#60472=DIRECTION('ref_axis',(0.,0.,-1.));
#60473=DIRECTION('center_axis',(0.,1.,0.));
#60474=DIRECTION('ref_axis',(0.,0.,1.));
#60475=DIRECTION('center_axis',(0.,1.,0.));
#60476=DIRECTION('ref_axis',(0.,0.,1.));
#60477=DIRECTION('',(0.,-1.,0.));
#60478=DIRECTION('center_axis',(0.,-1.,0.));
#60479=DIRECTION('ref_axis',(0.,0.,-1.));
#60480=DIRECTION('center_axis',(0.,1.,0.));
#60481=DIRECTION('ref_axis',(0.,0.,1.));
#60482=DIRECTION('center_axis',(0.,-1.,0.));
#60483=DIRECTION('ref_axis',(0.,0.,-1.));
#60484=DIRECTION('',(0.,1.,0.));
#60485=DIRECTION('center_axis',(0.,-1.,0.));
#60486=DIRECTION('ref_axis',(0.,0.,-1.));
#60487=DIRECTION('center_axis',(0.,1.,0.));
#60488=DIRECTION('ref_axis',(0.,0.,1.));
#60489=DIRECTION('center_axis',(0.,1.,0.));
#60490=DIRECTION('ref_axis',(0.,0.,1.));
#60491=DIRECTION('',(0.,-1.,0.));
#60492=DIRECTION('center_axis',(0.,-1.,0.));
#60493=DIRECTION('ref_axis',(0.,0.,-1.));
#60494=DIRECTION('center_axis',(0.,1.,0.));
#60495=DIRECTION('ref_axis',(0.,0.,1.));
#60496=DIRECTION('center_axis',(0.,-1.,0.));
#60497=DIRECTION('ref_axis',(0.,0.,-1.));
#60498=DIRECTION('',(0.,1.,0.));
#60499=DIRECTION('center_axis',(0.,-1.,0.));
#60500=DIRECTION('ref_axis',(0.,0.,-1.));
#60501=DIRECTION('center_axis',(0.,1.,0.));
#60502=DIRECTION('ref_axis',(0.,0.,1.));
#60503=DIRECTION('center_axis',(0.,1.,0.));
#60504=DIRECTION('ref_axis',(0.,0.,1.));
#60505=DIRECTION('',(0.,-1.,0.));
#60506=DIRECTION('center_axis',(0.,-1.,0.));
#60507=DIRECTION('ref_axis',(0.,0.,-1.));
#60508=DIRECTION('center_axis',(0.,1.,0.));
#60509=DIRECTION('ref_axis',(0.,0.,1.));
#60510=DIRECTION('center_axis',(0.,-1.,0.));
#60511=DIRECTION('ref_axis',(0.,0.,-1.));
#60512=DIRECTION('',(0.,1.,0.));
#60513=DIRECTION('center_axis',(0.,-1.,0.));
#60514=DIRECTION('ref_axis',(0.,0.,-1.));
#60515=DIRECTION('center_axis',(0.,1.,0.));
#60516=DIRECTION('ref_axis',(0.,0.,1.));
#60517=DIRECTION('center_axis',(0.,1.,0.));
#60518=DIRECTION('ref_axis',(0.,0.,1.));
#60519=DIRECTION('',(0.,-1.,0.));
#60520=DIRECTION('center_axis',(0.,-1.,0.));
#60521=DIRECTION('ref_axis',(0.,0.,-1.));
#60522=DIRECTION('center_axis',(0.,1.,0.));
#60523=DIRECTION('ref_axis',(0.,0.,1.));
#60524=DIRECTION('center_axis',(0.,-1.,0.));
#60525=DIRECTION('ref_axis',(0.,0.,-1.));
#60526=DIRECTION('',(0.,1.,0.));
#60527=DIRECTION('center_axis',(0.,-1.,0.));
#60528=DIRECTION('ref_axis',(0.,0.,-1.));
#60529=DIRECTION('center_axis',(0.,1.,0.));
#60530=DIRECTION('ref_axis',(0.,0.,1.));
#60531=DIRECTION('center_axis',(0.,1.,0.));
#60532=DIRECTION('ref_axis',(0.,0.,1.));
#60533=DIRECTION('',(0.,-1.,0.));
#60534=DIRECTION('center_axis',(0.,-1.,0.));
#60535=DIRECTION('ref_axis',(0.,0.,-1.));
#60536=DIRECTION('center_axis',(0.,1.,0.));
#60537=DIRECTION('ref_axis',(0.,0.,1.));
#60538=DIRECTION('center_axis',(0.,-1.,0.));
#60539=DIRECTION('ref_axis',(0.,0.,-1.));
#60540=DIRECTION('',(0.,1.,0.));
#60541=DIRECTION('center_axis',(0.,-1.,0.));
#60542=DIRECTION('ref_axis',(0.,0.,-1.));
#60543=DIRECTION('center_axis',(0.,1.,0.));
#60544=DIRECTION('ref_axis',(0.,0.,1.));
#60545=DIRECTION('center_axis',(0.,1.,0.));
#60546=DIRECTION('ref_axis',(0.,0.,1.));
#60547=DIRECTION('',(0.,-1.,0.));
#60548=DIRECTION('center_axis',(0.,-1.,0.));
#60549=DIRECTION('ref_axis',(0.,0.,-1.));
#60550=DIRECTION('center_axis',(0.,1.,0.));
#60551=DIRECTION('ref_axis',(0.,0.,1.));
#60552=DIRECTION('center_axis',(0.,-1.,0.));
#60553=DIRECTION('ref_axis',(0.,0.,-1.));
#60554=DIRECTION('',(0.,1.,0.));
#60555=DIRECTION('center_axis',(0.,-1.,0.));
#60556=DIRECTION('ref_axis',(0.,0.,-1.));
#60557=DIRECTION('center_axis',(0.,1.,0.));
#60558=DIRECTION('ref_axis',(0.,0.,1.));
#60559=DIRECTION('center_axis',(0.,1.,0.));
#60560=DIRECTION('ref_axis',(0.,0.,1.));
#60561=DIRECTION('',(0.,-1.,0.));
#60562=DIRECTION('center_axis',(0.,-1.,0.));
#60563=DIRECTION('ref_axis',(0.,0.,-1.));
#60564=DIRECTION('center_axis',(0.,1.,0.));
#60565=DIRECTION('ref_axis',(0.,0.,1.));
#60566=DIRECTION('center_axis',(0.,-1.,0.));
#60567=DIRECTION('ref_axis',(0.,0.,-1.));
#60568=DIRECTION('',(0.,1.,0.));
#60569=DIRECTION('center_axis',(0.,-1.,0.));
#60570=DIRECTION('ref_axis',(0.,0.,-1.));
#60571=DIRECTION('center_axis',(0.,1.,0.));
#60572=DIRECTION('ref_axis',(0.,0.,1.));
#60573=DIRECTION('center_axis',(0.,1.,0.));
#60574=DIRECTION('ref_axis',(0.,0.,1.));
#60575=DIRECTION('',(0.,-1.,0.));
#60576=DIRECTION('center_axis',(0.,-1.,0.));
#60577=DIRECTION('ref_axis',(0.,0.,-1.));
#60578=DIRECTION('center_axis',(0.,1.,0.));
#60579=DIRECTION('ref_axis',(0.,0.,1.));
#60580=DIRECTION('center_axis',(0.,-1.,0.));
#60581=DIRECTION('ref_axis',(0.,0.,-1.));
#60582=DIRECTION('',(0.,1.,0.));
#60583=DIRECTION('center_axis',(0.,-1.,0.));
#60584=DIRECTION('ref_axis',(0.,0.,-1.));
#60585=DIRECTION('center_axis',(0.,1.,0.));
#60586=DIRECTION('ref_axis',(0.,0.,1.));
#60587=DIRECTION('center_axis',(0.,1.,0.));
#60588=DIRECTION('ref_axis',(0.,0.,1.));
#60589=DIRECTION('',(0.,-1.,0.));
#60590=DIRECTION('center_axis',(0.,-1.,0.));
#60591=DIRECTION('ref_axis',(0.,0.,-1.));
#60592=DIRECTION('center_axis',(0.,1.,0.));
#60593=DIRECTION('ref_axis',(0.,0.,1.));
#60594=DIRECTION('center_axis',(0.,-1.,0.));
#60595=DIRECTION('ref_axis',(0.,0.,-1.));
#60596=DIRECTION('',(0.,1.,0.));
#60597=DIRECTION('center_axis',(0.,-1.,0.));
#60598=DIRECTION('ref_axis',(0.,0.,-1.));
#60599=DIRECTION('center_axis',(0.,1.,0.));
#60600=DIRECTION('ref_axis',(0.,0.,1.));
#60601=DIRECTION('center_axis',(0.,1.,0.));
#60602=DIRECTION('ref_axis',(0.,0.,1.));
#60603=DIRECTION('',(0.,-1.,0.));
#60604=DIRECTION('center_axis',(0.,-1.,0.));
#60605=DIRECTION('ref_axis',(0.,0.,-1.));
#60606=DIRECTION('center_axis',(0.,1.,0.));
#60607=DIRECTION('ref_axis',(0.,0.,1.));
#60608=DIRECTION('center_axis',(0.,-1.,0.));
#60609=DIRECTION('ref_axis',(0.,0.,-1.));
#60610=DIRECTION('',(0.,1.,0.));
#60611=DIRECTION('center_axis',(0.,-1.,0.));
#60612=DIRECTION('ref_axis',(0.,0.,-1.));
#60613=DIRECTION('center_axis',(0.,1.,0.));
#60614=DIRECTION('ref_axis',(0.,0.,1.));
#60615=DIRECTION('center_axis',(0.,1.,0.));
#60616=DIRECTION('ref_axis',(0.,0.,1.));
#60617=DIRECTION('',(0.,-1.,0.));
#60618=DIRECTION('center_axis',(0.,-1.,0.));
#60619=DIRECTION('ref_axis',(0.,0.,-1.));
#60620=DIRECTION('center_axis',(0.,1.,0.));
#60621=DIRECTION('ref_axis',(0.,0.,1.));
#60622=DIRECTION('center_axis',(0.,-1.,0.));
#60623=DIRECTION('ref_axis',(0.,0.,-1.));
#60624=DIRECTION('',(0.,1.,0.));
#60625=DIRECTION('center_axis',(0.,-1.,0.));
#60626=DIRECTION('ref_axis',(0.,0.,-1.));
#60627=DIRECTION('center_axis',(0.,1.,0.));
#60628=DIRECTION('ref_axis',(0.,0.,1.));
#60629=DIRECTION('center_axis',(0.,1.,0.));
#60630=DIRECTION('ref_axis',(0.,0.,1.));
#60631=DIRECTION('',(0.,-1.,0.));
#60632=DIRECTION('center_axis',(0.,-1.,0.));
#60633=DIRECTION('ref_axis',(0.,0.,-1.));
#60634=DIRECTION('center_axis',(0.,1.,0.));
#60635=DIRECTION('ref_axis',(0.,0.,1.));
#60636=DIRECTION('center_axis',(0.,-1.,0.));
#60637=DIRECTION('ref_axis',(0.,0.,-1.));
#60638=DIRECTION('',(0.,1.,0.));
#60639=DIRECTION('center_axis',(0.,-1.,0.));
#60640=DIRECTION('ref_axis',(0.,0.,-1.));
#60641=DIRECTION('center_axis',(0.,1.,0.));
#60642=DIRECTION('ref_axis',(0.,0.,1.));
#60643=DIRECTION('center_axis',(0.,1.,0.));
#60644=DIRECTION('ref_axis',(0.,0.,1.));
#60645=DIRECTION('',(0.,-1.,0.));
#60646=DIRECTION('center_axis',(0.,-1.,0.));
#60647=DIRECTION('ref_axis',(0.,0.,-1.));
#60648=DIRECTION('center_axis',(0.,1.,0.));
#60649=DIRECTION('ref_axis',(0.,0.,1.));
#60650=DIRECTION('center_axis',(0.,-1.,0.));
#60651=DIRECTION('ref_axis',(0.,0.,-1.));
#60652=DIRECTION('',(0.,1.,0.));
#60653=DIRECTION('center_axis',(0.,-1.,0.));
#60654=DIRECTION('ref_axis',(0.,0.,-1.));
#60655=DIRECTION('center_axis',(0.,1.,0.));
#60656=DIRECTION('ref_axis',(0.,0.,1.));
#60657=DIRECTION('center_axis',(0.,1.,0.));
#60658=DIRECTION('ref_axis',(0.,0.,1.));
#60659=DIRECTION('',(0.,-1.,0.));
#60660=DIRECTION('center_axis',(0.,-1.,0.));
#60661=DIRECTION('ref_axis',(0.,0.,-1.));
#60662=DIRECTION('center_axis',(0.,1.,0.));
#60663=DIRECTION('ref_axis',(0.,0.,1.));
#60664=DIRECTION('center_axis',(0.,-1.,0.));
#60665=DIRECTION('ref_axis',(0.,0.,-1.));
#60666=DIRECTION('',(0.,1.,0.));
#60667=DIRECTION('center_axis',(0.,-1.,0.));
#60668=DIRECTION('ref_axis',(0.,0.,-1.));
#60669=DIRECTION('center_axis',(0.,1.,0.));
#60670=DIRECTION('ref_axis',(0.,0.,1.));
#60671=DIRECTION('center_axis',(0.,1.,0.));
#60672=DIRECTION('ref_axis',(0.,0.,1.));
#60673=DIRECTION('',(0.,-1.,0.));
#60674=DIRECTION('center_axis',(0.,-1.,0.));
#60675=DIRECTION('ref_axis',(0.,0.,-1.));
#60676=DIRECTION('center_axis',(0.,1.,0.));
#60677=DIRECTION('ref_axis',(0.,0.,1.));
#60678=DIRECTION('center_axis',(0.,-1.,0.));
#60679=DIRECTION('ref_axis',(0.,0.,-1.));
#60680=DIRECTION('',(0.,1.,0.));
#60681=DIRECTION('center_axis',(0.,-1.,0.));
#60682=DIRECTION('ref_axis',(0.,0.,-1.));
#60683=DIRECTION('center_axis',(0.,1.,0.));
#60684=DIRECTION('ref_axis',(0.,0.,1.));
#60685=DIRECTION('center_axis',(0.,1.,0.));
#60686=DIRECTION('ref_axis',(0.,0.,1.));
#60687=DIRECTION('',(0.,-1.,0.));
#60688=DIRECTION('center_axis',(0.,-1.,0.));
#60689=DIRECTION('ref_axis',(0.,0.,-1.));
#60690=DIRECTION('center_axis',(0.,1.,0.));
#60691=DIRECTION('ref_axis',(0.,0.,1.));
#60692=DIRECTION('center_axis',(0.,-1.,0.));
#60693=DIRECTION('ref_axis',(0.,0.,-1.));
#60694=DIRECTION('',(0.,1.,0.));
#60695=DIRECTION('center_axis',(0.,-1.,0.));
#60696=DIRECTION('ref_axis',(0.,0.,-1.));
#60697=DIRECTION('center_axis',(0.,1.,0.));
#60698=DIRECTION('ref_axis',(0.,0.,1.));
#60699=DIRECTION('center_axis',(0.,1.,0.));
#60700=DIRECTION('ref_axis',(0.,0.,1.));
#60701=DIRECTION('',(0.,-1.,0.));
#60702=DIRECTION('center_axis',(0.,-1.,0.));
#60703=DIRECTION('ref_axis',(0.,0.,-1.));
#60704=DIRECTION('center_axis',(0.,1.,0.));
#60705=DIRECTION('ref_axis',(0.,0.,1.));
#60706=DIRECTION('center_axis',(0.,-1.,0.));
#60707=DIRECTION('ref_axis',(0.,0.,-1.));
#60708=DIRECTION('',(0.,1.,0.));
#60709=DIRECTION('center_axis',(0.,-1.,0.));
#60710=DIRECTION('ref_axis',(0.,0.,-1.));
#60711=DIRECTION('center_axis',(0.,1.,0.));
#60712=DIRECTION('ref_axis',(0.,0.,1.));
#60713=DIRECTION('center_axis',(0.,1.,0.));
#60714=DIRECTION('ref_axis',(0.,0.,1.));
#60715=DIRECTION('',(0.,-1.,0.));
#60716=DIRECTION('center_axis',(0.,-1.,0.));
#60717=DIRECTION('ref_axis',(0.,0.,-1.));
#60718=DIRECTION('center_axis',(0.,1.,0.));
#60719=DIRECTION('ref_axis',(0.,0.,1.));
#60720=DIRECTION('center_axis',(0.,-1.,0.));
#60721=DIRECTION('ref_axis',(0.,0.,-1.));
#60722=DIRECTION('',(0.,1.,0.));
#60723=DIRECTION('center_axis',(0.,-1.,0.));
#60724=DIRECTION('ref_axis',(0.,0.,-1.));
#60725=DIRECTION('center_axis',(0.,1.,0.));
#60726=DIRECTION('ref_axis',(0.,0.,1.));
#60727=DIRECTION('center_axis',(0.,1.,0.));
#60728=DIRECTION('ref_axis',(0.,0.,1.));
#60729=DIRECTION('',(0.,-1.,0.));
#60730=DIRECTION('center_axis',(0.,-1.,0.));
#60731=DIRECTION('ref_axis',(0.,0.,-1.));
#60732=DIRECTION('center_axis',(0.,1.,0.));
#60733=DIRECTION('ref_axis',(0.,0.,1.));
#60734=DIRECTION('center_axis',(0.,-1.,0.));
#60735=DIRECTION('ref_axis',(0.,0.,-1.));
#60736=DIRECTION('',(0.,1.,0.));
#60737=DIRECTION('center_axis',(0.,-1.,0.));
#60738=DIRECTION('ref_axis',(0.,0.,-1.));
#60739=DIRECTION('center_axis',(0.,1.,0.));
#60740=DIRECTION('ref_axis',(0.,0.,1.));
#60741=DIRECTION('center_axis',(0.,1.,0.));
#60742=DIRECTION('ref_axis',(0.,0.,1.));
#60743=DIRECTION('',(0.,-1.,0.));
#60744=DIRECTION('center_axis',(0.,-1.,0.));
#60745=DIRECTION('ref_axis',(0.,0.,-1.));
#60746=DIRECTION('center_axis',(0.,1.,0.));
#60747=DIRECTION('ref_axis',(0.,0.,1.));
#60748=DIRECTION('center_axis',(0.,-1.,0.));
#60749=DIRECTION('ref_axis',(0.,0.,-1.));
#60750=DIRECTION('',(0.,1.,0.));
#60751=DIRECTION('center_axis',(0.,-1.,0.));
#60752=DIRECTION('ref_axis',(0.,0.,-1.));
#60753=DIRECTION('center_axis',(0.,1.,0.));
#60754=DIRECTION('ref_axis',(0.,0.,1.));
#60755=DIRECTION('center_axis',(0.,1.,0.));
#60756=DIRECTION('ref_axis',(0.,0.,1.));
#60757=DIRECTION('',(0.,-1.,0.));
#60758=DIRECTION('center_axis',(0.,-1.,0.));
#60759=DIRECTION('ref_axis',(0.,0.,-1.));
#60760=DIRECTION('center_axis',(0.,1.,0.));
#60761=DIRECTION('ref_axis',(0.,0.,1.));
#60762=DIRECTION('center_axis',(0.,-1.,0.));
#60763=DIRECTION('ref_axis',(0.,0.,-1.));
#60764=DIRECTION('',(0.,1.,0.));
#60765=DIRECTION('center_axis',(0.,-1.,0.));
#60766=DIRECTION('ref_axis',(0.,0.,-1.));
#60767=DIRECTION('center_axis',(0.,1.,0.));
#60768=DIRECTION('ref_axis',(0.,0.,1.));
#60769=DIRECTION('center_axis',(0.,1.,0.));
#60770=DIRECTION('ref_axis',(0.,0.,1.));
#60771=DIRECTION('',(0.,-1.,0.));
#60772=DIRECTION('center_axis',(0.,-1.,0.));
#60773=DIRECTION('ref_axis',(0.,0.,-1.));
#60774=DIRECTION('center_axis',(0.,1.,0.));
#60775=DIRECTION('ref_axis',(0.,0.,1.));
#60776=DIRECTION('center_axis',(0.,-1.,0.));
#60777=DIRECTION('ref_axis',(0.,0.,-1.));
#60778=DIRECTION('',(0.,1.,0.));
#60779=DIRECTION('center_axis',(0.,-1.,0.));
#60780=DIRECTION('ref_axis',(0.,0.,-1.));
#60781=DIRECTION('center_axis',(0.,1.,0.));
#60782=DIRECTION('ref_axis',(0.,0.,1.));
#60783=DIRECTION('center_axis',(0.,1.,0.));
#60784=DIRECTION('ref_axis',(0.,0.,1.));
#60785=DIRECTION('',(0.,-1.,0.));
#60786=DIRECTION('center_axis',(0.,-1.,0.));
#60787=DIRECTION('ref_axis',(0.,0.,-1.));
#60788=DIRECTION('center_axis',(0.,1.,0.));
#60789=DIRECTION('ref_axis',(0.,0.,1.));
#60790=DIRECTION('center_axis',(0.,-1.,0.));
#60791=DIRECTION('ref_axis',(0.,0.,-1.));
#60792=DIRECTION('',(0.,1.,0.));
#60793=DIRECTION('center_axis',(0.,-1.,0.));
#60794=DIRECTION('ref_axis',(0.,0.,-1.));
#60795=DIRECTION('center_axis',(0.,1.,0.));
#60796=DIRECTION('ref_axis',(0.,0.,1.));
#60797=DIRECTION('center_axis',(0.,1.,0.));
#60798=DIRECTION('ref_axis',(0.,0.,1.));
#60799=DIRECTION('',(0.,-1.,0.));
#60800=DIRECTION('center_axis',(0.,-1.,0.));
#60801=DIRECTION('ref_axis',(0.,0.,-1.));
#60802=DIRECTION('center_axis',(0.,1.,0.));
#60803=DIRECTION('ref_axis',(0.,0.,1.));
#60804=DIRECTION('center_axis',(0.,-1.,0.));
#60805=DIRECTION('ref_axis',(0.,0.,-1.));
#60806=DIRECTION('',(0.,1.,0.));
#60807=DIRECTION('center_axis',(0.,-1.,0.));
#60808=DIRECTION('ref_axis',(0.,0.,-1.));
#60809=DIRECTION('center_axis',(0.,1.,0.));
#60810=DIRECTION('ref_axis',(0.,0.,1.));
#60811=DIRECTION('center_axis',(0.,1.,0.));
#60812=DIRECTION('ref_axis',(0.,0.,1.));
#60813=DIRECTION('',(0.,-1.,0.));
#60814=DIRECTION('center_axis',(0.,-1.,0.));
#60815=DIRECTION('ref_axis',(0.,0.,-1.));
#60816=DIRECTION('center_axis',(0.,1.,0.));
#60817=DIRECTION('ref_axis',(0.,0.,1.));
#60818=DIRECTION('center_axis',(0.,-1.,0.));
#60819=DIRECTION('ref_axis',(0.,0.,-1.));
#60820=DIRECTION('',(0.,1.,0.));
#60821=DIRECTION('center_axis',(0.,-1.,0.));
#60822=DIRECTION('ref_axis',(0.,0.,-1.));
#60823=DIRECTION('center_axis',(0.,1.,0.));
#60824=DIRECTION('ref_axis',(0.,0.,1.));
#60825=DIRECTION('center_axis',(0.,1.,0.));
#60826=DIRECTION('ref_axis',(0.,0.,1.));
#60827=DIRECTION('',(0.,-1.,0.));
#60828=DIRECTION('center_axis',(0.,-1.,0.));
#60829=DIRECTION('ref_axis',(0.,0.,-1.));
#60830=DIRECTION('center_axis',(0.,1.,0.));
#60831=DIRECTION('ref_axis',(0.,0.,1.));
#60832=DIRECTION('center_axis',(0.,-1.,0.));
#60833=DIRECTION('ref_axis',(0.,0.,-1.));
#60834=DIRECTION('',(0.,1.,0.));
#60835=DIRECTION('center_axis',(0.,-1.,0.));
#60836=DIRECTION('ref_axis',(0.,0.,-1.));
#60837=DIRECTION('center_axis',(0.,1.,0.));
#60838=DIRECTION('ref_axis',(0.,0.,1.));
#60839=DIRECTION('center_axis',(0.,1.,0.));
#60840=DIRECTION('ref_axis',(0.,0.,1.));
#60841=DIRECTION('',(0.,-1.,0.));
#60842=DIRECTION('center_axis',(0.,-1.,0.));
#60843=DIRECTION('ref_axis',(0.,0.,-1.));
#60844=DIRECTION('center_axis',(0.,1.,0.));
#60845=DIRECTION('ref_axis',(0.,0.,1.));
#60846=DIRECTION('center_axis',(0.,-1.,0.));
#60847=DIRECTION('ref_axis',(0.,0.,-1.));
#60848=DIRECTION('',(0.,1.,0.));
#60849=DIRECTION('center_axis',(0.,-1.,0.));
#60850=DIRECTION('ref_axis',(0.,0.,-1.));
#60851=DIRECTION('center_axis',(0.,1.,0.));
#60852=DIRECTION('ref_axis',(0.,0.,1.));
#60853=DIRECTION('center_axis',(0.,1.,0.));
#60854=DIRECTION('ref_axis',(0.,0.,1.));
#60855=DIRECTION('',(0.,-1.,0.));
#60856=DIRECTION('center_axis',(0.,-1.,0.));
#60857=DIRECTION('ref_axis',(0.,0.,-1.));
#60858=DIRECTION('center_axis',(0.,1.,0.));
#60859=DIRECTION('ref_axis',(0.,0.,1.));
#60860=DIRECTION('center_axis',(0.,-1.,0.));
#60861=DIRECTION('ref_axis',(0.,0.,-1.));
#60862=DIRECTION('',(0.,1.,0.));
#60863=DIRECTION('center_axis',(0.,-1.,0.));
#60864=DIRECTION('ref_axis',(0.,0.,-1.));
#60865=DIRECTION('center_axis',(0.,1.,0.));
#60866=DIRECTION('ref_axis',(0.,0.,1.));
#60867=DIRECTION('center_axis',(0.,1.,0.));
#60868=DIRECTION('ref_axis',(0.,0.,1.));
#60869=DIRECTION('',(0.,-1.,0.));
#60870=DIRECTION('center_axis',(0.,-1.,0.));
#60871=DIRECTION('ref_axis',(0.,0.,-1.));
#60872=DIRECTION('center_axis',(0.,1.,0.));
#60873=DIRECTION('ref_axis',(0.,0.,1.));
#60874=DIRECTION('center_axis',(0.,-1.,0.));
#60875=DIRECTION('ref_axis',(0.,0.,-1.));
#60876=DIRECTION('',(0.,1.,0.));
#60877=DIRECTION('center_axis',(0.,-1.,0.));
#60878=DIRECTION('ref_axis',(0.,0.,-1.));
#60879=DIRECTION('center_axis',(0.,1.,0.));
#60880=DIRECTION('ref_axis',(0.,0.,1.));
#60881=DIRECTION('center_axis',(0.,1.,0.));
#60882=DIRECTION('ref_axis',(0.,0.,1.));
#60883=DIRECTION('',(0.,-1.,0.));
#60884=DIRECTION('center_axis',(0.,-1.,0.));
#60885=DIRECTION('ref_axis',(0.,0.,-1.));
#60886=DIRECTION('center_axis',(0.,1.,0.));
#60887=DIRECTION('ref_axis',(0.,0.,1.));
#60888=DIRECTION('center_axis',(0.,-1.,0.));
#60889=DIRECTION('ref_axis',(0.,0.,-1.));
#60890=DIRECTION('',(0.,1.,0.));
#60891=DIRECTION('center_axis',(0.,-1.,0.));
#60892=DIRECTION('ref_axis',(0.,0.,-1.));
#60893=DIRECTION('center_axis',(0.,1.,0.));
#60894=DIRECTION('ref_axis',(0.,0.,1.));
#60895=DIRECTION('center_axis',(0.,1.,0.));
#60896=DIRECTION('ref_axis',(0.,0.,1.));
#60897=DIRECTION('',(0.,-1.,0.));
#60898=DIRECTION('center_axis',(0.,-1.,0.));
#60899=DIRECTION('ref_axis',(0.,0.,-1.));
#60900=DIRECTION('center_axis',(0.,1.,0.));
#60901=DIRECTION('ref_axis',(0.,0.,1.));
#60902=DIRECTION('center_axis',(0.,-1.,0.));
#60903=DIRECTION('ref_axis',(0.,0.,-1.));
#60904=DIRECTION('',(0.,1.,0.));
#60905=DIRECTION('center_axis',(0.,-1.,0.));
#60906=DIRECTION('ref_axis',(0.,0.,-1.));
#60907=DIRECTION('center_axis',(0.,1.,0.));
#60908=DIRECTION('ref_axis',(0.,0.,1.));
#60909=DIRECTION('center_axis',(0.,1.,0.));
#60910=DIRECTION('ref_axis',(0.,0.,1.));
#60911=DIRECTION('',(0.,-1.,0.));
#60912=DIRECTION('center_axis',(0.,-1.,0.));
#60913=DIRECTION('ref_axis',(0.,0.,-1.));
#60914=DIRECTION('center_axis',(0.,1.,0.));
#60915=DIRECTION('ref_axis',(0.,0.,1.));
#60916=DIRECTION('center_axis',(0.,-1.,0.));
#60917=DIRECTION('ref_axis',(0.,0.,-1.));
#60918=DIRECTION('',(0.,1.,0.));
#60919=DIRECTION('center_axis',(0.,-1.,0.));
#60920=DIRECTION('ref_axis',(0.,0.,-1.));
#60921=DIRECTION('center_axis',(0.,1.,0.));
#60922=DIRECTION('ref_axis',(0.,0.,1.));
#60923=DIRECTION('center_axis',(0.,1.,0.));
#60924=DIRECTION('ref_axis',(0.,0.,1.));
#60925=DIRECTION('',(0.,-1.,0.));
#60926=DIRECTION('center_axis',(0.,-1.,0.));
#60927=DIRECTION('ref_axis',(0.,0.,-1.));
#60928=DIRECTION('center_axis',(0.,1.,0.));
#60929=DIRECTION('ref_axis',(0.,0.,1.));
#60930=DIRECTION('center_axis',(0.,-1.,0.));
#60931=DIRECTION('ref_axis',(0.,0.,-1.));
#60932=DIRECTION('',(0.,1.,0.));
#60933=DIRECTION('center_axis',(0.,-1.,0.));
#60934=DIRECTION('ref_axis',(0.,0.,-1.));
#60935=DIRECTION('center_axis',(0.,1.,0.));
#60936=DIRECTION('ref_axis',(0.,0.,1.));
#60937=DIRECTION('center_axis',(0.,1.,0.));
#60938=DIRECTION('ref_axis',(0.,0.,1.));
#60939=DIRECTION('',(0.,-1.,0.));
#60940=DIRECTION('center_axis',(0.,-1.,0.));
#60941=DIRECTION('ref_axis',(0.,0.,-1.));
#60942=DIRECTION('center_axis',(0.,1.,0.));
#60943=DIRECTION('ref_axis',(0.,0.,1.));
#60944=DIRECTION('center_axis',(0.,-1.,0.));
#60945=DIRECTION('ref_axis',(0.,0.,-1.));
#60946=DIRECTION('',(0.,1.,0.));
#60947=DIRECTION('center_axis',(0.,-1.,0.));
#60948=DIRECTION('ref_axis',(0.,0.,-1.));
#60949=DIRECTION('center_axis',(0.,1.,0.));
#60950=DIRECTION('ref_axis',(0.,0.,1.));
#60951=DIRECTION('center_axis',(0.,1.,0.));
#60952=DIRECTION('ref_axis',(0.,0.,1.));
#60953=DIRECTION('',(0.,-1.,0.));
#60954=DIRECTION('center_axis',(0.,-1.,0.));
#60955=DIRECTION('ref_axis',(0.,0.,-1.));
#60956=DIRECTION('center_axis',(0.,1.,0.));
#60957=DIRECTION('ref_axis',(0.,0.,1.));
#60958=DIRECTION('center_axis',(0.,-1.,0.));
#60959=DIRECTION('ref_axis',(0.,0.,-1.));
#60960=DIRECTION('',(0.,1.,0.));
#60961=DIRECTION('center_axis',(0.,-1.,0.));
#60962=DIRECTION('ref_axis',(0.,0.,-1.));
#60963=DIRECTION('center_axis',(0.,1.,0.));
#60964=DIRECTION('ref_axis',(0.,0.,1.));
#60965=DIRECTION('center_axis',(0.,1.,0.));
#60966=DIRECTION('ref_axis',(0.,0.,1.));
#60967=DIRECTION('',(0.,-1.,0.));
#60968=DIRECTION('center_axis',(0.,-1.,0.));
#60969=DIRECTION('ref_axis',(0.,0.,-1.));
#60970=DIRECTION('center_axis',(0.,1.,0.));
#60971=DIRECTION('ref_axis',(0.,0.,1.));
#60972=DIRECTION('center_axis',(0.,-1.,0.));
#60973=DIRECTION('ref_axis',(0.,0.,-1.));
#60974=DIRECTION('',(0.,1.,0.));
#60975=DIRECTION('center_axis',(0.,-1.,0.));
#60976=DIRECTION('ref_axis',(0.,0.,-1.));
#60977=DIRECTION('center_axis',(0.,1.,0.));
#60978=DIRECTION('ref_axis',(0.,0.,1.));
#60979=DIRECTION('center_axis',(0.,1.,0.));
#60980=DIRECTION('ref_axis',(0.,0.,1.));
#60981=DIRECTION('',(0.,-1.,0.));
#60982=DIRECTION('center_axis',(0.,-1.,0.));
#60983=DIRECTION('ref_axis',(0.,0.,-1.));
#60984=DIRECTION('center_axis',(0.,1.,0.));
#60985=DIRECTION('ref_axis',(0.,0.,1.));
#60986=DIRECTION('center_axis',(0.,-1.,0.));
#60987=DIRECTION('ref_axis',(0.,0.,-1.));
#60988=DIRECTION('',(0.,1.,0.));
#60989=DIRECTION('center_axis',(0.,-1.,0.));
#60990=DIRECTION('ref_axis',(0.,0.,-1.));
#60991=DIRECTION('center_axis',(0.,1.,0.));
#60992=DIRECTION('ref_axis',(0.,0.,1.));
#60993=DIRECTION('center_axis',(0.,1.,0.));
#60994=DIRECTION('ref_axis',(0.,0.,1.));
#60995=DIRECTION('',(0.,-1.,0.));
#60996=DIRECTION('center_axis',(0.,-1.,0.));
#60997=DIRECTION('ref_axis',(0.,0.,-1.));
#60998=DIRECTION('center_axis',(0.,1.,0.));
#60999=DIRECTION('ref_axis',(0.,0.,1.));
#61000=DIRECTION('center_axis',(0.,-1.,0.));
#61001=DIRECTION('ref_axis',(0.,0.,-1.));
#61002=DIRECTION('',(0.,1.,0.));
#61003=DIRECTION('center_axis',(0.,-1.,0.));
#61004=DIRECTION('ref_axis',(0.,0.,-1.));
#61005=DIRECTION('center_axis',(0.,1.,0.));
#61006=DIRECTION('ref_axis',(0.,0.,1.));
#61007=DIRECTION('center_axis',(0.,1.,0.));
#61008=DIRECTION('ref_axis',(0.,0.,1.));
#61009=DIRECTION('',(0.,-1.,0.));
#61010=DIRECTION('center_axis',(0.,-1.,0.));
#61011=DIRECTION('ref_axis',(0.,0.,-1.));
#61012=DIRECTION('center_axis',(0.,1.,0.));
#61013=DIRECTION('ref_axis',(0.,0.,1.));
#61014=DIRECTION('center_axis',(0.,-1.,0.));
#61015=DIRECTION('ref_axis',(0.,0.,-1.));
#61016=DIRECTION('',(0.,1.,0.));
#61017=DIRECTION('center_axis',(0.,-1.,0.));
#61018=DIRECTION('ref_axis',(0.,0.,-1.));
#61019=DIRECTION('center_axis',(0.,1.,0.));
#61020=DIRECTION('ref_axis',(0.,0.,1.));
#61021=DIRECTION('center_axis',(0.,1.,0.));
#61022=DIRECTION('ref_axis',(0.,0.,1.));
#61023=DIRECTION('',(0.,-1.,0.));
#61024=DIRECTION('center_axis',(0.,-1.,0.));
#61025=DIRECTION('ref_axis',(0.,0.,-1.));
#61026=DIRECTION('center_axis',(0.,1.,0.));
#61027=DIRECTION('ref_axis',(0.,0.,1.));
#61028=DIRECTION('center_axis',(0.,-1.,0.));
#61029=DIRECTION('ref_axis',(0.,0.,-1.));
#61030=DIRECTION('',(0.,1.,0.));
#61031=DIRECTION('center_axis',(0.,-1.,0.));
#61032=DIRECTION('ref_axis',(0.,0.,-1.));
#61033=DIRECTION('center_axis',(0.,1.,0.));
#61034=DIRECTION('ref_axis',(0.,0.,1.));
#61035=DIRECTION('center_axis',(0.,1.,0.));
#61036=DIRECTION('ref_axis',(0.,0.,1.));
#61037=DIRECTION('',(0.,-1.,0.));
#61038=DIRECTION('center_axis',(0.,-1.,0.));
#61039=DIRECTION('ref_axis',(0.,0.,-1.));
#61040=DIRECTION('center_axis',(0.,1.,0.));
#61041=DIRECTION('ref_axis',(0.,0.,1.));
#61042=DIRECTION('center_axis',(0.,-1.,0.));
#61043=DIRECTION('ref_axis',(0.,0.,-1.));
#61044=DIRECTION('',(0.,1.,0.));
#61045=DIRECTION('center_axis',(0.,-1.,0.));
#61046=DIRECTION('ref_axis',(0.,0.,-1.));
#61047=DIRECTION('center_axis',(0.,1.,0.));
#61048=DIRECTION('ref_axis',(0.,0.,1.));
#61049=DIRECTION('center_axis',(0.,1.,0.));
#61050=DIRECTION('ref_axis',(0.,0.,1.));
#61051=DIRECTION('',(0.,-1.,0.));
#61052=DIRECTION('center_axis',(0.,-1.,0.));
#61053=DIRECTION('ref_axis',(0.,0.,-1.));
#61054=DIRECTION('center_axis',(0.,1.,0.));
#61055=DIRECTION('ref_axis',(0.,0.,1.));
#61056=DIRECTION('center_axis',(0.,-1.,0.));
#61057=DIRECTION('ref_axis',(0.,0.,-1.));
#61058=DIRECTION('',(0.,1.,0.));
#61059=DIRECTION('center_axis',(0.,-1.,0.));
#61060=DIRECTION('ref_axis',(0.,0.,-1.));
#61061=DIRECTION('center_axis',(0.,1.,0.));
#61062=DIRECTION('ref_axis',(0.,0.,1.));
#61063=DIRECTION('center_axis',(0.,1.,0.));
#61064=DIRECTION('ref_axis',(0.,0.,1.));
#61065=DIRECTION('',(0.,-1.,0.));
#61066=DIRECTION('center_axis',(0.,-1.,0.));
#61067=DIRECTION('ref_axis',(0.,0.,-1.));
#61068=DIRECTION('center_axis',(0.,1.,0.));
#61069=DIRECTION('ref_axis',(0.,0.,1.));
#61070=DIRECTION('center_axis',(0.,-1.,0.));
#61071=DIRECTION('ref_axis',(0.,0.,-1.));
#61072=DIRECTION('',(0.,1.,0.));
#61073=DIRECTION('center_axis',(0.,-1.,0.));
#61074=DIRECTION('ref_axis',(0.,0.,-1.));
#61075=DIRECTION('center_axis',(0.,1.,0.));
#61076=DIRECTION('ref_axis',(0.,0.,1.));
#61077=DIRECTION('center_axis',(0.,1.,0.));
#61078=DIRECTION('ref_axis',(0.,0.,1.));
#61079=DIRECTION('',(0.,-1.,0.));
#61080=DIRECTION('center_axis',(0.,-1.,0.));
#61081=DIRECTION('ref_axis',(0.,0.,-1.));
#61082=DIRECTION('center_axis',(0.,1.,0.));
#61083=DIRECTION('ref_axis',(0.,0.,1.));
#61084=DIRECTION('center_axis',(0.,-1.,0.));
#61085=DIRECTION('ref_axis',(0.,0.,-1.));
#61086=DIRECTION('',(0.,1.,0.));
#61087=DIRECTION('center_axis',(0.,-1.,0.));
#61088=DIRECTION('ref_axis',(0.,0.,-1.));
#61089=DIRECTION('center_axis',(0.,1.,0.));
#61090=DIRECTION('ref_axis',(0.,0.,1.));
#61091=DIRECTION('center_axis',(0.,1.,0.));
#61092=DIRECTION('ref_axis',(0.,0.,1.));
#61093=DIRECTION('',(0.,-1.,0.));
#61094=DIRECTION('center_axis',(0.,-1.,0.));
#61095=DIRECTION('ref_axis',(0.,0.,-1.));
#61096=DIRECTION('center_axis',(0.,1.,0.));
#61097=DIRECTION('ref_axis',(0.,0.,1.));
#61098=DIRECTION('center_axis',(0.,-1.,0.));
#61099=DIRECTION('ref_axis',(0.,0.,-1.));
#61100=DIRECTION('',(0.,1.,0.));
#61101=DIRECTION('center_axis',(0.,-1.,0.));
#61102=DIRECTION('ref_axis',(0.,0.,-1.));
#61103=DIRECTION('center_axis',(0.,1.,0.));
#61104=DIRECTION('ref_axis',(0.,0.,1.));
#61105=DIRECTION('center_axis',(0.,1.,0.));
#61106=DIRECTION('ref_axis',(0.,0.,1.));
#61107=DIRECTION('',(0.,-1.,0.));
#61108=DIRECTION('center_axis',(0.,-1.,0.));
#61109=DIRECTION('ref_axis',(0.,0.,-1.));
#61110=DIRECTION('center_axis',(0.,1.,0.));
#61111=DIRECTION('ref_axis',(0.,0.,1.));
#61112=DIRECTION('center_axis',(0.,-1.,0.));
#61113=DIRECTION('ref_axis',(0.,0.,-1.));
#61114=DIRECTION('',(0.,1.,0.));
#61115=DIRECTION('center_axis',(0.,-1.,0.));
#61116=DIRECTION('ref_axis',(0.,0.,-1.));
#61117=DIRECTION('center_axis',(0.,1.,0.));
#61118=DIRECTION('ref_axis',(0.,0.,1.));
#61119=DIRECTION('center_axis',(0.,1.,0.));
#61120=DIRECTION('ref_axis',(0.,0.,1.));
#61121=DIRECTION('',(0.,-1.,0.));
#61122=DIRECTION('center_axis',(0.,-1.,0.));
#61123=DIRECTION('ref_axis',(0.,0.,-1.));
#61124=DIRECTION('center_axis',(0.,1.,0.));
#61125=DIRECTION('ref_axis',(0.,0.,1.));
#61126=DIRECTION('center_axis',(0.,-1.,0.));
#61127=DIRECTION('ref_axis',(0.,0.,-1.));
#61128=DIRECTION('',(0.,1.,0.));
#61129=DIRECTION('center_axis',(0.,-1.,0.));
#61130=DIRECTION('ref_axis',(0.,0.,-1.));
#61131=DIRECTION('center_axis',(0.,1.,0.));
#61132=DIRECTION('ref_axis',(0.,0.,1.));
#61133=DIRECTION('center_axis',(0.,1.,0.));
#61134=DIRECTION('ref_axis',(0.,0.,1.));
#61135=DIRECTION('',(0.,-1.,0.));
#61136=DIRECTION('center_axis',(0.,-1.,0.));
#61137=DIRECTION('ref_axis',(0.,0.,-1.));
#61138=DIRECTION('center_axis',(0.,1.,0.));
#61139=DIRECTION('ref_axis',(0.,0.,1.));
#61140=DIRECTION('center_axis',(0.,-1.,0.));
#61141=DIRECTION('ref_axis',(0.,0.,-1.));
#61142=DIRECTION('',(0.,1.,0.));
#61143=DIRECTION('center_axis',(0.,-1.,0.));
#61144=DIRECTION('ref_axis',(0.,0.,-1.));
#61145=DIRECTION('center_axis',(0.,1.,0.));
#61146=DIRECTION('ref_axis',(0.,0.,1.));
#61147=DIRECTION('center_axis',(0.,1.,0.));
#61148=DIRECTION('ref_axis',(0.,0.,1.));
#61149=DIRECTION('',(0.,-1.,0.));
#61150=DIRECTION('center_axis',(0.,-1.,0.));
#61151=DIRECTION('ref_axis',(0.,0.,-1.));
#61152=DIRECTION('center_axis',(0.,1.,0.));
#61153=DIRECTION('ref_axis',(0.,0.,1.));
#61154=DIRECTION('center_axis',(0.,-1.,0.));
#61155=DIRECTION('ref_axis',(0.,0.,-1.));
#61156=DIRECTION('',(0.,1.,0.));
#61157=DIRECTION('center_axis',(0.,-1.,0.));
#61158=DIRECTION('ref_axis',(0.,0.,-1.));
#61159=DIRECTION('center_axis',(0.,1.,0.));
#61160=DIRECTION('ref_axis',(0.,0.,1.));
#61161=DIRECTION('center_axis',(0.,1.,0.));
#61162=DIRECTION('ref_axis',(0.,0.,1.));
#61163=DIRECTION('',(0.,-1.,0.));
#61164=DIRECTION('center_axis',(0.,-1.,0.));
#61165=DIRECTION('ref_axis',(0.,0.,-1.));
#61166=DIRECTION('center_axis',(0.,1.,0.));
#61167=DIRECTION('ref_axis',(0.,0.,1.));
#61168=DIRECTION('center_axis',(0.,-1.,0.));
#61169=DIRECTION('ref_axis',(0.,0.,-1.));
#61170=DIRECTION('',(0.,1.,0.));
#61171=DIRECTION('center_axis',(0.,-1.,0.));
#61172=DIRECTION('ref_axis',(0.,0.,-1.));
#61173=DIRECTION('center_axis',(0.,1.,0.));
#61174=DIRECTION('ref_axis',(0.,0.,1.));
#61175=DIRECTION('center_axis',(0.,1.,0.));
#61176=DIRECTION('ref_axis',(0.,0.,1.));
#61177=DIRECTION('',(0.,-1.,0.));
#61178=DIRECTION('center_axis',(0.,-1.,0.));
#61179=DIRECTION('ref_axis',(0.,0.,-1.));
#61180=DIRECTION('center_axis',(0.,1.,0.));
#61181=DIRECTION('ref_axis',(0.,0.,1.));
#61182=DIRECTION('center_axis',(0.,-1.,0.));
#61183=DIRECTION('ref_axis',(0.,0.,-1.));
#61184=DIRECTION('',(0.,1.,0.));
#61185=DIRECTION('center_axis',(0.,-1.,0.));
#61186=DIRECTION('ref_axis',(0.,0.,-1.));
#61187=DIRECTION('center_axis',(0.,1.,0.));
#61188=DIRECTION('ref_axis',(0.,0.,1.));
#61189=DIRECTION('center_axis',(0.,1.,0.));
#61190=DIRECTION('ref_axis',(0.,0.,1.));
#61191=DIRECTION('',(0.,-1.,0.));
#61192=DIRECTION('center_axis',(0.,-1.,0.));
#61193=DIRECTION('ref_axis',(0.,0.,-1.));
#61194=DIRECTION('center_axis',(0.,1.,0.));
#61195=DIRECTION('ref_axis',(0.,0.,1.));
#61196=DIRECTION('center_axis',(0.,-1.,0.));
#61197=DIRECTION('ref_axis',(0.,0.,-1.));
#61198=DIRECTION('',(0.,1.,0.));
#61199=DIRECTION('center_axis',(0.,-1.,0.));
#61200=DIRECTION('ref_axis',(0.,0.,-1.));
#61201=DIRECTION('center_axis',(0.,1.,0.));
#61202=DIRECTION('ref_axis',(0.,0.,1.));
#61203=DIRECTION('center_axis',(0.,1.,0.));
#61204=DIRECTION('ref_axis',(0.,0.,1.));
#61205=DIRECTION('',(0.,-1.,0.));
#61206=DIRECTION('center_axis',(0.,-1.,0.));
#61207=DIRECTION('ref_axis',(0.,0.,-1.));
#61208=DIRECTION('center_axis',(0.,1.,0.));
#61209=DIRECTION('ref_axis',(0.,0.,1.));
#61210=DIRECTION('center_axis',(0.,-1.,0.));
#61211=DIRECTION('ref_axis',(0.,0.,-1.));
#61212=DIRECTION('',(0.,1.,0.));
#61213=DIRECTION('center_axis',(0.,-1.,0.));
#61214=DIRECTION('ref_axis',(0.,0.,-1.));
#61215=DIRECTION('center_axis',(0.,1.,0.));
#61216=DIRECTION('ref_axis',(0.,0.,1.));
#61217=DIRECTION('center_axis',(0.,1.,0.));
#61218=DIRECTION('ref_axis',(0.,0.,1.));
#61219=DIRECTION('',(0.,-1.,0.));
#61220=DIRECTION('center_axis',(0.,-1.,0.));
#61221=DIRECTION('ref_axis',(0.,0.,-1.));
#61222=DIRECTION('center_axis',(0.,1.,0.));
#61223=DIRECTION('ref_axis',(0.,0.,1.));
#61224=DIRECTION('center_axis',(0.,-1.,0.));
#61225=DIRECTION('ref_axis',(0.,0.,-1.));
#61226=DIRECTION('',(0.,1.,0.));
#61227=DIRECTION('center_axis',(0.,-1.,0.));
#61228=DIRECTION('ref_axis',(0.,0.,-1.));
#61229=DIRECTION('center_axis',(0.,1.,0.));
#61230=DIRECTION('ref_axis',(0.,0.,1.));
#61231=DIRECTION('center_axis',(0.,1.,0.));
#61232=DIRECTION('ref_axis',(0.,0.,1.));
#61233=DIRECTION('',(0.,-1.,0.));
#61234=DIRECTION('center_axis',(0.,-1.,0.));
#61235=DIRECTION('ref_axis',(0.,0.,-1.));
#61236=DIRECTION('center_axis',(0.,1.,0.));
#61237=DIRECTION('ref_axis',(0.,0.,1.));
#61238=DIRECTION('center_axis',(0.,-1.,0.));
#61239=DIRECTION('ref_axis',(0.,0.,-1.));
#61240=DIRECTION('',(0.,1.,0.));
#61241=DIRECTION('center_axis',(0.,-1.,0.));
#61242=DIRECTION('ref_axis',(0.,0.,-1.));
#61243=DIRECTION('center_axis',(0.,1.,0.));
#61244=DIRECTION('ref_axis',(0.,0.,1.));
#61245=DIRECTION('center_axis',(0.,1.,0.));
#61246=DIRECTION('ref_axis',(0.,0.,1.));
#61247=DIRECTION('',(0.,-1.,0.));
#61248=DIRECTION('center_axis',(0.,-1.,0.));
#61249=DIRECTION('ref_axis',(0.,0.,-1.));
#61250=DIRECTION('center_axis',(0.,1.,0.));
#61251=DIRECTION('ref_axis',(0.,0.,1.));
#61252=DIRECTION('center_axis',(0.,-1.,0.));
#61253=DIRECTION('ref_axis',(0.,0.,-1.));
#61254=DIRECTION('',(0.,1.,0.));
#61255=DIRECTION('center_axis',(0.,-1.,0.));
#61256=DIRECTION('ref_axis',(0.,0.,-1.));
#61257=DIRECTION('center_axis',(0.,1.,0.));
#61258=DIRECTION('ref_axis',(0.,0.,1.));
#61259=DIRECTION('center_axis',(0.,1.,0.));
#61260=DIRECTION('ref_axis',(0.,0.,1.));
#61261=DIRECTION('',(0.,-1.,0.));
#61262=DIRECTION('center_axis',(0.,-1.,0.));
#61263=DIRECTION('ref_axis',(0.,0.,-1.));
#61264=DIRECTION('center_axis',(0.,1.,0.));
#61265=DIRECTION('ref_axis',(0.,0.,1.));
#61266=DIRECTION('center_axis',(0.,-1.,0.));
#61267=DIRECTION('ref_axis',(0.,0.,-1.));
#61268=DIRECTION('',(0.,1.,0.));
#61269=DIRECTION('center_axis',(0.,-1.,0.));
#61270=DIRECTION('ref_axis',(0.,0.,-1.));
#61271=DIRECTION('center_axis',(0.,1.,0.));
#61272=DIRECTION('ref_axis',(0.,0.,1.));
#61273=DIRECTION('center_axis',(0.,1.,0.));
#61274=DIRECTION('ref_axis',(0.,0.,1.));
#61275=DIRECTION('',(0.,-1.,0.));
#61276=DIRECTION('center_axis',(0.,-1.,0.));
#61277=DIRECTION('ref_axis',(0.,0.,-1.));
#61278=DIRECTION('center_axis',(0.,1.,0.));
#61279=DIRECTION('ref_axis',(0.,0.,1.));
#61280=DIRECTION('center_axis',(0.,-1.,0.));
#61281=DIRECTION('ref_axis',(0.,0.,-1.));
#61282=DIRECTION('',(0.,1.,0.));
#61283=DIRECTION('center_axis',(0.,-1.,0.));
#61284=DIRECTION('ref_axis',(0.,0.,-1.));
#61285=DIRECTION('center_axis',(0.,1.,0.));
#61286=DIRECTION('ref_axis',(0.,0.,1.));
#61287=DIRECTION('center_axis',(0.,1.,0.));
#61288=DIRECTION('ref_axis',(0.,0.,1.));
#61289=DIRECTION('',(0.,-1.,0.));
#61290=DIRECTION('center_axis',(0.,-1.,0.));
#61291=DIRECTION('ref_axis',(0.,0.,-1.));
#61292=DIRECTION('center_axis',(0.,1.,0.));
#61293=DIRECTION('ref_axis',(0.,0.,1.));
#61294=DIRECTION('center_axis',(0.,-1.,0.));
#61295=DIRECTION('ref_axis',(0.,0.,-1.));
#61296=DIRECTION('',(0.,1.,0.));
#61297=DIRECTION('center_axis',(0.,-1.,0.));
#61298=DIRECTION('ref_axis',(0.,0.,-1.));
#61299=DIRECTION('center_axis',(0.,1.,0.));
#61300=DIRECTION('ref_axis',(0.,0.,1.));
#61301=DIRECTION('center_axis',(0.,1.,0.));
#61302=DIRECTION('ref_axis',(0.,0.,1.));
#61303=DIRECTION('',(0.,-1.,0.));
#61304=DIRECTION('center_axis',(0.,-1.,0.));
#61305=DIRECTION('ref_axis',(0.,0.,-1.));
#61306=DIRECTION('center_axis',(0.,1.,0.));
#61307=DIRECTION('ref_axis',(0.,0.,1.));
#61308=DIRECTION('center_axis',(0.,-1.,0.));
#61309=DIRECTION('ref_axis',(0.,0.,-1.));
#61310=DIRECTION('',(0.,1.,0.));
#61311=DIRECTION('center_axis',(0.,-1.,0.));
#61312=DIRECTION('ref_axis',(0.,0.,-1.));
#61313=DIRECTION('center_axis',(0.,1.,0.));
#61314=DIRECTION('ref_axis',(0.,0.,1.));
#61315=DIRECTION('center_axis',(0.,1.,0.));
#61316=DIRECTION('ref_axis',(0.,0.,1.));
#61317=DIRECTION('',(0.,-1.,0.));
#61318=DIRECTION('center_axis',(0.,-1.,0.));
#61319=DIRECTION('ref_axis',(0.,0.,-1.));
#61320=DIRECTION('center_axis',(0.,1.,0.));
#61321=DIRECTION('ref_axis',(0.,0.,1.));
#61322=DIRECTION('center_axis',(0.,-1.,0.));
#61323=DIRECTION('ref_axis',(0.,0.,-1.));
#61324=DIRECTION('',(0.,1.,0.));
#61325=DIRECTION('center_axis',(0.,-1.,0.));
#61326=DIRECTION('ref_axis',(0.,0.,-1.));
#61327=DIRECTION('center_axis',(0.,1.,0.));
#61328=DIRECTION('ref_axis',(0.,0.,1.));
#61329=DIRECTION('center_axis',(0.,1.,0.));
#61330=DIRECTION('ref_axis',(0.,0.,1.));
#61331=DIRECTION('',(0.,-1.,0.));
#61332=DIRECTION('center_axis',(0.,-1.,0.));
#61333=DIRECTION('ref_axis',(0.,0.,-1.));
#61334=DIRECTION('center_axis',(0.,1.,0.));
#61335=DIRECTION('ref_axis',(0.,0.,1.));
#61336=DIRECTION('center_axis',(0.,-1.,0.));
#61337=DIRECTION('ref_axis',(0.,0.,-1.));
#61338=DIRECTION('',(0.,1.,0.));
#61339=DIRECTION('center_axis',(0.,-1.,0.));
#61340=DIRECTION('ref_axis',(0.,0.,-1.));
#61341=DIRECTION('center_axis',(0.,1.,0.));
#61342=DIRECTION('ref_axis',(0.,0.,1.));
#61343=DIRECTION('center_axis',(0.,1.,0.));
#61344=DIRECTION('ref_axis',(0.,0.,1.));
#61345=DIRECTION('',(0.,-1.,0.));
#61346=DIRECTION('center_axis',(0.,-1.,0.));
#61347=DIRECTION('ref_axis',(0.,0.,-1.));
#61348=DIRECTION('center_axis',(0.,1.,0.));
#61349=DIRECTION('ref_axis',(0.,0.,1.));
#61350=DIRECTION('center_axis',(0.,-1.,0.));
#61351=DIRECTION('ref_axis',(0.,0.,-1.));
#61352=DIRECTION('',(0.,1.,0.));
#61353=DIRECTION('center_axis',(0.,-1.,0.));
#61354=DIRECTION('ref_axis',(0.,0.,-1.));
#61355=DIRECTION('center_axis',(0.,1.,0.));
#61356=DIRECTION('ref_axis',(0.,0.,1.));
#61357=DIRECTION('center_axis',(0.,1.,0.));
#61358=DIRECTION('ref_axis',(0.,0.,1.));
#61359=DIRECTION('',(0.,-1.,0.));
#61360=DIRECTION('center_axis',(0.,-1.,0.));
#61361=DIRECTION('ref_axis',(0.,0.,-1.));
#61362=DIRECTION('center_axis',(0.,1.,0.));
#61363=DIRECTION('ref_axis',(0.,0.,1.));
#61364=DIRECTION('center_axis',(0.,-1.,0.));
#61365=DIRECTION('ref_axis',(0.,0.,-1.));
#61366=DIRECTION('',(0.,1.,0.));
#61367=DIRECTION('center_axis',(0.,-1.,0.));
#61368=DIRECTION('ref_axis',(0.,0.,-1.));
#61369=DIRECTION('center_axis',(0.,1.,0.));
#61370=DIRECTION('ref_axis',(0.,0.,1.));
#61371=DIRECTION('center_axis',(0.,1.,0.));
#61372=DIRECTION('ref_axis',(0.,0.,1.));
#61373=DIRECTION('',(0.,-1.,0.));
#61374=DIRECTION('center_axis',(0.,-1.,0.));
#61375=DIRECTION('ref_axis',(0.,0.,-1.));
#61376=DIRECTION('center_axis',(0.,1.,0.));
#61377=DIRECTION('ref_axis',(0.,0.,1.));
#61378=DIRECTION('center_axis',(0.,-1.,0.));
#61379=DIRECTION('ref_axis',(0.,0.,-1.));
#61380=DIRECTION('',(0.,1.,0.));
#61381=DIRECTION('center_axis',(0.,-1.,0.));
#61382=DIRECTION('ref_axis',(0.,0.,-1.));
#61383=DIRECTION('center_axis',(0.,1.,0.));
#61384=DIRECTION('ref_axis',(0.,0.,1.));
#61385=DIRECTION('center_axis',(0.,1.,0.));
#61386=DIRECTION('ref_axis',(0.,0.,1.));
#61387=DIRECTION('',(0.,-1.,0.));
#61388=DIRECTION('center_axis',(0.,-1.,0.));
#61389=DIRECTION('ref_axis',(0.,0.,-1.));
#61390=DIRECTION('center_axis',(0.,1.,0.));
#61391=DIRECTION('ref_axis',(0.,0.,1.));
#61392=DIRECTION('center_axis',(0.,-1.,0.));
#61393=DIRECTION('ref_axis',(0.,0.,-1.));
#61394=DIRECTION('',(0.,1.,0.));
#61395=DIRECTION('center_axis',(0.,-1.,0.));
#61396=DIRECTION('ref_axis',(0.,0.,-1.));
#61397=DIRECTION('center_axis',(0.,1.,0.));
#61398=DIRECTION('ref_axis',(0.,0.,1.));
#61399=DIRECTION('center_axis',(0.,1.,0.));
#61400=DIRECTION('ref_axis',(0.,0.,1.));
#61401=DIRECTION('',(0.,-1.,0.));
#61402=DIRECTION('center_axis',(0.,-1.,0.));
#61403=DIRECTION('ref_axis',(0.,0.,-1.));
#61404=DIRECTION('center_axis',(0.,1.,0.));
#61405=DIRECTION('ref_axis',(0.,0.,1.));
#61406=DIRECTION('center_axis',(0.,-1.,0.));
#61407=DIRECTION('ref_axis',(0.,0.,-1.));
#61408=DIRECTION('',(0.,1.,0.));
#61409=DIRECTION('center_axis',(0.,-1.,0.));
#61410=DIRECTION('ref_axis',(0.,0.,-1.));
#61411=DIRECTION('center_axis',(0.,1.,0.));
#61412=DIRECTION('ref_axis',(0.,0.,1.));
#61413=DIRECTION('center_axis',(0.,1.,0.));
#61414=DIRECTION('ref_axis',(0.,0.,1.));
#61415=DIRECTION('',(0.,-1.,0.));
#61416=DIRECTION('center_axis',(0.,-1.,0.));
#61417=DIRECTION('ref_axis',(0.,0.,-1.));
#61418=DIRECTION('center_axis',(0.,1.,0.));
#61419=DIRECTION('ref_axis',(0.,0.,1.));
#61420=DIRECTION('center_axis',(0.,-1.,0.));
#61421=DIRECTION('ref_axis',(0.,0.,-1.));
#61422=DIRECTION('',(0.,1.,0.));
#61423=DIRECTION('center_axis',(0.,-1.,0.));
#61424=DIRECTION('ref_axis',(0.,0.,-1.));
#61425=DIRECTION('center_axis',(0.,1.,0.));
#61426=DIRECTION('ref_axis',(0.,0.,1.));
#61427=DIRECTION('center_axis',(0.,1.,0.));
#61428=DIRECTION('ref_axis',(0.,0.,1.));
#61429=DIRECTION('',(0.,-1.,0.));
#61430=DIRECTION('center_axis',(0.,-1.,0.));
#61431=DIRECTION('ref_axis',(0.,0.,-1.));
#61432=DIRECTION('center_axis',(0.,1.,0.));
#61433=DIRECTION('ref_axis',(0.,0.,1.));
#61434=DIRECTION('center_axis',(0.,-1.,0.));
#61435=DIRECTION('ref_axis',(0.,0.,-1.));
#61436=DIRECTION('',(0.,1.,0.));
#61437=DIRECTION('center_axis',(0.,-1.,0.));
#61438=DIRECTION('ref_axis',(0.,0.,-1.));
#61439=DIRECTION('center_axis',(0.,1.,0.));
#61440=DIRECTION('ref_axis',(0.,0.,1.));
#61441=DIRECTION('center_axis',(0.,1.,0.));
#61442=DIRECTION('ref_axis',(0.,0.,1.));
#61443=DIRECTION('',(0.,-1.,0.));
#61444=DIRECTION('center_axis',(0.,-1.,0.));
#61445=DIRECTION('ref_axis',(0.,0.,-1.));
#61446=DIRECTION('center_axis',(0.,1.,0.));
#61447=DIRECTION('ref_axis',(0.,0.,1.));
#61448=DIRECTION('center_axis',(0.,-1.,0.));
#61449=DIRECTION('ref_axis',(0.,0.,-1.));
#61450=DIRECTION('',(0.,1.,0.));
#61451=DIRECTION('center_axis',(0.,-1.,0.));
#61452=DIRECTION('ref_axis',(0.,0.,-1.));
#61453=DIRECTION('center_axis',(0.,1.,0.));
#61454=DIRECTION('ref_axis',(0.,0.,1.));
#61455=DIRECTION('center_axis',(0.,1.,0.));
#61456=DIRECTION('ref_axis',(0.,0.,1.));
#61457=DIRECTION('',(0.,-1.,0.));
#61458=DIRECTION('center_axis',(0.,-1.,0.));
#61459=DIRECTION('ref_axis',(0.,0.,-1.));
#61460=DIRECTION('center_axis',(0.,1.,0.));
#61461=DIRECTION('ref_axis',(0.,0.,1.));
#61462=DIRECTION('center_axis',(0.,-1.,0.));
#61463=DIRECTION('ref_axis',(0.,0.,-1.));
#61464=DIRECTION('',(0.,1.,0.));
#61465=DIRECTION('center_axis',(0.,-1.,0.));
#61466=DIRECTION('ref_axis',(0.,0.,-1.));
#61467=DIRECTION('center_axis',(0.,1.,0.));
#61468=DIRECTION('ref_axis',(0.,0.,1.));
#61469=DIRECTION('center_axis',(0.,1.,0.));
#61470=DIRECTION('ref_axis',(0.,0.,1.));
#61471=DIRECTION('',(0.,-1.,0.));
#61472=DIRECTION('center_axis',(0.,-1.,0.));
#61473=DIRECTION('ref_axis',(0.,0.,-1.));
#61474=DIRECTION('center_axis',(0.,1.,0.));
#61475=DIRECTION('ref_axis',(0.,0.,1.));
#61476=DIRECTION('center_axis',(0.,-1.,0.));
#61477=DIRECTION('ref_axis',(0.,0.,-1.));
#61478=DIRECTION('',(0.,1.,0.));
#61479=DIRECTION('center_axis',(0.,-1.,0.));
#61480=DIRECTION('ref_axis',(0.,0.,-1.));
#61481=DIRECTION('center_axis',(0.,1.,0.));
#61482=DIRECTION('ref_axis',(0.,0.,1.));
#61483=DIRECTION('center_axis',(0.,1.,0.));
#61484=DIRECTION('ref_axis',(0.,0.,1.));
#61485=DIRECTION('',(0.,-1.,0.));
#61486=DIRECTION('center_axis',(0.,-1.,0.));
#61487=DIRECTION('ref_axis',(0.,0.,-1.));
#61488=DIRECTION('center_axis',(0.,1.,0.));
#61489=DIRECTION('ref_axis',(0.,0.,1.));
#61490=DIRECTION('center_axis',(0.,-1.,0.));
#61491=DIRECTION('ref_axis',(0.,0.,-1.));
#61492=DIRECTION('',(0.,1.,0.));
#61493=DIRECTION('center_axis',(0.,-1.,0.));
#61494=DIRECTION('ref_axis',(0.,0.,-1.));
#61495=DIRECTION('center_axis',(0.,1.,0.));
#61496=DIRECTION('ref_axis',(0.,0.,1.));
#61497=DIRECTION('center_axis',(0.,1.,0.));
#61498=DIRECTION('ref_axis',(0.,0.,1.));
#61499=DIRECTION('',(0.,-1.,0.));
#61500=DIRECTION('center_axis',(0.,-1.,0.));
#61501=DIRECTION('ref_axis',(0.,0.,-1.));
#61502=DIRECTION('center_axis',(0.,1.,0.));
#61503=DIRECTION('ref_axis',(0.,0.,1.));
#61504=DIRECTION('center_axis',(0.,-1.,0.));
#61505=DIRECTION('ref_axis',(0.,0.,-1.));
#61506=DIRECTION('',(0.,1.,0.));
#61507=DIRECTION('center_axis',(0.,-1.,0.));
#61508=DIRECTION('ref_axis',(0.,0.,-1.));
#61509=DIRECTION('center_axis',(0.,1.,0.));
#61510=DIRECTION('ref_axis',(0.,0.,1.));
#61511=DIRECTION('center_axis',(0.,1.,0.));
#61512=DIRECTION('ref_axis',(0.,0.,1.));
#61513=DIRECTION('',(0.,-1.,0.));
#61514=DIRECTION('center_axis',(0.,-1.,0.));
#61515=DIRECTION('ref_axis',(0.,0.,-1.));
#61516=DIRECTION('center_axis',(0.,1.,0.));
#61517=DIRECTION('ref_axis',(0.,0.,1.));
#61518=DIRECTION('center_axis',(0.,-1.,0.));
#61519=DIRECTION('ref_axis',(0.,0.,-1.));
#61520=DIRECTION('',(0.,1.,0.));
#61521=DIRECTION('center_axis',(0.,-1.,0.));
#61522=DIRECTION('ref_axis',(0.,0.,-1.));
#61523=DIRECTION('center_axis',(0.,1.,0.));
#61524=DIRECTION('ref_axis',(0.,0.,1.));
#61525=DIRECTION('center_axis',(0.,1.,0.));
#61526=DIRECTION('ref_axis',(0.,0.,1.));
#61527=DIRECTION('',(0.,-1.,0.));
#61528=DIRECTION('center_axis',(0.,-1.,0.));
#61529=DIRECTION('ref_axis',(0.,0.,-1.));
#61530=DIRECTION('center_axis',(0.,1.,0.));
#61531=DIRECTION('ref_axis',(0.,0.,1.));
#61532=DIRECTION('center_axis',(0.,-1.,0.));
#61533=DIRECTION('ref_axis',(0.,0.,-1.));
#61534=DIRECTION('',(0.,1.,0.));
#61535=DIRECTION('center_axis',(0.,-1.,0.));
#61536=DIRECTION('ref_axis',(0.,0.,-1.));
#61537=DIRECTION('center_axis',(0.,1.,0.));
#61538=DIRECTION('ref_axis',(0.,0.,1.));
#61539=DIRECTION('center_axis',(0.,1.,0.));
#61540=DIRECTION('ref_axis',(0.,0.,1.));
#61541=DIRECTION('',(0.,-1.,0.));
#61542=DIRECTION('center_axis',(0.,-1.,0.));
#61543=DIRECTION('ref_axis',(0.,0.,-1.));
#61544=DIRECTION('center_axis',(0.,1.,0.));
#61545=DIRECTION('ref_axis',(0.,0.,1.));
#61546=DIRECTION('center_axis',(0.,-1.,0.));
#61547=DIRECTION('ref_axis',(0.,0.,-1.));
#61548=DIRECTION('',(0.,1.,0.));
#61549=DIRECTION('center_axis',(0.,-1.,0.));
#61550=DIRECTION('ref_axis',(0.,0.,-1.));
#61551=DIRECTION('center_axis',(0.,1.,0.));
#61552=DIRECTION('ref_axis',(0.,0.,1.));
#61553=DIRECTION('center_axis',(0.,1.,0.));
#61554=DIRECTION('ref_axis',(0.,0.,1.));
#61555=DIRECTION('',(0.,-1.,0.));
#61556=DIRECTION('center_axis',(0.,-1.,0.));
#61557=DIRECTION('ref_axis',(0.,0.,-1.));
#61558=DIRECTION('center_axis',(0.,1.,0.));
#61559=DIRECTION('ref_axis',(0.,0.,1.));
#61560=DIRECTION('center_axis',(0.,-1.,0.));
#61561=DIRECTION('ref_axis',(0.,0.,-1.));
#61562=DIRECTION('',(0.,1.,0.));
#61563=DIRECTION('center_axis',(0.,-1.,0.));
#61564=DIRECTION('ref_axis',(0.,0.,-1.));
#61565=DIRECTION('center_axis',(0.,1.,0.));
#61566=DIRECTION('ref_axis',(0.,0.,1.));
#61567=DIRECTION('center_axis',(0.,1.,0.));
#61568=DIRECTION('ref_axis',(0.,0.,1.));
#61569=DIRECTION('',(0.,-1.,0.));
#61570=DIRECTION('center_axis',(0.,-1.,0.));
#61571=DIRECTION('ref_axis',(0.,0.,-1.));
#61572=DIRECTION('center_axis',(0.,1.,0.));
#61573=DIRECTION('ref_axis',(0.,0.,1.));
#61574=DIRECTION('center_axis',(0.,-1.,0.));
#61575=DIRECTION('ref_axis',(0.,0.,-1.));
#61576=DIRECTION('',(0.,1.,0.));
#61577=DIRECTION('center_axis',(0.,-1.,0.));
#61578=DIRECTION('ref_axis',(0.,0.,-1.));
#61579=DIRECTION('center_axis',(0.,1.,0.));
#61580=DIRECTION('ref_axis',(0.,0.,1.));
#61581=DIRECTION('center_axis',(0.,1.,0.));
#61582=DIRECTION('ref_axis',(0.,0.,1.));
#61583=DIRECTION('',(0.,-1.,0.));
#61584=DIRECTION('center_axis',(0.,-1.,0.));
#61585=DIRECTION('ref_axis',(0.,0.,-1.));
#61586=DIRECTION('center_axis',(0.,1.,0.));
#61587=DIRECTION('ref_axis',(0.,0.,1.));
#61588=DIRECTION('center_axis',(0.,-1.,0.));
#61589=DIRECTION('ref_axis',(0.,0.,-1.));
#61590=DIRECTION('',(0.,1.,0.));
#61591=DIRECTION('center_axis',(0.,-1.,0.));
#61592=DIRECTION('ref_axis',(0.,0.,-1.));
#61593=DIRECTION('center_axis',(0.,1.,0.));
#61594=DIRECTION('ref_axis',(0.,0.,1.));
#61595=DIRECTION('center_axis',(0.,1.,0.));
#61596=DIRECTION('ref_axis',(0.,0.,1.));
#61597=DIRECTION('',(0.,-1.,0.));
#61598=DIRECTION('center_axis',(0.,-1.,0.));
#61599=DIRECTION('ref_axis',(0.,0.,-1.));
#61600=DIRECTION('center_axis',(0.,1.,0.));
#61601=DIRECTION('ref_axis',(0.,0.,1.));
#61602=DIRECTION('center_axis',(0.,-1.,0.));
#61603=DIRECTION('ref_axis',(0.,0.,-1.));
#61604=DIRECTION('',(0.,1.,0.));
#61605=DIRECTION('center_axis',(0.,-1.,0.));
#61606=DIRECTION('ref_axis',(0.,0.,-1.));
#61607=DIRECTION('center_axis',(0.,1.,0.));
#61608=DIRECTION('ref_axis',(0.,0.,1.));
#61609=DIRECTION('center_axis',(0.,1.,0.));
#61610=DIRECTION('ref_axis',(0.,0.,1.));
#61611=DIRECTION('',(0.,-1.,0.));
#61612=DIRECTION('center_axis',(0.,-1.,0.));
#61613=DIRECTION('ref_axis',(0.,0.,-1.));
#61614=DIRECTION('center_axis',(0.,1.,0.));
#61615=DIRECTION('ref_axis',(0.,0.,1.));
#61616=DIRECTION('center_axis',(0.,-1.,0.));
#61617=DIRECTION('ref_axis',(0.,0.,-1.));
#61618=DIRECTION('',(0.,1.,0.));
#61619=DIRECTION('center_axis',(0.,-1.,0.));
#61620=DIRECTION('ref_axis',(0.,0.,-1.));
#61621=DIRECTION('center_axis',(0.,1.,0.));
#61622=DIRECTION('ref_axis',(0.,0.,1.));
#61623=DIRECTION('center_axis',(0.,1.,0.));
#61624=DIRECTION('ref_axis',(0.,0.,1.));
#61625=DIRECTION('',(0.,-1.,0.));
#61626=DIRECTION('center_axis',(0.,-1.,0.));
#61627=DIRECTION('ref_axis',(0.,0.,-1.));
#61628=DIRECTION('center_axis',(0.,1.,0.));
#61629=DIRECTION('ref_axis',(0.,0.,1.));
#61630=DIRECTION('center_axis',(0.,-1.,0.));
#61631=DIRECTION('ref_axis',(0.,0.,-1.));
#61632=DIRECTION('',(0.,1.,0.));
#61633=DIRECTION('center_axis',(0.,-1.,0.));
#61634=DIRECTION('ref_axis',(0.,0.,-1.));
#61635=DIRECTION('center_axis',(0.,1.,0.));
#61636=DIRECTION('ref_axis',(0.,0.,1.));
#61637=DIRECTION('center_axis',(0.,1.,0.));
#61638=DIRECTION('ref_axis',(0.,0.,1.));
#61639=DIRECTION('',(0.,-1.,0.));
#61640=DIRECTION('center_axis',(0.,-1.,0.));
#61641=DIRECTION('ref_axis',(0.,0.,-1.));
#61642=DIRECTION('center_axis',(0.,1.,0.));
#61643=DIRECTION('ref_axis',(0.,0.,1.));
#61644=DIRECTION('center_axis',(0.,-1.,0.));
#61645=DIRECTION('ref_axis',(0.,0.,-1.));
#61646=DIRECTION('',(0.,1.,0.));
#61647=DIRECTION('center_axis',(0.,-1.,0.));
#61648=DIRECTION('ref_axis',(0.,0.,-1.));
#61649=DIRECTION('center_axis',(0.,1.,0.));
#61650=DIRECTION('ref_axis',(0.,0.,1.));
#61651=DIRECTION('center_axis',(0.,1.,0.));
#61652=DIRECTION('ref_axis',(0.,0.,1.));
#61653=DIRECTION('',(0.,-1.,0.));
#61654=DIRECTION('center_axis',(0.,-1.,0.));
#61655=DIRECTION('ref_axis',(0.,0.,-1.));
#61656=DIRECTION('center_axis',(0.,1.,0.));
#61657=DIRECTION('ref_axis',(0.,0.,1.));
#61658=DIRECTION('center_axis',(0.,-1.,0.));
#61659=DIRECTION('ref_axis',(0.,0.,-1.));
#61660=DIRECTION('',(0.,1.,0.));
#61661=DIRECTION('center_axis',(0.,-1.,0.));
#61662=DIRECTION('ref_axis',(0.,0.,-1.));
#61663=DIRECTION('center_axis',(0.,1.,0.));
#61664=DIRECTION('ref_axis',(0.,0.,1.));
#61665=DIRECTION('center_axis',(0.,1.,0.));
#61666=DIRECTION('ref_axis',(0.,0.,1.));
#61667=DIRECTION('',(0.,-1.,0.));
#61668=DIRECTION('center_axis',(0.,-1.,0.));
#61669=DIRECTION('ref_axis',(0.,0.,-1.));
#61670=DIRECTION('center_axis',(0.,1.,0.));
#61671=DIRECTION('ref_axis',(0.,0.,1.));
#61672=DIRECTION('center_axis',(0.,-1.,0.));
#61673=DIRECTION('ref_axis',(0.,0.,-1.));
#61674=DIRECTION('',(0.,1.,0.));
#61675=DIRECTION('center_axis',(0.,-1.,0.));
#61676=DIRECTION('ref_axis',(0.,0.,-1.));
#61677=DIRECTION('center_axis',(0.,1.,0.));
#61678=DIRECTION('ref_axis',(0.,0.,1.));
#61679=DIRECTION('center_axis',(0.,1.,0.));
#61680=DIRECTION('ref_axis',(0.,0.,1.));
#61681=DIRECTION('',(0.,-1.,0.));
#61682=DIRECTION('center_axis',(0.,-1.,0.));
#61683=DIRECTION('ref_axis',(0.,0.,-1.));
#61684=DIRECTION('center_axis',(0.,1.,0.));
#61685=DIRECTION('ref_axis',(0.,0.,1.));
#61686=DIRECTION('center_axis',(0.,-1.,0.));
#61687=DIRECTION('ref_axis',(0.,0.,-1.));
#61688=DIRECTION('',(0.,1.,0.));
#61689=DIRECTION('center_axis',(0.,-1.,0.));
#61690=DIRECTION('ref_axis',(0.,0.,-1.));
#61691=DIRECTION('center_axis',(0.,1.,0.));
#61692=DIRECTION('ref_axis',(0.,0.,1.));
#61693=DIRECTION('center_axis',(0.,1.,0.));
#61694=DIRECTION('ref_axis',(0.,0.,1.));
#61695=DIRECTION('',(0.,-1.,0.));
#61696=DIRECTION('center_axis',(0.,-1.,0.));
#61697=DIRECTION('ref_axis',(0.,0.,-1.));
#61698=DIRECTION('center_axis',(0.,1.,0.));
#61699=DIRECTION('ref_axis',(0.,0.,1.));
#61700=DIRECTION('center_axis',(0.,-1.,0.));
#61701=DIRECTION('ref_axis',(0.,0.,-1.));
#61702=DIRECTION('',(0.,1.,0.));
#61703=DIRECTION('center_axis',(0.,-1.,0.));
#61704=DIRECTION('ref_axis',(0.,0.,-1.));
#61705=DIRECTION('center_axis',(0.,1.,0.));
#61706=DIRECTION('ref_axis',(0.,0.,1.));
#61707=DIRECTION('center_axis',(0.,1.,0.));
#61708=DIRECTION('ref_axis',(0.,0.,1.));
#61709=DIRECTION('',(0.,-1.,0.));
#61710=DIRECTION('center_axis',(0.,-1.,0.));
#61711=DIRECTION('ref_axis',(0.,0.,-1.));
#61712=DIRECTION('center_axis',(0.,1.,0.));
#61713=DIRECTION('ref_axis',(0.,0.,1.));
#61714=DIRECTION('center_axis',(0.,-1.,0.));
#61715=DIRECTION('ref_axis',(0.,0.,-1.));
#61716=DIRECTION('',(0.,1.,0.));
#61717=DIRECTION('center_axis',(0.,-1.,0.));
#61718=DIRECTION('ref_axis',(0.,0.,-1.));
#61719=DIRECTION('center_axis',(0.,1.,0.));
#61720=DIRECTION('ref_axis',(0.,0.,1.));
#61721=DIRECTION('center_axis',(0.,1.,0.));
#61722=DIRECTION('ref_axis',(0.,0.,1.));
#61723=DIRECTION('',(0.,-1.,0.));
#61724=DIRECTION('center_axis',(0.,-1.,0.));
#61725=DIRECTION('ref_axis',(0.,0.,-1.));
#61726=DIRECTION('center_axis',(0.,1.,0.));
#61727=DIRECTION('ref_axis',(0.,0.,1.));
#61728=DIRECTION('center_axis',(0.,-1.,0.));
#61729=DIRECTION('ref_axis',(0.,0.,-1.));
#61730=DIRECTION('',(0.,1.,0.));
#61731=DIRECTION('center_axis',(0.,-1.,0.));
#61732=DIRECTION('ref_axis',(0.,0.,-1.));
#61733=DIRECTION('center_axis',(0.,1.,0.));
#61734=DIRECTION('ref_axis',(0.,0.,1.));
#61735=DIRECTION('center_axis',(0.,1.,0.));
#61736=DIRECTION('ref_axis',(0.,0.,1.));
#61737=DIRECTION('',(0.,-1.,0.));
#61738=DIRECTION('center_axis',(0.,-1.,0.));
#61739=DIRECTION('ref_axis',(0.,0.,-1.));
#61740=DIRECTION('center_axis',(0.,1.,0.));
#61741=DIRECTION('ref_axis',(0.,0.,1.));
#61742=DIRECTION('center_axis',(0.,-1.,0.));
#61743=DIRECTION('ref_axis',(0.,0.,-1.));
#61744=DIRECTION('',(0.,1.,0.));
#61745=DIRECTION('center_axis',(0.,-1.,0.));
#61746=DIRECTION('ref_axis',(0.,0.,-1.));
#61747=DIRECTION('center_axis',(0.,1.,0.));
#61748=DIRECTION('ref_axis',(0.,0.,1.));
#61749=DIRECTION('center_axis',(0.,1.,0.));
#61750=DIRECTION('ref_axis',(0.,0.,1.));
#61751=DIRECTION('',(0.,-1.,0.));
#61752=DIRECTION('center_axis',(0.,-1.,0.));
#61753=DIRECTION('ref_axis',(0.,0.,-1.));
#61754=DIRECTION('center_axis',(0.,1.,0.));
#61755=DIRECTION('ref_axis',(0.,0.,1.));
#61756=DIRECTION('center_axis',(0.,-1.,0.));
#61757=DIRECTION('ref_axis',(0.,0.,-1.));
#61758=DIRECTION('',(0.,1.,0.));
#61759=DIRECTION('center_axis',(0.,-1.,0.));
#61760=DIRECTION('ref_axis',(0.,0.,-1.));
#61761=DIRECTION('center_axis',(0.,1.,0.));
#61762=DIRECTION('ref_axis',(0.,0.,1.));
#61763=DIRECTION('center_axis',(0.,1.,0.));
#61764=DIRECTION('ref_axis',(0.,0.,1.));
#61765=DIRECTION('',(0.,-1.,0.));
#61766=DIRECTION('center_axis',(0.,-1.,0.));
#61767=DIRECTION('ref_axis',(0.,0.,-1.));
#61768=DIRECTION('center_axis',(0.,1.,0.));
#61769=DIRECTION('ref_axis',(0.,0.,1.));
#61770=DIRECTION('center_axis',(0.,-1.,0.));
#61771=DIRECTION('ref_axis',(0.,0.,-1.));
#61772=DIRECTION('',(0.,1.,0.));
#61773=DIRECTION('center_axis',(0.,-1.,0.));
#61774=DIRECTION('ref_axis',(0.,0.,-1.));
#61775=DIRECTION('center_axis',(0.,1.,0.));
#61776=DIRECTION('ref_axis',(0.,0.,1.));
#61777=DIRECTION('center_axis',(0.,1.,0.));
#61778=DIRECTION('ref_axis',(0.,0.,1.));
#61779=DIRECTION('',(0.,-1.,0.));
#61780=DIRECTION('center_axis',(0.,-1.,0.));
#61781=DIRECTION('ref_axis',(0.,0.,-1.));
#61782=DIRECTION('center_axis',(0.,1.,0.));
#61783=DIRECTION('ref_axis',(0.,0.,1.));
#61784=DIRECTION('center_axis',(0.,-1.,0.));
#61785=DIRECTION('ref_axis',(0.,0.,-1.));
#61786=DIRECTION('',(0.,1.,0.));
#61787=DIRECTION('center_axis',(0.,-1.,0.));
#61788=DIRECTION('ref_axis',(0.,0.,-1.));
#61789=DIRECTION('center_axis',(0.,1.,0.));
#61790=DIRECTION('ref_axis',(0.,0.,1.));
#61791=DIRECTION('center_axis',(0.,1.,0.));
#61792=DIRECTION('ref_axis',(0.,0.,1.));
#61793=DIRECTION('',(0.,-1.,0.));
#61794=DIRECTION('center_axis',(0.,-1.,0.));
#61795=DIRECTION('ref_axis',(0.,0.,-1.));
#61796=DIRECTION('center_axis',(0.,1.,0.));
#61797=DIRECTION('ref_axis',(0.,0.,1.));
#61798=DIRECTION('center_axis',(0.,-1.,0.));
#61799=DIRECTION('ref_axis',(0.,0.,-1.));
#61800=DIRECTION('',(0.,1.,0.));
#61801=DIRECTION('center_axis',(0.,-1.,0.));
#61802=DIRECTION('ref_axis',(0.,0.,-1.));
#61803=DIRECTION('center_axis',(0.,1.,0.));
#61804=DIRECTION('ref_axis',(0.,0.,1.));
#61805=DIRECTION('center_axis',(0.,1.,0.));
#61806=DIRECTION('ref_axis',(0.,0.,1.));
#61807=DIRECTION('',(0.,-1.,0.));
#61808=DIRECTION('center_axis',(0.,-1.,0.));
#61809=DIRECTION('ref_axis',(0.,0.,-1.));
#61810=DIRECTION('center_axis',(0.,1.,0.));
#61811=DIRECTION('ref_axis',(0.,0.,1.));
#61812=DIRECTION('center_axis',(0.,-1.,0.));
#61813=DIRECTION('ref_axis',(0.,0.,-1.));
#61814=DIRECTION('',(0.,1.,0.));
#61815=DIRECTION('center_axis',(0.,-1.,0.));
#61816=DIRECTION('ref_axis',(0.,0.,-1.));
#61817=DIRECTION('center_axis',(0.,1.,0.));
#61818=DIRECTION('ref_axis',(0.,0.,1.));
#61819=DIRECTION('center_axis',(0.,1.,0.));
#61820=DIRECTION('ref_axis',(0.,0.,1.));
#61821=DIRECTION('',(0.,-1.,0.));
#61822=DIRECTION('center_axis',(0.,-1.,0.));
#61823=DIRECTION('ref_axis',(0.,0.,-1.));
#61824=DIRECTION('center_axis',(0.,1.,0.));
#61825=DIRECTION('ref_axis',(0.,0.,1.));
#61826=DIRECTION('center_axis',(0.,-1.,0.));
#61827=DIRECTION('ref_axis',(0.,0.,-1.));
#61828=DIRECTION('',(0.,1.,0.));
#61829=DIRECTION('center_axis',(0.,-1.,0.));
#61830=DIRECTION('ref_axis',(0.,0.,-1.));
#61831=DIRECTION('center_axis',(0.,1.,0.));
#61832=DIRECTION('ref_axis',(0.,0.,1.));
#61833=DIRECTION('center_axis',(0.,1.,0.));
#61834=DIRECTION('ref_axis',(0.,0.,1.));
#61835=DIRECTION('',(0.,-1.,0.));
#61836=DIRECTION('center_axis',(0.,-1.,0.));
#61837=DIRECTION('ref_axis',(0.,0.,-1.));
#61838=DIRECTION('center_axis',(0.,1.,0.));
#61839=DIRECTION('ref_axis',(0.,0.,1.));
#61840=DIRECTION('center_axis',(0.,-1.,0.));
#61841=DIRECTION('ref_axis',(0.,0.,-1.));
#61842=DIRECTION('',(0.,1.,0.));
#61843=DIRECTION('center_axis',(0.,-1.,0.));
#61844=DIRECTION('ref_axis',(0.,0.,-1.));
#61845=DIRECTION('center_axis',(0.,1.,0.));
#61846=DIRECTION('ref_axis',(0.,0.,1.));
#61847=DIRECTION('center_axis',(0.,1.,0.));
#61848=DIRECTION('ref_axis',(0.,0.,1.));
#61849=DIRECTION('',(0.,-1.,0.));
#61850=DIRECTION('center_axis',(0.,-1.,0.));
#61851=DIRECTION('ref_axis',(0.,0.,-1.));
#61852=DIRECTION('center_axis',(0.,1.,0.));
#61853=DIRECTION('ref_axis',(0.,0.,1.));
#61854=DIRECTION('center_axis',(0.,-1.,0.));
#61855=DIRECTION('ref_axis',(0.,0.,-1.));
#61856=DIRECTION('',(0.,1.,0.));
#61857=DIRECTION('center_axis',(0.,-1.,0.));
#61858=DIRECTION('ref_axis',(0.,0.,-1.));
#61859=DIRECTION('center_axis',(0.,1.,0.));
#61860=DIRECTION('ref_axis',(0.,0.,1.));
#61861=DIRECTION('center_axis',(0.,1.,0.));
#61862=DIRECTION('ref_axis',(0.,0.,1.));
#61863=DIRECTION('',(0.,-1.,0.));
#61864=DIRECTION('center_axis',(0.,-1.,0.));
#61865=DIRECTION('ref_axis',(0.,0.,-1.));
#61866=DIRECTION('center_axis',(0.,1.,0.));
#61867=DIRECTION('ref_axis',(0.,0.,1.));
#61868=DIRECTION('center_axis',(0.,-1.,0.));
#61869=DIRECTION('ref_axis',(0.,0.,-1.));
#61870=DIRECTION('',(0.,1.,0.));
#61871=DIRECTION('center_axis',(0.,-1.,0.));
#61872=DIRECTION('ref_axis',(0.,0.,-1.));
#61873=DIRECTION('center_axis',(0.,1.,0.));
#61874=DIRECTION('ref_axis',(0.,0.,1.));
#61875=DIRECTION('center_axis',(0.,1.,0.));
#61876=DIRECTION('ref_axis',(0.,0.,1.));
#61877=DIRECTION('',(0.,-1.,0.));
#61878=DIRECTION('center_axis',(0.,-1.,0.));
#61879=DIRECTION('ref_axis',(0.,0.,-1.));
#61880=DIRECTION('center_axis',(0.,1.,0.));
#61881=DIRECTION('ref_axis',(0.,0.,1.));
#61882=DIRECTION('center_axis',(0.,-1.,0.));
#61883=DIRECTION('ref_axis',(0.,0.,-1.));
#61884=DIRECTION('',(0.,1.,0.));
#61885=DIRECTION('center_axis',(0.,-1.,0.));
#61886=DIRECTION('ref_axis',(0.,0.,-1.));
#61887=DIRECTION('center_axis',(0.,1.,0.));
#61888=DIRECTION('ref_axis',(0.,0.,1.));
#61889=DIRECTION('center_axis',(0.,1.,0.));
#61890=DIRECTION('ref_axis',(0.,0.,1.));
#61891=DIRECTION('',(0.,-1.,0.));
#61892=DIRECTION('center_axis',(0.,-1.,0.));
#61893=DIRECTION('ref_axis',(0.,0.,-1.));
#61894=DIRECTION('center_axis',(0.,1.,0.));
#61895=DIRECTION('ref_axis',(0.,0.,1.));
#61896=DIRECTION('center_axis',(0.,-1.,0.));
#61897=DIRECTION('ref_axis',(0.,0.,-1.));
#61898=DIRECTION('',(0.,1.,0.));
#61899=DIRECTION('center_axis',(0.,-1.,0.));
#61900=DIRECTION('ref_axis',(0.,0.,-1.));
#61901=DIRECTION('center_axis',(0.,1.,0.));
#61902=DIRECTION('ref_axis',(0.,0.,1.));
#61903=DIRECTION('center_axis',(0.,1.,0.));
#61904=DIRECTION('ref_axis',(0.,0.,1.));
#61905=DIRECTION('',(0.,-1.,0.));
#61906=DIRECTION('center_axis',(0.,-1.,0.));
#61907=DIRECTION('ref_axis',(0.,0.,-1.));
#61908=DIRECTION('center_axis',(0.,1.,0.));
#61909=DIRECTION('ref_axis',(0.,0.,1.));
#61910=DIRECTION('center_axis',(0.,-1.,0.));
#61911=DIRECTION('ref_axis',(0.,0.,-1.));
#61912=DIRECTION('',(0.,1.,0.));
#61913=DIRECTION('center_axis',(0.,-1.,0.));
#61914=DIRECTION('ref_axis',(0.,0.,-1.));
#61915=DIRECTION('center_axis',(0.,1.,0.));
#61916=DIRECTION('ref_axis',(0.,0.,1.));
#61917=DIRECTION('center_axis',(0.,1.,0.));
#61918=DIRECTION('ref_axis',(0.,0.,1.));
#61919=DIRECTION('',(0.,-1.,0.));
#61920=DIRECTION('center_axis',(0.,-1.,0.));
#61921=DIRECTION('ref_axis',(0.,0.,-1.));
#61922=DIRECTION('center_axis',(0.,1.,0.));
#61923=DIRECTION('ref_axis',(0.,0.,1.));
#61924=DIRECTION('center_axis',(0.,-1.,0.));
#61925=DIRECTION('ref_axis',(0.,0.,-1.));
#61926=DIRECTION('',(0.,1.,0.));
#61927=DIRECTION('center_axis',(0.,-1.,0.));
#61928=DIRECTION('ref_axis',(0.,0.,-1.));
#61929=DIRECTION('center_axis',(0.,1.,0.));
#61930=DIRECTION('ref_axis',(0.,0.,1.));
#61931=DIRECTION('center_axis',(0.,1.,0.));
#61932=DIRECTION('ref_axis',(0.,0.,1.));
#61933=DIRECTION('',(0.,-1.,0.));
#61934=DIRECTION('center_axis',(0.,-1.,0.));
#61935=DIRECTION('ref_axis',(0.,0.,-1.));
#61936=DIRECTION('center_axis',(0.,1.,0.));
#61937=DIRECTION('ref_axis',(0.,0.,1.));
#61938=DIRECTION('center_axis',(0.,-1.,0.));
#61939=DIRECTION('ref_axis',(0.,0.,-1.));
#61940=DIRECTION('',(0.,1.,0.));
#61941=DIRECTION('center_axis',(0.,-1.,0.));
#61942=DIRECTION('ref_axis',(0.,0.,-1.));
#61943=DIRECTION('center_axis',(0.,1.,0.));
#61944=DIRECTION('ref_axis',(0.,0.,1.));
#61945=DIRECTION('center_axis',(0.,1.,0.));
#61946=DIRECTION('ref_axis',(0.,0.,1.));
#61947=DIRECTION('',(0.,-1.,0.));
#61948=DIRECTION('center_axis',(0.,-1.,0.));
#61949=DIRECTION('ref_axis',(0.,0.,-1.));
#61950=DIRECTION('center_axis',(0.,1.,0.));
#61951=DIRECTION('ref_axis',(0.,0.,1.));
#61952=DIRECTION('center_axis',(0.,-1.,0.));
#61953=DIRECTION('ref_axis',(0.,0.,-1.));
#61954=DIRECTION('',(0.,1.,0.));
#61955=DIRECTION('center_axis',(0.,-1.,0.));
#61956=DIRECTION('ref_axis',(0.,0.,-1.));
#61957=DIRECTION('center_axis',(0.,1.,0.));
#61958=DIRECTION('ref_axis',(0.,0.,1.));
#61959=DIRECTION('center_axis',(0.,1.,0.));
#61960=DIRECTION('ref_axis',(0.,0.,1.));
#61961=DIRECTION('',(0.,-1.,0.));
#61962=DIRECTION('center_axis',(0.,-1.,0.));
#61963=DIRECTION('ref_axis',(0.,0.,-1.));
#61964=DIRECTION('center_axis',(0.,1.,0.));
#61965=DIRECTION('ref_axis',(0.,0.,1.));
#61966=DIRECTION('center_axis',(0.,-1.,0.));
#61967=DIRECTION('ref_axis',(0.,0.,-1.));
#61968=DIRECTION('',(0.,1.,0.));
#61969=DIRECTION('center_axis',(0.,-1.,0.));
#61970=DIRECTION('ref_axis',(0.,0.,-1.));
#61971=DIRECTION('center_axis',(0.,1.,0.));
#61972=DIRECTION('ref_axis',(0.,0.,1.));
#61973=DIRECTION('center_axis',(0.,1.,0.));
#61974=DIRECTION('ref_axis',(0.,0.,1.));
#61975=DIRECTION('',(0.,-1.,0.));
#61976=DIRECTION('center_axis',(0.,-1.,0.));
#61977=DIRECTION('ref_axis',(0.,0.,-1.));
#61978=DIRECTION('center_axis',(0.,1.,0.));
#61979=DIRECTION('ref_axis',(0.,0.,1.));
#61980=DIRECTION('center_axis',(0.,-1.,0.));
#61981=DIRECTION('ref_axis',(0.,0.,-1.));
#61982=DIRECTION('',(0.,1.,0.));
#61983=DIRECTION('center_axis',(0.,-1.,0.));
#61984=DIRECTION('ref_axis',(0.,0.,-1.));
#61985=DIRECTION('center_axis',(0.,1.,0.));
#61986=DIRECTION('ref_axis',(0.,0.,1.));
#61987=DIRECTION('center_axis',(0.,1.,0.));
#61988=DIRECTION('ref_axis',(0.,0.,1.));
#61989=DIRECTION('',(0.,-1.,0.));
#61990=DIRECTION('center_axis',(0.,-1.,0.));
#61991=DIRECTION('ref_axis',(0.,0.,-1.));
#61992=DIRECTION('center_axis',(0.,1.,0.));
#61993=DIRECTION('ref_axis',(0.,0.,1.));
#61994=DIRECTION('center_axis',(0.,-1.,0.));
#61995=DIRECTION('ref_axis',(0.,0.,-1.));
#61996=DIRECTION('',(0.,1.,0.));
#61997=DIRECTION('center_axis',(0.,-1.,0.));
#61998=DIRECTION('ref_axis',(0.,0.,-1.));
#61999=DIRECTION('center_axis',(0.,1.,0.));
#62000=DIRECTION('ref_axis',(0.,0.,1.));
#62001=DIRECTION('center_axis',(0.,1.,0.));
#62002=DIRECTION('ref_axis',(0.,0.,1.));
#62003=DIRECTION('',(0.,-1.,0.));
#62004=DIRECTION('center_axis',(0.,-1.,0.));
#62005=DIRECTION('ref_axis',(0.,0.,-1.));
#62006=DIRECTION('center_axis',(0.,1.,0.));
#62007=DIRECTION('ref_axis',(0.,0.,1.));
#62008=DIRECTION('center_axis',(0.,-1.,0.));
#62009=DIRECTION('ref_axis',(0.,0.,-1.));
#62010=DIRECTION('',(0.,1.,0.));
#62011=DIRECTION('center_axis',(0.,-1.,0.));
#62012=DIRECTION('ref_axis',(0.,0.,-1.));
#62013=DIRECTION('center_axis',(0.,1.,0.));
#62014=DIRECTION('ref_axis',(0.,0.,1.));
#62015=DIRECTION('center_axis',(0.,1.,0.));
#62016=DIRECTION('ref_axis',(0.,0.,1.));
#62017=DIRECTION('',(0.,-1.,0.));
#62018=DIRECTION('center_axis',(0.,-1.,0.));
#62019=DIRECTION('ref_axis',(0.,0.,-1.));
#62020=DIRECTION('center_axis',(0.,1.,0.));
#62021=DIRECTION('ref_axis',(0.,0.,1.));
#62022=DIRECTION('center_axis',(0.,-1.,0.));
#62023=DIRECTION('ref_axis',(0.,0.,-1.));
#62024=DIRECTION('',(0.,1.,0.));
#62025=DIRECTION('center_axis',(0.,-1.,0.));
#62026=DIRECTION('ref_axis',(0.,0.,-1.));
#62027=DIRECTION('center_axis',(0.,1.,0.));
#62028=DIRECTION('ref_axis',(0.,0.,1.));
#62029=DIRECTION('center_axis',(0.,1.,0.));
#62030=DIRECTION('ref_axis',(0.,0.,1.));
#62031=DIRECTION('',(0.,-1.,0.));
#62032=DIRECTION('center_axis',(0.,-1.,0.));
#62033=DIRECTION('ref_axis',(0.,0.,-1.));
#62034=DIRECTION('center_axis',(0.,1.,0.));
#62035=DIRECTION('ref_axis',(0.,0.,1.));
#62036=DIRECTION('center_axis',(0.,-1.,0.));
#62037=DIRECTION('ref_axis',(0.,0.,-1.));
#62038=DIRECTION('',(0.,1.,0.));
#62039=DIRECTION('center_axis',(0.,-1.,0.));
#62040=DIRECTION('ref_axis',(0.,0.,-1.));
#62041=DIRECTION('center_axis',(0.,1.,0.));
#62042=DIRECTION('ref_axis',(0.,0.,1.));
#62043=DIRECTION('center_axis',(0.,1.,0.));
#62044=DIRECTION('ref_axis',(0.,0.,1.));
#62045=DIRECTION('',(0.,-1.,0.));
#62046=DIRECTION('center_axis',(0.,-1.,0.));
#62047=DIRECTION('ref_axis',(0.,0.,-1.));
#62048=DIRECTION('center_axis',(0.,1.,0.));
#62049=DIRECTION('ref_axis',(0.,0.,1.));
#62050=DIRECTION('center_axis',(0.,-1.,0.));
#62051=DIRECTION('ref_axis',(0.,0.,-1.));
#62052=DIRECTION('',(0.,1.,0.));
#62053=DIRECTION('center_axis',(0.,-1.,0.));
#62054=DIRECTION('ref_axis',(0.,0.,-1.));
#62055=DIRECTION('center_axis',(0.,1.,0.));
#62056=DIRECTION('ref_axis',(0.,0.,1.));
#62057=DIRECTION('center_axis',(0.,1.,0.));
#62058=DIRECTION('ref_axis',(0.,0.,1.));
#62059=DIRECTION('',(0.,-1.,0.));
#62060=DIRECTION('center_axis',(0.,-1.,0.));
#62061=DIRECTION('ref_axis',(0.,0.,-1.));
#62062=DIRECTION('center_axis',(0.,1.,0.));
#62063=DIRECTION('ref_axis',(0.,0.,1.));
#62064=DIRECTION('center_axis',(0.,-1.,0.));
#62065=DIRECTION('ref_axis',(0.,0.,-1.));
#62066=DIRECTION('',(0.,1.,0.));
#62067=DIRECTION('center_axis',(0.,-1.,0.));
#62068=DIRECTION('ref_axis',(0.,0.,-1.));
#62069=DIRECTION('center_axis',(0.,1.,0.));
#62070=DIRECTION('ref_axis',(0.,0.,1.));
#62071=DIRECTION('center_axis',(0.,1.,0.));
#62072=DIRECTION('ref_axis',(0.,0.,1.));
#62073=DIRECTION('',(0.,-1.,0.));
#62074=DIRECTION('center_axis',(0.,-1.,0.));
#62075=DIRECTION('ref_axis',(0.,0.,-1.));
#62076=DIRECTION('center_axis',(0.,1.,0.));
#62077=DIRECTION('ref_axis',(0.,0.,1.));
#62078=DIRECTION('center_axis',(0.,-1.,0.));
#62079=DIRECTION('ref_axis',(0.,0.,-1.));
#62080=DIRECTION('',(0.,1.,0.));
#62081=DIRECTION('center_axis',(0.,-1.,0.));
#62082=DIRECTION('ref_axis',(0.,0.,-1.));
#62083=DIRECTION('center_axis',(0.,1.,0.));
#62084=DIRECTION('ref_axis',(0.,0.,1.));
#62085=DIRECTION('center_axis',(0.,1.,0.));
#62086=DIRECTION('ref_axis',(0.,0.,1.));
#62087=DIRECTION('',(0.,-1.,0.));
#62088=DIRECTION('center_axis',(0.,-1.,0.));
#62089=DIRECTION('ref_axis',(0.,0.,-1.));
#62090=DIRECTION('center_axis',(0.,1.,0.));
#62091=DIRECTION('ref_axis',(0.,0.,1.));
#62092=DIRECTION('center_axis',(0.,-1.,0.));
#62093=DIRECTION('ref_axis',(0.,0.,-1.));
#62094=DIRECTION('',(0.,1.,0.));
#62095=DIRECTION('center_axis',(0.,-1.,0.));
#62096=DIRECTION('ref_axis',(0.,0.,-1.));
#62097=DIRECTION('center_axis',(0.,1.,0.));
#62098=DIRECTION('ref_axis',(0.,0.,1.));
#62099=DIRECTION('center_axis',(0.,1.,0.));
#62100=DIRECTION('ref_axis',(0.,0.,1.));
#62101=DIRECTION('',(0.,-1.,0.));
#62102=DIRECTION('center_axis',(0.,-1.,0.));
#62103=DIRECTION('ref_axis',(0.,0.,-1.));
#62104=DIRECTION('center_axis',(0.,1.,0.));
#62105=DIRECTION('ref_axis',(0.,0.,1.));
#62106=DIRECTION('center_axis',(0.,-1.,0.));
#62107=DIRECTION('ref_axis',(0.,0.,-1.));
#62108=DIRECTION('',(0.,1.,0.));
#62109=DIRECTION('center_axis',(0.,-1.,0.));
#62110=DIRECTION('ref_axis',(0.,0.,-1.));
#62111=DIRECTION('center_axis',(0.,1.,0.));
#62112=DIRECTION('ref_axis',(0.,0.,1.));
#62113=DIRECTION('center_axis',(0.,1.,0.));
#62114=DIRECTION('ref_axis',(0.,0.,1.));
#62115=DIRECTION('',(0.,-1.,0.));
#62116=DIRECTION('center_axis',(0.,-1.,0.));
#62117=DIRECTION('ref_axis',(0.,0.,-1.));
#62118=DIRECTION('center_axis',(0.,1.,0.));
#62119=DIRECTION('ref_axis',(0.,0.,1.));
#62120=DIRECTION('center_axis',(0.,-1.,0.));
#62121=DIRECTION('ref_axis',(0.,0.,-1.));
#62122=DIRECTION('',(0.,1.,0.));
#62123=DIRECTION('center_axis',(0.,-1.,0.));
#62124=DIRECTION('ref_axis',(0.,0.,-1.));
#62125=DIRECTION('center_axis',(0.,1.,0.));
#62126=DIRECTION('ref_axis',(0.,0.,1.));
#62127=DIRECTION('center_axis',(0.,1.,0.));
#62128=DIRECTION('ref_axis',(0.,0.,1.));
#62129=DIRECTION('',(0.,-1.,0.));
#62130=DIRECTION('center_axis',(0.,-1.,0.));
#62131=DIRECTION('ref_axis',(0.,0.,-1.));
#62132=DIRECTION('center_axis',(0.,1.,0.));
#62133=DIRECTION('ref_axis',(0.,0.,1.));
#62134=DIRECTION('center_axis',(0.,-1.,0.));
#62135=DIRECTION('ref_axis',(0.,0.,-1.));
#62136=DIRECTION('',(0.,1.,0.));
#62137=DIRECTION('center_axis',(0.,-1.,0.));
#62138=DIRECTION('ref_axis',(0.,0.,-1.));
#62139=DIRECTION('center_axis',(0.,1.,0.));
#62140=DIRECTION('ref_axis',(0.,0.,1.));
#62141=DIRECTION('center_axis',(0.,1.,0.));
#62142=DIRECTION('ref_axis',(0.,0.,1.));
#62143=DIRECTION('',(0.,-1.,0.));
#62144=DIRECTION('center_axis',(0.,-1.,0.));
#62145=DIRECTION('ref_axis',(0.,0.,-1.));
#62146=DIRECTION('center_axis',(0.,1.,0.));
#62147=DIRECTION('ref_axis',(0.,0.,1.));
#62148=DIRECTION('center_axis',(0.,-1.,0.));
#62149=DIRECTION('ref_axis',(0.,0.,-1.));
#62150=DIRECTION('',(0.,1.,0.));
#62151=DIRECTION('center_axis',(0.,-1.,0.));
#62152=DIRECTION('ref_axis',(0.,0.,-1.));
#62153=DIRECTION('center_axis',(0.,1.,0.));
#62154=DIRECTION('ref_axis',(0.,0.,1.));
#62155=DIRECTION('center_axis',(0.,1.,0.));
#62156=DIRECTION('ref_axis',(0.,0.,1.));
#62157=DIRECTION('',(0.,-1.,0.));
#62158=DIRECTION('center_axis',(0.,-1.,0.));
#62159=DIRECTION('ref_axis',(0.,0.,-1.));
#62160=DIRECTION('center_axis',(0.,1.,0.));
#62161=DIRECTION('ref_axis',(0.,0.,1.));
#62162=DIRECTION('center_axis',(0.,-1.,0.));
#62163=DIRECTION('ref_axis',(0.,0.,-1.));
#62164=DIRECTION('',(0.,1.,0.));
#62165=DIRECTION('center_axis',(0.,-1.,0.));
#62166=DIRECTION('ref_axis',(0.,0.,-1.));
#62167=DIRECTION('center_axis',(0.,1.,0.));
#62168=DIRECTION('ref_axis',(0.,0.,1.));
#62169=DIRECTION('center_axis',(0.,1.,0.));
#62170=DIRECTION('ref_axis',(0.,0.,1.));
#62171=DIRECTION('',(0.,-1.,0.));
#62172=DIRECTION('center_axis',(0.,-1.,0.));
#62173=DIRECTION('ref_axis',(0.,0.,-1.));
#62174=DIRECTION('center_axis',(0.,1.,0.));
#62175=DIRECTION('ref_axis',(0.,0.,1.));
#62176=DIRECTION('center_axis',(0.,-1.,0.));
#62177=DIRECTION('ref_axis',(0.,0.,-1.));
#62178=DIRECTION('',(0.,1.,0.));
#62179=DIRECTION('center_axis',(0.,-1.,0.));
#62180=DIRECTION('ref_axis',(0.,0.,-1.));
#62181=DIRECTION('center_axis',(0.,1.,0.));
#62182=DIRECTION('ref_axis',(0.,0.,1.));
#62183=DIRECTION('center_axis',(0.,1.,0.));
#62184=DIRECTION('ref_axis',(0.,0.,1.));
#62185=DIRECTION('',(0.,-1.,0.));
#62186=DIRECTION('center_axis',(0.,-1.,0.));
#62187=DIRECTION('ref_axis',(0.,0.,-1.));
#62188=DIRECTION('center_axis',(0.,1.,0.));
#62189=DIRECTION('ref_axis',(0.,0.,1.));
#62190=DIRECTION('center_axis',(0.,-1.,0.));
#62191=DIRECTION('ref_axis',(0.,0.,-1.));
#62192=DIRECTION('',(0.,1.,0.));
#62193=DIRECTION('center_axis',(0.,-1.,0.));
#62194=DIRECTION('ref_axis',(0.,0.,-1.));
#62195=DIRECTION('center_axis',(0.,1.,0.));
#62196=DIRECTION('ref_axis',(0.,0.,1.));
#62197=DIRECTION('center_axis',(0.,1.,0.));
#62198=DIRECTION('ref_axis',(0.,0.,1.));
#62199=DIRECTION('',(0.,-1.,0.));
#62200=DIRECTION('center_axis',(0.,-1.,0.));
#62201=DIRECTION('ref_axis',(0.,0.,-1.));
#62202=DIRECTION('center_axis',(0.,1.,0.));
#62203=DIRECTION('ref_axis',(0.,0.,1.));
#62204=DIRECTION('center_axis',(0.,-1.,0.));
#62205=DIRECTION('ref_axis',(0.,0.,-1.));
#62206=DIRECTION('',(0.,1.,0.));
#62207=DIRECTION('center_axis',(0.,-1.,0.));
#62208=DIRECTION('ref_axis',(0.,0.,-1.));
#62209=DIRECTION('center_axis',(0.,1.,0.));
#62210=DIRECTION('ref_axis',(0.,0.,1.));
#62211=DIRECTION('center_axis',(0.,1.,0.));
#62212=DIRECTION('ref_axis',(0.,0.,1.));
#62213=DIRECTION('',(0.,-1.,0.));
#62214=DIRECTION('center_axis',(0.,-1.,0.));
#62215=DIRECTION('ref_axis',(0.,0.,-1.));
#62216=DIRECTION('center_axis',(0.,1.,0.));
#62217=DIRECTION('ref_axis',(0.,0.,1.));
#62218=DIRECTION('center_axis',(0.,-1.,0.));
#62219=DIRECTION('ref_axis',(0.,0.,-1.));
#62220=DIRECTION('',(0.,1.,0.));
#62221=DIRECTION('center_axis',(0.,-1.,0.));
#62222=DIRECTION('ref_axis',(0.,0.,-1.));
#62223=DIRECTION('center_axis',(0.,1.,0.));
#62224=DIRECTION('ref_axis',(0.,0.,1.));
#62225=DIRECTION('center_axis',(0.,1.,0.));
#62226=DIRECTION('ref_axis',(0.,0.,1.));
#62227=DIRECTION('',(0.,-1.,0.));
#62228=DIRECTION('center_axis',(0.,-1.,0.));
#62229=DIRECTION('ref_axis',(0.,0.,-1.));
#62230=DIRECTION('center_axis',(0.,1.,0.));
#62231=DIRECTION('ref_axis',(0.,0.,1.));
#62232=DIRECTION('center_axis',(0.,-1.,0.));
#62233=DIRECTION('ref_axis',(0.,0.,-1.));
#62234=DIRECTION('',(0.,1.,0.));
#62235=DIRECTION('center_axis',(0.,-1.,0.));
#62236=DIRECTION('ref_axis',(0.,0.,-1.));
#62237=DIRECTION('center_axis',(0.,1.,0.));
#62238=DIRECTION('ref_axis',(0.,0.,1.));
#62239=DIRECTION('center_axis',(0.,1.,0.));
#62240=DIRECTION('ref_axis',(0.,0.,1.));
#62241=DIRECTION('',(0.,-1.,0.));
#62242=DIRECTION('center_axis',(0.,-1.,0.));
#62243=DIRECTION('ref_axis',(0.,0.,-1.));
#62244=DIRECTION('center_axis',(0.,1.,0.));
#62245=DIRECTION('ref_axis',(0.,0.,1.));
#62246=DIRECTION('center_axis',(0.,-1.,0.));
#62247=DIRECTION('ref_axis',(0.,0.,-1.));
#62248=DIRECTION('',(0.,1.,0.));
#62249=DIRECTION('center_axis',(0.,-1.,0.));
#62250=DIRECTION('ref_axis',(0.,0.,-1.));
#62251=DIRECTION('center_axis',(0.,1.,0.));
#62252=DIRECTION('ref_axis',(0.,0.,1.));
#62253=DIRECTION('center_axis',(0.,1.,0.));
#62254=DIRECTION('ref_axis',(0.,0.,1.));
#62255=DIRECTION('',(0.,-1.,0.));
#62256=DIRECTION('center_axis',(0.,-1.,0.));
#62257=DIRECTION('ref_axis',(0.,0.,-1.));
#62258=DIRECTION('center_axis',(0.,1.,0.));
#62259=DIRECTION('ref_axis',(0.,0.,1.));
#62260=DIRECTION('center_axis',(0.,-1.,0.));
#62261=DIRECTION('ref_axis',(0.,0.,-1.));
#62262=DIRECTION('',(0.,1.,0.));
#62263=DIRECTION('center_axis',(0.,-1.,0.));
#62264=DIRECTION('ref_axis',(0.,0.,-1.));
#62265=DIRECTION('center_axis',(0.,1.,0.));
#62266=DIRECTION('ref_axis',(0.,0.,1.));
#62267=DIRECTION('center_axis',(0.,1.,0.));
#62268=DIRECTION('ref_axis',(0.,0.,1.));
#62269=DIRECTION('',(0.,-1.,0.));
#62270=DIRECTION('center_axis',(0.,-1.,0.));
#62271=DIRECTION('ref_axis',(0.,0.,-1.));
#62272=DIRECTION('center_axis',(0.,1.,0.));
#62273=DIRECTION('ref_axis',(0.,0.,1.));
#62274=DIRECTION('center_axis',(0.,-1.,0.));
#62275=DIRECTION('ref_axis',(0.,0.,-1.));
#62276=DIRECTION('',(0.,1.,0.));
#62277=DIRECTION('center_axis',(0.,-1.,0.));
#62278=DIRECTION('ref_axis',(0.,0.,-1.));
#62279=DIRECTION('center_axis',(0.,1.,0.));
#62280=DIRECTION('ref_axis',(0.,0.,1.));
#62281=DIRECTION('center_axis',(0.,1.,0.));
#62282=DIRECTION('ref_axis',(0.,0.,1.));
#62283=DIRECTION('',(0.,-1.,0.));
#62284=DIRECTION('center_axis',(0.,-1.,0.));
#62285=DIRECTION('ref_axis',(0.,0.,-1.));
#62286=DIRECTION('center_axis',(0.,1.,0.));
#62287=DIRECTION('ref_axis',(0.,0.,1.));
#62288=DIRECTION('center_axis',(0.,-1.,0.));
#62289=DIRECTION('ref_axis',(0.,0.,-1.));
#62290=DIRECTION('',(0.,1.,0.));
#62291=DIRECTION('center_axis',(0.,-1.,0.));
#62292=DIRECTION('ref_axis',(0.,0.,-1.));
#62293=DIRECTION('center_axis',(0.,1.,0.));
#62294=DIRECTION('ref_axis',(0.,0.,1.));
#62295=DIRECTION('center_axis',(0.,1.,0.));
#62296=DIRECTION('ref_axis',(0.,0.,1.));
#62297=DIRECTION('',(0.,-1.,0.));
#62298=DIRECTION('center_axis',(0.,-1.,0.));
#62299=DIRECTION('ref_axis',(0.,0.,-1.));
#62300=DIRECTION('center_axis',(0.,1.,0.));
#62301=DIRECTION('ref_axis',(0.,0.,1.));
#62302=DIRECTION('center_axis',(0.,-1.,0.));
#62303=DIRECTION('ref_axis',(0.,0.,-1.));
#62304=DIRECTION('',(0.,1.,0.));
#62305=DIRECTION('center_axis',(0.,-1.,0.));
#62306=DIRECTION('ref_axis',(0.,0.,-1.));
#62307=DIRECTION('center_axis',(0.,1.,0.));
#62308=DIRECTION('ref_axis',(0.,0.,1.));
#62309=DIRECTION('center_axis',(0.,1.,0.));
#62310=DIRECTION('ref_axis',(0.,0.,1.));
#62311=DIRECTION('',(0.,-1.,0.));
#62312=DIRECTION('center_axis',(0.,-1.,0.));
#62313=DIRECTION('ref_axis',(0.,0.,-1.));
#62314=DIRECTION('center_axis',(0.,1.,0.));
#62315=DIRECTION('ref_axis',(0.,0.,1.));
#62316=DIRECTION('center_axis',(0.,-1.,0.));
#62317=DIRECTION('ref_axis',(0.,0.,-1.));
#62318=DIRECTION('',(0.,1.,0.));
#62319=DIRECTION('center_axis',(0.,-1.,0.));
#62320=DIRECTION('ref_axis',(0.,0.,-1.));
#62321=DIRECTION('center_axis',(0.,1.,0.));
#62322=DIRECTION('ref_axis',(0.,0.,1.));
#62323=DIRECTION('center_axis',(0.,1.,0.));
#62324=DIRECTION('ref_axis',(0.,0.,1.));
#62325=DIRECTION('',(0.,-1.,0.));
#62326=DIRECTION('center_axis',(0.,-1.,0.));
#62327=DIRECTION('ref_axis',(0.,0.,-1.));
#62328=DIRECTION('center_axis',(0.,1.,0.));
#62329=DIRECTION('ref_axis',(0.,0.,1.));
#62330=DIRECTION('center_axis',(0.,-1.,0.));
#62331=DIRECTION('ref_axis',(0.,0.,-1.));
#62332=DIRECTION('',(0.,1.,0.));
#62333=DIRECTION('center_axis',(0.,-1.,0.));
#62334=DIRECTION('ref_axis',(0.,0.,-1.));
#62335=DIRECTION('center_axis',(0.,1.,0.));
#62336=DIRECTION('ref_axis',(0.,0.,1.));
#62337=DIRECTION('center_axis',(0.,1.,0.));
#62338=DIRECTION('ref_axis',(0.,0.,1.));
#62339=DIRECTION('',(0.,-1.,0.));
#62340=DIRECTION('center_axis',(0.,-1.,0.));
#62341=DIRECTION('ref_axis',(0.,0.,-1.));
#62342=DIRECTION('center_axis',(0.,1.,0.));
#62343=DIRECTION('ref_axis',(0.,0.,1.));
#62344=DIRECTION('center_axis',(0.,-1.,0.));
#62345=DIRECTION('ref_axis',(0.,0.,-1.));
#62346=DIRECTION('',(0.,1.,0.));
#62347=DIRECTION('center_axis',(0.,-1.,0.));
#62348=DIRECTION('ref_axis',(0.,0.,-1.));
#62349=DIRECTION('center_axis',(0.,1.,0.));
#62350=DIRECTION('ref_axis',(0.,0.,1.));
#62351=DIRECTION('center_axis',(0.,1.,0.));
#62352=DIRECTION('ref_axis',(0.,0.,1.));
#62353=DIRECTION('',(0.,-1.,0.));
#62354=DIRECTION('center_axis',(0.,-1.,0.));
#62355=DIRECTION('ref_axis',(0.,0.,-1.));
#62356=DIRECTION('center_axis',(0.,1.,0.));
#62357=DIRECTION('ref_axis',(0.,0.,1.));
#62358=DIRECTION('center_axis',(0.,-1.,0.));
#62359=DIRECTION('ref_axis',(0.,0.,-1.));
#62360=DIRECTION('',(0.,1.,0.));
#62361=DIRECTION('center_axis',(0.,-1.,0.));
#62362=DIRECTION('ref_axis',(0.,0.,-1.));
#62363=DIRECTION('center_axis',(0.,1.,0.));
#62364=DIRECTION('ref_axis',(0.,0.,1.));
#62365=DIRECTION('center_axis',(0.,1.,0.));
#62366=DIRECTION('ref_axis',(0.,0.,1.));
#62367=DIRECTION('',(0.,-1.,0.));
#62368=DIRECTION('center_axis',(0.,-1.,0.));
#62369=DIRECTION('ref_axis',(0.,0.,-1.));
#62370=DIRECTION('center_axis',(0.,1.,0.));
#62371=DIRECTION('ref_axis',(0.,0.,1.));
#62372=DIRECTION('center_axis',(0.,-1.,0.));
#62373=DIRECTION('ref_axis',(0.,0.,-1.));
#62374=DIRECTION('',(0.,1.,0.));
#62375=DIRECTION('center_axis',(0.,-1.,0.));
#62376=DIRECTION('ref_axis',(0.,0.,-1.));
#62377=DIRECTION('center_axis',(0.,1.,0.));
#62378=DIRECTION('ref_axis',(0.,0.,1.));
#62379=DIRECTION('center_axis',(0.,1.,0.));
#62380=DIRECTION('ref_axis',(0.,0.,1.));
#62381=DIRECTION('',(0.,-1.,0.));
#62382=DIRECTION('center_axis',(0.,-1.,0.));
#62383=DIRECTION('ref_axis',(0.,0.,-1.));
#62384=DIRECTION('center_axis',(0.,1.,0.));
#62385=DIRECTION('ref_axis',(0.,0.,1.));
#62386=DIRECTION('center_axis',(0.,-1.,0.));
#62387=DIRECTION('ref_axis',(0.,0.,-1.));
#62388=DIRECTION('',(0.,1.,0.));
#62389=DIRECTION('center_axis',(0.,-1.,0.));
#62390=DIRECTION('ref_axis',(0.,0.,-1.));
#62391=DIRECTION('center_axis',(0.,1.,0.));
#62392=DIRECTION('ref_axis',(0.,0.,1.));
#62393=DIRECTION('center_axis',(0.,1.,0.));
#62394=DIRECTION('ref_axis',(0.,0.,1.));
#62395=DIRECTION('',(0.,-1.,0.));
#62396=DIRECTION('center_axis',(0.,-1.,0.));
#62397=DIRECTION('ref_axis',(0.,0.,-1.));
#62398=DIRECTION('center_axis',(0.,1.,0.));
#62399=DIRECTION('ref_axis',(0.,0.,1.));
#62400=DIRECTION('center_axis',(0.,-1.,0.));
#62401=DIRECTION('ref_axis',(0.,0.,-1.));
#62402=DIRECTION('',(0.,1.,0.));
#62403=DIRECTION('center_axis',(0.,-1.,0.));
#62404=DIRECTION('ref_axis',(0.,0.,-1.));
#62405=DIRECTION('center_axis',(0.,1.,0.));
#62406=DIRECTION('ref_axis',(0.,0.,1.));
#62407=DIRECTION('center_axis',(0.,1.,0.));
#62408=DIRECTION('ref_axis',(0.,0.,1.));
#62409=DIRECTION('',(0.,-1.,0.));
#62410=DIRECTION('center_axis',(0.,-1.,0.));
#62411=DIRECTION('ref_axis',(0.,0.,-1.));
#62412=DIRECTION('center_axis',(0.,1.,0.));
#62413=DIRECTION('ref_axis',(0.,0.,1.));
#62414=DIRECTION('center_axis',(0.,-1.,0.));
#62415=DIRECTION('ref_axis',(0.,0.,-1.));
#62416=DIRECTION('',(0.,1.,0.));
#62417=DIRECTION('center_axis',(0.,-1.,0.));
#62418=DIRECTION('ref_axis',(0.,0.,-1.));
#62419=DIRECTION('center_axis',(0.,1.,0.));
#62420=DIRECTION('ref_axis',(0.,0.,1.));
#62421=DIRECTION('center_axis',(0.,1.,0.));
#62422=DIRECTION('ref_axis',(0.,0.,1.));
#62423=DIRECTION('',(0.,-1.,0.));
#62424=DIRECTION('center_axis',(0.,-1.,0.));
#62425=DIRECTION('ref_axis',(0.,0.,-1.));
#62426=DIRECTION('center_axis',(0.,1.,0.));
#62427=DIRECTION('ref_axis',(0.,0.,1.));
#62428=DIRECTION('center_axis',(0.,-1.,0.));
#62429=DIRECTION('ref_axis',(0.,0.,-1.));
#62430=DIRECTION('',(0.,1.,0.));
#62431=DIRECTION('center_axis',(0.,-1.,0.));
#62432=DIRECTION('ref_axis',(0.,0.,-1.));
#62433=DIRECTION('center_axis',(0.,1.,0.));
#62434=DIRECTION('ref_axis',(0.,0.,1.));
#62435=DIRECTION('center_axis',(0.,1.,0.));
#62436=DIRECTION('ref_axis',(0.,0.,1.));
#62437=DIRECTION('',(0.,-1.,0.));
#62438=DIRECTION('center_axis',(0.,-1.,0.));
#62439=DIRECTION('ref_axis',(0.,0.,-1.));
#62440=DIRECTION('center_axis',(0.,1.,0.));
#62441=DIRECTION('ref_axis',(0.,0.,1.));
#62442=DIRECTION('center_axis',(0.,-1.,0.));
#62443=DIRECTION('ref_axis',(0.,0.,-1.));
#62444=DIRECTION('',(0.,1.,0.));
#62445=DIRECTION('center_axis',(0.,-1.,0.));
#62446=DIRECTION('ref_axis',(0.,0.,-1.));
#62447=DIRECTION('center_axis',(0.,1.,0.));
#62448=DIRECTION('ref_axis',(0.,0.,1.));
#62449=DIRECTION('center_axis',(0.,1.,0.));
#62450=DIRECTION('ref_axis',(0.,0.,1.));
#62451=DIRECTION('',(0.,-1.,0.));
#62452=DIRECTION('center_axis',(0.,-1.,0.));
#62453=DIRECTION('ref_axis',(0.,0.,-1.));
#62454=DIRECTION('center_axis',(0.,1.,0.));
#62455=DIRECTION('ref_axis',(0.,0.,1.));
#62456=DIRECTION('center_axis',(0.,-1.,0.));
#62457=DIRECTION('ref_axis',(0.,0.,-1.));
#62458=DIRECTION('',(0.,1.,0.));
#62459=DIRECTION('center_axis',(0.,-1.,0.));
#62460=DIRECTION('ref_axis',(0.,0.,-1.));
#62461=DIRECTION('center_axis',(0.,1.,0.));
#62462=DIRECTION('ref_axis',(0.,0.,1.));
#62463=DIRECTION('center_axis',(0.,1.,0.));
#62464=DIRECTION('ref_axis',(0.,0.,1.));
#62465=DIRECTION('',(0.,-1.,0.));
#62466=DIRECTION('center_axis',(0.,-1.,0.));
#62467=DIRECTION('ref_axis',(0.,0.,-1.));
#62468=DIRECTION('center_axis',(0.,1.,0.));
#62469=DIRECTION('ref_axis',(0.,0.,1.));
#62470=DIRECTION('center_axis',(0.,-1.,0.));
#62471=DIRECTION('ref_axis',(0.,0.,-1.));
#62472=DIRECTION('',(0.,1.,0.));
#62473=DIRECTION('center_axis',(0.,-1.,0.));
#62474=DIRECTION('ref_axis',(0.,0.,-1.));
#62475=DIRECTION('center_axis',(0.,1.,0.));
#62476=DIRECTION('ref_axis',(0.,0.,1.));
#62477=DIRECTION('center_axis',(0.,1.,0.));
#62478=DIRECTION('ref_axis',(0.,0.,1.));
#62479=DIRECTION('',(0.,-1.,0.));
#62480=DIRECTION('center_axis',(0.,-1.,0.));
#62481=DIRECTION('ref_axis',(0.,0.,-1.));
#62482=DIRECTION('center_axis',(0.,1.,0.));
#62483=DIRECTION('ref_axis',(0.,0.,1.));
#62484=DIRECTION('center_axis',(0.,-1.,0.));
#62485=DIRECTION('ref_axis',(0.,0.,-1.));
#62486=DIRECTION('',(0.,1.,0.));
#62487=DIRECTION('center_axis',(0.,-1.,0.));
#62488=DIRECTION('ref_axis',(0.,0.,-1.));
#62489=DIRECTION('center_axis',(0.,1.,0.));
#62490=DIRECTION('ref_axis',(0.,0.,1.));
#62491=DIRECTION('center_axis',(0.,1.,0.));
#62492=DIRECTION('ref_axis',(0.,0.,1.));
#62493=DIRECTION('',(0.,-1.,0.));
#62494=DIRECTION('center_axis',(0.,-1.,0.));
#62495=DIRECTION('ref_axis',(0.,0.,-1.));
#62496=DIRECTION('center_axis',(0.,1.,0.));
#62497=DIRECTION('ref_axis',(0.,0.,1.));
#62498=DIRECTION('center_axis',(0.,-1.,0.));
#62499=DIRECTION('ref_axis',(0.,0.,-1.));
#62500=DIRECTION('',(0.,1.,0.));
#62501=DIRECTION('center_axis',(0.,-1.,0.));
#62502=DIRECTION('ref_axis',(0.,0.,-1.));
#62503=DIRECTION('center_axis',(0.,1.,0.));
#62504=DIRECTION('ref_axis',(0.,0.,1.));
#62505=DIRECTION('center_axis',(0.,1.,0.));
#62506=DIRECTION('ref_axis',(0.,0.,1.));
#62507=DIRECTION('',(0.,-1.,0.));
#62508=DIRECTION('center_axis',(0.,-1.,0.));
#62509=DIRECTION('ref_axis',(0.,0.,-1.));
#62510=DIRECTION('center_axis',(0.,1.,0.));
#62511=DIRECTION('ref_axis',(0.,0.,1.));
#62512=DIRECTION('center_axis',(0.,-1.,0.));
#62513=DIRECTION('ref_axis',(0.,0.,-1.));
#62514=DIRECTION('',(0.,1.,0.));
#62515=DIRECTION('center_axis',(0.,-1.,0.));
#62516=DIRECTION('ref_axis',(0.,0.,-1.));
#62517=DIRECTION('center_axis',(0.,1.,0.));
#62518=DIRECTION('ref_axis',(0.,0.,1.));
#62519=DIRECTION('center_axis',(0.,1.,0.));
#62520=DIRECTION('ref_axis',(0.,0.,1.));
#62521=DIRECTION('',(0.,-1.,0.));
#62522=DIRECTION('center_axis',(0.,-1.,0.));
#62523=DIRECTION('ref_axis',(0.,0.,-1.));
#62524=DIRECTION('center_axis',(0.,1.,0.));
#62525=DIRECTION('ref_axis',(0.,0.,1.));
#62526=DIRECTION('center_axis',(0.,-1.,0.));
#62527=DIRECTION('ref_axis',(0.,0.,-1.));
#62528=DIRECTION('',(0.,1.,0.));
#62529=DIRECTION('center_axis',(0.,-1.,0.));
#62530=DIRECTION('ref_axis',(0.,0.,-1.));
#62531=DIRECTION('center_axis',(0.,1.,0.));
#62532=DIRECTION('ref_axis',(0.,0.,1.));
#62533=DIRECTION('center_axis',(0.,1.,0.));
#62534=DIRECTION('ref_axis',(0.,0.,1.));
#62535=DIRECTION('',(0.,-1.,0.));
#62536=DIRECTION('center_axis',(0.,-1.,0.));
#62537=DIRECTION('ref_axis',(0.,0.,-1.));
#62538=DIRECTION('center_axis',(0.,1.,0.));
#62539=DIRECTION('ref_axis',(0.,0.,1.));
#62540=DIRECTION('center_axis',(0.,-1.,0.));
#62541=DIRECTION('ref_axis',(0.,0.,-1.));
#62542=DIRECTION('',(0.,1.,0.));
#62543=DIRECTION('center_axis',(0.,-1.,0.));
#62544=DIRECTION('ref_axis',(0.,0.,-1.));
#62545=DIRECTION('center_axis',(0.,1.,0.));
#62546=DIRECTION('ref_axis',(0.,0.,1.));
#62547=DIRECTION('center_axis',(0.,1.,0.));
#62548=DIRECTION('ref_axis',(0.,0.,1.));
#62549=DIRECTION('',(0.,-1.,0.));
#62550=DIRECTION('center_axis',(0.,-1.,0.));
#62551=DIRECTION('ref_axis',(0.,0.,-1.));
#62552=DIRECTION('center_axis',(0.,1.,0.));
#62553=DIRECTION('ref_axis',(0.,0.,1.));
#62554=DIRECTION('center_axis',(0.,-1.,0.));
#62555=DIRECTION('ref_axis',(0.,0.,-1.));
#62556=DIRECTION('',(0.,1.,0.));
#62557=DIRECTION('center_axis',(0.,-1.,0.));
#62558=DIRECTION('ref_axis',(0.,0.,-1.));
#62559=DIRECTION('center_axis',(0.,1.,0.));
#62560=DIRECTION('ref_axis',(0.,0.,1.));
#62561=DIRECTION('center_axis',(0.,1.,0.));
#62562=DIRECTION('ref_axis',(0.,0.,1.));
#62563=DIRECTION('',(0.,-1.,0.));
#62564=DIRECTION('center_axis',(0.,-1.,0.));
#62565=DIRECTION('ref_axis',(0.,0.,-1.));
#62566=DIRECTION('center_axis',(0.,1.,0.));
#62567=DIRECTION('ref_axis',(0.,0.,1.));
#62568=DIRECTION('center_axis',(0.,-1.,0.));
#62569=DIRECTION('ref_axis',(0.,0.,-1.));
#62570=DIRECTION('',(0.,1.,0.));
#62571=DIRECTION('center_axis',(0.,-1.,0.));
#62572=DIRECTION('ref_axis',(0.,0.,-1.));
#62573=DIRECTION('center_axis',(0.,1.,0.));
#62574=DIRECTION('ref_axis',(0.,0.,1.));
#62575=DIRECTION('center_axis',(0.,1.,0.));
#62576=DIRECTION('ref_axis',(0.,0.,1.));
#62577=DIRECTION('',(0.,-1.,0.));
#62578=DIRECTION('center_axis',(0.,-1.,0.));
#62579=DIRECTION('ref_axis',(0.,0.,-1.));
#62580=DIRECTION('center_axis',(0.,1.,0.));
#62581=DIRECTION('ref_axis',(0.,0.,1.));
#62582=DIRECTION('center_axis',(0.,-1.,0.));
#62583=DIRECTION('ref_axis',(0.,0.,-1.));
#62584=DIRECTION('',(0.,1.,0.));
#62585=DIRECTION('center_axis',(0.,-1.,0.));
#62586=DIRECTION('ref_axis',(0.,0.,-1.));
#62587=DIRECTION('center_axis',(0.,1.,0.));
#62588=DIRECTION('ref_axis',(0.,0.,1.));
#62589=DIRECTION('center_axis',(0.,1.,0.));
#62590=DIRECTION('ref_axis',(0.,0.,1.));
#62591=DIRECTION('',(0.,-1.,0.));
#62592=DIRECTION('center_axis',(0.,-1.,0.));
#62593=DIRECTION('ref_axis',(0.,0.,-1.));
#62594=DIRECTION('center_axis',(0.,1.,0.));
#62595=DIRECTION('ref_axis',(0.,0.,1.));
#62596=DIRECTION('center_axis',(0.,-1.,0.));
#62597=DIRECTION('ref_axis',(0.,0.,-1.));
#62598=DIRECTION('',(0.,1.,0.));
#62599=DIRECTION('center_axis',(0.,-1.,0.));
#62600=DIRECTION('ref_axis',(0.,0.,-1.));
#62601=DIRECTION('center_axis',(0.,1.,0.));
#62602=DIRECTION('ref_axis',(0.,0.,1.));
#62603=DIRECTION('center_axis',(0.,1.,0.));
#62604=DIRECTION('ref_axis',(0.,0.,1.));
#62605=DIRECTION('',(0.,-1.,0.));
#62606=DIRECTION('center_axis',(0.,-1.,0.));
#62607=DIRECTION('ref_axis',(0.,0.,-1.));
#62608=DIRECTION('center_axis',(0.,1.,0.));
#62609=DIRECTION('ref_axis',(0.,0.,1.));
#62610=DIRECTION('center_axis',(0.,-1.,0.));
#62611=DIRECTION('ref_axis',(0.,0.,-1.));
#62612=DIRECTION('',(0.,1.,0.));
#62613=DIRECTION('center_axis',(0.,-1.,0.));
#62614=DIRECTION('ref_axis',(0.,0.,-1.));
#62615=DIRECTION('center_axis',(0.,1.,0.));
#62616=DIRECTION('ref_axis',(0.,0.,1.));
#62617=DIRECTION('center_axis',(0.,1.,0.));
#62618=DIRECTION('ref_axis',(0.,0.,1.));
#62619=DIRECTION('',(0.,-1.,0.));
#62620=DIRECTION('center_axis',(0.,-1.,0.));
#62621=DIRECTION('ref_axis',(0.,0.,-1.));
#62622=DIRECTION('center_axis',(0.,1.,0.));
#62623=DIRECTION('ref_axis',(0.,0.,1.));
#62624=DIRECTION('center_axis',(0.,-1.,0.));
#62625=DIRECTION('ref_axis',(0.,0.,-1.));
#62626=DIRECTION('',(0.,1.,0.));
#62627=DIRECTION('center_axis',(0.,-1.,0.));
#62628=DIRECTION('ref_axis',(0.,0.,-1.));
#62629=DIRECTION('center_axis',(0.,1.,0.));
#62630=DIRECTION('ref_axis',(0.,0.,1.));
#62631=DIRECTION('center_axis',(0.,1.,0.));
#62632=DIRECTION('ref_axis',(0.,0.,1.));
#62633=DIRECTION('',(0.,-1.,0.));
#62634=DIRECTION('center_axis',(0.,-1.,0.));
#62635=DIRECTION('ref_axis',(0.,0.,-1.));
#62636=DIRECTION('center_axis',(0.,1.,0.));
#62637=DIRECTION('ref_axis',(0.,0.,1.));
#62638=DIRECTION('center_axis',(0.,-1.,0.));
#62639=DIRECTION('ref_axis',(0.,0.,-1.));
#62640=DIRECTION('',(0.,1.,0.));
#62641=DIRECTION('center_axis',(0.,-1.,0.));
#62642=DIRECTION('ref_axis',(0.,0.,-1.));
#62643=DIRECTION('center_axis',(0.,1.,0.));
#62644=DIRECTION('ref_axis',(0.,0.,1.));
#62645=DIRECTION('center_axis',(0.,1.,0.));
#62646=DIRECTION('ref_axis',(0.,0.,1.));
#62647=DIRECTION('',(0.,-1.,0.));
#62648=DIRECTION('center_axis',(0.,-1.,0.));
#62649=DIRECTION('ref_axis',(0.,0.,-1.));
#62650=DIRECTION('center_axis',(0.,1.,0.));
#62651=DIRECTION('ref_axis',(0.,0.,1.));
#62652=DIRECTION('center_axis',(0.,-1.,0.));
#62653=DIRECTION('ref_axis',(0.,0.,-1.));
#62654=DIRECTION('',(0.,1.,0.));
#62655=DIRECTION('center_axis',(0.,-1.,0.));
#62656=DIRECTION('ref_axis',(0.,0.,-1.));
#62657=DIRECTION('center_axis',(0.,1.,0.));
#62658=DIRECTION('ref_axis',(0.,0.,1.));
#62659=DIRECTION('center_axis',(0.,1.,0.));
#62660=DIRECTION('ref_axis',(0.,0.,1.));
#62661=DIRECTION('',(0.,-1.,0.));
#62662=DIRECTION('center_axis',(0.,-1.,0.));
#62663=DIRECTION('ref_axis',(0.,0.,-1.));
#62664=DIRECTION('center_axis',(0.,1.,0.));
#62665=DIRECTION('ref_axis',(0.,0.,1.));
#62666=DIRECTION('center_axis',(0.,-1.,0.));
#62667=DIRECTION('ref_axis',(0.,0.,-1.));
#62668=DIRECTION('',(0.,1.,0.));
#62669=DIRECTION('center_axis',(0.,-1.,0.));
#62670=DIRECTION('ref_axis',(0.,0.,-1.));
#62671=DIRECTION('center_axis',(0.,1.,0.));
#62672=DIRECTION('ref_axis',(0.,0.,1.));
#62673=DIRECTION('center_axis',(0.,1.,0.));
#62674=DIRECTION('ref_axis',(0.,0.,1.));
#62675=DIRECTION('',(0.,-1.,0.));
#62676=DIRECTION('center_axis',(0.,-1.,0.));
#62677=DIRECTION('ref_axis',(0.,0.,-1.));
#62678=DIRECTION('center_axis',(0.,1.,0.));
#62679=DIRECTION('ref_axis',(0.,0.,1.));
#62680=DIRECTION('center_axis',(0.,-1.,0.));
#62681=DIRECTION('ref_axis',(0.,0.,-1.));
#62682=DIRECTION('',(0.,1.,0.));
#62683=DIRECTION('center_axis',(0.,-1.,0.));
#62684=DIRECTION('ref_axis',(0.,0.,-1.));
#62685=DIRECTION('center_axis',(0.,1.,0.));
#62686=DIRECTION('ref_axis',(0.,0.,1.));
#62687=DIRECTION('center_axis',(0.,1.,0.));
#62688=DIRECTION('ref_axis',(0.,0.,1.));
#62689=DIRECTION('',(0.,-1.,0.));
#62690=DIRECTION('center_axis',(0.,-1.,0.));
#62691=DIRECTION('ref_axis',(0.,0.,-1.));
#62692=DIRECTION('center_axis',(0.,1.,0.));
#62693=DIRECTION('ref_axis',(0.,0.,1.));
#62694=DIRECTION('center_axis',(0.,-1.,0.));
#62695=DIRECTION('ref_axis',(0.,0.,-1.));
#62696=DIRECTION('',(0.,1.,0.));
#62697=DIRECTION('center_axis',(0.,-1.,0.));
#62698=DIRECTION('ref_axis',(0.,0.,-1.));
#62699=DIRECTION('center_axis',(0.,1.,0.));
#62700=DIRECTION('ref_axis',(0.,0.,1.));
#62701=DIRECTION('center_axis',(0.,1.,0.));
#62702=DIRECTION('ref_axis',(0.,0.,1.));
#62703=DIRECTION('',(0.,-1.,0.));
#62704=DIRECTION('center_axis',(0.,-1.,0.));
#62705=DIRECTION('ref_axis',(0.,0.,-1.));
#62706=DIRECTION('center_axis',(0.,1.,0.));
#62707=DIRECTION('ref_axis',(0.,0.,1.));
#62708=DIRECTION('center_axis',(0.,-1.,0.));
#62709=DIRECTION('ref_axis',(0.,0.,-1.));
#62710=DIRECTION('',(0.,1.,0.));
#62711=DIRECTION('center_axis',(0.,-1.,0.));
#62712=DIRECTION('ref_axis',(0.,0.,-1.));
#62713=DIRECTION('center_axis',(0.,1.,0.));
#62714=DIRECTION('ref_axis',(0.,0.,1.));
#62715=DIRECTION('center_axis',(0.,1.,0.));
#62716=DIRECTION('ref_axis',(0.,0.,1.));
#62717=DIRECTION('',(0.,-1.,0.));
#62718=DIRECTION('center_axis',(0.,-1.,0.));
#62719=DIRECTION('ref_axis',(0.,0.,-1.));
#62720=DIRECTION('center_axis',(0.,1.,0.));
#62721=DIRECTION('ref_axis',(0.,0.,1.));
#62722=DIRECTION('center_axis',(0.,-1.,0.));
#62723=DIRECTION('ref_axis',(0.,0.,-1.));
#62724=DIRECTION('',(0.,1.,0.));
#62725=DIRECTION('center_axis',(0.,-1.,0.));
#62726=DIRECTION('ref_axis',(0.,0.,-1.));
#62727=DIRECTION('center_axis',(0.,1.,0.));
#62728=DIRECTION('ref_axis',(0.,0.,1.));
#62729=DIRECTION('center_axis',(0.,1.,0.));
#62730=DIRECTION('ref_axis',(0.,0.,1.));
#62731=DIRECTION('',(0.,-1.,0.));
#62732=DIRECTION('center_axis',(0.,-1.,0.));
#62733=DIRECTION('ref_axis',(0.,0.,-1.));
#62734=DIRECTION('center_axis',(0.,1.,0.));
#62735=DIRECTION('ref_axis',(0.,0.,1.));
#62736=DIRECTION('center_axis',(0.,-1.,0.));
#62737=DIRECTION('ref_axis',(0.,0.,-1.));
#62738=DIRECTION('',(0.,1.,0.));
#62739=DIRECTION('center_axis',(0.,-1.,0.));
#62740=DIRECTION('ref_axis',(0.,0.,-1.));
#62741=DIRECTION('center_axis',(0.,1.,0.));
#62742=DIRECTION('ref_axis',(0.,0.,1.));
#62743=DIRECTION('center_axis',(0.,1.,0.));
#62744=DIRECTION('ref_axis',(0.,0.,1.));
#62745=DIRECTION('',(0.,-1.,0.));
#62746=DIRECTION('center_axis',(0.,-1.,0.));
#62747=DIRECTION('ref_axis',(0.,0.,-1.));
#62748=DIRECTION('center_axis',(0.,1.,0.));
#62749=DIRECTION('ref_axis',(0.,0.,1.));
#62750=DIRECTION('center_axis',(0.,-1.,0.));
#62751=DIRECTION('ref_axis',(0.,0.,-1.));
#62752=DIRECTION('',(0.,1.,0.));
#62753=DIRECTION('center_axis',(0.,-1.,0.));
#62754=DIRECTION('ref_axis',(0.,0.,-1.));
#62755=DIRECTION('center_axis',(0.,1.,0.));
#62756=DIRECTION('ref_axis',(0.,0.,1.));
#62757=DIRECTION('center_axis',(0.,1.,0.));
#62758=DIRECTION('ref_axis',(0.,0.,1.));
#62759=DIRECTION('',(0.,-1.,0.));
#62760=DIRECTION('center_axis',(0.,-1.,0.));
#62761=DIRECTION('ref_axis',(0.,0.,-1.));
#62762=DIRECTION('center_axis',(0.,1.,0.));
#62763=DIRECTION('ref_axis',(0.,0.,1.));
#62764=DIRECTION('center_axis',(0.,-1.,0.));
#62765=DIRECTION('ref_axis',(0.,0.,-1.));
#62766=DIRECTION('',(0.,1.,0.));
#62767=DIRECTION('center_axis',(0.,-1.,0.));
#62768=DIRECTION('ref_axis',(0.,0.,-1.));
#62769=DIRECTION('center_axis',(0.,1.,0.));
#62770=DIRECTION('ref_axis',(0.,0.,1.));
#62771=DIRECTION('center_axis',(0.,1.,0.));
#62772=DIRECTION('ref_axis',(0.,0.,1.));
#62773=DIRECTION('',(0.,-1.,0.));
#62774=DIRECTION('center_axis',(0.,-1.,0.));
#62775=DIRECTION('ref_axis',(0.,0.,-1.));
#62776=DIRECTION('center_axis',(0.,1.,0.));
#62777=DIRECTION('ref_axis',(0.,0.,1.));
#62778=DIRECTION('center_axis',(0.,-1.,0.));
#62779=DIRECTION('ref_axis',(0.,0.,-1.));
#62780=DIRECTION('',(0.,1.,0.));
#62781=DIRECTION('center_axis',(0.,-1.,0.));
#62782=DIRECTION('ref_axis',(0.,0.,-1.));
#62783=DIRECTION('center_axis',(0.,1.,0.));
#62784=DIRECTION('ref_axis',(0.,0.,1.));
#62785=DIRECTION('center_axis',(0.,1.,0.));
#62786=DIRECTION('ref_axis',(0.,0.,1.));
#62787=DIRECTION('',(0.,-1.,0.));
#62788=DIRECTION('center_axis',(0.,-1.,0.));
#62789=DIRECTION('ref_axis',(0.,0.,-1.));
#62790=DIRECTION('center_axis',(0.,1.,0.));
#62791=DIRECTION('ref_axis',(0.,0.,1.));
#62792=DIRECTION('center_axis',(0.,-1.,0.));
#62793=DIRECTION('ref_axis',(0.,0.,-1.));
#62794=DIRECTION('',(0.,1.,0.));
#62795=DIRECTION('center_axis',(0.,-1.,0.));
#62796=DIRECTION('ref_axis',(0.,0.,-1.));
#62797=DIRECTION('center_axis',(0.,1.,0.));
#62798=DIRECTION('ref_axis',(0.,0.,1.));
#62799=DIRECTION('center_axis',(0.,1.,0.));
#62800=DIRECTION('ref_axis',(0.,0.,1.));
#62801=DIRECTION('',(0.,-1.,0.));
#62802=DIRECTION('center_axis',(0.,-1.,0.));
#62803=DIRECTION('ref_axis',(0.,0.,-1.));
#62804=DIRECTION('center_axis',(0.,1.,0.));
#62805=DIRECTION('ref_axis',(0.,0.,1.));
#62806=DIRECTION('center_axis',(0.,-1.,0.));
#62807=DIRECTION('ref_axis',(0.,0.,-1.));
#62808=DIRECTION('',(0.,1.,0.));
#62809=DIRECTION('center_axis',(0.,-1.,0.));
#62810=DIRECTION('ref_axis',(0.,0.,-1.));
#62811=DIRECTION('center_axis',(0.,1.,0.));
#62812=DIRECTION('ref_axis',(0.,0.,1.));
#62813=DIRECTION('center_axis',(0.,1.,0.));
#62814=DIRECTION('ref_axis',(0.,0.,1.));
#62815=DIRECTION('',(0.,-1.,0.));
#62816=DIRECTION('center_axis',(0.,-1.,0.));
#62817=DIRECTION('ref_axis',(0.,0.,-1.));
#62818=DIRECTION('center_axis',(0.,1.,0.));
#62819=DIRECTION('ref_axis',(0.,0.,1.));
#62820=DIRECTION('center_axis',(0.,-1.,0.));
#62821=DIRECTION('ref_axis',(0.,0.,-1.));
#62822=DIRECTION('',(0.,1.,0.));
#62823=DIRECTION('center_axis',(0.,-1.,0.));
#62824=DIRECTION('ref_axis',(0.,0.,-1.));
#62825=DIRECTION('center_axis',(0.,1.,0.));
#62826=DIRECTION('ref_axis',(0.,0.,1.));
#62827=DIRECTION('center_axis',(0.,1.,0.));
#62828=DIRECTION('ref_axis',(0.,0.,1.));
#62829=DIRECTION('',(0.,-1.,0.));
#62830=DIRECTION('center_axis',(0.,-1.,0.));
#62831=DIRECTION('ref_axis',(0.,0.,-1.));
#62832=DIRECTION('center_axis',(0.,1.,0.));
#62833=DIRECTION('ref_axis',(0.,0.,1.));
#62834=DIRECTION('center_axis',(0.,-1.,0.));
#62835=DIRECTION('ref_axis',(0.,0.,-1.));
#62836=DIRECTION('',(0.,1.,0.));
#62837=DIRECTION('center_axis',(0.,-1.,0.));
#62838=DIRECTION('ref_axis',(0.,0.,-1.));
#62839=DIRECTION('center_axis',(0.,1.,0.));
#62840=DIRECTION('ref_axis',(0.,0.,1.));
#62841=DIRECTION('center_axis',(0.,1.,0.));
#62842=DIRECTION('ref_axis',(0.,0.,1.));
#62843=DIRECTION('',(0.,-1.,0.));
#62844=DIRECTION('center_axis',(0.,-1.,0.));
#62845=DIRECTION('ref_axis',(0.,0.,-1.));
#62846=DIRECTION('center_axis',(0.,1.,0.));
#62847=DIRECTION('ref_axis',(0.,0.,1.));
#62848=DIRECTION('center_axis',(0.,-1.,0.));
#62849=DIRECTION('ref_axis',(0.,0.,-1.));
#62850=DIRECTION('',(0.,1.,0.));
#62851=DIRECTION('center_axis',(0.,-1.,0.));
#62852=DIRECTION('ref_axis',(0.,0.,-1.));
#62853=DIRECTION('center_axis',(0.,1.,0.));
#62854=DIRECTION('ref_axis',(0.,0.,1.));
#62855=DIRECTION('center_axis',(0.,1.,0.));
#62856=DIRECTION('ref_axis',(0.,0.,1.));
#62857=DIRECTION('',(0.,-1.,0.));
#62858=DIRECTION('center_axis',(0.,-1.,0.));
#62859=DIRECTION('ref_axis',(0.,0.,-1.));
#62860=DIRECTION('center_axis',(0.,1.,0.));
#62861=DIRECTION('ref_axis',(0.,0.,1.));
#62862=DIRECTION('center_axis',(0.,-1.,0.));
#62863=DIRECTION('ref_axis',(0.,0.,-1.));
#62864=DIRECTION('',(0.,1.,0.));
#62865=DIRECTION('center_axis',(0.,-1.,0.));
#62866=DIRECTION('ref_axis',(0.,0.,-1.));
#62867=DIRECTION('center_axis',(0.,1.,0.));
#62868=DIRECTION('ref_axis',(0.,0.,1.));
#62869=DIRECTION('center_axis',(0.,1.,0.));
#62870=DIRECTION('ref_axis',(0.,0.,1.));
#62871=DIRECTION('',(0.,-1.,0.));
#62872=DIRECTION('center_axis',(0.,-1.,0.));
#62873=DIRECTION('ref_axis',(0.,0.,-1.));
#62874=DIRECTION('center_axis',(0.,1.,0.));
#62875=DIRECTION('ref_axis',(0.,0.,1.));
#62876=DIRECTION('center_axis',(0.,-1.,0.));
#62877=DIRECTION('ref_axis',(0.,0.,-1.));
#62878=DIRECTION('',(0.,1.,0.));
#62879=DIRECTION('center_axis',(0.,-1.,0.));
#62880=DIRECTION('ref_axis',(0.,0.,-1.));
#62881=DIRECTION('center_axis',(0.,1.,0.));
#62882=DIRECTION('ref_axis',(0.,0.,1.));
#62883=DIRECTION('center_axis',(0.,1.,0.));
#62884=DIRECTION('ref_axis',(0.,0.,1.));
#62885=DIRECTION('',(0.,-1.,0.));
#62886=DIRECTION('center_axis',(0.,-1.,0.));
#62887=DIRECTION('ref_axis',(0.,0.,-1.));
#62888=DIRECTION('center_axis',(0.,1.,0.));
#62889=DIRECTION('ref_axis',(0.,0.,1.));
#62890=DIRECTION('center_axis',(0.,-1.,0.));
#62891=DIRECTION('ref_axis',(0.,0.,-1.));
#62892=DIRECTION('',(0.,1.,0.));
#62893=DIRECTION('center_axis',(0.,-1.,0.));
#62894=DIRECTION('ref_axis',(0.,0.,-1.));
#62895=DIRECTION('center_axis',(0.,1.,0.));
#62896=DIRECTION('ref_axis',(0.,0.,1.));
#62897=DIRECTION('center_axis',(0.,1.,0.));
#62898=DIRECTION('ref_axis',(0.,0.,1.));
#62899=DIRECTION('',(0.,-1.,0.));
#62900=DIRECTION('center_axis',(0.,-1.,0.));
#62901=DIRECTION('ref_axis',(0.,0.,-1.));
#62902=DIRECTION('center_axis',(0.,1.,0.));
#62903=DIRECTION('ref_axis',(0.,0.,1.));
#62904=DIRECTION('center_axis',(0.,-1.,0.));
#62905=DIRECTION('ref_axis',(0.,0.,-1.));
#62906=DIRECTION('',(0.,1.,0.));
#62907=DIRECTION('center_axis',(0.,-1.,0.));
#62908=DIRECTION('ref_axis',(0.,0.,-1.));
#62909=DIRECTION('center_axis',(0.,1.,0.));
#62910=DIRECTION('ref_axis',(0.,0.,1.));
#62911=DIRECTION('center_axis',(0.,1.,0.));
#62912=DIRECTION('ref_axis',(0.,0.,1.));
#62913=DIRECTION('',(0.,-1.,0.));
#62914=DIRECTION('center_axis',(0.,-1.,0.));
#62915=DIRECTION('ref_axis',(0.,0.,-1.));
#62916=DIRECTION('center_axis',(0.,1.,0.));
#62917=DIRECTION('ref_axis',(0.,0.,1.));
#62918=DIRECTION('center_axis',(0.,-1.,0.));
#62919=DIRECTION('ref_axis',(0.,0.,-1.));
#62920=DIRECTION('',(0.,1.,0.));
#62921=DIRECTION('center_axis',(0.,-1.,0.));
#62922=DIRECTION('ref_axis',(0.,0.,-1.));
#62923=DIRECTION('center_axis',(0.,1.,0.));
#62924=DIRECTION('ref_axis',(0.,0.,1.));
#62925=DIRECTION('center_axis',(0.,1.,0.));
#62926=DIRECTION('ref_axis',(0.,0.,1.));
#62927=DIRECTION('',(0.,-1.,0.));
#62928=DIRECTION('center_axis',(0.,-1.,0.));
#62929=DIRECTION('ref_axis',(0.,0.,-1.));
#62930=DIRECTION('center_axis',(0.,1.,0.));
#62931=DIRECTION('ref_axis',(0.,0.,1.));
#62932=DIRECTION('center_axis',(0.,-1.,0.));
#62933=DIRECTION('ref_axis',(0.,0.,-1.));
#62934=DIRECTION('',(0.,1.,0.));
#62935=DIRECTION('center_axis',(0.,-1.,0.));
#62936=DIRECTION('ref_axis',(0.,0.,-1.));
#62937=DIRECTION('center_axis',(0.,1.,0.));
#62938=DIRECTION('ref_axis',(0.,0.,1.));
#62939=DIRECTION('center_axis',(0.,1.,0.));
#62940=DIRECTION('ref_axis',(0.,0.,1.));
#62941=DIRECTION('',(0.,-1.,0.));
#62942=DIRECTION('center_axis',(0.,-1.,0.));
#62943=DIRECTION('ref_axis',(0.,0.,-1.));
#62944=DIRECTION('center_axis',(0.,1.,0.));
#62945=DIRECTION('ref_axis',(0.,0.,1.));
#62946=DIRECTION('center_axis',(0.,-1.,0.));
#62947=DIRECTION('ref_axis',(0.,0.,-1.));
#62948=DIRECTION('',(0.,1.,0.));
#62949=DIRECTION('center_axis',(0.,-1.,0.));
#62950=DIRECTION('ref_axis',(0.,0.,-1.));
#62951=DIRECTION('center_axis',(0.,1.,0.));
#62952=DIRECTION('ref_axis',(0.,0.,1.));
#62953=DIRECTION('center_axis',(0.,1.,0.));
#62954=DIRECTION('ref_axis',(0.,0.,1.));
#62955=DIRECTION('',(0.,-1.,0.));
#62956=DIRECTION('center_axis',(0.,-1.,0.));
#62957=DIRECTION('ref_axis',(0.,0.,-1.));
#62958=DIRECTION('center_axis',(0.,1.,0.));
#62959=DIRECTION('ref_axis',(0.,0.,1.));
#62960=DIRECTION('center_axis',(0.,-1.,0.));
#62961=DIRECTION('ref_axis',(0.,0.,-1.));
#62962=DIRECTION('',(0.,1.,0.));
#62963=DIRECTION('center_axis',(0.,-1.,0.));
#62964=DIRECTION('ref_axis',(0.,0.,-1.));
#62965=DIRECTION('center_axis',(0.,1.,0.));
#62966=DIRECTION('ref_axis',(0.,0.,1.));
#62967=DIRECTION('center_axis',(0.,1.,0.));
#62968=DIRECTION('ref_axis',(0.,0.,1.));
#62969=DIRECTION('',(0.,-1.,0.));
#62970=DIRECTION('center_axis',(0.,-1.,0.));
#62971=DIRECTION('ref_axis',(0.,0.,-1.));
#62972=DIRECTION('center_axis',(0.,1.,0.));
#62973=DIRECTION('ref_axis',(0.,0.,1.));
#62974=DIRECTION('center_axis',(0.,-1.,0.));
#62975=DIRECTION('ref_axis',(0.,0.,-1.));
#62976=DIRECTION('',(0.,1.,0.));
#62977=DIRECTION('center_axis',(0.,-1.,0.));
#62978=DIRECTION('ref_axis',(0.,0.,-1.));
#62979=DIRECTION('center_axis',(0.,1.,0.));
#62980=DIRECTION('ref_axis',(0.,0.,1.));
#62981=DIRECTION('center_axis',(0.,1.,0.));
#62982=DIRECTION('ref_axis',(0.,0.,1.));
#62983=DIRECTION('',(0.,-1.,0.));
#62984=DIRECTION('center_axis',(0.,-1.,0.));
#62985=DIRECTION('ref_axis',(0.,0.,-1.));
#62986=DIRECTION('center_axis',(0.,1.,0.));
#62987=DIRECTION('ref_axis',(0.,0.,1.));
#62988=DIRECTION('center_axis',(0.,-1.,0.));
#62989=DIRECTION('ref_axis',(0.,0.,-1.));
#62990=DIRECTION('',(0.,1.,0.));
#62991=DIRECTION('center_axis',(0.,-1.,0.));
#62992=DIRECTION('ref_axis',(0.,0.,-1.));
#62993=DIRECTION('center_axis',(0.,1.,0.));
#62994=DIRECTION('ref_axis',(0.,0.,1.));
#62995=DIRECTION('center_axis',(0.,1.,0.));
#62996=DIRECTION('ref_axis',(0.,0.,1.));
#62997=DIRECTION('',(0.,-1.,0.));
#62998=DIRECTION('center_axis',(0.,-1.,0.));
#62999=DIRECTION('ref_axis',(0.,0.,-1.));
#63000=DIRECTION('center_axis',(0.,1.,0.));
#63001=DIRECTION('ref_axis',(0.,0.,1.));
#63002=DIRECTION('center_axis',(0.,-1.,0.));
#63003=DIRECTION('ref_axis',(0.,0.,-1.));
#63004=DIRECTION('',(0.,1.,0.));
#63005=DIRECTION('center_axis',(0.,-1.,0.));
#63006=DIRECTION('ref_axis',(0.,0.,-1.));
#63007=DIRECTION('center_axis',(0.,1.,0.));
#63008=DIRECTION('ref_axis',(0.,0.,1.));
#63009=DIRECTION('center_axis',(0.,1.,0.));
#63010=DIRECTION('ref_axis',(0.,0.,1.));
#63011=DIRECTION('',(0.,-1.,0.));
#63012=DIRECTION('center_axis',(0.,-1.,0.));
#63013=DIRECTION('ref_axis',(0.,0.,-1.));
#63014=DIRECTION('center_axis',(0.,1.,0.));
#63015=DIRECTION('ref_axis',(0.,0.,1.));
#63016=DIRECTION('center_axis',(0.,-1.,0.));
#63017=DIRECTION('ref_axis',(0.,0.,-1.));
#63018=DIRECTION('',(0.,1.,0.));
#63019=DIRECTION('center_axis',(0.,-1.,0.));
#63020=DIRECTION('ref_axis',(0.,0.,-1.));
#63021=DIRECTION('center_axis',(0.,1.,0.));
#63022=DIRECTION('ref_axis',(0.,0.,1.));
#63023=DIRECTION('center_axis',(0.,1.,0.));
#63024=DIRECTION('ref_axis',(0.,0.,1.));
#63025=DIRECTION('',(0.,-1.,0.));
#63026=DIRECTION('center_axis',(0.,-1.,0.));
#63027=DIRECTION('ref_axis',(0.,0.,-1.));
#63028=DIRECTION('center_axis',(0.,1.,0.));
#63029=DIRECTION('ref_axis',(0.,0.,1.));
#63030=DIRECTION('center_axis',(0.,-1.,0.));
#63031=DIRECTION('ref_axis',(0.,0.,-1.));
#63032=DIRECTION('',(0.,1.,0.));
#63033=DIRECTION('center_axis',(0.,-1.,0.));
#63034=DIRECTION('ref_axis',(0.,0.,-1.));
#63035=DIRECTION('center_axis',(0.,1.,0.));
#63036=DIRECTION('ref_axis',(0.,0.,1.));
#63037=DIRECTION('center_axis',(0.,1.,0.));
#63038=DIRECTION('ref_axis',(0.,0.,1.));
#63039=DIRECTION('',(0.,-1.,0.));
#63040=DIRECTION('center_axis',(0.,-1.,0.));
#63041=DIRECTION('ref_axis',(0.,0.,-1.));
#63042=DIRECTION('center_axis',(0.,1.,0.));
#63043=DIRECTION('ref_axis',(0.,0.,1.));
#63044=DIRECTION('center_axis',(0.,-1.,0.));
#63045=DIRECTION('ref_axis',(0.,0.,-1.));
#63046=DIRECTION('',(0.,1.,0.));
#63047=DIRECTION('center_axis',(0.,-1.,0.));
#63048=DIRECTION('ref_axis',(0.,0.,-1.));
#63049=DIRECTION('center_axis',(0.,1.,0.));
#63050=DIRECTION('ref_axis',(0.,0.,1.));
#63051=DIRECTION('center_axis',(0.,1.,0.));
#63052=DIRECTION('ref_axis',(0.,0.,1.));
#63053=DIRECTION('',(0.,-1.,0.));
#63054=DIRECTION('center_axis',(0.,-1.,0.));
#63055=DIRECTION('ref_axis',(0.,0.,-1.));
#63056=DIRECTION('center_axis',(0.,1.,0.));
#63057=DIRECTION('ref_axis',(0.,0.,1.));
#63058=DIRECTION('center_axis',(0.,-1.,0.));
#63059=DIRECTION('ref_axis',(0.,0.,-1.));
#63060=DIRECTION('',(0.,1.,0.));
#63061=DIRECTION('center_axis',(0.,-1.,0.));
#63062=DIRECTION('ref_axis',(0.,0.,-1.));
#63063=DIRECTION('center_axis',(0.,1.,0.));
#63064=DIRECTION('ref_axis',(0.,0.,1.));
#63065=DIRECTION('center_axis',(0.,1.,0.));
#63066=DIRECTION('ref_axis',(0.,0.,1.));
#63067=DIRECTION('',(0.,-1.,0.));
#63068=DIRECTION('center_axis',(0.,-1.,0.));
#63069=DIRECTION('ref_axis',(0.,0.,-1.));
#63070=DIRECTION('center_axis',(0.,1.,0.));
#63071=DIRECTION('ref_axis',(0.,0.,1.));
#63072=DIRECTION('center_axis',(0.,-1.,0.));
#63073=DIRECTION('ref_axis',(0.,0.,-1.));
#63074=DIRECTION('',(0.,1.,0.));
#63075=DIRECTION('center_axis',(0.,-1.,0.));
#63076=DIRECTION('ref_axis',(0.,0.,-1.));
#63077=DIRECTION('center_axis',(0.,1.,0.));
#63078=DIRECTION('ref_axis',(0.,0.,1.));
#63079=DIRECTION('center_axis',(0.,1.,0.));
#63080=DIRECTION('ref_axis',(0.,0.,1.));
#63081=DIRECTION('',(0.,-1.,0.));
#63082=DIRECTION('center_axis',(0.,-1.,0.));
#63083=DIRECTION('ref_axis',(0.,0.,-1.));
#63084=DIRECTION('center_axis',(0.,1.,0.));
#63085=DIRECTION('ref_axis',(0.,0.,1.));
#63086=DIRECTION('center_axis',(0.,-1.,0.));
#63087=DIRECTION('ref_axis',(0.,0.,-1.));
#63088=DIRECTION('',(0.,1.,0.));
#63089=DIRECTION('center_axis',(0.,-1.,0.));
#63090=DIRECTION('ref_axis',(0.,0.,-1.));
#63091=DIRECTION('center_axis',(0.,1.,0.));
#63092=DIRECTION('ref_axis',(0.,0.,1.));
#63093=DIRECTION('center_axis',(0.,1.,0.));
#63094=DIRECTION('ref_axis',(0.,0.,1.));
#63095=DIRECTION('',(0.,-1.,0.));
#63096=DIRECTION('center_axis',(0.,-1.,0.));
#63097=DIRECTION('ref_axis',(0.,0.,-1.));
#63098=DIRECTION('center_axis',(0.,1.,0.));
#63099=DIRECTION('ref_axis',(0.,0.,1.));
#63100=DIRECTION('center_axis',(0.,-1.,0.));
#63101=DIRECTION('ref_axis',(0.,0.,-1.));
#63102=DIRECTION('',(0.,1.,0.));
#63103=DIRECTION('center_axis',(0.,-1.,0.));
#63104=DIRECTION('ref_axis',(0.,0.,-1.));
#63105=DIRECTION('center_axis',(0.,1.,0.));
#63106=DIRECTION('ref_axis',(0.,0.,1.));
#63107=DIRECTION('center_axis',(0.,1.,0.));
#63108=DIRECTION('ref_axis',(0.,0.,1.));
#63109=DIRECTION('',(0.,-1.,0.));
#63110=DIRECTION('center_axis',(0.,-1.,0.));
#63111=DIRECTION('ref_axis',(0.,0.,-1.));
#63112=DIRECTION('center_axis',(0.,1.,0.));
#63113=DIRECTION('ref_axis',(0.,0.,1.));
#63114=DIRECTION('center_axis',(0.,-1.,0.));
#63115=DIRECTION('ref_axis',(0.,0.,-1.));
#63116=DIRECTION('',(0.,1.,0.));
#63117=DIRECTION('center_axis',(0.,-1.,0.));
#63118=DIRECTION('ref_axis',(0.,0.,-1.));
#63119=DIRECTION('center_axis',(0.,1.,0.));
#63120=DIRECTION('ref_axis',(0.,0.,1.));
#63121=DIRECTION('center_axis',(0.,1.,0.));
#63122=DIRECTION('ref_axis',(0.,0.,1.));
#63123=DIRECTION('',(0.,-1.,0.));
#63124=DIRECTION('center_axis',(0.,-1.,0.));
#63125=DIRECTION('ref_axis',(0.,0.,-1.));
#63126=DIRECTION('center_axis',(0.,1.,0.));
#63127=DIRECTION('ref_axis',(0.,0.,1.));
#63128=DIRECTION('center_axis',(0.,-1.,0.));
#63129=DIRECTION('ref_axis',(0.,0.,-1.));
#63130=DIRECTION('',(0.,1.,0.));
#63131=DIRECTION('center_axis',(0.,-1.,0.));
#63132=DIRECTION('ref_axis',(0.,0.,-1.));
#63133=DIRECTION('center_axis',(0.,1.,0.));
#63134=DIRECTION('ref_axis',(0.,0.,1.));
#63135=DIRECTION('center_axis',(0.,1.,0.));
#63136=DIRECTION('ref_axis',(0.,0.,1.));
#63137=DIRECTION('',(0.,-1.,0.));
#63138=DIRECTION('center_axis',(0.,-1.,0.));
#63139=DIRECTION('ref_axis',(0.,0.,-1.));
#63140=DIRECTION('center_axis',(0.,1.,0.));
#63141=DIRECTION('ref_axis',(0.,0.,1.));
#63142=DIRECTION('center_axis',(0.,-1.,0.));
#63143=DIRECTION('ref_axis',(0.,0.,-1.));
#63144=DIRECTION('',(0.,1.,0.));
#63145=DIRECTION('center_axis',(0.,-1.,0.));
#63146=DIRECTION('ref_axis',(0.,0.,-1.));
#63147=DIRECTION('center_axis',(0.,1.,0.));
#63148=DIRECTION('ref_axis',(0.,0.,1.));
#63149=DIRECTION('center_axis',(0.,1.,0.));
#63150=DIRECTION('ref_axis',(0.,0.,1.));
#63151=DIRECTION('',(0.,-1.,0.));
#63152=DIRECTION('center_axis',(0.,-1.,0.));
#63153=DIRECTION('ref_axis',(0.,0.,-1.));
#63154=DIRECTION('center_axis',(0.,1.,0.));
#63155=DIRECTION('ref_axis',(0.,0.,1.));
#63156=DIRECTION('center_axis',(0.,-1.,0.));
#63157=DIRECTION('ref_axis',(0.,0.,-1.));
#63158=DIRECTION('',(0.,1.,0.));
#63159=DIRECTION('center_axis',(0.,-1.,0.));
#63160=DIRECTION('ref_axis',(0.,0.,-1.));
#63161=DIRECTION('center_axis',(0.,1.,0.));
#63162=DIRECTION('ref_axis',(0.,0.,1.));
#63163=DIRECTION('center_axis',(0.,1.,0.));
#63164=DIRECTION('ref_axis',(0.,0.,1.));
#63165=DIRECTION('',(0.,-1.,0.));
#63166=DIRECTION('center_axis',(0.,-1.,0.));
#63167=DIRECTION('ref_axis',(0.,0.,-1.));
#63168=DIRECTION('center_axis',(0.,1.,0.));
#63169=DIRECTION('ref_axis',(0.,0.,1.));
#63170=DIRECTION('center_axis',(0.,-1.,0.));
#63171=DIRECTION('ref_axis',(0.,0.,-1.));
#63172=DIRECTION('',(0.,1.,0.));
#63173=DIRECTION('center_axis',(0.,-1.,0.));
#63174=DIRECTION('ref_axis',(0.,0.,-1.));
#63175=DIRECTION('center_axis',(0.,1.,0.));
#63176=DIRECTION('ref_axis',(0.,0.,1.));
#63177=DIRECTION('center_axis',(0.,1.,0.));
#63178=DIRECTION('ref_axis',(0.,0.,1.));
#63179=DIRECTION('',(0.,-1.,0.));
#63180=DIRECTION('center_axis',(0.,-1.,0.));
#63181=DIRECTION('ref_axis',(0.,0.,-1.));
#63182=DIRECTION('center_axis',(0.,1.,0.));
#63183=DIRECTION('ref_axis',(0.,0.,1.));
#63184=DIRECTION('center_axis',(0.,-1.,0.));
#63185=DIRECTION('ref_axis',(0.,0.,-1.));
#63186=DIRECTION('',(0.,1.,0.));
#63187=DIRECTION('center_axis',(0.,-1.,0.));
#63188=DIRECTION('ref_axis',(0.,0.,-1.));
#63189=DIRECTION('center_axis',(0.,1.,0.));
#63190=DIRECTION('ref_axis',(0.,0.,1.));
#63191=DIRECTION('center_axis',(0.,1.,0.));
#63192=DIRECTION('ref_axis',(0.,0.,1.));
#63193=DIRECTION('',(0.,-1.,0.));
#63194=DIRECTION('center_axis',(0.,-1.,0.));
#63195=DIRECTION('ref_axis',(0.,0.,-1.));
#63196=DIRECTION('center_axis',(0.,1.,0.));
#63197=DIRECTION('ref_axis',(0.,0.,1.));
#63198=DIRECTION('center_axis',(0.,-1.,0.));
#63199=DIRECTION('ref_axis',(0.,0.,-1.));
#63200=DIRECTION('',(0.,1.,0.));
#63201=DIRECTION('center_axis',(0.,-1.,0.));
#63202=DIRECTION('ref_axis',(0.,0.,-1.));
#63203=DIRECTION('center_axis',(0.,1.,0.));
#63204=DIRECTION('ref_axis',(0.,0.,1.));
#63205=DIRECTION('center_axis',(0.,1.,0.));
#63206=DIRECTION('ref_axis',(0.,0.,1.));
#63207=DIRECTION('',(0.,-1.,0.));
#63208=DIRECTION('center_axis',(0.,-1.,0.));
#63209=DIRECTION('ref_axis',(0.,0.,-1.));
#63210=DIRECTION('center_axis',(0.,1.,0.));
#63211=DIRECTION('ref_axis',(0.,0.,1.));
#63212=DIRECTION('center_axis',(0.,-1.,0.));
#63213=DIRECTION('ref_axis',(0.,0.,-1.));
#63214=DIRECTION('',(0.,1.,0.));
#63215=DIRECTION('center_axis',(0.,-1.,0.));
#63216=DIRECTION('ref_axis',(0.,0.,-1.));
#63217=DIRECTION('center_axis',(0.,1.,0.));
#63218=DIRECTION('ref_axis',(0.,0.,1.));
#63219=DIRECTION('center_axis',(0.,1.,0.));
#63220=DIRECTION('ref_axis',(0.,0.,1.));
#63221=DIRECTION('',(0.,-1.,0.));
#63222=DIRECTION('center_axis',(0.,-1.,0.));
#63223=DIRECTION('ref_axis',(0.,0.,-1.));
#63224=DIRECTION('center_axis',(0.,1.,0.));
#63225=DIRECTION('ref_axis',(0.,0.,1.));
#63226=DIRECTION('center_axis',(0.,-1.,0.));
#63227=DIRECTION('ref_axis',(0.,0.,-1.));
#63228=DIRECTION('',(0.,1.,0.));
#63229=DIRECTION('center_axis',(0.,-1.,0.));
#63230=DIRECTION('ref_axis',(0.,0.,-1.));
#63231=DIRECTION('center_axis',(0.,1.,0.));
#63232=DIRECTION('ref_axis',(0.,0.,1.));
#63233=DIRECTION('center_axis',(0.,1.,0.));
#63234=DIRECTION('ref_axis',(0.,0.,1.));
#63235=DIRECTION('',(0.,-1.,0.));
#63236=DIRECTION('center_axis',(0.,-1.,0.));
#63237=DIRECTION('ref_axis',(0.,0.,-1.));
#63238=DIRECTION('center_axis',(0.,1.,0.));
#63239=DIRECTION('ref_axis',(0.,0.,1.));
#63240=DIRECTION('center_axis',(0.,-1.,0.));
#63241=DIRECTION('ref_axis',(0.,0.,-1.));
#63242=DIRECTION('',(0.,1.,0.));
#63243=DIRECTION('center_axis',(0.,-1.,0.));
#63244=DIRECTION('ref_axis',(0.,0.,-1.));
#63245=DIRECTION('center_axis',(0.,1.,0.));
#63246=DIRECTION('ref_axis',(0.,0.,1.));
#63247=DIRECTION('center_axis',(0.,1.,0.));
#63248=DIRECTION('ref_axis',(0.,0.,1.));
#63249=DIRECTION('',(0.,-1.,0.));
#63250=DIRECTION('center_axis',(0.,-1.,0.));
#63251=DIRECTION('ref_axis',(0.,0.,-1.));
#63252=DIRECTION('center_axis',(0.,1.,0.));
#63253=DIRECTION('ref_axis',(0.,0.,1.));
#63254=DIRECTION('center_axis',(0.,-1.,0.));
#63255=DIRECTION('ref_axis',(0.,0.,-1.));
#63256=DIRECTION('',(0.,1.,0.));
#63257=DIRECTION('center_axis',(0.,-1.,0.));
#63258=DIRECTION('ref_axis',(0.,0.,-1.));
#63259=DIRECTION('center_axis',(0.,1.,0.));
#63260=DIRECTION('ref_axis',(0.,0.,1.));
#63261=DIRECTION('center_axis',(0.,1.,0.));
#63262=DIRECTION('ref_axis',(0.,0.,1.));
#63263=DIRECTION('',(0.,-1.,0.));
#63264=DIRECTION('center_axis',(0.,-1.,0.));
#63265=DIRECTION('ref_axis',(0.,0.,-1.));
#63266=DIRECTION('center_axis',(0.,1.,0.));
#63267=DIRECTION('ref_axis',(0.,0.,1.));
#63268=DIRECTION('center_axis',(0.,-1.,0.));
#63269=DIRECTION('ref_axis',(0.,0.,-1.));
#63270=DIRECTION('',(0.,1.,0.));
#63271=DIRECTION('center_axis',(0.,-1.,0.));
#63272=DIRECTION('ref_axis',(0.,0.,-1.));
#63273=DIRECTION('center_axis',(0.,1.,0.));
#63274=DIRECTION('ref_axis',(0.,0.,1.));
#63275=DIRECTION('center_axis',(0.,1.,0.));
#63276=DIRECTION('ref_axis',(0.,0.,1.));
#63277=DIRECTION('',(0.,-1.,0.));
#63278=DIRECTION('center_axis',(0.,-1.,0.));
#63279=DIRECTION('ref_axis',(0.,0.,-1.));
#63280=DIRECTION('center_axis',(0.,1.,0.));
#63281=DIRECTION('ref_axis',(0.,0.,1.));
#63282=DIRECTION('center_axis',(0.,-1.,0.));
#63283=DIRECTION('ref_axis',(0.,0.,-1.));
#63284=DIRECTION('',(0.,1.,0.));
#63285=DIRECTION('center_axis',(0.,-1.,0.));
#63286=DIRECTION('ref_axis',(0.,0.,-1.));
#63287=DIRECTION('center_axis',(0.,1.,0.));
#63288=DIRECTION('ref_axis',(0.,0.,1.));
#63289=DIRECTION('center_axis',(0.,1.,0.));
#63290=DIRECTION('ref_axis',(0.,0.,1.));
#63291=DIRECTION('',(0.,-1.,0.));
#63292=DIRECTION('center_axis',(0.,-1.,0.));
#63293=DIRECTION('ref_axis',(0.,0.,-1.));
#63294=DIRECTION('center_axis',(0.,1.,0.));
#63295=DIRECTION('ref_axis',(0.,0.,1.));
#63296=DIRECTION('center_axis',(0.,-1.,0.));
#63297=DIRECTION('ref_axis',(0.,0.,-1.));
#63298=DIRECTION('',(0.,1.,0.));
#63299=DIRECTION('center_axis',(0.,-1.,0.));
#63300=DIRECTION('ref_axis',(0.,0.,-1.));
#63301=DIRECTION('center_axis',(0.,1.,0.));
#63302=DIRECTION('ref_axis',(0.,0.,1.));
#63303=DIRECTION('center_axis',(0.,1.,0.));
#63304=DIRECTION('ref_axis',(0.,0.,1.));
#63305=DIRECTION('',(0.,-1.,0.));
#63306=DIRECTION('center_axis',(0.,-1.,0.));
#63307=DIRECTION('ref_axis',(0.,0.,-1.));
#63308=DIRECTION('center_axis',(0.,1.,0.));
#63309=DIRECTION('ref_axis',(0.,0.,1.));
#63310=DIRECTION('center_axis',(0.,-1.,0.));
#63311=DIRECTION('ref_axis',(0.,0.,-1.));
#63312=DIRECTION('',(0.,1.,0.));
#63313=DIRECTION('center_axis',(0.,-1.,0.));
#63314=DIRECTION('ref_axis',(0.,0.,-1.));
#63315=DIRECTION('center_axis',(0.,1.,0.));
#63316=DIRECTION('ref_axis',(0.,0.,1.));
#63317=DIRECTION('center_axis',(0.,1.,0.));
#63318=DIRECTION('ref_axis',(0.,0.,1.));
#63319=DIRECTION('',(0.,-1.,0.));
#63320=DIRECTION('center_axis',(0.,-1.,0.));
#63321=DIRECTION('ref_axis',(0.,0.,-1.));
#63322=DIRECTION('center_axis',(0.,1.,0.));
#63323=DIRECTION('ref_axis',(0.,0.,1.));
#63324=DIRECTION('center_axis',(0.,-1.,0.));
#63325=DIRECTION('ref_axis',(0.,0.,-1.));
#63326=DIRECTION('',(0.,1.,0.));
#63327=DIRECTION('center_axis',(0.,-1.,0.));
#63328=DIRECTION('ref_axis',(0.,0.,-1.));
#63329=DIRECTION('center_axis',(0.,1.,0.));
#63330=DIRECTION('ref_axis',(0.,0.,1.));
#63331=DIRECTION('center_axis',(0.,1.,0.));
#63332=DIRECTION('ref_axis',(0.,0.,1.));
#63333=DIRECTION('',(0.,-1.,0.));
#63334=DIRECTION('center_axis',(0.,-1.,0.));
#63335=DIRECTION('ref_axis',(0.,0.,-1.));
#63336=DIRECTION('center_axis',(0.,1.,0.));
#63337=DIRECTION('ref_axis',(0.,0.,1.));
#63338=DIRECTION('center_axis',(0.,-1.,0.));
#63339=DIRECTION('ref_axis',(0.,0.,-1.));
#63340=DIRECTION('',(0.,1.,0.));
#63341=DIRECTION('center_axis',(0.,-1.,0.));
#63342=DIRECTION('ref_axis',(0.,0.,-1.));
#63343=DIRECTION('center_axis',(0.,1.,0.));
#63344=DIRECTION('ref_axis',(0.,0.,1.));
#63345=DIRECTION('center_axis',(0.,1.,0.));
#63346=DIRECTION('ref_axis',(0.,0.,1.));
#63347=DIRECTION('',(0.,-1.,0.));
#63348=DIRECTION('center_axis',(0.,-1.,0.));
#63349=DIRECTION('ref_axis',(0.,0.,-1.));
#63350=DIRECTION('center_axis',(0.,1.,0.));
#63351=DIRECTION('ref_axis',(0.,0.,1.));
#63352=DIRECTION('center_axis',(0.,-1.,0.));
#63353=DIRECTION('ref_axis',(0.,0.,-1.));
#63354=DIRECTION('',(0.,1.,0.));
#63355=DIRECTION('center_axis',(0.,-1.,0.));
#63356=DIRECTION('ref_axis',(0.,0.,-1.));
#63357=DIRECTION('center_axis',(0.,1.,0.));
#63358=DIRECTION('ref_axis',(0.,0.,1.));
#63359=DIRECTION('center_axis',(0.,1.,0.));
#63360=DIRECTION('ref_axis',(0.,0.,1.));
#63361=DIRECTION('',(0.,-1.,0.));
#63362=DIRECTION('center_axis',(0.,-1.,0.));
#63363=DIRECTION('ref_axis',(0.,0.,-1.));
#63364=DIRECTION('center_axis',(0.,1.,0.));
#63365=DIRECTION('ref_axis',(0.,0.,1.));
#63366=DIRECTION('center_axis',(0.,-1.,0.));
#63367=DIRECTION('ref_axis',(0.,0.,-1.));
#63368=DIRECTION('',(0.,1.,0.));
#63369=DIRECTION('center_axis',(0.,-1.,0.));
#63370=DIRECTION('ref_axis',(0.,0.,-1.));
#63371=DIRECTION('center_axis',(0.,1.,0.));
#63372=DIRECTION('ref_axis',(0.,0.,1.));
#63373=DIRECTION('center_axis',(0.,1.,0.));
#63374=DIRECTION('ref_axis',(0.,0.,1.));
#63375=DIRECTION('',(0.,-1.,0.));
#63376=DIRECTION('center_axis',(0.,-1.,0.));
#63377=DIRECTION('ref_axis',(0.,0.,-1.));
#63378=DIRECTION('center_axis',(0.,1.,0.));
#63379=DIRECTION('ref_axis',(0.,0.,1.));
#63380=DIRECTION('center_axis',(0.,-1.,0.));
#63381=DIRECTION('ref_axis',(0.,0.,-1.));
#63382=DIRECTION('',(0.,1.,0.));
#63383=DIRECTION('center_axis',(0.,-1.,0.));
#63384=DIRECTION('ref_axis',(0.,0.,-1.));
#63385=DIRECTION('center_axis',(0.,1.,0.));
#63386=DIRECTION('ref_axis',(0.,0.,1.));
#63387=DIRECTION('center_axis',(0.,1.,0.));
#63388=DIRECTION('ref_axis',(0.,0.,1.));
#63389=DIRECTION('',(0.,-1.,0.));
#63390=DIRECTION('center_axis',(0.,-1.,0.));
#63391=DIRECTION('ref_axis',(0.,0.,-1.));
#63392=DIRECTION('center_axis',(0.,1.,0.));
#63393=DIRECTION('ref_axis',(0.,0.,1.));
#63394=DIRECTION('center_axis',(0.,-1.,0.));
#63395=DIRECTION('ref_axis',(0.,0.,-1.));
#63396=DIRECTION('',(0.,1.,0.));
#63397=DIRECTION('center_axis',(0.,-1.,0.));
#63398=DIRECTION('ref_axis',(0.,0.,-1.));
#63399=DIRECTION('center_axis',(0.,1.,0.));
#63400=DIRECTION('ref_axis',(0.,0.,1.));
#63401=DIRECTION('center_axis',(0.,1.,0.));
#63402=DIRECTION('ref_axis',(0.,0.,1.));
#63403=DIRECTION('',(0.,-1.,0.));
#63404=DIRECTION('center_axis',(0.,-1.,0.));
#63405=DIRECTION('ref_axis',(0.,0.,-1.));
#63406=DIRECTION('center_axis',(0.,1.,0.));
#63407=DIRECTION('ref_axis',(0.,0.,1.));
#63408=DIRECTION('center_axis',(0.,-1.,0.));
#63409=DIRECTION('ref_axis',(0.,0.,-1.));
#63410=DIRECTION('',(0.,1.,0.));
#63411=DIRECTION('center_axis',(0.,-1.,0.));
#63412=DIRECTION('ref_axis',(0.,0.,-1.));
#63413=DIRECTION('center_axis',(0.,1.,0.));
#63414=DIRECTION('ref_axis',(0.,0.,1.));
#63415=DIRECTION('center_axis',(0.,1.,0.));
#63416=DIRECTION('ref_axis',(0.,0.,1.));
#63417=DIRECTION('',(0.,-1.,0.));
#63418=DIRECTION('center_axis',(0.,-1.,0.));
#63419=DIRECTION('ref_axis',(0.,0.,-1.));
#63420=DIRECTION('center_axis',(0.,1.,0.));
#63421=DIRECTION('ref_axis',(0.,0.,1.));
#63422=DIRECTION('center_axis',(0.,-1.,0.));
#63423=DIRECTION('ref_axis',(0.,0.,-1.));
#63424=DIRECTION('',(0.,1.,0.));
#63425=DIRECTION('center_axis',(0.,-1.,0.));
#63426=DIRECTION('ref_axis',(0.,0.,-1.));
#63427=DIRECTION('center_axis',(0.,1.,0.));
#63428=DIRECTION('ref_axis',(0.,0.,1.));
#63429=DIRECTION('center_axis',(0.,1.,0.));
#63430=DIRECTION('ref_axis',(0.,0.,1.));
#63431=DIRECTION('',(0.,-1.,0.));
#63432=DIRECTION('center_axis',(0.,-1.,0.));
#63433=DIRECTION('ref_axis',(0.,0.,-1.));
#63434=DIRECTION('center_axis',(0.,1.,0.));
#63435=DIRECTION('ref_axis',(0.,0.,1.));
#63436=DIRECTION('center_axis',(0.,-1.,0.));
#63437=DIRECTION('ref_axis',(0.,0.,-1.));
#63438=DIRECTION('',(0.,1.,0.));
#63439=DIRECTION('center_axis',(0.,-1.,0.));
#63440=DIRECTION('ref_axis',(0.,0.,-1.));
#63441=DIRECTION('center_axis',(0.,1.,0.));
#63442=DIRECTION('ref_axis',(0.,0.,1.));
#63443=DIRECTION('center_axis',(0.,1.,0.));
#63444=DIRECTION('ref_axis',(0.,0.,1.));
#63445=DIRECTION('',(0.,-1.,0.));
#63446=DIRECTION('center_axis',(0.,-1.,0.));
#63447=DIRECTION('ref_axis',(0.,0.,-1.));
#63448=DIRECTION('center_axis',(0.,1.,0.));
#63449=DIRECTION('ref_axis',(0.,0.,1.));
#63450=DIRECTION('center_axis',(0.,-1.,0.));
#63451=DIRECTION('ref_axis',(0.,0.,-1.));
#63452=DIRECTION('',(0.,1.,0.));
#63453=DIRECTION('center_axis',(0.,-1.,0.));
#63454=DIRECTION('ref_axis',(0.,0.,-1.));
#63455=DIRECTION('center_axis',(0.,1.,0.));
#63456=DIRECTION('ref_axis',(0.,0.,1.));
#63457=DIRECTION('center_axis',(0.,1.,0.));
#63458=DIRECTION('ref_axis',(0.,0.,1.));
#63459=DIRECTION('',(0.,-1.,0.));
#63460=DIRECTION('center_axis',(0.,-1.,0.));
#63461=DIRECTION('ref_axis',(0.,0.,-1.));
#63462=DIRECTION('center_axis',(0.,1.,0.));
#63463=DIRECTION('ref_axis',(0.,0.,1.));
#63464=DIRECTION('center_axis',(0.,-1.,0.));
#63465=DIRECTION('ref_axis',(0.,0.,-1.));
#63466=DIRECTION('',(0.,1.,0.));
#63467=DIRECTION('center_axis',(0.,-1.,0.));
#63468=DIRECTION('ref_axis',(0.,0.,-1.));
#63469=DIRECTION('center_axis',(0.,1.,0.));
#63470=DIRECTION('ref_axis',(0.,0.,1.));
#63471=DIRECTION('center_axis',(0.,1.,0.));
#63472=DIRECTION('ref_axis',(0.,0.,1.));
#63473=DIRECTION('',(0.,-1.,0.));
#63474=DIRECTION('center_axis',(0.,-1.,0.));
#63475=DIRECTION('ref_axis',(0.,0.,-1.));
#63476=DIRECTION('center_axis',(0.,1.,0.));
#63477=DIRECTION('ref_axis',(0.,0.,1.));
#63478=DIRECTION('center_axis',(0.,-1.,0.));
#63479=DIRECTION('ref_axis',(0.,0.,-1.));
#63480=DIRECTION('',(0.,1.,0.));
#63481=DIRECTION('center_axis',(0.,-1.,0.));
#63482=DIRECTION('ref_axis',(0.,0.,-1.));
#63483=DIRECTION('center_axis',(0.,1.,0.));
#63484=DIRECTION('ref_axis',(0.,0.,1.));
#63485=DIRECTION('center_axis',(0.,1.,0.));
#63486=DIRECTION('ref_axis',(0.,0.,1.));
#63487=DIRECTION('',(0.,-1.,0.));
#63488=DIRECTION('center_axis',(0.,-1.,0.));
#63489=DIRECTION('ref_axis',(0.,0.,-1.));
#63490=DIRECTION('center_axis',(0.,1.,0.));
#63491=DIRECTION('ref_axis',(0.,0.,1.));
#63492=DIRECTION('center_axis',(0.,-1.,0.));
#63493=DIRECTION('ref_axis',(0.,0.,-1.));
#63494=DIRECTION('',(0.,1.,0.));
#63495=DIRECTION('center_axis',(0.,-1.,0.));
#63496=DIRECTION('ref_axis',(0.,0.,-1.));
#63497=DIRECTION('center_axis',(0.,1.,0.));
#63498=DIRECTION('ref_axis',(0.,0.,1.));
#63499=DIRECTION('center_axis',(0.,1.,0.));
#63500=DIRECTION('ref_axis',(0.,0.,1.));
#63501=DIRECTION('',(0.,-1.,0.));
#63502=DIRECTION('center_axis',(0.,-1.,0.));
#63503=DIRECTION('ref_axis',(0.,0.,-1.));
#63504=DIRECTION('center_axis',(0.,1.,0.));
#63505=DIRECTION('ref_axis',(0.,0.,1.));
#63506=DIRECTION('center_axis',(0.,-1.,0.));
#63507=DIRECTION('ref_axis',(0.,0.,-1.));
#63508=DIRECTION('',(0.,1.,0.));
#63509=DIRECTION('center_axis',(0.,-1.,0.));
#63510=DIRECTION('ref_axis',(0.,0.,-1.));
#63511=DIRECTION('center_axis',(0.,1.,0.));
#63512=DIRECTION('ref_axis',(0.,0.,1.));
#63513=DIRECTION('center_axis',(0.,1.,0.));
#63514=DIRECTION('ref_axis',(0.,0.,1.));
#63515=DIRECTION('',(0.,-1.,0.));
#63516=DIRECTION('center_axis',(0.,-1.,0.));
#63517=DIRECTION('ref_axis',(0.,0.,-1.));
#63518=DIRECTION('center_axis',(0.,1.,0.));
#63519=DIRECTION('ref_axis',(0.,0.,1.));
#63520=DIRECTION('center_axis',(0.,-1.,0.));
#63521=DIRECTION('ref_axis',(0.,0.,-1.));
#63522=DIRECTION('',(0.,1.,0.));
#63523=DIRECTION('center_axis',(0.,-1.,0.));
#63524=DIRECTION('ref_axis',(0.,0.,-1.));
#63525=DIRECTION('center_axis',(0.,1.,0.));
#63526=DIRECTION('ref_axis',(0.,0.,1.));
#63527=DIRECTION('center_axis',(0.,1.,0.));
#63528=DIRECTION('ref_axis',(0.,0.,1.));
#63529=DIRECTION('',(0.,-1.,0.));
#63530=DIRECTION('center_axis',(0.,-1.,0.));
#63531=DIRECTION('ref_axis',(0.,0.,-1.));
#63532=DIRECTION('center_axis',(0.,1.,0.));
#63533=DIRECTION('ref_axis',(0.,0.,1.));
#63534=DIRECTION('center_axis',(0.,-1.,0.));
#63535=DIRECTION('ref_axis',(0.,0.,-1.));
#63536=DIRECTION('',(0.,1.,0.));
#63537=DIRECTION('center_axis',(0.,-1.,0.));
#63538=DIRECTION('ref_axis',(0.,0.,-1.));
#63539=DIRECTION('center_axis',(0.,1.,0.));
#63540=DIRECTION('ref_axis',(0.,0.,1.));
#63541=DIRECTION('center_axis',(0.,1.,0.));
#63542=DIRECTION('ref_axis',(0.,0.,1.));
#63543=DIRECTION('',(0.,-1.,0.));
#63544=DIRECTION('center_axis',(0.,-1.,0.));
#63545=DIRECTION('ref_axis',(0.,0.,-1.));
#63546=DIRECTION('center_axis',(0.,1.,0.));
#63547=DIRECTION('ref_axis',(0.,0.,1.));
#63548=DIRECTION('center_axis',(0.,-1.,0.));
#63549=DIRECTION('ref_axis',(0.,0.,-1.));
#63550=DIRECTION('',(0.,1.,0.));
#63551=DIRECTION('center_axis',(0.,-1.,0.));
#63552=DIRECTION('ref_axis',(0.,0.,-1.));
#63553=DIRECTION('center_axis',(0.,1.,0.));
#63554=DIRECTION('ref_axis',(0.,0.,1.));
#63555=DIRECTION('center_axis',(0.,1.,0.));
#63556=DIRECTION('ref_axis',(0.,0.,1.));
#63557=DIRECTION('',(0.,-1.,0.));
#63558=DIRECTION('center_axis',(0.,-1.,0.));
#63559=DIRECTION('ref_axis',(0.,0.,-1.));
#63560=DIRECTION('center_axis',(0.,1.,0.));
#63561=DIRECTION('ref_axis',(0.,0.,1.));
#63562=DIRECTION('center_axis',(0.,-1.,0.));
#63563=DIRECTION('ref_axis',(0.,0.,-1.));
#63564=DIRECTION('',(0.,1.,0.));
#63565=DIRECTION('center_axis',(0.,-1.,0.));
#63566=DIRECTION('ref_axis',(0.,0.,-1.));
#63567=DIRECTION('center_axis',(0.,1.,0.));
#63568=DIRECTION('ref_axis',(0.,0.,1.));
#63569=DIRECTION('center_axis',(0.,1.,0.));
#63570=DIRECTION('ref_axis',(0.,0.,1.));
#63571=DIRECTION('',(0.,-1.,0.));
#63572=DIRECTION('center_axis',(0.,-1.,0.));
#63573=DIRECTION('ref_axis',(0.,0.,-1.));
#63574=DIRECTION('center_axis',(0.,1.,0.));
#63575=DIRECTION('ref_axis',(0.,0.,1.));
#63576=DIRECTION('center_axis',(0.,-1.,0.));
#63577=DIRECTION('ref_axis',(0.,0.,-1.));
#63578=DIRECTION('',(0.,1.,0.));
#63579=DIRECTION('center_axis',(0.,-1.,0.));
#63580=DIRECTION('ref_axis',(0.,0.,-1.));
#63581=DIRECTION('center_axis',(0.,1.,0.));
#63582=DIRECTION('ref_axis',(0.,0.,1.));
#63583=DIRECTION('center_axis',(0.,1.,0.));
#63584=DIRECTION('ref_axis',(0.,0.,1.));
#63585=DIRECTION('',(0.,-1.,0.));
#63586=DIRECTION('center_axis',(0.,-1.,0.));
#63587=DIRECTION('ref_axis',(0.,0.,-1.));
#63588=DIRECTION('center_axis',(0.,1.,0.));
#63589=DIRECTION('ref_axis',(0.,0.,1.));
#63590=DIRECTION('center_axis',(0.,-1.,0.));
#63591=DIRECTION('ref_axis',(0.,0.,-1.));
#63592=DIRECTION('',(0.,1.,0.));
#63593=DIRECTION('center_axis',(0.,-1.,0.));
#63594=DIRECTION('ref_axis',(0.,0.,-1.));
#63595=DIRECTION('center_axis',(0.,1.,0.));
#63596=DIRECTION('ref_axis',(0.,0.,1.));
#63597=DIRECTION('center_axis',(0.,1.,0.));
#63598=DIRECTION('ref_axis',(0.,0.,1.));
#63599=DIRECTION('',(0.,-1.,0.));
#63600=DIRECTION('center_axis',(0.,-1.,0.));
#63601=DIRECTION('ref_axis',(0.,0.,-1.));
#63602=DIRECTION('center_axis',(0.,1.,0.));
#63603=DIRECTION('ref_axis',(0.,0.,1.));
#63604=DIRECTION('center_axis',(0.,-1.,0.));
#63605=DIRECTION('ref_axis',(0.,0.,-1.));
#63606=DIRECTION('',(0.,1.,0.));
#63607=DIRECTION('center_axis',(0.,-1.,0.));
#63608=DIRECTION('ref_axis',(0.,0.,-1.));
#63609=DIRECTION('center_axis',(0.,1.,0.));
#63610=DIRECTION('ref_axis',(0.,0.,1.));
#63611=DIRECTION('center_axis',(0.,1.,0.));
#63612=DIRECTION('ref_axis',(0.,0.,1.));
#63613=DIRECTION('',(0.,-1.,0.));
#63614=DIRECTION('center_axis',(0.,-1.,0.));
#63615=DIRECTION('ref_axis',(0.,0.,-1.));
#63616=DIRECTION('center_axis',(0.,1.,0.));
#63617=DIRECTION('ref_axis',(0.,0.,1.));
#63618=DIRECTION('center_axis',(0.,-1.,0.));
#63619=DIRECTION('ref_axis',(0.,0.,-1.));
#63620=DIRECTION('',(0.,1.,0.));
#63621=DIRECTION('center_axis',(0.,-1.,0.));
#63622=DIRECTION('ref_axis',(0.,0.,-1.));
#63623=DIRECTION('center_axis',(0.,1.,0.));
#63624=DIRECTION('ref_axis',(0.,0.,1.));
#63625=DIRECTION('center_axis',(0.,1.,0.));
#63626=DIRECTION('ref_axis',(0.,0.,1.));
#63627=DIRECTION('',(0.,-1.,0.));
#63628=DIRECTION('center_axis',(0.,-1.,0.));
#63629=DIRECTION('ref_axis',(0.,0.,-1.));
#63630=DIRECTION('center_axis',(0.,1.,0.));
#63631=DIRECTION('ref_axis',(0.,0.,1.));
#63632=DIRECTION('center_axis',(0.,-1.,0.));
#63633=DIRECTION('ref_axis',(0.,0.,-1.));
#63634=DIRECTION('',(0.,1.,0.));
#63635=DIRECTION('center_axis',(0.,-1.,0.));
#63636=DIRECTION('ref_axis',(0.,0.,-1.));
#63637=DIRECTION('center_axis',(0.,1.,0.));
#63638=DIRECTION('ref_axis',(0.,0.,1.));
#63639=DIRECTION('center_axis',(0.,1.,0.));
#63640=DIRECTION('ref_axis',(0.,0.,1.));
#63641=DIRECTION('',(0.,-1.,0.));
#63642=DIRECTION('center_axis',(0.,-1.,0.));
#63643=DIRECTION('ref_axis',(0.,0.,-1.));
#63644=DIRECTION('center_axis',(0.,1.,0.));
#63645=DIRECTION('ref_axis',(0.,0.,1.));
#63646=DIRECTION('center_axis',(0.,-1.,0.));
#63647=DIRECTION('ref_axis',(0.,0.,-1.));
#63648=DIRECTION('',(0.,1.,0.));
#63649=DIRECTION('center_axis',(0.,-1.,0.));
#63650=DIRECTION('ref_axis',(0.,0.,-1.));
#63651=DIRECTION('center_axis',(0.,1.,0.));
#63652=DIRECTION('ref_axis',(0.,0.,1.));
#63653=DIRECTION('center_axis',(0.,1.,0.));
#63654=DIRECTION('ref_axis',(0.,0.,1.));
#63655=DIRECTION('',(0.,-1.,0.));
#63656=DIRECTION('center_axis',(0.,-1.,0.));
#63657=DIRECTION('ref_axis',(0.,0.,-1.));
#63658=DIRECTION('center_axis',(0.,1.,0.));
#63659=DIRECTION('ref_axis',(0.,0.,1.));
#63660=DIRECTION('center_axis',(0.,-1.,0.));
#63661=DIRECTION('ref_axis',(0.,0.,-1.));
#63662=DIRECTION('',(0.,1.,0.));
#63663=DIRECTION('center_axis',(0.,-1.,0.));
#63664=DIRECTION('ref_axis',(0.,0.,-1.));
#63665=DIRECTION('center_axis',(0.,1.,0.));
#63666=DIRECTION('ref_axis',(0.,0.,1.));
#63667=DIRECTION('center_axis',(0.,1.,0.));
#63668=DIRECTION('ref_axis',(0.,0.,1.));
#63669=DIRECTION('',(0.,-1.,0.));
#63670=DIRECTION('center_axis',(0.,-1.,0.));
#63671=DIRECTION('ref_axis',(0.,0.,-1.));
#63672=DIRECTION('center_axis',(0.,1.,0.));
#63673=DIRECTION('ref_axis',(0.,0.,1.));
#63674=DIRECTION('center_axis',(0.,-1.,0.));
#63675=DIRECTION('ref_axis',(0.,0.,-1.));
#63676=DIRECTION('',(0.,1.,0.));
#63677=DIRECTION('center_axis',(0.,-1.,0.));
#63678=DIRECTION('ref_axis',(0.,0.,-1.));
#63679=DIRECTION('center_axis',(0.,1.,0.));
#63680=DIRECTION('ref_axis',(0.,0.,1.));
#63681=DIRECTION('center_axis',(0.,1.,0.));
#63682=DIRECTION('ref_axis',(0.,0.,1.));
#63683=DIRECTION('',(0.,-1.,0.));
#63684=DIRECTION('center_axis',(0.,-1.,0.));
#63685=DIRECTION('ref_axis',(0.,0.,-1.));
#63686=DIRECTION('center_axis',(0.,1.,0.));
#63687=DIRECTION('ref_axis',(0.,0.,1.));
#63688=DIRECTION('center_axis',(0.,-1.,0.));
#63689=DIRECTION('ref_axis',(0.,0.,-1.));
#63690=DIRECTION('',(0.,1.,0.));
#63691=DIRECTION('center_axis',(0.,-1.,0.));
#63692=DIRECTION('ref_axis',(0.,0.,-1.));
#63693=DIRECTION('center_axis',(0.,1.,0.));
#63694=DIRECTION('ref_axis',(0.,0.,1.));
#63695=DIRECTION('center_axis',(0.,1.,0.));
#63696=DIRECTION('ref_axis',(0.,0.,1.));
#63697=DIRECTION('',(0.,-1.,0.));
#63698=DIRECTION('center_axis',(0.,-1.,0.));
#63699=DIRECTION('ref_axis',(0.,0.,-1.));
#63700=DIRECTION('center_axis',(0.,1.,0.));
#63701=DIRECTION('ref_axis',(0.,0.,1.));
#63702=DIRECTION('center_axis',(0.,-1.,0.));
#63703=DIRECTION('ref_axis',(0.,0.,-1.));
#63704=DIRECTION('',(0.,1.,0.));
#63705=DIRECTION('center_axis',(0.,-1.,0.));
#63706=DIRECTION('ref_axis',(0.,0.,-1.));
#63707=DIRECTION('center_axis',(0.,1.,0.));
#63708=DIRECTION('ref_axis',(0.,0.,1.));
#63709=DIRECTION('center_axis',(0.,1.,0.));
#63710=DIRECTION('ref_axis',(0.,0.,1.));
#63711=DIRECTION('',(0.,-1.,0.));
#63712=DIRECTION('center_axis',(0.,-1.,0.));
#63713=DIRECTION('ref_axis',(0.,0.,-1.));
#63714=DIRECTION('center_axis',(0.,1.,0.));
#63715=DIRECTION('ref_axis',(0.,0.,1.));
#63716=DIRECTION('center_axis',(0.,-1.,0.));
#63717=DIRECTION('ref_axis',(0.,0.,-1.));
#63718=DIRECTION('',(0.,1.,0.));
#63719=DIRECTION('center_axis',(0.,-1.,0.));
#63720=DIRECTION('ref_axis',(0.,0.,-1.));
#63721=DIRECTION('center_axis',(0.,1.,0.));
#63722=DIRECTION('ref_axis',(0.,0.,1.));
#63723=DIRECTION('center_axis',(0.,1.,0.));
#63724=DIRECTION('ref_axis',(0.,0.,1.));
#63725=DIRECTION('',(0.,-1.,0.));
#63726=DIRECTION('center_axis',(0.,-1.,0.));
#63727=DIRECTION('ref_axis',(0.,0.,-1.));
#63728=DIRECTION('center_axis',(0.,1.,0.));
#63729=DIRECTION('ref_axis',(0.,0.,1.));
#63730=DIRECTION('center_axis',(0.,-1.,0.));
#63731=DIRECTION('ref_axis',(0.,0.,-1.));
#63732=DIRECTION('',(0.,1.,0.));
#63733=DIRECTION('center_axis',(0.,-1.,0.));
#63734=DIRECTION('ref_axis',(0.,0.,-1.));
#63735=DIRECTION('center_axis',(0.,1.,0.));
#63736=DIRECTION('ref_axis',(0.,0.,1.));
#63737=DIRECTION('center_axis',(0.,1.,0.));
#63738=DIRECTION('ref_axis',(0.,0.,1.));
#63739=DIRECTION('',(0.,-1.,0.));
#63740=DIRECTION('center_axis',(0.,-1.,0.));
#63741=DIRECTION('ref_axis',(0.,0.,-1.));
#63742=DIRECTION('center_axis',(0.,1.,0.));
#63743=DIRECTION('ref_axis',(0.,0.,1.));
#63744=DIRECTION('center_axis',(0.,-1.,0.));
#63745=DIRECTION('ref_axis',(0.,0.,-1.));
#63746=DIRECTION('',(0.,1.,0.));
#63747=DIRECTION('center_axis',(0.,-1.,0.));
#63748=DIRECTION('ref_axis',(0.,0.,-1.));
#63749=DIRECTION('center_axis',(0.,1.,0.));
#63750=DIRECTION('ref_axis',(0.,0.,1.));
#63751=DIRECTION('center_axis',(0.,1.,0.));
#63752=DIRECTION('ref_axis',(0.,0.,1.));
#63753=DIRECTION('',(0.,-1.,0.));
#63754=DIRECTION('center_axis',(0.,-1.,0.));
#63755=DIRECTION('ref_axis',(0.,0.,-1.));
#63756=DIRECTION('center_axis',(0.,1.,0.));
#63757=DIRECTION('ref_axis',(0.,0.,1.));
#63758=DIRECTION('center_axis',(0.,-1.,0.));
#63759=DIRECTION('ref_axis',(0.,0.,-1.));
#63760=DIRECTION('',(0.,1.,0.));
#63761=DIRECTION('center_axis',(0.,-1.,0.));
#63762=DIRECTION('ref_axis',(0.,0.,-1.));
#63763=DIRECTION('center_axis',(0.,1.,0.));
#63764=DIRECTION('ref_axis',(0.,0.,1.));
#63765=DIRECTION('center_axis',(0.,1.,0.));
#63766=DIRECTION('ref_axis',(0.,0.,1.));
#63767=DIRECTION('',(0.,-1.,0.));
#63768=DIRECTION('center_axis',(0.,-1.,0.));
#63769=DIRECTION('ref_axis',(0.,0.,-1.));
#63770=DIRECTION('center_axis',(0.,1.,0.));
#63771=DIRECTION('ref_axis',(0.,0.,1.));
#63772=DIRECTION('center_axis',(0.,-1.,0.));
#63773=DIRECTION('ref_axis',(0.,0.,-1.));
#63774=DIRECTION('',(0.,1.,0.));
#63775=DIRECTION('center_axis',(0.,-1.,0.));
#63776=DIRECTION('ref_axis',(0.,0.,-1.));
#63777=DIRECTION('center_axis',(0.,1.,0.));
#63778=DIRECTION('ref_axis',(0.,0.,1.));
#63779=DIRECTION('center_axis',(0.,1.,0.));
#63780=DIRECTION('ref_axis',(0.,0.,1.));
#63781=DIRECTION('',(0.,-1.,0.));
#63782=DIRECTION('center_axis',(0.,-1.,0.));
#63783=DIRECTION('ref_axis',(0.,0.,-1.));
#63784=DIRECTION('center_axis',(0.,1.,0.));
#63785=DIRECTION('ref_axis',(0.,0.,1.));
#63786=DIRECTION('center_axis',(0.,-1.,0.));
#63787=DIRECTION('ref_axis',(0.,0.,-1.));
#63788=DIRECTION('',(0.,1.,0.));
#63789=DIRECTION('center_axis',(0.,-1.,0.));
#63790=DIRECTION('ref_axis',(0.,0.,-1.));
#63791=DIRECTION('center_axis',(0.,1.,0.));
#63792=DIRECTION('ref_axis',(0.,0.,1.));
#63793=DIRECTION('center_axis',(0.,1.,0.));
#63794=DIRECTION('ref_axis',(0.,0.,1.));
#63795=DIRECTION('',(0.,-1.,0.));
#63796=DIRECTION('center_axis',(0.,-1.,0.));
#63797=DIRECTION('ref_axis',(0.,0.,-1.));
#63798=DIRECTION('center_axis',(0.,1.,0.));
#63799=DIRECTION('ref_axis',(0.,0.,1.));
#63800=DIRECTION('center_axis',(0.,-1.,0.));
#63801=DIRECTION('ref_axis',(0.,0.,-1.));
#63802=DIRECTION('',(0.,1.,0.));
#63803=DIRECTION('center_axis',(0.,-1.,0.));
#63804=DIRECTION('ref_axis',(0.,0.,-1.));
#63805=DIRECTION('center_axis',(0.,1.,0.));
#63806=DIRECTION('ref_axis',(0.,0.,1.));
#63807=DIRECTION('center_axis',(0.,1.,0.));
#63808=DIRECTION('ref_axis',(0.,0.,1.));
#63809=DIRECTION('',(0.,-1.,0.));
#63810=DIRECTION('center_axis',(0.,-1.,0.));
#63811=DIRECTION('ref_axis',(0.,0.,-1.));
#63812=DIRECTION('center_axis',(0.,1.,0.));
#63813=DIRECTION('ref_axis',(0.,0.,1.));
#63814=DIRECTION('center_axis',(0.,-1.,0.));
#63815=DIRECTION('ref_axis',(0.,0.,-1.));
#63816=DIRECTION('',(0.,1.,0.));
#63817=DIRECTION('center_axis',(0.,-1.,0.));
#63818=DIRECTION('ref_axis',(0.,0.,-1.));
#63819=DIRECTION('center_axis',(0.,1.,0.));
#63820=DIRECTION('ref_axis',(0.,0.,1.));
#63821=DIRECTION('center_axis',(0.,1.,0.));
#63822=DIRECTION('ref_axis',(0.,0.,1.));
#63823=DIRECTION('',(0.,-1.,0.));
#63824=DIRECTION('center_axis',(0.,-1.,0.));
#63825=DIRECTION('ref_axis',(0.,0.,-1.));
#63826=DIRECTION('center_axis',(0.,1.,0.));
#63827=DIRECTION('ref_axis',(0.,0.,1.));
#63828=DIRECTION('center_axis',(0.,-1.,0.));
#63829=DIRECTION('ref_axis',(0.,0.,-1.));
#63830=DIRECTION('',(0.,1.,0.));
#63831=DIRECTION('center_axis',(0.,-1.,0.));
#63832=DIRECTION('ref_axis',(0.,0.,-1.));
#63833=DIRECTION('center_axis',(0.,1.,0.));
#63834=DIRECTION('ref_axis',(0.,0.,1.));
#63835=DIRECTION('center_axis',(0.,1.,0.));
#63836=DIRECTION('ref_axis',(0.,0.,1.));
#63837=DIRECTION('',(0.,-1.,0.));
#63838=DIRECTION('center_axis',(0.,-1.,0.));
#63839=DIRECTION('ref_axis',(0.,0.,-1.));
#63840=DIRECTION('center_axis',(0.,1.,0.));
#63841=DIRECTION('ref_axis',(0.,0.,1.));
#63842=DIRECTION('center_axis',(0.,-1.,0.));
#63843=DIRECTION('ref_axis',(0.,0.,-1.));
#63844=DIRECTION('',(0.,1.,0.));
#63845=DIRECTION('center_axis',(0.,-1.,0.));
#63846=DIRECTION('ref_axis',(0.,0.,-1.));
#63847=DIRECTION('center_axis',(0.,1.,0.));
#63848=DIRECTION('ref_axis',(0.,0.,1.));
#63849=DIRECTION('center_axis',(0.,1.,0.));
#63850=DIRECTION('ref_axis',(0.,0.,1.));
#63851=DIRECTION('',(0.,-1.,0.));
#63852=DIRECTION('center_axis',(0.,-1.,0.));
#63853=DIRECTION('ref_axis',(0.,0.,-1.));
#63854=DIRECTION('center_axis',(0.,1.,0.));
#63855=DIRECTION('ref_axis',(0.,0.,1.));
#63856=DIRECTION('center_axis',(0.,-1.,0.));
#63857=DIRECTION('ref_axis',(0.,0.,-1.));
#63858=DIRECTION('',(0.,1.,0.));
#63859=DIRECTION('center_axis',(0.,-1.,0.));
#63860=DIRECTION('ref_axis',(0.,0.,-1.));
#63861=DIRECTION('center_axis',(0.,1.,0.));
#63862=DIRECTION('ref_axis',(0.,0.,1.));
#63863=DIRECTION('center_axis',(0.,1.,0.));
#63864=DIRECTION('ref_axis',(0.,0.,1.));
#63865=DIRECTION('',(0.,-1.,0.));
#63866=DIRECTION('center_axis',(0.,-1.,0.));
#63867=DIRECTION('ref_axis',(0.,0.,-1.));
#63868=DIRECTION('center_axis',(0.,1.,0.));
#63869=DIRECTION('ref_axis',(0.,0.,1.));
#63870=DIRECTION('center_axis',(0.,-1.,0.));
#63871=DIRECTION('ref_axis',(0.,0.,-1.));
#63872=DIRECTION('',(0.,1.,0.));
#63873=DIRECTION('center_axis',(0.,-1.,0.));
#63874=DIRECTION('ref_axis',(0.,0.,-1.));
#63875=DIRECTION('center_axis',(0.,1.,0.));
#63876=DIRECTION('ref_axis',(0.,0.,1.));
#63877=DIRECTION('center_axis',(0.,1.,0.));
#63878=DIRECTION('ref_axis',(0.,0.,1.));
#63879=DIRECTION('',(0.,-1.,0.));
#63880=DIRECTION('center_axis',(0.,-1.,0.));
#63881=DIRECTION('ref_axis',(0.,0.,-1.));
#63882=DIRECTION('center_axis',(0.,1.,0.));
#63883=DIRECTION('ref_axis',(0.,0.,1.));
#63884=DIRECTION('center_axis',(0.,-1.,0.));
#63885=DIRECTION('ref_axis',(0.,0.,-1.));
#63886=DIRECTION('',(0.,1.,0.));
#63887=DIRECTION('center_axis',(0.,-1.,0.));
#63888=DIRECTION('ref_axis',(0.,0.,-1.));
#63889=DIRECTION('center_axis',(0.,1.,0.));
#63890=DIRECTION('ref_axis',(0.,0.,1.));
#63891=DIRECTION('center_axis',(0.,1.,0.));
#63892=DIRECTION('ref_axis',(0.,0.,1.));
#63893=DIRECTION('',(0.,-1.,0.));
#63894=DIRECTION('center_axis',(0.,-1.,0.));
#63895=DIRECTION('ref_axis',(0.,0.,-1.));
#63896=DIRECTION('center_axis',(0.,1.,0.));
#63897=DIRECTION('ref_axis',(0.,0.,1.));
#63898=DIRECTION('center_axis',(0.,-1.,0.));
#63899=DIRECTION('ref_axis',(0.,0.,-1.));
#63900=DIRECTION('',(0.,1.,0.));
#63901=DIRECTION('center_axis',(0.,-1.,0.));
#63902=DIRECTION('ref_axis',(0.,0.,-1.));
#63903=DIRECTION('center_axis',(0.,1.,0.));
#63904=DIRECTION('ref_axis',(0.,0.,1.));
#63905=DIRECTION('center_axis',(0.,1.,0.));
#63906=DIRECTION('ref_axis',(0.,0.,1.));
#63907=DIRECTION('',(0.,-1.,0.));
#63908=DIRECTION('center_axis',(0.,-1.,0.));
#63909=DIRECTION('ref_axis',(0.,0.,-1.));
#63910=DIRECTION('center_axis',(0.,1.,0.));
#63911=DIRECTION('ref_axis',(0.,0.,1.));
#63912=DIRECTION('center_axis',(0.,-1.,0.));
#63913=DIRECTION('ref_axis',(0.,0.,-1.));
#63914=DIRECTION('',(0.,1.,0.));
#63915=DIRECTION('center_axis',(0.,-1.,0.));
#63916=DIRECTION('ref_axis',(0.,0.,-1.));
#63917=DIRECTION('center_axis',(0.,1.,0.));
#63918=DIRECTION('ref_axis',(0.,0.,1.));
#63919=DIRECTION('center_axis',(0.,1.,0.));
#63920=DIRECTION('ref_axis',(0.,0.,1.));
#63921=DIRECTION('',(0.,-1.,0.));
#63922=DIRECTION('center_axis',(0.,-1.,0.));
#63923=DIRECTION('ref_axis',(0.,0.,-1.));
#63924=DIRECTION('center_axis',(0.,1.,0.));
#63925=DIRECTION('ref_axis',(0.,0.,1.));
#63926=DIRECTION('center_axis',(0.,-1.,0.));
#63927=DIRECTION('ref_axis',(0.,0.,-1.));
#63928=DIRECTION('',(0.,1.,0.));
#63929=DIRECTION('center_axis',(0.,-1.,0.));
#63930=DIRECTION('ref_axis',(0.,0.,-1.));
#63931=DIRECTION('center_axis',(0.,1.,0.));
#63932=DIRECTION('ref_axis',(0.,0.,1.));
#63933=DIRECTION('center_axis',(0.,1.,0.));
#63934=DIRECTION('ref_axis',(0.,0.,1.));
#63935=DIRECTION('',(0.,-1.,0.));
#63936=DIRECTION('center_axis',(0.,-1.,0.));
#63937=DIRECTION('ref_axis',(0.,0.,-1.));
#63938=DIRECTION('center_axis',(0.,1.,0.));
#63939=DIRECTION('ref_axis',(0.,0.,1.));
#63940=DIRECTION('center_axis',(0.,-1.,0.));
#63941=DIRECTION('ref_axis',(0.,0.,-1.));
#63942=DIRECTION('',(0.,1.,0.));
#63943=DIRECTION('center_axis',(0.,-1.,0.));
#63944=DIRECTION('ref_axis',(0.,0.,-1.));
#63945=DIRECTION('center_axis',(0.,1.,0.));
#63946=DIRECTION('ref_axis',(0.,0.,1.));
#63947=DIRECTION('center_axis',(0.,1.,0.));
#63948=DIRECTION('ref_axis',(0.,0.,1.));
#63949=DIRECTION('',(0.,-1.,0.));
#63950=DIRECTION('center_axis',(0.,-1.,0.));
#63951=DIRECTION('ref_axis',(0.,0.,-1.));
#63952=DIRECTION('center_axis',(0.,1.,0.));
#63953=DIRECTION('ref_axis',(0.,0.,1.));
#63954=DIRECTION('center_axis',(0.,-1.,0.));
#63955=DIRECTION('ref_axis',(0.,0.,-1.));
#63956=DIRECTION('',(0.,1.,0.));
#63957=DIRECTION('center_axis',(0.,-1.,0.));
#63958=DIRECTION('ref_axis',(0.,0.,-1.));
#63959=DIRECTION('center_axis',(0.,1.,0.));
#63960=DIRECTION('ref_axis',(0.,0.,1.));
#63961=DIRECTION('center_axis',(0.,1.,0.));
#63962=DIRECTION('ref_axis',(0.,0.,1.));
#63963=DIRECTION('',(0.,-1.,0.));
#63964=DIRECTION('center_axis',(0.,-1.,0.));
#63965=DIRECTION('ref_axis',(0.,0.,-1.));
#63966=DIRECTION('center_axis',(0.,1.,0.));
#63967=DIRECTION('ref_axis',(0.,0.,1.));
#63968=DIRECTION('center_axis',(0.,-1.,0.));
#63969=DIRECTION('ref_axis',(0.,0.,-1.));
#63970=DIRECTION('',(0.,1.,0.));
#63971=DIRECTION('center_axis',(0.,-1.,0.));
#63972=DIRECTION('ref_axis',(0.,0.,-1.));
#63973=DIRECTION('center_axis',(0.,1.,0.));
#63974=DIRECTION('ref_axis',(0.,0.,1.));
#63975=DIRECTION('center_axis',(0.,1.,0.));
#63976=DIRECTION('ref_axis',(0.,0.,1.));
#63977=DIRECTION('',(0.,-1.,0.));
#63978=DIRECTION('center_axis',(0.,-1.,0.));
#63979=DIRECTION('ref_axis',(0.,0.,-1.));
#63980=DIRECTION('center_axis',(0.,1.,0.));
#63981=DIRECTION('ref_axis',(0.,0.,1.));
#63982=DIRECTION('center_axis',(0.,-1.,0.));
#63983=DIRECTION('ref_axis',(0.,0.,-1.));
#63984=DIRECTION('',(0.,1.,0.));
#63985=DIRECTION('center_axis',(0.,-1.,0.));
#63986=DIRECTION('ref_axis',(0.,0.,-1.));
#63987=DIRECTION('center_axis',(0.,1.,0.));
#63988=DIRECTION('ref_axis',(0.,0.,1.));
#63989=DIRECTION('center_axis',(0.,1.,0.));
#63990=DIRECTION('ref_axis',(0.,0.,1.));
#63991=DIRECTION('',(0.,-1.,0.));
#63992=DIRECTION('center_axis',(0.,-1.,0.));
#63993=DIRECTION('ref_axis',(0.,0.,-1.));
#63994=DIRECTION('center_axis',(0.,1.,0.));
#63995=DIRECTION('ref_axis',(0.,0.,1.));
#63996=DIRECTION('center_axis',(0.,-1.,0.));
#63997=DIRECTION('ref_axis',(0.,0.,-1.));
#63998=DIRECTION('',(0.,1.,0.));
#63999=DIRECTION('center_axis',(0.,-1.,0.));
#64000=DIRECTION('ref_axis',(0.,0.,-1.));
#64001=DIRECTION('center_axis',(0.,1.,0.));
#64002=DIRECTION('ref_axis',(0.,0.,1.));
#64003=DIRECTION('center_axis',(0.,1.,0.));
#64004=DIRECTION('ref_axis',(0.,0.,1.));
#64005=DIRECTION('',(0.,-1.,0.));
#64006=DIRECTION('center_axis',(0.,-1.,0.));
#64007=DIRECTION('ref_axis',(0.,0.,-1.));
#64008=DIRECTION('center_axis',(0.,1.,0.));
#64009=DIRECTION('ref_axis',(0.,0.,1.));
#64010=DIRECTION('center_axis',(0.,-1.,0.));
#64011=DIRECTION('ref_axis',(0.,0.,-1.));
#64012=DIRECTION('',(0.,1.,0.));
#64013=DIRECTION('center_axis',(0.,-1.,0.));
#64014=DIRECTION('ref_axis',(0.,0.,-1.));
#64015=DIRECTION('center_axis',(0.,1.,0.));
#64016=DIRECTION('ref_axis',(0.,0.,1.));
#64017=DIRECTION('center_axis',(0.,1.,0.));
#64018=DIRECTION('ref_axis',(0.,0.,1.));
#64019=DIRECTION('',(0.,-1.,0.));
#64020=DIRECTION('center_axis',(0.,-1.,0.));
#64021=DIRECTION('ref_axis',(0.,0.,-1.));
#64022=DIRECTION('center_axis',(0.,1.,0.));
#64023=DIRECTION('ref_axis',(0.,0.,1.));
#64024=DIRECTION('center_axis',(0.,-1.,0.));
#64025=DIRECTION('ref_axis',(0.,0.,-1.));
#64026=DIRECTION('',(0.,1.,0.));
#64027=DIRECTION('center_axis',(0.,-1.,0.));
#64028=DIRECTION('ref_axis',(0.,0.,-1.));
#64029=DIRECTION('center_axis',(0.,1.,0.));
#64030=DIRECTION('ref_axis',(0.,0.,1.));
#64031=DIRECTION('center_axis',(0.,1.,0.));
#64032=DIRECTION('ref_axis',(0.,0.,1.));
#64033=DIRECTION('',(0.,-1.,0.));
#64034=DIRECTION('center_axis',(0.,-1.,0.));
#64035=DIRECTION('ref_axis',(0.,0.,-1.));
#64036=DIRECTION('center_axis',(0.,1.,0.));
#64037=DIRECTION('ref_axis',(0.,0.,1.));
#64038=DIRECTION('center_axis',(0.,-1.,0.));
#64039=DIRECTION('ref_axis',(0.,0.,-1.));
#64040=DIRECTION('',(0.,1.,0.));
#64041=DIRECTION('center_axis',(0.,-1.,0.));
#64042=DIRECTION('ref_axis',(0.,0.,-1.));
#64043=DIRECTION('center_axis',(0.,-1.,0.));
#64044=DIRECTION('ref_axis',(0.,0.,-1.));
#64045=DIRECTION('center_axis',(-1.,0.,-1.22464679914735E-16));
#64046=DIRECTION('ref_axis',(-1.22464679914735E-16,0.,1.));
#64047=DIRECTION('center_axis',(0.,1.,0.));
#64048=DIRECTION('ref_axis',(0.,0.,-1.));
#64049=DIRECTION('center_axis',(0.,-1.,0.));
#64050=DIRECTION('ref_axis',(0.,0.,1.));
#64051=DIRECTION('center_axis',(0.,-1.,0.));
#64052=DIRECTION('ref_axis',(0.,0.,-1.));
#64053=DIRECTION('',(0.,1.,0.));
#64054=DIRECTION('center_axis',(0.,-1.,0.));
#64055=DIRECTION('ref_axis',(0.,0.,-1.));
#64056=DIRECTION('center_axis',(0.,-1.,2.84598943930249E-15));
#64057=DIRECTION('ref_axis',(0.,0.,-1.));
#64058=DIRECTION('center_axis',(0.,-1.,2.84598943930249E-15));
#64059=DIRECTION('ref_axis',(0.,-2.84598943930249E-15,-1.));
#64060=DIRECTION('center_axis',(-1.,-3.48533185724897E-31,-1.22464679914735E-16));
#64061=DIRECTION('ref_axis',(-1.22464679914735E-16,0.,1.));
#64062=DIRECTION('center_axis',(0.,1.,-2.84598943930249E-15));
#64063=DIRECTION('ref_axis',(0.,-2.84598943930249E-15,-1.));
#64064=DIRECTION('center_axis',(0.,1.,-2.84598943930249E-15));
#64065=DIRECTION('ref_axis',(0.,-2.84598943930249E-15,-1.));
#64066=DIRECTION('center_axis',(0.,1.,-2.84598943930249E-15));
#64067=DIRECTION('ref_axis',(0.,0.,1.));
#64068=DIRECTION('center_axis',(0.,1.,-2.84598943930249E-15));
#64069=DIRECTION('ref_axis',(0.,2.84598943930249E-15,1.));
#64070=DIRECTION('center_axis',(-1.,3.48533185724897E-31,1.22464679914735E-16));
#64071=DIRECTION('ref_axis',(-1.22464679914735E-16,0.,-1.));
#64072=DIRECTION('center_axis',(0.,-1.,2.84598943930249E-15));
#64073=DIRECTION('ref_axis',(0.,2.84598943930249E-15,1.));
#64074=DIRECTION('center_axis',(0.,1.,-2.84598943930249E-15));
#64075=DIRECTION('ref_axis',(0.,2.84598943930249E-15,1.));
#64076=DIRECTION('',(0.,-1.,2.84598943930249E-15));
#64077=DIRECTION('center_axis',(1.,0.,0.));
#64078=DIRECTION('ref_axis',(0.,0.,1.));
#64079=DIRECTION('center_axis',(0.,-1.,0.));
#64080=DIRECTION('ref_axis',(0.,0.,-1.));
#64081=DIRECTION('center_axis',(0.,-1.,0.));
#64082=DIRECTION('ref_axis',(0.,0.,-1.));
#64083=DIRECTION('center_axis',(0.,-1.,0.));
#64084=DIRECTION('ref_axis',(0.,0.,1.));
#64085=DIRECTION('center_axis',(-1.,0.,-1.22464679914735E-16));
#64086=DIRECTION('ref_axis',(-1.22464679914735E-16,0.,1.));
#64087=DIRECTION('center_axis',(0.,1.,0.));
#64088=DIRECTION('ref_axis',(0.,0.,-1.));
#64089=DIRECTION('center_axis',(0.,1.,0.));
#64090=DIRECTION('ref_axis',(0.,0.,1.));
#64091=DIRECTION('center_axis',(0.,1.,0.));
#64092=DIRECTION('ref_axis',(0.,0.,1.));
#64093=DIRECTION('center_axis',(-1.,0.,1.22464679914735E-16));
#64094=DIRECTION('ref_axis',(-1.22464679914735E-16,0.,-1.));
#64095=DIRECTION('center_axis',(0.,-1.,0.));
#64096=DIRECTION('ref_axis',(0.,0.,1.));
#64097=DIRECTION('center_axis',(0.,-1.,0.));
#64098=DIRECTION('ref_axis',(0.,0.,-1.));
#64099=DIRECTION('center_axis',(-1.,0.,-1.22464679914735E-16));
#64100=DIRECTION('ref_axis',(-1.22464679914735E-16,0.,1.));
#64101=DIRECTION('center_axis',(0.,1.,0.));
#64102=DIRECTION('ref_axis',(0.,0.,1.));
#64103=DIRECTION('center_axis',(0.,-1.,0.));
#64104=DIRECTION('ref_axis',(0.,0.,-1.));
#64105=DIRECTION('center_axis',(0.,1.,0.));
#64106=DIRECTION('ref_axis',(0.,0.,1.));
#64107=DIRECTION('',(9.85939117684628E-18,0.996753959471403,-0.0805080385929296));
#64108=DIRECTION('center_axis',(0.,-1.,0.));
#64109=DIRECTION('ref_axis',(0.,0.,-1.));
#64110=DIRECTION('center_axis',(0.,-1.,0.));
#64111=DIRECTION('ref_axis',(0.,0.,-1.));
#64112=DIRECTION('center_axis',(0.,-1.,0.));
#64113=DIRECTION('ref_axis',(0.,0.,-1.));
#64114=DIRECTION('center_axis',(-1.,0.,-1.22464679914735E-16));
#64115=DIRECTION('ref_axis',(-1.22464679914735E-16,0.,1.));
#64116=DIRECTION('center_axis',(0.,1.,0.));
#64117=DIRECTION('ref_axis',(0.,0.,-1.));
#64118=DIRECTION('center_axis',(0.,1.,0.));
#64119=DIRECTION('ref_axis',(0.,0.,1.));
#64120=DIRECTION('',(0.,-1.,0.));
#64121=DIRECTION('center_axis',(0.,1.,0.));
#64122=DIRECTION('ref_axis',(0.,0.,1.));
#64123=DIRECTION('',(0.,1.,0.));
#64124=DIRECTION('center_axis',(0.,-1.,0.));
#64125=DIRECTION('ref_axis',(0.,0.,-1.));
#64126=DIRECTION('center_axis',(0.,1.,0.));
#64127=DIRECTION('ref_axis',(0.,0.,1.));
#64128=DIRECTION('',(0.,-1.,0.));
#64129=DIRECTION('center_axis',(0.,1.,0.));
#64130=DIRECTION('ref_axis',(0.,0.,1.));
#64131=DIRECTION('center_axis',(0.,1.,0.));
#64132=DIRECTION('ref_axis',(0.,0.,1.));
#64133=DIRECTION('center_axis',(0.,-1.,0.));
#64134=DIRECTION('ref_axis',(0.,0.,-1.));
#64135=DIRECTION('center_axis',(0.,-1.,0.));
#64136=DIRECTION('ref_axis',(0.,0.,-1.));
#64137=DIRECTION('center_axis',(0.,1.,-2.84598943930249E-15));
#64138=DIRECTION('ref_axis',(0.,2.84598943930249E-15,1.));
#64139=DIRECTION('center_axis',(0.,-1.,2.84598943930249E-15));
#64140=DIRECTION('ref_axis',(0.,-2.84598943930249E-15,-1.));
#64141=DIRECTION('center_axis',(0.,1.,0.));
#64142=DIRECTION('ref_axis',(0.,0.,1.));
#64143=DIRECTION('center_axis',(0.,1.,0.));
#64144=DIRECTION('ref_axis',(0.,0.,1.));
#64145=DIRECTION('center_axis',(0.,1.,0.));
#64146=DIRECTION('ref_axis',(0.,0.,1.));
#64147=DIRECTION('center_axis',(0.,-1.,0.));
#64148=DIRECTION('ref_axis',(0.,0.,-1.));
#64149=DIRECTION('center_axis',(0.,1.,0.));
#64150=DIRECTION('ref_axis',(0.,0.,1.));
#64151=DIRECTION('center_axis',(0.,-1.,0.));
#64152=DIRECTION('ref_axis',(0.,0.,-1.));
#64153=DIRECTION('center_axis',(0.,1.,0.));
#64154=DIRECTION('ref_axis',(0.,0.,1.));
#64155=DIRECTION('center_axis',(0.,-1.,0.));
#64156=DIRECTION('ref_axis',(0.,0.,-1.));
#64157=DIRECTION('center_axis',(0.,1.,0.));
#64158=DIRECTION('ref_axis',(0.,0.,1.));
#64159=DIRECTION('center_axis',(0.,-1.,0.));
#64160=DIRECTION('ref_axis',(0.,0.,-1.));
#64161=DIRECTION('center_axis',(0.,1.,0.));
#64162=DIRECTION('ref_axis',(0.,0.,1.));
#64163=DIRECTION('center_axis',(0.,-1.,0.));
#64164=DIRECTION('ref_axis',(0.,0.,-1.));
#64165=DIRECTION('center_axis',(0.,1.,0.));
#64166=DIRECTION('ref_axis',(0.,0.,1.));
#64167=DIRECTION('center_axis',(0.,-1.,0.));
#64168=DIRECTION('ref_axis',(0.,0.,-1.));
#64169=DIRECTION('center_axis',(0.,1.,0.));
#64170=DIRECTION('ref_axis',(0.,0.,1.));
#64171=DIRECTION('center_axis',(0.,-1.,0.));
#64172=DIRECTION('ref_axis',(0.,0.,-1.));
#64173=DIRECTION('center_axis',(0.,1.,0.));
#64174=DIRECTION('ref_axis',(0.,0.,1.));
#64175=DIRECTION('center_axis',(0.,-1.,0.));
#64176=DIRECTION('ref_axis',(0.,0.,-1.));
#64177=DIRECTION('center_axis',(0.,1.,0.));
#64178=DIRECTION('ref_axis',(0.,0.,1.));
#64179=DIRECTION('center_axis',(0.,-1.,0.));
#64180=DIRECTION('ref_axis',(0.,0.,-1.));
#64181=DIRECTION('center_axis',(0.,1.,0.));
#64182=DIRECTION('ref_axis',(0.,0.,1.));
#64183=DIRECTION('center_axis',(0.,-1.,0.));
#64184=DIRECTION('ref_axis',(0.,0.,-1.));
#64185=DIRECTION('center_axis',(0.,1.,0.));
#64186=DIRECTION('ref_axis',(0.,0.,1.));
#64187=DIRECTION('center_axis',(0.,-1.,0.));
#64188=DIRECTION('ref_axis',(0.,0.,-1.));
#64189=DIRECTION('center_axis',(0.,1.,0.));
#64190=DIRECTION('ref_axis',(0.,0.,1.));
#64191=DIRECTION('center_axis',(0.,-1.,0.));
#64192=DIRECTION('ref_axis',(0.,0.,-1.));
#64193=DIRECTION('center_axis',(0.,1.,0.));
#64194=DIRECTION('ref_axis',(0.,0.,1.));
#64195=DIRECTION('center_axis',(0.,-1.,0.));
#64196=DIRECTION('ref_axis',(0.,0.,-1.));
#64197=DIRECTION('center_axis',(0.,1.,0.));
#64198=DIRECTION('ref_axis',(0.,0.,1.));
#64199=DIRECTION('center_axis',(0.,-1.,0.));
#64200=DIRECTION('ref_axis',(0.,0.,-1.));
#64201=DIRECTION('center_axis',(0.,1.,0.));
#64202=DIRECTION('ref_axis',(0.,0.,1.));
#64203=DIRECTION('center_axis',(0.,-1.,0.));
#64204=DIRECTION('ref_axis',(0.,0.,-1.));
#64205=DIRECTION('center_axis',(0.,1.,0.));
#64206=DIRECTION('ref_axis',(0.,0.,1.));
#64207=DIRECTION('center_axis',(0.,-1.,0.));
#64208=DIRECTION('ref_axis',(0.,0.,-1.));
#64209=DIRECTION('center_axis',(0.,1.,0.));
#64210=DIRECTION('ref_axis',(0.,0.,1.));
#64211=DIRECTION('center_axis',(0.,-1.,0.));
#64212=DIRECTION('ref_axis',(0.,0.,-1.));
#64213=DIRECTION('center_axis',(0.,1.,0.));
#64214=DIRECTION('ref_axis',(0.,0.,1.));
#64215=DIRECTION('center_axis',(0.,-1.,0.));
#64216=DIRECTION('ref_axis',(0.,0.,-1.));
#64217=DIRECTION('center_axis',(0.,1.,0.));
#64218=DIRECTION('ref_axis',(0.,0.,1.));
#64219=DIRECTION('center_axis',(0.,-1.,0.));
#64220=DIRECTION('ref_axis',(0.,0.,-1.));
#64221=DIRECTION('center_axis',(0.,1.,0.));
#64222=DIRECTION('ref_axis',(0.,0.,1.));
#64223=DIRECTION('center_axis',(0.,-1.,0.));
#64224=DIRECTION('ref_axis',(0.,0.,-1.));
#64225=DIRECTION('center_axis',(0.,1.,0.));
#64226=DIRECTION('ref_axis',(0.,0.,1.));
#64227=DIRECTION('center_axis',(0.,-1.,0.));
#64228=DIRECTION('ref_axis',(0.,0.,-1.));
#64229=DIRECTION('center_axis',(0.,1.,0.));
#64230=DIRECTION('ref_axis',(0.,0.,1.));
#64231=DIRECTION('center_axis',(0.,-1.,0.));
#64232=DIRECTION('ref_axis',(0.,0.,-1.));
#64233=DIRECTION('center_axis',(0.,1.,0.));
#64234=DIRECTION('ref_axis',(0.,0.,1.));
#64235=DIRECTION('center_axis',(0.,-1.,0.));
#64236=DIRECTION('ref_axis',(0.,0.,-1.));
#64237=DIRECTION('center_axis',(0.,1.,0.));
#64238=DIRECTION('ref_axis',(0.,0.,1.));
#64239=DIRECTION('center_axis',(0.,-1.,0.));
#64240=DIRECTION('ref_axis',(0.,0.,-1.));
#64241=DIRECTION('center_axis',(0.,1.,0.));
#64242=DIRECTION('ref_axis',(0.,0.,1.));
#64243=DIRECTION('center_axis',(0.,-1.,0.));
#64244=DIRECTION('ref_axis',(0.,0.,-1.));
#64245=DIRECTION('center_axis',(0.,1.,0.));
#64246=DIRECTION('ref_axis',(0.,0.,1.));
#64247=DIRECTION('center_axis',(0.,-1.,0.));
#64248=DIRECTION('ref_axis',(0.,0.,-1.));
#64249=DIRECTION('center_axis',(0.,1.,0.));
#64250=DIRECTION('ref_axis',(0.,0.,1.));
#64251=DIRECTION('center_axis',(0.,-1.,0.));
#64252=DIRECTION('ref_axis',(0.,0.,-1.));
#64253=DIRECTION('center_axis',(0.,1.,0.));
#64254=DIRECTION('ref_axis',(0.,0.,1.));
#64255=DIRECTION('center_axis',(0.,-1.,0.));
#64256=DIRECTION('ref_axis',(0.,0.,-1.));
#64257=DIRECTION('center_axis',(0.,1.,0.));
#64258=DIRECTION('ref_axis',(0.,0.,1.));
#64259=DIRECTION('center_axis',(0.,-1.,0.));
#64260=DIRECTION('ref_axis',(0.,0.,-1.));
#64261=DIRECTION('center_axis',(0.,1.,0.));
#64262=DIRECTION('ref_axis',(0.,0.,1.));
#64263=DIRECTION('center_axis',(0.,-1.,0.));
#64264=DIRECTION('ref_axis',(0.,0.,-1.));
#64265=DIRECTION('center_axis',(0.,1.,0.));
#64266=DIRECTION('ref_axis',(0.,0.,1.));
#64267=DIRECTION('center_axis',(0.,-1.,0.));
#64268=DIRECTION('ref_axis',(0.,0.,-1.));
#64269=DIRECTION('center_axis',(0.,1.,0.));
#64270=DIRECTION('ref_axis',(0.,0.,1.));
#64271=DIRECTION('center_axis',(0.,-1.,0.));
#64272=DIRECTION('ref_axis',(0.,0.,-1.));
#64273=DIRECTION('center_axis',(0.,1.,0.));
#64274=DIRECTION('ref_axis',(0.,0.,1.));
#64275=DIRECTION('center_axis',(0.,-1.,0.));
#64276=DIRECTION('ref_axis',(0.,0.,-1.));
#64277=DIRECTION('center_axis',(0.,1.,0.));
#64278=DIRECTION('ref_axis',(0.,0.,1.));
#64279=DIRECTION('center_axis',(0.,-1.,0.));
#64280=DIRECTION('ref_axis',(0.,0.,-1.));
#64281=DIRECTION('center_axis',(0.,1.,0.));
#64282=DIRECTION('ref_axis',(0.,0.,1.));
#64283=DIRECTION('center_axis',(0.,-1.,0.));
#64284=DIRECTION('ref_axis',(0.,0.,-1.));
#64285=DIRECTION('center_axis',(0.,1.,0.));
#64286=DIRECTION('ref_axis',(0.,0.,1.));
#64287=DIRECTION('center_axis',(0.,-1.,0.));
#64288=DIRECTION('ref_axis',(0.,0.,-1.));
#64289=DIRECTION('center_axis',(0.,1.,0.));
#64290=DIRECTION('ref_axis',(0.,0.,1.));
#64291=DIRECTION('center_axis',(0.,-1.,0.));
#64292=DIRECTION('ref_axis',(0.,0.,-1.));
#64293=DIRECTION('center_axis',(0.,1.,0.));
#64294=DIRECTION('ref_axis',(0.,0.,1.));
#64295=DIRECTION('center_axis',(0.,-1.,0.));
#64296=DIRECTION('ref_axis',(0.,0.,-1.));
#64297=DIRECTION('center_axis',(0.,1.,0.));
#64298=DIRECTION('ref_axis',(0.,0.,1.));
#64299=DIRECTION('center_axis',(0.,-1.,0.));
#64300=DIRECTION('ref_axis',(0.,0.,-1.));
#64301=DIRECTION('center_axis',(0.,1.,0.));
#64302=DIRECTION('ref_axis',(0.,0.,1.));
#64303=DIRECTION('center_axis',(0.,-1.,0.));
#64304=DIRECTION('ref_axis',(0.,0.,-1.));
#64305=DIRECTION('center_axis',(0.,1.,0.));
#64306=DIRECTION('ref_axis',(0.,0.,1.));
#64307=DIRECTION('center_axis',(0.,-1.,0.));
#64308=DIRECTION('ref_axis',(0.,0.,-1.));
#64309=DIRECTION('center_axis',(0.,1.,0.));
#64310=DIRECTION('ref_axis',(0.,0.,1.));
#64311=DIRECTION('center_axis',(0.,-1.,0.));
#64312=DIRECTION('ref_axis',(0.,0.,-1.));
#64313=DIRECTION('center_axis',(0.,1.,0.));
#64314=DIRECTION('ref_axis',(0.,0.,1.));
#64315=DIRECTION('center_axis',(0.,-1.,0.));
#64316=DIRECTION('ref_axis',(0.,0.,-1.));
#64317=DIRECTION('center_axis',(0.,1.,0.));
#64318=DIRECTION('ref_axis',(0.,0.,1.));
#64319=DIRECTION('center_axis',(0.,-1.,0.));
#64320=DIRECTION('ref_axis',(0.,0.,-1.));
#64321=DIRECTION('center_axis',(0.,1.,0.));
#64322=DIRECTION('ref_axis',(0.,0.,1.));
#64323=DIRECTION('center_axis',(0.,-1.,0.));
#64324=DIRECTION('ref_axis',(0.,0.,-1.));
#64325=DIRECTION('center_axis',(0.,1.,0.));
#64326=DIRECTION('ref_axis',(0.,0.,1.));
#64327=DIRECTION('center_axis',(0.,-1.,0.));
#64328=DIRECTION('ref_axis',(0.,0.,-1.));
#64329=DIRECTION('center_axis',(0.,1.,0.));
#64330=DIRECTION('ref_axis',(0.,0.,1.));
#64331=DIRECTION('center_axis',(0.,-1.,0.));
#64332=DIRECTION('ref_axis',(0.,0.,-1.));
#64333=DIRECTION('center_axis',(0.,1.,0.));
#64334=DIRECTION('ref_axis',(0.,0.,1.));
#64335=DIRECTION('center_axis',(0.,-1.,0.));
#64336=DIRECTION('ref_axis',(0.,0.,-1.));
#64337=DIRECTION('center_axis',(0.,1.,0.));
#64338=DIRECTION('ref_axis',(0.,0.,1.));
#64339=DIRECTION('center_axis',(0.,-1.,0.));
#64340=DIRECTION('ref_axis',(0.,0.,-1.));
#64341=DIRECTION('center_axis',(0.,1.,0.));
#64342=DIRECTION('ref_axis',(0.,0.,1.));
#64343=DIRECTION('center_axis',(0.,-1.,0.));
#64344=DIRECTION('ref_axis',(0.,0.,-1.));
#64345=DIRECTION('center_axis',(0.,1.,0.));
#64346=DIRECTION('ref_axis',(0.,0.,1.));
#64347=DIRECTION('center_axis',(0.,-1.,0.));
#64348=DIRECTION('ref_axis',(0.,0.,-1.));
#64349=DIRECTION('center_axis',(0.,1.,0.));
#64350=DIRECTION('ref_axis',(0.,0.,1.));
#64351=DIRECTION('center_axis',(0.,-1.,0.));
#64352=DIRECTION('ref_axis',(0.,0.,-1.));
#64353=DIRECTION('center_axis',(0.,1.,0.));
#64354=DIRECTION('ref_axis',(0.,0.,1.));
#64355=DIRECTION('center_axis',(0.,-1.,0.));
#64356=DIRECTION('ref_axis',(0.,0.,-1.));
#64357=DIRECTION('center_axis',(0.,1.,0.));
#64358=DIRECTION('ref_axis',(0.,0.,1.));
#64359=DIRECTION('center_axis',(0.,-1.,0.));
#64360=DIRECTION('ref_axis',(0.,0.,-1.));
#64361=DIRECTION('center_axis',(0.,1.,0.));
#64362=DIRECTION('ref_axis',(0.,0.,1.));
#64363=DIRECTION('center_axis',(0.,-1.,0.));
#64364=DIRECTION('ref_axis',(0.,0.,-1.));
#64365=DIRECTION('center_axis',(0.,1.,0.));
#64366=DIRECTION('ref_axis',(0.,0.,1.));
#64367=DIRECTION('center_axis',(0.,-1.,0.));
#64368=DIRECTION('ref_axis',(0.,0.,-1.));
#64369=DIRECTION('center_axis',(0.,1.,0.));
#64370=DIRECTION('ref_axis',(0.,0.,1.));
#64371=DIRECTION('center_axis',(0.,-1.,0.));
#64372=DIRECTION('ref_axis',(0.,0.,-1.));
#64373=DIRECTION('center_axis',(0.,1.,0.));
#64374=DIRECTION('ref_axis',(0.,0.,1.));
#64375=DIRECTION('center_axis',(0.,-1.,0.));
#64376=DIRECTION('ref_axis',(0.,0.,-1.));
#64377=DIRECTION('center_axis',(0.,1.,0.));
#64378=DIRECTION('ref_axis',(0.,0.,1.));
#64379=DIRECTION('center_axis',(0.,-1.,0.));
#64380=DIRECTION('ref_axis',(0.,0.,-1.));
#64381=DIRECTION('center_axis',(0.,1.,0.));
#64382=DIRECTION('ref_axis',(0.,0.,1.));
#64383=DIRECTION('center_axis',(0.,-1.,0.));
#64384=DIRECTION('ref_axis',(0.,0.,-1.));
#64385=DIRECTION('center_axis',(0.,1.,0.));
#64386=DIRECTION('ref_axis',(0.,0.,1.));
#64387=DIRECTION('center_axis',(0.,-1.,0.));
#64388=DIRECTION('ref_axis',(0.,0.,-1.));
#64389=DIRECTION('center_axis',(0.,1.,0.));
#64390=DIRECTION('ref_axis',(0.,0.,1.));
#64391=DIRECTION('center_axis',(0.,-1.,0.));
#64392=DIRECTION('ref_axis',(0.,0.,-1.));
#64393=DIRECTION('center_axis',(0.,1.,0.));
#64394=DIRECTION('ref_axis',(0.,0.,1.));
#64395=DIRECTION('center_axis',(0.,-1.,0.));
#64396=DIRECTION('ref_axis',(0.,0.,-1.));
#64397=DIRECTION('center_axis',(0.,1.,0.));
#64398=DIRECTION('ref_axis',(0.,0.,1.));
#64399=DIRECTION('center_axis',(0.,-1.,0.));
#64400=DIRECTION('ref_axis',(0.,0.,-1.));
#64401=DIRECTION('center_axis',(0.,1.,0.));
#64402=DIRECTION('ref_axis',(0.,0.,1.));
#64403=DIRECTION('center_axis',(0.,-1.,0.));
#64404=DIRECTION('ref_axis',(0.,0.,-1.));
#64405=DIRECTION('center_axis',(0.,1.,0.));
#64406=DIRECTION('ref_axis',(0.,0.,1.));
#64407=DIRECTION('center_axis',(0.,-1.,0.));
#64408=DIRECTION('ref_axis',(0.,0.,-1.));
#64409=DIRECTION('center_axis',(0.,1.,0.));
#64410=DIRECTION('ref_axis',(0.,0.,1.));
#64411=DIRECTION('center_axis',(0.,-1.,0.));
#64412=DIRECTION('ref_axis',(0.,0.,-1.));
#64413=DIRECTION('center_axis',(0.,1.,0.));
#64414=DIRECTION('ref_axis',(0.,0.,1.));
#64415=DIRECTION('center_axis',(0.,-1.,0.));
#64416=DIRECTION('ref_axis',(0.,0.,-1.));
#64417=DIRECTION('center_axis',(0.,1.,0.));
#64418=DIRECTION('ref_axis',(0.,0.,1.));
#64419=DIRECTION('center_axis',(0.,-1.,0.));
#64420=DIRECTION('ref_axis',(0.,0.,-1.));
#64421=DIRECTION('center_axis',(0.,1.,0.));
#64422=DIRECTION('ref_axis',(0.,0.,1.));
#64423=DIRECTION('center_axis',(0.,-1.,0.));
#64424=DIRECTION('ref_axis',(0.,0.,-1.));
#64425=DIRECTION('center_axis',(0.,1.,0.));
#64426=DIRECTION('ref_axis',(0.,0.,1.));
#64427=DIRECTION('center_axis',(0.,-1.,0.));
#64428=DIRECTION('ref_axis',(0.,0.,-1.));
#64429=DIRECTION('center_axis',(0.,1.,0.));
#64430=DIRECTION('ref_axis',(0.,0.,1.));
#64431=DIRECTION('center_axis',(0.,-1.,0.));
#64432=DIRECTION('ref_axis',(0.,0.,-1.));
#64433=DIRECTION('center_axis',(0.,1.,0.));
#64434=DIRECTION('ref_axis',(0.,0.,1.));
#64435=DIRECTION('center_axis',(0.,-1.,0.));
#64436=DIRECTION('ref_axis',(0.,0.,-1.));
#64437=DIRECTION('center_axis',(0.,1.,0.));
#64438=DIRECTION('ref_axis',(0.,0.,1.));
#64439=DIRECTION('center_axis',(0.,-1.,0.));
#64440=DIRECTION('ref_axis',(0.,0.,-1.));
#64441=DIRECTION('center_axis',(0.,1.,0.));
#64442=DIRECTION('ref_axis',(0.,0.,1.));
#64443=DIRECTION('center_axis',(0.,-1.,0.));
#64444=DIRECTION('ref_axis',(0.,0.,-1.));
#64445=DIRECTION('center_axis',(0.,1.,0.));
#64446=DIRECTION('ref_axis',(0.,0.,1.));
#64447=DIRECTION('center_axis',(0.,-1.,0.));
#64448=DIRECTION('ref_axis',(0.,0.,-1.));
#64449=DIRECTION('center_axis',(0.,1.,0.));
#64450=DIRECTION('ref_axis',(0.,0.,1.));
#64451=DIRECTION('center_axis',(0.,-1.,0.));
#64452=DIRECTION('ref_axis',(0.,0.,-1.));
#64453=DIRECTION('center_axis',(0.,1.,0.));
#64454=DIRECTION('ref_axis',(0.,0.,1.));
#64455=DIRECTION('center_axis',(0.,-1.,0.));
#64456=DIRECTION('ref_axis',(0.,0.,-1.));
#64457=DIRECTION('center_axis',(0.,1.,0.));
#64458=DIRECTION('ref_axis',(0.,0.,1.));
#64459=DIRECTION('center_axis',(0.,-1.,0.));
#64460=DIRECTION('ref_axis',(0.,0.,-1.));
#64461=DIRECTION('center_axis',(0.,1.,0.));
#64462=DIRECTION('ref_axis',(0.,0.,1.));
#64463=DIRECTION('center_axis',(0.,-1.,0.));
#64464=DIRECTION('ref_axis',(0.,0.,-1.));
#64465=DIRECTION('center_axis',(0.,1.,0.));
#64466=DIRECTION('ref_axis',(0.,0.,1.));
#64467=DIRECTION('center_axis',(0.,-1.,0.));
#64468=DIRECTION('ref_axis',(0.,0.,-1.));
#64469=DIRECTION('center_axis',(0.,1.,0.));
#64470=DIRECTION('ref_axis',(0.,0.,1.));
#64471=DIRECTION('center_axis',(0.,-1.,0.));
#64472=DIRECTION('ref_axis',(0.,0.,-1.));
#64473=DIRECTION('center_axis',(0.,1.,0.));
#64474=DIRECTION('ref_axis',(0.,0.,1.));
#64475=DIRECTION('center_axis',(0.,-1.,0.));
#64476=DIRECTION('ref_axis',(0.,0.,-1.));
#64477=DIRECTION('center_axis',(0.,1.,0.));
#64478=DIRECTION('ref_axis',(0.,0.,1.));
#64479=DIRECTION('center_axis',(0.,-1.,0.));
#64480=DIRECTION('ref_axis',(0.,0.,-1.));
#64481=DIRECTION('center_axis',(0.,1.,0.));
#64482=DIRECTION('ref_axis',(0.,0.,1.));
#64483=DIRECTION('center_axis',(0.,-1.,0.));
#64484=DIRECTION('ref_axis',(0.,0.,-1.));
#64485=DIRECTION('center_axis',(0.,1.,0.));
#64486=DIRECTION('ref_axis',(0.,0.,1.));
#64487=DIRECTION('center_axis',(0.,-1.,0.));
#64488=DIRECTION('ref_axis',(0.,0.,-1.));
#64489=DIRECTION('center_axis',(0.,1.,0.));
#64490=DIRECTION('ref_axis',(0.,0.,1.));
#64491=DIRECTION('center_axis',(0.,-1.,0.));
#64492=DIRECTION('ref_axis',(0.,0.,-1.));
#64493=DIRECTION('center_axis',(0.,1.,0.));
#64494=DIRECTION('ref_axis',(0.,0.,1.));
#64495=DIRECTION('center_axis',(0.,-1.,0.));
#64496=DIRECTION('ref_axis',(0.,0.,-1.));
#64497=DIRECTION('center_axis',(0.,1.,0.));
#64498=DIRECTION('ref_axis',(0.,0.,1.));
#64499=DIRECTION('center_axis',(0.,-1.,0.));
#64500=DIRECTION('ref_axis',(0.,0.,-1.));
#64501=DIRECTION('center_axis',(0.,1.,0.));
#64502=DIRECTION('ref_axis',(0.,0.,1.));
#64503=DIRECTION('center_axis',(0.,-1.,0.));
#64504=DIRECTION('ref_axis',(0.,0.,-1.));
#64505=DIRECTION('center_axis',(0.,1.,0.));
#64506=DIRECTION('ref_axis',(0.,0.,1.));
#64507=DIRECTION('center_axis',(0.,-1.,0.));
#64508=DIRECTION('ref_axis',(0.,0.,-1.));
#64509=DIRECTION('center_axis',(0.,1.,0.));
#64510=DIRECTION('ref_axis',(0.,0.,1.));
#64511=DIRECTION('center_axis',(0.,-1.,0.));
#64512=DIRECTION('ref_axis',(0.,0.,-1.));
#64513=DIRECTION('center_axis',(0.,1.,0.));
#64514=DIRECTION('ref_axis',(0.,0.,1.));
#64515=DIRECTION('center_axis',(0.,-1.,0.));
#64516=DIRECTION('ref_axis',(0.,0.,-1.));
#64517=DIRECTION('center_axis',(0.,1.,0.));
#64518=DIRECTION('ref_axis',(0.,0.,1.));
#64519=DIRECTION('center_axis',(0.,-1.,0.));
#64520=DIRECTION('ref_axis',(0.,0.,-1.));
#64521=DIRECTION('center_axis',(0.,1.,0.));
#64522=DIRECTION('ref_axis',(0.,0.,1.));
#64523=DIRECTION('center_axis',(0.,-1.,0.));
#64524=DIRECTION('ref_axis',(0.,0.,-1.));
#64525=DIRECTION('center_axis',(0.,1.,0.));
#64526=DIRECTION('ref_axis',(0.,0.,1.));
#64527=DIRECTION('center_axis',(0.,-1.,0.));
#64528=DIRECTION('ref_axis',(0.,0.,-1.));
#64529=DIRECTION('center_axis',(0.,1.,0.));
#64530=DIRECTION('ref_axis',(0.,0.,1.));
#64531=DIRECTION('center_axis',(0.,-1.,0.));
#64532=DIRECTION('ref_axis',(0.,0.,-1.));
#64533=DIRECTION('center_axis',(0.,1.,0.));
#64534=DIRECTION('ref_axis',(0.,0.,1.));
#64535=DIRECTION('center_axis',(0.,-1.,0.));
#64536=DIRECTION('ref_axis',(0.,0.,-1.));
#64537=DIRECTION('center_axis',(0.,1.,0.));
#64538=DIRECTION('ref_axis',(0.,0.,1.));
#64539=DIRECTION('center_axis',(0.,-1.,0.));
#64540=DIRECTION('ref_axis',(0.,0.,-1.));
#64541=DIRECTION('center_axis',(0.,1.,0.));
#64542=DIRECTION('ref_axis',(0.,0.,1.));
#64543=DIRECTION('center_axis',(0.,-1.,0.));
#64544=DIRECTION('ref_axis',(0.,0.,-1.));
#64545=DIRECTION('center_axis',(0.,1.,0.));
#64546=DIRECTION('ref_axis',(0.,0.,1.));
#64547=DIRECTION('center_axis',(0.,-1.,0.));
#64548=DIRECTION('ref_axis',(0.,0.,-1.));
#64549=DIRECTION('center_axis',(0.,1.,0.));
#64550=DIRECTION('ref_axis',(0.,0.,1.));
#64551=DIRECTION('center_axis',(0.,-1.,0.));
#64552=DIRECTION('ref_axis',(0.,0.,-1.));
#64553=DIRECTION('center_axis',(0.,1.,0.));
#64554=DIRECTION('ref_axis',(0.,0.,1.));
#64555=DIRECTION('center_axis',(0.,-1.,0.));
#64556=DIRECTION('ref_axis',(0.,0.,-1.));
#64557=DIRECTION('center_axis',(0.,1.,0.));
#64558=DIRECTION('ref_axis',(0.,0.,1.));
#64559=DIRECTION('center_axis',(0.,-1.,0.));
#64560=DIRECTION('ref_axis',(0.,0.,-1.));
#64561=DIRECTION('center_axis',(0.,1.,0.));
#64562=DIRECTION('ref_axis',(0.,0.,1.));
#64563=DIRECTION('center_axis',(0.,-1.,0.));
#64564=DIRECTION('ref_axis',(0.,0.,-1.));
#64565=DIRECTION('center_axis',(0.,1.,0.));
#64566=DIRECTION('ref_axis',(0.,0.,1.));
#64567=DIRECTION('center_axis',(0.,-1.,0.));
#64568=DIRECTION('ref_axis',(0.,0.,-1.));
#64569=DIRECTION('center_axis',(0.,1.,0.));
#64570=DIRECTION('ref_axis',(0.,0.,1.));
#64571=DIRECTION('center_axis',(0.,-1.,0.));
#64572=DIRECTION('ref_axis',(0.,0.,-1.));
#64573=DIRECTION('center_axis',(0.,1.,0.));
#64574=DIRECTION('ref_axis',(0.,0.,1.));
#64575=DIRECTION('center_axis',(0.,-1.,0.));
#64576=DIRECTION('ref_axis',(0.,0.,-1.));
#64577=DIRECTION('center_axis',(0.,1.,0.));
#64578=DIRECTION('ref_axis',(0.,0.,1.));
#64579=DIRECTION('center_axis',(0.,-1.,0.));
#64580=DIRECTION('ref_axis',(0.,0.,-1.));
#64581=DIRECTION('center_axis',(0.,1.,0.));
#64582=DIRECTION('ref_axis',(0.,0.,1.));
#64583=DIRECTION('center_axis',(0.,-1.,0.));
#64584=DIRECTION('ref_axis',(0.,0.,-1.));
#64585=DIRECTION('center_axis',(0.,1.,0.));
#64586=DIRECTION('ref_axis',(0.,0.,1.));
#64587=DIRECTION('center_axis',(0.,-1.,0.));
#64588=DIRECTION('ref_axis',(0.,0.,-1.));
#64589=DIRECTION('center_axis',(0.,1.,0.));
#64590=DIRECTION('ref_axis',(0.,0.,1.));
#64591=DIRECTION('center_axis',(0.,-1.,0.));
#64592=DIRECTION('ref_axis',(0.,0.,-1.));
#64593=DIRECTION('center_axis',(0.,1.,0.));
#64594=DIRECTION('ref_axis',(0.,0.,1.));
#64595=DIRECTION('center_axis',(0.,-1.,0.));
#64596=DIRECTION('ref_axis',(0.,0.,-1.));
#64597=DIRECTION('center_axis',(0.,1.,0.));
#64598=DIRECTION('ref_axis',(0.,0.,1.));
#64599=DIRECTION('center_axis',(0.,-1.,0.));
#64600=DIRECTION('ref_axis',(0.,0.,-1.));
#64601=DIRECTION('center_axis',(0.,1.,0.));
#64602=DIRECTION('ref_axis',(0.,0.,1.));
#64603=DIRECTION('center_axis',(0.,-1.,0.));
#64604=DIRECTION('ref_axis',(0.,0.,-1.));
#64605=DIRECTION('center_axis',(0.,1.,0.));
#64606=DIRECTION('ref_axis',(0.,0.,1.));
#64607=DIRECTION('center_axis',(0.,-1.,0.));
#64608=DIRECTION('ref_axis',(0.,0.,-1.));
#64609=DIRECTION('center_axis',(0.,1.,0.));
#64610=DIRECTION('ref_axis',(0.,0.,1.));
#64611=DIRECTION('center_axis',(0.,-1.,0.));
#64612=DIRECTION('ref_axis',(0.,0.,-1.));
#64613=DIRECTION('center_axis',(0.,1.,0.));
#64614=DIRECTION('ref_axis',(0.,0.,1.));
#64615=DIRECTION('center_axis',(0.,-1.,0.));
#64616=DIRECTION('ref_axis',(0.,0.,-1.));
#64617=DIRECTION('center_axis',(0.,1.,0.));
#64618=DIRECTION('ref_axis',(0.,0.,1.));
#64619=DIRECTION('center_axis',(0.,-1.,0.));
#64620=DIRECTION('ref_axis',(0.,0.,-1.));
#64621=DIRECTION('center_axis',(0.,1.,0.));
#64622=DIRECTION('ref_axis',(0.,0.,1.));
#64623=DIRECTION('center_axis',(0.,-1.,0.));
#64624=DIRECTION('ref_axis',(0.,0.,-1.));
#64625=DIRECTION('center_axis',(0.,1.,0.));
#64626=DIRECTION('ref_axis',(0.,0.,1.));
#64627=DIRECTION('center_axis',(0.,-1.,0.));
#64628=DIRECTION('ref_axis',(0.,0.,-1.));
#64629=DIRECTION('center_axis',(0.,1.,0.));
#64630=DIRECTION('ref_axis',(0.,0.,1.));
#64631=DIRECTION('center_axis',(0.,-1.,0.));
#64632=DIRECTION('ref_axis',(0.,0.,-1.));
#64633=DIRECTION('center_axis',(0.,1.,0.));
#64634=DIRECTION('ref_axis',(0.,0.,1.));
#64635=DIRECTION('center_axis',(0.,-1.,0.));
#64636=DIRECTION('ref_axis',(0.,0.,-1.));
#64637=DIRECTION('center_axis',(0.,1.,0.));
#64638=DIRECTION('ref_axis',(0.,0.,1.));
#64639=DIRECTION('center_axis',(0.,-1.,0.));
#64640=DIRECTION('ref_axis',(0.,0.,-1.));
#64641=DIRECTION('center_axis',(0.,1.,0.));
#64642=DIRECTION('ref_axis',(0.,0.,1.));
#64643=DIRECTION('center_axis',(0.,-1.,0.));
#64644=DIRECTION('ref_axis',(0.,0.,-1.));
#64645=DIRECTION('center_axis',(0.,1.,0.));
#64646=DIRECTION('ref_axis',(0.,0.,1.));
#64647=DIRECTION('center_axis',(0.,-1.,0.));
#64648=DIRECTION('ref_axis',(0.,0.,-1.));
#64649=DIRECTION('center_axis',(0.,1.,0.));
#64650=DIRECTION('ref_axis',(0.,0.,1.));
#64651=DIRECTION('center_axis',(0.,-1.,0.));
#64652=DIRECTION('ref_axis',(0.,0.,-1.));
#64653=DIRECTION('center_axis',(0.,1.,0.));
#64654=DIRECTION('ref_axis',(0.,0.,1.));
#64655=DIRECTION('center_axis',(0.,-1.,0.));
#64656=DIRECTION('ref_axis',(0.,0.,-1.));
#64657=DIRECTION('center_axis',(0.,1.,0.));
#64658=DIRECTION('ref_axis',(0.,0.,1.));
#64659=DIRECTION('center_axis',(0.,-1.,0.));
#64660=DIRECTION('ref_axis',(0.,0.,-1.));
#64661=DIRECTION('center_axis',(0.,1.,0.));
#64662=DIRECTION('ref_axis',(0.,0.,1.));
#64663=DIRECTION('center_axis',(0.,-1.,0.));
#64664=DIRECTION('ref_axis',(0.,0.,-1.));
#64665=DIRECTION('center_axis',(0.,1.,0.));
#64666=DIRECTION('ref_axis',(0.,0.,1.));
#64667=DIRECTION('center_axis',(0.,-1.,0.));
#64668=DIRECTION('ref_axis',(0.,0.,-1.));
#64669=DIRECTION('center_axis',(0.,1.,0.));
#64670=DIRECTION('ref_axis',(0.,0.,1.));
#64671=DIRECTION('center_axis',(0.,-1.,0.));
#64672=DIRECTION('ref_axis',(0.,0.,-1.));
#64673=DIRECTION('center_axis',(0.,1.,0.));
#64674=DIRECTION('ref_axis',(0.,0.,1.));
#64675=DIRECTION('center_axis',(0.,-1.,0.));
#64676=DIRECTION('ref_axis',(0.,0.,-1.));
#64677=DIRECTION('center_axis',(0.,1.,0.));
#64678=DIRECTION('ref_axis',(0.,0.,1.));
#64679=DIRECTION('center_axis',(0.,-1.,0.));
#64680=DIRECTION('ref_axis',(0.,0.,-1.));
#64681=DIRECTION('center_axis',(0.,1.,0.));
#64682=DIRECTION('ref_axis',(0.,0.,1.));
#64683=DIRECTION('center_axis',(0.,-1.,0.));
#64684=DIRECTION('ref_axis',(0.,0.,-1.));
#64685=DIRECTION('center_axis',(0.,1.,0.));
#64686=DIRECTION('ref_axis',(0.,0.,1.));
#64687=DIRECTION('center_axis',(0.,-1.,0.));
#64688=DIRECTION('ref_axis',(0.,0.,-1.));
#64689=DIRECTION('center_axis',(0.,1.,0.));
#64690=DIRECTION('ref_axis',(0.,0.,1.));
#64691=DIRECTION('center_axis',(0.,-1.,0.));
#64692=DIRECTION('ref_axis',(0.,0.,-1.));
#64693=DIRECTION('center_axis',(0.,1.,0.));
#64694=DIRECTION('ref_axis',(0.,0.,1.));
#64695=DIRECTION('center_axis',(0.,-1.,0.));
#64696=DIRECTION('ref_axis',(0.,0.,-1.));
#64697=DIRECTION('center_axis',(0.,1.,0.));
#64698=DIRECTION('ref_axis',(0.,0.,1.));
#64699=DIRECTION('center_axis',(0.,-1.,0.));
#64700=DIRECTION('ref_axis',(0.,0.,-1.));
#64701=DIRECTION('center_axis',(0.,1.,0.));
#64702=DIRECTION('ref_axis',(0.,0.,1.));
#64703=DIRECTION('center_axis',(0.,-1.,0.));
#64704=DIRECTION('ref_axis',(0.,0.,-1.));
#64705=DIRECTION('center_axis',(0.,1.,0.));
#64706=DIRECTION('ref_axis',(0.,0.,1.));
#64707=DIRECTION('center_axis',(0.,-1.,0.));
#64708=DIRECTION('ref_axis',(0.,0.,-1.));
#64709=DIRECTION('center_axis',(0.,1.,0.));
#64710=DIRECTION('ref_axis',(0.,0.,1.));
#64711=DIRECTION('center_axis',(0.,-1.,0.));
#64712=DIRECTION('ref_axis',(0.,0.,-1.));
#64713=DIRECTION('center_axis',(0.,1.,0.));
#64714=DIRECTION('ref_axis',(0.,0.,1.));
#64715=DIRECTION('center_axis',(0.,-1.,0.));
#64716=DIRECTION('ref_axis',(0.,0.,-1.));
#64717=DIRECTION('center_axis',(0.,1.,0.));
#64718=DIRECTION('ref_axis',(0.,0.,1.));
#64719=DIRECTION('center_axis',(0.,-1.,0.));
#64720=DIRECTION('ref_axis',(0.,0.,-1.));
#64721=DIRECTION('center_axis',(0.,1.,0.));
#64722=DIRECTION('ref_axis',(0.,0.,1.));
#64723=DIRECTION('center_axis',(0.,-1.,0.));
#64724=DIRECTION('ref_axis',(0.,0.,-1.));
#64725=DIRECTION('center_axis',(0.,1.,0.));
#64726=DIRECTION('ref_axis',(0.,0.,1.));
#64727=DIRECTION('center_axis',(0.,-1.,0.));
#64728=DIRECTION('ref_axis',(0.,0.,-1.));
#64729=DIRECTION('center_axis',(0.,1.,0.));
#64730=DIRECTION('ref_axis',(0.,0.,1.));
#64731=DIRECTION('center_axis',(0.,-1.,0.));
#64732=DIRECTION('ref_axis',(0.,0.,-1.));
#64733=DIRECTION('center_axis',(0.,1.,0.));
#64734=DIRECTION('ref_axis',(0.,0.,1.));
#64735=DIRECTION('center_axis',(0.,-1.,0.));
#64736=DIRECTION('ref_axis',(0.,0.,-1.));
#64737=DIRECTION('center_axis',(0.,1.,0.));
#64738=DIRECTION('ref_axis',(0.,0.,1.));
#64739=DIRECTION('center_axis',(0.,-1.,0.));
#64740=DIRECTION('ref_axis',(0.,0.,-1.));
#64741=DIRECTION('center_axis',(0.,1.,0.));
#64742=DIRECTION('ref_axis',(0.,0.,1.));
#64743=DIRECTION('center_axis',(0.,-1.,0.));
#64744=DIRECTION('ref_axis',(0.,0.,-1.));
#64745=DIRECTION('center_axis',(0.,1.,0.));
#64746=DIRECTION('ref_axis',(0.,0.,1.));
#64747=DIRECTION('center_axis',(0.,-1.,0.));
#64748=DIRECTION('ref_axis',(0.,0.,-1.));
#64749=DIRECTION('center_axis',(0.,1.,0.));
#64750=DIRECTION('ref_axis',(0.,0.,1.));
#64751=DIRECTION('center_axis',(0.,-1.,0.));
#64752=DIRECTION('ref_axis',(0.,0.,-1.));
#64753=DIRECTION('center_axis',(0.,1.,0.));
#64754=DIRECTION('ref_axis',(0.,0.,1.));
#64755=DIRECTION('center_axis',(0.,-1.,0.));
#64756=DIRECTION('ref_axis',(0.,0.,-1.));
#64757=DIRECTION('center_axis',(0.,1.,0.));
#64758=DIRECTION('ref_axis',(0.,0.,1.));
#64759=DIRECTION('center_axis',(0.,-1.,0.));
#64760=DIRECTION('ref_axis',(0.,0.,-1.));
#64761=DIRECTION('center_axis',(0.,1.,0.));
#64762=DIRECTION('ref_axis',(0.,0.,1.));
#64763=DIRECTION('center_axis',(0.,-1.,0.));
#64764=DIRECTION('ref_axis',(0.,0.,-1.));
#64765=DIRECTION('center_axis',(0.,1.,0.));
#64766=DIRECTION('ref_axis',(0.,0.,1.));
#64767=DIRECTION('center_axis',(0.,-1.,0.));
#64768=DIRECTION('ref_axis',(0.,0.,-1.));
#64769=DIRECTION('center_axis',(0.,1.,0.));
#64770=DIRECTION('ref_axis',(0.,0.,1.));
#64771=DIRECTION('center_axis',(0.,-1.,0.));
#64772=DIRECTION('ref_axis',(0.,0.,-1.));
#64773=DIRECTION('center_axis',(0.,1.,0.));
#64774=DIRECTION('ref_axis',(0.,0.,1.));
#64775=DIRECTION('center_axis',(0.,-1.,0.));
#64776=DIRECTION('ref_axis',(0.,0.,-1.));
#64777=DIRECTION('center_axis',(0.,1.,0.));
#64778=DIRECTION('ref_axis',(0.,0.,1.));
#64779=DIRECTION('center_axis',(0.,-1.,0.));
#64780=DIRECTION('ref_axis',(0.,0.,-1.));
#64781=DIRECTION('center_axis',(0.,1.,0.));
#64782=DIRECTION('ref_axis',(0.,0.,1.));
#64783=DIRECTION('center_axis',(0.,-1.,0.));
#64784=DIRECTION('ref_axis',(0.,0.,-1.));
#64785=DIRECTION('center_axis',(0.,1.,0.));
#64786=DIRECTION('ref_axis',(0.,0.,1.));
#64787=DIRECTION('center_axis',(0.,-1.,0.));
#64788=DIRECTION('ref_axis',(0.,0.,-1.));
#64789=DIRECTION('center_axis',(0.,1.,0.));
#64790=DIRECTION('ref_axis',(0.,0.,1.));
#64791=DIRECTION('center_axis',(0.,-1.,0.));
#64792=DIRECTION('ref_axis',(0.,0.,-1.));
#64793=DIRECTION('center_axis',(0.,1.,0.));
#64794=DIRECTION('ref_axis',(0.,0.,1.));
#64795=DIRECTION('center_axis',(0.,-1.,0.));
#64796=DIRECTION('ref_axis',(0.,0.,-1.));
#64797=DIRECTION('center_axis',(0.,1.,0.));
#64798=DIRECTION('ref_axis',(0.,0.,1.));
#64799=DIRECTION('center_axis',(0.,-1.,0.));
#64800=DIRECTION('ref_axis',(0.,0.,-1.));
#64801=DIRECTION('center_axis',(0.,1.,0.));
#64802=DIRECTION('ref_axis',(0.,0.,1.));
#64803=DIRECTION('center_axis',(0.,-1.,0.));
#64804=DIRECTION('ref_axis',(0.,0.,-1.));
#64805=DIRECTION('center_axis',(0.,1.,0.));
#64806=DIRECTION('ref_axis',(0.,0.,1.));
#64807=DIRECTION('center_axis',(0.,-1.,0.));
#64808=DIRECTION('ref_axis',(0.,0.,-1.));
#64809=DIRECTION('center_axis',(0.,1.,0.));
#64810=DIRECTION('ref_axis',(0.,0.,1.));
#64811=DIRECTION('center_axis',(0.,-1.,0.));
#64812=DIRECTION('ref_axis',(0.,0.,-1.));
#64813=DIRECTION('center_axis',(0.,1.,0.));
#64814=DIRECTION('ref_axis',(0.,0.,1.));
#64815=DIRECTION('center_axis',(0.,-1.,0.));
#64816=DIRECTION('ref_axis',(0.,0.,-1.));
#64817=DIRECTION('center_axis',(0.,1.,0.));
#64818=DIRECTION('ref_axis',(0.,0.,1.));
#64819=DIRECTION('center_axis',(0.,-1.,0.));
#64820=DIRECTION('ref_axis',(0.,0.,-1.));
#64821=DIRECTION('center_axis',(0.,1.,0.));
#64822=DIRECTION('ref_axis',(0.,0.,1.));
#64823=DIRECTION('center_axis',(0.,-1.,0.));
#64824=DIRECTION('ref_axis',(0.,0.,-1.));
#64825=DIRECTION('center_axis',(0.,1.,0.));
#64826=DIRECTION('ref_axis',(0.,0.,1.));
#64827=DIRECTION('center_axis',(0.,-1.,0.));
#64828=DIRECTION('ref_axis',(0.,0.,-1.));
#64829=DIRECTION('center_axis',(0.,1.,0.));
#64830=DIRECTION('ref_axis',(0.,0.,1.));
#64831=DIRECTION('center_axis',(0.,-1.,0.));
#64832=DIRECTION('ref_axis',(0.,0.,-1.));
#64833=DIRECTION('center_axis',(0.,1.,0.));
#64834=DIRECTION('ref_axis',(0.,0.,1.));
#64835=DIRECTION('center_axis',(0.,-1.,0.));
#64836=DIRECTION('ref_axis',(0.,0.,-1.));
#64837=DIRECTION('center_axis',(0.,1.,0.));
#64838=DIRECTION('ref_axis',(0.,0.,1.));
#64839=DIRECTION('center_axis',(0.,-1.,0.));
#64840=DIRECTION('ref_axis',(0.,0.,-1.));
#64841=DIRECTION('center_axis',(0.,1.,0.));
#64842=DIRECTION('ref_axis',(0.,0.,1.));
#64843=DIRECTION('center_axis',(0.,-1.,0.));
#64844=DIRECTION('ref_axis',(0.,0.,-1.));
#64845=DIRECTION('center_axis',(0.,1.,0.));
#64846=DIRECTION('ref_axis',(0.,0.,1.));
#64847=DIRECTION('center_axis',(0.,-1.,0.));
#64848=DIRECTION('ref_axis',(0.,0.,-1.));
#64849=DIRECTION('center_axis',(0.,1.,0.));
#64850=DIRECTION('ref_axis',(0.,0.,1.));
#64851=DIRECTION('center_axis',(0.,-1.,0.));
#64852=DIRECTION('ref_axis',(0.,0.,-1.));
#64853=DIRECTION('center_axis',(0.,1.,0.));
#64854=DIRECTION('ref_axis',(0.,0.,1.));
#64855=DIRECTION('center_axis',(0.,-1.,0.));
#64856=DIRECTION('ref_axis',(0.,0.,-1.));
#64857=DIRECTION('center_axis',(0.,1.,0.));
#64858=DIRECTION('ref_axis',(0.,0.,1.));
#64859=DIRECTION('center_axis',(0.,-1.,0.));
#64860=DIRECTION('ref_axis',(0.,0.,-1.));
#64861=DIRECTION('center_axis',(0.,1.,0.));
#64862=DIRECTION('ref_axis',(0.,0.,1.));
#64863=DIRECTION('center_axis',(0.,-1.,0.));
#64864=DIRECTION('ref_axis',(0.,0.,-1.));
#64865=DIRECTION('center_axis',(0.,1.,0.));
#64866=DIRECTION('ref_axis',(0.,0.,1.));
#64867=DIRECTION('center_axis',(0.,-1.,0.));
#64868=DIRECTION('ref_axis',(0.,0.,-1.));
#64869=DIRECTION('center_axis',(0.,1.,0.));
#64870=DIRECTION('ref_axis',(0.,0.,1.));
#64871=DIRECTION('center_axis',(0.,-1.,0.));
#64872=DIRECTION('ref_axis',(0.,0.,-1.));
#64873=DIRECTION('center_axis',(0.,1.,0.));
#64874=DIRECTION('ref_axis',(0.,0.,1.));
#64875=DIRECTION('center_axis',(0.,-1.,0.));
#64876=DIRECTION('ref_axis',(0.,0.,-1.));
#64877=DIRECTION('center_axis',(0.,1.,0.));
#64878=DIRECTION('ref_axis',(0.,0.,1.));
#64879=DIRECTION('center_axis',(0.,-1.,0.));
#64880=DIRECTION('ref_axis',(0.,0.,-1.));
#64881=DIRECTION('center_axis',(0.,1.,0.));
#64882=DIRECTION('ref_axis',(0.,0.,1.));
#64883=DIRECTION('center_axis',(0.,-1.,0.));
#64884=DIRECTION('ref_axis',(0.,0.,-1.));
#64885=DIRECTION('center_axis',(0.,1.,0.));
#64886=DIRECTION('ref_axis',(0.,0.,1.));
#64887=DIRECTION('center_axis',(0.,-1.,0.));
#64888=DIRECTION('ref_axis',(0.,0.,-1.));
#64889=DIRECTION('center_axis',(0.,1.,0.));
#64890=DIRECTION('ref_axis',(0.,0.,1.));
#64891=DIRECTION('center_axis',(0.,-1.,0.));
#64892=DIRECTION('ref_axis',(0.,0.,-1.));
#64893=DIRECTION('center_axis',(0.,1.,0.));
#64894=DIRECTION('ref_axis',(0.,0.,1.));
#64895=DIRECTION('center_axis',(0.,-1.,0.));
#64896=DIRECTION('ref_axis',(0.,0.,-1.));
#64897=DIRECTION('center_axis',(0.,1.,0.));
#64898=DIRECTION('ref_axis',(0.,0.,1.));
#64899=DIRECTION('center_axis',(0.,-1.,0.));
#64900=DIRECTION('ref_axis',(0.,0.,-1.));
#64901=DIRECTION('center_axis',(0.,1.,0.));
#64902=DIRECTION('ref_axis',(0.,0.,1.));
#64903=DIRECTION('center_axis',(0.,-1.,0.));
#64904=DIRECTION('ref_axis',(0.,0.,-1.));
#64905=DIRECTION('center_axis',(0.,1.,0.));
#64906=DIRECTION('ref_axis',(0.,0.,1.));
#64907=DIRECTION('center_axis',(0.,-1.,0.));
#64908=DIRECTION('ref_axis',(0.,0.,-1.));
#64909=DIRECTION('center_axis',(0.,1.,0.));
#64910=DIRECTION('ref_axis',(0.,0.,1.));
#64911=DIRECTION('center_axis',(0.,-1.,0.));
#64912=DIRECTION('ref_axis',(0.,0.,-1.));
#64913=DIRECTION('center_axis',(0.,1.,0.));
#64914=DIRECTION('ref_axis',(0.,0.,1.));
#64915=DIRECTION('center_axis',(0.,-1.,0.));
#64916=DIRECTION('ref_axis',(0.,0.,-1.));
#64917=DIRECTION('center_axis',(0.,1.,0.));
#64918=DIRECTION('ref_axis',(0.,0.,1.));
#64919=DIRECTION('center_axis',(0.,-1.,0.));
#64920=DIRECTION('ref_axis',(0.,0.,-1.));
#64921=DIRECTION('center_axis',(0.,1.,0.));
#64922=DIRECTION('ref_axis',(0.,0.,1.));
#64923=DIRECTION('center_axis',(0.,-1.,0.));
#64924=DIRECTION('ref_axis',(0.,0.,-1.));
#64925=DIRECTION('center_axis',(0.,1.,0.));
#64926=DIRECTION('ref_axis',(0.,0.,1.));
#64927=DIRECTION('center_axis',(0.,-1.,0.));
#64928=DIRECTION('ref_axis',(0.,0.,-1.));
#64929=DIRECTION('center_axis',(0.,1.,0.));
#64930=DIRECTION('ref_axis',(0.,0.,1.));
#64931=DIRECTION('center_axis',(0.,-1.,0.));
#64932=DIRECTION('ref_axis',(0.,0.,-1.));
#64933=DIRECTION('center_axis',(0.,1.,0.));
#64934=DIRECTION('ref_axis',(0.,0.,1.));
#64935=DIRECTION('center_axis',(0.,-1.,0.));
#64936=DIRECTION('ref_axis',(0.,0.,-1.));
#64937=DIRECTION('center_axis',(0.,1.,0.));
#64938=DIRECTION('ref_axis',(0.,0.,1.));
#64939=DIRECTION('center_axis',(0.,-1.,0.));
#64940=DIRECTION('ref_axis',(0.,0.,-1.));
#64941=DIRECTION('center_axis',(0.,1.,0.));
#64942=DIRECTION('ref_axis',(0.,0.,1.));
#64943=DIRECTION('center_axis',(0.,-1.,0.));
#64944=DIRECTION('ref_axis',(0.,0.,-1.));
#64945=DIRECTION('center_axis',(0.,1.,0.));
#64946=DIRECTION('ref_axis',(0.,0.,1.));
#64947=DIRECTION('center_axis',(0.,-1.,0.));
#64948=DIRECTION('ref_axis',(0.,0.,-1.));
#64949=DIRECTION('center_axis',(0.,1.,0.));
#64950=DIRECTION('ref_axis',(0.,0.,1.));
#64951=DIRECTION('center_axis',(0.,-1.,0.));
#64952=DIRECTION('ref_axis',(0.,0.,-1.));
#64953=DIRECTION('center_axis',(0.,1.,0.));
#64954=DIRECTION('ref_axis',(0.,0.,1.));
#64955=DIRECTION('center_axis',(0.,-1.,0.));
#64956=DIRECTION('ref_axis',(0.,0.,-1.));
#64957=DIRECTION('center_axis',(0.,1.,0.));
#64958=DIRECTION('ref_axis',(0.,0.,1.));
#64959=DIRECTION('center_axis',(0.,-1.,0.));
#64960=DIRECTION('ref_axis',(0.,0.,-1.));
#64961=DIRECTION('center_axis',(0.,1.,0.));
#64962=DIRECTION('ref_axis',(0.,0.,1.));
#64963=DIRECTION('center_axis',(0.,-1.,0.));
#64964=DIRECTION('ref_axis',(0.,0.,-1.));
#64965=DIRECTION('center_axis',(0.,1.,0.));
#64966=DIRECTION('ref_axis',(0.,0.,1.));
#64967=DIRECTION('center_axis',(0.,-1.,0.));
#64968=DIRECTION('ref_axis',(0.,0.,-1.));
#64969=DIRECTION('center_axis',(0.,1.,0.));
#64970=DIRECTION('ref_axis',(0.,0.,1.));
#64971=DIRECTION('center_axis',(0.,-1.,0.));
#64972=DIRECTION('ref_axis',(0.,0.,-1.));
#64973=DIRECTION('center_axis',(0.,1.,0.));
#64974=DIRECTION('ref_axis',(0.,0.,1.));
#64975=DIRECTION('center_axis',(0.,-1.,0.));
#64976=DIRECTION('ref_axis',(0.,0.,-1.));
#64977=DIRECTION('center_axis',(0.,1.,0.));
#64978=DIRECTION('ref_axis',(0.,0.,1.));
#64979=DIRECTION('center_axis',(0.,-1.,0.));
#64980=DIRECTION('ref_axis',(0.,0.,-1.));
#64981=DIRECTION('center_axis',(0.,1.,0.));
#64982=DIRECTION('ref_axis',(0.,0.,1.));
#64983=DIRECTION('center_axis',(0.,-1.,0.));
#64984=DIRECTION('ref_axis',(0.,0.,-1.));
#64985=DIRECTION('center_axis',(0.,1.,0.));
#64986=DIRECTION('ref_axis',(0.,0.,1.));
#64987=DIRECTION('center_axis',(0.,-1.,0.));
#64988=DIRECTION('ref_axis',(0.,0.,-1.));
#64989=DIRECTION('center_axis',(0.,1.,0.));
#64990=DIRECTION('ref_axis',(0.,0.,1.));
#64991=DIRECTION('center_axis',(0.,-1.,0.));
#64992=DIRECTION('ref_axis',(0.,0.,-1.));
#64993=DIRECTION('center_axis',(0.,1.,0.));
#64994=DIRECTION('ref_axis',(0.,0.,1.));
#64995=DIRECTION('center_axis',(0.,-1.,0.));
#64996=DIRECTION('ref_axis',(0.,0.,-1.));
#64997=DIRECTION('center_axis',(0.,1.,0.));
#64998=DIRECTION('ref_axis',(0.,0.,1.));
#64999=DIRECTION('center_axis',(0.,-1.,0.));
#65000=DIRECTION('ref_axis',(0.,0.,-1.));
#65001=DIRECTION('center_axis',(0.,1.,0.));
#65002=DIRECTION('ref_axis',(0.,0.,1.));
#65003=DIRECTION('center_axis',(0.,-1.,0.));
#65004=DIRECTION('ref_axis',(0.,0.,-1.));
#65005=DIRECTION('center_axis',(0.,1.,0.));
#65006=DIRECTION('ref_axis',(0.,0.,1.));
#65007=DIRECTION('center_axis',(0.,-1.,0.));
#65008=DIRECTION('ref_axis',(0.,0.,-1.));
#65009=DIRECTION('center_axis',(0.,1.,0.));
#65010=DIRECTION('ref_axis',(0.,0.,1.));
#65011=DIRECTION('center_axis',(0.,-1.,0.));
#65012=DIRECTION('ref_axis',(0.,0.,-1.));
#65013=DIRECTION('center_axis',(0.,1.,0.));
#65014=DIRECTION('ref_axis',(0.,0.,1.));
#65015=DIRECTION('center_axis',(0.,-1.,0.));
#65016=DIRECTION('ref_axis',(0.,0.,-1.));
#65017=DIRECTION('center_axis',(0.,1.,0.));
#65018=DIRECTION('ref_axis',(0.,0.,1.));
#65019=DIRECTION('center_axis',(0.,-1.,0.));
#65020=DIRECTION('ref_axis',(0.,0.,-1.));
#65021=DIRECTION('center_axis',(0.,1.,0.));
#65022=DIRECTION('ref_axis',(0.,0.,1.));
#65023=DIRECTION('center_axis',(0.,-1.,0.));
#65024=DIRECTION('ref_axis',(0.,0.,-1.));
#65025=DIRECTION('center_axis',(0.,1.,0.));
#65026=DIRECTION('ref_axis',(0.,0.,1.));
#65027=DIRECTION('center_axis',(0.,-1.,0.));
#65028=DIRECTION('ref_axis',(0.,0.,-1.));
#65029=DIRECTION('center_axis',(0.,1.,0.));
#65030=DIRECTION('ref_axis',(0.,0.,1.));
#65031=DIRECTION('center_axis',(0.,-1.,0.));
#65032=DIRECTION('ref_axis',(0.,0.,-1.));
#65033=DIRECTION('center_axis',(0.,1.,0.));
#65034=DIRECTION('ref_axis',(0.,0.,1.));
#65035=DIRECTION('center_axis',(0.,-1.,0.));
#65036=DIRECTION('ref_axis',(0.,0.,-1.));
#65037=DIRECTION('center_axis',(0.,1.,0.));
#65038=DIRECTION('ref_axis',(0.,0.,1.));
#65039=DIRECTION('center_axis',(0.,-1.,0.));
#65040=DIRECTION('ref_axis',(0.,0.,-1.));
#65041=DIRECTION('center_axis',(0.,1.,0.));
#65042=DIRECTION('ref_axis',(0.,0.,1.));
#65043=DIRECTION('center_axis',(0.,-1.,0.));
#65044=DIRECTION('ref_axis',(0.,0.,-1.));
#65045=DIRECTION('center_axis',(0.,1.,0.));
#65046=DIRECTION('ref_axis',(0.,0.,1.));
#65047=DIRECTION('center_axis',(0.,-1.,0.));
#65048=DIRECTION('ref_axis',(0.,0.,-1.));
#65049=DIRECTION('center_axis',(0.,1.,0.));
#65050=DIRECTION('ref_axis',(0.,0.,1.));
#65051=DIRECTION('center_axis',(0.,-1.,0.));
#65052=DIRECTION('ref_axis',(0.,0.,-1.));
#65053=DIRECTION('center_axis',(0.,1.,0.));
#65054=DIRECTION('ref_axis',(0.,0.,1.));
#65055=DIRECTION('center_axis',(0.,-1.,0.));
#65056=DIRECTION('ref_axis',(0.,0.,-1.));
#65057=DIRECTION('center_axis',(0.,1.,0.));
#65058=DIRECTION('ref_axis',(0.,0.,1.));
#65059=DIRECTION('center_axis',(0.,-1.,0.));
#65060=DIRECTION('ref_axis',(0.,0.,-1.));
#65061=DIRECTION('center_axis',(0.,1.,0.));
#65062=DIRECTION('ref_axis',(0.,0.,1.));
#65063=DIRECTION('center_axis',(0.,-1.,0.));
#65064=DIRECTION('ref_axis',(0.,0.,-1.));
#65065=DIRECTION('center_axis',(0.,1.,0.));
#65066=DIRECTION('ref_axis',(0.,0.,1.));
#65067=DIRECTION('center_axis',(0.,-1.,0.));
#65068=DIRECTION('ref_axis',(0.,0.,-1.));
#65069=DIRECTION('center_axis',(0.,1.,0.));
#65070=DIRECTION('ref_axis',(0.,0.,1.));
#65071=DIRECTION('center_axis',(0.,-1.,0.));
#65072=DIRECTION('ref_axis',(0.,0.,-1.));
#65073=DIRECTION('center_axis',(0.,1.,0.));
#65074=DIRECTION('ref_axis',(0.,0.,1.));
#65075=DIRECTION('center_axis',(0.,-1.,0.));
#65076=DIRECTION('ref_axis',(0.,0.,-1.));
#65077=DIRECTION('center_axis',(0.,1.,0.));
#65078=DIRECTION('ref_axis',(0.,0.,1.));
#65079=DIRECTION('center_axis',(0.,-1.,0.));
#65080=DIRECTION('ref_axis',(0.,0.,-1.));
#65081=DIRECTION('center_axis',(0.,1.,0.));
#65082=DIRECTION('ref_axis',(0.,0.,1.));
#65083=DIRECTION('center_axis',(0.,-1.,0.));
#65084=DIRECTION('ref_axis',(0.,0.,-1.));
#65085=DIRECTION('center_axis',(0.,1.,0.));
#65086=DIRECTION('ref_axis',(0.,0.,1.));
#65087=DIRECTION('center_axis',(0.,-1.,0.));
#65088=DIRECTION('ref_axis',(0.,0.,-1.));
#65089=DIRECTION('center_axis',(0.,1.,0.));
#65090=DIRECTION('ref_axis',(0.,0.,1.));
#65091=DIRECTION('center_axis',(0.,-1.,0.));
#65092=DIRECTION('ref_axis',(0.,0.,-1.));
#65093=DIRECTION('center_axis',(0.,1.,0.));
#65094=DIRECTION('ref_axis',(0.,0.,1.));
#65095=DIRECTION('center_axis',(0.,-1.,0.));
#65096=DIRECTION('ref_axis',(0.,0.,-1.));
#65097=DIRECTION('center_axis',(0.,1.,0.));
#65098=DIRECTION('ref_axis',(0.,0.,1.));
#65099=DIRECTION('center_axis',(0.,-1.,0.));
#65100=DIRECTION('ref_axis',(0.,0.,-1.));
#65101=DIRECTION('center_axis',(0.,1.,0.));
#65102=DIRECTION('ref_axis',(0.,0.,1.));
#65103=DIRECTION('center_axis',(0.,-1.,0.));
#65104=DIRECTION('ref_axis',(0.,0.,-1.));
#65105=DIRECTION('center_axis',(0.,1.,0.));
#65106=DIRECTION('ref_axis',(0.,0.,1.));
#65107=DIRECTION('center_axis',(0.,-1.,0.));
#65108=DIRECTION('ref_axis',(0.,0.,-1.));
#65109=DIRECTION('center_axis',(0.,1.,0.));
#65110=DIRECTION('ref_axis',(0.,0.,1.));
#65111=DIRECTION('center_axis',(0.,-1.,0.));
#65112=DIRECTION('ref_axis',(0.,0.,-1.));
#65113=DIRECTION('center_axis',(0.,1.,0.));
#65114=DIRECTION('ref_axis',(0.,0.,1.));
#65115=DIRECTION('center_axis',(0.,-1.,0.));
#65116=DIRECTION('ref_axis',(0.,0.,-1.));
#65117=DIRECTION('center_axis',(0.,1.,0.));
#65118=DIRECTION('ref_axis',(0.,0.,1.));
#65119=DIRECTION('center_axis',(0.,-1.,0.));
#65120=DIRECTION('ref_axis',(0.,0.,-1.));
#65121=DIRECTION('center_axis',(0.,1.,0.));
#65122=DIRECTION('ref_axis',(0.,0.,1.));
#65123=DIRECTION('center_axis',(0.,-1.,0.));
#65124=DIRECTION('ref_axis',(0.,0.,-1.));
#65125=DIRECTION('center_axis',(0.,1.,0.));
#65126=DIRECTION('ref_axis',(0.,0.,1.));
#65127=DIRECTION('center_axis',(0.,-1.,0.));
#65128=DIRECTION('ref_axis',(0.,0.,-1.));
#65129=DIRECTION('center_axis',(0.,1.,0.));
#65130=DIRECTION('ref_axis',(0.,0.,1.));
#65131=DIRECTION('center_axis',(0.,-1.,0.));
#65132=DIRECTION('ref_axis',(0.,0.,-1.));
#65133=DIRECTION('center_axis',(0.,1.,0.));
#65134=DIRECTION('ref_axis',(0.,0.,1.));
#65135=DIRECTION('center_axis',(0.,-1.,0.));
#65136=DIRECTION('ref_axis',(0.,0.,-1.));
#65137=DIRECTION('center_axis',(0.,1.,0.));
#65138=DIRECTION('ref_axis',(0.,0.,1.));
#65139=DIRECTION('center_axis',(0.,-1.,0.));
#65140=DIRECTION('ref_axis',(0.,0.,-1.));
#65141=DIRECTION('center_axis',(0.,1.,0.));
#65142=DIRECTION('ref_axis',(0.,0.,1.));
#65143=DIRECTION('center_axis',(0.,-1.,0.));
#65144=DIRECTION('ref_axis',(0.,0.,-1.));
#65145=DIRECTION('center_axis',(0.,1.,0.));
#65146=DIRECTION('ref_axis',(0.,0.,1.));
#65147=DIRECTION('center_axis',(0.,-1.,0.));
#65148=DIRECTION('ref_axis',(0.,0.,-1.));
#65149=DIRECTION('center_axis',(0.,1.,0.));
#65150=DIRECTION('ref_axis',(0.,0.,1.));
#65151=DIRECTION('center_axis',(0.,-1.,0.));
#65152=DIRECTION('ref_axis',(0.,0.,-1.));
#65153=DIRECTION('center_axis',(0.,1.,0.));
#65154=DIRECTION('ref_axis',(0.,0.,1.));
#65155=DIRECTION('center_axis',(0.,-1.,0.));
#65156=DIRECTION('ref_axis',(0.,0.,-1.));
#65157=DIRECTION('center_axis',(0.,1.,0.));
#65158=DIRECTION('ref_axis',(0.,0.,1.));
#65159=DIRECTION('center_axis',(0.,-1.,0.));
#65160=DIRECTION('ref_axis',(0.,0.,-1.));
#65161=DIRECTION('center_axis',(0.,1.,0.));
#65162=DIRECTION('ref_axis',(0.,0.,1.));
#65163=DIRECTION('center_axis',(0.,-1.,0.));
#65164=DIRECTION('ref_axis',(0.,0.,-1.));
#65165=DIRECTION('center_axis',(0.,1.,0.));
#65166=DIRECTION('ref_axis',(0.,0.,1.));
#65167=DIRECTION('center_axis',(0.,-1.,0.));
#65168=DIRECTION('ref_axis',(0.,0.,-1.));
#65169=DIRECTION('center_axis',(0.,1.,0.));
#65170=DIRECTION('ref_axis',(0.,0.,1.));
#65171=DIRECTION('center_axis',(0.,-1.,0.));
#65172=DIRECTION('ref_axis',(0.,0.,-1.));
#65173=DIRECTION('center_axis',(0.,1.,0.));
#65174=DIRECTION('ref_axis',(0.,0.,1.));
#65175=DIRECTION('center_axis',(0.,-1.,0.));
#65176=DIRECTION('ref_axis',(0.,0.,-1.));
#65177=DIRECTION('center_axis',(0.,1.,0.));
#65178=DIRECTION('ref_axis',(0.,0.,1.));
#65179=DIRECTION('center_axis',(0.,-1.,0.));
#65180=DIRECTION('ref_axis',(0.,0.,-1.));
#65181=DIRECTION('center_axis',(0.,1.,0.));
#65182=DIRECTION('ref_axis',(0.,0.,1.));
#65183=DIRECTION('center_axis',(0.,-1.,0.));
#65184=DIRECTION('ref_axis',(0.,0.,-1.));
#65185=DIRECTION('center_axis',(0.,1.,0.));
#65186=DIRECTION('ref_axis',(0.,0.,1.));
#65187=DIRECTION('center_axis',(0.,-1.,0.));
#65188=DIRECTION('ref_axis',(0.,0.,-1.));
#65189=DIRECTION('center_axis',(0.,1.,0.));
#65190=DIRECTION('ref_axis',(0.,0.,1.));
#65191=DIRECTION('center_axis',(0.,-1.,0.));
#65192=DIRECTION('ref_axis',(0.,0.,-1.));
#65193=DIRECTION('center_axis',(0.,1.,0.));
#65194=DIRECTION('ref_axis',(0.,0.,1.));
#65195=DIRECTION('center_axis',(0.,-1.,0.));
#65196=DIRECTION('ref_axis',(0.,0.,-1.));
#65197=DIRECTION('center_axis',(0.,1.,0.));
#65198=DIRECTION('ref_axis',(0.,0.,1.));
#65199=DIRECTION('center_axis',(0.,-1.,0.));
#65200=DIRECTION('ref_axis',(0.,0.,-1.));
#65201=DIRECTION('center_axis',(0.,1.,0.));
#65202=DIRECTION('ref_axis',(0.,0.,1.));
#65203=DIRECTION('center_axis',(0.,-1.,0.));
#65204=DIRECTION('ref_axis',(0.,0.,-1.));
#65205=DIRECTION('center_axis',(0.,1.,0.));
#65206=DIRECTION('ref_axis',(0.,0.,1.));
#65207=DIRECTION('center_axis',(0.,-1.,0.));
#65208=DIRECTION('ref_axis',(0.,0.,-1.));
#65209=DIRECTION('center_axis',(0.,1.,0.));
#65210=DIRECTION('ref_axis',(0.,0.,1.));
#65211=DIRECTION('center_axis',(0.,-1.,0.));
#65212=DIRECTION('ref_axis',(0.,0.,-1.));
#65213=DIRECTION('center_axis',(0.,1.,0.));
#65214=DIRECTION('ref_axis',(0.,0.,1.));
#65215=DIRECTION('center_axis',(0.,-1.,0.));
#65216=DIRECTION('ref_axis',(0.,0.,-1.));
#65217=DIRECTION('center_axis',(0.,1.,0.));
#65218=DIRECTION('ref_axis',(0.,0.,1.));
#65219=DIRECTION('center_axis',(0.,-1.,0.));
#65220=DIRECTION('ref_axis',(0.,0.,-1.));
#65221=DIRECTION('center_axis',(0.,1.,0.));
#65222=DIRECTION('ref_axis',(0.,0.,1.));
#65223=DIRECTION('center_axis',(0.,-1.,0.));
#65224=DIRECTION('ref_axis',(0.,0.,-1.));
#65225=DIRECTION('center_axis',(0.,1.,0.));
#65226=DIRECTION('ref_axis',(0.,0.,1.));
#65227=DIRECTION('center_axis',(0.,1.,0.));
#65228=DIRECTION('ref_axis',(0.,0.,1.));
#65229=DIRECTION('center_axis',(0.,1.,0.));
#65230=DIRECTION('ref_axis',(0.,0.,1.));
#65231=DIRECTION('center_axis',(0.,1.,0.));
#65232=DIRECTION('ref_axis',(0.,0.,1.));
#65233=DIRECTION('center_axis',(0.,1.,0.));
#65234=DIRECTION('ref_axis',(0.,0.,1.));
#65235=DIRECTION('center_axis',(0.,1.,0.));
#65236=DIRECTION('ref_axis',(0.,0.,1.));
#65237=DIRECTION('center_axis',(0.,1.,0.));
#65238=DIRECTION('ref_axis',(0.,0.,1.));
#65239=DIRECTION('center_axis',(0.,1.,0.));
#65240=DIRECTION('ref_axis',(0.,0.,1.));
#65241=DIRECTION('center_axis',(0.,1.,0.));
#65242=DIRECTION('ref_axis',(0.,0.,1.));
#65243=DIRECTION('center_axis',(0.,1.,0.));
#65244=DIRECTION('ref_axis',(0.,0.,1.));
#65245=DIRECTION('center_axis',(0.,1.,0.));
#65246=DIRECTION('ref_axis',(0.,0.,1.));
#65247=DIRECTION('center_axis',(0.,1.,0.));
#65248=DIRECTION('ref_axis',(0.,0.,1.));
#65249=DIRECTION('center_axis',(0.,1.,0.));
#65250=DIRECTION('ref_axis',(0.,0.,1.));
#65251=DIRECTION('center_axis',(0.,1.,0.));
#65252=DIRECTION('ref_axis',(0.,0.,1.));
#65253=DIRECTION('center_axis',(0.,1.,0.));
#65254=DIRECTION('ref_axis',(0.,0.,1.));
#65255=DIRECTION('center_axis',(0.,1.,0.));
#65256=DIRECTION('ref_axis',(0.,0.,1.));
#65257=DIRECTION('center_axis',(0.,1.,0.));
#65258=DIRECTION('ref_axis',(0.,0.,1.));
#65259=DIRECTION('center_axis',(0.,1.,0.));
#65260=DIRECTION('ref_axis',(0.,0.,1.));
#65261=DIRECTION('center_axis',(0.,1.,0.));
#65262=DIRECTION('ref_axis',(0.,0.,1.));
#65263=DIRECTION('center_axis',(0.,1.,0.));
#65264=DIRECTION('ref_axis',(0.,0.,1.));
#65265=DIRECTION('center_axis',(0.,1.,0.));
#65266=DIRECTION('ref_axis',(0.,0.,1.));
#65267=DIRECTION('center_axis',(0.,1.,0.));
#65268=DIRECTION('ref_axis',(0.,0.,1.));
#65269=DIRECTION('center_axis',(0.,1.,0.));
#65270=DIRECTION('ref_axis',(0.,0.,1.));
#65271=DIRECTION('center_axis',(0.,1.,0.));
#65272=DIRECTION('ref_axis',(0.,0.,1.));
#65273=DIRECTION('center_axis',(0.,1.,0.));
#65274=DIRECTION('ref_axis',(0.,0.,1.));
#65275=DIRECTION('center_axis',(0.,1.,0.));
#65276=DIRECTION('ref_axis',(0.,0.,1.));
#65277=DIRECTION('center_axis',(0.,1.,0.));
#65278=DIRECTION('ref_axis',(0.,0.,1.));
#65279=DIRECTION('center_axis',(0.,1.,0.));
#65280=DIRECTION('ref_axis',(0.,0.,1.));
#65281=DIRECTION('center_axis',(0.,1.,0.));
#65282=DIRECTION('ref_axis',(0.,0.,1.));
#65283=DIRECTION('center_axis',(0.,1.,0.));
#65284=DIRECTION('ref_axis',(0.,0.,1.));
#65285=DIRECTION('center_axis',(0.,1.,0.));
#65286=DIRECTION('ref_axis',(0.,0.,1.));
#65287=DIRECTION('center_axis',(0.,1.,0.));
#65288=DIRECTION('ref_axis',(0.,0.,1.));
#65289=DIRECTION('center_axis',(0.,1.,0.));
#65290=DIRECTION('ref_axis',(0.,0.,1.));
#65291=DIRECTION('center_axis',(0.,1.,0.));
#65292=DIRECTION('ref_axis',(0.,0.,1.));
#65293=DIRECTION('center_axis',(0.,1.,0.));
#65294=DIRECTION('ref_axis',(0.,0.,1.));
#65295=DIRECTION('center_axis',(0.,1.,0.));
#65296=DIRECTION('ref_axis',(0.,0.,1.));
#65297=DIRECTION('center_axis',(0.,1.,0.));
#65298=DIRECTION('ref_axis',(0.,0.,1.));
#65299=DIRECTION('center_axis',(0.,1.,0.));
#65300=DIRECTION('ref_axis',(0.,0.,1.));
#65301=DIRECTION('center_axis',(0.,1.,0.));
#65302=DIRECTION('ref_axis',(0.,0.,1.));
#65303=DIRECTION('center_axis',(0.,1.,0.));
#65304=DIRECTION('ref_axis',(0.,0.,1.));
#65305=DIRECTION('center_axis',(0.,1.,0.));
#65306=DIRECTION('ref_axis',(0.,0.,1.));
#65307=DIRECTION('center_axis',(0.,1.,0.));
#65308=DIRECTION('ref_axis',(0.,0.,1.));
#65309=DIRECTION('center_axis',(0.,1.,0.));
#65310=DIRECTION('ref_axis',(0.,0.,1.));
#65311=DIRECTION('center_axis',(0.,1.,0.));
#65312=DIRECTION('ref_axis',(0.,0.,1.));
#65313=DIRECTION('center_axis',(0.,1.,0.));
#65314=DIRECTION('ref_axis',(0.,0.,1.));
#65315=DIRECTION('center_axis',(0.,1.,0.));
#65316=DIRECTION('ref_axis',(0.,0.,1.));
#65317=DIRECTION('center_axis',(0.,1.,0.));
#65318=DIRECTION('ref_axis',(0.,0.,1.));
#65319=DIRECTION('center_axis',(0.,1.,0.));
#65320=DIRECTION('ref_axis',(0.,0.,1.));
#65321=DIRECTION('center_axis',(0.,1.,0.));
#65322=DIRECTION('ref_axis',(0.,0.,1.));
#65323=DIRECTION('center_axis',(0.,1.,0.));
#65324=DIRECTION('ref_axis',(0.,0.,1.));
#65325=DIRECTION('center_axis',(0.,1.,0.));
#65326=DIRECTION('ref_axis',(0.,0.,1.));
#65327=DIRECTION('center_axis',(0.,1.,0.));
#65328=DIRECTION('ref_axis',(0.,0.,1.));
#65329=DIRECTION('center_axis',(0.,1.,0.));
#65330=DIRECTION('ref_axis',(0.,0.,1.));
#65331=DIRECTION('center_axis',(0.,1.,0.));
#65332=DIRECTION('ref_axis',(0.,0.,1.));
#65333=DIRECTION('center_axis',(0.,1.,0.));
#65334=DIRECTION('ref_axis',(0.,0.,1.));
#65335=DIRECTION('center_axis',(0.,1.,0.));
#65336=DIRECTION('ref_axis',(0.,0.,1.));
#65337=DIRECTION('center_axis',(0.,1.,0.));
#65338=DIRECTION('ref_axis',(0.,0.,1.));
#65339=DIRECTION('center_axis',(0.,1.,0.));
#65340=DIRECTION('ref_axis',(0.,0.,1.));
#65341=DIRECTION('center_axis',(0.,1.,0.));
#65342=DIRECTION('ref_axis',(0.,0.,1.));
#65343=DIRECTION('center_axis',(0.,1.,0.));
#65344=DIRECTION('ref_axis',(0.,0.,1.));
#65345=DIRECTION('center_axis',(0.,1.,0.));
#65346=DIRECTION('ref_axis',(0.,0.,1.));
#65347=DIRECTION('center_axis',(0.,1.,0.));
#65348=DIRECTION('ref_axis',(0.,0.,1.));
#65349=DIRECTION('center_axis',(0.,1.,0.));
#65350=DIRECTION('ref_axis',(0.,0.,1.));
#65351=DIRECTION('center_axis',(0.,1.,0.));
#65352=DIRECTION('ref_axis',(0.,0.,1.));
#65353=DIRECTION('center_axis',(0.,1.,0.));
#65354=DIRECTION('ref_axis',(0.,0.,1.));
#65355=DIRECTION('center_axis',(0.,1.,0.));
#65356=DIRECTION('ref_axis',(0.,0.,1.));
#65357=DIRECTION('center_axis',(0.,1.,0.));
#65358=DIRECTION('ref_axis',(0.,0.,1.));
#65359=DIRECTION('center_axis',(0.,1.,0.));
#65360=DIRECTION('ref_axis',(0.,0.,1.));
#65361=DIRECTION('center_axis',(0.,1.,0.));
#65362=DIRECTION('ref_axis',(0.,0.,1.));
#65363=DIRECTION('center_axis',(0.,1.,0.));
#65364=DIRECTION('ref_axis',(0.,0.,1.));
#65365=DIRECTION('center_axis',(0.,1.,0.));
#65366=DIRECTION('ref_axis',(0.,0.,1.));
#65367=DIRECTION('center_axis',(0.,1.,0.));
#65368=DIRECTION('ref_axis',(0.,0.,1.));
#65369=DIRECTION('center_axis',(0.,1.,0.));
#65370=DIRECTION('ref_axis',(0.,0.,1.));
#65371=DIRECTION('center_axis',(0.,1.,0.));
#65372=DIRECTION('ref_axis',(0.,0.,1.));
#65373=DIRECTION('center_axis',(0.,1.,0.));
#65374=DIRECTION('ref_axis',(0.,0.,1.));
#65375=DIRECTION('center_axis',(0.,1.,0.));
#65376=DIRECTION('ref_axis',(0.,0.,1.));
#65377=DIRECTION('center_axis',(0.,1.,0.));
#65378=DIRECTION('ref_axis',(0.,0.,1.));
#65379=DIRECTION('center_axis',(0.,1.,0.));
#65380=DIRECTION('ref_axis',(0.,0.,1.));
#65381=DIRECTION('center_axis',(0.,1.,0.));
#65382=DIRECTION('ref_axis',(0.,0.,1.));
#65383=DIRECTION('center_axis',(0.,1.,0.));
#65384=DIRECTION('ref_axis',(0.,0.,1.));
#65385=DIRECTION('center_axis',(0.,1.,0.));
#65386=DIRECTION('ref_axis',(0.,0.,1.));
#65387=DIRECTION('center_axis',(0.,1.,0.));
#65388=DIRECTION('ref_axis',(0.,0.,1.));
#65389=DIRECTION('center_axis',(0.,1.,0.));
#65390=DIRECTION('ref_axis',(0.,0.,1.));
#65391=DIRECTION('center_axis',(0.,1.,0.));
#65392=DIRECTION('ref_axis',(0.,0.,1.));
#65393=DIRECTION('center_axis',(0.,1.,0.));
#65394=DIRECTION('ref_axis',(0.,0.,1.));
#65395=DIRECTION('center_axis',(0.,1.,0.));
#65396=DIRECTION('ref_axis',(0.,0.,1.));
#65397=DIRECTION('center_axis',(0.,1.,0.));
#65398=DIRECTION('ref_axis',(0.,0.,1.));
#65399=DIRECTION('center_axis',(0.,1.,0.));
#65400=DIRECTION('ref_axis',(0.,0.,1.));
#65401=DIRECTION('center_axis',(0.,1.,0.));
#65402=DIRECTION('ref_axis',(0.,0.,1.));
#65403=DIRECTION('center_axis',(0.,1.,0.));
#65404=DIRECTION('ref_axis',(0.,0.,1.));
#65405=DIRECTION('center_axis',(0.,1.,0.));
#65406=DIRECTION('ref_axis',(0.,0.,1.));
#65407=DIRECTION('center_axis',(0.,1.,0.));
#65408=DIRECTION('ref_axis',(0.,0.,1.));
#65409=DIRECTION('center_axis',(0.,1.,0.));
#65410=DIRECTION('ref_axis',(0.,0.,1.));
#65411=DIRECTION('center_axis',(0.,1.,0.));
#65412=DIRECTION('ref_axis',(0.,0.,1.));
#65413=DIRECTION('center_axis',(0.,1.,0.));
#65414=DIRECTION('ref_axis',(0.,0.,1.));
#65415=DIRECTION('center_axis',(0.,1.,0.));
#65416=DIRECTION('ref_axis',(0.,0.,1.));
#65417=DIRECTION('center_axis',(0.,1.,0.));
#65418=DIRECTION('ref_axis',(0.,0.,1.));
#65419=DIRECTION('center_axis',(0.,1.,0.));
#65420=DIRECTION('ref_axis',(0.,0.,1.));
#65421=DIRECTION('center_axis',(0.,1.,0.));
#65422=DIRECTION('ref_axis',(0.,0.,1.));
#65423=DIRECTION('center_axis',(0.,1.,0.));
#65424=DIRECTION('ref_axis',(0.,0.,1.));
#65425=DIRECTION('center_axis',(0.,1.,0.));
#65426=DIRECTION('ref_axis',(0.,0.,1.));
#65427=DIRECTION('center_axis',(0.,1.,0.));
#65428=DIRECTION('ref_axis',(0.,0.,1.));
#65429=DIRECTION('center_axis',(0.,1.,0.));
#65430=DIRECTION('ref_axis',(0.,0.,1.));
#65431=DIRECTION('center_axis',(0.,1.,0.));
#65432=DIRECTION('ref_axis',(0.,0.,1.));
#65433=DIRECTION('center_axis',(0.,1.,0.));
#65434=DIRECTION('ref_axis',(0.,0.,1.));
#65435=DIRECTION('center_axis',(0.,1.,0.));
#65436=DIRECTION('ref_axis',(0.,0.,1.));
#65437=DIRECTION('center_axis',(0.,1.,0.));
#65438=DIRECTION('ref_axis',(0.,0.,1.));
#65439=DIRECTION('center_axis',(0.,1.,0.));
#65440=DIRECTION('ref_axis',(0.,0.,1.));
#65441=DIRECTION('center_axis',(0.,1.,0.));
#65442=DIRECTION('ref_axis',(0.,0.,1.));
#65443=DIRECTION('center_axis',(0.,1.,0.));
#65444=DIRECTION('ref_axis',(0.,0.,1.));
#65445=DIRECTION('center_axis',(0.,1.,0.));
#65446=DIRECTION('ref_axis',(0.,0.,1.));
#65447=DIRECTION('center_axis',(0.,1.,0.));
#65448=DIRECTION('ref_axis',(0.,0.,1.));
#65449=DIRECTION('center_axis',(0.,1.,0.));
#65450=DIRECTION('ref_axis',(0.,0.,1.));
#65451=DIRECTION('center_axis',(0.,1.,0.));
#65452=DIRECTION('ref_axis',(0.,0.,1.));
#65453=DIRECTION('center_axis',(0.,1.,0.));
#65454=DIRECTION('ref_axis',(0.,0.,1.));
#65455=DIRECTION('center_axis',(0.,1.,0.));
#65456=DIRECTION('ref_axis',(0.,0.,1.));
#65457=DIRECTION('center_axis',(0.,1.,0.));
#65458=DIRECTION('ref_axis',(0.,0.,1.));
#65459=DIRECTION('center_axis',(0.,1.,0.));
#65460=DIRECTION('ref_axis',(0.,0.,1.));
#65461=DIRECTION('center_axis',(0.,1.,0.));
#65462=DIRECTION('ref_axis',(0.,0.,1.));
#65463=DIRECTION('',(0.,0.,1.));
#65464=DIRECTION('',(1.,0.,0.));
#65465=DIRECTION('',(0.,0.,1.));
#65466=DIRECTION('',(1.,0.,0.));
#65467=DIRECTION('',(0.,0.,1.));
#65468=DIRECTION('',(1.,0.,0.));
#65469=DIRECTION('',(0.,0.,1.));
#65470=DIRECTION('',(1.,0.,0.));
#65471=DIRECTION('',(0.,0.,1.));
#65472=DIRECTION('',(1.,0.,0.));
#65473=DIRECTION('',(0.,0.,1.));
#65474=DIRECTION('',(1.,0.,0.));
#65475=DIRECTION('',(0.,0.,1.));
#65476=DIRECTION('',(1.,0.,0.));
#65477=DIRECTION('',(0.,0.,1.));
#65478=DIRECTION('',(1.,0.,0.));
#65479=CARTESIAN_POINT('',(0.,0.,0.));
#65480=CARTESIAN_POINT('',(0.,0.,0.));
#65481=CARTESIAN_POINT('Origin',(0.,1148.83458861821,94.2994740882088));
#65482=CARTESIAN_POINT('',(1.40834381901946E-15,1148.83458861821,75.7994740882088));
#65483=CARTESIAN_POINT('Origin',(0.,1148.83458861821,64.2994740882088));
#65484=CARTESIAN_POINT('',(1.40834381901946E-15,1167.33458861821,94.2994740882088));
#65485=CARTESIAN_POINT('Origin',(1.40834381901946E-15,1148.83458861821,
94.2994740882088));
#65486=CARTESIAN_POINT('',(11.5,1178.83458861821,94.2994740882088));
#65487=CARTESIAN_POINT('Origin',(0.,1178.83458861821,94.2994740882088));
#65488=CARTESIAN_POINT('Origin',(0.,1178.83458861821,94.2994740882088));
#65489=CARTESIAN_POINT('Origin',(0.,1148.83458861821,394.620242579854));
#65490=CARTESIAN_POINT('',(1.40834381901946E-15,1167.33458861821,394.620242579854));
#65491=CARTESIAN_POINT('',(11.5,1178.83458861821,394.620242579854));
#65492=CARTESIAN_POINT('Origin',(0.,1178.83458861821,394.620242579854));
#65493=CARTESIAN_POINT('',(1.40834381901946E-15,1148.83458861821,413.120242579854));
#65494=CARTESIAN_POINT('Origin',(1.40834381901946E-15,1148.83458861821,
394.620242579854));
#65495=CARTESIAN_POINT('Origin',(0.,1148.83458861821,424.620242579854));
#65496=CARTESIAN_POINT('Origin',(0.,1178.83458861821,394.620242579854));
#65497=CARTESIAN_POINT('Origin',(0.,1148.83458861821,64.2994740882088));
#65498=CARTESIAN_POINT('',(-1.40834381901946E-15,737.065928490981,75.7994740882088));
#65499=CARTESIAN_POINT('Origin',(0.,737.065928490981,64.2994740882088));
#65500=CARTESIAN_POINT('',(-1.40834381901946E-15,1148.83458861821,75.7994740882088));
#65501=CARTESIAN_POINT('Origin',(0.,1178.83458861821,394.620242579854));
#65502=CARTESIAN_POINT('',(11.5,1178.83458861821,394.620242579854));
#65503=CARTESIAN_POINT('Origin',(0.,1134.14517683891,424.620242579854));
#65504=CARTESIAN_POINT('',(-1.40834381901946E-15,1134.14517683891,413.120242579854));
#65505=CARTESIAN_POINT('',(-1.40834381901946E-15,1134.14517683891,413.120242579854));
#65506=CARTESIAN_POINT('Origin',(0.,1134.14517683891,424.620242579854));
#65507=CARTESIAN_POINT('Origin',(0.,737.065928490981,76.7994740882088));
#65508=CARTESIAN_POINT('Origin',(0.,1134.14517683891,424.620242579854));
#65509=CARTESIAN_POINT('',(0.,0.,0.));
#65510=CARTESIAN_POINT('Origin',(52.8776183915471,752.330434448379,91.3216571729483));
#65511=CARTESIAN_POINT('',(44.574479425553,751.596144557082,91.2509530983505));
#65512=CARTESIAN_POINT('',(44.574479425553,744.926214295584,90.6087118617898));
#65513=CARTESIAN_POINT('',(44.574479425553,752.330434448379,91.3216571729483));
#65514=CARTESIAN_POINT('',(61.1807573575412,751.596144557082,91.2509530983505));
#65515=CARTESIAN_POINT('Origin',(52.8776183915471,751.59614455564,91.2509530980753));
#65516=CARTESIAN_POINT('',(61.1807573575412,744.926214295584,90.6087118617898));
#65517=CARTESIAN_POINT('',(61.1807573575412,752.330434448379,91.3216571729483));
#65518=CARTESIAN_POINT('',(52.8776183915471,744.926214295584,90.6087118617898));
#65519=CARTESIAN_POINT('Origin',(52.8776183915471,751.59614455564,90.6087118617898));
#65520=CARTESIAN_POINT('',(61.1807573575412,751.59614455564,90.6087118617898));
#65521=CARTESIAN_POINT('',(61.1807573575412,751.59614455564,90.6087118617898));
#65522=CARTESIAN_POINT('',(44.574479425553,751.59614455564,90.6087118617898));
#65523=CARTESIAN_POINT('Origin',(52.8776183915471,751.59614455564,90.6087118617898));
#65524=CARTESIAN_POINT('',(44.574479425553,751.59614455564,90.6087118617898));
#65525=CARTESIAN_POINT('Origin',(52.8776183915471,751.59614455564,112.60871186179));
#65526=CARTESIAN_POINT('',(44.574479425553,751.59614455564,112.60871186179));
#65527=CARTESIAN_POINT('',(61.1807573575412,751.59614455564,112.60871186179));
#65528=CARTESIAN_POINT('Origin',(61.1807573575412,751.59614455564,112.60871186179));
#65529=CARTESIAN_POINT('Origin',(44.574479425553,751.59614455564,112.60871186179));
#65530=CARTESIAN_POINT('Origin',(52.8776183915471,736.753459031024,105.895766550631));
#65531=CARTESIAN_POINT('',(61.1807573575412,737.487748923763,98.2698744426026));
#65532=CARTESIAN_POINT('',(61.1807573575412,738.225434976757,90.6087118617898));
#65533=CARTESIAN_POINT('',(61.1807573575412,736.753459031024,105.895766550631));
#65534=CARTESIAN_POINT('',(44.574479425553,737.487748923763,98.2698744426026));
#65535=CARTESIAN_POINT('Origin',(52.8776183915471,737.487748923763,98.2698744426026));
#65536=CARTESIAN_POINT('',(44.574479425553,738.225434976757,90.6087118617898));
#65537=CARTESIAN_POINT('',(44.574479425553,736.753459031024,105.895766550631));
#65538=CARTESIAN_POINT('Origin',(52.8776183915471,738.225434976757,90.6087118617898));
#65539=CARTESIAN_POINT('Origin',(44.574479425553,751.59614455564,112.60871186179));
#65540=CARTESIAN_POINT('',(44.574479425553,737.487748923763,90.6087118617898));
#65541=CARTESIAN_POINT('',(44.574479425553,737.487748923763,112.60871186179));
#65542=CARTESIAN_POINT('',(44.574479425553,751.59614455564,90.6087118617898));
#65543=CARTESIAN_POINT('Origin',(61.1807573575412,751.59614455564,112.60871186179));
#65544=CARTESIAN_POINT('',(61.1807573575412,737.487748923763,90.6087118617898));
#65545=CARTESIAN_POINT('',(61.1807573575412,737.487748923763,112.60871186179));
#65546=CARTESIAN_POINT('',(61.1807573575412,751.59614455564,90.6087118617898));
#65547=CARTESIAN_POINT('Origin',(52.8776183915471,751.59614455564,90.6087118617898));
#65548=CARTESIAN_POINT('Origin',(52.8776183915471,737.487748923763,90.6087118617898));
#65549=CARTESIAN_POINT('Origin',(52.8776183915471,737.487748923763,112.60871186179));
#65550=CARTESIAN_POINT('Origin',(18.9359428831647,828.055101296691,114.974210298));
#65551=CARTESIAN_POINT('',(18.9359428831647,825.603059199699,123.412429725824));
#65552=CARTESIAN_POINT('Origin',(18.9359428831647,825.131636969091,123.245813158557));
#65553=CARTESIAN_POINT('',(18.9359428831647,824.936592930631,125.298118648259));
#65554=CARTESIAN_POINT('',(18.9359428831647,828.5265235273,115.140826865267));
#65555=CARTESIAN_POINT('Origin',(18.9359428831647,824.465170700022,125.131502080992));
#65556=CARTESIAN_POINT('Origin',(18.9359428831647,828.055101296691,114.974210298));
#65557=CARTESIAN_POINT('',(18.9359428831647,826.174413048403,125.73560616057));
#65558=CARTESIAN_POINT('Origin',(18.9359428831647,824.465170700022,125.131502080992));
#65559=CARTESIAN_POINT('',(18.9359428831647,826.840879317471,123.849917238135));
#65560=CARTESIAN_POINT('',(18.9359428831647,829.764343645071,115.578314377579));
#65561=CARTESIAN_POINT('Origin',(18.9359428831647,825.131636969091,123.245813158557));
#65562=CARTESIAN_POINT('Origin',(37.0601473032809,800.968635034531,105.400936627455));
#65563=CARTESIAN_POINT('',(37.0601473032809,798.51659293754,113.839156055278));
#65564=CARTESIAN_POINT('Origin',(37.0601473032809,798.045170706931,113.672539488011));
#65565=CARTESIAN_POINT('',(37.0601473032809,797.850126668471,115.724844977713));
#65566=CARTESIAN_POINT('',(37.0601473032809,801.44005726514,105.567553194722));
#65567=CARTESIAN_POINT('Origin',(37.0601473032809,797.378704437862,115.558228410446));
#65568=CARTESIAN_POINT('Origin',(37.0601473032809,800.968635034531,105.400936627455));
#65569=CARTESIAN_POINT('',(37.0601473032809,799.087946786243,116.162332490025));
#65570=CARTESIAN_POINT('Origin',(37.0601473032809,797.378704437862,115.558228410446));
#65571=CARTESIAN_POINT('',(37.0601473032809,799.754413055311,114.276643567589));
#65572=CARTESIAN_POINT('',(37.0601473032809,802.677877382911,106.005040707033));
#65573=CARTESIAN_POINT('Origin',(37.0601473032809,798.045170706931,113.672539488011));
#65574=CARTESIAN_POINT('Origin',(71.0018228116636,802.224308791869,105.844734220082));
#65575=CARTESIAN_POINT('',(71.0018228116636,799.772266694878,114.282953647905));
#65576=CARTESIAN_POINT('Origin',(71.0018228116636,799.300844464269,114.116337080638));
#65577=CARTESIAN_POINT('',(71.0018228116636,799.105800425809,116.16864257034));
#65578=CARTESIAN_POINT('',(71.0018228116636,802.695731022478,106.011350787349));
#65579=CARTESIAN_POINT('Origin',(71.0018228116636,798.634378195201,116.002026003073));
#65580=CARTESIAN_POINT('Origin',(71.0018228116636,802.224308791869,105.844734220082));
#65581=CARTESIAN_POINT('',(71.0018228116636,800.343620543581,116.606130082651));
#65582=CARTESIAN_POINT('Origin',(71.0018228116636,798.634378195201,116.002026003073));
#65583=CARTESIAN_POINT('',(71.0018228116636,801.010086812649,114.720441160216));
#65584=CARTESIAN_POINT('',(71.0018228116636,803.933551140249,106.44883829966));
#65585=CARTESIAN_POINT('Origin',(71.0018228116636,799.300844464269,114.116337080638));
#65586=CARTESIAN_POINT('Origin',(86.81929389993,830.566448811367,115.861805483254));
#65587=CARTESIAN_POINT('',(86.81929389993,828.114406714375,124.300024911078));
#65588=CARTESIAN_POINT('Origin',(86.81929389993,827.642984483766,124.13340834381));
#65589=CARTESIAN_POINT('',(86.81929389993,827.447940445307,126.185713833513));
#65590=CARTESIAN_POINT('',(86.81929389993,831.037871041975,116.028422050521));
#65591=CARTESIAN_POINT('Origin',(86.81929389993,826.976518214698,126.019097266246));
#65592=CARTESIAN_POINT('Origin',(86.81929389993,830.566448811367,115.861805483254));
#65593=CARTESIAN_POINT('',(86.81929389993,828.685760563078,126.623201345824));
#65594=CARTESIAN_POINT('Origin',(86.81929389993,826.976518214698,126.019097266246));
#65595=CARTESIAN_POINT('',(86.81929389993,829.352226832147,124.737512423389));
#65596=CARTESIAN_POINT('',(86.81929389993,832.275691159747,116.465909562833));
#65597=CARTESIAN_POINT('Origin',(86.81929389993,827.642984483766,124.13340834381));
#65598=CARTESIAN_POINT('Origin',(68.6950894798137,857.652915073526,125.4350791538));
#65599=CARTESIAN_POINT('',(68.6950894798137,855.200872976535,133.873298581623));
#65600=CARTESIAN_POINT('Origin',(68.6950894798137,854.729450745926,133.706682014356));
#65601=CARTESIAN_POINT('',(68.6950894798137,854.534406707466,135.758987504058));
#65602=CARTESIAN_POINT('',(68.6950894798137,858.124337304135,125.601695721067));
#65603=CARTESIAN_POINT('Origin',(68.6950894798137,854.062984476858,135.592370936791));
#65604=CARTESIAN_POINT('Origin',(68.6950894798137,857.652915073526,125.4350791538));
#65605=CARTESIAN_POINT('',(68.6950894798137,855.772226825238,136.196475016369));
#65606=CARTESIAN_POINT('Origin',(68.6950894798137,854.062984476858,135.592370936791));
#65607=CARTESIAN_POINT('',(68.6950894798137,856.438693094306,134.310786093934));
#65608=CARTESIAN_POINT('',(68.6950894798137,859.362157421907,126.039183233378));
#65609=CARTESIAN_POINT('Origin',(68.6950894798137,854.729450745926,133.706682014356));
#65610=CARTESIAN_POINT('Origin',(34.7534139714311,856.397241316188,124.991281561173));
#65611=CARTESIAN_POINT('',(34.7534139714311,853.945199219197,133.429500988996));
#65612=CARTESIAN_POINT('Origin',(34.7534139714311,853.473776988588,133.262884421729));
#65613=CARTESIAN_POINT('',(34.7534139714311,853.278732950129,135.315189911431));
#65614=CARTESIAN_POINT('',(34.7534139714311,856.868663546797,125.15789812844));
#65615=CARTESIAN_POINT('Origin',(34.7534139714311,852.80731071952,135.148573344164));
#65616=CARTESIAN_POINT('Origin',(34.7534139714311,856.397241316188,124.991281561173));
#65617=CARTESIAN_POINT('',(34.7534139714311,854.5165530679,135.752677423742));
#65618=CARTESIAN_POINT('Origin',(34.7534139714311,852.80731071952,135.148573344164));
#65619=CARTESIAN_POINT('',(34.7534139714311,855.183019336969,133.866988501307));
#65620=CARTESIAN_POINT('',(34.7534139714311,858.106483664569,125.595385640751));
#65621=CARTESIAN_POINT('Origin',(34.7534139714311,853.473776988588,133.262884421729));
#65622=CARTESIAN_POINT('Origin',(-1.20267165682036,833.015540270651,116.727397272047));
#65623=CARTESIAN_POINT('',(-1.20267165682034,828.334694790224,127.12619746849));
#65624=CARTESIAN_POINT('',(-1.20267165689381,830.114166174335,127.781606968093));
#65625=CARTESIAN_POINT('Ctrl Pts',(-1.20267165682036,828.334694790224,127.12619746849));
#65626=CARTESIAN_POINT('Ctrl Pts',(-1.3291142188831,828.327437388836,127.146731443034));
#65627=CARTESIAN_POINT('Ctrl Pts',(-1.45430614477952,828.343822635535,127.176277230326));
#65628=CARTESIAN_POINT('Ctrl Pts',(-1.68514549780207,828.421280943045,127.249050764508));
#65629=CARTESIAN_POINT('Ctrl Pts',(-1.78913151791979,828.480813166934,127.291365400256));
#65630=CARTESIAN_POINT('Ctrl Pts',(-1.96268735299014,828.63467591294,127.382585424871));
#65631=CARTESIAN_POINT('Ctrl Pts',(-2.03128818522246,828.726948767031,127.430517553467));
#65632=CARTESIAN_POINT('Ctrl Pts',(-2.12497808078248,828.93287659233,127.525644047322));
#65633=CARTESIAN_POINT('Ctrl Pts',(-2.14960818542247,829.044222386194,127.571881210666));
#65634=CARTESIAN_POINT('Ctrl Pts',(-2.15183078840391,829.273431394245,127.657118282923));
#65635=CARTESIAN_POINT('Ctrl Pts',(-2.12918070135601,829.388843907327,127.695159946446));
#65636=CARTESIAN_POINT('Ctrl Pts',(-2.03824460180004,829.609963821869,127.758397540592));
#65637=CARTESIAN_POINT('Ctrl Pts',(-1.97014853040882,829.713054774199,127.782671606508));
#65638=CARTESIAN_POINT('Ctrl Pts',(-1.79626212620278,829.892523762626,127.814159147211));
#65639=CARTESIAN_POINT('Ctrl Pts',(-1.69155932791356,829.966552839317,127.82074104684));
#65640=CARTESIAN_POINT('Ctrl Pts',(-1.45854118760016,830.074434502816,127.815266376305));
#65641=CARTESIAN_POINT('Ctrl Pts',(-1.33197961484755,830.106424544809,127.80289079258));
#65642=CARTESIAN_POINT('Ctrl Pts',(-1.2041959927763,830.114076056837,127.781858267725));
#65643=CARTESIAN_POINT('Ctrl Pts',(-1.20368786395239,830.114106482911,127.781774632343));
#65644=CARTESIAN_POINT('Ctrl Pts',(-1.20317975185534,830.11413652206,127.781690865762));
#65645=CARTESIAN_POINT('Ctrl Pts',(-1.20267165696724,830.114166174335,127.781606968093));
#65646=CARTESIAN_POINT('',(-1.20267165682039,830.786433008964,125.879506018928));
#65647=CARTESIAN_POINT('',(-1.20267165682036,833.90943644327,117.043330425183));
#65648=CARTESIAN_POINT('Ctrl Pts',(-2.14826343637025,829.917241856529,125.699848416551));
#65649=CARTESIAN_POINT('Ctrl Pts',(-2.13968331783687,830.028581984869,125.739199785193));
#65650=CARTESIAN_POINT('Ctrl Pts',(-2.10906597586262,830.138399269345,125.774665152322));
#65651=CARTESIAN_POINT('Ctrl Pts',(-2.00423449611768,830.349368657819,125.835950927927));
#65652=CARTESIAN_POINT('Ctrl Pts',(-1.92876920194896,830.447515187103,125.860493869567));
#65653=CARTESIAN_POINT('Ctrl Pts',(-1.74517237638948,830.610903128901,125.89303488207));
#65654=CARTESIAN_POINT('Ctrl Pts',(-1.6393470870339,830.675148515068,125.901011837026));
#65655=CARTESIAN_POINT('Ctrl Pts',(-1.40805851153518,830.764006551829,125.900183193205));
#65656=CARTESIAN_POINT('Ctrl Pts',(-1.28442099189681,830.787154608998,125.891119405913));
#65657=CARTESIAN_POINT('Ctrl Pts',(-1.03549471494797,830.787627832663,125.856694388783));
#65658=CARTESIAN_POINT('Ctrl Pts',(-0.912507313011831,830.764379738259,
125.831453139541));
#65659=CARTESIAN_POINT('Ctrl Pts',(-0.685066390374408,830.673330581152,
125.767818087782));
#65660=CARTESIAN_POINT('Ctrl Pts',(-0.582847405174743,830.606301586927,
125.73000134134));
#65661=CARTESIAN_POINT('Ctrl Pts',(-0.417444637388589,830.440518446962,
125.648255064278));
#65662=CARTESIAN_POINT('Ctrl Pts',(-0.354334495380809,830.344757667241,
125.605401289678));
#65663=CARTESIAN_POINT('Ctrl Pts',(-0.272235940190863,830.137680511632,
125.519746988106));
#65664=CARTESIAN_POINT('Ctrl Pts',(-0.252596354959246,830.028841515062,
125.477755754259));
#65665=CARTESIAN_POINT('Ctrl Pts',(-0.256908479385002,829.807553875916,
125.397939782603));
#65666=CARTESIAN_POINT('Ctrl Pts',(-0.281063582749534,829.697120774919,
125.360871691001));
#65667=CARTESIAN_POINT('Ctrl Pts',(-0.371978455736119,829.48586098202,125.295656791375));
#65668=CARTESIAN_POINT('Ctrl Pts',(-0.438971591876693,829.387393335529,
125.268401313436));
#65669=CARTESIAN_POINT('Ctrl Pts',(-0.611791129636721,829.213469532326,
125.227497034506));
#65670=CARTESIAN_POINT('Ctrl Pts',(-0.71768204207598,829.141291221418,125.215068563833));
#65671=CARTESIAN_POINT('Ctrl Pts',(-0.94855904425708,829.040221526745,125.209010221274));
#65672=CARTESIAN_POINT('Ctrl Pts',(-1.07088004178212,829.01133993113,125.215023726535));
#65673=CARTESIAN_POINT('Ctrl Pts',(-1.31977016635572,828.998589587703,125.244637629106));
#65674=CARTESIAN_POINT('Ctrl Pts',(-1.44406179396237,829.015467658869,125.268205976454));
#65675=CARTESIAN_POINT('Ctrl Pts',(-1.67726982621071,829.094269915464,125.330137787643));
#65676=CARTESIAN_POINT('Ctrl Pts',(-1.78383407157677,829.15585890019,125.368044484481));
#65677=CARTESIAN_POINT('Ctrl Pts',(-1.9537147677774,829.307840573972,125.448382754829));
#65678=CARTESIAN_POINT('Ctrl Pts',(-2.01902459780627,829.393366107762,125.489290147882));
#65679=CARTESIAN_POINT('Ctrl Pts',(-2.1155257471177,829.588730151941,125.574991781173));
#65680=CARTESIAN_POINT('Ctrl Pts',(-2.14392988243959,829.697750196142,125.619071567142));
#65681=CARTESIAN_POINT('Ctrl Pts',(-2.1514912867446,829.845633941601,125.674194438292));
#65682=CARTESIAN_POINT('Ctrl Pts',(-2.15102207108058,829.881444362415,125.687196370892));
#65683=CARTESIAN_POINT('Ctrl Pts',(-2.14826343637024,829.917241856529,125.699848416551));
#65684=CARTESIAN_POINT('Ctrl Pts',(-1.20267165696725,830.114166174335,127.781606968093));
#65685=CARTESIAN_POINT('Ctrl Pts',(-1.08075513521124,830.121281188299,127.761475862289));
#65686=CARTESIAN_POINT('Ctrl Pts',(-0.959826602679901,830.106116474443,
127.733812530951));
#65687=CARTESIAN_POINT('Ctrl Pts',(-0.730868912708148,830.031822843933,
127.665555151892));
#65688=CARTESIAN_POINT('Ctrl Pts',(-0.625279805937704,829.97244057417,127.625319322289));
#65689=CARTESIAN_POINT('Ctrl Pts',(-0.447392920247649,829.816861543733,
127.537684702249));
#65690=CARTESIAN_POINT('Ctrl Pts',(-0.376667260732679,829.722425613006,
127.49118481603));
#65691=CARTESIAN_POINT('Ctrl Pts',(-0.280809829819228,829.512612223396,
127.39829819797));
#65692=CARTESIAN_POINT('Ctrl Pts',(-0.255751495196176,829.399818558959,
127.352855356984));
#65693=CARTESIAN_POINT('Ctrl Pts',(-0.253491139094301,829.167773722023,
127.267415838435));
#65694=CARTESIAN_POINT('Ctrl Pts',(-0.276786155720067,829.05091066254,127.228372802782));
#65695=CARTESIAN_POINT('Ctrl Pts',(-0.369939352279435,828.828729024651,
127.162251511837));
#65696=CARTESIAN_POINT('Ctrl Pts',(-0.439293744486302,828.725907820965,
127.136015715078));
#65697=CARTESIAN_POINT('Ctrl Pts',(-0.614808006592645,828.549194309779,
127.100810464247));
#65698=CARTESIAN_POINT('Ctrl Pts',(-0.719259927691373,828.477181737511,
127.09225800998));
#65699=CARTESIAN_POINT('Ctrl Pts',(-0.950157935397135,828.373046628809,
127.094515945668));
#65700=CARTESIAN_POINT('Ctrl Pts',(-1.07459576691847,828.342365977433,127.105523095909));
#65701=CARTESIAN_POINT('Ctrl Pts',(-1.20096012459087,828.33479410665,127.125919940975));
#65702=CARTESIAN_POINT('Ctrl Pts',(-1.20181591927738,828.33474390684,127.126058498727));
#65703=CARTESIAN_POINT('Ctrl Pts',(-1.20267165682035,828.334694790224,127.12619746849));
#65704=CARTESIAN_POINT('Origin',(-1.20267165682036,833.015540270651,116.727397272047));
#65705=CARTESIAN_POINT('',(-1.20267165682036,831.352123639145,122.934292515535));
#65706=CARTESIAN_POINT('Origin',(-1.20267165682036,830.880701408536,122.767675948268));
#65707=CARTESIAN_POINT('',(-1.2026716568203,829.69401966521,127.625705181122));
#65708=CARTESIAN_POINT('',(-1.20267165682036,833.48696250126,116.894013839314));
#65709=CARTESIAN_POINT('Ctrl Pts',(-1.20298789650297,828.755542369383,127.280115959316));
#65710=CARTESIAN_POINT('Ctrl Pts',(-1.26887122471697,828.751787433989,127.290865160166));
#65711=CARTESIAN_POINT('Ctrl Pts',(-1.33412418331166,828.760243626981,127.306140151335));
#65712=CARTESIAN_POINT('Ctrl Pts',(-1.45539836846876,828.800520225111,127.343823147789));
#65713=CARTESIAN_POINT('Ctrl Pts',(-1.51042491793021,828.831820515841,127.365848130137));
#65714=CARTESIAN_POINT('Ctrl Pts',(-1.60243301003513,828.912928606751,127.413422591274));
#65715=CARTESIAN_POINT('Ctrl Pts',(-1.63886413982435,828.961661140245,127.438463863894));
#65716=CARTESIAN_POINT('Ctrl Pts',(-1.68873358792721,829.070474044544,127.488316661981));
#65717=CARTESIAN_POINT('Ctrl Pts',(-1.7019139603871,829.129337809819,127.51262594284));
#65718=CARTESIAN_POINT('Ctrl Pts',(-1.70336818240946,829.250386378696,127.557595635152));
#65719=CARTESIAN_POINT('Ctrl Pts',(-1.69154803172257,829.311287908161,127.577763325018));
#65720=CARTESIAN_POINT('Ctrl Pts',(-1.64384832228144,829.427807146915,127.611468761738));
#65721=CARTESIAN_POINT('Ctrl Pts',(-1.60811863359135,829.482076408695,127.624540058091));
#65722=CARTESIAN_POINT('Ctrl Pts',(-1.51662342963629,829.576768936407,127.641807379075));
#65723=CARTESIAN_POINT('Ctrl Pts',(-1.46137405383466,829.61589349437,127.64562967002));
#65724=CARTESIAN_POINT('Ctrl Pts',(-1.3387017035892,829.672759375328,127.643299679692));
#65725=CARTESIAN_POINT('Ctrl Pts',(-1.27227880068162,829.689651767026,127.637030621277));
#65726=CARTESIAN_POINT('Ctrl Pts',(-1.13852642382636,829.698056300692,127.615272519426));
#65727=CARTESIAN_POINT('Ctrl Pts',(-1.07240032751607,829.689653389529,127.600037251621));
#65728=CARTESIAN_POINT('Ctrl Pts',(-0.949560991481654,829.648697322975,
127.562662456503));
#65729=CARTESIAN_POINT('Ctrl Pts',(-0.893904099793958,829.616719276534,
127.540922137783));
#65730=CARTESIAN_POINT('Ctrl Pts',(-0.801489156487562,829.534118127831,
127.494118858639));
#65731=CARTESIAN_POINT('Ctrl Pts',(-0.765173137461864,829.484772996318,
127.469596522221));
#65732=CARTESIAN_POINT('Ctrl Pts',(-0.715749284920526,829.374827607324,
127.420534890526));
#65733=CARTESIAN_POINT('Ctrl Pts',(-0.702925728831747,829.315445699046,
127.396489634076));
#65734=CARTESIAN_POINT('Ctrl Pts',(-0.702425039945017,829.193907478153,
127.351746728171));
#65735=CARTESIAN_POINT('Ctrl Pts',(-0.714756156375707,829.133015743589,
127.33151451947));
#65736=CARTESIAN_POINT('Ctrl Pts',(-0.763581488527736,829.016671918521,
127.2972799177));
#65737=CARTESIAN_POINT('Ctrl Pts',(-0.799999909523447,828.962580079425,
127.283766673945));
#65738=CARTESIAN_POINT('Ctrl Pts',(-0.892604933571247,828.868976250883,
127.26570534795));
#65739=CARTESIAN_POINT('Ctrl Pts',(-0.948103826096839,828.830643552855,
127.261474926263));
#65740=CARTESIAN_POINT('Ctrl Pts',(-1.07061270446102,828.775475790961,127.263227961856));
#65741=CARTESIAN_POINT('Ctrl Pts',(-1.13652913761774,828.759330100707,127.269272874018));
#65742=CARTESIAN_POINT('Ctrl Pts',(-1.20298789650297,828.755542369383,127.280115959316));
#65743=CARTESIAN_POINT('Origin',(6.55478737542994,847.253007595304,121.759399961329));
#65744=CARTESIAN_POINT('',(6.55478737542992,842.677000252971,131.641535184651));
#65745=CARTESIAN_POINT('',(6.55478737542993,844.584249391867,132.375487632912));
#65746=CARTESIAN_POINT('Ctrl Pts',(6.55478737542991,842.677000252971,131.641535184651));
#65747=CARTESIAN_POINT('Ctrl Pts',(6.55303790676142,842.676966746103,131.641629988445));
#65748=CARTESIAN_POINT('Ctrl Pts',(6.5512882317057,842.676937403425,131.641726498407));
#65749=CARTESIAN_POINT('Ctrl Pts',(6.41373413291095,842.674958404046,131.649447180971));
#65750=CARTESIAN_POINT('Ctrl Pts',(6.2794941213037,842.698132529524,131.66722321588));
#65751=CARTESIAN_POINT('Ctrl Pts',(6.03154658372636,842.791160631172,131.720813774759));
#65752=CARTESIAN_POINT('Ctrl Pts',(5.91994139510763,842.859481708406,131.755862738239));
#65753=CARTESIAN_POINT('Ctrl Pts',(5.73273525877527,843.032411930828,131.838382174141));
#65754=CARTESIAN_POINT('Ctrl Pts',(5.6587689273465,843.135292902605,131.88502954403));
#65755=CARTESIAN_POINT('Ctrl Pts',(5.55849985454393,843.362329295746,131.983106345019));
#65756=CARTESIAN_POINT('Ctrl Pts',(5.53294178186754,843.484253043593,132.033574133132));
#65757=CARTESIAN_POINT('Ctrl Pts',(5.53382741502631,843.731867371789,132.131263306231));
#65758=CARTESIAN_POINT('Ctrl Pts',(5.5602262917009,843.85513724034,132.177522209149));
#65759=CARTESIAN_POINT('Ctrl Pts',(5.66228992565744,844.087427841061,132.259627098616));
#65760=CARTESIAN_POINT('Ctrl Pts',(5.73714625520192,844.194049471479,132.294601117337));
#65761=CARTESIAN_POINT('Ctrl Pts',(5.92629383071629,844.376164218133,132.348689178051));
#65762=CARTESIAN_POINT('Ctrl Pts',(6.03893300012467,844.449643022453,132.367175469941));
#65763=CARTESIAN_POINT('Ctrl Pts',(6.28711596896352,844.552556231306,132.385476700563));
#65764=CARTESIAN_POINT('Ctrl Pts',(6.4203220368891,844.580860808567,132.3850752359));
#65765=CARTESIAN_POINT('Ctrl Pts',(6.5547873754299,844.584249391867,132.375487632912));
#65766=CARTESIAN_POINT('',(6.55478737646738,845.225288746624,130.561741212106));
#65767=CARTESIAN_POINT('',(6.55478737542994,848.216036735547,122.099767044397));
#65768=CARTESIAN_POINT('Ctrl Pts',(5.60999635886,844.61143003858,130.398176720001));
#65769=CARTESIAN_POINT('Ctrl Pts',(5.66060421325564,844.727579351653,130.439227817251));
#65770=CARTESIAN_POINT('Ctrl Pts',(5.73480526396349,844.833978699371,130.474516036691));
#65771=CARTESIAN_POINT('Ctrl Pts',(5.92197687730667,845.015281112435,130.529742818498));
#65772=CARTESIAN_POINT('Ctrl Pts',(6.03312264845888,845.088412618786,130.549147387708));
#65773=CARTESIAN_POINT('Ctrl Pts',(6.27847082239455,845.191632644705,130.569776359054));
#65774=CARTESIAN_POINT('Ctrl Pts',(6.41041618741639,845.220536970346,130.570730292764));
#65775=CARTESIAN_POINT('Ctrl Pts',(6.67790868490085,845.229442389718,130.554113051095));
#65776=CARTESIAN_POINT('Ctrl Pts',(6.81092204572145,845.209142652417,130.536625508053));
#65777=CARTESIAN_POINT('Ctrl Pts',(7.05983328010717,845.121243103356,130.485463008613));
#65778=CARTESIAN_POINT('Ctrl Pts',(7.17333222258342,845.054432865275,130.452260839241));
#65779=CARTESIAN_POINT('Ctrl Pts',(7.36432235367931,844.883570080731,130.37466281296));
#65780=CARTESIAN_POINT('Ctrl Pts',(7.44032470527312,844.781503834337,130.331108901728));
#65781=CARTESIAN_POINT('Ctrl Pts',(7.5462596693881,844.553385257458,130.238079676163));
#65782=CARTESIAN_POINT('Ctrl Pts',(7.57454430994381,844.429302892799,130.18944702958));
#65783=CARTESIAN_POINT('Ctrl Pts',(7.57770914177435,844.176793165481,130.093710651757));
#65784=CARTESIAN_POINT('Ctrl Pts',(7.55247229926116,844.050879973687,130.047557195243));
#65785=CARTESIAN_POINT('Ctrl Pts',(7.45175414255303,843.815798288611,129.964375202193));
#65786=CARTESIAN_POINT('Ctrl Pts',(7.37775872910222,843.70877597874,129.928074640688));
#65787=CARTESIAN_POINT('Ctrl Pts',(7.19052260488021,843.526789513878,129.869935499952));
#65788=CARTESIAN_POINT('Ctrl Pts',(7.0791397409318,843.453575009385,129.848659915797));
#65789=CARTESIAN_POINT('Ctrl Pts',(6.83389387739383,843.350924365173,129.824455764558));
#65790=CARTESIAN_POINT('Ctrl Pts',(6.70247479869712,843.322328360243,129.821707600764));
#65791=CARTESIAN_POINT('Ctrl Pts',(6.43533783189951,843.313366162955,129.835543150273));
#65792=CARTESIAN_POINT('Ctrl Pts',(6.30218241860372,843.333492045012,129.852161243939));
#65793=CARTESIAN_POINT('Ctrl Pts',(6.05154626048353,843.421068675173,129.903245440815));
#65794=CARTESIAN_POINT('Ctrl Pts',(5.93672077240539,843.48822147147,129.937421063615));
#65795=CARTESIAN_POINT('Ctrl Pts',(5.74402223653652,843.65999995787,130.01814503857));
#65796=CARTESIAN_POINT('Ctrl Pts',(5.66759854594246,843.762573828124,130.063778460294));
#65797=CARTESIAN_POINT('Ctrl Pts',(5.56246946534555,843.990325593362,130.160418011578));
#65798=CARTESIAN_POINT('Ctrl Pts',(5.53472239572821,844.113274934977,130.210474525316));
#65799=CARTESIAN_POINT('Ctrl Pts',(5.53277376714332,844.30146602845,130.283852718444));
#65800=CARTESIAN_POINT('Ctrl Pts',(5.53884227970387,844.364603779265,130.307934207726));
#65801=CARTESIAN_POINT('Ctrl Pts',(5.56440372553955,844.489907018077,130.354616535628));
#65802=CARTESIAN_POINT('Ctrl Pts',(5.5839832628442,844.55172777953,130.377075921576));
#65803=CARTESIAN_POINT('Ctrl Pts',(5.60999635885999,844.61143003858,130.398176720001));
#65804=CARTESIAN_POINT('Ctrl Pts',(6.5547873754299,844.584249391867,132.375487632912));
#65805=CARTESIAN_POINT('Ctrl Pts',(6.55480622813589,844.584249866963,132.375486288682));
#65806=CARTESIAN_POINT('Ctrl Pts',(6.55482508086662,844.58425034157,132.375484944272));
#65807=CARTESIAN_POINT('Ctrl Pts',(6.55484393362206,844.584250815686,132.375483599682));
#65808=CARTESIAN_POINT('Ctrl Pts',(6.68623894655647,844.587555190458,132.366112421274));
#65809=CARTESIAN_POINT('Ctrl Pts',(6.81642370072574,844.567003761885,132.348152635533));
#65810=CARTESIAN_POINT('Ctrl Pts',(7.06398759568666,844.478908057817,132.296499199516));
#65811=CARTESIAN_POINT('Ctrl Pts',(7.17839446645992,844.410728578013,132.262825655811));
#65812=CARTESIAN_POINT('Ctrl Pts',(7.37002394334276,844.23639007631,132.18469173527));
#65813=CARTESIAN_POINT('Ctrl Pts',(7.44575283668634,844.132356427329,132.141104935307));
#65814=CARTESIAN_POINT('Ctrl Pts',(7.54923081147987,843.901799809453,132.048801961113));
#65815=CARTESIAN_POINT('Ctrl Pts',(7.57598548488475,843.777573322673,132.000982234916));
#65816=CARTESIAN_POINT('Ctrl Pts',(7.57640419121021,843.525170126346,131.906562051835));
#65817=CARTESIAN_POINT('Ctrl Pts',(7.54985107163003,843.39949110052,131.860890489685));
#65818=CARTESIAN_POINT('Ctrl Pts',(7.44627657764221,843.1643784139,131.777803202536));
#65819=CARTESIAN_POINT('Ctrl Pts',(7.37028164579431,843.057273335293,131.741210390762));
#65820=CARTESIAN_POINT('Ctrl Pts',(7.17909431489495,842.876627618429,131.682596366717));
#65821=CARTESIAN_POINT('Ctrl Pts',(7.06594289073692,842.804729314389,131.661109320234));
#65822=CARTESIAN_POINT('Ctrl Pts',(6.81873561039477,842.705983821545,131.636976560333));
#65823=CARTESIAN_POINT('Ctrl Pts',(6.68735363927127,842.679539241202,131.634351412262));
#65824=CARTESIAN_POINT('Ctrl Pts',(6.55478737542991,842.677000252971,131.641535184651));
#65825=CARTESIAN_POINT('Origin',(6.55478737542994,847.253007595304,121.759399961329));
#65826=CARTESIAN_POINT('',(6.55478737542994,845.589590963798,127.966295204818));
#65827=CARTESIAN_POINT('Origin',(6.55478737542994,845.118168733189,127.799678637551));
#65828=CARTESIAN_POINT('',(6.55478737543003,844.09812975394,132.186211518965));
#65829=CARTESIAN_POINT('',(6.55478737542994,847.724429825913,121.926016528596));
#65830=CARTESIAN_POINT('Ctrl Pts',(6.55481851312468,843.164473852138,131.826980425391));
#65831=CARTESIAN_POINT('Ctrl Pts',(6.49382472049681,843.163209185906,131.830547252986));
#65832=CARTESIAN_POINT('Ctrl Pts',(6.43336250093996,843.172340323356,131.838191491812));
#65833=CARTESIAN_POINT('Ctrl Pts',(6.31517108154337,843.211873723551,131.861776761809));
#65834=CARTESIAN_POINT('Ctrl Pts',(6.25911871175114,843.24345373982,131.878076868745));
#65835=CARTESIAN_POINT('Ctrl Pts',(6.16392510454186,843.325110848359,131.916860147554));
#65836=CARTESIAN_POINT('Ctrl Pts',(6.12563808773415,843.37436783186,131.938957654843));
#65837=CARTESIAN_POINT('Ctrl Pts',(6.07204655748402,843.484148214731,131.98587934228));
#65838=CARTESIAN_POINT('Ctrl Pts',(6.05717241963223,843.54358604734,132.010242691029));
#65839=CARTESIAN_POINT('Ctrl Pts',(6.05293317978062,843.665034674381,132.057919717385));
#65840=CARTESIAN_POINT('Ctrl Pts',(6.06357636693077,843.725858898406,132.080767224076));
#65841=CARTESIAN_POINT('Ctrl Pts',(6.10927807047822,843.841077253218,132.121902922219));
#65842=CARTESIAN_POINT('Ctrl Pts',(6.14393797108856,843.894313107552,132.139772164867));
#65843=CARTESIAN_POINT('Ctrl Pts',(6.23305703868034,843.986063403245,132.168160912873));
#65844=CARTESIAN_POINT('Ctrl Pts',(6.28671435890372,844.023605589203,132.178370566321));
#65845=CARTESIAN_POINT('Ctrl Pts',(6.40605752914277,844.077640466166,132.189790697383));
#65846=CARTESIAN_POINT('Ctrl Pts',(6.47061868105095,844.093540264309,132.190865731911));
#65847=CARTESIAN_POINT('Ctrl Pts',(6.60263192308899,844.10124280269,132.183755074975));
#65848=CARTESIAN_POINT('Ctrl Pts',(6.66881976307734,844.092705764824,132.175541289738));
#65849=CARTESIAN_POINT('Ctrl Pts',(6.79335192706539,844.05171026747,132.150834900201));
#65850=CARTESIAN_POINT('Ctrl Pts',(6.85043847313586,844.019558982461,132.134552843621));
#65851=CARTESIAN_POINT('Ctrl Pts',(6.94696815080633,843.93604369985,132.096143876332));
#65852=CARTESIAN_POINT('Ctrl Pts',(6.98555744226268,843.885615368059,132.074427178142));
#65853=CARTESIAN_POINT('Ctrl Pts',(7.03907629503223,843.773133595323,132.028241411814));
#65854=CARTESIAN_POINT('Ctrl Pts',(7.05349101350017,843.712215014848,132.004231698388));
#65855=CARTESIAN_POINT('Ctrl Pts',(7.05591879218544,843.588034847224,131.95694833136));
#65856=CARTESIAN_POINT('Ctrl Pts',(7.04386252616135,843.526023081629,131.934149518317));
#65857=CARTESIAN_POINT('Ctrl Pts',(6.99459986187663,843.409564880055,131.892876156114));
#65858=CARTESIAN_POINT('Ctrl Pts',(6.95788872341961,843.356295342004,131.874818710348));
#65859=CARTESIAN_POINT('Ctrl Pts',(6.86471312661731,843.265977604734,131.846072563347));
#65860=CARTESIAN_POINT('Ctrl Pts',(6.80921918804558,843.229809044465,131.835663634095));
#65861=CARTESIAN_POINT('Ctrl Pts',(6.68682008321809,843.179487726841,131.824116116221));
#65862=CARTESIAN_POINT('Ctrl Pts',(6.62113381468758,843.165848856363,131.823102403754));
#65863=CARTESIAN_POINT('Ctrl Pts',(6.55481851312468,843.164473852138,131.826980425391));
#65864=CARTESIAN_POINT('Origin',(0.796070088965373,843.535854240486,120.445632192709));
#65865=CARTESIAN_POINT('',(0.796070088965328,838.864125149569,130.818638623573));
#65866=CARTESIAN_POINT('',(0.796070088870976,840.620830057273,131.538463224669));
#65867=CARTESIAN_POINT('Ctrl Pts',(0.796070088965304,838.864125149569,130.818638623573));
#65868=CARTESIAN_POINT('Ctrl Pts',(0.794827698097562,838.864057778329,130.818829242672));
#65869=CARTESIAN_POINT('Ctrl Pts',(0.793585218870054,838.863992651324,130.81902084043));
#65870=CARTESIAN_POINT('Ctrl Pts',(0.665663372755533,838.857518991375,130.838846563929));
#65871=CARTESIAN_POINT('Ctrl Pts',(0.540503522400223,838.874558326616,130.868296531431));
#65872=CARTESIAN_POINT('Ctrl Pts',(0.3092728956842,838.95277065554,130.942868566291));
#65873=CARTESIAN_POINT('Ctrl Pts',(0.205004865688482,839.012754838599,130.987154596652));
#65874=CARTESIAN_POINT('Ctrl Pts',(0.0315660344768318,839.167045965043,
131.083967170336));
#65875=CARTESIAN_POINT('Ctrl Pts',(-0.0366671735241947,839.259396874592,
131.135483488003));
#65876=CARTESIAN_POINT('Ctrl Pts',(-0.128592083149956,839.464373004797,
131.238526591522));
#65877=CARTESIAN_POINT('Ctrl Pts',(-0.152136571347762,839.574692592277,
131.289052191409));
#65878=CARTESIAN_POINT('Ctrl Pts',(-0.151891702170995,839.800490232602,
131.38283457539));
#65879=CARTESIAN_POINT('Ctrl Pts',(-0.128294067025386,839.913586090429,
131.425133728983));
#65880=CARTESIAN_POINT('Ctrl Pts',(-0.0360050571459805,840.129586582997,
131.496426943252));
#65881=CARTESIAN_POINT('Ctrl Pts',(0.0322173588675454,840.229979376594,
131.524472423262));
#65882=CARTESIAN_POINT('Ctrl Pts',(0.205944640509112,840.404927795732,131.562614261849));
#65883=CARTESIAN_POINT('Ctrl Pts',(0.310325571819949,840.477066589318,131.571943694023));
#65884=CARTESIAN_POINT('Ctrl Pts',(0.542115274605274,840.582108231562,131.570482146171));
#65885=CARTESIAN_POINT('Ctrl Pts',(0.667674821467832,840.613202212936,131.559325066392));
#65886=CARTESIAN_POINT('Ctrl Pts',(0.794285400310592,840.620725573823,131.538753807651));
#65887=CARTESIAN_POINT('Ctrl Pts',(0.794880322885515,840.620760924875,131.538657146642));
#65888=CARTESIAN_POINT('Ctrl Pts',(0.795475219297333,840.620795752662,131.538560285583));
#65889=CARTESIAN_POINT('Ctrl Pts',(0.796070088776574,840.620830057273,131.538463224669));
#65890=CARTESIAN_POINT('',(0.796070088965362,841.298123280429,129.622140692799));
#65891=CARTESIAN_POINT('',(0.796070088965373,844.429750413105,120.761565345845));
#65892=CARTESIAN_POINT('Ctrl Pts',(-0.114573768475245,840.621503109177,
129.483096530971));
#65893=CARTESIAN_POINT('Ctrl Pts',(-0.0816289370406585,840.72872824179,
129.520993520889));
#65894=CARTESIAN_POINT('Ctrl Pts',(-0.0276962030890162,840.830166871951,
129.553497588084));
#65895=CARTESIAN_POINT('Ctrl Pts',(0.12044651238664,841.016067290245,129.605923141397));
#65896=CARTESIAN_POINT('Ctrl Pts',(0.215202624761209,841.097345397984,129.624504212106));
#65897=CARTESIAN_POINT('Ctrl Pts',(0.429070634791453,841.221345788405,129.643124331242));
#65898=CARTESIAN_POINT('Ctrl Pts',(0.545729974921351,841.263543627242,129.643308936973));
#65899=CARTESIAN_POINT('Ctrl Pts',(0.789325626678496,841.305342087345,129.625847846461));
#65900=CARTESIAN_POINT('Ctrl Pts',(0.914171079203174,841.303866240822,129.608081138434));
#65901=CARTESIAN_POINT('Ctrl Pts',(1.15536541434991,841.255770008622,129.556490032213));
#65902=CARTESIAN_POINT('Ctrl Pts',(1.26935916895088,841.209037805329,129.522948704284));
#65903=CARTESIAN_POINT('Ctrl Pts',(1.46957291102217,841.075609376976,129.444335384128));
#65904=CARTESIAN_POINT('Ctrl Pts',(1.55379852050348,840.990104292807,129.399988562346));
#65905=CARTESIAN_POINT('Ctrl Pts',(1.67742500701556,840.795679236415,129.308119262895));
#65906=CARTESIAN_POINT('Ctrl Pts',(1.71741516907379,840.689701531423,129.261654481206));
#65907=CARTESIAN_POINT('Ctrl Pts',(1.75119228074715,840.471141451104,129.171941725508));
#65908=CARTESIAN_POINT('Ctrl Pts',(1.74615787971708,840.360855125383,129.129438956567));
#65909=CARTESIAN_POINT('Ctrl Pts',(1.69303143168079,840.145259473354,129.051634725752));
#65910=CARTESIAN_POINT('Ctrl Pts',(1.64518796173878,840.041961211094,129.017088327572));
#65911=CARTESIAN_POINT('Ctrl Pts',(1.51032859251117,839.8530749561,128.959780993269));
#65912=CARTESIAN_POINT('Ctrl Pts',(1.42360862026976,839.76983980922,128.937909196098));
#65913=CARTESIAN_POINT('Ctrl Pts',(1.21763762780869,839.633452990763,128.910271757672));
#65914=CARTESIAN_POINT('Ctrl Pts',(1.09905060553251,839.583519757645,128.905705450172));
#65915=CARTESIAN_POINT('Ctrl Pts',(0.852986550115753,839.529713465236,128.916351593169));
#65916=CARTESIAN_POINT('Ctrl Pts',(0.728093581363388,839.525330018705,128.931023573232));
#65917=CARTESIAN_POINT('Ctrl Pts',(0.484194615840542,839.561413569164,128.977897026239));
#65918=CARTESIAN_POINT('Ctrl Pts',(0.367560526885127,839.602166643071,129.009903607386));
#65919=CARTESIAN_POINT('Ctrl Pts',(0.159186954517308,839.724728288124,129.087301467092));
#65920=CARTESIAN_POINT('Ctrl Pts',(0.0696508749860938,839.805750216171,
129.13207642363));
#65921=CARTESIAN_POINT('Ctrl Pts',(-0.0611587166226164,839.987529379187,
129.222946134897));
#65922=CARTESIAN_POINT('Ctrl Pts',(-0.105441748260835,840.08391523088,129.267691931765));
#65923=CARTESIAN_POINT('Ctrl Pts',(-0.155599545862111,840.293812728813,
129.358530179364));
#65924=CARTESIAN_POINT('Ctrl Pts',(-0.158957976707979,840.40598034632,129.40372242424));
#65925=CARTESIAN_POINT('Ctrl Pts',(-0.133545652799168,840.552095120162,
129.458220080966));
#65926=CARTESIAN_POINT('Ctrl Pts',(-0.125166017890976,840.587028646908,
129.470912089532));
#65927=CARTESIAN_POINT('Ctrl Pts',(-0.114573768475226,840.621503109177,
129.483096530971));
#65928=CARTESIAN_POINT('Ctrl Pts',(0.796070088776549,840.620830057273,131.538463224669));
#65929=CARTESIAN_POINT('Ctrl Pts',(0.919117110633732,840.627925866344,131.518386456895));
#65930=CARTESIAN_POINT('Ctrl Pts',(1.04101449669179,840.612631456257,131.489773246558));
#65931=CARTESIAN_POINT('Ctrl Pts',(1.27106987721238,840.538183828132,131.418089116851));
#65932=CARTESIAN_POINT('Ctrl Pts',(1.37685998985184,840.478851109327,131.375388976825));
#65933=CARTESIAN_POINT('Ctrl Pts',(1.55418389755524,840.32403888529,131.282026824372));
#65934=CARTESIAN_POINT('Ctrl Pts',(1.62438039829403,840.230422130879,131.232331969497));
#65935=CARTESIAN_POINT('Ctrl Pts',(1.71997755586114,840.020721214871,131.13168195422));
#65936=CARTESIAN_POINT('Ctrl Pts',(1.74451008525223,839.906844836805,131.081747906321));
#65937=CARTESIAN_POINT('Ctrl Pts',(1.7437990867947,839.676499988517,130.98891715077));
#65938=CARTESIAN_POINT('Ctrl Pts',(1.71963538228123,839.562495315449,130.946831551189));
#65939=CARTESIAN_POINT('Ctrl Pts',(1.62521025709541,839.344576997806,130.874096289475));
#65940=CARTESIAN_POINT('Ctrl Pts',(1.55492888472768,839.243292762205,130.844512251832));
#65941=CARTESIAN_POINT('Ctrl Pts',(1.37774643215128,839.069982346398,130.803354915119));
#65942=CARTESIAN_POINT('Ctrl Pts',(1.27270211381144,838.999772092652,130.792226269154));
#65943=CARTESIAN_POINT('Ctrl Pts',(1.04253480033382,838.899769675012,130.790398083267));
#65944=CARTESIAN_POINT('Ctrl Pts',(0.919739196074592,838.870831365168,130.799664165218));
#65945=CARTESIAN_POINT('Ctrl Pts',(0.796070088965291,838.864125149569,130.818638623573));
#65946=CARTESIAN_POINT('Origin',(0.796070088965373,843.535854240486,120.445632192709));
#65947=CARTESIAN_POINT('',(0.796070088965373,841.87243760898,126.652527436197));
#65948=CARTESIAN_POINT('Origin',(0.796070088965373,841.401015378371,126.48591086893));
#65949=CARTESIAN_POINT('',(0.796070088965553,840.20622826248,131.366873312312));
#65950=CARTESIAN_POINT('',(0.796070088965373,844.007276471095,120.612248759976));
#65951=CARTESIAN_POINT('Ctrl Pts',(0.795562167795383,839.279741102276,130.987359868053));
#65952=CARTESIAN_POINT('Ctrl Pts',(0.731430348524241,839.276273003913,130.997367951997));
#65953=CARTESIAN_POINT('Ctrl Pts',(0.667960761387491,839.284234123323,131.012060478403));
#65954=CARTESIAN_POINT('Ctrl Pts',(0.546370658361078,839.322949872229,131.050091378513));
#65955=CARTESIAN_POINT('Ctrl Pts',(0.489756979218874,839.35443841009,131.073469241664));
#65956=CARTESIAN_POINT('Ctrl Pts',(0.396272683050392,839.435786511789,131.124336462737));
#65957=CARTESIAN_POINT('Ctrl Pts',(0.35962563070478,839.484265194161,131.151205415196));
#65958=CARTESIAN_POINT('Ctrl Pts',(0.3097598849944,839.592204362186,131.205143643489));
#65959=CARTESIAN_POINT('Ctrl Pts',(0.296659653429387,839.650449381564,131.231684608902));
#65960=CARTESIAN_POINT('Ctrl Pts',(0.295522146159853,839.769777315234,131.281163845474));
#65961=CARTESIAN_POINT('Ctrl Pts',(0.307379297042506,839.829607500631,131.303603261328));
#65962=CARTESIAN_POINT('Ctrl Pts',(0.354957946136456,839.943866973982,131.341673658187));
#65963=CARTESIAN_POINT('Ctrl Pts',(0.390394184750389,839.997002029084,131.356825299141));
#65964=CARTESIAN_POINT('Ctrl Pts',(0.48098165965852,840.089715368037,131.377829139342));
#65965=CARTESIAN_POINT('Ctrl Pts',(0.535518517417103,840.128053538018,131.383290349174));
#65966=CARTESIAN_POINT('Ctrl Pts',(0.657493684472937,840.184536999717,131.383631985095));
#65967=CARTESIAN_POINT('Ctrl Pts',(0.724034462236347,840.201509191044,131.378206313534));
#65968=CARTESIAN_POINT('Ctrl Pts',(0.858253621700997,840.210342346372,131.357106463382));
#65969=CARTESIAN_POINT('Ctrl Pts',(0.924704672466089,840.202192909004,131.341655540851));
#65970=CARTESIAN_POINT('Ctrl Pts',(1.04807337406688,840.161926284063,131.30296106932));
#65971=CARTESIAN_POINT('Ctrl Pts',(1.10395853967236,840.130363981493,131.280127550429));
#65972=CARTESIAN_POINT('Ctrl Pts',(1.19756615135367,840.048035258523,131.230056322029));
#65973=CARTESIAN_POINT('Ctrl Pts',(1.23453049148622,839.99819766724,131.203326248251));
#65974=CARTESIAN_POINT('Ctrl Pts',(1.28378485237463,839.888055818276,131.149983504672));
#65975=CARTESIAN_POINT('Ctrl Pts',(1.29625187582928,839.829164649058,131.123908659801));
#65976=CARTESIAN_POINT('Ctrl Pts',(1.29588526796899,839.709016475608,131.075132935204));
#65977=CARTESIAN_POINT('Ctrl Pts',(1.28318542618251,839.649007168727,131.052914243734));
#65978=CARTESIAN_POINT('Ctrl Pts',(1.23397083316012,839.535181990415,131.015043182221));
#65979=CARTESIAN_POINT('Ctrl Pts',(1.19784873878774,839.482592971347,130.99982322664));
#65980=CARTESIAN_POINT('Ctrl Pts',(1.10569639300086,839.390903804502,130.978341912658));
#65981=CARTESIAN_POINT('Ctrl Pts',(1.05014519878274,839.353176332159,130.972561536973));
#65982=CARTESIAN_POINT('Ctrl Pts',(0.927639293927917,839.299054603199,130.971861820969));
#65983=CARTESIAN_POINT('Ctrl Pts',(0.861843163686722,839.283325423069,130.977016394591));
#65984=CARTESIAN_POINT('Ctrl Pts',(0.795562167795383,839.279741102276,130.987359868053));
#65985=CARTESIAN_POINT('Origin',(11.5235903376672,855.941516570216,124.830213016114));
#65986=CARTESIAN_POINT('',(11.5235903376672,851.368643130532,134.703481225781));
#65987=CARTESIAN_POINT('',(11.5235903376673,853.266588565377,135.463757424364));
#65988=CARTESIAN_POINT('Ctrl Pts',(11.5235903376672,851.368643130532,134.703481225781));
#65989=CARTESIAN_POINT('Ctrl Pts',(11.5205021226678,851.368593808959,134.703620775445));
#65990=CARTESIAN_POINT('Ctrl Pts',(11.5174132752579,851.36855744311,134.703765698308));
#65991=CARTESIAN_POINT('Ctrl Pts',(11.3794022374267,851.367512362552,134.710480119367));
#65992=CARTESIAN_POINT('Ctrl Pts',(11.246127730073,851.391242846567,134.72719324216));
#65993=CARTESIAN_POINT('Ctrl Pts',(10.9990624023133,851.484833008573,134.779260202327));
#65994=CARTESIAN_POINT('Ctrl Pts',(10.8875292827729,851.55347968161,134.813990765133));
#65995=CARTESIAN_POINT('Ctrl Pts',(10.7003910944404,851.726799524684,134.896941108057));
#65996=CARTESIAN_POINT('Ctrl Pts',(10.626505033589,851.829800131095,134.944355825167));
#65997=CARTESIAN_POINT('Ctrl Pts',(10.5266345429849,852.056594180815,135.044993714505));
#65998=CARTESIAN_POINT('Ctrl Pts',(10.5013771736133,852.178179672887,135.097235730556));
#65999=CARTESIAN_POINT('Ctrl Pts',(10.503023411694,852.424395424166,135.199054871647));
#66000=CARTESIAN_POINT('Ctrl Pts',(10.5297458928562,852.546658827902,135.247651124626));
#66001=CARTESIAN_POINT('Ctrl Pts',(10.6322545121574,852.776515752824,135.33451099905));
#66002=CARTESIAN_POINT('Ctrl Pts',(10.7071100086572,852.881800419343,135.371887362115));
#66003=CARTESIAN_POINT('Ctrl Pts',(10.896054365022,853.061541060369,135.43039791291));
#66004=CARTESIAN_POINT('Ctrl Pts',(11.0084685942409,853.134002248043,135.450851545521));
#66005=CARTESIAN_POINT('Ctrl Pts',(11.2562712869861,853.23551591681,135.472220334527));
#66006=CARTESIAN_POINT('Ctrl Pts',(11.3893185237754,853.263374010964,135.472852632822));
#66007=CARTESIAN_POINT('Ctrl Pts',(11.5235903376673,853.266588565377,135.463757424364));
#66008=CARTESIAN_POINT('',(11.5235903391071,853.90899332006,133.646147763011));
#66009=CARTESIAN_POINT('',(11.5235903376672,856.904545710459,125.170580099181));
#66010=CARTESIAN_POINT('Ctrl Pts',(10.680142013218,853.477148071031,133.531621451738));
#66011=CARTESIAN_POINT('Ctrl Pts',(10.7552566727792,853.580838666919,133.568269216784));
#66012=CARTESIAN_POINT('Ctrl Pts',(10.8511384208992,853.670383328694,133.597600419919));
#66013=CARTESIAN_POINT('Ctrl Pts',(11.0735865855287,853.811093672709,133.638480591057));
#66014=CARTESIAN_POINT('Ctrl Pts',(11.1979838140956,853.86088358712,133.649635451893));
#66015=CARTESIAN_POINT('Ctrl Pts',(11.4596338352218,853.913861640245,133.652507210074));
#66016=CARTESIAN_POINT('Ctrl Pts',(11.5944280372036,853.916332889399,133.644118800169));
#66017=CARTESIAN_POINT('Ctrl Pts',(11.8566696033935,853.872743280832,133.608948039412));
#66018=CARTESIAN_POINT('Ctrl Pts',(11.9815853878325,853.826883552933,133.582426730849));
#66019=CARTESIAN_POINT('Ctrl Pts',(12.2042818130555,853.692249125062,133.514746543923));
#66020=CARTESIAN_POINT('Ctrl Pts',(12.2999034801377,853.604715673213,133.474220089617));
#66021=CARTESIAN_POINT('Ctrl Pts',(12.4478498336772,853.40026531813,133.384751079444));
#66022=CARTESIAN_POINT('Ctrl Pts',(12.4991659215438,853.285582203206,133.336737939971));
#66023=CARTESIAN_POINT('Ctrl Pts',(12.55162288623,853.0417674699,133.238161161633));
#66024=CARTESIAN_POINT('Ctrl Pts',(12.5515963550512,852.9148848129,133.188538796986));
#66025=CARTESIAN_POINT('Ctrl Pts',(12.4985600437562,852.667317196894,133.094549128521));
#66026=CARTESIAN_POINT('Ctrl Pts',(12.445994474123,852.549113986541,133.051120640321));
#66027=CARTESIAN_POINT('Ctrl Pts',(12.2956314640741,852.338913678305,132.97673256773));
#66028=CARTESIAN_POINT('Ctrl Pts',(12.1997586031175,852.248724795663,132.94638150898));
#66029=CARTESIAN_POINT('Ctrl Pts',(11.9769114666055,852.107376329575,132.902605212033));
#66030=CARTESIAN_POINT('Ctrl Pts',(11.8521364266482,852.057564352149,132.889600872787));
#66031=CARTESIAN_POINT('Ctrl Pts',(11.5904503957502,852.005149110542,132.883151612586));
#66032=CARTESIAN_POINT('Ctrl Pts',(11.4561071093275,852.002889344376,132.889711566681));
#66033=CARTESIAN_POINT('Ctrl Pts',(11.1940094503849,852.046372682254,132.922083142856));
#66034=CARTESIAN_POINT('Ctrl Pts',(11.0688603989777,852.092095747919,132.947748147312));
#66035=CARTESIAN_POINT('Ctrl Pts',(10.8444080174315,852.226752201474,133.01547194676));
#66036=CARTESIAN_POINT('Ctrl Pts',(10.7476233879218,852.314874914181,133.057059047555));
#66037=CARTESIAN_POINT('Ctrl Pts',(10.5984020412124,852.520536616746,133.14975849757));
#66038=CARTESIAN_POINT('Ctrl Pts',(10.5469174051594,852.635785811548,133.19987180787));
#66039=CARTESIAN_POINT('Ctrl Pts',(10.4954269424383,852.879058095224,133.301996835519));
#66040=CARTESIAN_POINT('Ctrl Pts',(10.4958558425417,853.00471458401,133.353010146666));
#66041=CARTESIAN_POINT('Ctrl Pts',(10.5359244585833,853.189128103142,133.425053217205));
#66042=CARTESIAN_POINT('Ctrl Pts',(10.5559055903532,853.249684413758,133.448222338175));
#66043=CARTESIAN_POINT('Ctrl Pts',(10.6087057436789,853.367222257402,133.492160112676));
#66044=CARTESIAN_POINT('Ctrl Pts',(10.6415321002965,853.423849754811,133.512784023393));
#66045=CARTESIAN_POINT('Ctrl Pts',(10.680142013218,853.477148071031,133.531621451738));
#66046=CARTESIAN_POINT('Ctrl Pts',(11.5235903376673,853.266588565377,135.463757424364));
#66047=CARTESIAN_POINT('Ctrl Pts',(11.5236943901661,853.266591056462,135.46375037613));
#66048=CARTESIAN_POINT('Ctrl Pts',(11.5237984434004,853.266593532747,135.463743322055));
#66049=CARTESIAN_POINT('Ctrl Pts',(11.5239024973665,853.266595994231,135.463736262138));
#66050=CARTESIAN_POINT('Ctrl Pts',(11.6551425361477,853.269700588689,135.454831808873));
#66051=CARTESIAN_POINT('Ctrl Pts',(11.7851296518499,853.249200036743,135.436812128387));
#66052=CARTESIAN_POINT('Ctrl Pts',(12.0334729099227,853.161290212145,135.383955763739));
#66053=CARTESIAN_POINT('Ctrl Pts',(12.1486654966744,853.092808126151,135.348975051315));
#66054=CARTESIAN_POINT('Ctrl Pts',(12.3408496401843,852.917885897015,135.26778523619));
#66055=CARTESIAN_POINT('Ctrl Pts',(12.4164867427695,852.813713385906,135.222532568282));
#66056=CARTESIAN_POINT('Ctrl Pts',(12.5190707641202,852.583469542574,135.127118673292));
#66057=CARTESIAN_POINT('Ctrl Pts',(12.5452809191628,852.459794537162,135.077909345789));
#66058=CARTESIAN_POINT('Ctrl Pts',(12.5447108915423,852.208730494133,134.980949860915));
#66059=CARTESIAN_POINT('Ctrl Pts',(12.5177773471651,852.083827409251,134.934148102748));
#66060=CARTESIAN_POINT('Ctrl Pts',(12.4135224748329,851.849957798997,134.848759380441));
#66061=CARTESIAN_POINT('Ctrl Pts',(12.3370911785135,851.743365151998,134.811036680661));
#66062=CARTESIAN_POINT('Ctrl Pts',(12.1449200415364,851.563846763306,134.750115378063));
#66063=CARTESIAN_POINT('Ctrl Pts',(12.0311862886986,851.492601493932,134.727487315331));
#66064=CARTESIAN_POINT('Ctrl Pts',(11.7845957909319,851.396167511552,134.701317415303));
#66065=CARTESIAN_POINT('Ctrl Pts',(11.6546626058585,851.370736472623,134.697558357399));
#66066=CARTESIAN_POINT('Ctrl Pts',(11.5235903376672,851.368643130532,134.703481225781));
#66067=CARTESIAN_POINT('Origin',(11.5235903376672,855.941516570216,124.830213016114));
#66068=CARTESIAN_POINT('',(11.5235903376672,854.27809993871,131.037108259602));
#66069=CARTESIAN_POINT('Origin',(11.5235903376672,853.806677708101,130.870491692335));
#66070=CARTESIAN_POINT('',(11.5235903376671,852.783421454099,135.266127479096));
#66071=CARTESIAN_POINT('',(11.5235903376672,856.412938800825,124.996829583381));
#66072=CARTESIAN_POINT('Ctrl Pts',(11.5234307913646,851.854317302887,134.894017809227));
#66073=CARTESIAN_POINT('Ctrl Pts',(11.4620605953806,851.8532288306,134.897156281172));
#66074=CARTESIAN_POINT('Ctrl Pts',(11.4012425456016,851.862628695986,134.904523912193));
#66075=CARTESIAN_POINT('Ctrl Pts',(11.2827884647596,851.902731625166,134.927852321044));
#66076=CARTESIAN_POINT('Ctrl Pts',(11.2268079678992,851.934490807818,134.944155309179));
#66077=CARTESIAN_POINT('Ctrl Pts',(11.1317720398537,852.016366574967,134.983364582381));
#66078=CARTESIAN_POINT('Ctrl Pts',(11.0935952813509,852.065685262024,135.005889850397));
#66079=CARTESIAN_POINT('Ctrl Pts',(11.0403322118733,852.175381959815,135.054046308876));
#66080=CARTESIAN_POINT('Ctrl Pts',(11.0256691663884,852.234683649601,135.079207243204));
#66081=CARTESIAN_POINT('Ctrl Pts',(11.0219278432404,852.355573996643,135.128693372122));
#66082=CARTESIAN_POINT('Ctrl Pts',(11.0328118469896,852.415992694243,135.15254086669));
#66083=CARTESIAN_POINT('Ctrl Pts',(11.0789341059454,852.530195117028,135.195700871793));
#66084=CARTESIAN_POINT('Ctrl Pts',(11.1137266837724,852.582852009129,135.214584939382));
#66085=CARTESIAN_POINT('Ctrl Pts',(11.2030012436641,852.673469967185,135.244856780591));
#66086=CARTESIAN_POINT('Ctrl Pts',(11.2566637199698,852.710476923002,135.255917874418));
#66087=CARTESIAN_POINT('Ctrl Pts',(11.3759898352345,852.763637145866,135.268732408905));
#66088=CARTESIAN_POINT('Ctrl Pts',(11.4405267510195,852.779181193359,135.270325149122));
#66089=CARTESIAN_POINT('Ctrl Pts',(11.5718381732654,852.786333960206,135.263867260214));
#66090=CARTESIAN_POINT('Ctrl Pts',(11.6373514964259,852.777824259386,135.255863124021));
#66091=CARTESIAN_POINT('Ctrl Pts',(11.7615714398395,852.73722955077,135.231158375251));
#66092=CARTESIAN_POINT('Ctrl Pts',(11.8189055150791,852.705119303221,135.214548792635));
#66093=CARTESIAN_POINT('Ctrl Pts',(11.9157287467566,852.621732954991,135.175170316205));
#66094=CARTESIAN_POINT('Ctrl Pts',(11.9543928728251,852.571416662468,135.152832569033));
#66095=CARTESIAN_POINT('Ctrl Pts',(12.0079060009128,852.459321242942,135.105288065939));
#66096=CARTESIAN_POINT('Ctrl Pts',(12.0223015627294,852.398693476501,135.08055888157));
#66097=CARTESIAN_POINT('Ctrl Pts',(12.0247151338561,852.275147512267,135.031782572753));
#66098=CARTESIAN_POINT('Ctrl Pts',(12.0126797276385,852.213469882361,135.008222185968));
#66099=CARTESIAN_POINT('Ctrl Pts',(11.9634580546866,852.097571840821,134.965378255875));
#66100=CARTESIAN_POINT('Ctrl Pts',(11.9267343509588,852.044534466716,134.946531893362));
#66101=CARTESIAN_POINT('Ctrl Pts',(11.8334642424212,851.954654908216,134.916244729229));
#66102=CARTESIAN_POINT('Ctrl Pts',(11.7778816295094,851.91870038575,134.905102603088));
#66103=CARTESIAN_POINT('Ctrl Pts',(11.6553877837247,851.868885618794,134.8922340432));
#66104=CARTESIAN_POINT('Ctrl Pts',(11.5897214869269,851.855493045995,134.890627702924));
#66105=CARTESIAN_POINT('Ctrl Pts',(11.5234307913646,851.854317302887,134.894017809227));
#66106=CARTESIAN_POINT('Origin',(5.07102541057036,853.43446399037,123.944135806152));
#66107=CARTESIAN_POINT('',(5.07102541057036,848.771152051143,134.293326883657));
#66108=CARTESIAN_POINT('',(5.07102541052708,850.506278886623,135.074204134598));
#66109=CARTESIAN_POINT('Ctrl Pts',(5.07102541057036,848.771152051143,134.293326883657));
#66110=CARTESIAN_POINT('Ctrl Pts',(5.0699582962581,848.771099914276,134.293474398867));
#66111=CARTESIAN_POINT('Ctrl Pts',(5.06889111868239,848.7710494163,134.293622683548));
#66112=CARTESIAN_POINT('Ctrl Pts',(4.94165327412791,848.765224438062,134.311393163062));
#66113=CARTESIAN_POINT('Ctrl Pts',(4.81710114981319,848.782464983614,134.33943824526));
#66114=CARTESIAN_POINT('Ctrl Pts',(4.58394097750445,848.860926766562,134.41368984665));
#66115=CARTESIAN_POINT('Ctrl Pts',(4.47773994242997,848.922069921972,134.459475719585));
#66116=CARTESIAN_POINT('Ctrl Pts',(4.30295154857553,849.07816947996,134.56079191155));
#66117=CARTESIAN_POINT('Ctrl Pts',(4.23491862264972,849.170822301041,134.615145628139));
#66118=CARTESIAN_POINT('Ctrl Pts',(4.14429105857174,849.375464639912,134.72504769072));
#66119=CARTESIAN_POINT('Ctrl Pts',(4.12168011923636,849.48521408266,134.77955337809));
#66120=CARTESIAN_POINT('Ctrl Pts',(4.12429471942459,849.70841290292,134.881590968212));
#66121=CARTESIAN_POINT('Ctrl Pts',(4.14893812838373,849.819580954806,134.928171807675));
#66122=CARTESIAN_POINT('Ctrl Pts',(4.24291571131902,850.03073743613,135.007798329004));
#66123=CARTESIAN_POINT('Ctrl Pts',(4.31142571246568,850.128392921735,135.039921708603));
#66124=CARTESIAN_POINT('Ctrl Pts',(4.48513736682712,850.298206835272,135.085630847371));
#66125=CARTESIAN_POINT('Ctrl Pts',(4.58907400449951,850.368022432266,135.098381587636));
#66126=CARTESIAN_POINT('Ctrl Pts',(4.81954792508221,850.469430147485,135.102577107638));
#66127=CARTESIAN_POINT('Ctrl Pts',(4.94413173609949,850.499233941933,135.093579592117));
#66128=CARTESIAN_POINT('Ctrl Pts',(5.06962996552313,850.506202346397,135.074417614505));
#66129=CARTESIAN_POINT('Ctrl Pts',(5.07009513240186,850.506228175216,135.074346589461));
#66130=CARTESIAN_POINT('Ctrl Pts',(5.07056028084347,850.506253688607,135.074275429459));
#66131=CARTESIAN_POINT('Ctrl Pts',(5.0710254104838,850.506278886623,135.074204134598));
#66132=CARTESIAN_POINT('',(5.07102541057036,851.188478953102,133.143998259299));
#66133=CARTESIAN_POINT('',(5.07102541057036,854.328360162989,124.260068959288));
#66134=CARTESIAN_POINT('Ctrl Pts',(4.23512898156332,850.693189667638,133.042771344765));
#66135=CARTESIAN_POINT('Ctrl Pts',(4.29099867867875,850.791613551705,133.07755767565));
#66136=CARTESIAN_POINT('Ctrl Pts',(4.36588968533656,850.88028614259,133.105549792614));
#66137=CARTESIAN_POINT('Ctrl Pts',(4.55086908900839,851.033175176208,133.146308005615));
#66138=CARTESIAN_POINT('Ctrl Pts',(4.66077472278794,851.094171929925,133.157720959576));
#66139=CARTESIAN_POINT('Ctrl Pts',(4.89556685899703,851.17371147003,133.160627109839));
#66140=CARTESIAN_POINT('Ctrl Pts',(5.01796167694315,851.192219771856,133.152439031636));
#66141=CARTESIAN_POINT('Ctrl Pts',(5.26321810607648,851.185574483663,133.11785628134));
#66142=CARTESIAN_POINT('Ctrl Pts',(5.38381514613692,851.159776035689,133.091493142985));
#66143=CARTESIAN_POINT('Ctrl Pts',(5.60673618965806,851.065687386839,133.023646760527));
#66144=CARTESIAN_POINT('Ctrl Pts',(5.70675422284467,850.997747268953,132.982609837993));
#66145=CARTESIAN_POINT('Ctrl Pts',(5.87099048308924,850.828202958375,132.891231943048));
#66146=CARTESIAN_POINT('Ctrl Pts',(5.93354165355819,850.728152743558,132.841744379948));
#66147=CARTESIAN_POINT('Ctrl Pts',(6.00998878810946,850.51390100233,132.742867659224));
#66148=CARTESIAN_POINT('Ctrl Pts',(6.02511120824281,850.402461808752,132.694472602674));
#66149=CARTESIAN_POINT('Ctrl Pts',(6.009090654539,850.182142107766,132.604137937494));
#66150=CARTESIAN_POINT('Ctrl Pts',(5.97960229472973,850.075276882214,132.562844301108));
#66151=CARTESIAN_POINT('Ctrl Pts',(5.87998340379096,849.874817826804,132.490389855698));
#66152=CARTESIAN_POINT('Ctrl Pts',(5.81054255648633,849.783142082205,132.459951248518));
#66153=CARTESIAN_POINT('Ctrl Pts',(5.63763269257999,849.624754818309,132.413423289628));
#66154=CARTESIAN_POINT('Ctrl Pts',(5.53497596315341,849.560286324222,132.398184262539));
#66155=CARTESIAN_POINT('Ctrl Pts',(5.30485543671926,849.467114843493,132.385820586694));
#66156=CARTESIAN_POINT('Ctrl Pts',(5.17875512652277,849.441429377766,132.389824260633));
#66157=CARTESIAN_POINT('Ctrl Pts',(4.9282581978398,849.43683076242,132.417862061688));
#66158=CARTESIAN_POINT('Ctrl Pts',(4.8062516798978,849.456914301006,132.441181502153));
#66159=CARTESIAN_POINT('Ctrl Pts',(4.57800342857582,849.53978619875,132.504591540214));
#66160=CARTESIAN_POINT('Ctrl Pts',(4.47412434763127,849.602391454363,132.544321421763));
#66161=CARTESIAN_POINT('Ctrl Pts',(4.2996921601432,849.762887981157,132.635126752235));
#66162=CARTESIAN_POINT('Ctrl Pts',(4.23109740276462,849.859580192221,132.685440117008));
#66163=CARTESIAN_POINT('Ctrl Pts',(4.14507592259544,850.062846652263,132.783904166084));
#66164=CARTESIAN_POINT('Ctrl Pts',(4.12375507032402,850.165733648502,132.830947687406));
#66165=CARTESIAN_POINT('Ctrl Pts',(4.1221327608723,850.380762396911,132.923599492544));
#66166=CARTESIAN_POINT('Ctrl Pts',(4.14396681404573,850.491099136668,132.968144643274));
#66167=CARTESIAN_POINT('Ctrl Pts',(4.20124222567194,850.629019808441,133.019746227074));
#66168=CARTESIAN_POINT('Ctrl Pts',(4.21716604956892,850.661544936641,133.031587026104));
#66169=CARTESIAN_POINT('Ctrl Pts',(4.23512898156325,850.693189667638,133.042771344765));
#66170=CARTESIAN_POINT('Ctrl Pts',(5.07102541048378,850.506278886623,135.074204134598));
#66171=CARTESIAN_POINT('Ctrl Pts',(5.19423078066677,850.512953436295,135.055319271343));
#66172=CARTESIAN_POINT('Ctrl Pts',(5.31611901355964,850.497498731957,135.026985023423));
#66173=CARTESIAN_POINT('Ctrl Pts',(5.54705036221113,850.423151972727,134.953923209424));
#66174=CARTESIAN_POINT('Ctrl Pts',(5.65355205997801,850.363656200473,134.90939339752));
#66175=CARTESIAN_POINT('Ctrl Pts',(5.83121312845475,850.209017353198,134.811222468209));
#66176=CARTESIAN_POINT('Ctrl Pts',(5.90123008407851,850.115815905014,134.75861491801));
#66177=CARTESIAN_POINT('Ctrl Pts',(5.99585789558844,849.90787126927,134.651654591827));
#66178=CARTESIAN_POINT('Ctrl Pts',(6.01988600047576,849.795357887299,134.598362087097));
#66179=CARTESIAN_POINT('Ctrl Pts',(6.01831170401472,849.567711146755,134.498395590651));
#66180=CARTESIAN_POINT('Ctrl Pts',(5.99371779675477,849.454975907878,134.452607245757));
#66181=CARTESIAN_POINT('Ctrl Pts',(5.89885078072835,849.241046241887,134.372903188918));
#66182=CARTESIAN_POINT('Ctrl Pts',(5.82913869410888,849.1422252107,134.339941444606));
#66183=CARTESIAN_POINT('Ctrl Pts',(5.65278354333737,848.972221136584,134.291760233714));
#66184=CARTESIAN_POINT('Ctrl Pts',(5.54766206537191,848.903127388101,134.277239294612));
#66185=CARTESIAN_POINT('Ctrl Pts',(5.31736144834189,848.805210438417,134.269484061337));
#66186=CARTESIAN_POINT('Ctrl Pts',(5.19461728992305,848.777190479516,134.276241851719));
#66187=CARTESIAN_POINT('Ctrl Pts',(5.07102541057036,848.771152051143,134.293326883657));
#66188=CARTESIAN_POINT('Origin',(5.07102541057036,853.43446399037,123.944135806152));
#66189=CARTESIAN_POINT('',(5.07102541057036,851.771047358864,130.15103104964));
#66190=CARTESIAN_POINT('Origin',(5.07102541057036,851.299625128255,129.984414482373));
#66191=CARTESIAN_POINT('',(5.07102541057048,850.097096174575,134.887281556846));
#66192=CARTESIAN_POINT('',(5.07102541057036,853.905886220979,124.110752373419));
#66193=CARTESIAN_POINT('Ctrl Pts',(5.0706266353229,849.181994456725,134.475554028475));
#66194=CARTESIAN_POINT('Ctrl Pts',(5.00538071894428,849.178772050676,134.484827609953));
#66195=CARTESIAN_POINT('Ctrl Pts',(4.94089660084872,849.187245813263,134.49932329689));
#66196=CARTESIAN_POINT('Ctrl Pts',(4.81872050007149,849.226996978315,134.537709047521));
#66197=CARTESIAN_POINT('Ctrl Pts',(4.76242595381707,849.258633076072,134.561535719969));
#66198=CARTESIAN_POINT('Ctrl Pts',(4.66924894253178,849.340049433716,134.614327125243));
#66199=CARTESIAN_POINT('Ctrl Pts',(4.63273407721486,849.388658790337,134.642690753026));
#66200=CARTESIAN_POINT('Ctrl Pts',(4.58357471445859,849.496406215602,134.700180626491));
#66201=CARTESIAN_POINT('Ctrl Pts',(4.570969969903,849.5543586624,134.728755879377));
#66202=CARTESIAN_POINT('Ctrl Pts',(4.57108058031632,849.672413088542,134.782444381829));
#66203=CARTESIAN_POINT('Ctrl Pts',(4.58350979218662,849.731306290975,134.807055202564));
#66204=CARTESIAN_POINT('Ctrl Pts',(4.63206290571102,849.843190482258,134.849348000012));
#66205=CARTESIAN_POINT('Ctrl Pts',(4.6677306976392,849.89497121084,134.866559374063));
#66206=CARTESIAN_POINT('Ctrl Pts',(4.7584701484939,849.985054915219,134.891392852513));
#66207=CARTESIAN_POINT('Ctrl Pts',(4.81284882588072,850.022167910333,134.898598615293));
#66208=CARTESIAN_POINT('Ctrl Pts',(4.93389009301996,850.076473238899,134.901886229569));
#66209=CARTESIAN_POINT('Ctrl Pts',(4.99954868223937,850.092655060561,134.897692010075));
#66210=CARTESIAN_POINT('Ctrl Pts',(5.13320829335458,850.101006435591,134.878245413705));
#66211=CARTESIAN_POINT('Ctrl Pts',(5.19995559405832,850.092681927241,134.862994352188));
#66212=CARTESIAN_POINT('Ctrl Pts',(5.32383274316292,850.052242247041,134.823711597774));
#66213=CARTESIAN_POINT('Ctrl Pts',(5.37990540190694,850.020624931118,134.800083176872));
#66214=CARTESIAN_POINT('Ctrl Pts',(5.47351575204461,849.938512202664,134.747726210205));
#66215=CARTESIAN_POINT('Ctrl Pts',(5.51036094006763,849.888945988342,134.71952470307));
#66216=CARTESIAN_POINT('Ctrl Pts',(5.55928135851067,849.779525665693,134.662740083004));
#66217=CARTESIAN_POINT('Ctrl Pts',(5.57152417748079,849.721020436217,134.634723276507));
#66218=CARTESIAN_POINT('Ctrl Pts',(5.57050061265669,849.602042816117,134.581957801238));
#66219=CARTESIAN_POINT('Ctrl Pts',(5.5574911359873,849.542792490688,134.557707958326));
#66220=CARTESIAN_POINT('Ctrl Pts',(5.50772101855733,849.430814536929,134.515872560121));
#66221=CARTESIAN_POINT('Ctrl Pts',(5.47148092102027,849.379252328022,134.498721208165));
#66222=CARTESIAN_POINT('Ctrl Pts',(5.37954247592785,849.289859054838,134.473632059099));
#66223=CARTESIAN_POINT('Ctrl Pts',(5.3244836160405,849.253247527649,134.466136803691));
#66224=CARTESIAN_POINT('Ctrl Pts',(5.20257928156474,849.200519585333,134.462286635868));
#66225=CARTESIAN_POINT('Ctrl Pts',(5.13683475959023,849.185264384898,134.466143685743));
#66226=CARTESIAN_POINT('Ctrl Pts',(5.0706266353229,849.181994456725,134.475554028475));
#66227=CARTESIAN_POINT('Origin',(18.2997627645019,863.466134352395,127.489667542144));
#66228=CARTESIAN_POINT('',(18.2997627645018,858.895801196787,137.355748312979));
#66229=CARTESIAN_POINT('',(18.2997627644989,860.785555989654,138.139198981994));
#66230=CARTESIAN_POINT('Ctrl Pts',(18.2997627645018,858.895801196787,137.355748312979));
#66231=CARTESIAN_POINT('Ctrl Pts',(18.2983068136417,858.895782959237,137.355799914008));
#66232=CARTESIAN_POINT('Ctrl Pts',(18.2968507168663,858.895767600436,137.355852711893));
#66233=CARTESIAN_POINT('Ctrl Pts',(18.1608616249801,858.89460231778,137.360895047597));
#66234=CARTESIAN_POINT('Ctrl Pts',(18.0278281919414,858.918050978786,137.37601610752));
#66235=CARTESIAN_POINT('Ctrl Pts',(17.7786029347692,859.011612283662,137.425711003125));
#66236=CARTESIAN_POINT('Ctrl Pts',(17.6651217807427,859.081309034422,137.460017191673));
#66237=CARTESIAN_POINT('Ctrl Pts',(17.4764533886176,859.256319335015,137.542854104322));
#66238=CARTESIAN_POINT('Ctrl Pts',(17.4025240193924,859.359427527541,137.590376644922));
#66239=CARTESIAN_POINT('Ctrl Pts',(17.3026195959521,859.586115931001,137.692365692213));
#66240=CARTESIAN_POINT('Ctrl Pts',(17.277421515798,859.707516946354,137.745845666951));
#66241=CARTESIAN_POINT('Ctrl Pts',(17.2793359665033,859.952765012574,137.851018357706));
#66242=CARTESIAN_POINT('Ctrl Pts',(17.3061982152061,860.074293963003,137.901713187695));
#66243=CARTESIAN_POINT('Ctrl Pts',(17.4088728257215,860.302144253813,137.993172112431));
#66244=CARTESIAN_POINT('Ctrl Pts',(17.4836394713146,860.406259319673,138.033042761101));
#66245=CARTESIAN_POINT('Ctrl Pts',(17.672197256176,860.58372504773,138.096468904178));
#66246=CARTESIAN_POINT('Ctrl Pts',(17.7842656183664,860.655152976418,138.119312482594));
#66247=CARTESIAN_POINT('Ctrl Pts',(18.0316171493468,860.755226628336,138.144865426948));
#66248=CARTESIAN_POINT('Ctrl Pts',(18.1645680107954,860.782589038475,138.147197677704));
#66249=CARTESIAN_POINT('Ctrl Pts',(18.2987622212797,860.785534481657,138.139258365774));
#66250=CARTESIAN_POINT('Ctrl Pts',(18.2990957438871,860.785541802181,138.139238633626));
#66251=CARTESIAN_POINT('Ctrl Pts',(18.2994292583314,860.785548971507,138.139218839026));
#66252=CARTESIAN_POINT('Ctrl Pts',(18.299762764496,860.785555989654,138.139198981994));
#66253=CARTESIAN_POINT('',(18.2997627661012,861.429330672107,136.317713269084));
#66254=CARTESIAN_POINT('',(18.2997627645019,864.429163492638,127.830034625211));
#66255=CARTESIAN_POINT('Ctrl Pts',(17.594519871266,861.155236423289,136.24531767004));
#66256=CARTESIAN_POINT('Ctrl Pts',(17.6908584649292,861.241936525388,136.275960419694));
#66257=CARTESIAN_POINT('Ctrl Pts',(17.804230417976,861.310744784423,136.297962676467));
#66258=CARTESIAN_POINT('Ctrl Pts',(18.0522330816735,861.404834888075,136.322365677225));
#66259=CARTESIAN_POINT('Ctrl Pts',(18.1844450118424,861.429195618522,136.324533004031));
#66260=CARTESIAN_POINT('Ctrl Pts',(18.4509615187008,861.429833981708,136.308906144829));
#66261=CARTESIAN_POINT('Ctrl Pts',(18.5827134042018,861.405891327604,136.291182167775));
#66262=CARTESIAN_POINT('Ctrl Pts',(18.8282428242795,861.311983164994,136.238227127449));
#66263=CARTESIAN_POINT('Ctrl Pts',(18.9396016131448,861.242709348448,136.203430487723));
#66264=CARTESIAN_POINT('Ctrl Pts',(19.1263503268062,861.067500157729,136.121409806725));
#66265=CARTESIAN_POINT('Ctrl Pts',(19.1999155927994,860.963200797497,136.074957713108));
#66266=CARTESIAN_POINT('Ctrl Pts',(19.2983522032081,860.734334643123,135.976859333337));
#66267=CARTESIAN_POINT('Ctrl Pts',(19.3227392680653,860.612149576957,135.92619475046));
#66268=CARTESIAN_POINT('Ctrl Pts',(19.3194256122495,860.363464891823,135.825896766366));
#66269=CARTESIAN_POINT('Ctrl Pts',(19.2910890688764,860.239392928892,135.777267796106));
#66270=CARTESIAN_POINT('Ctrl Pts',(19.1841695557557,860.007676446591,135.688880454628));
#66271=CARTESIAN_POINT('Ctrl Pts',(19.1065726266327,859.902371942357,135.65001080561));
#66272=CARTESIAN_POINT('Ctrl Pts',(18.9131363483052,859.726241093662,135.587664032789));
#66273=CARTESIAN_POINT('Ctrl Pts',(18.7995761439172,859.656806388201,135.564648202491));
#66274=CARTESIAN_POINT('Ctrl Pts',(18.5508574843179,859.562188652378,135.537388126793));
#66275=CARTESIAN_POINT('Ctrl Pts',(18.4181435363346,859.537893047305,135.533402136904));
#66276=CARTESIAN_POINT('Ctrl Pts',(18.1514542733364,859.537838183702,135.545458805947));
#66277=CARTESIAN_POINT('Ctrl Pts',(18.0200582254551,859.561912374016,135.561326071294));
#66278=CARTESIAN_POINT('Ctrl Pts',(17.7744547997471,859.655707338899,135.61147947879));
#66279=CARTESIAN_POINT('Ctrl Pts',(17.6627817243068,859.724898754097,135.645438992041));
#66280=CARTESIAN_POINT('Ctrl Pts',(17.4743227654491,859.900473460484,135.727624686544));
#66281=CARTESIAN_POINT('Ctrl Pts',(17.3998089472424,860.005571326227,135.775211380791));
#66282=CARTESIAN_POINT('Ctrl Pts',(17.3005864785872,860.235853052164,135.876612380104));
#66283=CARTESIAN_POINT('Ctrl Pts',(17.2762910227212,860.358611822648,135.929379828543));
#66284=CARTESIAN_POINT('Ctrl Pts',(17.2806895581755,860.606550772501,136.033154213921));
#66285=CARTESIAN_POINT('Ctrl Pts',(17.3092756830069,860.729331960926,136.083151296631));
#66286=CARTESIAN_POINT('Ctrl Pts',(17.3896103528833,860.901813882126,136.150977336745));
#66287=CARTESIAN_POINT('Ctrl Pts',(17.4226308325239,860.957117894915,136.172290117947));
#66288=CARTESIAN_POINT('Ctrl Pts',(17.5003620732768,861.06172047604,136.211656132999));
#66289=CARTESIAN_POINT('Ctrl Pts',(17.5450005799048,861.110671442074,136.229566897785));
#66290=CARTESIAN_POINT('Ctrl Pts',(17.5945198712659,861.155236423289,136.24531767004));
#66291=CARTESIAN_POINT('Ctrl Pts',(18.299762764496,860.785555989654,138.139198981994));
#66292=CARTESIAN_POINT('Ctrl Pts',(18.4310515283573,860.788318768667,138.131382019577));
#66293=CARTESIAN_POINT('Ctrl Pts',(18.5610575008464,860.767652691017,138.11389506776));
#66294=CARTESIAN_POINT('Ctrl Pts',(18.8072939520139,860.680553108331,138.061531489626));
#66295=CARTESIAN_POINT('Ctrl Pts',(18.9207645229621,860.613820608303,138.026744860966));
#66296=CARTESIAN_POINT('Ctrl Pts',(19.1134734904683,860.441564281237,137.944467023966));
#66297=CARTESIAN_POINT('Ctrl Pts',(19.1903967296927,860.337278540976,137.897641488792));
#66298=CARTESIAN_POINT('Ctrl Pts',(19.2944244219691,860.107094203539,137.798995600584));
#66299=CARTESIAN_POINT('Ctrl Pts',(19.3211066916547,859.983737438504,137.748200676581));
#66300=CARTESIAN_POINT('Ctrl Pts',(19.3212349898297,859.733815019667,137.648372605662));
#66301=CARTESIAN_POINT('Ctrl Pts',(19.2948235226952,859.609730037168,137.600301655224));
#66302=CARTESIAN_POINT('Ctrl Pts',(19.1918492603882,859.377156910803,137.512381797694));
#66303=CARTESIAN_POINT('Ctrl Pts',(19.116165062299,859.27102093137,137.47341188137));
#66304=CARTESIAN_POINT('Ctrl Pts',(18.9252420327866,859.091752276658,137.409732445018));
#66305=CARTESIAN_POINT('Ctrl Pts',(18.8118777132635,859.020399903431,137.385654923748));
#66306=CARTESIAN_POINT('Ctrl Pts',(18.5641974706985,858.923091316913,137.356286466893));
#66307=CARTESIAN_POINT('Ctrl Pts',(18.4325874854965,858.897464987428,137.351040810548));
#66308=CARTESIAN_POINT('Ctrl Pts',(18.2997627645018,858.895801196787,137.355748312979));
#66309=CARTESIAN_POINT('Origin',(18.2997627645019,863.466134352395,127.489667542144));
#66310=CARTESIAN_POINT('',(18.2997627645019,861.802717720889,133.696562785632));
#66311=CARTESIAN_POINT('Origin',(18.2997627645019,861.33129549028,133.529946218365));
#66312=CARTESIAN_POINT('',(18.299762764502,860.305153003216,137.933748266442));
#66313=CARTESIAN_POINT('',(18.2997627645019,863.937556583004,127.656284109411));
#66314=CARTESIAN_POINT('Ctrl Pts',(18.29939398446,859.38006602879,137.550272793039));
#66315=CARTESIAN_POINT('Ctrl Pts',(18.2379737606721,859.379200950101,137.55285637696));
#66316=CARTESIAN_POINT('Ctrl Pts',(18.1771136100427,859.38881406725,137.55975239348));
#66317=CARTESIAN_POINT('Ctrl Pts',(18.0575828896044,859.429646471273,137.582550689604));
#66318=CARTESIAN_POINT('Ctrl Pts',(18.00076816786,859.462274904145,137.598964230339));
#66319=CARTESIAN_POINT('Ctrl Pts',(17.9055516740868,859.545601002131,137.63864787193));
#66320=CARTESIAN_POINT('Ctrl Pts',(17.8677591905645,859.595188064968,137.661418479812));
#66321=CARTESIAN_POINT('Ctrl Pts',(17.8153741855982,859.705128586251,137.710432519616));
#66322=CARTESIAN_POINT('Ctrl Pts',(17.8012093834401,859.764415303675,137.736201186751));
#66323=CARTESIAN_POINT('Ctrl Pts',(17.7985313307441,859.884894677905,137.787164297783));
#66324=CARTESIAN_POINT('Ctrl Pts',(17.809949935042,859.944934259786,137.811871862339));
#66325=CARTESIAN_POINT('Ctrl Pts',(17.8570605234403,860.058029050945,137.856847222995));
#66326=CARTESIAN_POINT('Ctrl Pts',(17.8922619245073,860.109992517185,137.8766799161));
#66327=CARTESIAN_POINT('Ctrl Pts',(17.9821682557319,860.199082414306,137.908779616291));
#66328=CARTESIAN_POINT('Ctrl Pts',(18.0360273313281,860.235287778738,137.920708924167));
#66329=CARTESIAN_POINT('Ctrl Pts',(18.1555962784103,860.286929139148,137.93502439619));
#66330=CARTESIAN_POINT('Ctrl Pts',(18.2201700895372,860.301758691313,137.937228091227));
#66331=CARTESIAN_POINT('Ctrl Pts',(18.3514611526987,860.307659280882,137.931613387731));
#66332=CARTESIAN_POINT('Ctrl Pts',(18.4169046345712,860.298592812182,137.923820301848));
#66333=CARTESIAN_POINT('Ctrl Pts',(18.5397083677385,860.257453422974,137.899351328351));
#66334=CARTESIAN_POINT('Ctrl Pts',(18.595890064477,860.22576078684,137.882907870571));
#66335=CARTESIAN_POINT('Ctrl Pts',(18.6921251876924,860.14308502739,137.843265089781));
#66336=CARTESIAN_POINT('Ctrl Pts',(18.7309491520631,860.092609833795,137.820351574453));
#66337=CARTESIAN_POINT('Ctrl Pts',(18.7844040045152,859.980416734138,137.771490547314));
#66338=CARTESIAN_POINT('Ctrl Pts',(18.7986717946644,859.91988779825,137.746045105218));
#66339=CARTESIAN_POINT('Ctrl Pts',(18.8007306858124,859.796863325834,137.695837304615));
#66340=CARTESIAN_POINT('Ctrl Pts',(18.7885708633062,859.735601727313,137.671569735768));
#66341=CARTESIAN_POINT('Ctrl Pts',(18.7392248793321,859.620606992745,137.627292543392));
#66342=CARTESIAN_POINT('Ctrl Pts',(18.702523066407,859.568034582268,137.60772658718));
#66343=CARTESIAN_POINT('Ctrl Pts',(18.6093398118923,859.478950383452,137.575958450104));
#66344=CARTESIAN_POINT('Ctrl Pts',(18.5537944644497,859.443337588619,137.564076699109));
#66345=CARTESIAN_POINT('Ctrl Pts',(18.431346935512,859.394122374484,137.549769252772));
#66346=CARTESIAN_POINT('Ctrl Pts',(18.3656820900001,859.380999669599,137.547484446252));
#66347=CARTESIAN_POINT('Ctrl Pts',(18.29939398446,859.38006602879,137.550272793039));
#66348=CARTESIAN_POINT('Origin',(11.4353582469288,862.278752775433,127.070006716785));
#66349=CARTESIAN_POINT('',(11.4353582469287,857.622828056485,137.398296512269));
#66350=CARTESIAN_POINT('',(11.4353582469181,859.338553021224,138.234069103648));
#66351=CARTESIAN_POINT('Ctrl Pts',(11.4353582469287,857.622828056485,137.398296512269));
#66352=CARTESIAN_POINT('Ctrl Pts',(11.4320865847077,857.62269184695,137.398681901332));
#66353=CARTESIAN_POINT('Ctrl Pts',(11.4288143447741,857.622570916339,137.39907488024));
#66354=CARTESIAN_POINT('Ctrl Pts',(11.3000083658543,857.618413477821,137.414840308951));
#66355=CARTESIAN_POINT('Ctrl Pts',(11.1763214765735,857.636941059338,137.441069094707));
#66356=CARTESIAN_POINT('Ctrl Pts',(10.9451375843786,857.716774500484,137.512851098856));
#66357=CARTESIAN_POINT('Ctrl Pts',(10.8400642756321,857.777921112359,137.557999546846));
#66358=CARTESIAN_POINT('Ctrl Pts',(10.6656844460716,857.933799732246,137.660417061792));
#66359=CARTESIAN_POINT('Ctrl Pts',(10.5975262436369,858.026820199112,137.716661029169));
#66360=CARTESIAN_POINT('Ctrl Pts',(10.5072882989536,858.231586562797,137.831998211912));
#66361=CARTESIAN_POINT('Ctrl Pts',(10.4852163453759,858.341202487111,137.890013046486));
#66362=CARTESIAN_POINT('Ctrl Pts',(10.4895943608974,858.562777705946,137.999770984508));
#66363=CARTESIAN_POINT('Ctrl Pts',(10.5151728975665,858.672574961164,138.050559385957));
#66364=CARTESIAN_POINT('Ctrl Pts',(10.6108366295515,858.879630696045,138.138605941696));
#66365=CARTESIAN_POINT('Ctrl Pts',(10.6797107821902,858.974788226131,138.175003641196));
#66366=CARTESIAN_POINT('Ctrl Pts',(10.853433514803,859.139375609029,138.228935249572));
#66367=CARTESIAN_POINT('Ctrl Pts',(10.9567842004717,859.206682240259,138.24565223094));
#66368=CARTESIAN_POINT('Ctrl Pts',(11.1859684721632,859.304118626678,138.256987142537));
#66369=CARTESIAN_POINT('Ctrl Pts',(11.309772514178,859.332426008226,138.251037788143));
#66370=CARTESIAN_POINT('Ctrl Pts',(11.434431606882,859.338508219923,138.234194504867));
#66371=CARTESIAN_POINT('Ctrl Pts',(11.4347404960019,859.338523290858,138.234152769388));
#66372=CARTESIAN_POINT('Ctrl Pts',(11.4350493760453,859.338538224605,138.234110968965));
#66373=CARTESIAN_POINT('Ctrl Pts',(11.4353582469074,859.338553021224,138.234069103648));
#66374=CARTESIAN_POINT('',(11.4353582469288,860.025278981789,136.291057736552));
#66375=CARTESIAN_POINT('',(11.4353582469288,863.172648948052,127.385939869922));
#66376=CARTESIAN_POINT('Ctrl Pts',(10.7107419313788,859.692120499991,136.223297987356));
#66377=CARTESIAN_POINT('Ctrl Pts',(10.7870947203183,859.777441539487,136.253453329623));
#66378=CARTESIAN_POINT('Ctrl Pts',(10.879670903324,859.849518643311,136.275580039938));
#66379=CARTESIAN_POINT('Ctrl Pts',(11.0934025076228,859.962896633673,136.302373713363));
#66380=CARTESIAN_POINT('Ctrl Pts',(11.2136542592252,860.001085493384,136.305725585857));
#66381=CARTESIAN_POINT('Ctrl Pts',(11.4591089786043,860.03303403674,136.291811467588));
#66382=CARTESIAN_POINT('Ctrl Pts',(11.5818900335077,860.027246158317,136.275036297202));
#66383=CARTESIAN_POINT('Ctrl Pts',(11.8180883571915,859.972890174448,136.223590972723));
#66384=CARTESIAN_POINT('Ctrl Pts',(11.9291663154482,859.924133441659,136.189113599701));
#66385=CARTESIAN_POINT('Ctrl Pts',(12.1240713480493,859.788639504677,136.106633187435));
#66386=CARTESIAN_POINT('Ctrl Pts',(12.2057423918307,859.702694554128,136.05923274783));
#66387=CARTESIAN_POINT('Ctrl Pts',(12.3268232575814,859.504876187704,135.957861844871));
#66388=CARTESIAN_POINT('Ctrl Pts',(12.3649662027356,859.394847493541,135.904847549541));
#66389=CARTESIAN_POINT('Ctrl Pts',(12.3908928787125,859.170450820332,135.802385266591));
#66390=CARTESIAN_POINT('Ctrl Pts',(12.3804866345953,859.058544268114,135.753825029685));
#66391=CARTESIAN_POINT('Ctrl Pts',(12.3153685905864,858.84626515437,135.666332180096));
#66392=CARTESIAN_POINT('Ctrl Pts',(12.2627150548227,858.747539939813,135.62791549902));
#66393=CARTESIAN_POINT('Ctrl Pts',(12.1209575445399,858.571000548618,135.563915072285));
#66394=CARTESIAN_POINT('Ctrl Pts',(12.0329542181142,858.494927040812,135.538990823503));
#66395=CARTESIAN_POINT('Ctrl Pts',(11.8295508502949,858.373831268946,135.505642939685));
#66396=CARTESIAN_POINT('Ctrl Pts',(11.7154439553601,858.330843388052,135.497995888114));
#66397=CARTESIAN_POINT('Ctrl Pts',(11.4712312662008,858.284676880409,135.50224536021));
#66398=CARTESIAN_POINT('Ctrl Pts',(11.3431288567371,858.284182127883,135.515152284544));
#66399=CARTESIAN_POINT('Ctrl Pts',(11.0991469725864,858.328584852785,135.560508817244));
#66400=CARTESIAN_POINT('Ctrl Pts',(10.9853591757403,858.372034887868,135.592086768196));
#66401=CARTESIAN_POINT('Ctrl Pts',(10.7827371824602,858.497604711005,135.670587697811));
#66402=CARTESIAN_POINT('Ctrl Pts',(10.6961531238308,858.579084282088,135.716988401076));
#66403=CARTESIAN_POINT('Ctrl Pts',(10.5632858448346,858.77003324754,135.818556653753));
#66404=CARTESIAN_POINT('Ctrl Pts',(10.5186303296598,858.877948214756,135.872836520283));
#66405=CARTESIAN_POINT('Ctrl Pts',(10.4811565123898,859.093452681628,135.975625895056));
#66406=CARTESIAN_POINT('Ctrl Pts',(10.4837296630386,859.198197517844,136.023326039887));
#66407=CARTESIAN_POINT('Ctrl Pts',(10.530713744444,859.408731053183,136.114389084627));
#66408=CARTESIAN_POINT('Ctrl Pts',(10.5767860287417,859.512338482279,136.156555869277));
#66409=CARTESIAN_POINT('Ctrl Pts',(10.6634213177592,859.635998043111,136.203117093934));
#66410=CARTESIAN_POINT('Ctrl Pts',(10.6861933831297,859.664688526859,136.213602599867));
#66411=CARTESIAN_POINT('Ctrl Pts',(10.7107419313789,859.692120499991,136.223297987356));
#66412=CARTESIAN_POINT('Ctrl Pts',(11.4353582469074,859.338553021224,138.234069103648));
#66413=CARTESIAN_POINT('Ctrl Pts',(11.5585407700079,859.344454144118,138.217372561631));
#66414=CARTESIAN_POINT('Ctrl Pts',(11.6802640064212,859.328543777274,138.190361913439));
#66415=CARTESIAN_POINT('Ctrl Pts',(11.9117504582451,859.253850445023,138.117998610973));
#66416=CARTESIAN_POINT('Ctrl Pts',(12.0187722078778,859.194107831381,138.072641106697));
#66417=CARTESIAN_POINT('Ctrl Pts',(12.1968995691043,859.039470178997,137.97125906028));
#66418=CARTESIAN_POINT('Ctrl Pts',(12.2669116858857,858.946467335536,137.916298138233));
#66419=CARTESIAN_POINT('Ctrl Pts',(12.3609585691097,858.739753194833,137.803809423437));
#66420=CARTESIAN_POINT('Ctrl Pts',(12.3846034703439,858.628243661073,137.747373198729));
#66421=CARTESIAN_POINT('Ctrl Pts',(12.3821982225962,858.400942981135,137.639665883526));
#66422=CARTESIAN_POINT('Ctrl Pts',(12.356324383801,858.287491813633,137.589466738589));
#66423=CARTESIAN_POINT('Ctrl Pts',(12.2587335578108,858.076308145489,137.50262605921));
#66424=CARTESIAN_POINT('Ctrl Pts',(12.1890262960479,857.9804447875,137.466591781897));
#66425=CARTESIAN_POINT('Ctrl Pts',(12.012377014696,857.814748789332,137.411662720805));
#66426=CARTESIAN_POINT('Ctrl Pts',(11.9065264991529,857.747340837536,137.393769477282));
#66427=CARTESIAN_POINT('Ctrl Pts',(11.6772701963114,857.653954703855,137.380147881689));
#66428=CARTESIAN_POINT('Ctrl Pts',(11.556711719808,857.627880381267,137.384001545942));
#66429=CARTESIAN_POINT('Ctrl Pts',(11.4353582469287,857.622828056485,137.398296512269));
#66430=CARTESIAN_POINT('Origin',(11.4353582469288,862.278752775433,127.070006716785));
#66431=CARTESIAN_POINT('',(11.4353582469288,860.615336143927,133.276901960274));
#66432=CARTESIAN_POINT('Origin',(11.4353582469288,860.143913913318,133.110285393007));
#66433=CARTESIAN_POINT('',(11.4353582469292,858.934374098609,138.032988884704));
#66434=CARTESIAN_POINT('',(11.4353582469288,862.750175006042,127.236623284052));
#66435=CARTESIAN_POINT('Ctrl Pts',(11.4353409859824,858.029527342834,137.592245655571));
#66436=CARTESIAN_POINT('Ctrl Pts',(11.3714258466797,858.026771612524,137.600049295908));
#66437=CARTESIAN_POINT('Ctrl Pts',(11.3082664140231,858.035126649353,137.613183561539));
#66438=CARTESIAN_POINT('Ctrl Pts',(11.187192726061,858.073771395391,137.649568773904));
#66439=CARTESIAN_POINT('Ctrl Pts',(11.1308368061775,858.104791595968,137.672961899672));
#66440=CARTESIAN_POINT('Ctrl Pts',(11.0357617041929,858.185728686537,137.726636532982));
#66441=CARTESIAN_POINT('Ctrl Pts',(10.9980144608311,858.23503256091,137.756475064446));
#66442=CARTESIAN_POINT('Ctrl Pts',(10.9479256982084,858.343459450832,137.817334264073));
#66443=CARTESIAN_POINT('Ctrl Pts',(10.9352247351614,858.401245751621,137.847742836107));
#66444=CARTESIAN_POINT('Ctrl Pts',(10.9354916676171,858.518457696539,137.905498570289));
#66445=CARTESIAN_POINT('Ctrl Pts',(10.9480429333104,858.57672717557,137.932335231537));
#66446=CARTESIAN_POINT('Ctrl Pts',(10.9968288283811,858.686824604485,137.979127287851));
#66447=CARTESIAN_POINT('Ctrl Pts',(11.0324265036371,858.737547494408,137.998634075903));
#66448=CARTESIAN_POINT('Ctrl Pts',(11.1227658162271,858.825449110991,138.02792509068));
#66449=CARTESIAN_POINT('Ctrl Pts',(11.1766999687752,858.861548400801,138.037302469546));
#66450=CARTESIAN_POINT('Ctrl Pts',(11.2966265781814,858.914238670561,138.04457552041));
#66451=CARTESIAN_POINT('Ctrl Pts',(11.3615468796824,858.92990608801,138.042186163842));
#66452=CARTESIAN_POINT('Ctrl Pts',(11.4946528743705,858.938074061457,138.025654200299));
#66453=CARTESIAN_POINT('Ctrl Pts',(11.5615376947085,858.929791724399,138.011335589564));
#66454=CARTESIAN_POINT('Ctrl Pts',(11.6859232148725,858.889705148093,137.972878399885));
#66455=CARTESIAN_POINT('Ctrl Pts',(11.7423076352131,858.858319303421,137.949115413728));
#66456=CARTESIAN_POINT('Ctrl Pts',(11.8365300611981,858.776912540008,137.895577954623));
#66457=CARTESIAN_POINT('Ctrl Pts',(11.8736705998395,858.727769568308,137.866330839782));
#66458=CARTESIAN_POINT('Ctrl Pts',(11.9236019175578,858.618365478065,137.80622892357));
#66459=CARTESIAN_POINT('Ctrl Pts',(11.9361091204556,858.559230654604,137.775954595012));
#66460=CARTESIAN_POINT('Ctrl Pts',(11.9345598686111,858.440209979897,137.718936907514));
#66461=CARTESIAN_POINT('Ctrl Pts',(11.9212542753335,858.381556985196,137.692672767461));
#66462=CARTESIAN_POINT('Ctrl Pts',(11.8708786532403,858.271201026943,137.646825173002));
#66463=CARTESIAN_POINT('Ctrl Pts',(11.8344621486659,858.220592602821,137.627672546176));
#66464=CARTESIAN_POINT('Ctrl Pts',(11.7427775851303,858.133644866505,137.598827304036));
#66465=CARTESIAN_POINT('Ctrl Pts',(11.6883829066964,858.098287087514,137.589483483378));
#66466=CARTESIAN_POINT('Ctrl Pts',(11.5672638486872,858.047104506123,137.581955024154));
#66467=CARTESIAN_POINT('Ctrl Pts',(11.5015422870096,858.032381642046,137.584162889129));
#66468=CARTESIAN_POINT('Ctrl Pts',(11.4353409859824,858.029527342834,137.592245655571));
#66469=CARTESIAN_POINT('Origin',(26.5871534051988,869.497999037637,129.621532615152));
#66470=CARTESIAN_POINT('',(26.5871534051988,864.929584227576,139.482185650009));
#66471=CARTESIAN_POINT('',(26.5871534051999,866.812688940616,140.284451947729));
#66472=CARTESIAN_POINT('Ctrl Pts',(26.5871534051988,864.929584227576,139.482185650009));
#66473=CARTESIAN_POINT('Ctrl Pts',(26.5841573362241,864.929557222217,139.482262058535));
#66474=CARTESIAN_POINT('Ctrl Pts',(26.5811606574118,864.929542413547,139.482343517111));
#66475=CARTESIAN_POINT('Ctrl Pts',(26.4438450892314,864.929423400893,139.486307239835));
#66476=CARTESIAN_POINT('Ctrl Pts',(26.3111245569331,864.953832371642,139.500264749134));
#66477=CARTESIAN_POINT('Ctrl Pts',(26.0634220090255,865.048778496406,139.547580931716));
#66478=CARTESIAN_POINT('Ctrl Pts',(25.9509992542654,865.118604517996,139.580585753559));
#66479=CARTESIAN_POINT('Ctrl Pts',(25.7631707179859,865.293761695947,139.661567534247));
#66480=CARTESIAN_POINT('Ctrl Pts',(25.6893391335263,865.397164211242,139.708667886131));
#66481=CARTESIAN_POINT('Ctrl Pts',(25.5895898042354,865.624238507318,139.810905030994));
#66482=CARTESIAN_POINT('Ctrl Pts',(25.5645603817579,865.745751975618,139.865063001591));
#66483=CARTESIAN_POINT('Ctrl Pts',(25.5670106198202,865.990684247581,139.972625649828));
#66484=CARTESIAN_POINT('Ctrl Pts',(25.5942373034062,866.111810289127,140.025014472418));
#66485=CARTESIAN_POINT('Ctrl Pts',(25.6976267215419,866.338078488702,140.12047049549));
#66486=CARTESIAN_POINT('Ctrl Pts',(25.772631528245,866.441115147401,140.16264348319));
#66487=CARTESIAN_POINT('Ctrl Pts',(25.9613232969961,866.616044266393,140.230828193134));
#66488=CARTESIAN_POINT('Ctrl Pts',(26.0731963745589,866.686155071173,140.256132466736));
#66489=CARTESIAN_POINT('Ctrl Pts',(26.3199956490675,866.78393271988,140.286298227696));
#66490=CARTESIAN_POINT('Ctrl Pts',(26.452566411568,866.810359909426,140.2907382711));
#66491=CARTESIAN_POINT('Ctrl Pts',(26.5863839149178,866.812675889115,140.284488005616));
#66492=CARTESIAN_POINT('Ctrl Pts',(26.5866404166808,866.812680328392,140.284476025089));
#66493=CARTESIAN_POINT('Ctrl Pts',(26.5868969134595,866.812684678889,140.284464005791));
#66494=CARTESIAN_POINT('Ctrl Pts',(26.587153405201,866.812688940616,140.284451947729));
#66495=CARTESIAN_POINT('',(26.587153406672,867.457684615548,138.459511578372));
#66496=CARTESIAN_POINT('',(26.5871534051988,870.46102817788,129.96189969822));
#66497=CARTESIAN_POINT('Ctrl Pts',(26.0509384417415,867.310125790805,138.420663828409));
#66498=CARTESIAN_POINT('Ctrl Pts',(26.1642905106799,867.376046188621,138.443962327469));
#66499=CARTESIAN_POINT('Ctrl Pts',(26.2901977702864,867.421142608424,138.457584017948));
#66500=CARTESIAN_POINT('Ctrl Pts',(26.5529160266006,867.464621828609,138.464099420027));
#66501=CARTESIAN_POINT('Ctrl Pts',(26.6871643626009,867.462577160429,138.456934185508));
#66502=CARTESIAN_POINT('Ctrl Pts',(26.946899304951,867.411065612132,138.422875783052));
#66503=CARTESIAN_POINT('Ctrl Pts',(27.0698506843585,867.361882642322,138.396231024401));
#66504=CARTESIAN_POINT('Ctrl Pts',(27.2879371444874,867.222031561834,138.327038202379));
#66505=CARTESIAN_POINT('Ctrl Pts',(27.3808720243468,867.132512866614,138.285086337527));
#66506=CARTESIAN_POINT('Ctrl Pts',(27.5235112115396,866.924662340849,138.191529104276));
#66507=CARTESIAN_POINT('Ctrl Pts',(27.5718049213144,866.808287128267,138.140808995843));
#66508=CARTESIAN_POINT('Ctrl Pts',(27.616429636366,866.565244033439,138.037700005626));
#66509=CARTESIAN_POINT('Ctrl Pts',(27.6128218464575,866.440999804584,137.986307644981));
#66510=CARTESIAN_POINT('Ctrl Pts',(27.5538823927995,866.198484212482,137.888190027101));
#66511=CARTESIAN_POINT('Ctrl Pts',(27.4984742801511,866.082711089212,137.842494147576));
#66512=CARTESIAN_POINT('Ctrl Pts',(27.342344460985,865.877061992407,137.763319902144));
#66513=CARTESIAN_POINT('Ctrl Pts',(27.2431075305264,865.78928118362,137.730643720026));
#66514=CARTESIAN_POINT('Ctrl Pts',(27.0150520774923,865.654918878296,137.683059363707));
#66515=CARTESIAN_POINT('Ctrl Pts',(26.8887676555259,865.609252042839,137.668443902873));
#66516=CARTESIAN_POINT('Ctrl Pts',(26.6250476717488,865.565415411623,137.659131587765));
#66517=CARTESIAN_POINT('Ctrl Pts',(26.4901950520978,865.567634836273,137.66451690654));
#66518=CARTESIAN_POINT('Ctrl Pts',(26.2301581575115,865.619776926303,137.695021745125));
#66519=CARTESIAN_POINT('Ctrl Pts',(26.1074519859725,865.669031870551,137.719788740923));
#66520=CARTESIAN_POINT('Ctrl Pts',(25.8890768417382,865.808805694758,137.786192633038));
#66521=CARTESIAN_POINT('Ctrl Pts',(25.7957603915284,865.898310945924,137.827331743256));
#66522=CARTESIAN_POINT('Ctrl Pts',(25.6515314161874,866.106854010585,137.921169571086));
#66523=CARTESIAN_POINT('Ctrl Pts',(25.6025450206964,866.224190370345,137.973081763217));
#66524=CARTESIAN_POINT('Ctrl Pts',(25.5576579280982,866.468752913701,138.079530086611));
#66525=CARTESIAN_POINT('Ctrl Pts',(25.5616134804233,866.593527306509,138.133009924179));
#66526=CARTESIAN_POINT('Ctrl Pts',(25.6217087769471,866.835075114573,138.234525463799));
#66527=CARTESIAN_POINT('Ctrl Pts',(25.67720277568,866.949524219527,138.281577706287));
#66528=CARTESIAN_POINT('Ctrl Pts',(25.7942924888293,867.10244198729,138.342489112607));
#66529=CARTESIAN_POINT('Ctrl Pts',(25.8389091629305,867.150052395241,138.36108271354));
#66530=CARTESIAN_POINT('Ctrl Pts',(25.9381742628927,867.237115179535,138.394249570918));
#66531=CARTESIAN_POINT('Ctrl Pts',(25.9926740025924,867.276241848119,138.408688096572));
#66532=CARTESIAN_POINT('Ctrl Pts',(26.0509384417415,867.310125790805,138.420663828409));
#66533=CARTESIAN_POINT('Ctrl Pts',(26.587153405201,866.812688940616,140.284451947729));
#66534=CARTESIAN_POINT('Ctrl Pts',(26.7193793732077,866.814885935223,140.27823580659));
#66535=CARTESIAN_POINT('Ctrl Pts',(26.8502664503425,866.793494538863,140.261714995427));
#66536=CARTESIAN_POINT('Ctrl Pts',(27.0971885346626,866.705014039761,140.210141054699));
#66537=CARTESIAN_POINT('Ctrl Pts',(27.2105273651152,866.637908000364,140.175251086928));
#66538=CARTESIAN_POINT('Ctrl Pts',(27.4023994581216,866.465679384199,140.092020876916));
#66539=CARTESIAN_POINT('Ctrl Pts',(27.4787882987761,866.361916724528,140.044388992606));
#66540=CARTESIAN_POINT('Ctrl Pts',(27.5824289901366,866.132397663624,139.943336242273));
#66541=CARTESIAN_POINT('Ctrl Pts',(27.6089075312998,866.008996721649,139.890929576514));
#66542=CARTESIAN_POINT('Ctrl Pts',(27.6082114386975,865.759642775383,139.788074798368));
#66543=CARTESIAN_POINT('Ctrl Pts',(27.5814117467065,865.636169556493,139.738611745961));
#66544=CARTESIAN_POINT('Ctrl Pts',(27.477752251191,865.404971889854,139.648097208982));
#66545=CARTESIAN_POINT('Ctrl Pts',(27.4018173881855,865.299576554605,139.607941662044));
#66546=CARTESIAN_POINT('Ctrl Pts',(27.2102770903413,865.121570406777,139.541879144639));
#66547=CARTESIAN_POINT('Ctrl Pts',(27.0964598713859,865.050824388365,139.516659824231));
#66548=CARTESIAN_POINT('Ctrl Pts',(26.849268718363,864.955513020048,139.48520463439));
#66549=CARTESIAN_POINT('Ctrl Pts',(26.7188000123769,864.930770837042,139.478828276305));
#66550=CARTESIAN_POINT('Ctrl Pts',(26.5871534051988,864.929584227576,139.482185650009));
#66551=CARTESIAN_POINT('Origin',(26.5871534051988,869.497999037637,129.621532615152));
#66552=CARTESIAN_POINT('',(26.5871534051988,867.834582406131,135.828427858641));
#66553=CARTESIAN_POINT('Origin',(26.5871534051988,867.363160175522,135.661811291374));
#66554=CARTESIAN_POINT('',(26.5871534051989,866.334637698876,140.072347243623));
#66555=CARTESIAN_POINT('',(26.5871534051988,869.969421268246,129.788149182419));
#66556=CARTESIAN_POINT('Ctrl Pts',(26.5868406553291,865.412824171668,139.679609816816));
#66557=CARTESIAN_POINT('Ctrl Pts',(26.5255998020287,865.412183595571,139.681537205492));
#66558=CARTESIAN_POINT('Ctrl Pts',(26.4649104955618,865.421941243081,139.68780579045));
#66559=CARTESIAN_POINT('Ctrl Pts',(26.3457464565317,865.462873629541,139.709418190761));
#66560=CARTESIAN_POINT('Ctrl Pts',(26.2891055273704,865.495411593307,139.725285602752));
#66561=CARTESIAN_POINT('Ctrl Pts',(26.1937997484409,865.578522678673,139.764274150391));
#66562=CARTESIAN_POINT('Ctrl Pts',(26.1558424859167,865.628074988295,139.786932714436));
#66563=CARTESIAN_POINT('Ctrl Pts',(26.103082090476,865.737925353352,139.836204427724));
#66564=CARTESIAN_POINT('Ctrl Pts',(26.0887497271715,865.79717062609,139.862344963465));
#66565=CARTESIAN_POINT('Ctrl Pts',(26.0858142209995,865.917447595876,139.914486375135));
#66566=CARTESIAN_POINT('Ctrl Pts',(26.0971464162827,865.977336585021,139.939991349396));
#66567=CARTESIAN_POINT('Ctrl Pts',(26.1441282561774,866.089926265049,139.986829514137));
#66568=CARTESIAN_POINT('Ctrl Pts',(26.1792517930982,866.141567010159,140.007721422777));
#66569=CARTESIAN_POINT('Ctrl Pts',(26.2689503584317,866.229912144945,140.042023720481));
#66570=CARTESIAN_POINT('Ctrl Pts',(26.3226466874476,866.265743802293,140.055092849982));
#66571=CARTESIAN_POINT('Ctrl Pts',(26.441881427653,866.316758842355,140.071590853784));
#66572=CARTESIAN_POINT('Ctrl Pts',(26.5062738764259,866.331359924575,140.074821826206));
#66573=CARTESIAN_POINT('Ctrl Pts',(26.6373461264923,866.337029436076,140.070966439477));
#66574=CARTESIAN_POINT('Ctrl Pts',(26.7027421471079,866.327940656787,140.063877351223));
#66575=CARTESIAN_POINT('Ctrl Pts',(26.8256441219465,866.286918105112,140.04037031043));
#66576=CARTESIAN_POINT('Ctrl Pts',(26.881946610192,866.255328764845,140.024162420287));
#66577=CARTESIAN_POINT('Ctrl Pts',(26.9786069339817,866.172867767899,139.984500598062));
#66578=CARTESIAN_POINT('Ctrl Pts',(27.0176803150346,866.122451804828,139.96130813766));
#66579=CARTESIAN_POINT('Ctrl Pts',(27.0715216886377,866.010441767537,139.911553817448));
#66580=CARTESIAN_POINT('Ctrl Pts',(27.085940382297,865.950035340394,139.88550652597));
#66581=CARTESIAN_POINT('Ctrl Pts',(27.0882151259211,865.827369124149,139.83393799764));
#66582=CARTESIAN_POINT('Ctrl Pts',(27.0761576373045,865.766335361574,139.808922668868));
#66583=CARTESIAN_POINT('Ctrl Pts',(27.0269873600959,865.651790351316,139.763061341531));
#66584=CARTESIAN_POINT('Ctrl Pts',(26.9903600724254,865.599432603596,139.742672719495));
#66585=CARTESIAN_POINT('Ctrl Pts',(26.8972212757687,865.510709914048,139.709218650094));
#66586=CARTESIAN_POINT('Ctrl Pts',(26.8416271124669,865.475260573725,139.696497506621));
#66587=CARTESIAN_POINT('Ctrl Pts',(26.7190165790861,865.426428105236,139.68057103062));
#66588=CARTESIAN_POINT('Ctrl Pts',(26.6532462147938,865.413518770318,139.677519883112));
#66589=CARTESIAN_POINT('Ctrl Pts',(26.5868406553291,865.412824171668,139.679609816816));
#66590=CARTESIAN_POINT('Origin',(19.6109167136347,869.682182736162,129.686629366222));
#66591=CARTESIAN_POINT('',(19.6109167136347,865.032343784683,139.997700189292));
#66592=CARTESIAN_POINT('',(19.6109167136317,866.731743347019,140.879663611168));
#66593=CARTESIAN_POINT('Ctrl Pts',(19.6109167136347,865.032343784683,139.997700189293));
#66594=CARTESIAN_POINT('Ctrl Pts',(19.6079091554838,865.032244744606,139.997980411688));
#66595=CARTESIAN_POINT('Ctrl Pts',(19.6049010676707,865.032158534803,139.998267278442));
#66596=CARTESIAN_POINT('Ctrl Pts',(19.4766452794723,865.029030963697,140.010779980277));
#66597=CARTESIAN_POINT('Ctrl Pts',(19.3532338372231,865.048294548138,140.034265423507));
#66598=CARTESIAN_POINT('Ctrl Pts',(19.1229869647607,865.128765153076,140.101570012603));
#66599=CARTESIAN_POINT('Ctrl Pts',(19.0185497725543,865.189582551132,140.144935981));
#66600=CARTESIAN_POINT('Ctrl Pts',(18.8426550411811,865.345508921656,140.246549461264));
#66601=CARTESIAN_POINT('Ctrl Pts',(18.7732964870958,865.439673391445,140.304075495621));
#66602=CARTESIAN_POINT('Ctrl Pts',(18.6822541059607,865.645813434001,140.423536535197));
#66603=CARTESIAN_POINT('Ctrl Pts',(18.6603346908435,865.755588806299,140.484316542825));
#66604=CARTESIAN_POINT('Ctrl Pts',(18.6657293960687,865.976428794269,140.600814327004));
#66605=CARTESIAN_POINT('Ctrl Pts',(18.6920611528413,866.085448363961,140.655550665007));
#66606=CARTESIAN_POINT('Ctrl Pts',(18.7893203169287,866.289454747597,140.751818413044));
#66607=CARTESIAN_POINT('Ctrl Pts',(18.8587059789424,866.382580844235,140.792546559396));
#66608=CARTESIAN_POINT('Ctrl Pts',(19.0327570890426,866.542331936136,140.855025819383));
#66609=CARTESIAN_POINT('Ctrl Pts',(19.1356492734084,866.607153791863,140.876043211764));
#66610=CARTESIAN_POINT('Ctrl Pts',(19.3634697244148,866.700199832375,140.895524818092));
#66611=CARTESIAN_POINT('Ctrl Pts',(19.486253519577,866.726755317152,140.893386472135));
#66612=CARTESIAN_POINT('Ctrl Pts',(19.6099239036713,866.731704083989,140.879773141484));
#66613=CARTESIAN_POINT('Ctrl Pts',(19.6102548515049,866.731717327124,140.879736711563));
#66614=CARTESIAN_POINT('Ctrl Pts',(19.6105857882002,866.731730414779,140.879700201439));
#66615=CARTESIAN_POINT('Ctrl Pts',(19.6109167136287,866.731743347019,140.879663611168));
#66616=CARTESIAN_POINT('',(19.6109167136152,867.422358230611,138.925648987921));
#66617=CARTESIAN_POINT('',(19.6109167136347,870.576078908781,130.002562519359));
#66618=CARTESIAN_POINT('Ctrl Pts',(19.0292497216265,867.224999147202,138.885672182601));
#66619=CARTESIAN_POINT('Ctrl Pts',(19.1227486191325,867.293488403287,138.909878603093));
#66620=CARTESIAN_POINT('Ctrl Pts',(19.2289639550593,867.345865874679,138.925042796753));
#66621=CARTESIAN_POINT('Ctrl Pts',(19.4621066632783,867.414959985394,138.936185048728));
#66622=CARTESIAN_POINT('Ctrl Pts',(19.5874489541267,867.428811225524,138.930935182979));
#66623=CARTESIAN_POINT('Ctrl Pts',(19.8328387076159,867.412118580623,138.899829622964));
#66624=CARTESIAN_POINT('Ctrl Pts',(19.950639878208,867.382489738374,138.874628249283));
#66625=CARTESIAN_POINT('Ctrl Pts',(20.1674570962931,867.283241297794,138.807316411628));
#66626=CARTESIAN_POINT('Ctrl Pts',(20.2641613329589,867.21389398404,138.765561630593));
#66627=CARTESIAN_POINT('Ctrl Pts',(20.422532069456,867.04339149722,138.67070801227));
#66628=CARTESIAN_POINT('Ctrl Pts',(20.4822867073186,866.943431693524,138.618354249358));
#66629=CARTESIAN_POINT('Ctrl Pts',(20.5549203637325,866.726416809543,138.510198647565));
#66630=CARTESIAN_POINT('Ctrl Pts',(20.566988053838,866.611412394766,138.455425764211));
#66631=CARTESIAN_POINT('Ctrl Pts',(20.5412611510902,866.38699592464,138.352956484362));
#66632=CARTESIAN_POINT('Ctrl Pts',(20.505781045525,866.279636569542,138.306003380776));
#66633=CARTESIAN_POINT('Ctrl Pts',(20.3944114822048,866.084846838703,138.224691870873));
#66634=CARTESIAN_POINT('Ctrl Pts',(20.3208939826588,865.998624788428,138.19069423111));
#66635=CARTESIAN_POINT('Ctrl Pts',(20.1431933364602,865.853742724939,138.137882575139));
#66636=CARTESIAN_POINT('Ctrl Pts',(20.0404736985657,865.796569280442,138.11963824823));
#66637=CARTESIAN_POINT('Ctrl Pts',(19.8154665300435,865.717927684392,138.101295106619));
#66638=CARTESIAN_POINT('Ctrl Pts',(19.6948964884546,865.698195571221,138.101867430239));
#66639=CARTESIAN_POINT('Ctrl Pts',(19.4472649029493,865.70076932914,138.123343361353));
#66640=CARTESIAN_POINT('Ctrl Pts',(19.3227590842156,865.72530728058,138.145097690271));
#66641=CARTESIAN_POINT('Ctrl Pts',(19.0959554236896,865.816363415214,138.206943116528));
#66642=CARTESIAN_POINT('Ctrl Pts',(18.9953594206764,865.881058230151,138.246029691516));
#66643=CARTESIAN_POINT('Ctrl Pts',(18.827219238832,866.043369452561,138.33751627481));
#66644=CARTESIAN_POINT('Ctrl Pts',(18.7617143413566,866.139920574725,138.389243774185));
#66645=CARTESIAN_POINT('Ctrl Pts',(18.6762189085124,866.352508618056,138.498460009162));
#66646=CARTESIAN_POINT('Ctrl Pts',(18.6574542958356,866.466708326262,138.554961115806));
#66647=CARTESIAN_POINT('Ctrl Pts',(18.6701659270992,866.684666650145,138.658617766676));
#66648=CARTESIAN_POINT('Ctrl Pts',(18.6965206216375,866.786544825246,138.705304736474));
#66649=CARTESIAN_POINT('Ctrl Pts',(18.7900576640883,866.983153146354,138.791446139332));
#66650=CARTESIAN_POINT('Ctrl Pts',(18.8583545996072,867.07542693504,138.829607231979));
#66651=CARTESIAN_POINT('Ctrl Pts',(18.9705633881621,867.179381655039,138.869204099155));
#66652=CARTESIAN_POINT('Ctrl Pts',(18.9991884464773,867.202978840793,138.877889461241));
#66653=CARTESIAN_POINT('Ctrl Pts',(19.0292497216264,867.224999147202,138.885672182601));
#66654=CARTESIAN_POINT('Ctrl Pts',(19.6109167136287,866.731743347019,140.879663611168));
#66655=CARTESIAN_POINT('Ctrl Pts',(19.7350453890134,866.736594173375,140.865938761243));
#66656=CARTESIAN_POINT('Ctrl Pts',(19.8575890635283,866.719582206182,140.840940708518));
#66657=CARTESIAN_POINT('Ctrl Pts',(20.0901695612099,866.642879318333,140.770738181999));
#66658=CARTESIAN_POINT('Ctrl Pts',(20.1973571074338,866.582323959062,140.725481789898));
#66659=CARTESIAN_POINT('Ctrl Pts',(20.3754174637689,866.426657499236,140.622508788399));
#66660=CARTESIAN_POINT('Ctrl Pts',(20.4451444074523,866.333349007783,140.565863304855));
#66661=CARTESIAN_POINT('Ctrl Pts',(20.5380041418204,866.127030987397,140.448960690095));
#66662=CARTESIAN_POINT('Ctrl Pts',(20.5608936512099,866.016174028422,140.389818557589));
#66663=CARTESIAN_POINT('Ctrl Pts',(20.5568757972104,865.791108459228,140.27612392233));
#66664=CARTESIAN_POINT('Ctrl Pts',(20.5302903942735,865.679142892364,140.222655234495));
#66665=CARTESIAN_POINT('Ctrl Pts',(20.431342672214,865.471046158108,140.128893158474));
#66666=CARTESIAN_POINT('Ctrl Pts',(20.3609340088257,865.376737859219,140.089285391298));
#66667=CARTESIAN_POINT('Ctrl Pts',(20.1849676314699,865.216411830746,140.027945043353));
#66668=CARTESIAN_POINT('Ctrl Pts',(20.081302657797,865.151979964545,140.006799493586));
#66669=CARTESIAN_POINT('Ctrl Pts',(19.8541102059258,865.061508501907,139.985891334474));
#66670=CARTESIAN_POINT('Ctrl Pts',(19.7329498924299,865.036362385392,139.986330025201));
#66671=CARTESIAN_POINT('Ctrl Pts',(19.6109167136347,865.032343784683,139.997700189293));
#66672=CARTESIAN_POINT('Origin',(19.6109167136347,869.682182736162,129.686629366222));
#66673=CARTESIAN_POINT('',(19.6109167136347,868.018766104656,135.89352460971));
#66674=CARTESIAN_POINT('Origin',(19.6109167136347,867.547343874047,135.726908042443));
#66675=CARTESIAN_POINT('',(19.610916713635,866.331868113397,140.666406603934));
#66676=CARTESIAN_POINT('',(19.6109167136347,870.153604966771,129.853245933489));
#66677=CARTESIAN_POINT('Ctrl Pts',(19.6105158575642,865.435626868842,140.201315561332));
#66678=CARTESIAN_POINT('Ctrl Pts',(19.5445607754985,865.433403241226,140.207765736195));
#66679=CARTESIAN_POINT('Ctrl Pts',(19.4794591273816,865.442910966889,140.220171218638));
#66680=CARTESIAN_POINT('Ctrl Pts',(19.3574081226334,865.484197021565,140.255701685095));
#66681=CARTESIAN_POINT('Ctrl Pts',(19.3017731489761,865.515910048717,140.278645727799));
#66682=CARTESIAN_POINT('Ctrl Pts',(19.2081734914731,865.597527739722,140.332138008657));
#66683=CARTESIAN_POINT('Ctrl Pts',(19.171200496397,865.64683527457,140.362261189116));
#66684=CARTESIAN_POINT('Ctrl Pts',(19.1221696357718,865.755215094921,140.42482899266));
#66685=CARTESIAN_POINT('Ctrl Pts',(19.1100598110342,865.813135045759,140.456671002359));
#66686=CARTESIAN_POINT('Ctrl Pts',(19.1118515839942,865.929940662849,140.517783623131));
#66687=CARTESIAN_POINT('Ctrl Pts',(19.1252751719824,865.987726201218,140.546529918869));
#66688=CARTESIAN_POINT('Ctrl Pts',(19.1758037643967,866.09600162304,140.597229592055));
#66689=CARTESIAN_POINT('Ctrl Pts',(19.2121130439346,866.145496203584,140.618755424259));
#66690=CARTESIAN_POINT('Ctrl Pts',(19.3034447035421,866.230415067544,140.651972355631));
#66691=CARTESIAN_POINT('Ctrl Pts',(19.3575214778058,866.26491290037,140.663293686408));
#66692=CARTESIAN_POINT('Ctrl Pts',(19.4773038659371,866.314517498044,140.674213215849));
#66693=CARTESIAN_POINT('Ctrl Pts',(19.5418730777901,866.328797056902,140.673521190791));
#66694=CARTESIAN_POINT('Ctrl Pts',(19.6736152354049,866.334683065614,140.659959493424));
#66695=CARTESIAN_POINT('Ctrl Pts',(19.7394529565544,866.325710171844,140.64695922555));
#66696=CARTESIAN_POINT('Ctrl Pts',(19.8629345980097,866.284947722344,140.610242714423));
#66697=CARTESIAN_POINT('Ctrl Pts',(19.9192622420866,866.253198558701,140.586718168127));
#66698=CARTESIAN_POINT('Ctrl Pts',(20.0132730793094,866.171458568217,140.532754359423));
#66699=CARTESIAN_POINT('Ctrl Pts',(20.0502301346248,866.122304978792,140.502838248092));
#66700=CARTESIAN_POINT('Ctrl Pts',(20.0996784957012,866.013357514328,140.440711734639));
#66701=CARTESIAN_POINT('Ctrl Pts',(20.1119106306503,865.954641076045,140.409084347246));
#66702=CARTESIAN_POINT('Ctrl Pts',(20.1098221531946,865.836541728484,140.348768299185));
#66703=CARTESIAN_POINT('Ctrl Pts',(20.0961522190309,865.778328520145,140.320595559343));
#66704=CARTESIAN_POINT('Ctrl Pts',(20.0449647107109,865.669355314645,140.270849586179));
#66705=CARTESIAN_POINT('Ctrl Pts',(20.0082152325769,865.619618008665,140.249706310016));
#66706=CARTESIAN_POINT('Ctrl Pts',(19.9160806668646,865.534755094891,140.21696815546));
#66707=CARTESIAN_POINT('Ctrl Pts',(19.8616751765707,865.500496340684,140.205702364501));
#66708=CARTESIAN_POINT('Ctrl Pts',(19.7411182416906,865.451592425235,140.194505652039));
#66709=CARTESIAN_POINT('Ctrl Pts',(19.6760599579182,865.437836640507,140.194905579033));
#66710=CARTESIAN_POINT('Ctrl Pts',(19.6105158575642,865.435626868842,140.201315561332));
#66711=CARTESIAN_POINT('Origin',(36.023563521447,873.7734891951,131.132635501626));
#66712=CARTESIAN_POINT('',(36.0235635214469,869.206369897989,140.989623033016));
#66713=CARTESIAN_POINT('',(36.023563521447,871.084717611128,141.805348709603));
#66714=CARTESIAN_POINT('Ctrl Pts',(36.0235635214469,869.206369897989,140.989623033016));
#66715=CARTESIAN_POINT('Ctrl Pts',(36.0214735898105,869.206358310681,140.989655817959));
#66716=CARTESIAN_POINT('Ctrl Pts',(36.0193833524411,869.206352662864,140.989691046781));
#66717=CARTESIAN_POINT('Ctrl Pts',(35.882617727463,869.206372074219,140.992155845574));
#66718=CARTESIAN_POINT('Ctrl Pts',(35.749463090655,869.231065880043,141.004676089211));
#66719=CARTESIAN_POINT('Ctrl Pts',(35.5018229049838,869.326523954077,141.049072545613));
#66720=CARTESIAN_POINT('Ctrl Pts',(35.3897375564408,869.396230800334,141.080483069051));
#66721=CARTESIAN_POINT('Ctrl Pts',(35.2007289639281,869.572090641614,141.159163642578));
#66722=CARTESIAN_POINT('Ctrl Pts',(35.1259807189736,869.676783296143,141.205790862873));
#66723=CARTESIAN_POINT('Ctrl Pts',(35.0257778864496,869.90557827225,141.307681298877));
#66724=CARTESIAN_POINT('Ctrl Pts',(35.0008332545979,870.027310359311,141.361887441756));
#66725=CARTESIAN_POINT('Ctrl Pts',(35.0035814081167,870.272368126865,141.470698389129));
#66726=CARTESIAN_POINT('Ctrl Pts',(35.031104524426,870.393401514357,141.524273249009));
#66727=CARTESIAN_POINT('Ctrl Pts',(35.135198376659,870.618759041376,141.62296180998));
#66728=CARTESIAN_POINT('Ctrl Pts',(35.2105584998169,870.721042028848,141.667170482921));
#66729=CARTESIAN_POINT('Ctrl Pts',(35.3996779064446,870.893807170752,141.739826611328));
#66730=CARTESIAN_POINT('Ctrl Pts',(35.5115271934762,870.962665330356,141.767583474772));
#66731=CARTESIAN_POINT('Ctrl Pts',(35.7579249443527,871.057941141116,141.802619551707));
#66732=CARTESIAN_POINT('Ctrl Pts',(35.8900792569755,871.083250324898,141.809472095662));
#66733=CARTESIAN_POINT('Ctrl Pts',(36.0234917745249,871.084716824771,141.805350926948));
#66734=CARTESIAN_POINT('Ctrl Pts',(36.023515690209,871.084717087657,141.805350188182));
#66735=CARTESIAN_POINT('Ctrl Pts',(36.0235396058497,871.084717349776,141.805349449067));
#66736=CARTESIAN_POINT('Ctrl Pts',(36.023563521447,871.084717611128,141.805348709603));
#66737=CARTESIAN_POINT('',(36.0235635225402,871.730643764381,139.977775659879));
#66738=CARTESIAN_POINT('',(36.023563521447,874.736518335342,131.473002584693));
#66739=CARTESIAN_POINT('Ctrl Pts',(35.6798116547162,871.672817973783,139.962586861254));
#66740=CARTESIAN_POINT('Ctrl Pts',(35.8052231695942,871.71507762961,139.977522853514));
#66741=CARTESIAN_POINT('Ctrl Pts',(35.9381629843462,871.734523094844,139.982078628726));
#66742=CARTESIAN_POINT('Ctrl Pts',(36.2041147848115,871.725612726923,139.970077777723));
#66743=CARTESIAN_POINT('Ctrl Pts',(36.3345322301639,871.697340488082,139.9536428323));
#66744=CARTESIAN_POINT('Ctrl Pts',(36.5761339446808,871.596148008136,139.902025507603));
#66745=CARTESIAN_POINT('Ctrl Pts',(36.6849112527287,871.524001433083,139.867264633866));
#66746=CARTESIAN_POINT('Ctrl Pts',(36.8660233281058,871.34459099685,139.784090197));
#66747=CARTESIAN_POINT('Ctrl Pts',(36.9364725987585,871.238881431279,139.736415930733));
#66748=CARTESIAN_POINT('Ctrl Pts',(37.0287682425443,871.007749581237,139.63463028974));
#66749=CARTESIAN_POINT('Ctrl Pts',(37.0496797292442,870.884516345032,139.581486323711));
#66750=CARTESIAN_POINT('Ctrl Pts',(37.0385422347577,870.638154768914,139.477204469923));
#66751=CARTESIAN_POINT('Ctrl Pts',(37.0070972678148,870.517384161214,139.427039804527));
#66752=CARTESIAN_POINT('Ctrl Pts',(36.8951079532623,870.291807088037,139.334908832364));
#66753=CARTESIAN_POINT('Ctrl Pts',(36.8150498717391,870.189458250906,139.293957549782));
#66754=CARTESIAN_POINT('Ctrl Pts',(36.6165333688192,870.018953521555,139.227204512949));
#66755=CARTESIAN_POINT('Ctrl Pts',(36.4999935670778,869.952555527962,139.202085741226));
#66756=CARTESIAN_POINT('Ctrl Pts',(36.2472860569667,869.86583536407,139.1713397297));
#66757=CARTESIAN_POINT('Ctrl Pts',(36.113796652642,869.845911321467,139.165822642891));
#66758=CARTESIAN_POINT('Ctrl Pts',(35.846601173448,869.854686791253,139.175105224452));
#66759=CARTESIAN_POINT('Ctrl Pts',(35.7155035887039,869.883261068966,139.189805240037));
#66760=CARTESIAN_POINT('Ctrl Pts',(35.4734839226148,869.985155430913,139.237894214928));
#66761=CARTESIAN_POINT('Ctrl Pts',(35.3648304759233,870.057337406772,139.270764399454));
#66762=CARTESIAN_POINT('Ctrl Pts',(35.1832276548471,870.236747825837,139.351177205328));
#66763=CARTESIAN_POINT('Ctrl Pts',(35.1123462065239,870.342524587299,139.398067217846));
#66764=CARTESIAN_POINT('Ctrl Pts',(35.0186507130101,870.574645240218,139.500238163134));
#66765=CARTESIAN_POINT('Ctrl Pts',(34.9973326807799,870.698948554061,139.554612712571));
#66766=CARTESIAN_POINT('Ctrl Pts',(35.0087427455771,870.946828568636,139.662233542543));
#66767=CARTESIAN_POINT('Ctrl Pts',(35.0407764294759,871.068036538043,139.714452885408));
#66768=CARTESIAN_POINT('Ctrl Pts',(35.1539420342416,871.292414719914,139.809900098182));
#66769=CARTESIAN_POINT('Ctrl Pts',(35.2339185528415,871.393439110319,139.852207592312));
#66770=CARTESIAN_POINT('Ctrl Pts',(35.3826459269411,871.520015216523,139.903808964145));
#66771=CARTESIAN_POINT('Ctrl Pts',(35.4369088327499,871.557826960076,139.918939385534));
#66772=CARTESIAN_POINT('Ctrl Pts',(35.5533694307271,871.623511986515,139.944550619951));
#66773=CARTESIAN_POINT('Ctrl Pts',(35.6153485033544,871.651095960516,139.954909566782));
#66774=CARTESIAN_POINT('Ctrl Pts',(35.6798116547161,871.672817973783,139.962586861254));
#66775=CARTESIAN_POINT('Ctrl Pts',(36.023563521447,871.084717611128,141.805348709603));
#66776=CARTESIAN_POINT('Ctrl Pts',(36.1535485828446,871.086138099153,141.801329603676));
#66777=CARTESIAN_POINT('Ctrl Pts',(36.2822520299091,871.064895525646,141.786978732021));
#66778=CARTESIAN_POINT('Ctrl Pts',(36.5277296351162,870.977781321758,141.738902417381));
#66779=CARTESIAN_POINT('Ctrl Pts',(36.6415087243966,870.911149537884,141.704969375112));
#66780=CARTESIAN_POINT('Ctrl Pts',(36.8346602266769,870.740029154615,141.622421346045));
#66781=CARTESIAN_POINT('Ctrl Pts',(36.9118265070258,870.636834245981,141.574480960796));
#66782=CARTESIAN_POINT('Ctrl Pts',(37.0173134081556,870.408051769617,141.471727260535));
#66783=CARTESIAN_POINT('Ctrl Pts',(37.0446601784414,870.284713024406,141.417925385765));
#66784=CARTESIAN_POINT('Ctrl Pts',(37.0452748520624,870.035789658795,141.312099019871));
#66785=CARTESIAN_POINT('Ctrl Pts',(37.0191063125277,869.912675413112,141.261085179727));
#66786=CARTESIAN_POINT('Ctrl Pts',(36.9166621004451,869.682160318425,141.167510971958));
#66787=CARTESIAN_POINT('Ctrl Pts',(36.8413893433617,869.577047198559,141.125859475705));
#66788=CARTESIAN_POINT('Ctrl Pts',(36.6508038094406,869.399038736796,141.056715830726));
#66789=CARTESIAN_POINT('Ctrl Pts',(36.5371750424065,869.328106314267,141.029977428978));
#66790=CARTESIAN_POINT('Ctrl Pts',(36.2887995441781,869.231998274348,140.995352221373));
#66791=CARTESIAN_POINT('Ctrl Pts',(36.1568030641379,869.207108624384,140.987532892458));
#66792=CARTESIAN_POINT('Ctrl Pts',(36.0235635214469,869.206369897989,140.989623033016));
#66793=CARTESIAN_POINT('Origin',(36.023563521447,873.7734891951,131.132635501626));
#66794=CARTESIAN_POINT('',(36.023563521447,872.110072563594,137.339530745114));
#66795=CARTESIAN_POINT('Origin',(36.023563521447,871.638650332985,137.172914177847));
#66796=CARTESIAN_POINT('',(36.0235635214471,870.608405405657,141.588323604301));
#66797=CARTESIAN_POINT('',(36.023563521447,874.244911425709,131.299252068893));
#66798=CARTESIAN_POINT('Ctrl Pts',(36.023552436116,869.688940292305,141.188941320012));
#66799=CARTESIAN_POINT('Ctrl Pts',(35.9633631698392,869.688520842301,141.190132109607));
#66800=CARTESIAN_POINT('Ctrl Pts',(35.9036857119017,869.698133963336,141.195550737741));
#66801=CARTESIAN_POINT('Ctrl Pts',(35.7853286796557,869.738381949188,141.215393646171));
#66802=CARTESIAN_POINT('Ctrl Pts',(35.7285620503972,869.770665463377,141.230488710799));
#66803=CARTESIAN_POINT('Ctrl Pts',(35.6320548273116,869.853831216061,141.268507782764));
#66804=CARTESIAN_POINT('Ctrl Pts',(35.5933235777732,869.903939954933,141.29108002934));
#66805=CARTESIAN_POINT('Ctrl Pts',(35.5398537319471,870.014490714732,141.340430302232));
#66806=CARTESIAN_POINT('Ctrl Pts',(35.5253419006028,870.073746821741,141.366684028314));
#66807=CARTESIAN_POINT('Ctrl Pts',(35.5220958115816,870.193996208895,141.41954015403));
#66808=CARTESIAN_POINT('Ctrl Pts',(35.5333326526035,870.253850853304,141.445640232718));
#66809=CARTESIAN_POINT('Ctrl Pts',(35.5802108352733,870.366178452406,141.494031816885));
#66810=CARTESIAN_POINT('Ctrl Pts',(35.6153125063336,870.417611126486,141.51587339165));
#66811=CARTESIAN_POINT('Ctrl Pts',(35.7049419116693,870.505339114735,141.55225255951));
#66812=CARTESIAN_POINT('Ctrl Pts',(35.7585566921889,870.540813238459,141.566448497113));
#66813=CARTESIAN_POINT('Ctrl Pts',(35.8775574317109,870.591104860492,141.585201642523));
#66814=CARTESIAN_POINT('Ctrl Pts',(35.9417806479005,870.605391865572,141.589557400257));
#66815=CARTESIAN_POINT('Ctrl Pts',(36.0725734574083,870.610611423961,141.587762685552));
#66816=CARTESIAN_POINT('Ctrl Pts',(36.1378527847367,870.601397690208,141.581589950046));
#66817=CARTESIAN_POINT('Ctrl Pts',(36.2607138445109,870.560312018696,141.559533663607));
#66818=CARTESIAN_POINT('Ctrl Pts',(36.3170688658126,870.528758849371,141.54383433519));
#66819=CARTESIAN_POINT('Ctrl Pts',(36.4140299847881,870.44644218463,141.504705130878));
#66820=CARTESIAN_POINT('Ctrl Pts',(36.4533051342435,870.396097725773,141.481509106258));
#66821=CARTESIAN_POINT('Ctrl Pts',(36.507536546622,870.284320328245,141.431333906446));
#66822=CARTESIAN_POINT('Ctrl Pts',(36.5221437683816,870.224067148803,141.404876273121));
#66823=CARTESIAN_POINT('Ctrl Pts',(36.5247797852127,870.101801258789,141.352231451907));
#66824=CARTESIAN_POINT('Ctrl Pts',(36.5129148662676,870.041000669466,141.326558385375));
#66825=CARTESIAN_POINT('Ctrl Pts',(36.4641227992931,869.926876460825,141.279211080816));
#66826=CARTESIAN_POINT('Ctrl Pts',(36.4276685530675,869.874698686033,141.258007904886));
#66827=CARTESIAN_POINT('Ctrl Pts',(36.3347189194866,869.786196540001,141.222815192883));
#66828=CARTESIAN_POINT('Ctrl Pts',(36.279101758849,869.750821435053,141.209201905681));
#66829=CARTESIAN_POINT('Ctrl Pts',(36.1562325648716,869.702171695576,141.191512996649));
#66830=CARTESIAN_POINT('Ctrl Pts',(36.0902224625366,869.689404905759,141.187622314505));
#66831=CARTESIAN_POINT('Ctrl Pts',(36.023552436116,869.688940292305,141.188941320012));
#66832=CARTESIAN_POINT('Origin',(29.240389675011,875.321188457674,131.679644788733));
#66833=CARTESIAN_POINT('',(29.240389675011,870.675924374847,141.977771552158));
#66834=CARTESIAN_POINT('',(29.2403896750132,872.362839858081,142.895057226278));
#66835=CARTESIAN_POINT('Ctrl Pts',(29.240389675011,870.675924374847,141.977771552158));
#66836=CARTESIAN_POINT('Ctrl Pts',(29.2367816845808,870.675840918628,141.978007681839));
#66837=CARTESIAN_POINT('Ctrl Pts',(29.2331728647531,870.675775848065,141.978253596864));
#66838=CARTESIAN_POINT('Ctrl Pts',(29.1043285666561,870.674110361653,141.987381376002));
#66839=CARTESIAN_POINT('Ctrl Pts',(28.9809421210146,870.694687261028,142.007848186233));
#66840=CARTESIAN_POINT('Ctrl Pts',(28.7509635165537,870.777401026941,142.070066517537));
#66841=CARTESIAN_POINT('Ctrl Pts',(28.6468282149897,870.839029892949,142.111371712144));
#66842=CARTESIAN_POINT('Ctrl Pts',(28.471506017528,870.995818703683,142.210241340407));
#66843=CARTESIAN_POINT('Ctrl Pts',(28.4024845445846,871.089971733926,142.26710605341));
#66844=CARTESIAN_POINT('Ctrl Pts',(28.3113570012837,871.296145178495,142.387593174257));
#66845=CARTESIAN_POINT('Ctrl Pts',(28.2895286618689,871.406165584795,142.450083449862));
#66846=CARTESIAN_POINT('Ctrl Pts',(28.2955935390807,871.62674069641,142.57167116704));
#66847=CARTESIAN_POINT('Ctrl Pts',(28.3225857931083,871.7353464104,142.629746646865));
#66848=CARTESIAN_POINT('Ctrl Pts',(28.4213904548344,871.937131752257,142.733463409759));
#66849=CARTESIAN_POINT('Ctrl Pts',(28.4914745110623,872.028660429407,142.778324187968));
#66850=CARTESIAN_POINT('Ctrl Pts',(28.6663561746253,872.184110305666,142.849229501281));
#66851=CARTESIAN_POINT('Ctrl Pts',(28.7691430256071,872.246568056492,142.874634279215));
#66852=CARTESIAN_POINT('Ctrl Pts',(28.9959552138475,872.3348806794,142.902694767692));
#66853=CARTESIAN_POINT('Ctrl Pts',(29.1176930263198,872.359391999469,142.904812541878));
#66854=CARTESIAN_POINT('Ctrl Pts',(29.2403896750154,872.362839858081,142.895057226278));
#66855=CARTESIAN_POINT('',(29.240389674993,873.056476967889,140.93249156488));
#66856=CARTESIAN_POINT('',(29.240389675011,876.215084630293,131.99557794187));
#66857=CARTESIAN_POINT('Ctrl Pts',(28.8270936452429,872.962602665625,140.91353540268));
#66858=CARTESIAN_POINT('Ctrl Pts',(28.9336523008359,873.011266829159,140.930734964666));
#66859=CARTESIAN_POINT('Ctrl Pts',(29.0488646698254,873.041701491219,140.938143827054));
#66860=CARTESIAN_POINT('Ctrl Pts',(29.2912290268742,873.063674303931,140.932631817926));
#66861=CARTESIAN_POINT('Ctrl Pts',(29.4161837973998,873.052721869669,140.918615494393));
#66862=CARTESIAN_POINT('Ctrl Pts',(29.6507838752602,872.988463698336,140.870698667918));
#66863=CARTESIAN_POINT('Ctrl Pts',(29.7584566851137,872.936491073207,140.837600245346));
#66864=CARTESIAN_POINT('Ctrl Pts',(29.946416844765,872.797130430654,140.756111398283));
#66865=CARTESIAN_POINT('Ctrl Pts',(30.0245209206595,872.710460146978,140.708234093541));
#66866=CARTESIAN_POINT('Ctrl Pts',(30.1394357999211,872.51287589023,140.603808861391));
#66867=CARTESIAN_POINT('Ctrl Pts',(30.1746624674555,872.403503729237,140.548128452935));
#66868=CARTESIAN_POINT('Ctrl Pts',(30.1956744752123,872.177208845924,140.436692985381));
#66869=CARTESIAN_POINT('Ctrl Pts',(30.1811394943046,872.06244893213,140.382006516948));
#66870=CARTESIAN_POINT('Ctrl Pts',(30.1048834019336,871.848138665372,140.28310911132));
#66871=CARTESIAN_POINT('Ctrl Pts',(30.0458800857863,871.750142328819,140.239465215294));
#66872=CARTESIAN_POINT('Ctrl Pts',(29.8931263874831,871.581526406594,140.167404414969));
#66873=CARTESIAN_POINT('Ctrl Pts',(29.8019579916615,871.511624225611,140.13917476921));
#66874=CARTESIAN_POINT('Ctrl Pts',(29.5960805804867,871.404753576186,140.099797633118));
#66875=CARTESIAN_POINT('Ctrl Pts',(29.4831339722014,871.368951998056,140.089106846918));
#66876=CARTESIAN_POINT('Ctrl Pts',(29.246356895948,871.336071810407,140.086937335411));
#66877=CARTESIAN_POINT('Ctrl Pts',(29.1245931970823,871.340354230845,140.095997207761));
#66878=CARTESIAN_POINT('Ctrl Pts',(28.8843654037844,871.391273363315,140.134560030048));
#66879=CARTESIAN_POINT('Ctrl Pts',(28.7688976775041,871.439591960204,140.164719243706));
#66880=CARTESIAN_POINT('Ctrl Pts',(28.5691846488931,871.57291459618,140.24150308166));
#66881=CARTESIAN_POINT('Ctrl Pts',(28.4861769677574,871.655803975503,140.28702023133));
#66882=CARTESIAN_POINT('Ctrl Pts',(28.3598671301212,871.847294295614,140.388819695051));
#66883=CARTESIAN_POINT('Ctrl Pts',(28.3183042721467,871.954455505366,140.444297158382));
#66884=CARTESIAN_POINT('Ctrl Pts',(28.2839172461224,872.178923534258,140.557712182225));
#66885=CARTESIAN_POINT('Ctrl Pts',(28.29186363956,872.294195294952,140.614592188492));
#66886=CARTESIAN_POINT('Ctrl Pts',(28.3542051600735,872.504716080702,140.71562016173));
#66887=CARTESIAN_POINT('Ctrl Pts',(28.4031895718858,872.599128380444,140.759668438562));
#66888=CARTESIAN_POINT('Ctrl Pts',(28.539191557786,872.772990084837,140.837770417423));
#66889=CARTESIAN_POINT('Ctrl Pts',(28.6267282407186,872.849821237841,140.870473560104));
#66890=CARTESIAN_POINT('Ctrl Pts',(28.7596064663182,872.929488583218,140.901486447305));
#66891=CARTESIAN_POINT('Ctrl Pts',(28.79283346517,872.946956418997,140.908005489718));
#66892=CARTESIAN_POINT('Ctrl Pts',(28.8270936452429,872.962602665625,140.91353540268));
#66893=CARTESIAN_POINT('Ctrl Pts',(29.2403896750154,872.362839858081,142.895057226278));
#66894=CARTESIAN_POINT('Ctrl Pts',(29.2405343880238,872.362843924614,142.895045720495));
#66895=CARTESIAN_POINT('Ctrl Pts',(29.2406791023676,872.362847961838,142.895034198211));
#66896=CARTESIAN_POINT('Ctrl Pts',(29.2408238180354,872.36285196975,142.895022659426));
#66897=CARTESIAN_POINT('Ctrl Pts',(29.3621682470146,872.36621261347,142.885347361435));
#66898=CARTESIAN_POINT('Ctrl Pts',(29.4819887080006,872.348905343143,142.864265901722));
#66899=CARTESIAN_POINT('Ctrl Pts',(29.711794366194,872.273420916633,142.800706501727));
#66900=CARTESIAN_POINT('Ctrl Pts',(29.8186582549862,872.213860059979,142.757787166795));
#66901=CARTESIAN_POINT('Ctrl Pts',(29.9990404951428,872.05967678094,142.656582416295));
#66902=CARTESIAN_POINT('Ctrl Pts',(30.0705564373936,871.96610060915,142.599073633974));
#66903=CARTESIAN_POINT('Ctrl Pts',(30.1660633553242,871.759492852032,142.478737404305));
#66904=CARTESIAN_POINT('Ctrl Pts',(30.1898706208027,871.648600351706,142.417069812452));
#66905=CARTESIAN_POINT('Ctrl Pts',(30.1869698340323,871.424544776654,142.297613225431));
#66906=CARTESIAN_POINT('Ctrl Pts',(30.1609292067764,871.313545347621,142.240903072839));
#66907=CARTESIAN_POINT('Ctrl Pts',(30.0621397778283,871.105762271853,142.139169867226));
#66908=CARTESIAN_POINT('Ctrl Pts',(29.9906321851297,871.011024473981,142.095109691605));
#66909=CARTESIAN_POINT('Ctrl Pts',(29.8127632268166,870.852368043617,142.025877871808));
#66910=CARTESIAN_POINT('Ctrl Pts',(29.7089787024167,870.789466448968,142.00102846387));
#66911=CARTESIAN_POINT('Ctrl Pts',(29.4822392208746,870.70236091131,141.972947166182));
#66912=CARTESIAN_POINT('Ctrl Pts',(29.3617843938213,870.678732349099,141.969826715056));
#66913=CARTESIAN_POINT('Ctrl Pts',(29.240389675011,870.675924374847,141.977771552158));
#66914=CARTESIAN_POINT('Origin',(29.240389675011,875.321188457674,131.679644788733));
#66915=CARTESIAN_POINT('',(29.240389675011,873.657771826168,137.886540032222));
#66916=CARTESIAN_POINT('Origin',(29.240389675011,873.186349595559,137.719923464954));
#66917=CARTESIAN_POINT('',(29.2403896750113,871.966311801343,142.672329770708));
#66918=CARTESIAN_POINT('',(29.240389675011,875.792610688283,131.846261356));
#66919=CARTESIAN_POINT('Ctrl Pts',(29.2406093312764,871.076684303001,142.188525563727));
#66920=CARTESIAN_POINT('Ctrl Pts',(29.1766503670039,871.075101410464,142.192919855086));
#66921=CARTESIAN_POINT('Ctrl Pts',(29.1134480527164,871.08447829764,142.203123919309));
#66922=CARTESIAN_POINT('Ctrl Pts',(28.992504095938,871.124714337439,142.234746280417));
#66923=CARTESIAN_POINT('Ctrl Pts',(28.9363839134385,871.156158888874,142.256354888854));
#66924=CARTESIAN_POINT('Ctrl Pts',(28.8415260359534,871.237140896149,142.308141310702));
#66925=CARTESIAN_POINT('Ctrl Pts',(28.8038531092525,871.286088118937,142.337914947352));
#66926=CARTESIAN_POINT('Ctrl Pts',(28.7526370196238,871.394946036471,142.40164596502));
#66927=CARTESIAN_POINT('Ctrl Pts',(28.7397121645,871.453939292401,142.435051348497));
#66928=CARTESIAN_POINT('Ctrl Pts',(28.7410976817578,871.571637431497,142.499533406106));
#66929=CARTESIAN_POINT('Ctrl Pts',(28.7544777193056,871.629248844171,142.530081070611));
#66930=CARTESIAN_POINT('Ctrl Pts',(28.8051004198344,871.736636062784,142.584812959593));
#66931=CARTESIAN_POINT('Ctrl Pts',(28.8414633996518,871.785510712384,142.608573729047));
#66932=CARTESIAN_POINT('Ctrl Pts',(28.9327524760998,871.868747444632,142.646374157118));
#66933=CARTESIAN_POINT('Ctrl Pts',(28.9866219900859,871.902337699474,142.660080304813));
#66934=CARTESIAN_POINT('Ctrl Pts',(29.1057819299297,871.950168605278,142.675695243178));
#66935=CARTESIAN_POINT('Ctrl Pts',(29.1698765851482,871.963718616303,142.677330612537));
#66936=CARTESIAN_POINT('Ctrl Pts',(29.3005806209985,871.968579870734,142.668091050424));
#66937=CARTESIAN_POINT('Ctrl Pts',(29.3658219558896,871.959429472694,142.657088724495));
#66938=CARTESIAN_POINT('Ctrl Pts',(29.4887925124197,871.918887670554,142.623647814261));
#66939=CARTESIAN_POINT('Ctrl Pts',(29.5451141946069,871.887439870253,142.601311981726));
#66940=CARTESIAN_POINT('Ctrl Pts',(29.6401652702456,871.806187156151,142.548411193144));
#66941=CARTESIAN_POINT('Ctrl Pts',(29.6778518120375,871.75696139772,142.518260725676));
#66942=CARTESIAN_POINT('Ctrl Pts',(29.7284548414666,871.648039823179,142.454728397488));
#66943=CARTESIAN_POINT('Ctrl Pts',(29.7411139006961,871.589404978822,142.421942267325));
#66944=CARTESIAN_POINT('Ctrl Pts',(29.7396085708653,871.470797147763,142.358169018261));
#66945=CARTESIAN_POINT('Ctrl Pts',(29.7257062079282,871.411960181392,142.327766482922));
#66946=CARTESIAN_POINT('Ctrl Pts',(29.6735692326996,871.303236472631,142.273898165055));
#66947=CARTESIAN_POINT('Ctrl Pts',(29.6365554302358,871.254201035098,142.250779342196));
#66948=CARTESIAN_POINT('Ctrl Pts',(29.5440060903363,871.171100939789,142.214056048446));
#66949=CARTESIAN_POINT('Ctrl Pts',(29.4895324840044,871.137798929603,142.200768706667));
#66950=CARTESIAN_POINT('Ctrl Pts',(29.3696130132614,871.091101375852,142.185672833383));
#66951=CARTESIAN_POINT('Ctrl Pts',(29.3053785337554,871.07828724777,142.184075605069));
#66952=CARTESIAN_POINT('Ctrl Pts',(29.2406093312764,871.076684303001,142.188525563727));
#66953=CARTESIAN_POINT('Origin',(46.1965767102463,876.105745388824,131.956933754349));
#66954=CARTESIAN_POINT('',(46.1965767102464,871.539310156617,141.811985803522));
#66955=CARTESIAN_POINT('',(46.1965767102472,873.415048332981,142.635094861413));
#66956=CARTESIAN_POINT('Ctrl Pts',(46.1965767102464,871.539310156617,141.811985803522));
#66957=CARTESIAN_POINT('Ctrl Pts',(46.1937144929431,871.539304011668,141.812003189942));
#66958=CARTESIAN_POINT('Ctrl Pts',(46.1908517067503,871.539309014205,141.812025139295));
#66959=CARTESIAN_POINT('Ctrl Pts',(46.0534999164937,871.540084360332,141.813297227722));
#66960=CARTESIAN_POINT('Ctrl Pts',(45.9205687407884,871.565458979681,141.82457740446));
#66961=CARTESIAN_POINT('Ctrl Pts',(45.6732533278176,871.662243775346,141.86636373246));
#66962=CARTESIAN_POINT('Ctrl Pts',(45.5612848662722,871.73264076831,141.896452617147));
#66963=CARTESIAN_POINT('Ctrl Pts',(45.3727302369807,871.909663678627,141.972570662421));
#66964=CARTESIAN_POINT('Ctrl Pts',(45.2982635416768,872.014754229373,142.017961410119));
#66965=CARTESIAN_POINT('Ctrl Pts',(45.1984532575828,872.244160547686,142.118029234544));
#66966=CARTESIAN_POINT('Ctrl Pts',(45.173694385883,872.366101220885,142.171669705127));
#66967=CARTESIAN_POINT('Ctrl Pts',(45.1767763349096,872.611297248011,142.280401900152));
#66968=CARTESIAN_POINT('Ctrl Pts',(45.2045270734912,872.732242899625,142.334460899895));
#66969=CARTESIAN_POINT('Ctrl Pts',(45.3090871620149,872.956892070233,142.435187370653));
#66970=CARTESIAN_POINT('Ctrl Pts',(45.3847033292099,873.058580649317,142.480934171599));
#66971=CARTESIAN_POINT('Ctrl Pts',(45.5741277010826,873.229568847835,142.557408367027));
#66972=CARTESIAN_POINT('Ctrl Pts',(45.6859935378586,873.297356096951,142.587446034274));
#66973=CARTESIAN_POINT('Ctrl Pts',(45.9319537470132,873.39026526088,142.627317120645));
#66974=CARTESIAN_POINT('Ctrl Pts',(46.0636192986767,873.414464480635,142.636746803833));
#66975=CARTESIAN_POINT('Ctrl Pts',(46.196576710248,873.415048332981,142.635094861413));
#66976=CARTESIAN_POINT('',(46.1965767107091,874.061504505576,140.806022183502));
#66977=CARTESIAN_POINT('',(46.1965767102463,877.068774529067,132.297300837416));
#66978=CARTESIAN_POINT('Ctrl Pts',(46.0603115463226,874.052642389307,140.803697333072));
#66979=CARTESIAN_POINT('Ctrl Pts',(46.1923014221479,874.069394353401,140.809618043999));
#66980=CARTESIAN_POINT('Ctrl Pts',(46.3264636842238,874.062370818533,140.804818778975));
#66981=CARTESIAN_POINT('Ctrl Pts',(46.5840256589845,874.00158183426,140.774482269596));
#66982=CARTESIAN_POINT('Ctrl Pts',(46.7049123455155,873.948406123414,140.749245594537));
#66983=CARTESIAN_POINT('Ctrl Pts',(46.9178216779398,873.802172986762,140.681709377771));
#66984=CARTESIAN_POINT('Ctrl Pts',(47.0076708242949,873.710343136668,140.639991768634));
#66985=CARTESIAN_POINT('Ctrl Pts',(47.1438930481538,873.499485840497,140.545702947435));
#66986=CARTESIAN_POINT('Ctrl Pts',(47.1887777384192,873.382347031621,140.493989199866));
#66987=CARTESIAN_POINT('Ctrl Pts',(47.2266960762805,873.138311373662,140.387642916544));
#66988=CARTESIAN_POINT('Ctrl Pts',(47.2193114075928,873.013737671103,140.334025184349));
#66989=CARTESIAN_POINT('Ctrl Pts',(47.1528984655208,872.775061106413,140.232459473628));
#66990=CARTESIAN_POINT('Ctrl Pts',(47.0949906174885,872.6631450898,140.185424320325));
#66991=CARTESIAN_POINT('Ctrl Pts',(46.9348459124716,872.464535666884,140.102824628238));
#66992=CARTESIAN_POINT('Ctrl Pts',(46.8336367843973,872.380149856647,140.068222087155));
#66993=CARTESIAN_POINT('Ctrl Pts',(46.6014097214899,872.25233049921,140.016555505051));
#66994=CARTESIAN_POINT('Ctrl Pts',(46.4726603970214,872.210239908928,140.00002779212));
#66995=CARTESIAN_POINT('Ctrl Pts',(46.2063453606493,872.174953294334,139.987460137214));
#66996=CARTESIAN_POINT('Ctrl Pts',(46.0714851014881,872.181621883862,139.991341786384));
#66997=CARTESIAN_POINT('Ctrl Pts',(45.8124918514646,872.242541049771,140.019053714481));
#66998=CARTESIAN_POINT('Ctrl Pts',(45.6908788951564,872.296158170341,140.042604718078));
#66999=CARTESIAN_POINT('Ctrl Pts',(45.4774538783132,872.443185709471,140.106645284904));
#67000=CARTESIAN_POINT('Ctrl Pts',(45.3876018334669,872.53503897332,140.1464679682));
#67001=CARTESIAN_POINT('Ctrl Pts',(45.2507082502561,872.746011413384,140.238035860224));
#67002=CARTESIAN_POINT('Ctrl Pts',(45.2053596632383,872.86330621639,140.288996738346));
#67003=CARTESIAN_POINT('Ctrl Pts',(45.1662925942187,873.108583233809,140.395817588004));
#67004=CARTESIAN_POINT('Ctrl Pts',(45.1735746255535,873.234277472475,140.450683737337));
#67005=CARTESIAN_POINT('Ctrl Pts',(45.2407831731627,873.474366622656,140.555551012221));
#67006=CARTESIAN_POINT('Ctrl Pts',(45.299494962934,873.586581992753,140.604592066219));
#67007=CARTESIAN_POINT('Ctrl Pts',(45.460784995985,873.783762459085,140.690426686063));
#67008=CARTESIAN_POINT('Ctrl Pts',(45.5617486768193,873.866856228305,140.726396891969));
#67009=CARTESIAN_POINT('Ctrl Pts',(45.735613611947,873.961464421838,140.766699721802));
#67010=CARTESIAN_POINT('Ctrl Pts',(45.7971512000974,873.987800690086,140.777774321936));
#67011=CARTESIAN_POINT('Ctrl Pts',(45.9257174091181,874.029204308247,140.794803685085));
#67012=CARTESIAN_POINT('Ctrl Pts',(45.9924670317909,874.044031661671,140.800654010574));
#67013=CARTESIAN_POINT('Ctrl Pts',(46.0603115463226,874.052642389307,140.803697333072));
#67014=CARTESIAN_POINT('Ctrl Pts',(46.196576710248,873.415048332981,142.635094861413));
#67015=CARTESIAN_POINT('Ctrl Pts',(46.1967585223272,873.415049131367,142.635092602471));
#67016=CARTESIAN_POINT('Ctrl Pts',(46.1969403368227,873.415049885594,142.635090322854));
#67017=CARTESIAN_POINT('Ctrl Pts',(46.1971221537155,873.415050595624,142.635088022543));
#67018=CARTESIAN_POINT('Ctrl Pts',(46.3293223641573,873.415566862643,142.633415452066));
#67019=CARTESIAN_POINT('Ctrl Pts',(46.4601815023246,873.392724222154,142.62082390506));
#67020=CARTESIAN_POINT('Ctrl Pts',(46.7070847335911,873.301991730621,142.575215625585));
#67021=CARTESIAN_POINT('Ctrl Pts',(46.8203476425693,873.234141395486,142.542275498948));
#67022=CARTESIAN_POINT('Ctrl Pts',(47.0113946314043,873.061914923075,142.461033399297));
#67023=CARTESIAN_POINT('Ctrl Pts',(47.0872875550886,872.95912834712,142.413501722372));
#67024=CARTESIAN_POINT('Ctrl Pts',(47.191388287791,872.731128706094,142.310358062614));
#67025=CARTESIAN_POINT('Ctrl Pts',(47.2182095430374,872.607945942266,142.255692675743));
#67026=CARTESIAN_POINT('Ctrl Pts',(47.2177581155975,872.358734507253,142.147233054814));
#67027=CARTESIAN_POINT('Ctrl Pts',(47.1906112853271,872.23515978004,142.094499346869));
#67028=CARTESIAN_POINT('Ctrl Pts',(47.0859676846827,872.005453148782,141.998084602508));
#67029=CARTESIAN_POINT('Ctrl Pts',(47.0099705478659,871.901433474046,141.955257327032));
#67030=CARTESIAN_POINT('Ctrl Pts',(46.8187821282926,871.72628129303,141.884120969343));
#67031=CARTESIAN_POINT('Ctrl Pts',(46.7054924529518,871.656871990556,141.856490742835));
#67032=CARTESIAN_POINT('Ctrl Pts',(46.4588710796671,871.563505879996,141.820029177464));
#67033=CARTESIAN_POINT('Ctrl Pts',(46.3283266687638,871.539593013127,141.81118549387));
#67034=CARTESIAN_POINT('Ctrl Pts',(46.1965767102464,871.539310156617,141.811985803522));
#67035=CARTESIAN_POINT('Origin',(46.1965767102463,876.105745388824,131.956933754349));
#67036=CARTESIAN_POINT('',(46.1965767102463,874.442328757318,138.163828997837));
#67037=CARTESIAN_POINT('Origin',(46.1965767102463,873.970906526709,137.99721243057));
#67038=CARTESIAN_POINT('',(46.1965767102465,872.9397096753,142.415315215679));
#67039=CARTESIAN_POINT('',(46.1965767102463,876.577167619433,132.123550321616));
#67040=CARTESIAN_POINT('Ctrl Pts',(46.1968411429053,872.021533786227,142.012285430459));
#67041=CARTESIAN_POINT('Ctrl Pts',(46.1348931452708,872.021333101247,142.012754929298));
#67042=CARTESIAN_POINT('Ctrl Pts',(46.0734881842045,872.031753178132,142.017723413552));
#67043=CARTESIAN_POINT('Ctrl Pts',(45.9539222363994,872.074169732284,142.036888757063));
#67044=CARTESIAN_POINT('Ctrl Pts',(45.8975019133049,872.107219689185,142.051526873118));
#67045=CARTESIAN_POINT('Ctrl Pts',(45.8018160037468,872.191770318541,142.088792446426));
#67046=CARTESIAN_POINT('Ctrl Pts',(45.7635893227472,872.242503045512,142.111085597979));
#67047=CARTESIAN_POINT('Ctrl Pts',(45.7113639353332,872.353896025228,142.160089161092));
#67048=CARTESIAN_POINT('Ctrl Pts',(45.6975489663079,872.413342437864,142.186266910223));
#67049=CARTESIAN_POINT('Ctrl Pts',(45.6957048070797,872.533595683546,142.239294927549));
#67050=CARTESIAN_POINT('Ctrl Pts',(45.707655214252,872.593263119955,142.265641318822));
#67051=CARTESIAN_POINT('Ctrl Pts',(45.755874856025,872.704797681698,142.314839509429));
#67052=CARTESIAN_POINT('Ctrl Pts',(45.7915983533186,872.75564184062,142.33723653254));
#67053=CARTESIAN_POINT('Ctrl Pts',(45.8822487270904,872.841827223409,142.374943231437));
#67054=CARTESIAN_POINT('Ctrl Pts',(45.93624673542,872.876389215919,142.389908920414));
#67055=CARTESIAN_POINT('Ctrl Pts',(46.0557121402089,872.924688941862,142.410281649844));
#67056=CARTESIAN_POINT('Ctrl Pts',(46.1200085400123,872.937943820786,142.415482566568));
#67057=CARTESIAN_POINT('Ctrl Pts',(46.2507038369816,872.941158942785,142.415287982749));
#67058=CARTESIAN_POINT('Ctrl Pts',(46.3158069054221,872.930997240269,142.409854411394));
#67059=CARTESIAN_POINT('Ctrl Pts',(46.4381591803029,872.888206354577,142.389003820392));
#67060=CARTESIAN_POINT('Ctrl Pts',(46.4941628674793,872.855898190198,142.373751151953));
#67061=CARTESIAN_POINT('Ctrl Pts',(46.5892921029457,872.773168953882,142.335537771323));
#67062=CARTESIAN_POINT('Ctrl Pts',(46.6274605851056,872.723506146392,142.312933083704));
#67063=CARTESIAN_POINT('Ctrl Pts',(46.680824830468,872.612808685136,142.263274783167));
#67064=CARTESIAN_POINT('Ctrl Pts',(46.6952693168326,872.552740939566,142.236664232516));
#67065=CARTESIAN_POINT('Ctrl Pts',(46.6977194079068,872.430496918115,142.18317264406));
#67066=CARTESIAN_POINT('Ctrl Pts',(46.6855983534884,872.369519818791,142.156818143097));
#67067=CARTESIAN_POINT('Ctrl Pts',(46.6361791776284,872.255686822419,142.108158336933));
#67068=CARTESIAN_POINT('Ctrl Pts',(46.5995270010882,872.203913057215,142.086307973218));
#67069=CARTESIAN_POINT('Ctrl Pts',(46.506493373721,872.116527594763,142.049839061974));
#67070=CARTESIAN_POINT('Ctrl Pts',(46.4510803079727,872.081760306271,142.035567122818));
#67071=CARTESIAN_POINT('Ctrl Pts',(46.3287961632862,872.034129605604,142.01644344205));
#67072=CARTESIAN_POINT('Ctrl Pts',(46.2631519379868,872.021748604802,142.011782866332));
#67073=CARTESIAN_POINT('Ctrl Pts',(46.1968411429053,872.021533786227,142.012285430459));
#67074=CARTESIAN_POINT('Origin',(39.9029229553071,878.949318330988,132.961948646806));
#67075=CARTESIAN_POINT('',(39.9029229553071,874.306969838757,143.251826085178));
#67076=CARTESIAN_POINT('',(39.9029229553089,875.985831224642,144.191899892559));
#67077=CARTESIAN_POINT('Ctrl Pts',(39.9029229553071,874.306969838757,143.251826085178));
#67078=CARTESIAN_POINT('Ctrl Pts',(39.9009534307544,874.30694501926,143.251896309062));
#67079=CARTESIAN_POINT('Ctrl Pts',(39.8989836282631,874.306925665399,143.251969485561));
#67080=CARTESIAN_POINT('Ctrl Pts',(39.7715568737462,874.306027659273,143.256893792742));
#67081=CARTESIAN_POINT('Ctrl Pts',(39.647744719753,874.327347554828,143.273607956868));
#67082=CARTESIAN_POINT('Ctrl Pts',(39.4173398036129,874.41140713584,143.329072565374));
#67083=CARTESIAN_POINT('Ctrl Pts',(39.3131699848017,874.473363560329,143.367310208833));
#67084=CARTESIAN_POINT('Ctrl Pts',(39.1377884732739,874.629965346088,143.461038823805));
#67085=CARTESIAN_POINT('Ctrl Pts',(39.0686354901211,874.723405963652,143.515797110725));
#67086=CARTESIAN_POINT('Ctrl Pts',(38.9751238774499,874.930005668183,143.635280747051));
#67087=CARTESIAN_POINT('Ctrl Pts',(38.9522966177509,875.041537208258,143.699046013975));
#67088=CARTESIAN_POINT('Ctrl Pts',(38.9577679347267,875.263774022378,143.824633567473));
#67089=CARTESIAN_POINT('Ctrl Pts',(38.984895821811,875.372543450952,143.885386157237));
#67090=CARTESIAN_POINT('Ctrl Pts',(39.0844870246255,875.573527435018,143.995719560666));
#67091=CARTESIAN_POINT('Ctrl Pts',(39.1551805947154,875.664229356601,144.044498187797));
#67092=CARTESIAN_POINT('Ctrl Pts',(39.3309860528678,875.816648737464,144.123676489077));
#67093=CARTESIAN_POINT('Ctrl Pts',(39.4338855056939,875.877241726121,144.153527221637));
#67094=CARTESIAN_POINT('Ctrl Pts',(39.6600704936404,875.961350771491,144.190529796745));
#67095=CARTESIAN_POINT('Ctrl Pts',(39.7809437428096,875.983935484909,144.197263668013));
#67096=CARTESIAN_POINT('Ctrl Pts',(39.9029229553107,875.985831224642,144.191899892559));
#67097=CARTESIAN_POINT('',(39.9029229553206,876.681439899921,142.223755915584));
#67098=CARTESIAN_POINT('',(39.9029229553071,879.843214503607,133.277881799942));
#67099=CARTESIAN_POINT('Ctrl Pts',(39.6760609074945,876.65417024943,142.218260294109));
#67100=CARTESIAN_POINT('Ctrl Pts',(39.7910221966015,876.680882462951,142.227701294197));
#67101=CARTESIAN_POINT('Ctrl Pts',(39.9101962652796,876.688090144837,142.226900955887));
#67102=CARTESIAN_POINT('Ctrl Pts',(40.1511897857589,876.662163668026,142.204459717129));
#67103=CARTESIAN_POINT('Ctrl Pts',(40.2702959128896,876.627025544152,142.181895352544));
#67104=CARTESIAN_POINT('Ctrl Pts',(40.4838531659849,876.518356349961,142.118282167906));
#67105=CARTESIAN_POINT('Ctrl Pts',(40.5766917966377,876.446513653426,142.078160989779));
#67106=CARTESIAN_POINT('Ctrl Pts',(40.7275801369447,876.273574159347,141.984804240418));
#67107=CARTESIAN_POINT('Ctrl Pts',(40.7836705291662,876.173605613701,141.932226879937));
#67108=CARTESIAN_POINT('Ctrl Pts',(40.8501072195456,875.958049970237,141.821449951645));
#67109=CARTESIAN_POINT('Ctrl Pts',(40.8592663423443,875.844279312972,141.764214965779));
#67110=CARTESIAN_POINT('Ctrl Pts',(40.8277383758783,875.619026529051,141.653147811411));
#67111=CARTESIAN_POINT('Ctrl Pts',(40.7872359723692,875.509720651974,141.600388984095));
#67112=CARTESIAN_POINT('Ctrl Pts',(40.663783447529,875.315200899285,141.508486215769));
#67113=CARTESIAN_POINT('Ctrl Pts',(40.5838356488444,875.230974193866,141.469708973292));
#67114=CARTESIAN_POINT('Ctrl Pts',(40.3963738851674,875.096072584928,141.409563952035));
#67115=CARTESIAN_POINT('Ctrl Pts',(40.2915390894419,875.045593721648,141.388199163957));
#67116=CARTESIAN_POINT('Ctrl Pts',(40.0664827440692,874.981427291455,141.363915143875));
#67117=CARTESIAN_POINT('Ctrl Pts',(39.9482454741537,874.968535329637,141.361321391245));
#67118=CARTESIAN_POINT('Ctrl Pts',(39.7100467845826,874.982723789839,141.375787532497));
#67119=CARTESIAN_POINT('Ctrl Pts',(39.5924110863674,875.010729959418,141.393232180506));
#67120=CARTESIAN_POINT('Ctrl Pts',(39.3700861925856,875.107486650575,141.447995546985));
#67121=CARTESIAN_POINT('Ctrl Pts',(39.2687030524731,875.177294506076,141.485749791744));
#67122=CARTESIAN_POINT('Ctrl Pts',(39.1048090734562,875.346649486077,141.575268679262));
#67123=CARTESIAN_POINT('Ctrl Pts',(39.0430175481789,875.44388802455,141.625857307291));
#67124=CARTESIAN_POINT('Ctrl Pts',(38.964058400758,875.655719874202,141.734846155825));
#67125=CARTESIAN_POINT('Ctrl Pts',(38.9482540786183,875.768565996308,141.792332859536));
#67126=CARTESIAN_POINT('Ctrl Pts',(38.9664783374583,875.994635706068,141.906313971592));
#67127=CARTESIAN_POINT('Ctrl Pts',(39.0007884414862,876.105719976912,141.961713977259));
#67128=CARTESIAN_POINT('Ctrl Pts',(39.1100352276555,876.299236885488,142.056732204963));
#67129=CARTESIAN_POINT('Ctrl Pts',(39.1795085028925,876.381910390205,142.09663159444));
#67130=CARTESIAN_POINT('Ctrl Pts',(39.352031492848,876.525198211704,142.163927728593));
#67131=CARTESIAN_POINT('Ctrl Pts',(39.4549821501028,876.58315265103,142.189959201952));
#67132=CARTESIAN_POINT('Ctrl Pts',(39.6027223966637,876.635011562805,142.211143647796));
#67133=CARTESIAN_POINT('Ctrl Pts',(39.6390991567632,876.645581878637,142.215224873276));
#67134=CARTESIAN_POINT('Ctrl Pts',(39.6760609074945,876.65417024943,142.218260294109));
#67135=CARTESIAN_POINT('Ctrl Pts',(39.9029229553107,875.985831224642,144.191899892559));
#67136=CARTESIAN_POINT('Ctrl Pts',(39.9030874038895,875.985833780419,144.191892661284));
#67137=CARTESIAN_POINT('Ctrl Pts',(39.9032518544797,875.985836298579,144.191885408044));
#67138=CARTESIAN_POINT('Ctrl Pts',(39.903416307065,875.98583877912,144.191878132838));
#67139=CARTESIAN_POINT('Ctrl Pts',(40.0251817976164,875.987675443772,144.186491358095));
#67140=CARTESIAN_POINT('Ctrl Pts',(40.1454673356734,875.968858913891,144.169170410953));
#67141=CARTESIAN_POINT('Ctrl Pts',(40.3747002237885,875.890893894539,144.112074599829));
#67142=CARTESIAN_POINT('Ctrl Pts',(40.4806317218925,875.830953575662,144.072022552572));
#67143=CARTESIAN_POINT('Ctrl Pts',(40.6609684533752,875.676257671763,143.974339399571));
#67144=CARTESIAN_POINT('Ctrl Pts',(40.7328104936842,875.582157529378,143.917245070734));
#67145=CARTESIAN_POINT('Ctrl Pts',(40.8287772622849,875.374989520591,143.795799754419));
#67146=CARTESIAN_POINT('Ctrl Pts',(40.852578328741,875.263981598242,143.732618331064));
#67147=CARTESIAN_POINT('Ctrl Pts',(40.8492990764597,875.040632595631,143.608970566394));
#67148=CARTESIAN_POINT('Ctrl Pts',(40.822962703033,874.930358621375,143.549594774218));
#67149=CARTESIAN_POINT('Ctrl Pts',(40.7236050577374,874.724818305239,143.441853751764));
#67150=CARTESIAN_POINT('Ctrl Pts',(40.6519180075985,874.631458998882,143.39445059914));
#67151=CARTESIAN_POINT('Ctrl Pts',(40.473614022833,874.475647779633,143.31810069937));
#67152=CARTESIAN_POINT('Ctrl Pts',(40.3695340826542,874.41417502236,143.28955402088));
#67153=CARTESIAN_POINT('Ctrl Pts',(40.1431929620499,874.330531654497,143.254288726939));
#67154=CARTESIAN_POINT('Ctrl Pts',(40.0235798236697,874.308490328937,143.247524034764));
#67155=CARTESIAN_POINT('Ctrl Pts',(39.9029229553071,874.306969838757,143.251826085178));
#67156=CARTESIAN_POINT('Origin',(39.9029229553071,878.949318330988,132.961948646806));
#67157=CARTESIAN_POINT('',(39.9029229553071,877.285901699482,139.168843890294));
#67158=CARTESIAN_POINT('Origin',(39.9029229553071,876.814479468873,139.002227323027));
#67159=CARTESIAN_POINT('',(39.9029229553073,875.591487946798,143.962990858787));
#67160=CARTESIAN_POINT('',(39.9029229553071,879.420740561597,133.128565214073));
#67161=CARTESIAN_POINT('Ctrl Pts',(39.9029125861287,874.706111633602,143.46715827259));
#67162=CARTESIAN_POINT('Ctrl Pts',(39.8394125814979,874.705266289056,143.469554028673));
#67163=CARTESIAN_POINT('Ctrl Pts',(39.776620906851,874.715175936815,143.477814522341));
#67164=CARTESIAN_POINT('Ctrl Pts',(39.6560352456007,874.756218438025,143.505866775024));
#67165=CARTESIAN_POINT('Ctrl Pts',(39.5999333149543,874.787994049393,143.525943440243));
#67166=CARTESIAN_POINT('Ctrl Pts',(39.5051137443104,874.86924503659,143.575310541464));
#67167=CARTESIAN_POINT('Ctrl Pts',(39.4674503889586,874.918056839898,143.604189947962));
#67168=CARTESIAN_POINT('Ctrl Pts',(39.4159003605091,875.026297036297,143.667051502762));
#67169=CARTESIAN_POINT('Ctrl Pts',(39.4026875151781,875.084826141436,143.700503306233));
#67170=CARTESIAN_POINT('Ctrl Pts',(39.4031600074572,875.202109358987,143.766523330033));
#67171=CARTESIAN_POINT('Ctrl Pts',(39.4163122704492,875.259821781453,143.798523025633));
#67172=CARTESIAN_POINT('Ctrl Pts',(39.466789581369,875.36696636881,143.856818331159));
#67173=CARTESIAN_POINT('Ctrl Pts',(39.5032188927284,875.415560110795,143.882675862872));
#67174=CARTESIAN_POINT('Ctrl Pts',(39.5946098126277,875.497644378116,143.924914833303));
#67175=CARTESIAN_POINT('Ctrl Pts',(39.6484193347918,875.530516057664,143.940997221764));
#67176=CARTESIAN_POINT('Ctrl Pts',(39.7671645023835,875.576691676965,143.961401618141));
#67177=CARTESIAN_POINT('Ctrl Pts',(39.8308435880341,875.589497549965,143.965501203725));
#67178=CARTESIAN_POINT('Ctrl Pts',(39.9606812981915,875.593175112385,143.961031974467));
#67179=CARTESIAN_POINT('Ctrl Pts',(40.0254550063193,875.583696188365,143.952334245958));
#67180=CARTESIAN_POINT('Ctrl Pts',(40.1479332230503,875.542958292175,143.922963072296));
#67181=CARTESIAN_POINT('Ctrl Pts',(40.2041732943436,875.511641195688,143.902335419013));
#67182=CARTESIAN_POINT('Ctrl Pts',(40.2998867208973,875.43074791286,143.851772613677));
#67183=CARTESIAN_POINT('Ctrl Pts',(40.3381061536731,875.381620484094,143.822161237435));
#67184=CARTESIAN_POINT('Ctrl Pts',(40.3898919840359,875.273017444946,143.758620287658));
#67185=CARTESIAN_POINT('Ctrl Pts',(40.4031198235907,875.214565922328,143.725282428387));
#67186=CARTESIAN_POINT('Ctrl Pts',(40.4027233846304,875.096514204187,143.659534746794));
#67187=CARTESIAN_POINT('Ctrl Pts',(40.3893338580669,875.037997724845,143.627713405857));
#67188=CARTESIAN_POINT('Ctrl Pts',(40.3375528663649,874.928767732513,143.569742176593));
#67189=CARTESIAN_POINT('Ctrl Pts',(40.299830830971,874.879075145497,143.544120454941));
#67190=CARTESIAN_POINT('Ctrl Pts',(40.2060206396531,874.796466898826,143.503003556349));
#67191=CARTESIAN_POINT('Ctrl Pts',(40.1514502513785,874.763924057369,143.487638595844));
#67192=CARTESIAN_POINT('Ctrl Pts',(40.031578849116,874.718958482736,143.468406330896));
#67193=CARTESIAN_POINT('Ctrl Pts',(39.9675407015733,874.706971996137,143.464719954647));
#67194=CARTESIAN_POINT('Ctrl Pts',(39.9029125861287,874.706111633602,143.46715827259));
#67195=CARTESIAN_POINT('Origin',(56.6615834797138,876.392836831737,132.058401584256));
#67196=CARTESIAN_POINT('',(56.6615834797139,871.826484696526,141.913218520128));
#67197=CARTESIAN_POINT('',(56.6615834797138,873.701900949848,142.737238421883));
#67198=CARTESIAN_POINT('Ctrl Pts',(56.6615834797139,871.826484696526,141.913218520128));
#67199=CARTESIAN_POINT('Ctrl Pts',(56.6609946908177,871.826485410375,141.913216500375));
#67200=CARTESIAN_POINT('Ctrl Pts',(56.6604058766319,871.826486596065,141.913214673391));
#67201=CARTESIAN_POINT('Ctrl Pts',(56.5249017417484,871.826868056857,141.912838616704));
#67202=CARTESIAN_POINT('Ctrl Pts',(56.3913631648341,871.85202727222,141.922567460365));
#67203=CARTESIAN_POINT('Ctrl Pts',(56.1429026589535,871.948751438092,141.961234954755));
#67204=CARTESIAN_POINT('Ctrl Pts',(56.0303721644293,872.019212471289,141.989744021337));
#67205=CARTESIAN_POINT('Ctrl Pts',(55.8412133365598,872.1960898603,142.062545795087));
#67206=CARTESIAN_POINT('Ctrl Pts',(55.7664566066399,872.300752572678,142.106137665102));
#67207=CARTESIAN_POINT('Ctrl Pts',(55.66455851989,872.531309682226,142.203863605437));
#67208=CARTESIAN_POINT('Ctrl Pts',(55.638908707713,872.655089391935,142.257131608936));
#67209=CARTESIAN_POINT('Ctrl Pts',(55.6415222063443,872.902456466717,142.365462442173));
#67210=CARTESIAN_POINT('Ctrl Pts',(55.6691223250622,873.023665489806,142.419460728698));
#67211=CARTESIAN_POINT('Ctrl Pts',(55.773569354643,873.248580449788,142.521253485098));
#67212=CARTESIAN_POINT('Ctrl Pts',(55.8493012069038,873.350237199982,142.568103286156));
#67213=CARTESIAN_POINT('Ctrl Pts',(56.0389867145052,873.520509358991,142.647720348297));
#67214=CARTESIAN_POINT('Ctrl Pts',(56.150978431199,873.58768400378,142.679790881428));
#67215=CARTESIAN_POINT('Ctrl Pts',(56.3970138101901,873.678948589189,142.724285393482));
#67216=CARTESIAN_POINT('Ctrl Pts',(56.5286286481765,873.702232170148,142.736301272505));
#67217=CARTESIAN_POINT('Ctrl Pts',(56.6615834797138,873.701900949848,142.737238421883));
#67218=CARTESIAN_POINT('',(56.6615834794499,874.348423453521,140.907978067888));
#67219=CARTESIAN_POINT('',(56.6615834797138,877.355865971979,132.398768667323));
#67220=CARTESIAN_POINT('Ctrl Pts',(56.7387604601335,874.345589290753,140.907234680149));
#67221=CARTESIAN_POINT('Ctrl Pts',(56.8715601059757,874.336101421898,140.903881346266));
#67222=CARTESIAN_POINT('Ctrl Pts',(57.0010812807415,874.30294766371,140.889846776181));
#67223=CARTESIAN_POINT('Ctrl Pts',(57.2389967355791,874.193058379317,140.84215655939));
#67224=CARTESIAN_POINT('Ctrl Pts',(57.3450693350082,874.11739169635,140.808970813782));
#67225=CARTESIAN_POINT('Ctrl Pts',(57.5199811258611,873.932726670759,140.72785146709));
#67226=CARTESIAN_POINT('Ctrl Pts',(57.5869752716837,873.825354129399,140.680640544959));
#67227=CARTESIAN_POINT('Ctrl Pts',(57.6723540791752,873.592536847775,140.578590321866));
#67228=CARTESIAN_POINT('Ctrl Pts',(57.6897125127079,873.469229935417,140.524696557824));
#67229=CARTESIAN_POINT('Ctrl Pts',(57.6715963313277,873.223231944225,140.41765671954));
#67230=CARTESIAN_POINT('Ctrl Pts',(57.6362382527093,873.10289391739,140.365536018464));
#67231=CARTESIAN_POINT('Ctrl Pts',(57.5174524273053,872.882569984974,140.270456748966));
#67232=CARTESIAN_POINT('Ctrl Pts',(57.4356125490153,872.78450254126,140.228316149903));
#67233=CARTESIAN_POINT('Ctrl Pts',(57.234311545603,872.62171128422,140.158375809575));
#67234=CARTESIAN_POINT('Ctrl Pts',(57.1163746955299,872.559042171161,140.131448684077));
#67235=CARTESIAN_POINT('Ctrl Pts',(56.8605865096311,872.479583634516,140.09687445237));
#67236=CARTESIAN_POINT('Ctrl Pts',(56.7252546257234,872.463662685499,140.089595976134));
#67237=CARTESIAN_POINT('Ctrl Pts',(56.4569713081032,872.481353135161,140.09575220826));
#67238=CARTESIAN_POINT('Ctrl Pts',(56.326634234563,872.514301970465,140.108922185502));
#67239=CARTESIAN_POINT('Ctrl Pts',(56.087162461522,872.624617497883,140.154092459123));
#67240=CARTESIAN_POINT('Ctrl Pts',(55.9803492034041,872.700870958704,140.185643911285));
#67241=CARTESIAN_POINT('Ctrl Pts',(55.804846533169,872.886440043867,140.263306364565));
#67242=CARTESIAN_POINT('Ctrl Pts',(55.7377228556858,872.993849122406,140.308626999117));
#67243=CARTESIAN_POINT('Ctrl Pts',(55.6515214168156,873.226929597842,140.408008618885));
#67244=CARTESIAN_POINT('Ctrl Pts',(55.6336876419626,873.350485579954,140.461182409555));
#67245=CARTESIAN_POINT('Ctrl Pts',(55.650956415818,873.597922741854,140.568766727364));
#67246=CARTESIAN_POINT('Ctrl Pts',(55.6865202510053,873.719371085996,140.622132233908));
#67247=CARTESIAN_POINT('Ctrl Pts',(55.806589945394,873.94090153433,140.72044023561));
#67248=CARTESIAN_POINT('Ctrl Pts',(55.8894138540945,874.039091148948,140.764524113048));
#67249=CARTESIAN_POINT('Ctrl Pts',(56.0917791670309,874.20023448107,140.837621990316));
#67250=CARTESIAN_POINT('Ctrl Pts',(56.2093174127696,874.261675376655,140.865939338036));
#67251=CARTESIAN_POINT('Ctrl Pts',(56.4007211769631,874.320086557591,140.893448918861));
#67252=CARTESIAN_POINT('Ctrl Pts',(56.4668439595631,874.333772072963,140.900052314879));
#67253=CARTESIAN_POINT('Ctrl Pts',(56.6018968193636,874.349051846478,140.907848627408));
#67254=CARTESIAN_POINT('Ctrl Pts',(56.6704997132709,874.350466178866,140.908958337422));
#67255=CARTESIAN_POINT('Ctrl Pts',(56.7387604601335,874.345589290753,140.907234680149));
#67256=CARTESIAN_POINT('Ctrl Pts',(56.6615834797139,873.701900949848,142.737238421883));
#67257=CARTESIAN_POINT('Ctrl Pts',(56.6615908286669,873.701900931541,142.737238473683));
#67258=CARTESIAN_POINT('Ctrl Pts',(56.6615981776241,873.701900913178,142.737238525457));
#67259=CARTESIAN_POINT('Ctrl Pts',(56.6616055265853,873.701900894726,142.73723857719));
#67260=CARTESIAN_POINT('Ctrl Pts',(56.7920552216792,873.701573353253,142.73815686803));
#67261=CARTESIAN_POINT('Ctrl Pts',(56.9212693873624,873.678518937705,142.728390846398));
#67262=CARTESIAN_POINT('Ctrl Pts',(57.1668593346475,873.588131091588,142.68812134135));
#67263=CARTESIAN_POINT('Ctrl Pts',(57.2802745242113,873.520412040137,142.657423550219));
#67264=CARTESIAN_POINT('Ctrl Pts',(57.4723085051569,873.348581722697,142.579476613341));
#67265=CARTESIAN_POINT('Ctrl Pts',(57.5489049042427,873.245991264003,142.532933896641));
#67266=CARTESIAN_POINT('Ctrl Pts',(57.6541627852097,873.019492886243,142.430970318421));
#67267=CARTESIAN_POINT('Ctrl Pts',(57.681832787815,872.897736939774,142.376533693577));
#67268=CARTESIAN_POINT('Ctrl Pts',(57.6840938909722,872.649461894248,142.266717717683));
#67269=CARTESIAN_POINT('Ctrl Pts',(57.6579766086863,872.52533699858,142.212418898586));
#67270=CARTESIAN_POINT('Ctrl Pts',(57.554839527277,872.294897300328,142.112675071343));
#67271=CARTESIAN_POINT('Ctrl Pts',(57.4794877508656,872.190634193339,142.068093323857));
#67272=CARTESIAN_POINT('Ctrl Pts',(57.2894177385193,872.015132848579,141.993539452835));
#67273=CARTESIAN_POINT('Ctrl Pts',(57.176705659342,871.945522323037,141.964236815098));
#67274=CARTESIAN_POINT('Ctrl Pts',(56.9286459505039,871.850676119467,141.924128858445));
#67275=CARTESIAN_POINT('Ctrl Pts',(56.7957714512608,871.826322006757,141.913678831938));
#67276=CARTESIAN_POINT('Ctrl Pts',(56.6615834797138,871.826484696526,141.913218520128));
#67277=CARTESIAN_POINT('Origin',(56.6615834797138,876.392836831737,132.058401584256));
#67278=CARTESIAN_POINT('',(56.6615834797138,874.72942020023,138.265296827744));
#67279=CARTESIAN_POINT('Origin',(56.6615834797138,874.257997969622,138.098680260477));
#67280=CARTESIAN_POINT('',(56.661583479714,873.226683339969,142.517116285449));
#67281=CARTESIAN_POINT('',(56.6615834797138,876.864259062345,132.225018151523));
#67282=CARTESIAN_POINT('Ctrl Pts',(56.6615880190493,872.308665685004,142.113638585422));
#67283=CARTESIAN_POINT('Ctrl Pts',(56.6001364053008,872.308760865999,142.113367607646));
#67284=CARTESIAN_POINT('Ctrl Pts',(56.5392115878473,872.319304548476,142.117531372034));
#67285=CARTESIAN_POINT('Ctrl Pts',(56.419937753833,872.361849860724,142.13501247575));
#67286=CARTESIAN_POINT('Ctrl Pts',(56.3633877006692,872.395075829848,142.148862821418));
#67287=CARTESIAN_POINT('Ctrl Pts',(56.2676088882711,872.479846325149,142.184639702097));
#67288=CARTESIAN_POINT('Ctrl Pts',(56.2293515484587,872.530550570378,142.20621675157));
#67289=CARTESIAN_POINT('Ctrl Pts',(56.1763997004844,872.642841587476,142.254503154028));
#67290=CARTESIAN_POINT('Ctrl Pts',(56.1623578613256,872.703358814639,142.280758867163));
#67291=CARTESIAN_POINT('Ctrl Pts',(56.1608827404138,872.824741915519,142.333957573825));
#67292=CARTESIAN_POINT('Ctrl Pts',(56.173059875041,872.884430875959,142.360376943219));
#67293=CARTESIAN_POINT('Ctrl Pts',(56.2217698082996,872.995794763792,142.410142111349));
#67294=CARTESIAN_POINT('Ctrl Pts',(56.2577798059143,873.046441122238,142.433024237972));
#67295=CARTESIAN_POINT('Ctrl Pts',(56.348953330183,873.131911631132,142.47202087607));
#67296=CARTESIAN_POINT('Ctrl Pts',(56.4031767949244,873.165985195154,142.487787017585));
#67297=CARTESIAN_POINT('Ctrl Pts',(56.5228893958498,873.213074591051,142.509939180269));
#67298=CARTESIAN_POINT('Ctrl Pts',(56.5871943248138,873.225672192475,142.516124114616));
#67299=CARTESIAN_POINT('Ctrl Pts',(56.7177050294111,873.227581857597,142.517926403236));
#67300=CARTESIAN_POINT('Ctrl Pts',(56.7826190887181,873.216829601136,142.513504494232));
#67301=CARTESIAN_POINT('Ctrl Pts',(56.9045621441444,873.173036841854,142.494512977799));
#67302=CARTESIAN_POINT('Ctrl Pts',(56.9603425420374,873.140333886772,142.480089924366));
#67303=CARTESIAN_POINT('Ctrl Pts',(57.0551120863392,873.056999087507,142.443174197959));
#67304=CARTESIAN_POINT('Ctrl Pts',(57.0931127660954,873.007115390226,142.421016670206));
#67305=CARTESIAN_POINT('Ctrl Pts',(57.1459059727482,872.896715691287,142.372072783374));
#67306=CARTESIAN_POINT('Ctrl Pts',(57.160170788179,872.837245341146,142.345753833874));
#67307=CARTESIAN_POINT('Ctrl Pts',(57.1628182600068,872.715622211842,142.292131004574));
#67308=CARTESIAN_POINT('Ctrl Pts',(57.1507466719065,872.654639799362,142.265347796493));
#67309=CARTESIAN_POINT('Ctrl Pts',(57.1013501009362,872.540958533665,142.215589777814));
#67310=CARTESIAN_POINT('Ctrl Pts',(57.0646859878445,872.489327069808,142.193078327265));
#67311=CARTESIAN_POINT('Ctrl Pts',(56.9716045235116,872.402334668021,142.155167421734));
#67312=CARTESIAN_POINT('Ctrl Pts',(56.9161654721059,872.367800826181,142.140123523712));
#67313=CARTESIAN_POINT('Ctrl Pts',(56.7937562436668,872.320668501759,142.119399429729));
#67314=CARTESIAN_POINT('Ctrl Pts',(56.7280090715558,872.308562806958,142.113931476494));
#67315=CARTESIAN_POINT('Ctrl Pts',(56.6615880190493,872.308665685004,142.113638585422));
#67316=CARTESIAN_POINT('Origin',(51.1325126856635,880.408005670941,133.477498108665));
#67317=CARTESIAN_POINT('',(51.1325126856635,875.766823207888,143.764076402871));
#67318=CARTESIAN_POINT('',(51.1325126856635,877.442441730773,144.713325514568));
#67319=CARTESIAN_POINT('Ctrl Pts',(51.1325126856636,875.766823207888,143.764076402872));
#67320=CARTESIAN_POINT('Ctrl Pts',(51.131304761973,875.76682116675,143.764082178035));
#67321=CARTESIAN_POINT('Ctrl Pts',(51.1300967200539,875.766821180395,143.764089066902));
#67322=CARTESIAN_POINT('Ctrl Pts',(51.0035143611211,875.767038023791,143.76492759062));
#67323=CARTESIAN_POINT('Ctrl Pts',(50.8796062726843,875.789394490415,143.777723613443));
#67324=CARTESIAN_POINT('Ctrl Pts',(50.6488971671256,875.875493431376,143.825893678785));
#67325=CARTESIAN_POINT('Ctrl Pts',(50.5445508589289,875.938360214591,143.860790059619));
#67326=CARTESIAN_POINT('Ctrl Pts',(50.368954885655,876.09635398233,143.948721147385));
#67327=CARTESIAN_POINT('Ctrl Pts',(50.2997265485965,876.190109963413,144.001008999435));
#67328=CARTESIAN_POINT('Ctrl Pts',(50.2057276920398,876.396696616052,144.116947363144));
#67329=CARTESIAN_POINT('Ctrl Pts',(50.1825030142982,876.507816098029,144.179655123601));
#67330=CARTESIAN_POINT('Ctrl Pts',(50.1865848263252,876.730024323512,144.305847924143));
#67331=CARTESIAN_POINT('Ctrl Pts',(50.2134090577556,876.839168716171,144.368218448869));
#67332=CARTESIAN_POINT('Ctrl Pts',(50.3129358731998,877.040239015299,144.483589935969));
#67333=CARTESIAN_POINT('Ctrl Pts',(50.3840082053844,877.130689213192,144.535725492343));
#67334=CARTESIAN_POINT('Ctrl Pts',(50.5606018229957,877.281309892263,144.622514965763));
#67335=CARTESIAN_POINT('Ctrl Pts',(50.6638280461508,877.340603774865,144.656653127129));
#67336=CARTESIAN_POINT('Ctrl Pts',(50.8900959243223,877.421328513706,144.702583717026));
#67337=CARTESIAN_POINT('Ctrl Pts',(51.0106612922889,877.442186253871,144.714048356799));
#67338=CARTESIAN_POINT('Ctrl Pts',(51.1325126856635,877.442441730773,144.713325514568));
#67339=CARTESIAN_POINT('',(51.1325126856326,878.138848987347,142.742922044547));
#67340=CARTESIAN_POINT('',(51.1325126856635,881.30190184356,133.793431261802));
#67341=CARTESIAN_POINT('Ctrl Pts',(51.1019995799007,878.138362681097,142.742824118366));
#67342=CARTESIAN_POINT('Ctrl Pts',(51.2203391425413,878.141955492694,142.744093939551));
#67343=CARTESIAN_POINT('Ctrl Pts',(51.3382664322453,878.125667154056,142.73498931258));
#67344=CARTESIAN_POINT('Ctrl Pts',(51.5673565428978,878.053156825002,142.696083764234));
#67345=CARTESIAN_POINT('Ctrl Pts',(51.6754085173438,877.995508026985,142.66556336574));
#67346=CARTESIAN_POINT('Ctrl Pts',(51.8585894689507,877.847523288319,142.588054737409));
#67347=CARTESIAN_POINT('Ctrl Pts',(51.9325364267539,877.759152649319,142.542092025178));
#67348=CARTESIAN_POINT('Ctrl Pts',(52.0397584032032,877.5606352111,142.439695164907));
#67349=CARTESIAN_POINT('Ctrl Pts',(52.07138369246,877.451974309298,142.384045631647));
#67350=CARTESIAN_POINT('Ctrl Pts',(52.0864385917891,877.228343098163,142.270414524496));
#67351=CARTESIAN_POINT('Ctrl Pts',(52.0691298722353,877.115380041048,142.21346497185));
#67352=CARTESIAN_POINT('Ctrl Pts',(51.9864398549688,876.901445910502,142.10639821256));
#67353=CARTESIAN_POINT('Ctrl Pts',(51.9217401782439,876.802565238296,142.057324005392));
#67354=CARTESIAN_POINT('Ctrl Pts',(51.7564866886615,876.636655369949,141.975532938231));
#67355=CARTESIAN_POINT('Ctrl Pts',(51.6590885098741,876.570003109294,141.942967099181));
#67356=CARTESIAN_POINT('Ctrl Pts',(51.4451116594363,876.474882841051,141.89688214976));
#67357=CARTESIAN_POINT('Ctrl Pts',(51.3311922474334,876.446081851696,141.883179055817));
#67358=CARTESIAN_POINT('Ctrl Pts',(51.0967930100967,876.427446066606,141.874987106281));
#67359=CARTESIAN_POINT('Ctrl Pts',(50.9784326146121,876.438000210876,141.880680000862));
#67360=CARTESIAN_POINT('Ctrl Pts',(50.7492227374605,876.498507432607,141.911516759673));
#67361=CARTESIAN_POINT('Ctrl Pts',(50.6408562843865,876.548909725185,141.936876955342));
#67362=CARTESIAN_POINT('Ctrl Pts',(50.4461509548119,876.686992837895,142.006246477512));
#67363=CARTESIAN_POINT('Ctrl Pts',(50.3632833305802,876.775059381454,142.050453960429));
#67364=CARTESIAN_POINT('Ctrl Pts',(50.2423713544919,876.972637761829,142.149947952602));
#67365=CARTESIAN_POINT('Ctrl Pts',(50.2044965712362,877.079752927103,142.204027314726));
#67366=CARTESIAN_POINT('Ctrl Pts',(50.1763390076605,877.302199715689,142.316767841845));
#67367=CARTESIAN_POINT('Ctrl Pts',(50.1869839460711,877.415557116966,142.374435248914));
#67368=CARTESIAN_POINT('Ctrl Pts',(50.2570230022145,877.632880201761,142.485325007758));
#67369=CARTESIAN_POINT('Ctrl Pts',(50.3161973006486,877.734700453816,142.537450795729));
#67370=CARTESIAN_POINT('Ctrl Pts',(50.4675747436943,877.902390297205,142.623340864716));
#67371=CARTESIAN_POINT('Ctrl Pts',(50.5545005668584,877.969565128902,142.657762498737));
#67372=CARTESIAN_POINT('Ctrl Pts',(50.7560044783514,878.075788026719,142.711958634738));
#67373=CARTESIAN_POINT('Ctrl Pts',(50.8698696721942,878.112256677342,142.730396303378));
#67374=CARTESIAN_POINT('Ctrl Pts',(51.0260149820039,878.134001458524,142.740937396534));
#67375=CARTESIAN_POINT('Ctrl Pts',(51.06395166438,878.137207539156,142.742415852119));
#67376=CARTESIAN_POINT('Ctrl Pts',(51.1019995799007,878.138362681097,142.742824118366));
#67377=CARTESIAN_POINT('Ctrl Pts',(51.1325126856635,877.442441730773,144.713325514568));
#67378=CARTESIAN_POINT('Ctrl Pts',(51.1325199189838,877.442441745939,144.713325471659));
#67379=CARTESIAN_POINT('Ctrl Pts',(51.1325271523087,877.442441761051,144.713325428718));
#67380=CARTESIAN_POINT('Ctrl Pts',(51.1325343856381,877.442441776071,144.713325385723));
#67381=CARTESIAN_POINT('Ctrl Pts',(51.2516981149903,877.442689224519,144.712617074273));
#67382=CARTESIAN_POINT('Ctrl Pts',(51.3696091813458,877.423228035679,144.700269032771));
#67383=CARTESIAN_POINT('Ctrl Pts',(51.5966068087232,877.345147660409,144.652704913418));
#67384=CARTESIAN_POINT('Ctrl Pts',(51.702440326515,877.285339664995,144.616826217988));
#67385=CARTESIAN_POINT('Ctrl Pts',(51.8830714745084,877.131995260537,144.526111613188));
#67386=CARTESIAN_POINT('Ctrl Pts',(51.9554005077383,877.039315262831,144.4718160893));
#67387=CARTESIAN_POINT('Ctrl Pts',(52.0549496786397,876.833373267989,144.352618105642));
#67388=CARTESIAN_POINT('Ctrl Pts',(52.0806897870562,876.721757332879,144.288695108183));
#67389=CARTESIAN_POINT('Ctrl Pts',(52.0805052844136,876.497473999723,144.161740641726));
#67390=CARTESIAN_POINT('Ctrl Pts',(52.0553007572354,876.386836737815,144.099838102673));
#67391=CARTESIAN_POINT('Ctrl Pts',(51.9577591242723,876.181490947495,143.986155335694));
#67392=CARTESIAN_POINT('Ctrl Pts',(51.8869610300829,876.088520017704,143.935310368264));
#67393=CARTESIAN_POINT('Ctrl Pts',(51.7086733206128,875.932316781655,143.850685763962));
#67394=CARTESIAN_POINT('Ctrl Pts',(51.6031935937059,875.870504288221,143.817654977638));
#67395=CARTESIAN_POINT('Ctrl Pts',(51.374417798785,875.788047198342,143.774176101606));
#67396=CARTESIAN_POINT('Ctrl Pts',(51.2540638778635,875.767028603952,143.763495258558));
#67397=CARTESIAN_POINT('Ctrl Pts',(51.1325126856636,875.766823207888,143.764076402871));
#67398=CARTESIAN_POINT('Origin',(51.1325126856635,880.408005670941,133.477498108665));
#67399=CARTESIAN_POINT('',(51.1325126856635,878.744589039435,139.684393352153));
#67400=CARTESIAN_POINT('Origin',(51.1325126856635,878.273166808826,139.517776784886));
#67401=CARTESIAN_POINT('',(51.1325126856637,877.048983671841,144.481911856674));
#67402=CARTESIAN_POINT('',(51.1325126856635,880.87942790155,133.644114675932));
#67403=CARTESIAN_POINT('Ctrl Pts',(51.132518179114,876.16532192069,143.981228116023));
#67404=CARTESIAN_POINT('Ctrl Pts',(51.0700489071742,876.165209434297,143.981544323559));
#67405=CARTESIAN_POINT('Ctrl Pts',(51.0081976721465,876.175483592962,143.987602863164));
#67406=CARTESIAN_POINT('Ctrl Pts',(50.8882236513185,876.216940393256,144.011329545291));
#67407=CARTESIAN_POINT('Ctrl Pts',(50.8319197675561,876.249025053008,144.029491946118));
#67408=CARTESIAN_POINT('Ctrl Pts',(50.7365787284554,876.330774521863,144.075669314888));
#67409=CARTESIAN_POINT('Ctrl Pts',(50.6986313258318,876.379724500401,144.103284129777));
#67410=CARTESIAN_POINT('Ctrl Pts',(50.64635605161,876.488046712534,144.164492131436));
#67411=CARTESIAN_POINT('Ctrl Pts',(50.6327518447176,876.546490912549,144.197564296028));
#67412=CARTESIAN_POINT('Ctrl Pts',(50.6322781683162,876.664860241963,144.264690198484));
#67413=CARTESIAN_POINT('Ctrl Pts',(50.6455958134439,876.723721799899,144.298141347072));
#67414=CARTESIAN_POINT('Ctrl Pts',(50.6970449321914,876.831543867453,144.359477076571));
#67415=CARTESIAN_POINT('Ctrl Pts',(50.7339016926261,876.879821070422,144.386967878652));
#67416=CARTESIAN_POINT('Ctrl Pts',(50.8261041217096,876.960595270929,144.432870441603));
#67417=CARTESIAN_POINT('Ctrl Pts',(50.8802560923006,876.992589386614,144.450994984563));
#67418=CARTESIAN_POINT('Ctrl Pts',(50.9992790929795,877.036556088749,144.475618667509));
#67419=CARTESIAN_POINT('Ctrl Pts',(51.0628484643923,877.048220200473,144.481945783096));
#67420=CARTESIAN_POINT('Ctrl Pts',(51.1921045903496,877.049682395447,144.481909272916));
#67421=CARTESIAN_POINT('Ctrl Pts',(51.2564043337221,877.039294826231,144.475447594556));
#67422=CARTESIAN_POINT('Ctrl Pts',(51.3778238204396,876.997203424505,144.45028083773));
#67423=CARTESIAN_POINT('Ctrl Pts',(51.4334953538068,876.965570428101,144.431629797225));
#67424=CARTESIAN_POINT('Ctrl Pts',(51.528560079656,876.884538147418,144.384356054323));
#67425=CARTESIAN_POINT('Ctrl Pts',(51.5666325811411,876.835587573722,144.356007351641));
#67426=CARTESIAN_POINT('Ctrl Pts',(51.6189829601159,876.727008300879,144.293630177779));
#67427=CARTESIAN_POINT('Ctrl Pts',(51.6325178270963,876.668274436505,144.26012346701));
#67428=CARTESIAN_POINT('Ctrl Pts',(51.6325075804319,876.549983706729,144.193137461765));
#67429=CARTESIAN_POINT('Ctrl Pts',(51.6191678203549,876.491492888902,144.160258066154));
#67430=CARTESIAN_POINT('Ctrl Pts',(51.5674031509799,876.382850200371,144.099604111257));
#67431=CARTESIAN_POINT('Ctrl Pts',(51.5296988480654,876.333643902935,144.072350455167));
#67432=CARTESIAN_POINT('Ctrl Pts',(51.4358216161833,876.252131880027,144.027518483365));
#67433=CARTESIAN_POINT('Ctrl Pts',(51.3811186186126,876.220174302848,144.010117109192));
#67434=CARTESIAN_POINT('Ctrl Pts',(51.2611370152663,876.176674159055,143.986728644173));
#67435=CARTESIAN_POINT('Ctrl Pts',(51.1971591532616,876.165438317596,143.980900915744));
#67436=CARTESIAN_POINT('Ctrl Pts',(51.132518179114,876.16532192069,143.981228116023));
#67437=CARTESIAN_POINT('Origin',(66.9612128173492,874.622216250165,131.432604360284));
#67438=CARTESIAN_POINT('',(66.9612128173492,870.055347744271,141.288882307046));
#67439=CARTESIAN_POINT('',(66.9612128173492,871.932747002821,142.107291525763));
#67440=CARTESIAN_POINT('Ctrl Pts',(66.9612128173492,870.055347744271,141.288882307046));
#67441=CARTESIAN_POINT('Ctrl Pts',(66.9607167705809,870.055350023101,141.288875859362));
#67442=CARTESIAN_POINT('Ctrl Pts',(66.9602207056299,870.055352636768,141.288869548692));
#67443=CARTESIAN_POINT('Ctrl Pts',(66.8246828860381,870.056158236702,141.287182812833));
#67444=CARTESIAN_POINT('Ctrl Pts',(66.6910009462347,870.081773298768,141.295664265099));
#67445=CARTESIAN_POINT('Ctrl Pts',(66.4420819935384,870.179635238136,141.331805000495));
#67446=CARTESIAN_POINT('Ctrl Pts',(66.3292781831525,870.250838596208,141.359081080309));
#67447=CARTESIAN_POINT('Ctrl Pts',(66.1401342703794,870.429127841465,141.429249087433));
#67448=CARTESIAN_POINT('Ctrl Pts',(66.06553555221,870.534327130104,141.47141225971));
#67449=CARTESIAN_POINT('Ctrl Pts',(65.9642432607369,870.765176303953,141.566085423473));
#67450=CARTESIAN_POINT('Ctrl Pts',(65.938731577858,870.888601867314,141.617709928411));
#67451=CARTESIAN_POINT('Ctrl Pts',(65.9409408074312,871.135922922694,141.723700049532));
#67452=CARTESIAN_POINT('Ctrl Pts',(65.9683598824257,871.257416868622,141.777030695437));
#67453=CARTESIAN_POINT('Ctrl Pts',(66.0725601507498,871.482836964578,141.878621175579));
#67454=CARTESIAN_POINT('Ctrl Pts',(66.1483333041382,871.584643845217,141.925917988167));
#67455=CARTESIAN_POINT('Ctrl Pts',(66.3382430992424,871.754720048039,142.007542624859));
#67456=CARTESIAN_POINT('Ctrl Pts',(66.4504469292104,871.821545451402,142.041148859883));
#67457=CARTESIAN_POINT('Ctrl Pts',(66.6966715784841,871.911506422729,142.089495835615));
#67458=CARTESIAN_POINT('Ctrl Pts',(66.8282588619279,871.933967163154,142.103839223781));
#67459=CARTESIAN_POINT('Ctrl Pts',(66.9612128173492,871.932747002821,142.107291525763));
#67460=CARTESIAN_POINT('',(66.9612128163858,872.578864209794,140.279177911721));
#67461=CARTESIAN_POINT('',(66.9612128173492,875.585245390407,131.772971443351));
#67462=CARTESIAN_POINT('Ctrl Pts',(67.2484589377317,872.538855492815,140.268673823591));
#67463=CARTESIAN_POINT('Ctrl Pts',(67.3762643718234,872.503542456408,140.256193001679));
#67464=CARTESIAN_POINT('Ctrl Pts',(67.4954837624301,872.445739267827,140.233446488859));
#67465=CARTESIAN_POINT('Ctrl Pts',(67.7033546503243,872.29167391827,140.170142955904));
#67466=CARTESIAN_POINT('Ctrl Pts',(67.7899772810638,872.19691172647,140.130208211362));
#67467=CARTESIAN_POINT('Ctrl Pts',(67.9192470457648,871.982103237673,140.038435144843));
#67468=CARTESIAN_POINT('Ctrl Pts',(67.9604582254089,871.86400787901,139.987434416262));
#67469=CARTESIAN_POINT('Ctrl Pts',(67.9912621529526,871.619677243159,139.881314984221));
#67470=CARTESIAN_POINT('Ctrl Pts',(67.9803356829124,871.495732942861,139.827195945714));
#67471=CARTESIAN_POINT('Ctrl Pts',(67.9069767463482,871.258799856499,139.723359951516));
#67472=CARTESIAN_POINT('Ctrl Pts',(67.8451905755019,871.148088528114,139.6746416514));
#67473=CARTESIAN_POINT('Ctrl Pts',(67.6792233773331,870.955982750718,139.589535632671));
#67474=CARTESIAN_POINT('Ctrl Pts',(67.577028264178,870.876152612627,139.55384071449));
#67475=CARTESIAN_POINT('Ctrl Pts',(67.3433687821695,870.756464611354,139.499134523185));
#67476=CARTESIAN_POINT('Ctrl Pts',(67.2138586163694,870.718316741882,139.480874034868));
#67477=CARTESIAN_POINT('Ctrl Pts',(66.945688478612,870.690780874979,139.464651031496));
#67478=CARTESIAN_POINT('Ctrl Pts',(66.8096886879856,870.701748066281,139.466875733831));
#67479=CARTESIAN_POINT('Ctrl Pts',(66.5511623574619,870.771643743234,139.49148305969));
#67480=CARTESIAN_POINT('Ctrl Pts',(66.4310448250826,870.829411865114,139.513425012589));
#67481=CARTESIAN_POINT('Ctrl Pts',(66.2215605946194,870.9842175614,139.574319617251));
#67482=CARTESIAN_POINT('Ctrl Pts',(66.1342152866182,871.079711543178,139.612671320538));
#67483=CARTESIAN_POINT('Ctrl Pts',(66.0043052718372,871.295546092716,139.701030612986));
#67484=CARTESIAN_POINT('Ctrl Pts',(65.9628435885181,871.413715648899,139.750154364426));
#67485=CARTESIAN_POINT('Ctrl Pts',(65.9311017105071,871.658483946847,139.853666856138));
#67486=CARTESIAN_POINT('Ctrl Pts',(65.9415621693557,871.782770602058,139.907098891405));
#67487=CARTESIAN_POINT('Ctrl Pts',(66.0144120578042,872.02127727974,140.01152687392));
#67488=CARTESIAN_POINT('Ctrl Pts',(66.0767033865923,872.133028475974,140.061465080283));
#67489=CARTESIAN_POINT('Ctrl Pts',(66.2443866059568,872.326043489332,140.14969476242));
#67490=CARTESIAN_POINT('Ctrl Pts',(66.3477028313432,872.405787185121,140.18725922801));
#67491=CARTESIAN_POINT('Ctrl Pts',(66.5822990889336,872.523628960054,140.245052869823));
#67492=CARTESIAN_POINT('Ctrl Pts',(66.7112749142268,872.560641064037,140.264736256022));
#67493=CARTESIAN_POINT('Ctrl Pts',(66.9118522445325,872.580208115589,140.278517007198));
#67494=CARTESIAN_POINT('Ctrl Pts',(66.9796703386908,872.580620499121,140.280429229317));
#67495=CARTESIAN_POINT('Ctrl Pts',(67.1153073912448,872.569075728989,140.27874484049));
#67496=CARTESIAN_POINT('Ctrl Pts',(67.1827652807286,872.557006853263,140.275089128541));
#67497=CARTESIAN_POINT('Ctrl Pts',(67.2484589377317,872.538855492815,140.268673823591));
#67498=CARTESIAN_POINT('Ctrl Pts',(66.9612128173492,871.932747002821,142.107291525763));
#67499=CARTESIAN_POINT('Ctrl Pts',(66.9612307903993,871.932746837877,142.107291992453));
#67500=CARTESIAN_POINT('Ctrl Pts',(66.9612487634744,871.9327466725,142.107292458946));
#67501=CARTESIAN_POINT('Ctrl Pts',(66.9612667365744,871.93274650669,142.107292925239));
#67502=CARTESIAN_POINT('Ctrl Pts',(67.0922423889351,871.931538196034,142.110690951439));
#67503=CARTESIAN_POINT('Ctrl Pts',(67.2220163544519,871.907373314964,142.103447307919));
#67504=CARTESIAN_POINT('Ctrl Pts',(67.4676160932879,871.814778012017,142.067956275113));
#67505=CARTESIAN_POINT('Ctrl Pts',(67.5806061048436,871.746340964445,142.039620789915));
#67506=CARTESIAN_POINT('Ctrl Pts',(67.7721659932508,871.573417494683,141.965567349563));
#67507=CARTESIAN_POINT('Ctrl Pts',(67.8486260601588,871.470433340403,141.920494602424));
#67508=CARTESIAN_POINT('Ctrl Pts',(67.9538488821687,871.243381924432,141.820270582023));
#67509=CARTESIAN_POINT('Ctrl Pts',(67.9814997001897,871.121447991871,141.766076742079));
#67510=CARTESIAN_POINT('Ctrl Pts',(67.9836847296759,870.873817653467,141.656031680037));
#67511=CARTESIAN_POINT('Ctrl Pts',(67.9577540254432,870.750487314886,141.60124461176));
#67512=CARTESIAN_POINT('Ctrl Pts',(67.8549834052962,870.520631288988,141.499387847567));
#67513=CARTESIAN_POINT('Ctrl Pts',(67.7793370832508,870.416290831603,141.453283907477));
#67514=CARTESIAN_POINT('Ctrl Pts',(67.5887677448977,870.241420847348,141.375854989021));
#67515=CARTESIAN_POINT('Ctrl Pts',(67.476040165905,870.172345031139,141.345159267362));
#67516=CARTESIAN_POINT('Ctrl Pts',(67.2280588525592,870.078587319634,141.302364290857));
#67517=CARTESIAN_POINT('Ctrl Pts',(67.0953000153513,870.054731750144,141.290625190902));
#67518=CARTESIAN_POINT('Ctrl Pts',(66.9612128173492,870.055347744271,141.288882307046));
#67519=CARTESIAN_POINT('Origin',(66.9612128173492,874.622216250165,131.432604360284));
#67520=CARTESIAN_POINT('',(66.9612128173492,872.958799618659,137.639499603772));
#67521=CARTESIAN_POINT('Origin',(66.9612128173492,872.48737738805,137.472883036505));
#67522=CARTESIAN_POINT('',(66.9612128173494,871.456787053482,141.889269752637));
#67523=CARTESIAN_POINT('',(66.9612128173492,875.093638480774,131.599220927551));
#67524=CARTESIAN_POINT('Ctrl Pts',(66.961219998814,870.537790077594,141.488562927539));
#67525=CARTESIAN_POINT('Ctrl Pts',(66.9010760576186,870.538139679958,141.487571175934));
#67526=CARTESIAN_POINT('Ctrl Pts',(66.841417267067,870.548499587498,141.490822681978));
#67527=CARTESIAN_POINT('Ctrl Pts',(66.7229066632556,870.590348179204,141.506242708962));
#67528=CARTESIAN_POINT('Ctrl Pts',(66.6659945502401,870.623519583751,141.519155948664));
#67529=CARTESIAN_POINT('Ctrl Pts',(66.5694917223115,870.708265316722,141.55317061355));
#67530=CARTESIAN_POINT('Ctrl Pts',(66.5308478129759,870.758961653873,141.573922734633));
#67531=CARTESIAN_POINT('Ctrl Pts',(66.4771181048806,870.871150633871,141.620724975417));
#67532=CARTESIAN_POINT('Ctrl Pts',(66.4626144142707,870.931539358277,141.646320887713));
#67533=CARTESIAN_POINT('Ctrl Pts',(66.4599960159081,871.054070501487,141.699180043191));
#67534=CARTESIAN_POINT('Ctrl Pts',(66.4720801708997,871.114998491116,141.72592794606));
#67535=CARTESIAN_POINT('Ctrl Pts',(66.5211114613292,871.227511213839,141.776284817272));
#67536=CARTESIAN_POINT('Ctrl Pts',(66.5571264439551,871.278183036104,141.799464578186));
#67537=CARTESIAN_POINT('Ctrl Pts',(66.6483699129627,871.363513524511,141.839485506655));
#67538=CARTESIAN_POINT('Ctrl Pts',(66.7026693894346,871.39742288317,141.855967463947));
#67539=CARTESIAN_POINT('Ctrl Pts',(66.8224749324693,871.443959081405,141.87984779299));
#67540=CARTESIAN_POINT('Ctrl Pts',(66.886794061751,871.456211044856,141.887043560568));
#67541=CARTESIAN_POINT('Ctrl Pts',(67.0172155558393,871.457356377065,141.891005938955));
#67542=CARTESIAN_POINT('Ctrl Pts',(67.0820358816623,871.44624419388,141.887733838793));
#67543=CARTESIAN_POINT('Ctrl Pts',(67.2037935298491,871.401823665282,141.870981604617));
#67544=CARTESIAN_POINT('Ctrl Pts',(67.2594914802127,871.368884478593,141.857635292589));
#67545=CARTESIAN_POINT('Ctrl Pts',(67.354238085846,871.285188088802,141.822575885038));
#67546=CARTESIAN_POINT('Ctrl Pts',(67.392277055294,871.235179744322,141.801175926144));
#67547=CARTESIAN_POINT('Ctrl Pts',(67.4452703769498,871.124589667198,141.753283891179));
#67548=CARTESIAN_POINT('Ctrl Pts',(67.4596537585287,871.065049570772,141.727245902082));
#67549=CARTESIAN_POINT('Ctrl Pts',(67.4625607900712,870.943208554617,141.673658737767));
#67550=CARTESIAN_POINT('Ctrl Pts',(67.4505349671018,870.882082330638,141.646623366797));
#67551=CARTESIAN_POINT('Ctrl Pts',(67.4011072470207,870.768324913195,141.596056913241));
#67552=CARTESIAN_POINT('Ctrl Pts',(67.364382532302,870.716750383278,141.572996890378));
#67553=CARTESIAN_POINT('Ctrl Pts',(67.2711975628139,870.630101118888,141.533846914187));
#67554=CARTESIAN_POINT('Ctrl Pts',(67.2157489892355,870.595812493844,141.518110357346));
#67555=CARTESIAN_POINT('Ctrl Pts',(67.0933507907198,870.54922814529,141.49590606125));
#67556=CARTESIAN_POINT('Ctrl Pts',(67.0276271002878,870.537404068975,141.489657956368));
#67557=CARTESIAN_POINT('Ctrl Pts',(66.961219998814,870.537790077594,141.488562927539));
#67558=CARTESIAN_POINT('Origin',(62.4383719093132,879.633498841219,133.203761188948));
#67559=CARTESIAN_POINT('',(62.4383719093132,874.991697703936,143.49208995005));
#67560=CARTESIAN_POINT('',(62.4383719093099,876.669038396195,144.43646638347));
#67561=CARTESIAN_POINT('Ctrl Pts',(62.4383719093132,874.991697703936,143.49208995005));
#67562=CARTESIAN_POINT('Ctrl Pts',(62.3148834011908,874.992842777131,143.488850098404));
#67563=CARTESIAN_POINT('Ctrl Pts',(62.1925701437443,875.015475261366,143.497224099113));
#67564=CARTESIAN_POINT('Ctrl Pts',(61.9623649287828,875.101797335681,143.536566557516));
#67565=CARTESIAN_POINT('Ctrl Pts',(61.857190621639,875.165174958031,143.567458486917));
#67566=CARTESIAN_POINT('Ctrl Pts',(61.680055266306,875.324104920959,143.64812062898));
#67567=CARTESIAN_POINT('Ctrl Pts',(61.6100265481437,875.418087959246,143.697116123318));
#67568=CARTESIAN_POINT('Ctrl Pts',(61.5141957614568,875.624605575474,143.807569133984));
#67569=CARTESIAN_POINT('Ctrl Pts',(61.4898086927638,875.735289692519,143.868076311795));
#67570=CARTESIAN_POINT('Ctrl Pts',(61.4907877781008,875.959014181235,143.993218927626));
#67571=CARTESIAN_POINT('Ctrl Pts',(61.5168990793443,876.069995481957,144.056748614188));
#67572=CARTESIAN_POINT('Ctrl Pts',(61.6160440799812,876.273147684721,144.175878474448));
#67573=CARTESIAN_POINT('Ctrl Pts',(61.6872214527508,876.363929798732,144.230591602814));
#67574=CARTESIAN_POINT('Ctrl Pts',(61.8644179730801,876.514100247061,144.323908367462));
#67575=CARTESIAN_POINT('Ctrl Pts',(61.9681766740616,876.57272702324,144.361962979427));
#67576=CARTESIAN_POINT('Ctrl Pts',(62.1950042018106,876.650960072077,144.416339691797));
#67577=CARTESIAN_POINT('Ctrl Pts',(62.3155571194363,876.670356145296,144.432428136869));
#67578=CARTESIAN_POINT('Ctrl Pts',(62.4375722925693,876.669047270135,144.436440263785));
#67579=CARTESIAN_POINT('Ctrl Pts',(62.4378388367372,876.669044410875,144.436449028343));
#67580=CARTESIAN_POINT('Ctrl Pts',(62.4381053756728,876.669041452892,144.436457734904));
#67581=CARTESIAN_POINT('Ctrl Pts',(62.4383719093066,876.669038396195,144.436466383471));
#67582=CARTESIAN_POINT('',(62.4383719093132,877.365021216135,142.467263807625));
#67583=CARTESIAN_POINT('',(62.4383719093132,880.527395013838,133.519694342084));
#67584=CARTESIAN_POINT('Ctrl Pts',(62.6055413147402,877.350313629417,142.464300919196));
#67585=CARTESIAN_POINT('Ctrl Pts',(62.72208714417,877.330630015983,142.457344064197));
#67586=CARTESIAN_POINT('Ctrl Pts',(62.8336136664621,877.291603505312,142.440202997864));
#67587=CARTESIAN_POINT('Ctrl Pts',(63.0407880301549,877.175860699171,142.386017629309));
#67588=CARTESIAN_POINT('Ctrl Pts',(63.1330634621422,877.098360066963,142.348480920908));
#67589=CARTESIAN_POINT('Ctrl Pts',(63.2778622256759,876.917873540154,142.259485060922));
#67590=CARTESIAN_POINT('Ctrl Pts',(63.329685673737,876.817039438026,142.20911733911));
#67591=CARTESIAN_POINT('Ctrl Pts',(63.3885551714499,876.602062841949,142.100903255542));
#67592=CARTESIAN_POINT('Ctrl Pts',(63.394333180847,876.489695387477,142.043943701155));
#67593=CARTESIAN_POINT('Ctrl Pts',(63.3573483177835,876.268237368776,141.931080673741));
#67594=CARTESIAN_POINT('Ctrl Pts',(63.3143282299786,876.16125271223,141.87624409014));
#67595=CARTESIAN_POINT('Ctrl Pts',(63.1840901124571,875.968419109575,141.776634971362));
#67596=CARTESIAN_POINT('Ctrl Pts',(63.0980208488533,875.884479178917,141.732841327789));
#67597=CARTESIAN_POINT('Ctrl Pts',(62.8981887649957,875.754748175952,141.663837095797));
#67598=CARTESIAN_POINT('Ctrl Pts',(62.7875969738874,875.708707086128,141.638555941914));
#67599=CARTESIAN_POINT('Ctrl Pts',(62.5564568518299,875.657696550503,141.608060864491));
#67600=CARTESIAN_POINT('Ctrl Pts',(62.4384316484998,875.651880564185,141.602481448338));
#67601=CARTESIAN_POINT('Ctrl Pts',(62.2049338906412,875.679611942394,141.610677223185));
#67602=CARTESIAN_POINT('Ctrl Pts',(62.0916232868256,875.713123975188,141.62448421237));
#67603=CARTESIAN_POINT('Ctrl Pts',(61.881419793599,875.817175719986,141.670711078998));
#67604=CARTESIAN_POINT('Ctrl Pts',(61.7870587196657,875.887667691374,141.703171646909));
#67605=CARTESIAN_POINT('Ctrl Pts',(61.6284825114992,876.060759925578,141.784914577179));
#67606=CARTESIAN_POINT('Ctrl Pts',(61.5677521159699,876.163056594358,141.834151467837));
#67607=CARTESIAN_POINT('Ctrl Pts',(61.4951065763654,876.379815933426,141.940424659816));
#67608=CARTESIAN_POINT('Ctrl Pts',(61.4828038449027,876.49190353717,141.996261449943));
#67609=CARTESIAN_POINT('Ctrl Pts',(61.5066784858156,876.714774750312,142.10915198306));
#67610=CARTESIAN_POINT('Ctrl Pts',(61.5433074498874,876.823447452225,142.165163658863));
#67611=CARTESIAN_POINT('Ctrl Pts',(61.6621002604964,877.022057875704,142.26943973004));
#67612=CARTESIAN_POINT('Ctrl Pts',(61.7435525525451,877.109942462106,142.316640182244));
#67613=CARTESIAN_POINT('Ctrl Pts',(61.930444731815,877.244110818974,142.390682623665));
#67614=CARTESIAN_POINT('Ctrl Pts',(62.0310240273176,877.292704466039,142.418537038328));
#67615=CARTESIAN_POINT('Ctrl Pts',(62.2527021724929,877.356991314408,142.457911555512));
#67616=CARTESIAN_POINT('Ctrl Pts',(62.3725054475672,877.370304133369,142.468165169746));
#67617=CARTESIAN_POINT('Ctrl Pts',(62.5302315213295,877.36094521898,142.467713164468));
#67618=CARTESIAN_POINT('Ctrl Pts',(62.5680701109172,877.356642201572,142.466537650728));
#67619=CARTESIAN_POINT('Ctrl Pts',(62.6055413147402,877.350313629417,142.464300919196));
#67620=CARTESIAN_POINT('Ctrl Pts',(62.4383719093066,876.669038396195,144.436466383471));
#67621=CARTESIAN_POINT('Ctrl Pts',(62.555733234486,876.667692457565,144.440274560546));
#67622=CARTESIAN_POINT('Ctrl Pts',(62.6720670749973,876.647214147807,144.432827703646));
#67623=CARTESIAN_POINT('Ctrl Pts',(62.897044452594,876.567899624079,144.395156694303));
#67624=CARTESIAN_POINT('Ctrl Pts',(63.0024075453455,876.507839463088,144.364089835034));
#67625=CARTESIAN_POINT('Ctrl Pts',(63.1830615484687,876.354660027784,144.281800950729));
#67626=CARTESIAN_POINT('Ctrl Pts',(63.2558086950144,876.262483498011,144.231047193493));
#67627=CARTESIAN_POINT('Ctrl Pts',(63.3580066428205,876.056646754608,144.116235483613));
#67628=CARTESIAN_POINT('Ctrl Pts',(63.3852094653763,875.944453294448,144.052971918191));
#67629=CARTESIAN_POINT('Ctrl Pts',(63.3876075529805,875.719039320324,143.925081024894));
#67630=CARTESIAN_POINT('Ctrl Pts',(63.3632946319265,875.607847438087,143.861618541101));
#67631=CARTESIAN_POINT('Ctrl Pts',(63.2670637567054,875.402165648925,143.74348597352));
#67632=CARTESIAN_POINT('Ctrl Pts',(63.196723652669,875.309310840088,143.689762326666));
#67633=CARTESIAN_POINT('Ctrl Pts',(63.0193151739335,875.15402775659,143.598605428878));
#67634=CARTESIAN_POINT('Ctrl Pts',(62.9143276467654,875.092828857164,143.56189569621));
#67635=CARTESIAN_POINT('Ctrl Pts',(62.6849156051955,875.011174307758,143.510290460012));
#67636=CARTESIAN_POINT('Ctrl Pts',(62.5632257559092,874.990743073138,143.49547525302));
#67637=CARTESIAN_POINT('Ctrl Pts',(62.4395343550587,874.991687400951,143.492120704992));
#67638=CARTESIAN_POINT('Ctrl Pts',(62.4389531191745,874.991692314545,143.492105198705));
#67639=CARTESIAN_POINT('Ctrl Pts',(62.4383719093132,874.991697703936,143.49208995005));
#67640=CARTESIAN_POINT('Origin',(62.4383719093132,879.633498841219,133.203761188948));
#67641=CARTESIAN_POINT('',(62.4383719093132,877.970082209713,139.410656432436));
#67642=CARTESIAN_POINT('Origin',(62.4383719093132,877.498659979104,139.244039865169));
#67643=CARTESIAN_POINT('',(62.4383719093133,876.275109833979,144.206383959985));
#67644=CARTESIAN_POINT('',(62.4383719093132,880.104921071828,133.370377756215));
#67645=CARTESIAN_POINT('Ctrl Pts',(62.4383863925631,875.390537429112,143.708276808823));
#67646=CARTESIAN_POINT('Ctrl Pts',(62.376105965251,875.391147288516,143.706545868688));
#67647=CARTESIAN_POINT('Ctrl Pts',(62.3143704644587,875.402084130781,143.710517980071));
#67648=CARTESIAN_POINT('Ctrl Pts',(62.1951706705049,875.444615587081,143.729978894648));
#67649=CARTESIAN_POINT('Ctrl Pts',(62.1394034980978,875.476857064485,143.74588134496));
#67650=CARTESIAN_POINT('Ctrl Pts',(62.0441551526551,875.558908643506,143.788024886857));
#67651=CARTESIAN_POINT('Ctrl Pts',(62.005960028511,875.608132015386,143.813990237086));
#67652=CARTESIAN_POINT('Ctrl Pts',(61.9530905226921,875.716751261863,143.87259420486));
#67653=CARTESIAN_POINT('Ctrl Pts',(61.939128524658,875.775158862972,143.90471287974));
#67654=CARTESIAN_POINT('Ctrl Pts',(61.9376685681124,875.893313469618,143.970927050264));
#67655=CARTESIAN_POINT('Ctrl Pts',(61.9504235315678,875.951984282128,144.004431762463));
#67656=CARTESIAN_POINT('Ctrl Pts',(62.0008504069484,876.059930606694,144.067317152996));
#67657=CARTESIAN_POINT('Ctrl Pts',(62.0375913341877,876.108434873176,144.096220422258));
#67658=CARTESIAN_POINT('Ctrl Pts',(62.1298179415902,876.189173520707,144.145634475477));
#67659=CARTESIAN_POINT('Ctrl Pts',(62.1841270777158,876.220958291211,144.165839046227));
#67660=CARTESIAN_POINT('Ctrl Pts',(62.3033189923729,876.263969889562,144.194929658026));
#67661=CARTESIAN_POINT('Ctrl Pts',(62.3668774652493,876.275054758898,144.203681029958));
#67662=CARTESIAN_POINT('Ctrl Pts',(62.4958103337154,876.275232094091,144.208600339714));
#67663=CARTESIAN_POINT('Ctrl Pts',(62.5598205189458,876.264336616015,144.20472294943));
#67664=CARTESIAN_POINT('Ctrl Pts',(62.6807329013917,876.221492558253,144.184589799477));
#67665=CARTESIAN_POINT('Ctrl Pts',(62.7362168062647,876.189729164313,144.168388876152));
#67666=CARTESIAN_POINT('Ctrl Pts',(62.8312677686969,876.108822135668,144.125506319516));
#67667=CARTESIAN_POINT('Ctrl Pts',(62.8695264542933,876.06020301376,144.099081885462));
#67668=CARTESIAN_POINT('Ctrl Pts',(62.9232247192187,875.951866843773,144.039272469364));
#67669=CARTESIAN_POINT('Ctrl Pts',(62.9375602010487,875.892960850148,144.006318307079));
#67670=CARTESIAN_POINT('Ctrl Pts',(62.9391134300678,875.77432230511,143.939277709704));
#67671=CARTESIAN_POINT('Ctrl Pts',(62.9264289215955,875.715659761762,143.905800236594));
#67672=CARTESIAN_POINT('Ctrl Pts',(62.8758201252976,875.60689000501,143.843067465165));
#67673=CARTESIAN_POINT('Ctrl Pts',(62.8385821864005,875.557693083714,143.814342200385));
#67674=CARTESIAN_POINT('Ctrl Pts',(62.7444583446654,875.475483173381,143.76543488942));
#67675=CARTESIAN_POINT('Ctrl Pts',(62.6886427479659,875.443145833385,143.745659542972));
#67676=CARTESIAN_POINT('Ctrl Pts',(62.5672261067943,875.400453806565,143.718012081886));
#67677=CARTESIAN_POINT('Ctrl Pts',(62.5031730782759,875.389903028046,143.710077404602));
#67678=CARTESIAN_POINT('Ctrl Pts',(62.4383863925631,875.390537429112,143.708276808823));
#67679=CARTESIAN_POINT('Origin',(76.6453214979932,870.871268259904,130.106892424027));
#67680=CARTESIAN_POINT('',(76.6453214979932,866.303275397976,139.966351605635));
#67681=CARTESIAN_POINT('',(76.6453214979921,868.184856019917,140.772930142153));
#67682=CARTESIAN_POINT('Ctrl Pts',(76.6453214979932,866.303275397976,139.966351605635));
#67683=CARTESIAN_POINT('Ctrl Pts',(76.5119628738476,866.304347994492,139.963316818336));
#67684=CARTESIAN_POINT('Ctrl Pts',(76.379846768452,866.329598642102,139.970253809113));
#67685=CARTESIAN_POINT('Ctrl Pts',(76.1313319090301,866.426503413702,140.003110518868));
#67686=CARTESIAN_POINT('Ctrl Pts',(76.0176747985336,866.49784419209,140.028965220415));
#67687=CARTESIAN_POINT('Ctrl Pts',(75.8269771134016,866.676845950906,140.096285369625));
#67688=CARTESIAN_POINT('Ctrl Pts',(75.7516651901821,866.782573853334,140.137028281501));
#67689=CARTESIAN_POINT('Ctrl Pts',(75.6494772737211,867.01407916826,140.22863620336));
#67690=CARTESIAN_POINT('Ctrl Pts',(75.6234755046857,867.13750965737,140.278587256159));
#67691=CARTESIAN_POINT('Ctrl Pts',(75.6243652570395,867.386516400265,140.382275419247));
#67692=CARTESIAN_POINT('Ctrl Pts',(75.6516267692455,867.509619917659,140.435019246053));
#67693=CARTESIAN_POINT('Ctrl Pts',(75.756035101699,867.736839407519,140.535790665106));
#67694=CARTESIAN_POINT('Ctrl Pts',(75.8317723194575,867.838925833057,140.582888526695));
#67695=CARTESIAN_POINT('Ctrl Pts',(76.0218340465849,868.009264327836,140.665286730341));
#67696=CARTESIAN_POINT('Ctrl Pts',(76.1342919852252,868.075999606575,140.699831282128));
#67697=CARTESIAN_POINT('Ctrl Pts',(76.3807839141933,868.165078796819,140.750995183942));
#67698=CARTESIAN_POINT('Ctrl Pts',(76.5123700762829,868.186869794232,140.767232401553));
#67699=CARTESIAN_POINT('Ctrl Pts',(76.6453214979909,868.184856019917,140.772930142153));
#67700=CARTESIAN_POINT('',(76.6453214965781,868.830144724269,138.947160680077));
#67701=CARTESIAN_POINT('',(76.6453214979932,871.834297400147,130.447259507094));
#67702=CARTESIAN_POINT('Ctrl Pts',(77.1300827245181,868.711403932131,138.915922936985));
#67703=CARTESIAN_POINT('Ctrl Pts',(77.2473082361111,868.651809077314,138.89486009885));
#67704=CARTESIAN_POINT('Ctrl Pts',(77.351015383111,868.571914549659,138.864305759322));
#67705=CARTESIAN_POINT('Ctrl Pts',(77.5197567487852,868.38052807592,138.787811678289));
#67706=CARTESIAN_POINT('Ctrl Pts',(77.5831435862104,868.270900403944,138.742622970067));
#67707=CARTESIAN_POINT('Ctrl Pts',(77.6611216157373,868.035554291658,138.6435912125));
#67708=CARTESIAN_POINT('Ctrl Pts',(77.6747487028992,867.912024628227,138.590669816739));
#67709=CARTESIAN_POINT('Ctrl Pts',(77.6496314710478,867.667130458199,138.484351212652));
#67710=CARTESIAN_POINT('Ctrl Pts',(77.6108976366063,867.548107342416,138.431971487266));
#67711=CARTESIAN_POINT('Ctrl Pts',(77.4855020824012,867.330870219108,138.33509671284));
#67712=CARTESIAN_POINT('Ctrl Pts',(77.3999881714758,867.234755878982,138.291537482276));
#67713=CARTESIAN_POINT('Ctrl Pts',(77.1940931635023,867.079500510575,138.219455644948));
#67714=CARTESIAN_POINT('Ctrl Pts',(77.0760092323133,867.021499353061,138.191475827106));
#67715=CARTESIAN_POINT('Ctrl Pts',(76.8202033122931,866.950315878335,138.153912776674));
#67716=CARTESIAN_POINT('Ctrl Pts',(76.6847800464705,866.93842210285,138.144931373501));
#67717=CARTESIAN_POINT('Ctrl Pts',(76.415948278698,866.964101484819,138.147516439664));
#67718=CARTESIAN_POINT('Ctrl Pts',(76.2852244248027,867.001500174738,138.159082927942));
#67719=CARTESIAN_POINT('Ctrl Pts',(76.0477539225662,867.120547623079,138.201062152901));
#67720=CARTESIAN_POINT('Ctrl Pts',(75.9431056439005,867.200589350415,138.230876351615));
#67721=CARTESIAN_POINT('Ctrl Pts',(75.7727644221043,867.393034589059,138.305074044112));
#67722=CARTESIAN_POINT('Ctrl Pts',(75.7087044733088,867.503532369404,138.348728597479));
#67723=CARTESIAN_POINT('Ctrl Pts',(75.6300648050044,867.740033555641,138.444392178609));
#67724=CARTESIAN_POINT('Ctrl Pts',(75.6160771903657,867.863697967913,138.495457998115));
#67725=CARTESIAN_POINT('Ctrl Pts',(75.6401821455974,868.109223061586,138.599237967042));
#67726=CARTESIAN_POINT('Ctrl Pts',(75.6784796659013,868.228677949967,138.650962292424));
#67727=CARTESIAN_POINT('Ctrl Pts',(75.8037267792447,868.447553819744,138.748452083201));
#67728=CARTESIAN_POINT('Ctrl Pts',(75.8900231716582,868.544580426584,138.793186121453));
#67729=CARTESIAN_POINT('Ctrl Pts',(76.0979913546796,868.700369533179,138.86825890857));
#67730=CARTESIAN_POINT('Ctrl Pts',(76.2172844819361,868.758053321954,138.898026656606));
#67731=CARTESIAN_POINT('Ctrl Pts',(76.4738587020055,868.827221602551,138.938617438612));
#67732=CARTESIAN_POINT('Ctrl Pts',(76.6086352443932,868.838096652377,138.949063105502));
#67733=CARTESIAN_POINT('Ctrl Pts',(76.8096199490018,868.817870132611,138.948779462126));
#67734=CARTESIAN_POINT('Ctrl Pts',(76.8761693785757,868.804967104891,138.945985567369));
#67735=CARTESIAN_POINT('Ctrl Pts',(77.0064626338259,868.767069453388,138.934987178594));
#67736=CARTESIAN_POINT('Ctrl Pts',(77.0698272854177,868.742036463364,138.92674951));
#67737=CARTESIAN_POINT('Ctrl Pts',(77.130082724518,868.711403932131,138.915922936985));
#67738=CARTESIAN_POINT('Ctrl Pts',(76.6453214979909,868.184856019917,140.772930142153));
#67739=CARTESIAN_POINT('Ctrl Pts',(76.6455365781618,868.184852762164,140.772939359587));
#67740=CARTESIAN_POINT('Ctrl Pts',(76.6457516619049,868.184849442101,140.772948549453));
#67741=CARTESIAN_POINT('Ctrl Pts',(76.645966749189,868.184846059724,140.772957711745));
#67742=CARTESIAN_POINT('Ctrl Pts',(76.7758691670263,868.182803265772,140.778491297362));
#67743=CARTESIAN_POINT('Ctrl Pts',(76.9046277809621,868.158075778458,140.773848044284));
#67744=CARTESIAN_POINT('Ctrl Pts',(77.1491128882823,868.064720459959,140.743926410569));
#67745=CARTESIAN_POINT('Ctrl Pts',(77.2619724901293,867.995916165013,140.718416342906));
#67746=CARTESIAN_POINT('Ctrl Pts',(77.4536935388035,867.822471804786,140.649470931866));
#67747=CARTESIAN_POINT('Ctrl Pts',(77.5304169855189,867.719354765232,140.606626501274));
#67748=CARTESIAN_POINT('Ctrl Pts',(77.6366450292619,867.49203730869,140.50967863608));
#67749=CARTESIAN_POINT('Ctrl Pts',(77.6649018006034,867.369962760814,140.456488116416));
#67750=CARTESIAN_POINT('Ctrl Pts',(77.6683867627123,867.123261849436,140.34769961892));
#67751=CARTESIAN_POINT('Ctrl Pts',(77.6435639259179,867.000976223799,140.293149379933));
#67752=CARTESIAN_POINT('Ctrl Pts',(77.5430919170751,866.771200044504,140.189901410266));
#67753=CARTESIAN_POINT('Ctrl Pts',(77.4678598771213,866.666132679206,140.14229096986));
#67754=CARTESIAN_POINT('Ctrl Pts',(77.2778518533872,866.490435172365,140.061702718765));
#67755=CARTESIAN_POINT('Ctrl Pts',(77.1654208526084,866.421119586801,140.029332807694));
#67756=CARTESIAN_POINT('Ctrl Pts',(76.9175992267621,866.326859789564,139.983167794367));
#67757=CARTESIAN_POINT('Ctrl Pts',(76.7846945371961,866.30277197589,139.96977777939));
#67758=CARTESIAN_POINT('Ctrl Pts',(76.6486396341716,866.303252452217,139.966428656905));
#67759=CARTESIAN_POINT('Ctrl Pts',(76.6469804699811,866.30326205495,139.966389358177));
#67760=CARTESIAN_POINT('Ctrl Pts',(76.6453214979932,866.303275397976,139.966351605635));
#67761=CARTESIAN_POINT('Origin',(76.6453214979932,870.871268259904,130.106892424027));
#67762=CARTESIAN_POINT('',(76.6453214979932,869.207851628398,136.313787667516));
#67763=CARTESIAN_POINT('Origin',(76.6453214979932,868.736429397789,136.147171100248));
#67764=CARTESIAN_POINT('',(76.6453214979932,867.707356875089,140.55926334394));
#67765=CARTESIAN_POINT('',(76.6453214979932,871.342690490513,130.273508991294));
#67766=CARTESIAN_POINT('Ctrl Pts',(76.6455915157221,866.78629497717,140.164399194601));
#67767=CARTESIAN_POINT('Ctrl Pts',(76.5847002532572,866.786869833523,140.162674025301));
#67768=CARTESIAN_POINT('Ctrl Pts',(76.5242990128218,866.797712291959,140.165279069441));
#67769=CARTESIAN_POINT('Ctrl Pts',(76.4050919191034,866.840852512441,140.179454220941));
#67770=CARTESIAN_POINT('Ctrl Pts',(76.3481799042497,866.874635171996,140.191698659241));
#67771=CARTESIAN_POINT('Ctrl Pts',(76.2519029134282,866.960596605688,140.224409507011));
#67772=CARTESIAN_POINT('Ctrl Pts',(76.2134725269528,867.011866078816,140.24452996038));
#67773=CARTESIAN_POINT('Ctrl Pts',(76.1604395759368,867.124882016385,140.290073822061));
#67774=CARTESIAN_POINT('Ctrl Pts',(76.1463241275259,867.185474924495,140.315035239601));
#67775=CARTESIAN_POINT('Ctrl Pts',(76.1444190637503,867.307974733356,140.366715590104));
#67776=CARTESIAN_POINT('Ctrl Pts',(76.1567255732018,867.368664155497,140.392928419684));
#67777=CARTESIAN_POINT('Ctrl Pts',(76.2060536755482,867.480923818108,140.442751171601));
#67778=CARTESIAN_POINT('Ctrl Pts',(76.2423002723906,867.531524197334,140.465913652237));
#67779=CARTESIAN_POINT('Ctrl Pts',(76.3340138935697,867.616504965522,140.50632597579));
#67780=CARTESIAN_POINT('Ctrl Pts',(76.3885740530013,867.650117807156,140.523204417909));
#67781=CARTESIAN_POINT('Ctrl Pts',(76.5087908048966,867.695776913516,140.548223781975));
#67782=CARTESIAN_POINT('Ctrl Pts',(76.5732623406447,867.707472088686,140.556156355653));
#67783=CARTESIAN_POINT('Ctrl Pts',(76.7037400351171,867.707339181011,140.56181524903));
#67784=CARTESIAN_POINT('Ctrl Pts',(76.7684757215617,867.69556681531,140.55950677998));
#67785=CARTESIAN_POINT('Ctrl Pts',(76.8898618034568,867.649889340746,140.544752935997));
#67786=CARTESIAN_POINT('Ctrl Pts',(76.9452985494962,867.616407930743,140.532439542117));
#67787=CARTESIAN_POINT('Ctrl Pts',(77.0395056810008,867.53181158141,140.499307691243));
#67788=CARTESIAN_POINT('Ctrl Pts',(77.0772729664222,867.481467380607,140.478786840159));
#67789=CARTESIAN_POINT('Ctrl Pts',(77.1298095814109,867.370372348707,140.432305116792));
#67790=CARTESIAN_POINT('Ctrl Pts',(77.143979729308,867.31066847716,140.406782369924));
#67791=CARTESIAN_POINT('Ctrl Pts',(77.1464962024423,867.189247101387,140.354056506975));
#67792=CARTESIAN_POINT('Ctrl Pts',(77.1345177345304,867.128699899428,140.327356253872));
#67793=CARTESIAN_POINT('Ctrl Pts',(77.0854061738484,867.015453169631,140.276717501026));
#67794=CARTESIAN_POINT('Ctrl Pts',(77.0486577023117,866.963894880086,140.253287852374));
#67795=CARTESIAN_POINT('Ctrl Pts',(76.955439847223,866.877484477876,140.213166841424));
#67796=CARTESIAN_POINT('Ctrl Pts',(76.9000010858462,866.843386980729,140.196829321882));
#67797=CARTESIAN_POINT('Ctrl Pts',(76.7776540030803,866.797253892379,140.173272830889));
#67798=CARTESIAN_POINT('Ctrl Pts',(76.7119713163255,866.785668305157,140.166279864988));
#67799=CARTESIAN_POINT('Ctrl Pts',(76.6455915157221,866.78629497717,140.164399194601));
#67800=CARTESIAN_POINT('Origin',(73.3263803266512,876.659647506777,132.15270150458));
#67801=CARTESIAN_POINT('',(73.3263803266511,872.015461567959,142.447777784718));
#67802=CARTESIAN_POINT('',(73.3263803266511,873.699407765406,143.373464708198));
#67803=CARTESIAN_POINT('Ctrl Pts',(73.3263803266511,872.015461567959,142.447777784718));
#67804=CARTESIAN_POINT('Ctrl Pts',(73.3252176298833,872.015484770283,142.447712136436));
#67805=CARTESIAN_POINT('Ctrl Pts',(73.3240548025254,872.015509884549,142.447647496968));
#67806=CARTESIAN_POINT('Ctrl Pts',(73.2002688528243,872.018386715616,142.440874668704));
#67807=CARTESIAN_POINT('Ctrl Pts',(73.0787775891136,872.042455866726,142.445514355066));
#67808=CARTESIAN_POINT('Ctrl Pts',(72.8502948484491,872.13114453728,142.477079736634));
#67809=CARTESIAN_POINT('Ctrl Pts',(72.7459078121859,872.195304136686,142.503935208013));
#67810=CARTESIAN_POINT('Ctrl Pts',(72.5690591256913,872.355961412184,142.577013059498));
#67811=CARTESIAN_POINT('Ctrl Pts',(72.4988010419257,872.451067030189,142.622660201959));
#67812=CARTESIAN_POINT('Ctrl Pts',(72.4027730473336,872.659160424314,142.727125868623));
#67813=CARTESIAN_POINT('Ctrl Pts',(72.378220020111,872.770126231009,142.784966873483));
#67814=CARTESIAN_POINT('Ctrl Pts',(72.378373092551,872.993744226334,142.906062269608));
#67815=CARTESIAN_POINT('Ctrl Pts',(72.403730713248,873.104265330165,142.968231049123));
#67816=CARTESIAN_POINT('Ctrl Pts',(72.5013305992743,873.307813715298,143.087590079837));
#67817=CARTESIAN_POINT('Ctrl Pts',(72.5724781186642,873.399143569926,143.143755868877));
#67818=CARTESIAN_POINT('Ctrl Pts',(72.7501981240276,873.549623088657,143.241796329609));
#67819=CARTESIAN_POINT('Ctrl Pts',(72.8546655168054,873.607963600326,143.283029544791));
#67820=CARTESIAN_POINT('Ctrl Pts',(73.0826710213486,873.68433173699,143.344733798657));
#67821=CARTESIAN_POINT('Ctrl Pts',(73.2037128729335,873.70238934793,143.36499869336));
#67822=CARTESIAN_POINT('Ctrl Pts',(73.3263031053865,873.699409645139,143.37345938027));
#67823=CARTESIAN_POINT('Ctrl Pts',(73.3263288458507,873.699409019486,143.373461156774));
#67824=CARTESIAN_POINT('Ctrl Pts',(73.3263545862722,873.699408392909,143.373462932751));
#67825=CARTESIAN_POINT('Ctrl Pts',(73.3263803266511,873.699407765406,143.373464708199));
#67826=CARTESIAN_POINT('',(73.3263803266279,874.393769757164,141.408848077495));
#67827=CARTESIAN_POINT('',(73.3263803266512,877.553543679395,132.468634657717));
#67828=CARTESIAN_POINT('Ctrl Pts',(73.6839261380829,874.324464619427,141.394863496905));
#67829=CARTESIAN_POINT('Ctrl Pts',(73.7935846223079,874.282364849322,141.379984013668));
#67830=CARTESIAN_POINT('Ctrl Pts',(73.8938361330003,874.222351782337,141.355425588237));
#67831=CARTESIAN_POINT('Ctrl Pts',(74.0700402359082,874.068617340966,141.287812690312));
#67832=CARTESIAN_POINT('Ctrl Pts',(74.1425062462717,873.974791334929,141.244506042417));
#67833=CARTESIAN_POINT('Ctrl Pts',(74.242594420944,873.770037260412,141.146933209958));
#67834=CARTESIAN_POINT('Ctrl Pts',(74.2700294259057,873.66134888764,141.093789523144));
#67835=CARTESIAN_POINT('Ctrl Pts',(74.2779735653447,873.439751264166,140.983235344466));
#67836=CARTESIAN_POINT('Ctrl Pts',(74.2576517681451,873.328825054649,140.926785174812));
#67837=CARTESIAN_POINT('Ctrl Pts',(74.1702435586778,873.119694009547,140.818278916962));
#67838=CARTESIAN_POINT('Ctrl Pts',(74.1033922868915,873.023597269198,140.767290491347));
#67839=CARTESIAN_POINT('Ctrl Pts',(73.9312980998025,872.860723874628,140.678270323834));
#67840=CARTESIAN_POINT('Ctrl Pts',(73.8276208891447,872.795587240097,140.641122401338));
#67841=CARTESIAN_POINT('Ctrl Pts',(73.6019438319792,872.708022893533,140.587021292463));
#67842=CARTESIAN_POINT('Ctrl Pts',(73.4829918204992,872.684728893535,140.569779729792));
#67843=CARTESIAN_POINT('Ctrl Pts',(73.2447903592873,872.680228675476,140.555722972313));
#67844=CARTESIAN_POINT('Ctrl Pts',(73.1278176323637,872.69770026638,140.558374173904));
#67845=CARTESIAN_POINT('Ctrl Pts',(72.9054263264503,872.770608858555,140.582537104776));
#67846=CARTESIAN_POINT('Ctrl Pts',(72.802117731416,872.825587192415,140.603931011088));
#67847=CARTESIAN_POINT('Ctrl Pts',(72.6201075234333,872.968506117211,140.663894854231));
#67848=CARTESIAN_POINT('Ctrl Pts',(72.5438758603661,873.055903307858,140.702330298631));
#67849=CARTESIAN_POINT('Ctrl Pts',(72.4283593148395,873.256157296893,140.7936731121));
#67850=CARTESIAN_POINT('Ctrl Pts',(72.3924203577145,873.368033603299,140.84629577083));
#67851=CARTESIAN_POINT('Ctrl Pts',(72.371216213266,873.594093159447,140.955855974205));
#67852=CARTESIAN_POINT('Ctrl Pts',(72.3850232219967,873.706031693908,141.011640078203));
#67853=CARTESIAN_POINT('Ctrl Pts',(72.459886631027,873.91911826784,141.121072388753));
#67854=CARTESIAN_POINT('Ctrl Pts',(72.5208987592655,874.018115035693,141.173664262065));
#67855=CARTESIAN_POINT('Ctrl Pts',(72.6832535084843,874.188864594597,141.268093361005));
#67856=CARTESIAN_POINT('Ctrl Pts',(72.7834239381339,874.258750923942,141.308932620179));
#67857=CARTESIAN_POINT('Ctrl Pts',(72.9976627685876,874.353168422772,141.368925763367));
#67858=CARTESIAN_POINT('Ctrl Pts',(73.1074997385821,874.380910460523,141.389410513765));
#67859=CARTESIAN_POINT('Ctrl Pts',(73.3396637187662,874.400222940271,141.412889567333));
#67860=CARTESIAN_POINT('Ctrl Pts',(73.4601690970707,874.389721905566,141.41472655992));
#67861=CARTESIAN_POINT('Ctrl Pts',(73.6125825484943,874.349629111377,141.403412161613));
#67862=CARTESIAN_POINT('Ctrl Pts',(73.6486693173653,874.338000316709,141.399647470316));
#67863=CARTESIAN_POINT('Ctrl Pts',(73.6839261380829,874.324464619427,141.394863496905));
#67864=CARTESIAN_POINT('Ctrl Pts',(73.326380326651,873.699407765406,143.373464708198));
#67865=CARTESIAN_POINT('Ctrl Pts',(73.4455541865396,873.696502524816,143.381684749111));
#67866=CARTESIAN_POINT('Ctrl Pts',(73.5638127610191,873.673771001158,143.378576620235));
#67867=CARTESIAN_POINT('Ctrl Pts',(73.7891815913094,873.589628174773,143.349292845481));
#67868=CARTESIAN_POINT('Ctrl Pts',(73.8934150634961,873.528063536163,143.322787590984));
#67869=CARTESIAN_POINT('Ctrl Pts',(74.0722365373893,873.372608427554,143.24898823875));
#67870=CARTESIAN_POINT('Ctrl Pts',(74.1442639408735,873.279787856864,143.202101863764));
#67871=CARTESIAN_POINT('Ctrl Pts',(74.245332686204,873.074195514028,143.094021647677));
#67872=CARTESIAN_POINT('Ctrl Pts',(74.2724322038226,872.963098967145,143.03364064157));
#67873=CARTESIAN_POINT('Ctrl Pts',(74.2763024569755,872.738025842134,142.908222642779));
#67874=CARTESIAN_POINT('Ctrl Pts',(74.252376118135,872.626100339391,142.844299439973));
#67875=CARTESIAN_POINT('Ctrl Pts',(74.1564803184499,872.419702481987,142.723584293178));
#67876=CARTESIAN_POINT('Ctrl Pts',(74.0860193003306,872.326841366078,142.667777609939));
#67877=CARTESIAN_POINT('Ctrl Pts',(73.9084179013268,872.172564679373,142.571533546893));
#67878=CARTESIAN_POINT('Ctrl Pts',(73.8034116904804,872.112201763111,142.53179768104));
#67879=CARTESIAN_POINT('Ctrl Pts',(73.5731622181586,872.032298544407,142.473285703891));
#67880=CARTESIAN_POINT('Ctrl Pts',(73.450515317133,872.012984378416,142.454786704893));
#67881=CARTESIAN_POINT('Ctrl Pts',(73.3263803266512,872.015461567959,142.447777784718));
#67882=CARTESIAN_POINT('Origin',(73.3263803266512,876.659647506777,132.15270150458));
#67883=CARTESIAN_POINT('',(73.3263803266512,874.99623087527,138.359596748068));
#67884=CARTESIAN_POINT('Origin',(73.3263803266512,874.524808644662,138.192980180801));
#67885=CARTESIAN_POINT('',(73.3263803266513,873.3036828697,143.148464801744));
#67886=CARTESIAN_POINT('',(73.3263803266512,877.131069737385,132.319318071847));
#67887=CARTESIAN_POINT('Ctrl Pts',(73.3261543474481,872.415623888765,142.660222665343));
#67888=CARTESIAN_POINT('Ctrl Pts',(73.2635808346016,872.416966167653,142.656509710482));
#67889=CARTESIAN_POINT('Ctrl Pts',(73.2015028924454,872.428759538996,142.658477288826));
#67890=CARTESIAN_POINT('Ctrl Pts',(73.0828623177025,872.472884406954,142.6738385555));
#67891=CARTESIAN_POINT('Ctrl Pts',(73.0278008495359,872.505435760309,142.687455702834));
#67892=CARTESIAN_POINT('Ctrl Pts',(72.9328968960245,872.588203705615,142.725314756461));
#67893=CARTESIAN_POINT('Ctrl Pts',(72.8945586595841,872.637998254988,142.749439623196));
#67894=CARTESIAN_POINT('Ctrl Pts',(72.8414607066704,872.747505676854,142.804898884148));
#67895=CARTESIAN_POINT('Ctrl Pts',(72.8273702317476,872.806150475822,142.835708181034));
#67896=CARTESIAN_POINT('Ctrl Pts',(72.8254827966869,872.924488598716,142.900090056835));
#67897=CARTESIAN_POINT('Ctrl Pts',(72.8379339450748,872.983065601358,142.933077147691));
#67898=CARTESIAN_POINT('Ctrl Pts',(72.888135507535,873.09202877754,142.996761315637));
#67899=CARTESIAN_POINT('Ctrl Pts',(72.9256152790222,873.141367953334,143.026864461796));
#67900=CARTESIAN_POINT('Ctrl Pts',(73.0193759650266,873.222214252308,143.078896493632));
#67901=CARTESIAN_POINT('Ctrl Pts',(73.0742508764508,873.253498032805,143.100582891959));
#67902=CARTESIAN_POINT('Ctrl Pts',(73.1943348031452,873.294843230481,143.133063454025));
#67903=CARTESIAN_POINT('Ctrl Pts',(73.2582250952364,873.304879362383,143.143734410334));
#67904=CARTESIAN_POINT('Ctrl Pts',(73.387242507356,873.302633468585,143.152699660637));
#67905=CARTESIAN_POINT('Ctrl Pts',(73.4510382316342,873.290560858201,143.151003186636));
#67906=CARTESIAN_POINT('Ctrl Pts',(73.571118027379,873.245549422212,143.135288645358));
#67907=CARTESIAN_POINT('Ctrl Pts',(73.6260541677723,873.212962972271,143.121360974132));
#67908=CARTESIAN_POINT('Ctrl Pts',(73.7201443638919,873.130783389706,143.082748850287));
#67909=CARTESIAN_POINT('Ctrl Pts',(73.757999277323,873.081785889969,143.058298249754));
#67910=CARTESIAN_POINT('Ctrl Pts',(73.8111238250011,872.973256720484,143.001881207675));
#67911=CARTESIAN_POINT('Ctrl Pts',(73.8253525227939,872.914612735053,142.970335404131));
#67912=CARTESIAN_POINT('Ctrl Pts',(73.827311496767,872.795999726558,142.904726626321));
#67913=CARTESIAN_POINT('Ctrl Pts',(73.81473246018,872.737123639636,142.871251525938));
#67914=CARTESIAN_POINT('Ctrl Pts',(73.7642606016394,872.628265145637,142.807605786528));
#67915=CARTESIAN_POINT('Ctrl Pts',(73.7270004349945,872.579191091669,142.777980032369));
#67916=CARTESIAN_POINT('Ctrl Pts',(73.6328721718507,872.497629229533,142.726604661014));
#67917=CARTESIAN_POINT('Ctrl Pts',(73.5770519765085,872.4657615751,142.705265102881));
#67918=CARTESIAN_POINT('Ctrl Pts',(73.4554739759947,872.424152462769,142.674003993632));
#67919=CARTESIAN_POINT('Ctrl Pts',(73.3912060738502,872.414228449145,142.664082671164));
#67920=CARTESIAN_POINT('Ctrl Pts',(73.3261543474481,872.415623888765,142.660222665343));
#67921=CARTESIAN_POINT('Origin',(85.2906675027921,865.303927287174,128.139205748573));
#67922=CARTESIAN_POINT('',(85.2906675027921,860.734189796252,138.003601155341));
#67923=CARTESIAN_POINT('',(85.2906675027932,862.621926189382,138.792762652049));
#67924=CARTESIAN_POINT('Ctrl Pts',(85.2906675027921,860.734189796252,138.003601155341));
#67925=CARTESIAN_POINT('Ctrl Pts',(85.1569502915632,860.735734357018,137.999230999999));
#67926=CARTESIAN_POINT('Ctrl Pts',(85.0244838725072,860.761567555043,138.004939860221));
#67927=CARTESIAN_POINT('Ctrl Pts',(84.7760728436783,860.859607693897,138.035375001082));
#67928=CARTESIAN_POINT('Ctrl Pts',(84.6627547277935,860.931248053407,138.059952772527));
#67929=CARTESIAN_POINT('Ctrl Pts',(84.4722379734115,861.111004191591,138.124631954799));
#67930=CARTESIAN_POINT('Ctrl Pts',(84.3968810421119,861.217299815088,138.1640796615));
#67931=CARTESIAN_POINT('Ctrl Pts',(84.2947142013479,861.449979545937,138.252939966087));
#67932=CARTESIAN_POINT('Ctrl Pts',(84.2687517349878,861.573998336457,138.30145992044));
#67933=CARTESIAN_POINT('Ctrl Pts',(84.2697834501128,861.823678830441,138.402165922697));
#67934=CARTESIAN_POINT('Ctrl Pts',(84.2969413626358,861.946860844076,138.453381612405));
#67935=CARTESIAN_POINT('Ctrl Pts',(84.4009938711906,862.174540017638,138.551836427236));
#67936=CARTESIAN_POINT('Ctrl Pts',(84.476623662278,862.276920998404,138.598148073696));
#67937=CARTESIAN_POINT('Ctrl Pts',(84.6666190362455,862.447710551251,138.680043733148));
#67938=CARTESIAN_POINT('Ctrl Pts',(84.7791777149321,862.51451118956,138.714849843798));
#67939=CARTESIAN_POINT('Ctrl Pts',(85.0258844449915,862.603223168113,138.767654352663));
#67940=CARTESIAN_POINT('Ctrl Pts',(85.1576036840497,862.624581927685,138.78524854889));
#67941=CARTESIAN_POINT('Ctrl Pts',(85.2906675027942,862.621926189382,138.792762652049));
#67942=CARTESIAN_POINT('',(85.2906675011928,863.266061415442,136.970256822865));
#67943=CARTESIAN_POINT('',(85.2906675027921,866.266956427416,128.47957283164));
#67944=CARTESIAN_POINT('Ctrl Pts',(85.9517574437177,863.030512608055,136.908103725293));
#67945=CARTESIAN_POINT('Ctrl Pts',(86.0532797154454,862.94924051595,136.879379418033));
#67946=CARTESIAN_POINT('Ctrl Pts',(86.1369421188726,862.850778238061,136.842262607317));
#67947=CARTESIAN_POINT('Ctrl Pts',(86.2591791549355,862.630556693338,136.755577236539));
#67948=CARTESIAN_POINT('Ctrl Pts',(86.296559890087,862.510943262656,136.706859223314));
#67949=CARTESIAN_POINT('Ctrl Pts',(86.3198381703693,862.265562959298,136.604281043106));
#67950=CARTESIAN_POINT('Ctrl Pts',(86.30528559595,862.142125008828,136.551392061809));
#67951=CARTESIAN_POINT('Ctrl Pts',(86.2253449482614,861.907641753823,136.448753027354));
#67952=CARTESIAN_POINT('Ctrl Pts',(86.1604966038493,861.798883315632,136.400001186342));
#67953=CARTESIAN_POINT('Ctrl Pts',(85.9885448194371,861.611112405503,136.313540768668));
#67954=CARTESIAN_POINT('Ctrl Pts',(85.8830405366813,861.533927385015,136.276671800154));
#67955=CARTESIAN_POINT('Ctrl Pts',(85.6462163187424,861.422544139861,136.220095855634));
#67956=CARTESIAN_POINT('Ctrl Pts',(85.517404403943,861.389009606684,136.200763370681));
#67957=CARTESIAN_POINT('Ctrl Pts',(85.2506319921123,861.369612048728,136.181503215456));
#67958=CARTESIAN_POINT('Ctrl Pts',(85.1152142728158,861.384557787738,136.182007804843));
#67959=CARTESIAN_POINT('Ctrl Pts',(84.8574701132769,861.462419235978,136.20303577885));
#67960=CARTESIAN_POINT('Ctrl Pts',(84.7377354558107,861.524637599491,136.223374379572));
#67961=CARTESIAN_POINT('Ctrl Pts',(84.5316993823201,861.687635195048,136.280887073647));
#67962=CARTESIAN_POINT('Ctrl Pts',(84.4470939893041,861.78643138328,136.317329733415));
#67963=CARTESIAN_POINT('Ctrl Pts',(84.3233405049538,862.008020509159,136.401827861769));
#67964=CARTESIAN_POINT('Ctrl Pts',(84.2853656425202,862.12862962769,136.449056104176));
#67965=CARTESIAN_POINT('Ctrl Pts',(84.2614332515525,862.375295391752,136.548312191037));
#67966=CARTESIAN_POINT('Ctrl Pts',(84.275531031474,862.498948886981,136.59937415209));
#67967=CARTESIAN_POINT('Ctrl Pts',(84.3544293177363,862.734266673987,136.699546513469));
#67968=CARTESIAN_POINT('Ctrl Pts',(84.418890114086,862.843538527003,136.747671809601));
#67969=CARTESIAN_POINT('Ctrl Pts',(84.5910605524689,863.032941225698,136.834744784467));
#67970=CARTESIAN_POINT('Ctrl Pts',(84.6975904420636,863.110859336869,136.872725233798));
#67971=CARTESIAN_POINT('Ctrl Pts',(84.9367543812024,863.222339015667,136.932137569885));
#67972=CARTESIAN_POINT('Ctrl Pts',(85.0668107282356,863.255313033035,136.95317204863));
#67973=CARTESIAN_POINT('Ctrl Pts',(85.3341493861863,863.272563147414,136.975413193998));
#67974=CARTESIAN_POINT('Ctrl Pts',(85.4688362640369,863.256735195217,136.976421116455));
#67975=CARTESIAN_POINT('Ctrl Pts',(85.6614443469277,863.197504832214,136.962352195151));
#67976=CARTESIAN_POINT('Ctrl Pts',(85.723816582504,863.171826061194,136.955042920435));
#67977=CARTESIAN_POINT('Ctrl Pts',(85.8430715999771,863.109198937968,136.93530429961));
#67978=CARTESIAN_POINT('Ctrl Pts',(85.8995736743458,863.072287521466,136.922868393182));
#67979=CARTESIAN_POINT('Ctrl Pts',(85.9517574437177,863.030512608055,136.908103725293));
#67980=CARTESIAN_POINT('Ctrl Pts',(85.2906675027942,862.621926189382,138.792762652049));
#67981=CARTESIAN_POINT('Ctrl Pts',(85.290945444327,862.621920642119,138.792778347385));
#67982=CARTESIAN_POINT('Ctrl Pts',(85.2912233917269,862.621914990079,138.792793998729));
#67983=CARTESIAN_POINT('Ctrl Pts',(85.2915013449265,862.621909233251,138.792809606068));
#67984=CARTESIAN_POINT('Ctrl Pts',(85.4222739334188,862.619200736487,138.800152612201));
#67985=CARTESIAN_POINT('Ctrl Pts',(85.5518994590603,862.593351495863,138.797608133119));
#67986=CARTESIAN_POINT('Ctrl Pts',(85.7966451560299,862.497445813918,138.772211550131));
#67987=CARTESIAN_POINT('Ctrl Pts',(85.9090900912688,862.427638875522,138.749278284685));
#67988=CARTESIAN_POINT('Ctrl Pts',(86.1000182694894,862.252467028972,138.685371076264));
#67989=CARTESIAN_POINT('Ctrl Pts',(86.1763954703557,862.148680883902,138.644948266126));
#67990=CARTESIAN_POINT('Ctrl Pts',(86.2822289290466,861.920215182198,138.552015072588));
#67991=CARTESIAN_POINT('Ctrl Pts',(86.3103476954312,861.797682803914,138.500369231833));
#67992=CARTESIAN_POINT('Ctrl Pts',(86.3136533776107,861.550275897164,138.393491033601));
#67993=CARTESIAN_POINT('Ctrl Pts',(86.2886848594367,861.427774617121,138.339295280087));
#67994=CARTESIAN_POINT('Ctrl Pts',(86.1880560829598,861.198374157071,138.235949113747));
#67995=CARTESIAN_POINT('Ctrl Pts',(86.1129456851299,861.093827162204,138.187855010266));
#67996=CARTESIAN_POINT('Ctrl Pts',(85.922517161301,860.918403685406,138.105222472305));
#67997=CARTESIAN_POINT('Ctrl Pts',(85.8091606440087,860.849161672914,138.071459155492));
#67998=CARTESIAN_POINT('Ctrl Pts',(85.5601911825806,860.756144864372,138.022787569306));
#67999=CARTESIAN_POINT('Ctrl Pts',(85.4272341468802,860.732879332638,138.008174879463));
#68000=CARTESIAN_POINT('Ctrl Pts',(85.2921177777857,860.734173758729,138.003648848846));
#68001=CARTESIAN_POINT('Ctrl Pts',(85.2913926219043,860.734181420438,138.003624853735));
#68002=CARTESIAN_POINT('Ctrl Pts',(85.2906675027921,860.734189796252,138.003601155341));
#68003=CARTESIAN_POINT('Origin',(85.2906675027921,865.303927287174,128.139205748573));
#68004=CARTESIAN_POINT('',(85.2906675027921,863.640510655667,134.346100992061));
#68005=CARTESIAN_POINT('Origin',(85.2906675027921,863.169088425059,134.179484424794));
#68006=CARTESIAN_POINT('',(85.2906675027922,862.1422270283,138.585320544375));
#68007=CARTESIAN_POINT('',(85.2906675027921,865.775349517782,128.30582231584));
#68008=CARTESIAN_POINT('Ctrl Pts',(85.2909807609949,861.218133294598,138.199034698033));
#68009=CARTESIAN_POINT('Ctrl Pts',(85.2303434350245,861.218933212764,138.196657417334));
#68010=CARTESIAN_POINT('Ctrl Pts',(85.1701826148236,861.229928196416,138.198537549954));
#68011=CARTESIAN_POINT('Ctrl Pts',(85.0513057338549,861.27328301916,138.211091519141));
#68012=CARTESIAN_POINT('Ctrl Pts',(84.9944723623471,861.307143102732,138.222456500081));
#68013=CARTESIAN_POINT('Ctrl Pts',(84.8981098725595,861.39330282904,138.253406730414));
#68014=CARTESIAN_POINT('Ctrl Pts',(84.859547589708,861.444727407849,138.272677758026));
#68015=CARTESIAN_POINT('Ctrl Pts',(84.8061722049066,861.558144413647,138.316619598991));
#68016=CARTESIAN_POINT('Ctrl Pts',(84.7918688364119,861.618984002284,138.340846355856));
#68017=CARTESIAN_POINT('Ctrl Pts',(84.7896088285248,861.741938169565,138.391229715717));
#68018=CARTESIAN_POINT('Ctrl Pts',(84.8017276610717,861.802822562984,138.41688990679));
#68019=CARTESIAN_POINT('Ctrl Pts',(84.8511395108544,861.916493943517,138.466414463185));
#68020=CARTESIAN_POINT('Ctrl Pts',(84.8881037391214,861.968088688051,138.489773565644));
#68021=CARTESIAN_POINT('Ctrl Pts',(84.9810975338317,862.05352103395,138.530421121873));
#68022=CARTESIAN_POINT('Ctrl Pts',(85.0358750230947,862.086863109381,138.547428463491));
#68023=CARTESIAN_POINT('Ctrl Pts',(85.156432348358,862.131748439863,138.573113631298));
#68024=CARTESIAN_POINT('Ctrl Pts',(85.2210361814761,862.142942222118,138.581573766579));
#68025=CARTESIAN_POINT('Ctrl Pts',(85.3515751849396,862.141632752248,138.588611080981));
#68026=CARTESIAN_POINT('Ctrl Pts',(85.4162545362392,862.129221489918,138.587149859483));
#68027=CARTESIAN_POINT('Ctrl Pts',(85.5373232492208,862.082269081205,138.574274301085));
#68028=CARTESIAN_POINT('Ctrl Pts',(85.5925269194731,862.048196142289,138.562987216803));
#68029=CARTESIAN_POINT('Ctrl Pts',(85.6861999518173,861.962552220769,138.531886941751));
#68030=CARTESIAN_POINT('Ctrl Pts',(85.7236826757803,861.911777916675,138.512356609832));
#68031=CARTESIAN_POINT('Ctrl Pts',(85.7756902240541,861.799977902879,138.467601511756));
#68032=CARTESIAN_POINT('Ctrl Pts',(85.789600707965,861.740012884334,138.442797730877));
#68033=CARTESIAN_POINT('Ctrl Pts',(85.7916189117067,861.618851684643,138.391378021577));
#68034=CARTESIAN_POINT('Ctrl Pts',(85.7796409391956,861.558824243433,138.365259094939));
#68035=CARTESIAN_POINT('Ctrl Pts',(85.7308878325463,861.446273579123,138.315155727913));
#68036=CARTESIAN_POINT('Ctrl Pts',(85.6943308301417,861.394928575689,138.291686273606));
#68037=CARTESIAN_POINT('Ctrl Pts',(85.601258872647,861.308562553006,138.250914779803));
#68038=CARTESIAN_POINT('Ctrl Pts',(85.545606449769,861.274434173731,138.234029721826));
#68039=CARTESIAN_POINT('Ctrl Pts',(85.4230160348868,861.228610192363,138.209292316302));
#68040=CARTESIAN_POINT('Ctrl Pts',(85.3573492778565,861.217257771454,138.201636669536));
#68041=CARTESIAN_POINT('Ctrl Pts',(85.2909807609949,861.218133294598,138.199034698033));
#68042=CARTESIAN_POINT('Origin',(83.3206797233787,871.616423241051,130.370255407314));
#68043=CARTESIAN_POINT('',(83.3206797233786,866.96815944026,140.67686952441));
#68044=CARTESIAN_POINT('',(83.3206797233787,868.663281554644,141.570935488596));
#68045=CARTESIAN_POINT('Ctrl Pts',(83.3206797233786,866.96815944026,140.67686952441));
#68046=CARTESIAN_POINT('Ctrl Pts',(83.1979733150929,866.971842780361,140.666447941281));
#68047=CARTESIAN_POINT('Ctrl Pts',(83.076211935733,866.996854463994,140.667172424123));
#68048=CARTESIAN_POINT('Ctrl Pts',(82.8486585433656,867.087125090313,140.690637981941));
#68049=CARTESIAN_POINT('Ctrl Pts',(82.7451459390068,867.151320095247,140.713056669224));
#68050=CARTESIAN_POINT('Ctrl Pts',(82.5678423802552,867.312623517907,140.777509980887));
#68051=CARTESIAN_POINT('Ctrl Pts',(82.4966611313868,867.408697682202,140.819281052879));
#68052=CARTESIAN_POINT('Ctrl Pts',(82.3989366110453,867.618659328567,140.916691907774));
#68053=CARTESIAN_POINT('Ctrl Pts',(82.3734964306883,867.730386334333,140.971354297369));
#68054=CARTESIAN_POINT('Ctrl Pts',(82.3717326836918,867.95506733745,141.087157151649));
#68055=CARTESIAN_POINT('Ctrl Pts',(82.3958948815759,868.065798799513,141.147220798035));
#68056=CARTESIAN_POINT('Ctrl Pts',(82.491554647161,868.271676464125,141.265383137167));
#68057=CARTESIAN_POINT('Ctrl Pts',(82.5628631824429,868.364653210316,141.322345659536));
#68058=CARTESIAN_POINT('Ctrl Pts',(82.7414426939018,868.516808745593,141.423460415312));
#68059=CARTESIAN_POINT('Ctrl Pts',(82.8464994784539,868.575268072358,141.466953046361));
#68060=CARTESIAN_POINT('Ctrl Pts',(83.0756963723964,868.650648853518,141.53454681768));
#68061=CARTESIAN_POINT('Ctrl Pts',(83.1974017211958,868.667708457805,141.558410080125));
#68062=CARTESIAN_POINT('Ctrl Pts',(83.3206797233788,868.663281554644,141.570935488596));
#68063=CARTESIAN_POINT('',(83.3206797233787,869.354927286473,139.614004199963));
#68064=CARTESIAN_POINT('',(83.3206797233787,872.51031941367,130.68618856045));
#68065=CARTESIAN_POINT('Ctrl Pts',(83.8529754731604,869.193059772498,139.581251398577));
#68066=CARTESIAN_POINT('Ctrl Pts',(83.9509540102205,869.130383807693,139.55909959192));
#68067=CARTESIAN_POINT('Ctrl Pts',(84.0355490372359,869.052053013329,139.528067061837));
#68068=CARTESIAN_POINT('Ctrl Pts',(84.1730819145392,868.86722819535,139.44946577285));
#68069=CARTESIAN_POINT('Ctrl Pts',(84.2225713908958,868.761316773023,139.401887729917));
#68070=CARTESIAN_POINT('Ctrl Pts',(84.2735746431976,868.541589999515,139.299023039021));
#68071=CARTESIAN_POINT('Ctrl Pts',(84.2754221636958,868.429999817896,139.244853754776));
#68072=CARTESIAN_POINT('Ctrl Pts',(84.2320937478474,868.211908668153,139.135538882559));
#68073=CARTESIAN_POINT('Ctrl Pts',(84.1865603041033,868.107508511897,139.081395240941));
#68074=CARTESIAN_POINT('Ctrl Pts',(84.0525489064174,867.920319473664,138.980644030745));
#68075=CARTESIAN_POINT('Ctrl Pts',(83.9647881720151,867.839544310954,138.935070769086));
#68076=CARTESIAN_POINT('Ctrl Pts',(83.7583592571335,867.714181399806,138.859308075614));
#68077=CARTESIAN_POINT('Ctrl Pts',(83.6416052910264,867.670888821712,138.829880581775));
#68078=CARTESIAN_POINT('Ctrl Pts',(83.3999464308693,867.629636037344,138.79214754597));
#68079=CARTESIAN_POINT('Ctrl Pts',(83.2778329727144,867.630230889189,138.783349111841));
#68080=CARTESIAN_POINT('Ctrl Pts',(83.0429807192215,867.672608849585,138.78586068879));
#68081=CARTESIAN_POINT('Ctrl Pts',(82.9321727381681,867.712652813023,138.79648973059));
#68082=CARTESIAN_POINT('Ctrl Pts',(82.7306074514192,867.827574208798,138.835501407793));
#68083=CARTESIAN_POINT('Ctrl Pts',(82.6418159464984,867.901589075903,138.863623469071));
#68084=CARTESIAN_POINT('Ctrl Pts',(82.4959537432314,868.076999155354,138.935070785635));
#68085=CARTESIAN_POINT('Ctrl Pts',(82.4411831805063,868.177378266506,138.978094479996));
#68086=CARTESIAN_POINT('Ctrl Pts',(82.3737749249685,868.395759544687,139.075844090801));
#68087=CARTESIAN_POINT('Ctrl Pts',(82.3641981111281,868.512146324994,139.130060903623));
#68088=CARTESIAN_POINT('Ctrl Pts',(82.3953620846968,868.737218892493,139.239272271814));
#68089=CARTESIAN_POINT('Ctrl Pts',(82.4346754010858,868.84389336496,139.29319587819));
#68090=CARTESIAN_POINT('Ctrl Pts',(82.557255688024,869.0374138716,139.395712878524));
#68091=CARTESIAN_POINT('Ctrl Pts',(82.639984457656,869.122166355449,139.443270339902));
#68092=CARTESIAN_POINT('Ctrl Pts',(82.8388054638799,869.257124499995,139.525049541975));
#68093=CARTESIAN_POINT('Ctrl Pts',(82.9533161026836,869.305736591076,139.558369765515));
#68094=CARTESIAN_POINT('Ctrl Pts',(83.1855383193989,869.355911163594,139.602725961546));
#68095=CARTESIAN_POINT('Ctrl Pts',(83.2998325612397,869.361442482731,139.615360692469));
#68096=CARTESIAN_POINT('Ctrl Pts',(83.5323356964507,869.334707870404,139.622565145655));
#68097=CARTESIAN_POINT('Ctrl Pts',(83.6482765147052,869.300775739711,139.616120796109));
#68098=CARTESIAN_POINT('Ctrl Pts',(83.788716144608,869.231662099515,139.594549448878));
#68099=CARTESIAN_POINT('Ctrl Pts',(83.8214739277969,869.213211019984,139.588373531273));
#68100=CARTESIAN_POINT('Ctrl Pts',(83.8529754731605,869.193059772498,139.581251398577));
#68101=CARTESIAN_POINT('Ctrl Pts',(83.3206797233788,868.663281554644,141.570935488596));
#68102=CARTESIAN_POINT('Ctrl Pts',(83.3208136591537,868.663276745021,141.570949096866));
#68103=CARTESIAN_POINT('Ctrl Pts',(83.320947596785,868.663271910027,141.570962691749));
#68104=CARTESIAN_POINT('Ctrl Pts',(83.3210815362641,868.66326704966,141.570976273243));
#68105=CARTESIAN_POINT('Ctrl Pts',(83.4409190602393,868.658918411885,141.583127826063));
#68106=CARTESIAN_POINT('Ctrl Pts',(83.5599476170798,868.634346057652,141.584321333876));
#68107=CARTESIAN_POINT('Ctrl Pts',(83.7850979720042,868.546351202737,141.563918959409));
#68108=CARTESIAN_POINT('Ctrl Pts',(83.8886378549942,868.483357003621,141.542234991254));
#68109=CARTESIAN_POINT('Ctrl Pts',(84.0661297463215,868.325657417287,141.477894141923));
#68110=CARTESIAN_POINT('Ctrl Pts',(84.1376668760204,868.232228618615,141.435641327911));
#68111=CARTESIAN_POINT('Ctrl Pts',(84.2385262704065,868.025959966724,141.335701117012));
#68112=CARTESIAN_POINT('Ctrl Pts',(84.2658980052954,867.91492057408,141.278772343917));
#68113=CARTESIAN_POINT('Ctrl Pts',(84.2712520516383,867.689914391234,141.15817441664));
#68114=CARTESIAN_POINT('Ctrl Pts',(84.2482781067566,867.578078907386,141.095565824849));
#68115=CARTESIAN_POINT('Ctrl Pts',(84.1541862593483,867.370714845655,140.974594892567));
#68116=CARTESIAN_POINT('Ctrl Pts',(84.0838525790934,867.277055721332,140.91732411838));
#68117=CARTESIAN_POINT('Ctrl Pts',(83.9062265462893,867.122274782354,140.816925346475));
#68118=CARTESIAN_POINT('Ctrl Pts',(83.8010894313335,867.062087722414,140.774501488061));
#68119=CARTESIAN_POINT('Ctrl Pts',(83.5698228176162,866.982972971342,140.709594402539));
#68120=CARTESIAN_POINT('Ctrl Pts',(83.4461428096556,866.96441517511,140.687536555567));
#68121=CARTESIAN_POINT('Ctrl Pts',(83.3208024761302,866.96815576087,140.6768799527));
#68122=CARTESIAN_POINT('Ctrl Pts',(83.3207410996363,866.968157597897,140.67687473716));
#68123=CARTESIAN_POINT('Ctrl Pts',(83.3206797233786,866.968159440259,140.67686952441));
#68124=CARTESIAN_POINT('Origin',(83.3206797233787,871.616423241051,130.370255407314));
#68125=CARTESIAN_POINT('',(83.3206797233787,869.953006609545,136.577150650802));
#68126=CARTESIAN_POINT('Origin',(83.3206797233787,869.481584378936,136.410534083535));
#68127=CARTESIAN_POINT('',(83.3206797233786,868.264547749415,141.35444894226));
#68128=CARTESIAN_POINT('',(83.3206797233787,872.08784547166,130.536871974581));
#68129=CARTESIAN_POINT('Ctrl Pts',(83.3208923352077,867.370572634924,140.882945801216));
#68130=CARTESIAN_POINT('Ctrl Pts',(83.2585379255171,867.372510723548,140.877382636858));
#68131=CARTESIAN_POINT('Ctrl Pts',(83.1966100897607,867.384878590161,140.877314432226));
#68132=CARTESIAN_POINT('Ctrl Pts',(83.078181283712,867.43016320687,140.888377721573));
#68133=CARTESIAN_POINT('Ctrl Pts',(83.0231454578108,867.463267480699,140.899757361664));
#68134=CARTESIAN_POINT('Ctrl Pts',(82.9286860400494,867.546686619094,140.933039856722));
#68135=CARTESIAN_POINT('Ctrl Pts',(82.890537587744,867.596375775113,140.954753343466));
#68136=CARTESIAN_POINT('Ctrl Pts',(82.8368483641075,867.706138598117,141.006019179575));
#68137=CARTESIAN_POINT('Ctrl Pts',(82.822262021685,867.765208072751,141.035156313976));
#68138=CARTESIAN_POINT('Ctrl Pts',(82.8193298449488,867.884263474365,141.09691953464));
#68139=CARTESIAN_POINT('Ctrl Pts',(82.8312100648549,867.943076473732,141.128963473328));
#68140=CARTESIAN_POINT('Ctrl Pts',(82.8801593896866,868.0524566344,141.191772743508));
#68141=CARTESIAN_POINT('Ctrl Pts',(82.9170035013509,868.101937690783,141.221947076889));
#68142=CARTESIAN_POINT('Ctrl Pts',(83.009959191949,868.18342857881,141.275509009122));
#68143=CARTESIAN_POINT('Ctrl Pts',(83.0649190752211,868.215021557577,141.298539983206));
#68144=CARTESIAN_POINT('Ctrl Pts',(83.1853768504071,868.256450243687,141.334418913629));
#68145=CARTESIAN_POINT('Ctrl Pts',(83.2495943888809,868.266288666004,141.347114898385));
#68146=CARTESIAN_POINT('Ctrl Pts',(83.3790332430002,868.263175011208,141.36049940558));
#68147=CARTESIAN_POINT('Ctrl Pts',(83.4429676032448,868.250582689113,141.361226697384));
#68148=CARTESIAN_POINT('Ctrl Pts',(83.5630303392802,868.204478494439,141.350528099059));
#68149=CARTESIAN_POINT('Ctrl Pts',(83.6179099476324,868.17149099333,141.339236118848));
#68150=CARTESIAN_POINT('Ctrl Pts',(83.7120126809746,868.08870182261,141.305773167139));
#68151=CARTESIAN_POINT('Ctrl Pts',(83.7500132392623,868.039595570044,141.283833595494));
#68152=CARTESIAN_POINT('Ctrl Pts',(83.8038217444869,867.931080451226,141.231913675163));
#68153=CARTESIAN_POINT('Ctrl Pts',(83.8186384842597,867.872629644873,141.202336118948));
#68154=CARTESIAN_POINT('Ctrl Pts',(83.8223754593258,867.753598109998,141.139261029725));
#68155=CARTESIAN_POINT('Ctrl Pts',(83.8105849526875,867.694168199017,141.106304557215));
#68156=CARTESIAN_POINT('Ctrl Pts',(83.7614542221758,867.584234698682,141.042545515433));
#68157=CARTESIAN_POINT('Ctrl Pts',(83.7246512805773,867.534689143135,141.012311531101));
#68158=CARTESIAN_POINT('Ctrl Pts',(83.6312444949943,867.452512065021,140.958868320093));
#68159=CARTESIAN_POINT('Ctrl Pts',(83.5756574156258,867.420476026033,140.9360798409));
#68160=CARTESIAN_POINT('Ctrl Pts',(83.4531182214787,867.378352351999,140.900959048412));
#68161=CARTESIAN_POINT('Ctrl Pts',(83.3874399907159,867.368504212583,140.888883080505));
#68162=CARTESIAN_POINT('Ctrl Pts',(83.3208923352077,867.370572634924,140.882945801216));
#68163=CARTESIAN_POINT('Origin',(92.5194077263639,858.163512847548,125.615541683647));
#68164=CARTESIAN_POINT('',(92.5194077263639,853.591406436911,135.486639673687));
#68165=CARTESIAN_POINT('',(92.5194077263671,855.486945714773,136.253723814067));
#68166=CARTESIAN_POINT('Ctrl Pts',(92.5194077263639,853.591406436911,135.486639673687));
#68167=CARTESIAN_POINT('Ctrl Pts',(92.3869852387689,853.593396837675,135.481008065839));
#68168=CARTESIAN_POINT('Ctrl Pts',(92.2557551130715,853.619204273559,135.485269936815));
#68169=CARTESIAN_POINT('Ctrl Pts',(92.0085420427403,853.716672443918,135.512627696012));
#68170=CARTESIAN_POINT('Ctrl Pts',(91.8952729849214,853.788045926648,135.535713828907));
#68171=CARTESIAN_POINT('Ctrl Pts',(91.7041813968413,853.967450612033,135.597409337442));
#68172=CARTESIAN_POINT('Ctrl Pts',(91.6282910646732,854.073760618473,135.63542470618));
#68173=CARTESIAN_POINT('Ctrl Pts',(91.5248240399265,854.306889833465,135.721369193424));
#68174=CARTESIAN_POINT('Ctrl Pts',(91.498156989476,854.431366263457,135.768440963004));
#68175=CARTESIAN_POINT('Ctrl Pts',(91.4978432522669,854.681894117513,135.866103359209));
#68176=CARTESIAN_POINT('Ctrl Pts',(91.5242112377685,854.805465584329,135.915748516764));
#68177=CARTESIAN_POINT('Ctrl Pts',(91.6273321357412,855.035858649374,136.012159618501));
#68178=CARTESIAN_POINT('Ctrl Pts',(91.7035225991336,855.140199456724,136.05794316828));
#68179=CARTESIAN_POINT('Ctrl Pts',(91.894563280928,855.312867765503,136.138851218061));
#68180=CARTESIAN_POINT('Ctrl Pts',(92.0071264222377,855.37993844689,136.173317235713));
#68181=CARTESIAN_POINT('Ctrl Pts',(92.2540883379612,855.468855656258,136.226582411463));
#68182=CARTESIAN_POINT('Ctrl Pts',(92.3860910407434,855.490051831638,136.24493541706));
#68183=CARTESIAN_POINT('Ctrl Pts',(92.5194077263704,855.486945714773,136.253723814067));
#68184=CARTESIAN_POINT('',(92.5194077248472,856.129737102166,134.435020220354));
#68185=CARTESIAN_POINT('',(92.5194077263639,859.12654198779,125.955908766714));
#68186=CARTESIAN_POINT('Ctrl Pts',(93.32793357901,855.744463731389,134.332967522652));
#68187=CARTESIAN_POINT('Ctrl Pts',(93.4093156004398,855.64506638241,134.297837136329));
#68188=CARTESIAN_POINT('Ctrl Pts',(93.4692768118077,855.53237144291,134.255690021426));
#68189=CARTESIAN_POINT('Ctrl Pts',(93.5396671732254,855.293061111367,134.162258027501));
#68190=CARTESIAN_POINT('Ctrl Pts',(93.5494080886043,855.168778069024,134.111889615515));
#68191=CARTESIAN_POINT('Ctrl Pts',(93.516969247092,854.924305549308,134.009632276761));
#68192=CARTESIAN_POINT('Ctrl Pts',(93.4748730284245,854.806481321232,133.958727374903));
#68193=CARTESIAN_POINT('Ctrl Pts',(93.3436027548005,854.592928423506,133.863485836907));
#68194=CARTESIAN_POINT('Ctrl Pts',(93.2554740842456,854.499329540317,133.820091895569));
#68195=CARTESIAN_POINT('Ctrl Pts',(93.0444811877202,854.349507278583,133.747043814263));
#68196=CARTESIAN_POINT('Ctrl Pts',(92.9235975765563,854.29475660701,133.71810390374));
#68197=CARTESIAN_POINT('Ctrl Pts',(92.6661945033903,854.232349777071,133.678837881516));
#68198=CARTESIAN_POINT('Ctrl Pts',(92.5322843037635,854.224850203096,133.66870703206));
#68199=CARTESIAN_POINT('Ctrl Pts',(92.2662046346305,854.258256659072,133.668109602026));
#68200=CARTESIAN_POINT('Ctrl Pts',(92.136710866001,854.299454317514,133.677892507997));
#68201=CARTESIAN_POINT('Ctrl Pts',(91.9013189712622,854.426184042731,133.716192184587));
#68202=CARTESIAN_POINT('Ctrl Pts',(91.7978064893072,854.510525515979,133.744349840843));
#68203=CARTESIAN_POINT('Ctrl Pts',(91.6322096096441,854.710350802253,133.814878686914));
#68204=CARTESIAN_POINT('Ctrl Pts',(91.5713447639343,854.823562646887,133.85641632742));
#68205=CARTESIAN_POINT('Ctrl Pts',(91.499587638132,855.064526277156,133.947762061178));
#68206=CARTESIAN_POINT('Ctrl Pts',(91.4893575457721,855.189912359493,133.996678644227));
#68207=CARTESIAN_POINT('Ctrl Pts',(91.5211783924667,855.435796401683,134.095658444129));
#68208=CARTESIAN_POINT('Ctrl Pts',(91.562745426317,855.553933683864,134.144770788845));
#68209=CARTESIAN_POINT('Ctrl Pts',(91.6929888099045,855.768526170092,134.23761812767));
#68210=CARTESIAN_POINT('Ctrl Pts',(91.780795636183,855.862708766721,134.280410370037));
#68211=CARTESIAN_POINT('Ctrl Pts',(91.9923647252827,856.014084050154,134.354043169661));
#68212=CARTESIAN_POINT('Ctrl Pts',(92.1144722446957,856.069344892335,134.384015773502));
#68213=CARTESIAN_POINT('Ctrl Pts',(92.3743793281731,856.131368156919,134.425948539406));
#68214=CARTESIAN_POINT('Ctrl Pts',(92.5095148085389,856.13806247407,134.437694882898));
#68215=CARTESIAN_POINT('Ctrl Pts',(92.7759339221879,856.102418823341,134.441241581973));
#68216=CARTESIAN_POINT('Ctrl Pts',(92.9046446726391,856.060488970577,134.433024209589));
#68217=CARTESIAN_POINT('Ctrl Pts',(93.0804582363484,855.964749147531,134.406051609777));
#68218=CARTESIAN_POINT('Ctrl Pts',(93.1359273119399,855.927392662453,134.394615035788));
#68219=CARTESIAN_POINT('Ctrl Pts',(93.2389320751269,855.842740273728,134.367091940892));
#68220=CARTESIAN_POINT('Ctrl Pts',(93.2861021604945,855.795555262804,134.351024998579));
#68221=CARTESIAN_POINT('Ctrl Pts',(93.32793357901,855.744463731389,134.332967522652));
#68222=CARTESIAN_POINT('Ctrl Pts',(92.5194077263704,855.486945714773,136.253723814067));
#68223=CARTESIAN_POINT('Ctrl Pts',(92.5196238573676,855.486940679183,136.253738061683));
#68224=CARTESIAN_POINT('Ctrl Pts',(92.5198399918204,855.48693557973,136.253752284132));
#68225=CARTESIAN_POINT('Ctrl Pts',(92.5200561296971,855.486930416408,136.253766481407));
#68226=CARTESIAN_POINT('Ctrl Pts',(92.6499040778617,855.483828476222,136.262295699054));
#68227=CARTESIAN_POINT('Ctrl Pts',(92.7786346708171,855.457732528654,136.26158192679));
#68228=CARTESIAN_POINT('Ctrl Pts',(93.0225962035067,855.361385542605,136.240833318348));
#68229=CARTESIAN_POINT('Ctrl Pts',(93.1351240435946,855.291130048563,136.220571403863));
#68230=CARTESIAN_POINT('Ctrl Pts',(93.3262758568272,855.115108652454,136.162215494075));
#68231=CARTESIAN_POINT('Ctrl Pts',(93.4028833429568,855.010991636153,136.124644857631));
#68232=CARTESIAN_POINT('Ctrl Pts',(93.5095832636384,854.781822808916,136.036846104054));
#68233=CARTESIAN_POINT('Ctrl Pts',(93.5382981003373,854.658943603091,135.987427530001));
#68234=CARTESIAN_POINT('Ctrl Pts',(93.543028293216,854.410643148742,135.883789969737));
#68235=CARTESIAN_POINT('Ctrl Pts',(93.5187522798023,854.287643953618,135.830580521326));
#68236=CARTESIAN_POINT('Ctrl Pts',(93.4198665220468,854.058385092743,135.72843693595));
#68237=CARTESIAN_POINT('Ctrl Pts',(93.3461919613144,853.954308671273,135.680491457946));
#68238=CARTESIAN_POINT('Ctrl Pts',(93.157337423882,853.777631677803,135.596164976474));
#68239=CARTESIAN_POINT('Ctrl Pts',(93.0433585602817,853.707320562923,135.56082808586));
#68240=CARTESIAN_POINT('Ctrl Pts',(92.7931216418974,853.613345927679,135.509064500091));
#68241=CARTESIAN_POINT('Ctrl Pts',(92.6596620315709,853.589953134473,135.492874846329));
#68242=CARTESIAN_POINT('Ctrl Pts',(92.5229080805847,853.591357987078,135.486790254446));
#68243=CARTESIAN_POINT('Ctrl Pts',(92.521157799348,853.591380132115,135.486714100055));
#68244=CARTESIAN_POINT('Ctrl Pts',(92.5194077263639,853.591406436911,135.486639673688));
#68245=CARTESIAN_POINT('Origin',(92.5194077263639,858.163512847548,125.615541683647));
#68246=CARTESIAN_POINT('',(92.5194077263639,856.500096216042,131.822436927135));
#68247=CARTESIAN_POINT('Origin',(92.5194077263639,856.028673985433,131.655820359868));
#68248=CARTESIAN_POINT('',(92.5194077263641,855.004575041423,136.053840440156));
#68249=CARTESIAN_POINT('',(92.5194077263639,858.634935078157,125.782158250914));
#68250=CARTESIAN_POINT('Ctrl Pts',(92.5197874159677,854.076647188808,135.678402926227));
#68251=CARTESIAN_POINT('Ctrl Pts',(92.4585117931719,854.077656815856,135.675406667411));
#68252=CARTESIAN_POINT('Ctrl Pts',(92.3977223504281,854.089098293605,135.676698335242));
#68253=CARTESIAN_POINT('Ctrl Pts',(92.2785603320437,854.133529362063,135.688044747866));
#68254=CARTESIAN_POINT('Ctrl Pts',(92.2219767659596,854.167746440683,135.698683659406));
#68255=CARTESIAN_POINT('Ctrl Pts',(92.1260534852906,854.254541137588,135.728106029539));
#68256=CARTESIAN_POINT('Ctrl Pts',(92.0876826855216,854.3062519916,135.746594698822));
#68257=CARTESIAN_POINT('Ctrl Pts',(92.034624053689,854.420218150904,135.788973069629));
#68258=CARTESIAN_POINT('Ctrl Pts',(92.0204609285167,854.481324738186,135.81243758112));
#68259=CARTESIAN_POINT('Ctrl Pts',(92.0184661537579,854.604705873835,135.861361862463));
#68260=CARTESIAN_POINT('Ctrl Pts',(92.0306919009851,854.665742659649,135.886337827351));
#68261=CARTESIAN_POINT('Ctrl Pts',(92.0802382756373,854.779570179844,135.934687374985));
#68262=CARTESIAN_POINT('Ctrl Pts',(92.1172050570094,854.83116827952,135.95756949966));
#68263=CARTESIAN_POINT('Ctrl Pts',(92.2102277996603,854.91663570645,135.997708992039));
#68264=CARTESIAN_POINT('Ctrl Pts',(92.2650813235398,854.949957248097,136.01466711033));
#68265=CARTESIAN_POINT('Ctrl Pts',(92.3858052547534,854.99462728357,136.040691835628));
#68266=CARTESIAN_POINT('Ctrl Pts',(92.4505098709428,855.005607101473,136.049529447048));
#68267=CARTESIAN_POINT('Ctrl Pts',(92.5811610900851,855.003670969154,136.057712806867));
#68268=CARTESIAN_POINT('Ctrl Pts',(92.6458634843089,854.99086342945,136.057012613005));
#68269=CARTESIAN_POINT('Ctrl Pts',(92.7668257473756,854.943042171451,136.045937182797));
#68270=CARTESIAN_POINT('Ctrl Pts',(92.8219300964058,854.90853571467,136.035684857441));
#68271=CARTESIAN_POINT('Ctrl Pts',(92.9153449806096,854.822087121721,136.006748439735));
#68272=CARTESIAN_POINT('Ctrl Pts',(92.952700755937,854.770970449032,135.988334955313));
#68273=CARTESIAN_POINT('Ctrl Pts',(93.0045216658271,854.658567997623,135.945655893991));
#68274=CARTESIAN_POINT('Ctrl Pts',(93.0183716537132,854.598357073756,135.921791765898));
#68275=CARTESIAN_POINT('Ctrl Pts',(93.0203356164198,854.476759363803,135.871873177225));
#68276=CARTESIAN_POINT('Ctrl Pts',(93.0083336030846,854.416559419792,135.846303590804));
#68277=CARTESIAN_POINT('Ctrl Pts',(92.959785965243,854.304353847261,135.797112369177));
#68278=CARTESIAN_POINT('Ctrl Pts',(92.9236806560829,854.25343244026,135.773968282823));
#68279=CARTESIAN_POINT('Ctrl Pts',(92.8311363658633,854.166994431878,135.732989350332));
#68280=CARTESIAN_POINT('Ctrl Pts',(92.7752438274135,854.132642228019,135.715670430145));
#68281=CARTESIAN_POINT('Ctrl Pts',(92.6521955638388,854.086780861494,135.689912134253));
#68282=CARTESIAN_POINT('Ctrl Pts',(92.5863456734611,854.075550520771,135.681657495608));
#68283=CARTESIAN_POINT('Ctrl Pts',(92.5197874159677,854.076647188808,135.678402926227));
#68284=CARTESIAN_POINT('Origin',(91.9844712578892,864.72423914453,127.934324344724));
#68285=CARTESIAN_POINT('',(91.9844712578893,860.070334590592,138.256898317882));
#68286=CARTESIAN_POINT('',(91.9844712578948,861.780675301002,139.107905031699));
#68287=CARTESIAN_POINT('Ctrl Pts',(91.9844712578893,860.070334590592,138.256898317882));
#68288=CARTESIAN_POINT('Ctrl Pts',(91.8627158249353,860.075094927363,138.243429497726));
#68289=CARTESIAN_POINT('Ctrl Pts',(91.7417814147924,860.100971972796,138.240598889852));
#68290=CARTESIAN_POINT('Ctrl Pts',(91.5146801986006,860.193007929216,138.256390270714));
#68291=CARTESIAN_POINT('Ctrl Pts',(91.410885331243,860.258332094181,138.274897558361));
#68292=CARTESIAN_POINT('Ctrl Pts',(91.2338481590702,860.421363739986,138.331248363508));
#68293=CARTESIAN_POINT('Ctrl Pts',(91.162822221636,860.517698379504,138.368705872945));
#68294=CARTESIAN_POINT('Ctrl Pts',(91.0640827219528,860.729177979568,138.458223067825));
#68295=CARTESIAN_POINT('Ctrl Pts',(91.0379218314488,860.84226772842,138.509499129176));
#68296=CARTESIAN_POINT('Ctrl Pts',(91.0349795142351,861.06886741443,138.619135384539));
#68297=CARTESIAN_POINT('Ctrl Pts',(91.0583329386905,861.180068266577,138.67640787922));
#68298=CARTESIAN_POINT('Ctrl Pts',(91.1517636407079,861.386358342695,138.790233884351));
#68299=CARTESIAN_POINT('Ctrl Pts',(91.2214484393768,861.479291492061,138.845695359929));
#68300=CARTESIAN_POINT('Ctrl Pts',(91.3989637829188,861.634087737731,138.947624208233));
#68301=CARTESIAN_POINT('Ctrl Pts',(91.5057040424711,861.694093105123,138.993029281356));
#68302=CARTESIAN_POINT('Ctrl Pts',(91.7377050324959,861.769897318938,139.065243611614));
#68303=CARTESIAN_POINT('Ctrl Pts',(91.8603246959307,861.786317685181,139.091940560826));
#68304=CARTESIAN_POINT('Ctrl Pts',(91.9844712579004,861.780675301002,139.107905031699));
#68305=CARTESIAN_POINT('',(91.9844712578892,862.468675832393,137.161287414449));
#68306=CARTESIAN_POINT('',(91.9844712578892,865.618135317149,128.250257497861));
#68307=CARTESIAN_POINT('Ctrl Pts',(92.6682530675173,862.180366103655,137.102728175585));
#68308=CARTESIAN_POINT('Ctrl Pts',(92.7502695251889,862.099853184563,137.074272185756));
#68309=CARTESIAN_POINT('Ctrl Pts',(92.8155108599149,862.006674064341,137.037991754908));
#68310=CARTESIAN_POINT('Ctrl Pts',(92.9083616649202,861.799018927021,136.951321458583));
#68311=CARTESIAN_POINT('Ctrl Pts',(92.9327116796763,861.685790236625,136.901157245529));
#68312=CARTESIAN_POINT('Ctrl Pts',(92.9324009227412,861.461039991637,136.796517089838));
#68313=CARTESIAN_POINT('Ctrl Pts',(92.9085802132645,861.351627285942,136.743117399261));
#68314=CARTESIAN_POINT('Ctrl Pts',(92.8158729018139,861.14701686133,136.638567071437));
#68315=CARTESIAN_POINT('Ctrl Pts',(92.7471178415109,861.053942346796,136.588426294817));
#68316=CARTESIAN_POINT('Ctrl Pts',(92.5723601967429,860.897351377711,136.49848947757));
#68317=CARTESIAN_POINT('Ctrl Pts',(92.4675255649409,860.83566182762,136.459661717188));
#68318=CARTESIAN_POINT('Ctrl Pts',(92.2357838564043,860.753720287111,136.399245605298));
#68319=CARTESIAN_POINT('Ctrl Pts',(92.1110558434138,860.734357835676,136.378275827917));
#68320=CARTESIAN_POINT('Ctrl Pts',(91.8639768320607,860.741537481803,136.357660451801));
#68321=CARTESIAN_POINT('Ctrl Pts',(91.7440388713179,860.766118890054,136.35733967831));
#68322=CARTESIAN_POINT('Ctrl Pts',(91.5227999959679,860.853694088448,136.375825488455));
#68323=CARTESIAN_POINT('Ctrl Pts',(91.4229996012723,860.914608698739,136.393830923029));
#68324=CARTESIAN_POINT('Ctrl Pts',(91.251069703936,861.06654232663,136.445923975402));
#68325=CARTESIAN_POINT('Ctrl Pts',(91.1806759039626,861.15633197131,136.479621376828));
#68326=CARTESIAN_POINT('Ctrl Pts',(91.0773365836193,861.356437160706,136.559796780827));
#68327=CARTESIAN_POINT('Ctrl Pts',(91.0464208576457,861.465307521388,136.60582157008));
#68328=CARTESIAN_POINT('Ctrl Pts',(91.0300669563244,861.69198937351,136.706504884572));
#68329=CARTESIAN_POINT('Ctrl Pts',(91.0472708384882,861.807620334639,136.760454565323));
#68330=CARTESIAN_POINT('Ctrl Pts',(91.129440914888,862.0214618439,136.865696497521));
#68331=CARTESIAN_POINT('Ctrl Pts',(91.1925423583627,862.117987326432,136.916033107454));
#68332=CARTESIAN_POINT('Ctrl Pts',(91.3574821764649,862.283015468729,137.008479942166));
#68333=CARTESIAN_POINT('Ctrl Pts',(91.4583119432808,862.34957786219,137.049608410124));
#68334=CARTESIAN_POINT('Ctrl Pts',(91.6849097744894,862.442378299146,137.116487651892));
#68335=CARTESIAN_POINT('Ctrl Pts',(91.8087559580481,862.467369957056,137.141459615132));
#68336=CARTESIAN_POINT('Ctrl Pts',(92.0488123358252,862.470743163164,137.169274624711));
#68337=CARTESIAN_POINT('Ctrl Pts',(92.1625686427008,862.453675369375,137.173922064465));
#68338=CARTESIAN_POINT('Ctrl Pts',(92.3852494302583,862.381833420401,137.165184058635));
#68339=CARTESIAN_POINT('Ctrl Pts',(92.4915585183589,862.325877002723,137.150955580858));
#68340=CARTESIAN_POINT('Ctrl Pts',(92.6138864410115,862.230723900541,137.120181006694));
#68341=CARTESIAN_POINT('Ctrl Pts',(92.6418835662023,862.206252195131,137.111877196191));
#68342=CARTESIAN_POINT('Ctrl Pts',(92.6682530675173,862.180366103655,137.102728175585));
#68343=CARTESIAN_POINT('Ctrl Pts',(91.9844712579004,861.780675301002,139.107905031699));
#68344=CARTESIAN_POINT('Ctrl Pts',(91.9847252321603,861.78066375803,139.107937691199));
#68345=CARTESIAN_POINT('Ctrl Pts',(91.9849792128138,861.780652122725,139.107970305759));
#68346=CARTESIAN_POINT('Ctrl Pts',(91.9852331998028,861.780640395039,139.108002875342));
#68347=CARTESIAN_POINT('Ctrl Pts',(92.1041663410571,861.775148733354,139.12325406104));
#68348=CARTESIAN_POINT('Ctrl Pts',(92.2223724148456,861.749504142137,139.128370146541));
#68349=CARTESIAN_POINT('Ctrl Pts',(92.4465953442894,861.659347904305,139.11695403917));
#68350=CARTESIAN_POINT('Ctrl Pts',(92.5501112531231,861.595130822051,139.100179018847));
#68351=CARTESIAN_POINT('Ctrl Pts',(92.727211844383,861.435404183338,139.04585931993));
#68352=CARTESIAN_POINT('Ctrl Pts',(92.7986758536721,861.341441607929,139.008776037852));
#68353=CARTESIAN_POINT('Ctrl Pts',(92.900160658882,861.134354217937,138.918422742171));
#68354=CARTESIAN_POINT('Ctrl Pts',(92.9282801907244,861.023150295102,138.865850362895));
#68355=CARTESIAN_POINT('Ctrl Pts',(92.9360129240651,860.797535988778,138.752101290057));
#68356=CARTESIAN_POINT('Ctrl Pts',(92.9144813096627,860.68537949621,138.691920212741));
#68357=CARTESIAN_POINT('Ctrl Pts',(92.8232846241425,860.4763410989,138.573017588116));
#68358=CARTESIAN_POINT('Ctrl Pts',(92.7538593971312,860.381597900411,138.515432329864));
#68359=CARTESIAN_POINT('Ctrl Pts',(92.577630711232,860.225172745614,138.412564543943));
#68360=CARTESIAN_POINT('Ctrl Pts',(92.4728924209734,860.164443079223,138.368035922534));
#68361=CARTESIAN_POINT('Ctrl Pts',(92.242325525263,860.084831516747,138.297703692825));
#68362=CARTESIAN_POINT('Ctrl Pts',(92.1188845109012,860.066208098854,138.272330710447));
#68363=CARTESIAN_POINT('Ctrl Pts',(91.990564827285,860.070109586947,138.257579005833));
#68364=CARTESIAN_POINT('Ctrl Pts',(91.9875177857031,860.070215478877,138.257235330647));
#68365=CARTESIAN_POINT('Ctrl Pts',(91.9844712578893,860.070334590591,138.256898317882));
#68366=CARTESIAN_POINT('Origin',(91.9844712578892,864.72423914453,127.934324344724));
#68367=CARTESIAN_POINT('',(91.9844712578892,863.060822513024,134.141219588213));
#68368=CARTESIAN_POINT('Origin',(91.9844712578892,862.589400282415,133.974603020945));
#68369=CARTESIAN_POINT('',(91.9844712578892,861.377906466998,138.90283513076));
#68370=CARTESIAN_POINT('',(91.9844712578892,865.195661375139,128.100940911991));
#68371=CARTESIAN_POINT('Ctrl Pts',(91.9846725918056,860.475894112785,138.454072412269));
#68372=CARTESIAN_POINT('Ctrl Pts',(91.920362935665,860.478484117757,138.44666658428));
#68373=CARTESIAN_POINT('Ctrl Pts',(91.8564894643335,860.492246409255,138.444883783608));
#68374=CARTESIAN_POINT('Ctrl Pts',(91.7367744281551,860.540932435595,138.452791544227));
#68375=CARTESIAN_POINT('Ctrl Pts',(91.6821403542686,860.575344412562,138.462389293359));
#68376=CARTESIAN_POINT('Ctrl Pts',(91.5893477943355,860.660705211688,138.49183868113));
#68377=CARTESIAN_POINT('Ctrl Pts',(91.5521796696783,860.710782297006,138.511394943521));
#68378=CARTESIAN_POINT('Ctrl Pts',(91.4998807546353,860.821120474435,138.558444180532));
#68379=CARTESIAN_POINT('Ctrl Pts',(91.4857576205996,860.880386978147,138.585587421364));
#68380=CARTESIAN_POINT('Ctrl Pts',(91.4833370573924,860.999900945424,138.643966489552));
#68381=CARTESIAN_POINT('Ctrl Pts',(91.4953968609785,861.058927026634,138.674656249663));
#68382=CARTESIAN_POINT('Ctrl Pts',(91.5444300072723,861.168289090617,138.735417500556));
#68383=CARTESIAN_POINT('Ctrl Pts',(91.5811054278994,861.217528824092,138.764910926337));
#68384=CARTESIAN_POINT('Ctrl Pts',(91.6744672369076,861.299397019212,138.818756454622));
#68385=CARTESIAN_POINT('Ctrl Pts',(91.7304602702546,861.331162118061,138.842583962484));
#68386=CARTESIAN_POINT('Ctrl Pts',(91.8526214401056,861.371715525066,138.880466094217));
#68387=CARTESIAN_POINT('Ctrl Pts',(91.9174404826097,861.380692004442,138.894411746735));
#68388=CARTESIAN_POINT('Ctrl Pts',(92.0476183726505,861.37528556506,138.910772090592));
#68389=CARTESIAN_POINT('Ctrl Pts',(92.1117370714536,861.36136128817,138.913229966425));
#68390=CARTESIAN_POINT('Ctrl Pts',(92.2314396922143,861.312484217547,138.906295317189));
#68391=CARTESIAN_POINT('Ctrl Pts',(92.285884526361,861.27822964846,138.897083743854));
#68392=CARTESIAN_POINT('Ctrl Pts',(92.3786966175915,861.193272480086,138.867932763898));
#68393=CARTESIAN_POINT('Ctrl Pts',(92.4159843165664,861.143403781542,138.848254038664));
#68394=CARTESIAN_POINT('Ctrl Pts',(92.4685134912536,861.033772617879,138.800642507967));
#68395=CARTESIAN_POINT('Ctrl Pts',(92.482818936385,860.97503686455,138.773092214655));
#68396=CARTESIAN_POINT('Ctrl Pts',(92.4858877403505,860.855990276812,138.713567890834));
#68397=CARTESIAN_POINT('Ctrl Pts',(92.4740447195081,860.796878658118,138.682115382241));
#68398=CARTESIAN_POINT('Ctrl Pts',(92.4251369915085,860.687075956209,138.620034389912));
#68399=CARTESIAN_POINT('Ctrl Pts',(92.3882876298724,860.637490360132,138.589996275897));
#68400=CARTESIAN_POINT('Ctrl Pts',(92.2948713795416,860.555557021582,138.536029188218));
#68401=CARTESIAN_POINT('Ctrl Pts',(92.2392727738594,860.523816579573,138.512537365152));
#68402=CARTESIAN_POINT('Ctrl Pts',(92.1168172974433,860.482532432661,138.47525047117));
#68403=CARTESIAN_POINT('Ctrl Pts',(92.0511735362836,860.473215855938,138.461730586569));
#68404=CARTESIAN_POINT('Ctrl Pts',(91.9846725918056,860.475894112785,138.454072412269));
#68405=CARTESIAN_POINT('Origin',(98.0156115335941,849.762095315549,122.646196458769));
#68406=CARTESIAN_POINT('',(98.015611533594,845.187014905945,132.525709033565));
#68407=CARTESIAN_POINT('',(98.0156115335941,847.091594819924,133.267213743794));
#68408=CARTESIAN_POINT('Ctrl Pts',(98.015611533594,845.187014905945,132.525709033565));
#68409=CARTESIAN_POINT('Ctrl Pts',(97.8860206821817,845.189387618146,132.518995719895));
#68410=CARTESIAN_POINT('Ctrl Pts',(97.7575089471629,845.214593932317,132.521688408218));
#68411=CARTESIAN_POINT('Ctrl Pts',(97.5120105461576,845.310119933585,132.545461559902));
#68412=CARTESIAN_POINT('Ctrl Pts',(97.3980938198495,845.381109130524,132.566957650488));
#68413=CARTESIAN_POINT('Ctrl Pts',(97.2050733706479,845.560356389836,132.625726894498));
#68414=CARTESIAN_POINT('Ctrl Pts',(97.1280580197775,845.66700622652,132.662474778526));
#68415=CARTESIAN_POINT('Ctrl Pts',(97.0224968822141,845.901512098029,132.746010158396));
#68416=CARTESIAN_POINT('Ctrl Pts',(96.9949565268277,846.027021178794,132.79196184265));
#68417=CARTESIAN_POINT('Ctrl Pts',(96.9934840518301,846.279305202701,132.887078058931));
#68418=CARTESIAN_POINT('Ctrl Pts',(97.0193040736023,846.403578364203,132.935303568196));
#68419=CARTESIAN_POINT('Ctrl Pts',(97.1210286511537,846.63454771516,133.028555468656));
#68420=CARTESIAN_POINT('Ctrl Pts',(97.1959561217158,846.738944221774,133.072675894541));
#68421=CARTESIAN_POINT('Ctrl Pts',(97.3862532747563,846.914340584495,133.151917655163));
#68422=CARTESIAN_POINT('Ctrl Pts',(97.5001643386863,846.983197005934,133.186150376441));
#68423=CARTESIAN_POINT('Ctrl Pts',(97.749255929632,847.073593462009,133.23920802476));
#68424=CARTESIAN_POINT('Ctrl Pts',(97.8817488809734,847.094933194111,133.257735945125));
#68425=CARTESIAN_POINT('Ctrl Pts',(98.0155294910738,847.091596869053,133.267207936134));
#68426=CARTESIAN_POINT('Ctrl Pts',(98.01555683863,847.091596187038,133.267209872408));
#68427=CARTESIAN_POINT('Ctrl Pts',(98.0155841861368,847.091595503995,133.267211808294));
#68428=CARTESIAN_POINT('Ctrl Pts',(98.0156115335941,847.091594819924,133.267213743794));
#68429=CARTESIAN_POINT('',(98.015611532426,847.733004325138,131.452420025248));
#68430=CARTESIAN_POINT('',(98.0156115335941,850.725124455792,122.986563541837));
#68431=CARTESIAN_POINT('Ctrl Pts',(98.936236838463,847.171692600385,131.303060137992));
#68432=CARTESIAN_POINT('Ctrl Pts',(98.9939218247441,847.058514135643,131.263059039063));
#68433=CARTESIAN_POINT('Ctrl Pts',(99.0275612513901,846.936543658766,131.217633635405));
#68434=CARTESIAN_POINT('Ctrl Pts',(99.0430285415981,846.68872509615,131.121194544736));
#68435=CARTESIAN_POINT('Ctrl Pts',(99.0247039124607,846.565292673627,131.071126770575));
#68436=CARTESIAN_POINT('Ctrl Pts',(98.9379656821865,846.332630237766,130.97304351506));
#68437=CARTESIAN_POINT('Ctrl Pts',(98.8701656260265,846.225696394909,130.925987643825));
#68438=CARTESIAN_POINT('Ctrl Pts',(98.6933028673295,846.04267853967,130.841538223022));
#68439=CARTESIAN_POINT('Ctrl Pts',(98.5857455164236,845.968471543597,130.804998030732));
#68440=CARTESIAN_POINT('Ctrl Pts',(98.3449329098207,845.863421827441,130.74777408195));
#68441=CARTESIAN_POINT('Ctrl Pts',(98.2139531641199,845.83363004536,130.727655487479));
#68442=CARTESIAN_POINT('Ctrl Pts',(97.9472209851749,845.823163418232,130.706746890368));
#68443=CARTESIAN_POINT('Ctrl Pts',(97.8140650190188,845.842129285687,130.705969823394));
#68444=CARTESIAN_POINT('Ctrl Pts',(97.560307050921,845.927050063964,130.723579297893));
#68445=CARTESIAN_POINT('Ctrl Pts',(97.4423967320263,845.992764711925,130.742027337513));
#68446=CARTESIAN_POINT('Ctrl Pts',(97.239644857422,846.162913146625,130.795672655142));
#68447=CARTESIAN_POINT('Ctrl Pts',(97.156878543148,846.265714279697,130.830354579779));
#68448=CARTESIAN_POINT('Ctrl Pts',(97.0389582355761,846.493635253383,130.910813392422));
#68449=CARTESIAN_POINT('Ctrl Pts',(97.0044940229917,846.616293916566,130.955689858244));
#68450=CARTESIAN_POINT('Ctrl Pts',(96.9878693864634,846.866015909571,131.05013109374));
#68451=CARTESIAN_POINT('Ctrl Pts',(97.0058311683029,846.990635805093,131.098776880444));
#68452=CARTESIAN_POINT('Ctrl Pts',(97.092014528966,847.224825990711,131.193623675761));
#68453=CARTESIAN_POINT('Ctrl Pts',(97.1592341379057,847.332182848818,131.238925853845));
#68454=CARTESIAN_POINT('Ctrl Pts',(97.3351303579775,847.51643783525,131.321050893748));
#68455=CARTESIAN_POINT('Ctrl Pts',(97.4424456345311,847.591284427378,131.357009137874));
#68456=CARTESIAN_POINT('Ctrl Pts',(97.6841667899337,847.697740031898,131.414765803074));
#68457=CARTESIAN_POINT('Ctrl Pts',(97.8165152546305,847.727785063144,131.435826286133));
#68458=CARTESIAN_POINT('Ctrl Pts',(98.0858062957287,847.737366409717,131.459224303796));
#68459=CARTESIAN_POINT('Ctrl Pts',(98.2201148404824,847.717359646841,131.461533582153));
#68460=CARTESIAN_POINT('Ctrl Pts',(98.4739706161407,847.630158343464,131.446858062285));
#68461=CARTESIAN_POINT('Ctrl Pts',(98.5910799617756,847.563868469895,131.430031034307));
#68462=CARTESIAN_POINT('Ctrl Pts',(98.7424151099261,847.435709208592,131.391600308076));
#68463=CARTESIAN_POINT('Ctrl Pts',(98.7885567607571,847.388283410839,131.376604898282));
#68464=CARTESIAN_POINT('Ctrl Pts',(98.870809467233,847.285272572634,131.342593306167));
#68465=CARTESIAN_POINT('Ctrl Pts',(98.9065860045221,847.229867804717,131.323621223611));
#68466=CARTESIAN_POINT('Ctrl Pts',(98.936236838463,847.171692600385,131.303060137992));
#68467=CARTESIAN_POINT('Ctrl Pts',(98.0156115335941,847.091594819924,133.267213743794));
#68468=CARTESIAN_POINT('Ctrl Pts',(98.1445998794982,847.088368296269,133.27634281783));
#68469=CARTESIAN_POINT('Ctrl Pts',(98.2724871025139,847.062263821109,133.276878366808));
#68470=CARTESIAN_POINT('Ctrl Pts',(98.5159940599694,846.965770072614,133.259805381712));
#68471=CARTESIAN_POINT('Ctrl Pts',(98.6288368496251,846.895023685516,133.241812544452));
#68472=CARTESIAN_POINT('Ctrl Pts',(98.8203608187985,846.717967585965,133.188537930749));
#68473=CARTESIAN_POINT('Ctrl Pts',(98.8971756269128,846.613412536387,133.15377706999));
#68474=CARTESIAN_POINT('Ctrl Pts',(99.0044970511687,846.383468490965,133.071492895752));
#68475=CARTESIAN_POINT('Ctrl Pts',(99.0337108485038,846.260298058927,133.024740051622));
#68476=CARTESIAN_POINT('Ctrl Pts',(99.0398162769885,846.011238720184,132.925525072838));
#68477=CARTESIAN_POINT('Ctrl Pts',(99.0163400049041,845.887814160082,132.874029437785));
#68478=CARTESIAN_POINT('Ctrl Pts',(98.9190697926459,845.657464834316,132.773966888127));
#68479=CARTESIAN_POINT('Ctrl Pts',(98.8460794673428,845.552803403249,132.72638911324));
#68480=CARTESIAN_POINT('Ctrl Pts',(98.6591898310977,845.375795008331,132.642011323911));
#68481=CARTESIAN_POINT('Ctrl Pts',(98.5467424974315,845.305448130961,132.606138060299));
#68482=CARTESIAN_POINT('Ctrl Pts',(98.2981984872136,845.210182679547,132.551969565868));
#68483=CARTESIAN_POINT('Ctrl Pts',(98.1646041368167,845.18604461951,132.534146128871));
#68484=CARTESIAN_POINT('Ctrl Pts',(98.024693361461,845.186876679982,132.526190973292));
#68485=CARTESIAN_POINT('Ctrl Pts',(98.0201517849047,845.186931777317,132.525944236365));
#68486=CARTESIAN_POINT('Ctrl Pts',(98.015611533594,845.187014905945,132.525709033565));
#68487=CARTESIAN_POINT('Origin',(98.0156115335941,849.762095315549,122.646196458769));
#68488=CARTESIAN_POINT('',(98.0156115335941,848.098678684043,128.853091702258));
#68489=CARTESIAN_POINT('Origin',(98.0156115335941,847.627256453434,128.686475134991));
#68490=CARTESIAN_POINT('',(98.0156115335942,846.606301159591,133.075600622152));
#68491=CARTESIAN_POINT('',(98.0156115335941,850.233517546158,122.812813026036));
#68492=CARTESIAN_POINT('Ctrl Pts',(98.0158176429449,845.673946435203,132.712688122743));
#68493=CARTESIAN_POINT('Ctrl Pts',(97.9557714435446,845.675125151855,132.709278802009));
#68494=CARTESIAN_POINT('Ctrl Pts',(97.8961842020983,845.686350334974,132.70990421349));
#68495=CARTESIAN_POINT('Ctrl Pts',(97.7777646789254,845.730085723621,132.719534051333));
#68496=CARTESIAN_POINT('Ctrl Pts',(97.7208514348171,845.764265697177,132.729309055622));
#68497=CARTESIAN_POINT('Ctrl Pts',(97.6240779947701,845.851282269231,132.757040096443));
#68498=CARTESIAN_POINT('Ctrl Pts',(97.5852405293584,845.903285666734,132.774732778336));
#68499=CARTESIAN_POINT('Ctrl Pts',(97.5313805529879,846.018062097187,132.815590580301));
#68500=CARTESIAN_POINT('Ctrl Pts',(97.5168958887761,846.079669424561,132.838340589156));
#68501=CARTESIAN_POINT('Ctrl Pts',(97.5144934953664,846.203894714416,132.885832892649));
#68502=CARTESIAN_POINT('Ctrl Pts',(97.5265307410666,846.265258809389,132.910095601539));
#68503=CARTESIAN_POINT('Ctrl Pts',(97.5756135745257,846.379420823086,132.957054453336));
#68504=CARTESIAN_POINT('Ctrl Pts',(97.6121657000844,846.431077951219,132.979286002817));
#68505=CARTESIAN_POINT('Ctrl Pts',(97.7052144357998,846.517731302449,133.018934522713));
#68506=CARTESIAN_POINT('Ctrl Pts',(97.7608877180156,846.55177662378,133.03593394772));
#68507=CARTESIAN_POINT('Ctrl Pts',(97.8827489636195,846.596736518061,133.062031613723));
#68508=CARTESIAN_POINT('Ctrl Pts',(97.9475998140662,846.607579006291,133.071000881768));
#68509=CARTESIAN_POINT('Ctrl Pts',(98.0785141005218,846.605130157163,133.079858950843));
#68510=CARTESIAN_POINT('Ctrl Pts',(98.1433357321042,846.591935712411,133.079688276805));
#68511=CARTESIAN_POINT('Ctrl Pts',(98.2643323610686,846.543178024217,133.070008510938));
#68512=CARTESIAN_POINT('Ctrl Pts',(98.3193770988556,846.508158643057,133.060620053119));
#68513=CARTESIAN_POINT('Ctrl Pts',(98.4124730503905,846.420734531687,133.033627780465));
#68514=CARTESIAN_POINT('Ctrl Pts',(98.449625024441,846.369200341769,133.016292420463));
#68515=CARTESIAN_POINT('Ctrl Pts',(98.5010260186287,846.256121175603,132.975779766548));
#68516=CARTESIAN_POINT('Ctrl Pts',(98.5147027976635,846.195673548754,132.952989935427));
#68517=CARTESIAN_POINT('Ctrl Pts',(98.5164362709613,846.073700502084,132.904967362938));
#68518=CARTESIAN_POINT('Ctrl Pts',(98.5043714130655,846.013375760666,132.880202275878));
#68519=CARTESIAN_POINT('Ctrl Pts',(98.4557679898932,845.900960936697,132.832185571587));
#68520=CARTESIAN_POINT('Ctrl Pts',(98.4196344307866,845.849980782542,132.809406976519));
#68521=CARTESIAN_POINT('Ctrl Pts',(98.3270717501001,845.763555478679,132.768740178542));
#68522=CARTESIAN_POINT('Ctrl Pts',(98.2711793890321,845.729285195682,132.751360893904));
#68523=CARTESIAN_POINT('Ctrl Pts',(98.1481682221794,845.683688446436,132.725126126308));
#68524=CARTESIAN_POINT('Ctrl Pts',(98.082340963432,845.672640571612,132.716465203359));
#68525=CARTESIAN_POINT('Ctrl Pts',(98.0158176429449,845.673946435203,132.712688122743));
#68526=CARTESIAN_POINT('Origin',(98.9391056666407,856.284316734599,124.951370193141));
#68527=CARTESIAN_POINT('',(98.9391056666407,851.623398972203,135.2937872253));
#68528=CARTESIAN_POINT('',(98.9391056666684,853.352286325813,136.092318365703));
#68529=CARTESIAN_POINT('Ctrl Pts',(98.9391056666407,851.623398972202,135.2937872253));
#68530=CARTESIAN_POINT('Ctrl Pts',(98.8183330524074,851.629053230436,135.277789158166));
#68531=CARTESIAN_POINT('Ctrl Pts',(98.6983196784671,851.655643037619,135.271807650217));
#68532=CARTESIAN_POINT('Ctrl Pts',(98.4696960988426,851.75000232356,135.280508220464));
#68533=CARTESIAN_POINT('Ctrl Pts',(98.3639034533419,851.817950924658,135.29568569154));
#68534=CARTESIAN_POINT('Ctrl Pts',(98.1869989436827,851.984925764802,135.345082437744));
#68535=CARTESIAN_POINT('Ctrl Pts',(98.1170047732073,852.081550498225,135.378376918119));
#68536=CARTESIAN_POINT('Ctrl Pts',(98.0187924910619,852.294466426923,135.459840255075));
#68537=CARTESIAN_POINT('Ctrl Pts',(97.992575496003,852.408857935065,135.507449115179));
#68538=CARTESIAN_POINT('Ctrl Pts',(97.9895985571535,852.637951606723,135.6103718886));
#68539=CARTESIAN_POINT('Ctrl Pts',(98.0129429608198,852.750255777671,135.664633788996));
#68540=CARTESIAN_POINT('Ctrl Pts',(98.1063157764756,852.958199465322,135.773415305005));
#68541=CARTESIAN_POINT('Ctrl Pts',(98.1758294784201,853.051613466265,135.826864151084));
#68542=CARTESIAN_POINT('Ctrl Pts',(98.3527708738705,853.206970250865,135.926389951305));
#68543=CARTESIAN_POINT('Ctrl Pts',(98.4590917234256,853.266975125199,135.971421132707));
#68544=CARTESIAN_POINT('Ctrl Pts',(98.6911107358913,853.342817425497,136.045288422844));
#68545=CARTESIAN_POINT('Ctrl Pts',(98.8144028011606,853.358837770667,136.073781813223));
#68546=CARTESIAN_POINT('Ctrl Pts',(98.9391056666962,853.352286325813,136.092318365703));
#68547=CARTESIAN_POINT('',(98.9391056666407,854.035930319192,134.158027066904));
#68548=CARTESIAN_POINT('',(98.9391056666407,857.178212907218,125.267303346277));
#68549=CARTESIAN_POINT('Ctrl Pts',(99.7444889898849,853.592871976861,134.067617186048));
#68550=CARTESIAN_POINT('Ctrl Pts',(99.8069588554102,853.498040904391,134.034100676348));
#68551=CARTESIAN_POINT('Ctrl Pts',(99.8499951384563,853.394131802919,133.994027907069));
#68552=CARTESIAN_POINT('Ctrl Pts',(99.8941058454367,853.172904198033,133.90256064147));
#68553=CARTESIAN_POINT('Ctrl Pts',(99.892252186103,853.057446187517,133.851608511254));
#68554=CARTESIAN_POINT('Ctrl Pts',(99.8406410015003,852.83784124837,133.748786880744));
#68555=CARTESIAN_POINT('Ctrl Pts',(99.7921931413572,852.73559013722,133.697918339998));
#68556=CARTESIAN_POINT('Ctrl Pts',(99.654158688674,852.553845516766,133.601449561046));
#68557=CARTESIAN_POINT('Ctrl Pts',(99.5651869378705,852.476401247526,133.556833041976));
#68558=CARTESIAN_POINT('Ctrl Pts',(99.3573207936775,852.357727127421,133.480297322107));
#68559=CARTESIAN_POINT('Ctrl Pts',(99.2399940409375,852.318053092073,133.449250589549));
#68560=CARTESIAN_POINT('Ctrl Pts',(98.9930677634267,852.283546087162,133.405599447528));
#68561=CARTESIAN_POINT('Ctrl Pts',(98.8658169162329,852.289153971247,133.393455031611));
#68562=CARTESIAN_POINT('Ctrl Pts',(98.6241162920994,852.344770186552,133.389958777935));
#68563=CARTESIAN_POINT('Ctrl Pts',(98.5115956931786,852.392387528154,133.397779682731));
#68564=CARTESIAN_POINT('Ctrl Pts',(98.3136393964446,852.521503687909,133.430947474194));
#68565=CARTESIAN_POINT('Ctrl Pts',(98.2292083442512,852.600675071958,133.455405470348));
#68566=CARTESIAN_POINT('Ctrl Pts',(98.0944279978531,852.78300274833,133.518240807862));
#68567=CARTESIAN_POINT('Ctrl Pts',(98.0455084496729,852.884615981437,133.5561170655));
#68568=CARTESIAN_POINT('Ctrl Pts',(97.9892084364286,853.100540941266,133.641883711644));
#68569=CARTESIAN_POINT('Ctrl Pts',(97.9834987127821,853.213040772154,133.689191278475));
#68570=CARTESIAN_POINT('Ctrl Pts',(98.0189139096396,853.4378337081,133.789206986077));
#68571=CARTESIAN_POINT('Ctrl Pts',(98.0621465956036,853.547475589896,133.841039923547));
#68572=CARTESIAN_POINT('Ctrl Pts',(98.1917315482001,853.740332822469,133.938865302342));
#68573=CARTESIAN_POINT('Ctrl Pts',(98.2758632828868,853.822267946685,133.984045185969));
#68574=CARTESIAN_POINT('Ctrl Pts',(98.4759539706325,853.951122680629,134.063707114211));
#68575=CARTESIAN_POINT('Ctrl Pts',(98.5904779899877,853.996344171556,134.097292985126));
#68576=CARTESIAN_POINT('Ctrl Pts',(98.8349492336192,854.042463101807,134.147673402917));
#68577=CARTESIAN_POINT('Ctrl Pts',(98.9627182894318,854.04252045791,134.163832740225));
#68578=CARTESIAN_POINT('Ctrl Pts',(99.2001172126454,853.998579301805,134.174925253276));
#68579=CARTESIAN_POINT('Ctrl Pts',(99.3083638880813,853.95951169045,134.17179721312));
#68580=CARTESIAN_POINT('Ctrl Pts',(99.5114901090276,853.845473567317,134.148145651599));
#68581=CARTESIAN_POINT('Ctrl Pts',(99.6035212496963,853.769862238685,134.12697046325));
#68582=CARTESIAN_POINT('Ctrl Pts',(99.7023911478801,853.652789107984,134.088448609325));
#68583=CARTESIAN_POINT('Ctrl Pts',(99.7244040063591,853.623361565918,134.078393238462));
#68584=CARTESIAN_POINT('Ctrl Pts',(99.7444889898849,853.592871976861,134.067617186048));
#68585=CARTESIAN_POINT('Ctrl Pts',(98.9391056666962,853.352286325813,136.092318365703));
#68586=CARTESIAN_POINT('Ctrl Pts',(98.939500154013,853.352265600853,136.092377004571));
#68587=CARTESIAN_POINT('Ctrl Pts',(98.9398946554667,853.352244650014,136.092435543675));
#68588=CARTESIAN_POINT('Ctrl Pts',(98.9402891708356,853.352223473264,136.092493982953));
#68589=CARTESIAN_POINT('Ctrl Pts',(99.0592907010779,853.345835722816,136.110121594051));
#68590=CARTESIAN_POINT('Ctrl Pts',(99.1775484051736,853.319000264939,136.118369990443));
#68591=CARTESIAN_POINT('Ctrl Pts',(99.4018080526621,853.226000734966,136.114457120838));
#68592=CARTESIAN_POINT('Ctrl Pts',(99.5054334943449,853.160104158027,136.101993730068));
#68593=CARTESIAN_POINT('Ctrl Pts',(99.6819813946448,852.997273581419,136.056858318171));
#68594=CARTESIAN_POINT('Ctrl Pts',(99.7531172255607,852.902132804875,136.02470647874));
#68595=CARTESIAN_POINT('Ctrl Pts',(99.8541472207777,852.69315828628,135.944059927185));
#68596=CARTESIAN_POINT('Ctrl Pts',(99.8823574847066,852.581384720111,135.896238123706));
#68597=CARTESIAN_POINT('Ctrl Pts',(99.8909729788273,852.354888486021,135.790848550981));
#68598=CARTESIAN_POINT('Ctrl Pts',(99.8703042833721,852.242538680081,135.734223356735));
#68599=CARTESIAN_POINT('Ctrl Pts',(99.781359429257,852.032597516905,135.620203352314));
#68600=CARTESIAN_POINT('Ctrl Pts',(99.7130620675111,851.937340913477,135.563924601654));
#68601=CARTESIAN_POINT('Ctrl Pts',(99.537922545271,851.778765319224,135.460734879293));
#68602=CARTESIAN_POINT('Ctrl Pts',(99.4325126092684,851.716986994574,135.41479260724));
#68603=CARTESIAN_POINT('Ctrl Pts',(99.2005875282792,851.636760197283,135.340551393988));
#68604=CARTESIAN_POINT('Ctrl Pts',(99.0764838659736,851.618408610255,135.312666437792));
#68605=CARTESIAN_POINT('Ctrl Pts',(98.9467180969863,851.623063404591,135.294805444485));
#68606=CARTESIAN_POINT('Ctrl Pts',(98.9429115045806,851.623220792814,135.29429136319));
#68607=CARTESIAN_POINT('Ctrl Pts',(98.9391056666407,851.623398972202,135.2937872253));
#68608=CARTESIAN_POINT('Origin',(98.9391056666407,856.284316734599,124.951370193141));
#68609=CARTESIAN_POINT('',(98.9391056666407,854.620900103093,131.158265436629));
#68610=CARTESIAN_POINT('Origin',(98.9391056666407,854.149477872485,130.991648869362));
#68611=CARTESIAN_POINT('',(98.9391056666407,852.944699443349,135.90088057344));
#68612=CARTESIAN_POINT('',(98.9391056666407,856.755738965208,125.117986760408));
#68613=CARTESIAN_POINT('Ctrl Pts',(98.9395892642655,852.032885557983,135.479850729421));
#68614=CARTESIAN_POINT('Ctrl Pts',(98.8757180666484,852.035906692228,135.471117397303));
#68615=CARTESIAN_POINT('Ctrl Pts',(98.8122528025992,852.050048618326,135.467646859426));
#68616=CARTESIAN_POINT('Ctrl Pts',(98.692710416234,852.099580734955,135.471656287059));
#68617=CARTESIAN_POINT('Ctrl Pts',(98.6378647845073,852.13462307584,135.479166262806));
#68618=CARTESIAN_POINT('Ctrl Pts',(98.5448527029889,852.22127493928,135.504311011571));
#68619=CARTESIAN_POINT('Ctrl Pts',(98.5075784482175,852.271924965287,135.52164427711));
#68620=CARTESIAN_POINT('Ctrl Pts',(98.4550628489838,852.383312648024,135.56428857169));
#68621=CARTESIAN_POINT('Ctrl Pts',(98.4407340325358,852.443003475229,135.589264253722));
#68622=CARTESIAN_POINT('Ctrl Pts',(98.4377140072837,852.563652762671,135.643839450189));
#68623=CARTESIAN_POINT('Ctrl Pts',(98.4494848486265,852.623334697028,135.672933059764));
#68624=CARTESIAN_POINT('Ctrl Pts',(98.4980167772103,852.733901385318,135.731225969468));
#68625=CARTESIAN_POINT('Ctrl Pts',(98.5344774809786,852.783621350956,135.759849574892));
#68626=CARTESIAN_POINT('Ctrl Pts',(98.6274652847569,852.866234190975,135.8128740098));
#68627=CARTESIAN_POINT('Ctrl Pts',(98.6833111696002,852.898206244098,135.836745283202));
#68628=CARTESIAN_POINT('Ctrl Pts',(98.8056000180448,852.939039906398,135.875839621481));
#68629=CARTESIAN_POINT('Ctrl Pts',(98.8707933341061,852.947915416463,135.890856481481));
#68630=CARTESIAN_POINT('Ctrl Pts',(99.0016893108325,852.941762373625,135.910068249006));
#68631=CARTESIAN_POINT('Ctrl Pts',(99.0661955044237,852.927197696364,135.914270497187));
#68632=CARTESIAN_POINT('Ctrl Pts',(99.1862581541636,852.876723379701,135.911269008687));
#68633=CARTESIAN_POINT('Ctrl Pts',(99.2407711869484,852.841621887879,135.904259442341));
#68634=CARTESIAN_POINT('Ctrl Pts',(99.3333670282979,852.755072076452,135.879760025277));
#68635=CARTESIAN_POINT('Ctrl Pts',(99.37052279837,852.70457430827,135.86255320979));
#68636=CARTESIAN_POINT('Ctrl Pts',(99.4228570957353,852.593910665641,135.819807893051));
#68637=CARTESIAN_POINT('Ctrl Pts',(99.4372091362825,852.534838887248,135.794639379505));
#68638=CARTESIAN_POINT('Ctrl Pts',(99.4406829537521,852.41538414882,135.739416914261));
#68639=CARTESIAN_POINT('Ctrl Pts',(99.4292979567966,852.356248765524,135.709863105819));
#68640=CARTESIAN_POINT('Ctrl Pts',(99.3813658656915,852.245457750329,135.650155376543));
#68641=CARTESIAN_POINT('Ctrl Pts',(99.3446292315317,852.195136836004,135.620599435966));
#68642=CARTESIAN_POINT('Ctrl Pts',(99.2510883127142,852.112074251995,135.566591556355));
#68643=CARTESIAN_POINT('Ctrl Pts',(99.1951966748328,852.08002644877,135.542613499666));
#68644=CARTESIAN_POINT('Ctrl Pts',(99.0722054420159,852.038765923274,135.503668129575));
#68645=CARTESIAN_POINT('Ctrl Pts',(99.006312753062,852.029729509178,135.488974065284));
#68646=CARTESIAN_POINT('Ctrl Pts',(98.9395892642655,852.032885557983,135.479850729421));
#68647=CARTESIAN_POINT('Origin',(101.539068444395,840.466856951798,119.360944708767));
#68648=CARTESIAN_POINT('',(101.539068444395,835.888254215111,129.250423299054));
#68649=CARTESIAN_POINT('',(101.539068444395,837.802648617342,129.964159054369));
#68650=CARTESIAN_POINT('Ctrl Pts',(101.539068444395,835.888254215111,129.250423299054));
#68651=CARTESIAN_POINT('Ctrl Pts',(101.408193185807,835.891021178919,129.242594496241));
#68652=CARTESIAN_POINT('Ctrl Pts',(101.278433501112,835.917135843883,129.24419041653));
#68653=CARTESIAN_POINT('Ctrl Pts',(101.032404335379,836.014751255025,129.265891721646));
#68654=CARTESIAN_POINT('Ctrl Pts',(100.918992966955,836.086366368608,129.286212271391));
#68655=CARTESIAN_POINT('Ctrl Pts',(100.727010609144,836.266525518918,129.34258003759));
#68656=CARTESIAN_POINT('Ctrl Pts',(100.650479499543,836.37342753972,129.378110054304));
#68657=CARTESIAN_POINT('Ctrl Pts',(100.545469077725,836.608653519278,129.459226820863));
#68658=CARTESIAN_POINT('Ctrl Pts',(100.518149703322,836.734694021807,129.504025258485));
#68659=CARTESIAN_POINT('Ctrl Pts',(100.517185290251,836.988225471177,129.596699776211));
#68660=CARTESIAN_POINT('Ctrl Pts',(100.54336816205,837.113203518004,129.643659444668));
#68661=CARTESIAN_POINT('Ctrl Pts',(100.645838321594,837.345045509499,129.7340401625));
#68662=CARTESIAN_POINT('Ctrl Pts',(100.720971957318,837.449669182678,129.776598389277));
#68663=CARTESIAN_POINT('Ctrl Pts',(100.911075016139,837.625010276468,129.852712581925));
#68664=CARTESIAN_POINT('Ctrl Pts',(101.024400151761,837.693760928369,129.885468116527));
#68665=CARTESIAN_POINT('Ctrl Pts',(101.272801682029,837.784511923031,129.93662585663));
#68666=CARTESIAN_POINT('Ctrl Pts',(101.405308264756,837.806008945146,129.95465139703));
#68667=CARTESIAN_POINT('Ctrl Pts',(101.539068444395,837.802648617342,129.964159054369));
#68668=CARTESIAN_POINT('',(101.539068443729,838.442786669558,128.152962764451));
#68669=CARTESIAN_POINT('',(101.539068444395,841.429886092041,119.701311791834));
#68670=CARTESIAN_POINT('Ctrl Pts',(102.531557458013,837.686870450189,127.950803063132));
#68671=CARTESIAN_POINT('Ctrl Pts',(102.563024298442,837.564857311682,127.907679491566));
#68672=CARTESIAN_POINT('Ctrl Pts',(102.568871736002,837.438973807152,127.860871091535));
#68673=CARTESIAN_POINT('Ctrl Pts',(102.528739960197,837.193599419736,127.765295855082));
#68674=CARTESIAN_POINT('Ctrl Pts',(102.483150660768,837.076500672345,127.717466616018));
#68675=CARTESIAN_POINT('Ctrl Pts',(102.345903918612,836.866034463218,127.627228258059));
#68676=CARTESIAN_POINT('Ctrl Pts',(102.255363212755,836.774791706316,127.585718147521));
#68677=CARTESIAN_POINT('Ctrl Pts',(102.040637720221,836.630579050891,127.514983797339));
#68678=CARTESIAN_POINT('Ctrl Pts',(101.918352461316,836.579148755526,127.486493661749));
#68679=CARTESIAN_POINT('Ctrl Pts',(101.65824481109,836.523738707047,127.446814051124));
#68680=CARTESIAN_POINT('Ctrl Pts',(101.52289337425,836.520339531799,127.436023496924));
#68681=CARTESIAN_POINT('Ctrl Pts',(101.258489565672,836.562506858983,127.433717520182));
#68682=CARTESIAN_POINT('Ctrl Pts',(101.13190738766,836.607211983303,127.442037577493));
#68683=CARTESIAN_POINT('Ctrl Pts',(100.901561561467,836.740105969176,127.47660240677));
#68684=CARTESIAN_POINT('Ctrl Pts',(100.80038793904,836.827531166656,127.502723689185));
#68685=CARTESIAN_POINT('Ctrl Pts',(100.639137314404,837.033751137391,127.56911790816));
#68686=CARTESIAN_POINT('Ctrl Pts',(100.5807344529,837.150541704662,127.608744172187));
#68687=CARTESIAN_POINT('Ctrl Pts',(100.515644400704,837.396598446102,127.695612778794));
#68688=CARTESIAN_POINT('Ctrl Pts',(100.509087072713,837.523322218678,127.741925991822));
#68689=CARTESIAN_POINT('Ctrl Pts',(100.548321501849,837.770803650285,127.835575337108));
#68690=CARTESIAN_POINT('Ctrl Pts',(100.593690141832,837.88914769441,127.88200302558));
#68691=CARTESIAN_POINT('Ctrl Pts',(100.730469390048,838.1012429664,127.969040730821));
#68692=CARTESIAN_POINT('Ctrl Pts',(100.82040375461,838.19302634567,128.008838714542));
#68693=CARTESIAN_POINT('Ctrl Pts',(101.034265302307,838.33865752761,128.077312795068));
#68694=CARTESIAN_POINT('Ctrl Pts',(101.156398836596,838.390766443303,128.105234774994));
#68695=CARTESIAN_POINT('Ctrl Pts',(101.417707683903,838.447373310773,128.145373209846));
#68696=CARTESIAN_POINT('Ctrl Pts',(101.554512830897,838.450746041076,128.157006799272));
#68697=CARTESIAN_POINT('Ctrl Pts',(101.821418518916,838.4071919293,128.161624948071));
#68698=CARTESIAN_POINT('Ctrl Pts',(101.949030200169,838.361229671913,128.154760676441));
#68699=CARTESIAN_POINT('Ctrl Pts',(102.179227922305,838.226060145171,128.12313156339));
#68700=CARTESIAN_POINT('Ctrl Pts',(102.279617622767,838.13821678036,128.098686802327));
#68701=CARTESIAN_POINT('Ctrl Pts',(102.399860283198,837.983144987605,128.050744276872));
#68702=CARTESIAN_POINT('Ctrl Pts',(102.434657897715,837.927698355838,128.032914032947));
#68703=CARTESIAN_POINT('Ctrl Pts',(102.492563709514,837.810798236508,127.993993498926));
#68704=CARTESIAN_POINT('Ctrl Pts',(102.51538309237,837.749586791852,127.972969140337));
#68705=CARTESIAN_POINT('Ctrl Pts',(102.531557458013,837.686870450189,127.950803063132));
#68706=CARTESIAN_POINT('Ctrl Pts',(101.539068444395,837.802648617343,129.964159054369));
#68707=CARTESIAN_POINT('Ctrl Pts',(101.539102971817,837.802647749944,129.964161508574));
#68708=CARTESIAN_POINT('Ctrl Pts',(101.539137499323,837.802646880888,129.96416396221));
#68709=CARTESIAN_POINT('Ctrl Pts',(101.539172026912,837.802646010177,129.964166415277));
#68710=CARTESIAN_POINT('Ctrl Pts',(101.669676912657,837.799354961388,129.973438339675));
#68711=CARTESIAN_POINT('Ctrl Pts',(101.799001755468,837.772464643173,129.974424179339));
#68712=CARTESIAN_POINT('Ctrl Pts',(102.043583294327,837.67359624361,129.959030090533));
#68713=CARTESIAN_POINT('Ctrl Pts',(102.156230418727,837.601692148446,129.942446541966));
#68714=CARTESIAN_POINT('Ctrl Pts',(102.346855325263,837.422331778836,129.892852604008));
#68715=CARTESIAN_POINT('Ctrl Pts',(102.423091998765,837.316702513936,129.860351826956));
#68716=CARTESIAN_POINT('Ctrl Pts',(102.529109749153,837.084964808974,129.782959530906));
#68717=CARTESIAN_POINT('Ctrl Pts',(102.557728197776,836.96111900325,129.73880586743));
#68718=CARTESIAN_POINT('Ctrl Pts',(102.562863469046,836.710965174577,129.644414079336));
#68719=CARTESIAN_POINT('Ctrl Pts',(102.539021640317,836.58715827539,129.595095832061));
#68720=CARTESIAN_POINT('Ctrl Pts',(102.441167288692,836.356187406874,129.498391015763));
#68721=CARTESIAN_POINT('Ctrl Pts',(102.367882229711,836.251366198201,129.451977434468));
#68722=CARTESIAN_POINT('Ctrl Pts',(102.181334733362,836.075241602747,129.369240539844));
#68723=CARTESIAN_POINT('Ctrl Pts',(102.069827431732,836.005635100728,129.333727665471));
#68724=CARTESIAN_POINT('Ctrl Pts',(101.821459192417,835.910508245188,129.278628271386));
#68725=CARTESIAN_POINT('Ctrl Pts',(101.686695903781,835.886572425089,129.25982944876));
#68726=CARTESIAN_POINT('Ctrl Pts',(101.546490993202,835.888116081824,129.250874816581));
#68727=CARTESIAN_POINT('Ctrl Pts',(101.542779269904,835.888175760864,129.250645276237));
#68728=CARTESIAN_POINT('Ctrl Pts',(101.539068444395,835.888254215111,129.250423299054));
#68729=CARTESIAN_POINT('Origin',(101.539068444395,840.466856951798,119.360944708767));
#68730=CARTESIAN_POINT('',(101.539068444395,838.803440320292,125.567839952255));
#68731=CARTESIAN_POINT('Origin',(101.539068444395,838.332018089683,125.401223384988));
#68732=CARTESIAN_POINT('',(101.539068444395,837.314405062769,129.780892315957));
#68733=CARTESIAN_POINT('',(101.539068444395,840.938279182407,119.527561276034));
#68734=CARTESIAN_POINT('Ctrl Pts',(101.539325607471,836.377250220821,129.431561262802));
#68735=CARTESIAN_POINT('Ctrl Pts',(101.478599217227,836.378563737303,129.427751092737));
#68736=CARTESIAN_POINT('Ctrl Pts',(101.418348588659,836.390191952138,129.42795637229));
#68737=CARTESIAN_POINT('Ctrl Pts',(101.299561870893,836.434963708252,129.436671899503));
#68738=CARTESIAN_POINT('Ctrl Pts',(101.242859179905,836.469521653125,129.445845031852));
#68739=CARTESIAN_POINT('Ctrl Pts',(101.146561424509,836.557193391539,129.472232645901));
#68740=CARTESIAN_POINT('Ctrl Pts',(101.107965019525,836.609458055559,129.489191250003));
#68741=CARTESIAN_POINT('Ctrl Pts',(101.05448093305,836.72477574853,129.528532546431));
#68742=CARTESIAN_POINT('Ctrl Pts',(101.040163727406,836.786676466367,129.550522517419));
#68743=CARTESIAN_POINT('Ctrl Pts',(101.038095594994,836.911506260466,129.596503839619));
#68744=CARTESIAN_POINT('Ctrl Pts',(101.050324199247,836.973174531978,129.620030557596));
#68745=CARTESIAN_POINT('Ctrl Pts',(101.09979898472,837.087766866978,129.665544897754));
#68746=CARTESIAN_POINT('Ctrl Pts',(101.136514375652,837.139553119855,129.687082712585));
#68747=CARTESIAN_POINT('Ctrl Pts',(101.229740746087,837.226246637234,129.725488753147));
#68748=CARTESIAN_POINT('Ctrl Pts',(101.285380892132,837.260235735861,129.741963049638));
#68749=CARTESIAN_POINT('Ctrl Pts',(101.407240373126,837.305106476048,129.767432035295));
#68750=CARTESIAN_POINT('Ctrl Pts',(101.472149039858,837.315847036994,129.776276272621));
#68751=CARTESIAN_POINT('Ctrl Pts',(101.603175272831,837.313027043415,129.785315557002));
#68752=CARTESIAN_POINT('Ctrl Pts',(101.668051054937,837.299536686526,129.785438357248));
#68753=CARTESIAN_POINT('Ctrl Pts',(101.789039205539,837.250024635162,129.776751672538));
#68754=CARTESIAN_POINT('Ctrl Pts',(101.844033504356,837.214553736411,129.768052581997));
#68755=CARTESIAN_POINT('Ctrl Pts',(101.936865232963,837.126207584309,129.742747967812));
#68756=CARTESIAN_POINT('Ctrl Pts',(101.973843483836,837.074228458178,129.726402325773));
#68757=CARTESIAN_POINT('Ctrl Pts',(102.024840563852,836.96036444174,129.687995625057));
#68758=CARTESIAN_POINT('Ctrl Pts',(102.038330626816,836.899594262713,129.666306731107));
#68759=CARTESIAN_POINT('Ctrl Pts',(102.039750071531,836.777078728272,129.620357918605));
#68760=CARTESIAN_POINT('Ctrl Pts',(102.027569425668,836.716546909429,129.596546638139));
#68761=CARTESIAN_POINT('Ctrl Pts',(101.978789182878,836.603790937744,129.550088078679));
#68762=CARTESIAN_POINT('Ctrl Pts',(101.942578690059,836.552700977587,129.527903887479));
#68763=CARTESIAN_POINT('Ctrl Pts',(101.850290191676,836.466559787651,129.488184276716));
#68764=CARTESIAN_POINT('Ctrl Pts',(101.794893766359,836.432541051752,129.471097603998));
#68765=CARTESIAN_POINT('Ctrl Pts',(101.672245845522,836.386870444056,129.444727205074));
#68766=CARTESIAN_POINT('Ctrl Pts',(101.606132947174,836.375805172937,129.435752971297));
#68767=CARTESIAN_POINT('Ctrl Pts',(101.539325607471,836.377250220821,129.431561262802));
#68768=CARTESIAN_POINT('Origin',(103.880632053932,846.665521119814,121.551762362789));
#68769=CARTESIAN_POINT('',(103.880632053932,841.996470226746,131.917191143814));
#68770=CARTESIAN_POINT('',(103.880632054005,843.746368801472,132.656273473763));
#68771=CARTESIAN_POINT('Ctrl Pts',(103.880632053932,841.996470226746,131.917191143814));
#68772=CARTESIAN_POINT('Ctrl Pts',(103.761418994746,842.002764179425,131.899383135524));
#68773=CARTESIAN_POINT('Ctrl Pts',(103.642927426757,842.029653537582,131.890776429531));
#68774=CARTESIAN_POINT('Ctrl Pts',(103.415568339074,842.124451135479,131.892834505147));
#68775=CARTESIAN_POINT('Ctrl Pts',(103.309582766932,842.192992750961,131.904249163847));
#68776=CARTESIAN_POINT('Ctrl Pts',(103.131806387883,842.3615930436,131.945830480073));
#68777=CARTESIAN_POINT('Ctrl Pts',(103.061164311068,842.459284930544,131.975182682802));
#68778=CARTESIAN_POINT('Ctrl Pts',(102.961685480668,842.674661775683,132.048736802417));
#68779=CARTESIAN_POINT('Ctrl Pts',(102.934780773326,842.790397205374,132.092432269426));
#68780=CARTESIAN_POINT('Ctrl Pts',(102.930580638678,843.022320992322,132.187972370811));
#68781=CARTESIAN_POINT('Ctrl Pts',(102.953328321717,843.136043768445,132.238811317241));
#68782=CARTESIAN_POINT('Ctrl Pts',(103.04554288982,843.346392623877,132.341453813949));
#68783=CARTESIAN_POINT('Ctrl Pts',(103.114292890983,843.44077504051,132.392223053204));
#68784=CARTESIAN_POINT('Ctrl Pts',(103.289422454791,843.597819372278,132.487730165283));
#68785=CARTESIAN_POINT('Ctrl Pts',(103.394577644932,843.658540376311,132.531468337365));
#68786=CARTESIAN_POINT('Ctrl Pts',(103.627529007129,843.737014458413,132.605909436609));
#68787=CARTESIAN_POINT('Ctrl Pts',(103.753419529693,843.753606470952,132.635795328422));
#68788=CARTESIAN_POINT('Ctrl Pts',(103.880632054078,843.746368801472,132.656273473763));
#68789=CARTESIAN_POINT('',(103.880632053932,844.42519506336,130.735613386816));
#68790=CARTESIAN_POINT('',(103.880632053932,847.559417292433,121.867695515926));
#68791=CARTESIAN_POINT('Ctrl Pts',(104.772417774909,843.805892092828,130.608567344288));
#68792=CARTESIAN_POINT('Ctrl Pts',(104.8126108154,843.700887439897,130.571455147021));
#68793=CARTESIAN_POINT('Ctrl Pts',(104.831561154686,843.590835653455,130.52921134503));
#68794=CARTESIAN_POINT('Ctrl Pts',(104.82500391408,843.365886614736,130.436428798797));
#68795=CARTESIAN_POINT('Ctrl Pts',(104.797027594465,843.253384664035,130.386521440141));
#68796=CARTESIAN_POINT('Ctrl Pts',(104.69637163862,843.048868933494,130.289032846508));
#68797=CARTESIAN_POINT('Ctrl Pts',(104.625414031777,842.958450539467,130.242346388363));
#68798=CARTESIAN_POINT('Ctrl Pts',(104.448085205806,842.807957456829,130.156922960298));
#68799=CARTESIAN_POINT('Ctrl Pts',(104.342785256947,842.749764919734,130.119110654766));
#68800=CARTESIAN_POINT('Ctrl Pts',(104.110895361281,842.674669280196,130.057977044444));
#68801=CARTESIAN_POINT('Ctrl Pts',(103.986204229695,842.658978478078,130.035406798003));
#68802=CARTESIAN_POINT('Ctrl Pts',(103.734885246423,842.673846056906,130.009206304506));
#68803=CARTESIAN_POINT('Ctrl Pts',(103.610673037664,842.704373161885,130.005869184416));
#68804=CARTESIAN_POINT('Ctrl Pts',(103.384914277831,842.806313174553,130.018745328133));
#68805=CARTESIAN_POINT('Ctrl Pts',(103.284728730839,842.875009045625,130.034016098454));
#68806=CARTESIAN_POINT('Ctrl Pts',(103.118706652789,843.040194350758,130.079931946323));
#68807=CARTESIAN_POINT('Ctrl Pts',(103.053334985224,843.134210726847,130.109636664957));
#68808=CARTESIAN_POINT('Ctrl Pts',(102.961594737649,843.338985902304,130.180405708178));
#68809=CARTESIAN_POINT('Ctrl Pts',(102.936287460259,843.447954787142,130.220881702022));
#68810=CARTESIAN_POINT('Ctrl Pts',(102.929487334851,843.670132778008,130.308858380912));
#68811=CARTESIAN_POINT('Ctrl Pts',(102.949233155853,843.781241674513,130.355674344468));
#68812=CARTESIAN_POINT('Ctrl Pts',(103.034869636845,843.994038758867,130.451450312228));
#68813=CARTESIAN_POINT('Ctrl Pts',(103.10224165078,844.092720052682,130.499409407044));
#68814=CARTESIAN_POINT('Ctrl Pts',(103.273577995327,844.255756903701,130.586695254));
#68815=CARTESIAN_POINT('Ctrl Pts',(103.375063060711,844.31929796989,130.625374055142));
#68816=CARTESIAN_POINT('Ctrl Pts',(103.601559694902,844.405879202998,130.690095097829));
#68817=CARTESIAN_POINT('Ctrl Pts',(103.724772717604,844.42754167909,130.715354415762));
#68818=CARTESIAN_POINT('Ctrl Pts',(103.976432807209,844.424495509366,130.748358223679));
#68819=CARTESIAN_POINT('Ctrl Pts',(104.102540614433,844.399394443665,130.755625723465));
#68820=CARTESIAN_POINT('Ctrl Pts',(104.326906610974,844.309693794209,130.750545283255));
#68821=CARTESIAN_POINT('Ctrl Pts',(104.424912755827,844.250187158244,130.74019340023));
#68822=CARTESIAN_POINT('Ctrl Pts',(104.599606819597,844.098708198734,130.703308980291));
#68823=CARTESIAN_POINT('Ctrl Pts',(104.673337810374,844.006670349102,130.676328103615));
#68824=CARTESIAN_POINT('Ctrl Pts',(104.744428595113,843.872754633768,130.631853510398));
#68825=CARTESIAN_POINT('Ctrl Pts',(104.759495119332,843.839652638115,130.620499463309));
#68826=CARTESIAN_POINT('Ctrl Pts',(104.772417774909,843.805892092828,130.608567344288));
#68827=CARTESIAN_POINT('Ctrl Pts',(103.880632054078,843.746368801472,132.656273473763));
#68828=CARTESIAN_POINT('Ctrl Pts',(103.881160973326,843.746338708974,132.656358616993));
#68829=CARTESIAN_POINT('Ctrl Pts',(103.881689915481,843.746308204289,132.65644359717));
#68830=CARTESIAN_POINT('Ctrl Pts',(103.882218879997,843.746277287993,132.656528414428));
#68831=CARTESIAN_POINT('Ctrl Pts',(104.000111953979,843.739386812049,132.675432077867));
#68832=CARTESIAN_POINT('Ctrl Pts',(104.117202505183,843.712143462111,132.685935518663));
#68833=CARTESIAN_POINT('Ctrl Pts',(104.341086575488,843.617919766937,132.688493236018));
#68834=CARTESIAN_POINT('Ctrl Pts',(104.445405730643,843.550569397786,132.679921995478));
#68835=CARTESIAN_POINT('Ctrl Pts',(104.622400594513,843.384739558509,132.643405301328));
#68836=CARTESIAN_POINT('Ctrl Pts',(104.693630663002,843.288270086762,132.616029026027));
#68837=CARTESIAN_POINT('Ctrl Pts',(104.794656317807,843.077120754238,132.545243715783));
#68838=CARTESIAN_POINT('Ctrl Pts',(104.823133455667,842.964636400798,132.502515759332));
#68839=CARTESIAN_POINT('Ctrl Pts',(104.832904630706,842.736744645383,132.406576776194));
#68840=CARTESIAN_POINT('Ctrl Pts',(104.813221128518,842.623802822434,132.354239694833));
#68841=CARTESIAN_POINT('Ctrl Pts',(104.72683280558,842.412571907182,132.247131410046));
#68842=CARTESIAN_POINT('Ctrl Pts',(104.660136378731,842.316726408412,132.193427031619));
#68843=CARTESIAN_POINT('Ctrl Pts',(104.487180076312,842.155399720145,132.092336428288));
#68844=CARTESIAN_POINT('Ctrl Pts',(104.381734313182,842.092122389083,132.046070064516));
#68845=CARTESIAN_POINT('Ctrl Pts',(104.149121756987,842.009881560872,131.96947168897));
#68846=CARTESIAN_POINT('Ctrl Pts',(104.024314095971,841.991104888684,131.939632183285));
#68847=CARTESIAN_POINT('Ctrl Pts',(103.891939809102,841.995919629985,131.918900720637));
#68848=CARTESIAN_POINT('Ctrl Pts',(103.886285118654,841.996171768489,131.918035596797));
#68849=CARTESIAN_POINT('Ctrl Pts',(103.880632053932,841.996470226746,131.917191143814));
#68850=CARTESIAN_POINT('Origin',(103.880632053932,846.665521119814,121.551762362789));
#68851=CARTESIAN_POINT('',(103.880632053932,845.002104488308,127.758657606278));
#68852=CARTESIAN_POINT('Origin',(103.880632053932,844.530682257699,127.592041039011));
#68853=CARTESIAN_POINT('',(103.880632053932,843.333459423775,132.479895063748));
#68854=CARTESIAN_POINT('',(103.880632053932,847.136943350423,121.718378930056));
#68855=CARTESIAN_POINT('Ctrl Pts',(103.881088470536,842.410563859926,132.090219465587));
#68856=CARTESIAN_POINT('Ctrl Pts',(103.817092215407,842.413949745358,132.080464189414));
#68857=CARTESIAN_POINT('Ctrl Pts',(103.75351903137,842.428618923509,132.075655595089));
#68858=CARTESIAN_POINT('Ctrl Pts',(103.633730778617,842.479484772073,132.076489885268));
#68859=CARTESIAN_POINT('Ctrl Pts',(103.578725442098,842.515371453365,132.0822077029));
#68860=CARTESIAN_POINT('Ctrl Pts',(103.485742631032,842.603755906287,132.103520938011));
#68861=CARTESIAN_POINT('Ctrl Pts',(103.448557329042,842.655212023092,132.118810526531));
#68862=CARTESIAN_POINT('Ctrl Pts',(103.396625286578,842.767504521097,132.157065325446));
#68863=CARTESIAN_POINT('Ctrl Pts',(103.382440944718,842.827178549087,132.179638197222));
#68864=CARTESIAN_POINT('Ctrl Pts',(103.379101074122,842.948537065295,132.229852956544));
#68865=CARTESIAN_POINT('Ctrl Pts',(103.390690579609,843.00891419442,132.257076050657));
#68866=CARTESIAN_POINT('Ctrl Pts',(103.438881153461,843.120693738879,132.312143980886));
#68867=CARTESIAN_POINT('Ctrl Pts',(103.475122932878,843.170891088879,132.339427178499));
#68868=CARTESIAN_POINT('Ctrl Pts',(103.567612870714,843.254286502661,132.390561028732));
#68869=CARTESIAN_POINT('Ctrl Pts',(103.623151706139,843.28652571091,132.413890342806));
#68870=CARTESIAN_POINT('Ctrl Pts',(103.746193962561,843.32824636792,132.45337119734));
#68871=CARTESIAN_POINT('Ctrl Pts',(103.812668259895,843.33716584272,132.469105204232));
#68872=CARTESIAN_POINT('Ctrl Pts',(103.945240784138,843.32993698082,132.49015269318));
#68873=CARTESIAN_POINT('Ctrl Pts',(104.010142440204,843.314538856143,132.495556583241));
#68874=CARTESIAN_POINT('Ctrl Pts',(104.130534587574,843.2620111768,132.49553865509));
#68875=CARTESIAN_POINT('Ctrl Pts',(104.18505622567,843.225750167681,132.490300568786));
#68876=CARTESIAN_POINT('Ctrl Pts',(104.277094571263,843.136966665675,132.469753950187));
#68877=CARTESIAN_POINT('Ctrl Pts',(104.313843549289,843.085501608901,132.454748833412));
#68878=CARTESIAN_POINT('Ctrl Pts',(104.365170041522,842.973292777513,132.416594690365));
#68879=CARTESIAN_POINT('Ctrl Pts',(104.379095303301,842.913711995107,132.39381795739));
#68880=CARTESIAN_POINT('Ctrl Pts',(104.381951538699,842.79348344918,132.343127519791));
#68881=CARTESIAN_POINT('Ctrl Pts',(104.370444031482,842.734126561631,132.315683716556));
#68882=CARTESIAN_POINT('Ctrl Pts',(104.322715092642,842.623323395167,132.259674785956));
#68883=CARTESIAN_POINT('Ctrl Pts',(104.286455149685,842.573201116069,132.231671660714));
#68884=CARTESIAN_POINT('Ctrl Pts',(104.193572972612,842.489679052634,132.179265997727));
#68885=CARTESIAN_POINT('Ctrl Pts',(104.13753505549,842.457322967167,132.155419485912));
#68886=CARTESIAN_POINT('Ctrl Pts',(104.014163787141,842.415884110923,132.115845159717));
#68887=CARTESIAN_POINT('Ctrl Pts',(103.948010756191,842.407023165371,132.100420771544));
#68888=CARTESIAN_POINT('Ctrl Pts',(103.881088470536,842.410563859926,132.090219465587));
#68889=CARTESIAN_POINT('Origin',(102.935786484342,830.684044276295,115.903367699502));
#68890=CARTESIAN_POINT('',(102.935786484342,826.101475377183,125.804068085843));
#68891=CARTESIAN_POINT('',(102.935786484349,828.025971426816,126.489222402778));
#68892=CARTESIAN_POINT('Ctrl Pts',(102.935786484342,826.101475377183,125.804068085843));
#68893=CARTESIAN_POINT('Ctrl Pts',(102.806520930159,826.10448001969,125.795566798752));
#68894=CARTESIAN_POINT('Ctrl Pts',(102.678312485991,826.130360223824,125.79598194708));
#68895=CARTESIAN_POINT('Ctrl Pts',(102.433403951682,826.227124308982,125.814770529169));
#68896=CARTESIAN_POINT('Ctrl Pts',(102.319726709598,826.298624618765,125.833589843808));
#68897=CARTESIAN_POINT('Ctrl Pts',(102.127025707492,826.478590648783,125.887021052632));
#68898=CARTESIAN_POINT('Ctrl Pts',(102.050015789127,826.585389329037,125.921132104669));
#68899=CARTESIAN_POINT('Ctrl Pts',(101.943582951435,826.821037134934,125.999668746766));
#68900=CARTESIAN_POINT('Ctrl Pts',(101.915516701988,826.947665274344,126.043356460436));
#68901=CARTESIAN_POINT('Ctrl Pts',(101.913308128373,827.203050219501,126.133923369079));
#68902=CARTESIAN_POINT('Ctrl Pts',(101.939159834502,827.329260407403,126.179899382231));
#68903=CARTESIAN_POINT('Ctrl Pts',(102.041408202899,827.563187765812,126.267968264977));
#68904=CARTESIAN_POINT('Ctrl Pts',(102.116476686542,827.66870249053,126.309229803067));
#68905=CARTESIAN_POINT('Ctrl Pts',(102.305938517745,827.845039138649,126.382417259864));
#68906=CARTESIAN_POINT('Ctrl Pts',(102.418390800487,827.914181419715,126.413657184712));
#68907=CARTESIAN_POINT('Ctrl Pts',(102.666926931412,828.006894840134,126.462803160003));
#68908=CARTESIAN_POINT('Ctrl Pts',(102.800720750187,828.029186105331,126.480126843192));
#68909=CARTESIAN_POINT('Ctrl Pts',(102.935786484357,828.025971426816,126.489222402778));
#68910=CARTESIAN_POINT('',(102.935786484219,828.665071698505,124.680962392358));
#68911=CARTESIAN_POINT('',(102.935786484342,831.647073416538,116.243734782569));
#68912=CARTESIAN_POINT('Ctrl Pts',(103.956762674324,827.704529521989,124.422706018157));
#68913=CARTESIAN_POINT('Ctrl Pts',(103.960636116979,827.579014269356,124.378344680962));
#68914=CARTESIAN_POINT('Ctrl Pts',(103.938436004372,827.454751264983,124.332109020517));
#68915=CARTESIAN_POINT('Ctrl Pts',(103.844459113732,827.222666636853,124.241230834666));
#68916=CARTESIAN_POINT('Ctrl Pts',(103.773597615158,827.117107807912,124.197480193245));
#68917=CARTESIAN_POINT('Ctrl Pts',(103.591840702334,826.938253886779,124.118414687492));
#68918=CARTESIAN_POINT('Ctrl Pts',(103.482516410088,826.866817140815,124.083904691373));
#68919=CARTESIAN_POINT('Ctrl Pts',(103.239312718108,826.767983869091,124.029208950841));
#68920=CARTESIAN_POINT('Ctrl Pts',(103.107644003807,826.741719636915,124.009613353496));
#68921=CARTESIAN_POINT('Ctrl Pts',(102.839609262409,826.738646886536,123.988431514896));
#68922=CARTESIAN_POINT('Ctrl Pts',(102.705801641709,826.761920551898,123.987068045066));
#68923=CARTESIAN_POINT('Ctrl Pts',(102.455281918683,826.855115228523,124.00279686017));
#68924=CARTESIAN_POINT('Ctrl Pts',(102.340805777403,826.92370849611,124.019559795587));
#68925=CARTESIAN_POINT('Ctrl Pts',(102.143939311041,827.098937915499,124.069087399524));
#68926=CARTESIAN_POINT('Ctrl Pts',(102.063924157867,827.204318367303,124.101554676348));
#68927=CARTESIAN_POINT('Ctrl Pts',(101.95122220926,827.437686201415,124.177543868812));
#68928=CARTESIAN_POINT('Ctrl Pts',(101.919735285824,827.563384571856,124.220318451882));
#68929=CARTESIAN_POINT('Ctrl Pts',(101.910320236622,827.816824541311,124.309796541087));
#68930=CARTESIAN_POINT('Ctrl Pts',(101.931956379922,827.942054049341,124.355581630465));
#68931=CARTESIAN_POINT('Ctrl Pts',(102.025335141902,828.176393918699,124.444586302996));
#68932=CARTESIAN_POINT('Ctrl Pts',(102.096127812757,828.283226731668,124.486945532886));
#68933=CARTESIAN_POINT('Ctrl Pts',(102.277525039041,828.463791686724,124.562839357267));
#68934=CARTESIAN_POINT('Ctrl Pts',(102.386243595941,828.535889168149,124.5956796786));
#68935=CARTESIAN_POINT('Ctrl Pts',(102.628723695406,828.63629828649,124.648170751724));
#68936=CARTESIAN_POINT('Ctrl Pts',(102.76033766592,828.663261599384,124.667205424798));
#68937=CARTESIAN_POINT('Ctrl Pts',(103.029813754604,828.667269300677,124.688753534586));
#68938=CARTESIAN_POINT('Ctrl Pts',(103.165096542509,828.643678947569,124.690857458015));
#68939=CARTESIAN_POINT('Ctrl Pts',(103.417951818128,828.54861811161,124.677271387714));
#68940=CARTESIAN_POINT('Ctrl Pts',(103.53328939306,828.478580324885,124.661898009401));
#68941=CARTESIAN_POINT('Ctrl Pts',(103.729768316606,828.301128445595,124.615324882301));
#68942=CARTESIAN_POINT('Ctrl Pts',(103.80905086026,828.195480110099,124.584587242151));
#68943=CARTESIAN_POINT('Ctrl Pts',(103.892945851721,828.020178899464,124.529494955938));
#68944=CARTESIAN_POINT('Ctrl Pts',(103.914878607193,827.959110461282,124.509677775407));
#68945=CARTESIAN_POINT('Ctrl Pts',(103.945906762478,827.833397257411,124.467642399112));
#68946=CARTESIAN_POINT('Ctrl Pts',(103.954771674371,827.769045995908,124.44550832301));
#68947=CARTESIAN_POINT('Ctrl Pts',(103.956762674324,827.704529521989,124.422706018157));
#68948=CARTESIAN_POINT('Ctrl Pts',(102.935786484357,828.025971426816,126.489222402778));
#68949=CARTESIAN_POINT('Ctrl Pts',(102.936009125898,828.025966127759,126.489237395844));
#68950=CARTESIAN_POINT('Ctrl Pts',(102.936231770901,828.02596075942,126.489252366484));
#68951=CARTESIAN_POINT('Ctrl Pts',(102.93645441933,828.025955321793,126.489267314693));
#68952=CARTESIAN_POINT('Ctrl Pts',(103.066090593206,828.022789284825,126.497970851115));
#68953=CARTESIAN_POINT('Ctrl Pts',(103.194520386692,827.996185249279,126.4989298261));
#68954=CARTESIAN_POINT('Ctrl Pts',(103.438768938464,827.89765768665,126.484743511593));
#68955=CARTESIAN_POINT('Ctrl Pts',(103.551819217782,827.825349857432,126.469245354155));
#68956=CARTESIAN_POINT('Ctrl Pts',(103.742949719137,827.644788252355,126.422798925592));
#68957=CARTESIAN_POINT('Ctrl Pts',(103.81936605789,827.538401028909,126.392341299576));
#68958=CARTESIAN_POINT('Ctrl Pts',(103.925503874168,827.305224409805,126.319664335284));
#68959=CARTESIAN_POINT('Ctrl Pts',(103.954228823691,827.180739103681,126.278157789586));
#68960=CARTESIAN_POINT('Ctrl Pts',(103.959736028277,826.929431334742,126.18901812719));
#68961=CARTESIAN_POINT('Ctrl Pts',(103.936257027715,826.805122853584,126.142255913342));
#68962=CARTESIAN_POINT('Ctrl Pts',(103.839310186563,826.573014584314,126.049830578665));
#68963=CARTESIAN_POINT('Ctrl Pts',(103.766529342937,826.467617737881,126.005105066546));
#68964=CARTESIAN_POINT('Ctrl Pts',(103.580846949938,826.290260502289,125.924501776525));
#68965=CARTESIAN_POINT('Ctrl Pts',(103.469625196976,826.220105319395,125.889443620195));
#68966=CARTESIAN_POINT('Ctrl Pts',(103.222400347441,826.12439655287,125.834342041166));
#68967=CARTESIAN_POINT('Ctrl Pts',(103.088569987809,826.100182034503,125.814986042936));
#68968=CARTESIAN_POINT('Ctrl Pts',(102.947203763653,826.101254653806,125.80483616287));
#68969=CARTESIAN_POINT('Ctrl Pts',(102.941494092056,826.101342709816,125.804443452755));
#68970=CARTESIAN_POINT('Ctrl Pts',(102.935786484342,826.101475377183,125.804068085843));
#68971=CARTESIAN_POINT('Origin',(102.935786484342,830.684044276295,115.903367699502));
#68972=CARTESIAN_POINT('',(102.935786484342,829.020627644789,122.11026294299));
#68973=CARTESIAN_POINT('Origin',(102.935786484342,828.54920541418,121.943646375723));
#68974=CARTESIAN_POINT('',(102.935786484342,827.534953974529,126.313804085861));
#68975=CARTESIAN_POINT('',(102.935786484342,831.155466506904,116.069984266769));
#68976=CARTESIAN_POINT('Ctrl Pts',(102.936069390333,826.592865577367,125.978431996048));
#68977=CARTESIAN_POINT('Ctrl Pts',(102.874475063288,826.594269262267,125.974355848731));
#68978=CARTESIAN_POINT('Ctrl Pts',(102.813382543912,826.606334528243,125.974269675768));
#68979=CARTESIAN_POINT('Ctrl Pts',(102.694097165491,826.652275454842,125.982332226208));
#68980=CARTESIAN_POINT('Ctrl Pts',(102.637633481101,826.687254983315,125.991012593791));
#68981=CARTESIAN_POINT('Ctrl Pts',(102.541823826425,826.77573937831,126.016257939734));
#68982=CARTESIAN_POINT('Ctrl Pts',(102.503484011035,826.828406677805,126.032585966355));
#68983=CARTESIAN_POINT('Ctrl Pts',(102.451024353403,826.943445517041,126.070238122327));
#68984=CARTESIAN_POINT('Ctrl Pts',(102.437032368536,827.004523954009,126.091106467414));
#68985=CARTESIAN_POINT('Ctrl Pts',(102.43467602439,827.129071128835,126.135243922408));
#68986=CARTESIAN_POINT('Ctrl Pts',(102.446858456483,827.191297661732,126.15810438915));
#68987=CARTESIAN_POINT('Ctrl Pts',(102.496410196976,827.306804910587,126.202258301628));
#68988=CARTESIAN_POINT('Ctrl Pts',(102.53318051434,827.358955585124,126.223116337427));
#68989=CARTESIAN_POINT('Ctrl Pts',(102.626356702174,827.446043555937,126.260181537004));
#68990=CARTESIAN_POINT('Ctrl Pts',(102.681790369339,827.480148773743,126.276033643539));
#68991=CARTESIAN_POINT('Ctrl Pts',(102.804191383321,827.525687790986,126.300796577117));
#68992=CARTESIAN_POINT('Ctrl Pts',(102.869987789968,827.536584258163,126.309438485901));
#68993=CARTESIAN_POINT('Ctrl Pts',(103.00197251611,827.533314830037,126.318195636516));
#68994=CARTESIAN_POINT('Ctrl Pts',(103.066887885629,827.519502290332,126.318335541075));
#68995=CARTESIAN_POINT('Ctrl Pts',(103.187853521999,827.469163160649,126.310105508394));
#68996=CARTESIAN_POINT('Ctrl Pts',(103.242781380914,827.433173883405,126.301832843899));
#68997=CARTESIAN_POINT('Ctrl Pts',(103.335254496134,827.343738134208,126.277759976895));
#68998=CARTESIAN_POINT('Ctrl Pts',(103.371972275781,827.291208543319,126.262212102189));
#68999=CARTESIAN_POINT('Ctrl Pts',(103.422286201787,827.176391343456,126.225662856712));
#69000=CARTESIAN_POINT('Ctrl Pts',(103.435416496703,827.115238992875,126.205022925311));
#69001=CARTESIAN_POINT('Ctrl Pts',(103.436141839161,826.99216514814,126.161215576118));
#69002=CARTESIAN_POINT('Ctrl Pts',(103.423674641188,826.931463217743,126.138477589341));
#69003=CARTESIAN_POINT('Ctrl Pts',(103.374439161389,826.818496913598,126.093945388958));
#69004=CARTESIAN_POINT('Ctrl Pts',(103.338066005267,826.767379056222,126.072597250757));
#69005=CARTESIAN_POINT('Ctrl Pts',(103.245988382357,826.681699434716,126.034351642809));
#69006=CARTESIAN_POINT('Ctrl Pts',(103.191123271933,826.648011870649,126.017840711501));
#69007=CARTESIAN_POINT('Ctrl Pts',(103.06908825276,826.602406166871,125.991896511813));
#69008=CARTESIAN_POINT('Ctrl Pts',(103.002919813313,826.591342110291,125.982855977693));
#69009=CARTESIAN_POINT('Ctrl Pts',(102.936069390333,826.592865577367,125.978431996048));
#69010=CARTESIAN_POINT('Origin',(106.593082004564,836.288239824643,117.884080028985));
#69011=CARTESIAN_POINT('',(106.593082004564,831.610248993976,128.2748033254));
#69012=CARTESIAN_POINT('',(106.593082004635,833.382657080601,128.950197605091));
#69013=CARTESIAN_POINT('Ctrl Pts',(106.593082004564,831.610248993976,128.2748033254));
#69014=CARTESIAN_POINT('Ctrl Pts',(106.469739565798,831.61723941511,128.255024740483));
#69015=CARTESIAN_POINT('Ctrl Pts',(106.347303886464,831.64652201565,128.244402170008));
#69016=CARTESIAN_POINT('Ctrl Pts',(106.117480999544,831.747323237994,128.242611307471));
#69017=CARTESIAN_POINT('Ctrl Pts',(106.012399500629,831.818118670509,128.251564465386));
#69018=CARTESIAN_POINT('Ctrl Pts',(105.836647244662,831.991227608674,128.287581412267));
#69019=CARTESIAN_POINT('Ctrl Pts',(105.767133138537,832.091226896752,128.313942603965));
#69020=CARTESIAN_POINT('Ctrl Pts',(105.671659373922,832.308315912299,128.380321896406));
#69021=CARTESIAN_POINT('Ctrl Pts',(105.64644226575,832.42309642187,128.419581506658));
#69022=CARTESIAN_POINT('Ctrl Pts',(105.64363986978,832.655742776992,128.507039382574));
#69023=CARTESIAN_POINT('Ctrl Pts',(105.667249562721,832.771111027246,128.554492226706));
#69024=CARTESIAN_POINT('Ctrl Pts',(105.761343927845,832.983609420419,128.650543959949));
#69025=CARTESIAN_POINT('Ctrl Pts',(105.830797577804,833.078528931949,128.698148401477));
#69026=CARTESIAN_POINT('Ctrl Pts',(106.006514792163,833.235579097993,128.787930084183));
#69027=CARTESIAN_POINT('Ctrl Pts',(106.111252208483,833.295947377084,128.829193637811));
#69028=CARTESIAN_POINT('Ctrl Pts',(106.34260804147,833.373732025045,128.900310965665));
#69029=CARTESIAN_POINT('Ctrl Pts',(106.467281320242,833.390008779794,128.929396825915));
#69030=CARTESIAN_POINT('Ctrl Pts',(106.593082004706,833.382657080601,128.950197605091));
#69031=CARTESIAN_POINT('',(106.593082004564,834.056466383016,127.043732422434));
#69032=CARTESIAN_POINT('',(106.593082004564,837.182135997262,118.200013182122));
#69033=CARTESIAN_POINT('Ctrl Pts',(107.532294808004,833.247164435627,126.876755726751));
#69034=CARTESIAN_POINT('Ctrl Pts',(107.548454394724,833.136575409437,126.837669823023));
#69035=CARTESIAN_POINT('Ctrl Pts',(107.54249056949,833.025236699112,126.794971178588));
#69036=CARTESIAN_POINT('Ctrl Pts',(107.485551964177,832.806579904812,126.704412524435));
#69037=CARTESIAN_POINT('Ctrl Pts',(107.432675683693,832.702090199864,126.657336964529));
#69038=CARTESIAN_POINT('Ctrl Pts',(107.287374104876,832.521948109869,126.568462840168));
#69039=CARTESIAN_POINT('Ctrl Pts',(107.197007939246,832.447516409023,126.527426620317));
#69040=CARTESIAN_POINT('Ctrl Pts',(106.9881348606,832.3352947557,126.455529610318));
#69041=CARTESIAN_POINT('Ctrl Pts',(106.871108826735,832.299134044525,126.425504097532));
#69042=CARTESIAN_POINT('Ctrl Pts',(106.625329880769,832.271373928425,126.38110046283));
#69043=CARTESIAN_POINT('Ctrl Pts',(106.49872397112,832.280585895651,126.367331697681));
#69044=CARTESIAN_POINT('Ctrl Pts',(106.253996127618,832.34461020012,126.358504854285));
#69045=CARTESIAN_POINT('Ctrl Pts',(106.138251226854,832.39891632184,126.363572043295));
#69046=CARTESIAN_POINT('Ctrl Pts',(105.938301072436,832.543042787827,126.391358307029));
#69047=CARTESIAN_POINT('Ctrl Pts',(105.854829166522,832.629938551605,126.41306153524));
#69048=CARTESIAN_POINT('Ctrl Pts',(105.72799726863,832.824144791397,126.469234363367));
#69049=CARTESIAN_POINT('Ctrl Pts',(105.684542041252,832.928945580426,126.502750658433));
#69050=CARTESIAN_POINT('Ctrl Pts',(105.639851381538,833.147240642146,126.578298086916));
#69051=CARTESIAN_POINT('Ctrl Pts',(105.639262424399,833.25877576474,126.619681076013));
#69052=CARTESIAN_POINT('Ctrl Pts',(105.682259384937,833.477366759787,126.706389989212));
#69053=CARTESIAN_POINT('Ctrl Pts',(105.726597763458,833.582125107827,126.750961454064));
#69054=CARTESIAN_POINT('Ctrl Pts',(105.858712803437,833.773343681452,126.839110846006));
#69055=CARTESIAN_POINT('Ctrl Pts',(105.947279665046,833.856571908926,126.88160830431));
#69056=CARTESIAN_POINT('Ctrl Pts',(106.152879181124,833.982255567292,126.955692269105));
#69057=CARTESIAN_POINT('Ctrl Pts',(106.267282192868,834.024402784345,126.986809760084));
#69058=CARTESIAN_POINT('Ctrl Pts',(106.510285783741,834.064457978969,127.035086926522));
#69059=CARTESIAN_POINT('Ctrl Pts',(106.636802809456,834.061372969921,127.051599645854));
#69060=CARTESIAN_POINT('Ctrl Pts',(106.88465299152,834.008826857744,127.067108499236));
#69061=CARTESIAN_POINT('Ctrl Pts',(107.003588033846,833.959442793996,127.065793565877));
#69062=CARTESIAN_POINT('Ctrl Pts',(107.205115233036,833.827537429491,127.045796551336));
#69063=CARTESIAN_POINT('Ctrl Pts',(107.288597508492,833.750045845327,127.029088179082));
#69064=CARTESIAN_POINT('Ctrl Pts',(107.427224446225,833.567517731427,126.981229937407));
#69065=CARTESIAN_POINT('Ctrl Pts',(107.479432889011,833.462999668539,126.949838131088));
#69066=CARTESIAN_POINT('Ctrl Pts',(107.519637551879,833.318054914236,126.901465502322));
#69067=CARTESIAN_POINT('Ctrl Pts',(107.527099262435,833.282720439317,126.889322421523));
#69068=CARTESIAN_POINT('Ctrl Pts',(107.532294808004,833.247164435627,126.876755726751));
#69069=CARTESIAN_POINT('Ctrl Pts',(106.593082004706,833.382657080601,128.950197605091));
#69070=CARTESIAN_POINT('Ctrl Pts',(106.593566586252,833.382628762013,128.950277729248));
#69071=CARTESIAN_POINT('Ctrl Pts',(106.594051184575,833.382600092925,128.95035773022));
#69072=CARTESIAN_POINT('Ctrl Pts',(106.594535799255,833.38257107329,128.950437607906));
#69073=CARTESIAN_POINT('Ctrl Pts',(106.718490536038,833.375148431477,128.970868721557));
#69074=CARTESIAN_POINT('Ctrl Pts',(106.841376115117,833.344915423,128.982894032538));
#69075=CARTESIAN_POINT('Ctrl Pts',(107.069826980962,833.242557646128,128.988278417489));
#69076=CARTESIAN_POINT('Ctrl Pts',(107.173550330991,833.171754496403,128.981766361638));
#69077=CARTESIAN_POINT('Ctrl Pts',(107.347645321587,832.999315246611,128.950570955162));
#69078=CARTESIAN_POINT('Ctrl Pts',(107.41687218612,832.899849741347,128.926474465598));
#69079=CARTESIAN_POINT('Ctrl Pts',(107.51281361132,832.684051168875,128.863181751529));
#69080=CARTESIAN_POINT('Ctrl Pts',(107.538662259665,832.570042501173,128.824695839511));
#69081=CARTESIAN_POINT('Ctrl Pts',(107.543353913986,832.340478653054,128.737506920593));
#69082=CARTESIAN_POINT('Ctrl Pts',(107.52155108143,832.227438682135,128.68963989793));
#69083=CARTESIAN_POINT('Ctrl Pts',(107.431703158797,832.01661241602,128.590606090183));
#69084=CARTESIAN_POINT('Ctrl Pts',(107.363697477087,831.921395459319,128.54044669291));
#69085=CARTESIAN_POINT('Ctrl Pts',(107.189301746346,831.762226072258,128.445120679388));
#69086=CARTESIAN_POINT('Ctrl Pts',(107.083886573825,831.700446812157,128.401002341125));
#69087=CARTESIAN_POINT('Ctrl Pts',(106.850930292356,831.620656774394,128.326243839117));
#69088=CARTESIAN_POINT('Ctrl Pts',(106.725438767296,831.603433977474,128.29630366665));
#69089=CARTESIAN_POINT('Ctrl Pts',(106.596684952895,831.610049564228,128.275382995262));
#69090=CARTESIAN_POINT('Ctrl Pts',(106.594883381751,831.610146901093,128.275092185357));
#69091=CARTESIAN_POINT('Ctrl Pts',(106.593082004564,831.610248993975,128.2748033254));
#69092=CARTESIAN_POINT('Origin',(106.593082004564,836.288239824643,117.884080028985));
#69093=CARTESIAN_POINT('',(106.593082004564,834.624823193137,124.090975272474));
#69094=CARTESIAN_POINT('Origin',(106.593082004564,834.153400962528,123.924358705207));
#69095=CARTESIAN_POINT('',(106.593082004564,832.964211408695,128.789483496701));
#69096=CARTESIAN_POINT('',(106.593082004564,836.759662055252,118.050696596252));
#69097=CARTESIAN_POINT('Ctrl Pts',(106.593366660624,832.02945867497,128.433356001948));
#69098=CARTESIAN_POINT('Ctrl Pts',(106.529229872268,832.033084018716,128.422988938261));
#69099=CARTESIAN_POINT('Ctrl Pts',(106.465562429969,832.048176387402,128.417210567738));
#69100=CARTESIAN_POINT('Ctrl Pts',(106.344515676303,832.100634675078,128.415463730008));
#69101=CARTESIAN_POINT('Ctrl Pts',(106.288518675592,832.138112024034,128.419788627033));
#69102=CARTESIAN_POINT('Ctrl Pts',(106.195294077639,832.229555154974,128.43811226833));
#69103=CARTESIAN_POINT('Ctrl Pts',(106.158509650955,832.282139172819,128.451657695177));
#69104=CARTESIAN_POINT('Ctrl Pts',(106.107748472945,832.396354998587,128.486163431682));
#69105=CARTESIAN_POINT('Ctrl Pts',(106.09418295559,832.456768272901,128.506730952175));
#69106=CARTESIAN_POINT('Ctrl Pts',(106.092103923698,832.578126861548,128.552413755081));
#69107=CARTESIAN_POINT('Ctrl Pts',(106.103748191406,832.637801790198,128.577075359564));
#69108=CARTESIAN_POINT('Ctrl Pts',(106.151528610457,832.749639875857,128.627895107614));
#69109=CARTESIAN_POINT('Ctrl Pts',(106.187801996539,832.80036912786,128.653537993184));
#69110=CARTESIAN_POINT('Ctrl Pts',(106.280135616138,832.884421758021,128.701911539482));
#69111=CARTESIAN_POINT('Ctrl Pts',(106.33536955164,832.916828547416,128.72415136493));
#69112=CARTESIAN_POINT('Ctrl Pts',(106.457595851277,832.958840007983,128.762366164734));
#69113=CARTESIAN_POINT('Ctrl Pts',(106.523547910496,832.967875206953,128.777939067417));
#69114=CARTESIAN_POINT('Ctrl Pts',(106.657248103403,832.960845441647,128.800142247882));
#69115=CARTESIAN_POINT('Ctrl Pts',(106.723796670554,832.944694340638,128.806517052477));
#69116=CARTESIAN_POINT('Ctrl Pts',(106.845790324969,832.88983692334,128.808763319625));
#69117=CARTESIAN_POINT('Ctrl Pts',(106.90044739155,832.852405460387,128.804961284532));
#69118=CARTESIAN_POINT('Ctrl Pts',(106.99212519188,832.761229910569,128.787811655891));
#69119=CARTESIAN_POINT('Ctrl Pts',(107.028515633763,832.708620735536,128.774771708297));
#69120=CARTESIAN_POINT('Ctrl Pts',(107.078724348598,832.594535865148,128.740911588646));
#69121=CARTESIAN_POINT('Ctrl Pts',(107.092100143423,832.534283978702,128.720471727768));
#69122=CARTESIAN_POINT('Ctrl Pts',(107.093969569075,832.413137018149,128.674484579145));
#69123=CARTESIAN_POINT('Ctrl Pts',(107.082180859807,832.353551432732,128.649383923729));
#69124=CARTESIAN_POINT('Ctrl Pts',(107.034299560962,832.24257144573,128.59765875814));
#69125=CARTESIAN_POINT('Ctrl Pts',(106.998277536441,832.19250631668,128.571560224117));
#69126=CARTESIAN_POINT('Ctrl Pts',(106.905797872564,832.108583894106,128.521815529678));
#69127=CARTESIAN_POINT('Ctrl Pts',(106.849745265658,832.076014003546,128.498746767882));
#69128=CARTESIAN_POINT('Ctrl Pts',(106.726368574756,832.034423712299,128.459756828865));
#69129=CARTESIAN_POINT('Ctrl Pts',(106.660208106405,832.025680449965,128.444160246175));
#69130=CARTESIAN_POINT('Ctrl Pts',(106.593366660624,832.02945867497,128.433356001948));
#69131=CARTESIAN_POINT('Origin',(102.144722372893,820.841213146102,112.424578137575));
#69132=CARTESIAN_POINT('',(102.144722372892,816.254389947185,122.337315571232));
#69133=CARTESIAN_POINT('',(102.144722372897,818.188798096017,122.994424754414));
#69134=CARTESIAN_POINT('Ctrl Pts',(102.144722372892,816.254389947185,122.337315571232));
#69135=CARTESIAN_POINT('Ctrl Pts',(102.01448283502,816.257559043848,122.3283489802));
#69136=CARTESIAN_POINT('Ctrl Pts',(101.885333726022,816.284085748256,122.328050406789));
#69137=CARTESIAN_POINT('Ctrl Pts',(101.639205011226,816.382794367041,122.345203847486));
#69138=CARTESIAN_POINT('Ctrl Pts',(101.525237096631,816.455477147213,122.363071347237));
#69139=CARTESIAN_POINT('Ctrl Pts',(101.33324081447,816.637328130539,122.414444751396));
#69140=CARTESIAN_POINT('Ctrl Pts',(101.256924249962,816.744528982366,122.44735071358));
#69141=CARTESIAN_POINT('Ctrl Pts',(101.151828310525,816.980361239478,122.523340516029));
#69142=CARTESIAN_POINT('Ctrl Pts',(101.124248130998,817.106731592453,122.565686789286));
#69143=CARTESIAN_POINT('Ctrl Pts',(101.12242427395,817.361930091502,122.653628596318));
#69144=CARTESIAN_POINT('Ctrl Pts',(101.148341013592,817.488234278117,122.698352287058));
#69145=CARTESIAN_POINT('Ctrl Pts',(101.250666563817,817.722869309163,122.783883616561));
#69146=CARTESIAN_POINT('Ctrl Pts',(101.325914958908,817.828934815759,122.823867312529));
#69147=CARTESIAN_POINT('Ctrl Pts',(101.515724899758,818.006218208579,122.894269023263));
#69148=CARTESIAN_POINT('Ctrl Pts',(101.628300437093,818.075786292927,122.924039736244));
#69149=CARTESIAN_POINT('Ctrl Pts',(101.876649923645,818.169079109118,122.970299909665));
#69150=CARTESIAN_POINT('Ctrl Pts',(102.010057204773,818.19167386802,122.986288091447));
#69151=CARTESIAN_POINT('Ctrl Pts',(102.144722372902,818.188798096017,122.994424754414));
#69152=CARTESIAN_POINT('',(102.14472237325,818.827174390792,121.18821315261));
#69153=CARTESIAN_POINT('',(102.144722372893,821.804242286345,112.764945220642));
#69154=CARTESIAN_POINT('Ctrl Pts',(103.149564180549,817.660946014935,120.872963773621));
#69155=CARTESIAN_POINT('Ctrl Pts',(103.125674937399,817.537414267004,120.829303474101));
#69156=CARTESIAN_POINT('Ctrl Pts',(103.076397526074,817.420234466966,120.785571257734));
#69157=CARTESIAN_POINT('Ctrl Pts',(102.932682761671,817.211704355957,120.70301803522));
#69158=CARTESIAN_POINT('Ctrl Pts',(102.839646051471,817.122387338972,120.6650077997));
#69159=CARTESIAN_POINT('Ctrl Pts',(102.621322617236,816.983180158415,120.599954793548));
#69160=CARTESIAN_POINT('Ctrl Pts',(102.497992734769,816.934798730656,120.573593326978));
#69161=CARTESIAN_POINT('Ctrl Pts',(102.236940011704,816.8859357297,120.536558770922));
#69162=CARTESIAN_POINT('Ctrl Pts',(102.101642396639,816.886127045467,120.526313459366));
#69163=CARTESIAN_POINT('Ctrl Pts',(101.83739496844,816.935801832543,120.52377438526));
#69164=CARTESIAN_POINT('Ctrl Pts',(101.710979198984,816.984862841166,120.531525035075));
#69165=CARTESIAN_POINT('Ctrl Pts',(101.485292475534,817.125248122336,120.563932606559));
#69166=CARTESIAN_POINT('Ctrl Pts',(101.387925527677,817.214834393102,120.588115179616));
#69167=CARTESIAN_POINT('Ctrl Pts',(101.233142430397,817.424911210335,120.649959033043));
#69168=CARTESIAN_POINT('Ctrl Pts',(101.177782792624,817.543706890498,120.687167705484));
#69169=CARTESIAN_POINT('Ctrl Pts',(101.118555136005,817.794112423427,120.769178597195));
#69170=CARTESIAN_POINT('Ctrl Pts',(101.115360280281,817.923247652267,120.813167882312));
#69171=CARTESIAN_POINT('Ctrl Pts',(101.162031716901,818.172995627507,120.90134109584));
#69172=CARTESIAN_POINT('Ctrl Pts',(101.21091572821,818.291236803578,120.944656272247));
#69173=CARTESIAN_POINT('Ctrl Pts',(101.354357723054,818.502108459169,121.025366483967));
#69174=CARTESIAN_POINT('Ctrl Pts',(101.447480445364,818.592697757262,121.061984706085));
#69175=CARTESIAN_POINT('Ctrl Pts',(101.665567720486,818.733675018226,121.123886899891));
#69176=CARTESIAN_POINT('Ctrl Pts',(101.788318947099,818.782834550997,121.148620174046));
#69177=CARTESIAN_POINT('Ctrl Pts',(102.048820054437,818.833399767813,121.183494725859));
#69178=CARTESIAN_POINT('Ctrl Pts',(102.18416229911,818.833908535048,121.193179467386));
#69179=CARTESIAN_POINT('Ctrl Pts',(102.450028231007,818.784865476997,121.195977643805));
#69180=CARTESIAN_POINT('Ctrl Pts',(102.577876152832,818.735199674138,121.188865621007));
#69181=CARTESIAN_POINT('Ctrl Pts',(102.805630027172,818.592511939164,121.158446593098));
#69182=CARTESIAN_POINT('Ctrl Pts',(102.903652690307,818.501330804433,121.135600440196));
#69183=CARTESIAN_POINT('Ctrl Pts',(103.057825743493,818.289130385116,121.076746003304));
#69184=CARTESIAN_POINT('Ctrl Pts',(103.112536102743,818.170203762147,121.041315367079));
#69185=CARTESIAN_POINT('Ctrl Pts',(103.156416811535,817.982240369834,120.981747837426));
#69186=CARTESIAN_POINT('Ctrl Pts',(103.164526141302,817.918194852751,120.960878456479));
#69187=CARTESIAN_POINT('Ctrl Pts',(103.167320560797,817.789129935012,120.917658471095));
#69188=CARTESIAN_POINT('Ctrl Pts',(103.161843562539,817.724442941614,120.895405735981));
#69189=CARTESIAN_POINT('Ctrl Pts',(103.149564180549,817.660946014935,120.872963773621));
#69190=CARTESIAN_POINT('Ctrl Pts',(102.144722372902,818.188798096017,122.994424754414));
#69191=CARTESIAN_POINT('Ctrl Pts',(102.144921974185,818.188793833536,122.99443681461));
#69192=CARTESIAN_POINT('Ctrl Pts',(102.145121578235,818.188789515112,122.99444885751));
#69193=CARTESIAN_POINT('Ctrl Pts',(102.145321185027,818.188785140742,122.994460883112));
#69194=CARTESIAN_POINT('Ctrl Pts',(102.276018833491,818.185920910063,123.002334953166));
#69195=CARTESIAN_POINT('Ctrl Pts',(102.405450290849,818.159117399055,123.002667847017));
#69196=CARTESIAN_POINT('Ctrl Pts',(102.650512819559,818.059523212747,122.988014642784));
#69197=CARTESIAN_POINT('Ctrl Pts',(102.76345024988,817.986634529791,122.97280862151));
#69198=CARTESIAN_POINT('Ctrl Pts',(102.954123678733,817.804611259951,122.928076170702));
#69199=CARTESIAN_POINT('Ctrl Pts',(103.030215612037,817.697335910332,122.899013288643));
#69200=CARTESIAN_POINT('Ctrl Pts',(103.135434359748,817.462463797933,122.830052773349));
#69201=CARTESIAN_POINT('Ctrl Pts',(103.163681801997,817.337182959394,122.790834743897));
#69202=CARTESIAN_POINT('Ctrl Pts',(103.168279574962,817.08454906744,122.706661062042));
#69203=CARTESIAN_POINT('Ctrl Pts',(103.144479540307,816.959702721951,122.662524637957));
#69204=CARTESIAN_POINT('Ctrl Pts',(103.047084629083,816.726621903064,122.574967012687));
#69205=CARTESIAN_POINT('Ctrl Pts',(102.974184798905,816.62082493286,122.5324356244));
#69206=CARTESIAN_POINT('Ctrl Pts',(102.788264169511,816.442764856226,122.455239610837));
#69207=CARTESIAN_POINT('Ctrl Pts',(102.676884053809,816.372408509239,122.42138543827));
#69208=CARTESIAN_POINT('Ctrl Pts',(102.430524716656,816.277126019276,122.367880826043));
#69209=CARTESIAN_POINT('Ctrl Pts',(102.29788291689,816.253140111851,122.3487674368));
#69210=CARTESIAN_POINT('Ctrl Pts',(102.157209430967,816.254139835481,122.338194956278));
#69211=CARTESIAN_POINT('Ctrl Pts',(102.150964647552,816.254238054971,122.337745332615));
#69212=CARTESIAN_POINT('Ctrl Pts',(102.144722372892,816.254389947185,122.337315571232));
#69213=CARTESIAN_POINT('Origin',(102.144722372893,820.841213146102,112.424578137575));
#69214=CARTESIAN_POINT('',(102.144722372893,819.177796514596,118.631473381063));
#69215=CARTESIAN_POINT('Origin',(102.144722372893,818.706374283987,118.464856813796));
#69216=CARTESIAN_POINT('',(102.144722372893,817.695341518356,122.825907659524));
#69217=CARTESIAN_POINT('',(102.144722372893,821.312635376711,112.591194704842));
#69218=CARTESIAN_POINT('Ctrl Pts',(102.144732739577,816.748420555005,122.504208514761));
#69219=CARTESIAN_POINT('Ctrl Pts',(102.082926213998,816.749872861288,122.500095537239));
#69220=CARTESIAN_POINT('Ctrl Pts',(102.021641901999,816.76211826188,122.49983554938));
#69221=CARTESIAN_POINT('Ctrl Pts',(101.902064442961,816.808636819692,122.507325850532));
#69222=CARTESIAN_POINT('Ctrl Pts',(101.845509411206,816.844022033751,122.515598795588));
#69223=CARTESIAN_POINT('Ctrl Pts',(101.749938477978,816.933202929328,122.539823115067));
#69224=CARTESIAN_POINT('Ctrl Pts',(101.711824469246,816.986063262919,122.555508832254));
#69225=CARTESIAN_POINT('Ctrl Pts',(101.659266657108,817.102456110172,122.592085811327));
#69226=CARTESIAN_POINT('Ctrl Pts',(101.645383934472,817.164835103884,122.612612541681));
#69227=CARTESIAN_POINT('Ctrl Pts',(101.644106180934,817.290698493168,122.655611028783));
#69228=CARTESIAN_POINT('Ctrl Pts',(101.65675679843,817.352913990414,122.677649309188));
#69229=CARTESIAN_POINT('Ctrl Pts',(101.707115239758,817.468441092188,122.72016248875));
#69230=CARTESIAN_POINT('Ctrl Pts',(101.744281836181,817.520600863929,122.740213358666));
#69231=CARTESIAN_POINT('Ctrl Pts',(101.838182831566,817.607598727747,122.77570469556));
#69232=CARTESIAN_POINT('Ctrl Pts',(101.893952197496,817.641585061121,122.790799450178));
#69233=CARTESIAN_POINT('Ctrl Pts',(102.016836789362,817.686674346669,122.814181924386));
#69234=CARTESIAN_POINT('Ctrl Pts',(102.082758896603,817.697254907804,122.822218828137));
#69235=CARTESIAN_POINT('Ctrl Pts',(102.214775570901,817.69321892032,122.830091342823));
#69236=CARTESIAN_POINT('Ctrl Pts',(102.279591222087,817.678966204137,122.829957578635));
#69237=CARTESIAN_POINT('Ctrl Pts',(102.400208867725,817.627657586543,122.821614891196));
#69238=CARTESIAN_POINT('Ctrl Pts',(102.45488301693,817.591125059419,122.813496122556));
#69239=CARTESIAN_POINT('Ctrl Pts',(102.546662548993,817.500589627919,122.790178445001));
#69240=CARTESIAN_POINT('Ctrl Pts',(102.582955436481,817.447506317204,122.775221177029));
#69241=CARTESIAN_POINT('Ctrl Pts',(102.632278395286,817.331714167397,122.740216771296));
#69242=CARTESIAN_POINT('Ctrl Pts',(102.644883606345,817.270147421615,122.720516185985));
#69243=CARTESIAN_POINT('Ctrl Pts',(102.644557862627,817.146454664415,122.678761190402));
#69244=CARTESIAN_POINT('Ctrl Pts',(102.631604154655,817.085548920734,122.657115130615));
#69245=CARTESIAN_POINT('Ctrl Pts',(102.581493193793,816.972361457722,122.614685200656));
#69246=CARTESIAN_POINT('Ctrl Pts',(102.544745732041,816.921234710257,122.594327355879));
#69247=CARTESIAN_POINT('Ctrl Pts',(102.452028501185,816.835709539048,122.557770320426));
#69248=CARTESIAN_POINT('Ctrl Pts',(102.396899514493,816.802207792346,122.541947773768));
#69249=CARTESIAN_POINT('Ctrl Pts',(102.27553269161,816.757561985037,122.517228039019));
#69250=CARTESIAN_POINT('Ctrl Pts',(102.210446181577,816.746876445483,122.508581481974));
#69251=CARTESIAN_POINT('Ctrl Pts',(102.144732739577,816.748420555005,122.504208514761));
#69252=CARTESIAN_POINT('Origin',(106.957908439915,825.606009837406,114.108618509208));
#69253=CARTESIAN_POINT('',(106.957908439915,820.918639451936,124.525880166841));
#69254=CARTESIAN_POINT('',(106.957908439943,822.714037109275,125.136228125604));
#69255=CARTESIAN_POINT('Ctrl Pts',(106.957908439915,820.918639451935,124.525880166841));
#69256=CARTESIAN_POINT('Ctrl Pts',(106.834925181281,820.925791453,124.505644410275));
#69257=CARTESIAN_POINT('Ctrl Pts',(106.712929193591,820.955387903885,124.493716319717));
#69258=CARTESIAN_POINT('Ctrl Pts',(106.483232995468,821.05718149143,124.48782534621));
#69259=CARTESIAN_POINT('Ctrl Pts',(106.377868908004,821.128953076226,124.494135968551));
#69260=CARTESIAN_POINT('Ctrl Pts',(106.200587221442,821.305509989051,124.524310281196));
#69261=CARTESIAN_POINT('Ctrl Pts',(106.130232003092,821.408347994478,124.547757301054));
#69262=CARTESIAN_POINT('Ctrl Pts',(106.035173096044,821.630095879669,124.607839960344));
#69263=CARTESIAN_POINT('Ctrl Pts',(106.010538595136,821.746405328518,124.643583786556));
#69264=CARTESIAN_POINT('Ctrl Pts',(106.009133011291,821.980490748669,124.723295580061));
#69265=CARTESIAN_POINT('Ctrl Pts',(106.032860954363,822.095809796808,124.766502341402));
#69266=CARTESIAN_POINT('Ctrl Pts',(106.12680995675,822.309749177369,124.854856915442));
#69267=CARTESIAN_POINT('Ctrl Pts',(106.196498804425,822.405912616758,124.899089097247));
#69268=CARTESIAN_POINT('Ctrl Pts',(106.372588764774,822.564856895177,124.982741063986));
#69269=CARTESIAN_POINT('Ctrl Pts',(106.477298528654,822.625902635073,125.021302078196));
#69270=CARTESIAN_POINT('Ctrl Pts',(106.708338259671,822.704652344538,125.088258991379));
#69271=CARTESIAN_POINT('Ctrl Pts',(106.83262340867,822.721212144327,125.115927197065));
#69272=CARTESIAN_POINT('Ctrl Pts',(106.957908439971,822.714037109275,125.136228125604));
#69273=CARTESIAN_POINT('',(106.957908439915,823.382883520564,123.243804867125));
#69274=CARTESIAN_POINT('',(106.957908439915,826.499906010025,114.424551662345));
#69275=CARTESIAN_POINT('Ctrl Pts',(107.903500219465,822.378156070275,123.035280408344));
#69276=CARTESIAN_POINT('Ctrl Pts',(107.894920100932,822.266815941935,122.995929039701));
#69277=CARTESIAN_POINT('Ctrl Pts',(107.864302758957,822.159102313565,122.954511621887));
#69278=CARTESIAN_POINT('Ctrl Pts',(107.759471279212,821.956476440659,122.869618837775));
#69279=CARTESIAN_POINT('Ctrl Pts',(107.684005985044,821.864704993812,122.827038340615));
#69280=CARTESIAN_POINT('Ctrl Pts',(107.500409159485,821.717155731259,122.749683624278));
#69281=CARTESIAN_POINT('Ctrl Pts',(107.394583870129,821.662166004448,122.715518855886));
#69282=CARTESIAN_POINT('Ctrl Pts',(107.16329529463,821.593563026828,122.659038161755));
#69283=CARTESIAN_POINT('Ctrl Pts',(107.039657774991,821.581251338835,122.637441700713));
#69284=CARTESIAN_POINT('Ctrl Pts',(106.790731498044,821.602514999532,122.610364727493));
#69285=CARTESIAN_POINT('Ctrl Pts',(106.667744096107,821.636460901695,122.605337771844));
#69286=CARTESIAN_POINT('Ctrl Pts',(106.440303173469,821.747275688919,122.613048268249));
#69287=CARTESIAN_POINT('Ctrl Pts',(106.338084188269,821.823181366092,122.625749470995));
#69288=CARTESIAN_POINT('Ctrl Pts',(106.172681420484,822.003513190906,122.666331933578));
#69289=CARTESIAN_POINT('Ctrl Pts',(106.109571278476,822.104934787982,122.693169082771));
#69290=CARTESIAN_POINT('Ctrl Pts',(106.027472723286,822.319845397616,122.756659535749));
#69291=CARTESIAN_POINT('Ctrl Pts',(106.007833138054,822.430898689888,122.79238567702));
#69292=CARTESIAN_POINT('Ctrl Pts',(106.01214526248,822.653195141141,122.869347331955));
#69293=CARTESIAN_POINT('Ctrl Pts',(106.036300365844,822.762394930614,122.909904935309));
#69294=CARTESIAN_POINT('Ctrl Pts',(106.127215238831,822.967715671916,122.991923691824));
#69295=CARTESIAN_POINT('Ctrl Pts',(106.194208374972,823.061441406852,123.032595857908));
#69296=CARTESIAN_POINT('Ctrl Pts',(106.367027912732,823.22244189507,123.110065156012));
#69297=CARTESIAN_POINT('Ctrl Pts',(106.472918825171,823.286399950998,123.145751883668));
#69298=CARTESIAN_POINT('Ctrl Pts',(106.703795827351,823.368830119372,123.204548601583));
#69299=CARTESIAN_POINT('Ctrl Pts',(106.826116824876,823.387518710045,123.227375020255));
#69300=CARTESIAN_POINT('Ctrl Pts',(107.07500694945,823.378828739677,123.258423996052));
#69301=CARTESIAN_POINT('Ctrl Pts',(107.199298577057,823.350889359037,123.266152339495));
#69302=CARTESIAN_POINT('Ctrl Pts',(107.432506609306,823.250671846939,123.264812507143));
#69303=CARTESIAN_POINT('Ctrl Pts',(107.539070854672,823.17894149244,123.255599638526));
#69304=CARTESIAN_POINT('Ctrl Pts',(107.708951550872,823.010230739755,123.222594354461));
#69305=CARTESIAN_POINT('Ctrl Pts',(107.774261380901,822.917994312338,123.200674655697));
#69306=CARTESIAN_POINT('Ctrl Pts',(107.870762530212,822.712165723077,123.144581237638));
#69307=CARTESIAN_POINT('Ctrl Pts',(107.899166665534,822.599659199883,123.110366039151));
#69308=CARTESIAN_POINT('Ctrl Pts',(107.906728069839,822.449980974197,123.060320441437));
#69309=CARTESIAN_POINT('Ctrl Pts',(107.906258854175,822.413953564389,123.047932454002));
#69310=CARTESIAN_POINT('Ctrl Pts',(107.903500219465,822.378156070276,123.035280408344));
#69311=CARTESIAN_POINT('Ctrl Pts',(106.957908439971,822.714037109275,125.136228125604));
#69312=CARTESIAN_POINT('Ctrl Pts',(106.958225949864,822.714018925581,125.136279574254));
#69313=CARTESIAN_POINT('Ctrl Pts',(106.958543466198,822.71400058948,125.136330975481));
#69314=CARTESIAN_POINT('Ctrl Pts',(106.958860988855,822.713982100959,125.136382329263));
#69315=CARTESIAN_POINT('Ctrl Pts',(107.082183504009,822.706801350697,125.156327606682));
#69316=CARTESIAN_POINT('Ctrl Pts',(107.204315847898,822.676748446124,125.168784705021));
#69317=CARTESIAN_POINT('Ctrl Pts',(107.433103833348,822.574019529265,125.177189969658));
#69318=CARTESIAN_POINT('Ctrl Pts',(107.537700475697,822.501998097256,125.172968233913));
#69319=CARTESIAN_POINT('Ctrl Pts',(107.712795108306,822.326444658996,125.147723308565));
#69320=CARTESIAN_POINT('Ctrl Pts',(107.782301520331,822.225112537125,125.12723078329));
#69321=CARTESIAN_POINT('Ctrl Pts',(107.877977001318,822.005904816772,125.072143002326));
#69322=CARTESIAN_POINT('Ctrl Pts',(107.903664443433,821.890420768215,125.038250930893));
#69323=CARTESIAN_POINT('Ctrl Pts',(107.908029172466,821.65853590756,124.960632384663));
#69324=CARTESIAN_POINT('Ctrl Pts',(107.886442783627,821.544640051224,124.917698480754));
#69325=CARTESIAN_POINT('Ctrl Pts',(107.797513666835,821.332093544325,124.827822923118));
#69326=CARTESIAN_POINT('Ctrl Pts',(107.730340044753,821.236057615969,124.781807555512));
#69327=CARTESIAN_POINT('Ctrl Pts',(107.558029632007,821.075177001686,124.693188387097));
#69328=CARTESIAN_POINT('Ctrl Pts',(107.453962582539,821.012564342653,124.651570996227));
#69329=CARTESIAN_POINT('Ctrl Pts',(107.221766398994,820.930086273414,124.578987427032));
#69330=CARTESIAN_POINT('Ctrl Pts',(107.095367494674,820.91191116206,124.548954811932));
#69331=CARTESIAN_POINT('Ctrl Pts',(106.964318597556,820.918281957199,124.526940418755));
#69332=CARTESIAN_POINT('Ctrl Pts',(106.96111318255,820.918453082482,124.526407477571));
#69333=CARTESIAN_POINT('Ctrl Pts',(106.957908439915,820.918639451935,124.525880166841));
#69334=CARTESIAN_POINT('Origin',(106.957908439915,825.606009837406,114.108618509208));
#69335=CARTESIAN_POINT('',(106.957908439915,823.9425932059,120.315513752696));
#69336=CARTESIAN_POINT('Origin',(106.957908439915,823.471170975291,120.148897185429));
#69337=CARTESIAN_POINT('',(106.957908439915,822.290121186054,124.990991458137));
#69338=CARTESIAN_POINT('',(106.957908439915,826.077432068015,114.275235076475));
#69339=CARTESIAN_POINT('Ctrl Pts',(106.958222165921,821.343250545434,124.669150226088));
#69340=CARTESIAN_POINT('Ctrl Pts',(106.892818314994,821.346999101619,124.658420971245));
#69341=CARTESIAN_POINT('Ctrl Pts',(106.827973941537,821.362822182442,124.652039907669));
#69342=CARTESIAN_POINT('Ctrl Pts',(106.706127188088,821.417263436913,124.648701539818));
#69343=CARTESIAN_POINT('Ctrl Pts',(106.650342596402,821.455633557114,124.651879470715));
#69344=CARTESIAN_POINT('Ctrl Pts',(106.557641531978,821.549011664705,124.667387009783));
#69345=CARTESIAN_POINT('Ctrl Pts',(106.521165926485,821.60268099703,124.679330397564));
#69346=CARTESIAN_POINT('Ctrl Pts',(106.471381547181,821.718859927245,124.710292783712));
#69347=CARTESIAN_POINT('Ctrl Pts',(106.458365251161,821.780114158469,124.728931282838));
#69348=CARTESIAN_POINT('Ctrl Pts',(106.457475142972,821.902759510721,124.770570785216));
#69349=CARTESIAN_POINT('Ctrl Pts',(106.469617489539,821.962874942451,124.793139263138));
#69350=CARTESIAN_POINT('Ctrl Pts',(106.518091875654,822.075026388566,124.839711185584));
#69351=CARTESIAN_POINT('Ctrl Pts',(106.554351749362,822.125697829141,124.863239789614));
#69352=CARTESIAN_POINT('Ctrl Pts',(106.646693326278,822.210122721922,124.908110195148));
#69353=CARTESIAN_POINT('Ctrl Pts',(106.702091361353,822.24275767519,124.928957256173));
#69354=CARTESIAN_POINT('Ctrl Pts',(106.824493076789,822.284924682606,124.965086126507));
#69355=CARTESIAN_POINT('Ctrl Pts',(106.890407855879,822.29387030579,124.979979312455));
#69356=CARTESIAN_POINT('Ctrl Pts',(107.023922870188,822.286456511742,125.001761775637));
#69357=CARTESIAN_POINT('Ctrl Pts',(107.090317110489,822.269963943636,125.008388908033));
#69358=CARTESIAN_POINT('Ctrl Pts',(107.212406525572,822.214057763881,125.012129928141));
#69359=CARTESIAN_POINT('Ctrl Pts',(107.267258714984,822.175707090314,125.009439146229));
#69360=CARTESIAN_POINT('Ctrl Pts',(107.358868248356,822.082477678299,124.995170712216));
#69361=CARTESIAN_POINT('Ctrl Pts',(107.395075626198,822.028754809419,124.983875259776));
#69362=CARTESIAN_POINT('Ctrl Pts',(107.444481559075,821.912698140194,124.953991540321));
#69363=CARTESIAN_POINT('Ctrl Pts',(107.457416616252,821.851624437337,124.935777180103));
#69364=CARTESIAN_POINT('Ctrl Pts',(107.458374458683,821.729254849129,124.894454762244));
#69365=CARTESIAN_POINT('Ctrl Pts',(107.44629735527,821.669267360435,124.871770656094));
#69366=CARTESIAN_POINT('Ctrl Pts',(107.398096093024,821.557651868738,124.824619385304));
#69367=CARTESIAN_POINT('Ctrl Pts',(107.362122648394,821.507365458191,124.800638495034));
#69368=CARTESIAN_POINT('Ctrl Pts',(107.270199522723,821.423229564206,124.754549414011));
#69369=CARTESIAN_POINT('Ctrl Pts',(107.214773418277,821.390617372222,124.732966782589));
#69370=CARTESIAN_POINT('Ctrl Pts',(107.091840519965,821.348340849408,124.695551428081));
#69371=CARTESIAN_POINT('Ctrl Pts',(107.0253371481,821.339403917476,124.680160185553));
#69372=CARTESIAN_POINT('Ctrl Pts',(106.958222165921,821.343250545434,124.669150226088));
#69373=CARTESIAN_POINT('Origin',(99.2004494076648,811.368542512753,109.076615819925));
#69374=CARTESIAN_POINT('',(99.2004494076648,806.777379182049,119.001633152524));
#69375=CARTESIAN_POINT('',(99.200449407666,808.721073021462,119.632469552402));
#69376=CARTESIAN_POINT('Ctrl Pts',(99.2004494076648,806.777379182049,119.001633152524));
#69377=CARTESIAN_POINT('Ctrl Pts',(99.070502125323,806.780520677886,118.992744654824));
#69378=CARTESIAN_POINT('Ctrl Pts',(98.9416808923822,806.807078066664,118.992024529602));
#69379=CARTESIAN_POINT('Ctrl Pts',(98.6948096590929,806.906338889037,119.007670425697));
#69380=CARTESIAN_POINT('Ctrl Pts',(98.5799610544503,806.980050408541,119.024646475322));
#69381=CARTESIAN_POINT('Ctrl Pts',(98.3874632645327,807.163969124872,119.0740877708));
#69382=CARTESIAN_POINT('Ctrl Pts',(98.3112963781483,807.271951410195,119.10587854437));
#69383=CARTESIAN_POINT('Ctrl Pts',(98.2069661211874,807.508722169788,119.179510555792));
#69384=CARTESIAN_POINT('Ctrl Pts',(98.1797558642064,807.63514960335,119.220591621919));
#69385=CARTESIAN_POINT('Ctrl Pts',(98.1783519247404,807.890441700475,119.306045394217));
#69386=CARTESIAN_POINT('Ctrl Pts',(98.2043440701219,808.016792532354,119.349568694292));
#69387=CARTESIAN_POINT('Ctrl Pts',(98.3067294635506,808.251973127116,119.432723418524));
#69388=CARTESIAN_POINT('Ctrl Pts',(98.3821106445267,808.358483040857,119.47153464452));
#69389=CARTESIAN_POINT('Ctrl Pts',(98.5722066780431,808.536635542329,119.539347110914));
#69390=CARTESIAN_POINT('Ctrl Pts',(98.6849255663226,808.606633366165,119.567727414568));
#69391=CARTESIAN_POINT('Ctrl Pts',(98.9331184060169,808.700554506976,119.611047527071));
#69392=CARTESIAN_POINT('Ctrl Pts',(99.0661564394842,808.723512096891,119.625568471686));
#69393=CARTESIAN_POINT('Ctrl Pts',(99.2004494076673,808.721073021462,119.632469552402));
#69394=CARTESIAN_POINT('',(99.2004494083662,809.359064969247,117.827345415779));
#69395=CARTESIAN_POINT('',(99.2004494076648,812.331571652995,109.416982902992));
#69396=CARTESIAN_POINT('Ctrl Pts',(100.145240424235,807.995072722745,117.456717099162));
#69397=CARTESIAN_POINT('Ctrl Pts',(100.094632569839,807.878923409672,117.415666001911));
#69398=CARTESIAN_POINT('Ctrl Pts',(100.020431519131,807.773979948127,117.376258521595));
#69399=CARTESIAN_POINT('Ctrl Pts',(99.8332599057883,807.598239666649,117.305294334309));
#69400=CARTESIAN_POINT('Ctrl Pts',(99.7221141346367,807.529156510007,117.274435429664));
#69401=CARTESIAN_POINT('Ctrl Pts',(99.4767659606996,807.4358977698,117.225622157036));
#69402=CARTESIAN_POINT('Ctrl Pts',(99.3448205956772,807.412813339474,117.208201505304));
#69403=CARTESIAN_POINT('Ctrl Pts',(99.0773280981939,807.416327555735,117.18967883004));
#69404=CARTESIAN_POINT('Ctrl Pts',(98.9443147373734,807.44310766981,117.18883089946));
#69405=CARTESIAN_POINT('Ctrl Pts',(98.6954035029874,807.543634913197,117.204264804051));
#69406=CARTESIAN_POINT('Ctrl Pts',(98.5819045605111,807.61647073709,117.220418278023));
#69407=CARTESIAN_POINT('Ctrl Pts',(98.3909144294154,807.798147422045,117.267419628734));
#69408=CARTESIAN_POINT('Ctrl Pts',(98.3149120778216,807.904914060929,117.297674325197));
#69409=CARTESIAN_POINT('Ctrl Pts',(98.2089771137064,808.140827241832,117.368649623739));
#69410=CARTESIAN_POINT('Ctrl Pts',(98.180692473151,808.267911814532,117.408787871265));
#69411=CARTESIAN_POINT('Ctrl Pts',(98.1775276413204,808.524500252524,117.492984010829));
#69412=CARTESIAN_POINT('Ctrl Pts',(98.2027644838337,808.651451187789,117.536201292689));
#69413=CARTESIAN_POINT('Ctrl Pts',(98.3034826405417,808.886593304448,117.619212301592));
#69414=CARTESIAN_POINT('Ctrl Pts',(98.3774780539923,808.99265750479,117.658223722759));
#69415=CARTESIAN_POINT('Ctrl Pts',(98.5647141782149,809.170759968649,117.727352193347));
#69416=CARTESIAN_POINT('Ctrl Pts',(98.6760970421638,809.24108338769,117.756807768096));
#69417=CARTESIAN_POINT('Ctrl Pts',(98.9213429057008,809.336145749598,117.802482083006));
#69418=CARTESIAN_POINT('Ctrl Pts',(99.0527619843972,809.360117781331,117.818313242053));
#69419=CARTESIAN_POINT('Ctrl Pts',(99.319898951195,809.35839567637,117.834707685165));
#69420=CARTESIAN_POINT('Ctrl Pts',(99.4530543644905,809.332297145673,117.834988507322));
#69421=CARTESIAN_POINT('Ctrl Pts',(99.7036905226119,809.232070307862,117.819696604127));
#69422=CARTESIAN_POINT('Ctrl Pts',(99.8185160106895,809.158356311189,117.804085135945));
#69423=CARTESIAN_POINT('Ctrl Pts',(100.011214546557,808.974003026396,117.75894009294));
#69424=CARTESIAN_POINT('Ctrl Pts',(100.087638237152,808.865534790757,117.729984093654));
#69425=CARTESIAN_POINT('Ctrl Pts',(100.19276731775,808.627638321872,117.662047803397));
#69426=CARTESIAN_POINT('Ctrl Pts',(100.220514387367,808.500540419521,117.623729160557));
#69427=CARTESIAN_POINT('Ctrl Pts',(100.222463015951,808.308035479834,117.562556494394));
#69428=CARTESIAN_POINT('Ctrl Pts',(100.216394503391,808.243787723999,117.54161563543));
#69429=CARTESIAN_POINT('Ctrl Pts',(100.190833057555,808.116978949041,117.499193047242));
#69430=CARTESIAN_POINT('Ctrl Pts',(100.171253520251,808.054774981796,117.477817897587));
#69431=CARTESIAN_POINT('Ctrl Pts',(100.145240424235,807.995072722745,117.456717099161));
#69432=CARTESIAN_POINT('Ctrl Pts',(99.2004494076673,808.721073021462,119.632469552402));
#69433=CARTESIAN_POINT('Ctrl Pts',(99.200586744741,808.721070527098,119.632476609914));
#69434=CARTESIAN_POINT('Ctrl Pts',(99.200724083128,808.721068006178,119.632483659442));
#69435=CARTESIAN_POINT('Ctrl Pts',(99.2008614228201,808.7210654587,119.632490700987));
#69436=CARTESIAN_POINT('Ctrl Pts',(99.33388906559,808.71859796325,119.639311162565));
#69437=CARTESIAN_POINT('Ctrl Pts',(99.4655696532678,808.691255145031,119.63853277349));
#69438=CARTESIAN_POINT('Ctrl Pts',(99.712247169163,808.589609722891,119.622079579624));
#69439=CARTESIAN_POINT('Ctrl Pts',(99.8247810219441,808.515978218443,119.606464544674));
#69440=CARTESIAN_POINT('Ctrl Pts',(100.014384327843,808.332222414994,119.562047452818));
#69441=CARTESIAN_POINT('Ctrl Pts',(100.089785827074,808.22393248243,119.533688885553));
#69442=CARTESIAN_POINT('Ctrl Pts',(100.193249467711,807.987145590484,119.467265048762));
#69443=CARTESIAN_POINT('Ctrl Pts',(100.220519811164,807.860970612968,119.429851256551));
#69444=CARTESIAN_POINT('Ctrl Pts',(100.223098984371,807.607013193112,119.35006909109));
#69445=CARTESIAN_POINT('Ctrl Pts',(100.198405529581,807.481713981814,119.308472097133));
#69446=CARTESIAN_POINT('Ctrl Pts',(100.099517844319,807.248088427224,119.226081439652));
#69447=CARTESIAN_POINT('Ctrl Pts',(100.026095080398,807.142182897061,119.18611795792));
#69448=CARTESIAN_POINT('Ctrl Pts',(99.8393587726141,806.964053277967,119.113389542738));
#69449=CARTESIAN_POINT('Ctrl Pts',(99.7276750239694,806.893805083307,119.08140358225));
#69450=CARTESIAN_POINT('Ctrl Pts',(99.4807845745175,806.799011735487,119.030587569192));
#69451=CARTESIAN_POINT('Ctrl Pts',(99.3479058494294,806.775507972555,119.012302017345));
#69452=CARTESIAN_POINT('Ctrl Pts',(99.2090987505836,806.777196046337,119.002233713168));
#69453=CARTESIAN_POINT('Ctrl Pts',(99.2047734549445,806.77727464753,119.001928920805));
#69454=CARTESIAN_POINT('Ctrl Pts',(99.2004494076648,806.777379182049,119.001633152524));
#69455=CARTESIAN_POINT('Origin',(99.2004494076648,811.368542512753,109.076615819925));
#69456=CARTESIAN_POINT('',(99.2004494076648,809.705125881246,115.283511063413));
#69457=CARTESIAN_POINT('Origin',(99.2004494076648,809.233703650638,115.116894496146));
#69458=CARTESIAN_POINT('',(99.200449407665,808.225611598495,119.469624934516));
#69459=CARTESIAN_POINT('',(99.2004494076648,811.839964743362,109.243232387192));
#69460=CARTESIAN_POINT('Ctrl Pts',(99.2004115835223,807.274154639319,119.160759867218));
#69461=CARTESIAN_POINT('Ctrl Pts',(99.1397213644481,807.275531840299,119.156877014434));
#69462=CARTESIAN_POINT('Ctrl Pts',(99.0795379805894,807.287376987541,119.156535673506));
#69463=CARTESIAN_POINT('Ctrl Pts',(98.960417403472,807.332987270617,119.163351434566));
#69464=CARTESIAN_POINT('Ctrl Pts',(98.9033819848119,807.36837213651,119.171194805266));
#69465=CARTESIAN_POINT('Ctrl Pts',(98.8070984504213,807.457722147422,119.194382736858));
#69466=CARTESIAN_POINT('Ctrl Pts',(98.7686928520005,807.510685755188,119.209447504984));
#69467=CARTESIAN_POINT('Ctrl Pts',(98.7156373230637,807.627269030948,119.244647843334));
#69468=CARTESIAN_POINT('Ctrl Pts',(98.7014746143982,807.689707769768,119.264418740293));
#69469=CARTESIAN_POINT('Ctrl Pts',(98.6995305723522,807.815826186176,119.305877483558));
#69470=CARTESIAN_POINT('Ctrl Pts',(98.7117934003778,807.878240954595,119.327147245798));
#69471=CARTESIAN_POINT('Ctrl Pts',(98.7613718581357,807.99444038258,119.368183710536));
#69472=CARTESIAN_POINT('Ctrl Pts',(98.798189395984,808.047056399957,119.387537685907));
#69473=CARTESIAN_POINT('Ctrl Pts',(98.8915121173824,808.135102119885,119.421708911796));
#69474=CARTESIAN_POINT('Ctrl Pts',(98.9470626901652,808.169663840158,119.436190961412));
#69475=CARTESIAN_POINT('Ctrl Pts',(99.069580924823,808.215889230352,119.458476424783));
#69476=CARTESIAN_POINT('Ctrl Pts',(99.1353408400831,808.227049587905,119.466049692863));
#69477=CARTESIAN_POINT('Ctrl Pts',(99.2684764061568,808.224112205193,119.473361392877));
#69478=CARTESIAN_POINT('Ctrl Pts',(99.3345258202417,808.209884026469,119.472979998211));
#69479=CARTESIAN_POINT('Ctrl Pts',(99.4562573321618,808.158095773898,119.464319915616));
#69480=CARTESIAN_POINT('Ctrl Pts',(99.5109465614735,808.121458069389,119.456266835239));
#69481=CARTESIAN_POINT('Ctrl Pts',(99.6027239678335,808.03054605062,119.433507669961));
#69482=CARTESIAN_POINT('Ctrl Pts',(99.6389928983616,807.977181748975,119.419032476278));
#69483=CARTESIAN_POINT('Ctrl Pts',(99.6881807593334,807.860770555768,119.385380213024));
#69484=CARTESIAN_POINT('Ctrl Pts',(99.7007016654658,807.798867500261,119.366535657893));
#69485=CARTESIAN_POINT('Ctrl Pts',(99.7001896061441,807.674552715984,119.326735277047));
#69486=CARTESIAN_POINT('Ctrl Pts',(99.6871769384752,807.613355970545,119.306166858106));
#69487=CARTESIAN_POINT('Ctrl Pts',(99.6370076919849,807.499627299614,119.26588784107));
#69488=CARTESIAN_POINT('Ctrl Pts',(99.6002835803374,807.448247335238,119.246579276215));
#69489=CARTESIAN_POINT('Ctrl Pts',(99.507633262563,807.362223910903,119.211861011593));
#69490=CARTESIAN_POINT('Ctrl Pts',(99.4525465553774,807.32849823702,119.196813179721));
#69491=CARTESIAN_POINT('Ctrl Pts',(99.3312150161737,807.283471426747,119.173239863295));
#69492=CARTESIAN_POINT('Ctrl Pts',(99.2661202392978,807.272663558442,119.1649637907));
#69493=CARTESIAN_POINT('Ctrl Pts',(99.2004115835223,807.274154639319,119.160759867218));
#69494=CARTESIAN_POINT('Origin',(104.959166694129,815.085695867571,110.390383588546));
#69495=CARTESIAN_POINT('',(104.959166694129,810.388915181948,120.834270597794));
#69496=CARTESIAN_POINT('',(104.959166694201,812.206764196253,121.381095048935));
#69497=CARTESIAN_POINT('Ctrl Pts',(104.959166694129,810.388915181948,120.834270597794));
#69498=CARTESIAN_POINT('Ctrl Pts',(104.833354697547,810.396090006485,120.813970264862));
#69499=CARTESIAN_POINT('Ctrl Pts',(104.708759033778,810.427066256375,120.801480936088));
#69500=CARTESIAN_POINT('Ctrl Pts',(104.477220223402,810.532733747189,120.793740466415));
#69501=CARTESIAN_POINT('Ctrl Pts',(104.372257408679,810.606238567556,120.798463261266));
#69502=CARTESIAN_POINT('Ctrl Pts',(104.196557349567,810.786119026573,120.824322727236));
#69503=CARTESIAN_POINT('Ctrl Pts',(104.127207777786,810.890491609221,120.845060648666));
#69504=CARTESIAN_POINT('Ctrl Pts',(104.034135082436,811.115448129756,120.899100248007));
#69505=CARTESIAN_POINT('Ctrl Pts',(104.010557106957,811.233486460713,120.931626595927));
#69506=CARTESIAN_POINT('Ctrl Pts',(104.011622017921,811.469001588448,121.003997677175));
#69507=CARTESIAN_POINT('Ctrl Pts',(104.035980782298,811.584079574372,121.043055246401));
#69508=CARTESIAN_POINT('Ctrl Pts',(104.13038978535,811.79822607484,121.123250107242));
#69509=CARTESIAN_POINT('Ctrl Pts',(104.200081347412,811.894788176856,121.16356608195));
#69510=CARTESIAN_POINT('Ctrl Pts',(104.376274369614,812.055146075277,121.240129540311));
#69511=CARTESIAN_POINT('Ctrl Pts',(104.481238947464,812.116971344385,121.275548912842));
#69512=CARTESIAN_POINT('Ctrl Pts',(104.71173856663,812.196511893003,121.336909024889));
#69513=CARTESIAN_POINT('Ctrl Pts',(104.835002671733,812.213423877213,121.362252254993));
#69514=CARTESIAN_POINT('Ctrl Pts',(104.959166694272,812.206764196252,121.381095048935));
#69515=CARTESIAN_POINT('',(104.959166694129,812.870928637576,119.501918880835));
#69516=CARTESIAN_POINT('',(104.959166694129,815.979592040189,110.706316741682));
#69517=CARTESIAN_POINT('Ctrl Pts',(105.86981055157,811.673894817626,119.252032293924));
#69518=CARTESIAN_POINT('Ctrl Pts',(105.836865720135,811.566669685013,119.214135304005));
#69519=CARTESIAN_POINT('Ctrl Pts',(105.782932986183,811.467334710957,119.175679186124));
#69520=CARTESIAN_POINT('Ctrl Pts',(105.634790270708,811.289777808233,119.099646624304));
#69521=CARTESIAN_POINT('Ctrl Pts',(105.540034158333,811.21487478293,119.063027998075));
#69522=CARTESIAN_POINT('Ctrl Pts',(105.326166148304,811.106713071755,118.999594175106));
#69523=CARTESIAN_POINT('Ctrl Pts',(105.209506808175,811.073770892273,118.973221755938));
#69524=CARTESIAN_POINT('Ctrl Pts',(104.965911156416,811.052227491311,118.933373508499));
#69525=CARTESIAN_POINT('Ctrl Pts',(104.841065703891,811.064539707011,118.920479968192));
#69526=CARTESIAN_POINT('Ctrl Pts',(104.599871368744,811.134372823572,118.910569084063));
#69527=CARTESIAN_POINT('Ctrl Pts',(104.485877614143,811.191802834625,118.913842207101));
#69528=CARTESIAN_POINT('Ctrl Pts',(104.285663872071,811.344996893095,118.936530971902));
#69529=CARTESIAN_POINT('Ctrl Pts',(104.201438262591,811.439378660212,118.955762249989));
#69530=CARTESIAN_POINT('Ctrl Pts',(104.077811776079,811.648352401452,119.00646773496));
#69531=CARTESIAN_POINT('Ctrl Pts',(104.037821614021,811.7599909238,119.036915891242));
#69532=CARTESIAN_POINT('Ctrl Pts',(104.004044502348,811.986384458144,119.104464798348));
#69533=CARTESIAN_POINT('Ctrl Pts',(104.009078903378,812.098885079567,119.140702474712));
#69534=CARTESIAN_POINT('Ctrl Pts',(104.062205351414,812.315489543703,119.215652388806));
#69535=CARTESIAN_POINT('Ctrl Pts',(104.110048821356,812.417554494439,119.253688298738));
#69536=CARTESIAN_POINT('Ctrl Pts',(104.244908190584,812.600501697837,119.32779948993));
#69537=CARTESIAN_POINT('Ctrl Pts',(104.331628162827,812.678994933161,119.363087975246));
#69538=CARTESIAN_POINT('Ctrl Pts',(104.537599155287,812.802458436634,119.427290432846));
#69539=CARTESIAN_POINT('Ctrl Pts',(104.656186177563,812.84417141477,119.45511499733));
#69540=CARTESIAN_POINT('Ctrl Pts',(104.90225023298,812.879338180881,119.497207229687));
#69541=CARTESIAN_POINT('Ctrl Pts',(105.027143201732,812.87352862247,119.511375173558));
#69542=CARTESIAN_POINT('Ctrl Pts',(105.271042167254,812.816004758216,119.525164598919));
#69543=CARTESIAN_POINT('Ctrl Pts',(105.38767625621,812.764190374834,119.524454708563));
#69544=CARTESIAN_POINT('Ctrl Pts',(105.596049828579,812.620213474278,119.507648827693));
#69545=CARTESIAN_POINT('Ctrl Pts',(105.685585908109,812.529050176458,119.491567699377));
#69546=CARTESIAN_POINT('Ctrl Pts',(105.816395499718,812.330541934538,119.448030974393));
#69547=CARTESIAN_POINT('Ctrl Pts',(105.860678531356,812.227445189219,119.422272871814));
#69548=CARTESIAN_POINT('Ctrl Pts',(105.910836328957,812.007083146204,119.361042839447));
#69549=CARTESIAN_POINT('Ctrl Pts',(105.914194759803,811.891429049704,119.325715182053));
#69550=CARTESIAN_POINT('Ctrl Pts',(105.888782435894,811.743519795637,119.276294798763));
#69551=CARTESIAN_POINT('Ctrl Pts',(105.880402800986,811.708369279896,119.264216735362));
#69552=CARTESIAN_POINT('Ctrl Pts',(105.86981055157,811.673894817626,119.252032293924));
#69553=CARTESIAN_POINT('Ctrl Pts',(104.959166694272,812.206764196252,121.381095048935));
#69554=CARTESIAN_POINT('Ctrl Pts',(104.95976504612,812.206732102959,121.381185853182));
#69555=CARTESIAN_POINT('Ctrl Pts',(104.960363418914,812.206699462338,121.381276506184));
#69556=CARTESIAN_POINT('Ctrl Pts',(104.960961811862,812.206666274312,121.381367007803));
#69557=CARTESIAN_POINT('Ctrl Pts',(104.961270619604,812.20664914724,121.381413712231));
#69558=CARTESIAN_POINT('Ctrl Pts',(104.961579425527,812.20663187478,121.381460375256));
#69559=CARTESIAN_POINT('Ctrl Pts',(105.08829317379,812.199484690219,121.400590952754));
#69560=CARTESIAN_POINT('Ctrl Pts',(105.213220126502,812.168057685697,121.412579751966));
#69561=CARTESIAN_POINT('Ctrl Pts',(105.444394943492,812.061069588652,121.421057355886));
#69562=CARTESIAN_POINT('Ctrl Pts',(105.548796916412,811.986861848353,121.417613934371));
#69563=CARTESIAN_POINT('Ctrl Pts',(105.722606586098,811.80646593797,121.395560660536));
#69564=CARTESIAN_POINT('Ctrl Pts',(105.791053424735,811.702422734513,121.377392055017));
#69565=CARTESIAN_POINT('Ctrl Pts',(105.883424042089,811.478434068685,121.328333330863));
#69566=CARTESIAN_POINT('Ctrl Pts',(105.907181000798,811.360909031746,121.298113580969));
#69567=CARTESIAN_POINT('Ctrl Pts',(105.907320692346,811.126329823532,121.22882367717));
#69568=CARTESIAN_POINT('Ctrl Pts',(105.883889697256,811.011729202174,121.190508316358));
#69569=CARTESIAN_POINT('Ctrl Pts',(105.79189616721,810.798781561893,121.11002111123));
#69570=CARTESIAN_POINT('Ctrl Pts',(105.723811054966,810.702972235351,121.068691777476));
#69571=CARTESIAN_POINT('Ctrl Pts',(105.550353727072,810.542693327016,120.988421443388));
#69572=CARTESIAN_POINT('Ctrl Pts',(105.44611494346,810.480561578632,120.95039969055));
#69573=CARTESIAN_POINT('Ctrl Pts',(105.214531673714,810.399358552366,120.883442085345));
#69574=CARTESIAN_POINT('Ctrl Pts',(105.089028914393,810.381929682426,120.855358187615));
#69575=CARTESIAN_POINT('Ctrl Pts',(104.961339507698,810.388793050608,120.834621757548));
#69576=CARTESIAN_POINT('Ctrl Pts',(104.960253055459,810.388853228779,120.834445887092));
#69577=CARTESIAN_POINT('Ctrl Pts',(104.959166694129,810.388915181948,120.834270597794));
#69578=CARTESIAN_POINT('Origin',(104.959166694129,815.085695867571,110.390383588546));
#69579=CARTESIAN_POINT('',(104.959166694129,813.422279236064,116.597278832034));
#69580=CARTESIAN_POINT('Origin',(104.959166694129,812.950857005456,116.430662264767));
#69581=CARTESIAN_POINT('',(104.95916669413,811.777693521472,121.250443152468));
#69582=CARTESIAN_POINT('',(104.959166694129,815.557118098179,110.557000155813));
#69583=CARTESIAN_POINT('Ctrl Pts',(104.959670529459,810.818979506244,120.962111840113));
#69584=CARTESIAN_POINT('Ctrl Pts',(104.894942761524,810.822555013975,120.951799624401));
#69585=CARTESIAN_POINT('Ctrl Pts',(104.830824769369,810.838109254016,120.945314369594));
#69586=CARTESIAN_POINT('Ctrl Pts',(104.709436333555,810.892082012198,120.940681817555));
#69587=CARTESIAN_POINT('Ctrl Pts',(104.653463593158,810.930579058416,120.942788160454));
#69588=CARTESIAN_POINT('Ctrl Pts',(104.559429700388,811.025385114038,120.955629050457));
#69589=CARTESIAN_POINT('Ctrl Pts',(104.522160656818,811.080687145236,120.96618812564));
#69590=CARTESIAN_POINT('Ctrl Pts',(104.472191438664,811.199560019998,120.993985714608));
#69591=CARTESIAN_POINT('Ctrl Pts',(104.459349743312,811.261703340205,121.010761381756));
#69592=CARTESIAN_POINT('Ctrl Pts',(104.458988517942,811.385844599149,121.048419577696));
#69593=CARTESIAN_POINT('Ctrl Pts',(104.471338074762,811.446569770682,121.068891947692));
#69594=CARTESIAN_POINT('Ctrl Pts',(104.519900222239,811.559184108116,121.111032659457));
#69595=CARTESIAN_POINT('Ctrl Pts',(104.555717462033,811.609852674374,121.13226633793));
#69596=CARTESIAN_POINT('Ctrl Pts',(104.647365244939,811.695210236629,121.173222002652));
#69597=CARTESIAN_POINT('Ctrl Pts',(104.702733253995,811.72852066068,121.192454311888));
#69598=CARTESIAN_POINT('Ctrl Pts',(104.824904954755,811.771734163302,121.225910966599));
#69599=CARTESIAN_POINT('Ctrl Pts',(104.890536365835,811.781112203955,121.239785223859));
#69600=CARTESIAN_POINT('Ctrl Pts',(105.023429752435,811.774503425035,121.260426083977));
#69601=CARTESIAN_POINT('Ctrl Pts',(105.089467976359,811.758385156089,121.266948375166));
#69602=CARTESIAN_POINT('Ctrl Pts',(105.212859326362,811.70237139337,121.271621923929));
#69603=CARTESIAN_POINT('Ctrl Pts',(105.269039177046,811.662833636879,121.269677039047));
#69604=CARTESIAN_POINT('Ctrl Pts',(105.36163070635,811.567034614157,121.257482410398));
#69605=CARTESIAN_POINT('Ctrl Pts',(105.397798846797,811.512211077012,121.247609667748));
#69606=CARTESIAN_POINT('Ctrl Pts',(105.446628074815,811.394067836774,121.221177016886));
#69607=CARTESIAN_POINT('Ctrl Pts',(105.459169310893,811.332025327319,121.204972130901));
#69608=CARTESIAN_POINT('Ctrl Pts',(105.459164088117,811.208186328606,121.168069472528));
#69609=CARTESIAN_POINT('Ctrl Pts',(105.446725523884,811.147677185787,121.147773275748));
#69610=CARTESIAN_POINT('Ctrl Pts',(105.398035971004,811.035343098214,121.105407009963));
#69611=CARTESIAN_POINT('Ctrl Pts',(105.362081549874,810.984819644039,121.08377943449));
#69612=CARTESIAN_POINT('Ctrl Pts',(105.270614628522,810.900339483112,121.041960105072));
#69613=CARTESIAN_POINT('Ctrl Pts',(105.215732219555,810.867574479576,121.022241947609));
#69614=CARTESIAN_POINT('Ctrl Pts',(105.0933620194,810.824512770352,120.987420522973));
#69615=CARTESIAN_POINT('Ctrl Pts',(105.02679190406,810.815271777684,120.972805397389));
#69616=CARTESIAN_POINT('Ctrl Pts',(104.959670529459,810.818979506244,120.962111840113));
#69617=CARTESIAN_POINT('Origin',(94.2316464454274,802.680033537841,106.005802765141));
#69618=CARTESIAN_POINT('',(94.2316464454273,798.084680646679,115.94267397259));
#69619=CARTESIAN_POINT('',(94.2316464454283,800.036659745791,116.550068192181));
#69620=CARTESIAN_POINT('Ctrl Pts',(94.2316464454273,798.084680646679,115.94267397259));
#69621=CARTESIAN_POINT('Ctrl Pts',(94.1037999764411,798.087573511576,115.934488947264));
#69622=CARTESIAN_POINT('Ctrl Pts',(93.9770394345588,798.113304203478,115.933720303641));
#69623=CARTESIAN_POINT('Ctrl Pts',(93.7310611758891,798.210787294472,115.94805993517));
#69624=CARTESIAN_POINT('Ctrl Pts',(93.6153702918267,798.284480283536,115.964086371598));
#69625=CARTESIAN_POINT('Ctrl Pts',(93.4215142720861,798.468719806565,116.011286173827));
#69626=CARTESIAN_POINT('Ctrl Pts',(93.344747526796,798.576953819916,116.041784848021));
#69627=CARTESIAN_POINT('Ctrl Pts',(93.2393598302505,798.814238392117,116.112803621196));
#69628=CARTESIAN_POINT('Ctrl Pts',(93.2115917482419,798.940881351409,116.152571621789));
#69629=CARTESIAN_POINT('Ctrl Pts',(93.208974616995,799.197042906534,116.23565830297));
#69630=CARTESIAN_POINT('Ctrl Pts',(93.2344173963583,799.324033750943,116.27814988591));
#69631=CARTESIAN_POINT('Ctrl Pts',(93.3361029824329,799.561135843543,116.359462776658));
#69632=CARTESIAN_POINT('Ctrl Pts',(93.411528378302,799.668818063266,116.39744946001));
#69633=CARTESIAN_POINT('Ctrl Pts',(93.6022010781517,799.849092800142,116.463350069855));
#69634=CARTESIAN_POINT('Ctrl Pts',(93.715421127415,799.920017866629,116.490653651625));
#69635=CARTESIAN_POINT('Ctrl Pts',(93.9641490083928,800.015112070195,116.531380470685));
#69636=CARTESIAN_POINT('Ctrl Pts',(94.0970897622964,800.038582583248,116.54449292373));
#69637=CARTESIAN_POINT('Ctrl Pts',(94.2313049710666,800.036664680118,116.550054059785));
#69638=CARTESIAN_POINT('Ctrl Pts',(94.2314187968175,800.036663053575,116.550058776095));
#69639=CARTESIAN_POINT('Ctrl Pts',(94.2315326216066,800.036661408799,116.550063486893));
#69640=CARTESIAN_POINT('Ctrl Pts',(94.2316464454292,800.036659745791,116.550068192181));
#69641=CARTESIAN_POINT('',(94.2316464463135,800.674576417418,114.745157040706));
#69642=CARTESIAN_POINT('',(94.2316464454274,803.643062678083,106.346169848208));
#69643=CARTESIAN_POINT('Ctrl Pts',(95.0750947698766,799.129354690295,114.323272367424));
#69644=CARTESIAN_POINT('Ctrl Pts',(94.9999801103154,799.025664094407,114.286624602379));
#69645=CARTESIAN_POINT('Ctrl Pts',(94.9040983621953,798.937575318805,114.253174138367));
#69646=CARTESIAN_POINT('Ctrl Pts',(94.6816501975664,798.802427106374,114.19655656175));
#69647=CARTESIAN_POINT('Ctrl Pts',(94.5572529690001,798.756685541673,114.173947365479));
#69648=CARTESIAN_POINT('Ctrl Pts',(94.2956029478729,798.71366877426,114.142891306016));
#69649=CARTESIAN_POINT('Ctrl Pts',(94.160808745891,798.71701742042,114.1348129979));
#69650=CARTESIAN_POINT('Ctrl Pts',(93.8985671797012,798.773026664621,114.134843841723));
#69651=CARTESIAN_POINT('Ctrl Pts',(93.773651395262,798.825366769294,114.143029676665));
#69652=CARTESIAN_POINT('Ctrl Pts',(93.5509549700396,798.972628891492,114.174981268742));
#69653=CARTESIAN_POINT('Ctrl Pts',(93.4553333029572,799.066187929153,114.198459027646));
#69654=CARTESIAN_POINT('Ctrl Pts',(93.3073869494175,799.281452184646,114.25733136225));
#69655=CARTESIAN_POINT('Ctrl Pts',(93.2560708615511,799.400835692059,114.292045286953));
#69656=CARTESIAN_POINT('Ctrl Pts',(93.2036138968648,799.652445029388,114.368568138269));
#69657=CARTESIAN_POINT('Ctrl Pts',(93.2036404280434,799.78232989443,114.409696103859));
#69658=CARTESIAN_POINT('Ctrl Pts',(93.2566767393386,800.033976221112,114.492145534065));
#69659=CARTESIAN_POINT('Ctrl Pts',(93.309242308972,800.153217174935,114.53263784761));
#69660=CARTESIAN_POINT('Ctrl Pts',(93.4596053190206,800.363477914753,114.606854936056));
#69661=CARTESIAN_POINT('Ctrl Pts',(93.5554781799771,800.452708687867,114.639916854467));
#69662=CARTESIAN_POINT('Ctrl Pts',(93.7783253164892,800.590173152952,114.694682481267));
#69663=CARTESIAN_POINT('Ctrl Pts',(93.9031003564464,800.637094044925,114.715866811105));
#69664=CARTESIAN_POINT('Ctrl Pts',(94.1647863873439,800.681921004229,114.743786234978));
#69665=CARTESIAN_POINT('Ctrl Pts',(94.2991296737661,800.679556797199,114.750309276137));
#69666=CARTESIAN_POINT('Ctrl Pts',(94.5612273327101,800.625389157071,114.748167692582));
#69667=CARTESIAN_POINT('Ctrl Pts',(94.6863763841176,800.573693442765,114.739401603949));
#69668=CARTESIAN_POINT('Ctrl Pts',(94.9108287656632,800.426386781562,114.707470098182));
#69669=CARTESIAN_POINT('Ctrl Pts',(95.0076133951727,800.331702868478,114.684447152005));
#69670=CARTESIAN_POINT('Ctrl Pts',(95.1568347418816,800.11346636752,114.62732663394));
#69671=CARTESIAN_POINT('Ctrl Pts',(95.2083193779351,799.992322807333,114.593890746079));
#69672=CARTESIAN_POINT('Ctrl Pts',(95.2598098406563,799.738905820011,114.520468979456));
#69673=CARTESIAN_POINT('Ctrl Pts',(95.2593809405527,799.609100770489,114.481193539207));
#69674=CARTESIAN_POINT('Ctrl Pts',(95.2193123245112,799.420373405143,114.421355995634));
#69675=CARTESIAN_POINT('Ctrl Pts',(95.1993311927414,799.358707089507,114.401327504981));
#69676=CARTESIAN_POINT('Ctrl Pts',(95.1465310394155,799.239663709715,114.361649470194));
#69677=CARTESIAN_POINT('Ctrl Pts',(95.1137046827979,799.182653006514,114.34210979577));
#69678=CARTESIAN_POINT('Ctrl Pts',(95.0750947698766,799.129354690295,114.323272367424));
#69679=CARTESIAN_POINT('Ctrl Pts',(94.2316464454292,800.036659745791,116.550068192181));
#69680=CARTESIAN_POINT('Ctrl Pts',(94.3629815577469,800.03474089155,116.555497367452));
#69681=CARTESIAN_POINT('Ctrl Pts',(94.4930290911779,800.008544361815,116.553607102351));
#69682=CARTESIAN_POINT('Ctrl Pts',(94.7387571810064,799.909432676774,116.535734906483));
#69683=CARTESIAN_POINT('Ctrl Pts',(94.8517243323247,799.836549716512,116.519650101181));
#69684=CARTESIAN_POINT('Ctrl Pts',(95.0425762648668,799.653547815694,116.475207272092));
#69685=CARTESIAN_POINT('Ctrl Pts',(95.1186759198018,799.54518290088,116.447268899553));
#69686=CARTESIAN_POINT('Ctrl Pts',(95.2234050866694,799.30761221254,116.382725886987));
#69687=CARTESIAN_POINT('Ctrl Pts',(95.2512304695178,799.180719506938,116.346745494667));
#69688=CARTESIAN_POINT('Ctrl Pts',(95.2547001758982,798.9252096553,116.2707184679));
#69689=CARTESIAN_POINT('Ctrl Pts',(95.2304713001988,798.799051363495,116.231399994923));
#69690=CARTESIAN_POINT('Ctrl Pts',(95.1325932139514,798.563756070618,116.153912952651));
#69691=CARTESIAN_POINT('Ctrl Pts',(95.0598469876302,798.456974144627,116.116507492673));
#69692=CARTESIAN_POINT('Ctrl Pts',(94.8745204754859,798.276892259145,116.048434832477));
#69693=CARTESIAN_POINT('Ctrl Pts',(94.7635953773627,798.205571730331,116.018490318587));
#69694=CARTESIAN_POINT('Ctrl Pts',(94.51783746284,798.108448470284,115.970676477465));
#69695=CARTESIAN_POINT('Ctrl Pts',(94.3853136008111,798.083809800227,115.953347247582));
#69696=CARTESIAN_POINT('Ctrl Pts',(94.244581197857,798.084446452881,115.943520848752));
#69697=CARTESIAN_POINT('Ctrl Pts',(94.2381124317385,798.084534336617,115.943087939922));
#69698=CARTESIAN_POINT('Ctrl Pts',(94.2316464454274,798.084680646679,115.94267397259));
#69699=CARTESIAN_POINT('Origin',(94.2316464454274,802.680033537841,106.005802765141));
#69700=CARTESIAN_POINT('',(94.2316464454274,801.016616906335,112.212698008629));
#69701=CARTESIAN_POINT('Origin',(94.2316464454274,800.545194675726,112.046081441362));
#69702=CARTESIAN_POINT('',(94.2316464454273,799.539662874025,116.391567948387));
#69703=CARTESIAN_POINT('',(94.2316464454274,803.15145576845,106.172419332408));
#69704=CARTESIAN_POINT('Ctrl Pts',(94.2315455714384,798.584150826436,116.094176309146));
#69705=CARTESIAN_POINT('Ctrl Pts',(94.1720167839962,798.585389073316,116.090708873649));
#69706=CARTESIAN_POINT('Ctrl Pts',(94.1129792196732,798.59675826626,116.090478889328));
#69707=CARTESIAN_POINT('Ctrl Pts',(93.9946726488584,798.641170624584,116.096978630705));
#69708=CARTESIAN_POINT('Ctrl Pts',(93.9374123628351,798.676241270424,116.104496291945));
#69709=CARTESIAN_POINT('Ctrl Pts',(93.8405508411949,798.765138501411,116.12675935922));
#69710=CARTESIAN_POINT('Ctrl Pts',(93.8017859963506,798.817969151388,116.141237585891));
#69711=CARTESIAN_POINT('Ctrl Pts',(93.747874153489,798.934517249859,116.175145732248));
#69712=CARTESIAN_POINT('Ctrl Pts',(93.7332320968561,798.997065630691,116.194229136661));
#69713=CARTESIAN_POINT('Ctrl Pts',(93.7302997148241,799.123771859812,116.234338289418));
#69714=CARTESIAN_POINT('Ctrl Pts',(93.7421239774015,799.186659370225,116.254961776196));
#69715=CARTESIAN_POINT('Ctrl Pts',(93.7910594266082,799.304088700895,116.294762786258));
#69716=CARTESIAN_POINT('Ctrl Pts',(93.8277332777928,799.357420213033,116.313531040647));
#69717=CARTESIAN_POINT('Ctrl Pts',(93.9210127782908,799.44679212484,116.346498174468));
#69718=CARTESIAN_POINT('Ctrl Pts',(93.976636914046,799.481962276886,116.360374414023));
#69719=CARTESIAN_POINT('Ctrl Pts',(94.0991749479439,799.529119031612,116.381413843585));
#69720=CARTESIAN_POINT('Ctrl Pts',(94.1648222621132,799.540710146109,116.388393061611));
#69721=CARTESIAN_POINT('Ctrl Pts',(94.2974551609734,799.53863205019,116.39469475252));
#69722=CARTESIAN_POINT('Ctrl Pts',(94.3631216359456,799.524965765282,116.393953466352));
#69723=CARTESIAN_POINT('Ctrl Pts',(94.4858428735472,799.473824363662,116.384887449622));
#69724=CARTESIAN_POINT('Ctrl Pts',(94.5416225021999,799.436709724106,116.376607261033));
#69725=CARTESIAN_POINT('Ctrl Pts',(94.6342417498175,799.344776383757,116.353764068761));
#69726=CARTESIAN_POINT('Ctrl Pts',(94.6705215309892,799.291157621273,116.339530351243));
#69727=CARTESIAN_POINT('Ctrl Pts',(94.7196172889772,799.174109948565,116.306774352671));
#69728=CARTESIAN_POINT('Ctrl Pts',(94.7320397422235,799.111825090876,116.288573175419));
#69729=CARTESIAN_POINT('Ctrl Pts',(94.731235177814,798.986812617055,116.250406160606));
#69730=CARTESIAN_POINT('Ctrl Pts',(94.7180796550034,798.925294694194,116.230810008027));
#69731=CARTESIAN_POINT('Ctrl Pts',(94.6676781540853,798.811053796892,116.192631015984));
#69732=CARTESIAN_POINT('Ctrl Pts',(94.6309178831475,798.75946002571,116.174423147786));
#69733=CARTESIAN_POINT('Ctrl Pts',(94.5383015328304,798.67305163928,116.141785703591));
#69734=CARTESIAN_POINT('Ctrl Pts',(94.4833043525867,798.639145479472,116.127692793331));
#69735=CARTESIAN_POINT('Ctrl Pts',(94.3621547000017,798.593752761756,116.105678738551));
#69736=CARTESIAN_POINT('Ctrl Pts',(94.2971516425527,798.582786167145,116.097997734537));
#69737=CARTESIAN_POINT('Ctrl Pts',(94.2315455714384,798.584150826436,116.094176309146));
#69738=CARTESIAN_POINT('Origin',(100.684211372524,805.187086117687,106.891879975103));
#69739=CARTESIAN_POINT('',(100.684211372524,800.481296738109,117.361256037865));
#69740=CARTESIAN_POINT('',(100.684211372529,802.320089444705,117.848822743518));
#69741=CARTESIAN_POINT('Ctrl Pts',(100.684211372524,800.481296738109,117.361256037865));
#69742=CARTESIAN_POINT('Ctrl Pts',(100.565597463437,800.487609223464,117.34339559352));
#69743=CARTESIAN_POINT('Ctrl Pts',(100.448076354088,800.515369438104,117.331648409742));
#69744=CARTESIAN_POINT('Ctrl Pts',(100.219870360019,800.6139776104,117.321501328638));
#69745=CARTESIAN_POINT('Ctrl Pts',(100.112326389534,800.686724346148,117.324169705703));
#69746=CARTESIAN_POINT('Ctrl Pts',(99.9321222227121,800.866182147369,117.344893473142));
#69747=CARTESIAN_POINT('Ctrl Pts',(99.8606366181137,800.970741458563,117.362530678582));
#69748=CARTESIAN_POINT('Ctrl Pts',(99.7628167677313,801.198311150468,117.410042766362));
#69749=CARTESIAN_POINT('Ctrl Pts',(99.7370892623527,801.318928499893,117.439338383031));
#69750=CARTESIAN_POINT('Ctrl Pts',(99.7352187437462,801.561038000097,117.505395977054));
#69751=CARTESIAN_POINT('Ctrl Pts',(99.7590399517933,801.680005233789,117.541448176051));
#69752=CARTESIAN_POINT('Ctrl Pts',(99.8537940863741,801.900197902703,117.615189173687));
#69753=CARTESIAN_POINT('Ctrl Pts',(99.9237276110613,801.999066864586,117.652087516984));
#69754=CARTESIAN_POINT('Ctrl Pts',(100.100456009115,802.162851115463,117.721750207133));
#69755=CARTESIAN_POINT('Ctrl Pts',(100.205366872227,802.226036346363,117.753785216086));
#69756=CARTESIAN_POINT('Ctrl Pts',(100.436170978144,802.308107240893,117.809174515615));
#69757=CARTESIAN_POINT('Ctrl Pts',(100.559745617076,802.326050958506,117.83195533243));
#69758=CARTESIAN_POINT('Ctrl Pts',(100.684211372533,802.320089444705,117.848822743518));
#69759=CARTESIAN_POINT('',(100.684211372524,802.980040408452,115.981568120976));
#69760=CARTESIAN_POINT('',(100.684211372524,806.080982290306,107.207813128239));
#69761=CARTESIAN_POINT('Ctrl Pts',(101.520107801531,801.602208259166,115.69235748013));
#69762=CARTESIAN_POINT('Ctrl Pts',(101.464238104416,801.5037843751,115.657571149245));
#69763=CARTESIAN_POINT('Ctrl Pts',(101.389347097758,801.417215440319,115.623626981594));
#69764=CARTESIAN_POINT('Ctrl Pts',(101.204367694086,801.272669922271,115.559261760087));
#69765=CARTESIAN_POINT('Ctrl Pts',(101.094462060306,801.21804825099,115.529811250606));
#69766=CARTESIAN_POINT('Ctrl Pts',(100.859669924098,801.154347390131,115.482091396508));
#69767=CARTESIAN_POINT('Ctrl Pts',(100.737275106152,801.145094747659,115.464091661275));
#69768=CARTESIAN_POINT('Ctrl Pts',(100.492018677018,801.171995094994,115.44136507362));
#69769=CARTESIAN_POINT('Ctrl Pts',(100.371421636957,801.208629912145,115.437067963642));
#69770=CARTESIAN_POINT('Ctrl Pts',(100.148500593435,801.324455445357,115.443412355749));
#69771=CARTESIAN_POINT('Ctrl Pts',(100.048482560249,801.403093371002,115.454181073391));
#69772=CARTESIAN_POINT('Ctrl Pts',(99.884246300006,801.592403311696,115.489634412983));
#69773=CARTESIAN_POINT('Ctrl Pts',(99.8216951295365,801.70133020946,115.514006432386));
#69774=CARTESIAN_POINT('Ctrl Pts',(99.7452479949851,801.930130635538,115.571719338632));
#69775=CARTESIAN_POINT('Ctrl Pts',(99.7301255748518,802.047230646471,115.604097769774));
#69776=CARTESIAN_POINT('Ctrl Pts',(99.7461461285556,802.275383801483,115.672268586362));
#69777=CARTESIAN_POINT('Ctrl Pts',(99.775634488365,802.384463322736,115.707297130171));
#69778=CARTESIAN_POINT('Ctrl Pts',(99.8752533793037,802.585931190253,115.77689725886));
#69779=CARTESIAN_POINT('Ctrl Pts',(99.9446942266083,802.676373623328,115.810825377793));
#69780=CARTESIAN_POINT('Ctrl Pts',(100.117604090515,802.828821835627,115.874157193571));
#69781=CARTESIAN_POINT('Ctrl Pts',(100.220260819943,802.888548418159,115.902812908805));
#69782=CARTESIAN_POINT('Ctrl Pts',(100.450381346375,802.968796583903,115.951741603823));
#69783=CARTESIAN_POINT('Ctrl Pts',(100.57648165657,802.986261794649,115.970996186868));
#69784=CARTESIAN_POINT('Ctrl Pts',(100.826978585255,802.972220883698,115.995696761168));
#69785=CARTESIAN_POINT('Ctrl Pts',(100.948985103197,802.941944340169,116.001217244638));
#69786=CARTESIAN_POINT('Ctrl Pts',(101.177233354518,802.837632128631,115.998470084945));
#69787=CARTESIAN_POINT('Ctrl Pts',(101.281112435463,802.763965563543,115.990036894187));
#69788=CARTESIAN_POINT('Ctrl Pts',(101.455544622951,802.582053781247,115.959823542551));
#69789=CARTESIAN_POINT('Ctrl Pts',(101.52413938033,802.475220200409,115.938204005999));
#69790=CARTESIAN_POINT('Ctrl Pts',(101.610160860499,802.255224661463,115.887072943205));
#69791=CARTESIAN_POINT('Ctrl Pts',(101.631481712771,802.145626771598,115.859017116172));
#69792=CARTESIAN_POINT('Ctrl Pts',(101.633104022222,801.920133478107,115.795973526267));
#69793=CARTESIAN_POINT('Ctrl Pts',(101.611269969049,801.806310259357,115.761292963019));
#69794=CARTESIAN_POINT('Ctrl Pts',(101.553994557423,801.666595107358,115.714768652655));
#69795=CARTESIAN_POINT('Ctrl Pts',(101.538070733526,801.633852990164,115.70354179879));
#69796=CARTESIAN_POINT('Ctrl Pts',(101.520107801531,801.602208259166,115.69235748013));
#69797=CARTESIAN_POINT('Ctrl Pts',(100.684211372533,802.320089444705,117.848822743518));
#69798=CARTESIAN_POINT('Ctrl Pts',(100.684435662878,802.320078701911,117.848853139006));
#69799=CARTESIAN_POINT('Ctrl Pts',(100.68465995612,802.320067881495,117.848883515272));
#69800=CARTESIAN_POINT('Ctrl Pts',(100.684884252216,802.320056983452,117.848913872309));
#69801=CARTESIAN_POINT('Ctrl Pts',(100.802607848229,802.314337058754,117.864847005342));
#69802=CARTESIAN_POINT('Ctrl Pts',(100.919059102557,802.287333175311,117.87521746394));
#69803=CARTESIAN_POINT('Ctrl Pts',(101.147144227793,802.189808666365,117.884515701304));
#69804=CARTESIAN_POINT('Ctrl Pts',(101.255373087228,802.116609400356,117.882288300134));
#69805=CARTESIAN_POINT('Ctrl Pts',(101.435390440464,801.936613260541,117.864091786616));
#69806=CARTESIAN_POINT('Ctrl Pts',(101.506500565247,801.832286897255,117.848629204703));
#69807=CARTESIAN_POINT('Ctrl Pts',(101.603817387354,801.606453595449,117.806329558644));
#69808=CARTESIAN_POINT('Ctrl Pts',(101.629942246869,801.487327405553,117.780075013444));
#69809=CARTESIAN_POINT('Ctrl Pts',(101.634319351748,801.249250657437,117.719627397482));
#69810=CARTESIAN_POINT('Ctrl Pts',(101.613095827351,801.132674566714,117.686123284468));
#69811=CARTESIAN_POINT('Ctrl Pts',(101.525519281691,800.915574808855,117.615412566743));
#69812=CARTESIAN_POINT('Ctrl Pts',(101.459956708144,800.817438648366,117.578951020177));
#69813=CARTESIAN_POINT('Ctrl Pts',(101.291347353662,800.651683474917,117.507413567051));
#69814=CARTESIAN_POINT('Ctrl Pts',(101.189526852653,800.58641025219,117.473155863602));
#69815=CARTESIAN_POINT('Ctrl Pts',(100.962093260562,800.498315436644,117.411860821667));
#69816=CARTESIAN_POINT('Ctrl Pts',(100.838396201997,800.477202847779,117.385606217155));
#69817=CARTESIAN_POINT('Ctrl Pts',(100.703437945377,800.480414707131,117.364190083619));
#69818=CARTESIAN_POINT('Ctrl Pts',(100.693821067041,800.480785322067,117.362703030173));
#69819=CARTESIAN_POINT('Ctrl Pts',(100.684211372524,800.481296738109,117.361256037865));
#69820=CARTESIAN_POINT('Origin',(100.684211372524,805.187086117687,106.891879975103));
#69821=CARTESIAN_POINT('',(100.684211372524,803.523669486181,113.098775218591));
#69822=CARTESIAN_POINT('Origin',(100.684211372524,803.052247255572,112.932158651324));
#69823=CARTESIAN_POINT('',(100.684211372525,801.886384714253,117.731282369494));
#69824=CARTESIAN_POINT('',(100.684211372524,805.658508348296,107.05849654237));
#69825=CARTESIAN_POINT('Ctrl Pts',(100.68460553067,800.916635666742,117.47417310411));
#69826=CARTESIAN_POINT('Ctrl Pts',(100.621007780188,800.919891930241,117.464809433934));
#69827=CARTESIAN_POINT('Ctrl Pts',(100.558064699032,800.934856410941,117.458728634147));
#69828=CARTESIAN_POINT('Ctrl Pts',(100.437014956238,800.987800885012,117.453675701706));
#69829=CARTESIAN_POINT('Ctrl Pts',(100.380442230377,801.026501484678,117.455151425979));
#69830=CARTESIAN_POINT('Ctrl Pts',(100.285601512585,801.122037875001,117.466029264185));
#69831=CARTESIAN_POINT('Ctrl Pts',(100.248042152197,801.177825667902,117.475256698663));
#69832=CARTESIAN_POINT('Ctrl Pts',(100.197078508039,801.299145482615,117.500145751283));
#69833=CARTESIAN_POINT('Ctrl Pts',(100.184010548787,801.363408718905,117.515512547569));
#69834=CARTESIAN_POINT('Ctrl Pts',(100.184411022147,801.490348899504,117.549816644459));
#69835=CARTESIAN_POINT('Ctrl Pts',(100.19712771743,801.551744919999,117.568292146279));
#69836=CARTESIAN_POINT('Ctrl Pts',(100.246372778483,801.665394250182,117.606273737637));
#69837=CARTESIAN_POINT('Ctrl Pts',(100.282388052149,801.716469180971,117.625384893445));
#69838=CARTESIAN_POINT('Ctrl Pts',(100.374395891752,801.802641376072,117.662253270929));
#69839=CARTESIAN_POINT('Ctrl Pts',(100.429913984255,801.836325612348,117.679561067638));
#69840=CARTESIAN_POINT('Ctrl Pts',(100.552386419393,801.880116640256,117.709647845865));
#69841=CARTESIAN_POINT('Ctrl Pts',(100.618127726179,801.889650682728,117.722095834828));
#69842=CARTESIAN_POINT('Ctrl Pts',(100.751151899359,801.883076433634,117.740588031741));
#69843=CARTESIAN_POINT('Ctrl Pts',(100.817156319277,801.86680642142,117.74639924812));
#69844=CARTESIAN_POINT('Ctrl Pts',(100.940355474473,801.810232669805,117.750553218458));
#69845=CARTESIAN_POINT('Ctrl Pts',(100.996343911969,801.770249775246,117.748796216972));
#69846=CARTESIAN_POINT('Ctrl Pts',(101.088671570435,801.673147054687,117.737899059487));
#69847=CARTESIAN_POINT('Ctrl Pts',(101.1246722087,801.617342435969,117.729042799405));
#69848=CARTESIAN_POINT('Ctrl Pts',(101.172763582946,801.497233275492,117.705382376412));
#69849=CARTESIAN_POINT('Ctrl Pts',(101.184806915195,801.434193341402,117.690896042429));
#69850=CARTESIAN_POINT('Ctrl Pts',(101.183577064562,801.308768134617,117.657985660818));
#69851=CARTESIAN_POINT('Ctrl Pts',(101.170578582854,801.247637242075,117.639930834331));
#69852=CARTESIAN_POINT('Ctrl Pts',(101.120930273629,801.134485545129,117.602277962336));
#69853=CARTESIAN_POINT('Ctrl Pts',(101.08473464511,801.083700422408,117.583075919145));
#69854=CARTESIAN_POINT('Ctrl Pts',(100.993069398449,800.998815427795,117.545850400744));
#69855=CARTESIAN_POINT('Ctrl Pts',(100.938303975563,800.965888860509,117.528250577822));
#69856=CARTESIAN_POINT('Ctrl Pts',(100.816713774663,800.922634136733,117.497084754619));
#69857=CARTESIAN_POINT('Ctrl Pts',(100.750903588543,800.913241145012,117.483934347904));
#69858=CARTESIAN_POINT('Ctrl Pts',(100.68460553067,800.916635666742,117.47417310411));
#69859=CARTESIAN_POINT('Origin',(87.4554740185927,795.155415755662,103.346348239111));
#69860=CARTESIAN_POINT('',(87.4554740185928,790.556275448677,113.293935499859));
#69861=CARTESIAN_POINT('',(87.4554740185921,792.515241382411,113.881561282156));
#69862=CARTESIAN_POINT('Ctrl Pts',(87.4554740185928,790.556275448677,113.293935499859));
#69863=CARTESIAN_POINT('Ctrl Pts',(87.3253835403675,790.558833935716,113.286696557857));
#69864=CARTESIAN_POINT('Ctrl Pts',(87.196490100472,790.585213672252,113.286640186896));
#69865=CARTESIAN_POINT('Ctrl Pts',(86.9510050932038,790.68414220408,113.30175998056));
#69866=CARTESIAN_POINT('Ctrl Pts',(86.8373330070788,790.757222748724,113.317305304562));
#69867=CARTESIAN_POINT('Ctrl Pts',(86.6439779511395,790.941666492189,113.362990726077));
#69868=CARTESIAN_POINT('Ctrl Pts',(86.5666464608927,791.051678904515,113.392865238414));
#69869=CARTESIAN_POINT('Ctrl Pts',(86.4617431746276,791.291841553572,113.46226762902));
#69870=CARTESIAN_POINT('Ctrl Pts',(86.4346036414111,791.419372801328,113.500980286296));
#69871=CARTESIAN_POINT('Ctrl Pts',(86.4335451310337,791.676048198694,113.581630641002));
#69872=CARTESIAN_POINT('Ctrl Pts',(86.4594916050411,791.802665589228,113.622746811084));
#69873=CARTESIAN_POINT('Ctrl Pts',(86.5615665326647,792.038862265696,113.701322838691));
#69874=CARTESIAN_POINT('Ctrl Pts',(86.6368262096136,792.146066595192,113.737981543165));
#69875=CARTESIAN_POINT('Ctrl Pts',(86.8269999019267,792.326114157772,113.801356412446));
#69876=CARTESIAN_POINT('Ctrl Pts',(86.9400511911567,792.397174921811,113.827444669032));
#69877=CARTESIAN_POINT('Ctrl Pts',(87.1884857841945,792.492857385716,113.865606097001));
#69878=CARTESIAN_POINT('Ctrl Pts',(87.3213432683372,792.516721113301,113.877374555419));
#69879=CARTESIAN_POINT('Ctrl Pts',(87.4554740185915,792.515241382411,113.881561282156));
#69880=CARTESIAN_POINT('',(87.4554740194762,793.153312948626,112.076211874431));
#69881=CARTESIAN_POINT('',(87.4554740185927,796.118444895904,103.686715322178));
#69882=CARTESIAN_POINT('Ctrl Pts',(88.1607169118288,791.451266338037,111.609576149122));
#69883=CARTESIAN_POINT('Ctrl Pts',(88.0643783181657,791.364566235938,111.578933399469));
#69884=CARTESIAN_POINT('Ctrl Pts',(87.9510063651193,791.297213863075,111.55281188182));
#69885=CARTESIAN_POINT('Ctrl Pts',(87.703003701421,791.208685891007,111.512671475582));
#69886=CARTESIAN_POINT('Ctrl Pts',(87.5707917712519,791.18837351027,111.499049813342));
#69887=CARTESIAN_POINT('Ctrl Pts',(87.3042752643939,791.197696432798,111.486492371261));
#69888=CARTESIAN_POINT('Ctrl Pts',(87.1725233788929,791.227458982215,111.487749630293));
#69889=CARTESIAN_POINT('Ctrl Pts',(86.926993958815,791.333786780458,111.505564753685));
#69890=CARTESIAN_POINT('Ctrl Pts',(86.8156351699496,791.409540973779,111.522025919791));
#69891=CARTESIAN_POINT('Ctrl Pts',(86.6288864562886,791.597377858824,111.568318005939));
#69892=CARTESIAN_POINT('Ctrl Pts',(86.5553211902952,791.707702804868,111.597721404156));
#69893=CARTESIAN_POINT('Ctrl Pts',(86.4568845798862,791.947382859653,111.665223108358));
#69894=CARTESIAN_POINT('Ctrl Pts',(86.4324975150293,792.074268318309,111.702588476465));
#69895=CARTESIAN_POINT('Ctrl Pts',(86.4358111708451,792.330747607466,111.780832533536));
#69896=CARTESIAN_POINT('Ctrl Pts',(86.4641477142182,792.457821778439,111.82096710474));
#69897=CARTESIAN_POINT('Ctrl Pts',(86.571067227339,792.693616971415,111.897814207958));
#69898=CARTESIAN_POINT('Ctrl Pts',(86.6486641564619,792.799959219119,111.933747682322));
#69899=CARTESIAN_POINT('Ctrl Pts',(86.8421004347898,792.976150499397,111.995923470997));
#69900=CARTESIAN_POINT('Ctrl Pts',(86.9556606391781,793.04462709533,112.021650160957));
#69901=CARTESIAN_POINT('Ctrl Pts',(87.2043792987772,793.135360830149,112.059899566507));
#69902=CARTESIAN_POINT('Ctrl Pts',(87.3370932467606,793.15676534977,112.072065546988));
#69903=CARTESIAN_POINT('Ctrl Pts',(87.603782509758,793.14923193107,112.081479041617));
#69904=CARTESIAN_POINT('Ctrl Pts',(87.735178557639,793.120533767559,112.078694771524));
#69905=CARTESIAN_POINT('Ctrl Pts',(87.9807819833479,793.016054500426,112.058771356649));
#69906=CARTESIAN_POINT('Ctrl Pts',(88.0924550587883,792.940890436587,112.04171075922));
#69907=CARTESIAN_POINT('Ctrl Pts',(88.280914017646,792.752665522551,111.995317358397));
#69908=CARTESIAN_POINT('Ctrl Pts',(88.3554278358524,792.641006456432,111.966294818769));
#69909=CARTESIAN_POINT('Ctrl Pts',(88.4546503045072,792.398149932101,111.900472751406));
#69910=CARTESIAN_POINT('Ctrl Pts',(88.4789457603734,792.269496796233,111.864382725405));
#69911=CARTESIAN_POINT('Ctrl Pts',(88.4745472249191,792.011413142734,111.789311601055));
#69912=CARTESIAN_POINT('Ctrl Pts',(88.4459611000876,791.884483393573,111.751052389241));
#69913=CARTESIAN_POINT('Ctrl Pts',(88.3656264302111,791.707687626158,111.695431876093));
#69914=CARTESIAN_POINT('Ctrl Pts',(88.3326059505706,791.65127360835,111.677259725208));
#69915=CARTESIAN_POINT('Ctrl Pts',(88.2548747098177,791.545165491077,111.642153449871));
#69916=CARTESIAN_POINT('Ctrl Pts',(88.2102362031898,791.495831319252,111.625326921377));
#69917=CARTESIAN_POINT('Ctrl Pts',(88.1607169118288,791.451266338037,111.609576149122));
#69918=CARTESIAN_POINT('Ctrl Pts',(87.4554740185915,792.515241382411,113.881561282156));
#69919=CARTESIAN_POINT('Ctrl Pts',(87.4556313038014,792.51523964724,113.881566191621));
#69920=CARTESIAN_POINT('Ctrl Pts',(87.4557885907617,792.515237877217,113.881571090672));
#69921=CARTESIAN_POINT('Ctrl Pts',(87.4559458794601,792.51523607234,113.88157597931));
#69922=CARTESIAN_POINT('Ctrl Pts',(87.5897196818356,792.513701026646,113.885733758297));
#69923=CARTESIAN_POINT('Ctrl Pts',(87.7221304679224,792.48698234073,113.882287404633));
#69924=CARTESIAN_POINT('Ctrl Pts',(87.9692910476553,792.386040321447,113.861297284005));
#69925=CARTESIAN_POINT('Ctrl Pts',(88.0816233688188,792.312761486658,113.843958857174));
#69926=CARTESIAN_POINT('Ctrl Pts',(88.27107813599,792.128893080232,113.797858523711));
#69927=CARTESIAN_POINT('Ctrl Pts',(88.3463653590261,792.020033605798,113.769527284561));
#69928=CARTESIAN_POINT('Ctrl Pts',(88.4493240949078,791.781375308773,113.705355350815));
#69929=CARTESIAN_POINT('Ctrl Pts',(88.4761629535876,791.653875512941,113.670125305321));
#69930=CARTESIAN_POINT('Ctrl Pts',(88.4775703915665,791.397338462735,113.596761650743));
#69931=CARTESIAN_POINT('Ctrl Pts',(88.4523270331002,791.270732909266,113.559317028448));
#69932=CARTESIAN_POINT('Ctrl Pts',(88.352644593571,791.03491230642,113.486357641548));
#69933=CARTESIAN_POINT('Ctrl Pts',(88.2792053821163,790.927985879112,113.451541753603));
#69934=CARTESIAN_POINT('Ctrl Pts',(88.0928731410458,790.74781645978,113.38871562496));
#69935=CARTESIAN_POINT('Ctrl Pts',(87.9816782173191,790.67652309315,113.361362910284));
#69936=CARTESIAN_POINT('Ctrl Pts',(87.7355450627523,790.57956158465,113.318082029999));
#69937=CARTESIAN_POINT('Ctrl Pts',(87.602927570816,790.555130225739,113.302663470199));
#69938=CARTESIAN_POINT('Ctrl Pts',(87.46431459015,790.556129104338,113.294435645327));
#69939=CARTESIAN_POINT('Ctrl Pts',(87.4598936134117,790.556188528587,113.29418143016));
#69940=CARTESIAN_POINT('Ctrl Pts',(87.4554740185928,790.556275448677,113.293935499859));
#69941=CARTESIAN_POINT('Origin',(87.4554740185927,795.155415755662,103.346348239111));
#69942=CARTESIAN_POINT('',(87.4554740185927,793.491999124156,109.553243482599));
#69943=CARTESIAN_POINT('Origin',(87.4554740185927,793.020576893547,109.386626915332));
#69944=CARTESIAN_POINT('',(87.4554740185929,792.017155209494,113.726143089487));
#69945=CARTESIAN_POINT('',(87.4554740185927,795.626837986271,103.512964806378));
#69946=CARTESIAN_POINT('Ctrl Pts',(87.4558353843692,791.058204607979,113.438480800653));
#69947=CARTESIAN_POINT('Ctrl Pts',(87.395107247592,791.059227064835,113.435456167651));
#69948=CARTESIAN_POINT('Ctrl Pts',(87.3348995885395,791.070852031802,113.435634171487));
#69949=CARTESIAN_POINT('Ctrl Pts',(87.2167107569296,791.115870353922,113.442780376535));
#69950=CARTESIAN_POINT('Ctrl Pts',(87.1604601911993,791.150557842721,113.450245615535));
#69951=CARTESIAN_POINT('Ctrl Pts',(87.0639823201067,791.239230814299,113.472089618104));
#69952=CARTESIAN_POINT('Ctrl Pts',(87.0250007280466,791.292656297874,113.486368535044));
#69953=CARTESIAN_POINT('Ctrl Pts',(86.97120869868,791.410235149184,113.519607311488));
#69954=CARTESIAN_POINT('Ctrl Pts',(86.9567656762087,791.473148774376,113.538202487516));
#69955=CARTESIAN_POINT('Ctrl Pts',(86.9543510749744,791.600168419128,113.577075897066));
#69956=CARTESIAN_POINT('Ctrl Pts',(86.9663334441194,791.663006437193,113.596957774219));
#69957=CARTESIAN_POINT('Ctrl Pts',(87.0153338852697,791.780259083898,113.635175325558));
#69958=CARTESIAN_POINT('Ctrl Pts',(87.0518717596475,791.833495684237,113.653123712744));
#69959=CARTESIAN_POINT('Ctrl Pts',(87.1447619274761,791.92296559278,113.684508529733));
#69960=CARTESIAN_POINT('Ctrl Pts',(87.2001840939746,791.958299358853,113.697629236997));
#69961=CARTESIAN_POINT('Ctrl Pts',(87.3224539291836,792.006003370917,113.717251192452));
#69962=CARTESIAN_POINT('Ctrl Pts',(87.3880698750024,792.017908178443,113.723562835045));
#69963=CARTESIAN_POINT('Ctrl Pts',(87.520768401157,792.016428181589,113.728643294519));
#69964=CARTESIAN_POINT('Ctrl Pts',(87.5865243342633,792.003006760077,113.727350725679));
#69965=CARTESIAN_POINT('Ctrl Pts',(87.7094371416667,791.95220367027,113.717403344035));
#69966=CARTESIAN_POINT('Ctrl Pts',(87.7653025822814,791.915177376151,113.708804172052));
#69967=CARTESIAN_POINT('Ctrl Pts',(87.8580165693196,791.823281958596,113.685701418338));
#69968=CARTESIAN_POINT('Ctrl Pts',(87.8943120590452,791.769630662339,113.671529488309));
#69969=CARTESIAN_POINT('Ctrl Pts',(87.9434399741854,791.652359129353,113.639319851069));
#69970=CARTESIAN_POINT('Ctrl Pts',(87.9558689387087,791.589875652282,113.621594279242));
#69971=CARTESIAN_POINT('Ctrl Pts',(87.9550612009504,791.46438483847,113.584763385552));
#69972=CARTESIAN_POINT('Ctrl Pts',(87.941909781826,791.402578289912,113.566010139522));
#69973=CARTESIAN_POINT('Ctrl Pts',(87.8915435035756,791.28773862627,113.529745722553));
#69974=CARTESIAN_POINT('Ctrl Pts',(87.854835680133,791.235819579664,113.512584483153));
#69975=CARTESIAN_POINT('Ctrl Pts',(87.7623478554504,791.148734486793,113.482024002091));
#69976=CARTESIAN_POINT('Ctrl Pts',(87.7074350431466,791.114474968365,113.46893721144));
#69977=CARTESIAN_POINT('Ctrl Pts',(87.5863960038133,791.06838547699,113.448685678688));
#69978=CARTESIAN_POINT('Ctrl Pts',(87.5214233020689,791.057100328814,113.441747480497));
#69979=CARTESIAN_POINT('Ctrl Pts',(87.4558353843692,791.058204607979,113.438480800653));
#69980=CARTESIAN_POINT('Origin',(94.3198785361657,796.342797332624,103.766009064469));
#69981=CARTESIAN_POINT('',(94.3198785361658,791.628833734555,114.258513129312));
#69982=CARTESIAN_POINT('',(94.3198785361643,793.486184007617,114.693573355438));
#69983=CARTESIAN_POINT('Ctrl Pts',(94.3198785361657,791.628833734555,114.258513129312));
#69984=CARTESIAN_POINT('Ctrl Pts',(94.1999499248709,791.634446460657,114.242632572521));
#69985=CARTESIAN_POINT('Ctrl Pts',(94.0812954380223,791.662262567034,114.232209180336));
#69986=CARTESIAN_POINT('Ctrl Pts',(93.8516234337685,791.76205508106,114.223379074728));
#69987=CARTESIAN_POINT('Ctrl Pts',(93.7437966718754,791.835907160681,114.225910125099));
#69988=CARTESIAN_POINT('Ctrl Pts',(93.5637859343271,792.018065718583,114.244860681593));
#69989=CARTESIAN_POINT('Ctrl Pts',(93.4927273759246,792.124227158106,114.260909216245));
#69990=CARTESIAN_POINT('Ctrl Pts',(93.3965014592787,792.354666749605,114.304040522256));
#69991=CARTESIAN_POINT('Ctrl Pts',(93.3717288972453,792.476536734482,114.330575378483));
#69992=CARTESIAN_POINT('Ctrl Pts',(93.3718592883235,792.720755578022,114.390286018557));
#69993=CARTESIAN_POINT('Ctrl Pts',(93.396584521875,792.840619688169,114.422817130483));
#69994=CARTESIAN_POINT('Ctrl Pts',(93.4920515896565,793.060255122526,114.488485061245));
#69995=CARTESIAN_POINT('Ctrl Pts',(93.5608758781305,793.158154030557,114.520920811344));
#69996=CARTESIAN_POINT('Ctrl Pts',(93.7359386640734,793.323143670412,114.582575607507));
#69997=CARTESIAN_POINT('Ctrl Pts',(93.8410620672137,793.387779917198,114.611055630856));
#69998=CARTESIAN_POINT('Ctrl Pts',(94.0720804840438,793.472214532577,114.659675359076));
#69999=CARTESIAN_POINT('Ctrl Pts',(94.1955226391717,793.491216149227,114.679335495051));
#70000=CARTESIAN_POINT('Ctrl Pts',(94.3198785361628,793.486184007617,114.693573355438));
#70001=CARTESIAN_POINT('',(94.3198785361658,794.142531891777,112.836513228217));
#70002=CARTESIAN_POINT('',(94.3198785361657,797.236693505242,104.081942217606));
#70003=CARTESIAN_POINT('Ctrl Pts',(95.0444948517157,792.603277426813,112.511830837539));
#70004=CARTESIAN_POINT('Ctrl Pts',(94.9681420627759,792.517956387316,112.481675495271));
#70005=CARTESIAN_POINT('Ctrl Pts',(94.8755658797698,792.447982939598,112.45359673427));
#70006=CARTESIAN_POINT('Ctrl Pts',(94.6618342754716,792.342948464805,112.403196052339));
#70007=CARTESIAN_POINT('Ctrl Pts',(94.5415825238692,792.311134687531,112.381806624325));
#70008=CARTESIAN_POINT('Ctrl Pts',(94.2961278044905,792.29502482342,112.35090703876));
#70009=CARTESIAN_POINT('Ctrl Pts',(94.1733467495875,792.310068361198,112.341494395709));
#70010=CARTESIAN_POINT('Ctrl Pts',(93.9371484259024,792.384679404209,112.335630382237));
#70011=CARTESIAN_POINT('Ctrl Pts',(93.8260704676456,792.444272506174,112.339447506925));
#70012=CARTESIAN_POINT('Ctrl Pts',(93.6311654350456,792.601503327518,112.360425928841));
#70013=CARTESIAN_POINT('Ctrl Pts',(93.5494943912638,792.698146085825,112.377558163555));
#70014=CARTESIAN_POINT('Ctrl Pts',(93.4284135255128,792.915730082367,112.42300451116));
#70015=CARTESIAN_POINT('Ctrl Pts',(93.3902705803588,793.034635459477,112.450903262794));
#70016=CARTESIAN_POINT('Ctrl Pts',(93.3643439043819,793.273580817536,112.512201731264));
#70017=CARTESIAN_POINT('Ctrl Pts',(93.3747501484993,793.391148187109,112.544745342764));
#70018=CARTESIAN_POINT('Ctrl Pts',(93.4398681925082,793.611260754879,112.61007434376));
#70019=CARTESIAN_POINT('Ctrl Pts',(93.492521728272,793.712200265137,112.642225932259));
#70020=CARTESIAN_POINT('Ctrl Pts',(93.634279238555,793.889748468439,112.703372042273));
#70021=CARTESIAN_POINT('Ctrl Pts',(93.7222825649812,793.964588664721,112.731785802808));
#70022=CARTESIAN_POINT('Ctrl Pts',(93.9256859327996,794.079745384989,112.781937543513));
#70023=CARTESIAN_POINT('Ctrl Pts',(94.0397928277342,794.117991354328,112.80300128323));
#70024=CARTESIAN_POINT('Ctrl Pts',(94.2840055168934,794.151234546987,112.835316830307));
#70025=CARTESIAN_POINT('Ctrl Pts',(94.4121079263567,794.143509044532,112.845668162958));
#70026=CARTESIAN_POINT('Ctrl Pts',(94.6560898105082,794.080466793332,112.853050005612));
#70027=CARTESIAN_POINT('Ctrl Pts',(94.7698776073542,794.026823753307,112.850311978594));
#70028=CARTESIAN_POINT('Ctrl Pts',(94.9724996006353,793.879813616375,112.832473927347));
#70029=CARTESIAN_POINT('Ctrl Pts',(95.059083659264,793.787272735817,112.817369914873));
#70030=CARTESIAN_POINT('Ctrl Pts',(95.1919509382598,793.574908514864,112.776393641032));
#70031=CARTESIAN_POINT('Ctrl Pts',(95.2366064534347,793.456852177874,112.750807602725));
#70032=CARTESIAN_POINT('Ctrl Pts',(95.2740802707046,793.224618632098,112.695351214234));
#70033=CARTESIAN_POINT('Ctrl Pts',(95.2715071200559,793.113162902256,112.666638763691));
#70034=CARTESIAN_POINT('Ctrl Pts',(95.2245230386503,792.892164821833,112.605183934184));
#70035=CARTESIAN_POINT('Ctrl Pts',(95.1784507543524,792.785070913745,112.572881737015));
#70036=CARTESIAN_POINT('Ctrl Pts',(95.091815465336,792.659616872689,112.531397785795));
#70037=CARTESIAN_POINT('Ctrl Pts',(95.0690433999653,792.630709399946,112.521526225028));
#70038=CARTESIAN_POINT('Ctrl Pts',(95.0444948517157,792.603277426813,112.511830837539));
#70039=CARTESIAN_POINT('Ctrl Pts',(94.3198785361628,793.486184007617,114.693573355438));
#70040=CARTESIAN_POINT('Ctrl Pts',(94.3201814479661,793.486171750095,114.693608036672));
#70041=CARTESIAN_POINT('Ctrl Pts',(94.3204843651896,793.486159349951,114.693642685738));
#70042=CARTESIAN_POINT('Ctrl Pts',(94.3207872877309,793.486146807212,114.693677302633));
#70043=CARTESIAN_POINT('Ctrl Pts',(94.4423918214916,793.481111678678,114.707573830169));
#70044=CARTESIAN_POINT('Ctrl Pts',(94.5625357875021,793.453193046693,114.716031266773));
#70045=CARTESIAN_POINT('Ctrl Pts',(94.7922669428879,793.352783548108,114.72183342988));
#70046=CARTESIAN_POINT('Ctrl Pts',(94.8989193818404,793.27921826343,114.718591452997));
#70047=CARTESIAN_POINT('Ctrl Pts',(95.0771734259361,793.097584299186,114.700348787123));
#70048=CARTESIAN_POINT('Ctrl Pts',(95.1475849800514,792.991489731101,114.685632475545));
#70049=CARTESIAN_POINT('Ctrl Pts',(95.2428140827892,792.761842676514,114.646576000968));
#70050=CARTESIAN_POINT('Ctrl Pts',(95.2675201285011,792.640606010834,114.622726955487));
#70051=CARTESIAN_POINT('Ctrl Pts',(95.2683867434948,792.399142181889,114.56861189477));
#70052=CARTESIAN_POINT('Ctrl Pts',(95.2453382283517,792.281206003213,114.5389585584));
#70053=CARTESIAN_POINT('Ctrl Pts',(95.1543423974781,792.062682966526,114.476969392351));
#70054=CARTESIAN_POINT('Ctrl Pts',(95.0875621480027,791.964278660992,114.445284321032));
#70055=CARTESIAN_POINT('Ctrl Pts',(94.917408983588,791.798660843659,114.383399649576));
#70056=CARTESIAN_POINT('Ctrl Pts',(94.8155072818632,791.733605575997,114.353897130141));
#70057=CARTESIAN_POINT('Ctrl Pts',(94.5884072818366,791.645850916826,114.301068719493));
#70058=CARTESIAN_POINT('Ctrl Pts',(94.4652144984493,791.624923860551,114.278443245546));
#70059=CARTESIAN_POINT('Ctrl Pts',(94.3337109841025,791.628260380662,114.26036233615));
#70060=CARTESIAN_POINT('Ctrl Pts',(94.3267926411482,791.628510150573,114.259428672615));
#70061=CARTESIAN_POINT('Ctrl Pts',(94.3198785361657,791.628833734555,114.258513129312));
#70062=CARTESIAN_POINT('Origin',(94.3198785361657,796.342797332624,103.766009064469));
#70063=CARTESIAN_POINT('',(94.3198785361657,794.679380701117,109.972904307957));
#70064=CARTESIAN_POINT('Origin',(94.3198785361657,794.207958470509,109.80628774069));
#70065=CARTESIAN_POINT('',(94.3198785361661,793.048520242422,114.587234610521));
#70066=CARTESIAN_POINT('',(94.3198785361657,796.814219563232,103.932625631736));
#70067=CARTESIAN_POINT('Ctrl Pts',(94.320132853432,792.068989614922,114.357800917805));
#70068=CARTESIAN_POINT('Ctrl Pts',(94.2558845129119,792.071870312483,114.34955225228));
#70069=CARTESIAN_POINT('Ctrl Pts',(94.1923734261032,792.086837793992,114.344260223503));
#70070=CARTESIAN_POINT('Ctrl Pts',(94.0707675637118,792.140271091967,114.340101298925));
#70071=CARTESIAN_POINT('Ctrl Pts',(94.0142103222728,792.179363601755,114.341603445623));
#70072=CARTESIAN_POINT('Ctrl Pts',(93.9196147486483,792.275909218629,114.351676321105));
#70073=CARTESIAN_POINT('Ctrl Pts',(93.8822830362313,792.332341891131,114.360098786826));
#70074=CARTESIAN_POINT('Ctrl Pts',(93.831982898663,792.454929539717,114.382657156202));
#70075=CARTESIAN_POINT('Ctrl Pts',(93.8192954142479,792.519837184099,114.396528711945));
#70076=CARTESIAN_POINT('Ctrl Pts',(93.820486150406,792.64814158871,114.427423727633));
#70077=CARTESIAN_POINT('Ctrl Pts',(93.8336339592185,792.710277096339,114.44404492511));
#70078=CARTESIAN_POINT('Ctrl Pts',(93.8837406828856,792.825043932107,114.478024980643));
#70079=CARTESIAN_POINT('Ctrl Pts',(93.9200613152844,792.876551036056,114.495030166895));
#70080=CARTESIAN_POINT('Ctrl Pts',(94.0116076704564,792.962564793434,114.52731434934));
#70081=CARTESIAN_POINT('Ctrl Pts',(94.0659626484193,792.99609415452,114.542248458834));
#70082=CARTESIAN_POINT('Ctrl Pts',(94.1870028280717,793.040955950859,114.568392489085));
#70083=CARTESIAN_POINT('Ctrl Pts',(94.2526817079928,793.051211161219,114.579220108645));
#70084=CARTESIAN_POINT('Ctrl Pts',(94.38550251449,793.045894251701,114.595061971422));
#70085=CARTESIAN_POINT('Ctrl Pts',(94.4513180486207,793.030209918373,114.599883283801));
#70086=CARTESIAN_POINT('Ctrl Pts',(94.5742614986078,792.974690065251,114.602936647887));
#70087=CARTESIAN_POINT('Ctrl Pts',(94.6301533962583,792.935159572096,114.601082410372));
#70088=CARTESIAN_POINT('Ctrl Pts',(94.7239589495765,792.837293923143,114.590847168586));
#70089=CARTESIAN_POINT('Ctrl Pts',(94.7609089747412,792.779740229671,114.582519860644));
#70090=CARTESIAN_POINT('Ctrl Pts',(94.8091723737712,792.656692137025,114.560728524722));
#70091=CARTESIAN_POINT('Ctrl Pts',(94.820903005339,792.592637919736,114.547644054107));
#70092=CARTESIAN_POINT('Ctrl Pts',(94.8187304551029,792.465460926339,114.518211213071));
#70093=CARTESIAN_POINT('Ctrl Pts',(94.8052311361328,792.403555179987,114.502193492514));
#70094=CARTESIAN_POINT('Ctrl Pts',(94.7546532948325,792.289337576872,114.469035257421));
#70095=CARTESIAN_POINT('Ctrl Pts',(94.7182021582776,792.238167579766,114.452241610956));
#70096=CARTESIAN_POINT('Ctrl Pts',(94.6263637072458,792.152732315397,114.41981955295));
#70097=CARTESIAN_POINT('Ctrl Pts',(94.5717907076032,792.119552374481,114.404553672576));
#70098=CARTESIAN_POINT('Ctrl Pts',(94.4509524927302,792.075778742696,114.377581681358));
#70099=CARTESIAN_POINT('Ctrl Pts',(94.3857738824115,792.066046473503,114.366228386724));
#70100=CARTESIAN_POINT('Ctrl Pts',(94.320132853432,792.068989614922,114.357800917805));
#70101=CARTESIAN_POINT('Origin',(79.1680833778957,789.12355107042,101.214483166102));
#70102=CARTESIAN_POINT('',(79.1680833778957,784.521269383513,111.170958596584));
#70103=CARTESIAN_POINT('',(79.1680833778933,786.485704177605,111.743110873507));
#70104=CARTESIAN_POINT('Ctrl Pts',(79.1680833778957,784.521269383513,111.170958596584));
#70105=CARTESIAN_POINT('Ctrl Pts',(79.038495696276,784.523265496311,111.165310827197));
#70106=CARTESIAN_POINT('Ctrl Pts',(78.9101098282529,784.549054756029,111.166348335575));
#70107=CARTESIAN_POINT('Ctrl Pts',(78.6648563956979,784.64702740394,111.182602796984));
#70108=CARTESIAN_POINT('Ctrl Pts',(78.5510113593147,784.719983514685,111.198215982747));
#70109=CARTESIAN_POINT('Ctrl Pts',(78.3577721073245,784.904104430857,111.243062158392));
#70110=CARTESIAN_POINT('Ctrl Pts',(78.2805387846432,785.013781548247,111.271978423286));
#70111=CARTESIAN_POINT('Ctrl Pts',(78.1749393444207,785.254319059402,111.339231469695));
#70112=CARTESIAN_POINT('Ctrl Pts',(78.1474056758301,785.382730633137,111.376865511259));
#70113=CARTESIAN_POINT('Ctrl Pts',(78.1459781683731,785.640747173049,111.455208626358));
#70114=CARTESIAN_POINT('Ctrl Pts',(78.1717295877595,785.767807313328,111.495109588889));
#70115=CARTESIAN_POINT('Ctrl Pts',(78.273406477683,786.004861637992,111.571382975723));
#70116=CARTESIAN_POINT('Ctrl Pts',(78.3484317678547,786.112483420382,111.606975788103));
#70117=CARTESIAN_POINT('Ctrl Pts',(78.5384170098812,786.293721588223,111.668363723664));
#70118=CARTESIAN_POINT('Ctrl Pts',(78.651613522809,786.365445649623,111.693512375684));
#70119=CARTESIAN_POINT('Ctrl Pts',(78.9004957422719,786.462335228399,111.729575505573));
#70120=CARTESIAN_POINT('Ctrl Pts',(79.0336437867644,786.486733189265,111.740199404495));
#70121=CARTESIAN_POINT('Ctrl Pts',(79.1680833778909,786.485704177605,111.743110873507));
#70122=CARTESIAN_POINT('',(79.1680835138952,787.124199228011,109.936563266432));
#70123=CARTESIAN_POINT('',(79.1680833778957,790.086580210662,101.554850249169));
#70124=CARTESIAN_POINT('Ctrl Pts',(79.1681795594068,785.157640373189,109.370420786304));
#70125=CARTESIAN_POINT('Ctrl Pts',(79.0565797522559,785.159241406153,109.365859313369));
#70126=CARTESIAN_POINT('Ctrl Pts',(78.9457819465785,785.178473450502,109.366298254558));
#70127=CARTESIAN_POINT('Ctrl Pts',(78.7265698659691,785.253237743471,109.377746616587));
#70128=CARTESIAN_POINT('Ctrl Pts',(78.6206603918319,785.310837457545,109.389472296133));
#70129=CARTESIAN_POINT('Ctrl Pts',(78.4275363459733,785.463361212243,109.424812809634));
#70130=CARTESIAN_POINT('Ctrl Pts',(78.3437763000745,785.559247033304,109.448885211934));
#70131=CARTESIAN_POINT('Ctrl Pts',(78.2134481698245,785.781248379293,109.507869903562));
#70132=CARTESIAN_POINT('Ctrl Pts',(78.170515240135,785.906601377911,109.542743822392));
#70133=CARTESIAN_POINT('Ctrl Pts',(78.138113216936,786.162880012295,109.616690752767));
#70134=CARTESIAN_POINT('Ctrl Pts',(78.1479261701268,786.291213783879,109.654959003555));
#70135=CARTESIAN_POINT('Ctrl Pts',(78.2185590898771,786.537459021962,109.73045827924));
#70136=CARTESIAN_POINT('Ctrl Pts',(78.2790855396499,786.652878229769,109.766931827713));
#70137=CARTESIAN_POINT('Ctrl Pts',(78.4014042193265,786.80273854244,109.81573447721));
#70138=CARTESIAN_POINT('Ctrl Pts',(78.4464156775749,786.848044803181,109.830755023382));
#70139=CARTESIAN_POINT('Ctrl Pts',(78.5276488495495,786.915345202534,109.853522695068));
#70140=CARTESIAN_POINT('Ctrl Pts',(78.5613237813886,786.939871433717,109.861949059357));
#70141=CARTESIAN_POINT('Ctrl Pts',(78.6122234302917,786.972312574428,109.873294366734));
#70142=CARTESIAN_POINT('Ctrl Pts',(78.6282237847542,786.981900133383,109.876677423032));
#70143=CARTESIAN_POINT('Ctrl Pts',(78.6800743540025,787.011060352869,109.887066973852));
#70144=CARTESIAN_POINT('Ctrl Pts',(78.7169099836728,787.028960880562,109.893601975046));
#70145=CARTESIAN_POINT('Ctrl Pts',(78.8104233941452,787.06769306263,109.908178372036));
#70146=CARTESIAN_POINT('Ctrl Pts',(78.8681305988221,787.085897604127,109.915463717021));
#70147=CARTESIAN_POINT('Ctrl Pts',(79.0505347378378,787.126488872437,109.933433787981));
#70148=CARTESIAN_POINT('Ctrl Pts',(79.1783040990978,787.131582708756,109.939053170193));
#70149=CARTESIAN_POINT('Ctrl Pts',(79.4186547082694,787.098065123817,109.937057113325));
#70150=CARTESIAN_POINT('Ctrl Pts',(79.5298324975125,787.063489177882,109.9305786734));
#70151=CARTESIAN_POINT('Ctrl Pts',(79.7432385910014,786.956343208234,109.906549140195));
#70152=CARTESIAN_POINT('Ctrl Pts',(79.8424503831905,786.882079522847,109.888431314368));
#70153=CARTESIAN_POINT('Ctrl Pts',(80.0145709545595,786.696935900433,109.841223391061));
#70154=CARTESIAN_POINT('Ctrl Pts',(80.0835267510673,786.585589075789,109.811899048607));
#70155=CARTESIAN_POINT('Ctrl Pts',(80.1744357085788,786.342185570965,109.746150987676));
#70156=CARTESIAN_POINT('Ctrl Pts',(80.194744647275,786.212165496029,109.710248988596));
#70157=CARTESIAN_POINT('Ctrl Pts',(80.1821719388566,785.957447745236,109.638155686157));
#70158=CARTESIAN_POINT('Ctrl Pts',(80.151388104458,785.835021624015,109.602665897182));
#70159=CARTESIAN_POINT('Ctrl Pts',(80.0532344749418,785.628376756236,109.540856566718));
#70160=CARTESIAN_POINT('Ctrl Pts',(79.9938852893904,785.5425129798,109.51440542654));
#70161=CARTESIAN_POINT('Ctrl Pts',(79.8848830861954,785.429005086173,109.478057780923));
#70162=CARTESIAN_POINT('Ctrl Pts',(79.8449493356518,785.393657675966,109.466468752377));
#70163=CARTESIAN_POINT('Ctrl Pts',(79.7713452998875,785.338412853611,109.447843058239));
#70164=CARTESIAN_POINT('Ctrl Pts',(79.7390644081123,785.316994753261,109.44045036512));
#70165=CARTESIAN_POINT('Ctrl Pts',(79.6714344178052,785.277552470138,109.426460432741));
#70166=CARTESIAN_POINT('Ctrl Pts',(79.6361006665203,785.25963252552,109.419892656151));
#70167=CARTESIAN_POINT('Ctrl Pts',(79.5489861370645,785.221665691564,109.405416390313));
#70168=CARTESIAN_POINT('Ctrl Pts',(79.4963809031319,785.203648626529,109.398030619956));
#70169=CARTESIAN_POINT('Ctrl Pts',(79.353127519043,785.167153960785,109.381405109918));
#70170=CARTESIAN_POINT('Ctrl Pts',(79.2608542603522,785.156310843551,109.374208724212));
#70171=CARTESIAN_POINT('Ctrl Pts',(79.1681795594068,785.157640373189,109.370420786304));
#70172=CARTESIAN_POINT('Ctrl Pts',(79.1680833778909,786.485704177605,111.743110873507));
#70173=CARTESIAN_POINT('Ctrl Pts',(79.1683342559757,786.485702257363,111.743116306607));
#70174=CARTESIAN_POINT('Ctrl Pts',(79.1685851385565,786.485700248557,111.743121712917));
#70175=CARTESIAN_POINT('Ctrl Pts',(79.1688360255834,786.485698151175,111.743127092434));
#70176=CARTESIAN_POINT('Ctrl Pts',(79.3012650675521,786.484591062022,111.745966634573));
#70177=CARTESIAN_POINT('Ctrl Pts',(79.4323797174744,786.458827904345,111.741285419696));
#70178=CARTESIAN_POINT('Ctrl Pts',(79.6797094223275,786.359744177615,111.717947885726));
#70179=CARTESIAN_POINT('Ctrl Pts',(79.793137031013,786.286507288579,111.699276102561));
#70180=CARTESIAN_POINT('Ctrl Pts',(79.9834912650403,786.102592066859,111.651054921246));
#70181=CARTESIAN_POINT('Ctrl Pts',(80.0588282398736,785.993956923702,111.622054381437));
#70182=CARTESIAN_POINT('Ctrl Pts',(80.1619713641202,785.75518273005,111.557451980046));
#70183=CARTESIAN_POINT('Ctrl Pts',(80.1888360425792,785.627321415419,111.522459349039));
#70184=CARTESIAN_POINT('Ctrl Pts',(80.1901211924972,785.369735829489,111.450680705186));
#70185=CARTESIAN_POINT('Ctrl Pts',(80.1647227470622,785.242438260541,111.414560270241));
#70186=CARTESIAN_POINT('Ctrl Pts',(80.0647138465169,785.005337739439,111.345213681305));
#70187=CARTESIAN_POINT('Ctrl Pts',(79.9912014713939,784.897755455922,111.312628812));
#70188=CARTESIAN_POINT('Ctrl Pts',(79.8049953118768,784.716389260766,111.254659744362));
#70189=CARTESIAN_POINT('Ctrl Pts',(79.6940807464636,784.644452980825,111.229853398051));
#70190=CARTESIAN_POINT('Ctrl Pts',(79.4486018155069,784.546097890281,111.191277080136));
#70191=CARTESIAN_POINT('Ctrl Pts',(79.3163753921155,784.520912812566,111.177958377518));
#70192=CARTESIAN_POINT('Ctrl Pts',(79.17771772435,784.521153871509,111.171387654279));
#70193=CARTESIAN_POINT('Ctrl Pts',(79.1728997211776,784.521195194636,111.171168505395));
#70194=CARTESIAN_POINT('Ctrl Pts',(79.1680833778957,784.521269383513,111.170958596584));
#70195=CARTESIAN_POINT('Origin',(79.1680833778957,789.12355107042,101.214483166102));
#70196=CARTESIAN_POINT('',(79.1680833778957,787.460134438913,107.421378409591));
#70197=CARTESIAN_POINT('Origin',(79.1680833778957,786.988712208305,107.254761842323));
#70198=CARTESIAN_POINT('',(79.1680833778957,785.986909477983,111.589697374877));
#70199=CARTESIAN_POINT('',(79.1680833778957,789.594973301029,101.381099733369));
#70200=CARTESIAN_POINT('Ctrl Pts',(79.168391228125,785.025267490352,111.309649943081));
#70201=CARTESIAN_POINT('Ctrl Pts',(79.1078113239188,785.026049952496,111.307324126406));
#70202=CARTESIAN_POINT('Ctrl Pts',(79.0477543483745,785.037433740011,111.308041886352));
#70203=CARTESIAN_POINT('Ctrl Pts',(78.9296590831869,785.082033877263,111.315939718856));
#70204=CARTESIAN_POINT('Ctrl Pts',(78.8733783944443,785.116614078641,111.323598158908));
#70205=CARTESIAN_POINT('Ctrl Pts',(78.7767143522893,785.205313456759,111.345474505223));
#70206=CARTESIAN_POINT('Ctrl Pts',(78.7376263001179,785.258921662493,111.359603684456));
#70207=CARTESIAN_POINT('Ctrl Pts',(78.6837515456947,785.376962714069,111.39225754236));
#70208=CARTESIAN_POINT('Ctrl Pts',(78.6693173014704,785.440147786728,111.410425573342));
#70209=CARTESIAN_POINT('Ctrl Pts',(78.6670054811591,785.567666045195,111.448251480179));
#70210=CARTESIAN_POINT('Ctrl Pts',(78.6790458407191,785.630729446568,111.467524072511));
#70211=CARTESIAN_POINT('Ctrl Pts',(78.7281758927332,785.748442952833,111.504439064488));
#70212=CARTESIAN_POINT('Ctrl Pts',(78.764785065948,785.801911256534,111.521706560736));
#70213=CARTESIAN_POINT('Ctrl Pts',(78.8578837140739,785.891877981657,111.551701619793));
#70214=CARTESIAN_POINT('Ctrl Pts',(78.9134602960854,785.92745074866,111.564119512674));
#70215=CARTESIAN_POINT('Ctrl Pts',(79.0360374096544,785.97552759956,111.582295989573));
#70216=CARTESIAN_POINT('Ctrl Pts',(79.1017960228523,785.987568308633,111.587879222444));
#70217=CARTESIAN_POINT('Ctrl Pts',(79.2345371614157,785.986249018773,111.591520099771));
#70218=CARTESIAN_POINT('Ctrl Pts',(79.300189046162,785.972926127975,111.589552837808));
#70219=CARTESIAN_POINT('Ctrl Pts',(79.4226520444541,785.922417318756,111.578458139247));
#70220=CARTESIAN_POINT('Ctrl Pts',(79.4782117458125,785.885665419543,111.569424779973));
#70221=CARTESIAN_POINT('Ctrl Pts',(79.5707205852793,785.794147622431,111.545764836594));
#70222=CARTESIAN_POINT('Ctrl Pts',(79.6070148570429,785.74050344117,111.531441926772));
#70223=CARTESIAN_POINT('Ctrl Pts',(79.6561448310223,785.623044702354,111.499315924094));
#70224=CARTESIAN_POINT('Ctrl Pts',(79.6685427342927,785.560358099776,111.481820512201));
#70225=CARTESIAN_POINT('Ctrl Pts',(79.667599460703,785.434364550547,111.445870573146));
#70226=CARTESIAN_POINT('Ctrl Pts',(79.6543460022899,785.372256211283,111.42775664183));
#70227=CARTESIAN_POINT('Ctrl Pts',(79.6037679482855,785.256860725903,111.393118016673));
#70228=CARTESIAN_POINT('Ctrl Pts',(79.5669857453052,785.204666448264,111.376920019965));
#70229=CARTESIAN_POINT('Ctrl Pts',(79.4744461441153,785.117087834358,111.348427387096));
#70230=CARTESIAN_POINT('Ctrl Pts',(79.4195852814138,785.082576929838,111.33641404502));
#70231=CARTESIAN_POINT('Ctrl Pts',(79.2987116446366,785.035975259901,111.318181335789));
#70232=CARTESIAN_POINT('Ctrl Pts',(79.2338606263067,785.024421874527,111.312163479871));
#70233=CARTESIAN_POINT('Ctrl Pts',(79.168391228125,785.025267490352,111.309649943081));
#70234=CARTESIAN_POINT('Origin',(86.1443200694598,788.939367371895,101.149386415032));
#70235=CARTESIAN_POINT('',(86.1443200694599,784.218471557535,111.661504380944));
#70236=CARTESIAN_POINT('',(86.1443200694503,786.091238748752,112.052944227269));
#70237=CARTESIAN_POINT('Ctrl Pts',(86.1443200694599,784.218471557536,111.661504380944));
#70238=CARTESIAN_POINT('Ctrl Pts',(86.0232438014687,784.223073791487,111.64848289436));
#70239=CARTESIAN_POINT('Ctrl Pts',(85.9035767255775,784.250562154714,111.640293350206));
#70240=CARTESIAN_POINT('Ctrl Pts',(85.6727855885495,784.350654196083,111.634594772174));
#70241=CARTESIAN_POINT('Ctrl Pts',(85.5649088275317,784.425006936018,111.637854698421));
#70242=CARTESIAN_POINT('Ctrl Pts',(85.385137013404,784.608767941465,111.656521250761));
#70243=CARTESIAN_POINT('Ctrl Pts',(85.3144201570192,784.716099024219,111.671616691658));
#70244=CARTESIAN_POINT('Ctrl Pts',(85.2194105317485,784.948790966923,111.711418723205));
#70245=CARTESIAN_POINT('Ctrl Pts',(85.1953917516291,785.071771854287,111.735628162361));
#70246=CARTESIAN_POINT('Ctrl Pts',(85.1971198637617,785.317934859568,111.789674249004));
#70247=CARTESIAN_POINT('Ctrl Pts',(85.2225773921297,785.438692239883,111.818935351978));
#70248=CARTESIAN_POINT('Ctrl Pts',(85.319467638155,785.660230273347,111.877649929256));
#70249=CARTESIAN_POINT('Ctrl Pts',(85.3890318696257,785.759126606001,111.906487526506));
#70250=CARTESIAN_POINT('Ctrl Pts',(85.5636352728739,785.923988162167,111.960079069209));
#70251=CARTESIAN_POINT('Ctrl Pts',(85.6667991916973,785.988348088792,111.984291303336));
#70252=CARTESIAN_POINT('Ctrl Pts',(85.8957661859035,786.074845854189,112.025409242133));
#70253=CARTESIAN_POINT('Ctrl Pts',(86.0195494801765,786.095201758359,112.041731351737));
#70254=CARTESIAN_POINT('Ctrl Pts',(86.1443200694407,786.091238748751,112.052944227269));
#70255=CARTESIAN_POINT('',(86.1443200694599,786.744690678997,110.20407786539));
#70256=CARTESIAN_POINT('',(86.1443200694598,789.833263544514,101.465319568169));
#70257=CARTESIAN_POINT('Ctrl Pts',(86.7259870614681,785.070398779602,109.849456642294));
#70258=CARTESIAN_POINT('Ctrl Pts',(86.6324881639625,785.001909523517,109.825250221801));
#70259=CARTESIAN_POINT('Ctrl Pts',(86.5262728280359,784.95163570823,109.804133977455));
#70260=CARTESIAN_POINT('Ctrl Pts',(86.2931301198167,784.890885113085,109.769384716974));
#70261=CARTESIAN_POINT('Ctrl Pts',(86.1677878289683,784.883408955391,109.756597027203));
#70262=CARTESIAN_POINT('Ctrl Pts',(85.9223980754791,784.915940279537,109.742888883384));
#70263=CARTESIAN_POINT('Ctrl Pts',(85.804596904887,784.954824781141,109.741902443628));
#70264=CARTESIAN_POINT('Ctrl Pts',(85.5877796868017,785.074328280863,109.751904943332));
#70265=CARTESIAN_POINT('Ctrl Pts',(85.4910754501357,785.154511963793,109.762999476033));
#70266=CARTESIAN_POINT('Ctrl Pts',(85.3327047136388,785.346751334975,109.796351104006));
#70267=CARTESIAN_POINT('Ctrl Pts',(85.2729500757762,785.45740894643,109.818436662026));
#70268=CARTESIAN_POINT('Ctrl Pts',(85.2003164193624,785.694189460527,109.870667708466));
#70269=CARTESIAN_POINT('Ctrl Pts',(85.1882487292566,785.818070558252,109.900325048123));
#70270=CARTESIAN_POINT('Ctrl Pts',(85.2139756320044,786.057035713228,109.961630513494));
#70271=CARTESIAN_POINT('Ctrl Pts',(85.2494557375695,786.170055885681,109.992566991673));
#70272=CARTESIAN_POINT('Ctrl Pts',(85.3608253008893,786.372679070545,110.051714652982));
#70273=CARTESIAN_POINT('Ctrl Pts',(85.4343428004351,786.461115416521,110.079447200168));
#70274=CARTESIAN_POINT('Ctrl Pts',(85.6120434466344,786.607006292119,110.129404539419));
#70275=CARTESIAN_POINT('Ctrl Pts',(85.7147630845295,786.662946425091,110.151138378081));
#70276=CARTESIAN_POINT('Ctrl Pts',(85.9397702530505,786.735648969544,110.18628537658));
#70277=CARTESIAN_POINT('Ctrl Pts',(86.0603402946392,786.75063917116,110.199129741105));
#70278=CARTESIAN_POINT('Ctrl Pts',(86.307971880145,786.735142098257,110.214218829165));
#70279=CARTESIAN_POINT('Ctrl Pts',(86.4324776988788,786.702383891835,110.21572275723));
#70280=CARTESIAN_POINT('Ctrl Pts',(86.6592813594046,786.592688230903,110.206615706328));
#70281=CARTESIAN_POINT('Ctrl Pts',(86.7598773624179,786.517800411025,110.196369055275));
#70282=CARTESIAN_POINT('Ctrl Pts',(86.9280175442621,786.33404887482,110.165545350349));
#70283=CARTESIAN_POINT('Ctrl Pts',(86.9935224417377,786.226436443181,110.145114541764));
#70284=CARTESIAN_POINT('Ctrl Pts',(87.079017874582,785.992433144348,110.096490285624));
#70285=CARTESIAN_POINT('Ctrl Pts',(87.0977824872587,785.868092066369,110.068683007201));
#70286=CARTESIAN_POINT('Ctrl Pts',(87.0850708559952,785.633404663581,110.012359342614));
#70287=CARTESIAN_POINT('Ctrl Pts',(87.0587161614571,785.524815594854,109.984660067105));
#70288=CARTESIAN_POINT('Ctrl Pts',(86.9651791190065,785.317742728665,109.928126879479));
#70289=CARTESIAN_POINT('Ctrl Pts',(86.8968821834878,785.221982460985,109.899830374314));
#70290=CARTESIAN_POINT('Ctrl Pts',(86.7846733949305,785.116233260758,109.865310780573));
#70291=CARTESIAN_POINT('Ctrl Pts',(86.756048336616,785.09241908601,109.857239363654));
#70292=CARTESIAN_POINT('Ctrl Pts',(86.7259870614681,785.070398779602,109.849456642294));
#70293=CARTESIAN_POINT('Ctrl Pts',(86.1443200694407,786.091238748751,112.052944227269));
#70294=CARTESIAN_POINT('Ctrl Pts',(86.1446495235245,786.091228284509,112.052973834628));
#70295=CARTESIAN_POINT('Ctrl Pts',(86.1449789844855,786.091217650699,112.053003406431));
#70296=CARTESIAN_POINT('Ctrl Pts',(86.1453084521914,786.091206847301,112.053032942666));
#70297=CARTESIAN_POINT('Ctrl Pts',(86.2684868787339,786.08716776983,112.064075684971));
#70298=CARTESIAN_POINT('Ctrl Pts',(86.3901386013758,786.059510627326,112.069930167044));
#70299=CARTESIAN_POINT('Ctrl Pts',(86.6199199055224,785.959244886059,112.071277448783));
#70300=CARTESIAN_POINT('Ctrl Pts',(86.7253881253119,785.886477628309,112.066498366302));
#70301=CARTESIAN_POINT('Ctrl Pts',(86.9039325757279,785.704443352265,112.046848165786));
#70302=CARTESIAN_POINT('Ctrl Pts',(86.9748800396098,785.596346451338,112.032016692792));
#70303=CARTESIAN_POINT('Ctrl Pts',(87.0694458972329,785.362733236678,111.994548640001));
#70304=CARTESIAN_POINT('Ctrl Pts',(87.0932243693923,785.239656152849,111.972401425732));
#70305=CARTESIAN_POINT('Ctrl Pts',(87.0915567043042,784.994789033857,111.923368043958));
#70306=CARTESIAN_POINT('Ctrl Pts',(87.0670010783056,784.87522123426,111.897005218452));
#70307=CARTESIAN_POINT('Ctrl Pts',(86.9729694945433,784.654587721567,111.842899430378));
#70308=CARTESIAN_POINT('Ctrl Pts',(86.9049801725677,784.555495185941,111.815704126075));
#70309=CARTESIAN_POINT('Ctrl Pts',(86.7332512703618,784.389390804322,111.763339720698));
#70310=CARTESIAN_POINT('Ctrl Pts',(86.6312613812925,784.324240890815,111.738734258038));
#70311=CARTESIAN_POINT('Ctrl Pts',(86.404729652754,784.236310932174,111.695148800306));
#70312=CARTESIAN_POINT('Ctrl Pts',(86.2823161654338,784.215182880036,111.676744306655));
#70313=CARTESIAN_POINT('Ctrl Pts',(86.153871706826,784.218144173277,111.662538917529));
#70314=CARTESIAN_POINT('Ctrl Pts',(86.1490947922307,784.218290065393,111.662017891887));
#70315=CARTESIAN_POINT('Ctrl Pts',(86.1443200694599,784.218471557536,111.661504380944));
#70316=CARTESIAN_POINT('Origin',(86.1443200694598,788.939367371895,101.149386415032));
#70317=CARTESIAN_POINT('',(86.1443200694598,787.275950740389,107.356281658521));
#70318=CARTESIAN_POINT('Origin',(86.1443200694598,786.80452850978,107.189665091254));
#70319=CARTESIAN_POINT('',(86.1443200694602,785.650395405619,111.955601728935));
#70320=CARTESIAN_POINT('',(86.1443200694598,789.410789602504,101.316002982299));
#70321=CARTESIAN_POINT('Ctrl Pts',(86.1447175963381,784.662722492406,111.749205968351));
#70322=CARTESIAN_POINT('Ctrl Pts',(86.0790639755617,784.665072798417,111.742399408785));
#70323=CARTESIAN_POINT('Ctrl Pts',(86.0142265421774,784.680172569735,111.738315514435));
#70324=CARTESIAN_POINT('Ctrl Pts',(85.8916808562695,784.734517684191,111.736071683426));
#70325=CARTESIAN_POINT('Ctrl Pts',(85.8354078768984,784.773940501574,111.73811386647));
#70326=CARTESIAN_POINT('Ctrl Pts',(85.7415320712461,784.871287659228,111.748325758983));
#70327=CARTESIAN_POINT('Ctrl Pts',(85.7046579955178,784.928223230305,111.756366924686));
#70328=CARTESIAN_POINT('Ctrl Pts',(85.6553823759995,785.051794067799,111.777325443641));
#70329=CARTESIAN_POINT('Ctrl Pts',(85.6432461955908,785.117220056091,111.790011282445));
#70330=CARTESIAN_POINT('Ctrl Pts',(85.6455161442487,785.246771479336,111.817998634657));
#70331=CARTESIAN_POINT('Ctrl Pts',(85.6592911271632,785.309661546211,111.832963427702));
#70332=CARTESIAN_POINT('Ctrl Pts',(85.7106978120086,785.425525656657,111.863214412855));
#70333=CARTESIAN_POINT('Ctrl Pts',(85.7475800563947,785.477429862313,111.878189971105));
#70334=CARTESIAN_POINT('Ctrl Pts',(85.8399717853424,785.56385445823,111.906221565601));
#70335=CARTESIAN_POINT('Ctrl Pts',(85.8945059412723,785.59749810403,111.918988579773));
#70336=CARTESIAN_POINT('Ctrl Pts',(86.0152688124681,785.642383286418,111.94084131766));
#70337=CARTESIAN_POINT('Ctrl Pts',(86.0804048705909,785.652738356333,111.949627123714));
#70338=CARTESIAN_POINT('Ctrl Pts',(86.2125174373546,785.647901267344,111.961977841987));
#70339=CARTESIAN_POINT('Ctrl Pts',(86.2781371435774,785.632404365839,111.96534462441));
#70340=CARTESIAN_POINT('Ctrl Pts',(86.4004134430373,785.577245284638,111.96621938934));
#70341=CARTESIAN_POINT('Ctrl Pts',(86.4558315704492,785.537966698863,111.963685501028));
#70342=CARTESIAN_POINT('Ctrl Pts',(86.5488817521974,785.440581970136,111.953068499387));
#70343=CARTESIAN_POINT('Ctrl Pts',(86.5855214737621,785.383219071274,111.945039413769));
#70344=CARTESIAN_POINT('Ctrl Pts',(86.6337998151398,785.259613954274,111.92470894953));
#70345=CARTESIAN_POINT('Ctrl Pts',(86.6455115360651,785.194658947201,111.912674115002));
#70346=CARTESIAN_POINT('Ctrl Pts',(86.6429589584479,785.065677491729,111.886098320221));
#70347=CARTESIAN_POINT('Ctrl Pts',(86.6291498617514,785.00283709202,111.871843492542));
#70348=CARTESIAN_POINT('Ctrl Pts',(86.5778838978083,784.887159236913,111.842774131275));
#70349=CARTESIAN_POINT('Ctrl Pts',(86.5412040515293,784.835369261024,111.828254525587));
#70350=CARTESIAN_POINT('Ctrl Pts',(86.449203178204,784.749006572816,111.800581738242));
#70351=CARTESIAN_POINT('Ctrl Pts',(86.3948239620984,784.715383134124,111.787724194351));
#70352=CARTESIAN_POINT('Ctrl Pts',(86.2746031816651,784.670674004925,111.765270017627));
#70353=CARTESIAN_POINT('Ctrl Pts',(86.2099024020029,784.660388969307,111.755963924078));
#70354=CARTESIAN_POINT('Ctrl Pts',(86.1447175963381,784.662722492406,111.749205968351));
#70355=CARTESIAN_POINT('Origin',(58.6359451072587,790.091644456036,101.556640124838));
#70356=CARTESIAN_POINT('',(58.6359451072587,787.962812675165,112.230333666846));
#70357=CARTESIAN_POINT('Origin',(58.6359451072587,786.501713859367,111.713931907829));
#70358=CARTESIAN_POINT('',(58.6359451072371,788.629270889217,110.344667535143));
#70359=CARTESIAN_POINT('',(58.6359451072587,791.552743271833,102.073041883855));
#70360=CARTESIAN_POINT('Ctrl Pts',(58.6360112917652,785.683487034017,109.378598502357));
#70361=CARTESIAN_POINT('Ctrl Pts',(58.5934212586555,785.683433325671,109.378745005346));
#70362=CARTESIAN_POINT('Ctrl Pts',(58.5508491600315,785.685061751144,109.379400993085));
#70363=CARTESIAN_POINT('Ctrl Pts',(58.4173803867427,785.695459149166,109.383059322162));
#70364=CARTESIAN_POINT('Ctrl Pts',(58.3272019823704,785.710247041297,109.387879412916));
#70365=CARTESIAN_POINT('Ctrl Pts',(58.1169108226222,785.763387269929,109.404785756253));
#70366=CARTESIAN_POINT('Ctrl Pts',(57.9993169496857,785.808384142461,109.418879104229));
#70367=CARTESIAN_POINT('Ctrl Pts',(57.7083753933041,785.961349932394,109.466595888032));
#70368=CARTESIAN_POINT('Ctrl Pts',(57.549602335207,786.089615809777,109.506455074143));
#70369=CARTESIAN_POINT('Ctrl Pts',(57.3072455168803,786.381429583381,109.597965461416));
#70370=CARTESIAN_POINT('Ctrl Pts',(57.2194361224958,786.537537172826,109.647229099602));
#70371=CARTESIAN_POINT('Ctrl Pts',(57.1021429212925,786.880874522943,109.756900187524));
#70372=CARTESIAN_POINT('Ctrl Pts',(57.0772865499598,787.066323531765,109.816823279474));
#70373=CARTESIAN_POINT('Ctrl Pts',(57.1017554907427,787.447084244517,109.941562652666));
#70374=CARTESIAN_POINT('Ctrl Pts',(57.1554751227801,787.638481920637,110.005204307833));
#70375=CARTESIAN_POINT('Ctrl Pts',(57.3373200955687,787.986600043651,110.122429031596));
#70376=CARTESIAN_POINT('Ctrl Pts',(57.4624095156542,788.140469086084,110.175006241827));
#70377=CARTESIAN_POINT('Ctrl Pts',(57.7707058476356,788.395594787389,110.262919683401));
#70378=CARTESIAN_POINT('Ctrl Pts',(57.9517378698733,788.493398842964,110.297056511618));
#70379=CARTESIAN_POINT('Ctrl Pts',(58.2603293965507,788.590081206249,110.330899840703));
#70380=CARTESIAN_POINT('Ctrl Pts',(58.3768393456003,788.61302604832,110.338966249576));
#70381=CARTESIAN_POINT('Ctrl Pts',(58.5824662727724,788.630747755917,110.345190272108));
#70382=CARTESIAN_POINT('Ctrl Pts',(58.6704756685845,788.631255966232,110.345365104003));
#70383=CARTESIAN_POINT('Ctrl Pts',(58.846119991235,788.618166081974,110.340738557602));
#70384=CARTESIAN_POINT('Ctrl Pts',(58.9334289239458,788.60451362539,110.335918003867));
#70385=CARTESIAN_POINT('Ctrl Pts',(59.1324646379154,788.556625662076,110.319031637685));
#70386=CARTESIAN_POINT('Ctrl Pts',(59.2422582641522,788.517294170075,110.305172525968));
#70387=CARTESIAN_POINT('Ctrl Pts',(59.5300463347398,788.377244135138,110.255992915242));
#70388=CARTESIAN_POINT('Ctrl Pts',(59.69297781754,788.253988261049,110.21285265492));
#70389=CARTESIAN_POINT('Ctrl Pts',(59.9418603811138,787.97228364501,110.115406156515));
#70390=CARTESIAN_POINT('Ctrl Pts',(60.0328374740205,787.822121236338,110.063867581492));
#70391=CARTESIAN_POINT('Ctrl Pts',(60.1592605008424,787.488996131706,109.95100437375));
#70392=CARTESIAN_POINT('Ctrl Pts',(60.1900602977308,787.307524498111,109.890279344063));
#70393=CARTESIAN_POINT('Ctrl Pts',(60.179817887963,786.930798802891,109.766154932587));
#70394=CARTESIAN_POINT('Ctrl Pts',(60.134099569607,786.739118347925,109.704065529562));
#70395=CARTESIAN_POINT('Ctrl Pts',(59.9674977422645,786.38397477116,109.590909967842));
#70396=CARTESIAN_POINT('Ctrl Pts',(59.8485748527781,786.223833018589,109.540878268881));
#70397=CARTESIAN_POINT('Ctrl Pts',(59.5519042990591,785.955495691196,109.458296014561));
#70398=CARTESIAN_POINT('Ctrl Pts',(59.3767380367989,785.850226829109,109.426628824816));
#70399=CARTESIAN_POINT('Ctrl Pts',(59.0721263972114,785.739320213053,109.393885592828));
#70400=CARTESIAN_POINT('Ctrl Pts',(58.9543318038803,785.71092437552,109.385708176056));
#70401=CARTESIAN_POINT('Ctrl Pts',(58.768546670276,785.687730857853,109.379377275714));
#70402=CARTESIAN_POINT('Ctrl Pts',(58.7023139431371,785.683570645264,109.378370431706));
#70403=CARTESIAN_POINT('Ctrl Pts',(58.6360112917652,785.683487034017,109.378598502357));
#70404=CARTESIAN_POINT('Origin',(58.6359451072587,790.091644456036,101.556640124838));
#70405=CARTESIAN_POINT('',(58.6359451072587,788.42822782453,107.763535368326));
#70406=CARTESIAN_POINT('Origin',(58.6359451072587,787.956805593921,107.596918801059));
#70407=CARTESIAN_POINT('',(58.6359451072587,786.973136089976,111.880548475096));
#70408=CARTESIAN_POINT('',(58.6359451072587,790.563066686645,101.723256692105));
#70409=CARTESIAN_POINT('Origin',(58.6359451072587,786.501713859367,111.713931907829));
#70410=CARTESIAN_POINT('Origin',(63.9954594876854,787.256016761222,100.554433351629));
#70411=CARTESIAN_POINT('',(63.9954594876854,784.853467741515,111.131385959978));
#70412=CARTESIAN_POINT('Origin',(63.9954594876854,783.666086164553,110.71172513462));
#70413=CARTESIAN_POINT('',(63.9954594857071,785.501764606246,109.297105257399));
#70414=CARTESIAN_POINT('',(63.9954594876854,788.443398338184,100.974094176987));
#70415=CARTESIAN_POINT('Ctrl Pts',(63.9953219214531,783.079207789871,108.593010247634));
#70416=CARTESIAN_POINT('Ctrl Pts',(63.9634403507654,783.079109028351,108.593300132773));
#70417=CARTESIAN_POINT('Ctrl Pts',(63.9315697531246,783.080181855706,108.593908199));
#70418=CARTESIAN_POINT('Ctrl Pts',(63.8289234252417,783.087422140518,108.596893307604));
#70419=CARTESIAN_POINT('Ctrl Pts',(63.7586533599441,783.098216849211,108.600519814419));
#70420=CARTESIAN_POINT('Ctrl Pts',(63.5894835574832,783.138648577437,108.613170508994));
#70421=CARTESIAN_POINT('Ctrl Pts',(63.492731028879,783.174459467676,108.623847392199));
#70422=CARTESIAN_POINT('Ctrl Pts',(63.253827423507,783.29729116606,108.659648845313));
#70423=CARTESIAN_POINT('Ctrl Pts',(63.1233366762046,783.401071291594,108.689263983923));
#70424=CARTESIAN_POINT('Ctrl Pts',(62.9237206983426,783.638023348043,108.756633023886));
#70425=CARTESIAN_POINT('Ctrl Pts',(62.8510266210737,783.76488426197,108.792627068914));
#70426=CARTESIAN_POINT('Ctrl Pts',(62.7522703730241,784.044938749867,108.872466935751));
#70427=CARTESIAN_POINT('Ctrl Pts',(62.7300370223754,784.196796038279,108.915963009024));
#70428=CARTESIAN_POINT('Ctrl Pts',(62.7454369677152,784.509441867852,109.006232398207));
#70429=CARTESIAN_POINT('Ctrl Pts',(62.7866177928744,784.667138668229,109.052161077309));
#70430=CARTESIAN_POINT('Ctrl Pts',(62.9298158258099,784.955764713402,109.136849485736));
#70431=CARTESIAN_POINT('Ctrl Pts',(63.0296412381602,785.084217827181,109.174863410891));
#70432=CARTESIAN_POINT('Ctrl Pts',(63.2751955144117,785.296604402606,109.237831898397));
#70433=CARTESIAN_POINT('Ctrl Pts',(63.4184661898421,785.378531055751,109.262175722522));
#70434=CARTESIAN_POINT('Ctrl Pts',(63.667628860898,785.46356478289,109.287013767226));
#70435=CARTESIAN_POINT('Ctrl Pts',(63.764701445428,785.484786995277,109.293063915288));
#70436=CARTESIAN_POINT('Ctrl Pts',(63.9325074295607,785.501990879562,109.297504334598));
#70437=CARTESIAN_POINT('Ctrl Pts',(64.0021477557783,785.503592658949,109.297636891416));
#70438=CARTESIAN_POINT('Ctrl Pts',(64.1030708741173,785.497921031115,109.295349331963));
#70439=CARTESIAN_POINT('Ctrl Pts',(64.1344987271119,785.495018209405,109.294284466736));
#70440=CARTESIAN_POINT('Ctrl Pts',(64.2359926197191,785.481945868022,109.289698310745));
#70441=CARTESIAN_POINT('Ctrl Pts',(64.3052734101441,785.46725232174,109.284776957922));
#70442=CARTESIAN_POINT('Ctrl Pts',(64.4724952156569,785.417318882363,109.268421434084));
#70443=CARTESIAN_POINT('Ctrl Pts',(64.5678269053854,785.37583971053,109.25506930429));
#70444=CARTESIAN_POINT('Ctrl Pts',(64.7996433554226,785.239469992345,109.211746232437));
#70445=CARTESIAN_POINT('Ctrl Pts',(64.9234968634013,785.128812661035,109.177042998576));
#70446=CARTESIAN_POINT('Ctrl Pts',(65.1074081567735,784.882051521045,109.100960786265));
#70447=CARTESIAN_POINT('Ctrl Pts',(65.1716361928218,784.75219348862,109.061393699662));
#70448=CARTESIAN_POINT('Ctrl Pts',(65.2523304975,784.467614714687,108.976030377366));
#70449=CARTESIAN_POINT('Ctrl Pts',(65.2646432854445,784.314365839574,108.930768839063));
#70450=CARTESIAN_POINT('Ctrl Pts',(65.2284965205647,784.003194891884,108.840502095042));
#70451=CARTESIAN_POINT('Ctrl Pts',(65.1771813281799,783.848496517605,108.796520752538));
#70452=CARTESIAN_POINT('Ctrl Pts',(65.0163323663172,783.569217945263,108.718703210265));
#70453=CARTESIAN_POINT('Ctrl Pts',(64.9092886404542,783.446815684077,108.685434649322));
#70454=CARTESIAN_POINT('Ctrl Pts',(64.663337821583,783.256502698469,108.634942560308));
#70455=CARTESIAN_POINT('Ctrl Pts',(64.5298007662076,783.186419871577,108.617004866245));
#70456=CARTESIAN_POINT('Ctrl Pts',(64.3041632931217,783.114389570073,108.599522013241));
#70457=CARTESIAN_POINT('Ctrl Pts',(64.2190831819158,783.09634971238,108.595451984538));
#70458=CARTESIAN_POINT('Ctrl Pts',(64.0871325449022,783.081923075148,108.592835710093));
#70459=CARTESIAN_POINT('Ctrl Pts',(64.0412455965643,783.079350050488,108.592592683799));
#70460=CARTESIAN_POINT('Ctrl Pts',(63.9953219214531,783.079207789871,108.593010247634));
#70461=CARTESIAN_POINT('Origin',(63.9954594876854,787.256016761222,100.554433351629));
#70462=CARTESIAN_POINT('',(63.9954594876854,785.592600129715,106.761328595117));
#70463=CARTESIAN_POINT('Origin',(63.9954594876854,785.121177899107,106.59471202785));
#70464=CARTESIAN_POINT('',(63.9954594876854,784.137508395162,110.878341701887));
#70465=CARTESIAN_POINT('',(63.9954594876854,787.72743899183,100.721049918896));
#70466=CARTESIAN_POINT('Origin',(63.9954594876854,783.666086164553,110.71172513462));
#70467=CARTESIAN_POINT('Origin',(69.7316732616476,784.848060912957,99.7033802796288));
#70468=CARTESIAN_POINT('',(69.7316732616476,780.243496355298,109.666314827831));
#70469=CARTESIAN_POINT('',(69.7316732616476,782.211734062764,110.227707202932));
#70470=CARTESIAN_POINT('Ctrl Pts',(69.7316732616476,780.243496355298,109.666314827831));
#70471=CARTESIAN_POINT('Ctrl Pts',(69.6035672430037,780.244787361547,109.662662075552));
#70472=CARTESIAN_POINT('Ctrl Pts',(69.4766151361266,780.269448399822,109.66520829645));
#70473=CARTESIAN_POINT('Ctrl Pts',(69.2322800901463,780.365064241757,109.683393659838));
#70474=CARTESIAN_POINT('Ctrl Pts',(69.1181296682301,780.437328831716,109.699517539606));
#70475=CARTESIAN_POINT('Ctrl Pts',(68.9240377574953,780.620598551093,109.744397312699));
#70476=CARTESIAN_POINT('Ctrl Pts',(68.8462981895684,780.730166662832,109.772845259494));
#70477=CARTESIAN_POINT('Ctrl Pts',(68.7393590255276,780.971532284846,109.838678474064));
#70478=CARTESIAN_POINT('Ctrl Pts',(68.7112664462007,781.100986137373,109.875432840945));
#70479=CARTESIAN_POINT('Ctrl Pts',(68.7093271581908,781.360711137878,109.951681513805));
#70480=CARTESIAN_POINT('Ctrl Pts',(68.734888715193,781.48841604878,109.99038369636));
#70481=CARTESIAN_POINT('Ctrl Pts',(68.8361969648346,781.726416524879,110.064246696049));
#70482=CARTESIAN_POINT('Ctrl Pts',(68.9108964899515,781.834388247012,110.09866460518));
#70483=CARTESIAN_POINT('Ctrl Pts',(69.1003519106522,782.016639712931,110.157928290986));
#70484=CARTESIAN_POINT('Ctrl Pts',(69.2134117469588,782.088957655794,110.182124916369));
#70485=CARTESIAN_POINT('Ctrl Pts',(69.4627339866786,782.187316552922,110.216316324272));
#70486=CARTESIAN_POINT('Ctrl Pts',(69.5965420190118,782.212351494003,110.225960252934));
#70487=CARTESIAN_POINT('Ctrl Pts',(69.7316732616476,782.211734062764,110.227707202932));
#70488=CARTESIAN_POINT('',(69.7316732616702,782.827991978286,108.484076986977));
#70489=CARTESIAN_POINT('',(69.7316732616476,785.811090053199,100.043747362696));
#70490=CARTESIAN_POINT('Ctrl Pts',(69.7318153101166,780.843131484731,107.96971688462));
#70491=CARTESIAN_POINT('Ctrl Pts',(69.6375166661361,780.843123464971,107.969700221094));
#70492=CARTESIAN_POINT('Ctrl Pts',(69.5436863369083,780.855844728437,107.972854971));
#70493=CARTESIAN_POINT('Ctrl Pts',(69.3498604307255,780.909428975668,107.986198881597));
#70494=CARTESIAN_POINT('Ctrl Pts',(69.2520257946803,780.953570742773,107.997208303356));
#70495=CARTESIAN_POINT('Ctrl Pts',(69.066034155537,781.075016085042,108.027624702619));
#70496=CARTESIAN_POINT('Ctrl Pts',(68.9809430616127,781.154056140655,108.047476812565));
#70497=CARTESIAN_POINT('Ctrl Pts',(68.8369280171959,781.343018442622,108.09522531929));
#70498=CARTESIAN_POINT('Ctrl Pts',(68.7815223568898,781.453176152445,108.123203489822));
#70499=CARTESIAN_POINT('Ctrl Pts',(68.7120864656617,781.694966148047,108.185096763272));
#70500=CARTESIAN_POINT('Ctrl Pts',(68.7016897333903,781.825286227403,108.218711938315));
#70501=CARTESIAN_POINT('Ctrl Pts',(68.7331310173967,782.083699019231,108.285943406331));
#70502=CARTESIAN_POINT('Ctrl Pts',(68.7752474341524,782.209277021531,108.318911524792));
#70503=CARTESIAN_POINT('Ctrl Pts',(68.9042942849275,782.431927565488,108.377788983928));
#70504=CARTESIAN_POINT('Ctrl Pts',(68.9878862493639,782.52808328057,108.403427529047));
#70505=CARTESIAN_POINT('Ctrl Pts',(69.1679476320414,782.669766803881,108.441373804505));
#70506=CARTESIAN_POINT('Ctrl Pts',(69.2575787692492,782.720713653666,108.455089385681));
#70507=CARTESIAN_POINT('Ctrl Pts',(69.3974062319674,782.77466023747,108.469640517441));
#70508=CARTESIAN_POINT('Ctrl Pts',(69.4423610085247,782.78860039153,108.473406421392));
#70509=CARTESIAN_POINT('Ctrl Pts',(69.5193886940357,782.806907027757,108.478356459356));
#70510=CARTESIAN_POINT('Ctrl Pts',(69.5509692571673,782.812897783851,108.479977975895));
#70511=CARTESIAN_POINT('Ctrl Pts',(69.5972351897966,782.819495838748,108.481765566566));
#70512=CARTESIAN_POINT('Ctrl Pts',(69.6117239400673,782.821255703991,108.482242684802));
#70513=CARTESIAN_POINT('Ctrl Pts',(69.6598980083961,782.826093843841,108.483555443499));
#70514=CARTESIAN_POINT('Ctrl Pts',(69.6937024021389,782.82785262878,108.484034748969));
#70515=CARTESIAN_POINT('Ctrl Pts',(69.7812581577431,782.828192666179,108.484137200691));
#70516=CARTESIAN_POINT('Ctrl Pts',(69.8349132823111,782.824297482342,108.483090758963));
#70517=CARTESIAN_POINT('Ctrl Pts',(70.0101826552149,782.798006972545,108.476017453203));
#70518=CARTESIAN_POINT('Ctrl Pts',(70.1278787078675,782.758355117418,108.46533673211));
#70519=CARTESIAN_POINT('Ctrl Pts',(70.3339499104518,782.645177411981,108.435015348839));
#70520=CARTESIAN_POINT('Ctrl Pts',(70.4224938188007,782.575529540903,108.41640815476));
#70521=CARTESIAN_POINT('Ctrl Pts',(70.5788384608645,782.403800346269,108.370809734002));
#70522=CARTESIAN_POINT('Ctrl Pts',(70.6428826418601,782.300835790732,108.343609142235));
#70523=CARTESIAN_POINT('Ctrl Pts',(70.7337278085516,782.068686347582,108.282720458236));
#70524=CARTESIAN_POINT('Ctrl Pts',(70.756201634141,781.940232393222,108.249260428266));
#70525=CARTESIAN_POINT('Ctrl Pts',(70.7492205034136,781.680447870711,108.182080885617));
#70526=CARTESIAN_POINT('Ctrl Pts',(70.7191587872933,781.551574287505,108.149001405295));
#70527=CARTESIAN_POINT('Ctrl Pts',(70.6125196859197,781.319341010621,108.089744252411));
#70528=CARTESIAN_POINT('Ctrl Pts',(70.5396356529601,781.216909345899,108.063778162935));
#70529=CARTESIAN_POINT('Ctrl Pts',(70.3668838768826,781.050843319014,108.021841613514));
#70530=CARTESIAN_POINT('Ctrl Pts',(70.2712145987063,780.985782176087,108.005491425853));
#70531=CARTESIAN_POINT('Ctrl Pts',(70.1249540501647,780.918778107505,107.988680456899));
#70532=CARTESIAN_POINT('Ctrl Pts',(70.0823247393464,780.902550520314,107.984613344889));
#70533=CARTESIAN_POINT('Ctrl Pts',(70.0100858773551,780.880366181054,107.979055333505));
#70534=CARTESIAN_POINT('Ctrl Pts',(69.981070662606,780.872807249459,107.977162193431));
#70535=CARTESIAN_POINT('Ctrl Pts',(69.9385231381707,780.863659801175,107.9748710505));
#70536=CARTESIAN_POINT('Ctrl Pts',(69.9252359670773,780.861072118211,107.97422289459));
#70537=CARTESIAN_POINT('Ctrl Pts',(69.8812466666154,780.85338880199,107.972298086294));
#70538=CARTESIAN_POINT('Ctrl Pts',(69.8503570209193,780.849403477812,107.971299120077));
#70539=CARTESIAN_POINT('Ctrl Pts',(69.7902241224452,780.844357945566,107.970031639992));
#70540=CARTESIAN_POINT('Ctrl Pts',(69.7610268792052,780.84313396907,107.9697220466));
#70541=CARTESIAN_POINT('Ctrl Pts',(69.7318153101166,780.843131484731,107.96971688462));
#70542=CARTESIAN_POINT('Ctrl Pts',(69.7316732616476,782.211734062764,110.227707202932));
#70543=CARTESIAN_POINT('Ctrl Pts',(69.7316954699837,782.211733961292,110.227707490037));
#70544=CARTESIAN_POINT('Ctrl Pts',(69.7317176783555,782.211733859126,110.227707776929));
#70545=CARTESIAN_POINT('Ctrl Pts',(69.7317398867631,782.211733756267,110.227708063609));
#70546=CARTESIAN_POINT('Ctrl Pts',(69.8622261603718,782.211129405869,110.229392460867));
#70547=CARTESIAN_POINT('Ctrl Pts',(69.9914866175043,782.186613743472,110.223694823434));
#70548=CARTESIAN_POINT('Ctrl Pts',(70.2371565191121,782.090835500069,110.198437316032));
#70549=CARTESIAN_POINT('Ctrl Pts',(70.3506491877387,782.019141974026,110.178736812215));
#70550=CARTESIAN_POINT('Ctrl Pts',(70.543227682407,781.836814223691,110.128355921939));
#70551=CARTESIAN_POINT('Ctrl Pts',(70.6200878658936,781.72766524519,110.098098321078));
#70552=CARTESIAN_POINT('Ctrl Pts',(70.7247209820805,781.488141554969,110.031897147834));
#70553=CARTESIAN_POINT('Ctrl Pts',(70.7520158281456,781.360305818121,109.996652313396));
#70554=CARTESIAN_POINT('Ctrl Pts',(70.7540837955846,781.102112045273,109.925362383202));
#70555=CARTESIAN_POINT('Ctrl Pts',(70.7289530754057,780.974189437589,109.889977778559));
#70556=CARTESIAN_POINT('Ctrl Pts',(70.6293282700264,780.735611054836,109.823162945647));
#70557=CARTESIAN_POINT('Ctrl Pts',(70.5559653922169,780.627143860887,109.792333028749));
#70558=CARTESIAN_POINT('Ctrl Pts',(70.3701780264163,780.444035907159,109.738572393098));
#70559=CARTESIAN_POINT('Ctrl Pts',(70.2596061933404,780.371134110865,109.71614292612));
#70560=CARTESIAN_POINT('Ctrl Pts',(70.014929907433,780.270740964709,109.682309327284));
#70561=CARTESIAN_POINT('Ctrl Pts',(69.8831882168743,780.244411879854,109.671279865138));
#70562=CARTESIAN_POINT('Ctrl Pts',(69.7437009133202,780.243426643835,109.666671384854));
#70563=CARTESIAN_POINT('Ctrl Pts',(69.7376858169251,780.243435762934,109.666486266887));
#70564=CARTESIAN_POINT('Ctrl Pts',(69.7316732616476,780.243496355298,109.666314827831));
#70565=CARTESIAN_POINT('Origin',(69.7316732616476,784.848060912957,99.7033802796288));
#70566=CARTESIAN_POINT('',(69.7316732616476,783.184644281451,105.910275523117));
#70567=CARTESIAN_POINT('Origin',(69.7316732616476,782.713222050842,105.74365895585));
#70568=CARTESIAN_POINT('',(69.7316732616477,781.712527445781,110.075459176648));
#70569=CARTESIAN_POINT('',(69.7316732616476,785.319483143566,99.8699968468959));
#70570=CARTESIAN_POINT('Ctrl Pts',(69.7316871691062,780.74901083613,109.800715486367));
#70571=CARTESIAN_POINT('Ctrl Pts',(69.671752121605,780.74953320695,109.799232496016));
#70572=CARTESIAN_POINT('Ctrl Pts',(69.6123290057934,780.760469738631,109.800621919992));
#70573=CARTESIAN_POINT('Ctrl Pts',(69.4947140649738,780.804060409493,109.809524830073));
#70574=CARTESIAN_POINT('Ctrl Pts',(69.4383492748769,780.838298428812,109.81753740878));
#70575=CARTESIAN_POINT('Ctrl Pts',(69.3418554820246,780.926088143699,109.839629880153));
#70576=CARTESIAN_POINT('Ctrl Pts',(69.3028556001647,780.97898794651,109.853562786702));
#70577=CARTESIAN_POINT('Ctrl Pts',(69.248306083352,781.096348059627,109.885619453726));
#70578=CARTESIAN_POINT('Ctrl Pts',(69.2333981377799,781.159700758797,109.903446295939));
#70579=CARTESIAN_POINT('Ctrl Pts',(69.2302393778081,781.287681037935,109.940384059098));
#70580=CARTESIAN_POINT('Ctrl Pts',(69.2418695451783,781.351037439978,109.959120308888));
#70581=CARTESIAN_POINT('Ctrl Pts',(69.2902265851311,781.469464002387,109.994878145109));
#70582=CARTESIAN_POINT('Ctrl Pts',(69.3264580649211,781.523358506002,110.011539592825));
#70583=CARTESIAN_POINT('Ctrl Pts',(69.4189546875642,781.614390712454,110.040336968888));
#70584=CARTESIAN_POINT('Ctrl Pts',(69.47433436397,781.650573234726,110.052168466974));
#70585=CARTESIAN_POINT('Ctrl Pts',(69.5967834155184,781.699943203055,110.069178647964));
#70586=CARTESIAN_POINT('Ctrl Pts',(69.6626225671268,781.712621277087,110.074181823424));
#70587=CARTESIAN_POINT('Ctrl Pts',(69.7956063968911,781.712452000456,110.076645244186));
#70588=CARTESIAN_POINT('Ctrl Pts',(69.8614120152285,781.699661409441,110.074100249503));
#70589=CARTESIAN_POINT('Ctrl Pts',(69.9840574489736,781.650163219912,110.061939433147));
#70590=CARTESIAN_POINT('Ctrl Pts',(70.0396784273824,781.61396764452,110.052455127742));
#70591=CARTESIAN_POINT('Ctrl Pts',(70.1333093264964,781.522674617827,110.027916585964));
#70592=CARTESIAN_POINT('Ctrl Pts',(70.1703088101643,781.468407055534,110.013086799895));
#70593=CARTESIAN_POINT('Ctrl Pts',(70.2198014414364,781.350076068002,109.98043089558));
#70594=CARTESIAN_POINT('Ctrl Pts',(70.2321756068971,781.287299512487,109.96296408948));
#70595=CARTESIAN_POINT('Ctrl Pts',(70.2311408101823,781.160963301958,109.927482256949));
#70596=CARTESIAN_POINT('Ctrl Pts',(70.2177973847371,781.098603084693,109.909801900932));
#70597=CARTESIAN_POINT('Ctrl Pts',(70.1670042938586,780.982688784419,109.876431007625));
#70598=CARTESIAN_POINT('Ctrl Pts',(70.1301132607978,780.93021566454,109.861049269477));
#70599=CARTESIAN_POINT('Ctrl Pts',(70.0374327039456,780.842138208812,109.834445527333));
#70600=CARTESIAN_POINT('Ctrl Pts',(69.9825676271291,780.807371885577,109.823474718377));
#70601=CARTESIAN_POINT('Ctrl Pts',(69.8617888039196,780.760268603994,109.80733304511));
#70602=CARTESIAN_POINT('Ctrl Pts',(69.7970484500052,780.748441172346,109.802332739593));
#70603=CARTESIAN_POINT('Ctrl Pts',(69.7316871691062,780.74901083613,109.800715486367));
#70604=CARTESIAN_POINT('Origin',(76.5148471080835,783.300361650383,99.1563709925214));
#70605=CARTESIAN_POINT('',(76.5148471080835,778.574131435236,109.683582026066));
#70606=CARTESIAN_POINT('',(76.5148471080829,780.458567154633,110.042007126776));
#70607=CARTESIAN_POINT('Ctrl Pts',(76.514847108083,778.574131435236,109.683582026066));
#70608=CARTESIAN_POINT('Ctrl Pts',(76.3993676990878,778.577277784233,109.674679796912));
#70609=CARTESIAN_POINT('Ctrl Pts',(76.2850892439373,778.601440476607,109.669618110618));
#70610=CARTESIAN_POINT('Ctrl Pts',(76.0594426807239,778.693156619548,109.667865902568));
#70611=CARTESIAN_POINT('Ctrl Pts',(75.9517734184118,778.763815415005,109.672078130935));
#70612=CARTESIAN_POINT('Ctrl Pts',(75.7681870593439,778.942824194081,109.690747962663));
#70613=CARTESIAN_POINT('Ctrl Pts',(75.6944842980661,779.050091998023,109.705201132879));
#70614=CARTESIAN_POINT('Ctrl Pts',(75.5942072843244,779.284079485405,109.742375593649));
#70615=CARTESIAN_POINT('Ctrl Pts',(75.5678813662372,779.408400063706,109.764643013575));
#70616=CARTESIAN_POINT('Ctrl Pts',(75.565727455983,779.657383154022,109.81371832909));
#70617=CARTESIAN_POINT('Ctrl Pts',(75.5892879813095,779.779671946231,109.839993287732));
#70618=CARTESIAN_POINT('Ctrl Pts',(75.683429476057,780.00682706611,109.892701961643));
#70619=CARTESIAN_POINT('Ctrl Pts',(75.7528306138902,780.109481613965,109.918588311159));
#70620=CARTESIAN_POINT('Ctrl Pts',(75.9290060646397,780.281540500099,109.966063702635));
#70621=CARTESIAN_POINT('Ctrl Pts',(76.0339230674475,780.34912793396,109.987141839437));
#70622=CARTESIAN_POINT('Ctrl Pts',(76.2653154207896,780.439483817083,110.021351270875));
#70623=CARTESIAN_POINT('Ctrl Pts',(76.3893196857779,780.46129526995,110.034120738728));
#70624=CARTESIAN_POINT('Ctrl Pts',(76.514424819782,780.458576425092,110.041980614868));
#70625=CARTESIAN_POINT('Ctrl Pts',(76.5145655843954,780.458573365928,110.041989458569));
#70626=CARTESIAN_POINT('Ctrl Pts',(76.5147063471654,780.458570275774,110.041998295872));
#70627=CARTESIAN_POINT('Ctrl Pts',(76.5148471080822,780.458567154633,110.042007126776));
#70628=CARTESIAN_POINT('',(76.5148471806244,781.109526725105,108.200192607479));
#70629=CARTESIAN_POINT('',(76.5148471080835,784.194257823002,99.4723041456579));
#70630=CARTESIAN_POINT('Ctrl Pts',(76.514831644203,779.24561539752,107.783696123679));
#70631=CARTESIAN_POINT('Ctrl Pts',(76.4180353514781,779.247364784066,107.778751175432));
#70632=CARTESIAN_POINT('Ctrl Pts',(76.3219311476675,779.263698487753,107.777022587367));
#70633=CARTESIAN_POINT('Ctrl Pts',(76.1279621245816,779.327377634286,107.780321234634));
#70634=CARTESIAN_POINT('Ctrl Pts',(76.0323909289794,779.377369947571,107.786062306385));
#70635=CARTESIAN_POINT('Ctrl Pts',(75.8546355067824,779.511324331408,107.805933942219));
#70636=CARTESIAN_POINT('Ctrl Pts',(75.7756668708024,779.596699549882,107.820568463536));
#70637=CARTESIAN_POINT('Ctrl Pts',(75.6476359593787,779.797628781069,107.858447778253));
#70638=CARTESIAN_POINT('Ctrl Pts',(75.6024452365978,779.913162559872,107.88192076001));
#70639=CARTESIAN_POINT('Ctrl Pts',(75.5594285117788,780.154853299432,107.934096117601));
#70640=CARTESIAN_POINT('Ctrl Pts',(75.5623603358809,780.278831393633,107.962349095975));
#70641=CARTESIAN_POINT('Ctrl Pts',(75.615458548658,780.509909590215,108.017692493094));
#70642=CARTESIAN_POINT('Ctrl Pts',(75.6620100400825,780.615617596105,108.044259935867));
#70643=CARTESIAN_POINT('Ctrl Pts',(75.7837114236965,780.791750850276,108.090821603474));
#70644=CARTESIAN_POINT('Ctrl Pts',(75.8533174078007,780.863847185439,108.110907193139));
#70645=CARTESIAN_POINT('Ctrl Pts',(75.9649093399525,780.946983095817,108.135617499223));
#70646=CARTESIAN_POINT('Ctrl Pts',(75.9978133672779,780.968393995628,108.142187591245));
#70647=CARTESIAN_POINT('Ctrl Pts',(76.0540770976014,781.000133229645,108.152294329216));
#70648=CARTESIAN_POINT('Ctrl Pts',(76.0766440693645,781.011680863023,108.156074323909));
#70649=CARTESIAN_POINT('Ctrl Pts',(76.1099870320813,781.027069544935,108.161271590755));
#70650=CARTESIAN_POINT('Ctrl Pts',(76.1203879333148,781.031642925937,108.162840226802));
#70651=CARTESIAN_POINT('Ctrl Pts',(76.1543808544028,781.045860726047,108.167797903732));
#70652=CARTESIAN_POINT('Ctrl Pts',(76.1783011256814,781.054744321638,108.17102661096));
#70653=CARTESIAN_POINT('Ctrl Pts',(76.2404182218449,781.074994282979,108.178757274167));
#70654=CARTESIAN_POINT('Ctrl Pts',(76.279055543525,781.084951373524,108.182953898065));
#70655=CARTESIAN_POINT('Ctrl Pts',(76.4259133199425,781.113121698612,108.196663471679));
#70656=CARTESIAN_POINT('Ctrl Pts',(76.5366332654775,781.115159364184,108.202549062815));
#70657=CARTESIAN_POINT('Ctrl Pts',(76.7467266245878,781.083119054231,108.205515526864));
#70658=CARTESIAN_POINT('Ctrl Pts',(76.8449287800089,781.051754027594,108.203161155164));
#70659=CARTESIAN_POINT('Ctrl Pts',(77.0362488598872,780.95546122091,108.190693288838));
#70660=CARTESIAN_POINT('Ctrl Pts',(77.1265272632014,780.888412414372,108.179972970967));
#70661=CARTESIAN_POINT('Ctrl Pts',(77.2858000956765,780.720658390469,108.150152757721));
#70662=CARTESIAN_POINT('Ctrl Pts',(77.3510998144554,780.619139837436,108.130710489576));
#70663=CARTESIAN_POINT('Ctrl Pts',(77.4423037104024,780.392593318821,108.084936330138));
#70664=CARTESIAN_POINT('Ctrl Pts',(77.4651733722019,780.268754142177,108.058732275219));
#70665=CARTESIAN_POINT('Ctrl Pts',(77.460423090042,780.024264504341,108.004686491891));
#70666=CARTESIAN_POINT('Ctrl Pts',(77.4344837795554,779.90582397136,107.977404578711));
#70667=CARTESIAN_POINT('Ctrl Pts',(77.3403426958463,779.691325828456,107.925588225535));
#70668=CARTESIAN_POINT('Ctrl Pts',(77.275167465429,779.59625590887,107.901421104215));
#70669=CARTESIAN_POINT('Ctrl Pts',(77.1485457300168,779.470552156053,107.867262620632));
#70670=CARTESIAN_POINT('Ctrl Pts',(77.0986714243861,779.43040869639,107.855840432614));
#70671=CARTESIAN_POINT('Ctrl Pts',(77.0197460740544,779.379395763315,107.840465230297));
#70672=CARTESIAN_POINT('Ctrl Pts',(76.9937825261499,779.364346051898,107.835781128276));
#70673=CARTESIAN_POINT('Ctrl Pts',(76.9559862388099,779.344816952569,107.829475585546));
#70674=CARTESIAN_POINT('Ctrl Pts',(76.9447478175009,779.339294036391,107.827661933166));
#70675=CARTESIAN_POINT('Ctrl Pts',(76.9233453499745,779.329305838269,107.824322280644));
#70676=CARTESIAN_POINT('Ctrl Pts',(76.913207592371,779.324792731181,107.822787417808));
#70677=CARTESIAN_POINT('Ctrl Pts',(76.8806247515721,779.310976754472,107.818003065628));
#70678=CARTESIAN_POINT('Ctrl Pts',(76.8578814781205,779.302359717227,107.814885052182));
#70679=CARTESIAN_POINT('Ctrl Pts',(76.7995339020959,779.282805479904,107.80743700553));
#70680=CARTESIAN_POINT('Ctrl Pts',(76.7635447008317,779.273070095954,107.803345164877));
#70681=CARTESIAN_POINT('Ctrl Pts',(76.6573892522873,779.250975576363,107.792708414698));
#70682=CARTESIAN_POINT('Ctrl Pts',(76.5862038497717,779.244325497125,107.787342253638));
#70683=CARTESIAN_POINT('Ctrl Pts',(76.514831644203,779.24561539752,107.783696123679));
#70684=CARTESIAN_POINT('Ctrl Pts',(76.5148471080822,780.458567154633,110.042007126776));
#70685=CARTESIAN_POINT('Ctrl Pts',(76.6337470667696,780.455930744863,110.049466542098));
#70686=CARTESIAN_POINT('Ctrl Pts',(76.75132498731,780.431190888614,110.052357661743));
#70687=CARTESIAN_POINT('Ctrl Pts',(76.9783672850955,780.33771267233,110.049168030248));
#70688=CARTESIAN_POINT('Ctrl Pts',(77.0846276507624,780.267360411898,110.042582133196));
#70689=CARTESIAN_POINT('Ctrl Pts',(77.2653867807146,780.089441577228,110.020720096866));
#70690=CARTESIAN_POINT('Ctrl Pts',(77.3376895014433,779.983064117638,110.005538897587));
#70691=CARTESIAN_POINT('Ctrl Pts',(77.4361924532665,779.750562444307,109.968984768886));
#70692=CARTESIAN_POINT('Ctrl Pts',(77.4619661878394,779.6266845279,109.947991738727));
#70693=CARTESIAN_POINT('Ctrl Pts',(77.4638292103386,779.378852369871,109.902888612438));
#70694=CARTESIAN_POINT('Ctrl Pts',(77.4406618765805,779.257087152449,109.879215104217));
#70695=CARTESIAN_POINT('Ctrl Pts',(77.3488465804086,779.031885320795,109.831856464833));
#70696=CARTESIAN_POINT('Ctrl Pts',(77.2818291751373,778.930277434427,109.808610358476));
#70697=CARTESIAN_POINT('Ctrl Pts',(77.1120683540937,778.759369035873,109.7648949071));
#70698=CARTESIAN_POINT('Ctrl Pts',(77.0112915204305,778.691632890328,109.74485262965));
#70699=CARTESIAN_POINT('Ctrl Pts',(76.7871998036966,778.598293118821,109.710176384091));
#70700=CARTESIAN_POINT('Ctrl Pts',(76.666119806469,778.57411896189,109.695974807137));
#70701=CARTESIAN_POINT('Ctrl Pts',(76.5338265306903,778.573756358675,109.685070457189));
#70702=CARTESIAN_POINT('Ctrl Pts',(76.5243327688691,778.573872989167,109.684313269209));
#70703=CARTESIAN_POINT('Ctrl Pts',(76.514847108083,778.574131435236,109.683582026066));
#70704=CARTESIAN_POINT('Origin',(76.5148471080835,783.300361650383,99.1563709925214));
#70705=CARTESIAN_POINT('',(76.5148471080835,781.636945018877,105.36326623601));
#70706=CARTESIAN_POINT('Origin',(76.5148471080835,781.165522788268,105.196649668743));
#70707=CARTESIAN_POINT('',(76.5148471080838,780.015385701083,109.951280040382));
#70708=CARTESIAN_POINT('',(76.5148471080835,783.771783880992,99.3229875597885));
#70709=CARTESIAN_POINT('Ctrl Pts',(76.5148947017357,779.021561102855,109.762289290823));
#70710=CARTESIAN_POINT('Ctrl Pts',(76.4518262861511,779.023201131602,109.757631004561));
#70711=CARTESIAN_POINT('Ctrl Pts',(76.3894985517755,779.036703118335,109.7552102727));
#70712=CARTESIAN_POINT('Ctrl Pts',(76.2689368492823,779.087240744129,109.755141278728));
#70713=CARTESIAN_POINT('Ctrl Pts',(76.2124402604689,779.125265246733,109.75782168149));
#70714=CARTESIAN_POINT('Ctrl Pts',(76.1168758251058,779.220851900717,109.768409205877));
#70715=CARTESIAN_POINT('Ctrl Pts',(76.0788657754288,779.277710086336,109.776270092476));
#70716=CARTESIAN_POINT('Ctrl Pts',(76.027540498281,779.401750848085,109.796090763673));
#70717=CARTESIAN_POINT('Ctrl Pts',(76.0144959120489,779.467728702121,109.807838553993));
#70718=CARTESIAN_POINT('Ctrl Pts',(76.0152094779895,779.599784913144,109.833544517842));
#70719=CARTESIAN_POINT('Ctrl Pts',(76.0287247659368,779.664607941793,109.847236327804));
#70720=CARTESIAN_POINT('Ctrl Pts',(76.080163032521,779.783187552507,109.874308836184));
#70721=CARTESIAN_POINT('Ctrl Pts',(76.1169069858755,779.836044195316,109.887420776371));
#70722=CARTESIAN_POINT('Ctrl Pts',(76.2090455817878,779.92425976037,109.911502582937));
#70723=CARTESIAN_POINT('Ctrl Pts',(76.2633930890826,779.958818427281,109.922236706845));
#70724=CARTESIAN_POINT('Ctrl Pts',(76.383161440213,780.005285055043,109.939955024941));
#70725=CARTESIAN_POINT('Ctrl Pts',(76.4473757677932,780.016618263657,109.946739816801));
#70726=CARTESIAN_POINT('Ctrl Pts',(76.5786960284056,780.014232887792,109.955579176616));
#70727=CARTESIAN_POINT('Ctrl Pts',(76.6444324708125,779.999885421406,109.957415725242));
#70728=CARTESIAN_POINT('Ctrl Pts',(76.7672110100923,779.946704481258,109.955807955404));
#70729=CARTESIAN_POINT('Ctrl Pts',(76.8229528836136,779.908243036874,109.952347864267));
#70730=CARTESIAN_POINT('Ctrl Pts',(76.9168486009974,779.812057440101,109.940668067622));
#70731=CARTESIAN_POINT('Ctrl Pts',(76.9539474521059,779.7550646679,109.932516521091));
#70732=CARTESIAN_POINT('Ctrl Pts',(77.0038949556281,779.630161429046,109.912606063472));
#70733=CARTESIAN_POINT('Ctrl Pts',(77.0161343447144,779.563326456839,109.901006232884));
#70734=CARTESIAN_POINT('Ctrl Pts',(77.0133936677518,779.431600469514,109.876304221486));
#70735=CARTESIAN_POINT('Ctrl Pts',(76.9993563813161,779.367890126478,109.863483506371));
#70736=CARTESIAN_POINT('Ctrl Pts',(76.9475114155277,779.25069328556,109.837969434959));
#70737=CARTESIAN_POINT('Ctrl Pts',(76.9105617769154,779.198180512831,109.825516779465));
#70738=CARTESIAN_POINT('Ctrl Pts',(76.8182338016144,779.110685050023,109.802360911615));
#70739=CARTESIAN_POINT('Ctrl Pts',(76.7639017167637,779.076515588863,109.791885825037));
#70740=CARTESIAN_POINT('Ctrl Pts',(76.6440547087193,779.030765133784,109.77413470203));
#70741=CARTESIAN_POINT('Ctrl Pts',(76.5797369607959,779.019874947149,109.767078594656));
#70742=CARTESIAN_POINT('Ctrl Pts',(76.5148947017357,779.021561102855,109.762289290823));
#70743=CARTESIAN_POINT('Origin',(49.8616909408951,789.819881063962,101.460589746734));
#70744=CARTESIAN_POINT('',(49.8616909408951,787.691049283091,112.134283288743));
#70745=CARTESIAN_POINT('Origin',(49.8616909408951,786.229950467293,111.617881529726));
#70746=CARTESIAN_POINT('',(49.8616909408921,788.356889677166,110.250365206929));
#70747=CARTESIAN_POINT('',(49.8616909408951,791.28097987976,101.976991505752));
#70748=CARTESIAN_POINT('Ctrl Pts',(49.8617079781007,785.404291899084,109.303575373784));
#70749=CARTESIAN_POINT('Ctrl Pts',(49.7676926679438,785.404362943854,109.30337125909));
#70750=CARTESIAN_POINT('Ctrl Pts',(49.6738757965654,785.412651079779,109.305592005123));
#70751=CARTESIAN_POINT('Ctrl Pts',(49.4535286376546,785.45172627305,109.316630690403));
#70752=CARTESIAN_POINT('Ctrl Pts',(49.3291213344782,785.489761649913,109.327604661277));
#70753=CARTESIAN_POINT('Ctrl Pts',(49.0241319985413,785.625342980891,109.367331509502));
#70754=CARTESIAN_POINT('Ctrl Pts',(48.8562818266121,785.743328335843,109.402334396085));
#70755=CARTESIAN_POINT('Ctrl Pts',(48.5927373548287,786.019828245371,109.486021720799));
#70756=CARTESIAN_POINT('Ctrl Pts',(48.4935087823663,786.170739513764,109.532284505719));
#70757=CARTESIAN_POINT('Ctrl Pts',(48.3512585319294,786.507867112647,109.637402838476));
#70758=CARTESIAN_POINT('Ctrl Pts',(48.3131258693887,786.692615778466,109.695909053814));
#70759=CARTESIAN_POINT('Ctrl Pts',(48.3109094764101,787.07419402014,109.818734075163));
#70760=CARTESIAN_POINT('Ctrl Pts',(48.3504748358042,787.267409522545,109.881982780353));
#70761=CARTESIAN_POINT('Ctrl Pts',(48.5055399820578,787.625379184826,110.000744981419));
#70762=CARTESIAN_POINT('Ctrl Pts',(48.6186335944683,787.786982634862,110.055173428279));
#70763=CARTESIAN_POINT('Ctrl Pts',(48.8962360723346,788.05206050288,110.145208205056));
#70764=CARTESIAN_POINT('Ctrl Pts',(49.0551921775635,788.15595017432,110.180888215185));
#70765=CARTESIAN_POINT('Ctrl Pts',(49.3352507605499,788.274117089113,110.221619234482));
#70766=CARTESIAN_POINT('Ctrl Pts',(49.4452666326186,788.30724323978,110.233086243973));
#70767=CARTESIAN_POINT('Ctrl Pts',(49.6057395464989,788.337526862762,110.243593015385));
#70768=CARTESIAN_POINT('Ctrl Pts',(49.653754051446,788.344389614199,110.245979085644));
#70769=CARTESIAN_POINT('Ctrl Pts',(49.7453512028576,788.353348125892,110.24910349082));
#70770=CARTESIAN_POINT('Ctrl Pts',(49.7888422204462,788.355856881116,110.249984436697));
#70771=CARTESIAN_POINT('Ctrl Pts',(49.9254329935966,788.3582845325,110.250868019599));
#70772=CARTESIAN_POINT('Ctrl Pts',(50.0184483895708,788.35201288507,110.248730998659));
#70773=CARTESIAN_POINT('Ctrl Pts',(50.2366629592677,788.318458684918,110.237233788291));
#70774=CARTESIAN_POINT('Ctrl Pts',(50.359990076467,788.284298710163,110.225504745927));
#70775=CARTESIAN_POINT('Ctrl Pts',(50.6665356503412,788.158695640584,110.1825522443));
#70776=CARTESIAN_POINT('Ctrl Pts',(50.8373902774286,788.046281950615,110.144231210847));
#70777=CARTESIAN_POINT('Ctrl Pts',(51.1071657268225,787.779712973997,110.054512603112));
#70778=CARTESIAN_POINT('Ctrl Pts',(51.2097362504084,787.633520136832,110.005711544725));
#70779=CARTESIAN_POINT('Ctrl Pts',(51.3602314613403,787.304549943211,109.897343739963));
#70780=CARTESIAN_POINT('Ctrl Pts',(51.4034506949656,787.123097039,109.838301729158));
#70781=CARTESIAN_POINT('Ctrl Pts',(51.4177260726775,786.742509044268,109.716247190298));
#70782=CARTESIAN_POINT('Ctrl Pts',(51.3839977191523,786.546761045433,109.654435255415));
#70783=CARTESIAN_POINT('Ctrl Pts',(51.2392011316539,786.180937203769,109.540429527722));
#70784=CARTESIAN_POINT('Ctrl Pts',(51.1304148323752,786.014132992575,109.489219371059));
#70785=CARTESIAN_POINT('Ctrl Pts',(50.8554263874236,785.733905823956,109.403839258539));
#70786=CARTESIAN_POINT('Ctrl Pts',(50.6933678422754,785.621739854714,109.370007790432));
#70787=CARTESIAN_POINT('Ctrl Pts',(50.405460289627,785.493805216268,109.331324617886));
#70788=CARTESIAN_POINT('Ctrl Pts',(50.2918449324859,785.457865663585,109.320428626121));
#70789=CARTESIAN_POINT('Ctrl Pts',(50.1260492019831,785.425118040149,109.310356501147));
#70790=CARTESIAN_POINT('Ctrl Pts',(50.0765905941517,785.417724363462,109.308055221418));
#70791=CARTESIAN_POINT('Ctrl Pts',(49.9995534843385,785.409853193075,109.305547076538));
#70792=CARTESIAN_POINT('Ctrl Pts',(49.9721902681169,785.40776168142,109.304864181674));
#70793=CARTESIAN_POINT('Ctrl Pts',(49.9171162080564,785.404963658094,109.303906357104));
#70794=CARTESIAN_POINT('Ctrl Pts',(49.8894145804647,785.404270961971,109.303635527015));
#70795=CARTESIAN_POINT('Ctrl Pts',(49.8617079781007,785.404291899084,109.303575373784));
#70796=CARTESIAN_POINT('Origin',(49.8616909408951,789.819881063962,101.460589746734));
#70797=CARTESIAN_POINT('',(49.8616909408951,788.156464432456,107.667484990223));
#70798=CARTESIAN_POINT('Origin',(49.8616909408951,787.685042201847,107.500868422956));
#70799=CARTESIAN_POINT('',(49.8616909408951,786.701372697902,111.784498096993));
#70800=CARTESIAN_POINT('',(49.8616909408951,790.291303294571,101.627206314001));
#70801=CARTESIAN_POINT('Origin',(49.8616909408951,786.229950467293,111.617881529726));
#70802=CARTESIAN_POINT('Origin',(54.4787875961369,785.995601683377,100.108960015908));
#70803=CARTESIAN_POINT('',(54.4787875961369,783.593052663671,110.685912624258));
#70804=CARTESIAN_POINT('Origin',(54.4787875961369,782.405671086709,110.266251798899));
#70805=CARTESIAN_POINT('',(54.478787593146,784.202196751102,108.962410158872));
#70806=CARTESIAN_POINT('',(54.4787875961369,787.182983260339,100.528620841266));
#70807=CARTESIAN_POINT('Ctrl Pts',(54.4787613439502,781.7532554678,108.332966912952));
#70808=CARTESIAN_POINT('Ctrl Pts',(54.441743110491,781.753222920922,108.333061316267));
#70809=CARTESIAN_POINT('Ctrl Pts',(54.404743397955,781.754788427287,108.333532251668));
#70810=CARTESIAN_POINT('Ctrl Pts',(54.2822477200637,781.765282273289,108.336343481529));
#70811=CARTESIAN_POINT('Ctrl Pts',(54.19764331156,781.78117975144,108.340322846354));
#70812=CARTESIAN_POINT('Ctrl Pts',(53.9948553830075,781.840822325286,108.354981136571));
#70813=CARTESIAN_POINT('Ctrl Pts',(53.8805354429768,781.893729811182,108.367826941627));
#70814=CARTESIAN_POINT('Ctrl Pts',(53.6368509780762,782.053722918414,108.406735456799));
#70815=CARTESIAN_POINT('Ctrl Pts',(53.5177635875451,782.171407049685,108.435400678503));
#70816=CARTESIAN_POINT('Ctrl Pts',(53.3414506216402,782.433570469098,108.500102041471));
#70817=CARTESIAN_POINT('Ctrl Pts',(53.2813799982236,782.572883340683,108.53481473864));
#70818=CARTESIAN_POINT('Ctrl Pts',(53.2137683839407,782.873756350904,108.61085716836));
#70819=CARTESIAN_POINT('Ctrl Pts',(53.2101006971323,783.033403080544,108.651770527474));
#70820=CARTESIAN_POINT('Ctrl Pts',(53.2661104858377,783.348621422983,108.733700125082));
#70821=CARTESIAN_POINT('Ctrl Pts',(53.3267536550586,783.500952144515,108.773896898691));
#70822=CARTESIAN_POINT('Ctrl Pts',(53.504303031476,783.771396303741,108.846012919171));
#70823=CARTESIAN_POINT('Ctrl Pts',(53.6185214866455,783.887464323063,108.877357309535));
#70824=CARTESIAN_POINT('Ctrl Pts',(53.8606944177274,784.052893312023,108.922203052909));
#70825=CARTESIAN_POINT('Ctrl Pts',(53.9801599983939,784.109783748746,108.937697650171));
#70826=CARTESIAN_POINT('Ctrl Pts',(54.1913981916706,784.173035287721,108.954822938411));
#70827=CARTESIAN_POINT('Ctrl Pts',(54.2787172502997,784.189691046238,108.959292271416));
#70828=CARTESIAN_POINT('Ctrl Pts',(54.4058424335231,784.200693360855,108.962121681923));
#70829=CARTESIAN_POINT('Ctrl Pts',(54.4446999649238,784.202311169321,108.962502321777));
#70830=CARTESIAN_POINT('Ctrl Pts',(54.5201306433969,784.202077402492,108.962303774754));
#70831=CARTESIAN_POINT('Ctrl Pts',(54.556665812149,784.200426679941,108.961780463746));
#70832=CARTESIAN_POINT('Ctrl Pts',(54.6774398422457,784.189866283269,108.958633295975));
#70833=CARTESIAN_POINT('Ctrl Pts',(54.7608095113816,784.174286626917,108.954157454479));
#70834=CARTESIAN_POINT('Ctrl Pts',(54.9624804209552,784.115736682213,108.937574207204));
#70835=CARTESIAN_POINT('Ctrl Pts',(55.0768886143016,784.063463607035,108.922906058606));
#70836=CARTESIAN_POINT('Ctrl Pts',(55.3206565963673,783.905198823348,108.878991328144));
#70837=CARTESIAN_POINT('Ctrl Pts',(55.4397708406798,783.788705596441,108.846964888092));
#70838=CARTESIAN_POINT('Ctrl Pts',(55.615563991354,783.529311797718,108.776827455255));
#70839=CARTESIAN_POINT('Ctrl Pts',(55.6753801870606,783.391838660484,108.740105558444));
#70840=CARTESIAN_POINT('Ctrl Pts',(55.7433455670921,783.093937032578,108.661830405782));
#70841=CARTESIAN_POINT('Ctrl Pts',(55.747541805163,782.935359102455,108.620847036898));
#70842=CARTESIAN_POINT('Ctrl Pts',(55.6931651547547,782.619842413916,108.540746426938));
#70843=CARTESIAN_POINT('Ctrl Pts',(55.6330277655128,782.466165913169,108.502504324794));
#70844=CARTESIAN_POINT('Ctrl Pts',(55.4562033671363,782.192596973632,108.435558693061));
#70845=CARTESIAN_POINT('Ctrl Pts',(55.3421455779861,782.074729036396,108.407314164759));
#70846=CARTESIAN_POINT('Ctrl Pts',(55.102262000797,781.907952451745,108.367912857511));
#70847=CARTESIAN_POINT('Ctrl Pts',(54.9854616312421,781.85073328133,108.354635429623));
#70848=CARTESIAN_POINT('Ctrl Pts',(54.7769126032848,781.785401373428,108.339727471207));
#70849=CARTESIAN_POINT('Ctrl Pts',(54.6894493740972,781.767693079593,108.335791010007));
#70850=CARTESIAN_POINT('Ctrl Pts',(54.56023897283,781.755263741237,108.333215484316));
#70851=CARTESIAN_POINT('Ctrl Pts',(54.5195130740058,781.753291297213,108.332862988533));
#70852=CARTESIAN_POINT('Ctrl Pts',(54.4787613439502,781.7532554678,108.332966912952));
#70853=CARTESIAN_POINT('Origin',(54.4787875961369,785.995601683377,100.108960015908));
#70854=CARTESIAN_POINT('',(54.4787875961369,784.332185051871,106.315855259396));
#70855=CARTESIAN_POINT('Origin',(54.4787875961369,783.860762821262,106.149238692129));
#70856=CARTESIAN_POINT('',(54.4787875961369,782.877093317318,110.432868366167));
#70857=CARTESIAN_POINT('',(54.4787875961369,786.467023913986,100.275576583175));
#70858=CARTESIAN_POINT('Origin',(54.4787875961369,782.405671086709,110.266251798899));
#70859=CARTESIAN_POINT('Origin',(59.5586600728479,782.515804719233,98.8790820269056));
#70860=CARTESIAN_POINT('',(59.5586600728479,777.909975348877,108.845595215772));
#70861=CARTESIAN_POINT('',(59.5586600728476,779.880261212077,109.401192572043));
#70862=CARTESIAN_POINT('Ctrl Pts',(59.5586600728479,777.909975348877,108.845595215772));
#70863=CARTESIAN_POINT('Ctrl Pts',(59.4291990673829,777.91049817199,108.844115948479));
#70864=CARTESIAN_POINT('Ctrl Pts',(59.3009284172275,777.934959562234,108.848763253711));
#70865=CARTESIAN_POINT('Ctrl Pts',(59.0556946989573,778.030849155894,108.870598307995));
#70866=CARTESIAN_POINT('Ctrl Pts',(58.9418416420412,778.103121953752,108.88806442479));
#70867=CARTESIAN_POINT('Ctrl Pts',(58.74928633604,778.285885134678,108.934346625436));
#70868=CARTESIAN_POINT('Ctrl Pts',(58.6724738350208,778.394655560504,108.962745613571));
#70869=CARTESIAN_POINT('Ctrl Pts',(58.5662614311178,778.635055050951,109.027613408059));
#70870=CARTESIAN_POINT('Ctrl Pts',(58.5382704963566,778.764520150491,109.063524881249));
#70871=CARTESIAN_POINT('Ctrl Pts',(58.5362892225246,779.025665920847,109.137955372544));
#70872=CARTESIAN_POINT('Ctrl Pts',(58.5622340711796,779.154770996146,109.175734907046));
#70873=CARTESIAN_POINT('Ctrl Pts',(58.6646293609599,779.394225107181,109.247313761704));
#70874=CARTESIAN_POINT('Ctrl Pts',(58.7396089284805,779.502385677257,109.280427829676));
#70875=CARTESIAN_POINT('Ctrl Pts',(58.9290740373455,779.684475554637,109.337061172406));
#70876=CARTESIAN_POINT('Ctrl Pts',(59.0416896628259,779.756621160249,109.360005194922));
#70877=CARTESIAN_POINT('Ctrl Pts',(59.2900609887602,779.855132045876,109.391905804919));
#70878=CARTESIAN_POINT('Ctrl Pts',(59.4234209987155,779.880427292854,109.400506321648));
#70879=CARTESIAN_POINT('Ctrl Pts',(59.5581144817012,779.880262020816,109.401189846532));
#70880=CARTESIAN_POINT('Ctrl Pts',(59.5582963477946,779.880261797662,109.401190769442));
#70881=CARTESIAN_POINT('Ctrl Pts',(59.5584782115162,779.880261528082,109.401191677945));
#70882=CARTESIAN_POINT('Ctrl Pts',(59.5586600728473,779.880261212077,109.401192572043));
#70883=CARTESIAN_POINT('',(59.5586599619933,780.382502020465,107.980160521771));
#70884=CARTESIAN_POINT('',(59.5586600728479,783.478833859476,99.2194491099729));
#70885=CARTESIAN_POINT('Ctrl Pts',(59.5585491494349,778.363426758698,107.562607121697));
#70886=CARTESIAN_POINT('Ctrl Pts',(59.5294255770194,778.363280482099,107.563030485534));
#70887=CARTESIAN_POINT('Ctrl Pts',(59.5003138937717,778.364372249146,107.563688873113));
#70888=CARTESIAN_POINT('Ctrl Pts',(59.4015656073238,778.372291690413,107.56672194487));
#70889=CARTESIAN_POINT('Ctrl Pts',(59.3326533420484,778.384994224227,107.570198769266));
#70890=CARTESIAN_POINT('Ctrl Pts',(59.1636091293877,778.434441252366,107.582209556769));
#70891=CARTESIAN_POINT('Ctrl Pts',(59.0671044538631,778.479949504058,107.592353971292));
#70892=CARTESIAN_POINT('Ctrl Pts',(58.8827141924712,778.605073588118,107.619175068383));
#70893=CARTESIAN_POINT('Ctrl Pts',(58.7982697036429,778.686824389758,107.636226209408));
#70894=CARTESIAN_POINT('Ctrl Pts',(58.6572472071341,778.880408884885,107.676181399548));
#70895=CARTESIAN_POINT('Ctrl Pts',(58.6037710511383,778.992165009854,107.699055336428));
#70896=CARTESIAN_POINT('Ctrl Pts',(58.5378796772744,779.236225650972,107.749029077805));
#70897=CARTESIAN_POINT('Ctrl Pts',(58.5288235093464,779.367247621908,107.775874454381));
#70898=CARTESIAN_POINT('Ctrl Pts',(58.561979389092,779.629633019458,107.829819050094));
#70899=CARTESIAN_POINT('Ctrl Pts',(58.6055834773226,779.758412562268,107.856393029058));
#70900=CARTESIAN_POINT('Ctrl Pts',(58.7400981352003,779.989310878681,107.90400057502));
#70901=CARTESIAN_POINT('Ctrl Pts',(58.8287469694599,780.089759546732,107.924681723633));
#70902=CARTESIAN_POINT('Ctrl Pts',(59.0252516290962,780.239845227271,107.955078134323));
#70903=CARTESIAN_POINT('Ctrl Pts',(59.1270603864985,780.293646593864,107.965721056196));
#70904=CARTESIAN_POINT('Ctrl Pts',(59.3057541081849,780.352904596454,107.976669592383));
#70905=CARTESIAN_POINT('Ctrl Pts',(59.3779718308474,780.368590782434,107.979278478185));
#70906=CARTESIAN_POINT('Ctrl Pts',(59.4828077019629,780.379908954376,107.98051405783));
#70907=CARTESIAN_POINT('Ctrl Pts',(59.5144794615612,780.381868619709,107.98056231909));
#70908=CARTESIAN_POINT('Ctrl Pts',(59.575358043458,780.382844540222,107.98003169514));
#70909=CARTESIAN_POINT('Ctrl Pts',(59.6045295458972,780.382083679894,107.979503034302));
#70910=CARTESIAN_POINT('Ctrl Pts',(59.6983456308999,780.375675157192,107.976916910588));
#70911=CARTESIAN_POINT('Ctrl Pts',(59.7624609963608,780.365199776645,107.973785596302));
#70912=CARTESIAN_POINT('Ctrl Pts',(59.9149854483869,780.325301462213,107.962995276125));
#70913=CARTESIAN_POINT('Ctrl Pts',(60.0010793251777,780.289815471754,107.954011127531));
#70914=CARTESIAN_POINT('Ctrl Pts',(60.1978052761289,780.175483739639,107.926179956891));
#70915=CARTESIAN_POINT('Ctrl Pts',(60.2993869198372,780.085379168819,107.904985883879));
#70916=CARTESIAN_POINT('Ctrl Pts',(60.4529183290253,779.881546509522,107.858559180971));
#70917=CARTESIAN_POINT('Ctrl Pts',(60.5073867157846,779.772539579672,107.834288910627));
#70918=CARTESIAN_POINT('Ctrl Pts',(60.5767321158997,779.532917109774,107.782308502156));
#70919=CARTESIAN_POINT('Ctrl Pts',(60.5880863263182,779.40348322835,107.754948412995));
#70920=CARTESIAN_POINT('Ctrl Pts',(60.5603355536008,779.141304299766,107.701103856231));
#70921=CARTESIAN_POINT('Ctrl Pts',(60.5191745110486,779.011132679903,107.675221898375));
#70922=CARTESIAN_POINT('Ctrl Pts',(60.3890230476198,778.776360454652,107.630087794799));
#70923=CARTESIAN_POINT('Ctrl Pts',(60.3022131966845,778.673409220668,107.611109854969));
#70924=CARTESIAN_POINT('Ctrl Pts',(60.1106674953454,778.520005118074,107.584107313255));
#70925=CARTESIAN_POINT('Ctrl Pts',(60.0125986298598,778.464686810371,107.574958497107));
#70926=CARTESIAN_POINT('Ctrl Pts',(59.8387978799252,778.401096831037,107.565444890544));
#70927=CARTESIAN_POINT('Ctrl Pts',(59.7677184226025,778.38333941888,107.563158622208));
#70928=CARTESIAN_POINT('Ctrl Pts',(59.6500013167806,778.366942132872,107.561858168359));
#70929=CARTESIAN_POINT('Ctrl Pts',(59.6043070376603,778.363656583124,107.561941947973));
#70930=CARTESIAN_POINT('Ctrl Pts',(59.5585491494349,778.363426758698,107.562607121697));
#70931=CARTESIAN_POINT('Ctrl Pts',(59.5586600728473,779.880261212077,109.401192572043));
#70932=CARTESIAN_POINT('Ctrl Pts',(59.6914009222063,779.880030560098,109.401845175036));
#70933=CARTESIAN_POINT('Ctrl Pts',(59.8228682597227,779.855074343606,109.394801961274));
#70934=CARTESIAN_POINT('Ctrl Pts',(60.069947360309,779.757802072863,109.366432215607));
#70935=CARTESIAN_POINT('Ctrl Pts',(60.1829276319018,779.685886859264,109.345235094438));
#70936=CARTESIAN_POINT('Ctrl Pts',(60.3739939760634,779.503559113016,109.292043017165));
#70937=CARTESIAN_POINT('Ctrl Pts',(60.4499691725986,779.394731015658,109.260531934029));
#70938=CARTESIAN_POINT('Ctrl Pts',(60.5531420895566,779.155699974923,109.192357702164));
#70939=CARTESIAN_POINT('Ctrl Pts',(60.5797286821778,779.027987850295,109.156404113416));
#70940=CARTESIAN_POINT('Ctrl Pts',(60.5804013048047,778.769831416606,109.084656777137));
#70941=CARTESIAN_POINT('Ctrl Pts',(60.5545203707955,778.641837121719,109.049536430204));
#70942=CARTESIAN_POINT('Ctrl Pts',(60.4534436120453,778.403052677336,108.984414894268));
#70943=CARTESIAN_POINT('Ctrl Pts',(60.3793731555848,778.294441897652,108.954991469578));
#70944=CARTESIAN_POINT('Ctrl Pts',(60.1924972720798,778.111184060679,108.905023096645));
#70945=CARTESIAN_POINT('Ctrl Pts',(60.081585500179,778.038190504168,108.884915276922));
#70946=CARTESIAN_POINT('Ctrl Pts',(59.8367167955085,777.937641500065,108.856116983007));
#70947=CARTESIAN_POINT('Ctrl Pts',(59.7051391273397,777.911150010299,108.847721080187));
#70948=CARTESIAN_POINT('Ctrl Pts',(59.5675001500342,777.90996754457,108.845703368576));
#70949=CARTESIAN_POINT('Ctrl Pts',(59.5630794180022,777.909957501527,108.845645712775));
#70950=CARTESIAN_POINT('Ctrl Pts',(59.558660072848,777.909975348877,108.845595215772));
#70951=CARTESIAN_POINT('Origin',(59.5586600728479,782.515804719233,98.8790820269056));
#70952=CARTESIAN_POINT('',(59.5586600728479,780.852388087727,105.085977270394));
#70953=CARTESIAN_POINT('Origin',(59.5586600728479,780.380965857118,104.919360703127));
#70954=CARTESIAN_POINT('',(59.558660072848,779.380861865021,109.249489853121));
#70955=CARTESIAN_POINT('',(59.5586600728479,782.987226949842,99.0456985941727));
#70956=CARTESIAN_POINT('Ctrl Pts',(59.5586513681714,778.416331464684,108.977614565517));
#70957=CARTESIAN_POINT('Ctrl Pts',(59.497472789011,778.416545597769,108.977011897015));
#70958=CARTESIAN_POINT('Ctrl Pts',(59.4368314718854,778.427633987372,108.979335555447));
#70959=CARTESIAN_POINT('Ctrl Pts',(59.3183791845843,778.471987852838,108.990062024086));
#70960=CARTESIAN_POINT('Ctrl Pts',(59.2622836940566,778.506410872123,108.998802932055));
#70961=CARTESIAN_POINT('Ctrl Pts',(59.1669241754906,778.594167519378,109.02182532098));
#70962=CARTESIAN_POINT('Ctrl Pts',(59.1286095049931,778.646682464612,109.035897096814));
#70963=CARTESIAN_POINT('Ctrl Pts',(59.074886361842,778.763389551699,109.067824769961));
#70964=CARTESIAN_POINT('Ctrl Pts',(59.060231889012,778.826552703242,109.085407716669));
#70965=CARTESIAN_POINT('Ctrl Pts',(59.057321262279,778.954806178108,109.121715105653));
#70966=CARTESIAN_POINT('Ctrl Pts',(59.0692085890005,779.018633408671,109.140083886269));
#70967=CARTESIAN_POINT('Ctrl Pts',(59.1181801789798,779.137561600903,109.174798604849));
#70968=CARTESIAN_POINT('Ctrl Pts',(59.1546307622503,779.191532000205,109.190807514258));
#70969=CARTESIAN_POINT('Ctrl Pts',(59.2473241610817,779.282497734407,109.218149449029));
#70970=CARTESIAN_POINT('Ctrl Pts',(59.3026112008437,779.318612197079,109.229212283854));
#70971=CARTESIAN_POINT('Ctrl Pts',(59.4247318917649,779.367997348572,109.24469659038));
#70972=CARTESIAN_POINT('Ctrl Pts',(59.4903466069188,779.380766024055,109.248958240076));
#70973=CARTESIAN_POINT('Ctrl Pts',(59.6229829252642,779.380959468382,109.249992585328));
#70974=CARTESIAN_POINT('Ctrl Pts',(59.688676245608,779.368388609669,109.246758112561));
#70975=CARTESIAN_POINT('Ctrl Pts',(59.8112001817466,779.319349655604,109.233282829004));
#70976=CARTESIAN_POINT('Ctrl Pts',(59.8668001735035,779.283359637815,109.223177490479));
#70977=CARTESIAN_POINT('Ctrl Pts',(59.9603943689052,779.192424348506,109.197553856238));
#70978=CARTESIAN_POINT('Ctrl Pts',(59.99737193986,779.138308193386,109.182273464386));
#70979=CARTESIAN_POINT('Ctrl Pts',(60.04683244192,779.020164775574,109.149016356485));
#70980=CARTESIAN_POINT('Ctrl Pts',(60.0591832290489,778.957427159715,109.131403066181));
#70981=CARTESIAN_POINT('Ctrl Pts',(60.0581036627097,778.831005763246,109.096013690838));
#70982=CARTESIAN_POINT('Ctrl Pts',(60.0447172790343,778.768524164436,109.078572531174));
#70983=CARTESIAN_POINT('Ctrl Pts',(59.9938306790339,778.652266775422,109.046097033671));
#70984=CARTESIAN_POINT('Ctrl Pts',(59.9568864010481,778.599567405004,109.031359754466));
#70985=CARTESIAN_POINT('Ctrl Pts',(59.8641507641302,778.511006684921,109.00637202405));
#70986=CARTESIAN_POINT('Ctrl Pts',(59.8092933253543,778.475960331079,108.996348291178));
#70987=CARTESIAN_POINT('Ctrl Pts',(59.6886015082836,778.428265112025,108.982220333221));
#70988=CARTESIAN_POINT('Ctrl Pts',(59.6239434182865,778.416102933908,108.978257755708));
#70989=CARTESIAN_POINT('Ctrl Pts',(59.5586513681714,778.416331464684,108.977614565517));
#70990=CARTESIAN_POINT('Origin',(65.8523138277871,779.672231777069,97.874067134449));
#70991=CARTESIAN_POINT('',(65.8523138277871,774.942544771236,108.411058755856));
#70992=CARTESIAN_POINT('',(65.852313827786,776.834453268023,108.748340500639));
#70993=CARTESIAN_POINT('Ctrl Pts',(65.8523138277871,774.942544771236,108.411058755856));
#70994=CARTESIAN_POINT('Ctrl Pts',(65.7322417836214,774.944350535709,108.405949554955));
#70995=CARTESIAN_POINT('Ctrl Pts',(65.6135118178383,774.969019786884,108.404584777808));
#70996=CARTESIAN_POINT('Ctrl Pts',(65.3853653172308,775.063262639199,108.409857329762));
#70997=CARTESIAN_POINT('Ctrl Pts',(65.2791432926612,775.134129844452,108.416871158307));
#70998=CARTESIAN_POINT('Ctrl Pts',(65.0979365589389,775.314037132206,108.439338683121));
#70999=CARTESIAN_POINT('Ctrl Pts',(65.0255044176019,775.422226128488,108.454787173952));
#71000=CARTESIAN_POINT('Ctrl Pts',(64.9281324361108,775.658118649035,108.492073344462));
#71001=CARTESIAN_POINT('Ctrl Pts',(64.9035127580602,775.783470088651,108.513505234639));
#71002=CARTESIAN_POINT('Ctrl Pts',(64.9049679604501,776.033966376516,108.55933217769));
#71003=CARTESIAN_POINT('Ctrl Pts',(64.9303580011618,776.156810587794,108.583261877123));
#71004=CARTESIAN_POINT('Ctrl Pts',(65.0278868846264,776.384516462656,108.630174509819));
#71005=CARTESIAN_POINT('Ctrl Pts',(65.0987870954147,776.487254818492,108.652691131115));
#71006=CARTESIAN_POINT('Ctrl Pts',(65.2758838720473,776.657576442914,108.692440836573));
#71007=CARTESIAN_POINT('Ctrl Pts',(65.3796166526574,776.724077517478,108.709354965747));
#71008=CARTESIAN_POINT('Ctrl Pts',(65.6073879296887,776.813617520162,108.735323355696));
#71009=CARTESIAN_POINT('Ctrl Pts',(65.7290366671221,776.835873364083,108.744131991536));
#71010=CARTESIAN_POINT('Ctrl Pts',(65.8518246149033,776.834459028229,108.748323824041));
#71011=CARTESIAN_POINT('Ctrl Pts',(65.8519876882831,776.834457149864,108.748329391169));
#71012=CARTESIAN_POINT('Ctrl Pts',(65.8521507592488,776.834455229794,108.748334950035));
#71013=CARTESIAN_POINT('Ctrl Pts',(65.8523138277848,776.834453268023,108.748340500639));
#71014=CARTESIAN_POINT('',(65.852313813786,777.362147432391,107.255291135104));
#71015=CARTESIAN_POINT('',(65.8523138277871,780.566127949688,98.1900002875857));
#71016=CARTESIAN_POINT('Ctrl Pts',(65.8521676736201,775.46727685438,106.926390289016));
#71017=CARTESIAN_POINT('Ctrl Pts',(65.7938787655703,775.466892120574,106.92750581374));
#71018=CARTESIAN_POINT('Ctrl Pts',(65.7357126515191,775.471900601344,106.929492713395));
#71019=CARTESIAN_POINT('Ctrl Pts',(65.5552275269776,775.504466933521,106.938413702626));
#71020=CARTESIAN_POINT('Ctrl Pts',(65.4380309142196,775.550962449721,106.948301620205));
#71021=CARTESIAN_POINT('Ctrl Pts',(65.2435008496011,775.67720993831,106.972787148368));
#71022=CARTESIAN_POINT('Ctrl Pts',(65.1644084907303,775.750431692209,106.986348712562));
#71023=CARTESIAN_POINT('Ctrl Pts',(65.0290659387499,775.926769111364,107.018172304209));
#71024=CARTESIAN_POINT('Ctrl Pts',(64.976321495565,776.030372562027,107.036468342364));
#71025=CARTESIAN_POINT('Ctrl Pts',(64.9081731126887,776.259472346272,107.076464727966));
#71026=CARTESIAN_POINT('Ctrl Pts',(64.8965411565285,776.384020337214,107.097972551109));
#71027=CARTESIAN_POINT('Ctrl Pts',(64.9220490607854,776.632915868686,107.140648027606));
#71028=CARTESIAN_POINT('Ctrl Pts',(64.9599339375107,776.754973697645,107.161417845716));
#71029=CARTESIAN_POINT('Ctrl Pts',(65.0790786237519,776.972765128191,107.198024769879));
#71030=CARTESIAN_POINT('Ctrl Pts',(65.157423706574,777.06748124862,107.2137056887));
#71031=CARTESIAN_POINT('Ctrl Pts',(65.327869871706,777.207531871683,107.236126534395));
#71032=CARTESIAN_POINT('Ctrl Pts',(65.4133174380026,777.258017691905,107.243868632409));
#71033=CARTESIAN_POINT('Ctrl Pts',(65.5533429463574,777.313713915724,107.251634886811));
#71034=CARTESIAN_POINT('Ctrl Pts',(65.603046462404,777.328939096693,107.253564571878));
#71035=CARTESIAN_POINT('Ctrl Pts',(65.691202455759,777.34825438477,107.255572420587));
#71036=CARTESIAN_POINT('Ctrl Pts',(65.72910565202,777.354197115841,107.256001147787));
#71037=CARTESIAN_POINT('Ctrl Pts',(65.7851249769906,777.359548919515,107.255999937166));
#71038=CARTESIAN_POINT('Ctrl Pts',(65.8030275050721,777.360750787118,107.255905493694));
#71039=CARTESIAN_POINT('Ctrl Pts',(65.8642141912673,777.363126164254,107.255261695874));
#71040=CARTESIAN_POINT('Ctrl Pts',(65.9075288362554,777.3618553558,107.254258713131));
#71041=CARTESIAN_POINT('Ctrl Pts',(66.0215421744424,777.35069814177,107.25016831844));
#71042=CARTESIAN_POINT('Ctrl Pts',(66.0914119591671,777.335804392169,107.246164876582));
#71043=CARTESIAN_POINT('Ctrl Pts',(66.2777522215371,777.27351803522,107.23131969242));
#71044=CARTESIAN_POINT('Ctrl Pts',(66.3871548106612,777.210683193057,107.217750228743));
#71045=CARTESIAN_POINT('Ctrl Pts',(66.563117924055,777.056502548005,107.186360143025));
#71046=CARTESIAN_POINT('Ctrl Pts',(66.631886345624,776.970816324838,107.169518148369));
#71047=CARTESIAN_POINT('Ctrl Pts',(66.7411990064495,776.771970264116,107.131707116004));
#71048=CARTESIAN_POINT('Ctrl Pts',(66.7779141056529,776.658826566805,107.110842512559));
#71049=CARTESIAN_POINT('Ctrl Pts',(66.8088835662978,776.415907767078,107.067467884149));
#71050=CARTESIAN_POINT('Ctrl Pts',(66.7993393484381,776.287790441984,107.04536396087));
#71051=CARTESIAN_POINT('Ctrl Pts',(66.7311472726406,776.045441540949,107.005063032344));
#71052=CARTESIAN_POINT('Ctrl Pts',(66.6742419243611,775.933055037253,106.987133321718));
#71053=CARTESIAN_POINT('Ctrl Pts',(66.5213324548183,775.737620831312,106.95737404162));
#71054=CARTESIAN_POINT('Ctrl Pts',(66.4273149450998,775.655876932177,106.945712474531));
#71055=CARTESIAN_POINT('Ctrl Pts',(66.264699361539,775.562325212459,106.933579509576));
#71056=CARTESIAN_POINT('Ctrl Pts',(66.206184690539,775.536053303044,106.930454984566));
#71057=CARTESIAN_POINT('Ctrl Pts',(66.1075854805185,775.503247176792,106.927083624026));
#71058=CARTESIAN_POINT('Ctrl Pts',(66.0689740616965,775.493040979168,106.926199650991));
#71059=CARTESIAN_POINT('Ctrl Pts',(66.0125143587785,775.481867036827,106.92552098065));
#71060=CARTESIAN_POINT('Ctrl Pts',(65.9951093061857,775.478923975769,106.925393885891));
#71061=CARTESIAN_POINT('Ctrl Pts',(65.9607551680561,775.474097155938,106.925303286111));
#71062=CARTESIAN_POINT('Ctrl Pts',(65.943817948372,775.472181433331,106.925334324967));
#71063=CARTESIAN_POINT('Ctrl Pts',(65.9020012029613,775.468591689562,106.925596430788));
#71064=CARTESIAN_POINT('Ctrl Pts',(65.8770916458451,775.467441364147,106.925913297626));
#71065=CARTESIAN_POINT('Ctrl Pts',(65.8521676736201,775.46727685438,106.926390289016));
#71066=CARTESIAN_POINT('Ctrl Pts',(65.8523138277848,776.834453268023,108.748340500639));
#71067=CARTESIAN_POINT('Ctrl Pts',(65.9755932814574,776.832970173364,108.75253674477));
#71068=CARTESIAN_POINT('Ctrl Pts',(66.0974845196465,776.807660364505,108.752000220028));
#71069=CARTESIAN_POINT('Ctrl Pts',(66.3271173242504,776.711611238658,108.741919328901));
#71070=CARTESIAN_POINT('Ctrl Pts',(66.4321784934129,776.641010667136,108.732321657587));
#71071=CARTESIAN_POINT('Ctrl Pts',(66.6097011617382,776.463317298711,108.705744912834));
#71072=CARTESIAN_POINT('Ctrl Pts',(66.6801498205331,776.357660928064,108.688975507296));
#71073=CARTESIAN_POINT('Ctrl Pts',(66.7767014433819,776.124260080931,108.650642492643));
#71074=CARTESIAN_POINT('Ctrl Pts',(66.8012676906133,775.998380960927,108.629371044712));
#71075=CARTESIAN_POINT('Ctrl Pts',(66.7994991288181,775.74735913733,108.585763695408));
#71076=CARTESIAN_POINT('Ctrl Pts',(66.7741542057155,775.624422336652,108.56382675012));
#71077=CARTESIAN_POINT('Ctrl Pts',(66.6777954334382,775.397595837452,108.521749780387));
#71078=CARTESIAN_POINT('Ctrl Pts',(66.6084609820003,775.295441337757,108.501951703788));
#71079=CARTESIAN_POINT('Ctrl Pts',(66.4348223023411,775.124712757349,108.466479393225));
#71080=CARTESIAN_POINT('Ctrl Pts',(66.3326881832758,775.057397791066,108.451094710872));
#71081=CARTESIAN_POINT('Ctrl Pts',(66.1073521068603,774.965595399574,108.426235557521));
#71082=CARTESIAN_POINT('Ctrl Pts',(65.986522794371,774.942148754366,108.41703149008));
#71083=CARTESIAN_POINT('Ctrl Pts',(65.8602817427518,774.942450127446,108.411401868727));
#71084=CARTESIAN_POINT('Ctrl Pts',(65.8562970470197,774.942484867569,108.411228246327));
#71085=CARTESIAN_POINT('Ctrl Pts',(65.8523138277871,774.942544771236,108.411058755856));
#71086=CARTESIAN_POINT('Origin',(65.8523138277871,779.672231777069,97.874067134449));
#71087=CARTESIAN_POINT('',(65.8523138277871,778.008815145563,104.080962377937));
#71088=CARTESIAN_POINT('Origin',(65.8523138277871,777.537392914954,103.91434581067));
#71089=CARTESIAN_POINT('',(65.8523138277873,776.389806261283,108.661760026823));
#71090=CARTESIAN_POINT('',(65.8523138277871,780.143654007678,98.0406837017161));
#71091=CARTESIAN_POINT('Ctrl Pts',(65.8523236262048,775.392032337629,108.483943428478));
#71092=CARTESIAN_POINT('Ctrl Pts',(65.7878831210737,775.39295660244,108.481324538884));
#71093=CARTESIAN_POINT('Ctrl Pts',(65.7241978017977,775.406334757023,108.480843373498));
#71094=CARTESIAN_POINT('Ctrl Pts',(65.6030429989561,775.457117722179,108.484315352157));
#71095=CARTESIAN_POINT('Ctrl Pts',(65.547142292733,775.49486490529,108.488399771766));
#71096=CARTESIAN_POINT('Ctrl Pts',(65.4524055773241,775.590135292748,108.500900894481));
#71097=CARTESIAN_POINT('Ctrl Pts',(65.4147750191479,775.64705429602,108.509270128121));
#71098=CARTESIAN_POINT('Ctrl Pts',(65.3642116813439,775.771358807386,108.52915264891));
#71099=CARTESIAN_POINT('Ctrl Pts',(65.3515904232822,775.837563516921,108.540469630755));
#71100=CARTESIAN_POINT('Ctrl Pts',(65.3530953749288,775.97012946301,108.564479362415));
#71101=CARTESIAN_POINT('Ctrl Pts',(65.3670010612835,776.035275973097,108.57694019845));
#71102=CARTESIAN_POINT('Ctrl Pts',(65.4192307002952,776.154810754385,108.601026322507));
#71103=CARTESIAN_POINT('Ctrl Pts',(65.4565005520766,776.208278601099,108.612433029473));
#71104=CARTESIAN_POINT('Ctrl Pts',(65.5495777323318,776.297359004874,108.632697193855));
#71105=CARTESIAN_POINT('Ctrl Pts',(65.6042627705228,776.332258748866,108.641374072043));
#71106=CARTESIAN_POINT('Ctrl Pts',(65.7243323807721,776.379166233064,108.654827946433));
#71107=CARTESIAN_POINT('Ctrl Pts',(65.7884582310674,776.390729781173,108.65947181588));
#71108=CARTESIAN_POINT('Ctrl Pts',(65.9189746729532,776.388843611188,108.664149031545));
#71109=CARTESIAN_POINT('Ctrl Pts',(65.9839985847323,776.374979417501,108.66405355304));
#71110=CARTESIAN_POINT('Ctrl Pts',(66.105940596835,776.322870548642,108.659095610779));
#71111=CARTESIAN_POINT('Ctrl Pts',(66.1614612249993,776.284825042422,108.654220772858));
#71112=CARTESIAN_POINT('Ctrl Pts',(66.2547672156122,776.189536853153,108.640454625418));
#71113=CARTESIAN_POINT('Ctrl Pts',(66.291541390347,776.133108003367,108.631676658887));
#71114=CARTESIAN_POINT('Ctrl Pts',(66.3411916474218,776.00918888395,108.611441701454));
#71115=CARTESIAN_POINT('Ctrl Pts',(66.3534220149565,775.942748845708,108.600150043006));
#71116=CARTESIAN_POINT('Ctrl Pts',(66.351070325944,775.810535114789,108.5768357731));
#71117=CARTESIAN_POINT('Ctrl Pts',(66.3370086347315,775.745929364074,108.565033027938));
#71118=CARTESIAN_POINT('Ctrl Pts',(66.2848546751548,775.626960494077,108.542344463995));
#71119=CARTESIAN_POINT('Ctrl Pts',(66.2476407407646,775.573531554295,108.531650840516));
#71120=CARTESIAN_POINT('Ctrl Pts',(66.1548823701777,775.484555924095,108.512576100187));
#71121=CARTESIAN_POINT('Ctrl Pts',(66.1004778653315,775.44968513785,108.504355193393));
#71122=CARTESIAN_POINT('Ctrl Pts',(65.9808501232473,775.402702517939,108.491280639784));
#71123=CARTESIAN_POINT('Ctrl Pts',(65.9168825237981,775.391106374724,108.486567129591));
#71124=CARTESIAN_POINT('Ctrl Pts',(65.8523236262048,775.392032337629,108.483943428478));
#71125=CARTESIAN_POINT('Origin',(44.8921369270856,786.628267531093,100.332565533275));
#71126=CARTESIAN_POINT('',(44.8921369270856,784.225718511386,110.909518141625));
#71127=CARTESIAN_POINT('Origin',(44.8921369270856,783.038336934424,110.489857316266));
#71128=CARTESIAN_POINT('',(44.892136974638,784.857852423734,109.120968636072));
#71129=CARTESIAN_POINT('',(44.8921369270856,787.815649108055,100.752226358633));
#71130=CARTESIAN_POINT('Ctrl Pts',(44.8923073484297,782.422749479518,108.45237145031));
#71131=CARTESIAN_POINT('Ctrl Pts',(44.8162819691552,782.42299144979,108.451655950142));
#71132=CARTESIAN_POINT('Ctrl Pts',(44.7404232666641,782.429931891369,108.452646681253));
#71133=CARTESIAN_POINT('Ctrl Pts',(44.5603464969493,782.462552645622,108.459142731722));
#71134=CARTESIAN_POINT('Ctrl Pts',(44.4579575372025,782.494594811484,108.46629916939));
#71135=CARTESIAN_POINT('Ctrl Pts',(44.208852900756,782.608056538512,108.493019022734));
#71136=CARTESIAN_POINT('Ctrl Pts',(44.0725044195926,782.706041579602,108.517055867388));
#71137=CARTESIAN_POINT('Ctrl Pts',(43.85889975643,782.934951031857,108.575212430792));
#71138=CARTESIAN_POINT('Ctrl Pts',(43.7786615350378,783.059590779428,108.607576757387));
#71139=CARTESIAN_POINT('Ctrl Pts',(43.6637106530933,783.338132164978,108.681584485548));
#71140=CARTESIAN_POINT('Ctrl Pts',(43.6331172062892,783.49090718019,108.723031679013));
#71141=CARTESIAN_POINT('Ctrl Pts',(43.6324246149148,783.805991553284,108.810250709823));
#71142=CARTESIAN_POINT('Ctrl Pts',(43.6651931363107,783.965339218652,108.855280334504));
#71143=CARTESIAN_POINT('Ctrl Pts',(43.7923201765428,784.259766106586,108.939900381986));
#71144=CARTESIAN_POINT('Ctrl Pts',(43.8844794342416,784.392357994548,108.978738096277));
#71145=CARTESIAN_POINT('Ctrl Pts',(44.1057679513745,784.605258926542,109.041971711113));
#71146=CARTESIAN_POINT('Ctrl Pts',(44.2288314515859,784.687626790762,109.066871395095));
#71147=CARTESIAN_POINT('Ctrl Pts',(44.446078059077,784.783614759782,109.096393723432));
#71148=CARTESIAN_POINT('Ctrl Pts',(44.531919601865,784.811252398521,109.105054853075));
#71149=CARTESIAN_POINT('Ctrl Pts',(44.6575272967582,784.837700513626,109.113607669532));
#71150=CARTESIAN_POINT('Ctrl Pts',(44.6952917615232,784.843932240686,109.115672881431));
#71151=CARTESIAN_POINT('Ctrl Pts',(44.7676643818972,784.852630748071,109.118674765112));
#71152=CARTESIAN_POINT('Ctrl Pts',(44.8021976191136,784.855397046532,109.119699250864));
#71153=CARTESIAN_POINT('Ctrl Pts',(44.9118036736405,784.859814273518,109.121665797058));
#71154=CARTESIAN_POINT('Ctrl Pts',(44.9869414563982,784.856388765398,109.121112186209));
#71155=CARTESIAN_POINT('Ctrl Pts',(45.1659145638157,784.832726237737,109.115249535883));
#71156=CARTESIAN_POINT('Ctrl Pts',(45.2682965869261,784.806321184381,109.108122784627));
#71157=CARTESIAN_POINT('Ctrl Pts',(45.5212130708983,784.707055967686,109.080701233473));
#71158=CARTESIAN_POINT('Ctrl Pts',(45.6621889493315,784.617025423278,109.05540971265));
#71159=CARTESIAN_POINT('Ctrl Pts',(45.8868787027634,784.401100004618,108.994901346306));
#71160=CARTESIAN_POINT('Ctrl Pts',(45.973250561103,784.281702220923,108.961503594805));
#71161=CARTESIAN_POINT('Ctrl Pts',(46.1021019238818,784.011660239623,108.886550026756));
#71162=CARTESIAN_POINT('Ctrl Pts',(46.1406334213441,783.862007390482,108.845309057943));
#71163=CARTESIAN_POINT('Ctrl Pts',(46.1589399696531,783.547147245785,108.759302434206));
#71164=CARTESIAN_POINT('Ctrl Pts',(46.134740405625,783.384648516219,108.715324803664));
#71165=CARTESIAN_POINT('Ctrl Pts',(46.0227701768699,783.080537851574,108.633482615148));
#71166=CARTESIAN_POINT('Ctrl Pts',(45.9370116997564,782.941548162612,108.596303039931));
#71167=CARTESIAN_POINT('Ctrl Pts',(45.7159078965255,782.704871855997,108.532769262459));
#71168=CARTESIAN_POINT('Ctrl Pts',(45.5831741223873,782.609040411889,108.506898925147));
#71169=CARTESIAN_POINT('Ctrl Pts',(45.3471502485886,782.500099987671,108.476693369378));
#71170=CARTESIAN_POINT('Ctrl Pts',(45.2546051644565,782.469577723498,108.46798515072));
#71171=CARTESIAN_POINT('Ctrl Pts',(45.1243436765839,782.442489798182,108.459764223446));
#71172=CARTESIAN_POINT('Ctrl Pts',(45.0890639855754,782.436672235543,108.457924227011));
#71173=CARTESIAN_POINT('Ctrl Pts',(45.0270251652088,782.429074442781,108.455357726509));
#71174=CARTESIAN_POINT('Ctrl Pts',(45.0003760569042,782.426648194516,108.454468151232));
#71175=CARTESIAN_POINT('Ctrl Pts',(44.9465807318617,782.423430431719,108.453099584936));
#71176=CARTESIAN_POINT('Ctrl Pts',(44.9194473842637,782.422663099392,108.452626874227));
#71177=CARTESIAN_POINT('Ctrl Pts',(44.8923073484297,782.422749479518,108.45237145031));
#71178=CARTESIAN_POINT('Origin',(44.8921369270856,786.628267531093,100.332565533275));
#71179=CARTESIAN_POINT('',(44.8921369270856,784.964850899586,106.539460776763));
#71180=CARTESIAN_POINT('Origin',(44.8921369270856,784.493428668978,106.372844209496));
#71181=CARTESIAN_POINT('',(44.8921369270856,783.509759165033,110.656473883533));
#71182=CARTESIAN_POINT('',(44.8921369270856,787.099689761701,100.499182100542));
#71183=CARTESIAN_POINT('Origin',(44.8921369270856,783.038336934424,110.489857316266));
#71184=CARTESIAN_POINT('Origin',(49.0936533033807,782.22871327632,98.7776141969985));
#71185=CARTESIAN_POINT('',(49.0936533033807,777.622727263691,108.744570586988));
#71186=CARTESIAN_POINT('',(49.0936533033809,779.593263946518,109.299458278251));
#71187=CARTESIAN_POINT('Ctrl Pts',(49.0936533033807,777.622727263691,108.744570586988));
#71188=CARTESIAN_POINT('Ctrl Pts',(48.9632002870732,777.622428485583,108.745415944952));
#71189=CARTESIAN_POINT('Ctrl Pts',(48.833946065599,777.646453119096,108.752434741664));
#71190=CARTESIAN_POINT('Ctrl Pts',(48.5883527706715,777.741862477848,108.778574089776));
#71191=CARTESIAN_POINT('Ctrl Pts',(48.4749703105534,777.813617826965,108.79777836983));
#71192=CARTESIAN_POINT('Ctrl Pts',(48.2830436461297,777.995647923637,108.846516004725));
#71193=CARTESIAN_POINT('Ctrl Pts',(48.2064874701559,778.104274454239,108.875624111595));
#71194=CARTESIAN_POINT('Ctrl Pts',(48.1012232380387,778.343602206046,108.940563764105));
#71195=CARTESIAN_POINT('Ctrl Pts',(48.0735033741326,778.472013653152,108.97578880451));
#71196=CARTESIAN_POINT('Ctrl Pts',(48.0710564047158,778.732958464172,109.048553371529));
#71197=CARTESIAN_POINT('Ctrl Pts',(48.0969653472274,778.862958451878,109.08540613932));
#71198=CARTESIAN_POINT('Ctrl Pts',(48.1995298154465,779.103846631018,109.154765673716));
#71199=CARTESIAN_POINT('Ctrl Pts',(48.2745791925128,779.212586684015,109.186630601971));
#71200=CARTESIAN_POINT('Ctrl Pts',(48.4641597582515,779.395616161713,109.240795518626));
#71201=CARTESIAN_POINT('Ctrl Pts',(48.5767645661844,779.468158125872,109.262557898456));
#71202=CARTESIAN_POINT('Ctrl Pts',(48.8252757551249,779.5674830409,109.292254814351));
#71203=CARTESIAN_POINT('Ctrl Pts',(48.9587983910953,779.593131925164,109.299831817343));
#71204=CARTESIAN_POINT('Ctrl Pts',(49.0936533033811,779.593263946518,109.299458278251));
#71205=CARTESIAN_POINT('',(49.0936533269279,780.072861410571,107.94249294157));
#71206=CARTESIAN_POINT('',(49.0936533033807,783.191742416563,99.1179812800658));
#71207=CARTESIAN_POINT('Ctrl Pts',(49.0937056776217,778.048104433328,107.541015281665));
#71208=CARTESIAN_POINT('Ctrl Pts',(49.0271547441502,778.048321177872,107.540391787571));
#71209=CARTESIAN_POINT('Ctrl Pts',(48.9607903865118,778.055022080643,107.540940204712));
#71210=CARTESIAN_POINT('Ctrl Pts',(48.8117888491069,778.084877021327,107.544868878333));
#71211=CARTESIAN_POINT('Ctrl Pts',(48.7305237807704,778.112035075303,107.548991866279));
#71212=CARTESIAN_POINT('Ctrl Pts',(48.5304377372779,778.207843672871,107.564542383633));
#71213=CARTESIAN_POINT('Ctrl Pts',(48.4205566551283,778.290624354942,107.57871212594));
#71214=CARTESIAN_POINT('Ctrl Pts',(48.248797333885,778.483372358419,107.613207792825));
#71215=CARTESIAN_POINT('Ctrl Pts',(48.1846162168159,778.588357303446,107.63252937346));
#71216=CARTESIAN_POINT('Ctrl Pts',(48.0939316473472,778.822159595282,107.676842225506));
#71217=CARTESIAN_POINT('Ctrl Pts',(48.0707481447969,778.950081617404,107.701742704981));
#71218=CARTESIAN_POINT('Ctrl Pts',(48.073967176409,779.213418464044,107.754361930166));
#71219=CARTESIAN_POINT('Ctrl Pts',(48.1027752555812,779.346440990759,107.781666810885));
#71220=CARTESIAN_POINT('Ctrl Pts',(48.2106876020914,779.590992471309,107.833037117464));
#71221=CARTESIAN_POINT('Ctrl Pts',(48.2877948789974,779.700566598424,107.856657992685));
#71222=CARTESIAN_POINT('Ctrl Pts',(48.4740930495997,779.877463759995,107.895605643368));
#71223=CARTESIAN_POINT('Ctrl Pts',(48.5789813814141,779.945728191473,107.911061578461));
#71224=CARTESIAN_POINT('Ctrl Pts',(48.7673092303796,780.024177526603,107.92940720315));
#71225=CARTESIAN_POINT('Ctrl Pts',(48.8440766979462,780.046159153914,107.934755182649));
#71226=CARTESIAN_POINT('Ctrl Pts',(48.9564409588534,780.064664640844,107.939636414258));
#71227=CARTESIAN_POINT('Ctrl Pts',(48.9904403298714,780.068545523425,107.94074320737));
#71228=CARTESIAN_POINT('Ctrl Pts',(49.0557675827937,780.072739097664,107.942165936498));
#71229=CARTESIAN_POINT('Ctrl Pts',(49.0870359458949,780.073328819959,107.942541166276));
#71230=CARTESIAN_POINT('Ctrl Pts',(49.186430777403,780.070706768523,107.942764797524));
#71231=CARTESIAN_POINT('Ctrl Pts',(49.2542214653515,780.062191609398,107.941466692095));
#71232=CARTESIAN_POINT('Ctrl Pts',(49.4129475467574,780.026113842808,107.934975581307));
#71233=CARTESIAN_POINT('Ctrl Pts',(49.5017986747611,779.99260694913,107.928494380102));
#71234=CARTESIAN_POINT('Ctrl Pts',(49.7038721599177,779.882801061356,107.906730217753));
#71235=CARTESIAN_POINT('Ctrl Pts',(49.8086123473817,779.795323691912,107.889064186069));
#71236=CARTESIAN_POINT('Ctrl Pts',(49.9699044951568,779.594614101948,107.848576378668));
#71237=CARTESIAN_POINT('Ctrl Pts',(50.0285430722642,779.485966583569,107.826683787102));
#71238=CARTESIAN_POINT('Ctrl Pts',(50.1061786557834,779.246339681443,107.778767657688));
#71239=CARTESIAN_POINT('Ctrl Pts',(50.1218291289306,779.116500703771,107.752999600788));
#71240=CARTESIAN_POINT('Ctrl Pts',(50.1025559176442,778.852484042031,107.701053957671));
#71241=CARTESIAN_POINT('Ctrl Pts',(50.0656026602404,778.720801185339,107.675385835317));
#71242=CARTESIAN_POINT('Ctrl Pts',(49.9428080377817,778.48180386328,107.628961357646));
#71243=CARTESIAN_POINT('Ctrl Pts',(49.8590764708186,778.376243292557,107.608531686978));
#71244=CARTESIAN_POINT('Ctrl Pts',(49.6683817970023,778.214707142724,107.576927859538));
#71245=CARTESIAN_POINT('Ctrl Pts',(49.5674138549477,778.155205162263,107.56511209074));
#71246=CARTESIAN_POINT('Ctrl Pts',(49.385058364516,778.086339371718,107.550818021285));
#71247=CARTESIAN_POINT('Ctrl Pts',(49.3088046063118,778.067170383379,107.546599133708));
#71248=CARTESIAN_POINT('Ctrl Pts',(49.2085259745404,778.053932036756,107.543210601871));
#71249=CARTESIAN_POINT('Ctrl Pts',(49.1859256021635,778.051710488846,107.542584550007));
#71250=CARTESIAN_POINT('Ctrl Pts',(49.1401126226283,778.048741795942,107.54159245028));
#71251=CARTESIAN_POINT('Ctrl Pts',(49.1169122878013,778.04802885353,107.541232696863));
#71252=CARTESIAN_POINT('Ctrl Pts',(49.0937056776217,778.048104433328,107.541015281665));
#71253=CARTESIAN_POINT('Ctrl Pts',(49.093653303381,779.593263946518,109.299458278251));
#71254=CARTESIAN_POINT('Ctrl Pts',(49.0938253602664,779.593264114959,109.299457801665));
#71255=CARTESIAN_POINT('Ctrl Pts',(49.0939974193205,779.593264241851,109.299457312176));
#71256=CARTESIAN_POINT('Ctrl Pts',(49.0941694805274,779.59326432719,109.299456809783));
#71257=CARTESIAN_POINT('Ctrl Pts',(49.2265276323488,779.593329974147,109.299070344109));
#71258=CARTESIAN_POINT('Ctrl Pts',(49.3576186666871,779.568813570152,109.291030003779));
#71259=CARTESIAN_POINT('Ctrl Pts',(49.6047420471024,779.472477681339,109.260464064252));
#71260=CARTESIAN_POINT('Ctrl Pts',(49.7180437433462,779.400798422938,109.238004235613));
#71261=CARTESIAN_POINT('Ctrl Pts',(49.9087951730618,779.219487758016,109.182331489965));
#71262=CARTESIAN_POINT('Ctrl Pts',(49.9844406122878,779.111714188496,109.149707751261));
#71263=CARTESIAN_POINT('Ctrl Pts',(50.0882999563377,778.872938961531,109.079036770978));
#71264=CARTESIAN_POINT('Ctrl Pts',(50.1150962223982,778.744134562306,109.041666387846));
#71265=CARTESIAN_POINT('Ctrl Pts',(50.115027228245,778.484815561264,108.968211725716));
#71266=CARTESIAN_POINT('Ctrl Pts',(50.0887005288884,778.356819261407,108.932822778779));
#71267=CARTESIAN_POINT('Ctrl Pts',(49.9866264473733,778.117713653121,108.868221322591));
#71268=CARTESIAN_POINT('Ctrl Pts',(49.911937647475,778.008822967132,108.839593293666));
#71269=CARTESIAN_POINT('Ctrl Pts',(49.7239293003419,777.825088963006,108.792347678592));
#71270=CARTESIAN_POINT('Ctrl Pts',(49.6125313280592,777.751850570673,108.77412198634));
#71271=CARTESIAN_POINT('Ctrl Pts',(49.3672158233277,777.650964133216,108.749820142085));
#71272=CARTESIAN_POINT('Ctrl Pts',(49.2357088177524,777.624230107928,108.743950384203));
#71273=CARTESIAN_POINT('Ctrl Pts',(49.0996434064598,777.622753796935,108.744535038214));
#71274=CARTESIAN_POINT('Ctrl Pts',(49.0966480390014,777.62273412257,108.744551180586));
#71275=CARTESIAN_POINT('Ctrl Pts',(49.0936533033807,777.622727263691,108.744570586988));
#71276=CARTESIAN_POINT('Origin',(49.0936533033807,782.22871327632,98.7776141969985));
#71277=CARTESIAN_POINT('',(49.0936533033807,780.565296644814,104.984509440487));
#71278=CARTESIAN_POINT('Origin',(49.0936533033807,780.093874414205,104.81789287322));
#71279=CARTESIAN_POINT('',(49.0936533033808,779.093842445626,109.147818241034));
#71280=CARTESIAN_POINT('',(49.0936533033807,782.700135506929,98.9442307642656));
#71281=CARTESIAN_POINT('Ctrl Pts',(49.0936529529939,778.129187731554,108.876294684482));
#71282=CARTESIAN_POINT('Ctrl Pts',(49.0339299911541,778.129069875144,108.876628271105));
#71283=CARTESIAN_POINT('Ctrl Pts',(48.9746952099443,778.139320411379,108.879735639841));
#71284=CARTESIAN_POINT('Ctrl Pts',(48.8573329198357,778.18153746217,108.891789301062));
#71285=CARTESIAN_POINT('Ctrl Pts',(48.8010442575993,778.215116638054,108.901159973048));
#71286=CARTESIAN_POINT('Ctrl Pts',(48.7049742964704,778.301444764448,108.925117630472));
#71287=CARTESIAN_POINT('Ctrl Pts',(48.6661795247187,778.353406890188,108.939489958875));
#71288=CARTESIAN_POINT('Ctrl Pts',(48.6112999432858,778.469396243527,108.971680317644));
#71289=CARTESIAN_POINT('Ctrl Pts',(48.5960093741457,778.532414270852,108.989223232261));
#71290=CARTESIAN_POINT('Ctrl Pts',(48.5917898937807,778.66076063377,109.025170440976));
#71291=CARTESIAN_POINT('Ctrl Pts',(48.6030318506563,778.724832348016,109.04322517028));
#71292=CARTESIAN_POINT('Ctrl Pts',(48.6507951793941,778.844547241534,109.077148151531));
#71293=CARTESIAN_POINT('Ctrl Pts',(48.6866959785454,778.899058201511,109.09269200419));
#71294=CARTESIAN_POINT('Ctrl Pts',(48.778497345828,778.991364058649,109.119061017436));
#71295=CARTESIAN_POINT('Ctrl Pts',(48.8334672140009,779.028253422815,109.12962279123));
#71296=CARTESIAN_POINT('Ctrl Pts',(48.9553347524394,779.079321089152,109.144100974579));
#71297=CARTESIAN_POINT('Ctrl Pts',(49.0210330503128,779.0929322282,109.147851902656));
#71298=CARTESIAN_POINT('Ctrl Pts',(49.1541503834313,779.09466592974,109.147809453492));
#71299=CARTESIAN_POINT('Ctrl Pts',(49.2202266744672,779.082752256428,109.144010035709));
#71300=CARTESIAN_POINT('Ctrl Pts',(49.3434565507019,779.034810560724,109.129362668073));
#71301=CARTESIAN_POINT('Ctrl Pts',(49.3993906882173,778.999315633519,109.118679925339));
#71302=CARTESIAN_POINT('Ctrl Pts',(49.4934489760915,778.909406933719,109.092016312694));
#71303=CARTESIAN_POINT('Ctrl Pts',(49.530653525023,778.855912476024,109.076312562696));
#71304=CARTESIAN_POINT('Ctrl Pts',(49.5812722610349,778.737772260162,109.042098756154));
#71305=CARTESIAN_POINT('Ctrl Pts',(49.5940906052375,778.674262434235,109.023922964426));
#71306=CARTESIAN_POINT('Ctrl Pts',(49.5931995727275,778.546923013897,108.98797833082));
#71307=CARTESIAN_POINT('Ctrl Pts',(49.57987089725,778.484328380295,108.970551259103));
#71308=CARTESIAN_POINT('Ctrl Pts',(49.5290189689823,778.367655334965,108.938502065176));
#71309=CARTESIAN_POINT('Ctrl Pts',(49.492025321095,778.314666705199,108.924175652239));
#71310=CARTESIAN_POINT('Ctrl Pts',(49.3991635310428,778.225507085843,108.900409256669));
#71311=CARTESIAN_POINT('Ctrl Pts',(49.3442389574218,778.190136099238,108.891177247252));
#71312=CARTESIAN_POINT('Ctrl Pts',(49.2235176617433,778.141821358915,108.878883772904));
#71313=CARTESIAN_POINT('Ctrl Pts',(49.1589091968619,778.129316507261,108.87593019134));
#71314=CARTESIAN_POINT('Ctrl Pts',(49.0936529529939,778.129187731554,108.876294684482));
#71315=CARTESIAN_POINT('Origin',(54.622724097431,778.213544437116,97.3585176725896));
#71316=CARTESIAN_POINT('',(54.622724097431,773.482462218109,107.899456887669));
#71317=CARTESIAN_POINT('',(54.622724097431,775.377367353003,108.228259992878));
#71318=CARTESIAN_POINT('Ctrl Pts',(54.6227240974307,773.482462218109,107.899456887669));
#71319=CARTESIAN_POINT('Ctrl Pts',(54.5071908003515,773.482696433452,107.898794202553));
#71320=CARTESIAN_POINT('Ctrl Pts',(54.3927095887361,773.504165869956,107.90141402035));
#71321=CARTESIAN_POINT('Ctrl Pts',(54.1679886550712,773.590758299484,107.913586074231));
#71322=CARTESIAN_POINT('Ctrl Pts',(54.0614064897469,773.658443861292,107.923574140098));
#71323=CARTESIAN_POINT('Ctrl Pts',(53.8792311617861,773.831873819902,107.950262927227));
#71324=CARTESIAN_POINT('Ctrl Pts',(53.8059507901509,773.936483652477,107.966814225441));
#71325=CARTESIAN_POINT('Ctrl Pts',(53.7035028551231,774.16948192188,108.004940395586));
#71326=CARTESIAN_POINT('Ctrl Pts',(53.6761364981783,774.296106177837,108.026257726283));
#71327=CARTESIAN_POINT('Ctrl Pts',(53.6732822144116,774.550249009593,108.070375030963));
#71328=CARTESIAN_POINT('Ctrl Pts',(53.6971030856602,774.675439235575,108.092753169681));
#71329=CARTESIAN_POINT('Ctrl Pts',(53.7922038053258,774.907418348338,108.135309699879));
#71330=CARTESIAN_POINT('Ctrl Pts',(53.8619123252693,775.012258230956,108.155105398148));
#71331=CARTESIAN_POINT('Ctrl Pts',(54.0382646177959,775.188373499272,108.189078330288));
#71332=CARTESIAN_POINT('Ctrl Pts',(54.142876742799,775.25810793812,108.202938788058));
#71333=CARTESIAN_POINT('Ctrl Pts',(54.3737564245772,775.353177412434,108.222346328971));
#71334=CARTESIAN_POINT('Ctrl Pts',(54.4975757462634,775.377566653681,108.227689314813));
#71335=CARTESIAN_POINT('Ctrl Pts',(54.6227069807416,775.377367380385,108.228259914849));
#71336=CARTESIAN_POINT('Ctrl Pts',(54.6227126863074,775.377367371299,108.228259940867));
#71337=CARTESIAN_POINT('Ctrl Pts',(54.6227183918705,775.377367362191,108.22825996688));
#71338=CARTESIAN_POINT('Ctrl Pts',(54.622724097431,775.377367353003,108.228259992878));
#71339=CARTESIAN_POINT('',(54.6227240859897,775.748529403717,107.178100067398));
#71340=CARTESIAN_POINT('',(54.622724097431,779.107440609735,97.6744508257262));
#71341=CARTESIAN_POINT('Ctrl Pts',(54.622716580523,773.827866246708,106.922176294992));
#71342=CARTESIAN_POINT('Ctrl Pts',(54.5547214479639,773.827706518738,106.922629844528));
#71343=CARTESIAN_POINT('Ctrl Pts',(54.48695467043,773.835001109058,106.923941811772));
#71344=CARTESIAN_POINT('Ctrl Pts',(54.3341976754647,773.868608227771,106.92889428809));
#71345=CARTESIAN_POINT('Ctrl Pts',(54.2510658090552,773.899791884602,106.933087388114));
#71346=CARTESIAN_POINT('Ctrl Pts',(54.0627462365035,774.002529467038,106.946450719118));
#71347=CARTESIAN_POINT('Ctrl Pts',(53.965430143705,774.084527837828,106.956839943242));
#71348=CARTESIAN_POINT('Ctrl Pts',(53.813741224562,774.27409207907,106.980954385284));
#71349=CARTESIAN_POINT('Ctrl Pts',(53.758027625191,774.377889685351,106.994202828633));
#71350=CARTESIAN_POINT('Ctrl Pts',(53.6836643689704,774.607301028281,107.023918515021));
#71351=CARTESIAN_POINT('Ctrl Pts',(53.66837221503,774.732056379351,107.040308491224));
#71352=CARTESIAN_POINT('Ctrl Pts',(53.6858630334801,774.984738439568,107.074080228882));
#71353=CARTESIAN_POINT('Ctrl Pts',(53.7202694225296,775.110424799374,107.09118321926));
#71354=CARTESIAN_POINT('Ctrl Pts',(53.8349920837059,775.337509559787,107.122448519933));
#71355=CARTESIAN_POINT('Ctrl Pts',(53.912929941399,775.437441484146,107.136388643344));
#71356=CARTESIAN_POINT('Ctrl Pts',(54.0900558647598,775.58983252655,107.157590658501));
#71357=CARTESIAN_POINT('Ctrl Pts',(54.1833384098643,775.645864259133,107.165352934401));
#71358=CARTESIAN_POINT('Ctrl Pts',(54.3536483355174,775.711783249342,107.174173684347));
#71359=CARTESIAN_POINT('Ctrl Pts',(54.4260017437422,775.730362875771,107.176534938924));
#71360=CARTESIAN_POINT('Ctrl Pts',(54.532241205095,775.744561140108,107.178038880669));
#71361=CARTESIAN_POINT('Ctrl Pts',(54.5648533558934,775.747202740603,107.178243185922));
#71362=CARTESIAN_POINT('Ctrl Pts',(54.628232021751,775.749024807328,107.178141976805));
#71363=CARTESIAN_POINT('Ctrl Pts',(54.6589472785579,775.74840522504,107.177866856488));
#71364=CARTESIAN_POINT('Ctrl Pts',(54.7593635711179,775.741456415546,107.176226523946));
#71365=CARTESIAN_POINT('Ctrl Pts',(54.8283504852572,775.728864667926,107.17392188599));
#71366=CARTESIAN_POINT('Ctrl Pts',(54.9911292612032,775.679976819372,107.16562604374));
#71367=CARTESIAN_POINT('Ctrl Pts',(55.0816102887839,775.636136579799,107.158529661192));
#71368=CARTESIAN_POINT('Ctrl Pts',(55.2539895568943,775.515836505949,107.139718538326));
#71369=CARTESIAN_POINT('Ctrl Pts',(55.3325516100012,775.437401730338,107.127752856353));
#71370=CARTESIAN_POINT('Ctrl Pts',(55.4632320033908,775.251799922037,107.100265283793));
#71371=CARTESIAN_POINT('Ctrl Pts',(55.5122974996599,775.144706590069,107.084806196904));
#71372=CARTESIAN_POINT('Ctrl Pts',(55.5718394124838,774.910271451148,107.052025829815));
#71373=CARTESIAN_POINT('Ctrl Pts',(55.5787844982082,774.784042196732,107.034938701645));
#71374=CARTESIAN_POINT('Ctrl Pts',(55.5440059142545,774.532007887812,107.002014366974));
#71375=CARTESIAN_POINT('Ctrl Pts',(55.5010399322351,774.408502445413,106.986515261922));
#71376=CARTESIAN_POINT('Ctrl Pts',(55.3711866059429,774.188986879033,106.959985826081));
#71377=CARTESIAN_POINT('Ctrl Pts',(55.2868141078448,774.094130136453,106.949050756357));
#71378=CARTESIAN_POINT('Ctrl Pts',(55.10685794516,773.958321213211,106.934053534688));
#71379=CARTESIAN_POINT('Ctrl Pts',(55.0184126392753,773.911103993303,106.929122534429));
#71380=CARTESIAN_POINT('Ctrl Pts',(54.8565851010744,773.855460892064,106.923747053613));
#71381=CARTESIAN_POINT('Ctrl Pts',(54.7866558209677,773.840026945331,106.922445492453));
#71382=CARTESIAN_POINT('Ctrl Pts',(54.6847458860643,773.829564008447,106.921941855052));
#71383=CARTESIAN_POINT('Ctrl Pts',(54.6537438552632,773.827939133155,106.921969333031));
#71384=CARTESIAN_POINT('Ctrl Pts',(54.622716580523,773.827866246708,106.922176294992));
#71385=CARTESIAN_POINT('Ctrl Pts',(54.622724097431,775.377367353003,108.228259992878));
#71386=CARTESIAN_POINT('Ctrl Pts',(54.7413994181553,775.377176233909,108.228800742162));
#71387=CARTESIAN_POINT('Ctrl Pts',(54.8589252993588,775.354871874229,108.225040606538));
#71388=CARTESIAN_POINT('Ctrl Pts',(55.0856783861241,775.26607659639,108.209119800715));
#71389=CARTESIAN_POINT('Ctrl Pts',(55.1916913443785,775.198109872329,108.196676095123));
#71390=CARTESIAN_POINT('Ctrl Pts',(55.3716683219127,775.02490891286,108.165162909421));
#71391=CARTESIAN_POINT('Ctrl Pts',(55.4435478901821,774.921140142487,108.146374901502));
#71392=CARTESIAN_POINT('Ctrl Pts',(55.5433977550748,774.69045841209,108.105268754576));
#71393=CARTESIAN_POINT('Ctrl Pts',(55.5697381870677,774.565445575138,108.083306050231));
#71394=CARTESIAN_POINT('Ctrl Pts',(55.5718043512056,774.313882365095,108.039852320873));
#71395=CARTESIAN_POINT('Ctrl Pts',(55.5480284369105,774.189581291565,108.018739817575));
#71396=CARTESIAN_POINT('Ctrl Pts',(55.4541571370007,773.958887117895,107.980018294411));
#71397=CARTESIAN_POINT('Ctrl Pts',(55.3855739147925,773.854258479443,107.962689098121));
#71398=CARTESIAN_POINT('Ctrl Pts',(55.2130607587389,773.678553474488,107.933609686352));
#71399=CARTESIAN_POINT('Ctrl Pts',(55.1113512440305,773.608566369919,107.922029109468));
#71400=CARTESIAN_POINT('Ctrl Pts',(54.8870777334388,773.511594919478,107.905551238059));
#71401=CARTESIAN_POINT('Ctrl Pts',(54.7669522819423,773.48531221698,107.900770610043));
#71402=CARTESIAN_POINT('Ctrl Pts',(54.6375558568623,773.482519595948,107.899555498672));
#71403=CARTESIAN_POINT('Ctrl Pts',(54.6301378111837,773.482447188628,107.899499411841));
#71404=CARTESIAN_POINT('Ctrl Pts',(54.6227240974307,773.482462218109,107.899456887669));
#71405=CARTESIAN_POINT('Origin',(54.622724097431,778.213544437116,97.3585176725896));
#71406=CARTESIAN_POINT('',(54.622724097431,776.55012780561,103.565412916078));
#71407=CARTESIAN_POINT('Origin',(54.622724097431,776.078705575001,103.398796348811));
#71408=CARTESIAN_POINT('',(54.6227240974311,774.932139756061,108.143322231624));
#71409=CARTESIAN_POINT('',(54.622724097431,778.684966667725,97.5251342398567));
#71410=CARTESIAN_POINT('Ctrl Pts',(54.6227191556436,773.932781274095,107.969988956817));
#71411=CARTESIAN_POINT('Ctrl Pts',(54.561687772208,773.932899898407,107.969655133269));
#71412=CARTESIAN_POINT('Ctrl Pts',(54.50124623174,773.944221424331,107.97115222592));
#71413=CARTESIAN_POINT('Ctrl Pts',(54.3828385167216,773.989774403011,107.977947863272));
#71414=CARTESIAN_POINT('Ctrl Pts',(54.3267325112097,774.025310100391,107.98347519596));
#71415=CARTESIAN_POINT('Ctrl Pts',(54.2305902711695,774.11658962763,107.998107413849));
#71416=CARTESIAN_POINT('Ctrl Pts',(54.1918597388119,774.171805615782,108.007137886609));
#71417=CARTESIAN_POINT('Ctrl Pts',(54.1379246848474,774.294554828104,108.027653350482));
#71418=CARTESIAN_POINT('Ctrl Pts',(54.1235485762318,774.361091335508,108.038979723125));
#71419=CARTESIAN_POINT('Ctrl Pts',(54.1219744257417,774.495120721451,108.062235715201));
#71420=CARTESIAN_POINT('Ctrl Pts',(54.134587267002,774.561388536653,108.073949533389));
#71421=CARTESIAN_POINT('Ctrl Pts',(54.1850639422275,774.684427445897,108.096069747683));
#71422=CARTESIAN_POINT('Ctrl Pts',(54.2221935785743,774.740129991465,108.106277457678));
#71423=CARTESIAN_POINT('Ctrl Pts',(54.3151486312484,774.832544682185,108.123489914695));
#71424=CARTESIAN_POINT('Ctrl Pts',(54.3695203856928,774.86885143445,108.130406436861));
#71425=CARTESIAN_POINT('Ctrl Pts',(54.4891072638071,774.918557228744,108.140130263793));
#71426=CARTESIAN_POINT('Ctrl Pts',(54.5530376305238,774.931594169828,108.14286200799));
#71427=CARTESIAN_POINT('Ctrl Pts',(54.683310748962,774.932660053448,108.143730806839));
#71428=CARTESIAN_POINT('Ctrl Pts',(54.7482901945077,774.920352680989,108.141798928));
#71429=CARTESIAN_POINT('Ctrl Pts',(54.8706748106997,774.871194126728,108.133440911594));
#71430=CARTESIAN_POINT('Ctrl Pts',(54.9266391554852,774.834490789525,108.127037758269));
#71431=CARTESIAN_POINT('Ctrl Pts',(55.0212308234026,774.741354475557,108.110721338592));
#71432=CARTESIAN_POINT('Ctrl Pts',(55.0587548320678,774.685712231709,108.100949918147));
#71433=CARTESIAN_POINT('Ctrl Pts',(55.1100602100006,774.562690923574,108.079447781784));
#71434=CARTESIAN_POINT('Ctrl Pts',(55.1231033222687,774.49636817689,108.067904897197));
#71435=CARTESIAN_POINT('Ctrl Pts',(55.1223255313603,774.36219256659,108.044690970332));
#71436=CARTESIAN_POINT('Ctrl Pts',(55.1083339956401,774.295564275139,108.033232246365));
#71437=CARTESIAN_POINT('Ctrl Pts',(55.0556195402748,774.173902001322,108.012368859315));
#71438=CARTESIAN_POINT('Ctrl Pts',(55.0182397743535,774.119620555165,108.003088267979));
#71439=CARTESIAN_POINT('Ctrl Pts',(54.9251461528609,774.029090451328,107.987532467646));
#71440=CARTESIAN_POINT('Ctrl Pts',(54.8706037585573,773.993430164989,107.981356802045));
#71441=CARTESIAN_POINT('Ctrl Pts',(54.7509780106576,773.945032249884,107.972729045437));
#71442=CARTESIAN_POINT('Ctrl Pts',(54.6871837286973,773.932655976827,107.970341558893));
#71443=CARTESIAN_POINT('Ctrl Pts',(54.6227191556436,773.932781274095,107.969988956817));
#71444=CARTESIAN_POINT('Origin',(35.6544901166228,789.126363770955,101.215477269642));
#71445=CARTESIAN_POINT('',(35.6544901166228,786.723814751248,111.792429877991));
#71446=CARTESIAN_POINT('Origin',(35.6544901166228,785.536433174286,111.372769052633));
#71447=CARTESIAN_POINT('',(35.6544901166059,787.390150915315,109.907109072553));
#71448=CARTESIAN_POINT('',(35.6544901166228,790.313745347917,101.635138095));
#71449=CARTESIAN_POINT('Ctrl Pts',(35.6547954302602,784.997496551132,109.118408634909));
#71450=CARTESIAN_POINT('Ctrl Pts',(35.6023362552077,784.99746368276,109.118463466802));
#71451=CARTESIAN_POINT('Ctrl Pts',(35.5499276664424,785.000559817699,109.119501560811));
#71452=CARTESIAN_POINT('Ctrl Pts',(35.4748183637044,785.009515828586,109.122411075434));
#71453=CARTESIAN_POINT('Ctrl Pts',(35.451845283349,785.012873836572,109.12349567397));
#71454=CARTESIAN_POINT('Ctrl Pts',(35.3789035841627,785.025516809238,109.127563385561));
#71455=CARTESIAN_POINT('Ctrl Pts',(35.3294234991337,785.037086900285,109.131265659108));
#71456=CARTESIAN_POINT('Ctrl Pts',(35.2073924451325,785.073225428222,109.14279919142));
#71457=CARTESIAN_POINT('Ctrl Pts',(35.1362154876891,785.101338101937,109.151749240883));
#71458=CARTESIAN_POINT('Ctrl Pts',(34.9260028488811,785.206763856821,109.185308769177));
#71459=CARTESIAN_POINT('Ctrl Pts',(34.7994566209819,785.303343773512,109.216042429876));
#71460=CARTESIAN_POINT('Ctrl Pts',(34.6042763552335,785.521913936625,109.285961961862));
#71461=CARTESIAN_POINT('Ctrl Pts',(34.5317505805344,785.63769143293,109.323126754227));
#71462=CARTESIAN_POINT('Ctrl Pts',(34.4263153853796,785.895713696395,109.40648561012));
#71463=CARTESIAN_POINT('Ctrl Pts',(34.3973405094104,786.037171543863,109.45246585178));
#71464=CARTESIAN_POINT('Ctrl Pts',(34.3930164084478,786.332746671641,109.549353509024));
#71465=CARTESIAN_POINT('Ctrl Pts',(34.4215593604839,786.484350661742,109.599500429788));
#71466=CARTESIAN_POINT('Ctrl Pts',(34.5389873956959,786.773457383948,109.69605211633));
#71467=CARTESIAN_POINT('Ctrl Pts',(34.6286257756405,786.907518738343,109.741339307826));
#71468=CARTESIAN_POINT('Ctrl Pts',(34.8553936006824,787.13262266724,109.818025567516));
#71469=CARTESIAN_POINT('Ctrl Pts',(34.9894375292637,787.222324758519,109.84893812918));
#71470=CARTESIAN_POINT('Ctrl Pts',(35.2299877882829,787.324594196331,109.884326347562));
#71471=CARTESIAN_POINT('Ctrl Pts',(35.3268177589307,787.353138209337,109.894250096422));
#71472=CARTESIAN_POINT('Ctrl Pts',(35.4839021678214,787.380486101967,109.90375848326));
#71473=CARTESIAN_POINT('Ctrl Pts',(35.542263123963,787.386709856269,109.905923084951));
#71474=CARTESIAN_POINT('Ctrl Pts',(35.626202679431,787.390090766529,109.907091867684));
#71475=CARTESIAN_POINT('Ctrl Pts',(35.6515620585677,787.390388537154,109.907192438922));
#71476=CARTESIAN_POINT('Ctrl Pts',(35.7004714487293,787.389568306025,109.906899429126));
#71477=CARTESIAN_POINT('Ctrl Pts',(35.724012903159,787.38854914281,109.906540366245));
#71478=CARTESIAN_POINT('Ctrl Pts',(35.8018783737722,787.383107682481,109.904629781023));
#71479=CARTESIAN_POINT('Ctrl Pts',(35.8559278107591,787.375979306361,109.902133143967));
#71480=CARTESIAN_POINT('Ctrl Pts',(35.9917086189071,787.349495923221,109.892874204745));
#71481=CARTESIAN_POINT('Ctrl Pts',(36.0721871295654,787.325669420196,109.884554034847));
#71482=CARTESIAN_POINT('Ctrl Pts',(36.3031927842254,787.232397628624,109.852089575935));
#71483=CARTESIAN_POINT('Ctrl Pts',(36.4422395725919,787.142063105976,109.820751230696));
#71484=CARTESIAN_POINT('Ctrl Pts',(36.6612453160988,786.928442619778,109.747444288974));
#71485=CARTESIAN_POINT('Ctrl Pts',(36.7445262595779,786.811916635859,109.70773192335));
#71486=CARTESIAN_POINT('Ctrl Pts',(36.8684825246604,786.548578270246,109.618930130974));
#71487=CARTESIAN_POINT('Ctrl Pts',(36.9050534097343,786.40262360428,109.570192486408));
#71488=CARTESIAN_POINT('Ctrl Pts',(36.9202890269026,786.096231476617,109.469009300794));
#71489=CARTESIAN_POINT('Ctrl Pts',(36.8951923414051,785.93845968691,109.417510657593));
#71490=CARTESIAN_POINT('Ctrl Pts',(36.782221356325,785.641467927504,109.321522024938));
#71491=CARTESIAN_POINT('Ctrl Pts',(36.6956398814662,785.505082966989,109.277933140005));
#71492=CARTESIAN_POINT('Ctrl Pts',(36.4755872336333,785.275605637353,109.20510404788));
#71493=CARTESIAN_POINT('Ctrl Pts',(36.3456948455117,785.183375207323,109.176107924705));
#71494=CARTESIAN_POINT('Ctrl Pts',(36.0760626338526,785.059292373403,109.137303069111));
#71495=CARTESIAN_POINT('Ctrl Pts',(35.9418479810997,785.021839732685,109.125703610021));
#71496=CARTESIAN_POINT('Ctrl Pts',(35.7544543225039,785.000384650602,109.119192547212));
#71497=CARTESIAN_POINT('Ctrl Pts',(35.7046473858209,784.997527785947,109.118356528159));
#71498=CARTESIAN_POINT('Ctrl Pts',(35.6547954302602,784.997496551132,109.118408634909));
#71499=CARTESIAN_POINT('Origin',(35.6544901166228,789.126363770955,101.215477269642));
#71500=CARTESIAN_POINT('',(35.6544901166228,787.462947139449,107.42237251313));
#71501=CARTESIAN_POINT('Origin',(35.6544901166228,786.99152490884,107.255755945863));
#71502=CARTESIAN_POINT('',(35.6544901166228,786.007855404895,111.5393856199));
#71503=CARTESIAN_POINT('',(35.6544901166228,789.597786001564,101.382093836909));
#71504=CARTESIAN_POINT('Origin',(35.6544901166228,785.536433174286,111.372769052633));
#71505=CARTESIAN_POINT('Origin',(38.7940239657454,783.999333857892,99.403411420971));
#71506=CARTESIAN_POINT('',(38.7940239657454,779.394310614873,109.367643766138));
#71507=CARTESIAN_POINT('',(38.7940239657454,781.363295832901,109.926921146904));
#71508=CARTESIAN_POINT('Ctrl Pts',(38.7940239657453,779.394310614873,109.367643766138));
#71509=CARTESIAN_POINT('Ctrl Pts',(38.6635349461688,779.393207383636,109.370765230824));
#71510=CARTESIAN_POINT('Ctrl Pts',(38.5342083152401,779.416399346092,109.380182277251));
#71511=CARTESIAN_POINT('Ctrl Pts',(38.2888290241497,779.510170214757,109.410878727397));
#71512=CARTESIAN_POINT('Ctrl Pts',(38.1756822099265,779.580985895905,109.432143641909));
#71513=CARTESIAN_POINT('Ctrl Pts',(37.9838549896053,779.761485508096,109.484183819058));
#71514=CARTESIAN_POINT('Ctrl Pts',(37.9072551623842,779.869578073241,109.514504437028));
#71515=CARTESIAN_POINT('Ctrl Pts',(37.8017537134914,780.108411515024,109.58084224068));
#71516=CARTESIAN_POINT('Ctrl Pts',(37.7739374450261,780.236881950785,109.616244705413));
#71517=CARTESIAN_POINT('Ctrl Pts',(37.7713755000717,780.497798391027,109.688304510556));
#71518=CARTESIAN_POINT('Ctrl Pts',(37.7970878703195,780.627733019712,109.724281755939));
#71519=CARTESIAN_POINT('Ctrl Pts',(37.8994698608417,780.869972587616,109.791750369839));
#71520=CARTESIAN_POINT('Ctrl Pts',(37.9750248536947,780.979934395059,109.82258688857));
#71521=CARTESIAN_POINT('Ctrl Pts',(38.1654495596747,781.164254064518,109.8743032276));
#71522=CARTESIAN_POINT('Ctrl Pts',(38.2780994460044,781.237108238932,109.894745419256));
#71523=CARTESIAN_POINT('Ctrl Pts',(38.5263339759862,781.336877902731,109.921917474556));
#71524=CARTESIAN_POINT('Ctrl Pts',(38.6594853898809,781.362783466954,109.928351139963));
#71525=CARTESIAN_POINT('Ctrl Pts',(38.7939741509504,781.363295644351,109.926921676737));
#71526=CARTESIAN_POINT('Ctrl Pts',(38.7939907559017,781.363295707588,109.926921500245));
#71527=CARTESIAN_POINT('Ctrl Pts',(38.7940073608334,781.363295770438,109.926921323634));
#71528=CARTESIAN_POINT('Ctrl Pts',(38.7940239657454,781.363295832901,109.926921146904));
#71529=CARTESIAN_POINT('',(38.7940239785527,781.951092439748,108.263818899095));
#71530=CARTESIAN_POINT('',(38.7940239657454,784.962362998135,99.7437785040383));
#71531=CARTESIAN_POINT('Ctrl Pts',(38.7941252323501,779.956131957018,107.778035528783));
#71532=CARTESIAN_POINT('Ctrl Pts',(38.7717982570025,779.956215312796,107.77779304053));
#71533=CARTESIAN_POINT('Ctrl Pts',(38.7494784386769,779.957016493482,107.777716414688));
#71534=CARTESIAN_POINT('Ctrl Pts',(38.7071993034286,779.959896357852,107.77788640697));
#71535=CARTESIAN_POINT('Ctrl Pts',(38.6872412690192,779.961835607304,107.778100784944));
#71536=CARTESIAN_POINT('Ctrl Pts',(38.6234800619274,779.969892971348,107.779217291371));
#71537=CARTESIAN_POINT('Ctrl Pts',(38.5800189399609,779.978221365635,107.780635739443));
#71538=CARTESIAN_POINT('Ctrl Pts',(38.4733597888644,780.005786882482,107.785778436175));
#71539=CARTESIAN_POINT('Ctrl Pts',(38.4112650578069,780.028311812588,107.790282402133));
#71540=CARTESIAN_POINT('Ctrl Pts',(38.2304860384765,780.114081553115,107.808156405804));
#71541=CARTESIAN_POINT('Ctrl Pts',(38.1219923371333,780.194451284638,107.825696855367));
#71542=CARTESIAN_POINT('Ctrl Pts',(37.9547601499314,780.378227595285,107.867196662891));
#71543=CARTESIAN_POINT('Ctrl Pts',(37.8925536783812,780.475872236695,107.889709764016));
#71544=CARTESIAN_POINT('Ctrl Pts',(37.8011983956067,780.694807928319,107.941223168081));
#71545=CARTESIAN_POINT('Ctrl Pts',(37.7755572834675,780.815533665404,107.9701642364));
#71546=CARTESIAN_POINT('Ctrl Pts',(37.769954637119,781.068558963853,108.031937760385));
#71547=CARTESIAN_POINT('Ctrl Pts',(37.7935051652747,781.198683872671,108.064320940692));
#71548=CARTESIAN_POINT('Ctrl Pts',(37.8908118600368,781.441895243009,108.125910441481));
#71549=CARTESIAN_POINT('Ctrl Pts',(37.9634303911922,781.552718258361,108.154533590756));
#71550=CARTESIAN_POINT('Ctrl Pts',(38.1467671682822,781.738631312653,108.203399195271));
#71551=CARTESIAN_POINT('Ctrl Pts',(38.2549051097159,781.812684561484,108.22333946862));
#71552=CARTESIAN_POINT('Ctrl Pts',(38.449377361593,781.897268171814,108.246811960939));
#71553=CARTESIAN_POINT('Ctrl Pts',(38.5279083013846,781.920896627017,108.253607234217));
#71554=CARTESIAN_POINT('Ctrl Pts',(38.6568967577939,781.943672007042,108.260648257632));
#71555=CARTESIAN_POINT('Ctrl Pts',(38.7058364234343,781.948801804334,108.262417759953));
#71556=CARTESIAN_POINT('Ctrl Pts',(38.7968213338433,781.951914662628,108.264055971153));
#71557=CARTESIAN_POINT('Ctrl Pts',(38.838723164895,781.95084253162,108.264166302565));
#71558=CARTESIAN_POINT('Ctrl Pts',(38.9285392607002,781.943158445415,108.263020921169));
#71559=CARTESIAN_POINT('Ctrl Pts',(38.9762780876931,781.935735056933,108.261555365153));
#71560=CARTESIAN_POINT('Ctrl Pts',(39.0990243848424,781.907870141158,108.255546324818));
#71561=CARTESIAN_POINT('Ctrl Pts',(39.1724825034312,781.88234186469,108.249690030792));
#71562=CARTESIAN_POINT('Ctrl Pts',(39.3645106741623,781.790518890985,108.228062343069));
#71563=CARTESIAN_POINT('Ctrl Pts',(39.4734992058981,781.708941552887,108.208368670797));
#71564=CARTESIAN_POINT('Ctrl Pts',(39.6417942305272,781.520949901741,108.162743628668));
#71565=CARTESIAN_POINT('Ctrl Pts',(39.7041303056591,781.420051168054,108.138179679678));
#71566=CARTESIAN_POINT('Ctrl Pts',(39.7930469243524,781.194622883409,108.083395275582));
#71567=CARTESIAN_POINT('Ctrl Pts',(39.8161856608473,781.07090148787,108.053381528825));
#71568=CARTESIAN_POINT('Ctrl Pts',(39.8145910060359,780.813453807,107.991079118705));
#71569=CARTESIAN_POINT('Ctrl Pts',(39.7866483271373,780.682070359643,107.959366200801));
#71570=CARTESIAN_POINT('Ctrl Pts',(39.680502460119,780.439521693832,107.900731119095));
#71571=CARTESIAN_POINT('Ctrl Pts',(39.6040659813743,780.330365021441,107.874287509353));
#71572=CARTESIAN_POINT('Ctrl Pts',(39.4167249560214,780.151573518842,107.830468416537));
#71573=CARTESIAN_POINT('Ctrl Pts',(39.3093051606854,780.081890568166,107.813103271351));
#71574=CARTESIAN_POINT('Ctrl Pts',(39.1092107426472,779.999803301894,107.791801995607));
#71575=CARTESIAN_POINT('Ctrl Pts',(39.0228489620844,779.976801574484,107.785486260207));
#71576=CARTESIAN_POINT('Ctrl Pts',(38.8879679640875,779.958955767925,107.779787654166));
#71577=CARTESIAN_POINT('Ctrl Pts',(38.8410741021507,779.955956677588,107.778545429889));
#71578=CARTESIAN_POINT('Ctrl Pts',(38.7941252323501,779.956131957018,107.778035528783));
#71579=CARTESIAN_POINT('Ctrl Pts',(38.7940239657454,781.363295832901,109.926921146904));
#71580=CARTESIAN_POINT('Ctrl Pts',(38.9271033661578,781.36379643565,109.925504749551));
#71581=CARTESIAN_POINT('Ctrl Pts',(39.0589168714063,781.339426030814,109.916406030783));
#71582=CARTESIAN_POINT('Ctrl Pts',(39.3066501931785,781.243147914772,109.883523984144));
#71583=CARTESIAN_POINT('Ctrl Pts',(39.419915521759,781.171607115591,109.859889198305));
#71584=CARTESIAN_POINT('Ctrl Pts',(39.6103838098438,780.990699904101,109.801715818852));
#71585=CARTESIAN_POINT('Ctrl Pts',(39.6858212226316,780.883217206252,109.767797720514));
#71586=CARTESIAN_POINT('Ctrl Pts',(39.7890053443797,780.645542422123,109.694733020183));
#71587=CARTESIAN_POINT('Ctrl Pts',(39.8155355248429,780.517612882452,109.656308445813));
#71588=CARTESIAN_POINT('Ctrl Pts',(39.8153290314093,780.259446696781,109.581104571311));
#71589=CARTESIAN_POINT('Ctrl Pts',(39.7889372378603,780.131729598482,109.545052014377));
#71590=CARTESIAN_POINT('Ctrl Pts',(39.6867045289745,779.892704916431,109.479987305234));
#71591=CARTESIAN_POINT('Ctrl Pts',(39.6118483159403,779.78366064126,109.451584439574));
#71592=CARTESIAN_POINT('Ctrl Pts',(39.4234816594619,779.599339561651,109.405894216676));
#71593=CARTESIAN_POINT('Ctrl Pts',(39.3118682787941,779.525676509119,109.388982729106));
#71594=CARTESIAN_POINT('Ctrl Pts',(39.0663780401034,779.423854589174,109.368235081468));
#71595=CARTESIAN_POINT('Ctrl Pts',(38.9349087847057,779.396525332607,109.364541127432));
#71596=CARTESIAN_POINT('Ctrl Pts',(38.7992650647418,779.39436471664,109.36752095019));
#71597=CARTESIAN_POINT('Ctrl Pts',(38.7966442807793,779.394332768564,109.367581084842));
#71598=CARTESIAN_POINT('Ctrl Pts',(38.7940239657454,779.394310614874,109.367643766138));
#71599=CARTESIAN_POINT('Origin',(38.7940239657454,783.999333857892,99.403411420971));
#71600=CARTESIAN_POINT('',(38.7940239657454,782.335917226386,105.610306664459));
#71601=CARTESIAN_POINT('Origin',(38.7940239657454,781.864494995777,105.443690097192));
#71602=CARTESIAN_POINT('',(38.7940239657455,780.86401645488,109.774878989525));
#71603=CARTESIAN_POINT('',(38.7940239657454,784.470756088501,99.5700279882381));
#71604=CARTESIAN_POINT('Ctrl Pts',(38.7940134537644,779.900130022071,109.501181670678));
#71605=CARTESIAN_POINT('Ctrl Pts',(38.7331652254187,779.899685911755,109.502442068218));
#71606=CARTESIAN_POINT('Ctrl Pts',(38.6728198670922,779.909992103199,109.506617340839));
#71607=CARTESIAN_POINT('Ctrl Pts',(38.554769845173,779.952671412073,109.520882982605));
#71608=CARTESIAN_POINT('Ctrl Pts',(38.4987817926341,779.986234012438,109.531255916666));
#71609=CARTESIAN_POINT('Ctrl Pts',(38.4033499215098,780.072528529065,109.556908581401));
#71610=CARTESIAN_POINT('Ctrl Pts',(38.3649085626957,780.124480117025,109.571956667297));
#71611=CARTESIAN_POINT('Ctrl Pts',(38.3110385487116,780.239904350712,109.604916405902));
#71612=CARTESIAN_POINT('Ctrl Pts',(38.2961754871977,780.302280958421,109.622518437702));
#71613=CARTESIAN_POINT('Ctrl Pts',(38.2922864000264,780.429680183009,109.658246329906));
#71614=CARTESIAN_POINT('Ctrl Pts',(38.3035620976856,780.493479633859,109.676029847614));
#71615=CARTESIAN_POINT('Ctrl Pts',(38.3513481199104,780.613367305899,109.70928158051));
#71616=CARTESIAN_POINT('Ctrl Pts',(38.3874751602821,780.668243250305,109.724412540661));
#71617=CARTESIAN_POINT('Ctrl Pts',(38.4796635603617,780.760954307424,109.749677264535));
#71618=CARTESIAN_POINT('Ctrl Pts',(38.5347076160494,780.797957298672,109.759582328796));
#71619=CARTESIAN_POINT('Ctrl Pts',(38.6565040388531,780.849181732395,109.772649652012));
#71620=CARTESIAN_POINT('Ctrl Pts',(38.7220319881178,780.862905639468,109.775680761675));
#71621=CARTESIAN_POINT('Ctrl Pts',(38.8548068665812,780.865010636589,109.774218698247));
#71622=CARTESIAN_POINT('Ctrl Pts',(38.9207215027086,780.85334476714,109.769729672175));
#71623=CARTESIAN_POINT('Ctrl Pts',(39.0437830252023,780.805958802169,109.753726404538));
#71624=CARTESIAN_POINT('Ctrl Pts',(39.0996984050641,780.770725369361,109.742377051878));
#71625=CARTESIAN_POINT('Ctrl Pts',(39.1937617655332,780.681304018546,109.714429983369));
#71626=CARTESIAN_POINT('Ctrl Pts',(39.2309813150243,780.62802482522,109.698119994925));
#71627=CARTESIAN_POINT('Ctrl Pts',(39.2816007843049,780.510309578999,109.66286077316));
#71628=CARTESIAN_POINT('Ctrl Pts',(39.2944278342269,780.447020073884,109.644261590856));
#71629=CARTESIAN_POINT('Ctrl Pts',(39.2936060490897,780.319935487117,109.607738208716));
#71630=CARTESIAN_POINT('Ctrl Pts',(39.2803046369429,780.257381042135,109.590162038697));
#71631=CARTESIAN_POINT('Ctrl Pts',(39.2294872958762,780.140596593304,109.558184273771));
#71632=CARTESIAN_POINT('Ctrl Pts',(39.1924764666662,780.087469683158,109.544082686883));
#71633=CARTESIAN_POINT('Ctrl Pts',(39.099563435551,779.997919820937,109.521177493141));
#71634=CARTESIAN_POINT('Ctrl Pts',(39.0445971580782,779.962297891029,109.51257219115));
#71635=CARTESIAN_POINT('Ctrl Pts',(38.923852863808,779.913433836878,109.501856959151));
#71636=CARTESIAN_POINT('Ctrl Pts',(38.8592616191411,779.900606246017,109.499830133758));
#71637=CARTESIAN_POINT('Ctrl Pts',(38.7940134537644,779.900130022071,109.501181670678));
#71638=CARTESIAN_POINT('Origin',(43.3168648737812,778.988051266838,97.6322545923071));
#71639=CARTESIAN_POINT('',(43.3168648737812,774.257710238126,108.171096695511));
#71640=CARTESIAN_POINT('',(43.3168648737814,776.151024833139,108.504400048628));
#71641=CARTESIAN_POINT('Ctrl Pts',(43.3168648737811,774.257710238126,108.171096695511));
#71642=CARTESIAN_POINT('Ctrl Pts',(43.1997889459331,774.256411461088,108.174771434332));
#71643=CARTESIAN_POINT('Ctrl Pts',(43.0836809340222,774.276907434386,108.181853420389));
#71644=CARTESIAN_POINT('Ctrl Pts',(42.8587797518068,774.361923392078,108.202728140363));
#71645=CARTESIAN_POINT('Ctrl Pts',(42.7533149370578,774.427996104428,108.216658299341));
#71646=CARTESIAN_POINT('Ctrl Pts',(42.5725818214765,774.598386769129,108.249907769786));
#71647=CARTESIAN_POINT('Ctrl Pts',(42.4997983366597,774.701633843668,108.268988797232));
#71648=CARTESIAN_POINT('Ctrl Pts',(42.398003120726,774.931950151518,108.310324525063));
#71649=CARTESIAN_POINT('Ctrl Pts',(42.3707207599739,775.057192487492,108.33224420223));
#71650=CARTESIAN_POINT('Ctrl Pts',(42.3670375822734,775.310927938652,108.376041434313));
#71651=CARTESIAN_POINT('Ctrl Pts',(42.390728083664,775.437135635385,108.397529791516));
#71652=CARTESIAN_POINT('Ctrl Pts',(42.4858363338574,775.671275521423,108.436823330913));
#71653=CARTESIAN_POINT('Ctrl Pts',(42.5556801279478,775.777318844528,108.454316668448));
#71654=CARTESIAN_POINT('Ctrl Pts',(42.7322371250952,775.955721747957,108.48268721344));
#71655=CARTESIAN_POINT('Ctrl Pts',(42.8368789628639,776.026658532097,108.493338344764));
#71656=CARTESIAN_POINT('Ctrl Pts',(43.0677886888812,776.124200473689,108.505821338737));
#71657=CARTESIAN_POINT('Ctrl Pts',(43.1916145190988,776.149916964495,108.507534634318));
#71658=CARTESIAN_POINT('Ctrl Pts',(43.3168648737817,776.151024833139,108.504400048628));
#71659=CARTESIAN_POINT('',(43.3168650111487,776.615095621064,107.191365639192));
#71660=CARTESIAN_POINT('',(43.3168648737812,779.881947439457,97.9481877454437));
#71661=CARTESIAN_POINT('Ctrl Pts',(43.3169432955444,774.709698431335,106.892248594599));
#71662=CARTESIAN_POINT('Ctrl Pts',(43.2916025682699,774.709912156225,106.891637594698));
#71663=CARTESIAN_POINT('Ctrl Pts',(43.2662785675948,774.711151510538,106.891173520281));
#71664=CARTESIAN_POINT('Ctrl Pts',(43.1914778887744,774.717848091664,106.890238296377));
#71665=CARTESIAN_POINT('Ctrl Pts',(43.1423556364478,774.72620547009,106.89019199734));
#71666=CARTESIAN_POINT('Ctrl Pts',(43.0313357479768,774.754234755326,106.891415707021));
#71667=CARTESIAN_POINT('Ctrl Pts',(42.9703725212796,774.776475472245,106.893082917823));
#71668=CARTESIAN_POINT('Ctrl Pts',(42.8038921843578,774.857168113161,106.900603511246));
#71669=CARTESIAN_POINT('Ctrl Pts',(42.7066589318352,774.929552839227,106.908753210904));
#71670=CARTESIAN_POINT('Ctrl Pts',(42.5498762981391,775.099319630695,106.930126868861));
#71671=CARTESIAN_POINT('Ctrl Pts',(42.4892198667589,775.193263454763,106.942786202768));
#71672=CARTESIAN_POINT('Ctrl Pts',(42.3992430673852,775.404589368925,106.972970371438));
#71673=CARTESIAN_POINT('Ctrl Pts',(42.3732901755161,775.521580003357,106.990560624007));
#71674=CARTESIAN_POINT('Ctrl Pts',(42.3650763894248,775.766564702822,107.029159607396));
#71675=CARTESIAN_POINT('Ctrl Pts',(42.3859669946615,775.892605645028,107.049978821053));
#71676=CARTESIAN_POINT('Ctrl Pts',(42.4753790497857,776.126867070568,107.090377825187));
#71677=CARTESIAN_POINT('Ctrl Pts',(42.5422302186713,776.23318554235,107.109590038852));
#71678=CARTESIAN_POINT('Ctrl Pts',(42.7123975957046,776.411983125607,107.143434630939));
#71679=CARTESIAN_POINT('Ctrl Pts',(42.813289673547,776.483334619936,107.157809112372));
#71680=CARTESIAN_POINT('Ctrl Pts',(42.9976768306654,776.565590843421,107.175901933663));
#71681=CARTESIAN_POINT('Ctrl Pts',(43.0737952876244,776.588611330745,107.181514182836));
#71682=CARTESIAN_POINT('Ctrl Pts',(43.2050472441892,776.610831894175,107.18819191073));
#71683=CARTESIAN_POINT('Ctrl Pts',(43.2587849691808,776.615268834182,107.190126376709));
#71684=CARTESIAN_POINT('Ctrl Pts',(43.3368949521302,776.615048573204,107.191795193994));
#71685=CARTESIAN_POINT('Ctrl Pts',(43.3611452981077,776.614048983843,107.192153792773));
#71686=CARTESIAN_POINT('Ctrl Pts',(43.4380116491318,776.607922795436,107.192785236627));
#71687=CARTESIAN_POINT('Ctrl Pts',(43.4902448310117,776.599333853516,107.192458039042));
#71688=CARTESIAN_POINT('Ctrl Pts',(43.6143666224452,776.56814802355,107.189859135102));
#71689=CARTESIAN_POINT('Ctrl Pts',(43.6847685628978,776.54128895514,107.186834684274));
#71690=CARTESIAN_POINT('Ctrl Pts',(43.8636259881094,776.447702018633,107.17496477402));
#71691=CARTESIAN_POINT('Ctrl Pts',(43.9629224883099,776.367243756333,107.163671038405));
#71692=CARTESIAN_POINT('Ctrl Pts',(44.1160839257071,776.182866466268,107.136709568032));
#71693=CARTESIAN_POINT('Ctrl Pts',(44.172354506465,776.083624610569,107.121822623364));
#71694=CARTESIAN_POINT('Ctrl Pts',(44.2503317040309,775.863170793678,107.08831273556));
#71695=CARTESIAN_POINT('Ctrl Pts',(44.2687223641544,775.742707419449,107.069779404458));
#71696=CARTESIAN_POINT('Ctrl Pts',(44.259612352217,775.493922253699,107.031097509907));
#71697=CARTESIAN_POINT('Ctrl Pts',(44.2292053396555,775.367804321865,107.011264511283));
#71698=CARTESIAN_POINT('Ctrl Pts',(44.1217941034704,775.138808117992,106.974497329291));
#71699=CARTESIAN_POINT('Ctrl Pts',(44.0472299995365,775.037383156253,106.95781273974));
#71700=CARTESIAN_POINT('Ctrl Pts',(43.8645121774589,774.871228617837,106.92915962184));
#71701=CARTESIAN_POINT('Ctrl Pts',(43.7589390086845,774.807351301255,106.91736525756));
#71702=CARTESIAN_POINT('Ctrl Pts',(43.571472191739,774.739427657388,106.902928350702));
#71703=CARTESIAN_POINT('Ctrl Pts',(43.4962200622162,774.722243139992,106.898576271112));
#71704=CARTESIAN_POINT('Ctrl Pts',(43.3855168802414,774.710999060835,106.894170355902));
#71705=CARTESIAN_POINT('Ctrl Pts',(43.3512401635335,774.709409169933,106.893075539411));
#71706=CARTESIAN_POINT('Ctrl Pts',(43.3169432955444,774.709698431335,106.892248594599));
#71707=CARTESIAN_POINT('Ctrl Pts',(43.3168648737817,776.151024833139,108.504400048628));
#71708=CARTESIAN_POINT('Ctrl Pts',(43.3169501287949,776.151025587239,108.504397914989));
#71709=CARTESIAN_POINT('Ctrl Pts',(43.3170353844682,776.151026329935,108.504395779109));
#71710=CARTESIAN_POINT('Ctrl Pts',(43.3171206407995,776.151027061225,108.504393640989));
#71711=CARTESIAN_POINT('Ctrl Pts',(43.4355136039576,776.152042581919,108.501424496826));
#71712=CARTESIAN_POINT('Ctrl Pts',(43.5528642729635,776.131046769687,108.494177999891));
#71713=CARTESIAN_POINT('Ctrl Pts',(43.7797464004146,776.044763126869,108.471240762669));
#71714=CARTESIAN_POINT('Ctrl Pts',(43.8860081083987,775.977869599269,108.455327829206));
#71715=CARTESIAN_POINT('Ctrl Pts',(44.0658810353981,775.806796758588,108.417518461765));
#71716=CARTESIAN_POINT('Ctrl Pts',(44.1375564214189,775.704304443765,108.396013449576));
#71717=CARTESIAN_POINT('Ctrl Pts',(44.2370134195534,775.476452463699,108.350677577371));
#71718=CARTESIAN_POINT('Ctrl Pts',(44.263369533438,775.353125065724,108.327285004586));
#71719=CARTESIAN_POINT('Ctrl Pts',(44.2664140159794,775.101257501571,108.2820056959));
#71720=CARTESIAN_POINT('Ctrl Pts',(44.2423238519086,774.975022664943,108.260573808016));
#71721=CARTESIAN_POINT('Ctrl Pts',(44.1469186354503,774.741289399089,108.223349987931));
#71722=CARTESIAN_POINT('Ctrl Pts',(44.0774089508596,774.635485043324,108.207767424861));
#71723=CARTESIAN_POINT('Ctrl Pts',(43.9029192305033,774.45765507229,108.183950529821));
#71724=CARTESIAN_POINT('Ctrl Pts',(43.8001315532888,774.386653024556,108.17579414174));
#71725=CARTESIAN_POINT('Ctrl Pts',(43.5745041424813,774.288294926036,108.167394418138));
#71726=CARTESIAN_POINT('Ctrl Pts',(43.4541499450961,774.261311437038,108.167116988508));
#71727=CARTESIAN_POINT('Ctrl Pts',(43.3269438906221,774.257862392255,108.170786729149));
#71728=CARTESIAN_POINT('Ctrl Pts',(43.3219034854246,774.257766133759,108.170938545307));
#71729=CARTESIAN_POINT('Ctrl Pts',(43.3168648737811,774.257710238126,108.171096695511));
#71730=CARTESIAN_POINT('Origin',(43.3168648737812,778.988051266838,97.6322545923071));
#71731=CARTESIAN_POINT('',(43.3168648737812,777.324634635332,103.839149835795));
#71732=CARTESIAN_POINT('Origin',(43.3168648737812,776.853212404723,103.672533268528));
#71733=CARTESIAN_POINT('',(43.3168648737813,775.706104888437,108.418591821086));
#71734=CARTESIAN_POINT('',(43.3168648737812,779.459473497447,97.7988711595741));
#71735=CARTESIAN_POINT('Ctrl Pts',(43.3168503266343,774.70758740764,108.242879031684));
#71736=CARTESIAN_POINT('Ctrl Pts',(43.2550682844173,774.706935028639,108.244730256454));
#71737=CARTESIAN_POINT('Ctrl Pts',(43.193823506189,774.717759010054,108.248471851981));
#71738=CARTESIAN_POINT('Ctrl Pts',(43.0752989715982,774.762508820301,108.259670623897));
#71739=CARTESIAN_POINT('Ctrl Pts',(43.0197247862468,774.79724439007,108.267209108575));
#71740=CARTESIAN_POINT('Ctrl Pts',(42.9245342076126,774.886766279282,108.2852145568));
#71741=CARTESIAN_POINT('Ctrl Pts',(42.8861964492455,774.940962188479,108.295546493636));
#71742=CARTESIAN_POINT('Ctrl Pts',(42.8322758868149,775.062406211994,108.317906051551));
#71743=CARTESIAN_POINT('Ctrl Pts',(42.8178102587603,775.128756576984,108.329753951295));
#71744=CARTESIAN_POINT('Ctrl Pts',(42.8160129070241,775.262862992254,108.353142511379));
#71745=CARTESIAN_POINT('Ctrl Pts',(42.8285836005518,775.329393357407,108.364473180029));
#71746=CARTESIAN_POINT('Ctrl Pts',(42.8789928241664,775.453201577646,108.385013777053));
#71747=CARTESIAN_POINT('Ctrl Pts',(42.9161449838627,775.509428205282,108.394053274978));
#71748=CARTESIAN_POINT('Ctrl Pts',(43.0101178256596,775.603988858005,108.408505009329));
#71749=CARTESIAN_POINT('Ctrl Pts',(43.0658721367692,775.641536067018,108.413800454879));
#71750=CARTESIAN_POINT('Ctrl Pts',(43.1872698849458,775.692169429266,108.419674199264));
#71751=CARTESIAN_POINT('Ctrl Pts',(43.2513862686608,775.70540853512,108.420318980157));
#71752=CARTESIAN_POINT('Ctrl Pts',(43.3809545301484,775.706787231306,108.416901440254));
#71753=CARTESIAN_POINT('Ctrl Pts',(43.4450683019003,775.694967030789,108.41288325223));
#71754=CARTESIAN_POINT('Ctrl Pts',(43.5659481755348,775.647244426328,108.400577172761));
#71755=CARTESIAN_POINT('Ctrl Pts',(43.6212926952439,775.611458228687,108.39235270157));
#71756=CARTESIAN_POINT('Ctrl Pts',(43.7153285625206,775.520007538906,108.372796375814));
#71757=CARTESIAN_POINT('Ctrl Pts',(43.7527737650026,775.465010586555,108.361628112382));
#71758=CARTESIAN_POINT('Ctrl Pts',(43.8039815725099,775.343242807349,108.338041781264));
#71759=CARTESIAN_POINT('Ctrl Pts',(43.8170502786639,775.277577267703,108.325849305159));
#71760=CARTESIAN_POINT('Ctrl Pts',(43.8166738351301,775.144318022938,108.302185190506));
#71761=CARTESIAN_POINT('Ctrl Pts',(43.802996267905,775.077944109442,108.290940650918));
#71762=CARTESIAN_POINT('Ctrl Pts',(43.7508744080774,774.955503435521,108.271265687373));
#71763=CARTESIAN_POINT('Ctrl Pts',(43.7134089410029,774.900319559939,108.262951444371));
#71764=CARTESIAN_POINT('Ctrl Pts',(43.6199682076064,774.808010507736,108.250148038055));
#71765=CARTESIAN_POINT('Ctrl Pts',(43.5651553995317,774.771439202618,108.245711149419));
#71766=CARTESIAN_POINT('Ctrl Pts',(43.4452175081836,774.721463704055,108.241114382368));
#71767=CARTESIAN_POINT('Ctrl Pts',(43.3814051537084,774.708269065483,108.240944723743));
#71768=CARTESIAN_POINT('Ctrl Pts',(43.3168503266343,774.70758740764,108.242879031684));
#71769=CARTESIAN_POINT('Origin',(29.1099152851011,787.750281848153,100.729123357227));
#71770=CARTESIAN_POINT('',(29.1099152851011,783.147271975424,110.687659104939));
#71771=CARTESIAN_POINT('',(29.1099152851012,785.112934988763,111.256336278119));
#71772=CARTESIAN_POINT('Ctrl Pts',(29.1099152851011,783.147271975424,110.687659104939));
#71773=CARTESIAN_POINT('Ctrl Pts',(28.9787483332411,783.145433331028,110.692861335767));
#71774=CARTESIAN_POINT('Ctrl Pts',(28.8487346582336,783.168046709765,110.70469804998));
#71775=CARTESIAN_POINT('Ctrl Pts',(28.6032732367854,783.260735106295,110.74031249655));
#71776=CARTESIAN_POINT('Ctrl Pts',(28.4905625898534,783.330655829655,110.763922498915));
#71777=CARTESIAN_POINT('Ctrl Pts',(28.2993559915101,783.509432962389,110.820051965965));
#71778=CARTESIAN_POINT('Ctrl Pts',(28.2229742882335,783.6167202065,110.85206760072));
#71779=CARTESIAN_POINT('Ctrl Pts',(28.1175997654022,783.854467596885,110.920842468896));
#71780=CARTESIAN_POINT('Ctrl Pts',(28.0898122652965,783.98268545845,110.956961640161));
#71781=CARTESIAN_POINT('Ctrl Pts',(28.0872917990849,784.242317633029,111.029077359832));
#71782=CARTESIAN_POINT('Ctrl Pts',(28.1125710043552,784.371250162536,111.064400207693));
#71783=CARTESIAN_POINT('Ctrl Pts',(28.2140091567208,784.61408460271,111.130437573787));
#71784=CARTESIAN_POINT('Ctrl Pts',(28.2898721071226,784.725354188797,111.160436223417));
#71785=CARTESIAN_POINT('Ctrl Pts',(28.4810730060538,784.911526158526,111.209964033082));
#71786=CARTESIAN_POINT('Ctrl Pts',(28.5940093658696,784.985059931315,111.229130498158));
#71787=CARTESIAN_POINT('Ctrl Pts',(28.8424384690884,785.085710925819,111.253707018508));
#71788=CARTESIAN_POINT('Ctrl Pts',(28.975406862261,785.112001002839,111.258904477997));
#71789=CARTESIAN_POINT('Ctrl Pts',(29.1097268752779,785.112933697117,111.256339880534));
#71790=CARTESIAN_POINT('Ctrl Pts',(29.1097896788289,785.112934133213,111.256338681414));
#71791=CARTESIAN_POINT('Ctrl Pts',(29.1098524821037,785.112934563762,111.256337480609));
#71792=CARTESIAN_POINT('Ctrl Pts',(29.1099152851014,785.112934988763,111.256336278119));
#71793=CARTESIAN_POINT('',(29.1099152827985,785.751926387763,109.448384310331));
#71794=CARTESIAN_POINT('',(29.1099152851011,788.713310988396,101.069490440295));
#71795=CARTESIAN_POINT('Ctrl Pts',(29.1098761559961,783.783777209309,108.886741454917));
#71796=CARTESIAN_POINT('Ctrl Pts',(29.0202287505466,783.782651395279,108.889937120993));
#71797=CARTESIAN_POINT('Ctrl Pts',(28.9309471570873,783.792927405918,108.896289886262));
#71798=CARTESIAN_POINT('Ctrl Pts',(28.7990746032532,783.82557523518,108.910478138312));
#71799=CARTESIAN_POINT('Ctrl Pts',(28.7547021140882,783.839790686475,108.916140937024));
#71800=CARTESIAN_POINT('Ctrl Pts',(28.693668843277,783.864005294673,108.925208871393));
#71801=CARTESIAN_POINT('Ctrl Pts',(28.6760225836916,783.871586815564,108.927989911544));
#71802=CARTESIAN_POINT('Ctrl Pts',(28.6430773370826,783.886853839333,108.933487141561));
#71803=CARTESIAN_POINT('Ctrl Pts',(28.6277350233886,783.894438495488,108.936177399633));
#71804=CARTESIAN_POINT('Ctrl Pts',(28.5793647875507,783.919888781342,108.945080746947));
#71805=CARTESIAN_POINT('Ctrl Pts',(28.5471872541053,783.939173519489,108.951649044907));
#71806=CARTESIAN_POINT('Ctrl Pts',(28.4699608361721,783.991521328781,108.969076731593));
#71807=CARTESIAN_POINT('Ctrl Pts',(28.4265443682553,784.026590968006,108.980421608421));
#71808=CARTESIAN_POINT('Ctrl Pts',(28.3001221336293,784.147626083841,109.018661655491));
#71809=CARTESIAN_POINT('Ctrl Pts',(28.2301070425694,784.244716468015,109.048106650153));
#71810=CARTESIAN_POINT('Ctrl Pts',(28.132682303859,784.451124605322,109.108898530641));
#71811=CARTESIAN_POINT('Ctrl Pts',(28.1033621835979,784.55769513117,109.139553905886));
#71812=CARTESIAN_POINT('Ctrl Pts',(28.0815893348599,784.784169783905,109.203527275506));
#71813=CARTESIAN_POINT('Ctrl Pts',(28.0922331544423,784.902673246739,109.236368840142));
#71814=CARTESIAN_POINT('Ctrl Pts',(28.1584798739867,785.138465004452,109.300651731836));
#71815=CARTESIAN_POINT('Ctrl Pts',(28.2165006037512,785.252995534348,109.331270729447));
#71816=CARTESIAN_POINT('Ctrl Pts',(28.3766173930253,785.458603801005,109.384974672869));
#71817=CARTESIAN_POINT('Ctrl Pts',(28.4786090373902,785.546735662626,109.407239684852));
#71818=CARTESIAN_POINT('Ctrl Pts',(28.7084761035384,785.677932617153,109.438371460242));
#71819=CARTESIAN_POINT('Ctrl Pts',(28.8333423905459,785.721061493646,109.447326013261));
#71820=CARTESIAN_POINT('Ctrl Pts',(29.0806312716797,785.757873925994,109.450955844317));
#71821=CARTESIAN_POINT('Ctrl Pts',(29.200274304189,785.755550876228,109.446862986797));
#71822=CARTESIAN_POINT('Ctrl Pts',(29.3711115561848,785.723209312974,109.432419198064));
#71823=CARTESIAN_POINT('Ctrl Pts',(29.4245786574587,785.708632186141,109.426579559483));
#71824=CARTESIAN_POINT('Ctrl Pts',(29.5119641176442,785.67716942096,109.414763994875));
#71825=CARTESIAN_POINT('Ctrl Pts',(29.5466365298866,785.662506178878,109.409427815552));
#71826=CARTESIAN_POINT('Ctrl Pts',(29.5956714241808,785.638527670092,109.400916731226));
#71827=CARTESIAN_POINT('Ctrl Pts',(29.6107798755938,785.630666971371,109.398153735095));
#71828=CARTESIAN_POINT('Ctrl Pts',(29.6599117960034,785.603524165089,109.388698536729));
#71829=CARTESIAN_POINT('Ctrl Pts',(29.6929569172784,785.582698766549,109.381574653211));
#71830=CARTESIAN_POINT('Ctrl Pts',(29.7745389746346,785.524427593713,109.361950288889));
#71831=CARTESIAN_POINT('Ctrl Pts',(29.8208810640803,785.484435772604,109.348755521566));
#71832=CARTESIAN_POINT('Ctrl Pts',(29.9517215936083,785.348516600507,109.304700512644));
#71833=CARTESIAN_POINT('Ctrl Pts',(30.0208613487702,785.240743531152,109.270790110757));
#71834=CARTESIAN_POINT('Ctrl Pts',(30.1074039202553,785.018976884056,109.20297685208));
#71835=CARTESIAN_POINT('Ctrl Pts',(30.1291758558536,784.908726368771,109.170019179988));
#71836=CARTESIAN_POINT('Ctrl Pts',(30.1333197859797,784.677076963654,109.102504484767));
#71837=CARTESIAN_POINT('Ctrl Pts',(30.1125607153376,784.55741217819,109.068586766506));
#71838=CARTESIAN_POINT('Ctrl Pts',(30.024295720814,784.322417252564,109.004138224049));
#71839=CARTESIAN_POINT('Ctrl Pts',(29.954352866702,784.210271276886,108.974647794333));
#71840=CARTESIAN_POINT('Ctrl Pts',(29.7827806717245,784.027129496309,108.929036325172));
#71841=CARTESIAN_POINT('Ctrl Pts',(29.6862569985383,783.954587292616,108.91223455758));
#71842=CARTESIAN_POINT('Ctrl Pts',(29.5153336234898,783.867209843521,108.894253133582));
#71843=CARTESIAN_POINT('Ctrl Pts',(29.4483240993924,783.841142549999,108.889548585355));
#71844=CARTESIAN_POINT('Ctrl Pts',(29.2914060860322,783.797796476869,108.883536508149));
#71845=CARTESIAN_POINT('Ctrl Pts',(29.2008614875201,783.784919825343,108.883498095715));
#71846=CARTESIAN_POINT('Ctrl Pts',(29.1098761559961,783.783777209309,108.886741454917));
#71847=CARTESIAN_POINT('Ctrl Pts',(29.1099152851014,785.112934988763,111.256336278119));
#71848=CARTESIAN_POINT('Ctrl Pts',(29.2417187854962,785.113826929972,111.253812634032));
#71849=CARTESIAN_POINT('Ctrl Pts',(29.3723014451918,785.090289281962,111.243847695462));
#71850=CARTESIAN_POINT('Ctrl Pts',(29.6195013119506,784.995965598073,111.209284433721));
#71851=CARTESIAN_POINT('Ctrl Pts',(29.7332620403393,784.924991413875,111.184676204043));
#71852=CARTESIAN_POINT('Ctrl Pts',(29.9246539146689,784.745029752424,111.124318273611));
#71853=CARTESIAN_POINT('Ctrl Pts',(30.000521891227,784.63793575237,111.089210763936));
#71854=CARTESIAN_POINT('Ctrl Pts',(30.1041612235064,784.401495571549,111.013792466794));
#71855=CARTESIAN_POINT('Ctrl Pts',(30.1309721341953,784.274500123432,110.974249691163));
#71856=CARTESIAN_POINT('Ctrl Pts',(30.1316710389441,784.016053870509,110.896410747585));
#71857=CARTESIAN_POINT('Ctrl Pts',(30.105110186717,783.88715069737,110.858919261452));
#71858=CARTESIAN_POINT('Ctrl Pts',(30.0019418635203,783.64717626582,110.792216295676));
#71859=CARTESIAN_POINT('Ctrl Pts',(29.9268641669351,783.538233544062,110.763561784645));
#71860=CARTESIAN_POINT('Ctrl Pts',(29.7379565707489,783.353748398758,110.718399153832));
#71861=CARTESIAN_POINT('Ctrl Pts',(29.6259787794184,783.279879865624,110.702282096702));
#71862=CARTESIAN_POINT('Ctrl Pts',(29.3799365456471,783.177551001541,110.684210113816));
#71863=CARTESIAN_POINT('Ctrl Pts',(29.2482733293954,783.149880421077,110.682355112769));
#71864=CARTESIAN_POINT('Ctrl Pts',(29.1133855354354,783.147324894626,110.687522642653));
#71865=CARTESIAN_POINT('Ctrl Pts',(29.1116503093094,783.147296296281,110.687590291901));
#71866=CARTESIAN_POINT('Ctrl Pts',(29.1099152851011,783.147271975424,110.687659104939));
#71867=CARTESIAN_POINT('Origin',(29.1099152851011,787.750281848153,100.729123357227));
#71868=CARTESIAN_POINT('',(29.1099152851011,786.086865216647,106.936018600716));
#71869=CARTESIAN_POINT('Origin',(29.1099152851011,785.615442986038,106.769402033449));
#71870=CARTESIAN_POINT('',(29.1099152851012,784.6139997576,111.103320397167));
#71871=CARTESIAN_POINT('',(29.1099152851011,788.221704078762,100.895739924495));
#71872=CARTESIAN_POINT('Ctrl Pts',(29.1096415055408,783.651752382614,110.824985779127));
#71873=CARTESIAN_POINT('Ctrl Pts',(29.0494213811045,783.651046473984,110.827082017624));
#71874=CARTESIAN_POINT('Ctrl Pts',(28.9896823355468,783.660840914554,110.832115293449));
#71875=CARTESIAN_POINT('Ctrl Pts',(28.8721818261715,783.702224124192,110.848151793531));
#71876=CARTESIAN_POINT('Ctrl Pts',(28.8161719795131,783.735174074544,110.859463041959));
#71877=CARTESIAN_POINT('Ctrl Pts',(28.7205510696045,783.82032487939,110.886809468527));
#71878=CARTESIAN_POINT('Ctrl Pts',(28.681947966405,783.871751384858,110.902592576135));
#71879=CARTESIAN_POINT('Ctrl Pts',(28.6275938724069,783.98638894001,110.936708264004));
#71880=CARTESIAN_POINT('Ctrl Pts',(28.6124462165888,784.048514793948,110.954718856745));
#71881=CARTESIAN_POINT('Ctrl Pts',(28.6079643042431,784.175066905785,110.990715434349));
#71882=CARTESIAN_POINT('Ctrl Pts',(28.6186960189196,784.238278715916,111.008359168119));
#71883=CARTESIAN_POINT('Ctrl Pts',(28.6652534994828,784.358260734604,111.041294172221));
#71884=CARTESIAN_POINT('Ctrl Pts',(28.7010478762961,784.413712623193,111.056215116982));
#71885=CARTESIAN_POINT('Ctrl Pts',(28.792739146943,784.507606755541,111.080806383023));
#71886=CARTESIAN_POINT('Ctrl Pts',(28.8475916214523,784.545236136081,111.090267084053));
#71887=CARTESIAN_POINT('Ctrl Pts',(28.969089050239,784.597718776362,111.102322899475));
#71888=CARTESIAN_POINT('Ctrl Pts',(29.034495610272,784.612106187238,111.104810471845));
#71889=CARTESIAN_POINT('Ctrl Pts',(29.1672292978429,784.61557840484,111.102229458831));
#71890=CARTESIAN_POINT('Ctrl Pts',(29.2332258694233,784.604600092217,111.09717403284));
#71891=CARTESIAN_POINT('Ctrl Pts',(29.3567084403629,784.558499090403,111.0800019596));
#71892=CARTESIAN_POINT('Ctrl Pts',(29.412945752427,784.523824651056,111.068052336922));
#71893=CARTESIAN_POINT('Ctrl Pts',(29.5077136648204,784.435364605945,111.038885690367));
#71894=CARTESIAN_POINT('Ctrl Pts',(29.5453165048092,784.382491446767,111.021970912703));
#71895=CARTESIAN_POINT('Ctrl Pts',(29.5966542486413,784.265553629841,110.985598212997));
#71896=CARTESIAN_POINT('Ctrl Pts',(29.6098782986424,784.202659042162,110.966508949068));
#71897=CARTESIAN_POINT('Ctrl Pts',(29.6099522833995,784.075011066491,110.928847950516));
#71898=CARTESIAN_POINT('Ctrl Pts',(29.5966825891023,784.011526446793,110.91065924973));
#71899=CARTESIAN_POINT('Ctrl Pts',(29.5455296138344,783.893837807457,110.878130449407));
#71900=CARTESIAN_POINT('Ctrl Pts',(29.5085107025099,783.840634192522,110.864048011921));
#71901=CARTESIAN_POINT('Ctrl Pts',(29.4155234533503,783.750778963925,110.841586980028));
#71902=CARTESIAN_POINT('Ctrl Pts',(29.3604736528929,783.714946347179,110.833407470084));
#71903=CARTESIAN_POINT('Ctrl Pts',(29.2395914942158,783.665615214772,110.8239378139));
#71904=CARTESIAN_POINT('Ctrl Pts',(29.1749437335729,783.652517864365,110.822712634632));
#71905=CARTESIAN_POINT('Ctrl Pts',(29.1096415055408,783.651752382614,110.824985779127));
#71906=CARTESIAN_POINT('Origin',(32.4288564564431,781.96190260128,98.6833142766745));
#71907=CARTESIAN_POINT('',(32.4288564564431,777.234399375335,109.214127146458));
#71908=CARTESIAN_POINT('',(32.4288564564448,779.121595087564,109.564743167926));
#71909=CARTESIAN_POINT('Ctrl Pts',(32.4288564564431,777.234399375335,109.214127146458));
#71910=CARTESIAN_POINT('Ctrl Pts',(32.3101547171348,777.231595722789,109.222059755793));
#71911=CARTESIAN_POINT('Ctrl Pts',(32.1923352143316,777.251103332821,109.233757555294));
#71912=CARTESIAN_POINT('Ctrl Pts',(31.9671822172065,777.334478737508,109.263847146364));
#71913=CARTESIAN_POINT('Ctrl Pts',(31.8627895610585,777.398855105508,109.282112857103));
#71914=CARTESIAN_POINT('Ctrl Pts',(31.6837661754366,777.565695961093,109.323075248878));
#71915=CARTESIAN_POINT('Ctrl Pts',(31.6116352422431,777.667034631619,109.345412732826));
#71916=CARTESIAN_POINT('Ctrl Pts',(31.5103077358069,777.89417146595,109.39175065861));
#71917=CARTESIAN_POINT('Ctrl Pts',(31.4830297368684,778.018152703095,109.415323694428));
#71918=CARTESIAN_POINT('Ctrl Pts',(31.4787580499234,778.271183927327,109.46079925837));
#71919=CARTESIAN_POINT('Ctrl Pts',(31.5023951125465,778.397931822898,109.4822676082));
#71920=CARTESIAN_POINT('Ctrl Pts',(31.5975982095106,778.633539800542,109.519820243943));
#71921=CARTESIAN_POINT('Ctrl Pts',(31.6676565991942,778.740519737735,109.535640456385));
#71922=CARTESIAN_POINT('Ctrl Pts',(31.8445008416407,778.920733700444,109.55940470734));
#71923=CARTESIAN_POINT('Ctrl Pts',(31.949202460396,778.992660241787,109.567207699515));
#71924=CARTESIAN_POINT('Ctrl Pts',(32.1799990128611,779.09228918265,109.573273818901));
#71925=CARTESIAN_POINT('Ctrl Pts',(32.3036731310029,779.11920400299,109.57150846409));
#71926=CARTESIAN_POINT('Ctrl Pts',(32.4288564564465,779.121595087564,109.564743167926));
#71927=CARTESIAN_POINT('',(32.4288565295822,779.758468006617,107.762785193163));
#71928=CARTESIAN_POINT('',(32.4288564564431,782.855798773899,98.9992474298111));
#71929=CARTESIAN_POINT('Ctrl Pts',(32.4289098699438,777.886461794448,107.369192249501));
#71930=CARTESIAN_POINT('Ctrl Pts',(32.3637578802491,777.885807238946,107.371033223316));
#71931=CARTESIAN_POINT('Ctrl Pts',(32.2987643707776,777.891796036555,107.374231026386));
#71932=CARTESIAN_POINT('Ctrl Pts',(32.2096473094209,777.909320985861,107.38052044553));
#71933=CARTESIAN_POINT('Ctrl Pts',(32.1845614936939,777.915323247997,107.382509568572));
#71934=CARTESIAN_POINT('Ctrl Pts',(32.1431917498704,777.927021424797,107.386158045918));
#71935=CARTESIAN_POINT('Ctrl Pts',(32.1267554856739,777.932156741984,107.387707344574));
#71936=CARTESIAN_POINT('Ctrl Pts',(32.10308670609,777.940266420243,107.390084632186));
#71937=CARTESIAN_POINT('Ctrl Pts',(32.0957308859324,777.942888993599,107.390844370931));
#71938=CARTESIAN_POINT('Ctrl Pts',(32.0711923148809,777.9519818915,107.393449256827));
#71939=CARTESIAN_POINT('Ctrl Pts',(32.0541734470669,777.958858947601,107.395372687863));
#71940=CARTESIAN_POINT('Ctrl Pts',(32.0091600065378,777.978594060938,107.400776631465));
#71941=CARTESIAN_POINT('Ctrl Pts',(31.981595864868,777.992327796017,107.404423470151));
#71942=CARTESIAN_POINT('Ctrl Pts',(31.86030555755,778.060382594237,107.422034338184));
#71943=CARTESIAN_POINT('Ctrl Pts',(31.7760833968559,778.129138626915,107.438671915095));
#71944=CARTESIAN_POINT('Ctrl Pts',(31.6416384373393,778.284589931715,107.4746810714));
#71945=CARTESIAN_POINT('Ctrl Pts',(31.5898952076319,778.368154494824,107.493450566722));
#71946=CARTESIAN_POINT('Ctrl Pts',(31.5106696841909,778.557436045641,107.534958402962));
#71947=CARTESIAN_POINT('Ctrl Pts',(31.4868742502069,778.663182510197,107.557607942895));
#71948=CARTESIAN_POINT('Ctrl Pts',(31.4763124924462,778.886848161771,107.604564602141));
#71949=CARTESIAN_POINT('Ctrl Pts',(31.4928190226874,779.003232442255,107.628475197057));
#71950=CARTESIAN_POINT('Ctrl Pts',(31.5709857690768,779.232823306635,107.674597836214));
#71951=CARTESIAN_POINT('Ctrl Pts',(31.6352662925648,779.342931522523,107.696103966605));
#71952=CARTESIAN_POINT('Ctrl Pts',(31.8012862656198,779.52906909741,107.731049352303));
#71953=CARTESIAN_POINT('Ctrl Pts',(31.9002217088409,779.604351269389,107.744396594242));
#71954=CARTESIAN_POINT('Ctrl Pts',(32.1059129820279,779.705790038944,107.760427952354));
#71955=CARTESIAN_POINT('Ctrl Pts',(32.2080259836926,779.736725755301,107.764252910837));
#71956=CARTESIAN_POINT('Ctrl Pts',(32.4011468680326,779.761890836999,107.76429668748));
#71957=CARTESIAN_POINT('Ctrl Pts',(32.4902427056032,779.76115907177,107.761655079529));
#71958=CARTESIAN_POINT('Ctrl Pts',(32.6084649806787,779.743707004276,107.754577618871));
#71959=CARTESIAN_POINT('Ctrl Pts',(32.6388199915054,779.737709479938,107.752431875471));
#71960=CARTESIAN_POINT('Ctrl Pts',(32.6873290199313,779.725651121272,107.748466994289));
#71961=CARTESIAN_POINT('Ctrl Pts',(32.7056979419549,779.720494503792,107.746837721623));
#71962=CARTESIAN_POINT('Ctrl Pts',(32.7319460767755,779.712267143011,107.744323672343));
#71963=CARTESIAN_POINT('Ctrl Pts',(32.7399662388543,779.709635392808,107.743529986877));
#71964=CARTESIAN_POINT('Ctrl Pts',(32.7654359451088,779.700899982102,107.740927736297));
#71965=CARTESIAN_POINT('Ctrl Pts',(32.7827348481111,779.694396008882,107.739036758963));
#71966=CARTESIAN_POINT('Ctrl Pts',(32.8260733986865,779.676638522689,107.733983026282));
#71967=CARTESIAN_POINT('Ctrl Pts',(32.8518025663583,779.664717926169,107.730684761982));
#71968=CARTESIAN_POINT('Ctrl Pts',(32.9477030907431,779.614924131929,107.717234300634));
#71969=CARTESIAN_POINT('Ctrl Pts',(33.0133099159968,779.569450251953,107.705571309765));
#71970=CARTESIAN_POINT('Ctrl Pts',(33.1422003111067,779.453288462453,107.676912148343));
#71971=CARTESIAN_POINT('Ctrl Pts',(33.2019567319261,779.380150398644,107.659494344002));
#71972=CARTESIAN_POINT('Ctrl Pts',(33.3028562573453,779.209095036935,107.619979831064));
#71973=CARTESIAN_POINT('Ctrl Pts',(33.3401851525365,779.110475622494,107.597855895354));
#71974=CARTESIAN_POINT('Ctrl Pts',(33.3817915100074,778.895969171291,107.551083864768));
#71975=CARTESIAN_POINT('Ctrl Pts',(33.3825159827171,778.781052794483,107.52676400737));
#71976=CARTESIAN_POINT('Ctrl Pts',(33.340615761912,778.54767794391,107.478903837609));
#71977=CARTESIAN_POINT('Ctrl Pts',(33.2950359339541,778.431735421668,107.455999781223));
#71978=CARTESIAN_POINT('Ctrl Pts',(33.1602200989399,778.221636436189,107.416268778882));
#71979=CARTESIAN_POINT('Ctrl Pts',(33.0715905275148,778.129835781634,107.399915221269));
#71980=CARTESIAN_POINT('Ctrl Pts',(32.9032068320337,778.01331196114,107.380924465116));
#71981=CARTESIAN_POINT('Ctrl Pts',(32.8338108035281,777.976810683779,107.375501208513));
#71982=CARTESIAN_POINT('Ctrl Pts',(32.6546820911718,777.908854946885,107.366936997579));
#71983=CARTESIAN_POINT('Ctrl Pts',(32.5423259508394,777.887601239614,107.365987496492));
#71984=CARTESIAN_POINT('Ctrl Pts',(32.4289098699438,777.886461794448,107.369192249501));
#71985=CARTESIAN_POINT('Ctrl Pts',(32.4288564564465,779.121595087564,109.564743167926));
#71986=CARTESIAN_POINT('Ctrl Pts',(32.4290525561669,779.121598833199,109.564732570088));
#71987=CARTESIAN_POINT('Ctrl Pts',(32.4292486595918,779.121602518635,109.564721959994));
#71988=CARTESIAN_POINT('Ctrl Pts',(32.4294447666942,779.121606143867,109.564711337644));
#71989=CARTESIAN_POINT('Ctrl Pts',(32.5479650636094,779.123797107451,109.558291559722));
#71990=CARTESIAN_POINT('Ctrl Pts',(32.6655284664017,779.103957979382,109.547505888086));
#71991=CARTESIAN_POINT('Ctrl Pts',(32.8917401323626,779.020196791546,109.517398336627));
#71992=CARTESIAN_POINT('Ctrl Pts',(32.9973173386712,778.955090411697,109.498006966697));
#71993=CARTESIAN_POINT('Ctrl Pts',(33.1770386812934,778.787130123766,109.453481937324));
#71994=CARTESIAN_POINT('Ctrl Pts',(33.2489783367674,778.685696229256,109.428775728013));
#71995=CARTESIAN_POINT('Ctrl Pts',(33.3485088707922,778.460233422003,109.37799569508));
#71996=CARTESIAN_POINT('Ctrl Pts',(33.3749556280529,778.338418135868,109.352445590819));
#71997=CARTESIAN_POINT('Ctrl Pts',(33.3787327982746,778.089527534902,109.304228213008));
#71998=CARTESIAN_POINT('Ctrl Pts',(33.355459123767,777.964788289699,109.282066930245));
#71999=CARTESIAN_POINT('Ctrl Pts',(33.2610753639977,777.728947207022,109.244377166675));
#72000=CARTESIAN_POINT('Ctrl Pts',(33.1901692203057,777.620221547493,109.22928976029));
#72001=CARTESIAN_POINT('Ctrl Pts',(33.0127108190374,777.438787898314,109.208807515502));
#72002=CARTESIAN_POINT('Ctrl Pts',(32.9088501529068,777.36666055042,109.203300264579));
#72003=CARTESIAN_POINT('Ctrl Pts',(32.6815189326721,777.266530500913,109.20174319306));
#72004=CARTESIAN_POINT('Ctrl Pts',(32.5605210423891,777.238705364035,109.205534243894));
#72005=CARTESIAN_POINT('Ctrl Pts',(32.4348005148754,777.234553739407,109.213732320876));
#72006=CARTESIAN_POINT('Ctrl Pts',(32.4318282089087,777.234469566062,109.213928549946));
#72007=CARTESIAN_POINT('Ctrl Pts',(32.4288564564431,777.234399375335,109.214127146458));
#72008=CARTESIAN_POINT('Origin',(32.4288564564431,781.96190260128,98.6833142766745));
#72009=CARTESIAN_POINT('',(32.4288564564431,780.298485969774,104.890209520163));
#72010=CARTESIAN_POINT('Origin',(32.4288564564431,779.827063739165,104.723592952896));
#72011=CARTESIAN_POINT('',(32.4288564564431,778.677869419194,109.475555874173));
#72012=CARTESIAN_POINT('',(32.4288564564431,782.433324831889,98.8499308439416));
#72013=CARTESIAN_POINT('Ctrl Pts',(32.4290799508113,777.68259233814,109.290674899213));
#72014=CARTESIAN_POINT('Ctrl Pts',(32.3665334453012,777.681150919677,109.294669327409));
#72015=CARTESIAN_POINT('Ctrl Pts',(32.3044660597605,777.691430237481,109.300719408193));
#72016=CARTESIAN_POINT('Ctrl Pts',(32.1857666667416,777.735267561329,109.316547451625));
#72017=CARTESIAN_POINT('Ctrl Pts',(32.1306658993913,777.769142775006,109.326276325882));
#72018=CARTESIAN_POINT('Ctrl Pts',(32.0362583975027,777.856852174475,109.348218096714));
#72019=CARTESIAN_POINT('Ctrl Pts',(31.9982204294419,777.910059217511,109.36023628958));
#72020=CARTESIAN_POINT('Ctrl Pts',(31.9446687192663,778.029416818984,109.385193211902));
#72021=CARTESIAN_POINT('Ctrl Pts',(31.9301864927072,778.094613600829,109.397897869096));
#72022=CARTESIAN_POINT('Ctrl Pts',(31.9276892751721,778.227633723303,109.422265697251));
#72023=CARTESIAN_POINT('Ctrl Pts',(31.9399520972781,778.294234746654,109.433692986043));
#72024=CARTESIAN_POINT('Ctrl Pts',(31.989751865069,778.418596819799,109.453558877717));
#72025=CARTESIAN_POINT('Ctrl Pts',(32.0266601281827,778.475303485784,109.461840561142));
#72026=CARTESIAN_POINT('Ctrl Pts',(32.1201560115448,778.571116454262,109.47407505859));
#72027=CARTESIAN_POINT('Ctrl Pts',(32.1757253581395,778.609454002537,109.477942531954));
#72028=CARTESIAN_POINT('Ctrl Pts',(32.2970438717336,778.661951914601,109.48053467932));
#72029=CARTESIAN_POINT('Ctrl Pts',(32.361330718645,778.676188264655,109.479357549754));
#72030=CARTESIAN_POINT('Ctrl Pts',(32.4910841361272,778.679429649575,109.47205459791));
#72031=CARTESIAN_POINT('Ctrl Pts',(32.5552229102832,778.668592088853,109.466037804857));
#72032=CARTESIAN_POINT('Ctrl Pts',(32.675480520112,778.623066822056,109.449821046499));
#72033=CARTESIAN_POINT('Ctrl Pts',(32.7303336121286,778.588809263881,109.439782109346));
#72034=CARTESIAN_POINT('Ctrl Pts',(32.8246423274275,778.500017133566,109.416725069329));
#72035=CARTESIAN_POINT('Ctrl Pts',(32.8626062374142,778.44589451156,109.403881793554));
#72036=CARTESIAN_POINT('Ctrl Pts',(32.9147824306265,778.325695477516,109.37749955097));
#72037=CARTESIAN_POINT('Ctrl Pts',(32.9283833135647,778.260800967028,109.364230327539));
#72038=CARTESIAN_POINT('Ctrl Pts',(32.9293087524434,778.128738424644,109.339161010214));
#72039=CARTESIAN_POINT('Ctrl Pts',(32.9164313804879,778.062808208154,109.327612231577));
#72040=CARTESIAN_POINT('Ctrl Pts',(32.8655150618067,777.938880686931,109.307896134678));
#72041=CARTESIAN_POINT('Ctrl Pts',(32.8277569141518,777.88207133417,109.299933066946));
#72042=CARTESIAN_POINT('Ctrl Pts',(32.7335263655159,777.787373325686,109.288925300188));
#72043=CARTESIAN_POINT('Ctrl Pts',(32.6784224760383,777.749847132771,109.285847176004));
#72044=CARTESIAN_POINT('Ctrl Pts',(32.5579665365653,777.698144462057,109.284687314585));
#72045=CARTESIAN_POINT('Ctrl Pts',(32.493923646632,777.684086696613,109.28653376479));
#72046=CARTESIAN_POINT('Ctrl Pts',(32.4290799508113,777.68259233814,109.290674899213));
#72047=CARTESIAN_POINT('Origin',(20.4645692803024,793.317622820883,102.696810032682));
#72048=CARTESIAN_POINT('',(20.4645692803024,788.717535272518,112.647077402928));
#72049=CARTESIAN_POINT('',(20.4645692803045,790.678180117724,113.229952900161));
#72050=CARTESIAN_POINT('Ctrl Pts',(20.4645692803024,788.717535272518,112.647077402928));
#72051=CARTESIAN_POINT('Ctrl Pts',(20.3325219374791,788.715078477829,112.654028618235));
#72052=CARTESIAN_POINT('Ctrl Pts',(20.2016382854414,788.737261681635,112.668105133025));
#72053=CARTESIAN_POINT('Ctrl Pts',(19.955921009562,788.829133186696,112.708574079991));
#72054=CARTESIAN_POINT('Ctrl Pts',(19.843625220678,788.898242966989,112.73464303333));
#72055=CARTESIAN_POINT('Ctrl Pts',(19.653225199422,789.075233118174,112.795368281891));
#72056=CARTESIAN_POINT('Ctrl Pts',(19.5771916689324,789.181517184176,112.829456845998));
#72057=CARTESIAN_POINT('Ctrl Pts',(19.472166143186,789.417613506439,112.901588035092));
#72058=CARTESIAN_POINT('Ctrl Pts',(19.4444624805739,789.545202241544,112.938946875231));
#72059=CARTESIAN_POINT('Ctrl Pts',(19.4419466144868,789.804194947771,113.012522195203));
#72060=CARTESIAN_POINT('Ctrl Pts',(19.4672608066609,789.933106481549,113.048043093946));
#72061=CARTESIAN_POINT('Ctrl Pts',(19.5684801551307,790.175513753612,113.113318570561));
#72062=CARTESIAN_POINT('Ctrl Pts',(19.6438367318199,790.286513714994,113.142399952549));
#72063=CARTESIAN_POINT('Ctrl Pts',(19.8344868411345,790.473611921838,113.18989579132));
#72064=CARTESIAN_POINT('Ctrl Pts',(19.9477602472955,790.548015311287,113.207886612269));
#72065=CARTESIAN_POINT('Ctrl Pts',(20.1965535380417,790.649888329027,113.229885608953));
#72066=CARTESIAN_POINT('Ctrl Pts',(20.329457736696,790.676715811939,113.233770000985));
#72067=CARTESIAN_POINT('Ctrl Pts',(20.4637455691717,790.678171506983,113.229976266535));
#72068=CARTESIAN_POINT('Ctrl Pts',(20.4640201446788,790.678174483412,113.229968509566));
#72069=CARTESIAN_POINT('Ctrl Pts',(20.4642947150789,790.678177353655,113.229960720774));
#72070=CARTESIAN_POINT('Ctrl Pts',(20.4645692803066,790.678180117724,113.229952900161));
#72071=CARTESIAN_POINT('',(20.4645692794436,791.316321136848,111.424406983493));
#72072=CARTESIAN_POINT('',(20.4645692803024,794.280651961126,103.037177115749));
#72073=CARTESIAN_POINT('Ctrl Pts',(19.8034793393769,789.575990153271,110.94679009387));
#72074=CARTESIAN_POINT('Ctrl Pts',(19.7019570676491,789.657262245375,110.97551440113));
#72075=CARTESIAN_POINT('Ctrl Pts',(19.6182946642219,789.757180409438,111.008511950969));
#72076=CARTESIAN_POINT('Ctrl Pts',(19.4960576281591,789.982964085745,111.079459916268));
#72077=CARTESIAN_POINT('Ctrl Pts',(19.4586768930075,790.106625866136,111.116723594058));
#72078=CARTESIAN_POINT('Ctrl Pts',(19.4353986127253,790.361967455207,111.191117472984));
#72079=CARTESIAN_POINT('Ctrl Pts',(19.4499511871445,790.491225300991,111.227539736259));
#72080=CARTESIAN_POINT('Ctrl Pts',(19.5298918348331,790.738128191629,111.295038853781));
#72081=CARTESIAN_POINT('Ctrl Pts',(19.594740179245,790.853367006595,111.325455221171));
#72082=CARTESIAN_POINT('Ctrl Pts',(19.7666919636577,791.053765611051,111.376187043996));
#72083=CARTESIAN_POINT('Ctrl Pts',(19.8721962464135,791.13697621735,111.39600731711));
#72084=CARTESIAN_POINT('Ctrl Pts',(20.109020464352,791.259173362915,111.42198658606));
#72085=CARTESIAN_POINT('Ctrl Pts',(20.2378323791516,791.297408288582,111.428019856243));
#72086=CARTESIAN_POINT('Ctrl Pts',(20.5046047909829,791.324600450561,111.425226084446));
#72087=CARTESIAN_POINT('Ctrl Pts',(20.6400225102791,791.312656919593,111.416227096002));
#72088=CARTESIAN_POINT('Ctrl Pts',(20.8977666698177,791.238874182027,111.383658883735));
#72089=CARTESIAN_POINT('Ctrl Pts',(21.0175013272838,791.177693561985,111.36038410836));
#72090=CARTESIAN_POINT('Ctrl Pts',(21.2235374007743,791.014756398011,111.302700430138));
#72091=CARTESIAN_POINT('Ctrl Pts',(21.3081427937904,790.915002100251,111.268968630032));
#72092=CARTESIAN_POINT('Ctrl Pts',(21.4318962781407,790.689528973368,111.195459831531));
#72093=CARTESIAN_POINT('Ctrl Pts',(21.4698711405743,790.566028769384,111.156411579716));
#72094=CARTESIAN_POINT('Ctrl Pts',(21.493803531542,790.311774723019,111.078625656527));
#72095=CARTESIAN_POINT('Ctrl Pts',(21.4797057516203,790.183497254593,111.040646690727));
#72096=CARTESIAN_POINT('Ctrl Pts',(21.4008074653581,789.937495165339,110.97070432197));
#72097=CARTESIAN_POINT('Ctrl Pts',(21.3363466690085,789.822250663681,110.93947794166));
#72098=CARTESIAN_POINT('Ctrl Pts',(21.1641762306254,789.620197757338,110.888197260474));
#72099=CARTESIAN_POINT('Ctrl Pts',(21.0576463410307,789.535718445791,110.868780965762));
#72100=CARTESIAN_POINT('Ctrl Pts',(20.8184824018924,789.411663968598,110.844947561625));
#72101=CARTESIAN_POINT('Ctrl Pts',(20.688426054859,789.372795585845,110.840590505318));
#72102=CARTESIAN_POINT('Ctrl Pts',(20.4210873969079,789.345400767821,110.847052620977));
#72103=CARTESIAN_POINT('Ctrl Pts',(20.2864005190574,789.357080159282,110.857782569417));
#72104=CARTESIAN_POINT('Ctrl Pts',(20.093792436167,789.411996676071,110.884057017687));
#72105=CARTESIAN_POINT('Ctrl Pts',(20.0314202005905,789.43656544207,110.894506922721));
#72106=CARTESIAN_POINT('Ctrl Pts',(19.9121651831173,789.49768702915,110.918505283261));
#72107=CARTESIAN_POINT('Ctrl Pts',(19.8556631087487,789.53421523986,110.932025425981));
#72108=CARTESIAN_POINT('Ctrl Pts',(19.8034793393769,789.575990153271,110.94679009387));
#72109=CARTESIAN_POINT('Ctrl Pts',(20.4645692803066,790.678180117724,113.229952900161));
#72110=CARTESIAN_POINT('Ctrl Pts',(20.5946003758858,790.679489150697,113.22624914336));
#72111=CARTESIAN_POINT('Ctrl Pts',(20.7234710520815,790.656987854421,113.215398262081));
#72112=CARTESIAN_POINT('Ctrl Pts',(20.9698009034802,790.565163135047,113.179229742229));
#72113=CARTESIAN_POINT('Ctrl Pts',(21.0841491966429,790.494929565677,113.153699929834));
#72114=CARTESIAN_POINT('Ctrl Pts',(21.2769583706158,790.315968441955,113.091256578208));
#72115=CARTESIAN_POINT('Ctrl Pts',(21.3535542838551,790.209060509613,113.054978782971));
#72116=CARTESIAN_POINT('Ctrl Pts',(21.4581130112891,789.973151183668,112.977103531815));
#72117=CARTESIAN_POINT('Ctrl Pts',(21.4852877520556,789.846577752246,112.936315730743));
#72118=CARTESIAN_POINT('Ctrl Pts',(21.4866421167182,789.589763570253,112.856252698726));
#72119=CARTESIAN_POINT('Ctrl Pts',(21.4607577494378,789.462050385905,112.817787682342));
#72120=CARTESIAN_POINT('Ctrl Pts',(21.3583695124856,789.221166101082,112.748664112043));
#72121=CARTESIAN_POINT('Ctrl Pts',(21.2823071884363,789.110589209333,112.718802454285));
#72122=CARTESIAN_POINT('Ctrl Pts',(21.0915337930738,788.924847286338,112.672842408319));
#72123=CARTESIAN_POINT('Ctrl Pts',(20.9792448009946,788.850933017746,112.656971625891));
#72124=CARTESIAN_POINT('Ctrl Pts',(20.7325772743618,788.748297214449,112.640511611668));
#72125=CARTESIAN_POINT('Ctrl Pts',(20.6005809955413,788.720396088668,112.640014084162));
#72126=CARTESIAN_POINT('Ctrl Pts',(20.4663059453286,788.717568648235,112.64698629291));
#72127=CARTESIAN_POINT('Ctrl Pts',(20.4654375876425,788.717551427731,112.647031693631));
#72128=CARTESIAN_POINT('Ctrl Pts',(20.4645692803024,788.717535272518,112.647077402928));
#72129=CARTESIAN_POINT('Origin',(20.4645692803024,793.317622820883,102.696810032682));
#72130=CARTESIAN_POINT('',(20.4645692803024,791.654206189377,108.90370527617));
#72131=CARTESIAN_POINT('Origin',(20.4645692803024,791.182783958768,108.737088708903));
#72132=CARTESIAN_POINT('',(20.4645692803024,790.179862406587,113.075189817997));
#72133=CARTESIAN_POINT('',(20.4645692803024,793.789045051492,102.863426599949));
#72134=CARTESIAN_POINT('Ctrl Pts',(20.4639964622118,789.220082879986,112.789873469231));
#72135=CARTESIAN_POINT('Ctrl Pts',(20.4050339558016,789.219174851509,112.79264534018));
#72136=CARTESIAN_POINT('Ctrl Pts',(20.3465213477788,789.228291826247,112.798349454785));
#72137=CARTESIAN_POINT('Ctrl Pts',(20.2299791925496,789.267798967435,112.815878398925));
#72138=CARTESIAN_POINT('Ctrl Pts',(20.1737927019346,789.2999482079,112.828111760667));
#72139=CARTESIAN_POINT('Ctrl Pts',(20.0776751488463,789.383567300992,112.857245534214));
#72140=CARTESIAN_POINT('Ctrl Pts',(20.0387363811842,789.434255422457,112.873868829814));
#72141=CARTESIAN_POINT('Ctrl Pts',(19.9835030697374,789.547693532412,112.909441744593));
#72142=CARTESIAN_POINT('Ctrl Pts',(19.9678359233545,789.609367386774,112.928051657371));
#72143=CARTESIAN_POINT('Ctrl Pts',(19.9622134681862,789.735451156348,112.964932404433));
#72144=CARTESIAN_POINT('Ctrl Pts',(19.9723727478844,789.798644689578,112.982848956574));
#72145=CARTESIAN_POINT('Ctrl Pts',(20.0178714824198,789.919080901477,113.016025290741));
#72146=CARTESIAN_POINT('Ctrl Pts',(20.0532539728035,789.97498382296,113.03089898142));
#72147=CARTESIAN_POINT('Ctrl Pts',(20.1442906242766,790.069945619686,113.055092918069));
#72148=CARTESIAN_POINT('Ctrl Pts',(20.1988977292507,790.108193680832,113.06421575077));
#72149=CARTESIAN_POINT('Ctrl Pts',(20.3200200141217,790.161979710785,113.075418632704));
#72150=CARTESIAN_POINT('Ctrl Pts',(20.3852912578462,790.177072686822,113.077411380082));
#72151=CARTESIAN_POINT('Ctrl Pts',(20.5179768841985,790.182012331175,113.073774105504));
#72152=CARTESIAN_POINT('Ctrl Pts',(20.5840645289053,790.171777355984,113.068165953632));
#72153=CARTESIAN_POINT('Ctrl Pts',(20.7080517332299,790.127056361971,113.049829964805));
#72154=CARTESIAN_POINT('Ctrl Pts',(20.7646773179151,790.092962590222,113.037266694887));
#72155=CARTESIAN_POINT('Ctrl Pts',(20.8603329116298,790.005415513898,113.006807333327));
#72156=CARTESIAN_POINT('Ctrl Pts',(20.8984073744595,789.952857542019,112.989222595352));
#72157=CARTESIAN_POINT('Ctrl Pts',(20.9505461168486,789.836465323121,112.951552643713));
#72158=CARTESIAN_POINT('Ctrl Pts',(20.964152305626,789.773828708788,112.931856012379));
#72159=CARTESIAN_POINT('Ctrl Pts',(20.9649674299414,789.646774706997,112.893169870772));
#72160=CARTESIAN_POINT('Ctrl Pts',(20.9521660913145,789.583623642089,112.874570776244));
#72161=CARTESIAN_POINT('Ctrl Pts',(20.9015594798973,789.465059445714,112.841090127105));
#72162=CARTESIAN_POINT('Ctrl Pts',(20.8641227571364,789.410870859766,112.826565317502));
#72163=CARTESIAN_POINT('Ctrl Pts',(20.7703456159225,789.320112533352,112.803967063599));
#72164=CARTESIAN_POINT('Ctrl Pts',(20.7152216934108,789.28412977799,112.796004639445));
#72165=CARTESIAN_POINT('Ctrl Pts',(20.5941608260255,789.234412799054,112.787391251644));
#72166=CARTESIAN_POINT('Ctrl Pts',(20.5294013185598,789.221090121294,112.786798738656));
#72167=CARTESIAN_POINT('Ctrl Pts',(20.4639964622118,789.220082879986,112.789873469231));
#72168=CARTESIAN_POINT('Origin',(22.434557059716,787.005126867006,100.465760373941));
#72169=CARTESIAN_POINT('',(22.434557059716,782.282406564289,110.983040517812));
#72170=CARTESIAN_POINT('',(22.434557059716,784.159183512917,111.363135221129));
#72171=CARTESIAN_POINT('Ctrl Pts',(22.434557059716,782.282406564289,110.983040517812));
#72172=CARTESIAN_POINT('Ctrl Pts',(22.3145647956342,782.278220036892,110.994885810969));
#72173=CARTESIAN_POINT('Ctrl Pts',(22.1953761212331,782.296664917096,111.011054461859));
#72174=CARTESIAN_POINT('Ctrl Pts',(21.9699686706315,782.378103171931,111.050362783727));
#72175=CARTESIAN_POINT('Ctrl Pts',(21.8663333745128,782.440806687305,111.073167957544));
#72176=CARTESIAN_POINT('Ctrl Pts',(21.6888029197355,782.603965586086,111.122652988845));
#72177=CARTESIAN_POINT('Ctrl Pts',(21.6172849690108,782.703154860505,111.14884513235));
#72178=CARTESIAN_POINT('Ctrl Pts',(21.5165756055335,782.926141192785,111.201634645248));
#72179=CARTESIAN_POINT('Ctrl Pts',(21.489273406918,783.048043541804,111.227688637841));
#72180=CARTESIAN_POINT('Ctrl Pts',(21.4840352038534,783.298238922486,111.276558115142));
#72181=CARTESIAN_POINT('Ctrl Pts',(21.5070188487827,783.424204913184,111.298851887648));
#72182=CARTESIAN_POINT('Ctrl Pts',(21.6011223070221,783.660931494703,111.336591727571));
#72183=CARTESIAN_POINT('Ctrl Pts',(21.6715006688284,783.769520779225,111.351688252688));
#72184=CARTESIAN_POINT('Ctrl Pts',(21.8492291727829,783.952493435218,111.372363421747));
#72185=CARTESIAN_POINT('Ctrl Pts',(21.9544112999345,784.025697796313,111.377887946878));
#72186=CARTESIAN_POINT('Ctrl Pts',(22.1856973228963,784.127506336629,111.378346908484));
#72187=CARTESIAN_POINT('Ctrl Pts',(22.3093449109512,784.155565812865,111.37337108336));
#72188=CARTESIAN_POINT('Ctrl Pts',(22.434557059716,784.159183512917,111.363135221129));
#72189=CARTESIAN_POINT('',(22.4345565353571,784.811902018906,109.516343998021));
#72190=CARTESIAN_POINT('',(22.434557059716,787.899023039625,100.781693527078));
#72191=CARTESIAN_POINT('Ctrl Pts',(22.4341912064781,782.955910373024,109.077439905874));
#72192=CARTESIAN_POINT('Ctrl Pts',(22.3319455172926,782.953259645336,109.085058233456));
#72193=CARTESIAN_POINT('Ctrl Pts',(22.2302594739761,782.966838186319,109.096390842135));
#72194=CARTESIAN_POINT('Ctrl Pts',(22.0857147349296,783.010594491383,109.118060440226));
#72195=CARTESIAN_POINT('Ctrl Pts',(22.03964939657,783.028630720995,109.125897246329));
#72196=CARTESIAN_POINT('Ctrl Pts',(21.9638031770467,783.065544932245,109.140435804426));
#72197=CARTESIAN_POINT('Ctrl Pts',(21.9332233825504,783.082647231539,109.146800344347));
#72198=CARTESIAN_POINT('Ctrl Pts',(21.8745657646438,783.120006959674,109.160039888438));
#72199=CARTESIAN_POINT('Ctrl Pts',(21.8465144402259,783.140197898613,109.166897680218));
#72200=CARTESIAN_POINT('Ctrl Pts',(21.7829406417972,783.191690564646,109.183738895911));
#72201=CARTESIAN_POINT('Ctrl Pts',(21.748624641401,783.224249003488,109.193908821543));
#72202=CARTESIAN_POINT('Ctrl Pts',(21.6500854470938,783.333649529516,109.226727722468));
#72203=CARTESIAN_POINT('Ctrl Pts',(21.5961992886768,783.418421105743,109.250342260558));
#72204=CARTESIAN_POINT('Ctrl Pts',(21.5179717724287,783.603541053572,109.298860266041));
#72205=CARTESIAN_POINT('Ctrl Pts',(21.4946669617016,783.702832337023,109.323443667668));
#72206=CARTESIAN_POINT('Ctrl Pts',(21.481358554927,783.913726526315,109.373063675941));
#72207=CARTESIAN_POINT('Ctrl Pts',(21.4943742457734,784.024045980758,109.397591569015));
#72208=CARTESIAN_POINT('Ctrl Pts',(21.561203385517,784.243585087575,109.443685582558));
#72209=CARTESIAN_POINT('Ctrl Pts',(21.6173964599638,784.350248354268,109.46450956386));
#72210=CARTESIAN_POINT('Ctrl Pts',(21.770553698826,784.542666785869,109.498725550062));
#72211=CARTESIAN_POINT('Ctrl Pts',(21.8679207567976,784.625350123151,109.511387442897));
#72212=CARTESIAN_POINT('Ctrl Pts',(22.0861584324583,784.747450361711,109.525098704896));
#72213=CARTESIAN_POINT('Ctrl Pts',(22.2042453108566,784.786928099409,109.526342678263));
#72214=CARTESIAN_POINT('Ctrl Pts',(22.4498465842724,784.820054756526,109.517236101008));
#72215=CARTESIAN_POINT('Ctrl Pts',(22.5750169437994,784.812895137463,109.506847199228));
#72216=CARTESIAN_POINT('Ctrl Pts',(22.7483472112806,784.768498679961,109.484000899264));
#72217=CARTESIAN_POINT('Ctrl Pts',(22.8004886325275,784.750157708231,109.475905823453));
#72218=CARTESIAN_POINT('Ctrl Pts',(22.8838113679857,784.712317496645,109.46086572957));
#72219=CARTESIAN_POINT('Ctrl Pts',(22.9160638714698,784.695321524171,109.454464822773));
#72220=CARTESIAN_POINT('Ctrl Pts',(22.9611726951682,784.668041079933,109.4446457373));
#72221=CARTESIAN_POINT('Ctrl Pts',(22.9749311106217,784.659212428218,109.441525439157));
#72222=CARTESIAN_POINT('Ctrl Pts',(23.0186971033218,784.629453315632,109.431186098564));
#72223=CARTESIAN_POINT('Ctrl Pts',(23.0476449210594,784.60712631829,109.42369456889));
#72224=CARTESIAN_POINT('Ctrl Pts',(23.1167419282984,784.546887288026,109.404099395442));
#72225=CARTESIAN_POINT('Ctrl Pts',(23.1548544457957,784.506990149632,109.391645446958));
#72226=CARTESIAN_POINT('Ctrl Pts',(23.2609525475023,784.373336121114,109.351426617369));
#72227=CARTESIAN_POINT('Ctrl Pts',(23.3144028445643,784.27003570303,109.322325145207));
#72228=CARTESIAN_POINT('Ctrl Pts',(23.3759579552401,784.059388392483,109.266522815396));
#72229=CARTESIAN_POINT('Ctrl Pts',(23.3874433847075,783.954916956048,109.240273368974));
#72230=CARTESIAN_POINT('Ctrl Pts',(23.3736807622339,783.737700515715,109.188742314248));
#72231=CARTESIAN_POINT('Ctrl Pts',(23.3455640688954,783.626745545018,109.164131463533));
#72232=CARTESIAN_POINT('Ctrl Pts',(23.2468246171695,783.411393848005,109.120130746721));
#72233=CARTESIAN_POINT('Ctrl Pts',(23.1740611543256,783.31008566456,109.101678454116));
#72234=CARTESIAN_POINT('Ctrl Pts',(23.0069973980688,783.152118460831,109.077461305136));
#72235=CARTESIAN_POINT('Ctrl Pts',(22.9185796482836,783.092097603502,109.07037525928));
#72236=CARTESIAN_POINT('Ctrl Pts',(22.7668316838621,783.02154291635,109.065982529064));
#72237=CARTESIAN_POINT('Ctrl Pts',(22.7091762628634,783.000975149791,109.065805757572));
#72238=CARTESIAN_POINT('Ctrl Pts',(22.5793306231022,782.967876198178,109.068527071148));
#72239=CARTESIAN_POINT('Ctrl Pts',(22.5069179824542,782.957795820522,109.072021032885));
#72240=CARTESIAN_POINT('Ctrl Pts',(22.4341912064781,782.955910373024,109.077439905874));
#72241=CARTESIAN_POINT('Ctrl Pts',(22.434557059716,784.159183512916,111.363135221129));
#72242=CARTESIAN_POINT('Ctrl Pts',(22.4345899353016,784.159184462776,111.363132533611));
#72243=CARTESIAN_POINT('Ctrl Pts',(22.4346228109951,784.159185410951,111.363129845729));
#72244=CARTESIAN_POINT('Ctrl Pts',(22.4346556867964,784.15918635744,111.363127157485));
#72245=CARTESIAN_POINT('Ctrl Pts',(22.5528163031172,784.162588182837,111.35346520049));
#72246=CARTESIAN_POINT('Ctrl Pts',(22.6701261161492,784.144154849174,111.339290814618));
#72247=CARTESIAN_POINT('Ctrl Pts',(22.8972414404405,784.062970749404,111.30190779092));
#72248=CARTESIAN_POINT('Ctrl Pts',(23.0037970543271,783.998567263484,111.278611028557));
#72249=CARTESIAN_POINT('Ctrl Pts',(23.1840228811689,783.831951523415,111.2265530828));
#72250=CARTESIAN_POINT('Ctrl Pts',(23.2557926901844,783.73153169703,111.198354053641));
#72251=CARTESIAN_POINT('Ctrl Pts',(23.3548161962533,783.507967150304,111.141213130509));
#72252=CARTESIAN_POINT('Ctrl Pts',(23.3809709745847,783.387105574554,111.112876322306));
#72253=CARTESIAN_POINT('Ctrl Pts',(23.3841718939372,783.140133970266,111.060233344492));
#72254=CARTESIAN_POINT('Ctrl Pts',(23.360736107379,783.01643049486,111.036499466763));
#72255=CARTESIAN_POINT('Ctrl Pts',(23.2664302813607,782.782104439017,110.997192363948));
#72256=CARTESIAN_POINT('Ctrl Pts',(23.1957467150693,782.67389759727,110.982117502344));
#72257=CARTESIAN_POINT('Ctrl Pts',(23.018217947104,782.491565613827,110.963324471303));
#72258=CARTESIAN_POINT('Ctrl Pts',(22.9135927122306,782.418438310118,110.959561888858));
#72259=CARTESIAN_POINT('Ctrl Pts',(22.6847807346403,782.316346703612,110.963262832796));
#72260=CARTESIAN_POINT('Ctrl Pts',(22.5629895452002,782.287541742545,110.970489769422));
#72261=CARTESIAN_POINT('Ctrl Pts',(22.4378656680881,782.28252629713,110.982714739956));
#72262=CARTESIAN_POINT('Ctrl Pts',(22.4362112874469,782.282464280257,110.982877217181));
#72263=CARTESIAN_POINT('Ctrl Pts',(22.434557059716,782.282406564289,110.983040517812));
#72264=CARTESIAN_POINT('Origin',(22.434557059716,787.005126867006,100.465760373941));
#72265=CARTESIAN_POINT('',(22.434557059716,785.3417102355,106.672655617429));
#72266=CARTESIAN_POINT('Origin',(22.434557059716,784.870288004891,106.506039050162));
#72267=CARTESIAN_POINT('',(22.434557059716,783.717529955679,111.268085129529));
#72268=CARTESIAN_POINT('',(22.434557059716,787.476549097615,100.632376941208));
#72269=CARTESIAN_POINT('Ctrl Pts',(22.4343367025393,782.727746084943,111.067661749631));
#72270=CARTESIAN_POINT('Ctrl Pts',(22.3726006506608,782.725703330114,111.073523135672));
#72271=CARTESIAN_POINT('Ctrl Pts',(22.3112754249538,782.73500614065,111.081594388938));
#72272=CARTESIAN_POINT('Ctrl Pts',(22.1933973637207,782.77647171044,111.101696852075));
#72273=CARTESIAN_POINT('Ctrl Pts',(22.1383687395877,782.80910552941,111.113662513152));
#72274=CARTESIAN_POINT('Ctrl Pts',(22.0439914880774,782.894279111862,111.139852903109));
#72275=CARTESIAN_POINT('Ctrl Pts',(22.0058470515114,782.946124909647,111.15382062966));
#72276=CARTESIAN_POINT('Ctrl Pts',(21.9517697780768,783.062846215763,111.182106167447));
#72277=CARTESIAN_POINT('Ctrl Pts',(21.936799458975,783.126716842681,111.196133986485));
#72278=CARTESIAN_POINT('Ctrl Pts',(21.9327285656268,783.258661595137,111.222599196432));
#72279=CARTESIAN_POINT('Ctrl Pts',(21.9443532108643,783.325500261434,111.234727930421));
#72280=CARTESIAN_POINT('Ctrl Pts',(21.9931984200521,783.450943032292,111.255091508743));
#72281=CARTESIAN_POINT('Ctrl Pts',(22.0298801262911,783.508434903931,111.263156863517));
#72282=CARTESIAN_POINT('Ctrl Pts',(22.1230989462501,783.605896687254,111.274090436186));
#72283=CARTESIAN_POINT('Ctrl Pts',(22.1786153243142,783.645130577056,111.276903026751));
#72284=CARTESIAN_POINT('Ctrl Pts',(22.3010543292766,783.700005284196,111.276775953314));
#72285=CARTESIAN_POINT('Ctrl Pts',(22.3667029375574,783.715294105381,111.273878190394));
#72286=CARTESIAN_POINT('Ctrl Pts',(22.4978996032111,783.719620484652,111.26267793443));
#72287=CARTESIAN_POINT('Ctrl Pts',(22.5621006292266,783.70933723706,111.254636365592));
#72288=CARTESIAN_POINT('Ctrl Pts',(22.6821935273669,783.664944586968,111.234288495329));
#72289=CARTESIAN_POINT('Ctrl Pts',(22.7368752939048,783.631365466351,111.222203200013));
#72290=CARTESIAN_POINT('Ctrl Pts',(22.830343684457,783.544414068082,111.195303409615));
#72291=CARTESIAN_POINT('Ctrl Pts',(22.8678716260544,783.491661948801,111.180736044124));
#72292=CARTESIAN_POINT('Ctrl Pts',(22.9200963452349,783.373508134824,111.151123204493));
#72293=CARTESIAN_POINT('Ctrl Pts',(22.9338837698804,783.309167122121,111.13638881739));
#72294=CARTESIAN_POINT('Ctrl Pts',(22.9351871181484,783.177907773511,111.109036424678));
#72295=CARTESIAN_POINT('Ctrl Pts',(22.9224955483466,783.11226932585,111.096708180252));
#72296=CARTESIAN_POINT('Ctrl Pts',(22.8719994835884,782.988519520773,111.076266337587));
#72297=CARTESIAN_POINT('Ctrl Pts',(22.8344406021171,782.931627027859,111.068381887645));
#72298=CARTESIAN_POINT('Ctrl Pts',(22.7403204731203,782.835987918371,111.058395017031));
#72299=CARTESIAN_POINT('Ctrl Pts',(22.6849452223084,782.797760735205,111.056274121979));
#72300=CARTESIAN_POINT('Ctrl Pts',(22.5639127224996,782.744665805673,111.057868962667));
#72301=CARTESIAN_POINT('Ctrl Pts',(22.4995295038568,782.729903218508,111.061472170545));
#72302=CARTESIAN_POINT('Ctrl Pts',(22.4343367025393,782.727746084943,111.067661749631));
#72303=CARTESIAN_POINT('Origin',(13.2358290567306,800.458037260509,105.220474097608));
#72304=CARTESIAN_POINT('',(13.2358290567306,795.861581228149,115.160466514987));
#72305=CARTESIAN_POINT('',(13.2358290567306,797.815642116494,115.76197055367));
#72306=CARTESIAN_POINT('Ctrl Pts',(13.2358290567306,795.861581228149,115.160466514987));
#72307=CARTESIAN_POINT('Ctrl Pts',(13.1041212291136,795.858690928329,115.168644282725));
#72308=CARTESIAN_POINT('Ctrl Pts',(12.973562697341,795.880144614487,115.184392017813));
#72309=CARTESIAN_POINT('Ctrl Pts',(12.7282734162024,795.970123546666,115.228853097103));
#72310=CARTESIAN_POINT('Ctrl Pts',(12.616046168791,796.038139662565,115.257221950587));
#72311=CARTESIAN_POINT('Ctrl Pts',(12.4257398984536,796.212771683765,115.322601874734));
#72312=CARTESIAN_POINT('Ctrl Pts',(12.3496618273244,796.317767841094,115.358984279569));
#72313=CARTESIAN_POINT('Ctrl Pts',(12.2442054471236,796.551652098824,115.435220635439));
#72314=CARTESIAN_POINT('Ctrl Pts',(12.2161681956213,796.678332578655,115.474336159374));
#72315=CARTESIAN_POINT('Ctrl Pts',(12.2128246923721,796.93630278225,115.550549646238));
#72316=CARTESIAN_POINT('Ctrl Pts',(12.2377687821284,797.065077413602,115.586906141854));
#72317=CARTESIAN_POINT('Ctrl Pts',(12.3378734280937,797.30662427731,115.652500687538));
#72318=CARTESIAN_POINT('Ctrl Pts',(12.4120749207504,797.417086570966,115.681127350276));
#72319=CARTESIAN_POINT('Ctrl Pts',(12.6017910977174,797.606075689974,115.727617315544));
#72320=CARTESIAN_POINT('Ctrl Pts',(12.7160882481684,797.682172169096,115.744842792295));
#72321=CARTESIAN_POINT('Ctrl Pts',(12.9667210870214,797.786170619628,115.764616149613));
#72322=CARTESIAN_POINT('Ctrl Pts',(13.1002602974402,797.813718866267,115.767166354558));
#72323=CARTESIAN_POINT('Ctrl Pts',(13.235210494504,797.815633520053,115.761994314233));
#72324=CARTESIAN_POINT('Ctrl Pts',(13.2354166848091,797.815636445451,115.761986411876));
#72325=CARTESIAN_POINT('Ctrl Pts',(13.2356228722272,797.81563931093,115.761978491688));
#72326=CARTESIAN_POINT('Ctrl Pts',(13.2358290567306,797.815642116494,115.76197055367));
#72327=CARTESIAN_POINT('',(13.2358290558362,798.453583033059,113.956990803958));
#72328=CARTESIAN_POINT('',(13.2358290567306,801.421066400752,105.560841180675));
#72329=CARTESIAN_POINT('Ctrl Pts',(12.4273032040843,796.862039029937,113.521926296511));
#72330=CARTESIAN_POINT('Ctrl Pts',(12.3459211826545,796.961436378916,113.557056682833));
#72331=CARTESIAN_POINT('Ctrl Pts',(12.2859599712866,797.075587204588,113.59508453686));
#72332=CARTESIAN_POINT('Ctrl Pts',(12.215569609869,797.320459667716,113.672779125306));
#72333=CARTESIAN_POINT('Ctrl Pts',(12.20582869449,797.448791059769,113.711693201858));
#72334=CARTESIAN_POINT('Ctrl Pts',(12.2382675360023,797.703224865197,113.785766239328));
#72335=CARTESIAN_POINT('Ctrl Pts',(12.2803637546695,797.826868988588,113.820204423165));
#72336=CARTESIAN_POINT('Ctrl Pts',(12.4116340282938,798.052841521947,113.880306044229));
#72337=CARTESIAN_POINT('Ctrl Pts',(12.499762698849,798.152920781911,113.905364511945));
#72338=CARTESIAN_POINT('Ctrl Pts',(12.7107555953734,798.315370737971,113.942683998402));
#72339=CARTESIAN_POINT('Ctrl Pts',(12.8316392065375,798.376146995356,113.954575213524));
#72340=CARTESIAN_POINT('Ctrl Pts',(13.0890422797066,798.449367725707,113.963244560179));
#72341=CARTESIAN_POINT('Ctrl Pts',(13.2229524793323,798.46156769217,113.960076194865));
#72342=CARTESIAN_POINT('Ctrl Pts',(13.4890321484625,798.435955840218,113.938619697876));
#72343=CARTESIAN_POINT('Ctrl Pts',(13.618525917093,798.397760389817,113.920342392848));
#72344=CARTESIAN_POINT('Ctrl Pts',(13.8539178118326,798.275109375275,113.870502477999));
#72345=CARTESIAN_POINT('Ctrl Pts',(13.9574302937875,798.191805645498,113.839408647088));
#72346=CARTESIAN_POINT('Ctrl Pts',(14.1230271734505,797.992040790806,113.768708816872));
#72347=CARTESIAN_POINT('Ctrl Pts',(14.1838920191604,797.877870836644,113.729882036027));
#72348=CARTESIAN_POINT('Ctrl Pts',(14.2556491449628,797.633023205371,113.649525632122));
#72349=CARTESIAN_POINT('Ctrl Pts',(14.2658792373226,797.504746037582,113.608789039666));
#72350=CARTESIAN_POINT('Ctrl Pts',(14.2340583906279,797.251273713088,113.531279403436));
#72351=CARTESIAN_POINT('Ctrl Pts',(14.1924913567775,797.128512457711,113.495250053973));
#72352=CARTESIAN_POINT('Ctrl Pts',(14.0622479731902,796.903235669234,113.432632707769));
#72353=CARTESIAN_POINT('Ctrl Pts',(13.9744411469121,796.803080423965,113.406739381224));
#72354=CARTESIAN_POINT('Ctrl Pts',(13.7628720578125,796.639054932882,113.368898875281));
#72355=CARTESIAN_POINT('Ctrl Pts',(13.6407645383992,796.577232890325,113.357490426058));
#72356=CARTESIAN_POINT('Ctrl Pts',(13.3808574549199,796.502634827345,113.351136592103));
#72357=CARTESIAN_POINT('Ctrl Pts',(13.2457219745547,796.490046144811,113.35606767105));
#72358=CARTESIAN_POINT('Ctrl Pts',(12.9793028609075,796.515545091894,113.381224233002));
#72359=CARTESIAN_POINT('Ctrl Pts',(12.8505921104556,796.553326383922,113.401179476283));
#72360=CARTESIAN_POINT('Ctrl Pts',(12.6747785467436,796.644752360755,113.440357603061));
#72361=CARTESIAN_POINT('Ctrl Pts',(12.6193094711535,796.680998840812,113.454934807369));
#72362=CARTESIAN_POINT('Ctrl Pts',(12.516304707968,796.764145693389,113.486717641978));
#72363=CARTESIAN_POINT('Ctrl Pts',(12.4691346226,796.810947498522,113.503868820583));
#72364=CARTESIAN_POINT('Ctrl Pts',(12.4273032040843,796.862039029937,113.521926296511));
#72365=CARTESIAN_POINT('Ctrl Pts',(13.2358290567306,797.815642116494,115.76197055367));
#72366=CARTESIAN_POINT('Ctrl Pts',(13.3668381839024,797.817424765096,115.756926756439));
#72367=CARTESIAN_POINT('Ctrl Pts',(13.4966705402353,797.79501818008,115.744684286592));
#72368=CARTESIAN_POINT('Ctrl Pts',(13.7429834672164,797.703252865656,115.70589433082));
#72369=CARTESIAN_POINT('Ctrl Pts',(13.8565880736033,797.633581041091,115.679343320689));
#72370=CARTESIAN_POINT('Ctrl Pts',(14.0485151820788,797.455900294262,115.614936513227));
#72371=CARTESIAN_POINT('Ctrl Pts',(14.1248911380197,797.349587483375,115.577693034246));
#72372=CARTESIAN_POINT('Ctrl Pts',(14.2293664624442,797.11470288253,115.497676654686));
#72373=CARTESIAN_POINT('Ctrl Pts',(14.2565570706956,796.988489343664,115.455713402195));
#72374=CARTESIAN_POINT('Ctrl Pts',(14.2578921523234,796.73258620367,115.373250788514));
#72375=CARTESIAN_POINT('Ctrl Pts',(14.2320451601527,796.605413136226,115.333581681107));
#72376=CARTESIAN_POINT('Ctrl Pts',(14.1299427876524,796.365828693017,115.262335923215));
#72377=CARTESIAN_POINT('Ctrl Pts',(14.0542704661199,796.255947264145,115.23156063921));
#72378=CARTESIAN_POINT('Ctrl Pts',(13.8641237251078,796.070659717731,115.184267303577));
#72379=CARTESIAN_POINT('Ctrl Pts',(13.7519211761802,795.996662649226,115.16804993926));
#72380=CARTESIAN_POINT('Ctrl Pts',(13.5052398524324,795.893424010687,115.151906601647));
#72381=CARTESIAN_POINT('Ctrl Pts',(13.3731239816882,795.865071075193,115.152091801046));
#72382=CARTESIAN_POINT('Ctrl Pts',(13.2383415336434,795.861638576023,115.16031121011));
#72383=CARTESIAN_POINT('Ctrl Pts',(13.237085242904,795.861608794883,115.160388518114));
#72384=CARTESIAN_POINT('Ctrl Pts',(13.2358290567306,795.861581228149,115.160466514987));
#72385=CARTESIAN_POINT('Origin',(13.2358290567306,800.458037260509,105.220474097608));
#72386=CARTESIAN_POINT('',(13.2358290567306,798.794620629003,111.427369341096));
#72387=CARTESIAN_POINT('Origin',(13.2358290567306,798.323198398394,111.260752773829));
#72388=CARTESIAN_POINT('',(13.2358290567306,797.318300108841,115.604446831791));
#72389=CARTESIAN_POINT('',(13.2358290567306,800.929459491118,105.387090664875));
#72390=CARTESIAN_POINT('Ctrl Pts',(13.2354533120498,796.361757660371,115.309970985344));
#72391=CARTESIAN_POINT('Ctrl Pts',(13.1752379075312,796.360605246904,115.313367400001));
#72392=CARTESIAN_POINT('Ctrl Pts',(13.1154959366117,796.36985571648,115.319971852384));
#72393=CARTESIAN_POINT('Ctrl Pts',(12.9981428930495,796.409939133173,115.33961134581));
#72394=CARTESIAN_POINT('Ctrl Pts',(12.9422366428628,796.44208307235,115.352933503107));
#72395=CARTESIAN_POINT('Ctrl Pts',(12.8468224525815,796.525525714675,115.384236969571));
#72396=CARTESIAN_POINT('Ctrl Pts',(12.8082799589247,796.576029991166,115.401915191058));
#72397=CARTESIAN_POINT('Ctrl Pts',(12.7538475128707,796.689037826653,115.439382299639));
#72398=CARTESIAN_POINT('Ctrl Pts',(12.7385853584983,796.750464932062,115.458808831554));
#72399=CARTESIAN_POINT('Ctrl Pts',(12.7337447351938,796.87610395184,115.496952308307));
#72400=CARTESIAN_POINT('Ctrl Pts',(12.744301334523,796.93909251629,115.515296434828));
#72401=CARTESIAN_POINT('Ctrl Pts',(12.7901215243676,797.05798481727,115.54855854042));
#72402=CARTESIAN_POINT('Ctrl Pts',(12.8249689896076,797.112737150708,115.563156844004));
#72403=CARTESIAN_POINT('Ctrl Pts',(12.9153615496383,797.207392425631,115.586949603157));
#72404=CARTESIAN_POINT('Ctrl Pts',(12.9703955264301,797.2460467359,115.595799558701));
#72405=CARTESIAN_POINT('Ctrl Pts',(13.0922702046139,797.300271545736,115.606071285171));
#72406=CARTESIAN_POINT('Ctrl Pts',(13.1578123687506,797.315480168869,115.607445845313));
#72407=CARTESIAN_POINT('Ctrl Pts',(13.2906192914867,797.320495339603,115.602405918425));
#72408=CARTESIAN_POINT('Ctrl Pts',(13.356555221227,797.31035708358,115.596069310506));
#72409=CARTESIAN_POINT('Ctrl Pts',(13.4800532313852,797.266000197467,115.576293489835));
#72410=CARTESIAN_POINT('Ctrl Pts',(13.5363803104309,797.232231482656,115.563049591712));
#72411=CARTESIAN_POINT('Ctrl Pts',(13.6316289907162,797.145454251167,115.53126151422));
#72412=CARTESIAN_POINT('Ctrl Pts',(13.6695873623299,797.093309077365,115.513032813375));
#72413=CARTESIAN_POINT('Ctrl Pts',(13.7217020073133,796.977650458397,115.474076233999));
#72414=CARTESIAN_POINT('Ctrl Pts',(13.7353497047518,796.915302076225,115.453742496961));
#72415=CARTESIAN_POINT('Ctrl Pts',(13.7362840686973,796.788704020686,115.413854309931));
#72416=CARTESIAN_POINT('Ctrl Pts',(13.7235359348621,796.725719130352,115.394704459687));
#72417=CARTESIAN_POINT('Ctrl Pts',(13.6730191627257,796.607401935663,115.360333201665));
#72418=CARTESIAN_POINT('Ctrl Pts',(13.6356243685776,796.553297760889,115.345481743696));
#72419=CARTESIAN_POINT('Ctrl Pts',(13.5419009937708,796.462549287198,115.322568960372));
#72420=CARTESIAN_POINT('Ctrl Pts',(13.4867817211731,796.426508582014,115.314622935924));
#72421=CARTESIAN_POINT('Ctrl Pts',(13.3656941306241,796.376524780958,115.306448691272));
#72422=CARTESIAN_POINT('Ctrl Pts',(13.3008943237075,796.363010082466,115.306279823374));
#72423=CARTESIAN_POINT('Ctrl Pts',(13.2354533120498,796.361757660371,115.309970985344));
#72424=CARTESIAN_POINT('Origin',(13.7707655252052,793.897310963527,102.901691436531));
#72425=CARTESIAN_POINT('',(13.7707655252052,789.181066524569,113.400648875834));
#72426=CARTESIAN_POINT('',(13.7707655252132,791.043521315622,113.821266461007));
#72427=CARTESIAN_POINT('Ctrl Pts',(13.7707655252052,789.181066524569,113.400648875834));
#72428=CARTESIAN_POINT('Ctrl Pts',(13.6492784145032,789.175680293637,113.415888590839));
#72429=CARTESIAN_POINT('Ctrl Pts',(13.5285703655825,789.193261731801,113.436216379807));
#72430=CARTESIAN_POINT('Ctrl Pts',(13.3025153023418,789.273178909632,113.484449828108));
#72431=CARTESIAN_POINT('Ctrl Pts',(13.1993987229554,789.334524325493,113.511828328945));
#72432=CARTESIAN_POINT('Ctrl Pts',(13.0234167711003,789.494374366946,113.570254118077));
#72433=CARTESIAN_POINT('Ctrl Pts',(12.9526596650833,789.591384689429,113.600689697077));
#72434=CARTESIAN_POINT('Ctrl Pts',(12.8528934676997,789.810075625491,113.661124028342));
#72435=CARTESIAN_POINT('Ctrl Pts',(12.8257378275371,789.929805362413,113.690458608107));
#72436=CARTESIAN_POINT('Ctrl Pts',(12.8200631331498,790.176191048161,113.744419453954));
#72437=CARTESIAN_POINT('Ctrl Pts',(12.8424389481425,790.300465020687,113.768428489183));
#72438=CARTESIAN_POINT('Ctrl Pts',(12.9351494967828,790.536606222016,113.808198156768));
#72439=CARTESIAN_POINT('Ctrl Pts',(13.0054727532173,790.646007389772,113.82344242124));
#72440=CARTESIAN_POINT('Ctrl Pts',(13.1834024574027,790.830976922132,113.84264262536));
#72441=CARTESIAN_POINT('Ctrl Pts',(13.2889133176225,790.905326833515,113.846576875626));
#72442=CARTESIAN_POINT('Ctrl Pts',(13.5206220459066,791.009347472381,113.842562056751));
#72443=CARTESIAN_POINT('Ctrl Pts',(13.644390372637,791.038599593603,113.83479114981));
#72444=CARTESIAN_POINT('Ctrl Pts',(13.7697596530115,791.043482662353,113.821374226517));
#72445=CARTESIAN_POINT('Ctrl Pts',(13.7700949501014,791.043495722001,113.821338343282));
#72446=CARTESIAN_POINT('Ctrl Pts',(13.7704302408894,791.043508606022,113.821302421345));
#72447=CARTESIAN_POINT('Ctrl Pts',(13.7707655252212,791.043521315622,113.821266461007));
#72448=CARTESIAN_POINT('',(13.7707655251889,791.698900378754,111.966947500389));
#72449=CARTESIAN_POINT('',(13.7707655252052,794.791207136146,103.217624589667));
#72450=CARTESIAN_POINT('Ctrl Pts',(13.0869837155771,790.11503182315,111.63240064931));
#72451=CARTESIAN_POINT('Ctrl Pts',(13.0049672579053,790.195544742242,111.660856639139));
#72452=CARTESIAN_POINT('Ctrl Pts',(12.9397259231793,790.290827518569,111.6911850193));
#72453=CARTESIAN_POINT('Ctrl Pts',(12.8468751181743,790.506826171458,111.754248307119));
#72454=CARTESIAN_POINT('Ctrl Pts',(12.8225251034181,790.626429944291,111.786374964653));
#72455=CARTESIAN_POINT('Ctrl Pts',(12.8228358603533,790.867018868523,111.84620141651));
#72456=CARTESIAN_POINT('Ctrl Pts',(12.8466565698299,790.985687233574,111.87341329365));
#72457=CARTESIAN_POINT('Ctrl Pts',(12.9393638812806,791.210552717328,111.920654283523));
#72458=CARTESIAN_POINT('Ctrl Pts',(13.0081189415837,791.314463601038,111.94013481181));
#72459=CARTESIAN_POINT('Ctrl Pts',(13.1828765863515,791.492791454484,111.968569638707));
#72460=CARTESIAN_POINT('Ctrl Pts',(13.2877112181536,791.565178812335,111.977129194197));
#72461=CARTESIAN_POINT('Ctrl Pts',(13.5194529266911,791.666885982961,111.981620750733));
#72462=CARTESIAN_POINT('Ctrl Pts',(13.6441809396813,791.695125117343,111.977474984418));
#72463=CARTESIAN_POINT('Ctrl Pts',(13.8912599510332,791.702494156065,111.956926546054));
#72464=CARTESIAN_POINT('Ctrl Pts',(14.0111979117764,791.683573565169,111.941230694138));
#72465=CARTESIAN_POINT('Ctrl Pts',(14.2324367871271,791.603831820801,111.900581035401));
#72466=CARTESIAN_POINT('Ctrl Pts',(14.3322371818225,791.54513150621,111.876310508249));
#72467=CARTESIAN_POINT('Ctrl Pts',(14.5041670791584,791.394206690427,111.821363139156));
#72468=CARTESIAN_POINT('Ctrl Pts',(14.5745608791319,791.303183734224,111.791155249483));
#72469=CARTESIAN_POINT('Ctrl Pts',(14.6779001994751,791.09713949323,111.727783702372));
#72470=CARTESIAN_POINT('Ctrl Pts',(14.7088159254487,790.983527220993,111.695175601264));
#72471=CARTESIAN_POINT('Ctrl Pts',(14.72516982677,790.743922053886,111.631057305945));
#72472=CARTESIAN_POINT('Ctrl Pts',(14.7079659446061,790.620070837777,111.600365882178));
#72473=CARTESIAN_POINT('Ctrl Pts',(14.6257958682063,790.387589802217,111.547862325335));
#72474=CARTESIAN_POINT('Ctrl Pts',(14.5626944247314,790.280871314744,111.526365639337));
#72475=CARTESIAN_POINT('Ctrl Pts',(14.3977546066292,790.094402858652,111.494581682993));
#72476=CARTESIAN_POINT('Ctrl Pts',(14.2969248398132,790.016779155715,111.484749905825));
#72477=CARTESIAN_POINT('Ctrl Pts',(14.0703270086054,789.902563463259,111.478462642894));
#72478=CARTESIAN_POINT('Ctrl Pts',(13.9464808250464,789.867430435575,111.482184507875));
#72479=CARTESIAN_POINT('Ctrl Pts',(13.7064244472674,789.847328150563,111.501702484579));
#72480=CARTESIAN_POINT('Ctrl Pts',(13.5926681403926,789.857685050726,111.516042739114));
#72481=CARTESIAN_POINT('Ctrl Pts',(13.3699873528363,789.919062454618,111.554388960176));
#72482=CARTESIAN_POINT('Ctrl Pts',(13.2636782647354,789.971532393303,111.578482025435));
#72483=CARTESIAN_POINT('Ctrl Pts',(13.1413503420825,790.064891015258,111.614333873035));
#72484=CARTESIAN_POINT('Ctrl Pts',(13.113353216892,790.089145731674,111.623251628704));
#72485=CARTESIAN_POINT('Ctrl Pts',(13.0869837155771,790.11503182315,111.63240064931));
#72486=CARTESIAN_POINT('Ctrl Pts',(13.7707655252212,791.043521315622,113.821266461007));
#72487=CARTESIAN_POINT('Ctrl Pts',(13.8911012868655,791.04808287511,113.808360058089));
#72488=CARTESIAN_POINT('Ctrl Pts',(14.0106059580553,791.030100687515,113.790485308017));
#72489=CARTESIAN_POINT('Ctrl Pts',(14.2368210489679,790.949946485546,113.745783657447));
#72490=CARTESIAN_POINT('Ctrl Pts',(14.3410046451445,790.887881897924,113.719259733935));
#72491=CARTESIAN_POINT('Ctrl Pts',(14.5189034927078,790.726343959621,113.660593518157));
#72492=CARTESIAN_POINT('Ctrl Pts',(14.5904105476491,790.628171924739,113.629008416356));
#72493=CARTESIAN_POINT('Ctrl Pts',(14.6900521482705,790.408090704759,113.565126045315));
#72494=CARTESIAN_POINT('Ctrl Pts',(14.7167142995753,790.288290918272,113.533509985004));
#72495=CARTESIAN_POINT('Ctrl Pts',(14.7207463961015,790.043589576605,113.475233159204));
#72496=CARTESIAN_POINT('Ctrl Pts',(14.6979109393481,789.921159564621,113.449195572618));
#72497=CARTESIAN_POINT('Ctrl Pts',(14.6053240236367,789.689005947332,113.406546196425));
#72498=CARTESIAN_POINT('Ctrl Pts',(14.5359217725427,789.581678050486,113.390466256828));
#72499=CARTESIAN_POINT('Ctrl Pts',(14.3587046077869,789.39678406123,113.370879692966));
#72500=CARTESIAN_POINT('Ctrl Pts',(14.2519882513673,789.321358442444,113.367733513863));
#72501=CARTESIAN_POINT('Ctrl Pts',(14.0198183863037,789.216617046771,113.374961362592));
#72502=CARTESIAN_POINT('Ctrl Pts',(13.8970222289228,789.186910636597,113.384866626768));
#72503=CARTESIAN_POINT('Ctrl Pts',(13.7720311551946,789.181123259504,113.400490252153));
#72504=CARTESIAN_POINT('Ctrl Pts',(13.7713983296233,789.181094580473,113.400569494911));
#72505=CARTESIAN_POINT('Ctrl Pts',(13.7707655252052,789.181066524569,113.400648875834));
#72506=CARTESIAN_POINT('Origin',(13.7707655252052,793.897310963527,102.901691436531));
#72507=CARTESIAN_POINT('',(13.7707655252052,792.233894332021,109.108586680019));
#72508=CARTESIAN_POINT('Origin',(13.7707655252052,791.762472101412,108.941970112752));
#72509=CARTESIAN_POINT('',(13.7707655252051,790.604793599704,113.717938041125));
#72510=CARTESIAN_POINT('',(13.7707655252052,794.368733194136,103.068308003798));
#72511=CARTESIAN_POINT('Ctrl Pts',(13.7705656579046,789.622571644425,113.496119073646));
#72512=CARTESIAN_POINT('Ctrl Pts',(13.7079789944701,789.619914051806,113.503713500116));
#72513=CARTESIAN_POINT('Ctrl Pts',(13.6457874201933,789.628814405553,113.513869638531));
#72514=CARTESIAN_POINT('Ctrl Pts',(13.5274527452042,789.669636000176,113.538470417792));
#72515=CARTESIAN_POINT('Ctrl Pts',(13.4726695888231,789.701652930357,113.552754741715));
#72516=CARTESIAN_POINT('Ctrl Pts',(13.3790715125016,789.785315296323,113.583487719747));
#72517=CARTESIAN_POINT('Ctrl Pts',(13.3413318784207,789.836155196056,113.599616965602));
#72518=CARTESIAN_POINT('Ctrl Pts',(13.2878530989089,789.950824673352,113.631826576731));
#72519=CARTESIAN_POINT('Ctrl Pts',(13.2730365641952,790.013617018126,113.647559755922));
#72520=CARTESIAN_POINT('Ctrl Pts',(13.2689337098566,790.143331867244,113.676700604033));
#72521=CARTESIAN_POINT('Ctrl Pts',(13.2802379622306,790.208997031973,113.689759382511));
#72522=CARTESIAN_POINT('Ctrl Pts',(13.3281775282723,790.333634579579,113.711345037254));
#72523=CARTESIAN_POINT('Ctrl Pts',(13.3646690555538,790.391342894356,113.719614471265));
#72524=CARTESIAN_POINT('Ctrl Pts',(13.457598734647,790.489601360741,113.730056613978));
#72525=CARTESIAN_POINT('Ctrl Pts',(13.5130656544762,790.5293847229,113.732177343589));
#72526=CARTESIAN_POINT('Ctrl Pts',(13.6353884649001,790.585558085541,113.729928681215));
#72527=CARTESIAN_POINT('Ctrl Pts',(13.7010138313307,790.601612338272,113.725630069115));
#72528=CARTESIAN_POINT('Ctrl Pts',(13.8324207645165,790.607624549419,113.71114313671));
#72529=CARTESIAN_POINT('Ctrl Pts',(13.8968934152184,790.598176777658,113.70124278508));
#72530=CARTESIAN_POINT('Ctrl Pts',(14.0172914442885,790.555402151593,113.676949017842));
#72531=CARTESIAN_POINT('Ctrl Pts',(14.0720655339886,790.522704676629,113.662836096736));
#72532=CARTESIAN_POINT('Ctrl Pts',(14.1651508234348,790.437988080927,113.632043893543));
#72533=CARTESIAN_POINT('Ctrl Pts',(14.2024749867338,790.386827800339,113.615681598685));
#72534=CARTESIAN_POINT('Ctrl Pts',(14.2552963278157,790.271086038338,113.582449807667));
#72535=CARTESIAN_POINT('Ctrl Pts',(14.2695783894647,790.207416304052,113.565940175164));
#72536=CARTESIAN_POINT('Ctrl Pts',(14.2718152960103,790.077305573402,113.535577479682));
#72537=CARTESIAN_POINT('Ctrl Pts',(14.2596455275522,790.012186037977,113.522049402005));
#72538=CARTESIAN_POINT('Ctrl Pts',(14.210332779705,789.889083456448,113.499928736488));
#72539=CARTESIAN_POINT('Ctrl Pts',(14.1734685911125,789.832333077968,113.49158846207));
#72540=CARTESIAN_POINT('Ctrl Pts',(14.0796818308219,789.735083430543,113.48138693629));
#72541=CARTESIAN_POINT('Ctrl Pts',(14.0234642175206,789.695595617994,113.479667950468));
#72542=CARTESIAN_POINT('Ctrl Pts',(13.9010322090691,789.640799195777,113.48315987103));
#72543=CARTESIAN_POINT('Ctrl Pts',(13.836197853444,789.625358558263,113.488155094489));
#72544=CARTESIAN_POINT('Ctrl Pts',(13.7705656579046,789.622571644425,113.496119073646));
#72545=CARTESIAN_POINT('Origin',(7.73962524950056,808.859454792509,108.189819322485));
#72546=CARTESIAN_POINT('',(7.73962524950056,804.267101962135,118.118202206281));
#72547=CARTESIAN_POINT('',(7.73962524950039,806.213211761693,118.742202927456));
#72548=CARTESIAN_POINT('Ctrl Pts',(7.73962524950056,804.267101962135,118.118202206281));
#72549=CARTESIAN_POINT('Ctrl Pts',(7.73929993760265,804.267094191054,118.118224193655));
#72550=CARTESIAN_POINT('Ctrl Pts',(7.73897461814967,804.267086567046,118.118246231281));
#72551=CARTESIAN_POINT('Ctrl Pts',(7.60531324941621,804.264014660816,118.127321089998));
#72552=CARTESIAN_POINT('Ctrl Pts',(7.4732278130278,804.28571529985,118.144650731072));
#72553=CARTESIAN_POINT('Ctrl Pts',(7.22700336739817,804.376372539546,118.193171632574));
#72554=CARTESIAN_POINT('Ctrl Pts',(7.11513287093602,804.444293061202,118.223835269346));
#72555=CARTESIAN_POINT('Ctrl Pts',(6.92609483555976,804.618192584419,118.294059137281));
#72556=CARTESIAN_POINT('Ctrl Pts',(6.85077551572802,804.722462528698,118.332920483092));
#72557=CARTESIAN_POINT('Ctrl Pts',(6.74681866958897,804.954552184318,118.413770244575));
#72558=CARTESIAN_POINT('Ctrl Pts',(6.71943320781253,805.080146110677,118.45496182777));
#72559=CARTESIAN_POINT('Ctrl Pts',(6.71707351890575,805.336230349157,118.534550135433));
#72560=CARTESIAN_POINT('Ctrl Pts',(6.74240845697383,805.464196647438,118.572150775241));
#72561=CARTESIAN_POINT('Ctrl Pts',(6.84314685889307,805.704697604377,118.639200143135));
#72562=CARTESIAN_POINT('Ctrl Pts',(6.9176945787367,805.814870877432,118.667998289195));
#72563=CARTESIAN_POINT('Ctrl Pts',(7.10720753273267,806.002755049752,118.713620999227));
#72564=CARTESIAN_POINT('Ctrl Pts',(7.22068603978126,806.078348782568,118.729908655983));
#72565=CARTESIAN_POINT('Ctrl Pts',(7.47053559653812,806.18283418805,118.747546739802));
#72566=CARTESIAN_POINT('Ctrl Pts',(7.60437780516798,806.210886043958,118.748783275742));
#72567=CARTESIAN_POINT('Ctrl Pts',(7.73962524950022,806.213211761693,118.742202927456));
#72568=CARTESIAN_POINT('',(7.73962524873305,806.8511543926,116.937218327214));
#72569=CARTESIAN_POINT('',(7.73962524950056,809.822483932751,108.530186405553));
#72570=CARTESIAN_POINT('Ctrl Pts',(6.81899994463158,805.434810160941,116.55183368117));
#72571=CARTESIAN_POINT('Ctrl Pts',(6.76131495835045,805.547988625684,116.5918347801));
#72572=CARTESIAN_POINT('Ctrl Pts',(6.72767553170438,805.671414988733,116.633140922881));
#72573=CARTESIAN_POINT('Ctrl Pts',(6.71220824149641,805.924795682934,116.713842608071));
#72574=CARTESIAN_POINT('Ctrl Pts',(6.73053287063395,806.052276455167,116.752456046798));
#72575=CARTESIAN_POINT('Ctrl Pts',(6.81727110090787,806.29490017674,116.822355001029));
#72576=CARTESIAN_POINT('Ctrl Pts',(6.88507115706695,806.40765391491,116.852944154244));
#72577=CARTESIAN_POINT('Ctrl Pts',(7.06193391576527,806.603091405784,116.902253658114));
#72578=CARTESIAN_POINT('Ctrl Pts',(7.16949126667204,806.683778778631,116.920458376782));
#72579=CARTESIAN_POINT('Ctrl Pts',(7.41030387327418,806.801456189114,116.941953730715));
#72580=CARTESIAN_POINT('Ctrl Pts',(7.54128361897485,806.837273557006,116.945023629785));
#72581=CARTESIAN_POINT('Ctrl Pts',(7.80801579791962,806.858554084544,116.935335551326));
#72582=CARTESIAN_POINT('Ctrl Pts',(7.94117176407571,806.84428860958,116.92281340353));
#72583=CARTESIAN_POINT('Ctrl Pts',(8.19492973217388,806.767162435326,116.883150002009));
#72584=CARTESIAN_POINT('Ctrl Pts',(8.31284005106838,806.704449995406,116.856207563332));
#72585=CARTESIAN_POINT('Ctrl Pts',(8.51559192567223,806.538380271382,116.791022007443));
#72586=CARTESIAN_POINT('Ctrl Pts',(8.59835823994668,806.43661688178,116.753403908153));
#72587=CARTESIAN_POINT('Ctrl Pts',(8.71627854751855,806.208756339676,116.672774111363));
#72588=CARTESIAN_POINT('Ctrl Pts',(8.75074276010312,806.085139566965,116.630608505203));
#72589=CARTESIAN_POINT('Ctrl Pts',(8.76736739663133,805.831533572956,116.547156599559));
#72590=CARTESIAN_POINT('Ctrl Pts',(8.74940561479172,805.704022591982,116.506690803449));
#72591=CARTESIAN_POINT('Ctrl Pts',(8.66322225412873,805.462244124062,116.433314171803));
#72592=CARTESIAN_POINT('Ctrl Pts',(8.59600264518925,805.350263292758,116.401094988973));
#72593=CARTESIAN_POINT('Ctrl Pts',(8.42010642511699,805.155324004075,116.349199941691));
#72594=CARTESIAN_POINT('Ctrl Pts',(8.31279114856309,805.074504763307,116.330140613387));
#72595=CARTESIAN_POINT('Ctrl Pts',(8.07106999316088,804.955398951138,116.308176241868));
#72596=CARTESIAN_POINT('Ctrl Pts',(7.93872152846413,804.918792719516,116.305679913427));
#72597=CARTESIAN_POINT('Ctrl Pts',(7.66943048736669,804.896636574549,116.317860827714));
#72598=CARTESIAN_POINT('Ctrl Pts',(7.53512194261262,804.91074897204,116.332228971796));
#72599=CARTESIAN_POINT('Ctrl Pts',(7.28126616695447,804.98780557177,116.375607752691));
#72600=CARTESIAN_POINT('Ctrl Pts',(7.16415682131918,805.049946884604,116.404172651566));
#72601=CARTESIAN_POINT('Ctrl Pts',(7.01282167316582,805.173792299695,116.454808904763));
#72602=CARTESIAN_POINT('Ctrl Pts',(6.96668002233652,805.220108092428,116.472944944874));
#72603=CARTESIAN_POINT('Ctrl Pts',(6.88442731586288,805.321613394483,116.511216276703));
#72604=CARTESIAN_POINT('Ctrl Pts',(6.84865077857284,805.376634956608,116.531272595552));
#72605=CARTESIAN_POINT('Ctrl Pts',(6.81899994463153,805.434810160941,116.55183368117));
#72606=CARTESIAN_POINT('Ctrl Pts',(7.73962524950023,806.213211761693,118.742202927456));
#72607=CARTESIAN_POINT('Ctrl Pts',(7.73966507736922,806.213212446574,118.742200989665));
#72608=CARTESIAN_POINT('Ctrl Pts',(7.73970490535998,806.213213129224,118.742199051195));
#72609=CARTESIAN_POINT('Ctrl Pts',(7.73974473347228,806.213213809644,118.742197112044));
#72610=CARTESIAN_POINT('Ctrl Pts',(7.86972092356887,806.215434311411,118.735868832706));
#72611=CARTESIAN_POINT('Ctrl Pts',(7.99855463379575,806.193855978659,118.722427272111));
#72612=CARTESIAN_POINT('Ctrl Pts',(8.24422874222601,806.104026536541,118.68138442749));
#72613=CARTESIAN_POINT('Ctrl Pts',(8.35807038515727,806.035083011691,118.653698107887));
#72614=CARTESIAN_POINT('Ctrl Pts',(8.55091476656809,805.858369370529,118.586997037738));
#72615=CARTESIAN_POINT('Ctrl Pts',(8.62782091960456,805.752171957187,118.548577303902));
#72616=CARTESIAN_POINT('Ctrl Pts',(8.73310475984059,805.517085137047,118.466025251122));
#72617=CARTESIAN_POINT('Ctrl Pts',(8.76047806328709,805.390546161499,118.422718607167));
#72618=CARTESIAN_POINT('Ctrl Pts',(8.76156941761292,805.134638117182,118.337653443387));
#72619=CARTESIAN_POINT('Ctrl Pts',(8.73555670694445,805.007801765599,118.296741204908));
#72620=CARTESIAN_POINT('Ctrl Pts',(8.63347904356932,804.7699888555,118.223376934523));
#72621=CARTESIAN_POINT('Ctrl Pts',(8.55841972053927,804.661354389114,118.19166745545));
#72622=CARTESIAN_POINT('Ctrl Pts',(8.36795221021987,804.475801335955,118.142186475993));
#72623=CARTESIAN_POINT('Ctrl Pts',(8.25401916512692,804.40108967709,118.125073971573));
#72624=CARTESIAN_POINT('Ctrl Pts',(8.00520544493178,804.298210896697,118.108638494281));
#72625=CARTESIAN_POINT('Ctrl Pts',(7.87305008799637,804.270289227484,118.109184209061));
#72626=CARTESIAN_POINT('Ctrl Pts',(7.73962524950057,804.267101962135,118.118202206281));
#72627=CARTESIAN_POINT('Origin',(7.73962524950056,808.859454792509,108.189819322485));
#72628=CARTESIAN_POINT('',(7.73962524950056,807.196038161002,114.396714565974));
#72629=CARTESIAN_POINT('Origin',(7.73962524950056,806.724615930394,114.230097998707));
#72630=CARTESIAN_POINT('',(7.73962524950071,805.717276769695,118.580698218156));
#72631=CARTESIAN_POINT('',(7.73962524950056,809.330877023117,108.356435889752));
#72632=CARTESIAN_POINT('Ctrl Pts',(7.73942703132262,804.764632786182,118.275191812004));
#72633=CARTESIAN_POINT('Ctrl Pts',(7.6803069953167,804.763344197274,118.27890805784));
#72634=CARTESIAN_POINT('Ctrl Pts',(7.6216351072807,804.772026736497,118.285877779913));
#72635=CARTESIAN_POINT('Ctrl Pts',(7.50497069223838,804.810485868506,118.306576399115));
#72636=CARTESIAN_POINT('Ctrl Pts',(7.44878062387034,804.841967013201,118.320723743749));
#72637=CARTESIAN_POINT('Ctrl Pts',(7.35280716646198,804.924072931586,118.353854150928));
#72638=CARTESIAN_POINT('Ctrl Pts',(7.3139450565688,804.973877909452,118.372506437231));
#72639=CARTESIAN_POINT('Ctrl Pts',(7.25877394270037,805.085573767308,118.411883592206));
#72640=CARTESIAN_POINT('Ctrl Pts',(7.24306220635865,805.146384283711,118.432222756311));
#72641=CARTESIAN_POINT('Ctrl Pts',(7.23718461749696,805.271111529224,118.471992139086));
#72642=CARTESIAN_POINT('Ctrl Pts',(7.24717215376557,805.333806536062,118.491028612901));
#72643=CARTESIAN_POINT('Ctrl Pts',(7.29185694534469,805.452582953991,118.525369496033));
#72644=CARTESIAN_POINT('Ctrl Pts',(7.32618528592688,805.507493346813,118.540334741611));
#72645=CARTESIAN_POINT('Ctrl Pts',(7.41566526079609,805.602831926073,118.564508153228));
#72646=CARTESIAN_POINT('Ctrl Pts',(7.47033225120107,805.641998626575,118.573357622807));
#72647=CARTESIAN_POINT('Ctrl Pts',(7.5916655172645,805.69748301788,118.583323316583));
#72648=CARTESIAN_POINT('Ctrl Pts',(7.65704787848616,805.713424872029,118.584399185988));
#72649=CARTESIAN_POINT('Ctrl Pts',(7.78977309685976,805.720013409946,118.578574448473));
#72650=CARTESIAN_POINT('Ctrl Pts',(7.85579639670194,805.710696997823,118.571760280049));
#72651=CARTESIAN_POINT('Ctrl Pts',(7.97980651809698,805.667916211284,118.550908487762));
#72652=CARTESIAN_POINT('Ctrl Pts',(8.03654060555342,805.634850116953,118.537065832077));
#72653=CARTESIAN_POINT('Ctrl Pts',(8.13285433691024,805.549168836999,118.503954857943));
#72654=CARTESIAN_POINT('Ctrl Pts',(8.1714113386614,805.497367192946,118.485003329618));
#72655=CARTESIAN_POINT('Ctrl Pts',(8.22462677904391,805.382099483559,118.444530402764));
#72656=CARTESIAN_POINT('Ctrl Pts',(8.23875500815394,805.31980323468,118.423419601472));
#72657=CARTESIAN_POINT('Ctrl Pts',(8.24041517411517,805.193361333184,118.382075346817));
#72658=CARTESIAN_POINT('Ctrl Pts',(8.22800820244756,805.130490707571,118.36225839279));
#72659=CARTESIAN_POINT('Ctrl Pts',(8.17823550236331,805.012576685139,118.326773366923));
#72660=CARTESIAN_POINT('Ctrl Pts',(8.14138029080827,804.958704306977,118.311461483642));
#72661=CARTESIAN_POINT('Ctrl Pts',(8.04783721791141,804.867064539568,118.28756208062));
#72662=CARTESIAN_POINT('Ctrl Pts',(7.99198370064763,804.830288815083,118.279248410905));
#72663=CARTESIAN_POINT('Ctrl Pts',(7.8698833274836,804.779719352378,118.271028379672));
#72664=CARTESIAN_POINT('Ctrl Pts',(7.80497283984635,804.766061432163,118.271071646415));
#72665=CARTESIAN_POINT('Ctrl Pts',(7.73942703132262,804.764632786182,118.275191812004));
#72666=CARTESIAN_POINT('Origin',(6.8161311164539,802.337233373458,105.884645588114));
#72667=CARTESIAN_POINT('',(6.81613111645393,797.62882286912,116.361437819037));
#72668=CARTESIAN_POINT('',(6.81613111644524,799.473611621015,116.83203941074));
#72669=CARTESIAN_POINT('Ctrl Pts',(6.81613111645395,797.62882286912,116.361437819037));
#72670=CARTESIAN_POINT('Ctrl Pts',(6.81604355525754,797.628818358335,116.361450581781));
#72671=CARTESIAN_POINT('Ctrl Pts',(6.81595599336896,797.628813859282,116.361463347728));
#72672=CARTESIAN_POINT('Ctrl Pts',(6.69294816100052,797.622510078197,116.379401440403));
#72673=CARTESIAN_POINT('Ctrl Pts',(6.57085364087195,797.639445535317,116.403323434122));
#72674=CARTESIAN_POINT('Ctrl Pts',(6.34388761909424,797.718197941167,116.459742326899));
#72675=CARTESIAN_POINT('Ctrl Pts',(6.24095689020638,797.778570049065,116.491552034475));
#72676=CARTESIAN_POINT('Ctrl Pts',(6.06624785633576,797.935811287255,116.558993650833));
#72677=CARTESIAN_POINT('Ctrl Pts',(5.99624090564599,798.030950164683,116.59390349045));
#72678=CARTESIAN_POINT('Ctrl Pts',(5.89783051725714,798.245491134755,116.662757835106));
#72679=CARTESIAN_POINT('Ctrl Pts',(5.87106446850996,798.362848881483,116.695932839411));
#72680=CARTESIAN_POINT('Ctrl Pts',(5.86545622496071,798.605277690984,116.756533668511));
#72681=CARTESIAN_POINT('Ctrl Pts',(5.8876137635878,798.727906654488,116.783208304679));
#72682=CARTESIAN_POINT('Ctrl Pts',(5.97935436108149,798.961559238557,116.826681074512));
#72683=CARTESIAN_POINT('Ctrl Pts',(6.04891274062436,799.070074424253,116.84288196731));
#72684=CARTESIAN_POINT('Ctrl Pts',(6.22606528446883,799.255811493612,116.862470660604));
#72685=CARTESIAN_POINT('Ctrl Pts',(6.33215286282438,799.331286202517,116.865658921685));
#72686=CARTESIAN_POINT('Ctrl Pts',(6.56488788469013,799.437363932558,116.858520817398));
#72687=CARTESIAN_POINT('Ctrl Pts',(6.68912388985009,799.467641710427,116.848449614987));
#72688=CARTESIAN_POINT('Ctrl Pts',(6.81492901909246,799.47355585377,116.832194910747));
#72689=CARTESIAN_POINT('Ctrl Pts',(6.81532972689165,799.473574691185,116.832143137128));
#72690=CARTESIAN_POINT('Ctrl Pts',(6.81573042608588,799.473593280258,116.832091303782));
#72691=CARTESIAN_POINT('Ctrl Pts',(6.81613111643658,799.473611621015,116.83203941074));
#72692=CARTESIAN_POINT('',(6.81613111645102,800.132384730513,114.968117390021));
#72693=CARTESIAN_POINT('',(6.8161311164539,803.231129546077,106.200578741251));
#72694=CARTESIAN_POINT('Ctrl Pts',(6.01074779320954,798.702525949943,114.667511638846));
#72695=CARTESIAN_POINT('Ctrl Pts',(5.94827792768443,798.797357022413,114.701028148547));
#72696=CARTESIAN_POINT('Ctrl Pts',(5.9052416446383,798.90336977999,114.735148867139));
#72697=CARTESIAN_POINT('Ctrl Pts',(5.86113093765785,799.132940900446,114.803009124232));
#72698=CARTESIAN_POINT('Ctrl Pts',(5.86298459699158,799.254773993399,114.835923698928));
#72699=CARTESIAN_POINT('Ctrl Pts',(5.91459578159424,799.490217611791,114.893931625604));
#72700=CARTESIAN_POINT('Ctrl Pts',(5.96304364173721,799.601724382295,114.918612352913));
#72701=CARTESIAN_POINT('Ctrl Pts',(6.10107809442051,799.803724061892,114.957771793913));
#72702=CARTESIAN_POINT('Ctrl Pts',(6.19004984522366,799.892004700308,114.971728064651));
#72703=CARTESIAN_POINT('Ctrl Pts',(6.39791598941777,800.032415704775,114.98676179417));
#72704=CARTESIAN_POINT('Ctrl Pts',(6.51524274215751,800.082787547882,114.987540321836));
#72705=CARTESIAN_POINT('Ctrl Pts',(6.76216901966767,800.137060182909,114.975266908503));
#72706=CARTESIAN_POINT('Ctrl Pts',(6.88941986686158,800.140328981772,114.962295780724));
#72707=CARTESIAN_POINT('Ctrl Pts',(7.13112049099513,800.099261451316,114.92462821992));
#72708=CARTESIAN_POINT('Ctrl Pts',(7.243641089916,800.05730492707,114.900790689718));
#72709=CARTESIAN_POINT('Ctrl Pts',(7.44159738664962,799.93602222134,114.845459049661));
#72710=CARTESIAN_POINT('Ctrl Pts',(7.5260284388434,799.859065132993,114.814735960931));
#72711=CARTESIAN_POINT('Ctrl Pts',(7.66080878524161,799.677746268727,114.749046306696));
#72712=CARTESIAN_POINT('Ctrl Pts',(7.70972833342177,799.574899724096,114.714659560811));
#72713=CARTESIAN_POINT('Ctrl Pts',(7.76602834666594,799.35303571267,114.645696771555));
#72714=CARTESIAN_POINT('Ctrl Pts',(7.77173807031252,799.235793970228,114.611805892869));
#72715=CARTESIAN_POINT('Ctrl Pts',(7.73632287345495,798.998077719297,114.54835520444));
#72716=CARTESIAN_POINT('Ctrl Pts',(7.69309018749097,798.88021558252,114.519780523955));
#72717=CARTESIAN_POINT('Ctrl Pts',(7.56350523489464,798.66871882365,114.474693520515));
#72718=CARTESIAN_POINT('Ctrl Pts',(7.47937350020835,798.576590694492,114.458353560822));
#72719=CARTESIAN_POINT('Ctrl Pts',(7.27928281246208,798.426295646752,114.439354510948));
#72720=CARTESIAN_POINT('Ctrl Pts',(7.16475879310693,798.37001284635,114.437065330823));
#72721=CARTESIAN_POINT('Ctrl Pts',(6.9202875494757,798.302478660598,114.447276891869));
#72722=CARTESIAN_POINT('Ctrl Pts',(6.79251849366301,798.292279934721,114.459811382783));
#72723=CARTESIAN_POINT('Ctrl Pts',(6.5551195704484,798.319492011922,114.496051856014));
#72724=CARTESIAN_POINT('Ctrl Pts',(6.44687289501309,798.351848729651,114.518167590459));
#72725=CARTESIAN_POINT('Ctrl Pts',(6.24374667406768,798.455422307701,114.571427367212));
#72726=CARTESIAN_POINT('Ctrl Pts',(6.15171553339862,798.52754715734,114.602467143043));
#72727=CARTESIAN_POINT('Ctrl Pts',(6.05284563521359,798.642825807817,114.646066270405));
#72728=CARTESIAN_POINT('Ctrl Pts',(6.0308327767351,798.672036360887,114.656735586433));
#72729=CARTESIAN_POINT('Ctrl Pts',(6.01074779320959,798.702525949943,114.667511638846));
#72730=CARTESIAN_POINT('Ctrl Pts',(6.81613111643658,799.473611621015,116.83203941074));
#72731=CARTESIAN_POINT('Ctrl Pts',(6.93665525034905,799.479128359434,116.816430439957));
#72732=CARTESIAN_POINT('Ctrl Pts',(7.05637978296077,799.462177662245,116.795424117734));
#72733=CARTESIAN_POINT('Ctrl Pts',(7.28486648494508,799.383439235941,116.743426257329));
#72734=CARTESIAN_POINT('Ctrl Pts',(7.39079152683966,799.321029728914,116.712656173739));
#72735=CARTESIAN_POINT('Ctrl Pts',(7.56791944632267,799.16008888171,116.646186311464));
#72736=CARTESIAN_POINT('Ctrl Pts',(7.6380109240145,799.064003562227,116.611278377729));
#72737=CARTESIAN_POINT('Ctrl Pts',(7.73638929751765,798.847176413892,116.540457276636));
#72738=CARTESIAN_POINT('Ctrl Pts',(7.76266176660441,798.728252097948,116.505299866886));
#72739=CARTESIAN_POINT('Ctrl Pts',(7.76563629988533,798.485488138897,116.440662166943));
#72740=CARTESIAN_POINT('Ctrl Pts',(7.74229368430618,798.364173750922,116.411869578574));
#72741=CARTESIAN_POINT('Ctrl Pts',(7.64895664758895,798.134509339619,116.364886523339));
#72742=CARTESIAN_POINT('Ctrl Pts',(7.57953802933586,798.028539756959,116.347255576251));
#72743=CARTESIAN_POINT('Ctrl Pts',(7.40288190392766,797.845687558127,116.325994048102));
#72744=CARTESIAN_POINT('Ctrl Pts',(7.29677536501533,797.770950015637,116.322769350076));
#72745=CARTESIAN_POINT('Ctrl Pts',(7.06473329425217,797.665608558726,116.331537351354));
#72746=CARTESIAN_POINT('Ctrl Pts',(6.94113661840373,797.635262627994,116.343217269045));
#72747=CARTESIAN_POINT('Ctrl Pts',(6.81613111645396,797.62882286912,116.361437819037));
#72748=CARTESIAN_POINT('Origin',(6.8161311164539,802.337233373458,105.884645588114));
#72749=CARTESIAN_POINT('',(6.8161311164539,800.673816741952,112.091540831602));
#72750=CARTESIAN_POINT('Origin',(6.8161311164539,800.202394511343,111.924924264335));
#72751=CARTESIAN_POINT('',(6.8161311164541,799.038612298614,116.718161934316));
#72752=CARTESIAN_POINT('',(6.8161311164539,802.808655604067,106.051262155381));
#72753=CARTESIAN_POINT('Ctrl Pts',(6.81580794006168,798.065704838105,116.469988878972));
#72754=CARTESIAN_POINT('Ctrl Pts',(6.7543796153778,798.062661509509,116.47871877281));
#72755=CARTESIAN_POINT('Ctrl Pts',(6.69332155622728,798.070633238579,116.49025344683));
#72756=CARTESIAN_POINT('Ctrl Pts',(6.57572131339275,798.108967467512,116.518312508229));
#72757=CARTESIAN_POINT('Ctrl Pts',(6.52061302842095,798.139893322244,116.534754014128));
#72758=CARTESIAN_POINT('Ctrl Pts',(6.4266136932548,798.221243656218,116.569952156603));
#72759=CARTESIAN_POINT('Ctrl Pts',(6.3886468697899,798.270755429356,116.588332923346));
#72760=CARTESIAN_POINT('Ctrl Pts',(6.33456190763045,798.382768281265,116.624869201289));
#72761=CARTESIAN_POINT('Ctrl Pts',(6.31925762111652,798.444190102766,116.642626950885));
#72762=CARTESIAN_POINT('Ctrl Pts',(6.31381941331088,798.571424709535,116.675330894803));
#72763=CARTESIAN_POINT('Ctrl Pts',(6.32418796365442,798.635961269097,116.689882275963));
#72764=CARTESIAN_POINT('Ctrl Pts',(6.3701557089184,798.760009329424,116.713961899536));
#72765=CARTESIAN_POINT('Ctrl Pts',(6.40597239703097,798.818105205021,116.723108038333));
#72766=CARTESIAN_POINT('Ctrl Pts',(6.49792294837037,798.917744697554,116.734374023444));
#72767=CARTESIAN_POINT('Ctrl Pts',(6.55314738059275,798.95843843497,116.736417804411));
#72768=CARTESIAN_POINT('Ctrl Pts',(6.67518620580731,799.016665101815,116.733140858802));
#72769=CARTESIAN_POINT('Ctrl Pts',(6.74080209751259,799.03386033086,116.727909106));
#72770=CARTESIAN_POINT('Ctrl Pts',(6.87363166527902,799.04236903342,116.710754030943));
#72771=CARTESIAN_POINT('Ctrl Pts',(6.93955714260679,799.033781679734,116.69903933778));
#72772=CARTESIAN_POINT('Ctrl Pts',(7.06143948004197,798.99220535637,116.670801611149));
#72773=CARTESIAN_POINT('Ctrl Pts',(7.116420129854,798.960307081348,116.654695294223));
#72774=CARTESIAN_POINT('Ctrl Pts',(7.20970171777221,798.877245271801,116.619831929976));
#72775=CARTESIAN_POINT('Ctrl Pts',(7.24711464410287,798.827017237173,116.601442688545));
#72776=CARTESIAN_POINT('Ctrl Pts',(7.29989636346429,798.713693781464,116.564419428754));
#72777=CARTESIAN_POINT('Ctrl Pts',(7.31435912177347,798.651621065621,116.546181155725));
#72778=CARTESIAN_POINT('Ctrl Pts',(7.31762356009194,798.52358749062,116.512414208227));
#72779=CARTESIAN_POINT('Ctrl Pts',(7.305975167089,798.458935039213,116.497294475349));
#72780=CARTESIAN_POINT('Ctrl Pts',(7.25768541697495,798.336446873472,116.472618764187));
#72781=CARTESIAN_POINT('Ctrl Pts',(7.22137443733566,798.279868390151,116.463344637139));
#72782=CARTESIAN_POINT('Ctrl Pts',(7.12870284052068,798.18240642053,116.452059821675));
#72783=CARTESIAN_POINT('Ctrl Pts',(7.07303448450468,798.142563640943,116.450217458438));
#72784=CARTESIAN_POINT('Ctrl Pts',(6.94973861296488,798.085560492895,116.45439380324));
#72785=CARTESIAN_POINT('Ctrl Pts',(6.8831701538097,798.069042147929,116.460415689768));
#72786=CARTESIAN_POINT('Ctrl Pts',(6.81580794006168,798.065704838105,116.469988878972));
#72787=CARTESIAN_POINT('Origin',(4.21616833870003,818.154693156259,111.475071072488));
#72788=CARTESIAN_POINT('',(4.21616833870006,813.566663386125,121.391222359302));
#72789=CARTESIAN_POINT('',(4.21616833869997,815.503730966578,122.040806989507));
#72790=CARTESIAN_POINT('Ctrl Pts',(4.21616833870006,813.566663386125,121.391222359302));
#72791=CARTESIAN_POINT('Ctrl Pts',(4.21579739595471,813.566654326904,121.391247991317));
#72792=CARTESIAN_POINT('Ctrl Pts',(4.21542644360822,813.566645457546,121.391273692532));
#72793=CARTESIAN_POINT('Ctrl Pts',(4.08151962453409,813.563512416058,121.400576088745));
#72794=CARTESIAN_POINT('Ctrl Pts',(3.94927725818734,813.585048816235,121.4186585503));
#72795=CARTESIAN_POINT('Ctrl Pts',(3.70290827213485,813.675056767274,121.469733158647));
#72796=CARTESIAN_POINT('Ctrl Pts',(3.59101711651222,813.7424945632,121.502170135717));
#72797=CARTESIAN_POINT('Ctrl Pts',(3.40222886819611,813.915004724076,121.576569498705));
#72798=CARTESIAN_POINT('Ctrl Pts',(3.32706623318748,814.018333135414,121.61778141041));
#72799=CARTESIAN_POINT('Ctrl Pts',(3.22340449421018,814.24827939509,121.703389039361));
#72800=CARTESIAN_POINT('Ctrl Pts',(3.19605986775251,814.372671216344,121.746936556848));
#72801=CARTESIAN_POINT('Ctrl Pts',(3.19354318820913,814.626689524154,121.830781575904));
#72802=CARTESIAN_POINT('Ctrl Pts',(3.21870879655004,814.753790459032,121.87022216573));
#72803=CARTESIAN_POINT('Ctrl Pts',(3.3190825739423,814.99329705162,121.94007184856));
#72804=CARTESIAN_POINT('Ctrl Pts',(3.39352917219228,815.103278725567,121.969767839707));
#72805=CARTESIAN_POINT('Ctrl Pts',(3.5820490759131,815.290378121672,122.0158818445));
#72806=CARTESIAN_POINT('Ctrl Pts',(3.69433488590728,815.365693067524,122.03186961327));
#72807=CARTESIAN_POINT('Ctrl Pts',(3.94402218175684,815.471858923636,122.048509266252));
#72808=CARTESIAN_POINT('Ctrl Pts',(4.0793366716235,815.500912444094,122.048750602559));
#72809=CARTESIAN_POINT('Ctrl Pts',(4.21609103298932,815.503729376994,122.04081147827));
#72810=CARTESIAN_POINT('Ctrl Pts',(4.21611680160463,815.503729907789,122.040809982302));
#72811=CARTESIAN_POINT('Ctrl Pts',(4.21614257017483,815.50373043765,122.040808486047));
#72812=CARTESIAN_POINT('Ctrl Pts',(4.21616833869989,815.503730966578,122.040806989507));
#72813=CARTESIAN_POINT('',(4.21616833820598,816.141966729996,120.234993004862));
#72814=CARTESIAN_POINT('',(4.21616833870003,819.117722296501,111.815438155555));
#72815=CARTESIAN_POINT('Ctrl Pts',(3.22367932508172,814.919632311137,119.90409075603));
#72816=CARTESIAN_POINT('Ctrl Pts',(3.19221248465311,815.041645449644,119.947214327596));
#72817=CARTESIAN_POINT('Ctrl Pts',(3.18636504709321,815.168984840346,119.989903466751));
#72818=CARTESIAN_POINT('Ctrl Pts',(3.22649682289723,815.419921359348,120.069741297725));
#72819=CARTESIAN_POINT('Ctrl Pts',(3.27208612232692,815.541068456448,120.106116201354));
#72820=CARTESIAN_POINT('Ctrl Pts',(3.4093328644833,815.761495951288,120.16817025803));
#72821=CARTESIAN_POINT('Ctrl Pts',(3.49987357034009,815.858558603504,120.193213650547));
#72822=CARTESIAN_POINT('Ctrl Pts',(3.71459906287451,816.015190894562,120.228808083796));
#72823=CARTESIAN_POINT('Ctrl Pts',(3.8368843217803,816.073101566701,120.238962745765));
#72824=CARTESIAN_POINT('Ctrl Pts',(4.09699197200466,816.141139309507,120.242913761541));
#72825=CARTESIAN_POINT('Ctrl Pts',(4.23234340884442,816.150564070566,120.23665562034));
#72826=CARTESIAN_POINT('Ctrl Pts',(4.49674721742275,816.119210643793,120.208364921513));
#72827=CARTESIAN_POINT('Ctrl Pts',(4.62332939543466,816.079205911963,120.186745649431));
#72828=CARTESIAN_POINT('Ctrl Pts',(4.85367522162754,815.954106530113,120.130126893132));
#72829=CARTESIAN_POINT('Ctrl Pts',(4.95484884405447,815.869683540675,120.09551121166));
#72830=CARTESIAN_POINT('Ctrl Pts',(5.11609946869123,815.667542280614,120.017576754425));
#72831=CARTESIAN_POINT('Ctrl Pts',(5.17450233019456,815.551789456814,119.975014315745));
#72832=CARTESIAN_POINT('Ctrl Pts',(5.2395923823904,815.305793146957,119.887974724992));
#72833=CARTESIAN_POINT('Ctrl Pts',(5.24614971038165,815.178111264852,119.844372371625));
#72834=CARTESIAN_POINT('Ctrl Pts',(5.2069152812454,814.926745832242,119.761712356192));
#72835=CARTESIAN_POINT('Ctrl Pts',(5.16154664126315,814.805510702664,119.723464658313));
#72836=CARTESIAN_POINT('Ctrl Pts',(5.02476739304651,814.585827148372,119.657897116744));
#72837=CARTESIAN_POINT('Ctrl Pts',(4.93483302848475,814.489419795905,119.631182128276));
#72838=CARTESIAN_POINT('Ctrl Pts',(4.72097148078736,814.333104311715,119.592938040371));
#72839=CARTESIAN_POINT('Ctrl Pts',(4.59883794649819,814.275022747381,119.581914976267));
#72840=CARTESIAN_POINT('Ctrl Pts',(4.33752909919282,814.205765672262,119.577568835096));
#72841=CARTESIAN_POINT('Ctrl Pts',(4.20072395219808,814.195831741583,119.584499400288));
#72842=CARTESIAN_POINT('Ctrl Pts',(3.93381826417745,814.226811054965,119.615460183439));
#72843=CARTESIAN_POINT('Ctrl Pts',(3.80620658292549,814.266878946968,119.639001877507));
#72844=CARTESIAN_POINT('Ctrl Pts',(3.57600886078964,814.391903770064,119.699334251585));
#72845=CARTESIAN_POINT('Ctrl Pts',(3.47561916032804,814.475598574139,119.735516883545));
#72846=CARTESIAN_POINT('Ctrl Pts',(3.355376499897,814.62635652068,119.795664935966));
#72847=CARTESIAN_POINT('Ctrl Pts',(3.32057888538006,814.680693147426,119.816635810209));
#72848=CARTESIAN_POINT('Ctrl Pts',(3.26267307358109,814.796087730609,119.859816083944));
#72849=CARTESIAN_POINT('Ctrl Pts',(3.23985369072435,814.856915969473,119.881924678826));
#72850=CARTESIAN_POINT('Ctrl Pts',(3.22367932508172,814.919632311137,119.90409075603));
#72851=CARTESIAN_POINT('Ctrl Pts',(4.21616833869988,815.503730966578,122.040806989507));
#72852=CARTESIAN_POINT('Ctrl Pts',(4.347914315043,815.506435201059,122.033155672043));
#72853=CARTESIAN_POINT('Ctrl Pts',(4.47848121683415,815.484739441053,122.018051117122));
#72854=CARTESIAN_POINT('Ctrl Pts',(4.72499390664615,815.39419730065,121.973661824122));
#72855=CARTESIAN_POINT('Ctrl Pts',(4.83821063321016,815.325410607071,121.94454951115));
#72856=CARTESIAN_POINT('Ctrl Pts',(5.02957904846655,815.14947769508,121.875347618212));
#72857=CARTESIAN_POINT('Ctrl Pts',(5.10575399381212,815.043985810499,121.835898711131));
#72858=CARTESIAN_POINT('Ctrl Pts',(5.21013900292989,814.810264999246,121.751319288353));
#72859=CARTESIAN_POINT('Ctrl Pts',(5.2372210297118,814.68430473374,121.707007309095));
#72860=CARTESIAN_POINT('Ctrl Pts',(5.23792432954282,814.429332562611,121.619731263981));
#72861=CARTESIAN_POINT('Ctrl Pts',(5.21167957665196,814.302835549282,121.577632118039));
#72862=CARTESIAN_POINT('Ctrl Pts',(5.10914639550353,814.066009917319,121.501902354179));
#72863=CARTESIAN_POINT('Ctrl Pts',(5.03394315201209,813.957983982788,121.469023268446));
#72864=CARTESIAN_POINT('Ctrl Pts',(4.84358596990866,813.773904052068,121.417492551366));
#72865=CARTESIAN_POINT('Ctrl Pts',(4.73003738953763,813.699925994421,121.399478445952));
#72866=CARTESIAN_POINT('Ctrl Pts',(4.4816910942168,813.59771819199,121.381759167324));
#72867=CARTESIAN_POINT('Ctrl Pts',(4.34954949966834,813.569920841612,121.382005767238));
#72868=CARTESIAN_POINT('Ctrl Pts',(4.21616833870007,813.566663386125,121.391222359302));
#72869=CARTESIAN_POINT('Origin',(4.21616833870003,818.154693156259,111.475071072488));
#72870=CARTESIAN_POINT('',(4.21616833870003,816.491276524752,117.681966315976));
#72871=CARTESIAN_POINT('Origin',(4.21616833870003,816.019854294144,117.515349748709));
#72872=CARTESIAN_POINT('',(4.2161683387002,815.009671259245,121.873996379995));
#72873=CARTESIAN_POINT('',(4.21616833870003,818.626115386867,111.641687639755));
#72874=CARTESIAN_POINT('Ctrl Pts',(4.21591630885621,814.061445921076,121.555988002616));
#72875=CARTESIAN_POINT('Ctrl Pts',(4.15552196213932,814.06006265502,121.559993147844));
#72876=CARTESIAN_POINT('Ctrl Pts',(4.09561609080141,814.069024841709,121.567563518964));
#72877=CARTESIAN_POINT('Ctrl Pts',(3.97808181203072,814.108345878869,121.589863612151));
#72878=CARTESIAN_POINT('Ctrl Pts',(3.92213372965487,814.139987972191,121.604903509755));
#72879=CARTESIAN_POINT('Ctrl Pts',(3.82687081961698,814.222171178162,121.640013468081));
#72880=CARTESIAN_POINT('Ctrl Pts',(3.78843887181263,814.271878293051,121.659730173664));
#72881=CARTESIAN_POINT('Ctrl Pts',(3.7342215244729,814.383144228812,121.701216799812));
#72882=CARTESIAN_POINT('Ctrl Pts',(3.71899499190225,814.443619358232,121.72257857952));
#72883=CARTESIAN_POINT('Ctrl Pts',(3.71404760608176,814.567586012134,121.764179312166));
#72884=CARTESIAN_POINT('Ctrl Pts',(3.72447129863588,814.629856435003,121.784002021646));
#72885=CARTESIAN_POINT('Ctrl Pts',(3.76995848233187,814.747832107846,121.819548530303));
#72886=CARTESIAN_POINT('Ctrl Pts',(3.80466518948911,814.802353856866,121.83491178086));
#72887=CARTESIAN_POINT('Ctrl Pts',(3.89394549383036,814.896045752094,121.859198985713));
#72888=CARTESIAN_POINT('Ctrl Pts',(3.9476868533989,814.934292287786,121.867884107372));
#72889=CARTESIAN_POINT('Ctrl Pts',(4.06825440704684,814.989633510265,121.8775506611));
#72890=CARTESIAN_POINT('Ctrl Pts',(4.13411280462523,815.005766201399,121.878289859009));
#72891=CARTESIAN_POINT('Ctrl Pts',(4.26752485498035,815.012468557479,121.871423147378));
#72892=CARTESIAN_POINT('Ctrl Pts',(4.33374585310983,815.003161618151,121.863945434534));
#72893=CARTESIAN_POINT('Ctrl Pts',(4.45770354762203,814.960416980212,121.841647371366));
#72894=CARTESIAN_POINT('Ctrl Pts',(4.5142390171448,814.927495645059,121.827072175354));
#72895=CARTESIAN_POINT('Ctrl Pts',(4.61004378864544,814.842319992247,121.792524512427));
#72896=CARTESIAN_POINT('Ctrl Pts',(4.64834689317697,814.790915143196,121.772892696958));
#72897=CARTESIAN_POINT('Ctrl Pts',(4.70125386041098,814.676480271627,121.731066229657));
#72898=CARTESIAN_POINT('Ctrl Pts',(4.71530778575685,814.614593841588,121.709289011278));
#72899=CARTESIAN_POINT('Ctrl Pts',(4.7169515869088,814.488829597756,121.66660187769));
#72900=CARTESIAN_POINT('Ctrl Pts',(4.70454822428203,814.426216132537,121.646121994441));
#72901=CARTESIAN_POINT('Ctrl Pts',(4.65477641739308,814.308732600749,121.609400206655));
#72902=CARTESIAN_POINT('Ctrl Pts',(4.61790622062084,814.255038285866,121.593530522019));
#72903=CARTESIAN_POINT('Ctrl Pts',(4.52434712330669,814.163717598429,121.568741666655));
#72904=CARTESIAN_POINT('Ctrl Pts',(4.46850982709221,814.127074978406,121.560104934687));
#72905=CARTESIAN_POINT('Ctrl Pts',(4.34640555546615,814.076609567842,121.55157551949));
#72906=CARTESIAN_POINT('Ctrl Pts',(4.2814711554186,814.062947382702,121.551640630799));
#72907=CARTESIAN_POINT('Ctrl Pts',(4.21591630885621,814.061445921076,121.555988002616));
#72908=CARTESIAN_POINT('Origin',(1.87460472916284,811.956028988243,109.284253418465));
#72909=CARTESIAN_POINT('',(1.87460472916284,807.25641609678,119.736153825281));
#72910=CARTESIAN_POINT('',(1.87460472914096,809.080906302795,120.264187795611));
#72911=CARTESIAN_POINT('Ctrl Pts',(1.87460472916287,807.25641609678,119.736153825281));
#72912=CARTESIAN_POINT('Ctrl Pts',(1.75103549584412,807.24947860926,119.755782640683));
#72913=CARTESIAN_POINT('Ctrl Pts',(1.62836973988592,807.265718400088,119.78233157051));
#72914=CARTESIAN_POINT('Ctrl Pts',(1.40065186333159,807.342855758013,119.845485989263));
#72915=CARTESIAN_POINT('Ctrl Pts',(1.29742613189207,807.40234385158,119.881340847999));
#72916=CARTESIAN_POINT('Ctrl Pts',(1.12314017366551,807.557234499257,119.957439014239));
#72917=CARTESIAN_POINT('Ctrl Pts',(1.05351618053732,807.650714655165,119.996862573774));
#72918=CARTESIAN_POINT('Ctrl Pts',(0.956087033711997,807.861277422583,120.074560571483));
#72919=CARTESIAN_POINT('Ctrl Pts',(0.929579051060437,807.976212894383,120.111984351191));
#72920=CARTESIAN_POINT('Ctrl Pts',(0.923909377596282,808.214128449828,120.180375364673));
#72921=CARTESIAN_POINT('Ctrl Pts',(0.945672229366337,808.334631279297,120.210477268493));
#72922=CARTESIAN_POINT('Ctrl Pts',(1.03601846715911,808.564880083577,120.259459016282));
#72923=CARTESIAN_POINT('Ctrl Pts',(1.10451976956373,808.672072392336,120.277646302952));
#72924=CARTESIAN_POINT('Ctrl Pts',(1.28056330507626,808.858173895426,120.299796035088));
#72925=CARTESIAN_POINT('Ctrl Pts',(1.38723989220875,808.934688042217,120.303253530113));
#72926=CARTESIAN_POINT('Ctrl Pts',(1.62152018801628,809.042855486623,120.294711538717));
#72927=CARTESIAN_POINT('Ctrl Pts',(1.74674633614967,809.074099378817,120.282986895974));
#72928=CARTESIAN_POINT('Ctrl Pts',(1.8734622404411,809.080846138924,120.264355956543));
#72929=CARTESIAN_POINT('Ctrl Pts',(1.87384307751858,809.080866415908,120.264299962368));
#72930=CARTESIAN_POINT('Ctrl Pts',(1.87422390714615,809.080886470526,120.264243908713));
#72931=CARTESIAN_POINT('Ctrl Pts',(1.87460472911907,809.080906302795,120.264187795611));
#72932=CARTESIAN_POINT('',(1.87460472916012,809.743718201466,118.388838489889));
#72933=CARTESIAN_POINT('',(1.87460472916284,812.849925160862,109.600186571602));
#72934=CARTESIAN_POINT('Ctrl Pts',(0.982819008185952,808.489505833977,118.126561480607));
#72935=CARTESIAN_POINT('Ctrl Pts',(0.942625967695021,808.594510486907,118.163673677874));
#72936=CARTESIAN_POINT('Ctrl Pts',(0.923675628408658,808.706665929454,118.199965429178));
#72937=CARTESIAN_POINT('Ctrl Pts',(0.930232869014416,808.939958483743,118.269140966905));
#72938=CARTESIAN_POINT('Ctrl Pts',(0.958209188629994,809.05883551688,118.301010770041));
#72939=CARTESIAN_POINT('Ctrl Pts',(1.05886514447545,809.279189926667,118.35368565984));
#72940=CARTESIAN_POINT('Ctrl Pts',(1.129822751318,809.378863980049,118.374184304548));
#72941=CARTESIAN_POINT('Ctrl Pts',(1.307151577289,809.549612121828,118.402298394661));
#72942=CARTESIAN_POINT('Ctrl Pts',(1.41245152614895,809.6186410281,118.40945045186));
#72943=CARTESIAN_POINT('Ctrl Pts',(1.64434142181353,809.715473551999,118.409082071832));
#72944=CARTESIAN_POINT('Ctrl Pts',(1.76903255340026,809.741862161876,118.401384113382));
#72945=CARTESIAN_POINT('Ctrl Pts',(2.02035153667182,809.746760213165,118.371660051525));
#72946=CARTESIAN_POINT('Ctrl Pts',(2.14456374543044,809.725109791134,118.349881627919));
#72947=CARTESIAN_POINT('Ctrl Pts',(2.37032250526495,809.637718463314,118.295841669722));
#72948=CARTESIAN_POINT('Ctrl Pts',(2.47050805225589,809.574683409597,118.264554273995));
#72949=CARTESIAN_POINT('Ctrl Pts',(2.63653013030491,809.417331558491,118.196474577532));
#72950=CARTESIAN_POINT('Ctrl Pts',(2.70190179787091,809.325529478102,118.160504766322));
#72951=CARTESIAN_POINT('Ctrl Pts',(2.79364204544573,809.121763114752,118.08688140638));
#72952=CARTESIAN_POINT('Ctrl Pts',(2.81894932283529,809.011560918391,118.049894924289));
#72953=CARTESIAN_POINT('Ctrl Pts',(2.82574944824385,808.783443875928,117.978722102287));
#72954=CARTESIAN_POINT('Ctrl Pts',(2.80600362724193,808.667593067868,117.945322826876));
#72955=CARTESIAN_POINT('Ctrl Pts',(2.72036714624902,808.441872668529,117.886111878289));
#72956=CARTESIAN_POINT('Ctrl Pts',(2.65299513231454,808.334971119733,117.861411040457));
#72957=CARTESIAN_POINT('Ctrl Pts',(2.48165878776808,808.153294742417,117.826863568856));
#72958=CARTESIAN_POINT('Ctrl Pts',(2.38017372238493,808.079560671286,117.817024691649));
#72959=CARTESIAN_POINT('Ctrl Pts',(2.15367708819099,807.971539124383,117.81296652733));
#72960=CARTESIAN_POINT('Ctrl Pts',(2.03046406548969,807.938815338816,117.819003900188));
#72961=CARTESIAN_POINT('Ctrl Pts',(1.77880397588497,807.920446253038,117.846592071107));
#72962=CARTESIAN_POINT('Ctrl Pts',(1.65269616866143,807.935405948966,117.868018399543));
#72963=CARTESIAN_POINT('Ctrl Pts',(1.42833017212113,808.008377519518,117.920431826035));
#72964=CARTESIAN_POINT('Ctrl Pts',(1.33032402726732,808.061173261856,117.949771403349));
#72965=CARTESIAN_POINT('Ctrl Pts',(1.15562996349709,808.202187676284,118.01626403852));
#72966=CARTESIAN_POINT('Ctrl Pts',(1.08189897272091,808.290739046924,118.053109502678));
#72967=CARTESIAN_POINT('Ctrl Pts',(1.01080818798242,808.422860282031,118.102661369331));
#72968=CARTESIAN_POINT('Ctrl Pts',(0.995741663762431,808.455745288689,118.114629361585));
#72969=CARTESIAN_POINT('Ctrl Pts',(0.982819008185979,808.489505833977,118.126561480607));
#72970=CARTESIAN_POINT('Ctrl Pts',(1.87460472911908,809.080906302795,120.264187795611));
#72971=CARTESIAN_POINT('Ctrl Pts',(1.99072328499639,809.08695347077,120.247078036002));
#72972=CARTESIAN_POINT('Ctrl Pts',(2.10613151435791,809.072325787297,120.224449647386));
#72973=CARTESIAN_POINT('Ctrl Pts',(2.33134970731173,809.00036503431,120.168049079998));
#72974=CARTESIAN_POINT('Ctrl Pts',(2.43799701456852,808.940890665549,120.134168739612));
#72975=CARTESIAN_POINT('Ctrl Pts',(2.61920945920015,808.783876834124,120.060218809982));
#72976=CARTESIAN_POINT('Ctrl Pts',(2.69190568992126,808.688020815213,120.020918203225));
#72977=CARTESIAN_POINT('Ctrl Pts',(2.79289670773424,808.472524860687,119.941871820671));
#72978=CARTESIAN_POINT('Ctrl Pts',(2.82010327914144,808.355185743614,119.902969138478));
#72979=CARTESIAN_POINT('Ctrl Pts',(2.8249240987974,808.114954932764,119.831056598888));
#72980=CARTESIAN_POINT('Ctrl Pts',(2.80249149175379,807.99460496946,119.798816682038));
#72981=CARTESIAN_POINT('Ctrl Pts',(2.71086408106223,807.766515535603,119.745718689865));
#72982=CARTESIAN_POINT('Ctrl Pts',(2.64238875976384,807.661168277672,119.725471164478));
#72983=CARTESIAN_POINT('Ctrl Pts',(2.46772646343663,807.47885372346,119.700171889594));
#72984=CARTESIAN_POINT('Ctrl Pts',(2.36276911691211,807.404025681426,119.695569077496));
#72985=CARTESIAN_POINT('Ctrl Pts',(2.12960285019528,807.295668215198,119.703274012147));
#72986=CARTESIAN_POINT('Ctrl Pts',(2.00322961320662,807.263752966054,119.715757176099));
#72987=CARTESIAN_POINT('Ctrl Pts',(1.87519983982174,807.2564496419,119.736059333623));
#72988=CARTESIAN_POINT('Ctrl Pts',(1.87490228187681,807.256432802138,119.736106559411));
#72989=CARTESIAN_POINT('Ctrl Pts',(1.87460472916285,807.25641609678,119.736153825281));
#72990=CARTESIAN_POINT('Origin',(1.87460472916284,811.956028988243,109.284253418465));
#72991=CARTESIAN_POINT('',(1.87460472916284,810.292612356737,115.491148661954));
#72992=CARTESIAN_POINT('Origin',(1.87460472916284,809.821190126128,115.324532094686));
#72993=CARTESIAN_POINT('',(1.87460472916283,808.650347571495,120.137746182282));
#72994=CARTESIAN_POINT('',(1.87460472916284,812.427451218852,109.450869985732));
#72995=CARTESIAN_POINT('Ctrl Pts',(1.87415121283263,807.688135745084,119.859311375963));
#72996=CARTESIAN_POINT('Ctrl Pts',(1.81123905313606,807.684719945843,119.86914722499));
#72997=CARTESIAN_POINT('Ctrl Pts',(1.74876005479557,807.6927213796,119.882310692792));
#72998=CARTESIAN_POINT('Ctrl Pts',(1.63002655636162,807.73146338099,119.914217166966));
#72999=CARTESIAN_POINT('Ctrl Pts',(1.57503418290112,807.762342951292,119.93277936381));
#73000=CARTESIAN_POINT('Ctrl Pts',(1.48186889472678,807.843247470558,119.972450053152));
#73001=CARTESIAN_POINT('Ctrl Pts',(1.44446864217568,807.892267856135,119.99313112845));
#73002=CARTESIAN_POINT('Ctrl Pts',(1.39174295307579,808.002842937753,120.034135637593));
#73003=CARTESIAN_POINT('Ctrl Pts',(1.37706602145846,808.063263908712,120.054018864579));
#73004=CARTESIAN_POINT('Ctrl Pts',(1.37267743184874,808.188397163861,120.090588415092));
#73005=CARTESIAN_POINT('Ctrl Pts',(1.38340164071457,808.251816608146,120.106829571659));
#73006=CARTESIAN_POINT('Ctrl Pts',(1.42962580928306,808.373487772313,120.133572743112));
#73007=CARTESIAN_POINT('Ctrl Pts',(1.46517305774742,808.430358508466,120.143676182847));
#73008=CARTESIAN_POINT('Ctrl Pts',(1.55686256304649,808.529152863639,120.156235685135));
#73009=CARTESIAN_POINT('Ctrl Pts',(1.61245004635588,808.569888017684,120.158452324485));
#73010=CARTESIAN_POINT('Ctrl Pts',(1.73523469610953,808.628298955917,120.154543940035));
#73011=CARTESIAN_POINT('Ctrl Pts',(1.80125316755559,808.645590502154,120.148506330388));
#73012=CARTESIAN_POINT('Ctrl Pts',(1.93450917179671,808.654304616807,120.128978862922));
#73013=CARTESIAN_POINT('Ctrl Pts',(2.00049737710795,808.645885727578,120.115737376022));
#73014=CARTESIAN_POINT('Ctrl Pts',(2.12237961463586,808.60476778445,120.083969932862));
#73015=CARTESIAN_POINT('Ctrl Pts',(2.17733134395792,808.573117422367,120.065894989075));
#73016=CARTESIAN_POINT('Ctrl Pts',(2.27016201139863,808.490730810805,120.026935329761));
#73017=CARTESIAN_POINT('Ctrl Pts',(2.30724879376502,808.440993570416,120.006466421708));
#73018=CARTESIAN_POINT('Ctrl Pts',(2.35893381692117,808.329470149223,119.965558761407));
#73019=CARTESIAN_POINT('Ctrl Pts',(2.37297690792318,808.268834818019,119.945545079137));
#73020=CARTESIAN_POINT('Ctrl Pts',(2.37600694101095,808.142919188342,119.908165285883));
#73021=CARTESIAN_POINT('Ctrl Pts',(2.36426573934037,808.078918558869,119.891292908726));
#73022=CARTESIAN_POINT('Ctrl Pts',(2.31578907653539,807.957573271305,119.863643618579));
#73023=CARTESIAN_POINT('Ctrl Pts',(2.27941749384543,807.901516396578,119.853188989858));
#73024=CARTESIAN_POINT('Ctrl Pts',(2.18669906391868,807.804831068224,119.840287142195));
#73025=CARTESIAN_POINT('Ctrl Pts',(2.13106711651516,807.765275428406,119.838039605903));
#73026=CARTESIAN_POINT('Ctrl Pts',(2.00788629336271,807.708402984618,119.842281425572));
#73027=CARTESIAN_POINT('Ctrl Pts',(1.94137236530215,807.691785499959,119.848801847912));
#73028=CARTESIAN_POINT('Ctrl Pts',(1.87415121283263,807.688135745084,119.859311375963));
#73029=CARTESIAN_POINT('Origin',(-0.837845221469069,822.333310283414,112.951935752269));
#73030=CARTESIAN_POINT('',(-0.837845221469121,817.643030777277,123.37742842904));
#73031=CARTESIAN_POINT('',(-0.837845221469065,819.445433334314,123.967956837475));
#73032=CARTESIAN_POINT('Ctrl Pts',(-0.837845221469108,817.643030777277,
123.37742842904));
#73033=CARTESIAN_POINT('Ctrl Pts',(-0.838870544337092,817.642971214374,
123.377596955358));
#73034=CARTESIAN_POINT('Ctrl Pts',(-0.839895941276325,817.642913218051,
123.377766040561));
#73035=CARTESIAN_POINT('Ctrl Pts',(-0.965845396659871,817.635982543484,
123.398601934178));
#73036=CARTESIAN_POINT('Ctrl Pts',(-1.08962679456761,817.652486470228,123.427207421591));
#73037=CARTESIAN_POINT('Ctrl Pts',(-1.31856598867587,817.73013409283,123.496171760856));
#73038=CARTESIAN_POINT('Ctrl Pts',(-1.42199791702219,817.789827969577,123.535705754936));
#73039=CARTESIAN_POINT('Ctrl Pts',(-1.5953114515572,817.94447297846,123.620008575917));
#73040=CARTESIAN_POINT('Ctrl Pts',(-1.66405764291828,818.037361986833,123.663868162719));
#73041=CARTESIAN_POINT('Ctrl Pts',(-1.75888850861066,818.245520060921,123.750405240253));
#73042=CARTESIAN_POINT('Ctrl Pts',(-1.78412944892841,818.358527392692,123.792174138513));
#73043=CARTESIAN_POINT('Ctrl Pts',(-1.78756518092656,818.59188252935,123.8686854208));
#73044=CARTESIAN_POINT('Ctrl Pts',(-1.7651451040761,818.709747475906,123.902500385448));
#73045=CARTESIAN_POINT('Ctrl Pts',(-1.67415530367386,818.935425175148,123.95793561471));
#73046=CARTESIAN_POINT('Ctrl Pts',(-1.6056519868477,819.040614710209,123.978729192898));
#73047=CARTESIAN_POINT('Ctrl Pts',(-1.43041868743438,819.223396335037,124.004532279965));
#73048=CARTESIAN_POINT('Ctrl Pts',(-1.3246681546867,819.298638493162,124.008988335719));
#73049=CARTESIAN_POINT('Ctrl Pts',(-1.09143819615308,819.406436680195,124.000862648186));
#73050=CARTESIAN_POINT('Ctrl Pts',(-0.966039878408586,819.438016645367,
123.988356571581));
#73051=CARTESIAN_POINT('Ctrl Pts',(-0.839294955766421,819.445350508609,
123.968187856963));
#73052=CARTESIAN_POINT('Ctrl Pts',(-0.838811713835665,819.44537847052,123.968110959456));
#73053=CARTESIAN_POINT('Ctrl Pts',(-0.838328468930155,819.445406079099,
123.968033952939));
#73054=CARTESIAN_POINT('Ctrl Pts',(-0.837845221469056,819.445433334314,
123.967956837475));
#73055=CARTESIAN_POINT('',(-0.837845221469119,820.112801105241,122.079717220203));
#73056=CARTESIAN_POINT('',(-0.837845221469069,823.227206456033,113.267868905406));
#73057=CARTESIAN_POINT('Ctrl Pts',(-1.77705802490915,819.048233491177,121.858373098143));
#73058=CARTESIAN_POINT('Ctrl Pts',(-1.7932176116289,819.158822517368,121.897459001872));
#73059=CARTESIAN_POINT('Ctrl Pts',(-1.7872537863947,819.272264883798,121.934205595621));
#73060=CARTESIAN_POINT('Ctrl Pts',(-1.73031518108252,819.499265193667,122.001157241267));
#73061=CARTESIAN_POINT('Ctrl Pts',(-1.67743890059782,819.610129981052,122.030195245653));
#73062=CARTESIAN_POINT('Ctrl Pts',(-1.53213732178063,819.806110750292,122.07425566618));
#73063=CARTESIAN_POINT('Ctrl Pts',(-1.44177115614975,819.889798110493,122.089104072595));
#73064=CARTESIAN_POINT('Ctrl Pts',(-1.23289807750473,820.022274822958,122.103691744642));
#73065=CARTESIAN_POINT('Ctrl Pts',(-1.11587204363902,820.069271903309,122.103057009095));
#73066=CARTESIAN_POINT('Ctrl Pts',(-0.870093097674419,820.11876890377,122.085958653446));
#73067=CARTESIAN_POINT('Ctrl Pts',(-0.743487188025589,820.120254744304,
122.069459213704));
#73068=CARTESIAN_POINT('Ctrl Pts',(-0.498759344522085,820.075996069951,
122.022361501746));
#73069=CARTESIAN_POINT('Ctrl Pts',(-0.383014443759105,820.030566631178,
121.99217876904));
#73070=CARTESIAN_POINT('Ctrl Pts',(-0.183064289342193,819.900988850042,
121.923228690827));
#73071=CARTESIAN_POINT('Ctrl Pts',(-0.0995923834267395,819.819753903619,
121.885508837209));
#73072=CARTESIAN_POINT('Ctrl Pts',(0.0272395144654325,819.633381117852,
121.807172160489));
#73073=CARTESIAN_POINT('Ctrl Pts',(0.0706947418430991,819.530794624524,
121.767390772846));
#73074=CARTESIAN_POINT('Ctrl Pts',(0.11538540155723,819.313508374912,121.688989027642));
#73075=CARTESIAN_POINT('Ctrl Pts',(0.115974358696283,819.200739940794,121.651095550297));
#73076=CARTESIAN_POINT('Ctrl Pts',(0.0729773981583475,818.97620989415,121.581190493987));
#73077=CARTESIAN_POINT('Ctrl Pts',(0.0286390196368226,818.866709634554,
121.550035717279));
#73078=CARTESIAN_POINT('Ctrl Pts',(-0.103476020342342,818.662567745945,
121.498451344512));
#73079=CARTESIAN_POINT('Ctrl Pts',(-0.19204288195087,818.571119263489,121.479212143192));
#73080=CARTESIAN_POINT('Ctrl Pts',(-0.397642398028661,818.426796078826,
121.457866553751));
#73081=CARTESIAN_POINT('Ctrl Pts',(-0.512045409772581,818.374455856831,
121.455588986707));
#73082=CARTESIAN_POINT('Ctrl Pts',(-0.755049000647518,818.312960348412,
121.467974698637));
#73083=CARTESIAN_POINT('Ctrl Pts',(-0.881566026361287,818.304984047985,
121.482758670095));
#73084=CARTESIAN_POINT('Ctrl Pts',(-1.12941620842454,818.33611490466,121.52784179555));
#73085=CARTESIAN_POINT('Ctrl Pts',(-1.2483512507509,818.375357598635,121.557850557131));
#73086=CARTESIAN_POINT('Ctrl Pts',(-1.44987844994076,818.490533884236,121.625180557954));
#73087=CARTESIAN_POINT('Ctrl Pts',(-1.53336072539728,818.561314574774,121.660876624497));
#73088=CARTESIAN_POINT('Ctrl Pts',(-1.67198766313081,818.733378143591,121.738343081404));
#73089=CARTESIAN_POINT('Ctrl Pts',(-1.72419610591645,818.834409727487,121.779599475205));
#73090=CARTESIAN_POINT('Ctrl Pts',(-1.76440076878355,818.977560001563,121.833049377407));
#73091=CARTESIAN_POINT('Ctrl Pts',(-1.77186247933987,819.012677487488,121.845806403372));
#73092=CARTESIAN_POINT('Ctrl Pts',(-1.77705802490914,819.048233491177,121.858373098143));
#73093=CARTESIAN_POINT('Ctrl Pts',(-0.837845221469056,819.445433334314,
123.967956837475));
#73094=CARTESIAN_POINT('Ctrl Pts',(-0.837463437055385,819.445454867,123.967895913239));
#73095=CARTESIAN_POINT('Ctrl Pts',(-0.837081651046628,819.44547617913,123.967834921001));
#73096=CARTESIAN_POINT('Ctrl Pts',(-0.711701588183039,819.452402705841,
123.947782575134));
#73097=CARTESIAN_POINT('Ctrl Pts',(-0.587701893295878,819.435596050751,
123.920704421286));
#73098=CARTESIAN_POINT('Ctrl Pts',(-0.357004868804501,819.356342458806,
123.855293316923));
#73099=CARTESIAN_POINT('Ctrl Pts',(-0.252392382180456,819.294998403191,
123.81766184153));
#73100=CARTESIAN_POINT('Ctrl Pts',(-0.0777311002587548,819.136603506486,
123.736692949687));
#73101=CARTESIAN_POINT('Ctrl Pts',(-0.00884603348675146,819.041777621916,
123.69426066563));
#73102=CARTESIAN_POINT('Ctrl Pts',(0.0851971288872298,818.830539716007,
123.609334451121));
#73103=CARTESIAN_POINT('Ctrl Pts',(0.109637015562992,818.716408322916,123.567702195052));
#73104=CARTESIAN_POINT('Ctrl Pts',(0.110828055096987,818.481565818644,123.48987960165));
#73105=CARTESIAN_POINT('Ctrl Pts',(0.0868720204604159,818.363260089305,
123.454600933372));
#73106=CARTESIAN_POINT('Ctrl Pts',(-0.00744562183327744,818.138958151881,
123.395899461776));
#73107=CARTESIAN_POINT('Ctrl Pts',(-0.0772137185211807,818.035418763371,
123.373206376389));
#73108=CARTESIAN_POINT('Ctrl Pts',(-0.253364405911867,817.857499177711,
123.344247496048));
#73109=CARTESIAN_POINT('Ctrl Pts',(-0.358166509108883,817.78501276225,123.338355421415));
#73110=CARTESIAN_POINT('Ctrl Pts',(-0.588913932849431,817.680838923092,
123.344657928148));
#73111=CARTESIAN_POINT('Ctrl Pts',(-0.712830547148864,817.650293111087,
123.356880498781));
#73112=CARTESIAN_POINT('Ctrl Pts',(-0.837845221469107,817.643030777277,
123.37742842904));
#73113=CARTESIAN_POINT('Origin',(-0.837845221469069,822.333310283414,112.951935752269));
#73114=CARTESIAN_POINT('',(-0.837845221469069,820.669893651908,119.158830995758));
#73115=CARTESIAN_POINT('Origin',(-0.837845221469069,820.198471421299,118.992214428491));
#73116=CARTESIAN_POINT('',(-0.837845221469201,819.019888842168,123.827328016679));
#73117=CARTESIAN_POINT('',(-0.837845221469069,822.804732514023,113.118552319537));
#73118=CARTESIAN_POINT('Ctrl Pts',(-0.838127253371057,818.069328309183,
123.515926849969));
#73119=CARTESIAN_POINT('Ctrl Pts',(-0.903386802567897,818.065600594513,
123.52658445066));
#73120=CARTESIAN_POINT('Ctrl Pts',(-0.96810627933474,818.07400570268,123.541253699867));
#73121=CARTESIAN_POINT('Ctrl Pts',(-1.08869639284574,818.114227582888,123.576809526534));
#73122=CARTESIAN_POINT('Ctrl Pts',(-1.14354605159275,818.145532365327,123.59733483987));
#73123=CARTESIAN_POINT('Ctrl Pts',(-1.23565247345017,818.226895746216,123.641286165477));
#73124=CARTESIAN_POINT('Ctrl Pts',(-1.27227772680062,818.275879641158,123.664237576066));
#73125=CARTESIAN_POINT('Ctrl Pts',(-1.32296050700717,818.385686686851,123.709716037981));
#73126=CARTESIAN_POINT('Ctrl Pts',(-1.33658393458632,818.445317087223,123.731769586858));
#73127=CARTESIAN_POINT('Ctrl Pts',(-1.33895116164761,818.568338226321,123.772350546812));
#73128=CARTESIAN_POINT('Ctrl Pts',(-1.32742352957931,818.630432019446,123.790403742977));
#73129=CARTESIAN_POINT('Ctrl Pts',(-1.280059496147,818.749287811661,123.820213657924));
#73130=CARTESIAN_POINT('Ctrl Pts',(-1.24429665331102,818.804689147718,123.831544031392));
#73131=CARTESIAN_POINT('Ctrl Pts',(-1.1522982372719,818.901445669055,123.845948616437));
#73132=CARTESIAN_POINT('Ctrl Pts',(-1.09646639191691,818.941439069988,123.848661302589));
#73133=CARTESIAN_POINT('Ctrl Pts',(-0.973475719350933,818.998700737824,
123.844843178476));
#73134=CARTESIAN_POINT('Ctrl Pts',(-0.907483487113627,819.015558436254,
123.838392636998));
#73135=CARTESIAN_POINT('Ctrl Pts',(-0.774512181601959,819.023842503485,
123.817270075293));
#73136=CARTESIAN_POINT('Ctrl Pts',(-0.708732695548974,819.015384884699,
123.80284825954));
#73137=CARTESIAN_POINT('Ctrl Pts',(-0.58610711490321,818.974148875228,123.767809039508));
#73138=CARTESIAN_POINT('Ctrl Pts',(-0.530390937223295,818.941882381311,
123.747553670573));
#73139=CARTESIAN_POINT('Ctrl Pts',(-0.437826419359151,818.858565377267,
123.704221806289));
#73140=CARTESIAN_POINT('Ctrl Pts',(-0.401422293486539,818.80886555638,123.681659544998));
#73141=CARTESIAN_POINT('Ctrl Pts',(-0.351521899678847,818.697938420887,
123.636653869691));
#73142=CARTESIAN_POINT('Ctrl Pts',(-0.33842366126803,818.637910114495,123.61467090789));
#73143=CARTESIAN_POINT('Ctrl Pts',(-0.337301336556146,818.514783862232,
123.573950724408));
#73144=CARTESIAN_POINT('Ctrl Pts',(-0.349417725435632,818.452959187281,
123.555657405084));
#73145=CARTESIAN_POINT('Ctrl Pts',(-0.39809649811137,818.33437009056,123.524982773105));
#73146=CARTESIAN_POINT('Ctrl Pts',(-0.434792674234262,818.279047346598,
123.513103661662));
#73147=CARTESIAN_POINT('Ctrl Pts',(-0.527792894368055,818.183986419567,
123.498059527713));
#73148=CARTESIAN_POINT('Ctrl Pts',(-0.583239073177139,818.145239825183,
123.495075187514));
#73149=CARTESIAN_POINT('Ctrl Pts',(-0.705660969680285,818.089475828064,
123.498557023331));
#73150=CARTESIAN_POINT('Ctrl Pts',(-0.771587996691071,818.073129122493,
123.505060258999));
#73151=CARTESIAN_POINT('Ctrl Pts',(-0.838127253371057,818.069328309183,
123.515926849969));
#73152=CARTESIAN_POINT('Origin',(2.81945029875316,827.937505831762,114.932648081753));
#73153=CARTESIAN_POINT('',(2.81945029875317,823.353776244448,124.836632500591));
#73154=CARTESIAN_POINT('',(2.81945029874631,825.281064240076,125.513887330513));
#73155=CARTESIAN_POINT('Ctrl Pts',(2.81945029875317,823.353776244448,124.836632500591));
#73156=CARTESIAN_POINT('Ctrl Pts',(2.81791581258216,823.353739939602,124.836735220937));
#73157=CARTESIAN_POINT('Ctrl Pts',(2.81638116540465,823.353706863778,124.836839182085));
#73158=CARTESIAN_POINT('Ctrl Pts',(2.68102309435906,823.351074795614,124.846117234903));
#73159=CARTESIAN_POINT('Ctrl Pts',(2.54862698928472,823.373081668511,124.864568119099));
#73160=CARTESIAN_POINT('Ctrl Pts',(2.30214064245552,823.463765369885,124.917483105267));
#73161=CARTESIAN_POINT('Ctrl Pts',(2.19030299497781,823.531456705398,124.951390993351));
#73162=CARTESIAN_POINT('Ctrl Pts',(2.0021927260165,823.703984684317,125.029550081014));
#73163=CARTESIAN_POINT('Ctrl Pts',(1.92755636539819,823.807038105089,125.073003689809));
#73164=CARTESIAN_POINT('Ctrl Pts',(1.82531689718265,824.035726472811,125.163324160501));
#73165=CARTESIAN_POINT('Ctrl Pts',(1.7986825601708,824.159109076199,125.209294955413));
#73166=CARTESIAN_POINT('Ctrl Pts',(1.79742169351842,824.41077744021,125.297680541177));
#73167=CARTESIAN_POINT('Ctrl Pts',(1.82302350103118,824.536555735892,125.339193287099));
#73168=CARTESIAN_POINT('Ctrl Pts',(1.92397395762404,824.773806701183,125.412468330823));
#73169=CARTESIAN_POINT('Ctrl Pts',(1.99859537327238,824.882831159492,125.443455895961));
#73170=CARTESIAN_POINT('Ctrl Pts',(2.18740493361127,825.068660525225,125.491135776836));
#73171=CARTESIAN_POINT('Ctrl Pts',(2.29987719516671,825.143576314103,125.507343301605));
#73172=CARTESIAN_POINT('Ctrl Pts',(2.54883110033436,825.248869959957,125.523330091962));
#73173=CARTESIAN_POINT('Ctrl Pts',(2.6831123291743,825.277814208441,125.522816861722));
#73174=CARTESIAN_POINT('Ctrl Pts',(2.81878446568712,825.281048573515,125.513931005969));
#73175=CARTESIAN_POINT('Ctrl Pts',(2.8190064133322,825.281053864651,125.513916469493));
#73176=CARTESIAN_POINT('Ctrl Pts',(2.81922835769447,825.281059086836,125.513901911006));
#73177=CARTESIAN_POINT('Ctrl Pts',(2.81945029873946,825.281064240076,125.513887330513));
#73178=CARTESIAN_POINT('',(2.81945029873051,825.919929776281,123.70629147689));
#73179=CARTESIAN_POINT('',(2.81945029875316,828.900534972005,115.27301516482));
#73180=CARTESIAN_POINT('Ctrl Pts',(1.79847410877112,824.901973239337,123.432187801006));
#73181=CARTESIAN_POINT('Ctrl Pts',(1.7946006661164,825.027488491971,123.476549138201));
#73182=CARTESIAN_POINT('Ctrl Pts',(1.81680077872336,825.153207382516,123.518665537769));
#73183=CARTESIAN_POINT('Ctrl Pts',(1.91077766936289,825.390854142231,123.593806318141));
#73184=CARTESIAN_POINT('Ctrl Pts',(1.98163916793723,825.500461320881,123.626102624127));
#73185=CARTESIAN_POINT('Ctrl Pts',(2.16339608076163,825.689276527727,123.676983828598));
#73186=CARTESIAN_POINT('Ctrl Pts',(2.27272037300738,825.766533169006,123.695027106696));
#73187=CARTESIAN_POINT('Ctrl Pts',(2.51592406498725,825.877786076362,123.714582930294));
#73188=CARTESIAN_POINT('Ctrl Pts',(2.64759277928814,825.910530685313,123.715843054018));
#73189=CARTESIAN_POINT('Ctrl Pts',(2.91562752068664,825.926231130019,123.701296297768));
#73190=CARTESIAN_POINT('Ctrl Pts',(3.04943514138652,825.908983050468,123.685611072198));
#73191=CARTESIAN_POINT('Ctrl Pts',(3.29995486441188,825.826602274253,123.639285581525));
#73192=CARTESIAN_POINT('Ctrl Pts',(3.41443100569226,825.762709399156,123.609223431337));
#73193=CARTESIAN_POINT('Ctrl Pts',(3.61129747205381,825.595274583791,123.537641900378));
#73194=CARTESIAN_POINT('Ctrl Pts',(3.6913126252281,825.492896340028,123.496680224497));
#73195=CARTESIAN_POINT('Ctrl Pts',(3.80401457383471,825.26360721659,123.409150793774));
#73196=CARTESIAN_POINT('Ctrl Pts',(3.83550149727127,825.13894658962,123.36344003605));
#73197=CARTESIAN_POINT('Ctrl Pts',(3.84491654647323,824.885567051747,123.273790962698));
#73198=CARTESIAN_POINT('Ctrl Pts',(3.8232804031724,824.75937943419,123.230716732982));
#73199=CARTESIAN_POINT('Ctrl Pts',(3.72990164119277,824.521155563829,123.152701390303));
#73200=CARTESIAN_POINT('Ctrl Pts',(3.65910897033805,824.411431665406,123.118522151007));
#73201=CARTESIAN_POINT('Ctrl Pts',(3.47771174405423,824.223278428048,123.064098490298));
#73202=CARTESIAN_POINT('Ctrl Pts',(3.36899318715402,824.146556973427,123.044341164218));
#73203=CARTESIAN_POINT('Ctrl Pts',(3.12651308768783,824.035463552835,123.022080083715));
#73204=CARTESIAN_POINT('Ctrl Pts',(2.99489911717364,824.002527591301,123.019944326463));
#73205=CARTESIAN_POINT('Ctrl Pts',(2.72542302849062,823.985869682359,123.034188510356));
#73206=CARTESIAN_POINT('Ctrl Pts',(2.59014024058584,824.00289883509,123.050648741545));
#73207=CARTESIAN_POINT('Ctrl Pts',(2.33728496496612,824.085384872656,123.099813743796));
#73208=CARTESIAN_POINT('Ctrl Pts',(2.22194739003479,824.149528293997,123.131864544548));
#73209=CARTESIAN_POINT('Ctrl Pts',(2.02546846648917,824.31683546964,123.207140932675));
#73210=CARTESIAN_POINT('Ctrl Pts',(1.94618592283447,824.418335244401,123.249616443721));
#73211=CARTESIAN_POINT('Ctrl Pts',(1.86229093137326,824.589322608822,123.3169142569));
#73212=CARTESIAN_POINT('Ctrl Pts',(1.8403581759016,824.649281041984,123.339872067749));
#73213=CARTESIAN_POINT('Ctrl Pts',(1.80933002061679,824.773488709707,123.386167183759));
#73214=CARTESIAN_POINT('Ctrl Pts',(1.80046510872344,824.837456765419,123.409385496153));
#73215=CARTESIAN_POINT('Ctrl Pts',(1.79847410877112,824.901973239337,123.432187801006));
#73216=CARTESIAN_POINT('Ctrl Pts',(2.81945029873946,825.281064240076,125.513887330513));
#73217=CARTESIAN_POINT('Ctrl Pts',(2.95018225310641,825.284099699793,125.505298849708));
#73218=CARTESIAN_POINT('Ctrl Pts',(3.07976479896005,825.263206354084,125.489096445404));
#73219=CARTESIAN_POINT('Ctrl Pts',(3.32557482878724,825.174693257163,125.442353930516));
#73220=CARTESIAN_POINT('Ctrl Pts',(3.43897552087231,825.106775536387,125.411909442735));
#73221=CARTESIAN_POINT('Ctrl Pts',(3.63087432886115,824.932435262345,125.340134527275));
#73222=CARTESIAN_POINT('Ctrl Pts',(3.70738943235763,824.827654962982,125.299470901607));
#73223=CARTESIAN_POINT('Ctrl Pts',(3.81274670660058,824.594708319065,125.212386118258));
#73224=CARTESIAN_POINT('Ctrl Pts',(3.84026222369576,824.468742562579,125.166788721991));
#73225=CARTESIAN_POINT('Ctrl Pts',(3.84143550911825,824.213344401118,125.076788028346));
#73226=CARTESIAN_POINT('Ctrl Pts',(3.81510479130032,824.086454994449,125.033280863082));
#73227=CARTESIAN_POINT('Ctrl Pts',(3.71200697474968,823.849606391011,124.954883629206));
#73228=CARTESIAN_POINT('Ctrl Pts',(3.63655326772248,823.741883148951,124.920732856777));
#73229=CARTESIAN_POINT('Ctrl Pts',(3.44641415925407,823.559367339685,124.86698578621));
#73230=CARTESIAN_POINT('Ctrl Pts',(3.3336581971035,823.486322752695,124.847917398616));
#73231=CARTESIAN_POINT('Ctrl Pts',(3.08584832190646,823.384653308201,124.828176827905));
#73232=CARTESIAN_POINT('Ctrl Pts',(2.95326056976095,823.356942099808,124.827675080447));
#73233=CARTESIAN_POINT('Ctrl Pts',(2.81945029875316,823.353776244448,124.836632500591));
#73234=CARTESIAN_POINT('Origin',(2.81945029875316,827.937505831762,114.932648081753));
#73235=CARTESIAN_POINT('',(2.81945029875316,826.274089200256,121.139543325241));
#73236=CARTESIAN_POINT('Origin',(2.81945029875316,825.802666969647,120.972926757974));
#73237=CARTESIAN_POINT('',(2.81945029875316,824.789330259076,125.340496348389));
#73238=CARTESIAN_POINT('',(2.81945029875316,828.408928062371,115.09926464902));
#73239=CARTESIAN_POINT('Ctrl Pts',(2.81917054238824,823.845879038868,125.008980202828));
#73240=CARTESIAN_POINT('Ctrl Pts',(2.7598191810322,823.844516620611,125.012934660588));
#73241=CARTESIAN_POINT('Ctrl Pts',(2.70094339839517,823.853089617159,125.020489900141));
#73242=CARTESIAN_POINT('Ctrl Pts',(2.58398801401168,823.891174230767,125.043139335404));
#73243=CARTESIAN_POINT('Ctrl Pts',(2.5277096780785,823.922373774218,125.058708145184));
#73244=CARTESIAN_POINT('Ctrl Pts',(2.43182055000068,824.003656375447,125.095259561734));
#73245=CARTESIAN_POINT('Ctrl Pts',(2.39306971242166,824.052899522524,125.115870694418));
#73246=CARTESIAN_POINT('Ctrl Pts',(2.33827223814516,824.163183187804,125.15932074624));
#73247=CARTESIAN_POINT('Ctrl Pts',(2.32272841460622,824.223131749996,125.181729914033));
#73248=CARTESIAN_POINT('Ctrl Pts',(2.31709672244318,824.346106118589,125.225392637263));
#73249=CARTESIAN_POINT('Ctrl Pts',(2.32711354998336,824.407918514886,125.246210889237));
#73250=CARTESIAN_POINT('Ctrl Pts',(2.37173535253698,824.525276786811,125.283552464801));
#73251=CARTESIAN_POINT('Ctrl Pts',(2.40599117176568,824.579637174653,125.299692662541));
#73252=CARTESIAN_POINT('Ctrl Pts',(2.49446778498555,824.673421934029,125.32520988367));
#73253=CARTESIAN_POINT('Ctrl Pts',(2.54788723561534,824.711890374459,125.334323055125));
#73254=CARTESIAN_POINT('Ctrl Pts',(2.6679801840789,824.767975352769,125.344458703413));
#73255=CARTESIAN_POINT('Ctrl Pts',(2.7337029073108,824.784607576916,125.345220613515));
#73256=CARTESIAN_POINT('Ctrl Pts',(2.86700413355775,824.792473050555,125.338053006363));
#73257=CARTESIAN_POINT('Ctrl Pts',(2.9332601700801,824.783820174893,125.33025957484));
#73258=CARTESIAN_POINT('Ctrl Pts',(3.05748213479643,824.742442569745,125.307107502219));
#73259=CARTESIAN_POINT('Ctrl Pts',(3.11425445279668,824.710217417341,125.292002850164));
#73260=CARTESIAN_POINT('Ctrl Pts',(3.21080195129426,824.626295632984,125.256235997947));
#73261=CARTESIAN_POINT('Ctrl Pts',(3.24957772756914,824.575404495106,125.235917265404));
#73262=CARTESIAN_POINT('Ctrl Pts',(3.30355477045706,824.461635080464,125.192566698188));
#73263=CARTESIAN_POINT('Ctrl Pts',(3.31812602116394,824.399870523616,125.169961957814));
#73264=CARTESIAN_POINT('Ctrl Pts',(3.32060218684613,824.274098422348,125.12556746162));
#73265=CARTESIAN_POINT('Ctrl Pts',(3.30848418983936,824.211367414805,125.104228235675));
#73266=CARTESIAN_POINT('Ctrl Pts',(3.2590725721864,824.093792349117,125.065925050384));
#73267=CARTESIAN_POINT('Ctrl Pts',(3.22236516342835,824.040103744764,125.049334920485));
#73268=CARTESIAN_POINT('Ctrl Pts',(3.12928000770329,823.948993260361,125.023337325417));
#73269=CARTESIAN_POINT('Ctrl Pts',(3.07386495474634,823.912450896098,125.014181202832));
#73270=CARTESIAN_POINT('Ctrl Pts',(2.95145527750785,823.861359280484,125.004722558184));
#73271=CARTESIAN_POINT('Ctrl Pts',(2.88563042635011,823.84740463419,125.004552118992));
#73272=CARTESIAN_POINT('Ctrl Pts',(2.81917054238824,823.845879038868,125.008980202828));
#73273=CARTESIAN_POINT('Origin',(46.3540028286947,840.779950987597,119.47160273482));
#73274=CARTESIAN_POINT('',(46.3540028286947,838.188382810056,129.981749577168));
#73275=CARTESIAN_POINT('Origin',(46.3540028286947,837.190020390929,129.628894517811));
#73276=CARTESIAN_POINT('',(46.3540028286947,838.854849079124,128.096060654733));
#73277=CARTESIAN_POINT('',(46.3540028286947,841.778313406725,119.824457794176));
#73278=CARTESIAN_POINT('Origin',(46.3540028286947,837.856486659997,127.743205595376));
#73279=CARTESIAN_POINT('Origin',(46.3540028286947,840.779950987597,119.47160273482));
#73280=CARTESIAN_POINT('',(46.3540028286947,839.116534356091,125.678497978308));
#73281=CARTESIAN_POINT('Origin',(46.3540028286947,838.645112125482,125.511881411041));
#73282=CARTESIAN_POINT('',(46.3540028286947,837.661442621538,129.795511085078));
#73283=CARTESIAN_POINT('',(46.3540028286947,841.251373218206,119.638219302087));
#73284=CARTESIAN_POINT('Origin',(46.3540028286947,837.190020390929,129.628894517811));
#73285=CARTESIAN_POINT('Origin',(43.0684041447525,843.225670803329,120.336002870698));
#73286=CARTESIAN_POINT('',(43.0684041447525,840.857509486043,130.92510925662));
#73287=CARTESIAN_POINT('Origin',(43.0684041447525,839.63574020666,130.49329465369));
#73288=CARTESIAN_POINT('',(43.0684041447525,841.523975755111,129.039420334185));
#73289=CARTESIAN_POINT('',(43.0684041447525,844.447440082712,120.767817473629));
#73290=CARTESIAN_POINT('Origin',(43.0684041447525,840.302206475729,128.607605731254));
#73291=CARTESIAN_POINT('Origin',(43.0684041447525,843.225670803329,120.336002870698));
#73292=CARTESIAN_POINT('',(43.0684041447525,841.562254171823,126.542898114187));
#73293=CARTESIAN_POINT('Origin',(43.0684041447525,841.090831941214,126.37628154692));
#73294=CARTESIAN_POINT('',(43.0684041447525,840.107162437269,130.659911220957));
#73295=CARTESIAN_POINT('',(43.0684041447525,843.697093033938,120.502619437965));
#73296=CARTESIAN_POINT('Origin',(43.0684041447525,839.63574020666,130.49329465369));
#73297=CARTESIAN_POINT('Origin',(38.9324005984111,845.429042702751,121.114749052906));
#73298=CARTESIAN_POINT('',(38.9324005984111,843.353828508084,131.807392864075));
#73299=CARTESIAN_POINT('Origin',(38.9324005984111,841.839112106083,131.272040835897));
#73300=CARTESIAN_POINT('',(38.9324005984111,844.020294777152,129.92170394164));
#73301=CARTESIAN_POINT('',(38.9324005984111,846.943759104752,121.650101081084));
#73302=CARTESIAN_POINT('Origin',(38.9324005984111,842.505578375151,129.386351913462));
#73303=CARTESIAN_POINT('Origin',(38.9324005984111,845.429042702751,121.114749052906));
#73304=CARTESIAN_POINT('',(38.9324005984111,843.765626071245,127.321644296395));
#73305=CARTESIAN_POINT('Origin',(38.9324005984111,843.294203840636,127.155027729127));
#73306=CARTESIAN_POINT('',(38.9324005984111,842.310534336692,131.438657403165));
#73307=CARTESIAN_POINT('',(38.9324005984111,845.90046493336,121.281365620173));
#73308=CARTESIAN_POINT('Origin',(38.9324005984111,841.839112106083,131.272040835897));
#73309=CARTESIAN_POINT('Origin',(34.4222031106248,846.708386471252,121.566912428373));
#73310=CARTESIAN_POINT('',(34.4222031106248,844.84206801903,132.333387063086));
#73311=CARTESIAN_POINT('Origin',(34.4222031106248,843.118455874583,131.724204211364));
#73312=CARTESIAN_POINT('',(34.4222031106248,845.508534288098,130.447698140651));
#73313=CARTESIAN_POINT('',(34.4222031106248,848.431998615698,122.176095280095));
#73314=CARTESIAN_POINT('Origin',(34.4222031106248,843.784922143651,129.838515288929));
#73315=CARTESIAN_POINT('Origin',(34.4222031106248,846.708386471252,121.566912428373));
#73316=CARTESIAN_POINT('',(34.4222031106248,845.044969839745,127.773807671861));
#73317=CARTESIAN_POINT('Origin',(34.4222031106248,844.573547609136,127.607191104594));
#73318=CARTESIAN_POINT('',(34.4222031106248,843.589878105192,131.890820778631));
#73319=CARTESIAN_POINT('',(34.4222031106248,847.17980870186,121.73352899564));
#73320=CARTESIAN_POINT('Origin',(34.4222031106248,843.118455874583,131.724204211364));
#73321=CARTESIAN_POINT('Origin',(29.3744893768576,847.525235275903,121.855614434707));
#73322=CARTESIAN_POINT('',(29.3744893768576,845.687504076795,132.632192771945));
#73323=CARTESIAN_POINT('Origin',(29.3744893768576,843.935304679234,132.012906217698));
#73324=CARTESIAN_POINT('',(29.3744893768576,846.353970345864,130.74650384951));
#73325=CARTESIAN_POINT('',(29.3744893768576,849.277434673464,122.474900988954));
#73326=CARTESIAN_POINT('Origin',(29.3744893768576,844.601770948302,130.127217295263));
#73327=CARTESIAN_POINT('Origin',(29.3744893768576,847.525235275903,121.855614434707));
#73328=CARTESIAN_POINT('',(29.3744893768576,845.861818644396,128.062509678195));
#73329=CARTESIAN_POINT('Origin',(29.3744893768576,845.390396413787,127.895893110928));
#73330=CARTESIAN_POINT('',(29.3744893768576,844.406726909843,132.179522784965));
#73331=CARTESIAN_POINT('',(29.3744893768576,847.996657506511,122.022231001974));
#73332=CARTESIAN_POINT('Origin',(29.3744893768576,843.935304679234,132.012906217698));
#73333=CARTESIAN_POINT('Origin',(24.6354177384889,847.105053154204,121.707107855681));
#73334=CARTESIAN_POINT('',(24.6354177384889,845.224364905916,132.46850371825));
#73335=CARTESIAN_POINT('Origin',(24.6354177384889,843.515122557535,131.864399638672));
#73336=CARTESIAN_POINT('',(24.6354177384889,845.890831174984,130.582814795815));
#73337=CARTESIAN_POINT('',(24.6354177384889,848.814295502584,122.311211935259));
#73338=CARTESIAN_POINT('Origin',(24.6354177384889,844.181588826604,129.978710716237));
#73339=CARTESIAN_POINT('Origin',(24.6354177384889,847.105053154204,121.707107855681));
#73340=CARTESIAN_POINT('',(24.6354177384889,845.441636522697,127.914003099169));
#73341=CARTESIAN_POINT('Origin',(24.6354177384889,844.970214292089,127.747386531902));
#73342=CARTESIAN_POINT('',(24.6354177384889,843.986544788144,132.031016205939));
#73343=CARTESIAN_POINT('',(24.6354177384889,847.576475384813,121.873724422948));
#73344=CARTESIAN_POINT('Origin',(24.6354177384889,843.515122557535,131.864399638672));
#73345=CARTESIAN_POINT('Origin',(18.8286901708418,846.180691426412,121.380407144518));
#73346=CARTESIAN_POINT('',(18.8286901708418,844.392975979784,132.174662741008));
#73347=CARTESIAN_POINT('Origin',(18.8286901708418,842.590760829743,131.537698927509));
#73348=CARTESIAN_POINT('',(18.8286901708418,845.059442248852,130.288973818573));
#73349=CARTESIAN_POINT('',(18.8286901708418,847.982906576452,122.017370958017));
#73350=CARTESIAN_POINT('Origin',(18.8286901708418,843.257227098811,129.652010005074));
#73351=CARTESIAN_POINT('Origin',(18.8286901708418,846.180691426412,121.380407144518));
#73352=CARTESIAN_POINT('',(18.8286901708418,844.517274794905,127.587302388006));
#73353=CARTESIAN_POINT('Origin',(18.8286901708418,844.045852564297,127.420685820739));
#73354=CARTESIAN_POINT('',(18.8286901708418,843.062183060352,131.704315494776));
#73355=CARTESIAN_POINT('',(18.8286901708418,846.65211365702,121.547023711785));
#73356=CARTESIAN_POINT('Origin',(18.8286901708418,842.590760829743,131.537698927509));
#73357=CARTESIAN_POINT('Origin',(13.9747365845828,844.218509645117,120.686905710928));
#73358=CARTESIAN_POINT('',(13.9747365845828,842.089677864246,131.360599252937));
#73359=CARTESIAN_POINT('Origin',(13.9747365845828,840.628579048448,130.844197493919));
#73360=CARTESIAN_POINT('',(13.9747365845828,842.756144133314,129.474910330502));
#73361=CARTESIAN_POINT('',(13.9747365845828,845.679608460914,121.203307469945));
#73362=CARTESIAN_POINT('Origin',(13.9747365845828,841.295045317516,128.958508571484));
#73363=CARTESIAN_POINT('Origin',(13.9747365845828,844.218509645117,120.686905710928));
#73364=CARTESIAN_POINT('',(13.9747365845828,842.55509301361,126.893800954416));
#73365=CARTESIAN_POINT('Origin',(13.9747365845828,842.083670783002,126.727184387149));
#73366=CARTESIAN_POINT('',(13.9747365845828,841.100001279057,131.010814061186));
#73367=CARTESIAN_POINT('',(13.9747365845828,844.689931875726,120.853522278195));
#73368=CARTESIAN_POINT('Origin',(13.9747365845828,840.628579048448,130.844197493919));
#73369=CARTESIAN_POINT('Origin',(8.6903868869132,841.260133926098,119.641315632682));
#73370=CARTESIAN_POINT('',(8.6903868869132,838.857584906392,130.218268241032));
#73371=CARTESIAN_POINT('Origin',(8.6903868869132,837.67020332943,129.798607415673));
#73372=CARTESIAN_POINT('',(8.69038687124134,839.520801303739,128.341774453277));
#73373=CARTESIAN_POINT('',(8.6903868869132,842.44751550306,120.060976458041));
#73374=CARTESIAN_POINT('',(9.20983376921269,837.254998443755,127.530619307894));
#73375=CARTESIAN_POINT('Ctrl Pts',(8.69038687123737,839.520801303822,128.341774453042));
#73376=CARTESIAN_POINT('Ctrl Pts',(8.64508445351894,839.520560946243,128.342454515211));
#73377=CARTESIAN_POINT('Ctrl Pts',(8.59973500584719,839.518006330853,128.342347073248));
#73378=CARTESIAN_POINT('Ctrl Pts',(8.3885072590311,839.495195989871,128.338107439068));
#73379=CARTESIAN_POINT('Ctrl Pts',(8.22770820845667,839.446217715886,128.324053706448));
#73380=CARTESIAN_POINT('Ctrl Pts',(7.93598307619641,839.292425840023,128.275673458003));
#73381=CARTESIAN_POINT('Ctrl Pts',(7.80778813258912,839.189374835365,128.241898744099));
#73382=CARTESIAN_POINT('Ctrl Pts',(7.60164840112506,838.943588232457,128.158719926603));
#73383=CARTESIAN_POINT('Ctrl Pts',(7.52535695435235,838.803526026946,128.110226622501));
#73384=CARTESIAN_POINT('Ctrl Pts',(7.47983494279036,838.653883945332,128.057338047592));
#73385=CARTESIAN_POINT('Ctrl Pts',(7.46318547174112,838.599153026814,128.037994289121));
#73386=CARTESIAN_POINT('Ctrl Pts',(7.45073298503272,838.543405825278,128.01815863044));
#73387=CARTESIAN_POINT('Ctrl Pts',(7.42046193279149,838.33440932096,127.943319874755));
#73388=CARTESIAN_POINT('Ctrl Pts',(7.43016974680831,838.179445401286,127.886885132092));
#73389=CARTESIAN_POINT('Ctrl Pts',(7.51195492871686,837.882765369216,127.777376904774));
#73390=CARTESIAN_POINT('Ctrl Pts',(7.58300680585067,837.743796117878,127.725334933141));
#73391=CARTESIAN_POINT('Ctrl Pts',(7.77865108576784,837.498030616829,127.632340063583));
#73392=CARTESIAN_POINT('Ctrl Pts',(7.90188950339133,837.393924069373,127.59240811199));
#73393=CARTESIAN_POINT('Ctrl Pts',(8.17584855348552,837.240817866003,127.532976307217));
#73394=CARTESIAN_POINT('Ctrl Pts',(8.32216264264425,837.190204976988,127.512911156333));
#73395=CARTESIAN_POINT('Ctrl Pts',(8.62483087314532,837.141593624475,127.492538804799));
#73396=CARTESIAN_POINT('Ctrl Pts',(8.77849200804145,837.143199431036,127.492099195355));
#73397=CARTESIAN_POINT('Ctrl Pts',(9.02544731432327,837.188237595322,127.507157956335));
#73398=CARTESIAN_POINT('Ctrl Pts',(9.11997195076001,837.216636446791,127.517060880156));
#73399=CARTESIAN_POINT('Ctrl Pts',(9.20983376921266,837.254998443755,127.530619307894));
#73400=CARTESIAN_POINT('',(9.73894344514155,838.994312472096,128.145351736671));
#73401=CARTESIAN_POINT('Origin',(8.6903868869132,838.336669598498,127.912918493238));
#73402=CARTESIAN_POINT('Ctrl Pts',(9.73894344514147,838.994312472096,128.145351736671));
#73403=CARTESIAN_POINT('Ctrl Pts',(9.65588238431169,839.11204035232,128.186960752964));
#73404=CARTESIAN_POINT('Ctrl Pts',(9.551152040427,839.214779814469,128.22358824077));
#73405=CARTESIAN_POINT('Ctrl Pts',(9.30647723514233,839.381521455656,128.284220003819));
#73406=CARTESIAN_POINT('Ctrl Pts',(9.16812007029517,839.443556967977,128.307536040941));
#73407=CARTESIAN_POINT('Ctrl Pts',(8.91326191066645,839.507943838188,128.333650072219));
#73408=CARTESIAN_POINT('Ctrl Pts',(8.80196701421433,839.521393306068,128.340099455595));
#73409=CARTESIAN_POINT('Ctrl Pts',(8.69038687123737,839.520801303822,128.341774453042));
#73410=CARTESIAN_POINT('Origin',(8.6903868869132,841.260133926098,119.641315632682));
#73411=CARTESIAN_POINT('',(8.6903868869132,839.596717294592,125.84821087617));
#73412=CARTESIAN_POINT('Origin',(8.6903868869132,839.125295063983,125.681594308903));
#73413=CARTESIAN_POINT('',(8.6903868869132,838.141625560039,129.965223982941));
#73414=CARTESIAN_POINT('',(8.6903868869132,841.731556156707,119.807932199949));
#73415=CARTESIAN_POINT('Origin',(8.6903868869132,837.67020332943,129.798607415673));
#73416=CARTESIAN_POINT('Origin',(49.025689001695,841.80813580623,119.834998039228));
#73417=CARTESIAN_POINT('',(49.025689001695,839.216567628689,130.345144881576));
#73418=CARTESIAN_POINT('Origin',(49.025689001695,838.218205209562,129.992289822219));
#73419=CARTESIAN_POINT('',(49.025689001695,839.883033897757,128.45945595914));
#73420=CARTESIAN_POINT('',(49.025689001695,842.806498225357,120.187853098584));
#73421=CARTESIAN_POINT('Origin',(49.025689001695,838.88467147863,128.106600899784));
#73422=CARTESIAN_POINT('Origin',(49.025689001695,841.80813580623,119.834998039228));
#73423=CARTESIAN_POINT('',(49.025689001695,840.144719174724,126.041893282716));
#73424=CARTESIAN_POINT('Origin',(49.025689001695,839.673296944115,125.875276715449));
#73425=CARTESIAN_POINT('',(49.025689001695,838.68962744017,130.158906389486));
#73426=CARTESIAN_POINT('',(49.025689001695,842.279558036839,120.001614606495));
#73427=CARTESIAN_POINT('Origin',(49.025689001695,838.218205209562,129.992289822219));
#73428=CARTESIAN_POINT('Origin',(46.3512073306915,844.844481383473,120.908145303547));
#73429=CARTESIAN_POINT('',(46.3512073306915,842.476320066187,131.497251689469));
#73430=CARTESIAN_POINT('Origin',(46.3512073306915,841.254550786804,131.065437086538));
#73431=CARTESIAN_POINT('',(46.3512073306915,843.142786335256,129.611562767034));
#73432=CARTESIAN_POINT('',(46.3512073306915,846.066250662856,121.339959906477));
#73433=CARTESIAN_POINT('Origin',(46.3512073306915,841.921017055873,129.179748164103));
#73434=CARTESIAN_POINT('Origin',(46.3512073306915,844.844481383473,120.908145303547));
#73435=CARTESIAN_POINT('',(46.3512073306915,843.181064751967,127.115040547035));
#73436=CARTESIAN_POINT('Origin',(46.3512073306915,842.709642521358,126.948423979768));
#73437=CARTESIAN_POINT('',(46.3512073306915,841.725973017413,131.232053653805));
#73438=CARTESIAN_POINT('',(46.3512073306915,845.315903614082,121.074761870814));
#73439=CARTESIAN_POINT('Origin',(46.3512073306915,841.254550786804,131.065437086538));
#73440=CARTESIAN_POINT('Origin',(42.7914627445772,847.810478420552,121.956429013469));
#73441=CARTESIAN_POINT('',(42.7914627445772,845.735264225884,132.649072824638));
#73442=CARTESIAN_POINT('Origin',(42.7914627445772,844.220547823883,132.11372079646));
#73443=CARTESIAN_POINT('',(42.7914627445772,846.401730494952,130.763383902203));
#73444=CARTESIAN_POINT('',(42.7914627445772,849.325194822552,122.491781041647));
#73445=CARTESIAN_POINT('Origin',(42.7914627445772,844.887014092951,130.228031874025));
#73446=CARTESIAN_POINT('Origin',(42.7914627445772,847.810478420552,121.956429013469));
#73447=CARTESIAN_POINT('',(42.7914627445772,846.147061789045,128.163324256957));
#73448=CARTESIAN_POINT('Origin',(42.7914627445772,845.675639558437,127.99670768969));
#73449=CARTESIAN_POINT('',(42.7914627445772,844.691970054492,132.280337363727));
#73450=CARTESIAN_POINT('',(42.7914627445772,848.28190065116,122.123045580736));
#73451=CARTESIAN_POINT('Origin',(42.7914627445772,844.220547823883,132.11372079646));
#73452=CARTESIAN_POINT('Origin',(38.6619388515608,849.945992192791,122.711191837493));
#73453=CARTESIAN_POINT('',(38.6619388515608,848.079673740569,133.477666472207));
#73454=CARTESIAN_POINT('Origin',(38.6619388515608,846.356061596123,132.868483620484));
#73455=CARTESIAN_POINT('',(38.6619388515608,848.746140009638,131.591977549772));
#73456=CARTESIAN_POINT('',(38.6619388515608,851.669604337238,123.320374689216));
#73457=CARTESIAN_POINT('Origin',(38.6619388515608,847.022527865191,130.982794698049));
#73458=CARTESIAN_POINT('Origin',(38.6619388515608,849.945992192791,122.711191837493));
#73459=CARTESIAN_POINT('',(38.6619388515608,848.282575561285,128.918087080981));
#73460=CARTESIAN_POINT('Origin',(38.6619388515608,847.811153330676,128.751470513714));
#73461=CARTESIAN_POINT('',(38.6619388515608,846.827483826731,133.035100187751));
#73462=CARTESIAN_POINT('',(38.6619388515608,850.4174144234,122.87780840476));
#73463=CARTESIAN_POINT('Origin',(38.6619388515608,846.356061596123,132.868483620484));
#73464=CARTESIAN_POINT('Origin',(33.904657486265,851.734486067998,123.343306088194));
#73465=CARTESIAN_POINT('',(33.904657486265,849.896754868891,134.119884425433));
#73466=CARTESIAN_POINT('Origin',(33.904657486265,848.14455547133,133.500597871186));
#73467=CARTESIAN_POINT('',(33.904657486265,850.563221137959,132.234195502998));
#73468=CARTESIAN_POINT('',(33.904657486265,853.48668546556,123.962592642441));
#73469=CARTESIAN_POINT('Origin',(33.904657486265,848.811021740398,131.614908948751));
#73470=CARTESIAN_POINT('Origin',(33.904657486265,851.734486067998,123.343306088194));
#73471=CARTESIAN_POINT('',(33.904657486265,850.071069436492,129.550201331683));
#73472=CARTESIAN_POINT('Origin',(33.904657486265,849.599647205883,129.383584764416));
#73473=CARTESIAN_POINT('',(33.904657486265,848.615977701938,133.667214438453));
#73474=CARTESIAN_POINT('',(33.904657486265,852.205908298607,123.509922655461));
#73475=CARTESIAN_POINT('Origin',(33.904657486265,848.14455547133,133.500597871186));
#73476=CARTESIAN_POINT('Origin',(29.1764893194161,852.252478498716,123.526382139922));
#73477=CARTESIAN_POINT('',(29.1764893194161,850.371790250427,134.287778002492));
#73478=CARTESIAN_POINT('Origin',(29.1764893194161,848.662547902047,133.683673922913));
#73479=CARTESIAN_POINT('',(29.1764893194161,851.038256519496,132.402089080057));
#73480=CARTESIAN_POINT('',(29.1764893194161,853.961720847096,124.1304862195));
#73481=CARTESIAN_POINT('Origin',(29.1764893194161,849.329014171116,131.797985000478));
#73482=CARTESIAN_POINT('Origin',(29.1764893194161,852.252478498716,123.526382139922));
#73483=CARTESIAN_POINT('',(29.1764893194161,850.589061867209,129.73327738341));
#73484=CARTESIAN_POINT('Origin',(29.1764893194161,850.117639636601,129.566660816143));
#73485=CARTESIAN_POINT('',(29.1764893194161,849.133970132656,133.85029049018));
#73486=CARTESIAN_POINT('',(29.1764893194161,852.723900729324,123.692998707189));
#73487=CARTESIAN_POINT('Origin',(29.1764893194161,848.662547902047,133.683673922913));
#73488=CARTESIAN_POINT('Origin',(23.2928167169032,852.486599726132,123.609128503381));
#73489=CARTESIAN_POINT('',(23.2928167169032,850.698884279504,134.40338409987));
#73490=CARTESIAN_POINT('Origin',(23.2928167169032,848.896669129463,133.766420286372));
#73491=CARTESIAN_POINT('',(23.2928167169032,851.365350548572,132.517695177435));
#73492=CARTESIAN_POINT('',(23.2928167169032,854.288814876172,124.246092316879));
#73493=CARTESIAN_POINT('Origin',(23.2928167169032,849.563135398531,131.880731363937));
#73494=CARTESIAN_POINT('Origin',(23.2928167169032,852.486599726132,123.609128503381));
#73495=CARTESIAN_POINT('',(23.2928167169032,850.823183094625,129.816023746869));
#73496=CARTESIAN_POINT('Origin',(23.2928167169032,850.351760864016,129.649407179602));
#73497=CARTESIAN_POINT('',(23.2928167169032,849.368091360072,133.933036853639));
#73498=CARTESIAN_POINT('',(23.2928167169032,852.95802195674,123.775745070648));
#73499=CARTESIAN_POINT('Origin',(23.2928167169032,848.896669129463,133.766420286372));
#73500=CARTESIAN_POINT('Origin',(18.1122424300783,851.518809012321,123.267078519102));
#73501=CARTESIAN_POINT('',(18.1122424300783,849.38997723145,133.940772061111));
#73502=CARTESIAN_POINT('Origin',(18.1122424300783,847.928878415652,133.424370302094));
#73503=CARTESIAN_POINT('',(18.1122424300783,850.056443500518,132.055083138676));
#73504=CARTESIAN_POINT('',(18.1122424300783,852.979907828119,123.78348027812));
#73505=CARTESIAN_POINT('Origin',(18.1122424300783,848.595344684721,131.538681379659));
#73506=CARTESIAN_POINT('Origin',(18.1122424300783,851.518809012321,123.267078519102));
#73507=CARTESIAN_POINT('',(18.1122424300783,849.855392380815,129.473973762591));
#73508=CARTESIAN_POINT('Origin',(18.1122424300783,849.383970150206,129.307357195324));
#73509=CARTESIAN_POINT('',(18.1122424300783,848.400300646261,133.590986869361));
#73510=CARTESIAN_POINT('',(18.1122424300783,851.99023124293,123.43369508637));
#73511=CARTESIAN_POINT('Origin',(18.1122424300783,847.928878415652,133.424370302094));
#73512=CARTESIAN_POINT('Origin',(12.2910011493922,849.660963443569,122.610453033329));
#73513=CARTESIAN_POINT('',(12.2910011493922,847.258414423862,133.187405641679));
#73514=CARTESIAN_POINT('Origin',(12.2910011493922,846.0710328469,132.76774481632));
#73515=CARTESIAN_POINT('',(12.2910011421253,847.920148049266,131.315107184968));
#73516=CARTESIAN_POINT('',(12.2910011493922,850.848345020531,123.030113858687));
#73517=CARTESIAN_POINT('',(12.5605717611635,845.577638737166,130.472121991159));
#73518=CARTESIAN_POINT('Ctrl Pts',(12.2910011348584,847.920148049266,131.315107184968));
#73519=CARTESIAN_POINT('Ctrl Pts',(12.1670963424502,847.919423126756,131.317158264743));
#73520=CARTESIAN_POINT('Ctrl Pts',(12.0436279358354,847.901434025333,131.313177666126));
#73521=CARTESIAN_POINT('Ctrl Pts',(11.7655710010952,847.820082994309,131.289636036821));
#73522=CARTESIAN_POINT('Ctrl Pts',(11.6176364867692,847.744395575652,131.26553254008));
#73523=CARTESIAN_POINT('Ctrl Pts',(11.3620573685532,847.544363900691,131.198525062276));
#73524=CARTESIAN_POINT('Ctrl Pts',(11.2566171401221,847.422310749197,131.156396767216));
#73525=CARTESIAN_POINT('Ctrl Pts',(11.1790915154359,847.284862312556,131.107817839024));
#73526=CARTESIAN_POINT('Ctrl Pts',(11.1507368667833,847.234591164861,131.090050314461));
#73527=CARTESIAN_POINT('Ctrl Pts',(11.1262541876204,847.182504125465,131.071508280925));
#73528=CARTESIAN_POINT('Ctrl Pts',(11.0504903247229,846.984015357416,131.000383314775));
#73529=CARTESIAN_POINT('Ctrl Pts',(11.0256987007203,846.830546197247,130.944476870698));
#73530=CARTESIAN_POINT('Ctrl Pts',(11.0399519067323,846.524349054228,130.831604974351));
#73531=CARTESIAN_POINT('Ctrl Pts',(11.0786035845454,846.374508515622,130.775720721958));
#73532=CARTESIAN_POINT('Ctrl Pts',(11.2153525834717,846.095803855744,130.671084039146));
#73533=CARTESIAN_POINT('Ctrl Pts',(11.3127234995319,845.969835597046,130.62342541909));
#73534=CARTESIAN_POINT('Ctrl Pts',(11.546565107571,845.766407899241,130.546208295514));
#73535=CARTESIAN_POINT('Ctrl Pts',(11.6783701447436,845.688234254163,130.516402240896));
#73536=CARTESIAN_POINT('Ctrl Pts',(11.9634836843023,845.581375523282,130.475443294997));
#73537=CARTESIAN_POINT('Ctrl Pts',(12.1140712809063,845.552831209705,130.464347612941));
#73538=CARTESIAN_POINT('Ctrl Pts',(12.3655020970003,845.548480831299,130.461950791831));
#73539=CARTESIAN_POINT('Ctrl Pts',(12.4642142292712,845.557730509121,130.465085749757));
#73540=CARTESIAN_POINT('Ctrl Pts',(12.5605717611636,845.577638737166,130.47212199116));
#73541=CARTESIAN_POINT('',(13.461664589587,847.175224065062,131.036762701689));
#73542=CARTESIAN_POINT('Origin',(12.291001149392,846.737499115968,130.882055893885));
#73543=CARTESIAN_POINT('Ctrl Pts',(13.4616645895871,847.175224065062,131.036762701689));
#73544=CARTESIAN_POINT('Ctrl Pts',(13.4063794187397,847.306661634346,131.083217185975));
#73545=CARTESIAN_POINT('Ctrl Pts',(13.3266151996975,847.427683944249,131.126306450793));
#73546=CARTESIAN_POINT('Ctrl Pts',(13.1241739751137,847.638733418534,131.202598101252));
#73547=CARTESIAN_POINT('Ctrl Pts',(13.0026163741385,847.726525690388,131.235017448694));
#73548=CARTESIAN_POINT('Ctrl Pts',(12.7273317955889,847.858878443954,131.285730861966));
#73549=CARTESIAN_POINT('Ctrl Pts',(12.5750606879973,847.900659675509,131.303045913372));
#73550=CARTESIAN_POINT('Ctrl Pts',(12.3760093893508,847.918616263365,131.312991804535));
#73551=CARTESIAN_POINT('Ctrl Pts',(12.3334796188194,847.920396575643,131.314404009912));
#73552=CARTESIAN_POINT('Ctrl Pts',(12.2910011348584,847.920148049266,131.315107184968));
#73553=CARTESIAN_POINT('Origin',(12.2910011493922,849.660963443569,122.610453033329));
#73554=CARTESIAN_POINT('',(12.2910011493922,847.997546812062,128.817348276817));
#73555=CARTESIAN_POINT('Origin',(12.2910011493922,847.526124581453,128.65073170955));
#73556=CARTESIAN_POINT('',(12.2910011493922,846.542455077509,132.934361383587));
#73557=CARTESIAN_POINT('',(12.2910011493922,850.132385674177,122.777069600596));
#73558=CARTESIAN_POINT('Origin',(12.2910011493922,846.0710328469,132.76774481632));
#73559=CARTESIAN_POINT('Origin',(51.8657229726398,842.290125991002,120.005349679072));
#73560=CARTESIAN_POINT('',(51.8657229726398,839.69855781346,130.515496521419));
#73561=CARTESIAN_POINT('Origin',(51.8657229726398,838.700195394333,130.162641462063));
#73562=CARTESIAN_POINT('',(51.8657229726398,840.365024082528,128.629807598984));
#73563=CARTESIAN_POINT('',(51.8657229726398,843.288488410129,120.358204738428));
#73564=CARTESIAN_POINT('Origin',(51.8657229726398,839.366661663401,128.276952539628));
#73565=CARTESIAN_POINT('Origin',(51.8657229726398,842.290125991002,120.005349679072));
#73566=CARTESIAN_POINT('',(51.8657229726398,840.626709359495,126.21224492256));
#73567=CARTESIAN_POINT('Origin',(51.8657229726398,840.155287128887,126.045628355293));
#73568=CARTESIAN_POINT('',(51.8657229726398,839.171617624942,130.32925802933));
#73569=CARTESIAN_POINT('',(51.8657229726398,842.76154822161,120.171966246339));
#73570=CARTESIAN_POINT('Origin',(51.8657229726398,838.700195394333,130.162641462063));
#73571=CARTESIAN_POINT('Origin',(49.9192459971847,845.784394458028,121.240342386848));
#73572=CARTESIAN_POINT('',(49.9192459971847,843.416233140742,131.82944877277));
#73573=CARTESIAN_POINT('Origin',(49.9192459971847,842.194463861359,131.397634169839));
#73574=CARTESIAN_POINT('',(49.9192459971847,844.08269940981,129.943759850335));
#73575=CARTESIAN_POINT('',(49.9192459971847,847.006163737411,121.672156989779));
#73576=CARTESIAN_POINT('Origin',(49.9192459971847,842.860930130428,129.511945247404));
#73577=CARTESIAN_POINT('Origin',(49.9192459971847,845.784394458028,121.240342386848));
#73578=CARTESIAN_POINT('',(49.9192459971847,844.120977826522,127.447237630336));
#73579=CARTESIAN_POINT('Origin',(49.9192459971847,843.649555595913,127.280621063069));
#73580=CARTESIAN_POINT('',(49.9192459971847,842.665886091968,131.564250737106));
#73581=CARTESIAN_POINT('',(49.9192459971847,846.255816688637,121.406958954115));
#73582=CARTESIAN_POINT('Origin',(49.9192459971847,842.194463861359,131.397634169839));
#73583=CARTESIAN_POINT('Origin',(47.0913382912604,849.383388329809,122.512348596138));
#73584=CARTESIAN_POINT('',(47.0913382912604,847.308174135141,133.204992407307));
#73585=CARTESIAN_POINT('Origin',(47.0913382912604,845.793457733141,132.669640379129));
#73586=CARTESIAN_POINT('',(47.0913382912604,847.974640404209,131.319303484872));
#73587=CARTESIAN_POINT('',(47.0913382912604,850.89810473181,123.047700624315));
#73588=CARTESIAN_POINT('Origin',(47.0913382912604,846.459924002209,130.783951456694));
#73589=CARTESIAN_POINT('Origin',(47.0913382912604,849.383388329809,122.512348596138));
#73590=CARTESIAN_POINT('',(47.0913382912604,847.719971698303,128.719243839626));
#73591=CARTESIAN_POINT('Origin',(47.0913382912604,847.248549467694,128.552627272359));
#73592=CARTESIAN_POINT('',(47.0913382912604,846.264879963749,132.836256946396));
#73593=CARTESIAN_POINT('',(47.0913382912604,849.854810560418,122.678965163405));
#73594=CARTESIAN_POINT('Origin',(47.0913382912604,845.793457733141,132.669640379129));
#73595=CARTESIAN_POINT('Origin',(43.522968002793,852.281739906609,123.536724111556));
#73596=CARTESIAN_POINT('',(43.522968002793,850.415421454387,134.30319874627));
#73597=CARTESIAN_POINT('Origin',(43.522968002793,848.691809309941,133.694015894547));
#73598=CARTESIAN_POINT('',(43.522968002793,851.081887723456,132.417509823835));
#73599=CARTESIAN_POINT('',(43.522968002793,854.005352051056,124.145906963279));
#73600=CARTESIAN_POINT('Origin',(43.522968002793,849.358275579009,131.808326972112));
#73601=CARTESIAN_POINT('Origin',(43.522968002793,852.281739906609,123.536724111556));
#73602=CARTESIAN_POINT('',(43.522968002793,850.618323275103,129.743619355045));
#73603=CARTESIAN_POINT('Origin',(43.522968002793,850.146901044494,129.577002787777));
#73604=CARTESIAN_POINT('',(43.522968002793,849.16323154055,133.860632461815));
#73605=CARTESIAN_POINT('',(43.522968002793,852.753162137218,123.703340678823));
#73606=CARTESIAN_POINT('Origin',(43.522968002793,848.691809309941,133.694015894547));
#73607=CARTESIAN_POINT('Origin',(39.2640350296006,854.96371308788,124.484624180648));
#73608=CARTESIAN_POINT('',(39.2640350296006,853.125981888773,135.261202517887));
#73609=CARTESIAN_POINT('Origin',(39.2640350296006,851.373782491211,134.64191596364));
#73610=CARTESIAN_POINT('',(39.2640350296006,853.792448157841,133.375513595452));
#73611=CARTESIAN_POINT('',(39.2640350296006,856.715912485441,125.103910734895));
#73612=CARTESIAN_POINT('Origin',(39.2640350296006,852.04024876028,132.756227041205));
#73613=CARTESIAN_POINT('Origin',(39.2640350296006,854.96371308788,124.484624180648));
#73614=CARTESIAN_POINT('',(39.2640350296006,853.300296456374,130.691519424137));
#73615=CARTESIAN_POINT('Origin',(39.2640350296006,852.828874225765,130.52490285687));
#73616=CARTESIAN_POINT('',(39.2640350296006,851.84520472182,134.808532530907));
#73617=CARTESIAN_POINT('',(39.2640350296006,855.435135318489,124.651240747915));
#73618=CARTESIAN_POINT('Origin',(39.2640350296006,851.373782491211,134.64191596364));
#73619=CARTESIAN_POINT('Origin',(29.0499410597756,857.779613277735,125.479858586108));
#73620=CARTESIAN_POINT('',(29.0499410597756,855.991897831107,136.274114182598));
#73621=CARTESIAN_POINT('Origin',(29.0499410597756,854.189682681067,135.637150369099));
#73622=CARTESIAN_POINT('',(29.0499410597756,856.658364100176,134.388425260163));
#73623=CARTESIAN_POINT('',(29.0499410597756,859.581828427776,126.116822399607));
#73624=CARTESIAN_POINT('Origin',(29.0499410597756,854.856148950135,133.751461446664));
#73625=CARTESIAN_POINT('Origin',(29.0499410597756,857.779613277735,125.479858586108));
#73626=CARTESIAN_POINT('',(29.0499410597756,856.116196646229,131.686753829597));
#73627=CARTESIAN_POINT('Origin',(29.0499410597756,855.64477441562,131.520137262329));
#73628=CARTESIAN_POINT('',(29.0499410597756,854.661104911675,135.803766936367));
#73629=CARTESIAN_POINT('',(29.0499410597756,858.251035508344,125.646475153375));
#73630=CARTESIAN_POINT('Origin',(29.0499410597756,854.189682681067,135.637150369099));
#73631=CARTESIAN_POINT('Origin',(23.7691620278726,857.848510729578,125.504209276793));
#73632=CARTESIAN_POINT('',(23.7691620278726,855.719678948707,136.177902818801));
#73633=CARTESIAN_POINT('Origin',(23.7691620278726,854.258580132909,135.661501059784));
#73634=CARTESIAN_POINT('',(23.7691620278726,856.386145217775,134.292213896366));
#73635=CARTESIAN_POINT('',(23.7691620278726,859.309609545375,126.02061103581));
#73636=CARTESIAN_POINT('Origin',(23.7691620278726,854.925046401978,133.775812137349));
#73637=CARTESIAN_POINT('Origin',(23.7691620278726,857.848510729578,125.504209276793));
#73638=CARTESIAN_POINT('',(23.7691620278726,856.185094098072,131.711104520281));
#73639=CARTESIAN_POINT('Origin',(23.7691620278726,855.713671867463,131.544487953014));
#73640=CARTESIAN_POINT('',(23.7691620278726,854.730002363518,135.828117627051));
#73641=CARTESIAN_POINT('',(23.7691620278726,858.319932960187,125.67082584406));
#73642=CARTESIAN_POINT('Origin',(23.7691620278726,854.258580132909,135.661501059784));
#73643=CARTESIAN_POINT('Origin',(17.6654453415508,857.172392077378,125.265246068059));
#73644=CARTESIAN_POINT('',(17.6654453415508,854.769843057671,135.842198676409));
#73645=CARTESIAN_POINT('Origin',(17.6654453415508,853.582461480709,135.42253785105));
#73646=CARTESIAN_POINT('',(17.6654453366203,855.430023704928,133.974294191042));
#73647=CARTESIAN_POINT('',(17.6654453415508,858.35977365434,125.684906893417));
#73648=CARTESIAN_POINT('',(17.6733581535164,853.061569611098,133.117196387139));
#73649=CARTESIAN_POINT('Ctrl Pts',(17.6654453316897,855.430023704928,133.974294191042));
#73650=CARTESIAN_POINT('Ctrl Pts',(17.6295073639708,855.42981443297,133.974886300904));
#73651=CARTESIAN_POINT('Ctrl Pts',(17.59352668523,855.428157015281,133.974959520969));
#73652=CARTESIAN_POINT('Ctrl Pts',(17.3919526744461,855.410682439271,133.972410715024));
#73653=CARTESIAN_POINT('Ctrl Pts',(17.2307440375472,855.365630162799,133.959134714097));
#73654=CARTESIAN_POINT('Ctrl Pts',(16.9368955664509,855.220045084026,133.911370505633));
#73655=CARTESIAN_POINT('Ctrl Pts',(16.8069148003019,855.121321434135,133.877487645813));
#73656=CARTESIAN_POINT('Ctrl Pts',(16.7007738042995,855.002073798701,133.835341496605));
#73657=CARTESIAN_POINT('Ctrl Pts',(16.6619532122509,854.958459512211,133.819926732034));
#73658=CARTESIAN_POINT('Ctrl Pts',(16.6265103511939,854.912310910842,133.803483543428));
#73659=CARTESIAN_POINT('Ctrl Pts',(16.5085649220031,854.733018142063,133.739143092934));
#73660=CARTESIAN_POINT('Ctrl Pts',(16.4503573729137,854.587773946474,133.686143629637));
#73661=CARTESIAN_POINT('Ctrl Pts',(16.3964556695319,854.285505848461,133.574660390738));
#73662=CARTESIAN_POINT('Ctrl Pts',(16.4010178842328,854.131382945078,133.517262605736));
#73663=CARTESIAN_POINT('Ctrl Pts',(16.4728950147202,853.832004072906,133.405318956769));
#73664=CARTESIAN_POINT('Ctrl Pts',(16.5401428529477,853.689722598392,133.351894694273));
#73665=CARTESIAN_POINT('Ctrl Pts',(16.7236470185644,853.444937208962,133.260060363104));
#73666=CARTESIAN_POINT('Ctrl Pts',(16.8351824911558,853.342649262511,133.221731498453));
#73667=CARTESIAN_POINT('Ctrl Pts',(17.0902805099667,853.182257215964,133.161852067453));
#73668=CARTESIAN_POINT('Ctrl Pts',(17.2312131677073,853.124824135463,133.14054611769));
#73669=CARTESIAN_POINT('Ctrl Pts',(17.4761307604511,853.071287145555,133.120765083804));
#73670=CARTESIAN_POINT('Ctrl Pts',(17.5747161947025,853.060985237067,133.116989849583));
#73671=CARTESIAN_POINT('Ctrl Pts',(17.6733581535165,853.061569611098,133.117196387139));
#73672=CARTESIAN_POINT('',(18.9070520539092,854.447604093656,133.607067870924));
#73673=CARTESIAN_POINT('Origin',(17.6654453415506,854.248927749778,133.536848928615));
#73674=CARTESIAN_POINT('Ctrl Pts',(18.9070520539092,854.447604093656,133.607067870924));
#73675=CARTESIAN_POINT('Ctrl Pts',(18.8819590002978,854.587006899514,133.656337539326));
#73676=CARTESIAN_POINT('Ctrl Pts',(18.8306469852216,854.72101846392,133.704017646188));
#73677=CARTESIAN_POINT('Ctrl Pts',(18.6792869942737,854.967128558182,133.792700906052));
#73678=CARTESIAN_POINT('Ctrl Pts',(18.5798416076307,855.07682155118,133.832860709377));
#73679=CARTESIAN_POINT('Ctrl Pts',(18.3400311349627,855.260218651258,133.901614921833));
#73680=CARTESIAN_POINT('Ctrl Pts',(18.2004774636254,855.330918827193,133.929150906681));
#73681=CARTESIAN_POINT('Ctrl Pts',(17.9259064740675,855.412441796172,133.963152002444));
#73682=CARTESIAN_POINT('Ctrl Pts',(17.795957526262,855.43078369622,133.972143886994));
#73683=CARTESIAN_POINT('Ctrl Pts',(17.6654453316897,855.430023704928,133.974294191042));
#73684=CARTESIAN_POINT('Origin',(17.6654453415508,857.172392077378,125.265246068059));
#73685=CARTESIAN_POINT('',(17.6654453415508,855.508975445871,131.472141311547));
#73686=CARTESIAN_POINT('Origin',(17.6654453415508,855.037553215263,131.30552474428));
#73687=CARTESIAN_POINT('',(17.6654453415508,854.053883711318,135.589154418317));
#73688=CARTESIAN_POINT('',(17.6654453415508,857.643814307987,125.431862635326));
#73689=CARTESIAN_POINT('Origin',(17.6654453415508,853.582461480709,135.42253785105));
#73690=CARTESIAN_POINT('Origin',(54.7499816290036,842.204856257991,119.975212470252));
#73691=CARTESIAN_POINT('',(54.7499816290036,839.61328808045,130.4853593126));
#73692=CARTESIAN_POINT('Origin',(54.7499816290036,838.614925661323,130.132504253244));
#73693=CARTESIAN_POINT('',(54.7499816290036,840.279754349518,128.599670390165));
#73694=CARTESIAN_POINT('',(54.7499816290036,843.203218677118,120.328067529609));
#73695=CARTESIAN_POINT('Origin',(54.7499816290036,839.281391930391,128.246815330808));
#73696=CARTESIAN_POINT('Origin',(54.7499816290036,842.204856257991,119.975212470252));
#73697=CARTESIAN_POINT('',(54.7499816290036,840.541439626485,126.182107713741));
#73698=CARTESIAN_POINT('Origin',(54.7499816290036,840.070017395876,126.015491146474));
#73699=CARTESIAN_POINT('',(54.7499816290036,839.086347891931,130.299120820511));
#73700=CARTESIAN_POINT('',(54.7499816290036,842.6762784886,120.141829037519));
#73701=CARTESIAN_POINT('Origin',(54.7499816290036,838.614925661323,130.132504253244));
#73702=CARTESIAN_POINT('Origin',(53.6165797331573,846.004331315431,121.318075514004));
#73703=CARTESIAN_POINT('',(53.6165797331573,843.636169998145,131.907181899926));
#73704=CARTESIAN_POINT('Origin',(53.6165797331573,842.414400718763,131.475367296995));
#73705=CARTESIAN_POINT('',(53.6165797331573,844.302636267214,130.021492977491));
#73706=CARTESIAN_POINT('',(53.6165797331573,847.226100594814,121.749890116935));
#73707=CARTESIAN_POINT('Origin',(53.6165797331573,843.080866987831,129.58967837456));
#73708=CARTESIAN_POINT('Origin',(53.6165797331573,846.004331315431,121.318075514004));
#73709=CARTESIAN_POINT('',(53.6165797331573,844.340914683925,127.524970757492));
#73710=CARTESIAN_POINT('Origin',(53.6165797331573,843.869492453316,127.358354190225));
#73711=CARTESIAN_POINT('',(53.6165797331573,842.885822949371,131.641983864262));
#73712=CARTESIAN_POINT('',(53.6165797331573,846.47575354604,121.484692081271));
#73713=CARTESIAN_POINT('Origin',(53.6165797331573,842.414400718763,131.475367296995));
#73714=CARTESIAN_POINT('Origin',(51.6441020439785,850.07902871983,122.758211447552));
#73715=CARTESIAN_POINT('',(51.6441020439785,848.003814525162,133.450855258721));
#73716=CARTESIAN_POINT('Origin',(51.6441020439785,846.489098123162,132.915503230543));
#73717=CARTESIAN_POINT('',(51.6441020439785,848.67028079423,131.565166336286));
#73718=CARTESIAN_POINT('',(51.6441020439785,851.593745121831,123.29356347573));
#73719=CARTESIAN_POINT('Origin',(51.6441020439785,847.15556439223,131.029814308108));
#73720=CARTESIAN_POINT('Origin',(51.6441020439785,850.07902871983,122.758211447552));
#73721=CARTESIAN_POINT('',(51.6441020439785,848.415612088324,128.96510669104));
#73722=CARTESIAN_POINT('Origin',(51.6441020439785,847.944189857715,128.798490123773));
#73723=CARTESIAN_POINT('',(51.6441020439785,846.96052035377,133.08211979781));
#73724=CARTESIAN_POINT('',(51.6441020439785,850.550450950439,122.924828014819));
#73725=CARTESIAN_POINT('Origin',(51.6441020439785,846.489098123162,132.915503230543));
#73726=CARTESIAN_POINT('Origin',(48.7928402646065,853.613546229451,124.007429528842));
#73727=CARTESIAN_POINT('',(48.7928402646065,851.747227777229,134.773904163556));
#73728=CARTESIAN_POINT('Origin',(48.7928402646065,850.023615632782,134.164721311833));
#73729=CARTESIAN_POINT('',(48.7928402646065,852.413694046297,132.88821524112));
#73730=CARTESIAN_POINT('',(48.7928402646065,855.337158373898,124.616612380564));
#73731=CARTESIAN_POINT('Origin',(48.7928402646065,850.690081901851,132.279032389398));
#73732=CARTESIAN_POINT('Origin',(48.7928402646065,853.613546229451,124.007429528842));
#73733=CARTESIAN_POINT('',(48.7928402646065,851.950129597945,130.21432477233));
#73734=CARTESIAN_POINT('Origin',(48.7928402646065,851.478707367336,130.047708205063));
#73735=CARTESIAN_POINT('',(48.7928402646065,850.495037863391,134.3313378791));
#73736=CARTESIAN_POINT('',(48.7928402646065,854.08496846006,124.174046096109));
#73737=CARTESIAN_POINT('Origin',(48.7928402646065,850.023615632782,134.164721311833));
#73738=CARTESIAN_POINT('Origin',(45.2183914910739,857.071783619228,125.229687634777));
#73739=CARTESIAN_POINT('',(45.2183914910739,855.234052420121,136.006265972015));
#73740=CARTESIAN_POINT('Origin',(45.2183914910739,853.48185302256,135.386979417768));
#73741=CARTESIAN_POINT('',(45.2183914910739,855.900518689189,134.12057704958));
#73742=CARTESIAN_POINT('',(45.2183914910739,858.82398301679,125.848974189024));
#73743=CARTESIAN_POINT('Origin',(45.2183914910739,854.148319291628,133.501290495333));
#73744=CARTESIAN_POINT('Origin',(45.2183914910739,857.071783619228,125.229687634777));
#73745=CARTESIAN_POINT('',(45.2183914910739,855.408366987722,131.436582878265));
#73746=CARTESIAN_POINT('Origin',(45.2183914910739,854.936944757113,131.269966310998));
#73747=CARTESIAN_POINT('',(45.2183914910739,853.953275253168,135.553595985035));
#73748=CARTESIAN_POINT('',(45.2183914910739,857.543205849837,125.396304202044));
#73749=CARTESIAN_POINT('Origin',(45.2183914910739,853.48185302256,135.386979417768));
#73750=CARTESIAN_POINT('Origin',(41.1224533261868,859.358195582718,126.037782985357));
#73751=CARTESIAN_POINT('',(41.1224533261868,857.47750733443,136.799178847926));
#73752=CARTESIAN_POINT('Origin',(41.1224533261868,855.76826498605,136.195074768348));
#73753=CARTESIAN_POINT('',(41.1224533261868,858.143973603498,134.913489925491));
#73754=CARTESIAN_POINT('',(41.1224533261868,861.067437931099,126.641887064935));
#73755=CARTESIAN_POINT('Origin',(41.1224533261868,856.434731255118,134.309385845913));
#73756=CARTESIAN_POINT('Origin',(41.1224533261868,859.358195582718,126.037782985357));
#73757=CARTESIAN_POINT('',(41.1224533261868,857.694778951212,132.244678228845));
#73758=CARTESIAN_POINT('Origin',(41.1224533261868,857.223356720603,132.078061661578));
#73759=CARTESIAN_POINT('',(41.1224533261868,856.239687216658,136.361691335615));
#73760=CARTESIAN_POINT('',(41.1224533261868,859.829617813327,126.204399552624));
#73761=CARTESIAN_POINT('Origin',(41.1224533261868,855.76826498605,136.195074768348));
#73762=CARTESIAN_POINT('Origin',(35.8484492399277,861.828401990321,126.910837511327));
#73763=CARTESIAN_POINT('',(35.8484492399277,860.040686543693,137.705093107816));
#73764=CARTESIAN_POINT('Origin',(35.8484492399277,858.238471393652,137.068129294318));
#73765=CARTESIAN_POINT('',(35.8484492399277,860.707152812761,135.819404185381));
#73766=CARTESIAN_POINT('',(35.8484492399277,863.630617140361,127.547801324825));
#73767=CARTESIAN_POINT('Origin',(35.8484492399277,858.90493766272,135.182440371883));
#73768=CARTESIAN_POINT('Origin',(35.8484492399277,861.828401990321,126.910837511327));
#73769=CARTESIAN_POINT('',(35.8484492399277,860.164985358814,133.117732754815));
#73770=CARTESIAN_POINT('Origin',(35.8484492399277,859.693563128206,132.951116187548));
#73771=CARTESIAN_POINT('',(35.8484492399277,858.709893624261,137.234745861585));
#73772=CARTESIAN_POINT('',(35.8484492399277,862.299824220929,127.077454078594));
#73773=CARTESIAN_POINT('Origin',(35.8484492399277,858.238471393652,137.068129294318));
#73774=CARTESIAN_POINT('Origin',(30.69826084663,862.930976458564,127.300524634944));
#73775=CARTESIAN_POINT('',(30.69826084663,860.802144677693,137.974218176952));
#73776=CARTESIAN_POINT('Origin',(30.69826084663,859.341045861896,137.457816417935));
#73777=CARTESIAN_POINT('',(30.69826084663,861.468610946762,136.088529254517));
#73778=CARTESIAN_POINT('',(30.69826084663,864.392075274362,127.816926393961));
#73779=CARTESIAN_POINT('Origin',(30.69826084663,860.007512130964,135.5721274955));
#73780=CARTESIAN_POINT('Origin',(30.69826084663,862.930976458564,127.300524634944));
#73781=CARTESIAN_POINT('',(30.69826084663,861.267559827058,133.507419878432));
#73782=CARTESIAN_POINT('Origin',(30.69826084663,860.796137596449,133.340803311165));
#73783=CARTESIAN_POINT('',(30.69826084663,859.812468092504,137.624432985202));
#73784=CARTESIAN_POINT('',(30.69826084663,863.402398689173,127.467141202211));
#73785=CARTESIAN_POINT('Origin',(30.69826084663,859.341045861896,137.457816417935));
#73786=CARTESIAN_POINT('Origin',(24.5788304627471,863.466134352395,127.489667542144));
#73787=CARTESIAN_POINT('',(24.5788304627471,861.063585332689,138.066620150493));
#73788=CARTESIAN_POINT('Origin',(24.5788304627471,859.876203755726,137.646959325135));
#73789=CARTESIAN_POINT('',(24.5788304719421,861.72230180781,136.202858370173));
#73790=CARTESIAN_POINT('',(24.5788304627471,864.653515929357,127.909328367502));
#73791=CARTESIAN_POINT('',(24.3247396470537,859.379707374474,135.350240052251));
#73792=CARTESIAN_POINT('Ctrl Pts',(24.5788304811371,861.72230180781,136.202858370173));
#73793=CARTESIAN_POINT('Ctrl Pts',(24.4650951106064,861.721713023236,136.204524272744));
#73794=CARTESIAN_POINT('Ctrl Pts',(24.3516351742477,861.706668449823,136.200851948056));
#73795=CARTESIAN_POINT('Ctrl Pts',(24.0825158145281,861.635167682745,136.17869189312));
#73796=CARTESIAN_POINT('Ctrl Pts',(23.9336752938585,861.564074370878,136.154574529653));
#73797=CARTESIAN_POINT('Ctrl Pts',(23.8035577973859,861.46823923053,136.120703148391));
#73798=CARTESIAN_POINT('Ctrl Pts',(23.7559679080946,861.433187958849,136.10831484299));
#73799=CARTESIAN_POINT('Ctrl Pts',(23.7111138882448,861.394996533156,136.094683989506));
#73800=CARTESIAN_POINT('Ctrl Pts',(23.5561416739836,861.242749069374,136.039902264898));
#73801=CARTESIAN_POINT('Ctrl Pts',(23.4670621490132,861.11210057302,135.992061415569));
#73802=CARTESIAN_POINT('Ctrl Pts',(23.3473612993245,860.827035957846,135.8866584696));
#73803=CARTESIAN_POINT('Ctrl Pts',(23.3176346602385,860.67540677207,135.830142048776));
#73804=CARTESIAN_POINT('Ctrl Pts',(23.3214985467804,860.368522196417,135.715545630238));
#73805=CARTESIAN_POINT('Ctrl Pts',(23.3556842539537,860.216188967325,135.658568737564));
#73806=CARTESIAN_POINT('Ctrl Pts',(23.4808309645594,859.940817218659,135.555924152126));
#73807=CARTESIAN_POINT('Ctrl Pts',(23.5672222372109,859.81891533621,135.510663058839));
#73808=CARTESIAN_POINT('Ctrl Pts',(23.7811557277566,859.612043699473,135.43435616799));
#73809=CARTESIAN_POINT('Ctrl Pts',(23.9062740132204,859.528245783003,135.403731993118));
#73810=CARTESIAN_POINT('Ctrl Pts',(24.1339743085658,859.427873803726,135.367397889288));
#73811=CARTESIAN_POINT('Ctrl Pts',(24.2281243882554,859.398472394407,135.356872245226));
#73812=CARTESIAN_POINT('Ctrl Pts',(24.3247396470539,859.379707374475,135.350240052252));
#73813=CARTESIAN_POINT('',(25.8371162760489,860.493614653875,135.743932574787));
#73814=CARTESIAN_POINT('Origin',(24.5788304627464,860.542670024794,135.7612704027));
#73815=CARTESIAN_POINT('Ctrl Pts',(25.8371162760488,860.493614653875,135.743932574787));
#73816=CARTESIAN_POINT('Ctrl Pts',(25.8433120265261,860.634890124764,135.793864106374));
#73817=CARTESIAN_POINT('Ctrl Pts',(25.8226947966971,860.776029657672,135.844063478485));
#73818=CARTESIAN_POINT('Ctrl Pts',(25.7290311972954,861.046420841452,135.941328496956));
#73819=CARTESIAN_POINT('Ctrl Pts',(25.6560442655738,861.173201350605,135.987527606661));
#73820=CARTESIAN_POINT('Ctrl Pts',(25.4621887671792,861.399573424031,136.071470628793));
#73821=CARTESIAN_POINT('Ctrl Pts',(25.3414516971849,861.496067617522,136.108123092207));
#73822=CARTESIAN_POINT('Ctrl Pts',(25.0599300905018,861.646292595752,136.167054480677));
#73823=CARTESIAN_POINT('Ctrl Pts',(24.8999449549518,861.695586151695,136.187733337864));
#73824=CARTESIAN_POINT('Ctrl Pts',(24.6825627254731,861.719835765023,136.200231380237));
#73825=CARTESIAN_POINT('Ctrl Pts',(24.6306679924485,861.722570159924,136.202099096756));
#73826=CARTESIAN_POINT('Ctrl Pts',(24.5788304811371,861.72230180781,136.202858370173));
#73827=CARTESIAN_POINT('Origin',(24.5788304627471,863.466134352395,127.489667542144));
#73828=CARTESIAN_POINT('',(24.5788304627471,861.802717720889,133.696562785632));
#73829=CARTESIAN_POINT('Origin',(24.5788304627471,861.33129549028,133.529946218365));
#73830=CARTESIAN_POINT('',(24.5788304627471,860.347625986335,137.813575892402));
#73831=CARTESIAN_POINT('',(24.5788304627471,863.937556583004,127.656284109411));
#73832=CARTESIAN_POINT('Origin',(24.5788304627471,859.876203755726,137.646959325135));
#73833=CARTESIAN_POINT('Origin',(57.5524090272951,841.556053303701,119.74590355341));
#73834=CARTESIAN_POINT('',(57.5524090272951,838.96448512616,130.256050395757));
#73835=CARTESIAN_POINT('Origin',(57.5524090272951,837.966122707033,129.903195336401));
#73836=CARTESIAN_POINT('',(57.5524090272951,839.630951395229,128.370361473322));
#73837=CARTESIAN_POINT('',(57.5524090272951,842.554415722829,120.098758612766));
#73838=CARTESIAN_POINT('Origin',(57.5524090272951,838.632588976101,128.017506413966));
#73839=CARTESIAN_POINT('Origin',(57.5524090272951,841.556053303701,119.74590355341));
#73840=CARTESIAN_POINT('',(57.5524090272951,839.892636672195,125.952798796898));
#73841=CARTESIAN_POINT('Origin',(57.5524090272951,839.421214441586,125.786182229631));
#73842=CARTESIAN_POINT('',(57.5524090272951,838.437544937642,130.069811903668));
#73843=CARTESIAN_POINT('',(57.5524090272951,842.02747553431,119.912520120677));
#73844=CARTESIAN_POINT('Origin',(57.5524090272951,837.966122707033,129.903195336401));
#73845=CARTESIAN_POINT('Origin',(57.2816173125715,845.494679659641,121.137947374353));
#73846=CARTESIAN_POINT('',(57.2816173125715,843.126518342356,131.727053760275));
#73847=CARTESIAN_POINT('Origin',(57.2816173125715,841.904749062973,131.295239157344));
#73848=CARTESIAN_POINT('',(57.2816173125715,843.792984611424,129.84136483784));
#73849=CARTESIAN_POINT('',(57.2816173125715,846.716448939024,121.569761977284));
#73850=CARTESIAN_POINT('Origin',(57.2816173125715,842.571215332041,129.409550234909));
#73851=CARTESIAN_POINT('Origin',(57.2816173125715,845.494679659641,121.137947374353));
#73852=CARTESIAN_POINT('',(57.2816173125715,843.831263028135,127.344842617841));
#73853=CARTESIAN_POINT('Origin',(57.2816173125715,843.359840797526,127.178226050574));
#73854=CARTESIAN_POINT('',(57.2816173125715,842.376171293582,131.461855724611));
#73855=CARTESIAN_POINT('',(57.2816173125715,845.96610189025,121.30456394162));
#73856=CARTESIAN_POINT('Origin',(57.2816173125715,841.904749062973,131.295239157344));
#73857=CARTESIAN_POINT('Origin',(56.2507763801536,849.866996767518,122.683272181324));
#73858=CARTESIAN_POINT('',(56.2507763801536,847.79178257285,133.375915992493));
#73859=CARTESIAN_POINT('Origin',(56.2507763801536,846.277066170849,132.840563964316));
#73860=CARTESIAN_POINT('',(56.2507763801536,848.458248841918,131.490227070058));
#73861=CARTESIAN_POINT('',(56.2507763801536,851.381713169518,123.218624209502));
#73862=CARTESIAN_POINT('Origin',(56.2507763801536,846.943532439917,130.95487504188));
#73863=CARTESIAN_POINT('Origin',(56.2507763801536,849.866996767518,122.683272181324));
#73864=CARTESIAN_POINT('',(56.2507763801536,848.203580136011,128.890167424813));
#73865=CARTESIAN_POINT('Origin',(56.2507763801536,847.732157905402,128.723550857546));
#73866=CARTESIAN_POINT('',(56.2507763801536,846.748488401458,133.007180531583));
#73867=CARTESIAN_POINT('',(56.2507763801536,850.338418998126,122.849888748591));
#73868=CARTESIAN_POINT('Origin',(56.2507763801536,846.277066170849,132.840563964316));
#73869=CARTESIAN_POINT('Origin',(54.2412369315076,853.883204834292,124.10273600392));
#73870=CARTESIAN_POINT('',(54.2412369315076,852.01688638207,134.869210638633));
#73871=CARTESIAN_POINT('Origin',(54.2412369315076,850.293274237623,134.260027786911));
#73872=CARTESIAN_POINT('',(54.2412369315076,852.683352651138,132.983521716198));
#73873=CARTESIAN_POINT('',(54.2412369315076,855.606816978739,124.711918855642));
#73874=CARTESIAN_POINT('Origin',(54.2412369315076,850.959740506692,132.374338864476));
#73875=CARTESIAN_POINT('Origin',(54.2412369315076,853.883204834292,124.10273600392));
#73876=CARTESIAN_POINT('',(54.2412369315076,852.219788202786,130.309631247408));
#73877=CARTESIAN_POINT('Origin',(54.2412369315076,851.748365972177,130.143014680141));
#73878=CARTESIAN_POINT('',(54.2412369315076,850.764696468232,134.426644354178));
#73879=CARTESIAN_POINT('',(54.2412369315076,854.354627064901,124.269352571187));
#73880=CARTESIAN_POINT('Origin',(54.2412369315076,850.293274237623,134.260027786911));
#73881=CARTESIAN_POINT('Origin',(51.5074929211464,857.966564864178,125.545933602422));
#73882=CARTESIAN_POINT('',(51.5074929211464,856.128833665071,136.32251193966));
#73883=CARTESIAN_POINT('Origin',(51.5074929211464,854.37663426751,135.703225385413));
#73884=CARTESIAN_POINT('',(51.5074929211464,856.795299934139,134.436823017225));
#73885=CARTESIAN_POINT('',(51.5074929211464,859.71876426174,126.165220156669));
#73886=CARTESIAN_POINT('Origin',(51.5074929211464,855.043100536578,133.817536462978));
#73887=CARTESIAN_POINT('Origin',(51.5074929211464,857.966564864178,125.545933602422));
#73888=CARTESIAN_POINT('',(51.5074929211464,856.303148232672,131.75282884591));
#73889=CARTESIAN_POINT('Origin',(51.5074929211464,855.831726002063,131.586212278643));
#73890=CARTESIAN_POINT('',(51.5074929211464,854.848056498118,135.869841952681));
#73891=CARTESIAN_POINT('',(51.5074929211464,858.437987094787,125.712550169689));
#73892=CARTESIAN_POINT('Origin',(51.5074929211464,854.37663426751,135.703225385413));
#73893=CARTESIAN_POINT('Origin',(48.0052498018394,861.005933388624,126.620149278566));
#73894=CARTESIAN_POINT('',(48.0052498018394,859.125245140336,137.381545141136));
#73895=CARTESIAN_POINT('Origin',(48.0052498018394,857.416002791956,136.777441061558));
#73896=CARTESIAN_POINT('',(48.0052498018394,859.791711409404,135.495856218701));
#73897=CARTESIAN_POINT('',(48.0052498018394,862.715175737005,127.224253358145));
#73898=CARTESIAN_POINT('Origin',(48.0052498018394,858.082469061024,134.891752139123));
#73899=CARTESIAN_POINT('Origin',(48.0052498018394,861.005933388624,126.620149278566));
#73900=CARTESIAN_POINT('',(48.0052498018394,859.342516757118,132.827044522055));
#73901=CARTESIAN_POINT('Origin',(48.0052498018394,858.871094526509,132.660427954788));
#73902=CARTESIAN_POINT('',(48.0052498018394,857.887425022564,136.944057628825));
#73903=CARTESIAN_POINT('',(48.0052498018394,861.477355619233,126.786765845834));
#73904=CARTESIAN_POINT('Origin',(48.0052498018394,857.416002791956,136.777441061558));
#73905=CARTESIAN_POINT('Origin',(43.3912138270256,864.456014368904,127.839524633406));
#73906=CARTESIAN_POINT('',(43.3912138270256,862.668298922276,138.633780229895));
#73907=CARTESIAN_POINT('Origin',(43.3912138270256,860.866083772235,137.996816416397));
#73908=CARTESIAN_POINT('',(43.3912138270256,863.334765191344,136.74809130746));
#73909=CARTESIAN_POINT('',(43.3912138270256,866.258229518945,128.476488446904));
#73910=CARTESIAN_POINT('Origin',(43.3912138270256,861.532550041304,136.111127493962));
#73911=CARTESIAN_POINT('Origin',(43.3912138270256,864.456014368904,127.839524633406));
#73912=CARTESIAN_POINT('',(43.3912138270256,862.792597737398,134.046419876894));
#73913=CARTESIAN_POINT('Origin',(43.3912138270256,862.321175506789,133.879803309627));
#73914=CARTESIAN_POINT('',(43.3912138270256,861.337506002844,138.163432983664));
#73915=CARTESIAN_POINT('',(43.3912138270256,864.927436599513,128.006141200673));
#73916=CARTESIAN_POINT('Origin',(43.3912138270256,860.866083772235,137.996816416397));
#73917=CARTESIAN_POINT('Origin',(38.5967040184659,866.544078058546,128.577516992727));
#73918=CARTESIAN_POINT('',(38.5967040184659,864.415246277675,139.251210534735));
#73919=CARTESIAN_POINT('Origin',(38.5967040184659,862.954147461878,138.734808775718));
#73920=CARTESIAN_POINT('',(38.5967040184659,865.081712546744,137.3655216123));
#73921=CARTESIAN_POINT('',(38.5967040184659,868.005176874344,129.093918751744));
#73922=CARTESIAN_POINT('Origin',(38.5967040184659,863.620613730946,136.849119853283));
#73923=CARTESIAN_POINT('Origin',(38.5967040184659,866.544078058546,128.577516992727));
#73924=CARTESIAN_POINT('',(38.5967040184659,864.88066142704,134.784412236215));
#73925=CARTESIAN_POINT('Origin',(38.5967040184659,864.409239196431,134.617795668948));
#73926=CARTESIAN_POINT('',(38.5967040184659,863.425569692487,138.901425342985));
#73927=CARTESIAN_POINT('',(38.5967040184659,867.015500289155,128.744133559994));
#73928=CARTESIAN_POINT('Origin',(38.5967040184659,862.954147461878,138.734808775718));
#73929=CARTESIAN_POINT('Origin',(32.7290084090824,868.267123530476,129.186499563207));
#73930=CARTESIAN_POINT('',(32.7290084090824,865.864574510769,139.763452171557));
#73931=CARTESIAN_POINT('Origin',(32.7290084090824,864.677192933807,139.343791346199));
#73932=CARTESIAN_POINT('',(32.7290084119901,866.522075296429,137.90313004341));
#73933=CARTESIAN_POINT('',(32.7290084090824,869.454505107438,129.606160388566));
#73934=CARTESIAN_POINT('',(32.224018953637,864.255919089243,137.073658262999));
#73935=CARTESIAN_POINT('Ctrl Pts',(32.7290084148977,866.522075296429,137.90313004341));
#73936=CARTESIAN_POINT('Ctrl Pts',(32.7031571054404,866.521973103398,137.903419187084));
#73937=CARTESIAN_POINT('Ctrl Pts',(32.6772788326208,866.521125940755,137.903427495176));
#73938=CARTESIAN_POINT('Ctrl Pts',(32.4866202194529,866.50936005611,137.901396400289));
#73939=CARTESIAN_POINT('Ctrl Pts',(32.3254249892325,866.468990340329,137.888137795238));
#73940=CARTESIAN_POINT('Ctrl Pts',(32.1770177512588,866.40075615057,137.864021523816));
#73941=CARTESIAN_POINT('Ctrl Pts',(32.1227384712491,866.375799802465,137.855201105976));
#73942=CARTESIAN_POINT('Ctrl Pts',(32.0704336285077,866.347236523339,137.844973165265));
#73943=CARTESIAN_POINT('Ctrl Pts',(31.8852076585773,866.228701660669,137.802106614585));
#73944=CARTESIAN_POINT('Ctrl Pts',(31.7691493604183,866.118381696111,137.761450556226));
#73945=CARTESIAN_POINT('Ctrl Pts',(31.5888808659421,865.863043126858,137.666553800691));
#73946=CARTESIAN_POINT('Ctrl Pts',(31.5261645698418,865.720574753644,137.613275120991));
#73947=CARTESIAN_POINT('Ctrl Pts',(31.4618463420553,865.419681018586,137.500796068224));
#73948=CARTESIAN_POINT('Ctrl Pts',(31.4614758387299,865.263996806062,137.442634824622));
#73949=CARTESIAN_POINT('Ctrl Pts',(31.5227955825501,864.970146801218,137.333459398223));
#73950=CARTESIAN_POINT('Ctrl Pts',(31.5802669420954,864.833988571264,137.283159629352));
#73951=CARTESIAN_POINT('Ctrl Pts',(31.743685984272,864.589722450943,137.19363626273));
#73952=CARTESIAN_POINT('Ctrl Pts',(31.8475216280003,864.483235899298,137.154993156499));
#73953=CARTESIAN_POINT('Ctrl Pts',(32.0480530304138,864.340427466563,137.103660574143));
#73954=CARTESIAN_POINT('Ctrl Pts',(32.1336529452771,864.293213381728,137.086839327847));
#73955=CARTESIAN_POINT('Ctrl Pts',(32.2240189536389,864.255919089247,137.073658263001));
#73956=CARTESIAN_POINT('',(33.9489801953611,865.049016072261,137.353965571905));
#73957=CARTESIAN_POINT('Origin',(32.7290084090817,865.343659202875,137.458102423763));
#73958=CARTESIAN_POINT('Ctrl Pts',(33.948980195361,865.049016072261,137.353965571905));
#73959=CARTESIAN_POINT('Ctrl Pts',(33.9861939659006,865.185989792186,137.402376719148));
#73960=CARTESIAN_POINT('Ctrl Pts',(33.9971725931947,865.32808448117,137.452913675735));
#73961=CARTESIAN_POINT('Ctrl Pts',(33.9652989340809,865.610916023887,137.554575537985));
#73962=CARTESIAN_POINT('Ctrl Pts',(33.9219603364262,865.749224037751,137.604848857897));
#73963=CARTESIAN_POINT('Ctrl Pts',(33.7825322278083,866.008623498807,137.700464876327));
#73964=CARTESIAN_POINT('Ctrl Pts',(33.6858885484776,866.126659460691,137.744730929575));
#73965=CARTESIAN_POINT('Ctrl Pts',(33.4440501715648,866.328747814992,137.82199258999));
#73966=CARTESIAN_POINT('Ctrl Pts',(33.2986567258858,866.408303455729,137.853367091886));
#73967=CARTESIAN_POINT('Ctrl Pts',(33.0082071907687,866.501334098523,137.891757634516));
#73968=CARTESIAN_POINT('Ctrl Pts',(32.8690031975687,866.522628710994,137.901564219218));
#73969=CARTESIAN_POINT('Ctrl Pts',(32.7290084148977,866.522075296429,137.90313004341));
#73970=CARTESIAN_POINT('Origin',(32.7290084090824,868.267123530476,129.186499563207));
#73971=CARTESIAN_POINT('',(32.7290084090824,866.603706898969,135.393394806696));
#73972=CARTESIAN_POINT('Origin',(32.7290084090824,866.132284668361,135.226778239429));
#73973=CARTESIAN_POINT('',(32.7290084090824,865.148615164416,139.510407913466));
#73974=CARTESIAN_POINT('',(32.7290084090824,868.738545761084,129.353116130474));
#73975=CARTESIAN_POINT('Origin',(32.7290084090824,864.677192933807,139.343791346199));
#73976=CARTESIAN_POINT('Origin',(60.1505256426703,840.372072930537,119.327444828556));
#73977=CARTESIAN_POINT('',(60.1505256426703,837.780504752995,129.837591670903));
#73978=CARTESIAN_POINT('Origin',(60.1505256426703,836.782142333868,129.484736611547));
#73979=CARTESIAN_POINT('',(60.1505256426703,838.446971022064,127.951902748468));
#73980=CARTESIAN_POINT('',(60.1505256426703,841.370435349664,119.680299887912));
#73981=CARTESIAN_POINT('Origin',(60.1505256426703,837.448608602936,127.599047689112));
#73982=CARTESIAN_POINT('Origin',(60.1505256426703,840.372072930537,119.327444828556));
#73983=CARTESIAN_POINT('',(60.1505256426703,838.70865629903,125.534340072044));
#73984=CARTESIAN_POINT('Origin',(60.1505256426703,838.237234068422,125.367723504777));
#73985=CARTESIAN_POINT('',(60.1505256426703,837.253564564477,129.651353178814));
#73986=CARTESIAN_POINT('',(60.1505256426703,840.843495161145,119.494061395823));
#73987=CARTESIAN_POINT('Origin',(60.1505256426703,836.782142333868,129.484736611547));
#73988=CARTESIAN_POINT('Origin',(60.7541790064059,844.277713713595,120.707830431948));
#73989=CARTESIAN_POINT('',(60.7541790064059,841.909552396309,131.29693681787));
#73990=CARTESIAN_POINT('Origin',(60.7541790064059,840.687783116927,130.865122214939));
#73991=CARTESIAN_POINT('',(60.7541790064059,842.576018665377,129.411247895435));
#73992=CARTESIAN_POINT('',(60.7541790064059,845.499482992978,121.139645034879));
#73993=CARTESIAN_POINT('Origin',(60.7541790064059,841.354249385995,128.979433292504));
#73994=CARTESIAN_POINT('Origin',(60.7541790064059,844.277713713595,120.707830431948));
#73995=CARTESIAN_POINT('',(60.7541790064059,842.614297082089,126.914725675436));
#73996=CARTESIAN_POINT('Origin',(60.7541790064059,842.14287485148,126.748109108169));
#73997=CARTESIAN_POINT('',(60.7541790064059,841.159205347535,131.031738782206));
#73998=CARTESIAN_POINT('',(60.7541790064059,844.749135944204,120.874446999215));
#73999=CARTESIAN_POINT('Origin',(60.7541790064059,840.687783116927,130.865122214939));
#74000=CARTESIAN_POINT('Origin',(60.710027526019,848.756559286629,122.290806002987));
#74001=CARTESIAN_POINT('',(60.710027526019,846.681345091961,132.983449814156));
#74002=CARTESIAN_POINT('Origin',(60.710027526019,845.166628689961,132.448097785978));
#74003=CARTESIAN_POINT('',(60.710027526019,847.34781136103,131.097760891721));
#74004=CARTESIAN_POINT('',(60.710027526019,850.27127568863,122.826158031165));
#74005=CARTESIAN_POINT('Origin',(60.710027526019,845.833094959029,130.562408863543));
#74006=CARTESIAN_POINT('Origin',(60.710027526019,848.756559286629,122.290806002987));
#74007=CARTESIAN_POINT('',(60.710027526019,847.093142655123,128.497701246475));
#74008=CARTESIAN_POINT('Origin',(60.710027526019,846.621720424514,128.331084679208));
#74009=CARTESIAN_POINT('',(60.710027526019,845.63805092057,132.614714353245));
#74010=CARTESIAN_POINT('',(60.710027526019,849.227981517238,122.457422570254));
#74011=CARTESIAN_POINT('Origin',(60.710027526019,845.166628689961,132.448097785978));
#74012=CARTESIAN_POINT('Origin',(59.6300369248449,853.078930346135,123.818478186497));
#74013=CARTESIAN_POINT('',(59.6300369248449,851.212611893914,134.584952821211));
#74014=CARTESIAN_POINT('Origin',(59.6300369248449,849.488999749467,133.975769969489));
#74015=CARTESIAN_POINT('',(59.6300369248449,851.879078162982,132.699263898776));
#74016=CARTESIAN_POINT('',(59.6300369248449,854.802542490582,124.42766103822));
#74017=CARTESIAN_POINT('Origin',(59.6300369248449,850.155466018535,132.090081047054));
#74018=CARTESIAN_POINT('Origin',(59.6300369248449,853.078930346135,123.818478186497));
#74019=CARTESIAN_POINT('',(59.6300369248449,851.415513714629,130.025373429986));
#74020=CARTESIAN_POINT('Origin',(59.6300369248449,850.94409148402,129.858756862719));
#74021=CARTESIAN_POINT('',(59.6300369248449,849.960421980075,134.142386536756));
#74022=CARTESIAN_POINT('',(59.6300369248449,853.550352576744,123.985094753765));
#74023=CARTESIAN_POINT('Origin',(59.6300369248449,849.488999749467,133.975769969489));
#74024=CARTESIAN_POINT('Origin',(57.8564754088671,857.60895058869,125.419540617283));
#74025=CARTESIAN_POINT('',(57.8564754088671,855.771219389582,136.196118954521));
#74026=CARTESIAN_POINT('Origin',(57.8564754088671,854.019019992021,135.576832400274));
#74027=CARTESIAN_POINT('',(57.8564754088671,856.437685658651,134.310430032086));
#74028=CARTESIAN_POINT('',(57.8564754088671,859.361149986251,126.03882717153));
#74029=CARTESIAN_POINT('Origin',(57.8564754088671,854.685486261089,133.691143477839));
#74030=CARTESIAN_POINT('Origin',(57.8564754088671,857.60895058869,125.419540617283));
#74031=CARTESIAN_POINT('',(57.8564754088671,855.945533957183,131.626435860771));
#74032=CARTESIAN_POINT('Origin',(57.8564754088671,855.474111726575,131.459819293504));
#74033=CARTESIAN_POINT('',(57.8564754088671,854.49044222263,135.743448967541));
#74034=CARTESIAN_POINT('',(57.8564754088671,858.080372819298,125.58615718455));
#74035=CARTESIAN_POINT('Origin',(57.8564754088671,854.019019992021,135.576832400274));
#74036=CARTESIAN_POINT('Origin',(55.1009921650808,861.268440685064,126.712928239285));
#74037=CARTESIAN_POINT('',(55.1009921650808,859.387752436776,137.474324101854));
#74038=CARTESIAN_POINT('Origin',(55.1009921650808,857.678510088396,136.870220022276));
#74039=CARTESIAN_POINT('',(55.1009921650808,860.054218705844,135.588635179419));
#74040=CARTESIAN_POINT('',(55.1009921650808,862.977683033444,127.317032318863));
#74041=CARTESIAN_POINT('Origin',(55.1009921650808,858.344976357464,134.984531099841));
#74042=CARTESIAN_POINT('Origin',(55.1009921650808,861.268440685064,126.712928239285));
#74043=CARTESIAN_POINT('',(55.1009921650808,859.605024053558,132.919823482773));
#74044=CARTESIAN_POINT('Origin',(55.1009921650808,859.133601822949,132.753206915506));
#74045=CARTESIAN_POINT('',(55.1009921650808,858.149932319004,137.036836589543));
#74046=CARTESIAN_POINT('',(55.1009921650808,861.739862915673,126.879544806552));
#74047=CARTESIAN_POINT('Origin',(55.1009921650808,857.678510088396,136.870220022276));
#74048=CARTESIAN_POINT('Origin',(51.3485798144127,865.547611143858,128.225331868775));
#74049=CARTESIAN_POINT('',(51.3485798144127,863.75989569723,139.019587465264));
#74050=CARTESIAN_POINT('Origin',(51.3485798144127,861.957680547189,138.382623651766));
#74051=CARTESIAN_POINT('',(51.3485798144127,864.426361966298,137.133898542829));
#74052=CARTESIAN_POINT('',(51.3485798144127,867.349826293898,128.862295682273));
#74053=CARTESIAN_POINT('Origin',(51.3485798144127,862.624146816258,136.496934729331));
#74054=CARTESIAN_POINT('Origin',(51.3485798144127,865.547611143858,128.225331868775));
#74055=CARTESIAN_POINT('',(51.3485798144127,863.884194512352,134.432227112263));
#74056=CARTESIAN_POINT('Origin',(51.3485798144127,863.412772281743,134.265610544996));
#74057=CARTESIAN_POINT('',(51.3485798144127,862.429102777798,138.549240219033));
#74058=CARTESIAN_POINT('',(51.3485798144127,866.019033374467,128.391948436042));
#74059=CARTESIAN_POINT('Origin',(51.3485798144127,861.957680547189,138.382623651766));
#74060=CARTESIAN_POINT('Origin',(47.119291675836,868.529905652021,129.279375656417));
#74061=CARTESIAN_POINT('',(47.119291675836,866.40107387115,139.953069198425));
#74062=CARTESIAN_POINT('Origin',(47.119291675836,864.939975055353,139.436667439408));
#74063=CARTESIAN_POINT('',(47.119291675836,867.067540140218,138.06738027599));
#74064=CARTESIAN_POINT('',(47.119291675836,869.991004467819,129.795777415434));
#74065=CARTESIAN_POINT('Origin',(47.119291675836,865.606441324421,137.550978516973));
#74066=CARTESIAN_POINT('Origin',(47.119291675836,868.529905652021,129.279375656417));
#74067=CARTESIAN_POINT('',(47.119291675836,866.866489020515,135.486270899905));
#74068=CARTESIAN_POINT('Origin',(47.119291675836,866.395066789906,135.319654332638));
#74069=CARTESIAN_POINT('',(47.119291675836,865.411397285961,139.603284006675));
#74070=CARTESIAN_POINT('',(47.119291675836,869.00132788263,129.445992223684));
#74071=CARTESIAN_POINT('Origin',(47.119291675836,864.939975055353,139.436667439408));
#74072=CARTESIAN_POINT('Origin',(41.7597772954093,871.365533346835,130.281582429626));
#74073=CARTESIAN_POINT('',(41.7597772954093,868.962984327129,140.858535037976));
#74074=CARTESIAN_POINT('Origin',(41.7597772954093,867.775602750167,140.438874212617));
#74075=CARTESIAN_POINT('',(41.7597773059811,869.619655531143,139.000560114769));
#74076=CARTESIAN_POINT('',(41.7597772954093,872.552914923797,130.701243254984));
#74077=CARTESIAN_POINT('',(41.0259596626274,867.477090904821,138.212129373697));
#74078=CARTESIAN_POINT('Ctrl Pts',(41.7597773059816,869.619655531119,139.000560114837));
#74079=CARTESIAN_POINT('Ctrl Pts',(41.6573369345889,869.619422397947,139.001219740658));
#74080=CARTESIAN_POINT('Ctrl Pts',(41.555042709061,869.607515464247,138.997398768683));
#74081=CARTESIAN_POINT('Ctrl Pts',(41.4551932856153,869.584049900572,138.989105244503));
#74082=CARTESIAN_POINT('Ctrl Pts',(41.3965968798861,869.57027918821,138.984238208811));
#74083=CARTESIAN_POINT('Ctrl Pts',(41.339127186869,869.552594230335,138.977855034907));
#74084=CARTESIAN_POINT('Ctrl Pts',(41.1317427249637,869.472965862453,138.948739355919));
#74085=CARTESIAN_POINT('Ctrl Pts',(40.9937779581549,869.387818807864,138.91698025569));
#74086=CARTESIAN_POINT('Ctrl Pts',(40.7608204171255,869.173429676768,138.836556417158));
#74087=CARTESIAN_POINT('Ctrl Pts',(40.6678554670967,869.046388839606,138.788730350703));
#74088=CARTESIAN_POINT('Ctrl Pts',(40.5381661401692,868.764720660735,138.683046260005));
#74089=CARTESIAN_POINT('Ctrl Pts',(40.503255619118,868.612532689981,138.626120706543));
#74090=CARTESIAN_POINT('Ctrl Pts',(40.4980684291032,868.313120120479,138.51497928158));
#74091=CARTESIAN_POINT('Ctrl Pts',(40.5241081013521,868.168686202312,138.46175460448));
#74092=CARTESIAN_POINT('Ctrl Pts',(40.6298704988454,867.89774502338,138.362803369572));
#74093=CARTESIAN_POINT('Ctrl Pts',(40.7078853849485,867.773237639588,138.317791091509));
#74094=CARTESIAN_POINT('Ctrl Pts',(40.8724837098879,867.594245965953,138.253670127529));
#74095=CARTESIAN_POINT('Ctrl Pts',(40.9457923328914,867.53128453031,138.231283234632));
#74096=CARTESIAN_POINT('Ctrl Pts',(41.0259596626275,867.477090904821,138.212129373697));
#74097=CARTESIAN_POINT('',(42.8881164335297,867.914715447588,138.366800694508));
#74098=CARTESIAN_POINT('Origin',(41.7597772954084,868.442069019235,138.553185290182));
#74099=CARTESIAN_POINT('Ctrl Pts',(42.88811643353,867.914715447588,138.366800694508));
#74100=CARTESIAN_POINT('Ctrl Pts',(42.9547218037881,868.041401007716,138.41157565797));
#74101=CARTESIAN_POINT('Ctrl Pts',(42.9968164695112,868.178236295445,138.460253764197));
#74102=CARTESIAN_POINT('Ctrl Pts',(43.0281257825353,868.461123763136,138.561935392225));
#74103=CARTESIAN_POINT('Ctrl Pts',(43.0163296236268,868.604895462998,138.614139763637));
#74104=CARTESIAN_POINT('Ctrl Pts',(42.9374225821821,868.885931270645,138.717402799037));
#74105=CARTESIAN_POINT('Ctrl Pts',(42.8690960860492,869.02031527311,138.767446802976));
#74106=CARTESIAN_POINT('Ctrl Pts',(42.677510436449,869.265354624792,138.859888799149));
#74107=CARTESIAN_POINT('Ctrl Pts',(42.5530630718917,869.371650665748,138.900714263267));
#74108=CARTESIAN_POINT('Ctrl Pts',(42.2676632709367,869.532017614981,138.963368373441));
#74109=CARTESIAN_POINT('Ctrl Pts',(42.1096748558595,869.584750951896,138.984653116944));
#74110=CARTESIAN_POINT('Ctrl Pts',(41.8836861993185,869.615671233301,138.998125913844));
#74111=CARTESIAN_POINT('Ctrl Pts',(41.8217050457295,869.619796465891,139.000161354703));
#74112=CARTESIAN_POINT('Ctrl Pts',(41.7597773059816,869.619655531119,139.000560114837));
#74113=CARTESIAN_POINT('Origin',(41.7597772954093,871.365533346835,130.281582429626));
#74114=CARTESIAN_POINT('',(41.7597772954093,869.702116715329,136.488477673114));
#74115=CARTESIAN_POINT('Origin',(41.7597772954093,869.23069448472,136.321861105847));
#74116=CARTESIAN_POINT('',(41.7597772954093,868.247024980775,140.605490779884));
#74117=CARTESIAN_POINT('',(41.7597772954093,871.836955577444,130.448198996893));
#74118=CARTESIAN_POINT('Origin',(41.7597772954093,867.775602750167,140.438874212617));
#74119=CARTESIAN_POINT('Origin',(62.4307813118898,838.704660762172,118.738124949954));
#74120=CARTESIAN_POINT('',(62.4307813118898,836.113092584631,129.248271792302));
#74121=CARTESIAN_POINT('Origin',(62.4307813118898,835.114730165504,128.895416732946));
#74122=CARTESIAN_POINT('',(62.4307813118898,836.779558853699,127.362582869867));
#74123=CARTESIAN_POINT('',(62.4307813118898,839.703023181299,119.090980009311));
#74124=CARTESIAN_POINT('Origin',(62.4307813118898,835.781196434572,127.009727810511));
#74125=CARTESIAN_POINT('Origin',(62.4307813118898,838.704660762172,118.738124949954));
#74126=CARTESIAN_POINT('',(62.4307813118898,837.041244130666,124.945020193443));
#74127=CARTESIAN_POINT('Origin',(62.4307813118898,836.569821900057,124.778403626176));
#74128=CARTESIAN_POINT('',(62.4307813118898,835.586152396113,129.062033300213));
#74129=CARTESIAN_POINT('',(62.4307813118898,839.176082992781,118.904741517222));
#74130=CARTESIAN_POINT('Origin',(62.4307813118898,835.114730165504,128.895416732946));
#74131=CARTESIAN_POINT('Origin',(63.8824972054392,842.406620728786,120.046522861103));
#74132=CARTESIAN_POINT('',(63.8824972054392,840.0384594115,130.635629247025));
#74133=CARTESIAN_POINT('Origin',(63.8824972054392,838.816690132118,130.203814644094));
#74134=CARTESIAN_POINT('',(63.8824972054392,840.704925680569,128.74994032459));
#74135=CARTESIAN_POINT('',(63.8824972054392,843.628390008169,120.478337464034));
#74136=CARTESIAN_POINT('Origin',(63.8824972054392,839.483156401186,128.318125721659));
#74137=CARTESIAN_POINT('Origin',(63.8824972054392,842.406620728786,120.046522861103));
#74138=CARTESIAN_POINT('',(63.8824972054392,840.74320409728,126.253418104591));
#74139=CARTESIAN_POINT('Origin',(63.8824972054392,840.271781866671,126.086801537324));
#74140=CARTESIAN_POINT('',(63.8824972054392,839.288112362726,130.370431211361));
#74141=CARTESIAN_POINT('',(63.8824972054392,842.878042959395,120.21313942837));
#74142=CARTESIAN_POINT('Origin',(63.8824972054392,838.816690132118,130.203814644094));
#74143=CARTESIAN_POINT('Origin',(64.8269648086385,846.796247723552,121.597965567795));
#74144=CARTESIAN_POINT('',(64.8269648086385,844.721033528884,132.290609378964));
#74145=CARTESIAN_POINT('Origin',(64.8269648086385,843.206317126883,131.755257350787));
#74146=CARTESIAN_POINT('',(64.8269648086385,845.387499797952,130.404920456529));
#74147=CARTESIAN_POINT('',(64.8269648086385,848.310964125552,122.133317595973));
#74148=CARTESIAN_POINT('Origin',(64.8269648086385,843.872783395951,129.869568428351));
#74149=CARTESIAN_POINT('Origin',(64.8269648086385,846.796247723552,121.597965567795));
#74150=CARTESIAN_POINT('',(64.8269648086385,845.132831092045,127.804860811284));
#74151=CARTESIAN_POINT('Origin',(64.8269648086385,844.661408861436,127.638244244017));
#74152=CARTESIAN_POINT('',(64.8269648086385,843.677739357492,131.921873918054));
#74153=CARTESIAN_POINT('',(64.8269648086385,847.26766995416,121.764582135062));
#74154=CARTESIAN_POINT('Origin',(64.8269648086385,843.206317126883,131.755257350787));
#74155=CARTESIAN_POINT('Origin',(64.7237238265774,851.23587341945,123.167079507217));
#74156=CARTESIAN_POINT('',(64.7237238265774,849.369554967228,133.933554141931));
#74157=CARTESIAN_POINT('Origin',(64.7237238265774,847.645942822782,133.324371290208));
#74158=CARTESIAN_POINT('',(64.7237238265774,850.036021236297,132.047865219495));
#74159=CARTESIAN_POINT('',(64.7237238265774,852.959485563897,123.776262358939));
#74160=CARTESIAN_POINT('Origin',(64.7237238265774,848.31240909185,131.438682367773));
#74161=CARTESIAN_POINT('Origin',(64.7237238265774,851.23587341945,123.167079507217));
#74162=CARTESIAN_POINT('',(64.7237238265774,849.572456787944,129.373974750705));
#74163=CARTESIAN_POINT('Origin',(64.7237238265774,849.101034557335,129.207358183438));
#74164=CARTESIAN_POINT('',(64.7237238265774,848.117365053391,133.490987857475));
#74165=CARTESIAN_POINT('',(64.7237238265774,851.707295650059,123.333696074484));
#74166=CARTESIAN_POINT('Origin',(64.7237238265774,847.645942822782,133.324371290208));
#74167=CARTESIAN_POINT('Origin',(63.9878579537236,856.014570252624,124.85603265931));
#74168=CARTESIAN_POINT('',(63.9878579537236,854.176839053517,135.632610996548));
#74169=CARTESIAN_POINT('Origin',(63.9878579537236,852.424639655956,135.013324442301));
#74170=CARTESIAN_POINT('',(63.9878579537236,854.843305322585,133.746922074113));
#74171=CARTESIAN_POINT('',(63.9878579537236,857.766769650186,125.475319213557));
#74172=CARTESIAN_POINT('Origin',(63.9878579537236,853.091105925024,133.127635519866));
#74173=CARTESIAN_POINT('Origin',(63.9878579537236,856.014570252624,124.85603265931));
#74174=CARTESIAN_POINT('',(63.9878579537236,854.351153621118,131.062927902798));
#74175=CARTESIAN_POINT('Origin',(63.9878579537236,853.879731390509,130.896311335531));
#74176=CARTESIAN_POINT('',(63.9878579537236,852.896061886564,135.179941009568));
#74177=CARTESIAN_POINT('',(63.9878579537236,856.485992483233,125.022649226577));
#74178=CARTESIAN_POINT('Origin',(63.9878579537236,852.424639655956,135.013324442301));
#74179=CARTESIAN_POINT('Origin',(62.0995624254871,860.134244643534,126.312064981726));
#74180=CARTESIAN_POINT('',(62.0995624254871,858.253556395246,137.073460844295));
#74181=CARTESIAN_POINT('Origin',(62.0995624254871,856.544314046866,136.469356764717));
#74182=CARTESIAN_POINT('',(62.0995624254871,858.920022664315,135.18777192186));
#74183=CARTESIAN_POINT('',(62.0995624254871,861.843486991915,126.916169061304));
#74184=CARTESIAN_POINT('Origin',(62.0995624254871,857.210780315934,134.583667842282));
#74185=CARTESIAN_POINT('Origin',(62.0995624254871,860.134244643534,126.312064981726));
#74186=CARTESIAN_POINT('',(62.0995624254871,858.470828012028,132.518960225214));
#74187=CARTESIAN_POINT('Origin',(62.0995624254871,857.999405781419,132.352343657947));
#74188=CARTESIAN_POINT('',(62.0995624254871,857.015736277475,136.635973331984));
#74189=CARTESIAN_POINT('',(62.0995624254871,860.605666874143,126.478681548993));
#74190=CARTESIAN_POINT('Origin',(62.0995624254871,856.544314046866,136.469356764717));
#74191=CARTESIAN_POINT('Origin',(59.3727721247612,865.055484298055,128.05139758994));
#74192=CARTESIAN_POINT('',(59.3727721247612,863.267768851427,138.845653186429));
#74193=CARTESIAN_POINT('Origin',(59.3727721247612,861.465553701386,138.208689372931));
#74194=CARTESIAN_POINT('',(59.3727721247612,863.934235120495,136.959964263994));
#74195=CARTESIAN_POINT('',(59.3727721247612,866.857699448095,128.688361403438));
#74196=CARTESIAN_POINT('Origin',(59.3727721247612,862.132019970455,136.323000450496));
#74197=CARTESIAN_POINT('Origin',(59.3727721247612,865.055484298055,128.05139758994));
#74198=CARTESIAN_POINT('',(59.3727721247612,863.392067666549,134.258292833428));
#74199=CARTESIAN_POINT('Origin',(59.3727721247612,862.92064543594,134.091676266161));
#74200=CARTESIAN_POINT('',(59.3727721247612,861.936975931995,138.375305940198));
#74201=CARTESIAN_POINT('',(59.3727721247612,865.526906528664,128.218014157207));
#74202=CARTESIAN_POINT('Origin',(59.3727721247612,861.465553701386,138.208689372931));
#74203=CARTESIAN_POINT('Origin',(55.8935458421992,868.801669044095,129.37542603452));
#74204=CARTESIAN_POINT('',(55.8935458421992,866.672837263224,140.049119576529));
#74205=CARTESIAN_POINT('Origin',(55.8935458421992,865.211738447427,139.532717817511));
#74206=CARTESIAN_POINT('',(55.8935458421992,867.339303532293,138.163430654094));
#74207=CARTESIAN_POINT('',(55.8935458421992,870.262767859893,129.891827793537));
#74208=CARTESIAN_POINT('Origin',(55.8935458421992,865.878204716495,137.647028895076));
#74209=CARTESIAN_POINT('Origin',(55.8935458421992,868.801669044095,129.37542603452));
#74210=CARTESIAN_POINT('',(55.8935458421992,867.138252412589,135.582321278008));
#74211=CARTESIAN_POINT('Origin',(55.8935458421992,866.66683018198,135.415704710741));
#74212=CARTESIAN_POINT('',(55.8935458421992,865.683160678035,139.699334384778));
#74213=CARTESIAN_POINT('',(55.8935458421992,869.273091274704,129.542042601787));
#74214=CARTESIAN_POINT('Origin',(55.8935458421992,865.211738447427,139.532717817511));
#74215=CARTESIAN_POINT('Origin',(51.2764491869573,872.62594842468,130.727055765347));
#74216=CARTESIAN_POINT('',(51.2764491869573,870.223399404973,141.304008373696));
#74217=CARTESIAN_POINT('Origin',(51.2764491869573,869.036017828011,140.884347548338));
#74218=CARTESIAN_POINT('',(51.2764491871435,870.879723090442,139.447016713862));
#74219=CARTESIAN_POINT('',(51.2764491869573,873.813330001642,131.146716590705));
#74220=CARTESIAN_POINT('',(50.3458747286375,868.902442155958,138.715896733814));
#74221=CARTESIAN_POINT('Ctrl Pts',(51.2764491873298,870.879723090442,139.447016713862));
#74222=CARTESIAN_POINT('Ctrl Pts',(51.2618354165802,870.879718220088,139.447030493977));
#74223=CARTESIAN_POINT('Ctrl Pts',(51.2472113783088,870.879475947816,139.446952641435));
#74224=CARTESIAN_POINT('Ctrl Pts',(51.232583607977,870.878995268524,139.446782753109));
#74225=CARTESIAN_POINT('Ctrl Pts',(51.172231020632,870.877012038113,139.446081812378));
#74226=CARTESIAN_POINT('Ctrl Pts',(51.1121081786909,870.870980141333,139.443817224556));
#74227=CARTESIAN_POINT('Ctrl Pts',(50.8916289209462,870.833751761404,139.429687135951));
#74228=CARTESIAN_POINT('Ctrl Pts',(50.7377874078257,870.777521818001,139.408148321249));
#74229=CARTESIAN_POINT('Ctrl Pts',(50.4623221826389,870.613515830349,139.345531590367));
#74230=CARTESIAN_POINT('Ctrl Pts',(50.3431715930928,870.507494995374,139.305134703914));
#74231=CARTESIAN_POINT('Ctrl Pts',(50.1537792129284,870.257446839222,139.210626199135));
#74232=CARTESIAN_POINT('Ctrl Pts',(50.085854431441,870.115449532897,139.157302371292));
#74233=CARTESIAN_POINT('Ctrl Pts',(50.0143870126858,869.823633201028,139.048845713734));
#74234=CARTESIAN_POINT('Ctrl Pts',(50.0078569390086,869.677265941222,138.994937728282));
#74235=CARTESIAN_POINT('Ctrl Pts',(50.0513403675436,869.391534956718,138.890759275659));
#74236=CARTESIAN_POINT('Ctrl Pts',(50.1001248711416,869.254462140642,138.841305948666));
#74237=CARTESIAN_POINT('Ctrl Pts',(50.2215963819772,869.047121819918,138.767165613604));
#74238=CARTESIAN_POINT('Ctrl Pts',(50.2794097745223,868.971166592971,138.740186275205));
#74239=CARTESIAN_POINT('Ctrl Pts',(50.3458747286374,868.902442155957,138.715896733814));
#74240=CARTESIAN_POINT('',(52.2638418422125,868.965467966003,138.738172187616));
#74241=CARTESIAN_POINT('Origin',(51.2764491869568,869.70248409708,138.998658625903));
#74242=CARTESIAN_POINT('Ctrl Pts',(52.2638418422126,868.965467966004,138.738172187616));
#74243=CARTESIAN_POINT('Ctrl Pts',(52.3569278379003,869.076328599452,138.77735408654));
#74244=CARTESIAN_POINT('Ctrl Pts',(52.4282988031681,869.201919789666,138.822058148252));
#74245=CARTESIAN_POINT('Ctrl Pts',(52.5214227211125,869.472476304179,138.919381600198));
#74246=CARTESIAN_POINT('Ctrl Pts',(52.5416845496989,869.615409082029,138.971289468186));
#74247=CARTESIAN_POINT('Ctrl Pts',(52.5267471917766,869.905744583059,139.07783932989));
#74248=CARTESIAN_POINT('Ctrl Pts',(52.48972407459,870.050568410474,139.131573121207));
#74249=CARTESIAN_POINT('Ctrl Pts',(52.3567643645195,870.327769216161,139.235382063435));
#74250=CARTESIAN_POINT('Ctrl Pts',(52.2587020280801,870.456115288957,139.284000754887));
#74251=CARTESIAN_POINT('Ctrl Pts',(52.0153162405214,870.668883275139,139.365175164552));
#74252=CARTESIAN_POINT('Ctrl Pts',(51.8725921545554,870.751416302552,139.396992126975));
#74253=CARTESIAN_POINT('Ctrl Pts',(51.5758456035277,870.854733983497,139.437035579406));
#74254=CARTESIAN_POINT('Ctrl Pts',(51.4266900107678,870.879773161437,139.446875043663));
#74255=CARTESIAN_POINT('Ctrl Pts',(51.2764491873298,870.879723090442,139.447016713862));
#74256=CARTESIAN_POINT('Origin',(51.2764491869573,872.62594842468,130.727055765347));
#74257=CARTESIAN_POINT('',(51.2764491869573,870.962531793174,136.933951008835));
#74258=CARTESIAN_POINT('Origin',(51.2764491869573,870.491109562565,136.767334441568));
#74259=CARTESIAN_POINT('',(51.2764491869573,869.50744005862,141.050964115605));
#74260=CARTESIAN_POINT('',(51.2764491869573,873.097370655289,130.893672332614));
#74261=CARTESIAN_POINT('Origin',(51.2764491869573,869.036017828011,140.884347548338));
#74262=CARTESIAN_POINT('Origin',(64.2935179203293,836.626690711497,118.003700024172));
#74263=CARTESIAN_POINT('',(64.2935179203293,834.035122533956,128.513846866519));
#74264=CARTESIAN_POINT('Origin',(64.2935179203293,833.036760114829,128.160991807163));
#74265=CARTESIAN_POINT('',(64.2935179203293,834.701588803024,126.628157944084));
#74266=CARTESIAN_POINT('',(64.2935179203293,837.625053130624,118.356555083528));
#74267=CARTESIAN_POINT('Origin',(64.2935179203293,833.703226383897,126.275302884728));
#74268=CARTESIAN_POINT('Origin',(64.2935179203293,836.626690711497,118.003700024172));
#74269=CARTESIAN_POINT('',(64.2935179203293,834.963274079991,124.21059526766));
#74270=CARTESIAN_POINT('Origin',(64.2935179203293,834.491851849382,124.043978700393));
#74271=CARTESIAN_POINT('',(64.2935179203293,833.508182345437,128.32760837443));
#74272=CARTESIAN_POINT('',(64.2935179203293,837.098112942106,118.170316591439));
#74273=CARTESIAN_POINT('Origin',(64.2935179203293,833.036760114829,128.160991807163));
#74274=CARTESIAN_POINT('Origin',(66.5298493930383,839.963176447151,119.182926975969));
#74275=CARTESIAN_POINT('',(66.5298493930383,837.595015129865,129.772033361891));
#74276=CARTESIAN_POINT('Origin',(66.5298493930383,836.373245850482,129.34021875896));
#74277=CARTESIAN_POINT('',(66.5298493930383,838.261481398933,127.886344439456));
#74278=CARTESIAN_POINT('',(66.5298493930383,841.184945726533,119.6147415789));
#74279=CARTESIAN_POINT('Origin',(66.5298493930383,837.03971211955,127.454529836525));
#74280=CARTESIAN_POINT('Origin',(66.5298493930383,839.963176447151,119.182926975969));
#74281=CARTESIAN_POINT('',(66.5298493930383,838.299759815644,125.389822219457));
#74282=CARTESIAN_POINT('Origin',(66.5298493930383,837.828337585036,125.22320565219));
#74283=CARTESIAN_POINT('',(66.5298493930383,836.844668081091,129.506835326227));
#74284=CARTESIAN_POINT('',(66.5298493930383,840.434598677759,119.349543543236));
#74285=CARTESIAN_POINT('Origin',(66.5298493930383,836.373245850482,129.34021875896));
#74286=CARTESIAN_POINT('Origin',(68.4216583135058,844.071737100209,120.635031327384));
#74287=CARTESIAN_POINT('',(68.4216583135058,841.996522905541,131.327675138553));
#74288=CARTESIAN_POINT('Origin',(68.4216583135058,840.48180650354,130.792323110376));
#74289=CARTESIAN_POINT('',(68.4216583135058,842.662989174609,129.441986216118));
#74290=CARTESIAN_POINT('',(68.4216583135058,845.586453502209,121.170383355562));
#74291=CARTESIAN_POINT('Origin',(68.4216583135058,841.148272772608,128.906634187941));
#74292=CARTESIAN_POINT('Origin',(68.4216583135058,844.071737100209,120.635031327384));
#74293=CARTESIAN_POINT('',(68.4216583135058,842.408320468702,126.841926570873));
#74294=CARTESIAN_POINT('Origin',(68.4216583135058,841.936898238093,126.675310003606));
#74295=CARTESIAN_POINT('',(68.4216583135058,840.953228734149,130.958939677643));
#74296=CARTESIAN_POINT('',(68.4216583135058,844.543159330817,120.801647894651));
#74297=CARTESIAN_POINT('Origin',(68.4216583135058,840.48180650354,130.792323110376));
#74298=CARTESIAN_POINT('Origin',(69.2996790768792,848.434584485902,122.17700921412));
#74299=CARTESIAN_POINT('',(69.2996790768792,846.56826603368,132.943483848834));
#74300=CARTESIAN_POINT('Origin',(69.2996790768792,844.844653889233,132.334300997111));
#74301=CARTESIAN_POINT('',(69.2996790768792,847.234732302748,131.057794926399));
#74302=CARTESIAN_POINT('',(69.2996790768792,850.158196630348,122.786192065843));
#74303=CARTESIAN_POINT('Origin',(69.2996790768792,845.511120158302,130.448612074676));
#74304=CARTESIAN_POINT('Origin',(69.2996790768792,848.434584485902,122.17700921412));
#74305=CARTESIAN_POINT('',(69.2996790768792,846.771167854396,128.383904457608));
#74306=CARTESIAN_POINT('Origin',(69.2996790768792,846.299745623787,128.217287890341));
#74307=CARTESIAN_POINT('',(69.2996790768792,845.316076119842,132.500917564379));
#74308=CARTESIAN_POINT('',(69.2996790768792,848.906006716511,122.343625781387));
#74309=CARTESIAN_POINT('Origin',(69.2996790768792,844.844653889233,132.334300997111));
#74310=CARTESIAN_POINT('Origin',(69.6336697168692,853.253105927354,123.880037730278));
#74311=CARTESIAN_POINT('',(69.6336697168692,851.415374728247,134.656616067516));
#74312=CARTESIAN_POINT('Origin',(69.6336697168692,849.663175330685,134.03732951327));
#74313=CARTESIAN_POINT('',(69.6336697168692,852.081840997315,132.770927145081));
#74314=CARTESIAN_POINT('',(69.6336697168692,855.005305324915,124.499324284525));
#74315=CARTESIAN_POINT('Origin',(69.6336697168692,850.329641599754,132.151640590834));
#74316=CARTESIAN_POINT('Origin',(69.6336697168692,853.253105927354,123.880037730278));
#74317=CARTESIAN_POINT('',(69.6336697168692,851.589689295848,130.086932973767));
#74318=CARTESIAN_POINT('Origin',(69.6336697168692,851.118267065239,129.9203164065));
#74319=CARTESIAN_POINT('',(69.6336697168692,850.134597561294,134.203946080537));
#74320=CARTESIAN_POINT('',(69.6336697168692,853.724528157963,124.046654297545));
#74321=CARTESIAN_POINT('Origin',(69.6336697168692,849.663175330685,134.03732951327));
#74322=CARTESIAN_POINT('Origin',(67.1130950497633,863.001142136143,127.325323559515));
#74323=CARTESIAN_POINT('',(67.1130950497633,861.213426689515,138.119579156005));
#74324=CARTESIAN_POINT('Origin',(67.1130950497633,859.411211539474,137.482615342506));
#74325=CARTESIAN_POINT('',(67.1130950497633,861.879892958583,136.23389023357));
#74326=CARTESIAN_POINT('',(67.1130950497633,864.803357286184,127.962287373014));
#74327=CARTESIAN_POINT('Origin',(67.1130950497633,860.077677808543,135.596926420071));
#74328=CARTESIAN_POINT('Origin',(67.1130950497633,863.001142136143,127.325323559515));
#74329=CARTESIAN_POINT('',(67.1130950497633,861.337725504637,133.532218803004));
#74330=CARTESIAN_POINT('Origin',(67.1130950497633,860.866303274028,133.365602235737));
#74331=CARTESIAN_POINT('',(67.1130950497633,859.882633770083,137.649231909774));
#74332=CARTESIAN_POINT('',(67.1130950497633,863.472564366752,127.491940126782));
#74333=CARTESIAN_POINT('Origin',(67.1130950497633,859.411211539474,137.482615342506));
#74334=CARTESIAN_POINT('Origin',(64.535989506944,867.34749087047,128.861470264612));
#74335=CARTESIAN_POINT('',(64.535989506944,865.218659089599,139.535163806621));
#74336=CARTESIAN_POINT('Origin',(64.535989506944,863.757560273801,139.018762047603));
#74337=CARTESIAN_POINT('',(64.535989506944,865.885125358667,137.649474884186));
#74338=CARTESIAN_POINT('',(64.535989506944,868.808589686267,129.377872023629));
#74339=CARTESIAN_POINT('Origin',(64.535989506944,864.424026542869,137.133073125168));
#74340=CARTESIAN_POINT('Origin',(64.535989506944,867.34749087047,128.861470264612));
#74341=CARTESIAN_POINT('',(64.535989506944,865.684074238963,135.068365508101));
#74342=CARTESIAN_POINT('Origin',(64.535989506944,865.212652008354,134.901748940833));
#74343=CARTESIAN_POINT('',(64.535989506944,864.22898250441,139.185378614871));
#74344=CARTESIAN_POINT('',(64.535989506944,867.818913101078,129.028086831879));
#74345=CARTESIAN_POINT('Origin',(64.535989506944,863.757560273801,139.018762047603));
#74346=CARTESIAN_POINT('Origin',(60.8630998560088,871.993282576964,130.50345024798));
#74347=CARTESIAN_POINT('',(60.8630998560088,869.590733557258,141.080402856329));
#74348=CARTESIAN_POINT('Origin',(60.8630998560088,868.403351980296,140.660742030971));
#74349=CARTESIAN_POINT('',(60.8630998553805,870.247232404664,139.222915596134));
#74350=CARTESIAN_POINT('',(60.8630998560088,873.180664153927,130.923111073338));
#74351=CARTESIAN_POINT('',(59.7764391413702,868.469678153389,138.56294329237));
#74352=CARTESIAN_POINT('Ctrl Pts',(60.8630998547522,870.247232404664,139.222915596134));
#74353=CARTESIAN_POINT('Ctrl Pts',(60.7125947473751,870.247480485245,139.222213680484));
#74354=CARTESIAN_POINT('Ctrl Pts',(60.5631969146961,870.222538914215,139.211814297784));
#74355=CARTESIAN_POINT('Ctrl Pts',(60.2693839823579,870.120362912388,139.171234662913));
#74356=CARTESIAN_POINT('Ctrl Pts',(60.1292552058059,870.040035870772,139.139918832405));
#74357=CARTESIAN_POINT('Ctrl Pts',(59.8884371282248,869.83262025715,139.060478110665));
#74358=CARTESIAN_POINT('Ctrl Pts',(59.7904667251912,869.707062656979,139.012964631227));
#74359=CARTESIAN_POINT('Ctrl Pts',(59.655842546834,869.435669372995,138.911726169822));
#74360=CARTESIAN_POINT('Ctrl Pts',(59.6170281227853,869.293795614435,138.859406339753));
#74361=CARTESIAN_POINT('Ctrl Pts',(59.5963321478785,869.005806462867,138.754429774482));
#74362=CARTESIAN_POINT('Ctrl Pts',(59.6137541520704,868.86217278406,138.702657616607));
#74363=CARTESIAN_POINT('Ctrl Pts',(59.6867899608931,868.63555738197,138.621704815602));
#74364=CARTESIAN_POINT('Ctrl Pts',(59.7265814003054,868.549929814254,138.591306944703));
#74365=CARTESIAN_POINT('Ctrl Pts',(59.7764391413706,868.469678153389,138.562943292371));
#74366=CARTESIAN_POINT('',(61.6663922313285,868.155350700384,138.451849334943));
#74367=CARTESIAN_POINT('Origin',(60.8630998560082,869.069818249365,138.775053108536));
#74368=CARTESIAN_POINT('Ctrl Pts',(61.6663922313285,868.155350700384,138.451849334943));
#74369=CARTESIAN_POINT('Ctrl Pts',(61.7818905477588,868.245541265504,138.483725732331));
#74370=CARTESIAN_POINT('Ctrl Pts',(61.8794185589124,868.35439508296,138.522514240186));
#74371=CARTESIAN_POINT('Ctrl Pts',(62.0302871197043,868.600772687965,138.611292047399));
#74372=CARTESIAN_POINT('Ctrl Pts',(62.0817213966495,868.736600600712,138.66068881566));
#74373=CARTESIAN_POINT('Ctrl Pts',(62.1314065564681,869.023492700691,138.766021662923));
#74374=CARTESIAN_POINT('Ctrl Pts',(62.1273049061047,869.172391866978,138.821195816889));
#74375=CARTESIAN_POINT('Ctrl Pts',(62.0587821129058,869.469558973426,138.932061525383));
#74376=CARTESIAN_POINT('Ctrl Pts',(61.9913905992417,869.614301017483,138.98647510785));
#74377=CARTESIAN_POINT('Ctrl Pts',(61.8006559518915,869.870089012991,139.082854244429));
#74378=CARTESIAN_POINT('Ctrl Pts',(61.6794339224592,869.978778294368,139.123915712022));
#74379=CARTESIAN_POINT('Ctrl Pts',(61.399851307555,870.145341289405,139.186475194636));
#74380=CARTESIAN_POINT('Ctrl Pts',(61.2444721746654,870.201953729592,139.207493364977));
#74381=CARTESIAN_POINT('Ctrl Pts',(61.0818698441341,870.228996928008,139.217051346327));
#74382=CARTESIAN_POINT('Ctrl Pts',(61.0223987728464,870.238887856235,139.220547135031));
#74383=CARTESIAN_POINT('Ctrl Pts',(60.9622504386777,870.244774465707,139.222494950591));
#74384=CARTESIAN_POINT('Ctrl Pts',(60.8889550432104,870.24700405361,139.222964720184));
#74385=CARTESIAN_POINT('Ctrl Pts',(60.8760233670833,870.247211102579,139.222975867947));
#74386=CARTESIAN_POINT('Ctrl Pts',(60.8630998547522,870.247232404664,139.222915596135));
#74387=CARTESIAN_POINT('Origin',(60.8630998560088,871.993282576964,130.50345024798));
#74388=CARTESIAN_POINT('',(60.8630998560088,870.329865945458,136.710345491468));
#74389=CARTESIAN_POINT('Origin',(60.8630998560088,869.858443714849,136.543728924201));
#74390=CARTESIAN_POINT('',(60.8630998560088,868.874774210905,140.827358598238));
#74391=CARTESIAN_POINT('',(60.8630998560088,872.464704807573,130.670066815247));
#74392=CARTESIAN_POINT('Origin',(60.8630998560088,868.403351980296,140.660742030971));
#74393=CARTESIAN_POINT('Origin',(65.6573249397971,834.228980040933,117.156267944625));
#74394=CARTESIAN_POINT('',(65.6573249397971,831.637411863391,127.666414786973));
#74395=CARTESIAN_POINT('Origin',(65.6573249397971,830.639049444264,127.313559727617));
#74396=CARTESIAN_POINT('',(65.6573249397971,832.30387813246,125.780725864538));
#74397=CARTESIAN_POINT('',(65.6573249397971,835.22734246006,117.509123003982));
#74398=CARTESIAN_POINT('Origin',(65.6573249397971,831.305515713332,125.427870805181));
#74399=CARTESIAN_POINT('Origin',(65.6573249397971,834.228980040933,117.156267944625));
#74400=CARTESIAN_POINT('',(65.6573249397971,832.565563409427,123.363163188114));
#74401=CARTESIAN_POINT('Origin',(65.6573249397971,832.094141178818,123.196546620847));
#74402=CARTESIAN_POINT('',(65.6573249397971,831.110471674873,127.480176294884));
#74403=CARTESIAN_POINT('',(65.6573249397971,834.700402271542,117.322884511892));
#74404=CARTESIAN_POINT('Origin',(65.6573249397971,830.639049444264,127.313559727617));
#74405=CARTESIAN_POINT('Origin',(68.5805335751996,837.054171108743,118.154786060719));
#74406=CARTESIAN_POINT('',(68.5805335751996,834.686009791457,128.743892446641));
#74407=CARTESIAN_POINT('Origin',(68.5805335751996,833.464240512074,128.31207784371));
#74408=CARTESIAN_POINT('',(68.5805335751996,835.352476060525,126.858203524206));
#74409=CARTESIAN_POINT('',(68.5805335751996,838.275940388125,118.58660066365));
#74410=CARTESIAN_POINT('Origin',(68.5805335751996,834.130706781142,126.426388921275));
#74411=CARTESIAN_POINT('Origin',(68.5805335751996,837.054171108743,118.154786060719));
#74412=CARTESIAN_POINT('',(68.5805335751996,835.390754477236,124.361681304207));
#74413=CARTESIAN_POINT('Origin',(68.5805335751996,834.919332246628,124.19506473694));
#74414=CARTESIAN_POINT('',(68.5805335751996,833.935662742683,128.478694410977));
#74415=CARTESIAN_POINT('',(68.5805335751996,837.525593339351,118.321402627986));
#74416=CARTESIAN_POINT('Origin',(68.5805335751996,833.464240512074,128.31207784371));
#74417=CARTESIAN_POINT('Origin',(71.3370026852042,840.702101604493,119.444088128731));
#74418=CARTESIAN_POINT('',(71.3370026852042,838.626887409825,130.1367319399));
#74419=CARTESIAN_POINT('Origin',(71.3370026852042,837.112171007824,129.601379911722));
#74420=CARTESIAN_POINT('',(71.3370026852042,839.293353678893,128.251043017465));
#74421=CARTESIAN_POINT('',(71.3370026852042,842.216818006494,119.979440156909));
#74422=CARTESIAN_POINT('Origin',(71.3370026852042,837.778637276893,127.715690989287));
#74423=CARTESIAN_POINT('Origin',(71.3370026852042,840.702101604493,119.444088128731));
#74424=CARTESIAN_POINT('',(71.3370026852042,839.038684972987,125.650983372219));
#74425=CARTESIAN_POINT('Origin',(71.3370026852042,838.567262742378,125.484366804952));
#74426=CARTESIAN_POINT('',(71.3370026852042,837.583593238433,129.76799647899));
#74427=CARTESIAN_POINT('',(71.3370026852042,841.173523835102,119.610704695998));
#74428=CARTESIAN_POINT('Origin',(71.3370026852042,837.112171007824,129.601379911722));
#74429=CARTESIAN_POINT('Origin',(73.1579114734415,844.797493313962,120.8915381299));
#74430=CARTESIAN_POINT('',(73.1579114734415,842.93117486174,131.658012764614));
#74431=CARTESIAN_POINT('Origin',(73.1579114734415,841.207562717293,131.048829912891));
#74432=CARTESIAN_POINT('',(73.1579114734415,843.597641130808,129.772323842179));
#74433=CARTESIAN_POINT('',(73.1579114734415,846.521105458408,121.500720981622));
#74434=CARTESIAN_POINT('Origin',(73.1579114734415,841.874028986361,129.163140990456));
#74435=CARTESIAN_POINT('Origin',(73.1579114734415,844.797493313962,120.8915381299));
#74436=CARTESIAN_POINT('',(73.1579114734415,843.134076682455,127.098433373388));
#74437=CARTESIAN_POINT('Origin',(73.1579114734415,842.662654451847,126.931816806121));
#74438=CARTESIAN_POINT('',(73.1579114734415,841.678984947902,131.215446480159));
#74439=CARTESIAN_POINT('',(73.1579114734415,845.268915544571,121.058154697167));
#74440=CARTESIAN_POINT('Origin',(73.1579114734415,841.207562717293,131.048829912891));
#74441=CARTESIAN_POINT('Origin',(74.547161632643,849.445246854869,122.53421149193));
#74442=CARTESIAN_POINT('',(74.547161632643,847.607515655762,133.310789829168));
#74443=CARTESIAN_POINT('Origin',(74.547161632643,845.855316258201,132.691503274921));
#74444=CARTESIAN_POINT('',(74.547161632643,848.27398192483,131.425100906733));
#74445=CARTESIAN_POINT('',(74.547161632643,851.197446252431,123.153498046176));
#74446=CARTESIAN_POINT('Origin',(74.547161632643,846.521782527269,130.805814352486));
#74447=CARTESIAN_POINT('Origin',(74.547161632643,849.445246854869,122.53421149193));
#74448=CARTESIAN_POINT('',(74.547161632643,847.781830223363,128.741106735418));
#74449=CARTESIAN_POINT('Origin',(74.547161632643,847.310407992754,128.574490168151));
#74450=CARTESIAN_POINT('',(74.547161632643,846.32673848881,132.858119842188));
#74451=CARTESIAN_POINT('',(74.547161632643,849.916669085478,122.700828059197));
#74452=CARTESIAN_POINT('Origin',(74.547161632643,845.855316258201,132.691503274921));
#74453=CARTESIAN_POINT('Origin',(74.5993171469355,853.932897983989,124.120299244432));
#74454=CARTESIAN_POINT('',(74.5993171469355,852.052209735701,134.881695107002));
#74455=CARTESIAN_POINT('Origin',(74.5993171469355,850.342967387321,134.277591027424));
#74456=CARTESIAN_POINT('',(74.5993171469355,852.718676004769,132.996006184567));
#74457=CARTESIAN_POINT('',(74.5993171469355,855.64214033237,124.724403324011));
#74458=CARTESIAN_POINT('Origin',(74.5993171469355,851.009433656389,132.391902104989));
#74459=CARTESIAN_POINT('Origin',(74.5993171469355,853.932897983989,124.120299244432));
#74460=CARTESIAN_POINT('',(74.5993171469355,852.269481352483,130.327194487921));
#74461=CARTESIAN_POINT('Origin',(74.5993171469355,851.798059121874,130.160577920654));
#74462=CARTESIAN_POINT('',(74.5993171469355,850.814389617929,134.444207594691));
#74463=CARTESIAN_POINT('',(74.5993171469355,854.404320214598,124.2869158117));
#74464=CARTESIAN_POINT('Origin',(74.5993171469355,850.342967387321,134.277591027424));
#74465=CARTESIAN_POINT('Origin',(74.2312593354051,859.474369268425,126.07884269672));
#74466=CARTESIAN_POINT('',(74.2312593354051,857.686653821797,136.87309829321));
#74467=CARTESIAN_POINT('Origin',(74.2312593354051,855.884438671756,136.236134479712));
#74468=CARTESIAN_POINT('',(74.2312593354051,858.353120090865,134.987409370775));
#74469=CARTESIAN_POINT('',(74.2312593354051,861.276584418465,126.715806510219));
#74470=CARTESIAN_POINT('Origin',(74.2312593354051,856.550904940825,134.350445557277));
#74471=CARTESIAN_POINT('Origin',(74.2312593354051,859.474369268425,126.07884269672));
#74472=CARTESIAN_POINT('',(74.2312593354051,857.810952636918,132.285737940209));
#74473=CARTESIAN_POINT('Origin',(74.2312593354051,857.33953040631,132.119121372942));
#74474=CARTESIAN_POINT('',(74.2312593354051,856.355860902365,136.402751046979));
#74475=CARTESIAN_POINT('',(74.2312593354051,859.945791499033,126.245459263987));
#74476=CARTESIAN_POINT('Origin',(74.2312593354051,855.884438671756,136.236134479712));
#74477=CARTESIAN_POINT('Origin',(72.6689064108742,864.230925695252,127.759970680072));
#74478=CARTESIAN_POINT('',(72.6689064108742,862.102093914381,138.43366422208));
#74479=CARTESIAN_POINT('Origin',(72.6689064108742,860.640995098584,137.917262463063));
#74480=CARTESIAN_POINT('',(72.6689064108742,862.76856018345,136.547975299645));
#74481=CARTESIAN_POINT('',(72.6689064108742,865.69202451105,128.276372439089));
#74482=CARTESIAN_POINT('Origin',(72.6689064108742,861.307461367652,136.031573540628));
#74483=CARTESIAN_POINT('Origin',(72.6689064108742,864.230925695252,127.759970680072));
#74484=CARTESIAN_POINT('',(72.6689064108742,862.567509063746,133.96686592356));
#74485=CARTESIAN_POINT('Origin',(72.6689064108742,862.096086833137,133.800249356293));
#74486=CARTESIAN_POINT('',(72.6689064108742,861.112417329193,138.08387903033));
#74487=CARTESIAN_POINT('',(72.6689064108742,864.702347925861,127.926587247339));
#74488=CARTESIAN_POINT('Origin',(72.6689064108742,860.640995098584,137.917262463063));
#74489=CARTESIAN_POINT('Origin',(70.1007466664717,869.495186337102,129.620538511613));
#74490=CARTESIAN_POINT('',(70.1007466664717,867.092637317396,140.197491119963));
#74491=CARTESIAN_POINT('Origin',(70.1007466664717,865.905255740434,139.777830294604));
#74492=CARTESIAN_POINT('',(70.1007466531591,867.749813505509,138.338087402883));
#74493=CARTESIAN_POINT('',(70.1007466664717,870.682567914064,130.040199336972));
#74494=CARTESIAN_POINT('',(68.9054919831167,866.197712760658,137.759953848708));
#74495=CARTESIAN_POINT('Ctrl Pts',(70.1007466531577,867.749813505464,138.338087403012));
#74496=CARTESIAN_POINT('Ctrl Pts',(70.0385698236016,867.750027222959,138.337482712201));
#74497=CARTESIAN_POINT('Ctrl Pts',(69.976342079479,867.745935464751,138.335242039916));
#74498=CARTESIAN_POINT('Ctrl Pts',(69.7533901561324,867.715524071811,138.321283246897));
#74499=CARTESIAN_POINT('Ctrl Pts',(69.5984074925223,867.664441672665,138.300303462554));
#74500=CARTESIAN_POINT('Ctrl Pts',(69.3166886230872,867.508807874702,138.23916418655));
#74501=CARTESIAN_POINT('Ctrl Pts',(69.1929543752343,867.405220528364,138.199415738199));
#74502=CARTESIAN_POINT('Ctrl Pts',(69.0010571598675,867.166184517323,138.109613431888));
#74503=CARTESIAN_POINT('Ctrl Pts',(68.9316547620308,867.035034715326,138.061083810922));
#74504=CARTESIAN_POINT('Ctrl Pts',(68.8476838970957,866.757417727942,137.959773119425));
#74505=CARTESIAN_POINT('Ctrl Pts',(68.8329819766983,866.613514497137,137.907905692754));
#74506=CARTESIAN_POINT('Ctrl Pts',(68.8543900681979,866.37753999295,137.823645068394));
#74507=CARTESIAN_POINT('Ctrl Pts',(68.874420477635,866.285984262706,137.791151984273));
#74508=CARTESIAN_POINT('Ctrl Pts',(68.9054919831215,866.197712760659,137.759953848709));
#74509=CARTESIAN_POINT('',(70.6848310304297,865.51976966261,137.52034581908));
#74510=CARTESIAN_POINT('Origin',(70.1007466664716,866.571722009503,137.892141372169));
#74511=CARTESIAN_POINT('Ctrl Pts',(70.6848310304297,865.51976966261,137.52034581908));
#74512=CARTESIAN_POINT('Ctrl Pts',(70.8176938369516,865.585348398922,137.543523563405));
#74513=CARTESIAN_POINT('Ctrl Pts',(70.937116451913,865.672703071882,137.574713546154));
#74514=CARTESIAN_POINT('Ctrl Pts',(71.1391359754987,865.884110545421,137.651131725662));
#74515=CARTESIAN_POINT('Ctrl Pts',(71.2194947760908,866.006878166671,137.695912545002));
#74516=CARTESIAN_POINT('Ctrl Pts',(71.3316309737503,866.277734264315,137.795577726448));
#74517=CARTESIAN_POINT('Ctrl Pts',(71.3606300520131,866.424166171532,137.849879867578));
#74518=CARTESIAN_POINT('Ctrl Pts',(71.3595389505574,866.728231802344,137.963183747999));
#74519=CARTESIAN_POINT('Ctrl Pts',(71.325763592196,866.882999174463,138.021140620618));
#74520=CARTESIAN_POINT('Ctrl Pts',(71.1960161043892,867.170545970834,138.128744392009));
#74521=CARTESIAN_POINT('Ctrl Pts',(71.1015941158648,867.300604915829,138.177358621785));
#74522=CARTESIAN_POINT('Ctrl Pts',(70.8651064396571,867.518308900674,138.257993060595));
#74523=CARTESIAN_POINT('Ctrl Pts',(70.7256765621508,867.604136013465,138.289336684738));
#74524=CARTESIAN_POINT('Ctrl Pts',(70.5725909234467,867.662462925543,138.309951389007));
#74525=CARTESIAN_POINT('Ctrl Pts',(70.5166005394062,867.683795731382,138.317491124404));
#74526=CARTESIAN_POINT('Ctrl Pts',(70.4590554838378,867.70134539635,138.323561058407));
#74527=CARTESIAN_POINT('Ctrl Pts',(70.3021079592237,867.737816799193,138.335750016227));
#74528=CARTESIAN_POINT('Ctrl Pts',(70.2014941359312,867.749467210873,138.339067206542));
#74529=CARTESIAN_POINT('Ctrl Pts',(70.1007466531577,867.749813505464,138.338087403012));
#74530=CARTESIAN_POINT('Origin',(70.1007466664717,869.495186337102,129.620538511613));
#74531=CARTESIAN_POINT('',(70.1007466664717,867.831769705596,135.827433755101));
#74532=CARTESIAN_POINT('Origin',(70.1007466664717,867.360347474987,135.660817187834));
#74533=CARTESIAN_POINT('',(70.1007466664717,866.376677971043,139.944446861871));
#74534=CARTESIAN_POINT('',(70.1007466664717,869.966608567711,129.78715507888));
#74535=CARTESIAN_POINT('Origin',(70.1007466664717,865.905255740434,139.777830294604));
#74536=CARTESIAN_POINT('Origin',(66.4625974592707,831.616320212274,116.232865559622));
#74537=CARTESIAN_POINT('',(66.4625974592707,829.024752034733,126.74301240197));
#74538=CARTESIAN_POINT('Origin',(66.4625974592707,828.026389615606,126.390157342613));
#74539=CARTESIAN_POINT('',(66.4625974592707,829.691218303801,124.857323479535));
#74540=CARTESIAN_POINT('',(66.4625974592707,832.614682631402,116.585720618979));
#74541=CARTESIAN_POINT('Origin',(66.4625974592707,828.692855884674,124.504468420178));
#74542=CARTESIAN_POINT('Origin',(66.4625974592707,831.616320212274,116.232865559622));
#74543=CARTESIAN_POINT('',(66.4625974592707,829.952903580768,122.43976080311));
#74544=CARTESIAN_POINT('Origin',(66.4625974592707,829.481481350159,122.273144235843));
#74545=CARTESIAN_POINT('',(66.4625974592707,828.497811846215,126.55677390988));
#74546=CARTESIAN_POINT('',(66.4625974592707,832.087742442883,116.399482126889));
#74547=CARTESIAN_POINT('Origin',(66.4625974592707,828.026389615606,126.390157342613));
#74548=CARTESIAN_POINT('Origin',(69.9449250128882,833.806742205807,117.007034806917));
#74549=CARTESIAN_POINT('',(69.9449250128882,831.438580888521,127.59614119284));
#74550=CARTESIAN_POINT('Origin',(69.9449250128882,830.216811609138,127.164326589909));
#74551=CARTESIAN_POINT('',(69.9449250128882,832.105047157589,125.710452270404));
#74552=CARTESIAN_POINT('',(69.9449250128882,835.028511485189,117.438849409848));
#74553=CARTESIAN_POINT('Origin',(69.9449250128882,830.883277878207,125.278637667474));
#74554=CARTESIAN_POINT('Origin',(69.9449250128882,833.806742205807,117.007034806917));
#74555=CARTESIAN_POINT('',(69.9449250128882,832.1433255743,123.213930050406));
#74556=CARTESIAN_POINT('Origin',(69.9449250128882,831.671903343692,123.047313483139));
#74557=CARTESIAN_POINT('',(69.9449250128882,830.688233839747,127.330943157176));
#74558=CARTESIAN_POINT('',(69.9449250128882,834.278164436415,117.173651374185));
#74559=CARTESIAN_POINT('Origin',(69.9449250128882,830.216811609138,127.164326589909));
#74560=CARTESIAN_POINT('Origin',(73.4455833853166,836.834610476873,118.077185904396));
#74561=CARTESIAN_POINT('',(73.4455833853166,834.759396282205,128.769829715565));
#74562=CARTESIAN_POINT('Origin',(73.4455833853166,833.244679880204,128.234477687388));
#74563=CARTESIAN_POINT('',(73.4455833853166,835.425862551273,126.88414079313));
#74564=CARTESIAN_POINT('',(73.4455833853166,838.349326878873,118.612537932574));
#74565=CARTESIAN_POINT('Origin',(73.4455833853166,833.911146149272,126.348788764952));
#74566=CARTESIAN_POINT('Origin',(73.4455833853166,836.834610476873,118.077185904396));
#74567=CARTESIAN_POINT('',(73.4455833853166,835.171193845366,124.284081147885));
#74568=CARTESIAN_POINT('Origin',(73.4455833853166,834.699771614758,124.117464580618));
#74569=CARTESIAN_POINT('',(73.4455833853166,833.716102110813,128.401094254655));
#74570=CARTESIAN_POINT('',(73.4455833853166,837.306032707481,118.243802471663));
#74571=CARTESIAN_POINT('Origin',(73.4455833853166,833.244679880204,128.234477687388));
#74572=CARTESIAN_POINT('Origin',(76.129797746682,840.483558240543,119.366847509312));
#74573=CARTESIAN_POINT('',(76.129797746682,838.617239788321,130.133322144025));
#74574=CARTESIAN_POINT('Origin',(76.129797746682,836.893627643875,129.524139292303));
#74575=CARTESIAN_POINT('',(76.129797746682,839.28370605739,128.24763322159));
#74576=CARTESIAN_POINT('',(76.129797746682,842.20717038499,119.976030361034));
#74577=CARTESIAN_POINT('Origin',(76.129797746682,837.560093912943,127.638450369868));
#74578=CARTESIAN_POINT('Origin',(76.129797746682,840.483558240543,119.366847509312));
#74579=CARTESIAN_POINT('',(76.129797746682,838.820141609037,125.5737427528));
#74580=CARTESIAN_POINT('Origin',(76.129797746682,838.348719378428,125.407126185533));
#74581=CARTESIAN_POINT('',(76.129797746682,837.365049874483,129.69075585957));
#74582=CARTESIAN_POINT('',(76.129797746682,840.954980471152,119.533464076579));
#74583=CARTESIAN_POINT('Origin',(76.129797746682,836.893627643875,129.524139292303));
#74584=CARTESIAN_POINT('Origin',(78.5135905267759,844.757414748773,120.87737300887));
#74585=CARTESIAN_POINT('',(78.5135905267759,842.919683549666,131.653951346109));
#74586=CARTESIAN_POINT('Origin',(78.5135905267759,841.167484152104,131.034664791862));
#74587=CARTESIAN_POINT('',(78.5135905267759,843.586149818734,129.768262423673));
#74588=CARTESIAN_POINT('',(78.5135905267759,846.509614146334,121.496659563117));
#74589=CARTESIAN_POINT('Origin',(78.5135905267759,841.833950421173,129.148975869426));
#74590=CARTESIAN_POINT('Origin',(78.5135905267759,844.757414748773,120.87737300887));
#74591=CARTESIAN_POINT('',(78.5135905267759,843.093998117266,127.084268252359));
#74592=CARTESIAN_POINT('Origin',(78.5135905267759,842.622575886658,126.917651685091));
#74593=CARTESIAN_POINT('',(78.5135905267759,841.638906382713,131.201281359129));
#74594=CARTESIAN_POINT('',(78.5135905267759,845.228836979382,121.043989576137));
#74595=CARTESIAN_POINT('Origin',(78.5135905267759,841.167484152104,131.034664791862));
#74596=CARTESIAN_POINT('Origin',(79.5542023461718,849.136775972358,122.425187444677));
#74597=CARTESIAN_POINT('',(79.5542023461718,847.25608772407,133.186583307246));
#74598=CARTESIAN_POINT('Origin',(79.5542023461718,845.54684537569,132.582479227668));
#74599=CARTESIAN_POINT('',(79.5542023461718,847.922553993138,131.300894384811));
#74600=CARTESIAN_POINT('',(79.5542023461718,850.846018320739,123.029291524255));
#74601=CARTESIAN_POINT('Origin',(79.5542023461718,846.213311644758,130.696790305233));
#74602=CARTESIAN_POINT('Origin',(79.5542023461718,849.136775972358,122.425187444677));
#74603=CARTESIAN_POINT('',(79.5542023461718,847.473359340852,128.632082688165));
#74604=CARTESIAN_POINT('Origin',(79.5542023461718,847.001937110243,128.465466120898));
#74605=CARTESIAN_POINT('',(79.5542023461718,846.018267606298,132.749095794935));
#74606=CARTESIAN_POINT('',(79.5542023461718,849.608198202967,122.591804011944));
#74607=CARTESIAN_POINT('Origin',(79.5542023461718,845.54684537569,132.582479227668));
#74608=CARTESIAN_POINT('Origin',(80.4161670456629,854.629302592554,124.366432196538));
#74609=CARTESIAN_POINT('',(80.4161670456629,852.841587145926,135.160687793028));
#74610=CARTESIAN_POINT('Origin',(80.4161670456629,851.039371995885,134.523723979529));
#74611=CARTESIAN_POINT('',(80.4161670456629,853.508053414994,133.274998870593));
#74612=CARTESIAN_POINT('',(80.4161670456629,856.431517742594,125.003396010037));
#74613=CARTESIAN_POINT('Origin',(80.4161670456629,851.705838264953,132.638035057094));
#74614=CARTESIAN_POINT('Origin',(80.4161670456629,854.629302592554,124.366432196538));
#74615=CARTESIAN_POINT('',(80.4161670456629,852.965885961047,130.573327440026));
#74616=CARTESIAN_POINT('Origin',(80.4161670456629,852.494463730438,130.406710872759));
#74617=CARTESIAN_POINT('',(80.4161670456629,851.510794226494,134.690340546796));
#74618=CARTESIAN_POINT('',(80.4161670456629,855.100724823162,124.533048763805));
#74619=CARTESIAN_POINT('Origin',(80.4161670456629,851.039371995885,134.523723979529));
#74620=CARTESIAN_POINT('Origin',(79.9368490592233,859.58818237154,126.119068098324));
#74621=CARTESIAN_POINT('',(79.9368490592233,857.459350590669,136.792761640332));
#74622=CARTESIAN_POINT('Origin',(79.9368490592233,855.998251774872,136.276359881315));
#74623=CARTESIAN_POINT('',(79.9368490592233,858.125816859737,134.907072717897));
#74624=CARTESIAN_POINT('',(79.9368490592233,861.049281187338,126.635469857341));
#74625=CARTESIAN_POINT('Origin',(79.9368490592233,856.66471804394,134.39067095888));
#74626=CARTESIAN_POINT('Origin',(79.9368490592233,859.58818237154,126.119068098324));
#74627=CARTESIAN_POINT('',(79.9368490592233,857.924765740034,132.325963341812));
#74628=CARTESIAN_POINT('Origin',(79.9368490592233,857.453343509425,132.159346774545));
#74629=CARTESIAN_POINT('',(79.9368490592233,856.46967400548,136.442976448582));
#74630=CARTESIAN_POINT('',(79.9368490592233,860.059604602149,126.285684665591));
#74631=CARTESIAN_POINT('Origin',(79.9368490592233,855.998251774872,136.276359881315));
#74632=CARTESIAN_POINT('Origin',(78.5856601255815,865.24083849797,128.116908035806));
#74633=CARTESIAN_POINT('',(78.5856601255815,862.838289478264,138.693860644156));
#74634=CARTESIAN_POINT('Origin',(78.5856601255815,861.650907901302,138.274199818797));
#74635=CARTESIAN_POINT('',(78.5856601240841,863.496566482291,136.831342296269));
#74636=CARTESIAN_POINT('',(78.5856601255815,866.428220074932,128.536568861164));
#74637=CARTESIAN_POINT('',(77.3340498386503,862.185841767529,136.342022894688));
#74638=CARTESIAN_POINT('Ctrl Pts',(78.5856601225867,863.496566482291,136.831342296269));
#74639=CARTESIAN_POINT('Ctrl Pts',(78.4486937731582,863.497227928007,136.829470811441));
#74640=CARTESIAN_POINT('Ctrl Pts',(78.3124648687431,863.476938862574,136.819817687594));
#74641=CARTESIAN_POINT('Ctrl Pts',(78.0264738654205,863.387571443878,136.782579786376));
#74642=CARTESIAN_POINT('Ctrl Pts',(77.8823835531221,863.310524693534,136.752211682673));
#74643=CARTESIAN_POINT('Ctrl Pts',(77.6416001298824,863.114366012403,136.677563675543));
#74644=CARTESIAN_POINT('Ctrl Pts',(77.5446429760725,862.999701933924,136.634860667076));
#74645=CARTESIAN_POINT('Ctrl Pts',(77.4010671508439,862.744634128623,136.541519619498));
#74646=CARTESIAN_POINT('Ctrl Pts',(77.3548838503261,862.606764437272,136.49178464982));
#74647=CARTESIAN_POINT('Ctrl Pts',(77.3237285881768,862.371755847929,136.407865412448));
#74648=CARTESIAN_POINT('Ctrl Pts',(77.3231225426296,862.278275222544,136.374692005254));
#74649=CARTESIAN_POINT('Ctrl Pts',(77.3340498386502,862.185841767529,136.342022894688));
#74650=CARTESIAN_POINT('',(78.9250091887252,861.173912390952,135.984372813519));
#74651=CARTESIAN_POINT('Origin',(78.5856601255815,862.317374170371,136.388510896363));
#74652=CARTESIAN_POINT('Ctrl Pts',(78.9250091887252,861.173912390953,135.984372813519));
#74653=CARTESIAN_POINT('Ctrl Pts',(79.0694297431482,861.212013193,135.997838926136));
#74654=CARTESIAN_POINT('Ctrl Pts',(79.2055276205897,861.274046565504,136.020079504536));
#74655=CARTESIAN_POINT('Ctrl Pts',(79.4498688843905,861.441221048167,136.080864248408));
#74656=CARTESIAN_POINT('Ctrl Pts',(79.5556401434395,861.545543748934,136.11912600875));
#74657=CARTESIAN_POINT('Ctrl Pts',(79.7253264890131,861.78847209321,136.208920577197));
#74658=CARTESIAN_POINT('Ctrl Pts',(79.786158897029,861.926001974476,136.260076441147));
#74659=CARTESIAN_POINT('Ctrl Pts',(79.8525471736859,862.223596854638,136.371093339346));
#74660=CARTESIAN_POINT('Ctrl Pts',(79.8538641158598,862.381580756675,136.430187042472));
#74661=CARTESIAN_POINT('Ctrl Pts',(79.7907743754111,862.688237133456,136.544544786168));
#74662=CARTESIAN_POINT('Ctrl Pts',(79.72727912178,862.83394519488,136.598689943191));
#74663=CARTESIAN_POINT('Ctrl Pts',(79.5442220305133,863.093224784922,136.694018607624));
#74664=CARTESIAN_POINT('Ctrl Pts',(79.4268351630958,863.204501652834,136.734357036341));
#74665=CARTESIAN_POINT('Ctrl Pts',(79.2899567932164,863.291563112634,136.765127502032));
#74666=CARTESIAN_POINT('Ctrl Pts',(79.2398941448767,863.323405450102,136.776381661506));
#74667=CARTESIAN_POINT('Ctrl Pts',(79.1874673629681,863.351852988318,136.786303272653));
#74668=CARTESIAN_POINT('Ctrl Pts',(78.9856966443786,863.443980354888,136.817891881721));
#74669=CARTESIAN_POINT('Ctrl Pts',(78.8258553722391,863.483846736233,136.830316759686));
#74670=CARTESIAN_POINT('Ctrl Pts',(78.6368967142923,863.495587022015,136.831770148258));
#74671=CARTESIAN_POINT('Ctrl Pts',(78.6112655323327,863.496442827184,136.831692164219));
#74672=CARTESIAN_POINT('Ctrl Pts',(78.5856601225867,863.496566482291,136.831342296269));
#74673=CARTESIAN_POINT('Origin',(78.5856601255815,865.24083849797,128.116908035806));
#74674=CARTESIAN_POINT('',(78.5856601255815,863.577421866464,134.323803279294));
#74675=CARTESIAN_POINT('Origin',(78.5856601255815,863.105999635855,134.157186712027));
#74676=CARTESIAN_POINT('',(78.5856601255815,862.122330131911,138.440816386064));
#74677=CARTESIAN_POINT('',(78.5856601255815,865.712260728579,128.283524603073));
#74678=CARTESIAN_POINT('Origin',(78.5856601255815,861.650907901302,138.274199818797));
#74679=CARTESIAN_POINT('Origin',(66.6741412055227,828.902896996967,115.273849984363));
#74680=CARTESIAN_POINT('',(66.6741412055227,826.311328819426,125.783996826711));
#74681=CARTESIAN_POINT('Origin',(66.6741412055227,825.312966400299,125.431141767354));
#74682=CARTESIAN_POINT('',(66.6741412055227,826.977795088494,123.898307904275));
#74683=CARTESIAN_POINT('',(66.6741412055227,829.901259416094,115.626705043719));
#74684=CARTESIAN_POINT('Origin',(66.6741412055227,825.979432669367,123.545452844919));
#74685=CARTESIAN_POINT('Origin',(66.6741412055227,828.902896996967,115.273849984363));
#74686=CARTESIAN_POINT('',(66.6741412055227,827.239480365461,121.480745227851));
#74687=CARTESIAN_POINT('Origin',(66.6741412055227,826.768058134852,121.314128660584));
#74688=CARTESIAN_POINT('',(66.6741412055227,825.784388630908,125.597758334621));
#74689=CARTESIAN_POINT('',(66.6741412055227,829.374319227576,115.44046655163));
#74690=CARTESIAN_POINT('Origin',(66.6741412055227,825.312966400299,125.431141767354));
#74691=CARTESIAN_POINT('Origin',(70.5633932532005,830.362817964294,115.789835451877));
#74692=CARTESIAN_POINT('',(70.5633932532005,827.994656647008,126.378941837799));
#74693=CARTESIAN_POINT('Origin',(70.5633932532005,826.772887367626,125.947127234868));
#74694=CARTESIAN_POINT('',(70.5633932532005,828.661122916077,124.493252915364));
#74695=CARTESIAN_POINT('',(70.5633932532005,831.584587243677,116.221650054808));
#74696=CARTESIAN_POINT('Origin',(70.5633932532005,827.439353636694,124.061438312433));
#74697=CARTESIAN_POINT('Origin',(70.5633932532005,830.362817964294,115.789835451877));
#74698=CARTESIAN_POINT('',(70.5633932532005,828.699401332788,121.996730695365));
#74699=CARTESIAN_POINT('Origin',(70.5633932532005,828.227979102179,121.830114128098));
#74700=CARTESIAN_POINT('',(70.5633932532005,827.244309598234,126.113743802135));
#74701=CARTESIAN_POINT('',(70.5633932532005,830.834240194903,115.956452019144));
#74702=CARTESIAN_POINT('Origin',(70.5633932532005,826.772887367626,125.947127234868));
#74703=CARTESIAN_POINT('Origin',(74.6552453191549,832.638291637906,116.594064840708));
#74704=CARTESIAN_POINT('',(74.6552453191549,830.563077443238,127.286708651877));
#74705=CARTESIAN_POINT('Origin',(74.6552453191549,829.048361041238,126.751356623699));
#74706=CARTESIAN_POINT('',(74.6552453191549,831.229543712306,125.401019729442));
#74707=CARTESIAN_POINT('',(74.6552453191549,834.153008039907,117.129416868886));
#74708=CARTESIAN_POINT('Origin',(74.6552453191549,829.714827310306,124.865667701264));
#74709=CARTESIAN_POINT('Origin',(74.6552453191549,832.638291637906,116.594064840708));
#74710=CARTESIAN_POINT('',(74.6552453191549,830.9748750064,122.800960084196));
#74711=CARTESIAN_POINT('Origin',(74.6552453191549,830.503452775791,122.634343516929));
#74712=CARTESIAN_POINT('',(74.6552453191549,829.519783271846,126.917973190966));
#74713=CARTESIAN_POINT('',(74.6552453191549,833.109713868515,116.760681407975));
#74714=CARTESIAN_POINT('Origin',(74.6552453191549,829.048361041238,126.751356623699));
#74715=CARTESIAN_POINT('Origin',(78.0854522057672,835.681318928912,117.669573648752));
#74716=CARTESIAN_POINT('',(78.0854522057672,833.81500047669,128.436048283466));
#74717=CARTESIAN_POINT('Origin',(78.0854522057672,832.091388332243,127.826865431743));
#74718=CARTESIAN_POINT('',(78.0854522057672,834.481466745758,126.55035936103));
#74719=CARTESIAN_POINT('',(78.0854522057672,837.404931073359,118.278756500474));
#74720=CARTESIAN_POINT('Origin',(78.0854522057672,832.757854601311,125.941176509308));
#74721=CARTESIAN_POINT('Origin',(78.0854522057672,835.681318928912,117.669573648752));
#74722=CARTESIAN_POINT('',(78.0854522057672,834.017902297405,123.87646889224));
#74723=CARTESIAN_POINT('Origin',(78.0854522057672,833.546480066797,123.709852324973));
#74724=CARTESIAN_POINT('',(78.0854522057672,832.562810562852,127.99348199901));
#74725=CARTESIAN_POINT('',(78.0854522057672,836.152741159521,117.836190216019));
#74726=CARTESIAN_POINT('Origin',(78.0854522057672,832.091388332243,127.826865431743));
#74727=CARTESIAN_POINT('Origin',(81.3596044235566,839.394490366815,118.981934073203));
#74728=CARTESIAN_POINT('',(81.3596044235566,837.556759167708,129.758512410442));
#74729=CARTESIAN_POINT('Origin',(81.3596044235566,835.804559770147,129.139225856195));
#74730=CARTESIAN_POINT('',(81.3596044235566,838.223225436777,127.872823488007));
#74731=CARTESIAN_POINT('',(81.3596044235566,841.146689764377,119.601220627451));
#74732=CARTESIAN_POINT('Origin',(81.3596044235566,836.471026039215,127.25353693376));
#74733=CARTESIAN_POINT('Origin',(81.3596044235566,839.394490366815,118.981934073203));
#74734=CARTESIAN_POINT('',(81.3596044235566,837.731073735309,125.188829316692));
#74735=CARTESIAN_POINT('Origin',(81.3596044235566,837.2596515047,125.022212749425));
#74736=CARTESIAN_POINT('',(81.3596044235566,836.275982000755,129.305842423462));
#74737=CARTESIAN_POINT('',(81.3596044235566,839.865912597424,119.148550640471));
#74738=CARTESIAN_POINT('Origin',(81.3596044235566,835.804559770147,129.139225856195));
#74739=CARTESIAN_POINT('Origin',(83.343192818139,843.474162584889,120.423828274231));
#74740=CARTESIAN_POINT('',(83.343192818139,841.5934743366,131.185224136801));
#74741=CARTESIAN_POINT('Origin',(83.343192818139,839.88423198822,130.581120057222));
#74742=CARTESIAN_POINT('',(83.343192818139,842.259940605669,129.299535214366));
#74743=CARTESIAN_POINT('',(83.343192818139,845.183404933269,121.027932353809));
#74744=CARTESIAN_POINT('Origin',(83.343192818139,840.550698257288,128.695431134787));
#74745=CARTESIAN_POINT('Origin',(83.343192818139,843.474162584889,120.423828274231));
#74746=CARTESIAN_POINT('',(83.343192818139,841.810745953382,126.630723517719));
#74747=CARTESIAN_POINT('Origin',(83.343192818139,841.339323722773,126.464106950452));
#74748=CARTESIAN_POINT('',(83.343192818139,840.355654218829,130.747736624489));
#74749=CARTESIAN_POINT('',(83.343192818139,843.945584815497,120.590444841498));
#74750=CARTESIAN_POINT('Origin',(83.343192818139,839.88423198822,130.581120057222));
#74751=CARTESIAN_POINT('Origin',(85.3975080351181,848.677694771475,122.262932614884));
#74752=CARTESIAN_POINT('',(85.3975080351181,846.889979324847,133.057188211373));
#74753=CARTESIAN_POINT('Origin',(85.3975080351181,845.087764174806,132.420224397875));
#74754=CARTESIAN_POINT('',(85.3975080351181,847.556445593915,131.171499288938));
#74755=CARTESIAN_POINT('',(85.3975080351181,850.479909921515,122.899896428382));
#74756=CARTESIAN_POINT('Origin',(85.3975080351181,845.754230443874,130.53453547544));
#74757=CARTESIAN_POINT('Origin',(85.3975080351181,848.677694771475,122.262932614884));
#74758=CARTESIAN_POINT('',(85.3975080351181,847.014278139968,128.469827858372));
#74759=CARTESIAN_POINT('Origin',(85.3975080351181,846.542855909359,128.303211291105));
#74760=CARTESIAN_POINT('',(85.3975080351181,845.559186405414,132.586840965142));
#74761=CARTESIAN_POINT('',(85.3975080351181,849.149117002083,122.429549182151));
#74762=CARTESIAN_POINT('Origin',(85.3975080351181,845.087764174806,132.420224397875));
#74763=CARTESIAN_POINT('Origin',(86.0221734828003,853.622171060933,124.010477836116));
#74764=CARTESIAN_POINT('',(86.0221734828003,851.493339280062,134.684171378124));
#74765=CARTESIAN_POINT('Origin',(86.0221734828003,850.032240464264,134.167769619107));
#74766=CARTESIAN_POINT('',(86.0221734828003,852.15980554913,132.798482455689));
#74767=CARTESIAN_POINT('',(86.0221734828003,855.08326987673,124.526879595133));
#74768=CARTESIAN_POINT('Origin',(86.0221734828003,850.698706733332,132.282080696672));
#74769=CARTESIAN_POINT('Origin',(86.0221734828003,853.622171060933,124.010477836116));
#74770=CARTESIAN_POINT('',(86.0221734828003,851.958754429426,130.217373079604));
#74771=CARTESIAN_POINT('Origin',(86.0221734828003,851.487332198818,130.050756512337));
#74772=CARTESIAN_POINT('',(86.0221734828003,850.503662694873,134.334386186374));
#74773=CARTESIAN_POINT('',(86.0221734828003,854.093593291541,124.177094403383));
#74774=CARTESIAN_POINT('Origin',(86.0221734828003,850.032240464264,134.167769619107));
#74775=CARTESIAN_POINT('Origin',(85.9470088000432,859.416174474765,126.058274687571));
#74776=CARTESIAN_POINT('',(85.9470088000432,857.013625455059,136.635227295921));
#74777=CARTESIAN_POINT('Origin',(85.9470088000432,855.826243878096,136.215566470562));
#74778=CARTESIAN_POINT('',(85.9470087966831,857.673301053105,134.768751788653));
#74779=CARTESIAN_POINT('',(85.9470088000432,860.603556051727,126.477935512929));
#74780=CARTESIAN_POINT('',(84.6937442849622,856.609403187493,134.371120816987));
#74781=CARTESIAN_POINT('Ctrl Pts',(85.9470087933229,857.673301053105,134.768751788653));
#74782=CARTESIAN_POINT('Ctrl Pts',(85.898177953993,857.673578244451,134.767967507141));
#74783=CARTESIAN_POINT('Ctrl Pts',(85.8492938279539,857.671185445707,134.76621509686));
#74784=CARTESIAN_POINT('Ctrl Pts',(85.6371334459491,857.649028772594,134.754384637898));
#74785=CARTESIAN_POINT('Ctrl Pts',(85.4789845072744,857.601933009003,134.734602226331));
#74786=CARTESIAN_POINT('Ctrl Pts',(85.1998382671642,857.457297769682,134.678164346876));
#74787=CARTESIAN_POINT('Ctrl Pts',(85.0795638502545,857.364160676451,134.64306970338));
#74788=CARTESIAN_POINT('Ctrl Pts',(84.8826580172478,857.142833563675,134.561653758185));
#74789=CARTESIAN_POINT('Ctrl Pts',(84.8070117684544,857.017036808601,134.516185772685));
#74790=CARTESIAN_POINT('Ctrl Pts',(84.7246547871115,856.79327693593,134.436242212395));
#74791=CARTESIAN_POINT('Ctrl Pts',(84.7034387736784,856.701958809946,134.40383310566));
#74792=CARTESIAN_POINT('Ctrl Pts',(84.6937442849618,856.609403187493,134.371120816987));
#74793=CARTESIAN_POINT('',(86.0267913799356,855.307713701921,133.911059709021));
#74794=CARTESIAN_POINT('Origin',(85.9470088000436,856.492710147166,134.329877548128));
#74795=CARTESIAN_POINT('Ctrl Pts',(86.0267913799356,855.307713701921,133.911059709021));
#74796=CARTESIAN_POINT('Ctrl Pts',(86.1764578110232,855.316671381824,133.914225656189));
#74797=CARTESIAN_POINT('Ctrl Pts',(86.3232828206312,855.350667960248,133.926557082913));
#74798=CARTESIAN_POINT('Ctrl Pts',(86.5992669389399,855.466279786581,133.969117839372));
#74799=CARTESIAN_POINT('Ctrl Pts',(86.7258279448786,855.547579069414,133.999242344799));
#74800=CARTESIAN_POINT('Ctrl Pts',(86.9456483308198,855.751908486123,134.075394746216));
#74801=CARTESIAN_POINT('Ctrl Pts',(87.0356554004524,855.874490635807,134.121267576057));
#74802=CARTESIAN_POINT('Ctrl Pts',(87.1666215689656,856.15252829316,134.225372289979));
#74803=CARTESIAN_POINT('Ctrl Pts',(87.2029732549826,856.30677934918,134.283146679019));
#74804=CARTESIAN_POINT('Ctrl Pts',(87.2092985862878,856.619060905553,134.399492551516));
#74805=CARTESIAN_POINT('Ctrl Pts',(87.1795051148179,856.774013594738,134.456905072789));
#74806=CARTESIAN_POINT('Ctrl Pts',(87.0578790817858,857.063486351916,134.5629050241));
#74807=CARTESIAN_POINT('Ctrl Pts',(86.9676655938481,857.195335781048,134.610514492041));
#74808=CARTESIAN_POINT('Ctrl Pts',(86.8529767343722,857.307326785008,134.650095902151));
#74809=CARTESIAN_POINT('Ctrl Pts',(86.8110297996916,857.348286991164,134.66457262493));
#74810=CARTESIAN_POINT('Ctrl Pts',(86.7660125933822,857.386390931025,134.677907135151));
#74811=CARTESIAN_POINT('Ctrl Pts',(86.5888991837206,857.516064557618,134.722765862921));
#74812=CARTESIAN_POINT('Ctrl Pts',(86.4412266028949,857.586404622667,134.745961171809));
#74813=CARTESIAN_POINT('Ctrl Pts',(86.1737258624385,857.65758596838,134.767165773978));
#74814=CARTESIAN_POINT('Ctrl Pts',(86.0605112696524,857.672656749122,134.770574773776));
#74815=CARTESIAN_POINT('Ctrl Pts',(85.9470087933229,857.673301053105,134.768751788653));
#74816=CARTESIAN_POINT('Origin',(85.9470088000432,859.416174474765,126.058274687571));
#74817=CARTESIAN_POINT('',(85.9470088000432,857.752757843259,132.265169931059));
#74818=CARTESIAN_POINT('Origin',(85.9470088000432,857.28133561265,132.098553363792));
#74819=CARTESIAN_POINT('',(85.9470088000432,856.297666108705,136.382183037829));
#74820=CARTESIAN_POINT('',(85.9470088000432,859.887596705374,126.224891254838));
#74821=CARTESIAN_POINT('Origin',(85.9470088000432,855.826243878096,136.215566470562));
#74822=CARTESIAN_POINT('Origin',(66.2827107017424,826.207300009971,114.321134801354));
#74823=CARTESIAN_POINT('',(66.2827107017424,823.61573183243,124.831281643702));
#74824=CARTESIAN_POINT('Origin',(66.2827107017424,822.617369413302,124.478426584345));
#74825=CARTESIAN_POINT('',(66.2827107017424,824.282198101498,122.945592721267));
#74826=CARTESIAN_POINT('',(66.2827107017424,827.205662429098,114.67398986071));
#74827=CARTESIAN_POINT('Origin',(66.2827107017424,823.283835682371,122.59273766191));
#74828=CARTESIAN_POINT('Origin',(66.2827107017424,826.207300009971,114.321134801354));
#74829=CARTESIAN_POINT('',(66.2827107017424,824.543883378465,120.528030044842));
#74830=CARTESIAN_POINT('Origin',(66.2827107017424,824.072461147856,120.361413477575));
#74831=CARTESIAN_POINT('',(66.2827107017424,823.088791643911,124.645043151612));
#74832=CARTESIAN_POINT('',(66.2827107017424,826.67872224058,114.487751368621));
#74833=CARTESIAN_POINT('Origin',(66.2827107017424,822.617369413302,124.478426584345));
#74834=CARTESIAN_POINT('Origin',(70.4089082662952,826.872914399342,114.556385448183));
#74835=CARTESIAN_POINT('',(70.4089082662952,824.504753082056,125.145491834106));
#74836=CARTESIAN_POINT('Origin',(70.4089082662952,823.282983802673,124.713677231175));
#74837=CARTESIAN_POINT('',(70.4089082662952,825.171219351124,123.259802911671));
#74838=CARTESIAN_POINT('',(70.4089082662952,828.094683678724,114.988200051114));
#74839=CARTESIAN_POINT('Origin',(70.4089082662952,823.949450071741,122.82798830874));
#74840=CARTESIAN_POINT('Origin',(70.4089082662952,826.872914399342,114.556385448183));
#74841=CARTESIAN_POINT('',(70.4089082662952,825.209497767835,120.763280691672));
#74842=CARTESIAN_POINT('Origin',(70.4089082662952,824.738075537226,120.596664124405));
#74843=CARTESIAN_POINT('',(70.4089082662952,823.754406033282,124.880293798442));
#74844=CARTESIAN_POINT('',(70.4089082662952,827.34433662995,114.723002015451));
#74845=CARTESIAN_POINT('Origin',(70.4089082662952,823.282983802673,124.713677231175));
#74846=CARTESIAN_POINT('Origin',(74.9131204556088,828.296544357029,115.059544444954));
#74847=CARTESIAN_POINT('',(74.9131204556088,826.22133016236,125.752188256123));
#74848=CARTESIAN_POINT('Origin',(74.9131204556088,824.70661376036,125.216836227945));
#74849=CARTESIAN_POINT('',(74.9131204556088,826.887796431429,123.866499333688));
#74850=CARTESIAN_POINT('',(74.9131204556088,829.811260759029,115.594896473132));
#74851=CARTESIAN_POINT('Origin',(74.9131204556088,825.373080029428,123.33114730551));
#74852=CARTESIAN_POINT('Origin',(74.9131204556088,828.296544357029,115.059544444954));
#74853=CARTESIAN_POINT('',(74.9131204556088,826.633127725522,121.266439688442));
#74854=CARTESIAN_POINT('Origin',(74.9131204556088,826.161705494914,121.099823121175));
#74855=CARTESIAN_POINT('',(74.9131204556088,825.178035990969,125.383452795212));
#74856=CARTESIAN_POINT('',(74.9131204556088,828.767966587637,115.226161012221));
#74857=CARTESIAN_POINT('Origin',(74.9131204556088,824.70661376036,125.216836227945));
#74858=CARTESIAN_POINT('Origin',(78.9394033665642,830.600656280688,115.873895560351));
#74859=CARTESIAN_POINT('',(78.9394033665642,828.734337828466,126.640370195065));
#74860=CARTESIAN_POINT('Origin',(78.9394033665642,827.010725684019,126.031187343342));
#74861=CARTESIAN_POINT('',(78.9394033665642,829.400804097534,124.754681272629));
#74862=CARTESIAN_POINT('',(78.9394033665642,832.324268425134,116.483078412073));
#74863=CARTESIAN_POINT('Origin',(78.9394033665642,827.677191953087,124.145498420907));
#74864=CARTESIAN_POINT('Origin',(78.9394033665642,830.600656280688,115.873895560351));
#74865=CARTESIAN_POINT('',(78.9394033665642,828.937239649181,122.080790803839));
#74866=CARTESIAN_POINT('Origin',(78.9394033665642,828.465817418573,121.914174236572));
#74867=CARTESIAN_POINT('',(78.9394033665642,827.482147914628,126.197803910609));
#74868=CARTESIAN_POINT('',(78.9394033665642,831.072078511296,116.040512127618));
#74869=CARTESIAN_POINT('Origin',(78.9394033665642,827.010725684019,126.031187343342));
#74870=CARTESIAN_POINT('Origin',(82.9608188590062,833.590859238655,116.930734461743));
#74871=CARTESIAN_POINT('',(82.9608188590062,831.753128039548,127.707312798981));
#74872=CARTESIAN_POINT('Origin',(82.9608188590062,830.000928641986,127.088026244734));
#74873=CARTESIAN_POINT('',(82.9608188590062,832.419594308616,125.821623876546));
#74874=CARTESIAN_POINT('',(82.9608188590062,835.343058636216,117.55002101599));
#74875=CARTESIAN_POINT('Origin',(82.9608188590062,830.667394911054,125.202337322299));
#74876=CARTESIAN_POINT('Origin',(82.9608188590062,833.590859238655,116.930734461743));
#74877=CARTESIAN_POINT('',(82.9608188590062,831.927442607148,123.137629705231));
#74878=CARTESIAN_POINT('Origin',(82.9608188590062,831.45602037654,122.971013137964));
#74879=CARTESIAN_POINT('',(82.9608188590062,830.472350872595,127.254642812001));
#74880=CARTESIAN_POINT('',(82.9608188590062,834.062281469263,117.09735102901));
#74881=CARTESIAN_POINT('Origin',(82.9608188590062,830.000928641986,127.088026244734));
#74882=CARTESIAN_POINT('Origin',(85.8006914976185,837.192541198847,118.203690732431));
#74883=CARTESIAN_POINT('',(85.8006914976185,835.311852950559,128.965086595));
#74884=CARTESIAN_POINT('Origin',(85.8006914976185,833.602610602179,128.360982515422));
#74885=CARTESIAN_POINT('',(85.8006914976185,835.978319219627,127.079397672565));
#74886=CARTESIAN_POINT('',(85.8006914976185,838.901783547228,118.807794812009));
#74887=CARTESIAN_POINT('Origin',(85.8006914976185,834.269076871247,126.475293592987));
#74888=CARTESIAN_POINT('Origin',(85.8006914976185,837.192541198847,118.203690732431));
#74889=CARTESIAN_POINT('',(85.8006914976185,835.529124567341,124.410585975919));
#74890=CARTESIAN_POINT('Origin',(85.8006914976185,835.057702336732,124.243969408652));
#74891=CARTESIAN_POINT('',(85.8006914976185,834.074032832787,128.527599082689));
#74892=CARTESIAN_POINT('',(85.8006914976185,837.663963429456,118.370307299698));
#74893=CARTESIAN_POINT('Origin',(85.8006914976185,833.602610602179,128.360982515422));
#74894=CARTESIAN_POINT('Origin',(88.9575737994055,841.879659625952,119.860276977186));
#74895=CARTESIAN_POINT('',(88.9575737994055,840.091944179324,130.654532573676));
#74896=CARTESIAN_POINT('Origin',(88.9575737994055,838.289729029283,130.017568760178));
#74897=CARTESIAN_POINT('',(88.9575737994055,840.758410448393,128.768843651241));
#74898=CARTESIAN_POINT('',(88.9575737994055,843.681874775993,120.497240790685));
#74899=CARTESIAN_POINT('Origin',(88.9575737994055,838.956195298352,128.131879837743));
#74900=CARTESIAN_POINT('Origin',(88.9575737994055,841.879659625952,119.860276977186));
#74901=CARTESIAN_POINT('',(88.9575737994055,840.216242994446,126.067172220675));
#74902=CARTESIAN_POINT('Origin',(88.9575737994055,839.744820763837,125.900555653408));
#74903=CARTESIAN_POINT('',(88.9575737994055,838.761151259892,130.184185327445));
#74904=CARTESIAN_POINT('',(88.9575737994055,842.351081856561,120.026893544454));
#74905=CARTESIAN_POINT('Origin',(88.9575737994055,838.289729029283,130.017568760178));
#74906=CARTESIAN_POINT('Origin',(90.6589218036684,846.593635085803,121.526355406045));
#74907=CARTESIAN_POINT('',(90.6589218036684,844.464803304932,132.200048948054));
#74908=CARTESIAN_POINT('Origin',(90.6589218036684,843.003704489134,131.683647189036));
#74909=CARTESIAN_POINT('',(90.6589218036684,845.131269574,130.314360025618));
#74910=CARTESIAN_POINT('',(90.6589218036684,848.054733901601,122.042757165062));
#74911=CARTESIAN_POINT('Origin',(90.6589218036684,843.670170758203,129.797958266601));
#74912=CARTESIAN_POINT('Origin',(90.6589218036684,846.593635085803,121.526355406045));
#74913=CARTESIAN_POINT('',(90.6589218036684,844.930218454297,127.733250649533));
#74914=CARTESIAN_POINT('Origin',(90.6589218036684,844.458796223688,127.566634082266));
#74915=CARTESIAN_POINT('',(90.6589218036684,843.475126719743,131.850263756303));
#74916=CARTESIAN_POINT('',(90.6589218036684,847.065057316412,121.692971973312));
#74917=CARTESIAN_POINT('Origin',(90.6589218036684,843.003704489134,131.683647189036));
#74918=CARTESIAN_POINT('Origin',(91.8630664291128,852.27576003514,123.534610622645));
#74919=CARTESIAN_POINT('',(91.8630664291128,849.873211015433,134.111563230994));
#74920=CARTESIAN_POINT('Origin',(91.8630664291128,848.685829438471,133.691902405636));
#74921=CARTESIAN_POINT('',(91.8630664387515,850.534428209482,132.240725956837));
#74922=CARTESIAN_POINT('',(91.8630664291128,853.463141612102,123.954271448003));
#74923=CARTESIAN_POINT('',(90.662921359021,849.712114145219,131.933385493838));
#74924=CARTESIAN_POINT('Ctrl Pts',(91.8630664483903,850.534428209482,132.240725956837));
#74925=CARTESIAN_POINT('Ctrl Pts',(91.737992335004,850.53516728595,132.238634831534));
#74926=CARTESIAN_POINT('Ctrl Pts',(91.6133872467039,850.518326302074,132.230365038877));
#74927=CARTESIAN_POINT('Ctrl Pts',(91.3454402966626,850.442220816991,132.198798790733));
#74928=CARTESIAN_POINT('Ctrl Pts',(91.2071051858126,850.374711138186,132.17276174262));
#74929=CARTESIAN_POINT('Ctrl Pts',(90.9654750747892,850.196841598205,132.106705174074));
#74930=CARTESIAN_POINT('Ctrl Pts',(90.8636719817834,850.088629530986,132.067452212255));
#74931=CARTESIAN_POINT('Ctrl Pts',(90.7337126765244,849.885909553918,131.994944862974));
#74932=CARTESIAN_POINT('Ctrl Pts',(90.6928139367984,849.800746810279,131.964711276631));
#74933=CARTESIAN_POINT('Ctrl Pts',(90.6629213590209,849.712114145219,131.933385493838));
#74934=CARTESIAN_POINT('',(91.6797956441728,848.17755462737,131.391020237111));
#74935=CARTESIAN_POINT('Origin',(91.8630664291131,849.35229570754,131.806213483201));
#74936=CARTESIAN_POINT('Ctrl Pts',(91.6797956441728,848.17755462737,131.391020237111));
#74937=CARTESIAN_POINT('Ctrl Pts',(91.8281668107091,848.156977691535,131.383747651749));
#74938=CARTESIAN_POINT('Ctrl Pts',(91.9793019950186,848.161447324691,131.385643256946));
#74939=CARTESIAN_POINT('Ctrl Pts',(92.2748671375464,848.220420364746,131.408185949913));
#74940=CARTESIAN_POINT('Ctrl Pts',(92.416686567108,848.275123966036,131.428910641595));
#74941=CARTESIAN_POINT('Ctrl Pts',(92.6770337877353,848.431870239332,131.488245550114));
#74942=CARTESIAN_POINT('Ctrl Pts',(92.7922817781397,848.534112239401,131.526929482854));
#74943=CARTESIAN_POINT('Ctrl Pts',(92.9821019884994,848.780360946266,131.619798906068));
#74944=CARTESIAN_POINT('Ctrl Pts',(93.051899675246,848.924092923618,131.673855496785));
#74945=CARTESIAN_POINT('Ctrl Pts',(93.1273636309746,849.228269411424,131.787336763809));
#74946=CARTESIAN_POINT('Ctrl Pts',(93.1325740593341,849.385658205106,131.845610286839));
#74947=CARTESIAN_POINT('Ctrl Pts',(93.0776947258065,849.692622105076,131.95779219984));
#74948=CARTESIAN_POINT('Ctrl Pts',(93.0185973796637,849.83926778188,132.010631162352));
#74949=CARTESIAN_POINT('Ctrl Pts',(92.9311104840889,849.971293785735,132.057293619326));
#74950=CARTESIAN_POINT('Ctrl Pts',(92.8991125453979,850.019581703019,132.074360203157));
#74951=CARTESIAN_POINT('Ctrl Pts',(92.8634723826217,850.065678541835,132.090519674315));
#74952=CARTESIAN_POINT('Ctrl Pts',(92.7187569877708,850.227244420114,132.146650202932));
#74953=CARTESIAN_POINT('Ctrl Pts',(92.5897070986527,850.325006836843,132.179537498763));
#74954=CARTESIAN_POINT('Ctrl Pts',(92.2999886674533,850.468659422292,132.225657717503));
#74955=CARTESIAN_POINT('Ctrl Pts',(92.1421864000932,850.513398291368,132.238544411543));
#74956=CARTESIAN_POINT('Ctrl Pts',(91.9410083713401,850.532263460595,132.241428886593));
#74957=CARTESIAN_POINT('Ctrl Pts',(91.9020146658181,850.534198060251,132.241377135573));
#74958=CARTESIAN_POINT('Ctrl Pts',(91.8630664483903,850.534428209482,132.240725956837));
#74959=CARTESIAN_POINT('Origin',(91.8630664291128,852.27576003514,123.534610622645));
#74960=CARTESIAN_POINT('',(91.8630664291128,850.612343403633,129.741505866133));
#74961=CARTESIAN_POINT('Origin',(91.8630664291128,850.140921173025,129.574889298866));
#74962=CARTESIAN_POINT('',(91.8630664291128,849.15725166908,133.858518972903));
#74963=CARTESIAN_POINT('',(91.8630664291128,852.747182265749,123.701227189912));
#74964=CARTESIAN_POINT('Origin',(91.8630664291128,848.685829438471,133.691902405636));
#74965=CARTESIAN_POINT('Origin',(65.305413339237,823.647339774524,113.416358235727));
#74966=CARTESIAN_POINT('',(65.305413339237,821.055771596983,123.926505078075));
#74967=CARTESIAN_POINT('Origin',(65.305413339237,820.057409177856,123.573650018718));
#74968=CARTESIAN_POINT('',(65.305413339237,821.722237866051,122.04081615564));
#74969=CARTESIAN_POINT('',(65.305413339237,824.645702193652,113.769213295084));
#74970=CARTESIAN_POINT('Origin',(65.305413339237,820.723875446924,121.687961096283));
#74971=CARTESIAN_POINT('Origin',(65.305413339237,823.647339774524,113.416358235727));
#74972=CARTESIAN_POINT('',(65.305413339237,821.983923143018,119.623253479215));
#74973=CARTESIAN_POINT('Origin',(65.305413339237,821.512500912409,119.456636911948));
#74974=CARTESIAN_POINT('',(65.305413339237,820.528831408465,123.740266585986));
#74975=CARTESIAN_POINT('',(65.305413339237,824.118762005133,113.582974802994));
#74976=CARTESIAN_POINT('Origin',(65.305413339237,820.057409177856,123.573650018718));
#74977=CARTESIAN_POINT('Origin',(69.488221787401,823.489557043151,113.360592479748));
#74978=CARTESIAN_POINT('',(69.488221787401,821.121395725865,123.94969886567));
#74979=CARTESIAN_POINT('Origin',(69.488221787401,819.899626446483,123.517884262739));
#74980=CARTESIAN_POINT('',(69.488221787401,821.787861994934,122.064009943235));
#74981=CARTESIAN_POINT('',(69.488221787401,824.711326322534,113.792407082679));
#74982=CARTESIAN_POINT('Origin',(69.488221787401,820.566092715551,121.632195340304));
#74983=CARTESIAN_POINT('Origin',(69.488221787401,823.489557043151,113.360592479748));
#74984=CARTESIAN_POINT('',(69.488221787401,821.826140411645,119.567487723236));
#74985=CARTESIAN_POINT('Origin',(69.488221787401,821.354718181036,119.400871155969));
#74986=CARTESIAN_POINT('',(69.488221787401,820.371048677091,123.684500830006));
#74987=CARTESIAN_POINT('',(69.488221787401,823.96097927376,113.527209047015));
#74988=CARTESIAN_POINT('Origin',(69.488221787401,819.899626446483,123.517884262739));
#74989=CARTESIAN_POINT('Origin',(74.2079384137928,823.999123824428,113.540690621874));
#74990=CARTESIAN_POINT('',(74.2079384137928,821.92390962976,124.233334433043));
#74991=CARTESIAN_POINT('Origin',(74.2079384137928,820.409193227759,123.697982404865));
#74992=CARTESIAN_POINT('',(74.2079384137928,822.590375898829,122.347645510608));
#74993=CARTESIAN_POINT('',(74.2079384137928,825.513840226429,114.076042650052));
#74994=CARTESIAN_POINT('Origin',(74.2079384137928,821.075659496828,121.81229348243));
#74995=CARTESIAN_POINT('Origin',(74.2079384137928,823.999123824428,113.540690621874));
#74996=CARTESIAN_POINT('',(74.2079384137928,822.335707192922,119.747585865362));
#74997=CARTESIAN_POINT('Origin',(74.2079384137928,821.864284962313,119.580969298095));
#74998=CARTESIAN_POINT('',(74.2079384137928,820.880615458369,123.864598972132));
#74999=CARTESIAN_POINT('',(74.2079384137928,824.470546055037,113.707307189141));
#75000=CARTESIAN_POINT('Origin',(74.2079384137928,820.409193227759,123.697982404865));
#75001=CARTESIAN_POINT('Origin',(78.6543294656336,825.463619633321,114.058292993191));
#75002=CARTESIAN_POINT('',(78.6543294656336,823.597301181099,124.824767627905));
#75003=CARTESIAN_POINT('Origin',(78.6543294656336,821.873689036652,124.215584776183));
#75004=CARTESIAN_POINT('',(78.6543294656336,824.263767450167,122.93907870547));
#75005=CARTESIAN_POINT('',(78.6543294656336,827.187231777768,114.667475844914));
#75006=CARTESIAN_POINT('Origin',(78.6543294656336,822.540155305721,122.329895853747));
#75007=CARTESIAN_POINT('Origin',(78.6543294656336,825.463619633321,114.058292993191));
#75008=CARTESIAN_POINT('',(78.6543294656336,823.800203001815,120.26518823668));
#75009=CARTESIAN_POINT('Origin',(78.6543294656336,823.328780771206,120.098571669412));
#75010=CARTESIAN_POINT('',(78.6543294656336,822.345111267261,124.38220134345));
#75011=CARTESIAN_POINT('',(78.6543294656336,825.93504186393,114.224909560458));
#75012=CARTESIAN_POINT('Origin',(78.6543294656336,821.873689036652,124.215584776183));
#75013=CARTESIAN_POINT('Origin',(83.2472530788159,827.600167893503,114.813421440257));
#75014=CARTESIAN_POINT('',(83.2472530788159,825.762436694396,125.589999777496));
#75015=CARTESIAN_POINT('Origin',(83.2472530788159,824.010237296834,124.970713223248));
#75016=CARTESIAN_POINT('',(83.2472530788159,826.428902963464,123.70431085506));
#75017=CARTESIAN_POINT('',(83.2472530788159,829.352367291064,115.432707994504));
#75018=CARTESIAN_POINT('Origin',(83.2472530788159,824.676703565902,123.085024300813));
#75019=CARTESIAN_POINT('Origin',(83.2472530788159,827.600167893503,114.813421440257));
#75020=CARTESIAN_POINT('',(83.2472530788159,825.936751261997,121.020316683746));
#75021=CARTESIAN_POINT('Origin',(83.2472530788159,825.465329031388,120.853700116478));
#75022=CARTESIAN_POINT('',(83.2472530788159,824.481659527443,125.137329790516));
#75023=CARTESIAN_POINT('',(83.2472530788159,828.071590124112,114.980038007524));
#75024=CARTESIAN_POINT('Origin',(83.2472530788159,824.010237296834,124.970713223248));
#75025=CARTESIAN_POINT('Origin',(90.940772381535,834.532303912436,117.263472864034));
#75026=CARTESIAN_POINT('',(90.940772381535,832.744588465808,128.057728460524));
#75027=CARTESIAN_POINT('Origin',(90.940772381535,830.942373315767,127.420764647026));
#75028=CARTESIAN_POINT('',(90.940772381535,833.411054734876,126.172039538089));
#75029=CARTESIAN_POINT('',(90.940772381535,836.334519062477,117.900436677533));
#75030=CARTESIAN_POINT('Origin',(90.940772381535,831.608839584836,125.53507572459));
#75031=CARTESIAN_POINT('Origin',(90.940772381535,834.532303912436,117.263472864034));
#75032=CARTESIAN_POINT('',(90.940772381535,832.86888728093,123.470368107523));
#75033=CARTESIAN_POINT('Origin',(90.940772381535,832.397465050321,123.303751540255));
#75034=CARTESIAN_POINT('',(90.940772381535,831.413795546376,127.587381214293));
#75035=CARTESIAN_POINT('',(90.940772381535,835.003726143045,117.430089431301));
#75036=CARTESIAN_POINT('Origin',(90.940772381535,830.942373315767,127.420764647026));
#75037=CARTESIAN_POINT('Origin',(93.6444458706187,838.80975519492,118.775268878447));
#75038=CARTESIAN_POINT('',(93.6444458706187,836.680923414049,129.448962420455));
#75039=CARTESIAN_POINT('Origin',(93.6444458706187,835.219824598252,128.932560661438));
#75040=CARTESIAN_POINT('',(93.6444458706187,837.347389683118,127.56327349802));
#75041=CARTESIAN_POINT('',(93.6444458706187,840.270854010718,119.291670637464));
#75042=CARTESIAN_POINT('Origin',(93.6444458706187,835.88629086732,127.046871739003));
#75043=CARTESIAN_POINT('Origin',(93.6444458706187,838.80975519492,118.775268878447));
#75044=CARTESIAN_POINT('',(93.6444458706187,837.146338563414,124.982164121935));
#75045=CARTESIAN_POINT('Origin',(93.6444458706187,836.674916332805,124.815547554668));
#75046=CARTESIAN_POINT('',(93.6444458706187,835.691246828861,129.099177228705));
#75047=CARTESIAN_POINT('',(93.6444458706187,839.281177425529,118.941885445714));
#75048=CARTESIAN_POINT('Origin',(93.6444458706187,835.219824598252,128.932560661438));
#75049=CARTESIAN_POINT('Origin',(96.0752729060054,844.131665553615,120.656212070548));
#75050=CARTESIAN_POINT('',(96.0752729060054,841.729116533909,131.233164678898));
#75051=CARTESIAN_POINT('Origin',(96.0752729060054,840.541734956947,130.813503853539));
#75052=CARTESIAN_POINT('',(96.075272915159,842.391856517098,129.358018849683));
#75053=CARTESIAN_POINT('',(96.0752729060054,845.319047130577,121.075872895907));
#75054=CARTESIAN_POINT('',(94.9806993794011,841.795419268718,129.135357656415));
#75055=CARTESIAN_POINT('Ctrl Pts',(96.0752729243125,842.391856517098,129.358018849683));
#75056=CARTESIAN_POINT('Ctrl Pts',(96.0381869450381,842.392062128276,129.357437098348));
#75057=CARTESIAN_POINT('Ctrl Pts',(96.0010576020752,842.390718482093,129.356322901975));
#75058=CARTESIAN_POINT('Ctrl Pts',(95.8098139198172,842.375727679237,129.347827179232));
#75059=CARTESIAN_POINT('Ctrl Pts',(95.6594640231771,842.336825803051,129.331901096533));
#75060=CARTESIAN_POINT('Ctrl Pts',(95.3836700294588,842.210231411673,129.283966900442));
#75061=CARTESIAN_POINT('Ctrl Pts',(95.2601593759105,842.124347248646,129.252605375448));
#75062=CARTESIAN_POINT('Ctrl Pts',(95.0882775919892,841.951538801714,129.190669772999));
#75063=CARTESIAN_POINT('Ctrl Pts',(95.0294835971499,841.876255303615,129.163927846303));
#75064=CARTESIAN_POINT('Ctrl Pts',(94.9806993794009,841.795419268718,129.135357656415));
#75065=CARTESIAN_POINT('',(95.6369585689663,840.095057333157,128.534392215203));
#75066=CARTESIAN_POINT('Origin',(96.0752729060063,841.208201226016,128.927814931105));
#75067=CARTESIAN_POINT('Ctrl Pts',(95.6369585689663,840.095057333157,128.534392215203));
#75068=CARTESIAN_POINT('Ctrl Pts',(95.7775499390088,840.045845092418,128.516998944188));
#75069=CARTESIAN_POINT('Ctrl Pts',(95.9263899652387,840.020588098312,128.508388153485));
#75070=CARTESIAN_POINT('Ctrl Pts',(96.2286185169781,840.020321608885,128.509993592314));
#75071=CARTESIAN_POINT('Ctrl Pts',(96.3794981805657,840.046019623926,128.520466728387));
#75072=CARTESIAN_POINT('Ctrl Pts',(96.6689938130533,840.14827814966,128.560543823279));
#75073=CARTESIAN_POINT('Ctrl Pts',(96.8044458340276,840.225676544221,128.590447185228));
#75074=CARTESIAN_POINT('Ctrl Pts',(97.0448240321836,840.429293902598,128.668249247419));
#75075=CARTESIAN_POINT('Ctrl Pts',(97.1450172258218,840.556180302845,128.716352041202));
#75076=CARTESIAN_POINT('Ctrl Pts',(97.286321668992,840.838875704314,128.822241165483));
#75077=CARTESIAN_POINT('Ctrl Pts',(97.3263082764593,840.991785609775,128.878931697869));
#75078=CARTESIAN_POINT('Ctrl Pts',(97.3405741326517,841.302774181318,128.992536065982));
#75079=CARTESIAN_POINT('Ctrl Pts',(97.315175765911,841.457793125225,129.048334424406));
#75080=CARTESIAN_POINT('Ctrl Pts',(97.2587144313823,841.604083959076,129.100038554963));
#75081=CARTESIAN_POINT('Ctrl Pts',(97.2380639521442,841.657589173793,129.118949108238));
#75082=CARTESIAN_POINT('Ctrl Pts',(97.2133584790335,841.709666080833,129.137222137847));
#75083=CARTESIAN_POINT('Ctrl Pts',(97.1073658561724,841.896076358022,129.20213351767));
#75084=CARTESIAN_POINT('Ctrl Pts',(97.0025787581668,842.017011306053,129.243210770125));
#75085=CARTESIAN_POINT('Ctrl Pts',(96.7505467043735,842.214349710098,129.308305373662));
#75086=CARTESIAN_POINT('Ctrl Pts',(96.6058557131205,842.289064737309,129.331786656256));
#75087=CARTESIAN_POINT('Ctrl Pts',(96.3286812613534,842.372289415152,129.355764731473));
#75088=CARTESIAN_POINT('Ctrl Pts',(96.2022312191795,842.39115263803,129.360010388238));
#75089=CARTESIAN_POINT('Ctrl Pts',(96.0752729243125,842.391856517098,129.358018849683));
#75090=CARTESIAN_POINT('Origin',(96.0752729060054,844.131665553615,120.656212070548));
#75091=CARTESIAN_POINT('',(96.0752729060054,842.468248922109,126.863107314036));
#75092=CARTESIAN_POINT('Origin',(96.0752729060054,841.9968266915,126.696490746769));
#75093=CARTESIAN_POINT('',(96.0752729060054,841.013157187555,130.980120420807));
#75094=CARTESIAN_POINT('',(96.0752729060054,844.603087784224,120.822828637815));
#75095=CARTESIAN_POINT('Origin',(96.0752729060054,840.541734956947,130.813503853539));
#75096=CARTESIAN_POINT('Origin',(63.7849617023409,821.33489883697,112.599063365));
#75097=CARTESIAN_POINT('',(63.7849617023409,818.743330659428,123.109210207348));
#75098=CARTESIAN_POINT('Origin',(63.7849617023409,817.744968240301,122.756355147991));
#75099=CARTESIAN_POINT('',(63.7849617023409,819.409796928497,121.223521284913));
#75100=CARTESIAN_POINT('',(63.7849617023409,822.333261256097,112.951918424357));
#75101=CARTESIAN_POINT('Origin',(63.7849617023409,818.41143450937,120.870666225556));
#75102=CARTESIAN_POINT('Origin',(63.7849617023409,821.33489883697,112.599063365));
#75103=CARTESIAN_POINT('',(63.7849617023409,819.671482205463,118.805958608488));
#75104=CARTESIAN_POINT('Origin',(63.7849617023409,819.200059974855,118.639342041221));
#75105=CARTESIAN_POINT('',(63.7849617023409,818.21639047091,122.922971715259));
#75106=CARTESIAN_POINT('',(63.7849617023409,821.806321067579,112.765679932267));
#75107=CARTESIAN_POINT('Origin',(63.7849617023409,817.744968240301,122.756355147991));
#75108=CARTESIAN_POINT('Origin',(67.8415722335897,820.36061484734,112.254718437342));
#75109=CARTESIAN_POINT('',(67.8415722335897,817.992453530053,122.843824823264));
#75110=CARTESIAN_POINT('Origin',(67.8415722335897,816.770684250671,122.412010220333));
#75111=CARTESIAN_POINT('',(67.8415722335897,818.658919799122,120.958135900829));
#75112=CARTESIAN_POINT('',(67.8415722335897,821.582384126722,112.686533040273));
#75113=CARTESIAN_POINT('Origin',(67.8415722335897,817.437150519739,120.526321297898));
#75114=CARTESIAN_POINT('Origin',(67.8415722335897,820.36061484734,112.254718437342));
#75115=CARTESIAN_POINT('',(67.8415722335897,818.697198215833,118.46161368083));
#75116=CARTESIAN_POINT('Origin',(67.8415722335897,818.225775985225,118.294997113563));
#75117=CARTESIAN_POINT('',(67.8415722335897,817.24210648128,122.5786267876));
#75118=CARTESIAN_POINT('',(67.8415722335897,820.832037077948,112.421335004609));
#75119=CARTESIAN_POINT('Origin',(67.8415722335897,816.770684250671,122.412010220333));
#75120=CARTESIAN_POINT('Origin',(72.5705190327731,819.933847938692,112.103884571806));
#75121=CARTESIAN_POINT('',(72.5705190327731,817.858633744024,122.796528382975));
#75122=CARTESIAN_POINT('Origin',(72.5705190327731,816.343917342023,122.261176354798));
#75123=CARTESIAN_POINT('',(72.5705190327731,818.525100013092,120.91083946054));
#75124=CARTESIAN_POINT('',(72.5705190327731,821.448564340692,112.639236599984));
#75125=CARTESIAN_POINT('Origin',(72.5705190327731,817.010383611091,120.375487432362));
#75126=CARTESIAN_POINT('Origin',(72.5705190327731,819.933847938692,112.103884571806));
#75127=CARTESIAN_POINT('',(72.5705190327731,818.270431307185,118.310779815295));
#75128=CARTESIAN_POINT('Origin',(72.5705190327731,817.799009076576,118.144163248028));
#75129=CARTESIAN_POINT('',(72.5705190327731,816.815339572632,122.427792922065));
#75130=CARTESIAN_POINT('',(72.5705190327731,820.4052701693,112.270501139073));
#75131=CARTESIAN_POINT('Origin',(72.5705190327731,816.343917342023,122.261176354798));
#75132=CARTESIAN_POINT('Origin',(77.2426896003823,820.494722138539,112.302116491685));
#75133=CARTESIAN_POINT('',(77.2426896003823,818.628403686317,123.068591126399));
#75134=CARTESIAN_POINT('Origin',(77.2426896003823,816.904791541871,122.459408274677));
#75135=CARTESIAN_POINT('',(77.2426896003823,819.294869955385,121.182902203964));
#75136=CARTESIAN_POINT('',(77.2426896003823,822.218334282986,112.911299343408));
#75137=CARTESIAN_POINT('Origin',(77.2426896003823,817.571257810939,120.573719352242));
#75138=CARTESIAN_POINT('Origin',(77.2426896003823,820.494722138539,112.302116491685));
#75139=CARTESIAN_POINT('',(77.2426896003823,818.831305507033,118.509011735174));
#75140=CARTESIAN_POINT('Origin',(77.2426896003823,818.359883276424,118.342395167907));
#75141=CARTESIAN_POINT('',(77.2426896003823,817.376213772479,122.626024841944));
#75142=CARTESIAN_POINT('',(77.2426896003823,820.966144369148,112.468733058952));
#75143=CARTESIAN_POINT('Origin',(77.2426896003823,816.904791541871,122.459408274677));
#75144=CARTESIAN_POINT('Origin',(82.2063885331164,821.68423828967,112.72253174778));
#75145=CARTESIAN_POINT('',(82.2063885331164,819.846507090563,123.499110085019));
#75146=CARTESIAN_POINT('Origin',(82.2063885331164,818.094307693001,122.879823530771));
#75147=CARTESIAN_POINT('',(82.2063885331164,820.512973359631,121.613421162583));
#75148=CARTESIAN_POINT('',(82.2063885331164,823.436437687231,113.341818302027));
#75149=CARTESIAN_POINT('Origin',(82.2063885331164,818.760773962069,120.994134608336));
#75150=CARTESIAN_POINT('Origin',(82.2063885331164,821.68423828967,112.72253174778));
#75151=CARTESIAN_POINT('',(82.2063885331164,820.020821658163,118.929426991268));
#75152=CARTESIAN_POINT('Origin',(82.2063885331164,819.549399427555,118.762810424001));
#75153=CARTESIAN_POINT('',(82.2063885331164,818.56572992361,123.046440098039));
#75154=CARTESIAN_POINT('',(82.2063885331164,822.155660520279,112.889148315047));
#75155=CARTESIAN_POINT('Origin',(82.2063885331164,818.094307693001,122.879823530771));
#75156=CARTESIAN_POINT('Origin',(86.354482212296,823.885477455299,113.500524149703));
#75157=CARTESIAN_POINT('',(86.354482212296,822.004789207011,124.261920012272));
#75158=CARTESIAN_POINT('Origin',(86.354482212296,820.29554685863,123.657815932694));
#75159=CARTESIAN_POINT('',(86.354482212296,822.671255476079,122.376231089837));
#75160=CARTESIAN_POINT('',(86.354482212296,825.594719803679,114.104628229281));
#75161=CARTESIAN_POINT('Origin',(86.354482212296,820.962013127699,121.772127010259));
#75162=CARTESIAN_POINT('Origin',(86.354482212296,823.885477455299,113.500524149703));
#75163=CARTESIAN_POINT('',(86.354482212296,822.222060823793,119.707419393191));
#75164=CARTESIAN_POINT('Origin',(86.354482212296,821.750638593184,119.540802825924));
#75165=CARTESIAN_POINT('',(86.354482212296,820.766969089239,123.824432499961));
#75166=CARTESIAN_POINT('',(86.354482212296,824.356899685908,113.66714071697));
#75167=CARTESIAN_POINT('Origin',(86.354482212296,820.29554685863,123.657815932694));
#75168=CARTESIAN_POINT('Origin',(91.2604284870247,826.956742332132,114.586013076021));
#75169=CARTESIAN_POINT('',(91.2604284870247,825.169026885505,125.380268672511));
#75170=CARTESIAN_POINT('Origin',(91.2604284870247,823.366811735464,124.743304859012));
#75171=CARTESIAN_POINT('',(91.2604284870247,825.835493154573,123.494579750075));
#75172=CARTESIAN_POINT('',(91.2604284870247,828.758957482173,115.222976889519));
#75173=CARTESIAN_POINT('Origin',(91.2604284870247,824.033278004532,122.857615936577));
#75174=CARTESIAN_POINT('Origin',(91.2604284870247,826.956742332132,114.586013076021));
#75175=CARTESIAN_POINT('',(91.2604284870247,825.293325700626,120.792908319509));
#75176=CARTESIAN_POINT('Origin',(91.2604284870247,824.821903470017,120.626291752242));
#75177=CARTESIAN_POINT('',(91.2604284870247,823.838233966072,124.909921426279));
#75178=CARTESIAN_POINT('',(91.2604284870247,827.428164562741,114.752629643288));
#75179=CARTESIAN_POINT('Origin',(91.2604284870247,823.366811735464,124.743304859012));
#75180=CARTESIAN_POINT('Origin',(94.8482639557915,830.610724290717,115.877453935755));
#75181=CARTESIAN_POINT('',(94.8482639557915,828.481892509846,126.551147477763));
#75182=CARTESIAN_POINT('Origin',(94.8482639557915,827.020793694048,126.034745718746));
#75183=CARTESIAN_POINT('',(94.8482639557915,829.148358778914,124.665458555328));
#75184=CARTESIAN_POINT('',(94.8482639557915,832.071823106514,116.393855694772));
#75185=CARTESIAN_POINT('Origin',(94.8482639557915,827.687259963117,124.149056796311));
#75186=CARTESIAN_POINT('Origin',(94.8482639557915,830.610724290717,115.877453935755));
#75187=CARTESIAN_POINT('',(94.8482639557915,828.94730765921,122.084349179243));
#75188=CARTESIAN_POINT('Origin',(94.8482639557915,828.475885428602,121.917732611976));
#75189=CARTESIAN_POINT('',(94.8482639557915,827.492215924657,126.201362286013));
#75190=CARTESIAN_POINT('',(94.8482639557915,831.082146521326,116.044070503022));
#75191=CARTESIAN_POINT('Origin',(94.8482639557915,827.020793694048,126.034745718746));
#75192=CARTESIAN_POINT('Origin',(98.399534595272,835.339827038736,117.548878860097));
#75193=CARTESIAN_POINT('',(98.399534595272,832.937278019029,128.125831468446));
#75194=CARTESIAN_POINT('Origin',(98.399534595272,831.749896442067,127.706170643088));
#75195=CARTESIAN_POINT('',(98.3995346119163,833.601376047008,126.246843209188));
#75196=CARTESIAN_POINT('',(98.399534595272,836.527208615697,117.968539685455));
#75197=CARTESIAN_POINT('',(97.4583707276143,833.205316112613,126.099324547641));
#75198=CARTESIAN_POINT('Ctrl Pts',(98.3995346119195,833.601376047086,126.246843208968));
#75199=CARTESIAN_POINT('Ctrl Pts',(98.2960201644212,833.601860815876,126.245471616071));
#75200=CARTESIAN_POINT('Ctrl Pts',(98.1927006143714,833.590245389903,126.240034939902));
#75201=CARTESIAN_POINT('Ctrl Pts',(97.9441465608869,833.532056193237,126.216806144848));
#75202=CARTESIAN_POINT('Ctrl Pts',(97.8043263550253,833.472267314184,126.194667576166));
#75203=CARTESIAN_POINT('Ctrl Pts',(97.5980341511791,833.336934754523,126.145977220307));
#75204=CARTESIAN_POINT('Ctrl Pts',(97.5239144809264,833.274822594726,126.12389049023));
#75205=CARTESIAN_POINT('Ctrl Pts',(97.4583707276145,833.205316112613,126.099324547641));
#75206=CARTESIAN_POINT('',(97.7253331459279,831.413465735163,125.466023995477));
#75207=CARTESIAN_POINT('Origin',(98.3995345952731,832.416362711137,125.820481720653));
#75208=CARTESIAN_POINT('Ctrl Pts',(97.7253331459279,831.413465735163,125.466023995477));
#75209=CARTESIAN_POINT('Ctrl Pts',(97.8520002019731,831.337769000587,125.439270208214));
#75210=CARTESIAN_POINT('Ctrl Pts',(97.9920400467637,831.283884893482,125.420541627155));
#75211=CARTESIAN_POINT('Ctrl Pts',(98.2877231697512,831.22436718307,125.401205679672));
#75212=CARTESIAN_POINT('Ctrl Pts',(98.4410689020655,831.21991739046,125.401023560445));
#75213=CARTESIAN_POINT('Ctrl Pts',(98.7470605981185,831.263164940511,125.420244179844));
#75214=CARTESIAN_POINT('Ctrl Pts',(98.8967967463751,831.312302058446,125.44015905039));
#75215=CARTESIAN_POINT('Ctrl Pts',(99.1772272516042,831.46430886483,125.499720197219));
#75216=CARTESIAN_POINT('Ctrl Pts',(99.3034370287928,831.568759422086,125.539893404954));
#75217=CARTESIAN_POINT('Ctrl Pts',(99.5044062771853,831.817536546003,125.633794662295));
#75218=CARTESIAN_POINT('Ctrl Pts',(99.5774214571361,831.95924831943,125.686527395921));
#75219=CARTESIAN_POINT('Ctrl Pts',(99.6602090166774,832.260619193867,125.796732544454));
#75220=CARTESIAN_POINT('Ctrl Pts',(99.6696196598402,832.417222472356,125.853090860326));
#75221=CARTESIAN_POINT('Ctrl Pts',(99.6466515176081,832.571384524781,125.907576945857));
#75222=CARTESIAN_POINT('Ctrl Pts',(99.6382510228578,832.627768602301,125.927504986655));
#75223=CARTESIAN_POINT('Ctrl Pts',(99.6255599871384,832.683551389161,125.947087799584));
#75224=CARTESIAN_POINT('Ctrl Pts',(99.5629225224937,832.886672393037,126.01790531564));
#75225=CARTESIAN_POINT('Ctrl Pts',(99.4869779146069,833.025517301181,126.065312553998));
#75226=CARTESIAN_POINT('Ctrl Pts',(99.2836472483551,833.267980760135,126.146355878784));
#75227=CARTESIAN_POINT('Ctrl Pts',(99.1583912238311,833.369446712211,126.179291843365));
#75228=CARTESIAN_POINT('Ctrl Pts',(98.8728084678537,833.522624406972,126.227296997787));
#75229=CARTESIAN_POINT('Ctrl Pts',(98.7148885128273,833.572355949435,126.241736632413));
#75230=CARTESIAN_POINT('Ctrl Pts',(98.5009823002612,833.597998782357,126.247211076537));
#75231=CARTESIAN_POINT('Ctrl Pts',(98.4502350741954,833.601138611613,126.247515003057));
#75232=CARTESIAN_POINT('Ctrl Pts',(98.3995346119195,833.601376047086,126.246843208968));
#75233=CARTESIAN_POINT('Origin',(98.399534595272,835.339827038736,117.548878860097));
#75234=CARTESIAN_POINT('',(98.399534595272,833.676410407229,123.755774103585));
#75235=CARTESIAN_POINT('Origin',(98.399534595272,833.20498817662,123.589157536318));
#75236=CARTESIAN_POINT('',(98.399534595272,832.221318672676,127.872787210355));
#75237=CARTESIAN_POINT('',(98.399534595272,835.811249269344,117.715495427364));
#75238=CARTESIAN_POINT('Origin',(98.399534595272,831.749896442067,127.706170643088));
#75239=CARTESIAN_POINT('Origin',(61.7878068235231,819.371041962602,111.90496989684));
#75240=CARTESIAN_POINT('',(61.7878068235231,816.77947378506,122.415116739188));
#75241=CARTESIAN_POINT('Origin',(61.7878068235231,815.781111365933,122.062261679831));
#75242=CARTESIAN_POINT('',(61.7878068235231,817.445940054129,120.529427816752));
#75243=CARTESIAN_POINT('',(61.7878068235231,820.369404381729,112.257824956196));
#75244=CARTESIAN_POINT('Origin',(61.7878068235231,816.447577635001,120.176572757396));
#75245=CARTESIAN_POINT('Origin',(61.7878068235231,819.371041962602,111.90496989684));
#75246=CARTESIAN_POINT('',(61.7878068235231,817.707625331095,118.111865140328));
#75247=CARTESIAN_POINT('Origin',(61.7878068235231,817.236203100487,117.945248573061));
#75248=CARTESIAN_POINT('',(61.7878068235231,816.252533596542,122.228878247098));
#75249=CARTESIAN_POINT('',(61.7878068235231,819.84246419321,112.071586464107));
#75250=CARTESIAN_POINT('Origin',(61.7878068235231,815.781111365933,122.062261679831));
#75251=CARTESIAN_POINT('Origin',(65.540926091864,817.622837600195,111.287095323192));
#75252=CARTESIAN_POINT('',(65.540926091864,815.254676282909,121.876201709114));
#75253=CARTESIAN_POINT('Origin',(65.540926091864,814.032907003526,121.444387106183));
#75254=CARTESIAN_POINT('',(65.540926091864,815.921142551977,119.990512786679));
#75255=CARTESIAN_POINT('',(65.540926091864,818.844606879577,111.718909926123));
#75256=CARTESIAN_POINT('Origin',(65.540926091864,814.699373272594,119.558698183748));
#75257=CARTESIAN_POINT('Origin',(65.540926091864,817.622837600195,111.287095323192));
#75258=CARTESIAN_POINT('',(65.540926091864,815.959420968688,117.49399056668));
#75259=CARTESIAN_POINT('Origin',(65.540926091864,815.48799873808,117.327373999413));
#75260=CARTESIAN_POINT('',(65.540926091864,814.504329234135,121.61100367345));
#75261=CARTESIAN_POINT('',(65.540926091864,818.094259830803,111.453711890459));
#75262=CARTESIAN_POINT('Origin',(65.540926091864,814.032907003526,121.444387106183));
#75263=CARTESIAN_POINT('Origin',(70.0724253967104,816.278388763384,110.811921613699));
#75264=CARTESIAN_POINT('',(70.0724253967104,814.203174568716,121.504565424869));
#75265=CARTESIAN_POINT('Origin',(70.0724253967104,812.688458166716,120.969213396691));
#75266=CARTESIAN_POINT('',(70.0724253967104,814.869640837785,119.618876502433));
#75267=CARTESIAN_POINT('',(70.0724253967104,817.793105165385,111.347273641877));
#75268=CARTESIAN_POINT('Origin',(70.0724253967104,813.354924435784,119.083524474256));
#75269=CARTESIAN_POINT('Origin',(70.0724253967104,816.278388763384,110.811921613699));
#75270=CARTESIAN_POINT('',(70.0724253967104,814.614972131878,117.018816857188));
#75271=CARTESIAN_POINT('Origin',(70.0724253967104,814.143549901269,116.852200289921));
#75272=CARTESIAN_POINT('',(70.0724253967104,813.159880397325,121.135829963958));
#75273=CARTESIAN_POINT('',(70.0724253967104,816.749810993993,110.978538180967));
#75274=CARTESIAN_POINT('Origin',(70.0724253967104,812.688458166716,120.969213396691));
#75275=CARTESIAN_POINT('Origin',(74.7661792067218,815.91112846028,110.682119396019));
#75276=CARTESIAN_POINT('',(74.7661792067218,814.044810008058,121.448594030733));
#75277=CARTESIAN_POINT('Origin',(74.7661792067218,812.321197863611,120.839411179011));
#75278=CARTESIAN_POINT('',(74.7661792067218,814.711276277126,119.562905108298));
#75279=CARTESIAN_POINT('',(74.7661792067218,817.634740604727,111.291302247742));
#75280=CARTESIAN_POINT('Origin',(74.7661792067218,812.98766413268,118.953722256575));
#75281=CARTESIAN_POINT('Origin',(74.7661792067218,815.91112846028,110.682119396019));
#75282=CARTESIAN_POINT('',(74.7661792067218,814.247711828774,116.889014639508));
#75283=CARTESIAN_POINT('Origin',(74.7661792067218,813.776289598165,116.722398072241));
#75284=CARTESIAN_POINT('',(74.7661792067218,812.79262009422,121.006027746278));
#75285=CARTESIAN_POINT('',(74.7661792067218,816.382550690889,110.848735963286));
#75286=CARTESIAN_POINT('Origin',(74.7661792067218,812.321197863611,120.839411179011));
#75287=CARTESIAN_POINT('Origin',(79.8837159971768,816.101624938623,110.749447297075));
#75288=CARTESIAN_POINT('',(79.8837159971768,814.263893739516,121.526025634314));
#75289=CARTESIAN_POINT('Origin',(79.8837159971768,812.511694341955,120.906739080067));
#75290=CARTESIAN_POINT('',(79.8837159971768,814.930360008584,119.640336711878));
#75291=CARTESIAN_POINT('',(79.8837159971768,817.853824336185,111.368733851322));
#75292=CARTESIAN_POINT('Origin',(79.8837159971768,813.178160611023,119.021050157631));
#75293=CARTESIAN_POINT('Origin',(79.8837159971768,816.101624938623,110.749447297075));
#75294=CARTESIAN_POINT('',(79.8837159971768,814.438208307117,116.956342540564));
#75295=CARTESIAN_POINT('Origin',(79.8837159971768,813.966786076508,116.789725973297));
#75296=CARTESIAN_POINT('',(79.8837159971768,812.983116572563,121.073355647334));
#75297=CARTESIAN_POINT('',(79.8837159971768,816.573047169232,110.916063864342));
#75298=CARTESIAN_POINT('Origin',(79.8837159971768,812.511694341955,120.906739080067));
#75299=CARTESIAN_POINT('Origin',(84.4265709358799,817.441617637763,111.223046056738));
#75300=CARTESIAN_POINT('',(84.4265709358799,815.560929389475,121.984441919307));
#75301=CARTESIAN_POINT('Origin',(84.4265709358799,813.851687041094,121.380337839729));
#75302=CARTESIAN_POINT('',(84.4265709358799,816.227395658543,120.098752996872));
#75303=CARTESIAN_POINT('',(84.4265709358799,819.150859986143,111.827150136316));
#75304=CARTESIAN_POINT('Origin',(84.4265709358799,814.518153310162,119.494648917294));
#75305=CARTESIAN_POINT('Origin',(84.4265709358799,817.441617637763,111.223046056738));
#75306=CARTESIAN_POINT('',(84.4265709358799,815.778201006257,117.429941300226));
#75307=CARTESIAN_POINT('Origin',(84.4265709358799,815.306778775648,117.263324732959));
#75308=CARTESIAN_POINT('',(84.4265709358799,814.323109271703,121.546954406996));
#75309=CARTESIAN_POINT('',(84.4265709358799,817.913039868372,111.389662624005));
#75310=CARTESIAN_POINT('Origin',(84.4265709358799,813.851687041094,121.380337839729));
#75311=CARTESIAN_POINT('Origin',(89.9025716101847,819.484063277678,111.94491545376));
#75312=CARTESIAN_POINT('',(89.9025716101847,817.69634783105,122.739171050249));
#75313=CARTESIAN_POINT('Origin',(89.9025716101847,815.89413268101,122.102207236751));
#75314=CARTESIAN_POINT('',(89.9025716101847,818.362814100118,120.853482127814));
#75315=CARTESIAN_POINT('',(89.9025716101847,821.286278427719,112.581879267258));
#75316=CARTESIAN_POINT('Origin',(89.9025716101847,816.560598950078,120.216518314316));
#75317=CARTESIAN_POINT('Origin',(89.9025716101847,819.484063277678,111.94491545376));
#75318=CARTESIAN_POINT('',(89.9025716101847,817.820646646172,118.151810697248));
#75319=CARTESIAN_POINT('Origin',(89.9025716101847,817.349224415563,117.985194129981));
#75320=CARTESIAN_POINT('',(89.9025716101847,816.365554911618,122.268823804018));
#75321=CARTESIAN_POINT('',(89.9025716101847,819.955485508287,112.111532021027));
#75322=CARTESIAN_POINT('Origin',(89.9025716101847,815.89413268101,122.102207236751));
#75323=CARTESIAN_POINT('Origin',(94.2177634323048,822.354879367022,112.959558996225));
#75324=CARTESIAN_POINT('',(94.2177634323048,820.226047586151,123.633252538233));
#75325=CARTESIAN_POINT('Origin',(94.2177634323048,818.764948770354,123.116850779216));
#75326=CARTESIAN_POINT('',(94.2177634323048,820.892513855219,121.747563615798));
#75327=CARTESIAN_POINT('',(94.2177634323048,823.81597818282,113.475960755242));
#75328=CARTESIAN_POINT('Origin',(94.2177634323048,819.431415039422,121.231161856781));
#75329=CARTESIAN_POINT('Origin',(94.2177634323048,822.354879367022,112.959558996225));
#75330=CARTESIAN_POINT('',(94.2177634323048,820.691462735516,119.166454239713));
#75331=CARTESIAN_POINT('Origin',(94.2177634323048,820.220040504907,118.999837672446));
#75332=CARTESIAN_POINT('',(94.2177634323048,819.236371000962,123.283467346483));
#75333=CARTESIAN_POINT('',(94.2177634323048,822.826301597631,113.126175563492));
#75334=CARTESIAN_POINT('Origin',(94.2177634323048,818.764948770354,123.116850779216));
#75335=CARTESIAN_POINT('Origin',(98.7342701080466,826.284490021524,114.348416363226));
#75336=CARTESIAN_POINT('',(98.7342701080466,823.881941001817,124.925368971576));
#75337=CARTESIAN_POINT('Origin',(98.7342701080466,822.694559424855,124.505708146217));
#75338=CARTESIAN_POINT('',(98.7342701101916,824.547122491794,123.043315182399));
#75339=CARTESIAN_POINT('',(98.7342701080466,827.471871598486,114.768077188584));
#75340=CARTESIAN_POINT('',(97.9876492765575,824.317233404711,122.957975382871));
#75341=CARTESIAN_POINT('Ctrl Pts',(98.7342701123366,824.547122491794,123.043315182399));
#75342=CARTESIAN_POINT('Ctrl Pts',(98.7186233546984,824.547177168776,123.043160480388));
#75343=CARTESIAN_POINT('Ctrl Pts',(98.702965884564,824.546955160808,123.042913564466));
#75344=CARTESIAN_POINT('Ctrl Pts',(98.5349995581169,824.54159384245,123.039272550181));
#75345=CARTESIAN_POINT('Ctrl Pts',(98.384980613872,824.510527138023,123.027285369851));
#75346=CARTESIAN_POINT('Ctrl Pts',(98.1532939493101,824.418596946666,122.993934879506));
#75347=CARTESIAN_POINT('Ctrl Pts',(98.0670879888991,824.372372567245,122.977463428591));
#75348=CARTESIAN_POINT('Ctrl Pts',(97.9876492765573,824.317233404711,122.957975382871));
#75349=CARTESIAN_POINT('',(97.8536473849113,822.512207045121,122.320017992798));
#75350=CARTESIAN_POINT('Origin',(98.7342701080476,823.361025693924,122.620019223782));
#75351=CARTESIAN_POINT('Ctrl Pts',(97.8536473849113,822.512207045121,122.320017992798));
#75352=CARTESIAN_POINT('Ctrl Pts',(97.9608541687947,822.413334127242,122.285072958171));
#75353=CARTESIAN_POINT('Ctrl Pts',(98.0859734189423,822.333173563606,122.257057388288));
#75354=CARTESIAN_POINT('Ctrl Pts',(98.3621883418565,822.216982503381,122.21769116139));
#75355=CARTESIAN_POINT('Ctrl Pts',(98.5112981985599,822.182560285577,122.206915772957));
#75356=CARTESIAN_POINT('Ctrl Pts',(98.8204126527526,822.16485269463,122.204592783059));
#75357=CARTESIAN_POINT('Ctrl Pts',(98.9778887400996,822.183546018221,122.213747786592));
#75358=CARTESIAN_POINT('Ctrl Pts',(99.2861153936676,822.277218697885,122.252691679254));
#75359=CARTESIAN_POINT('Ctrl Pts',(99.4328257815214,822.354623700265,122.283306072786));
#75360=CARTESIAN_POINT('Ctrl Pts',(99.6846765146236,822.558527746896,122.361347666295));
#75361=CARTESIAN_POINT('Ctrl Pts',(99.787529153329,822.682811556581,122.407920767846));
#75362=CARTESIAN_POINT('Ctrl Pts',(99.9352202026085,822.96134270475,122.510053584314));
#75363=CARTESIAN_POINT('Ctrl Pts',(99.9790285654115,823.112672142274,122.564547946344));
#75364=CARTESIAN_POINT('Ctrl Pts',(99.9905574335051,823.267967791832,122.619434683458));
#75365=CARTESIAN_POINT('Ctrl Pts',(99.9947740651734,823.324766477407,122.639509260771));
#75366=CARTESIAN_POINT('Ctrl Pts',(99.9946521260043,823.381818990948,122.659540838072));
#75367=CARTESIAN_POINT('Ctrl Pts',(99.9781073773492,823.592786710345,122.733131648893));
#75368=CARTESIAN_POINT('Ctrl Pts',(99.9343244033688,823.743496256212,122.784732251672));
#75369=CARTESIAN_POINT('Ctrl Pts',(99.7885816504621,824.02055182496,122.878001598513));
#75370=CARTESIAN_POINT('Ctrl Pts',(99.6882348819836,824.144374324847,122.918839123543));
#75371=CARTESIAN_POINT('Ctrl Pts',(99.4422459149123,824.35022915398,122.985462159628));
#75372=CARTESIAN_POINT('Ctrl Pts',(99.2985261059392,824.429852275868,123.01046648983));
#75373=CARTESIAN_POINT('Ctrl Pts',(99.0112452426019,824.524339635425,123.038803592336));
#75374=CARTESIAN_POINT('Ctrl Pts',(98.873179893281,824.546637077005,123.044688605763));
#75375=CARTESIAN_POINT('Ctrl Pts',(98.7342701123366,824.547122491794,123.043315182399));
#75376=CARTESIAN_POINT('Origin',(98.7342701080466,826.284490021524,114.348416363226));
#75377=CARTESIAN_POINT('',(98.7342701080466,824.621073390018,120.555311606714));
#75378=CARTESIAN_POINT('Origin',(98.7342701080466,824.149651159408,120.388695039447));
#75379=CARTESIAN_POINT('',(98.7342701080466,823.165981655464,124.672324713484));
#75380=CARTESIAN_POINT('',(98.7342701080466,826.755912252132,114.515032930493));
#75381=CARTESIAN_POINT('Origin',(98.7342701080466,822.694559424855,124.505708146217));
#75382=CARTESIAN_POINT('Origin',(59.4012339544,817.84159912046,111.364413046435));
#75383=CARTESIAN_POINT('',(59.4012339544,815.250030942918,121.874559888782));
#75384=CARTESIAN_POINT('Origin',(59.4012339544,814.251668523791,121.521704829426));
#75385=CARTESIAN_POINT('',(59.4012339544,815.916497211987,119.988870966347));
#75386=CARTESIAN_POINT('',(59.4012339544,818.839961539587,111.717268105791));
#75387=CARTESIAN_POINT('Origin',(59.4012339544,814.91813479286,119.636015906991));
#75388=CARTESIAN_POINT('Origin',(59.4012339544,817.84159912046,111.364413046435));
#75389=CARTESIAN_POINT('',(59.4012339544,816.178182488954,117.571308289923));
#75390=CARTESIAN_POINT('Origin',(59.4012339544,815.706760258345,117.404691722656));
#75391=CARTESIAN_POINT('',(59.4012339544,814.7230907544,121.688321396693));
#75392=CARTESIAN_POINT('',(59.4012339544,818.313021351069,111.531029613702));
#75393=CARTESIAN_POINT('Origin',(59.4012339544,814.251668523791,121.521704829426));
#75394=CARTESIAN_POINT('Origin',(62.6868326383422,815.395879304728,110.500012910556));
#75395=CARTESIAN_POINT('',(62.6868326383422,813.027717987442,121.089119296479));
#75396=CARTESIAN_POINT('Origin',(62.6868326383422,811.80594870806,120.657304693548));
#75397=CARTESIAN_POINT('',(62.6868326383422,813.694184256511,119.203430374043));
#75398=CARTESIAN_POINT('',(62.6868326383422,816.617648584111,110.931827513487));
#75399=CARTESIAN_POINT('Origin',(62.6868326383422,812.472414977128,118.771615771112));
#75400=CARTESIAN_POINT('Origin',(62.6868326383422,815.395879304728,110.500012910556));
#75401=CARTESIAN_POINT('',(62.6868326383422,813.732462673222,116.706908154045));
#75402=CARTESIAN_POINT('Origin',(62.6868326383422,813.261040442613,116.540291586778));
#75403=CARTESIAN_POINT('',(62.6868326383422,812.277370938668,120.823921260815));
#75404=CARTESIAN_POINT('',(62.6868326383422,815.867301535337,110.666629477823));
#75405=CARTESIAN_POINT('Origin',(62.6868326383422,811.80594870806,120.657304693548));
#75406=CARTESIAN_POINT('Origin',(66.8228361846836,813.192507405306,109.721266728348));
#75407=CARTESIAN_POINT('',(66.8228361846836,811.117293210638,120.413910539517));
#75408=CARTESIAN_POINT('Origin',(66.8228361846836,809.602576808637,119.87855851134));
#75409=CARTESIAN_POINT('',(66.8228361846836,811.783759479706,118.528221617082));
#75410=CARTESIAN_POINT('',(66.8228361846836,814.707223807306,110.256618756526));
#75411=CARTESIAN_POINT('Origin',(66.8228361846836,810.269043077705,117.992869588904));
#75412=CARTESIAN_POINT('Origin',(66.8228361846836,813.192507405306,109.721266728348));
#75413=CARTESIAN_POINT('',(66.8228361846836,811.529090773799,115.928161971837));
#75414=CARTESIAN_POINT('Origin',(66.8228361846836,811.057668543191,115.76154540457));
#75415=CARTESIAN_POINT('',(66.8228361846836,810.073999039246,120.045175078607));
#75416=CARTESIAN_POINT('',(66.8228361846836,813.663929635914,109.887883295615));
#75417=CARTESIAN_POINT('Origin',(66.8228361846836,809.602576808637,119.87855851134));
#75418=CARTESIAN_POINT('Origin',(71.3330336724699,811.913163636806,109.269103352882));
#75419=CARTESIAN_POINT('',(71.3330336724699,810.046845184584,120.035577987596));
#75420=CARTESIAN_POINT('Origin',(71.3330336724699,808.323233040137,119.426395135873));
#75421=CARTESIAN_POINT('',(71.3330336724699,810.713311453652,118.14988906516));
#75422=CARTESIAN_POINT('',(71.3330336724699,813.636775781252,109.878286204604));
#75423=CARTESIAN_POINT('Origin',(71.3330336724699,808.989699309205,117.540706213438));
#75424=CARTESIAN_POINT('Origin',(71.3330336724699,811.913163636806,109.269103352882));
#75425=CARTESIAN_POINT('',(71.3330336724699,810.249747005299,115.47599859637));
#75426=CARTESIAN_POINT('Origin',(71.3330336724699,809.778324774691,115.309382029103));
#75427=CARTESIAN_POINT('',(71.3330336724699,808.794655270746,119.59301170314));
#75428=CARTESIAN_POINT('',(71.3330336724699,812.384585867414,109.435719920149));
#75429=CARTESIAN_POINT('Origin',(71.3330336724699,808.323233040137,119.426395135873));
#75430=CARTESIAN_POINT('Origin',(76.3807474062371,811.096314832155,108.980401346548));
#75431=CARTESIAN_POINT('',(76.3807474062371,809.258583633048,119.756979683786));
#75432=CARTESIAN_POINT('Origin',(76.3807474062371,807.506384235486,119.137693129539));
#75433=CARTESIAN_POINT('',(76.3807474062371,809.925049902116,117.871290761351));
#75434=CARTESIAN_POINT('',(76.3807474062371,812.848514229716,109.599687900795));
#75435=CARTESIAN_POINT('Origin',(76.3807474062371,808.172850504554,117.252004207104));
#75436=CARTESIAN_POINT('Origin',(76.3807474062371,811.096314832155,108.980401346548));
#75437=CARTESIAN_POINT('',(76.3807474062371,809.432898200648,115.187296590036));
#75438=CARTESIAN_POINT('Origin',(76.3807474062371,808.96147597004,115.020680022769));
#75439=CARTESIAN_POINT('',(76.3807474062371,807.977806466095,119.304309696806));
#75440=CARTESIAN_POINT('',(76.3807474062371,811.567737062763,109.147017913815));
#75441=CARTESIAN_POINT('Origin',(76.3807474062371,807.506384235486,119.137693129539));
#75442=CARTESIAN_POINT('Origin',(81.1198190446058,811.516496953853,109.128907925574));
#75443=CARTESIAN_POINT('',(81.1198190446058,809.635808705565,119.890303788143));
#75444=CARTESIAN_POINT('Origin',(81.1198190446058,807.926566357185,119.286199708565));
#75445=CARTESIAN_POINT('',(81.1198190446058,810.302274974634,118.004614865708));
#75446=CARTESIAN_POINT('',(81.1198190446058,813.225739302234,109.733012005152));
#75447=CARTESIAN_POINT('Origin',(81.1198190446058,808.593032626253,117.40051078613));
#75448=CARTESIAN_POINT('Origin',(81.1198190446058,811.516496953853,109.128907925574));
#75449=CARTESIAN_POINT('',(81.1198190446058,809.853080322347,115.335803169062));
#75450=CARTESIAN_POINT('Origin',(81.1198190446058,809.381658091738,115.169186601795));
#75451=CARTESIAN_POINT('',(81.1198190446058,808.397988587793,119.452816275832));
#75452=CARTESIAN_POINT('',(81.1198190446058,811.987919184462,109.295524492841));
#75453=CARTESIAN_POINT('Origin',(81.1198190446058,807.926566357185,119.286199708565));
#75454=CARTESIAN_POINT('Origin',(86.9265466122529,812.440858681645,109.455608636736));
#75455=CARTESIAN_POINT('',(86.9265466122529,810.653143235017,120.249864233226));
#75456=CARTESIAN_POINT('Origin',(86.9265466122529,808.850928084977,119.612900419728));
#75457=CARTESIAN_POINT('',(86.9265466122529,811.319609504086,118.364175310791));
#75458=CARTESIAN_POINT('',(86.9265466122529,814.243073831686,110.092572450235));
#75459=CARTESIAN_POINT('Origin',(86.9265466122529,809.517394354045,117.727211497293));
#75460=CARTESIAN_POINT('Origin',(86.9265466122529,812.440858681645,109.455608636736));
#75461=CARTESIAN_POINT('',(86.9265466122529,810.777442050139,115.662503880225));
#75462=CARTESIAN_POINT('Origin',(86.9265466122529,810.30601981953,115.495887312958));
#75463=CARTESIAN_POINT('',(86.9265466122529,809.322350315585,119.779516986995));
#75464=CARTESIAN_POINT('',(86.9265466122529,812.912280912254,109.622225204003));
#75465=CARTESIAN_POINT('Origin',(86.9265466122529,808.850928084977,119.612900419728));
#75466=CARTESIAN_POINT('Origin',(91.7805001985119,814.40304046294,110.149110070326));
#75467=CARTESIAN_POINT('',(91.7805001985119,812.274208682069,120.822803612335));
#75468=CARTESIAN_POINT('Origin',(91.7805001985119,810.813109866272,120.306401853318));
#75469=CARTESIAN_POINT('',(91.7805001985119,812.940674951138,118.9371146899));
#75470=CARTESIAN_POINT('',(91.7805001985119,815.864139278738,110.665511829344));
#75471=CARTESIAN_POINT('Origin',(91.7805001985119,811.47957613534,118.420712930883));
#75472=CARTESIAN_POINT('Origin',(91.7805001985119,814.40304046294,110.149110070326));
#75473=CARTESIAN_POINT('',(91.7805001985119,812.739623831434,116.356005313815));
#75474=CARTESIAN_POINT('Origin',(91.7805001985119,812.268201600825,116.189388746548));
#75475=CARTESIAN_POINT('',(91.7805001985119,811.28453209688,120.473018420585));
#75476=CARTESIAN_POINT('',(91.7805001985119,814.874462693549,110.315726637593));
#75477=CARTESIAN_POINT('Origin',(91.7805001985119,810.813109866272,120.306401853318));
#75478=CARTESIAN_POINT('Origin',(97.0648498961815,817.361416181959,111.194700148572));
#75479=CARTESIAN_POINT('',(97.0648498961815,814.958867162252,121.771652756922));
#75480=CARTESIAN_POINT('Origin',(97.0648498961815,813.77148558529,121.351991931564));
#75481=CARTESIAN_POINT('',(97.0648499049205,815.624798041961,119.887478656512));
#75482=CARTESIAN_POINT('',(97.0648498961815,818.548797758921,111.614360973931));
#75483=CARTESIAN_POINT('',(96.5454030138814,815.519623009101,119.848602194473));
#75484=CARTESIAN_POINT('Ctrl Pts',(97.0648499136594,815.624798041962,119.887478656512));
#75485=CARTESIAN_POINT('Ctrl Pts',(96.9852132592777,815.624972130868,119.886986095481));
#75486=CARTESIAN_POINT('Ctrl Pts',(96.905592296291,815.617976989133,119.884109694102));
#75487=CARTESIAN_POINT('Ctrl Pts',(96.7297894687742,815.586299535278,119.872302126068));
#75488=CARTESIAN_POINT('Ctrl Pts',(96.6352648323356,815.557985006066,119.862160622211));
#75489=CARTESIAN_POINT('Ctrl Pts',(96.5454030138814,815.519623009101,119.848602194473));
#75490=CARTESIAN_POINT('',(96.0162933379529,813.780308980762,119.233869765697));
#75491=CARTESIAN_POINT('Origin',(97.064849896183,814.437951854359,119.466303009129));
#75492=CARTESIAN_POINT('Ctrl Pts',(96.0162933379527,813.780308980762,119.233869765697));
#75493=CARTESIAN_POINT('Ctrl Pts',(96.0993543987815,813.662581100539,119.192260749403));
#75494=CARTESIAN_POINT('Ctrl Pts',(96.2040847426651,813.559643144079,119.156194878203));
#75495=CARTESIAN_POINT('Ctrl Pts',(96.4487595479483,813.391833502549,119.098584898114));
#75496=CARTESIAN_POINT('Ctrl Pts',(96.5871167127954,813.328924180813,119.077741203267));
#75497=CARTESIAN_POINT('Ctrl Pts',(96.8858441401799,813.250981315707,119.054129029369));
#75498=CARTESIAN_POINT('Ctrl Pts',(97.0441777059448,813.238378867134,119.0522230481));
#75499=CARTESIAN_POINT('Ctrl Pts',(97.3667295240589,813.269543326607,119.069074420728));
#75500=CARTESIAN_POINT('Ctrl Pts',(97.5275285746334,813.316475082749,119.088918537952));
#75501=CARTESIAN_POINT('Ctrl Pts',(97.8192537068948,813.466512421164,119.147921814152));
#75502=CARTESIAN_POINT('Ctrl Pts',(97.9474486505021,813.567900121045,119.186402655788));
#75503=CARTESIAN_POINT('Ctrl Pts',(98.153588381967,813.811367719415,119.276142827353));
#75504=CARTESIAN_POINT('Ctrl Pts',(98.2298798287403,813.950795632586,119.326430787979));
#75505=CARTESIAN_POINT('Ctrl Pts',(98.275401840303,814.1004377142,119.379319362887));
#75506=CARTESIAN_POINT('Ctrl Pts',(98.2920513113524,814.155168632718,119.398663121359));
#75507=CARTESIAN_POINT('Ctrl Pts',(98.304503798061,814.210999226654,119.418262830926));
#75508=CARTESIAN_POINT('Ctrl Pts',(98.3347748503032,814.420606711285,119.491372888756));
#75509=CARTESIAN_POINT('Ctrl Pts',(98.3250670362872,814.576617030885,119.544846964329));
#75510=CARTESIAN_POINT('Ctrl Pts',(98.24328185438,814.876219923119,119.646085298197));
#75511=CARTESIAN_POINT('Ctrl Pts',(98.1722299772469,815.017027505348,119.692925926032));
#75512=CARTESIAN_POINT('Ctrl Pts',(97.9765856973307,815.266646840541,119.775016819367));
#75513=CARTESIAN_POINT('Ctrl Pts',(97.8533472797075,815.372724707415,119.809371151566));
#75514=CARTESIAN_POINT('Ctrl Pts',(97.5793882296128,815.529173164405,119.859346437809));
#75515=CARTESIAN_POINT('Ctrl Pts',(97.4330741404546,815.581153925265,119.875541354133));
#75516=CARTESIAN_POINT('Ctrl Pts',(97.2091835566883,815.618596310145,119.886413968077));
#75517=CARTESIAN_POINT('Ctrl Pts',(97.1370102931382,815.62464029649,119.887924976));
#75518=CARTESIAN_POINT('Ctrl Pts',(97.0648499136594,815.624798041962,119.887478656512));
#75519=CARTESIAN_POINT('Origin',(97.0648498961815,817.361416181959,111.194700148572));
#75520=CARTESIAN_POINT('',(97.0648498961815,815.697999550452,117.401595392061));
#75521=CARTESIAN_POINT('Origin',(97.0648498961815,815.226577319843,117.234978824794));
#75522=CARTESIAN_POINT('',(97.0648498961815,814.242907815899,121.518608498831));
#75523=CARTESIAN_POINT('',(97.0648498961815,817.832838412567,111.361316715839));
#75524=CARTESIAN_POINT('Origin',(97.0648498961815,813.77148558529,121.351991931564));
#75525=CARTESIAN_POINT('Origin',(56.7295477813998,816.813414301827,111.001017742027));
#75526=CARTESIAN_POINT('',(56.7295477813998,814.221846124286,121.511164584375));
#75527=CARTESIAN_POINT('Origin',(56.7295477813998,813.223483705158,121.158309525018));
#75528=CARTESIAN_POINT('',(56.7295477813998,814.888312393354,119.625475661939));
#75529=CARTESIAN_POINT('',(56.7295477813998,817.811776720954,111.353872801383));
#75530=CARTESIAN_POINT('Origin',(56.7295477813998,813.889949974227,119.272620602583));
#75531=CARTESIAN_POINT('Origin',(56.7295477813998,816.813414301827,111.001017742027));
#75532=CARTESIAN_POINT('',(56.7295477813998,815.149997670321,117.207912985515));
#75533=CARTESIAN_POINT('Origin',(56.7295477813998,814.678575439712,117.041296418248));
#75534=CARTESIAN_POINT('',(56.7295477813998,813.694905935767,121.324926092285));
#75535=CARTESIAN_POINT('',(56.7295477813998,817.284836532436,111.167634309294));
#75536=CARTESIAN_POINT('Origin',(56.7295477813998,813.223483705158,121.158309525018));
#75537=CARTESIAN_POINT('Origin',(59.4040294524033,813.777068724584,109.927870477708));
#75538=CARTESIAN_POINT('',(59.4040294524033,811.408907407298,120.51697686363));
#75539=CARTESIAN_POINT('Origin',(59.4040294524033,810.187138127915,120.085162260699));
#75540=CARTESIAN_POINT('',(59.4040294524033,812.075373676366,118.631287941195));
#75541=CARTESIAN_POINT('',(59.4040294524033,814.998838003967,110.359685080639));
#75542=CARTESIAN_POINT('Origin',(59.4040294524033,810.853604396984,118.199473338264));
#75543=CARTESIAN_POINT('Origin',(59.4040294524033,813.777068724584,109.927870477708));
#75544=CARTESIAN_POINT('',(59.4040294524033,812.113652093078,116.134765721196));
#75545=CARTESIAN_POINT('Origin',(59.4040294524033,811.642229862469,115.968149153929));
#75546=CARTESIAN_POINT('',(59.4040294524033,810.658560358524,120.251778827966));
#75547=CARTESIAN_POINT('',(59.4040294524033,814.248490955193,110.094487044975));
#75548=CARTESIAN_POINT('Origin',(59.4040294524033,810.187138127915,120.085162260699));
#75549=CARTESIAN_POINT('Origin',(62.9637740385176,810.811071687506,108.879586767786));
#75550=CARTESIAN_POINT('',(62.9637740385176,808.735857492838,119.572230578955));
#75551=CARTESIAN_POINT('Origin',(62.9637740385176,807.221141090837,119.036878550777));
#75552=CARTESIAN_POINT('',(62.9637740385176,809.402323761906,117.68654165652));
#75553=CARTESIAN_POINT('',(62.9637740385176,812.325788089506,109.414938795964));
#75554=CARTESIAN_POINT('Origin',(62.9637740385176,807.887607359905,117.151189628342));
#75555=CARTESIAN_POINT('Origin',(62.9637740385176,810.811071687506,108.879586767786));
#75556=CARTESIAN_POINT('',(62.9637740385176,809.147655055999,115.086482011274));
#75557=CARTESIAN_POINT('Origin',(62.9637740385176,808.67623282539,114.919865444007));
#75558=CARTESIAN_POINT('',(62.9637740385176,807.692563321446,119.203495118044));
#75559=CARTESIAN_POINT('',(62.9637740385176,811.282493918114,109.046203335053));
#75560=CARTESIAN_POINT('Origin',(62.9637740385176,807.221141090837,119.036878550777));
#75561=CARTESIAN_POINT('Origin',(67.0932979315339,808.675557915266,108.124823943761));
#75562=CARTESIAN_POINT('',(67.0932979315339,806.809239463044,118.891298578475));
#75563=CARTESIAN_POINT('Origin',(67.0932979315339,805.085627318597,118.282115726753));
#75564=CARTESIAN_POINT('',(67.0932979315339,807.475705732112,117.00560965604));
#75565=CARTESIAN_POINT('',(67.0932979315339,810.399170059713,108.734006795484));
#75566=CARTESIAN_POINT('Origin',(67.0932979315339,805.752093587666,116.396426804318));
#75567=CARTESIAN_POINT('Origin',(67.0932979315339,808.675557915266,108.124823943761));
#75568=CARTESIAN_POINT('',(67.0932979315339,807.01214128376,114.33171918725));
#75569=CARTESIAN_POINT('Origin',(67.0932979315339,806.540719053151,114.165102619983));
#75570=CARTESIAN_POINT('',(67.0932979315339,805.557049549206,118.44873229402));
#75571=CARTESIAN_POINT('',(67.0932979315339,809.146980145875,108.291440511028));
#75572=CARTESIAN_POINT('Origin',(67.0932979315339,805.085627318597,118.282115726753));
#75573=CARTESIAN_POINT('Origin',(71.8505792968298,806.887064040059,107.49270969306));
#75574=CARTESIAN_POINT('',(71.8505792968298,805.049332840952,118.269288030299));
#75575=CARTESIAN_POINT('Origin',(71.8505792968298,803.29713344339,117.650001476052));
#75576=CARTESIAN_POINT('',(71.8505792968298,805.71579911002,116.383599107863));
#75577=CARTESIAN_POINT('',(71.8505792968298,808.63926343762,108.111996247307));
#75578=CARTESIAN_POINT('Origin',(71.8505792968298,803.963599712459,115.764312553616));
#75579=CARTESIAN_POINT('Origin',(71.8505792968298,806.887064040059,107.49270969306));
#75580=CARTESIAN_POINT('',(71.8505792968298,805.223647408553,113.699604936548));
#75581=CARTESIAN_POINT('Origin',(71.8505792968298,804.752225177944,113.532988369281));
#75582=CARTESIAN_POINT('',(71.8505792968298,803.768555673999,117.816618043319));
#75583=CARTESIAN_POINT('',(71.8505792968298,807.358486270668,107.659326260327));
#75584=CARTESIAN_POINT('Origin',(71.8505792968298,803.29713344339,117.650001476052));
#75585=CARTESIAN_POINT('Origin',(76.5787474636786,806.369071609341,107.309633641332));
#75586=CARTESIAN_POINT('',(76.5787474636786,804.488383361053,118.071029503902));
#75587=CARTESIAN_POINT('Origin',(76.5787474636786,802.779141012673,117.466925424324));
#75588=CARTESIAN_POINT('',(76.5787474636786,805.154849630121,116.185340581467));
#75589=CARTESIAN_POINT('',(76.5787474636786,808.078313957722,107.913737720911));
#75590=CARTESIAN_POINT('Origin',(76.5787474636786,803.445607281741,115.581236501889));
#75591=CARTESIAN_POINT('Origin',(76.5787474636786,806.369071609341,107.309633641332));
#75592=CARTESIAN_POINT('',(76.5787474636786,804.705654977835,113.516528884821));
#75593=CARTESIAN_POINT('Origin',(76.5787474636786,804.234232747226,113.349912317554));
#75594=CARTESIAN_POINT('',(76.5787474636786,803.250563243281,117.633541991591));
#75595=CARTESIAN_POINT('',(76.5787474636786,806.84049383995,107.4762502086));
#75596=CARTESIAN_POINT('Origin',(76.5787474636786,802.779141012673,117.466925424324));
#75597=CARTESIAN_POINT('Origin',(82.4624200661915,806.134950381925,107.226887277874));
#75598=CARTESIAN_POINT('',(82.4624200661915,804.347234935297,118.021142874364));
#75599=CARTESIAN_POINT('Origin',(82.4624200661915,802.545019785257,117.384179060865));
#75600=CARTESIAN_POINT('',(82.4624200661915,805.013701204366,116.135453951928));
#75601=CARTESIAN_POINT('',(82.4624200661915,807.937165531966,107.863851091372));
#75602=CARTESIAN_POINT('Origin',(82.4624200661915,803.211486054325,115.49849013843));
#75603=CARTESIAN_POINT('Origin',(82.4624200661915,806.134950381925,107.226887277874));
#75604=CARTESIAN_POINT('',(82.4624200661915,804.471533750419,113.433782521362));
#75605=CARTESIAN_POINT('Origin',(82.4624200661915,804.00011151981,113.267165954095));
#75606=CARTESIAN_POINT('',(82.4624200661915,803.016442015866,117.550795628132));
#75607=CARTESIAN_POINT('',(82.4624200661915,806.606372612534,107.393503845141));
#75608=CARTESIAN_POINT('Origin',(82.4624200661915,802.545019785257,117.384179060865));
#75609=CARTESIAN_POINT('Origin',(87.6429943530164,807.102741095736,107.568937262152));
#75610=CARTESIAN_POINT('',(87.6429943530164,804.973909314865,118.242630804161));
#75611=CARTESIAN_POINT('Origin',(87.6429943530164,803.512810499067,117.726229045143));
#75612=CARTESIAN_POINT('',(87.6429943530164,805.640375583933,116.356941881725));
#75613=CARTESIAN_POINT('',(87.6429943530164,808.563839911534,108.085339021169));
#75614=CARTESIAN_POINT('Origin',(87.6429943530164,804.179276768136,115.840540122708));
#75615=CARTESIAN_POINT('Origin',(87.6429943530164,807.102741095736,107.568937262152));
#75616=CARTESIAN_POINT('',(87.6429943530164,805.43932446423,113.77583250564));
#75617=CARTESIAN_POINT('Origin',(87.6429943530164,804.967902233621,113.609215938373));
#75618=CARTESIAN_POINT('',(87.6429943530164,803.984232729676,117.89284561241));
#75619=CARTESIAN_POINT('',(87.6429943530164,807.574163326345,107.735553829419));
#75620=CARTESIAN_POINT('Origin',(87.6429943530164,803.512810499067,117.726229045143));
#75621=CARTESIAN_POINT('Origin',(93.4642356337025,808.960586664488,108.225562747925));
#75622=CARTESIAN_POINT('',(93.4642356337025,806.558037644782,118.802515356275));
#75623=CARTESIAN_POINT('Origin',(93.4642356337025,805.37065606782,118.382854530917));
#75624=CARTESIAN_POINT('',(93.4642356337339,807.224380473639,116.917175693584));
#75625=CARTESIAN_POINT('',(93.4642356337025,810.14796824145,108.645223573284));
#75626=CARTESIAN_POINT('',(93.1946650219305,807.19698271569,116.907099511207));
#75627=CARTESIAN_POINT('Ctrl Pts',(93.4642356337653,807.224380473639,116.917175693584));
#75628=CARTESIAN_POINT('Ctrl Pts',(93.3734396015083,807.224468486999,116.916926670016));
#75629=CARTESIAN_POINT('Ctrl Pts',(93.2830615082368,807.215246128468,116.913554419244));
#75630=CARTESIAN_POINT('Ctrl Pts',(93.1946650260966,807.196982716551,116.907099511511));
#75631=CARTESIAN_POINT('',(92.2935721935075,805.599397387795,116.342458800678));
#75632=CARTESIAN_POINT('Origin',(93.464235633704,806.037122336889,116.497165608482));
#75633=CARTESIAN_POINT('Ctrl Pts',(92.2935721935074,805.599397387795,116.342458800678));
#75634=CARTESIAN_POINT('Ctrl Pts',(92.348857364355,805.46795981851,116.296004316392));
#75635=CARTESIAN_POINT('Ctrl Pts',(92.4286215833972,805.346739014297,116.25347666818));
#75636=CARTESIAN_POINT('Ctrl Pts',(92.6310628079813,805.134621539668,116.180206800681));
#75637=CARTESIAN_POINT('Ctrl Pts',(92.752620408957,805.045955458401,116.150259795513));
#75638=CARTESIAN_POINT('Ctrl Pts',(93.0279049875055,804.9111297565,116.106543302413));
#75639=CARTESIAN_POINT('Ctrl Pts',(93.1801760950964,804.867747333362,116.093758636667));
#75640=CARTESIAN_POINT('Ctrl Pts',(93.5029560155274,804.834961388344,116.088007772531));
#75641=CARTESIAN_POINT('Ctrl Pts',(93.6708160387134,804.849324033979,116.096340864099));
#75642=CARTESIAN_POINT('Ctrl Pts',(93.9896657820001,804.93885526688,116.133959235335));
#75643=CARTESIAN_POINT('Ctrl Pts',(94.1376002963257,805.01287938076,116.162768859809));
#75644=CARTESIAN_POINT('Ctrl Pts',(94.3931794145417,805.210592051185,116.236337691681));
#75645=CARTESIAN_POINT('Ctrl Pts',(94.4986196429727,805.33201091034,116.280260643265));
#75646=CARTESIAN_POINT('Ctrl Pts',(94.5761452676589,805.46945934698,116.328839571458));
#75647=CARTESIAN_POINT('Ctrl Pts',(94.6044999163115,805.519730494676,116.34660709602));
#75648=CARTESIAN_POINT('Ctrl Pts',(94.6289825954745,805.571900926472,116.364913180443));
#75649=CARTESIAN_POINT('Ctrl Pts',(94.7047464583719,805.771000674835,116.434309448738));
#75650=CARTESIAN_POINT('Ctrl Pts',(94.7295380823744,805.925516234931,116.487255225725));
#75651=CARTESIAN_POINT('Ctrl Pts',(94.7152848763623,806.234636238113,116.591857228622));
#75652=CARTESIAN_POINT('Ctrl Pts',(94.6766331985493,806.38631510761,116.642540137217));
#75653=CARTESIAN_POINT('Ctrl Pts',(94.5398841996231,806.66887360163,116.736272843806));
#75654=CARTESIAN_POINT('Ctrl Pts',(94.4425132835629,806.796813179746,116.778353844466));
#75655=CARTESIAN_POINT('Ctrl Pts',(94.2086716755231,807.003583131169,116.846114449512));
#75656=CARTESIAN_POINT('Ctrl Pts',(94.0768666383506,807.083124648092,116.872050269571));
#75657=CARTESIAN_POINT('Ctrl Pts',(93.7917530987918,807.191988806257,116.907335091828));
#75658=CARTESIAN_POINT('Ctrl Pts',(93.641165502188,807.221165990394,116.916640140119));
#75659=CARTESIAN_POINT('Ctrl Pts',(93.4805933409972,807.224289105858,116.91719520878));
#75660=CARTESIAN_POINT('Ctrl Pts',(93.4724127919216,807.224372547091,116.917198120831));
#75661=CARTESIAN_POINT('Ctrl Pts',(93.4642356337653,807.224380473639,116.917175693584));
#75662=CARTESIAN_POINT('Origin',(93.4642356337025,808.960586664488,108.225562747925));
#75663=CARTESIAN_POINT('',(93.4642356337025,807.297170032982,114.432457991414));
#75664=CARTESIAN_POINT('Origin',(93.4642356337025,806.825747802373,114.265841424147));
#75665=CARTESIAN_POINT('',(93.4642356337025,805.842078298429,118.549471098184));
#75666=CARTESIAN_POINT('',(93.4642356337025,809.432008895097,108.392179315193));
#75667=CARTESIAN_POINT('Origin',(93.4642356337025,805.37065606782,118.382854530917));
#75668=CARTESIAN_POINT('Origin',(53.889513810455,816.331424117056,110.830666102183));
#75669=CARTESIAN_POINT('',(53.889513810455,813.739855939514,121.340812944531));
#75670=CARTESIAN_POINT('Origin',(53.889513810455,812.741493520387,120.987957885174));
#75671=CARTESIAN_POINT('',(53.889513810455,814.406322208583,119.455124022096));
#75672=CARTESIAN_POINT('',(53.889513810455,817.329786536183,111.183521161539));
#75673=CARTESIAN_POINT('Origin',(53.889513810455,813.407959789456,119.102268962739));
#75674=CARTESIAN_POINT('Origin',(53.889513810455,816.331424117056,110.830666102183));
#75675=CARTESIAN_POINT('',(53.889513810455,814.668007485549,117.037561345671));
#75676=CARTESIAN_POINT('Origin',(53.889513810455,814.196585254941,116.870944778404));
#75677=CARTESIAN_POINT('',(53.889513810455,813.212915750996,121.154574452441));
#75678=CARTESIAN_POINT('',(53.889513810455,816.802846347665,110.99728266945));
#75679=CARTESIAN_POINT('Origin',(53.889513810455,812.741493520387,120.987957885174));
#75680=CARTESIAN_POINT('Origin',(55.83599078591,812.837155650029,109.595673394406));
#75681=CARTESIAN_POINT('',(55.83599078591,810.468994332743,120.184779780329));
#75682=CARTESIAN_POINT('Origin',(55.83599078591,809.247225053361,119.752965177398));
#75683=CARTESIAN_POINT('',(55.83599078591,811.135460601812,118.299090857894));
#75684=CARTESIAN_POINT('',(55.83599078591,814.058924929412,110.027487997337));
#75685=CARTESIAN_POINT('Origin',(55.83599078591,809.913691322429,117.867276254963));
#75686=CARTESIAN_POINT('Origin',(55.83599078591,812.837155650029,109.595673394406));
#75687=CARTESIAN_POINT('',(55.83599078591,811.173739018523,115.802568637895));
#75688=CARTESIAN_POINT('Origin',(55.83599078591,810.702316787914,115.635952070628));
#75689=CARTESIAN_POINT('',(55.83599078591,809.71864728397,119.919581744665));
#75690=CARTESIAN_POINT('',(55.83599078591,813.308577880638,109.762289961674));
#75691=CARTESIAN_POINT('Origin',(55.83599078591,809.247225053361,119.752965177398));
#75692=CARTESIAN_POINT('Origin',(58.6638984918342,809.238161778248,108.323667185117));
#75693=CARTESIAN_POINT('',(58.6638984918342,807.16294758358,119.016310996286));
#75694=CARTESIAN_POINT('Origin',(58.6638984918342,805.64823118158,118.480958968108));
#75695=CARTESIAN_POINT('',(58.6638984918342,807.829413852648,117.130622073851));
#75696=CARTESIAN_POINT('',(58.6638984918342,810.752878180249,108.859019213295));
#75697=CARTESIAN_POINT('Origin',(58.6638984918342,806.314697450648,116.595270045673));
#75698=CARTESIAN_POINT('Origin',(58.6638984918342,809.238161778248,108.323667185117));
#75699=CARTESIAN_POINT('',(58.6638984918342,807.574745146742,114.530562428605));
#75700=CARTESIAN_POINT('Origin',(58.6638984918342,807.103322916133,114.363945861338));
#75701=CARTESIAN_POINT('',(58.6638984918342,806.119653412188,118.647575535375));
#75702=CARTESIAN_POINT('',(58.6638984918342,809.709584008857,108.490283752384));
#75703=CARTESIAN_POINT('Origin',(58.6638984918342,805.64823118158,118.480958968108));
#75704=CARTESIAN_POINT('Origin',(62.2322687803016,806.339810201448,107.299291669698));
#75705=CARTESIAN_POINT('',(62.2322687803016,804.473491749226,118.065766304412));
#75706=CARTESIAN_POINT('Origin',(62.2322687803016,802.749879604779,117.45658345269));
#75707=CARTESIAN_POINT('',(62.2322687803016,805.139958018294,116.180077381977));
#75708=CARTESIAN_POINT('',(62.2322687803016,808.063422345894,107.908474521421));
#75709=CARTESIAN_POINT('Origin',(62.2322687803016,803.416345873847,115.570894530255));
#75710=CARTESIAN_POINT('Origin',(62.2322687803016,806.339810201448,107.299291669698));
#75711=CARTESIAN_POINT('',(62.2322687803016,804.676393569941,113.506186913187));
#75712=CARTESIAN_POINT('Origin',(62.2322687803016,804.204971339333,113.33957034592));
#75713=CARTESIAN_POINT('',(62.2322687803016,803.221301835388,117.623200019957));
#75714=CARTESIAN_POINT('',(62.2322687803016,806.811232432056,107.465908236965));
#75715=CARTESIAN_POINT('Origin',(62.2322687803016,802.749879604779,117.45658345269));
#75716=CARTESIAN_POINT('Origin',(66.491201753494,803.657837020177,106.351391600606));
#75717=CARTESIAN_POINT('',(66.491201753494,801.82010582107,117.127969937845));
#75718=CARTESIAN_POINT('Origin',(66.491201753494,800.067906423509,116.508683383598));
#75719=CARTESIAN_POINT('',(66.491201753494,802.486572090139,115.242281015409));
#75720=CARTESIAN_POINT('',(66.491201753494,805.410036417739,106.970678154853));
#75721=CARTESIAN_POINT('Origin',(66.491201753494,800.734372692577,114.622994461162));
#75722=CARTESIAN_POINT('Origin',(66.491201753494,803.657837020177,106.351391600606));
#75723=CARTESIAN_POINT('',(66.491201753494,801.994420388671,112.558286844094));
#75724=CARTESIAN_POINT('Origin',(66.491201753494,801.522998158062,112.391670276827));
#75725=CARTESIAN_POINT('',(66.491201753494,800.539328654118,116.675299950865));
#75726=CARTESIAN_POINT('',(66.491201753494,804.129259250786,106.518008167873));
#75727=CARTESIAN_POINT('Origin',(66.491201753494,800.067906423509,116.508683383598));
#75728=CARTESIAN_POINT('Origin',(76.705295723319,800.841936830322,105.356157195146));
#75729=CARTESIAN_POINT('',(76.705295723319,799.054221383694,116.150412791636));
#75730=CARTESIAN_POINT('Origin',(76.705295723319,797.252006233653,115.513448978138));
#75731=CARTESIAN_POINT('',(76.705295723319,799.720687652762,114.264723869201));
#75732=CARTESIAN_POINT('',(76.705295723319,802.644151980362,105.993121008645));
#75733=CARTESIAN_POINT('Origin',(76.705295723319,797.918472502722,113.627760055703));
#75734=CARTESIAN_POINT('Origin',(76.705295723319,800.841936830322,105.356157195146));
#75735=CARTESIAN_POINT('',(76.705295723319,799.178520198815,111.563052438635));
#75736=CARTESIAN_POINT('Origin',(76.705295723319,798.707097968207,111.396435871368));
#75737=CARTESIAN_POINT('',(76.705295723319,797.723428464262,115.680065545405));
#75738=CARTESIAN_POINT('',(76.705295723319,801.313359060931,105.522773762413));
#75739=CARTESIAN_POINT('Origin',(76.705295723319,797.252006233653,115.513448978138));
#75740=CARTESIAN_POINT('Origin',(81.986074755222,800.773039378479,105.331806504462));
#75741=CARTESIAN_POINT('',(81.986074755222,798.644207597608,116.00550004647));
#75742=CARTESIAN_POINT('Origin',(81.986074755222,797.183108781811,115.489098287453));
#75743=CARTESIAN_POINT('',(81.986074755222,799.310673866677,114.119811124035));
#75744=CARTESIAN_POINT('',(81.986074755222,802.234138194277,105.848208263479));
#75745=CARTESIAN_POINT('Origin',(81.986074755222,797.849575050879,113.603409365018));
#75746=CARTESIAN_POINT('Origin',(81.986074755222,800.773039378479,105.331806504462));
#75747=CARTESIAN_POINT('',(81.986074755222,799.109622746973,111.53870174795));
#75748=CARTESIAN_POINT('Origin',(81.986074755222,798.638200516364,111.372085180683));
#75749=CARTESIAN_POINT('',(81.986074755222,797.65453101242,115.65571485472));
#75750=CARTESIAN_POINT('',(81.986074755222,801.244461609088,105.498423071729));
#75751=CARTESIAN_POINT('Origin',(81.986074755222,797.183108781811,115.489098287453));
#75752=CARTESIAN_POINT('Origin',(88.0897914415438,801.449158030679,105.570769713196));
#75753=CARTESIAN_POINT('',(88.0897914415438,799.046609010973,116.147722321546));
#75754=CARTESIAN_POINT('Origin',(88.0897914415438,797.85922743401,115.728061496187));
#75755=CARTESIAN_POINT('',(88.0897914415438,799.713075280041,114.26203339911));
#75756=CARTESIAN_POINT('',(88.0897914415438,802.636539607641,105.990430538554));
#75757=CARTESIAN_POINT('',(88.0818786295781,799.713051841759,114.262025115228));
#75758=CARTESIAN_POINT('Ctrl Pts',(88.0897914415439,799.713075189938,114.262033654047));
#75759=CARTESIAN_POINT('Ctrl Pts',(88.0871539049629,799.71307525016,114.262033483656));
#75760=CARTESIAN_POINT('Ctrl Pts',(88.0845162887099,799.713067467756,114.262030637985));
#75761=CARTESIAN_POINT('Ctrl Pts',(88.0818786320383,799.713051841773,114.262025115233));
#75762=CARTESIAN_POINT('',(86.8481847291855,798.327017359201,113.772153631443));
#75763=CARTESIAN_POINT('Origin',(88.0897914415456,798.525693703079,113.842372573752));
#75764=CARTESIAN_POINT('Ctrl Pts',(86.8481847291853,798.327017359201,113.772153631443));
#75765=CARTESIAN_POINT('Ctrl Pts',(86.8732777827967,798.187614553342,113.722883963041));
#75766=CARTESIAN_POINT('Ctrl Pts',(86.9245897978729,798.053404494626,113.675765472785));
#75767=CARTESIAN_POINT('Ctrl Pts',(87.0759497888209,797.806226400021,113.590103995881));
#75768=CARTESIAN_POINT('Ctrl Pts',(87.175395175464,797.695659597608,113.552416534831));
#75769=CARTESIAN_POINT('Ctrl Pts',(87.4152056481323,797.509789549195,113.490659242545));
#75770=CARTESIAN_POINT('Ctrl Pts',(87.5547593194701,797.437488181679,113.467653643358));
#75771=CARTESIAN_POINT('Ctrl Pts',(87.8636603108241,797.342104587411,113.439778651934));
#75772=CARTESIAN_POINT('Ctrl Pts',(88.0312450181269,797.323225684679,113.436363055552));
#75773=CARTESIAN_POINT('Ctrl Pts',(88.3632841086485,797.348255821918,113.451184557132));
#75774=CARTESIAN_POINT('Ctrl Pts',(88.5244927455475,797.391644793613,113.469166685792));
#75775=CARTESIAN_POINT('Ctrl Pts',(88.8183412166434,797.53491086785,113.523492248324));
#75776=CARTESIAN_POINT('Ctrl Pts',(88.9483219827927,797.633000225401,113.559169764669));
#75777=CARTESIAN_POINT('Ctrl Pts',(89.0544629787952,797.752247860836,113.601315913876));
#75778=CARTESIAN_POINT('Ctrl Pts',(89.0932835708438,797.795862147326,113.616730678448));
#75779=CARTESIAN_POINT('Ctrl Pts',(89.1287264319009,797.842094141095,113.63293791794));
#75780=CARTESIAN_POINT('Ctrl Pts',(89.2466718610917,798.021997890187,113.695549670579));
#75781=CARTESIAN_POINT('Ctrl Pts',(89.304879410181,798.168288485704,113.745588466786));
#75782=CARTESIAN_POINT('Ctrl Pts',(89.3587811135626,798.47347944388,113.848801812235));
#75783=CARTESIAN_POINT('Ctrl Pts',(89.3542188988618,798.629440678153,113.900998253439));
#75784=CARTESIAN_POINT('Ctrl Pts',(89.2823417683743,798.932673384468,114.002037926182));
#75785=CARTESIAN_POINT('Ctrl Pts',(89.2150939301468,799.0769261784,114.049884569284));
#75786=CARTESIAN_POINT('Ctrl Pts',(89.0315897645301,799.325053821448,114.132262381922));
#75787=CARTESIAN_POINT('Ctrl Pts',(88.9200542919387,799.428709639743,114.166721012014));
#75788=CARTESIAN_POINT('Ctrl Pts',(88.6649562731285,799.591107113575,114.220926319372));
#75789=CARTESIAN_POINT('Ctrl Pts',(88.5240236153877,799.649173064636,114.240441635371));
#75790=CARTESIAN_POINT('Ctrl Pts',(88.2816857573755,799.702680388928,114.258502734602));
#75791=CARTESIAN_POINT('Ctrl Pts',(88.1857913741578,799.713072997999,114.262039855884));
#75792=CARTESIAN_POINT('Ctrl Pts',(88.0897914415439,799.713075189938,114.262033654047));
#75793=CARTESIAN_POINT('Origin',(88.0897914415438,801.449158030679,105.570769713196));
#75794=CARTESIAN_POINT('',(88.0897914415438,799.785741399173,111.777664956684));
#75795=CARTESIAN_POINT('Origin',(88.0897914415438,799.314319168564,111.611048389417));
#75796=CARTESIAN_POINT('',(88.0897914415438,798.330649664619,115.894678063454));
#75797=CARTESIAN_POINT('',(88.0897914415438,801.920580261288,105.737386280463));
#75798=CARTESIAN_POINT('Origin',(88.0897914415438,797.85922743401,115.728061496187));
#75799=CARTESIAN_POINT('Origin',(51.005255154091,816.416693850066,110.860803311002));
#75800=CARTESIAN_POINT('',(51.005255154091,813.825125672524,121.37095015335));
#75801=CARTESIAN_POINT('Origin',(51.005255154091,812.826763253397,121.018095093994));
#75802=CARTESIAN_POINT('',(51.005255154091,814.491591941593,119.485261230915));
#75803=CARTESIAN_POINT('',(51.005255154091,817.415056269193,111.213658370359));
#75804=CARTESIAN_POINT('Origin',(51.005255154091,813.493229522466,119.132406171558));
#75805=CARTESIAN_POINT('Origin',(51.005255154091,816.416693850066,110.860803311002));
#75806=CARTESIAN_POINT('',(51.005255154091,814.75327721856,117.067698554491));
#75807=CARTESIAN_POINT('Origin',(51.005255154091,814.281854987951,116.901081987224));
#75808=CARTESIAN_POINT('',(51.005255154091,813.298185484006,121.184711661261));
#75809=CARTESIAN_POINT('',(51.005255154091,816.888116080675,111.027419878269));
#75810=CARTESIAN_POINT('Origin',(51.005255154091,812.826763253397,121.018095093994));
#75811=CARTESIAN_POINT('Origin',(52.1386570499375,812.617218792626,109.51794026725));
#75812=CARTESIAN_POINT('',(52.1386570499375,810.24905747534,120.107046653173));
#75813=CARTESIAN_POINT('Origin',(52.1386570499375,809.027288195957,119.675232050242));
#75814=CARTESIAN_POINT('',(52.1386570499375,810.915523744408,118.221357730738));
#75815=CARTESIAN_POINT('',(52.1386570499375,813.838988072009,109.949754870181));
#75816=CARTESIAN_POINT('Origin',(52.1386570499375,809.693754465026,117.789543127807));
#75817=CARTESIAN_POINT('Origin',(52.1386570499375,812.617218792626,109.51794026725));
#75818=CARTESIAN_POINT('',(52.1386570499375,810.95380216112,115.724835510739));
#75819=CARTESIAN_POINT('Origin',(52.1386570499375,810.482379930511,115.558218943472));
#75820=CARTESIAN_POINT('',(52.1386570499375,809.498710426566,119.841848617509));
#75821=CARTESIAN_POINT('',(52.1386570499375,813.088641023235,109.684556834518));
#75822=CARTESIAN_POINT('Origin',(52.1386570499375,809.027288195957,119.675232050242));
#75823=CARTESIAN_POINT('Origin',(54.1111347391161,808.542521388227,108.077804333703));
#75824=CARTESIAN_POINT('',(54.1111347391161,806.467307193559,118.770448144872));
#75825=CARTESIAN_POINT('Origin',(54.1111347391161,804.952590791559,118.235096116694));
#75826=CARTESIAN_POINT('',(54.1111347391161,807.133773462628,116.884759222436));
#75827=CARTESIAN_POINT('',(54.1111347391161,810.057237790228,108.61315636188));
#75828=CARTESIAN_POINT('Origin',(54.1111347391161,805.619057060627,116.349407194259));
#75829=CARTESIAN_POINT('Origin',(54.1111347391161,808.542521388227,108.077804333703));
#75830=CARTESIAN_POINT('',(54.1111347391161,806.879104756721,114.284699577191));
#75831=CARTESIAN_POINT('Origin',(54.1111347391161,806.407682526112,114.118083009924));
#75832=CARTESIAN_POINT('',(54.1111347391161,805.424013022167,118.401712683961));
#75833=CARTESIAN_POINT('',(54.1111347391161,809.013943618836,108.24442090097));
#75834=CARTESIAN_POINT('Origin',(54.1111347391161,804.952590791559,118.235096116694));
#75835=CARTESIAN_POINT('Origin',(56.9623965184881,805.008003878606,106.828586252413));
#75836=CARTESIAN_POINT('',(56.9623965184881,803.141685426384,117.595060887126));
#75837=CARTESIAN_POINT('Origin',(56.9623965184881,801.418073281937,116.985878035404));
#75838=CARTESIAN_POINT('',(56.9623965184881,803.808151695452,115.709371964691));
#75839=CARTESIAN_POINT('',(56.9623965184881,806.731616023053,107.437769104135));
#75840=CARTESIAN_POINT('Origin',(56.9623965184881,802.084539551006,115.100189112969));
#75841=CARTESIAN_POINT('Origin',(56.9623965184881,805.008003878606,106.828586252413));
#75842=CARTESIAN_POINT('',(56.9623965184881,803.3445872471,113.035481495901));
#75843=CARTESIAN_POINT('Origin',(56.9623965184881,802.873165016491,112.868864928634));
#75844=CARTESIAN_POINT('',(56.9623965184881,801.889495512546,117.152494602671));
#75845=CARTESIAN_POINT('',(56.9623965184881,805.479426109215,106.99520281968));
#75846=CARTESIAN_POINT('Origin',(56.9623965184881,801.418073281937,116.985878035404));
#75847=CARTESIAN_POINT('Origin',(60.5368452920206,801.549766488829,105.606328146478));
#75848=CARTESIAN_POINT('',(60.5368452920206,799.712035289722,116.382906483716));
#75849=CARTESIAN_POINT('Origin',(60.5368452920206,797.959835892161,115.763619929469));
#75850=CARTESIAN_POINT('',(60.5368452920206,800.37850155879,114.497217561281));
#75851=CARTESIAN_POINT('',(60.5368452920206,803.301965886391,106.225614700725));
#75852=CARTESIAN_POINT('Origin',(60.5368452920206,798.626302161229,113.877931007034));
#75853=CARTESIAN_POINT('Origin',(60.5368452920206,801.549766488829,105.606328146478));
#75854=CARTESIAN_POINT('',(60.5368452920206,799.886349857323,111.813223389966));
#75855=CARTESIAN_POINT('Origin',(60.5368452920206,799.414927626714,111.646606822699));
#75856=CARTESIAN_POINT('',(60.5368452920206,798.431258122769,115.930236496736));
#75857=CARTESIAN_POINT('',(60.5368452920206,802.021188719438,105.772944713745));
#75858=CARTESIAN_POINT('Origin',(60.5368452920206,797.959835892161,115.763619929469));
#75859=CARTESIAN_POINT('Origin',(64.6327834569077,799.263354525339,104.798232795898));
#75860=CARTESIAN_POINT('',(64.6327834569077,797.382666277051,115.559628658467));
#75861=CARTESIAN_POINT('Origin',(64.6327834569077,795.67342392867,114.955524578889));
#75862=CARTESIAN_POINT('',(64.6327834569077,798.049132546119,113.673939736032));
#75863=CARTESIAN_POINT('',(64.6327834569077,800.972596873719,105.402336875476));
#75864=CARTESIAN_POINT('Origin',(64.6327834569077,796.339890197738,113.069835656454));
#75865=CARTESIAN_POINT('Origin',(64.6327834569077,799.263354525339,104.798232795898));
#75866=CARTESIAN_POINT('',(64.6327834569077,797.599937893832,111.005128039386));
#75867=CARTESIAN_POINT('Origin',(64.6327834569077,797.128515663224,110.838511472119));
#75868=CARTESIAN_POINT('',(64.6327834569077,796.144846159279,115.122141146156));
#75869=CARTESIAN_POINT('',(64.6327834569077,799.734776755947,104.964849363165));
#75870=CARTESIAN_POINT('Origin',(64.6327834569077,795.67342392867,114.955524578889));
#75871=CARTESIAN_POINT('Origin',(69.9067875431667,796.793148117736,103.925178269928));
#75872=CARTESIAN_POINT('',(69.9067875431667,795.005432671108,114.719433866418));
#75873=CARTESIAN_POINT('Origin',(69.9067875431667,793.203217521068,114.082470052919));
#75874=CARTESIAN_POINT('',(69.9067875431667,795.671898940177,112.833744943982));
#75875=CARTESIAN_POINT('',(69.9067875431667,798.595363267777,104.562142083426));
#75876=CARTESIAN_POINT('Origin',(69.9067875431667,793.869683790136,112.196781130484));
#75877=CARTESIAN_POINT('Origin',(69.9067875431667,796.793148117736,103.925178269928));
#75878=CARTESIAN_POINT('',(69.9067875431667,795.12973148623,110.132073513416));
#75879=CARTESIAN_POINT('Origin',(69.9067875431667,794.658309255621,109.965456946149));
#75880=CARTESIAN_POINT('',(69.9067875431667,793.674639751676,114.249086620186));
#75881=CARTESIAN_POINT('',(69.9067875431667,797.264570348345,104.091794837195));
#75882=CARTESIAN_POINT('Origin',(69.9067875431667,793.203217521068,114.082470052919));
#75883=CARTESIAN_POINT('Origin',(75.0569759364645,795.690573649493,103.535491146311));
#75884=CARTESIAN_POINT('',(75.0569759364645,793.561741868622,114.209184688319));
#75885=CARTESIAN_POINT('Origin',(75.0569759364645,792.100643052824,113.692782929302));
#75886=CARTESIAN_POINT('',(75.0569759364645,794.22820813769,112.323495765884));
#75887=CARTESIAN_POINT('',(75.0569759364645,797.151672465291,104.051892905328));
#75888=CARTESIAN_POINT('Origin',(75.0569759364645,792.767109321893,111.807094006867));
#75889=CARTESIAN_POINT('Origin',(75.0569759364645,795.690573649493,103.535491146311));
#75890=CARTESIAN_POINT('',(75.0569759364645,794.027157017987,109.742386389799));
#75891=CARTESIAN_POINT('Origin',(75.0569759364645,793.555734787378,109.575769822532));
#75892=CARTESIAN_POINT('',(75.0569759364645,792.572065283433,113.859399496569));
#75893=CARTESIAN_POINT('',(75.0569759364645,796.161995880102,103.702107713578));
#75894=CARTESIAN_POINT('Origin',(75.0569759364645,792.100643052824,113.692782929302));
#75895=CARTESIAN_POINT('Origin',(81.1764063203475,795.155415755662,103.346348239111));
#75896=CARTESIAN_POINT('',(81.1764063203475,792.752866735955,113.923300847461));
#75897=CARTESIAN_POINT('Origin',(81.1764063203475,791.565485158993,113.503640022102));
#75898=CARTESIAN_POINT('',(81.1764063203475,793.419333005024,112.037611925025));
#75899=CARTESIAN_POINT('',(81.1764063203475,796.342797332624,103.766009064469));
#75900=CARTESIAN_POINT('',(79.9181205070459,792.281006798982,111.63528892758));
#75901=CARTESIAN_POINT('Origin',(81.1764063203493,792.231951428062,111.617951099667));
#75902=CARTESIAN_POINT('',(81.4304971360407,793.394914078383,112.028981450115));
#75903=CARTESIAN_POINT('Ctrl Pts',(81.4304971360405,793.394914078382,112.028981450115));
#75904=CARTESIAN_POINT('Ctrl Pts',(81.5271123948389,793.37614905845,112.022349257141));
#75905=CARTESIAN_POINT('Ctrl Pts',(81.6212624745287,793.346663326874,112.012062193114));
#75906=CARTESIAN_POINT('Ctrl Pts',(81.8489627698746,793.245751417097,111.977255759942));
#75907=CARTESIAN_POINT('Ctrl Pts',(81.9740810553385,793.161320630065,111.948422218836));
#75908=CARTESIAN_POINT('Ctrl Pts',(82.1880145458838,792.952443566045,111.877789451628));
#75909=CARTESIAN_POINT('Ctrl Pts',(82.2744058185353,792.82917381175,111.8363985929));
#75910=CARTESIAN_POINT('Ctrl Pts',(82.3995525291408,792.550459809467,111.743210525993));
#75911=CARTESIAN_POINT('Ctrl Pts',(82.4337382363144,792.396155260957,111.691811252713));
#75912=CARTESIAN_POINT('Ctrl Pts',(82.4376021228561,792.085416851161,111.588118810398));
#75913=CARTESIAN_POINT('Ctrl Pts',(82.4078754837702,791.931949334495,111.536803733373));
#75914=CARTESIAN_POINT('Ctrl Pts',(82.2881746340815,791.643961859157,111.439670680854));
#75915=CARTESIAN_POINT('Ctrl Pts',(82.1990951091111,791.512266962877,111.394790498615));
#75916=CARTESIAN_POINT('Ctrl Pts',(82.0441228948492,791.35940851878,111.341737471862));
#75917=CARTESIAN_POINT('Ctrl Pts',(81.9992688749996,791.321133700687,111.328342567492));
#75918=CARTESIAN_POINT('Ctrl Pts',(81.9516789857087,791.286082429006,111.31595426209));
#75919=CARTESIAN_POINT('Ctrl Pts',(81.8215614892368,791.190247288659,111.282082880829));
#75920=CARTESIAN_POINT('Ctrl Pts',(81.6727209685682,791.119788269131,111.256170860838));
#75921=CARTESIAN_POINT('Ctrl Pts',(81.353445732818,791.037280881806,111.223319474081));
#75922=CARTESIAN_POINT('Ctrl Pts',(81.1860085643421,791.026459705763,111.216847906364));
#75923=CARTESIAN_POINT('Ctrl Pts',(80.8552918281437,791.067106646942,111.225238906537));
#75924=CARTESIAN_POINT('Ctrl Pts',(80.6953066925941,791.118446720726,111.240127379119));
#75925=CARTESIAN_POINT('Ctrl Pts',(80.4137850859091,791.27233939135,111.288681457831));
#75926=CARTESIAN_POINT('Ctrl Pts',(80.2930480159152,791.370434776423,111.320803535585));
#75927=CARTESIAN_POINT('Ctrl Pts',(80.0991925175211,791.599279798184,111.397749637547));
#75928=CARTESIAN_POINT('Ctrl Pts',(80.0262055857992,791.72693411675,111.441476404976));
#75929=CARTESIAN_POINT('Ctrl Pts',(79.9325419863974,791.998393300873,111.535719640487));
#75930=CARTESIAN_POINT('Ctrl Pts',(79.9119247565683,792.139731328094,111.585357395993));
#75931=CARTESIAN_POINT('Ctrl Pts',(79.9181205070457,792.281006798982,111.63528892758));
#75932=CARTESIAN_POINT('Origin',(81.1764063203493,792.231951428062,111.617951099667));
#75933=CARTESIAN_POINT('Origin',(81.1764063203475,795.155415755662,103.346348239111));
#75934=CARTESIAN_POINT('',(81.1764063203475,793.491999124156,109.553243482599));
#75935=CARTESIAN_POINT('Origin',(81.1764063203475,793.020576893547,109.386626915332));
#75936=CARTESIAN_POINT('',(81.1764063203475,792.036907389602,113.670256589369));
#75937=CARTESIAN_POINT('',(81.1764063203475,795.626837986271,103.512964806378));
#75938=CARTESIAN_POINT('Origin',(81.1764063203475,791.565485158993,113.503640022102));
#75939=CARTESIAN_POINT('Origin',(48.2028277557997,817.065496804356,111.090112227845));
#75940=CARTESIAN_POINT('',(48.2028277557997,814.473928626814,121.600259070193));
#75941=CARTESIAN_POINT('Origin',(48.2028277557997,813.475566207687,121.247404010836));
#75942=CARTESIAN_POINT('',(48.2028277557997,815.140394895883,119.714570147758));
#75943=CARTESIAN_POINT('',(48.2028277557997,818.063859223483,111.442967287202));
#75944=CARTESIAN_POINT('Origin',(48.2028277557997,814.142032476756,119.361715088401));
#75945=CARTESIAN_POINT('Origin',(48.2028277557997,817.065496804356,111.090112227845));
#75946=CARTESIAN_POINT('',(48.2028277557997,815.402080172849,117.297007471333));
#75947=CARTESIAN_POINT('Origin',(48.2028277557997,814.930657942241,117.130390904066));
#75948=CARTESIAN_POINT('',(48.2028277557997,813.946988438296,121.414020578103));
#75949=CARTESIAN_POINT('',(48.2028277557997,817.536919034965,111.256728795112));
#75950=CARTESIAN_POINT('Origin',(48.2028277557997,813.475566207687,121.247404010836));
#75951=CARTESIAN_POINT('Origin',(48.4736194705231,813.126870448416,109.698068406902));
#75952=CARTESIAN_POINT('',(48.4736194705231,810.75870913113,120.287174792824));
#75953=CARTESIAN_POINT('Origin',(48.4736194705231,809.536939851748,119.855360189893));
#75954=CARTESIAN_POINT('',(48.4736194705231,811.425175400199,118.401485870389));
#75955=CARTESIAN_POINT('',(48.4736194705231,814.348639727799,110.129883009833));
#75956=CARTESIAN_POINT('Origin',(48.4736194705231,810.203406120816,117.969671267458));
#75957=CARTESIAN_POINT('Origin',(48.4736194705231,813.126870448416,109.698068406902));
#75958=CARTESIAN_POINT('',(48.4736194705231,811.46345381691,115.90496365039));
#75959=CARTESIAN_POINT('Origin',(48.4736194705231,810.992031586301,115.738347083123));
#75960=CARTESIAN_POINT('',(48.4736194705231,810.008362082356,120.02197675716));
#75961=CARTESIAN_POINT('',(48.4736194705231,813.598292679025,109.864684974169));
#75962=CARTESIAN_POINT('Origin',(48.4736194705231,809.536939851748,119.855360189893));
#75963=CARTESIAN_POINT('Origin',(49.5044604029411,808.75455334054,108.15274359993));
#75964=CARTESIAN_POINT('',(49.5044604029411,806.679339145872,118.845387411099));
#75965=CARTESIAN_POINT('Origin',(49.5044604029411,805.164622743871,118.310035382922));
#75966=CARTESIAN_POINT('',(49.5044604029411,807.34580541494,116.959698488664));
#75967=CARTESIAN_POINT('',(49.5044604029411,810.269269742541,108.688095628108));
#75968=CARTESIAN_POINT('Origin',(49.5044604029411,805.83108901294,116.424346460486));
#75969=CARTESIAN_POINT('Origin',(49.5044604029411,808.75455334054,108.15274359993));
#75970=CARTESIAN_POINT('',(49.5044604029411,807.091136709034,114.359638843419));
#75971=CARTESIAN_POINT('Origin',(49.5044604029411,806.619714478425,114.193022276152));
#75972=CARTESIAN_POINT('',(49.5044604029411,805.63604497448,118.476651950189));
#75973=CARTESIAN_POINT('',(49.5044604029411,809.225975571149,108.319360167197));
#75974=CARTESIAN_POINT('Origin',(49.5044604029411,805.164622743871,118.310035382922));
#75975=CARTESIAN_POINT('Origin',(51.513999851587,804.738345273765,106.733279777335));
#75976=CARTESIAN_POINT('',(51.513999851587,802.872026821543,117.499754412049));
#75977=CARTESIAN_POINT('Origin',(51.513999851587,801.148414677097,116.890571560326));
#75978=CARTESIAN_POINT('',(51.513999851587,803.538493090612,115.614065489613));
#75979=CARTESIAN_POINT('',(51.513999851587,806.461957418212,107.342462629057));
#75980=CARTESIAN_POINT('Origin',(51.513999851587,801.814880946165,115.004882637891));
#75981=CARTESIAN_POINT('Origin',(51.513999851587,804.738345273765,106.733279777335));
#75982=CARTESIAN_POINT('',(51.513999851587,803.074928642259,112.940175020823));
#75983=CARTESIAN_POINT('Origin',(51.513999851587,802.60350641165,112.773558453556));
#75984=CARTESIAN_POINT('',(51.513999851587,801.619836907705,117.057188127593));
#75985=CARTESIAN_POINT('',(51.513999851587,805.209767504374,106.899896344602));
#75986=CARTESIAN_POINT('Origin',(51.513999851587,801.148414677097,116.890571560326));
#75987=CARTESIAN_POINT('Origin',(54.2477438619482,800.654985243879,105.290082178832));
#75988=CARTESIAN_POINT('',(54.2477438619482,798.817254044772,116.066660516071));
#75989=CARTESIAN_POINT('Origin',(54.2477438619482,797.06505464721,115.447373961824));
#75990=CARTESIAN_POINT('',(54.2477438619482,799.48372031384,114.180971593635));
#75991=CARTESIAN_POINT('',(54.2477438619482,802.40718464144,105.909368733079));
#75992=CARTESIAN_POINT('Origin',(54.2477438619482,797.731520916278,113.561685039388));
#75993=CARTESIAN_POINT('Origin',(54.2477438619482,800.654985243879,105.290082178832));
#75994=CARTESIAN_POINT('',(54.2477438619482,798.991568612372,111.496977422321));
#75995=CARTESIAN_POINT('Origin',(54.2477438619482,798.520146381764,111.330360855054));
#75996=CARTESIAN_POINT('',(54.2477438619482,797.536476877819,115.613990529091));
#75997=CARTESIAN_POINT('',(54.2477438619482,801.126407474487,105.456698746099));
#75998=CARTESIAN_POINT('Origin',(54.2477438619482,797.06505464721,115.447373961824));
#75999=CARTESIAN_POINT('Origin',(57.7499869812552,797.615616719433,104.215866502688));
#76000=CARTESIAN_POINT('',(57.7499869812552,795.734928471145,114.977262365258));
#76001=CARTESIAN_POINT('Origin',(57.7499869812552,794.025686122764,114.37315828568));
#76002=CARTESIAN_POINT('',(57.7499869812552,796.401394740213,113.091573442823));
#76003=CARTESIAN_POINT('',(57.7499869812552,799.324859067813,104.819970582266));
#76004=CARTESIAN_POINT('Origin',(57.7499869812552,794.692152391833,112.487469363244));
#76005=CARTESIAN_POINT('Origin',(57.7499869812552,797.615616719433,104.215866502688));
#76006=CARTESIAN_POINT('',(57.7499869812552,795.952200087927,110.422761746176));
#76007=CARTESIAN_POINT('Origin',(57.7499869812552,795.480777857318,110.256145178909));
#76008=CARTESIAN_POINT('',(57.7499869812552,794.497108353373,114.539774852947));
#76009=CARTESIAN_POINT('',(57.7499869812552,798.087038950042,104.382483069955));
#76010=CARTESIAN_POINT('Origin',(57.7499869812552,794.025686122764,114.37315828568));
#76011=CARTESIAN_POINT('Origin',(62.364022956069,794.165535739153,102.996491147849));
#76012=CARTESIAN_POINT('',(62.364022956069,792.377820292525,113.790746744339));
#76013=CARTESIAN_POINT('Origin',(62.364022956069,790.575605142485,113.15378293084));
#76014=CARTESIAN_POINT('',(62.364022956069,793.044286561593,111.905057821903));
#76015=CARTESIAN_POINT('',(62.364022956069,795.967750889194,103.633454961347));
#76016=CARTESIAN_POINT('Origin',(62.364022956069,791.242071411553,111.268094008405));
#76017=CARTESIAN_POINT('Origin',(62.364022956069,794.165535739153,102.996491147849));
#76018=CARTESIAN_POINT('',(62.364022956069,792.502119107647,109.203386391337));
#76019=CARTESIAN_POINT('Origin',(62.364022956069,792.030696877038,109.03676982407));
#76020=CARTESIAN_POINT('',(62.364022956069,791.047027373093,113.320399498107));
#76021=CARTESIAN_POINT('',(62.364022956069,794.636957969762,103.163107715116));
#76022=CARTESIAN_POINT('Origin',(62.364022956069,790.575605142485,113.15378293084));
#76023=CARTESIAN_POINT('Origin',(67.1585327646285,792.07747204951,102.258498788528));
#76024=CARTESIAN_POINT('',(67.1585327646285,789.94864026864,112.932192330537));
#76025=CARTESIAN_POINT('Origin',(67.1585327646285,788.487541452842,112.415790571519));
#76026=CARTESIAN_POINT('',(67.1585327646285,790.615106537832,111.04650340775));
#76027=CARTESIAN_POINT('',(67.1585327646285,793.538570865308,102.774900547545));
#76028=CARTESIAN_POINT('',(66.4584822850693,787.85048959706,110.069394238124));
#76029=CARTESIAN_POINT('Origin',(67.1585327646304,789.15400772191,110.530101649084));
#76030=CARTESIAN_POINT('',(67.5288831447128,787.735245668087,110.028663134249));
#76031=CARTESIAN_POINT('Ctrl Pts',(67.5288733605052,787.735245035326,110.02866291061));
#76032=CARTESIAN_POINT('Ctrl Pts',(67.4671620849654,787.720925260318,110.0236018176));
#76033=CARTESIAN_POINT('Ctrl Pts',(67.4045749097962,787.710195046386,110.019819666768));
#76034=CARTESIAN_POINT('Ctrl Pts',(67.2548610344048,787.693405932515,110.013913398071));
#76035=CARTESIAN_POINT('Ctrl Pts',(67.1675407850101,787.690603920603,110.012940933692));
#76036=CARTESIAN_POINT('Ctrl Pts',(67.0416065082334,787.696591904374,110.015068146693));
#76037=CARTESIAN_POINT('Ctrl Pts',(67.0028641856055,787.699815903729,110.016209079711));
#76038=CARTESIAN_POINT('Ctrl Pts',(66.8821639275677,787.714194190606,110.021288906651));
#76039=CARTESIAN_POINT('Ctrl Pts',(66.8009995388376,787.730169587177,110.026923647079));
#76040=CARTESIAN_POINT('Ctrl Pts',(66.6308922483411,787.777315396607,110.043554166242));
#76041=CARTESIAN_POINT('Ctrl Pts',(66.5428214394692,787.8102254516,110.055163526352));
#76042=CARTESIAN_POINT('Ctrl Pts',(66.4584818949366,787.850490113391,110.069394420613));
#76043=CARTESIAN_POINT('Origin',(67.1585327646304,789.15400772191,110.530101649084));
#76044=CARTESIAN_POINT('Origin',(67.1585327646285,792.07747204951,102.258498788528));
#76045=CARTESIAN_POINT('',(67.1585327646285,790.414055418004,108.465394032016));
#76046=CARTESIAN_POINT('Origin',(67.1585327646285,789.942633187395,108.298777464749));
#76047=CARTESIAN_POINT('',(67.1585327646285,788.958963683451,112.582407138786));
#76048=CARTESIAN_POINT('',(67.1585327646285,792.548894280119,102.425115355795));
#76049=CARTESIAN_POINT('Origin',(67.1585327646285,788.487541452842,112.415790571519));
#76050=CARTESIAN_POINT('Origin',(73.0262283740121,790.354426577582,101.649516218047));
#76051=CARTESIAN_POINT('',(73.0262283740121,787.951877557875,112.226468826397));
#76052=CARTESIAN_POINT('Origin',(73.0262283740121,786.764495980913,111.806808001039));
#76053=CARTESIAN_POINT('',(73.0262283740121,788.618343826943,110.340779903962));
#76054=CARTESIAN_POINT('',(73.0262283740121,791.541808154543,102.069177043406));
#76055=CARTESIAN_POINT('',(71.8612276196213,787.881917432482,110.080501898549));
#76056=CARTESIAN_POINT('Origin',(73.026228374014,787.430962249982,109.921119078603));
#76057=CARTESIAN_POINT('',(73.547638647088,788.511793322879,110.303121350599));
#76058=CARTESIAN_POINT('Ctrl Pts',(73.5476386478411,788.511793322897,110.303121350605));
#76059=CARTESIAN_POINT('Ctrl Pts',(73.6411231849667,788.471702806277,110.288952005535));
#76060=CARTESIAN_POINT('Ctrl Pts',(73.729056042615,788.420935975636,110.271151656072));
#76061=CARTESIAN_POINT('Ctrl Pts',(73.8817794828457,788.306353346367,110.231343155525));
#76062=CARTESIAN_POINT('Ctrl Pts',(73.9475471629768,788.244719253655,110.21006215985));
#76063=CARTESIAN_POINT('Ctrl Pts',(74.1079933820161,788.056975966865,110.145666872752));
#76064=CARTESIAN_POINT('Ctrl Pts',(74.1848486425081,787.919355348459,110.098916903248));
#76065=CARTESIAN_POINT('Ctrl Pts',(74.2760595756327,787.632863603953,110.002393768381));
#76066=CARTESIAN_POINT('Ctrl Pts',(74.293203957499,787.48758429983,109.953778221984));
#76067=CARTESIAN_POINT('Ctrl Pts',(74.2724489890072,787.207171966388,109.860239043525));
#76068=CARTESIAN_POINT('Ctrl Pts',(74.2380363542724,787.074013924212,109.815948173723));
#76069=CARTESIAN_POINT('Ctrl Pts',(74.1139149291181,786.803724199413,109.725899152577));
#76070=CARTESIAN_POINT('Ctrl Pts',(74.0171882043694,786.672308121852,109.682008166697));
#76071=CARTESIAN_POINT('Ctrl Pts',(73.8348841099355,786.50725247843,109.62630802448));
#76072=CARTESIAN_POINT('Ctrl Pts',(73.7677840018365,786.457770970221,109.609493877455));
#76073=CARTESIAN_POINT('Ctrl Pts',(73.6505262673303,786.388126103038,109.58558761328));
#76074=CARTESIAN_POINT('Ctrl Pts',(73.6033367136151,786.363944979445,109.577219223496));
#76075=CARTESIAN_POINT('Ctrl Pts',(73.5335192615212,786.333479727438,109.56656518841));
#76076=CARTESIAN_POINT('Ctrl Pts',(73.5121115414431,786.324815433283,109.563518615732));
#76077=CARTESIAN_POINT('Ctrl Pts',(73.4426717754365,786.298855829668,109.554334034923));
#76078=CARTESIAN_POINT('Ctrl Pts',(73.3937666214844,786.283794470383,109.54891317807));
#76079=CARTESIAN_POINT('Ctrl Pts',(73.2703323690151,786.253590252978,109.537774593641));
#76080=CARTESIAN_POINT('Ctrl Pts',(73.1950539083946,786.241959394905,109.533192361749));
#76081=CARTESIAN_POINT('Ctrl Pts',(72.9593318182645,786.226155947848,109.525592239343));
#76082=CARTESIAN_POINT('Ctrl Pts',(72.7987636659693,786.244536878615,109.529949011691));
#76083=CARTESIAN_POINT('Ctrl Pts',(72.5106810113424,786.332088715488,109.555992921144));
#76084=CARTESIAN_POINT('Ctrl Pts',(72.3835460494303,786.394616632969,109.575470922408));
#76085=CARTESIAN_POINT('Ctrl Pts',(72.1492360872349,786.562230779967,109.629231584724));
#76086=CARTESIAN_POINT('Ctrl Pts',(72.0457494325479,786.668422647191,109.663950958307));
#76087=CARTESIAN_POINT('Ctrl Pts',(71.8785559577171,786.91713604384,109.746731912045));
#76088=CARTESIAN_POINT('Ctrl Pts',(71.8190264473306,787.059150796,109.794708006097));
#76089=CARTESIAN_POINT('Ctrl Pts',(71.7675659500907,787.314715553241,109.882254532013));
#76090=CARTESIAN_POINT('Ctrl Pts',(71.761632694651,787.423919352526,109.920009091735));
#76091=CARTESIAN_POINT('Ctrl Pts',(71.7824174870735,787.652537898065,109.99966247971));
#76092=CARTESIAN_POINT('Ctrl Pts',(71.812679350666,787.770424668557,110.04109658337));
#76093=CARTESIAN_POINT('Ctrl Pts',(71.8612276196214,787.881917432482,110.080501898549));
#76094=CARTESIAN_POINT('Origin',(73.026228374014,787.430962249982,109.921119078603));
#76095=CARTESIAN_POINT('Origin',(73.0262283740121,790.354426577582,101.649516218047));
#76096=CARTESIAN_POINT('',(73.0262283740121,788.691009946075,107.856411461535));
#76097=CARTESIAN_POINT('Origin',(73.0262283740121,788.219587715466,107.689794894268));
#76098=CARTESIAN_POINT('',(73.0262283740121,787.235918211521,111.973424568306));
#76099=CARTESIAN_POINT('',(73.0262283740121,790.82584880819,101.816132785314));
#76100=CARTESIAN_POINT('Origin',(73.0262283740121,786.764495980913,111.806808001039));
#76101=CARTESIAN_POINT('Origin',(45.6047111404246,818.24947717752,111.508570952699));
#76102=CARTESIAN_POINT('',(45.6047111404246,815.657908999979,122.018717795047));
#76103=CARTESIAN_POINT('Origin',(45.6047111404246,814.659546580852,121.66586273569));
#76104=CARTESIAN_POINT('',(45.6047111404246,816.324375269047,120.133028872612));
#76105=CARTESIAN_POINT('',(45.6047111404246,819.247839596648,111.861426012055));
#76106=CARTESIAN_POINT('Origin',(45.6047111404246,815.32601284992,119.780173813255));
#76107=CARTESIAN_POINT('Origin',(45.6047111404246,818.24947717752,111.508570952699));
#76108=CARTESIAN_POINT('',(45.6047111404246,816.586060546014,117.715466196187));
#76109=CARTESIAN_POINT('Origin',(45.6047111404246,816.114638315406,117.54884962892));
#76110=CARTESIAN_POINT('',(45.6047111404246,815.130968811461,121.832479302957));
#76111=CARTESIAN_POINT('',(45.6047111404246,818.720899408129,111.675187519966));
#76112=CARTESIAN_POINT('Origin',(45.6047111404246,814.659546580852,121.66586273569));
#76113=CARTESIAN_POINT('Origin',(45.001057776689,814.343836394462,110.128185349306));
#76114=CARTESIAN_POINT('',(45.001057776689,811.975675077176,120.717291735229));
#76115=CARTESIAN_POINT('Origin',(45.001057776689,810.753905797794,120.285477132298));
#76116=CARTESIAN_POINT('',(45.001057776689,812.642141346244,118.831602812793));
#76117=CARTESIAN_POINT('',(45.001057776689,815.565605673845,110.559999952237));
#76118=CARTESIAN_POINT('Origin',(45.001057776689,811.420372066862,118.399788209863));
#76119=CARTESIAN_POINT('Origin',(45.001057776689,814.343836394462,110.128185349306));
#76120=CARTESIAN_POINT('',(45.001057776689,812.680419762956,116.335080592795));
#76121=CARTESIAN_POINT('Origin',(45.001057776689,812.208997532347,116.168464025528));
#76122=CARTESIAN_POINT('',(45.001057776689,811.225328028402,120.452093699565));
#76123=CARTESIAN_POINT('',(45.001057776689,814.815258625071,110.294801916574));
#76124=CARTESIAN_POINT('Origin',(45.001057776689,810.753905797794,120.285477132298));
#76125=CARTESIAN_POINT('Origin',(45.0452092570759,809.864990821428,108.545209778267));
#76126=CARTESIAN_POINT('',(45.0452092570759,807.78977662676,119.237853589437));
#76127=CARTESIAN_POINT('Origin',(45.0452092570759,806.275060224759,118.702501561259));
#76128=CARTESIAN_POINT('',(45.0452092570759,808.456242895828,117.352164667001));
#76129=CARTESIAN_POINT('',(45.0452092570759,811.379707223428,109.080561806445));
#76130=CARTESIAN_POINT('Origin',(45.0452092570759,806.941526493827,116.816812638824));
#76131=CARTESIAN_POINT('Origin',(45.0452092570759,809.864990821428,108.545209778267));
#76132=CARTESIAN_POINT('',(45.0452092570759,808.201574189921,114.752105021756));
#76133=CARTESIAN_POINT('Origin',(45.0452092570759,807.730151959312,114.585488454489));
#76134=CARTESIAN_POINT('',(45.0452092570759,806.746482455368,118.869118128526));
#76135=CARTESIAN_POINT('',(45.0452092570759,810.336413052037,108.711826345535));
#76136=CARTESIAN_POINT('Origin',(45.0452092570759,806.275060224759,118.702501561259));
#76137=CARTESIAN_POINT('Origin',(46.1251998582498,805.542619761922,107.017537594757));
#76138=CARTESIAN_POINT('',(46.1251998582498,803.6763013097,117.784012229471));
#76139=CARTESIAN_POINT('Origin',(46.1251998582498,801.952689165253,117.174829377748));
#76140=CARTESIAN_POINT('',(46.1251998582498,804.342767578769,115.898323307036));
#76141=CARTESIAN_POINT('',(46.1251998582498,807.266231906369,107.62672044648));
#76142=CARTESIAN_POINT('Origin',(46.1251998582498,802.619155434322,115.289140455313));
#76143=CARTESIAN_POINT('Origin',(46.1251998582498,805.542619761922,107.017537594757));
#76144=CARTESIAN_POINT('',(46.1251998582498,803.879203130416,113.224432838245));
#76145=CARTESIAN_POINT('Origin',(46.1251998582498,803.407780899807,113.057816270978));
#76146=CARTESIAN_POINT('',(46.1251998582498,802.424111395862,117.341445945016));
#76147=CARTESIAN_POINT('',(46.1251998582498,806.014041992531,107.184154162024));
#76148=CARTESIAN_POINT('Origin',(46.1251998582498,801.952689165253,117.174829377748));
#76149=CARTESIAN_POINT('Origin',(47.8987613742277,801.012599519368,105.416475163972));
#76150=CARTESIAN_POINT('',(47.8987613742277,799.174868320261,116.19305350121));
#76151=CARTESIAN_POINT('Origin',(47.8987613742277,797.422668922699,115.573766946963));
#76152=CARTESIAN_POINT('',(47.8987613742277,799.841334589329,114.307364578775));
#76153=CARTESIAN_POINT('',(47.8987613742277,802.764798916929,106.035761718219));
#76154=CARTESIAN_POINT('Origin',(47.8987613742277,798.089135191767,113.688078024528));
#76155=CARTESIAN_POINT('Origin',(47.8987613742277,801.012599519368,105.416475163972));
#76156=CARTESIAN_POINT('',(47.8987613742277,799.349182887861,111.62337040746));
#76157=CARTESIAN_POINT('Origin',(47.8987613742277,798.877760657253,111.456753840193));
#76158=CARTESIAN_POINT('',(47.8987613742277,797.894091153308,115.74038351423));
#76159=CARTESIAN_POINT('',(47.8987613742277,801.484021749976,105.583091731239));
#76160=CARTESIAN_POINT('Origin',(47.8987613742277,797.422668922699,115.573766946963));
#76161=CARTESIAN_POINT('Origin',(50.6542446180139,797.353109422993,104.12308754197));
#76162=CARTESIAN_POINT('',(50.6542446180139,795.472421174705,114.884483404539));
#76163=CARTESIAN_POINT('Origin',(50.6542446180139,793.763178826324,114.280379324961));
#76164=CARTESIAN_POINT('',(50.6542446180139,796.138887443773,112.998794482104));
#76165=CARTESIAN_POINT('',(50.6542446180139,799.062351771373,104.727191621548));
#76166=CARTESIAN_POINT('Origin',(50.6542446180139,794.429645095393,112.394690402526));
#76167=CARTESIAN_POINT('Origin',(50.6542446180139,797.353109422993,104.12308754197));
#76168=CARTESIAN_POINT('',(50.6542446180139,795.689692791486,110.329982785458));
#76169=CARTESIAN_POINT('Origin',(50.6542446180139,795.218270560878,110.163366218191));
#76170=CARTESIAN_POINT('',(50.6542446180139,794.234601056933,114.446995892228));
#76171=CARTESIAN_POINT('',(50.6542446180139,797.824531653602,104.289704109237));
#76172=CARTESIAN_POINT('Origin',(50.6542446180139,793.763178826324,114.280379324961));
#76173=CARTESIAN_POINT('Origin',(54.406656968682,793.073938964199,102.61068391248));
#76174=CARTESIAN_POINT('',(54.406656968682,791.286223517571,113.40493950897));
#76175=CARTESIAN_POINT('Origin',(54.406656968682,789.48400836753,112.767975695471));
#76176=CARTESIAN_POINT('',(54.406656968682,791.952689786913,111.519250585761));
#76177=CARTESIAN_POINT('',(54.406656968682,794.87615411424,103.247647725978));
#76178=CARTESIAN_POINT('',(53.0282509976584,788.901890948758,110.440995050868));
#76179=CARTESIAN_POINT('Origin',(54.4066569686837,790.150474636598,110.882286773036));
#76180=CARTESIAN_POINT('',(55.7276395803606,788.847878514773,110.421905229141));
#76181=CARTESIAN_POINT('Ctrl Pts',(55.7276395634569,788.847878682488,110.421905288417));
#76182=CARTESIAN_POINT('Ctrl Pts',(55.5456566202033,788.683820399216,110.363921539188));
#76183=CARTESIAN_POINT('Ctrl Pts',(55.3310737782485,788.555040568309,110.319135204066));
#76184=CARTESIAN_POINT('Ctrl Pts',(54.9643199501897,788.420973591252,110.272735437511));
#76185=CARTESIAN_POINT('Ctrl Pts',(54.8271319930196,788.386712853143,110.260948684297));
#76186=CARTESIAN_POINT('Ctrl Pts',(54.5812541501973,788.352204133832,110.249104533157));
#76187=CARTESIAN_POINT('Ctrl Pts',(54.4741664289805,788.34577865309,110.24691602536));
#76188=CARTESIAN_POINT('Ctrl Pts',(54.2597596859153,788.349965233717,110.248396777475));
#76189=CARTESIAN_POINT('Ctrl Pts',(54.1528214814057,788.360605741338,110.252075734691));
#76190=CARTESIAN_POINT('Ctrl Pts',(53.9076157883093,788.404957435148,110.267398592785));
#76191=CARTESIAN_POINT('Ctrl Pts',(53.7712598392015,788.4449186278,110.281197882194));
#76192=CARTESIAN_POINT('Ctrl Pts',(53.4105721629827,788.593926845041,110.33287678729));
#76193=CARTESIAN_POINT('Ctrl Pts',(53.2023852593083,788.730998225782,110.38059577992));
#76194=CARTESIAN_POINT('Ctrl Pts',(53.0282510499295,788.901890998491,110.440995068445));
#76195=CARTESIAN_POINT('Origin',(54.4066569686837,790.150474636598,110.882286773036));
#76196=CARTESIAN_POINT('Origin',(54.406656968682,793.073938964199,102.61068391248));
#76197=CARTESIAN_POINT('',(54.406656968682,791.410522332693,108.817579155968));
#76198=CARTESIAN_POINT('Origin',(54.406656968682,790.939100102084,108.650962588701));
#76199=CARTESIAN_POINT('',(54.406656968682,789.955430598139,112.934592262738));
#76200=CARTESIAN_POINT('',(54.406656968682,793.545361194808,102.777300479747));
#76201=CARTESIAN_POINT('Origin',(54.406656968682,789.48400836753,112.767975695471));
#76202=CARTESIAN_POINT('Origin',(43.3244554712047,819.916889345885,112.0978908313));
#76203=CARTESIAN_POINT('',(43.3244554712047,817.325321168344,122.608037673648));
#76204=CARTESIAN_POINT('Origin',(43.3244554712047,816.326958749216,122.255182614291));
#76205=CARTESIAN_POINT('',(43.3244554712047,817.991787437412,120.722348751213));
#76206=CARTESIAN_POINT('',(43.3244554712047,820.915251765012,112.450745890657));
#76207=CARTESIAN_POINT('Origin',(43.3244554712047,816.993425018285,120.369493691856));
#76208=CARTESIAN_POINT('Origin',(43.3244554712047,819.916889345885,112.0978908313));
#76209=CARTESIAN_POINT('',(43.3244554712047,818.253472714379,118.304786074788));
#76210=CARTESIAN_POINT('Origin',(43.3244554712047,817.78205048377,118.138169507521));
#76211=CARTESIAN_POINT('',(43.3244554712047,816.798380979825,122.421799181559));
#76212=CARTESIAN_POINT('',(43.3244554712047,820.388311576494,112.264507398567));
#76213=CARTESIAN_POINT('Origin',(43.3244554712047,816.326958749216,122.255182614291));
#76214=CARTESIAN_POINT('Origin',(41.8727395776554,816.214929379271,110.789492920152));
#76215=CARTESIAN_POINT('',(41.8727395776554,813.846768061985,121.378599306074));
#76216=CARTESIAN_POINT('Origin',(41.8727395776554,812.624998782603,120.946784703143));
#76217=CARTESIAN_POINT('',(41.8727395776554,814.513234331054,119.492910383639));
#76218=CARTESIAN_POINT('',(41.8727395776554,817.436698658654,111.221307523083));
#76219=CARTESIAN_POINT('Origin',(41.8727395776554,813.291465051671,119.061095780708));
#76220=CARTESIAN_POINT('Origin',(41.8727395776554,816.214929379271,110.789492920152));
#76221=CARTESIAN_POINT('',(41.8727395776554,814.551512747765,116.99638816364));
#76222=CARTESIAN_POINT('Origin',(41.8727395776554,814.080090517156,116.829771596373));
#76223=CARTESIAN_POINT('',(41.8727395776554,813.096421013212,121.11340127041));
#76224=CARTESIAN_POINT('',(41.8727395776554,816.68635160988,110.956109487419));
#76225=CARTESIAN_POINT('Origin',(41.8727395776554,812.624998782603,120.946784703143));
#76226=CARTESIAN_POINT('Origin',(40.9282719744559,811.825302384506,109.238050213459));
#76227=CARTESIAN_POINT('',(40.9282719744559,809.750088189838,119.930694024628));
#76228=CARTESIAN_POINT('Origin',(40.9282719744559,808.235371787837,119.395341996451));
#76229=CARTESIAN_POINT('',(40.9282719744559,810.416554458906,118.045005102193));
#76230=CARTESIAN_POINT('',(40.9282719744559,813.340018786506,109.773402241637));
#76231=CARTESIAN_POINT('Origin',(40.9282719744559,808.901838056905,117.509653074015));
#76232=CARTESIAN_POINT('Origin',(40.9282719744559,811.825302384506,109.238050213459));
#76233=CARTESIAN_POINT('',(40.9282719744559,810.161885753,115.444945456948));
#76234=CARTESIAN_POINT('Origin',(40.9282719744559,809.69046352239,115.27832888968));
#76235=CARTESIAN_POINT('',(40.9282719744559,808.706794018446,119.561958563718));
#76236=CARTESIAN_POINT('',(40.9282719744559,812.296724615114,109.404666780726));
#76237=CARTESIAN_POINT('Origin',(40.9282719744559,808.235371787837,119.395341996451));
#76238=CARTESIAN_POINT('Origin',(41.031512956517,807.385676688607,107.668936274038));
#76239=CARTESIAN_POINT('',(41.031512956517,805.519358236385,118.435410908752));
#76240=CARTESIAN_POINT('Origin',(41.031512956517,803.795746091938,117.826228057029));
#76241=CARTESIAN_POINT('',(41.031512956517,806.185824505454,116.549721986316));
#76242=CARTESIAN_POINT('',(41.031512956517,809.109288833054,108.27811912576));
#76243=CARTESIAN_POINT('Origin',(41.031512956517,804.462212361007,115.940539134594));
#76244=CARTESIAN_POINT('Origin',(41.031512956517,807.385676688607,107.668936274038));
#76245=CARTESIAN_POINT('',(41.031512956517,805.722260057101,113.875831517526));
#76246=CARTESIAN_POINT('Origin',(41.031512956517,805.250837826492,113.709214950259));
#76247=CARTESIAN_POINT('',(41.031512956517,804.267168322547,117.992844624296));
#76248=CARTESIAN_POINT('',(41.031512956517,807.857098919216,107.835552841305));
#76249=CARTESIAN_POINT('Origin',(41.031512956517,803.795746091938,117.826228057029));
#76250=CARTESIAN_POINT('Origin',(41.7673788293708,802.606979855433,105.979983121944));
#76251=CARTESIAN_POINT('',(41.7673788293708,800.769248656326,116.756561459183));
#76252=CARTESIAN_POINT('Origin',(41.7673788293708,799.017049258764,116.137274904936));
#76253=CARTESIAN_POINT('',(41.7673788293708,801.435714925394,114.870872536748));
#76254=CARTESIAN_POINT('',(41.7673788293708,804.359179252995,106.599269676191));
#76255=CARTESIAN_POINT('Origin',(41.7673788293708,799.683515527833,114.251585982501));
#76256=CARTESIAN_POINT('Origin',(41.7673788293708,802.606979855433,105.979983121944));
#76257=CARTESIAN_POINT('',(41.7673788293708,800.943563223927,112.186878365433));
#76258=CARTESIAN_POINT('Origin',(41.7673788293708,800.472140993318,112.020261798166));
#76259=CARTESIAN_POINT('',(41.7673788293708,799.488471489373,116.303891472203));
#76260=CARTESIAN_POINT('',(41.7673788293708,803.078402086042,106.146599689212));
#76261=CARTESIAN_POINT('Origin',(41.7673788293708,799.017049258764,116.137274904936));
#76262=CARTESIAN_POINT('Origin',(43.6556743576072,798.487305464523,104.523950799529));
#76263=CARTESIAN_POINT('',(43.6556743576072,796.606617216234,115.285346662099));
#76264=CARTESIAN_POINT('Origin',(43.6556743576072,794.897374867854,114.68124258252));
#76265=CARTESIAN_POINT('',(43.6556743576072,797.273083485303,113.399657739663));
#76266=CARTESIAN_POINT('',(43.6556743576072,800.196547812903,105.128054879107));
#76267=CARTESIAN_POINT('Origin',(43.6556743576072,795.563841136923,112.795553660085));
#76268=CARTESIAN_POINT('Origin',(43.6556743576072,798.487305464523,104.523950799529));
#76269=CARTESIAN_POINT('',(43.6556743576072,796.823888833016,110.730846043017));
#76270=CARTESIAN_POINT('Origin',(43.6556743576072,796.352466602408,110.56422947575));
#76271=CARTESIAN_POINT('',(43.6556743576072,795.368797098463,114.847859149787));
#76272=CARTESIAN_POINT('',(43.6556743576072,798.958727695131,104.690567366796));
#76273=CARTESIAN_POINT('Origin',(43.6556743576072,794.897374867854,114.68124258252));
#76274=CARTESIAN_POINT('Origin',(46.3824646583332,793.566065810002,102.784618191315));
#76275=CARTESIAN_POINT('',(46.3824646583332,791.778350363374,113.578873787805));
#76276=CARTESIAN_POINT('Origin',(46.3824646583332,789.976135213334,112.941909974306));
#76277=CARTESIAN_POINT('',(46.3824646583332,792.444816632443,111.693184865369));
#76278=CARTESIAN_POINT('',(46.3824646583332,795.368280960043,103.421582004813));
#76279=CARTESIAN_POINT('Origin',(46.3824646583332,790.642601482402,111.056221051871));
#76280=CARTESIAN_POINT('Origin',(46.3824646583332,793.566065810002,102.784618191315));
#76281=CARTESIAN_POINT('',(46.3824646583332,791.902649178496,108.991513434803));
#76282=CARTESIAN_POINT('Origin',(46.3824646583332,791.431226947887,108.824896867536));
#76283=CARTESIAN_POINT('',(46.3824646583332,790.447557443943,113.108526541573));
#76284=CARTESIAN_POINT('',(46.3824646583332,794.037488040611,102.951234758582));
#76285=CARTESIAN_POINT('Origin',(46.3824646583332,789.976135213334,112.941909974306));
#76286=CARTESIAN_POINT('Origin',(41.4617188627654,821.99485939656,112.832315757083));
#76287=CARTESIAN_POINT('',(41.4617188627654,819.403291219019,123.342462599431));
#76288=CARTESIAN_POINT('Origin',(41.4617188627654,818.404928799891,122.989607540074));
#76289=CARTESIAN_POINT('',(41.4617188627654,820.069757488087,121.456773676996));
#76290=CARTESIAN_POINT('',(41.4617188627654,822.993221815687,113.18517081644));
#76291=CARTESIAN_POINT('Origin',(41.4617188627654,819.07139506896,121.103918617639));
#76292=CARTESIAN_POINT('Origin',(41.4617188627654,821.99485939656,112.832315757083));
#76293=CARTESIAN_POINT('',(41.4617188627654,820.331442765054,119.039211000571));
#76294=CARTESIAN_POINT('Origin',(41.4617188627654,819.860020534445,118.872594433304));
#76295=CARTESIAN_POINT('',(41.4617188627654,818.8763510305,123.156224107341));
#76296=CARTESIAN_POINT('',(41.4617188627654,822.466281627169,112.99893232435));
#76297=CARTESIAN_POINT('Origin',(41.4617188627654,818.404928799891,122.989607540074));
#76298=CARTESIAN_POINT('Origin',(39.2253873900563,818.658373660907,111.653088805286));
#76299=CARTESIAN_POINT('',(39.2253873900563,816.290212343621,122.242195191208));
#76300=CARTESIAN_POINT('Origin',(39.2253873900563,815.068443064238,121.810380588277));
#76301=CARTESIAN_POINT('',(39.2253873900563,816.956678612689,120.356506268773));
#76302=CARTESIAN_POINT('',(39.2253873900563,819.880142940289,112.084903408217));
#76303=CARTESIAN_POINT('Origin',(39.2253873900563,815.734909333306,119.924691665842));
#76304=CARTESIAN_POINT('Origin',(39.2253873900563,818.658373660907,111.653088805286));
#76305=CARTESIAN_POINT('',(39.2253873900563,816.9949570294,117.859984048774));
#76306=CARTESIAN_POINT('Origin',(39.2253873900563,816.523534798792,117.693367481507));
#76307=CARTESIAN_POINT('',(39.2253873900563,815.539865294847,121.976997155544));
#76308=CARTESIAN_POINT('',(39.2253873900563,819.129795891515,111.819705372553));
#76309=CARTESIAN_POINT('Origin',(39.2253873900563,815.068443064238,121.810380588277));
#76310=CARTESIAN_POINT('Origin',(37.333578469589,814.549813007849,110.20098445387));
#76311=CARTESIAN_POINT('',(37.333578469589,812.474598813181,120.893628265039));
#76312=CARTESIAN_POINT('Origin',(37.333578469589,810.95988241118,120.358276236862));
#76313=CARTESIAN_POINT('',(37.333578469589,813.141065082249,119.007939342604));
#76314=CARTESIAN_POINT('',(37.333578469589,816.064529409849,110.736336482048));
#76315=CARTESIAN_POINT('Origin',(37.333578469589,811.626348680248,118.472587314426));
#76316=CARTESIAN_POINT('Origin',(37.333578469589,814.549813007849,110.20098445387));
#76317=CARTESIAN_POINT('',(37.333578469589,812.886396376342,116.407879697359));
#76318=CARTESIAN_POINT('Origin',(37.333578469589,812.414974145734,116.241263130091));
#76319=CARTESIAN_POINT('',(37.333578469589,811.431304641789,120.524892804129));
#76320=CARTESIAN_POINT('',(37.333578469589,815.021235238458,110.367601021137));
#76321=CARTESIAN_POINT('Origin',(37.333578469589,810.95988241118,120.358276236862));
#76322=CARTESIAN_POINT('Origin',(36.4555577062156,810.186965622156,108.659006567134));
#76323=CARTESIAN_POINT('',(36.4555577062156,808.320647169934,119.425481201848));
#76324=CARTESIAN_POINT('Origin',(36.4555577062156,806.597035025487,118.816298350126));
#76325=CARTESIAN_POINT('',(36.4555577062156,808.987113439002,117.539792279413));
#76326=CARTESIAN_POINT('',(36.4555577062156,811.910577766602,109.268189418857));
#76327=CARTESIAN_POINT('Origin',(36.4555577062156,807.263501294555,116.930609427691));
#76328=CARTESIAN_POINT('Origin',(36.4555577062156,810.186965622156,108.659006567134));
#76329=CARTESIAN_POINT('',(36.4555577062156,808.523548990649,114.865901810623));
#76330=CARTESIAN_POINT('Origin',(36.4555577062156,808.05212676004,114.699285243356));
#76331=CARTESIAN_POINT('',(36.4555577062156,807.068457256096,118.982914917393));
#76332=CARTESIAN_POINT('',(36.4555577062156,810.658387852764,108.825623134402));
#76333=CARTESIAN_POINT('Origin',(36.4555577062156,806.597035025487,118.816298350126));
#76334=CARTESIAN_POINT('Origin',(36.1215670662255,805.368444180703,106.955978050976));
#76335=CARTESIAN_POINT('',(36.1215670662255,803.530712981596,117.732556388215));
#76336=CARTESIAN_POINT('Origin',(36.1215670662255,801.778513584035,117.113269833968));
#76337=CARTESIAN_POINT('',(36.1215670662255,804.197179250664,115.846867465779));
#76338=CARTESIAN_POINT('',(36.1215670662255,807.120643578265,107.575264605223));
#76339=CARTESIAN_POINT('Origin',(36.1215670662255,802.444979853103,115.227580911532));
#76340=CARTESIAN_POINT('Origin',(36.1215670662255,805.368444180703,106.955978050976));
#76341=CARTESIAN_POINT('',(36.1215670662255,803.705027549197,113.162873294465));
#76342=CARTESIAN_POINT('Origin',(36.1215670662255,803.233605318588,112.996256727198));
#76343=CARTESIAN_POINT('',(36.1215670662255,802.249935814643,117.279886401235));
#76344=CARTESIAN_POINT('',(36.1215670662255,805.839866411312,107.122594618243));
#76345=CARTESIAN_POINT('Origin',(36.1215670662255,801.778513584035,117.113269833968));
#76346=CARTESIAN_POINT('Origin',(38.6421417333314,795.620407971914,103.510692221739));
#76347=CARTESIAN_POINT('',(38.6421417333314,793.832692525286,114.304947818229));
#76348=CARTESIAN_POINT('Origin',(38.6421417333314,792.030477375246,113.667984004731));
#76349=CARTESIAN_POINT('',(38.6421417333314,794.499158794355,112.419258895794));
#76350=CARTESIAN_POINT('',(38.6421417333314,797.422623121955,104.147656035238));
#76351=CARTESIAN_POINT('Origin',(38.6421417333314,792.696943644314,111.782295082296));
#76352=CARTESIAN_POINT('Origin',(38.6421417333314,795.620407971914,103.510692221739));
#76353=CARTESIAN_POINT('',(38.6421417333314,793.956991340408,109.717587465228));
#76354=CARTESIAN_POINT('Origin',(38.6421417333314,793.485569109799,109.550970897961));
#76355=CARTESIAN_POINT('',(38.6421417333314,792.501899605855,113.834600571998));
#76356=CARTESIAN_POINT('',(38.6421417333314,796.091830202523,103.677308789006));
#76357=CARTESIAN_POINT('Origin',(38.6421417333314,792.030477375246,113.667984004731));
#76358=CARTESIAN_POINT('Origin',(41.2192472761507,791.274059237588,101.974545516642));
#76359=CARTESIAN_POINT('',(41.2192472761507,789.145227456717,112.648239058651));
#76360=CARTESIAN_POINT('Origin',(41.2192472761507,787.684128640919,112.131837299634));
#76361=CARTESIAN_POINT('',(41.2192472761507,789.811693725789,110.762550136206));
#76362=CARTESIAN_POINT('',(41.2192472761507,792.735158053385,102.49094727566));
#76363=CARTESIAN_POINT('',(39.7442317533746,787.902560458671,110.087797842478));
#76364=CARTESIAN_POINT('Origin',(41.2192472761522,788.350594909987,110.246148377198));
#76365=CARTESIAN_POINT('',(42.7661923053508,788.263967910344,110.215531464427));
#76366=CARTESIAN_POINT('Ctrl Pts',(42.7661922957563,788.263967909607,110.215531464166));
#76367=CARTESIAN_POINT('Ctrl Pts',(42.7576496927167,788.128357840798,110.167602277356));
#76368=CARTESIAN_POINT('Ctrl Pts',(42.729089354505,787.994387123929,110.120716649006));
#76369=CARTESIAN_POINT('Ctrl Pts',(42.627691869533,787.721691289648,110.026032551387));
#76370=CARTESIAN_POINT('Ctrl Pts',(42.5504466448361,787.586099090374,109.97941496988));
#76371=CARTESIAN_POINT('Ctrl Pts',(42.3277194563926,787.30916137911,109.884730050415));
#76372=CARTESIAN_POINT('Ctrl Pts',(42.1716038272599,787.179045937569,109.840642865158));
#76373=CARTESIAN_POINT('Ctrl Pts',(41.889457604766,787.025002344919,109.78838353968));
#76374=CARTESIAN_POINT('Ctrl Pts',(41.7791159733533,786.979941045624,109.773079760154));
#76375=CARTESIAN_POINT('Ctrl Pts',(41.5826242356446,786.924183406791,109.754005617275));
#76376=CARTESIAN_POINT('Ctrl Pts',(41.4989623551683,786.90742981042,109.748218661099));
#76377=CARTESIAN_POINT('Ctrl Pts',(41.3756211561855,786.892678768829,109.743001632323));
#76378=CARTESIAN_POINT('Ctrl Pts',(41.3368035967877,786.889441333856,109.741828028186));
#76379=CARTESIAN_POINT('Ctrl Pts',(41.2095058860293,786.88340089315,109.739505704016));
#76380=CARTESIAN_POINT('Ctrl Pts',(41.1208920861614,786.886399441584,109.740290711422));
#76381=CARTESIAN_POINT('Ctrl Pts',(40.9019145860912,786.911704903613,109.74823340755));
#76382=CARTESIAN_POINT('Ctrl Pts',(40.7733674323024,786.94268665391,109.758303443042));
#76383=CARTESIAN_POINT('Ctrl Pts',(40.458350410294,787.060702263822,109.797357332023));
#76384=CARTESIAN_POINT('Ctrl Pts',(40.2832716228728,787.168316322986,109.833418795446));
#76385=CARTESIAN_POINT('Ctrl Pts',(40.0416454203311,787.392022078613,109.909768279067));
#76386=CARTESIAN_POINT('Ctrl Pts',(39.9597641668178,787.489881377695,109.943441271257));
#76387=CARTESIAN_POINT('Ctrl Pts',(39.830368156229,787.69271580738,110.013947340926));
#76388=CARTESIAN_POINT('Ctrl Pts',(39.7808072878434,787.795518055038,110.049965435164));
#76389=CARTESIAN_POINT('Ctrl Pts',(39.7442317638745,787.902560455324,110.087797841296));
#76390=CARTESIAN_POINT('Origin',(41.2192472761522,788.350594909987,110.246148377198));
#76391=CARTESIAN_POINT('Origin',(41.2192472761507,791.274059237588,101.974545516642));
#76392=CARTESIAN_POINT('',(41.2192472761507,789.610642606081,108.181440760131));
#76393=CARTESIAN_POINT('Origin',(41.2192472761507,789.139220375473,108.014824192864));
#76394=CARTESIAN_POINT('',(41.2192472761507,788.155550871528,112.298453866901));
#76395=CARTESIAN_POINT('',(41.2192472761507,791.745481468196,102.141162083909));
#76396=CARTESIAN_POINT('Origin',(41.2192472761507,787.684128640919,112.131837299634));
#76397=CARTESIAN_POINT('Origin',(40.0979118432977,824.392570067125,113.679747836629));
#76398=CARTESIAN_POINT('',(40.0979118432977,821.801001889583,124.189894678977));
#76399=CARTESIAN_POINT('Origin',(40.0979118432977,820.802639470456,123.837039619621));
#76400=CARTESIAN_POINT('',(40.0979118432977,822.467468158652,122.304205756542));
#76401=CARTESIAN_POINT('',(40.0979118432977,825.390932486252,114.032602895986));
#76402=CARTESIAN_POINT('Origin',(40.0979118432977,821.469105739524,121.951350697185));
#76403=CARTESIAN_POINT('Origin',(40.0979118432977,824.392570067125,113.679747836629));
#76404=CARTESIAN_POINT('',(40.0979118432977,822.729153435618,119.886643080118));
#76405=CARTESIAN_POINT('Origin',(40.0979118432977,822.257731205009,119.720026512851));
#76406=CARTESIAN_POINT('',(40.0979118432977,821.274061701065,124.003656186888));
#76407=CARTESIAN_POINT('',(40.0979118432977,824.863992297733,113.846364403896));
#76408=CARTESIAN_POINT('Origin',(40.0979118432977,820.802639470456,123.837039619621));
#76409=CARTESIAN_POINT('Origin',(37.1747032078952,821.567378999314,112.681229720536));
#76410=CARTESIAN_POINT('',(37.1747032078952,819.199217682029,123.270336106458));
#76411=CARTESIAN_POINT('Origin',(37.1747032078952,817.977448402646,122.838521503527));
#76412=CARTESIAN_POINT('',(37.1747032078952,819.865683951097,121.384647184023));
#76413=CARTESIAN_POINT('',(37.1747032078952,822.789148278697,113.113044323467));
#76414=CARTESIAN_POINT('Origin',(37.1747032078952,818.643914671714,120.952832581092));
#76415=CARTESIAN_POINT('Origin',(37.1747032078952,821.567378999314,112.681229720536));
#76416=CARTESIAN_POINT('',(37.1747032078952,819.903962367808,118.888124964024));
#76417=CARTESIAN_POINT('Origin',(37.1747032078952,819.432540137199,118.721508396757));
#76418=CARTESIAN_POINT('',(37.1747032078952,818.448870633255,123.005138070794));
#76419=CARTESIAN_POINT('',(37.1747032078952,822.038801229923,112.847846287803));
#76420=CARTESIAN_POINT('Origin',(37.1747032078952,817.977448402646,122.838521503527));
#76421=CARTESIAN_POINT('Origin',(34.4182340978906,817.919448503564,111.391927652523));
#76422=CARTESIAN_POINT('',(34.4182340978906,815.844234308896,122.084571463692));
#76423=CARTESIAN_POINT('Origin',(34.4182340978906,814.329517906896,121.549219435515));
#76424=CARTESIAN_POINT('',(34.4182340978906,816.510700577964,120.198882541257));
#76425=CARTESIAN_POINT('',(34.4182340978906,819.434164905565,111.927279680701));
#76426=CARTESIAN_POINT('Origin',(34.4182340978906,814.995984175964,119.66353051308));
#76427=CARTESIAN_POINT('Origin',(34.4182340978906,817.919448503564,111.391927652523));
#76428=CARTESIAN_POINT('',(34.4182340978906,816.256031872058,117.598822896012));
#76429=CARTESIAN_POINT('Origin',(34.4182340978906,815.784609641449,117.432206328745));
#76430=CARTESIAN_POINT('',(34.4182340978906,814.800940137504,121.715836002782));
#76431=CARTESIAN_POINT('',(34.4182340978906,818.390870734173,111.558544219791));
#76432=CARTESIAN_POINT('Origin',(34.4182340978906,814.329517906896,121.549219435515));
#76433=CARTESIAN_POINT('Origin',(32.5973253096532,813.824056794096,109.944477651355));
#76434=CARTESIAN_POINT('',(32.5973253096532,811.957738341874,120.710952286068));
#76435=CARTESIAN_POINT('Origin',(32.5973253096532,810.234126197427,120.101769434346));
#76436=CARTESIAN_POINT('',(32.5973253096532,812.624204610942,118.825263363633));
#76437=CARTESIAN_POINT('',(32.5973253096532,815.547668938542,110.553660503077));
#76438=CARTESIAN_POINT('Origin',(32.5973253096532,810.900592466495,118.216080511911));
#76439=CARTESIAN_POINT('Origin',(32.5973253096532,813.824056794096,109.944477651355));
#76440=CARTESIAN_POINT('',(32.5973253096532,812.160640162589,116.151372894843));
#76441=CARTESIAN_POINT('Origin',(32.5973253096532,811.68921793198,115.984756327576));
#76442=CARTESIAN_POINT('',(32.5973253096532,810.705548428036,120.268386001613));
#76443=CARTESIAN_POINT('',(32.5973253096532,814.295479024704,110.111094218622));
#76444=CARTESIAN_POINT('Origin',(32.5973253096532,810.234126197427,120.101769434346));
#76445=CARTESIAN_POINT('Origin',(31.2080751504518,809.176303253188,108.301804289325));
#76446=CARTESIAN_POINT('',(31.2080751504518,807.338572054081,119.078382626563));
#76447=CARTESIAN_POINT('Origin',(31.2080751504518,805.586372656519,118.459096072316));
#76448=CARTESIAN_POINT('',(31.2080751504518,808.005038323149,117.192693704128));
#76449=CARTESIAN_POINT('',(31.2080751504518,810.928502650749,108.921090843572));
#76450=CARTESIAN_POINT('Origin',(31.2080751504518,806.252838925588,116.573407149881));
#76451=CARTESIAN_POINT('Origin',(31.2080751504518,809.176303253188,108.301804289325));
#76452=CARTESIAN_POINT('',(31.2080751504518,807.512886621681,114.508699532813));
#76453=CARTESIAN_POINT('Origin',(31.2080751504518,807.041464391073,114.342082965546));
#76454=CARTESIAN_POINT('',(31.2080751504518,806.057794887128,118.625712639584));
#76455=CARTESIAN_POINT('',(31.2080751504518,809.647725483797,108.468420856592));
#76456=CARTESIAN_POINT('Origin',(31.2080751504518,805.586372656519,118.459096072316));
#76457=CARTESIAN_POINT('Origin',(31.1559196361592,804.688652124068,106.715716536822));
#76458=CARTESIAN_POINT('',(31.1559196361592,802.80796387578,117.477112399392));
#76459=CARTESIAN_POINT('Origin',(31.1559196361592,801.0987215274,116.873008319814));
#76460=CARTESIAN_POINT('',(31.1559196361592,803.474430144848,115.591423476957));
#76461=CARTESIAN_POINT('',(31.1559196361592,806.397894472449,107.319820616401));
#76462=CARTESIAN_POINT('Origin',(31.1559196361592,801.765187796468,114.987319397378));
#76463=CARTESIAN_POINT('Origin',(31.1559196361592,804.688652124068,106.715716536822));
#76464=CARTESIAN_POINT('',(31.1559196361592,803.025235492562,112.922611780311));
#76465=CARTESIAN_POINT('Origin',(31.1559196361592,802.553813261953,112.755995213043));
#76466=CARTESIAN_POINT('',(31.1559196361592,801.570143758008,117.039624887081));
#76467=CARTESIAN_POINT('',(31.1559196361592,805.160074354677,106.882333104089));
#76468=CARTESIAN_POINT('Origin',(31.1559196361592,801.0987215274,116.873008319814));
#76469=CARTESIAN_POINT('Origin',(31.5239774476895,799.147180839632,104.757173084534));
#76470=CARTESIAN_POINT('',(31.5239774476895,797.359465393004,115.551428681024));
#76471=CARTESIAN_POINT('Origin',(31.5239774476895,795.557250242964,114.914464867526));
#76472=CARTESIAN_POINT('',(31.5239774476895,798.025931662073,113.665739758589));
#76473=CARTESIAN_POINT('',(31.5239774476895,800.949395989673,105.394136898033));
#76474=CARTESIAN_POINT('Origin',(31.5239774476895,796.223716512032,113.02877594509));
#76475=CARTESIAN_POINT('Origin',(31.5239774476895,799.147180839632,104.757173084534));
#76476=CARTESIAN_POINT('',(31.5239774476895,797.483764208126,110.964068328022));
#76477=CARTESIAN_POINT('Origin',(31.5239774476895,797.012341977518,110.797451760755));
#76478=CARTESIAN_POINT('',(31.5239774476895,796.028672473573,115.081081434793));
#76479=CARTESIAN_POINT('',(31.5239774476895,799.618603070241,104.923789651801));
#76480=CARTESIAN_POINT('Origin',(31.5239774476895,795.557250242964,114.914464867526));
#76481=CARTESIAN_POINT('Origin',(33.0863303722204,794.390624412805,103.076045101183));
#76482=CARTESIAN_POINT('',(33.0863303722204,792.261792631934,113.749738643192));
#76483=CARTESIAN_POINT('Origin',(33.0863303722204,790.800693816136,113.233336884174));
#76484=CARTESIAN_POINT('',(33.0863303722204,792.928258901002,111.864049720756));
#76485=CARTESIAN_POINT('',(33.0863303722204,795.851723228602,103.5924468602));
#76486=CARTESIAN_POINT('Origin',(33.0863303722204,791.467160085205,111.347647961739));
#76487=CARTESIAN_POINT('Origin',(33.0863303722204,794.390624412805,103.076045101183));
#76488=CARTESIAN_POINT('',(33.0863303722204,792.727207781298,109.282940344671));
#76489=CARTESIAN_POINT('Origin',(33.0863303722204,792.25578555069,109.116323777404));
#76490=CARTESIAN_POINT('',(33.0863303722204,791.272116046745,113.399953451442));
#76491=CARTESIAN_POINT('',(33.0863303722204,794.862046643414,103.24266166845));
#76492=CARTESIAN_POINT('Origin',(33.0863303722204,790.800693816136,113.233336884174));
#76493=CARTESIAN_POINT('Origin',(39.2926393238238,827.005229895783,114.603150221633));
#76494=CARTESIAN_POINT('',(39.2926393238238,824.413661718241,125.11329706398));
#76495=CARTESIAN_POINT('Origin',(39.2926393238238,823.415299299114,124.760442004624));
#76496=CARTESIAN_POINT('',(39.2926393238238,825.08012798731,123.227608141545));
#76497=CARTESIAN_POINT('',(39.2926393238238,828.00359231491,114.956005280989));
#76498=CARTESIAN_POINT('Origin',(39.2926393238238,824.081765568183,122.874753082189));
#76499=CARTESIAN_POINT('Origin',(39.2926393238238,827.005229895783,114.603150221633));
#76500=CARTESIAN_POINT('',(39.2926393238238,825.341813264276,120.810045465121));
#76501=CARTESIAN_POINT('Origin',(39.2926393238238,824.870391033668,120.643428897854));
#76502=CARTESIAN_POINT('',(39.2926393238238,823.886721529723,124.927058571891));
#76503=CARTESIAN_POINT('',(39.2926393238238,827.476652126392,114.7697667889));
#76504=CARTESIAN_POINT('Origin',(39.2926393238238,823.415299299114,124.760442004624));
#76505=CARTESIAN_POINT('Origin',(35.8103117702064,824.81480790225,113.828980974337));
#76506=CARTESIAN_POINT('',(35.8103117702064,822.446646584964,124.418087360259));
#76507=CARTESIAN_POINT('Origin',(35.8103117702064,821.224877305582,123.986272757328));
#76508=CARTESIAN_POINT('',(35.8103117702064,823.113112854032,122.532398437824));
#76509=CARTESIAN_POINT('',(35.8103117702064,826.036577181633,114.260795577268));
#76510=CARTESIAN_POINT('Origin',(35.8103117702064,821.89134357465,122.100583834893));
#76511=CARTESIAN_POINT('Origin',(35.8103117702064,824.81480790225,113.828980974337));
#76512=CARTESIAN_POINT('',(35.8103117702064,823.151391270744,120.035876217825));
#76513=CARTESIAN_POINT('Origin',(35.8103117702064,822.679969040135,119.869259650558));
#76514=CARTESIAN_POINT('',(35.8103117702064,821.69629953619,124.152889324596));
#76515=CARTESIAN_POINT('',(35.8103117702064,825.286230132859,113.995597541604));
#76516=CARTESIAN_POINT('Origin',(35.8103117702064,821.224877305582,123.986272757328));
#76517=CARTESIAN_POINT('Origin',(32.3096533977779,821.786939631185,112.758829876858));
#76518=CARTESIAN_POINT('',(32.3096533977779,819.711725436516,123.451473688027));
#76519=CARTESIAN_POINT('Origin',(32.3096533977779,818.197009034516,122.91612165985));
#76520=CARTESIAN_POINT('',(32.3096533977779,820.378191705585,121.565784765592));
#76521=CARTESIAN_POINT('',(32.3096533977779,823.301656033185,113.294181905036));
#76522=CARTESIAN_POINT('Origin',(32.3096533977779,818.863475303584,121.030432737414));
#76523=CARTESIAN_POINT('Origin',(32.3096533977779,821.786939631185,112.758829876858));
#76524=CARTESIAN_POINT('',(32.3096533977779,820.123522999678,118.965725120347));
#76525=CARTESIAN_POINT('Origin',(32.3096533977779,819.652100769069,118.79910855308));
#76526=CARTESIAN_POINT('',(32.3096533977779,818.668431265125,123.082738227117));
#76527=CARTESIAN_POINT('',(32.3096533977779,822.258361861793,112.925446444125));
#76528=CARTESIAN_POINT('Origin',(32.3096533977779,818.197009034516,122.91612165985));
#76529=CARTESIAN_POINT('Origin',(29.6254390364126,818.137991867514,111.469168271943));
#76530=CARTESIAN_POINT('',(29.6254390364126,816.271673415292,122.235642906657));
#76531=CARTESIAN_POINT('Origin',(29.6254390364126,814.548061270846,121.626460054934));
#76532=CARTESIAN_POINT('',(29.6254390364126,816.93813968436,120.349953984221));
#76533=CARTESIAN_POINT('',(29.6254390364126,819.861604011961,112.078351123665));
#76534=CARTESIAN_POINT('Origin',(29.6254390364126,815.214527539914,119.740771132499));
#76535=CARTESIAN_POINT('Origin',(29.6254390364126,818.137991867514,111.469168271943));
#76536=CARTESIAN_POINT('',(29.6254390364126,816.474575236008,117.676063515431));
#76537=CARTESIAN_POINT('Origin',(29.6254390364126,816.003153005399,117.509446948164));
#76538=CARTESIAN_POINT('',(29.6254390364126,815.019483501454,121.793076622201));
#76539=CARTESIAN_POINT('',(29.6254390364126,818.609414098123,111.63578483921));
#76540=CARTESIAN_POINT('Origin',(29.6254390364126,814.548061270846,121.626460054934));
#76541=CARTESIAN_POINT('Origin',(27.2416462563186,813.864135359284,109.958642772384));
#76542=CARTESIAN_POINT('',(27.2416462563186,812.026404160177,120.735221109623));
#76543=CARTESIAN_POINT('Origin',(27.2416462563186,810.274204762616,120.115934555376));
#76544=CARTESIAN_POINT('',(27.2416462563186,812.692870429245,118.849532187187));
#76545=CARTESIAN_POINT('',(27.2416462563186,815.616334756846,110.577929326631));
#76546=CARTESIAN_POINT('Origin',(27.2416462563186,810.940671031684,118.23024563294));
#76547=CARTESIAN_POINT('Origin',(27.2416462563186,813.864135359284,109.958642772384));
#76548=CARTESIAN_POINT('',(27.2416462563186,812.200718727778,116.165538015873));
#76549=CARTESIAN_POINT('Origin',(27.2416462563186,811.729296497169,115.998921448606));
#76550=CARTESIAN_POINT('',(27.2416462563186,810.745626993224,120.282551122643));
#76551=CARTESIAN_POINT('',(27.2416462563186,814.335557589893,110.125259339651));
#76552=CARTESIAN_POINT('Origin',(27.2416462563186,810.274204762616,120.115934555376));
#76553=CARTESIAN_POINT('Origin',(26.2010344369226,809.484774135699,108.410828336578));
#76554=CARTESIAN_POINT('',(26.2010344369226,807.604085887411,119.172224199147));
#76555=CARTESIAN_POINT('Origin',(26.2010344369226,805.89484353903,118.568120119569));
#76556=CARTESIAN_POINT('',(26.2010344369226,808.270552156479,117.286535276712));
#76557=CARTESIAN_POINT('',(26.2010344369226,811.194016484079,109.014932416156));
#76558=CARTESIAN_POINT('Origin',(26.2010344369226,806.561309808099,116.682431197134));
#76559=CARTESIAN_POINT('Origin',(26.2010344369226,809.484774135699,108.410828336578));
#76560=CARTESIAN_POINT('',(26.2010344369226,807.821357504193,114.617723580066));
#76561=CARTESIAN_POINT('Origin',(26.2010344369226,807.349935273584,114.451107012799));
#76562=CARTESIAN_POINT('',(26.2010344369226,806.366265769639,118.734736686836));
#76563=CARTESIAN_POINT('',(26.2010344369226,809.956196366308,108.577444903845));
#76564=CARTESIAN_POINT('Origin',(26.2010344369226,805.89484353903,118.568120119569));
#76565=CARTESIAN_POINT('Origin',(25.3390697374316,803.992247515504,106.469583584716));
#76566=CARTESIAN_POINT('',(25.3390697374316,802.204532068876,117.263839181206));
#76567=CARTESIAN_POINT('Origin',(25.3390697374316,800.402316918835,116.626875367708));
#76568=CARTESIAN_POINT('',(25.3390697374316,802.870998337944,115.378150258771));
#76569=CARTESIAN_POINT('',(25.3390697374316,805.794462665544,107.106547398215));
#76570=CARTESIAN_POINT('Origin',(25.3390697374316,801.068783187903,114.741186445273));
#76571=CARTESIAN_POINT('Origin',(25.3390697374316,803.992247515504,106.469583584716));
#76572=CARTESIAN_POINT('',(25.3390697374316,802.328830883997,112.676478828205));
#76573=CARTESIAN_POINT('Origin',(25.3390697374316,801.857408653389,112.509862260938));
#76574=CARTESIAN_POINT('',(25.3390697374316,800.873739149444,116.793491934975));
#76575=CARTESIAN_POINT('',(25.3390697374316,804.463669746112,106.636200151984));
#76576=CARTESIAN_POINT('Origin',(25.3390697374316,800.402316918835,116.626875367708));
#76577=CARTESIAN_POINT('Origin',(25.818387723871,799.033367736517,104.716947682931));
#76578=CARTESIAN_POINT('',(25.818387723871,796.904535955646,115.390641224939));
#76579=CARTESIAN_POINT('Origin',(25.818387723871,795.443437139849,114.874239465922));
#76580=CARTESIAN_POINT('',(25.818387723871,797.571002224714,113.504952302504));
#76581=CARTESIAN_POINT('',(25.818387723871,800.494466552315,105.233349441948));
#76582=CARTESIAN_POINT('Origin',(25.818387723871,796.109903408917,112.988550543487));
#76583=CARTESIAN_POINT('Origin',(25.818387723871,799.033367736517,104.716947682931));
#76584=CARTESIAN_POINT('',(25.818387723871,797.369951105011,110.923842926419));
#76585=CARTESIAN_POINT('Origin',(25.818387723871,796.898528874402,110.757226359152));
#76586=CARTESIAN_POINT('',(25.818387723871,795.914859370457,115.040856033189));
#76587=CARTESIAN_POINT('',(25.818387723871,799.504789967126,104.883564250198));
#76588=CARTESIAN_POINT('Origin',(25.818387723871,795.443437139849,114.874239465922));
#76589=CARTESIAN_POINT('Origin',(27.1695766575127,793.380711610087,102.719107745449));
#76590=CARTESIAN_POINT('',(27.1695766575127,790.97816259038,113.296060353798));
#76591=CARTESIAN_POINT('Origin',(27.1695766575127,789.790781013418,112.87639952844));
#76592=CARTESIAN_POINT('',(27.1695766575127,791.644628859449,111.410371431363));
#76593=CARTESIAN_POINT('',(27.1695766575127,794.568093187049,103.138768570807));
#76594=CARTESIAN_POINT('',(26.8302275943695,791.600709061904,111.394848688847));
#76595=CARTESIAN_POINT('Origin',(27.1695766575141,790.457247282485,110.990710606004));
#76596=CARTESIAN_POINT('',(25.9127399611503,790.376124123725,110.981073928445));
#76597=CARTESIAN_POINT('Ctrl Pts',(25.9127399611504,790.376124123725,110.981073928445));
#76598=CARTESIAN_POINT('Ctrl Pts',(25.9055874800323,790.483136414161,111.016781431184));
#76599=CARTESIAN_POINT('Ctrl Pts',(25.9136369112483,790.590820092905,111.052683799123));
#76600=CARTESIAN_POINT('Ctrl Pts',(25.9690778860656,790.842405034397,111.136728108892));
#76601=CARTESIAN_POINT('Ctrl Pts',(26.0299102940817,790.981536107245,111.183353587182));
#76602=CARTESIAN_POINT('Ctrl Pts',(26.1995966396547,791.226937399855,111.266151235457));
#76603=CARTESIAN_POINT('Ctrl Pts',(26.3053678987038,791.332133910036,111.301940653525));
#76604=CARTESIAN_POINT('Ctrl Pts',(26.5497091625053,791.500376393043,111.359703614437));
#76605=CARTESIAN_POINT('Ctrl Pts',(26.6858070399473,791.562608259858,111.381382576231));
#76606=CARTESIAN_POINT('Ctrl Pts',(26.8302275943693,791.600709061904,111.394848688848));
#76607=CARTESIAN_POINT('',(28.4218514091029,790.583031932634,111.035167157397));
#76608=CARTESIAN_POINT('Ctrl Pts',(28.4218514095886,790.583031931885,111.035167157132));
#76609=CARTESIAN_POINT('Ctrl Pts',(28.4337689638032,790.477559435438,110.997889608137));
#76610=CARTESIAN_POINT('Ctrl Pts',(28.430643339413,790.371000767451,110.960403070916));
#76611=CARTESIAN_POINT('Ctrl Pts',(28.3962813721003,790.171821902233,110.890856204986));
#76612=CARTESIAN_POINT('Ctrl Pts',(28.3680120124044,790.079599353015,110.858882283526));
#76613=CARTESIAN_POINT('Ctrl Pts',(28.2650618942256,789.850809070196,110.780282222341));
#76614=CARTESIAN_POINT('Ctrl Pts',(28.1737123951907,789.722733212863,110.737038440023));
#76615=CARTESIAN_POINT('Ctrl Pts',(27.9518861123843,789.512401256264,110.667606548889));
#76616=CARTESIAN_POINT('Ctrl Pts',(27.8259459980945,789.429555555268,110.641103162105));
#76617=CARTESIAN_POINT('Ctrl Pts',(27.5578613172935,789.313752584681,110.605707845539));
#76618=CARTESIAN_POINT('Ctrl Pts',(27.4191425282237,789.278839242261,110.596067471477));
#76619=CARTESIAN_POINT('Ctrl Pts',(27.1259918700454,789.253550609447,110.59206710079));
#76620=CARTESIAN_POINT('Ctrl Pts',(26.9735308851987,789.266538812695,110.598802966545));
#76621=CARTESIAN_POINT('Ctrl Pts',(26.75335717898,789.324487291314,110.62142302944));
#76622=CARTESIAN_POINT('Ctrl Pts',(26.6814475117158,789.350361655281,110.631098020792));
#76623=CARTESIAN_POINT('Ctrl Pts',(26.563258185529,789.405151119292,110.651011114534));
#76624=CARTESIAN_POINT('Ctrl Pts',(26.5156521743354,789.431027062694,110.660277588935));
#76625=CARTESIAN_POINT('Ctrl Pts',(26.44898174078,789.473016771392,110.675134208564));
#76626=CARTESIAN_POINT('Ctrl Pts',(26.4283985204782,789.486849842576,110.68000507493));
#76627=CARTESIAN_POINT('Ctrl Pts',(26.3605541410553,789.535436747924,110.697037838876));
#76628=CARTESIAN_POINT('Ctrl Pts',(26.3154825093639,789.57281589133,110.710020416739));
#76629=CARTESIAN_POINT('Ctrl Pts',(26.2055383718527,789.67809999404,110.746308960983));
#76630=CARTESIAN_POINT('Ctrl Pts',(26.1458120891379,789.750329498672,110.77094586298));
#76631=CARTESIAN_POINT('Ctrl Pts',(26.0364130077358,789.919666471888,110.828284944853));
#76632=CARTESIAN_POINT('Ctrl Pts',(25.9906709130046,790.018147111709,110.861386421255));
#76633=CARTESIAN_POINT('Ctrl Pts',(25.9341567116865,790.204254288454,110.92370472727));
#76634=CARTESIAN_POINT('Ctrl Pts',(25.9185125677585,790.289756911455,110.952255206282));
#76635=CARTESIAN_POINT('Ctrl Pts',(25.9127399611503,790.376124123725,110.981073928445));
#76636=CARTESIAN_POINT('Origin',(27.1695766575141,790.457247282485,110.990710606004));
#76637=CARTESIAN_POINT('Origin',(27.1695766575127,793.380711610087,102.719107745449));
#76638=CARTESIAN_POINT('',(27.1695766575127,791.717294978581,108.926002988937));
#76639=CARTESIAN_POINT('Origin',(27.1695766575127,791.245872747972,108.75938642167));
#76640=CARTESIAN_POINT('',(27.1695766575127,790.262203244027,113.043016095707));
#76641=CARTESIAN_POINT('',(27.1695766575127,793.852133840696,102.885724312716));
#76642=CARTESIAN_POINT('Origin',(27.1695766575127,789.790781013418,112.87639952844));
#76643=CARTESIAN_POINT('Origin',(39.0810955775722,829.718653111089,115.562165796892));
#76644=CARTESIAN_POINT('',(39.0810955775722,827.127084933548,126.072312639239));
#76645=CARTESIAN_POINT('Origin',(39.0810955775722,826.128722514421,125.719457579883));
#76646=CARTESIAN_POINT('',(39.0810955775722,827.793551202616,124.186623716804));
#76647=CARTESIAN_POINT('',(39.0810955775722,830.717015530217,115.915020856248));
#76648=CARTESIAN_POINT('Origin',(39.0810955775722,826.795188783489,123.833768657448));
#76649=CARTESIAN_POINT('Origin',(39.0810955775722,829.718653111089,115.562165796892));
#76650=CARTESIAN_POINT('',(39.0810955775722,828.055236479583,121.76906104038));
#76651=CARTESIAN_POINT('Origin',(39.0810955775722,827.583814248974,121.602444473113));
#76652=CARTESIAN_POINT('',(39.0810955775722,826.60014474503,125.88607414715));
#76653=CARTESIAN_POINT('',(39.0810955775722,830.190075341698,115.728782364159));
#76654=CARTESIAN_POINT('Origin',(39.0810955775722,826.128722514421,125.719457579883));
#76655=CARTESIAN_POINT('Origin',(35.1918435298943,828.258732143763,115.046180329378));
#76656=CARTESIAN_POINT('',(35.1918435298943,825.890570826477,125.6352867153));
#76657=CARTESIAN_POINT('Origin',(35.1918435298943,824.668801547094,125.203472112369));
#76658=CARTESIAN_POINT('',(35.1918435298943,826.557037095545,123.749597792865));
#76659=CARTESIAN_POINT('',(35.1918435298943,829.480501423146,115.477994932309));
#76660=CARTESIAN_POINT('Origin',(35.1918435298943,825.335267816163,123.317783189934));
#76661=CARTESIAN_POINT('Origin',(35.1918435298943,828.258732143763,115.046180329378));
#76662=CARTESIAN_POINT('',(35.1918435298943,826.595315512257,121.253075572866));
#76663=CARTESIAN_POINT('Origin',(35.1918435298943,826.123893281648,121.086459005599));
#76664=CARTESIAN_POINT('',(35.1918435298943,825.140223777703,125.370088679636));
#76665=CARTESIAN_POINT('',(35.1918435298943,828.730154374372,115.212796896645));
#76666=CARTESIAN_POINT('Origin',(35.1918435298943,824.668801547094,125.203472112369));
#76667=CARTESIAN_POINT('Origin',(31.0999914639398,825.983258470151,114.241950940547));
#76668=CARTESIAN_POINT('',(31.0999914639398,823.908044275483,124.934594751716));
#76669=CARTESIAN_POINT('Origin',(31.0999914639398,822.393327873482,124.399242723538));
#76670=CARTESIAN_POINT('',(31.0999914639398,824.574510544551,123.048905829281));
#76671=CARTESIAN_POINT('',(31.0999914639398,827.497974872151,114.777302968724));
#76672=CARTESIAN_POINT('Origin',(31.0999914639398,823.05979414255,122.513553801103));
#76673=CARTESIAN_POINT('Origin',(31.0999914639398,825.983258470151,114.241950940547));
#76674=CARTESIAN_POINT('',(31.0999914639398,824.319841838645,120.448846184035));
#76675=CARTESIAN_POINT('Origin',(31.0999914639398,823.848419608036,120.282229616768));
#76676=CARTESIAN_POINT('',(31.0999914639398,822.864750104091,124.565859290805));
#76677=CARTESIAN_POINT('',(31.0999914639398,826.45468070076,114.408567507814));
#76678=CARTESIAN_POINT('Origin',(31.0999914639398,822.393327873482,124.399242723538));
#76679=CARTESIAN_POINT('Origin',(27.6697845773275,822.940231179145,113.166442132503));
#76680=CARTESIAN_POINT('',(27.6697845773275,821.073912726923,123.932916767216));
#76681=CARTESIAN_POINT('Origin',(27.6697845773275,819.350300582477,123.323733915494));
#76682=CARTESIAN_POINT('',(27.6697845773275,821.740378995992,122.047227844781));
#76683=CARTESIAN_POINT('',(27.6697845773275,824.663843323592,113.775624984225));
#76684=CARTESIAN_POINT('Origin',(27.6697845773275,820.016766851545,121.438044993059));
#76685=CARTESIAN_POINT('Origin',(27.6697845773275,822.940231179145,113.166442132503));
#76686=CARTESIAN_POINT('',(27.6697845773275,821.276814547639,119.373337375991));
#76687=CARTESIAN_POINT('Origin',(27.6697845773275,820.80539231703,119.206720808724));
#76688=CARTESIAN_POINT('',(27.6697845773275,819.821722813085,123.490350482761));
#76689=CARTESIAN_POINT('',(27.6697845773275,823.411653409754,113.33305869977));
#76690=CARTESIAN_POINT('Origin',(27.6697845773275,819.350300582477,123.323733915494));
#76691=CARTESIAN_POINT('Origin',(24.3956323595381,819.227059741242,111.854081708051));
#76692=CARTESIAN_POINT('',(24.3956323595381,817.389328542135,122.630660045289));
#76693=CARTESIAN_POINT('Origin',(24.3956323595381,815.637129144574,122.011373491042));
#76694=CARTESIAN_POINT('',(24.3956323595381,818.055794811203,120.744971122854));
#76695=CARTESIAN_POINT('',(24.3956323595381,820.979259138803,112.473368262298));
#76696=CARTESIAN_POINT('Origin',(24.3956323595381,816.303595413642,120.125684568607));
#76697=CARTESIAN_POINT('Origin',(24.3956323595381,819.227059741242,111.854081708051));
#76698=CARTESIAN_POINT('',(24.3956323595381,817.563643109736,118.060976951539));
#76699=CARTESIAN_POINT('Origin',(24.3956323595381,817.092220879127,117.894360384272));
#76700=CARTESIAN_POINT('',(24.3956323595381,816.108551375182,122.177990058309));
#76701=CARTESIAN_POINT('',(24.3956323595381,819.698481971851,112.020698275318));
#76702=CARTESIAN_POINT('Origin',(24.3956323595381,815.637129144574,122.011373491042));
#76703=CARTESIAN_POINT('Origin',(22.4120439649557,815.147387523168,110.412187507023));
#76704=CARTESIAN_POINT('',(22.4120439649557,813.26669927488,121.173583369593));
#76705=CARTESIAN_POINT('Origin',(22.4120439649557,811.5574569265,120.569479290015));
#76706=CARTESIAN_POINT('',(22.4120439649557,813.933165543949,119.287894447158));
#76707=CARTESIAN_POINT('',(22.4120439649557,816.856629871549,111.016291586602));
#76708=CARTESIAN_POINT('Origin',(22.4120439649557,812.223923195568,118.68379036758));
#76709=CARTESIAN_POINT('Origin',(22.4120439649557,815.147387523168,110.412187507023));
#76710=CARTESIAN_POINT('',(22.4120439649557,813.483970891662,116.619082750512));
#76711=CARTESIAN_POINT('Origin',(22.4120439649557,813.012548661053,116.452466183245));
#76712=CARTESIAN_POINT('',(22.4120439649557,812.028879157109,120.736095857282));
#76713=CARTESIAN_POINT('',(22.4120439649557,815.618809753777,110.578804074291));
#76714=CARTESIAN_POINT('Origin',(22.4120439649557,811.5574569265,120.569479290015));
#76715=CARTESIAN_POINT('Origin',(20.3577287479766,809.943855336583,108.573083166371));
#76716=CARTESIAN_POINT('',(20.3577287479766,808.156139889955,119.367338762861));
#76717=CARTESIAN_POINT('Origin',(20.3577287479766,806.353924739914,118.730374949362));
#76718=CARTESIAN_POINT('',(20.3577287479766,808.822606159023,117.481649840425));
#76719=CARTESIAN_POINT('',(20.3577287479766,811.746070486623,109.210046979869));
#76720=CARTESIAN_POINT('Origin',(20.3577287479766,807.020391008982,116.844686026927));
#76721=CARTESIAN_POINT('Origin',(20.3577287479766,809.943855336583,108.573083166371));
#76722=CARTESIAN_POINT('',(20.3577287479766,808.280438705076,114.779978409859));
#76723=CARTESIAN_POINT('Origin',(20.3577287479766,807.809016474468,114.613361842592));
#76724=CARTESIAN_POINT('',(20.3577287479766,806.825346970523,118.896991516629));
#76725=CARTESIAN_POINT('',(20.3577287479766,810.415277567191,108.739699733638));
#76726=CARTESIAN_POINT('Origin',(20.3577287479766,806.353924739914,118.730374949362));
#76727=CARTESIAN_POINT('Origin',(19.7330633002943,804.999379047125,106.825537945139));
#76728=CARTESIAN_POINT('',(19.7330633002943,802.870547266253,117.499231487147));
#76729=CARTESIAN_POINT('Origin',(19.7330633002943,801.409448450456,116.98282972813));
#76730=CARTESIAN_POINT('',(19.7330633002943,803.537013535322,115.613542564712));
#76731=CARTESIAN_POINT('',(19.7330633002943,806.460477862922,107.341939704156));
#76732=CARTESIAN_POINT('Origin',(19.7330633002943,802.075914719524,115.097140805695));
#76733=CARTESIAN_POINT('Origin',(19.7330633002943,804.999379047125,106.825537945139));
#76734=CARTESIAN_POINT('',(19.7330633002943,803.335962415618,113.032433188627));
#76735=CARTESIAN_POINT('Origin',(19.7330633002943,802.864540185009,112.86581662136));
#76736=CARTESIAN_POINT('',(19.7330633002943,801.880870681065,117.149446295397));
#76737=CARTESIAN_POINT('',(19.7330633002943,805.470801277733,106.992154512406));
#76738=CARTESIAN_POINT('Origin',(19.7330633002943,801.409448450456,116.98282972813));
#76739=CARTESIAN_POINT('Origin',(19.8082279830515,799.205375633292,104.777741093684));
#76740=CARTESIAN_POINT('',(19.8082279830515,796.802826613586,115.354693702033));
#76741=CARTESIAN_POINT('Origin',(19.8082279830515,795.615445036624,114.935032876675));
#76742=CARTESIAN_POINT('',(19.8082279830515,797.469292882654,113.469004779598));
#76743=CARTESIAN_POINT('',(19.8082279830515,800.392757210254,105.197401919042));
#76744=CARTESIAN_POINT('',(19.7284454031586,797.466907750936,113.468161793346));
#76745=CARTESIAN_POINT('Origin',(19.8082279830522,796.281911305691,113.049343954239));
#76746=CARTESIAN_POINT('',(21.061492498137,796.165218265362,113.008100685379));
#76747=CARTESIAN_POINT('Ctrl Pts',(21.0614924981326,796.165218265362,113.008100685379));
#76748=CARTESIAN_POINT('Ctrl Pts',(21.051798009416,796.072662642909,112.975388396707));
#76749=CARTESIAN_POINT('Ctrl Pts',(21.030581995983,795.981260194669,112.943217870007));
#76750=CARTESIAN_POINT('Ctrl Pts',(20.9482250146403,795.756960391498,112.864801980375));
#76751=CARTESIAN_POINT('Ctrl Pts',(20.8725787658467,795.630530765864,112.821124628641));
#76752=CARTESIAN_POINT('Ctrl Pts',(20.67567293284,795.407198225804,112.745382807087));
#76753=CARTESIAN_POINT('Ctrl Pts',(20.5553985159303,795.312693260727,112.71415839815));
#76754=CARTESIAN_POINT('Ctrl Pts',(20.2762522758205,795.164715767788,112.667177037225));
#76755=CARTESIAN_POINT('Ctrl Pts',(20.118103337146,795.11564868478,112.652972245053));
#76756=CARTESIAN_POINT('Ctrl Pts',(19.792769730301,795.077819089887,112.645735012025));
#76757=CARTESIAN_POINT('Ctrl Pts',(19.6287529031382,795.088828338619,112.652551589102));
#76758=CARTESIAN_POINT('Ctrl Pts',(19.3140101801986,795.16965780951,112.685770924614));
#76759=CARTESIAN_POINT('Ctrl Pts',(19.1663375993738,795.238951474633,112.711926900593));
#76760=CARTESIAN_POINT('Ctrl Pts',(18.9892241897138,795.368014120911,112.758514326216));
#76761=CARTESIAN_POINT('Ctrl Pts',(18.9442069834037,795.406034668372,112.772084785551));
#76762=CARTESIAN_POINT('Ctrl Pts',(18.9022600487226,795.446994874529,112.78656150833));
#76763=CARTESIAN_POINT('Ctrl Pts',(18.7875711892465,795.558985878489,112.82614291844));
#76764=CARTESIAN_POINT('Ctrl Pts',(18.6973577013089,795.69146959996,112.871957729857));
#76765=CARTESIAN_POINT('Ctrl Pts',(18.5757316682768,795.983261361675,112.9713963271));
#76766=CARTESIAN_POINT('Ctrl Pts',(18.5459381968071,796.139877355637,113.024102720641));
#76767=CARTESIAN_POINT('Ctrl Pts',(18.5522635281122,796.455913449457,113.129825565382));
#76768=CARTESIAN_POINT('Ctrl Pts',(18.5886152141294,796.612211023319,113.181809569817));
#76769=CARTESIAN_POINT('Ctrl Pts',(18.7195813826428,796.893916373066,113.275536973982));
#76770=CARTESIAN_POINT('Ctrl Pts',(18.8095884522755,797.018099714331,113.316879418162));
#76771=CARTESIAN_POINT('Ctrl Pts',(19.0294088382157,797.224902079374,113.386034899408));
#76772=CARTESIAN_POINT('Ctrl Pts',(19.1559698441546,797.307075171622,113.413687062561));
#76773=CARTESIAN_POINT('Ctrl Pts',(19.4319539624635,797.423754998297,113.45322603606));
#76774=CARTESIAN_POINT('Ctrl Pts',(19.5787789720714,797.457950071032,113.464995846177));
#76775=CARTESIAN_POINT('Ctrl Pts',(19.7284454031586,797.466907750936,113.468161793346));
#76776=CARTESIAN_POINT('Origin',(19.8082279830522,796.281911305691,113.049343954239));
#76777=CARTESIAN_POINT('Origin',(19.8082279830515,799.205375633292,104.777741093684));
#76778=CARTESIAN_POINT('',(19.8082279830515,797.541959001786,110.984636337172));
#76779=CARTESIAN_POINT('Origin',(19.8082279830515,797.070536771177,110.818019769905));
#76780=CARTESIAN_POINT('',(19.8082279830515,796.086867267232,115.101649443942));
#76781=CARTESIAN_POINT('',(19.8082279830515,799.676797863901,104.944357660951));
#76782=CARTESIAN_POINT('Origin',(19.8082279830515,795.615445036624,114.935032876675));
#76783=CARTESIAN_POINT('Origin',(39.4725260813523,832.414250098087,116.514880979901));
#76784=CARTESIAN_POINT('',(39.4725260813523,829.822681920545,127.025027822248));
#76785=CARTESIAN_POINT('Origin',(39.4725260813523,828.824319501418,126.672172762892));
#76786=CARTESIAN_POINT('',(39.4725260813523,830.489148189613,125.139338899813));
#76787=CARTESIAN_POINT('',(39.4725260813523,833.412612517214,116.867736039257));
#76788=CARTESIAN_POINT('Origin',(39.4725260813523,829.490785770486,124.786483840457));
#76789=CARTESIAN_POINT('Origin',(39.4725260813523,832.414250098087,116.514880979901));
#76790=CARTESIAN_POINT('',(39.4725260813523,830.75083346658,122.721776223389));
#76791=CARTESIAN_POINT('Origin',(39.4725260813523,830.279411235971,122.555159656122));
#76792=CARTESIAN_POINT('',(39.4725260813523,829.295741732027,126.838789330159));
#76793=CARTESIAN_POINT('',(39.4725260813523,832.885672328695,116.681497547168));
#76794=CARTESIAN_POINT('Origin',(39.4725260813523,828.824319501418,126.672172762892));
#76795=CARTESIAN_POINT('Origin',(35.3463285167995,831.748635708716,116.279630333071));
#76796=CARTESIAN_POINT('',(35.3463285167995,829.38047439143,126.868736718993));
#76797=CARTESIAN_POINT('Origin',(35.3463285167995,828.158705112047,126.436922116062));
#76798=CARTESIAN_POINT('',(35.3463285167995,830.046940660498,124.983047796558));
#76799=CARTESIAN_POINT('',(35.3463285167995,832.970404988099,116.711444936002));
#76800=CARTESIAN_POINT('Origin',(35.3463285167995,828.825171381116,124.551233193627));
#76801=CARTESIAN_POINT('Origin',(35.3463285167995,831.748635708716,116.279630333071));
#76802=CARTESIAN_POINT('',(35.3463285167995,830.08521907721,122.48652557656));
#76803=CARTESIAN_POINT('Origin',(35.3463285167995,829.613796846601,122.319909009292));
#76804=CARTESIAN_POINT('',(35.3463285167995,828.630127342656,126.60353868333));
#76805=CARTESIAN_POINT('',(35.3463285167995,832.220057939325,116.446246900338));
#76806=CARTESIAN_POINT('Origin',(35.3463285167995,828.158705112047,126.436922116062));
#76807=CARTESIAN_POINT('Origin',(30.8421163274859,830.325005751029,115.776471336301));
#76808=CARTESIAN_POINT('',(30.8421163274859,828.249791556361,126.46911514747));
#76809=CARTESIAN_POINT('Origin',(30.8421163274859,826.73507515436,125.933763119292));
#76810=CARTESIAN_POINT('',(30.8421163274859,828.916257825429,124.583426225035));
#76811=CARTESIAN_POINT('',(30.8421163274859,831.839722153029,116.311823364479));
#76812=CARTESIAN_POINT('Origin',(30.8421163274859,827.401541423429,124.048074196857));
#76813=CARTESIAN_POINT('Origin',(30.8421163274859,830.325005751029,115.776471336301));
#76814=CARTESIAN_POINT('',(30.8421163274859,828.661589119523,121.983366579789));
#76815=CARTESIAN_POINT('Origin',(30.8421163274859,828.190166888914,121.816750012522));
#76816=CARTESIAN_POINT('',(30.8421163274859,827.206497384969,126.100379686559));
#76817=CARTESIAN_POINT('',(30.8421163274859,830.796427981638,115.943087903568));
#76818=CARTESIAN_POINT('Origin',(30.8421163274859,826.73507515436,125.933763119292));
#76819=CARTESIAN_POINT('Origin',(26.8158334165305,828.02089382737,114.962120220904));
#76820=CARTESIAN_POINT('',(26.8158334165305,826.154575375148,125.728594855617));
#76821=CARTESIAN_POINT('Origin',(26.8158334165305,824.430963230701,125.119412003895));
#76822=CARTESIAN_POINT('',(26.8158334165305,826.821041644216,123.842905933182));
#76823=CARTESIAN_POINT('',(26.8158334165305,829.744505971817,115.571303072626));
#76824=CARTESIAN_POINT('Origin',(26.8158334165305,825.09742949977,123.23372308146));
#76825=CARTESIAN_POINT('Origin',(26.8158334165305,828.02089382737,114.962120220904));
#76826=CARTESIAN_POINT('',(26.8158334165305,826.357477195864,121.169015464392));
#76827=CARTESIAN_POINT('Origin',(26.8158334165305,825.886054965255,121.002398897125));
#76828=CARTESIAN_POINT('',(26.8158334165305,824.90238546131,125.286028571162));
#76829=CARTESIAN_POINT('',(26.8158334165305,828.492316057979,115.128736788171));
#76830=CARTESIAN_POINT('Origin',(26.8158334165305,824.430963230701,125.119412003895));
#76831=CARTESIAN_POINT('Origin',(22.7944179240885,825.030690869403,113.905281319512));
#76832=CARTESIAN_POINT('',(22.7944179240885,823.192959670296,124.68185965675));
#76833=CARTESIAN_POINT('Origin',(22.7944179240885,821.440760272734,124.062573102503));
#76834=CARTESIAN_POINT('',(22.7944179240885,823.859425939364,122.796170734315));
#76835=CARTESIAN_POINT('',(22.7944179240885,826.782890266964,114.524567873759));
#76836=CARTESIAN_POINT('Origin',(22.7944179240885,822.107226541802,122.176884180068));
#76837=CARTESIAN_POINT('Origin',(22.7944179240885,825.030690869403,113.905281319512));
#76838=CARTESIAN_POINT('',(22.7944179240885,823.367274237896,120.112176563));
#76839=CARTESIAN_POINT('Origin',(22.7944179240885,822.895852007288,119.945559995733));
#76840=CARTESIAN_POINT('',(22.7944179240885,821.912182503343,124.22918966977));
#76841=CARTESIAN_POINT('',(22.7944179240885,825.502113100012,114.071897886779));
#76842=CARTESIAN_POINT('Origin',(22.7944179240885,821.440760272734,124.062573102503));
#76843=CARTESIAN_POINT('Origin',(19.9545452854761,821.42900890921,112.632325048824));
#76844=CARTESIAN_POINT('',(19.9545452854761,819.548320660922,123.393720911393));
#76845=CARTESIAN_POINT('Origin',(19.9545452854761,817.839078312542,122.789616831815));
#76846=CARTESIAN_POINT('',(19.9545452854761,820.21478692999,121.508031988958));
#76847=CARTESIAN_POINT('',(19.9545452854761,823.138251257591,113.236429128402));
#76848=CARTESIAN_POINT('Origin',(19.9545452854761,818.50554458161,120.90392790938));
#76849=CARTESIAN_POINT('Origin',(19.9545452854761,821.42900890921,112.632325048824));
#76850=CARTESIAN_POINT('',(19.9545452854761,819.765592277704,118.839220292312));
#76851=CARTESIAN_POINT('Origin',(19.9545452854761,819.294170047095,118.672603725045));
#76852=CARTESIAN_POINT('',(19.9545452854761,818.31050054315,122.956233399082));
#76853=CARTESIAN_POINT('',(19.9545452854761,821.900431139819,112.798941616091));
#76854=CARTESIAN_POINT('Origin',(19.9545452854761,817.839078312542,122.789616831815));
#76855=CARTESIAN_POINT('Origin',(16.7976629836891,816.741890482106,110.975738804068));
#76856=CARTESIAN_POINT('',(16.7976629836891,814.954175035478,121.769994400558));
#76857=CARTESIAN_POINT('Origin',(16.7976629836891,813.151959885437,121.13303058706));
#76858=CARTESIAN_POINT('',(16.7976629836891,815.620641304546,119.884305478123));
#76859=CARTESIAN_POINT('',(16.7976629836891,818.544105632146,111.612702617567));
#76860=CARTESIAN_POINT('Origin',(16.7976629836891,813.818426154505,119.247341664624));
#76861=CARTESIAN_POINT('Origin',(16.7976629836891,816.741890482106,110.975738804068));
#76862=CARTESIAN_POINT('',(16.7976629836891,815.078473850599,117.182634047557));
#76863=CARTESIAN_POINT('Origin',(16.7976629836891,814.60705161999,117.016017480289));
#76864=CARTESIAN_POINT('',(16.7976629836891,813.623382116046,121.299647154327));
#76865=CARTESIAN_POINT('',(16.7976629836891,817.213312712714,111.142355371335));
#76866=CARTESIAN_POINT('Origin',(16.7976629836891,813.151959885437,121.13303058706));
#76867=CARTESIAN_POINT('Origin',(15.0963149794262,812.027915022255,109.30966037521));
#76868=CARTESIAN_POINT('',(15.0963149794262,809.899083241384,119.983353917218));
#76869=CARTESIAN_POINT('Origin',(15.0963149794262,808.437984425586,119.466952158201));
#76870=CARTESIAN_POINT('',(15.0963149794262,810.565549510452,118.097664994783));
#76871=CARTESIAN_POINT('',(15.0963149794262,813.489013838052,109.826062134227));
#76872=CARTESIAN_POINT('Origin',(15.0963149794262,809.104450694654,117.581263235766));
#76873=CARTESIAN_POINT('Origin',(15.0963149794262,812.027915022255,109.30966037521));
#76874=CARTESIAN_POINT('',(15.0963149794262,810.364498390749,115.516555618698));
#76875=CARTESIAN_POINT('Origin',(15.0963149794262,809.893076160139,115.349939051431));
#76876=CARTESIAN_POINT('',(15.0963149794262,808.909406656195,119.633568725468));
#76877=CARTESIAN_POINT('',(15.0963149794262,812.499337252864,109.476276942477));
#76878=CARTESIAN_POINT('Origin',(15.0963149794262,808.437984425586,119.466952158201));
#76879=CARTESIAN_POINT('Origin',(13.8921703539818,806.345790072918,107.30140515861));
#76880=CARTESIAN_POINT('',(13.8921703539818,803.943241053211,117.87835776696));
#76881=CARTESIAN_POINT('Origin',(13.8921703539818,802.755859476249,117.458696941601));
#76882=CARTESIAN_POINT('',(13.8921703526055,804.609653252271,115.992821829335));
#76883=CARTESIAN_POINT('',(13.8921703539818,807.53317164988,107.721065983968));
#76884=CARTESIAN_POINT('',(15.0923154240742,803.062507307636,115.445836008528));
#76885=CARTESIAN_POINT('Ctrl Pts',(13.892170353543,804.609653252273,115.992821829331));
#76886=CARTESIAN_POINT('Ctrl Pts',(13.8039600128603,804.609598801071,115.992975892591));
#76887=CARTESIAN_POINT('Ctrl Pts',(13.7158062647662,804.600761138376,115.990168610606));
#76888=CARTESIAN_POINT('Ctrl Pts',(13.4803696455484,804.552934593457,115.97461895202));
#76889=CARTESIAN_POINT('Ctrl Pts',(13.3385502159868,804.497357182754,115.956366602613));
#76890=CARTESIAN_POINT('Ctrl Pts',(13.078202995359,804.338137961123,115.904028614265));
#76891=CARTESIAN_POINT('Ctrl Pts',(12.9629550049546,804.234294769472,115.869875067184));
#76892=CARTESIAN_POINT('Ctrl Pts',(12.7731347945951,803.984378370213,115.787382953728));
#76893=CARTESIAN_POINT('Ctrl Pts',(12.7033371078485,803.838599875019,115.739116747616));
#76894=CARTESIAN_POINT('Ctrl Pts',(12.6278731521198,803.530668849765,115.636258508348));
#76895=CARTESIAN_POINT('Ctrl Pts',(12.6226627237605,803.371616751307,115.58269111305));
#76896=CARTESIAN_POINT('Ctrl Pts',(12.677542057288,803.0623338468,115.477070554118));
#76897=CARTESIAN_POINT('Ctrl Pts',(12.7366394034306,802.915053877657,115.426026248129));
#76898=CARTESIAN_POINT('Ctrl Pts',(12.8241262990056,802.783027873801,115.379363791155));
#76899=CARTESIAN_POINT('Ctrl Pts',(12.8561242376968,802.734739956517,115.362297207324));
#76900=CARTESIAN_POINT('Ctrl Pts',(12.8917644004736,802.688726510102,115.345901787053));
#76901=CARTESIAN_POINT('Ctrl Pts',(13.0364797953235,802.527771612137,115.288042560581));
#76902=CARTESIAN_POINT('Ctrl Pts',(13.1655296844413,802.431055595334,115.25219459766));
#76903=CARTESIAN_POINT('Ctrl Pts',(13.4552481156411,802.290325870049,115.19780448547));
#76904=CARTESIAN_POINT('Ctrl Pts',(13.613050383001,802.247425331864,115.179716447631));
#76905=CARTESIAN_POINT('Ctrl Pts',(13.9391917620889,802.220695745209,115.164136281486));
#76906=CARTESIAN_POINT('Ctrl Pts',(14.104487459637,802.237710452545,115.167012679576));
#76907=CARTESIAN_POINT('Ctrl Pts',(14.4097964864331,802.327770213418,115.193523954294));
#76908=CARTESIAN_POINT('Ctrl Pts',(14.5481315972824,802.396647764069,115.215690767848));
#76909=CARTESIAN_POINT('Ctrl Pts',(14.7897617083049,802.576522731334,115.276073212751));
#76910=CARTESIAN_POINT('Ctrl Pts',(14.8915648013111,802.685367669113,115.313535540805));
#76911=CARTESIAN_POINT('Ctrl Pts',(15.02152410657,802.888627576681,115.384515219428));
#76912=CARTESIAN_POINT('Ctrl Pts',(15.0624228462959,802.973874642577,115.414510225735));
#76913=CARTESIAN_POINT('Ctrl Pts',(15.0923154240733,803.062507307637,115.445836008528));
#76914=CARTESIAN_POINT('',(14.0754411389211,804.597066825487,115.988201265256));
#76915=CARTESIAN_POINT('Origin',(13.8921703539826,803.422325745316,115.573008019166));
#76916=CARTESIAN_POINT('Ctrl Pts',(14.0754411389211,804.597066825487,115.988201265256));
#76917=CARTESIAN_POINT('Ctrl Pts',(14.0146511156019,804.605497522896,115.99118095898));
#76918=CARTESIAN_POINT('Ctrl Pts',(13.9533971024774,804.609691046822,115.992714894107));
#76919=CARTESIAN_POINT('Ctrl Pts',(13.892170353543,804.609653252273,115.992821829331));
#76920=CARTESIAN_POINT('Origin',(13.8921703539818,806.345790072918,107.30140515861));
#76921=CARTESIAN_POINT('',(13.8921703539818,804.682373441412,113.508300402098));
#76922=CARTESIAN_POINT('Origin',(13.8921703539818,804.210951210803,113.341683834831));
#76923=CARTESIAN_POINT('',(13.8921703539818,803.227281706858,117.625313508868));
#76924=CARTESIAN_POINT('',(13.8921703539818,806.817212303527,107.468021725877));
#76925=CARTESIAN_POINT('Origin',(13.8921703539818,802.755859476249,117.458696941601));
#76926=CARTESIAN_POINT('Origin',(40.4498234438578,834.974210333533,117.419657545528));
#76927=CARTESIAN_POINT('',(40.4498234438578,832.382642155992,127.929804387875));
#76928=CARTESIAN_POINT('Origin',(40.4498234438578,831.384279736864,127.576949328519));
#76929=CARTESIAN_POINT('',(40.4498234438578,833.04910842506,126.04411546544));
#76930=CARTESIAN_POINT('',(40.4498234438578,835.97257275266,117.772512604884));
#76931=CARTESIAN_POINT('Origin',(40.4498234438578,832.050746005933,125.691260406084));
#76932=CARTESIAN_POINT('Origin',(40.4498234438578,834.974210333533,117.419657545528));
#76933=CARTESIAN_POINT('',(40.4498234438578,833.310793702027,123.626552789016));
#76934=CARTESIAN_POINT('Origin',(40.4498234438578,832.839371471418,123.459936221749));
#76935=CARTESIAN_POINT('',(40.4498234438578,831.855701967473,127.743565895786));
#76936=CARTESIAN_POINT('',(40.4498234438578,835.445632564142,117.586274112795));
#76937=CARTESIAN_POINT('Origin',(40.4498234438578,831.384279736864,127.576949328519));
#76938=CARTESIAN_POINT('Origin',(36.2670149956938,835.131993064906,117.475423301507));
#76939=CARTESIAN_POINT('',(36.2670149956938,832.76383174762,128.064529687429));
#76940=CARTESIAN_POINT('Origin',(36.2670149956938,831.542062468237,127.632715084498));
#76941=CARTESIAN_POINT('',(36.2670149956938,833.430298016688,126.178840764994));
#76942=CARTESIAN_POINT('',(36.2670149956938,836.353762344289,117.907237904438));
#76943=CARTESIAN_POINT('Origin',(36.2670149956938,832.208528737306,125.747026162063));
#76944=CARTESIAN_POINT('Origin',(36.2670149956938,835.131993064906,117.475423301507));
#76945=CARTESIAN_POINT('',(36.2670149956938,833.4685764334,123.682318544995));
#76946=CARTESIAN_POINT('Origin',(36.2670149956938,832.997154202791,123.515701977728));
#76947=CARTESIAN_POINT('',(36.2670149956938,832.013484698846,127.799331651765));
#76948=CARTESIAN_POINT('',(36.2670149956938,835.603415295515,117.642039868774));
#76949=CARTESIAN_POINT('Origin',(36.2670149956938,831.542062468237,127.632715084498));
#76950=CARTESIAN_POINT('Origin',(31.547298369302,834.622426283629,117.295325159381));
#76951=CARTESIAN_POINT('',(31.547298369302,832.547212088961,127.98796897055));
#76952=CARTESIAN_POINT('Origin',(31.547298369302,831.032495686961,127.452616942372));
#76953=CARTESIAN_POINT('',(31.547298369302,833.21367835803,126.102280048115));
#76954=CARTESIAN_POINT('',(31.547298369302,836.13714268563,117.830677187558));
#76955=CARTESIAN_POINT('Origin',(31.547298369302,831.698961956029,125.566928019937));
#76956=CARTESIAN_POINT('Origin',(31.547298369302,834.622426283629,117.295325159381));
#76957=CARTESIAN_POINT('',(31.547298369302,832.959009652123,123.502220402869));
#76958=CARTESIAN_POINT('Origin',(31.547298369302,832.487587421514,123.335603835602));
#76959=CARTESIAN_POINT('',(31.547298369302,831.503917917569,127.619233509639));
#76960=CARTESIAN_POINT('',(31.547298369302,835.093848514238,117.461941726648));
#76961=CARTESIAN_POINT('Origin',(31.547298369302,831.032495686961,127.452616942372));
#76962=CARTESIAN_POINT('Origin',(27.1009073174613,833.157930474737,116.777722788063));
#76963=CARTESIAN_POINT('',(27.1009073174613,831.291612022515,127.544197422777));
#76964=CARTESIAN_POINT('Origin',(27.1009073174613,829.567999878068,126.935014571055));
#76965=CARTESIAN_POINT('',(27.1009073174613,831.958078291583,125.658508500342));
#76966=CARTESIAN_POINT('',(27.1009073174613,834.881542619183,117.386905639786));
#76967=CARTESIAN_POINT('Origin',(27.1009073174613,830.234466147136,125.04932564862));
#76968=CARTESIAN_POINT('Origin',(27.1009073174613,833.157930474737,116.777722788063));
#76969=CARTESIAN_POINT('',(27.1009073174613,831.49451384323,122.984618031552));
#76970=CARTESIAN_POINT('Origin',(27.1009073174613,831.023091612622,122.818001464285));
#76971=CARTESIAN_POINT('',(27.1009073174613,830.039422108677,127.101631138322));
#76972=CARTESIAN_POINT('',(27.1009073174613,833.629352705345,116.944339355331));
#76973=CARTESIAN_POINT('Origin',(27.1009073174613,829.567999878068,126.935014571055));
#76974=CARTESIAN_POINT('Origin',(22.5079837042789,831.021382214555,116.022594340998));
#76975=CARTESIAN_POINT('',(22.5079837042789,829.183651015447,126.799172678236));
#76976=CARTESIAN_POINT('Origin',(22.5079837042789,827.431451617886,126.179886123989));
#76977=CARTESIAN_POINT('',(22.5079837042789,829.850117284516,124.913483755801));
#76978=CARTESIAN_POINT('',(22.5079837042789,832.773581612116,116.641880895245));
#76979=CARTESIAN_POINT('Origin',(22.5079837042789,828.097917886954,124.294197201554));
#76980=CARTESIAN_POINT('Origin',(22.5079837042789,831.021382214555,116.022594340998));
#76981=CARTESIAN_POINT('',(22.5079837042789,829.357965583048,122.229489584486));
#76982=CARTESIAN_POINT('Origin',(22.5079837042789,828.88654335244,122.062873017219));
#76983=CARTESIAN_POINT('',(22.5079837042789,827.902873848495,126.346502691256));
#76984=CARTESIAN_POINT('',(22.5079837042789,831.492804445163,116.189210908265));
#76985=CARTESIAN_POINT('Origin',(22.5079837042789,827.431451617886,126.179886123989));
#76986=CARTESIAN_POINT('Origin',(14.8144644015597,824.089246195621,113.57254291722));
#76987=CARTESIAN_POINT('',(14.8144644015597,822.301530748994,124.36679851371));
#76988=CARTESIAN_POINT('Origin',(14.8144644015597,820.499315598953,123.729834700212));
#76989=CARTESIAN_POINT('',(14.8144644015597,822.967997018062,122.481109591275));
#76990=CARTESIAN_POINT('',(14.8144644015597,825.891461345662,114.209506730719));
#76991=CARTESIAN_POINT('Origin',(14.8144644015597,821.165781868021,121.844145777777));
#76992=CARTESIAN_POINT('Origin',(14.8144644015597,824.089246195621,113.57254291722));
#76993=CARTESIAN_POINT('',(14.8144644015597,822.425829564115,119.779438160709));
#76994=CARTESIAN_POINT('Origin',(14.8144644015597,821.954407333506,119.612821593442));
#76995=CARTESIAN_POINT('',(14.8144644015597,820.970737829562,123.896451267479));
#76996=CARTESIAN_POINT('',(14.8144644015597,824.56066842623,113.739159484487));
#76997=CARTESIAN_POINT('Origin',(14.8144644015597,820.499315598953,123.729834700212));
#76998=CARTESIAN_POINT('Origin',(12.110790912476,819.811794913137,112.060746902808));
#76999=CARTESIAN_POINT('',(12.110790912476,817.682963132266,122.734440444817));
#77000=CARTESIAN_POINT('Origin',(12.110790912476,816.221864316469,122.218038685799));
#77001=CARTESIAN_POINT('',(12.110790912476,818.349429401335,120.848751522381));
#77002=CARTESIAN_POINT('',(12.110790912476,821.272893728935,112.577148661825));
#77003=CARTESIAN_POINT('Origin',(12.110790912476,816.888330585537,120.332349763364));
#77004=CARTESIAN_POINT('Origin',(12.110790912476,819.811794913137,112.060746902808));
#77005=CARTESIAN_POINT('',(12.110790912476,818.148378281631,118.267642146296));
#77006=CARTESIAN_POINT('Origin',(12.110790912476,817.676956051022,118.101025579029));
#77007=CARTESIAN_POINT('',(12.110790912476,816.693286547077,122.384655253066));
#77008=CARTESIAN_POINT('',(12.110790912476,820.283217143746,112.227363470075));
#77009=CARTESIAN_POINT('Origin',(12.110790912476,816.221864316469,122.218038685799));
#77010=CARTESIAN_POINT('Origin',(9.67996387708925,814.489884554442,110.179803710707));
#77011=CARTESIAN_POINT('',(9.67996387708925,812.087335534736,120.756756319056));
#77012=CARTESIAN_POINT('Origin',(9.67996387708925,810.899953957774,120.337095493698));
#77013=CARTESIAN_POINT('',(9.67996387708875,812.75343949573,118.872092505248));
#77014=CARTESIAN_POINT('',(9.67996387708925,815.677266131404,110.599464536065));
#77015=CARTESIAN_POINT('',(10.7745374036936,810.979202184137,118.243863845951));
#77016=CARTESIAN_POINT('Ctrl Pts',(9.67996387708853,812.75343949573,118.872092505248));
#77017=CARTESIAN_POINT('Ctrl Pts',(9.67956979645961,812.753438801654,118.872094469055));
#77018=CARTESIAN_POINT('Ctrl Pts',(9.67917570725331,812.753437932054,118.872096374398));
#77019=CARTESIAN_POINT('Ctrl Pts',(9.52661826611054,812.753033349318,118.872811309619));
#77020=CARTESIAN_POINT('Ctrl Pts',(9.37573860252287,812.726461524862,118.86481051582));
#77021=CARTESIAN_POINT('Ctrl Pts',(9.08624297003607,812.621730050792,118.831730341099));
#77022=CARTESIAN_POINT('Ctrl Pts',(8.95079094906213,812.542730464648,118.80635736481));
#77023=CARTESIAN_POINT('Ctrl Pts',(8.71041275090674,812.335445413876,118.738932612376));
#77024=CARTESIAN_POINT('Ctrl Pts',(8.61021955726934,812.206512495788,118.696620203197));
#77025=CARTESIAN_POINT('Ctrl Pts',(8.46891511410034,811.920062556869,118.601354106671));
#77026=CARTESIAN_POINT('Ctrl Pts',(8.4289285066343,811.765489346632,118.549369702018));
#77027=CARTESIAN_POINT('Ctrl Pts',(8.41466265044363,811.452181770553,118.442326687973));
#77028=CARTESIAN_POINT('Ctrl Pts',(8.44006101718495,811.296528534306,118.388322986074));
#77029=CARTESIAN_POINT('Ctrl Pts',(8.49652235171455,811.150237700456,118.336618855517));
#77030=CARTESIAN_POINT('Ctrl Pts',(8.51717283095315,811.096732485738,118.317708302242));
#77031=CARTESIAN_POINT('Ctrl Pts',(8.54187830406437,811.044738971098,118.299199323518));
#77032=CARTESIAN_POINT('Ctrl Pts',(8.64787092692629,810.858939674224,118.232559245842));
#77033=CARTESIAN_POINT('Ctrl Pts',(8.75265802493252,810.739051126119,118.188521326296));
#77034=CARTESIAN_POINT('Ctrl Pts',(9.004690078727,810.54463558224,118.11515682931));
#77035=CARTESIAN_POINT('Ctrl Pts',(9.14938106998037,810.47175888592,118.086474202917));
#77036=CARTESIAN_POINT('Ctrl Pts',(9.46207627804917,810.381722544442,118.04851928758));
#77037=CARTESIAN_POINT('Ctrl Pts',(9.62729451931023,810.365984329808,118.039819694823));
#77038=CARTESIAN_POINT('Ctrl Pts',(9.94542286328407,810.394263351174,118.044495565795));
#77039=CARTESIAN_POINT('Ctrl Pts',(10.0957727599236,810.434533099207,118.056551413935));
#77040=CARTESIAN_POINT('Ctrl Pts',(10.3715667536406,810.56313291787,118.098811486384));
#77041=CARTESIAN_POINT('Ctrl Pts',(10.4950774071888,810.649649951457,118.128382377614));
#77042=CARTESIAN_POINT('Ctrl Pts',(10.6669591911075,810.822998328889,118.188790309404));
#77043=CARTESIAN_POINT('Ctrl Pts',(10.725753185945,810.898366149242,118.215293656064));
#77044=CARTESIAN_POINT('Ctrl Pts',(10.7745374036927,810.979202184137,118.243863845952));
#77045=CARTESIAN_POINT('',(10.1182782141275,812.679564119701,118.844829287164));
#77046=CARTESIAN_POINT('Origin',(9.67996387708958,811.566420226841,118.451406571262));
#77047=CARTESIAN_POINT('Ctrl Pts',(10.1182782141275,812.679564119701,118.844829287164));
#77048=CARTESIAN_POINT('Ctrl Pts',(9.97805606177369,812.728647120432,118.862176880387));
#77049=CARTESIAN_POINT('Ctrl Pts',(9.82962852093729,812.753703093081,118.871346687152));
#77050=CARTESIAN_POINT('Ctrl Pts',(9.67996387708853,812.75343949573,118.872092505248));
#77051=CARTESIAN_POINT('Origin',(9.67996387708925,814.489884554442,110.179803710707));
#77052=CARTESIAN_POINT('',(9.67996387708925,812.826467922936,116.386698954195));
#77053=CARTESIAN_POINT('Origin',(9.67996387708925,812.355045692327,116.220082386928));
#77054=CARTESIAN_POINT('',(9.67996387708925,811.371376188383,120.503712060965));
#77055=CARTESIAN_POINT('',(9.67996387708925,814.961306785051,110.346420277974));
#77056=CARTESIAN_POINT('Origin',(9.67996387708925,810.899953957774,120.337095493698));
#77057=CARTESIAN_POINT('Origin',(41.970275080754,837.286651271087,118.236952416254));
#77058=CARTESIAN_POINT('',(41.970275080754,834.695083093546,128.747099258602));
#77059=CARTESIAN_POINT('Origin',(41.970275080754,833.696720674418,128.394244199246));
#77060=CARTESIAN_POINT('',(41.970275080754,835.361549362614,126.861410336167));
#77061=CARTESIAN_POINT('',(41.970275080754,838.285013690214,118.589807475611));
#77062=CARTESIAN_POINT('Origin',(41.970275080754,834.363186943487,126.50855527681));
#77063=CARTESIAN_POINT('Origin',(41.970275080754,837.286651271087,118.236952416254));
#77064=CARTESIAN_POINT('',(41.970275080754,835.623234639581,124.443847659743));
#77065=CARTESIAN_POINT('Origin',(41.970275080754,835.151812408972,124.277231092476));
#77066=CARTESIAN_POINT('',(41.970275080754,834.168142905027,128.560860766513));
#77067=CARTESIAN_POINT('',(41.970275080754,837.758073501696,118.403568983521));
#77068=CARTESIAN_POINT('Origin',(41.970275080754,833.696720674418,128.394244199246));
#77069=CARTESIAN_POINT('Origin',(37.9136645495052,838.260935260717,118.581297343913));
#77070=CARTESIAN_POINT('',(37.9136645495052,835.892773943431,129.170403729835));
#77071=CARTESIAN_POINT('Origin',(37.9136645495052,834.671004664049,128.738589126904));
#77072=CARTESIAN_POINT('',(37.9136645495052,836.5592402125,127.2847148074));
#77073=CARTESIAN_POINT('',(37.9136645495052,839.4827045401,119.013111946843));
#77074=CARTESIAN_POINT('Origin',(37.9136645495052,835.337470933117,126.852900204469));
#77075=CARTESIAN_POINT('Origin',(37.9136645495052,838.260935260717,118.581297343913));
#77076=CARTESIAN_POINT('',(37.9136645495052,836.597518629211,124.788192587401));
#77077=CARTESIAN_POINT('Origin',(37.9136645495052,836.126096398602,124.621576020134));
#77078=CARTESIAN_POINT('',(37.9136645495052,835.142426894657,128.905205694171));
#77079=CARTESIAN_POINT('',(37.9136645495052,838.732357491326,118.74791391118));
#77080=CARTESIAN_POINT('Origin',(37.9136645495052,834.671004664049,128.738589126904));
#77081=CARTESIAN_POINT('Origin',(33.1847177503218,838.687702169366,118.732131209448));
#77082=CARTESIAN_POINT('',(33.1847177503218,836.612487974698,129.424775020617));
#77083=CARTESIAN_POINT('Origin',(33.1847177503218,835.097771572697,128.889422992439));
#77084=CARTESIAN_POINT('',(33.1847177503218,837.278954243766,127.539086098182));
#77085=CARTESIAN_POINT('',(33.1847177503218,840.202418571366,119.267483237626));
#77086=CARTESIAN_POINT('Origin',(33.1847177503218,835.764237841765,127.003734070004));
#77087=CARTESIAN_POINT('Origin',(33.1847177503218,838.687702169366,118.732131209448));
#77088=CARTESIAN_POINT('',(33.1847177503218,837.024285537859,124.939026452937));
#77089=CARTESIAN_POINT('Origin',(33.1847177503218,836.552863307251,124.772409885669));
#77090=CARTESIAN_POINT('',(33.1847177503218,835.569193803306,129.056039559707));
#77091=CARTESIAN_POINT('',(33.1847177503218,839.159124399974,118.898747776715));
#77092=CARTESIAN_POINT('Origin',(33.1847177503218,835.097771572697,128.889422992439));
#77093=CARTESIAN_POINT('Origin',(28.5125471827126,838.126827969518,118.533899289569));
#77094=CARTESIAN_POINT('',(28.5125471827126,836.260509517296,129.300373924283));
#77095=CARTESIAN_POINT('Origin',(28.5125471827126,834.536897372849,128.69119107256));
#77096=CARTESIAN_POINT('',(28.5125471827126,836.926975786364,127.414685001848));
#77097=CARTESIAN_POINT('',(28.5125471827126,839.850440113965,119.143082141291));
#77098=CARTESIAN_POINT('Origin',(28.5125471827126,835.203363641918,126.805502150125));
#77099=CARTESIAN_POINT('Origin',(28.5125471827126,838.126827969518,118.533899289569));
#77100=CARTESIAN_POINT('',(28.5125471827126,836.463411338012,124.740794533057));
#77101=CARTESIAN_POINT('Origin',(28.5125471827126,835.991989107403,124.57417796579));
#77102=CARTESIAN_POINT('',(28.5125471827126,835.008319603458,128.857807639828));
#77103=CARTESIAN_POINT('',(28.5125471827126,838.598250200127,118.700515856836));
#77104=CARTESIAN_POINT('Origin',(28.5125471827126,834.536897372849,128.69119107256));
#77105=CARTESIAN_POINT('Origin',(23.5488482499785,836.937311818387,118.113484033474));
#77106=CARTESIAN_POINT('',(23.5488482499785,835.09958061928,128.890062370713));
#77107=CARTESIAN_POINT('Origin',(23.5488482499785,833.347381221719,128.270775816466));
#77108=CARTESIAN_POINT('',(23.5488482499785,835.766046888348,127.004373448277));
#77109=CARTESIAN_POINT('',(23.5488482499785,838.689511215949,118.732770587721));
#77110=CARTESIAN_POINT('Origin',(23.5488482499785,834.013847490787,126.385086894031));
#77111=CARTESIAN_POINT('Origin',(23.5488482499785,836.937311818387,118.113484033474));
#77112=CARTESIAN_POINT('',(23.5488482499785,835.273895186881,124.320379276963));
#77113=CARTESIAN_POINT('Origin',(23.5488482499785,834.802472956272,124.153762709696));
#77114=CARTESIAN_POINT('',(23.5488482499785,833.818803452328,128.437392383733));
#77115=CARTESIAN_POINT('',(23.5488482499785,837.408734048996,118.280100600741));
#77116=CARTESIAN_POINT('Origin',(23.5488482499785,833.347381221719,128.270775816466));
#77117=CARTESIAN_POINT('Origin',(19.4007545707989,834.736072652758,117.335491631552));
#77118=CARTESIAN_POINT('',(19.4007545707989,832.85538440447,128.096887494121));
#77119=CARTESIAN_POINT('Origin',(19.4007545707989,831.14614205609,127.492783414543));
#77120=CARTESIAN_POINT('',(19.4007545707989,833.521850673538,126.211198571686));
#77121=CARTESIAN_POINT('',(19.4007545707989,836.445315001138,117.93959571113));
#77122=CARTESIAN_POINT('Origin',(19.4007545707989,831.812608325158,125.607094492108));
#77123=CARTESIAN_POINT('Origin',(19.4007545707989,834.736072652758,117.335491631552));
#77124=CARTESIAN_POINT('',(19.4007545707989,833.072656021252,123.54238687504));
#77125=CARTESIAN_POINT('Origin',(19.4007545707989,832.601233790643,123.375770307773));
#77126=CARTESIAN_POINT('',(19.4007545707989,831.617564286698,127.65939998181));
#77127=CARTESIAN_POINT('',(19.4007545707989,835.207494883367,117.502108198819));
#77128=CARTESIAN_POINT('Origin',(19.4007545707989,831.14614205609,127.492783414543));
#77129=CARTESIAN_POINT('Origin',(14.4948082960701,831.664807775925,116.250002705234));
#77130=CARTESIAN_POINT('',(14.4948082960701,829.877092329297,127.044258301724));
#77131=CARTESIAN_POINT('Origin',(14.4948082960701,828.074877179256,126.407294488225));
#77132=CARTESIAN_POINT('',(14.4948082960701,830.543558598365,125.158569379288));
#77133=CARTESIAN_POINT('',(14.4948082960701,833.467022925965,116.886966518732));
#77134=CARTESIAN_POINT('Origin',(14.4948082960701,828.741343448324,124.52160556579));
#77135=CARTESIAN_POINT('Origin',(14.4948082960701,831.664807775925,116.250002705234));
#77136=CARTESIAN_POINT('',(14.4948082960701,830.001391144418,122.456897948722));
#77137=CARTESIAN_POINT('Origin',(14.4948082960701,829.52996891381,122.290281381455));
#77138=CARTESIAN_POINT('',(14.4948082960701,828.546299409865,126.573911055492));
#77139=CARTESIAN_POINT('',(14.4948082960701,832.136230006534,116.416619272501));
#77140=CARTESIAN_POINT('Origin',(14.4948082960701,828.074877179256,126.407294488225));
#77141=CARTESIAN_POINT('Origin',(10.9069728273033,828.01082581734,114.9585618455));
#77142=CARTESIAN_POINT('',(10.9069728273033,825.881994036469,125.632255387508));
#77143=CARTESIAN_POINT('Origin',(10.9069728273033,824.420895220671,125.115853628491));
#77144=CARTESIAN_POINT('',(10.9069728273033,826.548460305538,123.746566465073));
#77145=CARTESIAN_POINT('',(10.9069728273033,829.471924633138,115.474963604517));
#77146=CARTESIAN_POINT('Origin',(10.9069728273033,825.08736148974,123.230164706056));
#77147=CARTESIAN_POINT('Origin',(10.9069728273033,828.01082581734,114.9585618455));
#77148=CARTESIAN_POINT('',(10.9069728273033,826.347409185834,121.165457088988));
#77149=CARTESIAN_POINT('Origin',(10.9069728273033,825.875986955225,120.998840521721));
#77150=CARTESIAN_POINT('',(10.9069728273033,824.892317451281,125.282470195758));
#77151=CARTESIAN_POINT('',(10.9069728273033,828.482248047949,115.125178412767));
#77152=CARTESIAN_POINT('Origin',(10.9069728273033,824.420895220671,125.115853628491));
#77153=CARTESIAN_POINT('Origin',(7.35570218782278,823.281723069322,113.287136921158));
#77154=CARTESIAN_POINT('',(7.35570218782278,820.879174049615,123.864089529508));
#77155=CARTESIAN_POINT('Origin',(7.35570218782278,819.691792472653,123.444428704149));
#77156=CARTESIAN_POINT('',(7.35570217511657,821.544643257089,121.981221677081));
#77157=CARTESIAN_POINT('',(7.35570218782278,824.469104646284,113.706797746516));
#77158=CARTESIAN_POINT('',(8.29686605548008,819.569305340243,121.279896954726));
#77159=CARTESIAN_POINT('Ctrl Pts',(7.35570217511549,821.544643257128,121.981221676971));
#77160=CARTESIAN_POINT('Ctrl Pts',(7.29157612797449,821.544446918859,121.981777191364));
#77161=CARTESIAN_POINT('Ctrl Pts',(7.22741742029148,821.539601725858,121.98078819253));
#77162=CARTESIAN_POINT('Ctrl Pts',(7.00817618497621,821.506843259943,121.972029984534));
#77163=CARTESIAN_POINT('Ctrl Pts',(6.85844003671936,821.456104950426,121.956645499649));
#77164=CARTESIAN_POINT('Ctrl Pts',(6.57800953149111,821.300430451649,121.907461662577));
#77165=CARTESIAN_POINT('Ctrl Pts',(6.45179975430232,821.193933376551,121.873078839447));
#77166=CARTESIAN_POINT('Ctrl Pts',(6.25083050590953,820.941401715186,121.789800609862));
#77167=CARTESIAN_POINT('Ctrl Pts',(6.17781532595884,820.798026636983,121.741774003968));
#77168=CARTESIAN_POINT('Ctrl Pts',(6.09502776641756,820.494336758009,121.638130209503));
#77169=CARTESIAN_POINT('Ctrl Pts',(6.08561712325453,820.337099187181,121.583566550156));
#77170=CARTESIAN_POINT('Ctrl Pts',(6.10858526548658,820.182937134755,121.529080464625));
#77171=CARTESIAN_POINT('Ctrl Pts',(6.11698576023683,820.126553057236,121.509152423826));
#77172=CARTESIAN_POINT('Ctrl Pts',(6.12967679595621,820.070853662776,121.489333661784));
#77173=CARTESIAN_POINT('Ctrl Pts',(6.19231426060091,819.868343639213,121.416787447873));
#77174=CARTESIAN_POINT('Ctrl Pts',(6.26825886848808,819.730545130996,121.366419542425));
#77175=CARTESIAN_POINT('Ctrl Pts',(6.47158953473939,819.491004532206,121.277106324189));
#77176=CARTESIAN_POINT('Ctrl Pts',(6.59684555926346,819.39137691102,121.238969015809));
#77177=CARTESIAN_POINT('Ctrl Pts',(6.88242831524046,819.242053050402,121.180059885164));
#77178=CARTESIAN_POINT('Ctrl Pts',(7.04034827026691,819.194292827357,121.160042631143));
#77179=CARTESIAN_POINT('Ctrl Pts',(7.35739219623943,819.15962821654,121.142472092751));
#77180=CARTESIAN_POINT('Ctrl Pts',(7.51318586672746,819.169560072011,121.143805503151));
#77181=CARTESIAN_POINT('Ctrl Pts',(7.81109022220729,819.241308136301,121.165972241978));
#77182=CARTESIAN_POINT('Ctrl Pts',(7.950910428069,819.301729885915,121.186320176895));
#77183=CARTESIAN_POINT('Ctrl Pts',(8.15720263191499,819.437602376076,121.233482862095));
#77184=CARTESIAN_POINT('Ctrl Pts',(8.23132230216756,819.499798858129,121.255331012136));
#77185=CARTESIAN_POINT('Ctrl Pts',(8.29686605547942,819.569305340243,121.279896954726));
#77186=CARTESIAN_POINT('',(8.02990363716613,821.361155717694,121.91319750689));
#77187=CARTESIAN_POINT('Origin',(7.355702187823,820.35825874172,121.558739781714));
#77188=CARTESIAN_POINT('Ctrl Pts',(8.02990363716613,821.361155717694,121.91319750689));
#77189=CARTESIAN_POINT('Ctrl Pts',(7.90323658112111,821.43685245227,121.939951294153));
#77190=CARTESIAN_POINT('Ctrl Pts',(7.76319673633093,821.490538065063,121.959241491818));
#77191=CARTESIAN_POINT('Ctrl Pts',(7.53050212542476,821.536536404112,121.976836420245));
#77192=CARTESIAN_POINT('Ctrl Pts',(7.44313250309093,821.544910947404,121.980464281065));
#77193=CARTESIAN_POINT('Ctrl Pts',(7.35570217511549,821.544643257128,121.981221676971));
#77194=CARTESIAN_POINT('Origin',(7.35570218782278,823.281723069322,113.287136921158));
#77195=CARTESIAN_POINT('',(7.35570218782278,821.618306437815,119.494032164646));
#77196=CARTESIAN_POINT('Origin',(7.35570218782278,821.146884207207,119.327415597379));
#77197=CARTESIAN_POINT('',(7.35570218782278,820.163214703262,123.611045271416));
#77198=CARTESIAN_POINT('',(7.35570218782278,823.75314529993,113.453753488425));
#77199=CARTESIAN_POINT('Origin',(7.35570218782278,819.691792472653,123.444428704149));
#77200=CARTESIAN_POINT('Origin',(43.9674299595719,839.250508145456,118.931045884415));
#77201=CARTESIAN_POINT('',(43.9674299595719,836.658939967914,129.441192726762));
#77202=CARTESIAN_POINT('Origin',(43.9674299595719,835.660577548787,129.088337667406));
#77203=CARTESIAN_POINT('',(43.9674299595719,837.325406236982,127.555503804327));
#77204=CARTESIAN_POINT('',(43.9674299595719,840.248870564583,119.283900943771));
#77205=CARTESIAN_POINT('Origin',(43.9674299595719,836.327043817855,127.202648744971));
#77206=CARTESIAN_POINT('Origin',(43.9674299595719,839.250508145456,118.931045884415));
#77207=CARTESIAN_POINT('',(43.9674299595719,837.587091513949,125.137941127903));
#77208=CARTESIAN_POINT('Origin',(43.9674299595719,837.11566928334,124.971324560636));
#77209=CARTESIAN_POINT('',(43.9674299595719,836.131999779396,129.254954234673));
#77210=CARTESIAN_POINT('',(43.9674299595719,839.721930376064,119.097662451682));
#77211=CARTESIAN_POINT('Origin',(43.9674299595719,835.660577548787,129.088337667406));
#77212=CARTESIAN_POINT('Origin',(40.214310691231,840.998712507863,119.548920458063));
#77213=CARTESIAN_POINT('',(40.214310691231,838.630551190577,130.138026843985));
#77214=CARTESIAN_POINT('Origin',(40.214310691231,837.408781911194,129.706212241054));
#77215=CARTESIAN_POINT('',(40.214310691231,839.297017459645,128.25233792155));
#77216=CARTESIAN_POINT('',(40.214310691231,842.220481787245,119.980735060994));
#77217=CARTESIAN_POINT('Origin',(40.214310691231,838.075248180263,127.820523318619));
#77218=CARTESIAN_POINT('Origin',(40.214310691231,840.998712507863,119.548920458063));
#77219=CARTESIAN_POINT('',(40.214310691231,839.335295876356,125.755815701551));
#77220=CARTESIAN_POINT('Origin',(40.214310691231,838.863873645748,125.589199134284));
#77221=CARTESIAN_POINT('',(40.214310691231,837.880204141803,129.872828808321));
#77222=CARTESIAN_POINT('',(40.214310691231,841.470134738472,119.71553702533));
#77223=CARTESIAN_POINT('Origin',(40.214310691231,837.408781911194,129.706212241054));
#77224=CARTESIAN_POINT('Origin',(35.6828113863847,842.343161344673,120.024094167555));
#77225=CARTESIAN_POINT('',(35.6828113863847,840.267947150005,130.716737978724));
#77226=CARTESIAN_POINT('Origin',(35.6828113863847,838.753230748005,130.181385950546));
#77227=CARTESIAN_POINT('',(35.6828113863847,840.934413419073,128.831049056289));
#77228=CARTESIAN_POINT('',(35.6828113863847,843.857877746674,120.559446195733));
#77229=CARTESIAN_POINT('Origin',(35.6828113863847,839.419697017073,128.295697028111));
#77230=CARTESIAN_POINT('Origin',(35.6828113863847,842.343161344673,120.024094167555));
#77231=CARTESIAN_POINT('',(35.6828113863847,840.679744713167,126.230989411044));
#77232=CARTESIAN_POINT('Origin',(35.6828113863847,840.208322482558,126.064372843776));
#77233=CARTESIAN_POINT('',(35.6828113863847,839.224652978613,130.348002517814));
#77234=CARTESIAN_POINT('',(35.6828113863847,842.814583575282,120.190710734822));
#77235=CARTESIAN_POINT('Origin',(35.6828113863847,838.753230748005,130.181385950546));
#77236=CARTESIAN_POINT('Origin',(30.9890575763733,842.710421647777,120.153896385235));
#77237=CARTESIAN_POINT('',(30.9890575763733,840.844103195556,130.920371019949));
#77238=CARTESIAN_POINT('Origin',(30.9890575763733,839.120491051109,130.311188168227));
#77239=CARTESIAN_POINT('',(30.9890575763733,841.510569464624,129.034682097514));
#77240=CARTESIAN_POINT('',(30.9890575763733,844.434033792224,120.763079236958));
#77241=CARTESIAN_POINT('Origin',(30.9890575763733,839.786957320177,128.425499245791));
#77242=CARTESIAN_POINT('Origin',(30.9890575763733,842.710421647777,120.153896385235));
#77243=CARTESIAN_POINT('',(30.9890575763733,841.047005016271,126.360791628724));
#77244=CARTESIAN_POINT('Origin',(30.9890575763733,840.575582785662,126.194175061457));
#77245=CARTESIAN_POINT('',(30.9890575763733,839.591913281718,130.477804735494));
#77246=CARTESIAN_POINT('',(30.9890575763733,843.181843878386,120.320512952502));
#77247=CARTESIAN_POINT('Origin',(30.9890575763733,839.120491051109,130.311188168227));
#77248=CARTESIAN_POINT('Origin',(25.8715207859182,842.519925169434,120.086568484179));
#77249=CARTESIAN_POINT('',(25.8715207859182,840.682193970327,130.863146821418));
#77250=CARTESIAN_POINT('Origin',(25.8715207859182,838.929994572766,130.243860267171));
#77251=CARTESIAN_POINT('',(25.8715207859182,841.348660239395,128.977457898982));
#77252=CARTESIAN_POINT('',(25.8715207859182,844.272124566995,120.705855038426));
#77253=CARTESIAN_POINT('Origin',(25.8715207859182,839.596460841834,128.358171344736));
#77254=CARTESIAN_POINT('Origin',(25.8715207859182,842.519925169434,120.086568484179));
#77255=CARTESIAN_POINT('',(25.8715207859182,840.856508537928,126.293463727668));
#77256=CARTESIAN_POINT('Origin',(25.8715207859182,840.385086307319,126.126847160401));
#77257=CARTESIAN_POINT('',(25.8715207859182,839.401416803374,130.410476834438));
#77258=CARTESIAN_POINT('',(25.8715207859182,842.991347400043,120.253185051446));
#77259=CARTESIAN_POINT('Origin',(25.8715207859182,838.929994572766,130.243860267171));
#77260=CARTESIAN_POINT('Origin',(21.3286658472151,841.179932470295,119.612969724517));
#77261=CARTESIAN_POINT('',(21.3286658472151,839.299244222006,130.374365587087));
#77262=CARTESIAN_POINT('Origin',(21.3286658472151,837.590001873626,129.770261507508));
#77263=CARTESIAN_POINT('',(21.3286658472151,839.965710491075,128.488676664651));
#77264=CARTESIAN_POINT('',(21.3286658472151,842.889174818675,120.217073804095));
#77265=CARTESIAN_POINT('Origin',(21.3286658472151,838.256468142695,127.884572585073));
#77266=CARTESIAN_POINT('Origin',(21.3286658472151,841.179932470295,119.612969724517));
#77267=CARTESIAN_POINT('',(21.3286658472151,839.516515838788,125.819864968005));
#77268=CARTESIAN_POINT('Origin',(21.3286658472151,839.04509360818,125.653248400738));
#77269=CARTESIAN_POINT('',(21.3286658472151,838.061424104235,129.936878074775));
#77270=CARTESIAN_POINT('',(21.3286658472151,841.651354700903,119.779586291784));
#77271=CARTESIAN_POINT('Origin',(21.3286658472151,837.590001873626,129.770261507508));
#77272=CARTESIAN_POINT('Origin',(15.8526651729103,839.137486830379,118.891100327495));
#77273=CARTESIAN_POINT('',(15.8526651729103,837.349771383751,129.685355923985));
#77274=CARTESIAN_POINT('Origin',(15.8526651729103,835.547556233711,129.048392110486));
#77275=CARTESIAN_POINT('',(15.8526651729103,838.016237652819,127.799667001549));
#77276=CARTESIAN_POINT('',(15.8526651729103,840.93970198042,119.528064140993));
#77277=CARTESIAN_POINT('Origin',(15.8526651729103,836.214022502779,127.162703188051));
#77278=CARTESIAN_POINT('Origin',(15.8526651729103,839.137486830379,118.891100327495));
#77279=CARTESIAN_POINT('',(15.8526651729103,837.474070198873,125.097995570983));
#77280=CARTESIAN_POINT('Origin',(15.8526651729103,837.002647968264,124.931379003716));
#77281=CARTESIAN_POINT('',(15.8526651729103,836.018978464319,129.215008677753));
#77282=CARTESIAN_POINT('',(15.8526651729103,839.608909060988,119.057716894762));
#77283=CARTESIAN_POINT('Origin',(15.8526651729103,835.547556233711,129.048392110486));
#77284=CARTESIAN_POINT('Origin',(11.5374733507902,836.266670741035,117.87645678503));
#77285=CARTESIAN_POINT('',(11.5374733507902,834.137838960164,128.550150327038));
#77286=CARTESIAN_POINT('Origin',(11.5374733507902,832.676740144367,128.033748568021));
#77287=CARTESIAN_POINT('',(11.5374733507902,834.804305229233,126.664461404603));
#77288=CARTESIAN_POINT('',(11.5374733507902,837.727769556833,118.392858544047));
#77289=CARTESIAN_POINT('Origin',(11.5374733507902,833.343206413435,126.148059645586));
#77290=CARTESIAN_POINT('Origin',(11.5374733507902,836.266670741035,117.87645678503));
#77291=CARTESIAN_POINT('',(11.5374733507902,834.603254109529,124.083352028518));
#77292=CARTESIAN_POINT('Origin',(11.5374733507902,834.13183187892,123.916735461251));
#77293=CARTESIAN_POINT('',(11.5374733507902,833.148162374975,128.200365135288));
#77294=CARTESIAN_POINT('',(11.5374733507902,836.738092971644,118.043073352297));
#77295=CARTESIAN_POINT('Origin',(11.5374733507902,832.676740144367,128.033748568021));
#77296=CARTESIAN_POINT('Origin',(7.02096667504837,832.337060086534,116.487599418029));
#77297=CARTESIAN_POINT('',(7.02096667504837,829.934511066827,127.064552026378));
#77298=CARTESIAN_POINT('Origin',(7.02096667504837,828.747129489865,126.64489120102));
#77299=CARTESIAN_POINT('',(7.02096666994515,830.599004089277,125.184446176129));
#77300=CARTESIAN_POINT('',(7.02096667504837,833.524441663496,116.907260243387));
#77301=CARTESIAN_POINT('',(7.76758750653674,828.457388048144,124.421246119495));
#77302=CARTESIAN_POINT('Ctrl Pts',(7.02096666484195,830.599004089278,125.184446176129));
#77303=CARTESIAN_POINT('Ctrl Pts',(6.88754184176866,830.598428459883,125.186074849416));
#77304=CARTESIAN_POINT('Ctrl Pts',(6.75480841283368,830.577742800318,125.180967780531));
#77305=CARTESIAN_POINT('Ctrl Pts',(6.46912138942601,830.487520618593,125.154490180543));
#77306=CARTESIAN_POINT('Ctrl Pts',(6.32241100157311,830.408069098372,125.129666171615));
#77307=CARTESIAN_POINT('Ctrl Pts',(6.0705602684719,830.200410514294,125.062247605861));
#77308=CARTESIAN_POINT('Ctrl Pts',(5.9677076297661,830.074463399832,125.020380632044));
#77309=CARTESIAN_POINT('Ctrl Pts',(5.82001658048626,829.793613247126,124.924809169643));
#77310=CARTESIAN_POINT('Ctrl Pts',(5.77620821768348,829.641649517263,124.872109464138));
#77311=CARTESIAN_POINT('Ctrl Pts',(5.76467934958987,829.486353867704,124.817222727024));
#77312=CARTESIAN_POINT('Ctrl Pts',(5.76046271792157,829.42955518213,124.79714814971));
#77313=CARTESIAN_POINT('Ctrl Pts',(5.7605846570906,829.372586060989,124.776880623296));
#77314=CARTESIAN_POINT('Ctrl Pts',(5.77712940574573,829.162229321906,124.70156111462));
#77315=CARTESIAN_POINT('Ctrl Pts',(5.82091237972588,829.012566175966,124.646999844751));
#77316=CARTESIAN_POINT('Ctrl Pts',(5.96665513263313,828.738433467381,124.545460604461));
#77317=CARTESIAN_POINT('Ctrl Pts',(6.0670019011125,828.616449298384,124.499421735631));
#77318=CARTESIAN_POINT('Ctrl Pts',(6.31299086818166,828.414448303395,124.421894723324));
#77319=CARTESIAN_POINT('Ctrl Pts',(6.456710677155,828.336796500924,124.391312773727));
#77320=CARTESIAN_POINT('Ctrl Pts',(6.75881384421649,828.240776304019,124.352057095193));
#77321=CARTESIAN_POINT('Ctrl Pts',(6.91324235757128,828.219966088468,124.34252521751));
#77322=CARTESIAN_POINT('Ctrl Pts',(7.22023722497622,828.23177048709,124.343505836645));
#77323=CARTESIAN_POINT('Ctrl Pts',(7.37025616922219,828.263470062076,124.35370238321));
#77324=CARTESIAN_POINT('Ctrl Pts',(7.60194283378443,828.355940183934,124.385525202896));
#77325=CARTESIAN_POINT('Ctrl Pts',(7.68814879419479,828.402248885612,124.401758073776));
#77326=CARTESIAN_POINT('Ctrl Pts',(7.76758750653594,828.457388048145,124.421246119495));
#77327=CARTESIAN_POINT('',(7.90158939818299,830.262414407737,125.059203509569));
#77328=CARTESIAN_POINT('Origin',(7.02096667504848,829.413595758933,124.759202278584));
#77329=CARTESIAN_POINT('Ctrl Pts',(7.90158939818298,830.262414407737,125.059203509569));
#77330=CARTESIAN_POINT('Ctrl Pts',(7.79438261430018,830.361287325615,125.094148544196));
#77331=CARTESIAN_POINT('Ctrl Pts',(7.66926336415262,830.44124939494,125.122725730685));
#77332=CARTESIAN_POINT('Ctrl Pts',(7.39304844123785,830.556372454823,125.165113740543));
#77333=CARTESIAN_POINT('Ctrl Pts',(7.24393858453375,830.589920863212,125.17836147125));
#77334=CARTESIAN_POINT('Ctrl Pts',(7.06833649789207,830.598575376114,125.18365593624));
#77335=CARTESIAN_POINT('Ctrl Pts',(7.04464069952261,830.599106225221,125.184157194911));
#77336=CARTESIAN_POINT('Ctrl Pts',(7.02096666484194,830.599004089278,125.184446176129));
#77337=CARTESIAN_POINT('Origin',(7.02096667504837,832.337060086534,116.487599418029));
#77338=CARTESIAN_POINT('',(7.02096667504837,830.673643455028,122.694494661517));
#77339=CARTESIAN_POINT('Origin',(7.02096667504837,830.202221224419,122.52787809425));
#77340=CARTESIAN_POINT('',(7.02096667504837,829.218551720474,126.811507768287));
#77341=CARTESIAN_POINT('',(7.02096667504837,832.808482317143,116.654215985296));
#77342=CARTESIAN_POINT('Origin',(7.02096667504837,828.747129489865,126.64489120102));
#77343=CARTESIAN_POINT('Ctrl Pts',(17.2487640684582,778.138083759694,108.757942040107));
#77344=CARTESIAN_POINT('Ctrl Pts',(-19.6797178494731,802.718757630444,117.445583893923));
#77345=CARTESIAN_POINT('Ctrl Pts',(-6.00421854062202,843.341877796349,131.803169078188));
#77346=CARTESIAN_POINT('Ctrl Pts',(7.67128076822907,883.964997962254,146.160754262452));
#77347=CARTESIAN_POINT('Ctrl Pts',(52.875234385587,883.966642709865,146.161335571909));
#77348=CARTESIAN_POINT('Ctrl Pts',(98.0791880029448,883.968287457475,146.161916881366));
#77349=CARTESIAN_POINT('Ctrl Pts',(111.75801268726,843.346162579713,131.804683465608));
#77350=CARTESIAN_POINT('Ctrl Pts',(125.436837371576,802.72403770195,117.447450049849));
#77351=CARTESIAN_POINT('Ctrl Pts',(88.5103677421852,778.140676615915,108.758858443227));
#77352=CARTESIAN_POINT('Ctrl Pts',(21.9700649362988,785.109903755238,109.100778471584));
#77353=CARTESIAN_POINT('Ctrl Pts',(-10.0648980335876,806.433308789172,116.637191306022));
#77354=CARTESIAN_POINT('Ctrl Pts',(1.79841427173159,841.673320905785,129.092203963653));
#77355=CARTESIAN_POINT('Ctrl Pts',(13.6617265770508,876.913333022398,141.547216621283));
#77356=CARTESIAN_POINT('Ctrl Pts',(52.8755502983386,876.914759818899,141.547720899443));
#77357=CARTESIAN_POINT('Ctrl Pts',(92.0893740196265,876.9161866154,141.548225177604));
#77358=CARTESIAN_POINT('Ctrl Pts',(103.955571043578,841.677037897907,129.093517674436));
#77359=CARTESIAN_POINT('Ctrl Pts',(115.82176806753,806.437889180414,116.638810171269));
#77360=CARTESIAN_POINT('Ctrl Pts',(83.7885507309743,785.112153023248,109.101573439004));
#77361=CARTESIAN_POINT('Ctrl Pts',(26.83022759437,791.600709061904,111.394848688847));
#77362=CARTESIAN_POINT('Ctrl Pts',(-0.167289399587949,809.571043234409,
117.746172826868));
#77363=CARTESIAN_POINT('Ctrl Pts',(9.83053628444845,839.269620594397,128.242654942375));
#77364=CARTESIAN_POINT('Ctrl Pts',(19.8283619684848,868.968197954386,138.739137057882));
#77365=CARTESIAN_POINT('Ctrl Pts',(52.8758755026418,868.969400389451,138.739562039119));
#77366=CARTESIAN_POINT('Ctrl Pts',(85.9233890367988,868.970602824516,138.739987020357));
#77367=CARTESIAN_POINT('Ctrl Pts',(95.9236458221411,839.272753095536,128.243762074268));
#77368=CARTESIAN_POINT('Ctrl Pts',(105.923902607483,809.574903366556,117.74753712818));
#77369=CARTESIAN_POINT('Ctrl Pts',(78.9278567488456,791.602604636167,111.39551864893));
#77370=CARTESIAN_POINT('',(17.244803233355,778.140660313945,108.758852681557));
#77371=CARTESIAN_POINT('',(88.5104020101015,778.140638997398,108.758845147568));
#77372=CARTESIAN_POINT('Origin',(52.8776183915471,825.72084445736,125.575299673619));
#77373=CARTESIAN_POINT('Origin',(26.8353066323039,768.271008451119,177.392764388526));
#77374=CARTESIAN_POINT('Origin',(52.8776183915471,826.387310726428,123.689610751183));
#77375=CARTESIAN_POINT('Origin',(52.8776183915471,826.387310726428,123.689610751183));
#77376=CARTESIAN_POINT('Origin',(52.8776183915471,826.387310726428,123.689610751183));
#77377=CARTESIAN_POINT('Origin',(52.8776183915471,826.387310726428,123.689610751183));
#77378=CARTESIAN_POINT('Origin',(52.8776183915471,826.387310726428,123.689610751183));
#77379=CARTESIAN_POINT('Origin',(52.8776183915471,826.387310726428,123.689610751183));
#77380=CARTESIAN_POINT('Origin',(52.8776183915471,826.387310726428,123.689610751183));
#77381=CARTESIAN_POINT('Origin',(52.8776183915471,826.387310726428,123.689610751183));
#77382=CARTESIAN_POINT('Origin',(52.8776183915471,826.387310726428,123.689610751183));
#77383=CARTESIAN_POINT('Origin',(52.8776183915471,826.387310726428,123.689610751183));
#77384=CARTESIAN_POINT('Origin',(52.8776183915471,826.387310726428,123.689610751183));
#77385=CARTESIAN_POINT('Origin',(52.8776183915471,826.387310726428,123.689610751183));
#77386=CARTESIAN_POINT('Origin',(52.8776183915471,826.387310726428,123.689610751183));
#77387=CARTESIAN_POINT('Origin',(52.8776183915471,826.387310726428,123.689610751183));
#77388=CARTESIAN_POINT('Origin',(52.8776183915471,826.387310726428,123.689610751183));
#77389=CARTESIAN_POINT('Origin',(52.8776183915471,826.387310726428,123.689610751183));
#77390=CARTESIAN_POINT('Origin',(52.8776183915471,826.387310726428,123.689610751183));
#77391=CARTESIAN_POINT('Origin',(52.8776183915471,826.387310726428,123.689610751183));
#77392=CARTESIAN_POINT('Origin',(52.8776183915471,826.387310726428,123.689610751183));
#77393=CARTESIAN_POINT('Origin',(52.8776183915471,826.387310726428,123.689610751183));
#77394=CARTESIAN_POINT('Origin',(52.8776183915471,826.387310726428,123.689610751183));
#77395=CARTESIAN_POINT('Origin',(52.8776183915471,826.387310726428,123.689610751183));
#77396=CARTESIAN_POINT('Origin',(52.8776183915471,826.387310726428,123.689610751183));
#77397=CARTESIAN_POINT('Origin',(52.8776183915471,826.387310726428,123.689610751183));
#77398=CARTESIAN_POINT('',(78.9278568228492,791.602604685434,111.395518666343));
#77399=CARTESIAN_POINT('Origin',(52.8776183915471,826.387310726428,123.689610751183));
#77400=CARTESIAN_POINT('Origin',(78.9278568223621,768.27628526772,177.394630951443));
#77401=CARTESIAN_POINT('',(3.61051440984461,833.840239926159,126.494338492581));
#77402=CARTESIAN_POINT('',(3.61051441020205,835.757685720563,127.199440688052));
#77403=CARTESIAN_POINT('Ctrl Pts',(3.61051440984449,833.840239926159,126.494338492581));
#77404=CARTESIAN_POINT('Ctrl Pts',(3.55313771416574,833.838958115137,126.497965228091));
#77405=CARTESIAN_POINT('Ctrl Pts',(3.49573635195613,833.842193256988,126.503319790014));
#77406=CARTESIAN_POINT('Ctrl Pts',(3.30520855208768,833.868273506038,126.526964401137));
#77407=CARTESIAN_POINT('Ctrl Pts',(3.17736063026302,833.911378108521,126.552640578553));
#77408=CARTESIAN_POINT('Ctrl Pts',(2.94960675592224,834.041491045101,126.618638538412));
#77409=CARTESIAN_POINT('Ctrl Pts',(2.85158409278753,834.126777814448,126.658162113752));
#77410=CARTESIAN_POINT('Ctrl Pts',(2.6974110396019,834.328833530119,126.745719811672));
#77411=CARTESIAN_POINT('Ctrl Pts',(2.64270068035171,834.443611592352,126.792888318793));
#77412=CARTESIAN_POINT('Ctrl Pts',(2.59881997156012,834.627261138451,126.864661375413));
#77413=CARTESIAN_POINT('Ctrl Pts',(2.59071064179276,834.690196650513,126.888671386677));
#77414=CARTESIAN_POINT('Ctrl Pts',(2.58791622229759,834.817756032106,126.936151111776));
#77415=CARTESIAN_POINT('Ctrl Pts',(2.59339322055599,834.882059819712,126.959488083182));
#77416=CARTESIAN_POINT('Ctrl Pts',(2.60567260254573,834.945556746391,126.981930045542));
#77417=CARTESIAN_POINT('Ctrl Pts',(2.62956184569571,835.069088494322,127.025590345062));
#77418=CARTESIAN_POINT('Ctrl Pts',(2.67883925702017,835.187724180532,127.065203300552));
#77419=CARTESIAN_POINT('Ctrl Pts',(2.82255402142357,835.401816423126,127.132019117587));
#77420=CARTESIAN_POINT('Ctrl Pts',(2.91559073162443,835.495181789821,127.158575017672));
#77421=CARTESIAN_POINT('Ctrl Pts',(3.13391416585918,835.644350256091,127.195443722542));
#77422=CARTESIAN_POINT('Ctrl Pts',(3.25724404832662,835.698551579164,127.20533847109));
#77423=CARTESIAN_POINT('Ctrl Pts',(3.46087175387042,835.746353580736,127.206816337373));
#77424=CARTESIAN_POINT('Ctrl Pts',(3.53566947643406,835.755896971539,127.204501745718));
#77425=CARTESIAN_POINT('Ctrl Pts',(3.61051441020204,835.757685720563,127.199440688052));
#77426=CARTESIAN_POINT('Ctrl Pts',(3.61051441020204,835.757685720563,127.199440688052));
#77427=CARTESIAN_POINT('Ctrl Pts',(3.66908123832854,835.759085432626,127.195480365296));
#77428=CARTESIAN_POINT('Ctrl Pts',(3.72767695938084,835.755737011247,127.18983816472));
#77429=CARTESIAN_POINT('Ctrl Pts',(3.9178418146544,835.729076184011,127.165953427404));
#77430=CARTESIAN_POINT('Ctrl Pts',(4.04425758411047,835.686040761199,127.141154082189));
#77431=CARTESIAN_POINT('Ctrl Pts',(4.26994430756122,835.556469380439,127.078149835135));
#77432=CARTESIAN_POINT('Ctrl Pts',(4.36731125541824,835.471583502163,127.040668047308));
#77433=CARTESIAN_POINT('Ctrl Pts',(4.52209435269776,835.269301288954,126.956770266859));
#77434=CARTESIAN_POINT('Ctrl Pts',(4.57745399047076,835.153507816833,126.911067195361));
#77435=CARTESIAN_POINT('Ctrl Pts',(4.6366816470894,834.907180994579,126.817516065391));
#77436=CARTESIAN_POINT('Ctrl Pts',(4.63987650281397,834.779083509209,126.770590605619));
#77437=CARTESIAN_POINT('Ctrl Pts',(4.59320506619355,834.529395965551,126.682246407946));
#77438=CARTESIAN_POINT('Ctrl Pts',(4.54432105488512,834.410196679952,126.6416420912));
#77439=CARTESIAN_POINT('Ctrl Pts',(4.40087906004098,834.195441023357,126.571921209333));
#77440=CARTESIAN_POINT('Ctrl Pts',(4.30775633773022,834.101960639812,126.543482977807));
#77441=CARTESIAN_POINT('Ctrl Pts',(4.08966906260932,833.953395096546,126.503050947673));
#77442=CARTESIAN_POINT('Ctrl Pts',(3.96691783599692,833.899611590578,126.491400668772));
#77443=CARTESIAN_POINT('Ctrl Pts',(3.76264653461912,833.851582931137,126.487758649126));
#77444=CARTESIAN_POINT('Ctrl Pts',(3.68660214370276,833.841939746873,126.489529047161));
#77445=CARTESIAN_POINT('Ctrl Pts',(3.61051440984449,833.840239926159,126.494338492581));
#77446=CARTESIAN_POINT('Origin',(52.8776183915471,825.82081439772,125.292446335253));
#77447=CARTESIAN_POINT('',(89.6658953216452,777.849661941175,108.656004010442));
#77448=CARTESIAN_POINT('',(16.0893414616814,777.849661941191,108.656004010448));
#77449=CARTESIAN_POINT('Origin',(52.8776183915471,825.72084445736,125.575299673619));
#77450=CARTESIAN_POINT('',(89.8419123794813,777.72172974858,108.288790430857));
#77451=CARTESIAN_POINT('Origin',(89.6658475858845,777.949599270907,108.373139155083));
#77452=CARTESIAN_POINT('',(90.0889201803354,777.892818101182,108.344695672232));
#77453=CARTESIAN_POINT('Ctrl Pts',(89.8419355198187,777.722828038471,108.285587078659));
#77454=CARTESIAN_POINT('Ctrl Pts',(89.9244204729452,777.77927806364,108.305192971918));
#77455=CARTESIAN_POINT('Ctrl Pts',(90.0067649765183,777.835914159845,108.324880126932));
#77456=CARTESIAN_POINT('Ctrl Pts',(90.0889691576735,777.892731478081,108.344662072744));
#77457=CARTESIAN_POINT('',(93.6680441109739,780.557861377815,109.278881970676));
#77458=CARTESIAN_POINT('Ctrl Pts',(90.0889201803354,777.892818101182,108.344695672232));
#77459=CARTESIAN_POINT('Ctrl Pts',(91.3154631687481,778.7366822112,108.651320889096));
#77460=CARTESIAN_POINT('Ctrl Pts',(92.5094987365803,779.625048288525,108.965299465377));
#77461=CARTESIAN_POINT('Ctrl Pts',(93.667901465805,780.558016866062,109.278945885626));
#77462=CARTESIAN_POINT('',(52.8776183915471,885.221162372646,146.286427926904));
#77463=CARTESIAN_POINT('Ctrl Pts',(93.6680441109739,780.557861377815,109.278881970676));
#77464=CARTESIAN_POINT('Ctrl Pts',(94.197024709261,780.980338314738,109.431683914032));
#77465=CARTESIAN_POINT('Ctrl Pts',(94.7185981290245,781.41128110683,109.586717706928));
#77466=CARTESIAN_POINT('Ctrl Pts',(95.2324518299379,781.850431742364,109.744058725421));
#77467=CARTESIAN_POINT('Ctrl Pts',(95.8193315364788,782.351992002905,109.923760166893));
#77468=CARTESIAN_POINT('Ctrl Pts',(96.3961413415951,782.864258158874,110.106471169126));
#77469=CARTESIAN_POINT('Ctrl Pts',(96.9624586130382,783.386794371866,110.292284981594));
#77470=CARTESIAN_POINT('Ctrl Pts',(97.6184571070962,783.992078699396,110.507524013319));
#77471=CARTESIAN_POINT('Ctrl Pts',(98.2603768782123,784.611142413407,110.726926031512));
#77472=CARTESIAN_POINT('Ctrl Pts',(98.8876154581229,785.243257192534,110.950615259769));
#77473=CARTESIAN_POINT('Ctrl Pts',(99.4301896715193,785.790049418086,111.144111021914));
#77474=CARTESIAN_POINT('Ctrl Pts',(99.9617797418856,786.346606065637,111.340814223757));
#77475=CARTESIAN_POINT('Ctrl Pts',(100.482019891401,786.912438172296,111.540798435659));
#77476=CARTESIAN_POINT('Ctrl Pts',(101.131349594451,787.618672772097,111.790405639273));
#77477=CARTESIAN_POINT('Ctrl Pts',(101.762996785547,788.339359682015,112.04512077829));
#77478=CARTESIAN_POINT('Ctrl Pts',(102.376257962256,789.073696230874,112.304660161555));
#77479=CARTESIAN_POINT('Ctrl Pts',(102.989518339807,789.808031822797,112.564199206606));
#77480=CARTESIAN_POINT('Ctrl Pts',(103.584392649411,790.556016896556,112.82856244038));
#77481=CARTESIAN_POINT('Ctrl Pts',(104.160218346474,791.316818379583,113.097455426844));
#77482=CARTESIAN_POINT('Ctrl Pts',(104.736043308847,792.077618891913,113.36634807023));
#77483=CARTESIAN_POINT('Ctrl Pts',(105.292819612004,792.851235654898,113.639770410246));
#77484=CARTESIAN_POINT('Ctrl Pts',(105.829927144797,793.63680705073,113.917417922006));
#77485=CARTESIAN_POINT('Ctrl Pts',(106.367034006896,794.422377465605,114.195065087063));
#77486=CARTESIAN_POINT('Ctrl Pts',(106.884472058878,795.219902353467,114.476937367362));
#77487=CARTESIAN_POINT('Ctrl Pts',(107.381665004123,796.028493470983,114.762720827657));
#77488=CARTESIAN_POINT('Ctrl Pts',(107.878857342036,796.837083600788,115.048503938861));
#77489=CARTESIAN_POINT('Ctrl Pts',(108.355804540403,797.656739799398,115.338198173211));
#77490=CARTESIAN_POINT('Ctrl Pts',(108.811975400586,798.486549176966,115.631480884545));
#77491=CARTESIAN_POINT('Ctrl Pts',(109.268145715963,799.31635756349,115.924763245612));
#77492=CARTESIAN_POINT('Ctrl Pts',(109.703539667303,800.156318967395,116.221634026556));
#77493=CARTESIAN_POINT('Ctrl Pts',(110.117672336942,801.0054978862,116.521762589149));
#77494=CARTESIAN_POINT('Ctrl Pts',(110.531804523245,801.854675813923,116.82189080146));
#77495=CARTESIAN_POINT('Ctrl Pts',(110.924675408953,802.713071094501,117.125276738147));
#77496=CARTESIAN_POINT('Ctrl Pts',(111.295847437258,803.579727697054,117.431582505548));
#77497=CARTESIAN_POINT('Ctrl Pts',(111.667019042458,804.446383311692,117.737887923787));
#77498=CARTESIAN_POINT('Ctrl Pts',(112.016491778313,805.321300086051,118.047113115394));
#77499=CARTESIAN_POINT('Ctrl Pts',(112.343876423242,806.203503590788,118.35891368407));
#77500=CARTESIAN_POINT('Ctrl Pts',(112.671260703895,807.08570611391,118.67071390581));
#77501=CARTESIAN_POINT('Ctrl Pts',(112.97655688861,807.975195205204,118.985089447289));
#77502=CARTESIAN_POINT('Ctrl Pts',(113.259424957734,808.870980207768,119.301690176839));
#77503=CARTESIAN_POINT('Ctrl Pts',(113.54229271982,809.766764238006,119.618290562735));
#77504=CARTESIAN_POINT('Ctrl Pts',(113.802732368204,810.668844017608,119.937116079479));
#77505=CARTESIAN_POINT('Ctrl Pts',(114.040453842246,811.576214869137,120.25781164007));
#77506=CARTESIAN_POINT('Ctrl Pts',(114.27817506469,812.483584760335,120.578506861247));
#77507=CARTESIAN_POINT('Ctrl Pts',(114.493178121551,813.396245562106,120.901072069243));
#77508=CARTESIAN_POINT('Ctrl Pts',(114.685223556998,814.313180814713,121.225148012794));
#77509=CARTESIAN_POINT('Ctrl Pts',(114.87726879443,815.230115121885,121.549223622197));
#77510=CARTESIAN_POINT('Ctrl Pts',(115.046356426019,816.151323719344,121.874809910411));
#77511=CARTESIAN_POINT('Ctrl Pts',(115.19229813381,817.075780629512,122.201544262246));
#77512=CARTESIAN_POINT('Ctrl Pts',(115.3382396951,818.000236611673,122.528278286091));
#77513=CARTESIAN_POINT('Ctrl Pts',(115.46103535492,818.927940747042,122.856160317185));
#77514=CARTESIAN_POINT('Ctrl Pts',(115.560548352345,819.857859825842,123.184825184231));
#77515=CARTESIAN_POINT('Ctrl Pts',(115.660061252576,820.78777799639,123.513489730271));
#77516=CARTESIAN_POINT('Ctrl Pts',(115.736291519433,821.71991095216,123.842937056347));
#77517=CARTESIAN_POINT('Ctrl Pts',(115.789154253324,822.6532205529,124.172800248569));
#77518=CARTESIAN_POINT('Ctrl Pts',(115.842016937023,823.586529267472,124.502663127588));
#77519=CARTESIAN_POINT('Ctrl Pts',(115.87151212339,824.521014470338,124.832941817379));
#77520=CARTESIAN_POINT('Ctrl Pts',(115.877606962946,825.455635403465,125.163268478836));
#77521=CARTESIAN_POINT('Ctrl Pts',(115.883969825378,826.431356645674,125.508121380186));
#77522=CARTESIAN_POINT('Ctrl Pts',(115.864828583856,827.407225640495,125.853026502308));
#77523=CARTESIAN_POINT('Ctrl Pts',(115.820206471894,828.382057884472,126.197565201603));
#77524=CARTESIAN_POINT('Ctrl Pts',(115.776978800931,829.326426620824,126.531337066545));
#77525=CARTESIAN_POINT('Ctrl Pts',(115.709838235661,830.269822231259,126.864764995862));
#77526=CARTESIAN_POINT('Ctrl Pts',(115.61886125874,831.211170053946,127.197469167699));
#77527=CARTESIAN_POINT('Ctrl Pts',(115.528902022302,832.141987214704,127.526451447297));
#77528=CARTESIAN_POINT('Ctrl Pts',(115.415636810722,833.070801999554,127.854726019497));
#77529=CARTESIAN_POINT('Ctrl Pts',(115.279191779543,833.996579888444,128.181927249908));
#77530=CARTESIAN_POINT('Ctrl Pts',(115.142747206403,834.922354669536,128.509127381919));
#77531=CARTESIAN_POINT('Ctrl Pts',(114.983122991902,835.845092421845,128.835254125198));
#77532=CARTESIAN_POINT('Ctrl Pts',(114.800496925351,836.763765400855,129.159944240057));
#77533=CARTESIAN_POINT('Ctrl Pts',(114.617871451988,837.682435395922,129.48463330029));
#77534=CARTESIAN_POINT('Ctrl Pts',(114.412244306252,838.597040492061,129.807885687703));
#77535=CARTESIAN_POINT('Ctrl Pts',(114.183844513994,839.506562009519,130.129341366402));
#77536=CARTESIAN_POINT('Ctrl Pts',(113.955445438748,840.416080671732,130.450796035962));
#77537=CARTESIAN_POINT('Ctrl Pts',(113.704273897785,841.320515636666,130.770453954891));
#77538=CARTESIAN_POINT('Ctrl Pts',(113.430609642179,842.218859558297,131.087959093022));
#77539=CARTESIAN_POINT('Ctrl Pts',(113.1569462159,843.117200757535,131.405463268968));
#77540=CARTESIAN_POINT('Ctrl Pts',(112.86079025662,844.009450801726,131.720814624619));
#77541=CARTESIAN_POINT('Ctrl Pts',(112.54247161638,844.894615922248,132.033661928523));
#77542=CARTESIAN_POINT('Ctrl Pts',(112.224153906152,845.779778456638,132.346508318399));
#77543=CARTESIAN_POINT('Ctrl Pts',(111.883673697169,846.657855962279,132.656850619388));
#77544=CARTESIAN_POINT('Ctrl Pts',(111.52141020664,847.527870461329,132.964343181029));
#77545=CARTESIAN_POINT('Ctrl Pts',(111.159147735086,848.397882513203,133.271834877755));
#77546=CARTESIAN_POINT('Ctrl Pts',(110.775102164503,849.259831459875,133.57647680028));
#77547=CARTESIAN_POINT('Ctrl Pts',(110.369701231559,850.112757292431,133.877929648973));
#77548=CARTESIAN_POINT('Ctrl Pts',(109.96430139481,850.965680818696,134.179381682544));
#77549=CARTESIAN_POINT('Ctrl Pts',(109.5375463783,851.809581138503,134.477644609644));
#77550=CARTESIAN_POINT('Ctrl Pts',(109.08991148443,852.643518349956,134.772386237143));
#77551=CARTESIAN_POINT('Ctrl Pts',(108.642277752234,853.477453397227,135.067127099746));
#77552=CARTESIAN_POINT('Ctrl Pts',(108.173764325148,854.30142524986,135.358346632251));
#77553=CARTESIAN_POINT('Ctrl Pts',(107.684893011688,855.114516206239,135.645720487856));
#77554=CARTESIAN_POINT('Ctrl Pts',(107.196022913727,855.927605140998,135.933093628952));
#77555=CARTESIAN_POINT('Ctrl Pts',(106.686795111545,856.729813099066,136.216621064718));
#77556=CARTESIAN_POINT('Ctrl Pts',(106.157776756618,857.520246622884,136.495987017022));
#77557=CARTESIAN_POINT('Ctrl Pts',(105.628759659444,858.310678267429,136.775352305128));
#77558=CARTESIAN_POINT('Ctrl Pts',(105.079952191192,859.089335402919,137.050556083333));
#77559=CARTESIAN_POINT('Ctrl Pts',(104.511965582211,859.855350805601,137.321291845419));
#77560=CARTESIAN_POINT('Ctrl Pts',(103.943980261838,860.621364470401,137.59202699328));
#77561=CARTESIAN_POINT('Ctrl Pts',(103.356815981767,861.374736333003,137.858294100498));
#77562=CARTESIAN_POINT('Ctrl Pts',(102.751126689003,862.114627334749,138.119796615353));
#77563=CARTESIAN_POINT('Ctrl Pts',(102.145438704458,862.854516738416,138.381298565393));
#77564=CARTESIAN_POINT('Ctrl Pts',(101.521225887489,863.580925217035,138.638035900382));
#77565=CARTESIAN_POINT('Ctrl Pts',(100.87918344445,864.293043745578,138.889722683502));
#77566=CARTESIAN_POINT('Ctrl Pts',(100.237142318287,865.005160813513,139.141408950394));
#77567=CARTESIAN_POINT('Ctrl Pts',(99.5772717454529,865.702987872164,139.388044644489));
#77568=CARTESIAN_POINT('Ctrl Pts',(98.9003066425044,866.385747731757,139.629355080627));
#77569=CARTESIAN_POINT('Ctrl Pts',(98.2233428544031,867.068506265249,139.870665048076));
#77570=CARTESIAN_POINT('Ctrl Pts',(97.5292847146265,867.736197545241,140.106649738324));
#77571=CARTESIAN_POINT('Ctrl Pts',(96.8189052123928,868.388077947923,140.337046329557));
#77572=CARTESIAN_POINT('Ctrl Pts',(96.0929140815661,869.054284375921,140.57250622287));
#77573=CARTESIAN_POINT('Ctrl Pts',(95.3498763203634,869.703977103575,140.802129615725));
#77574=CARTESIAN_POINT('Ctrl Pts',(94.5906562273834,870.336400410859,141.025649411097));
#77575=CARTESIAN_POINT('Ctrl Pts',(93.8477364929531,870.955245670409,141.244370264975));
#77576=CARTESIAN_POINT('Ctrl Pts',(93.089322087264,871.557555123933,141.4572468055));
#77577=CARTESIAN_POINT('Ctrl Pts',(92.3162577333526,872.142657918312,141.664041930481));
#77578=CARTESIAN_POINT('Ctrl Pts',(91.5431983690533,872.727756936244,141.870835720739));
#77579=CARTESIAN_POINT('Ctrl Pts',(90.7554893736169,873.295649420353,142.071548139746));
#77580=CARTESIAN_POINT('Ctrl Pts',(89.9540080871138,873.845702859351,142.265955636611));
#77581=CARTESIAN_POINT('Ctrl Pts',(89.1525316247205,874.395752987581,142.460361963339));
#77582=CARTESIAN_POINT('Ctrl Pts',(88.3372831697205,874.927964194455,142.648463411664));
#77583=CARTESIAN_POINT('Ctrl Pts',(87.5091707243506,875.441743717161,142.830050479154));
#77584=CARTESIAN_POINT('Ctrl Pts',(86.681062902896,875.955520371087,143.011636532719));
#77585=CARTESIAN_POINT('Ctrl Pts',(85.8400913717978,876.450865461692,143.186708248159));
#77586=CARTESIAN_POINT('Ctrl Pts',(84.9871927725203,876.927227292831,143.355070637389));
#77587=CARTESIAN_POINT('Ctrl Pts',(84.1342985643052,877.403586671469,143.523432159822));
#77588=CARTESIAN_POINT('Ctrl Pts',(83.269477551886,877.860962907313,143.685084397281));
#77589=CARTESIAN_POINT('Ctrl Pts',(82.3936929294395,878.2988465977,143.839847309629));
#77590=CARTESIAN_POINT('Ctrl Pts',(81.5179124346959,878.736728224277,143.994609492556));
#77591=CARTESIAN_POINT('Ctrl Pts',(80.6311685782169,879.15511741671,144.142482389715));
#77592=CARTESIAN_POINT('Ctrl Pts',(79.7344489614346,879.553548198539,144.283301309255));
#77593=CARTESIAN_POINT('Ctrl Pts',(78.8377331806933,879.951977275936,144.424119626392));
#77594=CARTESIAN_POINT('Ctrl Pts',(77.9310418734027,880.330448047585,144.557884002972));
#77595=CARTESIAN_POINT('Ctrl Pts',(77.0153848486169,880.688538999341,144.684445461633));
#77596=CARTESIAN_POINT('Ctrl Pts',(76.0620139019287,881.061378938789,144.816219711588));
#77597=CARTESIAN_POINT('Ctrl Pts',(75.0989234943549,881.412125271284,144.940185333291));
#77598=CARTESIAN_POINT('Ctrl Pts',(74.1272763932478,881.740354530471,145.056192659402));
#77599=CARTESIAN_POINT('Ctrl Pts',(73.1940407178224,882.055608138538,145.167613951365));
#77600=CARTESIAN_POINT('Ctrl Pts',(72.2529117951107,882.350090054414,145.271693824481));
#77601=CARTESIAN_POINT('Ctrl Pts',(71.3049378455667,882.623472286938,145.368316355574));
#77602=CARTESIAN_POINT('Ctrl Pts',(70.3569750989512,882.896851288697,145.464937744805));
#77603=CARTESIAN_POINT('Ctrl Pts',(69.4021676441985,883.149131060654,145.554101952314));
#77604=CARTESIAN_POINT('Ctrl Pts',(68.441578911655,883.380030622634,145.6357096702));
#77605=CARTESIAN_POINT('Ctrl Pts',(67.4809998585701,883.610927857934,145.717316565758));
#77606=CARTESIAN_POINT('Ctrl Pts',(66.514639803188,883.820445276004,145.791367110503));
#77607=CARTESIAN_POINT('Ctrl Pts',(65.5435750210444,884.00834952855,145.857778831252));
#77608=CARTESIAN_POINT('Ctrl Pts',(64.5799300420301,884.194818024608,145.923683107079));
#77609=CARTESIAN_POINT('Ctrl Pts',(63.6116521277509,884.360002410964,145.98206485837));
#77610=CARTESIAN_POINT('Ctrl Pts',(62.6398032780485,884.503721514643,146.032860052468));
#77611=CARTESIAN_POINT('Ctrl Pts',(61.6632079549134,884.648142537049,146.083903328394));
#77612=CARTESIAN_POINT('Ctrl Pts',(60.6830046352858,884.770888340889,146.127285848679));
#77613=CARTESIAN_POINT('Ctrl Pts',(59.7002803969362,884.871822593871,146.162959428879));
#77614=CARTESIAN_POINT('Ctrl Pts',(58.7171808562614,884.972795393638,146.198646632816));
#77615=CARTESIAN_POINT('Ctrl Pts',(57.7315589965718,885.051939905625,146.226618981274));
#77616=CARTESIAN_POINT('Ctrl Pts',(56.7445099147395,885.109168319521,146.246845439117));
#77617=CARTESIAN_POINT('Ctrl Pts',(55.7574501536532,885.166397352592,146.267072115797));
#77618=CARTESIAN_POINT('Ctrl Pts',(54.768963305234,885.201709803786,146.279552730875));
#77619=CARTESIAN_POINT('Ctrl Pts',(53.7801476712614,885.215066915775,146.284273586201));
#77620=CARTESIAN_POINT('Ctrl Pts',(53.4793246798471,885.219130490669,146.285709791063));
#77621=CARTESIAN_POINT('Ctrl Pts',(53.1784712709463,885.221162372646,146.286427926904));
#77622=CARTESIAN_POINT('Ctrl Pts',(52.8776183915471,885.221162372646,146.286427926904));
#77623=CARTESIAN_POINT('',(12.0877107975547,780.556697717533,109.280534704239));
#77624=CARTESIAN_POINT('Ctrl Pts',(52.8776183915471,885.221162372646,146.286427926904));
#77625=CARTESIAN_POINT('Ctrl Pts',(51.8886967717354,885.221162372646,146.286427926904));
#77626=CARTESIAN_POINT('Ctrl Pts',(50.8997695057188,885.199204645394,146.278667323135));
#77627=CARTESIAN_POINT('Ctrl Pts',(49.9119353918395,885.155313002713,146.263154531501));
#77628=CARTESIAN_POINT('Ctrl Pts',(48.9241072223979,885.111421624157,146.247641833217));
#77629=CARTESIAN_POINT('Ctrl Pts',(47.9373723577675,885.045596601369,146.224377042919));
#77630=CARTESIAN_POINT('Ctrl Pts',(46.9528271634588,884.957910840272,146.193385928025));
#77631=CARTESIAN_POINT('Ctrl Pts',(45.96861372072,884.8702546257,146.162405255874));
#77632=CARTESIAN_POINT('Ctrl Pts',(44.9865886376979,884.760752420113,146.123703471319));
#77633=CARTESIAN_POINT('Ctrl Pts',(44.0078422813454,884.629525928522,146.077323589032));
#77634=CARTESIAN_POINT('Ctrl Pts',(43.0258069589663,884.497858465203,146.030787852415));
#77635=CARTESIAN_POINT('Ctrl Pts',(42.0470723074263,884.344320502467,145.976522341297));
#77636=CARTESIAN_POINT('Ctrl Pts',(41.0727270204261,884.169082909413,145.914587446599));
#77637=CARTESIAN_POINT('Ctrl Pts',(40.0989774107091,883.993952449893,145.852690416518));
#77638=CARTESIAN_POINT('Ctrl Pts',(39.129612715469,883.797149013145,145.78313342296));
#77639=CARTESIAN_POINT('Ctrl Pts',(38.1657125620015,883.578891788462,145.705993934839));
#77640=CARTESIAN_POINT('Ctrl Pts',(37.2018135599169,883.360634824488,145.628854538862));
#77641=CARTESIAN_POINT('Ctrl Pts',(36.243379246057,883.120924159959,145.544132679205));
#77642=CARTESIAN_POINT('Ctrl Pts',(35.2914770714854,882.860026771341,145.451922714383));
#77643=CARTESIAN_POINT('Ctrl Pts',(34.3395760080784,882.59912968727,145.359712857199));
#77644=CARTESIAN_POINT('Ctrl Pts',(33.39420722623,882.317045971755,145.260014927594));
#77645=CARTESIAN_POINT('Ctrl Pts',(32.4564236228807,882.014089793283,145.152939963344));
#77646=CARTESIAN_POINT('Ctrl Pts',(31.518641088697,881.711133960212,145.04586512117));
#77647=CARTESIAN_POINT('Ctrl Pts',(30.5884438708996,881.38730576192,144.931413278892));
#77648=CARTESIAN_POINT('Ctrl Pts',(29.6668679668588,881.042965858658,144.809711906048));
#77649=CARTESIAN_POINT('Ctrl Pts',(28.7452930884338,880.69862633861,144.688010668644));
#77650=CARTESIAN_POINT('Ctrl Pts',(27.832339657076,880.333775216237,144.559059936951));
#77651=CARTESIAN_POINT('Ctrl Pts',(26.9290244628079,879.948818839737,144.423003328171));
#77652=CARTESIAN_POINT('Ctrl Pts',(26.0257102492375,879.56386288117,144.286946867103));
#77653=CARTESIAN_POINT('Ctrl Pts',(25.1320344013059,879.158801775842,144.143784566895));
#77654=CARTESIAN_POINT('Ctrl Pts',(24.2489922367168,878.734086654315,143.993675872352));
#77655=CARTESIAN_POINT('Ctrl Pts',(23.3659510068373,878.309371982354,143.843567336701));
#77656=CARTESIAN_POINT('Ctrl Pts',(22.49354358391,877.865003406093,143.686512446264));
#77657=CARTESIAN_POINT('Ctrl Pts',(21.6327415962015,877.401475833138,143.522686118134));
#77658=CARTESIAN_POINT('Ctrl Pts',(20.7719404962203,876.937948738209,143.358859958955));
#77659=CARTESIAN_POINT('Ctrl Pts',(19.9227449499613,876.455262762814,143.188262403162));
#77660=CARTESIAN_POINT('Ctrl Pts',(19.086100731926,875.953955488774,143.01108345036));
#77661=CARTESIAN_POINT('Ctrl Pts',(18.2494573539578,875.452648718092,142.833904675462));
#77662=CARTESIAN_POINT('Ctrl Pts',(17.4253654174497,874.932720769122,142.650144546094));
#77663=CARTESIAN_POINT('Ctrl Pts',(16.6147427364191,874.394750700022,142.460007721002));
#77664=CARTESIAN_POINT('Ctrl Pts',(15.8041208472464,873.85678115644,142.269871081646));
#77665=CARTESIAN_POINT('Ctrl Pts',(15.0069683213714,873.300769617006,142.073357790489));
#77666=CARTESIAN_POINT('Ctrl Pts',(14.2241729679096,872.727335325964,141.8706867094));
#77667=CARTESIAN_POINT('Ctrl Pts',(13.4413783578525,872.1539015795,141.668015820784));
#77668=CARTESIAN_POINT('Ctrl Pts',(12.6729410224688,871.563045209417,141.459187187472));
#77669=CARTESIAN_POINT('Ctrl Pts',(11.9197167884083,870.955424266287,141.244433386801));
#77670=CARTESIAN_POINT('Ctrl Pts',(11.1332002832681,870.320946671129,141.020187536586));
#77671=CARTESIAN_POINT('Ctrl Pts',(10.3632718518326,869.66818958464,140.789481095633));
#77672=CARTESIAN_POINT('Ctrl Pts',(9.61086642972582,868.997945659523,140.552594214226));
#77673=CARTESIAN_POINT('Ctrl Pts',(8.88197367705985,868.348646857067,140.323110047864));
#77674=CARTESIAN_POINT('Ctrl Pts',(8.16952578585541,867.682937388807,140.087825796938));
#77675=CARTESIAN_POINT('Ctrl Pts',(7.47433468430374,867.001575918348,139.847009598836));
#77676=CARTESIAN_POINT('Ctrl Pts',(6.78706819199614,866.327981410663,139.60893850818));
#77677=CARTESIAN_POINT('Ctrl Pts',(6.11666734831014,865.639089886227,139.365460934217));
#77678=CARTESIAN_POINT('Ctrl Pts',(5.46387885017508,864.935668637012,139.116848063891));
#77679=CARTESIAN_POINT('Ctrl Pts',(4.81109254389226,864.232249749657,138.868236028327));
#77680=CARTESIAN_POINT('Ctrl Pts',(4.17591857290188,863.514301351529,138.614488772037));
#77681=CARTESIAN_POINT('Ctrl Pts',(3.55906439345839,862.782623092972,138.355888918511));
#77682=CARTESIAN_POINT('Ctrl Pts',(2.94221221808227,862.050947211529,138.097289905136));
#77683=CARTESIAN_POINT('Ctrl Pts',(2.34367981728249,861.305541679978,137.833838368859));
#77684=CARTESIAN_POINT('Ctrl Pts',(1.76413383163206,860.547236725002,137.565827739881));
#77685=CARTESIAN_POINT('Ctrl Pts',(1.18458966576892,859.78893415112,137.297817952462));
#77686=CARTESIAN_POINT('Ctrl Pts',(0.624031891709943,859.017732360335,137.025249145334));
#77687=CARTESIAN_POINT('Ctrl Pts',(0.083084850274769,858.234490305603,136.748424901534));
#77688=CARTESIAN_POINT('Ctrl Pts',(-0.457860551453115,857.451250625018,
136.471601496838));
#77689=CARTESIAN_POINT('Ctrl Pts',(-0.979195249943123,856.655970883114,
136.190522727086));
#77690=CARTESIAN_POINT('Ctrl Pts',(-1.48033859396631,855.849536845141,135.905501651689));
#77691=CARTESIAN_POINT('Ctrl Pts',(-1.98148047346789,855.043105163859,135.620481409226));
#77692=CARTESIAN_POINT('Ctrl Pts',(-2.46243103360221,854.225519385171,135.331518931331));
#77693=CARTESIAN_POINT('Ctrl Pts',(-2.92265460524362,853.397690112986,135.038936056237));
#77694=CARTESIAN_POINT('Ctrl Pts',(-3.38287688203091,852.569863169926,134.746354004335));
#77695=CARTESIAN_POINT('Ctrl Pts',(-3.82237221081663,851.731792928016,134.450151624029));
#77696=CARTESIAN_POINT('Ctrl Pts',(-4.24065109689235,850.884412800929,134.150658815293));
#77697=CARTESIAN_POINT('Ctrl Pts',(-4.65892885164612,850.037034965757,133.851166816597));
#77698=CARTESIAN_POINT('Ctrl Pts',(-5.05599020925946,849.18034743601,133.548384456837));
#77699=CARTESIAN_POINT('Ctrl Pts',(-5.43139293890597,848.31530435549,133.242648962717));
#77700=CARTESIAN_POINT('Ctrl Pts',(-5.80679469402922,847.450263520572,132.936914262269));
#77701=CARTESIAN_POINT('Ctrl Pts',(-6.16053787153141,846.576867321423,132.62822649339));
#77702=CARTESIAN_POINT('Ctrl Pts',(-6.49222848866201,845.696088506238,132.316929458208));
#77703=CARTESIAN_POINT('Ctrl Pts',(-6.82391828088239,844.815311881538,132.005633197217));
#77704=CARTESIAN_POINT('Ctrl Pts',(-7.13355556755057,843.927152823285,131.691727734417));
#77705=CARTESIAN_POINT('Ctrl Pts',(-7.42079549072711,843.032600516941,131.375562681421));
#77706=CARTESIAN_POINT('Ctrl Pts',(-7.70803473077437,842.138050338069,131.059398380346));
#77707=CARTESIAN_POINT('Ctrl Pts',(-7.97287666634953,841.237107089555,130.740974552144));
#77708=CARTESIAN_POINT('Ctrl Pts',(-8.21502633165284,840.330774190458,130.420645839062));
#77709=CARTESIAN_POINT('Ctrl Pts',(-8.4571754474035,839.42444334826,130.100317852959));
#77710=CARTESIAN_POINT('Ctrl Pts',(-8.67663235582913,838.512723029929,129.778085043633));
#77711=CARTESIAN_POINT('Ctrl Pts',(-8.87315263948633,837.5966286528,129.454306293927));
#77712=CARTESIAN_POINT('Ctrl Pts',(-9.06967249854039,836.68053625499,129.13052824378));
#77713=CARTESIAN_POINT('Ctrl Pts',(-9.2432557994382,835.760069968883,128.805204313514));
#77714=CARTESIAN_POINT('Ctrl Pts',(-9.39370921673994,834.836254948099,128.478696827106));
#77715=CARTESIAN_POINT('Ctrl Pts',(-9.54416232533976,833.912441822809,128.15219001063));
#77716=CARTESIAN_POINT('Ctrl Pts',(-9.67148562038048,832.985280129458,127.8244996969));
#77717=CARTESIAN_POINT('Ctrl Pts',(-9.77553729829627,832.055802474329,127.495990843915));
#77718=CARTESIAN_POINT('Ctrl Pts',(-9.87958877403793,831.12632662519,127.167482629228));
#77719=CARTESIAN_POINT('Ctrl Pts',(-9.96036870588743,830.194534977082,126.838155932827));
#77720=CARTESIAN_POINT('Ctrl Pts',(-10.0177871272924,829.261465288766,126.508377533774));
#77721=CARTESIAN_POINT('Ctrl Pts',(-10.0764915750459,828.307497216711,126.171212938794));
#77722=CARTESIAN_POINT('Ctrl Pts',(-10.1107761009928,827.352193369348,125.833576235622));
#77723=CARTESIAN_POINT('Ctrl Pts',(-10.1206007926555,826.396665867741,125.495860485472));
#77724=CARTESIAN_POINT('Ctrl Pts',(-10.130210591096,825.4620383995,125.165531514285));
#77725=CARTESIAN_POINT('Ctrl Pts',(-10.1164190566398,824.527197115671,124.835126973434));
#77726=CARTESIAN_POINT('Ctrl Pts',(-10.0792415503186,823.593183243885,124.505014867996));
#77727=CARTESIAN_POINT('Ctrl Pts',(-10.0420642840558,822.659175403107,124.174904894119));
#77728=CARTESIAN_POINT('Ctrl Pts',(-9.98150135414635,821.72599511826,123.84508740651));
#77729=CARTESIAN_POINT('Ctrl Pts',(-9.89762021480198,820.794681753534,123.515929751641));
#77730=CARTESIAN_POINT('Ctrl Pts',(-9.81373958056812,819.863373996936,123.186774078873));
#77731=CARTESIAN_POINT('Ctrl Pts',(-9.70654103166478,818.933933292096,122.85827828537));
#77732=CARTESIAN_POINT('Ctrl Pts',(-9.57614396301838,818.007394825643,122.530808241113));
#77733=CARTESIAN_POINT('Ctrl Pts',(-9.44574762282193,817.080861535203,122.203340026234));
#77734=CARTESIAN_POINT('Ctrl Pts',(-9.29215304370139,816.157230604051,121.876897603331));
#77735=CARTESIAN_POINT('Ctrl Pts',(-9.11553129335159,815.237530736552,121.551844551334));
#77736=CARTESIAN_POINT('Ctrl Pts',(-8.93891045280868,814.317835606575,121.226793173737));
#77737=CARTESIAN_POINT('Ctrl Pts',(-8.73926270754151,813.402071651942,120.903131206522));
#77738=CARTESIAN_POINT('Ctrl Pts',(-8.51681041518808,812.491258804582,120.581219128141));
#77739=CARTESIAN_POINT('Ctrl Pts',(-8.29435917190049,811.580450252537,120.259308567871));
#77740=CARTESIAN_POINT('Ctrl Pts',(-8.04910363346647,810.674592911782,119.939147933199));
#77741=CARTESIAN_POINT('Ctrl Pts',(-7.78131695061947,809.774695671244,119.621093799608));
#77742=CARTESIAN_POINT('Ctrl Pts',(-7.51353141406179,808.874802282812,119.303041027482));
#77743=CARTESIAN_POINT('Ctrl Pts',(-7.22321497033357,807.980869092476,118.987094791032));
#77744=CARTESIAN_POINT('Ctrl Pts',(-6.91069095350244,807.093891700248,118.673606968988));
#77745=CARTESIAN_POINT('Ctrl Pts',(-6.58504807005736,806.169681527588,118.346959822537));
#77746=CARTESIAN_POINT('Ctrl Pts',(-6.23529373717443,805.253023668774,118.022981919338));
#77747=CARTESIAN_POINT('Ctrl Pts',(-5.86185086381152,804.345026509845,117.702065000521));
#77748=CARTESIAN_POINT('Ctrl Pts',(-5.5034427310267,803.473585147543,117.394068137128));
#77749=CARTESIAN_POINT('Ctrl Pts',(-5.12321546462664,802.610121193389,117.088890759696));
#77750=CARTESIAN_POINT('Ctrl Pts',(-4.72159255818815,801.755596365468,116.786872771939));
#77751=CARTESIAN_POINT('Ctrl Pts',(-4.3199744018931,800.901081644331,116.48485835626));
#77752=CARTESIAN_POINT('Ctrl Pts',(-3.89696117822355,800.055505979351,116.186003305489));
#77753=CARTESIAN_POINT('Ctrl Pts',(-3.45302402421467,799.219811142534,115.890640473716));
#77754=CARTESIAN_POINT('Ctrl Pts',(-3.00909134785035,798.384124734713,115.595280621036));
#77755=CARTESIAN_POINT('Ctrl Pts',(-2.54423523677349,797.558319093993,115.303412965772));
#77756=CARTESIAN_POINT('Ctrl Pts',(-2.05897342069375,796.743313954683,115.015362573152));
#77757=CARTESIAN_POINT('Ctrl Pts',(-1.57371565419147,795.928315616704,114.727314584352));
#77758=CARTESIAN_POINT('Ctrl Pts',(-1.06805260362502,795.124117734704,114.443083842138));
#77759=CARTESIAN_POINT('Ctrl Pts',(-0.54254743770422,794.331615962585,114.162986900903));
#77760=CARTESIAN_POINT('Ctrl Pts',(-0.0170308548852931,793.539096972915,
113.882883874403));
#77761=CARTESIAN_POINT('Ctrl Pts',(0.528328618654131,792.758274732585,113.606914874889));
#77762=CARTESIAN_POINT('Ctrl Pts',(1.09292357699108,791.990018899273,113.335387268811));
#77763=CARTESIAN_POINT('Ctrl Pts',(1.65750755153488,791.221778011831,113.063864945109));
#77764=CARTESIAN_POINT('Ctrl Pts',(2.24132616889006,790.466103169512,112.796783886936));
#77765=CARTESIAN_POINT('Ctrl Pts',(2.8437292137206,789.723835988798,112.534441550034));
#77766=CARTESIAN_POINT('Ctrl Pts',(3.4461352662169,788.981565102108,112.272097903314));
#77767=CARTESIAN_POINT('Ctrl Pts',(4.06712583211287,788.252702133763,112.014493068606));
#77768=CARTESIAN_POINT('Ctrl Pts',(4.70600928971643,787.538058847205,111.761913950576));
#77769=CARTESIAN_POINT('Ctrl Pts',(4.89369464802301,787.328117456952,111.687713559716));
#77770=CARTESIAN_POINT('Ctrl Pts',(5.08292392017445,787.119403041301,111.613946823196));
#77771=CARTESIAN_POINT('Ctrl Pts',(5.27367891242885,786.911935667425,111.540620833434));
#77772=CARTESIAN_POINT('Ctrl Pts',(5.8889578504258,786.242751055482,111.304108349146));
#77773=CARTESIAN_POINT('Ctrl Pts',(6.52011267108288,785.586541088171,111.072184698428));
#77774=CARTESIAN_POINT('Ctrl Pts',(7.16653231814136,784.944093264104,110.844773330027));
#77775=CARTESIAN_POINT('Ctrl Pts',(7.76297552640692,784.351314806528,110.634943745203));
#77776=CARTESIAN_POINT('Ctrl Pts',(8.37241468131322,783.770253293932,110.428955962841));
#77777=CARTESIAN_POINT('Ctrl Pts',(8.99433775587323,783.201503264864,110.22674055518));
#77778=CARTESIAN_POINT('Ctrl Pts',(9.53777057157126,782.704532751359,110.050045891711));
#77779=CARTESIAN_POINT('Ctrl Pts',(10.0907350345358,782.216962646337,109.876231644642));
#77780=CARTESIAN_POINT('Ctrl Pts',(10.6528630950096,781.7391645579,109.70524141257));
#77781=CARTESIAN_POINT('Ctrl Pts',(11.1247663754188,781.338055805001,109.561696094151));
#77782=CARTESIAN_POINT('Ctrl Pts',(11.6031274536375,780.94383391265,109.42014094233));
#77783=CARTESIAN_POINT('Ctrl Pts',(12.0877107975547,780.556697717533,109.280534704239));
#77784=CARTESIAN_POINT('',(15.6662215388589,777.892883824876,108.344718533713));
#77785=CARTESIAN_POINT('Ctrl Pts',(12.0879058517676,780.556909685729,109.280623951409));
#77786=CARTESIAN_POINT('Ctrl Pts',(13.2461021182051,779.624779114207,108.965204337006));
#77787=CARTESIAN_POINT('Ctrl Pts',(14.4399142821894,778.736588450391,108.651287750854));
#77788=CARTESIAN_POINT('Ctrl Pts',(15.6662215388589,777.892883824876,108.344718533713));
#77789=CARTESIAN_POINT('',(15.9133244032209,777.721729749158,108.288790421306));
#77790=CARTESIAN_POINT('Ctrl Pts',(15.6661725562014,777.892797194896,108.344684931383));
#77791=CARTESIAN_POINT('Ctrl Pts',(15.7484074658122,777.83595842687,108.324895482652));
#77792=CARTESIAN_POINT('Ctrl Pts',(15.8307836517621,777.779300419268,108.305200714399));
#77793=CARTESIAN_POINT('Ctrl Pts',(15.9133012616994,777.722828034493,108.285587077081));
#77794=CARTESIAN_POINT('Origin',(16.0893891985929,777.949599269962,108.373139154749));
#77795=CARTESIAN_POINT('Origin',(52.8776183915471,826.553927293695,123.218188520575));
#77796=CARTESIAN_POINT('',(52.8776183915471,817.923891256083,120.210169373246));
#77797=CARTESIAN_POINT('',(52.8776183915471,835.157491445947,126.301106793786));
#77798=CARTESIAN_POINT('Origin',(52.8776183915471,826.540691351014,123.255638083516));
#77799=CARTESIAN_POINT('',(52.8776183915471,836.515175234928,127.233000992115));
#77800=CARTESIAN_POINT('',(52.8776183915471,835.030963717011,126.214260020273));
#77801=CARTESIAN_POINT('Origin',(52.8776183915471,826.39866537014,123.657484105229));
#77802=CARTESIAN_POINT('Origin',(52.8776183915471,826.540691351014,123.255638083516));
#77803=CARTESIAN_POINT('Origin',(52.8776183915471,826.720543860959,122.746766289965));
#77804=CARTESIAN_POINT('',(52.8776183915471,836.747846694345,127.351374719744));
#77805=CARTESIAN_POINT('Origin',(52.8776183915471,837.081079828879,126.408530258526));
#77806=CARTESIAN_POINT('Origin',(52.8776183915471,826.387310726425,123.689610751182));
#77807=CARTESIAN_POINT('Origin',(52.8776183915471,826.605067049179,123.073494520463));
#77808=CARTESIAN_POINT('',(52.8776183915471,818.128030625863,120.077423020765));
#77809=CARTESIAN_POINT('Origin',(52.8776183915471,817.93946173362,120.010776393858));
#77810=CARTESIAN_POINT('',(52.8776183915471,835.082103472494,126.069566020161));
#77811=CARTESIAN_POINT('Origin',(52.8776183915471,826.605067049179,123.073494520463));
#77812=CARTESIAN_POINT('Origin',(52.8776183915471,826.605067049179,123.073494520463));
#77813=CARTESIAN_POINT('Origin',(52.8776183915471,826.387310726428,123.689610751183));
#77814=CARTESIAN_POINT('',(11.859543044092,780.20945181141,109.457020834635));
#77815=CARTESIAN_POINT('',(93.8960334963338,780.209723961161,109.457117026756));
#77816=CARTESIAN_POINT('Origin',(52.8776183915471,825.731304036591,125.545705508684));
#77817=CARTESIAN_POINT('',(94.9631204076456,779.681651525798,107.182848479366));
#77818=CARTESIAN_POINT('Ctrl Pts',(94.9630822777178,779.681610364452,107.182867696666));
#77819=CARTESIAN_POINT('Ctrl Pts',(94.9631775102079,779.603493726972,107.402215219776));
#77820=CARTESIAN_POINT('Ctrl Pts',(94.9366427780809,779.555592945074,107.631525596045));
#77821=CARTESIAN_POINT('Ctrl Pts',(94.8338455012492,779.524285459544,108.083418924359));
#77822=CARTESIAN_POINT('Ctrl Pts',(94.7576080457245,779.540886396965,108.305891585224));
#77823=CARTESIAN_POINT('Ctrl Pts',(94.564542439954,779.636618923506,108.71737180854));
#77824=CARTESIAN_POINT('Ctrl Pts',(94.4477614101949,779.715727147703,108.90627894322));
#77825=CARTESIAN_POINT('Ctrl Pts',(94.1876223298964,779.926998404112,109.227910928672));
#77826=CARTESIAN_POINT('Ctrl Pts',(94.0443277701068,780.059109872482,109.360557280451));
#77827=CARTESIAN_POINT('Ctrl Pts',(93.8961044974596,780.209688803323,109.456966042443));
#77828=CARTESIAN_POINT('',(10.7920801946104,779.681690583154,107.182830244375));
#77829=CARTESIAN_POINT('Origin',(52.8776183915471,826.387310726428,123.689610751183));
#77830=CARTESIAN_POINT('Ctrl Pts',(10.7921545066383,779.681610363091,107.182867697302));
#77831=CARTESIAN_POINT('Ctrl Pts',(10.7929881005113,779.604523358188,107.401313219156));
#77832=CARTESIAN_POINT('Ctrl Pts',(10.8194412281584,779.556508528823,107.630605497856));
#77833=CARTESIAN_POINT('Ctrl Pts',(10.9221008132029,779.524954693993,108.082505965785));
#77834=CARTESIAN_POINT('Ctrl Pts',(10.9982822164968,779.541423389251,108.305003868565));
#77835=CARTESIAN_POINT('Ctrl Pts',(11.1912682486577,779.636889115481,108.716575677992));
#77836=CARTESIAN_POINT('Ctrl Pts',(11.3080257792239,779.715862848014,108.905549140411));
#77837=CARTESIAN_POINT('Ctrl Pts',(11.5681536396292,779.926879240623,109.227347596125));
#77838=CARTESIAN_POINT('Ctrl Pts',(11.7114604851836,780.058870402084,109.360094054407));
#77839=CARTESIAN_POINT('Ctrl Pts',(11.8594721313973,780.209416745796,109.456869892554));
#77840=CARTESIAN_POINT('Origin',(52.8776183915471,640.625373764374,98.8443190641064));
#77841=CARTESIAN_POINT('',(68.1332263705066,640.627119090081,81.6674251557765));
#77842=CARTESIAN_POINT('',(37.6220104125875,640.627119090085,81.6674251557765));
#77843=CARTESIAN_POINT('Origin',(52.8776183915471,640.627119090081,98.8443190641064));
#77844=CARTESIAN_POINT('',(67.8012014212036,640.125373764374,82.0412652109852));
#77845=CARTESIAN_POINT('Origin',(67.8012014212036,640.625373764374,82.0412652109852));
#77846=CARTESIAN_POINT('',(37.9540353618905,640.125373764374,82.0412652109853));
#77847=CARTESIAN_POINT('Origin',(52.8776183915471,640.125373764374,98.8443190641064));
#77848=CARTESIAN_POINT('Origin',(37.9540353618905,640.625373764374,82.0412652109853));
#77849=CARTESIAN_POINT('Origin',(68.3051174347811,640.625373764374,82.3731046594733));
#77850=CARTESIAN_POINT('',(68.3051174347811,640.125373764374,83.1627853766115));
#77851=CARTESIAN_POINT('',(68.8051174347811,640.625373764374,83.1627853766115));
#77852=CARTESIAN_POINT('Origin',(68.3051174347811,640.625373764374,83.1627853766115));
#77853=CARTESIAN_POINT('',(68.80511438861,640.627119090084,83.1627853766115));
#77854=CARTESIAN_POINT('Origin',(68.3051174347811,640.625373764374,83.1627853766115));
#77855=CARTESIAN_POINT('',(68.80511438861,640.627119090078,98.0546383469682));
#77856=CARTESIAN_POINT('',(68.80511438861,640.627119090081,82.287785267134));
#77857=CARTESIAN_POINT('',(68.3051174347811,640.125373764374,98.0546383469682));
#77858=CARTESIAN_POINT('Origin',(68.3051174347811,640.625373764374,98.0546383469682));
#77859=CARTESIAN_POINT('',(68.3051174347811,640.125373764374,82.3731046594733));
#77860=CARTESIAN_POINT('Origin',(52.8776183915471,825.829705040065,125.267291295063));
#77861=CARTESIAN_POINT('Ctrl Pts',(93.6680386448423,780.55786728502,109.278884568687));
#77862=CARTESIAN_POINT('Ctrl Pts',(93.6684006063571,780.552263632436,109.293364314974));
#77863=CARTESIAN_POINT('Ctrl Pts',(93.6695470714606,780.54579059155,109.307535012193));
#77864=CARTESIAN_POINT('Ctrl Pts',(93.6714688592443,780.53853308618,109.321188415692));
#77865=CARTESIAN_POINT('Ctrl Pts',(93.6735703333615,780.530597007171,109.336118406563));
#77866=CARTESIAN_POINT('Ctrl Pts',(93.6765985254415,780.521723742468,109.350428795394));
#77867=CARTESIAN_POINT('Ctrl Pts',(93.6805040104157,780.512054570306,109.363893905088));
#77868=CARTESIAN_POINT('Ctrl Pts',(93.6845685330264,780.501991653885,109.377907335729));
#77869=CARTESIAN_POINT('Ctrl Pts',(93.6895823854221,780.491067718938,109.391005393111));
#77870=CARTESIAN_POINT('Ctrl Pts',(93.695461822842,780.479457398172,109.402989163316));
#77871=CARTESIAN_POINT('Ctrl Pts',(93.702041769321,780.46646375885,109.416400746931));
#77872=CARTESIAN_POINT('Ctrl Pts',(93.7097054443003,780.452610794498,109.428417101803));
#77873=CARTESIAN_POINT('Ctrl Pts',(93.718312273728,780.438149357518,109.438824117562));
#77874=CARTESIAN_POINT('Ctrl Pts',(93.7241837646935,780.428283913187,109.445923677222));
#77875=CARTESIAN_POINT('Ctrl Pts',(93.7304938312127,780.418135258818,109.4522756276));
#77876=CARTESIAN_POINT('Ctrl Pts',(93.7371927454339,780.407785047693,109.457824301935));
#77877=CARTESIAN_POINT('Ctrl Pts',(93.7480264169828,780.391046396609,109.466797773349));
#77878=CARTESIAN_POINT('Ctrl Pts',(93.7598269340027,780.37385921059,109.473625169796));
#77879=CARTESIAN_POINT('Ctrl Pts',(93.7723431068519,780.356589301551,109.478180574098));
#77880=CARTESIAN_POINT('Ctrl Pts',(93.782596465795,780.342441640088,109.48191240139));
#77881=CARTESIAN_POINT('Ctrl Pts',(93.7933303813018,780.328237953836,109.484119948096));
#77882=CARTESIAN_POINT('Ctrl Pts',(93.804388447967,780.31419121037,109.484765154944));
#77883=CARTESIAN_POINT('Ctrl Pts',(93.8147461868357,780.301034073125,109.485369499649));
#77884=CARTESIAN_POINT('Ctrl Pts',(93.8253884059732,780.288014795392,109.4846023526));
#77885=CARTESIAN_POINT('Ctrl Pts',(93.836166085422,780.275321659614,109.482467289298));
#77886=CARTESIAN_POINT('Ctrl Pts',(93.8462299626048,780.263469186162,109.480473630556));
#77887=CARTESIAN_POINT('Ctrl Pts',(93.8564115840146,780.251901722966,109.47728674108));
#77888=CARTESIAN_POINT('Ctrl Pts',(93.8665734130811,780.240778459561,109.472950114439));
#77889=CARTESIAN_POINT('Ctrl Pts',(93.8764579813262,780.22995868927,109.468731810656));
#77890=CARTESIAN_POINT('Ctrl Pts',(93.8863232420543,780.219560060177,109.463425299444));
#77891=CARTESIAN_POINT('Ctrl Pts',(93.8960335411076,780.209723997027,109.457117039439));
#77892=CARTESIAN_POINT('Origin',(11.8936587105147,780.345763542483,109.19196327747));
#77893=CARTESIAN_POINT('Origin',(52.8776183915471,826.720543860962,122.746766289966));
#77894=CARTESIAN_POINT('',(52.8776183915471,818.163626601955,119.976708339595));
#77895=CARTESIAN_POINT('',(52.8776183915471,835.117699448586,125.968851338991));
#77896=CARTESIAN_POINT('Origin',(52.8776183915471,826.64066302527,122.972779839293));
#77897=CARTESIAN_POINT('',(52.8776183915471,835.197580284278,125.742837789664));
#77898=CARTESIAN_POINT('Origin',(52.8776183915471,826.64066302527,122.972779839293));
#77899=CARTESIAN_POINT('Origin',(52.8776183915471,826.64066302527,122.972779839293));
#77900=CARTESIAN_POINT('',(52.8776183915471,818.246409367408,120.213087978549));
#77901=CARTESIAN_POINT('Origin',(52.8776183915471,818.352195494198,120.043354966502));
#77902=CARTESIAN_POINT('Origin',(52.8776183915471,826.575588168114,123.156901591529));
#77903=CARTESIAN_POINT('Origin',(3.61051441020205,837.780336961955,118.41143764368));
#77904=CARTESIAN_POINT('',(3.61051441020205,836.116920330448,124.618332887168));
#77905=CARTESIAN_POINT('Origin',(3.61051441020205,835.645498099839,124.451716319901));
#77906=CARTESIAN_POINT('',(3.61051441020237,834.62882423843,128.828727991124));
#77907=CARTESIAN_POINT('',(3.61051441020205,838.251759192563,118.578054210947));
#77908=CARTESIAN_POINT('Ctrl Pts',(3.61023855880141,833.690302175803,128.48326536002));
#77909=CARTESIAN_POINT('Ctrl Pts',(3.54970624529949,833.688968919781,128.487137870804));
#77910=CARTESIAN_POINT('Ctrl Pts',(3.48969016814101,833.697918586839,128.494902083681));
#77911=CARTESIAN_POINT('Ctrl Pts',(3.37188423689048,833.737039310482,128.518373667602));
#77912=CARTESIAN_POINT('Ctrl Pts',(3.31579912354491,833.768524751875,128.534458727518));
#77913=CARTESIAN_POINT('Ctrl Pts',(3.22048458350583,833.850144207547,128.572392016225));
#77914=CARTESIAN_POINT('Ctrl Pts',(3.1821019261915,833.899442320513,128.593857577818));
#77915=CARTESIAN_POINT('Ctrl Pts',(3.12820529820177,834.009523847839,128.639201274647));
#77916=CARTESIAN_POINT('Ctrl Pts',(3.1131494283263,834.069215464973,128.66263211001));
#77917=CARTESIAN_POINT('Ctrl Pts',(3.10851033861788,834.191402337082,128.708319672525));
#77918=CARTESIAN_POINT('Ctrl Pts',(3.1189842716532,834.25269542384,128.730124180922));
#77919=CARTESIAN_POINT('Ctrl Pts',(3.16441820688302,834.368927344028,128.769238568114));
#77920=CARTESIAN_POINT('Ctrl Pts',(3.1990099353471,834.42268871086,128.786145498392));
#77921=CARTESIAN_POINT('Ctrl Pts',(3.28805051477577,834.515358321064,128.812847356105));
#77922=CARTESIAN_POINT('Ctrl Pts',(3.34169967361902,834.553298184813,128.822356138207));
#77923=CARTESIAN_POINT('Ctrl Pts',(3.46101423119602,834.607921907473,128.832756247285));
#77924=CARTESIAN_POINT('Ctrl Pts',(3.52555294689342,834.624039698791,128.833535305143));
#77925=CARTESIAN_POINT('Ctrl Pts',(3.65798399987879,834.63204521721,128.826236604458));
#77926=CARTESIAN_POINT('Ctrl Pts',(3.72460865089341,834.623439329546,128.818083126898));
#77927=CARTESIAN_POINT('Ctrl Pts',(3.84924104636131,834.582078715853,128.793884832996));
#77928=CARTESIAN_POINT('Ctrl Pts',(3.90608099408457,834.549896254268,128.778130750541));
#77929=CARTESIAN_POINT('Ctrl Pts',(4.00244766333427,834.466234776723,128.740977444715));
#77930=CARTESIAN_POINT('Ctrl Pts',(4.04105590966,834.415630846942,128.719955933113));
#77931=CARTESIAN_POINT('Ctrl Pts',(4.09472970727648,834.302600429106,128.6751956904));
#77932=CARTESIAN_POINT('Ctrl Pts',(4.1092069337592,834.241289170898,128.651897825474));
#77933=CARTESIAN_POINT('Ctrl Pts',(4.1116547785933,834.116320260818,128.606071945226));
#77934=CARTESIAN_POINT('Ctrl Pts',(4.09955730020252,834.053924847908,128.584007358413));
#77935=CARTESIAN_POINT('Ctrl Pts',(4.05018166696433,833.936857875505,128.544242066616));
#77936=CARTESIAN_POINT('Ctrl Pts',(4.01344192677525,833.883355043824,128.526937604381));
#77937=CARTESIAN_POINT('Ctrl Pts',(3.9202568917958,833.792623252911,128.499637264666));
#77938=CARTESIAN_POINT('Ctrl Pts',(3.86478659222662,833.756269032296,128.489904210129));
#77939=CARTESIAN_POINT('Ctrl Pts',(3.74236795433918,833.705563571832,128.479531579772));
#77940=CARTESIAN_POINT('Ctrl Pts',(3.67661606883661,833.69176417535,128.479018907034));
#77941=CARTESIAN_POINT('Ctrl Pts',(3.61023855880141,833.690302175803,128.48326536002));
#77942=CARTESIAN_POINT('Origin',(3.61051441020205,837.780336961955,118.41143764368));
#77943=CARTESIAN_POINT('',(3.610514410202,833.200671336708,128.303923553727));
#77944=CARTESIAN_POINT('',(3.61051441019541,835.117863715507,129.009742759232));
#77945=CARTESIAN_POINT('Ctrl Pts',(3.61051441020201,833.200671336708,128.303923553727));
#77946=CARTESIAN_POINT('Ctrl Pts',(3.607420505753,833.200603853511,128.304114489599));
#77947=CARTESIAN_POINT('Ctrl Pts',(3.60432596997758,833.200549435127,128.304310645018));
#77948=CARTESIAN_POINT('Ctrl Pts',(3.4673576701867,833.198720168197,128.313222308701));
#77949=CARTESIAN_POINT('Ctrl Pts',(3.33506769578121,833.221432861026,128.331556653784));
#77950=CARTESIAN_POINT('Ctrl Pts',(3.08885719489787,833.31315177346,128.385241364804));
#77951=CARTESIAN_POINT('Ctrl Pts',(2.97723197304173,833.381238660411,128.420056263876));
#77952=CARTESIAN_POINT('Ctrl Pts',(2.78989253690627,833.554051605796,128.501007325928));
#77953=CARTESIAN_POINT('Ctrl Pts',(2.71578278492597,833.657007447089,128.546322414568));
#77954=CARTESIAN_POINT('Ctrl Pts',(2.61493637022606,833.884781048766,128.640900564318));
#77955=CARTESIAN_POINT('Ctrl Pts',(2.58903224367024,834.007350332351,128.689230558964));
#77956=CARTESIAN_POINT('Ctrl Pts',(2.58918047884613,834.256867321233,128.782327108995));
#77957=CARTESIAN_POINT('Ctrl Pts',(2.61533535784576,834.381343663168,128.826155651171));
#77958=CARTESIAN_POINT('Ctrl Pts',(2.71714194869618,834.616112757335,128.90357578295));
#77959=CARTESIAN_POINT('Ctrl Pts',(2.7920532267335,834.723959726474,128.936334868865));
#77960=CARTESIAN_POINT('Ctrl Pts',(2.98137159503634,834.907968170851,128.986643990243));
#77961=CARTESIAN_POINT('Ctrl Pts',(3.09410414598422,834.982164030165,129.003640167242));
#77962=CARTESIAN_POINT('Ctrl Pts',(3.34231950686057,835.085908810425,129.020009783769));
#77963=CARTESIAN_POINT('Ctrl Pts',(3.47545047883008,835.11442517967,129.019227036856));
#77964=CARTESIAN_POINT('Ctrl Pts',(3.60989644190229,835.117848159014,129.009786213532));
#77965=CARTESIAN_POINT('Ctrl Pts',(3.61010243425556,835.117853403556,129.009771748707));
#77966=CARTESIAN_POINT('Ctrl Pts',(3.61030842369358,835.117858589052,129.009757263938));
#77967=CARTESIAN_POINT('Ctrl Pts',(3.6105144101888,835.117863715506,129.009742759232));
#77968=CARTESIAN_POINT('',(3.61051441020205,838.743366102197,118.751804726747));
#77969=CARTESIAN_POINT('Ctrl Pts',(3.6105144101888,835.117863715507,129.009742759232));
#77970=CARTESIAN_POINT('Ctrl Pts',(3.74358702873083,835.121175537834,129.000372342509));
#77971=CARTESIAN_POINT('Ctrl Pts',(3.87543331537735,835.099838142981,128.982703984738));
#77972=CARTESIAN_POINT('Ctrl Pts',(4.12318024047454,835.009653073117,128.932477177548));
#77973=CARTESIAN_POINT('Ctrl Pts',(4.23646391221276,834.941155999679,128.900240030458));
#77974=CARTESIAN_POINT('Ctrl Pts',(4.42691427816867,834.766191500003,128.82512706458));
#77975=CARTESIAN_POINT('Ctrl Pts',(4.50235825038151,834.661612991776,128.783019910645));
#77976=CARTESIAN_POINT('Ctrl Pts',(4.60556281030655,834.429622981205,128.693411449959));
#77977=CARTESIAN_POINT('Ctrl Pts',(4.63210431266964,834.304430572222,128.646760959523));
#77978=CARTESIAN_POINT('Ctrl Pts',(4.63173866563419,834.050426145918,128.554659044094));
#77979=CARTESIAN_POINT('Ctrl Pts',(4.60467802583654,833.924134376609,128.510120334094));
#77980=CARTESIAN_POINT('Ctrl Pts',(4.50013123319633,833.688443712997,128.429552133629));
#77981=CARTESIAN_POINT('Ctrl Pts',(4.42384712657423,833.581316578468,128.394299832691));
#77982=CARTESIAN_POINT('Ctrl Pts',(4.23230042940205,833.400593907936,128.33847956846));
#77983=CARTESIAN_POINT('Ctrl Pts',(4.11906927618906,833.328650323819,128.318425858318));
#77984=CARTESIAN_POINT('Ctrl Pts',(3.87260447181931,833.230048980955,128.297143385851));
#77985=CARTESIAN_POINT('Ctrl Pts',(3.74213002483795,833.203542091986,128.295801085002));
#77986=CARTESIAN_POINT('Ctrl Pts',(3.610514410202,833.200671336708,128.303923553727));
#77987=CARTESIAN_POINT('Ctrl Pts',(4.82708931360096,834.938756820481,128.868207249531));
#77988=CARTESIAN_POINT('Ctrl Pts',(4.6896478039067,834.31354365703,128.647235762952));
#77989=CARTESIAN_POINT('Ctrl Pts',(4.56596057298178,833.685782312016,128.425363662788));
#77990=CARTESIAN_POINT('Ctrl Pts',(4.45608061274202,833.055741740253,128.202686006771));
#77991=CARTESIAN_POINT('Ctrl Pts',(3.82123976285279,835.120615159236,128.979286076428));
#77992=CARTESIAN_POINT('Ctrl Pts',(3.68092116765224,834.482314306813,128.753688957733));
#77993=CARTESIAN_POINT('Ctrl Pts',(3.55464477177853,833.841411931325,128.527172372761));
#77994=CARTESIAN_POINT('Ctrl Pts',(3.4424646764359,833.198182617664,128.299833369106));
#77995=CARTESIAN_POINT('Ctrl Pts',(2.79286361328544,835.287202884736,129.147582594022));
#77996=CARTESIAN_POINT('Ctrl Pts',(2.6496034985378,834.635521236761,128.917256249428));
#77997=CARTESIAN_POINT('Ctrl Pts',(2.52067995182663,833.981183529609,128.685991163651));
#77998=CARTESIAN_POINT('Ctrl Pts',(2.40614820848774,833.324470104333,128.453886418704));
#77999=CARTESIAN_POINT('Origin',(52.8776183915471,827.175936191914,121.458286566849));
#78000=CARTESIAN_POINT('Origin',(52.8776183915471,839.88934933413,85.4871602829437));
#78001=CARTESIAN_POINT('Origin',(44.574479425553,750.796902408053,107.247996346823));
#78002=CARTESIAN_POINT('',(44.574479425553,751.028294523684,104.84489734479));
#78003=CARTESIAN_POINT('',(44.574479425553,751.190391228939,103.16145621705));
#78004=CARTESIAN_POINT('',(44.574479425553,750.796902408053,107.247996346823));
#78005=CARTESIAN_POINT('',(44.5744737598758,740.123648048838,102.671482055163));
#78006=CARTESIAN_POINT('Ctrl Pts',(44.574479425553,751.190390984301,103.161456255756));
#78007=CARTESIAN_POINT('Ctrl Pts',(44.574479425553,749.674634276855,102.996991076383));
#78008=CARTESIAN_POINT('Ctrl Pts',(44.5744794185563,748.157236956516,102.868136570664));
#78009=CARTESIAN_POINT('Ctrl Pts',(44.5744794208369,746.637666420114,102.785395558612));
#78010=CARTESIAN_POINT('Ctrl Pts',(44.5744794212215,746.381436650187,102.771443780808));
#78011=CARTESIAN_POINT('Ctrl Pts',(44.5744794220274,746.125145008676,102.75880305028));
#78012=CARTESIAN_POINT('Ctrl Pts',(44.5744794229963,745.868788828836,102.747523631887));
#78013=CARTESIAN_POINT('Ctrl Pts',(44.5744794232527,745.800952768154,102.744538912302));
#78014=CARTESIAN_POINT('Ctrl Pts',(44.5744794235174,745.733112429613,102.741646736372));
#78015=CARTESIAN_POINT('Ctrl Pts',(44.5744794237779,745.66526790518,102.738845268841));
#78016=CARTESIAN_POINT('Ctrl Pts',(44.5744794271895,744.776818912522,102.702159021465));
#78017=CARTESIAN_POINT('Ctrl Pts',(44.5744794246643,743.887633214054,102.68114827826));
#78018=CARTESIAN_POINT('Ctrl Pts',(44.57447942518,742.997909741617,102.671614854512));
#78019=CARTESIAN_POINT('Ctrl Pts',(44.5744794251997,742.963938779512,102.67125085425));
#78020=CARTESIAN_POINT('Ctrl Pts',(44.5744794252212,742.929967047581,102.670903547168));
#78021=CARTESIAN_POINT('Ctrl Pts',(44.5744794252439,742.895994571136,102.670572357382));
#78022=CARTESIAN_POINT('Ctrl Pts',(44.5744794257199,742.184192104095,102.663633160374));
#78023=CARTESIAN_POINT('Ctrl Pts',(44.5744805176467,741.472051967534,102.663812317252));
#78024=CARTESIAN_POINT('Ctrl Pts',(44.5744783292307,740.759831783239,102.666908058489));
#78025=CARTESIAN_POINT('Ctrl Pts',(44.5744776776485,740.547774267963,102.667829789169));
#78026=CARTESIAN_POINT('Ctrl Pts',(44.5744765953231,740.335709718464,102.669010137175));
#78027=CARTESIAN_POINT('Ctrl Pts',(44.5744741956371,740.123643706643,102.670338613259));
#78028=CARTESIAN_POINT('',(44.574479425553,737.487748923763,102.682654164686));
#78029=CARTESIAN_POINT('',(44.574479425553,740.123646440349,102.672625562047));
#78030=CARTESIAN_POINT('',(44.5744794255551,737.051924408278,102.796187237243));
#78031=CARTESIAN_POINT('Ctrl Pts',(44.574479425553,737.487748923764,102.682654164686));
#78032=CARTESIAN_POINT('Ctrl Pts',(44.574479425553,737.483496025753,102.683718797301));
#78033=CARTESIAN_POINT('Ctrl Pts',(44.574479425553,737.479243465217,102.684784786436));
#78034=CARTESIAN_POINT('Ctrl Pts',(44.574479425553,737.406445987069,102.703057328914));
#78035=CARTESIAN_POINT('Ctrl Pts',(44.5744794246898,737.337998433286,102.72060842095));
#78036=CARTESIAN_POINT('Ctrl Pts',(44.5744794246898,737.196963765955,102.757400510756));
#78037=CARTESIAN_POINT('Ctrl Pts',(44.574479425553,737.124447291944,102.776662229155));
#78038=CARTESIAN_POINT('Ctrl Pts',(44.574479425553,737.051933705082,102.796186515614));
#78039=CARTESIAN_POINT('',(44.574479425553,736.984851146654,103.492667548598));
#78040=CARTESIAN_POINT('',(44.574479425553,736.753459031024,105.895766550631));
#78041=CARTESIAN_POINT('',(44.574479425553,751.028294523684,104.84489734479));
#78042=CARTESIAN_POINT('Origin',(52.8776183915471,736.753459031024,105.895766550631));
#78043=CARTESIAN_POINT('',(61.1807573575412,736.984851146654,103.492667548599));
#78044=CARTESIAN_POINT('',(60.8450373933169,734.658443669204,103.268659986875));
#78045=CARTESIAN_POINT('Origin',(52.8776183915471,736.984851146654,103.492667548598));
#78046=CARTESIAN_POINT('',(61.1807573575412,737.051933882625,102.795986698316));
#78047=CARTESIAN_POINT('Ctrl Pts',(60.8450364033132,734.658440391634,103.268658813673));
#78048=CARTESIAN_POINT('Ctrl Pts',(60.9043602784127,734.86592469736,103.223858487515));
#78049=CARTESIAN_POINT('Ctrl Pts',(60.9560530979001,735.075773134149,103.1806805371));
#78050=CARTESIAN_POINT('Ctrl Pts',(60.9999054241525,735.287413267627,103.138859881021));
#78051=CARTESIAN_POINT('Ctrl Pts',(61.0381189952664,735.471839636361,103.102416737598));
#78052=CARTESIAN_POINT('Ctrl Pts',(61.07037943333,735.657626095902,103.067004230362));
#78053=CARTESIAN_POINT('Ctrl Pts',(61.096578180922,735.84438204548,103.032445812295));
#78054=CARTESIAN_POINT('Ctrl Pts',(61.1218367646853,736.024436102613,102.999127551779));
#78055=CARTESIAN_POINT('Ctrl Pts',(61.1414225510105,736.205129994327,102.966676983641));
#78056=CARTESIAN_POINT('Ctrl Pts',(61.1553113009867,736.38614342945,102.933437414957));
#78057=CARTESIAN_POINT('Ctrl Pts',(61.1568911442891,736.406733681532,102.929656418824));
#78058=CARTESIAN_POINT('Ctrl Pts',(61.1583973289327,736.427328066591,102.925865213634));
#78059=CARTESIAN_POINT('Ctrl Pts',(61.1598298619551,736.447926112677,102.922061360995));
#78060=CARTESIAN_POINT('Ctrl Pts',(61.1657763651597,736.53342944499,102.90627141301));
#78061=CARTESIAN_POINT('Ctrl Pts',(61.1704619101878,736.619114102371,102.890867626113));
#78062=CARTESIAN_POINT('Ctrl Pts',(61.1738683606914,736.704671003371,102.874266030665));
#78063=CARTESIAN_POINT('Ctrl Pts',(61.1772935325301,736.790698112117,102.857573195367));
#78064=CARTESIAN_POINT('Ctrl Pts',(61.1794255194344,736.876595794494,102.839669324177));
#78065=CARTESIAN_POINT('Ctrl Pts',(61.180298716096,736.962049331845,102.818944138484));
#78066=CARTESIAN_POINT('Ctrl Pts',(61.1806054804515,736.99207017419,102.811663134659));
#78067=CARTESIAN_POINT('Ctrl Pts',(61.1807573575412,737.022036214132,102.804033925453));
#78068=CARTESIAN_POINT('Ctrl Pts',(61.1807573575412,737.051933882625,102.795986698316));
#78069=CARTESIAN_POINT('',(61.1807573575412,736.753459031024,105.895766550631));
#78070=CARTESIAN_POINT('Origin',(52.8776183915471,736.984851146654,103.492667548598));
#78071=CARTESIAN_POINT('',(59.2182833240547,732.044715789226,103.727362864435));
#78072=CARTESIAN_POINT('Ctrl Pts',(60.8450391521548,734.658446660987,103.268691491693));
#78073=CARTESIAN_POINT('Ctrl Pts',(60.808566415916,734.530888123547,103.296230653766));
#78074=CARTESIAN_POINT('Ctrl Pts',(60.7665091025834,734.403593561596,103.322321835396));
#78075=CARTESIAN_POINT('Ctrl Pts',(60.6844080075902,734.183682229405,103.366659532388));
#78076=CARTESIAN_POINT('Ctrl Pts',(60.6462367344819,734.089804826984,103.385276064217));
#78077=CARTESIAN_POINT('Ctrl Pts',(60.5779754381771,733.934622540943,103.4157764696));
#78078=CARTESIAN_POINT('Ctrl Pts',(60.5492824792608,733.872619393186,103.427884070048));
#78079=CARTESIAN_POINT('Ctrl Pts',(60.5057507842612,733.783010299744,103.44528574064));
#78080=CARTESIAN_POINT('Ctrl Pts',(60.4918352280297,733.754981403043,103.450714514658));
#78081=CARTESIAN_POINT('Ctrl Pts',(60.4457279638996,733.664072444659,103.468275193877));
#78082=CARTESIAN_POINT('Ctrl Pts',(60.4125546154033,733.601679353953,103.480254800349));
#78083=CARTESIAN_POINT('Ctrl Pts',(60.323194734268,733.441055008029,103.510868758104));
#78084=CARTESIAN_POINT('Ctrl Pts',(60.2652170234325,733.343914031774,103.529162067083));
#78085=CARTESIAN_POINT('Ctrl Pts',(60.0834842500503,733.05878163104,103.581795960366));
#78086=CARTESIAN_POINT('Ctrl Pts',(59.9521350216947,732.876983742758,103.613928489012));
#78087=CARTESIAN_POINT('Ctrl Pts',(59.6261861561843,732.470798745779,103.678791567783));
#78088=CARTESIAN_POINT('Ctrl Pts',(59.4281892680164,732.254744633062,103.707859181998));
#78089=CARTESIAN_POINT('Ctrl Pts',(59.2182845115635,732.044714413234,103.72736082686));
#78090=CARTESIAN_POINT('',(60.8878641387277,736.917077965099,104.196518950431));
#78091=CARTESIAN_POINT('Origin',(60.1807573575412,736.984851146654,103.492667548598));
#78092=CARTESIAN_POINT('Origin',(52.8776183915471,736.917077965099,104.196518950431));
#78093=CARTESIAN_POINT('Origin',(52.8776183915471,750.796902408053,107.247996346823));
#78094=CARTESIAN_POINT('',(61.1807573575412,751.190390849763,103.161460105204));
#78095=CARTESIAN_POINT('',(61.1807573575412,751.59614455564,98.947549280963));
#78096=CARTESIAN_POINT('',(61.1807573575412,750.796902408053,107.247996346823));
#78097=CARTESIAN_POINT('',(44.574479425553,751.59614455564,98.947549280963));
#78098=CARTESIAN_POINT('Origin',(52.8776183915471,751.59614455564,98.947549280963));
#78099=CARTESIAN_POINT('',(44.574479425553,750.796902408053,107.247996346823));
#78100=CARTESIAN_POINT('',(61.1807573575412,751.028294523684,104.84489734479));
#78101=CARTESIAN_POINT('Origin',(52.8776183915471,751.028294523684,104.84489734479));
#78102=CARTESIAN_POINT('',(61.1807573575412,750.796902408053,107.247996346823));
#78103=CARTESIAN_POINT('Origin',(52.8776183915471,736.753459031024,105.895766550631));
#78104=CARTESIAN_POINT('',(44.9102331003523,734.658332041414,103.268620312408));
#78105=CARTESIAN_POINT('Ctrl Pts',(44.5744794255595,737.051924855535,102.796188898326));
#78106=CARTESIAN_POINT('Ctrl Pts',(44.5744791286989,736.807354199727,102.86204099027));
#78107=CARTESIAN_POINT('Ctrl Pts',(44.5834464915899,736.379766761261,102.933369831913));
#78108=CARTESIAN_POINT('Ctrl Pts',(44.7152766932813,735.441353648989,103.107028422208));
#78109=CARTESIAN_POINT('Ctrl Pts',(44.7992091262746,735.046632082973,103.184616559007));
#78110=CARTESIAN_POINT('Ctrl Pts',(44.9102335588522,734.658333245328,103.268591502399));
#78111=CARTESIAN_POINT('Origin',(52.8776183915471,736.984851146654,103.492667548598));
#78112=CARTESIAN_POINT('Origin',(61.1807573575412,750.796902408053,107.247996346823));
#78113=CARTESIAN_POINT('',(61.1807573575412,737.487748923763,102.682654164686));
#78114=CARTESIAN_POINT('',(61.1807605165803,740.123621968703,102.670910437332));
#78115=CARTESIAN_POINT('',(61.1807573575412,737.487748923763,102.682654164686));
#78116=CARTESIAN_POINT('Ctrl Pts',(61.1807586638608,740.12361543648,102.669195273733));
#78117=CARTESIAN_POINT('Ctrl Pts',(61.1807560496647,741.047936554133,102.664564349666));
#78118=CARTESIAN_POINT('Ctrl Pts',(61.1807573574534,741.972239121777,102.661547405019));
#78119=CARTESIAN_POINT('Ctrl Pts',(61.180757357629,742.89597670391,102.67056249796));
#78120=CARTESIAN_POINT('Ctrl Pts',(61.1807573576322,742.912710422517,102.67072580844));
#78121=CARTESIAN_POINT('Ctrl Pts',(61.1807573576353,742.929443959488,102.670893055289));
#78122=CARTESIAN_POINT('Ctrl Pts',(61.1807573576383,742.946177311763,102.671064307693));
#78123=CARTESIAN_POINT('Ctrl Pts',(61.1807573578003,743.853161319358,102.680346559628));
#78124=CARTESIAN_POINT('Ctrl Pts',(61.1807573561954,744.759591967292,102.701437959504));
#78125=CARTESIAN_POINT('Ctrl Pts',(61.1807573589444,745.665256166094,102.738838654994));
#78126=CARTESIAN_POINT('Ctrl Pts',(61.1807573591155,745.721625214061,102.74116649527));
#78127=CARTESIAN_POINT('Ctrl Pts',(61.1807573592889,745.777991366072,102.743557133276));
#78128=CARTESIAN_POINT('Ctrl Pts',(61.1807573594589,745.834354568082,102.746011643787));
#78129=CARTESIAN_POINT('Ctrl Pts',(61.1807573641388,747.38638228969,102.813599506415));
#78130=CARTESIAN_POINT('Ctrl Pts',(61.1807573577533,748.936047138209,102.931108441007));
#78131=CARTESIAN_POINT('Ctrl Pts',(61.1807573575642,750.483918388405,103.087438878833));
#78132=CARTESIAN_POINT('Ctrl Pts',(61.1807573575354,750.719450082243,103.111226886276));
#78133=CARTESIAN_POINT('Ctrl Pts',(61.1807573575412,750.95494017589,103.135913703081));
#78134=CARTESIAN_POINT('Ctrl Pts',(61.1807573575412,751.190390600116,103.161460144679));
#78135=CARTESIAN_POINT('',(61.1807573575412,736.984851146654,103.492667548599));
#78136=CARTESIAN_POINT('Ctrl Pts',(61.180829512521,737.051935013493,102.795969534154));
#78137=CARTESIAN_POINT('Ctrl Pts',(61.180808006567,737.148389738621,102.770016804829));
#78138=CARTESIAN_POINT('Ctrl Pts',(61.1807835398961,737.244967673439,102.744516726847));
#78139=CARTESIAN_POINT('Ctrl Pts',(61.1807690759748,737.341710445985,102.719649607981));
#78140=CARTESIAN_POINT('Ctrl Pts',(61.1807626840078,737.384463486494,102.708660208853));
#78141=CARTESIAN_POINT('Ctrl Pts',(61.1807584586882,737.427248534081,102.697795029881));
#78142=CARTESIAN_POINT('Ctrl Pts',(61.1807575470676,737.470068261744,102.687072865374));
#78143=CARTESIAN_POINT('Ctrl Pts',(61.1807574216098,737.475961142441,102.685597273639));
#78144=CARTESIAN_POINT('Ctrl Pts',(61.1807573575412,737.481855369893,102.684127065464));
#78145=CARTESIAN_POINT('Ctrl Pts',(61.1807573575412,737.487748923763,102.682654164686));
#78146=CARTESIAN_POINT('Origin',(52.8776183915471,750.796902408053,107.247996346823));
#78147=CARTESIAN_POINT('',(46.9886929879261,750.796902408053,107.247996346823));
#78148=CARTESIAN_POINT('',(46.9886929879261,736.753459031024,105.895766550631));
#78149=CARTESIAN_POINT('',(46.9886929879261,750.796902408053,107.247996346823));
#78150=CARTESIAN_POINT('',(58.7665437951681,736.753459031024,105.895766550631));
#78151=CARTESIAN_POINT('Origin',(52.8776183915471,736.753459031024,105.895766550631));
#78152=CARTESIAN_POINT('',(58.7665437951681,750.796902408053,107.247996346823));
#78153=CARTESIAN_POINT('',(58.7665437951681,750.796902408053,107.247996346823));
#78154=CARTESIAN_POINT('Origin',(52.8776183915471,750.796902408053,107.247996346823));
#78155=CARTESIAN_POINT('Origin',(59.1807573575412,750.796902408053,107.247996346823));
#78156=CARTESIAN_POINT('',(59.4736505763546,750.824974979019,106.956451550289));
#78157=CARTESIAN_POINT('',(60.8878641387277,750.960521342129,105.548748746623));
#78158=CARTESIAN_POINT('',(59.1807573575412,750.796902408053,107.247996346823));
#78159=CARTESIAN_POINT('',(59.4736505763546,736.781531601989,105.604221754097));
#78160=CARTESIAN_POINT('',(59.4736505763546,750.824974979019,106.956451550289));
#78161=CARTESIAN_POINT('',(61.1807573575412,736.945150536064,103.904974153897));
#78162=CARTESIAN_POINT('',(60.8878641387277,750.960521342129,105.548748746623));
#78163=CARTESIAN_POINT('Origin',(52.8776183915471,750.796902408053,107.247996346823));
#78164=CARTESIAN_POINT('',(46.2815862067395,750.824974979019,106.956451550289));
#78165=CARTESIAN_POINT('',(44.8673726443664,750.960521342129,105.548748746623));
#78166=CARTESIAN_POINT('',(46.574479425553,750.796902408053,107.247996346823));
#78167=CARTESIAN_POINT('Origin',(52.8776183915471,750.824974979019,106.956451550289));
#78168=CARTESIAN_POINT('Origin',(52.8776183915471,750.960521342129,105.548748746623));
#78169=CARTESIAN_POINT('Origin',(52.8776183915471,736.753459031024,105.895766550631));
#78170=CARTESIAN_POINT('',(58.3219300063767,731.218651083621,103.766631312401));
#78171=CARTESIAN_POINT('Ctrl Pts',(59.2182826984074,732.044716514228,103.727363937984));
#78172=CARTESIAN_POINT('Ctrl Pts',(59.1410053172168,731.967395409693,103.734545295664));
#78173=CARTESIAN_POINT('Ctrl Pts',(59.0625975079218,731.891133513513,103.741163687107));
#78174=CARTESIAN_POINT('Ctrl Pts',(58.9833028731213,731.815787977957,103.746880332788));
#78175=CARTESIAN_POINT('Ctrl Pts',(58.9043155133724,731.740734414278,103.752574825866));
#78176=CARTESIAN_POINT('Ctrl Pts',(58.8244484793124,731.666589906708,103.757374527535));
#78177=CARTESIAN_POINT('Ctrl Pts',(58.7439078609761,731.59317536338,103.76094093225));
#78178=CARTESIAN_POINT('Ctrl Pts',(58.6638424024685,731.520193938676,103.764486296498));
#78179=CARTESIAN_POINT('Ctrl Pts',(58.5831115382727,731.447933633485,103.766812848102));
#78180=CARTESIAN_POINT('Ctrl Pts',(58.5018793316936,731.376184532491,103.76758476604));
#78181=CARTESIAN_POINT('Ctrl Pts',(58.4421511530334,731.323429063898,103.768152339598));
#78182=CARTESIAN_POINT('Ctrl Pts',(58.3821511559648,731.270949246123,103.767879358289));
#78183=CARTESIAN_POINT('Ctrl Pts',(58.3219300063767,731.218651083621,103.766631312401));
#78184=CARTESIAN_POINT('',(46.2815862067395,736.781531601989,105.604221754097));
#78185=CARTESIAN_POINT('Origin',(52.8776183915471,736.781531601989,105.604221754097));
#78186=CARTESIAN_POINT('',(44.8673726443664,736.917077965099,104.196518950431));
#78187=CARTESIAN_POINT('',(44.574479425553,736.945150536064,103.904974153897));
#78188=CARTESIAN_POINT('',(46.5369840943911,732.044637214649,103.727329693178));
#78189=CARTESIAN_POINT('Origin',(52.8776183915471,736.917077965099,104.196518950431));
#78190=CARTESIAN_POINT('',(47.4333208409147,731.218654873935,103.766631507277));
#78191=CARTESIAN_POINT('Ctrl Pts',(47.4333199694293,731.218655630363,103.766645149501));
#78192=CARTESIAN_POINT('Ctrl Pts',(47.2825110232573,731.349638140042,103.769783701346));
#78193=CARTESIAN_POINT('Ctrl Pts',(47.1293091961631,731.484318580969,103.766191622297));
#78194=CARTESIAN_POINT('Ctrl Pts',(46.8277456416006,731.760758895609,103.751646950206));
#78195=CARTESIAN_POINT('Ctrl Pts',(46.6809723070849,731.900553502369,103.7406976256));
#78196=CARTESIAN_POINT('Ctrl Pts',(46.5369645910256,732.044621808575,103.727301634748));
#78197=CARTESIAN_POINT('Ctrl Pts',(58.3219249040931,731.21864665262,103.766631206657));
#78198=CARTESIAN_POINT('Ctrl Pts',(58.2440956171014,731.151056992137,103.765018172219));
#78199=CARTESIAN_POINT('Ctrl Pts',(58.1647207776151,731.084673275731,103.763443633293));
#78200=CARTESIAN_POINT('Ctrl Pts',(58.084094661515,731.019772305155,103.761912350037));
#78201=CARTESIAN_POINT('Ctrl Pts',(58.0034573035392,730.954862285294,103.760380853271));
#78202=CARTESIAN_POINT('Ctrl Pts',(57.92156855916,730.891435630024,103.758892624238));
#78203=CARTESIAN_POINT('Ctrl Pts',(57.8387558587535,730.82972881865,103.75745242509));
#78204=CARTESIAN_POINT('Ctrl Pts',(57.8050394303558,730.804605458621,103.756866061269));
#78205=CARTESIAN_POINT('Ctrl Pts',(57.7711702037205,730.779766703224,103.756287659056));
#78206=CARTESIAN_POINT('Ctrl Pts',(57.7371716948611,730.755226485564,103.755717539843));
#78207=CARTESIAN_POINT('Ctrl Pts',(57.6043222460252,730.659335386223,103.753489794402));
#78208=CARTESIAN_POINT('Ctrl Pts',(57.4691061887164,730.567711554512,103.75138016625));
#78209=CARTESIAN_POINT('Ctrl Pts',(57.3315633396149,730.480289249374,103.7493829085));
#78210=CARTESIAN_POINT('Ctrl Pts',(57.261007256714,730.435443767046,103.748358364626));
#78211=CARTESIAN_POINT('Ctrl Pts',(57.1898382886597,730.391704490583,103.74736339031));
#78212=CARTESIAN_POINT('Ctrl Pts',(57.1180583559394,730.349066580572,103.7463972098));
#78213=CARTESIAN_POINT('Ctrl Pts',(56.9774193116041,730.26552575392,103.744504163952));
#78214=CARTESIAN_POINT('Ctrl Pts',(56.8344421594333,730.1862135713,103.742720926515));
#78215=CARTESIAN_POINT('Ctrl Pts',(56.6891216129092,730.111126398369,103.741044697022));
#78216=CARTESIAN_POINT('Ctrl Pts',(56.5430260983871,730.035638799226,103.739359528502));
#78217=CARTESIAN_POINT('Ctrl Pts',(56.3945615921378,729.964421061701,103.737782512277));
#78218=CARTESIAN_POINT('Ctrl Pts',(56.2437010615264,729.897518087519,103.736310802839));
#78219=CARTESIAN_POINT('Ctrl Pts',(56.092840530915,729.830615113337,103.7348390934));
#78220=CARTESIAN_POINT('Ctrl Pts',(55.9395833889696,729.768026641657,103.733472690748));
#78221=CARTESIAN_POINT('Ctrl Pts',(55.7838894679809,729.709850421025,103.732208749374));
#78222=CARTESIAN_POINT('Ctrl Pts',(55.6765488700272,729.669741788205,103.731337345904));
#78223=CARTESIAN_POINT('Ctrl Pts',(55.5682311649451,729.631805000722,103.730517048397));
#78224=CARTESIAN_POINT('Ctrl Pts',(55.4593025183271,729.596169629469,103.729748945441));
#78225=CARTESIAN_POINT('Ctrl Pts',(55.3502206571051,729.560484134952,103.728979762102));
#78226=CARTESIAN_POINT('Ctrl Pts',(55.2405264652308,729.527106629751,103.728262920248));
#78227=CARTESIAN_POINT('Ctrl Pts',(55.1306025848533,729.496117118348,103.727599513066));
#78228=CARTESIAN_POINT('Ctrl Pts',(55.1118928282375,729.490842502733,103.727486596866));
#78229=CARTESIAN_POINT('Ctrl Pts',(55.0931764455505,729.485636948906,103.727375228681));
#78230=CARTESIAN_POINT('Ctrl Pts',(55.074455355652,729.480500704696,103.727265413902));
#78231=CARTESIAN_POINT('Ctrl Pts',(54.9159162785624,729.437004550303,103.726335450221));
#78232=CARTESIAN_POINT('Ctrl Pts',(54.7565538689342,729.398340894392,103.725512891532));
#78233=CARTESIAN_POINT('Ctrl Pts',(54.5963803385134,729.364450698395,103.724794379583));
#78234=CARTESIAN_POINT('Ctrl Pts',(54.5155470402871,729.34734764577,103.724431774786));
#78235=CARTESIAN_POINT('Ctrl Pts',(54.4345068451812,729.331461078676,103.724095668872));
#78236=CARTESIAN_POINT('Ctrl Pts',(54.3532597720157,729.316788196599,103.723785630211));
#78237=CARTESIAN_POINT('Ctrl Pts',(54.1931230587091,729.287868175004,103.72317454885));
#78238=CARTESIAN_POINT('Ctrl Pts',(54.0321913209344,729.263661319254,103.722663775038));
#78239=CARTESIAN_POINT('Ctrl Pts',(53.8704525191743,729.244181911624,103.72225375967));
#78240=CARTESIAN_POINT('Ctrl Pts',(53.706657913141,729.224454908186,103.721838532742));
#78241=CARTESIAN_POINT('Ctrl Pts',(53.5420349654433,729.20957610299,103.721526641947));
#78242=CARTESIAN_POINT('Ctrl Pts',(53.3765697975624,729.199614985232,103.721318555591));
#78243=CARTESIAN_POINT('Ctrl Pts',(53.2111046296815,729.189653867473,103.721110469236));
#78244=CARTESIAN_POINT('Ctrl Pts',(53.0447965770304,729.184610396008,103.721006187319));
#78245=CARTESIAN_POINT('Ctrl Pts',(52.8776401587059,729.184609957798,103.721006178149));
#78246=CARTESIAN_POINT('Ctrl Pts',(52.7137023104169,729.184609528025,103.721006169156));
#78247=CARTESIAN_POINT('Ctrl Pts',(52.5505758965974,729.189460030891,103.721106467457));
#78248=CARTESIAN_POINT('Ctrl Pts',(52.3882588644791,729.199043117555,103.721306625593));
#78249=CARTESIAN_POINT('Ctrl Pts',(52.2222003373688,729.208847099526,103.721511397481));
#78250=CARTESIAN_POINT('Ctrl Pts',(52.0569883213915,729.223604188265,103.721820685908));
#78251=CARTESIAN_POINT('Ctrl Pts',(51.8926120674172,729.243242920974,103.722234011753));
#78252=CARTESIAN_POINT('Ctrl Pts',(51.7282358134428,729.262881653682,103.722647337599));
#78253=CARTESIAN_POINT('Ctrl Pts',(51.564694672195,729.287402108584,103.723164700862));
#78254=CARTESIAN_POINT('Ctrl Pts',(51.4019790523234,729.316787827959,103.723785622422));
#78255=CARTESIAN_POINT('Ctrl Pts',(51.2409737783516,729.34586466645,103.724400017315));
#78256=CARTESIAN_POINT('Ctrl Pts',(51.0807815335725,729.379704317724,103.725116773544));
#78257=CARTESIAN_POINT('Ctrl Pts',(50.9214059654977,729.418340665856,103.725939243923));
#78258=CARTESIAN_POINT('Ctrl Pts',(50.8409931639961,729.437834601035,103.726354220623));
#78259=CARTESIAN_POINT('Ctrl Pts',(50.7607884800892,729.458550422199,103.726796108954));
#78260=CARTESIAN_POINT('Ctrl Pts',(50.680794100972,729.480497227648,103.727265339561));
#78261=CARTESIAN_POINT('Ctrl Pts',(50.5704196242906,729.51077894485,103.727912773585));
#78262=CARTESIAN_POINT('Ctrl Pts',(50.4602121832636,729.543473259537,103.72861418246));
#78263=CARTESIAN_POINT('Ctrl Pts',(50.3505563395933,729.578509132596,103.729368495549));
#78264=CARTESIAN_POINT('Ctrl Pts',(50.2410631623908,729.613493032486,103.73012168967));
#78265=CARTESIAN_POINT('Ctrl Pts',(50.1321202807258,729.650811465402,103.730927631162));
#78266=CARTESIAN_POINT('Ctrl Pts',(50.0240965575535,729.690343596891,103.731785254144));
#78267=CARTESIAN_POINT('Ctrl Pts',(50.0064974381545,729.696784133116,103.731924977242));
#78268=CARTESIAN_POINT('Ctrl Pts',(49.9889226791992,729.703283320467,103.732066072102));
#78269=CARTESIAN_POINT('Ctrl Pts',(49.9713738312623,729.709840513116,103.732208534114));
#78270=CARTESIAN_POINT('Ctrl Pts',(49.8177009328862,729.767260966198,103.733456054769));
#78271=CARTESIAN_POINT('Ctrl Pts',(49.6664031093005,729.828979546795,103.734803384278));
#78272=CARTESIAN_POINT('Ctrl Pts',(49.5174415848815,729.894901729426,103.736253254073));
#78273=CARTESIAN_POINT('Ctrl Pts',(49.365930849862,729.961952052545,103.737727935801));
#78274=CARTESIAN_POINT('Ctrl Pts',(49.2168364407443,730.033351192812,103.739308697432));
#78275=CARTESIAN_POINT('Ctrl Pts',(49.0701306934366,730.109052960563,103.740998413044));
#78276=CARTESIAN_POINT('Ctrl Pts',(48.9234249461288,730.184754728315,103.742688128655));
#78277=CARTESIAN_POINT('Ctrl Pts',(48.7791072888848,730.264759419022,103.744486798248));
#78278=CARTESIAN_POINT('Ctrl Pts',(48.6371720308017,730.349070380066,103.746397295897));
#78279=CARTESIAN_POINT('Ctrl Pts',(48.4972332733578,730.432195399787,103.748280919957));
#78280=CARTESIAN_POINT('Ctrl Pts',(48.3596156778622,730.519503358546,103.750273968768));
#78281=CARTESIAN_POINT('Ctrl Pts',(48.2243412484543,730.611039789433,103.752382185054));
#78282=CARTESIAN_POINT('Ctrl Pts',(48.154963352582,730.657985875241,103.753463421254));
#78283=CARTESIAN_POINT('Ctrl Pts',(48.0862022998346,730.706044851327,103.754574950341));
#78284=CARTESIAN_POINT('Ctrl Pts',(48.0180646604849,730.755226794314,103.755717547016));
#78285=CARTESIAN_POINT('Ctrl Pts',(47.9345157570287,730.815532631816,103.757118574411));
#78286=CARTESIAN_POINT('Ctrl Pts',(47.8517492715001,730.877644568796,103.758569627446));
#78287=CARTESIAN_POINT('Ctrl Pts',(47.77010514203,730.941343414278,103.760065946964));
#78288=CARTESIAN_POINT('Ctrl Pts',(47.6884928602638,731.005017412145,103.761561682797));
#78289=CARTESIAN_POINT('Ctrl Pts',(47.6080023160632,731.070276898363,103.763102649804));
#78290=CARTESIAN_POINT('Ctrl Pts',(47.5289415695104,731.136861352564,103.764684094393));
#78291=CARTESIAN_POINT('Ctrl Pts',(47.4968230726771,731.163911344812,103.765326557628));
#78292=CARTESIAN_POINT('Ctrl Pts',(47.4649401663363,731.191179547578,103.765975701273));
#78293=CARTESIAN_POINT('Ctrl Pts',(47.4333118811382,731.218646650764,103.766631206613));
#78294=CARTESIAN_POINT('Origin',(46.574479425553,750.796902408053,107.247996346823));
#78295=CARTESIAN_POINT('',(46.2815862067395,750.824974979019,106.956451550289));
#78296=CARTESIAN_POINT('',(44.8673726443664,736.917077965099,104.196518950431));
#78297=CARTESIAN_POINT('Origin',(52.8776183915471,750.892748160574,106.252600148456));
#78298=CARTESIAN_POINT('Origin',(58.7665437951681,750.892748160574,106.252600148456));
#78299=CARTESIAN_POINT('Origin',(46.9886929879261,750.892748160574,106.252600148456));
#78300=CARTESIAN_POINT('Origin',(46.9886929879261,750.892748160574,106.252600148456));
#78301=CARTESIAN_POINT('Origin',(46.9886929879261,736.849304783544,104.900370352264));
#78302=CARTESIAN_POINT('Origin',(58.7665437951681,750.892748160574,106.252600148456));
#78303=CARTESIAN_POINT('Origin',(58.7665437951681,736.849304783544,104.900370352264));
#78304=CARTESIAN_POINT('Origin',(52.8776183915471,736.849304783544,104.900370352264));
#78305=CARTESIAN_POINT('Origin',(52.8776183915471,736.984851146654,103.492667548598));
#78306=CARTESIAN_POINT('Ctrl Pts',(46.5369645921949,732.044621809289,103.727301632047));
#78307=CARTESIAN_POINT('Ctrl Pts',(46.3225264216533,732.259153081262,103.707349715149));
#78308=CARTESIAN_POINT('Ctrl Pts',(46.1205233504414,732.480034869399,103.677463263573));
#78309=CARTESIAN_POINT('Ctrl Pts',(45.7933717648021,732.89018316908,103.611665037245));
#78310=CARTESIAN_POINT('Ctrl Pts',(45.664030910038,733.070178870018,103.579805976886));
#78311=CARTESIAN_POINT('Ctrl Pts',(45.4855803385425,733.351362146652,103.527862348267));
#78312=CARTESIAN_POINT('Ctrl Pts',(45.4289758251606,733.446475095519,103.509933886774));
#78313=CARTESIAN_POINT('Ctrl Pts',(45.3415828623108,733.603808834803,103.479938974266));
#78314=CARTESIAN_POINT('Ctrl Pts',(45.3090974516336,733.6649463005,103.468193759419));
#78315=CARTESIAN_POINT('Ctrl Pts',(45.2638137275495,733.754201624595,103.450940497582));
#78316=CARTESIAN_POINT('Ctrl Pts',(45.2500770414093,733.781852806832,103.445580763039));
#78317=CARTESIAN_POINT('Ctrl Pts',(45.2066141899079,733.871237044652,103.42820896964));
#78318=CARTESIAN_POINT('Ctrl Pts',(45.1778247696134,733.933397521809,103.416059205064));
#78319=CARTESIAN_POINT('Ctrl Pts',(45.1085970074955,734.090669669677,103.385121922763));
#78320=CARTESIAN_POINT('Ctrl Pts',(45.0696884673827,734.186463068881,103.36611067962));
#78321=CARTESIAN_POINT('Ctrl Pts',(44.9876931506015,734.406729887678,103.321673608498));
#78322=CARTESIAN_POINT('Ctrl Pts',(44.946241754629,734.532389344382,103.295830687479));
#78323=CARTESIAN_POINT('Ctrl Pts',(44.9102342133583,734.658330962292,103.268591994624));
#78324=CARTESIAN_POINT('Origin',(45.574479425553,736.984851146654,103.492667548598));
#78325=CARTESIAN_POINT('Origin',(45.574479425553,751.028294523684,104.84489734479));
#78326=CARTESIAN_POINT('Origin',(45.574479425553,751.028294523684,104.84489734479));
#78327=CARTESIAN_POINT('Origin',(60.1807573575412,751.028294523684,104.84489734479));
#78328=CARTESIAN_POINT('Origin',(60.1807573575412,751.028294523684,104.84489734479));
#78329=CARTESIAN_POINT('Origin',(52.8776183915471,751.028294523684,104.84489734479));
#78330=CARTESIAN_POINT('Ctrl Pts',(44.574479425553,739.297010529679,102.671020968754));
#78331=CARTESIAN_POINT('Ctrl Pts',(44.5744794255741,739.29810258077,103.433937572034));
#78332=CARTESIAN_POINT('Ctrl Pts',(43.8749449432361,739.298063899118,103.129485841296));
#78333=CARTESIAN_POINT('Ctrl Pts',(44.574479425553,740.530857021924,102.667286233968));
#78334=CARTESIAN_POINT('Ctrl Pts',(44.5744794255372,740.537828296885,103.430114647369));
#78335=CARTESIAN_POINT('Ctrl Pts',(43.874983425004,740.533976463203,103.125741677408));
#78336=CARTESIAN_POINT('Ctrl Pts',(44.574479425553,741.764892155927,102.658402212418));
#78337=CARTESIAN_POINT('Ctrl Pts',(44.5744794255229,741.762501809108,103.421959943614));
#78338=CARTESIAN_POINT('Ctrl Pts',(43.8746011421895,741.765219958194,103.116745243982));
#78339=CARTESIAN_POINT('Ctrl Pts',(44.574479425553,743.955576229434,102.681842604063));
#78340=CARTESIAN_POINT('Ctrl Pts',(44.5744794255763,743.938984899097,103.440683584674));
#78341=CARTESIAN_POINT('Ctrl Pts',(43.8771264840893,743.946601258126,103.141178205667));
#78342=CARTESIAN_POINT('Ctrl Pts',(44.574479425553,744.912616217256,102.705438138897));
#78343=CARTESIAN_POINT('Ctrl Pts',(44.574479425553,744.883170807362,103.459905019968));
#78344=CARTESIAN_POINT('Ctrl Pts',(43.8793242348887,744.898138964526,103.165604660246));
#78345=CARTESIAN_POINT('Ctrl Pts',(44.574479425553,748.056063398855,102.843629112592));
#78346=CARTESIAN_POINT('Ctrl Pts',(44.574479425553,747.973884049545,103.575040888373));
#78347=CARTESIAN_POINT('Ctrl Pts',(43.8912182783842,748.022533230734,103.307895376711));
#78348=CARTESIAN_POINT('Ctrl Pts',(44.5744794255529,750.238556260715,103.039162325259));
#78349=CARTESIAN_POINT('Ctrl Pts',(44.5744794256417,750.101103921648,103.736030596296));
#78350=CARTESIAN_POINT('Ctrl Pts',(43.9071717466752,750.190640286152,103.508440148698));
#78351=CARTESIAN_POINT('Ctrl Pts',(44.574479425553,752.418162461714,103.302274539183));
#78352=CARTESIAN_POINT('Ctrl Pts',(44.5744794255157,752.338363272777,103.97656838147));
#78353=CARTESIAN_POINT('Ctrl Pts',(43.9260235934534,752.361394691197,103.776329042103));
#78354=CARTESIAN_POINT('',(43.8763887996152,740.125375114458,103.127134598756));
#78355=CARTESIAN_POINT('Origin',(44.074479425553,740.123635038617,102.66805173472));
#78356=CARTESIAN_POINT('',(44.574479425553,751.59614455564,103.206327301003));
#78357=CARTESIAN_POINT('Ctrl Pts',(44.574479425553,751.59614455564,103.206327301003));
#78358=CARTESIAN_POINT('Ctrl Pts',(44.574479425553,751.460907273987,103.19109258465));
#78359=CARTESIAN_POINT('Ctrl Pts',(44.574479425553,751.325656135411,103.176133022638));
#78360=CARTESIAN_POINT('Ctrl Pts',(44.574479425553,751.190391221941,103.161456281541));
#78361=CARTESIAN_POINT('',(43.9196965836671,751.54292215966,103.678777984592));
#78362=CARTESIAN_POINT('Origin',(44.074479425553,751.59614455564,103.206327301003));
#78363=CARTESIAN_POINT('Ctrl Pts',(43.8763918793368,740.125375235339,103.127136791686));
#78364=CARTESIAN_POINT('Ctrl Pts',(43.8761609839388,740.382537008607,103.12606196984));
#78365=CARTESIAN_POINT('Ctrl Pts',(43.8760246822405,740.639656652116,103.12503062257));
#78366=CARTESIAN_POINT('Ctrl Pts',(43.8759483580193,740.896786009906,103.124321807132));
#78367=CARTESIAN_POINT('Ctrl Pts',(43.8758735861635,741.14868559011,103.123627408357));
#78368=CARTESIAN_POINT('Ctrl Pts',(43.8758561270906,741.400594538677,103.12324269677));
#78369=CARTESIAN_POINT('Ctrl Pts',(43.8758880528351,741.652523518746,103.123411688851));
#78370=CARTESIAN_POINT('Ctrl Pts',(43.8759192074444,741.898367399276,103.123576599093));
#78371=CARTESIAN_POINT('Ctrl Pts',(43.8759972035132,742.144230284881,103.12426888698));
#78372=CARTESIAN_POINT('Ctrl Pts',(43.8761415145388,742.390085708688,103.12569590925));
#78373=CARTESIAN_POINT('Ctrl Pts',(43.8762581050598,742.588715105541,103.126848816794));
#78374=CARTESIAN_POINT('Ctrl Pts',(43.876418424685,742.787338947153,103.128480971918));
#78375=CARTESIAN_POINT('Ctrl Pts',(43.8766472931601,742.985925842393,103.130691443671));
#78376=CARTESIAN_POINT('Ctrl Pts',(43.8769322533183,743.233182932084,103.13344366361));
#78377=CARTESIAN_POINT('Ctrl Pts',(43.8773287442974,743.480413177981,103.137095886245));
#78378=CARTESIAN_POINT('Ctrl Pts',(43.8777960574979,743.727640306692,103.141770103925));
#78379=CARTESIAN_POINT('Ctrl Pts',(43.8782647951713,743.975621037748,103.146458569643));
#78380=CARTESIAN_POINT('Ctrl Pts',(43.8788046918661,744.223598486502,103.152175306106));
#78381=CARTESIAN_POINT('Ctrl Pts',(43.8794071456804,744.471561541077,103.159021276459));
#78382=CARTESIAN_POINT('Ctrl Pts',(43.8800141469592,744.721396279667,103.165918921822));
#78383=CARTESIAN_POINT('Ctrl Pts',(43.880684554495,744.97121626136,103.173962947854));
#78384=CARTESIAN_POINT('Ctrl Pts',(43.881444002068,745.220976746973,103.183233610531));
#78385=CARTESIAN_POINT('Ctrl Pts',(43.8820768967054,745.429117608275,103.190959427165));
#78386=CARTESIAN_POINT('Ctrl Pts',(43.8827722350252,745.637216499217,103.199536718816));
#78387=CARTESIAN_POINT('Ctrl Pts',(43.8835635166994,745.84523122278,103.208999702177));
#78388=CARTESIAN_POINT('Ctrl Pts',(43.8846113185723,746.1206808181,103.221530425449));
#78389=CARTESIAN_POINT('Ctrl Pts',(43.8858848744824,746.395912657287,103.23563536325));
#78390=CARTESIAN_POINT('Ctrl Pts',(43.88729096164,746.671006938799,103.251288589859));
#78391=CARTESIAN_POINT('Ctrl Pts',(43.8887485706763,746.956181231446,103.267515382366));
#78392=CARTESIAN_POINT('Ctrl Pts',(43.8903487160162,747.241207475621,103.285405858764));
#78393=CARTESIAN_POINT('Ctrl Pts',(43.8920261956294,747.52613890873,103.304907908265));
#78394=CARTESIAN_POINT('Ctrl Pts',(43.8937725314076,747.822766034346,103.325210466056));
#78395=CARTESIAN_POINT('Ctrl Pts',(43.8956028269719,748.119290175308,103.34725943002));
#78396=CARTESIAN_POINT('Ctrl Pts',(43.8974826562651,748.415736514845,103.370973860377));
#78397=CARTESIAN_POINT('Ctrl Pts',(43.8994982690507,748.733595713221,103.396401227217));
#78398=CARTESIAN_POINT('Ctrl Pts',(43.9015708694549,749.05136534484,103.4237431833));
#78399=CARTESIAN_POINT('Ctrl Pts',(43.9037009210375,749.369039730519,103.452877636005));
#78400=CARTESIAN_POINT('Ctrl Pts',(43.9059365213006,749.702455571738,103.483455764097));
#78401=CARTESIAN_POINT('Ctrl Pts',(43.9082357098795,750.035766184794,103.516008089841));
#78402=CARTESIAN_POINT('Ctrl Pts',(43.9106417524483,750.368929551215,103.55037389145));
#78403=CARTESIAN_POINT('Ctrl Pts',(43.9132468091299,750.729650290319,103.58758223608));
#78404=CARTESIAN_POINT('Ctrl Pts',(43.9159773869033,751.090198191152,103.626916043815));
#78405=CARTESIAN_POINT('Ctrl Pts',(43.9189330996857,751.450483445277,103.668154957693));
#78406=CARTESIAN_POINT('Ctrl Pts',(43.9191858990892,751.481298312631,103.671682084176));
#78407=CARTESIAN_POINT('Ctrl Pts',(43.9194403687895,751.512111239579,103.675223140215));
#78408=CARTESIAN_POINT('Ctrl Pts',(43.9196965836671,751.54292215966,103.678777984592));
#78409=CARTESIAN_POINT('Ctrl Pts',(44.5744794255529,751.59614455564,103.206327301003));
#78410=CARTESIAN_POINT('Ctrl Pts',(44.5744794255529,751.519059169342,103.890607720566));
#78411=CARTESIAN_POINT('Ctrl Pts',(43.9196965836671,751.54292215966,103.678777984592));
#78412=CARTESIAN_POINT('Ctrl Pts',(44.5744794255529,752.148115347472,103.272252174199));
#78413=CARTESIAN_POINT('Ctrl Pts',(44.5694175928971,752.047430714789,103.941138173534));
#78414=CARTESIAN_POINT('Ctrl Pts',(43.9245398403207,752.125343909066,103.745975546382));
#78415=CARTESIAN_POINT('Ctrl Pts',(44.6288816340649,752.687363884647,103.360500944369));
#78416=CARTESIAN_POINT('Ctrl Pts',(44.6138450657875,752.573635763871,104.010544030293));
#78417=CARTESIAN_POINT('Ctrl Pts',(43.9880971321887,752.695085898244,103.83582173207));
#78418=CARTESIAN_POINT('Ctrl Pts',(44.786533250981,753.480032342672,103.51306294943));
#78419=CARTESIAN_POINT('Ctrl Pts',(44.759884698206,753.364651507361,104.137065762323));
#78420=CARTESIAN_POINT('Ctrl Pts',(44.1649153929541,753.533629601795,103.990943559498));
#78421=CARTESIAN_POINT('Ctrl Pts',(44.8518746516715,753.741539999995,103.567315461367));
#78422=CARTESIAN_POINT('Ctrl Pts',(44.8206625872923,753.624759284194,104.182208679739));
#78423=CARTESIAN_POINT('Ctrl Pts',(44.2375623083812,753.810449016713,104.046078043825));
#78424=CARTESIAN_POINT('Ctrl Pts',(45.0085265998517,754.259352877323,103.680782752095));
#78425=CARTESIAN_POINT('Ctrl Pts',(44.9690396895463,754.142216340654,104.278001051109));
#78426=CARTESIAN_POINT('Ctrl Pts',(44.4106063671844,754.358904400579,104.161327568411));
#78427=CARTESIAN_POINT('Ctrl Pts',(45.1002504493515,754.516305080123,103.74017707805));
#78428=CARTESIAN_POINT('Ctrl Pts',(45.0566143202729,754.400226022768,104.328716018458));
#78429=CARTESIAN_POINT('Ctrl Pts',(44.5114523561693,754.631227769305,104.221624502903));
#78430=CARTESIAN_POINT('Ctrl Pts',(45.4089475002517,755.263809131338,103.919511248394));
#78431=CARTESIAN_POINT('Ctrl Pts',(45.3524248984368,755.147282537831,104.482366235933));
#78432=CARTESIAN_POINT('Ctrl Pts',(44.8495485943442,755.423863452299,104.403592609289));
#78433=CARTESIAN_POINT('Ctrl Pts',(45.6603645608836,755.736496797567,104.041550175918));
#78434=CARTESIAN_POINT('Ctrl Pts',(45.5975986674501,755.628487215605,104.590077208969));
#78435=CARTESIAN_POINT('Ctrl Pts',(45.1233896323209,755.925647089536,104.527303365006));
#78436=CARTESIAN_POINT('Ctrl Pts',(46.1061076400661,756.40873710487,104.220441809427));
#78437=CARTESIAN_POINT('Ctrl Pts',(46.0413560410478,756.317625207438,104.751047110497));
#78438=CARTESIAN_POINT('Ctrl Pts',(45.6068395559476,756.639778449399,104.708487339111));
#78439=CARTESIAN_POINT('Ctrl Pts',(46.2668483778836,756.627399620023,104.279627720028));
#78440=CARTESIAN_POINT('Ctrl Pts',(46.2008832979289,756.540949210339,104.804363833508));
#78441=CARTESIAN_POINT('Ctrl Pts',(45.7808868346458,756.872158644901,104.768404935654));
#78442=CARTESIAN_POINT('Ctrl Pts',(46.6095956365525,757.048455848963,104.394751624816));
#78443=CARTESIAN_POINT('Ctrl Pts',(46.5423197953537,756.971159154162,104.908585762778));
#78444=CARTESIAN_POINT('Ctrl Pts',(46.151447281953,757.319765230662,104.884904813448));
#78445=CARTESIAN_POINT('Ctrl Pts',(46.7901385762444,757.249215258982,104.45023537906));
#78446=CARTESIAN_POINT('Ctrl Pts',(46.7227447552921,757.176852686386,104.959173188352));
#78447=CARTESIAN_POINT('Ctrl Pts',(46.3463802154442,757.533253384794,104.941027707592));
#78448=CARTESIAN_POINT('Ctrl Pts',(47.3587160332289,757.823009112407,104.609666709733));
#78449=CARTESIAN_POINT('Ctrl Pts',(47.2893552731759,757.761581290454,105.104277070691));
#78450=CARTESIAN_POINT('Ctrl Pts',(46.9595638789727,758.143567934702,105.102237696256));
#78451=CARTESIAN_POINT('Ctrl Pts',(47.7734412621022,758.167848086674,104.706595789808));
#78452=CARTESIAN_POINT('Ctrl Pts',(47.706990188793,758.117175996062,105.194224195243));
#78453=CARTESIAN_POINT('Ctrl Pts',(47.4059222897145,758.510547383819,105.200167705424));
#78454=CARTESIAN_POINT('Ctrl Pts',(48.4514501703775,758.626478847941,104.835483439563));
#78455=CARTESIAN_POINT('Ctrl Pts',(48.3932481566116,758.589939004014,105.314345113022));
#78456=CARTESIAN_POINT('Ctrl Pts',(48.134519768385,758.998737734966,105.330317611021));
#78457=CARTESIAN_POINT('Ctrl Pts',(48.6874818606445,758.76966617092,104.875741471088));
#78458=CARTESIAN_POINT('Ctrl Pts',(48.6316846628547,758.737249348849,105.351893075696));
#78459=CARTESIAN_POINT('Ctrl Pts',(48.38798759889,759.151176514627,105.370956824011));
#78460=CARTESIAN_POINT('Ctrl Pts',(49.1677758503293,759.029429484382,104.948719148144));
#78461=CARTESIAN_POINT('Ctrl Pts',(49.1170905060348,759.004243100467,105.420023263218));
#78462=CARTESIAN_POINT('Ctrl Pts',(48.9034665725843,759.427748450228,105.444608450082));
#78463=CARTESIAN_POINT('Ctrl Pts',(49.4132813461956,759.146937273221,104.981702524249));
#78464=CARTESIAN_POINT('Ctrl Pts',(49.3655541140878,759.125201002094,105.45093035461));
#78465=CARTESIAN_POINT('Ctrl Pts',(49.1668145853464,759.552873463948,105.477887235526));
#78466=CARTESIAN_POINT('Ctrl Pts',(49.9148905872182,759.35748115349,105.040728766851));
#78467=CARTESIAN_POINT('Ctrl Pts',(49.8732615932761,759.341703719427,105.506261540841));
#78468=CARTESIAN_POINT('Ctrl Pts',(49.7046495990986,759.77707896997,105.537431528601));
#78469=CARTESIAN_POINT('Ctrl Pts',(50.1709940815575,759.450517538234,105.066772942566));
#78470=CARTESIAN_POINT('Ctrl Pts',(50.132764946986,759.437496221055,105.530750099739));
#78471=CARTESIAN_POINT('Ctrl Pts',(49.9791362390332,759.876159864622,105.563698346379));
#78472=CARTESIAN_POINT('Ctrl Pts',(50.6939870257785,759.611675989273,105.11183475266));
#78473=CARTESIAN_POINT('Ctrl Pts',(50.6626659053261,759.60326155973,105.573119554025));
#78474=CARTESIAN_POINT('Ctrl Pts',(50.5394972721225,760.047795397873,105.60913954858));
#78475=CARTESIAN_POINT('Ctrl Pts',(50.9619905198647,759.680016906257,105.130914271761));
#78476=CARTESIAN_POINT('Ctrl Pts',(50.9344582158919,759.673639259957,105.591104788454));
#78477=CARTESIAN_POINT('Ctrl Pts',(50.8265645638574,760.120583193639,105.628376318847));
#78478=CARTESIAN_POINT('Ctrl Pts',(51.7753420479021,759.84436412666,105.176763005322));
#78479=CARTESIAN_POINT('Ctrl Pts',(51.7582264576729,759.842529266706,105.634258674167));
#78480=CARTESIAN_POINT('Ctrl Pts',(51.6975998109845,760.295628418505,105.674599430838));
#78481=CARTESIAN_POINT('Ctrl Pts',(52.3204317814714,759.89866305656,105.191873856739));
#78482=CARTESIAN_POINT('Ctrl Pts',(52.3123691280982,759.898645098071,105.648594749949));
#78483=CARTESIAN_POINT('Ctrl Pts',(52.2811255874571,760.35346752339,105.689829315887));
#78484=CARTESIAN_POINT('Ctrl Pts',(53.1422255185264,759.899585901188,105.192131310029));
#78485=CARTESIAN_POINT('Ctrl Pts',(53.1460494438434,759.899594647449,105.64883774948));
#78486=CARTESIAN_POINT('Ctrl Pts',(53.1608917437895,760.354450523046,105.690088828146));
#78487=CARTESIAN_POINT('Ctrl Pts',(53.4168551254893,759.886373409819,105.188450617713));
#78488=CARTESIAN_POINT('Ctrl Pts',(53.4247959624678,759.885985202566,105.645359420836));
#78489=CARTESIAN_POINT('Ctrl Pts',(53.4548903834744,760.340376857288,105.686378827854));
#78490=CARTESIAN_POINT('Ctrl Pts',(53.9675536213112,759.832084811908,105.17332453908));
#78491=CARTESIAN_POINT('Ctrl Pts',(53.9833766930975,759.830129923587,105.631089132305));
#78492=CARTESIAN_POINT('Ctrl Pts',(54.0444787668349,760.28255157886,105.671131426169));
#78493=CARTESIAN_POINT('Ctrl Pts',(54.2419099682168,759.791027458344,105.161883921301));
#78494=CARTESIAN_POINT('Ctrl Pts',(54.2617662228772,759.787844040971,105.620286614436));
#78495=CARTESIAN_POINT('Ctrl Pts',(54.3382358524801,760.238819943468,105.659598813989));
#78496=CARTESIAN_POINT('Ctrl Pts',(55.0489471047564,759.629112297025,105.116715339214));
#78497=CARTESIAN_POINT('Ctrl Pts',(55.0809094134985,759.621093926842,105.577680193947));
#78498=CARTESIAN_POINT('Ctrl Pts',(55.2025043190926,760.066364963711,105.61406153305));
#78499=CARTESIAN_POINT('Ctrl Pts',(55.5710463976871,759.469419747382,105.072109809235));
#78500=CARTESIAN_POINT('Ctrl Pts',(55.6111133398768,759.456081709598,105.535495281444));
#78501=CARTESIAN_POINT('Ctrl Pts',(55.7618470107023,759.896281612356,105.569087544629));
#78502=CARTESIAN_POINT('Ctrl Pts',(56.3303163159383,759.152348544857,104.983223153246));
#78503=CARTESIAN_POINT('Ctrl Pts',(56.3779146260612,759.130763073273,105.452353711034));
#78504=CARTESIAN_POINT('Ctrl Pts',(56.5759381906951,759.558635651997,105.479421434344));
#78505=CARTESIAN_POINT('Ctrl Pts',(56.5802727164515,759.033027300629,104.94973178096));
#78506=CARTESIAN_POINT('Ctrl Pts',(56.6308781790121,759.007942241034,105.42097037371));
#78507=CARTESIAN_POINT('Ctrl Pts',(56.8440578657723,759.431579412207,105.445630264923));
#78508=CARTESIAN_POINT('Ctrl Pts',(57.0615059695379,758.773327759877,104.876773293326));
#78509=CARTESIAN_POINT('Ctrl Pts',(57.1172413600607,758.741012612513,105.352855148836));
#78510=CARTESIAN_POINT('Ctrl Pts',(57.3605396045951,759.155074860993,105.371998350356));
#78511=CARTESIAN_POINT('Ctrl Pts',(57.294018868685,758.632543759301,104.83719138845));
#78512=CARTESIAN_POINT('Ctrl Pts',(57.3521149071898,758.596181765672,105.315938102217));
#78513=CARTESIAN_POINT('Ctrl Pts',(57.6102260026136,759.005194380144,105.332041857984));
#78514=CARTESIAN_POINT('Ctrl Pts',(57.7432907980298,758.329697775192,104.75208224537));
#78515=CARTESIAN_POINT('Ctrl Pts',(57.8052249848145,758.285129533451,105.236897381044));
#78516=CARTESIAN_POINT('Ctrl Pts',(58.0930084527051,758.682827936322,105.246100041666));
#78517=CARTESIAN_POINT('Ctrl Pts',(57.9600487684303,758.167634829186,104.706552727405));
#78518=CARTESIAN_POINT('Ctrl Pts',(58.0236467810424,758.118539254183,105.194680055239));
#78519=CARTESIAN_POINT('Ctrl Pts',(58.3261033342161,758.510340844161,105.20011241727));
#78520=CARTESIAN_POINT('Ctrl Pts',(58.3778094652649,757.822177088784,104.609756284298));
#78521=CARTESIAN_POINT('Ctrl Pts',(58.4437597202967,757.76411531061,105.105383013978));
#78522=CARTESIAN_POINT('Ctrl Pts',(58.7757333828905,758.142735072835,105.102306949991));
#78523=CARTESIAN_POINT('Ctrl Pts',(58.5797093488485,757.637852690173,104.558228376542));
#78524=CARTESIAN_POINT('Ctrl Pts',(58.6465023262139,757.574888333299,105.057958577838));
#78525=CARTESIAN_POINT('Ctrl Pts',(58.9932364046669,757.94662755088,105.050225183338));
#78526=CARTESIAN_POINT('Ctrl Pts',(59.1544072875436,757.058734139539,104.397303612921));
#78527=CARTESIAN_POINT('Ctrl Pts',(59.2251233187521,756.97865409733,104.909978577497));
#78528=CARTESIAN_POINT('Ctrl Pts',(59.6130103989281,757.330647109462,104.887506015757));
#78529=CARTESIAN_POINT('Ctrl Pts',(59.4935762137873,756.641866404394,104.282546238651));
#78530=CARTESIAN_POINT('Ctrl Pts',(59.562918319445,756.550559643376,104.805531171682));
#78531=CARTESIAN_POINT('Ctrl Pts',(59.9797033840178,756.887441018598,104.771385918518));
#78532=CARTESIAN_POINT('Ctrl Pts',(59.9394997893029,755.971526865868,104.104068709291));
#78533=CARTESIAN_POINT('Ctrl Pts',(60.0010294218336,755.87243549109,104.647027891106));
#78534=CARTESIAN_POINT('Ctrl Pts',(60.4633225313643,756.175320476182,104.590623776178));
#78535=CARTESIAN_POINT('Ctrl Pts',(60.0775910818274,755.74051238977,104.043534590738));
#78536=CARTESIAN_POINT('Ctrl Pts',(60.1369009815706,755.637390179665,104.593249818085));
#78537=CARTESIAN_POINT('Ctrl Pts',(60.6133744486101,755.929997358585,104.529288381377));
#78538=CARTESIAN_POINT('Ctrl Pts',(60.3322391296729,755.262753497981,103.921522025463));
#78539=CARTESIAN_POINT('Ctrl Pts',(60.3862493070344,755.153147854279,104.485863090903));
#78540=CARTESIAN_POINT('Ctrl Pts',(60.8906892901628,755.422887310523,104.405602436978));
#78541=CARTESIAN_POINT('Ctrl Pts',(60.447901738291,755.017429606684,103.860427381585));
#78542=CARTESIAN_POINT('Ctrl Pts',(60.4986089402268,754.905013930175,104.432563256064));
#78543=CARTESIAN_POINT('Ctrl Pts',(61.0169814111351,755.162609709595,104.343640628005));
#78544=CARTESIAN_POINT('Ctrl Pts',(60.7560740078579,754.27217004841,103.681568565603));
#78545=CARTESIAN_POINT('Ctrl Pts',(60.7986572104131,754.148276419581,104.276856895969));
#78546=CARTESIAN_POINT('Ctrl Pts',(61.3544921187512,754.372350029824,104.162155689742));
#78547=CARTESIAN_POINT('Ctrl Pts',(60.9123307712354,753.759154140586,103.567040624627));
#78548=CARTESIAN_POINT('Ctrl Pts',(60.9446633007839,753.63474809668,104.180498188071));
#78549=CARTESIAN_POINT('Ctrl Pts',(61.5271361446121,753.828916680788,104.045825043828));
#78550=CARTESIAN_POINT('Ctrl Pts',(61.1251758119162,752.697511926956,103.362211444783));
#78551=CARTESIAN_POINT('Ctrl Pts',(61.1403990245377,752.583507919546,104.011897615359));
#78552=CARTESIAN_POINT('Ctrl Pts',(61.7657767399434,752.705810036518,103.837562632188));
#78553=CARTESIAN_POINT('Ctrl Pts',(61.1807573575412,752.146129805475,103.272018526422));
#78554=CARTESIAN_POINT('Ctrl Pts',(61.1858008747042,752.04551697713,103.940958574835));
#78555=CARTESIAN_POINT('Ctrl Pts',(61.8307144309821,752.123237070503,103.745735973319));
#78556=CARTESIAN_POINT('Ctrl Pts',(61.1807573575412,751.59614455564,103.206330589227));
#78557=CARTESIAN_POINT('Ctrl Pts',(61.1807573575412,751.519058933453,103.89061093067));
#78558=CARTESIAN_POINT('Ctrl Pts',(61.8355401657986,751.54292199161,103.678781264903));
#78559=CARTESIAN_POINT('',(61.1807573575412,751.59614455564,103.206330589227));
#78560=CARTESIAN_POINT('',(61.8355401657986,751.54292199161,103.678781264903));
#78561=CARTESIAN_POINT('Origin',(61.6807573575412,751.59614455564,103.206330589227));
#78562=CARTESIAN_POINT('Ctrl Pts',(43.9196965836672,751.54292215966,103.678777984592));
#78563=CARTESIAN_POINT('Ctrl Pts',(43.9222882420743,751.854579858462,103.714735840723));
#78564=CARTESIAN_POINT('Ctrl Pts',(43.9416843025476,752.162082511931,103.757115234728));
#78565=CARTESIAN_POINT('Ctrl Pts',(43.9770626340715,752.465825441172,103.804485148761));
#78566=CARTESIAN_POINT('Ctrl Pts',(44.0079926061767,752.731376695964,103.845898919748));
#78567=CARTESIAN_POINT('Ctrl Pts',(44.0511391087946,752.994054039292,103.891127868557));
#78568=CARTESIAN_POINT('Ctrl Pts',(44.1059768732623,753.254114812661,103.939236516006));
#78569=CARTESIAN_POINT('Ctrl Pts',(44.1070628642689,753.259264979954,103.940189245552));
#78570=CARTESIAN_POINT('Ctrl Pts',(44.1081534842892,753.264414115119,103.941143116971));
#78571=CARTESIAN_POINT('Ctrl Pts',(44.1092487338049,753.26956221924,103.942098124302));
#78572=CARTESIAN_POINT('Ctrl Pts',(44.1676695835732,753.54416322397,103.993038425126));
#78573=CARTESIAN_POINT('Ctrl Pts',(44.239273149121,753.815847378745,104.047214475678));
#78574=CARTESIAN_POINT('Ctrl Pts',(44.3240881220502,754.084675390243,104.103703645877));
#78575=CARTESIAN_POINT('Ctrl Pts',(44.3261337935242,754.091159313724,104.105066120923));
#78576=CARTESIAN_POINT('Ctrl Pts',(44.328187400331,754.097641960348,104.106430043822));
#78577=CARTESIAN_POINT('Ctrl Pts',(44.3302489077782,754.104123247547,104.107795383506));
#78578=CARTESIAN_POINT('Ctrl Pts',(44.4077281650296,754.347714566551,104.159110019675));
#78579=CARTESIAN_POINT('Ctrl Pts',(44.4964062601969,754.589472508106,104.212446643126));
#78580=CARTESIAN_POINT('Ctrl Pts',(44.5944959003185,754.825061900319,104.266177546448));
#78581=CARTESIAN_POINT('Ctrl Pts',(44.6042892519893,754.848583342186,104.271542084754));
#78582=CARTESIAN_POINT('Ctrl Pts',(44.6141764317493,754.872043333742,104.27691056703));
#78583=CARTESIAN_POINT('Ctrl Pts',(44.6241556689194,754.8954375867,104.282281382562));
#78584=CARTESIAN_POINT('Ctrl Pts',(44.6271462429718,754.902448367652,104.283890906546));
#78585=CARTESIAN_POINT('Ctrl Pts',(44.6301452662658,754.909454266755,104.285500809474));
#78586=CARTESIAN_POINT('Ctrl Pts',(44.6331527373413,754.916455286669,104.287111078783));
#78587=CARTESIAN_POINT('Ctrl Pts',(44.8234368635388,755.359413148416,104.388993584289));
#78588=CARTESIAN_POINT('Ctrl Pts',(45.0475806350685,755.783008851131,104.492369940441));
#78589=CARTESIAN_POINT('Ctrl Pts',(45.3053136151034,756.187928903774,104.594105064536));
#78590=CARTESIAN_POINT('Ctrl Pts',(45.3510494184664,756.2597836734,104.612158391006));
#78591=CARTESIAN_POINT('Ctrl Pts',(45.3978429047043,756.331050318697,104.630160157722));
#78592=CARTESIAN_POINT('Ctrl Pts',(45.4456925075793,756.401732640839,104.64809300649));
#78593=CARTESIAN_POINT('Ctrl Pts',(45.45003966964,756.408154167679,104.649722215409));
#78594=CARTESIAN_POINT('Ctrl Pts',(45.4543961181741,756.414571424984,104.651351039854));
#78595=CARTESIAN_POINT('Ctrl Pts',(45.4587618192155,756.420984356023,104.652979456487));
#78596=CARTESIAN_POINT('Ctrl Pts',(45.6163109922364,756.652413849778,104.711745664119));
#78597=CARTESIAN_POINT('Ctrl Pts',(45.7859551656581,756.878279376204,104.769998200999));
#78598=CARTESIAN_POINT('Ctrl Pts',(45.9661679585971,757.095961187712,104.826654941289));
#78599=CARTESIAN_POINT('Ctrl Pts',(46.1514947957323,757.319820332065,104.884919475725));
#78600=CARTESIAN_POINT('Ctrl Pts',(46.3464184182909,757.533287259426,104.941037304803));
#78601=CARTESIAN_POINT('Ctrl Pts',(46.5507789485454,757.736687387445,104.994764523293));
#78602=CARTESIAN_POINT('Ctrl Pts',(46.5553762786402,757.741263112164,104.995973180162));
#78603=CARTESIAN_POINT('Ctrl Pts',(46.5599783502191,757.745833779824,104.997180627251));
#78604=CARTESIAN_POINT('Ctrl Pts',(46.5645851663029,757.750399388697,104.998386862409));
#78605=CARTESIAN_POINT('Ctrl Pts',(46.9137288383299,758.096420028114,105.089805613366));
#78606=CARTESIAN_POINT('Ctrl Pts',(47.2901206721729,758.413385452472,105.174261793583));
#78607=CARTESIAN_POINT('Ctrl Pts',(47.6947821660368,758.700291748076,105.250752122856));
#78608=CARTESIAN_POINT('Ctrl Pts',(47.7596785582558,758.746303498074,105.263019033557));
#78609=CARTESIAN_POINT('Ctrl Pts',(47.8253019526046,758.791542230477,105.275081093836));
#78610=CARTESIAN_POINT('Ctrl Pts',(47.8916564802653,758.836003896006,105.286934195027));
#78611=CARTESIAN_POINT('Ctrl Pts',(47.8956664048994,758.838690795215,105.287650499462));
#78612=CARTESIAN_POINT('Ctrl Pts',(47.8996792064592,758.841374880698,105.288366053528));
#78613=CARTESIAN_POINT('Ctrl Pts',(47.9036948563414,758.844056135095,105.289080852419));
#78614=CARTESIAN_POINT('Ctrl Pts',(48.1428788724764,759.003759598727,105.331656394186));
#78615=CARTESIAN_POINT('Ctrl Pts',(48.3922085638967,759.153441202998,105.371559916014));
#78616=CARTESIAN_POINT('Ctrl Pts',(48.6457272938702,759.28946210282,105.407782617332));
#78617=CARTESIAN_POINT('Ctrl Pts',(48.6491409775775,759.291293653214,105.408270363722));
#78618=CARTESIAN_POINT('Ctrl Pts',(48.6525556554173,759.293122900299,105.408757489342));
#78619=CARTESIAN_POINT('Ctrl Pts',(48.6559713274725,759.294949844451,105.4092439943));
#78620=CARTESIAN_POINT('Ctrl Pts',(48.9104046830959,759.431038884519,105.445483740654));
#78621=CARTESIAN_POINT('Ctrl Pts',(49.1703412219104,759.554343580572,105.478277671731));
#78622=CARTESIAN_POINT('Ctrl Pts',(49.4357322277162,759.664975899792,105.507659360736));
#78623=CARTESIAN_POINT('Ctrl Pts',(49.4384950114107,759.666127608633,105.507965231129));
#78624=CARTESIAN_POINT('Ctrl Pts',(49.4412583861498,759.667277944231,105.508270731881));
#78625=CARTESIAN_POINT('Ctrl Pts',(49.444022352054,759.668426906305,105.508575862942));
#78626=CARTESIAN_POINT('Ctrl Pts',(49.7102673651492,759.779103171087,105.537968274488));
#78627=CARTESIAN_POINT('Ctrl Pts',(49.9820143411467,759.877040020028,105.563931608773));
#78628=CARTESIAN_POINT('Ctrl Pts',(50.2593169608851,759.961976978418,105.586418896536));
#78629=CARTESIAN_POINT('Ctrl Pts',(50.261424521963,759.962622518038,105.586589804883));
#78630=CARTESIAN_POINT('Ctrl Pts',(50.2635324714005,759.963267320058,105.586760516006));
#78631=CARTESIAN_POINT('Ctrl Pts',(50.2656408076297,759.963911383872,105.586931029756));
#78632=CARTESIAN_POINT('Ctrl Pts',(50.5437951360706,760.048883190283,105.60942703249));
#78633=CARTESIAN_POINT('Ctrl Pts',(50.8287372405806,760.121019818447,105.628491616469));
#78634=CARTESIAN_POINT('Ctrl Pts',(51.1169098357794,760.178930684446,105.643783944634));
#78635=CARTESIAN_POINT('Ctrl Pts',(51.1183173872021,760.179213544521,105.643858638546));
#78636=CARTESIAN_POINT('Ctrl Pts',(51.1197249553105,760.179496058764,105.643933240885));
#78637=CARTESIAN_POINT('Ctrl Pts',(51.1211325401031,760.179778227198,105.644007751659));
#78638=CARTESIAN_POINT('Ctrl Pts',(51.537483728184,760.263241165698,105.666047382542));
#78639=CARTESIAN_POINT('Ctrl Pts',(51.9553898405354,760.316467744201,105.680080083813));
#78640=CARTESIAN_POINT('Ctrl Pts',(52.3748207884131,760.340038026233,105.686291460172));
#78641=CARTESIAN_POINT('Ctrl Pts',(52.5388480286482,760.349255677751,105.688720548744));
#78642=CARTESIAN_POINT('Ctrl Pts',(52.7031084285715,760.353938347338,105.689953616226));
#78643=CARTESIAN_POINT('Ctrl Pts',(52.8676000187963,760.354122807732,105.690002312588));
#78644=CARTESIAN_POINT('Ctrl Pts',(52.8676121319811,760.354122821316,105.690002316174));
#78645=CARTESIAN_POINT('Ctrl Pts',(52.8676242451673,760.354122834875,105.690002319753));
#78646=CARTESIAN_POINT('Ctrl Pts',(52.8676363583547,760.35412284841,105.690002323327));
#78647=CARTESIAN_POINT('Ctrl Pts',(53.1601792657639,760.354449726949,105.690088617979));
#78648=CARTESIAN_POINT('Ctrl Pts',(53.4534590064905,760.340443962875,105.686396550651));
#78649=CARTESIAN_POINT('Ctrl Pts',(53.7474975400303,760.311678350027,105.678811605977));
#78650=CARTESIAN_POINT('Ctrl Pts',(53.7482265437083,760.311607032036,105.67879280078));
#78651=CARTESIAN_POINT('Ctrl Pts',(53.7489555522463,760.311535623303,105.67877397165));
#78652=CARTESIAN_POINT('Ctrl Pts',(53.7496845656449,760.311464123822,105.678755118587));
#78653=CARTESIAN_POINT('Ctrl Pts',(54.0430101818375,760.28269561375,105.671169405409));
#78654=CARTESIAN_POINT('Ctrl Pts',(54.3353080121679,760.239254752756,105.659713477702));
#78655=CARTESIAN_POINT('Ctrl Pts',(54.621997755479,760.182196535239,105.644647363647));
#78656=CARTESIAN_POINT('Ctrl Pts',(54.6234403711711,760.181909419701,105.644571551334));
#78657=CARTESIAN_POINT('Ctrl Pts',(54.6248828455483,760.18162195925,105.644495647578));
#78658=CARTESIAN_POINT('Ctrl Pts',(54.626325178025,760.181334154021,105.644419652411));
#78659=CARTESIAN_POINT('Ctrl Pts',(55.0237698139674,760.102027443378,105.623478661413));
#78660=CARTESIAN_POINT('Ctrl Pts',(55.4132143245847,759.996489629965,105.595581455059));
#78661=CARTESIAN_POINT('Ctrl Pts',(55.7946463204337,759.864793743759,105.560676652494));
#78662=CARTESIAN_POINT('Ctrl Pts',(55.9633680415354,759.806539698937,105.545236945213));
#78663=CARTESIAN_POINT('Ctrl Pts',(56.130522226761,759.743168128376,105.528426281525));
#78664=CARTESIAN_POINT('Ctrl Pts',(56.2961088088657,759.674688336685,105.51024101466));
#78665=CARTESIAN_POINT('Ctrl Pts',(56.2989309021838,759.6735212351,105.509931083025));
#78666=CARTESIAN_POINT('Ctrl Pts',(56.3017525423132,759.672352648481,105.509620751853));
#78667=CARTESIAN_POINT('Ctrl Pts',(56.3045737292892,759.671182576856,105.50931002112));
#78668=CARTESIAN_POINT('Ctrl Pts',(56.5723103313437,759.56014030856,105.479821018315));
#78669=CARTESIAN_POINT('Ctrl Pts',(56.8368504016774,759.434989847435,105.446537269546));
#78670=CARTESIAN_POINT('Ctrl Pts',(57.0918297542857,759.298919797329,105.410304083083));
#78671=CARTESIAN_POINT('Ctrl Pts',(57.0953207503219,759.297056822933,105.409808004052));
#78672=CARTESIAN_POINT('Ctrl Pts',(57.0988099745461,759.295191792752,105.40931136945));
#78673=CARTESIAN_POINT('Ctrl Pts',(57.102297410318,759.293324715008,105.408814181461));
#78674=CARTESIAN_POINT('Ctrl Pts',(57.3562133100673,759.157385085934,105.372614536862));
#78675=CARTESIAN_POINT('Ctrl Pts',(57.6019269575373,759.010170269504,105.333368585133));
#78676=CARTESIAN_POINT('Ctrl Pts',(57.8395823891179,758.852032502038,105.291209524237));
#78677=CARTESIAN_POINT('Ctrl Pts',(57.8435961886419,758.849361688703,105.290497493305));
#78678=CARTESIAN_POINT('Ctrl Pts',(57.8476076982969,758.846687755669,105.289784630274));
#78679=CARTESIAN_POINT('Ctrl Pts',(57.8516169192593,758.844010704458,105.289070935729));
#78680=CARTESIAN_POINT('Ctrl Pts',(58.0882524163231,758.686003612812,105.246946676398));
#78681=CARTESIAN_POINT('Ctrl Pts',(58.3169134960859,758.517132591522,105.201923457535));
#78682=CARTESIAN_POINT('Ctrl Pts',(58.5376144473366,758.337392970489,105.154098018575));
#78683=CARTESIAN_POINT('Ctrl Pts',(58.5420522017946,758.333778847849,105.153136366377));
#78684=CARTESIAN_POINT('Ctrl Pts',(58.546486708164,758.330160353861,105.152173587515));
#78685=CARTESIAN_POINT('Ctrl Pts',(58.550917968495,758.326537487121,105.151209682423));
#78686=CARTESIAN_POINT('Ctrl Pts',(58.7332547760087,758.177464332762,105.111547066319));
#78687=CARTESIAN_POINT('Ctrl Pts',(58.9107348333014,758.020340398815,105.069804813504));
#78688=CARTESIAN_POINT('Ctrl Pts',(59.0815559882096,757.856699493983,105.026498262851));
#78689=CARTESIAN_POINT('Ctrl Pts',(59.1165412024408,757.823184838755,105.017628817184));
#78690=CARTESIAN_POINT('Ctrl Pts',(59.1512469848355,757.789396703121,105.008693726704));
#78691=CARTESIAN_POINT('Ctrl Pts',(59.1856576422419,757.755348095664,104.999697380079));
#78692=CARTESIAN_POINT('Ctrl Pts',(59.1903858204453,757.750669664742,104.998461241823));
#78693=CARTESIAN_POINT('Ctrl Pts',(59.195108372811,757.745986371901,104.997223961393));
#78694=CARTESIAN_POINT('Ctrl Pts',(59.1998252568978,757.74129825323,104.995985550773));
#78695=CARTESIAN_POINT('Ctrl Pts',(59.4544505926583,757.488225722995,104.929134062762));
#78696=CARTESIAN_POINT('Ctrl Pts',(59.6914823033983,757.222735724059,104.859365942784));
#78697=CARTESIAN_POINT('Ctrl Pts',(59.9114777383397,756.944951075768,104.787414134271));
#78698=CARTESIAN_POINT('Ctrl Pts',(60.043401849949,756.778372651292,104.744266973425));
#78699=CARTESIAN_POINT('Ctrl Pts',(60.1691988731846,756.607372436143,104.700334462475));
#78700=CARTESIAN_POINT('Ctrl Pts',(60.2889819139123,756.431971457055,104.655774342994));
#78701=CARTESIAN_POINT('Ctrl Pts',(60.2933667668142,756.425550619118,104.654143147393));
#78702=CARTESIAN_POINT('Ctrl Pts',(60.2977435424752,756.419123894807,104.652511115576));
#78703=CARTESIAN_POINT('Ctrl Pts',(60.302112246228,756.412691285737,104.650878255422));
#78704=CARTESIAN_POINT('Ctrl Pts',(60.4587645447275,756.182031791949,104.592327410428));
#78705=CARTESIAN_POINT('Ctrl Pts',(60.604959123994,755.94374589697,104.532726165884));
#78706=CARTESIAN_POINT('Ctrl Pts',(60.7404635896536,755.697527263392,104.472591813655));
#78707=CARTESIAN_POINT('Ctrl Pts',(60.7443280641775,755.690505312992,104.470876832005));
#78708=CARTESIAN_POINT('Ctrl Pts',(60.7481838759298,755.683476843825,104.469161401562));
#78709=CARTESIAN_POINT('Ctrl Pts',(60.7520310175676,755.676441850253,104.467445534873));
#78710=CARTESIAN_POINT('Ctrl Pts',(60.8868425647486,755.429921587369,104.407318129921));
#78711=CARTESIAN_POINT('Ctrl Pts',(61.0100891296998,755.176812867826,104.347021350455));
#78712=CARTESIAN_POINT('Ctrl Pts',(61.120367510098,754.920453707401,104.288034421268));
#78713=CARTESIAN_POINT('Ctrl Pts',(61.1234156256758,754.913367891055,104.286404011235));
#78714=CARTESIAN_POINT('Ctrl Pts',(61.1264538819749,754.906279489723,104.284774578093));
#78715=CARTESIAN_POINT('Ctrl Pts',(61.1294822492254,754.899188572816,104.283146152984));
#78716=CARTESIAN_POINT('Ctrl Pts',(61.2851753799673,754.534633364785,104.199426252964));
#78717=CARTESIAN_POINT('Ctrl Pts',(61.4160669876604,754.161503146051,104.117788101251));
#78718=CARTESIAN_POINT('Ctrl Pts',(61.5215771637907,753.779210947047,104.04077912677));
#78719=CARTESIAN_POINT('Ctrl Pts',(61.5667510621108,753.615533569567,104.007807941331));
#78720=CARTESIAN_POINT('Ctrl Pts',(61.6072722405618,753.450176565982,103.975685963823));
#78721=CARTESIAN_POINT('Ctrl Pts',(61.6430949649522,753.28309321559,103.944615964494));
#78722=CARTESIAN_POINT('Ctrl Pts',(61.6442187866902,753.277851517633,103.943641244083));
#78723=CARTESIAN_POINT('Ctrl Pts',(61.6453380248863,753.272607919378,103.942667522459));
#78724=CARTESIAN_POINT('Ctrl Pts',(61.6464526753947,753.267362426993,103.94169480763));
#78725=CARTESIAN_POINT('Ctrl Pts',(61.6800280803303,753.109358165033,103.912394776783));
#78726=CARTESIAN_POINT('Ctrl Pts',(61.7093532644357,752.94940376462,103.884017215441));
#78727=CARTESIAN_POINT('Ctrl Pts',(61.734231455373,752.788230657605,103.856889346437));
#78728=CARTESIAN_POINT('Ctrl Pts',(61.7530337256528,752.666420340786,103.836386829738));
#78729=CARTESIAN_POINT('Ctrl Pts',(61.7692967927551,752.543914606322,103.81659808501));
#78730=CARTESIAN_POINT('Ctrl Pts',(61.7829539548099,752.421035328951,103.79765983892));
#78731=CARTESIAN_POINT('Ctrl Pts',(61.7971811141958,752.293027543925,103.777931183397));
#78732=CARTESIAN_POINT('Ctrl Pts',(61.8085787756287,752.164678612146,103.759133442712));
#78733=CARTESIAN_POINT('Ctrl Pts',(61.8171072456853,752.035968727419,103.741364412261));
#78734=CARTESIAN_POINT('Ctrl Pts',(61.8254209279602,751.910500374928,103.724042891224));
#78735=CARTESIAN_POINT('Ctrl Pts',(61.8310081021847,751.784688356559,103.707698629829));
#78736=CARTESIAN_POINT('Ctrl Pts',(61.8337861166434,751.658514124101,103.692440352553));
#78737=CARTESIAN_POINT('Ctrl Pts',(61.8346337139604,751.620017225506,103.687784914263));
#78738=CARTESIAN_POINT('Ctrl Pts',(61.8352194731405,751.581486643892,103.683230718558));
#78739=CARTESIAN_POINT('Ctrl Pts',(61.8355401657986,751.54292199161,103.678781264903));
#78740=CARTESIAN_POINT('Ctrl Pts',(61.1807573575412,751.59614455564,103.206330589227));
#78741=CARTESIAN_POINT('Ctrl Pts',(61.1807573575412,751.718279376357,103.220917861222));
#78742=CARTESIAN_POINT('Ctrl Pts',(61.1780202994061,751.840070301746,103.236662403929));
#78743=CARTESIAN_POINT('Ctrl Pts',(61.1726298703664,751.961534761204,103.253447745652));
#78744=CARTESIAN_POINT('Ctrl Pts',(61.1671114860814,752.085882481826,103.270631529224));
#78745=CARTESIAN_POINT('Ctrl Pts',(61.1588122816436,752.209888772891,103.288906439657));
#78746=CARTESIAN_POINT('Ctrl Pts',(61.1477725027734,752.333573159067,103.308169159173));
#78747=CARTESIAN_POINT('Ctrl Pts',(61.1452162792684,752.36221186088,103.312629376807));
#78748=CARTESIAN_POINT('Ctrl Pts',(61.1425129174128,752.390833280895,103.317142632079));
#78749=CARTESIAN_POINT('Ctrl Pts',(61.1396625485833,752.419437602569,103.321707772919));
#78750=CARTESIAN_POINT('Ctrl Pts',(61.1242164768869,752.574443649098,103.346446147822));
#78751=CARTESIAN_POINT('Ctrl Pts',(61.1044561303026,752.728875719466,103.37269840247));
#78752=CARTESIAN_POINT('Ctrl Pts',(61.080504106868,752.88200547624,103.40014979494));
#78753=CARTESIAN_POINT('Ctrl Pts',(61.0623131367301,752.998303743913,103.42099844942));
#78754=CARTESIAN_POINT('Ctrl Pts',(61.0417054555287,753.113850750621,103.44253827644));
#78755=CARTESIAN_POINT('Ctrl Pts',(61.0187532924489,753.228333029416,103.464626059596));
#78756=CARTESIAN_POINT('Ctrl Pts',(61.0187372299444,753.228413147012,103.464641517186));
#78757=CARTESIAN_POINT('Ctrl Pts',(61.0187211663153,753.228493264148,103.464656975041));
#78758=CARTESIAN_POINT('Ctrl Pts',(61.0187051015615,753.228573380827,103.464672433162));
#78759=CARTESIAN_POINT('Ctrl Pts',(60.9357145300591,753.642456409306,103.544529137881));
#78760=CARTESIAN_POINT('Ctrl Pts',(60.8224631198419,754.045356768554,103.631716926695));
#78761=CARTESIAN_POINT('Ctrl Pts',(60.6792876136371,754.438138498757,103.722736038756));
#78762=CARTESIAN_POINT('Ctrl Pts',(60.6389128222857,754.548901022487,103.748402982466));
#78763=CARTESIAN_POINT('Ctrl Pts',(60.5961581529625,754.658858791047,103.774374719279));
#78764=CARTESIAN_POINT('Ctrl Pts',(60.5510305085273,754.768030931921,103.800573012368));
#78765=CARTESIAN_POINT('Ctrl Pts',(60.5508956397594,754.768357204482,103.800651308755));
#78766=CARTESIAN_POINT('Ctrl Pts',(60.5507607497986,754.768683470021,103.800729607164));
#78767=CARTESIAN_POINT('Ctrl Pts',(60.5506258386452,754.769009728538,103.800807907594));
#78768=CARTESIAN_POINT('Ctrl Pts',(60.4478944370174,755.017447265838,103.860431687568));
#78769=CARTESIAN_POINT('Ctrl Pts',(60.3322348600846,755.262761506947,103.921524154167));
#78770=CARTESIAN_POINT('Ctrl Pts',(60.2049151155111,755.501632925562,103.982528405725));
#78771=CARTESIAN_POINT('Ctrl Pts',(60.0780610014804,755.73963074968,104.04330955408));
#78772=CARTESIAN_POINT('Ctrl Pts',(59.9405192295365,755.969823047112,104.103622339393));
#78773=CARTESIAN_POINT('Ctrl Pts',(59.7924856214108,756.192526600842,104.162909900451));
#78774=CARTESIAN_POINT('Ctrl Pts',(59.7919434243098,756.19334228873,104.16312705076));
#78775=CARTESIAN_POINT('Ctrl Pts',(59.7914010865019,756.19415787607,104.163344187296));
#78776=CARTESIAN_POINT('Ctrl Pts',(59.7908586079975,756.194973362876,104.163561310031));
#78777=CARTESIAN_POINT('Ctrl Pts',(59.5103527670844,756.616646867508,104.275831556317));
#78778=CARTESIAN_POINT('Ctrl Pts',(59.1925105038488,757.011662044582,104.384358291729));
#78779=CARTESIAN_POINT('Ctrl Pts',(58.8354949001653,757.379387741009,104.486417413724));
#78780=CARTESIAN_POINT('Ctrl Pts',(58.8152435256669,757.40024663545,104.492206621476));
#78781=CARTESIAN_POINT('Ctrl Pts',(58.7948660949876,757.421017715167,104.497975015419));
#78782=CARTESIAN_POINT('Ctrl Pts',(58.7743622687371,757.441700862214,104.503722097022));
#78783=CARTESIAN_POINT('Ctrl Pts',(58.7733336125057,757.442738514788,104.504010422295));
#78784=CARTESIAN_POINT('Ctrl Pts',(58.7723046378064,757.443775946385,104.504298694041));
#78785=CARTESIAN_POINT('Ctrl Pts',(58.771275344601,757.444813156983,104.504586912195));
#78786=CARTESIAN_POINT('Ctrl Pts',(58.5808516562452,757.636701597139,104.557908515421));
#78787=CARTESIAN_POINT('Ctrl Pts',(58.3801742618017,757.820019718356,104.609153555221));
#78788=CARTESIAN_POINT('Ctrl Pts',(58.1725590383603,757.991902528665,104.657313147226));
#78789=CARTESIAN_POINT('Ctrl Pts',(58.1713493088757,757.992904053023,104.657593762865));
#78790=CARTESIAN_POINT('Ctrl Pts',(58.1701393423884,757.993905190394,104.657874274123));
#78791=CARTESIAN_POINT('Ctrl Pts',(58.1689291395544,757.994905940208,104.658154680801));
#78792=CARTESIAN_POINT('Ctrl Pts',(57.9613202248094,758.166583428389,104.70625812639));
#78793=CARTESIAN_POINT('Ctrl Pts',(57.74586879823,758.327772728434,104.751541429878));
#78794=CARTESIAN_POINT('Ctrl Pts',(57.5225977213104,758.478461299949,104.793889430685));
#78795=CARTESIAN_POINT('Ctrl Pts',(57.521283696778,758.479348152301,104.794138662751));
#78796=CARTESIAN_POINT('Ctrl Pts',(57.5199694010075,758.480234641255,104.794387793235));
#78797=CARTESIAN_POINT('Ctrl Pts',(57.5186548339968,758.481120766816,104.794636822115));
#78798=CARTESIAN_POINT('Ctrl Pts',(57.2953041107844,758.631677401157,104.836947925182));
#78799=CARTESIAN_POINT('Ctrl Pts',(57.06412449074,758.771744807745,104.876328247103));
#78800=CARTESIAN_POINT('Ctrl Pts',(56.8248820252568,758.901021457148,104.912646842755));
#78801=CARTESIAN_POINT('Ctrl Pts',(56.8235513819219,758.901740481304,104.912848843253));
#78802=CARTESIAN_POINT('Ctrl Pts',(56.8222204887008,758.902459171897,104.91305074912));
#78803=CARTESIAN_POINT('Ctrl Pts',(56.8208893455624,758.903177528867,104.913252560329));
#78804=CARTESIAN_POINT('Ctrl Pts',(56.581479531921,759.032376037715,104.949548870375));
#78805=CARTESIAN_POINT('Ctrl Pts',(56.3327598991671,759.151183230584,104.982896590313));
#78806=CARTESIAN_POINT('Ctrl Pts',(56.0808986448664,759.25650434361,105.012422175321));
#78807=CARTESIAN_POINT('Ctrl Pts',(56.0796746295836,759.257016191502,105.012565666098));
#78808=CARTESIAN_POINT('Ctrl Pts',(56.0784505393988,759.257527721218,105.012709066717));
#78809=CARTESIAN_POINT('Ctrl Pts',(56.0772263750149,759.258038932408,105.012852377078));
#78810=CARTESIAN_POINT('Ctrl Pts',(55.5718655807993,759.469077658888,105.072013906959));
#78811=CARTESIAN_POINT('Ctrl Pts',(55.0504843965195,759.628654703179,105.116587532522));
#78812=CARTESIAN_POINT('Ctrl Pts',(54.5131113124341,759.736616264493,105.146705257487));
#78813=CARTESIAN_POINT('Ctrl Pts',(54.5123816890383,759.736762850326,105.146746150114));
#78814=CARTESIAN_POINT('Ctrl Pts',(54.5116520360825,759.736909341028,105.146787016095));
#78815=CARTESIAN_POINT('Ctrl Pts',(54.5109223535671,759.737055736599,105.146827855433));
#78816=CARTESIAN_POINT('Ctrl Pts',(54.2422928154709,759.790950648254,105.161862685196));
#78817=CARTESIAN_POINT('Ctrl Pts',(53.9682976582015,759.831974635287,105.173293918456));
#78818=CARTESIAN_POINT('Ctrl Pts',(53.6932892470521,759.859122090062,105.18085779993));
#78819=CARTESIAN_POINT('Ctrl Pts',(53.6929276245361,759.859157787628,105.180867746061));
#78820=CARTESIAN_POINT('Ctrl Pts',(53.6925660003232,759.859193461195,105.180877685505));
#78821=CARTESIAN_POINT('Ctrl Pts',(53.692204374423,759.859229110763,105.180887618259));
#78822=CARTESIAN_POINT('Ctrl Pts',(53.4168449209188,759.886374415834,105.188450898013));
#78823=CARTESIAN_POINT('Ctrl Pts',(53.1422198606357,759.899585894834,105.192131319773));
#78824=CARTESIAN_POINT('Ctrl Pts',(52.8682942728391,759.899278286312,105.19204549995));
#78825=CARTESIAN_POINT('Ctrl Pts',(52.8682575431499,759.899278245066,105.192045488443));
#78826=CARTESIAN_POINT('Ctrl Pts',(52.8682208134732,759.899278203579,105.192045476869));
#78827=CARTESIAN_POINT('Ctrl Pts',(52.868184083809,759.89927816185,105.192045465227));
#78828=CARTESIAN_POINT('Ctrl Pts',(52.3556480524019,759.898695868066,105.191883015616));
#78829=CARTESIAN_POINT('Ctrl Pts',(51.845582323436,759.851133811666,105.178646938558));
#78830=CARTESIAN_POINT('Ctrl Pts',(51.3379868705484,759.755295894061,105.151914842749));
#78831=CARTESIAN_POINT('Ctrl Pts',(51.3030154172992,759.748693015261,105.150073100012));
#78832=CARTESIAN_POINT('Ctrl Pts',(51.2680556907327,759.741860965531,105.148167290173));
#78833=CARTESIAN_POINT('Ctrl Pts',(51.2331076912966,759.734799312132,105.146197272619));
#78834=CARTESIAN_POINT('Ctrl Pts',(51.2323200163315,759.734640153162,105.146152871407));
#78835=CARTESIAN_POINT('Ctrl Pts',(51.23153236758,759.734480879735,105.146108438146));
#78836=CARTESIAN_POINT('Ctrl Pts',(51.230744745125,759.734321491882,105.146063972844));
#78837=CARTESIAN_POINT('Ctrl Pts',(50.960387914189,759.679610513937,105.130800951599));
#78838=CARTESIAN_POINT('Ctrl Pts',(50.6931888913391,759.611430047017,105.111766049666));
#78839=CARTESIAN_POINT('Ctrl Pts',(50.4324905512462,759.531096763007,105.089303880242));
#78840=CARTESIAN_POINT('Ctrl Pts',(50.4314101557122,759.530763842892,105.089210791704));
#78841=CARTESIAN_POINT('Ctrl Pts',(50.4303298528035,759.530430710309,105.089117643243));
#78842=CARTESIAN_POINT('Ctrl Pts',(50.429249642512,759.530097365272,105.089024434863));
#78843=CARTESIAN_POINT('Ctrl Pts',(50.1688396973573,759.449736750779,105.066554375817));
#78844=CARTESIAN_POINT('Ctrl Pts',(49.9138178176667,759.357030872691,105.040602588784));
#78845=CARTESIAN_POINT('Ctrl Pts',(49.6640859638924,759.252209212174,105.011215675376));
#78846=CARTESIAN_POINT('Ctrl Pts',(49.6628163442094,759.251676306013,105.011066274316));
#78847=CARTESIAN_POINT('Ctrl Pts',(49.6615468612612,759.251143086695,105.010916784436));
#78848=CARTESIAN_POINT('Ctrl Pts',(49.660277515055,759.250609554202,105.010767205733));
#78849=CARTESIAN_POINT('Ctrl Pts',(49.4107594812073,759.14573195828,104.981364207807));
#78850=CARTESIAN_POINT('Ctrl Pts',(49.1665103026534,759.028745024005,104.948526855206));
#78851=CARTESIAN_POINT('Ctrl Pts',(48.9276288233629,758.899547810277,104.912230599334));
#78852=CARTESIAN_POINT('Ctrl Pts',(48.9262603815349,758.898807699023,104.912022674823));
#78853=CARTESIAN_POINT('Ctrl Pts',(48.924892075464,758.898067156868,104.911814628255));
#78854=CARTESIAN_POINT('Ctrl Pts',(48.9235239062514,758.897326184491,104.91160645983));
#78855=CARTESIAN_POINT('Ctrl Pts',(48.6847697427405,758.768021827698,104.875279755613));
#78856=CARTESIAN_POINT('Ctrl Pts',(48.4501209010315,758.625579680219,104.835230789));
#78857=CARTESIAN_POINT('Ctrl Pts',(48.2254471982682,758.473601925703,104.792520911464));
#78858=CARTESIAN_POINT('Ctrl Pts',(48.224084691537,758.472680274834,104.792261902533));
#78859=CARTESIAN_POINT('Ctrl Pts',(48.22272252582,758.471758270358,104.792002794067));
#78860=CARTESIAN_POINT('Ctrl Pts',(48.2213607010834,758.470835912327,104.791743586116));
#78861=CARTESIAN_POINT('Ctrl Pts',(47.7707693013975,758.165652297368,104.705978604487));
#78862=CARTESIAN_POINT('Ctrl Pts',(47.357436514095,757.821717855496,104.609307927081));
#78863=CARTESIAN_POINT('Ctrl Pts',(46.9796643865617,757.440479868033,104.503379222176));
#78864=CARTESIAN_POINT('Ctrl Pts',(46.9786124252374,757.439418255519,104.503084248321));
#78865=CARTESIAN_POINT('Ctrl Pts',(46.9775607416614,757.438356351503,104.502789202658));
#78866=CARTESIAN_POINT('Ctrl Pts',(46.9765093358634,757.437294155939,104.502494085233));
#78867=CARTESIAN_POINT('Ctrl Pts',(46.7881027111374,757.246954059582,104.449610528658));
#78868=CARTESIAN_POINT('Ctrl Pts',(46.608619434504,757.047256610765,104.39442382041));
#78869=CARTESIAN_POINT('Ctrl Pts',(46.4382219947662,756.837927719196,104.337189771042));
#78870=CARTESIAN_POINT('Ctrl Pts',(46.2668310118311,756.627378285251,104.279622004803));
#78871=CARTESIAN_POINT('Ctrl Pts',(46.1060960213913,756.408719586273,104.220437312538));
#78872=CARTESIAN_POINT('Ctrl Pts',(45.9575265766773,756.184656946643,104.160811584938));
#78873=CARTESIAN_POINT('Ctrl Pts',(45.956968192286,756.183814828124,104.160587487206));
#78874=CARTESIAN_POINT('Ctrl Pts',(45.9564099695286,756.182972623177,104.160363379714));
#78875=CARTESIAN_POINT('Ctrl Pts',(45.9558519084036,756.182130331792,104.160139262496));
#78876=CARTESIAN_POINT('Ctrl Pts',(45.6869748935028,755.776309565548,104.052158315929));
#78877=CARTESIAN_POINT('Ctrl Pts',(45.4556141963641,755.350424500661,103.941918440707));
#78878=CARTESIAN_POINT('Ctrl Pts',(45.2616365426822,754.903580844173,103.833307486465));
#78879=CARTESIAN_POINT('Ctrl Pts',(45.241747857797,754.857765604591,103.82217151795));
#78880=CARTESIAN_POINT('Ctrl Pts',(45.2222522042453,754.811730014642,103.811052673536));
#78881=CARTESIAN_POINT('Ctrl Pts',(45.2031494655285,754.765473095282,103.799955144725));
#78882=CARTESIAN_POINT('Ctrl Pts',(45.2029977238449,754.765105655674,103.79986699204));
#78883=CARTESIAN_POINT('Ctrl Pts',(45.2028460064544,754.764738199117,103.799778840185));
#78884=CARTESIAN_POINT('Ctrl Pts',(45.2026943133641,754.764370725629,103.799690689167));
#78885=CARTESIAN_POINT('Ctrl Pts',(45.0999909574253,754.515573892939,103.740008304287));
#78886=CARTESIAN_POINT('Ctrl Pts',(45.0084219713795,754.259007028087,103.680706966827));
#78887=CARTESIAN_POINT('Ctrl Pts',(44.9302006255377,754.000446437919,103.624049110639));
#78888=CARTESIAN_POINT('Ctrl Pts',(44.9301647802918,754.00032795149,103.624023146949));
#78889=CARTESIAN_POINT('Ctrl Pts',(44.9301289377625,754.000209464507,103.623997183776));
#78890=CARTESIAN_POINT('Ctrl Pts',(44.9300930979498,754.000090976969,103.623971221122));
#78891=CARTESIAN_POINT('Ctrl Pts',(44.8518477686917,753.741409481043,103.567289661503));
#78892=CARTESIAN_POINT('Ctrl Pts',(44.7865499756604,753.480086321699,103.513075105129));
#78893=CARTESIAN_POINT('Ctrl Pts',(44.7340181312022,753.215987600015,103.462243225474));
#78894=CARTESIAN_POINT('Ctrl Pts',(44.7340063241217,753.21592824107,103.462231800478));
#78895=CARTESIAN_POINT('Ctrl Pts',(44.7339945176863,753.215868881986,103.462220375653));
#78896=CARTESIAN_POINT('Ctrl Pts',(44.7339827118959,753.215809522762,103.462208951));
#78897=CARTESIAN_POINT('Ctrl Pts',(44.6664310985141,752.876161669581,103.39683816619));
#78898=CARTESIAN_POINT('Ctrl Pts',(44.619802503244,752.531965278004,103.337008941954));
#78899=CARTESIAN_POINT('Ctrl Pts',(44.5951181145293,752.182622649644,103.28507900627));
#78900=CARTESIAN_POINT('Ctrl Pts',(44.5814191394018,751.988749670565,103.256259702477));
#78901=CARTESIAN_POINT('Ctrl Pts',(44.5744794255529,751.79329153799,103.229873637158));
#78902=CARTESIAN_POINT('Ctrl Pts',(44.5744794255529,751.59614455564,103.206327301003));
#78903=CARTESIAN_POINT('Origin',(44.0744794081648,738.805700682709,102.677639949919));
#78904=CARTESIAN_POINT('',(43.8756325293234,737.489494249471,103.141409944702));
#78905=CARTESIAN_POINT('Origin',(44.074479425553,737.487748923763,102.682654164686));
#78906=CARTESIAN_POINT('',(43.8756325293234,737.489494249471,103.141409944702));
#78907=CARTESIAN_POINT('Ctrl Pts',(61.1807573575412,752.432433191562,103.304005925674));
#78908=CARTESIAN_POINT('Ctrl Pts',(61.1807573572072,752.352624036457,103.978124555041));
#78909=CARTESIAN_POINT('Ctrl Pts',(61.8291002976553,752.375611223793,103.778088716576));
#78910=CARTESIAN_POINT('Ctrl Pts',(61.1807573575412,750.236642473856,103.038617574031));
#78911=CARTESIAN_POINT('Ctrl Pts',(61.1807573583187,750.098025106155,103.735420913324));
#78912=CARTESIAN_POINT('Ctrl Pts',(61.8481071279839,750.188704031144,103.507887504724));
#78913=CARTESIAN_POINT('Ctrl Pts',(61.1807573575412,748.037926488067,102.841853249379));
#78914=CARTESIAN_POINT('Ctrl Pts',(61.1807573576092,747.955742160344,103.573549866495));
#78915=CARTESIAN_POINT('Ctrl Pts',(61.8641730445071,748.004525375531,103.306069819682));
#78916=CARTESIAN_POINT('Ctrl Pts',(61.1807573575412,744.872422398288,102.704110639652));
#78917=CARTESIAN_POINT('Ctrl Pts',(61.1807573575109,744.843334627062,103.45882252758));
#78918=CARTESIAN_POINT('Ctrl Pts',(61.8760420486351,744.858180968395,103.164229826639));
#78919=CARTESIAN_POINT('Ctrl Pts',(61.1807573575411,743.909613176086,102.680905707402));
#78920=CARTESIAN_POINT('Ctrl Pts',(61.1807573575511,743.893463278854,103.439935530219));
#78921=CARTESIAN_POINT('Ctrl Pts',(61.8782104710529,743.900885214033,103.140202681235));
#78922=CARTESIAN_POINT('Ctrl Pts',(61.1807573575411,741.72559338774,102.658573823938));
#78923=CARTESIAN_POINT('Ctrl Pts',(61.1807573575284,741.72352117949,103.422147088387));
#78924=CARTESIAN_POINT('Ctrl Pts',(61.8806437790432,741.726018999221,103.11691165222));
#78925=CARTESIAN_POINT('Ctrl Pts',(61.1807573575413,740.504024682783,102.667452033055));
#78926=CARTESIAN_POINT('Ctrl Pts',(61.1807573574781,740.51080807793,103.430288184586));
#78927=CARTESIAN_POINT('Ctrl Pts',(61.8802581399683,740.50712798626,103.125906581776));
#78928=CARTESIAN_POINT('Ctrl Pts',(61.1807573575412,739.28265565772,102.671032434937));
#78929=CARTESIAN_POINT('Ctrl Pts',(61.1807573575944,739.283824549444,103.433975186531));
#78930=CARTESIAN_POINT('Ctrl Pts',(61.8803059240399,739.283702376469,103.129490493437));
#78931=CARTESIAN_POINT('',(61.8788481782903,740.125366496447,103.127135084915));
#78932=CARTESIAN_POINT('Origin',(61.6807577676043,740.123614817939,102.668051724002));
#78933=CARTESIAN_POINT('Ctrl Pts',(61.8355401657986,751.54292199161,103.678781264903));
#78934=CARTESIAN_POINT('Ctrl Pts',(61.8384787588597,751.189543606527,103.638009712643));
#78935=CARTESIAN_POINT('Ctrl Pts',(61.8411871116658,750.835827677254,103.599045405492));
#78936=CARTESIAN_POINT('Ctrl Pts',(61.8437662515124,750.481892841926,103.562101738362));
#78937=CARTESIAN_POINT('Ctrl Pts',(61.8461724288251,750.151693619869,103.527635591126));
#78938=CARTESIAN_POINT('Ctrl Pts',(61.8484664081269,749.821304102811,103.494928513058));
#78939=CARTESIAN_POINT('Ctrl Pts',(61.8506962759595,749.490793109622,103.464141507031));
#78940=CARTESIAN_POINT('Ctrl Pts',(61.8527456212718,749.187039163024,103.435846912365));
#78941=CARTESIAN_POINT('Ctrl Pts',(61.8547408431025,748.883182682306,103.409174260207));
#78942=CARTESIAN_POINT('Ctrl Pts',(61.8566878402505,748.579251128213,103.384234339186));
#78943=CARTESIAN_POINT('Ctrl Pts',(61.8585623243818,748.286639053391,103.360223268478));
#78944=CARTESIAN_POINT('Ctrl Pts',(61.860392300632,747.993957621667,103.337818478434));
#78945=CARTESIAN_POINT('Ctrl Pts',(61.8621507591059,747.701203844434,103.317102277541));
#78946=CARTESIAN_POINT('Ctrl Pts',(61.8638506124278,747.418206839903,103.297076497333));
#78947=CARTESIAN_POINT('Ctrl Pts',(61.8654837934075,747.135142455684,103.278628807288));
#78948=CARTESIAN_POINT('Ctrl Pts',(61.8669926368471,746.851978532029,103.261814975452));
#78949=CARTESIAN_POINT('Ctrl Pts',(61.8684390595075,746.580529086019,103.245696731016));
#78950=CARTESIAN_POINT('Ctrl Pts',(61.8697712776325,746.308988318233,103.231080061492));
#78951=CARTESIAN_POINT('Ctrl Pts',(61.8709059450773,746.037297746506,103.217994751078));
#78952=CARTESIAN_POINT('Ctrl Pts',(61.8711766714067,745.972473650647,103.214872657399));
#78953=CARTESIAN_POINT('Ctrl Pts',(61.8714359983516,745.907640880863,103.211837646742));
#78954=CARTESIAN_POINT('Ctrl Pts',(61.8716824986774,745.842798358752,103.208889941404));
#78955=CARTESIAN_POINT('Ctrl Pts',(61.8726385106581,745.591317035963,103.197457738992));
#78956=CARTESIAN_POINT('Ctrl Pts',(61.8734562291384,745.339774682026,103.187322776724));
#78957=CARTESIAN_POINT('Ctrl Pts',(61.8741903578932,745.088218203332,103.178420629519));
#78958=CARTESIAN_POINT('Ctrl Pts',(61.874920260042,744.83811001295,103.169569734724));
#78959=CARTESIAN_POINT('Ctrl Pts',(61.8755674729943,744.587988035432,103.161937492574));
#78960=CARTESIAN_POINT('Ctrl Pts',(61.876151387719,744.337867954568,103.155437940408));
#78961=CARTESIAN_POINT('Ctrl Pts',(61.8767310399504,744.089573714229,103.148985834036));
#78962=CARTESIAN_POINT('Ctrl Pts',(61.8772482273628,743.841281493753,103.14364991165));
#78963=CARTESIAN_POINT('Ctrl Pts',(61.8776890558787,743.59297415862,103.139323989149));
#78964=CARTESIAN_POINT('Ctrl Pts',(61.8780489409083,743.390260201962,103.135792378349));
#78965=CARTESIAN_POINT('Ctrl Pts',(61.8783573098943,743.187535613118,103.132933500598));
#78966=CARTESIAN_POINT('Ctrl Pts',(61.8785908136361,742.98477378795,103.130678769005));
#78967=CARTESIAN_POINT('Ctrl Pts',(61.8788741515892,742.738738670584,103.127942834113));
#78968=CARTESIAN_POINT('Ctrl Pts',(61.8790532116822,742.492644581835,103.126094962502));
#78969=CARTESIAN_POINT('Ctrl Pts',(61.8791721169013,742.246547775394,103.124944588732));
#78970=CARTESIAN_POINT('Ctrl Pts',(61.879292724808,741.996926935346,103.12377774195));
#78971=CARTESIAN_POINT('Ctrl Pts',(61.8793512245671,741.747303367807,103.123328391134));
#78972=CARTESIAN_POINT('Ctrl Pts',(61.8793620402373,741.49769720654,103.123375262688));
#78973=CARTESIAN_POINT('Ctrl Pts',(61.8793731911177,741.240355000058,103.123423586932));
#78974=CARTESIAN_POINT('Ctrl Pts',(61.8793334631664,740.983031397289,103.123999270504));
#78975=CARTESIAN_POINT('Ctrl Pts',(61.8792283444092,740.725706244935,103.124837783144));
#78976=CARTESIAN_POINT('Ctrl Pts',(61.8791466023763,740.525606076093,103.125489824032));
#78977=CARTESIAN_POINT('Ctrl Pts',(61.8790246531794,740.325504073412,103.126300315418));
#78978=CARTESIAN_POINT('Ctrl Pts',(61.8788449024366,740.125373764374,103.127136797834));
#78979=CARTESIAN_POINT('Ctrl Pts',(61.1807573575412,751.190390842625,103.161460170991));
#78980=CARTESIAN_POINT('Ctrl Pts',(61.1807573575412,751.325655907648,103.176136471429));
#78981=CARTESIAN_POINT('Ctrl Pts',(61.1807573575412,751.460907175924,103.191095813468));
#78982=CARTESIAN_POINT('Ctrl Pts',(61.1807573575412,751.59614455564,103.206330589227));
#78983=CARTESIAN_POINT('Origin',(61.6807573751531,738.813605060629,102.677609876716));
#78984=CARTESIAN_POINT('',(61.8796042537708,737.489494249471,103.141409944702));
#78985=CARTESIAN_POINT('Origin',(61.6807573575412,737.487748923763,102.682654164686));
#78986=CARTESIAN_POINT('',(61.8796869430852,740.125382453445,103.131345527102));
#78987=CARTESIAN_POINT('Origin',(52.8776183915471,737.487748923763,112.60871186179));
#78988=CARTESIAN_POINT('Ctrl Pts',(47.4333208409147,731.218654873935,103.766631507276));
#78989=CARTESIAN_POINT('Ctrl Pts',(47.4903874665928,731.169089705094,103.783146874125));
#78990=CARTESIAN_POINT('Ctrl Pts',(47.5481332189328,731.120299570413,103.799578343581));
#78991=CARTESIAN_POINT('Ctrl Pts',(47.6065015949763,731.072342124072,103.815890137194));
#78992=CARTESIAN_POINT('Ctrl Pts',(47.7742018602631,730.934553872641,103.862756133846));
#78993=CARTESIAN_POINT('Ctrl Pts',(47.9463966762133,730.80405183503,103.908474318674));
#78994=CARTESIAN_POINT('Ctrl Pts',(48.1231892969836,730.680578747284,103.952726980298));
#78995=CARTESIAN_POINT('Ctrl Pts',(48.1670582502311,730.649940392074,103.963707743723));
#78996=CARTESIAN_POINT('Ctrl Pts',(48.211210436374,730.619735036351,103.974598241531));
#78997=CARTESIAN_POINT('Ctrl Pts',(48.2556476994714,730.589959161072,103.985393549995));
#78998=CARTESIAN_POINT('Ctrl Pts',(48.3758656235744,730.509405282078,104.014598534351));
#78999=CARTESIAN_POINT('Ctrl Pts',(48.4981525688067,730.431967570665,104.043110482607));
#79000=CARTESIAN_POINT('Ctrl Pts',(48.6226013076915,730.357666854282,104.070828813816));
#79001=CARTESIAN_POINT('Ctrl Pts',(48.8327809759369,730.232181453146,104.117641900956));
#79002=CARTESIAN_POINT('Ctrl Pts',(49.049022413504,730.1157090445,104.162170387175));
#79003=CARTESIAN_POINT('Ctrl Pts',(49.2715626044912,730.008466747415,104.203884195918));
#79004=CARTESIAN_POINT('Ctrl Pts',(49.4070320348871,729.943183919914,104.22927711881));
#79005=CARTESIAN_POINT('Ctrl Pts',(49.5448501968965,729.881314641415,104.253629756634));
#79006=CARTESIAN_POINT('Ctrl Pts',(49.6850608216465,729.822914101572,104.276820177489));
#79007=CARTESIAN_POINT('Ctrl Pts',(49.7751789073598,729.785378109812,104.291725441182));
#79008=CARTESIAN_POINT('Ctrl Pts',(49.8657653920901,729.749494357006,104.306061555955));
#79009=CARTESIAN_POINT('Ctrl Pts',(49.9568153069889,729.715260451392,104.319811060496));
#79010=CARTESIAN_POINT('Ctrl Pts',(50.292244015169,729.589142434159,104.370464359309));
#79011=CARTESIAN_POINT('Ctrl Pts',(50.6338992149115,729.485434904179,104.413149724166));
#79012=CARTESIAN_POINT('Ctrl Pts',(50.9817695313361,729.403915246444,104.447033878752));
#79013=CARTESIAN_POINT('Ctrl Pts',(51.0701525460672,729.383203639933,104.45564278728));
#79014=CARTESIAN_POINT('Ctrl Pts',(51.1589368158667,729.363924516919,104.463683470189));
#79015=CARTESIAN_POINT('Ctrl Pts',(51.2481222818587,729.346074702995,104.471142049786));
#79016=CARTESIAN_POINT('Ctrl Pts',(51.2949743914626,729.336697598451,104.475060291226));
#79017=CARTESIAN_POINT('Ctrl Pts',(51.3419389862517,729.32771747114,104.478817985273));
#79018=CARTESIAN_POINT('Ctrl Pts',(51.3890171418665,729.319136999466,104.482412896601));
#79019=CARTESIAN_POINT('Ctrl Pts',(51.6108100758792,729.278712986187,104.499349115119));
#79020=CARTESIAN_POINT('Ctrl Pts',(51.8351262404447,729.247160032436,104.512672795294));
#79021=CARTESIAN_POINT('Ctrl Pts',(52.0620115376169,729.224765071157,104.522147068232));
#79022=CARTESIAN_POINT('Ctrl Pts',(52.3357794585568,729.197742509249,104.53357906509));
#79023=CARTESIAN_POINT('Ctrl Pts',(52.6114066564425,729.18439443935,104.539260772721));
#79024=CARTESIAN_POINT('Ctrl Pts',(52.8842892071817,729.184612644427,104.539167920817));
#79025=CARTESIAN_POINT('Ctrl Pts',(52.8855117861528,729.184613622038,104.539167504818));
#79026=CARTESIAN_POINT('Ctrl Pts',(52.8867343109061,729.184614871909,104.539166972943));
#79027=CARTESIAN_POINT('Ctrl Pts',(52.8879567810331,729.18461639403,104.539166325188));
#79028=CARTESIAN_POINT('Ctrl Pts',(53.3857239796833,729.185236173512,104.538902571453));
#79029=CARTESIAN_POINT('Ctrl Pts',(53.8790018614575,729.230179734849,104.519658858136));
#79030=CARTESIAN_POINT('Ctrl Pts',(54.3677408399323,729.31940537429,104.48229740503));
#79031=CARTESIAN_POINT('Ctrl Pts',(54.4173351519301,729.328459459181,104.478506187951));
#79032=CARTESIAN_POINT('Ctrl Pts',(54.4668853995529,729.337969958316,104.474529220779));
#79033=CARTESIAN_POINT('Ctrl Pts',(54.5163907755215,729.347936778366,104.470366910493));
#79034=CARTESIAN_POINT('Ctrl Pts',(54.7114157407302,729.387200771329,104.453969612161));
#79035=CARTESIAN_POINT('Ctrl Pts',(54.9064965795643,729.433888389138,104.434574530941));
#79036=CARTESIAN_POINT('Ctrl Pts',(55.098754983177,729.487234225264,104.412598792644));
#79037=CARTESIAN_POINT('Ctrl Pts',(55.1714270378057,729.507398501282,104.404292148961));
#79038=CARTESIAN_POINT('Ctrl Pts',(55.2436845065661,729.528510694318,104.395622861317));
#79039=CARTESIAN_POINT('Ctrl Pts',(55.315381563322,729.550531060602,104.386614149159));
#79040=CARTESIAN_POINT('Ctrl Pts',(55.4815118393699,729.601554766387,104.365739933323));
#79041=CARTESIAN_POINT('Ctrl Pts',(55.6450583157892,729.657475260353,104.343033475127));
#79042=CARTESIAN_POINT('Ctrl Pts',(55.8061710715705,729.718206206078,104.318638781474));
#79043=CARTESIAN_POINT('Ctrl Pts',(55.8987084970164,729.753087897072,104.304627338778));
#79044=CARTESIAN_POINT('Ctrl Pts',(55.9904286757707,729.789551686463,104.290061032122));
#79045=CARTESIAN_POINT('Ctrl Pts',(56.0813462694638,729.827576316513,104.274969868601));
#79046=CARTESIAN_POINT('Ctrl Pts',(56.4436427840962,729.979100244693,104.214833257817));
#79047=CARTESIAN_POINT('Ctrl Pts',(56.7932824124638,730.155215020753,104.146356969981));
#79048=CARTESIAN_POINT('Ctrl Pts',(57.1303788166724,730.356323264058,104.071323822942));
#79049=CARTESIAN_POINT('Ctrl Pts',(57.2572760202182,730.432028828896,104.043078204142));
#79050=CARTESIAN_POINT('Ctrl Pts',(57.3824601776219,730.511315078268,104.013889115566));
#79051=CARTESIAN_POINT('Ctrl Pts',(57.5059168719087,730.594203401661,103.983853486297));
#79052=CARTESIAN_POINT('Ctrl Pts',(57.5875886668259,730.649037513236,103.963983654466));
#79053=CARTESIAN_POINT('Ctrl Pts',(57.6681015618492,730.705188433614,103.943841378445));
#79054=CARTESIAN_POINT('Ctrl Pts',(57.7474430225457,730.762630072087,103.923470734033));
#79055=CARTESIAN_POINT('Ctrl Pts',(57.8947007825111,730.869241759545,103.885662815717));
#79056=CARTESIAN_POINT('Ctrl Pts',(58.0376550195572,730.98009982637,103.847138414877));
#79057=CARTESIAN_POINT('Ctrl Pts',(58.17643809902,731.09513910412,103.808134434802));
#79058=CARTESIAN_POINT('Ctrl Pts',(58.225462290879,731.135775957299,103.794356540481));
#79059=CARTESIAN_POINT('Ctrl Pts',(58.2739656903081,731.176934899041,103.780518722733));
#79060=CARTESIAN_POINT('Ctrl Pts',(58.3219531024995,731.218614186682,103.766631207477));
#79061=CARTESIAN_POINT('Ctrl Pts',(18.2205457342854,776.218453213852,107.756965262063));
#79062=CARTESIAN_POINT('Ctrl Pts',(18.2213549247058,776.117573843427,108.040792094665));
#79063=CARTESIAN_POINT('Ctrl Pts',(18.0556468322312,775.880815322444,107.955814427592));
#79064=CARTESIAN_POINT('Ctrl Pts',(17.3544392369962,776.755270180238,107.950249975219));
#79065=CARTESIAN_POINT('Ctrl Pts',(17.3244896481851,776.666856095555,108.259553418174));
#79066=CARTESIAN_POINT('Ctrl Pts',(17.1727637467093,776.406561520024,108.145113036192));
#79067=CARTESIAN_POINT('Ctrl Pts',(16.5030075315832,777.315984535372,108.138886510896));
#79068=CARTESIAN_POINT('Ctrl Pts',(16.488670529682,777.214259844005,108.458076806816));
#79069=CARTESIAN_POINT('Ctrl Pts',(16.3091708822954,776.961315153559,108.329900767511));
#79070=CARTESIAN_POINT('Ctrl Pts',(15.6662338972256,777.89550680801,108.337269960847));
#79071=CARTESIAN_POINT('Ctrl Pts',(15.6646166993499,777.782008928933,108.661951401639));
#79072=CARTESIAN_POINT('Ctrl Pts',(15.4635632798279,777.538177789599,108.526207820323));
#79073=CARTESIAN_POINT('',(15.4635632798629,777.538177785738,108.526207827222));
#79074=CARTESIAN_POINT('Origin',(15.4890368307271,777.667265994068,108.256601934497));
#79075=CARTESIAN_POINT('',(18.0556466141873,775.880815148244,107.955814158127));
#79076=CARTESIAN_POINT('Ctrl Pts',(18.0556467918663,775.880815346481,107.955814436247));
#79077=CARTESIAN_POINT('Ctrl Pts',(17.1738808373735,776.405896305826,108.144873521151));
#79078=CARTESIAN_POINT('Ctrl Pts',(16.3101489074236,776.96064795568,108.329673719029));
#79079=CARTESIAN_POINT('Ctrl Pts',(15.4635632805302,777.53817778912,108.52620782016));
#79080=CARTESIAN_POINT('',(18.2205407156876,776.21798090548,107.758260909884));
#79081=CARTESIAN_POINT('Origin',(18.0555120549653,775.982245018246,107.673481293432));
#79082=CARTESIAN_POINT('Ctrl Pts',(18.2205473657951,776.218126918571,107.757885251456));
#79083=CARTESIAN_POINT('Ctrl Pts',(17.4395547310011,776.702515187951,107.931255171408));
#79084=CARTESIAN_POINT('Ctrl Pts',(16.670513723768,777.206050004925,108.101619406009));
#79085=CARTESIAN_POINT('Ctrl Pts',(15.9133489649393,777.722889497859,108.285610804169));
#79086=CARTESIAN_POINT('Ctrl Pts',(87.534693420407,776.218613999725,107.756513650752));
#79087=CARTESIAN_POINT('Ctrl Pts',(87.5336178514962,776.117952853449,108.0409278003));
#79088=CARTESIAN_POINT('Ctrl Pts',(87.699590784449,775.880815944701,107.955814324766));
#79089=CARTESIAN_POINT('Ctrl Pts',(86.259537844912,775.428266754528,107.471942382034));
#79090=CARTESIAN_POINT('Ctrl Pts',(86.2555670717131,775.325475361612,107.756754598578));
#79091=CARTESIAN_POINT('Ctrl Pts',(86.4183730487532,775.085504287272,107.66948244197));
#79092=CARTESIAN_POINT('Ctrl Pts',(84.9560677605553,774.684903718524,107.197696734793));
#79093=CARTESIAN_POINT('Ctrl Pts',(84.9508894325089,774.58120275026,107.483989729736));
#79094=CARTESIAN_POINT('Ctrl Pts',(85.1091907908226,774.337094526585,107.393435206673));
#79095=CARTESIAN_POINT('Ctrl Pts',(82.2927499621516,773.285117635406,106.689234302032));
#79096=CARTESIAN_POINT('Ctrl Pts',(82.2887487103214,773.181142922102,106.978515953765));
#79097=CARTESIAN_POINT('Ctrl Pts',(82.4355140915199,772.928856409756,106.881939604336));
#79098=CARTESIAN_POINT('Ctrl Pts',(80.9329000613502,772.628392057774,106.455863954993));
#79099=CARTESIAN_POINT('Ctrl Pts',(80.9331460203576,772.526276326062,106.74708687405));
#79100=CARTESIAN_POINT('Ctrl Pts',(81.0710134534976,772.268715768294,106.647338926234));
#79101=CARTESIAN_POINT('Ctrl Pts',(78.1562200818106,771.392761835475,106.058942628791));
#79102=CARTESIAN_POINT('Ctrl Pts',(78.1613397634359,771.292476595305,106.351216827985));
#79103=CARTESIAN_POINT('Ctrl Pts',(78.2856477557455,771.028649273413,106.248771326341));
#79104=CARTESIAN_POINT('Ctrl Pts',(76.7382747560354,770.813290309123,105.895701125155));
#79105=CARTESIAN_POINT('Ctrl Pts',(76.7523463957842,770.716575263587,106.188097519309));
#79106=CARTESIAN_POINT('Ctrl Pts',(76.8636742037813,770.448155127505,106.085112151117));
#79107=CARTESIAN_POINT('Ctrl Pts',(73.8483529833387,769.729793727005,105.659592442164));
#79108=CARTESIAN_POINT('Ctrl Pts',(73.8695654291816,769.63647611085,105.948354019399));
#79109=CARTESIAN_POINT('Ctrl Pts',(73.9654526952167,769.365276516662,105.848948952432));
#79110=CARTESIAN_POINT('Ctrl Pts',(72.3942858815777,769.232288195398,105.58842925458));
#79111=CARTESIAN_POINT('Ctrl Pts',(72.4254204189451,769.142497596095,105.873763703825));
#79112=CARTESIAN_POINT('Ctrl Pts',(72.5071730554801,768.869421251228,105.778146304558));
#79113=CARTESIAN_POINT('Ctrl Pts',(69.4682809012006,768.323985331645,105.531976527412));
#79114=CARTESIAN_POINT('Ctrl Pts',(69.505130570297,768.237853395557,105.808378836195));
#79115=CARTESIAN_POINT('Ctrl Pts',(69.5714410518175,767.966563923016,105.72289441824));
#79116=CARTESIAN_POINT('Ctrl Pts',(67.9963263139418,767.913184640725,105.546636240739));
#79117=CARTESIAN_POINT('Ctrl Pts',(68.039107434635,767.829022250898,105.81678292199));
#79118=CARTESIAN_POINT('Ctrl Pts',(68.0939695200466,767.559560119585,105.738387788275));
#79119=CARTESIAN_POINT('Ctrl Pts',(65.0323690485381,767.186623681901,105.630322411241));
#79120=CARTESIAN_POINT('Ctrl Pts',(65.0760847078406,767.105299652801,105.88863578277));
#79121=CARTESIAN_POINT('Ctrl Pts',(65.116643660827,766.841456434063,105.823831389765));
#79122=CARTESIAN_POINT('Ctrl Pts',(63.5403268572924,766.870997823238,105.698903803921));
#79123=CARTESIAN_POINT('Ctrl Pts',(63.582537797136,766.789660577686,105.950808131252));
#79124=CARTESIAN_POINT('Ctrl Pts',(63.6167373626631,766.530467814802,105.893331175143));
#79125=CARTESIAN_POINT('Ctrl Pts',(60.5319701718021,766.351593356512,105.842003024112));
#79126=CARTESIAN_POINT('Ctrl Pts',(60.5693321518246,766.271904121821,106.083181145775));
#79127=CARTESIAN_POINT('Ctrl Pts',(60.5900264012593,766.019480612874,106.038035999016));
#79128=CARTESIAN_POINT('Ctrl Pts',(59.0156050355678,766.148059099485,105.915801308287));
#79129=CARTESIAN_POINT('Ctrl Pts',(59.0440098927689,766.067318380161,106.152731837784));
#79130=CARTESIAN_POINT('Ctrl Pts',(59.06316201519,765.819700469343,106.112522123908));
#79131=CARTESIAN_POINT('Ctrl Pts',(56.7192697416383,765.941250026258,105.99565564567));
#79132=CARTESIAN_POINT('Ctrl Pts',(56.7344612356701,765.860453468508,106.228099156722));
#79133=CARTESIAN_POINT('Ctrl Pts',(56.7496613191456,765.616810173469,106.19308711179));
#79134=CARTESIAN_POINT('Ctrl Pts',(55.9501937298133,765.888725246282,106.017218851542));
#79135=CARTESIAN_POINT('Ctrl Pts',(55.9619069202598,765.807911798399,106.248500301597));
#79136=CARTESIAN_POINT('Ctrl Pts',(55.9746367498585,765.565310282087,106.214834552912));
#79137=CARTESIAN_POINT('Ctrl Pts',(54.4042994258696,765.818508090254,106.046441318916));
#79138=CARTESIAN_POINT('Ctrl Pts',(54.4107850600319,765.737853040583,106.276099275293));
#79139=CARTESIAN_POINT('Ctrl Pts',(54.4165611592209,765.496472547381,106.244304592913));
#79140=CARTESIAN_POINT('Ctrl Pts',(53.630716477118,765.801038717635,106.05399145759));
#79141=CARTESIAN_POINT('Ctrl Pts',(53.6333631037709,765.720370934785,106.283261246584));
#79142=CARTESIAN_POINT('Ctrl Pts',(53.6367679636054,765.479352894896,106.25191739984));
#79143=CARTESIAN_POINT('Ctrl Pts',(51.320944157274,765.801809480288,106.053661913636));
#79144=CARTESIAN_POINT('Ctrl Pts',(51.3154236794076,765.721140016323,106.282949676225));
#79145=CARTESIAN_POINT('Ctrl Pts',(51.308435374231,765.480108275012,106.251585096457));
#79146=CARTESIAN_POINT('Ctrl Pts',(49.7905213129482,765.873238298318,106.021911621623));
#79147=CARTESIAN_POINT('Ctrl Pts',(49.7713984809396,765.793164808446,106.252609550755));
#79148=CARTESIAN_POINT('Ctrl Pts',(49.765754962707,765.55008826985,106.219576265668));
#79149=CARTESIAN_POINT('Ctrl Pts',(46.7466364047402,766.14748500395,105.916026945306));
#79150=CARTESIAN_POINT('Ctrl Pts',(46.7183488694763,766.066737371129,106.152947518903));
#79151=CARTESIAN_POINT('Ctrl Pts',(46.6991326128801,765.819137212082,106.112749731659));
#79152=CARTESIAN_POINT('Ctrl Pts',(45.233155034996,766.350078747165,105.842479913589));
#79153=CARTESIAN_POINT('Ctrl Pts',(45.1957740955227,766.270398907609,106.083623748225));
#79154=CARTESIAN_POINT('Ctrl Pts',(45.1751630890169,766.017991986964,106.03851775086));
#79155=CARTESIAN_POINT('Ctrl Pts',(42.2198738993365,766.869948931633,105.699133802545));
#79156=CARTESIAN_POINT('Ctrl Pts',(42.1776265700307,766.78862042883,105.95101607769));
#79157=CARTESIAN_POINT('Ctrl Pts',(42.1434897954953,766.529434177947,105.893564182041));
#79158=CARTESIAN_POINT('Ctrl Pts',(40.7200336640549,767.186966131458,105.6300621503));
#79159=CARTESIAN_POINT('Ctrl Pts',(40.6760645500492,767.105704617896,105.888384255489));
#79160=CARTESIAN_POINT('Ctrl Pts',(40.6357383690942,766.841788106103,105.823569143026));
#79161=CARTESIAN_POINT('Ctrl Pts',(38.4781056808001,767.737064430316,105.567037591417));
#79162=CARTESIAN_POINT('Ctrl Pts',(38.4461641720026,767.650888832438,105.834581014409));
#79163=CARTESIAN_POINT('Ctrl Pts',(38.3837285294506,767.38548886143,105.759216213041));
#79164=CARTESIAN_POINT('Ctrl Pts',(37.7308829200252,767.933261549124,105.552759622542));
#79165=CARTESIAN_POINT('Ctrl Pts',(37.7000110194929,767.846293937843,105.823313156379));
#79166=CARTESIAN_POINT('Ctrl Pts',(37.6334210776661,767.579653875514,105.744505442416));
#79167=CARTESIAN_POINT('Ctrl Pts',(36.2480250617279,768.346763858315,105.542525881567));
#79168=CARTESIAN_POINT('Ctrl Pts',(36.2190919362398,768.258082697861,105.818526797865));
#79169=CARTESIAN_POINT('Ctrl Pts',(36.1448885168633,767.98950585078,105.73348100182));
#79170=CARTESIAN_POINT('Ctrl Pts',(35.5117601149707,768.564176759389,105.546532407994));
#79171=CARTESIAN_POINT('Ctrl Pts',(35.4847637878845,768.474492412453,105.825126547508));
#79172=CARTESIAN_POINT('Ctrl Pts',(35.4060306581063,768.205298543414,105.737129671795));
#79173=CARTESIAN_POINT('Ctrl Pts',(33.3181340307008,769.246512188562,105.590106103946));
#79174=CARTESIAN_POINT('Ctrl Pts',(33.2871615303783,769.156654004714,105.875553753093));
#79175=CARTESIAN_POINT('Ctrl Pts',(33.2051169048726,768.88358612718,105.779810199754));
#79176=CARTESIAN_POINT('Ctrl Pts',(31.8758516711713,769.741242509528,105.661953891397));
#79177=CARTESIAN_POINT('Ctrl Pts',(31.8548850892463,769.647824959646,105.950746346646));
#79178=CARTESIAN_POINT('Ctrl Pts',(31.7586628738894,769.376713512273,105.851309487688));
#79179=CARTESIAN_POINT('Ctrl Pts',(29.0310841033454,770.80817936637,105.894731397872));
#79180=CARTESIAN_POINT('Ctrl Pts',(29.0171468783213,770.711418792167,106.187091334568));
#79181=CARTESIAN_POINT('Ctrl Pts',(28.905725568513,770.443052104303,106.084143587));
#79182=CARTESIAN_POINT('Ctrl Pts',(27.6285945736765,771.380493418822,106.055391376126));
#79183=CARTESIAN_POINT('Ctrl Pts',(27.6233671814146,771.280254931325,106.347667830369));
#79184=CARTESIAN_POINT('Ctrl Pts',(27.4992526397927,771.016354716152,106.245209657368));
#79185=CARTESIAN_POINT('Ctrl Pts',(24.8642886953906,772.608850120777,106.449213695433));
#79186=CARTESIAN_POINT('Ctrl Pts',(24.863940674956,772.506772873493,106.740473669186));
#79187=CARTESIAN_POINT('Ctrl Pts',(24.7263127094394,772.249086217425,106.640656841136));
#79188=CARTESIAN_POINT('Ctrl Pts',(23.5024732025465,773.265020652559,106.682018558467));
#79189=CARTESIAN_POINT('Ctrl Pts',(23.5064761400537,773.16103442948,106.971337918364));
#79190=CARTESIAN_POINT('Ctrl Pts',(23.3598548361072,772.90864623969,106.874683104988));
#79191=CARTESIAN_POINT('Ctrl Pts',(20.8213555103874,774.672343951284,107.193055298186));
#79192=CARTESIAN_POINT('Ctrl Pts',(20.8265704347935,774.568617899291,107.479369892601));
#79193=CARTESIAN_POINT('Ctrl Pts',(20.6683281599921,774.324450877034,107.388763799337));
#79194=CARTESIAN_POINT('Ctrl Pts',(19.498862029959,775.42630609411,107.471237036644));
#79195=CARTESIAN_POINT('Ctrl Pts',(19.5028455397015,775.323505963338,107.75604902853));
#79196=CARTESIAN_POINT('Ctrl Pts',(19.3400444664692,775.083529671144,107.668772140042));
#79197=CARTESIAN_POINT('Ctrl Pts',(18.2205442368837,776.218613355413,107.756513745616));
#79198=CARTESIAN_POINT('Ctrl Pts',(18.2216197623594,776.117952235154,108.040927907501));
#79199=CARTESIAN_POINT('Ctrl Pts',(18.055646832231,775.880815322444,107.955814427592));
#79200=CARTESIAN_POINT('',(87.6995909938491,775.880815775522,107.955814071221));
#79201=CARTESIAN_POINT('',(87.5347015018662,776.217932075331,107.758391194347));
#79202=CARTESIAN_POINT('Origin',(87.6997256064195,775.9822456651,107.673481199464));
#79203=CARTESIAN_POINT('',(72.9143353470373,769.422151368467,105.625740702768));
#79204=CARTESIAN_POINT('Ctrl Pts',(72.9143353591496,769.422151372559,105.625740703389));
#79205=CARTESIAN_POINT('Ctrl Pts',(73.5595632056107,769.640073855905,105.658870605513));
#79206=CARTESIAN_POINT('Ctrl Pts',(74.2034293583074,769.866876365016,105.700518523386));
#79207=CARTESIAN_POINT('Ctrl Pts',(74.8434686433405,770.101754837589,105.750415037215));
#79208=CARTESIAN_POINT('Ctrl Pts',(75.4835079283737,770.336633310163,105.800311551044));
#79209=CARTESIAN_POINT('Ctrl Pts',(76.1197187903174,770.579587235218,105.858456457505));
#79210=CARTESIAN_POINT('Ctrl Pts',(76.7496513514779,770.829776339044,105.924543673933));
#79211=CARTESIAN_POINT('Ctrl Pts',(76.7924259359966,770.846765038513,105.929031222917));
#79212=CARTESIAN_POINT('Ctrl Pts',(76.8351735163699,770.863787902504,105.933555445468));
#79213=CARTESIAN_POINT('Ctrl Pts',(76.8778934067034,770.880844703162,105.93811626543));
#79214=CARTESIAN_POINT('Ctrl Pts',(77.7781956810092,771.240309025396,106.034233473409));
#79215=CARTESIAN_POINT('Ctrl Pts',(78.668175288905,771.615443511941,106.146422411895));
#79216=CARTESIAN_POINT('Ctrl Pts',(79.5476437017226,772.006933824121,106.27197850604));
#79217=CARTESIAN_POINT('Ctrl Pts',(79.8555809468298,772.144010319947,106.315940741834));
#79218=CARTESIAN_POINT('Ctrl Pts',(80.1622296910544,772.283091693059,106.361541443976));
#79219=CARTESIAN_POINT('Ctrl Pts',(80.4675823874359,772.424206324646,106.408663614685));
#79220=CARTESIAN_POINT('Ctrl Pts',(80.7735702594751,772.565614494099,106.455883805998));
#79221=CARTESIAN_POINT('Ctrl Pts',(81.0782698798938,772.709073078691,106.504626295143));
#79222=CARTESIAN_POINT('Ctrl Pts',(81.3816836495893,772.854616733058,106.554771887758));
#79223=CARTESIAN_POINT('Ctrl Pts',(82.8526350110214,773.560213043846,106.797877953118));
#79224=CARTESIAN_POINT('Ctrl Pts',(84.2933577349007,774.31508394129,107.073196647605));
#79225=CARTESIAN_POINT('Ctrl Pts',(85.7035661425854,775.124749342466,107.365756396725));
#79226=CARTESIAN_POINT('Ctrl Pts',(86.31979169175,775.47855272625,107.493597637128));
#79227=CARTESIAN_POINT('Ctrl Pts',(86.9301910915229,775.842921633408,107.624435383555));
#79228=CARTESIAN_POINT('Ctrl Pts',(87.5347015018662,776.217932075331,107.758391194347));
#79229=CARTESIAN_POINT('',(32.8408501865509,769.421912550842,105.626344597616));
#79230=CARTESIAN_POINT('Ctrl Pts',(32.8408501865664,769.421912550837,105.626344597615));
#79231=CARTESIAN_POINT('Ctrl Pts',(33.0236782934409,769.360223677481,105.616839744328));
#79232=CARTESIAN_POINT('Ctrl Pts',(33.2068891034353,769.299142362413,105.608032051533));
#79233=CARTESIAN_POINT('Ctrl Pts',(33.3904861083511,769.238669866531,105.599921157552));
#79234=CARTESIAN_POINT('Ctrl Pts',(34.0174987635566,769.03214677958,105.572221178602));
#79235=CARTESIAN_POINT('Ctrl Pts',(34.6501640698298,768.832460864523,105.552522928579));
#79236=CARTESIAN_POINT('Ctrl Pts',(35.2846233311591,768.64112189397,105.540132327312));
#79237=CARTESIAN_POINT('Ctrl Pts',(35.4438452852828,768.593104051614,105.537022819946));
#79238=CARTESIAN_POINT('Ctrl Pts',(35.6031689190437,768.545616536284,105.534370539334));
#79239=CARTESIAN_POINT('Ctrl Pts',(35.7625331951534,768.498681780911,105.532168229936));
#79240=CARTESIAN_POINT('Ctrl Pts',(36.4241388190288,768.303830721013,105.523025275701));
#79241=CARTESIAN_POINT('Ctrl Pts',(37.0868545409594,768.118322885106,105.521569713914));
#79242=CARTESIAN_POINT('Ctrl Pts',(37.7508739084941,767.942395758076,105.526470077786));
#79243=CARTESIAN_POINT('Ctrl Pts',(37.8841707688899,767.90707971936,105.527453788731));
#79244=CARTESIAN_POINT('Ctrl Pts',(38.0175179372388,767.872150705027,105.528692784248));
#79245=CARTESIAN_POINT('Ctrl Pts',(38.15091594521,767.837610987588,105.530176143381));
#79246=CARTESIAN_POINT('Ctrl Pts',(39.6666985187674,767.445141095529,105.54703134203));
#79247=CARTESIAN_POINT('Ctrl Pts',(41.1890080909103,767.102716903944,105.595773740223));
#79248=CARTESIAN_POINT('Ctrl Pts',(42.7192171003575,766.817008028999,105.653936404576));
#79249=CARTESIAN_POINT('Ctrl Pts',(42.8000135837808,766.801922330094,105.657007448281));
#79250=CARTESIAN_POINT('Ctrl Pts',(42.8808320901257,766.786994821904,105.660104552257));
#79251=CARTESIAN_POINT('Ctrl Pts',(42.9616728208353,766.772226487832,105.663224405103));
#79252=CARTESIAN_POINT('Ctrl Pts',(44.5466204718882,766.482681400938,105.724391633511));
#79253=CARTESIAN_POINT('Ctrl Pts',(46.1401706839877,766.254624596373,105.793419872345));
#79254=CARTESIAN_POINT('Ctrl Pts',(47.7440902907559,766.097195410041,105.845350382395));
#79255=CARTESIAN_POINT('Ctrl Pts',(47.7713529131537,766.094519507556,105.846233071203));
#79256=CARTESIAN_POINT('Ctrl Pts',(47.7986185487758,766.091864008652,105.84711082102));
#79257=CARTESIAN_POINT('Ctrl Pts',(47.8258872054595,766.089228958453,105.847983508994));
#79258=CARTESIAN_POINT('Ctrl Pts',(49.3118883269248,765.945632315735,105.895540501731));
#79259=CARTESIAN_POINT('Ctrl Pts',(50.8069096666398,765.863014317756,105.927387474233));
#79260=CARTESIAN_POINT('Ctrl Pts',(52.3117085411413,765.846417767268,105.933827740143));
#79261=CARTESIAN_POINT('Ctrl Pts',(52.459091258596,765.844792271161,105.934458511408));
#79262=CARTESIAN_POINT('Ctrl Pts',(52.6065677619598,765.843800053509,105.934845580706));
#79263=CARTESIAN_POINT('Ctrl Pts',(52.754138758307,765.843445826145,105.934979848475));
#79264=CARTESIAN_POINT('Ctrl Pts',(52.7818089890395,765.843379406909,105.93500502429));
#79265=CARTESIAN_POINT('Ctrl Pts',(52.8094831122868,765.843335361707,105.935021625747));
#79266=CARTESIAN_POINT('Ctrl Pts',(52.8371610676647,765.843313695639,105.935029674915));
#79267=CARTESIAN_POINT('Ctrl Pts',(53.636861059485,765.842687697291,105.935262239763));
#79268=CARTESIAN_POINT('Ctrl Pts',(54.4398528135242,765.860749498513,105.928342777723));
#79269=CARTESIAN_POINT('Ctrl Pts',(55.244613964507,765.897618906657,105.914824361016));
#79270=CARTESIAN_POINT('Ctrl Pts',(55.3003085386821,765.900170503469,105.913888800867));
#79271=CARTESIAN_POINT('Ctrl Pts',(55.3559839602243,765.902810734082,105.912922266593));
#79272=CARTESIAN_POINT('Ctrl Pts',(55.4116402817597,765.905539243272,105.911925431088));
#79273=CARTESIAN_POINT('Ctrl Pts',(56.1880255318818,765.943600944657,105.898019941792));
#79274=CARTESIAN_POINT('Ctrl Pts',(56.960722155325,765.99885130209,105.878192146322));
#79275=CARTESIAN_POINT('Ctrl Pts',(57.7299521592197,766.070328053399,105.854281130698));
#79276=CARTESIAN_POINT('Ctrl Pts',(57.8126622929001,766.078013468198,105.851710139852));
#79277=CARTESIAN_POINT('Ctrl Pts',(57.8953323483527,766.085886453703,105.849091074128));
#79278=CARTESIAN_POINT('Ctrl Pts',(57.9779626577588,766.093945617801,105.846427342593));
#79279=CARTESIAN_POINT('Ctrl Pts',(59.5424882901759,766.246538157971,105.795992141575));
#79280=CARTESIAN_POINT('Ctrl Pts',(61.0927572405591,766.465921133663,105.729413145712));
#79281=CARTESIAN_POINT('Ctrl Pts',(62.630986689335,766.742742837056,105.669539025615));
#79282=CARTESIAN_POINT('Ctrl Pts',(62.7663823010022,766.767108801369,105.664268880046));
#79283=CARTESIAN_POINT('Ctrl Pts',(62.9016851664723,766.791917627592,105.659057180489));
#79284=CARTESIAN_POINT('Ctrl Pts',(63.0368965356465,766.817164168077,105.653919296428));
#79285=CARTESIAN_POINT('Ctrl Pts',(64.5189523589357,767.093892246284,105.597602797022));
#79286=CARTESIAN_POINT('Ctrl Pts',(65.990029631157,767.423147191921,105.550338785539));
#79287=CARTESIAN_POINT('Ctrl Pts',(67.451755462978,767.798254419419,105.532062337455));
#79288=CARTESIAN_POINT('Ctrl Pts',(67.6384506822806,767.846164037334,105.529728024542));
#79289=CARTESIAN_POINT('Ctrl Pts',(67.8249938600168,767.894819691892,105.52787330476));
#79290=CARTESIAN_POINT('Ctrl Pts',(68.0113863289532,767.944216390829,105.526521579779));
#79291=CARTESIAN_POINT('Ctrl Pts',(68.8926978463568,768.177776684027,105.52013027652));
#79292=CARTESIAN_POINT('Ctrl Pts',(69.7707970311868,768.427894891168,105.52513974266));
#79293=CARTESIAN_POINT('Ctrl Pts',(70.6455470696625,768.69398372115,105.543974097712));
#79294=CARTESIAN_POINT('Ctrl Pts',(71.166422612617,768.852428028317,105.555189135703));
#79295=CARTESIAN_POINT('Ctrl Pts',(71.6861109237649,769.016534162042,105.571305670155));
#79296=CARTESIAN_POINT('Ctrl Pts',(72.2045860049618,769.186171538845,105.592830330109));
#79297=CARTESIAN_POINT('Ctrl Pts',(72.4413593070117,769.263640260705,105.602660049989));
#79298=CARTESIAN_POINT('Ctrl Pts',(72.6779786088689,769.342312155877,105.61363557759));
#79299=CARTESIAN_POINT('Ctrl Pts',(72.914335334925,769.422151364376,105.625740702148));
#79300=CARTESIAN_POINT('Ctrl Pts',(18.2205382491878,776.217926749776,107.758400240177));
#79301=CARTESIAN_POINT('Ctrl Pts',(18.8176899041017,775.847482616211,107.626072229285));
#79302=CARTESIAN_POINT('Ctrl Pts',(19.42029013547,775.487607707795,107.496852123233));
#79303=CARTESIAN_POINT('Ctrl Pts',(20.0282637453734,775.13819782016,107.370606446288));
#79304=CARTESIAN_POINT('Ctrl Pts',(21.4287261468346,774.333334907756,107.079800528026));
#79305=CARTESIAN_POINT('Ctrl Pts',(22.8577001927037,773.583478723244,106.806304167243));
#79306=CARTESIAN_POINT('Ctrl Pts',(24.3145822062801,772.88293906295,106.564536635338));
#79307=CARTESIAN_POINT('Ctrl Pts',(24.6415401841664,772.725721780682,106.510278416338));
#79308=CARTESIAN_POINT('Ctrl Pts',(24.9699031440383,772.570975547355,106.457655516378));
#79309=CARTESIAN_POINT('Ctrl Pts',(25.2996699862003,772.418653078543,106.406814871278));
#79310=CARTESIAN_POINT('Ctrl Pts',(26.4393021087457,771.892246065315,106.231116089962));
#79311=CARTESIAN_POINT('Ctrl Pts',(27.595697848614,771.394747224638,106.076817314253));
#79312=CARTESIAN_POINT('Ctrl Pts',(28.768817589677,770.924268391335,105.949795981634));
#79313=CARTESIAN_POINT('Ctrl Pts',(28.8500363924492,770.891695648559,105.941001891652));
#79314=CARTESIAN_POINT('Ctrl Pts',(28.931335326977,770.859251953746,105.932339804482));
#79315=CARTESIAN_POINT('Ctrl Pts',(29.0127144902168,770.826937363433,105.923810175765));
#79316=CARTESIAN_POINT('Ctrl Pts',(30.0912177658905,770.398677964881,105.810768554961));
#79317=CARTESIAN_POINT('Ctrl Pts',(31.183803955927,769.993060962209,105.721095643046));
#79318=CARTESIAN_POINT('Ctrl Pts',(32.2906732771414,769.610038346885,105.656385894741));
#79319=CARTESIAN_POINT('Ctrl Pts',(32.4736749782796,769.546712181063,105.645687256886));
#79320=CARTESIAN_POINT('Ctrl Pts',(32.6570670106512,769.484003647625,105.635671053798));
#79321=CARTESIAN_POINT('Ctrl Pts',(32.8408501865509,769.421912550842,105.626344597616));
#79322=CARTESIAN_POINT('Ctrl Pts',(87.699590784449,775.880815944701,107.955814324766));
#79323=CARTESIAN_POINT('Ctrl Pts',(86.8582777839384,775.358573691995,107.767794186879));
#79324=CARTESIAN_POINT('Ctrl Pts',(86.0060117989125,774.857236858343,107.584458176575));
#79325=CARTESIAN_POINT('Ctrl Pts',(85.1428195414831,774.375835906652,107.408556668802));
#79326=CARTESIAN_POINT('Ctrl Pts',(84.6890166633739,774.122750761921,107.316080618647));
#79327=CARTESIAN_POINT('Ctrl Pts',(84.2321935891412,773.875176311381,107.225658799374));
#79328=CARTESIAN_POINT('Ctrl Pts',(83.7723522027849,773.632975867124,107.137687555858));
#79329=CARTESIAN_POINT('Ctrl Pts',(83.7596177450129,773.626268573216,107.13525135477));
#79330=CARTESIAN_POINT('Ctrl Pts',(83.7468809718159,773.619565372531,107.132817109852));
#79331=CARTESIAN_POINT('Ctrl Pts',(83.7341418825031,773.612866261111,107.130384833086));
#79332=CARTESIAN_POINT('Ctrl Pts',(82.8766542607943,773.161938806444,106.966664556956));
#79333=CARTESIAN_POINT('Ctrl Pts',(82.008669068268,772.729536592449,106.811865103256));
#79334=CARTESIAN_POINT('Ctrl Pts',(81.1301611010632,772.314552117029,106.669650327641));
#79335=CARTESIAN_POINT('Ctrl Pts',(80.6493702975054,772.0874389583,106.591818869306));
#79336=CARTESIAN_POINT('Ctrl Pts',(80.1654278484269,771.865542814205,106.517755856902));
#79337=CARTESIAN_POINT('Ctrl Pts',(79.6783303541909,771.648683021283,106.448055320323));
#79338=CARTESIAN_POINT('Ctrl Pts',(79.6565647520409,771.638992796983,106.44494080184));
#79339=CARTESIAN_POINT('Ctrl Pts',(79.6347925795945,771.629312489993,106.441835068224));
#79340=CARTESIAN_POINT('Ctrl Pts',(79.6130138468199,771.619642097175,106.438738156145));
#79341=CARTESIAN_POINT('Ctrl Pts',(78.5915534579615,771.166083880045,106.29348760144));
#79342=CARTESIAN_POINT('Ctrl Pts',(77.5557294924615,770.734362664327,106.167655588074));
#79343=CARTESIAN_POINT('Ctrl Pts',(76.5063986710057,770.324083567929,106.064972094903));
#79344=CARTESIAN_POINT('Ctrl Pts',(76.1440527569051,770.182409511301,106.029514312252));
#79345=CARTESIAN_POINT('Ctrl Pts',(75.7800960624704,770.043292390726,105.996816390673));
#79346=CARTESIAN_POINT('Ctrl Pts',(75.4145631715615,769.906716507234,105.967030809491));
#79347=CARTESIAN_POINT('Ctrl Pts',(75.3880786252614,769.896820953647,105.964872706558));
#79348=CARTESIAN_POINT('Ctrl Pts',(75.361591806201,769.886940921773,105.962730460533));
#79349=CARTESIAN_POINT('Ctrl Pts',(75.3351027106994,769.877076401201,105.960604043418));
#79350=CARTESIAN_POINT('Ctrl Pts',(74.2930654068928,769.489022440684,105.876954303209));
#79351=CARTESIAN_POINT('Ctrl Pts',(73.246276649245,769.124516422601,105.817703826413));
#79352=CARTESIAN_POINT('Ctrl Pts',(72.194795767384,768.783191202966,105.781328240662));
#79353=CARTESIAN_POINT('Ctrl Pts',(71.8102591048826,768.658365290246,105.768025339409));
#79354=CARTESIAN_POINT('Ctrl Pts',(71.4250949828742,768.536639299448,105.757781452103));
#79355=CARTESIAN_POINT('Ctrl Pts',(71.0393065916545,768.417994044972,105.750520851269));
#79356=CARTESIAN_POINT('Ctrl Pts',(71.0112581482468,768.409368034491,105.749992974961));
#79357=CARTESIAN_POINT('Ctrl Pts',(70.98320639808,768.400758307566,105.749480846806));
#79358=CARTESIAN_POINT('Ctrl Pts',(70.9551513342617,768.392164889373,105.748984355338));
#79359=CARTESIAN_POINT('Ctrl Pts',(69.8779620116377,768.062215958136,105.729921297378));
#79360=CARTESIAN_POINT('Ctrl Pts',(68.795896327465,767.756312172852,105.733909550365));
#79361=CARTESIAN_POINT('Ctrl Pts',(67.7085751978045,767.475856479629,105.754634331229));
#79362=CARTESIAN_POINT('Ctrl Pts',(67.3414226561117,767.381155826997,105.761632407292));
#79363=CARTESIAN_POINT('Ctrl Pts',(66.9736710071267,767.289356325921,105.770538728799));
#79364=CARTESIAN_POINT('Ctrl Pts',(66.6053060211355,767.200510675188,105.781110245067));
#79365=CARTESIAN_POINT('Ctrl Pts',(66.5767807618794,767.193630691158,105.781928876733));
#79366=CARTESIAN_POINT('Ctrl Pts',(66.5482518057202,767.186768460588,105.782757328545));
#79367=CARTESIAN_POINT('Ctrl Pts',(66.5197191417406,767.179924035241,105.783595431181));
#79368=CARTESIAN_POINT('Ctrl Pts',(65.5464684356867,766.946460317778,105.81218315726));
#79369=CARTESIAN_POINT('Ctrl Pts',(64.5689095968792,766.733710819704,105.851994672493));
#79370=CARTESIAN_POINT('Ctrl Pts',(63.5865249767008,766.543694768022,105.896332474997));
#79371=CARTESIAN_POINT('Ctrl Pts',(63.093381349984,766.448309312126,105.9185894447));
#79372=CARTESIAN_POINT('Ctrl Pts',(62.5990218002459,766.358652022941,105.941987598611));
#79373=CARTESIAN_POINT('Ctrl Pts',(62.1033816701624,766.274975514481,105.965683853526));
#79374=CARTESIAN_POINT('Ctrl Pts',(62.0766203065504,766.27045752384,105.966963298138));
#79375=CARTESIAN_POINT('Ctrl Pts',(62.0498551911242,766.265957036811,105.968243387741));
#79376=CARTESIAN_POINT('Ctrl Pts',(62.0230863151129,766.261474100584,105.969523995523));
#79377=CARTESIAN_POINT('Ctrl Pts',(60.993793818126,766.0891003102,106.01876476236));
#79378=CARTESIAN_POINT('Ctrl Pts',(59.9589403298854,765.942670793626,106.068766207129));
#79379=CARTESIAN_POINT('Ctrl Pts',(58.9178662167072,765.824834760521,106.112355741571));
#79380=CARTESIAN_POINT('Ctrl Pts',(58.4534442810074,765.772268244941,106.131800981546));
#79381=CARTESIAN_POINT('Ctrl Pts',(57.9877844352259,765.725391859862,106.149970946558));
#79382=CARTESIAN_POINT('Ctrl Pts',(57.52082820375,765.684440438175,106.166232140873));
#79383=CARTESIAN_POINT('Ctrl Pts',(57.4987351198496,765.682502904989,106.167001506193));
#79384=CARTESIAN_POINT('Ctrl Pts',(57.4766391419228,765.680578635084,106.167766670019));
#79385=CARTESIAN_POINT('Ctrl Pts',(57.4545402658822,765.678667649798,106.168527587898));
#79386=CARTESIAN_POINT('Ctrl Pts',(56.7926258462055,765.621429050229,106.19131890613));
#79387=CARTESIAN_POINT('Ctrl Pts',(56.1282177310631,765.576115938076,106.210298714617));
#79388=CARTESIAN_POINT('Ctrl Pts',(55.4608823872178,765.54328039121,106.22428065565));
#79389=CARTESIAN_POINT('Ctrl Pts',(55.3725062494401,765.53893193456,106.226132303339));
#79390=CARTESIAN_POINT('Ctrl Pts',(55.2840787559664,765.534802380145,106.227896276555));
#79391=CARTESIAN_POINT('Ctrl Pts',(55.1955988834149,765.530893075335,106.229569797693));
#79392=CARTESIAN_POINT('Ctrl Pts',(55.17689430288,765.530066651149,106.229923578841));
#79393=CARTESIAN_POINT('Ctrl Pts',(55.1581892595765,765.529250195679,106.230273254402));
#79394=CARTESIAN_POINT('Ctrl Pts',(55.1394838074096,765.528443709585,106.230618816138));
#79395=CARTESIAN_POINT('Ctrl Pts',(54.5347612060503,765.502371077699,106.241790371378));
#79396=CARTESIAN_POINT('Ctrl Pts',(53.9299116628076,765.486731543858,106.248659101124));
#79397=CARTESIAN_POINT('Ctrl Pts',(53.3266615204972,765.481538125481,106.250951479058));
#79398=CARTESIAN_POINT('Ctrl Pts',(53.1712106389157,765.480199839074,106.251542199467));
#79399=CARTESIAN_POINT('Ctrl Pts',(53.0158659657042,765.479555459939,106.251828930165));
#79400=CARTESIAN_POINT('Ctrl Pts',(52.8606571008079,765.479605727691,106.251806767246));
#79401=CARTESIAN_POINT('Ctrl Pts',(52.8459297524962,765.479610497461,106.251804664267));
#79402=CARTESIAN_POINT('Ctrl Pts',(52.8312031599683,765.479621520867,106.251799699673));
#79403=CARTESIAN_POINT('Ctrl Pts',(52.8164773180528,765.479638793933,106.251791882204));
#79404=CARTESIAN_POINT('Ctrl Pts',(51.7356232332715,765.480906610322,106.25121809205));
#79405=CARTESIAN_POINT('Ctrl Pts',(50.6591814899032,765.515843034854,106.235276753435));
#79406=CARTESIAN_POINT('Ctrl Pts',(49.5868625183453,765.582849136413,106.20744904546));
#79407=CARTESIAN_POINT('Ctrl Pts',(49.1346634480453,765.611105744411,106.195714044953));
#79408=CARTESIAN_POINT('Ctrl Pts',(48.6831976373843,765.645066027333,106.181865118927));
#79409=CARTESIAN_POINT('Ctrl Pts',(48.2324437882054,765.684612745822,106.166162999396));
#79410=CARTESIAN_POINT('Ctrl Pts',(48.2248448904869,765.68527943224,106.165898289953));
#79411=CARTESIAN_POINT('Ctrl Pts',(48.2172461944353,765.685947701091,106.165633068221));
#79412=CARTESIAN_POINT('Ctrl Pts',(48.209647699823,765.686617551509,106.165367336933));
#79413=CARTESIAN_POINT('Ctrl Pts',(47.1353654230241,765.781321630261,106.127797998829));
#79414=CARTESIAN_POINT('Ctrl Pts',(46.0651042888957,765.907638791474,106.08003928013));
#79415=CARTESIAN_POINT('Ctrl Pts',(44.9983540051326,766.063114396604,106.029843226538));
#79416=CARTESIAN_POINT('Ctrl Pts',(44.5514076839244,766.12825546177,106.00881211754));
#79417=CARTESIAN_POINT('Ctrl Pts',(44.1050776793143,766.198515194267,105.987353729809));
#79418=CARTESIAN_POINT('Ctrl Pts',(43.6593264839041,766.273713338407,105.966041018857));
#79419=CARTESIAN_POINT('Ctrl Pts',(43.6565741099716,766.27417766338,105.965909419547));
#79420=CARTESIAN_POINT('Ctrl Pts',(43.6538217579502,766.274642175869,105.965777828192));
#79421=CARTESIAN_POINT('Ctrl Pts',(43.6510694278281,766.275106875837,105.965646244939));
#79422=CARTESIAN_POINT('Ctrl Pts',(42.6536499926894,766.443509923196,105.917961669528));
#79423=CARTESIAN_POINT('Ctrl Pts',(41.6591048139389,766.636536152419,105.871336956417));
#79424=CARTESIAN_POINT('Ctrl Pts',(40.6670269579103,766.852398103184,105.832815900152));
#79425=CARTESIAN_POINT('Ctrl Pts',(40.1555137236564,766.963696066259,105.812954525405));
#79426=CARTESIAN_POINT('Ctrl Pts',(39.6446563246227,767.081064302483,105.795248236246));
#79427=CARTESIAN_POINT('Ctrl Pts',(39.1343984934061,767.204255349575,105.780667209758));
#79428=CARTESIAN_POINT('Ctrl Pts',(39.1337133432591,767.204420764702,105.780647631044));
#79429=CARTESIAN_POINT('Ctrl Pts',(39.1330281931599,767.204586190663,105.780628057937));
#79430=CARTESIAN_POINT('Ctrl Pts',(39.1323430431126,767.204751627457,105.78060849044));
#79431=CARTESIAN_POINT('Ctrl Pts',(38.382626037155,767.385778802471,105.759196997366));
#79432=CARTESIAN_POINT('Ctrl Pts',(37.632946947243,767.579784422389,105.744501930844));
#79433=CARTESIAN_POINT('Ctrl Pts',(36.8891547984958,767.784579867596,105.738993223485));
#79434=CARTESIAN_POINT('Ctrl Pts',(36.8885834704922,767.78473717683,105.73898899209));
#79435=CARTESIAN_POINT('Ctrl Pts',(36.8880121455897,767.784894492491,105.738984766092));
#79436=CARTESIAN_POINT('Ctrl Pts',(36.8874408237884,767.785051814578,105.738980545492));
#79437=CARTESIAN_POINT('Ctrl Pts',(36.1438767224033,767.989803420957,105.733487517914));
#79438=CARTESIAN_POINT('Ctrl Pts',(35.4055582568506,768.205444130159,105.737138832528));
#79439=CARTESIAN_POINT('Ctrl Pts',(34.6723927466888,768.431394424583,105.75135652115));
#79440=CARTESIAN_POINT('Ctrl Pts',(34.6716125182536,768.431634878944,105.751371651492));
#79441=CARTESIAN_POINT('Ctrl Pts',(34.6708322956372,768.431875344902,105.751386794007));
#79442=CARTESIAN_POINT('Ctrl Pts',(34.6700520788396,768.432115822456,105.751401948695));
#79443=CARTESIAN_POINT('Ctrl Pts',(33.6254395721809,768.754085127844,105.771692176961));
#79444=CARTESIAN_POINT('Ctrl Pts',(32.5912678029789,769.096841452481,105.813806788475));
#79445=CARTESIAN_POINT('Ctrl Pts',(31.5674456454017,769.459993643089,105.878413923118));
#79446=CARTESIAN_POINT('Ctrl Pts',(31.1540099390576,769.606640286086,105.904503313886));
#79447=CARTESIAN_POINT('Ctrl Pts',(30.7422617233729,769.75661244681,105.934260091256));
#79448=CARTESIAN_POINT('Ctrl Pts',(30.3321942334713,769.909882838522,105.967726548718));
#79449=CARTESIAN_POINT('Ctrl Pts',(30.3308081024758,769.910400930899,105.96783967374));
#79450=CARTESIAN_POINT('Ctrl Pts',(30.3294219906938,769.910919061048,105.967952840895));
#79451=CARTESIAN_POINT('Ctrl Pts',(30.3280358981258,769.91143722897,105.968066050175));
#79452=CARTESIAN_POINT('Ctrl Pts',(29.1299440841663,770.359324159757,106.065920345501));
#79453=CARTESIAN_POINT('Ctrl Pts',(27.9462089779132,770.835436553784,106.195249342647));
#79454=CARTESIAN_POINT('Ctrl Pts',(26.7770031279921,771.341380969508,106.351250345135));
#79455=CARTESIAN_POINT('Ctrl Pts',(26.5550725248336,771.437415854515,106.380861381188));
#79456=CARTESIAN_POINT('Ctrl Pts',(26.3336653434522,771.534525429352,106.411433324955));
#79457=CARTESIAN_POINT('Ctrl Pts',(26.1127826892852,771.63272049615,106.442933260637));
#79458=CARTESIAN_POINT('Ctrl Pts',(26.1114327061628,771.633320641432,106.443125780877));
#79459=CARTESIAN_POINT('Ctrl Pts',(26.110082742642,771.633920827386,106.443318335444));
#79460=CARTESIAN_POINT('Ctrl Pts',(26.1087327987236,771.634521054016,106.443510924326));
#79461=CARTESIAN_POINT('Ctrl Pts',(24.8834028164008,772.179340490833,106.618321839375));
#79462=CARTESIAN_POINT('Ctrl Pts',(23.6742287046315,772.75767287839,106.821400751351));
#79463=CARTESIAN_POINT('Ctrl Pts',(22.4816817734695,773.372951908832,107.043515560356));
#79464=CARTESIAN_POINT('Ctrl Pts',(22.3255329513332,773.453514856401,107.072598663838));
#79465=CARTESIAN_POINT('Ctrl Pts',(22.1696691850727,773.534711197042,107.102008189595));
#79466=CARTESIAN_POINT('Ctrl Pts',(22.0140915237079,773.616548601358,107.131723468372));
#79467=CARTESIAN_POINT('Ctrl Pts',(22.0139887749509,773.616602649551,107.131743093349));
#79468=CARTESIAN_POINT('Ctrl Pts',(22.0138860262999,773.616656698041,107.131762718459));
#79469=CARTESIAN_POINT('Ctrl Pts',(22.0137832777549,773.616710746827,107.131782343701));
#79470=CARTESIAN_POINT('Ctrl Pts',(21.5862139423887,773.84162491469,107.213449213102));
#79471=CARTESIAN_POINT('Ctrl Pts',(21.1607365610572,774.071528113583,107.297369892082));
#79472=CARTESIAN_POINT('Ctrl Pts',(20.7377097588874,774.306260864954,107.383126887167));
#79473=CARTESIAN_POINT('Ctrl Pts',(20.3168766744112,774.539776347379,107.468439166606));
#79474=CARTESIAN_POINT('Ctrl Pts',(19.898467575598,774.778072073164,107.555569538841));
#79475=CARTESIAN_POINT('Ctrl Pts',(19.4828625856908,775.021031750083,107.64412093627));
#79476=CARTESIAN_POINT('Ctrl Pts',(19.0865928171878,775.252688196147,107.728552650547));
#79477=CARTESIAN_POINT('Ctrl Pts',(18.6928715455575,775.488585453396,107.81427690553));
#79478=CARTESIAN_POINT('Ctrl Pts',(18.3020670071316,775.728649501869,107.900951830872));
#79479=CARTESIAN_POINT('Ctrl Pts',(18.2197962836763,775.779186895889,107.919198315014));
#79480=CARTESIAN_POINT('Ctrl Pts',(18.1376549866794,775.829909027471,107.937486919332));
#79481=CARTESIAN_POINT('Ctrl Pts',(18.0556468322311,775.880815322444,107.955814427592));
#79482=CARTESIAN_POINT('Ctrl Pts',(11.8385912118569,780.22624452509,109.46295982623));
#79483=CARTESIAN_POINT('Ctrl Pts',(12.0670832072855,780.458609040937,109.611864051783));
#79484=CARTESIAN_POINT('Ctrl Pts',(12.0670501393615,780.578030861977,109.274058255276));
#79485=CARTESIAN_POINT('Ctrl Pts',(13.0097844767455,779.287129064763,109.130812234977));
#79486=CARTESIAN_POINT('Ctrl Pts',(13.2324907967292,779.524274195338,109.281682936946));
#79487=CARTESIAN_POINT('Ctrl Pts',(13.231839594492,779.644266255903,108.943836855405));
#79488=CARTESIAN_POINT('Ctrl Pts',(14.2171090900043,778.388492815856,108.815571055468));
#79489=CARTESIAN_POINT('Ctrl Pts',(14.4032018227789,778.651087036577,108.97403106638));
#79490=CARTESIAN_POINT('Ctrl Pts',(14.4327918077321,778.749748784589,108.629696114708));
#79491=CARTESIAN_POINT('Ctrl Pts',(15.4635632812157,777.538177788623,108.526207819986));
#79492=CARTESIAN_POINT('Ctrl Pts',(15.6646167008071,777.782008927919,108.661951401308));
#79493=CARTESIAN_POINT('Ctrl Pts',(15.6662338981911,777.895506807342,108.337269960618));
#79494=CARTESIAN_POINT('Ctrl Pts',(15.4635632805302,777.53817778912,108.52620782016));
#79495=CARTESIAN_POINT('Ctrl Pts',(14.7152684519203,778.048654902706,108.699923801311));
#79496=CARTESIAN_POINT('Ctrl Pts',(13.9814260101745,778.576348492687,108.882905465017));
#79497=CARTESIAN_POINT('Ctrl Pts',(13.2611376128576,779.119610429859,109.073211560677));
#79498=CARTESIAN_POINT('Ctrl Pts',(12.7881788749144,779.476329323478,109.198171134039));
#79499=CARTESIAN_POINT('Ctrl Pts',(12.3210644993871,779.839761579878,109.326288922373));
#79500=CARTESIAN_POINT('Ctrl Pts',(11.859543044092,780.20945181141,109.457020834635));
#79501=CARTESIAN_POINT('Ctrl Pts',(90.0889078210223,777.895440968217,108.337247425881));
#79502=CARTESIAN_POINT('Ctrl Pts',(90.0905250557564,777.781943458107,108.661927889749));
#79503=CARTESIAN_POINT('Ctrl Pts',(90.2915774330859,777.538112255547,108.526185523131));
#79504=CARTESIAN_POINT('Ctrl Pts',(89.2520735400448,777.315878912135,108.138850533236));
#79505=CARTESIAN_POINT('Ctrl Pts',(89.2664127847706,777.214156416844,108.458039407528));
#79506=CARTESIAN_POINT('Ctrl Pts',(89.445908281308,776.961210264209,108.329865285142));
#79507=CARTESIAN_POINT('Ctrl Pts',(88.4006672002774,776.755189453486,107.950220772475));
#79508=CARTESIAN_POINT('Ctrl Pts',(88.4306076665784,776.666770743405,108.259519276078));
#79509=CARTESIAN_POINT('Ctrl Pts',(88.5823401442266,776.406482463236,108.145084435913));
#79510=CARTESIAN_POINT('Ctrl Pts',(87.5346919229366,776.218453858122,107.756965167182));
#79511=CARTESIAN_POINT('Ctrl Pts',(87.5338826891535,776.117574461731,108.040791987471));
#79512=CARTESIAN_POINT('Ctrl Pts',(87.6995907844487,775.880815944701,107.955814324766));
#79513=CARTESIAN_POINT('',(90.2915774337827,777.538112255959,108.526185523262));
#79514=CARTESIAN_POINT('Origin',(90.2661044385266,777.667199844411,108.256579289987));
#79515=CARTESIAN_POINT('Ctrl Pts',(89.8418878191544,777.722889498519,108.285610804474));
#79516=CARTESIAN_POINT('Ctrl Pts',(89.0846481267868,777.205998632613,108.101601829559));
#79517=CARTESIAN_POINT('Ctrl Pts',(88.3156024019357,776.702465886418,107.93123726532));
#79518=CARTESIAN_POINT('Ctrl Pts',(87.5346940946149,776.217967276064,107.758346187656));
#79519=CARTESIAN_POINT('Ctrl Pts',(90.2915774337827,777.538112255959,108.526185523262));
#79520=CARTESIAN_POINT('Ctrl Pts',(89.4450227738296,776.960606185036,108.329659716473));
#79521=CARTESIAN_POINT('Ctrl Pts',(88.5813231070643,776.405876829861,108.144866373145));
#79522=CARTESIAN_POINT('Ctrl Pts',(87.6995908232158,775.880815967783,107.955814333077));
#79523=CARTESIAN_POINT('Ctrl Pts',(93.6887548566012,780.578486380469,109.274219348021));
#79524=CARTESIAN_POINT('Ctrl Pts',(93.6887212389462,780.45906415542,109.612024882815));
#79525=CARTESIAN_POINT('Ctrl Pts',(93.9172164533292,780.22670229016,109.463121730127));
#79526=CARTESIAN_POINT('Ctrl Pts',(92.5237579617488,779.644534103879,108.943928297855));
#79527=CARTESIAN_POINT('Ctrl Pts',(92.5231064640288,779.52454057462,109.281777811047));
#79528=CARTESIAN_POINT('Ctrl Pts',(92.7458176037906,779.287396872426,109.130903091125));
#79529=CARTESIAN_POINT('Ctrl Pts',(91.322583073976,778.74984115456,108.62972748294));
#79530=CARTESIAN_POINT('Ctrl Pts',(91.352184971522,778.65118685501,108.97406731076));
#79531=CARTESIAN_POINT('Ctrl Pts',(91.5382669500913,778.388583935177,108.815601759781));
#79532=CARTESIAN_POINT('Ctrl Pts',(90.0889078212206,777.895440968355,108.337247425928));
#79533=CARTESIAN_POINT('Ctrl Pts',(90.0905250557281,777.781943458083,108.661927889755));
#79534=CARTESIAN_POINT('Ctrl Pts',(90.2915774330965,777.538112255541,108.526185523126));
#79535=CARTESIAN_POINT('Ctrl Pts',(93.8960334963338,780.209723961161,109.457117026756));
#79536=CARTESIAN_POINT('Ctrl Pts',(93.1510424308948,779.612954242215,109.246081306523));
#79537=CARTESIAN_POINT('Ctrl Pts',(92.3913732828177,779.0324108185,109.041831100158));
#79538=CARTESIAN_POINT('Ctrl Pts',(91.6160271246919,778.470077943857,108.846679892652));
#79539=CARTESIAN_POINT('Ctrl Pts',(91.1795712666005,778.153530973496,108.736825878626));
#79540=CARTESIAN_POINT('Ctrl Pts',(90.7381479858848,777.842755555208,108.629855897371));
#79541=CARTESIAN_POINT('Ctrl Pts',(90.2915774337562,777.538112255991,108.526185523279));
#79542=CARTESIAN_POINT('Ctrl Pts',(68.80511438861,640.627119090081,98.0546383469682));
#79543=CARTESIAN_POINT('Ctrl Pts',(68.8068658173116,640.125373764374,98.0546383469682));
#79544=CARTESIAN_POINT('Ctrl Pts',(68.3051174347811,640.125373764374,98.0546383469682));
#79545=CARTESIAN_POINT('Ctrl Pts',(68.8051141943977,640.627174727561,98.1965353136778));
#79546=CARTESIAN_POINT('Ctrl Pts',(68.8069216424176,640.125373764374,98.1966675010902));
#79547=CARTESIAN_POINT('Ctrl Pts',(68.305117426757,640.125373764374,98.1610611371843));
#79548=CARTESIAN_POINT('Ctrl Pts',(68.7901809021704,640.62721634467,98.3359104357707));
#79549=CARTESIAN_POINT('Ctrl Pts',(68.7920160644509,640.125373764374,98.3361724571032));
#79550=CARTESIAN_POINT('Ctrl Pts',(68.2939175755223,640.125373764374,98.2655925281767));
#79551=CARTESIAN_POINT('Ctrl Pts',(68.7316262194072,640.627272620042,98.6097537558797));
#79552=CARTESIAN_POINT('Ctrl Pts',(68.7334618482997,640.125373764374,98.610284735857));
#79553=CARTESIAN_POINT('Ctrl Pts',(68.2500017088632,640.125373764374,98.4709750840453));
#79554=CARTESIAN_POINT('Ctrl Pts',(68.687173049619,640.627287130011,98.7456950617399));
#79555=CARTESIAN_POINT('Ctrl Pts',(68.6889804824384,640.125373764374,98.7463587242848));
#79556=CARTESIAN_POINT('Ctrl Pts',(68.2166618686685,640.125373764374,98.5729310799066));
#79557=CARTESIAN_POINT('Ctrl Pts',(68.5146759823964,640.627287252338,99.1299181624823));
#79558=CARTESIAN_POINT('Ctrl Pts',(68.516317865413,640.125373764374,99.1309508939863));
#79559=CARTESIAN_POINT('Ctrl Pts',(68.0872890739678,640.125373764374,98.8610984080293));
#79560=CARTESIAN_POINT('Ctrl Pts',(68.3463456555463,640.627230853324,99.3607167776682));
#79561=CARTESIAN_POINT('Ctrl Pts',(68.3477940984104,640.125373764374,99.3619233451112));
#79562=CARTESIAN_POINT('Ctrl Pts',(67.9610411711621,640.125373764374,99.0341972964163));
#79563=CARTESIAN_POINT('Ctrl Pts',(68.1332263705067,640.627119090081,99.5499985678032));
#79564=CARTESIAN_POINT('Ctrl Pts',(68.134389413644,640.125373764374,99.5513080841862));
#79565=CARTESIAN_POINT('Ctrl Pts',(67.8012014212036,640.125373764374,99.1761585125944));
#79566=CARTESIAN_POINT('',(68.1332263705066,640.627119090085,99.5499985678032));
#79567=CARTESIAN_POINT('Origin',(66.8051226640402,640.625373779613,98.0546365904861));
#79568=CARTESIAN_POINT('',(67.8012014212036,640.125373764374,99.1761585125944));
#79569=CARTESIAN_POINT('Origin',(67.8012014212036,640.625373764374,99.1761585125944));
#79570=CARTESIAN_POINT('Ctrl Pts',(68.3051174347811,640.125373764374,98.0546383469682));
#79571=CARTESIAN_POINT('Ctrl Pts',(68.3051174347811,640.125373764374,98.16106912087));
#79572=CARTESIAN_POINT('Ctrl Pts',(68.2939175755208,640.125373764374,98.2655925281833));
#79573=CARTESIAN_POINT('Ctrl Pts',(68.2719596426717,640.125373764374,98.3682838062134));
#79574=CARTESIAN_POINT('Ctrl Pts',(68.2500017098227,640.125373764374,98.4709750842436));
#79575=CARTESIAN_POINT('Ctrl Pts',(68.2166618704369,640.125373764374,98.5729310807814));
#79576=CARTESIAN_POINT('Ctrl Pts',(68.1735376049674,640.125373764374,98.6689868564858));
#79577=CARTESIAN_POINT('Ctrl Pts',(68.1453423196876,640.125373764374,98.7317895493379));
#79578=CARTESIAN_POINT('Ctrl Pts',(68.1128287472829,640.125373764374,98.7926468994039));
#79579=CARTESIAN_POINT('Ctrl Pts',(68.0762480466093,640.125373764374,98.8510410845592));
#79580=CARTESIAN_POINT('Ctrl Pts',(68.0385887645426,640.125373764374,98.9111570213597));
#79581=CARTESIAN_POINT('Ctrl Pts',(67.9966191995703,640.125373764374,98.9686613932213));
#79582=CARTESIAN_POINT('Ctrl Pts',(67.9506628544449,640.125373764374,99.0230191503698));
#79583=CARTESIAN_POINT('Ctrl Pts',(67.9047065093195,640.125373764374,99.0773769075182));
#79584=CARTESIAN_POINT('Ctrl Pts',(67.8547638793613,640.125373764374,99.1285871723741));
#79585=CARTESIAN_POINT('Ctrl Pts',(67.8012014212036,640.125373764374,99.1761585125944));
#79586=CARTESIAN_POINT('Origin',(52.8776183915471,640.625373764374,82.3731046594733));
#79587=CARTESIAN_POINT('',(37.6220104125875,640.627119090081,99.5499985678032));
#79588=CARTESIAN_POINT('',(37.9540353618906,640.125373764374,99.1761585125945));
#79589=CARTESIAN_POINT('Origin',(37.9540353618906,640.625373764375,99.1761585125944));
#79590=CARTESIAN_POINT('Origin',(52.8776183915471,640.125373764374,82.3731046594733));
#79591=CARTESIAN_POINT('Origin',(52.8776183915471,640.627119090082,82.3731046594733));
#79592=CARTESIAN_POINT('Ctrl Pts',(37.6220104125875,640.627119090081,99.5499985678032));
#79593=CARTESIAN_POINT('Ctrl Pts',(37.6208473694502,640.125373764374,99.5513080841862));
#79594=CARTESIAN_POINT('Ctrl Pts',(37.9540353618906,640.125373764374,99.1761585125945));
#79595=CARTESIAN_POINT('Ctrl Pts',(37.5159163554561,640.627174727549,99.4557711821737));
#79596=CARTESIAN_POINT('Ctrl Pts',(37.5146172779777,640.125373764374,99.4570348037583));
#79597=CARTESIAN_POINT('Ctrl Pts',(37.8744646789089,640.125373764374,99.1054880329923));
#79598=CARTESIAN_POINT('Ctrl Pts',(37.4216242255084,640.627216344653,99.3520531890113));
#79599=CARTESIAN_POINT('Ctrl Pts',(37.4202096694391,640.125373764374,99.3532513153967));
#79600=CARTESIAN_POINT('Ctrl Pts',(37.8037454661792,640.125373764374,99.0276995934824));
#79601=CARTESIAN_POINT('Ctrl Pts',(37.2557592423392,640.627272620036,99.1264260137889));
#79602=CARTESIAN_POINT('Ctrl Pts',(37.25414328015,640.125373764374,99.1274458860118));
#79603=CARTESIAN_POINT('Ctrl Pts',(37.6793465830514,640.125373764374,98.8584792771019));
#79604=CARTESIAN_POINT('Ctrl Pts',(37.1836373152616,640.627287130011,99.0029167000581));
#79605=CARTESIAN_POINT('Ctrl Pts',(37.181940872061,640.125373764374,99.0038273821317));
#79606=CARTESIAN_POINT('Ctrl Pts',(37.6252551007653,640.125373764374,98.7658473086436));
#79607=CARTESIAN_POINT('Ctrl Pts',(37.0109069525407,640.627287252338,98.6187984225216));
#79608=CARTESIAN_POINT('Ctrl Pts',(37.0090444961387,640.125373764374,98.6193402438448));
#79609=CARTESIAN_POINT('Ctrl Pts',(37.495707323009,640.125373764374,98.4777586030618));
#79610=CARTESIAN_POINT('Ctrl Pts',(36.9501227846132,640.627230853348,98.3396776876425));
#79611=CARTESIAN_POINT('Ctrl Pts',(36.9482588084213,640.125373764374,98.3399594403062));
#79612=CARTESIAN_POINT('Ctrl Pts',(37.4501193563501,640.125373764374,98.2684179824933));
#79613=CARTESIAN_POINT('Ctrl Pts',(36.9501223944842,640.627119090081,98.0546383469683));
#79614=CARTESIAN_POINT('Ctrl Pts',(36.9483709657826,640.125373764374,98.0546383469683));
#79615=CARTESIAN_POINT('Ctrl Pts',(37.4501193483131,640.125373764374,98.0546383469682));
#79616=CARTESIAN_POINT('',(36.9501223944842,640.627119090084,98.0546383469682));
#79617=CARTESIAN_POINT('',(37.4501193483131,640.125373764374,98.0546383469682));
#79618=CARTESIAN_POINT('Origin',(37.4501193483131,640.625373764374,98.0546383469682));
#79619=CARTESIAN_POINT('Ctrl Pts',(37.9540353618906,640.125373764374,99.1761585125945));
#79620=CARTESIAN_POINT('Ctrl Pts',(37.8744587042996,640.125373764374,99.1054827373954));
#79621=CARTESIAN_POINT('Ctrl Pts',(37.8037454661753,640.125373764374,99.0276995934772));
#79622=CARTESIAN_POINT('Ctrl Pts',(37.7415460242206,640.125373764374,98.9430894355824));
#79623=CARTESIAN_POINT('Ctrl Pts',(37.6793465822659,640.125373764374,98.8584792776875));
#79624=CARTESIAN_POINT('Ctrl Pts',(37.6252550989367,640.125373764374,98.7658473093854));
#79625=CARTESIAN_POINT('Ctrl Pts',(37.5820725069809,640.125373764374,98.6698177406556));
#79626=CARTESIAN_POINT('Ctrl Pts',(37.5538390869676,640.125373764374,98.6070321822894));
#79627=CARTESIAN_POINT('Ctrl Pts',(37.5299277455258,640.125373764374,98.5423097194069));
#79628=CARTESIAN_POINT('Ctrl Pts',(37.5105588672889,640.125373764374,98.4761820014583));
#79629=CARTESIAN_POINT('Ctrl Pts',(37.490618897988,640.125373764374,98.4081045088073));
#79630=CARTESIAN_POINT('Ctrl Pts',(37.4754938161077,640.125373764374,98.3385385037225));
#79631=CARTESIAN_POINT('Ctrl Pts',(37.4653688468807,640.125373764374,98.268081166164));
#79632=CARTESIAN_POINT('Ctrl Pts',(37.4552438776536,640.125373764374,98.1976238286054));
#79633=CARTESIAN_POINT('Ctrl Pts',(37.450119348313,640.125373764374,98.1262761116766));
#79634=CARTESIAN_POINT('Ctrl Pts',(37.4501193483131,640.125373764374,98.0546383469682));
#79635=CARTESIAN_POINT('Origin',(38.9501141189669,640.625373779629,98.0546365905253));
#79636=CARTESIAN_POINT('Ctrl Pts',(68.1332263705066,640.627119090081,81.6674251557765));
#79637=CARTESIAN_POINT('Ctrl Pts',(68.134389413644,640.125373764374,81.6661156393935));
#79638=CARTESIAN_POINT('Ctrl Pts',(67.8012014212035,640.125373764374,82.0412652109852));
#79639=CARTESIAN_POINT('Ctrl Pts',(68.2393204276379,640.62717472755,81.7616525414059));
#79640=CARTESIAN_POINT('Ctrl Pts',(68.2406195051122,640.125373764374,81.7603889198256));
#79641=CARTESIAN_POINT('Ctrl Pts',(67.8807721041838,640.125373764374,82.1119356905887));
#79642=CARTESIAN_POINT('Ctrl Pts',(68.3336125575859,640.627216344653,81.8653705345686));
#79643=CARTESIAN_POINT('Ctrl Pts',(68.3350271136558,640.125373764374,81.864172408183));
#79644=CARTESIAN_POINT('Ctrl Pts',(67.9514913169153,640.125373764374,82.1897241300973));
#79645=CARTESIAN_POINT('Ctrl Pts',(68.4994775407548,640.627272620036,82.0909977097906));
#79646=CARTESIAN_POINT('Ctrl Pts',(68.5010935029434,640.125373764374,82.0899778375679));
#79647=CARTESIAN_POINT('Ctrl Pts',(68.0758902000424,640.125373764374,82.3589444464778));
#79648=CARTESIAN_POINT('Ctrl Pts',(68.5715994678325,640.627287130011,82.2145070235214));
#79649=CARTESIAN_POINT('Ctrl Pts',(68.5732959110343,640.125373764374,82.2135963414472));
#79650=CARTESIAN_POINT('Ctrl Pts',(68.1299816823292,640.125373764374,82.4515764149354));
#79651=CARTESIAN_POINT('Ctrl Pts',(68.7443298305536,640.627287252338,82.5986253010585));
#79652=CARTESIAN_POINT('Ctrl Pts',(68.7461922869533,640.125373764374,82.5980834797364));
#79653=CARTESIAN_POINT('Ctrl Pts',(68.2595294600845,640.125373764374,82.7396651205193));
#79654=CARTESIAN_POINT('Ctrl Pts',(68.805113998481,640.627230853348,82.877746035937));
#79655=CARTESIAN_POINT('Ctrl Pts',(68.8069779746714,640.125373764374,82.8774642832724));
#79656=CARTESIAN_POINT('Ctrl Pts',(68.3051174267426,640.125373764374,82.9490057410853));
#79657=CARTESIAN_POINT('Ctrl Pts',(68.80511438861,640.627119090081,83.1627853766115));
#79658=CARTESIAN_POINT('Ctrl Pts',(68.8068658173116,640.125373764374,83.1627853766115));
#79659=CARTESIAN_POINT('Ctrl Pts',(68.3051174347811,640.125373764374,83.1627853766115));
#79660=CARTESIAN_POINT('Origin',(66.8051226640255,640.625373779627,83.1627871331001));
#79661=CARTESIAN_POINT('Ctrl Pts',(67.8012014212036,640.125373764374,82.0412652109852));
#79662=CARTESIAN_POINT('Ctrl Pts',(67.8807780787945,640.125373764374,82.1119409861843));
#79663=CARTESIAN_POINT('Ctrl Pts',(67.951491316919,640.125373764374,82.1897241301024));
#79664=CARTESIAN_POINT('Ctrl Pts',(68.0136907588737,640.125373764374,82.2743342879973));
#79665=CARTESIAN_POINT('Ctrl Pts',(68.0758902008283,640.125373764374,82.3589444458922));
#79666=CARTESIAN_POINT('Ctrl Pts',(68.1299816841575,640.125373764374,82.4515764141943));
#79667=CARTESIAN_POINT('Ctrl Pts',(68.173164276113,640.125373764374,82.5476059829244));
#79668=CARTESIAN_POINT('Ctrl Pts',(68.2013976961101,640.125373764374,82.6103915412553));
#79669=CARTESIAN_POINT('Ctrl Pts',(68.2253090375408,640.125373764374,82.6751140041001));
#79670=CARTESIAN_POINT('Ctrl Pts',(68.244677915772,640.125373764374,82.7412417220098));
#79671=CARTESIAN_POINT('Ctrl Pts',(68.2646178850837,640.125373764374,82.8093192146777));
#79672=CARTESIAN_POINT('Ctrl Pts',(68.2797429669723,640.125373764374,82.8788852197806));
#79673=CARTESIAN_POINT('Ctrl Pts',(68.289867936205,640.125373764374,82.9493425573579));
#79674=CARTESIAN_POINT('Ctrl Pts',(68.2999929054377,640.125373764374,83.0197998949352));
#79675=CARTESIAN_POINT('Ctrl Pts',(68.3051174347812,640.125373764374,83.0911476118835));
#79676=CARTESIAN_POINT('Ctrl Pts',(68.3051174347811,640.125373764374,83.1627853766115));
#79677=CARTESIAN_POINT('Origin',(37.4501193483131,640.625373764374,82.287785267134));
#79678=CARTESIAN_POINT('',(36.9501223944842,640.627119090078,83.1627853766115));
#79679=CARTESIAN_POINT('',(37.4501193483131,640.125373764374,83.1627853766115));
#79680=CARTESIAN_POINT('Origin',(37.4501193483131,640.62537376437,83.1627853766115));
#79681=CARTESIAN_POINT('',(37.4501193483131,640.125373764374,83.1619984528873));
#79682=CARTESIAN_POINT('',(36.9501223944842,640.627119090081,98.0554252706924));
#79683=CARTESIAN_POINT('Ctrl Pts',(36.9501223944842,640.627119090081,83.1627853766114));
#79684=CARTESIAN_POINT('Ctrl Pts',(36.9483709657826,640.125373764374,83.1627853766115));
#79685=CARTESIAN_POINT('Ctrl Pts',(37.4501193483131,640.125373764374,83.1627853766115));
#79686=CARTESIAN_POINT('Ctrl Pts',(36.9501225886964,640.627174727561,83.0208884099024));
#79687=CARTESIAN_POINT('Ctrl Pts',(36.9483151406832,640.125373764374,83.0207562224895));
#79688=CARTESIAN_POINT('Ctrl Pts',(37.4501193563416,640.125373764374,83.0563625863953));
#79689=CARTESIAN_POINT('Ctrl Pts',(36.9650558809238,640.62721634467,82.8815132878083));
#79690=CARTESIAN_POINT('Ctrl Pts',(36.9632207186425,640.125373764374,82.8812512664765));
#79691=CARTESIAN_POINT('Ctrl Pts',(37.4613192075715,640.125373764374,82.951831195403));
#79692=CARTESIAN_POINT('Ctrl Pts',(37.0236105636868,640.627272620042,82.6076699677006));
#79693=CARTESIAN_POINT('Ctrl Pts',(37.0217749347951,640.125373764374,82.6071389877227));
#79694=CARTESIAN_POINT('Ctrl Pts',(37.5052350742313,640.125373764374,82.7464486395343));
#79695=CARTESIAN_POINT('Ctrl Pts',(37.0680637334749,640.627287130011,82.4717286618402));
#79696=CARTESIAN_POINT('Ctrl Pts',(37.066256300655,640.125373764374,82.4710649992963));
#79697=CARTESIAN_POINT('Ctrl Pts',(37.5385749144261,640.125373764374,82.6444926436739));
#79698=CARTESIAN_POINT('Ctrl Pts',(37.2405608006982,640.627287252338,82.0875055610965));
#79699=CARTESIAN_POINT('Ctrl Pts',(37.2389189176825,640.125373764374,82.0864728295907));
#79700=CARTESIAN_POINT('Ctrl Pts',(37.6679477091256,640.125373764374,82.356325315549));
#79701=CARTESIAN_POINT('Ctrl Pts',(37.4088911275473,640.627230853324,81.856706945912));
#79702=CARTESIAN_POINT('Ctrl Pts',(37.4074426846854,640.125373764374,81.8555003784741));
#79703=CARTESIAN_POINT('Ctrl Pts',(37.794195611936,640.125373764374,82.1832264271683));
#79704=CARTESIAN_POINT('Ctrl Pts',(37.6220104125875,640.627119090081,81.6674251557765));
#79705=CARTESIAN_POINT('Ctrl Pts',(37.6208473694501,640.125373764374,81.6661156393935));
#79706=CARTESIAN_POINT('Ctrl Pts',(37.9540353618906,640.125373764374,82.0412652109853));
#79707=CARTESIAN_POINT('Origin',(38.9501141190175,640.62537377961,83.1627871330772));
#79708=CARTESIAN_POINT('Ctrl Pts',(37.4501193483131,640.125373764374,83.1627853766115));
#79709=CARTESIAN_POINT('Ctrl Pts',(37.4501193483131,640.125373764374,83.0563546027096));
#79710=CARTESIAN_POINT('Ctrl Pts',(37.4613192075729,640.125373764374,82.9518311953963));
#79711=CARTESIAN_POINT('Ctrl Pts',(37.4832771404222,640.125373764374,82.8491399173662));
#79712=CARTESIAN_POINT('Ctrl Pts',(37.5052350732715,640.125373764374,82.7464486393361));
#79713=CARTESIAN_POINT('Ctrl Pts',(37.5385749126573,640.125373764374,82.6444926427984));
#79714=CARTESIAN_POINT('Ctrl Pts',(37.5816991781264,640.125373764374,82.5484368670937));
#79715=CARTESIAN_POINT('Ctrl Pts',(37.6098944633952,640.125373764374,82.4856341742655));
#79716=CARTESIAN_POINT('Ctrl Pts',(37.6424080357855,640.125373764374,82.4247768242222));
#79717=CARTESIAN_POINT('Ctrl Pts',(37.6789887364421,640.125373764374,82.3663826390874));
#79718=CARTESIAN_POINT('Ctrl Pts',(37.7166480185124,640.125373764374,82.3062667022739));
#79719=CARTESIAN_POINT('Ctrl Pts',(37.7586175834904,640.125373764374,82.2487623304001));
#79720=CARTESIAN_POINT('Ctrl Pts',(37.8045739286231,640.125373764374,82.1944045732403));
#79721=CARTESIAN_POINT('Ctrl Pts',(37.8505302737557,640.125373764374,82.1400468160806));
#79722=CARTESIAN_POINT('Ctrl Pts',(37.9004729037229,640.125373764374,82.0888365512145));
#79723=CARTESIAN_POINT('Ctrl Pts',(37.9540353618905,640.125373764374,82.0412652109853));
#79724=CARTESIAN_POINT('Ctrl Pts',(10.5317017736754,779.984261556367,107.006332650571));
#79725=CARTESIAN_POINT('Ctrl Pts',(10.3604849461703,779.152731480618,108.803696199278));
#79726=CARTESIAN_POINT('Ctrl Pts',(11.5614808152667,780.530792792794,109.582854450735));
#79727=CARTESIAN_POINT('Ctrl Pts',(10.5733299874904,779.865842760521,107.219090474412));
#79728=CARTESIAN_POINT('Ctrl Pts',(10.5582433475702,779.256981704553,108.887216975226));
#79729=CARTESIAN_POINT('Ctrl Pts',(11.7093120354819,780.435428829693,109.551490669409));
#79730=CARTESIAN_POINT('Ctrl Pts',(10.7318267936817,779.743920761265,107.158653158791));
#79731=CARTESIAN_POINT('Ctrl Pts',(10.7068785033582,779.120077753409,108.835843568229));
#79732=CARTESIAN_POINT('Ctrl Pts',(11.8566239029334,780.315075067507,109.508795773261));
#79733=CARTESIAN_POINT('Ctrl Pts',(10.9216035979647,779.592391477705,107.105565628044));
#79734=CARTESIAN_POINT('Ctrl Pts',(10.8970342369242,778.968863920289,108.782484477585));
#79735=CARTESIAN_POINT('Ctrl Pts',(12.0415407060361,780.167617208107,109.456683482087));
#79736=CARTESIAN_POINT('Ctrl Pts',(10.9595078561701,779.562175400004,107.095035038181));
#79737=CARTESIAN_POINT('Ctrl Pts',(10.9350411255372,778.938762360073,108.771872584246));
#79738=CARTESIAN_POINT('Ctrl Pts',(12.0784988928585,780.138215973205,109.446293459633));
#79739=CARTESIAN_POINT('Ctrl Pts',(11.0732462957153,779.471645605594,107.063645836025));
#79740=CARTESIAN_POINT('Ctrl Pts',(11.0491718823668,778.848720729622,108.74015903354));
#79741=CARTESIAN_POINT('Ctrl Pts',(12.1894723235861,780.050134608815,109.415168109637));
#79742=CARTESIAN_POINT('Ctrl Pts',(11.1491060843021,779.411450286746,107.042989781577));
#79743=CARTESIAN_POINT('Ctrl Pts',(11.125405322853,778.789043900988,108.719179562979));
#79744=CARTESIAN_POINT('Ctrl Pts',(12.26358634686,779.991576829024,109.394477502784));
#79745=CARTESIAN_POINT('Ctrl Pts',(11.3767577611053,779.231301369849,106.981776204739));
#79746=CARTESIAN_POINT('Ctrl Pts',(11.3544757071218,778.611001152522,108.656698819988));
#79747=CARTESIAN_POINT('Ctrl Pts',(12.4862824988523,779.816350545124,109.33256920393));
#79748=CARTESIAN_POINT('Ctrl Pts',(11.5286209740312,779.111784371392,106.941972898753));
#79749=CARTESIAN_POINT('Ctrl Pts',(11.50768553079,778.493617265097,108.615653000625));
#79750=CARTESIAN_POINT('Ctrl Pts',(12.635218701962,779.70012801209,109.291514647201));
#79751=CARTESIAN_POINT('Ctrl Pts',(11.9842915999363,778.754706931681,106.82514494408));
#79752=CARTESIAN_POINT('Ctrl Pts',(11.9682792420486,778.144895323507,108.494096092455));
#79753=CARTESIAN_POINT('Ctrl Pts',(13.0831312259875,779.352924298943,109.168887274619));
#79754=CARTESIAN_POINT('Ctrl Pts',(12.2881684816843,778.51861469024,106.750692042409));
#79755=CARTESIAN_POINT('Ctrl Pts',(12.2767214939561,777.916865625875,108.415119273732));
#79756=CARTESIAN_POINT('Ctrl Pts',(13.3832175329536,779.123384899081,109.087842851556));
#79757=CARTESIAN_POINT('Ctrl Pts',(13.3131173672748,777.725974089015,106.507342906962));
#79758=CARTESIAN_POINT('Ctrl Pts',(13.3177396755757,777.158567029708,108.153655030184));
#79759=CARTESIAN_POINT('Ctrl Pts',(14.3987831512332,778.352459845658,108.815709181203));
#79760=CARTESIAN_POINT('Ctrl Pts',(14.0325982015706,777.175560053502,106.349270625002));
#79761=CARTESIAN_POINT('Ctrl Pts',(14.0533667512555,776.640899205561,107.977072247212));
#79762=CARTESIAN_POINT('Ctrl Pts',(15.1179090626436,777.816088388095,108.626470714689));
#79763=CARTESIAN_POINT('Ctrl Pts',(14.7464540540325,776.626446606295,106.193899773879));
#79764=CARTESIAN_POINT('Ctrl Pts',(14.7919275351275,776.119102455067,107.799271902089));
#79765=CARTESIAN_POINT('Ctrl Pts',(15.8356919568668,777.277268015822,108.43638579439));
#79766=CARTESIAN_POINT('',(14.3866390709116,776.891105572714,106.313407256592));
#79767=CARTESIAN_POINT('Ctrl Pts',(14.3866390402624,776.891105535654,106.313407246381));
#79768=CARTESIAN_POINT('Ctrl Pts',(14.3889611516474,776.87128206777,106.378381133509));
#79769=CARTESIAN_POINT('Ctrl Pts',(14.3934547660474,776.854060889204,106.444094869398));
#79770=CARTESIAN_POINT('Ctrl Pts',(14.400093388946,776.839542736536,106.51017865051));
#79771=CARTESIAN_POINT('Ctrl Pts',(14.4069781065082,776.824486393953,106.578712166474));
#79772=CARTESIAN_POINT('Ctrl Pts',(14.416169310853,776.812336724029,106.64764312285));
#79773=CARTESIAN_POINT('Ctrl Pts',(14.4276103046054,776.80316153864,106.716583175345));
#79774=CARTESIAN_POINT('Ctrl Pts',(14.4399117991466,776.793296268593,106.790708351689));
#79775=CARTESIAN_POINT('Ctrl Pts',(14.4548137441145,776.78686922282,106.864843683666));
#79776=CARTESIAN_POINT('Ctrl Pts',(14.472222712476,776.78392174325,106.938541809043));
#79777=CARTESIAN_POINT('Ctrl Pts',(14.4758003829653,776.783316014613,106.953687313521));
#79778=CARTESIAN_POINT('Ctrl Pts',(14.4794838753247,776.782857120754,106.96881447167));
#79779=CARTESIAN_POINT('Ctrl Pts',(14.4832722978711,776.782545250895,106.983919577223));
#79780=CARTESIAN_POINT('Ctrl Pts',(14.5008198470155,776.781100704622,107.053884735218));
#79781=CARTESIAN_POINT('Ctrl Pts',(14.5206170789698,776.782814197739,107.123360471363));
#79782=CARTESIAN_POINT('Ctrl Pts',(14.5425448232576,776.787676006415,107.191926901758));
#79783=CARTESIAN_POINT('Ctrl Pts',(14.5650401209042,776.792663652742,107.262268029421));
#79784=CARTESIAN_POINT('Ctrl Pts',(14.5897774106074,776.800964417161,107.331652085065));
#79785=CARTESIAN_POINT('Ctrl Pts',(14.6166037709663,776.812526033795,107.39965284292));
#79786=CARTESIAN_POINT('Ctrl Pts',(14.6442355350974,776.824434763102,107.469695177276));
#79787=CARTESIAN_POINT('Ctrl Pts',(14.6740836141183,776.83980295605,107.538269973234));
#79788=CARTESIAN_POINT('Ctrl Pts',(14.7059579927268,776.85853302803,107.604939969069));
#79789=CARTESIAN_POINT('Ctrl Pts',(14.7090669241534,776.860359903155,107.611442760789));
#79790=CARTESIAN_POINT('Ctrl Pts',(14.7121951155176,776.862218731124,107.617927452371));
#79791=CARTESIAN_POINT('Ctrl Pts',(14.7153423794039,776.864109401912,107.624393651513));
#79792=CARTESIAN_POINT('Ctrl Pts',(14.7471339629307,776.883207710938,107.689710929489));
#79793=CARTESIAN_POINT('Ctrl Pts',(14.7808684292452,776.905555339565,107.753128713198));
#79794=CARTESIAN_POINT('Ctrl Pts',(14.8163336489197,776.931011584379,107.814248718621));
#79795=CARTESIAN_POINT('Ctrl Pts',(14.8528604552702,776.957229815458,107.877198239947));
#79796=CARTESIAN_POINT('Ctrl Pts',(14.8912233634063,776.986745851564,107.937710200034));
#79797=CARTESIAN_POINT('Ctrl Pts',(14.9311656072414,777.019362440652,107.995378735158));
#79798=CARTESIAN_POINT('Ctrl Pts',(14.968877269302,777.050157550468,108.04982676059));
#79799=CARTESIAN_POINT('Ctrl Pts',(15.0079966692538,777.083716400361,108.101740112061));
#79800=CARTESIAN_POINT('Ctrl Pts',(15.0482858219991,777.119834762961,108.150803170287));
#79801=CARTESIAN_POINT('Ctrl Pts',(15.0506688580393,777.121971103736,108.15370516817));
#79802=CARTESIAN_POINT('Ctrl Pts',(15.0530559801051,777.12411638773,108.156597202236));
#79803=CARTESIAN_POINT('Ctrl Pts',(15.0554471365295,777.126270568379,108.159479210262));
#79804=CARTESIAN_POINT('Ctrl Pts',(15.0974465589804,777.164107634247,108.210100186517));
#79805=CARTESIAN_POINT('Ctrl Pts',(15.1406848085548,777.204685542196,108.257617141791));
#79806=CARTESIAN_POINT('Ctrl Pts',(15.1848969486944,777.247755041553,108.301740662617));
#79807=CARTESIAN_POINT('Ctrl Pts',(15.2271686575255,777.288934259085,108.343927641556));
#79808=CARTESIAN_POINT('Ctrl Pts',(15.2703307319288,777.33239141631,108.38301211459));
#79809=CARTESIAN_POINT('Ctrl Pts',(15.3141296941221,777.377872296008,108.418761739622));
#79810=CARTESIAN_POINT('Ctrl Pts',(15.35581599226,777.421159383548,108.452786964257));
#79811=CARTESIAN_POINT('Ctrl Pts',(15.3980790830262,777.466279671584,108.483790788085));
#79812=CARTESIAN_POINT('Ctrl Pts',(15.4406805907297,777.512978560241,108.511598648713));
#79813=CARTESIAN_POINT('Ctrl Pts',(15.4482978589518,777.521328451589,108.516570771637));
#79814=CARTESIAN_POINT('Ctrl Pts',(15.4559258968458,777.529728716795,108.52144079969));
#79815=CARTESIAN_POINT('Ctrl Pts',(15.4635632778611,777.538177775594,108.526207848409));
#79816=CARTESIAN_POINT('Ctrl Pts',(14.3866390862365,776.891105591244,106.313407261698));
#79817=CARTESIAN_POINT('Ctrl Pts',(14.1635282499457,777.062166931795,106.362258830835));
#79818=CARTESIAN_POINT('Ctrl Pts',(13.9402770911972,777.233217022154,106.411497164547));
#79819=CARTESIAN_POINT('Ctrl Pts',(13.7171561772671,777.404295799324,106.461350719229));
#79820=CARTESIAN_POINT('Ctrl Pts',(13.5059079782952,777.566271128857,106.508551465469));
#79821=CARTESIAN_POINT('Ctrl Pts',(13.2947768511875,777.728271930287,106.556303545477));
#79822=CARTESIAN_POINT('Ctrl Pts',(13.0839822957079,777.890366583229,106.604830521648));
#79823=CARTESIAN_POINT('Ctrl Pts',(12.8883440114655,778.040806520893,106.649868375382));
#79824=CARTESIAN_POINT('Ctrl Pts',(12.6929958066475,778.191327236408,106.695573695199));
#79825=CARTESIAN_POINT('Ctrl Pts',(12.4981009461385,778.342015811371,106.742152379873));
#79826=CARTESIAN_POINT('Ctrl Pts',(12.3101448643633,778.487339469698,106.78707273869));
#79827=CARTESIAN_POINT('Ctrl Pts',(12.1226106083063,778.632819007354,106.832805230861));
#79828=CARTESIAN_POINT('Ctrl Pts',(11.9356302264546,778.778566284359,106.87956213152));
#79829=CARTESIAN_POINT('Ctrl Pts',(11.7548581546475,778.919474314193,106.924766562699));
#79830=CARTESIAN_POINT('Ctrl Pts',(11.5746039399841,779.060632360689,106.970928362183));
#79831=CARTESIAN_POINT('Ctrl Pts',(11.3949707652917,779.202177093405,107.018267738977));
#79832=CARTESIAN_POINT('Ctrl Pts',(11.2229617632804,779.337714241574,107.063597890114));
#79833=CARTESIAN_POINT('Ctrl Pts',(11.051522286338,779.47360579314,107.110007706059));
#79834=CARTESIAN_POINT('Ctrl Pts',(10.8807262369361,779.610007641348,107.15771846644));
#79835=CARTESIAN_POINT('Ctrl Pts',(10.8510478741863,779.6337094983,107.166008923149));
#79836=CARTESIAN_POINT('Ctrl Pts',(10.8213888951291,779.65742685787,107.174338733481));
#79837=CARTESIAN_POINT('Ctrl Pts',(10.791749630326,779.68116066072,107.182709152208));
#79838=CARTESIAN_POINT('Ctrl Pts',(93.9784435005612,780.377188811389,109.530513700775));
#79839=CARTESIAN_POINT('Ctrl Pts',(95.1084144693317,779.190184574876,108.861662561019));
#79840=CARTESIAN_POINT('Ctrl Pts',(95.0949273018122,779.794272325681,107.197683299583));
#79841=CARTESIAN_POINT('Ctrl Pts',(93.9029214534442,780.319268354671,109.510319941364));
#79842=CARTESIAN_POINT('Ctrl Pts',(95.0270033001491,779.15409027672,108.854135188967));
#79843=CARTESIAN_POINT('Ctrl Pts',(95.0299861041092,779.732879674436,107.2059504738));
#79844=CARTESIAN_POINT('Ctrl Pts',(93.8271635469066,780.258099564455,109.488660207096));
#79845=CARTESIAN_POINT('Ctrl Pts',(94.9497485946087,779.087848677435,108.829971302735));
#79846=CARTESIAN_POINT('Ctrl Pts',(94.9503799339584,779.670399483667,107.179461492168));
#79847=CARTESIAN_POINT('Ctrl Pts',(93.7145339590534,780.168283129866,109.456918645028));
#79848=CARTESIAN_POINT('Ctrl Pts',(94.8340030377784,778.995794648529,108.797486372228));
#79849=CARTESIAN_POINT('Ctrl Pts',(94.8347839700442,779.578107160797,107.147122444466));
#79850=CARTESIAN_POINT('Ctrl Pts',(93.6777850797537,780.139047238446,109.446587044326));
#79851=CARTESIAN_POINT('Ctrl Pts',(94.7962349321268,778.965876172659,108.786938170426));
#79852=CARTESIAN_POINT('Ctrl Pts',(94.797091755628,779.548063554189,107.13664949813));
#79853=CARTESIAN_POINT('Ctrl Pts',(93.5674424188274,780.051462002609,109.415636978074));
#79854=CARTESIAN_POINT('Ctrl Pts',(94.6828244381048,778.87637858051,108.755412779786));
#79855=CARTESIAN_POINT('Ctrl Pts',(94.6839894976143,779.458054320114,107.105430896486));
#79856=CARTESIAN_POINT('Ctrl Pts',(93.4937527041494,779.993235106026,109.395063251624));
#79857=CARTESIAN_POINT('Ctrl Pts',(94.6070763781049,778.81705748974,108.734554862737));
#79858=CARTESIAN_POINT('Ctrl Pts',(94.608553905792,779.398210244639,107.084885469161));
#79859=CARTESIAN_POINT('Ctrl Pts',(93.2723395706119,779.819001952487,109.33350570485));
#79860=CARTESIAN_POINT('Ctrl Pts',(94.3794751460829,778.640062134937,108.672427820456));
#79861=CARTESIAN_POINT('Ctrl Pts',(94.3821747887695,779.219127121472,107.023995285396));
#79862=CARTESIAN_POINT('Ctrl Pts',(93.1242721691852,779.703442160639,109.292685135209));
#79863=CARTESIAN_POINT('Ctrl Pts',(94.2272622385821,778.523350322706,108.631603283016));
#79864=CARTESIAN_POINT('Ctrl Pts',(94.2311597815261,779.10033662908,106.984396198984));
#79865=CARTESIAN_POINT('Ctrl Pts',(92.6789965002652,779.358229445953,109.170760515774));
#79866=CARTESIAN_POINT('Ctrl Pts',(93.7696917507482,778.176575029635,108.510672591972));
#79867=CARTESIAN_POINT('Ctrl Pts',(93.7780323027825,778.745482414722,106.868153397216));
#79868=CARTESIAN_POINT('Ctrl Pts',(92.3807087316349,779.130021392018,109.090185763539));
#79869=CARTESIAN_POINT('Ctrl Pts',(93.463312097639,777.949755097055,108.432064949768));
#79870=CARTESIAN_POINT('Ctrl Pts',(93.4758459227127,778.510928031655,106.794052998108));
#79871=CARTESIAN_POINT('Ctrl Pts',(91.436392783065,778.413053495081,108.837097455752));
#79872=CARTESIAN_POINT('Ctrl Pts',(92.4955494384007,777.24368808485,108.188425098313));
#79873=CARTESIAN_POINT('Ctrl Pts',(92.522429303692,777.774489190713,106.567468299851));
#79874=CARTESIAN_POINT('Ctrl Pts',(90.7875519064439,777.928254343851,108.666045113778));
#79875=CARTESIAN_POINT('Ctrl Pts',(91.8317630359771,776.774133286743,108.027925378993));
#79876=CARTESIAN_POINT('Ctrl Pts',(91.8723885912789,777.277552943272,106.423405302575));
#79877=CARTESIAN_POINT('Ctrl Pts',(90.1393011458404,777.442136168392,108.494548400935));
#79878=CARTESIAN_POINT('Ctrl Pts',(91.1655083296893,776.302751793624,107.867095841556));
#79879=CARTESIAN_POINT('Ctrl Pts',(91.2264327071444,776.782084773983,106.282319498487));
#79880=CARTESIAN_POINT('',(91.3685977607863,776.891105610866,106.313407267717));
#79881=CARTESIAN_POINT('Origin',(90.121757461417,778.398696175795,106.728810633623));
#79882=CARTESIAN_POINT('Ctrl Pts',(94.9634854797312,779.681065915379,107.182982656498));
#79883=CARTESIAN_POINT('Ctrl Pts',(94.9335364154961,779.65678741413,107.175391806428));
#79884=CARTESIAN_POINT('Ctrl Pts',(94.9028729284262,779.632469682793,107.166170964834));
#79885=CARTESIAN_POINT('Ctrl Pts',(94.8724662944701,779.608192893332,107.157664425742));
#79886=CARTESIAN_POINT('Ctrl Pts',(94.8347859453406,779.578108737883,107.147122997074));
#79887=CARTESIAN_POINT('Ctrl Pts',(94.7970943095949,779.548065586691,107.136650203078));
#79888=CARTESIAN_POINT('Ctrl Pts',(94.7593910029568,779.518060476164,107.126243297582));
#79889=CARTESIAN_POINT('Ctrl Pts',(94.6840066344572,779.458067957986,107.105435626615));
#79890=CARTESIAN_POINT('Ctrl Pts',(94.6085756769736,779.398227467302,107.084891325052));
#79891=CARTESIAN_POINT('Ctrl Pts',(94.5330942001178,779.33851587025,107.064588741239));
#79892=CARTESIAN_POINT('Ctrl Pts',(94.3823169310425,779.219239566836,107.024033518026));
#79893=CARTESIAN_POINT('Ctrl Pts',(94.2313389024036,779.100476902626,106.984442149658));
#79894=CARTESIAN_POINT('Ctrl Pts',(94.0801172886116,778.982051890961,106.945648598395));
#79895=CARTESIAN_POINT('Ctrl Pts',(93.7791781886844,778.746379783477,106.868447356408));
#79896=CARTESIAN_POINT('Ctrl Pts',(93.4772813584262,778.512036792077,106.794394137293));
#79897=CARTESIAN_POINT('Ctrl Pts',(93.1739656948357,778.277749460308,106.722309503209));
#79898=CARTESIAN_POINT('Ctrl Pts',(93.0983585117683,778.219348898419,106.704341040714));
#79899=CARTESIAN_POINT('Ctrl Pts',(93.0226642310308,778.16095067228,106.686492238259));
#79900=CARTESIAN_POINT('Ctrl Pts',(92.9468736313629,778.10253749141,106.668748929446));
#79901=CARTESIAN_POINT('Ctrl Pts',(92.6334775012801,777.860997446724,106.595379879182));
#79902=CARTESIAN_POINT('Ctrl Pts',(92.3192632623904,777.61984344963,106.524012845445));
#79903=CARTESIAN_POINT('Ctrl Pts',(92.0047568357767,777.37872161051,106.453859054074));
#79904=CARTESIAN_POINT('Ctrl Pts',(91.7927819712388,777.216207382311,106.40657594898));
#79905=CARTESIAN_POINT('Ctrl Pts',(91.580674607973,777.053707086829,106.359842876413));
#79906=CARTESIAN_POINT('Ctrl Pts',(91.3685977607864,776.891105610866,106.313407267717));
#79907=CARTESIAN_POINT('Origin',(52.8776183915471,825.72084445736,125.575299673618));
#79908=CARTESIAN_POINT('',(109.287160197048,801.327730363652,97.6776808736006));
#79909=CARTESIAN_POINT('Ctrl Pts',(94.9631204076456,779.681651525798,107.182848479366));
#79910=CARTESIAN_POINT('Ctrl Pts',(97.9566175222976,782.913141020044,105.674139401781));
#79911=CARTESIAN_POINT('Ctrl Pts',(100.611942429969,786.348058684875,104.108803322329));
#79912=CARTESIAN_POINT('Ctrl Pts',(105.362756559923,793.572374302806,100.924218762755));
#79913=CARTESIAN_POINT('Ctrl Pts',(107.456885361,797.362462511322,99.3044501680741));
#79914=CARTESIAN_POINT('Ctrl Pts',(109.287160197048,801.327730363652,97.6776808736006));
#79915=CARTESIAN_POINT('',(110.414493061984,803.264712503322,98.3625359087414));
#79916=CARTESIAN_POINT('Ctrl Pts',(109.286997799662,801.327818017083,97.6777118772549));
#79917=CARTESIAN_POINT('Ctrl Pts',(109.602099673755,801.846665738832,97.8613333644607));
#79918=CARTESIAN_POINT('Ctrl Pts',(109.909319285169,802.370215427769,98.0464022479971));
#79919=CARTESIAN_POINT('Ctrl Pts',(110.20842933104,802.89807608039,98.2329603445207));
#79920=CARTESIAN_POINT('Ctrl Pts',(110.277550970416,803.020059926052,98.2760722414585));
#79921=CARTESIAN_POINT('Ctrl Pts',(110.346239709757,803.142273864574,98.3192636277638));
#79922=CARTESIAN_POINT('Ctrl Pts',(110.414493061994,803.264712840779,98.3625349539297));
#79923=CARTESIAN_POINT('',(-4.65925699042498,803.26469939074,98.3625770753546));
#79924=CARTESIAN_POINT('Origin',(52.8776183915471,831.777100559639,108.439826246791));
#79925=CARTESIAN_POINT('',(-3.53191933480331,801.327721522442,97.6776844983083));
#79926=CARTESIAN_POINT('Ctrl Pts',(-4.65925699042498,803.264699682484,98.3625762498996));
#79927=CARTESIAN_POINT('Ctrl Pts',(-4.29564935142747,802.612431997225,98.132044141205));
#79928=CARTESIAN_POINT('Ctrl Pts',(-3.91967758749859,801.966556600686,97.9037821557117));
#79929=CARTESIAN_POINT('Ctrl Pts',(-3.53175694823092,801.327809177577,97.6777154785989));
#79930=CARTESIAN_POINT('Ctrl Pts',(-3.53191933480331,801.327721522442,97.6776844983083));
#79931=CARTESIAN_POINT('Ctrl Pts',(-1.70164478141682,797.362455407221,99.3044531792666));
#79932=CARTESIAN_POINT('Ctrl Pts',(0.39248354271191,793.572368800321,100.924221150267));
#79933=CARTESIAN_POINT('Ctrl Pts',(5.14328675973971,786.348070686369,104.108798069958));
#79934=CARTESIAN_POINT('Ctrl Pts',(7.79859897771313,782.91316749669,105.674127349588));
#79935=CARTESIAN_POINT('Ctrl Pts',(10.7920801946104,779.681690583154,107.182830244375));
#79936=CARTESIAN_POINT('Ctrl Pts',(37.9812496537119,740.125372558701,99.4034193855844));
#79937=CARTESIAN_POINT('Ctrl Pts',(37.2974432564443,740.126812599378,98.8057432472127));
#79938=CARTESIAN_POINT('Ctrl Pts',(37.2974382339422,740.125373764374,97.8975538623548));
#79939=CARTESIAN_POINT('Ctrl Pts',(37.9848781973332,741.131801150289,99.40192578217));
#79940=CARTESIAN_POINT('Ctrl Pts',(37.3009560358114,741.133144619624,98.8042413548037));
#79941=CARTESIAN_POINT('Ctrl Pts',(37.3009513751051,741.131810483968,97.8959593541246));
#79942=CARTESIAN_POINT('Ctrl Pts',(37.9866262292947,742.10800476726,99.4028220357934));
#79943=CARTESIAN_POINT('Ctrl Pts',(37.3013602990247,742.104570379522,98.8049161509109));
#79944=CARTESIAN_POINT('Ctrl Pts',(37.3017025845383,742.109496105312,97.8954725494215));
#79945=CARTESIAN_POINT('Ctrl Pts',(37.932153261221,744.017093575077,99.4504961368679));
#79946=CARTESIAN_POINT('Ctrl Pts',(37.2320445091758,743.994011092838,98.8508878191548));
#79947=CARTESIAN_POINT('Ctrl Pts',(37.2320605227026,744.020040901463,97.9291756497104));
#79948=CARTESIAN_POINT('Ctrl Pts',(37.8766679946406,744.950872239177,99.4961335269924));
#79949=CARTESIAN_POINT('Ctrl Pts',(37.1633838585167,744.915439122629,98.8953866888645));
#79950=CARTESIAN_POINT('Ctrl Pts',(37.1628307039845,744.953765972469,97.9629589076155));
#79951=CARTESIAN_POINT('Ctrl Pts',(37.6873075163571,746.798808429708,99.6375574552887));
#79952=CARTESIAN_POINT('Ctrl Pts',(36.9403996269704,746.729163892062,99.0355904635441));
#79953=CARTESIAN_POINT('Ctrl Pts',(36.9342019053666,746.7964768367,98.076166342412));
#79954=CARTESIAN_POINT('Ctrl Pts',(37.5538636559385,747.712920381025,99.7328632917094));
#79955=CARTESIAN_POINT('Ctrl Pts',(36.7859775201029,747.62350503362,99.1313049156982));
#79956=CARTESIAN_POINT('Ctrl Pts',(36.7753843913839,747.705400843227,98.1553201925244));
#79957=CARTESIAN_POINT('Ctrl Pts',(37.2017809758576,749.533161016737,99.9688263843864));
#79958=CARTESIAN_POINT('Ctrl Pts',(36.3903788991122,749.39639674591,99.3709651407066));
#79959=CARTESIAN_POINT('Ctrl Pts',(36.3652226953077,749.50796954038,98.3603489337074));
#79960=CARTESIAN_POINT('Ctrl Pts',(36.9833127647707,750.439165145003,100.109343103989));
#79961=CARTESIAN_POINT('Ctrl Pts',(36.148555591448,750.275876693628,99.5152612287328));
#79962=CARTESIAN_POINT('Ctrl Pts',(36.1141069873064,750.401487464794,98.4860982992872));
#79963=CARTESIAN_POINT('Ctrl Pts',(36.4594369785795,752.247460839569,100.429869034596));
#79964=CARTESIAN_POINT('Ctrl Pts',(35.5806904318709,752.02583524078,99.8466826136125));
#79965=CARTESIAN_POINT('Ctrl Pts',(35.522610606527,752.177098593973,98.781314739587));
#79966=CARTESIAN_POINT('Ctrl Pts',(36.1573629783603,753.137997262295,100.607797664768));
#79967=CARTESIAN_POINT('Ctrl Pts',(35.2576419586772,752.884926267611,100.031972820423));
#79968=CARTESIAN_POINT('Ctrl Pts',(35.1860607782106,753.047665087694,98.9488503591591));
#79969=CARTESIAN_POINT('Ctrl Pts',(35.4833922952658,754.885078669401,100.989350703394));
#79970=CARTESIAN_POINT('Ctrl Pts',(34.5471212341506,754.568275972171,100.430525778272));
#79971=CARTESIAN_POINT('Ctrl Pts',(34.446248605843,754.749366369677,99.3142469989865));
#79972=CARTESIAN_POINT('Ctrl Pts',(35.1109298655096,755.743586990137,101.193363601259));
#79973=CARTESIAN_POINT('Ctrl Pts',(34.1586862018381,755.393720711171,100.644289501562));
#79974=CARTESIAN_POINT('Ctrl Pts',(34.0423388546041,755.582452785822,99.5124350021307));
#79975=CARTESIAN_POINT('Ctrl Pts',(33.8962272695194,758.278760713144,101.836914643919));
#79976=CARTESIAN_POINT('Ctrl Pts',(32.8995224205562,757.840128068945,101.321091231123));
#79977=CARTESIAN_POINT('Ctrl Pts',(32.7411531447682,758.03610031727,100.143047832541));
#79978=CARTESIAN_POINT('Ctrl Pts',(32.9572524321006,759.915278556649,102.307851274058));
#79979=CARTESIAN_POINT('Ctrl Pts',(31.9441149171027,759.409670588889,101.814372592625));
#79980=CARTESIAN_POINT('Ctrl Pts',(31.7554250151974,759.611504553537,100.61146803336));
#79981=CARTESIAN_POINT('Ctrl Pts',(30.8570361245727,763.093346528461,103.30000026461));
#79982=CARTESIAN_POINT('Ctrl Pts',(29.825466232898,762.462865228477,102.845341032932));
#79983=CARTESIAN_POINT('Ctrl Pts',(29.5870230864445,762.666413683269,101.592593895766));
#79984=CARTESIAN_POINT('Ctrl Pts',(29.7125386287475,764.609757915344,103.813459947128));
#79985=CARTESIAN_POINT('Ctrl Pts',(28.6759889607061,763.920191194033,103.375458895112));
#79986=CARTESIAN_POINT('Ctrl Pts',(28.421165172366,764.121697471862,102.097362675171));
#79987=CARTESIAN_POINT('Ctrl Pts',(27.2672007424541,767.51635281373,104.842469498997));
#79988=CARTESIAN_POINT('Ctrl Pts',(26.225714610018,766.706197784119,104.425707712909));
#79989=CARTESIAN_POINT('Ctrl Pts',(25.9520288338402,766.91296491144,103.085302829331));
#79990=CARTESIAN_POINT('Ctrl Pts',(25.9651032199003,768.907107240029,105.358419148589));
#79991=CARTESIAN_POINT('Ctrl Pts',(24.9148601580403,768.039581315371,104.948653383042));
#79992=CARTESIAN_POINT('Ctrl Pts',(24.6473500139942,768.249130815112,103.568680493393));
#79993=CARTESIAN_POINT('Ctrl Pts',(23.2176003801495,771.582105405033,106.362164464073));
#79994=CARTESIAN_POINT('Ctrl Pts',(22.1528427787513,770.579303463978,105.9503202526));
#79995=CARTESIAN_POINT('Ctrl Pts',(21.9084442478426,770.82737375778,104.47103030333));
#79996=CARTESIAN_POINT('Ctrl Pts',(21.7706855706201,772.865970272614,106.849323966766));
#79997=CARTESIAN_POINT('Ctrl Pts',(20.6827182904449,771.793794132029,106.432116222091));
#79998=CARTESIAN_POINT('Ctrl Pts',(20.4732983628028,772.068583075469,104.888224483132));
#79999=CARTESIAN_POINT('Ctrl Pts',(19.5143472122575,774.730385301656,107.538946728448));
#80000=CARTESIAN_POINT('Ctrl Pts',(18.4132817282156,773.523297302945,107.095600274954));
#80001=CARTESIAN_POINT('Ctrl Pts',(18.2396670183582,773.892291450409,105.45248981662));
#80002=CARTESIAN_POINT('Ctrl Pts',(18.7480232299384,775.341818771779,107.762053723911));
#80003=CARTESIAN_POINT('Ctrl Pts',(17.6323627611125,774.094371854445,107.310495542271));
#80004=CARTESIAN_POINT('Ctrl Pts',(17.4816920982757,774.494237769663,105.630707165859));
#80005=CARTESIAN_POINT('Ctrl Pts',(17.1984668818591,776.548230578555,108.195765565376));
#80006=CARTESIAN_POINT('Ctrl Pts',(16.049679031786,775.22424377604,107.7256534537));
#80007=CARTESIAN_POINT('Ctrl Pts',(15.9460577282015,775.693942761,105.975651051878));
#80008=CARTESIAN_POINT('Ctrl Pts',(16.4159441921319,777.142527752461,108.406078863569));
#80009=CARTESIAN_POINT('Ctrl Pts',(15.2486973592712,775.781848806884,107.925169073805));
#80010=CARTESIAN_POINT('Ctrl Pts',(15.1690942862755,776.291189365633,106.142083265953));
#80011=CARTESIAN_POINT('Ctrl Pts',(15.6333869345031,777.732299565987,108.614524175997));
#80012=CARTESIAN_POINT('Ctrl Pts',(14.451947512053,776.338746499521,108.121995372869));
#80013=CARTESIAN_POINT('Ctrl Pts',(14.386546670293,776.891176447478,106.31342749679));
#80014=CARTESIAN_POINT('',(37.9809447552159,740.125373764374,99.4032758153525));
#80015=CARTESIAN_POINT('Ctrl Pts',(18.0556461947237,775.880814855153,107.955813432072));
#80016=CARTESIAN_POINT('Ctrl Pts',(18.6359399718752,775.428232050397,107.792932399321));
#80017=CARTESIAN_POINT('Ctrl Pts',(19.2109756852516,774.971301297233,107.626641737905));
#80018=CARTESIAN_POINT('Ctrl Pts',(19.7787947443054,774.508909152344,107.456599405267));
#80019=CARTESIAN_POINT('Ctrl Pts',(19.9419616392958,774.376037440226,107.407736516656));
#80020=CARTESIAN_POINT('Ctrl Pts',(20.1045324232678,774.242714570337,107.358563696084));
#80021=CARTESIAN_POINT('Ctrl Pts',(20.2664599983784,774.108913625309,107.309072474554));
#80022=CARTESIAN_POINT('Ctrl Pts',(20.7762113255627,773.687705506431,107.153273094234));
#80023=CARTESIAN_POINT('Ctrl Pts',(21.2795378908958,773.261673546964,106.994279935223));
#80024=CARTESIAN_POINT('Ctrl Pts',(21.776120368853,772.830028841967,106.832474695738));
#80025=CARTESIAN_POINT('Ctrl Pts',(21.901530240627,772.721018738896,106.791611444945));
#80026=CARTESIAN_POINT('Ctrl Pts',(22.026509775505,772.611650510322,106.750568787163));
#80027=CARTESIAN_POINT('Ctrl Pts',(22.1510534016441,772.501911135818,106.70935277429));
#80028=CARTESIAN_POINT('Ctrl Pts',(22.7300047215739,771.991778600838,106.517756738467));
#80029=CARTESIAN_POINT('Ctrl Pts',(23.299430327368,771.473724094565,106.322450258449));
#80030=CARTESIAN_POINT('Ctrl Pts',(23.8584057417782,770.946731145025,106.124160150832));
#80031=CARTESIAN_POINT('Ctrl Pts',(24.1047781349485,770.714455250925,106.0367623743));
#80032=CARTESIAN_POINT('Ctrl Pts',(24.3491198830283,770.480442524666,105.948785039611));
#80033=CARTESIAN_POINT('Ctrl Pts',(24.5913492318159,770.244603979373,105.860290778658));
#80034=CARTESIAN_POINT('Ctrl Pts',(25.0521007996099,769.796008546848,105.691963242467));
#80035=CARTESIAN_POINT('Ctrl Pts',(25.5053803166802,769.34085066765,105.521836468159));
#80036=CARTESIAN_POINT('Ctrl Pts',(25.9509163291252,768.878635306682,105.350453253166));
#80037=CARTESIAN_POINT('Ctrl Pts',(26.5018720881807,768.30705364339,105.138518489941));
#80038=CARTESIAN_POINT('Ctrl Pts',(27.0409759418072,767.724707271522,104.924672333782));
#80039=CARTESIAN_POINT('Ctrl Pts',(27.5676119325008,767.130683387953,104.709978953184));
#80040=CARTESIAN_POINT('Ctrl Pts',(27.8794361966021,766.778958356572,104.582857741198));
#80041=CARTESIAN_POINT('Ctrl Pts',(28.1868887145181,766.423138784951,104.455439922943));
#80042=CARTESIAN_POINT('Ctrl Pts',(28.4898357301289,766.063030294278,104.327950500425));
#80043=CARTESIAN_POINT('Ctrl Pts',(28.8000158409975,765.69432393374,104.197417168939));
#80044=CARTESIAN_POINT('Ctrl Pts',(29.1055538570495,765.321084701143,104.066782989571));
#80045=CARTESIAN_POINT('Ctrl Pts',(29.4061629237366,764.943095807458,103.936306435134));
#80046=CARTESIAN_POINT('Ctrl Pts',(29.7677270420684,764.488461412724,103.779372910514));
#80047=CARTESIAN_POINT('Ctrl Pts',(30.1222178891466,764.026933172879,103.622662560985));
#80048=CARTESIAN_POINT('Ctrl Pts',(30.469238091311,763.557975992853,103.466594024389));
#80049=CARTESIAN_POINT('Ctrl Pts',(30.6453260113138,763.320013782336,103.387400410254));
#80050=CARTESIAN_POINT('Ctrl Pts',(30.8194897665024,763.080138267366,103.308372271751));
#80051=CARTESIAN_POINT('Ctrl Pts',(30.9916735359252,762.838276475935,103.229565859888));
#80052=CARTESIAN_POINT('Ctrl Pts',(31.3035038206331,762.400257076461,103.086844940661));
#80053=CARTESIAN_POINT('Ctrl Pts',(31.6088768919138,761.955597818807,102.944803289155));
#80054=CARTESIAN_POINT('Ctrl Pts',(31.9071207213202,761.504299136386,102.8039146946));
#80055=CARTESIAN_POINT('Ctrl Pts',(32.098100365209,761.215311223952,102.71369705734));
#80056=CARTESIAN_POINT('Ctrl Pts',(32.2856033689663,760.924432957779,102.62420875733));
#80057=CARTESIAN_POINT('Ctrl Pts',(32.4694461051648,760.631695630178,102.535578116741));
#80058=CARTESIAN_POINT('Ctrl Pts',(32.7850951211746,760.129079909168,102.383403627454));
#80059=CARTESIAN_POINT('Ctrl Pts',(33.0901687852529,759.620779524475,102.233712226929));
#80060=CARTESIAN_POINT('Ctrl Pts',(33.384057549731,759.106366696422,102.087002002915));
#80061=CARTESIAN_POINT('Ctrl Pts',(33.6704511511639,758.605073145063,101.944033388593));
#80062=CARTESIAN_POINT('Ctrl Pts',(33.9462231170835,758.097974964884,101.803895702305));
#80063=CARTESIAN_POINT('Ctrl Pts',(34.210766568814,757.584662151294,101.667069515409));
#80064=CARTESIAN_POINT('Ctrl Pts',(34.380532980657,757.255252090504,101.579263558984));
#80065=CARTESIAN_POINT('Ctrl Pts',(34.5456743815257,756.923282422653,101.492821749334));
#80066=CARTESIAN_POINT('Ctrl Pts',(34.7060206085897,756.588641542112,101.40787591758));
#80067=CARTESIAN_POINT('Ctrl Pts',(34.804502824199,756.383110199388,101.355703478783));
#80068=CARTESIAN_POINT('Ctrl Pts',(34.9011674635956,756.17656816369,101.304097107596));
#80069=CARTESIAN_POINT('Ctrl Pts',(34.9959622034492,755.968977218687,101.253097355651));
#80070=CARTESIAN_POINT('Ctrl Pts',(35.2891642151148,755.326894305936,101.095354110744));
#80071=CARTESIAN_POINT('Ctrl Pts',(35.5645845671724,754.674582533358,100.94337441152));
#80072=CARTESIAN_POINT('Ctrl Pts',(35.8203705047122,754.011535722312,100.798569763282));
#80073=CARTESIAN_POINT('Ctrl Pts',(35.8858189728303,753.841880586103,100.761518303398));
#80074=CARTESIAN_POINT('Ctrl Pts',(35.9500034519668,753.671448552098,100.724922033871));
#80075=CARTESIAN_POINT('Ctrl Pts',(36.0128772187498,753.500267400008,100.688820064372));
#80076=CARTESIAN_POINT('Ctrl Pts',(36.1327878772717,753.173796667875,100.619967645342));
#80077=CARTESIAN_POINT('Ctrl Pts',(36.2479329813418,752.844593841339,100.552907119306));
#80078=CARTESIAN_POINT('Ctrl Pts',(36.3580946322322,752.512498828401,100.487847755715));
#80079=CARTESIAN_POINT('Ctrl Pts',(36.3896867780702,752.417260657984,100.469190038751));
#80080=CARTESIAN_POINT('Ctrl Pts',(36.4208687868851,752.321784548089,100.450697037795));
#80081=CARTESIAN_POINT('Ctrl Pts',(36.4516348136901,752.226066545188,100.432374031466));
#80082=CARTESIAN_POINT('Ctrl Pts',(36.5455194837096,751.933976403869,100.376460103615));
#80083=CARTESIAN_POINT('Ctrl Pts',(36.6355420462419,751.639583202857,100.32212010209));
#80084=CARTESIAN_POINT('Ctrl Pts',(36.7213730733827,751.343312580103,100.269604830608));
#80085=CARTESIAN_POINT('Ctrl Pts',(36.7617470615855,751.203950078844,100.244902214062));
#80086=CARTESIAN_POINT('Ctrl Pts',(36.8011148436526,751.064451733841,100.220652624616));
#80087=CARTESIAN_POINT('Ctrl Pts',(36.839467518245,750.924843089873,100.196873854367));
#80088=CARTESIAN_POINT('Ctrl Pts',(36.9440720163877,750.544069329141,100.132018760044));
#80089=CARTESIAN_POINT('Ctrl Pts',(37.041311835785,750.161767483015,100.070543566056));
#80090=CARTESIAN_POINT('Ctrl Pts',(37.1310665907186,749.778084619037,100.012767251748));
#80091=CARTESIAN_POINT('Ctrl Pts',(37.2208213456522,749.394401755058,99.9549909374389));
#80092=CARTESIAN_POINT('Ctrl Pts',(37.3030910876506,749.009337679417,99.9009137567967));
#80093=CARTESIAN_POINT('Ctrl Pts',(37.3778087353439,748.623038694641,99.8508345064501));
#80094=CARTESIAN_POINT('Ctrl Pts',(37.450080637764,748.249384499219,99.8023945085907));
#80095=CARTESIAN_POINT('Ctrl Pts',(37.5152581745136,747.874595933607,99.7577188420942));
#80096=CARTESIAN_POINT('Ctrl Pts',(37.5735213054274,747.498556700093,99.7169961397917));
#80097=CARTESIAN_POINT('Ctrl Pts',(37.6323548151807,747.118836153572,99.6758747742641));
#80098=CARTESIAN_POINT('Ctrl Pts',(37.6841380810966,746.737839878748,99.6387843384986));
#80099=CARTESIAN_POINT('Ctrl Pts',(37.7291029119305,746.355452828044,99.6058939719244));
#80100=CARTESIAN_POINT('Ctrl Pts',(37.7479124219616,746.195494190758,99.592135403983));
#80101=CARTESIAN_POINT('Ctrl Pts',(37.7655293233452,746.035292279684,99.5791114827409));
#80102=CARTESIAN_POINT('Ctrl Pts',(37.7819728263361,745.874839208236,99.5668331851581));
#80103=CARTESIAN_POINT('Ctrl Pts',(37.7913011847699,745.783814579051,99.5598677374143));
#80104=CARTESIAN_POINT('Ctrl Pts',(37.800247750642,745.692709568112,99.5531469001629));
#80105=CARTESIAN_POINT('Ctrl Pts',(37.8088230074611,745.601517934398,99.5466675895096));
#80106=CARTESIAN_POINT('Ctrl Pts',(37.8378956419644,745.292351562745,99.5247008269473));
#80107=CARTESIAN_POINT('Ctrl Pts',(37.8626795852361,744.982343338724,99.5055209995584));
#80108=CARTESIAN_POINT('Ctrl Pts',(37.8835913732746,744.671551091498,99.4890037412289));
#80109=CARTESIAN_POINT('Ctrl Pts',(37.9046205324492,744.359014467413,99.4723937768443));
#80110=CARTESIAN_POINT('Ctrl Pts',(37.9217347366429,744.045684201553,99.4584761186185));
#80111=CARTESIAN_POINT('Ctrl Pts',(37.935389011644,743.73165097331,99.4470976139473));
#80112=CARTESIAN_POINT('Ctrl Pts',(37.9450719184635,743.508954822322,99.439028565941));
#80113=CARTESIAN_POINT('Ctrl Pts',(37.9530155354597,743.28590580784,99.4322358706036));
#80114=CARTESIAN_POINT('Ctrl Pts',(37.9593883250465,743.062549141665,99.4266578585726));
#80115=CARTESIAN_POINT('Ctrl Pts',(37.9611590765629,743.000486970937,99.4251079449706));
#80116=CARTESIAN_POINT('Ctrl Pts',(37.9628054655143,742.938397342271,99.4236565976025));
#80117=CARTESIAN_POINT('Ctrl Pts',(37.9643355819159,742.876282072794,99.4222976730097));
#80118=CARTESIAN_POINT('Ctrl Pts',(37.9711642729064,742.599070495545,99.4162329866146));
#80119=CARTESIAN_POINT('Ctrl Pts',(37.9756774229465,742.321457256423,99.4120103254435));
#80120=CARTESIAN_POINT('Ctrl Pts',(37.9785774429603,742.04357831077,99.4090836139286));
#80121=CARTESIAN_POINT('Ctrl Pts',(37.9813521913033,741.777702854617,99.4062833270727));
#80122=CARTESIAN_POINT('Ctrl Pts',(37.9826505919109,741.51158419174,99.4046691230041));
#80123=CARTESIAN_POINT('Ctrl Pts',(37.9830568749844,741.245367381578,99.4037857245824));
#80124=CARTESIAN_POINT('Ctrl Pts',(37.9834441189532,740.991625936664,99.4029437236892));
#80125=CARTESIAN_POINT('Ctrl Pts',(37.9830211040447,740.737795411156,99.4027654800549));
#80126=CARTESIAN_POINT('Ctrl Pts',(37.9822605484979,740.484024606801,99.4028814909415));
#80127=CARTESIAN_POINT('Ctrl Pts',(37.9819021957661,740.364454824696,99.4029361520616));
#80128=CARTESIAN_POINT('Ctrl Pts',(37.9814683990284,740.244898636289,99.4030565185439));
#80129=CARTESIAN_POINT('Ctrl Pts',(37.9810056935186,740.125373441235,99.4032061173321));
#80130=CARTESIAN_POINT('',(37.2974382384014,740.125373959151,97.8976768136687));
#80131=CARTESIAN_POINT('Ctrl Pts',(37.2974382384014,740.125373959151,97.8976768136687));
#80132=CARTESIAN_POINT('Ctrl Pts',(37.2983318605475,740.381377378649,97.8972387441088));
#80133=CARTESIAN_POINT('Ctrl Pts',(37.2990577839814,740.637542123138,97.8968757675639));
#80134=CARTESIAN_POINT('Ctrl Pts',(37.2990427906181,740.89368310615,97.8968686277991));
#80135=CARTESIAN_POINT('Ctrl Pts',(37.2990273004109,741.158311982312,97.8968612514397));
#80136=CARTESIAN_POINT('Ctrl Pts',(37.2982206538606,741.422915451805,97.8972338428727));
#80137=CARTESIAN_POINT('Ctrl Pts',(37.2959428630901,741.687311531574,97.8983197957206));
#80138=CARTESIAN_POINT('Ctrl Pts',(37.2935027332017,741.970551232522,97.8994831448904));
#80139=CARTESIAN_POINT('Ctrl Pts',(37.289373995854,742.253552746991,97.9014653049404));
#80140=CARTESIAN_POINT('Ctrl Pts',(37.2826709803646,742.536119324456,97.904700903467));
#80141=CARTESIAN_POINT('Ctrl Pts',(37.2787647974619,742.700785023872,97.9065864488107));
#80142=CARTESIAN_POINT('Ctrl Pts',(37.2739834986708,742.865303533007,97.9088981060954));
#80143=CARTESIAN_POINT('Ctrl Pts',(37.2681456938219,743.02964000767,97.9117249392825));
#80144=CARTESIAN_POINT('Ctrl Pts',(37.2677296940343,743.041350563318,97.9119263783568));
#80145=CARTESIAN_POINT('Ctrl Pts',(37.2673083352308,743.05305998757,97.9121304239047));
#80146=CARTESIAN_POINT('Ctrl Pts',(37.2668815517067,743.064768267401,97.912337108483));
#80147=CARTESIAN_POINT('Ctrl Pts',(37.2549444530568,743.392247852373,97.9181180584528));
#80148=CARTESIAN_POINT('Ctrl Pts',(37.2388984624568,743.71892997045,97.9259165344839));
#80149=CARTESIAN_POINT('Ctrl Pts',(37.2182112729509,744.044672112233,97.9360228946803));
#80150=CARTESIAN_POINT('Ctrl Pts',(37.1978608651249,744.365111262726,97.9459647261492));
#80151=CARTESIAN_POINT('Ctrl Pts',(37.1730184144701,744.68464151184,97.9581403117403));
#80152=CARTESIAN_POINT('Ctrl Pts',(37.1432044022258,745.003166375805,97.9728135962615));
#80153=CARTESIAN_POINT('Ctrl Pts',(37.1159189644583,745.294676632188,97.9862424158504));
#80154=CARTESIAN_POINT('Ctrl Pts',(37.084469352093,745.585345608254,98.0017633380483));
#80155=CARTESIAN_POINT('Ctrl Pts',(37.048516313891,745.875121266209,98.019564990037));
#80156=CARTESIAN_POINT('Ctrl Pts',(37.0475376309818,745.883009291759,98.0200495714085));
#80157=CARTESIAN_POINT('Ctrl Pts',(37.0465556556594,745.890896651898,98.0205358219973));
#80158=CARTESIAN_POINT('Ctrl Pts',(37.0455703870231,745.898783342991,98.0210237422502));
#80159=CARTESIAN_POINT('Ctrl Pts',(37.0005242361305,746.259360208962,98.0433312922155));
#80160=CARTESIAN_POINT('Ctrl Pts',(36.9485888662299,746.61854987502,98.0691300902769));
#80161=CARTESIAN_POINT('Ctrl Pts',(36.8896598941157,746.976332159384,98.0984675551207));
#80162=CARTESIAN_POINT('Ctrl Pts',(36.8310145410884,747.332392474381,98.1276638217611));
#80163=CARTESIAN_POINT('Ctrl Pts',(36.7654426559371,747.687059243834,98.1603648150365));
#80164=CARTESIAN_POINT('Ctrl Pts',(36.6928858986749,748.040325201541,98.1965946320511));
#80165=CARTESIAN_POINT('Ctrl Pts',(36.6540288333409,748.229513347716,98.2159971580169));
#80166=CARTESIAN_POINT('Ctrl Pts',(36.6131692518367,748.418299923063,98.2364113721441));
#80167=CARTESIAN_POINT('Ctrl Pts',(36.5703036120726,748.606684822443,98.2578382276742));
#80168=CARTESIAN_POINT('Ctrl Pts',(36.5622919438916,748.641894312199,98.2618429470162));
#80169=CARTESIAN_POINT('Ctrl Pts',(36.5542105589542,748.677089578501,98.2658828432146));
#80170=CARTESIAN_POINT('Ctrl Pts',(36.5460596373825,748.712270459513,98.2699577847131));
#80171=CARTESIAN_POINT('Ctrl Pts',(36.4518792628445,749.118770328411,98.3170419718421));
#80172=CARTESIAN_POINT('Ctrl Pts',(36.3484727645248,749.523118577006,98.3687797969891));
#80173=CARTESIAN_POINT('Ctrl Pts',(36.2359718696286,749.925751497935,98.4250421952344));
#80174=CARTESIAN_POINT('Ctrl Pts',(36.1220206095073,750.333575175681,98.4820299301625));
#80175=CARTESIAN_POINT('Ctrl Pts',(35.9987389341516,750.739638875786,98.5436597116707));
#80176=CARTESIAN_POINT('Ctrl Pts',(35.8662168994976,751.144387313592,98.6098212405897));
#80177=CARTESIAN_POINT('Ctrl Pts',(35.8503959760103,751.192707535077,98.6177198250747));
#80178=CARTESIAN_POINT('Ctrl Pts',(35.8344433014094,751.241009002355,98.6256830246782));
#80179=CARTESIAN_POINT('Ctrl Pts',(35.8183589852451,751.28929246544,98.6337106734054));
#80180=CARTESIAN_POINT('Ctrl Pts',(35.7985042220638,751.348894422736,98.6436201443927));
#80181=CARTESIAN_POINT('Ctrl Pts',(35.7784661312112,751.408416995377,98.6536191168439));
#80182=CARTESIAN_POINT('Ctrl Pts',(35.7582467256096,751.46786022694,98.6637062638557));
#80183=CARTESIAN_POINT('Ctrl Pts',(35.6169690124689,751.883203980482,98.7341875178566));
#80184=CARTESIAN_POINT('Ctrl Pts',(35.4672072907378,752.293604308015,98.8087915984105));
#80185=CARTESIAN_POINT('Ctrl Pts',(35.3097956950983,752.699018411369,98.8869972042913));
#80186=CARTESIAN_POINT('Ctrl Pts',(35.1526148447416,753.103838229457,98.9650881707481));
#80187=CARTESIAN_POINT('Ctrl Pts',(34.9878061137368,753.503686549661,99.0467703748835));
#80188=CARTESIAN_POINT('Ctrl Pts',(34.8161547712006,753.898515570349,99.1315496716264));
#80189=CARTESIAN_POINT('Ctrl Pts',(34.6273932430672,754.332701101294,99.2247797586786));
#80190=CARTESIAN_POINT('Ctrl Pts',(34.4301879091346,754.76132641945,99.3218404923965));
#80191=CARTESIAN_POINT('Ctrl Pts',(34.2251022209785,755.184974100915,99.4222726360482));
#80192=CARTESIAN_POINT('Ctrl Pts',(34.026814638703,755.594578862951,99.5193756914906));
#80193=CARTESIAN_POINT('Ctrl Pts',(33.8211599493022,755.999530207921,99.6196307211958));
#80194=CARTESIAN_POINT('Ctrl Pts',(33.6086106613834,756.400334739729,99.7226425127427));
#80195=CARTESIAN_POINT('Ctrl Pts',(33.5646169352091,756.483293779463,99.7439640264227));
#80196=CARTESIAN_POINT('Ctrl Pts',(33.5203303039215,756.566076272598,99.7654035652552));
#80197=CARTESIAN_POINT('Ctrl Pts',(33.4757529967058,756.648685564578,99.7869579643792));
#80198=CARTESIAN_POINT('Ctrl Pts',(33.2095740132058,757.14196025388,99.9156630927762));
#80199=CARTESIAN_POINT('Ctrl Pts',(32.9332035131286,757.628747618622,100.048378087605));
#80200=CARTESIAN_POINT('Ctrl Pts',(32.6472123512702,758.109614982728,100.184390926258));
#80201=CARTESIAN_POINT('Ctrl Pts',(32.3393089393483,758.627325743886,100.33082488182));
#80202=CARTESIAN_POINT('Ctrl Pts',(32.0202543965417,759.13817469299,100.481081454425));
#80203=CARTESIAN_POINT('Ctrl Pts',(31.6907105830928,759.642842532214,100.634303710862));
#80204=CARTESIAN_POINT('Ctrl Pts',(31.3611667696439,760.147510371438,100.787525967299));
#80205=CARTESIAN_POINT('Ctrl Pts',(31.0211333110752,760.64599686594,100.943714382247));
#80206=CARTESIAN_POINT('Ctrl Pts',(30.6712252726902,761.138957940082,101.102037752359));
#80207=CARTESIAN_POINT('Ctrl Pts',(30.611648803568,761.222891079623,101.128994399066));
#80208=CARTESIAN_POINT('Ctrl Pts',(30.5518367470566,761.306590851968,101.15598902283));
#80209=CARTESIAN_POINT('Ctrl Pts',(30.4917908266565,761.390060526202,101.183017748532));
#80210=CARTESIAN_POINT('Ctrl Pts',(30.1140681869024,761.915131763029,101.353043647931));
#80211=CARTESIAN_POINT('Ctrl Pts',(29.7273147134851,762.430793603965,101.52431280613));
#80212=CARTESIAN_POINT('Ctrl Pts',(29.3320083504767,762.937818247023,101.695852328439));
#80213=CARTESIAN_POINT('Ctrl Pts',(28.9175690820682,763.469382982118,101.875694397228));
#80214=CARTESIAN_POINT('Ctrl Pts',(28.4937289681027,763.991454179029,102.05583405897));
#80215=CARTESIAN_POINT('Ctrl Pts',(28.0609982131296,764.504885059978,102.235171026141));
#80216=CARTESIAN_POINT('Ctrl Pts',(27.7734124900033,764.846102755915,102.354355416884));
#80217=CARTESIAN_POINT('Ctrl Pts',(27.4818991808668,765.183503509633,102.473185705651));
#80218=CARTESIAN_POINT('Ctrl Pts',(27.1865989652666,765.517329651811,102.591342117818));
#80219=CARTESIAN_POINT('Ctrl Pts',(27.1237204576095,765.58841151538,102.61650125579));
#80220=CARTESIAN_POINT('Ctrl Pts',(27.0606665961456,765.659331758786,102.641630381738));
#80221=CARTESIAN_POINT('Ctrl Pts',(26.9974376972065,765.730092673734,102.666726864875));
#80222=CARTESIAN_POINT('Ctrl Pts',(26.3736370873112,766.428202282502,102.914322533149));
#80223=CARTESIAN_POINT('Ctrl Pts',(25.7329957515788,767.110586820099,103.158643462115));
#80224=CARTESIAN_POINT('Ctrl Pts',(25.0762978115619,767.778941189329,103.397017695192));
#80225=CARTESIAN_POINT('Ctrl Pts',(24.4894741349809,768.376181022608,103.610028328136));
#80226=CARTESIAN_POINT('Ctrl Pts',(23.8898288617463,768.962217177825,103.818291018878));
#80227=CARTESIAN_POINT('Ctrl Pts',(23.2779107817818,769.538240064334,104.01992680827));
#80228=CARTESIAN_POINT('Ctrl Pts',(23.2208829292338,769.591922655701,104.038718304129));
#80229=CARTESIAN_POINT('Ctrl Pts',(23.1637468817857,769.645516760381,104.0574491783));
#80230=CARTESIAN_POINT('Ctrl Pts',(23.1065035427576,769.699024062558,104.076118974889));
#80231=CARTESIAN_POINT('Ctrl Pts',(22.521837427674,770.245531429594,104.26680661866));
#80232=CARTESIAN_POINT('Ctrl Pts',(21.9259462054306,770.783010238342,104.451060584945));
#80233=CARTESIAN_POINT('Ctrl Pts',(21.3201444618659,771.312948153102,104.628323437275));
#80234=CARTESIAN_POINT('Ctrl Pts',(20.7202763727252,771.837695477895,104.803850050778));
#80235=CARTESIAN_POINT('Ctrl Pts',(20.1106918453103,772.355050307892,104.972521471847));
#80236=CARTESIAN_POINT('Ctrl Pts',(19.492693694308,772.866451768922,105.133838046219));
#80237=CARTESIAN_POINT('Ctrl Pts',(19.3238196104963,773.006197256917,105.177919389595));
#80238=CARTESIAN_POINT('Ctrl Pts',(19.1543173848269,773.145498103519,105.221451797222));
#80239=CARTESIAN_POINT('Ctrl Pts',(18.9842138166466,773.28438339178,105.264425669065));
#80240=CARTESIAN_POINT('Ctrl Pts',(18.9443923702578,773.316896601937,105.274485903263));
#80241=CARTESIAN_POINT('Ctrl Pts',(18.9045381239163,773.349388165791,105.284516625319));
#80242=CARTESIAN_POINT('Ctrl Pts',(18.8646517458932,773.38185861452,105.294518478373));
#80243=CARTESIAN_POINT('Ctrl Pts',(18.285662894482,773.853198173206,105.439704922939));
#80244=CARTESIAN_POINT('Ctrl Pts',(17.699937037803,774.32007178252,105.578734506063));
#80245=CARTESIAN_POINT('Ctrl Pts',(17.1099015562802,774.783789023184,105.713499937743));
#80246=CARTESIAN_POINT('Ctrl Pts',(16.9780991288093,774.887374417441,105.74360390876));
#80247=CARTESIAN_POINT('Ctrl Pts',(16.8460816480295,774.990802127088,105.773495035281));
#80248=CARTESIAN_POINT('Ctrl Pts',(16.7138761071789,775.094086374212,105.803194238856));
#80249=CARTESIAN_POINT('Ctrl Pts',(16.6899503361007,775.11277814187,105.808569023766));
#80250=CARTESIAN_POINT('Ctrl Pts',(16.6660190814303,775.131464713226,105.813937236859));
#80251=CARTESIAN_POINT('Ctrl Pts',(16.6420825015631,775.150146217236,105.819299208366));
#80252=CARTESIAN_POINT('Ctrl Pts',(16.2574274119396,775.450353499937,105.905464802704));
#80253=CARTESIAN_POINT('Ctrl Pts',(15.8714060853263,775.749252883057,105.98999114635));
#80254=CARTESIAN_POINT('Ctrl Pts',(15.4846980450322,776.047354453647,106.074219552651));
#80255=CARTESIAN_POINT('Ctrl Pts',(15.119102964531,776.329180680002,106.153849370947));
#80256=CARTESIAN_POINT('Ctrl Pts',(14.7528942828154,776.61029400738,106.23321330142));
#80257=CARTESIAN_POINT('Ctrl Pts',(14.386639086236,776.891105591243,106.313407261698));
#80258=CARTESIAN_POINT('Origin',(39.2974260110815,740.1183815439,97.8977997828924));
#80259=CARTESIAN_POINT('Ctrl Pts',(68.457798550648,740.125373335778,97.8975538630338));
#80260=CARTESIAN_POINT('Ctrl Pts',(68.457793528146,740.126812170783,98.8057432478524));
#80261=CARTESIAN_POINT('Ctrl Pts',(67.7739871309274,740.125372130105,99.4034193862205));
#80262=CARTESIAN_POINT('Ctrl Pts',(68.4543137644914,741.123686977417,97.8959722242474));
#80263=CARTESIAN_POINT('Ctrl Pts',(68.4543091225958,741.125015728932,98.8042534866716));
#80264=CARTESIAN_POINT('Ctrl Pts',(67.770387876316,741.123676987505,99.4019378389631));
#80265=CARTESIAN_POINT('Ctrl Pts',(68.4534660468998,742.089834211708,97.895444103238));
#80266=CARTESIAN_POINT('Ctrl Pts',(68.4537977237444,742.085024899139,98.8048439523186));
#80267=CARTESIAN_POINT('Ctrl Pts',(67.7685829871235,742.088371346622,99.4027417427996));
#80268=CARTESIAN_POINT('Ctrl Pts',(68.5212719805811,743.985087877402,97.9282498249378));
#80269=CARTESIAN_POINT('Ctrl Pts',(68.5213036800754,743.959475863193,98.8496547973229));
#80270=CARTESIAN_POINT('Ctrl Pts',(67.8215691081142,743.982153788961,99.4492253539828));
#80271=CARTESIAN_POINT('Ctrl Pts',(68.5888690257085,744.914529948807,97.961220943636));
#80272=CARTESIAN_POINT('Ctrl Pts',(68.5883730543687,744.876767240832,98.8931590717075));
#80273=CARTESIAN_POINT('Ctrl Pts',(67.8756945555098,744.911598667171,99.493863121479));
#80274=CARTESIAN_POINT('Ctrl Pts',(68.8148134713651,746.756613909965,98.0730736941144));
#80275=CARTESIAN_POINT('Ctrl Pts',(68.8087869122143,746.689940361214,99.0318249317338));
#80276=CARTESIAN_POINT('Ctrl Pts',(68.0627239309321,746.758761162693,99.6337887080991));
#80277=CARTESIAN_POINT('Ctrl Pts',(68.9726401474251,747.669153697586,98.1517196268434));
#80278=CARTESIAN_POINT('Ctrl Pts',(68.9622942131984,747.587911596858,99.1270386428823));
#80279=CARTESIAN_POINT('Ctrl Pts',(68.195245132507,747.676396788027,99.7286309912845));
#80280=CARTESIAN_POINT('Ctrl Pts',(69.3842051708727,749.48685510545,98.3574424080094));
#80281=CARTESIAN_POINT('Ctrl Pts',(69.3592786500214,749.37567200458,99.3676317906573));
#80282=CARTESIAN_POINT('Ctrl Pts',(68.548409408609,749.511762264063,99.9655665671925));
#80283=CARTESIAN_POINT('Ctrl Pts',(69.6397214138926,750.396327035182,98.4853933992926));
#80284=CARTESIAN_POINT('Ctrl Pts',(69.6053161375638,750.270768604279,99.5144439610128));
#80285=CARTESIAN_POINT('Ctrl Pts',(68.7707035402597,750.433935418948,100.108551651481));
#80286=CARTESIAN_POINT('Ctrl Pts',(70.5222777867757,753.048462277384,98.9258874811848));
#80287=CARTESIAN_POINT('Ctrl Pts',(70.4561632372631,752.895496196554,100.011085429209));
#80288=CARTESIAN_POINT('Ctrl Pts',(69.5522866245713,753.134812078005,100.586887702835));
#80289=CARTESIAN_POINT('Ctrl Pts',(71.2666661634435,754.737397951853,99.2960490283313));
#80290=CARTESIAN_POINT('Ctrl Pts',(71.170949083334,754.563260077608,100.415280341793));
#80291=CARTESIAN_POINT('Ctrl Pts',(70.2279620290083,754.870567597945,100.972451671599));
#80292=CARTESIAN_POINT('Ctrl Pts',(72.9942145650824,758.002166447748,100.133539302775));
#80293=CARTESIAN_POINT('Ctrl Pts',(72.8364708956345,757.80629690058,101.310996337131));
#80294=CARTESIAN_POINT('Ctrl Pts',(71.8402373204914,758.243588198102,101.82729685542));
#80295=CARTESIAN_POINT('Ctrl Pts',(73.9775035669035,759.577384533899,100.601048495267));
#80296=CARTESIAN_POINT('Ctrl Pts',(73.7894427854517,759.375625735358,101.803417053148));
#80297=CARTESIAN_POINT('Ctrl Pts',(72.776593891794,759.879822520825,102.297356153672));
#80298=CARTESIAN_POINT('Ctrl Pts',(76.1447884375183,762.636049603697,101.582311656938));
#80299=CARTESIAN_POINT('Ctrl Pts',(75.9067736606732,762.432506681983,102.834553788344));
#80300=CARTESIAN_POINT('Ctrl Pts',(74.8752981911426,763.061721698698,103.289564156708));
#80301=CARTESIAN_POINT('Ctrl Pts',(77.3113370175406,764.094348930254,102.087808588578));
#80302=CARTESIAN_POINT('Ctrl Pts',(77.0568033578485,763.892857490299,103.365391981035));
#80303=CARTESIAN_POINT('Ctrl Pts',(76.0203013175091,764.581271199176,103.803653935234));
#80304=CARTESIAN_POINT('Ctrl Pts',(79.782400865438,766.891062887789,103.077422528602));
#80305=CARTESIAN_POINT('Ctrl Pts',(79.5087647074557,766.684405458065,104.417255532439));
#80306=CARTESIAN_POINT('Ctrl Pts',(78.46730944119,767.493556992294,104.834121508641));
#80307=CARTESIAN_POINT('Ctrl Pts',(81.0886284163067,768.230099673479,103.561888384961));
#80308=CARTESIAN_POINT('Ctrl Pts',(80.8210769288954,768.020758453429,104.941255173866));
#80309=CARTESIAN_POINT('Ctrl Pts',(79.7708698338623,768.887323474605,105.35104305306));
#80310=CARTESIAN_POINT('Ctrl Pts',(83.831887455577,770.81423378035,104.4665568788));
#80311=CARTESIAN_POINT('Ctrl Pts',(83.5872932985924,770.566505473212,105.94524619932));
#80312=CARTESIAN_POINT('Ctrl Pts',(82.5226269516004,771.568512635756,106.357013415668));
#80313=CARTESIAN_POINT('Ctrl Pts',(85.2698557482559,772.058456227081,104.884970895144));
#80314=CARTESIAN_POINT('Ctrl Pts',(85.060286287709,771.784116881193,106.428343407822));
#80315=CARTESIAN_POINT('Ctrl Pts',(83.9723523533647,772.855556135977,106.845426196585));
#80316=CARTESIAN_POINT('Ctrl Pts',(87.5086332117794,773.886757355081,105.450835609297));
#80317=CARTESIAN_POINT('Ctrl Pts',(87.3348509098558,773.518063834734,107.093622744994));
#80318=CARTESIAN_POINT('Ctrl Pts',(86.2338780036532,774.724758211298,107.536886595124));
#80319=CARTESIAN_POINT('Ctrl Pts',(88.2686884844878,774.490412833172,105.629591813404));
#80320=CARTESIAN_POINT('Ctrl Pts',(88.1178962276606,774.090775432108,107.309158083682));
#80321=CARTESIAN_POINT('Ctrl Pts',(87.0023075858948,775.337952653219,107.760653532829));
#80322=CARTESIAN_POINT('Ctrl Pts',(89.8066747417754,775.692017030682,105.975112203932));
#80323=CARTESIAN_POINT('Ctrl Pts',(89.7029989420519,775.222460255136,107.72501381451));
#80324=CARTESIAN_POINT('Ctrl Pts',(88.5542478926562,776.546313317911,108.19508593578));
#80325=CARTESIAN_POINT('Ctrl Pts',(90.5848365181571,776.290187893291,106.141797634399));
#80326=CARTESIAN_POINT('Ctrl Pts',(90.5052198785861,775.780926684455,107.92484290776));
#80327=CARTESIAN_POINT('Ctrl Pts',(89.3379859242012,777.141542501245,108.405730641429));
#80328=CARTESIAN_POINT('Ctrl Pts',(91.3685977607865,776.891105610866,106.313407267717));
#80329=CARTESIAN_POINT('Ctrl Pts',(91.30319437909,776.338680147618,108.121971920454));
#80330=CARTESIAN_POINT('Ctrl Pts',(90.121757463342,777.732229909622,108.614499557081));
#80331=CARTESIAN_POINT('',(67.7742920278783,740.125373764374,99.4032758153525));
#80332=CARTESIAN_POINT('Ctrl Pts',(67.7742310895756,740.125373441235,99.4032061173321));
#80333=CARTESIAN_POINT('Ctrl Pts',(67.7732877224663,740.369027246431,99.4029012766841));
#80334=CARTESIAN_POINT('Ctrl Pts',(67.7724586522842,740.612704432908,99.4027119719534));
#80335=CARTESIAN_POINT('Ctrl Pts',(67.7721484590144,740.856295764963,99.4029559530873));
#80336=CARTESIAN_POINT('Ctrl Pts',(67.7718267965963,741.108893691921,99.4032089552288));
#80337=CARTESIAN_POINT('Ctrl Pts',(67.7720634371067,741.361399339847,99.4039281453025));
#80338=CARTESIAN_POINT('Ctrl Pts',(67.773344281289,741.613730131199,99.4054937540533));
#80339=CARTESIAN_POINT('Ctrl Pts',(67.774726999303,741.886130424322,99.4071838858059));
#80340=CARTESIAN_POINT('Ctrl Pts',(67.7773270520541,742.158326800835,99.4098607599035));
#80341=CARTESIAN_POINT('Ctrl Pts',(67.7817898558437,742.430261486565,99.4140279754738));
#80342=CARTESIAN_POINT('Ctrl Pts',(67.7841872781943,742.576345052909,99.4162666075578));
#80343=CARTESIAN_POINT('Ctrl Pts',(67.7871227905514,742.72235387932,99.4189357188471));
#80344=CARTESIAN_POINT('Ctrl Pts',(67.7906992152466,742.868283965283,99.4221154035058));
#80345=CARTESIAN_POINT('Ctrl Pts',(67.7920636549196,742.923957666184,99.4233284831219));
#80346=CARTESIAN_POINT('Ctrl Pts',(67.7935213617819,742.979617114786,99.4246157929733));
#80347=CARTESIAN_POINT('Ctrl Pts',(67.7950781312413,743.035262525335,99.4259817466451));
#80348=CARTESIAN_POINT('Ctrl Pts',(67.8039732671529,743.353211651789,99.4337865911499));
#80349=CARTESIAN_POINT('Ctrl Pts',(67.8160290747519,743.670739140473,99.4440434513336));
#80350=CARTESIAN_POINT('Ctrl Pts',(67.8317599909462,743.987754340686,99.4569482517995));
#80351=CARTESIAN_POINT('Ctrl Pts',(67.8472830920453,744.300581574783,99.4696825719004));
#80352=CARTESIAN_POINT('Ctrl Pts',(67.8663857089031,744.612910887329,99.4849956039512));
#80353=CARTESIAN_POINT('Ctrl Pts',(67.8895371977891,744.924690182995,99.503051025853));
#80354=CARTESIAN_POINT('Ctrl Pts',(67.9060712787972,745.147353362738,99.5159456526232));
#80355=CARTESIAN_POINT('Ctrl Pts',(67.9246699523343,745.369736771215,99.5302385027949));
#80356=CARTESIAN_POINT('Ctrl Pts',(67.9454925408185,745.591828666883,99.5459802086122));
#80357=CARTESIAN_POINT('Ctrl Pts',(67.9531016634615,745.672986899129,99.5517326428144));
#80358=CARTESIAN_POINT('Ctrl Pts',(67.9610071024784,745.754102616515,99.5576783730213));
#80359=CARTESIAN_POINT('Ctrl Pts',(67.9692166012849,745.835179366707,99.563819843913));
#80360=CARTESIAN_POINT('Ctrl Pts',(68.0044365618116,746.183010581337,99.5901676597151));
#80361=CARTESIAN_POINT('Ctrl Pts',(68.0452020240616,746.530112578135,99.6200570912663));
#80362=CARTESIAN_POINT('Ctrl Pts',(68.0917401161303,746.876470855017,99.6533875148075));
#80363=CARTESIAN_POINT('Ctrl Pts',(68.1374417447843,747.216603779416,99.6861188660909));
#80364=CARTESIAN_POINT('Ctrl Pts',(68.1887105364043,747.55601987355,99.7221684631195));
#80365=CARTESIAN_POINT('Ctrl Pts',(68.2457178514693,747.894706722461,99.7614164359059));
#80366=CARTESIAN_POINT('Ctrl Pts',(68.2677433897189,748.025562914106,99.7765804148591));
#80367=CARTESIAN_POINT('Ctrl Pts',(68.2906250723667,748.156310229622,99.7922215858955));
#80368=CARTESIAN_POINT('Ctrl Pts',(68.3143709022457,748.286947818455,99.8083321054578));
#80369=CARTESIAN_POINT('Ctrl Pts',(68.3329980045785,748.38942474801,99.8209697895502));
#80370=CARTESIAN_POINT('Ctrl Pts',(68.352148729185,748.491793122839,99.8338915643058));
#80371=CARTESIAN_POINT('Ctrl Pts',(68.3718306053814,748.594079036638,99.8470962397665));
#80372=CARTESIAN_POINT('Ctrl Pts',(68.4249845802106,748.870318091961,99.8827575242933));
#80373=CARTESIAN_POINT('Ctrl Pts',(68.4821587598131,749.146356983718,99.9205610463555));
#80374=CARTESIAN_POINT('Ctrl Pts',(68.5431875418258,749.421829357746,99.9603143446058));
#80375=CARTESIAN_POINT('Ctrl Pts',(68.5580569543216,749.488947072135,99.9700000727206));
#80376=CARTESIAN_POINT('Ctrl Pts',(68.5731553965728,749.556031213665,99.9798016632362));
#80377=CARTESIAN_POINT('Ctrl Pts',(68.5884808649365,749.623076561152,99.989716548589));
#80378=CARTESIAN_POINT('Ctrl Pts',(68.6560448371755,749.918653171852,100.03342738488));
#80379=CARTESIAN_POINT('Ctrl Pts',(68.727998815401,750.213369552359,100.079327842352));
#80380=CARTESIAN_POINT('Ctrl Pts',(68.8039642538315,750.505968120847,100.127062363807));
#80381=CARTESIAN_POINT('Ctrl Pts',(68.8421391725935,750.653007706384,100.151050397264));
#80382=CARTESIAN_POINT('Ctrl Pts',(68.8813264975892,750.799512856937,100.175501330819));
#80383=CARTESIAN_POINT('Ctrl Pts',(68.921474642866,750.945327316819,100.200368733094));
#80384=CARTESIAN_POINT('Ctrl Pts',(68.9572967666306,751.075430054879,100.222556636317));
#80385=CARTESIAN_POINT('Ctrl Pts',(68.9939077941583,751.205085505603,100.245096046841));
#80386=CARTESIAN_POINT('Ctrl Pts',(69.0312825981136,751.334215880537,100.267961608868));
#80387=CARTESIAN_POINT('Ctrl Pts',(69.2398705795402,752.054889740941,100.395573821447));
#80388=CARTESIAN_POINT('Ctrl Pts',(69.4725174329772,752.762848064153,100.53347495977));
#80389=CARTESIAN_POINT('Ctrl Pts',(69.7271516357318,753.459062406438,100.679829134532));
#80390=CARTESIAN_POINT('Ctrl Pts',(69.9667703347098,754.114221741294,100.81755296176));
#80391=CARTESIAN_POINT('Ctrl Pts',(70.2258594541185,754.758981441764,100.962762134576));
#80392=CARTESIAN_POINT('Ctrl Pts',(70.5027061196983,755.394128388056,101.113965705465));
#80393=CARTESIAN_POINT('Ctrl Pts',(70.5855287331775,755.584141621284,101.159200402015));
#80394=CARTESIAN_POINT('Ctrl Pts',(70.6699407413637,755.773294352767,101.204971877759));
#80395=CARTESIAN_POINT('Ctrl Pts',(70.7558965790219,755.961607205061,101.251240971544));
#80396=CARTESIAN_POINT('Ctrl Pts',(70.8469099664253,756.161000184593,101.300232489423));
#80397=CARTESIAN_POINT('Ctrl Pts',(70.9396654517017,756.359475081021,101.349787412258));
#80398=CARTESIAN_POINT('Ctrl Pts',(71.0341165657173,756.557071161423,101.399864795737));
#80399=CARTESIAN_POINT('Ctrl Pts',(71.2796304629115,757.070697541326,101.530034711754));
#80400=CARTESIAN_POINT('Ctrl Pts',(71.5365755788152,757.578291245017,101.663805397549));
#80401=CARTESIAN_POINT('Ctrl Pts',(71.8043655001815,758.080232588601,101.80070691016));
#80402=CARTESIAN_POINT('Ctrl Pts',(72.0790115985549,758.595025045778,101.941113487481));
#80403=CARTESIAN_POINT('Ctrl Pts',(72.365064950169,759.103871994686,102.084813401217));
#80404=CARTESIAN_POINT('Ctrl Pts',(72.6619410691463,759.607169089028,102.231322895338));
#80405=CARTESIAN_POINT('Ctrl Pts',(72.861480151622,759.945449718549,102.329796191646));
#80406=CARTESIAN_POINT('Ctrl Pts',(73.065909504308,760.281222856161,102.429539216931));
#80407=CARTESIAN_POINT('Ctrl Pts',(73.2750632326797,760.614605117607,102.530410239635));
#80408=CARTESIAN_POINT('Ctrl Pts',(73.4551718214064,760.901690645955,102.617273322038));
#80409=CARTESIAN_POINT('Ctrl Pts',(73.6388660691381,761.187093199647,102.70499474763));
#80410=CARTESIAN_POINT('Ctrl Pts',(73.8259682109547,761.470759519602,102.793449721858));
#80411=CARTESIAN_POINT('Ctrl Pts',(74.1273614208162,761.927702993742,102.93593728695));
#80412=CARTESIAN_POINT('Ctrl Pts',(74.4361683805267,762.377984729352,103.079663214883));
#80413=CARTESIAN_POINT('Ctrl Pts',(74.751624296169,762.821500601673,103.224103473275));
#80414=CARTESIAN_POINT('Ctrl Pts',(75.0805888348608,763.28400894945,103.374729030172));
#80415=CARTESIAN_POINT('Ctrl Pts',(75.4168296426776,763.73930700147,103.526184694805));
#80416=CARTESIAN_POINT('Ctrl Pts',(75.759965128326,764.187892650595,103.678080246159));
#80417=CARTESIAN_POINT('Ctrl Pts',(75.9501426745341,764.436514322159,103.762266010805));
#80418=CARTESIAN_POINT('Ctrl Pts',(76.1424388529362,764.683073556509,103.846587192504));
#80419=CARTESIAN_POINT('Ctrl Pts',(76.3367939550992,764.927651198528,103.930979227673));
#80420=CARTESIAN_POINT('Ctrl Pts',(76.6343722691297,765.30212555784,104.060192401207));
#80421=CARTESIAN_POINT('Ctrl Pts',(76.9368184677876,765.671978786484,104.189577407643));
#80422=CARTESIAN_POINT('Ctrl Pts',(77.2438372520424,766.037390595207,104.318874365421));
#80423=CARTESIAN_POINT('Ctrl Pts',(77.7681161939748,766.661384064896,104.539667605755));
#80424=CARTESIAN_POINT('Ctrl Pts',(78.3060132783773,767.272616928675,104.760302519951));
#80425=CARTESIAN_POINT('Ctrl Pts',(78.8568288139819,767.872053720357,104.979603558284));
#80426=CARTESIAN_POINT('Ctrl Pts',(79.1650161183708,768.207445148229,105.102304882929));
#80427=CARTESIAN_POINT('Ctrl Pts',(79.4772482099342,768.539143253834,105.224589148224));
#80428=CARTESIAN_POINT('Ctrl Pts',(79.7934071938624,768.867313120509,105.346254087456));
#80429=CARTESIAN_POINT('Ctrl Pts',(80.2368843417532,769.327637969384,105.516913859885));
#80430=CARTESIAN_POINT('Ctrl Pts',(80.6880872333938,769.781011256299,105.686350506972));
#80431=CARTESIAN_POINT('Ctrl Pts',(81.1467510511712,770.227915631652,105.854027170534));
#80432=CARTESIAN_POINT('Ctrl Pts',(81.6973635034992,770.764411218467,106.055318084148));
#80433=CARTESIAN_POINT('Ctrl Pts',(82.2589714532759,771.291524419039,106.253970999396));
#80434=CARTESIAN_POINT('Ctrl Pts',(82.8306295792313,771.810281649119,106.44924471571));
#80435=CARTESIAN_POINT('Ctrl Pts',(83.0843259953669,772.040501152946,106.535905325864));
#80436=CARTESIAN_POINT('Ctrl Pts',(83.3400023623642,772.269074524743,106.621900498031));
#80437=CARTESIAN_POINT('Ctrl Pts',(83.5975786343429,772.496089563158,106.707165791572));
#80438=CARTESIAN_POINT('Ctrl Pts',(84.1242886014654,772.960305783469,106.88152222438));
#80439=CARTESIAN_POINT('Ctrl Pts',(84.6589209701514,773.417991363861,107.052821094596));
#80440=CARTESIAN_POINT('Ctrl Pts',(85.2009816334199,773.870020876545,107.220562746921));
#80441=CARTESIAN_POINT('Ctrl Pts',(85.2937827633958,773.947408616335,107.249280224382));
#80442=CARTESIAN_POINT('Ctrl Pts',(85.3868017127355,774.024630507358,107.277893419594));
#80443=CARTESIAN_POINT('Ctrl Pts',(85.4800361202237,774.101690852858,107.306399795611));
#80444=CARTESIAN_POINT('Ctrl Pts',(86.0719655882021,774.590933939642,107.487381950637));
#80445=CARTESIAN_POINT('Ctrl Pts',(86.6726364164098,775.073886492312,107.664146507473));
#80446=CARTESIAN_POINT('Ctrl Pts',(87.2790233367975,775.551280939275,107.836892391151));
#80447=CARTESIAN_POINT('Ctrl Pts',(87.4189205946676,775.66141882617,107.876745947721));
#80448=CARTESIAN_POINT('Ctrl Pts',(87.5591222556294,775.771260752326,107.916385519452));
#80449=CARTESIAN_POINT('Ctrl Pts',(87.6995913966809,775.880815488401,107.955813389664));
#80450=CARTESIAN_POINT('',(68.4577985453727,740.125373764361,97.8976768139577));
#80451=CARTESIAN_POINT('Origin',(66.4578107338363,740.118392461545,97.897799765561));
#80452=CARTESIAN_POINT('Ctrl Pts',(91.3685977607861,776.891105610866,106.313407267717));
#80453=CARTESIAN_POINT('Ctrl Pts',(90.9807645122238,776.59374991394,106.228488649706));
#80454=CARTESIAN_POINT('Ctrl Pts',(90.5929827521625,776.296055513399,106.144500887552));
#80455=CARTESIAN_POINT('Ctrl Pts',(90.2059289296751,775.997535867259,106.060142229145));
#80456=CARTESIAN_POINT('Ctrl Pts',(89.840429621133,775.715640384224,105.980481392523));
#80457=CARTESIAN_POINT('Ctrl Pts',(89.4755797478288,775.433008439386,105.900488671419));
#80458=CARTESIAN_POINT('Ctrl Pts',(89.1119557798394,775.149210594843,105.819030848735));
#80459=CARTESIAN_POINT('Ctrl Pts',(89.0871916323187,775.129882903857,105.813483267401));
#80460=CARTESIAN_POINT('Ctrl Pts',(89.0624331052717,775.110549722594,105.807928988557));
#80461=CARTESIAN_POINT('Ctrl Pts',(89.03768037791,775.091210911155,105.802367647203));
#80462=CARTESIAN_POINT('Ctrl Pts',(88.3981541217163,774.591561822048,105.65868150855));
#80463=CARTESIAN_POINT('Ctrl Pts',(87.762336284931,774.088004973204,105.510337467111));
#80464=CARTESIAN_POINT('Ctrl Pts',(87.1340806565533,773.579504623176,105.355121991748));
#80465=CARTESIAN_POINT('Ctrl Pts',(87.0514946058935,773.512660756172,105.334718460872));
#80466=CARTESIAN_POINT('Ctrl Pts',(86.9690392655668,773.445731408773,105.314196174729));
#80467=CARTESIAN_POINT('Ctrl Pts',(86.886723406743,773.378714186383,105.293550101408));
#80468=CARTESIAN_POINT('Ctrl Pts',(86.8452368118931,773.344937993156,105.283144630441));
#80469=CARTESIAN_POINT('Ctrl Pts',(86.803785640428,773.311139432702,105.272708072074));
#80470=CARTESIAN_POINT('Ctrl Pts',(86.7623708602348,773.277318075086,105.262239751732));
#80471=CARTESIAN_POINT('Ctrl Pts',(86.1451910388785,772.773298511194,105.106236603869));
#80472=CARTESIAN_POINT('Ctrl Pts',(85.535985930652,772.263834583666,104.942883567379));
#80473=CARTESIAN_POINT('Ctrl Pts',(84.9360365702387,771.747549276272,104.772668100744));
#80474=CARTESIAN_POINT('Ctrl Pts',(84.3294429878634,771.225546296015,104.60056755944));
#80475=CARTESIAN_POINT('Ctrl Pts',(83.7323121895133,770.696568606511,104.42145207513));
#80476=CARTESIAN_POINT('Ctrl Pts',(83.145943842104,770.15918257094,104.235869825657));
#80477=CARTESIAN_POINT('Ctrl Pts',(82.9764651492521,770.003861289926,104.18223078256));
#80478=CARTESIAN_POINT('Ctrl Pts',(82.8078853384044,769.847837593609,104.12805177399));
#80479=CARTESIAN_POINT('Ctrl Pts',(82.6402352490262,769.691076967123,104.073346646529));
#80480=CARTESIAN_POINT('Ctrl Pts',(82.5801185630709,769.634865071338,104.053730247994));
#80481=CARTESIAN_POINT('Ctrl Pts',(82.5201210385646,769.578558067279,104.034046834186));
#80482=CARTESIAN_POINT('Ctrl Pts',(82.4602437160975,769.522154014666,104.01429694718));
#80483=CARTESIAN_POINT('Ctrl Pts',(81.775386691458,768.877023102676,103.788404267034));
#80484=CARTESIAN_POINT('Ctrl Pts',(81.1060195434944,768.219416764147,103.554258150673));
#80485=CARTESIAN_POINT('Ctrl Pts',(80.4528992274308,767.547678951716,103.314503189542));
#80486=CARTESIAN_POINT('Ctrl Pts',(79.8714268663558,766.949631452334,103.101049588575));
#80487=CARTESIAN_POINT('Ctrl Pts',(79.3028325727198,766.340382487871,102.883150733177));
#80488=CARTESIAN_POINT('Ctrl Pts',(78.7476614911316,765.718744550908,102.662699893706));
#80489=CARTESIAN_POINT('Ctrl Pts',(78.6805303972213,765.643576307985,102.636043054944));
#80490=CARTESIAN_POINT('Ctrl Pts',(78.6135988172079,765.56823053418,102.609350414184));
#80491=CARTESIAN_POINT('Ctrl Pts',(78.5468669476994,765.492704343741,102.582625076989));
#80492=CARTESIAN_POINT('Ctrl Pts',(78.1183922109045,765.007762668828,102.411025930964));
#80493=CARTESIAN_POINT('Ctrl Pts',(77.6979420020796,764.515310703848,102.238036237578));
#80494=CARTESIAN_POINT('Ctrl Pts',(77.2859484879984,764.01461866131,102.064638291515));
#80495=CARTESIAN_POINT('Ctrl Pts',(76.8937139601728,763.537939538511,101.899556417225));
#80496=CARTESIAN_POINT('Ctrl Pts',(76.5091443987673,763.053791770041,101.734104044716));
#80497=CARTESIAN_POINT('Ctrl Pts',(76.1326468908731,762.561516463863,101.569139898605));
#80498=CARTESIAN_POINT('Ctrl Pts',(75.8347136960172,762.171965001654,101.438599074146));
#80499=CARTESIAN_POINT('Ctrl Pts',(75.5418358252766,761.777323557447,101.308364096761));
#80500=CARTESIAN_POINT('Ctrl Pts',(75.254231642613,761.377251511711,101.178868608371));
#80501=CARTESIAN_POINT('Ctrl Pts',(75.1895924136379,761.287335056633,101.149764412292));
#80502=CARTESIAN_POINT('Ctrl Pts',(75.1252294081678,761.197157836843,101.120702138367));
#80503=CARTESIAN_POINT('Ctrl Pts',(75.0611448173126,761.106715923497,101.091686671466));
#80504=CARTESIAN_POINT('Ctrl Pts',(74.7252379190504,760.632654028437,100.939598699018));
#80505=CARTESIAN_POINT('Ctrl Pts',(74.3986534810529,760.153737745643,100.789588600975));
#80506=CARTESIAN_POINT('Ctrl Pts',(74.0818958041657,759.669396971228,100.642377223156));
#80507=CARTESIAN_POINT('Ctrl Pts',(73.7599137942162,759.17706788996,100.492737865451));
#80508=CARTESIAN_POINT('Ctrl Pts',(73.4480848800937,758.679134181147,100.34598977661));
#80509=CARTESIAN_POINT('Ctrl Pts',(73.1469854009512,758.174974131377,100.202914164611));
#80510=CARTESIAN_POINT('Ctrl Pts',(72.8687762443246,757.709141567831,100.070715512321));
#80511=CARTESIAN_POINT('Ctrl Pts',(72.5997274327346,757.23799325803,99.9416521346038));
#80512=CARTESIAN_POINT('Ctrl Pts',(72.3403334658204,756.761018795067,99.8163640668633));
#80513=CARTESIAN_POINT('Ctrl Pts',(72.3189912079547,756.721774582471,99.8060556919961));
#80514=CARTESIAN_POINT('Ctrl Pts',(72.2977143320303,756.682490917786,99.7957728888851));
#80515=CARTESIAN_POINT('Ctrl Pts',(72.2765031258968,756.643167510428,99.7855160220318));
#80516=CARTESIAN_POINT('Ctrl Pts',(72.227461953983,756.552250192083,99.7618017283947));
#80517=CARTESIAN_POINT('Ctrl Pts',(72.1787729826753,756.461122589529,99.7382267680948));
#80518=CARTESIAN_POINT('Ctrl Pts',(72.1304401703867,756.36978191241,99.7147958362881));
#80519=CARTESIAN_POINT('Ctrl Pts',(71.8690884406554,755.875872230153,99.5880969278873));
#80520=CARTESIAN_POINT('Ctrl Pts',(71.6181356407634,755.375790462634,99.4655907782217));
#80521=CARTESIAN_POINT('Ctrl Pts',(71.3787125423155,754.86877041419,99.3480968719145));
#80522=CARTESIAN_POINT('Ctrl Pts',(71.1430487323805,754.369711312941,99.2324477896664));
#80523=CARTESIAN_POINT('Ctrl Pts',(70.918555297956,753.86393017412,99.1216546996797));
#80524=CARTESIAN_POINT('Ctrl Pts',(70.7063483157787,753.350674498194,99.0165239863566));
#80525=CARTESIAN_POINT('Ctrl Pts',(70.4985310074892,752.84803593305,98.9135679872786));
#80526=CARTESIAN_POINT('Ctrl Pts',(70.3024970383778,752.338228909847,98.8160424711298));
#80527=CARTESIAN_POINT('Ctrl Pts',(70.1193322626677,751.82052474662,98.724729886038));
#80528=CARTESIAN_POINT('Ctrl Pts',(70.0806268960185,751.711126368161,98.7054342159401));
#80529=CARTESIAN_POINT('Ctrl Pts',(70.0424963259886,751.601375271595,98.6864160694099));
#80530=CARTESIAN_POINT('Ctrl Pts',(70.0049510239408,751.49126444936,98.6676829807012));
#80531=CARTESIAN_POINT('Ctrl Pts',(69.9810239029901,751.421092288852,98.6557446327624));
#80532=CARTESIAN_POINT('Ctrl Pts',(69.9573427321779,751.350798301254,98.6439264166418));
#80533=CARTESIAN_POINT('Ctrl Pts',(69.9339067018654,751.280371607074,98.6322285107702));
#80534=CARTESIAN_POINT('Ctrl Pts',(69.8522878701283,751.03510206162,98.5914891279363));
#80535=CARTESIAN_POINT('Ctrl Pts',(69.7736131636686,750.787790163411,98.5521884983569));
#80536=CARTESIAN_POINT('Ctrl Pts',(69.6980134816527,750.538580321834,98.514405391234));
#80537=CARTESIAN_POINT('Ctrl Pts',(69.6558192522898,750.399489561998,98.4933176161869));
#80538=CARTESIAN_POINT('Ctrl Pts',(69.6145836640669,750.259807269986,98.4727029314975));
#80539=CARTESIAN_POINT('Ctrl Pts',(69.5743357876118,750.119557537408,98.452578198471));
#80540=CARTESIAN_POINT('Ctrl Pts',(69.4412691722878,749.655867055873,98.386042263063));
#80541=CARTESIAN_POINT('Ctrl Pts',(69.3196158156649,749.18811805896,98.3251703911877));
#80542=CARTESIAN_POINT('Ctrl Pts',(69.2109107377535,748.719717791463,98.2708381534396));
#80543=CARTESIAN_POINT('Ctrl Pts',(69.1999501987674,748.672489828504,98.265359930881));
#80544=CARTESIAN_POINT('Ctrl Pts',(69.1891200775681,748.625249855634,98.2599472155666));
#80545=CARTESIAN_POINT('Ctrl Pts',(69.1784222872972,748.578002387959,98.2546010785117));
#80546=CARTESIAN_POINT('Ctrl Pts',(69.1033489490578,748.246436239071,98.2170837646336));
#80547=CARTESIAN_POINT('Ctrl Pts',(69.0345597878175,747.913927214286,98.1827308961769));
#80548=CARTESIAN_POINT('Ctrl Pts',(68.9719999552296,747.580534775366,98.1515240467797));
#80549=CARTESIAN_POINT('Ctrl Pts',(68.9085608240518,747.242456398371,98.1198785750663));
#80550=CARTESIAN_POINT('Ctrl Pts',(68.8515272981591,746.903469292199,98.0914681468127));
#80551=CARTESIAN_POINT('Ctrl Pts',(68.8007944554575,746.563639967713,98.0662489751074));
#80552=CARTESIAN_POINT('Ctrl Pts',(68.7672748745265,746.33911210887,98.0495864736197));
#80553=CARTESIAN_POINT('Ctrl Pts',(68.7365047781278,746.1142166938,98.0343165602586));
#80554=CARTESIAN_POINT('Ctrl Pts',(68.7084429883808,745.888974959709,98.0204209926115));
#80555=CARTESIAN_POINT('Ctrl Pts',(68.7062255233766,745.871176178258,98.0193229537747));
#80556=CARTESIAN_POINT('Ctrl Pts',(68.7040249428091,745.85337505384,98.0182334644857));
#80557=CARTESIAN_POINT('Ctrl Pts',(68.7018412289294,745.83557162853,98.0171525161574));
#80558=CARTESIAN_POINT('Ctrl Pts',(68.6632110913049,745.520627085521,97.9980304218781));
#80559=CARTESIAN_POINT('Ctrl Pts',(68.6299239732758,745.204972885799,97.9816106203079));
#80560=CARTESIAN_POINT('Ctrl Pts',(68.6015127569383,744.888652305022,97.967637146246));
#80561=CARTESIAN_POINT('Ctrl Pts',(68.5720603542791,744.560739518615,97.9531515860457));
#80562=CARTESIAN_POINT('Ctrl Pts',(68.5478470658136,744.232109684,97.9412945386335));
#80563=CARTESIAN_POINT('Ctrl Pts',(68.5283084725441,743.902839265685,97.9317593780112));
#80564=CARTESIAN_POINT('Ctrl Pts',(68.5112191275066,743.614844336287,97.9234194915304));
#80565=CARTESIAN_POINT('Ctrl Pts',(68.497704854417,743.32635947197,97.9168553037103));
#80566=CARTESIAN_POINT('Ctrl Pts',(68.4873690146543,743.037460938716,97.9118529049428));
#80567=CARTESIAN_POINT('Ctrl Pts',(68.4871628646808,743.031698811367,97.911753131301));
#80568=CARTESIAN_POINT('Ctrl Pts',(68.4869580177625,743.025936507947,97.9116539921842));
#80569=CARTESIAN_POINT('Ctrl Pts',(68.4867544660922,743.020174028313,97.9115554837351));
#80570=CARTESIAN_POINT('Ctrl Pts',(68.4769948303666,742.743882008606,97.9068323263289));
#80571=CARTESIAN_POINT('Ctrl Pts',(68.4702128160218,742.467233873008,97.9035600998517));
#80572=CARTESIAN_POINT('Ctrl Pts',(68.4655567364647,742.190285780326,97.9013210273558));
#80573=CARTESIAN_POINT('Ctrl Pts',(68.4611688045257,741.929287366015,97.8992109049669));
#80574=CARTESIAN_POINT('Ctrl Pts',(68.4586682871477,741.668022513426,97.898018015762));
#80575=CARTESIAN_POINT('Ctrl Pts',(68.4573689622943,741.406570728667,97.8974060106253));
#80576=CARTESIAN_POINT('Ctrl Pts',(68.4561510499872,741.161500879099,97.8968323522473));
#80577=CARTESIAN_POINT('Ctrl Pts',(68.4559881997955,740.916266870814,97.896768909083));
#80578=CARTESIAN_POINT('Ctrl Pts',(68.4563461801979,740.670963156096,97.8969540896854));
#80579=CARTESIAN_POINT('Ctrl Pts',(68.4566115484957,740.489121276497,97.8970913627342));
#80580=CARTESIAN_POINT('Ctrl Pts',(68.4571637055702,740.307241660318,97.8973655500502));
#80581=CARTESIAN_POINT('Ctrl Pts',(68.4577985453727,740.125373764361,97.8976768139577));
#80582=CARTESIAN_POINT('Ctrl Pts',(37.2974370684329,740.1250398719,82.4370095290715));
#80583=CARTESIAN_POINT('Ctrl Pts',(37.3424884707948,753.031264614585,82.4563563944262));
#80584=CARTESIAN_POINT('Ctrl Pts',(37.3879041226833,765.937472681678,82.4756378033222));
#80585=CARTESIAN_POINT('Ctrl Pts',(13.9672995497186,779.915230707551,88.5489395495829));
#80586=CARTESIAN_POINT('Ctrl Pts',(2.77065801251735,790.645214141688,92.3412787532726));
#80587=CARTESIAN_POINT('Ctrl Pts',(-4.44817956388518,803.379710979161,96.8420808181083));
#80588=CARTESIAN_POINT('Ctrl Pts',(37.2974370944911,740.125047336989,83.2541797519407));
#80589=CARTESIAN_POINT('Ctrl Pts',(37.3414812482621,752.742717755302,83.2719940286304));
#80590=CARTESIAN_POINT('Ctrl Pts',(37.3858793646116,765.36036823179,83.2897413519787));
#80591=CARTESIAN_POINT('Ctrl Pts',(14.6269734057586,779.259941132568,89.4579435538414));
#80592=CARTESIAN_POINT('Ctrl Pts',(3.52773834636104,789.585631506022,93.0954993990444));
#80593=CARTESIAN_POINT('Ctrl Pts',(-3.81134624434443,801.905170120104,97.4384971415098));
#80594=CARTESIAN_POINT('Ctrl Pts',(37.297437120366,740.125054749569,84.07134997481));
#80595=CARTESIAN_POINT('Ctrl Pts',(37.3404811104892,752.456200521121,84.0876316628422));
#80596=CARTESIAN_POINT('Ctrl Pts',(37.3838684935262,764.787322986573,84.1038448845999));
#80597=CARTESIAN_POINT('Ctrl Pts',(15.3048815505885,778.617102553909,90.3217738647409));
#80598=CARTESIAN_POINT('Ctrl Pts',(4.3028141604402,788.543880887858,93.8278683544787));
#80599=CARTESIAN_POINT('Ctrl Pts',(-3.14516449837338,800.450285635656,98.0345313843018));
#80600=CARTESIAN_POINT('Ctrl Pts',(37.2974371460461,740.125062106342,84.8885201976793));
#80601=CARTESIAN_POINT('Ctrl Pts',(37.3394885023999,752.171840373793,84.9032692970658));
#80602=CARTESIAN_POINT('Ctrl Pts',(37.3818727361078,764.21859183176,84.9179478797552));
#80603=CARTESIAN_POINT('Ctrl Pts',(15.9793268060979,777.989735996571,91.1817234896819));
#80604=CARTESIAN_POINT('Ctrl Pts',(5.08782990810792,787.523121454333,94.5593122958652));
#80605=CARTESIAN_POINT('Ctrl Pts',(-2.44951120227387,799.014953473008,98.6297577392777));
#80606=CARTESIAN_POINT('Ctrl Pts',(37.2974371715198,740.125069404011,85.7056904205486));
#80607=CARTESIAN_POINT('Ctrl Pts',(37.3385038689179,751.88976477507,85.7189069313054));
#80608=CARTESIAN_POINT('Ctrl Pts',(37.37989331662,763.654429651608,85.7320498163745));
#80609=CARTESIAN_POINT('Ctrl Pts',(16.6287677270449,777.38095747515,92.07906222547));
#80610=CARTESIAN_POINT('Ctrl Pts',(5.87488577558581,786.526607362185,95.3107346888993));
#80611=CARTESIAN_POINT('Ctrl Pts',(-1.72410749947928,797.599164568951,99.2237271886367));
#80612=CARTESIAN_POINT('Ctrl Pts',(37.2974372094038,740.125080256911,86.9314457548525));
#80613=CARTESIAN_POINT('Ctrl Pts',(37.3370395479918,751.470269392525,86.9423633826947));
#80614=CARTESIAN_POINT('Ctrl Pts',(37.376950526235,762.815422167125,86.9532003527393));
#80615=CARTESIAN_POINT('Ctrl Pts',(17.5333967744215,776.500515238856,93.5430042314188));
#80616=CARTESIAN_POINT('Ctrl Pts',(7.04696637151271,785.073254941205,96.4991366952518));
#80617=CARTESIAN_POINT('Ctrl Pts',(-0.590671714732331,795.504951976006,
100.112068018336));
#80618=CARTESIAN_POINT('Ctrl Pts',(37.2974372219773,740.125083858944,87.3400308662872));
#80619=CARTESIAN_POINT('Ctrl Pts',(37.3365535459,751.331040600932,87.3501821998278));
#80620=CARTESIAN_POINT('Ctrl Pts',(37.3759739088114,762.536959012098,87.3602503005129));
#80621=CARTESIAN_POINT('Ctrl Pts',(17.8283182521832,776.209771644634,94.040091612404));
#80622=CARTESIAN_POINT('Ctrl Pts',(7.43772026798971,784.59385178339,96.9000225008642));
#80623=CARTESIAN_POINT('Ctrl Pts',(-0.205304748057507,794.811792905548,
100.407746070846));
#80624=CARTESIAN_POINT('Ctrl Pts',(37.2974372344949,740.125087444965,87.7486159777218));
#80625=CARTESIAN_POINT('Ctrl Pts',(37.3360697043082,751.192430744648,87.7580010169631));
#80626=CARTESIAN_POINT('Ctrl Pts',(37.37500167387,762.259733741229,87.7673000996059));
#80627=CARTESIAN_POINT('Ctrl Pts',(18.1192890407701,775.921049293556,94.5419441749148));
#80628=CARTESIAN_POINT('Ctrl Pts',(7.82954922493632,784.118890694556,97.3033652604152));
#80629=CARTESIAN_POINT('Ctrl Pts',(0.187675975419192,794.123558618551,100.702927900473));
#80630=CARTESIAN_POINT('Ctrl Pts',(37.2974372469552,740.12509101456,88.1572010891565));
#80631=CARTESIAN_POINT('Ctrl Pts',(37.3355880788326,751.05445575639,88.1658198340999));
#80632=CARTESIAN_POINT('Ctrl Pts',(37.3740338910031,761.9837782321,88.1743498323877));
#80633=CARTESIAN_POINT('Ctrl Pts',(18.4089919196902,775.633639338812,95.0442181190076));
#80634=CARTESIAN_POINT('Ctrl Pts',(8.22347986897346,783.647773155753,97.7068678552149));
#80635=CARTESIAN_POINT('Ctrl Pts',(0.588341104726402,793.440269165873,100.99755057259));
#80636=CARTESIAN_POINT('Ctrl Pts',(37.2974372717582,740.125098120077,88.9743713120258));
#80637=CARTESIAN_POINT('Ctrl Pts',(37.3346293713467,750.779807381366,88.9814574683739));
#80638=CARTESIAN_POINT('Ctrl Pts',(37.3721073681987,761.434470492247,88.9884493301505));
#80639=CARTESIAN_POINT('Ctrl Pts',(18.9912534758669,775.060041775275,96.0409158137305));
#80640=CARTESIAN_POINT('Ctrl Pts',(9.01762384312406,782.712043387227,98.5095931211922));
#80641=CARTESIAN_POINT('Ctrl Pts',(1.40520753171264,792.083635277775,101.585546375814));
#80642=CARTESIAN_POINT('Ctrl Pts',(37.297437284101,740.125101655998,89.3829564234604));
#80643=CARTESIAN_POINT('Ctrl Pts',(37.3341522893364,750.6431339946,89.3892762855112));
#80644=CARTESIAN_POINT('Ctrl Pts',(37.3711486282413,761.161118261416,89.3954990950289));
#80645=CARTESIAN_POINT('Ctrl Pts',(19.2838134375432,774.773861036257,96.5353461798798));
#80646=CARTESIAN_POINT('Ctrl Pts',(9.41783717323752,782.247431157503,98.9088157923697));
#80647=CARTESIAN_POINT('Ctrl Pts',(1.82140882939167,791.410290842356,101.87891950692));
#80648=CARTESIAN_POINT('Ctrl Pts',(37.2974372963835,740.125105174671,89.7915415348951));
#80649=CARTESIAN_POINT('Ctrl Pts',(37.333677534675,750.507127341298,89.7970951026478));
#80650=CARTESIAN_POINT('Ctrl Pts',(37.3701944834603,760.889099547344,89.8025489584973));
#80651=CARTESIAN_POINT('Ctrl Pts',(19.5802186903287,774.487584241543,97.0214998392773));
#80652=CARTESIAN_POINT('Ctrl Pts',(9.8222315023368,781.785480686826,99.3035987046764));
#80653=CARTESIAN_POINT('Ctrl Pts',(2.24546188961201,790.741946589879,102.171602254524));
#80654=CARTESIAN_POINT('Ctrl Pts',(37.2974373086044,740.125108675681,90.2001266463297));
#80655=CARTESIAN_POINT('Ctrl Pts',(37.3332051629788,750.37180335418,90.2049139197827));
#80656=CARTESIAN_POINT('Ctrl Pts',(37.3692450073853,760.618446227576,90.2095990031906));
#80657=CARTESIAN_POINT('Ctrl Pts',(19.8828983710714,774.200504916139,97.4950158880135));
#80658=CARTESIAN_POINT('Ctrl Pts',(10.2318595156963,781.325608703157,99.6916393826827));
#80659=CARTESIAN_POINT('Ctrl Pts',(2.67746342005582,790.078637818108,102.463526327259));
#80660=CARTESIAN_POINT('Ctrl Pts',(37.2974373450777,740.125119124492,91.4258819806337));
#80661=CARTESIAN_POINT('Ctrl Pts',(37.3317953636346,749.967927189533,91.4283703711791));
#80662=CARTESIAN_POINT('Ctrl Pts',(37.3664108052091,759.810678083431,91.4307499289936));
#80663=CARTESIAN_POINT('Ctrl Pts',(20.8170904917175,773.334764479849,98.8645592276937));
#80664=CARTESIAN_POINT('Ctrl Pts',(11.4796450483815,779.950502954021,100.828618024696));
#80665=CARTESIAN_POINT('Ctrl Pts',(3.99764592910691,788.103948395176,103.336808383945));
#80666=CARTESIAN_POINT('Ctrl Pts',(37.297437369141,740.125126018071,92.243052203503));
#80667=CARTESIAN_POINT('Ctrl Pts',(37.3308652517341,749.701470808714,92.244008005429));
#80668=CARTESIAN_POINT('Ctrl Pts',(37.3645400286259,759.277754923748,92.2448519400639));
#80669=CARTESIAN_POINT('Ctrl Pts',(21.4925708184156,772.761294515867,99.6877915698248));
#80670=CARTESIAN_POINT('Ctrl Pts',(12.345371211636,779.043417932929,101.539440317288));
#80671=CARTESIAN_POINT('Ctrl Pts',(4.91000482543385,786.807804636397,103.915676206375));
#80672=CARTESIAN_POINT('Ctrl Pts',(37.2974373929403,740.125132836058,93.0602224263723));
#80673=CARTESIAN_POINT('Ctrl Pts',(37.329945339088,749.437936285258,93.0596456396654));
#80674=CARTESIAN_POINT('Ctrl Pts',(37.3626890028486,758.750675605608,93.0589551285022));
#80675=CARTESIAN_POINT('Ctrl Pts',(22.2098244807151,772.193286281927,100.442875982628));
#80676=CARTESIAN_POINT('Ctrl Pts',(13.2416248126661,778.147949114238,102.213865617469));
#80677=CARTESIAN_POINT('Ctrl Pts',(5.85548763085168,785.532324601494,104.490652781672));
#80678=CARTESIAN_POINT('Ctrl Pts',(37.2974374164643,740.125139575155,93.8773926492416));
#80679=CARTESIAN_POINT('Ctrl Pts',(37.3290360706217,749.177451080918,93.8752832738895));
#80680=CARTESIAN_POINT('Ctrl Pts',(37.3608587836402,758.229695032105,93.8730592785752));
#80681=CARTESIAN_POINT('Ctrl Pts',(22.9581652826313,771.632642151683,101.151411686076));
#80682=CARTESIAN_POINT('Ctrl Pts',(14.1652901957973,777.266191525838,102.862610999887));
#80683=CARTESIAN_POINT('Ctrl Pts',(6.83520707883987,784.277987128319,105.061117676372));
#80684=CARTESIAN_POINT('Ctrl Pts',(37.2974374629385,740.125152888974,95.5117330949803));
#80685=CARTESIAN_POINT('Ctrl Pts',(37.3272397119003,748.662834233973,95.5065585423147));
#80686=CARTESIAN_POINT('Ctrl Pts',(37.3572420617776,757.200441175945,95.501269072464));
#80687=CARTESIAN_POINT('Ctrl Pts',(24.4961711849034,770.530184767746,102.51845911973));
#80688=CARTESIAN_POINT('Ctrl Pts',(16.0617356260895,775.534586787255,104.13005108402));
#80689=CARTESIAN_POINT('Ctrl Pts',(8.86586713809172,781.812852902991,106.191658243183));
#80690=CARTESIAN_POINT('Ctrl Pts',(37.2974374858887,740.125159463696,96.3289033178496));
#80691=CARTESIAN_POINT('Ctrl Pts',(37.3263526216414,748.408702591369,96.3221961765227));
#80692=CARTESIAN_POINT('Ctrl Pts',(37.3554559164072,756.692167907054,96.3153740553816));
#80693=CARTESIAN_POINT('Ctrl Pts',(25.2628191432126,769.98748460851,103.21954759762));
#80694=CARTESIAN_POINT('Ctrl Pts',(17.0243325801041,774.68595208428,104.770644970324));
#80695=CARTESIAN_POINT('Ctrl Pts',(9.91680774935538,780.602056150836,106.751733915294));
#80696=CARTESIAN_POINT('Ctrl Pts',(37.2974375085405,740.125165952933,97.146073540719));
#80697=CARTESIAN_POINT('Ctrl Pts',(37.3254770654129,748.157875191384,97.1378338107217));
#80698=CARTESIAN_POINT('Ctrl Pts',(37.353692747676,756.190503271047,97.1294794255097));
#80699=CARTESIAN_POINT('Ctrl Pts',(26.0354102597506,769.450667095891,103.92649548435));
#80700=CARTESIAN_POINT('Ctrl Pts',(18.0055779592141,773.852731336532,105.411629333519));
#80701=CARTESIAN_POINT('Ctrl Pts',(11.0047328813242,779.413657557974,107.305932045411));
#80702=CARTESIAN_POINT('Ctrl Pts',(37.2974375308824,740.125172353387,97.9632437635883));
#80703=CARTESIAN_POINT('Ctrl Pts',(37.3246134881434,747.91047949577,97.9534714449075));
#80704=CARTESIAN_POINT('Ctrl Pts',(37.3519533126077,755.695702239311,97.9435854850557));
#80705=CARTESIAN_POINT('Ctrl Pts',(26.8225038911607,768.9172353047,104.627534930461));
#80706=CARTESIAN_POINT('Ctrl Pts',(19.0100071552343,773.033319793847,106.046458309024));
#80707=CARTESIAN_POINT('Ctrl Pts',(12.1312776786533,778.248433884114,107.853507205599));
#80708=CARTESIAN_POINT('Ctrl Pts',(37.2974375529029,740.125178661761,98.7804139864576));
#80709=CARTESIAN_POINT('Ctrl Pts',(37.3237623347616,747.666642966279,98.7691090790754));
#80710=CARTESIAN_POINT('Ctrl Pts',(37.3502383636256,755.208019780636,98.7576925374003));
#80711=CARTESIAN_POINT('Ctrl Pts',(27.6329557572476,768.384859261124,105.310822493709));
#80712=CARTESIAN_POINT('Ctrl Pts',(20.0424519231406,772.226279657433,106.668510439474));
#80713=CARTESIAN_POINT('Ctrl Pts',(13.2983736491593,777.107328840337,108.39363837514));
#80714=CARTESIAN_POINT('',(37.297438237489,740.125373936259,83.3197325254973));
#80715=CARTESIAN_POINT('Ctrl Pts',(-3.53207921104705,801.327714069793,97.6774171598034));
#80716=CARTESIAN_POINT('Ctrl Pts',(-3.52587249025034,801.317418707077,97.6740101620181));
#80717=CARTESIAN_POINT('Ctrl Pts',(-3.51962667648031,801.307146848781,97.6703505307767));
#80718=CARTESIAN_POINT('Ctrl Pts',(-3.51334807640392,801.296826345139,97.6666767907112));
#80719=CARTESIAN_POINT('Ctrl Pts',(-3.5106008964837,801.292310644183,97.6650693583509));
#80720=CARTESIAN_POINT('Ctrl Pts',(-3.50784744134078,801.287785628975,97.6634592331446));
#80721=CARTESIAN_POINT('Ctrl Pts',(-3.50508824012168,801.283252220773,97.6618466990113));
#80722=CARTESIAN_POINT('Ctrl Pts',(-3.49201375725401,801.261770653046,97.6542057014094));
#80723=CARTESIAN_POINT('Ctrl Pts',(-3.47868041561161,801.239995695538,97.646128608076));
#80724=CARTESIAN_POINT('Ctrl Pts',(-3.46537855240211,801.218215478767,97.6383364608635));
#80725=CARTESIAN_POINT('Ctrl Pts',(-3.46229474298644,801.213166108127,97.636529984841));
#80726=CARTESIAN_POINT('Ctrl Pts',(-3.4592126975727,801.208116512442,97.6347390358641));
#80727=CARTESIAN_POINT('Ctrl Pts',(-3.45613613830592,801.203070365482,97.6329729068014));
#80728=CARTESIAN_POINT('Ctrl Pts',(-3.4304744809274,801.160980328153,97.6182415803537));
#80729=CARTESIAN_POINT('Ctrl Pts',(-3.40459867550778,801.118642251537,97.6034680866934));
#80730=CARTESIAN_POINT('Ctrl Pts',(-3.37884385789892,801.076686597832,97.5886127519183));
#80731=CARTESIAN_POINT('Ctrl Pts',(-3.32744721036587,800.992959351992,97.5589672534716));
#80732=CARTESIAN_POINT('Ctrl Pts',(-3.27586200981757,800.909393845096,97.529356289513));
#80733=CARTESIAN_POINT('Ctrl Pts',(-3.22408722923495,800.825990597834,97.4997811184006));
#80734=CARTESIAN_POINT('Ctrl Pts',(-3.19288321141107,800.775724495596,97.4819565297466));
#80735=CARTESIAN_POINT('Ctrl Pts',(-3.16161031478435,800.725517304614,97.464144933854));
#80736=CARTESIAN_POINT('Ctrl Pts',(-3.13026831930153,800.675369158711,97.4463466147331));
#80737=CARTESIAN_POINT('Ctrl Pts',(-3.05760287905582,800.559102244513,97.4050817662566));
#80738=CARTESIAN_POINT('Ctrl Pts',(-2.98456554311726,800.443153214223,97.3638884681123));
#80739=CARTESIAN_POINT('Ctrl Pts',(-2.91115554479481,800.3275217629,97.3227696504956));
#80740=CARTESIAN_POINT('Ctrl Pts',(-2.76326137054251,800.094566873895,97.2399303409108));
#80741=CARTESIAN_POINT('Ctrl Pts',(-2.61385506024094,799.86290132501,97.1573933949809));
#80742=CARTESIAN_POINT('Ctrl Pts',(-2.46292804567857,799.632522498369,97.0751821615028));
#80743=CARTESIAN_POINT('Ctrl Pts',(-2.39939935499147,799.535550692089,97.0405775412644));
#80744=CARTESIAN_POINT('Ctrl Pts',(-2.3356003334188,799.438808100775,97.0060312761693));
#80745=CARTESIAN_POINT('Ctrl Pts',(-2.27153217997277,799.342292332637,96.9715441428051));
#80746=CARTESIAN_POINT('Ctrl Pts',(-1.92974275328136,798.827402059012,96.7875629148974));
#80747=CARTESIAN_POINT('Ctrl Pts',(-1.58030992268464,798.318982584886,96.6052745778218));
#80748=CARTESIAN_POINT('Ctrl Pts',(-1.22344040148274,797.816762200364,96.4248254346384));
#80749=CARTESIAN_POINT('Ctrl Pts',(-1.17154198831683,797.743725867845,96.3985832827258));
#80750=CARTESIAN_POINT('Ctrl Pts',(-1.11948623212914,797.670820699189,96.3723800465563));
#80751=CARTESIAN_POINT('Ctrl Pts',(-1.06727370425656,797.59804591967,96.3462161961521));
#80752=CARTESIAN_POINT('Ctrl Pts',(-1.02414389435495,797.537930799138,96.3246037222842));
#80753=CARTESIAN_POINT('Ctrl Pts',(-0.980906989626348,797.477905472924,
96.3030187351991));
#80754=CARTESIAN_POINT('Ctrl Pts',(-0.937563757151817,797.417968716901,
96.2814610407467));
#80755=CARTESIAN_POINT('Ctrl Pts',(-0.405606907320748,796.682357501429,
96.0168807919786));
#80756=CARTESIAN_POINT('Ctrl Pts',(0.1423611097153,795.960080192847,95.7564278130585));
#80757=CARTESIAN_POINT('Ctrl Pts',(0.704521420287423,795.249490032763,95.4999771464207));
#80758=CARTESIAN_POINT('Ctrl Pts',(1.10745352353966,794.740169857773,95.3161644429169));
#80759=CARTESIAN_POINT('Ctrl Pts',(1.51767785039838,794.236855021861,95.1344083618379));
#80760=CARTESIAN_POINT('Ctrl Pts',(1.93453138702115,793.738951725696,94.954670179249));
#80761=CARTESIAN_POINT('Ctrl Pts',(1.93694797209831,793.736065278612,94.9536282003003));
#80762=CARTESIAN_POINT('Ctrl Pts',(1.93936478014842,793.73317901318,94.9525862891865));
#80763=CARTESIAN_POINT('Ctrl Pts',(1.9417818110133,793.730292929321,94.9515444459138));
#80764=CARTESIAN_POINT('Ctrl Pts',(2.46152573053298,793.10968664788,94.727512674564));
#80765=CARTESIAN_POINT('Ctrl Pts',(2.99136899894459,792.497326343745,94.5065323530685));
#80766=CARTESIAN_POINT('Ctrl Pts',(3.52988153404372,791.89198649273,94.288351414471));
#80767=CARTESIAN_POINT('Ctrl Pts',(4.07175701103376,791.282866371786,94.0688079638234));
#80768=CARTESIAN_POINT('Ctrl Pts',(4.62241032479021,790.680854621645,93.8520989609514));
#80769=CARTESIAN_POINT('Ctrl Pts',(5.18034579587942,790.084667031274,93.6379591178906));
#80770=CARTESIAN_POINT('Ctrl Pts',(5.74430546766639,789.482042220322,93.4215071411534));
#80771=CARTESIAN_POINT('Ctrl Pts',(6.31570537878925,788.885367999664,93.2076801009325));
#80772=CARTESIAN_POINT('Ctrl Pts',(6.8929619902048,788.293282271603,92.996195468457));
#80773=CARTESIAN_POINT('Ctrl Pts',(7.35536276565974,787.819002905412,92.8267895991787));
#80774=CARTESIAN_POINT('Ctrl Pts',(7.82152073377076,787.347667044819,92.6588865708896));
#80775=CARTESIAN_POINT('Ctrl Pts',(8.29060449945157,786.878558472934,92.4923373092731));
#80776=CARTESIAN_POINT('Ctrl Pts',(8.37840289062202,786.790755438787,92.4611642901017));
#80777=CARTESIAN_POINT('Ctrl Pts',(8.4663027434857,786.70303137381,92.4300390763354));
#80778=CARTESIAN_POINT('Ctrl Pts',(8.55429849135774,786.615381572838,92.3989606884239));
#80779=CARTESIAN_POINT('Ctrl Pts',(9.2020771922392,785.970149552205,92.1701778411428));
#80780=CARTESIAN_POINT('Ctrl Pts',(9.85516593914095,785.328922519864,91.9438905224339));
#80781=CARTESIAN_POINT('Ctrl Pts',(10.5119316825118,784.690249367814,91.7199934851448));
#80782=CARTESIAN_POINT('Ctrl Pts',(11.1784195477638,784.042121919023,91.492782093678));
#80783=CARTESIAN_POINT('Ctrl Pts',(11.8486939692838,783.396624421051,91.2680322692314));
#80784=CARTESIAN_POINT('Ctrl Pts',(12.5210102394924,782.752202308121,91.0456283092697));
#80785=CARTESIAN_POINT('Ctrl Pts',(13.2092167288867,782.092549255413,90.8179678237289));
#80786=CARTESIAN_POINT('Ctrl Pts',(13.8995626461569,781.434022950849,90.5927654025733));
#80787=CARTESIAN_POINT('Ctrl Pts',(14.5901383989481,780.77491761496,90.3698910252198));
#80788=CARTESIAN_POINT('Ctrl Pts',(14.7454939012683,780.626641860816,90.3197520495779));
#80789=CARTESIAN_POINT('Ctrl Pts',(14.9008608885752,780.478336654654,90.2697308715161));
#80790=CARTESIAN_POINT('Ctrl Pts',(15.0562173685823,780.329982323209,90.2198259708646));
#80791=CARTESIAN_POINT('Ctrl Pts',(15.2025918930187,780.190205117184,90.172806328687));
#80792=CARTESIAN_POINT('Ctrl Pts',(15.3489560630232,780.050385112899,90.1258907692892));
#80793=CARTESIAN_POINT('Ctrl Pts',(15.4952926315725,779.910504634489,90.0790775852241));
#80794=CARTESIAN_POINT('Ctrl Pts',(16.1928584000468,779.2437141365,89.855925743953));
#80795=CARTESIAN_POINT('Ctrl Pts',(16.889954019786,778.575674525802,89.6351177879038));
#80796=CARTESIAN_POINT('Ctrl Pts',(17.5847563840439,777.904658212687,89.4168036934157));
#80797=CARTESIAN_POINT('Ctrl Pts',(18.2975118197521,777.216303438401,89.1928485580525));
#80798=CARTESIAN_POINT('Ctrl Pts',(19.0078543826094,776.524816528801,88.9715177779207));
#80799=CARTESIAN_POINT('Ctrl Pts',(19.7137724683992,775.828294175026,88.7529787110537));
#80800=CARTESIAN_POINT('Ctrl Pts',(20.3772626986632,775.173634964287,88.54757451655));
#80801=CARTESIAN_POINT('Ctrl Pts',(21.0368441158626,774.514527240835,88.3446365659295));
#80802=CARTESIAN_POINT('Ctrl Pts',(21.6908079933751,773.849356636992,88.1443086044901));
#80803=CARTESIAN_POINT('Ctrl Pts',(21.7326266723076,773.806821327514,88.1314983392924));
#80804=CARTESIAN_POINT('Ctrl Pts',(21.7744223670276,773.764261214263,88.1186987483769));
#80805=CARTESIAN_POINT('Ctrl Pts',(21.8161946252474,773.721675870246,88.1059098700103));
#80806=CARTESIAN_POINT('Ctrl Pts',(21.9874035471954,773.547134412572,88.053493022768));
#80807=CARTESIAN_POINT('Ctrl Pts',(22.1582247673597,773.372162484028,88.0012561601995));
#80808=CARTESIAN_POINT('Ctrl Pts',(22.3286263866547,773.196731155624,87.9492018283233));
#80809=CARTESIAN_POINT('Ctrl Pts',(22.9217001552904,772.586151752073,87.7680294961155));
#80810=CARTESIAN_POINT('Ctrl Pts',(23.5096391298023,771.969986601658,87.5891234565314));
#80811=CARTESIAN_POINT('Ctrl Pts',(24.0901190310581,771.347652427082,87.4129600323426));
#80812=CARTESIAN_POINT('Ctrl Pts',(24.4191223749035,770.994926994243,87.3131144468262));
#80813=CARTESIAN_POINT('Ctrl Pts',(24.7457287032067,770.640219608101,87.2141500896773));
#80814=CARTESIAN_POINT('Ctrl Pts',(25.0695077938623,770.283422208196,87.1161552851402));
#80815=CARTESIAN_POINT('Ctrl Pts',(25.2378156931276,770.097950624099,87.0652153073388));
#80816=CARTESIAN_POINT('Ctrl Pts',(25.4053776088423,769.911894013562,87.0145331826002));
#80817=CARTESIAN_POINT('Ctrl Pts',(25.5721341822133,769.725234149169,86.9641212714148));
#80818=CARTESIAN_POINT('Ctrl Pts',(26.0657199242206,769.172736302715,86.8149061605171));
#80819=CARTESIAN_POINT('Ctrl Pts',(26.5524710659009,768.614757993071,86.667993036751));
#80820=CARTESIAN_POINT('Ctrl Pts',(27.0309765036493,768.050324506237,86.5236723647956));
#80821=CARTESIAN_POINT('Ctrl Pts',(27.4081607721694,767.605407029726,86.4099108841739));
#80822=CARTESIAN_POINT('Ctrl Pts',(27.7802208709166,767.15647821111,86.2977603859367));
#80823=CARTESIAN_POINT('Ctrl Pts',(28.1464464456118,766.703049004253,86.1873675997798));
#80824=CARTESIAN_POINT('Ctrl Pts',(28.2997018283907,766.513301287377,86.14117123921));
#80825=CARTESIAN_POINT('Ctrl Pts',(28.4519381960058,766.322761541815,86.0952825656747));
#80826=CARTESIAN_POINT('Ctrl Pts',(28.6031049900163,766.131389970733,86.049711726047));
#80827=CARTESIAN_POINT('Ctrl Pts',(29.0146873705057,765.610341897316,85.9256358350576));
#80828=CARTESIAN_POINT('Ctrl Pts',(29.4183518970935,765.083145013738,85.8039128044781));
#80829=CARTESIAN_POINT('Ctrl Pts',(29.8128239835195,764.548824944325,85.6848253174677));
#80830=CARTESIAN_POINT('Ctrl Pts',(30.1808879757273,764.050275149214,85.5737101906962));
#80831=CARTESIAN_POINT('Ctrl Pts',(30.5409489517119,763.545523878989,85.4648895910462));
#80832=CARTESIAN_POINT('Ctrl Pts',(30.8919292568867,763.033753666233,85.3586037439776));
#80833=CARTESIAN_POINT('Ctrl Pts',(30.9171116196388,762.997034844825,85.3509778780335));
#80834=CARTESIAN_POINT('Ctrl Pts',(30.9422472176289,762.960279879347,85.3433650653162));
#80835=CARTESIAN_POINT('Ctrl Pts',(30.9673356440519,762.923488462468,85.3357653967386));
#80836=CARTESIAN_POINT('Ctrl Pts',(31.0931562269573,762.738976391463,85.2976524153105));
#80837=CARTESIAN_POINT('Ctrl Pts',(31.2177928973397,762.553543736145,85.2598702174453));
#80838=CARTESIAN_POINT('Ctrl Pts',(31.3411923375727,762.367153525296,85.2224307953528));
#80839=CARTESIAN_POINT('Ctrl Pts',(31.67162055091,761.868054143339,85.1221787899384));
#80840=CARTESIAN_POINT('Ctrl Pts',(31.9931781805276,761.362119302838,85.0243785666424));
#80841=CARTESIAN_POINT('Ctrl Pts',(32.3046347587608,760.848393719462,84.9293386946084));
#80842=CARTESIAN_POINT('Ctrl Pts',(32.6103846810005,760.344080861276,84.8360401884446));
#80843=CARTESIAN_POINT('Ctrl Pts',(32.9064003732124,759.83226018293,84.745401791375));
#80844=CARTESIAN_POINT('Ctrl Pts',(33.191477489211,759.311999617512,84.6577259631547));
#80845=CARTESIAN_POINT('Ctrl Pts',(33.2722338246568,759.164620770238,84.6328892498695));
#80846=CARTESIAN_POINT('Ctrl Pts',(33.3521121179694,759.016564468346,84.6082903403824));
#80847=CARTESIAN_POINT('Ctrl Pts',(33.4310843780547,758.867809091466,84.5839362708936));
#80848=CARTESIAN_POINT('Ctrl Pts',(33.5184886981044,758.703170741799,84.5569818582706));
#80849=CARTESIAN_POINT('Ctrl Pts',(33.604784507844,758.537673273943,84.5303280434968));
#80850=CARTESIAN_POINT('Ctrl Pts',(33.6899309478928,758.371291959995,84.5039849906636));
#80851=CARTESIAN_POINT('Ctrl Pts',(33.9690198476379,757.825935303612,84.4176390010139));
#80852=CARTESIAN_POINT('Ctrl Pts',(34.235731054912,757.271036232819,84.3346450446765));
#80853=CARTESIAN_POINT('Ctrl Pts',(34.4885049018037,756.705379129562,84.2554525761138));
#80854=CARTESIAN_POINT('Ctrl Pts',(34.5543284959757,756.558079145551,84.2348304548925));
#80855=CARTESIAN_POINT('Ctrl Pts',(34.6192302660274,756.409996636499,84.2144591104201));
#80856=CARTESIAN_POINT('Ctrl Pts',(34.683162161741,756.261152515248,84.1943530418467));
#80857=CARTESIAN_POINT('Ctrl Pts',(34.7794358499984,756.037011304225,84.1640757388463));
#80858=CARTESIAN_POINT('Ctrl Pts',(34.8731112642366,755.81203754227,84.134524996995));
#80859=CARTESIAN_POINT('Ctrl Pts',(34.9640667158625,755.586434948884,84.1057441504196));
#80860=CARTESIAN_POINT('Ctrl Pts',(35.1154224134244,755.211017782751,84.0578509781911));
#80861=CARTESIAN_POINT('Ctrl Pts',(35.2592674497983,754.833824929926,84.0120879836128));
#80862=CARTESIAN_POINT('Ctrl Pts',(35.3954459345825,754.454814897335,83.968523258549));
#80863=CARTESIAN_POINT('Ctrl Pts',(35.4390765570408,754.33338276607,83.9545654290521));
#80864=CARTESIAN_POINT('Ctrl Pts',(35.4819193465824,754.211765261265,83.9408333754645));
#80865=CARTESIAN_POINT('Ctrl Pts',(35.5239629769602,754.08997669971,83.9273314983401));
#80866=CARTESIAN_POINT('Ctrl Pts',(35.6660146583664,753.678492967467,83.8817130698071));
#80867=CARTESIAN_POINT('Ctrl Pts',(35.7989765135005,753.264811291308,83.8387082730724));
#80868=CARTESIAN_POINT('Ctrl Pts',(35.92285624938,752.848949522755,83.7983768427954));
#80869=CARTESIAN_POINT('Ctrl Pts',(36.0471797986685,752.431597881562,83.7579009205283));
#80870=CARTESIAN_POINT('Ctrl Pts',(36.1623561247641,752.012050272139,83.7201175790626));
#80871=CARTESIAN_POINT('Ctrl Pts',(36.268442795898,751.590333930163,83.6850727875611));
#80872=CARTESIAN_POINT('Ctrl Pts',(36.3750616706859,751.166501969178,83.6498521872997));
#80873=CARTESIAN_POINT('Ctrl Pts',(36.4724995532146,750.740479226775,83.6173977076522));
#80874=CARTESIAN_POINT('Ctrl Pts',(36.5608637350915,750.312306102992,83.5877411049482));
#80875=CARTESIAN_POINT('Ctrl Pts',(36.5947655315134,750.148033229442,83.5763630546332));
#80876=CARTESIAN_POINT('Ctrl Pts',(36.6273322267701,749.983443982138,83.5653966803727));
#80877=CARTESIAN_POINT('Ctrl Pts',(36.6585717280759,749.818541249099,83.5548431863892));
#80878=CARTESIAN_POINT('Ctrl Pts',(36.6697841668005,749.759354587583,83.5510553408836));
#80879=CARTESIAN_POINT('Ctrl Pts',(36.6808256450559,749.700127543216,83.547320581778));
#80880=CARTESIAN_POINT('Ctrl Pts',(36.6916965257908,749.640860451538,83.5436389647139));
#80881=CARTESIAN_POINT('Ctrl Pts',(36.7715340805677,749.205593080501,83.5166005571378));
#80882=CARTESIAN_POINT('Ctrl Pts',(36.8420681306053,748.768117375119,83.4924835988422));
#80883=CARTESIAN_POINT('Ctrl Pts',(36.9040112041995,748.328578403737,83.4710984305574));
#80884=CARTESIAN_POINT('Ctrl Pts',(36.9678585923859,747.875526695119,83.4490558184996));
#80885=CARTESIAN_POINT('Ctrl Pts',(37.0225793411126,747.420282447104,83.4299153750923));
#80886=CARTESIAN_POINT('Ctrl Pts',(37.0689991241824,746.963034706298,83.4134539836569));
#80887=CARTESIAN_POINT('Ctrl Pts',(37.117061798547,746.489604030473,83.3964099898287));
#80888=CARTESIAN_POINT('Ctrl Pts',(37.1562263895217,746.014024962391,83.3822378239292));
#80889=CARTESIAN_POINT('Ctrl Pts',(37.1874453911839,745.536547323445,83.3706765172477));
#80890=CARTESIAN_POINT('Ctrl Pts',(37.1988089751989,745.362747490762,83.3664682507177));
#80891=CARTESIAN_POINT('Ctrl Pts',(37.209120094727,745.188696526882,83.3626057969649));
#80892=CARTESIAN_POINT('Ctrl Pts',(37.2184254531716,745.014407957878,83.3590762444424));
#80893=CARTESIAN_POINT('Ctrl Pts',(37.2187740305499,745.00787913335,83.3589440279166));
#80894=CARTESIAN_POINT('Ctrl Pts',(37.2191211971741,745.00134996549,83.3588122778083));
#80895=CARTESIAN_POINT('Ctrl Pts',(37.2194669555068,744.994820454777,83.3586809934331));
#80896=CARTESIAN_POINT('Ctrl Pts',(37.2425322364403,744.559241656856,83.3499231105201));
#80897=CARTESIAN_POINT('Ctrl Pts',(37.2594390596283,744.122700322152,83.343187806879));
#80898=CARTESIAN_POINT('Ctrl Pts',(37.2716207511684,743.685890065863,83.3380039330951));
#80899=CARTESIAN_POINT('Ctrl Pts',(37.2818457931714,743.31924121392,83.3336527042856));
#80900=CARTESIAN_POINT('Ctrl Pts',(37.2887414425155,742.952402928708,83.3303946352932));
#80901=CARTESIAN_POINT('Ctrl Pts',(37.293128367296,742.585781657886,83.3279600207453));
#80902=CARTESIAN_POINT('Ctrl Pts',(37.2931885805528,742.580749554113,83.3279266041543));
#80903=CARTESIAN_POINT('Ctrl Pts',(37.2932483203103,742.575717439987,83.3278933422545));
#80904=CARTESIAN_POINT('Ctrl Pts',(37.2933075895563,742.570685315405,83.3278602340709));
#80905=CARTESIAN_POINT('Ctrl Pts',(37.2974212094887,742.221427489737,83.3255623394062));
#80906=CARTESIAN_POINT('Ctrl Pts',(37.2992717289621,741.872143582838,83.3240043233008));
#80907=CARTESIAN_POINT('Ctrl Pts',(37.2998365932158,741.522834600892,83.3228583018915));
#80908=CARTESIAN_POINT('Ctrl Pts',(37.3003789001298,741.187474955125,83.3217580458038));
#80909=CARTESIAN_POINT('Ctrl Pts',(37.299736351987,740.852092203344,83.3210374820026));
#80910=CARTESIAN_POINT('Ctrl Pts',(37.2987309819122,740.516704184972,83.320420517403));
#80911=CARTESIAN_POINT('Ctrl Pts',(37.2983399605194,740.386260785713,83.3201805596371));
#80912=CARTESIAN_POINT('Ctrl Pts',(37.2978935698031,740.255816775995,83.3199564322173));
#80913=CARTESIAN_POINT('Ctrl Pts',(37.297438237489,740.125373936259,83.3197325254973));
#80914=CARTESIAN_POINT('',(37.2974382339422,740.125373764374,83.3197325252249));
#80915=CARTESIAN_POINT('Ctrl Pts',(68.4577991911175,740.125189855522,98.7804139696777));
#80916=CARTESIAN_POINT('Ctrl Pts',(68.4314744168991,747.666651921185,98.7691090655225));
#80917=CARTESIAN_POINT('Ctrl Pts',(68.4050070734591,755.208031515623,98.7576983734677));
#80918=CARTESIAN_POINT('Ctrl Pts',(78.1222855324702,768.384861541845,105.310823299793));
#80919=CARTESIAN_POINT('Ctrl Pts',(85.7127868619961,772.226281106417,106.668510951594));
#80920=CARTESIAN_POINT('Ctrl Pts',(92.4568631339348,777.107328840337,108.39363837514));
#80921=CARTESIAN_POINT('Ctrl Pts',(68.4577992118746,740.125183909083,97.9632437490832));
#80922=CARTESIAN_POINT('Ctrl Pts',(68.430623262492,747.910488740229,97.953471433172));
#80923=CARTESIAN_POINT('Ctrl Pts',(68.4032928480487,755.695714014116,97.9435914375012));
#80924=CARTESIAN_POINT('Ctrl Pts',(78.9327187735727,768.917219170172,104.62754444939));
#80925=CARTESIAN_POINT('Ctrl Pts',(86.7452316640843,773.033321350878,106.046458844125));
#80926=CARTESIAN_POINT('Ctrl Pts',(93.6239591044408,778.248433884114,107.853507205599));
#80927=CARTESIAN_POINT('Ctrl Pts',(68.4577992329346,740.125177875847,97.1460735284887));
#80928=CARTESIAN_POINT('Ctrl Pts',(68.4297596841829,748.157884729622,97.1378338008051));
#80929=CARTESIAN_POINT('Ctrl Pts',(68.4015541154982,756.190515080161,97.1294854786493));
#80930=CARTESIAN_POINT('Ctrl Pts',(79.7198124540396,769.450651027237,103.926505090804));
#80931=CARTESIAN_POINT('Ctrl Pts',(87.7496608967702,773.852732995686,105.411629894754));
#80932=CARTESIAN_POINT('Ctrl Pts',(94.75050390177,779.413657557974,107.305932045411));
#80933=CARTESIAN_POINT('Ctrl Pts',(68.4577992542868,740.125171758922,96.3289033078942));
#80934=CARTESIAN_POINT('Ctrl Pts',(68.4288841269008,748.408712427461,96.3221961684255));
#80935=CARTESIAN_POINT('Ctrl Pts',(68.3997916362531,756.69217974737,96.3153802040162));
#80936=CARTESIAN_POINT('Ctrl Pts',(80.4924129928722,769.987477901082,103.219552953207));
#80937=CARTESIAN_POINT('Ctrl Pts',(88.7309063108587,774.685953843899,104.770645558223));
#80938=CARTESIAN_POINT('Ctrl Pts',(95.8384290337387,780.602056150837,106.751733915294));
#80939=CARTESIAN_POINT('Ctrl Pts',(68.4577992759202,740.125165561416,95.5117330872998));
#80940=CARTESIAN_POINT('Ctrl Pts',(68.4279970355747,748.662844371844,95.5065585360376));
#80941=CARTESIAN_POINT('Ctrl Pts',(68.3980061750953,757.200453046912,95.5012753218122));
#80942=CARTESIAN_POINT('Ctrl Pts',(81.2590704459109,770.530187531119,102.518460172987));
#80943=CARTESIAN_POINT('Ctrl Pts',(89.6935032939934,775.534588649946,104.130051696489));
#80944=CARTESIAN_POINT('Ctrl Pts',(96.8893696450024,781.812852902992,106.191658243183));
#80945=CARTESIAN_POINT('Ctrl Pts',(68.457799319728,740.125153011461,93.8773926461109));
#80946=CARTESIAN_POINT('Ctrl Pts',(68.4262006746925,749.177461829888,93.8752832712527));
#80947=CARTESIAN_POINT('Ctrl Pts',(68.3943908261618,758.229706968641,93.8730657605118));
#80948=CARTESIAN_POINT('Ctrl Pts',(82.7970768809045,771.632645704261,101.151412605607));
#80949=CARTESIAN_POINT('Ctrl Pts',(91.5899487624662,777.266193608426,102.862611652065));
#80950=CARTESIAN_POINT('Ctrl Pts',(98.9200297042542,784.277987128321,105.061117676372));
#80951=CARTESIAN_POINT('Ctrl Pts',(68.4577993419023,740.125146659012,93.0602224255164));
#80952=CARTESIAN_POINT('Ctrl Pts',(68.4252914051331,749.437947343551,93.0596456388496));
#80953=CARTESIAN_POINT('Ctrl Pts',(68.3925612750287,758.750687577726,93.0589617044525));
#80954=CARTESIAN_POINT('Ctrl Pts',(83.5454184581273,772.193289626093,100.442877153979));
#80955=CARTESIAN_POINT('Ctrl Pts',(92.5136141758915,778.147951298143,102.213866283972));
#80956=CARTESIAN_POINT('Ctrl Pts',(99.8997491522424,785.532324601496,104.490652781672));
#80957=CARTESIAN_POINT('Ctrl Pts',(68.4577993643362,740.125140232198,92.2430522049219));
#80958=CARTESIAN_POINT('Ctrl Pts',(68.4243714913817,749.70148217995,92.2440080064353));
#80959=CARTESIAN_POINT('Ctrl Pts',(68.3907108896609,759.277766932611,92.2448585685712));
#80960=CARTESIAN_POINT('Ctrl Pts',(84.2626728179383,772.761297551471,99.6877930536026));
#80961=CARTESIAN_POINT('Ctrl Pts',(93.4098678056052,779.043420219821,101.539441004633));
#80962=CARTESIAN_POINT('Ctrl Pts',(100.84523195766,786.807804636399,103.915676206375));
#80963=CARTESIAN_POINT('Ctrl Pts',(68.4577993870189,740.125133734129,91.4258819843274));
#80964=CARTESIAN_POINT('Ctrl Pts',(68.4234413783645,749.967938877182,91.4283703740089));
#80965=CARTESIAN_POINT('Ctrl Pts',(68.3888407163122,759.810690128692,91.430756549369));
#80966=CARTESIAN_POINT('Ctrl Pts',(84.9381531776121,773.334767609609,98.8645608264283));
#80967=CARTESIAN_POINT('Ctrl Pts',(94.275593983119,779.950505355874,100.828618751446));
#80968=CARTESIAN_POINT('Ctrl Pts',(101.757590853987,788.103948395178,103.336808383945));
#80969=CARTESIAN_POINT('Ctrl Pts',(68.4577994213996,740.125123884805,90.2001266534357));
#80970=CARTESIAN_POINT('Ctrl Pts',(68.4220315773295,750.371815521424,90.20491392535));
#80971=CARTESIAN_POINT('Ctrl Pts',(68.3860073486596,760.618458324829,90.2096054914207));
#80972=CARTESIAN_POINT('Ctrl Pts',(85.8723434708061,774.20050954551,97.4950169758646));
#80973=CARTESIAN_POINT('Ctrl Pts',(95.5233794963349,781.325611310863,99.6916402144542));
#80974=CARTESIAN_POINT('Ctrl Pts',(103.077773363038,790.07863781811,102.463526327259));
#80975=CARTESIAN_POINT('Ctrl Pts',(68.4577994329193,740.12512058466,89.7915415431385));
#80976=CARTESIAN_POINT('Ctrl Pts',(68.4215592050669,750.507139669237,89.797095109128));
#80977=CARTESIAN_POINT('Ctrl Pts',(68.3850581429893,760.889111659347,89.8025553875324));
#80978=CARTESIAN_POINT('Ctrl Pts',(86.1750232524054,774.487588917475,97.0215011063112));
#80979=CARTESIAN_POINT('Ctrl Pts',(95.933007509302,781.785483359929,99.3035995687804));
#80980=CARTESIAN_POINT('Ctrl Pts',(103.509774893482,790.741946589881,102.171602254524));
#80981=CARTESIAN_POINT('Ctrl Pts',(68.4577994444972,740.125117267868,89.3829564328412));
#80982=CARTESIAN_POINT('Ctrl Pts',(68.4210844498364,750.643146484044,89.3892762929044));
#80983=CARTESIAN_POINT('Ctrl Pts',(68.3841042630244,761.161130386228,89.3955054536124));
#80984=CARTESIAN_POINT('Ctrl Pts',(86.4714289387005,774.773865563578,96.5353477393156));
#80985=CARTESIAN_POINT('Ctrl Pts',(96.3374018422195,782.247433893577,98.9088166869112));
#80986=CARTESIAN_POINT('Ctrl Pts',(103.933827953702,791.410290842359,101.87891950692));
#80987=CARTESIAN_POINT('Ctrl Pts',(68.4577994561318,740.125113934815,88.9743713225439));
#80988=CARTESIAN_POINT('Ctrl Pts',(68.4206073672543,750.779820033107,88.9814574766802));
#80989=CARTESIAN_POINT('Ctrl Pts',(68.3831457844632,761.434482628579,88.9884556109133));
#80990=CARTESIAN_POINT('Ctrl Pts',(86.763989289185,775.060046216945,96.0409175425288));
#80991=CARTESIAN_POINT('Ctrl Pts',(96.7376151784749,782.712046184646,98.5095940450559));
#80992=CARTESIAN_POINT('Ctrl Pts',(104.350029251381,792.083635277778,101.585546375814));
#80993=CARTESIAN_POINT('Ctrl Pts',(68.4577994795118,740.125107236968,88.1572011019495));
#80994=CARTESIAN_POINT('Ctrl Pts',(68.4196486586195,751.054468734271,88.1658198442325));
#80995=CARTESIAN_POINT('Ctrl Pts',(68.3812197819262,761.983790390204,88.17435595054));
#80996=CARTESIAN_POINT('Ctrl Pts',(87.3462507788668,775.633644251365,95.0442194679357));
#80997=CARTESIAN_POINT('Ctrl Pts',(97.5317591657831,783.647776074199,97.7068688370514));
#80998=CARTESIAN_POINT('Ctrl Pts',(105.166895678368,793.440269165875,100.99755057259));
#80999=CARTESIAN_POINT('Ctrl Pts',(68.4577994912571,740.125103872174,87.7486159916522));
#81000=CARTESIAN_POINT('Ctrl Pts',(68.4191670325668,751.192443886372,87.758001028009));
#81001=CARTESIAN_POINT('Ctrl Pts',(68.3802522579229,762.259745909587,87.767306132953));
#81002=CARTESIAN_POINT('Ctrl Pts',(87.6359537956839,775.921054293985,94.5419456284517));
#81003=CARTESIAN_POINT('Ctrl Pts',(97.9256898168359,784.118893672684,97.3033662709022));
#81004=CARTESIAN_POINT('Ctrl Pts',(105.567560807675,794.123558618553,100.702927900473));
#81005=CARTESIAN_POINT('Ctrl Pts',(68.4577995030566,740.125100491896,87.3400308813549));
#81006=CARTESIAN_POINT('Ctrl Pts',(68.4186831903952,751.331053907253,87.3501822117867));
#81007=CARTESIAN_POINT('Ctrl Pts',(68.3792802829773,762.536971190724,87.3602562494283));
#81008=CARTESIAN_POINT('Ctrl Pts',(87.9269247718117,776.209776667823,94.0400932925943));
#81009=CARTESIAN_POINT('Ctrl Pts',(98.3175187793482,784.593854821168,96.9000235404456));
#81010=CARTESIAN_POINT('Ctrl Pts',(105.960541531152,794.81179290555,100.407746070846));
#81011=CARTESIAN_POINT('Ctrl Pts',(68.4577995149088,740.125097096526,86.9314457710577));
#81012=CARTESIAN_POINT('Ctrl Pts',(68.418197187721,751.470282864177,86.9423633955665));
#81013=CARTESIAN_POINT('Ctrl Pts',(68.3783039290729,762.815434356689,86.9532062214676));
#81014=CARTESIAN_POINT('Ctrl Pts',(88.2218463652581,776.500520302144,93.543006087808));
#81015=CARTESIAN_POINT('Ctrl Pts',(98.7082726780542,785.073258039394,96.4991377651511));
#81016=CARTESIAN_POINT('Ctrl Pts',(106.345908497826,795.504951976008,100.112068018336));
#81017=CARTESIAN_POINT('Ctrl Pts',(68.4577995506192,740.125086866296,85.7056904401659));
#81018=CARTESIAN_POINT('Ctrl Pts',(68.4167328650399,751.889778744866,85.7189069469152));
#81019=CARTESIAN_POINT('Ctrl Pts',(68.3753619469564,763.654441877978,85.7320554688825));
#81020=CARTESIAN_POINT('Ctrl Pts',(89.126475179618,777.380962958098,92.079063941594));
#81021=CARTESIAN_POINT('Ctrl Pts',(99.8803532649971,786.526610646288,95.310735855761));
#81022=CARTESIAN_POINT('Ctrl Pts',(107.479344282573,797.599164568952,99.2237271886368));
#81023=CARTESIAN_POINT('Ctrl Pts',(68.4577995746314,740.125079987321,84.8885202195714));
#81024=CARTESIAN_POINT('Ctrl Pts',(68.415748230377,752.171854678547,84.9032693144991));
#81025=CARTESIAN_POINT('Ctrl Pts',(68.3733831076234,764.218604097713,84.9179534581158));
#81026=CARTESIAN_POINT('Ctrl Pts',(89.7759151781224,777.989739099571,91.1817265572392));
#81027=CARTESIAN_POINT('Ctrl Pts',(100.667408968764,787.523124895316,94.5593136514548));
#81028=CARTESIAN_POINT('Ctrl Pts',(108.204747985368,799.014953473009,98.6297577392777));
#81029=CARTESIAN_POINT('Ctrl Pts',(68.4577995988381,740.125073052633,84.0713499989769));
#81030=CARTESIAN_POINT('Ctrl Pts',(68.4147556210969,752.456215163547,84.0876316820978));
#81031=CARTESIAN_POINT('Ctrl Pts',(68.3713879526406,764.787335304437,84.1038504221104));
#81032=CARTESIAN_POINT('Ctrl Pts',(90.4503596257349,778.617103253815,90.3217783746812));
#81033=CARTESIAN_POINT('Ctrl Pts',(101.452424543665,788.543884485768,93.8278698898637));
#81034=CARTESIAN_POINT('Ctrl Pts',(108.900401281468,800.450285635657,98.0345313843018));
#81035=CARTESIAN_POINT('Ctrl Pts',(68.4577996232285,740.12506606534,83.2541797783824));
#81036=CARTESIAN_POINT('Ctrl Pts',(68.4137554821241,752.742732737961,83.2719940497075));
#81037=CARTESIAN_POINT('Ctrl Pts',(68.3693776870735,765.36038061127,83.289746845202));
#81038=CARTESIAN_POINT('Ctrl Pts',(91.1282679588575,779.259942042811,89.4579482431207));
#81039=CARTESIAN_POINT('Ctrl Pts',(102.227500324588,789.585635228018,93.0955009722738));
#81040=CARTESIAN_POINT('Ctrl Pts',(109.566583027439,801.905170120104,97.4384971415098));
#81041=CARTESIAN_POINT('Ctrl Pts',(68.4577996477916,740.125059028551,82.4370095577878));
#81042=CARTESIAN_POINT('Ctrl Pts',(68.4127482583835,753.031279939886,82.4563564173248));
#81043=CARTESIAN_POINT('Ctrl Pts',(68.3673535182661,765.937485129951,82.4756432120661));
#81044=CARTESIAN_POINT('Ctrl Pts',(91.7879438810236,779.915237078138,88.5489418011639));
#81045=CARTESIAN_POINT('Ctrl Pts',(102.984580913554,790.645217922039,92.3412800893767));
#81046=CARTESIAN_POINT('Ctrl Pts',(110.203416346979,803.379710979161,96.8420808181083));
#81047=CARTESIAN_POINT('',(68.4577985491519,740.125373764374,83.3197325252249));
#81048=CARTESIAN_POINT('',(68.4577985491519,740.125373764374,83.3197325252249));
#81049=CARTESIAN_POINT('Ctrl Pts',(68.4577985491519,740.125373764374,83.3197325252249));
#81050=CARTESIAN_POINT('Ctrl Pts',(68.4521142211524,741.75380716905,83.3224194785555));
#81051=CARTESIAN_POINT('Ctrl Pts',(68.4499256999464,743.382130664584,83.3261020865078));
#81052=CARTESIAN_POINT('Ctrl Pts',(68.5797134472817,745.820412963062,83.3752834133531));
#81053=CARTESIAN_POINT('Ctrl Pts',(68.6448130821809,746.634567916206,83.3988648178505));
#81054=CARTESIAN_POINT('Ctrl Pts',(68.8296879542825,748.245163355258,83.4636594090421));
#81055=CARTESIAN_POINT('Ctrl Pts',(68.9493582190413,749.04253454444,83.5048356188137));
#81056=CARTESIAN_POINT('Ctrl Pts',(69.3984362959591,751.408519901678,83.656381909957));
#81057=CARTESIAN_POINT('Ctrl Pts',(69.8191726784943,752.950650995558,83.7950334335352));
#81058=CARTESIAN_POINT('Ctrl Pts',(70.6317188459528,755.211605983176,84.0548612189204));
#81059=CARTESIAN_POINT('Ctrl Pts',(70.9324330224284,755.95665758029,84.1500172544934));
#81060=CARTESIAN_POINT('Ctrl Pts',(71.4258868704458,757.062054538247,84.3045997067613));
#81061=CARTESIAN_POINT('Ctrl Pts',(71.5976113189271,757.428799566548,84.3581584224953));
#81062=CARTESIAN_POINT('Ctrl Pts',(71.9513538712402,758.15192384479,84.4680386926666));
#81063=CARTESIAN_POINT('Ctrl Pts',(72.1337262198999,758.509139597191,84.5244719529524));
#81064=CARTESIAN_POINT('Ctrl Pts',(73.0709910162594,760.27515071812,84.813518540632));
#81065=CARTESIAN_POINT('Ctrl Pts',(73.9015561965611,761.624180220335,85.0665674297279));
#81066=CARTESIAN_POINT('Ctrl Pts',(75.6790516558849,764.230121938606,85.6050503921944));
#81067=CARTESIAN_POINT('Ctrl Pts',(76.6261100820584,765.486924428665,85.8905575072476));
#81068=CARTESIAN_POINT('Ctrl Pts',(78.6034328418404,767.934229456814,86.4866793099093));
#81069=CARTESIAN_POINT('Ctrl Pts',(79.6338181982263,769.124636451881,86.7973264992592));
#81070=CARTESIAN_POINT('Ctrl Pts',(81.7524708372019,771.458757542837,87.4386664033878));
#81071=CARTESIAN_POINT('Ctrl Pts',(82.8414898324954,772.603045483691,87.7695806430336));
#81072=CARTESIAN_POINT('Ctrl Pts',(86.1553991306081,775.980737157317,88.7843870404448));
#81073=CARTESIAN_POINT('Ctrl Pts',(88.4295363397,778.162606809164,89.4905766503777));
#81074=CARTESIAN_POINT('Ctrl Pts',(92.9793970190661,782.507828567648,90.9525504249873));
#81075=CARTESIAN_POINT('Ctrl Pts',(95.256518702732,784.669931234052,91.708224027398));
#81076=CARTESIAN_POINT('Ctrl Pts',(99.6798110453827,789.094244285017,93.2790928565411));
#81077=CARTESIAN_POINT('Ctrl Pts',(101.826042863888,791.356276291902,94.0946429907112));
#81078=CARTESIAN_POINT('Ctrl Pts',(104.820439166947,794.933117908512,95.3858318597951));
#81079=CARTESIAN_POINT('Ctrl Pts',(105.780609774061,796.156382916215,95.827771932233));
#81080=CARTESIAN_POINT('Ctrl Pts',(107.150002788981,798.050254358706,96.5089305255182));
#81081=CARTESIAN_POINT('Ctrl Pts',(107.594705916051,798.691342353046,96.7389844066105));
#81082=CARTESIAN_POINT('Ctrl Pts',(108.243331370894,799.668541513458,97.0881426854701));
#81083=CARTESIAN_POINT('Ctrl Pts',(108.456477837002,799.996861973796,97.2052035713835));
#81084=CARTESIAN_POINT('Ctrl Pts',(108.771609297049,800.493252018569,97.3817121458909));
#81085=CARTESIAN_POINT('Ctrl Pts',(108.875889222769,800.65936627551,97.4407009280924));
#81086=CARTESIAN_POINT('Ctrl Pts',(109.082932430931,800.992892849213,97.5589647600582));
#81087=CARTESIAN_POINT('Ctrl Pts',(109.186653881671,801.161883674408,97.6187977856326));
#81088=CARTESIAN_POINT('Ctrl Pts',(109.28716016657,801.327730313361,97.677680855745));
#81089=CARTESIAN_POINT('Origin',(52.8776183915471,763.53825870998,301.513705792983));
#81090=CARTESIAN_POINT('',(109.164743594634,804.5210255586,96.7791116555879));
#81091=CARTESIAN_POINT('',(-3.40942206489524,804.520974706055,96.7791223637616));
#81092=CARTESIAN_POINT('Ctrl Pts',(109.164743594634,804.5210255586,96.7791116555879));
#81093=CARTESIAN_POINT('Ctrl Pts',(108.81785985458,804.8963810802,96.7588565871085));
#81094=CARTESIAN_POINT('Ctrl Pts',(108.468245873048,805.269049622901,96.7392277597907));
#81095=CARTESIAN_POINT('Ctrl Pts',(108.11577894047,805.639042885829,96.720204176775));
#81096=CARTESIAN_POINT('Ctrl Pts',(107.74545819184,806.027777741361,96.7002169755574));
#81097=CARTESIAN_POINT('Ctrl Pts',(107.37198808282,806.413559445882,96.6808978891222));
#81098=CARTESIAN_POINT('Ctrl Pts',(106.995272778489,806.7963641143,96.6622233680472));
#81099=CARTESIAN_POINT('Ctrl Pts',(106.613731311482,807.184072957255,96.643309604564));
#81100=CARTESIAN_POINT('Ctrl Pts',(106.228861219377,807.568727757392,96.6250570349512));
#81101=CARTESIAN_POINT('Ctrl Pts',(105.840607577229,807.950268251547,96.6074419190684));
#81102=CARTESIAN_POINT('Ctrl Pts',(105.434092518505,808.349754410979,96.5889982804513));
#81103=CARTESIAN_POINT('Ctrl Pts',(105.023868199041,808.74582631095,96.5712534762176));
#81104=CARTESIAN_POINT('Ctrl Pts',(104.609918091164,809.138378549129,96.5541809523683));
#81105=CARTESIAN_POINT('Ctrl Pts',(104.248161472504,809.481435278985,96.5392610420162));
#81106=CARTESIAN_POINT('Ctrl Pts',(103.883560272872,809.821803233661,96.5248545843592));
#81107=CARTESIAN_POINT('Ctrl Pts',(103.516129310237,810.159392437004,96.5109442003283));
#81108=CARTESIAN_POINT('Ctrl Pts',(103.06479988911,810.574066090609,96.4938575467505));
#81109=CARTESIAN_POINT('Ctrl Pts',(102.60906554779,810.98464433311,96.4775075766846));
#81110=CARTESIAN_POINT('Ctrl Pts',(102.148842854877,811.391053015295,96.4618608159888));
#81111=CARTESIAN_POINT('Ctrl Pts',(101.653703754645,811.828295316299,96.4450269589631));
#81112=CARTESIAN_POINT('Ctrl Pts',(101.153369718894,812.260711381115,96.4290070688144));
#81113=CARTESIAN_POINT('Ctrl Pts',(100.64777226437,812.688159362852,96.4137620187931));
#81114=CARTESIAN_POINT('Ctrl Pts',(100.087326977579,813.161977426152,96.3968631670388));
#81115=CARTESIAN_POINT('Ctrl Pts',(99.5204148958492,813.629691121572,96.3809163971792));
#81116=CARTESIAN_POINT('Ctrl Pts',(98.9469783994167,814.09104744428,96.3658713278112));
#81117=CARTESIAN_POINT('Ctrl Pts',(98.4269437329283,814.509439511936,96.3522273451213));
#81118=CARTESIAN_POINT('Ctrl Pts',(97.901544405208,814.922601805145,96.3393250150671));
#81119=CARTESIAN_POINT('Ctrl Pts',(97.3707511754493,815.330311529557,96.3271282343743));
#81120=CARTESIAN_POINT('Ctrl Pts',(96.666210865658,815.87147882303,96.310939023273));
#81121=CARTESIAN_POINT('Ctrl Pts',(95.9550708055675,816.40080863672,96.2960592932168));
#81122=CARTESIAN_POINT('Ctrl Pts',(95.2375484879537,816.917927766701,96.2823758101844));
#81123=CARTESIAN_POINT('Ctrl Pts',(94.6380435770987,817.349991620758,96.2709429737775));
#81124=CARTESIAN_POINT('Ctrl Pts',(94.0340839728432,817.773530116061,96.2603453667684));
#81125=CARTESIAN_POINT('Ctrl Pts',(93.4257633003275,818.18833773882,96.250518440248));
#81126=CARTESIAN_POINT('Ctrl Pts',(92.8704692631059,818.566987043239,96.2415481159642));
#81127=CARTESIAN_POINT('Ctrl Pts',(92.3115417089347,818.938360749592,96.2332200210036));
#81128=CARTESIAN_POINT('Ctrl Pts',(91.74901452317,819.302323611573,96.2254853180879));
#81129=CARTESIAN_POINT('Ctrl Pts',(91.2207405796963,819.644124152493,96.2182215944595));
#81130=CARTESIAN_POINT('Ctrl Pts',(90.6892923056537,819.979388560072,96.2114812282335));
#81131=CARTESIAN_POINT('Ctrl Pts',(90.154658713138,820.3080299507,96.2052234643063));
#81132=CARTESIAN_POINT('Ctrl Pts',(89.6564796614257,820.614262590454,96.1993923924419));
#81133=CARTESIAN_POINT('Ctrl Pts',(89.1555349269183,820.914744481525,96.1939803706782));
#81134=CARTESIAN_POINT('Ctrl Pts',(88.6517785687755,821.209430866217,96.188953827893));
#81135=CARTESIAN_POINT('Ctrl Pts',(88.164171040949,821.494670540519,96.1840884201193));
#81136=CARTESIAN_POINT('Ctrl Pts',(87.6739294792162,821.774480098891,96.1795841890942));
#81137=CARTESIAN_POINT('Ctrl Pts',(87.1809740020025,822.048846495541,96.1754098686499));
#81138=CARTESIAN_POINT('Ctrl Pts',(86.7101113032903,822.310916617355,96.1714226286647));
#81139=CARTESIAN_POINT('Ctrl Pts',(86.236772571269,822.568020427466,96.167736400845));
#81140=CARTESIAN_POINT('Ctrl Pts',(85.7608508452064,822.820174359809,96.1643229932653));
#81141=CARTESIAN_POINT('Ctrl Pts',(85.3585836922947,823.03330445853,96.1614378512899));
#81142=CARTESIAN_POINT('Ctrl Pts',(84.9544706744878,823.242898585414,96.1587476093714));
#81143=CARTESIAN_POINT('Ctrl Pts',(84.5484240257377,823.448984348812,96.1562345944108));
#81144=CARTESIAN_POINT('Ctrl Pts',(84.3196278766203,823.56510802376,96.15481857941));
#81145=CARTESIAN_POINT('Ctrl Pts',(84.0902168468878,823.680118401631,96.1534588149677));
#81146=CARTESIAN_POINT('Ctrl Pts',(83.860148425969,823.794016828468,96.1521530930805));
#81147=CARTESIAN_POINT('Ctrl Pts',(83.4412841428411,824.001381153896,96.1497758860737));
#81148=CARTESIAN_POINT('Ctrl Pts',(83.0206056486588,824.204892507276,96.1475840276166));
#81149=CARTESIAN_POINT('Ctrl Pts',(82.5979699841252,824.404530042682,96.1455626897761));
#81150=CARTESIAN_POINT('Ctrl Pts',(82.1749665556623,824.604341296235,96.1435395930324));
#81151=CARTESIAN_POINT('Ctrl Pts',(81.7500025546443,824.800271983972,96.1416873134641));
#81152=CARTESIAN_POINT('Ctrl Pts',(81.3229848179643,824.992286687618,96.1399910525799));
#81153=CARTESIAN_POINT('Ctrl Pts',(80.8953263404622,825.184589509646,96.1382922464535));
#81154=CARTESIAN_POINT('Ctrl Pts',(80.465607961045,825.372964584677,96.1367499272253));
#81155=CARTESIAN_POINT('Ctrl Pts',(80.0337863500513,825.5573618177,96.135349303189));
#81156=CARTESIAN_POINT('Ctrl Pts',(79.6015643180971,825.741930039194,96.1339473803775));
#81157=CARTESIAN_POINT('Ctrl Pts',(79.1672351601097,825.922513033928,96.132687415312));
#81158=CARTESIAN_POINT('Ctrl Pts',(78.7308056556793,826.099046084197,96.1315546539312));
#81159=CARTESIAN_POINT('Ctrl Pts',(78.293687855145,826.275857546007,96.1304201060643));
#81160=CARTESIAN_POINT('Ctrl Pts',(77.8544630820329,826.448606275714,96.1294131630575));
#81161=CARTESIAN_POINT('Ctrl Pts',(77.4131884314279,826.617212779452,96.1285190853947));
#81162=CARTESIAN_POINT('Ctrl Pts',(77.1269068793251,826.72659801497,96.1279390431452));
#81163=CARTESIAN_POINT('Ctrl Pts',(76.839763575618,826.834239534435,96.1274065065369));
#81164=CARTESIAN_POINT('Ctrl Pts',(76.5517853843881,826.94011239358,96.1269174709266));
#81165=CARTESIAN_POINT('Ctrl Pts',(76.1094254387221,827.102742459485,96.1261662690211));
#81166=CARTESIAN_POINT('Ctrl Pts',(75.6649961893313,827.261246404981,96.1255203741796));
#81167=CARTESIAN_POINT('Ctrl Pts',(75.2184220958277,827.415588632804,96.1249665290083));
#81168=CARTESIAN_POINT('Ctrl Pts',(74.777972940969,827.567813996506,96.1244202800404));
#81169=CARTESIAN_POINT('Ctrl Pts',(74.3354373538775,827.715991025202,96.1239635813572));
#81170=CARTESIAN_POINT('Ctrl Pts',(73.8907836577821,827.860056255693,96.1235840476201));
#81171=CARTESIAN_POINT('Ctrl Pts',(73.5114595775302,827.982955067808,96.1232602759142));
#81172=CARTESIAN_POINT('Ctrl Pts',(73.1305946682942,828.102861107367,96.122992668282));
#81173=CARTESIAN_POINT('Ctrl Pts',(72.7481937098735,828.219717553959,96.1227736657644));
#81174=CARTESIAN_POINT('Ctrl Pts',(72.3376562878923,828.345172114858,96.1225385493846));
#81175=CARTESIAN_POINT('Ctrl Pts',(71.925008210908,828.467179924549,96.1223492899608));
#81176=CARTESIAN_POINT('Ctrl Pts',(71.5109237265998,828.585474558666,96.122201589357));
#81177=CARTESIAN_POINT('Ctrl Pts',(71.0891856621001,828.705955648695,96.1220511587827));
#81178=CARTESIAN_POINT('Ctrl Pts',(70.665957780851,828.822584769025,96.1219438236296));
#81179=CARTESIAN_POINT('Ctrl Pts',(70.242000467664,828.935106602914,96.1218746129595));
#81180=CARTESIAN_POINT('Ctrl Pts',(69.9067472443637,829.024085625872,96.1218198831565));
#81181=CARTESIAN_POINT('Ctrl Pts',(69.571038934021,829.110496760903,96.1217889821186));
#81182=CARTESIAN_POINT('Ctrl Pts',(69.2352705986298,829.194226670312,96.1217793560992));
#81183=CARTESIAN_POINT('Ctrl Pts',(69.1074681048227,829.226096534444,96.1217756921764));
#81184=CARTESIAN_POINT('Ctrl Pts',(68.979657110544,829.257578070376,96.1217751100857));
#81185=CARTESIAN_POINT('Ctrl Pts',(68.8518554245239,829.288669335678,96.1217775923678));
#81186=CARTESIAN_POINT('Ctrl Pts',(68.3162220814629,829.418976837027,96.121787995932));
#81187=CARTESIAN_POINT('Ctrl Pts',(67.7796819487752,829.542652600751,96.1218398401812));
#81188=CARTESIAN_POINT('Ctrl Pts',(67.2424596078188,829.659711642437,96.1219241710703));
#81189=CARTESIAN_POINT('Ctrl Pts',(66.7045825480914,829.776913345263,96.1220086047345));
#81190=CARTESIAN_POINT('Ctrl Pts',(66.1660216083883,829.887482190453,96.1221256049698));
#81191=CARTESIAN_POINT('Ctrl Pts',(65.6269501649236,829.991428532487,96.1222666012994));
#81192=CARTESIAN_POINT('Ctrl Pts',(65.0870382729811,830.095536933828,96.1224078174518));
#81193=CARTESIAN_POINT('Ctrl Pts',(64.5466142815548,830.193002168601,96.1225731052528));
#81194=CARTESIAN_POINT('Ctrl Pts',(64.0058002959459,830.283829877612,96.1227542611935));
#81195=CARTESIAN_POINT('Ctrl Pts',(63.4645517895842,830.374730562776,96.1229355626852));
#81196=CARTESIAN_POINT('Ctrl Pts',(62.9229126551899,830.458983054191,96.1231327585445));
#81197=CARTESIAN_POINT('Ctrl Pts',(62.3809532481644,830.536588205254,96.1233380223962));
#81198=CARTESIAN_POINT('Ctrl Pts',(61.8386286725166,830.614245646149,96.1235434245533));
#81199=CARTESIAN_POINT('Ctrl Pts',(61.2959833867929,830.685246788226,96.1237569062999));
#81200=CARTESIAN_POINT('Ctrl Pts',(60.7530358914191,830.749587646318,96.1239710119053));
#81201=CARTESIAN_POINT('Ctrl Pts',(60.2097935247798,830.813963447514,96.12418523379));
#81202=CARTESIAN_POINT('Ctrl Pts',(59.6662486156575,830.871671731051,96.1244000809341));
#81203=CARTESIAN_POINT('Ctrl Pts',(59.1223677365911,830.922703623813,96.1246084613678));
#81204=CARTESIAN_POINT('Ctrl Pts',(58.5781800982875,830.97376429954,96.124816959332));
#81205=CARTESIAN_POINT('Ctrl Pts',(58.0336561089993,831.01814105406,96.1250189840038));
#81206=CARTESIAN_POINT('Ctrl Pts',(57.4887103301528,831.055820072134,96.1252077968563));
#81207=CARTESIAN_POINT('Ctrl Pts',(56.943659265322,831.093506369965,96.1253966461883));
#81208=CARTESIAN_POINT('Ctrl Pts',(56.3981862451516,831.124492345937,96.1255722793249));
#81209=CARTESIAN_POINT('Ctrl Pts',(55.8521538618925,831.148759205987,96.1257283084493));
#81210=CARTESIAN_POINT('Ctrl Pts',(55.3060711495201,831.173028302772,96.1258843519552));
#81211=CARTESIAN_POINT('Ctrl Pts',(54.7594289696607,831.190577048051,96.1260207885621));
#81212=CARTESIAN_POINT('Ctrl Pts',(54.2120379841324,831.201381626344,96.1261315723995));
#81213=CARTESIAN_POINT('Ctrl Pts',(53.8259906871007,831.209001551326,96.1262097026613));
#81214=CARTESIAN_POINT('Ctrl Pts',(53.4395698705124,831.213266977978,96.1262750810007));
#81215=CARTESIAN_POINT('Ctrl Pts',(53.0526936028336,831.214168039196,96.1263256865));
#81216=CARTESIAN_POINT('Ctrl Pts',(53.0507674189968,831.21417252541,96.1263259384553));
#81217=CARTESIAN_POINT('Ctrl Pts',(53.0488412238427,831.214176928223,96.1263261900445));
#81218=CARTESIAN_POINT('Ctrl Pts',(53.0469150173836,831.214181247634,96.126326441268));
#81219=CARTESIAN_POINT('Ctrl Pts',(52.3346198024729,831.215778530047,96.1264193416725));
#81220=CARTESIAN_POINT('Ctrl Pts',(51.6215169228228,831.205826030126,96.1264155205298));
#81221=CARTESIAN_POINT('Ctrl Pts',(50.9075293471847,831.184317742721,96.1263391289961));
#81222=CARTESIAN_POINT('Ctrl Pts',(50.1715641524487,831.162147397649,96.1262603860152));
#81223=CARTESIAN_POINT('Ctrl Pts',(49.4346598209972,831.127701084149,96.1261044758506));
#81224=CARTESIAN_POINT('Ctrl Pts',(48.6967885724123,831.080969582942,96.125896924031));
#81225=CARTESIAN_POINT('Ctrl Pts',(48.000718975506,831.036885500157,96.1257011303723));
#81226=CARTESIAN_POINT('Ctrl Pts',(47.3037901271249,830.981870161356,96.1254593251443));
#81227=CARTESIAN_POINT('Ctrl Pts',(46.6060121350389,830.915887966615,96.125192980259));
#81228=CARTESIAN_POINT('Ctrl Pts',(46.0831370663034,830.866444669461,96.1249933965779));
#81229=CARTESIAN_POINT('Ctrl Pts',(45.5597859324478,830.810842890367,96.124780029375));
#81230=CARTESIAN_POINT('Ctrl Pts',(45.0359707212101,830.749049777422,96.1245622001286));
#81231=CARTESIAN_POINT('Ctrl Pts',(44.4025671667175,830.674328813725,96.1242987984251));
#81232=CARTESIAN_POINT('Ctrl Pts',(43.7714150067874,830.590901454991,96.1240300924934));
#81233=CARTESIAN_POINT('Ctrl Pts',(43.1426290306698,830.498910823778,96.1237662142207));
#81234=CARTESIAN_POINT('Ctrl Pts',(42.5654376360675,830.414468417718,96.12352398829));
#81235=CARTESIAN_POINT('Ctrl Pts',(41.9902401605419,830.322810512071,96.1232858165673));
#81236=CARTESIAN_POINT('Ctrl Pts',(41.4171018972515,830.224010399001,96.1230601152048));
#81237=CARTESIAN_POINT('Ctrl Pts',(40.8646821681992,830.128781838654,96.1228425727836));
#81238=CARTESIAN_POINT('Ctrl Pts',(40.3141756799341,830.026918383084,96.1226366023955));
#81239=CARTESIAN_POINT('Ctrl Pts',(39.7656155656075,829.918446237259,96.1224504934597));
#81240=CARTESIAN_POINT('Ctrl Pts',(39.2433139742531,829.815166445487,96.1222732932026));
#81241=CARTESIAN_POINT('Ctrl Pts',(38.7227769897778,829.705895614109,96.1221140905957));
#81242=CARTESIAN_POINT('Ctrl Pts',(38.2040076146669,829.590617471609,96.1219808803541));
#81243=CARTESIAN_POINT('Ctrl Pts',(37.8404778949911,829.509835851031,96.1218875327432));
#81244=CARTESIAN_POINT('Ctrl Pts',(37.4778156605375,829.426103522171,96.1218069655784));
#81245=CARTESIAN_POINT('Ctrl Pts',(37.1160133445364,829.339402126673,96.1217422273291));
#81246=CARTESIAN_POINT('Ctrl Pts',(36.9923124132681,829.30975874715,96.1217200931929));
#81247=CARTESIAN_POINT('Ctrl Pts',(36.8687142495218,829.279774758988,96.1217017401159));
#81248=CARTESIAN_POINT('Ctrl Pts',(36.7452224780983,829.249449924558,96.1216872005585));
#81249=CARTESIAN_POINT('Ctrl Pts',(36.2993203358342,829.139953490261,96.121634701354));
#81250=CARTESIAN_POINT('Ctrl Pts',(35.8548008687036,829.02601443886,96.1216319013983));
#81251=CARTESIAN_POINT('Ctrl Pts',(35.4115522887877,828.907694732824,96.1216850275004));
#81252=CARTESIAN_POINT('Ctrl Pts',(34.9603240819995,828.787244964451,96.1217391100104));
#81253=CARTESIAN_POINT('Ctrl Pts',(34.5104129852087,828.662255071877,96.1218511518375));
#81254=CARTESIAN_POINT('Ctrl Pts',(34.0617533635338,828.532776578757,96.1220280134034));
#81255=CARTESIAN_POINT('Ctrl Pts',(33.6002876660254,828.399602385552,96.1222099231228));
#81256=CARTESIAN_POINT('Ctrl Pts',(33.1401459038875,828.261679322302,96.1224604071805));
#81257=CARTESIAN_POINT('Ctrl Pts',(32.6813112387729,828.119054297259,96.1227872133734));
#81258=CARTESIAN_POINT('Ctrl Pts',(32.2149424150519,827.974087340269,96.1231193857905));
#81259=CARTESIAN_POINT('Ctrl Pts',(31.749924115111,827.824262281401,96.1235304099026));
#81260=CARTESIAN_POINT('Ctrl Pts',(31.2862929699484,827.669625492323,96.1240286780445));
#81261=CARTESIAN_POINT('Ctrl Pts',(30.812451946628,827.511583360892,96.1245379188251));
#81262=CARTESIAN_POINT('Ctrl Pts',(30.3400599943064,827.348514711429,96.1251382913234));
#81263=CARTESIAN_POINT('Ctrl Pts',(29.8692102824549,827.180473645186,96.1258389792862));
#81264=CARTESIAN_POINT('Ctrl Pts',(29.7316433704635,827.131377532374,96.1260436974307));
#81265=CARTESIAN_POINT('Ctrl Pts',(29.5942084434188,827.081857023802,96.1262569799536));
#81266=CARTESIAN_POINT('Ctrl Pts',(29.4569086376803,827.031913643688,96.1264790588299));
#81267=CARTESIAN_POINT('Ctrl Pts',(28.9763315010338,826.857101694897,96.1272563798895));
#81268=CARTESIAN_POINT('Ctrl Pts',(28.4972902395431,826.677116185297,96.1281568157707));
#81269=CARTESIAN_POINT('Ctrl Pts',(28.0197389778897,826.491962153884,96.1291981422069));
#81270=CARTESIAN_POINT('Ctrl Pts',(27.5380280346519,826.305195349401,96.1302485390545));
#81271=CARTESIAN_POINT('Ctrl Pts',(27.0578334044021,826.113168931253,96.1314422860078));
#81272=CARTESIAN_POINT('Ctrl Pts',(26.5791611724838,825.915895118084,96.1327981858621));
#81273=CARTESIAN_POINT('Ctrl Pts',(26.2452186745877,825.778268354828,96.1337441203744));
#81274=CARTESIAN_POINT('Ctrl Pts',(25.9120209680096,825.638088956988,96.1347689780978));
#81275=CARTESIAN_POINT('Ctrl Pts',(25.579575465666,825.495361925563,96.1358793542484));
#81276=CARTESIAN_POINT('Ctrl Pts',(25.1043935615804,825.291354645937,96.1374664734899));
#81277=CARTESIAN_POINT('Ctrl Pts',(24.6307299666174,825.082134386464,96.1392283111973));
#81278=CARTESIAN_POINT('Ctrl Pts',(24.1585815459311,824.867703385282,96.1411851424814));
#81279=CARTESIAN_POINT('Ctrl Pts',(24.0645301183577,824.824988974106,96.1415749410442));
#81280=CARTESIAN_POINT('Ctrl Pts',(23.9705389615557,824.782067872531,96.1419724803075));
#81281=CARTESIAN_POINT('Ctrl Pts',(23.8766082699099,824.738940216866,96.142377925612));
#81282=CARTESIAN_POINT('Ctrl Pts',(23.5242791952853,824.57717065311,96.1438987295842));
#81283=CARTESIAN_POINT('Ctrl Pts',(23.1726904806387,824.412439784918,96.1455313567798));
#81284=CARTESIAN_POINT('Ctrl Pts',(22.8225264021466,824.245069168157,96.1472764201388));
#81285=CARTESIAN_POINT('Ctrl Pts',(22.5641059405136,824.121549953298,96.1485642737667));
#81286=CARTESIAN_POINT('Ctrl Pts',(22.3064613514965,823.996594101978,96.1499133413435));
#81287=CARTESIAN_POINT('Ctrl Pts',(22.0498649176053,823.870348867314,96.1513233720859));
#81288=CARTESIAN_POINT('Ctrl Pts',(21.8205654519541,823.757533718598,96.1525834024413));
#81289=CARTESIAN_POINT('Ctrl Pts',(21.5919627696193,823.643633984308,96.1538967179459));
#81290=CARTESIAN_POINT('Ctrl Pts',(21.3640843664886,823.528679500814,96.1552654445697));
#81291=CARTESIAN_POINT('Ctrl Pts',(20.6897210395786,823.188493301213,96.1593159338962));
#81292=CARTESIAN_POINT('Ctrl Pts',(20.0216970167957,822.839071979066,96.1638516478053));
#81293=CARTESIAN_POINT('Ctrl Pts',(19.3597612622417,822.48059179808,96.1689367561272));
#81294=CARTESIAN_POINT('Ctrl Pts',(18.6797438547955,822.11231925559,96.174160770926));
#81295=CARTESIAN_POINT('Ctrl Pts',(18.0061520763646,821.734486260633,96.1799646020606));
#81296=CARTESIAN_POINT('Ctrl Pts',(17.3387696085509,821.34728998514,96.1864183552341));
#81297=CARTESIAN_POINT('Ctrl Pts',(16.6518654105832,820.94876775853,96.1930608883562));
#81298=CARTESIAN_POINT('Ctrl Pts',(15.9715393097476,820.540326539864,96.2003919176625));
#81299=CARTESIAN_POINT('Ctrl Pts',(15.2976106450826,820.122186493828,96.2084884921846));
#81300=CARTESIAN_POINT('Ctrl Pts',(14.5906904817536,819.683576823195,96.2169814263535));
#81301=CARTESIAN_POINT('Ctrl Pts',(13.8908095443592,819.234295555008,96.2263166860551));
#81302=CARTESIAN_POINT('Ctrl Pts',(13.1978169881674,818.774601332847,96.2365839510869));
#81303=CARTESIAN_POINT('Ctrl Pts',(12.4824725211103,818.300080047702,96.2471823783956));
#81304=CARTESIAN_POINT('Ctrl Pts',(11.7744682831821,817.814463333678,96.258773896731));
#81305=CARTESIAN_POINT('Ctrl Pts',(11.0736948546628,817.318039228885,96.2714580313752));
#81306=CARTESIAN_POINT('Ctrl Pts',(10.334954086467,816.794719266112,96.2848293822136));
#81307=CARTESIAN_POINT('Ctrl Pts',(9.60424912359563,816.259389196666,96.2994149405681));
#81308=CARTESIAN_POINT('Ctrl Pts',(8.88150935089614,815.712389091413,96.3153324022128));
#81309=CARTESIAN_POINT('Ctrl Pts',(8.737364605695,815.603294236287,96.318507014348));
#81310=CARTESIAN_POINT('Ctrl Pts',(8.59353685960559,815.493735186086,96.3217346094189));
#81311=CARTESIAN_POINT('Ctrl Pts',(8.45002579119955,815.38371464605,96.3250161265263));
#81312=CARTESIAN_POINT('Ctrl Pts',(7.73485923702806,814.835443273122,96.3413690901561));
#81313=CARTESIAN_POINT('Ctrl Pts',(7.02744314731507,814.275599585686,96.3590559958425));
#81314=CARTESIAN_POINT('Ctrl Pts',(6.32763648910812,813.704382912701,96.3781977036289));
#81315=CARTESIAN_POINT('Ctrl Pts',(5.98839153239689,813.427474464879,96.387477020642));
#81316=CARTESIAN_POINT('Ctrl Pts',(5.65093560132485,813.147893119755,96.3970982758466));
#81317=CARTESIAN_POINT('Ctrl Pts',(5.31525674903631,812.865660336836,96.4070755760922));
#81318=CARTESIAN_POINT('Ctrl Pts',(4.88604189826204,812.504784157183,96.4198330238934));
#81319=CARTESIAN_POINT('Ctrl Pts',(4.45941044659712,812.139296345883,96.4331827773792));
#81320=CARTESIAN_POINT('Ctrl Pts',(4.03593287282361,811.769745606281,96.4471373618657));
#81321=CARTESIAN_POINT('Ctrl Pts',(3.60939542391928,811.397524644717,96.461192776452));
#81322=CARTESIAN_POINT('Ctrl Pts',(3.18605779243993,811.021182033279,96.4758618462414));
#81323=CARTESIAN_POINT('Ctrl Pts',(2.76646984314789,810.641319253384,96.4911510252356));
#81324=CARTESIAN_POINT('Ctrl Pts',(2.60477662834758,810.494934605856,96.4970428925007));
#81325=CARTESIAN_POINT('Ctrl Pts',(2.44363989332385,810.348027610871,96.5030267777089));
#81326=CARTESIAN_POINT('Ctrl Pts',(2.28308971551838,810.200634184955,96.5091027768158));
#81327=CARTESIAN_POINT('Ctrl Pts',(1.59637390937374,809.57019330546,96.5350914408076));
#81328=CARTESIAN_POINT('Ctrl Pts',(0.920061146645233,808.930567192885,96.562778850032));
#81329=CARTESIAN_POINT('Ctrl Pts',(0.253832209561208,808.28208074038,96.5922727164801));
#81330=CARTESIAN_POINT('Ctrl Pts',(-0.434923194360932,807.611667728168,
96.6227638266195));
#81331=CARTESIAN_POINT('Ctrl Pts',(-1.11290049535978,806.931785155324,96.6551855659363));
#81332=CARTESIAN_POINT('Ctrl Pts',(-1.78043670077545,806.242737817501,96.6896592282327));
#81333=CARTESIAN_POINT('Ctrl Pts',(-2.33045840547436,805.674991846132,96.7180640733178));
#81334=CARTESIAN_POINT('Ctrl Pts',(-2.87339101909581,805.101022796369,96.7478620175358));
#81335=CARTESIAN_POINT('Ctrl Pts',(-3.40942206489524,804.520974706055,96.7791223637616));
#81336=CARTESIAN_POINT('Origin',(52.8776183915471,832.414102583906,106.637502983816));
#81337=CARTESIAN_POINT('Ctrl Pts',(68.4577985491519,740.125373764374,82.4370100295875));
#81338=CARTESIAN_POINT('Ctrl Pts',(68.4127473761225,753.031531728391,82.4563567944567));
#81339=CARTESIAN_POINT('Ctrl Pts',(68.3676962032424,765.937689649662,82.4757320753115));
#81340=CARTESIAN_POINT('Ctrl Pts',(91.7880530990439,779.91534174428,88.5489787937199));
#81341=CARTESIAN_POINT('Ctrl Pts',(102.984616121786,790.64528003164,92.3413020410111));
#81342=CARTESIAN_POINT('Ctrl Pts',(110.203416346979,803.379710979161,96.8420808181083));
#81343=CARTESIAN_POINT('Ctrl Pts',(68.146245887415,740.125373764374,82.1411634292565));
#81344=CARTESIAN_POINT('Ctrl Pts',(68.1013386355289,753.27209360235,82.1623170532707));
#81345=CARTESIAN_POINT('Ctrl Pts',(68.0564326571535,766.41881340126,82.1834984289274));
#81346=CARTESIAN_POINT('Ctrl Pts',(90.6389575804412,780.789138080197,88.3851212990028));
#81347=CARTESIAN_POINT('Ctrl Pts',(101.882701838135,791.724397584064,92.2074425549413));
#81348=CARTESIAN_POINT('Ctrl Pts',(109.112490425402,804.596520123409,96.7733914942943));
#81349=CARTESIAN_POINT('Ctrl Pts',(67.8275991955539,740.125373764374,81.8527984530498));
#81350=CARTESIAN_POINT('Ctrl Pts',(67.7829212500557,753.508784911136,81.8757450226982));
#81351=CARTESIAN_POINT('Ctrl Pts',(67.7382457320547,766.892196022395,81.8987186035317));
#81352=CARTESIAN_POINT('Ctrl Pts',(89.4941280640034,781.614609851677,88.2295744554866));
#81353=CARTESIAN_POINT('Ctrl Pts',(100.768263665002,792.773015962468,92.0801584109773));
#81354=CARTESIAN_POINT('Ctrl Pts',(107.999153078758,805.790564251154,96.7101361882138));
#81355=CARTESIAN_POINT('Ctrl Pts',(67.5021302853703,740.125373764374,81.5720908670709));
#81356=CARTESIAN_POINT('Ctrl Pts',(67.4577640330222,753.741304019782,81.5968129309024));
#81357=CARTESIAN_POINT('Ctrl Pts',(67.4134012477569,767.357234243137,81.6215612893473));
#81358=CARTESIAN_POINT('Ctrl Pts',(88.3519233861698,782.395636392562,88.0819107242408));
#81359=CARTESIAN_POINT('Ctrl Pts',(99.6387825034722,793.793017584272,91.9592106396445));
#81360=CARTESIAN_POINT('Ctrl Pts',(106.860546215042,806.962773547768,96.6519976135905));
#81361=CARTESIAN_POINT('Ctrl Pts',(67.1701109686658,740.125373764374,81.2992164374233));
#81362=CARTESIAN_POINT('Ctrl Pts',(67.1261357977477,753.969349293325,81.3256930060463));
#81363=CARTESIAN_POINT('Ctrl Pts',(67.0821650240712,767.813324793557,81.3521951765969));
#81364=CARTESIAN_POINT('Ctrl Pts',(87.2125822519353,783.134553009413,87.941736205412));
#81365=CARTESIAN_POINT('Ctrl Pts',(98.4936191231884,794.784740839621,91.8443939105452));
#81366=CARTESIAN_POINT('Ctrl Pts',(105.695691610809,808.11253417135,96.598692123225));
#81367=CARTESIAN_POINT('Ctrl Pts',(66.4935151458177,740.125373764374,80.7694854229978));
#81368=CARTESIAN_POINT('Ctrl Pts',(66.4504749173554,754.415888900274,80.7994219465401));
#81369=CARTESIAN_POINT('Ctrl Pts',(66.4074407375454,768.706404013894,80.8293827344099));
#81370=CARTESIAN_POINT('Ctrl Pts',(84.9422477192991,784.531226837734,87.6756031833855));
#81371=CARTESIAN_POINT('Ctrl Pts',(96.1727927030411,796.71069722726,91.6266372665226));
#81372=CARTESIAN_POINT('Ctrl Pts',(103.313673713057,810.364320218198,96.501205407115));
#81373=CARTESIAN_POINT('Ctrl Pts',(66.1489386396743,740.125373764374,80.5126288382199));
#81374=CARTESIAN_POINT('Ctrl Pts',(66.1064422722375,754.63438323368,80.5442708118899));
#81375=CARTESIAN_POINT('Ctrl Pts',(66.0639526747054,769.143392683811,80.5759364049731));
#81376=CARTESIAN_POINT('Ctrl Pts',(83.8113135756256,785.189269489409,87.5495985783604));
#81377=CARTESIAN_POINT('Ctrl Pts',(94.9971296631777,797.644930359551,91.5236973515995));
#81378=CARTESIAN_POINT('Ctrl Pts',(102.096510419537,811.466345641466,96.4570241813705));
#81379=CARTESIAN_POINT('Ctrl Pts',(65.798355350613,740.125373764374,80.2639569419803));
#81380=CARTESIAN_POINT('Ctrl Pts',(65.7564762355172,754.847800462054,80.2972763005058));
#81381=CARTESIAN_POINT('Ctrl Pts',(65.7146045120992,769.570227143548,80.330618657416));
#81382=CARTESIAN_POINT('Ctrl Pts',(82.6856346728155,785.808275750055,87.4303886685735));
#81383=CARTESIAN_POINT('Ctrl Pts',(93.8066491824885,798.549951735236,91.4265032086189));
#81384=CARTESIAN_POINT('Ctrl Pts',(100.853286177248,812.543084537451,96.4171341359893));
#81385=CARTESIAN_POINT('Ctrl Pts',(65.4420370904355,740.125373764374,80.0236455003826));
#81386=CARTESIAN_POINT('Ctrl Pts',(65.4008456205139,755.05583895043,80.058610640551));
#81387=CARTESIAN_POINT('Ctrl Pts',(65.3596620695378,769.986304123174,80.0935981819611));
#81388=CARTESIAN_POINT('Ctrl Pts',(81.5673047484096,786.388698405906,87.317718938527));
#81389=CARTESIAN_POINT('Ctrl Pts',(92.60285526926,799.424489574021,91.3348748976876));
#81390=CARTESIAN_POINT('Ctrl Pts',(99.5851660013872,813.592312893813,96.3812770142762));
#81391=CARTESIAN_POINT('Ctrl Pts',(64.3566928319587,740.125373764374,79.3283198378255));
#81392=CARTESIAN_POINT('Ctrl Pts',(64.3177664806126,755.662913290672,79.3681168994633));
#81393=CARTESIAN_POINT('Ctrl Pts',(64.2788493614205,771.200452811937,79.4079346425718));
#81394=CARTESIAN_POINT('Ctrl Pts',(78.241433233292,788.015375488293,86.9985419953978));
#81395=CARTESIAN_POINT('Ctrl Pts',(88.9568353670791,801.952638709294,91.0761228956451));
#81396=CARTESIAN_POINT('Ctrl Pts',(95.7104028289416,816.650595877495,96.2850049043395));
#81397=CARTESIAN_POINT('Ctrl Pts',(63.6112773557153,740.125373764374,78.8989142791022));
#81398=CARTESIAN_POINT('Ctrl Pts',(63.5741306608233,756.044908017652,78.9417920571076));
#81399=CARTESIAN_POINT('Ctrl Pts',(63.5369937154316,771.964442270956,78.9846894656125));
#81400=CARTESIAN_POINT('Ctrl Pts',(76.0642641288587,788.948173418263,86.8103724461283));
#81401=CARTESIAN_POINT('Ctrl Pts',(86.4799712156315,803.510785624701,90.925132135285));
#81402=CARTESIAN_POINT('Ctrl Pts',(93.0333571874941,818.570248419414,96.2358891713181));
#81403=CARTESIAN_POINT('Ctrl Pts',(62.8461837366256,740.125373764374,78.5050597321885));
#81404=CARTESIAN_POINT('Ctrl Pts',(62.8110622877333,756.401768165066,78.5508493584264));
#81405=CARTESIAN_POINT('Ctrl Pts',(62.7759507873526,772.678162570383,78.5966576597357));
#81406=CARTESIAN_POINT('Ctrl Pts',(73.9439429760598,789.735427319849,86.6451094909407));
#81407=CARTESIAN_POINT('Ctrl Pts',(83.9710618745184,804.930943310987,90.7941464415347));
#81408=CARTESIAN_POINT('Ctrl Pts',(90.273868435174,820.35237693673,96.1997070697605));
#81409=CARTESIAN_POINT('Ctrl Pts',(62.0635864691022,740.125373764374,78.1481623259125));
#81410=CARTESIAN_POINT('Ctrl Pts',(62.030711867897,756.731080653197,78.1966666287248));
#81411=CARTESIAN_POINT('Ctrl Pts',(61.9978471356711,773.336787550785,78.2451887467233));
#81412=CARTESIAN_POINT('Ctrl Pts',(71.9014530756279,790.382188332322,86.5009126672756));
#81413=CARTESIAN_POINT('Ctrl Pts',(81.4484602921453,806.201350089842,90.6815283295111));
#81414=CARTESIAN_POINT('Ctrl Pts',(87.4475775756694,821.977601894745,96.1741945803691));
#81415=CARTESIAN_POINT('Ctrl Pts',(60.8666968367854,740.125373764374,77.6703611206971));
#81416=CARTESIAN_POINT('Ctrl Pts',(60.8374889278549,757.180108276895,77.7225992255993));
#81417=CARTESIAN_POINT('Ctrl Pts',(60.8082904104759,774.2348428037,77.7748539991746));
#81418=CARTESIAN_POINT('Ctrl Pts',(68.9534649735206,791.183049009015,86.3122526659036));
#81419=CARTESIAN_POINT('Ctrl Pts',(77.6390738981942,807.898573162258,90.5364930374217));
#81420=CARTESIAN_POINT('Ctrl Pts',(83.0989245500585,824.184896473511,96.1473309662659));
#81421=CARTESIAN_POINT('Ctrl Pts',(60.4639013375078,740.125373764374,77.5206848696584));
#81422=CARTESIAN_POINT('Ctrl Pts',(60.4359650627929,757.322293966711,77.574111206462));
#81423=CARTESIAN_POINT('Ctrl Pts',(60.4080379607987,774.519214185056,77.6275538536533));
#81424=CARTESIAN_POINT('Ctrl Pts',(67.9937609712978,791.419007894659,86.2538360757553));
#81425=CARTESIAN_POINT('Ctrl Pts',(76.3668683465713,808.42881848167,90.4919822112373));
#81426=CARTESIAN_POINT('Ctrl Pts',(81.6311707521293,824.882237523391,96.1402772815622));
#81427=CARTESIAN_POINT('Ctrl Pts',(60.0575929071003,740.125373764374,77.3806599983877));
#81428=CARTESIAN_POINT('Ctrl Pts',(60.0309746715761,757.456687836812,77.435214660357));
#81429=CARTESIAN_POINT('Ctrl Pts',(60.0043653352274,774.788001926869,77.4897852983144));
#81430=CARTESIAN_POINT('Ctrl Pts',(67.0520671834915,791.628107124824,86.1997490225217));
#81431=CARTESIAN_POINT('Ctrl Pts',(75.0880088655532,808.924844429388,90.4511382932003));
#81432=CARTESIAN_POINT('Ctrl Pts',(80.1413037501949,825.541048987406,96.1348595437315));
#81433=CARTESIAN_POINT('Ctrl Pts',(59.6480909029385,740.125373764374,77.2503470692863));
#81434=CARTESIAN_POINT('Ctrl Pts',(59.6228341130978,757.582988252235,77.3059666117453));
#81435=CARTESIAN_POINT('Ctrl Pts',(59.5975858991469,775.040602759208,77.3616018196785));
#81436=CARTESIAN_POINT('Ctrl Pts',(66.1262266721434,791.81364749282,86.1498551125073));
#81437=CARTESIAN_POINT('Ctrl Pts',(73.801043158822,809.387093113981,90.4137980666451));
#81438=CARTESIAN_POINT('Ctrl Pts',(78.6282046757473,826.160390864936,96.1308169926819));
#81439=CARTESIAN_POINT('Ctrl Pts',(58.8233384618568,740.125373764374,77.0092662202253));
#81440=CARTESIAN_POINT('Ctrl Pts',(58.8008853794041,757.818798903791,77.066881558431));
#81441=CARTESIAN_POINT('Ctrl Pts',(58.7784401367371,775.51222406508,77.1245119888545));
#81442=CARTESIAN_POINT('Ctrl Pts',(64.307521418656,792.142543642154,86.0581890842577));
#81443=CARTESIAN_POINT('Ctrl Pts',(71.2135777935067,810.243251725114,90.3458068558984));
#81444=CARTESIAN_POINT('Ctrl Pts',(75.5588877370191,827.316586996844,96.1249690366928));
#81445=CARTESIAN_POINT('Ctrl Pts',(58.4080880249371,740.125373764374,76.8984983002657));
#81446=CARTESIAN_POINT('Ctrl Pts',(58.3870772041889,757.928309139926,76.9570445537283));
#81447=CARTESIAN_POINT('Ctrl Pts',(58.3660738104078,775.731244538614,77.0156056366663));
#81448=CARTESIAN_POINT('Ctrl Pts',(63.4143078482157,792.286216796038,86.0164198990661));
#81449=CARTESIAN_POINT('Ctrl Pts',(69.9130781349227,810.637161651653,90.315155871707));
#81450=CARTESIAN_POINT('Ctrl Pts',(74.0026698727384,827.853441251222,96.1231636317532));
#81451=CARTESIAN_POINT('Ctrl Pts',(57.9902827290137,740.125373764374,76.7975634472785));
#81452=CARTESIAN_POINT('Ctrl Pts',(57.9707515794984,758.029122651452,76.8569700954413));
#81453=CARTESIAN_POINT('Ctrl Pts',(57.9512274043388,775.932871562816,76.9163913342226));
#81454=CARTESIAN_POINT('Ctrl Pts',(62.5378525327461,792.410646110844,85.9786120728594));
#81455=CARTESIAN_POINT('Ctrl Pts',(68.6071507501991,810.996510083265,90.2876904383976));
#81456=CARTESIAN_POINT('Ctrl Pts',(72.4265652911377,828.347277468934,96.1222201861425));
#81457=CARTESIAN_POINT('Ctrl Pts',(57.5702419314624,740.125373764374,76.7065222236651));
#81458=CARTESIAN_POINT('Ctrl Pts',(57.5522248642258,758.120937803404,76.7667152080309));
#81459=CARTESIAN_POINT('Ctrl Pts',(57.534214283915,776.116501867756,76.8269225680443));
#81460=CARTESIAN_POINT('Ctrl Pts',(61.6815662170187,792.516528443811,85.9446672820555));
#81461=CARTESIAN_POINT('Ctrl Pts',(67.2999264352273,811.320070679581,90.2632556320363));
#81462=CARTESIAN_POINT('Ctrl Pts',(70.8350382159185,828.795487200422,96.1218862325003));
#81463=CARTESIAN_POINT('Ctrl Pts',(56.3043711060502,740.125373764374,76.4632611281508));
#81464=CARTESIAN_POINT('Ctrl Pts',(56.2909905233413,758.368483275649,76.5255803318131));
#81465=CARTESIAN_POINT('Ctrl Pts',(56.2776148757333,776.611592815006,76.5879133378671));
#81466=CARTESIAN_POINT('Ctrl Pts',(59.1918211416932,792.778122395503,85.8541394842021));
#81467=CARTESIAN_POINT('Ctrl Pts',(63.3951297255563,812.177207268129,90.198590761091));
#81468=CARTESIAN_POINT('Ctrl Pts',(66.0359568188235,829.992908914138,96.1219678844952));
#81469=CARTESIAN_POINT('Ctrl Pts',(55.4527926454315,740.125373764374,76.3409038315759));
#81470=CARTESIAN_POINT('Ctrl Pts',(55.4426287026627,758.496313612328,76.4043301290191));
#81471=CARTESIAN_POINT('Ctrl Pts',(55.4324685410653,776.867253489743,76.4677699422263));
#81472=CARTESIAN_POINT('Ctrl Pts',(57.5776163014075,792.896237715016,85.8093161318793));
#81473=CARTESIAN_POINT('Ctrl Pts',(60.7859907751168,812.60335257697,90.1671799470646));
#81474=CARTESIAN_POINT('Ctrl Pts',(62.8039023255101,830.594913415615,96.1234670030539));
#81475=CARTESIAN_POINT('Ctrl Pts',(54.5961044668057,740.125373764374,76.2588478013141));
#81476=CARTESIAN_POINT('Ctrl Pts',(54.5892588263739,758.584530891138,76.3230425032652));
#81477=CARTESIAN_POINT('Ctrl Pts',(54.5824157335954,777.043688048284,76.3872505298953));
#81478=CARTESIAN_POINT('Ctrl Pts',(56.0185052693372,792.968126815447,85.7796391878122));
#81479=CARTESIAN_POINT('Ctrl Pts',(58.1928767330255,812.887876650848,90.1467431470515));
#81480=CARTESIAN_POINT('Ctrl Pts',(59.5658196544964,831.000797356562,96.1253259192129));
#81481=CARTESIAN_POINT('Ctrl Pts',(53.7368614291764,740.125373764374,76.2175775365774));
#81482=CARTESIAN_POINT('Ctrl Pts',(53.7334117656202,758.630722032363,76.2821736502402));
#81483=CARTESIAN_POINT('Ctrl Pts',(53.7299633764019,777.136070331194,76.3467829930399));
#81484=CARTESIAN_POINT('Ctrl Pts',(54.4988708269895,793.001912967943,85.7649011332908));
#81485=CARTESIAN_POINT('Ctrl Pts',(55.6126678348459,813.032506180276,90.1367298610748));
#81486=CARTESIAN_POINT('Ctrl Pts',(56.3232617065557,831.208785659394,96.126634332624));
#81487=CARTESIAN_POINT('Ctrl Pts',(52.0183753539178,740.125373764373,76.2175775365774));
#81488=CARTESIAN_POINT('Ctrl Pts',(52.0218250174741,758.634225880209,76.2821858810255));
#81489=CARTESIAN_POINT('Ctrl Pts',(52.0252734087246,777.143078026885,76.3468074546121));
#81490=CARTESIAN_POINT('Ctrl Pts',(51.4571490512008,793.00566360327,85.7652369378129));
#81491=CARTESIAN_POINT('Ctrl Pts',(50.4216491638841,813.041567215157,90.1367984891347));
#81492=CARTESIAN_POINT('Ctrl Pts',(49.782129424813,831.22155851757,96.126678725148));
#81493=CARTESIAN_POINT('Ctrl Pts',(51.1591323162885,740.125373764374,76.2588478013141));
#81494=CARTESIAN_POINT('Ctrl Pts',(51.1659789780672,758.5910875414,76.3230649827209));
#81495=CARTESIAN_POINT('Ctrl Pts',(51.1728230942121,777.056801348808,76.3872954888097));
#81496=CARTESIAN_POINT('Ctrl Pts',(49.8704945841611,792.973408011051,85.7797762908131));
#81497=CARTESIAN_POINT('Ctrl Pts',(47.7800644164022,812.905202797824,90.1466343865574));
#81498=CARTESIAN_POINT('Ctrl Pts',(46.4835550910109,831.026343072914,96.1254147042609));
#81499=CARTESIAN_POINT('Ctrl Pts',(50.3024441376628,740.125373764374,76.3409038315759));
#81500=CARTESIAN_POINT('Ctrl Pts',(50.3126108891353,758.505475285689,76.404360988347));
#81501=CARTESIAN_POINT('Ctrl Pts',(50.3227738614307,776.885576836465,76.4678316608864));
#81502=CARTESIAN_POINT('Ctrl Pts',(48.2415589467887,792.894397192007,85.8089306098157));
#81503=CARTESIAN_POINT('Ctrl Pts',(45.1221815361918,812.620221612385,90.1667651019422));
#81504=CARTESIAN_POINT('Ctrl Pts',(43.1856486711625,830.624454929622,96.1236765570555));
#81505=CARTESIAN_POINT('Ctrl Pts',(49.450865677044,740.125373764374,76.4632611281508));
#81506=CARTESIAN_POINT('Ctrl Pts',(49.464251366487,758.379805458904,76.5256178155316));
#81507=CARTESIAN_POINT('Ctrl Pts',(49.4776321227852,776.634237181515,76.5879883053097));
#81508=CARTESIAN_POINT('Ctrl Pts',(46.6096800057099,792.777563498267,85.8527801984682));
#81509=CARTESIAN_POINT('Ctrl Pts',(42.4936032603387,812.200458494583,90.1975206582424));
#81510=CARTESIAN_POINT('Ctrl Pts',(39.9329117299652,830.032379931876,96.122113162747));
#81511=CARTESIAN_POINT('Ctrl Pts',(48.1849948516318,740.125373764374,76.706522223665));
#81512=CARTESIAN_POINT('Ctrl Pts',(48.2030208556531,758.134838880861,76.7667601650879));
#81513=CARTESIAN_POINT('Ctrl Pts',(48.2210403746284,776.14430402267,76.8270124821659));
#81514=CARTESIAN_POINT('Ctrl Pts',(44.1793258575781,792.534315599669,85.9415459155213));
#81515=CARTESIAN_POINT('Ctrl Pts',(38.6259692778301,811.364731598803,90.2609142626241));
#81516=CARTESIAN_POINT('Ctrl Pts',(35.1511853022989,828.859054345708,96.1218314935801));
#81517=CARTESIAN_POINT('Ctrl Pts',(47.7649540540804,740.125373764374,76.7975634472784));
#81518=CARTESIAN_POINT('Ctrl Pts',(47.7844954808982,758.043773048535,76.8570171330699));
#81519=CARTESIAN_POINT('Ctrl Pts',(47.8040299352114,775.962172356984,76.9164854094881));
#81520=CARTESIAN_POINT('Ctrl Pts',(43.3440936170016,792.434158289661,85.9750736900068));
#81521=CARTESIAN_POINT('Ctrl Pts',(37.3360276518998,811.04929213267,90.2849869594039));
#81522=CARTESIAN_POINT('Ctrl Pts',(33.5735063237651,828.420410302061,96.1220815075737));
#81523=CARTESIAN_POINT('Ctrl Pts',(47.3471487581571,740.125373764374,76.8984983002657));
#81524=CARTESIAN_POINT('Ctrl Pts',(47.3681712286424,757.943598953128,76.957093275552));
#81525=CARTESIAN_POINT('Ctrl Pts',(47.3891862739802,775.761824165019,77.0157030803224));
#81526=CARTESIAN_POINT('Ctrl Pts',(42.4812723007942,792.314724749067,86.0125874141734));
#81527=CARTESIAN_POINT('Ctrl Pts',(36.0421742699118,810.6977140878,90.3121448688152));
#81528=CARTESIAN_POINT('Ctrl Pts',(32.0080856465946,827.935994030087,96.122920038645));
#81529=CARTESIAN_POINT('Ctrl Pts',(46.9318983212373,740.125373764374,77.0092662202253));
#81530=CARTESIAN_POINT('Ctrl Pts',(46.954364425862,757.834618637866,77.0669315822377));
#81531=CARTESIAN_POINT('Ctrl Pts',(46.9768226924855,775.543863533231,77.124612036477));
#81532=CARTESIAN_POINT('Ctrl Pts',(41.5917117805538,792.174400912347,86.0541498402097));
#81533=CARTESIAN_POINT('Ctrl Pts',(34.7445524302651,810.309310207566,90.3425477128121));
#81534=CARTESIAN_POINT('Ctrl Pts',(30.4542764974918,827.40615630429,96.1246077047976));
#81535=CARTESIAN_POINT('Ctrl Pts',(46.1071458801556,740.125373764374,77.2503470692862));
#81536=CARTESIAN_POINT('Ctrl Pts',(46.1324183732037,757.599649654093,77.3060185034231));
#81537=CARTESIAN_POINT('Ctrl Pts',(46.1576822920703,775.073925562926,77.361705603044));
#81538=CARTESIAN_POINT('Ctrl Pts',(39.7649974382762,791.849864134419,86.1455125141571));
#81539=CARTESIAN_POINT('Ctrl Pts',(32.146243795526,809.458595881956,90.4101776276437));
#81540=CARTESIAN_POINT('Ctrl Pts',(27.3727730719043,826.257459112895,96.1302174570309));
#81541=CARTESIAN_POINT('Ctrl Pts',(45.6976438759937,740.125373764374,77.3806599983876));
#81542=CARTESIAN_POINT('Ctrl Pts',(45.724279123326,757.473660985582,77.4352671179228));
#81543=CARTESIAN_POINT('Ctrl Pts',(45.7509054731498,774.821948224408,77.4898902134563));
#81544=CARTESIAN_POINT('Ctrl Pts',(38.8267914620367,791.663318494346,86.1953136093372));
#81545=CARTESIAN_POINT('Ctrl Pts',(30.8455570004336,808.99628543658,90.4474046984785));
#81546=CARTESIAN_POINT('Ctrl Pts',(25.8450787954196,825.638599647297,96.1341395431115));
#81547=CARTESIAN_POINT('Ctrl Pts',(45.2913354455863,740.125373764374,77.5206848696584));
#81548=CARTESIAN_POINT('Ctrl Pts',(45.3192899768756,757.339470183674,77.574163876033));
#81549=CARTESIAN_POINT('Ctrl Pts',(45.347235337067,774.553566618983,77.627659192806));
#81550=CARTESIAN_POINT('Ctrl Pts',(37.8665259645302,791.450598279842,86.2493786341431));
#81551=CARTESIAN_POINT('Ctrl Pts',(29.5455737075545,808.496894261427,90.4882110615655));
#81552=CARTESIAN_POINT('Ctrl Pts',(24.3318878634854,824.976139895723,96.139446914039));
#81553=CARTESIAN_POINT('Ctrl Pts',(44.8885399463087,740.125373764374,77.6703611206971));
#81554=CARTESIAN_POINT('Ctrl Pts',(44.9177672608288,757.197379291599,77.7226517674573));
#81555=CARTESIAN_POINT('Ctrl Pts',(44.9469851853724,774.269384833108,77.7749590829014));
#81556=CARTESIAN_POINT('Ctrl Pts',(36.8890829111274,791.210365977003,86.3078592168729));
#81557=CARTESIAN_POINT('Ctrl Pts',(28.2506225783616,807.960854718712,90.5327713526171));
#81558=CARTESIAN_POINT('Ctrl Pts',(22.8367388658799,824.271550251516,96.146415101575));
#81559=CARTESIAN_POINT('Ctrl Pts',(43.6916503139919,740.125373764374,78.1481623259125));
#81560=CARTESIAN_POINT('Ctrl Pts',(43.7245473848271,756.748312474556,78.1967178107824));
#81561=CARTESIAN_POINT('Ctrl Pts',(43.7574345881057,773.371251193502,78.2452911108501));
#81562=CARTESIAN_POINT('Ctrl Pts',(33.9224488004764,790.410716654602,86.4969992510776));
#81563=CARTESIAN_POINT('Ctrl Pts',(24.3964334873945,806.251684467338,90.6782346441511));
#81564=CARTESIAN_POINT('Ctrl Pts',(18.4186152665191,822.043399213847,96.1731254366424));
#81565=CARTESIAN_POINT('Ctrl Pts',(42.9090530464685,740.125373764375,78.5050597321886));
#81566=CARTESIAN_POINT('Ctrl Pts',(42.9441984970111,756.418542408771,78.5508983317358));
#81567=CARTESIAN_POINT('Ctrl Pts',(42.9793340003503,772.711711057793,78.596755606366));
#81568=CARTESIAN_POINT('Ctrl Pts',(31.8698675756471,789.759693991976,86.6416659528865));
#81569=CARTESIAN_POINT('Ctrl Pts',(21.8539209894605,804.971856467956,90.7911736909535));
#81570=CARTESIAN_POINT('Ctrl Pts',(15.5629640582194,820.40545571534,96.1986733566335));
#81571=CARTESIAN_POINT('Ctrl Pts',(42.1439594273788,740.125373764375,78.8989142791023));
#81572=CARTESIAN_POINT('Ctrl Pts',(42.1811308899313,756.060796501059,78.9418376327706));
#81573=CARTESIAN_POINT('Ctrl Pts',(42.2182926041646,771.99621923777,78.9847806169498));
#81574=CARTESIAN_POINT('Ctrl Pts',(29.7482325355677,788.975322800262,86.8070049453425));
#81575=CARTESIAN_POINT('Ctrl Pts',(19.3392894961986,803.552080430039,90.922021074782));
#81576=CARTESIAN_POINT('Ctrl Pts',(12.7933854819489,818.622207535651,96.2344984406095));
#81577=CARTESIAN_POINT('Ctrl Pts',(41.3985439511354,740.125373764375,79.3283198378255));
#81578=CARTESIAN_POINT('Ctrl Pts',(41.4374948148052,755.67749109725,79.3681580018985));
#81579=CARTESIAN_POINT('Ctrl Pts',(41.4764364473626,771.229608425092,79.4080168474528));
#81580=CARTESIAN_POINT('Ctrl Pts',(27.5697855394546,788.045868489416,86.9951801697774));
#81581=CARTESIAN_POINT('Ctrl Pts',(16.8599436396416,801.99648030487,91.0727866099062));
#81582=CARTESIAN_POINT('Ctrl Pts',(10.1126581685345,816.704550291679,96.2832018189664));
#81583=CARTESIAN_POINT('Ctrl Pts',(39.9514182731664,740.125373764374,80.255420721235));
#81584=CARTESIAN_POINT('Ctrl Pts',(39.9933862308964,754.864593989093,80.2888054523636));
#81585=CARTESIAN_POINT('Ctrl Pts',(40.0353467081538,769.603814197741,80.3222131579999));
#81586=CARTESIAN_POINT('Ctrl Pts',(23.126009607612,785.876577822194,87.421096066829));
#81587=CARTESIAN_POINT('Ctrl Pts',(11.9888907180205,798.625133155414,91.4177387128464));
#81588=CARTESIAN_POINT('Ctrl Pts',(4.93672158308855,812.625462281788,96.4111325267945));
#81589=CARTESIAN_POINT('Ctrl Pts',(39.2497080714407,740.125373764374,80.7531160459211));
#81590=CARTESIAN_POINT('Ctrl Pts',(39.2929137221135,754.435002284747,80.7831325337009));
#81591=CARTESIAN_POINT('Ctrl Pts',(39.3361131257469,768.74463078307,80.8131732380438));
#81592=CARTESIAN_POINT('Ctrl Pts',(20.8607795467825,784.637676843055,87.6588066532497));
#81593=CARTESIAN_POINT('Ctrl Pts',(9.5971836529565,796.809386131128,91.6119252806624));
#81594=CARTESIAN_POINT('Ctrl Pts',(2.44151231105709,810.46403151587,96.4903598562657));
#81595=CARTESIAN_POINT('Ctrl Pts',(38.5720250013864,740.125373764374,81.2835501247607));
#81596=CARTESIAN_POINT('Ctrl Pts',(38.6161732477199,753.984683775961,81.3100852591544));
#81597=CARTESIAN_POINT('Ctrl Pts',(38.6603168783517,767.84399375906,81.3366459477096));
#81598=CARTESIAN_POINT('Ctrl Pts',(18.5683916561005,783.235903460189,87.9242593021168));
#81599=CARTESIAN_POINT('Ctrl Pts',(7.25782974268059,794.869316294976,91.8296147298744));
#81600=CARTESIAN_POINT('Ctrl Pts',(0.0429698175526117,808.193236292288,
96.5872328424701));
#81601=CARTESIAN_POINT('Ctrl Pts',(37.9205435574161,740.125373764374,81.8453168289255));
#81602=CARTESIAN_POINT('Ctrl Pts',(37.9653150589334,753.516054808566,81.8682859167358));
#81603=CARTESIAN_POINT('Ctrl Pts',(38.010084013782,766.906735817371,81.8912819918484));
#81604=CARTESIAN_POINT('Ctrl Pts',(16.2661593276306,781.664267601813,88.2202259887619));
#81605=CARTESIAN_POINT('Ctrl Pts',(4.98049187324324,792.812300971065,92.0723819763127));
#81606=CARTESIAN_POINT('Ctrl Pts',(-2.25386901258056,805.827225600765,96.7039177173643));
#81607=CARTESIAN_POINT('Ctrl Pts',(37.2974382339422,740.125373764374,82.4370100295875));
#81608=CARTESIAN_POINT('Ctrl Pts',(37.3424894069716,753.031531728391,82.4563567944567));
#81609=CARTESIAN_POINT('Ctrl Pts',(37.3875405798517,765.937689649662,82.4757320753115));
#81610=CARTESIAN_POINT('Ctrl Pts',(13.9671836840501,779.915341744281,88.5489787937201));
#81611=CARTESIAN_POINT('Ctrl Pts',(2.77062066130783,790.64528003164,92.3413020410112));
#81612=CARTESIAN_POINT('Ctrl Pts',(-4.44817956388518,803.379710979161,96.8420808181083));
#81613=CARTESIAN_POINT('',(-2.3072174972792,802.626345096273,96.1096278308841));
#81614=CARTESIAN_POINT('Ctrl Pts',(-2.30689020010939,802.626560388343,96.1095808375407));
#81615=CARTESIAN_POINT('Ctrl Pts',(-2.68639626067645,803.251812836745,96.330577960684));
#81616=CARTESIAN_POINT('Ctrl Pts',(-3.05421750819845,803.883231163271,96.5538081011059));
#81617=CARTESIAN_POINT('Ctrl Pts',(-3.40944118612444,804.520983132338,96.7791293074463));
#81618=CARTESIAN_POINT('',(108.062487312194,802.626301820665,96.1096219232672));
#81619=CARTESIAN_POINT('Ctrl Pts',(109.164772626437,804.521007661288,96.7791165021265));
#81620=CARTESIAN_POINT('Ctrl Pts',(108.987923875025,804.201654960381,96.666601644594));
#81621=CARTESIAN_POINT('Ctrl Pts',(108.807152759608,803.884339316512,96.5544638713983));
#81622=CARTESIAN_POINT('Ctrl Pts',(108.623155796259,803.568713813167,96.4428324932515));
#81623=CARTESIAN_POINT('Ctrl Pts',(108.439158832909,803.253088309821,96.3312011151047));
#81624=CARTESIAN_POINT('Ctrl Pts',(108.252007023091,802.939107479159,96.2200864522011));
#81625=CARTESIAN_POINT('Ctrl Pts',(108.062323461338,802.626409591658,96.1095984083762));
#81626=CARTESIAN_POINT('',(67.774347942193,740.125373764374,81.8141824275666));
#81627=CARTESIAN_POINT('Ctrl Pts',(108.062487312194,802.626301820665,96.1096219232672));
#81628=CARTESIAN_POINT('Ctrl Pts',(107.640412981026,801.930681948247,95.8638046150634));
#81629=CARTESIAN_POINT('Ctrl Pts',(107.203256492765,801.24328772892,95.620741919965));
#81630=CARTESIAN_POINT('Ctrl Pts',(106.75236567008,800.565958331003,95.3807586268188));
#81631=CARTESIAN_POINT('Ctrl Pts',(106.325982702208,799.925444698033,95.1538194574609));
#81632=CARTESIAN_POINT('Ctrl Pts',(105.8873187214,799.293931975707,94.9296340745444));
#81633=CARTESIAN_POINT('Ctrl Pts',(105.437552836549,798.67295949173,94.7084711043448));
#81634=CARTESIAN_POINT('Ctrl Pts',(105.42652693745,798.657736505321,94.7030493489913));
#81635=CARTESIAN_POINT('Ctrl Pts',(105.415494274884,798.642519698899,94.697629359652));
#81636=CARTESIAN_POINT('Ctrl Pts',(105.404454864429,798.627309092915,94.6922111394988));
#81637=CARTESIAN_POINT('Ctrl Pts',(104.79826132232,797.79206783104,94.394687093275));
#81638=CARTESIAN_POINT('Ctrl Pts',(104.171417072003,796.974168319304,94.1020990225107));
#81639=CARTESIAN_POINT('Ctrl Pts',(103.526885548805,796.171143140921,93.8138832266392));
#81640=CARTESIAN_POINT('Ctrl Pts',(103.198040541494,795.761433435264,93.6668332809201));
#81641=CARTESIAN_POINT('Ctrl Pts',(102.864592019392,795.35559515563,93.5209213547615));
#81642=CARTESIAN_POINT('Ctrl Pts',(102.52693755488,794.953297460646,93.37607176917));
#81643=CARTESIAN_POINT('Ctrl Pts',(102.504551389322,794.926625511211,93.3664683812544));
#81644=CARTESIAN_POINT('Ctrl Pts',(102.482146735223,794.899969102788,93.3568696590447));
#81645=CARTESIAN_POINT('Ctrl Pts',(102.4597237084,794.873328137208,93.3472755801077));
#81646=CARTESIAN_POINT('Ctrl Pts',(101.728050389849,794.004021604738,93.0342165257061));
#81647=CARTESIAN_POINT('Ctrl Pts',(100.977128069926,793.150865667694,92.7260164575441));
#81648=CARTESIAN_POINT('Ctrl Pts',(100.211177215851,792.310090537155,92.4222827468567));
#81649=CARTESIAN_POINT('Ctrl Pts',(99.380591387708,791.398366365341,92.0929183832238));
#81650=CARTESIAN_POINT('Ctrl Pts',(98.5323338124084,790.501200490887,91.7688059920466));
#81651=CARTESIAN_POINT('Ctrl Pts',(97.6718328280343,789.613743392316,91.4494366429952));
#81652=CARTESIAN_POINT('Ctrl Pts',(97.152518953693,789.07816145512,91.2566966728924));
#81653=CARTESIAN_POINT('Ctrl Pts',(96.6287467376884,788.546114787712,91.0656840262139));
#81654=CARTESIAN_POINT('Ctrl Pts',(96.1017159269538,788.016531543047,90.8762855451684));
#81655=CARTESIAN_POINT('Ctrl Pts',(96.0590994158765,787.973708638289,90.8609704965961));
#81656=CARTESIAN_POINT('Ctrl Pts',(96.0164615787842,787.930901903599,90.8456660040061));
#81657=CARTESIAN_POINT('Ctrl Pts',(95.9738030426657,787.888110760593,90.830372003895));
#81658=CARTESIAN_POINT('Ctrl Pts',(94.8209136774377,786.73163756233,90.4170364400377));
#81659=CARTESIAN_POINT('Ctrl Pts',(93.6527406381072,785.58666301832,90.0114150472833));
#81660=CARTESIAN_POINT('Ctrl Pts',(92.4789028667217,784.444304507527,89.6134588224494));
#81661=CARTESIAN_POINT('Ctrl Pts',(91.4230801131926,783.416796160305,89.2555122242647));
#81662=CARTESIAN_POINT('Ctrl Pts',(90.3626752475194,782.39140318791,88.903766858798));
#81663=CARTESIAN_POINT('Ctrl Pts',(89.3047136290314,781.361636814038,88.5581860807789));
#81664=CARTESIAN_POINT('Ctrl Pts',(89.2467119251352,781.305180886662,88.5392399549379));
#81665=CARTESIAN_POINT('Ctrl Pts',(89.1887176192233,781.248711946809,88.5203123802324));
#81666=CARTESIAN_POINT('Ctrl Pts',(89.1307318277863,781.192228889795,88.5014033367873));
#81667=CARTESIAN_POINT('Ctrl Pts',(88.0211876752418,780.111439198484,88.139583344944));
#81668=CARTESIAN_POINT('Ctrl Pts',(86.9143542908349,779.025811538966,87.7845303670263));
#81669=CARTESIAN_POINT('Ctrl Pts',(85.8179698161622,777.927924518351,87.4370122370397));
#81670=CARTESIAN_POINT('Ctrl Pts',(84.9020308283374,777.010730277063,87.1466894428158));
#81671=CARTESIAN_POINT('Ctrl Pts',(83.9933842451906,776.084980050413,86.8616255566873));
#81672=CARTESIAN_POINT('Ctrl Pts',(83.0965727816879,775.146316117423,86.582276091458));
#81673=CARTESIAN_POINT('Ctrl Pts',(82.9198955321183,774.961393679764,86.5272425674744));
#81674=CARTESIAN_POINT('Ctrl Pts',(82.7436777330877,774.775969931733,86.4724308521597));
#81675=CARTESIAN_POINT('Ctrl Pts',(82.5679542960686,774.590011378811,86.4178444648264));
#81676=CARTESIAN_POINT('Ctrl Pts',(82.5012260278146,774.519396482961,86.3971161251195));
#81677=CARTESIAN_POINT('Ctrl Pts',(82.4345687142384,774.448703746333,86.3764201674801));
#81678=CARTESIAN_POINT('Ctrl Pts',(82.3679844602655,774.377931547985,86.3557568467796));
#81679=CARTESIAN_POINT('Ctrl Pts',(81.4237317729819,773.374288276671,86.0627236604705));
#81680=CARTESIAN_POINT('Ctrl Pts',(80.4945540723926,772.354776636511,85.7764377798638));
#81681=CARTESIAN_POINT('Ctrl Pts',(79.5903226433914,771.317053989318,85.4989930367865));
#81682=CARTESIAN_POINT('Ctrl Pts',(79.5114235124355,771.226507020465,85.4747844675917));
#81683=CARTESIAN_POINT('Ctrl Pts',(79.4327142911312,771.135821426451,85.4506431946544));
#81684=CARTESIAN_POINT('Ctrl Pts',(79.3542015223261,771.044995666001,85.4265705989427));
#81685=CARTESIAN_POINT('Ctrl Pts',(79.2872510851058,770.967545533169,85.406043099627));
#81686=CARTESIAN_POINT('Ctrl Pts',(79.220441547077,770.88999082999,85.3855649455497));
#81687=CARTESIAN_POINT('Ctrl Pts',(79.1537766614075,770.812330210894,85.3651369027868));
#81688=CARTESIAN_POINT('Ctrl Pts',(78.5551663921203,770.114984919695,85.1817054597342));
#81689=CARTESIAN_POINT('Ctrl Pts',(77.9679052424419,769.408810509424,85.0022174634512));
#81690=CARTESIAN_POINT('Ctrl Pts',(77.3946133745915,768.69196912988,84.8272162256116));
#81691=CARTESIAN_POINT('Ctrl Pts',(77.0383014961175,768.246438479898,84.7184496037794));
#81692=CARTESIAN_POINT('Ctrl Pts',(76.687386434515,767.796786822786,84.611416309622));
#81693=CARTESIAN_POINT('Ctrl Pts',(76.3425054304563,767.342566840531,84.5062485763837));
#81694=CARTESIAN_POINT('Ctrl Pts',(76.2787833852224,767.25864274522,84.48681722767));
#81695=CARTESIAN_POINT('Ctrl Pts',(76.2152675101717,767.174562113752,84.467449653553));
#81696=CARTESIAN_POINT('Ctrl Pts',(76.1519616252091,767.090321815678,84.4481466294127));
#81697=CARTESIAN_POINT('Ctrl Pts',(75.705965492299,766.49684070096,84.3121549419864));
#81698=CARTESIAN_POINT('Ctrl Pts',(75.2703804789971,765.89544498154,84.1793611878219));
#81699=CARTESIAN_POINT('Ctrl Pts',(74.8469145710805,765.284861908932,84.0501684628422));
#81700=CARTESIAN_POINT('Ctrl Pts',(74.4554953372686,764.720485995804,83.9307526693148));
#81701=CARTESIAN_POINT('Ctrl Pts',(74.0744302930709,764.148260661885,83.8144134988996));
#81702=CARTESIAN_POINT('Ctrl Pts',(73.7051075794581,763.56715370259,83.7014789981592));
#81703=CARTESIAN_POINT('Ctrl Pts',(73.6748700141567,763.51957672186,83.6922327097099));
#81704=CARTESIAN_POINT('Ctrl Pts',(73.6447111835826,763.471940189732,83.6830092491982));
#81705=CARTESIAN_POINT('Ctrl Pts',(73.6146318625107,763.424243530879,83.6738087998238));
#81706=CARTESIAN_POINT('Ctrl Pts',(73.5590966011547,763.336181489556,83.6568220679962));
#81707=CARTESIAN_POINT('Ctrl Pts',(73.5038324872464,763.247913812902,83.6399138783004));
#81708=CARTESIAN_POINT('Ctrl Pts',(73.4488444080641,763.159436842759,83.6230853925887));
#81709=CARTESIAN_POINT('Ctrl Pts',(73.1132302252477,762.619426599187,83.520374431156));
#81710=CARTESIAN_POINT('Ctrl Pts',(72.7879129157079,762.071637465489,83.4206318480089));
#81711=CARTESIAN_POINT('Ctrl Pts',(72.474219014269,761.515064802767,83.3242202553888));
#81712=CARTESIAN_POINT('Ctrl Pts',(72.1726286046254,760.979966808905,83.2315285850079));
#81713=CARTESIAN_POINT('Ctrl Pts',(71.8817818330543,760.436750090596,83.1419157855282));
#81714=CARTESIAN_POINT('Ctrl Pts',(71.6028966763131,759.884495600035,83.0557144828276));
#81715=CARTESIAN_POINT('Ctrl Pts',(71.4907939020061,759.662507233072,83.0210643591189));
#81716=CARTESIAN_POINT('Ctrl Pts',(71.3806243244004,759.439058250873,82.9869655811785));
#81717=CARTESIAN_POINT('Ctrl Pts',(71.2724690060563,759.214087653493,82.9534402731627));
#81718=CARTESIAN_POINT('Ctrl Pts',(71.2313548746967,759.128567395828,82.9406959722931));
#81719=CARTESIAN_POINT('Ctrl Pts',(71.1905294946928,759.042821726578,82.9280338870646));
#81720=CARTESIAN_POINT('Ctrl Pts',(71.1499985653014,758.956849457591,82.9154556285894));
#81721=CARTESIAN_POINT('Ctrl Pts',(70.9502324773323,758.533115185837,82.8534607637595));
#81722=CARTESIAN_POINT('Ctrl Pts',(70.7572982590349,758.102842316802,82.7934040808962));
#81723=CARTESIAN_POINT('Ctrl Pts',(70.5729745362041,757.668912681433,82.7358431182547));
#81724=CARTESIAN_POINT('Ctrl Pts',(70.4749971365992,757.438257090107,82.7052465496105));
#81725=CARTESIAN_POINT('Ctrl Pts',(70.3794524660278,757.20656932707,82.6753551137604));
#81726=CARTESIAN_POINT('Ctrl Pts',(70.2866057688366,756.974287643936,82.6462520783323));
#81727=CARTESIAN_POINT('Ctrl Pts',(70.2549725135742,756.895148309984,82.6363365533168));
#81728=CARTESIAN_POINT('Ctrl Pts',(70.2236466597481,756.815928101304,82.6265104736713));
#81729=CARTESIAN_POINT('Ctrl Pts',(70.1926389310556,756.736643983384,82.6167772222424));
#81730=CARTESIAN_POINT('Ctrl Pts',(70.0008322429551,756.246210639236,82.5565695643541));
#81731=CARTESIAN_POINT('Ctrl Pts',(69.8207380469322,755.752537000797,82.4997730334338));
#81732=CARTESIAN_POINT('Ctrl Pts',(69.6526436142649,755.25574335944,82.4465134247772));
#81733=CARTESIAN_POINT('Ctrl Pts',(69.5876584443764,755.063683344895,82.4259233037255));
#81734=CARTESIAN_POINT('Ctrl Pts',(69.5244662353335,754.871157182456,82.4058616953423));
#81735=CARTESIAN_POINT('Ctrl Pts',(69.4630816345515,754.678172457831,82.3863354291315));
#81736=CARTESIAN_POINT('Ctrl Pts',(69.4414146562721,754.610054464336,82.3794432252159));
#81737=CARTESIAN_POINT('Ctrl Pts',(69.4199715886117,754.541876553508,82.3726171766097));
#81738=CARTESIAN_POINT('Ctrl Pts',(69.3987530496711,754.473639090163,82.3658575497437));
#81739=CARTESIAN_POINT('Ctrl Pts',(69.2456839785206,753.981378753056,82.31709406944));
#81740=CARTESIAN_POINT('Ctrl Pts',(69.1044146638885,753.486041628445,82.2718223599259));
#81741=CARTESIAN_POINT('Ctrl Pts',(68.9747603029794,752.987670002935,82.2300252477364));
#81742=CARTESIAN_POINT('Ctrl Pts',(68.8429790834064,752.481123056502,82.1875424929695));
#81743=CARTESIAN_POINT('Ctrl Pts',(68.7231969358553,751.971441077823,82.1486492709651));
#81744=CARTESIAN_POINT('Ctrl Pts',(68.6151684215416,751.458678722048,82.1133126209994));
#81745=CARTESIAN_POINT('Ctrl Pts',(68.5098860997668,750.958951296583,82.0788742639066));
#81746=CARTESIAN_POINT('Ctrl Pts',(68.4157670280329,750.456298046548,82.0478138616348));
#81747=CARTESIAN_POINT('Ctrl Pts',(68.3325396635622,749.950780797533,82.020087648334));
#81748=CARTESIAN_POINT('Ctrl Pts',(68.3261422655682,749.911923445082,82.0179564307653));
#81749=CARTESIAN_POINT('Ctrl Pts',(68.3198091607959,749.873049471991,82.0158448547));
#81750=CARTESIAN_POINT('Ctrl Pts',(68.3135402277496,749.834158963291,82.0137529034267));
#81751=CARTESIAN_POINT('Ctrl Pts',(68.2338355712915,749.339696091785,81.9871553538386));
#81752=CARTESIAN_POINT('Ctrl Pts',(68.1644146011459,748.842528149145,81.9637035184728));
#81753=CARTESIAN_POINT('Ctrl Pts',(68.104550932947,748.34284804846,81.9432166527108));
#81754=CARTESIAN_POINT('Ctrl Pts',(68.0718651149346,748.070020583542,81.9320307366772));
#81755=CARTESIAN_POINT('Ctrl Pts',(68.0420276545082,747.796444564669,81.9217284836477));
#81756=CARTESIAN_POINT('Ctrl Pts',(68.0149147410762,747.522154173909,81.9122787837859));
#81757=CARTESIAN_POINT('Ctrl Pts',(68.0125303604343,747.498032358317,81.9114477524222));
#81758=CARTESIAN_POINT('Ctrl Pts',(68.0101670378479,747.473905194498,81.9106232965028));
#81759=CARTESIAN_POINT('Ctrl Pts',(68.0078246793461,747.449772635794,81.9098053910308));
#81760=CARTESIAN_POINT('Ctrl Pts',(67.9624381839498,746.982170318031,81.8939573204166));
#81761=CARTESIAN_POINT('Ctrl Pts',(67.9249638118947,746.512338386814,81.8805821287688));
#81762=CARTESIAN_POINT('Ctrl Pts',(67.8943950412482,746.041844248718,81.8693983373665));
#81763=CARTESIAN_POINT('Ctrl Pts',(67.8731624008485,745.715045603139,81.8616302323322));
#81764=CARTESIAN_POINT('Ctrl Pts',(67.8552623904349,745.387926532362,81.8549196791735));
#81765=CARTESIAN_POINT('Ctrl Pts',(67.8403691802505,745.061004150737,81.8491758738642));
#81766=CARTESIAN_POINT('Ctrl Pts',(67.8398151425495,745.048842412437,81.8489622003412));
#81767=CARTESIAN_POINT('Ctrl Pts',(67.839265268583,745.036681055243,81.8487498640869));
#81768=CARTESIAN_POINT('Ctrl Pts',(67.838719541966,745.024520113673,81.8485388605921));
#81769=CARTESIAN_POINT('Ctrl Pts',(67.809929228428,744.382958368549,81.8374071756329));
#81770=CARTESIAN_POINT('Ctrl Pts',(67.7929166955335,743.741046577285,81.830088040421));
#81771=CARTESIAN_POINT('Ctrl Pts',(67.7832106745823,743.098909519817,81.8251575416515));
#81772=CARTESIAN_POINT('Ctrl Pts',(67.775657710959,742.599215787377,81.8213207605402));
#81773=CARTESIAN_POINT('Ctrl Pts',(67.7725283304721,742.099386023544,81.8189301434773));
#81774=CARTESIAN_POINT('Ctrl Pts',(67.7717437536218,741.599490031252,81.8173236497979));
#81775=CARTESIAN_POINT('Ctrl Pts',(67.770972615075,741.10815630284,81.8157446722878));
#81776=CARTESIAN_POINT('Ctrl Pts',(67.7724654094933,740.616758542271,81.8149227882236));
#81777=CARTESIAN_POINT('Ctrl Pts',(67.774294136204,740.125373479123,81.8142439628221));
#81778=CARTESIAN_POINT('',(37.9808888409178,740.125373764374,81.814182427552));
#81779=CARTESIAN_POINT('Ctrl Pts',(67.774347942193,740.125373764374,81.8141824275666));
#81780=CARTESIAN_POINT('Ctrl Pts',(67.5900718265523,740.125373764374,81.6531996590034));
#81781=CARTESIAN_POINT('Ctrl Pts',(67.0763564188786,740.125373764374,81.2162773885272));
#81782=CARTESIAN_POINT('Ctrl Pts',(66.5464115392411,740.125373764374,80.7985912178955));
#81783=CARTESIAN_POINT('Ctrl Pts',(65.3066539796418,740.125373764381,79.8939539311288));
#81784=CARTESIAN_POINT('Ctrl Pts',(63.9938241652593,740.125373764356,79.0958415525578));
#81785=CARTESIAN_POINT('Ctrl Pts',(62.8461837366256,740.125373764374,78.5050597321885));
#81786=CARTESIAN_POINT('Ctrl Pts',(60.4983919340555,740.125373764374,77.4343675133605));
#81787=CARTESIAN_POINT('Ctrl Pts',(58.0126377452945,740.125373764374,76.7089447197242));
#81788=CARTESIAN_POINT('Ctrl Pts',(56.3145905420647,740.125373764374,76.3826585955248));
#81789=CARTESIAN_POINT('Ctrl Pts',(52.8776183915509,740.125373764374,76.052496477614));
#81790=CARTESIAN_POINT('Ctrl Pts',(49.4406462410274,740.125373764373,76.3826585955353));
#81791=CARTESIAN_POINT('Ctrl Pts',(47.742599037804,740.125373764375,76.7089447197054));
#81792=CARTESIAN_POINT('Ctrl Pts',(45.2568448490267,740.125373764369,77.4343675134104));
#81793=CARTESIAN_POINT('Ctrl Pts',(42.2948993868004,740.125373764376,78.785139739208));
#81794=CARTESIAN_POINT('Ctrl Pts',(40.9539042355239,740.125373764374,79.5398396982121));
#81795=CARTESIAN_POINT('Ctrl Pts',(39.6810271869632,740.125373764374,80.4042681496218));
#81796=CARTESIAN_POINT('Ctrl Pts',(38.4886305678844,740.125373764374,81.3704310402807));
#81797=CARTESIAN_POINT('Ctrl Pts',(37.9808888409178,740.125373764374,81.814182427552));
#81798=CARTESIAN_POINT('Ctrl Pts',(37.9809426469069,740.125373479124,81.8142439628075));
#81799=CARTESIAN_POINT('Ctrl Pts',(37.9827466960379,740.59524704715,81.8148446402991));
#81800=CARTESIAN_POINT('Ctrl Pts',(37.9844092385585,741.06512079536,81.8155325195939));
#81801=CARTESIAN_POINT('Ctrl Pts',(37.9840335952872,741.534967841274,81.8169143815015));
#81802=CARTESIAN_POINT('Ctrl Pts',(37.9837494506095,741.890370287103,81.8179596516719));
#81803=CARTESIAN_POINT('Ctrl Pts',(37.9822977692306,742.245757495851,81.8194024431643));
#81804=CARTESIAN_POINT('Ctrl Pts',(37.97883925489,742.601120543275,81.8215114577564));
#81805=CARTESIAN_POINT('Ctrl Pts',(37.9788240082044,742.602687143306,81.8215207552406));
#81806=CARTESIAN_POINT('Ctrl Pts',(37.9788087225029,742.604253741534,81.8215300656766));
#81807=CARTESIAN_POINT('Ctrl Pts',(37.9787933977119,742.605820337965,81.8215393890886));
#81808=CARTESIAN_POINT('Ctrl Pts',(37.9737782986691,743.118495274342,81.8245905128916));
#81809=CARTESIAN_POINT('Ctrl Pts',(37.9645767685362,743.631503793139,81.8290294628732));
#81810=CARTESIAN_POINT('Ctrl Pts',(37.9492753233026,744.14400294551,81.835443517788));
#81811=CARTESIAN_POINT('Ctrl Pts',(37.940075009395,744.452153777489,81.8393001024266));
#81812=CARTESIAN_POINT('Ctrl Pts',(37.9286685542766,744.760120076633,81.8438710044871));
#81813=CARTESIAN_POINT('Ctrl Pts',(37.9146320060792,745.067715043578,81.8492863515391));
#81814=CARTESIAN_POINT('Ctrl Pts',(37.9145109708903,745.070367391891,81.8493330473181));
#81815=CARTESIAN_POINT('Ctrl Pts',(37.9143897370563,745.073019691594,81.8493798067728));
#81816=CARTESIAN_POINT('Ctrl Pts',(37.9142683044256,745.075671942701,81.8494266299454));
#81817=CARTESIAN_POINT('Ctrl Pts',(37.8866198583192,745.679550993783,81.8600875862031));
#81818=CARTESIAN_POINT('Ctrl Pts',(37.8486433540992,746.281212927868,81.8740631070229));
#81819=CARTESIAN_POINT('Ctrl Pts',(37.7985599020469,746.880257424195,81.8918453024477));
#81820=CARTESIAN_POINT('Ctrl Pts',(37.7539545794202,747.413778416287,81.9076824808256));
#81821=CARTESIAN_POINT('Ctrl Pts',(37.6997452435811,747.945223820169,81.9265392815381));
#81822=CARTESIAN_POINT('Ctrl Pts',(37.6347063987271,748.474332613323,81.9487526687549));
#81823=CARTESIAN_POINT('Ctrl Pts',(37.5766710855168,748.946465760858,81.9685740676049));
#81824=CARTESIAN_POINT('Ctrl Pts',(37.5100128380444,749.416738761758,81.9910680943248));
#81825=CARTESIAN_POINT('Ctrl Pts',(37.4338923550026,749.884978811516,82.0164642440168));
#81826=CARTESIAN_POINT('Ctrl Pts',(37.4299124359474,749.909460494001,82.0177920682246));
#81827=CARTESIAN_POINT('Ctrl Pts',(37.4259068238323,749.93393682343,82.019127764189));
#81828=CARTESIAN_POINT('Ctrl Pts',(37.42187547866,749.958407780289,82.0204713395027));
#81829=CARTESIAN_POINT('Ctrl Pts',(37.3372425300594,750.472144298872,82.048677989048));
#81830=CARTESIAN_POINT('Ctrl Pts',(37.2412646275997,750.983457551872,82.0803621354665));
#81831=CARTESIAN_POINT('Ctrl Pts',(37.1335886143222,751.492258643645,82.115588980578));
#81832=CARTESIAN_POINT('Ctrl Pts',(37.0243826544436,752.008289186781,82.1513163567762));
#81833=CARTESIAN_POINT('Ctrl Pts',(36.903143375796,752.521735767981,82.1906879120542));
#81834=CARTESIAN_POINT('Ctrl Pts',(36.7695549149236,753.032515831067,82.233756080504));
#81835=CARTESIAN_POINT('Ctrl Pts',(36.6359664540512,753.543295894153,82.2768242489537));
#81836=CARTESIAN_POINT('Ctrl Pts',(36.4900285286155,754.051409567256,82.3235890827042));
#81837=CARTESIAN_POINT('Ctrl Pts',(36.3314825399832,754.556782671789,82.3740865194685));
#81838=CARTESIAN_POINT('Ctrl Pts',(36.3162234058514,754.605421909245,82.3789466056022));
#81839=CARTESIAN_POINT('Ctrl Pts',(36.3008472050756,754.654038994412,82.3838413589757));
#81840=CARTESIAN_POINT('Ctrl Pts',(36.2853543869488,754.702633073474,82.388770610727));
#81841=CARTESIAN_POINT('Ctrl Pts',(36.1002458846035,755.283236106727,82.4476654097167));
#81842=CARTESIAN_POINT('Ctrl Pts',(35.8983907512341,755.860820660562,82.5115195397896));
#81843=CARTESIAN_POINT('Ctrl Pts',(35.6804717557189,756.434123844787,82.5800712398139));
#81844=CARTESIAN_POINT('Ctrl Pts',(35.6280069590958,756.572148686965,82.5965753127674));
#81845=CARTESIAN_POINT('Ctrl Pts',(35.5746112583638,756.709925496093,82.6133516164342));
#81846=CARTESIAN_POINT('Ctrl Pts',(35.5202945448795,756.847436900889,82.6303964032376));
#81847=CARTESIAN_POINT('Ctrl Pts',(35.497861482644,756.904229768204,82.6374359816403));
#81848=CARTESIAN_POINT('Ctrl Pts',(35.4752936356645,756.960922884651,82.6445143553775));
#81849=CARTESIAN_POINT('Ctrl Pts',(35.4525923201978,757.017516942744,82.651631118668));
#81850=CARTESIAN_POINT('Ctrl Pts',(35.1875439041849,757.678278891777,82.734722639952));
#81851=CARTESIAN_POINT('Ctrl Pts',(34.9042764143143,758.325612285822,82.8230551210942));
#81852=CARTESIAN_POINT('Ctrl Pts',(34.6047070769484,758.960937830743,82.9160405142498));
#81853=CARTESIAN_POINT('Ctrl Pts',(34.5867726694948,758.998973055872,82.9216072986969));
#81854=CARTESIAN_POINT('Ctrl Pts',(34.5687798227313,759.036965234549,82.9271907631233));
#81855=CARTESIAN_POINT('Ctrl Pts',(34.5507289434783,759.074914668111,82.9327907826882));
#81856=CARTESIAN_POINT('Ctrl Pts',(34.5222206321713,759.134849381028,82.9416350666061));
#81857=CARTESIAN_POINT('Ctrl Pts',(34.4935678348722,759.194677750235,82.950520481513));
#81858=CARTESIAN_POINT('Ctrl Pts',(34.4647721445413,759.254400744103,82.9594465899417));
#81859=CARTESIAN_POINT('Ctrl Pts',(34.1949133510472,759.814094742889,83.0430976093646));
#81860=CARTESIAN_POINT('Ctrl Pts',(33.912510712514,760.364551038498,83.1303190024909));
#81861=CARTESIAN_POINT('Ctrl Pts',(33.618793061381,760.90667060331,83.220776067925));
#81862=CARTESIAN_POINT('Ctrl Pts',(33.3134812904446,761.470189628311,83.3148038076091));
#81863=CARTESIAN_POINT('Ctrl Pts',(32.9959434573165,762.024700696235,83.4123277444519));
#81864=CARTESIAN_POINT('Ctrl Pts',(32.6675131954889,762.571185853467,83.512984538312));
#81865=CARTESIAN_POINT('Ctrl Pts',(32.5238668199846,762.810203450891,83.5570090551986));
#81866=CARTESIAN_POINT('Ctrl Pts',(32.3781362077929,763.047685365439,83.6016330258509));
#81867=CARTESIAN_POINT('Ctrl Pts',(32.230430415535,763.283712134329,83.6468267333961));
#81868=CARTESIAN_POINT('Ctrl Pts',(32.1941831345178,763.341633550198,83.6579173547763));
#81869=CARTESIAN_POINT('Ctrl Pts',(32.1578171062028,763.39946717192,83.6690422855322));
#81870=CARTESIAN_POINT('Ctrl Pts',(32.1213337000335,763.457214005624,83.6802012019161));
#81871=CARTESIAN_POINT('Ctrl Pts',(31.7502871493371,764.044515623252,83.7936905349721));
#81872=CARTESIAN_POINT('Ctrl Pts',(31.3671032562343,764.62286796126,83.910692328112));
#81873=CARTESIAN_POINT('Ctrl Pts',(30.9732032066471,765.193301121279,84.0308718910516));
#81874=CARTESIAN_POINT('Ctrl Pts',(30.5580738785247,765.794477827669,84.1575285423251));
#81875=CARTESIAN_POINT('Ctrl Pts',(30.1310419378069,766.386858621788,84.2877147689403));
#81876=CARTESIAN_POINT('Ctrl Pts',(29.6937240880705,766.971618419196,84.4210507830968));
#81877=CARTESIAN_POINT('Ctrl Pts',(29.6303795406661,767.056319614744,84.4403642171918));
#81878=CARTESIAN_POINT('Ctrl Pts',(29.5668191133517,767.140860866817,84.4597437554177));
#81879=CARTESIAN_POINT('Ctrl Pts',(29.503047648562,767.225245698764,84.4791882620394));
#81880=CARTESIAN_POINT('Ctrl Pts',(29.4655179406033,767.274906438242,84.4906314154517));
#81881=CARTESIAN_POINT('Ctrl Pts',(29.4279150906882,767.32451295757,84.5020971038909));
#81882=CARTESIAN_POINT('Ctrl Pts',(29.3902398839613,767.374065886495,84.5135851689969));
#81883=CARTESIAN_POINT('Ctrl Pts',(28.8372399597301,768.101408038588,84.6822079765435));
#81884=CARTESIAN_POINT('Ctrl Pts',(28.2686639470961,768.817231510892,84.85564644981));
#81885=CARTESIAN_POINT('Ctrl Pts',(27.6870997968389,769.523343990526,85.0333678725965));
#81886=CARTESIAN_POINT('Ctrl Pts',(27.2888276362705,770.006910494313,85.1550767072989));
#81887=CARTESIAN_POINT('Ctrl Pts',(26.8844630765403,770.485921879645,85.278794462455));
#81888=CARTESIAN_POINT('Ctrl Pts',(26.4748262094946,770.960950931432,85.4043528068919));
#81889=CARTESIAN_POINT('Ctrl Pts',(26.4409425167201,771.000243631246,85.4147385429192));
#81890=CARTESIAN_POINT('Ctrl Pts',(26.4070217053255,771.039510056123,85.4251371961802));
#81891=CARTESIAN_POINT('Ctrl Pts',(26.3730642728265,771.078750367021,85.4355486646748));
#81892=CARTESIAN_POINT('Ctrl Pts',(25.7100717721007,771.8448869662,85.638824502258));
#81893=CARTESIAN_POINT('Ctrl Pts',(25.0328724614708,772.601367096943,85.8470613974414));
#81894=CARTESIAN_POINT('Ctrl Pts',(24.3457466839457,773.348724068689,86.0593230190846));
#81895=CARTESIAN_POINT('Ctrl Pts',(23.9775445712505,773.749201572131,86.1730651898625));
#81896=CARTESIAN_POINT('Ctrl Pts',(23.6064930208942,774.147060117326,86.287962674055));
#81897=CARTESIAN_POINT('Ctrl Pts',(23.2332540233972,774.542385963715,86.4038694764088));
#81898=CARTESIAN_POINT('Ctrl Pts',(23.2062709433082,774.570965798742,86.4122488862554));
#81899=CARTESIAN_POINT('Ctrl Pts',(23.1792765535914,774.599532492652,86.4206334784754));
#81900=CARTESIAN_POINT('Ctrl Pts',(23.1522710105224,774.628086137261,86.4290232311268));
#81901=CARTESIAN_POINT('Ctrl Pts',(22.4054414532268,775.417727941851,86.6610391266233));
#81902=CARTESIAN_POINT('Ctrl Pts',(21.6500097546164,776.197495325431,86.8970247415881));
#81903=CARTESIAN_POINT('Ctrl Pts',(20.8885671226297,776.970039421042,87.1367381864585));
#81904=CARTESIAN_POINT('Ctrl Pts',(20.0199236634596,777.851347279813,87.4102000432217));
#81905=CARTESIAN_POINT('Ctrl Pts',(19.143457320241,778.723254574552,87.6885131079581));
#81906=CARTESIAN_POINT('Ctrl Pts',(18.2629623050438,779.589646932752,87.9713327580525));
#81907=CARTESIAN_POINT('Ctrl Pts',(17.6497070459899,780.193079843671,88.1683135867802));
#81908=CARTESIAN_POINT('Ctrl Pts',(17.0344962824946,780.793836325147,88.3674808723051));
#81909=CARTESIAN_POINT('Ctrl Pts',(16.4186020601252,781.39321950309,88.5687220124197));
#81910=CARTESIAN_POINT('Ctrl Pts',(16.4153549874364,781.396379527452,88.5697829813105));
#81911=CARTESIAN_POINT('Ctrl Pts',(16.4121078922666,781.39953951086,88.5708440079859));
#81912=CARTESIAN_POINT('Ctrl Pts',(16.408860774807,781.402699453514,88.5719050924519));
#81913=CARTESIAN_POINT('Ctrl Pts',(15.0040136404545,782.769830897858,89.0309773280409));
#81914=CARTESIAN_POINT('Ctrl Pts',(13.5950748355171,784.129278826655,89.5008398450487));
#81915=CARTESIAN_POINT('Ctrl Pts',(12.1980182279082,785.496799332103,89.9818285700894));
#81916=CARTESIAN_POINT('Ctrl Pts',(11.3291011844497,786.347346022903,90.2809855968148));
#81917=CARTESIAN_POINT('Ctrl Pts',(10.4647792418779,787.201014039128,90.584447359179));
#81918=CARTESIAN_POINT('Ctrl Pts',(9.60890053120187,788.061597029217,90.8923018138587));
#81919=CARTESIAN_POINT('Ctrl Pts',(9.58424946245066,788.0863835909,90.9011686558925));
#81920=CARTESIAN_POINT('Ctrl Pts',(9.55960541231716,788.111175895238,90.9100391396316));
#81921=CARTESIAN_POINT('Ctrl Pts',(9.53496847334693,788.135974031963,90.91891326703));
#81922=CARTESIAN_POINT('Ctrl Pts',(8.59423498486735,789.082862673328,91.2577617268507));
#81923=CARTESIAN_POINT('Ctrl Pts',(7.66378701510754,790.038210513089,91.6018883436517));
#81924=CARTESIAN_POINT('Ctrl Pts',(6.75031466068051,791.008392590562,91.9520631261947));
#81925=CARTESIAN_POINT('Ctrl Pts',(6.60468479907203,791.163063370682,92.0078895613061));
#81926=CARTESIAN_POINT('Ctrl Pts',(6.45948646854013,791.318111255008,92.0638697355003));
#81927=CARTESIAN_POINT('Ctrl Pts',(6.31474687067201,791.473562167901,92.1200067905554));
#81928=CARTESIAN_POINT('Ctrl Pts',(5.82689730392431,791.997514573619,92.309218577727));
#81929=CARTESIAN_POINT('Ctrl Pts',(5.34457107578471,792.525722147699,92.5000943886224));
#81930=CARTESIAN_POINT('Ctrl Pts',(4.86909463668608,793.058804009112,92.6926189943811));
#81931=CARTESIAN_POINT('Ctrl Pts',(4.42763029014315,793.553753109111,92.871371803744));
#81932=CARTESIAN_POINT('Ctrl Pts',(3.99207103417591,794.052904312235,93.0515459213008));
#81933=CARTESIAN_POINT('Ctrl Pts',(3.56344441385697,794.556723524126,93.233121145656));
#81934=CARTESIAN_POINT('Ctrl Pts',(3.43512442690785,794.707554274318,93.2874801829043));
#81935=CARTESIAN_POINT('Ctrl Pts',(3.30742552153365,794.858803170986,93.3419647388763));
#81936=CARTESIAN_POINT('Ctrl Pts',(3.18037457161906,795.0104821055,93.3965741249367));
#81937=CARTESIAN_POINT('Ctrl Pts',(3.13179027251589,795.068484148988,93.4174567609814));
#81938=CARTESIAN_POINT('Ctrl Pts',(3.08329934447481,795.126550660042,93.4383582328862));
#81939=CARTESIAN_POINT('Ctrl Pts',(3.03490304960601,795.184682618555,93.4592786115396));
#81940=CARTESIAN_POINT('Ctrl Pts',(2.5486063539281,795.768805420002,93.6694912122997));
#81941=CARTESIAN_POINT('Ctrl Pts',(2.07201161992725,796.359670351005,93.88165210726));
#81942=CARTESIAN_POINT('Ctrl Pts',(1.60626353450439,796.958089247717,94.0959442263557));
#81943=CARTESIAN_POINT('Ctrl Pts',(1.15619334881705,797.536364311837,94.3030228958153));
#81944=CARTESIAN_POINT('Ctrl Pts',(0.71625188401368,798.121693370953,94.5120917355322));
#81945=CARTESIAN_POINT('Ctrl Pts',(0.28743872356641,798.714778005,94.7233075671941));
#81946=CARTESIAN_POINT('Ctrl Pts',(0.224074940183661,798.802415441874,94.754517976386));
#81947=CARTESIAN_POINT('Ctrl Pts',(0.160953410662966,798.890220616696,94.785775156932));
#81948=CARTESIAN_POINT('Ctrl Pts',(0.0980770791788375,798.978196277738,
94.8170797440185));
#81949=CARTESIAN_POINT('Ctrl Pts',(-0.369182434230171,799.63197908599,95.0497168235724));
#81950=CARTESIAN_POINT('Ctrl Pts',(-0.822955604702935,800.295117632775,
95.2849851591274));
#81951=CARTESIAN_POINT('Ctrl Pts',(-1.26279292192534,800.967941700168,95.5231915489782));
#81952=CARTESIAN_POINT('Ctrl Pts',(-1.48341606559332,801.305431392541,95.6426762777924));
#81953=CARTESIAN_POINT('Ctrl Pts',(-1.70054450132931,801.64534585775,95.7629004304533));
#81954=CARTESIAN_POINT('Ctrl Pts',(-1.91420412082378,801.98764121032,95.8839019515004));
#81955=CARTESIAN_POINT('Ctrl Pts',(-2.02120199779361,802.15905814024,95.9444978932736));
#81956=CARTESIAN_POINT('Ctrl Pts',(-2.12733090562511,802.331071173192,96.0052887647587));
#81957=CARTESIAN_POINT('Ctrl Pts',(-2.23260018314948,802.503668568799,96.0662790978337));
#81958=CARTESIAN_POINT('Ctrl Pts',(-2.25752083667438,802.544527972382,96.0807174885463));
#81959=CARTESIAN_POINT('Ctrl Pts',(-2.2823890579689,802.585424172706,96.0951666815795));
#81960=CARTESIAN_POINT('Ctrl Pts',(-2.3072174972792,802.626345096273,96.1096278308841));
#81961=CARTESIAN_POINT('Origin',(52.8776183915471,831.777100559639,108.439826246791));
#81962=CARTESIAN_POINT('Ctrl Pts',(-3.40945017935348,804.520999278367,96.7791350119252));
#81963=CARTESIAN_POINT('Ctrl Pts',(-3.46667793432084,804.486019404866,96.7878665218692));
#81964=CARTESIAN_POINT('Ctrl Pts',(-3.52304849176604,804.450364686567,96.7998559185783));
#81965=CARTESIAN_POINT('Ctrl Pts',(-3.57823712091559,804.414238076631,96.8150416942174));
#81966=CARTESIAN_POINT('Ctrl Pts',(-3.63506842586774,804.377036167147,96.8306794706866));
#81967=CARTESIAN_POINT('Ctrl Pts',(-3.69064613886921,804.339334172832,96.8497062468343));
#81968=CARTESIAN_POINT('Ctrl Pts',(-3.7446495153042,804.301350628926,96.8720101986567));
#81969=CARTESIAN_POINT('Ctrl Pts',(-3.80177576206803,804.261170598614,96.8956039281553));
#81970=CARTESIAN_POINT('Ctrl Pts',(-3.85714010926235,804.22067577032,96.9228644349813));
#81971=CARTESIAN_POINT('Ctrl Pts',(-3.91040432059931,804.180116757718,96.953616843281));
#81972=CARTESIAN_POINT('Ctrl Pts',(-3.96553462626411,804.138136773296,96.9854466522077));
#81973=CARTESIAN_POINT('Ctrl Pts',(-4.0184152243734,804.096088090149,97.021016895017));
#81974=CARTESIAN_POINT('Ctrl Pts',(-4.06871448527445,804.054237640207,97.0600961959471));
#81975=CARTESIAN_POINT('Ctrl Pts',(-4.12125356143182,804.010523598741,97.1009156897322));
#81976=CARTESIAN_POINT('Ctrl Pts',(-4.17097653717914,803.967025723494,97.1455636479873));
#81977=CARTESIAN_POINT('Ctrl Pts',(-4.21754878663746,803.924036824183,97.193740329175));
#81978=CARTESIAN_POINT('Ctrl Pts',(-4.2510073136189,803.893152654657,97.2283515151526));
#81979=CARTESIAN_POINT('Ctrl Pts',(-4.28284057407814,803.862530918084,97.2647832827392));
#81980=CARTESIAN_POINT('Ctrl Pts',(-4.31293627306915,803.83227757975,97.3029132850214));
#81981=CARTESIAN_POINT('Ctrl Pts',(-4.35503392302775,803.789959424999,97.3562492613505));
#81982=CARTESIAN_POINT('Ctrl Pts',(-4.3936829806961,803.748409996973,97.412849490922));
#81983=CARTESIAN_POINT('Ctrl Pts',(-4.4286303447873,803.707907145932,97.4723270319076));
#81984=CARTESIAN_POINT('Ctrl Pts',(-4.46264936649609,803.668480213324,97.5302246104687));
#81985=CARTESIAN_POINT('Ctrl Pts',(-4.4931608496782,803.630044812499,97.5908490142823));
#81986=CARTESIAN_POINT('Ctrl Pts',(-4.51996545111149,803.592850417633,97.6538087985575));
#81987=CARTESIAN_POINT('Ctrl Pts',(-4.54516688592327,803.557880596503,97.713002997103));
#81988=CARTESIAN_POINT('Ctrl Pts',(-4.56709154016755,803.524007777126,97.7742616441211));
#81989=CARTESIAN_POINT('Ctrl Pts',(-4.58560390336969,803.491434394108,97.8372257077396));
#81990=CARTESIAN_POINT('Ctrl Pts',(-4.60352285616161,803.459905144913,97.8981714698365));
#81991=CARTESIAN_POINT('Ctrl Pts',(-4.61824441404098,803.429593543633,97.9607151154782));
#81992=CARTESIAN_POINT('Ctrl Pts',(-4.62967815148095,803.40067698333,98.0244973547518));
#81993=CARTESIAN_POINT('Ctrl Pts',(-4.64062622635985,803.372988690758,98.085570362172));
#81994=CARTESIAN_POINT('Ctrl Pts',(-4.64855954807306,803.346579693476,98.1477787580681));
#81995=CARTESIAN_POINT('Ctrl Pts',(-4.6534337763171,803.321596805669,98.2107770840891));
#81996=CARTESIAN_POINT('Ctrl Pts',(-4.65731484044172,803.30170438686,98.2609389827098));
#81997=CARTESIAN_POINT('Ctrl Pts',(-4.65925699042526,803.282716040417,98.3116010570751));
#81998=CARTESIAN_POINT('Ctrl Pts',(-4.659256990425,803.264699682484,98.3625762498986));
#81999=CARTESIAN_POINT('Origin',(108.644128965869,804.142030366665,98.6726132747675));
#82000=CARTESIAN_POINT('Ctrl Pts',(110.421072908878,803.276519768482,98.366706730931));
#82001=CARTESIAN_POINT('Ctrl Pts',(110.421014271246,803.768657750697,96.9739242975922));
#82002=CARTESIAN_POINT('Ctrl Pts',(109.171101223695,804.532439790988,96.7831441306878));
#82003=CARTESIAN_POINT('Ctrl Pts',(110.052254005922,802.614532539069,98.1328076646065));
#82004=CARTESIAN_POINT('Ctrl Pts',(110.052305119154,803.10632016932,96.7416534710974));
#82005=CARTESIAN_POINT('Ctrl Pts',(108.812286380141,803.884051253074,96.5547193989541));
#82006=CARTESIAN_POINT('Ctrl Pts',(109.671712416757,801.960951606285,97.901782698405));
#82007=CARTESIAN_POINT('Ctrl Pts',(109.671681841165,802.453140325948,96.5090374725116));
#82008=CARTESIAN_POINT('Ctrl Pts',(108.437995444743,803.245379043133,96.3283029022672));
#82009=CARTESIAN_POINT('Ctrl Pts',(109.279637963697,801.31562045008,97.6736561886769));
#82010=CARTESIAN_POINT('Ctrl Pts',(109.279678408479,801.807888527408,96.2810525353335));
#82011=CARTESIAN_POINT('Ctrl Pts',(108.054721885659,802.614266885493,96.105245090354));
#82012=CARTESIAN_POINT('Ctrl Pts',(108.062487312194,802.626301820665,96.1096219232672));
#82013=CARTESIAN_POINT('Ctrl Pts',(108.118602839649,802.589390382965,96.1176812397369));
#82014=CARTESIAN_POINT('Ctrl Pts',(108.173877147318,802.55183405875,96.1290098394246));
#82015=CARTESIAN_POINT('Ctrl Pts',(108.227991810621,802.513846617947,96.1435497736361));
#82016=CARTESIAN_POINT('Ctrl Pts',(108.283722724182,802.474724600908,96.1585239741071));
#82017=CARTESIAN_POINT('Ctrl Pts',(108.338223437648,802.435145655062,96.1769037122149));
#82018=CARTESIAN_POINT('Ctrl Pts',(108.391179399861,802.395339000355,96.198580674604));
#82019=CARTESIAN_POINT('Ctrl Pts',(108.447209799911,802.353221310585,96.2215161255675));
#82020=CARTESIAN_POINT('Ctrl Pts',(108.501510662581,802.31084896716,96.2481423888305));
#82021=CARTESIAN_POINT('Ctrl Pts',(108.55375011033,802.268483950337,96.2782882195284));
#82022=CARTESIAN_POINT('Ctrl Pts',(108.607829357391,802.224626897663,96.3094957436591));
#82023=CARTESIAN_POINT('Ctrl Pts',(108.659699593296,802.180777751386,96.3444746782031));
#82024=CARTESIAN_POINT('Ctrl Pts',(108.709035256812,802.137214687147,96.3829971093564));
#82025=CARTESIAN_POINT('Ctrl Pts',(108.760576879989,802.091703775133,96.4232420050129));
#82026=CARTESIAN_POINT('Ctrl Pts',(108.809352452134,802.046504974408,96.4673542972343));
#82027=CARTESIAN_POINT('Ctrl Pts',(108.855033248751,802.001922593523,96.515037567581));
#82028=CARTESIAN_POINT('Ctrl Pts',(108.887652344881,801.970087838538,96.5490865617847));
#82029=CARTESIAN_POINT('Ctrl Pts',(108.918694344536,801.938567095153,96.5849556525495));
#82030=CARTESIAN_POINT('Ctrl Pts',(108.948050870766,801.90746822385,96.6225258003466));
#82031=CARTESIAN_POINT('Ctrl Pts',(108.989460056698,801.863601353023,96.6755208047089));
#82032=CARTESIAN_POINT('Ctrl Pts',(109.027466079045,801.820625240543,96.7318402448099));
#82033=CARTESIAN_POINT('Ctrl Pts',(109.061816904743,801.778823729021,96.7910956325936));
#82034=CARTESIAN_POINT('Ctrl Pts',(109.095235650154,801.738156465776,96.8487431760892));
#82035=CARTESIAN_POINT('Ctrl Pts',(109.125194979059,801.698600727609,96.9091698637508));
#82036=CARTESIAN_POINT('Ctrl Pts',(109.151496205164,801.660409921191,96.9719830641364));
#82037=CARTESIAN_POINT('Ctrl Pts',(109.17619271011,801.624549256907,97.030963832098));
#82038=CARTESIAN_POINT('Ctrl Pts',(109.197663830857,801.589892049051,97.0920488555737));
#82039=CARTESIAN_POINT('Ctrl Pts',(109.215774451259,801.556642318281,97.1548789506565));
#82040=CARTESIAN_POINT('Ctrl Pts',(109.233295236484,801.524475480332,97.2156627657432));
#82041=CARTESIAN_POINT('Ctrl Pts',(109.247670494366,801.493626127562,97.2780798931909));
#82042=CARTESIAN_POINT('Ctrl Pts',(109.258809538119,801.464271879396,97.3417709039283));
#82043=CARTESIAN_POINT('Ctrl Pts',(109.26947065127,801.436177101411,97.4027291950817));
#82044=CARTESIAN_POINT('Ctrl Pts',(109.277166990319,801.409452143862,97.464854188198));
#82045=CARTESIAN_POINT('Ctrl Pts',(109.281853279706,801.384242796069,97.5278001497676));
#82046=CARTESIAN_POINT('Ctrl Pts',(109.285533189291,801.364447151169,97.5772284774392));
#82047=CARTESIAN_POINT('Ctrl Pts',(109.287357614049,801.345585947171,97.627162373131));
#82048=CARTESIAN_POINT('Ctrl Pts',(109.287322495866,801.327723325276,97.6774220453723));
#82049=CARTESIAN_POINT('Ctrl Pts',(109.295214075855,801.340715062203,97.6820532174938));
#82050=CARTESIAN_POINT('Ctrl Pts',(109.294861021846,801.8329774859,96.2899062835287));
#82051=CARTESIAN_POINT('Ctrl Pts',(108.069824947897,802.638398299217,96.1138965465646));
#82052=CARTESIAN_POINT('Ctrl Pts',(108.442187483773,799.934658383676,97.18505161579));
#82053=CARTESIAN_POINT('Ctrl Pts',(108.441981829264,800.427131807017,95.7932530139787));
#82054=CARTESIAN_POINT('Ctrl Pts',(107.235749064159,801.263000987828,95.6278638607556));
#82055=CARTESIAN_POINT('Ctrl Pts',(107.52710530691,798.562162368243,96.6932753022757));
#82056=CARTESIAN_POINT('Ctrl Pts',(107.52535987795,799.057721670121,95.3079216776574));
#82057=CARTESIAN_POINT('Ctrl Pts',(106.344056162865,799.922005251717,95.1533860412624));
#82058=CARTESIAN_POINT('Ctrl Pts',(105.602319018081,795.920775113123,95.7428524103056));
#82059=CARTESIAN_POINT('Ctrl Pts',(105.598173918827,796.419036535808,94.3684927787303));
#82060=CARTESIAN_POINT('Ctrl Pts',(104.467575793977,797.336433927823,94.2323842521393));
#82061=CARTESIAN_POINT('Ctrl Pts',(104.592399256266,794.648346650005,95.2830219901209));
#82062=CARTESIAN_POINT('Ctrl Pts',(104.587966674248,795.147046217482,93.9135888475786));
#82063=CARTESIAN_POINT('Ctrl Pts',(103.482351883554,796.088345213852,93.7848284793472));
#82064=CARTESIAN_POINT('Ctrl Pts',(101.456168750866,790.944845315593,93.9462813965269));
#82065=CARTESIAN_POINT('Ctrl Pts',(101.457735490723,791.445279193071,92.5880663369688));
#82066=CARTESIAN_POINT('Ctrl Pts',(100.414443555522,792.44331512699,92.4721670616595));
#82067=CARTESIAN_POINT('Ctrl Pts',(99.226526723945,788.625058813487,93.1106895076422));
#82068=CARTESIAN_POINT('Ctrl Pts',(99.233925577768,789.118118434763,91.7524962811977));
#82069=CARTESIAN_POINT('Ctrl Pts',(98.2219969540277,790.143303030444,91.6363993045642));
#82070=CARTESIAN_POINT('Ctrl Pts',(94.6762234756949,784.109404432082,91.5115703119863));
#82071=CARTESIAN_POINT('Ctrl Pts',(94.6930413876074,784.581658178514,90.1568569234352));
#82072=CARTESIAN_POINT('Ctrl Pts',(93.7255485233951,785.632982415435,90.02433712775));
#82073=CARTESIAN_POINT('Ctrl Pts',(92.3541248459539,781.91348973001,90.7476546813426));
#82074=CARTESIAN_POINT('Ctrl Pts',(92.3791378846776,782.376338799843,89.3979289669664));
#82075=CARTESIAN_POINT('Ctrl Pts',(91.4209323280296,783.423079983555,89.248233527896));
#82076=CARTESIAN_POINT('Ctrl Pts',(87.7513528206951,777.511282938626,89.2780543750025));
#82077=CARTESIAN_POINT('Ctrl Pts',(87.7764466266993,777.940567375721,87.9475638320085));
#82078=CARTESIAN_POINT('Ctrl Pts',(86.8404914765804,778.961421974556,87.7545659796536));
#82079=CARTESIAN_POINT('Ctrl Pts',(85.4690225979344,775.306343516102,88.5725577284606));
#82080=CARTESIAN_POINT('Ctrl Pts',(85.4979413206163,775.72389797577,87.259453067688));
#82081=CARTESIAN_POINT('Ctrl Pts',(84.5629483705987,776.711061799412,87.0369300296726));
#82082=CARTESIAN_POINT('Ctrl Pts',(82.1733222236736,771.902715674148,87.5663060875807));
#82083=CARTESIAN_POINT('Ctrl Pts',(82.183750371381,772.274875821215,86.2839817908659));
#82084=CARTESIAN_POINT('Ctrl Pts',(81.270476661061,773.211393613522,86.0151631449675));
#82085=CARTESIAN_POINT('Ctrl Pts',(81.096556296596,770.752364778805,87.2398363086889));
#82086=CARTESIAN_POINT('Ctrl Pts',(81.1046082428451,771.113387291667,85.9707508669623));
#82087=CARTESIAN_POINT('Ctrl Pts',(80.1941410218622,772.02430508146,85.6839344533105));
#82088=CARTESIAN_POINT('Ctrl Pts',(79.014739726505,768.4123957434,86.6105536288388));
#82089=CARTESIAN_POINT('Ctrl Pts',(79.0162099655969,768.746782235972,85.3710221059379));
#82090=CARTESIAN_POINT('Ctrl Pts',(78.1134036875601,769.600363807285,85.0463364454658));
#82091=CARTESIAN_POINT('Ctrl Pts',(78.0087611740672,767.221939997721,86.307466040044));
#82092=CARTESIAN_POINT('Ctrl Pts',(78.0071437361477,767.543114000067,85.0845274729088));
#82093=CARTESIAN_POINT('Ctrl Pts',(77.1080622694572,768.362630795394,84.7396761820318));
#82094=CARTESIAN_POINT('Ctrl Pts',(76.0927241109205,764.783750194135,85.7297309016138));
#82095=CARTESIAN_POINT('Ctrl Pts',(76.084470878905,765.073533320776,84.5431656020163));
#82096=CARTESIAN_POINT('Ctrl Pts',(75.19584029529,765.818031164947,84.1566085998454));
#82097=CARTESIAN_POINT('Ctrl Pts',(75.182623032252,763.536105161568,85.4550691342351));
#82098=CARTESIAN_POINT('Ctrl Pts',(75.1713154649656,763.81013185858,84.2883909459588));
#82099=CARTESIAN_POINT('Ctrl Pts',(74.2889243477987,764.511199556224,83.8801784199441));
#82100=CARTESIAN_POINT('Ctrl Pts',(73.4901734252389,760.96320744885,84.941329020355));
#82101=CARTESIAN_POINT('Ctrl Pts',(73.4741566583351,761.20056361727,83.8175931584094));
#82102=CARTESIAN_POINT('Ctrl Pts',(72.6087386229698,761.807693786518,83.3659796212416));
#82103=CARTESIAN_POINT('Ctrl Pts',(72.707836081372,759.63815168905,84.7022138549167));
#82104=CARTESIAN_POINT('Ctrl Pts',(72.6897377638328,759.856915801337,83.6014313699369));
#82105=CARTESIAN_POINT('Ctrl Pts',(71.8355785722929,760.411115842064,83.128212093595));
#82106=CARTESIAN_POINT('Ctrl Pts',(71.658920438192,757.571059475316,84.3774661637953));
#82107=CARTESIAN_POINT('Ctrl Pts',(71.6373194821546,757.752838052951,83.3119628596065));
#82108=CARTESIAN_POINT('Ctrl Pts',(70.8072004200214,758.229721199251,82.8090726008211));
#82109=CARTESIAN_POINT('Ctrl Pts',(71.3290696884154,756.865866044856,84.2745652736144));
#82110=CARTESIAN_POINT('Ctrl Pts',(71.3074689206998,757.037084857487,83.2213327932257));
#82111=CARTESIAN_POINT('Ctrl Pts',(70.4853541094165,757.485138318237,82.7086553235673));
#82112=CARTESIAN_POINT('Ctrl Pts',(70.7257249999294,755.447684184856,84.0846957456631));
#82113=CARTESIAN_POINT('Ctrl Pts',(70.7050549298059,755.597824860978,83.0557025153916));
#82114=CARTESIAN_POINT('Ctrl Pts',(69.899878526431,755.98817308601,82.5248701016234));
#82115=CARTESIAN_POINT('Ctrl Pts',(70.4511377454858,754.732937305474,83.9973933941209));
#82116=CARTESIAN_POINT('Ctrl Pts',(70.4310337524815,754.872430959252,82.9802998082194));
#82117=CARTESIAN_POINT('Ctrl Pts',(69.6351681246828,755.233941812227,82.441172093944));
#82118=CARTESIAN_POINT('Ctrl Pts',(69.7105470631533,752.568708941546,83.7594876855879));
#82119=CARTESIAN_POINT('Ctrl Pts',(69.6954059045199,752.682705696041,82.7772948998672));
#82120=CARTESIAN_POINT('Ctrl Pts',(68.9259081577405,752.953039927856,82.2152182103315));
#82121=CARTESIAN_POINT('Ctrl Pts',(69.3286692857491,751.099448039298,83.6331406219163));
#82122=CARTESIAN_POINT('Ctrl Pts',(69.3150421947875,751.190991418035,82.6713974262477));
#82123=CARTESIAN_POINT('Ctrl Pts',(68.5672888315565,751.408381407968,82.0984264432094));
#82124=CARTESIAN_POINT('Ctrl Pts',(68.9176924348934,748.838880031761,83.4940017770909));
#82125=CARTESIAN_POINT('Ctrl Pts',(68.9082513720638,748.899344003655,82.5559441007562));
#82126=CARTESIAN_POINT('Ctrl Pts',(68.1866424032589,749.047053332051,81.97139742283));
#82127=CARTESIAN_POINT('Ctrl Pts',(68.8074764353244,748.075842023577,83.4559769694687));
#82128=CARTESIAN_POINT('Ctrl Pts',(68.7995471274378,748.127296138224,82.5246052204508));
#82129=CARTESIAN_POINT('Ctrl Pts',(68.0857361905741,748.252477165913,81.9370102412519));
#82130=CARTESIAN_POINT('Ctrl Pts',(68.6358788294816,746.527801456371,83.3956678993834));
#82131=CARTESIAN_POINT('Ctrl Pts',(68.6309578842129,746.563507408634,82.4749758028119));
#82132=CARTESIAN_POINT('Ctrl Pts',(67.9299075561181,746.647068940509,81.8825958600769));
#82133=CARTESIAN_POINT('Ctrl Pts',(68.5746540239514,745.742195057558,83.3734373232148));
#82134=CARTESIAN_POINT('Ctrl Pts',(68.5710208199205,745.770325190704,82.456671026825));
#82135=CARTESIAN_POINT('Ctrl Pts',(67.8751177828609,745.835626086142,81.8626119544358));
#82136=CARTESIAN_POINT('Ctrl Pts',(68.4511339891996,743.3692333769,83.3264891742176));
#82137=CARTESIAN_POINT('Ctrl Pts',(68.4507140403186,743.380436487727,82.41788350119));
#82138=CARTESIAN_POINT('Ctrl Pts',(67.7656841774958,743.397293078928,81.8202937869079));
#82139=CARTESIAN_POINT('Ctrl Pts',(68.4520573306559,741.761597715518,83.3224477769537));
#82140=CARTESIAN_POINT('Ctrl Pts',(68.4520660684083,741.763107158896,82.4141868365033));
#82141=CARTESIAN_POINT('Ctrl Pts',(67.768181414692,741.761742048572,81.8164948678625));
#82142=CARTESIAN_POINT('Ctrl Pts',(68.4578519957978,740.110102294567,83.3198423992737));
#82143=CARTESIAN_POINT('Ctrl Pts',(68.4578585200934,740.111539480387,82.4117286275963));
#82144=CARTESIAN_POINT('Ctrl Pts',(67.7741541147992,740.110097758569,81.8140506910839));
#82145=CARTESIAN_POINT('Origin',(66.4578107338364,740.118392461545,83.3196239580187));
#82146=CARTESIAN_POINT('Origin',(52.8776183915471,640.125373764374,98.8443190641064));
#82147=CARTESIAN_POINT('Ctrl Pts',(67.7745968623189,740.125373764374,81.8142915850038));
#82148=CARTESIAN_POINT('Ctrl Pts',(67.8942035323011,706.959289447806,81.7651023987915));
#82149=CARTESIAN_POINT('Ctrl Pts',(68.0137456503395,673.793204547609,81.7161493121274));
#82150=CARTESIAN_POINT('Ctrl Pts',(68.1332263705164,640.627119090081,81.66742515578));
#82151=CARTESIAN_POINT('Ctrl Pts',(37.622010412585,640.627119090085,81.6674251557736));
#82152=CARTESIAN_POINT('Ctrl Pts',(37.7161153406155,666.749258887989,81.7058010809911));
#82153=CARTESIAN_POINT('Ctrl Pts',(37.8102583547102,692.871398339875,81.7443190218601));
#82154=CARTESIAN_POINT('Ctrl Pts',(37.9044409990548,718.993537433499,81.7829824784269));
#82155=CARTESIAN_POINT('Ctrl Pts',(37.9298377480952,726.037482903233,81.793408243283));
#82156=CARTESIAN_POINT('Ctrl Pts',(37.9552373778878,733.081428123876,81.803844588833));
#82157=CARTESIAN_POINT('Ctrl Pts',(37.9806399232851,740.125374460328,81.8142915860359));
#82158=CARTESIAN_POINT('Ctrl Pts',(-2.54756887983518,803.022417447735,96.2501688554413));
#82159=CARTESIAN_POINT('Ctrl Pts',(-3.76067897315835,802.223917717087,96.4241939687641));
#82160=CARTESIAN_POINT('Ctrl Pts',(-3.77095614126524,801.727425136398,97.8000254103195));
#82161=CARTESIAN_POINT('Ctrl Pts',(-2.49510594629795,802.935978449927,96.219371864756));
#82162=CARTESIAN_POINT('Ctrl Pts',(-3.71075325311643,802.135854698797,96.393779692249));
#82163=CARTESIAN_POINT('Ctrl Pts',(-3.71892210633938,801.640324877161,97.7731993356308));
#82164=CARTESIAN_POINT('Ctrl Pts',(-2.44263599469854,802.849517379784,96.1886494506309));
#82165=CARTESIAN_POINT('Ctrl Pts',(-3.66085515329841,802.047826199787,96.363461972859));
#82166=CARTESIAN_POINT('Ctrl Pts',(-3.66686675102868,801.553206555292,97.7464448827534));
#82167=CARTESIAN_POINT('Ctrl Pts',(-2.36392313096885,802.719800352555,96.1426793912113));
#82168=CARTESIAN_POINT('Ctrl Pts',(-3.58602456746336,801.915795967737,96.3181154713988));
#82169=CARTESIAN_POINT('Ctrl Pts',(-3.58875388690028,801.422509800265,97.7064217180787));
#82170=CARTESIAN_POINT('Ctrl Pts',(-2.3376840822935,802.676556934075,96.1273749027454));
#82171=CARTESIAN_POINT('Ctrl Pts',(-3.56107010939721,801.871763815172,96.3030133965861));
#82172=CARTESIAN_POINT('Ctrl Pts',(-3.56271119025831,801.378940829508,97.693098694744));
#82173=CARTESIAN_POINT('Ctrl Pts',(-2.28520294972504,802.590061552113,96.0968035718952));
#82174=CARTESIAN_POINT('Ctrl Pts',(-3.51115718317375,801.78368761136,96.2728469833879));
#82175=CARTESIAN_POINT('Ctrl Pts',(-3.5106154032456,801.291796406231,97.6664885739323));
#82176=CARTESIAN_POINT('Ctrl Pts',(-2.25892246716778,802.546846114927,96.0815333620853));
#82177=CARTESIAN_POINT('Ctrl Pts',(-3.482711717244,801.739390886515,96.2567977055715));
#82178=CARTESIAN_POINT('Ctrl Pts',(-3.48307491491547,801.247085257979,97.6489167037903));
#82179=CARTESIAN_POINT('Ctrl Pts',(-2.12724597762409,802.331001389362,96.0052527348621));
#82180=CARTESIAN_POINT('Ctrl Pts',(-3.34800333457594,801.51876669674,96.1788407103674));
#82181=CARTESIAN_POINT('Ctrl Pts',(-3.34838159956812,801.026426926903,97.5708484797001));
#82182=CARTESIAN_POINT('Ctrl Pts',(-2.02110379157191,802.158997158457,95.9444602975967));
#82183=CARTESIAN_POINT('Ctrl Pts',(-3.23932659433289,801.342952870263,96.1166961159775));
#82184=CARTESIAN_POINT('Ctrl Pts',(-3.23975939827196,800.850558213657,97.5085238064614));
#82185=CARTESIAN_POINT('Ctrl Pts',(-1.70025205868664,801.645032317437,95.7627637886631));
#82186=CARTESIAN_POINT('Ctrl Pts',(-2.91059639593457,800.817621326081,95.9309328218339));
#82187=CARTESIAN_POINT('Ctrl Pts',(-2.91128616137831,800.324991032427,97.3219922775962));
#82188=CARTESIAN_POINT('Ctrl Pts',(-1.48311342467661,801.305123534837,95.64254057864));
#82189=CARTESIAN_POINT('Ctrl Pts',(-2.68784390047268,800.470220965194,95.8079863882428));
#82190=CARTESIAN_POINT('Ctrl Pts',(-2.68882416246288,799.977336107303,97.1982295895679));
#82191=CARTESIAN_POINT('Ctrl Pts',(-0.821956157160209,800.293715588133,
95.2844669131353));
#82192=CARTESIAN_POINT('Ctrl Pts',(-2.0092020871634,799.436803763087,95.4418913907417));
#82193=CARTESIAN_POINT('Ctrl Pts',(-2.01113581282655,798.942895026148,96.8290880220157));
#82194=CARTESIAN_POINT('Ctrl Pts',(-0.368150041841871,799.630582229875,
95.0492110213477));
#82195=CARTESIAN_POINT('Ctrl Pts',(-1.54281133857619,798.759443153596,95.2014321306635));
#82196=CARTESIAN_POINT('Ctrl Pts',(-1.54556290786924,798.264694255303,96.5858881514787));
#82197=CARTESIAN_POINT('Ctrl Pts',(1.03061030691538,797.673484553947,94.3528071728653));
#82198=CARTESIAN_POINT('Ctrl Pts',(-0.106711134755086,796.762712146839,
94.4910767743835));
#82199=CARTESIAN_POINT('Ctrl Pts',(-0.110695325855799,796.264745392156,
95.8668830489244));
#82200=CARTESIAN_POINT('Ctrl Pts',(2.01312465174172,796.412063159207,93.9009736591558));
#82201=CARTESIAN_POINT('Ctrl Pts',(0.901311526995951,795.476698050913,94.0314310313919));
#82202=CARTESIAN_POINT('Ctrl Pts',(0.896808093594574,794.97805572051,95.4019733112351));
#82203=CARTESIAN_POINT('Ctrl Pts',(5.07849924016303,792.729956164408,92.5758839929726));
#82204=CARTESIAN_POINT('Ctrl Pts',(4.0306470527666,791.735946530686,92.6922147735793));
#82205=CARTESIAN_POINT('Ctrl Pts',(4.03172924159146,791.23476686307,94.0506880453146));
#82206=CARTESIAN_POINT('Ctrl Pts',(7.27664404461848,790.409107078949,91.7323566158703));
#82207=CARTESIAN_POINT('Ctrl Pts',(6.26157209028423,789.386372296047,91.8480320390701));
#82208=CARTESIAN_POINT('Ctrl Pts',(6.26821503959616,788.89247683333,93.2063626670902));
#82209=CARTESIAN_POINT('Ctrl Pts',(11.7933103381052,785.862859302431,90.1054677611424));
#82210=CARTESIAN_POINT('Ctrl Pts',(10.8240801502024,784.811849964826,90.2364798435984));
#82211=CARTESIAN_POINT('Ctrl Pts',(10.8403820254109,784.338281826247,91.5915713698604));
#82212=CARTESIAN_POINT('Ctrl Pts',(14.1122918869024,783.637701417767,89.3223002813892));
#82213=CARTESIAN_POINT('Ctrl Pts',(13.1527770859699,782.590309602832,89.4700943476909));
#82214=CARTESIAN_POINT('Ctrl Pts',(13.1774368624816,782.126095976334,90.8205764507483));
#82215=CARTESIAN_POINT('Ctrl Pts',(18.7249146873591,779.148740308681,87.8151433083763));
#82216=CARTESIAN_POINT('Ctrl Pts',(17.7880690821033,778.125688253418,88.0056748348046));
#82217=CARTESIAN_POINT('Ctrl Pts',(17.8131492667992,777.694891150616,89.3376463120531));
#82218=CARTESIAN_POINT('Ctrl Pts',(21.0203075585196,776.886334924432,87.0910859533607));
#82219=CARTESIAN_POINT('Ctrl Pts',(20.0843546720735,775.896396719256,87.3109957127761));
#82220=CARTESIAN_POINT('Ctrl Pts',(20.1135073946011,775.477223638155,88.6259100659374));
#82221=CARTESIAN_POINT('Ctrl Pts',(24.3397387087871,773.370423560442,86.0602581245099));
#82222=CARTESIAN_POINT('Ctrl Pts',(23.425414865776,772.43036838436,86.3263153651351));
#82223=CARTESIAN_POINT('Ctrl Pts',(23.4361862275068,772.056471333472,87.6108938714464));
#82224=CARTESIAN_POINT('Ctrl Pts',(25.4253996464263,772.17790967056,85.7260139011157));
#82225=CARTESIAN_POINT('Ctrl Pts',(24.5138126607302,771.263228374096,86.0100516271665));
#82226=CARTESIAN_POINT('Ctrl Pts',(24.5222414514152,770.900436422346,87.2815154680637));
#82227=CARTESIAN_POINT('Ctrl Pts',(27.5242571088241,769.743996468356,85.0826902645603));
#82228=CARTESIAN_POINT('Ctrl Pts',(26.6201843438213,768.886224410496,85.4045996990067));
#82229=CARTESIAN_POINT('Ctrl Pts',(26.6220269177733,768.550030010176,86.6467338844264));
#82230=CARTESIAN_POINT('Ctrl Pts',(28.5384523052729,768.50166160768,84.7733012266733));
#82231=CARTESIAN_POINT('Ctrl Pts',(27.6379911920885,767.677778332248,85.1154060870583));
#82232=CARTESIAN_POINT('Ctrl Pts',(27.6367436421517,767.35476598226,86.3410381049848));
#82233=CARTESIAN_POINT('Ctrl Pts',(30.4676562121875,765.948841552032,84.1850699287477));
#82234=CARTESIAN_POINT('Ctrl Pts',(29.5774139914747,765.199660947832,84.5689922057617));
#82235=CARTESIAN_POINT('Ctrl Pts',(29.5694662193078,764.908010092887,85.7584008538283));
#82236=CARTESIAN_POINT('Ctrl Pts',(31.3826991203075,764.638386759695,83.9062051751521));
#82237=CARTESIAN_POINT('Ctrl Pts',(30.4985460010245,763.932521667716,84.3118728786106));
#82238=CARTESIAN_POINT('Ctrl Pts',(30.4875123616944,763.656602738954,85.4814464761971));
#82239=CARTESIAN_POINT('Ctrl Pts',(33.0781796764642,761.929051245223,83.3874395020897));
#82240=CARTESIAN_POINT('Ctrl Pts',(32.2107225236239,761.316951014723,83.8367566227028));
#82241=CARTESIAN_POINT('Ctrl Pts',(32.1948719624217,761.077699450203,84.9634374215801));
#82242=CARTESIAN_POINT('Ctrl Pts',(33.8585030159751,760.530256860817,83.147540342318));
#82243=CARTESIAN_POINT('Ctrl Pts',(33.0021498927262,759.971065301871,83.6186294465493));
#82244=CARTESIAN_POINT('Ctrl Pts',(32.9841687445563,759.750391677565,84.7223482483494));
#82245=CARTESIAN_POINT('Ctrl Pts',(34.8968479257256,758.347247245236,82.8254124815966));
#82246=CARTESIAN_POINT('Ctrl Pts',(34.0644292190259,757.865367363984,83.3264590338104));
#82247=CARTESIAN_POINT('Ctrl Pts',(34.0428118160153,757.681740104667,84.3948146040165));
#82248=CARTESIAN_POINT('Ctrl Pts',(35.2209007078652,757.605400534592,82.7243472537898));
#82249=CARTESIAN_POINT('Ctrl Pts',(34.3963889580535,757.15231636156,83.2352634977894));
#82250=CARTESIAN_POINT('Ctrl Pts',(34.3747602646247,756.979163746297,84.2913421825726));
#82251=CARTESIAN_POINT('Ctrl Pts',(35.8196885745711,756.089473367867,82.536445429766));
#82252=CARTESIAN_POINT('Ctrl Pts',(35.0123043239642,755.694916051544,83.0659664510821));
#82253=CARTESIAN_POINT('Ctrl Pts',(34.9915640255228,755.54314104189,84.0973654783811));
#82254=CARTESIAN_POINT('Ctrl Pts',(36.0904492393661,755.325097075514,82.4508556938986));
#82255=CARTESIAN_POINT('Ctrl Pts',(35.292528911043,754.959832059304,82.988886942784));
#82256=CARTESIAN_POINT('Ctrl Pts',(35.2723340002733,754.818874589516,84.008141624083));
#82257=CARTESIAN_POINT('Ctrl Pts',(36.8135735373189,753.020164341297,82.2205312756795));
#82258=CARTESIAN_POINT('Ctrl Pts',(36.042391668946,752.747409898035,82.7820512032344));
#82259=CARTESIAN_POINT('Ctrl Pts',(36.0272207560278,752.632179790114,83.7657201066036));
#82260=CARTESIAN_POINT('Ctrl Pts',(37.1771034358654,751.464582237428,82.1021362636218));
#82261=CARTESIAN_POINT('Ctrl Pts',(36.4280933234008,751.245242086986,82.6747341408129));
#82262=CARTESIAN_POINT('Ctrl Pts',(36.414375945687,751.152783996483,83.6375840405036));
#82263=CARTESIAN_POINT('Ctrl Pts',(37.6907126543852,748.305382907416,81.9307673070529));
#82264=CARTESIAN_POINT('Ctrl Pts',(36.9762334614121,748.184766944419,82.5192847281391));
#82265=CARTESIAN_POINT('Ctrl Pts',(36.9690167893174,748.128934992039,83.4497201824271));
#82266=CARTESIAN_POINT('Ctrl Pts',(37.8401034447293,746.700925585337,81.8780397031153));
#82267=CARTESIAN_POINT('Ctrl Pts',(37.1400301940856,746.619999140862,82.4708341127755));
#82268=CARTESIAN_POINT('Ctrl Pts',(37.1353188681197,746.583923140769,83.3906420629135));
#82269=CARTESIAN_POINT('Ctrl Pts',(37.9518992948506,744.251109993819,81.8349070904933));
#82270=CARTESIAN_POINT('Ctrl Pts',(37.263127800321,744.216555382476,82.4312579044147));
#82271=CARTESIAN_POINT('Ctrl Pts',(37.2615409843506,744.200268989692,83.3427055344115));
#82272=CARTESIAN_POINT('Ctrl Pts',(37.9707386166179,743.429305592017,81.8264396253836));
#82273=CARTESIAN_POINT('Ctrl Pts',(37.2842851583786,743.40744096781,82.4234417302218));
#82274=CARTESIAN_POINT('Ctrl Pts',(37.2834266463915,743.396567644625,83.3333441910137));
#82275=CARTESIAN_POINT('Ctrl Pts',(37.9868489066019,741.782335097605,81.8166385183344));
#82276=CARTESIAN_POINT('Ctrl Pts',(37.3028776730937,741.778675123994,82.4143081461178));
#82277=CARTESIAN_POINT('Ctrl Pts',(37.3028300875899,741.774995661547,83.3225770714669));
#82278=CARTESIAN_POINT('Ctrl Pts',(37.9841298949872,740.955816068756,81.8153066626739));
#82279=CARTESIAN_POINT('Ctrl Pts',(37.3003420559413,740.957253716847,82.412981445933));
#82280=CARTESIAN_POINT('Ctrl Pts',(37.3003369686651,740.955796719301,83.3211559311962));
#82281=CARTESIAN_POINT('Ctrl Pts',(37.9811378013137,740.125371330475,81.8140733335412));
#82282=CARTESIAN_POINT('Ctrl Pts',(37.2974432528674,740.126811574677,82.4117412974523));
#82283=CARTESIAN_POINT('Ctrl Pts',(37.2974382339422,740.125373764374,83.3198410924311));
#82284=CARTESIAN_POINT('Origin',(39.2974260809896,740.118401563543,83.3196239724233));
#82285=CARTESIAN_POINT('Ctrl Pts',(-2.30721749727922,802.626345096273,96.1096278308841));
#82286=CARTESIAN_POINT('Ctrl Pts',(-2.36327072866609,802.589348633611,96.1176523786537));
#82287=CARTESIAN_POINT('Ctrl Pts',(-2.41849852049417,802.551715366678,96.1289510061921));
#82288=CARTESIAN_POINT('Ctrl Pts',(-2.47257991396617,802.513656987001,96.1434674812622));
#82289=CARTESIAN_POINT('Ctrl Pts',(-2.52823332824809,802.474492338403,96.1584059166302));
#82290=CARTESIAN_POINT('Ctrl Pts',(-2.58267247133486,802.434877827384,96.1767515168295));
#82291=CARTESIAN_POINT('Ctrl Pts',(-2.63558008449285,802.395040475326,96.1983975246404));
#82292=CARTESIAN_POINT('Ctrl Pts',(-2.69144357855432,802.352977461192,96.2212528673146));
#82293=CARTESIAN_POINT('Ctrl Pts',(-2.74559941542201,802.310666270982,96.2477873359821));
#82294=CARTESIAN_POINT('Ctrl Pts',(-2.79771392683107,802.268365353768,96.2778317474554));
#82295=CARTESIAN_POINT('Ctrl Pts',(-2.85156635968805,802.224653780112,96.3088780838374));
#82296=CARTESIAN_POINT('Ctrl Pts',(-2.90323918786958,802.180953239413,96.3436719467398));
#82297=CARTESIAN_POINT('Ctrl Pts',(-2.95240600655323,802.13753719224,96.3819880306071));
#82298=CARTESIAN_POINT('Ctrl Pts',(-3.00361526460589,802.092317598561,96.4218958033462));
#82299=CARTESIAN_POINT('Ctrl Pts',(-3.05210620578357,802.047406519098,96.4656244285225));
#82300=CARTESIAN_POINT('Ctrl Pts',(-3.09755173275986,802.003100720221,96.5128822403463));
#82301=CARTESIAN_POINT('Ctrl Pts',(-3.13083736450424,801.970649858636,96.5474952424627));
#82302=CARTESIAN_POINT('Ctrl Pts',(-3.16249016323363,801.938523416787,96.5840007665001));
#82303=CARTESIAN_POINT('Ctrl Pts',(-3.19239386993921,801.906834880987,96.6222719698307));
#82304=CARTESIAN_POINT('Ctrl Pts',(-3.23322357536797,801.863568218598,96.6745264269044));
#82305=CARTESIAN_POINT('Ctrl Pts',(-3.2707467664661,801.821165312288,96.730017165873));
#82306=CARTESIAN_POINT('Ctrl Pts',(-3.30472114590546,801.779906743377,96.7883698877386));
#82307=CARTESIAN_POINT('Ctrl Pts',(-3.33789162255928,801.739624435962,96.8453418657488));
#82308=CARTESIAN_POINT('Ctrl Pts',(-3.36767931860476,801.70043280346,96.9050422820145));
#82309=CARTESIAN_POINT('Ctrl Pts',(-3.39389274176312,801.662584602277,96.9670880638343));
#82310=CARTESIAN_POINT('Ctrl Pts',(-3.41866210564239,801.626821403337,97.0257158339574));
#82311=CARTESIAN_POINT('Ctrl Pts',(-3.44024009918937,801.592257712198,97.0864377315033));
#82312=CARTESIAN_POINT('Ctrl Pts',(-3.45849568331896,801.559100137027,97.1488969208789));
#82313=CARTESIAN_POINT('Ctrl Pts',(-3.47620000246389,801.526943823171,97.2094700263129));
#82314=CARTESIAN_POINT('Ctrl Pts',(-3.49077920080706,801.496110179152,97.271677116829));
#82315=CARTESIAN_POINT('Ctrl Pts',(-3.50214642651331,801.466779625618,97.3351593149313));
#82316=CARTESIAN_POINT('Ctrl Pts',(-3.51304904452183,801.438647887107,97.3960468326192));
#82317=CARTESIAN_POINT('Ctrl Pts',(-3.52099660020155,801.411899132525,97.4581071320463));
#82318=CARTESIAN_POINT('Ctrl Pts',(-3.52594744762757,801.386681807434,97.5209938678202));
#82319=CARTESIAN_POINT('Ctrl Pts',(-3.53001391253826,801.365969117504,97.5726469854316));
#82320=CARTESIAN_POINT('Ctrl Pts',(-3.53205915571888,801.346289518382,97.6248570357437));
#82321=CARTESIAN_POINT('Ctrl Pts',(-3.53208119303051,801.3277173574,97.6774182477473));
#82322=CARTESIAN_POINT('Ctrl Pts',(-3.40946931693737,804.521033637143,96.7791471510659));
#82323=CARTESIAN_POINT('Ctrl Pts',(-4.65925736534058,803.756954223787,96.969801323411));
#82324=CARTESIAN_POINT('Ctrl Pts',(-4.65925854064561,803.26470246339,98.3625772327603));
#82325=CARTESIAN_POINT('Ctrl Pts',(-3.05089567652535,803.877265759675,96.5517004996727));
#82326=CARTESIAN_POINT('Ctrl Pts',(-4.29249081153572,803.098952748285,96.7374561156329));
#82327=CARTESIAN_POINT('Ctrl Pts',(-4.29249163071458,802.606767441921,98.1300418153432));
#82328=CARTESIAN_POINT('Ctrl Pts',(-2.68053925162189,803.241833344296,96.3270499699154));
#82329=CARTESIAN_POINT('Ctrl Pts',(-3.91415453452997,802.44937988459,96.5076786811755));
#82330=CARTESIAN_POINT('Ctrl Pts',(-3.91414269854377,801.957105620144,97.9004419917104));
#82331=CARTESIAN_POINT('Ctrl Pts',(-2.29945272409813,802.614310079946,96.105250940801));
#82332=CARTESIAN_POINT('Ctrl Pts',(-3.52444864420587,801.807911322885,96.2810249800505));
#82333=CARTESIAN_POINT('Ctrl Pts',(-3.52439708867275,801.31561163008,97.6736597068728));
#82334=CARTESIAN_POINT('Ctrl Pts',(37.6198584342843,640.029588266083,99.5508769219774));
#82335=CARTESIAN_POINT('Ctrl Pts',(36.9480411577294,640.030997493993,98.9541445975251));
#82336=CARTESIAN_POINT('Ctrl Pts',(36.9480366099606,640.029588266083,98.0555746669669));
#82337=CARTESIAN_POINT('Ctrl Pts',(37.7400559519511,673.39485105406,99.5018629213698));
#82338=CARTESIAN_POINT('Ctrl Pts',(37.0645737053678,673.414978395905,98.9047878032409));
#82339=CARTESIAN_POINT('Ctrl Pts',(37.0645038212888,673.394851054046,98.0032473080201));
#82340=CARTESIAN_POINT('Ctrl Pts',(37.8603155876735,706.760113449952,99.4526172749795));
#82341=CARTESIAN_POINT('Ctrl Pts',(37.1810433321196,706.780933775647,98.8552405413389));
#82342=CARTESIAN_POINT('Ctrl Pts',(37.1809710312484,706.760113449936,97.9506580829349));
#82343=CARTESIAN_POINT('Ctrl Pts',(37.9806405542058,740.125375436351,99.4031326849135));
#82344=CARTESIAN_POINT('Ctrl Pts',(37.2974428811024,740.126813453391,98.8055008811664));
#82345=CARTESIAN_POINT('Ctrl Pts',(37.2974382397787,740.125375436351,97.8977989293328));
#82346=CARTESIAN_POINT('Ctrl Pts',(36.9501223944842,640.627119090084,98.0546383469715));
#82347=CARTESIAN_POINT('Ctrl Pts',(37.0658943424063,673.793204392933,98.0026202559452));
#82348=CARTESIAN_POINT('Ctrl Pts',(37.1816662884245,706.959289150332,97.9503433686471));
#82349=CARTESIAN_POINT('Ctrl Pts',(37.2974382346222,740.125373959158,97.8977997652524));
#82350=CARTESIAN_POINT('Ctrl Pts',(37.9806399237917,740.125374600818,99.4031321373354));
#82351=CARTESIAN_POINT('Ctrl Pts',(37.9617902823362,734.898502237979,99.4108842010231));
#82352=CARTESIAN_POINT('Ctrl Pts',(37.9429422647548,729.671635581994,99.4186303922604));
#82353=CARTESIAN_POINT('Ctrl Pts',(37.9240958291834,724.444766469215,99.4263707511508));
#82354=CARTESIAN_POINT('Ctrl Pts',(37.8233558620347,696.505551081905,99.4677453387957));
#82355=CARTESIAN_POINT('Ctrl Pts',(37.722661352726,668.56633528394,99.5089531833321));
#82356=CARTESIAN_POINT('Ctrl Pts',(37.622010412585,640.627119090081,99.549998567806));
#82357=CARTESIAN_POINT('Origin',(52.8776183915471,640.125373764374,82.3731046594733));
#82358=CARTESIAN_POINT('Ctrl Pts',(67.7745962349168,740.125373763053,99.4031326874004));
#82359=CARTESIAN_POINT('Ctrl Pts',(68.4577939078287,740.126811780092,98.8055008836706));
#82360=CARTESIAN_POINT('Ctrl Pts',(68.4577985491564,740.125373763053,97.8977989319926));
#82361=CARTESIAN_POINT('Ctrl Pts',(67.8949211990607,706.760112339463,99.4526172769356));
#82362=CARTESIAN_POINT('Ctrl Pts',(68.5741934539237,706.78093266449,98.8552405439302));
#82363=CARTESIAN_POINT('Ctrl Pts',(68.5742657557221,706.760112339449,97.9506580860804));
#82364=CARTESIAN_POINT('Ctrl Pts',(68.0151808329475,673.394850504227,99.5018629223341));
#82365=CARTESIAN_POINT('Ctrl Pts',(68.6906630793029,673.414977845443,98.9047878029075));
#82366=CARTESIAN_POINT('Ctrl Pts',(68.6907329637246,673.394850504214,98.0032473081996));
#82367=CARTESIAN_POINT('Ctrl Pts',(68.1353783487679,640.029588276093,99.5508769219679));
#82368=CARTESIAN_POINT('Ctrl Pts',(68.8071956253259,640.030997504003,98.9541445975185));
#82369=CARTESIAN_POINT('Ctrl Pts',(68.8072001730986,640.029588276093,98.05557466696));
#82370=CARTESIAN_POINT('Ctrl Pts',(68.1332263705092,640.627119090085,99.5499985678061));
#82371=CARTESIAN_POINT('Ctrl Pts',(68.0137456499717,673.793204547633,99.501274411779));
#82372=CARTESIAN_POINT('Ctrl Pts',(67.8942035319655,706.959289448019,99.4523213250808));
#82373=CARTESIAN_POINT('Ctrl Pts',(67.7745968623189,740.125373764374,99.4031321385759));
#82374=CARTESIAN_POINT('Ctrl Pts',(68.4577985491519,740.125373764374,97.897799765561));
#82375=CARTESIAN_POINT('Ctrl Pts',(68.5735704941848,706.959289289235,97.9503433698041));
#82376=CARTESIAN_POINT('Ctrl Pts',(68.6893424406885,673.793204392753,98.0026202555698));
#82377=CARTESIAN_POINT('Ctrl Pts',(68.80511438861,640.627119090078,98.0546383469682));
#82378=CARTESIAN_POINT('Ctrl Pts',(68.1353783487637,640.029588276122,81.6665468016082));
#82379=CARTESIAN_POINT('Ctrl Pts',(68.8071956253297,640.030997504033,82.2632791260614));
#82380=CARTESIAN_POINT('Ctrl Pts',(68.8072001730985,640.029588276122,83.1618490566285));
#82381=CARTESIAN_POINT('Ctrl Pts',(68.0151808335876,673.394850502988,81.7155608018083));
#82382=CARTESIAN_POINT('Ctrl Pts',(68.6906630786356,673.414977844198,82.3126359204306));
#82383=CARTESIAN_POINT('Ctrl Pts',(68.690732963729,673.394850502972,83.2141764146837));
#82384=CARTESIAN_POINT('Ctrl Pts',(67.8949211993995,706.760112337766,81.7648064469326));
#82385=CARTESIAN_POINT('Ctrl Pts',(68.5741934539143,706.780932662796,82.3621831796554));
#82386=CARTESIAN_POINT('Ctrl Pts',(68.574265755728,706.760112337753,83.2667656382088));
#82387=CARTESIAN_POINT('Ctrl Pts',(67.7745962349126,740.125373763053,81.8142910361756));
#82388=CARTESIAN_POINT('Ctrl Pts',(68.4577939078327,740.126811780092,82.4119228399093));
#82389=CARTESIAN_POINT('Ctrl Pts',(68.4577985491564,740.125373763053,83.319624791596));
#82390=CARTESIAN_POINT('Ctrl Pts',(68.80511438861,640.627119090084,83.1627853766079));
#82391=CARTESIAN_POINT('Ctrl Pts',(68.6893424406879,673.793204392933,83.2148034676149));
#82392=CARTESIAN_POINT('Ctrl Pts',(68.5735704941839,706.95928928949,83.2670803544752));
#82393=CARTESIAN_POINT('Ctrl Pts',(68.4577985491519,740.125373764374,83.3196239580187));
#82394=CARTESIAN_POINT('Ctrl Pts',(37.9806405532016,740.12537515524,81.8142910382409));
#82395=CARTESIAN_POINT('Ctrl Pts',(37.2974428801211,740.12681317228,82.4119228419864));
#82396=CARTESIAN_POINT('Ctrl Pts',(37.2974382387975,740.12537515524,83.3196247938016));
#82397=CARTESIAN_POINT('Ctrl Pts',(37.86031558737,706.760113264802,81.7648064480086));
#82398=CARTESIAN_POINT('Ctrl Pts',(37.1810433314535,706.780933590387,82.362183181023));
#82399=CARTESIAN_POINT('Ctrl Pts',(37.1809710306022,706.76011326479,83.2667656389741));
#82400=CARTESIAN_POINT('Ctrl Pts',(37.740055951603,673.394850962724,81.7155608020926));
#82401=CARTESIAN_POINT('Ctrl Pts',(37.0645737050292,673.414978304463,82.3126359218093));
#82402=CARTESIAN_POINT('Ctrl Pts',(37.06450382097,673.394850962711,83.2141764151761));
#82403=CARTESIAN_POINT('Ctrl Pts',(37.6198584342997,640.029588267741,81.6665468015964));
#82404=CARTESIAN_POINT('Ctrl Pts',(36.9480411577352,640.030997495651,82.2632791260495));
#82405=CARTESIAN_POINT('Ctrl Pts',(36.9480366099664,640.029588267741,83.1618490566154));
#82406=CARTESIAN_POINT('Ctrl Pts',(37.2974382345426,740.12537393637,83.3196239582912));
#82407=CARTESIAN_POINT('Ctrl Pts',(37.1816662880619,706.959289046462,83.2670803533975));
#82408=CARTESIAN_POINT('Ctrl Pts',(37.0658943424057,673.793204392754,83.2148034673805));
#82409=CARTESIAN_POINT('Ctrl Pts',(36.9501223944842,640.627119090078,83.1627853766038));
#82410=CARTESIAN_POINT('Origin',(36.9483709657826,640.125373764374,82.287785267134));
#82411=CARTESIAN_POINT('Origin',(68.8068658173115,640.125373764374,82.287785267134));
#82412=CARTESIAN_POINT('Ctrl Pts',(37.2974381894958,740.125361031455,98.7804137130792));
#82413=CARTESIAN_POINT('Ctrl Pts',(37.3237628455944,747.666788861133,98.7691088591345));
#82414=CARTESIAN_POINT('Ctrl Pts',(37.350097372228,755.208210967482,98.7577876187542));
#82415=CARTESIAN_POINT('Ctrl Pts',(27.632882335034,768.384896418847,105.310835626506));
#82416=CARTESIAN_POINT('Ctrl Pts',(20.0424193057215,772.226303264399,106.668518782974));
#82417=CARTESIAN_POINT('Ctrl Pts',(13.2983736491593,777.107328840337,108.39363837514));
#82418=CARTESIAN_POINT('Ctrl Pts',(39.7898594872664,740.125360272474,101.147186527103));
#82419=CARTESIAN_POINT('Ctrl Pts',(39.8138888831648,748.116316296691,101.129143905661));
#82420=CARTESIAN_POINT('Ctrl Pts',(39.8379218896383,756.107266958529,101.11108900417));
#82421=CARTESIAN_POINT('Ctrl Pts',(32.8646428197398,769.386481710472,105.664840290342));
#82422=CARTESIAN_POINT('Ctrl Pts',(26.4798688189832,773.811767639453,107.228875594274));
#82423=CARTESIAN_POINT('Ctrl Pts',(21.001327165595,779.233378063583,109.145056107309));
#82424=CARTESIAN_POINT('Ctrl Pts',(42.7362987166043,740.12535970087,103.0351353954));
#82425=CARTESIAN_POINT('Ctrl Pts',(42.7558869385823,748.454864485732,103.011405070401));
#82426=CARTESIAN_POINT('Ctrl Pts',(42.7754757177386,756.784364143077,102.987665643325));
#82427=CARTESIAN_POINT('Ctrl Pts',(37.9535760120706,770.177419744143,105.944385861491));
#82428=CARTESIAN_POINT('Ctrl Pts',(33.008775321197,775.040599666662,107.663186445134));
#82429=CARTESIAN_POINT('Ctrl Pts',(28.8582165463779,780.867648688703,109.722662643155));
#82430=CARTESIAN_POINT('Ctrl Pts',(46.0036740674455,740.125359318221,104.339521998396));
#82431=CARTESIAN_POINT('Ctrl Pts',(46.0173362799933,748.681498353339,104.311576952405));
#82432=CARTESIAN_POINT('Ctrl Pts',(46.0309981446169,757.237632403596,104.283624962077));
#82433=CARTESIAN_POINT('Ctrl Pts',(42.9549355603365,770.721385630642,106.136637190634));
#82434=CARTESIAN_POINT('Ctrl Pts',(39.606300767173,775.876482116324,107.958615601677));
#82435=CARTESIAN_POINT('Ctrl Pts',(36.8253774496378,781.973823505111,110.113622251634));
#82436=CARTESIAN_POINT('Ctrl Pts',(49.4406462293589,740.125359126107,104.9998462381));
#82437=CARTESIAN_POINT('Ctrl Pts',(49.4475586751773,748.795282824599,104.969582372301));
#82438=CARTESIAN_POINT('Ctrl Pts',(49.4544709472461,757.465201607624,104.939312647404));
#82439=CARTESIAN_POINT('Ctrl Pts',(47.9163274999357,770.996796588943,106.233969488297));
#82440=CARTESIAN_POINT('Ctrl Pts',(46.241959498809,776.297839866931,108.107537689874));
#82441=CARTESIAN_POINT('Ctrl Pts',(44.8514979205924,782.530327410416,110.31030956155));
#82442=CARTESIAN_POINT('Ctrl Pts',(56.3145905537352,740.125359126107,104.9998462381));
#82443=CARTESIAN_POINT('Ctrl Pts',(56.3076781079168,748.7952828246,104.969582372301));
#82444=CARTESIAN_POINT('Ctrl Pts',(56.3007658357219,757.465201607906,104.939312647392));
#82445=CARTESIAN_POINT('Ctrl Pts',(57.8390930067729,770.996827303478,106.233967161403));
#82446=CARTESIAN_POINT('Ctrl Pts',(59.5132769913723,776.297839943397,108.107537701204));
#82447=CARTESIAN_POINT('Ctrl Pts',(60.9037388625016,782.530327410416,110.31030956155));
#82448=CARTESIAN_POINT('Ctrl Pts',(59.7515627156487,740.125359318221,104.339521998396));
#82449=CARTESIAN_POINT('Ctrl Pts',(59.7379005030991,748.681498353538,104.311576952411));
#82450=CARTESIAN_POINT('Ctrl Pts',(59.7242386383603,757.237632404556,104.283624962066));
#82451=CARTESIAN_POINT('Ctrl Pts',(62.8004665740107,770.721447059711,106.136632536847));
#82452=CARTESIAN_POINT('Ctrl Pts',(66.1489357522997,775.876482269256,107.958615624337));
#82453=CARTESIAN_POINT('Ctrl Pts',(68.9298593334563,781.973823505111,110.113622251634));
#82454=CARTESIAN_POINT('Ctrl Pts',(63.0189380664898,740.12535970087,103.0351353954));
#82455=CARTESIAN_POINT('Ctrl Pts',(62.9993498445084,748.454864486128,103.011405070414));
#82456=CARTESIAN_POINT('Ctrl Pts',(62.9797610652604,756.784364144573,102.98766564332));
#82457=CARTESIAN_POINT('Ctrl Pts',(67.8017893775537,770.17749653048,105.944380044258));
#82458=CARTESIAN_POINT('Ctrl Pts',(72.7464612568582,775.040599857826,107.66318647346));
#82459=CARTESIAN_POINT('Ctrl Pts',(76.8970202367163,780.867648688703,109.722662643155));
#82460=CARTESIAN_POINT('Ctrl Pts',(65.9653772958277,740.125360272474,101.147186527103));
#82461=CARTESIAN_POINT('Ctrl Pts',(65.9413478999259,748.116316297088,101.129143905674));
#82462=CARTESIAN_POINT('Ctrl Pts',(65.9173148933985,756.107266959884,101.111089004171));
#82463=CARTESIAN_POINT('Ctrl Pts',(72.8906674528,769.386543139541,105.664835636555));
#82464=CARTESIAN_POINT('Ctrl Pts',(79.2753678469458,773.811767792385,107.228875616935));
#82465=CARTESIAN_POINT('Ctrl Pts',(84.7539096174991,779.233378063583,109.145056107309));
#82466=CARTESIAN_POINT('Ctrl Pts',(68.4577985935984,740.125361031455,98.7804137130792));
#82467=CARTESIAN_POINT('Ctrl Pts',(68.4314739374997,747.666788861133,98.7691088591345));
#82468=CARTESIAN_POINT('Ctrl Pts',(68.4051394108661,755.208210967482,98.7577876187542));
#82469=CARTESIAN_POINT('Ctrl Pts',(78.12235444806,768.384896418847,105.310835626506));
#82470=CARTESIAN_POINT('Ctrl Pts',(85.7128174773725,772.226303264399,106.668518782974));
#82471=CARTESIAN_POINT('Ctrl Pts',(92.4568631339348,777.107328840337,108.39363837514));
#82472=CARTESIAN_POINT('Origin',(49.7723662973504,740.125373764374,87.0815594473992));
#82473=CARTESIAN_POINT('Origin',(55.9828704857687,740.125373764387,87.0815594474413));
#82474=CARTESIAN_POINT('Origin',(52.8776183915471,640.125373764374,82.3731046594733));
#82475=CARTESIAN_POINT('Ctrl Pts',(61.8796042537708,737.489494249471,103.141409944702));
#82476=CARTESIAN_POINT('Ctrl Pts',(61.8795904670124,737.049866679283,103.143088473426));
#82477=CARTESIAN_POINT('Ctrl Pts',(61.8462475343457,736.616839151068,103.159344525209));
#82478=CARTESIAN_POINT('Ctrl Pts',(61.7810191782632,736.190073934242,103.188826529972));
#82479=CARTESIAN_POINT('Ctrl Pts',(61.7588991064281,736.045350414904,103.198824391368));
#82480=CARTESIAN_POINT('Ctrl Pts',(61.7331118049536,735.901347140534,103.210343460409));
#82481=CARTESIAN_POINT('Ctrl Pts',(61.7037124152504,735.758051166241,103.223331663321));
#82482=CARTESIAN_POINT('Ctrl Pts',(61.7024284846643,735.751793142312,103.223898884312));
#82483=CARTESIAN_POINT('Ctrl Pts',(61.7011376103645,735.745536471594,103.224468906265));
#82484=CARTESIAN_POINT('Ctrl Pts',(61.6998397898271,735.739281153977,103.225041724595));
#82485=CARTESIAN_POINT('Ctrl Pts',(61.6473911496994,735.486485876722,103.24819095175));
#82486=CARTESIAN_POINT('Ctrl Pts',(61.5836086936033,735.235957110305,103.275902401703));
#82487=CARTESIAN_POINT('Ctrl Pts',(61.5083050324455,734.987567502205,103.307883344724));
#82488=CARTESIAN_POINT('Ctrl Pts',(61.5011236194725,734.963879565568,103.310933241045));
#82489=CARTESIAN_POINT('Ctrl Pts',(61.4938373887345,734.940211087047,103.314021982181));
#82490=CARTESIAN_POINT('Ctrl Pts',(61.4864461547222,734.916561958224,103.317149323662));
#82491=CARTESIAN_POINT('Ctrl Pts',(61.4836783635224,734.907706082395,103.31832041745));
#82492=CARTESIAN_POINT('Ctrl Pts',(61.4808959536254,734.898853893324,103.319496860068));
#82493=CARTESIAN_POINT('Ctrl Pts',(61.4780989983619,734.890005548072,103.32067860039));
#82494=CARTESIAN_POINT('Ctrl Pts',(61.3930671039362,734.621001760591,103.356605388201));
#82495=CARTESIAN_POINT('Ctrl Pts',(61.2946694414231,734.355838081379,103.397395085336));
#82496=CARTESIAN_POINT('Ctrl Pts',(61.1850563833084,734.099023223897,103.441579862578));
#82497=CARTESIAN_POINT('Ctrl Pts',(61.1804741420644,734.088287389569,103.443426953719));
#82498=CARTESIAN_POINT('Ctrl Pts',(61.1758717233044,734.077563534859,103.445280281205));
#82499=CARTESIAN_POINT('Ctrl Pts',(61.171249132145,734.066851644088,103.447139790914));
#82500=CARTESIAN_POINT('Ctrl Pts',(61.0302565652223,733.740130780315,103.503856259691));
#82501=CARTESIAN_POINT('Ctrl Pts',(60.8704863579398,733.424488578447,103.566326522464));
#82502=CARTESIAN_POINT('Ctrl Pts',(60.6921688089864,733.119635342625,103.632993159259));
#82503=CARTESIAN_POINT('Ctrl Pts',(60.5866039466843,732.93916073398,103.672460134747));
#82504=CARTESIAN_POINT('Ctrl Pts',(60.4745396709947,732.7624668695,103.713397939859));
#82505=CARTESIAN_POINT('Ctrl Pts',(60.3560312363458,732.589489897496,103.755485520567));
#82506=CARTESIAN_POINT('Ctrl Pts',(60.347596357518,732.577178201681,103.758481118682));
#82507=CARTESIAN_POINT('Ctrl Pts',(60.3391264396999,732.564883413902,103.761483211003));
#82508=CARTESIAN_POINT('Ctrl Pts',(60.3306220595767,732.552606246971,103.764491483777));
#82509=CARTESIAN_POINT('Ctrl Pts',(60.2054970233299,732.371972157826,103.808752233466));
#82510=CARTESIAN_POINT('Ctrl Pts',(60.0728060717286,732.195023121539,103.85438736651));
#82511=CARTESIAN_POINT('Ctrl Pts',(59.9344436855003,732.024134138079,103.900375897542));
#82512=CARTESIAN_POINT('Ctrl Pts',(59.9003812038466,731.982064157771,103.911697496838));
#82513=CARTESIAN_POINT('Ctrl Pts',(59.8659751152151,731.940361241186,103.923040526528));
#82514=CARTESIAN_POINT('Ctrl Pts',(59.8312538652178,731.899060345914,103.934389804448));
#82515=CARTESIAN_POINT('Ctrl Pts',(59.821130197731,731.887018252653,103.937698911001));
#82516=CARTESIAN_POINT('Ctrl Pts',(59.8109780058676,731.875007261272,103.941009221813));
#82517=CARTESIAN_POINT('Ctrl Pts',(59.8007973552984,731.863027348642,103.944320590203));
#82518=CARTESIAN_POINT('Ctrl Pts',(59.6242019572846,731.655221626935,104.001760182566));
#82519=CARTESIAN_POINT('Ctrl Pts',(59.4389525551288,731.456653794244,104.059546382713));
#82520=CARTESIAN_POINT('Ctrl Pts',(59.2452344512833,731.267076299754,104.116965618561));
#82521=CARTESIAN_POINT('Ctrl Pts',(59.2338983396636,731.255982490784,104.120325711675));
#82522=CARTESIAN_POINT('Ctrl Pts',(59.2225323659722,731.2449184774,104.123684829486));
#82523=CARTESIAN_POINT('Ctrl Pts',(59.2111365846961,731.233884354556,104.127042811653));
#82524=CARTESIAN_POINT('Ctrl Pts',(59.0732523283383,731.100376016158,104.1676730118));
#82525=CARTESIAN_POINT('Ctrl Pts',(58.9310931515999,730.971347054013,104.208111285362));
#82526=CARTESIAN_POINT('Ctrl Pts',(58.7846121092527,730.846778632298,104.248118262814));
#82527=CARTESIAN_POINT('Ctrl Pts',(58.7121076139363,730.785120342569,104.26792072778));
#82528=CARTESIAN_POINT('Ctrl Pts',(58.6385436048391,730.724555332511,104.287617604263));
#82529=CARTESIAN_POINT('Ctrl Pts',(58.5639105593564,730.665084102829,104.307180093771));
#82530=CARTESIAN_POINT('Ctrl Pts',(58.446848215123,730.571803150457,104.337863966661));
#82531=CARTESIAN_POINT('Ctrl Pts',(58.327000083616,730.481096837117,104.368256829114));
#82532=CARTESIAN_POINT('Ctrl Pts',(58.2045733181375,730.393210204539,104.398180402797));
#82533=CARTESIAN_POINT('Ctrl Pts',(58.1032142839657,730.320447486682,104.422954597523));
#82534=CARTESIAN_POINT('Ctrl Pts',(58.0000884337886,730.249616951538,104.447407062917));
#82535=CARTESIAN_POINT('Ctrl Pts',(57.8953327097942,730.180838956165,104.471439405193));
#82536=CARTESIAN_POINT('Ctrl Pts',(57.8829736747637,730.172724558004,104.474274730545));
#82537=CARTESIAN_POINT('Ctrl Pts',(57.8706004834804,730.164644069944,104.477102260258));
#82538=CARTESIAN_POINT('Ctrl Pts',(57.858213342344,730.156597577331,104.479921881953));
#82539=CARTESIAN_POINT('Ctrl Pts',(57.4392032376927,729.884415184763,104.575299012839));
#82540=CARTESIAN_POINT('Ctrl Pts',(57.0021628088544,729.649538680741,104.662096415195));
#82541=CARTESIAN_POINT('Ctrl Pts',(56.547072539648,729.450947454989,104.737462545629));
#82542=CARTESIAN_POINT('Ctrl Pts',(56.4820482176787,729.42257229367,104.748231027978));
#82543=CARTESIAN_POINT('Ctrl Pts',(56.4166554466581,729.394937957736,104.758766192916));
#82544=CARTESIAN_POINT('Ctrl Pts',(56.3508942152867,729.368041516593,104.769059779925));
#82545=CARTESIAN_POINT('Ctrl Pts',(56.3404401460206,729.363765786761,104.77069615244));
#82546=CARTESIAN_POINT('Ctrl Pts',(56.329976698201,729.35950885027,104.772326424363));
#82547=CARTESIAN_POINT('Ctrl Pts',(56.3195038552598,729.355270730177,104.773950560435));
#82548=CARTESIAN_POINT('Ctrl Pts',(56.0754485372618,729.256507122941,104.811798836003));
#82549=CARTESIAN_POINT('Ctrl Pts',(55.8262484873397,729.167949961071,104.84631974904));
#82550=CARTESIAN_POINT('Ctrl Pts',(55.5718285705163,729.089905039709,104.877053064662));
#82551=CARTESIAN_POINT('Ctrl Pts',(55.5547359345939,729.084661765349,104.879117814077));
#82552=CARTESIAN_POINT('Ctrl Pts',(55.5376197452286,729.079465921373,104.881165475601));
#82553=CARTESIAN_POINT('Ctrl Pts',(55.520479982504,729.074317593171,104.883195912995));
#82554=CARTESIAN_POINT('Ctrl Pts',(55.511843802133,729.071723514613,104.884218985709));
#82555=CARTESIAN_POINT('Ctrl Pts',(55.5032005793578,729.069141445982,104.885237709746));
#82556=CARTESIAN_POINT('Ctrl Pts',(55.4945505473297,729.066571444255,104.88625205199));
#82557=CARTESIAN_POINT('Ctrl Pts',(55.2191338591722,728.98474268781,104.918548670129));
#82558=CARTESIAN_POINT('Ctrl Pts',(54.9366264377297,728.915110056549,104.946425904167));
#82559=CARTESIAN_POINT('Ctrl Pts',(54.6542663207744,728.859520795137,104.968821856728));
#82560=CARTESIAN_POINT('Ctrl Pts',(54.6481856147052,728.858323664455,104.969304159987));
#82561=CARTESIAN_POINT('Ctrl Pts',(54.6421043009935,728.857132748841,104.969784023243));
#82562=CARTESIAN_POINT('Ctrl Pts',(54.6360223788474,728.855948047957,104.970261445308));
#82563=CARTESIAN_POINT('Ctrl Pts',(54.059132722657,728.743575401716,105.015546446442));
#82564=CARTESIAN_POINT('Ctrl Pts',(53.4767411004789,728.68707816909,105.038869503257));
#82565=CARTESIAN_POINT('Ctrl Pts',(52.8888265844506,728.686362168155,105.039162721828));
#82566=CARTESIAN_POINT('Ctrl Pts',(52.88871717262,728.686362034906,105.039162776396));
#82567=CARTESIAN_POINT('Ctrl Pts',(52.8886077603945,728.686361903625,105.039162830157));
#82568=CARTESIAN_POINT('Ctrl Pts',(52.8884983477746,728.686361774311,105.039162883111));
#82569=CARTESIAN_POINT('Ctrl Pts',(52.6528529895801,728.686083267348,105.039276930853));
#82570=CARTESIAN_POINT('Ctrl Pts',(52.4154382016483,728.694925935922,105.035647251309));
#82571=CARTESIAN_POINT('Ctrl Pts',(52.1785782191425,728.712949886856,105.028285481323));
#82572=CARTESIAN_POINT('Ctrl Pts',(52.11990863315,728.717414371435,105.026461990531));
#82573=CARTESIAN_POINT('Ctrl Pts',(52.0612730714328,728.72244239549,105.024409426725));
#82574=CARTESIAN_POINT('Ctrl Pts',(52.0027068898726,728.728035331038,105.02212778052));
#82575=CARTESIAN_POINT('Ctrl Pts',(51.999601646668,728.728331874618,105.022006805135));
#82576=CARTESIAN_POINT('Ctrl Pts',(51.9964966087559,728.728630004985,105.021885186128));
#82577=CARTESIAN_POINT('Ctrl Pts',(51.9933917816137,728.728929722308,105.021762923512));
#82578=CARTESIAN_POINT('Ctrl Pts',(51.7015274348803,728.757104173523,105.010269820423));
#82579=CARTESIAN_POINT('Ctrl Pts',(51.4134962561136,728.798950066402,104.993234307881));
#82580=CARTESIAN_POINT('Ctrl Pts',(51.1290331392348,728.854038354221,104.971030027237));
#82581=CARTESIAN_POINT('Ctrl Pts',(51.1230292865439,728.855201042617,104.970561385708));
#82582=CARTESIAN_POINT('Ctrl Pts',(51.1170270590945,728.856369626789,104.970090443887));
#82583=CARTESIAN_POINT('Ctrl Pts',(51.1110264549796,728.857544102496,104.969617205344));
#82584=CARTESIAN_POINT('Ctrl Pts',(50.760369668679,728.926176838348,104.941962605324));
#82585=CARTESIAN_POINT('Ctrl Pts',(50.4151645113868,729.014797017035,104.90646128262));
#82586=CARTESIAN_POINT('Ctrl Pts',(50.0754187952665,729.123669682408,104.86374653985));
#82587=CARTESIAN_POINT('Ctrl Pts',(49.8641924928849,729.191357866383,104.837189980799));
#82588=CARTESIAN_POINT('Ctrl Pts',(49.6550766140004,729.266875282715,104.807844895762));
#82589=CARTESIAN_POINT('Ctrl Pts',(49.4480747596083,729.350295343021,104.775860965201));
#82590=CARTESIAN_POINT('Ctrl Pts',(49.4375295289826,729.354544985022,104.774231617845));
#82591=CARTESIAN_POINT('Ctrl Pts',(49.4269898221273,729.358815150135,104.772595427554));
#82592=CARTESIAN_POINT('Ctrl Pts',(49.4164556399806,729.363105847858,104.770952414218));
#82593=CARTESIAN_POINT('Ctrl Pts',(49.0488154420395,729.512850074624,104.713611679116));
#82594=CARTESIAN_POINT('Ctrl Pts',(48.6958839685112,729.684306267898,104.649249296768));
#82595=CARTESIAN_POINT('Ctrl Pts',(48.35682671435,729.876945078386,104.579525681863));
#82596=CARTESIAN_POINT('Ctrl Pts',(48.2028987101414,729.964400831854,104.54787198103));
#82597=CARTESIAN_POINT('Ctrl Pts',(48.0518304648117,730.056223118857,104.515113321302));
#82598=CARTESIAN_POINT('Ctrl Pts',(47.9035448503638,730.15236579935,104.481405401508));
#82599=CARTESIAN_POINT('Ctrl Pts',(47.8912655859373,730.160327201411,104.478614109433));
#82600=CARTESIAN_POINT('Ctrl Pts',(47.8790055110362,730.168318239008,104.475816332613));
#82601=CARTESIAN_POINT('Ctrl Pts',(47.8667645865555,730.176338880992,104.473012161201));
#82602=CARTESIAN_POINT('Ctrl Pts',(47.6376248244894,730.326478521067,104.420520442044));
#82603=CARTESIAN_POINT('Ctrl Pts',(47.4152527800419,730.487078105255,104.365776743866));
#82604=CARTESIAN_POINT('Ctrl Pts',(47.1996985589347,730.658424243244,104.309365278181));
#82605=CARTESIAN_POINT('Ctrl Pts',(47.1874393157864,730.668169234353,104.306156981583));
#82606=CARTESIAN_POINT('Ctrl Pts',(47.1752017887997,730.677949282337,104.302943203536));
#82607=CARTESIAN_POINT('Ctrl Pts',(47.1629860410042,730.687764410395,104.299724064378));
#82608=CARTESIAN_POINT('Ctrl Pts',(46.9909866530897,730.825962746382,104.254398147855));
#82609=CARTESIAN_POINT('Ctrl Pts',(46.8239310400841,730.970725125754,104.208155267803));
#82610=CARTESIAN_POINT('Ctrl Pts',(46.6632891329359,731.120607145755,104.161798643899));
#82611=CARTESIAN_POINT('Ctrl Pts',(46.6240170718333,731.157248741663,104.150465859081));
#82612=CARTESIAN_POINT('Ctrl Pts',(46.5851282064136,731.194196104456,104.139126316237));
#82613=CARTESIAN_POINT('Ctrl Pts',(46.5466437390096,731.231427760247,104.127791806588));
#82614=CARTESIAN_POINT('Ctrl Pts',(46.5351811948828,731.242517156209,104.124415838937));
#82615=CARTESIAN_POINT('Ctrl Pts',(46.5237536592718,731.2536325835,104.12104006282));
#82616=CARTESIAN_POINT('Ctrl Pts',(46.5123616699023,731.264773517811,104.117664779297));
#82617=CARTESIAN_POINT('Ctrl Pts',(46.2843633878658,731.4877472058,104.050112149143));
#82618=CARTESIAN_POINT('Ctrl Pts',(46.0692250098231,731.721847303384,103.982410465341));
#82619=CARTESIAN_POINT('Ctrl Pts',(45.8670654960537,731.967312670592,103.915718237435));
#82620=CARTESIAN_POINT('Ctrl Pts',(45.7143536769484,732.152737843293,103.865338756135));
#82621=CARTESIAN_POINT('Ctrl Pts',(45.569047152536,732.344647880411,103.815535785514));
#82622=CARTESIAN_POINT('Ctrl Pts',(45.4311812997561,732.543135231252,103.766813632448));
#82623=CARTESIAN_POINT('Ctrl Pts',(45.4226395749163,732.555432869144,103.763794964542));
#82624=CARTESIAN_POINT('Ctrl Pts',(45.4141262937154,732.56775599969,103.760780405758));
#82625=CARTESIAN_POINT('Ctrl Pts',(45.4056414672279,732.580104644677,103.757770077436));
#82626=CARTESIAN_POINT('Ctrl Pts',(45.2628995841321,732.787848296452,103.707126739694));
#82627=CARTESIAN_POINT('Ctrl Pts',(45.1277025931781,733.004005641326,103.657461813213));
#82628=CARTESIAN_POINT('Ctrl Pts',(45.0025610201077,733.224954135452,103.610237725581));
#82629=CARTESIAN_POINT('Ctrl Pts',(44.9916710856471,733.244181276051,103.606128242165));
#82630=CARTESIAN_POINT('Ctrl Pts',(44.9808573007471,733.263444667264,103.602037248998));
#82631=CARTESIAN_POINT('Ctrl Pts',(44.9701213212071,733.282741905032,103.597965713246));
#82632=CARTESIAN_POINT('Ctrl Pts',(44.9634793631087,733.294680400649,103.595446802907));
#82633=CARTESIAN_POINT('Ctrl Pts',(44.9568671680185,733.306631773498,103.592935333914));
#82634=CARTESIAN_POINT('Ctrl Pts',(44.9502851239598,733.318595466034,103.590431533745));
#82635=CARTESIAN_POINT('Ctrl Pts',(44.8167011978043,733.561401045296,103.539616398831));
#82636=CARTESIAN_POINT('Ctrl Pts',(44.6953101553414,733.809279305862,103.491905524418));
#82637=CARTESIAN_POINT('Ctrl Pts',(44.5859555352944,734.062282106168,103.447931161836));
#82638=CARTESIAN_POINT('Ctrl Pts',(44.5813216007246,734.073003175127,103.446067735134));
#82639=CARTESIAN_POINT('Ctrl Pts',(44.57670927537,734.083733432462,103.444211017472));
#82640=CARTESIAN_POINT('Ctrl Pts',(44.5721185456116,734.094472880908,103.442361056568));
#82641=CARTESIAN_POINT('Ctrl Pts',(44.4105096418914,734.472537062695,103.377236300951));
#82642=CARTESIAN_POINT('Ctrl Pts',(44.2754369813562,734.861905124845,103.32045882081));
#82643=CARTESIAN_POINT('Ctrl Pts',(44.1681996948913,735.263402492546,103.274231479426));
#82644=CARTESIAN_POINT('Ctrl Pts',(44.1276253708223,735.415313127801,103.256740892039));
#82645=CARTESIAN_POINT('Ctrl Pts',(44.0910361632143,735.568960400019,103.240760963358));
#82646=CARTESIAN_POINT('Ctrl Pts',(44.0585035980047,735.724389967507,103.226412308778));
#82647=CARTESIAN_POINT('Ctrl Pts',(44.0571410537863,735.730899741857,103.225811351669));
#82648=CARTESIAN_POINT('Ctrl Pts',(44.0557855452771,735.737413050662,103.22521322064));
#82649=CARTESIAN_POINT('Ctrl Pts',(44.054437086145,735.743929870542,103.224617928189));
#82650=CARTESIAN_POINT('Ctrl Pts',(44.0251843913813,735.885302002801,103.211703997045));
#82651=CARTESIAN_POINT('Ctrl Pts',(43.9994306999042,736.027799875058,103.200209958833));
#82652=CARTESIAN_POINT('Ctrl Pts',(43.9772758840869,736.170913964547,103.19020770992));
#82653=CARTESIAN_POINT('Ctrl Pts',(43.9551210682695,736.314028054035,103.180205461008));
#82654=CARTESIAN_POINT('Ctrl Pts',(43.9365652126234,736.457757751576,103.17169511312));
#82655=CARTESIAN_POINT('Ctrl Pts',(43.9216507621959,736.6015839673,103.164724639108));
#82656=CARTESIAN_POINT('Ctrl Pts',(43.9063925566538,736.74872515581,103.157593506404));
#82657=CARTESIAN_POINT('Ctrl Pts',(43.8949033349003,736.896283772816,103.152054681657));
#82658=CARTESIAN_POINT('Ctrl Pts',(43.8872145218739,737.044266546973,103.148150887835));
#82659=CARTESIAN_POINT('Ctrl Pts',(43.8795257088476,737.192249321131,103.144247094013));
#82660=CARTESIAN_POINT('Ctrl Pts',(43.8756371967118,737.340656799868,103.141978216393));
#82661=CARTESIAN_POINT('Ctrl Pts',(43.8756325293234,737.489494249471,103.141409944702));
#82662=CARTESIAN_POINT('Ctrl Pts',(15.7871623891209,777.809475003739,108.316029302452));
#82663=CARTESIAN_POINT('Ctrl Pts',(15.7828592118407,777.701521672783,108.603706188413));
#82664=CARTESIAN_POINT('Ctrl Pts',(15.9637713943952,777.935743349876,108.686420476388));
#82665=CARTESIAN_POINT('Ctrl Pts',(17.1698777637827,776.859899239153,107.980583473227));
#82666=CARTESIAN_POINT('Ctrl Pts',(17.1658604835569,776.751736583642,108.268251210865));
#82667=CARTESIAN_POINT('Ctrl Pts',(17.339905451348,776.990753940025,108.352595674445));
#82668=CARTESIAN_POINT('Ctrl Pts',(18.5839869581375,775.970726517344,107.663779924925));
#82669=CARTESIAN_POINT('Ctrl Pts',(18.5775897517564,775.864254818958,107.951030268325));
#82670=CARTESIAN_POINT('Ctrl Pts',(18.7474923713148,776.104630519359,108.036859377413));
#82671=CARTESIAN_POINT('Ctrl Pts',(21.4288123221645,774.335785651368,107.073001766124));
#82672=CARTESIAN_POINT('Ctrl Pts',(21.4233211378568,774.229827357484,107.357671335684));
#82673=CARTESIAN_POINT('Ctrl Pts',(21.5778907227146,774.475289361177,107.448008465933));
#82674=CARTESIAN_POINT('Ctrl Pts',(22.8577706644518,773.585932431183,106.799533790745));
#82675=CARTESIAN_POINT('Ctrl Pts',(22.8530525134455,773.479965851209,107.082603184221));
#82676=CARTESIAN_POINT('Ctrl Pts',(22.998957483572,773.728099094563,107.175447339692));
#82677=CARTESIAN_POINT('Ctrl Pts',(25.7716023470914,772.18478907632,106.316079490884));
#82678=CARTESIAN_POINT('Ctrl Pts',(25.7641886004944,772.080644591425,106.598115865289));
#82679=CARTESIAN_POINT('Ctrl Pts',(25.8953600097582,772.333644099618,106.694294509729));
#82680=CARTESIAN_POINT('Ctrl Pts',(27.2563198999602,771.533314665731,106.106856054866));
#82681=CARTESIAN_POINT('Ctrl Pts',(27.251586921119,771.427992638627,106.388475167844));
#82682=CARTESIAN_POINT('Ctrl Pts',(27.3707066300181,771.686096682895,106.486434551977));
#82683=CARTESIAN_POINT('Ctrl Pts',(30.2816206589377,770.320021916191,105.779318909421));
#82684=CARTESIAN_POINT('Ctrl Pts',(30.2707752197921,770.215782961016,106.063698689885));
#82685=CARTESIAN_POINT('Ctrl Pts',(30.3762932668855,770.482514096521,106.162191817292));
#82686=CARTESIAN_POINT('Ctrl Pts',(31.8218958654417,769.758147156968,105.661459556942));
#82687=CARTESIAN_POINT('Ctrl Pts',(31.8149887412563,769.651659865527,105.948249651328));
#82688=CARTESIAN_POINT('Ctrl Pts',(31.906520346948,769.926326252646,106.04624309019));
#82689=CARTESIAN_POINT('Ctrl Pts',(34.1753342422536,768.982641272906,105.558519931726));
#82690=CARTESIAN_POINT('Ctrl Pts',(34.1546169585506,768.877637047113,105.851399684763));
#82691=CARTESIAN_POINT('Ctrl Pts',(34.2448266873315,769.16068073807,105.946414538527));
#82692=CARTESIAN_POINT('Ctrl Pts',(34.9686229099064,768.734994611625,105.536323043755));
#82693=CARTESIAN_POINT('Ctrl Pts',(34.947012343891,768.629165255762,105.831524846475));
#82694=CARTESIAN_POINT('Ctrl Pts',(35.0332146223605,768.916496206878,105.92529234965));
#82695=CARTESIAN_POINT('Ctrl Pts',(36.5574672658585,768.267097781214,105.514313342663));
#82696=CARTESIAN_POINT('Ctrl Pts',(36.5323909593653,768.159538131973,105.814595596256));
#82697=CARTESIAN_POINT('Ctrl Pts',(36.6126042630737,768.455745087938,105.9054342665));
#82698=CARTESIAN_POINT('Ctrl Pts',(37.3535733947877,768.046590379996,105.514400128375));
#82699=CARTESIAN_POINT('Ctrl Pts',(37.3276962200189,767.937856780718,105.817623550911));
#82700=CARTESIAN_POINT('Ctrl Pts',(37.4041927108883,768.238916686194,105.906602202054));
#82701=CARTESIAN_POINT('Ctrl Pts',(39.7470698872341,767.426930329457,105.540910201916));
#82702=CARTESIAN_POINT('Ctrl Pts',(39.731369122651,767.310558107932,105.853533619489));
#82703=CARTESIAN_POINT('Ctrl Pts',(39.7851879275338,767.63026353926,105.936276431145));
#82704=CARTESIAN_POINT('Ctrl Pts',(41.3501040612565,767.069220619382,105.593941179774));
#82705=CARTESIAN_POINT('Ctrl Pts',(41.3351409056594,766.950282574883,105.914278418857));
#82706=CARTESIAN_POINT('Ctrl Pts',(41.3808256323271,767.280032673843,105.991321543562));
#82707=CARTESIAN_POINT('Ctrl Pts',(44.5738166034429,766.480398389306,105.718196950375));
#82708=CARTESIAN_POINT('Ctrl Pts',(44.5615972127706,766.353558912604,106.052595889704));
#82709=CARTESIAN_POINT('Ctrl Pts',(44.5923634296551,766.704367233879,106.118970464199));
#82710=CARTESIAN_POINT('Ctrl Pts',(46.1946605516339,766.249522535964,105.78850353175));
#82711=CARTESIAN_POINT('Ctrl Pts',(46.1795127759105,766.120994876181,106.129399020199));
#82712=CARTESIAN_POINT('Ctrl Pts',(46.2083274763445,766.479215938456,106.190660953083));
#82713=CARTESIAN_POINT('Ctrl Pts',(49.4574855150692,765.934275375266,105.892868516371));
#82714=CARTESIAN_POINT('Ctrl Pts',(49.4546256912783,765.799410469687,106.243931276121));
#82715=CARTESIAN_POINT('Ctrl Pts',(49.463598562072,766.171873580197,106.296940787133));
#82716=CARTESIAN_POINT('Ctrl Pts',(51.099964532512,765.850120640634,105.926129110136));
#82717=CARTESIAN_POINT('Ctrl Pts',(51.0910382647445,765.714667095532,106.279827188356));
#82718=CARTESIAN_POINT('Ctrl Pts',(51.102948592707,766.089969488739,106.330715610695));
#82719=CARTESIAN_POINT('Ctrl Pts',(53.5812393839398,765.844168786106,105.928376604794));
#82720=CARTESIAN_POINT('Ctrl Pts',(53.5850396314526,765.708577852611,106.282289428977));
#82721=CARTESIAN_POINT('Ctrl Pts',(53.5800634567942,766.084172742205,106.33299999645));
#82722=CARTESIAN_POINT('Ctrl Pts',(54.411880554151,765.86217585081,105.92146709385));
#82723=CARTESIAN_POINT('Ctrl Pts',(54.4179864165666,765.726919467555,106.274755736027));
#82724=CARTESIAN_POINT('Ctrl Pts',(54.4092728216049,766.101706740817,106.325979308644));
#82725=CARTESIAN_POINT('Ctrl Pts',(56.0769319609754,765.93844695356,105.893509488094));
#82726=CARTESIAN_POINT('Ctrl Pts',(56.0911552800048,765.80490169404,106.244116471363));
#82727=CARTESIAN_POINT('Ctrl Pts',(56.0712773854469,766.176009378732,106.297551934537));
#82728=CARTESIAN_POINT('Ctrl Pts',(56.9052458395736,765.996396478854,105.872599600657));
#82729=CARTESIAN_POINT('Ctrl Pts',(56.9214628881391,765.863871224801,106.221288358478));
#82730=CARTESIAN_POINT('Ctrl Pts',(56.8979108032853,766.232465009037,106.276287758478));
#82731=CARTESIAN_POINT('Ctrl Pts',(59.3783911870065,766.226174100899,105.795738329226));
#82732=CARTESIAN_POINT('Ctrl Pts',(59.3931930839897,766.097281081923,106.13732691571));
#82733=CARTESIAN_POINT('Ctrl Pts',(59.3652210008115,766.456444148206,106.198036053344));
#82734=CARTESIAN_POINT('Ctrl Pts',(61.0112655596819,766.453952146128,105.725310064261));
#82735=CARTESIAN_POINT('Ctrl Pts',(61.0230698567076,766.326720958392,106.060446968748));
#82736=CARTESIAN_POINT('Ctrl Pts',(60.9932650699687,766.678550277211,106.126240847154));
#82737=CARTESIAN_POINT('Ctrl Pts',(64.2501406514068,767.036718468604,105.599412980091));
#82738=CARTESIAN_POINT('Ctrl Pts',(64.2650219723685,766.917450919191,105.920451345278));
#82739=CARTESIAN_POINT('Ctrl Pts',(64.220087663195,767.248223944424,105.99697671647));
#82740=CARTESIAN_POINT('Ctrl Pts',(65.8563267979194,767.391477721513,105.544877839256));
#82741=CARTESIAN_POINT('Ctrl Pts',(65.8720329977456,767.274797690945,105.858171285359));
#82742=CARTESIAN_POINT('Ctrl Pts',(65.8189446590444,767.595514746263,105.940437566371));
#82743=CARTESIAN_POINT('Ctrl Pts',(69.0465943635938,768.210053193601,105.505173430379));
#82744=CARTESIAN_POINT('Ctrl Pts',(69.057730705995,768.098890004912,105.806099333311));
#82745=CARTESIAN_POINT('Ctrl Pts',(68.9922854012551,768.399315245165,105.896535263205));
#82746=CARTESIAN_POINT('Ctrl Pts',(70.6305164306212,768.673731102989,105.52051972908));
#82747=CARTESIAN_POINT('Ctrl Pts',(70.644943034338,768.565368486617,105.815477540819));
#82748=CARTESIAN_POINT('Ctrl Pts',(70.5668278970275,768.855706852748,105.909665906585));
#82749=CARTESIAN_POINT('Ctrl Pts',(73.7781993814608,769.703475797329,105.65147939074));
#82750=CARTESIAN_POINT('Ctrl Pts',(73.785156923816,769.596881243375,105.938580705688));
#82751=CARTESIAN_POINT('Ctrl Pts',(73.6945831500112,769.872258227292,106.036461068767));
#82752=CARTESIAN_POINT('Ctrl Pts',(75.3459978283876,770.271662966608,105.767902085136));
#82753=CARTESIAN_POINT('Ctrl Pts',(75.3568953147369,770.167357396806,106.052433260717));
#82754=CARTESIAN_POINT('Ctrl Pts',(75.2521594979732,770.434601013187,106.150924723143));
#82755=CARTESIAN_POINT('Ctrl Pts',(78.4094844858746,771.494821615298,106.09492936714));
#82756=CARTESIAN_POINT('Ctrl Pts',(78.414133676991,771.389464389472,106.376558566266));
#82757=CARTESIAN_POINT('Ctrl Pts',(78.2956674291651,771.647853007347,106.474594343472));
#82758=CARTESIAN_POINT('Ctrl Pts',(79.9105925242892,772.151408559331,106.30497861231));
#82759=CARTESIAN_POINT('Ctrl Pts',(79.9180899961921,772.047304534831,106.587006825142));
#82760=CARTESIAN_POINT('Ctrl Pts',(79.7872875510178,772.300446180308,106.683256580676));
#82761=CARTESIAN_POINT('Ctrl Pts',(82.8525638161391,773.562668707001,106.791100861697));
#82762=CARTESIAN_POINT('Ctrl Pts',(82.8572888565633,773.456721640073,107.074131615572));
#82763=CARTESIAN_POINT('Ctrl Pts',(82.7116297096421,773.704923756985,107.16704469137));
#82764=CARTESIAN_POINT('Ctrl Pts',(84.2932699293538,774.317537975393,107.066385590134));
#82765=CARTESIAN_POINT('Ctrl Pts',(84.298806954681,774.211617420184,107.351034210259));
#82766=CARTESIAN_POINT('Ctrl Pts',(84.1443675648991,774.457105296261,107.44141406158));
#82767=CARTESIAN_POINT('Ctrl Pts',(87.1578941883669,775.962233307482,107.660731979537));
#82768=CARTESIAN_POINT('Ctrl Pts',(87.1643322846048,775.855786966959,107.947981090005));
#82769=CARTESIAN_POINT('Ctrl Pts',(86.9944506659982,776.09616644414,108.033821604836));
#82770=CARTESIAN_POINT('Ctrl Pts',(88.5799295501548,776.856148047137,107.979260687991));
#82771=CARTESIAN_POINT('Ctrl Pts',(88.5839431068136,776.747982826875,108.26692813987));
#82772=CARTESIAN_POINT('Ctrl Pts',(88.4099278287071,776.987021304641,108.351279441427));
#82773=CARTESIAN_POINT('Ctrl Pts',(89.9686252865639,777.809853363037,108.316162883459));
#82774=CARTESIAN_POINT('Ctrl Pts',(89.9729284260661,777.701900006605,108.603839733057));
#82775=CARTESIAN_POINT('Ctrl Pts',(89.792013646137,777.936119871348,108.686553408827));
#82776=CARTESIAN_POINT('Ctrl Pts',(16.0893414574741,777.849661935782,108.656004008529));
#82777=CARTESIAN_POINT('Ctrl Pts',(17.4250549733219,776.937175921057,108.333500400375));
#82778=CARTESIAN_POINT('Ctrl Pts',(18.78943598776,776.080497252125,108.028135460872));
#82779=CARTESIAN_POINT('Ctrl Pts',(21.5746899384678,774.476977569018,107.448620490165));
#82780=CARTESIAN_POINT('Ctrl Pts',(22.9955938975846,773.729725682315,107.176024929388));
#82781=CARTESIAN_POINT('Ctrl Pts',(25.8934985433138,772.334397900271,106.694534848672));
#82782=CARTESIAN_POINT('Ctrl Pts',(27.3704856350576,771.686064132665,106.486387701304));
#82783=CARTESIAN_POINT('Ctrl Pts',(30.3808686758457,770.480671981398,106.161721933409));
#82784=CARTESIAN_POINT('Ctrl Pts',(31.9142587560915,769.923462674222,106.04565513536));
#82785=CARTESIAN_POINT('Ctrl Pts',(34.2576802253298,769.15654052208,105.945964322096));
#82786=CARTESIAN_POINT('Ctrl Pts',(35.0478636523885,768.911965834192,105.924938629994));
#82787=CARTESIAN_POINT('Ctrl Pts',(36.6303099055664,768.450709294541,105.905345473651));
#82788=CARTESIAN_POINT('Ctrl Pts',(37.4232324031954,768.233741281857,105.906677444993));
#82789=CARTESIAN_POINT('Ctrl Pts',(39.8074008004172,767.625011695292,105.936830078864));
#82790=CARTESIAN_POINT('Ctrl Pts',(41.4040107345446,767.275207462003,105.99215472231));
#82791=CARTESIAN_POINT('Ctrl Pts',(44.6144245059283,766.700953763019,106.119909037887));
#82792=CARTESIAN_POINT('Ctrl Pts',(46.2282835033238,766.476775822931,106.191423389735));
#82793=CARTESIAN_POINT('Ctrl Pts',(49.4766332220309,766.171063900259,106.297232632525));
#82794=CARTESIAN_POINT('Ctrl Pts',(51.1111753031026,766.089792523124,106.330747957394));
#82795=CARTESIAN_POINT('Ctrl Pts',(53.5801372868367,766.084145679822,106.332973315604));
#82796=CARTESIAN_POINT('Ctrl Pts',(54.4064440289033,766.101597865186,106.325986242852));
#82797=CARTESIAN_POINT('Ctrl Pts',(56.0628277007067,766.175473742229,106.297718036996));
#82798=CARTESIAN_POINT('Ctrl Pts',(56.8869548009683,766.231598277818,106.276572947795));
#82799=CARTESIAN_POINT('Ctrl Pts',(59.3478646853131,766.454407478501,106.198677774663));
#82800=CARTESIAN_POINT('Ctrl Pts',(60.9731755266814,766.675510114496,106.127094439787));
#82801=CARTESIAN_POINT('Ctrl Pts',(64.1977890163342,767.243651270107,105.997794517429));
#82802=CARTESIAN_POINT('Ctrl Pts',(65.7971573448773,767.590423963616,105.941009947412));
#82803=CARTESIAN_POINT('Ctrl Pts',(68.9737932300432,768.394076466195,105.896488785951));
#82804=CARTESIAN_POINT('Ctrl Pts',(70.5510930280338,768.850829333817,105.909275429647));
#82805=CARTESIAN_POINT('Ctrl Pts',(73.6851181293508,769.868817507906,106.035790294461));
#82806=CARTESIAN_POINT('Ctrl Pts',(75.2463606945133,770.432304387266,106.15035314656));
#82807=CARTESIAN_POINT('Ctrl Pts',(78.2952107601735,771.647525172689,106.474453855161));
#82808=CARTESIAN_POINT('Ctrl Pts',(79.7886644455849,772.300974854605,106.683420921211));
#82809=CARTESIAN_POINT('Ctrl Pts',(82.7147733195567,773.706431016707,107.167578148489));
#82810=CARTESIAN_POINT('Ctrl Pts',(84.1474203625525,774.458709583747,107.441995642768));
#82811=CARTESIAN_POINT('Ctrl Pts',(86.9521465126742,776.071846592112,108.025029756641));
#82812=CARTESIAN_POINT('Ctrl Pts',(88.3242703519922,776.933137527661,108.332073090122));
#82813=CARTESIAN_POINT('Ctrl Pts',(89.6658953259192,777.849661935669,108.656004008489));
#82814=CARTESIAN_POINT('Ctrl Pts',(88.5738513044493,778.181878049576,108.773653956565));
#82815=CARTESIAN_POINT('Ctrl Pts',(83.8434238890686,785.148186360683,109.114308839679));
#82816=CARTESIAN_POINT('Ctrl Pts',(78.9738504955049,791.633263347778,111.406354474977));
#82817=CARTESIAN_POINT('Ctrl Pts',(87.9149776371255,777.742127291872,108.618238413247));
#82818=CARTESIAN_POINT('Ctrl Pts',(83.2725051483006,784.767138659038,108.979633688774));
#82819=CARTESIAN_POINT('Ctrl Pts',(78.4934733905516,791.312643755968,111.293036662796));
#82820=CARTESIAN_POINT('Ctrl Pts',(87.2882571412732,777.341259228713,108.47646064782));
#82821=CARTESIAN_POINT('Ctrl Pts',(82.7150583236353,784.410224910016,108.853488293304));
#82822=CARTESIAN_POINT('Ctrl Pts',(78.0073420881403,791.00099847986,111.182890677438));
#82823=CARTESIAN_POINT('Ctrl Pts',(86.0362516952194,776.570985822674,108.20271274568));
#82824=CARTESIAN_POINT('Ctrl Pts',(81.604148087287,783.72393950889,108.610931811799));
#82825=CARTESIAN_POINT('Ctrl Pts',(77.0417726934468,790.401519506022,110.971014524206));
#82826=CARTESIAN_POINT('Ctrl Pts',(85.4124909221331,776.201653664868,108.070824267304));
#82827=CARTESIAN_POINT('Ctrl Pts',(81.0515796632365,783.39441895453,108.494468098035));
#82828=CARTESIAN_POINT('Ctrl Pts',(76.5625713693442,790.113291377843,110.869144951265));
#82829=CARTESIAN_POINT('Ctrl Pts',(84.0792612027146,775.445672384301,107.800616740213));
#82830=CARTESIAN_POINT('Ctrl Pts',(79.8976647185069,782.734867224681,108.261360200414));
#82831=CARTESIAN_POINT('Ctrl Pts',(75.5934183244409,789.553692399723,110.671363737892));
#82832=CARTESIAN_POINT('Ctrl Pts',(83.3720539242186,775.059903900003,107.6624783517));
#82833=CARTESIAN_POINT('Ctrl Pts',(79.2974971757814,782.405212171218,108.144848950272));
#82834=CARTESIAN_POINT('Ctrl Pts',(75.1035387365079,789.2822084411,110.575412121025));
#82835=CARTESIAN_POINT('Ctrl Pts',(82.1654585207305,774.436382978644,107.442289651568));
#82836=CARTESIAN_POINT('Ctrl Pts',(78.3167674194848,781.898680004742,107.965823343682));
#82837=CARTESIAN_POINT('Ctrl Pts',(74.3552830957901,788.896051377323,110.438931148736));
#82838=CARTESIAN_POINT('Ctrl Pts',(81.7385250148577,774.220948387259,107.366715554214));
#82839=CARTESIAN_POINT('Ctrl Pts',(77.976199525919,781.727802549079,107.905429469083));
#82840=CARTESIAN_POINT('Ctrl Pts',(74.1035832785893,788.77090952714,110.394701784601));
#82841=CARTESIAN_POINT('Ctrl Pts',(80.8079497421642,773.765682033111,107.209530118557));
#82842=CARTESIAN_POINT('Ctrl Pts',(77.2531183817485,781.378821137396,107.78208763009));
#82843=CARTESIAN_POINT('Ctrl Pts',(73.5938901808835,788.530494361478,110.309730930405));
#82844=CARTESIAN_POINT('Ctrl Pts',(80.3034332507445,773.525337785074,107.127690866966));
#82845=CARTESIAN_POINT('Ctrl Pts',(76.8698599874927,781.200311547758,107.718996301082));
#82846=CARTESIAN_POINT('Ctrl Pts',(73.3353014539425,788.414941956932,110.268890800825));
#82847=CARTESIAN_POINT('Ctrl Pts',(79.1770575653734,773.008703161511,106.957283814441));
#82848=CARTESIAN_POINT('Ctrl Pts',(76.0409616383071,780.833266548411,107.589270179072));
#82849=CARTESIAN_POINT('Ctrl Pts',(72.8120842823484,788.199188971456,110.192636395573));
#82850=CARTESIAN_POINT('Ctrl Pts',(78.5568496943687,772.73295592847,106.868769852518));
#82851=CARTESIAN_POINT('Ctrl Pts',(75.5965095740638,780.645113872109,107.522770656896));
#82852=CARTESIAN_POINT('Ctrl Pts',(72.5482099436597,788.099250448862,110.157314740184));
#82853=CARTESIAN_POINT('Ctrl Pts',(77.4911048517436,772.281537917275,106.732807228027));
#82854=CARTESIAN_POINT('Ctrl Pts',(74.8588910374908,780.353097020446,107.419562020953));
#82855=CARTESIAN_POINT('Ctrl Pts',(72.1475773980314,787.966232967754,110.110301861602));
#82856=CARTESIAN_POINT('Ctrl Pts',(77.112950447673,772.124710631934,106.686988491034));
#82857=CARTESIAN_POINT('Ctrl Pts',(74.6010028008535,780.254108042824,107.384575966848));
#82858=CARTESIAN_POINT('Ctrl Pts',(72.0132232095821,787.924731631362,110.095633885088));
#82859=CARTESIAN_POINT('Ctrl Pts',(76.3037627940189,771.798066830141,106.59588420746));
#82860=CARTESIAN_POINT('Ctrl Pts',(74.0574741870081,780.053376333228,107.313630588775));
#82861=CARTESIAN_POINT('Ctrl Pts',(71.7425915643583,787.848467048447,110.068679401009));
#82862=CARTESIAN_POINT('Ctrl Pts',(75.8722540562148,771.628097477578,106.550578461549));
#82863=CARTESIAN_POINT('Ctrl Pts',(73.7715798531127,779.951560540875,107.277645442728));
#82864=CARTESIAN_POINT('Ctrl Pts',(71.6063114236022,787.813713205088,110.05639621684));
#82865=CARTESIAN_POINT('Ctrl Pts',(74.9599655844954,771.279645950925,106.46373018065));
#82866=CARTESIAN_POINT('Ctrl Pts',(73.1736720938016,779.748117469616,107.205741777664));
#82867=CARTESIAN_POINT('Ctrl Pts',(71.3315223578334,787.752013970454,110.034589619675));
#82868=CARTESIAN_POINT('Ctrl Pts',(74.4788746718596,771.101147210338,106.422253178248));
#82869=CARTESIAN_POINT('Ctrl Pts',(72.8614810857166,779.646493791832,107.169824531404));
#82870=CARTESIAN_POINT('Ctrl Pts',(71.1930079058333,787.725087942696,110.0250730504));
#82871=CARTESIAN_POINT('Ctrl Pts',(73.496993747821,770.748822516026,106.347734551176));
#82872=CARTESIAN_POINT('Ctrl Pts',(72.2258102743165,779.450406994966,107.100520822657));
#82873=CARTESIAN_POINT('Ctrl Pts',(70.9135678426254,787.679683282299,110.009025507111));
#82874=CARTESIAN_POINT('Ctrl Pts',(72.9972861502008,770.575443021603,106.314830495441));
#82875=CARTESIAN_POINT('Ctrl Pts',(71.9028611425821,779.356169439202,107.067214081826));
#82876=CARTESIAN_POINT('Ctrl Pts',(70.7726394832558,787.661214277631,110.002497935947));
#82877=CARTESIAN_POINT('Ctrl Pts',(72.0255934206576,770.249325984699,106.260112822916));
#82878=CARTESIAN_POINT('Ctrl Pts',(71.2697212485457,779.18247231621,107.005823641377));
#82879=CARTESIAN_POINT('Ctrl Pts',(70.4884658286637,787.632393555839,109.992311717692));
#82880=CARTESIAN_POINT('Ctrl Pts',(71.5536373679969,770.096525865296,106.238228677174));
#82881=CARTESIAN_POINT('Ctrl Pts',(70.9594066510123,779.102962134233,106.977722052762));
#82882=CARTESIAN_POINT('Ctrl Pts',(70.344949670124,787.622012052336,109.988642543087));
#82883=CARTESIAN_POINT('Ctrl Pts',(70.6681422002458,769.818470054936,106.204087028555));
#82884=CARTESIAN_POINT('Ctrl Pts',(70.3679066564915,778.961275090666,106.927645057479));
#82885=CARTESIAN_POINT('Ctrl Pts',(70.0571733336436,787.608223198133,109.983769095454));
#82886=CARTESIAN_POINT('Ctrl Pts',(70.2562198335574,769.693596329677,106.191779838153));
#82887=CARTESIAN_POINT('Ctrl Pts',(70.0879120630911,778.899274121479,106.905731817103));
#82888=CARTESIAN_POINT('Ctrl Pts',(69.9136476562238,787.604807391686,109.982561833879));
#82889=CARTESIAN_POINT('Ctrl Pts',(69.1075565099042,769.354665279132,106.164335933203));
#82890=CARTESIAN_POINT('Ctrl Pts',(69.2923238767039,778.734902877756,106.847637457941));
#82891=CARTESIAN_POINT('Ctrl Pts',(69.4839004401929,787.602523253,109.981754541982));
#82892=CARTESIAN_POINT('Ctrl Pts',(68.4559672015376,769.17518744114,106.158151845178));
#82893=CARTESIAN_POINT('Ctrl Pts',(68.8203566681227,778.653557517144,106.818887255123));
#82894=CARTESIAN_POINT('Ctrl Pts',(69.1984902703543,787.611441170196,109.984906435664));
#82895=CARTESIAN_POINT('Ctrl Pts',(67.2950904119738,768.868275425604,106.154657878201));
#82896=CARTESIAN_POINT('Ctrl Pts',(67.9491799021657,778.522040766329,106.772404785367));
#82897=CARTESIAN_POINT('Ctrl Pts',(68.6288985832237,787.641067693366,109.995377451391));
#82898=CARTESIAN_POINT('Ctrl Pts',(66.7851640278802,768.740976392566,106.157639466173));
#82899=CARTESIAN_POINT('Ctrl Pts',(67.549698766656,778.472018174541,106.754725108905));
#82900=CARTESIAN_POINT('Ctrl Pts',(68.3447257023204,787.661859177433,110.002725865358));
#82901=CARTESIAN_POINT('Ctrl Pts',(65.8509965373988,768.516718306576,106.167242031038));
#82902=CARTESIAN_POINT('Ctrl Pts',(66.794624228746,778.390000059683,106.725737131935));
#82903=CARTESIAN_POINT('Ctrl Pts',(67.7770957888854,787.710311740259,110.019850640494));
#82904=CARTESIAN_POINT('Ctrl Pts',(65.4272737571728,768.420031205163,106.173980523856));
#82905=CARTESIAN_POINT('Ctrl Pts',(66.4393274595632,778.358174956261,106.714489063581));
#82906=CARTESIAN_POINT('Ctrl Pts',(67.4936435311311,787.738018639783,110.029643196272));
#82907=CARTESIAN_POINT('Ctrl Pts',(64.6361872575302,768.246354011442,106.188976594821));
#82908=CARTESIAN_POINT('Ctrl Pts',(65.7576292395194,778.305889398473,106.69600957831));
#82909=CARTESIAN_POINT('Ctrl Pts',(66.9271483164738,787.797360269187,110.050616535977));
#82910=CARTESIAN_POINT('Ctrl Pts',(64.2691108829029,768.169487022388,106.197273275863));
#82911=CARTESIAN_POINT('Ctrl Pts',(65.4313953294225,778.285505642855,106.68880526938));
#82912=CARTESIAN_POINT('Ctrl Pts',(66.6441075879408,787.829016383441,110.061804877866));
#82913=CARTESIAN_POINT('Ctrl Pts',(63.2269996462562,767.959563358908,106.222950194576));
#82914=CARTESIAN_POINT('Ctrl Pts',(64.4828994295554,778.235670861743,106.671191971545));
#82915=CARTESIAN_POINT('Ctrl Pts',(65.7953010971783,787.927014271945,110.096440647505));
#82916=CARTESIAN_POINT('Ctrl Pts',(62.6097075508497,767.846709151702,106.241045178976));
#82917=CARTESIAN_POINT('Ctrl Pts',(63.8904323523067,778.21725275906,106.664682390869));
#82918=CARTESIAN_POINT('Ctrl Pts',(65.2298349915925,787.99623168283,110.120904422542));
#82919=CARTESIAN_POINT('Ctrl Pts',(61.4590052374346,767.651437052883,106.275936414629));
#82920=CARTESIAN_POINT('Ctrl Pts',(62.748362851604,778.194057714248,106.656484477185));
#82921=CARTESIAN_POINT('Ctrl Pts',(64.0987686108381,788.133378954464,110.169376908831));
#82922=CARTESIAN_POINT('Ctrl Pts',(60.926821211362,767.569468956964,106.292826110456));
#82923=CARTESIAN_POINT('Ctrl Pts',(62.1994558233975,778.18956414367,106.654896297299));
#82924=CARTESIAN_POINT('Ctrl Pts',(63.5331799072629,788.201419861245,110.193424867509));
#82925=CARTESIAN_POINT('Ctrl Pts',(59.4092177133849,767.354659251409,106.340244800808));
#82926=CARTESIAN_POINT('Ctrl Pts',(60.592599303396,778.186156421342,106.65369189296));
#82927=CARTESIAN_POINT('Ctrl Pts',(61.8354805457418,788.396586698252,110.262403431342));
#82928=CARTESIAN_POINT('Ctrl Pts',(58.5007011856502,767.252229641939,106.36749379104));
#82929=CARTESIAN_POINT('Ctrl Pts',(59.5741477724552,778.196813737576,106.657458549082));
#82930=CARTESIAN_POINT('Ctrl Pts',(60.7023962859907,788.514369519008,110.304031865479));
#82931=CARTESIAN_POINT('Ctrl Pts',(56.7697487845424,767.09500330296,106.41105217881));
#82932=CARTESIAN_POINT('Ctrl Pts',(57.579404677287,778.218730226506,106.665204577855));
#82933=CARTESIAN_POINT('Ctrl Pts',(58.4317005834261,788.706490328621,110.371933860166));
#82934=CARTESIAN_POINT('Ctrl Pts',(55.9515831390504,767.041203218348,106.427412017473));
#82935=CARTESIAN_POINT('Ctrl Pts',(56.6066138022518,778.230530097354,106.669375051334));
#82936=CARTESIAN_POINT('Ctrl Pts',(57.2963394038202,788.780952969837,110.398251477078));
#82937=CARTESIAN_POINT('Ctrl Pts',(54.354843997501,766.971158844204,106.448937284848));
#82938=CARTESIAN_POINT('Ctrl Pts',(54.6828513340098,778.246666962928,106.675078365885));
#82939=CARTESIAN_POINT('Ctrl Pts',(55.0285659862819,788.879478327426,110.433073672139));
#82940=CARTESIAN_POINT('Ctrl Pts',(53.5768772428552,766.955076749816,106.454128934655));
#82941=CARTESIAN_POINT('Ctrl Pts',(53.7321495971161,778.251150846421,106.676663121963));
#82942=CARTESIAN_POINT('Ctrl Pts',(53.8957206869194,788.90368428377,110.44162887614));
#82943=CARTESIAN_POINT('Ctrl Pts',(52.0222390159911,766.957423826263,106.453384325924));
#82944=CARTESIAN_POINT('Ctrl Pts',(51.8322941590422,778.250536615474,106.67644603184));
#82945=CARTESIAN_POINT('Ctrl Pts',(51.6321856100123,788.900233488439,110.44040924831));
#82946=CARTESIAN_POINT('Ctrl Pts',(51.2442658197987,766.975858807195,106.447448325547));
#82947=CARTESIAN_POINT('Ctrl Pts',(50.8826289700665,778.245446491303,106.674647009886));
#82948=CARTESIAN_POINT('Ctrl Pts',(50.5014953947721,788.872587267927,110.430638138547));
#82949=CARTESIAN_POINT('Ctrl Pts',(49.6481191527577,767.050640179407,106.424565547509));
#82950=CARTESIAN_POINT('Ctrl Pts',(48.9632488386254,778.228521988974,106.668665317918));
#82951=CARTESIAN_POINT('Ctrl Pts',(48.2421630907403,788.768016093984,110.393679147422));
#82952=CARTESIAN_POINT('Ctrl Pts',(48.8307699445029,767.106785567727,106.407600455105));
#82953=CARTESIAN_POINT('Ctrl Pts',(47.9941274109117,778.216541598047,106.664431042419));
#82954=CARTESIAN_POINT('Ctrl Pts',(47.113525345716,788.690986627767,110.366454327704));
#82955=CARTESIAN_POINT('Ctrl Pts',(47.099562606948,767.269023789712,106.3630646157));
#82956=CARTESIAN_POINT('Ctrl Pts',(46.0065892381932,778.19512484894,106.656861638777));
#82957=CARTESIAN_POINT('Ctrl Pts',(44.8579854286538,788.495169122572,110.297245795717));
#82958=CARTESIAN_POINT('Ctrl Pts',(46.1884599507835,767.374227192424,106.33538318268));
#82959=CARTESIAN_POINT('Ctrl Pts',(44.9898074938279,778.185072718314,106.65330887556));
#82960=CARTESIAN_POINT('Ctrl Pts',(43.7310987807227,788.376007567032,110.255130070057));
#82961=CARTESIAN_POINT('Ctrl Pts',(44.6599688000924,767.595039520773,106.287523900011));
#82962=CARTESIAN_POINT('Ctrl Pts',(43.3812833108911,778.190851690929,106.655351360106));
#82963=CARTESIAN_POINT('Ctrl Pts',(42.0414880433933,788.179960166242,110.185840285188));
#82964=CARTESIAN_POINT('Ctrl Pts',(44.1229651056719,767.679321827364,106.270522681015));
#82965=CARTESIAN_POINT('Ctrl Pts',(42.8311204157762,778.196385262059,106.65730711133));
#82966=CARTESIAN_POINT('Ctrl Pts',(41.478400047932,788.111830043881,110.161760794705));
#82967=CARTESIAN_POINT('Ctrl Pts',(42.9585131381123,767.880518992648,106.235593765515));
#82968=CARTESIAN_POINT('Ctrl Pts',(41.684402157246,778.222618365023,106.666578777572));
#82969=CARTESIAN_POINT('Ctrl Pts',(40.3522402774629,787.97517952959,110.113463879269));
#82970=CARTESIAN_POINT('Ctrl Pts',(42.3324438370369,767.996929545801,106.21756013989));
#82971=CARTESIAN_POINT('Ctrl Pts',(41.0886358099137,778.243004169485,106.673783810619));
#82972=CARTESIAN_POINT('Ctrl Pts',(39.7892076533655,787.906542750337,110.089205319098));
#82973=CARTESIAN_POINT('Ctrl Pts',(41.2706386875018,768.214470254944,106.192394945541));
#82974=CARTESIAN_POINT('Ctrl Pts',(40.1319615807423,778.29735667139,106.69299382386));
#82975=CARTESIAN_POINT('Ctrl Pts',(38.9442264979715,787.810332049824,110.055201202166));
#82976=CARTESIAN_POINT('Ctrl Pts',(40.8958775623199,768.294267732256,106.18434076263));
#82977=CARTESIAN_POINT('Ctrl Pts',(39.8024487847689,778.319513361772,106.700824747908));
#82978=CARTESIAN_POINT('Ctrl Pts',(38.662488217245,787.779426833836,110.044278253132));
#82979=CARTESIAN_POINT('Ctrl Pts',(40.0857541413549,768.475159029144,106.170123670993));
#82980=CARTESIAN_POINT('Ctrl Pts',(39.1123933899711,778.376231169052,106.720870740139));
#82981=CARTESIAN_POINT('Ctrl Pts',(38.0987161989031,787.722035297116,110.023994142163));
#82982=CARTESIAN_POINT('Ctrl Pts',(39.6507046877265,768.576114921759,106.163914476279));
#82983=CARTESIAN_POINT('Ctrl Pts',(38.7520321209999,778.410706406896,106.733055455671));
#82984=CARTESIAN_POINT('Ctrl Pts',(37.8166840316626,787.695525489556,110.01462467919));
#82985=CARTESIAN_POINT('Ctrl Pts',(38.6875932077418,768.811386493074,106.156016095358));
#82986=CARTESIAN_POINT('Ctrl Pts',(37.9837524896163,778.499588578614,106.764469422558));
#82987=CARTESIAN_POINT('Ctrl Pts',(37.2521088113107,787.650146756091,109.998586299356));
#82988=CARTESIAN_POINT('Ctrl Pts',(38.16001983477,768.945417238923,106.154189393271));
#82989=CARTESIAN_POINT('Ctrl Pts',(37.5761167951056,778.553814431039,106.7836346736));
#82990=CARTESIAN_POINT('Ctrl Pts',(36.9695690548407,787.631228525103,109.99189995641));
#82991=CARTESIAN_POINT('Ctrl Pts',(36.9532834034759,769.270474682901,106.161569740109));
#82992=CARTESIAN_POINT('Ctrl Pts',(36.6834835598239,778.696633881445,106.834111899758));
#82993=CARTESIAN_POINT('Ctrl Pts',(36.4036171345023,787.606439911982,109.983138821789));
#82994=CARTESIAN_POINT('Ctrl Pts',(36.2725027848239,769.461655907321,106.170500609688));
#82995=CARTESIAN_POINT('Ctrl Pts',(36.1977184022626,778.785219903999,106.865421197509));
#82996=CARTESIAN_POINT('Ctrl Pts',(36.1202098960075,787.600495865408,109.981037994608));
#82997=CARTESIAN_POINT('Ctrl Pts',(35.0747520244915,769.822544499692,106.204756011053));
#82998=CARTESIAN_POINT('Ctrl Pts',(35.3790433873196,778.963412841933,106.928400611112));
#82999=CARTESIAN_POINT('Ctrl Pts',(35.6939666874706,787.608515394358,109.983872367487));
#83000=CARTESIAN_POINT('Ctrl Pts',(34.6457340436867,769.955453947562,106.219805597645));
#83001=CARTESIAN_POINT('Ctrl Pts',(35.0910332971829,779.030509162521,106.95211472106));
#83002=CARTESIAN_POINT('Ctrl Pts',(35.5516937213439,787.614058603793,109.98583152526));
#83003=CARTESIAN_POINT('Ctrl Pts',(33.7312343792939,770.249022021035,106.260244813743));
#83004=CARTESIAN_POINT('Ctrl Pts',(34.4862671715431,779.18240510027,107.005799884985));
#83005=CARTESIAN_POINT('Ctrl Pts',(35.2666546143195,787.632521014431,109.992356765871));
#83006=CARTESIAN_POINT('Ctrl Pts',(33.2440379163932,770.410411212385,106.285871093897));
#83007=CARTESIAN_POINT('Ctrl Pts',(34.1684624290794,779.267617800876,107.03591693661));
#83008=CARTESIAN_POINT('Ctrl Pts',(35.1235149780168,787.645538139296,109.996957458244));
#83009=CARTESIAN_POINT('Ctrl Pts',(32.259690132129,770.748325877485,106.347650981772));
#83010=CARTESIAN_POINT('Ctrl Pts',(33.5298937723489,779.450220385751,107.100454868647));
#83011=CARTESIAN_POINT('Ctrl Pts',(34.8411271130687,787.679795133055,110.009065038953));
#83012=CARTESIAN_POINT('Ctrl Pts',(31.762501164651,770.924854912313,106.383805863243));
#83013=CARTESIAN_POINT('Ctrl Pts',(33.2088787785457,779.547622607324,107.134880109408));
#83014=CARTESIAN_POINT('Ctrl Pts',(34.7014294761367,787.70105383366,110.016578583053));
#83015=CARTESIAN_POINT('Ctrl Pts',(30.8016313863479,771.277106071563,106.463016442903));
#83016=CARTESIAN_POINT('Ctrl Pts',(32.5854182318755,779.746708986598,107.20524397213));
#83017=CARTESIAN_POINT('Ctrl Pts',(34.4249901431715,787.751730477205,110.034489423568));
#83018=CARTESIAN_POINT('Ctrl Pts',(30.338486235497,771.452534880892,106.505935931361));
#83019=CARTESIAN_POINT('Ctrl Pts',(32.2832227399766,779.848236956052,107.241127391809));
#83020=CARTESIAN_POINT('Ctrl Pts',(34.2882421003274,787.781130901128,110.044880528171));
#83021=CARTESIAN_POINT('Ctrl Pts',(29.030519462635,771.961590961752,106.638170728346));
#83022=CARTESIAN_POINT('Ctrl Pts',(31.4200055420069,780.150349731569,107.347904268904));
#83023=CARTESIAN_POINT('Ctrl Pts',(33.8819357641858,787.880201606199,110.079895467484));
#83024=CARTESIAN_POINT('Ctrl Pts',(28.2689843845276,772.276572686069,106.730103740878));
#83025=CARTESIAN_POINT('Ctrl Pts',(30.9030724009608,780.347718738259,107.417661154068));
#83026=CARTESIAN_POINT('Ctrl Pts',(33.6162769933636,787.960635684765,110.108323592405));
#83027=CARTESIAN_POINT('Ctrl Pts',(26.9222137772097,772.854600754735,106.907363636004));
#83028=CARTESIAN_POINT('Ctrl Pts',(29.9621884190293,780.727290843087,107.551814778971));
#83029=CARTESIAN_POINT('Ctrl Pts',(33.092297454712,788.141758829008,110.172338640035));
#83030=CARTESIAN_POINT('Ctrl Pts',(26.3325994493358,773.11952290612,106.993320051036));
#83031=CARTESIAN_POINT('Ctrl Pts',(29.5359678693991,780.910440753884,107.616546154532));
#83032=CARTESIAN_POINT('Ctrl Pts',(32.8339653751143,788.242416670986,110.207914527233));
#83033=CARTESIAN_POINT('Ctrl Pts',(25.2579283778626,773.617013896509,107.158722030965));
#83034=CARTESIAN_POINT('Ctrl Pts',(28.7390226055063,781.26782836661,107.742859029362));
#83035=CARTESIAN_POINT('Ctrl Pts',(32.3224322386645,788.457895445242,110.284072016962));
#83036=CARTESIAN_POINT('Ctrl Pts',(24.7730747796453,773.849677797855,107.238310108299));
#83037=CARTESIAN_POINT('Ctrl Pts',(28.3683890273826,781.442147786514,107.804469410656));
#83038=CARTESIAN_POINT('Ctrl Pts',(32.069242790029,788.572748419678,110.324664944275));
#83039=CARTESIAN_POINT('Ctrl Pts',(23.8701844394258,774.294398766932,107.392397926644));
#83040=CARTESIAN_POINT('Ctrl Pts',(27.6628084392416,781.785649366179,107.925874491486));
#83041=CARTESIAN_POINT('Ctrl Pts',(31.5665966864075,788.81275794636,110.40949243193));
#83042=CARTESIAN_POINT('Ctrl Pts',(23.4527729129437,774.506259872119,107.466876025996));
#83043=CARTESIAN_POINT('Ctrl Pts',(27.3282358841123,781.95473047245,107.985633475494));
#83044=CARTESIAN_POINT('Ctrl Pts',(31.3172707008355,788.937895174379,110.453720162436));
#83045=CARTESIAN_POINT('Ctrl Pts',(22.2749915223958,775.118189983364,107.68330074963));
#83046=CARTESIAN_POINT('Ctrl Pts',(26.3668555933542,782.454445946986,108.162249832477));
#83047=CARTESIAN_POINT('Ctrl Pts',(30.5786420327287,789.322073679573,110.589501845176));
#83048=CARTESIAN_POINT('Ctrl Pts',(21.5833243793265,775.497036466794,107.818980673689));
#83049=CARTESIAN_POINT('Ctrl Pts',(25.778292337407,782.77915976542,108.277014682795));
#83050=CARTESIAN_POINT('Ctrl Pts',(30.0963148301091,789.590657952587,110.684428615035));
#83051=CARTESIAN_POINT('Ctrl Pts',(20.2781860531485,776.23958244733,108.084377327684));
#83052=CARTESIAN_POINT('Ctrl Pts',(24.646734284643,783.428111818108,108.506376296241));
#83053=CARTESIAN_POINT('Ctrl Pts',(29.1436129446067,790.142589946348,110.879500056716));
#83054=CARTESIAN_POINT('Ctrl Pts',(19.6668691668151,776.602439087497,108.213913923102));
#83055=CARTESIAN_POINT('Ctrl Pts',(24.104872557406,783.75198935753,108.620845577318));
#83056=CARTESIAN_POINT('Ctrl Pts',(28.6733263532804,790.426046475611,110.979683185149));
#83057=CARTESIAN_POINT('Ctrl Pts',(18.4402065432691,777.358402958426,108.482528589129));
#83058=CARTESIAN_POINT('Ctrl Pts',(23.01638179156,784.425478984283,108.858879599368));
#83059=CARTESIAN_POINT('Ctrl Pts',(27.7271624247458,791.014305376711,111.187593785036));
#83060=CARTESIAN_POINT('Ctrl Pts',(17.8263068741335,777.751461542779,108.621536767266));
#83061=CARTESIAN_POINT('Ctrl Pts',(22.4706348085142,784.775231435535,108.982493950034));
#83062=CARTESIAN_POINT('Ctrl Pts',(27.2515765493364,791.319458697228,111.295445293627));
#83063=CARTESIAN_POINT('Ctrl Pts',(17.1827964457161,778.180936484659,108.773321213211));
#83064=CARTESIAN_POINT('Ctrl Pts',(21.9130382745855,785.147368653583,109.1140198343));
#83065=CARTESIAN_POINT('Ctrl Pts',(26.7824206252748,791.632573132854,111.406110529669));
#83066=CARTESIAN_POINT('Ctrl Pts',(55.7276456603534,788.847878152655,110.421905101156));
#83067=CARTESIAN_POINT('Ctrl Pts',(55.8725641695401,788.842398318866,110.41996834248));
#83068=CARTESIAN_POINT('Ctrl Pts',(56.0174997454617,788.836507669495,110.417886387678));
#83069=CARTESIAN_POINT('Ctrl Pts',(56.1624523198427,788.830207971405,110.415659861218));
#83070=CARTESIAN_POINT('Ctrl Pts',(57.296339635109,788.780928765541,110.398242922464));
#83071=CARTESIAN_POINT('Ctrl Pts',(58.4317006497298,788.706476146093,110.371928847582));
#83072=CARTESIAN_POINT('Ctrl Pts',(59.567047823892,788.610423506175,110.337980594612));
#83073=CARTESIAN_POINT('Ctrl Pts',(60.0784213303319,788.567160285554,110.322689908596));
#83074=CARTESIAN_POINT('Ctrl Pts',(60.5893354360563,788.519489778419,110.305841538403));
#83075=CARTESIAN_POINT('Ctrl Pts',(61.0998792915351,788.46826787082,110.287737983121));
#83076=CARTESIAN_POINT('Ctrl Pts',(61.7228414790833,788.405767242783,110.265648146411));
#83077=CARTESIAN_POINT('Ctrl Pts',(62.345254962281,788.337983235991,110.241690984881));
#83078=CARTESIAN_POINT('Ctrl Pts',(62.9672801200892,788.266475473581,110.21641772212));
#83079=CARTESIAN_POINT('Ctrl Pts',(63.2383859190671,788.235309259774,110.205402527625));
#83080=CARTESIAN_POINT('Ctrl Pts',(63.5094202672636,788.203457902004,110.194145180072));
#83081=CARTESIAN_POINT('Ctrl Pts',(63.7804110897448,788.171191083345,110.182740994583));
#83082=CARTESIAN_POINT('Ctrl Pts',(64.0750803558359,788.136104877523,110.170340342274));
#83083=CARTESIAN_POINT('Ctrl Pts',(64.3696983593313,788.100525711438,110.157765461128));
#83084=CARTESIAN_POINT('Ctrl Pts',(64.6643013465014,788.064801985003,110.145139487464));
#83085=CARTESIAN_POINT('Ctrl Pts',(65.2298341777321,787.996225150983,110.120902113966));
#83086=CARTESIAN_POINT('Ctrl Pts',(65.7953001791059,787.927004653761,110.096437248114));
#83087=CARTESIAN_POINT('Ctrl Pts',(66.3611718962303,787.86168084646,110.073349604327));
#83088=CARTESIAN_POINT('Ctrl Pts',(66.3936068769028,787.857936576578,110.07202625266));
#83089=CARTESIAN_POINT('Ctrl Pts',(66.4260432428301,787.854205614206,110.070707604317));
#83090=CARTESIAN_POINT('Ctrl Pts',(66.4584811470731,787.850489430807,110.069394179364));
#83091=CARTESIAN_POINT('Ctrl Pts',(42.7661933181638,788.263968022319,110.215531504003));
#83092=CARTESIAN_POINT('Ctrl Pts',(43.8388165649104,788.387349366501,110.259138645749));
#83093=CARTESIAN_POINT('Ctrl Pts',(44.9118861838019,788.499848583716,110.298899675619));
#83094=CARTESIAN_POINT('Ctrl Pts',(45.9857553871849,788.593077875169,110.33185006171));
#83095=CARTESIAN_POINT('Ctrl Pts',(46.6204803621889,788.648182313867,110.351325834851));
#83096=CARTESIAN_POINT('Ctrl Pts',(47.2554797595624,788.69667299997,110.368464084043));
#83097=CARTESIAN_POINT('Ctrl Pts',(47.8907831607379,788.737861036833,110.383021329903));
#83098=CARTESIAN_POINT('Ctrl Pts',(48.3842772970703,788.769855285001,110.394329179758));
#83099=CARTESIAN_POINT('Ctrl Pts',(48.8779550586805,788.797440912187,110.404078873788));
#83100=CARTESIAN_POINT('Ctrl Pts',(49.3718294922987,788.820296888119,110.412156949034));
#83101=CARTESIAN_POINT('Ctrl Pts',(50.5014957115572,788.872576621917,110.430634375888));
#83102=CARTESIAN_POINT('Ctrl Pts',(51.6321862379869,788.900215353204,110.440402838705));
#83103=CARTESIAN_POINT('Ctrl Pts',(52.7639531549206,788.901955122284,110.441017731963));
#83104=CARTESIAN_POINT('Ctrl Pts',(52.8520451148785,788.902090538566,110.441065592659));
#83105=CARTESIAN_POINT('Ctrl Pts',(52.9401436011452,788.902068984546,110.441057974739));
#83106=CARTESIAN_POINT('Ctrl Pts',(53.0282485972464,788.901890883653,110.440995027858));
#83107=CARTESIAN_POINT('Ctrl Pts',(28.4218514088844,790.583031932319,111.035167157285));
#83108=CARTESIAN_POINT('Ctrl Pts',(28.8178561793361,790.339188506334,110.948984639894));
#83109=CARTESIAN_POINT('Ctrl Pts',(29.2170541634323,790.100042996678,110.864462525091));
#83110=CARTESIAN_POINT('Ctrl Pts',(29.6199625150174,789.866621843685,110.781963591621));
#83111=CARTESIAN_POINT('Ctrl Pts',(29.9403508812464,789.681007865825,110.716361331439));
#83112=CARTESIAN_POINT('Ctrl Pts',(30.2630464352065,789.498965415945,110.652021370092));
#83113=CARTESIAN_POINT('Ctrl Pts',(30.5891590962137,789.32205998929,110.589497006568));
#83114=CARTESIAN_POINT('Ctrl Pts',(30.7244461380251,789.248671204633,110.5635589269));
#83115=CARTESIAN_POINT('Ctrl Pts',(30.8603209078513,789.176166054629,110.537933153616));
#83116=CARTESIAN_POINT('Ctrl Pts',(30.9968610193644,789.104654262708,110.512658466691));
#83117=CARTESIAN_POINT('Ctrl Pts',(31.0215692479453,789.091713525503,110.508084772302));
#83118=CARTESIAN_POINT('Ctrl Pts',(31.0462980416312,789.078806144513,110.503522867128));
#83119=CARTESIAN_POINT('Ctrl Pts',(31.0710482020822,789.065932555418,110.498972905153));
#83120=CARTESIAN_POINT('Ctrl Pts',(31.317568884694,788.937706882794,110.453653613826));
#83121=CARTESIAN_POINT('Ctrl Pts',(31.5668006079514,788.812638621386,110.409450258449));
#83122=CARTESIAN_POINT('Ctrl Pts',(31.8179138799322,788.692742276541,110.367074833385));
#83123=CARTESIAN_POINT('Ctrl Pts',(31.990334141305,788.610418634494,110.337978872795));
#83124=CARTESIAN_POINT('Ctrl Pts',(32.1635810675995,788.530542075654,110.30974779421));
#83125=CARTESIAN_POINT('Ctrl Pts',(32.3379854760787,788.453693822171,110.282587021203));
#83126=CARTESIAN_POINT('Ctrl Pts',(32.4178161094536,788.418517849253,110.270154642165));
#83127=CARTESIAN_POINT('Ctrl Pts',(32.4978789650267,788.383983087561,110.257948888871));
#83128=CARTESIAN_POINT('Ctrl Pts',(32.5781960071056,788.35015014966,110.24599118385));
#83129=CARTESIAN_POINT('Ctrl Pts',(32.8339631335456,788.242410209518,110.207912243532));
#83130=CARTESIAN_POINT('Ctrl Pts',(33.0922962422252,788.141755327546,110.1723374025));
#83131=CARTESIAN_POINT('Ctrl Pts',(33.354286616325,788.051195694031,110.140330563854));
#83132=CARTESIAN_POINT('Ctrl Pts',(33.4778110484393,788.008498219588,110.12523983168));
#83133=CARTESIAN_POINT('Ctrl Pts',(33.6021510102252,787.968051834242,110.110944710562));
#83134=CARTESIAN_POINT('Ctrl Pts',(33.7274682578125,787.930302473205,110.097602809089));
#83135=CARTESIAN_POINT('Ctrl Pts',(33.8679812561842,787.887975690515,110.082643091924));
#83136=CARTESIAN_POINT('Ctrl Pts',(34.0096692762972,787.849054278572,110.068886948005));
#83137=CARTESIAN_POINT('Ctrl Pts',(34.1528056083597,787.814150653876,110.056550826044));
#83138=CARTESIAN_POINT('Ctrl Pts',(34.2882334261246,787.781126741243,110.044879057927));
#83139=CARTESIAN_POINT('Ctrl Pts',(34.424967282988,787.751725783049,110.034487764496));
#83140=CARTESIAN_POINT('Ctrl Pts',(34.563207601984,787.726381449949,110.025530219632));
#83141=CARTESIAN_POINT('Ctrl Pts',(34.7013791320057,787.701049728298,110.01657713208));
#83142=CARTESIAN_POINT('Ctrl Pts',(34.8410619689514,787.679788099456,110.009062553043));
#83143=CARTESIAN_POINT('Ctrl Pts',(34.9823190110975,787.662651728054,110.003005979566));
#83144=CARTESIAN_POINT('Ctrl Pts',(35.054858148777,787.653851758966,109.999895772735));
#83145=CARTESIAN_POINT('Ctrl Pts',(35.1279311989363,787.646134864626,109.997168361168));
#83146=CARTESIAN_POINT('Ctrl Pts',(35.201196182069,787.639458454135,109.994808691798));
#83147=CARTESIAN_POINT('Ctrl Pts',(35.2704926162082,787.633143685196,109.99257683879));
#83148=CARTESIAN_POINT('Ctrl Pts',(35.3399150435733,787.627763108406,109.990675160896));
#83149=CARTESIAN_POINT('Ctrl Pts',(35.40917327038,787.623277492044,109.989089792298));
#83150=CARTESIAN_POINT('Ctrl Pts',(35.5517549337684,787.61404296971,109.985825999648));
#83151=CARTESIAN_POINT('Ctrl Pts',(35.6940149178129,787.608502739353,109.983867894781));
#83152=CARTESIAN_POINT('Ctrl Pts',(35.8360475033717,787.605830235265,109.98292334141));
#83153=CARTESIAN_POINT('Ctrl Pts',(36.0908674215757,787.601035509672,109.981228723152));
#83154=CARTESIAN_POINT('Ctrl Pts',(36.3449657656687,787.605316731778,109.982741851903));
#83155=CARTESIAN_POINT('Ctrl Pts',(36.5987997780528,787.6151913345,109.98623187062));
#83156=CARTESIAN_POINT('Ctrl Pts',(36.6280676541629,787.616329907879,109.986634280977));
#83157=CARTESIAN_POINT('Ctrl Pts',(36.6573320118389,787.617542895409,109.987062991812));
#83158=CARTESIAN_POINT('Ctrl Pts',(36.686593549319,787.618824991082,109.987516127804));
#83159=CARTESIAN_POINT('Ctrl Pts',(36.6986198925109,787.619351925889,109.987702364394));
#83160=CARTESIAN_POINT('Ctrl Pts',(36.7106457504267,787.61989066731,109.987892773841));
#83161=CARTESIAN_POINT('Ctrl Pts',(36.7226711608112,787.620441007396,109.988087282649));
#83162=CARTESIAN_POINT('Ctrl Pts',(36.9935849295287,787.632839312507,109.992469263181));
#83163=CARTESIAN_POINT('Ctrl Pts',(37.2641062977475,787.651109175024,109.998926450771));
#83164=CARTESIAN_POINT('Ctrl Pts',(37.5343966207417,787.67283391909,110.006604710399));
#83165=CARTESIAN_POINT('Ctrl Pts',(37.7681335687267,787.691620664088,110.013244581747));
#83166=CARTESIAN_POINT('Ctrl Pts',(38.0016954672153,787.713024821358,110.020809535154));
#83167=CARTESIAN_POINT('Ctrl Pts',(38.2351440760971,787.736118419525,110.028971594138));
#83168=CARTESIAN_POINT('Ctrl Pts',(38.2836351952192,787.740915340034,110.030666988154));
#83169=CARTESIAN_POINT('Ctrl Pts',(38.3321214618988,787.745785478162,110.032388259753));
#83170=CARTESIAN_POINT('Ctrl Pts',(38.3806034200487,787.750720481976,110.034132457081));
#83171=CARTESIAN_POINT('Ctrl Pts',(38.6624894118298,787.779413804146,110.044273647999));
#83172=CARTESIAN_POINT('Ctrl Pts',(38.9442281267435,787.810323481981,110.055198174001));
#83173=CARTESIAN_POINT('Ctrl Pts',(39.2258874928907,787.842397522499,110.066534225172));
#83174=CARTESIAN_POINT('Ctrl Pts',(39.3986909004619,787.86207555974,110.073489109356));
#83175=CARTESIAN_POINT('Ctrl Pts',(39.5714666607601,787.882176445889,110.080593442651));
#83176=CARTESIAN_POINT('Ctrl Pts',(39.7442240872993,787.902559549599,110.087797521182));
#83177=CARTESIAN_POINT('Ctrl Pts',(17.244803233355,778.140660313945,108.758852681557));
#83178=CARTESIAN_POINT('Ctrl Pts',(17.4302427942975,778.017216179823,108.715223348388));
#83179=CARTESIAN_POINT('Ctrl Pts',(17.6161195650913,777.895023168326,108.672035343682));
#83180=CARTESIAN_POINT('Ctrl Pts',(17.8025176283173,777.773958439212,108.629218349539));
#83181=CARTESIAN_POINT('Ctrl Pts',(17.9870250009404,777.654121705398,108.586835660812));
#83182=CARTESIAN_POINT('Ctrl Pts',(18.1720429482635,777.535390196698,108.544816419935));
#83183=CARTESIAN_POINT('Ctrl Pts',(18.3576213362097,777.417677845536,108.503114059011));
#83184=CARTESIAN_POINT('Ctrl Pts',(18.5421857868206,777.300608634714,108.461639545635));
#83185=CARTESIAN_POINT('Ctrl Pts',(18.7273043691045,777.184547269975,108.420478415007));
#83186=CARTESIAN_POINT('Ctrl Pts',(18.912997562236,777.069445629894,108.379607264944));
#83187=CARTESIAN_POINT('Ctrl Pts',(19.1038171142841,776.951166424126,108.337607801123));
#83188=CARTESIAN_POINT('Ctrl Pts',(19.2952433373739,776.833900304558,108.295914413569));
#83189=CARTESIAN_POINT('Ctrl Pts',(19.4872703008399,776.717638363243,108.254526995366));
#83190=CARTESIAN_POINT('Ctrl Pts',(19.6751476855667,776.603888767441,108.214033932558));
#83191=CARTESIAN_POINT('Ctrl Pts',(19.8635997887069,776.491100501578,108.173833868963));
#83192=CARTESIAN_POINT('Ctrl Pts',(20.052598145976,776.379307612994,108.133950440718));
#83193=CARTESIAN_POINT('Ctrl Pts',(20.2478580091165,776.263811031752,108.092745676544));
#83194=CARTESIAN_POINT('Ctrl Pts',(20.4437007248949,776.149376625192,108.051878811667));
#83195=CARTESIAN_POINT('Ctrl Pts',(20.6400739635806,776.036089498082,108.01140147736));
#83196=CARTESIAN_POINT('Ctrl Pts',(20.8364472022663,775.922802370972,107.970924143053));
#83197=CARTESIAN_POINT('Ctrl Pts',(21.0333506142589,775.810662609105,107.93083646242));
#83198=CARTESIAN_POINT('Ctrl Pts',(21.230715589858,775.69980296013,107.891214563218));
#83199=CARTESIAN_POINT('Ctrl Pts',(21.4510621334662,775.576034594425,107.846979011728));
#83200=CARTESIAN_POINT('Ctrl Pts',(21.6721167421861,775.453725728634,107.803275358442));
#83201=CARTESIAN_POINT('Ctrl Pts',(21.8938661721106,775.332765884813,107.760111498484));
#83202=CARTESIAN_POINT('Ctrl Pts',(22.1268288785303,775.205689424709,107.714764957397));
#83203=CARTESIAN_POINT('Ctrl Pts',(22.3605582172284,775.080102215295,107.670014400197));
#83204=CARTESIAN_POINT('Ctrl Pts',(22.5950407446481,774.955928755215,107.625894992143));
#83205=CARTESIAN_POINT('Ctrl Pts',(22.8503193797093,774.820742429185,107.577862661582));
#83206=CARTESIAN_POINT('Ctrl Pts',(23.1064903655798,774.687231914115,107.53057856877));
#83207=CARTESIAN_POINT('Ctrl Pts',(23.3635434284907,774.555356825587,107.48411523043));
#83208=CARTESIAN_POINT('Ctrl Pts',(23.6348421915746,774.416173312291,107.435076926519));
#83209=CARTESIAN_POINT('Ctrl Pts',(23.9071230928796,774.278812126388,107.386953297135));
#83210=CARTESIAN_POINT('Ctrl Pts',(24.1803878516845,774.143279983621,107.339853560423));
#83211=CARTESIAN_POINT('Ctrl Pts',(24.476664170325,773.9963347116,107.288787566174));
#83212=CARTESIAN_POINT('Ctrl Pts',(24.7740963725344,773.851540100502,107.238925693366));
#83213=CARTESIAN_POINT('Ctrl Pts',(25.0727111866745,773.708957217398,107.190427006648));
#83214=CARTESIAN_POINT('Ctrl Pts',(25.1730175253031,773.661062852222,107.174136034257));
#83215=CARTESIAN_POINT('Ctrl Pts',(25.2734575369564,773.613418408341,107.157998991203));
#83216=CARTESIAN_POINT('Ctrl Pts',(25.3740329818863,773.566027188085,107.142022184744));
#83217=CARTESIAN_POINT('Ctrl Pts',(25.6843444268857,773.419808217358,107.092727986718));
#83218=CARTESIAN_POINT('Ctrl Pts',(25.9959755695988,773.2758580971,107.04490895962));
#83219=CARTESIAN_POINT('Ctrl Pts',(26.3088451966942,773.134131453208,106.998692394593));
#83220=CARTESIAN_POINT('Ctrl Pts',(26.6298522170826,772.988718655909,106.951273787776));
#83221=CARTESIAN_POINT('Ctrl Pts',(26.9521628990224,772.8456475125,106.905542763938));
#83222=CARTESIAN_POINT('Ctrl Pts',(27.2757410475479,772.704884152336,106.861629835336));
#83223=CARTESIAN_POINT('Ctrl Pts',(27.5998714259456,772.563880560462,106.817641963384));
#83224=CARTESIAN_POINT('Ctrl Pts',(27.9252738053818,772.425193467478,106.775478905283));
#83225=CARTESIAN_POINT('Ctrl Pts',(28.2519616068956,772.288789746552,106.735255966003));
#83226=CARTESIAN_POINT('Ctrl Pts',(28.5781188910106,772.152607535418,106.695098345872));
#83227=CARTESIAN_POINT('Ctrl Pts',(28.9055577145741,772.018701882974,106.656874901712));
#83228=CARTESIAN_POINT('Ctrl Pts',(29.2343372719155,771.887030087691,106.620678159765));
#83229=CARTESIAN_POINT('Ctrl Pts',(29.3798300670145,771.828762178073,106.604660238207));
#83230=CARTESIAN_POINT('Ctrl Pts',(29.5255859903457,771.770931537783,106.589038877081));
#83231=CARTESIAN_POINT('Ctrl Pts',(29.6716128056531,771.71353344704,106.573820461869));
#83232=CARTESIAN_POINT('Ctrl Pts',(29.98499083181,771.590355383173,106.54116127588));
#83233=CARTESIAN_POINT('Ctrl Pts',(30.2996186961208,771.469154223282,106.510354321007));
#83234=CARTESIAN_POINT('Ctrl Pts',(30.6154250134758,771.349953382847,106.48146631183));
#83235=CARTESIAN_POINT('Ctrl Pts',(30.9329624820416,771.230099120781,106.452419947644));
#83236=CARTESIAN_POINT('Ctrl Pts',(31.2516915141686,771.112267420327,106.425313820703));
#83237=CARTESIAN_POINT('Ctrl Pts',(31.5715845956891,770.996474616581,106.400189136909));
#83238=CARTESIAN_POINT('Ctrl Pts',(31.8930543690029,770.88011109226,106.374940618357));
#83239=CARTESIAN_POINT('Ctrl Pts',(32.2156998911378,770.765806805995,106.351693262802));
#83240=CARTESIAN_POINT('Ctrl Pts',(32.5395359463363,770.653567465855,106.330459565991));
#83241=CARTESIAN_POINT('Ctrl Pts',(32.8669620803978,770.540083829177,106.308990470297));
#83242=CARTESIAN_POINT('Ctrl Pts',(33.1956054823697,770.428711338438,106.289580054316));
#83243=CARTESIAN_POINT('Ctrl Pts',(33.5255221042312,770.319442106759,106.272209275265));
#83244=CARTESIAN_POINT('Ctrl Pts',(33.7242078623965,770.253636873856,106.261748067259));
#83245=CARTESIAN_POINT('Ctrl Pts',(33.9233561640316,770.188594174724,106.252025971253));
#83246=CARTESIAN_POINT('Ctrl Pts',(34.1229857448722,770.124309587169,106.243033090213));
#83247=CARTESIAN_POINT('Ctrl Pts',(34.4053309678074,770.03338896244,106.230314048319));
#83248=CARTESIAN_POINT('Ctrl Pts',(34.6888310896164,769.943954899535,106.219056503782));
#83249=CARTESIAN_POINT('Ctrl Pts',(34.9731646028604,769.856111120652,106.209232445828));
#83250=CARTESIAN_POINT('Ctrl Pts',(35.2621382182265,769.766833799519,106.199248066878));
#83251=CARTESIAN_POINT('Ctrl Pts',(35.551972690203,769.679199164546,106.190744375241));
#83252=CARTESIAN_POINT('Ctrl Pts',(35.8423794454014,769.593326894789,106.18367117377));
#83253=CARTESIAN_POINT('Ctrl Pts',(36.0301478417598,769.53780443157,106.179097851444));
#83254=CARTESIAN_POINT('Ctrl Pts',(36.2181564792175,769.483018947022,106.175122122085));
#83255=CARTESIAN_POINT('Ctrl Pts',(36.4063377647076,769.429004905351,106.171725880262));
#83256=CARTESIAN_POINT('Ctrl Pts',(36.7463662342535,769.331405870062,106.16558914405));
#83257=CARTESIAN_POINT('Ctrl Pts',(37.0867097552781,769.236368553691,106.161342180024));
#83258=CARTESIAN_POINT('Ctrl Pts',(37.4273506666537,769.143933968207,106.158823323891));
#83259=CARTESIAN_POINT('Ctrl Pts',(37.7829651679578,769.047436225504,106.156193746122));
#83260=CARTESIAN_POINT('Ctrl Pts',(38.1389040062214,768.953775170179,106.155447471501));
#83261=CARTESIAN_POINT('Ctrl Pts',(38.4951922026422,768.862988805248,106.156367580926));
#83262=CARTESIAN_POINT('Ctrl Pts',(38.5660483213149,768.844933844371,106.15655056589));
#83263=CARTESIAN_POINT('Ctrl Pts',(38.6369183876645,768.826992549612,106.156799359364));
#83264=CARTESIAN_POINT('Ctrl Pts',(38.7078027855985,768.809165175802,106.157112113951));
#83265=CARTESIAN_POINT('Ctrl Pts',(39.0660941928767,768.71905515108,106.158692959443));
#83266=CARTESIAN_POINT('Ctrl Pts',(39.4247842952702,768.631843714424,106.161909448324));
#83267=CARTESIAN_POINT('Ctrl Pts',(39.7838264747246,768.54761783095,106.166513137719));
#83268=CARTESIAN_POINT('Ctrl Pts',(40.1704981466507,768.456910485,106.171471096358));
#83269=CARTESIAN_POINT('Ctrl Pts',(40.5575782622505,768.36966600186,106.178037739708));
#83270=CARTESIAN_POINT('Ctrl Pts',(40.9450618818424,768.285989009415,106.185873456951));
#83271=CARTESIAN_POINT('Ctrl Pts',(41.3721816802832,768.193752593886,106.194510699404));
#83272=CARTESIAN_POINT('Ctrl Pts',(41.7997918445297,768.105851072209,106.204689398667));
#83273=CARTESIAN_POINT('Ctrl Pts',(42.2279470420453,768.022416903132,106.215926170645));
#83274=CARTESIAN_POINT('Ctrl Pts',(42.5983746669712,767.950232047574,106.225647904212));
#83275=CARTESIAN_POINT('Ctrl Pts',(42.9692116538452,767.881391015369,106.236160711799));
#83276=CARTESIAN_POINT('Ctrl Pts',(43.3405227698438,767.815973740261,106.247143043839));
#83277=CARTESIAN_POINT('Ctrl Pts',(43.7894092447679,767.73688930471,106.260419835465));
#83278=CARTESIAN_POINT('Ctrl Pts',(44.2389602380122,767.662833944119,106.274384781587));
#83279=CARTESIAN_POINT('Ctrl Pts',(44.6891574273935,767.594001659024,106.288473974073));
#83280=CARTESIAN_POINT('Ctrl Pts',(45.1319036972893,767.5263085721,106.302329985541));
#83281=CARTESIAN_POINT('Ctrl Pts',(45.5752759585645,767.463667274342,106.316304786023));
#83282=CARTESIAN_POINT('Ctrl Pts',(46.0192976440156,767.406257685716,106.329888910912));
#83283=CARTESIAN_POINT('Ctrl Pts',(46.4363813545946,767.352331030709,106.342648912056));
#83284=CARTESIAN_POINT('Ctrl Pts',(46.8540388223096,767.303020623235,106.355063538047));
#83285=CARTESIAN_POINT('Ctrl Pts',(47.2723132478599,767.258469809936,106.366748379134));
#83286=CARTESIAN_POINT('Ctrl Pts',(47.5207984325909,767.232003412766,106.37369001773));
#83287=CARTESIAN_POINT('Ctrl Pts',(47.7695017500408,767.207216663347,106.380374877173));
#83288=CARTESIAN_POINT('Ctrl Pts',(48.0184352890197,767.184138393967,106.386730603336));
#83289=CARTESIAN_POINT('Ctrl Pts',(48.4103491489587,767.14780462524,106.396736877234));
#83290=CARTESIAN_POINT('Ctrl Pts',(48.8028254789344,767.115718004464,106.405926142084));
#83291=CARTESIAN_POINT('Ctrl Pts',(49.1958617553921,767.087969142023,106.414049755935));
#83292=CARTESIAN_POINT('Ctrl Pts',(49.5712128370626,767.061468876891,106.421807836878));
#83293=CARTESIAN_POINT('Ctrl Pts',(49.9470747019511,767.038924816821,106.428593946834));
#83294=CARTESIAN_POINT('Ctrl Pts',(50.32345337455,767.020411253827,106.434239309414));
#83295=CARTESIAN_POINT('Ctrl Pts',(50.6934444934781,767.002211886047,106.439788864078));
#83296=CARTESIAN_POINT('Ctrl Pts',(51.0639350090242,766.987907416256,106.444235893158));
#83297=CARTESIAN_POINT('Ctrl Pts',(51.4349383309662,766.97756326832,106.44746932169));
#83298=CARTESIAN_POINT('Ctrl Pts',(51.799639404856,766.967394836832,106.450647823845));
#83299=CARTESIAN_POINT('Ctrl Pts',(52.1648359513474,766.961053359176,106.452653536912));
#83300=CARTESIAN_POINT('Ctrl Pts',(52.5305487998093,766.958595366651,106.453430683641));
#83301=CARTESIAN_POINT('Ctrl Pts',(52.6032085014127,766.95810701355,106.453585086883));
#83302=CARTESIAN_POINT('Ctrl Pts',(52.6758886111045,766.957771936566,106.453691155307));
#83303=CARTESIAN_POINT('Ctrl Pts',(52.7485893348995,766.957590550071,106.453748693095));
#83304=CARTESIAN_POINT('Ctrl Pts',(52.7916024730424,766.957483233362,106.453782735133));
#83305=CARTESIAN_POINT('Ctrl Pts',(52.8346226593573,766.957429629665,106.453799778285));
#83306=CARTESIAN_POINT('Ctrl Pts',(52.8776498831824,766.957429760005,106.453799787005));
#83307=CARTESIAN_POINT('Ctrl Pts',(53.2527766899241,766.957430896356,106.453799863031));
#83308=CARTESIAN_POINT('Ctrl Pts',(53.6284390702103,766.961516813679,106.452500231006));
#83309=CARTESIAN_POINT('Ctrl Pts',(54.0046343511746,766.969707371652,106.4499239518));
#83310=CARTESIAN_POINT('Ctrl Pts',(54.380829632139,766.977897929626,106.447347672594));
#83311=CARTESIAN_POINT('Ctrl Pts',(54.7575577055266,766.990193160191,106.44349480217));
#83312=CARTESIAN_POINT('Ctrl Pts',(55.1348251867634,767.006606943788,106.438447973463));
#83313=CARTESIAN_POINT('Ctrl Pts',(55.4561641097655,767.020587442521,106.434149319108));
#83314=CARTESIAN_POINT('Ctrl Pts',(55.7778622926501,767.037583043997,106.428988897936));
#83315=CARTESIAN_POINT('Ctrl Pts',(56.0993921197504,767.057497379615,106.423055564023));
#83316=CARTESIAN_POINT('Ctrl Pts',(56.4262826167593,767.077743734757,106.417023307267));
#83317=CARTESIAN_POINT('Ctrl Pts',(56.7529993434126,767.101006852348,106.410192320713));
#83318=CARTESIAN_POINT('Ctrl Pts',(57.0789741399141,767.12720391569,106.402704938146));
#83319=CARTESIAN_POINT('Ctrl Pts',(57.228415709256,767.139213832715,106.39927238381));
#83320=CARTESIAN_POINT('Ctrl Pts',(57.3777011350278,767.151840645628,106.395702527817));
#83321=CARTESIAN_POINT('Ctrl Pts',(57.5267745005702,767.16507773094,106.392012248412));
#83322=CARTESIAN_POINT('Ctrl Pts',(57.9483269317961,767.202509806585,106.381576807787));
#83323=CARTESIAN_POINT('Ctrl Pts',(58.3687655186023,767.244817320047,106.370151825623));
#83324=CARTESIAN_POINT('Ctrl Pts',(58.7881688820604,767.291834998808,106.358094002693));
#83325=CARTESIAN_POINT('Ctrl Pts',(59.2221899539139,767.340491411964,106.345615921474));
#83326=CARTESIAN_POINT('Ctrl Pts',(59.6551028890472,767.394191898677,106.332460922299));
#83327=CARTESIAN_POINT('Ctrl Pts',(60.0869645521638,767.452745062953,106.319073080512));
#83328=CARTESIAN_POINT('Ctrl Pts',(60.5251884576043,767.512160840079,106.305488007294));
#83329=CARTESIAN_POINT('Ctrl Pts',(60.9623305926084,767.576573131153,106.29166436926));
#83330=CARTESIAN_POINT('Ctrl Pts',(61.3984106399046,767.645776298645,106.278099940895));
#83331=CARTESIAN_POINT('Ctrl Pts',(61.6818255091146,767.690752460212,106.269284218381));
#83332=CARTESIAN_POINT('Ctrl Pts',(61.9647909508895,767.737752127751,106.26057863376));
#83333=CARTESIAN_POINT('Ctrl Pts',(62.2473011154386,767.786718213586,106.252123551089));
#83334=CARTESIAN_POINT('Ctrl Pts',(62.6665970293828,767.859392695035,106.23957468715));
#83335=CARTESIAN_POINT('Ctrl Pts',(63.0848727254616,767.936378587464,106.227575522707));
#83336=CARTESIAN_POINT('Ctrl Pts',(63.5022363713141,768.017536835016,106.216582523638));
#83337=CARTESIAN_POINT('Ctrl Pts',(63.8968659205552,768.094274334717,106.206188321098));
#83338=CARTESIAN_POINT('Ctrl Pts',(64.2906803943568,768.174741854941,106.1966943297));
#83339=CARTESIAN_POINT('Ctrl Pts',(64.6837303810336,768.258815228337,106.188472833452));
#83340=CARTESIAN_POINT('Ctrl Pts',(65.0524210672923,768.337678148536,106.18076086501));
#83341=CARTESIAN_POINT('Ctrl Pts',(65.4204392441859,768.419713694752,106.174168906627));
#83342=CARTESIAN_POINT('Ctrl Pts',(65.7877865032849,768.504815487676,106.168985000604));
#83343=CARTESIAN_POINT('Ctrl Pts',(66.1551337623839,768.589917280599,106.163801094582));
#83344=CARTESIAN_POINT('Ctrl Pts',(66.5218106947982,768.67808522904,106.160025715033));
#83345=CARTESIAN_POINT('Ctrl Pts',(66.8877713295124,768.769210484844,106.157920728899));
#83346=CARTESIAN_POINT('Ctrl Pts',(67.2493508831965,768.859244838809,106.15584094251));
#83347=CARTESIAN_POINT('Ctrl Pts',(67.6102184648288,768.95214837915,106.155388024597));
#83348=CARTESIAN_POINT('Ctrl Pts',(67.9704601261528,769.047897806214,106.15679353994));
#83349=CARTESIAN_POINT('Ctrl Pts',(68.313064781029,769.138959454368,106.158130242911));
#83350=CARTESIAN_POINT('Ctrl Pts',(68.6551034662053,769.232595028966,106.161147869937));
#83351=CARTESIAN_POINT('Ctrl Pts',(68.9966145154768,769.328774634844,106.166016326262));
#83352=CARTESIAN_POINT('Ctrl Pts',(69.3301256614168,769.422701231482,106.170770738898));
#83353=CARTESIAN_POINT('Ctrl Pts',(69.6631338605876,769.519053985963,106.177290356695));
#83354=CARTESIAN_POINT('Ctrl Pts',(69.995636649277,769.617796797526,106.185704017807));
#83355=CARTESIAN_POINT('Ctrl Pts',(70.3185030507481,769.713677906873,106.193873839471));
#83356=CARTESIAN_POINT('Ctrl Pts',(70.6408930762567,769.811812450673,106.203829498684));
#83357=CARTESIAN_POINT('Ctrl Pts',(70.9627650543597,769.912160796529,106.21566052958));
#83358=CARTESIAN_POINT('Ctrl Pts',(71.1279096933335,769.963647078266,106.221730742145));
#83359=CARTESIAN_POINT('Ctrl Pts',(71.2929172974997,770.01571603625,106.228294174781));
#83360=CARTESIAN_POINT('Ctrl Pts',(71.4577778171004,770.068361747236,106.235359916851));
#83361=CARTESIAN_POINT('Ctrl Pts',(71.7847090879655,770.172762298928,106.249371834562));
#83362=CARTESIAN_POINT('Ctrl Pts',(72.111113040878,770.279454187517,106.26536517023));
#83363=CARTESIAN_POINT('Ctrl Pts',(72.437015064023,770.388454389171,106.283403068439));
#83364=CARTESIAN_POINT('Ctrl Pts',(72.755745340328,770.495055950141,106.301044027599));
#83365=CARTESIAN_POINT('Ctrl Pts',(73.0739957493183,770.603865216048,106.320640490581));
#83366=CARTESIAN_POINT('Ctrl Pts',(73.3917516221727,770.714885580109,106.342222081288));
#83367=CARTESIAN_POINT('Ctrl Pts',(73.5005165936022,770.75288685013,106.349609265278));
#83368=CARTESIAN_POINT('Ctrl Pts',(73.6092232721889,770.791147079065,106.357228779375));
#83369=CARTESIAN_POINT('Ctrl Pts',(73.717869934504,770.829666103205,106.365081018644));
#83370=CARTESIAN_POINT('Ctrl Pts',(73.9939731299839,770.927554298068,106.385035873287));
#83371=CARTESIAN_POINT('Ctrl Pts',(74.2698322480944,771.027190750308,106.406514466711));
#83372=CARTESIAN_POINT('Ctrl Pts',(74.5451525422015,771.128450377454,106.42948314097));
#83373=CARTESIAN_POINT('Ctrl Pts',(74.8190712176449,771.22919450543,106.452334884791));
#83374=CARTESIAN_POINT('Ctrl Pts',(75.0924565785729,771.331545169713,106.476661452536));
#83375=CARTESIAN_POINT('Ctrl Pts',(75.3649710421158,771.435390477115,106.502412606952));
#83376=CARTESIAN_POINT('Ctrl Pts',(75.5631914758016,771.510925043617,106.521143374229));
#83377=CARTESIAN_POINT('Ctrl Pts',(75.7609501554619,771.587250611355,106.540627487359));
#83378=CARTESIAN_POINT('Ctrl Pts',(75.95810121129,771.664328638783,106.560840536383));
#83379=CARTESIAN_POINT('Ctrl Pts',(76.2903210760871,771.79421306544,106.594901608922));
#83380=CARTESIAN_POINT('Ctrl Pts',(76.6210076059917,771.926275982453,106.631041202677));
#83381=CARTESIAN_POINT('Ctrl Pts',(76.9502435149238,772.060562462679,106.66917485183));
#83382=CARTESIAN_POINT('Ctrl Pts',(77.2812602282517,772.195575285166,106.707514762111));
#83383=CARTESIAN_POINT('Ctrl Pts',(77.6108109014645,772.332835291012,106.747870059369));
#83384=CARTESIAN_POINT('Ctrl Pts',(77.938935474115,772.472374376002,106.790129678487));
#83385=CARTESIAN_POINT('Ctrl Pts',(78.266895980731,772.611843689855,106.832368167314));
#83386=CARTESIAN_POINT('Ctrl Pts',(78.5934320342002,772.753589087331,106.87650862444));
#83387=CARTESIAN_POINT('Ctrl Pts',(78.918535562098,772.897637659967,106.922420647974));
#83388=CARTESIAN_POINT('Ctrl Pts',(79.2380344310416,773.03920289098,106.967541165997));
#83389=CARTESIAN_POINT('Ctrl Pts',(79.5561497471268,773.182991674586,107.014372093433));
#83390=CARTESIAN_POINT('Ctrl Pts',(79.872826046708,773.32903705898,107.062778666628));
#83391=CARTESIAN_POINT('Ctrl Pts',(80.0205711758635,773.397174441564,107.085362723023));
#83392=CARTESIAN_POINT('Ctrl Pts',(80.1680023906269,773.465803200904,107.108289644626));
#83393=CARTESIAN_POINT('Ctrl Pts',(80.3151104245496,773.53492818077,107.131545519252));
#83394=CARTESIAN_POINT('Ctrl Pts',(80.6192289859328,773.677831249161,107.179622724464));
#83395=CARTESIAN_POINT('Ctrl Pts',(80.9220023028729,773.822986743339,107.229153229747));
#83396=CARTESIAN_POINT('Ctrl Pts',(81.2234700330845,773.970314254708,107.27996471884));
#83397=CARTESIAN_POINT('Ctrl Pts',(81.5008857271214,774.10588751752,107.326722308788));
#83398=CARTESIAN_POINT('Ctrl Pts',(81.7771952718529,774.243299530907,107.374564166958));
#83399=CARTESIAN_POINT('Ctrl Pts',(82.052408977665,774.382524341856,107.423368824163));
#83400=CARTESIAN_POINT('Ctrl Pts',(82.306318838869,774.510971987005,107.468395592364));
#83401=CARTESIAN_POINT('Ctrl Pts',(82.5592955474459,774.640962327582,107.514241591404));
#83402=CARTESIAN_POINT('Ctrl Pts',(82.8113354824272,774.772513053793,107.560827758554));
#83403=CARTESIAN_POINT('Ctrl Pts',(83.0511584124714,774.897687187852,107.605155777866));
#83404=CARTESIAN_POINT('Ctrl Pts',(83.2901329115115,775.02427369952,107.65015367622));
#83405=CARTESIAN_POINT('Ctrl Pts',(83.528249378592,775.152328972771,107.695772667662));
#83406=CARTESIAN_POINT('Ctrl Pts',(83.7512300445672,775.272244451365,107.73849190173));
#83407=CARTESIAN_POINT('Ctrl Pts',(83.9734580736361,775.393447712216,107.781755638271));
#83408=CARTESIAN_POINT('Ctrl Pts',(84.1949231770313,775.516025956021,107.825543948619));
#83409=CARTESIAN_POINT('Ctrl Pts',(84.2966126723844,775.572309856115,107.845650101297));
#83410=CARTESIAN_POINT('Ctrl Pts',(84.3981413012444,775.628884255573,107.865867154406));
#83411=CARTESIAN_POINT('Ctrl Pts',(84.4995080719372,775.685760960997,107.886194872769));
#83412=CARTESIAN_POINT('Ctrl Pts',(84.6944224660258,775.795127062923,107.925282286531));
#83413=CARTESIAN_POINT('Ctrl Pts',(84.8888430390403,775.905714468591,107.964815559485));
#83414=CARTESIAN_POINT('Ctrl Pts',(85.0827036691784,776.017394830005,108.004720940244));
#83415=CARTESIAN_POINT('Ctrl Pts',(85.2743324103567,776.127789431823,108.044166896215));
#83416=CARTESIAN_POINT('Ctrl Pts',(85.4654137438478,776.239251980637,108.083976376863));
#83417=CARTESIAN_POINT('Ctrl Pts',(85.6558986329479,776.351701355677,108.124100247506));
#83418=CARTESIAN_POINT('Ctrl Pts',(85.8449854023638,776.463325375565,108.163929617237));
#83419=CARTESIAN_POINT('Ctrl Pts',(86.0334841976882,776.575921840707,108.204068743911));
#83420=CARTESIAN_POINT('Ctrl Pts',(86.2213657472959,776.689453432604,108.244492225632));
#83421=CARTESIAN_POINT('Ctrl Pts',(86.4146817443415,776.806268909854,108.286084950886));
#83422=CARTESIAN_POINT('Ctrl Pts',(86.6073438841338,776.924074263358,108.327978577234));
#83423=CARTESIAN_POINT('Ctrl Pts',(86.799345208022,777.042874482526,108.37017106729));
#83424=CARTESIAN_POINT('Ctrl Pts',(86.9860289092342,777.15838443928,108.411195004248));
#83425=CARTESIAN_POINT('Ctrl Pts',(87.1720877947107,777.274835274588,108.45250161709));
#83426=CARTESIAN_POINT('Ctrl Pts',(87.3575419166461,777.392271729837,108.49411256191));
#83427=CARTESIAN_POINT('Ctrl Pts',(87.5509199363648,777.514725892203,108.537501417461));
#83428=CARTESIAN_POINT('Ctrl Pts',(87.7436399756386,777.638251699538,108.581221070523));
#83429=CARTESIAN_POINT('Ctrl Pts',(87.9357584155001,777.762942100741,108.625322094426));
#83430=CARTESIAN_POINT('Ctrl Pts',(88.1278768553616,777.887632501944,108.66942311833));
#83431=CARTESIAN_POINT('Ctrl Pts',(88.3193935291358,778.013487920609,108.713905655094));
#83432=CARTESIAN_POINT('Ctrl Pts',(88.5104020101015,778.140638997398,108.758845147568));
#83433=CARTESIAN_POINT('Ctrl Pts',(73.5476386472354,788.511793322588,110.303121350496));
#83434=CARTESIAN_POINT('Ctrl Pts',(73.6485328417201,788.557253210302,110.319188412988));
#83435=CARTESIAN_POINT('Ctrl Pts',(73.7489162064673,788.603615273794,110.335574334926));
#83436=CARTESIAN_POINT('Ctrl Pts',(73.8487392078304,788.650697274009,110.352214706861));
#83437=CARTESIAN_POINT('Ctrl Pts',(74.1035309214589,788.770871015049,110.394688173126));
#83438=CARTESIAN_POINT('Ctrl Pts',(74.355266481156,788.896015030648,110.438918302596));
#83439=CARTESIAN_POINT('Ctrl Pts',(74.6047148824487,789.024747592744,110.484416745817));
#83440=CARTESIAN_POINT('Ctrl Pts',(74.7184820864584,789.083459308589,110.505167452757));
#83441=CARTESIAN_POINT('Ctrl Pts',(74.8317823705978,789.142903575577,110.526177068057));
#83442=CARTESIAN_POINT('Ctrl Pts',(74.9446503073713,789.203009286023,110.547420459854));
#83443=CARTESIAN_POINT('Ctrl Pts',(75.3267059948401,789.406465902505,110.61932891224));
#83444=CARTESIAN_POINT('Ctrl Pts',(75.7039441998201,789.617479744584,110.693908343871));
#83445=CARTESIAN_POINT('Ctrl Pts',(76.0780101827947,789.833468278297,110.77024599984));
#83446=CARTESIAN_POINT('Ctrl Pts',(76.1516852545629,789.876008823139,110.785281267783));
#83447=CARTESIAN_POINT('Ctrl Pts',(76.2252355766988,789.918744947225,110.800385660048));
#83448=CARTESIAN_POINT('Ctrl Pts',(76.2986648253408,789.961670797666,110.815557108025));
#83449=CARTESIAN_POINT('Ctrl Pts',(76.7081990718776,790.201079563819,110.900172266577));
#83450=CARTESIAN_POINT('Ctrl Pts',(77.1139902758252,790.446347379196,110.986858211375));
#83451=CARTESIAN_POINT('Ctrl Pts',(77.5167337817441,790.696396899066,111.075234172333));
#83452=CARTESIAN_POINT('Ctrl Pts',(77.9916855340511,790.991278022859,111.179455139034));
#83453=CARTESIAN_POINT('Ctrl Pts',(78.4624432629204,791.292761109192,111.286009462679));
#83454=CARTESIAN_POINT('Ctrl Pts',(78.9278568223611,791.602604685109,111.395518666228));
#83455=CARTESIAN_POINT('Ctrl Pts',(67.5289020028163,787.735242207091,110.028661911016));
#83456=CARTESIAN_POINT('Ctrl Pts',(67.7061220726526,787.717742978049,110.022477091371));
#83457=CARTESIAN_POINT('Ctrl Pts',(67.883445519993,787.70123378808,110.016642185034));
#83458=CARTESIAN_POINT('Ctrl Pts',(68.0609107392751,787.686085392946,110.011288229635));
#83459=CARTESIAN_POINT('Ctrl Pts',(68.2456467398798,787.670316365394,110.005714921739));
#83460=CARTESIAN_POINT('Ctrl Pts',(68.4305343439629,787.656002508816,110.000655920503));
#83461=CARTESIAN_POINT('Ctrl Pts',(68.6156463726316,787.643845166967,109.99635910454));
#83462=CARTESIAN_POINT('Ctrl Pts',(68.7149270954738,787.637324846838,109.994054602785));
#83463=CARTESIAN_POINT('Ctrl Pts',(68.8142727465984,787.631424983268,109.991969391373));
#83464=CARTESIAN_POINT('Ctrl Pts',(68.9136943681619,787.626253429796,109.990141589392));
#83465=CARTESIAN_POINT('Ctrl Pts',(69.1777263035479,787.612519442652,109.985287533634));
#83466=CARTESIAN_POINT('Ctrl Pts',(69.4422864352835,787.603850726593,109.982223716065));
#83467=CARTESIAN_POINT('Ctrl Pts',(69.7077490719245,787.603862578117,109.982227904797));
#83468=CARTESIAN_POINT('Ctrl Pts',(69.7286265902763,787.603863510189,109.982228234223));
#83469=CARTESIAN_POINT('Ctrl Pts',(69.749509735423,787.603918333592,109.982247610669));
#83470=CARTESIAN_POINT('Ctrl Pts',(69.7703986871635,787.604028793531,109.982286650949));
#83471=CARTESIAN_POINT('Ctrl Pts',(69.9136472752219,787.604786286317,109.982554374532));
#83472=CARTESIAN_POINT('Ctrl Pts',(70.0571734867388,787.608204434059,109.983762463599));
#83473=CARTESIAN_POINT('Ctrl Pts',(70.2010623316121,787.615102231534,109.986200378618));
#83474=CARTESIAN_POINT('Ctrl Pts',(70.344950365047,787.621999990109,109.988638279889));
#83475=CARTESIAN_POINT('Ctrl Pts',(70.4884664923808,787.632385806578,109.992308978842));
#83476=CARTESIAN_POINT('Ctrl Pts',(70.6305534917093,787.64679659127,109.997402237753));
#83477=CARTESIAN_POINT('Ctrl Pts',(70.6883193644943,787.65265533668,109.999472916616));
#83478=CARTESIAN_POINT('Ctrl Pts',(70.7458938079884,787.659184277743,110.0017804653));
#83479=CARTESIAN_POINT('Ctrl Pts',(70.8032735414792,787.666394845197,110.004328923814));
#83480=CARTESIAN_POINT('Ctrl Pts',(70.8870312365736,787.676920173105,110.008048930831));
#83481=CARTESIAN_POINT('Ctrl Pts',(70.9703735131096,787.688901299224,110.012283466193));
#83482=CARTESIAN_POINT('Ctrl Pts',(71.053289968927,787.702374152363,110.017045228358));
#83483=CARTESIAN_POINT('Ctrl Pts',(71.1930103788716,787.725076914381,110.025069152622));
#83484=CARTESIAN_POINT('Ctrl Pts',(71.3315243908326,787.752005750895,110.034586714605));
#83485=CARTESIAN_POINT('Ctrl Pts',(71.4689182867618,787.782858060651,110.045490964787));
#83486=CARTESIAN_POINT('Ctrl Pts',(71.6006684907306,787.812443058411,110.055947304028));
#83487=CARTESIAN_POINT('Ctrl Pts',(71.731393808425,787.845618024237,110.067672459454));
#83488=CARTESIAN_POINT('Ctrl Pts',(71.8612276196213,787.881917432482,110.080501898549));
#83489=CARTESIAN_POINT('Origin',(52.8776183915471,826.387310726428,123.689610751183));
#83490=CARTESIAN_POINT('Origin',(52.8776183915471,887.005734436498,147.235453418339));
#83491=CARTESIAN_POINT('Origin',(51.305620893586,644.631864177561,61.5723267466062));
#83492=CARTESIAN_POINT('Origin',(54.4496157591678,644.63186463643,61.5723269068127));
#83493=CARTESIAN_POINT('Ctrl Pts',(37.2974382339422,740.125373764374,98.7804136939922));
#83494=CARTESIAN_POINT('Ctrl Pts',(37.3237628811582,747.666799047464,98.7691088438472));
#83495=CARTESIAN_POINT('Ctrl Pts',(37.3500875283232,755.208224315958,98.7577942572374));
#83496=CARTESIAN_POINT('Ctrl Pts',(27.6328772087504,768.384899013174,105.310836543429));
#83497=CARTESIAN_POINT('Ctrl Pts',(20.0424170283973,772.22630491262,106.668519365511));
#83498=CARTESIAN_POINT('Ctrl Pts',(13.2983736491593,777.107328840337,108.39363837514));
#83499=CARTESIAN_POINT('Ctrl Pts',(39.7898595278376,740.125373764374,101.14718649664));
#83500=CARTESIAN_POINT('Ctrl Pts',(39.8138889156218,748.116327090208,101.129143881277));
#83501=CARTESIAN_POINT('Ctrl Pts',(39.8379148254437,756.107280410872,101.111093617291));
#83502=CARTESIAN_POINT('Ctrl Pts',(32.8646385077286,769.386484699126,105.664841346626));
#83503=CARTESIAN_POINT('Ctrl Pts',(26.4798669689934,773.811769470219,107.228876241329));
#83504=CARTESIAN_POINT('Ctrl Pts',(21.001327165595,779.233378063583,109.145056107309));
#83505=CARTESIAN_POINT('Ctrl Pts',(42.736298749677,740.125373764374,103.035135355334));
#83506=CARTESIAN_POINT('Ctrl Pts',(42.755886965038,748.454875736532,103.011405038338));
#83507=CARTESIAN_POINT('Ctrl Pts',(42.7754708329722,756.784377710745,102.987668638594));
#83508=CARTESIAN_POINT('Ctrl Pts',(37.9535726725575,770.177423028533,105.944387022298));
#83509=CARTESIAN_POINT('Ctrl Pts',(33.0087739196395,775.040601634335,107.663187140576));
#83510=CARTESIAN_POINT('Ctrl Pts',(28.8582165463779,780.867648688703,109.722662643155));
#83511=CARTESIAN_POINT('Ctrl Pts',(46.0036740905127,740.125373764374,104.339521951214));
#83512=CARTESIAN_POINT('Ctrl Pts',(46.0173362984446,748.681509910258,104.311576914651));
#83513=CARTESIAN_POINT('Ctrl Pts',(46.0309950284494,757.237646063144,104.283626839249));
#83514=CARTESIAN_POINT('Ctrl Pts',(42.9549332988076,770.72138911218,106.136638421123));
#83515=CARTESIAN_POINT('Ctrl Pts',(39.6062998281129,775.87648417527,107.958616329378));
#83516=CARTESIAN_POINT('Ctrl Pts',(36.8253774496378,781.973823505111,110.113622251634));
#83517=CARTESIAN_POINT('Ctrl Pts',(49.4406462410299,740.125373764373,104.999846187002));
#83518=CARTESIAN_POINT('Ctrl Pts',(49.4475586845128,748.795294535209,104.969582331416));
#83519=CARTESIAN_POINT('Ctrl Pts',(49.4544693890487,757.465215315637,104.93931395894));
#83520=CARTESIAN_POINT('Ctrl Pts',(47.9163263691371,770.996800169048,106.233970753627));
#83521=CARTESIAN_POINT('Ctrl Pts',(46.2419590292789,776.297841971512,108.107538433704));
#83522=CARTESIAN_POINT('Ctrl Pts',(44.8514979205924,782.530327410416,110.31030956155));
#83523=CARTESIAN_POINT('Ctrl Pts',(56.3145905420643,740.125373764374,104.999846187002));
#83524=CARTESIAN_POINT('Ctrl Pts',(56.3076780985813,748.79529453521,104.969582331416));
#83525=CARTESIAN_POINT('Ctrl Pts',(56.3007673941054,757.465215315951,104.939313958926));
#83526=CARTESIAN_POINT('Ctrl Pts',(57.8390941374472,770.996830883562,106.233968426735));
#83527=CARTESIAN_POINT('Ctrl Pts',(59.5132774609024,776.297842047978,108.107538445034));
#83528=CARTESIAN_POINT('Ctrl Pts',(60.9037388625016,782.530327410416,110.31030956155));
#83529=CARTESIAN_POINT('Ctrl Pts',(59.7515626925815,740.125373764374,104.339521951214));
#83530=CARTESIAN_POINT('Ctrl Pts',(59.7379004846479,748.681509910457,104.311576914657));
#83531=CARTESIAN_POINT('Ctrl Pts',(59.7242417546954,757.237646064166,104.283626839233));
#83532=CARTESIAN_POINT('Ctrl Pts',(62.8004688354278,770.721450541208,106.136633767339));
#83533=CARTESIAN_POINT('Ctrl Pts',(66.1489366913599,775.876484328201,107.958616352038));
#83534=CARTESIAN_POINT('Ctrl Pts',(68.9298593334563,781.973823505111,110.113622251634));
#83535=CARTESIAN_POINT('Ctrl Pts',(63.0189380334171,740.125373764374,103.035135355334));
#83536=CARTESIAN_POINT('Ctrl Pts',(62.9993498180528,748.454875736928,103.011405038351));
#83537=CARTESIAN_POINT('Ctrl Pts',(62.9797659501571,756.784377712319,102.987668638583));
#83538=CARTESIAN_POINT('Ctrl Pts',(67.8017927169798,770.177499814818,105.944381205068));
#83539=CARTESIAN_POINT('Ctrl Pts',(72.7464626584159,775.0406018255,107.663187168902));
#83540=CARTESIAN_POINT('Ctrl Pts',(76.8970202367163,780.867648688703,109.722662643155));
#83541=CARTESIAN_POINT('Ctrl Pts',(65.9653772552566,740.125373764374,101.14718649664));
#83542=CARTESIAN_POINT('Ctrl Pts',(65.9413478674689,748.116327090604,101.12914388129));
#83543=CARTESIAN_POINT('Ctrl Pts',(65.9173219576676,756.107280412289,101.111093617287));
#83544=CARTESIAN_POINT('Ctrl Pts',(72.8906717647615,769.386546128155,105.664836692843));
#83545=CARTESIAN_POINT('Ctrl Pts',(79.2753696969357,773.81176962315,107.228876263989));
#83546=CARTESIAN_POINT('Ctrl Pts',(84.7539096174991,779.233378063583,109.145056107309));
#83547=CARTESIAN_POINT('Ctrl Pts',(68.4577985491519,740.125373764374,98.7804136939922));
#83548=CARTESIAN_POINT('Ctrl Pts',(68.4314739019359,747.666799047464,98.7691088438472));
#83549=CARTESIAN_POINT('Ctrl Pts',(68.4051492547709,755.208224315958,98.7577942572374));
#83550=CARTESIAN_POINT('Ctrl Pts',(78.1223595743435,768.384899013174,105.310836543429));
#83551=CARTESIAN_POINT('Ctrl Pts',(85.7128197546968,772.22630491262,106.668519365511));
#83552=CARTESIAN_POINT('Ctrl Pts',(92.4568631339348,777.107328840337,108.39363837514));
#83553=CARTESIAN_POINT('Ctrl Pts',(61.1807573575412,737.487748923763,102.682654164686));
#83554=CARTESIAN_POINT('Ctrl Pts',(61.1807573575412,737.490646661967,103.444319534016));
#83555=CARTESIAN_POINT('Ctrl Pts',(61.8796042537708,737.489494249471,103.141409944702));
#83556=CARTESIAN_POINT('Ctrl Pts',(61.1807573575412,736.932983697653,102.684891852733));
#83557=CARTESIAN_POINT('Ctrl Pts',(61.1809509020401,736.958112818667,103.4462282913));
#83558=CARTESIAN_POINT('Ctrl Pts',(61.8795858086402,736.901322056595,103.143655627156));
#83559=CARTESIAN_POINT('Ctrl Pts',(61.1257247484325,736.388809219359,102.712651269588));
#83560=CARTESIAN_POINT('Ctrl Pts',(61.1315244238093,736.439502901679,103.467444860905));
#83561=CARTESIAN_POINT('Ctrl Pts',(61.8199032205241,736.324378385116,103.172000328419));
#83562=CARTESIAN_POINT('Ctrl Pts',(60.9649930899463,735.587567421577,102.788007703544));
#83563=CARTESIAN_POINT('Ctrl Pts',(60.981820887591,735.660697899481,103.527070137866));
#83564=CARTESIAN_POINT('Ctrl Pts',(61.6456182738998,735.474887256523,103.248996797997));
#83565=CARTESIAN_POINT('Ctrl Pts',(60.8982825197972,735.322998250083,102.818743893064));
#83566=CARTESIAN_POINT('Ctrl Pts',(60.9199522152394,735.404098567403,103.551302444857));
#83567=CARTESIAN_POINT('Ctrl Pts',(61.5732848924775,735.19438620833,103.280406636733));
#83568=CARTESIAN_POINT('Ctrl Pts',(60.7381098070039,734.798906562277,102.890642890349));
#83569=CARTESIAN_POINT('Ctrl Pts',(60.7697965738214,734.892509407837,103.608706401083));
#83570=CARTESIAN_POINT('Ctrl Pts',(61.3996158945904,734.638734667783,103.353888537477));
#83571=CARTESIAN_POINT('Ctrl Pts',(60.6447435666911,734.540287656224,102.931744025724));
#83572=CARTESIAN_POINT('Ctrl Pts',(60.6820947269692,734.63910185468,103.641656972148));
#83573=CARTESIAN_POINT('Ctrl Pts',(61.2983842846201,734.364542199337,103.395897601165));
#83574=CARTESIAN_POINT('Ctrl Pts',(60.3311877109548,733.788965343319,103.065815369317));
#83575=CARTESIAN_POINT('Ctrl Pts',(60.3866007381818,733.90349987622,103.749743252493));
#83576=CARTESIAN_POINT('Ctrl Pts',(60.958418488567,733.567976616374,103.532937356843));
#83577=CARTESIAN_POINT('Ctrl Pts',(60.0762481608013,733.314787297901,103.170272691237));
#83578=CARTESIAN_POINT('Ctrl Pts',(60.1442935975249,733.43158872955,103.835289846909));
#83579=CARTESIAN_POINT('Ctrl Pts',(60.6820115486397,733.065244427314,103.639715549476));
#83580=CARTESIAN_POINT('Ctrl Pts',(59.6252595505857,732.641678750238,103.34014197422));
#83581=CARTESIAN_POINT('Ctrl Pts',(59.7019880275959,732.748764058181,103.979323506016));
#83582=CARTESIAN_POINT('Ctrl Pts',(60.1930545417937,732.351602501481,103.813365835641));
#83583=CARTESIAN_POINT('Ctrl Pts',(59.4626751707199,732.42299274092,103.399206463738));
#83584=CARTESIAN_POINT('Ctrl Pts',(59.5432261215717,732.527629412984,104.029360742554));
#83585=CARTESIAN_POINT('Ctrl Pts',(60.0167833769942,732.119747616557,103.873746066075));
#83586=CARTESIAN_POINT('Ctrl Pts',(59.1204278078766,732.006685289033,103.517848709794));
#83587=CARTESIAN_POINT('Ctrl Pts',(59.2067025055535,732.105084204966,104.130742222411));
#83588=CARTESIAN_POINT('Ctrl Pts',(59.6457267679576,731.678370883142,103.995032772172));
#83589=CARTESIAN_POINT('Ctrl Pts',(58.9402283766131,731.808090210619,103.577647519589));
#83590=CARTESIAN_POINT('Ctrl Pts',(59.0287912923034,731.902472536105,104.182228416435));
#83591=CARTESIAN_POINT('Ctrl Pts',(59.4503597030529,731.467816768717,104.056165212955));
#83592=CARTESIAN_POINT('Ctrl Pts',(58.3726318318003,731.240067038385,103.756066170503));
#83593=CARTESIAN_POINT('Ctrl Pts',(58.4698094265145,731.326084508652,104.335651640274));
#83594=CARTESIAN_POINT('Ctrl Pts',(58.8349904857801,730.865588269116,104.238564540963));
#83595=CARTESIAN_POINT('Ctrl Pts',(57.9571860672587,730.897183698347,103.874066021539));
#83596=CARTESIAN_POINT('Ctrl Pts',(58.0545173909263,730.970975749466,104.439583656015));
#83597=CARTESIAN_POINT('Ctrl Pts',(58.3845815167719,730.50205711538,104.35919918526));
#83598=CARTESIAN_POINT('Ctrl Pts',(57.0546474823471,730.291222974584,104.09363972318));
#83599=CARTESIAN_POINT('Ctrl Pts',(57.1452072958055,730.343809488644,104.634257597851));
#83600=CARTESIAN_POINT('Ctrl Pts',(57.4060930165886,729.859606532818,104.583677606931));
#83601=CARTESIAN_POINT('Ctrl Pts',(56.5798557797467,730.036068845983,104.192221461437));
#83602=CARTESIAN_POINT('Ctrl Pts',(56.6630499090508,730.07624833159,104.723128595975));
#83603=CARTESIAN_POINT('Ctrl Pts',(56.891349737683,729.58908748456,104.684462416802));
#83604=CARTESIAN_POINT('Ctrl Pts',(55.8320913800377,729.723329995616,104.31634306445));
#83605=CARTESIAN_POINT('Ctrl Pts',(55.8988443964391,729.748595063217,104.83536748852));
#83606=CARTESIAN_POINT('Ctrl Pts',(56.0806674621493,729.257516067056,104.811358313865));
#83607=CARTESIAN_POINT('Ctrl Pts',(55.5768657910945,729.630840873543,104.353761308194));
#83608=CARTESIAN_POINT('Ctrl Pts',(55.6386235138817,729.651816413208,104.869210413042));
#83609=CARTESIAN_POINT('Ctrl Pts',(55.8039673529785,729.159457417016,104.84961300737));
#83610=CARTESIAN_POINT('Ctrl Pts',(55.0538963656352,729.470220949813,104.419458032274));
#83611=CARTESIAN_POINT('Ctrl Pts',(55.1051328898357,729.483964632797,104.928620527236));
#83612=CARTESIAN_POINT('Ctrl Pts',(55.2369964086371,728.989165252824,104.916778416946));
#83613=CARTESIAN_POINT('Ctrl Pts',(54.7851014678237,729.402035764568,104.447762052157));
#83614=CARTESIAN_POINT('Ctrl Pts',(54.8302761550589,729.412455456162,104.954337757205));
#83615=CARTESIAN_POINT('Ctrl Pts',(54.9455860846029,728.916874079002,104.945715242535));
#83616=CARTESIAN_POINT('Ctrl Pts',(53.9789685647692,729.239738639677,104.515565791446));
#83617=CARTESIAN_POINT('Ctrl Pts',(54.0082608735909,729.243006873554,105.015710454987));
#83618=CARTESIAN_POINT('Ctrl Pts',(54.0716288994501,728.744803714473,105.015034956347));
#83619=CARTESIAN_POINT('Ctrl Pts',(53.4361694424363,729.185298984108,104.538875891959));
#83620=CARTESIAN_POINT('Ctrl Pts',(53.4496161456551,729.185332137448,105.037159942866));
#83621=CARTESIAN_POINT('Ctrl Pts',(53.4831622362376,728.68708580134,105.038866301411));
#83622=CARTESIAN_POINT('Ctrl Pts',(52.6138504499604,729.184275098991,104.539310798033));
#83623=CARTESIAN_POINT('Ctrl Pts',(52.6075136823759,729.184259004066,105.037555700089));
#83624=CARTESIAN_POINT('Ctrl Pts',(52.5916587586709,728.686000260307,105.039310932355));
#83625=CARTESIAN_POINT('Ctrl Pts',(52.3370055315343,729.197621489013,104.533629664186));
#83626=CARTESIAN_POINT('Ctrl Pts',(52.3236418415964,729.198286299786,105.032370697334));
#83627=CARTESIAN_POINT('Ctrl Pts',(52.2915219403397,728.700150345916,105.033502765101));
#83628=CARTESIAN_POINT('Ctrl Pts',(51.7870175816165,729.251908649559,104.510663500195));
#83629=CARTESIAN_POINT('Ctrl Pts',(51.7606605684528,729.255166215058,105.01148612717));
#83630=CARTESIAN_POINT('Ctrl Pts',(51.695261374346,728.757706580342,105.010023081021));
#83631=CARTESIAN_POINT('Ctrl Pts',(51.5157722085268,729.292506544129,104.493525021637));
#83632=CARTESIAN_POINT('Ctrl Pts',(51.482794014801,729.297802076253,104.995868437499));
#83633=CARTESIAN_POINT('Ctrl Pts',(51.4011949421538,728.800749207109,104.99250139366));
#83634=CARTESIAN_POINT('Ctrl Pts',(50.7128226027646,729.453210985855,104.426373808672));
#83635=CARTESIAN_POINT('Ctrl Pts',(50.659795046494,729.466453778642,104.934771634819));
#83636=CARTESIAN_POINT('Ctrl Pts',(50.5306889001451,728.971130979045,104.923848793536));
#83637=CARTESIAN_POINT('Ctrl Pts',(50.1916745911165,729.611899298158,104.360612213778));
#83638=CARTESIAN_POINT('Ctrl Pts',(50.12567436779,729.634048243943,104.874648394563));
#83639=CARTESIAN_POINT('Ctrl Pts',(49.9656928764268,729.13937521528,104.856616947866));
#83640=CARTESIAN_POINT('Ctrl Pts',(49.1784470909822,730.033928888822,104.193027849295));
#83641=CARTESIAN_POINT('Ctrl Pts',(49.0951325681358,730.074079498543,104.723829183479));
#83642=CARTESIAN_POINT('Ctrl Pts',(48.8672111471257,729.586818662584,104.68528682235));
#83643=CARTESIAN_POINT('Ctrl Pts',(48.7027982162775,730.290339076695,104.094018837663));
#83644=CARTESIAN_POINT('Ctrl Pts',(48.6124016060787,730.342788849866,104.634629987258));
#83645=CARTESIAN_POINT('Ctrl Pts',(48.3515385393433,729.858669408582,104.584065199752));
#83646=CARTESIAN_POINT('Ctrl Pts',(48.0320729801837,730.739768842028,103.931077496968));
#83647=CARTESIAN_POINT('Ctrl Pts',(47.9412391106486,730.804777879081,104.491144118451));
#83648=CARTESIAN_POINT('Ctrl Pts',(47.624370852353,730.335163020942,104.417484147719));
#83649=CARTESIAN_POINT('Ctrl Pts',(47.8156813845902,730.900472889617,103.874347068112));
#83650=CARTESIAN_POINT('Ctrl Pts',(47.7238916112771,730.970992477136,104.44101889853));
#83651=CARTESIAN_POINT('Ctrl Pts',(47.389768913752,730.505544375239,104.359486753798));
#83652=CARTESIAN_POINT('Ctrl Pts',(47.3973220744942,731.244211137401,103.757431495977));
#83653=CARTESIAN_POINT('Ctrl Pts',(47.3052179858964,731.324859887805,104.338424006517));
#83654=CARTESIAN_POINT('Ctrl Pts',(46.9362012231384,730.869981918465,104.239960877132));
#83655=CARTESIAN_POINT('Ctrl Pts',(47.1963552596799,731.426598283342,103.697495897006));
#83656=CARTESIAN_POINT('Ctrl Pts',(47.1049878887212,731.512287596286,104.286106464377));
#83657=CARTESIAN_POINT('Ctrl Pts',(46.718320595536,731.063352088166,104.178687517304));
#83658=CARTESIAN_POINT('Ctrl Pts',(46.6264326450995,731.996527007362,103.518418939747));
#83659=CARTESIAN_POINT('Ctrl Pts',(46.5346004165947,732.099997089064,104.129613768312));
#83660=CARTESIAN_POINT('Ctrl Pts',(46.100429550514,731.667600888059,103.995615183088));
#83661=CARTESIAN_POINT('Ctrl Pts',(46.2862941213449,732.409628760885,103.398906187144));
#83662=CARTESIAN_POINT('Ctrl Pts',(46.2017494877472,732.520766276813,104.02759395401));
#83663=CARTESIAN_POINT('Ctrl Pts',(45.7316592763466,732.105578881428,103.873438096382));
#83664=CARTESIAN_POINT('Ctrl Pts',(45.8352318176212,733.080982096968,103.229178588061));
#83665=CARTESIAN_POINT('Ctrl Pts',(45.7665725264928,733.190705968255,103.886013091801));
#83666=CARTESIAN_POINT('Ctrl Pts',(45.2426224560662,732.817359900666,103.699932564948));
#83667=CARTESIAN_POINT('Ctrl Pts',(45.6941245720904,733.31484502054,103.173914949951));
#83668=CARTESIAN_POINT('Ctrl Pts',(45.6304395608493,733.424882397453,103.840011653334));
#83669=CARTESIAN_POINT('Ctrl Pts',(45.0896344539317,733.065305626168,103.643439885389));
#83670=CARTESIAN_POINT('Ctrl Pts',(45.4370595664475,733.792644756091,103.070197444028));
#83671=CARTESIAN_POINT('Ctrl Pts',(45.3833924746706,733.900859143644,103.754294935155));
#83672=CARTESIAN_POINT('Ctrl Pts',(44.8109232393786,733.571877596802,103.537418520231));
#83673=CARTESIAN_POINT('Ctrl Pts',(45.3208753235868,734.036579304987,103.021686463586));
#83674=CARTESIAN_POINT('Ctrl Pts',(45.2728079392524,734.142444713245,103.714681228453));
#83675=CARTESIAN_POINT('Ctrl Pts',(44.6849544916996,733.830501442806,103.487831436724));
#83676=CARTESIAN_POINT('Ctrl Pts',(45.0086600428394,734.783512511873,102.888228488882));
#83677=CARTESIAN_POINT('Ctrl Pts',(44.9743839861276,734.884162275861,103.605552967253));
#83678=CARTESIAN_POINT('Ctrl Pts',(44.3464422296916,734.622413615477,103.351418560461));
#83679=CARTESIAN_POINT('Ctrl Pts',(44.8485632569221,735.301485450629,102.81531169835));
#83680=CARTESIAN_POINT('Ctrl Pts',(44.8268749830078,735.387060666504,103.548333060095));
#83681=CARTESIAN_POINT('Ctrl Pts',(44.1728555580203,735.171577946915,103.276895349789));
#83682=CARTESIAN_POINT('Ctrl Pts',(44.6301364121208,736.381170716927,102.712981257937));
#83683=CARTESIAN_POINT('Ctrl Pts',(44.6242435666643,736.43229980519,103.467685458753));
#83684=CARTESIAN_POINT('Ctrl Pts',(43.93601074888,736.316279906073,103.172337185597));
#83685=CARTESIAN_POINT('Ctrl Pts',(44.574479425553,736.934722944003,102.684884837068));
#83686=CARTESIAN_POINT('Ctrl Pts',(44.574286483178,736.959771156344,103.446222347099));
#83687=CARTESIAN_POINT('Ctrl Pts',(43.8756509159712,736.903165979843,103.143648586643));
#83688=CARTESIAN_POINT('Ctrl Pts',(44.574479425553,737.487748923763,102.682654164686));
#83689=CARTESIAN_POINT('Ctrl Pts',(44.574479425553,737.490646661967,103.444319534016));
#83690=CARTESIAN_POINT('Ctrl Pts',(43.8756325293234,737.489494249471,103.141409944702));
#83691=CARTESIAN_POINT('Origin',(61.1807573575412,751.59614455564,112.60871186179));
#83692=CARTESIAN_POINT('',(61.1807573575412,751.59614455564,112.60871186179));
#83693=CARTESIAN_POINT('Origin',(44.574479425553,751.59614455564,112.60871186179));
#83694=CARTESIAN_POINT('',(44.574479425553,751.59614455564,112.60871186179));
#83695=CARTESIAN_POINT('Origin',(52.8776183915471,751.59614455564,112.60871186179));
#83696=CARTESIAN_POINT('Origin',(52.8776183915471,827.175936191914,121.458286566849));
#83697=CARTESIAN_POINT('Origin',(52.8776183915471,825.559694878252,125.51834395973));
#83698=CARTESIAN_POINT('Origin',(52.8776183915471,827.175936191914,121.458286566849));
#83699=CARTESIAN_POINT('Origin',(52.8776183915471,825.559694878252,125.51834395973));
#83700=CARTESIAN_POINT('Origin',(52.8776183915471,827.175936191914,121.458286566849));
#83701=CARTESIAN_POINT('Origin',(52.8776183915471,825.559694878252,125.51834395973));
#83702=CARTESIAN_POINT('Origin',(52.8776183915471,827.175936191914,121.458286566849));
#83703=CARTESIAN_POINT('Origin',(52.8776183915471,825.559694878252,125.51834395973));
#83704=CARTESIAN_POINT('Origin',(52.8776183915471,827.175936191914,121.458286566849));
#83705=CARTESIAN_POINT('Origin',(52.8776183915471,825.559694878252,125.51834395973));
#83706=CARTESIAN_POINT('Origin',(52.8776183915471,827.175936191914,121.458286566849));
#83707=CARTESIAN_POINT('Origin',(52.8776183915471,825.559694878252,125.51834395973));
#83708=CARTESIAN_POINT('Origin',(52.8776183915471,827.175936191914,121.458286566849));
#83709=CARTESIAN_POINT('Origin',(52.8776183915471,825.559694878252,125.51834395973));
#83710=CARTESIAN_POINT('Origin',(52.8776183915471,827.175936191914,121.458286566849));
#83711=CARTESIAN_POINT('Origin',(52.8776183915471,825.559694878252,125.51834395973));
#83712=CARTESIAN_POINT('Origin',(52.8776183915471,827.175936191914,121.458286566849));
#83713=CARTESIAN_POINT('Origin',(52.8776183915471,825.559694878252,125.51834395973));
#83714=CARTESIAN_POINT('Origin',(52.8776183915471,827.175936191914,121.458286566849));
#83715=CARTESIAN_POINT('Origin',(52.8776183915471,825.559694878252,125.51834395973));
#83716=CARTESIAN_POINT('Origin',(52.8776183915471,827.175936191914,121.458286566849));
#83717=CARTESIAN_POINT('Origin',(52.8776183915471,825.559694878252,125.51834395973));
#83718=CARTESIAN_POINT('Origin',(52.8776183915471,827.175936191914,121.458286566849));
#83719=CARTESIAN_POINT('Origin',(52.8776183915471,825.559694878252,125.51834395973));
#83720=CARTESIAN_POINT('Origin',(52.8776183915471,827.175936191914,121.458286566849));
#83721=CARTESIAN_POINT('Origin',(52.8776183915471,825.559694878252,125.51834395973));
#83722=CARTESIAN_POINT('Origin',(52.8776183915471,827.175936191914,121.458286566849));
#83723=CARTESIAN_POINT('Origin',(52.8776183915471,825.559694878252,125.51834395973));
#83724=CARTESIAN_POINT('Origin',(52.8776183915471,827.175936191914,121.458286566849));
#83725=CARTESIAN_POINT('Origin',(52.8776183915471,825.559694878252,125.51834395973));
#83726=CARTESIAN_POINT('Origin',(52.8776183915471,827.175936191914,121.458286566849));
#83727=CARTESIAN_POINT('Origin',(52.8776183915471,825.559694878252,125.51834395973));
#83728=CARTESIAN_POINT('Origin',(52.8776183915471,827.175936191914,121.458286566849));
#83729=CARTESIAN_POINT('Origin',(52.8776183915471,825.559694878252,125.51834395973));
#83730=CARTESIAN_POINT('Origin',(52.8776183915471,827.175936191914,121.458286566849));
#83731=CARTESIAN_POINT('Origin',(52.8776183915471,825.559694878252,125.51834395973));
#83732=CARTESIAN_POINT('Origin',(52.8776183915471,827.175936191914,121.458286566849));
#83733=CARTESIAN_POINT('Origin',(52.8776183915471,825.559694878252,125.51834395973));
#83734=CARTESIAN_POINT('Origin',(52.8776183915471,827.175936191914,121.458286566849));
#83735=CARTESIAN_POINT('Origin',(52.8776183915471,825.559694878252,125.51834395973));
#83736=CARTESIAN_POINT('Origin',(52.8776183915471,827.175936191914,121.458286566849));
#83737=CARTESIAN_POINT('Origin',(52.8776183915471,825.559694878252,125.51834395973));
#83738=CARTESIAN_POINT('Origin',(52.8776183915471,827.175936191914,121.458286566849));
#83739=CARTESIAN_POINT('Origin',(52.8776183915471,825.559694878252,125.51834395973));
#83740=CARTESIAN_POINT('Origin',(52.8776183915471,827.175936191914,121.458286566849));
#83741=CARTESIAN_POINT('Origin',(52.8776183915471,825.559694878252,125.51834395973));
#83742=CARTESIAN_POINT('Origin',(52.8776183915471,827.175936191914,121.458286566849));
#83743=CARTESIAN_POINT('Origin',(52.8776183915471,825.559694878252,125.51834395973));
#83744=CARTESIAN_POINT('Origin',(52.8776183915471,827.175936191914,121.458286566849));
#83745=CARTESIAN_POINT('Origin',(52.8776183915471,825.559694878252,125.51834395973));
#83746=CARTESIAN_POINT('Origin',(52.8776183915471,827.175936191914,121.458286566849));
#83747=CARTESIAN_POINT('Origin',(52.8776183915471,825.559694878252,125.51834395973));
#83748=CARTESIAN_POINT('Origin',(52.8776183915471,827.175936191914,121.458286566849));
#83749=CARTESIAN_POINT('Origin',(52.8776183915471,825.559694878252,125.51834395973));
#83750=CARTESIAN_POINT('Origin',(52.8776183915471,827.175936191914,121.458286566849));
#83751=CARTESIAN_POINT('Origin',(52.8776183915471,825.559694878252,125.51834395973));
#83752=CARTESIAN_POINT('Origin',(52.8776183915471,827.175936191914,121.458286566849));
#83753=CARTESIAN_POINT('Origin',(52.8776183915471,825.559694878252,125.51834395973));
#83754=CARTESIAN_POINT('Origin',(52.8776183915471,827.175936191914,121.458286566849));
#83755=CARTESIAN_POINT('Origin',(52.8776183915471,825.559694878252,125.51834395973));
#83756=CARTESIAN_POINT('Origin',(52.8776183915471,827.175936191914,121.458286566849));
#83757=CARTESIAN_POINT('Origin',(52.8776183915471,825.559694878252,125.51834395973));
#83758=CARTESIAN_POINT('Origin',(52.8776183915471,827.175936191914,121.458286566849));
#83759=CARTESIAN_POINT('Origin',(52.8776183915471,825.559694878252,125.51834395973));
#83760=CARTESIAN_POINT('Origin',(52.8776183915471,827.175936191914,121.458286566849));
#83761=CARTESIAN_POINT('Origin',(52.8776183915471,825.559694878252,125.51834395973));
#83762=CARTESIAN_POINT('Origin',(52.8776183915471,827.175936191914,121.458286566849));
#83763=CARTESIAN_POINT('Origin',(52.8776183915471,825.559694878252,125.51834395973));
#83764=CARTESIAN_POINT('Origin',(52.8776183915471,827.175936191914,121.458286566849));
#83765=CARTESIAN_POINT('Origin',(52.8776183915471,825.559694878252,125.51834395973));
#83766=CARTESIAN_POINT('Origin',(52.8776183915471,827.175936191914,121.458286566849));
#83767=CARTESIAN_POINT('Origin',(52.8776183915471,825.559694878252,125.51834395973));
#83768=CARTESIAN_POINT('Origin',(52.8776183915471,827.175936191914,121.458286566849));
#83769=CARTESIAN_POINT('Origin',(52.8776183915471,825.559694878252,125.51834395973));
#83770=CARTESIAN_POINT('Origin',(52.8776183915471,827.175936191914,121.458286566849));
#83771=CARTESIAN_POINT('Origin',(52.8776183915471,825.559694878252,125.51834395973));
#83772=CARTESIAN_POINT('Origin',(52.8776183915471,827.175936191914,121.458286566849));
#83773=CARTESIAN_POINT('Origin',(52.8776183915471,825.559694878252,125.51834395973));
#83774=CARTESIAN_POINT('Origin',(52.8776183915471,827.175936191914,121.458286566849));
#83775=CARTESIAN_POINT('Origin',(52.8776183915471,825.559694878252,125.51834395973));
#83776=CARTESIAN_POINT('Origin',(52.8776183915471,827.175936191914,121.458286566849));
#83777=CARTESIAN_POINT('Origin',(52.8776183915471,825.559694878252,125.51834395973));
#83778=CARTESIAN_POINT('Origin',(52.8776183915471,827.175936191914,121.458286566849));
#83779=CARTESIAN_POINT('Origin',(52.8776183915471,825.559694878252,125.51834395973));
#83780=CARTESIAN_POINT('Origin',(52.8776183915471,827.175936191914,121.458286566849));
#83781=CARTESIAN_POINT('Origin',(52.8776183915471,825.559694878252,125.51834395973));
#83782=CARTESIAN_POINT('Origin',(52.8776183915471,827.175936191914,121.458286566849));
#83783=CARTESIAN_POINT('Origin',(52.8776183915471,825.559694878252,125.51834395973));
#83784=CARTESIAN_POINT('Origin',(52.8776183915471,827.175936191914,121.458286566849));
#83785=CARTESIAN_POINT('Origin',(52.8776183915471,825.559694878252,125.51834395973));
#83786=CARTESIAN_POINT('Origin',(52.8776183915471,827.175936191914,121.458286566849));
#83787=CARTESIAN_POINT('Origin',(52.8776183915471,825.559694878252,125.51834395973));
#83788=CARTESIAN_POINT('Origin',(52.8776183915471,827.175936191914,121.458286566849));
#83789=CARTESIAN_POINT('Origin',(52.8776183915471,825.559694878252,125.51834395973));
#83790=CARTESIAN_POINT('Origin',(52.8776183915471,827.175936191914,121.458286566849));
#83791=CARTESIAN_POINT('Origin',(52.8776183915471,825.559694878252,125.51834395973));
#83792=CARTESIAN_POINT('Origin',(52.8776183915471,827.175936191914,121.458286566849));
#83793=CARTESIAN_POINT('Origin',(52.8776183915471,825.559694878252,125.51834395973));
#83794=CARTESIAN_POINT('Origin',(52.8776183915471,827.175936191914,121.458286566849));
#83795=CARTESIAN_POINT('Origin',(52.8776183915471,825.559694878252,125.51834395973));
#83796=CARTESIAN_POINT('Origin',(52.8776183915471,827.175936191914,121.458286566849));
#83797=CARTESIAN_POINT('Origin',(52.8776183915471,825.559694878252,125.51834395973));
#83798=CARTESIAN_POINT('Origin',(52.8776183915471,827.175936191914,121.458286566849));
#83799=CARTESIAN_POINT('Origin',(52.8776183915471,825.559694878252,125.51834395973));
#83800=CARTESIAN_POINT('Origin',(52.8776183915471,827.175936191914,121.458286566849));
#83801=CARTESIAN_POINT('Origin',(52.8776183915471,825.559694878252,125.51834395973));
#83802=CARTESIAN_POINT('Origin',(52.8776183915471,827.175936191914,121.458286566849));
#83803=CARTESIAN_POINT('Origin',(52.8776183915471,825.559694878252,125.51834395973));
#83804=CARTESIAN_POINT('Origin',(52.8776183915471,827.175936191914,121.458286566849));
#83805=CARTESIAN_POINT('Origin',(52.8776183915471,825.559694878252,125.51834395973));
#83806=CARTESIAN_POINT('Origin',(52.8776183915471,827.175936191914,121.458286566849));
#83807=CARTESIAN_POINT('Origin',(52.8776183915471,825.559694878252,125.51834395973));
#83808=CARTESIAN_POINT('Origin',(52.8776183915471,827.175936191914,121.458286566849));
#83809=CARTESIAN_POINT('Origin',(52.8776183915471,825.559694878252,125.51834395973));
#83810=CARTESIAN_POINT('Origin',(52.8776183915471,827.175936191914,121.458286566849));
#83811=CARTESIAN_POINT('Origin',(52.8776183915471,825.559694878252,125.51834395973));
#83812=CARTESIAN_POINT('Origin',(52.8776183915471,827.175936191914,121.458286566849));
#83813=CARTESIAN_POINT('Origin',(52.8776183915471,825.559694878252,125.51834395973));
#83814=CARTESIAN_POINT('Origin',(52.8776183915471,827.175936191914,121.458286566849));
#83815=CARTESIAN_POINT('Origin',(52.8776183915471,825.559694878252,125.51834395973));
#83816=CARTESIAN_POINT('Origin',(52.8776183915471,827.175936191914,121.458286566849));
#83817=CARTESIAN_POINT('Origin',(52.8776183915471,825.559694878252,125.51834395973));
#83818=CARTESIAN_POINT('Origin',(52.8776183915471,827.175936191914,121.458286566849));
#83819=CARTESIAN_POINT('Origin',(52.8776183915471,825.559694878252,125.51834395973));
#83820=CARTESIAN_POINT('Origin',(52.8776183915471,827.175936191914,121.458286566849));
#83821=CARTESIAN_POINT('Origin',(52.8776183915471,825.559694878252,125.51834395973));
#83822=CARTESIAN_POINT('Origin',(52.8776183915471,827.175936191914,121.458286566849));
#83823=CARTESIAN_POINT('Origin',(52.8776183915471,825.559694878252,125.51834395973));
#83824=CARTESIAN_POINT('Origin',(52.8776183915471,827.175936191914,121.458286566849));
#83825=CARTESIAN_POINT('Origin',(52.8776183915471,825.559694878252,125.51834395973));
#83826=CARTESIAN_POINT('Origin',(52.8776183915471,827.175936191914,121.458286566849));
#83827=CARTESIAN_POINT('Origin',(52.8776183915471,825.559694878252,125.51834395973));
#83828=CARTESIAN_POINT('Origin',(52.8776183915471,827.175936191914,121.458286566849));
#83829=CARTESIAN_POINT('Origin',(52.8776183915471,825.559694878252,125.51834395973));
#83830=CARTESIAN_POINT('Origin',(52.8776183915471,827.175936191914,121.458286566849));
#83831=CARTESIAN_POINT('Origin',(52.8776183915471,825.559694878252,125.51834395973));
#83832=CARTESIAN_POINT('Origin',(52.8776183915471,827.175936191914,121.458286566849));
#83833=CARTESIAN_POINT('Origin',(52.8776183915471,825.559694878252,125.51834395973));
#83834=CARTESIAN_POINT('Origin',(52.8776183915471,827.175936191914,121.458286566849));
#83835=CARTESIAN_POINT('Origin',(52.8776183915471,825.559694878252,125.51834395973));
#83836=CARTESIAN_POINT('Origin',(52.8776183915471,827.175936191914,121.458286566849));
#83837=CARTESIAN_POINT('Origin',(52.8776183915471,825.559694878252,125.51834395973));
#83838=CARTESIAN_POINT('Origin',(52.8776183915471,827.175936191914,121.458286566849));
#83839=CARTESIAN_POINT('Origin',(52.8776183915471,825.559694878252,125.51834395973));
#83840=CARTESIAN_POINT('Origin',(52.8776183915471,827.175936191914,121.458286566849));
#83841=CARTESIAN_POINT('Origin',(52.8776183915471,825.559694878252,125.51834395973));
#83842=CARTESIAN_POINT('Origin',(52.8776183915471,827.175936191914,121.458286566849));
#83843=CARTESIAN_POINT('Origin',(52.8776183915471,825.559694878252,125.51834395973));
#83844=CARTESIAN_POINT('Origin',(52.8776183915471,827.175936191914,121.458286566849));
#83845=CARTESIAN_POINT('Origin',(52.8776183915471,825.559694878252,125.51834395973));
#83846=CARTESIAN_POINT('Origin',(52.8776183915471,827.175936191914,121.458286566849));
#83847=CARTESIAN_POINT('Origin',(52.8776183915471,825.559694878252,125.51834395973));
#83848=CARTESIAN_POINT('Origin',(52.8776183915471,827.175936191914,121.458286566849));
#83849=CARTESIAN_POINT('Origin',(52.8776183915471,825.559694878252,125.51834395973));
#83850=CARTESIAN_POINT('Origin',(52.8776183915471,827.175936191914,121.458286566849));
#83851=CARTESIAN_POINT('Origin',(52.8776183915471,825.559694878252,125.51834395973));
#83852=CARTESIAN_POINT('Origin',(52.8776183915471,827.175936191914,121.458286566849));
#83853=CARTESIAN_POINT('Origin',(52.8776183915471,825.559694878252,125.51834395973));
#83854=CARTESIAN_POINT('Origin',(52.8776183915471,827.175936191914,121.458286566849));
#83855=CARTESIAN_POINT('Origin',(52.8776183915471,825.559694878252,125.51834395973));
#83856=CARTESIAN_POINT('Origin',(52.8776183915471,827.175936191914,121.458286566849));
#83857=CARTESIAN_POINT('Origin',(52.8776183915471,825.559694878252,125.51834395973));
#83858=CARTESIAN_POINT('Origin',(52.8776183915471,827.175936191914,121.458286566849));
#83859=CARTESIAN_POINT('Origin',(52.8776183915471,825.559694878252,125.51834395973));
#83860=CARTESIAN_POINT('Origin',(52.8776183915471,827.175936191914,121.458286566849));
#83861=CARTESIAN_POINT('Origin',(52.8776183915471,825.559694878252,125.51834395973));
#83862=CARTESIAN_POINT('Origin',(52.8776183915471,827.175936191914,121.458286566849));
#83863=CARTESIAN_POINT('Origin',(52.8776183915471,825.559694878252,125.51834395973));
#83864=CARTESIAN_POINT('Origin',(52.8776183915471,827.175936191914,121.458286566849));
#83865=CARTESIAN_POINT('Origin',(52.8776183915471,825.559694878252,125.51834395973));
#83866=CARTESIAN_POINT('Origin',(52.8776183915471,827.175936191914,121.458286566849));
#83867=CARTESIAN_POINT('Origin',(52.8776183915471,825.559694878252,125.51834395973));
#83868=CARTESIAN_POINT('Origin',(52.8776183915471,827.175936191914,121.458286566849));
#83869=CARTESIAN_POINT('Origin',(52.8776183915471,825.559694878252,125.51834395973));
#83870=CARTESIAN_POINT('Origin',(52.8776183915471,827.175936191914,121.458286566849));
#83871=CARTESIAN_POINT('Origin',(52.8776183915471,825.559694878252,125.51834395973));
#83872=CARTESIAN_POINT('Origin',(52.8776183915471,827.175936191914,121.458286566849));
#83873=CARTESIAN_POINT('Origin',(52.8776183915471,825.559694878252,125.51834395973));
#83874=CARTESIAN_POINT('Origin',(52.8776183915471,827.175936191914,121.458286566849));
#83875=CARTESIAN_POINT('Origin',(52.8776183915471,825.559694878252,125.51834395973));
#83876=CARTESIAN_POINT('Origin',(52.8776183915471,827.175936191914,121.458286566849));
#83877=CARTESIAN_POINT('Origin',(52.8776183915471,825.559694878252,125.51834395973));
#83878=CARTESIAN_POINT('Origin',(52.8776183915471,827.175936191914,121.458286566849));
#83879=CARTESIAN_POINT('Origin',(52.8776183915471,825.559694878252,125.51834395973));
#83880=CARTESIAN_POINT('Origin',(52.8776183915471,827.175936191914,121.458286566849));
#83881=CARTESIAN_POINT('Origin',(52.8776183915471,825.559694878252,125.51834395973));
#83882=CARTESIAN_POINT('Origin',(52.8776183915471,827.175936191914,121.458286566849));
#83883=CARTESIAN_POINT('Origin',(52.8776183915471,825.559694878252,125.51834395973));
#83884=CARTESIAN_POINT('Origin',(52.8776183915471,827.175936191914,121.458286566849));
#83885=CARTESIAN_POINT('Origin',(52.8776183915471,825.559694878252,125.51834395973));
#83886=CARTESIAN_POINT('Origin',(52.8776183915471,827.175936191914,121.458286566849));
#83887=CARTESIAN_POINT('Origin',(52.8776183915471,825.559694878252,125.51834395973));
#83888=CARTESIAN_POINT('Origin',(52.8776183915471,827.175936191914,121.458286566849));
#83889=CARTESIAN_POINT('Origin',(52.8776183915471,825.559694878252,125.51834395973));
#83890=CARTESIAN_POINT('Origin',(52.8776183915471,827.175936191914,121.458286566849));
#83891=CARTESIAN_POINT('Origin',(52.8776183915471,825.559694878252,125.51834395973));
#83892=CARTESIAN_POINT('Origin',(52.8776183915471,827.175936191914,121.458286566849));
#83893=CARTESIAN_POINT('Origin',(52.8776183915471,825.559694878252,125.51834395973));
#83894=CARTESIAN_POINT('Origin',(52.8776183915471,827.175936191914,121.458286566849));
#83895=CARTESIAN_POINT('Origin',(52.8776183915471,825.559694878252,125.51834395973));
#83896=CARTESIAN_POINT('Origin',(52.8776183915471,827.175936191914,121.458286566849));
#83897=CARTESIAN_POINT('Origin',(52.8776183915471,825.559694878252,125.51834395973));
#83898=CARTESIAN_POINT('Origin',(52.8776183915471,827.175936191914,121.458286566849));
#83899=CARTESIAN_POINT('Origin',(52.8776183915471,825.559694878252,125.51834395973));
#83900=CARTESIAN_POINT('Origin',(52.8776183915471,827.175936191914,121.458286566849));
#83901=CARTESIAN_POINT('Origin',(52.8776183915471,825.559694878252,125.51834395973));
#83902=CARTESIAN_POINT('Origin',(52.8776183915471,827.175936191914,121.458286566849));
#83903=CARTESIAN_POINT('Origin',(52.8776183915471,825.559694878252,125.51834395973));
#83904=CARTESIAN_POINT('Origin',(52.8776183915471,827.175936191914,121.458286566849));
#83905=CARTESIAN_POINT('Origin',(52.8776183915471,825.559694878252,125.51834395973));
#83906=CARTESIAN_POINT('Origin',(52.8776183915471,827.175936191914,121.458286566849));
#83907=CARTESIAN_POINT('Origin',(52.8776183915471,825.559694878252,125.51834395973));
#83908=CARTESIAN_POINT('Origin',(52.8776183915471,827.175936191914,121.458286566849));
#83909=CARTESIAN_POINT('Origin',(52.8776183915471,825.559694878252,125.51834395973));
#83910=CARTESIAN_POINT('Origin',(52.8776183915471,827.175936191914,121.458286566849));
#83911=CARTESIAN_POINT('Origin',(52.8776183915471,825.559694878252,125.51834395973));
#83912=CARTESIAN_POINT('Origin',(52.8776183915471,827.175936191914,121.458286566849));
#83913=CARTESIAN_POINT('Origin',(52.8776183915471,825.559694878252,125.51834395973));
#83914=CARTESIAN_POINT('Origin',(52.8776183915471,827.175936191914,121.458286566849));
#83915=CARTESIAN_POINT('Origin',(52.8776183915471,825.559694878252,125.51834395973));
#83916=CARTESIAN_POINT('Origin',(52.8776183915471,827.175936191914,121.458286566849));
#83917=CARTESIAN_POINT('Origin',(52.8776183915471,825.559694878252,125.51834395973));
#83918=CARTESIAN_POINT('Origin',(52.8776183915471,827.175936191914,121.458286566849));
#83919=CARTESIAN_POINT('Origin',(52.8776183915471,825.559694878252,125.51834395973));
#83920=CARTESIAN_POINT('Origin',(52.8776183915471,827.175936191914,121.458286566849));
#83921=CARTESIAN_POINT('Origin',(52.8776183915471,825.559694878252,125.51834395973));
#83922=CARTESIAN_POINT('Origin',(52.8776183915471,827.175936191914,121.458286566849));
#83923=CARTESIAN_POINT('Origin',(52.8776183915471,825.559694878252,125.51834395973));
#83924=CARTESIAN_POINT('Origin',(52.8776183915471,827.175936191914,121.458286566849));
#83925=CARTESIAN_POINT('Origin',(52.8776183915471,825.559694878252,125.51834395973));
#83926=CARTESIAN_POINT('Origin',(52.8776183915471,827.175936191914,121.458286566849));
#83927=CARTESIAN_POINT('Origin',(52.8776183915471,825.559694878252,125.51834395973));
#83928=CARTESIAN_POINT('Origin',(52.8776183915471,827.175936191914,121.458286566849));
#83929=CARTESIAN_POINT('Origin',(52.8776183915471,825.559694878252,125.51834395973));
#83930=CARTESIAN_POINT('Origin',(52.8776183915471,827.175936191914,121.458286566849));
#83931=CARTESIAN_POINT('Origin',(52.8776183915471,825.559694878252,125.51834395973));
#83932=CARTESIAN_POINT('Origin',(52.8776183915471,827.175936191914,121.458286566849));
#83933=CARTESIAN_POINT('Origin',(52.8776183915471,825.559694878252,125.51834395973));
#83934=CARTESIAN_POINT('Origin',(52.8776183915471,827.175936191914,121.458286566849));
#83935=CARTESIAN_POINT('Origin',(52.8776183915471,825.559694878252,125.51834395973));
#83936=CARTESIAN_POINT('Origin',(52.8776183915471,827.175936191914,121.458286566849));
#83937=CARTESIAN_POINT('Origin',(52.8776183915471,825.559694878252,125.51834395973));
#83938=CARTESIAN_POINT('Origin',(52.8776183915471,827.175936191914,121.458286566849));
#83939=CARTESIAN_POINT('Origin',(52.8776183915471,825.559694878252,125.51834395973));
#83940=CARTESIAN_POINT('Origin',(52.8776183915471,827.175936191914,121.458286566849));
#83941=CARTESIAN_POINT('Origin',(52.8776183915471,825.559694878252,125.51834395973));
#83942=CARTESIAN_POINT('Origin',(52.8776183915471,827.175936191914,121.458286566849));
#83943=CARTESIAN_POINT('Origin',(52.8776183915471,825.559694878252,125.51834395973));
#83944=CARTESIAN_POINT('Origin',(52.8776183915471,827.175936191914,121.458286566849));
#83945=CARTESIAN_POINT('Origin',(52.8776183915471,825.559694878252,125.51834395973));
#83946=CARTESIAN_POINT('Origin',(52.8776183915471,827.175936191914,121.458286566849));
#83947=CARTESIAN_POINT('Origin',(52.8776183915471,825.559694878252,125.51834395973));
#83948=CARTESIAN_POINT('Origin',(52.8776183915471,827.175936191914,121.458286566849));
#83949=CARTESIAN_POINT('Origin',(52.8776183915471,825.559694878252,125.51834395973));
#83950=CARTESIAN_POINT('Origin',(52.8776183915471,827.175936191914,121.458286566849));
#83951=CARTESIAN_POINT('Origin',(52.8776183915471,825.559694878252,125.51834395973));
#83952=CARTESIAN_POINT('Origin',(52.8776183915471,827.175936191914,121.458286566849));
#83953=CARTESIAN_POINT('Origin',(52.8776183915471,825.559694878252,125.51834395973));
#83954=CARTESIAN_POINT('Origin',(52.8776183915471,827.175936191914,121.458286566849));
#83955=CARTESIAN_POINT('Origin',(52.8776183915471,825.559694878252,125.51834395973));
#83956=CARTESIAN_POINT('Origin',(52.8776183915471,827.175936191914,121.458286566849));
#83957=CARTESIAN_POINT('Origin',(52.8776183915471,825.559694878252,125.51834395973));
#83958=CARTESIAN_POINT('Origin',(52.8776183915471,827.175936191914,121.458286566849));
#83959=CARTESIAN_POINT('Origin',(52.8776183915471,825.559694878252,125.51834395973));
#83960=CARTESIAN_POINT('Origin',(52.8776183915471,827.175936191914,121.458286566849));
#83961=CARTESIAN_POINT('Origin',(52.8776183915471,825.559694878252,125.51834395973));
#83962=CARTESIAN_POINT('Origin',(52.8776183915471,827.175936191914,121.458286566849));
#83963=CARTESIAN_POINT('Origin',(52.8776183915471,825.559694878252,125.51834395973));
#83964=CARTESIAN_POINT('Origin',(52.8776183915471,827.175936191914,121.458286566849));
#83965=CARTESIAN_POINT('Origin',(52.8776183915471,825.559694878252,125.51834395973));
#83966=CARTESIAN_POINT('Origin',(52.8776183915471,827.175936191914,121.458286566849));
#83967=CARTESIAN_POINT('Origin',(52.8776183915471,825.559694878252,125.51834395973));
#83968=CARTESIAN_POINT('Origin',(52.8776183915471,827.175936191914,121.458286566849));
#83969=CARTESIAN_POINT('Origin',(52.8776183915471,825.559694878252,125.51834395973));
#83970=CARTESIAN_POINT('Origin',(52.8776183915471,827.175936191914,121.458286566849));
#83971=CARTESIAN_POINT('Origin',(52.8776183915471,825.559694878252,125.51834395973));
#83972=CARTESIAN_POINT('Origin',(52.8776183915471,827.175936191914,121.458286566849));
#83973=CARTESIAN_POINT('Origin',(52.8776183915471,825.559694878252,125.51834395973));
#83974=CARTESIAN_POINT('Origin',(52.8776183915471,827.175936191914,121.458286566849));
#83975=CARTESIAN_POINT('Origin',(52.8776183915471,825.559694878252,125.51834395973));
#83976=CARTESIAN_POINT('Origin',(52.8776183915471,827.175936191914,121.458286566849));
#83977=CARTESIAN_POINT('Origin',(52.8776183915471,825.559694878252,125.51834395973));
#83978=CARTESIAN_POINT('Origin',(52.8776183915471,827.175936191914,121.458286566849));
#83979=CARTESIAN_POINT('Origin',(52.8776183915471,825.559694878252,125.51834395973));
#83980=CARTESIAN_POINT('Origin',(52.8776183915471,827.175936191914,121.458286566849));
#83981=CARTESIAN_POINT('Origin',(52.8776183915471,825.559694878252,125.51834395973));
#83982=CARTESIAN_POINT('Origin',(52.8776183915471,827.175936191914,121.458286566849));
#83983=CARTESIAN_POINT('Origin',(52.8776183915471,825.559694878252,125.51834395973));
#83984=CARTESIAN_POINT('Origin',(52.8776183915471,827.175936191914,121.458286566849));
#83985=CARTESIAN_POINT('Origin',(52.8776183915471,825.559694878252,125.51834395973));
#83986=CARTESIAN_POINT('Origin',(52.8776183915471,827.175936191914,121.458286566849));
#83987=CARTESIAN_POINT('Origin',(52.8776183915471,825.559694878252,125.51834395973));
#83988=CARTESIAN_POINT('Origin',(52.8776183915471,827.175936191914,121.458286566849));
#83989=CARTESIAN_POINT('Origin',(52.8776183915471,825.559694878252,125.51834395973));
#83990=CARTESIAN_POINT('Origin',(52.8776183915471,827.175936191914,121.458286566849));
#83991=CARTESIAN_POINT('Origin',(52.8776183915471,825.559694878252,125.51834395973));
#83992=CARTESIAN_POINT('Origin',(52.8776183915471,827.175936191914,121.458286566849));
#83993=CARTESIAN_POINT('Origin',(52.8776183915471,825.559694878252,125.51834395973));
#83994=CARTESIAN_POINT('Origin',(52.8776183915471,827.175936191914,121.458286566849));
#83995=CARTESIAN_POINT('Origin',(52.8776183915471,825.559694878252,125.51834395973));
#83996=CARTESIAN_POINT('Origin',(52.8776183915471,827.175936191914,121.458286566849));
#83997=CARTESIAN_POINT('Origin',(52.8776183915471,825.559694878252,125.51834395973));
#83998=CARTESIAN_POINT('Origin',(52.8776183915471,827.175936191914,121.458286566849));
#83999=CARTESIAN_POINT('Origin',(52.8776183915471,825.559694878252,125.51834395973));
#84000=CARTESIAN_POINT('Origin',(52.8776183915471,827.175936191914,121.458286566849));
#84001=CARTESIAN_POINT('Origin',(52.8776183915471,825.559694878252,125.51834395973));
#84002=CARTESIAN_POINT('Origin',(52.8776183915471,827.175936191914,121.458286566849));
#84003=CARTESIAN_POINT('Origin',(52.8776183915471,825.559694878252,125.51834395973));
#84004=CARTESIAN_POINT('Origin',(52.8776183915471,827.175936191914,121.458286566849));
#84005=CARTESIAN_POINT('Origin',(52.8776183915471,825.559694878252,125.51834395973));
#84006=CARTESIAN_POINT('Origin',(52.8776183915471,827.175936191914,121.458286566849));
#84007=CARTESIAN_POINT('Origin',(52.8776183915471,825.559694878252,125.51834395973));
#84008=CARTESIAN_POINT('Origin',(52.8776183915471,827.175936191914,121.458286566849));
#84009=CARTESIAN_POINT('Origin',(52.8776183915471,825.559694878252,125.51834395973));
#84010=CARTESIAN_POINT('Origin',(52.8776183915471,827.175936191914,121.458286566849));
#84011=CARTESIAN_POINT('Origin',(52.8776183915471,825.559694878252,125.51834395973));
#84012=CARTESIAN_POINT('Origin',(52.8776183915471,827.175936191914,121.458286566849));
#84013=CARTESIAN_POINT('Origin',(52.8776183915471,825.559694878252,125.51834395973));
#84014=CARTESIAN_POINT('Origin',(52.8776183915471,827.175936191914,121.458286566849));
#84015=CARTESIAN_POINT('Origin',(52.8776183915471,825.559694878252,125.51834395973));
#84016=CARTESIAN_POINT('Origin',(52.8776183915471,827.175936191914,121.458286566849));
#84017=CARTESIAN_POINT('Origin',(52.8776183915471,825.559694878252,125.51834395973));
#84018=CARTESIAN_POINT('Origin',(52.8776183915471,827.175936191914,121.458286566849));
#84019=CARTESIAN_POINT('Origin',(52.8776183915471,825.559694878252,125.51834395973));
#84020=CARTESIAN_POINT('Origin',(52.8776183915471,827.175936191914,121.458286566849));
#84021=CARTESIAN_POINT('Origin',(52.8776183915471,825.559694878252,125.51834395973));
#84022=CARTESIAN_POINT('Origin',(52.8776183915471,827.175936191914,121.458286566849));
#84023=CARTESIAN_POINT('Origin',(52.8776183915471,825.559694878252,125.51834395973));
#84024=CARTESIAN_POINT('Origin',(52.8776183915471,827.175936191914,121.458286566849));
#84025=CARTESIAN_POINT('Origin',(52.8776183915471,825.559694878252,125.51834395973));
#84026=CARTESIAN_POINT('Origin',(52.8776183915471,827.175936191914,121.458286566849));
#84027=CARTESIAN_POINT('Origin',(52.8776183915471,825.559694878252,125.51834395973));
#84028=CARTESIAN_POINT('Origin',(52.8776183915471,827.175936191914,121.458286566849));
#84029=CARTESIAN_POINT('Origin',(52.8776183915471,825.559694878252,125.51834395973));
#84030=CARTESIAN_POINT('Origin',(52.8776183915471,827.175936191914,121.458286566849));
#84031=CARTESIAN_POINT('Origin',(52.8776183915471,825.559694878252,125.51834395973));
#84032=CARTESIAN_POINT('Origin',(52.8776183915471,827.175936191914,121.458286566849));
#84033=CARTESIAN_POINT('Origin',(52.8776183915471,825.559694878252,125.51834395973));
#84034=CARTESIAN_POINT('Origin',(52.8776183915471,827.175936191914,121.458286566849));
#84035=CARTESIAN_POINT('Origin',(52.8776183915471,825.559694878252,125.51834395973));
#84036=CARTESIAN_POINT('Origin',(52.8776183915471,827.175936191914,121.458286566849));
#84037=CARTESIAN_POINT('Origin',(52.8776183915471,825.559694878252,125.51834395973));
#84038=CARTESIAN_POINT('Origin',(52.8776183915471,827.175936191914,121.458286566849));
#84039=CARTESIAN_POINT('Origin',(52.8776183915471,825.559694878252,125.51834395973));
#84040=CARTESIAN_POINT('Origin',(52.8776183915471,827.175936191914,121.458286566849));
#84041=CARTESIAN_POINT('Origin',(52.8776183915471,825.559694878252,125.51834395973));
#84042=CARTESIAN_POINT('Origin',(52.8776183915471,827.175936191914,121.458286566849));
#84043=CARTESIAN_POINT('Origin',(52.8776183915471,825.559694878252,125.51834395973));
#84044=CARTESIAN_POINT('Origin',(52.8776183915471,827.175936191914,121.458286566849));
#84045=CARTESIAN_POINT('Origin',(52.8776183915471,825.559694878252,125.51834395973));
#84046=CARTESIAN_POINT('Origin',(52.8776183915471,827.175936191914,121.458286566849));
#84047=CARTESIAN_POINT('Origin',(52.8776183915471,825.559694878252,125.51834395973));
#84048=CARTESIAN_POINT('Origin',(52.8776183915471,827.175936191914,121.458286566849));
#84049=CARTESIAN_POINT('Origin',(52.8776183915471,825.559694878252,125.51834395973));
#84050=CARTESIAN_POINT('Origin',(52.8776183915471,827.175936191914,121.458286566849));
#84051=CARTESIAN_POINT('Origin',(52.8776183915471,825.559694878252,125.51834395973));
#84052=CARTESIAN_POINT('Origin',(52.8776183915471,827.175936191914,121.458286566849));
#84053=CARTESIAN_POINT('Origin',(52.8776183915471,825.559694878252,125.51834395973));
#84054=CARTESIAN_POINT('Origin',(52.8776183915471,827.175936191914,121.458286566849));
#84055=CARTESIAN_POINT('Origin',(52.8776183915471,825.559694878252,125.51834395973));
#84056=CARTESIAN_POINT('Origin',(52.8776183915471,827.175936191914,121.458286566849));
#84057=CARTESIAN_POINT('Origin',(52.8776183915471,825.559694878252,125.51834395973));
#84058=CARTESIAN_POINT('Origin',(52.8776183915471,827.175936191914,121.458286566849));
#84059=CARTESIAN_POINT('Origin',(52.8776183915471,825.559694878252,125.51834395973));
#84060=CARTESIAN_POINT('Origin',(52.8776183915471,827.175936191914,121.458286566849));
#84061=CARTESIAN_POINT('Origin',(52.8776183915471,825.559694878252,125.51834395973));
#84062=CARTESIAN_POINT('Origin',(52.8776183915471,827.175936191914,121.458286566849));
#84063=CARTESIAN_POINT('Origin',(52.8776183915471,825.559694878252,125.51834395973));
#84064=CARTESIAN_POINT('Origin',(52.8776183915471,827.175936191914,121.458286566849));
#84065=CARTESIAN_POINT('Origin',(52.8776183915471,825.559694878252,125.51834395973));
#84066=CARTESIAN_POINT('Origin',(52.8776183915471,827.175936191914,121.458286566849));
#84067=CARTESIAN_POINT('Origin',(52.8776183915471,825.559694878252,125.51834395973));
#84068=CARTESIAN_POINT('Origin',(52.8776183915471,827.175936191914,121.458286566849));
#84069=CARTESIAN_POINT('Origin',(52.8776183915471,825.559694878252,125.51834395973));
#84070=CARTESIAN_POINT('Origin',(52.8776183915471,827.175936191914,121.458286566849));
#84071=CARTESIAN_POINT('Origin',(52.8776183915471,825.559694878252,125.51834395973));
#84072=CARTESIAN_POINT('Origin',(52.8776183915471,827.175936191914,121.458286566849));
#84073=CARTESIAN_POINT('Origin',(52.8776183915471,825.559694878252,125.51834395973));
#84074=CARTESIAN_POINT('Origin',(52.8776183915471,827.175936191914,121.458286566849));
#84075=CARTESIAN_POINT('Origin',(52.8776183915471,825.559694878252,125.51834395973));
#84076=CARTESIAN_POINT('Origin',(52.8776183915471,827.175936191914,121.458286566849));
#84077=CARTESIAN_POINT('Origin',(52.8776183915471,825.559694878252,125.51834395973));
#84078=CARTESIAN_POINT('Origin',(52.8776183915471,827.175936191914,121.458286566849));
#84079=CARTESIAN_POINT('Origin',(52.8776183915471,825.559694878252,125.51834395973));
#84080=CARTESIAN_POINT('Origin',(52.8776183915471,827.175936191914,121.458286566849));
#84081=CARTESIAN_POINT('Origin',(52.8776183915471,825.559694878252,125.51834395973));
#84082=CARTESIAN_POINT('Origin',(52.8776183915471,827.175936191914,121.458286566849));
#84083=CARTESIAN_POINT('Origin',(52.8776183915471,825.559694878252,125.51834395973));
#84084=CARTESIAN_POINT('Origin',(52.8776183915471,827.175936191914,121.458286566849));
#84085=CARTESIAN_POINT('Origin',(52.8776183915471,825.559694878252,125.51834395973));
#84086=CARTESIAN_POINT('Origin',(52.8776183915471,827.175936191914,121.458286566849));
#84087=CARTESIAN_POINT('Origin',(52.8776183915471,825.559694878252,125.51834395973));
#84088=CARTESIAN_POINT('Origin',(52.8776183915471,827.175936191914,121.458286566849));
#84089=CARTESIAN_POINT('Origin',(52.8776183915471,825.559694878252,125.51834395973));
#84090=CARTESIAN_POINT('Origin',(52.8776183915471,827.175936191914,121.458286566849));
#84091=CARTESIAN_POINT('Origin',(52.8776183915471,825.559694878252,125.51834395973));
#84092=CARTESIAN_POINT('Origin',(52.8776183915471,827.175936191914,121.458286566849));
#84093=CARTESIAN_POINT('Origin',(52.8776183915471,825.559694878252,125.51834395973));
#84094=CARTESIAN_POINT('Origin',(52.8776183915471,827.175936191914,121.458286566849));
#84095=CARTESIAN_POINT('Origin',(52.8776183915471,825.559694878252,125.51834395973));
#84096=CARTESIAN_POINT('Origin',(52.8776183915471,827.175936191914,121.458286566849));
#84097=CARTESIAN_POINT('Origin',(52.8776183915471,825.559694878252,125.51834395973));
#84098=CARTESIAN_POINT('Origin',(52.8776183915471,827.175936191914,121.458286566849));
#84099=CARTESIAN_POINT('Origin',(52.8776183915471,825.559694878252,125.51834395973));
#84100=CARTESIAN_POINT('Origin',(52.8776183915471,827.175936191914,121.458286566849));
#84101=CARTESIAN_POINT('Origin',(52.8776183915471,825.559694878252,125.51834395973));
#84102=CARTESIAN_POINT('Origin',(52.8776183915471,827.175936191914,121.458286566849));
#84103=CARTESIAN_POINT('Origin',(52.8776183915471,825.559694878252,125.51834395973));
#84104=CARTESIAN_POINT('Origin',(52.8776183915471,827.175936191914,121.458286566849));
#84105=CARTESIAN_POINT('Origin',(52.8776183915471,825.559694878252,125.51834395973));
#84106=CARTESIAN_POINT('Origin',(52.8776183915471,827.175936191914,121.458286566849));
#84107=CARTESIAN_POINT('Origin',(52.8776183915471,825.559694878252,125.51834395973));
#84108=CARTESIAN_POINT('Origin',(52.8776183915471,827.175936191914,121.458286566849));
#84109=CARTESIAN_POINT('Origin',(52.8776183915471,825.559694878252,125.51834395973));
#84110=CARTESIAN_POINT('Origin',(52.8776183915471,827.175936191914,121.458286566849));
#84111=CARTESIAN_POINT('Origin',(52.8776183915471,825.559694878252,125.51834395973));
#84112=CARTESIAN_POINT('Origin',(52.8776183915471,827.175936191914,121.458286566849));
#84113=CARTESIAN_POINT('Origin',(52.8776183915471,825.559694878252,125.51834395973));
#84114=CARTESIAN_POINT('Origin',(52.8776183915471,827.175936191914,121.458286566849));
#84115=CARTESIAN_POINT('Origin',(52.8776183915471,825.559694878252,125.51834395973));
#84116=CARTESIAN_POINT('Origin',(52.8776183915471,827.175936191914,121.458286566849));
#84117=CARTESIAN_POINT('Origin',(52.8776183915471,825.559694878252,125.51834395973));
#84118=CARTESIAN_POINT('Origin',(52.8776183915471,827.175936191914,121.458286566849));
#84119=CARTESIAN_POINT('Origin',(52.8776183915471,825.559694878252,125.51834395973));
#84120=CARTESIAN_POINT('Origin',(52.8776183915471,827.175936191914,121.458286566849));
#84121=CARTESIAN_POINT('Origin',(52.8776183915471,825.559694878252,125.51834395973));
#84122=CARTESIAN_POINT('Origin',(52.8776183915471,827.175936191914,121.458286566849));
#84123=CARTESIAN_POINT('Origin',(52.8776183915471,825.559694878252,125.51834395973));
#84124=CARTESIAN_POINT('Origin',(52.8776183915471,827.175936191914,121.458286566849));
#84125=CARTESIAN_POINT('Origin',(52.8776183915471,825.559694878252,125.51834395973));
#84126=CARTESIAN_POINT('Origin',(52.8776183915471,827.175936191914,121.458286566849));
#84127=CARTESIAN_POINT('Origin',(52.8776183915471,825.559694878252,125.51834395973));
#84128=CARTESIAN_POINT('Origin',(52.8776183915471,827.175936191914,121.458286566849));
#84129=CARTESIAN_POINT('Origin',(52.8776183915471,825.559694878252,125.51834395973));
#84130=CARTESIAN_POINT('Origin',(52.8776183915471,827.175936191914,121.458286566849));
#84131=CARTESIAN_POINT('Origin',(52.8776183915471,825.559694878252,125.51834395973));
#84132=CARTESIAN_POINT('Origin',(52.8776183915471,827.175936191914,121.458286566849));
#84133=CARTESIAN_POINT('Origin',(52.8776183915471,825.559694878252,125.51834395973));
#84134=CARTESIAN_POINT('Origin',(52.8776183915471,827.175936191914,121.458286566849));
#84135=CARTESIAN_POINT('Origin',(52.8776183915471,825.559694878252,125.51834395973));
#84136=CARTESIAN_POINT('Origin',(52.8776183915471,827.175936191914,121.458286566849));
#84137=CARTESIAN_POINT('Origin',(52.8776183915471,825.559694878252,125.51834395973));
#84138=CARTESIAN_POINT('Origin',(52.8776183915471,827.175936191914,121.458286566849));
#84139=CARTESIAN_POINT('Origin',(52.8776183915471,825.559694878252,125.51834395973));
#84140=CARTESIAN_POINT('Origin',(52.8776183915471,827.175936191914,121.458286566849));
#84141=CARTESIAN_POINT('Origin',(52.8776183915471,825.559694878252,125.51834395973));
#84142=CARTESIAN_POINT('Origin',(52.8776183915471,827.175936191914,121.458286566849));
#84143=CARTESIAN_POINT('Origin',(52.8776183915471,825.559694878252,125.51834395973));
#84144=CARTESIAN_POINT('Origin',(52.8776183915471,827.175936191914,121.458286566849));
#84145=CARTESIAN_POINT('Origin',(52.8776183915471,825.559694878252,125.51834395973));
#84146=CARTESIAN_POINT('Origin',(52.8776183915471,827.175936191914,121.458286566849));
#84147=CARTESIAN_POINT('Origin',(52.8776183915471,825.559694878252,125.51834395973));
#84148=CARTESIAN_POINT('Origin',(52.8776183915471,827.175936191914,121.458286566849));
#84149=CARTESIAN_POINT('Origin',(52.8776183915471,825.559694878252,125.51834395973));
#84150=CARTESIAN_POINT('Origin',(52.8776183915471,827.175936191914,121.458286566849));
#84151=CARTESIAN_POINT('Origin',(52.8776183915471,825.559694878252,125.51834395973));
#84152=CARTESIAN_POINT('Origin',(52.8776183915471,827.175936191914,121.458286566849));
#84153=CARTESIAN_POINT('Origin',(52.8776183915471,825.559694878252,125.51834395973));
#84154=CARTESIAN_POINT('Origin',(52.8776183915471,827.175936191914,121.458286566849));
#84155=CARTESIAN_POINT('Origin',(52.8776183915471,825.559694878252,125.51834395973));
#84156=CARTESIAN_POINT('Origin',(52.8776183915471,827.175936191914,121.458286566849));
#84157=CARTESIAN_POINT('Origin',(52.8776183915471,825.559694878252,125.51834395973));
#84158=CARTESIAN_POINT('Origin',(52.8776183915471,827.175936191914,121.458286566849));
#84159=CARTESIAN_POINT('Origin',(52.8776183915471,825.559694878252,125.51834395973));
#84160=CARTESIAN_POINT('Origin',(52.8776183915471,827.175936191914,121.458286566849));
#84161=CARTESIAN_POINT('Origin',(52.8776183915471,825.559694878252,125.51834395973));
#84162=CARTESIAN_POINT('Origin',(52.8776183915471,827.175936191914,121.458286566849));
#84163=CARTESIAN_POINT('Origin',(52.8776183915471,825.559694878252,125.51834395973));
#84164=CARTESIAN_POINT('Origin',(52.8776183915471,827.175936191914,121.458286566849));
#84165=CARTESIAN_POINT('Origin',(52.8776183915471,825.559694878252,125.51834395973));
#84166=CARTESIAN_POINT('Origin',(52.8776183915471,827.175936191914,121.458286566849));
#84167=CARTESIAN_POINT('Origin',(52.8776183915471,825.559694878252,125.51834395973));
#84168=CARTESIAN_POINT('Origin',(52.8776183915471,827.175936191914,121.458286566849));
#84169=CARTESIAN_POINT('Origin',(52.8776183915471,825.559694878252,125.51834395973));
#84170=CARTESIAN_POINT('Origin',(52.8776183915471,827.175936191914,121.458286566849));
#84171=CARTESIAN_POINT('Origin',(52.8776183915471,825.559694878252,125.51834395973));
#84172=CARTESIAN_POINT('Origin',(52.8776183915471,827.175936191914,121.458286566849));
#84173=CARTESIAN_POINT('Origin',(52.8776183915471,825.559694878252,125.51834395973));
#84174=CARTESIAN_POINT('Origin',(52.8776183915471,827.175936191914,121.458286566849));
#84175=CARTESIAN_POINT('Origin',(52.8776183915471,825.559694878252,125.51834395973));
#84176=CARTESIAN_POINT('Origin',(52.8776183915471,827.175936191914,121.458286566849));
#84177=CARTESIAN_POINT('Origin',(52.8776183915471,825.559694878252,125.51834395973));
#84178=CARTESIAN_POINT('Origin',(52.8776183915471,827.175936191914,121.458286566849));
#84179=CARTESIAN_POINT('Origin',(52.8776183915471,825.559694878252,125.51834395973));
#84180=CARTESIAN_POINT('Origin',(52.8776183915471,827.175936191914,121.458286566849));
#84181=CARTESIAN_POINT('Origin',(52.8776183915471,825.559694878252,125.51834395973));
#84182=CARTESIAN_POINT('Origin',(52.8776183915471,827.175936191914,121.458286566849));
#84183=CARTESIAN_POINT('Origin',(52.8776183915471,825.559694878252,125.51834395973));
#84184=CARTESIAN_POINT('Origin',(52.8776183915471,827.175936191914,121.458286566849));
#84185=CARTESIAN_POINT('Origin',(52.8776183915471,825.559694878252,125.51834395973));
#84186=CARTESIAN_POINT('Origin',(52.8776183915471,827.175936191914,121.458286566849));
#84187=CARTESIAN_POINT('Origin',(52.8776183915471,825.559694878252,125.51834395973));
#84188=CARTESIAN_POINT('Origin',(52.8776183915471,827.175936191914,121.458286566849));
#84189=CARTESIAN_POINT('Origin',(52.8776183915471,825.559694878252,125.51834395973));
#84190=CARTESIAN_POINT('Origin',(52.8776183915471,827.175936191914,121.458286566849));
#84191=CARTESIAN_POINT('Origin',(52.8776183915471,825.559694878252,125.51834395973));
#84192=CARTESIAN_POINT('Origin',(52.8776183915471,827.175936191914,121.458286566849));
#84193=CARTESIAN_POINT('Origin',(52.8776183915471,825.559694878252,125.51834395973));
#84194=CARTESIAN_POINT('Origin',(52.8776183915471,827.175936191914,121.458286566849));
#84195=CARTESIAN_POINT('Origin',(52.8776183915471,825.559694878252,125.51834395973));
#84196=CARTESIAN_POINT('Origin',(52.8776183915471,827.175936191914,121.458286566849));
#84197=CARTESIAN_POINT('Origin',(52.8776183915471,825.559694878252,125.51834395973));
#84198=CARTESIAN_POINT('Origin',(52.8776183915471,827.175936191914,121.458286566849));
#84199=CARTESIAN_POINT('Origin',(52.8776183915471,825.559694878252,125.51834395973));
#84200=CARTESIAN_POINT('Origin',(52.8776183915471,827.175936191914,121.458286566849));
#84201=CARTESIAN_POINT('Origin',(52.8776183915471,825.559694878252,125.51834395973));
#84202=CARTESIAN_POINT('Origin',(52.8776183915471,827.175936191914,121.458286566849));
#84203=CARTESIAN_POINT('Origin',(52.8776183915471,825.559694878252,125.51834395973));
#84204=CARTESIAN_POINT('Origin',(52.8776183915471,827.175936191914,121.458286566849));
#84205=CARTESIAN_POINT('Origin',(52.8776183915471,825.559694878252,125.51834395973));
#84206=CARTESIAN_POINT('Origin',(52.8776183915471,827.175936191914,121.458286566849));
#84207=CARTESIAN_POINT('Origin',(52.8776183915471,825.559694878252,125.51834395973));
#84208=CARTESIAN_POINT('Origin',(52.8776183915471,827.175936191914,121.458286566849));
#84209=CARTESIAN_POINT('Origin',(52.8776183915471,825.559694878252,125.51834395973));
#84210=CARTESIAN_POINT('Origin',(52.8776183915471,827.175936191914,121.458286566849));
#84211=CARTESIAN_POINT('Origin',(52.8776183915471,825.559694878252,125.51834395973));
#84212=CARTESIAN_POINT('Origin',(52.8776183915471,827.175936191914,121.458286566849));
#84213=CARTESIAN_POINT('Ctrl Pts',(3.84082565589434,825.316688336501,125.465893547845));
#84214=CARTESIAN_POINT('Ctrl Pts',(3.8442236582366,824.679598781654,125.240724542698));
#84215=CARTESIAN_POINT('Ctrl Pts',(3.86158552590586,824.042711504904,125.015627029475));
#84216=CARTESIAN_POINT('Ctrl Pts',(3.89290384275382,823.406298553624,124.790697158922));
#84217=CARTESIAN_POINT('Ctrl Pts',(2.81394584476287,825.297442889065,125.504849768887));
#84218=CARTESIAN_POINT('Ctrl Pts',(2.81741500469536,824.647012037505,125.274965498068));
#84219=CARTESIAN_POINT('Ctrl Pts',(2.83514044735389,823.996787699948,125.045154216285));
#84220=CARTESIAN_POINT('Ctrl Pts',(2.86711460128858,823.347047620715,124.815514087779));
#84221=CARTESIAN_POINT('Ctrl Pts',(1.76405870526505,825.258413667814,125.599434679541));
#84222=CARTESIAN_POINT('Ctrl Pts',(1.76760061707955,824.594342606667,125.364729497126));
#84223=CARTESIAN_POINT('Ctrl Pts',(1.78569778065552,823.930482390338,125.130098834403));
#84224=CARTESIAN_POINT('Ctrl Pts',(1.8183424657619,823.267116587731,124.895642914219));
#84225=CARTESIAN_POINT('Origin',(52.8776183915471,827.175936191914,121.458286566849));
#84226=CARTESIAN_POINT('Ctrl Pts',(0.000492700221437848,819.600382093278,
123.878802654728));
#84227=CARTESIAN_POINT('Ctrl Pts',(0.0733770646291771,819.010988593857,
123.670491049405));
#84228=CARTESIAN_POINT('Ctrl Pts',(0.157334275777137,818.422906232969,123.462642844803));
#84229=CARTESIAN_POINT('Ctrl Pts',(0.252337935209915,817.836319919877,123.255323394113));
#84230=CARTESIAN_POINT('Ctrl Pts',(-0.948554213994308,819.448222594439,
123.977266388053));
#84231=CARTESIAN_POINT('Ctrl Pts',(-0.87436170962564,818.848250568395,123.765215973488));
#84232=CARTESIAN_POINT('Ctrl Pts',(-0.788897621333276,818.249613213403,
123.553637276833));
#84233=CARTESIAN_POINT('Ctrl Pts',(-0.692188821376213,817.652498757506,
123.342596824246));
#84234=CARTESIAN_POINT('Ctrl Pts',(-1.91572574332748,819.278466654302,124.11917574241));
#84235=CARTESIAN_POINT('Ctrl Pts',(-1.84020011653079,818.667714076086,123.903315115938));
#84236=CARTESIAN_POINT('Ctrl Pts',(-1.75320037320342,818.058320150858,123.687934683404));
#84237=CARTESIAN_POINT('Ctrl Pts',(-1.65475386845653,817.450476488823,123.473102166337));
#84238=CARTESIAN_POINT('Origin',(52.8776183915471,827.175936191914,121.458286566849));
#84239=CARTESIAN_POINT('Ctrl Pts',(2.46855401679697,809.370840123866,120.258308875262));
#84240=CARTESIAN_POINT('Ctrl Pts',(2.67073628760838,808.806131617377,120.058721781679));
#84241=CARTESIAN_POINT('Ctrl Pts',(2.88355991138435,808.244909852193,119.86036702045));
#84242=CARTESIAN_POINT('Ctrl Pts',(3.10695729599134,807.687353070633,119.663307588441));
#84243=CARTESIAN_POINT('Ctrl Pts',(1.56447923623846,809.035572744419,120.291078774796));
#84244=CARTESIAN_POINT('Ctrl Pts',(1.77028759879318,808.460736322933,120.087912133367));
#84245=CARTESIAN_POINT('Ctrl Pts',(1.98692816448921,807.889449176641,119.885999925883));
#84246=CARTESIAN_POINT('Ctrl Pts',(2.21433212894391,807.321892744598,119.685406279047));
#84247=CARTESIAN_POINT('Ctrl Pts',(0.643150928951218,808.679241949644,120.36596729256));
#84248=CARTESIAN_POINT('Ctrl Pts',(0.852654584240296,808.094084330198,120.159152790545));
#84249=CARTESIAN_POINT('Ctrl Pts',(1.07318493506676,807.512539713244,119.95361524586));
#84250=CARTESIAN_POINT('Ctrl Pts',(1.30467194166409,806.934792795578,119.749419936601));
#84251=CARTESIAN_POINT('Origin',(52.8776183915471,827.175936191914,121.458286566849));
#84252=CARTESIAN_POINT('Ctrl Pts',(5.00031415269847,815.719484412942,122.072244000229));
#84253=CARTESIAN_POINT('Ctrl Pts',(5.14465313820655,815.094556777728,121.85137342899));
#84254=CARTESIAN_POINT('Ctrl Pts',(5.30272291144696,814.472589472092,121.631549138388));
#84255=CARTESIAN_POINT('Ctrl Pts',(5.47445532125263,813.853850654815,121.412865904811));
#84256=CARTESIAN_POINT('Ctrl Pts',(3.99763435701107,815.499604445748,122.039117284757));
#84257=CARTESIAN_POINT('Ctrl Pts',(4.14499618991626,814.86158914147,121.813621088437));
#84258=CARTESIAN_POINT('Ctrl Pts',(4.30637637025783,814.226596164049,121.589193084692));
#84259=CARTESIAN_POINT('Ctrl Pts',(4.48170531959961,813.594899288235,121.365930034782));
#84260=CARTESIAN_POINT('Ctrl Pts',(2.9724864061455,815.255447616079,122.059996186536));
#84261=CARTESIAN_POINT('Ctrl Pts',(3.12293882273279,814.604051372859,121.82977071364));
#84262=CARTESIAN_POINT('Ctrl Pts',(3.28770359012886,813.95574084302,121.600635836259));
#84263=CARTESIAN_POINT('Ctrl Pts',(3.466709670646,813.31079554312,121.372690345005));
#84264=CARTESIAN_POINT('Origin',(52.8776183915471,827.175936191914,121.458286566849));
#84265=CARTESIAN_POINT('Ctrl Pts',(7.14679452608843,799.846737018268,116.886459225876));
#84266=CARTESIAN_POINT('Ctrl Pts',(7.46834327891507,799.335514201564,116.705775784797));
#84267=CARTESIAN_POINT('Ctrl Pts',(7.79948339953489,798.829763525227,116.527026383277));
#84268=CARTESIAN_POINT('Ctrl Pts',(8.14011016077353,798.329644939187,116.350267553035));
#84269=CARTESIAN_POINT('Ctrl Pts',(6.32653782350611,799.340882241166,116.857967319315));
#84270=CARTESIAN_POINT('Ctrl Pts',(6.65385407618119,798.820489811793,116.674043026856));
#84271=CARTESIAN_POINT('Ctrl Pts',(6.99093373343021,798.305667674524,116.492087464103));
#84272=CARTESIAN_POINT('Ctrl Pts',(7.3376701896266,797.796578648251,116.31215817676));
#84273=CARTESIAN_POINT('Ctrl Pts',(5.49062488819893,798.810708086188,116.870422046865));
#84274=CARTESIAN_POINT('Ctrl Pts',(5.82381872494313,798.280971023826,116.683195044925));
#84275=CARTESIAN_POINT('Ctrl Pts',(6.16695128670662,797.756904278727,116.497972124965));
#84276=CARTESIAN_POINT('Ctrl Pts',(6.5199140535566,797.238673593504,116.314811866034));
#84277=CARTESIAN_POINT('Origin',(52.8776183915471,827.175936191914,121.458286566849));
#84278=CARTESIAN_POINT('Ctrl Pts',(8.25143832150338,806.549530642949,118.829815173907));
#84279=CARTESIAN_POINT('Ctrl Pts',(8.53030342011268,805.96729913711,118.624034859448));
#84280=CARTESIAN_POINT('Ctrl Pts',(8.8219243969931,805.390649719661,118.420227443901));
#84281=CARTESIAN_POINT('Ctrl Pts',(9.12617563318484,804.819830788713,118.218480719563));
#84282=CARTESIAN_POINT('Ctrl Pts',(7.31405734151393,806.13669890325,118.72757413102));
#84283=CARTESIAN_POINT('Ctrl Pts',(7.59878005193337,805.542237519374,118.517471363854));
#84284=CARTESIAN_POINT('Ctrl Pts',(7.89652658015303,804.953475476663,118.309382936699));
#84285=CARTESIAN_POINT('Ctrl Pts',(8.20716866856419,804.370666390877,118.103398485944));
#84286=CARTESIAN_POINT('Ctrl Pts',(6.35560773678644,805.695128252369,118.678095158437));
#84287=CARTESIAN_POINT('Ctrl Pts',(6.64631971501044,805.088162111066,118.463572786888));
#84288=CARTESIAN_POINT('Ctrl Pts',(6.95032947278689,804.487015199085,118.25110712788));
#84289=CARTESIAN_POINT('Ctrl Pts',(7.26750605455168,803.891946467103,118.040789703343));
#84290=CARTESIAN_POINT('Origin',(52.8776183915471,827.175936191914,121.458286566849));
#84291=CARTESIAN_POINT('Ctrl Pts',(13.820198976375,791.445139376217,113.912623895849));
#84292=CARTESIAN_POINT('Ctrl Pts',(14.2485767358446,791.00733451784,113.757888845401));
#84293=CARTESIAN_POINT('Ctrl Pts',(14.6851662425343,790.576801200474,113.605723803585));
#84294=CARTESIAN_POINT('Ctrl Pts',(15.1298286699926,790.153676324828,113.456177155743));
#84295=CARTESIAN_POINT('Ctrl Pts',(13.1175861709652,790.78687998019,113.829937150564));
#84296=CARTESIAN_POINT('Ctrl Pts',(13.5536701154277,790.341199350592,113.672418536083));
#84297=CARTESIAN_POINT('Ctrl Pts',(13.9981135300995,789.902921071413,113.517516162705));
#84298=CARTESIAN_POINT('Ctrl Pts',(14.4507750911487,789.472184506096,113.365279286186));
#84299=CARTESIAN_POINT('Ctrl Pts',(12.4015228153398,790.101272006005,113.787392724708));
#84300=CARTESIAN_POINT('Ctrl Pts',(12.8454604690467,789.647564834443,113.627037258712));
#84301=CARTESIAN_POINT('Ctrl Pts',(13.2979081439044,789.201393326868,113.469345151344));
#84302=CARTESIAN_POINT('Ctrl Pts',(13.7587219708917,788.762899356612,113.314366545442));
#84303=CARTESIAN_POINT('Origin',(52.8776183915471,827.175936191914,121.458286566849));
#84304=CARTESIAN_POINT('Ctrl Pts',(13.4452714124558,798.220327738148,115.884933356194));
#84305=CARTESIAN_POINT('Ctrl Pts',(13.8473572187005,797.70461362743,115.702662539843));
#84306=CARTESIAN_POINT('Ctrl Pts',(14.2607352601467,797.196897982581,115.523218651965));
#84307=CARTESIAN_POINT('Ctrl Pts',(14.6852266063437,796.697400568031,115.346679364745));
#84308=CARTESIAN_POINT('Ctrl Pts',(12.6187070497033,797.63399734938,115.720502517623));
#84309=CARTESIAN_POINT('Ctrl Pts',(13.0292212104253,797.107473055197,115.534411016664));
#84310=CARTESIAN_POINT('Ctrl Pts',(13.4512643094595,796.589114887379,115.35120570107));
#84311=CARTESIAN_POINT('Ctrl Pts',(13.8846536656899,796.079147216966,115.170965871158));
#84312=CARTESIAN_POINT('Ctrl Pts',(11.7736026754359,797.015140000607,115.607204037821));
#84313=CARTESIAN_POINT('Ctrl Pts',(12.1927342403887,796.477563048284,115.417206153499));
#84314=CARTESIAN_POINT('Ctrl Pts',(12.6236367560647,795.948323643482,115.230155040579));
#84315=CARTESIAN_POINT('Ctrl Pts',(13.0661237065545,795.427650867176,115.046131664029));
#84316=CARTESIAN_POINT('Origin',(52.8776183915471,827.175936191914,121.458286566849));
#84317=CARTESIAN_POINT('Ctrl Pts',(22.1980264899163,784.534083757446,111.466793902928));
#84318=CARTESIAN_POINT('Ctrl Pts',(22.713880531712,784.189975556137,111.345174421393));
#84319=CARTESIAN_POINT('Ctrl Pts',(23.2361643237017,783.854600088267,111.226641383336));
#84320=CARTESIAN_POINT('Ctrl Pts',(23.7647115850361,783.528064128199,111.111232526427));
#84321=CARTESIAN_POINT('Ctrl Pts',(21.6467475207342,783.752542356409,111.339802088341));
#84322=CARTESIAN_POINT('Ctrl Pts',(22.1718708997924,783.402250904191,111.215997236719));
#84323=CARTESIAN_POINT('Ctrl Pts',(22.7035395646771,783.060849103155,111.095334288614));
#84324=CARTESIAN_POINT('Ctrl Pts',(23.2415842466528,782.728445646282,110.977851659803));
#84325=CARTESIAN_POINT('Ctrl Pts',(21.0849267323589,782.941344425908,111.252006419899));
#84326=CARTESIAN_POINT('Ctrl Pts',(21.6194967013644,782.58475148371,111.125974408502));
#84327=CARTESIAN_POINT('Ctrl Pts',(22.1607297011565,782.237208111092,111.003140821195));
#84328=CARTESIAN_POINT('Ctrl Pts',(22.7084534179776,781.898824956343,110.883544764827));
#84329=CARTESIAN_POINT('Origin',(52.8776183915471,827.175936191914,121.458286566849));
#84330=CARTESIAN_POINT('Ctrl Pts',(20.3722156592907,791.094625888558,113.365198749342));
#84331=CARTESIAN_POINT('Ctrl Pts',(20.8778391407687,790.670597907231,113.215332913395));
#84332=CARTESIAN_POINT('Ctrl Pts',(21.3926859167994,790.256553475804,113.068995601785));
#84333=CARTESIAN_POINT('Ctrl Pts',(21.916534279872,789.852670893462,112.926249831477));
#84334=CARTESIAN_POINT('Ctrl Pts',(19.689809879067,790.358096599145,113.146794345208));
#84335=CARTESIAN_POINT('Ctrl Pts',(20.2060482232254,789.925166739327,112.9937822842));
#84336=CARTESIAN_POINT('Ctrl Pts',(20.7317034921946,789.502430020172,112.844372823996));
#84337=CARTESIAN_POINT('Ctrl Pts',(21.2665493240224,789.090068484008,112.698630304515));
#84338=CARTESIAN_POINT('Ctrl Pts',(18.9920735300533,789.585590955693,112.978457958024));
#84339=CARTESIAN_POINT('Ctrl Pts',(19.5191652048056,789.143559232471,112.82222899052));
#84340=CARTESIAN_POINT('Ctrl Pts',(20.0558717846221,788.71193494923,112.66967836445));
#84341=CARTESIAN_POINT('Ctrl Pts',(20.6019621485449,788.290903975535,112.520871772407));
#84342=CARTESIAN_POINT('Origin',(52.8776183915471,827.175936191914,121.458286566849));
#84343=CARTESIAN_POINT('Ctrl Pts',(31.9219622709691,779.417686408915,109.655646046072));
#84344=CARTESIAN_POINT('Ctrl Pts',(32.5011814287363,779.183130129333,109.572745920458));
#84345=CARTESIAN_POINT('Ctrl Pts',(33.0847382986841,778.958334790098,109.493295641431));
#84346=CARTESIAN_POINT('Ctrl Pts',(33.6724478603244,778.743371664027,109.417320399219));
#84347=CARTESIAN_POINT('Ctrl Pts',(31.5451527574604,778.543748134616,109.495603117894));
#84348=CARTESIAN_POINT('Ctrl Pts',(32.1347870168974,778.304974232972,109.411212341936));
#84349=CARTESIAN_POINT('Ctrl Pts',(32.7288369861309,778.076136785871,109.330333445222));
#84350=CARTESIAN_POINT('Ctrl Pts',(33.3271143177676,777.857308347711,109.252992070931));
#84351=CARTESIAN_POINT('Ctrl Pts',(31.161132595897,777.638356388944,109.374173686482));
#84352=CARTESIAN_POINT('Ctrl Pts',(31.7613812609754,777.395284156583,109.288263735011));
#84353=CARTESIAN_POINT('Ctrl Pts',(32.366125126033,777.162327251614,109.205928882501));
#84354=CARTESIAN_POINT('Ctrl Pts',(32.9751724531075,776.939559534534,109.12719523375));
#84355=CARTESIAN_POINT('Origin',(52.8776183915471,827.175936191914,121.458286566849));
#84356=CARTESIAN_POINT('Ctrl Pts',(28.7148160478869,785.478954218345,111.379630155249));
#84357=CARTESIAN_POINT('Ctrl Pts',(29.3048316403161,785.162691727128,111.267852289844));
#84358=CARTESIAN_POINT('Ctrl Pts',(29.9017032114044,784.858080026341,111.160192207991));
#84359=CARTESIAN_POINT('Ctrl Pts',(30.5051719961012,784.565251175986,111.056696584164));
#84360=CARTESIAN_POINT('Ctrl Pts',(28.2069988999599,784.623787837421,111.118728900438));
#84361=CARTESIAN_POINT('Ctrl Pts',(28.8094145456246,784.30087862063,111.004601857317));
#84362=CARTESIAN_POINT('Ctrl Pts',(29.4188302585139,783.989865052919,110.894679139081));
#84363=CARTESIAN_POINT('Ctrl Pts',(30.0349818352457,783.690881969727,110.789008401135));
#84364=CARTESIAN_POINT('Ctrl Pts',(27.6877606464623,783.729919130396,110.90704547314));
#84365=CARTESIAN_POINT('Ctrl Pts',(28.3028552298343,783.400213699273,110.790516417919));
#84366=CARTESIAN_POINT('Ctrl Pts',(28.9250972096328,783.082654282895,110.678280175279));
#84367=CARTESIAN_POINT('Ctrl Pts',(29.5542168218329,782.777378554559,110.570385403623));
#84368=CARTESIAN_POINT('Origin',(52.8776183915471,827.175936191914,121.458286566849));
#84369=CARTESIAN_POINT('Ctrl Pts',(42.5551319591545,776.317087718572,108.558576546772));
#84370=CARTESIAN_POINT('Ctrl Pts',(43.1748960382436,776.20126800047,108.517641939537));
#84371=CARTESIAN_POINT('Ctrl Pts',(43.796753920824,776.095896381883,108.480400044191));
#84372=CARTESIAN_POINT('Ctrl Pts',(44.4205074850962,776.00100643385,108.446862725874));
#84373=CARTESIAN_POINT('Ctrl Pts',(42.3696630121901,775.388170827814,108.378775171248));
#84374=CARTESIAN_POINT('Ctrl Pts',(43.0005626826765,775.270270122607,108.337105072758));
#84375=CARTESIAN_POINT('Ctrl Pts',(43.6335937770019,775.163005242812,108.29919403484));
#84376=CARTESIAN_POINT('Ctrl Pts',(44.2685546136197,775.066410362653,108.265054135823));
#84377=CARTESIAN_POINT('Ctrl Pts',(42.1806476137204,774.426785367898,108.237145342521));
#84378=CARTESIAN_POINT('Ctrl Pts',(42.8228958052374,774.306763883913,108.194725689052));
#84379=CARTESIAN_POINT('Ctrl Pts',(43.4673137603,774.197569540843,108.156132713528));
#84380=CARTESIAN_POINT('Ctrl Pts',(44.1136961695466,774.099237127634,108.12137871154));
#84381=CARTESIAN_POINT('Origin',(52.8776183915471,827.175936191914,121.458286566849));
#84382=CARTESIAN_POINT('Ctrl Pts',(38.1133381600097,781.620808531784,110.015513754693));
#84383=CARTESIAN_POINT('Ctrl Pts',(38.7603804515547,781.427496535375,109.947190754287));
#84384=CARTESIAN_POINT('Ctrl Pts',(39.4115526444503,781.246932435716,109.883373291929));
#84385=CARTESIAN_POINT('Ctrl Pts',(40.0665722423738,781.079194566457,109.82408905338));
#84386=CARTESIAN_POINT('Ctrl Pts',(37.8031710004168,780.685060281388,109.725715192468));
#84387=CARTESIAN_POINT('Ctrl Pts',(38.4638063196311,780.48768719755,109.655956866354));
#84388=CARTESIAN_POINT('Ctrl Pts',(39.1286583009287,780.303329817553,109.590798730375));
#84389=CARTESIAN_POINT('Ctrl Pts',(39.7974385133204,780.132068120674,109.530269051914));
#84390=CARTESIAN_POINT('Ctrl Pts',(37.486030705108,779.708823383608,109.484436565335));
#84391=CARTESIAN_POINT('Ctrl Pts',(38.160564648583,779.507297911529,109.413210644717));
#84392=CARTESIAN_POINT('Ctrl Pts',(38.839403965417,779.319061971182,109.346681694276));
#84393=CARTESIAN_POINT('Ctrl Pts',(39.5222541565317,779.144197224472,109.284878576092));
#84394=CARTESIAN_POINT('Origin',(52.8776183915471,827.175936191914,121.458286566849));
#84395=CARTESIAN_POINT('Origin',(52.8776183915471,825.559694878252,125.51834395973));
#84396=CARTESIAN_POINT('Origin',(52.8776183915471,827.175936191914,121.458286566849));
#84397=CARTESIAN_POINT('Ctrl Pts',(53.6435222021547,775.36779391924,108.222950328633));
#84398=CARTESIAN_POINT('Ctrl Pts',(54.2751643466901,775.376386049419,108.22598707816));
#84399=CARTESIAN_POINT('Ctrl Pts',(54.9065432779137,775.395604598973,108.232779563848));
#84400=CARTESIAN_POINT('Ctrl Pts',(55.5374579069272,775.425443446955,108.243325622348));
#84401=CARTESIAN_POINT('Ctrl Pts',(53.6572481924173,774.424257074307,108.037580241535));
#84402=CARTESIAN_POINT('Ctrl Pts',(54.3002101839168,774.43300318661,108.040671413555));
#84403=CARTESIAN_POINT('Ctrl Pts',(54.9429042449805,774.452566157514,108.047585629402));
#84404=CARTESIAN_POINT('Ctrl Pts',(55.5851256829359,774.482939756375,108.058320686956));
#84405=CARTESIAN_POINT('Ctrl Pts',(53.6712359705142,773.44809401445,107.890070523166));
#84406=CARTESIAN_POINT('Ctrl Pts',(54.3257337058396,773.456997045688,107.893217155647));
#84407=CARTESIAN_POINT('Ctrl Pts',(54.979958703638,773.476911006889,107.900255423342));
#84408=CARTESIAN_POINT('Ctrl Pts',(55.6337025987302,773.507829555624,107.91118308462));
#84409=CARTESIAN_POINT('Origin',(52.8776183915471,827.175936191914,121.458286566849));
#84410=CARTESIAN_POINT('Ctrl Pts',(48.1619991748231,779.687415153512,109.332005249395));
#84411=CARTESIAN_POINT('Ctrl Pts',(48.8357364265094,779.625835415267,109.310240886297));
#84412=CARTESIAN_POINT('Ctrl Pts',(49.5106850110303,779.577464239345,109.293144876046));
#84413=CARTESIAN_POINT('Ctrl Pts',(50.1865536600841,779.542322499915,109.280724596282));
#84414=CARTESIAN_POINT('Ctrl Pts',(48.0629532561413,778.711286166964,109.02778511079));
#84415=CARTESIAN_POINT('Ctrl Pts',(48.7508415497114,778.648413020268,109.005563613381));
#84416=CARTESIAN_POINT('Ctrl Pts',(49.4399666187075,778.599025865885,108.988108521966));
#84417=CARTESIAN_POINT('Ctrl Pts',(50.130031077087,778.56314601642,108.97542736914));
#84418=CARTESIAN_POINT('Ctrl Pts',(47.9616810252838,777.693773274732,108.771738246455));
#84419=CARTESIAN_POINT('Ctrl Pts',(48.6640384418585,777.629577646898,108.749049339465));
#84420=CARTESIAN_POINT('Ctrl Pts',(49.3676586483386,777.57915167732,108.731227095611));
#84421=CARTESIAN_POINT('Ctrl Pts',(50.0722380034285,777.542517126896,108.71827920593));
#84422=CARTESIAN_POINT('Origin',(52.8776183915471,827.175936191914,121.458286566849));
#84423=CARTESIAN_POINT('Origin',(52.8776183915471,825.559694878252,125.51834395973));
#84424=CARTESIAN_POINT('Origin',(52.8776183915471,827.175936191914,121.458286566849));
#84425=CARTESIAN_POINT('Ctrl Pts',(64.7036892859012,776.620201057868,108.665594837008));
#84426=CARTESIAN_POINT('Ctrl Pts',(65.3179672524269,776.752533429287,108.712365574645));
#84427=CARTESIAN_POINT('Ctrl Pts',(65.929649521093,776.89515429438,108.762772614066));
#84428=CARTESIAN_POINT('Ctrl Pts',(66.5385422613663,777.048018459292,108.816799982235));
#84429=CARTESIAN_POINT('Ctrl Pts',(64.9163700462617,775.695883179202,108.487536320395));
#84430=CARTESIAN_POINT('Ctrl Pts',(65.5416952241698,775.830595423837,108.535148185752));
#84431=CARTESIAN_POINT('Ctrl Pts',(66.164378023034,775.975781191025,108.586461748359));
#84432=CARTESIAN_POINT('Ctrl Pts',(66.7842211264615,776.131394474147,108.641460747921));
#84433=CARTESIAN_POINT('Ctrl Pts',(65.1331213486505,774.739141244516,108.347756181132));
#84434=CARTESIAN_POINT('Ctrl Pts',(65.7697051728548,774.876278911263,108.39622527273));
#84435=CARTESIAN_POINT('Ctrl Pts',(66.4035990433899,775.024078670752,108.448462708663));
#84436=CARTESIAN_POINT('Ctrl Pts',(67.0346020912866,775.182493688035,108.504451935877));
#84437=CARTESIAN_POINT('Origin',(52.8776183915471,827.175936191914,121.458286566849));
#84438=CARTESIAN_POINT('Ctrl Pts',(58.4091473829218,779.76738491836,109.360315888696));
#84439=CARTESIAN_POINT('Ctrl Pts',(59.0834071649073,779.839801671071,109.385910419386));
#84440=CARTESIAN_POINT('Ctrl Pts',(59.7559212371808,779.925441548512,109.416178449772));
#84441=CARTESIAN_POINT('Ctrl Pts',(60.4263979154771,780.02426740677,109.451106851937));
#84442=CARTESIAN_POINT('Ctrl Pts',(58.5251440477691,778.794488373911,109.057209042452));
#84443=CARTESIAN_POINT('Ctrl Pts',(59.2135431185612,778.868423712496,109.083340292773));
#84444=CARTESIAN_POINT('Ctrl Pts',(59.9001598719503,778.955859465938,109.114243046502));
#84445=CARTESIAN_POINT('Ctrl Pts',(60.5846965070255,779.05675771141,109.149903900429));
#84446=CARTESIAN_POINT('Ctrl Pts',(58.6437438476791,777.780377886812,108.802135529116));
#84447=CARTESIAN_POINT('Ctrl Pts',(59.3465995136287,777.855865890564,108.828815543843));
#84448=CARTESIAN_POINT('Ctrl Pts',(60.0476354329541,777.945137822094,108.860367265037));
#84449=CARTESIAN_POINT('Ctrl Pts',(60.7465475508325,778.048154962186,108.896777008017));
#84450=CARTESIAN_POINT('Origin',(52.8776183915471,827.175936191914,121.458286566849));
#84451=CARTESIAN_POINT('Origin',(52.8776183915471,825.559694878252,125.51834395973));
#84452=CARTESIAN_POINT('Origin',(52.8776183915471,827.175936191914,121.458286566849));
#84453=CARTESIAN_POINT('Origin',(52.8776183915471,825.559694878252,125.51834395973));
#84454=CARTESIAN_POINT('Origin',(52.8776183915471,827.175936191914,121.458286566849));
#84455=CARTESIAN_POINT('Ctrl Pts',(75.2378334424178,780.001886138673,109.86318891898));
#84456=CARTESIAN_POINT('Ctrl Pts',(75.8111772114877,780.252813357473,109.951875088439));
#84457=CARTESIAN_POINT('Ctrl Pts',(76.3796786218251,780.51335069488,110.04395779898));
#84458=CARTESIAN_POINT('Ctrl Pts',(76.9431564894166,780.783415116447,110.139407703419));
#84459=CARTESIAN_POINT('Ctrl Pts',(75.6395522221989,779.139143914756,109.707161743586));
#84460=CARTESIAN_POINT('Ctrl Pts',(76.2231965612223,779.394579237611,109.797441229553));
#84461=CARTESIAN_POINT('Ctrl Pts',(76.8019115447451,779.659797332383,109.891178278124));
#84462=CARTESIAN_POINT('Ctrl Pts',(77.3755127336413,779.934713672844,109.98834301487));
#84463=CARTESIAN_POINT('Ctrl Pts',(76.0489516266781,778.245201444726,109.589757869781));
#84464=CARTESIAN_POINT('Ctrl Pts',(76.6430934764404,778.505231063911,109.681661135523));
#84465=CARTESIAN_POINT('Ctrl Pts',(77.2322173106074,778.77521940935,109.777084152086));
#84466=CARTESIAN_POINT('Ctrl Pts',(77.8161353727047,779.055080434516,109.875996507714));
#84467=CARTESIAN_POINT('Origin',(52.8776183915471,827.175936191914,121.458286566849));
#84468=CARTESIAN_POINT('Ctrl Pts',(68.4183096607616,781.857910547663,110.099377322435));
#84469=CARTESIAN_POINT('Ctrl Pts',(69.0612797297983,782.061204974069,110.171228451366));
#84470=CARTESIAN_POINT('Ctrl Pts',(69.6996238599015,782.277070010889,110.247522459354));
#84471=CARTESIAN_POINT('Ctrl Pts',(70.333065618516,782.505412178569,110.328226307563));
#84472=CARTESIAN_POINT('Ctrl Pts',(68.7452591349629,780.925783914164,109.810967425304));
#84473=CARTESIAN_POINT('Ctrl Pts',(69.4017561908213,781.133355306418,109.884330178681));
#84474=CARTESIAN_POINT('Ctrl Pts',(70.0535299859299,781.353761773157,109.962229281665));
#84475=CARTESIAN_POINT('Ctrl Pts',(70.7002982720667,781.586907868177,110.044631000341));
#84476=CARTESIAN_POINT('Ctrl Pts',(69.0795696415712,779.95316335926,109.571259129136));
#84477=CARTESIAN_POINT('Ctrl Pts',(69.7498982346366,780.165108010175,109.646167540096));
#84478=CARTESIAN_POINT('Ctrl Pts',(70.4154040540052,780.390158153862,109.725707875637));
#84479=CARTESIAN_POINT('Ctrl Pts',(71.0757989048528,780.628216333193,109.809845691112));
#84480=CARTESIAN_POINT('Origin',(52.8776183915471,827.175936191914,121.458286566849));
#84481=CARTESIAN_POINT('Origin',(52.8776183915471,825.559694878252,125.51834395973));
#84482=CARTESIAN_POINT('Origin',(52.8776183915471,827.175936191914,121.458286566849));
#84483=CARTESIAN_POINT('Origin',(52.8776183915471,825.559694878252,125.51834395973));
#84484=CARTESIAN_POINT('Origin',(52.8776183915471,827.175936191914,121.458286566849));
#84485=CARTESIAN_POINT('Ctrl Pts',(84.7978201531078,785.382466127243,111.767254473936));
#84486=CARTESIAN_POINT('Ctrl Pts',(85.3021477216854,785.739908233174,111.893586608527));
#84487=CARTESIAN_POINT('Ctrl Pts',(85.799642046942,786.105763910382,112.022892383889));
#84488=CARTESIAN_POINT('Ctrl Pts',(86.2901452539088,786.479917058139,112.155130766095));
#84489=CARTESIAN_POINT('Ctrl Pts',(85.3722795647444,784.614952542165,111.645559022608));
#84490=CARTESIAN_POINT('Ctrl Pts',(85.8856833829171,784.978827438946,111.774164723145));
#84491=CARTESIAN_POINT('Ctrl Pts',(86.3921309816998,785.351267323819,111.905797580278));
#84492=CARTESIAN_POINT('Ctrl Pts',(86.8914616448896,785.732154006619,112.040415821602));
#84493=CARTESIAN_POINT('Ctrl Pts',(85.9577410185038,783.817981991301,111.563287639805));
#84494=CARTESIAN_POINT('Ctrl Pts',(86.4803949145324,784.188412879694,111.694210449606));
#84495=CARTESIAN_POINT('Ctrl Pts',(86.9959672598652,784.567563072923,111.828214956761));
#84496=CARTESIAN_POINT('Ctrl Pts',(87.50429444265,784.955312251376,111.965258636247));
#84497=CARTESIAN_POINT('Origin',(52.8776183915471,827.175936191914,121.458286566849));
#84498=CARTESIAN_POINT('Ctrl Pts',(77.7523941907489,785.863531124246,111.515718880779));
#84499=CARTESIAN_POINT('Ctrl Pts',(78.3358113354591,786.188591421181,111.630606188406));
#84500=CARTESIAN_POINT('Ctrl Pts',(78.9119357508628,786.525015861201,111.749509968715));
#84501=CARTESIAN_POINT('Ctrl Pts',(79.4805184652575,786.872659058756,111.872378837532));
#84502=CARTESIAN_POINT('Ctrl Pts',(78.274356371013,785.017733856259,111.258191966894));
#84503=CARTESIAN_POINT('Ctrl Pts',(78.8700157038463,785.349615086282,111.375490023066));
#84504=CARTESIAN_POINT('Ctrl Pts',(79.458229279707,785.693098919947,111.496888831949));
#84505=CARTESIAN_POINT('Ctrl Pts',(80.0387429025715,786.048036920993,111.622335931147));
#84506=CARTESIAN_POINT('Ctrl Pts',(78.808039345768,784.133535105251,111.049797417012));
#84507=CARTESIAN_POINT('Ctrl Pts',(79.4162157681955,784.472390434162,111.169560355706));
#84508=CARTESIAN_POINT('Ctrl Pts',(80.0167899697085,784.823092181966,111.29351021967));
#84509=CARTESIAN_POINT('Ctrl Pts',(80.6095024126493,785.185488793185,111.421593444071));
#84510=CARTESIAN_POINT('Origin',(52.8776183915471,827.175936191914,121.458286566849));
#84511=CARTESIAN_POINT('Ctrl Pts',(92.9661650926069,792.518247313548,114.29315925778));
#84512=CARTESIAN_POINT('Ctrl Pts',(93.3806595130324,792.967234459711,114.451846507093));
#84513=CARTESIAN_POINT('Ctrl Pts',(93.7866039081684,793.423113039347,114.612969422174));
#84514=CARTESIAN_POINT('Ctrl Pts',(94.1838694119097,793.885738334861,114.776476854927));
#84515=CARTESIAN_POINT('Ctrl Pts',(93.6856293079454,791.88073464461,114.217671724052));
#84516=CARTESIAN_POINT('Ctrl Pts',(94.1075626087368,792.337779707844,114.379206913905));
#84517=CARTESIAN_POINT('Ctrl Pts',(94.5207924379869,792.80183988426,114.543221482119));
#84518=CARTESIAN_POINT('Ctrl Pts',(94.9251876168462,793.272767859034,114.709663362651));
#84519=CARTESIAN_POINT('Ctrl Pts',(94.4188341119727,791.216367871884,114.182274053281));
#84520=CARTESIAN_POINT('Ctrl Pts',(94.8483483635669,791.681624745213,114.346711574676));
#84521=CARTESIAN_POINT('Ctrl Pts',(95.2690027667957,792.154022773513,114.513673021864));
#84522=CARTESIAN_POINT('Ctrl Pts',(95.6806637858958,792.633411995128,114.683105393322));
#84523=CARTESIAN_POINT('Origin',(52.8776183915471,827.175936191914,121.458286566849));
#84524=CARTESIAN_POINT('Ctrl Pts',(85.9972328647244,791.603786356977,113.5456214498));
#84525=CARTESIAN_POINT('Ctrl Pts',(86.4968504914115,792.037099733043,113.698769058426));
#84526=CARTESIAN_POINT('Ctrl Pts',(86.9867952965917,792.48012280452,113.855348401947));
#84527=CARTESIAN_POINT('Ctrl Pts',(87.4668550512191,792.932663667419,114.015291654998));
#84528=CARTESIAN_POINT('Ctrl Pts',(86.6918182644616,790.878584527844,113.331530897999));
#84529=CARTESIAN_POINT('Ctrl Pts',(87.2019138847627,791.320985363089,113.487890322181));
#84530=CARTESIAN_POINT('Ctrl Pts',(87.7021338248975,791.773299525725,113.647753451688));
#84531=CARTESIAN_POINT('Ctrl Pts',(88.192261404947,792.235331087145,113.811051038723));
#84532=CARTESIAN_POINT('Ctrl Pts',(87.4019915546031,790.117715985974,113.167502367862));
#84533=CARTESIAN_POINT('Ctrl Pts',(87.9228003157242,790.569408221219,113.327145687187));
#84534=CARTESIAN_POINT('Ctrl Pts',(88.4335259854642,791.031221985746,113.49036629743));
#84535=CARTESIAN_POINT('Ctrl Pts',(88.9339473331445,791.502957236012,113.657093496435));
#84536=CARTESIAN_POINT('Origin',(52.8776183915471,827.175936191914,121.458286566849));
#84537=CARTESIAN_POINT('Ctrl Pts',(99.3836913129681,801.093665801638,117.329369223643));
#84538=CARTESIAN_POINT('Ctrl Pts',(99.6902065779454,801.614669831695,117.513509676477));
#84539=CARTESIAN_POINT('Ctrl Pts',(99.9868254004947,802.140741376905,117.69944116063));
#84540=CARTESIAN_POINT('Ctrl Pts',(100.273453568563,802.671713346455,117.887104620555));
#84541=CARTESIAN_POINT('Ctrl Pts',(100.217916781638,800.61003260618,117.30912382607));
#84542=CARTESIAN_POINT('Ctrl Pts',(100.529930314357,801.140382401292,117.496567388496));
#84543=CARTESIAN_POINT('Ctrl Pts',(100.831869882365,801.675890612593,117.685834109743));
#84544=CARTESIAN_POINT('Ctrl Pts',(101.123639583632,802.216387151997,117.876863874926));
#84545=CARTESIAN_POINT('Ctrl Pts',(101.068066047063,800.102499844735,117.32999314988));
#84546=CARTESIAN_POINT('Ctrl Pts',(101.385682799126,800.642373797997,117.520802872055));
#84547=CARTESIAN_POINT('Ctrl Pts',(101.693044675624,801.187498803613,117.713468493806));
#84548=CARTESIAN_POINT('Ctrl Pts',(101.990054052297,801.737701719013,117.907928820689));
#84549=CARTESIAN_POINT('Origin',(52.8776183915471,827.175936191914,121.458286566849));
#84550=CARTESIAN_POINT('Ctrl Pts',(92.7914283577236,798.843631763094,116.10536273626));
#84551=CARTESIAN_POINT('Ctrl Pts',(93.1830725017883,799.363954194011,116.289262288895));
#84552=CARTESIAN_POINT('Ctrl Pts',(93.5631886174356,799.891821941612,116.475828611749));
#84553=CARTESIAN_POINT('Ctrl Pts',(93.9316132340898,800.427007994094,116.664981471169));
#84554=CARTESIAN_POINT('Ctrl Pts',(93.6299721692471,798.269043655217,115.945277016441));
#84555=CARTESIAN_POINT('Ctrl Pts',(94.0298443119319,798.800297469402,116.133040089796));
#84556=CARTESIAN_POINT('Ctrl Pts',(94.4179462354163,799.339255118804,116.323525959183));
#84557=CARTESIAN_POINT('Ctrl Pts',(94.7941110347935,799.88568482236,116.516652705331));
#84558=CARTESIAN_POINT('Ctrl Pts',(94.4873670344129,797.662074949797,115.836662038794));
#84559=CARTESIAN_POINT('Ctrl Pts',(94.8956521469038,798.204505892421,116.028375487527));
#84560=CARTESIAN_POINT('Ctrl Pts',(95.2919194047924,798.754802752404,116.222869017605));
#84561=CARTESIAN_POINT('Ctrl Pts',(95.6759983916348,799.312728872205,116.420058986245));
#84562=CARTESIAN_POINT('Origin',(52.8776183915471,827.175936191914,121.458286566849));
#84563=CARTESIAN_POINT('Ctrl Pts',(103.763049025154,810.745309098518,120.745216801789));
#84564=CARTESIAN_POINT('Ctrl Pts',(103.947373053888,811.313710833613,120.946109207325));
#84565=CARTESIAN_POINT('Ctrl Pts',(104.120955679622,811.885110913332,121.148061329302));
#84566=CARTESIAN_POINT('Ctrl Pts',(104.283742090387,812.459328907384,121.351009397552));
#84567=CARTESIAN_POINT('Ctrl Pts',(104.677088626,810.434154205991,120.786938235321));
#84568=CARTESIAN_POINT('Ctrl Pts',(104.864723611516,811.012765969549,120.99143921038));
#84569=CARTESIAN_POINT('Ctrl Pts',(105.041424249458,811.594429936087,121.197018937247));
#84570=CARTESIAN_POINT('Ctrl Pts',(105.207134743288,812.178962434302,121.403612500268));
#84571=CARTESIAN_POINT('Ctrl Pts',(105.60859894153,810.102340362435,120.871081935004));
#84572=CARTESIAN_POINT('Ctrl Pts',(105.799608168593,810.691357306277,121.079260452844));
#84573=CARTESIAN_POINT('Ctrl Pts',(105.979486415616,811.283481340892,121.288537121695));
#84574=CARTESIAN_POINT('Ctrl Pts',(106.148176882671,811.878525492014,121.498845858524));
#84575=CARTESIAN_POINT('Origin',(52.8776183915471,827.175936191914,121.458286566849));
#84576=CARTESIAN_POINT('Ctrl Pts',(97.844501095678,807.253538512874,119.079062323388));
#84577=CARTESIAN_POINT('Ctrl Pts',(98.1134360590212,807.841098387078,119.286725863517));
#84578=CARTESIAN_POINT('Ctrl Pts',(98.3693602313756,808.433801630878,119.496207244492));
#84579=CARTESIAN_POINT('Ctrl Pts',(98.6121630384352,809.031392161588,119.707415958026));
#84580=CARTESIAN_POINT('Ctrl Pts',(98.7871151231428,806.85621056334,118.982521982872));
#84581=CARTESIAN_POINT('Ctrl Pts',(99.0616876102297,807.456087105858,119.194538650328));
#84582=CARTESIAN_POINT('Ctrl Pts',(99.3229765688517,808.061214835372,119.408411264947));
#84583=CARTESIAN_POINT('Ctrl Pts',(99.5708691067994,808.671332301084,119.624047421171));
#84584=CARTESIAN_POINT('Ctrl Pts',(99.7508719466112,806.430588090693,118.938656702047));
#84585=CARTESIAN_POINT('Ctrl Pts',(100.03120840688,807.043057563918,119.155124137308));
#84586=CARTESIAN_POINT('Ctrl Pts',(100.297982483717,807.660888459877,119.373486480771));
#84587=CARTESIAN_POINT('Ctrl Pts',(100.551078915019,808.283813839258,119.593649387051));
#84588=CARTESIAN_POINT('Origin',(52.8776183915471,827.175936191914,121.458286566849));
#84589=CARTESIAN_POINT('Ctrl Pts',(105.922015646428,821.04073406854,124.389683333783));
#84590=CARTESIAN_POINT('Ctrl Pts',(105.976969940256,821.633474172943,124.599177742542));
#84591=CARTESIAN_POINT('Ctrl Pts',(106.020740371651,822.227041648839,124.808964572381));
#84592=CARTESIAN_POINT('Ctrl Pts',(106.053313108912,822.821248925566,125.018977529483));
#84593=CARTESIAN_POINT('Ctrl Pts',(106.872914726583,820.914491596563,124.497433171603));
#84594=CARTESIAN_POINT('Ctrl Pts',(106.928854157205,821.517857441841,124.710683076718));
#84595=CARTESIAN_POINT('Ctrl Pts',(106.97340923816,822.122065490465,124.924230644992));
#84596=CARTESIAN_POINT('Ctrl Pts',(107.006565889793,822.726924809295,125.138008394194));
#84597=CARTESIAN_POINT('Ctrl Pts',(107.841951609362,820.771184791302,124.648706674861));
#84598=CARTESIAN_POINT('Ctrl Pts',(107.898894967643,821.385379056786,124.865783710065));
#84599=CARTESIAN_POINT('Ctrl Pts',(107.944249664856,822.000430640379,125.083163750497));
#84600=CARTESIAN_POINT('Ctrl Pts',(107.97800136866,822.616145182324,125.300778102843));
#84601=CARTESIAN_POINT('Origin',(52.8776183915471,827.175936191914,121.458286566849));
#84602=CARTESIAN_POINT('Ctrl Pts',(100.932612370989,816.47036724468,122.338107749172));
#84603=CARTESIAN_POINT('Ctrl Pts',(101.065805084989,817.097055564791,122.559600606029));
#84604=CARTESIAN_POINT('Ctrl Pts',(101.185180748678,817.726214116847,122.781966526437));
#84605=CARTESIAN_POINT('Ctrl Pts',(101.290687985324,818.357572124469,123.005109808863));
#84606=CARTESIAN_POINT('Ctrl Pts',(101.939753753683,816.265959562204,122.310820246181));
#84607=CARTESIAN_POINT('Ctrl Pts',(102.075737933939,816.905782078971,122.536955172542));
#84608=CARTESIAN_POINT('Ctrl Pts',(102.197615484758,817.548126599052,122.763981460209));
#84609=CARTESIAN_POINT('Ctrl Pts',(102.30533395265,818.192716671109,122.991801401925));
#84610=CARTESIAN_POINT('Ctrl Pts',(102.969479515644,816.037588240675,122.337754166415));
#84611=CARTESIAN_POINT('Ctrl Pts',(103.108317758664,816.690839478466,122.568635257159));
#84612=CARTESIAN_POINT('Ctrl Pts',(103.232753299529,817.346665651872,122.800426417274));
#84613=CARTESIAN_POINT('Ctrl Pts',(103.342732583845,818.004784507343,123.033027888805));
#84614=CARTESIAN_POINT('Origin',(52.8776183915471,827.175936191914,121.458286566849));
#84615=CARTESIAN_POINT('Ctrl Pts',(105.761429506502,831.539389861825,128.105886396078));
#84616=CARTESIAN_POINT('Ctrl Pts',(105.684526018595,832.12929698831,128.314379534585));
#84617=CARTESIAN_POINT('Ctrl Pts',(105.596532411993,832.717824608245,128.5223851088));
#84618=CARTESIAN_POINT('Ctrl Pts',(105.497476395537,833.304787396605,128.729837618589));
#84619=CARTESIAN_POINT('Ctrl Pts',(106.709627746758,831.601093240578,128.28105038138));
#84620=CARTESIAN_POINT('Ctrl Pts',(106.631345391663,832.201577307103,128.493281768376));
#84621=CARTESIAN_POINT('Ctrl Pts',(106.541774073826,832.800657132747,128.705016849131));
#84622=CARTESIAN_POINT('Ctrl Pts',(106.440941998903,833.398144069637,128.916188949105));
#84623=CARTESIAN_POINT('Ctrl Pts',(107.675914903239,831.649307998338,128.501051019185));
#84624=CARTESIAN_POINT('Ctrl Pts',(107.596227376105,832.260570782731,128.717091969783));
#84625=CARTESIAN_POINT('Ctrl Pts',(107.505048248806,832.870404120053,128.932627705419));
#84626=CARTESIAN_POINT('Ctrl Pts',(107.402406233289,833.478615976192,129.147590354741));
#84627=CARTESIAN_POINT('Origin',(52.8776183915471,827.175936191914,121.458286566849));
#84628=CARTESIAN_POINT('Ctrl Pts',(101.919463205941,826.096733439178,125.741939549448));
#84629=CARTESIAN_POINT('Ctrl Pts',(101.911465154775,826.733418377351,125.966965549372));
#84630=CARTESIAN_POINT('Ctrl Pts',(101.889523384275,827.369811805957,126.191888519951));
#84631=CARTESIAN_POINT('Ctrl Pts',(101.853647253075,828.005642289612,126.416612526737));
#84632=CARTESIAN_POINT('Ctrl Pts',(102.946478823582,826.093748663403,125.786887623192));
#84633=CARTESIAN_POINT('Ctrl Pts',(102.938313280277,826.743766814824,126.016626031818));
#84634=CARTESIAN_POINT('Ctrl Pts',(102.915912013585,827.393487351997,126.246259253499));
#84635=CARTESIAN_POINT('Ctrl Pts',(102.879284578122,828.042633155239,126.475689344762));
#84636=CARTESIAN_POINT('Ctrl Pts',(103.996505226553,826.071342075713,125.887605326046));
#84637=CARTESIAN_POINT('Ctrl Pts',(103.988168438367,826.734992177522,126.122161727189));
#84638=CARTESIAN_POINT('Ctrl Pts',(103.965297380245,827.398338423622,126.356610735442));
#84639=CARTESIAN_POINT('Ctrl Pts',(103.927901807182,828.061097882676,126.590852353298));
#84640=CARTESIAN_POINT('Origin',(52.8776183915471,827.175936191914,121.458286566849));
#84641=CARTESIAN_POINT('Ctrl Pts',(103.290428074605,841.770498106016,131.727402106468));
#84642=CARTESIAN_POINT('Ctrl Pts',(103.084642224443,842.334153467199,131.926616982866));
#84643=CARTESIAN_POINT('Ctrl Pts',(102.868256026129,842.89426875693,132.124580678231));
#84644=CARTESIAN_POINT('Ctrl Pts',(102.64133793703,843.450666773438,132.321230563463));
#84645=CARTESIAN_POINT('Ctrl Pts',(104.192978406205,842.015017669718,131.967882763203));
#84646=CARTESIAN_POINT('Ctrl Pts',(103.983508331965,842.588764262402,132.170664222258));
#84647=CARTESIAN_POINT('Ctrl Pts',(103.763248129479,843.158907405048,132.372172100145));
#84648=CARTESIAN_POINT('Ctrl Pts',(103.53226748172,843.725266723403,132.572342646498));
#84649=CARTESIAN_POINT('Ctrl Pts',(105.112720530425,842.249568871481,132.25432659535));
#84650=CARTESIAN_POINT('Ctrl Pts',(104.899496054949,842.8335989136,132.460742573385));
#84651=CARTESIAN_POINT('Ctrl Pts',(104.6752880562,843.413960919856,132.665862143435));
#84652=CARTESIAN_POINT('Ctrl Pts',(104.4401674661,843.990471283092,132.869620412519));
#84653=CARTESIAN_POINT('Origin',(52.8776183915471,827.175936191914,121.458286566849));
#84654=CARTESIAN_POINT('Ctrl Pts',(100.765958536865,835.701990838064,129.138530074238));
#84655=CARTESIAN_POINT('Ctrl Pts',(100.617419197977,836.324774219662,129.358642793697));
#84656=CARTESIAN_POINT('Ctrl Pts',(100.455247155973,836.94452713004,129.577684442088));
#84657=CARTESIAN_POINT('Ctrl Pts',(100.279511819792,837.56098431761,129.795561270526));
#84658=CARTESIAN_POINT('Ctrl Pts',(101.767197580229,835.89946903489,129.255457648539));
#84659=CARTESIAN_POINT('Ctrl Pts',(101.615552613017,836.535273436538,129.480172437062));
#84660=CARTESIAN_POINT('Ctrl Pts',(101.449989913085,837.16798400653,129.703793760794));
#84661=CARTESIAN_POINT('Ctrl Pts',(101.270580340559,837.797329947456,129.92622591077));
#84662=CARTESIAN_POINT('Ctrl Pts',(102.790832383946,836.0820659331,129.429603528724));
#84663=CARTESIAN_POINT('Ctrl Pts',(102.636012321573,836.731182609566,129.659023325598));
#84664=CARTESIAN_POINT('Ctrl Pts',(102.466983121322,837.377140676691,129.887326763058));
#84665=CARTESIAN_POINT('Ctrl Pts',(102.283817126965,838.019663667193,130.11441612821));
#84666=CARTESIAN_POINT('Origin',(52.8776183915471,827.175936191914,121.458286566849));
#84667=CARTESIAN_POINT('Ctrl Pts',(98.6188091293693,851.302769029011,135.10252964045));
#84668=CARTESIAN_POINT('Ctrl Pts',(98.2939262573026,851.812906345545,135.282829429041));
#84669=CARTESIAN_POINT('Ctrl Pts',(97.9594953788288,852.317528965392,135.461180137228));
#84670=CARTESIAN_POINT('Ctrl Pts',(97.6156217655107,852.816478044332,135.63752562409));
#84671=CARTESIAN_POINT('Ctrl Pts',(99.4361478251386,851.716860219949,135.403672389488));
#84672=CARTESIAN_POINT('Ctrl Pts',(99.1054596966138,852.23611306151,135.587193913055));
#84673=CARTESIAN_POINT('Ctrl Pts',(98.7650529505767,852.749752665553,135.768731528554));
#84674=CARTESIAN_POINT('Ctrl Pts',(98.4150347396632,853.257617349506,135.948228091895));
#84675=CARTESIAN_POINT('Ctrl Pts',(100.26902456131,852.124249564078,135.751775289756));
#84676=CARTESIAN_POINT('Ctrl Pts',(99.9324208153347,852.652791221614,135.938579795183));
#84677=CARTESIAN_POINT('Ctrl Pts',(99.5859245973349,853.175619227485,136.123364902786));
#84678=CARTESIAN_POINT('Ctrl Pts',(99.2296449767795,853.692569006813,136.306072446233));
#84679=CARTESIAN_POINT('Origin',(52.8776183915471,827.175936191914,121.458286566849));
#84680=CARTESIAN_POINT('Ctrl Pts',(97.5139865755203,844.864516615738,132.378233576775));
#84681=CARTESIAN_POINT('Ctrl Pts',(97.2312091993379,845.445397385802,132.583536495507));
#84682=CARTESIAN_POINT('Ctrl Pts',(96.9357387751277,846.020634534243,132.786844767402));
#84683=CARTESIAN_POINT('Ctrl Pts',(96.627701932469,846.589981532028,132.988071260757));
#84684=CARTESIAN_POINT('Ctrl Pts',(98.4487596583488,845.253923252333,132.563977905155));
#84685=CARTESIAN_POINT('Ctrl Pts',(98.1600603693754,845.846968804844,132.773580269611));
#84686=CARTESIAN_POINT('Ctrl Pts',(97.8584022150573,846.434252547228,132.981146215412));
#84687=CARTESIAN_POINT('Ctrl Pts',(97.5439144768452,847.015522787652,133.186586786147));
#84688=CARTESIAN_POINT('Ctrl Pts',(99.4044750958214,845.632687821054,132.808678028001));
#84689=CARTESIAN_POINT('Ctrl Pts',(99.1097212214331,846.238170691874,133.022676161574));
#84690=CARTESIAN_POINT('Ctrl Pts',(98.8017367090974,846.837770916207,133.234595168834));
#84691=CARTESIAN_POINT('Ctrl Pts',(98.4806535515487,847.43123152375,133.444344227781));
#84692=CARTESIAN_POINT('Origin',(52.8776183915471,827.175936191914,121.458286566849));
#84693=CARTESIAN_POINT('Ctrl Pts',(91.9417831532315,859.700313020388,138.074190482449));
#84694=CARTESIAN_POINT('Ctrl Pts',(91.5121277434549,860.135379853124,138.227957821992));
#84695=CARTESIAN_POINT('Ctrl Pts',(91.074364555794,860.563201391009,138.379164429184));
#84696=CARTESIAN_POINT('Ctrl Pts',(90.6286310070099,860.983643338031,138.52776283927));
#84697=CARTESIAN_POINT('Ctrl Pts',(92.6415135252399,860.265659888805,138.429787896317));
#84698=CARTESIAN_POINT('Ctrl Pts',(92.2041619841994,860.708519784021,138.586309567825));
#84699=CARTESIAN_POINT('Ctrl Pts',(91.7585574360481,861.144004604244,138.740224638289));
#84700=CARTESIAN_POINT('Ctrl Pts',(91.3048397590019,861.571977647906,138.891484792749));
#84701=CARTESIAN_POINT('Ctrl Pts',(93.3545782125711,860.827132606148,138.833605402784));
#84702=CARTESIAN_POINT('Ctrl Pts',(92.9093838800028,861.277934071264,138.992933893805));
#84703=CARTESIAN_POINT('Ctrl Pts',(92.4557885435564,861.721228208107,139.149609040998));
#84704=CARTESIAN_POINT('Ctrl Pts',(91.9939345898091,862.156875863715,139.303581662996));
#84705=CARTESIAN_POINT('Origin',(52.8776183915471,827.175936191914,121.458286566849));
#84706=CARTESIAN_POINT('Ctrl Pts',(92.3139898798326,853.195701951383,135.324194005371));
#84707=CARTESIAN_POINT('Ctrl Pts',(91.9087941278747,853.709482121067,135.505781301524));
#84708=CARTESIAN_POINT('Ctrl Pts',(91.492392464683,854.215234701004,135.68453137584));
#84709=CARTESIAN_POINT('Ctrl Pts',(91.0649637439505,854.712742459312,135.860367451222));
#84710=CARTESIAN_POINT('Ctrl Pts',(93.1370644539869,853.757382363456,135.571601530681));
#84711=CARTESIAN_POINT('Ctrl Pts',(92.7234118813732,854.28188561385,135.756978726381));
#84712=CARTESIAN_POINT('Ctrl Pts',(92.2983195195021,854.798193731065,135.939459484727));
#84713=CARTESIAN_POINT('Ctrl Pts',(91.8619699549135,855.306084949383,136.118965426209));
#84714=CARTESIAN_POINT('Ctrl Pts',(93.9785156047657,854.312363461301,135.87896966896));
#84715=CARTESIAN_POINT('Ctrl Pts',(93.5562173982128,854.8478292039,136.068221380331));
#84716=CARTESIAN_POINT('Ctrl Pts',(93.122240302644,855.374928529188,136.254516116739));
#84717=CARTESIAN_POINT('Ctrl Pts',(92.676770720788,855.893435036387,136.43777386049));
#84718=CARTESIAN_POINT('Origin',(52.8776183915471,827.175936191914,121.458286566849));
#84719=CARTESIAN_POINT('Ctrl Pts',(83.5602516028411,866.611482450665,140.520652182709));
#84720=CARTESIAN_POINT('Ctrl Pts',(83.0432523771499,866.953693687156,140.641601212692));
#84721=CARTESIAN_POINT('Ctrl Pts',(82.5198948914167,867.287202629092,140.759474557329));
#84722=CARTESIAN_POINT('Ctrl Pts',(81.9903439038852,867.611904284474,140.874235108896));
#84723=CARTESIAN_POINT('Ctrl Pts',(84.1086002196864,867.298879563462,140.919669805206));
#84724=CARTESIAN_POINT('Ctrl Pts',(83.5823613759883,867.647206671981,141.042780391299));
#84725=CARTESIAN_POINT('Ctrl Pts',(83.0496506397879,867.986675961771,141.162760324541));
#84726=CARTESIAN_POINT('Ctrl Pts',(82.5106357138271,868.317180564455,141.279571834033));
#84727=CARTESIAN_POINT('Ctrl Pts',(84.667374327897,867.984762138475,141.367536623201));
#84728=CARTESIAN_POINT('Ctrl Pts',(84.1317201977308,868.339321397187,141.492849862042));
#84729=CARTESIAN_POINT('Ctrl Pts',(83.589478382162,868.684864356089,141.614976435456));
#84730=CARTESIAN_POINT('Ctrl Pts',(83.0408195844131,869.021282234752,141.733877896759));
#84731=CARTESIAN_POINT('Origin',(52.8776183915471,827.175936191914,121.458286566849));
#84732=CARTESIAN_POINT('Ctrl Pts',(85.3908378832772,860.329215965232,137.846832736418));
#84733=CARTESIAN_POINT('Ctrl Pts',(84.8819518685354,860.752084986696,137.996288956734));
#84734=CARTESIAN_POINT('Ctrl Pts',(84.3638957786647,861.164937009303,138.142204830721));
#84735=CARTESIAN_POINT('Ctrl Pts',(83.8368913789253,861.5675953027,138.284517895892));
#84736=CARTESIAN_POINT('Ctrl Pts',(86.0696628273966,861.03975848912,138.147777713084));
#84737=CARTESIAN_POINT('Ctrl Pts',(85.5501520721363,861.471456351417,138.300354344482));
#84738=CARTESIAN_POINT('Ctrl Pts',(85.0212797849848,861.892928075657,138.449316712681));
#84739=CARTESIAN_POINT('Ctrl Pts',(84.4832723613125,862.303993241637,138.594601051076));
#84740=CARTESIAN_POINT('Ctrl Pts',(86.7636485216625,861.74691198598,138.509932643049));
#84741=CARTESIAN_POINT('Ctrl Pts',(86.2332757349034,862.187635870799,138.66569937621));
#84742=CARTESIAN_POINT('Ctrl Pts',(85.6933456835311,862.617919807489,138.817776278457));
#84743=CARTESIAN_POINT('Ctrl Pts',(85.1440894964343,863.037579603581,138.96609824994));
#84744=CARTESIAN_POINT('Origin',(52.8776183915471,827.175936191914,121.458286566849));
#84745=CARTESIAN_POINT('Ctrl Pts',(73.8390976335837,871.728561617911,142.332123170967));
#84746=CARTESIAN_POINT('Ctrl Pts',(73.2579608975552,871.962320061041,142.414741314184));
#84747=CARTESIAN_POINT('Ctrl Pts',(72.6725173783085,872.186321648689,142.493911054542));
#84748=CARTESIAN_POINT('Ctrl Pts',(72.0829513316637,872.400495881149,142.56960747506));
#84749=CARTESIAN_POINT('Ctrl Pts',(74.2138218059742,872.50749828857,142.764025385591));
#84750=CARTESIAN_POINT('Ctrl Pts',(73.6222962047354,872.74543558464,142.848120476832));
#84751=CARTESIAN_POINT('Ctrl Pts',(73.0263868287761,872.973441603873,142.928705518806));
#84752=CARTESIAN_POINT('Ctrl Pts',(72.4262812278209,873.191444586254,143.005755149094));
#84753=CARTESIAN_POINT('Ctrl Pts',(74.59567234048,873.286654376598,143.245433677184));
#84754=CARTESIAN_POINT('Ctrl Pts',(73.9935603025345,873.528849997446,143.331033804486));
#84755=CARTESIAN_POINT('Ctrl Pts',(73.3869860341711,873.760936603024,143.413061063744));
#84756=CARTESIAN_POINT('Ctrl Pts',(72.776140441661,873.98284114904,143.491489638634));
#84757=CARTESIAN_POINT('Origin',(52.8776183915471,827.175936191914,121.458286566849));
#84758=CARTESIAN_POINT('Ctrl Pts',(77.0446291096948,865.943081673865,139.831814242213));
#84759=CARTESIAN_POINT('Ctrl Pts',(76.4547328300808,866.25679917775,139.942692622983));
#84760=CARTESIAN_POINT('Ctrl Pts',(75.8580915804765,866.558965055531,140.049488268229));
#84761=CARTESIAN_POINT('Ctrl Pts',(75.2549597919521,866.849450451907,140.152155636127));
#84762=CARTESIAN_POINT('Ctrl Pts',(77.5495692953528,866.771277650764,140.174917758729));
#84763=CARTESIAN_POINT('Ctrl Pts',(76.9473478531268,867.091549898902,140.288112807904));
#84764=CARTESIAN_POINT('Ctrl Pts',(76.3382405129968,867.400029163813,140.39713981778));
#84765=CARTESIAN_POINT('Ctrl Pts',(75.7225070220598,867.69658389792,140.501952294994));
#84766=CARTESIAN_POINT('Ctrl Pts',(78.0657947333568,867.598694356786,140.580266045052));
#84767=CARTESIAN_POINT('Ctrl Pts',(77.4509726650595,867.925667845626,140.695829539433));
#84768=CARTESIAN_POINT('Ctrl Pts',(76.8291206212506,868.240601599858,140.807137784228));
#84769=CARTESIAN_POINT('Ctrl Pts',(76.2005037838652,868.54336131946,140.914143313267));
#84770=CARTESIAN_POINT('Origin',(52.8776183915471,827.175936191914,121.458286566849));
#84771=CARTESIAN_POINT('Ctrl Pts',(63.2008179182801,874.827293699973,143.428853925027));
#84772=CARTESIAN_POINT('Ctrl Pts',(62.5808898780519,874.942399752043,143.469536298538));
#84773=CARTESIAN_POINT('Ctrl Pts',(61.9588939175424,875.047120272489,143.506548073772));
#84774=CARTESIAN_POINT('Ctrl Pts',(61.3350257412051,875.141422312107,143.539877605362));
#84775=CARTESIAN_POINT('Ctrl Pts',(63.3851735065715,875.660694606795,143.880098746674));
#84776=CARTESIAN_POINT('Ctrl Pts',(62.7541745577303,875.777856266129,143.921507641346));
#84777=CARTESIAN_POINT('Ctrl Pts',(62.1210707589078,875.884446925102,143.959180386812));
#84778=CARTESIAN_POINT('Ctrl Pts',(61.4860613095217,875.980433046089,143.993105129741));
#84779=CARTESIAN_POINT('Ctrl Pts',(63.5730314472391,876.495363235131,144.381126406714));
#84780=CARTESIAN_POINT('Ctrl Pts',(62.9307512667703,876.614619553766,144.423275624858));
#84781=CARTESIAN_POINT('Ctrl Pts',(62.2863286050369,876.723115879801,144.461621897544));
#84782=CARTESIAN_POINT('Ctrl Pts',(61.6399662228172,876.820818076015,144.496153159522));
#84783=CARTESIAN_POINT('Origin',(52.8776183915471,827.175936191914,121.458286566849));
#84784=CARTESIAN_POINT('Ctrl Pts',(67.6425933777688,869.801569588793,141.196238235659));
#84785=CARTESIAN_POINT('Ctrl Pts',(66.9957449747181,869.993416316922,141.264043360677));
#84786=CARTESIAN_POINT('Ctrl Pts',(66.3448291753891,870.172616751141,141.327378857528));
#84787=CARTESIAN_POINT('Ctrl Pts',(65.6901240748378,870.339094330465,141.386217666971));
#84788=CARTESIAN_POINT('Ctrl Pts',(67.9507110880758,870.709135201805,141.567772915938));
#84789=CARTESIAN_POINT('Ctrl Pts',(67.2903641556304,870.904985416202,141.636993008463));
#84790=CARTESIAN_POINT('Ctrl Pts',(66.6258649478717,871.087925431933,141.701650199953));
#84791=CARTESIAN_POINT('Ctrl Pts',(65.9574973631851,871.257877090326,141.761716866487));
#84792=CARTESIAN_POINT('Ctrl Pts',(68.2657065447386,871.617715220731,142.002049885831));
#84793=CARTESIAN_POINT('Ctrl Pts',(67.5915597712301,871.817658286473,142.072716530507));
#84794=CARTESIAN_POINT('Ctrl Pts',(66.9131739487192,872.00442135796,142.138724919257));
#84795=CARTESIAN_POINT('Ctrl Pts',(66.2308389084616,872.177924643171,142.200046850881));
#84796=CARTESIAN_POINT('Origin',(52.8776183915471,827.175936191914,121.458286566849));
#84797=CARTESIAN_POINT('Ctrl Pts',(52.1069565671731,875.776490730993,143.765284624484));
#84798=CARTESIAN_POINT('Ctrl Pts',(51.4765013855252,875.767916475681,143.76225419254));
#84799=CARTESIAN_POINT('Ctrl Pts',(50.8463059048213,875.748823152766,143.755505966183));
#84800=CARTESIAN_POINT('Ctrl Pts',(50.2165675427821,875.719216743503,143.745042059391));
#84801=CARTESIAN_POINT('Ctrl Pts',(52.0932323946971,876.624413877709,144.221380036531));
#84802=CARTESIAN_POINT('Ctrl Pts',(51.4515498817118,876.615686929536,144.218295637763));
#84803=CARTESIAN_POINT('Ctrl Pts',(50.8101316945012,876.59625358711,144.211427237006));
#84804=CARTESIAN_POINT('Ctrl Pts',(50.1691787664591,876.566119938201,144.200776985884));
#84805=CARTESIAN_POINT('Ctrl Pts',(52.0792482260038,877.473916293593,144.727097056353));
#84806=CARTESIAN_POINT('Ctrl Pts',(51.4261256866218,877.465033759884,144.723957668392));
#84807=CARTESIAN_POINT('Ctrl Pts',(50.7732721854601,877.445253956481,144.716966816603));
#84808=CARTESIAN_POINT('Ctrl Pts',(50.1208922381873,877.414583079688,144.706126690969));
#84809=CARTESIAN_POINT('Origin',(52.8776183915471,827.175936191914,121.458286566849));
#84810=CARTESIAN_POINT('Ctrl Pts',(57.5979609920746,871.730424908023,141.878222226749));
#84811=CARTESIAN_POINT('Ctrl Pts',(56.9224864915348,871.791797290229,141.899913303207));
#84812=CARTESIAN_POINT('Ctrl Pts',(56.2458102319545,871.83998496928,141.916944459455));
#84813=CARTESIAN_POINT('Ctrl Pts',(55.5682216841954,871.874967331285,141.929308409845));
#84814=CARTESIAN_POINT('Ctrl Pts',(57.6964400038153,872.677944444343,142.264027428917));
#84815=CARTESIAN_POINT('Ctrl Pts',(57.0068732928368,872.740597219109,142.286171039429));
#84816=CARTESIAN_POINT('Ctrl Pts',(56.3160797508998,872.789790222437,142.303557511292));
#84817=CARTESIAN_POINT('Ctrl Pts',(55.6243548880048,872.825502410374,142.316179406861));
#84818=CARTESIAN_POINT('Ctrl Pts',(57.7971166535088,873.627373797714,142.712864928224));
#84819=CARTESIAN_POINT('Ctrl Pts',(57.0931432531388,873.691335538026,142.73547117145));
#84820=CARTESIAN_POINT('Ctrl Pts',(56.3879173903922,873.741556300245,142.75322088808));
#84821=CARTESIAN_POINT('Ctrl Pts',(55.6817407491769,873.778014600765,142.766106485082));
#84822=CARTESIAN_POINT('Origin',(52.8776183915471,827.175936191914,121.458286566849));
#84823=CARTESIAN_POINT('Ctrl Pts',(41.05568276073,874.527241609199,143.322686086998));
#84824=CARTESIAN_POINT('Ctrl Pts',(40.4400310058198,874.395533889448,143.276136122395));
#84825=CARTESIAN_POINT('Ctrl Pts',(39.8269516528412,874.25355950477,143.225957571027));
#84826=CARTESIAN_POINT('Ctrl Pts',(39.2166372801776,874.101363051674,143.172166194807));
#84827=CARTESIAN_POINT('Ctrl Pts',(40.8444331847336,875.355795549055,143.772293777475));
#84828=CARTESIAN_POINT('Ctrl Pts',(40.2177801711254,875.221734306089,143.724911998135));
#84829=CARTESIAN_POINT('Ctrl Pts',(39.5937455264405,875.077222940201,143.673836791766));
#84830=CARTESIAN_POINT('Ctrl Pts',(38.9725252703009,874.922306844807,143.619084201937));
#84831=CARTESIAN_POINT('Ctrl Pts',(40.6291678739282,876.185517036185,144.27170857765));
#84832=CARTESIAN_POINT('Ctrl Pts',(39.9913044739241,876.04905753086,144.223479171246));
#84833=CARTESIAN_POINT('Ctrl Pts',(39.3561062836415,875.901960957186,144.171490264972));
#84834=CARTESIAN_POINT('Ctrl Pts',(38.7237728293571,875.744273520633,144.115758189407));
#84835=CARTESIAN_POINT('Origin',(52.8776183915471,827.175936191914,121.458286566849));
#84836=CARTESIAN_POINT('Ctrl Pts',(47.3453867844678,871.652360600451,141.850744181654));
#84837=CARTESIAN_POINT('Ctrl Pts',(46.6707644356192,871.580401462171,141.825311387387));
#84838=CARTESIAN_POINT('Ctrl Pts',(45.9978656469194,871.495297131312,141.795232637284));
#84839=CARTESIAN_POINT('Ctrl Pts',(45.3269785201039,871.397084045309,141.760520809568));
#84840=CARTESIAN_POINT('Ctrl Pts',(47.2301660207634,872.5966204711,142.235380472072));
#84841=CARTESIAN_POINT('Ctrl Pts',(46.541493193235,872.523162627151,142.209417984512));
#84842=CARTESIAN_POINT('Ctrl Pts',(45.8545798227468,872.436285813379,142.178712778975));
#84843=CARTESIAN_POINT('Ctrl Pts',(45.16972001138,872.336027226107,142.143278001899));
#84844=CARTESIAN_POINT('Ctrl Pts',(47.1123783978066,873.542746553868,142.682824237962));
#84845=CARTESIAN_POINT('Ctrl Pts',(46.4093420785613,873.467756616462,142.656320256735));
#84846=CARTESIAN_POINT('Ctrl Pts',(45.7081019129495,873.379067832847,142.624974639746));
#84847=CARTESIAN_POINT('Ctrl Pts',(45.008958137072,873.276718175141,142.588800807625));
#84848=CARTESIAN_POINT('Origin',(52.8776183915471,827.175936191914,121.458286566849));
#84849=CARTESIAN_POINT('Ctrl Pts',(30.5176874370867,871.137829742988,142.122382291291));
#84850=CARTESIAN_POINT('Ctrl Pts',(29.9434493604142,870.888251874385,142.034173027849));
#84851=CARTESIAN_POINT('Ctrl Pts',(29.3740019118244,870.629100035184,141.942579999254));
#84852=CARTESIAN_POINT('Ctrl Pts',(28.8095246350419,870.360455934569,141.847632084296));
#84853=CARTESIAN_POINT('Ctrl Pts',(30.1182334177546,871.905731565912,142.550119765185));
#84854=CARTESIAN_POINT('Ctrl Pts',(29.5337367357112,871.6516950573,142.460334667502));
#84855=CARTESIAN_POINT('Ctrl Pts',(28.9541162650043,871.387913541738,142.367105354631));
#84856=CARTESIAN_POINT('Ctrl Pts',(28.3795547568576,871.114470188121,142.270461221276));
#84857=CARTESIAN_POINT('Ctrl Pts',(29.7111878117354,872.673653539381,143.027221090879));
#84858=CARTESIAN_POINT('Ctrl Pts',(29.1162375604751,872.41507365472,142.93583021037));
#84859=CARTESIAN_POINT('Ctrl Pts',(28.5262507303067,872.146574476225,142.840933515793));
#84860=CARTESIAN_POINT('Ctrl Pts',(27.9414133409115,871.868240660246,142.742560927566));
#84861=CARTESIAN_POINT('Origin',(52.8776183915471,827.175936191914,121.458286566849));
#84862=CARTESIAN_POINT('Ctrl Pts',(37.3302788892939,869.558176849511,141.109984760151));
#84863=CARTESIAN_POINT('Ctrl Pts',(36.6878228196305,869.3564263923,141.038679322175));
#84864=CARTESIAN_POINT('Ctrl Pts',(36.0499205843609,869.142215425391,140.96296991846));
#84865=CARTESIAN_POINT('Ctrl Pts',(35.4168440128105,868.915635230518,140.88288881106));
#84866=CARTESIAN_POINT('Ctrl Pts',(37.0052885994072,870.462226073617,141.480217953634));
#84867=CARTESIAN_POINT('Ctrl Pts',(36.3494030948049,870.256258371419,141.407421998586));
#84868=CARTESIAN_POINT('Ctrl Pts',(35.6981666146422,870.037569694081,141.330130020498));
#84869=CARTESIAN_POINT('Ctrl Pts',(35.0518566703672,869.806253231424,141.248374955807));
#84870=CARTESIAN_POINT('Ctrl Pts',(36.6730316785943,871.367181199195,141.913359744775));
#84871=CARTESIAN_POINT('Ctrl Pts',(36.003416463167,871.156901956384,141.839039945389));
#84872=CARTESIAN_POINT('Ctrl Pts',(35.3385475906301,870.933635449105,141.760130007306));
#84873=CARTESIAN_POINT('Ctrl Pts',(34.6787083816039,870.69747681793,141.676663556422));
#84874=CARTESIAN_POINT('Origin',(52.8776183915471,827.175936191914,121.458286566849));
#84875=CARTESIAN_POINT('Ctrl Pts',(20.9538218835522,865.756712404766,140.217399249458));
#84876=CARTESIAN_POINT('Ctrl Pts',(20.4480094289833,865.400980192249,140.091671449054));
#84877=CARTESIAN_POINT('Ctrl Pts',(19.9489644671128,865.036850228768,139.962975599315));
#84878=CARTESIAN_POINT('Ctrl Pts',(19.4568438183336,864.664436938889,139.831352141753));
#84879=CARTESIAN_POINT('Ctrl Pts',(20.3821255088437,866.430260973763,140.611649556182));
#84880=CARTESIAN_POINT('Ctrl Pts',(19.8672548851911,866.068158252769,140.483670202531));
#84881=CARTESIAN_POINT('Ctrl Pts',(19.3592729475619,865.697507392565,140.352669647249));
#84882=CARTESIAN_POINT('Ctrl Pts',(18.8583393247131,865.31842486685,140.218689056083));
#84883=CARTESIAN_POINT('Ctrl Pts',(19.7995374347198,867.101999092337,141.054840453057));
#84884=CARTESIAN_POINT('Ctrl Pts',(19.2754360698645,866.733404494836,140.92456665059));
#84885=CARTESIAN_POINT('Ctrl Pts',(18.7583468932775,866.356108504748,140.791217481564));
#84886=CARTESIAN_POINT('Ctrl Pts',(18.248432395584,865.970229683947,140.654834849756));
#84887=CARTESIAN_POINT('Origin',(52.8776183915471,827.175936191914,121.458286566849));
#84888=CARTESIAN_POINT('Ctrl Pts',(28.0016339850113,865.558805254534,139.696003784806));
#84889=CARTESIAN_POINT('Ctrl Pts',(27.4171903968369,865.23579664227,139.581841611962));
#84890=CARTESIAN_POINT('Ctrl Pts',(26.8399476456599,864.901475271192,139.463681127377));
#84891=CARTESIAN_POINT('Ctrl Pts',(26.270152024064,864.555983786442,139.34157274667));
#84892=CARTESIAN_POINT('Ctrl Pts',(27.48299472275,866.377213147581,140.035543517094));
#84893=CARTESIAN_POINT('Ctrl Pts',(26.8863660734158,866.047470130534,139.919001177736));
#84894=CARTESIAN_POINT('Ctrl Pts',(26.2970883912899,865.706178495026,139.798377165856));
#84895=CARTESIAN_POINT('Ctrl Pts',(25.715413103909,865.353483860208,139.67372294819));
#84896=CARTESIAN_POINT('Ctrl Pts',(26.9527888856775,867.194666383688,140.436998441805));
#84897=CARTESIAN_POINT('Ctrl Pts',(26.3437034267223,866.858038772694,140.318022854));
#84898=CARTESIAN_POINT('Ctrl Pts',(25.7421224133561,866.509621423506,140.194880373801));
#84899=CARTESIAN_POINT('Ctrl Pts',(25.148302522587,866.149562995606,140.0676235425));
#84900=CARTESIAN_POINT('Origin',(52.8776183915471,827.175936191914,121.458286566849));
#84901=CARTESIAN_POINT('Ctrl Pts',(12.7865428347925,858.62672781395,137.694349954101));
#84902=CARTESIAN_POINT('Ctrl Pts',(12.3703603268689,858.180246532437,137.536548362142));
#84903=CARTESIAN_POINT('Ctrl Pts',(11.9626324102089,857.726883713927,137.376314602166));
#84904=CARTESIAN_POINT('Ctrl Pts',(11.5634870604064,857.266781657667,137.213698967542));
#84905=CARTESIAN_POINT('Ctrl Pts',(12.0704861765269,859.171290255116,138.042086111739));
#84906=CARTESIAN_POINT('Ctrl Pts',(11.6468703370773,858.716834483271,137.881466065073));
#84907=CARTESIAN_POINT('Ctrl Pts',(11.2318600942279,858.255374265021,137.718370410047));
#84908=CARTESIAN_POINT('Ctrl Pts',(10.8255857093128,857.787054441183,137.552850338305));
#84909=CARTESIAN_POINT('Ctrl Pts',(11.3408233400644,859.711637129034,138.437634367714));
#84910=CARTESIAN_POINT('Ctrl Pts',(10.9096329243531,859.249055339272,138.274142311366));
#84911=CARTESIAN_POINT('Ctrl Pts',(10.4872019799126,858.779343858228,138.10813038088));
#84912=CARTESIAN_POINT('Ctrl Pts',(10.0736630972495,858.302650116585,137.939650683247));
#84913=CARTESIAN_POINT('Origin',(52.8776183915471,827.175936191914,121.458286566849));
#84914=CARTESIAN_POINT('Ctrl Pts',(19.7613090894358,859.806810803219,137.661702909781));
#84915=CARTESIAN_POINT('Ctrl Pts',(19.2595092245227,859.375617365219,137.509304558998));
#84916=CARTESIAN_POINT('Ctrl Pts',(18.7672892142599,858.934717240451,137.353475536676));
#84917=CARTESIAN_POINT('Ctrl Pts',(18.2848602345987,858.484299587218,137.194282697761));
#84918=CARTESIAN_POINT('Ctrl Pts',(19.0699494553796,860.506484585855,137.958487139599));
#84919=CARTESIAN_POINT('Ctrl Pts',(18.557673659474,860.066289246865,137.802907212419));
#84920=CARTESIAN_POINT('Ctrl Pts',(18.0551777140801,859.616184577407,137.64382499256));
#84921=CARTESIAN_POINT('Ctrl Pts',(17.5626772038086,859.156363684789,137.48130873068));
#84922=CARTESIAN_POINT('Ctrl Pts',(18.3631501702965,861.202530292096,138.316374507908));
#84923=CARTESIAN_POINT('Ctrl Pts',(17.8401644917606,860.753132018958,138.157541952411));
#84924=CARTESIAN_POINT('Ctrl Pts',(17.3271631259654,860.293617246153,137.995133883631));
#84925=CARTESIAN_POINT('Ctrl Pts',(16.8243661646366,859.824183118185,137.829219979106));
#84926=CARTESIAN_POINT('Origin',(52.8776183915471,827.175936191914,121.458286566849));
#84927=CARTESIAN_POINT('Ctrl Pts',(6.37745532491532,850.043581143414,134.655040109612));
#84928=CARTESIAN_POINT('Ctrl Pts',(6.06790703385583,849.52418619948,134.471468362258));
#84929=CARTESIAN_POINT('Ctrl Pts',(5.76819589177487,848.999687435667,134.286092752267));
#84930=CARTESIAN_POINT('Ctrl Pts',(5.47841652993691,848.470250458033,134.098971810424));
#84931=CARTESIAN_POINT('Ctrl Pts',(5.54555081826099,850.435760948325,134.948213821533));
#84932=CARTESIAN_POINT('Ctrl Pts',(5.23046459784004,849.907073843545,134.761357910128));
#84933=CARTESIAN_POINT('Ctrl Pts',(4.92539151650234,849.373191609727,134.572665864339));
#84934=CARTESIAN_POINT('Ctrl Pts',(4.63042789849945,848.834282815682,134.382197262089));
#84935=CARTESIAN_POINT('Ctrl Pts',(4.69781197294163,850.820797936038,135.288297996182));
#84936=CARTESIAN_POINT('Ctrl Pts',(4.37708241508856,850.282641804893,135.098095410468));
#84937=CARTESIAN_POINT('Ctrl Pts',(4.06654533619126,849.739197497587,134.906023804368));
#84938=CARTESIAN_POINT('Ctrl Pts',(3.76629878571242,849.190636602077,134.712143822873));
#84939=CARTESIAN_POINT('Origin',(52.8776183915471,827.175936191914,121.458286566849));
#84940=CARTESIAN_POINT('Ctrl Pts',(12.9650774688681,852.569047898116,135.10234465102));
#84941=CARTESIAN_POINT('Ctrl Pts',(12.5693265975477,852.049404581664,134.918685120414));
#84942=CARTESIAN_POINT('Ctrl Pts',(12.1850749352458,851.522145076098,134.732333770876));
#84943=CARTESIAN_POINT('Ctrl Pts',(11.8124873105256,850.987495554614,134.543370539665));
#84944=CARTESIAN_POINT('Ctrl Pts',(12.1299603114578,853.119108286907,135.345529079686));
#84945=CARTESIAN_POINT('Ctrl Pts',(11.7259288763082,852.588592120988,135.158026716186));
#84946=CARTESIAN_POINT('Ctrl Pts',(11.3336372559245,852.050300407265,134.967776211001));
#84947=CARTESIAN_POINT('Ctrl Pts',(10.9532537276901,851.504464051312,134.774859173973));
#84948=CARTESIAN_POINT('Ctrl Pts',(11.2761503952751,853.662144956265,135.648865597357));
#84949=CARTESIAN_POINT('Ctrl Pts',(10.8636530491497,853.120512569574,135.457434385311));
#84950=CARTESIAN_POINT('Ctrl Pts',(10.4631415091117,852.570941709401,135.263197448131));
#84951=CARTESIAN_POINT('Ctrl Pts',(10.0747875785606,852.013668119621,135.066238105679));
#84952=CARTESIAN_POINT('Origin',(52.8776183915471,827.175936191914,121.458286566849));
#84953=CARTESIAN_POINT('Ctrl Pts',(1.99652577628784,840.395005721243,131.239611548762));
#84954=CARTESIAN_POINT('Ctrl Pts',(1.80814586333338,839.826414148728,131.038652048258));
#84955=CARTESIAN_POINT('Ctrl Pts',(1.6305160883364,839.254755063331,130.83660838491));
#84956=CARTESIAN_POINT('Ctrl Pts',(1.46369258826633,838.680209128505,130.633544411295));
#84957=CARTESIAN_POINT('Ctrl Pts',(1.08432921088779,840.615282592914,131.471458943975));
#84958=CARTESIAN_POINT('Ctrl Pts',(0.892572021606208,840.036497306922,131.266896640215));
#84959=CARTESIAN_POINT('Ctrl Pts',(0.711757698826617,839.454589513656,131.061230736733));
#84960=CARTESIAN_POINT('Ctrl Pts',(0.541943385942385,838.869743115505,130.854526230854));
#84961=CARTESIAN_POINT('Ctrl Pts',(0.154732817407261,840.825095759158,131.749222818875));
#84962=CARTESIAN_POINT('Ctrl Pts',(-0.0404660685574277,840.235922318195,
131.540988989657));
#84963=CARTESIAN_POINT('Ctrl Pts',(-0.224525683246545,839.643570326568,
131.331631753086));
#84964=CARTESIAN_POINT('Ctrl Pts',(-0.397387857645575,839.048226987384,
131.121217273072));
#84965=CARTESIAN_POINT('Origin',(52.8776183915471,827.175936191914,121.458286566849));
#84966=CARTESIAN_POINT('Ctrl Pts',(7.91273499456057,844.159523714638,132.128757411956));
#84967=CARTESIAN_POINT('Ctrl Pts',(7.64025937140726,843.574324363908,131.921928160693));
#84968=CARTESIAN_POINT('Ctrl Pts',(7.38069155747312,842.983931954819,131.713263506894));
#84969=CARTESIAN_POINT('Ctrl Pts',(7.13414281207972,842.388599549019,131.502852891109));
#84970=CARTESIAN_POINT('Ctrl Pts',(6.9725451158367,844.533646352629,132.30882139234));
#84971=CARTESIAN_POINT('Ctrl Pts',(6.69437218394524,843.936210819682,132.09766746026));
#84972=CARTESIAN_POINT('Ctrl Pts',(6.42937695614795,843.333473644509,131.884639748432));
#84973=CARTESIAN_POINT('Ctrl Pts',(6.17767301813491,842.725693180133,131.669829567555));
#84974=CARTESIAN_POINT('Ctrl Pts',(6.01132405391079,844.896832714271,132.547534652228));
#84975=CARTESIAN_POINT('Ctrl Pts',(5.72732636972265,844.286887286961,132.331959300197));
#84976=CARTESIAN_POINT('Ctrl Pts',(5.45678232180392,843.671529204637,132.114470932742));
#84977=CARTESIAN_POINT('Ctrl Pts',(5.19980787425188,843.051022230058,131.895162772548));
#84978=CARTESIAN_POINT('Origin',(52.8776183915471,827.175936191914,121.458286566849));
#84979=CARTESIAN_POINT('Ctrl Pts',(-0.162078610920046,830.096471860791,
127.594334646973));
#84980=CARTESIAN_POINT('Ctrl Pts',(-0.220920824684921,829.504313278728,
127.385045767885));
#84981=CARTESIAN_POINT('Ctrl Pts',(-0.268599504446354,828.911262785418,
127.175441657185));
#84982=CARTESIAN_POINT('Ctrl Pts',(-0.305099610353358,828.317507453808,
126.965588432779));
#84983=CARTESIAN_POINT('Ctrl Pts',(-1.11256710860028,830.132360300293,127.760025246802));
#84984=CARTESIAN_POINT('Ctrl Pts',(-1.17246379383695,829.529590045222,127.546985843418));
#84985=CARTESIAN_POINT('Ctrl Pts',(-1.22099689093594,828.925911895566,127.333625559369));
#84986=CARTESIAN_POINT('Ctrl Pts',(-1.25815109052729,828.32151627668,127.120011697418));
#84987=CARTESIAN_POINT('Ctrl Pts',(-2.08117880382292,830.154283943356,127.970323009527));
#84988=CARTESIAN_POINT('Ctrl Pts',(-2.14215006639781,829.540699679902,127.75346156968));
#84989=CARTESIAN_POINT('Ctrl Pts',(-2.19155387221951,828.926191233768,127.536273492403));
#84990=CARTESIAN_POINT('Ctrl Pts',(-2.22937463726006,828.310952446636,127.318827287906));
#84991=CARTESIAN_POINT('Origin',(52.8776183915471,825.559694878252,125.51834395973));
#84992=CARTESIAN_POINT('Origin',(52.8776183915471,826.387310726428,123.689610751183));
#84993=CARTESIAN_POINT('Origin',(52.8776183915471,825.559694878252,125.51834395973));
#84994=CARTESIAN_POINT('Origin',(52.8776183915471,826.387310726428,123.689610751183));
#84995=CARTESIAN_POINT('Origin',(52.8776183915471,825.559694878252,125.51834395973));
#84996=CARTESIAN_POINT('Origin',(52.8776183915471,826.387310726428,123.689610751183));
#84997=CARTESIAN_POINT('Origin',(52.8776183915471,825.559694878252,125.51834395973));
#84998=CARTESIAN_POINT('Origin',(52.8776183915471,826.387310726428,123.689610751183));
#84999=CARTESIAN_POINT('Origin',(52.8776183915471,825.559694878252,125.51834395973));
#85000=CARTESIAN_POINT('Origin',(52.8776183915471,826.387310726428,123.689610751183));
#85001=CARTESIAN_POINT('Origin',(52.8776183915471,825.559694878252,125.51834395973));
#85002=CARTESIAN_POINT('Origin',(52.8776183915471,826.387310726428,123.689610751183));
#85003=CARTESIAN_POINT('',(0.,0.,0.));
#85004=CARTESIAN_POINT('Origin',(52.8776183915471,639.625373764374,90.6087118617898));
#85005=CARTESIAN_POINT('',(52.8776183915471,639.604463591086,79.6305155808287));
#85006=CARTESIAN_POINT('',(52.8776183915471,639.604463591086,101.586908142751));
#85007=CARTESIAN_POINT('Origin',(52.8776183915471,639.604463591086,90.6087118617898));
#85008=CARTESIAN_POINT('Origin',(52.8776183915471,639.604463591086,90.6087118617898));
#85009=CARTESIAN_POINT('',(52.8776183915471,640.125373764374,101.08734556944));
#85010=CARTESIAN_POINT('Origin',(52.8776183915471,639.625373764374,101.08734556944));
#85011=CARTESIAN_POINT('Origin',(52.8776183915471,640.125373764374,90.6087118617898));
#85012=CARTESIAN_POINT('Origin',(52.8776183915471,604.14887537019,90.6087118617898));
#85013=CARTESIAN_POINT('',(52.8776183915471,604.127965196902,81.1154541424767));
#85014=CARTESIAN_POINT('Origin',(52.8776183915471,604.127965196902,90.6087118617898));
#85015=CARTESIAN_POINT('',(52.8776183915471,603.64887537019,81.6150167157877));
#85016=CARTESIAN_POINT('Origin',(52.8776183915471,604.14887537019,81.6150167157877));
#85017=CARTESIAN_POINT('Origin',(52.8776183915471,603.64887537019,90.6087118617898));
#85018=CARTESIAN_POINT('Origin',(52.8776183915471,603.64887537019,90.6087118617898));
#85019=CARTESIAN_POINT('',(52.8776183915471,603.64887537019,81.1355073887209));
#85020=CARTESIAN_POINT('Ctrl Pts',(20.,-22.143643036685,76.7830741855192));
#85021=CARTESIAN_POINT('Ctrl Pts',(20.,-27.8457920778109,76.7830741857566));
#85022=CARTESIAN_POINT('Ctrl Pts',(20.0165214330532,-33.485592853313,76.7809705517141));
#85023=CARTESIAN_POINT('Ctrl Pts',(20.0854446608167,-44.638917128667,76.7729088380163));
#85024=CARTESIAN_POINT('Ctrl Pts',(20.1238292955523,-50.1526654673148,76.7668988331685));
#85025=CARTESIAN_POINT('Ctrl Pts',(20.4301340697073,-66.5001303791202,76.743985515181));
#85026=CARTESIAN_POINT('Ctrl Pts',(20.7188936123879,-77.141599114471,76.7227141396145));
#85027=CARTESIAN_POINT('Ctrl Pts',(21.8028495683285,-108.277666955853,76.643040982027));
#85028=CARTESIAN_POINT('Ctrl Pts',(22.8522177208893,-127.983498586547,76.568779347995));
#85029=CARTESIAN_POINT('Ctrl Pts',(27.2962882348799,-183.793342140183,76.3120470559144));
#85030=CARTESIAN_POINT('Ctrl Pts',(31.9889018993299,-216.590007789356,76.0958804243854));
#85031=CARTESIAN_POINT('Ctrl Pts',(42.752586146367,-258.54916325461,75.8385782220632));
#85032=CARTESIAN_POINT('Ctrl Pts',(46.9602598342624,-271.329384640549,75.7640306692479));
#85033=CARTESIAN_POINT('Ctrl Pts',(56.7935789905011,-294.374861216214,75.6600037328577));
#85034=CARTESIAN_POINT('Ctrl Pts',(62.4190261651095,-304.639843280753,75.6305279269569));
#85035=CARTESIAN_POINT('Ctrl Pts',(75.2624672361846,-322.558676299804,75.6391115492116));
#85036=CARTESIAN_POINT('Ctrl Pts',(82.4798249428642,-330.212646288195,75.6771562180411));
#85037=CARTESIAN_POINT('Ctrl Pts',(98.6902707967944,-342.825622479896,75.8431732977935));
#85038=CARTESIAN_POINT('Ctrl Pts',(107.683690787476,-347.785594002476,75.9711317990764));
#85039=CARTESIAN_POINT('Ctrl Pts',(126.023069913222,-354.340138637006,76.3098567703564));
#85040=CARTESIAN_POINT('Ctrl Pts',(135.083207114917,-356.371635015224,76.501925570174));
#85041=CARTESIAN_POINT('Ctrl Pts',(148.924338523526,-357.668316903019,76.9207856483578));
#85042=CARTESIAN_POINT('Ctrl Pts',(153.579247220674,-357.810711475144,77.0819658816335));
#85043=CARTESIAN_POINT('Ctrl Pts',(160.521670574454,-357.554693148273,77.3648314770126));
#85044=CARTESIAN_POINT('Ctrl Pts',(162.82915793653,-357.391086631896,77.4659695920693));
#85045=CARTESIAN_POINT('Ctrl Pts',(167.413894984383,-356.901529412086,77.6834093931112));
#85046=CARTESIAN_POINT('Ctrl Pts',(169.690165914981,-356.571218959933,77.800168876217));
#85047=CARTESIAN_POINT('Ctrl Pts',(180.410587995582,-354.672149675074,78.3871286663314));
#85048=CARTESIAN_POINT('Ctrl Pts',(188.539471171489,-351.990508745272,78.9676971116917));
#85049=CARTESIAN_POINT('Ctrl Pts',(203.935932366808,-344.394636660447,80.2994244971851));
#85050=CARTESIAN_POINT('Ctrl Pts',(211.203510672235,-339.480369996828,81.0505889748358));
#85051=CARTESIAN_POINT('Ctrl Pts',(231.426270328895,-321.586439483533,83.4642765655722));
#85052=CARTESIAN_POINT('Ctrl Pts',(242.801650331,-305.454778835795,85.2871564557421));
#85053=CARTESIAN_POINT('Ctrl Pts',(259.787422523192,-265.857198323714,88.846412059781));
#85054=CARTESIAN_POINT('Ctrl Pts',(265.396961479631,-242.39170484102,90.582652202398));
#85055=CARTESIAN_POINT('Ctrl Pts',(269.303802179431,-189.217670775394,93.4513081720829));
#85056=CARTESIAN_POINT('Ctrl Pts',(267.601212650846,-159.509605592023,94.5836348018781));
#85057=CARTESIAN_POINT('Ctrl Pts',(260.488092878426,-122.007461671797,95.2483440922483));
#85058=CARTESIAN_POINT('Ctrl Pts',(259.365919995518,-116.723004281873,95.3235942479774));
#85059=CARTESIAN_POINT('Ctrl Pts',(256.932101050909,-106.048555274698,95.4495336771278));
#85060=CARTESIAN_POINT('Ctrl Pts',(255.614336154295,-100.659660585315,95.4992578713651));
#85061=CARTESIAN_POINT('Ctrl Pts',(251.40188561101,-84.3843231292077,95.6128833960036));
#85062=CARTESIAN_POINT('Ctrl Pts',(248.248043744655,-73.3892261805465,95.6412376442078));
#85063=CARTESIAN_POINT('Ctrl Pts',(238.097187851482,-40.3402024940961,95.6176286794984));
#85064=CARTESIAN_POINT('Ctrl Pts',(230.410833839506,-18.2225145274556,95.4569933696899));
#85065=CARTESIAN_POINT('Ctrl Pts',(201.530604066263,61.5570672312919,94.6440942086903));
#85066=CARTESIAN_POINT('Ctrl Pts',(180.38355994371,113.231534550229,93.6242109681347));
#85067=CARTESIAN_POINT('Ctrl Pts',(140.797124795906,209.938840593949,91.236348118932));
#85068=CARTESIAN_POINT('Ctrl Pts',(122.357793139117,254.971482304575,89.8683893074086));
#85069=CARTESIAN_POINT('Ctrl Pts',(90.7794276043238,345.543709944167,87.281854516083));
#85070=CARTESIAN_POINT('Ctrl Pts',(77.6398467041473,391.083508984014,86.0632256586685));
#85071=CARTESIAN_POINT('Ctrl Pts',(59.2526292615706,489.828486097094,84.2723560895427));
#85072=CARTESIAN_POINT('Ctrl Pts',(54.0050807366749,543.034307838934,83.7001064546653));
#85073=CARTESIAN_POINT('Ctrl Pts',(54.0050807343608,603.648875370191,83.7001064550861));
#85074=CARTESIAN_POINT('Ctrl Pts',(34.,-22.143643036685,76.7830741855191));
#85075=CARTESIAN_POINT('Ctrl Pts',(33.9999999999839,-27.818749567832,76.7830741857369));
#85076=CARTESIAN_POINT('Ctrl Pts',(34.0164436970964,-33.4297565255892,76.7809804490342));
#85077=CARTESIAN_POINT('Ctrl Pts',(34.0849877845006,-44.5217274543659,76.7729629323669));
#85078=CARTESIAN_POINT('Ctrl Pts',(34.1231742300284,-50.0028679006344,76.7389494577223));
#85079=CARTESIAN_POINT('Ctrl Pts',(34.4276899601393,-66.246853907463,76.8982463815691));
#85080=CARTESIAN_POINT('Ctrl Pts',(34.7126441433325,-76.8114792097519,77.0127755335157));
#85081=CARTESIAN_POINT('Ctrl Pts',(35.7801701648313,-107.689013837462,77.2436000455983));
#85082=CARTESIAN_POINT('Ctrl Pts',(36.8122807199099,-127.185635036684,77.3200887338452));
#85083=CARTESIAN_POINT('Ctrl Pts',(41.1733655791691,-182.212078558018,77.4363129347258));
#85084=CARTESIAN_POINT('Ctrl Pts',(45.7887675371877,-214.28465811726,77.3652387134946));
#85085=CARTESIAN_POINT('Ctrl Pts',(56.1071091638816,-254.559565379267,77.2809282374505));
#85086=CARTESIAN_POINT('Ctrl Pts',(60.1071507567796,-266.675138787952,77.2549720220375));
#85087=CARTESIAN_POINT('Ctrl Pts',(69.2672710615284,-288.157823623031,77.2351548953765));
#85088=CARTESIAN_POINT('Ctrl Pts',(74.4235442697514,-297.51883236657,77.241288185783));
#85089=CARTESIAN_POINT('Ctrl Pts',(85.8799878791956,-313.508885526083,77.3068472367312));
#85090=CARTESIAN_POINT('Ctrl Pts',(92.1662088124034,-320.140602612327,77.3659108227464));
#85091=CARTESIAN_POINT('Ctrl Pts',(106.074791507621,-330.965616389605,77.5558022149426));
#85092=CARTESIAN_POINT('Ctrl Pts',(113.704741593858,-335.180562056838,77.6863058336575));
#85093=CARTESIAN_POINT('Ctrl Pts',(129.547452308994,-340.84513890228,78.019344686732));
#85094=CARTESIAN_POINT('Ctrl Pts',(137.504622410254,-342.63348319117,78.1724169021146));
#85095=CARTESIAN_POINT('Ctrl Pts',(149.585403594227,-343.765248871106,78.5379883229279));
#85096=CARTESIAN_POINT('Ctrl Pts',(153.635968157751,-343.887687412075,78.6783580728553));
#85097=CARTESIAN_POINT('Ctrl Pts',(159.628436780843,-343.666700644404,78.9225120249749));
#85098=CARTESIAN_POINT('Ctrl Pts',(161.61206380368,-343.525732039158,79.0094845712665));
#85099=CARTESIAN_POINT('Ctrl Pts',(165.532545967561,-343.107103515031,79.1954129140516));
#85100=CARTESIAN_POINT('Ctrl Pts',(167.468098111069,-342.826090867219,79.3037431318874));
#85101=CARTESIAN_POINT('Ctrl Pts',(176.532101218951,-341.217569579924,79.6978427041489));
#85102=CARTESIAN_POINT('Ctrl Pts',(183.383375567806,-338.959436198211,80.1037808086076));
#85103=CARTESIAN_POINT('Ctrl Pts',(196.476071197198,-332.501375371133,81.0647133327792));
#85104=CARTESIAN_POINT('Ctrl Pts',(202.718744012329,-328.297008645753,81.6202751258499));
#85105=CARTESIAN_POINT('Ctrl Pts',(220.341909241066,-312.716811913614,83.4515942144793));
#85106=CARTESIAN_POINT('Ctrl Pts',(230.624134911047,-298.333852015906,84.8966292281925));
#85107=CARTESIAN_POINT('Ctrl Pts',(246.265932818144,-261.956042751922,87.7965104150377));
#85108=CARTESIAN_POINT('Ctrl Pts',(251.601872159868,-239.986217448384,89.2479470149237));
#85109=CARTESIAN_POINT('Ctrl Pts',(255.356970654638,-189.502920762821,91.6411093546763));
#85110=CARTESIAN_POINT('Ctrl Pts',(253.780180374585,-160.998128460726,92.5820596772374));
#85111=CARTESIAN_POINT('Ctrl Pts',(246.932276322894,-124.751374927772,93.0704364824261));
#85112=CARTESIAN_POINT('Ctrl Pts',(245.842235402124,-119.627034808441,93.1558629346225));
#85113=CARTESIAN_POINT('Ctrl Pts',(243.475097814891,-109.245042637674,93.2783520239457));
#85114=CARTESIAN_POINT('Ctrl Pts',(242.190038398626,-103.98905174219,93.3268821124474));
#85115=CARTESIAN_POINT('Ctrl Pts',(238.072169272926,-88.0791416638133,93.4379565165972));
#85116=CARTESIAN_POINT('Ctrl Pts',(234.976567368465,-77.2836801120869,93.4659513934413));
#85117=CARTESIAN_POINT('Ctrl Pts',(224.980111926361,-44.7373516402995,93.4427019766555));
#85118=CARTESIAN_POINT('Ctrl Pts',(217.369979234584,-22.8302137815567,93.2841181941716));
#85119=CARTESIAN_POINT('Ctrl Pts',(188.65251219865,56.4997474834766,92.4758003573277));
#85120=CARTESIAN_POINT('Ctrl Pts',(167.598367439946,107.953240075026,91.4612213775221));
#85121=CARTESIAN_POINT('Ctrl Pts',(128.017986339935,204.645755313006,89.0737264657378));
#85122=CARTESIAN_POINT('Ctrl Pts',(109.483389981347,249.892586601305,87.6997062527036));
#85123=CARTESIAN_POINT('Ctrl Pts',(77.5768324188997,341.406124610584,85.0862925379845));
#85124=CARTESIAN_POINT('Ctrl Pts',(64.215495896169,387.677233373842,83.8475365004758));
#85125=CARTESIAN_POINT('Ctrl Pts',(45.5165434104212,488.096320975175,82.0263070967131));
#85126=CARTESIAN_POINT('Ctrl Pts',(40.1878699233725,542.222624701163,81.4451817692483));
#85127=CARTESIAN_POINT('Ctrl Pts',(40.1878699209532,603.648875370192,81.4451817694587));
#85128=CARTESIAN_POINT('Ctrl Pts',(34.,-22.143643036685,90.7830741855191));
#85129=CARTESIAN_POINT('Ctrl Pts',(33.9999999999666,-27.822192816507,90.7830741857369));
#85130=CARTESIAN_POINT('Ctrl Pts',(34.0164537550708,-33.4365739834866,90.7809791784461));
#85131=CARTESIAN_POINT('Ctrl Pts',(34.0850387982778,-44.5351482419418,90.7729568888413));
#85132=CARTESIAN_POINT('Ctrl Pts',(34.1512904613084,-50.0190681308895,90.7390437618613));
#85133=CARTESIAN_POINT('Ctrl Pts',(34.2738860204776,-66.275150464231,90.8979005786987));
#85134=CARTESIAN_POINT('Ctrl Pts',(34.4233619248085,-76.8497861166896,91.0101176438938));
#85135=CARTESIAN_POINT('Ctrl Pts',(35.1819506943524,-107.760797693274,91.2321643624032));
#85136=CARTESIAN_POINT('Ctrl Pts',(36.0651110374872,-127.285189611952,91.3003474514556));
#85137=CARTESIAN_POINT('Ctrl Pts',(40.0636907101652,-182.413148706558,91.3930827017859));
#85138=CARTESIAN_POINT('Ctrl Pts',(44.5459926487259,-214.577066409288,91.3077501454067));
#85139=CARTESIAN_POINT('Ctrl Pts',(54.7471862739539,-255.049764636043,91.2063086160594));
#85140=CARTESIAN_POINT('Ctrl Pts',(58.7239589095343,-267.241778858765,91.1752276768338));
#85141=CARTESIAN_POINT('Ctrl Pts',(67.8755199829761,-288.900859668629,91.1462563801209));
#85142=CARTESIAN_POINT('Ctrl Pts',(73.0468995042606,-298.36236982239,91.148353067284));
#85143=CARTESIAN_POINT('Ctrl Pts',(84.5856302727223,-314.566486013887,91.2071810262364));
#85144=CARTESIAN_POINT('Ctrl Pts',(90.9403044324173,-321.311526658035,91.2635796420002));
#85145=CARTESIAN_POINT('Ctrl Pts',(105.034746410925,-332.341129151079,91.4498791587053));
#85146=CARTESIAN_POINT('Ctrl Pts',(112.781438867057,-336.645409342233,91.5794836918854));
#85147=CARTESIAN_POINT('Ctrl Pts',(128.84379162978,-342.431310881406,91.9118603910799));
#85148=CARTESIAN_POINT('Ctrl Pts',(136.882331514546,-344.218066302979,92.06862737911));
#85149=CARTESIAN_POINT('Ctrl Pts',(149.042319260545,-345.35723535437,92.4365976867908));
#85150=CARTESIAN_POINT('Ctrl Pts',(153.113390074031,-345.479917353382,92.5777083987872));
#85151=CARTESIAN_POINT('Ctrl Pts',(159.128250624564,-345.258098659325,92.8227754054756));
#85152=CARTESIAN_POINT('Ctrl Pts',(161.117941330513,-345.116650646867,92.910018487043));
#85153=CARTESIAN_POINT('Ctrl Pts',(165.047777667848,-344.697015385526,93.0963913730309));
#85154=CARTESIAN_POINT('Ctrl Pts',(166.988577813154,-344.424194906112,93.2039800042653));
#85155=CARTESIAN_POINT('Ctrl Pts',(176.041505784734,-342.714803975454,93.6091367219815));
#85156=CARTESIAN_POINT('Ctrl Pts',(182.872054436279,-340.375843599256,94.0228196827679));
#85157=CARTESIAN_POINT('Ctrl Pts',(195.898526230413,-333.760723015434,94.9962526493361));
#85158=CARTESIAN_POINT('Ctrl Pts',(202.095700336024,-329.480194547591,95.5565589536698));
#85159=CARTESIAN_POINT('Ctrl Pts',(219.550609434862,-313.688603271014,97.3965554226442));
#85160=CARTESIAN_POINT('Ctrl Pts',(229.677969866178,-299.18923380383,98.8396419135539));
#85161=CARTESIAN_POINT('Ctrl Pts',(244.985390793916,-262.650450662216,101.721757946628));
#85162=CARTESIAN_POINT('Ctrl Pts',(250.143524864557,-240.635208284846,103.157649060994));
#85163=CARTESIAN_POINT('Ctrl Pts',(253.569471045668,-190.114279597768,105.514063707513));
#85164=CARTESIAN_POINT('Ctrl Pts',(251.841116264558,-161.616321569825,106.433990219553));
#85165=CARTESIAN_POINT('Ctrl Pts',(244.840413337758,-125.392448579826,106.898437331156));
#85166=CARTESIAN_POINT('Ctrl Pts',(243.762458422889,-120.265193874764,106.985804413879));
#85167=CARTESIAN_POINT('Ctrl Pts',(241.394977423079,-109.881694957916,107.108311299953));
#85168=CARTESIAN_POINT('Ctrl Pts',(240.109726258598,-104.624918046502,107.156848712739));
#85169=CARTESIAN_POINT('Ctrl Pts',(235.991218325549,-88.712539478757,107.267940365215));
#85170=CARTESIAN_POINT('Ctrl Pts',(232.89510653369,-77.9152866016949,107.295940488026));
#85171=CARTESIAN_POINT('Ctrl Pts',(222.896820184299,-45.3629955827255,107.272686881542));
#85172=CARTESIAN_POINT('Ctrl Pts',(215.28508460652,-23.4511547129986,107.114074507951));
#85173=CARTESIAN_POINT('Ctrl Pts',(186.559040616919,55.9024997794776,106.305515254125));
#85174=CARTESIAN_POINT('Ctrl Pts',(165.493582228552,107.38447679482,105.290480713943));
#85175=CARTESIAN_POINT('Ctrl Pts',(125.879107090836,204.160288949093,102.900929517052));
#85176=CARTESIAN_POINT('Ctrl Pts',(107.321611573323,249.462326772125,101.52526697662));
#85177=CARTESIAN_POINT('Ctrl Pts',(75.3707137533804,341.103048649986,98.9082216417973));
#85178=CARTESIAN_POINT('Ctrl Pts',(61.9890301742715,387.445708532525,97.6675820645533));
#85179=CARTESIAN_POINT('Ctrl Pts',(43.265762695917,487.995387928407,95.8439845955144));
#85180=CARTESIAN_POINT('Ctrl Pts',(37.9329452373243,542.179444956935,95.2623925830766));
#85181=CARTESIAN_POINT('Ctrl Pts',(37.9329452353258,603.648875370192,95.2623925828662));
#85182=CARTESIAN_POINT('Ctrl Pts',(20.,-22.143643036685,90.7830741855191));
#85183=CARTESIAN_POINT('Ctrl Pts',(20.0000000000198,-27.8492353264858,90.7830741857566));
#85184=CARTESIAN_POINT('Ctrl Pts',(20.016531491053,-33.4924103112104,90.7809692811259));
#85185=CARTESIAN_POINT('Ctrl Pts',(20.0854956745684,-44.652337916243,90.7729027944908));
#85186=CARTESIAN_POINT('Ctrl Pts',(20.1519455268513,-50.1688656975699,90.7669931373075));
#85187=CARTESIAN_POINT('Ctrl Pts',(20.2763301300078,-66.5284269358881,90.7436397123106));
#85188=CARTESIAN_POINT('Ctrl Pts',(20.4296113938976,-77.1799060213726,90.7200562499926));
#85189=CARTESIAN_POINT('Ctrl Pts',(21.204630097782,-108.349450811737,90.6316052988318));
#85190=CARTESIAN_POINT('Ctrl Pts',(22.10504803841,-128.083053161685,90.5490380656054));
#85191=CARTESIAN_POINT('Ctrl Pts',(26.1866133659894,-183.994412288981,90.2688168229746));
#85192=CARTESIAN_POINT('Ctrl Pts',(30.746127010843,-216.882416081384,90.0383918562974));
#85193=CARTESIAN_POINT('Ctrl Pts',(41.3926632564519,-259.039362511386,89.7639586006721));
#85194=CARTESIAN_POINT('Ctrl Pts',(45.5770679869517,-271.896024711361,89.6842863240442));
#85195=CARTESIAN_POINT('Ctrl Pts',(55.4018279120142,-295.117897261812,89.5711052176021));
#85196=CARTESIAN_POINT('Ctrl Pts',(61.0423813996187,-305.483380736572,89.537592808458));
#85197=CARTESIAN_POINT('Ctrl Pts',(73.9681096297112,-323.616276787607,89.5394453387168));
#85198=CARTESIAN_POINT('Ctrl Pts',(81.2539205629141,-331.38357033419,89.574825037295));
#85199=CARTESIAN_POINT('Ctrl Pts',(97.6502257000617,-344.201135241083,89.7372502415561));
#85200=CARTESIAN_POINT('Ctrl Pts',(106.760388060712,-349.250441287872,89.8643096573043));
#85201=CARTESIAN_POINT('Ctrl Pts',(125.319409233977,-355.926310616132,90.2023724747043));
#85202=CARTESIAN_POINT('Ctrl Pts',(134.460916219209,-357.956218127161,90.3981360471693));
#85203=CARTESIAN_POINT('Ctrl Pts',(148.381254189844,-359.260303386218,90.8193950122208));
#85204=CARTESIAN_POINT('Ctrl Pts',(153.056669136986,-359.402941416322,90.9813162075653));
#85205=CARTESIAN_POINT('Ctrl Pts',(160.021484418159,-359.146091163259,91.2650948575132));
#85206=CARTESIAN_POINT('Ctrl Pts',(162.335035463347,-358.982005239573,91.3665035078458));
#85207=CARTESIAN_POINT('Ctrl Pts',(166.929126684686,-358.491441282613,91.5843878520904));
#85208=CARTESIAN_POINT('Ctrl Pts',(169.210645617082,-358.169322998826,91.7004057485949));
#85209=CARTESIAN_POINT('Ctrl Pts',(179.919992561305,-356.169384070604,92.298422684164));
#85210=CARTESIAN_POINT('Ctrl Pts',(188.028150039962,-353.406916146197,92.886735985852));
#85211=CARTESIAN_POINT('Ctrl Pts',(203.358387400023,-345.653984304867,94.2309638137419));
#85212=CARTESIAN_POINT('Ctrl Pts',(210.580466995992,-340.663555898792,94.9868728026557));
#85213=CARTESIAN_POINT('Ctrl Pts',(230.634970522565,-322.558230840682,97.4092377737371));
#85214=CARTESIAN_POINT('Ctrl Pts',(241.855485286281,-306.310160623718,99.2301691411035));
#85215=CARTESIAN_POINT('Ctrl Pts',(258.506880498815,-266.551606234007,102.771659591371));
#85216=CARTESIAN_POINT('Ctrl Pts',(263.93861418432,-243.040695677481,104.492354248469));
#85217=CARTESIAN_POINT('Ctrl Pts',(267.516302570461,-189.829029610341,107.32426252492));
#85218=CARTESIAN_POINT('Ctrl Pts',(265.662148540819,-160.127798701236,108.435565344194));
#85219=CARTESIAN_POINT('Ctrl Pts',(258.396229893289,-122.648535323832,109.076344940978));
#85220=CARTESIAN_POINT('Ctrl Pts',(257.286143016284,-117.361163348158,109.153535727234));
#85221=CARTESIAN_POINT('Ctrl Pts',(254.851980659096,-106.685207594979,109.279492953135));
#85222=CARTESIAN_POINT('Ctrl Pts',(253.534024014268,-101.295526889627,109.329224471656));
#85223=CARTESIAN_POINT('Ctrl Pts',(249.320934663633,-85.0177209441514,109.442867244621));
#85224=CARTESIAN_POINT('Ctrl Pts',(246.16658290972,-74.0208326701545,109.471226738793));
#85225=CARTESIAN_POINT('Ctrl Pts',(236.013896109739,-40.9658464365221,109.447613584385));
#85226=CARTESIAN_POINT('Ctrl Pts',(228.325939211598,-18.8434554588877,109.28694968347));
#85227=CARTESIAN_POINT('Ctrl Pts',(199.4371324841,60.9598195272659,108.473809105488));
#85228=CARTESIAN_POINT('Ctrl Pts',(178.278774731953,112.662771270022,107.453470304555));
#85229=CARTESIAN_POINT('Ctrl Pts',(138.658245547169,209.453374230036,105.063551170246));
#85230=CARTESIAN_POINT('Ctrl Pts',(120.196014730927,254.541222475395,103.693950031325));
#85231=CARTESIAN_POINT('Ctrl Pts',(88.5733089389711,345.240633983569,101.103783619896));
#85232=CARTESIAN_POINT('Ctrl Pts',(75.4133809825114,390.851984142697,99.8832712227459));
#85233=CARTESIAN_POINT('Ctrl Pts',(57.0018485468049,489.727553050326,98.090033588344));
#85234=CARTESIAN_POINT('Ctrl Pts',(51.7501560506267,542.991128087974,97.5173172684936));
#85235=CARTESIAN_POINT('Ctrl Pts',(51.7501560487334,603.648875370191,97.5173172684936));
#85236=CARTESIAN_POINT('Ctrl Pts',(6.,-22.143643036685,90.7830741855191));
#85237=CARTESIAN_POINT('Ctrl Pts',(6.00000000007298,-27.8762778364647,90.7830741857764));
#85238=CARTESIAN_POINT('Ctrl Pts',(6.01660922703522,-33.5482466389342,90.7809593838058));
#85239=CARTESIAN_POINT('Ctrl Pts',(6.08595255085911,-44.7695275905442,90.7728487001403));
#85240=CARTESIAN_POINT('Ctrl Pts',(6.15260059239406,-50.3186632642503,90.7949425127537));
#85241=CARTESIAN_POINT('Ctrl Pts',(6.27877423953789,-66.7817034075453,90.5893788459225));
#85242=CARTESIAN_POINT('Ctrl Pts',(6.43586086298679,-77.5100259260557,90.4299948560914));
#85243=CARTESIAN_POINT('Ctrl Pts',(7.22730950121153,-108.9381039302,90.0310462352604));
#85244=CARTESIAN_POINT('Ctrl Pts',(8.14498503933279,-128.880916711419,89.7977286797552));
#85245=CARTESIAN_POINT('Ctrl Pts',(12.3095360218137,-185.575675871405,89.1445509441633));
#85246=CARTESIAN_POINT('Ctrl Pts',(16.9462613729601,-219.18776575348,88.7690335671882));
#85247=CARTESIAN_POINT('Ctrl Pts',(28.0381402389499,-263.028960386728,88.3216085852849));
#85248=CARTESIAN_POINT('Ctrl Pts',(32.4301770643691,-276.550270563958,88.1933449712546));
#85249=CARTESIAN_POINT('Ctrl Pts',(42.9281358410523,-301.334934854994,87.9959540550834));
#85250=CARTESIAN_POINT('Ctrl Pts',(49.0378632949769,-312.604391650755,87.9268325496319));
#85251=CARTESIAN_POINT('Ctrl Pts',(63.3505889867002,-332.666067561327,87.8717096511972));
#85252=CARTESIAN_POINT('Ctrl Pts',(71.5675366934108,-341.455614010345,87.8860704325898));
#85253=CARTESIAN_POINT('Ctrl Pts',(90.2657049891989,-356.061141331087,88.024621324407));
#85254=CARTESIAN_POINT('Ctrl Pts',(100.739337254366,-361.85547323351,88.1491356227232));
#85255=CARTESIAN_POINT('Ctrl Pts',(121.795026838174,-369.421310350857,88.4928845583287));
#85256=CARTESIAN_POINT('Ctrl Pts',(132.039500923872,-371.694369951344,88.7276447152287));
#85257=CARTESIAN_POINT('Ctrl Pts',(147.720189119143,-373.163371418067,89.2021923376507));
#85258=CARTESIAN_POINT('Ctrl Pts',(152.999948199941,-373.325965479262,89.3849240163435));
#85259=CARTESIAN_POINT('Ctrl Pts',(160.914718211754,-373.034083667193,89.7074143095509));
#85260=CARTESIAN_POINT('Ctrl Pts',(163.552129596181,-372.84735983228,89.8229885286486));
#85261=CARTESIAN_POINT('Ctrl Pts',(168.810475701525,-372.285867179701,90.07238433115));
#85262=CARTESIAN_POINT('Ctrl Pts',(171.43271342101,-371.91445109154,90.1968314929245));
#85263=CARTESIAN_POINT('Ctrl Pts',(183.798479337875,-369.623964165754,90.9877086463466));
#85264=CARTESIAN_POINT('Ctrl Pts',(193.184245643645,-366.437988693138,91.7506522889361));
#85265=CARTESIAN_POINT('Ctrl Pts',(210.818248569633,-357.5472455943,93.4656749781478));
#85266=CARTESIAN_POINT('Ctrl Pts',(219.06523365596,-351.846917249993,94.4171866516416));
#85267=CARTESIAN_POINT('Ctrl Pts',(241.719331610269,-331.42785841035,97.42192012483));
#85268=CARTESIAN_POINT('Ctrl Pts',(254.033000706385,-313.431087443606,99.6206963686531));
#85269=CARTESIAN_POINT('Ctrl Pts',(272.028370203714,-270.452761805799,103.821561236115));
#85270=CARTESIAN_POINT('Ctrl Pts',(277.733703504083,-245.446183070117,105.827059435943));
#85271=CARTESIAN_POINT('Ctrl Pts',(281.463134095255,-189.543779622914,109.134461342326));
#85272=CARTESIAN_POINT('Ctrl Pts',(279.48318081708,-158.639275832648,110.437140468834));
#85273=CARTESIAN_POINT('Ctrl Pts',(271.952046448821,-119.904622067839,111.2542525508));
#85274=CARTESIAN_POINT('Ctrl Pts',(270.809827609678,-114.457132821552,111.321267040589));
#85275=CARTESIAN_POINT('Ctrl Pts',(268.308983895114,-103.488720232041,111.450674606317));
#85276=CARTESIAN_POINT('Ctrl Pts',(266.958321769937,-97.9661357327517,111.501600230574));
#85277=CARTESIAN_POINT('Ctrl Pts',(262.650651001717,-81.3229024095457,111.617794124028));
#85278=CARTESIAN_POINT('Ctrl Pts',(259.438059285751,-70.1263787386142,111.646512989559));
#85279=CARTESIAN_POINT('Ctrl Pts',(249.130972035179,-36.5686972903188,111.622540287227));
#85280=CARTESIAN_POINT('Ctrl Pts',(241.366793816677,-14.2357562047768,111.459824858988));
#85281=CARTESIAN_POINT('Ctrl Pts',(212.315224351282,66.0171392750542,110.64210295685));
#85282=CARTESIAN_POINT('Ctrl Pts',(191.063967235354,117.941065745225,109.616459895168));
#85283=CARTESIAN_POINT('Ctrl Pts',(151.437384003502,214.746459510979,107.22617282344));
#85284=CARTESIAN_POINT('Ctrl Pts',(133.070417888531,259.620118178664,105.86263308603));
#85285=CARTESIAN_POINT('Ctrl Pts',(101.775904124562,349.378219317153,103.299345597994));
#85286=CARTESIAN_POINT('Ctrl Pts',(88.8377317907513,394.25825975287,102.098960380939));
#85287=CARTESIAN_POINT('Ctrl Pts',(70.7379343976928,491.459718172245,100.336082581174));
#85288=CARTESIAN_POINT('Ctrl Pts',(65.5673668639291,543.802811219013,99.7722419539107));
#85289=CARTESIAN_POINT('Ctrl Pts',(65.567366862141,603.648875370191,99.772241954121));
#85290=CARTESIAN_POINT('Ctrl Pts',(6.,-22.143643036685,76.7830741855191));
#85291=CARTESIAN_POINT('Ctrl Pts',(6.00000000001608,-27.8728345877897,76.7830741857764));
#85292=CARTESIAN_POINT('Ctrl Pts',(6.01659916901003,-33.5414291810368,76.7809606543939));
#85293=CARTESIAN_POINT('Ctrl Pts',(6.08590153713278,-44.7561068029682,76.7728547436659));
#85294=CARTESIAN_POINT('Ctrl Pts',(6.12448436107623,-50.3024630339952,76.7948482086147));
#85295=CARTESIAN_POINT('Ctrl Pts',(6.43257817927521,-66.7534068507774,76.5897246487929));
#85296=CARTESIAN_POINT('Ctrl Pts',(6.72514308144325,-77.47171901919,76.4326527457133));
#85297=CARTESIAN_POINT('Ctrl Pts',(7.82552897182559,-108.866320074244,76.0424819184556));
#85298=CARTESIAN_POINT('Ctrl Pts',(8.89215472186884,-128.78136213641,75.8174699621448));
#85299=CARTESIAN_POINT('Ctrl Pts',(13.4192108905908,-185.374605722347,75.1877811771031));
#85300=CARTESIAN_POINT('Ctrl Pts',(18.189036261472,-218.895357461452,74.8265221352761));
#85301=CARTESIAN_POINT('Ctrl Pts',(29.3980631288525,-262.538761129952,74.3962282066761));
#85302=CARTESIAN_POINT('Ctrl Pts',(33.8133689117452,-275.983630493145,74.2730893164583));
#85303=CARTESIAN_POINT('Ctrl Pts',(44.3198869194738,-300.591898809396,74.0848525703389));
#85304=CARTESIAN_POINT('Ctrl Pts',(50.4145080604677,-311.760854194936,74.0197676681309));
#85305=CARTESIAN_POINT('Ctrl Pts',(64.6449465931735,-331.608467073524,73.9713758616919));
#85306=CARTESIAN_POINT('Ctrl Pts',(72.793441073325,-340.284689964064,73.9884016133359));
#85307=CARTESIAN_POINT('Ctrl Pts',(91.3057500859674,-354.685628570187,74.1305443806443));
#85308=CARTESIAN_POINT('Ctrl Pts',(101.662639981094,-360.390625948114,74.2559577644952));
#85309=CARTESIAN_POINT('Ctrl Pts',(122.498687517451,-367.835138371731,74.6003688539808));
#85310=CARTESIAN_POINT('Ctrl Pts',(132.66179181958,-370.109786839278,74.8314342382333));
#85311=CARTESIAN_POINT('Ctrl Pts',(148.263273452825,-371.571384934932,75.3035829737878));
#85312=CARTESIAN_POINT('Ctrl Pts',(153.522526283597,-371.733735538213,75.4855736904116));
#85313=CARTESIAN_POINT('Ctrl Pts',(161.414904368065,-371.442685652143,75.8071509290502));
#85314=CARTESIAN_POINT('Ctrl Pts',(164.04625206938,-371.256441224634,75.922454612872));
#85315=CARTESIAN_POINT('Ctrl Pts',(169.295244001206,-370.695955309142,76.1714058721708));
#85316=CARTESIAN_POINT('Ctrl Pts',(171.912233718893,-370.316347052647,76.2965946205466));
#85317=CARTESIAN_POINT('Ctrl Pts',(184.289074772213,-368.126729770224,77.0764146285139));
#85318=CARTESIAN_POINT('Ctrl Pts',(193.695566775172,-365.021581292332,77.8316134147758));
#85319=CARTESIAN_POINT('Ctrl Pts',(211.395793536418,-356.28789794976,79.5341356615909));
#85320=CARTESIAN_POINT('Ctrl Pts',(219.68827733214,-350.663731347904,80.4809028238217));
#85321=CARTESIAN_POINT('Ctrl Pts',(242.510631416724,-330.456067053452,83.4769589166651));
#85322=CARTESIAN_POINT('Ctrl Pts',(254.979165750953,-312.575705655683,85.6776836832917));
#85323=CARTESIAN_POINT('Ctrl Pts',(273.308912228241,-269.758353895505,89.8963137045242));
#85324=CARTESIAN_POINT('Ctrl Pts',(279.192050799395,-244.797192233655,91.9173573898723));
#85325=CARTESIAN_POINT('Ctrl Pts',(283.250633704224,-188.932420787966,95.2615069894894));
#85326=CARTESIAN_POINT('Ctrl Pts',(281.422244927106,-158.021082723321,96.5852099265189));
#85327=CARTESIAN_POINT('Ctrl Pts',(274.043909433957,-119.263548415822,97.4262517020704));
#85328=CARTESIAN_POINT('Ctrl Pts',(272.889604588913,-113.818973755306,97.4913255613324));
#85329=CARTESIAN_POINT('Ctrl Pts',(270.389104286926,-102.852067911723,97.6207153303099));
#85330=CARTESIAN_POINT('Ctrl Pts',(269.038633909964,-97.3302694284403,97.6716336302827));
#85331=CARTESIAN_POINT('Ctrl Pts',(264.731601949094,-80.689504594602,97.78781027541));
#85332=CARTESIAN_POINT('Ctrl Pts',(261.519520120845,-69.4947722490061,97.8165238949743));
#85333=CARTESIAN_POINT('Ctrl Pts',(251.214263776602,-35.9430533478927,97.7925553823412));
#85334=CARTESIAN_POINT('Ctrl Pts',(243.451688444427,-13.6148152733545,97.6298685452083));
#85335=CARTESIAN_POINT('Ctrl Pts',(214.408695933877,66.6143869791072,96.812388060053));
#85336=CARTESIAN_POINT('Ctrl Pts',(193.168752447473,118.509829025431,95.7872005587473));
#85337=CARTESIAN_POINT('Ctrl Pts',(153.576263251876,215.231925874893,93.3989697721262));
#85338=CARTESIAN_POINT('Ctrl Pts',(135.232196296888,260.050378007844,92.0370723621136));
#85339=CARTESIAN_POINT('Ctrl Pts',(103.982022789748,349.68129527775,89.4774164941815));
#85340=CARTESIAN_POINT('Ctrl Pts',(91.0641975121257,394.489784594186,88.2789148168611));
#85341=CARTESIAN_POINT('Ctrl Pts',(72.9887151127201,491.560651219013,86.5184050823723));
#85342=CARTESIAN_POINT('Ctrl Pts',(67.8222915499773,543.845990976705,85.9550311400823));
#85343=CARTESIAN_POINT('Ctrl Pts',(67.8222915477683,603.648875370191,85.9550311407135));
#85344=CARTESIAN_POINT('Ctrl Pts',(20.,-22.143643036685,76.7830741855192));
#85345=CARTESIAN_POINT('Ctrl Pts',(20.,-27.8457920778109,76.7830741857566));
#85346=CARTESIAN_POINT('Ctrl Pts',(20.0165214330532,-33.485592853313,76.7809705517141));
#85347=CARTESIAN_POINT('Ctrl Pts',(20.0854446608167,-44.638917128667,76.7729088380163));
#85348=CARTESIAN_POINT('Ctrl Pts',(20.1238292955523,-50.1526654673148,76.7668988331685));
#85349=CARTESIAN_POINT('Ctrl Pts',(20.4301340697073,-66.5001303791202,76.743985515181));
#85350=CARTESIAN_POINT('Ctrl Pts',(20.7188936123879,-77.141599114471,76.7227141396145));
#85351=CARTESIAN_POINT('Ctrl Pts',(21.8028495683285,-108.277666955853,76.643040982027));
#85352=CARTESIAN_POINT('Ctrl Pts',(22.8522177208893,-127.983498586547,76.568779347995));
#85353=CARTESIAN_POINT('Ctrl Pts',(27.2962882348799,-183.793342140183,76.3120470559144));
#85354=CARTESIAN_POINT('Ctrl Pts',(31.9889018993299,-216.590007789356,76.0958804243854));
#85355=CARTESIAN_POINT('Ctrl Pts',(42.752586146367,-258.54916325461,75.8385782220632));
#85356=CARTESIAN_POINT('Ctrl Pts',(46.9602598342624,-271.329384640549,75.7640306692479));
#85357=CARTESIAN_POINT('Ctrl Pts',(56.7935789905011,-294.374861216214,75.6600037328577));
#85358=CARTESIAN_POINT('Ctrl Pts',(62.4190261651095,-304.639843280753,75.6305279269569));
#85359=CARTESIAN_POINT('Ctrl Pts',(75.2624672361846,-322.558676299804,75.6391115492116));
#85360=CARTESIAN_POINT('Ctrl Pts',(82.4798249428642,-330.212646288195,75.6771562180411));
#85361=CARTESIAN_POINT('Ctrl Pts',(98.6902707967944,-342.825622479896,75.8431732977935));
#85362=CARTESIAN_POINT('Ctrl Pts',(107.683690787476,-347.785594002476,75.9711317990764));
#85363=CARTESIAN_POINT('Ctrl Pts',(126.023069913222,-354.340138637006,76.3098567703564));
#85364=CARTESIAN_POINT('Ctrl Pts',(135.083207114917,-356.371635015224,76.501925570174));
#85365=CARTESIAN_POINT('Ctrl Pts',(148.924338523526,-357.668316903019,76.9207856483578));
#85366=CARTESIAN_POINT('Ctrl Pts',(153.579247220674,-357.810711475144,77.0819658816335));
#85367=CARTESIAN_POINT('Ctrl Pts',(160.521670574454,-357.554693148273,77.3648314770126));
#85368=CARTESIAN_POINT('Ctrl Pts',(162.82915793653,-357.391086631896,77.4659695920693));
#85369=CARTESIAN_POINT('Ctrl Pts',(167.413894984383,-356.901529412086,77.6834093931112));
#85370=CARTESIAN_POINT('Ctrl Pts',(169.690165914981,-356.571218959933,77.800168876217));
#85371=CARTESIAN_POINT('Ctrl Pts',(180.410587995582,-354.672149675074,78.3871286663314));
#85372=CARTESIAN_POINT('Ctrl Pts',(188.539471171489,-351.990508745272,78.9676971116917));
#85373=CARTESIAN_POINT('Ctrl Pts',(203.935932366808,-344.394636660447,80.2994244971851));
#85374=CARTESIAN_POINT('Ctrl Pts',(211.203510672235,-339.480369996828,81.0505889748358));
#85375=CARTESIAN_POINT('Ctrl Pts',(231.426270328895,-321.586439483533,83.4642765655722));
#85376=CARTESIAN_POINT('Ctrl Pts',(242.801650331,-305.454778835795,85.2871564557421));
#85377=CARTESIAN_POINT('Ctrl Pts',(259.787422523192,-265.857198323714,88.846412059781));
#85378=CARTESIAN_POINT('Ctrl Pts',(265.396961479631,-242.39170484102,90.582652202398));
#85379=CARTESIAN_POINT('Ctrl Pts',(269.303802179431,-189.217670775394,93.4513081720829));
#85380=CARTESIAN_POINT('Ctrl Pts',(267.601212650846,-159.509605592023,94.5836348018781));
#85381=CARTESIAN_POINT('Ctrl Pts',(260.488092878426,-122.007461671797,95.2483440922483));
#85382=CARTESIAN_POINT('Ctrl Pts',(259.365919995518,-116.723004281873,95.3235942479774));
#85383=CARTESIAN_POINT('Ctrl Pts',(256.932101050909,-106.048555274698,95.4495336771278));
#85384=CARTESIAN_POINT('Ctrl Pts',(255.614336154295,-100.659660585315,95.4992578713651));
#85385=CARTESIAN_POINT('Ctrl Pts',(251.40188561101,-84.3843231292077,95.6128833960036));
#85386=CARTESIAN_POINT('Ctrl Pts',(248.248043744655,-73.3892261805465,95.6412376442078));
#85387=CARTESIAN_POINT('Ctrl Pts',(238.097187851482,-40.3402024940961,95.6176286794984));
#85388=CARTESIAN_POINT('Ctrl Pts',(230.410833839506,-18.2225145274556,95.4569933696899));
#85389=CARTESIAN_POINT('Ctrl Pts',(201.530604066263,61.5570672312919,94.6440942086903));
#85390=CARTESIAN_POINT('Ctrl Pts',(180.38355994371,113.231534550229,93.6242109681347));
#85391=CARTESIAN_POINT('Ctrl Pts',(140.797124795906,209.938840593949,91.236348118932));
#85392=CARTESIAN_POINT('Ctrl Pts',(122.357793139117,254.971482304575,89.8683893074086));
#85393=CARTESIAN_POINT('Ctrl Pts',(90.7794276043238,345.543709944167,87.281854516083));
#85394=CARTESIAN_POINT('Ctrl Pts',(77.6398467041473,391.083508984014,86.0632256586685));
#85395=CARTESIAN_POINT('Ctrl Pts',(59.2526292615706,489.828486097094,84.2723560895427));
#85396=CARTESIAN_POINT('Ctrl Pts',(54.0050807366749,543.034307838934,83.7001064546653));
#85397=CARTESIAN_POINT('Ctrl Pts',(54.0050807343608,603.648875370191,83.7001064550861));
#85398=CARTESIAN_POINT('',(20.,-22.143643036685,76.7830741855192));
#85399=CARTESIAN_POINT('',(20.,-22.143643036685,90.7830741855191));
#85400=CARTESIAN_POINT('Origin',(20.,-22.143643036685,83.7830741855192));
#85401=CARTESIAN_POINT('',(51.7501560487334,603.648875370191,97.5173172684936));
#85402=CARTESIAN_POINT('Ctrl Pts',(20.,-22.143643036685,90.7830741855191));
#85403=CARTESIAN_POINT('Ctrl Pts',(20.0000000000198,-27.8492353264858,90.7830741857566));
#85404=CARTESIAN_POINT('Ctrl Pts',(20.016531491053,-33.4924103112104,90.7809692811259));
#85405=CARTESIAN_POINT('Ctrl Pts',(20.0854956745684,-44.652337916243,90.7729027944908));
#85406=CARTESIAN_POINT('Ctrl Pts',(20.1519455268513,-50.1688656975699,90.7669931373075));
#85407=CARTESIAN_POINT('Ctrl Pts',(20.2763301300078,-66.5284269358881,90.7436397123106));
#85408=CARTESIAN_POINT('Ctrl Pts',(20.4296113938976,-77.1799060213726,90.7200562499926));
#85409=CARTESIAN_POINT('Ctrl Pts',(21.204630097782,-108.349450811737,90.6316052988318));
#85410=CARTESIAN_POINT('Ctrl Pts',(22.10504803841,-128.083053161685,90.5490380656054));
#85411=CARTESIAN_POINT('Ctrl Pts',(26.1866133659894,-183.994412288981,90.2688168229746));
#85412=CARTESIAN_POINT('Ctrl Pts',(30.746127010843,-216.882416081384,90.0383918562974));
#85413=CARTESIAN_POINT('Ctrl Pts',(41.3926632564519,-259.039362511386,89.7639586006721));
#85414=CARTESIAN_POINT('Ctrl Pts',(45.5770679869517,-271.896024711361,89.6842863240442));
#85415=CARTESIAN_POINT('Ctrl Pts',(55.4018279120142,-295.117897261812,89.5711052176021));
#85416=CARTESIAN_POINT('Ctrl Pts',(61.0423813996187,-305.483380736572,89.537592808458));
#85417=CARTESIAN_POINT('Ctrl Pts',(73.9681096297112,-323.616276787607,89.5394453387168));
#85418=CARTESIAN_POINT('Ctrl Pts',(81.2539205629141,-331.38357033419,89.574825037295));
#85419=CARTESIAN_POINT('Ctrl Pts',(97.6502257000617,-344.201135241083,89.7372502415561));
#85420=CARTESIAN_POINT('Ctrl Pts',(106.760388060712,-349.250441287872,89.8643096573043));
#85421=CARTESIAN_POINT('Ctrl Pts',(125.319409233977,-355.926310616132,90.2023724747043));
#85422=CARTESIAN_POINT('Ctrl Pts',(134.460916219209,-357.956218127161,90.3981360471693));
#85423=CARTESIAN_POINT('Ctrl Pts',(148.381254189844,-359.260303386218,90.8193950122208));
#85424=CARTESIAN_POINT('Ctrl Pts',(153.056669136986,-359.402941416322,90.9813162075653));
#85425=CARTESIAN_POINT('Ctrl Pts',(160.021484418159,-359.146091163259,91.2650948575132));
#85426=CARTESIAN_POINT('Ctrl Pts',(162.335035463347,-358.982005239573,91.3665035078458));
#85427=CARTESIAN_POINT('Ctrl Pts',(166.929126684686,-358.491441282613,91.5843878520904));
#85428=CARTESIAN_POINT('Ctrl Pts',(169.210645617082,-358.169322998826,91.7004057485949));
#85429=CARTESIAN_POINT('Ctrl Pts',(179.919992561305,-356.169384070604,92.298422684164));
#85430=CARTESIAN_POINT('Ctrl Pts',(188.028150039962,-353.406916146197,92.886735985852));
#85431=CARTESIAN_POINT('Ctrl Pts',(203.358387400023,-345.653984304867,94.2309638137419));
#85432=CARTESIAN_POINT('Ctrl Pts',(210.580466995992,-340.663555898792,94.9868728026557));
#85433=CARTESIAN_POINT('Ctrl Pts',(230.634970522565,-322.558230840682,97.4092377737371));
#85434=CARTESIAN_POINT('Ctrl Pts',(241.855485286281,-306.310160623718,99.2301691411035));
#85435=CARTESIAN_POINT('Ctrl Pts',(258.506880498815,-266.551606234007,102.771659591371));
#85436=CARTESIAN_POINT('Ctrl Pts',(263.93861418432,-243.040695677481,104.492354248469));
#85437=CARTESIAN_POINT('Ctrl Pts',(267.516302570461,-189.829029610341,107.32426252492));
#85438=CARTESIAN_POINT('Ctrl Pts',(265.662148540819,-160.127798701236,108.435565344194));
#85439=CARTESIAN_POINT('Ctrl Pts',(258.396229893289,-122.648535323832,109.076344940978));
#85440=CARTESIAN_POINT('Ctrl Pts',(257.286143016284,-117.361163348158,109.153535727234));
#85441=CARTESIAN_POINT('Ctrl Pts',(254.851980659096,-106.685207594979,109.279492953135));
#85442=CARTESIAN_POINT('Ctrl Pts',(253.534024014268,-101.295526889627,109.329224471656));
#85443=CARTESIAN_POINT('Ctrl Pts',(249.320934663633,-85.0177209441514,109.442867244621));
#85444=CARTESIAN_POINT('Ctrl Pts',(246.16658290972,-74.0208326701545,109.471226738793));
#85445=CARTESIAN_POINT('Ctrl Pts',(236.013896109739,-40.9658464365221,109.447613584385));
#85446=CARTESIAN_POINT('Ctrl Pts',(228.325939211598,-18.8434554588877,109.28694968347));
#85447=CARTESIAN_POINT('Ctrl Pts',(199.4371324841,60.9598195272659,108.473809105488));
#85448=CARTESIAN_POINT('Ctrl Pts',(178.278774731953,112.662771270022,107.453470304555));
#85449=CARTESIAN_POINT('Ctrl Pts',(138.658245547169,209.453374230036,105.063551170246));
#85450=CARTESIAN_POINT('Ctrl Pts',(120.196014730927,254.541222475395,103.693950031325));
#85451=CARTESIAN_POINT('Ctrl Pts',(88.5733089389711,345.240633983569,101.103783619896));
#85452=CARTESIAN_POINT('Ctrl Pts',(75.4133809825114,390.851984142697,99.8832712227459));
#85453=CARTESIAN_POINT('Ctrl Pts',(57.0018485468049,489.727553050326,98.090033588344));
#85454=CARTESIAN_POINT('Ctrl Pts',(51.7501560506267,542.991128087974,97.5173172684936));
#85455=CARTESIAN_POINT('Ctrl Pts',(51.7501560487334,603.648875370191,97.5173172684936));
#85456=CARTESIAN_POINT('',(54.0050807343608,603.648875370191,83.700106455086));
#85457=CARTESIAN_POINT('Origin',(52.8776183915471,603.648875370191,90.6087118617898));
#85458=CARTESIAN_POINT('Ctrl Pts',(20.,-22.143643036685,76.7830741855192));
#85459=CARTESIAN_POINT('Ctrl Pts',(20.,-27.8457920778109,76.7830741857566));
#85460=CARTESIAN_POINT('Ctrl Pts',(20.0165214330532,-33.485592853313,76.7809705517141));
#85461=CARTESIAN_POINT('Ctrl Pts',(20.0854446608167,-44.638917128667,76.7729088380163));
#85462=CARTESIAN_POINT('Ctrl Pts',(20.1238292955523,-50.1526654673148,76.7668988331685));
#85463=CARTESIAN_POINT('Ctrl Pts',(20.4301340697073,-66.5001303791202,76.743985515181));
#85464=CARTESIAN_POINT('Ctrl Pts',(20.7188936123879,-77.141599114471,76.7227141396145));
#85465=CARTESIAN_POINT('Ctrl Pts',(21.8028495683285,-108.277666955853,76.643040982027));
#85466=CARTESIAN_POINT('Ctrl Pts',(22.8522177208893,-127.983498586547,76.568779347995));
#85467=CARTESIAN_POINT('Ctrl Pts',(27.2962882348799,-183.793342140183,76.3120470559144));
#85468=CARTESIAN_POINT('Ctrl Pts',(31.9889018993299,-216.590007789356,76.0958804243854));
#85469=CARTESIAN_POINT('Ctrl Pts',(42.752586146367,-258.54916325461,75.8385782220632));
#85470=CARTESIAN_POINT('Ctrl Pts',(46.9602598342624,-271.329384640549,75.7640306692479));
#85471=CARTESIAN_POINT('Ctrl Pts',(56.7935789905011,-294.374861216214,75.6600037328577));
#85472=CARTESIAN_POINT('Ctrl Pts',(62.4190261651095,-304.639843280753,75.6305279269569));
#85473=CARTESIAN_POINT('Ctrl Pts',(75.2624672361846,-322.558676299804,75.6391115492116));
#85474=CARTESIAN_POINT('Ctrl Pts',(82.4798249428642,-330.212646288195,75.6771562180411));
#85475=CARTESIAN_POINT('Ctrl Pts',(98.6902707967944,-342.825622479896,75.8431732977935));
#85476=CARTESIAN_POINT('Ctrl Pts',(107.683690787476,-347.785594002476,75.9711317990764));
#85477=CARTESIAN_POINT('Ctrl Pts',(126.023069913222,-354.340138637006,76.3098567703564));
#85478=CARTESIAN_POINT('Ctrl Pts',(135.083207114917,-356.371635015224,76.501925570174));
#85479=CARTESIAN_POINT('Ctrl Pts',(148.924338523526,-357.668316903019,76.9207856483578));
#85480=CARTESIAN_POINT('Ctrl Pts',(153.579247220674,-357.810711475144,77.0819658816335));
#85481=CARTESIAN_POINT('Ctrl Pts',(160.521670574454,-357.554693148273,77.3648314770126));
#85482=CARTESIAN_POINT('Ctrl Pts',(162.82915793653,-357.391086631896,77.4659695920693));
#85483=CARTESIAN_POINT('Ctrl Pts',(167.413894984383,-356.901529412086,77.6834093931112));
#85484=CARTESIAN_POINT('Ctrl Pts',(169.690165914981,-356.571218959933,77.800168876217));
#85485=CARTESIAN_POINT('Ctrl Pts',(180.410587995582,-354.672149675074,78.3871286663314));
#85486=CARTESIAN_POINT('Ctrl Pts',(188.539471171489,-351.990508745272,78.9676971116917));
#85487=CARTESIAN_POINT('Ctrl Pts',(203.935932366808,-344.394636660447,80.2994244971851));
#85488=CARTESIAN_POINT('Ctrl Pts',(211.203510672235,-339.480369996828,81.0505889748358));
#85489=CARTESIAN_POINT('Ctrl Pts',(231.426270328895,-321.586439483533,83.4642765655722));
#85490=CARTESIAN_POINT('Ctrl Pts',(242.801650331,-305.454778835795,85.2871564557421));
#85491=CARTESIAN_POINT('Ctrl Pts',(259.787422523192,-265.857198323714,88.846412059781));
#85492=CARTESIAN_POINT('Ctrl Pts',(265.396961479631,-242.39170484102,90.582652202398));
#85493=CARTESIAN_POINT('Ctrl Pts',(269.303802179431,-189.217670775394,93.4513081720829));
#85494=CARTESIAN_POINT('Ctrl Pts',(267.601212650846,-159.509605592023,94.5836348018781));
#85495=CARTESIAN_POINT('Ctrl Pts',(260.488092878426,-122.007461671797,95.2483440922483));
#85496=CARTESIAN_POINT('Ctrl Pts',(259.365919995518,-116.723004281873,95.3235942479774));
#85497=CARTESIAN_POINT('Ctrl Pts',(256.932101050909,-106.048555274698,95.4495336771278));
#85498=CARTESIAN_POINT('Ctrl Pts',(255.614336154295,-100.659660585315,95.4992578713651));
#85499=CARTESIAN_POINT('Ctrl Pts',(251.40188561101,-84.3843231292077,95.6128833960036));
#85500=CARTESIAN_POINT('Ctrl Pts',(248.248043744655,-73.3892261805465,95.6412376442078));
#85501=CARTESIAN_POINT('Ctrl Pts',(238.097187851482,-40.3402024940961,95.6176286794984));
#85502=CARTESIAN_POINT('Ctrl Pts',(230.410833839506,-18.2225145274556,95.4569933696899));
#85503=CARTESIAN_POINT('Ctrl Pts',(201.530604066263,61.5570672312919,94.6440942086903));
#85504=CARTESIAN_POINT('Ctrl Pts',(180.38355994371,113.231534550229,93.6242109681347));
#85505=CARTESIAN_POINT('Ctrl Pts',(140.797124795906,209.938840593949,91.236348118932));
#85506=CARTESIAN_POINT('Ctrl Pts',(122.357793139117,254.971482304575,89.8683893074086));
#85507=CARTESIAN_POINT('Ctrl Pts',(90.7794276043238,345.543709944167,87.281854516083));
#85508=CARTESIAN_POINT('Ctrl Pts',(77.6398467041473,391.083508984014,86.0632256586685));
#85509=CARTESIAN_POINT('Ctrl Pts',(59.2526292615706,489.828486097094,84.2723560895427));
#85510=CARTESIAN_POINT('Ctrl Pts',(54.0050807366749,543.034307838934,83.7001064546653));
#85511=CARTESIAN_POINT('Ctrl Pts',(54.0050807343608,603.648875370191,83.700106455086));
#85512=CARTESIAN_POINT('Origin',(20.,-21.143643036685,83.7830741855192));
#85513=CARTESIAN_POINT('',(20.,-21.1844254061993,74.7958939977414));
#85514=CARTESIAN_POINT('Origin',(20.,-21.1844254061993,83.7830741855192));
#85515=CARTESIAN_POINT('',(20.,-22.143643036685,75.795062050842));
#85516=CARTESIAN_POINT('Origin',(20.,-21.143643036685,75.795062050842));
#85517=CARTESIAN_POINT('Origin',(20.,-22.143643036685,83.7830741855192));
#85518=CARTESIAN_POINT('Origin',(20.,-22.143643036685,83.7830741855192));
#85519=CARTESIAN_POINT('',(20.,3.62965999324553,73.7830741855192));
#85520=CARTESIAN_POINT('Origin',(20.,3.62965999324553,83.7830741855192));
#85521=CARTESIAN_POINT('',(20.,-22.143643036685,74.8350457377612));
#85522=CARTESIAN_POINT('Origin',(20.,3.62965999324553,73.7830741855192));
#85523=CARTESIAN_POINT('Origin',(20.,-22.143643036685,83.7830741855192));
#85524=CARTESIAN_POINT('Origin',(20.,-22.143643036685,83.7830741855192));
#85525=CARTESIAN_POINT('Ctrl Pts',(20.,-22.143643036685,76.7830741855192));
#85526=CARTESIAN_POINT('Ctrl Pts',(20.,-27.8457920778109,76.7830741857566));
#85527=CARTESIAN_POINT('Ctrl Pts',(20.0165214330532,-33.485592853313,76.7809705517141));
#85528=CARTESIAN_POINT('Ctrl Pts',(20.0854446608167,-44.638917128667,76.7729088380163));
#85529=CARTESIAN_POINT('Ctrl Pts',(20.1238292955523,-50.1526654673148,76.7668988331685));
#85530=CARTESIAN_POINT('Ctrl Pts',(20.4301340697073,-66.5001303791202,76.743985515181));
#85531=CARTESIAN_POINT('Ctrl Pts',(20.7188936123879,-77.141599114471,76.7227141396145));
#85532=CARTESIAN_POINT('Ctrl Pts',(21.8028495683285,-108.277666955853,76.643040982027));
#85533=CARTESIAN_POINT('Ctrl Pts',(22.8522177208893,-127.983498586547,76.568779347995));
#85534=CARTESIAN_POINT('Ctrl Pts',(27.2962882348799,-183.793342140183,76.3120470559144));
#85535=CARTESIAN_POINT('Ctrl Pts',(31.9889018993299,-216.590007789356,76.0958804243854));
#85536=CARTESIAN_POINT('Ctrl Pts',(42.752586146367,-258.54916325461,75.8385782220632));
#85537=CARTESIAN_POINT('Ctrl Pts',(46.9602598342624,-271.329384640549,75.7640306692479));
#85538=CARTESIAN_POINT('Ctrl Pts',(56.7935789905011,-294.374861216214,75.6600037328577));
#85539=CARTESIAN_POINT('Ctrl Pts',(62.4190261651095,-304.639843280753,75.6305279269569));
#85540=CARTESIAN_POINT('Ctrl Pts',(75.2624672361846,-322.558676299804,75.6391115492116));
#85541=CARTESIAN_POINT('Ctrl Pts',(82.4798249428642,-330.212646288195,75.6771562180411));
#85542=CARTESIAN_POINT('Ctrl Pts',(98.6902707967944,-342.825622479896,75.8431732977935));
#85543=CARTESIAN_POINT('Ctrl Pts',(107.683690787476,-347.785594002476,75.9711317990764));
#85544=CARTESIAN_POINT('Ctrl Pts',(126.023069913222,-354.340138637006,76.3098567703564));
#85545=CARTESIAN_POINT('Ctrl Pts',(135.083207114917,-356.371635015224,76.501925570174));
#85546=CARTESIAN_POINT('Ctrl Pts',(148.924338523526,-357.668316903019,76.9207856483578));
#85547=CARTESIAN_POINT('Ctrl Pts',(153.579247220674,-357.810711475144,77.0819658816335));
#85548=CARTESIAN_POINT('Ctrl Pts',(160.521670574454,-357.554693148273,77.3648314770126));
#85549=CARTESIAN_POINT('Ctrl Pts',(162.82915793653,-357.391086631896,77.4659695920693));
#85550=CARTESIAN_POINT('Ctrl Pts',(167.413894984383,-356.901529412086,77.6834093931112));
#85551=CARTESIAN_POINT('Ctrl Pts',(169.690165914981,-356.571218959933,77.800168876217));
#85552=CARTESIAN_POINT('Ctrl Pts',(180.410587995582,-354.672149675074,78.3871286663314));
#85553=CARTESIAN_POINT('Ctrl Pts',(188.539471171489,-351.990508745272,78.9676971116917));
#85554=CARTESIAN_POINT('Ctrl Pts',(203.935932366808,-344.394636660447,80.2994244971851));
#85555=CARTESIAN_POINT('Ctrl Pts',(211.203510672235,-339.480369996828,81.0505889748358));
#85556=CARTESIAN_POINT('Ctrl Pts',(231.426270328895,-321.586439483533,83.4642765655722));
#85557=CARTESIAN_POINT('Ctrl Pts',(242.801650331,-305.454778835795,85.2871564557421));
#85558=CARTESIAN_POINT('Ctrl Pts',(259.787422523192,-265.857198323714,88.846412059781));
#85559=CARTESIAN_POINT('Ctrl Pts',(265.396961479631,-242.39170484102,90.582652202398));
#85560=CARTESIAN_POINT('Ctrl Pts',(269.303802179431,-189.217670775394,93.4513081720829));
#85561=CARTESIAN_POINT('Ctrl Pts',(267.601212650846,-159.509605592023,94.5836348018781));
#85562=CARTESIAN_POINT('Ctrl Pts',(260.488092878426,-122.007461671797,95.2483440922483));
#85563=CARTESIAN_POINT('Ctrl Pts',(259.365919995518,-116.723004281873,95.3235942479774));
#85564=CARTESIAN_POINT('Ctrl Pts',(256.932101050909,-106.048555274698,95.4495336771278));
#85565=CARTESIAN_POINT('Ctrl Pts',(255.614336154295,-100.659660585315,95.4992578713651));
#85566=CARTESIAN_POINT('Ctrl Pts',(251.40188561101,-84.3843231292077,95.6128833960036));
#85567=CARTESIAN_POINT('Ctrl Pts',(248.248043744655,-73.3892261805465,95.6412376442078));
#85568=CARTESIAN_POINT('Ctrl Pts',(238.097187851482,-40.3402024940961,95.6176286794984));
#85569=CARTESIAN_POINT('Ctrl Pts',(230.410833839506,-18.2225145274556,95.4569933696899));
#85570=CARTESIAN_POINT('Ctrl Pts',(201.530604066263,61.5570672312919,94.6440942086903));
#85571=CARTESIAN_POINT('Ctrl Pts',(180.38355994371,113.231534550229,93.6242109681347));
#85572=CARTESIAN_POINT('Ctrl Pts',(140.797124795906,209.938840593949,91.236348118932));
#85573=CARTESIAN_POINT('Ctrl Pts',(122.357793139117,254.971482304575,89.8683893074086));
#85574=CARTESIAN_POINT('Ctrl Pts',(90.7794276043238,345.543709944167,87.281854516083));
#85575=CARTESIAN_POINT('Ctrl Pts',(77.6398467041473,391.083508984014,86.0632256586685));
#85576=CARTESIAN_POINT('Ctrl Pts',(59.2526292615706,489.828486097094,84.2723560895427));
#85577=CARTESIAN_POINT('Ctrl Pts',(54.0050807366749,543.034307838934,83.7001064546653));
#85578=CARTESIAN_POINT('Ctrl Pts',(54.0050807343608,603.648875370191,83.7001064550861));
#85579=CARTESIAN_POINT('Ctrl Pts',(34.,-22.143643036685,76.7830741855191));
#85580=CARTESIAN_POINT('Ctrl Pts',(33.9999999999839,-27.818749567832,76.7830741857369));
#85581=CARTESIAN_POINT('Ctrl Pts',(34.0164436970964,-33.4297565255892,76.7809804490342));
#85582=CARTESIAN_POINT('Ctrl Pts',(34.0849877845006,-44.5217274543659,76.7729629323669));
#85583=CARTESIAN_POINT('Ctrl Pts',(34.1231742300284,-50.0028679006344,76.7389494577223));
#85584=CARTESIAN_POINT('Ctrl Pts',(34.4276899601393,-66.246853907463,76.8982463815691));
#85585=CARTESIAN_POINT('Ctrl Pts',(34.7126441433325,-76.8114792097519,77.0127755335157));
#85586=CARTESIAN_POINT('Ctrl Pts',(35.7801701648313,-107.689013837462,77.2436000455983));
#85587=CARTESIAN_POINT('Ctrl Pts',(36.8122807199099,-127.185635036684,77.3200887338452));
#85588=CARTESIAN_POINT('Ctrl Pts',(41.1733655791691,-182.212078558018,77.4363129347258));
#85589=CARTESIAN_POINT('Ctrl Pts',(45.7887675371877,-214.28465811726,77.3652387134946));
#85590=CARTESIAN_POINT('Ctrl Pts',(56.1071091638816,-254.559565379267,77.2809282374505));
#85591=CARTESIAN_POINT('Ctrl Pts',(60.1071507567796,-266.675138787952,77.2549720220375));
#85592=CARTESIAN_POINT('Ctrl Pts',(69.2672710615284,-288.157823623031,77.2351548953765));
#85593=CARTESIAN_POINT('Ctrl Pts',(74.4235442697514,-297.51883236657,77.241288185783));
#85594=CARTESIAN_POINT('Ctrl Pts',(85.8799878791956,-313.508885526083,77.3068472367312));
#85595=CARTESIAN_POINT('Ctrl Pts',(92.1662088124034,-320.140602612327,77.3659108227464));
#85596=CARTESIAN_POINT('Ctrl Pts',(106.074791507621,-330.965616389605,77.5558022149426));
#85597=CARTESIAN_POINT('Ctrl Pts',(113.704741593858,-335.180562056838,77.6863058336575));
#85598=CARTESIAN_POINT('Ctrl Pts',(129.547452308994,-340.84513890228,78.019344686732));
#85599=CARTESIAN_POINT('Ctrl Pts',(137.504622410254,-342.63348319117,78.1724169021146));
#85600=CARTESIAN_POINT('Ctrl Pts',(149.585403594227,-343.765248871106,78.5379883229279));
#85601=CARTESIAN_POINT('Ctrl Pts',(153.635968157751,-343.887687412075,78.6783580728553));
#85602=CARTESIAN_POINT('Ctrl Pts',(159.628436780843,-343.666700644404,78.9225120249749));
#85603=CARTESIAN_POINT('Ctrl Pts',(161.61206380368,-343.525732039158,79.0094845712665));
#85604=CARTESIAN_POINT('Ctrl Pts',(165.532545967561,-343.107103515031,79.1954129140516));
#85605=CARTESIAN_POINT('Ctrl Pts',(167.468098111069,-342.826090867219,79.3037431318874));
#85606=CARTESIAN_POINT('Ctrl Pts',(176.532101218951,-341.217569579924,79.6978427041489));
#85607=CARTESIAN_POINT('Ctrl Pts',(183.383375567806,-338.959436198211,80.1037808086076));
#85608=CARTESIAN_POINT('Ctrl Pts',(196.476071197198,-332.501375371133,81.0647133327792));
#85609=CARTESIAN_POINT('Ctrl Pts',(202.718744012329,-328.297008645753,81.6202751258499));
#85610=CARTESIAN_POINT('Ctrl Pts',(220.341909241066,-312.716811913614,83.4515942144793));
#85611=CARTESIAN_POINT('Ctrl Pts',(230.624134911047,-298.333852015906,84.8966292281925));
#85612=CARTESIAN_POINT('Ctrl Pts',(246.265932818144,-261.956042751922,87.7965104150377));
#85613=CARTESIAN_POINT('Ctrl Pts',(251.601872159868,-239.986217448384,89.2479470149237));
#85614=CARTESIAN_POINT('Ctrl Pts',(255.356970654638,-189.502920762821,91.6411093546763));
#85615=CARTESIAN_POINT('Ctrl Pts',(253.780180374585,-160.998128460726,92.5820596772374));
#85616=CARTESIAN_POINT('Ctrl Pts',(246.932276322894,-124.751374927772,93.0704364824261));
#85617=CARTESIAN_POINT('Ctrl Pts',(245.842235402124,-119.627034808441,93.1558629346225));
#85618=CARTESIAN_POINT('Ctrl Pts',(243.475097814891,-109.245042637674,93.2783520239457));
#85619=CARTESIAN_POINT('Ctrl Pts',(242.190038398626,-103.98905174219,93.3268821124474));
#85620=CARTESIAN_POINT('Ctrl Pts',(238.072169272926,-88.0791416638133,93.4379565165972));
#85621=CARTESIAN_POINT('Ctrl Pts',(234.976567368465,-77.2836801120869,93.4659513934413));
#85622=CARTESIAN_POINT('Ctrl Pts',(224.980111926361,-44.7373516402995,93.4427019766555));
#85623=CARTESIAN_POINT('Ctrl Pts',(217.369979234584,-22.8302137815567,93.2841181941716));
#85624=CARTESIAN_POINT('Ctrl Pts',(188.65251219865,56.4997474834766,92.4758003573277));
#85625=CARTESIAN_POINT('Ctrl Pts',(167.598367439946,107.953240075026,91.4612213775221));
#85626=CARTESIAN_POINT('Ctrl Pts',(128.017986339935,204.645755313006,89.0737264657378));
#85627=CARTESIAN_POINT('Ctrl Pts',(109.483389981347,249.892586601305,87.6997062527036));
#85628=CARTESIAN_POINT('Ctrl Pts',(77.5768324188997,341.406124610584,85.0862925379845));
#85629=CARTESIAN_POINT('Ctrl Pts',(64.215495896169,387.677233373842,83.8475365004758));
#85630=CARTESIAN_POINT('Ctrl Pts',(45.5165434104212,488.096320975175,82.0263070967131));
#85631=CARTESIAN_POINT('Ctrl Pts',(40.1878699233725,542.222624701163,81.4451817692483));
#85632=CARTESIAN_POINT('Ctrl Pts',(40.1878699209532,603.648875370192,81.4451817694587));
#85633=CARTESIAN_POINT('Ctrl Pts',(34.,-22.143643036685,90.7830741855191));
#85634=CARTESIAN_POINT('Ctrl Pts',(33.9999999999666,-27.822192816507,90.7830741857369));
#85635=CARTESIAN_POINT('Ctrl Pts',(34.0164537550708,-33.4365739834866,90.7809791784461));
#85636=CARTESIAN_POINT('Ctrl Pts',(34.0850387982778,-44.5351482419418,90.7729568888413));
#85637=CARTESIAN_POINT('Ctrl Pts',(34.1512904613084,-50.0190681308895,90.7390437618613));
#85638=CARTESIAN_POINT('Ctrl Pts',(34.2738860204776,-66.275150464231,90.8979005786987));
#85639=CARTESIAN_POINT('Ctrl Pts',(34.4233619248085,-76.8497861166896,91.0101176438938));
#85640=CARTESIAN_POINT('Ctrl Pts',(35.1819506943524,-107.760797693274,91.2321643624032));
#85641=CARTESIAN_POINT('Ctrl Pts',(36.0651110374872,-127.285189611952,91.3003474514556));
#85642=CARTESIAN_POINT('Ctrl Pts',(40.0636907101652,-182.413148706558,91.3930827017859));
#85643=CARTESIAN_POINT('Ctrl Pts',(44.5459926487259,-214.577066409288,91.3077501454067));
#85644=CARTESIAN_POINT('Ctrl Pts',(54.7471862739539,-255.049764636043,91.2063086160594));
#85645=CARTESIAN_POINT('Ctrl Pts',(58.7239589095343,-267.241778858765,91.1752276768338));
#85646=CARTESIAN_POINT('Ctrl Pts',(67.8755199829761,-288.900859668629,91.1462563801209));
#85647=CARTESIAN_POINT('Ctrl Pts',(73.0468995042606,-298.36236982239,91.148353067284));
#85648=CARTESIAN_POINT('Ctrl Pts',(84.5856302727223,-314.566486013887,91.2071810262364));
#85649=CARTESIAN_POINT('Ctrl Pts',(90.9403044324173,-321.311526658035,91.2635796420002));
#85650=CARTESIAN_POINT('Ctrl Pts',(105.034746410925,-332.341129151079,91.4498791587053));
#85651=CARTESIAN_POINT('Ctrl Pts',(112.781438867057,-336.645409342233,91.5794836918854));
#85652=CARTESIAN_POINT('Ctrl Pts',(128.84379162978,-342.431310881406,91.9118603910799));
#85653=CARTESIAN_POINT('Ctrl Pts',(136.882331514546,-344.218066302979,92.06862737911));
#85654=CARTESIAN_POINT('Ctrl Pts',(149.042319260545,-345.35723535437,92.4365976867908));
#85655=CARTESIAN_POINT('Ctrl Pts',(153.113390074031,-345.479917353382,92.5777083987872));
#85656=CARTESIAN_POINT('Ctrl Pts',(159.128250624564,-345.258098659325,92.8227754054756));
#85657=CARTESIAN_POINT('Ctrl Pts',(161.117941330513,-345.116650646867,92.910018487043));
#85658=CARTESIAN_POINT('Ctrl Pts',(165.047777667848,-344.697015385526,93.0963913730309));
#85659=CARTESIAN_POINT('Ctrl Pts',(166.988577813154,-344.424194906112,93.2039800042653));
#85660=CARTESIAN_POINT('Ctrl Pts',(176.041505784734,-342.714803975454,93.6091367219815));
#85661=CARTESIAN_POINT('Ctrl Pts',(182.872054436279,-340.375843599256,94.0228196827679));
#85662=CARTESIAN_POINT('Ctrl Pts',(195.898526230413,-333.760723015434,94.9962526493361));
#85663=CARTESIAN_POINT('Ctrl Pts',(202.095700336024,-329.480194547591,95.5565589536698));
#85664=CARTESIAN_POINT('Ctrl Pts',(219.550609434862,-313.688603271014,97.3965554226442));
#85665=CARTESIAN_POINT('Ctrl Pts',(229.677969866178,-299.18923380383,98.8396419135539));
#85666=CARTESIAN_POINT('Ctrl Pts',(244.985390793916,-262.650450662216,101.721757946628));
#85667=CARTESIAN_POINT('Ctrl Pts',(250.143524864557,-240.635208284846,103.157649060994));
#85668=CARTESIAN_POINT('Ctrl Pts',(253.569471045668,-190.114279597768,105.514063707513));
#85669=CARTESIAN_POINT('Ctrl Pts',(251.841116264558,-161.616321569825,106.433990219553));
#85670=CARTESIAN_POINT('Ctrl Pts',(244.840413337758,-125.392448579826,106.898437331156));
#85671=CARTESIAN_POINT('Ctrl Pts',(243.762458422889,-120.265193874764,106.985804413879));
#85672=CARTESIAN_POINT('Ctrl Pts',(241.394977423079,-109.881694957916,107.108311299953));
#85673=CARTESIAN_POINT('Ctrl Pts',(240.109726258598,-104.624918046502,107.156848712739));
#85674=CARTESIAN_POINT('Ctrl Pts',(235.991218325549,-88.712539478757,107.267940365215));
#85675=CARTESIAN_POINT('Ctrl Pts',(232.89510653369,-77.9152866016949,107.295940488026));
#85676=CARTESIAN_POINT('Ctrl Pts',(222.896820184299,-45.3629955827255,107.272686881542));
#85677=CARTESIAN_POINT('Ctrl Pts',(215.28508460652,-23.4511547129986,107.114074507951));
#85678=CARTESIAN_POINT('Ctrl Pts',(186.559040616919,55.9024997794776,106.305515254125));
#85679=CARTESIAN_POINT('Ctrl Pts',(165.493582228552,107.38447679482,105.290480713943));
#85680=CARTESIAN_POINT('Ctrl Pts',(125.879107090836,204.160288949093,102.900929517052));
#85681=CARTESIAN_POINT('Ctrl Pts',(107.321611573323,249.462326772125,101.52526697662));
#85682=CARTESIAN_POINT('Ctrl Pts',(75.3707137533804,341.103048649986,98.9082216417973));
#85683=CARTESIAN_POINT('Ctrl Pts',(61.9890301742715,387.445708532525,97.6675820645533));
#85684=CARTESIAN_POINT('Ctrl Pts',(43.265762695917,487.995387928407,95.8439845955144));
#85685=CARTESIAN_POINT('Ctrl Pts',(37.9329452373243,542.179444956935,95.2623925830766));
#85686=CARTESIAN_POINT('Ctrl Pts',(37.9329452353258,603.648875370192,95.2623925828662));
#85687=CARTESIAN_POINT('Ctrl Pts',(20.,-22.143643036685,90.7830741855191));
#85688=CARTESIAN_POINT('Ctrl Pts',(20.0000000000198,-27.8492353264858,90.7830741857566));
#85689=CARTESIAN_POINT('Ctrl Pts',(20.016531491053,-33.4924103112104,90.7809692811259));
#85690=CARTESIAN_POINT('Ctrl Pts',(20.0854956745684,-44.652337916243,90.7729027944908));
#85691=CARTESIAN_POINT('Ctrl Pts',(20.1519455268513,-50.1688656975699,90.7669931373075));
#85692=CARTESIAN_POINT('Ctrl Pts',(20.2763301300078,-66.5284269358881,90.7436397123106));
#85693=CARTESIAN_POINT('Ctrl Pts',(20.4296113938976,-77.1799060213726,90.7200562499926));
#85694=CARTESIAN_POINT('Ctrl Pts',(21.204630097782,-108.349450811737,90.6316052988318));
#85695=CARTESIAN_POINT('Ctrl Pts',(22.10504803841,-128.083053161685,90.5490380656054));
#85696=CARTESIAN_POINT('Ctrl Pts',(26.1866133659894,-183.994412288981,90.2688168229746));
#85697=CARTESIAN_POINT('Ctrl Pts',(30.746127010843,-216.882416081384,90.0383918562974));
#85698=CARTESIAN_POINT('Ctrl Pts',(41.3926632564519,-259.039362511386,89.7639586006721));
#85699=CARTESIAN_POINT('Ctrl Pts',(45.5770679869517,-271.896024711361,89.6842863240442));
#85700=CARTESIAN_POINT('Ctrl Pts',(55.4018279120142,-295.117897261812,89.5711052176021));
#85701=CARTESIAN_POINT('Ctrl Pts',(61.0423813996187,-305.483380736572,89.537592808458));
#85702=CARTESIAN_POINT('Ctrl Pts',(73.9681096297112,-323.616276787607,89.5394453387168));
#85703=CARTESIAN_POINT('Ctrl Pts',(81.2539205629141,-331.38357033419,89.574825037295));
#85704=CARTESIAN_POINT('Ctrl Pts',(97.6502257000617,-344.201135241083,89.7372502415561));
#85705=CARTESIAN_POINT('Ctrl Pts',(106.760388060712,-349.250441287872,89.8643096573043));
#85706=CARTESIAN_POINT('Ctrl Pts',(125.319409233977,-355.926310616132,90.2023724747043));
#85707=CARTESIAN_POINT('Ctrl Pts',(134.460916219209,-357.956218127161,90.3981360471693));
#85708=CARTESIAN_POINT('Ctrl Pts',(148.381254189844,-359.260303386218,90.8193950122208));
#85709=CARTESIAN_POINT('Ctrl Pts',(153.056669136986,-359.402941416322,90.9813162075653));
#85710=CARTESIAN_POINT('Ctrl Pts',(160.021484418159,-359.146091163259,91.2650948575132));
#85711=CARTESIAN_POINT('Ctrl Pts',(162.335035463347,-358.982005239573,91.3665035078458));
#85712=CARTESIAN_POINT('Ctrl Pts',(166.929126684686,-358.491441282613,91.5843878520904));
#85713=CARTESIAN_POINT('Ctrl Pts',(169.210645617082,-358.169322998826,91.7004057485949));
#85714=CARTESIAN_POINT('Ctrl Pts',(179.919992561305,-356.169384070604,92.298422684164));
#85715=CARTESIAN_POINT('Ctrl Pts',(188.028150039962,-353.406916146197,92.886735985852));
#85716=CARTESIAN_POINT('Ctrl Pts',(203.358387400023,-345.653984304867,94.2309638137419));
#85717=CARTESIAN_POINT('Ctrl Pts',(210.580466995992,-340.663555898792,94.9868728026557));
#85718=CARTESIAN_POINT('Ctrl Pts',(230.634970522565,-322.558230840682,97.4092377737371));
#85719=CARTESIAN_POINT('Ctrl Pts',(241.855485286281,-306.310160623718,99.2301691411035));
#85720=CARTESIAN_POINT('Ctrl Pts',(258.506880498815,-266.551606234007,102.771659591371));
#85721=CARTESIAN_POINT('Ctrl Pts',(263.93861418432,-243.040695677481,104.492354248469));
#85722=CARTESIAN_POINT('Ctrl Pts',(267.516302570461,-189.829029610341,107.32426252492));
#85723=CARTESIAN_POINT('Ctrl Pts',(265.662148540819,-160.127798701236,108.435565344194));
#85724=CARTESIAN_POINT('Ctrl Pts',(258.396229893289,-122.648535323832,109.076344940978));
#85725=CARTESIAN_POINT('Ctrl Pts',(257.286143016284,-117.361163348158,109.153535727234));
#85726=CARTESIAN_POINT('Ctrl Pts',(254.851980659096,-106.685207594979,109.279492953135));
#85727=CARTESIAN_POINT('Ctrl Pts',(253.534024014268,-101.295526889627,109.329224471656));
#85728=CARTESIAN_POINT('Ctrl Pts',(249.320934663633,-85.0177209441514,109.442867244621));
#85729=CARTESIAN_POINT('Ctrl Pts',(246.16658290972,-74.0208326701545,109.471226738793));
#85730=CARTESIAN_POINT('Ctrl Pts',(236.013896109739,-40.9658464365221,109.447613584385));
#85731=CARTESIAN_POINT('Ctrl Pts',(228.325939211598,-18.8434554588877,109.28694968347));
#85732=CARTESIAN_POINT('Ctrl Pts',(199.4371324841,60.9598195272659,108.473809105488));
#85733=CARTESIAN_POINT('Ctrl Pts',(178.278774731953,112.662771270022,107.453470304555));
#85734=CARTESIAN_POINT('Ctrl Pts',(138.658245547169,209.453374230036,105.063551170246));
#85735=CARTESIAN_POINT('Ctrl Pts',(120.196014730927,254.541222475395,103.693950031325));
#85736=CARTESIAN_POINT('Ctrl Pts',(88.5733089389711,345.240633983569,101.103783619896));
#85737=CARTESIAN_POINT('Ctrl Pts',(75.4133809825114,390.851984142697,99.8832712227459));
#85738=CARTESIAN_POINT('Ctrl Pts',(57.0018485468049,489.727553050326,98.090033588344));
#85739=CARTESIAN_POINT('Ctrl Pts',(51.7501560506267,542.991128087974,97.5173172684936));
#85740=CARTESIAN_POINT('Ctrl Pts',(51.7501560487334,603.648875370191,97.5173172684936));
#85741=CARTESIAN_POINT('Ctrl Pts',(6.,-22.143643036685,90.7830741855191));
#85742=CARTESIAN_POINT('Ctrl Pts',(6.00000000007298,-27.8762778364647,90.7830741857764));
#85743=CARTESIAN_POINT('Ctrl Pts',(6.01660922703522,-33.5482466389342,90.7809593838058));
#85744=CARTESIAN_POINT('Ctrl Pts',(6.08595255085911,-44.7695275905442,90.7728487001403));
#85745=CARTESIAN_POINT('Ctrl Pts',(6.15260059239406,-50.3186632642503,90.7949425127537));
#85746=CARTESIAN_POINT('Ctrl Pts',(6.27877423953789,-66.7817034075453,90.5893788459225));
#85747=CARTESIAN_POINT('Ctrl Pts',(6.43586086298679,-77.5100259260557,90.4299948560914));
#85748=CARTESIAN_POINT('Ctrl Pts',(7.22730950121153,-108.9381039302,90.0310462352604));
#85749=CARTESIAN_POINT('Ctrl Pts',(8.14498503933279,-128.880916711419,89.7977286797552));
#85750=CARTESIAN_POINT('Ctrl Pts',(12.3095360218137,-185.575675871405,89.1445509441633));
#85751=CARTESIAN_POINT('Ctrl Pts',(16.9462613729601,-219.18776575348,88.7690335671882));
#85752=CARTESIAN_POINT('Ctrl Pts',(28.0381402389499,-263.028960386728,88.3216085852849));
#85753=CARTESIAN_POINT('Ctrl Pts',(32.4301770643691,-276.550270563958,88.1933449712546));
#85754=CARTESIAN_POINT('Ctrl Pts',(42.9281358410523,-301.334934854994,87.9959540550834));
#85755=CARTESIAN_POINT('Ctrl Pts',(49.0378632949769,-312.604391650755,87.9268325496319));
#85756=CARTESIAN_POINT('Ctrl Pts',(63.3505889867002,-332.666067561327,87.8717096511972));
#85757=CARTESIAN_POINT('Ctrl Pts',(71.5675366934108,-341.455614010345,87.8860704325898));
#85758=CARTESIAN_POINT('Ctrl Pts',(90.2657049891989,-356.061141331087,88.024621324407));
#85759=CARTESIAN_POINT('Ctrl Pts',(100.739337254366,-361.85547323351,88.1491356227232));
#85760=CARTESIAN_POINT('Ctrl Pts',(121.795026838174,-369.421310350857,88.4928845583287));
#85761=CARTESIAN_POINT('Ctrl Pts',(132.039500923872,-371.694369951344,88.7276447152287));
#85762=CARTESIAN_POINT('Ctrl Pts',(147.720189119143,-373.163371418067,89.2021923376507));
#85763=CARTESIAN_POINT('Ctrl Pts',(152.999948199941,-373.325965479262,89.3849240163435));
#85764=CARTESIAN_POINT('Ctrl Pts',(160.914718211754,-373.034083667193,89.7074143095509));
#85765=CARTESIAN_POINT('Ctrl Pts',(163.552129596181,-372.84735983228,89.8229885286486));
#85766=CARTESIAN_POINT('Ctrl Pts',(168.810475701525,-372.285867179701,90.07238433115));
#85767=CARTESIAN_POINT('Ctrl Pts',(171.43271342101,-371.91445109154,90.1968314929245));
#85768=CARTESIAN_POINT('Ctrl Pts',(183.798479337875,-369.623964165754,90.9877086463466));
#85769=CARTESIAN_POINT('Ctrl Pts',(193.184245643645,-366.437988693138,91.7506522889361));
#85770=CARTESIAN_POINT('Ctrl Pts',(210.818248569633,-357.5472455943,93.4656749781478));
#85771=CARTESIAN_POINT('Ctrl Pts',(219.06523365596,-351.846917249993,94.4171866516416));
#85772=CARTESIAN_POINT('Ctrl Pts',(241.719331610269,-331.42785841035,97.42192012483));
#85773=CARTESIAN_POINT('Ctrl Pts',(254.033000706385,-313.431087443606,99.6206963686531));
#85774=CARTESIAN_POINT('Ctrl Pts',(272.028370203714,-270.452761805799,103.821561236115));
#85775=CARTESIAN_POINT('Ctrl Pts',(277.733703504083,-245.446183070117,105.827059435943));
#85776=CARTESIAN_POINT('Ctrl Pts',(281.463134095255,-189.543779622914,109.134461342326));
#85777=CARTESIAN_POINT('Ctrl Pts',(279.48318081708,-158.639275832648,110.437140468834));
#85778=CARTESIAN_POINT('Ctrl Pts',(271.952046448821,-119.904622067839,111.2542525508));
#85779=CARTESIAN_POINT('Ctrl Pts',(270.809827609678,-114.457132821552,111.321267040589));
#85780=CARTESIAN_POINT('Ctrl Pts',(268.308983895114,-103.488720232041,111.450674606317));
#85781=CARTESIAN_POINT('Ctrl Pts',(266.958321769937,-97.9661357327517,111.501600230574));
#85782=CARTESIAN_POINT('Ctrl Pts',(262.650651001717,-81.3229024095457,111.617794124028));
#85783=CARTESIAN_POINT('Ctrl Pts',(259.438059285751,-70.1263787386142,111.646512989559));
#85784=CARTESIAN_POINT('Ctrl Pts',(249.130972035179,-36.5686972903188,111.622540287227));
#85785=CARTESIAN_POINT('Ctrl Pts',(241.366793816677,-14.2357562047768,111.459824858988));
#85786=CARTESIAN_POINT('Ctrl Pts',(212.315224351282,66.0171392750542,110.64210295685));
#85787=CARTESIAN_POINT('Ctrl Pts',(191.063967235354,117.941065745225,109.616459895168));
#85788=CARTESIAN_POINT('Ctrl Pts',(151.437384003502,214.746459510979,107.22617282344));
#85789=CARTESIAN_POINT('Ctrl Pts',(133.070417888531,259.620118178664,105.86263308603));
#85790=CARTESIAN_POINT('Ctrl Pts',(101.775904124562,349.378219317153,103.299345597994));
#85791=CARTESIAN_POINT('Ctrl Pts',(88.8377317907513,394.25825975287,102.098960380939));
#85792=CARTESIAN_POINT('Ctrl Pts',(70.7379343976928,491.459718172245,100.336082581174));
#85793=CARTESIAN_POINT('Ctrl Pts',(65.5673668639291,543.802811219013,99.7722419539107));
#85794=CARTESIAN_POINT('Ctrl Pts',(65.567366862141,603.648875370191,99.772241954121));
#85795=CARTESIAN_POINT('Ctrl Pts',(6.,-22.143643036685,76.7830741855191));
#85796=CARTESIAN_POINT('Ctrl Pts',(6.00000000001608,-27.8728345877897,76.7830741857764));
#85797=CARTESIAN_POINT('Ctrl Pts',(6.01659916901003,-33.5414291810368,76.7809606543939));
#85798=CARTESIAN_POINT('Ctrl Pts',(6.08590153713278,-44.7561068029682,76.7728547436659));
#85799=CARTESIAN_POINT('Ctrl Pts',(6.12448436107623,-50.3024630339952,76.7948482086147));
#85800=CARTESIAN_POINT('Ctrl Pts',(6.43257817927521,-66.7534068507774,76.5897246487929));
#85801=CARTESIAN_POINT('Ctrl Pts',(6.72514308144325,-77.47171901919,76.4326527457133));
#85802=CARTESIAN_POINT('Ctrl Pts',(7.82552897182559,-108.866320074244,76.0424819184556));
#85803=CARTESIAN_POINT('Ctrl Pts',(8.89215472186884,-128.78136213641,75.8174699621448));
#85804=CARTESIAN_POINT('Ctrl Pts',(13.4192108905908,-185.374605722347,75.1877811771031));
#85805=CARTESIAN_POINT('Ctrl Pts',(18.189036261472,-218.895357461452,74.8265221352761));
#85806=CARTESIAN_POINT('Ctrl Pts',(29.3980631288525,-262.538761129952,74.3962282066761));
#85807=CARTESIAN_POINT('Ctrl Pts',(33.8133689117452,-275.983630493145,74.2730893164583));
#85808=CARTESIAN_POINT('Ctrl Pts',(44.3198869194738,-300.591898809396,74.0848525703389));
#85809=CARTESIAN_POINT('Ctrl Pts',(50.4145080604677,-311.760854194936,74.0197676681309));
#85810=CARTESIAN_POINT('Ctrl Pts',(64.6449465931735,-331.608467073524,73.9713758616919));
#85811=CARTESIAN_POINT('Ctrl Pts',(72.793441073325,-340.284689964064,73.9884016133359));
#85812=CARTESIAN_POINT('Ctrl Pts',(91.3057500859674,-354.685628570187,74.1305443806443));
#85813=CARTESIAN_POINT('Ctrl Pts',(101.662639981094,-360.390625948114,74.2559577644952));
#85814=CARTESIAN_POINT('Ctrl Pts',(122.498687517451,-367.835138371731,74.6003688539808));
#85815=CARTESIAN_POINT('Ctrl Pts',(132.66179181958,-370.109786839278,74.8314342382333));
#85816=CARTESIAN_POINT('Ctrl Pts',(148.263273452825,-371.571384934932,75.3035829737878));
#85817=CARTESIAN_POINT('Ctrl Pts',(153.522526283597,-371.733735538213,75.4855736904116));
#85818=CARTESIAN_POINT('Ctrl Pts',(161.414904368065,-371.442685652143,75.8071509290502));
#85819=CARTESIAN_POINT('Ctrl Pts',(164.04625206938,-371.256441224634,75.922454612872));
#85820=CARTESIAN_POINT('Ctrl Pts',(169.295244001206,-370.695955309142,76.1714058721708));
#85821=CARTESIAN_POINT('Ctrl Pts',(171.912233718893,-370.316347052647,76.2965946205466));
#85822=CARTESIAN_POINT('Ctrl Pts',(184.289074772213,-368.126729770224,77.0764146285139));
#85823=CARTESIAN_POINT('Ctrl Pts',(193.695566775172,-365.021581292332,77.8316134147758));
#85824=CARTESIAN_POINT('Ctrl Pts',(211.395793536418,-356.28789794976,79.5341356615909));
#85825=CARTESIAN_POINT('Ctrl Pts',(219.68827733214,-350.663731347904,80.4809028238217));
#85826=CARTESIAN_POINT('Ctrl Pts',(242.510631416724,-330.456067053452,83.4769589166651));
#85827=CARTESIAN_POINT('Ctrl Pts',(254.979165750953,-312.575705655683,85.6776836832917));
#85828=CARTESIAN_POINT('Ctrl Pts',(273.308912228241,-269.758353895505,89.8963137045242));
#85829=CARTESIAN_POINT('Ctrl Pts',(279.192050799395,-244.797192233655,91.9173573898723));
#85830=CARTESIAN_POINT('Ctrl Pts',(283.250633704224,-188.932420787966,95.2615069894894));
#85831=CARTESIAN_POINT('Ctrl Pts',(281.422244927106,-158.021082723321,96.5852099265189));
#85832=CARTESIAN_POINT('Ctrl Pts',(274.043909433957,-119.263548415822,97.4262517020704));
#85833=CARTESIAN_POINT('Ctrl Pts',(272.889604588913,-113.818973755306,97.4913255613324));
#85834=CARTESIAN_POINT('Ctrl Pts',(270.389104286926,-102.852067911723,97.6207153303099));
#85835=CARTESIAN_POINT('Ctrl Pts',(269.038633909964,-97.3302694284403,97.6716336302827));
#85836=CARTESIAN_POINT('Ctrl Pts',(264.731601949094,-80.689504594602,97.78781027541));
#85837=CARTESIAN_POINT('Ctrl Pts',(261.519520120845,-69.4947722490061,97.8165238949743));
#85838=CARTESIAN_POINT('Ctrl Pts',(251.214263776602,-35.9430533478927,97.7925553823412));
#85839=CARTESIAN_POINT('Ctrl Pts',(243.451688444427,-13.6148152733545,97.6298685452083));
#85840=CARTESIAN_POINT('Ctrl Pts',(214.408695933877,66.6143869791072,96.812388060053));
#85841=CARTESIAN_POINT('Ctrl Pts',(193.168752447473,118.509829025431,95.7872005587473));
#85842=CARTESIAN_POINT('Ctrl Pts',(153.576263251876,215.231925874893,93.3989697721262));
#85843=CARTESIAN_POINT('Ctrl Pts',(135.232196296888,260.050378007844,92.0370723621136));
#85844=CARTESIAN_POINT('Ctrl Pts',(103.982022789748,349.68129527775,89.4774164941815));
#85845=CARTESIAN_POINT('Ctrl Pts',(91.0641975121257,394.489784594186,88.2789148168611));
#85846=CARTESIAN_POINT('Ctrl Pts',(72.9887151127201,491.560651219013,86.5184050823723));
#85847=CARTESIAN_POINT('Ctrl Pts',(67.8222915499773,543.845990976705,85.9550311400823));
#85848=CARTESIAN_POINT('Ctrl Pts',(67.8222915477683,603.648875370191,85.9550311407135));
#85849=CARTESIAN_POINT('Ctrl Pts',(20.,-22.143643036685,76.7830741855192));
#85850=CARTESIAN_POINT('Ctrl Pts',(20.,-27.8457920778109,76.7830741857566));
#85851=CARTESIAN_POINT('Ctrl Pts',(20.0165214330532,-33.485592853313,76.7809705517141));
#85852=CARTESIAN_POINT('Ctrl Pts',(20.0854446608167,-44.638917128667,76.7729088380163));
#85853=CARTESIAN_POINT('Ctrl Pts',(20.1238292955523,-50.1526654673148,76.7668988331685));
#85854=CARTESIAN_POINT('Ctrl Pts',(20.4301340697073,-66.5001303791202,76.743985515181));
#85855=CARTESIAN_POINT('Ctrl Pts',(20.7188936123879,-77.141599114471,76.7227141396145));
#85856=CARTESIAN_POINT('Ctrl Pts',(21.8028495683285,-108.277666955853,76.643040982027));
#85857=CARTESIAN_POINT('Ctrl Pts',(22.8522177208893,-127.983498586547,76.568779347995));
#85858=CARTESIAN_POINT('Ctrl Pts',(27.2962882348799,-183.793342140183,76.3120470559144));
#85859=CARTESIAN_POINT('Ctrl Pts',(31.9889018993299,-216.590007789356,76.0958804243854));
#85860=CARTESIAN_POINT('Ctrl Pts',(42.752586146367,-258.54916325461,75.8385782220632));
#85861=CARTESIAN_POINT('Ctrl Pts',(46.9602598342624,-271.329384640549,75.7640306692479));
#85862=CARTESIAN_POINT('Ctrl Pts',(56.7935789905011,-294.374861216214,75.6600037328577));
#85863=CARTESIAN_POINT('Ctrl Pts',(62.4190261651095,-304.639843280753,75.6305279269569));
#85864=CARTESIAN_POINT('Ctrl Pts',(75.2624672361846,-322.558676299804,75.6391115492116));
#85865=CARTESIAN_POINT('Ctrl Pts',(82.4798249428642,-330.212646288195,75.6771562180411));
#85866=CARTESIAN_POINT('Ctrl Pts',(98.6902707967944,-342.825622479896,75.8431732977935));
#85867=CARTESIAN_POINT('Ctrl Pts',(107.683690787476,-347.785594002476,75.9711317990764));
#85868=CARTESIAN_POINT('Ctrl Pts',(126.023069913222,-354.340138637006,76.3098567703564));
#85869=CARTESIAN_POINT('Ctrl Pts',(135.083207114917,-356.371635015224,76.501925570174));
#85870=CARTESIAN_POINT('Ctrl Pts',(148.924338523526,-357.668316903019,76.9207856483578));
#85871=CARTESIAN_POINT('Ctrl Pts',(153.579247220674,-357.810711475144,77.0819658816335));
#85872=CARTESIAN_POINT('Ctrl Pts',(160.521670574454,-357.554693148273,77.3648314770126));
#85873=CARTESIAN_POINT('Ctrl Pts',(162.82915793653,-357.391086631896,77.4659695920693));
#85874=CARTESIAN_POINT('Ctrl Pts',(167.413894984383,-356.901529412086,77.6834093931112));
#85875=CARTESIAN_POINT('Ctrl Pts',(169.690165914981,-356.571218959933,77.800168876217));
#85876=CARTESIAN_POINT('Ctrl Pts',(180.410587995582,-354.672149675074,78.3871286663314));
#85877=CARTESIAN_POINT('Ctrl Pts',(188.539471171489,-351.990508745272,78.9676971116917));
#85878=CARTESIAN_POINT('Ctrl Pts',(203.935932366808,-344.394636660447,80.2994244971851));
#85879=CARTESIAN_POINT('Ctrl Pts',(211.203510672235,-339.480369996828,81.0505889748358));
#85880=CARTESIAN_POINT('Ctrl Pts',(231.426270328895,-321.586439483533,83.4642765655722));
#85881=CARTESIAN_POINT('Ctrl Pts',(242.801650331,-305.454778835795,85.2871564557421));
#85882=CARTESIAN_POINT('Ctrl Pts',(259.787422523192,-265.857198323714,88.846412059781));
#85883=CARTESIAN_POINT('Ctrl Pts',(265.396961479631,-242.39170484102,90.582652202398));
#85884=CARTESIAN_POINT('Ctrl Pts',(269.303802179431,-189.217670775394,93.4513081720829));
#85885=CARTESIAN_POINT('Ctrl Pts',(267.601212650846,-159.509605592023,94.5836348018781));
#85886=CARTESIAN_POINT('Ctrl Pts',(260.488092878426,-122.007461671797,95.2483440922483));
#85887=CARTESIAN_POINT('Ctrl Pts',(259.365919995518,-116.723004281873,95.3235942479774));
#85888=CARTESIAN_POINT('Ctrl Pts',(256.932101050909,-106.048555274698,95.4495336771278));
#85889=CARTESIAN_POINT('Ctrl Pts',(255.614336154295,-100.659660585315,95.4992578713651));
#85890=CARTESIAN_POINT('Ctrl Pts',(251.40188561101,-84.3843231292077,95.6128833960036));
#85891=CARTESIAN_POINT('Ctrl Pts',(248.248043744655,-73.3892261805465,95.6412376442078));
#85892=CARTESIAN_POINT('Ctrl Pts',(238.097187851482,-40.3402024940961,95.6176286794984));
#85893=CARTESIAN_POINT('Ctrl Pts',(230.410833839506,-18.2225145274556,95.4569933696899));
#85894=CARTESIAN_POINT('Ctrl Pts',(201.530604066263,61.5570672312919,94.6440942086903));
#85895=CARTESIAN_POINT('Ctrl Pts',(180.38355994371,113.231534550229,93.6242109681347));
#85896=CARTESIAN_POINT('Ctrl Pts',(140.797124795906,209.938840593949,91.236348118932));
#85897=CARTESIAN_POINT('Ctrl Pts',(122.357793139117,254.971482304575,89.8683893074086));
#85898=CARTESIAN_POINT('Ctrl Pts',(90.7794276043238,345.543709944167,87.281854516083));
#85899=CARTESIAN_POINT('Ctrl Pts',(77.6398467041473,391.083508984014,86.0632256586685));
#85900=CARTESIAN_POINT('Ctrl Pts',(59.2526292615706,489.828486097094,84.2723560895427));
#85901=CARTESIAN_POINT('Ctrl Pts',(54.0050807366749,543.034307838934,83.7001064546653));
#85902=CARTESIAN_POINT('Ctrl Pts',(54.0050807343608,603.648875370191,83.7001064550861));
#85903=CARTESIAN_POINT('Origin',(52.8776183915471,603.648875370191,90.6087118617898));
#85904=CARTESIAN_POINT('Origin',(52.8776183915471,640.125373764374,79.6087118617898));
#85905=CARTESIAN_POINT('Origin',(52.8776183915471,603.64887537019,90.6087118617898));
#85906=CARTESIAN_POINT('',(0.,0.,0.));
#85907=CARTESIAN_POINT('Origin',(121.691000639221,53.9,183.212899484195));
#85908=CARTESIAN_POINT('',(121.691000639221,53.9,183.712899484196));
#85909=CARTESIAN_POINT('',(121.691000639221,54.8,183.712899484196));
#85910=CARTESIAN_POINT('',(121.691000639221,53.9,183.712899484196));
#85911=CARTESIAN_POINT('',(121.691000639221,54.8,182.712899484195));
#85912=CARTESIAN_POINT('Origin',(121.691000639221,54.8,183.212899484195));
#85913=CARTESIAN_POINT('',(121.691000639221,53.9,182.712899484195));
#85914=CARTESIAN_POINT('',(121.691000639221,53.9,182.712899484195));
#85915=CARTESIAN_POINT('Origin',(121.691000639221,53.9,183.212899484195));
#85916=CARTESIAN_POINT('Origin',(121.691000639221,53.9,183.712899484196));
#85917=CARTESIAN_POINT('',(106.90475031663,53.9,183.712899484195));
#85918=CARTESIAN_POINT('',(106.90475031663,54.8,183.712899484195));
#85919=CARTESIAN_POINT('',(106.90475031663,53.9,183.712899484195));
#85920=CARTESIAN_POINT('',(-205.7,54.8,183.712899484194));
#85921=CARTESIAN_POINT('',(121.691000639221,53.9,183.712899484196));
#85922=CARTESIAN_POINT('Origin',(106.90475031663,53.9,183.212899484195));
#85923=CARTESIAN_POINT('',(106.90475031663,53.9,182.712899484196));
#85924=CARTESIAN_POINT('',(106.90475031663,54.8,182.712899484196));
#85925=CARTESIAN_POINT('',(106.90475031663,53.9,182.712899484196));
#85926=CARTESIAN_POINT('Origin',(106.90475031663,54.8,183.212899484195));
#85927=CARTESIAN_POINT('Origin',(106.90475031663,53.9,183.212899484195));
#85928=CARTESIAN_POINT('Origin',(121.691000639221,53.9,182.712899484195));
#85929=CARTESIAN_POINT('',(-205.7,54.8,182.712899484197));
#85930=CARTESIAN_POINT('',(121.691000639221,53.9,182.712899484195));
#85931=CARTESIAN_POINT('Origin',(121.691000639221,53.9,183.212899484195));
#85932=CARTESIAN_POINT('Origin',(-205.7,54.8,197.697003183159));
#85933=CARTESIAN_POINT('Origin',(128.895960652199,53.9,183.212899484195));
#85934=CARTESIAN_POINT('',(128.895960652199,53.9,182.712899484195));
#85935=CARTESIAN_POINT('',(128.895960652199,53.9,183.712899484196));
#85936=CARTESIAN_POINT('Origin',(128.895960652199,53.9,183.212899484195));
#85937=CARTESIAN_POINT('',(143.682210974789,53.9,183.712899484195));
#85938=CARTESIAN_POINT('',(128.895960652199,53.9,183.712899484196));
#85939=CARTESIAN_POINT('',(143.682210974789,53.9,182.712899484196));
#85940=CARTESIAN_POINT('Origin',(143.682210974789,53.9,183.212899484195));
#85941=CARTESIAN_POINT('',(128.895960652199,53.9,182.712899484195));
#85942=CARTESIAN_POINT('Origin',(128.895960652199,53.9,183.712899484196));
#85943=CARTESIAN_POINT('',(128.895960652199,54.8,183.712899484196));
#85944=CARTESIAN_POINT('',(128.895960652199,53.9,183.712899484196));
#85945=CARTESIAN_POINT('',(143.682210974789,54.8,183.712899484195));
#85946=CARTESIAN_POINT('',(-205.7,54.8,183.712899484197));
#85947=CARTESIAN_POINT('',(143.682210974789,53.9,183.712899484195));
#85948=CARTESIAN_POINT('Origin',(143.682210974789,53.9,183.212899484195));
#85949=CARTESIAN_POINT('',(143.682210974789,54.8,182.712899484196));
#85950=CARTESIAN_POINT('Origin',(143.682210974789,54.8,183.212899484195));
#85951=CARTESIAN_POINT('',(143.682210974789,53.9,182.712899484196));
#85952=CARTESIAN_POINT('Origin',(128.895960652199,53.9,182.712899484195));
#85953=CARTESIAN_POINT('',(128.895960652199,54.8,182.712899484195));
#85954=CARTESIAN_POINT('',(-205.7,54.8,182.712899484194));
#85955=CARTESIAN_POINT('',(128.895960652199,53.9,182.712899484195));
#85956=CARTESIAN_POINT('Origin',(128.895960652199,53.9,183.212899484195));
#85957=CARTESIAN_POINT('Origin',(128.895960652199,54.8,183.212899484195));
#85958=CARTESIAN_POINT('Origin',(-205.7,54.8,197.697003183159));
#85959=CARTESIAN_POINT('Origin',(125.29348064571,25.4505574462982,200.));
#85960=CARTESIAN_POINT('',(96.7708826633735,25.4505574465334,196.229576409449));
#85961=CARTESIAN_POINT('',(96.8114851745877,23.9291040663932,194.272013743528));
#85962=CARTESIAN_POINT('Ctrl Pts',(96.7708826633735,25.4505574465334,196.229576409449));
#85963=CARTESIAN_POINT('Ctrl Pts',(96.770884572667,25.3888168379312,196.215660891132));
#85964=CARTESIAN_POINT('Ctrl Pts',(96.7710859278689,25.328300044412,196.198742499774));
#85965=CARTESIAN_POINT('Ctrl Pts',(96.7714629075156,25.2689905570161,196.178935869129));
#85966=CARTESIAN_POINT('Ctrl Pts',(96.7718468277933,25.2085891133962,196.158764575518));
#85967=CARTESIAN_POINT('Ctrl Pts',(96.7724129528313,25.1494394923947,196.135597518842));
#85968=CARTESIAN_POINT('Ctrl Pts',(96.7731397544311,25.0915407352726,196.109504170528));
#85969=CARTESIAN_POINT('Ctrl Pts',(96.7736290811383,25.0525597971678,196.091936553429));
#85970=CARTESIAN_POINT('Ctrl Pts',(96.7741913136005,25.0141461969243,196.073041442187));
#85971=CARTESIAN_POINT('Ctrl Pts',(96.7748205968608,24.9763049437873,196.052827902151));
#85972=CARTESIAN_POINT('Ctrl Pts',(96.775605887767,24.9290823433476,196.02760315811));
#85973=CARTESIAN_POINT('Ctrl Pts',(96.7764993817748,24.8825802014245,196.000147388779));
#85974=CARTESIAN_POINT('Ctrl Pts',(96.7774766184748,24.8371623486203,195.970690132415));
#85975=CARTESIAN_POINT('Ctrl Pts',(96.7785956662022,24.7851537155424,195.936958206682));
#85976=CARTESIAN_POINT('Ctrl Pts',(96.7798169585537,24.7349116033477,195.900837873986));
#85977=CARTESIAN_POINT('Ctrl Pts',(96.7811015898682,24.686931282354,195.862746601214));
#85978=CARTESIAN_POINT('Ctrl Pts',(96.78117851315,24.6840582372147,195.860465708885));
#85979=CARTESIAN_POINT('Ctrl Pts',(96.7812556644065,24.6811933013905,195.85817773446));
#85980=CARTESIAN_POINT('Ctrl Pts',(96.7813330355974,24.6783365813196,195.855882761992));
#85981=CARTESIAN_POINT('Ctrl Pts',(96.7827143680617,24.6273346498515,195.814909889032));
#85982=CARTESIAN_POINT('Ctrl Pts',(96.7841695078232,24.5786282396643,195.771582834397));
#85983=CARTESIAN_POINT('Ctrl Pts',(96.7856684582633,24.5321043729733,195.725832497918));
#85984=CARTESIAN_POINT('Ctrl Pts',(96.786903293901,24.4937780033667,195.688143362636));
#85985=CARTESIAN_POINT('Ctrl Pts',(96.7881679285545,24.4569334037587,195.648808966062));
#85986=CARTESIAN_POINT('Ctrl Pts',(96.7894462372192,24.4215244761583,195.607770307954));
#85987=CARTESIAN_POINT('Ctrl Pts',(96.7903511917988,24.3964573917586,195.578717761713));
#85988=CARTESIAN_POINT('Ctrl Pts',(96.7912621271681,24.3721489380842,195.548811846036));
#85989=CARTESIAN_POINT('Ctrl Pts',(96.7921699928626,24.3486689952047,195.518156906328));
#85990=CARTESIAN_POINT('Ctrl Pts',(96.7935847249944,24.3120800703772,195.470387144268));
#85991=CARTESIAN_POINT('Ctrl Pts',(96.7949823397169,24.2777486344132,195.421117146607));
#85992=CARTESIAN_POINT('Ctrl Pts',(96.7963302088508,24.2458601081044,195.37075500768));
#85993=CARTESIAN_POINT('Ctrl Pts',(96.7968332917952,24.2339579335512,195.351957683446));
#85994=CARTESIAN_POINT('Ctrl Pts',(96.7973294572306,24.2223963168555,195.333007722924));
#85995=CARTESIAN_POINT('Ctrl Pts',(96.7978170366339,24.2111858784597,195.3139248247));
#85996=CARTESIAN_POINT('Ctrl Pts',(96.7991683406123,24.1801166620386,195.261037446533));
#85997=CARTESIAN_POINT('Ctrl Pts',(96.8004619805254,24.151517163759,195.20689229819));
#85998=CARTESIAN_POINT('Ctrl Pts',(96.8016796026155,24.1253390270934,195.151352643979));
#85999=CARTESIAN_POINT('Ctrl Pts',(96.8028512729684,24.1001488249169,195.097908996089));
#86000=CARTESIAN_POINT('Ctrl Pts',(96.8039526057457,24.0772008393268,195.043174016525));
#86001=CARTESIAN_POINT('Ctrl Pts',(96.8049660037159,24.0564914865203,194.987003196263));
#86002=CARTESIAN_POINT('Ctrl Pts',(96.8053085104808,24.0494921697253,194.968018664525));
#86003=CARTESIAN_POINT('Ctrl Pts',(96.8056393130589,24.0427722122427,194.948929948601));
#86004=CARTESIAN_POINT('Ctrl Pts',(96.8059580529338,24.0363324515711,194.929737855852));
#86005=CARTESIAN_POINT('Ctrl Pts',(96.8068918795025,24.0174655946617,194.873509917246));
#86006=CARTESIAN_POINT('Ctrl Pts',(96.8077148336768,24.0011508604124,194.816857349836));
#86007=CARTESIAN_POINT('Ctrl Pts',(96.8084222566688,23.9873133973046,194.759798812559));
#86008=CARTESIAN_POINT('Ctrl Pts',(96.8091332048146,23.9734069808486,194.702455947356));
#86009=CARTESIAN_POINT('Ctrl Pts',(96.8097274986935,23.9620025122422,194.644702547731));
#86010=CARTESIAN_POINT('Ctrl Pts',(96.8101983286926,23.9530743260575,194.586541266325));
#86011=CARTESIAN_POINT('Ctrl Pts',(96.8106680291585,23.9441675588171,194.528519515303));
#86012=CARTESIAN_POINT('Ctrl Pts',(96.8110148873442,23.9377251529057,194.470091329796));
#86013=CARTESIAN_POINT('Ctrl Pts',(96.8112296232299,23.9337724353167,194.41125080931));
#86014=CARTESIAN_POINT('Ctrl Pts',(96.8113980719359,23.9306717418256,194.365093598536));
#86015=CARTESIAN_POINT('Ctrl Pts',(96.8114851744842,23.9291040683311,194.31868240643));
#86016=CARTESIAN_POINT('Ctrl Pts',(96.8114851745877,23.9291040663932,194.272013743528));
#86017=CARTESIAN_POINT('',(96.8114851745877,23.9291040663932,152.608250755187));
#86018=CARTESIAN_POINT('',(96.8114851745877,23.9291040663932,200.));
#86019=CARTESIAN_POINT('',(108.710714013295,2.24386148976204,152.608250755187));
#86020=CARTESIAN_POINT('Origin',(125.29348064571,25.4505574462982,152.608250755187));
#86021=CARTESIAN_POINT('',(111.239793308547,0.630550221611421,150.608250755187));
#86022=CARTESIAN_POINT('Ctrl Pts',(108.710714013295,2.24386148976203,152.608250755187));
#86023=CARTESIAN_POINT('Ctrl Pts',(108.853554035459,2.14179255423786,152.608250752516));
#86024=CARTESIAN_POINT('Ctrl Pts',(108.996115566955,2.04191344387966,152.597109166573));
#86025=CARTESIAN_POINT('Ctrl Pts',(109.138428228549,1.94410762303756,152.574931667418));
#86026=CARTESIAN_POINT('Ctrl Pts',(109.261361350294,1.85962058761654,152.555774206844));
#86027=CARTESIAN_POINT('Ctrl Pts',(109.384108759692,1.77668082196495,152.528380974701));
#86028=CARTESIAN_POINT('Ctrl Pts',(109.506688753907,1.69521934777192,152.492789418762));
#86029=CARTESIAN_POINT('Ctrl Pts',(109.509657719578,1.69324629889127,152.491927368569));
#86030=CARTESIAN_POINT('Ctrl Pts',(109.512625826965,1.6912746327679,152.491060749244));
#86031=CARTESIAN_POINT('Ctrl Pts',(109.515593066985,1.689304352752,152.490189550154));
#86032=CARTESIAN_POINT('Ctrl Pts',(109.648551129122,1.60101873682548,152.451152282539));
#86033=CARTESIAN_POINT('Ctrl Pts',(109.779549079908,1.51566120719707,152.402991156227));
#86034=CARTESIAN_POINT('Ctrl Pts',(109.907692820099,1.43356899326917,152.344885850416));
#86035=CARTESIAN_POINT('Ctrl Pts',(110.032432777243,1.35365733131867,152.288323950896));
#86036=CARTESIAN_POINT('Ctrl Pts',(110.154467914824,1.27683990420537,152.222338990309));
#86037=CARTESIAN_POINT('Ctrl Pts',(110.272995112549,1.20341533113175,152.146214709741));
#86038=CARTESIAN_POINT('Ctrl Pts',(110.277494300693,1.20062819893815,152.143325099026));
#86039=CARTESIAN_POINT('Ctrl Pts',(110.281989807978,1.19784513176216,152.14041918704));
#86040=CARTESIAN_POINT('Ctrl Pts',(110.286481320508,1.19506630191825,152.137497018263));
#86041=CARTESIAN_POINT('Ctrl Pts',(110.35623096888,1.15191326533487,152.092118041067));
#86042=CARTESIAN_POINT('Ctrl Pts',(110.425074014063,1.10974719909899,152.042776226069));
#86043=CARTESIAN_POINT('Ctrl Pts',(110.491771329291,1.06925349349879,151.989678218464));
#86044=CARTESIAN_POINT('Ctrl Pts',(110.537415615272,1.04154163924302,151.953340614231));
#86045=CARTESIAN_POINT('Ctrl Pts',(110.58205524589,1.01461277564984,151.915244580614));
#86046=CARTESIAN_POINT('Ctrl Pts',(110.62530262364,0.988680169120933,151.875465066187));
#86047=CARTESIAN_POINT('Ctrl Pts',(110.629563036415,0.986125479938043,151.871546281737));
#86048=CARTESIAN_POINT('Ctrl Pts',(110.633811274977,0.983579621774255,151.867610985757));
#86049=CARTESIAN_POINT('Ctrl Pts',(110.638047119709,0.981042694525639,151.863658939861));
#86050=CARTESIAN_POINT('Ctrl Pts',(110.70070725821,0.943514356544463,151.805196989804));
#86051=CARTESIAN_POINT('Ctrl Pts',(110.760624068134,0.907958530544358,151.743130385674));
#86052=CARTESIAN_POINT('Ctrl Pts',(110.817254839353,0.874600052649044,151.676514300529));
#86053=CARTESIAN_POINT('Ctrl Pts',(110.85673195265,0.851345973939509,151.630076459685));
#86054=CARTESIAN_POINT('Ctrl Pts',(110.894611970937,0.82915999987308,151.581427616684));
#86055=CARTESIAN_POINT('Ctrl Pts',(110.93070160126,0.808125250386176,151.53023744095));
#86056=CARTESIAN_POINT('Ctrl Pts',(110.933778433361,0.806331926601132,151.525873207387));
#86057=CARTESIAN_POINT('Ctrl Pts',(110.936838861941,0.804548941091073,151.521495117895));
#86058=CARTESIAN_POINT('Ctrl Pts',(110.939882620671,0.802776422030424,151.517103032953));
#86059=CARTESIAN_POINT('Ctrl Pts',(110.980020267636,0.779402445768727,151.459185185155));
#86060=CARTESIAN_POINT('Ctrl Pts',(111.017089051938,0.757947186283859,151.39911365981));
#86061=CARTESIAN_POINT('Ctrl Pts',(111.050594740143,0.738635777139546,151.336542541543));
#86062=CARTESIAN_POINT('Ctrl Pts',(111.080229497341,0.72155542595697,151.281200299767));
#86063=CARTESIAN_POINT('Ctrl Pts',(111.107077475512,0.706152002360059,151.223902600443));
#86064=CARTESIAN_POINT('Ctrl Pts',(111.1307673688,0.692600311320128,151.164386072023));
#86065=CARTESIAN_POINT('Ctrl Pts',(111.139079110306,0.687845619033563,151.143504340159));
#86066=CARTESIAN_POINT('Ctrl Pts',(111.147001767321,0.683319072810068,151.122349238626));
#86067=CARTESIAN_POINT('Ctrl Pts',(111.154518126295,0.679028925038091,151.100908592914));
#86068=CARTESIAN_POINT('Ctrl Pts',(111.155644514676,0.678386011012504,151.097695535328));
#86069=CARTESIAN_POINT('Ctrl Pts',(111.156760455762,0.677749140970417,151.094479455626));
#86070=CARTESIAN_POINT('Ctrl Pts',(111.157865910725,0.677118333770718,151.091260344968));
#86071=CARTESIAN_POINT('Ctrl Pts',(111.178503113567,0.665342099939013,151.031164328541));
#86072=CARTESIAN_POINT('Ctrl Pts',(111.195422514671,0.655714867320027,150.970227054675));
#86073=CARTESIAN_POINT('Ctrl Pts',(111.208427711382,0.648327212263957,150.908408142258));
#86074=CARTESIAN_POINT('Ctrl Pts',(111.220857230375,0.641266573284417,150.849325656765));
#86075=CARTESIAN_POINT('Ctrl Pts',(111.229711584529,0.636251567041951,150.78943767752));
#86076=CARTESIAN_POINT('Ctrl Pts',(111.234779728312,0.633384247886193,150.728697997016));
#86077=CARTESIAN_POINT('Ctrl Pts',(111.238098863481,0.63150643615474,150.688919486701));
#86078=CARTESIAN_POINT('Ctrl Pts',(111.239793303854,0.630550224268599,150.648775470141));
#86079=CARTESIAN_POINT('Ctrl Pts',(111.239793308547,0.630550221611425,150.608250755187));
#86080=CARTESIAN_POINT('',(111.239793308547,0.630550221611421,41.));
#86081=CARTESIAN_POINT('',(111.239793308547,0.630550221611421,200.));
#86082=CARTESIAN_POINT('',(148.327056352437,8.62815343953651,41.));
#86083=CARTESIAN_POINT('Origin',(125.29348064571,25.4505574462982,41.));
#86084=CARTESIAN_POINT('',(148.327056352437,8.62815343953651,150.608250755186));
#86085=CARTESIAN_POINT('',(148.327056352437,8.62815343953651,200.));
#86086=CARTESIAN_POINT('',(150.023036902254,11.238311537975,152.608250755187));
#86087=CARTESIAN_POINT('Ctrl Pts',(148.327056352437,8.62815343953653,150.608250755186));
#86088=CARTESIAN_POINT('Ctrl Pts',(148.327056355648,8.62815344393261,150.653182845415));
#86089=CARTESIAN_POINT('Ctrl Pts',(148.328597783066,8.63025784593123,150.697882422423));
#86090=CARTESIAN_POINT('Ctrl Pts',(148.331544689823,8.63429111208799,150.742200419329));
#86091=CARTESIAN_POINT('Ctrl Pts',(148.334586530884,8.63845430950751,150.787946116039));
#86092=CARTESIAN_POINT('Ctrl Pts',(148.339126089743,8.6446729210104,150.833286146418));
#86093=CARTESIAN_POINT('Ctrl Pts',(148.345047922207,8.65280026655287,150.878059836472));
#86094=CARTESIAN_POINT('Ctrl Pts',(148.351129064247,8.66114625454908,150.924038031663));
#86095=CARTESIAN_POINT('Ctrl Pts',(148.358668143408,8.67150540995371,150.969420095879));
#86096=CARTESIAN_POINT('Ctrl Pts',(148.367571470274,8.68376212324061,151.014020080674));
#86097=CARTESIAN_POINT('Ctrl Pts',(148.373624358134,8.69209479620402,151.044341185425));
#86098=CARTESIAN_POINT('Ctrl Pts',(148.380308440668,8.70130540278121,151.074300568726));
#86099=CARTESIAN_POINT('Ctrl Pts',(148.387601113806,8.7113672249093,151.103832740569));
#86100=CARTESIAN_POINT('Ctrl Pts',(148.388415597221,8.71249098119087,151.107131046104));
#86101=CARTESIAN_POINT('Ctrl Pts',(148.389237458434,8.71362506083807,151.110423262381));
#86102=CARTESIAN_POINT('Ctrl Pts',(148.390066647454,8.71476940103632,151.113709253066));
#86103=CARTESIAN_POINT('Ctrl Pts',(148.410348874067,8.74276032549509,151.194085628184));
#86104=CARTESIAN_POINT('Ctrl Pts',(148.434884633381,8.77673358153417,151.271196363152));
#86105=CARTESIAN_POINT('Ctrl Pts',(148.462667315314,8.81542934375246,151.344668023511));
#86106=CARTESIAN_POINT('Ctrl Pts',(148.487557673704,8.85009667328186,151.410490896992));
#86107=CARTESIAN_POINT('Ctrl Pts',(148.515054073122,8.88855439426902,151.473392480735));
#86108=CARTESIAN_POINT('Ctrl Pts',(148.544415056844,8.92987551455189,151.533081539737));
#86109=CARTESIAN_POINT('Ctrl Pts',(148.546552570807,8.93288374044883,151.537426973061));
#86110=CARTESIAN_POINT('Ctrl Pts',(148.548699885631,8.93590702948339,151.541755336793));
#86111=CARTESIAN_POINT('Ctrl Pts',(148.55085670104,8.93894500455668,151.546066510681));
#86112=CARTESIAN_POINT('Ctrl Pts',(148.587783204918,8.9909577071013,151.619877453696));
#86113=CARTESIAN_POINT('Ctrl Pts',(148.627416081672,9.04719548373904,151.689016296417));
#86114=CARTESIAN_POINT('Ctrl Pts',(148.669115490153,9.10686606773614,151.753729104497));
#86115=CARTESIAN_POINT('Ctrl Pts',(148.712668400571,9.16918895657458,151.821318339832));
#86116=CARTESIAN_POINT('Ctrl Pts',(148.758475300866,9.23525621682179,151.884079380573));
#86117=CARTESIAN_POINT('Ctrl Pts',(148.805779372373,9.30412622234888,151.94232646711));
#86118=CARTESIAN_POINT('Ctrl Pts',(148.857157944997,9.37892829472724,152.00559062325));
#86119=CARTESIAN_POINT('Ctrl Pts',(148.91030228072,9.45703626517374,152.06352962054));
#86120=CARTESIAN_POINT('Ctrl Pts',(148.964216374769,9.53720504806013,152.116585972851));
#86121=CARTESIAN_POINT('Ctrl Pts',(148.975223846884,9.55357285795584,152.127418322515));
#86122=CARTESIAN_POINT('Ctrl Pts',(148.986263339059,9.57002646799165,152.138047268404));
#86123=CARTESIAN_POINT('Ctrl Pts',(148.997326284789,9.58655513910883,152.148476762181));
#86124=CARTESIAN_POINT('Ctrl Pts',(149.00027597909,9.59096215042319,152.151257560271));
#86125=CARTESIAN_POINT('Ctrl Pts',(149.003227532453,9.59537478430998,152.154024316336));
#86126=CARTESIAN_POINT('Ctrl Pts',(149.006180782728,9.59979283861002,152.156777099669));
#86127=CARTESIAN_POINT('Ctrl Pts',(149.065723470318,9.68886853571161,152.212278023329));
#86128=CARTESIAN_POINT('Ctrl Pts',(149.12656226372,9.78102167254516,152.262422515793));
#86129=CARTESIAN_POINT('Ctrl Pts',(149.188058090848,9.87538467355686,152.307308751997));
#86130=CARTESIAN_POINT('Ctrl Pts',(149.254297541489,9.97702658390632,152.355657392324));
#86131=CARTESIAN_POINT('Ctrl Pts',(149.321298638721,10.0812316646319,152.397904945431));
#86132=CARTESIAN_POINT('Ctrl Pts',(149.388246614364,10.1868826220101,152.434224145398));
#86133=CARTESIAN_POINT('Ctrl Pts',(149.429229226741,10.2515575011517,152.456457165587));
#86134=CARTESIAN_POINT('Ctrl Pts',(149.470191659495,10.3167736033849,152.476469621483));
#86135=CARTESIAN_POINT('Ctrl Pts',(149.510946200718,10.3822714058908,152.494309993715));
#86136=CARTESIAN_POINT('Ctrl Pts',(149.512747991317,10.3851671157005,152.495098730724));
#86137=CARTESIAN_POINT('Ctrl Pts',(149.51454941295,10.3880634359148,152.495883238571));
#86138=CARTESIAN_POINT('Ctrl Pts',(149.516350450608,10.3909603461317,152.496663521671));
#86139=CARTESIAN_POINT('Ctrl Pts',(149.686680714973,10.6649310101692,152.570457551552));
#86140=CARTESIAN_POINT('Ctrl Pts',(149.855757811428,10.9472429965344,152.608250749998));
#86141=CARTESIAN_POINT('Ctrl Pts',(150.023036902254,11.238311537975,152.608250755187));
#86142=CARTESIAN_POINT('',(153.775476116832,23.9291040663932,152.608250755187));
#86143=CARTESIAN_POINT('Origin',(125.29348064571,25.4505574462982,152.608250755187));
#86144=CARTESIAN_POINT('',(153.775476116832,23.9291040663932,184.081718857688));
#86145=CARTESIAN_POINT('',(153.775476116832,23.9291040663932,200.));
#86146=CARTESIAN_POINT('',(153.812479229218,24.9971192497139,186.033932954965));
#86147=CARTESIAN_POINT('Ctrl Pts',(153.775476116832,23.9291040663932,184.081718857688));
#86148=CARTESIAN_POINT('Ctrl Pts',(153.775476116833,23.9291040664218,184.18683784592));
#86149=CARTESIAN_POINT('Ctrl Pts',(153.775835918749,23.9356932216278,184.291821685737));
#86150=CARTESIAN_POINT('Ctrl Pts',(153.776527304571,23.9488156066092,184.395645925698));
#86151=CARTESIAN_POINT('Ctrl Pts',(153.777122987151,23.9601215603797,184.48509857161));
#86152=CARTESIAN_POINT('Ctrl Pts',(153.777964738683,23.9762763343269,184.573689668976));
#86153=CARTESIAN_POINT('Ctrl Pts',(153.779032729615,23.9972132828232,184.660762130601));
#86154=CARTESIAN_POINT('Ctrl Pts',(153.77905396866,23.9976296541279,184.662493733201));
#86155=CARTESIAN_POINT('Ctrl Pts',(153.779075297335,23.9980479198028,184.664224752928));
#86156=CARTESIAN_POINT('Ctrl Pts',(153.779096715495,23.9984680795417,184.665955185441));
#86157=CARTESIAN_POINT('Ctrl Pts',(153.780335726001,24.0227737306845,184.76605827737));
#86158=CARTESIAN_POINT('Ctrl Pts',(153.781891347461,24.0537766428393,184.86522683398));
#86159=CARTESIAN_POINT('Ctrl Pts',(153.783676643627,24.0912021740848,184.961913456917));
#86160=CARTESIAN_POINT('Ctrl Pts',(153.785213510754,24.1234198362054,185.04514586126));
#86161=CARTESIAN_POINT('Ctrl Pts',(153.786920623228,24.1603976715318,185.126539185878));
#86162=CARTESIAN_POINT('Ctrl Pts',(153.788742263954,24.2019772886183,185.205080004687));
#86163=CARTESIAN_POINT('Ctrl Pts',(153.788798993319,24.2032721571579,185.207525915508));
#86164=CARTESIAN_POINT('Ctrl Pts',(153.788855834083,24.204571498343,185.209969085199));
#86165=CARTESIAN_POINT('Ctrl Pts',(153.78891278456,24.2058753078926,185.212409482336));
#86166=CARTESIAN_POINT('Ctrl Pts',(153.790943205448,24.2523592400329,185.299415483266));
#86167=CARTESIAN_POINT('Ctrl Pts',(153.793125302327,24.3048539183938,185.383361160768));
#86168=CARTESIAN_POINT('Ctrl Pts',(153.795342394988,24.3629513380175,185.463342843834));
#86169=CARTESIAN_POINT('Ctrl Pts',(153.79741974315,24.4173868472074,185.538283240013));
#86170=CARTESIAN_POINT('Ctrl Pts',(153.799527849837,24.4767414351666,185.609743667113));
#86171=CARTESIAN_POINT('Ctrl Pts',(153.801567334367,24.540682359021,185.676939406521));
#86172=CARTESIAN_POINT('Ctrl Pts',(153.802750453586,24.5777749355041,185.715920124237));
#86173=CARTESIAN_POINT('Ctrl Pts',(153.803904141896,24.6162117466583,185.753262592201));
#86174=CARTESIAN_POINT('Ctrl Pts',(153.805012744829,24.6560073896456,185.788953519961));
#86175=CARTESIAN_POINT('Ctrl Pts',(153.806106344776,24.6952644687927,185.824161433962));
#86176=CARTESIAN_POINT('Ctrl Pts',(153.807156145169,24.7358442672836,185.857762680895));
#86177=CARTESIAN_POINT('Ctrl Pts',(153.808146151009,24.7777933705704,185.889706633511));
#86178=CARTESIAN_POINT('Ctrl Pts',(153.809105866949,24.8184590126162,185.920673239251));
#86179=CARTESIAN_POINT('Ctrl Pts',(153.81000945025,24.8604118596032,185.950082728695));
#86180=CARTESIAN_POINT('Ctrl Pts',(153.81084045852,24.9037190593713,185.97784759324));
#86181=CARTESIAN_POINT('Ctrl Pts',(153.811424818388,24.9341724139999,185.997371674011));
#86182=CARTESIAN_POINT('Ctrl Pts',(153.811973254734,24.965295980978,186.016081687442));
#86183=CARTESIAN_POINT('Ctrl Pts',(153.812479229218,24.9971192497139,186.033932954965));
#86184=CARTESIAN_POINT('',(153.816083724746,25.4505574462842,186.284526408638));
#86185=CARTESIAN_POINT('Origin',(133.440794228452,34.3467674767392,169.944726356503));
#86186=CARTESIAN_POINT('',(153.816083724746,25.4505574462982,199.));
#86187=CARTESIAN_POINT('',(153.816083724746,25.4505574462982,200.));
#86188=CARTESIAN_POINT('Origin',(125.29348064571,25.4505574462982,199.));
#86189=CARTESIAN_POINT('',(150.625700340104,38.5584761124776,190.698119455572));
#86190=CARTESIAN_POINT('Ctrl Pts',(153.816083724746,25.4505574462982,186.284526408646));
#86191=CARTESIAN_POINT('Ctrl Pts',(153.816083724746,26.5106419398841,186.861657876856));
#86192=CARTESIAN_POINT('Ctrl Pts',(153.757166391213,27.588785058979,187.388187067696));
#86193=CARTESIAN_POINT('Ctrl Pts',(153.569780012624,29.2312207216284,188.104076474668));
#86194=CARTESIAN_POINT('Ctrl Pts',(153.490782930083,29.7829196479227,188.330345814086));
#86195=CARTESIAN_POINT('Ctrl Pts',(153.297393809188,30.8946428510959,188.757964813333));
#86196=CARTESIAN_POINT('Ctrl Pts',(153.182766552402,31.4549710261938,188.959285999996));
#86197=CARTESIAN_POINT('Ctrl Pts',(152.788570289629,33.1228706277751,189.517224242465));
#86198=CARTESIAN_POINT('Ctrl Pts',(152.457618579669,34.2256840028288,189.831355971386));
#86199=CARTESIAN_POINT('Ctrl Pts',(151.652438549957,36.4095069388551,190.348448095162));
#86200=CARTESIAN_POINT('Ctrl Pts',(151.178289930999,37.4905475363332,190.551395655298));
#86201=CARTESIAN_POINT('Ctrl Pts',(150.625700340104,38.5584761124776,190.698119455572));
#86202=CARTESIAN_POINT('',(127.30024332107,53.9024781190581,194.634660522392));
#86203=CARTESIAN_POINT('Ctrl Pts',(150.625700340104,38.5584761124776,190.698119455572));
#86204=CARTESIAN_POINT('Ctrl Pts',(150.061469174662,39.6489030677709,190.847934331189));
#86205=CARTESIAN_POINT('Ctrl Pts',(149.431181026365,40.695257042216,191.009583714252));
#86206=CARTESIAN_POINT('Ctrl Pts',(148.735694662152,41.6986800582058,191.179338039736));
#86207=CARTESIAN_POINT('Ctrl Pts',(148.735673295998,41.6987108845328,191.179343254787));
#86208=CARTESIAN_POINT('Ctrl Pts',(148.73565192978,41.698741710823,191.179348469846));
#86209=CARTESIAN_POINT('Ctrl Pts',(148.735630563497,41.6987725370764,191.179353684914));
#86210=CARTESIAN_POINT('Ctrl Pts',(148.387874587815,42.20049826009,191.2642337292));
#86211=CARTESIAN_POINT('Ctrl Pts',(148.022946011743,42.6924701456368,191.35134309563));
#86212=CARTESIAN_POINT('Ctrl Pts',(147.643370795097,43.1712035043443,191.439657777885));
#86213=CARTESIAN_POINT('Ctrl Pts',(147.643369837125,43.1712047125725,191.439658000774));
#86214=CARTESIAN_POINT('Ctrl Pts',(147.643368879152,43.1712059208007,191.439658223663));
#86215=CARTESIAN_POINT('Ctrl Pts',(147.643367921179,43.1712071290287,191.439658446552));
#86216=CARTESIAN_POINT('Ctrl Pts',(147.263793588568,43.6499392126947,191.527972912004));
#86217=CARTESIAN_POINT('Ctrl Pts',(146.870881838364,44.1139344808582,191.617196054609));
#86218=CARTESIAN_POINT('Ctrl Pts',(146.464931838332,44.5636037969635,191.70694380284));
#86219=CARTESIAN_POINT('Ctrl Pts',(146.464890465031,44.5636496260163,191.706952949682));
#86220=CARTESIAN_POINT('Ctrl Pts',(146.464849091595,44.5636954549204,191.70696209653));
#86221=CARTESIAN_POINT('Ctrl Pts',(146.464807718023,44.5637412836756,191.706971243383));
#86222=CARTESIAN_POINT('Ctrl Pts',(145.652941727099,45.4630305166459,191.886458259871));
#86223=CARTESIAN_POINT('Ctrl Pts',(144.789083501741,46.3052025359163,192.067991850579));
#86224=CARTESIAN_POINT('Ctrl Pts',(143.873620601989,47.0911971228637,192.249227483336));
#86225=CARTESIAN_POINT('Ctrl Pts',(143.873463960051,47.0913316118918,192.249258493987));
#86226=CARTESIAN_POINT('Ctrl Pts',(143.873307316601,47.0914660992751,192.24928950463));
#86227=CARTESIAN_POINT('Ctrl Pts',(143.873150671641,47.0916005850136,192.249320515264));
#86228=CARTESIAN_POINT('Ctrl Pts',(142.957780102958,47.8774815154557,192.430534271331));
#86229=CARTESIAN_POINT('Ctrl Pts',(141.990826816845,48.6072058722179,192.611464291541));
#86230=CARTESIAN_POINT('Ctrl Pts',(140.970103221489,49.2787422497132,192.790511107359));
#86231=CARTESIAN_POINT('Ctrl Pts',(140.969808649731,49.2789360491434,192.790562778679));
#86232=CARTESIAN_POINT('Ctrl Pts',(140.969514073494,49.2791298437284,192.790614449842));
#86233=CARTESIAN_POINT('Ctrl Pts',(140.969219492776,49.2793236334683,192.790666120848));
#86234=CARTESIAN_POINT('Ctrl Pts',(140.459049412573,49.6149386998141,192.880152635069));
#86235=CARTESIAN_POINT('Ctrl Pts',(139.938175750855,49.9340294827454,192.968677353463));
#86236=CARTESIAN_POINT('Ctrl Pts',(139.410618693711,50.2345300845201,193.055482746109));
#86237=CARTESIAN_POINT('Ctrl Pts',(139.410267290937,50.2347302462726,193.055540566691));
#86238=CARTESIAN_POINT('Ctrl Pts',(139.409915885195,50.2349303997783,193.05559838651));
#86239=CARTESIAN_POINT('Ctrl Pts',(139.409564476487,50.2351305450365,193.055656205566));
#86240=CARTESIAN_POINT('Ctrl Pts',(138.882045294331,50.5355797384922,193.142451611038));
#86241=CARTESIAN_POINT('Ctrl Pts',(138.346664242735,50.8182249900564,193.227736381437));
#86242=CARTESIAN_POINT('Ctrl Pts',(137.803522272346,51.0833049561888,193.311458624612));
#86243=CARTESIAN_POINT('Ctrl Pts',(137.803136062597,51.0834934455209,193.311518156646));
#86244=CARTESIAN_POINT('Ctrl Pts',(137.802749848923,51.0836819259721,193.311577687891));
#86245=CARTESIAN_POINT('Ctrl Pts',(137.802363631325,51.0838703975427,193.311637218346));
#86246=CARTESIAN_POINT('Ctrl Pts',(136.715720182944,51.6141450354221,193.479129271527));
#86247=CARTESIAN_POINT('Ctrl Pts',(135.598096689337,52.0743333349272,193.640350049973));
#86248=CARTESIAN_POINT('Ctrl Pts',(134.449176632172,52.4637415868922,193.795169694551));
#86249=CARTESIAN_POINT('Ctrl Pts',(134.448795563475,52.4638707440901,193.795221044443));
#86250=CARTESIAN_POINT('Ctrl Pts',(134.448414491335,52.4639998935016,193.79527239363));
#86251=CARTESIAN_POINT('Ctrl Pts',(134.448033415752,52.4641290351266,193.795323742113));
#86252=CARTESIAN_POINT('Ctrl Pts',(133.873739902698,52.6587497372968,193.872707605266));
#86253=CARTESIAN_POINT('Ctrl Pts',(133.291604977981,52.8356331717541,193.948497219751));
#86254=CARTESIAN_POINT('Ctrl Pts',(132.701448837108,52.9943569968444,194.022701543398));
#86255=CARTESIAN_POINT('Ctrl Pts',(132.701112354813,52.9944474945164,194.022743851593));
#86256=CARTESIAN_POINT('Ctrl Pts',(132.700775869911,52.9945379862852,194.022786159272));
#86257=CARTESIAN_POINT('Ctrl Pts',(132.7004393824,52.9946284721507,194.022828466437));
#86258=CARTESIAN_POINT('Ctrl Pts',(132.110218972949,53.1533464123654,194.097037912924));
#86259=CARTESIAN_POINT('Ctrl Pts',(131.511183281109,53.2939014558829,194.169734986987));
#86260=CARTESIAN_POINT('Ctrl Pts',(130.912612387922,53.4141810466492,194.239880283632));
#86261=CARTESIAN_POINT('Ctrl Pts',(130.912355373884,53.4142326922331,194.23991040258));
#86262=CARTESIAN_POINT('Ctrl Pts',(130.912098359931,53.4142843340791,194.239940521058));
#86263=CARTESIAN_POINT('Ctrl Pts',(130.911841346064,53.414335972187,194.239970639066));
#86264=CARTESIAN_POINT('Ctrl Pts',(129.714274871677,53.6549458171522,194.380306710062));
#86265=CARTESIAN_POINT('Ctrl Pts',(128.510331618815,53.8171285197205,194.51151055066));
#86266=CARTESIAN_POINT('Ctrl Pts',(127.30024332107,53.9024781190581,194.634660522392));
#86267=CARTESIAN_POINT('',(123.286717970418,53.9024781190629,195.01289889797));
#86268=CARTESIAN_POINT('Ctrl Pts',(127.30024332107,53.9024781190581,194.634660522392));
#86269=CARTESIAN_POINT('Ctrl Pts',(126.632621052928,53.949566660614,194.702604046515));
#86270=CARTESIAN_POINT('Ctrl Pts',(125.963635221528,53.9731507806434,194.765349588697));
#86271=CARTESIAN_POINT('Ctrl Pts',(124.624155818791,53.9731702639907,194.891453422566));
#86272=CARTESIAN_POINT('Ctrl Pts',(123.955253370733,53.9496310653927,194.954665574162));
#86273=CARTESIAN_POINT('Ctrl Pts',(123.286717970418,53.9024781190629,195.01289889797));
#86274=CARTESIAN_POINT('',(96.9910158671794,28.9874167683923,196.445393189885));
#86275=CARTESIAN_POINT('Ctrl Pts',(123.286717970418,53.9024781190629,195.01289889797));
#86276=CARTESIAN_POINT('Ctrl Pts',(123.051828692201,53.8859109761352,195.033359121005));
#86277=CARTESIAN_POINT('Ctrl Pts',(122.816379187764,53.8663568090316,195.05358701849));
#86278=CARTESIAN_POINT('Ctrl Pts',(122.581140823996,53.8438729171098,195.073525055871));
#86279=CARTESIAN_POINT('Ctrl Pts',(122.407062679345,53.827234669302,195.08827935232));
#86280=CARTESIAN_POINT('Ctrl Pts',(122.233100354408,53.8089931799125,195.102875013651));
#86281=CARTESIAN_POINT('Ctrl Pts',(122.059565244225,53.7891899052099,195.117290547141));
#86282=CARTESIAN_POINT('Ctrl Pts',(121.77966601252,53.757248695338,195.140541730975));
#86283=CARTESIAN_POINT('Ctrl Pts',(121.500846574299,53.7212485547933,195.1633276292));
#86284=CARTESIAN_POINT('Ctrl Pts',(121.223097074563,53.6812169890033,195.1856676816));
#86285=CARTESIAN_POINT('Ctrl Pts',(121.095940822165,53.6628901733355,195.195895161197));
#86286=CARTESIAN_POINT('Ctrl Pts',(120.969008930784,53.6437177097922,195.206029122082));
#86287=CARTESIAN_POINT('Ctrl Pts',(120.842301392603,53.6236987276649,195.216071038628));
#86288=CARTESIAN_POINT('Ctrl Pts',(120.842169588707,53.6236779034908,195.216081484445));
#86289=CARTESIAN_POINT('Ctrl Pts',(120.842037785115,53.6236570784102,195.216091930157));
#86290=CARTESIAN_POINT('Ctrl Pts',(120.841905981827,53.6236362524229,195.216102375765));
#86291=CARTESIAN_POINT('Ctrl Pts',(120.03508769286,53.4961524272351,195.280043932537));
#86292=CARTESIAN_POINT('Ctrl Pts',(119.237312586138,53.3346392699969,195.340284676336));
#86293=CARTESIAN_POINT('Ctrl Pts',(118.448469507687,53.139629459016,195.397278038018));
#86294=CARTESIAN_POINT('Ctrl Pts',(118.448244786133,53.1395739056253,195.397294273993));
#86295=CARTESIAN_POINT('Ctrl Pts',(118.448020065304,53.1395183495163,195.397310509705));
#86296=CARTESIAN_POINT('Ctrl Pts',(118.4477953452,53.1394627906889,195.397326745153));
#86297=CARTESIAN_POINT('Ctrl Pts',(116.870086353624,52.7493968376374,195.511312153296));
#86298=CARTESIAN_POINT('Ctrl Pts',(115.327903406651,52.2260862500057,195.612365054023));
#86299=CARTESIAN_POINT('Ctrl Pts',(113.822703841679,51.5649244867685,195.703261304229));
#86300=CARTESIAN_POINT('Ctrl Pts',(113.822385722138,51.5647847521568,195.703280514886));
#86301=CARTESIAN_POINT('Ctrl Pts',(113.822067604247,51.5646450113871,195.70329972509));
#86302=CARTESIAN_POINT('Ctrl Pts',(113.821749488008,51.5645052644595,195.703318934841));
#86303=CARTESIAN_POINT('Ctrl Pts',(113.44571802119,51.3993164571522,195.726025951065));
#86304=CARTESIAN_POINT('Ctrl Pts',(113.071361950894,51.2251071050355,195.748130225883));
#86305=CARTESIAN_POINT('Ctrl Pts',(112.702797713323,51.0437907256687,195.769437135944));
#86306=CARTESIAN_POINT('Ctrl Pts',(112.702474366697,51.0436316542412,195.769455828798));
#86307=CARTESIAN_POINT('Ctrl Pts',(112.702151024526,51.0434725773416,195.769474521039));
#86308=CARTESIAN_POINT('Ctrl Pts',(112.701827686811,51.0433134949714,195.769493212665));
#86309=CARTESIAN_POINT('Ctrl Pts',(112.333285153187,50.8619903238695,195.790798056524));
#86310=CARTESIAN_POINT('Ctrl Pts',(111.969800119671,50.6732726224591,195.811351687744));
#86311=CARTESIAN_POINT('Ctrl Pts',(111.611298768909,50.4772788755021,195.831212048309));
#86312=CARTESIAN_POINT('Ctrl Pts',(111.610976846822,50.4771028797467,195.831229882241));
#86313=CARTESIAN_POINT('Ctrl Pts',(111.610654928752,50.4769268781238,195.831247715614));
#86314=CARTESIAN_POINT('Ctrl Pts',(111.610333014701,50.4767508706336,195.831265548428));
#86315=CARTESIAN_POINT('Ctrl Pts',(110.893041082789,50.0845693177917,195.871000793435));
#86316=CARTESIAN_POINT('Ctrl Pts',(110.195668715804,49.6632963076804,195.907966652454));
#86317=CARTESIAN_POINT('Ctrl Pts',(109.517936153566,49.2133662529799,195.942552628765));
#86318=CARTESIAN_POINT('Ctrl Pts',(109.517627457568,49.213161317265,195.942568382106));
#86319=CARTESIAN_POINT('Ctrl Pts',(109.517318765645,49.2129563756048,195.942584134954));
#86320=CARTESIAN_POINT('Ctrl Pts',(109.517010077796,49.2127514279993,195.942599887308));
#86321=CARTESIAN_POINT('Ctrl Pts',(108.161281119207,48.3126401828122,196.011782793513));
#86322=CARTESIAN_POINT('Ctrl Pts',(106.883700856073,47.2985001737882,196.071502648147));
#86323=CARTESIAN_POINT('Ctrl Pts',(105.687270783624,46.1661414654911,196.123962833256));
#86324=CARTESIAN_POINT('Ctrl Pts',(105.687018511028,46.1659027026272,196.123973894719));
#86325=CARTESIAN_POINT('Ctrl Pts',(105.68676624204,46.1656639345064,196.123984955859));
#86326=CARTESIAN_POINT('Ctrl Pts',(105.686513976658,46.1654251611288,196.123996016677));
#86327=CARTESIAN_POINT('Ctrl Pts',(105.387599175031,45.8824973320413,196.13710222288));
#86328=CARTESIAN_POINT('Ctrl Pts',(105.093849245306,45.5921177194927,196.149746269813));
#86329=CARTESIAN_POINT('Ctrl Pts',(104.808073524937,45.2971435883637,196.161843863493));
#86330=CARTESIAN_POINT('Ctrl Pts',(104.807841819524,45.2969044249286,196.161853672157));
#86331=CARTESIAN_POINT('Ctrl Pts',(104.80761011935,45.29666525847,196.161863480461));
#86332=CARTESIAN_POINT('Ctrl Pts',(104.807378424416,45.2964260889894,196.161873288407));
#86333=CARTESIAN_POINT('Ctrl Pts',(104.521606158111,45.0014347250463,196.17397039717));
#86334=CARTESIAN_POINT('Ctrl Pts',(104.243057792459,44.7011568357949,196.185554290362));
#86335=CARTESIAN_POINT('Ctrl Pts',(103.971628652771,44.3956759203509,196.196665129066));
#86336=CARTESIAN_POINT('Ctrl Pts',(103.971418658918,44.3954395820027,196.196673725077));
#86337=CARTESIAN_POINT('Ctrl Pts',(103.971208669325,44.3952032405395,196.196682320804));
#86338=CARTESIAN_POINT('Ctrl Pts',(103.970998683993,44.3949668959614,196.196690916249));
#86339=CARTESIAN_POINT('Ctrl Pts',(103.427932303613,43.7837299434221,196.218920549917));
#86340=CARTESIAN_POINT('Ctrl Pts',(102.913323228656,43.1516872362662,196.239261316819));
#86341=CARTESIAN_POINT('Ctrl Pts',(102.426794049151,42.4991213301067,196.257972789619));
#86342=CARTESIAN_POINT('Ctrl Pts',(102.426626494949,42.4988965950563,196.257979233602));
#86343=CARTESIAN_POINT('Ctrl Pts',(102.426458944077,42.4986718575718,196.257985677392));
#86344=CARTESIAN_POINT('Ctrl Pts',(102.426291396536,42.4984471176532,196.257992120989));
#86345=CARTESIAN_POINT('Ctrl Pts',(101.453063032674,41.1930071125781,196.295420847925));
#86346=CARTESIAN_POINT('Ctrl Pts',(100.591557999332,39.8059105229358,196.326383225952));
#86347=CARTESIAN_POINT('Ctrl Pts',(99.8463073435662,38.3338899863526,196.352178614945));
#86348=CARTESIAN_POINT('Ctrl Pts',(99.8462171346804,38.333711805587,196.352181737349));
#86349=CARTESIAN_POINT('Ctrl Pts',(99.846126927498,38.333533623577,196.352184859677));
#86350=CARTESIAN_POINT('Ctrl Pts',(99.8460367220189,38.3333554403228,196.352187981929));
#86351=CARTESIAN_POINT('Ctrl Pts',(99.4734515242212,37.5973863649595,196.365084149053));
#86352=CARTESIAN_POINT('Ctrl Pts',(99.1340435629579,36.8475297378679,196.376538124842));
#86353=CARTESIAN_POINT('Ctrl Pts',(98.8291431339836,36.0890595245597,196.386657820445));
#86354=CARTESIAN_POINT('Ctrl Pts',(98.8290868940062,36.0889196220092,196.38665968706));
#86355=CARTESIAN_POINT('Ctrl Pts',(98.8290306552028,36.0887797191656,196.386661553628));
#86356=CARTESIAN_POINT('Ctrl Pts',(98.8289744175735,36.0886398160288,196.386663420152));
#86357=CARTESIAN_POINT('Ctrl Pts',(98.5240691405042,35.3301226957862,196.396783206952));
#86358=CARTESIAN_POINT('Ctrl Pts',(98.252880212789,34.5614226416425,196.405595343169));
#86359=CARTESIAN_POINT('Ctrl Pts',(98.0150109184552,33.7826625670746,196.413227915146));
#86360=CARTESIAN_POINT('Ctrl Pts',(98.0149812430995,33.7825654129534,196.413228867347));
#86361=CARTESIAN_POINT('Ctrl Pts',(98.0149515682624,33.7824682586759,196.413229819529));
#86362=CARTESIAN_POINT('Ctrl Pts',(98.0149218939439,33.7823711042421,196.413230771693));
#86363=CARTESIAN_POINT('Ctrl Pts',(97.6450275225364,32.5713280160703,196.425099622736));
#86364=CARTESIAN_POINT('Ctrl Pts',(97.3552447935968,31.3360957625847,196.434146130749));
#86365=CARTESIAN_POINT('Ctrl Pts',(97.1483025685318,30.0758530500492,196.440544914249));
#86366=CARTESIAN_POINT('Ctrl Pts',(97.0890634582333,29.715097012816,196.442376624725));
#86367=CARTESIAN_POINT('Ctrl Pts',(97.036612966678,29.3522914170678,196.44399135908));
#86368=CARTESIAN_POINT('Ctrl Pts',(96.9910158671796,28.9874167683946,196.445393189885));
#86369=CARTESIAN_POINT('',(96.7715712560824,25.6494824928011,196.263237066376));
#86370=CARTESIAN_POINT('Ctrl Pts',(96.9910158671794,28.9874167683923,196.445393189885));
#86371=CARTESIAN_POINT('Ctrl Pts',(96.8801655539068,28.1003763742528,196.448801156303));
#86372=CARTESIAN_POINT('Ctrl Pts',(96.81145956153,27.2127811520719,196.411604298023));
#86373=CARTESIAN_POINT('Ctrl Pts',(96.7842616286642,26.3247722192935,196.33198398003));
#86374=CARTESIAN_POINT('Ctrl Pts',(96.777368162748,26.0997014633065,196.311803771812));
#86375=CARTESIAN_POINT('Ctrl Pts',(96.7731413589317,25.8746041252277,196.288898122989));
#86376=CARTESIAN_POINT('Ctrl Pts',(96.7715712560824,25.6494824928014,196.263237066376));
#86377=CARTESIAN_POINT('Origin',(96.8900428237467,25.8589582227839,194.418219598777));
#86378=CARTESIAN_POINT('Origin',(125.29348064571,25.4505574462982,199.));
#86379=CARTESIAN_POINT('',(152.816083724746,25.4505574462982,200.));
#86380=CARTESIAN_POINT('Origin',(152.816083724746,25.4505574462982,199.));
#86381=CARTESIAN_POINT('Origin',(125.29348064571,25.4505574462982,200.));
#86382=CARTESIAN_POINT('Origin',(-34.5950649486897,26.6830679909832,173.608250755187));
#86383=CARTESIAN_POINT('',(-18.1943440740468,24.8757620423259,173.608250755187));
#86384=CARTESIAN_POINT('',(-50.9957858233326,24.8757620423259,173.608250755187));
#86385=CARTESIAN_POINT('Origin',(-34.5950649486897,26.6830679909832,173.608250755187));
#86386=CARTESIAN_POINT('',(-50.9957858233326,24.8757620423259,152.608250755187));
#86387=CARTESIAN_POINT('',(-50.9957858233326,24.8757620423259,173.608250755187));
#86388=CARTESIAN_POINT('',(-50.8544940072586,23.8757620423259,151.608250755187));
#86389=CARTESIAN_POINT('Ctrl Pts',(-50.9957858233326,24.8757620423259,152.608250755187));
#86390=CARTESIAN_POINT('Ctrl Pts',(-50.9957858233326,24.8757620423259,152.482802647827));
#86391=CARTESIAN_POINT('Ctrl Pts',(-50.9930852122888,24.8507057023964,152.349039676494));
#86392=CARTESIAN_POINT('Ctrl Pts',(-50.9814007950441,24.7490003445042,152.103116732228));
#86393=CARTESIAN_POINT('Ctrl Pts',(-50.9723338669737,24.6723550602491,151.990959171534));
#86394=CARTESIAN_POINT('Ctrl Pts',(-50.9495732713337,24.4948810766518,151.812827976054));
#86395=CARTESIAN_POINT('Ctrl Pts',(-50.9342825703181,24.3818609440281,151.735479916628));
#86396=CARTESIAN_POINT('Ctrl Pts',(-50.897590189515,24.1348809622359,151.633200800084));
#86397=CARTESIAN_POINT('Ctrl Pts',(-50.8761070582787,24.0009410845208,151.608250755187));
#86398=CARTESIAN_POINT('Ctrl Pts',(-50.8544940072586,23.8757620423259,151.608250755187));
#86399=CARTESIAN_POINT('',(-18.3356358901209,23.8757620423259,151.608250755187));
#86400=CARTESIAN_POINT('Origin',(-34.5950649486897,26.6830679909832,151.608250755187));
#86401=CARTESIAN_POINT('',(-18.1943440740468,24.8757620423259,152.608250755187));
#86402=CARTESIAN_POINT('Ctrl Pts',(-18.3356358901209,23.8757620423259,151.608250755187));
#86403=CARTESIAN_POINT('Ctrl Pts',(-18.3140228391008,24.0009410845208,151.608250755187));
#86404=CARTESIAN_POINT('Ctrl Pts',(-18.2925397078645,24.1348809622359,151.633200800084));
#86405=CARTESIAN_POINT('Ctrl Pts',(-18.2558473270613,24.3818609440281,151.735479916628));
#86406=CARTESIAN_POINT('Ctrl Pts',(-18.2405566260457,24.4948810766518,151.812827976054));
#86407=CARTESIAN_POINT('Ctrl Pts',(-18.2177960304058,24.6723550602491,151.990959171534));
#86408=CARTESIAN_POINT('Ctrl Pts',(-18.2087291023353,24.7490003445041,152.103116732228));
#86409=CARTESIAN_POINT('Ctrl Pts',(-18.1970446850907,24.8507057023964,152.349039676494));
#86410=CARTESIAN_POINT('Ctrl Pts',(-18.1943440740468,24.8757620423259,152.482802647827));
#86411=CARTESIAN_POINT('Ctrl Pts',(-18.1943440740468,24.8757620423259,152.608250755187));
#86412=CARTESIAN_POINT('',(-18.1943440740468,24.8757620423259,173.608250755187));
#86413=CARTESIAN_POINT('Origin',(35.4049350513103,26.6830679909832,173.608250755187));
#86414=CARTESIAN_POINT('',(51.8056559259532,24.8757620423259,173.608250755187));
#86415=CARTESIAN_POINT('',(19.0042141766674,24.8757620423259,173.608250755187));
#86416=CARTESIAN_POINT('Origin',(35.4049350513103,26.6830679909832,173.608250755187));
#86417=CARTESIAN_POINT('',(19.0042141766674,24.8757620423259,152.608250755187));
#86418=CARTESIAN_POINT('',(19.0042141766674,24.8757620423259,173.608250755187));
#86419=CARTESIAN_POINT('',(19.1455059927414,23.8757620423259,151.608250755187));
#86420=CARTESIAN_POINT('Ctrl Pts',(19.0042141766674,24.8757620423259,152.608250755187));
#86421=CARTESIAN_POINT('Ctrl Pts',(19.0042141766674,24.8757620423259,152.482802647827));
#86422=CARTESIAN_POINT('Ctrl Pts',(19.0069147877113,24.8507057023964,152.349039676494));
#86423=CARTESIAN_POINT('Ctrl Pts',(19.0185992049559,24.7490003445042,152.103116732228));
#86424=CARTESIAN_POINT('Ctrl Pts',(19.0276661330263,24.6723550602491,151.990959171534));
#86425=CARTESIAN_POINT('Ctrl Pts',(19.0504267286663,24.4948810766518,151.812827976054));
#86426=CARTESIAN_POINT('Ctrl Pts',(19.0657174296819,24.3818609440281,151.735479916628));
#86427=CARTESIAN_POINT('Ctrl Pts',(19.102409810485,24.1348809622359,151.633200800084));
#86428=CARTESIAN_POINT('Ctrl Pts',(19.1238929417213,24.0009410845208,151.608250755187));
#86429=CARTESIAN_POINT('Ctrl Pts',(19.1455059927414,23.8757620423259,151.608250755187));
#86430=CARTESIAN_POINT('',(51.6643641098791,23.8757620423259,151.608250755187));
#86431=CARTESIAN_POINT('Origin',(35.4049350513103,26.6830679909832,151.608250755187));
#86432=CARTESIAN_POINT('',(51.8056559259533,24.8757620423259,152.608250755187));
#86433=CARTESIAN_POINT('Ctrl Pts',(51.6643641098791,23.8757620423259,151.608250755187));
#86434=CARTESIAN_POINT('Ctrl Pts',(51.6859771608993,24.0009410845208,151.608250755187));
#86435=CARTESIAN_POINT('Ctrl Pts',(51.7074602921355,24.1348809622359,151.633200800084));
#86436=CARTESIAN_POINT('Ctrl Pts',(51.7441526729387,24.3818609440281,151.735479916628));
#86437=CARTESIAN_POINT('Ctrl Pts',(51.7594433739543,24.4948810766518,151.812827976054));
#86438=CARTESIAN_POINT('Ctrl Pts',(51.7822039695942,24.6723550602491,151.990959171534));
#86439=CARTESIAN_POINT('Ctrl Pts',(51.7912708976647,24.7490003445041,152.103116732228));
#86440=CARTESIAN_POINT('Ctrl Pts',(51.8029553149093,24.8507057023964,152.349039676494));
#86441=CARTESIAN_POINT('Ctrl Pts',(51.8056559259532,24.8757620423259,152.482802647827));
#86442=CARTESIAN_POINT('Ctrl Pts',(51.8056559259532,24.8757620423259,152.608250755187));
#86443=CARTESIAN_POINT('',(51.8056559259532,24.8757620423259,173.608250755187));
#86444=CARTESIAN_POINT('Origin',(-104.59506494869,26.6830679909832,173.608250755187));
#86445=CARTESIAN_POINT('',(-88.1943440740468,24.8757620423259,173.608250755187));
#86446=CARTESIAN_POINT('',(-120.995785823333,24.8757620423259,173.608250755187));
#86447=CARTESIAN_POINT('Origin',(-104.59506494869,26.6830679909832,173.608250755187));
#86448=CARTESIAN_POINT('',(-120.995785823333,24.8757620423259,152.608250755187));
#86449=CARTESIAN_POINT('',(-120.995785823333,24.8757620423259,173.608250755187));
#86450=CARTESIAN_POINT('',(-120.854494007259,23.8757620423259,151.608250755187));
#86451=CARTESIAN_POINT('Ctrl Pts',(-120.995785823333,24.8757620423259,152.608250755187));
#86452=CARTESIAN_POINT('Ctrl Pts',(-120.995785823333,24.8757620423259,152.482802647827));
#86453=CARTESIAN_POINT('Ctrl Pts',(-120.993085212289,24.8507057023964,152.349039676494));
#86454=CARTESIAN_POINT('Ctrl Pts',(-120.981400795044,24.7490003445042,152.103116732228));
#86455=CARTESIAN_POINT('Ctrl Pts',(-120.972333866974,24.6723550602491,151.990959171534));
#86456=CARTESIAN_POINT('Ctrl Pts',(-120.949573271334,24.4948810766518,151.812827976054));
#86457=CARTESIAN_POINT('Ctrl Pts',(-120.934282570318,24.3818609440281,151.735479916628));
#86458=CARTESIAN_POINT('Ctrl Pts',(-120.897590189515,24.1348809622359,151.633200800084));
#86459=CARTESIAN_POINT('Ctrl Pts',(-120.876107058279,24.0009410845208,151.608250755187));
#86460=CARTESIAN_POINT('Ctrl Pts',(-120.854494007259,23.8757620423259,151.608250755187));
#86461=CARTESIAN_POINT('',(-88.3356358901209,23.8757620423259,151.608250755187));
#86462=CARTESIAN_POINT('Origin',(-104.59506494869,26.6830679909832,151.608250755187));
#86463=CARTESIAN_POINT('',(-88.1943440740468,24.8757620423259,152.608250755187));
#86464=CARTESIAN_POINT('Ctrl Pts',(-88.3356358901209,23.8757620423259,151.608250755187));
#86465=CARTESIAN_POINT('Ctrl Pts',(-88.3140228391008,24.0009410845208,151.608250755187));
#86466=CARTESIAN_POINT('Ctrl Pts',(-88.2925397078645,24.1348809622359,151.633200800084));
#86467=CARTESIAN_POINT('Ctrl Pts',(-88.2558473270613,24.3818609440281,151.735479916628));
#86468=CARTESIAN_POINT('Ctrl Pts',(-88.2405566260458,24.4948810766518,151.812827976054));
#86469=CARTESIAN_POINT('Ctrl Pts',(-88.2177960304058,24.6723550602491,151.990959171534));
#86470=CARTESIAN_POINT('Ctrl Pts',(-88.2087291023354,24.7490003445041,152.103116732228));
#86471=CARTESIAN_POINT('Ctrl Pts',(-88.1970446850907,24.8507057023964,152.349039676494));
#86472=CARTESIAN_POINT('Ctrl Pts',(-88.1943440740468,24.8757620423259,152.482802647827));
#86473=CARTESIAN_POINT('Ctrl Pts',(-88.1943440740468,24.8757620423259,152.608250755187));
#86474=CARTESIAN_POINT('',(-88.1943440740468,24.8757620423259,173.608250755187));
#86475=CARTESIAN_POINT('Origin',(-104.59506494869,26.6830679909832,171.608250755187));
#86476=CARTESIAN_POINT('',(-120.59506494869,26.6830679909832,152.108250755187));
#86477=CARTESIAN_POINT('',(-88.5950649486898,26.6830679909832,152.108250755187));
#86478=CARTESIAN_POINT('Origin',(-104.59506494869,26.6830679909832,152.108250755187));
#86479=CARTESIAN_POINT('',(-88.5950649486898,26.6830679909832,171.108250755187));
#86480=CARTESIAN_POINT('',(-88.5950649486898,26.6830679909832,171.608250755187));
#86481=CARTESIAN_POINT('',(-112.492659345135,12.768040044578,171.108250755187));
#86482=CARTESIAN_POINT('Origin',(-104.59506494869,26.6830679909832,171.108250755187));
#86483=CARTESIAN_POINT('',(-112.492659345135,12.768040044578,153.608250755187));
#86484=CARTESIAN_POINT('',(-112.492659345135,12.768040044578,171.608250755187));
#86485=CARTESIAN_POINT('',(-113.345699320966,13.2880540647967,152.608250755187));
#86486=CARTESIAN_POINT('Ctrl Pts',(-113.345699320966,13.2880540647967,152.608250755187));
#86487=CARTESIAN_POINT('Ctrl Pts',(-113.314805388695,13.2678718158554,152.60825075831));
#86488=CARTESIAN_POINT('Ctrl Pts',(-113.283882083917,13.247833572522,152.610400982822));
#86489=CARTESIAN_POINT('Ctrl Pts',(-113.253143854674,13.2280604794924,152.614563215046));
#86490=CARTESIAN_POINT('Ctrl Pts',(-113.221265174007,13.207553764109,152.618879874633));
#86491=CARTESIAN_POINT('Ctrl Pts',(-113.189584552444,13.1873316127548,152.625360599392));
#86492=CARTESIAN_POINT('Ctrl Pts',(-113.158319731925,13.1675195649457,152.633903745459));
#86493=CARTESIAN_POINT('Ctrl Pts',(-113.126367003894,13.147271600464,152.642634862998));
#86494=CARTESIAN_POINT('Ctrl Pts',(-113.094847362014,13.1274512359853,152.653520253598));
#86495=CARTESIAN_POINT('Ctrl Pts',(-113.063988424239,13.1081932943863,152.666504445662));
#86496=CARTESIAN_POINT('Ctrl Pts',(-113.051791630358,13.1005817185771,152.671636362887));
#86497=CARTESIAN_POINT('Ctrl Pts',(-113.039698098786,13.0930580740493,152.677096714824));
#86498=CARTESIAN_POINT('Ctrl Pts',(-113.027722336541,13.0856311228787,152.682884240715));
#86499=CARTESIAN_POINT('Ctrl Pts',(-113.026049232486,13.0845935219426,152.68369280161));
#86500=CARTESIAN_POINT('Ctrl Pts',(-113.024377683382,13.0835573316238,152.684508023839));
#86501=CARTESIAN_POINT('Ctrl Pts',(-113.022707717151,13.0825225645949,152.685329889022));
#86502=CARTESIAN_POINT('Ctrl Pts',(-112.972795707585,13.0515954111635,152.709893824593));
#86503=CARTESIAN_POINT('Ctrl Pts',(-112.924466199263,13.0220440815315,152.74032765976));
#86504=CARTESIAN_POINT('Ctrl Pts',(-112.878864738381,12.9944473172043,152.775796511354));
#86505=CARTESIAN_POINT('Ctrl Pts',(-112.837356246389,12.96932750637,152.808081848577));
#86506=CARTESIAN_POINT('Ctrl Pts',(-112.798108353315,12.9458272165739,152.844537973071));
#86507=CARTESIAN_POINT('Ctrl Pts',(-112.7619450575,12.9243594466032,152.884524370354));
#86508=CARTESIAN_POINT('Ctrl Pts',(-112.758379154776,12.9222426047144,152.888467252212));
#86509=CARTESIAN_POINT('Ctrl Pts',(-112.754843207173,12.9201455042233,152.892444455782));
#86510=CARTESIAN_POINT('Ctrl Pts',(-112.751337979856,12.9180685269604,152.896455365444));
#86511=CARTESIAN_POINT('Ctrl Pts',(-112.749642377971,12.917063819921,152.898395583685));
#86512=CARTESIAN_POINT('Ctrl Pts',(-112.747953361917,12.916063438456,152.900344344348));
#86513=CARTESIAN_POINT('Ctrl Pts',(-112.746270995886,12.9150674101679,152.902301551646));
#86514=CARTESIAN_POINT('Ctrl Pts',(-112.707269815393,12.89197714424,152.947674195699));
#86515=CARTESIAN_POINT('Ctrl Pts',(-112.67183902809,12.8712238657582,152.997605490933));
#86516=CARTESIAN_POINT('Ctrl Pts',(-112.640718851925,12.8531192060996,153.051009927998));
#86517=CARTESIAN_POINT('Ctrl Pts',(-112.609598675759,12.8350145464411,153.104414365064));
#86518=CARTESIAN_POINT('Ctrl Pts',(-112.582788322685,12.8195581462718,153.161292777412));
#86519=CARTESIAN_POINT('Ctrl Pts',(-112.561022072452,12.8070625461649,153.22061351513));
#86520=CARTESIAN_POINT('Ctrl Pts',(-112.56036537399,12.8066855477713,153.222403250928));
#86521=CARTESIAN_POINT('Ctrl Pts',(-112.559713246063,12.8063112214621,153.22419533454));
#86522=CARTESIAN_POINT('Ctrl Pts',(-112.559065695038,12.8059395694613,153.225989728665));
#86523=CARTESIAN_POINT('Ctrl Pts',(-112.546565934931,12.7987655234449,153.260627147536));
#86524=CARTESIAN_POINT('Ctrl Pts',(-112.53581288098,12.7926115974439,153.296006270051));
#86525=CARTESIAN_POINT('Ctrl Pts',(-112.526803176794,12.7874655986588,153.331953347758));
#86526=CARTESIAN_POINT('Ctrl Pts',(-112.517741491554,12.7822899102814,153.368107820401));
#86527=CARTESIAN_POINT('Ctrl Pts',(-112.510443061843,12.7781337002311,153.404837909206));
#86528=CARTESIAN_POINT('Ctrl Pts',(-112.504946453002,12.7750090296612,153.441987310219));
#86529=CARTESIAN_POINT('Ctrl Pts',(-112.499569035295,12.7719521159637,153.478331145599));
#86530=CARTESIAN_POINT('Ctrl Pts',(-112.495916044603,12.7698824718338,153.515077343027));
#86531=CARTESIAN_POINT('Ctrl Pts',(-112.494066058465,12.7688355319706,153.552083286413));
#86532=CARTESIAN_POINT('Ctrl Pts',(-112.493133072646,12.7683075388002,153.57074613999));
#86533=CARTESIAN_POINT('Ctrl Pts',(-112.492659348059,12.7680400462376,153.589475021945));
#86534=CARTESIAN_POINT('Ctrl Pts',(-112.492659345135,12.768040044578,153.608250755187));
#86535=CARTESIAN_POINT('',(-118.077578311569,18.0678585669597,152.608250755187));
#86536=CARTESIAN_POINT('Origin',(-104.59506494869,26.6830679909832,152.608250755187));
#86537=CARTESIAN_POINT('',(-118.588969902809,18.9260953769367,153.608250755187));
#86538=CARTESIAN_POINT('Ctrl Pts',(-118.588969902809,18.9260953769367,153.608250755187));
#86539=CARTESIAN_POINT('Ctrl Pts',(-118.588969902308,18.9260953760319,153.570920583163));
#86540=CARTESIAN_POINT('Ctrl Pts',(-118.587912104855,18.9241774989277,153.533707722385));
#86541=CARTESIAN_POINT('Ctrl Pts',(-118.58584346415,18.9204434093274,153.496805212604));
#86542=CARTESIAN_POINT('Ctrl Pts',(-118.584596475761,18.9181924788664,153.474560169703));
#86543=CARTESIAN_POINT('Ctrl Pts',(-118.582981660905,18.9152806425285,153.452427631481));
#86544=CARTESIAN_POINT('Ctrl Pts',(-118.581004941819,18.911722257265,153.430449466818));
#86545=CARTESIAN_POINT('Ctrl Pts',(-118.577602099565,18.9055966404222,153.39261494198));
#86546=CARTESIAN_POINT('Ctrl Pts',(-118.573130216493,18.8975612058818,153.355237560415));
#86547=CARTESIAN_POINT('Ctrl Pts',(-118.567637196493,18.8877211995476,153.318533572216));
#86548=CARTESIAN_POINT('Ctrl Pts',(-118.565894155589,18.8845987762653,153.306886690759));
#86549=CARTESIAN_POINT('Ctrl Pts',(-118.564048110786,18.8812943178558,153.295307498788));
#86550=CARTESIAN_POINT('Ctrl Pts',(-118.562100070791,18.8778102513036,153.283802686776));
#86551=CARTESIAN_POINT('Ctrl Pts',(-118.559067410454,18.8723863429266,153.265892280843));
#86552=CARTESIAN_POINT('Ctrl Pts',(-118.555788379196,18.8665286220844,153.24816250223));
#86553=CARTESIAN_POINT('Ctrl Pts',(-118.552268294674,18.8602489158523,153.230639181705));
#86554=CARTESIAN_POINT('Ctrl Pts',(-118.551651723925,18.8591489754537,153.227569833004));
#86555=CARTESIAN_POINT('Ctrl Pts',(-118.551027749158,18.8580360733877,153.224506614159));
#86556=CARTESIAN_POINT('Ctrl Pts',(-118.550396496785,18.8569104466983,153.221450561457));
#86557=CARTESIAN_POINT('Ctrl Pts',(-118.549451041215,18.8552245440869,153.216873371454));
#86558=CARTESIAN_POINT('Ctrl Pts',(-118.548488694798,18.8535092116976,153.212308955191));
#86559=CARTESIAN_POINT('Ctrl Pts',(-118.547510041777,18.8517655750918,153.207760541832));
#86560=CARTESIAN_POINT('Ctrl Pts',(-118.539440539885,18.8373883866629,153.170256513932));
#86561=CARTESIAN_POINT('Ctrl Pts',(-118.530248612225,18.8210621214486,153.133776898268));
#86562=CARTESIAN_POINT('Ctrl Pts',(-118.519979370497,18.8029154201173,153.098570203321));
#86563=CARTESIAN_POINT('Ctrl Pts',(-118.514671326566,18.7935356148284,153.080372298509));
#86564=CARTESIAN_POINT('Ctrl Pts',(-118.509075277567,18.7836691588754,153.062515275874));
#86565=CARTESIAN_POINT('Ctrl Pts',(-118.50319668039,18.7733327882725,153.045038768438));
#86566=CARTESIAN_POINT('Ctrl Pts',(-118.494570848663,18.7581659396509,153.019394995308));
#86567=CARTESIAN_POINT('Ctrl Pts',(-118.485337290662,18.7419883607805,152.994565543546));
#86568=CARTESIAN_POINT('Ctrl Pts',(-118.475513996705,18.7248554116565,152.970664496244));
#86569=CARTESIAN_POINT('Ctrl Pts',(-118.465690702749,18.7077224625325,152.946763448943));
#86570=CARTESIAN_POINT('Ctrl Pts',(-118.455275811572,18.6896309027286,152.923794471748));
#86571=CARTESIAN_POINT('Ctrl Pts',(-118.444290799697,18.6706436778748,152.901863691503));
#86572=CARTESIAN_POINT('Ctrl Pts',(-118.443473437761,18.6692308951631,152.900231887624));
#86573=CARTESIAN_POINT('Ctrl Pts',(-118.442653055338,18.6678133893012,152.898605923768));
#86574=CARTESIAN_POINT('Ctrl Pts',(-118.441829667636,18.6663911970232,152.896985860847));
#86575=CARTESIAN_POINT('Ctrl Pts',(-118.420960697625,18.6303453732945,152.855924955523));
#86576=CARTESIAN_POINT('Ctrl Pts',(-118.398127427616,18.5912435035496,152.818486237725));
#86577=CARTESIAN_POINT('Ctrl Pts',(-118.373607653542,18.5497069642611,152.785209355589));
#86578=CARTESIAN_POINT('Ctrl Pts',(-118.348072099179,18.5064496914209,152.750553912586));
#86579=CARTESIAN_POINT('Ctrl Pts',(-118.320707604461,18.4605523877565,152.720413135382));
#86580=CARTESIAN_POINT('Ctrl Pts',(-118.2918537178,18.4127621747986,152.695377210154));
#86581=CARTESIAN_POINT('Ctrl Pts',(-118.287748531666,18.4059628232293,152.691815224405));
#86582=CARTESIAN_POINT('Ctrl Pts',(-118.283613234898,18.3991252184581,152.688356527975));
#86583=CARTESIAN_POINT('Ctrl Pts',(-118.279448841604,18.3922515717701,152.685002773781));
#86584=CARTESIAN_POINT('Ctrl Pts',(-118.278651700618,18.3909358301689,152.684360803933));
#86585=CARTESIAN_POINT('Ctrl Pts',(-118.277853564481,18.3896188851033,152.683722731272));
#86586=CARTESIAN_POINT('Ctrl Pts',(-118.277054437491,18.3883007472027,152.683088562518));
#86587=CARTESIAN_POINT('Ctrl Pts',(-118.256302811182,18.3540715127057,152.666620550358));
#86588=CARTESIAN_POINT('Ctrl Pts',(-118.234954792237,18.319160553495,152.652827752379));
#86589=CARTESIAN_POINT('Ctrl Pts',(-118.213106927497,18.283743787874,152.641735383215));
#86590=CARTESIAN_POINT('Ctrl Pts',(-118.191390078416,18.2485394068949,152.630709531951));
#86591=CARTESIAN_POINT('Ctrl Pts',(-118.169178909844,18.212834480398,152.622351680357));
#86592=CARTESIAN_POINT('Ctrl Pts',(-118.146561622526,18.1767968967697,152.616737045581));
#86593=CARTESIAN_POINT('Ctrl Pts',(-118.123944335209,18.1407593131414,152.611122410806));
#86594=CARTESIAN_POINT('Ctrl Pts',(-118.100920482758,18.1043882808045,152.608250762682));
#86595=CARTESIAN_POINT('Ctrl Pts',(-118.077578311569,18.0678585669597,152.608250755187));
#86596=CARTESIAN_POINT('',(-118.588969902809,18.9260953769367,171.108250755187));
#86597=CARTESIAN_POINT('',(-118.588969902809,18.9260953769367,171.608250755187));
#86598=CARTESIAN_POINT('Origin',(-104.59506494869,26.6830679909832,171.108250755187));
#86599=CARTESIAN_POINT('Origin',(-104.59506494869,26.6830679909832,152.108250755187));
#86600=CARTESIAN_POINT('Origin',(-104.59506494869,26.6830679909832,153.108250755187));
#86601=CARTESIAN_POINT('',(-101.803422330775,23.8631510023956,172.108250755187));
#86602=CARTESIAN_POINT('',(-107.386707566605,29.5029849795709,172.108250755187));
#86603=CARTESIAN_POINT('Origin',(-104.59506494869,26.6830679909832,172.108250755187));
#86604=CARTESIAN_POINT('',(-107.386707566605,29.5029849795709,172.608250755187));
#86605=CARTESIAN_POINT('',(-107.386707566605,29.5029849795709,153.108250755187));
#86606=CARTESIAN_POINT('',(-101.803422330775,23.8631510023956,172.608250755187));
#86607=CARTESIAN_POINT('Origin',(-104.59506494869,26.6830679909832,172.608250755187));
#86608=CARTESIAN_POINT('',(-101.803422330775,23.8631510023956,153.108250755187));
#86609=CARTESIAN_POINT('Origin',(-104.59506494869,26.6830679909832,172.108250755187));
#86610=CARTESIAN_POINT('',(-101.451654817389,23.5078207102358,171.608250755187));
#86611=CARTESIAN_POINT('Origin',(-101.451654817389,23.5078207102358,172.108250755187));
#86612=CARTESIAN_POINT('',(-107.738475079991,29.8583152717307,171.608250755187));
#86613=CARTESIAN_POINT('Origin',(-104.59506494869,26.6830679909832,171.608250755187));
#86614=CARTESIAN_POINT('Origin',(-107.738475079991,29.8583152717307,172.108250755187));
#86615=CARTESIAN_POINT('Origin',(-104.59506494869,26.6830679909832,171.108250755187));
#86616=CARTESIAN_POINT('',(-118.286142887994,19.4164054241714,171.608250755187));
#86617=CARTESIAN_POINT('Ctrl Pts',(-118.286142887994,19.4164054241713,171.608250755187));
#86618=CARTESIAN_POINT('Ctrl Pts',(-118.302185325772,19.3896971879647,171.608250755187));
#86619=CARTESIAN_POINT('Ctrl Pts',(-118.318199921039,19.3631642033379,171.606119035114));
#86620=CARTESIAN_POINT('Ctrl Pts',(-118.33408048304,19.3369687870384,171.601866237762));
#86621=CARTESIAN_POINT('Ctrl Pts',(-118.349524991939,19.3114926521192,171.59773021496));
#86622=CARTESIAN_POINT('Ctrl Pts',(-118.36484326585,19.2863349716358,171.59158772586));
#86623=CARTESIAN_POINT('Ctrl Pts',(-118.379930666554,19.2616587919161,171.583402532591));
#86624=CARTESIAN_POINT('Ctrl Pts',(-118.386479406906,19.2509480076639,171.579849720115));
#86625=CARTESIAN_POINT('Ctrl Pts',(-118.39298451303,19.240328189853,171.575911483355));
#86626=CARTESIAN_POINT('Ctrl Pts',(-118.399436615525,19.2298141093875,171.57158222553));
#86627=CARTESIAN_POINT('Ctrl Pts',(-118.413723814319,19.2065322787209,171.561995743106));
#86628=CARTESIAN_POINT('Ctrl Pts',(-118.4276586612,19.1839180856243,171.550546208524));
#86629=CARTESIAN_POINT('Ctrl Pts',(-118.441115563924,19.1621551516899,171.537246666312));
#86630=CARTESIAN_POINT('Ctrl Pts',(-118.453872254784,19.1415246227997,171.52463914792));
#86631=CARTESIAN_POINT('Ctrl Pts',(-118.466199710331,19.1216587053993,171.510368657222));
#86632=CARTESIAN_POINT('Ctrl Pts',(-118.477968777846,19.1027490964865,171.494425144437));
#86633=CARTESIAN_POINT('Ctrl Pts',(-118.482589906378,19.0953242318429,171.488164918489));
#86634=CARTESIAN_POINT('Ctrl Pts',(-118.487124674916,19.0880472321337,171.48164655399));
#86635=CARTESIAN_POINT('Ctrl Pts',(-118.491564119309,19.0809314970593,171.474868716253));
#86636=CARTESIAN_POINT('Ctrl Pts',(-118.493589137647,19.0776857093564,171.471777057816));
#86637=CARTESIAN_POINT('Ctrl Pts',(-118.495593035932,19.0744755040767,171.468633337136));
#86638=CARTESIAN_POINT('Ctrl Pts',(-118.497574879897,19.0713022787009,171.465437794362));
#86639=CARTESIAN_POINT('Ctrl Pts',(-118.509817058045,19.051700740414,171.445698397808));
#86640=CARTESIAN_POINT('Ctrl Pts',(-118.521194139698,19.0335459229592,171.423959301334));
#86641=CARTESIAN_POINT('Ctrl Pts',(-118.531468150003,19.0171904481872,171.400512409472));
#86642=CARTESIAN_POINT('Ctrl Pts',(-118.54099374159,19.002026401407,171.378773525704));
#86643=CARTESIAN_POINT('Ctrl Pts',(-118.549570988509,18.9884092853584,171.355566752543));
#86644=CARTESIAN_POINT('Ctrl Pts',(-118.556992948035,18.9766454465187,171.331150570564));
#86645=CARTESIAN_POINT('Ctrl Pts',(-118.55979681479,18.9722013052469,171.321926628999));
#86646=CARTESIAN_POINT('Ctrl Pts',(-118.562436589657,18.9680203916148,171.312526353858));
#86647=CARTESIAN_POINT('Ctrl Pts',(-118.56489645112,18.964126514061,171.302980969397));
#86648=CARTESIAN_POINT('Ctrl Pts',(-118.566941566645,18.9608891653092,171.295044988349));
#86649=CARTESIAN_POINT('Ctrl Pts',(-118.568864875742,18.9578459265386,171.286995184802));
#86650=CARTESIAN_POINT('Ctrl Pts',(-118.570661329118,18.9550044569664,171.278854434802));
#86651=CARTESIAN_POINT('Ctrl Pts',(-118.575332050019,18.9476167276229,171.257688747076));
#86652=CARTESIAN_POINT('Ctrl Pts',(-118.579148064562,18.9415884594895,171.235909909701));
#86653=CARTESIAN_POINT('Ctrl Pts',(-118.582070947222,18.9369745864019,171.213680494807));
#86654=CARTESIAN_POINT('Ctrl Pts',(-118.584872012388,18.9325530065136,171.192377539143));
#86655=CARTESIAN_POINT('Ctrl Pts',(-118.586852864555,18.9294303689664,171.170659720195));
#86656=CARTESIAN_POINT('Ctrl Pts',(-118.587954670714,18.9276943711425,171.148671871491));
#86657=CARTESIAN_POINT('Ctrl Pts',(-118.588625418196,18.9266375462553,171.13528630994));
#86658=CARTESIAN_POINT('Ctrl Pts',(-118.588969902809,18.9260953769367,171.121800772669));
#86659=CARTESIAN_POINT('Ctrl Pts',(-118.588969902809,18.9260953769367,171.108250755187));
#86660=CARTESIAN_POINT('',(-111.999322625392,13.0659108626764,171.608250755187));
#86661=CARTESIAN_POINT('Origin',(-104.59506494869,26.6830679909832,171.608250755187));
#86662=CARTESIAN_POINT('Ctrl Pts',(-112.492659345135,12.768040044578,171.108250755187));
#86663=CARTESIAN_POINT('Ctrl Pts',(-112.492659345135,12.768040044578,171.13083841899));
#86664=CARTESIAN_POINT('Ctrl Pts',(-112.491148987968,12.7689784818048,171.153252246832));
#86665=CARTESIAN_POINT('Ctrl Pts',(-112.488239747042,12.770782703053,171.17533199473));
#86666=CARTESIAN_POINT('Ctrl Pts',(-112.485198504088,12.7726687878766,171.19841357492));
#86667=CARTESIAN_POINT('Ctrl Pts',(-112.48062856265,12.7755010159135,171.221131109194));
#86668=CARTESIAN_POINT('Ctrl Pts',(-112.474611075407,12.7792252792491,171.243315149928));
#86669=CARTESIAN_POINT('Ctrl Pts',(-112.4731153884,12.7801509699996,171.248829142754));
#86670=CARTESIAN_POINT('Ctrl Pts',(-112.471530056724,12.7811319046715,171.254310195157));
#86671=CARTESIAN_POINT('Ctrl Pts',(-112.469855909556,12.7821675113977,171.259755708108));
#86672=CARTESIAN_POINT('Ctrl Pts',(-112.465313911514,12.7849771351943,171.27452950436));
#86673=CARTESIAN_POINT('Ctrl Pts',(-112.460117552039,12.7881895603694,171.289041238678));
#86674=CARTESIAN_POINT('Ctrl Pts',(-112.45429845138,12.7917840756337,171.303197876379));
#86675=CARTESIAN_POINT('Ctrl Pts',(-112.451837145533,12.7933044482744,171.309185711473));
#86676=CARTESIAN_POINT('Ctrl Pts',(-112.449263349994,12.7948937448599,171.315113565351));
#86677=CARTESIAN_POINT('Ctrl Pts',(-112.446581969183,12.7965487469991,171.320976176106));
#86678=CARTESIAN_POINT('Ctrl Pts',(-112.433991994688,12.8043195323466,171.348503082977));
#86679=CARTESIAN_POINT('Ctrl Pts',(-112.419032456129,12.813537291141,171.374583846366));
#86680=CARTESIAN_POINT('Ctrl Pts',(-112.402171437491,12.8238954967047,171.398817826505));
#86681=CARTESIAN_POINT('Ctrl Pts',(-112.386488190105,12.8335301637326,171.421359021305));
#86682=CARTESIAN_POINT('Ctrl Pts',(-112.369160238947,12.8441512616082,171.442302499413));
#86683=CARTESIAN_POINT('Ctrl Pts',(-112.350556132769,12.8555190964742,171.461373719866));
#86684=CARTESIAN_POINT('Ctrl Pts',(-112.349159012588,12.8563727914249,171.462805919119));
#86685=CARTESIAN_POINT('Ctrl Pts',(-112.347754689754,12.8572307021413,171.464227583082));
#86686=CARTESIAN_POINT('Ctrl Pts',(-112.346343317434,12.858092729399,171.465638607126));
#86687=CARTESIAN_POINT('Ctrl Pts',(-112.343322278299,12.8599378967184,171.468658900776));
#86688=CARTESIAN_POINT('Ctrl Pts',(-112.340265588914,12.8618039160818,171.471633649355));
#86689=CARTESIAN_POINT('Ctrl Pts',(-112.337175174345,12.8636895691223,171.474562315445));
#86690=CARTESIAN_POINT('Ctrl Pts',(-112.320153524577,12.8740755302676,171.490693073098));
#86691=CARTESIAN_POINT('Ctrl Pts',(-112.302126698691,12.8850431839654,171.5054110965));
#86692=CARTESIAN_POINT('Ctrl Pts',(-112.283339116041,12.896436216056,171.518686045026));
#86693=CARTESIAN_POINT('Ctrl Pts',(-112.263152157685,12.9086778475984,171.532949765808));
#86694=CARTESIAN_POINT('Ctrl Pts',(-112.242086394472,12.9214109244347,171.545548160215));
#86695=CARTESIAN_POINT('Ctrl Pts',(-112.220395747739,12.9344717190782,171.556423719585));
#86696=CARTESIAN_POINT('Ctrl Pts',(-112.209365692527,12.941113350736,171.561954122703));
#86697=CARTESIAN_POINT('Ctrl Pts',(-112.198173339535,12.9478401579873,171.567038641577));
#86698=CARTESIAN_POINT('Ctrl Pts',(-112.186848432126,12.9546327985747,171.571666998134));
#86699=CARTESIAN_POINT('Ctrl Pts',(-112.163706014081,12.9685135414746,171.581125032396));
#86700=CARTESIAN_POINT('Ctrl Pts',(-112.139785120082,12.9828022164443,171.58875486132));
#86701=CARTESIAN_POINT('Ctrl Pts',(-112.115420185619,12.9972962282834,171.594560491601));
#86702=CARTESIAN_POINT('Ctrl Pts',(-112.090440971411,13.0121556578048,171.600512491292));
#86703=CARTESIAN_POINT('Ctrl Pts',(-112.064993329893,13.0272319598494,171.604547546384));
#86704=CARTESIAN_POINT('Ctrl Pts',(-112.039420334739,13.0423156811498,171.606621211165));
#86705=CARTESIAN_POINT('Ctrl Pts',(-112.026072225888,13.0501887970118,171.60770358353));
#86706=CARTESIAN_POINT('Ctrl Pts',(-112.01268984259,13.0580639808388,171.608250755187));
#86707=CARTESIAN_POINT('Ctrl Pts',(-111.999322625392,13.0659108626764,171.608250755187));
#86708=CARTESIAN_POINT('Origin',(-104.59506494869,26.6830679909832,172.608250755187));
#86709=CARTESIAN_POINT('',(-107.034940053219,29.147654687411,173.108250755187));
#86710=CARTESIAN_POINT('Origin',(-107.034940053219,29.147654687411,172.608250755187));
#86711=CARTESIAN_POINT('',(-102.15518984416,24.2184812945555,173.108250755187));
#86712=CARTESIAN_POINT('Origin',(-104.59506494869,26.6830679909832,173.108250755187));
#86713=CARTESIAN_POINT('Origin',(-102.15518984416,24.2184812945555,172.608250755187));
#86714=CARTESIAN_POINT('Origin',(-104.59506494869,26.6830679909832,152.108250755187));
#86715=CARTESIAN_POINT('',(-120.09506494869,26.6830679909832,151.608250755187));
#86716=CARTESIAN_POINT('Origin',(-120.09506494869,26.6830679909832,152.108250755187));
#86717=CARTESIAN_POINT('Origin',(-104.59506494869,26.6830679909832,151.608250755187));
#86718=CARTESIAN_POINT('Origin',(-34.5950649486897,26.6830679909832,171.608250755187));
#86719=CARTESIAN_POINT('',(-50.5950649486897,26.6830679909832,152.108250755187));
#86720=CARTESIAN_POINT('',(-18.5950649486897,26.6830679909832,152.108250755187));
#86721=CARTESIAN_POINT('Origin',(-34.5950649486897,26.6830679909832,152.108250755187));
#86722=CARTESIAN_POINT('',(-18.5950649486897,26.6830679909832,171.108250755187));
#86723=CARTESIAN_POINT('',(-18.5950649486897,26.6830679909832,171.608250755187));
#86724=CARTESIAN_POINT('',(-42.4926593451348,12.768040044578,171.108250755187));
#86725=CARTESIAN_POINT('Origin',(-34.5950649486897,26.6830679909832,171.108250755187));
#86726=CARTESIAN_POINT('',(-42.4926593451348,12.768040044578,153.608250755187));
#86727=CARTESIAN_POINT('',(-42.4926593451348,12.768040044578,171.608250755187));
#86728=CARTESIAN_POINT('',(-43.3456993209664,13.2880540647968,152.608250755187));
#86729=CARTESIAN_POINT('Ctrl Pts',(-43.3456993209664,13.2880540647967,152.608250755187));
#86730=CARTESIAN_POINT('Ctrl Pts',(-43.3148053886973,13.2678718158571,152.60825075831));
#86731=CARTESIAN_POINT('Ctrl Pts',(-43.283882083922,13.2478335725253,152.610400982821));
#86732=CARTESIAN_POINT('Ctrl Pts',(-43.2531438546813,13.2280604794972,152.614563215045));
#86733=CARTESIAN_POINT('Ctrl Pts',(-43.2212651740174,13.2075537641154,152.618879874632));
#86734=CARTESIAN_POINT('Ctrl Pts',(-43.1895845524561,13.1873316127627,152.625360599389));
#86735=CARTESIAN_POINT('Ctrl Pts',(-43.1583197319398,13.1675195649551,152.633903745455));
#86736=CARTESIAN_POINT('Ctrl Pts',(-43.126367003911,13.1472716004751,152.642634862993));
#86737=CARTESIAN_POINT('Ctrl Pts',(-43.094847362034,13.1274512359979,152.653520253591));
#86738=CARTESIAN_POINT('Ctrl Pts',(-43.0639884242618,13.1081932944003,152.666504445653));
#86739=CARTESIAN_POINT('Ctrl Pts',(-43.0517916303728,13.1005817185864,152.671636362881));
#86740=CARTESIAN_POINT('Ctrl Pts',(-43.0396980987932,13.0930580740539,152.677096714821));
#86741=CARTESIAN_POINT('Ctrl Pts',(-43.0277223365409,13.0856311228787,152.682884240716));
#86742=CARTESIAN_POINT('Ctrl Pts',(-43.0260492324864,13.0845935219426,152.68369280161));
#86743=CARTESIAN_POINT('Ctrl Pts',(-43.0243776833816,13.0835573316238,152.684508023839));
#86744=CARTESIAN_POINT('Ctrl Pts',(-43.0227077171508,13.0825225645949,152.685329889023));
#86745=CARTESIAN_POINT('Ctrl Pts',(-42.9727957075848,13.0515954111635,152.709893824594));
#86746=CARTESIAN_POINT('Ctrl Pts',(-42.9244661992627,13.0220440815316,152.74032765976));
#86747=CARTESIAN_POINT('Ctrl Pts',(-42.8788647383815,12.9944473172044,152.775796511355));
#86748=CARTESIAN_POINT('Ctrl Pts',(-42.8373562463308,12.9693275063351,152.808081848623));
#86749=CARTESIAN_POINT('Ctrl Pts',(-42.7981083532053,12.9458272165084,152.844537973172));
#86750=CARTESIAN_POINT('Ctrl Pts',(-42.7619450573485,12.9243594465134,152.884524370521));
#86751=CARTESIAN_POINT('Ctrl Pts',(-42.7583791546756,12.922242604655,152.888467252324));
#86752=CARTESIAN_POINT('Ctrl Pts',(-42.7548432071236,12.9201455041938,152.892444455838));
#86753=CARTESIAN_POINT('Ctrl Pts',(-42.7513379798555,12.9180685269602,152.896455365443));
#86754=CARTESIAN_POINT('Ctrl Pts',(-42.7496423779711,12.9170638199208,152.898395583684));
#86755=CARTESIAN_POINT('Ctrl Pts',(-42.7479533619165,12.9160634384558,152.900344344347));
#86756=CARTESIAN_POINT('Ctrl Pts',(-42.7462709958856,12.9150674101677,152.902301551645));
#86757=CARTESIAN_POINT('Ctrl Pts',(-42.707269815392,12.8919771442397,152.947674195698));
#86758=CARTESIAN_POINT('Ctrl Pts',(-42.6718390280897,12.871223865758,152.997605490932));
#86759=CARTESIAN_POINT('Ctrl Pts',(-42.6407188519244,12.8531192060995,153.051009927998));
#86760=CARTESIAN_POINT('Ctrl Pts',(-42.6095986757592,12.835014546441,153.104414365063));
#86761=CARTESIAN_POINT('Ctrl Pts',(-42.582788322685,12.8195581462718,153.161292777412));
#86762=CARTESIAN_POINT('Ctrl Pts',(-42.5610220724519,12.8070625461647,153.22061351513));
#86763=CARTESIAN_POINT('Ctrl Pts',(-42.5603653739899,12.8066855477711,153.222403250928));
#86764=CARTESIAN_POINT('Ctrl Pts',(-42.5597132460627,12.8063112214619,153.22419533454));
#86765=CARTESIAN_POINT('Ctrl Pts',(-42.5590656950375,12.8059395694612,153.225989728665));
#86766=CARTESIAN_POINT('Ctrl Pts',(-42.5465659349297,12.7987655234443,153.260627147538));
#86767=CARTESIAN_POINT('Ctrl Pts',(-42.535812880978,12.7926115974429,153.296006270054));
#86768=CARTESIAN_POINT('Ctrl Pts',(-42.5268031767919,12.7874655986576,153.331953347763));
#86769=CARTESIAN_POINT('Ctrl Pts',(-42.5177414915513,12.7822899102801,153.368107820407));
#86770=CARTESIAN_POINT('Ctrl Pts',(-42.5104430618402,12.7781337002298,153.404837909212));
#86771=CARTESIAN_POINT('Ctrl Pts',(-42.504946453,12.7750090296599,153.441987310225));
#86772=CARTESIAN_POINT('Ctrl Pts',(-42.4995690352926,12.7719521159626,153.478331145603));
#86773=CARTESIAN_POINT('Ctrl Pts',(-42.4959160446013,12.7698824718329,153.515077343029));
#86774=CARTESIAN_POINT('Ctrl Pts',(-42.4940660584642,12.76883553197,153.552083286413));
#86775=CARTESIAN_POINT('Ctrl Pts',(-42.4931330726453,12.7683075387998,153.57074613999));
#86776=CARTESIAN_POINT('Ctrl Pts',(-42.4926593480585,12.7680400462373,153.589475021945));
#86777=CARTESIAN_POINT('Ctrl Pts',(-42.4926593451348,12.768040044578,153.608250755187));
#86778=CARTESIAN_POINT('',(-48.0775783115689,18.0678585669597,152.608250755187));
#86779=CARTESIAN_POINT('Origin',(-34.5950649486897,26.6830679909832,152.608250755187));
#86780=CARTESIAN_POINT('',(-48.5889699028093,18.9260953769367,153.608250755187));
#86781=CARTESIAN_POINT('Ctrl Pts',(-48.5889699028093,18.9260953769367,153.608250755187));
#86782=CARTESIAN_POINT('Ctrl Pts',(-48.5889699023077,18.9260953760317,153.570920583159));
#86783=CARTESIAN_POINT('Ctrl Pts',(-48.5879121048548,18.9241774989272,153.533707722378));
#86784=CARTESIAN_POINT('Ctrl Pts',(-48.5858434641496,18.9204434093262,153.496805212593));
#86785=CARTESIAN_POINT('Ctrl Pts',(-48.5845964757606,18.9181924788654,153.474560169695));
#86786=CARTESIAN_POINT('Ctrl Pts',(-48.5829816609043,18.9152806425278,153.452427631477));
#86787=CARTESIAN_POINT('Ctrl Pts',(-48.5810049418185,18.911722257265,153.430449466818));
#86788=CARTESIAN_POINT('Ctrl Pts',(-48.577602099566,18.9055966404233,153.392614941987));
#86789=CARTESIAN_POINT('Ctrl Pts',(-48.5731302164946,18.8975612058847,153.355237560429));
#86790=CARTESIAN_POINT('Ctrl Pts',(-48.5676371964959,18.8877211995531,153.318533572236));
#86791=CARTESIAN_POINT('Ctrl Pts',(-48.5658941555907,18.8845987762691,153.306886690772));
#86792=CARTESIAN_POINT('Ctrl Pts',(-48.5640481107871,18.8812943178578,153.295307498794));
#86793=CARTESIAN_POINT('Ctrl Pts',(-48.5621000707914,18.8778102513037,153.283802686776));
#86794=CARTESIAN_POINT('Ctrl Pts',(-48.5590674104541,18.8723863429266,153.265892280843));
#86795=CARTESIAN_POINT('Ctrl Pts',(-48.5557883791962,18.8665286220844,153.24816250223));
#86796=CARTESIAN_POINT('Ctrl Pts',(-48.5522682946736,18.8602489158523,153.230639181705));
#86797=CARTESIAN_POINT('Ctrl Pts',(-48.5516517239249,18.8591489754537,153.227569833004));
#86798=CARTESIAN_POINT('Ctrl Pts',(-48.5510277491576,18.8580360733877,153.224506614159));
#86799=CARTESIAN_POINT('Ctrl Pts',(-48.5503964967849,18.8569104466983,153.221450561457));
#86800=CARTESIAN_POINT('Ctrl Pts',(-48.5494510412146,18.855224544087,153.216873371454));
#86801=CARTESIAN_POINT('Ctrl Pts',(-48.5484886947976,18.8535092116976,153.212308955191));
#86802=CARTESIAN_POINT('Ctrl Pts',(-48.5475100417767,18.8517655750918,153.207760541832));
#86803=CARTESIAN_POINT('Ctrl Pts',(-48.5394405398847,18.8373883866618,153.170256513929));
#86804=CARTESIAN_POINT('Ctrl Pts',(-48.530248612224,18.8210621214462,153.133776898263));
#86805=CARTESIAN_POINT('Ctrl Pts',(-48.5199793704951,18.8029154201132,153.098570203313));
#86806=CARTESIAN_POINT('Ctrl Pts',(-48.5146713265647,18.7935356148255,153.080372298504));
#86807=CARTESIAN_POINT('Ctrl Pts',(-48.5090752775665,18.783669158874,153.062515275872));
#86808=CARTESIAN_POINT('Ctrl Pts',(-48.5031966803903,18.7733327882725,153.045038768438));
#86809=CARTESIAN_POINT('Ctrl Pts',(-48.494570848663,18.758165939651,153.019394995308));
#86810=CARTESIAN_POINT('Ctrl Pts',(-48.4853372906616,18.7419883607805,152.994565543546));
#86811=CARTESIAN_POINT('Ctrl Pts',(-48.4755139967052,18.7248554116565,152.970664496244));
#86812=CARTESIAN_POINT('Ctrl Pts',(-48.4656907027488,18.7077224625325,152.946763448943));
#86813=CARTESIAN_POINT('Ctrl Pts',(-48.455275811572,18.6896309027286,152.923794471748));
#86814=CARTESIAN_POINT('Ctrl Pts',(-48.4442907996973,18.6706436778748,152.901863691503));
#86815=CARTESIAN_POINT('Ctrl Pts',(-48.4434734377613,18.6692308951631,152.900231887624));
#86816=CARTESIAN_POINT('Ctrl Pts',(-48.4426530553384,18.6678133893012,152.898605923768));
#86817=CARTESIAN_POINT('Ctrl Pts',(-48.4418296676355,18.6663911970232,152.896985860847));
#86818=CARTESIAN_POINT('Ctrl Pts',(-48.4209606976304,18.6303453733033,152.855924955533));
#86819=CARTESIAN_POINT('Ctrl Pts',(-48.3981274276271,18.5912435035687,152.818486237743));
#86820=CARTESIAN_POINT('Ctrl Pts',(-48.3736076535603,18.5497069642916,152.785209355613));
#86821=CARTESIAN_POINT('Ctrl Pts',(-48.3480720992044,18.5064496914645,152.750553912618));
#86822=CARTESIAN_POINT('Ctrl Pts',(-48.3207076044961,18.4605523878146,152.720413135418));
#86823=CARTESIAN_POINT('Ctrl Pts',(-48.291853717844,18.4127621748717,152.695377210192));
#86824=CARTESIAN_POINT('Ctrl Pts',(-48.2877485316961,18.4059628232783,152.691815224429));
#86825=CARTESIAN_POINT('Ctrl Pts',(-48.283613234913,18.3991252184827,152.688356527986));
#86826=CARTESIAN_POINT('Ctrl Pts',(-48.279448841604,18.3922515717701,152.68500277378));
#86827=CARTESIAN_POINT('Ctrl Pts',(-48.2786517006176,18.3909358301689,152.684360803933));
#86828=CARTESIAN_POINT('Ctrl Pts',(-48.2778535644812,18.3896188851034,152.683722731272));
#86829=CARTESIAN_POINT('Ctrl Pts',(-48.277054437491,18.3883007472027,152.683088562518));
#86830=CARTESIAN_POINT('Ctrl Pts',(-48.2563028111771,18.3540715126977,152.666620550354));
#86831=CARTESIAN_POINT('Ctrl Pts',(-48.2349547922275,18.3191605534787,152.652827752373));
#86832=CARTESIAN_POINT('Ctrl Pts',(-48.2131069274817,18.2837437878493,152.641735383207));
#86833=CARTESIAN_POINT('Ctrl Pts',(-48.1913900784035,18.248539406874,152.630709531945));
#86834=CARTESIAN_POINT('Ctrl Pts',(-48.1691789098335,18.2128344803812,152.622351680354));
#86835=CARTESIAN_POINT('Ctrl Pts',(-48.1465616225185,18.1767968967571,152.616737045579));
#86836=CARTESIAN_POINT('Ctrl Pts',(-48.1239443352035,18.1407593131329,152.611122410805));
#86837=CARTESIAN_POINT('Ctrl Pts',(-48.1009204827551,18.1043882808003,152.608250762682));
#86838=CARTESIAN_POINT('Ctrl Pts',(-48.0775783115689,18.0678585669597,152.608250755187));
#86839=CARTESIAN_POINT('',(-48.5889699028093,18.9260953769367,171.108250755187));
#86840=CARTESIAN_POINT('',(-48.5889699028093,18.9260953769367,171.608250755187));
#86841=CARTESIAN_POINT('Origin',(-34.5950649486897,26.6830679909832,171.108250755187));
#86842=CARTESIAN_POINT('Origin',(-34.5950649486897,26.6830679909832,152.108250755187));
#86843=CARTESIAN_POINT('Origin',(-34.5950649486897,26.6830679909832,153.108250755187));
#86844=CARTESIAN_POINT('',(-31.8034223307746,23.8631510023956,172.108250755187));
#86845=CARTESIAN_POINT('',(-37.3867075666049,29.5029849795709,172.108250755187));
#86846=CARTESIAN_POINT('Origin',(-34.5950649486897,26.6830679909832,172.108250755187));
#86847=CARTESIAN_POINT('',(-37.3867075666049,29.5029849795709,172.608250755187));
#86848=CARTESIAN_POINT('',(-37.3867075666049,29.5029849795709,153.108250755187));
#86849=CARTESIAN_POINT('',(-31.8034223307746,23.8631510023956,172.608250755187));
#86850=CARTESIAN_POINT('Origin',(-34.5950649486897,26.6830679909832,172.608250755187));
#86851=CARTESIAN_POINT('',(-31.8034223307746,23.8631510023956,153.108250755187));
#86852=CARTESIAN_POINT('Origin',(-34.5950649486897,26.6830679909832,172.108250755187));
#86853=CARTESIAN_POINT('',(-31.4516548173888,23.5078207102358,171.608250755187));
#86854=CARTESIAN_POINT('Origin',(-31.4516548173888,23.5078207102358,172.108250755187));
#86855=CARTESIAN_POINT('',(-37.7384750799907,29.8583152717307,171.608250755187));
#86856=CARTESIAN_POINT('Origin',(-34.5950649486897,26.6830679909832,171.608250755187));
#86857=CARTESIAN_POINT('Origin',(-37.7384750799907,29.8583152717307,172.108250755187));
#86858=CARTESIAN_POINT('Origin',(-34.5950649486897,26.6830679909832,171.108250755187));
#86859=CARTESIAN_POINT('',(-48.2861428879937,19.4164054241714,171.608250755187));
#86860=CARTESIAN_POINT('Ctrl Pts',(-48.2861428879937,19.4164054241714,171.608250755187));
#86861=CARTESIAN_POINT('Ctrl Pts',(-48.3021853257697,19.3896971879684,171.608250755187));
#86862=CARTESIAN_POINT('Ctrl Pts',(-48.3181999210346,19.3631642033453,171.606119035115));
#86863=CARTESIAN_POINT('Ctrl Pts',(-48.3340804830342,19.3369687870493,171.601866237764));
#86864=CARTESIAN_POINT('Ctrl Pts',(-48.3495249919314,19.3114926521329,171.597730214963));
#86865=CARTESIAN_POINT('Ctrl Pts',(-48.3648432658407,19.2863349716523,171.591587725864));
#86866=CARTESIAN_POINT('Ctrl Pts',(-48.3799306665435,19.2616587919351,171.583402532597));
#86867=CARTESIAN_POINT('Ctrl Pts',(-48.3864794068996,19.2509480076768,171.57984972012));
#86868=CARTESIAN_POINT('Ctrl Pts',(-48.392984513027,19.2403281898597,171.575911483358));
#86869=CARTESIAN_POINT('Ctrl Pts',(-48.399436615526,19.2298141093882,171.57158222553));
#86870=CARTESIAN_POINT('Ctrl Pts',(-48.4137238143177,19.2065322787241,171.561995743107));
#86871=CARTESIAN_POINT('Ctrl Pts',(-48.4276586611977,19.1839180856298,171.550546208526));
#86872=CARTESIAN_POINT('Ctrl Pts',(-48.4411155639197,19.1621551516974,171.537246666316));
#86873=CARTESIAN_POINT('Ctrl Pts',(-48.4538722547784,19.1415246228092,171.524639147927));
#86874=CARTESIAN_POINT('Ctrl Pts',(-48.4661997103245,19.1216587054105,171.51036865723));
#86875=CARTESIAN_POINT('Ctrl Pts',(-48.4779687778381,19.1027490964993,171.494425144447));
#86876=CARTESIAN_POINT('Ctrl Pts',(-48.4825899063729,19.0953242318513,171.488164918496));
#86877=CARTESIAN_POINT('Ctrl Pts',(-48.4871246749138,19.0880472321378,171.481646553994));
#86878=CARTESIAN_POINT('Ctrl Pts',(-48.4915641193089,19.0809314970594,171.474868716253));
#86879=CARTESIAN_POINT('Ctrl Pts',(-48.4935891376473,19.0776857093565,171.471777057816));
#86880=CARTESIAN_POINT('Ctrl Pts',(-48.4955930359323,19.0744755040767,171.468633337136));
#86881=CARTESIAN_POINT('Ctrl Pts',(-48.4975748798971,19.071302278701,171.465437794362));
#86882=CARTESIAN_POINT('Ctrl Pts',(-48.5098170580377,19.0517007404259,171.44569839782));
#86883=CARTESIAN_POINT('Ctrl Pts',(-48.5211941396845,19.0335459229812,171.42395930136));
#86884=CARTESIAN_POINT('Ctrl Pts',(-48.531468149985,19.0171904482168,171.400512409514));
#86885=CARTESIAN_POINT('Ctrl Pts',(-48.5409937415793,19.0020264014248,171.378773525734));
#86886=CARTESIAN_POINT('Ctrl Pts',(-48.5495709885045,18.9884092853662,171.355566752559));
#86887=CARTESIAN_POINT('Ctrl Pts',(-48.5569929480345,18.9766454465188,171.331150570564));
#86888=CARTESIAN_POINT('Ctrl Pts',(-48.5597968147904,18.972201305247,171.321926628999));
#86889=CARTESIAN_POINT('Ctrl Pts',(-48.5624365896571,18.9680203916148,171.312526353858));
#86890=CARTESIAN_POINT('Ctrl Pts',(-48.5648964511201,18.964126514061,171.302980969397));
#86891=CARTESIAN_POINT('Ctrl Pts',(-48.5669415666449,18.9608891653093,171.295044988349));
#86892=CARTESIAN_POINT('Ctrl Pts',(-48.5688648757415,18.9578459265386,171.286995184802));
#86893=CARTESIAN_POINT('Ctrl Pts',(-48.5706613291176,18.9550044569664,171.278854434802));
#86894=CARTESIAN_POINT('Ctrl Pts',(-48.5753320500147,18.947616727629,171.257688747093));
#86895=CARTESIAN_POINT('Ctrl Pts',(-48.5791480645553,18.9415884594994,171.235909909737));
#86896=CARTESIAN_POINT('Ctrl Pts',(-48.5820709472144,18.9369745864134,171.213680494862));
#86897=CARTESIAN_POINT('Ctrl Pts',(-48.5848720123792,18.9325530065268,171.192377539217));
#86898=CARTESIAN_POINT('Ctrl Pts',(-48.5868528645474,18.9294303689789,171.17065972029));
#86899=CARTESIAN_POINT('Ctrl Pts',(-48.5879546707082,18.9276943711517,171.148671871607));
#86900=CARTESIAN_POINT('Ctrl Pts',(-48.5886254181942,18.9266375462585,171.135286310018));
#86901=CARTESIAN_POINT('Ctrl Pts',(-48.5889699028093,18.9260953769367,171.121800772708));
#86902=CARTESIAN_POINT('Ctrl Pts',(-48.5889699028093,18.9260953769367,171.108250755187));
#86903=CARTESIAN_POINT('',(-41.9993226253918,13.0659108626764,171.608250755187));
#86904=CARTESIAN_POINT('Origin',(-34.5950649486897,26.6830679909832,171.608250755187));
#86905=CARTESIAN_POINT('Ctrl Pts',(-42.4926593451348,12.768040044578,171.108250755187));
#86906=CARTESIAN_POINT('Ctrl Pts',(-42.4926593451348,12.768040044578,171.130838418967));
#86907=CARTESIAN_POINT('Ctrl Pts',(-42.4911489879713,12.7689784818031,171.153252246788));
#86908=CARTESIAN_POINT('Ctrl Pts',(-42.488239747051,12.7707827030479,171.175331994665));
#86909=CARTESIAN_POINT('Ctrl Pts',(-42.4851985041028,12.7726687878681,171.198413574834));
#86910=CARTESIAN_POINT('Ctrl Pts',(-42.4806285626732,12.7755010158997,171.221131109087));
#86911=CARTESIAN_POINT('Ctrl Pts',(-42.4746110754411,12.7792252792283,171.243315149802));
#86912=CARTESIAN_POINT('Ctrl Pts',(-42.4731153884239,12.7801509699851,171.248829142671));
#86913=CARTESIAN_POINT('Ctrl Pts',(-42.4715300567366,12.781131904664,171.254310195115));
#86914=CARTESIAN_POINT('Ctrl Pts',(-42.4698559095559,12.782167511398,171.259755708107));
#86915=CARTESIAN_POINT('Ctrl Pts',(-42.4653139115146,12.7849771351945,171.27452950436));
#86916=CARTESIAN_POINT('Ctrl Pts',(-42.4601175520392,12.7881895603695,171.289041238678));
#86917=CARTESIAN_POINT('Ctrl Pts',(-42.4542984513799,12.7917840756337,171.303197876379));
#86918=CARTESIAN_POINT('Ctrl Pts',(-42.4518371455332,12.7933044482744,171.309185711473));
#86919=CARTESIAN_POINT('Ctrl Pts',(-42.4492633499944,12.7948937448598,171.315113565351));
#86920=CARTESIAN_POINT('Ctrl Pts',(-42.4465819691828,12.796548746999,171.320976176106));
#86921=CARTESIAN_POINT('Ctrl Pts',(-42.4339919946876,12.8043195323464,171.348503082977));
#86922=CARTESIAN_POINT('Ctrl Pts',(-42.4190324561286,12.8135372911409,171.374583846366));
#86923=CARTESIAN_POINT('Ctrl Pts',(-42.4021714374908,12.8238954967045,171.398817826505));
#86924=CARTESIAN_POINT('Ctrl Pts',(-42.3864881901019,12.8335301637344,171.42135902131));
#86925=CARTESIAN_POINT('Ctrl Pts',(-42.3691602389399,12.8441512616124,171.442302499421));
#86926=CARTESIAN_POINT('Ctrl Pts',(-42.3505561327577,12.855519096481,171.461373719878));
#86927=CARTESIAN_POINT('Ctrl Pts',(-42.3491590125803,12.8563727914294,171.462805919127));
#86928=CARTESIAN_POINT('Ctrl Pts',(-42.3477546897505,12.8572307021435,171.464227583086));
#86929=CARTESIAN_POINT('Ctrl Pts',(-42.3463433174337,12.858092729399,171.465638607126));
#86930=CARTESIAN_POINT('Ctrl Pts',(-42.3433222782986,12.8599378967184,171.468658900776));
#86931=CARTESIAN_POINT('Ctrl Pts',(-42.3402655889138,12.8618039160818,171.471633649355));
#86932=CARTESIAN_POINT('Ctrl Pts',(-42.3371751743445,12.8636895691222,171.474562315445));
#86933=CARTESIAN_POINT('Ctrl Pts',(-42.3201535245773,12.8740755302671,171.490693073097));
#86934=CARTESIAN_POINT('Ctrl Pts',(-42.3021266986922,12.8850431839643,171.505411096499));
#86935=CARTESIAN_POINT('Ctrl Pts',(-42.2833391160437,12.8964362160542,171.518686045024));
#86936=CARTESIAN_POINT('Ctrl Pts',(-42.2631521576885,12.9086778475957,171.532949765805));
#86937=CARTESIAN_POINT('Ctrl Pts',(-42.2420863944765,12.9214109244311,171.545548160212));
#86938=CARTESIAN_POINT('Ctrl Pts',(-42.2203957477446,12.9344717190736,171.556423719582));
#86939=CARTESIAN_POINT('Ctrl Pts',(-42.2093656925312,12.9411133507326,171.561954122701));
#86940=CARTESIAN_POINT('Ctrl Pts',(-42.1981733395362,12.9478401579852,171.567038641576));
#86941=CARTESIAN_POINT('Ctrl Pts',(-42.1868484321251,12.9546327985739,171.571666998134));
#86942=CARTESIAN_POINT('Ctrl Pts',(-42.1637060140812,12.9685135414727,171.581125032395));
#86943=CARTESIAN_POINT('Ctrl Pts',(-42.1397851200849,12.9828022164415,171.588754861319));
#86944=CARTESIAN_POINT('Ctrl Pts',(-42.115420185623,12.9972962282797,171.594560491599));
#86945=CARTESIAN_POINT('Ctrl Pts',(-42.0904409714184,13.0121556577995,171.60051249129));
#86946=CARTESIAN_POINT('Ctrl Pts',(-42.0649933299033,13.0272319598426,171.604547546382));
#86947=CARTESIAN_POINT('Ctrl Pts',(-42.0394203347526,13.0423156811413,171.606621211164));
#86948=CARTESIAN_POINT('Ctrl Pts',(-42.0260722258977,13.0501887970062,171.607703583529));
#86949=CARTESIAN_POINT('Ctrl Pts',(-42.0126898425947,13.0580639808361,171.608250755187));
#86950=CARTESIAN_POINT('Ctrl Pts',(-41.9993226253918,13.0659108626764,171.608250755187));
#86951=CARTESIAN_POINT('Origin',(-34.5950649486897,26.6830679909832,172.608250755187));
#86952=CARTESIAN_POINT('',(-37.0349400532192,29.147654687411,173.108250755187));
#86953=CARTESIAN_POINT('Origin',(-37.0349400532192,29.147654687411,172.608250755187));
#86954=CARTESIAN_POINT('',(-32.1551898441603,24.2184812945555,173.108250755187));
#86955=CARTESIAN_POINT('Origin',(-34.5950649486897,26.6830679909832,173.108250755187));
#86956=CARTESIAN_POINT('Origin',(-32.1551898441603,24.2184812945555,172.608250755187));
#86957=CARTESIAN_POINT('Origin',(-34.5950649486897,26.6830679909832,152.108250755187));
#86958=CARTESIAN_POINT('',(-50.0950649486897,26.6830679909832,151.608250755187));
#86959=CARTESIAN_POINT('Origin',(-50.0950649486897,26.6830679909832,152.108250755187));
#86960=CARTESIAN_POINT('Origin',(-34.5950649486897,26.6830679909832,151.608250755187));
#86961=CARTESIAN_POINT('Origin',(35.4049350513103,26.6830679909832,171.608250755187));
#86962=CARTESIAN_POINT('',(19.4049350513103,26.6830679909833,152.108250755187));
#86963=CARTESIAN_POINT('',(51.4049350513103,26.6830679909832,152.108250755187));
#86964=CARTESIAN_POINT('Origin',(35.4049350513103,26.6830679909832,152.108250755187));
#86965=CARTESIAN_POINT('',(51.4049350513103,26.6830679909832,171.108250755187));
#86966=CARTESIAN_POINT('',(51.4049350513103,26.6830679909832,171.608250755187));
#86967=CARTESIAN_POINT('',(27.5073406548652,12.768040044578,171.108250755187));
#86968=CARTESIAN_POINT('Origin',(35.4049350513103,26.6830679909832,171.108250755187));
#86969=CARTESIAN_POINT('',(27.5073406548652,12.768040044578,153.608250755187));
#86970=CARTESIAN_POINT('',(27.5073406548652,12.768040044578,171.608250755187));
#86971=CARTESIAN_POINT('',(26.6543006790336,13.2880540647968,152.608250755187));
#86972=CARTESIAN_POINT('Ctrl Pts',(26.6543006790336,13.2880540647968,152.608250755187));
#86973=CARTESIAN_POINT('Ctrl Pts',(26.6851946113006,13.2678718158584,152.60825075831));
#86974=CARTESIAN_POINT('Ctrl Pts',(26.7161179160738,13.247833572528,152.610400982821));
#86975=CARTESIAN_POINT('Ctrl Pts',(26.7468561453125,13.2280604795012,152.614563215044));
#86976=CARTESIAN_POINT('Ctrl Pts',(26.7787348259742,13.2075537641208,152.61887987463));
#86977=CARTESIAN_POINT('Ctrl Pts',(26.8104154475333,13.1873316127695,152.625360599387));
#86978=CARTESIAN_POINT('Ctrl Pts',(26.8416802680476,13.1675195649632,152.633903745451));
#86979=CARTESIAN_POINT('Ctrl Pts',(26.873632996074,13.1472716004846,152.642634862988));
#86980=CARTESIAN_POINT('Ctrl Pts',(26.9051526379488,13.1274512360087,152.653520253585));
#86981=CARTESIAN_POINT('Ctrl Pts',(26.9360115757189,13.1081932944124,152.666504445645));
#86982=CARTESIAN_POINT('Ctrl Pts',(26.9482083696144,13.1005817185943,152.671636362875));
#86983=CARTESIAN_POINT('Ctrl Pts',(26.9603019012005,13.0930580740578,152.677096714818));
#86984=CARTESIAN_POINT('Ctrl Pts',(26.9722776634591,13.0856311228788,152.682884240716));
#86985=CARTESIAN_POINT('Ctrl Pts',(26.9739507675136,13.0845935219426,152.68369280161));
#86986=CARTESIAN_POINT('Ctrl Pts',(26.9756223166184,13.0835573316238,152.684508023839));
#86987=CARTESIAN_POINT('Ctrl Pts',(26.9772922828492,13.082522564595,152.685329889023));
#86988=CARTESIAN_POINT('Ctrl Pts',(27.0272042924152,13.0515954111636,152.709893824594));
#86989=CARTESIAN_POINT('Ctrl Pts',(27.0755338007373,13.0220440815316,152.74032765976));
#86990=CARTESIAN_POINT('Ctrl Pts',(27.1211352616185,12.9944473172044,152.775796511355));
#86991=CARTESIAN_POINT('Ctrl Pts',(27.1626437536728,12.969327506333,152.808081848625));
#86992=CARTESIAN_POINT('Ctrl Pts',(27.2018916468014,12.9458272165044,152.844537973178));
#86993=CARTESIAN_POINT('Ctrl Pts',(27.2380549426608,12.9243594465078,152.884524370531));
#86994=CARTESIAN_POINT('Ctrl Pts',(27.2416208453306,12.9222426046513,152.888467252331));
#86995=CARTESIAN_POINT('Ctrl Pts',(27.2451567928795,12.9201455041919,152.892444455841));
#86996=CARTESIAN_POINT('Ctrl Pts',(27.2486620201446,12.9180685269602,152.896455365443));
#86997=CARTESIAN_POINT('Ctrl Pts',(27.250357622029,12.9170638199208,152.898395583684));
#86998=CARTESIAN_POINT('Ctrl Pts',(27.2520466380835,12.9160634384558,152.900344344347));
#86999=CARTESIAN_POINT('Ctrl Pts',(27.2537290041144,12.9150674101677,152.902301551645));
#87000=CARTESIAN_POINT('Ctrl Pts',(27.2927301846081,12.8919771442397,152.947674195698));
#87001=CARTESIAN_POINT('Ctrl Pts',(27.3281609719104,12.8712238657579,152.997605490932));
#87002=CARTESIAN_POINT('Ctrl Pts',(27.3592811480756,12.8531192060994,153.051009927998));
#87003=CARTESIAN_POINT('Ctrl Pts',(27.3904013242408,12.835014546441,153.104414365063));
#87004=CARTESIAN_POINT('Ctrl Pts',(27.417211677315,12.8195581462718,153.161292777412));
#87005=CARTESIAN_POINT('Ctrl Pts',(27.4389779275479,12.8070625461649,153.22061351513));
#87006=CARTESIAN_POINT('Ctrl Pts',(27.4396346260099,12.8066855477713,153.222403250928));
#87007=CARTESIAN_POINT('Ctrl Pts',(27.4402867539371,12.8063112214621,153.22419533454));
#87008=CARTESIAN_POINT('Ctrl Pts',(27.4409343049623,12.8059395694613,153.225989728665));
#87009=CARTESIAN_POINT('Ctrl Pts',(27.4534340650697,12.7987655234446,153.260627147537));
#87010=CARTESIAN_POINT('Ctrl Pts',(27.4641871190213,12.7926115974433,153.296006270053));
#87011=CARTESIAN_POINT('Ctrl Pts',(27.4731968232073,12.7874655986581,153.331953347762));
#87012=CARTESIAN_POINT('Ctrl Pts',(27.4822585084477,12.7822899102806,153.368107820404));
#87013=CARTESIAN_POINT('Ctrl Pts',(27.4895569381589,12.7781337002303,153.404837909208));
#87014=CARTESIAN_POINT('Ctrl Pts',(27.4950535469991,12.7750090296604,153.441987310221));
#87015=CARTESIAN_POINT('Ctrl Pts',(27.5004309647065,12.7719521159632,153.478331145598));
#87016=CARTESIAN_POINT('Ctrl Pts',(27.5040839553981,12.7698824718333,153.515077343023));
#87017=CARTESIAN_POINT('Ctrl Pts',(27.5059339415353,12.7688355319703,153.552083286406));
#87018=CARTESIAN_POINT('Ctrl Pts',(27.5068669273545,12.7683075387999,153.570746139986));
#87019=CARTESIAN_POINT('Ctrl Pts',(27.5073406519415,12.7680400462374,153.589475021942));
#87020=CARTESIAN_POINT('Ctrl Pts',(27.5073406548652,12.768040044578,153.608250755187));
#87021=CARTESIAN_POINT('',(21.9224216884311,18.0678585669597,152.608250755187));
#87022=CARTESIAN_POINT('Origin',(35.4049350513103,26.6830679909832,152.608250755187));
#87023=CARTESIAN_POINT('',(21.4110300971907,18.9260953769367,153.608250755187));
#87024=CARTESIAN_POINT('Ctrl Pts',(21.4110300971907,18.9260953769367,153.608250755187));
#87025=CARTESIAN_POINT('Ctrl Pts',(21.4110300976924,18.9260953760316,153.570920583161));
#87026=CARTESIAN_POINT('Ctrl Pts',(21.4120878951452,18.9241774989273,153.533707722381));
#87027=CARTESIAN_POINT('Ctrl Pts',(21.4141565358502,18.9204434093267,153.496805212598));
#87028=CARTESIAN_POINT('Ctrl Pts',(21.4154035242392,18.9181924788658,153.474560169699));
#87029=CARTESIAN_POINT('Ctrl Pts',(21.4170183390955,18.9152806425281,153.452427631479));
#87030=CARTESIAN_POINT('Ctrl Pts',(21.4189950581815,18.911722257265,153.430449466818));
#87031=CARTESIAN_POINT('Ctrl Pts',(21.4223979004345,18.9055966404225,153.392614941982));
#87032=CARTESIAN_POINT('Ctrl Pts',(21.4268697835066,18.8975612058826,153.355237560419));
#87033=CARTESIAN_POINT('Ctrl Pts',(21.4323628035064,18.8877211995491,153.318533572221));
#87034=CARTESIAN_POINT('Ctrl Pts',(21.4341058444109,18.8845987762663,153.306886690763));
#87035=CARTESIAN_POINT('Ctrl Pts',(21.4359518892137,18.8812943178563,153.295307498789));
#87036=CARTESIAN_POINT('Ctrl Pts',(21.4378999292086,18.8778102513037,153.283802686776));
#87037=CARTESIAN_POINT('Ctrl Pts',(21.4409325895459,18.8723863429266,153.265892280843));
#87038=CARTESIAN_POINT('Ctrl Pts',(21.4442116208038,18.8665286220844,153.248162502229));
#87039=CARTESIAN_POINT('Ctrl Pts',(21.4477317053264,18.8602489158523,153.230639181705));
#87040=CARTESIAN_POINT('Ctrl Pts',(21.4483482760751,18.8591489754537,153.227569833004));
#87041=CARTESIAN_POINT('Ctrl Pts',(21.4489722508424,18.8580360733877,153.224506614159));
#87042=CARTESIAN_POINT('Ctrl Pts',(21.4496035032151,18.8569104466983,153.221450561457));
#87043=CARTESIAN_POINT('Ctrl Pts',(21.4505489587854,18.855224544087,153.216873371454));
#87044=CARTESIAN_POINT('Ctrl Pts',(21.4515113052024,18.8535092116976,153.212308955191));
#87045=CARTESIAN_POINT('Ctrl Pts',(21.4524899582233,18.8517655750918,153.207760541832));
#87046=CARTESIAN_POINT('Ctrl Pts',(21.4605594601156,18.8373883866613,153.170256513927));
#87047=CARTESIAN_POINT('Ctrl Pts',(21.4697513877767,18.8210621214449,153.13377689826));
#87048=CARTESIAN_POINT('Ctrl Pts',(21.480020629506,18.8029154201111,153.098570203309));
#87049=CARTESIAN_POINT('Ctrl Pts',(21.4853286734362,18.7935356148241,153.080372298501));
#87050=CARTESIAN_POINT('Ctrl Pts',(21.490924722434,18.7836691588732,153.062515275871));
#87051=CARTESIAN_POINT('Ctrl Pts',(21.4968033196097,18.7733327882725,153.045038768438));
#87052=CARTESIAN_POINT('Ctrl Pts',(21.505429151337,18.758165939651,153.019394995308));
#87053=CARTESIAN_POINT('Ctrl Pts',(21.5146627093384,18.7419883607805,152.994565543546));
#87054=CARTESIAN_POINT('Ctrl Pts',(21.5244860032948,18.7248554116565,152.970664496244));
#87055=CARTESIAN_POINT('Ctrl Pts',(21.5343092972512,18.7077224625325,152.946763448943));
#87056=CARTESIAN_POINT('Ctrl Pts',(21.544724188428,18.6896309027287,152.923794471748));
#87057=CARTESIAN_POINT('Ctrl Pts',(21.5557092003027,18.6706436778749,152.901863691503));
#87058=CARTESIAN_POINT('Ctrl Pts',(21.5565265622387,18.6692308951631,152.900231887624));
#87059=CARTESIAN_POINT('Ctrl Pts',(21.5573469446616,18.6678133893012,152.898605923768));
#87060=CARTESIAN_POINT('Ctrl Pts',(21.5581703323645,18.6663911970232,152.896985860847));
#87061=CARTESIAN_POINT('Ctrl Pts',(21.5790393023703,18.630345373302,152.855924955531));
#87062=CARTESIAN_POINT('Ctrl Pts',(21.6018725723745,18.5912435035659,152.818486237741));
#87063=CARTESIAN_POINT('Ctrl Pts',(21.6263923464424,18.5497069642871,152.785209355609));
#87064=CARTESIAN_POINT('Ctrl Pts',(21.6519279007995,18.5064496914579,152.750553912613));
#87065=CARTESIAN_POINT('Ctrl Pts',(21.6792923955092,18.4605523878058,152.720413135413));
#87066=CARTESIAN_POINT('Ctrl Pts',(21.7081462821627,18.4127621748605,152.695377210186));
#87067=CARTESIAN_POINT('Ctrl Pts',(21.7122514683085,18.4059628232708,152.691815224426));
#87068=CARTESIAN_POINT('Ctrl Pts',(21.7163867650893,18.399125218479,152.688356527985));
#87069=CARTESIAN_POINT('Ctrl Pts',(21.720551158396,18.3922515717701,152.68500277378));
#87070=CARTESIAN_POINT('Ctrl Pts',(21.7213482993824,18.3909358301689,152.684360803933));
#87071=CARTESIAN_POINT('Ctrl Pts',(21.7221464355189,18.3896188851033,152.683722731272));
#87072=CARTESIAN_POINT('Ctrl Pts',(21.722945562509,18.3883007472027,152.683088562518));
#87073=CARTESIAN_POINT('Ctrl Pts',(21.7436971888205,18.3540715127016,152.666620550356));
#87074=CARTESIAN_POINT('Ctrl Pts',(21.7650452077676,18.3191605534867,152.652827752376));
#87075=CARTESIAN_POINT('Ctrl Pts',(21.7868930725109,18.2837437878615,152.641735383211));
#87076=CARTESIAN_POINT('Ctrl Pts',(21.8086099215902,18.2485394068843,152.630709531948));
#87077=CARTESIAN_POINT('Ctrl Pts',(21.8308210901613,18.2128344803894,152.622351680356));
#87078=CARTESIAN_POINT('Ctrl Pts',(21.8534383774776,18.1767968967633,152.61673704558));
#87079=CARTESIAN_POINT('Ctrl Pts',(21.8760556647939,18.1407593131371,152.611122410805));
#87080=CARTESIAN_POINT('Ctrl Pts',(21.8990795172436,18.1043882808024,152.608250762682));
#87081=CARTESIAN_POINT('Ctrl Pts',(21.9224216884311,18.0678585669597,152.608250755187));
#87082=CARTESIAN_POINT('',(21.4110300971907,18.9260953769367,171.108250755187));
#87083=CARTESIAN_POINT('',(21.4110300971907,18.9260953769367,171.608250755187));
#87084=CARTESIAN_POINT('Origin',(35.4049350513103,26.6830679909832,171.108250755187));
#87085=CARTESIAN_POINT('Origin',(35.4049350513103,26.6830679909832,152.108250755187));
#87086=CARTESIAN_POINT('Origin',(35.4049350513103,26.6830679909832,153.108250755187));
#87087=CARTESIAN_POINT('',(38.1965776692254,23.8631510023956,172.108250755187));
#87088=CARTESIAN_POINT('',(32.6132924333951,29.5029849795709,172.108250755187));
#87089=CARTESIAN_POINT('Origin',(35.4049350513103,26.6830679909832,172.108250755187));
#87090=CARTESIAN_POINT('',(32.6132924333951,29.5029849795709,172.608250755187));
#87091=CARTESIAN_POINT('',(32.6132924333951,29.5029849795709,153.108250755187));
#87092=CARTESIAN_POINT('',(38.1965776692254,23.8631510023956,172.608250755187));
#87093=CARTESIAN_POINT('Origin',(35.4049350513103,26.6830679909832,172.608250755187));
#87094=CARTESIAN_POINT('',(38.1965776692254,23.8631510023956,153.108250755187));
#87095=CARTESIAN_POINT('Origin',(35.4049350513103,26.6830679909832,172.108250755187));
#87096=CARTESIAN_POINT('',(38.5483451826112,23.5078207102358,171.608250755187));
#87097=CARTESIAN_POINT('Origin',(38.5483451826112,23.5078207102358,172.108250755187));
#87098=CARTESIAN_POINT('',(32.2615249200093,29.8583152717307,171.608250755187));
#87099=CARTESIAN_POINT('Origin',(35.4049350513103,26.6830679909832,171.608250755187));
#87100=CARTESIAN_POINT('Origin',(32.2615249200093,29.8583152717307,172.108250755187));
#87101=CARTESIAN_POINT('Origin',(35.4049350513103,26.6830679909832,171.108250755187));
#87102=CARTESIAN_POINT('',(21.7138571120063,19.4164054241714,171.608250755187));
#87103=CARTESIAN_POINT('Ctrl Pts',(21.7138571120063,19.4164054241714,171.608250755187));
#87104=CARTESIAN_POINT('Ctrl Pts',(21.6978146742301,19.3896971879681,171.608250755187));
#87105=CARTESIAN_POINT('Ctrl Pts',(21.6818000789652,19.3631642033449,171.606119035115));
#87106=CARTESIAN_POINT('Ctrl Pts',(21.6659195169656,19.3369687870488,171.601866237764));
#87107=CARTESIAN_POINT('Ctrl Pts',(21.6504750080682,19.311492652132,171.597730214963));
#87108=CARTESIAN_POINT('Ctrl Pts',(21.6351567341587,19.2863349716511,171.591587725864));
#87109=CARTESIAN_POINT('Ctrl Pts',(21.6200693334557,19.2616587919335,171.583402532597));
#87110=CARTESIAN_POINT('Ctrl Pts',(21.6135205931,19.2509480076757,171.579849720119));
#87111=CARTESIAN_POINT('Ctrl Pts',(21.6070154869729,19.2403281898591,171.575911483357));
#87112=CARTESIAN_POINT('Ctrl Pts',(21.6005633844741,19.2298141093881,171.57158222553));
#87113=CARTESIAN_POINT('Ctrl Pts',(21.5862761856819,19.2065322787234,171.561995743107));
#87114=CARTESIAN_POINT('Ctrl Pts',(21.5723413388016,19.1839180856286,171.550546208526));
#87115=CARTESIAN_POINT('Ctrl Pts',(21.5588844360793,19.1621551516958,171.537246666315));
#87116=CARTESIAN_POINT('Ctrl Pts',(21.5461277452202,19.1415246228069,171.524639147925));
#87117=CARTESIAN_POINT('Ctrl Pts',(21.5338002896738,19.1216587054077,171.510368657228));
#87118=CARTESIAN_POINT('Ctrl Pts',(21.5220312221599,19.102749096496,171.494425144445));
#87119=CARTESIAN_POINT('Ctrl Pts',(21.5174100936258,19.0953242318491,171.488164918495));
#87120=CARTESIAN_POINT('Ctrl Pts',(21.5128753250856,19.0880472321367,171.481646553993));
#87121=CARTESIAN_POINT('Ctrl Pts',(21.5084358806911,19.0809314970593,171.474868716253));
#87122=CARTESIAN_POINT('Ctrl Pts',(21.5064108623527,19.0776857093565,171.471777057816));
#87123=CARTESIAN_POINT('Ctrl Pts',(21.5044069640677,19.0744755040767,171.468633337136));
#87124=CARTESIAN_POINT('Ctrl Pts',(21.502425120103,19.0713022787009,171.465437794362));
#87125=CARTESIAN_POINT('Ctrl Pts',(21.4901829419552,19.0517007404143,171.445698397808));
#87126=CARTESIAN_POINT('Ctrl Pts',(21.4788058603021,19.0335459229596,171.423959301334));
#87127=CARTESIAN_POINT('Ctrl Pts',(21.4685318499969,19.0171904481876,171.400512409473));
#87128=CARTESIAN_POINT('Ctrl Pts',(21.4590062584099,19.0020264014073,171.378773525704));
#87129=CARTESIAN_POINT('Ctrl Pts',(21.4504290114908,18.9884092853585,171.355566752544));
#87130=CARTESIAN_POINT('Ctrl Pts',(21.4430070519656,18.9766454465187,171.331150570564));
#87131=CARTESIAN_POINT('Ctrl Pts',(21.4402031852097,18.9722013052469,171.321926628999));
#87132=CARTESIAN_POINT('Ctrl Pts',(21.437563410343,18.9680203916148,171.312526353858));
#87133=CARTESIAN_POINT('Ctrl Pts',(21.4351035488799,18.964126514061,171.302980969397));
#87134=CARTESIAN_POINT('Ctrl Pts',(21.433058433355,18.9608891653093,171.295044988349));
#87135=CARTESIAN_POINT('Ctrl Pts',(21.4311351242584,18.9578459265386,171.286995184802));
#87136=CARTESIAN_POINT('Ctrl Pts',(21.4293386708823,18.9550044569664,171.278854434802));
#87137=CARTESIAN_POINT('Ctrl Pts',(21.4246679499804,18.9476167276214,171.257688747072));
#87138=CARTESIAN_POINT('Ctrl Pts',(21.4208519354368,18.941588459487,171.235909909692));
#87139=CARTESIAN_POINT('Ctrl Pts',(21.4179290527765,18.9369745863991,171.213680494794));
#87140=CARTESIAN_POINT('Ctrl Pts',(21.4151279876107,18.932553006511,171.192377539128));
#87141=CARTESIAN_POINT('Ctrl Pts',(21.4131471354433,18.9294303689643,171.170659720179));
#87142=CARTESIAN_POINT('Ctrl Pts',(21.412045329285,18.9276943711411,171.148671871474));
#87143=CARTESIAN_POINT('Ctrl Pts',(21.4113745818035,18.9266375462549,171.135286309929));
#87144=CARTESIAN_POINT('Ctrl Pts',(21.4110300971907,18.9260953769367,171.121800772663));
#87145=CARTESIAN_POINT('Ctrl Pts',(21.4110300971907,18.9260953769367,171.108250755187));
#87146=CARTESIAN_POINT('',(28.0006773746082,13.0659108626764,171.608250755187));
#87147=CARTESIAN_POINT('Origin',(35.4049350513103,26.6830679909832,171.608250755187));
#87148=CARTESIAN_POINT('Ctrl Pts',(27.5073406548652,12.768040044578,171.108250755187));
#87149=CARTESIAN_POINT('Ctrl Pts',(27.5073406548652,12.768040044578,171.13083841897));
#87150=CARTESIAN_POINT('Ctrl Pts',(27.508851012029,12.7689784818034,171.153252246793));
#87151=CARTESIAN_POINT('Ctrl Pts',(27.5117602529499,12.7707827030486,171.175331994673));
#87152=CARTESIAN_POINT('Ctrl Pts',(27.5148014958989,12.7726687878693,171.198413574845));
#87153=CARTESIAN_POINT('Ctrl Pts',(27.5193714373296,12.7755010159017,171.221131109101));
#87154=CARTESIAN_POINT('Ctrl Pts',(27.5253889245633,12.7792252792313,171.243315149819));
#87155=CARTESIAN_POINT('Ctrl Pts',(27.5268846115792,12.7801509699872,171.248829142682));
#87156=CARTESIAN_POINT('Ctrl Pts',(27.5284699432649,12.7811319046652,171.254310195121));
#87157=CARTESIAN_POINT('Ctrl Pts',(27.5301440904439,12.7821675113981,171.259755708108));
#87158=CARTESIAN_POINT('Ctrl Pts',(27.5346860884853,12.7849771351945,171.27452950436));
#87159=CARTESIAN_POINT('Ctrl Pts',(27.5398824479607,12.7881895603696,171.289041238678));
#87160=CARTESIAN_POINT('Ctrl Pts',(27.5457015486201,12.7917840756337,171.303197876379));
#87161=CARTESIAN_POINT('Ctrl Pts',(27.5481628544669,12.7933044482744,171.309185711473));
#87162=CARTESIAN_POINT('Ctrl Pts',(27.5507366500057,12.7948937448598,171.315113565351));
#87163=CARTESIAN_POINT('Ctrl Pts',(27.5534180308173,12.796548746999,171.320976176106));
#87164=CARTESIAN_POINT('Ctrl Pts',(27.5660080053126,12.8043195323464,171.348503082977));
#87165=CARTESIAN_POINT('Ctrl Pts',(27.5809675438715,12.8135372911409,171.374583846366));
#87166=CARTESIAN_POINT('Ctrl Pts',(27.5978285625092,12.8238954967046,171.398817826505));
#87167=CARTESIAN_POINT('Ctrl Pts',(27.6135118098975,12.8335301637343,171.421359021309));
#87168=CARTESIAN_POINT('Ctrl Pts',(27.6308397610588,12.8441512616119,171.44230249942));
#87169=CARTESIAN_POINT('Ctrl Pts',(27.6494438672404,12.8555190964801,171.461373719876));
#87170=CARTESIAN_POINT('Ctrl Pts',(27.6508409874183,12.8563727914288,171.462805919126));
#87171=CARTESIAN_POINT('Ctrl Pts',(27.6522453102488,12.8572307021433,171.464227583086));
#87172=CARTESIAN_POINT('Ctrl Pts',(27.6536566825661,12.8580927293991,171.465638607126));
#87173=CARTESIAN_POINT('Ctrl Pts',(27.6566777217013,12.8599378967185,171.468658900776));
#87174=CARTESIAN_POINT('Ctrl Pts',(27.6597344110861,12.8618039160819,171.471633649355));
#87175=CARTESIAN_POINT('Ctrl Pts',(27.6628248256553,12.8636895691224,171.474562315445));
#87176=CARTESIAN_POINT('Ctrl Pts',(27.6798464754228,12.8740755302673,171.490693073097));
#87177=CARTESIAN_POINT('Ctrl Pts',(27.697873301308,12.8850431839646,171.505411096499));
#87178=CARTESIAN_POINT('Ctrl Pts',(27.7166608839567,12.8964362160547,171.518686045025));
#87179=CARTESIAN_POINT('Ctrl Pts',(27.736847842312,12.9086778475964,171.532949765806));
#87180=CARTESIAN_POINT('Ctrl Pts',(27.7579136055242,12.921410924432,171.545548160212));
#87181=CARTESIAN_POINT('Ctrl Pts',(27.7796042522562,12.9344717190747,171.556423719583));
#87182=CARTESIAN_POINT('Ctrl Pts',(27.7906343074692,12.9411133507335,171.561954122701));
#87183=CARTESIAN_POINT('Ctrl Pts',(27.8018266604637,12.9478401579859,171.567038641576));
#87184=CARTESIAN_POINT('Ctrl Pts',(27.8131515678744,12.9546327985744,171.571666998134));
#87185=CARTESIAN_POINT('Ctrl Pts',(27.8362939859182,12.9685135414732,171.581125032396));
#87186=CARTESIAN_POINT('Ctrl Pts',(27.8602148799146,12.982802216442,171.588754861319));
#87187=CARTESIAN_POINT('Ctrl Pts',(27.8845798143767,12.9972962282802,171.5945604916));
#87188=CARTESIAN_POINT('Ctrl Pts',(27.9095590285816,13.0121556578,171.60051249129));
#87189=CARTESIAN_POINT('Ctrl Pts',(27.9350066700969,13.027231959843,171.604547546382));
#87190=CARTESIAN_POINT('Ctrl Pts',(27.9605796652478,13.0423156811417,171.606621211164));
#87191=CARTESIAN_POINT('Ctrl Pts',(27.9739277741026,13.0501887970065,171.607703583529));
#87192=CARTESIAN_POINT('Ctrl Pts',(27.9873101574055,13.0580639808362,171.608250755187));
#87193=CARTESIAN_POINT('Ctrl Pts',(28.0006773746082,13.0659108626764,171.608250755187));
#87194=CARTESIAN_POINT('Origin',(35.4049350513103,26.6830679909832,172.608250755187));
#87195=CARTESIAN_POINT('',(32.9650599467808,29.147654687411,173.108250755187));
#87196=CARTESIAN_POINT('Origin',(32.9650599467808,29.147654687411,172.608250755187));
#87197=CARTESIAN_POINT('',(37.8448101558397,24.2184812945555,173.108250755187));
#87198=CARTESIAN_POINT('Origin',(35.4049350513103,26.6830679909832,173.108250755187));
#87199=CARTESIAN_POINT('Origin',(37.8448101558397,24.2184812945555,172.608250755187));
#87200=CARTESIAN_POINT('Origin',(35.4049350513103,26.6830679909832,152.108250755187));
#87201=CARTESIAN_POINT('',(19.9049350513103,26.6830679909832,151.608250755187));
#87202=CARTESIAN_POINT('Origin',(19.9049350513103,26.6830679909832,152.108250755187));
#87203=CARTESIAN_POINT('Origin',(35.4049350513103,26.6830679909832,151.608250755187));
#87204=CARTESIAN_POINT('Origin',(125.29348064571,25.4505574462982,227.));
#87205=CARTESIAN_POINT('',(151.316083724746,25.4505574462982,200.));
#87206=CARTESIAN_POINT('Origin',(125.29348064571,25.4505574462982,200.));
#87207=CARTESIAN_POINT('',(151.316083724746,25.4505574462982,226.3));
#87208=CARTESIAN_POINT('',(151.316083724746,25.4505574462982,227.));
#87209=CARTESIAN_POINT('',(119.980756553526,50.9250708612662,226.3));
#87210=CARTESIAN_POINT('Origin',(125.29348064571,25.4505574462982,226.3));
#87211=CARTESIAN_POINT('',(119.980756553526,50.9250708612662,202.7));
#87212=CARTESIAN_POINT('',(119.980756553526,50.9250708612662,227.));
#87213=CARTESIAN_POINT('',(121.344083479533,51.1717186376762,201.3));
#87214=CARTESIAN_POINT('Ctrl Pts',(121.344083479533,51.1717186376762,201.3));
#87215=CARTESIAN_POINT('Ctrl Pts',(121.296814940039,51.164460713567,201.300000001764));
#87216=CARTESIAN_POINT('Ctrl Pts',(121.249631520094,51.1570730071936,201.30261647433));
#87217=CARTESIAN_POINT('Ctrl Pts',(121.202809575166,51.1496136039449,201.307693045627));
#87218=CARTESIAN_POINT('Ctrl Pts',(121.154373252809,51.1418970073598,201.312944652415));
#87219=CARTESIAN_POINT('Ctrl Pts',(121.106322691563,51.1341034996569,201.320828920817));
#87220=CARTESIAN_POINT('Ctrl Pts',(121.058940661441,51.1262905985135,201.331225416489));
#87221=CARTESIAN_POINT('Ctrl Pts',(121.010426286528,51.1182909831689,201.341870369596));
#87222=CARTESIAN_POINT('Ctrl Pts',(120.96261148805,51.1102708092942,201.355149130815));
#87223=CARTESIAN_POINT('Ctrl Pts',(120.915794212708,51.1022880243849,201.370986079636));
#87224=CARTESIAN_POINT('Ctrl Pts',(120.885078842197,51.0970507653943,201.381376213347));
#87225=CARTESIAN_POINT('Ctrl Pts',(120.854792756682,51.0918295287459,201.392868556026));
#87226=CARTESIAN_POINT('Ctrl Pts',(120.825022979086,51.0866405538404,201.405453604755));
#87227=CARTESIAN_POINT('Ctrl Pts',(120.822614540357,51.0862207546636,201.406471762135));
#87228=CARTESIAN_POINT('Ctrl Pts',(120.820208501303,51.0858010088545,201.407497395078));
#87229=CARTESIAN_POINT('Ctrl Pts',(120.817804891954,51.0853813251034,201.408530483275));
#87230=CARTESIAN_POINT('Ctrl Pts',(120.748752458259,51.0733243806588,201.438209704743));
#87231=CARTESIAN_POINT('Ctrl Pts',(120.681875427084,51.0613482917229,201.473987104567));
#87232=CARTESIAN_POINT('Ctrl Pts',(120.618293835989,51.0497349272812,201.51508560388));
#87233=CARTESIAN_POINT('Ctrl Pts',(120.558229638025,51.0387640250305,201.553910495744));
#87234=CARTESIAN_POINT('Ctrl Pts',(120.501106992418,51.0281170259462,201.597483053204));
#87235=CARTESIAN_POINT('Ctrl Pts',(120.447829239022,51.0180241909268,201.645128573345));
#87236=CARTESIAN_POINT('Ctrl Pts',(120.42575040754,51.0138416196026,201.664873351287));
#87237=CARTESIAN_POINT('Ctrl Pts',(120.404331325271,51.0097541109278,201.685317440809));
#87238=CARTESIAN_POINT('Ctrl Pts',(120.383633686815,51.0057775363715,201.706412319778));
#87239=CARTESIAN_POINT('Ctrl Pts',(120.381288649471,51.0053269914529,201.708802364374));
#87240=CARTESIAN_POINT('Ctrl Pts',(120.378951141237,51.0048775527908,201.711202451161));
#87241=CARTESIAN_POINT('Ctrl Pts',(120.376621298644,51.0044292543624,201.713612409408));
#87242=CARTESIAN_POINT('Ctrl Pts',(120.329918672461,50.9954429331492,201.761920985893));
#87243=CARTESIAN_POINT('Ctrl Pts',(120.286217524176,50.986899636637,201.814296128758));
#87244=CARTESIAN_POINT('Ctrl Pts',(120.246644234098,50.9790767475013,201.869390093657));
#87245=CARTESIAN_POINT('Ctrl Pts',(120.235032869601,50.9767814008927,201.885555444244));
#87246=CARTESIAN_POINT('Ctrl Pts',(120.223776558923,50.974548012121,201.901954831386));
#87247=CARTESIAN_POINT('Ctrl Pts',(120.212902870258,50.9723834091261,201.91855423109));
#87248=CARTESIAN_POINT('Ctrl Pts',(120.211224597556,50.9720493188068,201.921116224565));
#87249=CARTESIAN_POINT('Ctrl Pts',(120.209555106758,50.9717168083916,201.923682941432));
#87250=CARTESIAN_POINT('Ctrl Pts',(120.207894399138,50.9713858827489,201.926254375486));
#87251=CARTESIAN_POINT('Ctrl Pts',(120.166433470862,50.9631240525672,201.990452336396));
#87252=CARTESIAN_POINT('Ctrl Pts',(120.130429392281,50.9558466678358,202.057605589415));
#87253=CARTESIAN_POINT('Ctrl Pts',(120.099834407458,50.9496146107615,202.127787837188));
#87254=CARTESIAN_POINT('Ctrl Pts',(120.095136748583,50.9486577193494,202.138563860156));
#87255=CARTESIAN_POINT('Ctrl Pts',(120.090566696606,50.9477254852738,202.149411345588));
#87256=CARTESIAN_POINT('Ctrl Pts',(120.086124170858,50.9468181437796,202.1603306173));
#87257=CARTESIAN_POINT('Ctrl Pts',(120.085241450897,50.9466378570477,202.162500252244));
#87258=CARTESIAN_POINT('Ctrl Pts',(120.084364128845,50.9464586358352,202.164672249676));
#87259=CARTESIAN_POINT('Ctrl Pts',(120.083492209333,50.9462804820366,202.166846579406));
#87260=CARTESIAN_POINT('Ctrl Pts',(120.065306140488,50.9425646376238,202.212197680753));
#87261=CARTESIAN_POINT('Ctrl Pts',(120.049527707131,50.9393249175896,202.258413140069));
#87262=CARTESIAN_POINT('Ctrl Pts',(120.036138534255,50.936566193575,202.305307920115));
#87263=CARTESIAN_POINT('Ctrl Pts',(120.02267110342,50.9337913451802,202.352476794));
#87264=CARTESIAN_POINT('Ctrl Pts',(120.011620718125,50.9315030569102,202.400333921084));
#87265=CARTESIAN_POINT('Ctrl Pts',(120.00301661756,50.9297157845129,202.448711398113));
#87266=CARTESIAN_POINT('Ctrl Pts',(119.994561270883,50.9279594117685,202.496252490468));
#87267=CARTESIAN_POINT('Ctrl Pts',(119.988468284927,50.9266868395961,202.544297037827));
#87268=CARTESIAN_POINT('Ctrl Pts',(119.984813469459,50.9259217362925,202.592691092945));
#87269=CARTESIAN_POINT('Ctrl Pts',(119.982124767438,50.9253588802969,202.628292669809));
#87270=CARTESIAN_POINT('Ctrl Pts',(119.980756556636,50.925070861915,202.664083573468));
#87271=CARTESIAN_POINT('Ctrl Pts',(119.980756553526,50.9250708612662,202.7));
#87272=CARTESIAN_POINT('',(129.242877811887,51.1717186376762,201.3));
#87273=CARTESIAN_POINT('Origin',(125.29348064571,25.4505574462982,201.3));
#87274=CARTESIAN_POINT('',(130.606204737894,50.9250708612662,202.7));
#87275=CARTESIAN_POINT('Ctrl Pts',(130.606204737894,50.9250708612662,202.7));
#87276=CARTESIAN_POINT('Ctrl Pts',(130.606204736907,50.9250708614721,202.649823152623));
#87277=CARTESIAN_POINT('Ctrl Pts',(130.603493048605,50.9256415257708,202.599732878103));
#87278=CARTESIAN_POINT('Ctrl Pts',(130.598216123741,50.9267435592911,202.550016081281));
#87279=CARTESIAN_POINT('Ctrl Pts',(130.592800185238,50.9278746244338,202.49898956089));
#87280=CARTESIAN_POINT('Ctrl Pts',(130.584681986303,50.9295654689291,202.44835525433));
#87281=CARTESIAN_POINT('Ctrl Pts',(130.573966511743,50.9317850515479,202.398409849753));
#87282=CARTESIAN_POINT('Ctrl Pts',(130.563222416445,50.934010562611,202.348331042373));
#87283=CARTESIAN_POINT('Ctrl Pts',(130.549866888012,50.9367677238324,202.298943529959));
#87284=CARTESIAN_POINT('Ctrl Pts',(130.533955804295,50.9400355548964,202.250551985476));
#87285=CARTESIAN_POINT('Ctrl Pts',(130.52453817908,50.9419697542745,202.221909472014));
#87286=CARTESIAN_POINT('Ctrl Pts',(130.514224327984,50.9440830480728,202.193616080543));
#87287=CARTESIAN_POINT('Ctrl Pts',(130.503018172532,50.9463726044773,202.165738725987));
#87288=CARTESIAN_POINT('Ctrl Pts',(130.502391057095,50.946500731931,202.164178662017));
#87289=CARTESIAN_POINT('Ctrl Pts',(130.501761172559,50.9466294061949,202.162619958756));
#87290=CARTESIAN_POINT('Ctrl Pts',(130.501128521321,50.9467586264223,202.161062631988));
#87291=CARTESIAN_POINT('Ctrl Pts',(130.467437757633,50.9536400294536,202.07812984855));
#87292=CARTESIAN_POINT('Ctrl Pts',(130.425599590938,50.9621200262788,201.998148794283));
#87293=CARTESIAN_POINT('Ctrl Pts',(130.376670295168,50.9718651713917,201.92287275644));
#87294=CARTESIAN_POINT('Ctrl Pts',(130.327740999398,50.9816103165046,201.847596718597));
#87295=CARTESIAN_POINT('Ctrl Pts',(130.271720626042,50.9926205787292,201.777026086224));
#87296=CARTESIAN_POINT('Ctrl Pts',(130.20970669802,51.0045511176674,201.712958049445));
#87297=CARTESIAN_POINT('Ctrl Pts',(130.207830086632,51.0049121492283,201.71101927841));
#87298=CARTESIAN_POINT('Ctrl Pts',(130.205947872494,51.0052740452498,201.709086313541));
#87299=CARTESIAN_POINT('Ctrl Pts',(130.204060089613,51.0056367953596,201.707159214017));
#87300=CARTESIAN_POINT('Ctrl Pts',(130.163509016277,51.0134289553865,201.665763588018));
#87301=CARTESIAN_POINT('Ctrl Pts',(130.119885380912,51.0217082832857,201.626558866243));
#87302=CARTESIAN_POINT('Ctrl Pts',(130.074141666999,51.0302581165978,201.590396521904));
#87303=CARTESIAN_POINT('Ctrl Pts',(130.050982804967,51.0345866765929,201.572088460059));
#87304=CARTESIAN_POINT('Ctrl Pts',(130.027281461632,51.0389844001929,201.554560066656));
#87305=CARTESIAN_POINT('Ctrl Pts',(130.00316572107,51.043422400071,201.5379199304));
#87306=CARTESIAN_POINT('Ctrl Pts',(130.001082367498,51.0438057979135,201.536482392654));
#87307=CARTESIAN_POINT('Ctrl Pts',(129.998995800011,51.0441895186937,201.535051370118));
#87308=CARTESIAN_POINT('Ctrl Pts',(129.996906096631,51.0445735445554,201.533626931406));
#87309=CARTESIAN_POINT('Ctrl Pts',(129.930621956132,51.0567546150476,201.488444588001));
#87310=CARTESIAN_POINT('Ctrl Pts',(129.86081854997,51.0693171758067,201.449358588045));
#87311=CARTESIAN_POINT('Ctrl Pts',(129.787469755343,51.0821772615741,201.416548723103));
#87312=CARTESIAN_POINT('Ctrl Pts',(129.78103100378,51.0833061539812,201.413668586214));
#87313=CARTESIAN_POINT('Ctrl Pts',(129.774564952339,51.0844373354015,201.410836785548));
#87314=CARTESIAN_POINT('Ctrl Pts',(129.768071595154,51.0855707469888,201.408053427281));
#87315=CARTESIAN_POINT('Ctrl Pts',(129.766264252068,51.0858862176364,201.407278715036));
#87316=CARTESIAN_POINT('Ctrl Pts',(129.764454981671,51.0862018282248,201.4065078337));
#87317=CARTESIAN_POINT('Ctrl Pts',(129.762643778742,51.0865175784956,201.405740780295));
#87318=CARTESIAN_POINT('Ctrl Pts',(129.714272775736,51.0949501826254,201.385255421096));
#87319=CARTESIAN_POINT('Ctrl Pts',(129.664883221933,51.1034125934789,201.367706325503));
#87320=CARTESIAN_POINT('Ctrl Pts',(129.614679793085,51.1118624165726,201.35310702986));
#87321=CARTESIAN_POINT('Ctrl Pts',(129.564594471029,51.1202923609145,201.338542079997));
#87322=CARTESIAN_POINT('Ctrl Pts',(129.51369823572,51.1287099459605,201.326912907498));
#87323=CARTESIAN_POINT('Ctrl Pts',(129.46218278672,51.1370724391893,201.318283262024));
#87324=CARTESIAN_POINT('Ctrl Pts',(129.41177367354,51.1452553411305,201.309838945148));
#87325=CARTESIAN_POINT('Ctrl Pts',(129.360770860779,51.1533856413995,201.304266683087));
#87326=CARTESIAN_POINT('Ctrl Pts',(129.309355143587,51.1614203559357,201.301675514577));
#87327=CARTESIAN_POINT('Ctrl Pts',(129.287267165588,51.1648720358419,201.300562359376));
#87328=CARTESIAN_POINT('Ctrl Pts',(129.265103069234,51.1683060247023,201.300000002005));
#87329=CARTESIAN_POINT('Ctrl Pts',(129.242877811887,51.1717186376762,201.3));
#87330=CARTESIAN_POINT('',(130.606204737894,50.9250708612662,226.3));
#87331=CARTESIAN_POINT('',(130.606204737894,50.9250708612662,227.));
#87332=CARTESIAN_POINT('Origin',(125.29348064571,25.4505574462982,226.3));
#87333=CARTESIAN_POINT('Origin',(125.29348064571,25.4505574462982,226.3));
#87334=CARTESIAN_POINT('',(130.749115378049,50.178482477843,227.));
#87335=CARTESIAN_POINT('Ctrl Pts',(130.606204737894,50.9250708612662,226.3));
#87336=CARTESIAN_POINT('Ctrl Pts',(130.606204737894,50.9250708612662,226.327283375706));
#87337=CARTESIAN_POINT('Ctrl Pts',(130.606521196537,50.9233280888925,226.354433744169));
#87338=CARTESIAN_POINT('Ctrl Pts',(130.607134490211,50.9199608865016,226.381298026589));
#87339=CARTESIAN_POINT('Ctrl Pts',(130.607772970913,50.9164553982781,226.409265583844));
#87340=CARTESIAN_POINT('Ctrl Pts',(130.608733160752,50.9111893063652,226.436924230535));
#87341=CARTESIAN_POINT('Ctrl Pts',(130.610002771111,50.9042414687086,226.464113586868));
#87342=CARTESIAN_POINT('Ctrl Pts',(130.610977695644,50.8989062748601,226.484992095236));
#87343=CARTESIAN_POINT('Ctrl Pts',(130.612135280192,50.8925782669583,226.505594295321));
#87344=CARTESIAN_POINT('Ctrl Pts',(130.613473681732,50.8852727968182,226.525845500815));
#87345=CARTESIAN_POINT('Ctrl Pts',(130.614470475815,50.8798319413003,226.540927881695));
#87346=CARTESIAN_POINT('Ctrl Pts',(130.615567141013,50.8738512343175,226.555805651625));
#87347=CARTESIAN_POINT('Ctrl Pts',(130.616760678055,50.8673492154425,226.570416316965));
#87348=CARTESIAN_POINT('Ctrl Pts',(130.618997538772,50.8551634934195,226.597798813054));
#87349=CARTESIAN_POINT('Ctrl Pts',(130.621587650642,50.8410803822523,226.624424058888));
#87350=CARTESIAN_POINT('Ctrl Pts',(130.624488519249,50.8253628624445,226.649987233896));
#87351=CARTESIAN_POINT('Ctrl Pts',(130.625554698216,50.8195860792457,226.659382667889));
#87352=CARTESIAN_POINT('Ctrl Pts',(130.62666277844,50.8135889080171,226.668634944449));
#87353=CARTESIAN_POINT('Ctrl Pts',(130.62781040101,50.8073856540369,226.677730163301));
#87354=CARTESIAN_POINT('Ctrl Pts',(130.631954405204,50.7849860331286,226.710572515881));
#87355=CARTESIAN_POINT('Ctrl Pts',(130.636632724928,50.7597985255623,226.741511971335));
#87356=CARTESIAN_POINT('Ctrl Pts',(130.641763810671,50.7323297966851,226.770042486735));
#87357=CARTESIAN_POINT('Ctrl Pts',(130.643470156645,50.7231950526413,226.779530328593));
#87358=CARTESIAN_POINT('Ctrl Pts',(130.645226560496,50.7138080496165,226.788752180359));
#87359=CARTESIAN_POINT('Ctrl Pts',(130.647029992641,50.7041874189799,226.797690746489));
#87360=CARTESIAN_POINT('Ctrl Pts',(130.647571851327,50.7012968071615,226.800376425409));
#87361=CARTESIAN_POINT('Ctrl Pts',(130.648118782333,50.6983807626333,226.803040587555));
#87362=CARTESIAN_POINT('Ctrl Pts',(130.64867056125,50.6954405413581,226.805682465323));
#87363=CARTESIAN_POINT('Ctrl Pts',(130.653661469249,50.6688458792137,226.829578573851));
#87364=CARTESIAN_POINT('Ctrl Pts',(130.659056798759,50.6402484831699,226.851675168384));
#87365=CARTESIAN_POINT('Ctrl Pts',(130.664705914535,50.6104938033034,226.871445497822));
#87366=CARTESIAN_POINT('Ctrl Pts',(130.665956597121,50.6039062838658,226.875822538006));
#87367=CARTESIAN_POINT('Ctrl Pts',(130.667219752626,50.5972618524138,226.880085629563));
#87368=CARTESIAN_POINT('Ctrl Pts',(130.668493801137,50.5905693773403,226.884229173985));
#87369=CARTESIAN_POINT('Ctrl Pts',(130.676235766143,50.5499014534891,226.909408102141));
#87370=CARTESIAN_POINT('Ctrl Pts',(130.684436648208,50.5071526195933,226.930546414023));
#87371=CARTESIAN_POINT('Ctrl Pts',(130.693116168835,50.4623179858518,226.947750095497));
#87372=CARTESIAN_POINT('Ctrl Pts',(130.693628527943,50.4596713612343,226.9487656427));
#87373=CARTESIAN_POINT('Ctrl Pts',(130.694142145785,50.4570196470152,226.949766385399));
#87374=CARTESIAN_POINT('Ctrl Pts',(130.694656993051,50.4543629986236,226.950752326852));
#87375=CARTESIAN_POINT('Ctrl Pts',(130.700229539504,50.4256082638754,226.961423850053));
#87376=CARTESIAN_POINT('Ctrl Pts',(130.705926064316,50.3963849653276,226.970325357774));
#87377=CARTESIAN_POINT('Ctrl Pts',(130.711726791672,50.3668025158223,226.977508176548));
#87378=CARTESIAN_POINT('Ctrl Pts',(130.717754981156,50.3360600588667,226.984972652975));
#87379=CARTESIAN_POINT('Ctrl Pts',(130.723895866631,50.3049288077942,226.990581437737));
#87380=CARTESIAN_POINT('Ctrl Pts',(130.730132469486,50.2735099108083,226.994338233717));
#87381=CARTESIAN_POINT('Ctrl Pts',(130.73636907234,50.2420910138223,226.998095029697));
#87382=CARTESIAN_POINT('Ctrl Pts',(130.742701591324,50.2103833747577,227.));
#87383=CARTESIAN_POINT('Ctrl Pts',(130.749115378049,50.178482477843,227.));
#87384=CARTESIAN_POINT('',(119.837845913371,50.178482477843,227.));
#87385=CARTESIAN_POINT('Origin',(125.29348064571,25.4505574462982,227.));
#87386=CARTESIAN_POINT('Ctrl Pts',(119.980756553526,50.9250708612662,226.3));
#87387=CARTESIAN_POINT('Ctrl Pts',(119.980756553526,50.9250708612662,226.330760525798));
#87388=CARTESIAN_POINT('Ctrl Pts',(119.980359541554,50.9228826666961,226.361320229286));
#87389=CARTESIAN_POINT('Ctrl Pts',(119.979587330222,50.918642522777,226.39147985655));
#87390=CARTESIAN_POINT('Ctrl Pts',(119.978786079618,50.9142429267913,226.422773646943));
#87391=CARTESIAN_POINT('Ctrl Pts',(119.97758088991,50.9076341444555,226.453637771802));
#87392=CARTESIAN_POINT('Ctrl Pts',(119.97598628326,50.898913553164,226.48386189553));
#87393=CARTESIAN_POINT('Ctrl Pts',(119.974422187669,50.8903598208746,226.513507713618));
#87394=CARTESIAN_POINT('Ctrl Pts',(119.972483366779,50.8797738865834,226.542538859668));
#87395=CARTESIAN_POINT('Ctrl Pts',(119.970174805301,50.8671999665045,226.570752225921));
#87396=CARTESIAN_POINT('Ctrl Pts',(119.969982103564,50.8661503881186,226.573107270269));
#87397=CARTESIAN_POINT('Ctrl Pts',(119.969786983124,50.8650878548648,226.575455559618));
#87398=CARTESIAN_POINT('Ctrl Pts',(119.96958943686,50.8640123484877,226.577797141023));
#87399=CARTESIAN_POINT('Ctrl Pts',(119.966196766862,50.8455415451015,226.618011583879));
#87400=CARTESIAN_POINT('Ctrl Pts',(119.962106793885,50.8233369857853,226.656038781937));
#87401=CARTESIAN_POINT('Ctrl Pts',(119.957332733188,50.7975628028764,226.691909536739));
#87402=CARTESIAN_POINT('Ctrl Pts',(119.953498572278,50.7768629477846,226.720718187204));
#87403=CARTESIAN_POINT('Ctrl Pts',(119.949209307764,50.7537894010272,226.748100234994));
#87404=CARTESIAN_POINT('Ctrl Pts',(119.944585796445,50.7290437736179,226.773441873749));
#87405=CARTESIAN_POINT('Ctrl Pts',(119.943048816176,50.720817657481,226.781866120184));
#87406=CARTESIAN_POINT('Ctrl Pts',(119.941474871115,50.7124065814287,226.790065256546));
#87407=CARTESIAN_POINT('Ctrl Pts',(119.939868307432,50.7038357163588,226.798017899287));
#87408=CARTESIAN_POINT('Ctrl Pts',(119.939373357799,50.7011952069503,226.800467946955));
#87409=CARTESIAN_POINT('Ctrl Pts',(119.938874561918,50.6985355852531,226.802898076406));
#87410=CARTESIAN_POINT('Ctrl Pts',(119.938372010707,50.6958573802167,226.80530808448));
#87411=CARTESIAN_POINT('Ctrl Pts',(119.933610160355,50.670480440854,226.828143762831));
#87412=CARTESIAN_POINT('Ctrl Pts',(119.928517223032,50.6434770554831,226.849139888348));
#87413=CARTESIAN_POINT('Ctrl Pts',(119.923155669031,50.6152163475391,226.868195456293));
#87414=CARTESIAN_POINT('Ctrl Pts',(119.917432532216,50.5850497395014,226.888536130357));
#87415=CARTESIAN_POINT('Ctrl Pts',(119.911403216501,50.5534497793912,226.906666565703));
#87416=CARTESIAN_POINT('Ctrl Pts',(119.905133396445,50.5208108759897,226.92244047314));
#87417=CARTESIAN_POINT('Ctrl Pts',(119.901430938444,50.5015369306507,226.931755290674));
#87418=CARTESIAN_POINT('Ctrl Pts',(119.897644428727,50.4818997258722,226.94024784624));
#87419=CARTESIAN_POINT('Ctrl Pts',(119.89378614051,50.4619741917207,226.947882574378));
#87420=CARTESIAN_POINT('Ctrl Pts',(119.887076253848,50.4273220174062,226.961160006656));
#87421=CARTESIAN_POINT('Ctrl Pts',(119.8800777526,50.391437659274,226.971955518833));
#87422=CARTESIAN_POINT('Ctrl Pts',(119.872890492327,50.3548503848194,226.98021787587));
#87423=CARTESIAN_POINT('Ctrl Pts',(119.865851227239,50.3190164906886,226.988310100059));
#87424=CARTESIAN_POINT('Ctrl Pts',(119.858630540141,50.2825064549341,226.993972516927));
#87425=CARTESIAN_POINT('Ctrl Pts',(119.851320043032,50.245811059138,226.997110112562));
#87426=CARTESIAN_POINT('Ctrl Pts',(119.846855087645,50.2233989984148,226.999026428829));
#87427=CARTESIAN_POINT('Ctrl Pts',(119.842356609805,50.2009177829365,227.));
#87428=CARTESIAN_POINT('Ctrl Pts',(119.837845913371,50.178482477843,227.));
#87429=CARTESIAN_POINT('Origin',(-190.5,58.8,211.4));
#87430=CARTESIAN_POINT('',(-190.,58.8,102.225104347671));
#87431=CARTESIAN_POINT('',(-189.999800857363,58.8,102.333498885934));
#87432=CARTESIAN_POINT('Origin',(-160.5,58.8,102.225104347671));
#87433=CARTESIAN_POINT('',(1.15828019241431E-14,58.8,195.5));
#87434=CARTESIAN_POINT('Ctrl Pts',(-189.999800857363,58.8,102.333498885934));
#87435=CARTESIAN_POINT('Ctrl Pts',(-189.98025109905,58.8,107.654006604893));
#87436=CARTESIAN_POINT('Ctrl Pts',(-189.93589337482,58.7999999999999,112.972770159136));
#87437=CARTESIAN_POINT('Ctrl Pts',(-189.816879937051,58.7999999999999,118.286284921046));
#87438=CARTESIAN_POINT('Ctrl Pts',(-189.757373218167,58.7999999999999,120.943042302001));
#87439=CARTESIAN_POINT('Ctrl Pts',(-189.678761610221,58.7999999999999,123.598456482408));
#87440=CARTESIAN_POINT('Ctrl Pts',(-189.570666695347,58.7999999999999,126.251797790585));
#87441=CARTESIAN_POINT('Ctrl Pts',(-189.462571780473,58.7999999999999,128.905139098762));
#87442=CARTESIAN_POINT('Ctrl Pts',(-189.325139639205,58.8,131.556417805139));
#87443=CARTESIAN_POINT('Ctrl Pts',(-189.143206561331,58.8,134.204567800212));
#87444=CARTESIAN_POINT('Ctrl Pts',(-188.961273483458,58.8,136.852717795285));
#87445=CARTESIAN_POINT('Ctrl Pts',(-188.735101605105,58.8,139.497757508966));
#87446=CARTESIAN_POINT('Ctrl Pts',(-188.441756887885,58.8,142.138074526077));
#87447=CARTESIAN_POINT('Ctrl Pts',(-188.148412170664,58.8,144.778391543189));
#87448=CARTESIAN_POINT('Ctrl Pts',(-187.788398583062,58.8,147.41402129609));
#87449=CARTESIAN_POINT('Ctrl Pts',(-187.325444057625,58.8,150.042413617553));
#87450=CARTESIAN_POINT('Ctrl Pts',(-187.093966794906,58.8,151.356609778285));
#87451=CARTESIAN_POINT('Ctrl Pts',(-186.83650703826,58.8,152.668979197212));
#87452=CARTESIAN_POINT('Ctrl Pts',(-186.546468546693,58.8,153.979058114737));
#87453=CARTESIAN_POINT('Ctrl Pts',(-186.256430055127,58.8,155.289137032263));
#87454=CARTESIAN_POINT('Ctrl Pts',(-185.933727730554,58.8,156.596161198099));
#87455=CARTESIAN_POINT('Ctrl Pts',(-185.574584035801,58.8,157.885628894788));
#87456=CARTESIAN_POINT('Ctrl Pts',(-184.856296646294,58.8,160.464564288164));
#87457=CARTESIAN_POINT('Ctrl Pts',(-183.99092543291,58.8,162.986625821545));
#87458=CARTESIAN_POINT('Ctrl Pts',(-182.913145481925,58.8,165.426553885135));
#87459=CARTESIAN_POINT('Ctrl Pts',(-182.374255506433,58.8,166.646517916931));
#87460=CARTESIAN_POINT('Ctrl Pts',(-181.781931362085,58.8,167.845820210719));
#87461=CARTESIAN_POINT('Ctrl Pts',(-181.12595295987,58.8,169.020508898055));
#87462=CARTESIAN_POINT('Ctrl Pts',(-180.797963758762,58.8,169.607853241724));
#87463=CARTESIAN_POINT('Ctrl Pts',(-180.452895188786,58.8,170.190776016641));
#87464=CARTESIAN_POINT('Ctrl Pts',(-180.094025945826,58.8,170.761526129557));
#87465=CARTESIAN_POINT('Ctrl Pts',(-179.735156702866,58.8,171.332276242472));
#87466=CARTESIAN_POINT('Ctrl Pts',(-179.362497837563,58.7999999999999,171.891096446703));
#87467=CARTESIAN_POINT('Ctrl Pts',(-178.975721840832,58.7999999999999,172.437703402131));
#87468=CARTESIAN_POINT('Ctrl Pts',(-177.428617853909,58.7999999999999,174.624131223845));
#87469=CARTESIAN_POINT('Ctrl Pts',(-175.653687288283,58.8,176.613457906034));
#87470=CARTESIAN_POINT('Ctrl Pts',(-173.645004150579,58.8,178.400556654236));
#87471=CARTESIAN_POINT('Ctrl Pts',(-173.142833366153,58.8,178.847331341286));
#87472=CARTESIAN_POINT('Ctrl Pts',(-172.624619471942,58.8,179.282785482727));
#87473=CARTESIAN_POINT('Ctrl Pts',(-172.095993754087,58.8,179.702765830952));
#87474=CARTESIAN_POINT('Ctrl Pts',(-171.567368036232,58.8,180.122746179177));
#87475=CARTESIAN_POINT('Ctrl Pts',(-171.029630345955,58.7999999999999,180.526399139266));
#87476=CARTESIAN_POINT('Ctrl Pts',(-170.483419960298,58.7999999999999,180.914870206751));
#87477=CARTESIAN_POINT('Ctrl Pts',(-169.390999188983,58.7999999999999,181.691812341722));
#87478=CARTESIAN_POINT('Ctrl Pts',(-168.264719930409,58.8,182.408084773304));
#87479=CARTESIAN_POINT('Ctrl Pts',(-167.109367700984,58.8,183.07226248173));
#87480=CARTESIAN_POINT('Ctrl Pts',(-164.798663242132,58.8,184.400617898584));
#87481=CARTESIAN_POINT('Ctrl Pts',(-162.372251203749,58.8,185.521641414205));
#87482=CARTESIAN_POINT('Ctrl Pts',(-159.861852893949,58.8,186.492173204115));
#87483=CARTESIAN_POINT('Ctrl Pts',(-158.606653739049,58.8,186.97743909907));
#87484=CARTESIAN_POINT('Ctrl Pts',(-157.337498640633,58.7999999999999,187.422033931911));
#87485=CARTESIAN_POINT('Ctrl Pts',(-156.060779329092,58.7999999999999,187.832008793431));
#87486=CARTESIAN_POINT('Ctrl Pts',(-154.784060017551,58.7999999999999,188.241983654951));
#87487=CARTESIAN_POINT('Ctrl Pts',(-153.498376682177,58.7999999999999,188.61784576423));
#87488=CARTESIAN_POINT('Ctrl Pts',(-152.205313605643,58.7999999999999,188.965624137122));
#87489=CARTESIAN_POINT('Ctrl Pts',(-149.619187452575,58.7999999999999,189.661180882907));
#87490=CARTESIAN_POINT('Ctrl Pts',(-147.003773115772,58.7999999999999,190.24528092407));
#87491=CARTESIAN_POINT('Ctrl Pts',(-144.368026627399,58.7999999999999,190.752006600492));
#87492=CARTESIAN_POINT('Ctrl Pts',(-143.050153383213,58.7999999999999,191.005369438703));
#87493=CARTESIAN_POINT('Ctrl Pts',(-141.726406587005,58.8,191.239238184733));
#87494=CARTESIAN_POINT('Ctrl Pts',(-140.40217354554,58.8,191.455987813524));
#87495=CARTESIAN_POINT('Ctrl Pts',(-139.077940504076,58.8,191.672737442316));
#87496=CARTESIAN_POINT('Ctrl Pts',(-137.752328543611,58.7999999999999,191.87255073608));
#87497=CARTESIAN_POINT('Ctrl Pts',(-136.425559458292,58.7999999999999,192.058151843066));
#87498=CARTESIAN_POINT('Ctrl Pts',(-133.772021287655,58.7999999999999,192.429354057037));
#87499=CARTESIAN_POINT('Ctrl Pts',(-131.113885005295,58.8,192.744080755892));
#87500=CARTESIAN_POINT('Ctrl Pts',(-128.45244324479,58.8,193.018208488718));
#87501=CARTESIAN_POINT('Ctrl Pts',(-123.129559723779,58.8,193.56646395437));
#87502=CARTESIAN_POINT('Ctrl Pts',(-117.793666862818,58.8,193.954934442914));
#87503=CARTESIAN_POINT('Ctrl Pts',(-112.450694014707,58.8,194.256446208796));
#87504=CARTESIAN_POINT('Ctrl Pts',(-107.107721166596,58.8,194.557957974678));
#87505=CARTESIAN_POINT('Ctrl Pts',(-101.757516044789,58.8,194.770640584592));
#87506=CARTESIAN_POINT('Ctrl Pts',(-96.4031808681222,58.8,194.932596507142));
#87507=CARTESIAN_POINT('Ctrl Pts',(-91.0488456914553,58.8,195.094552429692));
#87508=CARTESIAN_POINT('Ctrl Pts',(-85.6929541823069,58.8,195.204966816985));
#87509=CARTESIAN_POINT('Ctrl Pts',(-80.3374898338037,58.8,195.285751221278));
#87510=CARTESIAN_POINT('Ctrl Pts',(-74.9820254853004,58.8,195.366535625571));
#87511=CARTESIAN_POINT('Ctrl Pts',(-69.6263951900152,58.8,195.417356847769));
#87512=CARTESIAN_POINT('Ctrl Pts',(-64.2706727216169,58.8,195.451535386383));
#87513=CARTESIAN_POINT('Ctrl Pts',(-53.5592277848204,58.8,195.519892463612));
#87514=CARTESIAN_POINT('Ctrl Pts',(-42.8474268145233,58.8,195.523964494124));
#87515=CARTESIAN_POINT('Ctrl Pts',(-32.1355782419999,58.8,195.51944151511));
#87516=CARTESIAN_POINT('Ctrl Pts',(-21.4237296694766,58.8,195.514918536095));
#87517=CARTESIAN_POINT('Ctrl Pts',(-10.7118235226534,58.8,195.500000000149));
#87518=CARTESIAN_POINT('Ctrl Pts',(1.15828019241431E-14,58.8,195.5));
#87519=CARTESIAN_POINT('',(189.999800857363,58.8,102.333498885935));
#87520=CARTESIAN_POINT('Ctrl Pts',(8.88178419700125E-15,58.8,195.5));
#87521=CARTESIAN_POINT('Ctrl Pts',(10.6608822212759,58.8,195.500000000296));
#87522=CARTESIAN_POINT('Ctrl Pts',(21.3218250169713,58.8,195.514760894626));
#87523=CARTESIAN_POINT('Ctrl Pts',(31.9827261779419,58.8,195.51937615705));
#87524=CARTESIAN_POINT('Ctrl Pts',(42.6436273389126,58.8,195.523991419473));
#87525=CARTESIAN_POINT('Ctrl Pts',(53.3044940402517,58.8,195.520209490269));
#87526=CARTESIAN_POINT('Ctrl Pts',(63.9651023694078,58.8,195.453466915477));
#87527=CARTESIAN_POINT('Ctrl Pts',(69.2954065339858,58.8,195.420095628081));
#87528=CARTESIAN_POINT('Ctrl Pts',(74.6256438146957,58.8,195.370425946996));
#87529=CARTESIAN_POINT('Ctrl Pts',(79.9557608635996,58.8,195.291457941204));
#87530=CARTESIAN_POINT('Ctrl Pts',(85.2858779125034,58.8,195.212489935411));
#87531=CARTESIAN_POINT('Ctrl Pts',(90.617169770423,58.8,195.10450581883));
#87532=CARTESIAN_POINT('Ctrl Pts',(95.9430357498042,58.8,194.946385956025));
#87533=CARTESIAN_POINT('Ctrl Pts',(101.268901729185,58.8,194.78826609322));
#87534=CARTESIAN_POINT('Ctrl Pts',(106.58996338726,58.8,194.580711495765));
#87535=CARTESIAN_POINT('Ctrl Pts',(111.902657189983,58.8,194.287054682287));
#87536=CARTESIAN_POINT('Ctrl Pts',(117.215350992707,58.8,193.993397868808));
#87537=CARTESIAN_POINT('Ctrl Pts',(122.519844509403,58.8,193.615363067472));
#87538=CARTESIAN_POINT('Ctrl Pts',(127.809401981597,58.8,193.083641750981));
#87539=CARTESIAN_POINT('Ctrl Pts',(130.454180717694,58.8,192.817781092736));
#87540=CARTESIAN_POINT('Ctrl Pts',(133.095165732892,58.8,192.512884413637));
#87541=CARTESIAN_POINT('Ctrl Pts',(135.730906077612,58.8,192.154021965476));
#87542=CARTESIAN_POINT('Ctrl Pts',(138.366646422331,58.8,191.795159517316));
#87543=CARTESIAN_POINT('Ctrl Pts',(140.997169684096,58.8000000000001,191.382615165556));
#87544=CARTESIAN_POINT('Ctrl Pts',(143.620258990582,58.8000000000001,190.893578093325));
#87545=CARTESIAN_POINT('Ctrl Pts',(146.243348297067,58.8000000000001,190.404541021094));
#87546=CARTESIAN_POINT('Ctrl Pts',(148.859060109816,58.8,189.839592196665));
#87547=CARTESIAN_POINT('Ctrl Pts',(151.463804706251,58.8,189.161794669432));
#87548=CARTESIAN_POINT('Ctrl Pts',(152.766177004469,58.8,188.822895905815));
#87549=CARTESIAN_POINT('Ctrl Pts',(154.063722484329,58.8,188.455855238128));
#87550=CARTESIAN_POINT('Ctrl Pts',(155.345610999807,58.8,188.057834736658));
#87551=CARTESIAN_POINT('Ctrl Pts',(156.627499515284,58.8,187.659814235188));
#87552=CARTESIAN_POINT('Ctrl Pts',(157.896230834775,58.8,187.230200792086));
#87553=CARTESIAN_POINT('Ctrl Pts',(159.149225485557,58.8,186.762800600376));
#87554=CARTESIAN_POINT('Ctrl Pts',(161.655214787121,58.8,185.828000216956));
#87555=CARTESIAN_POINT('Ctrl Pts',(164.099002476109,58.8,184.743841876054));
#87556=CARTESIAN_POINT('Ctrl Pts',(166.452402824297,58.8,183.442646258576));
#87557=CARTESIAN_POINT('Ctrl Pts',(167.040752911344,58.8,183.117347354207));
#87558=CARTESIAN_POINT('Ctrl Pts',(167.623396019085,58.8,182.778344901958));
#87559=CARTESIAN_POINT('Ctrl Pts',(168.19976750543,58.8,182.42428308841));
#87560=CARTESIAN_POINT('Ctrl Pts',(168.776138991775,58.8,182.070221274862));
#87561=CARTESIAN_POINT('Ctrl Pts',(169.345685170054,58.8,181.701285645968));
#87562=CARTESIAN_POINT('Ctrl Pts',(169.901687100616,58.8,181.320740058355));
#87563=CARTESIAN_POINT('Ctrl Pts',(171.013690961741,58.8,180.559648883128));
#87564=CARTESIAN_POINT('Ctrl Pts',(172.078138682642,58.8,179.748063563893));
#87565=CARTESIAN_POINT('Ctrl Pts',(173.091864655936,58.8,178.882622922976));
#87566=CARTESIAN_POINT('Ctrl Pts',(175.119316602522,58.8,177.151741641143));
#87567=CARTESIAN_POINT('Ctrl Pts',(176.942436203403,58.8,175.203904423765));
#87568=CARTESIAN_POINT('Ctrl Pts',(178.549784955921,58.8,173.026966100971));
#87569=CARTESIAN_POINT('Ctrl Pts',(178.951622144051,58.8,172.482731520272));
#87570=CARTESIAN_POINT('Ctrl Pts',(179.340199864675,58.8,171.923832776685));
#87571=CARTESIAN_POINT('Ctrl Pts',(179.710556657438,58.8,171.358822781541));
#87572=CARTESIAN_POINT('Ctrl Pts',(180.080913450202,58.8,170.793812786397));
#87573=CARTESIAN_POINT('Ctrl Pts',(180.434508985294,58.8,170.220810507793));
#87574=CARTESIAN_POINT('Ctrl Pts',(180.772486437532,58.8,169.640361046698));
#87575=CARTESIAN_POINT('Ctrl Pts',(181.44844134201,58.8,168.47946212451));
#87576=CARTESIAN_POINT('Ctrl Pts',(182.061965606304,58.8,167.288794351923));
#87577=CARTESIAN_POINT('Ctrl Pts',(182.621837291323,58.8,166.072543378534));
#87578=CARTESIAN_POINT('Ctrl Pts',(183.181708976343,58.8,164.856292405145));
#87579=CARTESIAN_POINT('Ctrl Pts',(183.68794311769,58.8,163.614465400397));
#87580=CARTESIAN_POINT('Ctrl Pts',(184.148570796702,58.8,162.350891830973));
#87581=CARTESIAN_POINT('Ctrl Pts',(184.609198475714,58.8,161.087318261549));
#87582=CARTESIAN_POINT('Ctrl Pts',(185.025180861451,58.8,159.798417119322));
#87583=CARTESIAN_POINT('Ctrl Pts',(185.399766833237,58.8,158.501874284172));
#87584=CARTESIAN_POINT('Ctrl Pts',(186.148938776808,58.8,155.908788613871));
#87585=CARTESIAN_POINT('Ctrl Pts',(186.736003435447,58.8,153.285009470254));
#87586=CARTESIAN_POINT('Ctrl Pts',(187.218096335368,58.8,150.641354922102));
#87587=CARTESIAN_POINT('Ctrl Pts',(187.70018923529,58.8,147.99770037395));
#87588=CARTESIAN_POINT('Ctrl Pts',(188.076546005177,58.8,145.334025694806));
#87589=CARTESIAN_POINT('Ctrl Pts',(188.383194380381,58.8,142.657152393827));
#87590=CARTESIAN_POINT('Ctrl Pts',(188.689842755585,58.8,139.980279092848));
#87591=CARTESIAN_POINT('Ctrl Pts',(188.925895877108,58.8,137.293871517216));
#87592=CARTESIAN_POINT('Ctrl Pts',(189.115096080232,58.8,134.608587766533));
#87593=CARTESIAN_POINT('Ctrl Pts',(189.304296283357,58.8,131.923304015851));
#87594=CARTESIAN_POINT('Ctrl Pts',(189.446683812067,58.8,129.236274241946));
#87595=CARTESIAN_POINT('Ctrl Pts',(189.558470527221,58.8,126.548103116225));
#87596=CARTESIAN_POINT('Ctrl Pts',(189.670257242375,58.8,123.859931990504));
#87597=CARTESIAN_POINT('Ctrl Pts',(189.751276588566,58.8,121.170613300767));
#87598=CARTESIAN_POINT('Ctrl Pts',(189.812493834118,58.8,118.480556030551));
#87599=CARTESIAN_POINT('Ctrl Pts',(189.934928325222,58.8,113.100441490117));
#87600=CARTESIAN_POINT('Ctrl Pts',(189.980018010671,58.8,107.717442136363));
#87601=CARTESIAN_POINT('Ctrl Pts',(189.999800857363,58.8,102.333498885935));
#87602=CARTESIAN_POINT('',(190.,58.8,102.225104347672));
#87603=CARTESIAN_POINT('Origin',(160.5,58.8,102.225104347672));
#87604=CARTESIAN_POINT('',(190.,58.8,40.5));
#87605=CARTESIAN_POINT('',(190.,58.8,211.4));
#87606=CARTESIAN_POINT('',(-190.,58.8,40.5));
#87607=CARTESIAN_POINT('',(-190.5,58.8,40.5));
#87608=CARTESIAN_POINT('',(-190.,58.8,211.4));
#87609=CARTESIAN_POINT('Origin',(-160.5,51.6013867006571,102.225104347671));
#87610=CARTESIAN_POINT('',(-190.499797482064,58.2999999999999,102.335336081498));
#87611=CARTESIAN_POINT('',(-190.499797482064,55.3,102.335336081498));
#87612=CARTESIAN_POINT('',(-190.499797482064,58.8,102.335336081498));
#87613=CARTESIAN_POINT('',(-190.5,58.2999999999999,102.225104347671));
#87614=CARTESIAN_POINT('Origin',(-160.5,58.3,102.225104347671));
#87615=CARTESIAN_POINT('',(-190.5,55.3,102.225104347671));
#87616=CARTESIAN_POINT('',(-190.5,58.8,102.225104347671));
#87617=CARTESIAN_POINT('Origin',(-160.5,55.3,102.225104347671));
#87618=CARTESIAN_POINT('Ctrl Pts',(-190.499797482064,55.2999999999999,102.335336081498));
#87619=CARTESIAN_POINT('Ctrl Pts',(-190.499797482064,58.9,102.335336081498));
#87620=CARTESIAN_POINT('Ctrl Pts',(-190.141509581597,55.2999999999999,199.844139409912));
#87621=CARTESIAN_POINT('Ctrl Pts',(-190.141509581597,58.9,199.844139409912));
#87622=CARTESIAN_POINT('Ctrl Pts',(-180.969631132311,55.2999999999999,196.));
#87623=CARTESIAN_POINT('Ctrl Pts',(-180.969631132311,58.9,196.));
#87624=CARTESIAN_POINT('Ctrl Pts',(1.20290037631083E-14,55.3,196.));
#87625=CARTESIAN_POINT('Ctrl Pts',(1.20290037631083E-14,58.9,196.));
#87626=CARTESIAN_POINT('',(1.20290037631083E-14,55.3,196.));
#87627=CARTESIAN_POINT('',(1.16465450439953E-14,58.3,196.));
#87628=CARTESIAN_POINT('',(3.34339434094657E-14,-112.6,196.));
#87629=CARTESIAN_POINT('Ctrl Pts',(1.16465450439953E-14,58.3,196.));
#87630=CARTESIAN_POINT('Ctrl Pts',(-10.7117531408873,58.3,196.));
#87631=CARTESIAN_POINT('Ctrl Pts',(-21.4235888453057,58.3000000000004,196.014918521175));
#87632=CARTESIAN_POINT('Ctrl Pts',(-32.1353671216415,58.3000000000002,196.019441470522));
#87633=CARTESIAN_POINT('Ctrl Pts',(-37.9435658896329,58.3000000000001,196.021893928756));
#87634=CARTESIAN_POINT('Ctrl Pts',(-43.7517506038881,58.3000000000219,196.02182007439));
#87635=CARTESIAN_POINT('Ctrl Pts',(-49.5598722236178,58.3000000000338,196.010342241869));
#87636=CARTESIAN_POINT('Ctrl Pts',(-54.4645909813284,58.3000000000439,196.000649686488));
#87637=CARTESIAN_POINT('Ctrl Pts',(-59.3692646648713,58.300000000047,195.982824814488));
#87638=CARTESIAN_POINT('Ctrl Pts',(-64.2738634995991,58.3000000000241,195.951525205213));
#87639=CARTESIAN_POINT('Ctrl Pts',(-69.6310359294076,58.299999999999,195.917337413403));
#87640=CARTESIAN_POINT('Ctrl Pts',(-74.9881325496685,58.3000000000011,195.866500385808));
#87641=CARTESIAN_POINT('Ctrl Pts',(-80.3450312167436,58.3000000000005,195.785694345575));
#87642=CARTESIAN_POINT('Ctrl Pts',(-82.3276213464493,58.3000000000003,195.755788000926));
#87643=CARTESIAN_POINT('Ctrl Pts',(-84.3102735136791,58.2999999999996,195.721822619659));
#87644=CARTESIAN_POINT('Ctrl Pts',(-86.2928865664701,58.2999999999997,195.68268720698));
#87645=CARTESIAN_POINT('Ctrl Pts',(-89.6683095657664,58.3,195.616058687683));
#87646=CARTESIAN_POINT('Ctrl Pts',(-93.0436168853548,58.3000000000031,195.534444015978));
#87647=CARTESIAN_POINT('Ctrl Pts',(-96.4182977668297,58.3000000000172,195.432367934214));
#87648=CARTESIAN_POINT('Ctrl Pts',(-99.0028780309804,58.300000000028,195.354190519628));
#87649=CARTESIAN_POINT('Ctrl Pts',(-101.58649661917,58.3000000000233,195.264202002625));
#87650=CARTESIAN_POINT('Ctrl Pts',(-104.168805586391,58.3000000000169,195.158122276966));
#87651=CARTESIAN_POINT('Ctrl Pts',(-106.940478976983,58.30000000001,195.044263572752));
#87652=CARTESIAN_POINT('Ctrl Pts',(-109.710642796453,58.3,194.911866797889));
#87653=CARTESIAN_POINT('Ctrl Pts',(-112.478864925773,58.3,194.755651977743));
#87654=CARTESIAN_POINT('Ctrl Pts',(-114.594746753345,58.3,194.636249674133));
#87655=CARTESIAN_POINT('Ctrl Pts',(-116.709518796986,58.3000000000003,194.50322857681));
#87656=CARTESIAN_POINT('Ctrl Pts',(-118.822815220673,58.3000000000008,194.352073391081));
#87657=CARTESIAN_POINT('Ctrl Pts',(-121.558136194221,58.3000000000013,194.156427411107));
#87658=CARTESIAN_POINT('Ctrl Pts',(-124.290983473982,58.3000000000019,193.930399062793));
#87659=CARTESIAN_POINT('Ctrl Pts',(-127.020560439236,58.3000000000014,193.664236652735));
#87660=CARTESIAN_POINT('Ctrl Pts',(-127.515039874691,58.3000000000013,193.61601971658));
#87661=CARTESIAN_POINT('Ctrl Pts',(-128.009411994897,58.3000000000012,193.566485817347));
#87662=CARTESIAN_POINT('Ctrl Pts',(-128.503672075522,58.300000000001,193.515577171767));
#87663=CARTESIAN_POINT('Ctrl Pts',(-130.44029839942,58.3000000000004,193.316105219635));
#87664=CARTESIAN_POINT('Ctrl Pts',(-132.375178704953,58.3000000000097,193.09517822546));
#87665=CARTESIAN_POINT('Ctrl Pts',(-134.307814874518,58.3000000000101,192.846714080737));
#87666=CARTESIAN_POINT('Ctrl Pts',(-135.037148072975,58.3000000000103,192.752949329654));
#87667=CARTESIAN_POINT('Ctrl Pts',(-135.766161858712,58.3000000000092,192.655263232269));
#87668=CARTESIAN_POINT('Ctrl Pts',(-136.494829730514,58.3000000000057,192.553330224408));
#87669=CARTESIAN_POINT('Ctrl Pts',(-136.887919456177,58.3000000000039,192.498341086494));
#87670=CARTESIAN_POINT('Ctrl Pts',(-137.280910057353,58.3000000000028,192.442107471789));
#87671=CARTESIAN_POINT('Ctrl Pts',(-137.673799736929,58.3000000000017,192.384558364539));
#87672=CARTESIAN_POINT('Ctrl Pts',(-138.610834557934,58.2999999999991,192.247304778573));
#87673=CARTESIAN_POINT('Ctrl Pts',(-139.547276794965,58.299999999998,192.10257023963));
#87674=CARTESIAN_POINT('Ctrl Pts',(-140.482938496475,58.3000000000027,191.949421722643));
#87675=CARTESIAN_POINT('Ctrl Pts',(-140.735750537704,58.300000000004,191.908041607235));
#87676=CARTESIAN_POINT('Ctrl Pts',(-140.988534787172,58.3000000000047,191.866041232622));
#87677=CARTESIAN_POINT('Ctrl Pts',(-141.241276754389,58.300000000005,191.823400409433));
#87678=CARTESIAN_POINT('Ctrl Pts',(-142.316874391201,58.3000000000062,191.641933242905));
#87679=CARTESIAN_POINT('Ctrl Pts',(-143.391615355279,58.3000000000001,191.448879234469));
#87680=CARTESIAN_POINT('Ctrl Pts',(-144.462423620222,58.3000000000008,191.243014958559));
#87681=CARTESIAN_POINT('Ctrl Pts',(-144.849418251539,58.300000000001,191.16861473943));
#87682=CARTESIAN_POINT('Ctrl Pts',(-145.235966544853,58.3000000000006,191.092555291249));
#87683=CARTESIAN_POINT('Ctrl Pts',(-145.622053820955,58.3000000000003,191.014726875239));
#87684=CARTESIAN_POINT('Ctrl Pts',(-147.026899875961,58.2999999999989,190.731534576587));
#87685=CARTESIAN_POINT('Ctrl Pts',(-148.425594601788,58.2999999999958,190.424926449121));
#87686=CARTESIAN_POINT('Ctrl Pts',(-149.816784842427,58.2999999999984,190.089768387871));
#87687=CARTESIAN_POINT('Ctrl Pts',(-150.659099143544,58.2999999999999,189.886842562288));
#87688=CARTESIAN_POINT('Ctrl Pts',(-151.498662614194,58.3000000000036,189.673451611131));
#87689=CARTESIAN_POINT('Ctrl Pts',(-152.33517708753,58.3000000000109,189.448465183433));
#87690=CARTESIAN_POINT('Ctrl Pts',(-152.632968472974,58.3000000000135,189.368372104178));
#87691=CARTESIAN_POINT('Ctrl Pts',(-152.930371233519,58.3000000000145,189.286797584502));
#87692=CARTESIAN_POINT('Ctrl Pts',(-153.227374012079,58.3000000000153,189.203666691527));
#87693=CARTESIAN_POINT('Ctrl Pts',(-154.162302092042,58.300000000018,188.941980903497));
#87694=CARTESIAN_POINT('Ctrl Pts',(-155.093230771767,58.3000000000155,188.664878377644));
#87695=CARTESIAN_POINT('Ctrl Pts',(-156.019362355789,58.3000000000071,188.370172325877));
#87696=CARTESIAN_POINT('Ctrl Pts',(-156.084148129711,58.3000000000066,188.349556724409));
#87697=CARTESIAN_POINT('Ctrl Pts',(-156.148910434322,58.3000000000059,188.328855002121));
#87698=CARTESIAN_POINT('Ctrl Pts',(-156.213648998875,58.3000000000053,188.308066420174));
#87699=CARTESIAN_POINT('Ctrl Pts',(-156.416564742649,58.3000000000033,188.242906949971));
#87700=CARTESIAN_POINT('Ctrl Pts',(-156.619277404117,58.300000000003,188.176883122836));
#87701=CARTESIAN_POINT('Ctrl Pts',(-156.821789346548,58.300000000003,188.109962018534));
#87702=CARTESIAN_POINT('Ctrl Pts',(-157.674439750132,58.3000000000032,187.82819934367));
#87703=CARTESIAN_POINT('Ctrl Pts',(-158.523442517442,58.3000000000126,187.530554246495));
#87704=CARTESIAN_POINT('Ctrl Pts',(-159.366711643314,58.3000000000119,187.215315791802));
#87705=CARTESIAN_POINT('Ctrl Pts',(-159.592281256958,58.3000000000117,187.130991328533));
#87706=CARTESIAN_POINT('Ctrl Pts',(-159.817440715442,58.3000000000108,187.045408267945));
#87707=CARTESIAN_POINT('Ctrl Pts',(-160.042150350673,58.3000000000089,186.958534466439));
#87708=CARTESIAN_POINT('Ctrl Pts',(-160.341043439003,58.3000000000062,186.842980993174));
#87709=CARTESIAN_POINT('Ctrl Pts',(-160.638745189105,58.3000000000063,186.725316023782));
#87710=CARTESIAN_POINT('Ctrl Pts',(-160.93521712623,58.3000000000063,186.605440004865));
#87711=CARTESIAN_POINT('Ctrl Pts',(-162.043912968536,58.3000000000061,186.157147849276));
#87712=CARTESIAN_POINT('Ctrl Pts',(-163.135358586009,58.3000000000134,185.67794905054));
#87713=CARTESIAN_POINT('Ctrl Pts',(-164.206821638704,58.3000000000175,185.16295321028));
#87714=CARTESIAN_POINT('Ctrl Pts',(-165.21381224214,58.3000000000213,184.678945879701));
#87715=CARTESIAN_POINT('Ctrl Pts',(-166.203152864415,58.3000000000223,184.163320138608));
#87716=CARTESIAN_POINT('Ctrl Pts',(-167.172600014669,58.3000000000118,183.612061847702));
#87717=CARTESIAN_POINT('Ctrl Pts',(-167.234668748967,58.3000000000112,183.576767603576));
#87718=CARTESIAN_POINT('Ctrl Pts',(-167.296655944745,58.3000000000105,183.541327310698));
#87719=CARTESIAN_POINT('Ctrl Pts',(-167.358561016714,58.3000000000097,183.505739922036));
#87720=CARTESIAN_POINT('Ctrl Pts',(-168.394805402409,58.2999999999968,182.910033778262));
#87721=CARTESIAN_POINT('Ctrl Pts',(-169.407907923029,58.3000000000085,182.272891065632));
#87722=CARTESIAN_POINT('Ctrl Pts',(-170.394542881228,58.3000000000045,181.588329914564));
#87723=CARTESIAN_POINT('Ctrl Pts',(-170.521203484904,58.300000000004,181.500448446422));
#87724=CARTESIAN_POINT('Ctrl Pts',(-170.647427870475,58.3000000000033,181.411785539936));
#87725=CARTESIAN_POINT('Ctrl Pts',(-170.77320899952,58.3000000000023,181.322328563753));
#87726=CARTESIAN_POINT('Ctrl Pts',(-170.892813072123,58.3000000000014,181.237264780691));
#87727=CARTESIAN_POINT('Ctrl Pts',(-171.012017677299,58.3000000000012,181.151481007302));
#87728=CARTESIAN_POINT('Ctrl Pts',(-171.130802553357,58.300000000001,181.064975844131));
#87729=CARTESIAN_POINT('Ctrl Pts',(-171.508826193717,58.3000000000003,180.789679882414));
#87730=CARTESIAN_POINT('Ctrl Pts',(-171.882642934083,58.3000000000006,180.507051767321));
#87731=CARTESIAN_POINT('Ctrl Pts',(-172.252308609757,58.3000000000003,180.216507805986));
#87732=CARTESIAN_POINT('Ctrl Pts',(-172.303960387306,58.3000000000002,180.175911361559));
#87733=CARTESIAN_POINT('Ctrl Pts',(-172.355531082787,58.3000000000002,180.135160300748));
#87734=CARTESIAN_POINT('Ctrl Pts',(-172.407020808966,58.3000000000001,180.094252958564));
#87735=CARTESIAN_POINT('Ctrl Pts',(-172.455054775942,58.3,180.056091133491));
#87736=CARTESIAN_POINT('Ctrl Pts',(-172.503007691249,58.3,180.017800246934));
#87737=CARTESIAN_POINT('Ctrl Pts',(-172.550875975171,58.3,179.979382822756));
#87738=CARTESIAN_POINT('Ctrl Pts',(-172.597530076584,58.3,179.94193985934));
#87739=CARTESIAN_POINT('Ctrl Pts',(-172.644097658298,58.3,179.904381602751));
#87740=CARTESIAN_POINT('Ctrl Pts',(-172.690571407457,58.3,179.866713790957));
#87741=CARTESIAN_POINT('Ctrl Pts',(-173.036090106872,58.3000000000001,179.586664654043));
#87742=CARTESIAN_POINT('Ctrl Pts',(-173.37649834377,58.3000000000002,179.300504243075));
#87743=CARTESIAN_POINT('Ctrl Pts',(-173.710509907641,58.3000000000002,179.00917403755));
#87744=CARTESIAN_POINT('Ctrl Pts',(-173.799924383646,58.3000000000003,178.93118530755));
#87745=CARTESIAN_POINT('Ctrl Pts',(-173.888880292515,58.3000000000003,178.85282585907));
#87746=CARTESIAN_POINT('Ctrl Pts',(-173.977352529315,58.3000000000003,178.77411328332));
#87747=CARTESIAN_POINT('Ctrl Pts',(-174.08688548205,58.3000000000003,178.676663267914));
#87748=CARTESIAN_POINT('Ctrl Pts',(-174.195746814185,58.3000000000004,178.578606695465));
#87749=CARTESIAN_POINT('Ctrl Pts',(-174.303919105548,58.3000000000005,178.47996099629));
#87750=CARTESIAN_POINT('Ctrl Pts',(-174.958585105133,58.3000000000017,177.882950574851));
#87751=CARTESIAN_POINT('Ctrl Pts',(-175.588161570033,58.3000000000061,177.264237400956));
#87752=CARTESIAN_POINT('Ctrl Pts',(-176.192889049001,58.3000000000103,176.624027669967));
#87753=CARTESIAN_POINT('Ctrl Pts',(-176.801495037263,58.3000000000146,175.979711859004));
#87754=CARTESIAN_POINT('Ctrl Pts',(-177.384932288338,58.3000000000186,175.313622817443));
#87755=CARTESIAN_POINT('Ctrl Pts',(-177.94340602101,58.3000000000187,174.625935950806));
#87756=CARTESIAN_POINT('Ctrl Pts',(-178.443543937974,58.3000000000188,174.010081960041));
#87757=CARTESIAN_POINT('Ctrl Pts',(-178.92366058504,58.3000000000158,173.376906024021));
#87758=CARTESIAN_POINT('Ctrl Pts',(-179.383876297428,58.3000000000071,172.726511192076));
#87759=CARTESIAN_POINT('Ctrl Pts',(-179.775881961455,58.2999999999996,172.172513466414));
#87760=CARTESIAN_POINT('Ctrl Pts',(-180.153586615474,58.2999999999989,171.606136536173));
#87761=CARTESIAN_POINT('Ctrl Pts',(-180.517306782578,58.3000000000017,171.027671453041));
#87762=CARTESIAN_POINT('Ctrl Pts',(-180.773257891743,58.3000000000037,170.620603621693));
#87763=CARTESIAN_POINT('Ctrl Pts',(-181.02228224259,58.3000000000012,170.207421559621));
#87764=CARTESIAN_POINT('Ctrl Pts',(-181.263216377716,58.3000000000022,169.790863880058));
#87765=CARTESIAN_POINT('Ctrl Pts',(-181.364433854457,58.3000000000026,169.615866189419));
#87766=CARTESIAN_POINT('Ctrl Pts',(-181.464223374814,58.3000000000036,169.440272954189));
#87767=CARTESIAN_POINT('Ctrl Pts',(-181.562498312604,58.3000000000056,169.264287803901));
#87768=CARTESIAN_POINT('Ctrl Pts',(-181.963798132055,58.3000000000141,168.545662988413));
#87769=CARTESIAN_POINT('Ctrl Pts',(-182.341570768327,58.3000000000098,167.817936557716));
#87770=CARTESIAN_POINT('Ctrl Pts',(-182.698077172536,58.3000000000056,167.081982270718));
#87771=CARTESIAN_POINT('Ctrl Pts',(-182.931096083592,58.3000000000029,166.600949491171));
#87772=CARTESIAN_POINT('Ctrl Pts',(-183.155029793797,58.3,166.11640183649));
#87773=CARTESIAN_POINT('Ctrl Pts',(-183.370511496512,58.3,165.628584399065));
#87774=CARTESIAN_POINT('Ctrl Pts',(-183.755752982814,58.3,164.756456917848));
#87775=CARTESIAN_POINT('Ctrl Pts',(-184.114155312767,58.3,163.873945558567));
#87776=CARTESIAN_POINT('Ctrl Pts',(-184.448595069682,58.3000000000002,162.982163713652));
#87777=CARTESIAN_POINT('Ctrl Pts',(-184.791126443434,58.3000000000005,162.068805615186));
#87778=CARTESIAN_POINT('Ctrl Pts',(-185.108521692177,58.3000000000011,161.145723081237));
#87779=CARTESIAN_POINT('Ctrl Pts',(-185.403902451678,58.3000000000022,160.21412405169));
#87780=CARTESIAN_POINT('Ctrl Pts',(-185.613943251761,58.300000000003,159.551678041825));
#87781=CARTESIAN_POINT('Ctrl Pts',(-185.812853271099,58.300000000004,158.884925982554));
#87782=CARTESIAN_POINT('Ctrl Pts',(-186.001763980044,58.3000000000055,158.214305556729));
#87783=CARTESIAN_POINT('Ctrl Pts',(-186.020019206364,58.3000000000056,158.149500720008));
#87784=CARTESIAN_POINT('Ctrl Pts',(-186.038181070206,58.3000000000058,158.084659736397));
#87785=CARTESIAN_POINT('Ctrl Pts',(-186.056250572068,58.3000000000059,158.019783088719));
#87786=CARTESIAN_POINT('Ctrl Pts',(-186.248767774588,58.3000000000077,157.32857030296));
#87787=CARTESIAN_POINT('Ctrl Pts',(-186.430890237263,58.3000000000059,156.632353763643));
#87788=CARTESIAN_POINT('Ctrl Pts',(-186.603184824574,58.3000000000038,155.93332206803));
#87789=CARTESIAN_POINT('Ctrl Pts',(-186.726566962198,58.3000000000024,155.432737422754));
#87790=CARTESIAN_POINT('Ctrl Pts',(-186.844909305794,58.3000000000008,154.930709352884));
#87791=CARTESIAN_POINT('Ctrl Pts',(-186.958421382134,58.3000000000002,154.428044798887));
#87792=CARTESIAN_POINT('Ctrl Pts',(-186.984076158333,58.3000000000001,154.314437973502));
#87793=CARTESIAN_POINT('Ctrl Pts',(-187.009484242047,58.3,154.200798493157));
#87794=CARTESIAN_POINT('Ctrl Pts',(-187.034647948172,58.3000000000001,154.087136197121));
#87795=CARTESIAN_POINT('Ctrl Pts',(-187.249235323321,58.3000000000005,153.117863481938));
#87796=CARTESIAN_POINT('Ctrl Pts',(-187.446091763184,58.3000000000003,152.147365334446));
#87797=CARTESIAN_POINT('Ctrl Pts',(-187.627848879965,58.3000000000049,151.175800942874));
#87798=CARTESIAN_POINT('Ctrl Pts',(-187.693091881787,58.3000000000065,150.827051036998));
#87799=CARTESIAN_POINT('Ctrl Pts',(-187.756389540824,58.3000000000085,150.478163535845));
#87800=CARTESIAN_POINT('Ctrl Pts',(-187.817864007364,58.3000000000118,150.129146500694));
#87801=CARTESIAN_POINT('Ctrl Pts',(-188.069630134647,58.3000000000257,148.699761713139));
#87802=CARTESIAN_POINT('Ctrl Pts',(-188.291104381093,58.300000000021,147.268244389129));
#87803=CARTESIAN_POINT('Ctrl Pts',(-188.488029483918,58.3000000000165,145.834998732404));
#87804=CARTESIAN_POINT('Ctrl Pts',(-188.654658778524,58.3000000000128,144.622249776835));
#87805=CARTESIAN_POINT('Ctrl Pts',(-188.803712708488,58.3000000000085,143.408263442865));
#87806=CARTESIAN_POINT('Ctrl Pts',(-188.938699247615,58.3000000000175,142.193285856765));
#87807=CARTESIAN_POINT('Ctrl Pts',(-189.136760752398,58.3000000000306,140.410587444496));
#87808=CARTESIAN_POINT('Ctrl Pts',(-189.304299635183,58.3000000000179,138.625740791404));
#87809=CARTESIAN_POINT('Ctrl Pts',(-189.448306843471,58.300000000011,136.83923745387));
#87810=CARTESIAN_POINT('Ctrl Pts',(-189.518148309857,58.3000000000076,135.972808514095));
#87811=CARTESIAN_POINT('Ctrl Pts',(-189.582455698063,58.3000000000052,135.105989966169));
#87812=CARTESIAN_POINT('Ctrl Pts',(-189.642030732453,58.3000000000086,134.238837995223));
#87813=CARTESIAN_POINT('Ctrl Pts',(-189.792507729526,58.3000000000171,132.048550974295));
#87814=CARTESIAN_POINT('Ctrl Pts',(-189.912606188582,58.3000000000056,129.85612495635));
#87815=CARTESIAN_POINT('Ctrl Pts',(-190.010855650094,58.3000000000114,127.66216080368));
#87816=CARTESIAN_POINT('Ctrl Pts',(-190.031601675758,58.3000000000126,127.198890716326));
#87817=CARTESIAN_POINT('Ctrl Pts',(-190.05137369699,58.3000000000145,126.73555206654));
#87818=CARTESIAN_POINT('Ctrl Pts',(-190.070252291175,58.3000000000178,126.272150491644));
#87819=CARTESIAN_POINT('Ctrl Pts',(-190.155978461159,58.3000000000328,124.167881402989));
#87820=CARTESIAN_POINT('Ctrl Pts',(-190.223187158372,58.3000000000361,122.062308228899));
#87821=CARTESIAN_POINT('Ctrl Pts',(-190.277034713559,58.3000000000306,119.955794495884));
#87822=CARTESIAN_POINT('Ctrl Pts',(-190.291163272368,58.3000000000292,119.403085964254));
#87823=CARTESIAN_POINT('Ctrl Pts',(-190.304372107163,58.300000000027,118.850312644463));
#87824=CARTESIAN_POINT('Ctrl Pts',(-190.316754563799,58.3000000000245,118.297481238444));
#87825=CARTESIAN_POINT('Ctrl Pts',(-190.39715529836,58.3000000000085,114.707882466758));
#87826=CARTESIAN_POINT('Ctrl Pts',(-190.443516404958,58.300000000003,111.115886215597));
#87827=CARTESIAN_POINT('Ctrl Pts',(-190.471166980605,58.300000000001,107.522572735381));
#87828=CARTESIAN_POINT('Ctrl Pts',(-190.484470219448,58.3000000000001,105.793758548108));
#87829=CARTESIAN_POINT('Ctrl Pts',(-190.493443302044,58.3,104.064639496642));
#87830=CARTESIAN_POINT('Ctrl Pts',(-190.499797482064,58.3,102.335336081498));
#87831=CARTESIAN_POINT('Ctrl Pts',(-190.499797482064,55.2999999999999,102.335336081498));
#87832=CARTESIAN_POINT('Ctrl Pts',(-190.486691892323,55.3,105.902049807941));
#87833=CARTESIAN_POINT('Ctrl Pts',(-190.462485288409,55.2999999999994,109.468349270102));
#87834=CARTESIAN_POINT('Ctrl Pts',(-190.4120617449,55.2999999999994,113.033670360094));
#87835=CARTESIAN_POINT('Ctrl Pts',(-190.386326129341,55.2999999999994,114.853370574095));
#87836=CARTESIAN_POINT('Ctrl Pts',(-190.353761766739,55.2999999999996,116.6728159339));
#87837=CARTESIAN_POINT('Ctrl Pts',(-190.312364415728,55.2999999999999,118.491931513318));
#87838=CARTESIAN_POINT('Ctrl Pts',(-190.26239910735,55.3000000000004,120.687547142897));
#87839=CARTESIAN_POINT('Ctrl Pts',(-190.199254190876,55.2999999999999,122.882671101962));
#87840=CARTESIAN_POINT('Ctrl Pts',(-190.116985654538,55.2999999999998,125.077081385043));
#87841=CARTESIAN_POINT('Ctrl Pts',(-190.098341748212,55.2999999999998,125.574384261422));
#87842=CARTESIAN_POINT('Ctrl Pts',(-190.078715787918,55.2999999999998,126.071650491612));
#87843=CARTESIAN_POINT('Ctrl Pts',(-190.058038765853,55.2999999999997,126.568877497678));
#87844=CARTESIAN_POINT('Ctrl Pts',(-190.005527764093,55.2999999999996,127.831626461638));
#87845=CARTESIAN_POINT('Ctrl Pts',(-189.946274541593,55.3000000000004,129.094132890502));
#87846=CARTESIAN_POINT('Ctrl Pts',(-189.878604951289,55.2999999999989,130.356321825266));
#87847=CARTESIAN_POINT('Ctrl Pts',(-189.801961025494,55.2999999999971,131.785902152592));
#87848=CARTESIAN_POINT('Ctrl Pts',(-189.714520017616,55.2999999999926,133.215074811835));
#87849=CARTESIAN_POINT('Ctrl Pts',(-189.613859593324,55.2999999999818,134.643729735402));
#87850=CARTESIAN_POINT('Ctrl Pts',(-189.567223188341,55.2999999999768,135.30563167021));
#87851=CARTESIAN_POINT('Ctrl Pts',(-189.51774671133,55.2999999999746,135.967606041755));
#87852=CARTESIAN_POINT('Ctrl Pts',(-189.465075917415,55.2999999999738,136.629493724172));
#87853=CARTESIAN_POINT('Ctrl Pts',(-189.329240119307,55.2999999999716,138.336474669696));
#87854=CARTESIAN_POINT('Ctrl Pts',(-189.172155668906,55.2999999999801,140.042873666388));
#87855=CARTESIAN_POINT('Ctrl Pts',(-188.987779803917,55.2999999999871,141.745933189677));
#87856=CARTESIAN_POINT('Ctrl Pts',(-188.952829258419,55.2999999999884,142.068767522461));
#87857=CARTESIAN_POINT('Ctrl Pts',(-188.916898181551,55.2999999999897,142.391481893429));
#87858=CARTESIAN_POINT('Ctrl Pts',(-188.879945626183,55.2999999999908,142.714057575824));
#87859=CARTESIAN_POINT('Ctrl Pts',(-188.750614226618,55.2999999999948,143.843050254512));
#87860=CARTESIAN_POINT('Ctrl Pts',(-188.608928166082,55.2999999999971,144.969702294663));
#87861=CARTESIAN_POINT('Ctrl Pts',(-188.452204690944,55.2999999999979,146.093506559918));
#87862=CARTESIAN_POINT('Ctrl Pts',(-188.257218139742,55.299999999999,147.491680749931));
#87863=CARTESIAN_POINT('Ctrl Pts',(-188.038953458898,55.2999999999974,148.885446027331));
#87864=CARTESIAN_POINT('Ctrl Pts',(-187.792286254426,55.2999999999928,150.273830439671));
#87865=CARTESIAN_POINT('Ctrl Pts',(-187.765197067702,55.2999999999923,150.426303909631));
#87866=CARTESIAN_POINT('Ctrl Pts',(-187.737765380842,55.2999999999918,150.578712491456));
#87867=CARTESIAN_POINT('Ctrl Pts',(-187.709984445717,55.2999999999912,150.731054904143));
#87868=CARTESIAN_POINT('Ctrl Pts',(-187.493624536488,55.2999999999867,151.917508507399));
#87869=CARTESIAN_POINT('Ctrl Pts',(-187.256237229441,55.2999999999887,153.099979686043));
#87870=CARTESIAN_POINT('Ctrl Pts',(-186.992719010159,55.2999999999906,154.277501006747));
#87871=CARTESIAN_POINT('Ctrl Pts',(-186.740879122074,55.2999999999925,155.402838140671));
#87872=CARTESIAN_POINT('Ctrl Pts',(-186.465172879604,55.2999999999945,156.523654431007));
#87873=CARTESIAN_POINT('Ctrl Pts',(-186.161192902748,55.2999999999918,157.639113379179));
#87874=CARTESIAN_POINT('Ctrl Pts',(-186.070081234826,55.2999999999909,157.973448970351));
#87875=CARTESIAN_POINT('Ctrl Pts',(-185.976429868101,55.2999999999897,158.307303327867));
#87876=CARTESIAN_POINT('Ctrl Pts',(-185.88012104457,55.2999999999879,158.640654079262));
#87877=CARTESIAN_POINT('Ctrl Pts',(-185.612786098818,55.2999999999829,159.56597225648));
#87878=CARTESIAN_POINT('Ctrl Pts',(-185.324526062901,55.2999999999913,160.487428138369));
#87879=CARTESIAN_POINT('Ctrl Pts',(-185.014202918841,55.2999999999948,161.398696211986));
#87880=CARTESIAN_POINT('Ctrl Pts',(-184.886035202094,55.2999999999962,161.775062430795));
#87881=CARTESIAN_POINT('Ctrl Pts',(-184.75410415523,55.2999999999968,162.149691352719));
#87882=CARTESIAN_POINT('Ctrl Pts',(-184.618330478778,55.2999999999954,162.522139724443));
#87883=CARTESIAN_POINT('Ctrl Pts',(-184.23064261954,55.2999999999914,163.585627991711));
#87884=CARTESIAN_POINT('Ctrl Pts',(-183.810946185528,55.2999999999973,164.633847666811));
#87885=CARTESIAN_POINT('Ctrl Pts',(-183.354597012639,55.2999999999993,165.664583381619));
#87886=CARTESIAN_POINT('Ctrl Pts',(-183.263221822042,55.2999999999997,165.870968487565));
#87887=CARTESIAN_POINT('Ctrl Pts',(-183.170377275705,55.3,166.076652697458));
#87888=CARTESIAN_POINT('Ctrl Pts',(-183.076026323033,55.2999999999999,166.281618301401));
#87889=CARTESIAN_POINT('Ctrl Pts',(-182.580805460325,55.2999999999997,167.35742347703));
#87890=CARTESIAN_POINT('Ctrl Pts',(-182.044068007193,55.2999999999999,168.413424777875));
#87891=CARTESIAN_POINT('Ctrl Pts',(-181.45994811726,55.2999999999962,169.446823583728));
#87892=CARTESIAN_POINT('Ctrl Pts',(-181.375812919564,55.2999999999957,169.59567181562));
#87893=CARTESIAN_POINT('Ctrl Pts',(-181.290694734727,55.2999999999953,169.744051101896));
#87894=CARTESIAN_POINT('Ctrl Pts',(-181.204575998837,55.2999999999944,169.891953198675));
#87895=CARTESIAN_POINT('Ctrl Pts',(-180.915435634367,55.2999999999914,170.3885288361));
#87896=CARTESIAN_POINT('Ctrl Pts',(-180.615009421971,55.2999999999974,170.879720750648));
#87897=CARTESIAN_POINT('Ctrl Pts',(-180.302607188989,55.2999999999992,171.365199942073));
#87898=CARTESIAN_POINT('Ctrl Pts',(-180.245054999167,55.2999999999995,171.454637172764));
#87899=CARTESIAN_POINT('Ctrl Pts',(-180.187096430933,55.2999999999997,171.543880399659));
#87900=CARTESIAN_POINT('Ctrl Pts',(-180.128726879727,55.2999999999996,171.632927989696));
#87901=CARTESIAN_POINT('Ctrl Pts',(-179.894241861513,55.2999999999995,171.990654327147));
#87902=CARTESIAN_POINT('Ctrl Pts',(-179.652545955628,55.2999999999997,172.345968524669));
#87903=CARTESIAN_POINT('Ctrl Pts',(-179.404876266101,55.2999999999998,172.696746542243));
#87904=CARTESIAN_POINT('Ctrl Pts',(-179.255994389225,55.2999999999999,172.907610010127));
#87905=CARTESIAN_POINT('Ctrl Pts',(-179.104954749709,55.3,173.116833074002));
#87906=CARTESIAN_POINT('Ctrl Pts',(-178.952022467963,55.3,173.323959339789));
#87907=CARTESIAN_POINT('Ctrl Pts',(-178.41719983759,55.3,174.048304867251));
#87908=CARTESIAN_POINT('Ctrl Pts',(-177.858788574558,55.3,174.747631024544));
#87909=CARTESIAN_POINT('Ctrl Pts',(-177.277237712592,55.3,175.422402984304));
#87910=CARTESIAN_POINT('Ctrl Pts',(-176.681725802524,55.3,176.113373912038));
#87911=CARTESIAN_POINT('Ctrl Pts',(-176.061949956807,55.3,176.778597639781));
#87912=CARTESIAN_POINT('Ctrl Pts',(-175.418353704452,55.3,177.41853304461));
#87913=CARTESIAN_POINT('Ctrl Pts',(-174.774757452097,55.3,178.05846844944));
#87914=CARTESIAN_POINT('Ctrl Pts',(-174.107341075041,55.3000000000009,178.673115079697));
#87915=CARTESIAN_POINT('Ctrl Pts',(-173.416509908913,55.2999999999999,179.26289316856));
#87916=CARTESIAN_POINT('Ctrl Pts',(-172.902930290524,55.2999999999991,179.70134762844));
#87917=CARTESIAN_POINT('Ctrl Pts',(-172.376508960269,55.2999999999991,180.126166505602));
#87918=CARTESIAN_POINT('Ctrl Pts',(-171.837640512919,55.2999999999989,180.537771132798));
#87919=CARTESIAN_POINT('Ctrl Pts',(-171.568206289244,55.2999999999988,180.743573446396));
#87920=CARTESIAN_POINT('Ctrl Pts',(-171.295660191796,55.2999999999986,180.946072091014));
#87921=CARTESIAN_POINT('Ctrl Pts',(-171.020051006383,55.2999999999983,181.145319119996));
#87922=CARTESIAN_POINT('Ctrl Pts',(-170.876736551081,55.2999999999981,181.248925897057));
#87923=CARTESIAN_POINT('Ctrl Pts',(-170.732593857952,55.2999999999978,181.351653459219));
#87924=CARTESIAN_POINT('Ctrl Pts',(-170.587629750578,55.2999999999975,181.453509083908));
#87925=CARTESIAN_POINT('Ctrl Pts',(-170.453812213327,55.2999999999972,181.547532832943));
#87926=CARTESIAN_POINT('Ctrl Pts',(-170.319291857913,55.2999999999971,181.640815489386));
#87927=CARTESIAN_POINT('Ctrl Pts',(-170.184091336249,55.2999999999959,181.733351070885));
#87928=CARTESIAN_POINT('Ctrl Pts',(-169.902739839192,55.2999999999936,181.925917076294));
#87929=CARTESIAN_POINT('Ctrl Pts',(-169.618005644094,55.2999999999945,182.115519126605));
#87930=CARTESIAN_POINT('Ctrl Pts',(-169.330645353429,55.299999999996,182.301804073465));
#87931=CARTESIAN_POINT('Ctrl Pts',(-169.186572407503,55.2999999999967,182.395201184853));
#87932=CARTESIAN_POINT('Ctrl Pts',(-169.041839246008,55.2999999999975,182.487764336891));
#87933=CARTESIAN_POINT('Ctrl Pts',(-168.89654087646,55.2999999999981,182.579448043434));
#87934=CARTESIAN_POINT('Ctrl Pts',(-168.834229760776,55.2999999999984,182.618766544133));
#87935=CARTESIAN_POINT('Ctrl Pts',(-168.771814695492,55.2999999999986,182.657923295422));
#87936=CARTESIAN_POINT('Ctrl Pts',(-168.709303172194,55.2999999999988,182.696914667427));
#87937=CARTESIAN_POINT('Ctrl Pts',(-168.650733708525,55.2999999999989,182.733447191761));
#87938=CARTESIAN_POINT('Ctrl Pts',(-168.59208268385,55.299999999999,182.76983257515));
#87939=CARTESIAN_POINT('Ctrl Pts',(-168.533364737283,55.299999999999,182.806062700292));
#87940=CARTESIAN_POINT('Ctrl Pts',(-168.509414306756,55.299999999999,182.82084058586));
#87941=CARTESIAN_POINT('Ctrl Pts',(-168.485452338166,55.299999999999,182.835592892692));
#87942=CARTESIAN_POINT('Ctrl Pts',(-168.46147926487,55.299999999999,182.850319418911));
#87943=CARTESIAN_POINT('Ctrl Pts',(-168.169963101635,55.2999999999989,183.029396184255));
#87944=CARTESIAN_POINT('Ctrl Pts',(-167.876944721106,55.2999999999992,183.204614901524));
#87945=CARTESIAN_POINT('Ctrl Pts',(-167.582420661782,55.2999999999995,183.376193981152));
#87946=CARTESIAN_POINT('Ctrl Pts',(-167.384297559265,55.2999999999997,183.491613345061));
#87947=CARTESIAN_POINT('Ctrl Pts',(-167.185493054643,55.2999999999999,183.605385566813));
#87948=CARTESIAN_POINT('Ctrl Pts',(-166.986005355678,55.3,183.717575256982));
#87949=CARTESIAN_POINT('Ctrl Pts',(-166.888940425809,55.3,183.772163507109));
#87950=CARTESIAN_POINT('Ctrl Pts',(-166.791714965253,55.3,183.826376357779));
#87951=CARTESIAN_POINT('Ctrl Pts',(-166.694335930232,55.3,183.880217249607));
#87952=CARTESIAN_POINT('Ctrl Pts',(-165.743362040703,55.3,184.40601094131));
#87953=CARTESIAN_POINT('Ctrl Pts',(-164.777788310111,55.3,184.896759395401));
#87954=CARTESIAN_POINT('Ctrl Pts',(-163.799410499353,55.3,185.356773166156));
#87955=CARTESIAN_POINT('Ctrl Pts',(-162.812239834025,55.3,185.820921162096));
#87956=CARTESIAN_POINT('Ctrl Pts',(-161.812033992515,55.2999999999999,186.253779761824));
#87957=CARTESIAN_POINT('Ctrl Pts',(-160.800656964796,55.2999999999999,186.659825139884));
#87958=CARTESIAN_POINT('Ctrl Pts',(-160.31097753273,55.2999999999999,186.856420538704));
#87959=CARTESIAN_POINT('Ctrl Pts',(-159.818679305665,55.3000000000012,187.046731154551));
#87960=CARTESIAN_POINT('Ctrl Pts',(-159.323976398265,55.2999999999994,187.231268441749));
#87961=CARTESIAN_POINT('Ctrl Pts',(-158.693118416369,55.299999999997,187.466595177949));
#87962=CARTESIAN_POINT('Ctrl Pts',(-158.058297774248,55.2999999999972,187.692418003419));
#87963=CARTESIAN_POINT('Ctrl Pts',(-157.419838084174,55.2999999999965,187.909507127552));
#87964=CARTESIAN_POINT('Ctrl Pts',(-157.019499284202,55.2999999999961,188.045630364137));
#87965=CARTESIAN_POINT('Ctrl Pts',(-156.617729738341,55.2999999999953,188.178319823437));
#87966=CARTESIAN_POINT('Ctrl Pts',(-156.214609655659,55.2999999999934,188.307766485117));
#87967=CARTESIAN_POINT('Ctrl Pts',(-155.974834462964,55.2999999999922,188.384761156387));
#87968=CARTESIAN_POINT('Ctrl Pts',(-155.734577656072,55.2999999999914,188.460609746169));
#87969=CARTESIAN_POINT('Ctrl Pts',(-155.493876194086,55.299999999987,188.535346445525));
#87970=CARTESIAN_POINT('Ctrl Pts',(-154.849286915679,55.2999999999753,188.735488458418));
#87971=CARTESIAN_POINT('Ctrl Pts',(-154.200851882109,55.2999999999802,188.927821054047));
#87972=CARTESIAN_POINT('Ctrl Pts',(-153.549758382643,55.2999999999871,189.112746132645));
#87973=CARTESIAN_POINT('Ctrl Pts',(-153.22421163291,55.2999999999906,189.205208671944));
#87974=CARTESIAN_POINT('Ctrl Pts',(-152.898000237317,55.2999999999945,189.295819123002));
#87975=CARTESIAN_POINT('Ctrl Pts',(-152.571272698333,55.2999999999971,189.384626541979));
#87976=CARTESIAN_POINT('Ctrl Pts',(-152.406379380498,55.2999999999984,189.429445996161));
#87977=CARTESIAN_POINT('Ctrl Pts',(-152.241354602361,55.2999999999993,189.473806200192));
#87978=CARTESIAN_POINT('Ctrl Pts',(-152.076217481013,55.2999999999997,189.517713389758));
#87979=CARTESIAN_POINT('Ctrl Pts',(-151.943218512572,55.3,189.553075583744));
#87980=CARTESIAN_POINT('Ctrl Pts',(-151.810145280887,55.2999999999999,189.588144270557));
#87981=CARTESIAN_POINT('Ctrl Pts',(-151.677027873674,55.2999999999993,189.622917512509));
#87982=CARTESIAN_POINT('Ctrl Pts',(-151.647927448919,55.2999999999991,189.630519193853));
#87983=CARTESIAN_POINT('Ctrl Pts',(-151.618824705037,55.2999999999989,189.638106811891));
#87984=CARTESIAN_POINT('Ctrl Pts',(-151.58971975818,55.2999999999988,189.645680399349));
#87985=CARTESIAN_POINT('Ctrl Pts',(-150.2812980681,55.29999999999,189.98615331447));
#87986=CARTESIAN_POINT('Ctrl Pts',(-148.970507516151,55.2999999999809,190.298209232362));
#87987=CARTESIAN_POINT('Ctrl Pts',(-147.657489395253,55.2999999999767,190.586549148109));
#87988=CARTESIAN_POINT('Ctrl Pts',(-147.000980334804,55.2999999999746,190.730719105983));
#87989=CARTESIAN_POINT('Ctrl Pts',(-146.34391436091,55.2999999999738,190.868959783947));
#87990=CARTESIAN_POINT('Ctrl Pts',(-145.686309051212,55.2999999999748,191.00185772528));
#87991=CARTESIAN_POINT('Ctrl Pts',(-145.236865028949,55.2999999999755,191.092687565646));
#87992=CARTESIAN_POINT('Ctrl Pts',(-144.787169075752,55.2999999999771,191.181021739963));
#87993=CARTESIAN_POINT('Ctrl Pts',(-144.33722679863,55.2999999999798,191.267047451344));
#87994=CARTESIAN_POINT('Ctrl Pts',(-144.128834743028,55.299999999981,191.3068905062));
#87995=CARTESIAN_POINT('Ctrl Pts',(-143.920388717415,55.2999999999825,191.346238574216));
#87996=CARTESIAN_POINT('Ctrl Pts',(-143.711897764384,55.2999999999843,191.385108697693));
#87997=CARTESIAN_POINT('Ctrl Pts',(-141.950706217328,55.3000000000001,191.71345739535));
#87998=CARTESIAN_POINT('Ctrl Pts',(-140.186182407371,55.3000000000011,192.007447721363));
#87999=CARTESIAN_POINT('Ctrl Pts',(-138.418979168621,55.2999999999956,192.273910691535));
#88000=CARTESIAN_POINT('Ctrl Pts',(-137.546066740989,55.2999999999928,192.405530435697));
#88001=CARTESIAN_POINT('Ctrl Pts',(-136.672500176854,55.2999999999896,192.530434732744));
#88002=CARTESIAN_POINT('Ctrl Pts',(-135.79835995011,55.2999999999832,192.64945104723));
#88003=CARTESIAN_POINT('Ctrl Pts',(-133.742775638351,55.2999999999681,192.929323842712));
#88004=CARTESIAN_POINT('Ctrl Pts',(-131.684009902325,55.2999999999751,193.176457453746));
#88005=CARTESIAN_POINT('Ctrl Pts',(-129.622742521771,55.2999999999818,193.397881768966));
#88006=CARTESIAN_POINT('Ctrl Pts',(-129.035163425207,55.2999999999837,193.461000363051));
#88007=CARTESIAN_POINT('Ctrl Pts',(-128.447380807758,55.2999999999854,193.522030170679));
#88008=CARTESIAN_POINT('Ctrl Pts',(-127.859411366078,55.2999999999871,193.581134526229));
#88009=CARTESIAN_POINT('Ctrl Pts',(-125.144150681436,55.2999999999946,193.854080229763));
#88010=CARTESIAN_POINT('Ctrl Pts',(-122.424955472583,55.2999999999977,194.086609801097));
#88011=CARTESIAN_POINT('Ctrl Pts',(-119.702735665975,55.2999999999966,194.288037001772));
#88012=CARTESIAN_POINT('Ctrl Pts',(-117.522588010382,55.2999999999957,194.449354261406));
#88013=CARTESIAN_POINT('Ctrl Pts',(-115.340500490943,55.2999999999921,194.590723897809));
#88014=CARTESIAN_POINT('Ctrl Pts',(-113.156942060905,55.299999999986,194.716950287514));
#88015=CARTESIAN_POINT('Ctrl Pts',(-112.748096052287,55.2999999999848,194.740584716025));
#88016=CARTESIAN_POINT('Ctrl Pts',(-112.339198609107,55.2999999999837,194.763688283965));
#88017=CARTESIAN_POINT('Ctrl Pts',(-111.930252346801,55.2999999999822,194.786292608757));
#88018=CARTESIAN_POINT('Ctrl Pts',(-107.974707073947,55.2999999999682,195.004933634036));
#88019=CARTESIAN_POINT('Ctrl Pts',(-104.014517429673,55.2999999999849,195.175894152784));
#88020=CARTESIAN_POINT('Ctrl Pts',(-100.051160906159,55.2999999999941,195.314262519372));
#88021=CARTESIAN_POINT('Ctrl Pts',(-98.6870868231336,55.2999999999972,195.361884957993));
#88022=CARTESIAN_POINT('Ctrl Pts',(-97.3226375965247,55.2999999999995,195.405647209011));
#88023=CARTESIAN_POINT('Ctrl Pts',(-95.9578737332236,55.2999999999994,195.446165741684));
#88024=CARTESIAN_POINT('Ctrl Pts',(-93.2937797771208,55.2999999999991,195.525260141021));
#88025=CARTESIAN_POINT('Ctrl Pts',(-90.6283351791982,55.2999999999899,195.591817563438));
#88026=CARTESIAN_POINT('Ctrl Pts',(-87.9622980004871,55.2999999999833,195.648477101291));
#88027=CARTESIAN_POINT('Ctrl Pts',(-86.4341087402463,55.2999999999795,195.680954704353));
#88028=CARTESIAN_POINT('Ctrl Pts',(-84.9057247909427,55.2999999999766,195.710180235644));
#88029=CARTESIAN_POINT('Ctrl Pts',(-83.3772890352257,55.2999999999766,195.736651020953));
#88030=CARTESIAN_POINT('Ctrl Pts',(-82.3556648250435,55.2999999999767,195.754344401283));
#88031=CARTESIAN_POINT('Ctrl Pts',(-81.3340174708388,55.299999999978,195.770807037021));
#88032=CARTESIAN_POINT('Ctrl Pts',(-80.3123896643528,55.2999999999814,195.786187504847));
#88033=CARTESIAN_POINT('Ctrl Pts',(-80.1959820125014,55.2999999999818,195.787940006231));
#88034=CARTESIAN_POINT('Ctrl Pts',(-80.0795746244709,55.2999999999822,195.789678457632));
#88035=CARTESIAN_POINT('Ctrl Pts',(-79.9631677685342,55.2999999999827,195.791403075907));
#88036=CARTESIAN_POINT('Ctrl Pts',(-76.1297427206355,55.2999999999984,195.848196937737));
#88037=CARTESIAN_POINT('Ctrl Pts',(-72.2961721091227,55.3000000000004,195.889842603839));
#88038=CARTESIAN_POINT('Ctrl Pts',(-68.4625314791343,55.3000000000001,195.921169797769));
#88039=CARTESIAN_POINT('Ctrl Pts',(-66.964441063854,55.3,195.933411677876));
#88040=CARTESIAN_POINT('Ctrl Pts',(-65.4663401615409,55.2999999999993,195.944077956465));
#88041=CARTESIAN_POINT('Ctrl Pts',(-63.9682326441714,55.2999999999994,195.953457116585));
#88042=CARTESIAN_POINT('Ctrl Pts',(-58.6374128389523,55.2999999999997,195.986831632062));
#88043=CARTESIAN_POINT('Ctrl Pts',(-53.3064763293846,55.2999999999998,196.004466674216));
#88044=CARTESIAN_POINT('Ctrl Pts',(-47.9754976701425,55.2999999999999,196.01317970203));
#88045=CARTESIAN_POINT('Ctrl Pts',(-44.2886966671822,55.2999999999999,196.019205462352));
#88046=CARTESIAN_POINT('Ctrl Pts',(-40.6018755026786,55.3,196.020964151304));
#88047=CARTESIAN_POINT('Ctrl Pts',(-36.915058817711,55.3,196.020712339862));
#88048=CARTESIAN_POINT('Ctrl Pts',(-35.2708741678306,55.3,196.020600041219));
#88049=CARTESIAN_POINT('Ctrl Pts',(-33.6266905523897,55.2999999999999,196.020087900419));
#88050=CARTESIAN_POINT('Ctrl Pts',(-31.9825097205406,55.2999999999999,196.019376110131));
#88051=CARTESIAN_POINT('Ctrl Pts',(-21.3216725475468,55.2999999999999,196.014760875474));
#88052=CARTESIAN_POINT('Ctrl Pts',(-10.6608381121449,55.3,196.));
#88053=CARTESIAN_POINT('Ctrl Pts',(1.06581410364015E-14,55.3,196.));
#88054=CARTESIAN_POINT('Origin',(160.5,51.6013867006572,102.225104347672));
#88055=CARTESIAN_POINT('',(190.5,58.3,102.225104347672));
#88056=CARTESIAN_POINT('',(190.5,55.3,102.225104347672));
#88057=CARTESIAN_POINT('',(190.5,51.6013867006572,102.225104347672));
#88058=CARTESIAN_POINT('',(190.499797482064,58.3,102.335336081499));
#88059=CARTESIAN_POINT('Origin',(160.5,58.3,102.225104347672));
#88060=CARTESIAN_POINT('',(190.499797482064,55.3,102.335336081499));
#88061=CARTESIAN_POINT('',(190.499797482064,51.6013867006573,102.335336081499));
#88062=CARTESIAN_POINT('Origin',(160.5,55.3,102.225104347672));
#88063=CARTESIAN_POINT('Ctrl Pts',(1.20290037631083E-14,55.2999999999999,
196.));
#88064=CARTESIAN_POINT('Ctrl Pts',(1.15700533001727E-14,58.9,196.));
#88065=CARTESIAN_POINT('Ctrl Pts',(180.96963113231,55.3,196.));
#88066=CARTESIAN_POINT('Ctrl Pts',(180.96963113231,58.9,196.));
#88067=CARTESIAN_POINT('Ctrl Pts',(190.141509581597,55.3,199.844139409912));
#88068=CARTESIAN_POINT('Ctrl Pts',(190.141509581597,58.9,199.844139409912));
#88069=CARTESIAN_POINT('Ctrl Pts',(190.499797482064,55.3,102.335336081499));
#88070=CARTESIAN_POINT('Ctrl Pts',(190.499797482064,58.9,102.335336081499));
#88071=CARTESIAN_POINT('Ctrl Pts',(190.499797482064,58.3,102.335336081499));
#88072=CARTESIAN_POINT('Ctrl Pts',(190.486691892692,58.3,105.902049707337));
#88073=CARTESIAN_POINT('Ctrl Pts',(190.462485289776,58.3,109.468349068915));
#88074=CARTESIAN_POINT('Ctrl Pts',(190.412061749167,58.3,113.033670058396));
#88075=CARTESIAN_POINT('Ctrl Pts',(190.386326132941,58.3,114.853370372991));
#88076=CARTESIAN_POINT('Ctrl Pts',(190.353761769027,58.3,116.672815833366));
#88077=CARTESIAN_POINT('Ctrl Pts',(190.312364415728,58.3,118.491931513319));
#88078=CARTESIAN_POINT('Ctrl Pts',(190.262398908667,58.3,120.687555873587));
#88079=CARTESIAN_POINT('Ctrl Pts',(190.19925368868,58.3,122.882688559424));
#88080=CARTESIAN_POINT('Ctrl Pts',(190.116984673134,58.3,125.077107562727));
#88081=CARTESIAN_POINT('Ctrl Pts',(190.098341059481,58.3,125.574401711925));
#88082=CARTESIAN_POINT('Ctrl Pts',(190.07871542511,58.3,126.071659216176));
#88083=CARTESIAN_POINT('Ctrl Pts',(190.058038765853,58.3,126.568877497679));
#88084=CARTESIAN_POINT('Ctrl Pts',(190.005527904509,58.3,127.831623085003));
#88085=CARTESIAN_POINT('Ctrl Pts',(189.946274858486,58.3000000000002,129.094126138524));
#88086=CARTESIAN_POINT('Ctrl Pts',(189.878605494142,58.3000000000003,130.356311699848));
#88087=CARTESIAN_POINT('Ctrl Pts',(189.801961438374,58.3000000000005,131.785895404238));
#88088=CARTESIAN_POINT('Ctrl Pts',(189.714520255269,58.3000000000007,133.215071438881));
#88089=CARTESIAN_POINT('Ctrl Pts',(189.613859593324,58.3000000000004,134.643729735403));
#88090=CARTESIAN_POINT('Ctrl Pts',(189.567223198167,58.3000000000003,135.305631530741));
#88091=CARTESIAN_POINT('Ctrl Pts',(189.51774673218,58.3000000000036,135.967605762786));
#88092=CARTESIAN_POINT('Ctrl Pts',(189.46507595071,58.3000000000082,136.629493305773));
#88093=CARTESIAN_POINT('Ctrl Pts',(189.329240157618,58.3000000000201,138.336474231981));
#88094=CARTESIAN_POINT('Ctrl Pts',(189.172155713213,58.3000000000407,140.042873209594));
#88095=CARTESIAN_POINT('Ctrl Pts',(188.9877798554,58.3000000000341,141.745932714139));
#88096=CARTESIAN_POINT('Ctrl Pts',(188.952829293703,58.3000000000328,142.068767205554));
#88097=CARTESIAN_POINT('Ctrl Pts',(188.916898199695,58.3000000000306,142.391481735044));
#88098=CARTESIAN_POINT('Ctrl Pts',(188.879945626183,58.3000000000271,142.714057575825));
#88099=CARTESIAN_POINT('Ctrl Pts',(188.750614304397,58.3000000000151,143.843049575544));
#88100=CARTESIAN_POINT('Ctrl Pts',(188.608928336502,58.3000000000094,144.969700939541));
#88101=CARTESIAN_POINT('Ctrl Pts',(188.452204973701,58.3000000000058,146.093504532372));
#88102=CARTESIAN_POINT('Ctrl Pts',(188.25721844303,58.3000000000012,147.491678740773));
#88103=CARTESIAN_POINT('Ctrl Pts',(188.038953784735,58.3000000000009,148.885444036944));
#88104=CARTESIAN_POINT('Ctrl Pts',(187.792286604651,58.3000000000004,150.273828468404));
#88105=CARTESIAN_POINT('Ctrl Pts',(187.765197304137,58.3000000000004,150.426302596012));
#88106=CARTESIAN_POINT('Ctrl Pts',(187.737765500565,58.3000000000003,150.578711834932));
#88107=CARTESIAN_POINT('Ctrl Pts',(187.709984445717,58.3000000000003,150.731054904144));
#88108=CARTESIAN_POINT('Ctrl Pts',(187.493624541263,58.2999999999998,151.917508481214));
#88109=CARTESIAN_POINT('Ctrl Pts',(187.256237239919,58.3000000000075,153.09997963385));
#88110=CARTESIAN_POINT('Ctrl Pts',(186.992719027606,58.3000000000135,154.277500928785));
#88111=CARTESIAN_POINT('Ctrl Pts',(186.740879139795,58.3000000000192,155.402838066619));
#88112=CARTESIAN_POINT('Ctrl Pts',(186.465172897544,58.3000000000235,156.523654360854));
#88113=CARTESIAN_POINT('Ctrl Pts',(186.161192920807,58.3000000000189,157.639113312908));
#88114=CARTESIAN_POINT('Ctrl Pts',(186.070081247201,58.3000000000175,157.973448926234));
#88115=CARTESIAN_POINT('Ctrl Pts',(185.976429874464,58.3000000000152,158.307303305843));
#88116=CARTESIAN_POINT('Ctrl Pts',(185.880121044569,58.300000000012,158.640654079262));
#88117=CARTESIAN_POINT('Ctrl Pts',(185.61278602088,58.300000000003,159.565972526244));
#88118=CARTESIAN_POINT('Ctrl Pts',(185.324525894825,58.3000000000103,160.487428675641));
#88119=CARTESIAN_POINT('Ctrl Pts',(185.014202647431,58.3000000000117,161.398697008986));
#88120=CARTESIAN_POINT('Ctrl Pts',(184.886035015842,58.3000000000123,161.775062959677));
#88121=CARTESIAN_POINT('Ctrl Pts',(184.754104059391,58.3000000000119,162.14969161562));
#88122=CARTESIAN_POINT('Ctrl Pts',(184.618330478778,58.3000000000092,162.522139724444));
#88123=CARTESIAN_POINT('Ctrl Pts',(184.230642847717,58.3000000000013,163.585627365785));
#88124=CARTESIAN_POINT('Ctrl Pts',(183.810946679566,58.3000000000002,164.633846432934));
#88125=CARTESIAN_POINT('Ctrl Pts',(183.354597818405,58.3000000000001,165.66458156167));
#88126=CARTESIAN_POINT('Ctrl Pts',(183.263222367858,58.3000000000001,165.870967278386));
#88127=CARTESIAN_POINT('Ctrl Pts',(183.17037755304,58.3000000000001,166.076652094981));
#88128=CARTESIAN_POINT('Ctrl Pts',(183.076026323032,58.3000000000001,166.281618301402));
#88129=CARTESIAN_POINT('Ctrl Pts',(182.580804157945,58.3000000000003,167.357426306289));
#88130=CARTESIAN_POINT('Ctrl Pts',(182.044065184055,58.3000000000001,168.413430332222));
#88131=CARTESIAN_POINT('Ctrl Pts',(181.459943508732,58.3000000000056,169.446831736928));
#88132=CARTESIAN_POINT('Ctrl Pts',(181.375809811316,58.3000000000064,169.595677233963));
#88133=CARTESIAN_POINT('Ctrl Pts',(181.290693162334,58.300000000007,169.744053802355));
#88134=CARTESIAN_POINT('Ctrl Pts',(181.204575998837,58.3000000000083,169.891953198676));
#88135=CARTESIAN_POINT('Ctrl Pts',(180.915435742078,58.3000000000128,170.388528651114));
#88136=CARTESIAN_POINT('Ctrl Pts',(180.6150096458,58.3000000000038,170.879720384691));
#88137=CARTESIAN_POINT('Ctrl Pts',(180.302607538116,58.3000000000012,171.365199399522));
#88138=CARTESIAN_POINT('Ctrl Pts',(180.245055233562,58.3000000000007,171.454636811847));
#88139=CARTESIAN_POINT('Ctrl Pts',(180.187096548962,58.3000000000004,171.543880219597));
#88140=CARTESIAN_POINT('Ctrl Pts',(180.128726879727,58.3000000000005,171.632927989697));
#88141=CARTESIAN_POINT('Ctrl Pts',(179.894241878965,58.3000000000007,171.990654300523));
#88142=CARTESIAN_POINT('Ctrl Pts',(179.652545991606,58.3000000000004,172.345968471778));
#88143=CARTESIAN_POINT('Ctrl Pts',(179.404876321403,58.3000000000002,172.696746463919));
#88144=CARTESIAN_POINT('Ctrl Pts',(179.255994426627,58.3000000000001,172.907609958317));
#88145=CARTESIAN_POINT('Ctrl Pts',(179.104954768645,58.3,173.116833048357));
#88146=CARTESIAN_POINT('Ctrl Pts',(178.952022467963,58.3,173.323959339789));
#88147=CARTESIAN_POINT('Ctrl Pts',(178.417199844465,58.3,174.04830485794));
#88148=CARTESIAN_POINT('Ctrl Pts',(177.858788588915,58.3,174.747631006561));
#88149=CARTESIAN_POINT('Ctrl Pts',(177.277237735021,58.3,175.422402958276));
#88150=CARTESIAN_POINT('Ctrl Pts',(176.681725821823,58.3,176.113373890994));
#88151=CARTESIAN_POINT('Ctrl Pts',(176.061949972666,58.3,176.778597623392));
#88152=CARTESIAN_POINT('Ctrl Pts',(175.418353716571,58.3,177.418533032557));
#88153=CARTESIAN_POINT('Ctrl Pts',(174.774757460475,58.3,178.058468441722));
#88154=CARTESIAN_POINT('Ctrl Pts',(174.107341079373,58.3,178.673115075999));
#88155=CARTESIAN_POINT('Ctrl Pts',(173.416509908913,58.3,179.262893168561));
#88156=CARTESIAN_POINT('Ctrl Pts',(172.902930290527,58.3,179.701347628437));
#88157=CARTESIAN_POINT('Ctrl Pts',(172.376508960271,58.3,180.126166505599));
#88158=CARTESIAN_POINT('Ctrl Pts',(171.83764051292,58.3,180.537771132796));
#88159=CARTESIAN_POINT('Ctrl Pts',(171.568206289245,58.3,180.743573446395));
#88160=CARTESIAN_POINT('Ctrl Pts',(171.295660191797,58.3,180.946072091013));
#88161=CARTESIAN_POINT('Ctrl Pts',(171.020051006383,58.3,181.145319119995));
#88162=CARTESIAN_POINT('Ctrl Pts',(170.87673654841,58.3,181.248925898987));
#88163=CARTESIAN_POINT('Ctrl Pts',(170.73259385258,58.3,181.351653463048));
#88164=CARTESIAN_POINT('Ctrl Pts',(170.587629742474,58.3,181.453509089602));
#88165=CARTESIAN_POINT('Ctrl Pts',(170.453812207896,58.3,181.547532836709));
#88166=CARTESIAN_POINT('Ctrl Pts',(170.319291855183,58.3,181.640815491254));
#88167=CARTESIAN_POINT('Ctrl Pts',(170.184091336249,58.3,181.733351070886));
#88168=CARTESIAN_POINT('Ctrl Pts',(169.902739839191,58.3,181.925917076294));
#88169=CARTESIAN_POINT('Ctrl Pts',(169.618005644093,58.3,182.115519126606));
#88170=CARTESIAN_POINT('Ctrl Pts',(169.330645353427,58.3,182.301804073466));
#88171=CARTESIAN_POINT('Ctrl Pts',(169.186572409167,58.3,182.395201183774));
#88172=CARTESIAN_POINT('Ctrl Pts',(169.041839249353,58.3,182.487764334752));
#88173=CARTESIAN_POINT('Ctrl Pts',(168.896540881497,58.3,182.579448040255));
#88174=CARTESIAN_POINT('Ctrl Pts',(168.834229775528,58.3,182.618766534837));
#88175=CARTESIAN_POINT('Ctrl Pts',(168.771814719992,58.3,182.657923280058));
#88176=CARTESIAN_POINT('Ctrl Pts',(168.70930320647,58.3,182.696914646047));
#88177=CARTESIAN_POINT('Ctrl Pts',(168.65073375144,58.3,182.73344716507));
#88178=CARTESIAN_POINT('Ctrl Pts',(168.592082735421,58.3,182.769832543196));
#88179=CARTESIAN_POINT('Ctrl Pts',(168.53336479753,58.3,182.806062663119));
#88180=CARTESIAN_POINT('Ctrl Pts',(168.50941434694,58.3,182.820840561121));
#88181=CARTESIAN_POINT('Ctrl Pts',(168.485452358266,58.3,182.835592880344));
#88182=CARTESIAN_POINT('Ctrl Pts',(168.46147926487,58.3,182.850319418911));
#88183=CARTESIAN_POINT('Ctrl Pts',(168.16996310164,58.3,183.029396184252));
#88184=CARTESIAN_POINT('Ctrl Pts',(167.876944721109,58.3,183.204614901521));
#88185=CARTESIAN_POINT('Ctrl Pts',(167.582420661783,58.3,183.376193981151));
#88186=CARTESIAN_POINT('Ctrl Pts',(167.384297562419,58.3,183.491613343224));
#88187=CARTESIAN_POINT('Ctrl Pts',(167.185493060971,58.3,183.605385563191));
#88188=CARTESIAN_POINT('Ctrl Pts',(166.986005365204,58.3,183.717575251625));
#88189=CARTESIAN_POINT('Ctrl Pts',(166.88894043217,58.3,183.772163503562));
#88190=CARTESIAN_POINT('Ctrl Pts',(166.791714968437,58.3,183.826376356018));
#88191=CARTESIAN_POINT('Ctrl Pts',(166.694335930232,58.3,183.880217249608));
#88192=CARTESIAN_POINT('Ctrl Pts',(165.743362022725,58.3,184.40601095125));
#88193=CARTESIAN_POINT('Ctrl Pts',(164.77778827359,58.300000000006,184.896759413961));
#88194=CARTESIAN_POINT('Ctrl Pts',(163.799410443834,58.3000000000113,185.356773192257));
#88195=CARTESIAN_POINT('Ctrl Pts',(162.812239974668,58.3000000000167,185.820921094562));
#88196=CARTESIAN_POINT('Ctrl Pts',(161.812034334544,58.3000000000215,186.253779613209));
#88197=CARTESIAN_POINT('Ctrl Pts',(160.800657512328,58.3000000000187,186.65982492006));
#88198=CARTESIAN_POINT('Ctrl Pts',(160.310977899702,58.3000000000174,186.85642039684));
#88199=CARTESIAN_POINT('Ctrl Pts',(159.818679490042,58.3000000000149,187.046731085773));
#88200=CARTESIAN_POINT('Ctrl Pts',(159.323976398265,58.3000000000085,187.23126844175));
#88201=CARTESIAN_POINT('Ctrl Pts',(158.693118416376,58.3000000000002,187.466595177947));
#88202=CARTESIAN_POINT('Ctrl Pts',(158.058297774254,58.2999999999984,187.692418003417));
#88203=CARTESIAN_POINT('Ctrl Pts',(157.419838084178,58.2999999999987,187.90950712755));
#88204=CARTESIAN_POINT('Ctrl Pts',(157.019499271022,58.2999999999989,188.045630368619));
#88205=CARTESIAN_POINT('Ctrl Pts',(156.617729711881,58.2999999999999,188.178319832175));
#88206=CARTESIAN_POINT('Ctrl Pts',(156.214609615834,58.3000000000006,188.307766497905));
#88207=CARTESIAN_POINT('Ctrl Pts',(155.974834436361,58.300000000001,188.384761164785));
#88208=CARTESIAN_POINT('Ctrl Pts',(155.734577642747,58.3000000000014,188.460609750306));
#88209=CARTESIAN_POINT('Ctrl Pts',(155.493876194085,58.3000000000011,188.535346445525));
#88210=CARTESIAN_POINT('Ctrl Pts',(154.849286915676,58.3000000000005,188.735488458419));
#88211=CARTESIAN_POINT('Ctrl Pts',(154.200851882107,58.3000000000027,188.927821054048));
#88212=CARTESIAN_POINT('Ctrl Pts',(153.549758382642,58.3000000000043,189.112746132646));
#88213=CARTESIAN_POINT('Ctrl Pts',(153.22421163291,58.3000000000051,189.205208671945));
#88214=CARTESIAN_POINT('Ctrl Pts',(152.898000237318,58.3000000000059,189.295819123002));
#88215=CARTESIAN_POINT('Ctrl Pts',(152.571272698334,58.300000000006,189.384626541979));
#88216=CARTESIAN_POINT('Ctrl Pts',(152.40637937128,58.3000000000061,189.429445998667));
#88217=CARTESIAN_POINT('Ctrl Pts',(152.241354583909,58.3000000000061,189.473806205152));
#88218=CARTESIAN_POINT('Ctrl Pts',(152.076217453316,58.3000000000058,189.517713397122));
#88219=CARTESIAN_POINT('Ctrl Pts',(151.943218487967,58.3000000000057,189.553075590242));
#88220=CARTESIAN_POINT('Ctrl Pts',(151.810145259381,58.3000000000053,189.588144276204));
#88221=CARTESIAN_POINT('Ctrl Pts',(151.677027855266,58.3000000000049,189.622917517318));
#88222=CARTESIAN_POINT('Ctrl Pts',(151.647927436647,58.3000000000048,189.630519197052));
#88223=CARTESIAN_POINT('Ctrl Pts',(151.6188246989,58.3000000000047,189.638106813488));
#88224=CARTESIAN_POINT('Ctrl Pts',(151.58971975818,58.3000000000046,189.645680399349));
#88225=CARTESIAN_POINT('Ctrl Pts',(150.281298068072,58.2999999999996,189.986153314478));
#88226=CARTESIAN_POINT('Ctrl Pts',(148.970507516125,58.2999999999987,190.29820923237));
#88227=CARTESIAN_POINT('Ctrl Pts',(147.657489395235,58.3000000000009,190.586549148116));
#88228=CARTESIAN_POINT('Ctrl Pts',(147.000980334791,58.3000000000021,190.730719105988));
#88229=CARTESIAN_POINT('Ctrl Pts',(146.343914360902,58.3000000000039,190.86895978395));
#88230=CARTESIAN_POINT('Ctrl Pts',(145.686309051208,58.3000000000064,191.001857725282));
#88231=CARTESIAN_POINT('Ctrl Pts',(145.236864991416,58.3000000000082,191.092687573232));
#88232=CARTESIAN_POINT('Ctrl Pts',(144.787169000648,58.3000000000102,191.181021754716));
#88233=CARTESIAN_POINT('Ctrl Pts',(144.337226685912,58.3000000000124,191.267047472895));
#88234=CARTESIAN_POINT('Ctrl Pts',(144.128834667865,58.3000000000135,191.306890520389));
#88235=CARTESIAN_POINT('Ctrl Pts',(143.920388679827,58.3000000000144,191.346238581224));
#88236=CARTESIAN_POINT('Ctrl Pts',(143.711897764384,58.3000000000166,191.385108697693));
#88237=CARTESIAN_POINT('Ctrl Pts',(141.950705915482,58.3000000000348,191.713457451624));
#88238=CARTESIAN_POINT('Ctrl Pts',(140.18618180257,58.3000000000201,192.00744782213));
#88239=CARTESIAN_POINT('Ctrl Pts',(138.418978260056,58.3000000000199,192.273910828531));
#88240=CARTESIAN_POINT('Ctrl Pts',(137.546066134828,58.3000000000198,192.405530522368));
#88241=CARTESIAN_POINT('Ctrl Pts',(136.67249987358,58.3000000000189,192.530434774035));
#88242=CARTESIAN_POINT('Ctrl Pts',(135.798359950109,58.300000000037,192.64945104723));
#88243=CARTESIAN_POINT('Ctrl Pts',(133.742775355374,58.3000000000793,192.92932388124));
#88244=CARTESIAN_POINT('Ctrl Pts',(131.684009335516,58.3000000000285,193.176457521784));
#88245=CARTESIAN_POINT('Ctrl Pts',(129.622741670531,58.3000000000104,193.397881860408));
#88246=CARTESIAN_POINT('Ctrl Pts',(129.035162857518,58.3000000000053,193.461000421995));
#88247=CARTESIAN_POINT('Ctrl Pts',(128.447380523824,58.3000000000026,193.522030199221));
#88248=CARTESIAN_POINT('Ctrl Pts',(127.859411366078,58.300000000006,193.581134526229));
#88249=CARTESIAN_POINT('Ctrl Pts',(125.144150532821,58.3000000000217,193.854080244702));
#88250=CARTESIAN_POINT('Ctrl Pts',(122.424955174928,58.3000000000296,194.086609826551));
#88251=CARTESIAN_POINT('Ctrl Pts',(119.702735219,58.3000000000308,194.288037034846));
#88252=CARTESIAN_POINT('Ctrl Pts',(117.52258727193,58.3000000000318,194.449354313301));
#88253=CARTESIAN_POINT('Ctrl Pts',(115.34049946053,58.3000000000286,194.590723963524));
#88254=CARTESIAN_POINT('Ctrl Pts',(113.156940738231,58.3000000000219,194.716950363975));
#88255=CARTESIAN_POINT('Ctrl Pts',(112.748095170393,58.3000000000206,194.740584765853));
#88256=CARTESIAN_POINT('Ctrl Pts',(112.339198168107,58.3000000000193,194.763688308341));
#88257=CARTESIAN_POINT('Ctrl Pts',(111.930252346801,58.3000000000176,194.786292608757));
#88258=CARTESIAN_POINT('Ctrl Pts',(107.974706849214,58.3000000000011,195.004933646458));
#88259=CARTESIAN_POINT('Ctrl Pts',(104.014516979677,58.3000000000813,195.175894172209));
#88260=CARTESIAN_POINT('Ctrl Pts',(100.051160230625,58.3000000000906,195.314262542956));
#88261=CARTESIAN_POINT('Ctrl Pts',(98.6870863726536,58.3000000000937,195.361884972441));
#88262=CARTESIAN_POINT('Ctrl Pts',(97.3226373712284,58.3000000000908,195.4056472157));
#88263=CARTESIAN_POINT('Ctrl Pts',(95.9578737332232,58.3000000000677,195.446165741684));
#88264=CARTESIAN_POINT('Ctrl Pts',(93.2937797771291,58.3000000000226,195.525260141021));
#88265=CARTESIAN_POINT('Ctrl Pts',(90.6283351792062,58.3000000000059,195.591817563437));
#88266=CARTESIAN_POINT('Ctrl Pts',(87.9622980004928,58.3000000000006,195.648477101291));
#88267=CARTESIAN_POINT('Ctrl Pts',(86.4341094435501,58.2999999999976,195.680954689406));
#88268=CARTESIAN_POINT('Ctrl Pts',(84.9057261977232,58.2999999999983,195.710180208743));
#88269=CARTESIAN_POINT('Ctrl Pts',(83.3772911454653,58.2999999999996,195.736650984406));
#88270=CARTESIAN_POINT('Ctrl Pts',(82.3556671155038,58.3000000000005,195.75434436331));
#88271=CARTESIAN_POINT('Ctrl Pts',(81.3340199414989,58.3000000000017,195.770806997954));
#88272=CARTESIAN_POINT('Ctrl Pts',(80.3123923151694,58.3000000000021,195.78618746494));
#88273=CARTESIAN_POINT('Ctrl Pts',(80.1959837797084,58.3000000000022,195.787939979839));
#88274=CARTESIAN_POINT('Ctrl Pts',(80.07957550807,58.3000000000022,195.789678444541));
#88275=CARTESIAN_POINT('Ctrl Pts',(79.963167768534,58.3000000000022,195.791403075907));
#88276=CARTESIAN_POINT('Ctrl Pts',(76.1297303378317,58.3000000000006,195.848197121193));
#88277=CARTESIAN_POINT('Ctrl Pts',(72.296147342554,58.3000000000581,195.889842872884));
#88278=CARTESIAN_POINT('Ctrl Pts',(68.4624943285942,58.3000000000755,195.92117010135));
#88279=CARTESIAN_POINT('Ctrl Pts',(66.9644162966496,58.3000000000824,195.933411854215));
#88280=CARTESIAN_POINT('Ctrl Pts',(65.4663277778819,58.3000000000841,195.944078033995));
#88281=CARTESIAN_POINT('Ctrl Pts',(63.9682326441713,58.3000000000717,195.953457116585));
#88282=CARTESIAN_POINT('Ctrl Pts',(58.6374128389633,58.3000000000276,195.986831632062));
#88283=CARTESIAN_POINT('Ctrl Pts',(53.3064763293957,58.3000000000836,196.004466674216));
#88284=CARTESIAN_POINT('Ctrl Pts',(47.9754976701507,58.3000000001318,196.01317970203));
#88285=CARTESIAN_POINT('Ctrl Pts',(44.2887044272162,58.3000000001652,196.019205449669));
#88286=CARTESIAN_POINT('Ctrl Pts',(40.6018910228219,58.3000000001949,196.020964143901));
#88287=CARTESIAN_POINT('Ctrl Pts',(36.9150820978944,58.3000000001853,196.020712341452));
#88288=CARTESIAN_POINT('Ctrl Pts',(35.270889687944,58.300000000181,196.020600046054));
#88289=CARTESIAN_POINT('Ctrl Pts',(33.6266983124335,58.3000000001696,196.020087903778));
#88290=CARTESIAN_POINT('Ctrl Pts',(31.9825097205404,58.3000000001458,196.019376110131));
#88291=CARTESIAN_POINT('Ctrl Pts',(21.3216725475386,58.2999999999912,196.014760875474));
#88292=CARTESIAN_POINT('Ctrl Pts',(10.6608381121449,58.3,196.));
#88293=CARTESIAN_POINT('Ctrl Pts',(1.06581410364015E-14,58.3,196.));
#88294=CARTESIAN_POINT('Ctrl Pts',(1.20290037631083E-14,55.3,196.));
#88295=CARTESIAN_POINT('Ctrl Pts',(10.7117531408873,55.3,196.));
#88296=CARTESIAN_POINT('Ctrl Pts',(21.4235888453034,55.3,196.014918521175));
#88297=CARTESIAN_POINT('Ctrl Pts',(32.1353671216414,55.3,196.019441470522));
#88298=CARTESIAN_POINT('Ctrl Pts',(37.9435392315241,55.2999999999999,196.0218939175));
#88299=CARTESIAN_POINT('Ctrl Pts',(43.751697287797,55.2999999999995,196.021820075071));
#88300=CARTESIAN_POINT('Ctrl Pts',(49.5597922503515,55.2999999999992,196.010342399909));
#88301=CARTESIAN_POINT('Ctrl Pts',(54.4645376663083,55.2999999999989,196.000649880244));
#88302=CARTESIAN_POINT('Ctrl Pts',(59.3692380077688,55.2999999999989,195.982824984605));
#88303=CARTESIAN_POINT('Ctrl Pts',(64.273863499599,55.2999999999994,195.951525205213));
#88304=CARTESIAN_POINT('Ctrl Pts',(69.6310359294058,55.2999999999999,195.917337413403));
#88305=CARTESIAN_POINT('Ctrl Pts',(74.9881325496578,55.299999999963,195.866500385808));
#88306=CARTESIAN_POINT('Ctrl Pts',(80.3450312167435,55.2999999999824,195.785694345575));
#88307=CARTESIAN_POINT('Ctrl Pts',(82.3276173506661,55.2999999999896,195.7557880612));
#88308=CARTESIAN_POINT('Ctrl Pts',(84.310265521851,55.2999999999926,195.72182275657));
#88309=CARTESIAN_POINT('Ctrl Pts',(86.2928745789687,55.2999999999948,195.682687443605));
#88310=CARTESIAN_POINT('Ctrl Pts',(89.6683015743703,55.2999999999986,195.616058880913));
#88311=CARTESIAN_POINT('Ctrl Pts',(93.0436128903952,55.2999999999982,195.534444136816));
#88312=CARTESIAN_POINT('Ctrl Pts',(96.4182977668295,55.2999999999993,195.432367934215));
#88313=CARTESIAN_POINT('Ctrl Pts',(99.0028738236992,55.3000000000002,195.354190646888));
#88314=CARTESIAN_POINT('Ctrl Pts',(101.586488207725,55.2999999999912,195.264202295603));
#88315=CARTESIAN_POINT('Ctrl Pts',(104.168792975622,55.2999999999847,195.15812279501));
#88316=CARTESIAN_POINT('Ctrl Pts',(106.940470574378,55.2999999999776,195.044263974341));
#88317=CARTESIAN_POINT('Ctrl Pts',(109.71063859809,55.2999999999726,194.911867034808));
#88318=CARTESIAN_POINT('Ctrl Pts',(112.478864925772,55.2999999999828,194.755651977743));
#88319=CARTESIAN_POINT('Ctrl Pts',(114.594741665139,55.2999999999906,194.636249961268));
#88320=CARTESIAN_POINT('Ctrl Pts',(116.709508625892,55.2999999999934,194.503229216588));
#88321=CARTESIAN_POINT('Ctrl Pts',(118.822799974681,55.2999999999957,194.352074481563));
#88322=CARTESIAN_POINT('Ctrl Pts',(121.558121076672,55.2999999999986,194.156428605941));
#88323=CARTESIAN_POINT('Ctrl Pts',(124.290968486144,55.299999999999,193.930400377491));
#88324=CARTESIAN_POINT('Ctrl Pts',(127.020545582271,55.2999999999995,193.664238101445));
#88325=CARTESIAN_POINT('Ctrl Pts',(127.515029972198,55.2999999999997,193.616020708766));
#88326=CARTESIAN_POINT('Ctrl Pts',(128.009407044772,55.2999999999998,193.566486327208));
#88327=CARTESIAN_POINT('Ctrl Pts',(128.503672075522,55.2999999999999,193.515577171767));
#88328=CARTESIAN_POINT('Ctrl Pts',(130.440299623163,55.3000000000005,193.316105093589));
#88329=CARTESIAN_POINT('Ctrl Pts',(132.375181150211,55.2999999999988,193.095177946254));
#88330=CARTESIAN_POINT('Ctrl Pts',(134.307818538159,55.2999999999985,192.846713609731));
#88331=CARTESIAN_POINT('Ctrl Pts',(135.03715051433,55.2999999999985,192.752949002519));
#88332=CARTESIAN_POINT('Ctrl Pts',(135.766163078809,55.2999999999985,192.655263061591));
#88333=CARTESIAN_POINT('Ctrl Pts',(136.494829730513,55.2999999999989,192.553330224408));
#88334=CARTESIAN_POINT('Ctrl Pts',(136.887919350373,55.2999999999991,192.498341101294));
#88335=CARTESIAN_POINT('Ctrl Pts',(137.280909845793,55.2999999999986,192.442107502062));
#88336=CARTESIAN_POINT('Ctrl Pts',(137.673799419673,55.2999999999978,192.38455841101));
#88337=CARTESIAN_POINT('Ctrl Pts',(138.610834346566,55.299999999996,192.247304811242));
#88338=CARTESIAN_POINT('Ctrl Pts',(139.547276689375,55.299999999993,192.102570256913));
#88339=CARTESIAN_POINT('Ctrl Pts',(140.482938496474,55.299999999998,191.949421722643));
#88340=CARTESIAN_POINT('Ctrl Pts',(140.735750542117,55.2999999999994,191.908041606513));
#88341=CARTESIAN_POINT('Ctrl Pts',(140.988534796001,55.2999999999993,191.866041231155));
#88342=CARTESIAN_POINT('Ctrl Pts',(141.241276767632,55.2999999999987,191.823400407199));
#88343=CARTESIAN_POINT('Ctrl Pts',(142.316874400025,55.2999999999962,191.64193324132));
#88344=CARTESIAN_POINT('Ctrl Pts',(143.391615359688,55.2999999999831,191.448879233622));
#88345=CARTESIAN_POINT('Ctrl Pts',(144.462423620222,55.2999999999908,191.243014958559));
#88346=CARTESIAN_POINT('Ctrl Pts',(144.849418372946,55.2999999999936,191.168614716089));
#88347=CARTESIAN_POINT('Ctrl Pts',(145.235966787396,55.2999999999938,191.092555243525));
#88348=CARTESIAN_POINT('Ctrl Pts',(145.622054184335,55.2999999999945,191.014726801987));
#88349=CARTESIAN_POINT('Ctrl Pts',(147.026900291875,55.2999999999974,190.731534488493));
#88350=CARTESIAN_POINT('Ctrl Pts',(148.425595069659,55.2999999999977,190.424926343951));
#88351=CARTESIAN_POINT('Ctrl Pts',(149.816785361501,55.2999999999978,190.089768262817));
#88352=CARTESIAN_POINT('Ctrl Pts',(150.659099488471,55.2999999999978,189.886842474617));
#88353=CARTESIAN_POINT('Ctrl Pts',(151.498662786036,55.2999999999977,189.673451564913));
#88354=CARTESIAN_POINT('Ctrl Pts',(152.33517708753,55.299999999998,189.448465183433));
#88355=CARTESIAN_POINT('Ctrl Pts',(152.632968543411,55.2999999999981,189.368372085234));
#88356=CARTESIAN_POINT('Ctrl Pts',(152.930371374219,55.2999999999987,189.286797545909));
#88357=CARTESIAN_POINT('Ctrl Pts',(153.227374222845,55.2999999999992,189.203666632533));
#88358=CARTESIAN_POINT('Ctrl Pts',(154.1623023375,55.3000000000009,188.941980832308));
#88359=CARTESIAN_POINT('Ctrl Pts',(155.093231051561,55.3000000000026,188.664878292928));
#88360=CARTESIAN_POINT('Ctrl Pts',(156.019362669451,55.2999999999938,188.370172226066));
#88361=CARTESIAN_POINT('Ctrl Pts',(156.084148338743,55.2999999999931,188.349556657591));
#88362=CARTESIAN_POINT('Ctrl Pts',(156.148910538799,55.2999999999925,188.328854968572));
#88363=CARTESIAN_POINT('Ctrl Pts',(156.213648998874,55.2999999999917,188.308066420174));
#88364=CARTESIAN_POINT('Ctrl Pts',(156.416564746944,55.2999999999895,188.242906948592));
#88365=CARTESIAN_POINT('Ctrl Pts',(156.619277412703,55.2999999999878,188.17688312004));
#88366=CARTESIAN_POINT('Ctrl Pts',(156.821789359415,55.299999999986,188.109962014282));
#88367=CARTESIAN_POINT('Ctrl Pts',(157.67443976817,55.2999999999783,187.828199337537));
#88368=CARTESIAN_POINT('Ctrl Pts',(158.523442540595,55.2999999999708,187.530554238279));
#88369=CARTESIAN_POINT('Ctrl Pts',(159.36671167149,55.2999999999747,187.215315781269));
#88370=CARTESIAN_POINT('Ctrl Pts',(159.592281275708,55.2999999999758,187.130991321406));
#88371=CARTESIAN_POINT('Ctrl Pts',(159.817440724798,55.2999999999776,187.045408264328));
#88372=CARTESIAN_POINT('Ctrl Pts',(160.042150350672,55.2999999999805,186.958534466439));
#88373=CARTESIAN_POINT('Ctrl Pts',(160.341043434012,55.2999999999843,186.842980995103));
#88374=CARTESIAN_POINT('Ctrl Pts',(160.638745179164,55.2999999999854,186.725316027712));
#88375=CARTESIAN_POINT('Ctrl Pts',(160.935217111381,55.2999999999872,186.605440010869));
#88376=CARTESIAN_POINT('Ctrl Pts',(162.043912956315,55.2999999999939,186.157147854555));
#88377=CARTESIAN_POINT('Ctrl Pts',(163.135358576353,55.2999999999986,185.677949054978));
#88378=CARTESIAN_POINT('Ctrl Pts',(164.206821631529,55.2999999999996,185.162953213729));
#88379=CARTESIAN_POINT('Ctrl Pts',(165.213812236743,55.3000000000006,184.678945882486));
#88380=CARTESIAN_POINT('Ctrl Pts',(166.203152860742,55.2999999999984,184.163320140631));
#88381=CARTESIAN_POINT('Ctrl Pts',(167.172600012654,55.2999999999914,183.612061848847));
#88382=CARTESIAN_POINT('Ctrl Pts',(167.234668747626,55.299999999991,183.576767604343));
#88383=CARTESIAN_POINT('Ctrl Pts',(167.296655944075,55.2999999999905,183.541327311083));
#88384=CARTESIAN_POINT('Ctrl Pts',(167.358561016714,55.29999999999,183.505739922036));
#88385=CARTESIAN_POINT('Ctrl Pts',(168.39480559842,55.2999999999819,182.910033665581));
#88386=CARTESIAN_POINT('Ctrl Pts',(169.407908306295,55.299999999996,182.272890824595));
#88387=CARTESIAN_POINT('Ctrl Pts',(170.394543441111,55.2999999999993,181.588329526098));
#88388=CARTESIAN_POINT('Ctrl Pts',(170.521203856873,55.2999999999997,181.500448185142));
#88389=CARTESIAN_POINT('Ctrl Pts',(170.647428055806,55.3,181.411785408126));
#88390=CARTESIAN_POINT('Ctrl Pts',(170.773208999519,55.3,181.322328563753));
#88391=CARTESIAN_POINT('Ctrl Pts',(170.892813073087,55.3,181.237264780005));
#88392=CARTESIAN_POINT('Ctrl Pts',(171.01201767922,55.3,181.151481005919));
#88393=CARTESIAN_POINT('Ctrl Pts',(171.130802556229,55.3,181.064975842039));
#88394=CARTESIAN_POINT('Ctrl Pts',(171.50882619844,55.3,180.789679878921));
#88395=CARTESIAN_POINT('Ctrl Pts',(171.882642940618,55.3,180.507051762352));
#88396=CARTESIAN_POINT('Ctrl Pts',(172.252308618058,55.3,180.216507799462));
#88397=CARTESIAN_POINT('Ctrl Pts',(172.303960392832,55.3,180.175911357193));
#88398=CARTESIAN_POINT('Ctrl Pts',(172.355531085545,55.3,180.135160298557));
#88399=CARTESIAN_POINT('Ctrl Pts',(172.407020808966,55.3,180.094252958565));
#88400=CARTESIAN_POINT('Ctrl Pts',(172.455054775581,55.3,180.056091133778));
#88401=CARTESIAN_POINT('Ctrl Pts',(172.503007690529,55.3,180.017800247509));
#88402=CARTESIAN_POINT('Ctrl Pts',(172.550875974094,55.3,179.979382823621));
#88403=CARTESIAN_POINT('Ctrl Pts',(172.597530075614,55.3,179.941939860122));
#88404=CARTESIAN_POINT('Ctrl Pts',(172.644097657435,55.3,179.904381603449));
#88405=CARTESIAN_POINT('Ctrl Pts',(172.6905714067,55.3,179.866713791571));
#88406=CARTESIAN_POINT('Ctrl Pts',(173.036090102331,55.3,179.586664657738));
#88407=CARTESIAN_POINT('Ctrl Pts',(173.37649833556,55.3,179.300504249984));
#88408=CARTESIAN_POINT('Ctrl Pts',(173.710509895914,55.3,179.009174047778));
#88409=CARTESIAN_POINT('Ctrl Pts',(173.799924375868,55.3,178.931185314401));
#88410=CARTESIAN_POINT('Ctrl Pts',(173.888880288647,55.3,178.852825862511));
#88411=CARTESIAN_POINT('Ctrl Pts',(173.977352529315,55.3,178.77411328332));
#88412=CARTESIAN_POINT('Ctrl Pts',(174.086885478565,55.3,178.676663271014));
#88413=CARTESIAN_POINT('Ctrl Pts',(174.195746807261,55.3,178.578606701701));
#88414=CARTESIAN_POINT('Ctrl Pts',(174.303919095228,55.3,178.479961005701));
#88415=CARTESIAN_POINT('Ctrl Pts',(174.958585095774,55.3,177.882950583855));
#88416=CARTESIAN_POINT('Ctrl Pts',(175.588161561579,55.3,177.264237409506));
#88417=CARTESIAN_POINT('Ctrl Pts',(176.192889041399,55.3,176.624027678017));
#88418=CARTESIAN_POINT('Ctrl Pts',(176.801495030497,55.3,175.979711866572));
#88419=CARTESIAN_POINT('Ctrl Pts',(177.384932282356,55.3,175.313622824482));
#88420=CARTESIAN_POINT('Ctrl Pts',(177.943406015761,55.3,174.62593595727));
#88421=CARTESIAN_POINT('Ctrl Pts',(178.443543934614,55.3,174.010081964474));
#88422=CARTESIAN_POINT('Ctrl Pts',(178.923660583429,55.3,173.376906026298));
#88423=CARTESIAN_POINT('Ctrl Pts',(179.383876297428,55.3,172.726511192076));
#88424=CARTESIAN_POINT('Ctrl Pts',(179.775881961457,55.3,172.172513466411));
#88425=CARTESIAN_POINT('Ctrl Pts',(180.153586615474,55.3,171.606136536173));
#88426=CARTESIAN_POINT('Ctrl Pts',(180.517306782578,55.3,171.027671453042));
#88427=CARTESIAN_POINT('Ctrl Pts',(180.773257893905,55.3,170.620603618255));
#88428=CARTESIAN_POINT('Ctrl Pts',(181.022282246798,55.3,170.20742155264));
#88429=CARTESIAN_POINT('Ctrl Pts',(181.263216383822,55.3,169.7908638695));
#88430=CARTESIAN_POINT('Ctrl Pts',(181.364433858471,55.3,169.615866182357));
#88431=CARTESIAN_POINT('Ctrl Pts',(181.46422337679,55.2999999999999,169.44027295065));
#88432=CARTESIAN_POINT('Ctrl Pts',(181.562498312604,55.2999999999999,169.264287803902));
#88433=CARTESIAN_POINT('Ctrl Pts',(181.963798726816,55.2999999999999,168.545661923348));
#88434=CARTESIAN_POINT('Ctrl Pts',(182.341571888111,55.3,167.817934400603));
#88435=CARTESIAN_POINT('Ctrl Pts',(182.698078757659,55.3,167.081978998468));
#88436=CARTESIAN_POINT('Ctrl Pts',(182.93109709914,55.3,166.600947293731));
#88437=CARTESIAN_POINT('Ctrl Pts',(183.155030282405,55.3,166.116400730355));
#88438=CARTESIAN_POINT('Ctrl Pts',(183.370511496512,55.3,165.628584399066));
#88439=CARTESIAN_POINT('Ctrl Pts',(183.755753078273,55.3,164.756456701743));
#88440=CARTESIAN_POINT('Ctrl Pts',(184.114155490382,55.3,163.873945121211));
#88441=CARTESIAN_POINT('Ctrl Pts',(184.448595318293,55.3,162.982163050726));
#88442=CARTESIAN_POINT('Ctrl Pts',(184.791126490202,55.3,162.068805453339));
#88443=CARTESIAN_POINT('Ctrl Pts',(185.108521565696,55.3,161.145723431531));
#88444=CARTESIAN_POINT('Ctrl Pts',(185.403902175355,55.3,160.21412492318));
#88445=CARTESIAN_POINT('Ctrl Pts',(185.613942848109,55.3,159.551679349462));
#88446=CARTESIAN_POINT('Ctrl Pts',(185.812852754154,55.3,158.884927731768));
#88447=CARTESIAN_POINT('Ctrl Pts',(186.001763361621,55.3,158.21430775209));
#88448=CARTESIAN_POINT('Ctrl Pts',(186.02001879619,55.3,158.149502184398));
#88449=CARTESIAN_POINT('Ctrl Pts',(186.038180866162,55.3,158.084660468995));
#88450=CARTESIAN_POINT('Ctrl Pts',(186.056250572068,55.3,158.01978308872));
#88451=CARTESIAN_POINT('Ctrl Pts',(186.24876776852,55.3,157.328570324747));
#88452=CARTESIAN_POINT('Ctrl Pts',(186.430890225782,55.3,156.63235380753));
#88453=CARTESIAN_POINT('Ctrl Pts',(186.603184808282,55.3,155.933322134126));
#88454=CARTESIAN_POINT('Ctrl Pts',(186.726566943441,55.3,155.43273750078));
#88455=CARTESIAN_POINT('Ctrl Pts',(186.8449092848,55.3,154.930709442874));
#88456=CARTESIAN_POINT('Ctrl Pts',(186.958421359116,55.3,154.428044900815));
#88457=CARTESIAN_POINT('Ctrl Pts',(186.984076143135,55.3,154.314438041474));
#88458=CARTESIAN_POINT('Ctrl Pts',(187.009484234522,55.3,154.20079852715));
#88459=CARTESIAN_POINT('Ctrl Pts',(187.034647948172,55.3,154.087136197122));
#88460=CARTESIAN_POINT('Ctrl Pts',(187.249235230063,55.3,153.117863903177));
#88461=CARTESIAN_POINT('Ctrl Pts',(187.446091592081,55.2999999999899,152.147366177988));
#88462=CARTESIAN_POINT('Ctrl Pts',(187.627848642994,55.2999999999872,151.175802209577));
#88463=CARTESIAN_POINT('Ctrl Pts',(187.693091728517,55.2999999999863,150.8270518818));
#88464=CARTESIAN_POINT('Ctrl Pts',(187.756389466396,55.2999999999861,150.478163958403));
#88465=CARTESIAN_POINT('Ctrl Pts',(187.817864007364,55.2999999999881,150.129146500694));
#88466=CARTESIAN_POINT('Ctrl Pts',(188.069630152066,55.2999999999964,148.699761614247));
#88467=CARTESIAN_POINT('Ctrl Pts',(188.291104411737,55.2999999999992,147.268244191048));
#88468=CARTESIAN_POINT('Ctrl Pts',(188.488029524791,55.2999999999999,145.834998434922));
#88469=CARTESIAN_POINT('Ctrl Pts',(188.654658802898,55.3000000000006,144.622249578312));
#88470=CARTESIAN_POINT('Ctrl Pts',(188.803712719525,55.2999999999995,143.408263343521));
#88471=CARTESIAN_POINT('Ctrl Pts',(188.938699247615,55.2999999999996,142.193285856766));
#88472=CARTESIAN_POINT('Ctrl Pts',(189.136760801143,55.2999999999999,140.410587005753));
#88473=CARTESIAN_POINT('Ctrl Pts',(189.304299717647,55.2999999999999,138.625739912856));
#88474=CARTESIAN_POINT('Ctrl Pts',(189.448306949797,55.3,136.839236134823));
#88475=CARTESIAN_POINT('Ctrl Pts',(189.518148375124,55.3,135.972807634335));
#88476=CARTESIAN_POINT('Ctrl Pts',(189.582455728296,55.3,135.105989526119));
#88477=CARTESIAN_POINT('Ctrl Pts',(189.642030732453,55.3,134.238837995224));
#88478=CARTESIAN_POINT('Ctrl Pts',(189.792507914843,55.3,132.048548276901));
#88479=CARTESIAN_POINT('Ctrl Pts',(189.91260648438,55.3,129.856119556288));
#88480=CARTESIAN_POINT('Ctrl Pts',(190.010856013085,55.3,127.662152697902));
#88481=CARTESIAN_POINT('Ctrl Pts',(190.031601906391,55.3,127.198885311674));
#88482=CARTESIAN_POINT('Ctrl Pts',(190.051373807095,55.3,126.735549363847));
#88483=CARTESIAN_POINT('Ctrl Pts',(190.070252291175,55.3,126.272150491645));
#88484=CARTESIAN_POINT('Ctrl Pts',(190.155978348671,55.3,124.167884164185));
#88485=CARTESIAN_POINT('Ctrl Pts',(190.223186981995,55.3,122.062313754707));
#88486=CARTESIAN_POINT('Ctrl Pts',(190.277034501585,55.3,119.955802788295));
#88487=CARTESIAN_POINT('Ctrl Pts',(190.291163140251,55.3,119.403091493176));
#88488=CARTESIAN_POINT('Ctrl Pts',(190.304372045238,55.3,118.850315409215));
#88489=CARTESIAN_POINT('Ctrl Pts',(190.316754563799,55.3,118.297481238445));
#88490=CARTESIAN_POINT('Ctrl Pts',(190.397155299449,55.3,114.707882418131));
#88491=CARTESIAN_POINT('Ctrl Pts',(190.443516406214,55.3,111.115886118275));
#88492=CARTESIAN_POINT('Ctrl Pts',(190.471166981729,55.3,107.522572589343));
#88493=CARTESIAN_POINT('Ctrl Pts',(190.484470219953,55.3,105.793758450732));
#88494=CARTESIAN_POINT('Ctrl Pts',(190.493443302223,55.3,104.064639447949));
#88495=CARTESIAN_POINT('Ctrl Pts',(190.499797482064,55.3,102.335336081499));
#88496=CARTESIAN_POINT('Origin',(-122.710817715584,2.44173312008429,40.));
#88497=CARTESIAN_POINT('',(190.,55.3,40.));
#88498=CARTESIAN_POINT('',(-190.,55.3,40.));
#88499=CARTESIAN_POINT('',(-190.5,55.3,40.));
#88500=CARTESIAN_POINT('',(-190.,58.2999999999999,40.));
#88501=CARTESIAN_POINT('',(-190.,58.8,40.));
#88502=CARTESIAN_POINT('',(190.,58.3,40.));
#88503=CARTESIAN_POINT('',(190.5,58.3,40.));
#88504=CARTESIAN_POINT('',(190.,54.8,40.));
#88505=CARTESIAN_POINT('Origin',(-190.5,58.8,211.4));
#88506=CARTESIAN_POINT('',(-190.5,58.2999999999999,40.5));
#88507=CARTESIAN_POINT('',(-190.5,58.2999999999999,211.4));
#88508=CARTESIAN_POINT('',(-190.5,55.3,40.5));
#88509=CARTESIAN_POINT('',(-190.5,54.8,40.5));
#88510=CARTESIAN_POINT('',(-190.5,55.3,211.4));
#88511=CARTESIAN_POINT('Origin',(190.5,58.8,211.4));
#88512=CARTESIAN_POINT('',(190.5,55.3,40.5));
#88513=CARTESIAN_POINT('',(190.5,58.3,40.5));
#88514=CARTESIAN_POINT('',(190.5,58.8,40.5));
#88515=CARTESIAN_POINT('',(190.5,58.3,211.4));
#88516=CARTESIAN_POINT('',(190.5,55.3,211.4));
#88517=CARTESIAN_POINT('Ctrl Pts',(1.19489048671551E-14,54.8498893695668,
195.717716375983));
#88518=CARTESIAN_POINT('Ctrl Pts',(1.20290037631083E-14,54.9864286189535,
196.));
#88519=CARTESIAN_POINT('Ctrl Pts',(1.20290037631083E-14,55.3,196.));
#88520=CARTESIAN_POINT('Ctrl Pts',(10.7116410653504,54.8498893695294,195.717716376117));
#88521=CARTESIAN_POINT('Ctrl Pts',(10.7114086955983,54.9864286188836,196.000000000093));
#88522=CARTESIAN_POINT('Ctrl Pts',(10.7114086955983,55.3,196.));
#88523=CARTESIAN_POINT('Ctrl Pts',(21.4234737060142,54.8498893695169,195.732634823405));
#88524=CARTESIAN_POINT('Ctrl Pts',(21.4231418325433,54.9864286188603,196.014918332448));
#88525=CARTESIAN_POINT('Ctrl Pts',(21.4231418325433,55.3,196.014918332428));
#88526=CARTESIAN_POINT('Ctrl Pts',(42.8474989205484,54.8498893696167,195.741680919933));
#88527=CARTESIAN_POINT('Ctrl Pts',(42.8475924107395,54.9864286190467,196.023964608597));
#88528=CARTESIAN_POINT('Ctrl Pts',(42.8475924107395,55.3,196.023964608617));
#88529=CARTESIAN_POINT('Ctrl Pts',(53.5596882551516,54.8498893695668,195.737610334586));
#88530=CARTESIAN_POINT('Ctrl Pts',(53.560285285152,54.9864286189535,196.01989589653));
#88531=CARTESIAN_POINT('Ctrl Pts',(53.5602852851508,55.3,196.019895896344));
#88532=CARTESIAN_POINT('Ctrl Pts',(69.6282490087062,54.8498893695668,195.635065826431));
#88533=CARTESIAN_POINT('Ctrl Pts',(69.6306526068224,54.9864286189535,195.917339859554));
#88534=CARTESIAN_POINT('Ctrl Pts',(69.630652606823,55.3,195.917339859647));
#88535=CARTESIAN_POINT('Ctrl Pts',(74.9844823357142,54.8498893695756,195.584239709646));
#88536=CARTESIAN_POINT('Ctrl Pts',(74.9876678041973,54.986428618963,195.866507396292));
#88537=CARTESIAN_POINT('Ctrl Pts',(74.9876678041967,55.2999999999628,195.866507396253));
#88538=CARTESIAN_POINT('Ctrl Pts',(85.6970648621475,54.849889369558,195.422645953774));
#88539=CARTESIAN_POINT('Ctrl Pts',(85.7023946292896,54.9864286189441,195.704881294858));
#88540=CARTESIAN_POINT('Ctrl Pts',(85.7023946292902,55.3000000000371,195.704881294897));
#88541=CARTESIAN_POINT('Ctrl Pts',(91.054003880559,54.8498893696168,195.312212356202));
#88542=CARTESIAN_POINT('Ctrl Pts',(91.0606918125482,54.9864286190468,195.594422789953));
#88543=CARTESIAN_POINT('Ctrl Pts',(91.0606918125484,55.3,195.594422789964));
#88544=CARTESIAN_POINT('Ctrl Pts',(101.765522641295,54.8498893695169,194.988214353708));
#88545=CARTESIAN_POINT('Ctrl Pts',(101.775903721111,54.9864286188603,195.270313078475));
#88546=CARTESIAN_POINT('Ctrl Pts',(101.77590372111,55.3,195.270313078465));
#88547=CARTESIAN_POINT('Ctrl Pts',(107.117519783562,54.8498893695382,194.77546778461));
#88548=CARTESIAN_POINT('Ctrl Pts',(107.130224336095,54.9864286188931,195.057483582449));
#88549=CARTESIAN_POINT('Ctrl Pts',(107.130224336101,55.2999999999628,195.057483582545));
#88550=CARTESIAN_POINT('Ctrl Pts',(117.808401320513,54.8498893695954,194.172165716499));
#88551=CARTESIAN_POINT('Ctrl Pts',(117.827505515449,54.9864286190139,194.453820373037));
#88552=CARTESIAN_POINT('Ctrl Pts',(117.827505515444,55.3000000000371,194.453820372941));
#88553=CARTESIAN_POINT('Ctrl Pts',(123.147415580818,54.8498893695419,193.783493005426));
#88554=CARTESIAN_POINT('Ctrl Pts',(123.170566875688,54.986428618907,194.064885467392));
#88555=CARTESIAN_POINT('Ctrl Pts',(123.170566875683,55.3,194.06488546734));
#88556=CARTESIAN_POINT('Ctrl Pts',(131.138417142893,54.8498893695793,192.960422151946));
#88557=CARTESIAN_POINT('Ctrl Pts',(131.170224675439,54.9864286189768,193.240923023955));
#88558=CARTESIAN_POINT('Ctrl Pts',(131.170224675442,55.3,193.240923023981));
#88559=CARTESIAN_POINT('Ctrl Pts',(133.799118380507,54.8498893695668,192.645399766939));
#88560=CARTESIAN_POINT('Ctrl Pts',(133.834251546586,54.9864286189535,192.925517262466));
#88561=CARTESIAN_POINT('Ctrl Pts',(133.834251546587,55.3,192.925517262471));
#88562=CARTESIAN_POINT('Ctrl Pts',(137.784023815075,54.8498893695668,192.08795320905));
#88563=CARTESIAN_POINT('Ctrl Pts',(137.825118822477,54.9864286189535,192.367236705379));
#88564=CARTESIAN_POINT('Ctrl Pts',(137.825118822477,55.3,192.367236705376));
#88565=CARTESIAN_POINT('Ctrl Pts',(139.111294699818,54.8498893695628,191.887891561296));
#88566=CARTESIAN_POINT('Ctrl Pts',(139.154540611869,54.9864286189442,192.166853050329));
#88567=CARTESIAN_POINT('Ctrl Pts',(139.154540611864,55.2999999999907,192.1668530503));
#88568=CARTESIAN_POINT('Ctrl Pts',(141.763387800952,54.8498893695709,191.453798635637));
#88569=CARTESIAN_POINT('Ctrl Pts',(141.81133638108,54.9864286189629,191.731990394956));
#88570=CARTESIAN_POINT('Ctrl Pts',(141.811336381084,55.3000000000093,191.731990394986));
#88571=CARTESIAN_POINT('Ctrl Pts',(143.089104272173,54.8498893695493,191.219584409738));
#88572=CARTESIAN_POINT('Ctrl Pts',(143.139606665644,54.9864286189174,191.497328231536));
#88573=CARTESIAN_POINT('Ctrl Pts',(143.139606665632,55.2999999999813,191.497328231471));
#88574=CARTESIAN_POINT('Ctrl Pts',(147.049181964921,54.8498893696018,190.458254343683));
#88575=CARTESIAN_POINT('Ctrl Pts',(147.108057529376,54.9864286190258,190.734388412604));
#88576=CARTESIAN_POINT('Ctrl Pts',(147.108057529402,55.3000000000372,190.734388412735));
#88577=CARTESIAN_POINT('Ctrl Pts',(149.669629595343,54.8498893695668,189.873067582401));
#88578=CARTESIAN_POINT('Ctrl Pts',(149.735031156397,54.9864286189535,190.147792646745));
#88579=CARTESIAN_POINT('Ctrl Pts',(149.73503115636,55.2999999999999,190.147792646608));
#88580=CARTESIAN_POINT('Ctrl Pts',(153.557975830725,54.8498893695668,188.827269622761));
#88581=CARTESIAN_POINT('Ctrl Pts',(153.635250053096,54.9864286189535,189.098801451777));
#88582=CARTESIAN_POINT('Ctrl Pts',(153.635250053114,55.2999999999999,189.098801451845));
#88583=CARTESIAN_POINT('Ctrl Pts',(154.846981325738,54.8498893695781,188.450444611742));
#88584=CARTESIAN_POINT('Ctrl Pts',(154.928562946898,54.986428618978,188.720727975022));
#88585=CARTESIAN_POINT('Ctrl Pts',(154.928562946869,55.3000000000186,188.720727974942));
#88586=CARTESIAN_POINT('Ctrl Pts',(157.407706254429,54.8498893695556,187.628155140046));
#88587=CARTESIAN_POINT('Ctrl Pts',(157.49873505085,54.9864286189291,187.895404865325));
#88588=CARTESIAN_POINT('Ctrl Pts',(157.498735050879,55.2999999999814,187.895404865405));
#88589=CARTESIAN_POINT('Ctrl Pts',(158.680831044999,54.8498893695443,187.182182108568));
#88590=CARTESIAN_POINT('Ctrl Pts',(158.777006808679,54.9864286189044,187.447644908267));
#88591=CARTESIAN_POINT('Ctrl Pts',(158.777006808638,55.2999999999626,187.447644908161));
#88592=CARTESIAN_POINT('Ctrl Pts',(162.459418845047,54.8498893696119,185.721362298639));
#88593=CARTESIAN_POINT('Ctrl Pts',(162.572437434659,54.9864286190517,185.980313582784));
#88594=CARTESIAN_POINT('Ctrl Pts',(162.572437434741,55.3000000000747,185.980313582995));
#88595=CARTESIAN_POINT('Ctrl Pts',(164.895888522176,54.849889369586,184.595853659769));
#88596=CARTESIAN_POINT('Ctrl Pts',(165.021947502581,54.9864286189963,184.848989685788));
#88597=CARTESIAN_POINT('Ctrl Pts',(165.021947502437,55.300000000037,184.848989685601));
#88598=CARTESIAN_POINT('Ctrl Pts',(168.378867687188,54.8498893695572,182.593592304728));
#88599=CARTESIAN_POINT('Ctrl Pts',(168.526867773781,54.9864286189321,182.83411504016));
#88600=CARTESIAN_POINT('Ctrl Pts',(168.526867773853,55.2999999999815,182.834115040254));
#88601=CARTESIAN_POINT('Ctrl Pts',(169.511081787078,54.8498893695574,181.873572185375));
#88602=CARTESIAN_POINT('Ctrl Pts',(169.66677678621,54.986428618936,182.109235796402));
#88603=CARTESIAN_POINT('Ctrl Pts',(169.666776786129,55.3,182.109235796287));
#88604=CARTESIAN_POINT('Ctrl Pts',(171.158864505137,54.8498893695715,180.701650287951));
#88605=CARTESIAN_POINT('Ctrl Pts',(171.326425106174,54.9864286189623,180.928874947428));
#88606=CARTESIAN_POINT('Ctrl Pts',(171.326425106214,55.3,180.928874947486));
#88607=CARTESIAN_POINT('Ctrl Pts',(171.699692855963,54.8498893695652,180.295680572782));
#88608=CARTESIAN_POINT('Ctrl Pts',(171.871260701908,54.9864286189506,180.519901406498));
#88609=CARTESIAN_POINT('Ctrl Pts',(171.871260701868,55.3,180.51990140644));
#88610=CARTESIAN_POINT('Ctrl Pts',(172.763157385062,54.8498893695684,179.45078372375));
#88611=CARTESIAN_POINT('Ctrl Pts',(172.942780916024,54.9864286189565,179.668604510632));
#88612=CARTESIAN_POINT('Ctrl Pts',(172.942780916064,55.3,179.668604510689));
#88613=CARTESIAN_POINT('Ctrl Pts',(173.284486233779,54.8498893695692,179.012714799304));
#88614=CARTESIAN_POINT('Ctrl Pts',(173.468148508341,54.9864286189579,179.227145347657));
#88615=CARTESIAN_POINT('Ctrl Pts',(173.468148508335,55.3,179.227145347651));
#88616=CARTESIAN_POINT('Ctrl Pts',(175.810652663565,54.8498893695574,176.76521802901));
#88617=CARTESIAN_POINT('Ctrl Pts',(176.014168613212,54.986428618936,176.961985025973));
#88618=CARTESIAN_POINT('Ctrl Pts',(176.014168613234,55.3,176.961985025999));
#88619=CARTESIAN_POINT('Ctrl Pts',(177.597042024351,54.8498893695856,174.763030220158));
#88620=CARTESIAN_POINT('Ctrl Pts',(177.815415056872,54.9864286189885,174.94312191924));
#88621=CARTESIAN_POINT('Ctrl Pts',(177.81541505695,55.3,174.943121919295));
#88622=CARTESIAN_POINT('Ctrl Pts',(179.542546567764,54.8498893695622,172.013567161068));
#88623=CARTESIAN_POINT('Ctrl Pts',(179.775991607566,54.9864286189448,172.172358510285));
#88624=CARTESIAN_POINT('Ctrl Pts',(179.775991607547,55.3,172.172358510271));
#88625=CARTESIAN_POINT('Ctrl Pts',(179.917402670385,54.8498893695668,171.451447836108));
#88626=CARTESIAN_POINT('Ctrl Pts',(180.153696573191,54.9864286189535,171.605961657991));
#88627=CARTESIAN_POINT('Ctrl Pts',(180.153696573218,55.3,171.605961658008));
#88628=CARTESIAN_POINT('Ctrl Pts',(180.639269900445,54.8498893695668,170.303381204245));
#88629=CARTESIAN_POINT('Ctrl Pts',(180.880916991964,54.9864286189535,170.449381248092));
#88630=CARTESIAN_POINT('Ctrl Pts',(180.880916991938,55.3,170.449381248076));
#88631=CARTESIAN_POINT('Ctrl Pts',(180.986269545301,54.8498893695668,169.71719072451));
#88632=CARTESIAN_POINT('Ctrl Pts',(181.230420402754,54.9864286189535,169.858953973853));
#88633=CARTESIAN_POINT('Ctrl Pts',(181.230420402816,55.3,169.858953973888));
#88634=CARTESIAN_POINT('Ctrl Pts',(181.9755782218,54.8498893695668,167.945593204617));
#88635=CARTESIAN_POINT('Ctrl Pts',(182.226654132303,54.9864286189535,168.074955463999));
#88636=CARTESIAN_POINT('Ctrl Pts',(182.226654132179,55.3,168.07495546393));
#88637=CARTESIAN_POINT('Ctrl Pts',(182.570885742225,54.8498893695668,166.740197827949));
#88638=CARTESIAN_POINT('Ctrl Pts',(182.825829796685,54.9864286189535,166.86166000408));
#88639=CARTESIAN_POINT('Ctrl Pts',(182.825829796816,55.3,166.861660004138));
#88640=CARTESIAN_POINT('Ctrl Pts',(184.195121388266,54.8498893695668,163.063178107394));
#88641=CARTESIAN_POINT('Ctrl Pts',(184.459874896166,54.9864286189535,163.162433189036));
#88642=CARTESIAN_POINT('Ctrl Pts',(184.459874895903,55.3,163.16243318892));
#88643=CARTESIAN_POINT('Ctrl Pts',(185.06372001807,54.8498893695668,160.531273278361));
#88644=CARTESIAN_POINT('Ctrl Pts',(185.332658084462,54.9864286189535,160.617765878982));
#88645=CARTESIAN_POINT('Ctrl Pts',(185.332658084646,55.3,160.617765879034));
#88646=CARTESIAN_POINT('Ctrl Pts',(186.144616122717,54.8498893695668,156.650429397757));
#88647=CARTESIAN_POINT('Ctrl Pts',(186.418046815871,54.9864286189535,156.720791693588));
#88648=CARTESIAN_POINT('Ctrl Pts',(186.418046815779,55.3,156.720791693563));
#88649=CARTESIAN_POINT('Ctrl Pts',(186.46824053002,54.8498893695543,155.339625317485));
#88650=CARTESIAN_POINT('Ctrl Pts',(186.742866764419,54.9864286189301,155.405086705306));
#88651=CARTESIAN_POINT('Ctrl Pts',(186.742866764507,55.3,155.405086705325));
#88652=CARTESIAN_POINT('Ctrl Pts',(187.049835163757,54.8498893695793,152.712612385649));
#88653=CARTESIAN_POINT('Ctrl Pts',(187.326429131926,54.9864286189768,152.769185688938));
#88654=CARTESIAN_POINT('Ctrl Pts',(187.326429131838,55.3,152.769185688918));
#88655=CARTESIAN_POINT('Ctrl Pts',(187.307891131261,54.8498893695494,151.397166218267));
#88656=CARTESIAN_POINT('Ctrl Pts',(187.585258126244,54.9864286189176,151.449750314472));
#88657=CARTESIAN_POINT('Ctrl Pts',(187.585258126311,55.2999999999814,151.449750314484));
#88658=CARTESIAN_POINT('Ctrl Pts',(188.00379723173,54.8498893696016,147.446207430077));
#88659=CARTESIAN_POINT('Ctrl Pts',(188.283075769604,54.9864286190254,147.487938873138));
#88660=CARTESIAN_POINT('Ctrl Pts',(188.283075769471,55.300000000037,147.487938873115));
#88661=CARTESIAN_POINT('Ctrl Pts',(188.364385942478,54.8498893695668,144.806133531479));
#88662=CARTESIAN_POINT('Ctrl Pts',(188.644410165646,54.9864286189535,144.842102846927));
#88663=CARTESIAN_POINT('Ctrl Pts',(188.644410165762,55.3,144.84210284694));
#88664=CARTESIAN_POINT('Ctrl Pts',(188.951897791745,54.8498893695668,139.51809716399));
#88665=CARTESIAN_POINT('Ctrl Pts',(189.232988329585,54.9864286189535,139.544468866606));
#88666=CARTESIAN_POINT('Ctrl Pts',(189.232988329468,55.3,139.544468866593));
#88667=CARTESIAN_POINT('Ctrl Pts',(189.178308705455,54.8498893695668,136.870102382931));
#88668=CARTESIAN_POINT('Ctrl Pts',(189.45970916863,54.9864286189535,136.892642646069));
#88669=CARTESIAN_POINT('Ctrl Pts',(189.459709168719,55.3,136.892642646075));
#88670=CARTESIAN_POINT('Ctrl Pts',(189.542513180321,54.8498893695668,131.568877948139));
#88671=CARTESIAN_POINT('Ctrl Pts',(189.824352296276,54.9864286189535,131.585033344378));
#88672=CARTESIAN_POINT('Ctrl Pts',(189.824352296186,55.3,131.585033344372));
#88673=CARTESIAN_POINT('Ctrl Pts',(189.68004124865,54.8498893695668,128.915632750363));
#88674=CARTESIAN_POINT('Ctrl Pts',(189.962004740436,54.9864286189535,128.929238460971));
#88675=CARTESIAN_POINT('Ctrl Pts',(189.962004740445,55.3,128.929238460971));
#88676=CARTESIAN_POINT('Ctrl Pts',(189.89636400371,54.8498893695668,123.605687296072));
#88677=CARTESIAN_POINT('Ctrl Pts',(190.178499841913,54.9864286189535,123.615062522318));
#88678=CARTESIAN_POINT('Ctrl Pts',(190.178499841904,55.3,123.615062522318));
#88679=CARTESIAN_POINT('Ctrl Pts',(189.975011236078,54.8498893695668,120.9489786286));
#88680=CARTESIAN_POINT('Ctrl Pts',(190.257193263767,54.9864286189535,120.956675467105));
#88681=CARTESIAN_POINT('Ctrl Pts',(190.257193263798,55.3,120.956675467117));
#88682=CARTESIAN_POINT('Ctrl Pts',(190.155938877336,54.8498893695668,112.871221107224));
#88683=CARTESIAN_POINT('Ctrl Pts',(190.438214558407,54.9864286189535,112.874736662693));
#88684=CARTESIAN_POINT('Ctrl Pts',(190.438214558344,55.3,112.874736662668));
#88685=CARTESIAN_POINT('Ctrl Pts',(190.199675585056,54.8498893695475,107.446717574517));
#88686=CARTESIAN_POINT('Ctrl Pts',(190.481953816303,54.9864286189174,107.448676238389));
#88687=CARTESIAN_POINT('Ctrl Pts',(190.481953816244,55.3,107.448676238409));
#88688=CARTESIAN_POINT('Ctrl Pts',(190.218638436563,54.849889369568,102.021063856015));
#88689=CARTESIAN_POINT('Ctrl Pts',(190.500920367765,54.9864286189556,102.022043932952));
#88690=CARTESIAN_POINT('Ctrl Pts',(190.500920367768,55.3,102.022043932951));
#88691=CARTESIAN_POINT('',(119.410706527861,54.8500000000013,194.026226514646));
#88692=CARTESIAN_POINT('',(1.20290037631083E-14,54.8500000000093,195.717944947196));
#88693=CARTESIAN_POINT('Ctrl Pts',(119.410743668763,54.8500000000039,194.026733883575));
#88694=CARTESIAN_POINT('Ctrl Pts',(117.096090401041,54.8500000000093,194.196173327592));
#88695=CARTESIAN_POINT('Ctrl Pts',(114.779973647168,54.8500000000123,194.343293250508));
#88696=CARTESIAN_POINT('Ctrl Pts',(112.462973430155,54.8499999999998,194.474044958672));
#88697=CARTESIAN_POINT('Ctrl Pts',(110.006841798142,54.8499999999867,194.612648055902));
#88698=CARTESIAN_POINT('Ctrl Pts',(107.549690002739,54.8499999999751,194.732460623929));
#88699=CARTESIAN_POINT('Ctrl Pts',(105.091970605807,54.8499999999712,194.837192076906));
#88700=CARTESIAN_POINT('Ctrl Pts',(103.554266624083,54.8499999999688,194.902718667311));
#88701=CARTESIAN_POINT('Ctrl Pts',(102.0163496059,54.8499999999694,194.962341604715));
#88702=CARTESIAN_POINT('Ctrl Pts',(100.478225211469,54.8499999999746,195.016972545393));
#88703=CARTESIAN_POINT('Ctrl Pts',(99.122234956026,54.8499999999792,195.065134464853));
#88704=CARTESIAN_POINT('Ctrl Pts',(97.7660827406174,54.8499999999872,195.109416587705));
#88705=CARTESIAN_POINT('Ctrl Pts',(96.4097701715019,54.8499999999999,195.150441821658));
#88706=CARTESIAN_POINT('Ctrl Pts',(94.6308236322866,54.8500000000165,195.204250729445));
#88707=CARTESIAN_POINT('Ctrl Pts',(92.8518861601934,54.8500000000211,195.252366591768));
#88708=CARTESIAN_POINT('Ctrl Pts',(91.0729256581933,54.8500000000201,195.29559716179));
#88709=CARTESIAN_POINT('Ctrl Pts',(90.1129897448902,54.8500000000196,195.318924591865));
#88710=CARTESIAN_POINT('Ctrl Pts',(89.1530495490921,54.8500000000175,195.340829459218));
#88711=CARTESIAN_POINT('Ctrl Pts',(88.1930835376938,54.8500000000148,195.361438701481));
#88712=CARTESIAN_POINT('Ctrl Pts',(85.5757330912171,54.8500000000074,195.417629867416));
#88713=CARTESIAN_POINT('Ctrl Pts',(82.9582317068191,54.8499999999956,195.464188429785));
#88714=CARTESIAN_POINT('Ctrl Pts',(80.3407770464166,54.8499999999998,195.503671376904));
#88715=CARTESIAN_POINT('Ctrl Pts',(78.4437598294776,54.8500000000029,195.532286898538));
#88716=CARTESIAN_POINT('Ctrl Pts',(76.5466931771328,54.8500000000039,195.557143922092));
#88717=CARTESIAN_POINT('Ctrl Pts',(74.6495706553743,54.8500000000037,195.578833932771));
#88718=CARTESIAN_POINT('Ctrl Pts',(71.1904981133586,54.8500000000035,195.618381890013));
#88719=CARTESIAN_POINT('Ctrl Pts',(67.7313184321388,54.8500276561664,195.647457113546));
#88720=CARTESIAN_POINT('Ctrl Pts',(64.2720640515808,54.8500381138508,195.669554571807));
#88721=CARTESIAN_POINT('Ctrl Pts',(62.7549036160415,54.850042700384,195.679246079199));
#88722=CARTESIAN_POINT('Ctrl Pts',(61.2377288142738,54.8500439773173,195.687641278906));
#88723=CARTESIAN_POINT('Ctrl Pts',(59.7205427111412,54.8500381593574,195.694890495738));
#88724=CARTESIAN_POINT('Ctrl Pts',(50.5258276199189,54.8500029003453,195.738823460365));
#88725=CARTESIAN_POINT('Ctrl Pts',(41.3306706881903,54.8500518450573,195.741376041741));
#88726=CARTESIAN_POINT('Ctrl Pts',(32.1354861856875,54.8500356591211,195.737460054359));
#88727=CARTESIAN_POINT('Ctrl Pts',(31.3771645488717,54.8500343242762,195.737137105106));
#88728=CARTESIAN_POINT('Ctrl Pts',(30.6188427437782,54.8500325464933,195.736761144975));
#88729=CARTESIAN_POINT('Ctrl Pts',(29.8605210106052,54.8500302420968,195.736340981459));
#88730=CARTESIAN_POINT('Ctrl Pts',(19.9070136065305,54.849999995267,195.730826039073));
#88731=CARTESIAN_POINT('Ctrl Pts',(9.95351054027871,54.849999999965,195.717944947301));
#88732=CARTESIAN_POINT('Ctrl Pts',(1.20290037631102E-14,54.8500000000093,
195.717944947196));
#88733=CARTESIAN_POINT('',(123.142835173977,54.8703625774417,193.770443909236));
#88734=CARTESIAN_POINT('Ctrl Pts',(123.142835173977,54.8703625774417,193.770443909236));
#88735=CARTESIAN_POINT('Ctrl Pts',(121.899340181671,54.863377344104,193.863435857888));
#88736=CARTESIAN_POINT('Ctrl Pts',(120.654374052645,54.8500000000005,193.934853431518));
#88737=CARTESIAN_POINT('Ctrl Pts',(119.410687750229,54.85,194.025969999953));
#88738=CARTESIAN_POINT('',(127.218111007812,54.870362430323,193.399408941216));
#88739=CARTESIAN_POINT('Ctrl Pts',(127.218115807736,54.8703459680316,193.399454348143));
#88740=CARTESIAN_POINT('Ctrl Pts',(126.904655624744,54.8721034990734,193.433239035163));
#88741=CARTESIAN_POINT('Ctrl Pts',(126.589462087755,54.8733936915971,193.465799923233));
#88742=CARTESIAN_POINT('Ctrl Pts',(126.069842054209,54.8748466726111,193.517494280518));
#88743=CARTESIAN_POINT('Ctrl Pts',(125.863371183883,54.8752481439835,193.53751566446));
#88744=CARTESIAN_POINT('Ctrl Pts',(125.565865345439,54.8755920729016,193.565665507521));
#88745=CARTESIAN_POINT('Ctrl Pts',(125.474374710482,54.8756657856571,193.574226747018));
#88746=CARTESIAN_POINT('Ctrl Pts',(125.315939112259,54.8757392663103,193.588890198462));
#88747=CARTESIAN_POINT('Ctrl Pts',(125.2489457798,54.8757535671162,193.595040325144));
#88748=CARTESIAN_POINT('Ctrl Pts',(125.113301273444,54.8757490110628,193.607392178321));
#88749=CARTESIAN_POINT('Ctrl Pts',(125.044551562222,54.8757293328324,193.613600376908));
#88750=CARTESIAN_POINT('Ctrl Pts',(124.876641589548,54.8756381943028,193.628634589557));
#88751=CARTESIAN_POINT('Ctrl Pts',(124.777384795725,54.8755475890981,193.63741238751));
#88752=CARTESIAN_POINT('Ctrl Pts',(124.429631300409,54.87509793653,193.667777337326));
#88753=CARTESIAN_POINT('Ctrl Pts',(124.18023801191,54.8745385967918,193.688857592025));
#88754=CARTESIAN_POINT('Ctrl Pts',(123.669067795424,54.8728573299448,193.730536953319));
#88755=CARTESIAN_POINT('Ctrl Pts',(123.405543514086,54.8716993004467,193.751193535519));
#88756=CARTESIAN_POINT('Ctrl Pts',(123.14286640231,54.8702154555249,193.770850279654));
#88757=CARTESIAN_POINT('',(130.93851195015,54.8499999998387,192.9690053296));
#88758=CARTESIAN_POINT('Ctrl Pts',(130.938511950113,54.85,192.969005329269));
#88759=CARTESIAN_POINT('Ctrl Pts',(130.748438209165,54.8499991196594,192.990502729015));
#88760=CARTESIAN_POINT('Ctrl Pts',(130.558419310946,54.8503671322184,193.012402086984));
#88761=CARTESIAN_POINT('Ctrl Pts',(130.368421134895,54.8509960128742,193.034550306987));
#88762=CARTESIAN_POINT('Ctrl Pts',(130.248410110378,54.8513932409601,193.048540075883));
#88763=CARTESIAN_POINT('Ctrl Pts',(130.128408438622,54.8518944712188,193.062628779303));
#88764=CARTESIAN_POINT('Ctrl Pts',(130.008417669627,54.8524737295353,193.076774905918));
#88765=CARTESIAN_POINT('Ctrl Pts',(129.89218384073,54.8530348511332,193.090478113876));
#88766=CARTESIAN_POINT('Ctrl Pts',(129.775956712028,54.8536688413448,193.104236291091));
#88767=CARTESIAN_POINT('Ctrl Pts',(129.659732098805,54.8543528373223,193.118014480271));
#88768=CARTESIAN_POINT('Ctrl Pts',(129.60888383052,54.8546520855624,193.124042438037));
#88769=CARTESIAN_POINT('Ctrl Pts',(129.558036045364,54.8549609249045,193.130074240602));
#88770=CARTESIAN_POINT('Ctrl Pts',(129.507188402119,54.8552775416311,193.136107031175));
#88771=CARTESIAN_POINT('Ctrl Pts',(129.365399712784,54.8561604275981,193.152929471974));
#88772=CARTESIAN_POINT('Ctrl Pts',(129.223606656697,54.8571005169143,193.16976679798));
#88773=CARTESIAN_POINT('Ctrl Pts',(129.081819468307,54.8580660163222,193.18654630739));
#88774=CARTESIAN_POINT('Ctrl Pts',(128.857087329936,54.8595963291029,193.213141764098));
#88775=CARTESIAN_POINT('Ctrl Pts',(128.632345894176,54.8611886270791,193.23958486306));
#88776=CARTESIAN_POINT('Ctrl Pts',(128.407552504352,54.8627477135206,193.265688218895));
#88777=CARTESIAN_POINT('Ctrl Pts',(128.166437604382,54.8644200001108,193.293686853711));
#88778=CARTESIAN_POINT('Ctrl Pts',(127.925263358931,54.8660541928077,193.321294884794));
#88779=CARTESIAN_POINT('Ctrl Pts',(127.684011178606,54.867575440588,193.348250932464));
#88780=CARTESIAN_POINT('Ctrl Pts',(127.528742633054,54.8685545070983,193.365599693042));
#88781=CARTESIAN_POINT('Ctrl Pts',(127.3734424732,54.8694876782735,193.382677751082));
#88782=CARTESIAN_POINT('Ctrl Pts',(127.218111007812,54.870362430323,193.399408941216));
#88783=CARTESIAN_POINT('',(190.217744333281,54.85,102.334299700915));
#88784=CARTESIAN_POINT('Ctrl Pts',(190.217744333281,54.85,102.334299700915));
#88785=CARTESIAN_POINT('Ctrl Pts',(190.198438372667,54.8500000000001,107.588457360702));
#88786=CARTESIAN_POINT('Ctrl Pts',(190.154899230013,54.85,112.84243630191));
#88787=CARTESIAN_POINT('Ctrl Pts',(189.981234566109,54.8499999999999,120.721692135521));
#88788=CARTESIAN_POINT('Ctrl Pts',(189.90484649384,54.85,123.347975843259));
#88789=CARTESIAN_POINT('Ctrl Pts',(189.695312595311,54.85,128.595739803922));
#88790=CARTESIAN_POINT('Ctrl Pts',(189.562294604773,54.85,131.217600991548));
#88791=CARTESIAN_POINT('Ctrl Pts',(189.210995417379,54.85,136.455224502561));
#88792=CARTESIAN_POINT('Ctrl Pts',(188.992951237667,54.85,139.071003779748));
#88793=CARTESIAN_POINT('Ctrl Pts',(188.428934412368,54.85,144.293411630326));
#88794=CARTESIAN_POINT('Ctrl Pts',(188.082255525325,54.85,146.905440395189));
#88795=CARTESIAN_POINT('Ctrl Pts',(187.202193126973,54.85,152.075325431284));
#88796=CARTESIAN_POINT('Ctrl Pts',(186.669269532277,54.85,154.635271282323));
#88797=CARTESIAN_POINT('Ctrl Pts',(185.327632557779,54.85,159.680949962078));
#88798=CARTESIAN_POINT('Ctrl Pts',(184.519597931304,54.8499999999999,162.16686543837));
#88799=CARTESIAN_POINT('Ctrl Pts',(182.999398653294,54.85,165.812818448613));
#88800=CARTESIAN_POINT('Ctrl Pts',(182.437877250581,54.85,167.018905464543));
#88801=CARTESIAN_POINT('Ctrl Pts',(181.213923690437,54.85,169.351657826097));
#88802=CARTESIAN_POINT('Ctrl Pts',(180.550121170522,54.85,170.48259474114));
#88803=CARTESIAN_POINT('Ctrl Pts',(179.10880585684,54.85,172.666711676218));
#88804=CARTESIAN_POINT('Ctrl Pts',(178.331265907326,54.85,173.71987312672));
#88805=CARTESIAN_POINT('Ctrl Pts',(177.073364034008,54.85,175.23698326999));
#88806=CARTESIAN_POINT('Ctrl Pts',(176.638813994407,54.85,175.732258858291));
#88807=CARTESIAN_POINT('Ctrl Pts',(175.738392615775,54.85,176.701392031852));
#88808=CARTESIAN_POINT('Ctrl Pts',(175.271411249757,54.85,177.176171676685));
#88809=CARTESIAN_POINT('Ctrl Pts',(172.887512343756,54.8500000000001,179.467132277965));
#88810=CARTESIAN_POINT('Ctrl Pts',(170.80436878542,54.85,181.056284046568));
#88811=CARTESIAN_POINT('Ctrl Pts',(167.464200921113,54.85,183.141826753163));
#88812=CARTESIAN_POINT('Ctrl Pts',(166.313975611903,54.85,183.787918097031));
#88813=CARTESIAN_POINT('Ctrl Pts',(163.954209381834,54.8499999999999,184.990236396472));
#88814=CARTESIAN_POINT('Ctrl Pts',(162.757917664203,54.85,185.540014896745));
#88815=CARTESIAN_POINT('Ctrl Pts',(159.128777137195,54.85,187.063266469322));
#88816=CARTESIAN_POINT('Ctrl Pts',(156.656109556117,54.85,187.912054070198));
#88817=CARTESIAN_POINT('Ctrl Pts',(151.638015130561,54.85,189.38179645165));
#88818=CARTESIAN_POINT('Ctrl Pts',(149.092379741324,54.85,190.002098211036));
#88819=CARTESIAN_POINT('Ctrl Pts',(145.235296685317,54.8499999999999,190.811587895128));
#88820=CARTESIAN_POINT('Ctrl Pts',(143.942303135459,54.85,191.061144118388));
#88821=CARTESIAN_POINT('Ctrl Pts',(141.353031978865,54.8499999999999,191.524375610374));
#88822=CARTESIAN_POINT('Ctrl Pts',(140.055900136512,54.85,191.738245937891));
#88823=CARTESIAN_POINT('Ctrl Pts',(136.158198163361,54.85,192.33502571568));
#88824=CARTESIAN_POINT('Ctrl Pts',(133.551375018438,54.8499999999999,192.673483797853));
#88825=CARTESIAN_POINT('Ctrl Pts',(130.938511950113,54.8499999999999,192.969005329269));
#88826=CARTESIAN_POINT('Origin',(189.999800857363,55.3,102.333498885935));
#88827=CARTESIAN_POINT('Origin',(1.20290037631083E-14,55.3,195.5));
#88828=CARTESIAN_POINT('Ctrl Pts',(-190.217744333281,54.85,102.334299700914));
#88829=CARTESIAN_POINT('Ctrl Pts',(-190.499797482064,54.9866054968633,102.335336081498));
#88830=CARTESIAN_POINT('Ctrl Pts',(-190.499797482064,55.2999999999999,102.335336081498));
#88831=CARTESIAN_POINT('Ctrl Pts',(-190.197958800231,54.8499999999032,107.718974084326));
#88832=CARTESIAN_POINT('Ctrl Pts',(-190.480008298463,54.9866054967246,107.721003970568));
#88833=CARTESIAN_POINT('Ctrl Pts',(-190.480008298168,55.3000000002241,107.72100397055));
#88834=CARTESIAN_POINT('Ctrl Pts',(-190.15286634701,54.8499999999749,113.103225357617));
#88835=CARTESIAN_POINT('Ctrl Pts',(-190.434912437381,54.9866054968165,113.106828120184));
#88836=CARTESIAN_POINT('Ctrl Pts',(-190.434912437369,55.3,113.106828120207));
#88837=CARTESIAN_POINT('Ctrl Pts',(-189.969140380158,54.8500000000125,121.176659053989));
#88838=CARTESIAN_POINT('Ctrl Pts',(-190.251090404902,54.9866054968868,121.184483209885));
#88839=CARTESIAN_POINT('Ctrl Pts',(-190.251090404908,55.3,121.184483209874));
#88840=CARTESIAN_POINT('Ctrl Pts',(-189.888083875663,54.8500000000125,123.867306750675));
#88841=CARTESIAN_POINT('Ctrl Pts',(-190.169985811631,54.9866054968868,123.876850850686));
#88842=CARTESIAN_POINT('Ctrl Pts',(-190.16998581157,55.2999999999999,123.876850850684));
#88843=CARTESIAN_POINT('Ctrl Pts',(-189.66437067227,54.8499999999874,129.247010167646));
#88844=CARTESIAN_POINT('Ctrl Pts',(-189.946091720074,54.98660549684,129.260904144669));
#88845=CARTESIAN_POINT('Ctrl Pts',(-189.946091720136,55.2999999999999,129.260904144672));
#88846=CARTESIAN_POINT('Ctrl Pts',(-189.52188207134,54.8500000000226,131.936069993364));
#88847=CARTESIAN_POINT('Ctrl Pts',(-189.803472315591,54.9866054969124,131.952591176849));
#88848=CARTESIAN_POINT('Ctrl Pts',(-189.803472315518,55.3000000000373,131.952591176844));
#88849=CARTESIAN_POINT('Ctrl Pts',(-189.143122039148,54.8499999999774,137.311741597895));
#88850=CARTESIAN_POINT('Ctrl Pts',(-189.424246871058,54.9866054968143,137.334868293955));
#88851=CARTESIAN_POINT('Ctrl Pts',(-189.424246871131,55.2999999999626,137.33486829396));
#88852=CARTESIAN_POINT('Ctrl Pts',(-188.906813700382,54.849999999973,140.001224223251));
#88853=CARTESIAN_POINT('Ctrl Pts',(-189.18760824081,54.9866054968095,140.028330517394));
#88854=CARTESIAN_POINT('Ctrl Pts',(-189.187608240719,55.2999999999813,140.028330517384));
#88855=CARTESIAN_POINT('Ctrl Pts',(-188.292632756423,54.850000000027,145.362689351932));
#88856=CARTESIAN_POINT('Ctrl Pts',(-188.572283011556,54.9866054969172,145.399784634254));
#88857=CARTESIAN_POINT('Ctrl Pts',(-188.572283011647,55.3000000000187,145.399784634264));
#88858=CARTESIAN_POINT('Ctrl Pts',(-187.915655912286,54.8500000000144,148.031000011928));
#88859=CARTESIAN_POINT('Ctrl Pts',(-188.194503693629,54.9866054968937,148.07409498288));
#88860=CARTESIAN_POINT('Ctrl Pts',(-188.194503693513,55.3000000000186,148.074094982859));
#88861=CARTESIAN_POINT('Ctrl Pts',(-186.949354871226,54.8499999999856,153.329908463642));
#88862=CARTESIAN_POINT('Ctrl Pts',(-187.225465197805,54.986605496833,153.388014825406));
#88863=CARTESIAN_POINT('Ctrl Pts',(-187.225465197921,55.2999999999813,153.388014825428));
#88864=CARTESIAN_POINT('Ctrl Pts',(-186.360811154485,54.8500000000352,155.960659886914));
#88865=CARTESIAN_POINT('Ctrl Pts',(-186.635007346912,54.9866054969361,156.027789475615));
#88866=CARTESIAN_POINT('Ctrl Pts',(-186.635007346693,55.3000000000374,156.027789475552));
#88867=CARTESIAN_POINT('Ctrl Pts',(-185.233316992153,54.8499999999824,159.8632205481));
#88868=CARTESIAN_POINT('Ctrl Pts',(-185.502677893398,54.986605496827,159.947086381085));
#88869=CARTESIAN_POINT('Ctrl Pts',(-185.502677893508,55.2999999999813,159.947086381116));
#88870=CARTESIAN_POINT('Ctrl Pts',(-184.815825918778,54.8500000000041,161.156850396224));
#88871=CARTESIAN_POINT('Ctrl Pts',(-185.083234340623,54.9866054968727,161.246835918567));
#88872=CARTESIAN_POINT('Ctrl Pts',(-185.083234340539,55.3000000000093,161.246835918536));
#88873=CARTESIAN_POINT('Ctrl Pts',(-183.890842670928,54.8499999999959,163.694223718077));
#88874=CARTESIAN_POINT('Ctrl Pts',(-184.153426616934,54.986605496854,163.797443530319));
#88875=CARTESIAN_POINT('Ctrl Pts',(-184.153426617017,55.2999999999906,163.79744353035));
#88876=CARTESIAN_POINT('Ctrl Pts',(-183.382385037553,54.8500000000062,164.94156139573));
#88877=CARTESIAN_POINT('Ctrl Pts',(-183.642091434846,54.986605496875,165.051912885639));
#88878=CARTESIAN_POINT('Ctrl Pts',(-183.642091434722,55.3,165.051912885581));
#88879=CARTESIAN_POINT('Ctrl Pts',(-182.257242363085,54.8499999999937,167.38579265337));
#88880=CARTESIAN_POINT('Ctrl Pts',(-182.509961211219,54.9866054968517,167.511323717164));
#88881=CARTESIAN_POINT('Ctrl Pts',(-182.509961211343,55.3,167.511323717221));
#88882=CARTESIAN_POINT('Ctrl Pts',(-181.640539237098,54.8500000000066,168.58268067929));
#88883=CARTESIAN_POINT('Ctrl Pts',(-181.889144137789,54.9866054968791,168.716261729528));
#88884=CARTESIAN_POINT('Ctrl Pts',(-181.889144137688,55.3000000000186,168.71626172947));
#88885=CARTESIAN_POINT('Ctrl Pts',(-180.620975247538,54.8499999999967,170.333700945188));
#88886=CARTESIAN_POINT('Ctrl Pts',(-180.862291929361,54.9866054968555,170.479798933249));
#88887=CARTESIAN_POINT('Ctrl Pts',(-180.862291929412,55.2999999999906,170.479798933278));
#88888=CARTESIAN_POINT('Ctrl Pts',(-180.26535921273,54.8500000000008,170.90998258945));
#88889=CARTESIAN_POINT('Ctrl Pts',(-180.504061049894,54.9866054968648,171.06032459263));
#88890=CARTESIAN_POINT('Ctrl Pts',(-180.504061049845,55.3,171.060324592604));
#88891=CARTESIAN_POINT('Ctrl Pts',(-179.520306450127,54.8499999999992,172.046622354047));
#88892=CARTESIAN_POINT('Ctrl Pts',(-179.75339270956,54.9866054968619,172.205531386762));
#88893=CARTESIAN_POINT('Ctrl Pts',(-179.753392709609,55.3,172.205531386788));
#88894=CARTESIAN_POINT('Ctrl Pts',(-179.129400936759,54.8499999999992,172.608873025932));
#88895=CARTESIAN_POINT('Ctrl Pts',(-179.359474666008,54.9866054968619,172.772119981196));
#88896=CARTESIAN_POINT('Ctrl Pts',(-179.359474666011,55.3,172.772119981188));
#88897=CARTESIAN_POINT('Ctrl Pts',(-177.107977365711,54.8500000000031,175.346620158582));
#88898=CARTESIAN_POINT('Ctrl Pts',(-177.322213675783,54.9866054968692,175.53131677416));
#88899=CARTESIAN_POINT('Ctrl Pts',(-177.322213675773,55.3,175.531316774194));
#88900=CARTESIAN_POINT('Ctrl Pts',(-175.273059695142,54.8500000000093,177.307053577842));
#88901=CARTESIAN_POINT('Ctrl Pts',(-175.472027446834,54.9866054968808,177.508051660724));
#88902=CARTESIAN_POINT('Ctrl Pts',(-175.472027446897,55.3,177.508051660799));
#88903=CARTESIAN_POINT('Ctrl Pts',(-172.213531513844,54.8499999999953,179.919041531276));
#88904=CARTESIAN_POINT('Ctrl Pts',(-172.388751139953,54.9866054968547,180.140313922478));
#88905=CARTESIAN_POINT('Ctrl Pts',(-172.388751139921,55.3,180.140313922441));
#88906=CARTESIAN_POINT('Ctrl Pts',(-171.14287675774,54.8500000000066,180.735334590373));
#88907=CARTESIAN_POINT('Ctrl Pts',(-171.310063503819,54.9866054968792,180.962699537817));
#88908=CARTESIAN_POINT('Ctrl Pts',(-171.310063503861,55.3000000000187,180.96269953789));
#88909=CARTESIAN_POINT('Ctrl Pts',(-169.465738000691,54.8499999999967,181.883222248313));
#88910=CARTESIAN_POINT('Ctrl Pts',(-169.621105252464,54.9866054968555,182.11867683742));
#88911=CARTESIAN_POINT('Ctrl Pts',(-169.621105252443,55.2999999999906,182.118676837383));
#88912=CARTESIAN_POINT('Ctrl Pts',(-168.893167994943,54.85,182.254113120666));
#88913=CARTESIAN_POINT('Ctrl Pts',(-169.04462193827,54.9866054968634,182.492098102623));
#88914=CARTESIAN_POINT('Ctrl Pts',(-169.04462193831,55.3,182.492098102688));
#88915=CARTESIAN_POINT('Ctrl Pts',(-167.734522038227,54.85,182.965862918278));
#88916=CARTESIAN_POINT('Ctrl Pts',(-167.87833659147,54.9866054968634,183.208540735198));
#88917=CARTESIAN_POINT('Ctrl Pts',(-167.87833659143,55.3,183.208540735133));
#88918=CARTESIAN_POINT('Ctrl Pts',(-167.149001871247,54.8499999999969,183.306536007332));
#88919=CARTESIAN_POINT('Ctrl Pts',(-167.289093057181,54.9866054968575,183.551375891323));
#88920=CARTESIAN_POINT('Ctrl Pts',(-167.289093057217,55.3,183.551375891388));
#88921=CARTESIAN_POINT('Ctrl Pts',(-164.193287616351,54.8500000000125,184.940751128666));
#88922=CARTESIAN_POINT('Ctrl Pts',(-164.315307422436,54.9866054968868,185.195582682745));
#88923=CARTESIAN_POINT('Ctrl Pts',(-164.315307422292,55.3,185.195582682486));
#88924=CARTESIAN_POINT('Ctrl Pts',(-161.739738382499,54.85,186.029085306811));
#88925=CARTESIAN_POINT('Ctrl Pts',(-161.84912521402,54.9866054968633,186.289321051958));
#88926=CARTESIAN_POINT('Ctrl Pts',(-161.849125214096,55.2999999999999,186.289321052161));
#88927=CARTESIAN_POINT('Ctrl Pts',(-157.968227272373,54.85,187.435958843901));
#88928=CARTESIAN_POINT('Ctrl Pts',(-158.061401990388,54.9866054968633,187.702242136645));
#88929=CARTESIAN_POINT('Ctrl Pts',(-158.06140199035,55.2999999999999,187.702242136544));
#88930=CARTESIAN_POINT('Ctrl Pts',(-156.695660864883,54.8500000000162,187.866859457223));
#88931=CARTESIAN_POINT('Ctrl Pts',(-156.783872375767,54.9866054969007,188.134808550894));
#88932=CARTESIAN_POINT('Ctrl Pts',(-156.783872375788,55.3000000000372,188.134808550961));
#88933=CARTESIAN_POINT('Ctrl Pts',(-154.124815734453,54.8499999999838,188.665095072689));
#88934=CARTESIAN_POINT('Ctrl Pts',(-154.203880012405,54.9866054968261,188.935884340155));
#88935=CARTESIAN_POINT('Ctrl Pts',(-154.203880012384,55.2999999999627,188.935884340088));
#88936=CARTESIAN_POINT('Ctrl Pts',(-152.824031066258,54.8500000000135,189.033044232236));
#88937=CARTESIAN_POINT('Ctrl Pts',(-152.898903324984,54.9866054968902,189.305009231248));
#88938=CARTESIAN_POINT('Ctrl Pts',(-152.898903325004,55.3000000000093,189.305009231326));
#88939=CARTESIAN_POINT('Ctrl Pts',(-148.908007282254,54.849999999973,190.052058242771));
#88940=CARTESIAN_POINT('Ctrl Pts',(-148.971352624573,54.9866054968096,190.32702273555));
#88941=CARTESIAN_POINT('Ctrl Pts',(-148.971352624532,55.2999999999813,190.327022735394));
#88942=CARTESIAN_POINT('Ctrl Pts',(-146.287439493149,54.8499999999776,190.618021136898));
#88943=CARTESIAN_POINT('Ctrl Pts',(-146.344500438236,54.9866054968147,190.894297995684));
#88944=CARTESIAN_POINT('Ctrl Pts',(-146.344500438254,55.2999999999629,190.894297995781));
#88945=CARTESIAN_POINT('Ctrl Pts',(-141.032967318856,54.8500000000224,191.597641496055));
#88946=CARTESIAN_POINT('Ctrl Pts',(-141.079295090532,54.986605496912,191.875919399702));
#88947=CARTESIAN_POINT('Ctrl Pts',(-141.079295090514,55.300000000037,191.875919399605));
#88948=CARTESIAN_POINT('Ctrl Pts',(-138.399009626471,54.8500000000471,192.010708935057));
#88949=CARTESIAN_POINT('Ctrl Pts',(-138.440892704756,54.9866054969581,192.289663795972));
#88950=CARTESIAN_POINT('Ctrl Pts',(-138.44089270476,55.3000000000369,192.289663796002));
#88951=CARTESIAN_POINT('Ctrl Pts',(-133.121607451461,54.8499999999529,192.729240056066));
#88952=CARTESIAN_POINT('Ctrl Pts',(-133.155827195463,54.9866054967686,193.009238298489));
#88953=CARTESIAN_POINT('Ctrl Pts',(-133.155827195459,55.2999999999631,193.009238298459));
#88954=CARTESIAN_POINT('Ctrl Pts',(-130.47813816516,54.849999999992,193.034416151033));
#88955=CARTESIAN_POINT('Ctrl Pts',(-130.509142871666,54.9866054968449,193.314776001578));
#88956=CARTESIAN_POINT('Ctrl Pts',(-130.509142871667,55.2999999999815,193.31477600159));
#88957=CARTESIAN_POINT('Ctrl Pts',(-122.537325370419,54.8500000000161,193.832649170543));
#88958=CARTESIAN_POINT('Ctrl Pts',(-122.559948354902,54.9866054969003,194.11385157553));
#88959=CARTESIAN_POINT('Ctrl Pts',(-122.559948354899,55.3000000000369,194.113851575506));
#88960=CARTESIAN_POINT('Ctrl Pts',(-117.229788845083,54.8499999999913,194.210877457251));
#88961=CARTESIAN_POINT('Ctrl Pts',(-117.248473697759,54.986605496854,194.492330262601));
#88962=CARTESIAN_POINT('Ctrl Pts',(-117.248473697781,55.3000000000369,194.492330262574));
#88963=CARTESIAN_POINT('Ctrl Pts',(-106.599582434858,54.8500000000087,194.798457441269));
#88964=CARTESIAN_POINT('Ctrl Pts',(-106.612030995843,54.9866054968727,195.080254954912));
#88965=CARTESIAN_POINT('Ctrl Pts',(-106.612030995821,55.299999999963,195.08025495494));
#88966=CARTESIAN_POINT('Ctrl Pts',(-101.276765722829,54.85,195.006073597426));
#88967=CARTESIAN_POINT('Ctrl Pts',(-101.286942967898,54.9866054968634,195.287950777376));
#88968=CARTESIAN_POINT('Ctrl Pts',(-101.286942967899,55.3,195.28795077739));
#88969=CARTESIAN_POINT('Ctrl Pts',(-90.6222412308268,54.85,195.32239623046));
#88970=CARTESIAN_POINT('Ctrl Pts',(-90.6288044985487,54.9866054968634,195.604380705992));
#88971=CARTESIAN_POINT('Ctrl Pts',(-90.6288044985483,55.3,195.604380705979));
#88972=CARTESIAN_POINT('Ctrl Pts',(-85.2899196297656,54.849999999959,195.430398920617));
#88973=CARTESIAN_POINT('Ctrl Pts',(-85.2951502477932,54.98660549678,195.712407433009));
#88974=CARTESIAN_POINT('Ctrl Pts',(-85.295150247793,55.299999999963,195.712407432997));
#88975=CARTESIAN_POINT('Ctrl Pts',(-74.628059287452,54.8500000000409,195.588359025636));
#88976=CARTESIAN_POINT('Ctrl Pts',(-74.6311852892752,54.9866054969467,195.870398718805));
#88977=CARTESIAN_POINT('Ctrl Pts',(-74.6311852892754,55.3000000000369,195.870398718817));
#88978=CARTESIAN_POINT('Ctrl Pts',(-69.2972283472756,54.85,195.6380334407));
#88979=CARTESIAN_POINT('Ctrl Pts',(-69.2995860602678,54.9866054968634,195.920079260338));
#88980=CARTESIAN_POINT('Ctrl Pts',(-69.2995860602679,55.3,195.920079260345));
#88981=CARTESIAN_POINT('Ctrl Pts',(-53.3049437790784,54.85,195.73815589255));
#88982=CARTESIAN_POINT('Ctrl Pts',(-53.3055258119786,54.9866054968634,196.02021282908));
#88983=CARTESIAN_POINT('Ctrl Pts',(-53.3055258119785,55.3,196.020212829065));
#88984=CARTESIAN_POINT('Ctrl Pts',(-42.6436940741756,54.85,195.741936415933));
#88985=CARTESIAN_POINT('Ctrl Pts',(-42.6437804403081,54.9866054968634,196.023991532525));
#88986=CARTESIAN_POINT('Ctrl Pts',(-42.6437804403082,55.3,196.023991532478));
#88987=CARTESIAN_POINT('Ctrl Pts',(-21.3215695785207,54.85,195.732705751546));
#88988=CARTESIAN_POINT('Ctrl Pts',(-21.321239000773,54.9866054968634,196.014760687738));
#88989=CARTESIAN_POINT('Ctrl Pts',(-21.3212390007729,55.3,196.014760687785));
#88990=CARTESIAN_POINT('Ctrl Pts',(-10.6607012638122,54.8499999999627,195.71794494731));
#88991=CARTESIAN_POINT('Ctrl Pts',(-10.6604701165162,54.9866054967938,196.000000000093));
#88992=CARTESIAN_POINT('Ctrl Pts',(-10.6604701165162,55.3,196.));
#88993=CARTESIAN_POINT('Ctrl Pts',(1.20290037631083E-14,54.85,195.717944947177));
#88994=CARTESIAN_POINT('Ctrl Pts',(1.20290037631083E-14,54.9866054968634,
196.));
#88995=CARTESIAN_POINT('Ctrl Pts',(1.20290037631083E-14,55.3,196.));
#88996=CARTESIAN_POINT('',(-190.217744333281,54.85,102.334299700914));
#88997=CARTESIAN_POINT('Ctrl Pts',(8.09400652964437E-15,54.8500000000093,
195.717944947196));
#88998=CARTESIAN_POINT('Ctrl Pts',(-10.6608823663659,54.8499999999628,195.71794494731));
#88999=CARTESIAN_POINT('Ctrl Pts',(-21.3217703135716,54.8500173325644,195.732741622938));
#89000=CARTESIAN_POINT('Ctrl Pts',(-31.9826318183453,54.8500089537298,195.737339569908));
#89001=CARTESIAN_POINT('Ctrl Pts',(-32.0538745521929,54.850008897737,195.737370296347));
#89002=CARTESIAN_POINT('Ctrl Pts',(-32.1251172845683,54.8500088405961,195.737400645486));
#89003=CARTESIAN_POINT('Ctrl Pts',(-32.1963600154795,54.8500087822941,195.737430601013));
#89004=CARTESIAN_POINT('Ctrl Pts',(-42.7864993946942,54.8500001157824,195.741883451166));
#89005=CARTESIAN_POINT('Ctrl Pts',(-53.376605619207,54.8500178679623,195.737744132389));
#89006=CARTESIAN_POINT('Ctrl Pts',(-63.966466909668,54.8500065855881,195.671421188064));
#89007=CARTESIAN_POINT('Ctrl Pts',(-64.1084275988407,54.850006434344,195.670532106458));
#89008=CARTESIAN_POINT('Ctrl Pts',(-64.2503882446953,54.8500062778827,195.669631454805));
#89009=CARTESIAN_POINT('Ctrl Pts',(-64.3923488470745,54.8500061160708,195.668718987262));
#89010=CARTESIAN_POINT('Ctrl Pts',(-69.5813056237556,54.8500002015057,195.635366391111));
#89011=CARTESIAN_POINT('Ctrl Pts',(-74.7702705239252,54.8500177709199,195.586288797379));
#89012=CARTESIAN_POINT('Ctrl Pts',(-79.9589897750587,54.8500103466269,195.509400332601));
#89013=CARTESIAN_POINT('Ctrl Pts',(-80.1359326075558,54.8500100934478,195.506778324725));
#89014=CARTESIAN_POINT('Ctrl Pts',(-80.3128765776078,54.850009811204,195.504124288698));
#89015=CARTESIAN_POINT('Ctrl Pts',(-80.4898214380652,54.8500094979738,195.501437448281));
#89016=CARTESIAN_POINT('Ctrl Pts',(-84.2161548089894,54.8500029015686,195.444854493121));
#89017=CARTESIAN_POINT('Ctrl Pts',(-87.9419352769354,54.8500219794238,195.373821829301));
#89018=CARTESIAN_POINT('Ctrl Pts',(-91.6663092609427,54.8500269293056,195.281029095046));
#89019=CARTESIAN_POINT('Ctrl Pts',(-93.0942640584976,54.8500288271299,195.245451617964));
#89020=CARTESIAN_POINT('Ctrl Pts',(-94.5220120877842,54.8500286476275,195.20667493315));
#89021=CARTESIAN_POINT('Ctrl Pts',(-95.9495049562082,54.8500241474107,195.164284743112));
#89022=CARTESIAN_POINT('Ctrl Pts',(-96.160010222454,54.8500234837861,195.158033672835));
#89023=CARTESIAN_POINT('Ctrl Pts',(-96.3705108978206,54.8500227262081,195.151705119376));
#89024=CARTESIAN_POINT('Ctrl Pts',(-96.5810070229234,54.850021867489,195.145296789444));
#89025=CARTESIAN_POINT('Ctrl Pts',(-100.153755735135,54.8500072924569,195.036528266986));
#89026=CARTESIAN_POINT('Ctrl Pts',(-103.725065610368,54.8500509518181,194.904965551832));
#89027=CARTESIAN_POINT('Ctrl Pts',(-107.294222030251,54.8500655366034,194.739296744632));
#89028=CARTESIAN_POINT('Ctrl Pts',(-108.834799786133,54.8500718319273,194.667788060453));
#89029=CARTESIAN_POINT('Ctrl Pts',(-110.374976159483,54.8500727069131,194.589924501481));
#89030=CARTESIAN_POINT('Ctrl Pts',(-111.914692604448,54.8500611385557,194.50479344714));
#89031=CARTESIAN_POINT('Ctrl Pts',(-112.160365253972,54.8500592927425,194.491210185271));
#89032=CARTESIAN_POINT('Ctrl Pts',(-112.40602650628,54.8500571301813,194.477445607957));
#89033=CARTESIAN_POINT('Ctrl Pts',(-112.65167584228,54.8500546224071,194.46349276727));
#89034=CARTESIAN_POINT('Ctrl Pts',(-115.322724624506,54.8500273543214,194.311777648746));
#89035=CARTESIAN_POINT('Ctrl Pts',(-117.992372106993,54.8500268152894,194.137946722465));
#89036=CARTESIAN_POINT('Ctrl Pts',(-120.660060774621,54.8500287491632,193.933064820058));
#89037=CARTESIAN_POINT('Ctrl Pts',(-123.052153184648,54.8500304832505,193.749349062801));
#89038=CARTESIAN_POINT('Ctrl Pts',(-125.442670690351,54.8500342081856,193.540666594926));
#89039=CARTESIAN_POINT('Ctrl Pts',(-127.83120520213,54.8500224481125,193.300539935285));
#89040=CARTESIAN_POINT('Ctrl Pts',(-128.116308822552,54.8500210443901,193.271877598741));
#89041=CARTESIAN_POINT('Ctrl Pts',(-128.401383566503,54.8500194200674,193.242760058163));
#89042=CARTESIAN_POINT('Ctrl Pts',(-128.686428059558,54.8500175454592,193.213168377398));
#89043=CARTESIAN_POINT('Ctrl Pts',(-130.749050770458,54.8500039805263,192.999038744005));
#89044=CARTESIAN_POINT('Ctrl Pts',(-132.810104968374,54.850025848303,192.760185452714));
#89045=CARTESIAN_POINT('Ctrl Pts',(-134.869143324983,54.8500268298807,192.489305956972));
#89046=CARTESIAN_POINT('Ctrl Pts',(-135.166243246818,54.8500269715132,192.450220586486));
#89047=CARTESIAN_POINT('Ctrl Pts',(-135.463301170148,54.8500266782594,192.41046835331));
#89048=CARTESIAN_POINT('Ctrl Pts',(-135.760315719154,54.8500257809353,192.370027231952));
#89049=CARTESIAN_POINT('Ctrl Pts',(-136.067578585864,54.8500248526495,192.328190712754));
#89050=CARTESIAN_POINT('Ctrl Pts',(-136.374795369895,54.8500232778804,192.285620846307));
#89051=CARTESIAN_POINT('Ctrl Pts',(-136.681963465636,54.8500208694187,192.242280665229));
#89052=CARTESIAN_POINT('Ctrl Pts',(-137.619433940555,54.8500135188449,192.11000735722));
#89053=CARTESIAN_POINT('Ctrl Pts',(-138.556477977294,54.8500184166363,191.970592697317));
#89054=CARTESIAN_POINT('Ctrl Pts',(-139.49227471986,54.8500261469767,191.823104689008));
#89055=CARTESIAN_POINT('Ctrl Pts',(-140.361449919136,54.8500333269763,191.686116694519));
#89056=CARTESIAN_POINT('Ctrl Pts',(-141.229549084268,54.8500429514451,191.542163698025));
#89057=CARTESIAN_POINT('Ctrl Pts',(-142.095917433607,54.850047472919,191.390543532221));
#89058=CARTESIAN_POINT('Ctrl Pts',(-142.618028305764,54.8500501977539,191.299170691714));
#89059=CARTESIAN_POINT('Ctrl Pts',(-143.139510640945,54.8500510690445,191.20501418281));
#89060=CARTESIAN_POINT('Ctrl Pts',(-143.660221729556,54.8500484348223,191.107929600065));
#89061=CARTESIAN_POINT('Ctrl Pts',(-143.986659753988,54.8500467834069,191.047066484055));
#89062=CARTESIAN_POINT('Ctrl Pts',(-144.312795498642,54.850043754279,190.985061831075));
#89063=CARTESIAN_POINT('Ctrl Pts',(-144.638591532731,54.8500389409188,190.921854313299));
#89064=CARTESIAN_POINT('Ctrl Pts',(-145.864982398198,54.8500208220335,190.683922864423));
#89065=CARTESIAN_POINT('Ctrl Pts',(-147.086704129731,54.8500111358652,190.428986178105));
#89066=CARTESIAN_POINT('Ctrl Pts',(-148.303814497845,54.8500062423224,190.153475973731));
#89067=CARTESIAN_POINT('Ctrl Pts',(-149.379024500777,54.8500019193077,189.910086930786));
#89068=CARTESIAN_POINT('Ctrl Pts',(-150.45063586881,54.8500013371218,189.650643680963));
#89069=CARTESIAN_POINT('Ctrl Pts',(-151.518690840111,54.8500019909062,189.372719547259));
#89070=CARTESIAN_POINT('Ctrl Pts',(-151.840538674191,54.8500021879176,189.288969850029));
#89071=CARTESIAN_POINT('Ctrl Pts',(-152.161936727543,54.8500024971687,189.203546240927));
#89072=CARTESIAN_POINT('Ctrl Pts',(-152.482731128704,54.8500028501313,189.116409021106));
#89073=CARTESIAN_POINT('Ctrl Pts',(-153.059659884567,54.8500034849125,188.959698156955));
#89074=CARTESIAN_POINT('Ctrl Pts',(-153.635450160572,54.8500037883794,188.797226731405));
#89075=CARTESIAN_POINT('Ctrl Pts',(-154.209635529004,54.8500037516326,188.628574338648));
#89076=CARTESIAN_POINT('Ctrl Pts',(-154.610676144961,54.8500037259667,188.510778826619));
#89077=CARTESIAN_POINT('Ctrl Pts',(-155.010933537627,54.8500035343333,188.389967202185));
#89078=CARTESIAN_POINT('Ctrl Pts',(-155.41024024276,54.8500031737061,188.265983522997));
#89079=CARTESIAN_POINT('Ctrl Pts',(-155.722702261715,54.8500028915113,188.168964889905));
#89080=CARTESIAN_POINT('Ctrl Pts',(-156.034729938686,54.850002505833,188.069967506862));
#89081=CARTESIAN_POINT('Ctrl Pts',(-156.346359438258,54.850002015223,187.968862642223));
#89082=CARTESIAN_POINT('Ctrl Pts',(-156.829044177179,54.8500012553143,187.81226073111));
#89083=CARTESIAN_POINT('Ctrl Pts',(-157.310905250608,54.8500072780007,187.650569111632));
#89084=CARTESIAN_POINT('Ctrl Pts',(-157.791044491721,54.8500142606259,187.483641634521));
#89085=CARTESIAN_POINT('Ctrl Pts',(-158.236870292617,54.8500207442335,187.328643730158));
#89086=CARTESIAN_POINT('Ctrl Pts',(-158.681211585458,54.8500280556456,187.169131631849));
#89087=CARTESIAN_POINT('Ctrl Pts',(-159.123367174125,54.8500315308054,187.005034533807));
#89088=CARTESIAN_POINT('Ctrl Pts',(-159.157398132692,54.8500317982746,186.99240463228));
#89089=CARTESIAN_POINT('Ctrl Pts',(-159.191416152949,54.8500320430176,186.979747594348));
#89090=CARTESIAN_POINT('Ctrl Pts',(-159.225420919937,54.8500322629076,186.967063399997));
#89091=CARTESIAN_POINT('Ctrl Pts',(-159.535627988313,54.8500342688443,186.851352366136));
#89092=CARTESIAN_POINT('Ctrl Pts',(-159.844743764922,54.8500342064119,186.7334078408));
#89093=CARTESIAN_POINT('Ctrl Pts',(-160.152517177576,54.8500304615589,186.613187307355));
#89094=CARTESIAN_POINT('Ctrl Pts',(-160.837757657589,54.8500221238508,186.345522939161));
#89095=CARTESIAN_POINT('Ctrl Pts',(-161.516997750355,54.8500160688841,186.066368496853));
#89096=CARTESIAN_POINT('Ctrl Pts',(-162.189598467762,54.8500116711269,185.774498421334));
#89097=CARTESIAN_POINT('Ctrl Pts',(-162.851405567252,54.8500073439431,185.487312155979));
#89098=CARTESIAN_POINT('Ctrl Pts',(-163.506784615461,54.8500046212496,185.187814946701));
#89099=CARTESIAN_POINT('Ctrl Pts',(-164.155145741996,54.8500029079638,184.874885718999));
#89100=CARTESIAN_POINT('Ctrl Pts',(-164.790397041045,54.8500012293207,184.568283903634));
#89101=CARTESIAN_POINT('Ctrl Pts',(-165.418911321688,54.8500005197017,184.248787686258));
#89102=CARTESIAN_POINT('Ctrl Pts',(-166.040152646954,54.8500002197043,183.915389170481));
#89103=CARTESIAN_POINT('Ctrl Pts',(-166.213290015513,54.8500001360962,183.822472393449));
#89104=CARTESIAN_POINT('Ctrl Pts',(-166.385862599876,54.8500000843048,183.728476092638));
#89105=CARTESIAN_POINT('Ctrl Pts',(-166.55785907244,54.8500000522222,183.633379125962));
#89106=CARTESIAN_POINT('Ctrl Pts',(-166.837832170401,54.8499999999985,183.478581809656));
#89107=CARTESIAN_POINT('Ctrl Pts',(-167.116264884686,54.8499999999984,183.320836486654));
#89108=CARTESIAN_POINT('Ctrl Pts',(-167.393094984824,54.8499999999988,183.160022261953));
#89109=CARTESIAN_POINT('Ctrl Pts',(-167.685523875221,54.8499999999991,182.990146496039));
#89110=CARTESIAN_POINT('Ctrl Pts',(-167.975956522574,54.8499999999999,182.816972220691));
#89111=CARTESIAN_POINT('Ctrl Pts',(-168.264823575429,54.8500000866495,182.640056525926));
#89112=CARTESIAN_POINT('Ctrl Pts',(-168.281169085329,54.8500000915526,182.630045771111));
#89113=CARTESIAN_POINT('Ctrl Pts',(-168.297509577167,54.8500000967331,182.620023023886));
#89114=CARTESIAN_POINT('Ctrl Pts',(-168.313845127043,54.8500001022067,182.609988199285));
#89115=CARTESIAN_POINT('Ctrl Pts',(-168.602860109673,54.8500001990484,182.432448129943));
#89116=CARTESIAN_POINT('Ctrl Pts',(-168.890192672684,54.8500003876472,182.251177618191));
#89117=CARTESIAN_POINT('Ctrl Pts',(-169.175478680366,54.850000754949,182.066258513183));
#89118=CARTESIAN_POINT('Ctrl Pts',(-169.437780750684,54.8500010926593,181.896237331706));
#89119=CARTESIAN_POINT('Ctrl Pts',(-169.698353639928,54.8500015814379,181.723130682223));
#89120=CARTESIAN_POINT('Ctrl Pts',(-169.956876365831,54.8500022888712,181.546974119049));
#89121=CARTESIAN_POINT('Ctrl Pts',(-169.979529142198,54.8500023508592,181.531538589282));
#89122=CARTESIAN_POINT('Ctrl Pts',(-170.002166146793,54.8500024145262,181.516079628883));
#89123=CARTESIAN_POINT('Ctrl Pts',(-170.024787145037,54.8500024799174,181.500597254396));
#89124=CARTESIAN_POINT('Ctrl Pts',(-170.276030180198,54.8500032061933,181.32864026489));
#89125=CARTESIAN_POINT('Ctrl Pts',(-170.52563717389,54.8500041451709,181.153591409795));
#89126=CARTESIAN_POINT('Ctrl Pts',(-170.773852761769,54.8500053591626,180.975118583254));
#89127=CARTESIAN_POINT('Ctrl Pts',(-170.997400265556,54.8500064525057,180.814382687463));
#89128=CARTESIAN_POINT('Ctrl Pts',(-171.219836911137,54.8500072970219,180.65084691465));
#89129=CARTESIAN_POINT('Ctrl Pts',(-171.4405992899,54.8500076440165,180.484811934086));
#89130=CARTESIAN_POINT('Ctrl Pts',(-171.658857749817,54.8500079870754,180.320660146299));
#89131=CARTESIAN_POINT('Ctrl Pts',(-171.875479669646,54.8500078438299,180.154065488974));
#89132=CARTESIAN_POINT('Ctrl Pts',(-172.089955276584,54.8500069739881,179.985355854544));
#89133=CARTESIAN_POINT('Ctrl Pts',(-172.190228162052,54.8500065673145,179.906479743213));
#89134=CARTESIAN_POINT('Ctrl Pts',(-172.290032406048,54.8500060018222,179.827141877461));
#89135=CARTESIAN_POINT('Ctrl Pts',(-172.389318587393,54.8500052529633,179.747378636735));
#89136=CARTESIAN_POINT('Ctrl Pts',(-172.674702066623,54.8500031004787,179.518110969828));
#89137=CARTESIAN_POINT('Ctrl Pts',(-172.956068640285,54.8500017378943,179.285125620791));
#89138=CARTESIAN_POINT('Ctrl Pts',(-173.233384096643,54.8500073519304,179.048390424515));
#89139=CARTESIAN_POINT('Ctrl Pts',(-173.467638136679,54.8500120942215,178.848415360469));
#89140=CARTESIAN_POINT('Ctrl Pts',(-173.698981502201,54.8500218139805,178.645743109414));
#89141=CARTESIAN_POINT('Ctrl Pts',(-173.927415809643,54.8500402477035,178.440378355981));
#89142=CARTESIAN_POINT('Ctrl Pts',(-174.411601717874,54.8500793195445,178.005090326029));
#89143=CARTESIAN_POINT('Ctrl Pts',(-174.882407081437,54.8500970763827,177.557823667813));
#89144=CARTESIAN_POINT('Ctrl Pts',(-175.340006494809,54.8501017502797,177.098439362564));
#89145=CARTESIAN_POINT('Ctrl Pts',(-175.794576229559,54.8501063932317,176.642096553368));
#89146=CARTESIAN_POINT('Ctrl Pts',(-176.236114350063,54.850098130278,176.173796068497));
#89147=CARTESIAN_POINT('Ctrl Pts',(-176.664760320395,54.850085069284,175.693361571846));
#89148=CARTESIAN_POINT('Ctrl Pts',(-177.089022890663,54.8500721418538,175.217840072748));
#89149=CARTESIAN_POINT('Ctrl Pts',(-177.500655675424,54.8500545155468,174.730431470717));
#89150=CARTESIAN_POINT('Ctrl Pts',(-177.899762155142,54.8500400462237,174.230925044469));
#89151=CARTESIAN_POINT('Ctrl Pts',(-178.181106114092,54.8500298462974,173.878805691306));
#89152=CARTESIAN_POINT('Ctrl Pts',(-178.45622468802,54.8500212147052,173.520673709915));
#89153=CARTESIAN_POINT('Ctrl Pts',(-178.725144291181,54.8500168999681,173.156443177018));
#89154=CARTESIAN_POINT('Ctrl Pts',(-178.900331371547,54.8500140891421,172.919166002398));
#89155=CARTESIAN_POINT('Ctrl Pts',(-179.072930945669,54.8500131102433,172.679236747959));
#89156=CARTESIAN_POINT('Ctrl Pts',(-179.242558922419,54.8500147234712,172.437343705895));
#89157=CARTESIAN_POINT('Ctrl Pts',(-179.409540825703,54.8500163115338,172.199224019927));
#89158=CARTESIAN_POINT('Ctrl Pts',(-179.574369077232,54.8500137889583,171.958134845391));
#89159=CARTESIAN_POINT('Ctrl Pts',(-179.736323660477,54.8500104070973,171.715126362041));
#89160=CARTESIAN_POINT('Ctrl Pts',(-179.788806911429,54.8500093111662,171.636376659751));
#89161=CARTESIAN_POINT('Ctrl Pts',(-179.840988586092,54.8500081249988,171.557425766626));
#89162=CARTESIAN_POINT('Ctrl Pts',(-179.892844848329,54.8500069592319,171.478310348672));
#89163=CARTESIAN_POINT('Ctrl Pts',(-180.05189632116,54.850003383638,171.235650673513));
#89164=CARTESIAN_POINT('Ctrl Pts',(-180.208151077888,54.8499999999998,170.991096913461));
#89165=CARTESIAN_POINT('Ctrl Pts',(-180.361429505763,54.8499999999993,170.745090323767));
#89166=CARTESIAN_POINT('Ctrl Pts',(-180.566661136845,54.8499999999987,170.415700634953));
#89167=CARTESIAN_POINT('Ctrl Pts',(-180.766380808872,54.8500000984341,170.083978833131));
#89168=CARTESIAN_POINT('Ctrl Pts',(-180.96083020235,54.8500001634391,169.750027693026));
#89169=CARTESIAN_POINT('Ctrl Pts',(-181.105064833824,54.8500002116571,169.50231635404));
#89170=CARTESIAN_POINT('Ctrl Pts',(-181.24640142172,54.8500002414793,169.253379552386));
#89171=CARTESIAN_POINT('Ctrl Pts',(-181.384934465216,54.8500001990872,169.003256361499));
#89172=CARTESIAN_POINT('Ctrl Pts',(-181.776611235903,54.8500000792315,168.296078916981));
#89173=CARTESIAN_POINT('Ctrl Pts',(-182.145884496243,54.8500012930554,167.579420745079));
#89174=CARTESIAN_POINT('Ctrl Pts',(-182.494841975545,54.8500020250206,166.854169935699));
#89175=CARTESIAN_POINT('Ctrl Pts',(-182.605177175342,54.8500022564572,166.624856343923));
#89176=CARTESIAN_POINT('Ctrl Pts',(-182.713480983087,54.8500024397198,166.394683554933));
#89177=CARTESIAN_POINT('Ctrl Pts',(-182.819818421831,54.8500025174166,166.163679197984));
#89178=CARTESIAN_POINT('Ctrl Pts',(-182.935798630709,54.850002602159,165.911727167849));
#89179=CARTESIAN_POINT('Ctrl Pts',(-183.049440450245,54.8500025613201,165.658786155025));
#89180=CARTESIAN_POINT('Ctrl Pts',(-183.160821296697,54.8500023204387,165.404887883679));
#89181=CARTESIAN_POINT('Ctrl Pts',(-183.365125754767,54.8500018785932,164.939165541063));
#89182=CARTESIAN_POINT('Ctrl Pts',(-183.561639829366,54.8500055588454,164.470674968065));
#89183=CARTESIAN_POINT('Ctrl Pts',(-183.750988391072,54.8500111929849,163.999314478622));
#89184=CARTESIAN_POINT('Ctrl Pts',(-183.947592530409,54.850017043017,163.509892100606));
#89185=CARTESIAN_POINT('Ctrl Pts',(-184.136471310677,54.8500249997458,163.017375565003));
#89186=CARTESIAN_POINT('Ctrl Pts',(-184.318273619788,54.8500326353226,162.521628197236));
#89187=CARTESIAN_POINT('Ctrl Pts',(-184.330012024327,54.8500331283278,162.489619345532));
#89188=CARTESIAN_POINT('Ctrl Pts',(-184.341720911643,54.8500336199935,162.457597017546));
#89189=CARTESIAN_POINT('Ctrl Pts',(-184.353400449796,54.8500341096657,162.425561173513));
#89190=CARTESIAN_POINT('Ctrl Pts',(-184.543743154348,54.8500420899082,161.903469536315));
#89191=CARTESIAN_POINT('Ctrl Pts',(-184.726458531671,54.8500495408636,161.377181095366));
#89192=CARTESIAN_POINT('Ctrl Pts',(-184.901911923505,54.8500536313765,160.847476946169));
#89193=CARTESIAN_POINT('Ctrl Pts',(-185.083025533198,54.8500578538514,160.300684265064));
#89194=CARTESIAN_POINT('Ctrl Pts',(-185.256401042875,54.8500584951217,159.750250429398));
#89195=CARTESIAN_POINT('Ctrl Pts',(-185.422386623896,54.8500524422723,159.197025985645));
#89196=CARTESIAN_POINT('Ctrl Pts',(-185.48573987968,54.8500501320251,158.985871682508));
#89197=CARTESIAN_POINT('Ctrl Pts',(-185.548016034937,54.8500468466359,158.774310881095));
#89198=CARTESIAN_POINT('Ctrl Pts',(-185.60923249047,54.8500424133448,158.562391294959));
#89199=CARTESIAN_POINT('Ctrl Pts',(-185.679701723209,54.8500373099683,158.318440375111));
#89200=CARTESIAN_POINT('Ctrl Pts',(-185.748797650257,54.8500306854296,158.074012769126));
#89201=CARTESIAN_POINT('Ctrl Pts',(-185.816571022676,54.8500222767591,157.829073160196));
#89202=CARTESIAN_POINT('Ctrl Pts',(-185.918406796886,54.8500096419523,157.461028693464));
#89203=CARTESIAN_POINT('Ctrl Pts',(-186.017319103435,54.8500041741207,157.091670527571));
#89204=CARTESIAN_POINT('Ctrl Pts',(-186.113234906169,54.8500018069331,156.721804640251));
#89205=CARTESIAN_POINT('Ctrl Pts',(-186.186449970179,54.8499999999964,156.439476245519));
#89206=CARTESIAN_POINT('Ctrl Pts',(-186.257920283618,54.8500000000129,156.156852248164));
#89207=CARTESIAN_POINT('Ctrl Pts',(-186.327633325725,54.8500000000123,155.874294898771));
#89208=CARTESIAN_POINT('Ctrl Pts',(-186.488674327249,54.8500000000109,155.221571718727));
#89209=CARTESIAN_POINT('Ctrl Pts',(-186.640602570786,54.8500000000075,154.568170282113));
#89210=CARTESIAN_POINT('Ctrl Pts',(-186.784395313844,54.8500000000042,153.914165865284));
#89211=CARTESIAN_POINT('Ctrl Pts',(-186.967585480598,54.8500000000001,153.080972370057));
#89212=CARTESIAN_POINT('Ctrl Pts',(-187.137593562521,54.8500103689392,152.246804668101));
#89213=CARTESIAN_POINT('Ctrl Pts',(-187.296351738213,54.8500156959195,151.411830799846));
#89214=CARTESIAN_POINT('Ctrl Pts',(-187.342692041962,54.8500172508245,151.168108279678));
#89215=CARTESIAN_POINT('Ctrl Pts',(-187.388073498977,54.8500183760775,150.924317036446));
#89216=CARTESIAN_POINT('Ctrl Pts',(-187.43254334808,54.8500186882901,150.680461159443));
#89217=CARTESIAN_POINT('Ctrl Pts',(-187.474893892218,54.8500189856236,150.448226751392));
#89218=CARTESIAN_POINT('Ctrl Pts',(-187.516411642212,54.850018545554,150.21593254165));
#89219=CARTESIAN_POINT('Ctrl Pts',(-187.557122720677,54.8500170370286,149.983579406153));
#89220=CARTESIAN_POINT('Ctrl Pts',(-187.723025465295,54.8500108895986,149.036711272131));
#89221=CARTESIAN_POINT('Ctrl Pts',(-187.87557598185,54.850011114299,148.08892712507));
#89222=CARTESIAN_POINT('Ctrl Pts',(-188.016548444847,54.8500131636224,147.140288699541));
#89223=CARTESIAN_POINT('Ctrl Pts',(-188.165405941458,54.8500153275708,146.138589940715));
#89224=CARTESIAN_POINT('Ctrl Pts',(-188.301353764444,54.8500195263539,145.135938648905));
#89225=CARTESIAN_POINT('Ctrl Pts',(-188.426422471049,54.8500204062576,144.132398367695));
#89226=CARTESIAN_POINT('Ctrl Pts',(-188.486651809581,54.8500208299929,143.649123462496));
#89227=CARTESIAN_POINT('Ctrl Pts',(-188.544357357385,54.8500204840077,143.165642262192));
#89228=CARTESIAN_POINT('Ctrl Pts',(-188.599761728483,54.850018770448,142.681961197956));
#89229=CARTESIAN_POINT('Ctrl Pts',(-188.622338005758,54.8500180722034,142.48486992876));
#89230=CARTESIAN_POINT('Ctrl Pts',(-188.644527321077,54.8500171468879,142.287765317132));
#89231=CARTESIAN_POINT('Ctrl Pts',(-188.666339692097,54.8500159540699,142.090649333442));
#89232=CARTESIAN_POINT('Ctrl Pts',(-188.793874655865,54.850008979771,140.938129975725));
#89233=CARTESIAN_POINT('Ctrl Pts',(-188.90862770106,54.8500087186653,139.78461609317));
#89234=CARTESIAN_POINT('Ctrl Pts',(-189.012550625685,54.8500098332402,138.63033201508));
#89235=CARTESIAN_POINT('Ctrl Pts',(-189.132704196567,54.8500111218891,137.295772250766));
#89236=CARTESIAN_POINT('Ctrl Pts',(-189.238379958311,54.8500142498538,135.960182025919));
#89237=CARTESIAN_POINT('Ctrl Pts',(-189.332524646315,54.8500109691833,134.623907387355));
#89238=CARTESIAN_POINT('Ctrl Pts',(-189.343237480957,54.850010595872,134.471851126477));
#89239=CARTESIAN_POINT('Ctrl Pts',(-189.353801068778,54.8500101395807,134.319776825197));
#89240=CARTESIAN_POINT('Ctrl Pts',(-189.364218337543,54.8500095881607,134.167683191866));
#89241=CARTESIAN_POINT('Ctrl Pts',(-189.493454219205,54.8500027472846,132.280820594396));
#89242=CARTESIAN_POINT('Ctrl Pts',(-189.600125024046,54.8500055486022,130.392311238613));
#89243=CARTESIAN_POINT('Ctrl Pts',(-189.689765383739,54.850006017259,128.50255729975));
#89244=CARTESIAN_POINT('Ctrl Pts',(-189.720518645157,54.8500061780429,127.854232180394));
#89245=CARTESIAN_POINT('Ctrl Pts',(-189.749267897846,54.8500060642914,127.205760606272));
#89246=CARTESIAN_POINT('Ctrl Pts',(-189.776237985562,54.8500051925039,126.557158904599));
#89247=CARTESIAN_POINT('Ctrl Pts',(-189.780843967841,54.850005043619,126.446389967722));
#89248=CARTESIAN_POINT('Ctrl Pts',(-189.785397775027,54.8500048726252,126.335617228642));
#89249=CARTESIAN_POINT('Ctrl Pts',(-189.789900160442,54.8500046771144,126.224840759492));
#89250=CARTESIAN_POINT('Ctrl Pts',(-189.883899653494,54.8500005952975,123.912081858822));
#89251=CARTESIAN_POINT('Ctrl Pts',(-189.955534459011,54.8500116062881,121.597690348618));
#89252=CARTESIAN_POINT('Ctrl Pts',(-190.011686299581,54.8500111214795,119.282167861307));
#89253=CARTESIAN_POINT('Ctrl Pts',(-190.01812560416,54.8500110658833,119.016631515502));
#89254=CARTESIAN_POINT('Ctrl Pts',(-190.0243613518,54.8500108591021,118.751080301671));
#89255=CARTESIAN_POINT('Ctrl Pts',(-190.030403961542,54.8500104610399,118.485514979907));
#89256=CARTESIAN_POINT('Ctrl Pts',(-190.032047390757,54.8500103527776,118.413288272079));
#89257=CARTESIAN_POINT('Ctrl Pts',(-190.033676869816,54.8500102303663,118.341060525259));
#89258=CARTESIAN_POINT('Ctrl Pts',(-190.035292521922,54.8500100929995,118.268831752682));
#89259=CARTESIAN_POINT('Ctrl Pts',(-190.104937525408,54.8500041716088,115.155306818301));
#89260=CARTESIAN_POINT('Ctrl Pts',(-190.148948120071,54.8500017243381,112.039912168456));
#89261=CARTESIAN_POINT('Ctrl Pts',(-190.177365979128,54.850000712722,108.923379427127));
#89262=CARTESIAN_POINT('Ctrl Pts',(-190.197388942463,54.8499999999465,106.727498988393));
#89263=CARTESIAN_POINT('Ctrl Pts',(-190.209672545854,54.8499999999605,104.531053605748));
#89264=CARTESIAN_POINT('Ctrl Pts',(-190.217744333281,54.85,102.334299700914));
#89265=CARTESIAN_POINT('Origin',(-189.999800857363,55.3,102.333498885934));
#89266=CARTESIAN_POINT('Origin',(160.5,55.3,102.225104347672));
#89267=CARTESIAN_POINT('',(190.217944947177,54.85,102.225104347672));
#89268=CARTESIAN_POINT('Origin',(160.5,54.85,102.225104347672));
#89269=CARTESIAN_POINT('Origin',(190.,55.3,102.225104347672));
#89270=CARTESIAN_POINT('Origin',(-160.5,55.3,102.225104347671));
#89271=CARTESIAN_POINT('',(-190.217944947177,54.85,102.225104347671));
#89272=CARTESIAN_POINT('Origin',(-160.5,54.85,102.225104347671));
#89273=CARTESIAN_POINT('Origin',(-190.,55.3,102.225104347671));
#89274=CARTESIAN_POINT('Origin',(190.,55.3,211.4));
#89275=CARTESIAN_POINT('',(190.104681191176,54.811080938995,40.5));
#89276=CARTESIAN_POINT('',(190.217944947177,54.85,41.));
#89277=CARTESIAN_POINT('Ctrl Pts',(190.104681191175,54.8110809389947,40.5000000000008));
#89278=CARTESIAN_POINT('Ctrl Pts',(190.12358091403,54.8151275096016,40.5320279313255));
#89279=CARTESIAN_POINT('Ctrl Pts',(190.140604162343,54.8199259241617,40.5679467634758));
#89280=CARTESIAN_POINT('Ctrl Pts',(190.199161359621,54.8390668735187,40.725766780693));
#89281=CARTESIAN_POINT('Ctrl Pts',(190.217944947177,54.85,40.8634110132489));
#89282=CARTESIAN_POINT('Ctrl Pts',(190.217944947177,54.85,41.));
#89283=CARTESIAN_POINT('Origin',(190.,55.3,40.5));
#89284=CARTESIAN_POINT('',(190.217944947177,54.85,71.6125521738359));
#89285=CARTESIAN_POINT('Origin',(-190.,55.3,211.4));
#89286=CARTESIAN_POINT('',(-190.217944947177,54.85,41.));
#89287=CARTESIAN_POINT('',(-190.217944947177,54.85,71.6125521738355));
#89288=CARTESIAN_POINT('',(-190.104681191184,54.8110809389967,40.5));
#89289=CARTESIAN_POINT('Origin',(-190.,55.3,40.5));
#89290=CARTESIAN_POINT('Ctrl Pts',(-190.217944947177,54.85,41.));
#89291=CARTESIAN_POINT('Ctrl Pts',(-190.217944947177,54.85,40.9938389177394));
#89292=CARTESIAN_POINT('Ctrl Pts',(-190.217905298598,54.8499807908613,40.9876799790596));
#89293=CARTESIAN_POINT('Ctrl Pts',(-190.216401080532,54.849252755359,40.8708492263633));
#89294=CARTESIAN_POINT('Ctrl Pts',(-190.202442092343,54.8416051156352,40.7575089701039));
#89295=CARTESIAN_POINT('Ctrl Pts',(-190.15302607478,54.8236016547333,40.595037086274));
#89296=CARTESIAN_POINT('Ctrl Pts',(-190.130450467364,54.8165983318361,40.5436692439569));
#89297=CARTESIAN_POINT('Ctrl Pts',(-190.104681191177,54.8110809389952,40.5000000000045));
#89298=CARTESIAN_POINT('Origin',(-205.7,55.3,40.5));
#89299=CARTESIAN_POINT('',(-189.999999999997,54.811080938995,40.3953188088242));
#89300=CARTESIAN_POINT('',(-189.5,54.85,40.282055052823));
#89301=CARTESIAN_POINT('Ctrl Pts',(-189.999999999997,54.811080938995,40.3953188088242));
#89302=CARTESIAN_POINT('Ctrl Pts',(-189.967972070583,54.8151275093604,40.3764190870962));
#89303=CARTESIAN_POINT('Ctrl Pts',(-189.932053240841,54.8199259235839,40.3593958397075));
#89304=CARTESIAN_POINT('Ctrl Pts',(-189.774233224941,54.8390668729966,40.3008386411371));
#89305=CARTESIAN_POINT('Ctrl Pts',(-189.636588989633,54.85,40.282055052823));
#89306=CARTESIAN_POINT('Ctrl Pts',(-189.5,54.85,40.282055052823));
#89307=CARTESIAN_POINT('Origin',(-190.,55.3,40.5));
#89308=CARTESIAN_POINT('',(190.,54.8110809389967,40.3953188088159));
#89309=CARTESIAN_POINT('Origin',(190.,55.3,40.5));
#89310=CARTESIAN_POINT('',(189.5,54.85,40.282055052823));
#89311=CARTESIAN_POINT('Ctrl Pts',(189.5,54.85,40.282055052823));
#89312=CARTESIAN_POINT('Ctrl Pts',(189.506161082261,54.85,40.282055052823));
#89313=CARTESIAN_POINT('Ctrl Pts',(189.51232002094,54.8499807908613,40.2820947014021));
#89314=CARTESIAN_POINT('Ctrl Pts',(189.629150773595,54.8492527553593,40.283598919467));
#89315=CARTESIAN_POINT('Ctrl Pts',(189.742491029857,54.8416051156395,40.2975579076449));
#89316=CARTESIAN_POINT('Ctrl Pts',(189.904962913708,54.8236016547353,40.3469739252141));
#89317=CARTESIAN_POINT('Ctrl Pts',(189.95633075603,54.8165983318378,40.3695495326286));
#89318=CARTESIAN_POINT('Ctrl Pts',(189.999999999996,54.8110809389952,40.3953188088232));
#89319=CARTESIAN_POINT('',(-2.77555756156289E-14,54.85,40.282055052823));
#89320=CARTESIAN_POINT('Origin',(190.,55.3,40.5));
#89321=CARTESIAN_POINT('Ctrl Pts',(189.999999999995,54.8110809389952,40.3953188088232));
#89322=CARTESIAN_POINT('Ctrl Pts',(190.02146654402,54.8083687474021,40.4079862436505));
#89323=CARTESIAN_POINT('Ctrl Pts',(190.042396677867,54.8069935753319,40.4245436742059));
#89324=CARTESIAN_POINT('Ctrl Pts',(190.075456325793,54.8069935753319,40.457603322132));
#89325=CARTESIAN_POINT('Ctrl Pts',(190.092013756348,54.8083687474019,40.4785334559779));
#89326=CARTESIAN_POINT('Ctrl Pts',(190.104681191175,54.8110809389947,40.5000000000008));
#89327=CARTESIAN_POINT('Origin',(190.,55.3,40.5));
#89328=CARTESIAN_POINT('Origin',(-190.,55.3,40.5));
#89329=CARTESIAN_POINT('Ctrl Pts',(-190.104681191177,54.8110809389952,40.5000000000045));
#89330=CARTESIAN_POINT('Ctrl Pts',(-190.09201375635,54.8083687474021,40.4785334559804));
#89331=CARTESIAN_POINT('Ctrl Pts',(-190.075456325794,54.8069935753319,40.457603322133));
#89332=CARTESIAN_POINT('Ctrl Pts',(-190.042396677867,54.8069935753319,40.4245436742064));
#89333=CARTESIAN_POINT('Ctrl Pts',(-190.021466544021,54.808368747402,40.4079862436513));
#89334=CARTESIAN_POINT('Ctrl Pts',(-189.999999999997,54.811080938995,40.3953188088242));
#89335=CARTESIAN_POINT('Origin',(-190.,55.3,40.5));
#89336=CARTESIAN_POINT('Origin',(190.,58.8,40.5));
#89337=CARTESIAN_POINT('Origin',(190.,58.3,40.5));
#89338=CARTESIAN_POINT('Origin',(-190.,58.8,40.5));
#89339=CARTESIAN_POINT('Origin',(-190.,58.2999999999999,40.5));
#89340=CARTESIAN_POINT('Origin',(-190.5,58.2999999999999,40.5));
#89341=CARTESIAN_POINT('Origin',(190.,58.3,40.5));
#89342=CARTESIAN_POINT('Origin',(-190.,58.2999999999999,40.5));
#89343=CARTESIAN_POINT('Origin',(190.,58.3,40.5));
#89344=CARTESIAN_POINT('Origin',(190.,58.3,40.5));
#89345=CARTESIAN_POINT('Origin',(-190.,58.2999999999999,40.5));
#89346=CARTESIAN_POINT('Origin',(-190.,58.2999999999999,40.5));
#89347=CARTESIAN_POINT('Origin',(190.,58.3,211.4));
#89348=CARTESIAN_POINT('Origin',(190.,58.3,102.225104347672));
#89349=CARTESIAN_POINT('Origin',(-190.,58.2999999999999,211.4));
#89350=CARTESIAN_POINT('Origin',(-190.,58.2999999999999,102.225104347671));
#89351=CARTESIAN_POINT('Origin',(160.5,58.3,102.225104347672));
#89352=CARTESIAN_POINT('Origin',(189.999800857363,58.3,102.333498885935));
#89353=CARTESIAN_POINT('Origin',(-160.5,58.3,102.225104347671));
#89354=CARTESIAN_POINT('Origin',(-189.999800857363,58.2999999999999,102.333498885934));
#89355=CARTESIAN_POINT('Ctrl Pts',(189.999800857363,58.8,102.333498885935));
#89356=CARTESIAN_POINT('Ctrl Pts',(190.499797482064,58.8,102.335336081499));
#89357=CARTESIAN_POINT('Ctrl Pts',(190.499797482064,58.3,102.335336081499));
#89358=CARTESIAN_POINT('Ctrl Pts',(189.98001814498,58.8,107.717405584026));
#89359=CARTESIAN_POINT('Ctrl Pts',(190.48000829834,58.8000000000187,107.721003970607));
#89360=CARTESIAN_POINT('Ctrl Pts',(190.480008298168,58.3,107.721003970608));
#89361=CARTESIAN_POINT('Ctrl Pts',(189.934928325224,58.8,113.100441490038));
#89362=CARTESIAN_POINT('Ctrl Pts',(190.434912437463,58.8,113.106828120133));
#89363=CARTESIAN_POINT('Ctrl Pts',(190.434912437371,58.3,113.106828120131));
#89364=CARTESIAN_POINT('Ctrl Pts',(189.751276588517,58.8,121.170613300806));
#89365=CARTESIAN_POINT('Ctrl Pts',(190.251090404861,58.8,121.184483209912));
#89366=CARTESIAN_POINT('Ctrl Pts',(190.251090404907,58.3,121.184483209913));
#89367=CARTESIAN_POINT('Ctrl Pts',(189.670257242378,58.8,123.859931990418));
#89368=CARTESIAN_POINT('Ctrl Pts',(190.16998581163,58.7999999999253,123.876850850614));
#89369=CARTESIAN_POINT('Ctrl Pts',(190.169985811573,58.3,123.876850850612));
#89370=CARTESIAN_POINT('Ctrl Pts',(189.446683812013,58.8,129.236274242029));
#89371=CARTESIAN_POINT('Ctrl Pts',(189.946091720075,58.8000000000747,129.260904144743));
#89372=CARTESIAN_POINT('Ctrl Pts',(189.946091720133,58.3,129.260904144745));
#89373=CARTESIAN_POINT('Ctrl Pts',(189.304296283357,58.8,131.923304015849));
#89374=CARTESIAN_POINT('Ctrl Pts',(189.803472315597,58.8000000000374,131.952591176853));
#89375=CARTESIAN_POINT('Ctrl Pts',(189.803472315518,58.3,131.952591176848));
#89376=CARTESIAN_POINT('Ctrl Pts',(188.925895877044,58.8,137.293871517213));
#89377=CARTESIAN_POINT('Ctrl Pts',(189.424246871052,58.7999999999626,137.334868293952));
#89378=CARTESIAN_POINT('Ctrl Pts',(189.424246871131,58.3,137.334868293958));
#89379=CARTESIAN_POINT('Ctrl Pts',(188.689842755583,58.8,139.98027909287));
#89380=CARTESIAN_POINT('Ctrl Pts',(189.187608240863,58.8000000000561,140.028330517364));
#89381=CARTESIAN_POINT('Ctrl Pts',(189.187608240723,58.3000000000561,140.028330517352));
#89382=CARTESIAN_POINT('Ctrl Pts',(188.076546005068,58.8,145.334025694771));
#89383=CARTESIAN_POINT('Ctrl Pts',(188.572283011502,58.799999999944,145.399784634286));
#89384=CARTESIAN_POINT('Ctrl Pts',(188.572283011643,58.2999999999439,145.399784634298));
#89385=CARTESIAN_POINT('Ctrl Pts',(187.700189235296,58.8,147.997700373917));
#89386=CARTESIAN_POINT('Ctrl Pts',(188.194503693773,58.8,148.07409498293));
#89387=CARTESIAN_POINT('Ctrl Pts',(188.194503693509,58.3,148.074094982882));
#89388=CARTESIAN_POINT('Ctrl Pts',(186.736003435206,58.8,153.285009470243));
#89389=CARTESIAN_POINT('Ctrl Pts',(187.225465197661,58.8,153.388014825357));
#89390=CARTESIAN_POINT('Ctrl Pts',(187.225465197925,58.3,153.388014825405));
#89391=CARTESIAN_POINT('Ctrl Pts',(186.148938776817,58.8,155.908788613842));
#89392=CARTESIAN_POINT('Ctrl Pts',(186.635007347117,58.8000000000187,156.027789475654));
#89393=CARTESIAN_POINT('Ctrl Pts',(186.635007346696,58.3000000000375,156.027789475543));
#89394=CARTESIAN_POINT('Ctrl Pts',(185.02518086126,58.8,159.798417119283));
#89395=CARTESIAN_POINT('Ctrl Pts',(185.502677893295,58.7999999999906,159.947086381067));
#89396=CARTESIAN_POINT('Ctrl Pts',(185.502677893506,58.2999999999813,159.947086381122));
#89397=CARTESIAN_POINT('Ctrl Pts',(184.609198475717,58.8,161.087318261543));
#89398=CARTESIAN_POINT('Ctrl Pts',(185.083234340728,58.8000000000093,161.246835918548));
#89399=CARTESIAN_POINT('Ctrl Pts',(185.083234340555,58.3000000000187,161.246835918492));
#89400=CARTESIAN_POINT('Ctrl Pts',(183.687943117541,58.8,163.61446540035));
#89401=CARTESIAN_POINT('Ctrl Pts',(184.153426616828,58.7999999999907,163.797443530339));
#89402=CARTESIAN_POINT('Ctrl Pts',(184.153426617001,58.2999999999813,163.797443530395));
#89403=CARTESIAN_POINT('Ctrl Pts',(183.181708976339,58.8,164.856292405152));
#89404=CARTESIAN_POINT('Ctrl Pts',(183.64209143492,58.8,165.051912885673));
#89405=CARTESIAN_POINT('Ctrl Pts',(183.642091434722,58.3,165.051912885582));
#89406=CARTESIAN_POINT('Ctrl Pts',(182.06196560612,58.8,167.28879435183));
#89407=CARTESIAN_POINT('Ctrl Pts',(182.509961211144,58.8,167.51132371713));
#89408=CARTESIAN_POINT('Ctrl Pts',(182.509961211343,58.3,167.511323717222));
#89409=CARTESIAN_POINT('Ctrl Pts',(181.448441342018,58.8,168.479462124495));
#89410=CARTESIAN_POINT('Ctrl Pts',(181.889144137848,58.7999999999627,168.716261729601));
#89411=CARTESIAN_POINT('Ctrl Pts',(181.889144137668,58.299999999972,168.716261729504));
#89412=CARTESIAN_POINT('Ctrl Pts',(180.434508985192,58.8,170.220810507743));
#89413=CARTESIAN_POINT('Ctrl Pts',(180.862291929331,58.8000000000186,170.479798933213));
#89414=CARTESIAN_POINT('Ctrl Pts',(180.862291929421,58.300000000014,170.479798933262));
#89415=CARTESIAN_POINT('Ctrl Pts',(180.080913450215,58.8,170.793812786376));
#89416=CARTESIAN_POINT('Ctrl Pts',(180.504061049942,58.800000000007,171.060324592655));
#89417=CARTESIAN_POINT('Ctrl Pts',(180.50406104985,58.3,171.060324592596));
#89418=CARTESIAN_POINT('Ctrl Pts',(179.340199864572,58.8,171.923832776648));
#89419=CARTESIAN_POINT('Ctrl Pts',(179.753392709512,58.7999999999929,172.205531386738));
#89420=CARTESIAN_POINT('Ctrl Pts',(179.753392709603,58.3,172.205531386798));
#89421=CARTESIAN_POINT('Ctrl Pts',(178.951622144051,58.8,172.482731520272));
#89422=CARTESIAN_POINT('Ctrl Pts',(179.359474666006,58.7999999999953,172.772119981183));
#89423=CARTESIAN_POINT('Ctrl Pts',(179.359474666015,58.3,172.772119981182));
#89424=CARTESIAN_POINT('Ctrl Pts',(176.94243620339,58.8,175.203904423759));
#89425=CARTESIAN_POINT('Ctrl Pts',(177.322213675789,58.8000000000187,175.531316774216));
#89426=CARTESIAN_POINT('Ctrl Pts',(177.322213675755,58.3,175.531316774218));
#89427=CARTESIAN_POINT('Ctrl Pts',(175.119316602416,58.8,177.151741641064));
#89428=CARTESIAN_POINT('Ctrl Pts',(175.472027446722,58.8,177.508051660755));
#89429=CARTESIAN_POINT('Ctrl Pts',(175.472027446818,58.3,177.508051660867));
#89430=CARTESIAN_POINT('Ctrl Pts',(172.078138682654,58.8,179.748063563884));
#89431=CARTESIAN_POINT('Ctrl Pts',(172.388751140008,58.8,180.140313922463));
#89432=CARTESIAN_POINT('Ctrl Pts',(172.38875113996,58.3,180.140313922407));
#89433=CARTESIAN_POINT('Ctrl Pts',(171.013690961684,58.8,180.55964888304));
#89434=CARTESIAN_POINT('Ctrl Pts',(171.310063503812,58.8,180.962699537774));
#89435=CARTESIAN_POINT('Ctrl Pts',(171.310063503882,58.3,180.962699537876));
#89436=CARTESIAN_POINT('Ctrl Pts',(169.345685170052,58.8,181.701285645969));
#89437=CARTESIAN_POINT('Ctrl Pts',(169.621105252467,58.8,182.118676837442));
#89438=CARTESIAN_POINT('Ctrl Pts',(169.621105252432,58.3,182.118676837391));
#89439=CARTESIAN_POINT('Ctrl Pts',(168.776138991726,58.8,182.070221274742));
#89440=CARTESIAN_POINT('Ctrl Pts',(169.044621938208,58.8000000000094,182.492098102594));
#89441=CARTESIAN_POINT('Ctrl Pts',(169.044621938292,58.3,182.4920981027));
#89442=CARTESIAN_POINT('Ctrl Pts',(167.623396019067,58.8,182.778344901968));
#89443=CARTESIAN_POINT('Ctrl Pts',(167.878336591531,58.7999999999906,183.208540735228));
#89444=CARTESIAN_POINT('Ctrl Pts',(167.878336591447,58.3,183.208540735122));
#89445=CARTESIAN_POINT('Ctrl Pts',(167.040752911306,58.8,183.117347354141));
#89446=CARTESIAN_POINT('Ctrl Pts',(167.289093057169,58.7999999999999,183.551375891322));
#89447=CARTESIAN_POINT('Ctrl Pts',(167.289093057208,58.3,183.551375891393));
#89448=CARTESIAN_POINT('Ctrl Pts',(164.099002476116,58.8,184.743841876051));
#89449=CARTESIAN_POINT('Ctrl Pts',(164.315307422483,58.7999999999999,185.19558268275));
#89450=CARTESIAN_POINT('Ctrl Pts',(164.315307422327,58.3,185.195582682467));
#89451=CARTESIAN_POINT('Ctrl Pts',(161.655214786853,58.8,185.828000216715));
#89452=CARTESIAN_POINT('Ctrl Pts',(161.849125213937,58.8000000000928,186.289321051912));
#89453=CARTESIAN_POINT('Ctrl Pts',(161.849125214018,58.3000000000371,186.28932105219));
#89454=CARTESIAN_POINT('Ctrl Pts',(157.896230834854,58.8,187.230200792056));
#89455=CARTESIAN_POINT('Ctrl Pts',(158.061401990429,58.7999999999536,187.702242136669));
#89456=CARTESIAN_POINT('Ctrl Pts',(158.061401990388,58.2999999999814,187.702242136529));
#89457=CARTESIAN_POINT('Ctrl Pts',(156.627499515221,58.8,187.65981423508));
#89458=CARTESIAN_POINT('Ctrl Pts',(156.783872375754,58.8,188.134808550835));
#89459=CARTESIAN_POINT('Ctrl Pts',(156.783872375793,58.3,188.13480855096));
#89460=CARTESIAN_POINT('Ctrl Pts',(154.063722484356,58.8,188.45585523812));
#89461=CARTESIAN_POINT('Ctrl Pts',(154.203880012417,58.8,188.935884340214));
#89462=CARTESIAN_POINT('Ctrl Pts',(154.203880012378,58.3,188.93588434009));
#89463=CARTESIAN_POINT('Ctrl Pts',(152.766177004478,58.8,188.822895905688));
#89464=CARTESIAN_POINT('Ctrl Pts',(152.898903325027,58.800000000014,189.305009231201));
#89465=CARTESIAN_POINT('Ctrl Pts',(152.898903325061,58.3000000000094,189.305009231311));
#89466=CARTESIAN_POINT('Ctrl Pts',(148.859060109736,58.8,189.839592196685));
#89467=CARTESIAN_POINT('Ctrl Pts',(148.971352624484,58.799999999972,190.327022735643));
#89468=CARTESIAN_POINT('Ctrl Pts',(148.971352624418,58.2999999999813,190.327022735424));
#89469=CARTESIAN_POINT('Ctrl Pts',(146.243348297063,58.8000000000001,190.40454102088));
#89470=CARTESIAN_POINT('Ctrl Pts',(146.344500438298,58.7999999999816,190.894297995552));
#89471=CARTESIAN_POINT('Ctrl Pts',(146.344500438332,58.299999999963,190.894297995767));
#89472=CARTESIAN_POINT('Ctrl Pts',(140.997169684061,58.8000000000001,191.382615165563));
#89473=CARTESIAN_POINT('Ctrl Pts',(141.079295090469,58.8000000000186,191.875919399834));
#89474=CARTESIAN_POINT('Ctrl Pts',(141.079295090435,58.3000000000371,191.87591939962));
#89475=CARTESIAN_POINT('Ctrl Pts',(138.366646422257,58.8,191.79515951725));
#89476=CARTESIAN_POINT('Ctrl Pts',(138.44089270479,58.7999999998615,192.28966379588));
#89477=CARTESIAN_POINT('Ctrl Pts',(138.440892704796,58.2999999999077,192.289663795997));
#89478=CARTESIAN_POINT('Ctrl Pts',(133.095165732956,58.8,192.512884413628));
#89479=CARTESIAN_POINT('Ctrl Pts',(133.155827195428,58.8000000001384,193.009238298581));
#89480=CARTESIAN_POINT('Ctrl Pts',(133.155827195422,58.3000000000922,193.009238298464));
#89481=CARTESIAN_POINT('Ctrl Pts',(130.454180717654,58.8,192.817781092679));
#89482=CARTESIAN_POINT('Ctrl Pts',(130.509142871665,58.7999999999723,193.314776001534));
#89483=CARTESIAN_POINT('Ctrl Pts',(130.50914287167,58.2999999999815,193.31477600159));
#89484=CARTESIAN_POINT('Ctrl Pts',(122.519844509471,58.8,193.615363067465));
#89485=CARTESIAN_POINT('Ctrl Pts',(122.559948354903,58.8000000000553,194.113851575618));
#89486=CARTESIAN_POINT('Ctrl Pts',(122.559948354892,58.3000000000369,194.113851575507));
#89487=CARTESIAN_POINT('Ctrl Pts',(117.215350992657,58.8,193.993397868622));
#89488=CARTESIAN_POINT('Ctrl Pts',(117.248473697783,58.8000000000554,194.492330262396));
#89489=CARTESIAN_POINT('Ctrl Pts',(117.248473697793,58.3000000000369,194.492330262573));
#89490=CARTESIAN_POINT('Ctrl Pts',(106.589963387299,58.8,194.580711495763));
#89491=CARTESIAN_POINT('Ctrl Pts',(106.612030995818,58.7999999999446,195.080254955117));
#89492=CARTESIAN_POINT('Ctrl Pts',(106.612030995808,58.2999999999631,195.08025495494));
#89493=CARTESIAN_POINT('Ctrl Pts',(101.268901729087,58.8,194.788266093034));
#89494=CARTESIAN_POINT('Ctrl Pts',(101.28694296775,58.8000000002218,195.28795077722));
#89495=CARTESIAN_POINT('Ctrl Pts',(101.286942967794,58.3000000001479,195.287950777393));
#89496=CARTESIAN_POINT('Ctrl Pts',(90.6171697705162,58.8,195.104505818827));
#89497=CARTESIAN_POINT('Ctrl Pts',(90.6288044986965,58.7999999997782,195.604380706148));
#89498=CARTESIAN_POINT('Ctrl Pts',(90.6288044986522,58.2999999998521,195.604380705975));
#89499=CARTESIAN_POINT('Ctrl Pts',(85.285877912414,58.8,195.212489935321));
#89500=CARTESIAN_POINT('Ctrl Pts',(85.2951502476821,58.800000000074,195.712407432941));
#89501=CARTESIAN_POINT('Ctrl Pts',(85.2951502476829,58.3,195.712407432999));
#89502=CARTESIAN_POINT('Ctrl Pts',(74.6256438147839,58.8,195.370425946995));
#89503=CARTESIAN_POINT('Ctrl Pts',(74.6311852893859,58.799999999926,195.870398718872));
#89504=CARTESIAN_POINT('Ctrl Pts',(74.6311852893851,58.3,195.870398718815));
#89505=CARTESIAN_POINT('Ctrl Pts',(69.2954065338737,58.8,195.420095627817));
#89506=CARTESIAN_POINT('Ctrl Pts',(69.2995860601197,58.800000000037,195.920079260185));
#89507=CARTESIAN_POINT('Ctrl Pts',(69.2995860601212,58.300000000111,195.920079260346));
#89508=CARTESIAN_POINT('Ctrl Pts',(53.3044940404725,58.8,195.520209490268));
#89509=CARTESIAN_POINT('Ctrl Pts',(53.3055258122745,58.799999999926,196.020212829384));
#89510=CARTESIAN_POINT('Ctrl Pts',(53.3055258122716,58.2999999997781,196.020212829063));
#89511=CARTESIAN_POINT('Ctrl Pts',(42.6436273390892,58.8,195.523991419473));
#89512=CARTESIAN_POINT('Ctrl Pts',(42.6437804406409,58.8000000004438,196.0239915327));
#89513=CARTESIAN_POINT('Ctrl Pts',(42.6437804406409,58.3000000002959,196.023991532478));
#89514=CARTESIAN_POINT('Ctrl Pts',(21.3218250167947,58.8,195.514760894498));
#89515=CARTESIAN_POINT('Ctrl Pts',(21.32123900044,58.7999999995561,196.014760687562));
#89516=CARTESIAN_POINT('Ctrl Pts',(21.32123900044,58.2999999997041,196.014760687785));
#89517=CARTESIAN_POINT('Ctrl Pts',(10.6608798724039,58.8,195.500000000296));
#89518=CARTESIAN_POINT('Ctrl Pts',(10.6604701167662,58.799999999778,196.000000000296));
#89519=CARTESIAN_POINT('Ctrl Pts',(10.6604701167663,58.3,196.));
#89520=CARTESIAN_POINT('Ctrl Pts',(1.14409252987596E-14,58.8,195.5));
#89521=CARTESIAN_POINT('Ctrl Pts',(1.15828019241431E-14,58.8,196.));
#89522=CARTESIAN_POINT('Ctrl Pts',(1.16465450439953E-14,58.3,196.));
#89523=CARTESIAN_POINT('Origin',(1.15046684186118E-14,58.3,195.5));
#89524=CARTESIAN_POINT('Ctrl Pts',(1.15828019241431E-14,58.8,195.5));
#89525=CARTESIAN_POINT('Ctrl Pts',(1.15828019241431E-14,58.8,196.));
#89526=CARTESIAN_POINT('Ctrl Pts',(1.16465450439953E-14,58.3,196.));
#89527=CARTESIAN_POINT('Ctrl Pts',(-10.7118202846616,58.8,195.500000000149));
#89528=CARTESIAN_POINT('Ctrl Pts',(-10.7114086955145,58.7999999998885,196.000000000149));
#89529=CARTESIAN_POINT('Ctrl Pts',(-10.7114086955145,58.3,196.));
#89530=CARTESIAN_POINT('Ctrl Pts',(-21.4237296695725,58.8,195.514918536095));
#89531=CARTESIAN_POINT('Ctrl Pts',(-21.4231418326548,58.8000000001487,196.01491833246));
#89532=CARTESIAN_POINT('Ctrl Pts',(-21.4231418326549,58.3,196.014918332428));
#89533=CARTESIAN_POINT('Ctrl Pts',(-42.8474268144279,58.8,195.523964494094));
#89534=CARTESIAN_POINT('Ctrl Pts',(-42.8475924106281,58.7999999998513,196.023964608585));
#89535=CARTESIAN_POINT('Ctrl Pts',(-42.8475924106281,58.3,196.023964608617));
#89536=CARTESIAN_POINT('Ctrl Pts',(-53.5592277847632,58.8,195.519892463612));
#89537=CARTESIAN_POINT('Ctrl Pts',(-53.5602852850042,58.8000000001115,196.019895896343));
#89538=CARTESIAN_POINT('Ctrl Pts',(-53.5602852850042,58.3000000000743,196.019895896345));
#89539=CARTESIAN_POINT('Ctrl Pts',(-69.6263951900445,58.8,195.417356847765));
#89540=CARTESIAN_POINT('Ctrl Pts',(-69.6306526068966,58.7999999999442,195.917339859648));
#89541=CARTESIAN_POINT('Ctrl Pts',(-69.6306526068966,58.2999999999628,195.917339859647));
#89542=CARTESIAN_POINT('Ctrl Pts',(-74.982025485357,58.8,195.36653562557));
#89543=CARTESIAN_POINT('Ctrl Pts',(-74.9876678043093,58.7999999999256,195.86650739624));
#89544=CARTESIAN_POINT('Ctrl Pts',(-74.9876678043095,58.3,195.866507396251));
#89545=CARTESIAN_POINT('Ctrl Pts',(-85.6929541822509,58.8,195.204966816963));
#89546=CARTESIAN_POINT('Ctrl Pts',(-85.7023946291779,58.8000000000743,195.704881294909));
#89547=CARTESIAN_POINT('Ctrl Pts',(-85.7023946291777,58.3,195.704881294898));
#89548=CARTESIAN_POINT('Ctrl Pts',(-91.0488456914488,58.8,195.094552429692));
#89549=CARTESIAN_POINT('Ctrl Pts',(-91.0606918125482,58.7999999998699,195.594422790096));
#89550=CARTESIAN_POINT('Ctrl Pts',(-91.0606918125442,58.2999999999628,195.594422789964));
#89551=CARTESIAN_POINT('Ctrl Pts',(-101.757516044794,58.8,194.770640584481));
#89552=CARTESIAN_POINT('Ctrl Pts',(-101.775903721111,58.8000000001301,195.270313078333));
#89553=CARTESIAN_POINT('Ctrl Pts',(-101.775903721115,58.3000000000371,195.270313078465));
#89554=CARTESIAN_POINT('Ctrl Pts',(-107.107721166644,58.8,194.557957974675));
#89555=CARTESIAN_POINT('Ctrl Pts',(-107.130224336241,58.7999999999257,195.057483582615));
#89556=CARTESIAN_POINT('Ctrl Pts',(-107.130224336237,58.2999999999999,195.057483582537));
#89557=CARTESIAN_POINT('Ctrl Pts',(-117.793666862769,58.8,193.954934442877));
#89558=CARTESIAN_POINT('Ctrl Pts',(-117.827505515304,58.8000000000742,194.453820372871));
#89559=CARTESIAN_POINT('Ctrl Pts',(-117.827505515308,58.2999999999999,194.453820372949));
#89560=CARTESIAN_POINT('Ctrl Pts',(-123.129559723837,58.8,193.566463954364));
#89561=CARTESIAN_POINT('Ctrl Pts',(-123.170566875692,58.7999999999999,194.064885467423));
#89562=CARTESIAN_POINT('Ctrl Pts',(-123.170566875683,58.3,194.06488546734));
#89563=CARTESIAN_POINT('Ctrl Pts',(-131.113885005264,58.8,192.74408075586));
#89564=CARTESIAN_POINT('Ctrl Pts',(-131.170224675438,58.7999999999999,193.240923023939));
#89565=CARTESIAN_POINT('Ctrl Pts',(-131.170224675442,58.3,193.240923023981));
#89566=CARTESIAN_POINT('Ctrl Pts',(-133.772021287641,58.8,192.429354057039));
#89567=CARTESIAN_POINT('Ctrl Pts',(-133.834251546661,58.8000000000557,192.925517262575));
#89568=CARTESIAN_POINT('Ctrl Pts',(-133.834251546645,58.3000000000185,192.925517262463));
#89569=CARTESIAN_POINT('Ctrl Pts',(-137.752328543611,58.8,191.872550736023));
#89570=CARTESIAN_POINT('Ctrl Pts',(-137.82511882244,58.7999999999721,192.367236705325));
#89571=CARTESIAN_POINT('Ctrl Pts',(-137.825118822448,58.2999999999907,192.36723670538));
#89572=CARTESIAN_POINT('Ctrl Pts',(-139.077940504066,58.8,191.672737442318));
#89573=CARTESIAN_POINT('Ctrl Pts',(-139.154540611854,58.7999999999906,192.166853050365));
#89574=CARTESIAN_POINT('Ctrl Pts',(-139.154540611843,58.2999999999906,192.166853050303));
#89575=CARTESIAN_POINT('Ctrl Pts',(-141.726406587006,58.8,191.239238184666));
#89576=CARTESIAN_POINT('Ctrl Pts',(-141.811336381096,58.8000000000093,191.73199039492));
#89577=CARTESIAN_POINT('Ctrl Pts',(-141.811336381106,58.3000000000093,191.731990394982));
#89578=CARTESIAN_POINT('Ctrl Pts',(-143.050153383207,58.7999999999999,191.005369438704));
#89579=CARTESIAN_POINT('Ctrl Pts',(-143.139606665615,58.7999999999999,191.497328231557));
#89580=CARTESIAN_POINT('Ctrl Pts',(-143.1396066656,58.2999999999999,191.497328231477));
#89581=CARTESIAN_POINT('Ctrl Pts',(-147.003773115755,58.7999999999999,190.245280923907));
#89582=CARTESIAN_POINT('Ctrl Pts',(-147.108057529436,58.7999999999999,190.734388412564));
#89583=CARTESIAN_POINT('Ctrl Pts',(-147.108057529467,58.2999999999999,190.734388412723));
#89584=CARTESIAN_POINT('Ctrl Pts',(-149.619187452484,58.7999999999999,189.661180882931));
#89585=CARTESIAN_POINT('Ctrl Pts',(-149.735031156308,58.7999999999442,190.147792646827));
#89586=CARTESIAN_POINT('Ctrl Pts',(-149.735031156257,58.2999999999628,190.147792646636));
#89587=CARTESIAN_POINT('Ctrl Pts',(-153.498376682197,58.7999999999999,188.617845764116));
#89588=CARTESIAN_POINT('Ctrl Pts',(-153.635250053141,58.8000000000278,189.098801451736));
#89589=CARTESIAN_POINT('Ctrl Pts',(-153.635250053166,58.3000000000185,189.098801451831));
#89590=CARTESIAN_POINT('Ctrl Pts',(-154.784060017518,58.7999999999999,188.241983654962));
#89591=CARTESIAN_POINT('Ctrl Pts',(-154.928562946898,58.8000000000278,188.720727975089));
#89592=CARTESIAN_POINT('Ctrl Pts',(-154.928562946852,58.3000000000185,188.720727974947));
#89593=CARTESIAN_POINT('Ctrl Pts',(-157.337498640619,58.7999999999999,187.422033931746));
#89594=CARTESIAN_POINT('Ctrl Pts',(-157.498735050851,58.799999999972,187.895404865258));
#89595=CARTESIAN_POINT('Ctrl Pts',(-157.498735050897,58.2999999999813,187.8954048654));
#89596=CARTESIAN_POINT('Ctrl Pts',(-158.606653739105,58.8,186.977439099048));
#89597=CARTESIAN_POINT('Ctrl Pts',(-158.777006808703,58.800000000028,187.447644908311));
#89598=CARTESIAN_POINT('Ctrl Pts',(-158.777006808644,58.3000000000187,187.447644908159));
#89599=CARTESIAN_POINT('Ctrl Pts',(-162.372251203529,58.8,185.52164141396));
#89600=CARTESIAN_POINT('Ctrl Pts',(-162.572437434611,58.799999999944,185.980313582696));
#89601=CARTESIAN_POINT('Ctrl Pts',(-162.572437434729,58.2999999999626,185.980313583));
#89602=CARTESIAN_POINT('Ctrl Pts',(-164.798663242189,58.8,184.400617898551));
#89603=CARTESIAN_POINT('Ctrl Pts',(-165.02194750263,58.8000000000555,184.848989685973));
#89604=CARTESIAN_POINT('Ctrl Pts',(-165.021947502421,58.300000000037,184.84898968561));
#89605=CARTESIAN_POINT('Ctrl Pts',(-168.264719930277,58.8,182.408084773135));
#89606=CARTESIAN_POINT('Ctrl Pts',(-168.526867773756,58.7999999999722,182.834115040067));
#89607=CARTESIAN_POINT('Ctrl Pts',(-168.526867773861,58.2999999999815,182.834115040249));
#89608=CARTESIAN_POINT('Ctrl Pts',(-169.390999188975,58.7999999999999,181.691812341728));
#89609=CARTESIAN_POINT('Ctrl Pts',(-169.666776786259,58.7999999999906,182.109235796414));
#89610=CARTESIAN_POINT('Ctrl Pts',(-169.666776786143,58.3000000000092,182.109235796277));
#89611=CARTESIAN_POINT('Ctrl Pts',(-171.029630345911,58.7999999999999,180.526399139192));
#89612=CARTESIAN_POINT('Ctrl Pts',(-171.32642510615,58.8000000000046,180.928874947422));
#89613=CARTESIAN_POINT('Ctrl Pts',(-171.326425106208,58.2999999999953,180.92887494749));
#89614=CARTESIAN_POINT('Ctrl Pts',(-171.567368036222,58.8,180.122746179185));
#89615=CARTESIAN_POINT('Ctrl Pts',(-171.871260701913,58.8000000000046,180.519901406522));
#89616=CARTESIAN_POINT('Ctrl Pts',(-171.871260701861,58.3,180.519901406445));
#89617=CARTESIAN_POINT('Ctrl Pts',(-172.624619471896,58.8,179.282785482643));
#89618=CARTESIAN_POINT('Ctrl Pts',(-172.942780916019,58.7999999999953,179.668604510607));
#89619=CARTESIAN_POINT('Ctrl Pts',(-172.942780916071,58.3,179.668604510684));
#89620=CARTESIAN_POINT('Ctrl Pts',(-173.142833366156,58.8,178.847331341283));
#89621=CARTESIAN_POINT('Ctrl Pts',(-173.468148508335,58.800000000007,179.227145347679));
#89622=CARTESIAN_POINT('Ctrl Pts',(-173.468148508321,58.3,179.227145347663));
#89623=CARTESIAN_POINT('Ctrl Pts',(-175.653687288211,58.8,176.613457905974));
#89624=CARTESIAN_POINT('Ctrl Pts',(-176.014168613236,58.799999999972,176.961985025883));
#89625=CARTESIAN_POINT('Ctrl Pts',(-176.014168613293,58.3,176.961985025947));
#89626=CARTESIAN_POINT('Ctrl Pts',(-177.428617853825,58.7999999999999,174.624131223718));
#89627=CARTESIAN_POINT('Ctrl Pts',(-177.815415056938,58.8000000000464,174.943121919096));
#89628=CARTESIAN_POINT('Ctrl Pts',(-177.81541505701,58.3000000000371,174.94312191921));
#89629=CARTESIAN_POINT('Ctrl Pts',(-179.362497837556,58.7999999999999,171.891096446713));
#89630=CARTESIAN_POINT('Ctrl Pts',(-179.77599160755,58.7999999999883,172.17235851032));
#89631=CARTESIAN_POINT('Ctrl Pts',(-179.775991607532,58.2999999999906,172.172358510292));
#89632=CARTESIAN_POINT('Ctrl Pts',(-179.735156702828,58.8,171.332276242436));
#89633=CARTESIAN_POINT('Ctrl Pts',(-180.153696573167,58.7999999999789,171.605961657972));
#89634=CARTESIAN_POINT('Ctrl Pts',(-180.153696573215,58.2999999999953,171.605961658012));
#89635=CARTESIAN_POINT('Ctrl Pts',(-180.452895188782,58.8,170.190776016648));
#89636=CARTESIAN_POINT('Ctrl Pts',(-180.880916991989,58.800000000021,170.449381248111));
#89637=CARTESIAN_POINT('Ctrl Pts',(-180.88091699194,58.3000000000046,170.449381248071));
#89638=CARTESIAN_POINT('Ctrl Pts',(-180.797963758657,58.8,169.607853241695));
#89639=CARTESIAN_POINT('Ctrl Pts',(-181.230420402717,58.7999999999766,169.858953973832));
#89640=CARTESIAN_POINT('Ctrl Pts',(-181.230420402812,58.2999999999906,169.858953973894));
#89641=CARTESIAN_POINT('Ctrl Pts',(-181.781931362112,58.8,167.84582021067));
#89642=CARTESIAN_POINT('Ctrl Pts',(-182.226654132377,58.8000000000467,168.074955464039));
#89643=CARTESIAN_POINT('Ctrl Pts',(-182.226654132187,58.3000000000186,168.074955463915));
#89644=CARTESIAN_POINT('Ctrl Pts',(-182.374255506228,58.8,166.646517916866));
#89645=CARTESIAN_POINT('Ctrl Pts',(-182.825829796625,58.8,166.861660004045));
#89646=CARTESIAN_POINT('Ctrl Pts',(-182.825829796819,58.3,166.861660004131));
#89647=CARTESIAN_POINT('Ctrl Pts',(-183.99092543293,58.8,162.986625821498));
#89648=CARTESIAN_POINT('Ctrl Pts',(-184.459874896285,58.8,163.162433189105));
#89649=CARTESIAN_POINT('Ctrl Pts',(-184.459874895897,58.3,163.162433188933));
#89650=CARTESIAN_POINT('Ctrl Pts',(-184.856296646016,58.8,160.464564288146));
#89651=CARTESIAN_POINT('Ctrl Pts',(-185.332658084315,58.8000000000093,160.617765879063));
#89652=CARTESIAN_POINT('Ctrl Pts',(-185.332658084617,58.2999999999814,160.617765879137));
#89653=CARTESIAN_POINT('Ctrl Pts',(-185.933727730562,58.8,156.59616119807));
#89654=CARTESIAN_POINT('Ctrl Pts',(-186.418046815945,58.7999999999953,156.720791693547));
#89655=CARTESIAN_POINT('Ctrl Pts',(-186.418046815794,58.3000000000093,156.72079169351));
#89656=CARTESIAN_POINT('Ctrl Pts',(-186.256430054963,58.8,155.289137032266));
#89657=CARTESIAN_POINT('Ctrl Pts',(-186.742866764348,58.7999999999813,155.405086705275));
#89658=CARTESIAN_POINT('Ctrl Pts',(-186.74286676451,58.3,155.405086705311));
#89659=CARTESIAN_POINT('Ctrl Pts',(-186.836507038269,58.8,152.668979197173));
#89660=CARTESIAN_POINT('Ctrl Pts',(-187.326429131997,58.8000000000186,152.769185688968));
#89661=CARTESIAN_POINT('Ctrl Pts',(-187.326429131835,58.3,152.769185688932));
#89662=CARTESIAN_POINT('Ctrl Pts',(-187.093966794783,58.8,151.356609778289));
#89663=CARTESIAN_POINT('Ctrl Pts',(-187.585258126186,58.7999999999722,151.449750314483));
#89664=CARTESIAN_POINT('Ctrl Pts',(-187.585258126307,58.2999999999814,151.449750314505));
#89665=CARTESIAN_POINT('Ctrl Pts',(-187.788398583071,58.8,147.414021296038));
#89666=CARTESIAN_POINT('Ctrl Pts',(-188.283075769721,58.8000000000555,147.487938873115));
#89667=CARTESIAN_POINT('Ctrl Pts',(-188.283075769478,58.300000000037,147.487938873072));
#89668=CARTESIAN_POINT('Ctrl Pts',(-188.148412170526,58.8,144.778391543178));
#89669=CARTESIAN_POINT('Ctrl Pts',(-188.644410165613,58.7999999999447,144.842102846955));
#89670=CARTESIAN_POINT('Ctrl Pts',(-188.644410165759,58.2999999999631,144.842102846971));
#89671=CARTESIAN_POINT('Ctrl Pts',(-188.735101605106,58.8,139.49775750896));
#89672=CARTESIAN_POINT('Ctrl Pts',(-189.232988329617,58.8000000000553,139.544468866576));
#89673=CARTESIAN_POINT('Ctrl Pts',(-189.232988329472,58.3000000000369,139.54446886656));
#89674=CARTESIAN_POINT('Ctrl Pts',(-188.961273483377,58.8,136.852717795317));
#89675=CARTESIAN_POINT('Ctrl Pts',(-189.459709168613,58.7999999999723,136.892642646102));
#89676=CARTESIAN_POINT('Ctrl Pts',(-189.459709168717,58.2999999999815,136.892642646109));
#89677=CARTESIAN_POINT('Ctrl Pts',(-189.325139639208,58.8,131.556417805101));
#89678=CARTESIAN_POINT('Ctrl Pts',(-189.824352296292,58.8000000000276,131.585033344344));
#89679=CARTESIAN_POINT('Ctrl Pts',(-189.824352296188,58.3000000000184,131.585033344337));
#89680=CARTESIAN_POINT('Ctrl Pts',(-189.462571780471,58.7999999999999,128.905139098825));
#89681=CARTESIAN_POINT('Ctrl Pts',(-189.962004740431,58.7999999999078,128.929238461044));
#89682=CARTESIAN_POINT('Ctrl Pts',(-189.962004740442,58.2999999999631,128.929238461044));
#89683=CARTESIAN_POINT('Ctrl Pts',(-189.678761610221,58.7999999999999,123.598456482345));
#89684=CARTESIAN_POINT('Ctrl Pts',(-190.178499841919,58.800000000092,123.615062522244));
#89685=CARTESIAN_POINT('Ctrl Pts',(-190.178499841907,58.3000000000368,123.615062522244));
#89686=CARTESIAN_POINT('Ctrl Pts',(-189.757373218151,58.7999999999999,120.943042302021));
#89687=CARTESIAN_POINT('Ctrl Pts',(-190.257193263786,58.8000000000552,120.956675467134));
#89688=CARTESIAN_POINT('Ctrl Pts',(-190.257193263798,58.3000000000368,120.956675467134));
#89689=CARTESIAN_POINT('Ctrl Pts',(-189.935893374821,58.7999999999999,112.972770159095));
#89690=CARTESIAN_POINT('Ctrl Pts',(-190.435877163826,58.7999999998893,112.979092781064));
#89691=CARTESIAN_POINT('Ctrl Pts',(-190.435877163802,58.2999999999262,112.979092781063));
#89692=CARTESIAN_POINT('Ctrl Pts',(-189.980251348956,58.8,107.653938592502));
#89693=CARTESIAN_POINT('Ctrl Pts',(-190.480241583042,58.7999999991693,107.657514868693));
#89694=CARTESIAN_POINT('Ctrl Pts',(-190.480241583535,58.299999999557,107.657514868695));
#89695=CARTESIAN_POINT('Ctrl Pts',(-189.999800857363,58.8,102.333498885934));
#89696=CARTESIAN_POINT('Ctrl Pts',(-190.499797482064,58.8,102.335336081498));
#89697=CARTESIAN_POINT('Ctrl Pts',(-190.499797482064,58.3,102.335336081498));
#89698=CARTESIAN_POINT('Origin',(125.29348064571,25.4505574462982,228.3));
#89699=CARTESIAN_POINT('',(121.237845913371,25.4505574462982,229.));
#89700=CARTESIAN_POINT('',(120.537845913371,25.4505574462982,228.3));
#89701=CARTESIAN_POINT('Origin',(121.237845913371,25.4505574462982,228.3));
#89702=CARTESIAN_POINT('',(130.049115378049,25.4505574462982,228.3));
#89703=CARTESIAN_POINT('Origin',(125.29348064571,25.4505574462982,228.3));
#89704=CARTESIAN_POINT('',(129.349115378049,25.4505574462982,229.));
#89705=CARTESIAN_POINT('Origin',(129.349115378049,25.4505574462982,228.3));
#89706=CARTESIAN_POINT('Origin',(125.29348064571,25.4505574462982,229.));
#89707=CARTESIAN_POINT('Origin',(129.349115378049,25.4505574462982,228.3));
#89708=CARTESIAN_POINT('',(130.049115378049,53.4601166829598,228.3));
#89709=CARTESIAN_POINT('',(129.349115378049,53.4601166829598,229.));
#89710=CARTESIAN_POINT('Origin',(129.349115378049,53.4601166829598,228.3));
#89711=CARTESIAN_POINT('',(129.349115378049,25.4505574462982,229.));
#89712=CARTESIAN_POINT('',(130.049115378049,25.4505574462982,228.3));
#89713=CARTESIAN_POINT('Origin',(121.237845913371,25.4505574462982,228.3));
#89714=CARTESIAN_POINT('',(121.237845913371,53.4601166829598,229.));
#89715=CARTESIAN_POINT('',(120.537845913371,53.4601166829598,228.3));
#89716=CARTESIAN_POINT('Origin',(121.237845913371,53.4601166829598,228.3));
#89717=CARTESIAN_POINT('',(120.537845913371,25.4505574462982,228.3));
#89718=CARTESIAN_POINT('',(121.237845913371,25.4505574462982,229.));
#89719=CARTESIAN_POINT('Origin',(125.29348064571,53.4601166829598,228.3));
#89720=CARTESIAN_POINT('Origin',(125.29348064571,53.4601166829598,228.3));
#89721=CARTESIAN_POINT('Origin',(125.29348064571,53.4601166829598,229.));
#89722=CARTESIAN_POINT('Origin',(119.837845913371,51.61032741828,227.));
#89723=CARTESIAN_POINT('',(120.537845913371,51.61032741828,226.3));
#89724=CARTESIAN_POINT('Origin',(119.837845913371,51.61032741828,226.3));
#89725=CARTESIAN_POINT('',(120.537845913371,51.61032741828,202.7));
#89726=CARTESIAN_POINT('',(120.537845913371,51.61032741828,202.));
#89727=CARTESIAN_POINT('Origin',(119.837845913371,51.61032741828,202.7));
#89728=CARTESIAN_POINT('Ctrl Pts',(119.980756553526,50.9250708612662,202.7));
#89729=CARTESIAN_POINT('Ctrl Pts',(120.537845913371,51.0412521604076,202.7));
#89730=CARTESIAN_POINT('Ctrl Pts',(120.537845913371,51.61032741828,202.7));
#89731=CARTESIAN_POINT('Ctrl Pts',(119.980756569514,50.9250708646006,202.515401659683));
#89732=CARTESIAN_POINT('Ctrl Pts',(120.53784592438,51.0412521623395,202.592003939902));
#89733=CARTESIAN_POINT('Ctrl Pts',(120.537845913371,51.6103274217032,202.607700830635));
#89734=CARTESIAN_POINT('Ctrl Pts',(120.016933348296,50.9326865962307,202.330393020895));
#89735=CARTESIAN_POINT('Ctrl Pts',(120.563210336327,51.0457300061094,202.483460486543));
#89736=CARTESIAN_POINT('Ctrl Pts',(120.556420880425,51.6181480150106,202.515196509376));
#89737=CARTESIAN_POINT('Ctrl Pts',(120.12071246513,50.9538824639444,202.075296318228));
#89738=CARTESIAN_POINT('Ctrl Pts',(120.632852328253,51.0577402793023,202.34004784784));
#89739=CARTESIAN_POINT('Ctrl Pts',(120.609706255931,51.6399140437658,202.38764815965));
#89740=CARTESIAN_POINT('Ctrl Pts',(120.163000282663,50.9624493988279,201.994724706521));
#89741=CARTESIAN_POINT('Ctrl Pts',(120.661125768475,51.0625838875446,202.295519980409));
#89742=CARTESIAN_POINT('Ctrl Pts',(120.631418928709,51.648711427579,202.347362353776));
#89743=CARTESIAN_POINT('Ctrl Pts',(120.262801434937,50.9823166185813,201.842380942087));
#89744=CARTESIAN_POINT('Ctrl Pts',(120.726488287769,51.0736408783625,202.213784518412));
#89745=CARTESIAN_POINT('Ctrl Pts',(120.682661813548,51.6691130682172,202.271190470529));
#89746=CARTESIAN_POINT('Ctrl Pts',(120.320608134591,50.9936686129295,201.770645389731));
#89747=CARTESIAN_POINT('Ctrl Pts',(120.763864029259,51.0798986385742,202.176621792572));
#89748=CARTESIAN_POINT('Ctrl Pts',(120.712342654789,51.6807704288856,202.235322694426));
#89749=CARTESIAN_POINT('Ctrl Pts',(120.509667057382,51.0299919759325,201.57792765521));
#89750=CARTESIAN_POINT('Ctrl Pts',(120.883631159183,51.0996738601009,202.080620018702));
#89751=CARTESIAN_POINT('Ctrl Pts',(120.809414931026,51.7180708774407,202.138963828484));
#89752=CARTESIAN_POINT('Ctrl Pts',(120.661556892567,51.0581478200239,201.474556554105));
#89753=CARTESIAN_POINT('Ctrl Pts',(120.976009362001,51.1145360804081,202.03632174739));
#89754=CARTESIAN_POINT('Ctrl Pts',(120.887402742536,51.746984107053,202.087278277309));
#89755=CARTESIAN_POINT('Ctrl Pts',(120.988479548833,51.1151316286093,201.336326839815));
#89756=CARTESIAN_POINT('Ctrl Pts',(121.161594565797,51.1436937459234,201.989169936985));
#89757=CARTESIAN_POINT('Ctrl Pts',(121.055261129938,51.805500760816,202.018163419651));
#89758=CARTESIAN_POINT('Ctrl Pts',(121.168035486324,51.1446870647112,201.300000006569));
#89759=CARTESIAN_POINT('Ctrl Pts',(121.257345167804,51.1584002645244,201.986437757956));
#89760=CARTESIAN_POINT('Ctrl Pts',(121.147464824898,51.8358545236066,202.));
#89761=CARTESIAN_POINT('Ctrl Pts',(121.344083479533,51.1717186376762,201.3));
#89762=CARTESIAN_POINT('Ctrl Pts',(121.344083479533,51.1717186376762,202.));
#89763=CARTESIAN_POINT('Ctrl Pts',(121.237845913371,51.8636099438334,202.));
#89764=CARTESIAN_POINT('',(121.237845913371,51.8636099438334,202.));
#89765=CARTESIAN_POINT('Origin',(121.237845913371,51.8636099438334,201.3));
#89766=CARTESIAN_POINT('Ctrl Pts',(120.537845913371,51.61032741828,202.7));
#89767=CARTESIAN_POINT('Ctrl Pts',(120.537845913371,51.61032741828,202.66960977505));
#89768=CARTESIAN_POINT('Ctrl Pts',(120.539855658745,51.6111733231747,202.639425914894));
#89769=CARTESIAN_POINT('Ctrl Pts',(120.54375094998,51.612797640954,202.60963193772));
#89770=CARTESIAN_POINT('Ctrl Pts',(120.547805934794,51.6144885501911,202.578616509673));
#89771=CARTESIAN_POINT('Ctrl Pts',(120.553904211385,51.6170230548541,202.548022544351));
#89772=CARTESIAN_POINT('Ctrl Pts',(120.561957633332,51.620347527652,202.51804567938));
#89773=CARTESIAN_POINT('Ctrl Pts',(120.57001105528,51.6236720004499,202.48806881441));
#89774=CARTESIAN_POINT('Ctrl Pts',(120.580019901367,51.6277866249341,202.458707903137));
#89775=CARTESIAN_POINT('Ctrl Pts',(120.591944490529,51.6326578298738,202.430164212952));
#89776=CARTESIAN_POINT('Ctrl Pts',(120.592593281725,51.632922861636,202.428611212287));
#89777=CARTESIAN_POINT('Ctrl Pts',(120.593247373301,51.6331899634816,202.427061118066));
#89778=CARTESIAN_POINT('Ctrl Pts',(120.593906770483,51.633459131624,202.425513916105));
#89779=CARTESIAN_POINT('Ctrl Pts',(120.611371061272,51.6405881137296,202.384535905139));
#89780=CARTESIAN_POINT('Ctrl Pts',(120.632459420528,51.6491254533931,202.345815672698));
#89781=CARTESIAN_POINT('Ctrl Pts',(120.65704038842,51.6589119690931,202.309276386448));
#89782=CARTESIAN_POINT('Ctrl Pts',(120.678024081841,51.667266288012,202.2780844015));
#89783=CARTESIAN_POINT('Ctrl Pts',(120.701651295733,51.6765655446655,202.248497154293));
#89784=CARTESIAN_POINT('Ctrl Pts',(120.727118155272,51.6864222072939,202.221305435165));
#89785=CARTESIAN_POINT('Ctrl Pts',(120.732887337535,51.6886551046452,202.215145508636));
#89786=CARTESIAN_POINT('Ctrl Pts',(120.738751061304,51.6909166731422,202.209108367204));
#89787=CARTESIAN_POINT('Ctrl Pts',(120.744700214597,51.6932025229427,202.203202939035));
#89788=CARTESIAN_POINT('Ctrl Pts',(120.746092792191,51.693737594584,202.201820596616));
#89789=CARTESIAN_POINT('Ctrl Pts',(120.74749123962,51.6942744329583,202.200444341435));
#89790=CARTESIAN_POINT('Ctrl Pts',(120.748895476413,51.6948129989188,202.199074212284));
#89791=CARTESIAN_POINT('Ctrl Pts',(120.772718863232,51.7039499658979,202.175829473978));
#89792=CARTESIAN_POINT('Ctrl Pts',(120.798162272373,51.7135669523555,202.154387377056));
#89793=CARTESIAN_POINT('Ctrl Pts',(120.824895788136,51.7234982117892,202.134874709475));
#89794=CARTESIAN_POINT('Ctrl Pts',(120.85282975049,51.733875426279,202.114485841566));
#89795=CARTESIAN_POINT('Ctrl Pts',(120.882173281514,51.7445963236697,202.096202574251));
#89796=CARTESIAN_POINT('Ctrl Pts',(120.912593768197,51.7554862438252,202.08020234405));
#89797=CARTESIAN_POINT('Ctrl Pts',(120.931770422228,51.7623510988628,202.070116020245));
#89798=CARTESIAN_POINT('Ctrl Pts',(120.951375867509,51.7692833814873,202.060937650301));
#89799=CARTESIAN_POINT('Ctrl Pts',(120.971332224645,51.7762404987801,202.052720729726));
#89800=CARTESIAN_POINT('Ctrl Pts',(121.00280605992,51.7872128000952,202.039761550711));
#89801=CARTESIAN_POINT('Ctrl Pts',(121.035480957547,51.7983527205708,202.029088055337));
#89802=CARTESIAN_POINT('Ctrl Pts',(121.068916659086,51.8094930078735,202.020802179907));
#89803=CARTESIAN_POINT('Ctrl Pts',(121.09993022458,51.8198262748305,202.013116546632));
#89804=CARTESIAN_POINT('Ctrl Pts',(121.131599665853,51.8301602846134,202.007485376878));
#89805=CARTESIAN_POINT('Ctrl Pts',(121.163565450452,51.8403542638175,202.004031182709));
#89806=CARTESIAN_POINT('Ctrl Pts',(121.188207937351,51.8482128226525,202.001368337558));
#89807=CARTESIAN_POINT('Ctrl Pts',(121.213026553804,51.8559880865824,202.));
#89808=CARTESIAN_POINT('Ctrl Pts',(121.237845913371,51.8636099438334,202.));
#89809=CARTESIAN_POINT('Ctrl Pts',(120.537845913371,51.61032741828,226.3));
#89810=CARTESIAN_POINT('Ctrl Pts',(120.537845913371,51.0412521604076,226.3));
#89811=CARTESIAN_POINT('Ctrl Pts',(119.980756553526,50.9250708612662,226.3));
#89812=CARTESIAN_POINT('Ctrl Pts',(120.537845913371,51.6103274014729,226.485230527047));
#89813=CARTESIAN_POINT('Ctrl Pts',(120.537845913371,51.0412521492249,226.40834300785));
#89814=CARTESIAN_POINT('Ctrl Pts',(119.980756550258,50.9250708605847,226.392615262739));
#89815=CARTESIAN_POINT('Ctrl Pts',(120.537845913371,51.5720784940094,226.670993650709));
#89816=CARTESIAN_POINT('Ctrl Pts',(120.537845913372,51.0154718436456,226.517300435127));
#89817=CARTESIAN_POINT('Ctrl Pts',(119.977147933168,50.905195322387,226.485496826417));
#89818=CARTESIAN_POINT('Ctrl Pts',(120.537845913371,51.4624739877832,226.926759478812));
#89819=CARTESIAN_POINT('Ctrl Pts',(120.53784591337,50.9435849182146,226.662349946297));
#89820=CARTESIAN_POINT('Ctrl Pts',(119.966685777936,50.8482018526639,226.613379738875));
#89821=CARTESIAN_POINT('Ctrl Pts',(120.537845913371,51.4178168105653,227.007514343431));
#89822=CARTESIAN_POINT('Ctrl Pts',(120.537845913371,50.9143149102838,226.707540176998));
#89823=CARTESIAN_POINT('Ctrl Pts',(119.962410036061,50.8249762936204,226.653757171192));
#89824=CARTESIAN_POINT('Ctrl Pts',(120.537845913371,51.312438648417,227.160123469212));
#89825=CARTESIAN_POINT('Ctrl Pts',(120.537845913371,50.8461079001102,226.790822267366));
#89826=CARTESIAN_POINT('Ctrl Pts',(119.952253732179,50.7701490700559,226.73006173513));
#89827=CARTESIAN_POINT('Ctrl Pts',(120.537845913371,51.2514663528816,227.23186217591));
#89828=CARTESIAN_POINT('Ctrl Pts',(120.537845913371,50.8069032828533,226.828843822385));
#89829=CARTESIAN_POINT('Ctrl Pts',(119.946347697567,50.7384162488755,226.765931088417));
#89830=CARTESIAN_POINT('Ctrl Pts',(120.537845913371,51.0522284602922,227.424379532362));
#89831=CARTESIAN_POINT('Ctrl Pts',(120.537845913371,50.6803088645031,226.927203621114));
#89832=CARTESIAN_POINT('Ctrl Pts',(119.926892953773,50.6346729547807,226.862189765258));
#89833=CARTESIAN_POINT('Ctrl Pts',(120.537845913371,50.8924503496942,227.527224116548));
#89834=CARTESIAN_POINT('Ctrl Pts',(120.537845913373,50.5809974336902,226.973017056931));
#89835=CARTESIAN_POINT('Ctrl Pts',(119.911093129127,50.5514121280869,226.913612058182));
#89836=CARTESIAN_POINT('Ctrl Pts',(120.537845913371,50.549650402769,227.664303698141));
#89837=CARTESIAN_POINT('Ctrl Pts',(120.537845913368,50.378975163546,227.019149612712));
#89838=CARTESIAN_POINT('Ctrl Pts',(119.876462473964,50.3725357589363,226.982151849163));
#89839=CARTESIAN_POINT('Ctrl Pts',(120.537845913371,50.3620142055013,227.699999994234));
#89840=CARTESIAN_POINT('Ctrl Pts',(120.537845913371,50.2731525920023,227.019033760568));
#89841=CARTESIAN_POINT('Ctrl Pts',(119.857153207514,50.2745131115586,227.));
#89842=CARTESIAN_POINT('Ctrl Pts',(120.537845913371,50.1784824778425,227.7));
#89843=CARTESIAN_POINT('Ctrl Pts',(120.537845913371,50.1784824778428,227.));
#89844=CARTESIAN_POINT('Ctrl Pts',(119.83784591337,50.1784824778428,227.));
#89845=CARTESIAN_POINT('',(120.537845913371,50.178482477843,227.7));
#89846=CARTESIAN_POINT('Origin',(119.837845913371,50.178482477843,227.7));
#89847=CARTESIAN_POINT('Ctrl Pts',(120.537845913371,50.178482477843,227.7));
#89848=CARTESIAN_POINT('Ctrl Pts',(120.537845913371,50.2266182247457,227.699999998488));
#89849=CARTESIAN_POINT('Ctrl Pts',(120.537845913371,50.2746956243944,227.697548388819));
#89850=CARTESIAN_POINT('Ctrl Pts',(120.53784591337,50.3224646868022,227.69277495358));
#89851=CARTESIAN_POINT('Ctrl Pts',(120.53784591337,50.3716410766915,227.687860887852));
#89852=CARTESIAN_POINT('Ctrl Pts',(120.537845913368,50.4204918776408,227.680486173035));
#89853=CARTESIAN_POINT('Ctrl Pts',(120.537845913367,50.4687648579522,227.670738951763));
#89854=CARTESIAN_POINT('Ctrl Pts',(120.537845913365,50.5174165969936,227.660915251991));
#89855=CARTESIAN_POINT('Ctrl Pts',(120.537845913364,50.5654827340969,227.648681512488));
#89856=CARTESIAN_POINT('Ctrl Pts',(120.537845913363,50.6127063716968,227.634075950352));
#89857=CARTESIAN_POINT('Ctrl Pts',(120.537845913363,50.6493708477602,227.622736178353));
#89858=CARTESIAN_POINT('Ctrl Pts',(120.537845913364,50.6855276842963,227.609965612803));
#89859=CARTESIAN_POINT('Ctrl Pts',(120.537845913366,50.7210494651645,227.595761629006));
#89860=CARTESIAN_POINT('Ctrl Pts',(120.537845913366,50.7215096846164,227.595577602488));
#89861=CARTESIAN_POINT('Ctrl Pts',(120.537845913366,50.7219698305945,227.595393324582));
#89862=CARTESIAN_POINT('Ctrl Pts',(120.537845913366,50.7224299029115,227.595208795376));
#89863=CARTESIAN_POINT('Ctrl Pts',(120.537845913373,50.8577361254776,227.540939175357));
#89864=CARTESIAN_POINT('Ctrl Pts',(120.537845913368,50.9857915093738,227.465273532112));
#89865=CARTESIAN_POINT('Ctrl Pts',(120.537845913369,51.0990063730544,227.37257058707));
#89866=CARTESIAN_POINT('Ctrl Pts',(120.537845913369,51.1287591671713,227.348208312116));
#89867=CARTESIAN_POINT('Ctrl Pts',(120.53784591337,51.1574871836322,227.322669608678));
#89868=CARTESIAN_POINT('Ctrl Pts',(120.53784591337,51.1850531176328,227.296034002577));
#89869=CARTESIAN_POINT('Ctrl Pts',(120.53784591337,51.1852908868274,227.2958042579));
#89870=CARTESIAN_POINT('Ctrl Pts',(120.53784591337,51.1855285862015,227.295574416347));
#89871=CARTESIAN_POINT('Ctrl Pts',(120.53784591337,51.1857662156247,227.295344478058));
#89872=CARTESIAN_POINT('Ctrl Pts',(120.537845913371,51.2518975783998,227.231353528472));
#89873=CARTESIAN_POINT('Ctrl Pts',(120.537845913371,51.3126273026802,227.159850257429));
#89874=CARTESIAN_POINT('Ctrl Pts',(120.53784591337,51.3651275337233,227.083818771142));
#89875=CARTESIAN_POINT('Ctrl Pts',(120.53784591337,51.3652690148093,227.083613876477));
#89876=CARTESIAN_POINT('Ctrl Pts',(120.53784591337,51.3654104379503,227.083408949767));
#89877=CARTESIAN_POINT('Ctrl Pts',(120.53784591337,51.3655518031444,227.08320399101));
#89878=CARTESIAN_POINT('Ctrl Pts',(120.53784591337,51.418056152811,227.007080400097));
#89879=CARTESIAN_POINT('Ctrl Pts',(120.53784591337,51.4625703069915,226.926533129112));
#89880=CARTESIAN_POINT('Ctrl Pts',(120.53784591337,51.4990085348243,226.841504079202));
#89881=CARTESIAN_POINT('Ctrl Pts',(120.53784591337,51.4990739390667,226.841351457603));
#89882=CARTESIAN_POINT('Ctrl Pts',(120.53784591337,51.4991393154205,226.841198823767));
#89883=CARTESIAN_POINT('Ctrl Pts',(120.53784591337,51.4992046638834,226.841046177703));
#89884=CARTESIAN_POINT('Ctrl Pts',(120.537845913371,51.5143302327706,226.805714687968));
#89885=CARTESIAN_POINT('Ctrl Pts',(120.537845913371,51.5280125310827,226.769597689428));
#89886=CARTESIAN_POINT('Ctrl Pts',(120.537845913371,51.5401513369114,226.7329742214));
#89887=CARTESIAN_POINT('Ctrl Pts',(120.537845913371,51.552355291154,226.6961541969));
#89888=CARTESIAN_POINT('Ctrl Pts',(120.537845913371,51.5629989358661,226.658823004492));
#89889=CARTESIAN_POINT('Ctrl Pts',(120.537845913371,51.5720303361862,226.621280362417));
#89890=CARTESIAN_POINT('Ctrl Pts',(120.537845913371,51.5756770373127,226.606121384818));
#89891=CARTESIAN_POINT('Ctrl Pts',(120.537845913371,51.5790614626629,226.590928052307));
#89892=CARTESIAN_POINT('Ctrl Pts',(120.537845913371,51.5821825826778,226.575720403825));
#89893=CARTESIAN_POINT('Ctrl Pts',(120.537845913371,51.5900124195483,226.537569545728));
#89894=CARTESIAN_POINT('Ctrl Pts',(120.537845913371,51.5962282679499,226.499143671121));
#89895=CARTESIAN_POINT('Ctrl Pts',(120.537845913371,51.6008158826798,226.460436009908));
#89896=CARTESIAN_POINT('Ctrl Pts',(120.537845913371,51.6053222463237,226.422413898744));
#89897=CARTESIAN_POINT('Ctrl Pts',(120.537845913371,51.608257592452,226.384119167664));
#89898=CARTESIAN_POINT('Ctrl Pts',(120.537845913371,51.6095585651145,226.345544518822));
#89899=CARTESIAN_POINT('Ctrl Pts',(120.537845913371,51.6100691246589,226.330406110686));
#89900=CARTESIAN_POINT('Ctrl Pts',(120.537845913371,51.6103274168984,226.315224640044));
#89901=CARTESIAN_POINT('Ctrl Pts',(120.537845913371,51.6103274182798,226.3));
#89902=CARTESIAN_POINT('Origin',(121.237845913371,25.4505574462982,202.7));
#89903=CARTESIAN_POINT('',(120.537845913371,53.4601166829598,202.7));
#89904=CARTESIAN_POINT('',(121.237845913371,53.4601166829598,202.));
#89905=CARTESIAN_POINT('Origin',(121.237845913371,53.4601166829598,202.7));
#89906=CARTESIAN_POINT('',(121.237845913371,53.4601166829598,202.));
#89907=CARTESIAN_POINT('',(120.537845913371,51.0349239481607,202.7));
#89908=CARTESIAN_POINT('Origin',(125.29348064571,25.4505574462982,201.3));
#89909=CARTESIAN_POINT('',(129.349115378049,51.8636099438334,202.));
#89910=CARTESIAN_POINT('Origin',(129.349115378049,51.8636099438334,201.3));
#89911=CARTESIAN_POINT('Origin',(125.29348064571,25.4505574462982,202.));
#89912=CARTESIAN_POINT('Origin',(119.837845913371,25.4505574462982,227.7));
#89913=CARTESIAN_POINT('',(119.837845913371,25.4505574462982,227.));
#89914=CARTESIAN_POINT('',(120.537845913371,25.4505574462982,227.7));
#89915=CARTESIAN_POINT('Origin',(119.837845913371,25.4505574462982,227.7));
#89916=CARTESIAN_POINT('',(120.537845913371,25.4505574462982,227.7));
#89917=CARTESIAN_POINT('',(119.837845913371,51.0349239481607,227.));
#89918=CARTESIAN_POINT('Origin',(125.29348064571,53.4601166829598,202.7));
#89919=CARTESIAN_POINT('',(130.049115378049,53.4601166829598,202.7));
#89920=CARTESIAN_POINT('',(129.349115378049,53.4601166829598,202.));
#89921=CARTESIAN_POINT('Origin',(129.349115378049,53.4601166829598,202.7));
#89922=CARTESIAN_POINT('Origin',(125.29348064571,53.4601166829598,202.));
#89923=CARTESIAN_POINT('Origin',(125.29348064571,53.4601166829598,202.7));
#89924=CARTESIAN_POINT('Ctrl Pts',(129.242877811887,51.1717186376762,201.3));
#89925=CARTESIAN_POINT('Ctrl Pts',(129.242877811887,51.1717186376762,202.));
#89926=CARTESIAN_POINT('Ctrl Pts',(129.349115378049,51.8636099438334,202.));
#89927=CARTESIAN_POINT('Ctrl Pts',(129.420790531699,51.1444007422584,201.30000001605));
#89928=CARTESIAN_POINT('Ctrl Pts',(129.330552739425,51.1582564503628,201.986291315068));
#89929=CARTESIAN_POINT('Ctrl Pts',(129.440457412025,51.8355594232403,202.));
#89930=CARTESIAN_POINT('Ctrl Pts',(129.598075339384,51.1152070969532,201.336045209247));
#89931=CARTESIAN_POINT('Ctrl Pts',(129.4251056608,51.1437356540326,201.989044028215));
#89932=CARTESIAN_POINT('Ctrl Pts',(129.531491494697,51.8055782590138,202.018022602192));
#89933=CARTESIAN_POINT('Ctrl Pts',(129.844929320498,51.0721725887805,201.440585262543));
#89934=CARTESIAN_POINT('Ctrl Pts',(129.566019525609,51.1215950595266,202.024935223531));
#89935=CARTESIAN_POINT('Ctrl Pts',(129.658238631884,51.7613861374496,202.070292632487));
#89936=CARTESIAN_POINT('Ctrl Pts',(129.922998586318,51.0581555745418,201.483235952924));
#89937=CARTESIAN_POINT('Ctrl Pts',(129.611787002084,51.1143254180597,202.041693414839));
#89938=CARTESIAN_POINT('Ctrl Pts',(129.698323284282,51.7469920688305,202.091617977236));
#89939=CARTESIAN_POINT('Ctrl Pts',(130.070819619104,51.0309904096655,201.584008547698));
#89940=CARTESIAN_POINT('Ctrl Pts',(129.700624875494,51.1000325324506,202.085699650362));
#89941=CARTESIAN_POINT('Ctrl Pts',(129.774221971894,51.719096170358,202.142004273075));
#89942=CARTESIAN_POINT('Ctrl Pts',(130.141021021261,51.0177501887032,201.642790906908));
#89943=CARTESIAN_POINT('Ctrl Pts',(129.744060773163,51.0929493134279,202.113213517417));
#89944=CARTESIAN_POINT('Ctrl Pts',(129.810266870854,51.705499790411,202.171395452989));
#89945=CARTESIAN_POINT('Ctrl Pts',(130.330155491038,50.981406690983,201.835877820745));
#89946=CARTESIAN_POINT('Ctrl Pts',(129.862797424543,51.0733422962284,202.208553654803));
#89947=CARTESIAN_POINT('Ctrl Pts',(129.907377934003,51.6681786657293,202.267938911302));
#89948=CARTESIAN_POINT('Ctrl Pts',(130.432435875125,50.9607892587758,201.991913652187));
#89949=CARTESIAN_POINT('Ctrl Pts',(129.931172038655,51.0616962900198,202.292657911015));
#89950=CARTESIAN_POINT('Ctrl Pts',(129.959893782294,51.6470066287864,202.345956826036));
#89951=CARTESIAN_POINT('Ctrl Pts',(130.569841134829,50.9327239155203,202.330202935899));
#89952=CARTESIAN_POINT('Ctrl Pts',(130.023631529767,51.0457502346248,202.483369876793));
#89953=CARTESIAN_POINT('Ctrl Pts',(130.030444491613,51.6181863382183,202.515101468007));
#89954=CARTESIAN_POINT('Ctrl Pts',(130.606204734282,50.9250708620194,202.516399404814));
#89955=CARTESIAN_POINT('Ctrl Pts',(130.049115375546,51.0412521608442,202.592582962827));
#89956=CARTESIAN_POINT('Ctrl Pts',(130.049115378049,51.6103274190584,202.60819970236));
#89957=CARTESIAN_POINT('Ctrl Pts',(130.606204737894,50.9250708612662,202.7));
#89958=CARTESIAN_POINT('Ctrl Pts',(130.049115378049,51.0412521604076,202.7));
#89959=CARTESIAN_POINT('Ctrl Pts',(130.049115378049,51.61032741828,202.7));
#89960=CARTESIAN_POINT('',(130.049115378049,51.61032741828,202.7));
#89961=CARTESIAN_POINT('Origin',(130.749115378049,51.61032741828,202.7));
#89962=CARTESIAN_POINT('Ctrl Pts',(129.349115378049,51.8636099438334,202.));
#89963=CARTESIAN_POINT('Ctrl Pts',(129.378353274608,51.8546311836304,202.));
#89964=CARTESIAN_POINT('Ctrl Pts',(129.407352909326,51.8455186460904,202.001842190722));
#89965=CARTESIAN_POINT('Ctrl Pts',(129.436016335062,51.8363253799306,202.005435824546));
#89966=CARTESIAN_POINT('Ctrl Pts',(129.466313728877,51.8266080485878,202.009234314657));
#89967=CARTESIAN_POINT('Ctrl Pts',(129.496236566828,51.8168001521295,202.014989357515));
#89968=CARTESIAN_POINT('Ctrl Pts',(129.525671916517,51.8069563789023,202.022654975898));
#89969=CARTESIAN_POINT('Ctrl Pts',(129.555107266207,51.7971126056752,202.03032059428));
#89970=CARTESIAN_POINT('Ctrl Pts',(129.584056310451,51.7872324900621,202.039897017501));
#89971=CARTESIAN_POINT('Ctrl Pts',(129.612391438466,51.7773694907784,202.05139719529));
#89972=CARTESIAN_POINT('Ctrl Pts',(129.613592056781,51.7769515749824,202.051884481745));
#89973=CARTESIAN_POINT('Ctrl Pts',(129.614791403714,51.7765337478366,202.052375163507));
#89974=CARTESIAN_POINT('Ctrl Pts',(129.615989462678,51.7761160158889,202.052869238133));
#89975=CARTESIAN_POINT('Ctrl Pts',(129.658186901675,51.7614028682804,202.070271289727));
#89976=CARTESIAN_POINT('Ctrl Pts',(129.698259377414,51.7470135279152,202.091575579855));
#89977=CARTESIAN_POINT('Ctrl Pts',(129.736272329953,51.7330417822806,202.11681092723));
#89978=CARTESIAN_POINT('Ctrl Pts',(129.768808503909,51.7210830388506,202.138410450477));
#89979=CARTESIAN_POINT('Ctrl Pts',(129.800007889183,51.7093596806358,202.16313533375));
#89980=CARTESIAN_POINT('Ctrl Pts',(129.828750982204,51.6983779810147,202.190153705326));
#89981=CARTESIAN_POINT('Ctrl Pts',(129.831763959202,51.6972268311251,202.192985889462));
#89982=CARTESIAN_POINT('Ctrl Pts',(129.834749901387,51.6960838481987,202.195843270102));
#89983=CARTESIAN_POINT('Ctrl Pts',(129.837707485871,51.694949628585,202.198724884211));
#89984=CARTESIAN_POINT('Ctrl Pts',(129.839359638223,51.6943160359987,202.200334598338));
#89985=CARTESIAN_POINT('Ctrl Pts',(129.841002890048,51.693685195333,202.201951824494));
#89986=CARTESIAN_POINT('Ctrl Pts',(129.842637012104,51.6930572101032,202.203576393868));
#89987=CARTESIAN_POINT('Ctrl Pts',(129.872259007364,51.6816736200997,202.233025226127));
#89988=CARTESIAN_POINT('Ctrl Pts',(129.899402602918,51.6710350326229,202.265409408267));
#89989=CARTESIAN_POINT('Ctrl Pts',(129.923562110217,51.6614414622518,202.300131331105));
#89990=CARTESIAN_POINT('Ctrl Pts',(129.945932245253,51.6525584390168,202.332281577094));
#89991=CARTESIAN_POINT('Ctrl Pts',(129.965744082943,51.6445712156073,202.366436892053));
#89992=CARTESIAN_POINT('Ctrl Pts',(129.982555408054,51.637736668221,202.402115810062));
#89993=CARTESIAN_POINT('Ctrl Pts',(129.986969969209,51.6359419538121,202.411484896942));
#89994=CARTESIAN_POINT('Ctrl Pts',(129.99117738931,51.6342268363493,202.420958971512));
#89995=CARTESIAN_POINT('Ctrl Pts',(129.995169129062,51.6325962227829,202.430529128101));
#89996=CARTESIAN_POINT('Ctrl Pts',(130.009842100651,51.6266023584496,202.465707432407));
#89997=CARTESIAN_POINT('Ctrl Pts',(130.021713385473,51.6217126940862,202.502527760224));
#89998=CARTESIAN_POINT('Ctrl Pts',(130.030551890778,51.6180547683919,202.540342857465));
#89999=CARTESIAN_POINT('Ctrl Pts',(130.038818443306,51.6146335524908,202.575710883717));
#90000=CARTESIAN_POINT('Ctrl Pts',(130.044431912552,51.6122898468198,202.611949523054));
#90001=CARTESIAN_POINT('Ctrl Pts',(130.047175263708,51.6111411941615,202.648495735808));
#90002=CARTESIAN_POINT('Ctrl Pts',(130.048460491453,51.6106030639031,202.665617206574));
#90003=CARTESIAN_POINT('Ctrl Pts',(130.049115378049,51.61032741828,202.682805650654));
#90004=CARTESIAN_POINT('Ctrl Pts',(130.049115378049,51.61032741828,202.7));
#90005=CARTESIAN_POINT('Ctrl Pts',(130.049115378049,50.178482477843,227.7));
#90006=CARTESIAN_POINT('Ctrl Pts',(130.049115378049,50.178482477843,227.));
#90007=CARTESIAN_POINT('Ctrl Pts',(130.749115378049,50.178482477843,227.));
#90008=CARTESIAN_POINT('Ctrl Pts',(130.049115378049,50.3640529785653,227.699999985699));
#90009=CARTESIAN_POINT('Ctrl Pts',(130.049115378046,50.2742101005222,227.019246371374));
#90010=CARTESIAN_POINT('Ctrl Pts',(130.729594026839,50.2755777892112,227.));
#90011=CARTESIAN_POINT('Ctrl Pts',(130.049115378049,50.5491164643398,227.664615075625));
#90012=CARTESIAN_POINT('Ctrl Pts',(130.049115378049,50.3786321825897,227.019287176017));
#90013=CARTESIAN_POINT('Ctrl Pts',(130.710551910362,50.3722574264186,226.982307540039));
#90014=CARTESIAN_POINT('Ctrl Pts',(130.049115378049,50.8080062597781,227.560942587807));
#90015=CARTESIAN_POINT('Ctrl Pts',(130.049115378049,50.5320966264688,226.984154463904));
#90016=CARTESIAN_POINT('Ctrl Pts',(130.6843993777,50.5073482333576,226.93047129279));
#90017=CARTESIAN_POINT('Ctrl Pts',(130.049115378049,50.8899726556653,227.518580284352));
#90018=CARTESIAN_POINT('Ctrl Pts',(130.049115378049,50.581618854421,226.967154819554));
#90019=CARTESIAN_POINT('Ctrl Pts',(130.676202303086,50.5500914608447,226.909290141361));
#90020=CARTESIAN_POINT('Ctrl Pts',(130.049115378049,51.04529430901,227.418334861381));
#90021=CARTESIAN_POINT('Ctrl Pts',(130.049115378049,50.676931026749,226.922196051976));
#90022=CARTESIAN_POINT('Ctrl Pts',(130.660793255904,50.6310467935792,226.859167431505));
#90023=CARTESIAN_POINT('Ctrl Pts',(130.049115378049,51.1192364398054,227.359716859222));
#90024=CARTESIAN_POINT('Ctrl Pts',(130.049115378048,50.7232221818321,226.893911925771));
#90025=CARTESIAN_POINT('Ctrl Pts',(130.653524972478,50.6695641554132,226.8298584301));
#90026=CARTESIAN_POINT('Ctrl Pts',(130.049115378049,51.3187163915109,227.166709167936));
#90027=CARTESIAN_POINT('Ctrl Pts',(130.049115378052,50.8489603384451,226.796066144146));
#90028=CARTESIAN_POINT('Ctrl Pts',(130.634047549317,50.7734331756717,226.733354582991));
#90029=CARTESIAN_POINT('Ctrl Pts',(130.049115378049,51.4266877775246,227.010514764464));
#90030=CARTESIAN_POINT('Ctrl Pts',(130.049115378049,50.9199140373353,226.710257286212));
#90031=CARTESIAN_POINT('Ctrl Pts',(130.62369129701,50.8295933572578,226.655257382363));
#90032=CARTESIAN_POINT('Ctrl Pts',(130.049115378049,51.5719050301311,226.671150503398));
#90033=CARTESIAN_POINT('Ctrl Pts',(130.049115378049,51.0153618694534,226.517377439877));
#90034=CARTESIAN_POINT('Ctrl Pts',(130.609830059099,50.9051050736271,226.485575251568));
#90035=CARTESIAN_POINT('Ctrl Pts',(130.049115378049,51.6103274150268,226.484470451835));
#90036=CARTESIAN_POINT('Ctrl Pts',(130.049115378049,51.0412521582374,226.407900947214));
#90037=CARTESIAN_POINT('Ctrl Pts',(130.606204738526,50.9250708611343,226.392235226019));
#90038=CARTESIAN_POINT('Ctrl Pts',(130.049115378049,51.61032741828,226.3));
#90039=CARTESIAN_POINT('Ctrl Pts',(130.049115378049,51.0412521604076,226.3));
#90040=CARTESIAN_POINT('Ctrl Pts',(130.606204737894,50.9250708612662,226.3));
#90041=CARTESIAN_POINT('',(130.049115378049,51.61032741828,226.3));
#90042=CARTESIAN_POINT('',(130.049115378049,50.178482477843,227.7));
#90043=CARTESIAN_POINT('Ctrl Pts',(130.049115378049,51.61032741828,226.3));
#90044=CARTESIAN_POINT('Ctrl Pts',(130.049115378049,51.6103274173581,226.352275490756));
#90045=CARTESIAN_POINT('Ctrl Pts',(130.049115378049,51.6072458611602,226.40444186111));
#90046=CARTESIAN_POINT('Ctrl Pts',(130.04911537805,51.6012540856931,226.456167219767));
#90047=CARTESIAN_POINT('Ctrl Pts',(130.04911537805,51.5950870508888,226.509405544342));
#90048=CARTESIAN_POINT('Ctrl Pts',(130.049115378051,51.5858369917708,226.562177812294));
#90049=CARTESIAN_POINT('Ctrl Pts',(130.049115378052,51.5736365792281,226.614138230052));
#90050=CARTESIAN_POINT('Ctrl Pts',(130.049115378054,51.5612855538423,226.666740093844));
#90051=CARTESIAN_POINT('Ctrl Pts',(130.049115378054,51.5459106783256,226.718511224708));
#90052=CARTESIAN_POINT('Ctrl Pts',(130.049115378053,51.5275972011629,226.769090547588));
#90053=CARTESIAN_POINT('Ctrl Pts',(130.049115378053,51.5188348162022,226.793291058184));
#90054=CARTESIAN_POINT('Ctrl Pts',(130.049115378052,51.5093989505799,226.817218572867));
#90055=CARTESIAN_POINT('Ctrl Pts',(130.049115378051,51.4992949803203,226.840832024798));
#90056=CARTESIAN_POINT('Ctrl Pts',(130.049115378051,51.4991039032287,226.841278580915));
#90057=CARTESIAN_POINT('Ctrl Pts',(130.049115378051,51.4989125789814,226.841725048981));
#90058=CARTESIAN_POINT('Ctrl Pts',(130.049115378051,51.498721007717,226.842171428811));
#90059=CARTESIAN_POINT('Ctrl Pts',(130.049115378049,51.4829426914355,226.878936452861));
#90060=CARTESIAN_POINT('Ctrl Pts',(130.049115378049,51.4654314885516,226.915223527298));
#90061=CARTESIAN_POINT('Ctrl Pts',(130.049115378049,51.4463326897367,226.950746995099));
#90062=CARTESIAN_POINT('Ctrl Pts',(130.049115378049,51.4270191511954,226.986669875442));
#90063=CARTESIAN_POINT('Ctrl Pts',(130.049115378049,51.4060825500491,227.021811110712));
#90064=CARTESIAN_POINT('Ctrl Pts',(130.049115378049,51.3837210648003,227.055897707461));
#90065=CARTESIAN_POINT('Ctrl Pts',(130.049115378049,51.3772329873993,227.065787769574));
#90066=CARTESIAN_POINT('Ctrl Pts',(130.049115378049,51.3706252381693,227.075589231533));
#90067=CARTESIAN_POINT('Ctrl Pts',(130.049115378049,51.3639033150166,227.085295915543));
#90068=CARTESIAN_POINT('Ctrl Pts',(130.049115378049,51.3417215427007,227.117327143775));
#90069=CARTESIAN_POINT('Ctrl Pts',(130.049115378049,51.3183237725072,227.14829466271));
#90070=CARTESIAN_POINT('Ctrl Pts',(130.049115378049,51.2937326377604,227.1782127794));
#90071=CARTESIAN_POINT('Ctrl Pts',(130.049115378049,51.2692357654807,227.208016214294));
#90072=CARTESIAN_POINT('Ctrl Pts',(130.04911537805,51.243554116965,227.236778933117));
#90073=CARTESIAN_POINT('Ctrl Pts',(130.04911537805,51.2166697232773,227.264483603619));
#90074=CARTESIAN_POINT('Ctrl Pts',(130.04911537805,51.2065284811418,227.274934267863));
#90075=CARTESIAN_POINT('Ctrl Pts',(130.04911537805,51.1962157273765,227.285234007762));
#90076=CARTESIAN_POINT('Ctrl Pts',(130.049115378049,51.1857292329141,227.295380420424));
#90077=CARTESIAN_POINT('Ctrl Pts',(130.049115378049,51.1854959240312,227.295606162994));
#90078=CARTESIAN_POINT('Ctrl Pts',(130.049115378049,51.1852625144088,227.295831843945));
#90079=CARTESIAN_POINT('Ctrl Pts',(130.049115378049,51.1850290041207,227.296057463206));
#90080=CARTESIAN_POINT('Ctrl Pts',(130.049115378049,51.1187206958901,227.360125010799));
#90081=CARTESIAN_POINT('Ctrl Pts',(130.049115378049,51.0450217810817,227.418510753969));
#90082=CARTESIAN_POINT('Ctrl Pts',(130.049115378049,50.9676333634749,227.468457388699));
#90083=CARTESIAN_POINT('Ctrl Pts',(130.049115378049,50.9674289789469,227.468589298869));
#90084=CARTESIAN_POINT('Ctrl Pts',(130.049115378049,50.9672245646234,227.468721155272));
#90085=CARTESIAN_POINT('Ctrl Pts',(130.049115378049,50.9670201205043,227.468852957906));
#90086=CARTESIAN_POINT('Ctrl Pts',(130.049115378049,50.8895409876893,227.51880281126));
#90087=CARTESIAN_POINT('Ctrl Pts',(130.049115378049,50.8077835053153,227.561031606915));
#90088=CARTESIAN_POINT('Ctrl Pts',(130.049115378049,50.721709619144,227.595499978478));
#90089=CARTESIAN_POINT('Ctrl Pts',(130.049115378049,50.7215582076484,227.595560611359));
#90090=CARTESIAN_POINT('Ctrl Pts',(130.049115378049,50.721406786528,227.595621218291));
#90091=CARTESIAN_POINT('Ctrl Pts',(130.049115378049,50.7212553557907,227.595681799273));
#90092=CARTESIAN_POINT('Ctrl Pts',(130.049115378049,50.6710671469183,227.615759962087));
#90093=CARTESIAN_POINT('Ctrl Pts',(130.049115378049,50.6199526275822,227.632940553192));
#90094=CARTESIAN_POINT('Ctrl Pts',(130.049115378049,50.5681013780827,227.647244653797));
#90095=CARTESIAN_POINT('Ctrl Pts',(130.049115378049,50.5160514903066,227.661603552347));
#90096=CARTESIAN_POINT('Ctrl Pts',(130.049115378049,50.4632583681232,227.673064024006));
#90097=CARTESIAN_POINT('Ctrl Pts',(130.049115378049,50.4098993109671,227.681596908351));
#90098=CARTESIAN_POINT('Ctrl Pts',(130.049115378049,50.3572232257564,227.690020575613));
#90099=CARTESIAN_POINT('Ctrl Pts',(130.049115378049,50.3039947720342,227.695591155994));
#90100=CARTESIAN_POINT('Ctrl Pts',(130.049115378049,50.2503829577808,227.698230353047));
#90101=CARTESIAN_POINT('Ctrl Pts',(130.049115378049,50.2264870648022,227.699406697686));
#90102=CARTESIAN_POINT('Ctrl Pts',(130.049115378049,50.2025150640935,227.699999998148));
#90103=CARTESIAN_POINT('Ctrl Pts',(130.049115378049,50.178482477843,227.7));
#90104=CARTESIAN_POINT('Origin',(130.749115378049,50.178482477843,227.7));
#90105=CARTESIAN_POINT('Origin',(130.749115378049,51.61032741828,226.3));
#90106=CARTESIAN_POINT('Origin',(125.29348064571,25.4505574462982,227.7));
#90107=CARTESIAN_POINT('',(130.749115378049,25.4505574462982,227.));
#90108=CARTESIAN_POINT('',(130.049115378049,25.4505574462982,227.7));
#90109=CARTESIAN_POINT('Origin',(130.749115378049,25.4505574462982,227.7));
#90110=CARTESIAN_POINT('Origin',(125.29348064571,25.4505574462982,227.7));
#90111=CARTESIAN_POINT('Origin',(125.29348064571,25.4505574462982,227.));
#90112=CARTESIAN_POINT('Origin',(129.349115378049,25.4505574462982,202.7));
#90113=CARTESIAN_POINT('',(130.049115378049,53.4601166829598,202.7));
#90114=CARTESIAN_POINT('',(129.349115378049,51.0349239481607,202.));
#90115=CARTESIAN_POINT('Origin',(130.749115378049,51.61032741828,227.));
#90116=CARTESIAN_POINT('',(130.049115378049,51.61032741828,202.));
#90117=CARTESIAN_POINT('Origin',(130.749115378049,25.4505574462982,227.7));
#90118=CARTESIAN_POINT('',(130.049115378049,51.0349239481607,227.7));
#90119=CARTESIAN_POINT('',(130.749115378049,25.4505574462982,227.));
#90120=CARTESIAN_POINT('Origin',(125.29348064571,25.4505574462982,229.));
#90121=CARTESIAN_POINT('Origin',(125.29348064571,25.4505574462982,202.));
#90122=CARTESIAN_POINT('Origin',(125.29348064571,53.4601166829598,202.));
#90123=CARTESIAN_POINT('',(120.537845913371,53.4601166829598,202.));
#90124=CARTESIAN_POINT('',(130.049115378049,53.4601166829598,202.));
#90125=CARTESIAN_POINT('Origin',(125.29348064571,25.4505574462982,202.));
#90126=CARTESIAN_POINT('',(130.049115378049,25.4505574462982,202.));
#90127=CARTESIAN_POINT('',(120.537845913371,25.4505574462982,202.));
#90128=CARTESIAN_POINT('Origin',(130.049115378049,25.4505574462982,202.));
#90129=CARTESIAN_POINT('Origin',(120.537845913371,25.4505574462982,202.));
#90130=CARTESIAN_POINT('Origin',(125.29348064571,25.4505574462982,227.));
#90131=CARTESIAN_POINT('Origin',(37.8448101558397,24.2184812945555,172.608250755187));
#90132=CARTESIAN_POINT('',(16.5267601345175,3.11418027746145,173.108250755187));
#90133=CARTESIAN_POINT('',(16.8785276479032,2.7588499853016,172.608250755187));
#90134=CARTESIAN_POINT('Origin',(16.5267601345175,3.11418027746145,172.608250755187));
#90135=CARTESIAN_POINT('',(38.1965776692254,23.8631510023956,172.608250755187));
#90136=CARTESIAN_POINT('',(37.8448101558397,24.2184812945555,173.108250755187));
#90137=CARTESIAN_POINT('Origin',(14.0868850299881,5.57876697388923,172.608250755187));
#90138=CARTESIAN_POINT('',(11.6470099254586,8.043353670317,173.108250755187));
#90139=CARTESIAN_POINT('',(11.2952424120729,8.39868396247686,172.608250755187));
#90140=CARTESIAN_POINT('Origin',(11.6470099254586,8.043353670317,172.608250755187));
#90141=CARTESIAN_POINT('Origin',(14.0868850299881,5.57876697388923,172.608250755187));
#90142=CARTESIAN_POINT('Origin',(14.0868850299881,5.57876697388923,173.108250755187));
#90143=CARTESIAN_POINT('Origin',(32.9650599467808,29.147654687411,172.608250755187));
#90144=CARTESIAN_POINT('',(32.6132924333951,29.5029849795709,172.608250755187));
#90145=CARTESIAN_POINT('',(32.9650599467808,29.147654687411,173.108250755187));
#90146=CARTESIAN_POINT('Origin',(35.4049350513103,26.6830679909832,152.608250755187));
#90147=CARTESIAN_POINT('',(21.5010931458411,17.798633272459,153.108250755187));
#90148=CARTESIAN_POINT('Origin',(21.5010931458411,17.798633272459,152.608250755187));
#90149=CARTESIAN_POINT('',(26.3808433549,12.8694598796034,153.108250755187));
#90150=CARTESIAN_POINT('Origin',(26.3808433549,12.8694598796034,152.608250755187));
#90151=CARTESIAN_POINT('Origin',(35.4049350513103,26.6830679909832,153.108250755187));
#90152=CARTESIAN_POINT('Ctrl Pts',(27.5073406548652,12.768040044578,153.608250755187));
#90153=CARTESIAN_POINT('Ctrl Pts',(27.1779404377158,12.9549939852504,153.608250755187));
#90154=CARTESIAN_POINT('Ctrl Pts',(26.9087733165906,12.6885257134127,153.608250755187));
#90155=CARTESIAN_POINT('Ctrl Pts',(27.5073406342015,12.7680400563058,153.475551801171));
#90156=CARTESIAN_POINT('Ctrl Pts',(27.1779404229081,12.9549939942968,153.527723751245));
#90157=CARTESIAN_POINT('Ctrl Pts',(26.9087733118706,12.68852570874,153.541901279333));
#90158=CARTESIAN_POINT('Ctrl Pts',(27.4836651381883,12.7814084763901,153.342399703391));
#90159=CARTESIAN_POINT('Ctrl Pts',(27.1606400720877,12.965534956355,153.446619353193));
#90160=CARTESIAN_POINT('Ctrl Pts',(26.893846651724,12.6927270912806,153.475325227732));
#90161=CARTESIAN_POINT('Ctrl Pts',(27.3943038776747,12.8327090607538,153.098820706789));
#90162=CARTESIAN_POINT('Ctrl Pts',(27.0980595223776,13.0041108087012,153.3049590945));
#90163=CARTESIAN_POINT('Ctrl Pts',(26.8377244017675,12.7092343374354,153.353535732545));
#90164=CARTESIAN_POINT('Ctrl Pts',(27.3285209197659,12.8707492134963,152.987832794725));
#90165=CARTESIAN_POINT('Ctrl Pts',(27.0522238475563,13.0325418769711,153.243730625338));
#90166=CARTESIAN_POINT('Ctrl Pts',(26.7964812241876,12.7215983775456,153.298041773782));
#90167=CARTESIAN_POINT('Ctrl Pts',(27.168815411942,12.9653805575585,152.805062971569));
#90168=CARTESIAN_POINT('Ctrl Pts',(26.9473919563668,13.0985506777719,153.152596157915));
#90169=CARTESIAN_POINT('Ctrl Pts',(26.696939992414,12.7533719782571,153.206656864552));
#90170=CARTESIAN_POINT('Ctrl Pts',(27.0735561471923,13.0228217613016,152.731827736181));
#90171=CARTESIAN_POINT('Ctrl Pts',(26.8870893049663,13.136998440275,153.1222986856));
#90172=CARTESIAN_POINT('Ctrl Pts',(26.637823732227,12.7730921439478,153.170039246316));
#90173=CARTESIAN_POINT('Ctrl Pts',(26.8710052246367,13.1484367358317,152.633922888492));
#90174=CARTESIAN_POINT('Ctrl Pts',(26.7679788506669,13.2138353374613,153.093277185672));
#90175=CARTESIAN_POINT('Ctrl Pts',(26.5130205024505,12.8177036267266,153.121086821207));
#90176=CARTESIAN_POINT('Ctrl Pts',(26.760985873486,13.2183592414295,152.608250765972));
#90177=CARTESIAN_POINT('Ctrl Pts',(26.7075856545808,13.2532442939392,153.094953472493));
#90178=CARTESIAN_POINT('Ctrl Pts',(26.4456558529318,12.8432444717969,153.108250755187));
#90179=CARTESIAN_POINT('Ctrl Pts',(26.6543006790336,13.2880540647968,152.608250755187));
#90180=CARTESIAN_POINT('Ctrl Pts',(26.6543006790336,13.2880540647968,153.108250755187));
#90181=CARTESIAN_POINT('Ctrl Pts',(26.3808433549,12.8694598796034,153.108250755187));
#90182=CARTESIAN_POINT('',(26.9087733165906,12.6885257134127,153.608250755187));
#90183=CARTESIAN_POINT('Origin',(27.2605408299763,12.3331954212528,153.608250755187));
#90184=CARTESIAN_POINT('Ctrl Pts',(26.9087733165906,12.6885257134127,153.608250755187));
#90185=CARTESIAN_POINT('Ctrl Pts',(26.9087733165906,12.6885257134127,153.58561192993));
#90186=CARTESIAN_POINT('Ctrl Pts',(26.9070395695061,12.6890138059481,153.563154237045));
#90187=CARTESIAN_POINT('Ctrl Pts',(26.9037135366198,12.6899636529495,153.541035429084));
#90188=CARTESIAN_POINT('Ctrl Pts',(26.900229546794,12.6909586092238,153.517866174742));
#90189=CARTESIAN_POINT('Ctrl Pts',(26.8949984104558,12.6924601686093,153.495067766235));
#90190=CARTESIAN_POINT('Ctrl Pts',(26.8881298385863,12.6944521653016,153.472807844592));
#90191=CARTESIAN_POINT('Ctrl Pts',(26.886517484165,12.6949197741052,153.467582466775));
#90192=CARTESIAN_POINT('Ctrl Pts',(26.8848146808982,12.6954144688681,153.462386743418));
#90193=CARTESIAN_POINT('Ctrl Pts',(26.8830224554071,12.6959361508752,153.457222835554));
#90194=CARTESIAN_POINT('Ctrl Pts',(26.8779742821994,12.6974055759806,153.442677622656));
#90195=CARTESIAN_POINT('Ctrl Pts',(26.8722166021153,12.699089141154,153.428386396435));
#90196=CARTESIAN_POINT('Ctrl Pts',(26.8657855267457,12.700980714358,153.414430480138));
#90197=CARTESIAN_POINT('Ctrl Pts',(26.8632008765685,12.7017409379188,153.408821595238));
#90198=CARTESIAN_POINT('Ctrl Pts',(26.860507107671,12.7025352357299,153.40326444683));
#90199=CARTESIAN_POINT('Ctrl Pts',(26.8577089907892,12.7033627973938,153.397762970209));
#90200=CARTESIAN_POINT('Ctrl Pts',(26.8434713128181,12.7075736852767,153.369769767704));
#90201=CARTESIAN_POINT('Ctrl Pts',(26.826539106381,12.7126442230621,153.343230009335));
#90202=CARTESIAN_POINT('Ctrl Pts',(26.8074888665516,12.7184791208889,153.318537883336));
#90203=CARTESIAN_POINT('Ctrl Pts',(26.7890492187098,12.7241270005001,153.294637181194));
#90204=CARTESIAN_POINT('Ctrl Pts',(26.7686251816549,12.7304910090134,153.272467520466));
#90205=CARTESIAN_POINT('Ctrl Pts',(26.7467118251245,12.7374867495037,153.252349061816));
#90206=CARTESIAN_POINT('Ctrl Pts',(26.7447051617612,12.738127367755,153.250506761946));
#90207=CARTESIAN_POINT('Ctrl Pts',(26.7426846595016,12.7387737898784,153.248680454799));
#90208=CARTESIAN_POINT('Ctrl Pts',(26.7406507833593,12.7394259068857,153.246870287867));
#90209=CARTESIAN_POINT('Ctrl Pts',(26.7219609664006,12.7454183797056,153.230236193034));
#90210=CARTESIAN_POINT('Ctrl Pts',(26.7021655132865,12.751883330314,153.214981265978));
#90211=CARTESIAN_POINT('Ctrl Pts',(26.6815451859053,12.7587610622873,153.201166192582));
#90212=CARTESIAN_POINT('Ctrl Pts',(26.6596871824718,12.7660516104105,153.186521909001));
#90213=CARTESIAN_POINT('Ctrl Pts',(26.6369012258168,12.7738061414819,153.173494523172));
#90214=CARTESIAN_POINT('Ctrl Pts',(26.6134755587766,12.7819706583732,153.162187747804));
#90215=CARTESIAN_POINT('Ctrl Pts',(26.6009612965353,12.7863322377159,153.156147537644));
#90216=CARTESIAN_POINT('Ctrl Pts',(26.5882638090727,12.7908110879768,153.150598972776));
#90217=CARTESIAN_POINT('Ctrl Pts',(26.5754238802881,12.7954005301352,153.145562771898));
#90218=CARTESIAN_POINT('Ctrl Pts',(26.5512362102307,12.8040460541516,153.13607565034));
#90219=CARTESIAN_POINT('Ctrl Pts',(26.5262911060842,12.8131811825813,153.128328353012));
#90220=CARTESIAN_POINT('Ctrl Pts',(26.500936708412,12.822692741828,153.12238823827));
#90221=CARTESIAN_POINT('Ctrl Pts',(26.477347025937,12.8315422781244,153.116861567023));
#90222=CARTESIAN_POINT('Ctrl Pts',(26.453401570454,12.8407182262646,153.112899483272));
#90223=CARTESIAN_POINT('Ctrl Pts',(26.4293898763036,12.8501313371653,153.110597998101));
#90224=CARTESIAN_POINT('Ctrl Pts',(26.4132055677847,12.8564759411731,153.1090467562));
#90225=CARTESIAN_POINT('Ctrl Pts',(26.3969913673361,12.8629283194239,153.108250755187));
#90226=CARTESIAN_POINT('Ctrl Pts',(26.3808433549,12.8694598796034,153.108250755187));
#90227=CARTESIAN_POINT('Ctrl Pts',(21.9224216884311,18.0678585669597,152.608250755187));
#90228=CARTESIAN_POINT('Ctrl Pts',(21.9224216884311,18.0678585669597,153.108250755187));
#90229=CARTESIAN_POINT('Ctrl Pts',(21.5010931458411,17.798633272459,153.108250755187));
#90230=CARTESIAN_POINT('Ctrl Pts',(21.8529692250382,18.1765493392546,152.60825077749));
#90231=CARTESIAN_POINT('Ctrl Pts',(21.8877231275685,18.1221606460453,153.094787604517));
#90232=CARTESIAN_POINT('Ctrl Pts',(21.4752187820791,17.8645045048257,153.108250755187));
#90233=CARTESIAN_POINT('Ctrl Pts',(21.7851621994479,18.2856761107434,152.633710236017));
#90234=CARTESIAN_POINT('Ctrl Pts',(21.8494711012016,18.1820886305035,153.093185957657));
#90235=CARTESIAN_POINT('Ctrl Pts',(21.4507281499402,17.9311502346664,153.120980492262));
#90236=CARTESIAN_POINT('Ctrl Pts',(21.6607280584935,18.4909268139007,152.732462696752));
#90237=CARTESIAN_POINT('Ctrl Pts',(21.7732901420723,18.3028399523544,153.122507989483));
#90238=CARTESIAN_POINT('Ctrl Pts',(21.4070763536337,18.0572865403012,153.170356729309));
#90239=CARTESIAN_POINT('Ctrl Pts',(21.6047379954083,18.5859573989266,152.805334639289));
#90240=CARTESIAN_POINT('Ctrl Pts',(21.7357414624187,18.3630692431353,153.152707467856));
#90241=CARTESIAN_POINT('Ctrl Pts',(21.388124909213,18.1161056718009,153.206792695945));
#90242=CARTESIAN_POINT('Ctrl Pts',(21.5115995501989,18.7468303826906,152.988630571688));
#90243=CARTESIAN_POINT('Ctrl Pts',(21.6706947362434,18.4687247489851,153.244147548454));
#90244=CARTESIAN_POINT('Ctrl Pts',(21.3573191318963,18.2161018881959,153.29844066473));
#90245=CARTESIAN_POINT('Ctrl Pts',(21.4742934531536,18.8128807906121,153.099898214101));
#90246=CARTESIAN_POINT('Ctrl Pts',(21.6427661294028,18.5147847472079,153.30558183398));
#90247=CARTESIAN_POINT('Ctrl Pts',(21.345396035639,18.2573986678047,153.354074484501));
#90248=CARTESIAN_POINT('Ctrl Pts',(21.4242056493653,18.9022051021532,153.342371533405));
#90249=CARTESIAN_POINT('Ctrl Pts',(21.6050533759232,18.5773697525719,153.446616730793));
#90250=CARTESIAN_POINT('Ctrl Pts',(21.3295538767565,18.3133407705917,153.475311144439));
#90251=CARTESIAN_POINT('Ctrl Pts',(21.4110300989696,18.9260953737276,153.475893601961));
#90252=CARTESIAN_POINT('Ctrl Pts',(21.5946552032658,18.5948279601094,153.527930080756));
#90253=CARTESIAN_POINT('Ctrl Pts',(21.3254880800282,18.3283596898632,153.542072178464));
#90254=CARTESIAN_POINT('Ctrl Pts',(21.4110300971907,18.9260953769367,153.608250755187));
#90255=CARTESIAN_POINT('Ctrl Pts',(21.5946552018854,18.5948279624256,153.608250755187));
#90256=CARTESIAN_POINT('Ctrl Pts',(21.3254880807602,18.3283596905879,153.608250755187));
#90257=CARTESIAN_POINT('',(21.3254880807602,18.3283596905879,153.608250755187));
#90258=CARTESIAN_POINT('Origin',(20.9737205673745,18.6836899827478,153.608250755187));
#90259=CARTESIAN_POINT('Ctrl Pts',(21.5010931458411,17.798633272459,153.108250755187));
#90260=CARTESIAN_POINT('Ctrl Pts',(21.4905730502976,17.8254154443586,153.108250755187));
#90261=CARTESIAN_POINT('Ctrl Pts',(21.4803463693722,17.8521593410534,153.110350857061));
#90262=CARTESIAN_POINT('Ctrl Pts',(21.4704609701153,17.8786538141028,153.114447252937));
#90263=CARTESIAN_POINT('Ctrl Pts',(21.4603139997298,17.9058493401941,153.118652040884));
#90264=CARTESIAN_POINT('Ctrl Pts',(21.4505262446712,17.9327832401005,153.124960207408));
#90265=CARTESIAN_POINT('Ctrl Pts',(21.4411536697561,17.9592354635942,153.13331284971));
#90266=CARTESIAN_POINT('Ctrl Pts',(21.43698585605,17.9709982865785,153.137027117921));
#90267=CARTESIAN_POINT('Ctrl Pts',(21.4329002292475,17.9826658616096,153.141146354449));
#90268=CARTESIAN_POINT('Ctrl Pts',(21.4289022644077,17.9942183957151,153.145668609543));
#90269=CARTESIAN_POINT('Ctrl Pts',(21.4200063910211,18.0199239446167,153.155731081412));
#90270=CARTESIAN_POINT('Ctrl Pts',(21.4115784694086,18.0449504539261,153.167751327949));
#90271=CARTESIAN_POINT('Ctrl Pts',(21.4036467411062,18.0690479409556,153.181631702462));
#90272=CARTESIAN_POINT('Ctrl Pts',(21.3960731025622,18.0920575108276,153.19488542667));
#90273=CARTESIAN_POINT('Ctrl Pts',(21.3889517927388,18.1142208889259,153.209835861403));
#90274=CARTESIAN_POINT('Ctrl Pts',(21.3823199823874,18.1352871692309,153.226428438647));
#90275=CARTESIAN_POINT('Ctrl Pts',(21.3797305551073,18.143512615681,153.232907102826));
#90276=CARTESIAN_POINT('Ctrl Pts',(21.3772159005764,18.1515703676921,153.239636401772));
#90277=CARTESIAN_POINT('Ctrl Pts',(21.3747788264842,18.1594436001056,153.246614074428));
#90278=CARTESIAN_POINT('Ctrl Pts',(21.374086775673,18.1616793453772,153.248595509476));
#90279=CARTESIAN_POINT('Ctrl Pts',(21.3734011788201,18.1638995706237,153.250596415344));
#90280=CARTESIAN_POINT('Ctrl Pts',(21.3727221102163,18.1661038480104,153.252616665764));
#90281=CARTESIAN_POINT('Ctrl Pts',(21.3657201020249,18.1888325800269,153.273447860005));
#90282=CARTESIAN_POINT('Ctrl Pts',(21.3593972300783,18.2098942489177,153.296424536252));
#90283=CARTESIAN_POINT('Ctrl Pts',(21.3538250978631,18.2287912078363,153.321170461488));
#90284=CARTESIAN_POINT('Ctrl Pts',(21.3485511315198,18.2466769868303,153.344592227481));
#90285=CARTESIAN_POINT('Ctrl Pts',(21.3439497209919,18.2626236397157,153.369599261715));
#90286=CARTESIAN_POINT('Ctrl Pts',(21.3400895512389,18.2761669413073,153.395852653192));
#90287=CARTESIAN_POINT('Ctrl Pts',(21.3391761782763,18.2793714857415,153.402064591911));
#90288=CARTESIAN_POINT('Ctrl Pts',(21.3383043412798,18.2824412753061,153.408346207007));
#90289=CARTESIAN_POINT('Ctrl Pts',(21.3374750195038,18.2853697768887,153.414692806039));
#90290=CARTESIAN_POINT('Ctrl Pts',(21.3340535782225,18.297451572515,153.4408762689));
#90291=CARTESIAN_POINT('Ctrl Pts',(21.3313279236915,18.3072005590295,153.468385102508));
#90292=CARTESIAN_POINT('Ctrl Pts',(21.3293445811899,18.3143466012112,153.49672275683));
#90293=CARTESIAN_POINT('Ctrl Pts',(21.3274524666984,18.3211639461519,153.523756961136));
#90294=CARTESIAN_POINT('Ctrl Pts',(21.3262359632126,18.3256122792073,153.551545730234));
#90295=CARTESIAN_POINT('Ctrl Pts',(21.3257408437783,18.3274298612427,153.579619100729));
#90296=CARTESIAN_POINT('Ctrl Pts',(21.3255729780825,18.3280460957344,153.589137119097));
#90297=CARTESIAN_POINT('Ctrl Pts',(21.3254880807602,18.3283596905879,153.598687494769));
#90298=CARTESIAN_POINT('Ctrl Pts',(21.3254880807602,18.3283596905879,153.608250755187));
#90299=CARTESIAN_POINT('Origin',(27.2605408299763,12.3331954212528,171.608250755187));
#90300=CARTESIAN_POINT('',(26.9087733165906,12.6885257134127,171.108250755187));
#90301=CARTESIAN_POINT('Origin',(27.2605408299763,12.3331954212528,171.108250755187));
#90302=CARTESIAN_POINT('',(26.9087733165906,12.6885257134127,153.108250755187));
#90303=CARTESIAN_POINT('Origin',(37.8448101558397,24.2184812945555,153.608250755187));
#90304=CARTESIAN_POINT('',(16.8785276479032,2.7588499853016,153.608250755187));
#90305=CARTESIAN_POINT('',(16.5267601345175,3.11418027746145,153.108250755187));
#90306=CARTESIAN_POINT('Origin',(16.5267601345175,3.11418027746145,153.608250755187));
#90307=CARTESIAN_POINT('',(16.5267601345175,3.11418027746145,153.108250755187));
#90308=CARTESIAN_POINT('',(27.1812285825866,12.9582491609851,153.608250755187));
#90309=CARTESIAN_POINT('Origin',(32.9650599467808,29.147654687411,153.608250755187));
#90310=CARTESIAN_POINT('',(11.6470099254586,8.043353670317,153.108250755187));
#90311=CARTESIAN_POINT('',(11.2952424120729,8.39868396247686,153.608250755187));
#90312=CARTESIAN_POINT('Origin',(11.6470099254586,8.04335367031701,153.608250755187));
#90313=CARTESIAN_POINT('',(11.2952424120729,8.39868396247685,153.608250755187));
#90314=CARTESIAN_POINT('',(21.949710860142,18.2427528460005,153.108250755187));
#90315=CARTESIAN_POINT('Origin',(20.9737205673745,18.6836899827478,171.608250755187));
#90316=CARTESIAN_POINT('',(21.3254880807602,18.3283596905879,171.108250755187));
#90317=CARTESIAN_POINT('Origin',(20.9737205673745,18.6836899827478,171.108250755187));
#90318=CARTESIAN_POINT('',(21.3254880807602,18.3283596905879,153.108250755187));
#90319=CARTESIAN_POINT('Ctrl Pts',(26.9087733165906,12.6885257134127,171.108250755187));
#90320=CARTESIAN_POINT('Ctrl Pts',(27.1779404377158,12.9549939852504,171.108250755187));
#90321=CARTESIAN_POINT('Ctrl Pts',(27.5073406548652,12.768040044578,171.108250755187));
#90322=CARTESIAN_POINT('Ctrl Pts',(26.9087733340747,12.6885257307215,171.241737242521));
#90323=CARTESIAN_POINT('Ctrl Pts',(27.177940450083,12.9549939974924,171.189238482122));
#90324=CARTESIAN_POINT('Ctrl Pts',(27.5073406604818,12.7680400413903,171.174993997722));
#90325=CARTESIAN_POINT('Ctrl Pts',(26.9289558292315,12.7085058627054,171.375809742194));
#90326=CARTESIAN_POINT('Ctrl Pts',(27.1924226045785,12.9693309442371,171.270872142595));
#90327=CARTESIAN_POINT('Ctrl Pts',(27.5205585322336,12.7762529890485,171.242030250225));
#90328=CARTESIAN_POINT('Ctrl Pts',(27.0054626143324,12.784245539693,171.620480252948));
#90329=CARTESIAN_POINT('Ctrl Pts',(27.2458363457333,13.0222091235587,171.414405744627));
#90330=CARTESIAN_POINT('Ctrl Pts',(27.5708445650066,12.8073151622189,171.364365502532));
#90331=CARTESIAN_POINT('Ctrl Pts',(27.0619560851888,12.8401725692881,171.731805299994));
#90332=CARTESIAN_POINT('Ctrl Pts',(27.2853253179226,13.0613021529443,171.477100056791));
#90333=CARTESIAN_POINT('Ctrl Pts',(27.608034085531,12.8302288792103,171.420028028856));
#90334=CARTESIAN_POINT('Ctrl Pts',(27.1998136024674,12.9766478350469,171.914243767979));
#90335=CARTESIAN_POINT('Ctrl Pts',(27.3778758818511,13.1529247431196,171.570720798637));
#90336=CARTESIAN_POINT('Ctrl Pts',(27.6992900235444,12.8859483002505,171.511247260317));
#90337=CARTESIAN_POINT('Ctrl Pts',(27.2823137807828,13.0583208114866,171.986819299416));
#90338=CARTESIAN_POINT('Ctrl Pts',(27.4322874234685,13.2067907182887,171.602133212335));
#90339=CARTESIAN_POINT('Ctrl Pts',(27.7541210219345,12.9192082849093,171.547535027057));
#90340=CARTESIAN_POINT('Ctrl Pts',(27.458765263205,13.2330030735239,172.083342412463));
#90341=CARTESIAN_POINT('Ctrl Pts',(27.541996530637,13.3153998086924,171.630196458045));
#90342=CARTESIAN_POINT('Ctrl Pts',(27.8721997120763,12.9900408536816,171.595796584069));
#90343=CARTESIAN_POINT('Ctrl Pts',(27.5549119618052,13.3281857411239,172.108250746497));
#90344=CARTESIAN_POINT('Ctrl Pts',(27.5989314668852,13.3717638772494,171.626173327528));
#90345=CARTESIAN_POINT('Ctrl Pts',(27.9369238543391,13.0284859943162,171.608250755187));
#90346=CARTESIAN_POINT('Ctrl Pts',(27.6489098612225,13.4212411548363,172.108250755187));
#90347=CARTESIAN_POINT('Ctrl Pts',(27.6489098612225,13.4212411548363,171.608250755187));
#90348=CARTESIAN_POINT('Ctrl Pts',(28.0006773746082,13.0659108626764,171.608250755187));
#90349=CARTESIAN_POINT('',(27.6489098612224,13.4212411548363,172.108250755187));
#90350=CARTESIAN_POINT('Origin',(28.0006773746082,13.0659108626764,172.108250755187));
#90351=CARTESIAN_POINT('Ctrl Pts',(27.6489098612224,13.4212411548363,172.108250755187));
#90352=CARTESIAN_POINT('Ctrl Pts',(27.6221197748791,13.3947196837871,172.10825075271));
#90353=CARTESIAN_POINT('Ctrl Pts',(27.595366665669,13.368234819114,172.106231383603));
#90354=CARTESIAN_POINT('Ctrl Pts',(27.5688036575348,13.3419381494357,172.102298699115));
#90355=CARTESIAN_POINT('Ctrl Pts',(27.5414606876917,13.3148693384654,172.098250540381));
#90356=CARTESIAN_POINT('Ctrl Pts',(27.5143182183118,13.2879990176061,172.092175073618));
#90357=CARTESIAN_POINT('Ctrl Pts',(27.4875298095769,13.2614792073432,172.084134831723));
#90358=CARTESIAN_POINT('Ctrl Pts',(27.4607131615435,13.234931440928,172.076086114118));
#90359=CARTESIAN_POINT('Ctrl Pts',(27.4342503195365,13.2087339330439,172.066068297256));
#90360=CARTESIAN_POINT('Ctrl Pts',(27.4082967712959,13.1830406124086,172.054093236391));
#90361=CARTESIAN_POINT('Ctrl Pts',(27.3955823048237,13.1704536296674,172.048226735654));
#90362=CARTESIAN_POINT('Ctrl Pts',(27.3829901821132,13.1579877639881,172.041889749808));
#90363=CARTESIAN_POINT('Ctrl Pts',(27.3705399239133,13.1456623403913,172.035079401128));
#90364=CARTESIAN_POINT('Ctrl Pts',(27.3703156689721,13.1454403339799,172.034956732641));
#90365=CARTESIAN_POINT('Ctrl Pts',(27.3700914459051,13.1452183591231,172.034833904296));
#90366=CARTESIAN_POINT('Ctrl Pts',(27.3698672547917,13.1449964158994,172.034710916136));
#90367=CARTESIAN_POINT('Ctrl Pts',(27.2819022951275,13.0579134516647,171.98645454965));
#90368=CARTESIAN_POINT('Ctrl Pts',(27.1996383705023,12.9764743600704,171.914009179875));
#90369=CARTESIAN_POINT('Ctrl Pts',(27.1308853210348,12.908410674588,171.823023819991));
#90370=CARTESIAN_POINT('Ctrl Pts',(27.1307685101586,12.9082950349356,171.822869236599));
#90371=CARTESIAN_POINT('Ctrl Pts',(27.1306517350126,12.9081794306553,171.822714595501));
#90372=CARTESIAN_POINT('Ctrl Pts',(27.1305349956251,12.9080638617748,171.822559896743));
#90373=CARTESIAN_POINT('Ctrl Pts',(27.0617656524892,12.8399840459953,171.731429283186));
#90374=CARTESIAN_POINT('Ctrl Pts',(27.0053994467863,12.7841830055056,171.620275542505));
#90375=CARTESIAN_POINT('Ctrl Pts',(26.9672095752599,12.7463760511325,171.498144778716));
#90376=CARTESIAN_POINT('Ctrl Pts',(26.9671771612793,12.7463439621561,171.498041119185));
#90377=CARTESIAN_POINT('Ctrl Pts',(26.9671447602716,12.7463118860226,171.497937451223));
#90378=CARTESIAN_POINT('Ctrl Pts',(26.9671123722381,12.7462798227331,171.497833774838));
#90379=CARTESIAN_POINT('Ctrl Pts',(26.9560651316504,12.7353433491563,171.462470776877));
#90380=CARTESIAN_POINT('Ctrl Pts',(26.9465607587732,12.725934273468,171.426245512338));
#90381=CARTESIAN_POINT('Ctrl Pts',(26.9386061022959,12.7180593756882,171.389360653073));
#90382=CARTESIAN_POINT('Ctrl Pts',(26.9306441693041,12.7101772743531,171.352442053416));
#90383=CARTESIAN_POINT('Ctrl Pts',(26.9242345978251,12.7038319695175,171.314861536714));
#90384=CARTESIAN_POINT('Ctrl Pts',(26.9194191830746,12.6990648373308,171.276805373256));
#90385=CARTESIAN_POINT('Ctrl Pts',(26.9147383382688,12.6944309258006,171.239812714414));
#90386=CARTESIAN_POINT('Ctrl Pts',(26.9115637593677,12.6912881773473,171.202369605235));
#90387=CARTESIAN_POINT('Ctrl Pts',(26.9099682233711,12.6897086392599,171.164646810882));
#90388=CARTESIAN_POINT('Ctrl Pts',(26.9091757117165,12.6889240738564,171.145909687915));
#90389=CARTESIAN_POINT('Ctrl Pts',(26.9087733190599,12.6885257158573,171.127103649704));
#90390=CARTESIAN_POINT('Ctrl Pts',(26.9087733165906,12.6885257134127,171.108250755187));
#90391=CARTESIAN_POINT('Origin',(14.0868850299881,5.57876697388923,153.608250755187));
#90392=CARTESIAN_POINT('Origin',(14.0868850299881,5.57876697388923,153.608250755187));
#90393=CARTESIAN_POINT('Origin',(14.0868850299881,5.57876697388923,153.108250755187));
#90394=CARTESIAN_POINT('Ctrl Pts',(22.0656246253921,19.0610751320115,172.108250755187));
#90395=CARTESIAN_POINT('Ctrl Pts',(22.0656246253921,19.0610751320115,171.608250755187));
#90396=CARTESIAN_POINT('Ctrl Pts',(21.7138571120063,19.4164054241714,171.608250755187));
#90397=CARTESIAN_POINT('Ctrl Pts',(21.970440150776,18.9668450404955,172.108250736963));
#90398=CARTESIAN_POINT('Ctrl Pts',(22.0150140548495,19.0109720168265,171.626400023775));
#90399=CARTESIAN_POINT('Ctrl Pts',(21.6753131026798,19.352235470221,171.608250755187));
#90400=CARTESIAN_POINT('Ctrl Pts',(21.8758188843882,18.873172510106,172.083590099036));
#90401=CARTESIAN_POINT('Ctrl Pts',(21.9589405696991,18.9554607618996,171.630295894894));
#90402=CARTESIAN_POINT('Ctrl Pts',(21.6368349074759,19.2889233489516,171.595920429989));
#90403=CARTESIAN_POINT('Ctrl Pts',(21.6980773333364,18.6972131145286,171.986236425372));
#90404=CARTESIAN_POINT('Ctrl Pts',(21.8484160221931,18.8460444073025,171.601943545762));
#90405=CARTESIAN_POINT('Ctrl Pts',(21.5642889040396,19.1707080971489,171.547243587402));
#90406=CARTESIAN_POINT('Ctrl Pts',(21.6164317208276,18.616386135448,171.914220536541));
#90407=CARTESIAN_POINT('Ctrl Pts',(21.7945323741985,18.7927010327448,171.570727890217));
#90408=CARTESIAN_POINT('Ctrl Pts',(21.530827148552,19.1167826550556,171.511235647295));
#90409=CARTESIAN_POINT('Ctrl Pts',(21.4781632900135,18.4795040762473,171.73102847759));
#90410=CARTESIAN_POINT('Ctrl Pts',(21.7016983911598,18.7007978652084,171.476689446385));
#90411=CARTESIAN_POINT('Ctrl Pts',(21.474021706278,19.0258237386761,171.419639614958));
#90412=CARTESIAN_POINT('Ctrl Pts',(21.4218647858374,18.4237700584664,171.619640310305));
#90413=CARTESIAN_POINT('Ctrl Pts',(21.6623323229597,18.6618265074946,171.413915961975));
#90414=CARTESIAN_POINT('Ctrl Pts',(21.450814218412,18.9889959729158,171.363945533082));
#90415=CARTESIAN_POINT('Ctrl Pts',(21.345712062812,18.3483808934915,171.37578205691));
#90416=CARTESIAN_POINT('Ctrl Pts',(21.6091642396647,18.6091915229033,171.270846895345));
#90417=CARTESIAN_POINT('Ctrl Pts',(21.4193928793478,18.9392570552062,171.242016405712));
#90418=CARTESIAN_POINT('Ctrl Pts',(21.3254880824681,18.3283596922787,171.241710900386));
#90419=CARTESIAN_POINT('Ctrl Pts',(21.5946552031017,18.5948279636278,171.189221495563));
#90420=CARTESIAN_POINT('Ctrl Pts',(21.4110300968858,18.9260953774867,171.17498082804));
#90421=CARTESIAN_POINT('Ctrl Pts',(21.3254880807602,18.3283596905879,171.108250755187));
#90422=CARTESIAN_POINT('Ctrl Pts',(21.5946552018854,18.5948279624256,171.108250755187));
#90423=CARTESIAN_POINT('Ctrl Pts',(21.4110300971907,18.9260953769367,171.108250755187));
#90424=CARTESIAN_POINT('',(22.0656246253921,19.0610751320115,172.108250755187));
#90425=CARTESIAN_POINT('Origin',(21.7138571120063,19.4164054241714,172.108250755187));
#90426=CARTESIAN_POINT('Ctrl Pts',(21.3254880807602,18.3283596905879,171.108250755187));
#90427=CARTESIAN_POINT('Ctrl Pts',(21.3254880812526,18.3283596910754,171.146726782705));
#90428=CARTESIAN_POINT('Ctrl Pts',(21.3271964240235,18.3300508975486,171.185041427676));
#90429=CARTESIAN_POINT('Ctrl Pts',(21.3305183422912,18.333339538009,171.22298649035));
#90430=CARTESIAN_POINT('Ctrl Pts',(21.3321922826555,18.3349967094283,171.242107301556));
#90431=CARTESIAN_POINT('Ctrl Pts',(21.334276539325,18.3370600938913,171.261134517834));
#90432=CARTESIAN_POINT('Ctrl Pts',(21.3367624462568,18.3395211258692,171.280042307355));
#90433=CARTESIAN_POINT('Ctrl Pts',(21.3418914454626,18.3445988023093,171.319053436934));
#90434=CARTESIAN_POINT('Ctrl Pts',(21.3487258208062,18.3513648861209,171.357556066236));
#90435=CARTESIAN_POINT('Ctrl Pts',(21.357163993125,18.3597187357998,171.395315415654));
#90436=CARTESIAN_POINT('Ctrl Pts',(21.3599099796439,18.3624372816807,171.407603226396));
#90437=CARTESIAN_POINT('Ctrl Pts',(21.3628260701827,18.365324228437,171.419812520361));
#90438=CARTESIAN_POINT('Ctrl Pts',(21.3659095386159,18.3683768672509,171.431935680483));
#90439=CARTESIAN_POINT('Ctrl Pts',(21.3706190483618,18.3730392896352,171.450451887793));
#90440=CARTESIAN_POINT('Ctrl Pts',(21.3757178706185,18.3780870998679,171.46876644342));
#90441=CARTESIAN_POINT('Ctrl Pts',(21.3811942208671,18.3835085796861,171.486850966306));
#90442=CARTESIAN_POINT('Ctrl Pts',(21.3822539081404,18.3845576493959,171.490350366066));
#90443=CARTESIAN_POINT('Ctrl Pts',(21.3833277549178,18.3856207337022,171.493841420748));
#90444=CARTESIAN_POINT('Ctrl Pts',(21.3844155368878,18.3866976107387,171.497323013247));
#90445=CARTESIAN_POINT('Ctrl Pts',(21.3857871789431,18.3880555021843,171.501713138128));
#90446=CARTESIAN_POINT('Ctrl Pts',(21.387181459874,18.3894358011567,171.506090294806));
#90447=CARTESIAN_POINT('Ctrl Pts',(21.3885977255394,18.3908378605866,171.510452436845));
#90448=CARTESIAN_POINT('Ctrl Pts',(21.4016701057897,18.4037791147949,171.550715772199));
#90449=CARTESIAN_POINT('Ctrl Pts',(21.4166313641888,18.4185899911857,171.58974450264));
#90450=CARTESIAN_POINT('Ctrl Pts',(21.4333457746744,18.4351365211234,171.627226319309));
#90451=CARTESIAN_POINT('Ctrl Pts',(21.4409833846734,18.4426974185065,171.644353546022));
#90452=CARTESIAN_POINT('Ctrl Pts',(21.4489871451359,18.4506208105774,171.661157055623));
#90453=CARTESIAN_POINT('Ctrl Pts',(21.4573442130695,18.4588939974157,171.677603438498));
#90454=CARTESIAN_POINT('Ctrl Pts',(21.4757377303701,18.4771028963323,171.713801161234));
#90455=CARTESIAN_POINT('Ctrl Pts',(21.4958432302445,18.497006759284,171.748272860834));
#90456=CARTESIAN_POINT('Ctrl Pts',(21.5175216452097,18.5184678018636,171.78069958324));
#90457=CARTESIAN_POINT('Ctrl Pts',(21.5271409181195,18.5279906210289,171.795088157907));
#90458=CARTESIAN_POINT('Ctrl Pts',(21.5370700702229,18.5378202177446,171.809073466704));
#90459=CARTESIAN_POINT('Ctrl Pts',(21.547297552772,18.5479451527243,171.8226244363));
#90460=CARTESIAN_POINT('Ctrl Pts',(21.547411296165,18.5480577556501,171.822775141349));
#90461=CARTESIAN_POINT('Ctrl Pts',(21.5475250755806,18.5481703942374,171.822925793229));
#90462=CARTESIAN_POINT('Ctrl Pts',(21.5476388910036,18.5482830684709,171.82307639192));
#90463=CARTESIAN_POINT('Ctrl Pts',(21.6089370659646,18.6089666269991,171.904185126494));
#90464=CARTESIAN_POINT('Ctrl Pts',(21.6800387968247,18.6793554444288,171.969901908548));
#90465=CARTESIAN_POINT('Ctrl Pts',(21.757287760541,18.7558298584533,172.017635952684));
#90466=CARTESIAN_POINT('Ctrl Pts',(21.767078251159,18.7655221830751,172.02368573884));
#90467=CARTESIAN_POINT('Ctrl Pts',(21.776967510281,18.7753122858817,172.029446612593));
#90468=CARTESIAN_POINT('Ctrl Pts',(21.7869481132028,18.7851928166143,172.034913246513));
#90469=CARTESIAN_POINT('Ctrl Pts',(21.7870212219941,18.785265192368,172.034953290086));
#90470=CARTESIAN_POINT('Ctrl Pts',(21.7870943346886,18.7853375719858,172.034993317412));
#90471=CARTESIAN_POINT('Ctrl Pts',(21.7871674512835,18.7854099554649,172.035033328492));
#90472=CARTESIAN_POINT('Ctrl Pts',(21.8164243108428,18.8143734662146,172.051043353842));
#90473=CARTESIAN_POINT('Ctrl Pts',(21.8462312070523,18.8438814985796,172.064416117585));
#90474=CARTESIAN_POINT('Ctrl Pts',(21.8764714094513,18.8738184925171,172.07518031916));
#90475=CARTESIAN_POINT('Ctrl Pts',(21.9072499164823,18.9042883936849,172.086136133856));
#90476=CARTESIAN_POINT('Ctrl Pts',(21.9384778938109,18.9352032584609,172.094389922825));
#90477=CARTESIAN_POINT('Ctrl Pts',(21.9700412343799,18.9664501239016,172.09991854538));
#90478=CARTESIAN_POINT('Ctrl Pts',(22.001604574949,18.9976969893423,172.105447167935));
#90479=CARTESIAN_POINT('Ctrl Pts',(22.03350392535,19.029276495556,172.108250749037));
#90480=CARTESIAN_POINT('Ctrl Pts',(22.0656246253921,19.0610751320115,172.108250755187));
#90481=CARTESIAN_POINT('Origin',(38.5483451826112,23.5078207102358,172.108250755187));
#90482=CARTESIAN_POINT('',(38.1965776692254,23.8631510023956,172.108250755187));
#90483=CARTESIAN_POINT('',(27.5329960959723,12.6029188688252,171.608250755187));
#90484=CARTESIAN_POINT('Origin',(32.2615249200093,29.8583152717307,172.108250755187));
#90485=CARTESIAN_POINT('',(32.2615249200093,29.8583152717307,171.608250755187));
#90486=CARTESIAN_POINT('',(21.5979433467562,18.5980831381603,172.108250755187));
#90487=CARTESIAN_POINT('Origin',(35.4049350513103,26.6830679909832,173.108250755187));
#90488=CARTESIAN_POINT('Origin',(35.4049350513103,26.6830679909832,153.108250755187));
#90489=CARTESIAN_POINT('Origin',(14.0868850299881,5.57876697388923,153.108250755187));
#90490=CARTESIAN_POINT('',(11.2952424120729,8.39868396247686,153.108250755187));
#90491=CARTESIAN_POINT('',(16.8785276479032,2.7588499853016,153.108250755187));
#90492=CARTESIAN_POINT('Origin',(32.6132924333951,29.5029849795709,153.108250755187));
#90493=CARTESIAN_POINT('Origin',(38.1965776692254,23.8631510023956,153.108250755187));
#90494=CARTESIAN_POINT('Origin',(35.4049350513103,26.6830679909832,171.608250755187));
#90495=CARTESIAN_POINT('Origin',(-32.1551898441603,24.2184812945555,172.608250755187));
#90496=CARTESIAN_POINT('',(-53.4732398654825,3.11418027746144,173.108250755187));
#90497=CARTESIAN_POINT('',(-53.1214723520968,2.75884998530159,172.608250755187));
#90498=CARTESIAN_POINT('Origin',(-53.4732398654825,3.11418027746144,172.608250755187));
#90499=CARTESIAN_POINT('',(-31.8034223307746,23.8631510023956,172.608250755187));
#90500=CARTESIAN_POINT('',(-32.1551898441603,24.2184812945555,173.108250755187));
#90501=CARTESIAN_POINT('Origin',(-55.9131149700119,5.57876697388922,172.608250755187));
#90502=CARTESIAN_POINT('',(-58.3529900745414,8.04335367031699,173.108250755187));
#90503=CARTESIAN_POINT('',(-58.7047575879271,8.39868396247685,172.608250755187));
#90504=CARTESIAN_POINT('Origin',(-58.3529900745414,8.04335367031699,172.608250755187));
#90505=CARTESIAN_POINT('Origin',(-55.9131149700119,5.57876697388922,172.608250755187));
#90506=CARTESIAN_POINT('Origin',(-55.9131149700119,5.57876697388922,173.108250755187));
#90507=CARTESIAN_POINT('Origin',(-37.0349400532192,29.147654687411,172.608250755187));
#90508=CARTESIAN_POINT('',(-37.3867075666049,29.5029849795709,172.608250755187));
#90509=CARTESIAN_POINT('',(-37.0349400532192,29.147654687411,173.108250755187));
#90510=CARTESIAN_POINT('Origin',(-34.5950649486897,26.6830679909832,152.608250755187));
#90511=CARTESIAN_POINT('',(-48.4989068541589,17.798633272459,153.108250755187));
#90512=CARTESIAN_POINT('Origin',(-48.4989068541589,17.798633272459,152.608250755187));
#90513=CARTESIAN_POINT('',(-43.6191566451,12.8694598796034,153.108250755187));
#90514=CARTESIAN_POINT('Origin',(-43.6191566451,12.8694598796034,152.608250755187));
#90515=CARTESIAN_POINT('Origin',(-34.5950649486897,26.6830679909832,153.108250755187));
#90516=CARTESIAN_POINT('Ctrl Pts',(-42.4926593451348,12.768040044578,153.608250755187));
#90517=CARTESIAN_POINT('Ctrl Pts',(-42.8220595622842,12.9549939852504,153.608250755187));
#90518=CARTESIAN_POINT('Ctrl Pts',(-43.0912266834094,12.6885257134127,153.608250755187));
#90519=CARTESIAN_POINT('Ctrl Pts',(-42.4926593657982,12.7680400563057,153.475551801171));
#90520=CARTESIAN_POINT('Ctrl Pts',(-42.8220595770889,12.954993994298,153.527723751245));
#90521=CARTESIAN_POINT('Ctrl Pts',(-43.091226688129,12.6885257087404,153.541901279333));
#90522=CARTESIAN_POINT('Ctrl Pts',(-42.516334861811,12.7814084763897,153.342399703391));
#90523=CARTESIAN_POINT('Ctrl Pts',(-42.8393599279114,12.9655349563554,153.446619353193));
#90524=CARTESIAN_POINT('Ctrl Pts',(-43.1061533482757,12.6927270912809,153.475325227732));
#90525=CARTESIAN_POINT('Ctrl Pts',(-42.605696122326,12.8327090607542,153.098820706789));
#90526=CARTESIAN_POINT('Ctrl Pts',(-42.9019404776233,13.0041108087007,153.3049590945));
#90527=CARTESIAN_POINT('Ctrl Pts',(-43.1622755982328,12.7092343374352,153.353535732545));
#90528=CARTESIAN_POINT('Ctrl Pts',(-42.6714790802343,12.8707492134964,152.987832794725));
#90529=CARTESIAN_POINT('Ctrl Pts',(-42.947776152444,13.0325418769712,153.243730625338));
#90530=CARTESIAN_POINT('Ctrl Pts',(-43.2035187758124,12.7215983775455,153.298041773782));
#90531=CARTESIAN_POINT('Ctrl Pts',(-42.8311845880579,12.9653805575584,152.805062971569));
#90532=CARTESIAN_POINT('Ctrl Pts',(-43.052608043633,13.0985506777718,153.152596157915));
#90533=CARTESIAN_POINT('Ctrl Pts',(-43.303060007586,12.7533719782572,153.206656864552));
#90534=CARTESIAN_POINT('Ctrl Pts',(-42.9264438528075,13.0228217613015,152.731827736181));
#90535=CARTESIAN_POINT('Ctrl Pts',(-43.112910695034,13.1369984402745,153.1222986856));
#90536=CARTESIAN_POINT('Ctrl Pts',(-43.3621762677728,12.7730921439476,153.170039246316));
#90537=CARTESIAN_POINT('Ctrl Pts',(-43.1289947753635,13.1484367358318,152.633922888492));
#90538=CARTESIAN_POINT('Ctrl Pts',(-43.2320211493329,13.2138353374619,153.093277185672));
#90539=CARTESIAN_POINT('Ctrl Pts',(-43.4869794975497,12.8177036267268,153.121086821207));
#90540=CARTESIAN_POINT('Ctrl Pts',(-43.2390141265139,13.2183592414294,152.608250765972));
#90541=CARTESIAN_POINT('Ctrl Pts',(-43.2924143454201,13.2532442939382,153.094953472492));
#90542=CARTESIAN_POINT('Ctrl Pts',(-43.5543441470683,12.8432444717964,153.108250755187));
#90543=CARTESIAN_POINT('Ctrl Pts',(-43.3456993209664,13.2880540647967,152.608250755187));
#90544=CARTESIAN_POINT('Ctrl Pts',(-43.3456993209664,13.2880540647967,153.108250755187));
#90545=CARTESIAN_POINT('Ctrl Pts',(-43.6191566451,12.8694598796034,153.108250755187));
#90546=CARTESIAN_POINT('',(-43.0912266834095,12.6885257134127,153.608250755187));
#90547=CARTESIAN_POINT('Origin',(-42.7394591700237,12.3331954212528,153.608250755187));
#90548=CARTESIAN_POINT('Ctrl Pts',(-43.0912266834094,12.6885257134127,153.608250755187));
#90549=CARTESIAN_POINT('Ctrl Pts',(-43.0912266834094,12.6885257134127,153.585611929926));
#90550=CARTESIAN_POINT('Ctrl Pts',(-43.0929604304944,12.6890138059483,153.563154237037));
#90551=CARTESIAN_POINT('Ctrl Pts',(-43.0962864633818,12.6899636529501,153.541035429073));
#90552=CARTESIAN_POINT('Ctrl Pts',(-43.0997704532087,12.6909586092248,153.517866174726));
#90553=CARTESIAN_POINT('Ctrl Pts',(-43.1050015895489,12.6924601686109,153.495067766215));
#90554=CARTESIAN_POINT('Ctrl Pts',(-43.1118701614209,12.6944521653039,153.472807844568));
#90555=CARTESIAN_POINT('Ctrl Pts',(-43.11348251584,12.6949197741068,153.46758246676));
#90556=CARTESIAN_POINT('Ctrl Pts',(-43.1151853191043,12.695414468869,153.46238674341));
#90557=CARTESIAN_POINT('Ctrl Pts',(-43.1169775445928,12.6959361508754,153.457222835554));
#90558=CARTESIAN_POINT('Ctrl Pts',(-43.1220257178005,12.6974055759807,153.442677622656));
#90559=CARTESIAN_POINT('Ctrl Pts',(-43.1277833978846,12.6990891411541,153.428386396435));
#90560=CARTESIAN_POINT('Ctrl Pts',(-43.1342144732543,12.700980714358,153.414430480138));
#90561=CARTESIAN_POINT('Ctrl Pts',(-43.1367991234315,12.7017409379188,153.408821595238));
#90562=CARTESIAN_POINT('Ctrl Pts',(-43.1394928923291,12.7025352357298,153.40326444683));
#90563=CARTESIAN_POINT('Ctrl Pts',(-43.1422910092109,12.7033627973937,153.397762970209));
#90564=CARTESIAN_POINT('Ctrl Pts',(-43.1565286871827,12.7075736852767,153.369769767703));
#90565=CARTESIAN_POINT('Ctrl Pts',(-43.1734608936206,12.7126442230623,153.343230009333));
#90566=CARTESIAN_POINT('Ctrl Pts',(-43.1925111334509,12.7184791208895,153.318537883333));
#90567=CARTESIAN_POINT('Ctrl Pts',(-43.210950781292,12.7241270005005,153.294637181192));
#90568=CARTESIAN_POINT('Ctrl Pts',(-43.2313748183461,12.7304910090136,153.272467520466));
#90569=CARTESIAN_POINT('Ctrl Pts',(-43.2532881748755,12.7374867495036,153.252349061816));
#90570=CARTESIAN_POINT('Ctrl Pts',(-43.2552948382388,12.738127367755,153.250506761946));
#90571=CARTESIAN_POINT('Ctrl Pts',(-43.2573153404985,12.7387737898784,153.248680454799));
#90572=CARTESIAN_POINT('Ctrl Pts',(-43.2593492166407,12.7394259068856,153.246870287867));
#90573=CARTESIAN_POINT('Ctrl Pts',(-43.2780390336002,12.7454183797058,153.230236193034));
#90574=CARTESIAN_POINT('Ctrl Pts',(-43.2978344867151,12.7518833303144,153.214981265976));
#90575=CARTESIAN_POINT('Ctrl Pts',(-43.3184548140972,12.7587610622881,153.201166192581));
#90576=CARTESIAN_POINT('Ctrl Pts',(-43.3403128175315,12.7660516104115,153.186521908999));
#90577=CARTESIAN_POINT('Ctrl Pts',(-43.3630987741874,12.7738061414832,153.173494523169));
#90578=CARTESIAN_POINT('Ctrl Pts',(-43.3865244412286,12.7819706583749,153.162187747801));
#90579=CARTESIAN_POINT('Ctrl Pts',(-43.3990387034681,12.786332237717,153.156147537642));
#90580=CARTESIAN_POINT('Ctrl Pts',(-43.4117361909291,12.7908110879773,153.150598972776));
#90581=CARTESIAN_POINT('Ctrl Pts',(-43.424576119712,12.7954005301352,153.145562771898));
#90582=CARTESIAN_POINT('Ctrl Pts',(-43.4487637897704,12.804046054152,153.136075650339));
#90583=CARTESIAN_POINT('Ctrl Pts',(-43.473708893918,12.813181182582,153.128328353011));
#90584=CARTESIAN_POINT('Ctrl Pts',(-43.4990632915912,12.8226927418291,153.122388238269));
#90585=CARTESIAN_POINT('Ctrl Pts',(-43.5226529740675,12.831542278126,153.116861567022));
#90586=CARTESIAN_POINT('Ctrl Pts',(-43.5465984295517,12.8407182262666,153.112899483271));
#90587=CARTESIAN_POINT('Ctrl Pts',(-43.5706101237033,12.8501313371678,153.1105979981));
#90588=CARTESIAN_POINT('Ctrl Pts',(-43.5867944322199,12.8564759411747,153.1090467562));
#90589=CARTESIAN_POINT('Ctrl Pts',(-43.6030086326662,12.8629283194247,153.108250755187));
#90590=CARTESIAN_POINT('Ctrl Pts',(-43.6191566451001,12.8694598796034,153.108250755187));
#90591=CARTESIAN_POINT('Ctrl Pts',(-48.0775783115689,18.0678585669597,152.608250755187));
#90592=CARTESIAN_POINT('Ctrl Pts',(-48.0775783115689,18.0678585669597,153.108250755187));
#90593=CARTESIAN_POINT('Ctrl Pts',(-48.4989068541589,17.798633272459,153.108250755187));
#90594=CARTESIAN_POINT('Ctrl Pts',(-48.1470307749619,18.1765493392547,152.60825077749));
#90595=CARTESIAN_POINT('Ctrl Pts',(-48.1122768724314,18.1221606460454,153.094787604517));
#90596=CARTESIAN_POINT('Ctrl Pts',(-48.5247812179203,17.864504504826,153.108250755187));
#90597=CARTESIAN_POINT('Ctrl Pts',(-48.214837800552,18.2856761107432,152.633710236017));
#90598=CARTESIAN_POINT('Ctrl Pts',(-48.150528898798,18.1820886305035,153.093185957657));
#90599=CARTESIAN_POINT('Ctrl Pts',(-48.5492718500596,17.9311502346665,153.120980492262));
#90600=CARTESIAN_POINT('Ctrl Pts',(-48.3392719415066,18.4909268139009,152.732462696752));
#90601=CARTESIAN_POINT('Ctrl Pts',(-48.2267098579281,18.3028399523544,153.122507989483));
#90602=CARTESIAN_POINT('Ctrl Pts',(-48.5929236463666,18.0572865403011,153.170356729309));
#90603=CARTESIAN_POINT('Ctrl Pts',(-48.3952620045917,18.5859573989267,152.805334639289));
#90604=CARTESIAN_POINT('Ctrl Pts',(-48.2642585375815,18.3630692431352,153.152707467858));
#90605=CARTESIAN_POINT('Ctrl Pts',(-48.6118750907876,18.1161056718007,153.206792695945));
#90606=CARTESIAN_POINT('Ctrl Pts',(-48.488400449801,18.7468303826905,152.988630571688));
#90607=CARTESIAN_POINT('Ctrl Pts',(-48.3293052637564,18.468724748985,153.244147548452));
#90608=CARTESIAN_POINT('Ctrl Pts',(-48.6426808681032,18.2161018881961,153.29844066473));
#90609=CARTESIAN_POINT('Ctrl Pts',(-48.5257065468464,18.8128807906121,153.099898214101));
#90610=CARTESIAN_POINT('Ctrl Pts',(-48.357233870597,18.5147847472079,153.30558183398));
#90611=CARTESIAN_POINT('Ctrl Pts',(-48.6546039643613,18.2573986678045,153.354074484501));
#90612=CARTESIAN_POINT('Ctrl Pts',(-48.5757943506347,18.9022051021532,153.342371533405));
#90613=CARTESIAN_POINT('Ctrl Pts',(-48.3949466240771,18.5773697525719,153.446616730793));
#90614=CARTESIAN_POINT('Ctrl Pts',(-48.6704461232433,18.3133407705919,153.475311144438));
#90615=CARTESIAN_POINT('Ctrl Pts',(-48.5889699010307,18.926095373728,153.475893601961));
#90616=CARTESIAN_POINT('Ctrl Pts',(-48.4053447967376,18.5948279601089,153.527930080756));
#90617=CARTESIAN_POINT('Ctrl Pts',(-48.6745119199733,18.3283596898617,153.542072178464));
#90618=CARTESIAN_POINT('Ctrl Pts',(-48.5889699028093,18.9260953769367,153.608250755187));
#90619=CARTESIAN_POINT('Ctrl Pts',(-48.4053447981146,18.5948279624256,153.608250755187));
#90620=CARTESIAN_POINT('Ctrl Pts',(-48.6745119192398,18.3283596905879,153.608250755187));
#90621=CARTESIAN_POINT('',(-48.6745119192398,18.3283596905879,153.608250755187));
#90622=CARTESIAN_POINT('Origin',(-49.0262794326256,18.6836899827478,153.608250755187));
#90623=CARTESIAN_POINT('Ctrl Pts',(-48.4989068541589,17.798633272459,153.108250755187));
#90624=CARTESIAN_POINT('Ctrl Pts',(-48.5094269497017,17.8254154443576,153.108250755187));
#90625=CARTESIAN_POINT('Ctrl Pts',(-48.5196536306266,17.8521593410513,153.110350857061));
#90626=CARTESIAN_POINT('Ctrl Pts',(-48.5295390298831,17.8786538140997,153.114447252937));
#90627=CARTESIAN_POINT('Ctrl Pts',(-48.5396860002682,17.9058493401896,153.118652040883));
#90628=CARTESIAN_POINT('Ctrl Pts',(-48.5494737553264,17.9327832400945,153.124960207407));
#90629=CARTESIAN_POINT('Ctrl Pts',(-48.5588463302412,17.9592354635869,153.133312849708));
#90630=CARTESIAN_POINT('Ctrl Pts',(-48.5630141439483,17.9709982865737,153.13702711792));
#90631=CARTESIAN_POINT('Ctrl Pts',(-48.5670997707517,17.9826658616072,153.141146354448));
#90632=CARTESIAN_POINT('Ctrl Pts',(-48.5710977355924,17.994218395715,153.145668609543));
#90633=CARTESIAN_POINT('Ctrl Pts',(-48.5799936089787,18.0199239446154,153.155731081411));
#90634=CARTESIAN_POINT('Ctrl Pts',(-48.5884215305909,18.0449504539237,153.167751327948));
#90635=CARTESIAN_POINT('Ctrl Pts',(-48.5963532588931,18.0690479409521,153.18163170246));
#90636=CARTESIAN_POINT('Ctrl Pts',(-48.6039268974369,18.0920575108232,153.194885426667));
#90637=CARTESIAN_POINT('Ctrl Pts',(-48.6110482072602,18.1142208889207,153.209835861399));
#90638=CARTESIAN_POINT('Ctrl Pts',(-48.6176800176114,18.1352871692251,153.226428438643));
#90639=CARTESIAN_POINT('Ctrl Pts',(-48.6202694448921,18.143512615677,153.232907102823));
#90640=CARTESIAN_POINT('Ctrl Pts',(-48.6227840994235,18.15157036769,153.23963640177));
#90641=CARTESIAN_POINT('Ctrl Pts',(-48.6252211735162,18.1594436001053,153.246614074428));
#90642=CARTESIAN_POINT('Ctrl Pts',(-48.6259132243274,18.1616793453769,153.248595509476));
#90643=CARTESIAN_POINT('Ctrl Pts',(-48.6265988211803,18.1638995706234,153.250596415344));
#90644=CARTESIAN_POINT('Ctrl Pts',(-48.6272778897841,18.1661038480101,153.252616665764));
#90645=CARTESIAN_POINT('Ctrl Pts',(-48.6342798979749,18.1888325800255,153.273447860004));
#90646=CARTESIAN_POINT('Ctrl Pts',(-48.6406027699211,18.2098942489154,153.29642453625));
#90647=CARTESIAN_POINT('Ctrl Pts',(-48.6461749021359,18.2287912078335,153.321170461484));
#90648=CARTESIAN_POINT('Ctrl Pts',(-48.6514488684785,18.2466769868256,153.344592227475));
#90649=CARTESIAN_POINT('Ctrl Pts',(-48.6560502790058,18.2626236397099,153.369599261704));
#90650=CARTESIAN_POINT('Ctrl Pts',(-48.6599104487583,18.2761669413009,153.395852653178));
#90651=CARTESIAN_POINT('Ctrl Pts',(-48.6608238217216,18.2793714857378,153.402064591901));
#90652=CARTESIAN_POINT('Ctrl Pts',(-48.6616956587186,18.2824412753048,153.408346207002));
#90653=CARTESIAN_POINT('Ctrl Pts',(-48.6625249804952,18.2853697768896,153.414692806039));
#90654=CARTESIAN_POINT('Ctrl Pts',(-48.6659464217758,18.2974515725152,153.440876268898));
#90655=CARTESIAN_POINT('Ctrl Pts',(-48.6686720763068,18.3072005590288,153.468385102503));
#90656=CARTESIAN_POINT('Ctrl Pts',(-48.6706554188086,18.3143466012101,153.496722756822));
#90657=CARTESIAN_POINT('Ctrl Pts',(-48.6725475333005,18.3211639461509,153.523756961128));
#90658=CARTESIAN_POINT('Ctrl Pts',(-48.6737640367869,18.3256122792063,153.551545730225));
#90659=CARTESIAN_POINT('Ctrl Pts',(-48.6742591562215,18.3274298612422,153.579619100719));
#90660=CARTESIAN_POINT('Ctrl Pts',(-48.6744270219174,18.3280460957343,153.589137119091));
#90661=CARTESIAN_POINT('Ctrl Pts',(-48.6745119192398,18.3283596905879,153.598687494766));
#90662=CARTESIAN_POINT('Ctrl Pts',(-48.6745119192398,18.3283596905879,153.608250755187));
#90663=CARTESIAN_POINT('Origin',(-42.7394591700237,12.3331954212528,171.608250755187));
#90664=CARTESIAN_POINT('',(-43.0912266834095,12.6885257134127,171.108250755187));
#90665=CARTESIAN_POINT('Origin',(-42.7394591700237,12.3331954212528,171.108250755187));
#90666=CARTESIAN_POINT('',(-43.0912266834095,12.6885257134127,153.108250755187));
#90667=CARTESIAN_POINT('Origin',(-32.1551898441603,24.2184812945555,153.608250755187));
#90668=CARTESIAN_POINT('',(-53.1214723520968,2.75884998530159,153.608250755187));
#90669=CARTESIAN_POINT('',(-53.4732398654825,3.11418027746144,153.108250755187));
#90670=CARTESIAN_POINT('Origin',(-53.4732398654825,3.11418027746144,153.608250755187));
#90671=CARTESIAN_POINT('',(-53.4732398654825,3.11418027746144,153.108250755187));
#90672=CARTESIAN_POINT('',(-42.8187714174134,12.9582491609851,153.608250755187));
#90673=CARTESIAN_POINT('Origin',(-37.0349400532192,29.147654687411,153.608250755187));
#90674=CARTESIAN_POINT('',(-58.3529900745414,8.04335367031699,153.108250755187));
#90675=CARTESIAN_POINT('',(-58.7047575879271,8.39868396247685,153.608250755187));
#90676=CARTESIAN_POINT('Origin',(-58.3529900745414,8.043353670317,153.608250755187));
#90677=CARTESIAN_POINT('',(-58.7047575879271,8.39868396247684,153.608250755187));
#90678=CARTESIAN_POINT('',(-48.050289139858,18.2427528460005,153.108250755187));
#90679=CARTESIAN_POINT('Origin',(-49.0262794326255,18.6836899827478,171.608250755187));
#90680=CARTESIAN_POINT('',(-48.6745119192398,18.3283596905879,171.108250755187));
#90681=CARTESIAN_POINT('Origin',(-49.0262794326256,18.6836899827478,171.108250755187));
#90682=CARTESIAN_POINT('',(-48.6745119192398,18.3283596905879,153.108250755187));
#90683=CARTESIAN_POINT('Ctrl Pts',(-43.0912266834094,12.6885257134127,171.108250755187));
#90684=CARTESIAN_POINT('Ctrl Pts',(-42.8220595622842,12.9549939852504,171.108250755187));
#90685=CARTESIAN_POINT('Ctrl Pts',(-42.4926593451348,12.768040044578,171.108250755187));
#90686=CARTESIAN_POINT('Ctrl Pts',(-43.0912266659252,12.6885257307216,171.241737242521));
#90687=CARTESIAN_POINT('Ctrl Pts',(-42.8220595499177,12.9549939974934,171.189238482122));
#90688=CARTESIAN_POINT('Ctrl Pts',(-42.4926593395179,12.76804004139,171.174993997722));
#90689=CARTESIAN_POINT('Ctrl Pts',(-43.0710441707684,12.7085058627055,171.375809742194));
#90690=CARTESIAN_POINT('Ctrl Pts',(-42.8075773954216,12.9693309442371,171.270872142595));
#90691=CARTESIAN_POINT('Ctrl Pts',(-42.4794414677661,12.7762529890484,171.242030250225));
#90692=CARTESIAN_POINT('Ctrl Pts',(-42.9945373856677,12.7842455396928,171.620480252948));
#90693=CARTESIAN_POINT('Ctrl Pts',(-42.7541636542667,13.0222091235587,171.414405744627));
#90694=CARTESIAN_POINT('Ctrl Pts',(-42.4291554349937,12.807315162219,171.364365502532));
#90695=CARTESIAN_POINT('Ctrl Pts',(-42.9380439148113,12.840172569288,171.731805299994));
#90696=CARTESIAN_POINT('Ctrl Pts',(-42.7146746820777,13.061302152944,171.477100056791));
#90697=CARTESIAN_POINT('Ctrl Pts',(-42.3919659144686,12.83022887921,171.420028028856));
#90698=CARTESIAN_POINT('Ctrl Pts',(-42.8001863975324,12.976647835047,171.914243767979));
#90699=CARTESIAN_POINT('Ctrl Pts',(-42.6221241181486,13.1529247431198,171.570720798637));
#90700=CARTESIAN_POINT('Ctrl Pts',(-42.300709976456,12.8859483002507,171.511247260317));
#90701=CARTESIAN_POINT('Ctrl Pts',(-42.7176862192175,13.0583208114862,171.986819299416));
#90702=CARTESIAN_POINT('Ctrl Pts',(-42.5677125765317,13.2067907182888,171.602133212335));
#90703=CARTESIAN_POINT('Ctrl Pts',(-42.245878978066,12.9192082849093,171.547535027057));
#90704=CARTESIAN_POINT('Ctrl Pts',(-42.5412347367947,13.2330030735242,172.083342412463));
#90705=CARTESIAN_POINT('Ctrl Pts',(-42.4580034693628,13.3153998086923,171.630196458045));
#90706=CARTESIAN_POINT('Ctrl Pts',(-42.1278002879233,12.9900408536815,171.595796584069));
#90707=CARTESIAN_POINT('Ctrl Pts',(-42.4450880381951,13.3281857411236,172.108250746497));
#90708=CARTESIAN_POINT('Ctrl Pts',(-42.4010685331158,13.3717638772503,171.626173327528));
#90709=CARTESIAN_POINT('Ctrl Pts',(-42.0630761456614,13.0284859943164,171.608250755187));
#90710=CARTESIAN_POINT('Ctrl Pts',(-42.3510901387775,13.4212411548363,172.108250755187));
#90711=CARTESIAN_POINT('Ctrl Pts',(-42.3510901387775,13.4212411548362,171.608250755187));
#90712=CARTESIAN_POINT('Ctrl Pts',(-41.9993226253918,13.0659108626764,171.608250755187));
#90713=CARTESIAN_POINT('',(-42.3510901387776,13.4212411548362,172.108250755187));
#90714=CARTESIAN_POINT('Origin',(-41.9993226253918,13.0659108626764,172.108250755187));
#90715=CARTESIAN_POINT('Ctrl Pts',(-42.3510901387776,13.4212411548362,172.108250755187));
#90716=CARTESIAN_POINT('Ctrl Pts',(-42.3778802251244,13.3947196837837,172.10825075271));
#90717=CARTESIAN_POINT('Ctrl Pts',(-42.404633334338,13.368234819107,172.106231383602));
#90718=CARTESIAN_POINT('Ctrl Pts',(-42.4311963424757,13.3419381494253,172.102298699113));
#90719=CARTESIAN_POINT('Ctrl Pts',(-42.4585393123223,13.3148693384515,172.098250540379));
#90720=CARTESIAN_POINT('Ctrl Pts',(-42.4856817817057,13.2879990175887,172.092175073614));
#90721=CARTESIAN_POINT('Ctrl Pts',(-42.512470190444,13.2614792073225,172.084134831717));
#90722=CARTESIAN_POINT('Ctrl Pts',(-42.5392868384809,13.2349314409038,172.076086114109));
#90723=CARTESIAN_POINT('Ctrl Pts',(-42.5657496804913,13.2087339330164,172.066068297245));
#90724=CARTESIAN_POINT('Ctrl Pts',(-42.591703228735,13.183040612378,172.054093236376));
#90725=CARTESIAN_POINT('Ctrl Pts',(-42.6044176951968,13.1704536296472,172.048226735644));
#90726=CARTESIAN_POINT('Ctrl Pts',(-42.6170098178969,13.157987763978,172.041889749803));
#90727=CARTESIAN_POINT('Ctrl Pts',(-42.6294600760868,13.1456623403912,172.035079401128));
#90728=CARTESIAN_POINT('Ctrl Pts',(-42.6296843310279,13.1454403339798,172.034956732641));
#90729=CARTESIAN_POINT('Ctrl Pts',(-42.6299085540949,13.1452183591231,172.034833904296));
#90730=CARTESIAN_POINT('Ctrl Pts',(-42.6301327452084,13.1449964158994,172.034710916136));
#90731=CARTESIAN_POINT('Ctrl Pts',(-42.7180977048726,13.0579134516646,171.98645454965));
#90732=CARTESIAN_POINT('Ctrl Pts',(-42.8003616294977,12.9764743600703,171.914009179875));
#90733=CARTESIAN_POINT('Ctrl Pts',(-42.8691146789652,12.908410674588,171.823023819991));
#90734=CARTESIAN_POINT('Ctrl Pts',(-42.8692314898414,12.9082950349356,171.822869236599));
#90735=CARTESIAN_POINT('Ctrl Pts',(-42.8693482649874,12.9081794306552,171.822714595501));
#90736=CARTESIAN_POINT('Ctrl Pts',(-42.8694650043749,12.9080638617748,171.822559896743));
#90737=CARTESIAN_POINT('Ctrl Pts',(-42.9382343475108,12.8399840459953,171.731429283186));
#90738=CARTESIAN_POINT('Ctrl Pts',(-42.9946005532137,12.7841830055056,171.620275542505));
#90739=CARTESIAN_POINT('Ctrl Pts',(-43.0327904247401,12.7463760511325,171.498144778716));
#90740=CARTESIAN_POINT('Ctrl Pts',(-43.0328228387206,12.7463439621562,171.498041119184));
#90741=CARTESIAN_POINT('Ctrl Pts',(-43.0328552397283,12.7463118860226,171.497937451222));
#90742=CARTESIAN_POINT('Ctrl Pts',(-43.0328876277619,12.7462798227331,171.497833774838));
#90743=CARTESIAN_POINT('Ctrl Pts',(-43.0439348683491,12.7353433491568,171.462470776879));
#90744=CARTESIAN_POINT('Ctrl Pts',(-43.053439241226,12.7259342734689,171.426245512341));
#90745=CARTESIAN_POINT('Ctrl Pts',(-43.061393897703,12.7180593756894,171.389360653077));
#90746=CARTESIAN_POINT('Ctrl Pts',(-43.0693558306946,12.7101772743544,171.352442053422));
#90747=CARTESIAN_POINT('Ctrl Pts',(-43.0757654021736,12.7038319695189,171.314861536722));
#90748=CARTESIAN_POINT('Ctrl Pts',(-43.0805808169241,12.6990648373321,171.276805373266));
#90749=CARTESIAN_POINT('Ctrl Pts',(-43.08526166173,12.6944309258018,171.239812714425));
#90750=CARTESIAN_POINT('Ctrl Pts',(-43.0884362406313,12.6912881773483,171.202369605247));
#90751=CARTESIAN_POINT('Ctrl Pts',(-43.0900317766283,12.6897086392606,171.164646810896));
#90752=CARTESIAN_POINT('Ctrl Pts',(-43.0908242882833,12.6889240738566,171.145909687925));
#90753=CARTESIAN_POINT('Ctrl Pts',(-43.0912266809401,12.6885257158573,171.127103649709));
#90754=CARTESIAN_POINT('Ctrl Pts',(-43.0912266834094,12.6885257134127,171.108250755187));
#90755=CARTESIAN_POINT('Origin',(-55.9131149700119,5.57876697388922,153.608250755187));
#90756=CARTESIAN_POINT('Origin',(-55.9131149700119,5.57876697388922,153.608250755187));
#90757=CARTESIAN_POINT('Origin',(-55.9131149700119,5.57876697388922,153.108250755187));
#90758=CARTESIAN_POINT('Ctrl Pts',(-47.9343753746079,19.0610751320115,172.108250755187));
#90759=CARTESIAN_POINT('Ctrl Pts',(-47.9343753746079,19.0610751320115,171.608250755187));
#90760=CARTESIAN_POINT('Ctrl Pts',(-48.2861428879937,19.4164054241714,171.608250755187));
#90761=CARTESIAN_POINT('Ctrl Pts',(-48.0295598492238,18.9668450404957,172.108250736963));
#90762=CARTESIAN_POINT('Ctrl Pts',(-47.9849859451505,19.0109720168265,171.626400023775));
#90763=CARTESIAN_POINT('Ctrl Pts',(-48.32468689732,19.3522354702212,171.608250755187));
#90764=CARTESIAN_POINT('Ctrl Pts',(-48.1241811156121,18.8731725101058,172.083590099036));
#90765=CARTESIAN_POINT('Ctrl Pts',(-48.0410594303009,18.9554607618994,171.630295894894));
#90766=CARTESIAN_POINT('Ctrl Pts',(-48.3631650925245,19.2889233489514,171.595920429989));
#90767=CARTESIAN_POINT('Ctrl Pts',(-48.3019226666633,18.6972131145288,171.986236425372));
#90768=CARTESIAN_POINT('Ctrl Pts',(-48.151583977807,18.8460444073028,171.601943545762));
#90769=CARTESIAN_POINT('Ctrl Pts',(-48.43571109596,19.1707080971491,171.547243587402));
#90770=CARTESIAN_POINT('Ctrl Pts',(-48.3835682791724,18.616386135448,171.914220536541));
#90771=CARTESIAN_POINT('Ctrl Pts',(-48.2054676258018,18.7927010327451,171.570727890217));
#90772=CARTESIAN_POINT('Ctrl Pts',(-48.4691728514479,19.1167826550556,171.511235647295));
#90773=CARTESIAN_POINT('Ctrl Pts',(-48.5218367099866,18.4795040762473,171.73102847759));
#90774=CARTESIAN_POINT('Ctrl Pts',(-48.29830160884,18.7007978652082,171.476689446385));
#90775=CARTESIAN_POINT('Ctrl Pts',(-48.5259782937221,19.0258237386761,171.419639614957));
#90776=CARTESIAN_POINT('Ctrl Pts',(-48.5781352141625,18.4237700584665,171.619640310305));
#90777=CARTESIAN_POINT('Ctrl Pts',(-48.3376676770396,18.6618265074951,171.413915961973));
#90778=CARTESIAN_POINT('Ctrl Pts',(-48.5491857815886,18.9889959729155,171.363945533081));
#90779=CARTESIAN_POINT('Ctrl Pts',(-48.6542879371882,18.3483808934914,171.37578205691));
#90780=CARTESIAN_POINT('Ctrl Pts',(-48.390835760336,18.6091915229028,171.270846895347));
#90781=CARTESIAN_POINT('Ctrl Pts',(-48.5806071206517,18.9392570552066,171.242016405713));
#90782=CARTESIAN_POINT('Ctrl Pts',(-48.6745119175319,18.3283596922787,171.241710900385));
#90783=CARTESIAN_POINT('Ctrl Pts',(-48.4053447968997,18.5948279636275,171.189221495561));
#90784=CARTESIAN_POINT('Ctrl Pts',(-48.5889699031145,18.9260953774872,171.174980828039));
#90785=CARTESIAN_POINT('Ctrl Pts',(-48.6745119192398,18.3283596905879,171.108250755187));
#90786=CARTESIAN_POINT('Ctrl Pts',(-48.4053447981146,18.5948279624256,171.108250755187));
#90787=CARTESIAN_POINT('Ctrl Pts',(-48.5889699028093,18.9260953769367,171.108250755187));
#90788=CARTESIAN_POINT('',(-47.9343753746079,19.0610751320115,172.108250755187));
#90789=CARTESIAN_POINT('Origin',(-48.2861428879937,19.4164054241714,172.108250755187));
#90790=CARTESIAN_POINT('Ctrl Pts',(-48.6745119192398,18.3283596905879,171.108250755187));
#90791=CARTESIAN_POINT('Ctrl Pts',(-48.6745119187474,18.3283596910754,171.146726782702));
#90792=CARTESIAN_POINT('Ctrl Pts',(-48.6728035759767,18.3300508975484,171.185041427672));
#90793=CARTESIAN_POINT('Ctrl Pts',(-48.6694816577094,18.3333395380085,171.222986490344));
#90794=CARTESIAN_POINT('Ctrl Pts',(-48.6678077173449,18.3349967094278,171.242107301551));
#90795=CARTESIAN_POINT('Ctrl Pts',(-48.6657234606753,18.337060093891,171.261134517832));
#90796=CARTESIAN_POINT('Ctrl Pts',(-48.6632375537432,18.3395211258692,171.280042307355));
#90797=CARTESIAN_POINT('Ctrl Pts',(-48.6581085545367,18.34459880231,171.319053436939));
#90798=CARTESIAN_POINT('Ctrl Pts',(-48.6512741791919,18.3513648861228,171.357556066246));
#90799=CARTESIAN_POINT('Ctrl Pts',(-48.6428360068715,18.3597187358033,171.39531541567));
#90800=CARTESIAN_POINT('Ctrl Pts',(-48.6400900203536,18.3624372816831,171.407603226407));
#90801=CARTESIAN_POINT('Ctrl Pts',(-48.637173929816,18.3653242284384,171.419812520366));
#90802=CARTESIAN_POINT('Ctrl Pts',(-48.6340904613841,18.3683768672509,171.431935680483));
#90803=CARTESIAN_POINT('Ctrl Pts',(-48.6293809516382,18.3730392896352,171.450451887793));
#90804=CARTESIAN_POINT('Ctrl Pts',(-48.6242821293815,18.3780870998679,171.46876644342));
#90805=CARTESIAN_POINT('Ctrl Pts',(-48.6188057791329,18.3835085796861,171.486850966306));
#90806=CARTESIAN_POINT('Ctrl Pts',(-48.6177460918596,18.3845576493959,171.490350366066));
#90807=CARTESIAN_POINT('Ctrl Pts',(-48.6166722450822,18.3856207337022,171.493841420748));
#90808=CARTESIAN_POINT('Ctrl Pts',(-48.6155844631122,18.3866976107387,171.497323013247));
#90809=CARTESIAN_POINT('Ctrl Pts',(-48.6142128210569,18.3880555021843,171.501713138128));
#90810=CARTESIAN_POINT('Ctrl Pts',(-48.612818540126,18.3894358011566,171.506090294806));
#90811=CARTESIAN_POINT('Ctrl Pts',(-48.6114022744607,18.3908378605866,171.510452436845));
#90812=CARTESIAN_POINT('Ctrl Pts',(-48.5983298942098,18.4037791147954,171.550715772201));
#90813=CARTESIAN_POINT('Ctrl Pts',(-48.5833686358101,18.4185899911868,171.589744502643));
#90814=CARTESIAN_POINT('Ctrl Pts',(-48.5666542253237,18.4351365211253,171.627226319313));
#90815=CARTESIAN_POINT('Ctrl Pts',(-48.5590166153253,18.4426974185078,171.644353546025));
#90816=CARTESIAN_POINT('Ctrl Pts',(-48.5510128548635,18.450620810578,171.661157055624));
#90817=CARTESIAN_POINT('Ctrl Pts',(-48.5426557869305,18.4588939974157,171.677603438498));
#90818=CARTESIAN_POINT('Ctrl Pts',(-48.524262269629,18.4771028963332,171.713801161236));
#90819=CARTESIAN_POINT('Ctrl Pts',(-48.5041567697535,18.4970067592859,171.748272860838));
#90820=CARTESIAN_POINT('Ctrl Pts',(-48.4824783547872,18.5184678018667,171.780699583245));
#90821=CARTESIAN_POINT('Ctrl Pts',(-48.4728590818784,18.527990621031,171.79508815791));
#90822=CARTESIAN_POINT('Ctrl Pts',(-48.462929929776,18.5378202177457,171.809073466706));
#90823=CARTESIAN_POINT('Ctrl Pts',(-48.4527024472281,18.5479451527243,171.8226244363));
#90824=CARTESIAN_POINT('Ctrl Pts',(-48.4525887038351,18.5480577556501,171.822775141349));
#90825=CARTESIAN_POINT('Ctrl Pts',(-48.4524749244194,18.5481703942374,171.822925793229));
#90826=CARTESIAN_POINT('Ctrl Pts',(-48.4523611089964,18.5482830684709,171.82307639192));
#90827=CARTESIAN_POINT('Ctrl Pts',(-48.3910629342879,18.6089666267492,171.90418512616));
#90828=CARTESIAN_POINT('Ctrl Pts',(-48.3199612037609,18.679355443849,171.969901908007));
#90829=CARTESIAN_POINT('Ctrl Pts',(-48.2427122404135,18.7558298575084,172.017635952094));
#90830=CARTESIAN_POINT('Ctrl Pts',(-48.2329217494837,18.7655221824388,172.023685738466));
#90831=CARTESIAN_POINT('Ctrl Pts',(-48.2230324900434,18.7753122855606,172.029446612416));
#90832=CARTESIAN_POINT('Ctrl Pts',(-48.2130518867972,18.7851928166143,172.034913246513));
#90833=CARTESIAN_POINT('Ctrl Pts',(-48.2129787780059,18.785265192368,172.034953290086));
#90834=CARTESIAN_POINT('Ctrl Pts',(-48.2129056653114,18.7853375719858,172.034993317412));
#90835=CARTESIAN_POINT('Ctrl Pts',(-48.2128325487165,18.7854099554649,172.035033328492));
#90836=CARTESIAN_POINT('Ctrl Pts',(-48.1835756891614,18.8143734662104,172.051043353839));
#90837=CARTESIAN_POINT('Ctrl Pts',(-48.1537687929565,18.843881498571,172.064416117581));
#90838=CARTESIAN_POINT('Ctrl Pts',(-48.123528590562,18.873818492504,172.075180319155));
#90839=CARTESIAN_POINT('Ctrl Pts',(-48.0927500835289,18.9042883936738,172.086136133853));
#90840=CARTESIAN_POINT('Ctrl Pts',(-48.0615221061982,18.935203258452,172.094389922823));
#90841=CARTESIAN_POINT('Ctrl Pts',(-48.0299587656269,18.9664501238949,172.099918545379));
#90842=CARTESIAN_POINT('Ctrl Pts',(-47.9983954250556,18.9976969893378,172.105447167934));
#90843=CARTESIAN_POINT('Ctrl Pts',(-47.9664960746524,19.0292764955537,172.108250749037));
#90844=CARTESIAN_POINT('Ctrl Pts',(-47.9343753746079,19.0610751320115,172.108250755187));
#90845=CARTESIAN_POINT('Origin',(-31.4516548173888,23.5078207102358,172.108250755187));
#90846=CARTESIAN_POINT('',(-31.8034223307746,23.8631510023956,172.108250755187));
#90847=CARTESIAN_POINT('',(-42.4670039040277,12.6029188688252,171.608250755187));
#90848=CARTESIAN_POINT('Origin',(-37.7384750799907,29.8583152717307,172.108250755187));
#90849=CARTESIAN_POINT('',(-37.7384750799907,29.8583152717307,171.608250755187));
#90850=CARTESIAN_POINT('',(-48.4020566532438,18.5980831381603,172.108250755187));
#90851=CARTESIAN_POINT('Origin',(-34.5950649486897,26.6830679909832,173.108250755187));
#90852=CARTESIAN_POINT('Origin',(-34.5950649486897,26.6830679909832,153.108250755187));
#90853=CARTESIAN_POINT('Origin',(-55.9131149700119,5.57876697388922,153.108250755187));
#90854=CARTESIAN_POINT('',(-58.7047575879271,8.39868396247685,153.108250755187));
#90855=CARTESIAN_POINT('',(-53.1214723520968,2.75884998530159,153.108250755187));
#90856=CARTESIAN_POINT('Origin',(-37.3867075666049,29.5029849795709,153.108250755187));
#90857=CARTESIAN_POINT('Origin',(-31.8034223307746,23.8631510023956,153.108250755187));
#90858=CARTESIAN_POINT('Origin',(-34.5950649486897,26.6830679909832,171.608250755187));
#90859=CARTESIAN_POINT('Origin',(-102.15518984416,24.2184812945555,172.608250755187));
#90860=CARTESIAN_POINT('',(-123.473239865483,3.11418027746143,173.108250755187));
#90861=CARTESIAN_POINT('',(-123.121472352097,2.75884998530158,172.608250755187));
#90862=CARTESIAN_POINT('Origin',(-123.473239865483,3.11418027746143,172.608250755187));
#90863=CARTESIAN_POINT('',(-101.803422330775,23.8631510023956,172.608250755187));
#90864=CARTESIAN_POINT('',(-102.15518984416,24.2184812945555,173.108250755187));
#90865=CARTESIAN_POINT('Origin',(-125.913114970012,5.57876697388921,172.608250755187));
#90866=CARTESIAN_POINT('',(-128.352990074541,8.04335367031698,173.108250755187));
#90867=CARTESIAN_POINT('',(-128.704757587927,8.39868396247684,172.608250755187));
#90868=CARTESIAN_POINT('Origin',(-128.352990074541,8.04335367031698,172.608250755187));
#90869=CARTESIAN_POINT('Origin',(-125.913114970012,5.57876697388921,172.608250755187));
#90870=CARTESIAN_POINT('Origin',(-125.913114970012,5.57876697388921,173.108250755187));
#90871=CARTESIAN_POINT('Origin',(-107.034940053219,29.147654687411,172.608250755187));
#90872=CARTESIAN_POINT('',(-107.386707566605,29.5029849795709,172.608250755187));
#90873=CARTESIAN_POINT('',(-107.034940053219,29.147654687411,173.108250755187));
#90874=CARTESIAN_POINT('Origin',(-104.59506494869,26.6830679909832,152.608250755187));
#90875=CARTESIAN_POINT('',(-118.498906854159,17.798633272459,153.108250755187));
#90876=CARTESIAN_POINT('Origin',(-118.498906854159,17.798633272459,152.608250755187));
#90877=CARTESIAN_POINT('',(-113.6191566451,12.8694598796034,153.108250755187));
#90878=CARTESIAN_POINT('Origin',(-113.6191566451,12.8694598796034,152.608250755187));
#90879=CARTESIAN_POINT('Origin',(-104.59506494869,26.6830679909832,153.108250755187));
#90880=CARTESIAN_POINT('Ctrl Pts',(-112.492659345135,12.768040044578,153.608250755187));
#90881=CARTESIAN_POINT('Ctrl Pts',(-112.822059562284,12.9549939852504,153.608250755187));
#90882=CARTESIAN_POINT('Ctrl Pts',(-113.091226683409,12.6885257134127,153.608250755187));
#90883=CARTESIAN_POINT('Ctrl Pts',(-112.492659365801,12.7680400563074,153.475551801171));
#90884=CARTESIAN_POINT('Ctrl Pts',(-112.822059577098,12.9549939942945,153.527723751245));
#90885=CARTESIAN_POINT('Ctrl Pts',(-113.091226688129,12.6885257087402,153.541901279333));
#90886=CARTESIAN_POINT('Ctrl Pts',(-112.516334861812,12.7814084763901,153.342399703391));
#90887=CARTESIAN_POINT('Ctrl Pts',(-112.839359927912,12.9655349563554,153.446619353193));
#90888=CARTESIAN_POINT('Ctrl Pts',(-113.106153348276,12.6927270912805,153.475325227732));
#90889=CARTESIAN_POINT('Ctrl Pts',(-112.605696122325,12.8327090607538,153.098820706789));
#90890=CARTESIAN_POINT('Ctrl Pts',(-112.901940477622,13.0041108087007,153.3049590945));
#90891=CARTESIAN_POINT('Ctrl Pts',(-113.162275598232,12.7092343374356,153.353535732545));
#90892=CARTESIAN_POINT('Ctrl Pts',(-112.671479080234,12.8707492134964,152.987832794727));
#90893=CARTESIAN_POINT('Ctrl Pts',(-112.947776152446,13.0325418769711,153.243730625338));
#90894=CARTESIAN_POINT('Ctrl Pts',(-113.203518775813,12.7215983775457,153.298041773782));
#90895=CARTESIAN_POINT('Ctrl Pts',(-112.831184588058,12.9653805575584,152.805062971567));
#90896=CARTESIAN_POINT('Ctrl Pts',(-113.052608043631,13.0985506777719,153.152596157915));
#90897=CARTESIAN_POINT('Ctrl Pts',(-113.303060007586,12.7533719782569,153.206656864552));
#90898=CARTESIAN_POINT('Ctrl Pts',(-112.926443852807,13.0228217613013,152.731827736181));
#90899=CARTESIAN_POINT('Ctrl Pts',(-113.112910695034,13.1369984402749,153.1222986856));
#90900=CARTESIAN_POINT('Ctrl Pts',(-113.362176267773,12.7730921439476,153.170039246316));
#90901=CARTESIAN_POINT('Ctrl Pts',(-113.128994775364,13.148436735832,152.633922888492));
#90902=CARTESIAN_POINT('Ctrl Pts',(-113.232021149333,13.2138353374614,153.093277185672));
#90903=CARTESIAN_POINT('Ctrl Pts',(-113.486979497549,12.8177036267268,153.121086821207));
#90904=CARTESIAN_POINT('Ctrl Pts',(-113.239014126514,13.2183592414292,152.608250765972));
#90905=CARTESIAN_POINT('Ctrl Pts',(-113.29241434542,13.2532442939391,153.094953472492));
#90906=CARTESIAN_POINT('Ctrl Pts',(-113.554344147068,12.8432444717975,153.108250755187));
#90907=CARTESIAN_POINT('Ctrl Pts',(-113.345699320966,13.2880540647967,152.608250755187));
#90908=CARTESIAN_POINT('Ctrl Pts',(-113.345699320966,13.2880540647967,153.108250755187));
#90909=CARTESIAN_POINT('Ctrl Pts',(-113.6191566451,12.8694598796034,153.108250755187));
#90910=CARTESIAN_POINT('',(-113.091226683409,12.6885257134127,153.608250755187));
#90911=CARTESIAN_POINT('Origin',(-112.739459170024,12.3331954212528,153.608250755187));
#90912=CARTESIAN_POINT('Ctrl Pts',(-113.091226683409,12.6885257134127,153.608250755187));
#90913=CARTESIAN_POINT('Ctrl Pts',(-113.091226683409,12.6885257134127,153.585611929932));
#90914=CARTESIAN_POINT('Ctrl Pts',(-113.092960430494,12.6890138059481,153.563154237047));
#90915=CARTESIAN_POINT('Ctrl Pts',(-113.09628646338,12.6899636529493,153.541035429088));
#90916=CARTESIAN_POINT('Ctrl Pts',(-113.099770453205,12.6909586092235,153.517866174747));
#90917=CARTESIAN_POINT('Ctrl Pts',(-113.105001589543,12.6924601686088,153.495067766241));
#90918=CARTESIAN_POINT('Ctrl Pts',(-113.111870161412,12.694452165301,153.472807844599));
#90919=CARTESIAN_POINT('Ctrl Pts',(-113.113482515834,12.6949197741047,153.46758246678));
#90920=CARTESIAN_POINT('Ctrl Pts',(-113.115185319101,12.6954144688678,153.46238674342));
#90921=CARTESIAN_POINT('Ctrl Pts',(-113.116977544593,12.6959361508752,153.457222835554));
#90922=CARTESIAN_POINT('Ctrl Pts',(-113.122025717801,12.6974055759806,153.442677622656));
#90923=CARTESIAN_POINT('Ctrl Pts',(-113.127783397885,12.699089141154,153.428386396435));
#90924=CARTESIAN_POINT('Ctrl Pts',(-113.134214473254,12.700980714358,153.414430480138));
#90925=CARTESIAN_POINT('Ctrl Pts',(-113.136799123432,12.7017409379188,153.408821595238));
#90926=CARTESIAN_POINT('Ctrl Pts',(-113.139492892329,12.7025352357299,153.40326444683));
#90927=CARTESIAN_POINT('Ctrl Pts',(-113.142291009211,12.7033627973938,153.397762970209));
#90928=CARTESIAN_POINT('Ctrl Pts',(-113.156528687181,12.7075736852766,153.369769767705));
#90929=CARTESIAN_POINT('Ctrl Pts',(-113.173460893617,12.7126442230616,153.343230009338));
#90930=CARTESIAN_POINT('Ctrl Pts',(-113.192511133445,12.7184791208881,153.31853788334));
#90931=CARTESIAN_POINT('Ctrl Pts',(-113.210950781288,12.7241270004995,153.294637181197));
#90932=CARTESIAN_POINT('Ctrl Pts',(-113.231374818344,12.7304910090131,153.272467520468));
#90933=CARTESIAN_POINT('Ctrl Pts',(-113.253288174875,12.7374867495037,153.252349061816));
#90934=CARTESIAN_POINT('Ctrl Pts',(-113.255294838239,12.738127367755,153.250506761946));
#90935=CARTESIAN_POINT('Ctrl Pts',(-113.257315340498,12.7387737898784,153.248680454799));
#90936=CARTESIAN_POINT('Ctrl Pts',(-113.259349216641,12.7394259068857,153.246870287867));
#90937=CARTESIAN_POINT('Ctrl Pts',(-113.278039033598,12.745418379705,153.230236193036));
#90938=CARTESIAN_POINT('Ctrl Pts',(-113.29783448671,12.7518833303128,153.21498126598));
#90939=CARTESIAN_POINT('Ctrl Pts',(-113.318454814089,12.7587610622854,153.201166192586));
#90940=CARTESIAN_POINT('Ctrl Pts',(-113.340312817521,12.766051610408,153.186521909005));
#90941=CARTESIAN_POINT('Ctrl Pts',(-113.363098774174,12.7738061414787,153.173494523177));
#90942=CARTESIAN_POINT('Ctrl Pts',(-113.386524441212,12.7819706583693,153.162187747809));
#90943=CARTESIAN_POINT('Ctrl Pts',(-113.399038703457,12.7863322377132,153.156147537647));
#90944=CARTESIAN_POINT('Ctrl Pts',(-113.411736190924,12.7908110879754,153.150598972778));
#90945=CARTESIAN_POINT('Ctrl Pts',(-113.424576119712,12.7954005301353,153.145562771898));
#90946=CARTESIAN_POINT('Ctrl Pts',(-113.448763789768,12.8040460541511,153.13607565034));
#90947=CARTESIAN_POINT('Ctrl Pts',(-113.473708893912,12.8131811825802,153.128328353013));
#90948=CARTESIAN_POINT('Ctrl Pts',(-113.499063291583,12.8226927418264,153.122388238271));
#90949=CARTESIAN_POINT('Ctrl Pts',(-113.522652974056,12.8315422781222,153.116861567024));
#90950=CARTESIAN_POINT('Ctrl Pts',(-113.546598429537,12.8407182262617,153.112899483273));
#90951=CARTESIAN_POINT('Ctrl Pts',(-113.570610123686,12.8501313371616,153.110597998102));
#90952=CARTESIAN_POINT('Ctrl Pts',(-113.586794432208,12.8564759411706,153.109046756201));
#90953=CARTESIAN_POINT('Ctrl Pts',(-113.60300863266,12.8629283194227,153.108250755187));
#90954=CARTESIAN_POINT('Ctrl Pts',(-113.6191566451,12.8694598796034,153.108250755187));
#90955=CARTESIAN_POINT('Ctrl Pts',(-118.077578311569,18.0678585669597,152.608250755187));
#90956=CARTESIAN_POINT('Ctrl Pts',(-118.077578311569,18.0678585669597,153.108250755187));
#90957=CARTESIAN_POINT('Ctrl Pts',(-118.498906854159,17.798633272459,153.108250755187));
#90958=CARTESIAN_POINT('Ctrl Pts',(-118.147030774962,18.1765493392544,152.60825077749));
#90959=CARTESIAN_POINT('Ctrl Pts',(-118.112276872432,18.1221606460463,153.094787604524));
#90960=CARTESIAN_POINT('Ctrl Pts',(-118.524781217919,17.8645045048263,153.108250755187));
#90961=CARTESIAN_POINT('Ctrl Pts',(-118.214837800552,18.2856761107436,152.633710236017));
#90962=CARTESIAN_POINT('Ctrl Pts',(-118.150528898799,18.1820886305035,153.093185957657));
#90963=CARTESIAN_POINT('Ctrl Pts',(-118.54927185006,17.9311502346664,153.120980492262));
#90964=CARTESIAN_POINT('Ctrl Pts',(-118.339271941506,18.4909268139004,152.732462696752));
#90965=CARTESIAN_POINT('Ctrl Pts',(-118.226709857927,18.3028399523544,153.122507989483));
#90966=CARTESIAN_POINT('Ctrl Pts',(-118.592923646367,18.0572865403011,153.170356729309));
#90967=CARTESIAN_POINT('Ctrl Pts',(-118.395262004592,18.5859573989267,152.805334639289));
#90968=CARTESIAN_POINT('Ctrl Pts',(-118.264258537582,18.3630692431351,153.152707467856));
#90969=CARTESIAN_POINT('Ctrl Pts',(-118.611875090787,18.1161056718008,153.206792695945));
#90970=CARTESIAN_POINT('Ctrl Pts',(-118.488400449801,18.7468303826905,152.988630571688));
#90971=CARTESIAN_POINT('Ctrl Pts',(-118.329305263756,18.4687247489854,153.244147548454));
#90972=CARTESIAN_POINT('Ctrl Pts',(-118.642680868104,18.216101888196,153.298440664731));
#90973=CARTESIAN_POINT('Ctrl Pts',(-118.525706546847,18.8128807906123,153.099898214101));
#90974=CARTESIAN_POINT('Ctrl Pts',(-118.357233870597,18.5147847472074,153.30558183398));
#90975=CARTESIAN_POINT('Ctrl Pts',(-118.654603964361,18.2573986678045,153.354074484501));
#90976=CARTESIAN_POINT('Ctrl Pts',(-118.575794350635,18.902205102153,153.342371533405));
#90977=CARTESIAN_POINT('Ctrl Pts',(-118.394946624077,18.5773697525724,153.446616730793));
#90978=CARTESIAN_POINT('Ctrl Pts',(-118.670446123243,18.3133407705919,153.475311144438));
#90979=CARTESIAN_POINT('Ctrl Pts',(-118.588969901031,18.9260953737285,153.475893601961));
#90980=CARTESIAN_POINT('Ctrl Pts',(-118.405344796735,18.5948279601087,153.527930080756));
#90981=CARTESIAN_POINT('Ctrl Pts',(-118.674511919973,18.3283596898625,153.542072178464));
#90982=CARTESIAN_POINT('Ctrl Pts',(-118.588969902809,18.9260953769367,153.608250755187));
#90983=CARTESIAN_POINT('Ctrl Pts',(-118.405344798115,18.5948279624256,153.608250755187));
#90984=CARTESIAN_POINT('Ctrl Pts',(-118.67451191924,18.3283596905879,153.608250755187));
#90985=CARTESIAN_POINT('',(-118.67451191924,18.3283596905879,153.608250755187));
#90986=CARTESIAN_POINT('Origin',(-119.026279432626,18.6836899827478,153.608250755187));
#90987=CARTESIAN_POINT('Ctrl Pts',(-118.498906854159,17.798633272459,153.108250755187));
#90988=CARTESIAN_POINT('Ctrl Pts',(-118.509426949702,17.825415444359,153.108250755187));
#90989=CARTESIAN_POINT('Ctrl Pts',(-118.519653630627,17.852159341054,153.110350857061));
#90990=CARTESIAN_POINT('Ctrl Pts',(-118.529539029884,17.8786538141036,153.114447252937));
#90991=CARTESIAN_POINT('Ctrl Pts',(-118.53968600027,17.9058493401947,153.118652040884));
#90992=CARTESIAN_POINT('Ctrl Pts',(-118.549473755328,17.9327832401008,153.124960207408));
#90993=CARTESIAN_POINT('Ctrl Pts',(-118.558846330244,17.9592354635942,153.13331284971));
#90994=CARTESIAN_POINT('Ctrl Pts',(-118.56301414395,17.9709982865785,153.137027117921));
#90995=CARTESIAN_POINT('Ctrl Pts',(-118.567099770752,17.9826658616096,153.141146354449));
#90996=CARTESIAN_POINT('Ctrl Pts',(-118.571097735592,17.994218395715,153.145668609543));
#90997=CARTESIAN_POINT('Ctrl Pts',(-118.579993608979,18.0199239446165,153.155731081412));
#90998=CARTESIAN_POINT('Ctrl Pts',(-118.588421530591,18.0449504539258,153.167751327949));
#90999=CARTESIAN_POINT('Ctrl Pts',(-118.596353258894,18.0690479409552,153.181631702461));
#91000=CARTESIAN_POINT('Ctrl Pts',(-118.603926897438,18.0920575108272,153.19488542667));
#91001=CARTESIAN_POINT('Ctrl Pts',(-118.611048207261,18.1142208889254,153.209835861402));
#91002=CARTESIAN_POINT('Ctrl Pts',(-118.617680017612,18.1352871692305,153.226428438647));
#91003=CARTESIAN_POINT('Ctrl Pts',(-118.620269444893,18.1435126156807,153.232907102825));
#91004=CARTESIAN_POINT('Ctrl Pts',(-118.622784099424,18.151570367692,153.239636401772));
#91005=CARTESIAN_POINT('Ctrl Pts',(-118.625221173516,18.1594436001056,153.246614074428));
#91006=CARTESIAN_POINT('Ctrl Pts',(-118.625913224327,18.1616793453773,153.248595509476));
#91007=CARTESIAN_POINT('Ctrl Pts',(-118.62659882118,18.1638995706237,153.250596415344));
#91008=CARTESIAN_POINT('Ctrl Pts',(-118.627277889784,18.1661038480104,153.252616665764));
#91009=CARTESIAN_POINT('Ctrl Pts',(-118.634279897975,18.1888325800265,153.273447860005));
#91010=CARTESIAN_POINT('Ctrl Pts',(-118.640602769921,18.2098942489168,153.296424536251));
#91011=CARTESIAN_POINT('Ctrl Pts',(-118.646174902136,18.2287912078352,153.321170461487));
#91012=CARTESIAN_POINT('Ctrl Pts',(-118.65144886848,18.2466769868291,153.344592227479));
#91013=CARTESIAN_POINT('Ctrl Pts',(-118.656050279007,18.2626236397145,153.369599261712));
#91014=CARTESIAN_POINT('Ctrl Pts',(-118.65991044876,18.2761669413062,153.395852653189));
#91015=CARTESIAN_POINT('Ctrl Pts',(-118.660823821723,18.2793714857411,153.402064591909));
#91016=CARTESIAN_POINT('Ctrl Pts',(-118.661695658719,18.2824412753062,153.408346207006));
#91017=CARTESIAN_POINT('Ctrl Pts',(-118.662524980496,18.2853697768892,153.414692806039));
#91018=CARTESIAN_POINT('Ctrl Pts',(-118.665946421777,18.2974515725156,153.4408762689));
#91019=CARTESIAN_POINT('Ctrl Pts',(-118.668672076308,18.3072005590298,153.468385102507));
#91020=CARTESIAN_POINT('Ctrl Pts',(-118.670655418809,18.3143466012114,153.496722756828));
#91021=CARTESIAN_POINT('Ctrl Pts',(-118.672547533301,18.3211639461522,153.523756961136));
#91022=CARTESIAN_POINT('Ctrl Pts',(-118.673764036787,18.3256122792076,153.551545730234));
#91023=CARTESIAN_POINT('Ctrl Pts',(-118.674259156222,18.3274298612428,153.579619100731));
#91024=CARTESIAN_POINT('Ctrl Pts',(-118.674427021917,18.3280460957345,153.589137119098));
#91025=CARTESIAN_POINT('Ctrl Pts',(-118.67451191924,18.3283596905879,153.59868749477));
#91026=CARTESIAN_POINT('Ctrl Pts',(-118.67451191924,18.3283596905879,153.608250755187));
#91027=CARTESIAN_POINT('Origin',(-112.739459170024,12.3331954212528,171.608250755187));
#91028=CARTESIAN_POINT('',(-113.091226683409,12.6885257134127,171.108250755187));
#91029=CARTESIAN_POINT('Origin',(-112.739459170024,12.3331954212528,171.108250755187));
#91030=CARTESIAN_POINT('',(-113.091226683409,12.6885257134127,153.108250755187));
#91031=CARTESIAN_POINT('Origin',(-102.15518984416,24.2184812945555,153.608250755187));
#91032=CARTESIAN_POINT('',(-123.121472352097,2.75884998530158,153.608250755187));
#91033=CARTESIAN_POINT('',(-123.473239865483,3.11418027746143,153.108250755187));
#91034=CARTESIAN_POINT('Origin',(-123.473239865483,3.11418027746144,153.608250755187));
#91035=CARTESIAN_POINT('',(-123.473239865483,3.11418027746143,153.108250755187));
#91036=CARTESIAN_POINT('',(-112.818771417413,12.9582491609851,153.608250755187));
#91037=CARTESIAN_POINT('Origin',(-107.034940053219,29.147654687411,153.608250755187));
#91038=CARTESIAN_POINT('',(-128.352990074541,8.04335367031699,153.108250755187));
#91039=CARTESIAN_POINT('',(-128.704757587927,8.39868396247684,153.608250755187));
#91040=CARTESIAN_POINT('Origin',(-128.352990074541,8.04335367031699,153.608250755187));
#91041=CARTESIAN_POINT('',(-128.704757587927,8.39868396247683,153.608250755187));
#91042=CARTESIAN_POINT('',(-118.050289139858,18.2427528460005,153.108250755187));
#91043=CARTESIAN_POINT('Origin',(-119.026279432626,18.6836899827478,171.608250755187));
#91044=CARTESIAN_POINT('',(-118.67451191924,18.3283596905879,171.108250755187));
#91045=CARTESIAN_POINT('Origin',(-119.026279432626,18.6836899827478,171.108250755187));
#91046=CARTESIAN_POINT('',(-118.67451191924,18.3283596905879,153.108250755187));
#91047=CARTESIAN_POINT('Ctrl Pts',(-113.091226683409,12.6885257134127,171.108250755187));
#91048=CARTESIAN_POINT('Ctrl Pts',(-112.822059562284,12.9549939852504,171.108250755187));
#91049=CARTESIAN_POINT('Ctrl Pts',(-112.492659345135,12.768040044578,171.108250755187));
#91050=CARTESIAN_POINT('Ctrl Pts',(-113.091226665924,12.6885257307224,171.241737242521));
#91051=CARTESIAN_POINT('Ctrl Pts',(-112.822059549918,12.9549939974928,171.189238482124));
#91052=CARTESIAN_POINT('Ctrl Pts',(-112.492659339517,12.7680400413896,171.174993997723));
#91053=CARTESIAN_POINT('Ctrl Pts',(-113.071044170768,12.7085058627058,171.375809742194));
#91054=CARTESIAN_POINT('Ctrl Pts',(-112.807577395421,12.9693309442375,171.270872142593));
#91055=CARTESIAN_POINT('Ctrl Pts',(-112.479441467766,12.7762529890477,171.242030250224));
#91056=CARTESIAN_POINT('Ctrl Pts',(-112.994537385668,12.7842455396925,171.620480252948));
#91057=CARTESIAN_POINT('Ctrl Pts',(-112.754163654268,13.0222091235583,171.414405744629));
#91058=CARTESIAN_POINT('Ctrl Pts',(-112.429155434994,12.8073151622197,171.364365502534));
#91059=CARTESIAN_POINT('Ctrl Pts',(-112.938043914811,12.8401725692882,171.731805299994));
#91060=CARTESIAN_POINT('Ctrl Pts',(-112.714674682077,13.0613021529447,171.477100056791));
#91061=CARTESIAN_POINT('Ctrl Pts',(-112.391965914469,12.8302288792103,171.420028028857));
#91062=CARTESIAN_POINT('Ctrl Pts',(-112.800186397533,12.9766478350468,171.914243767979));
#91063=CARTESIAN_POINT('Ctrl Pts',(-112.62212411815,13.1529247431191,171.570720798637));
#91064=CARTESIAN_POINT('Ctrl Pts',(-112.300709976456,12.8859483002505,171.511247260317));
#91065=CARTESIAN_POINT('Ctrl Pts',(-112.717686219217,13.0583208114866,171.986819299416));
#91066=CARTESIAN_POINT('Ctrl Pts',(-112.567712576532,13.2067907182878,171.602133212335));
#91067=CARTESIAN_POINT('Ctrl Pts',(-112.245878978066,12.9192082849092,171.547535027057));
#91068=CARTESIAN_POINT('Ctrl Pts',(-112.541234736795,13.2330030735238,172.083342412463));
#91069=CARTESIAN_POINT('Ctrl Pts',(-112.458003469363,13.3153998086934,171.630196458045));
#91070=CARTESIAN_POINT('Ctrl Pts',(-112.127800287923,12.9900408536816,171.595796584069));
#91071=CARTESIAN_POINT('Ctrl Pts',(-112.445088038195,13.3281857411239,172.108250746497));
#91072=CARTESIAN_POINT('Ctrl Pts',(-112.401068533116,13.3717638772499,171.626173327527));
#91073=CARTESIAN_POINT('Ctrl Pts',(-112.063076145661,13.0284859943151,171.608250755187));
#91074=CARTESIAN_POINT('Ctrl Pts',(-112.351090138778,13.4212411548363,172.108250755187));
#91075=CARTESIAN_POINT('Ctrl Pts',(-112.351090138778,13.4212411548362,171.608250755187));
#91076=CARTESIAN_POINT('Ctrl Pts',(-111.999322625392,13.0659108626764,171.608250755187));
#91077=CARTESIAN_POINT('',(-112.351090138778,13.4212411548362,172.108250755187));
#91078=CARTESIAN_POINT('Origin',(-111.999322625392,13.0659108626764,172.108250755187));
#91079=CARTESIAN_POINT('Ctrl Pts',(-112.351090138778,13.4212411548362,172.108250755187));
#91080=CARTESIAN_POINT('Ctrl Pts',(-112.37788022512,13.3947196837876,172.10825075271));
#91081=CARTESIAN_POINT('Ctrl Pts',(-112.40463333433,13.3682348191149,172.106231383603));
#91082=CARTESIAN_POINT('Ctrl Pts',(-112.431196342464,13.3419381494371,172.102298699115));
#91083=CARTESIAN_POINT('Ctrl Pts',(-112.458539312306,13.3148693384673,172.098250540382));
#91084=CARTESIAN_POINT('Ctrl Pts',(-112.485681781686,13.2879990176084,172.092175073619));
#91085=CARTESIAN_POINT('Ctrl Pts',(-112.51247019042,13.261479207346,172.084134831724));
#91086=CARTESIAN_POINT('Ctrl Pts',(-112.539286838453,13.2349314409313,172.076086114119));
#91087=CARTESIAN_POINT('Ctrl Pts',(-112.56574968046,13.2087339330476,172.066068297258));
#91088=CARTESIAN_POINT('Ctrl Pts',(-112.5917032287,13.1830406124129,172.054093236393));
#91089=CARTESIAN_POINT('Ctrl Pts',(-112.604417695173,13.1704536296702,172.048226735655));
#91090=CARTESIAN_POINT('Ctrl Pts',(-112.617009817885,13.1579877639894,172.041889749809));
#91091=CARTESIAN_POINT('Ctrl Pts',(-112.629460076087,13.1456623403912,172.035079401128));
#91092=CARTESIAN_POINT('Ctrl Pts',(-112.629684331028,13.1454403339799,172.034956732641));
#91093=CARTESIAN_POINT('Ctrl Pts',(-112.629908554095,13.1452183591231,172.034833904296));
#91094=CARTESIAN_POINT('Ctrl Pts',(-112.630132745208,13.1449964158994,172.034710916136));
#91095=CARTESIAN_POINT('Ctrl Pts',(-112.718097704872,13.0579134516647,171.98645454965));
#91096=CARTESIAN_POINT('Ctrl Pts',(-112.800361629498,12.9764743600703,171.914009179875));
#91097=CARTESIAN_POINT('Ctrl Pts',(-112.869114678965,12.908410674588,171.823023819991));
#91098=CARTESIAN_POINT('Ctrl Pts',(-112.869231489841,12.9082950349356,171.822869236599));
#91099=CARTESIAN_POINT('Ctrl Pts',(-112.869348264987,12.9081794306553,171.822714595501));
#91100=CARTESIAN_POINT('Ctrl Pts',(-112.869465004375,12.9080638617748,171.822559896743));
#91101=CARTESIAN_POINT('Ctrl Pts',(-112.938234347511,12.8399840459954,171.731429283186));
#91102=CARTESIAN_POINT('Ctrl Pts',(-112.994600553214,12.7841830055055,171.620275542505));
#91103=CARTESIAN_POINT('Ctrl Pts',(-113.03279042474,12.7463760511326,171.498144778716));
#91104=CARTESIAN_POINT('Ctrl Pts',(-113.032822838721,12.7463439621563,171.498041119184));
#91105=CARTESIAN_POINT('Ctrl Pts',(-113.032855239728,12.7463118860227,171.497937451222));
#91106=CARTESIAN_POINT('Ctrl Pts',(-113.032887627762,12.7462798227332,171.497833774838));
#91107=CARTESIAN_POINT('Ctrl Pts',(-113.043934868349,12.735343349157,171.462470776879));
#91108=CARTESIAN_POINT('Ctrl Pts',(-113.053439241226,12.7259342734692,171.426245512342));
#91109=CARTESIAN_POINT('Ctrl Pts',(-113.061393897703,12.7180593756897,171.389360653078));
#91110=CARTESIAN_POINT('Ctrl Pts',(-113.069355830694,12.7101772743547,171.352442053422));
#91111=CARTESIAN_POINT('Ctrl Pts',(-113.075765402173,12.7038319695192,171.314861536721));
#91112=CARTESIAN_POINT('Ctrl Pts',(-113.080580816924,12.6990648373324,171.276805373265));
#91113=CARTESIAN_POINT('Ctrl Pts',(-113.08526166173,12.694430925802,171.239812714423));
#91114=CARTESIAN_POINT('Ctrl Pts',(-113.088436240631,12.6912881773485,171.202369605244));
#91115=CARTESIAN_POINT('Ctrl Pts',(-113.090031776628,12.6897086392607,171.164646810892));
#91116=CARTESIAN_POINT('Ctrl Pts',(-113.090824288283,12.6889240738568,171.145909687922));
#91117=CARTESIAN_POINT('Ctrl Pts',(-113.09122668094,12.6885257158574,171.127103649708));
#91118=CARTESIAN_POINT('Ctrl Pts',(-113.091226683409,12.6885257134127,171.108250755187));
#91119=CARTESIAN_POINT('Origin',(-125.913114970012,5.57876697388921,153.608250755187));
#91120=CARTESIAN_POINT('Origin',(-125.913114970012,5.57876697388921,153.608250755187));
#91121=CARTESIAN_POINT('Origin',(-125.913114970012,5.57876697388921,153.108250755187));
#91122=CARTESIAN_POINT('Ctrl Pts',(-117.934375374608,19.0610751320115,172.108250755187));
#91123=CARTESIAN_POINT('Ctrl Pts',(-117.934375374608,19.0610751320115,171.608250755187));
#91124=CARTESIAN_POINT('Ctrl Pts',(-118.286142887994,19.4164054241713,171.608250755187));
#91125=CARTESIAN_POINT('Ctrl Pts',(-118.029559849224,18.9668450404955,172.108250736963));
#91126=CARTESIAN_POINT('Ctrl Pts',(-117.984985945151,19.0109720168266,171.626400023775));
#91127=CARTESIAN_POINT('Ctrl Pts',(-118.324686897321,19.3522354702217,171.608250755187));
#91128=CARTESIAN_POINT('Ctrl Pts',(-118.124181115612,18.873172510106,172.083590099036));
#91129=CARTESIAN_POINT('Ctrl Pts',(-118.0410594303,18.9554607618992,171.630295894894));
#91130=CARTESIAN_POINT('Ctrl Pts',(-118.363165092524,19.2889233489514,171.595920429989));
#91131=CARTESIAN_POINT('Ctrl Pts',(-118.301922666664,18.6972131145286,171.986236425372));
#91132=CARTESIAN_POINT('Ctrl Pts',(-118.151583977807,18.846044407303,171.601943545762));
#91133=CARTESIAN_POINT('Ctrl Pts',(-118.43571109596,19.1707080971491,171.547243587402));
#91134=CARTESIAN_POINT('Ctrl Pts',(-118.383568279172,18.6163861354481,171.914220536541));
#91135=CARTESIAN_POINT('Ctrl Pts',(-118.205467625802,18.7927010327455,171.570727890218));
#91136=CARTESIAN_POINT('Ctrl Pts',(-118.469172851448,19.1167826550558,171.511235647295));
#91137=CARTESIAN_POINT('Ctrl Pts',(-118.521836709987,18.4795040762472,171.73102847759));
#91138=CARTESIAN_POINT('Ctrl Pts',(-118.29830160884,18.7007978652077,171.476689446383));
#91139=CARTESIAN_POINT('Ctrl Pts',(-118.525978293722,19.0258237386759,171.419639614957));
#91140=CARTESIAN_POINT('Ctrl Pts',(-118.578135214163,18.4237700584662,171.619640310305));
#91141=CARTESIAN_POINT('Ctrl Pts',(-118.337667677041,18.6618265074946,171.413915961975));
#91142=CARTESIAN_POINT('Ctrl Pts',(-118.549185781588,18.988995972916,171.363945533082));
#91143=CARTESIAN_POINT('Ctrl Pts',(-118.654287937188,18.3483808934916,171.37578205691));
#91144=CARTESIAN_POINT('Ctrl Pts',(-118.390835760335,18.6091915229033,171.270846895345));
#91145=CARTESIAN_POINT('Ctrl Pts',(-118.580607120652,18.9392570552061,171.242016405712));
#91146=CARTESIAN_POINT('Ctrl Pts',(-118.674511917534,18.3283596922771,171.241710900386));
#91147=CARTESIAN_POINT('Ctrl Pts',(-118.405344796902,18.5948279636271,171.189221495563));
#91148=CARTESIAN_POINT('Ctrl Pts',(-118.588969903115,18.926095377489,171.17498082804));
#91149=CARTESIAN_POINT('Ctrl Pts',(-118.67451191924,18.3283596905879,171.108250755187));
#91150=CARTESIAN_POINT('Ctrl Pts',(-118.405344798115,18.5948279624256,171.108250755187));
#91151=CARTESIAN_POINT('Ctrl Pts',(-118.588969902809,18.9260953769367,171.108250755187));
#91152=CARTESIAN_POINT('',(-117.934375374608,19.0610751320115,172.108250755187));
#91153=CARTESIAN_POINT('Origin',(-118.286142887994,19.4164054241713,172.108250755187));
#91154=CARTESIAN_POINT('Ctrl Pts',(-118.67451191924,18.3283596905879,171.108250755187));
#91155=CARTESIAN_POINT('Ctrl Pts',(-118.674511918748,18.3283596910749,171.146726782688));
#91156=CARTESIAN_POINT('Ctrl Pts',(-118.672803575978,18.3300508975469,171.185041427643));
#91157=CARTESIAN_POINT('Ctrl Pts',(-118.669481657713,18.3333395380046,171.222986490301));
#91158=CARTESIAN_POINT('Ctrl Pts',(-118.667807717348,18.3349967094246,171.242107301523));
#91159=CARTESIAN_POINT('Ctrl Pts',(-118.665723460677,18.3370600938892,171.261134517818));
#91160=CARTESIAN_POINT('Ctrl Pts',(-118.663237553743,18.3395211258692,171.280042307355));
#91161=CARTESIAN_POINT('Ctrl Pts',(-118.658108554535,18.3445988023115,171.31905343695));
#91162=CARTESIAN_POINT('Ctrl Pts',(-118.651274179188,18.3513648861267,171.357556066268));
#91163=CARTESIAN_POINT('Ctrl Pts',(-118.642836006864,18.3597187358104,171.395315415702));
#91164=CARTESIAN_POINT('Ctrl Pts',(-118.640090020348,18.3624372816882,171.407603226428));
#91165=CARTESIAN_POINT('Ctrl Pts',(-118.637173929813,18.365324228441,171.419812520377));
#91166=CARTESIAN_POINT('Ctrl Pts',(-118.634090461384,18.3683768672509,171.431935680483));
#91167=CARTESIAN_POINT('Ctrl Pts',(-118.629380951638,18.3730392896352,171.450451887793));
#91168=CARTESIAN_POINT('Ctrl Pts',(-118.624282129381,18.3780870998679,171.46876644342));
#91169=CARTESIAN_POINT('Ctrl Pts',(-118.618805779133,18.3835085796861,171.486850966306));
#91170=CARTESIAN_POINT('Ctrl Pts',(-118.61774609186,18.3845576493959,171.490350366066));
#91171=CARTESIAN_POINT('Ctrl Pts',(-118.616672245082,18.3856207337022,171.493841420748));
#91172=CARTESIAN_POINT('Ctrl Pts',(-118.615584463112,18.3866976107387,171.497323013247));
#91173=CARTESIAN_POINT('Ctrl Pts',(-118.614212821057,18.3880555021842,171.501713138128));
#91174=CARTESIAN_POINT('Ctrl Pts',(-118.612818540126,18.3894358011566,171.506090294806));
#91175=CARTESIAN_POINT('Ctrl Pts',(-118.611402274461,18.3908378605866,171.510452436845));
#91176=CARTESIAN_POINT('Ctrl Pts',(-118.59832989421,18.403779114795,171.550715772199));
#91177=CARTESIAN_POINT('Ctrl Pts',(-118.583368635811,18.4185899911859,171.589744502641));
#91178=CARTESIAN_POINT('Ctrl Pts',(-118.566654225325,18.4351365211238,171.62722631931));
#91179=CARTESIAN_POINT('Ctrl Pts',(-118.559016615326,18.4426974185068,171.644353546023));
#91180=CARTESIAN_POINT('Ctrl Pts',(-118.551012854864,18.4506208105775,171.661157055623));
#91181=CARTESIAN_POINT('Ctrl Pts',(-118.542655786931,18.4588939974157,171.677603438498));
#91182=CARTESIAN_POINT('Ctrl Pts',(-118.52426226963,18.4771028963319,171.713801161233));
#91183=CARTESIAN_POINT('Ctrl Pts',(-118.504156769756,18.4970067592832,171.748272860833));
#91184=CARTESIAN_POINT('Ctrl Pts',(-118.482478354792,18.5184678018624,171.780699583238));
#91185=CARTESIAN_POINT('Ctrl Pts',(-118.472859081881,18.527990621028,171.795088157906));
#91186=CARTESIAN_POINT('Ctrl Pts',(-118.462929929778,18.5378202177442,171.809073466704));
#91187=CARTESIAN_POINT('Ctrl Pts',(-118.452702447228,18.5479451527244,171.8226244363));
#91188=CARTESIAN_POINT('Ctrl Pts',(-118.452588703835,18.5480577556501,171.822775141349));
#91189=CARTESIAN_POINT('Ctrl Pts',(-118.452474924419,18.5481703942374,171.822925793229));
#91190=CARTESIAN_POINT('Ctrl Pts',(-118.452361108996,18.5482830684709,171.82307639192));
#91191=CARTESIAN_POINT('Ctrl Pts',(-118.391062933909,18.6089666271241,171.904185126661));
#91192=CARTESIAN_POINT('Ctrl Pts',(-118.319961202882,18.6793554447188,171.969901908819));
#91193=CARTESIAN_POINT('Ctrl Pts',(-118.242712238982,18.7558298589259,172.017635952979));
#91194=CARTESIAN_POINT('Ctrl Pts',(-118.23292174852,18.7655221833933,172.023685739028));
#91195=CARTESIAN_POINT('Ctrl Pts',(-118.223032489557,18.7753122860422,172.029446612682));
#91196=CARTESIAN_POINT('Ctrl Pts',(-118.213051886797,18.7851928166143,172.034913246513));
#91197=CARTESIAN_POINT('Ctrl Pts',(-118.212978778006,18.785265192368,172.034953290086));
#91198=CARTESIAN_POINT('Ctrl Pts',(-118.212905665311,18.7853375719858,172.034993317412));
#91199=CARTESIAN_POINT('Ctrl Pts',(-118.212832548717,18.7854099554649,172.035033328492));
#91200=CARTESIAN_POINT('Ctrl Pts',(-118.183575689157,18.8143734662143,172.051043353842));
#91201=CARTESIAN_POINT('Ctrl Pts',(-118.153768792948,18.843881498579,172.064416117585));
#91202=CARTESIAN_POINT('Ctrl Pts',(-118.12352859055,18.8738184925162,172.07518031916));
#91203=CARTESIAN_POINT('Ctrl Pts',(-118.092750083519,18.9042883936841,172.086136133856));
#91204=CARTESIAN_POINT('Ctrl Pts',(-118.06152210619,18.9352032584602,172.094389922825));
#91205=CARTESIAN_POINT('Ctrl Pts',(-118.029958765621,18.9664501239011,172.09991854538));
#91206=CARTESIAN_POINT('Ctrl Pts',(-117.998395425051,18.997696989342,172.105447167935));
#91207=CARTESIAN_POINT('Ctrl Pts',(-117.96649607465,19.0292764955558,172.108250749037));
#91208=CARTESIAN_POINT('Ctrl Pts',(-117.934375374608,19.0610751320115,172.108250755187));
#91209=CARTESIAN_POINT('Origin',(-101.451654817389,23.5078207102358,172.108250755187));
#91210=CARTESIAN_POINT('',(-101.803422330775,23.8631510023956,172.108250755187));
#91211=CARTESIAN_POINT('',(-112.467003904028,12.6029188688252,171.608250755187));
#91212=CARTESIAN_POINT('Origin',(-107.738475079991,29.8583152717307,172.108250755187));
#91213=CARTESIAN_POINT('',(-107.738475079991,29.8583152717307,171.608250755187));
#91214=CARTESIAN_POINT('',(-118.402056653244,18.5980831381603,172.108250755187));
#91215=CARTESIAN_POINT('Origin',(-104.59506494869,26.6830679909832,173.108250755187));
#91216=CARTESIAN_POINT('Origin',(-104.59506494869,26.6830679909832,153.108250755187));
#91217=CARTESIAN_POINT('Origin',(-125.913114970012,5.57876697388921,153.108250755187));
#91218=CARTESIAN_POINT('',(-128.704757587927,8.39868396247684,153.108250755187));
#91219=CARTESIAN_POINT('',(-123.121472352097,2.75884998530158,153.108250755187));
#91220=CARTESIAN_POINT('Origin',(-107.386707566605,29.5029849795709,153.108250755187));
#91221=CARTESIAN_POINT('Origin',(-101.803422330775,23.8631510023956,153.108250755187));
#91222=CARTESIAN_POINT('Origin',(-104.59506494869,26.6830679909832,171.608250755187));
#91223=CARTESIAN_POINT('Origin',(-104.59506494869,26.6830679909832,173.608250755187));
#91224=CARTESIAN_POINT('',(-205.7,24.8757620423259,173.608250755187));
#91225=CARTESIAN_POINT('Origin',(35.4049350513103,26.6830679909832,173.608250755187));
#91226=CARTESIAN_POINT('',(-205.7,24.8757620423259,173.608250755187));
#91227=CARTESIAN_POINT('Origin',(-34.5950649486897,26.6830679909832,173.608250755187));
#91228=CARTESIAN_POINT('',(-205.7,24.8757620423259,173.608250755187));
#91229=CARTESIAN_POINT('Origin',(190.,54.4,211.4));
#91230=CARTESIAN_POINT('',(190.5,54.4,41.));
#91231=CARTESIAN_POINT('Origin',(190.,54.4,41.));
#91232=CARTESIAN_POINT('',(190.5,54.4,102.225104347672));
#91233=CARTESIAN_POINT('Origin',(190.,54.4,102.225104347672));
#91234=CARTESIAN_POINT('',(190.5,54.4,211.4));
#91235=CARTESIAN_POINT('Origin',(160.5,54.4,102.225104347672));
#91236=CARTESIAN_POINT('',(190.499797482064,54.4,102.335336081499));
#91237=CARTESIAN_POINT('Origin',(189.999800857363,54.4,102.333498885935));
#91238=CARTESIAN_POINT('Origin',(160.5,54.4,102.225104347672));
#91239=CARTESIAN_POINT('Ctrl Pts',(189.5,54.85,40.282055052823));
#91240=CARTESIAN_POINT('Ctrl Pts',(190.217944947177,54.85,40.282055052823));
#91241=CARTESIAN_POINT('Ctrl Pts',(190.217944947177,54.85,41.));
#91242=CARTESIAN_POINT('Ctrl Pts',(189.5,54.7133945031366,40.));
#91243=CARTESIAN_POINT('Ctrl Pts',(190.5,54.7133945031366,40.));
#91244=CARTESIAN_POINT('Ctrl Pts',(190.5,54.7133945031366,41.));
#91245=CARTESIAN_POINT('Ctrl Pts',(189.5,54.4,40.));
#91246=CARTESIAN_POINT('Ctrl Pts',(190.5,54.4,40.));
#91247=CARTESIAN_POINT('Ctrl Pts',(190.5,54.4,41.));
#91248=CARTESIAN_POINT('',(189.5,54.4,40.));
#91249=CARTESIAN_POINT('Origin',(189.5,54.4,41.));
#91250=CARTESIAN_POINT('Origin',(189.5,54.4,40.5));
#91251=CARTESIAN_POINT('Ctrl Pts',(190.219194548401,54.8501814482227,101.816662400769));
#91252=CARTESIAN_POINT('Ctrl Pts',(190.501623088573,54.7136847329578,101.817606429853));
#91253=CARTESIAN_POINT('Ctrl Pts',(190.501623088584,54.4000000000002,101.817606429849));
#91254=CARTESIAN_POINT('Ctrl Pts',(190.200871934805,54.8501814482482,107.235732213123));
#91255=CARTESIAN_POINT('Ctrl Pts',(190.483296758343,54.7136847330045,107.23763909223));
#91256=CARTESIAN_POINT('Ctrl Pts',(190.483296758234,54.399999999995,107.23763909227));
#91257=CARTESIAN_POINT('Ctrl Pts',(190.158430844455,54.8501814482705,112.654414896875));
#91258=CARTESIAN_POINT('Ctrl Pts',(190.440853585033,54.713684733061,112.657855156237));
#91259=CARTESIAN_POINT('Ctrl Pts',(190.440853584981,54.4000000000751,112.657855156188));
#91260=CARTESIAN_POINT('Ctrl Pts',(189.981599530965,54.8501814482032,120.693291671663));
#91261=CARTESIAN_POINT('Ctrl Pts',(190.263931815988,54.7136847329145,120.700844105146));
#91262=CARTESIAN_POINT('Ctrl Pts',(190.263931816014,54.3999999999636,120.700844105169));
#91263=CARTESIAN_POINT('Ctrl Pts',(189.905525199068,54.8501814482593,123.31496616946));
#91264=CARTESIAN_POINT('Ctrl Pts',(190.187813351298,54.7136847330329,123.324152150651));
#91265=CARTESIAN_POINT('Ctrl Pts',(190.187813351256,54.4000000000363,123.324152150649));
#91266=CARTESIAN_POINT('Ctrl Pts',(189.696750321874,54.850181448191,128.556852744112));
#91267=CARTESIAN_POINT('Ctrl Pts',(189.978874876793,54.7136847328917,128.570146301895));
#91268=CARTESIAN_POINT('Ctrl Pts',(189.978874876835,54.3999999999636,128.570146301897));
#91269=CARTESIAN_POINT('Ctrl Pts',(189.564190785202,54.8501814482593,131.177068260088));
#91270=CARTESIAN_POINT('Ctrl Pts',(189.846197509667,54.7136847330329,131.192833544529));
#91271=CARTESIAN_POINT('Ctrl Pts',(189.84619750958,54.4000000000363,131.192833544524));
#91272=CARTESIAN_POINT('Ctrl Pts',(189.21373904357,54.850181448191,136.415271144211));
#91273=CARTESIAN_POINT('Ctrl Pts',(189.495332574474,54.7136847328916,136.437212434963));
#91274=CARTESIAN_POINT('Ctrl Pts',(189.495332574561,54.3999999999636,136.437212434969));
#91275=CARTESIAN_POINT('Ctrl Pts',(188.995975118318,54.8501814482251,139.034428718839));
#91276=CARTESIAN_POINT('Ctrl Pts',(189.277277045309,54.7136847329623,139.060072711156));
#91277=CARTESIAN_POINT('Ctrl Pts',(189.277277045221,54.3999999999999,139.060072711146));
#91278=CARTESIAN_POINT('Ctrl Pts',(188.432225703268,54.8501814482251,144.264463671248));
#91279=CARTESIAN_POINT('Ctrl Pts',(188.71253077521,54.7136847329623,144.299355721209));
#91280=CARTESIAN_POINT('Ctrl Pts',(188.712530775298,54.3999999999999,144.299355721219));
#91281=CARTESIAN_POINT('Ctrl Pts',(188.087304668474,54.8501814482349,146.868271499025));
#91282=CARTESIAN_POINT('Ctrl Pts',(188.366914065688,54.7136847329872,146.908694703911));
#91283=CARTESIAN_POINT('Ctrl Pts',(188.366914065557,54.4000000000363,146.908694703889));
#91284=CARTESIAN_POINT('Ctrl Pts',(187.208321751508,54.8501814482154,152.042290376387));
#91285=CARTESIAN_POINT('Ctrl Pts',(187.485593746244,54.7136847329374,152.096472398439));
#91286=CARTESIAN_POINT('Ctrl Pts',(187.485593746376,54.3999999999636,152.096472398462));
#91287=CARTESIAN_POINT('Ctrl Pts',(186.674882433875,54.8501814482251,154.612621948317));
#91288=CARTESIAN_POINT('Ctrl Pts',(186.950529717102,54.7136847329623,154.675038288882));
#91289=CARTESIAN_POINT('Ctrl Pts',(186.950529716886,54.3999999999999,154.675038288824));
#91290=CARTESIAN_POINT('Ctrl Pts',(185.829068982087,54.8501814482251,157.793689708649));
#91291=CARTESIAN_POINT('Ctrl Pts',(186.101340342461,54.7136847329623,157.868802749258));
#91292=CARTESIAN_POINT('Ctrl Pts',(186.101340342515,54.3999999999999,157.868802749272));
#91293=CARTESIAN_POINT('Ctrl Pts',(185.650840070459,54.850181448231,158.428289553895));
#91294=CARTESIAN_POINT('Ctrl Pts',(185.922366535571,54.713684732974,158.50606230595));
#91295=CARTESIAN_POINT('Ctrl Pts',(185.922366535509,54.4000000000045,158.506062305931));
#91296=CARTESIAN_POINT('Ctrl Pts',(185.274189105931,54.8501814482193,159.693888916717));
#91297=CARTESIAN_POINT('Ctrl Pts',(185.544055877709,54.7136847329506,159.77723846825));
#91298=CARTESIAN_POINT('Ctrl Pts',(185.544055877772,54.3999999999954,159.777238468269));
#91299=CARTESIAN_POINT('Ctrl Pts',(185.075603523205,54.8501814482251,160.325278084653));
#91300=CARTESIAN_POINT('Ctrl Pts',(185.344554566279,54.7136847329623,160.411547100408));
#91301=CARTESIAN_POINT('Ctrl Pts',(185.344554566236,54.3999999999999,160.411547100394));
#91302=CARTESIAN_POINT('Ctrl Pts',(184.449826482446,54.8501814482251,162.202753795278));
#91303=CARTESIAN_POINT('Ctrl Pts',(184.715740727713,54.7136847329623,162.298133906292));
#91304=CARTESIAN_POINT('Ctrl Pts',(184.715740727799,54.3999999999999,162.298133906321));
#91305=CARTESIAN_POINT('Ctrl Pts',(183.991757248688,54.8501814482251,163.43542835655));
#91306=CARTESIAN_POINT('Ctrl Pts',(184.255257809005,54.7136847329623,163.537370813413));
#91307=CARTESIAN_POINT('Ctrl Pts',(184.255257808904,54.3999999999999,163.53737081337));
#91308=CARTESIAN_POINT('Ctrl Pts',(182.473253277925,54.8501814482251,167.066305711601));
#91309=CARTESIAN_POINT('Ctrl Pts',(182.727934619225,54.7136847329623,167.189335701864));
#91310=CARTESIAN_POINT('Ctrl Pts',(182.727934619428,54.3999999999999,167.189335701949));
#91311=CARTESIAN_POINT('Ctrl Pts',(181.268987344943,54.8501814481749,169.397698176221));
#91312=CARTESIAN_POINT('Ctrl Pts',(181.515620921969,54.7136847328548,169.536771595712));
#91313=CARTESIAN_POINT('Ctrl Pts',(181.515620921781,54.3999999999268,169.536771595573));
#91314=CARTESIAN_POINT('Ctrl Pts',(179.441582135828,54.8501814482377,172.160422815342));
#91315=CARTESIAN_POINT('Ctrl Pts',(179.674375772127,54.7136847329892,172.32041986224));
#91316=CARTESIAN_POINT('Ctrl Pts',(179.674375772174,54.4000000000182,172.320419862275));
#91317=CARTESIAN_POINT('Ctrl Pts',(179.058647571677,54.8501814482279,172.707019013959));
#91318=CARTESIAN_POINT('Ctrl Pts',(179.288478943293,54.7136847329684,172.871248799738));
#91319=CARTESIAN_POINT('Ctrl Pts',(179.288478943292,54.4000000000046,172.871248799737));
#91320=CARTESIAN_POINT('Ctrl Pts',(178.268178494805,54.8501814482224,173.771202442769));
#91321=CARTESIAN_POINT('Ctrl Pts',(178.491798868746,54.7136847329563,173.943793897587));
#91322=CARTESIAN_POINT('Ctrl Pts',(178.491798868747,54.3999999999954,173.943793897587));
#91323=CARTESIAN_POINT('Ctrl Pts',(177.860133057982,54.8501814482298,174.289776895294));
#91324=CARTESIAN_POINT('Ctrl Pts',(178.080501288023,54.7136847329709,174.466503936161));
#91325=CARTESIAN_POINT('Ctrl Pts',(178.080501288033,54.4,174.466503936169));
#91326=CARTESIAN_POINT('Ctrl Pts',(176.597748388822,54.8501814482161,175.805008910674));
#91327=CARTESIAN_POINT('Ctrl Pts',(176.80798357003,54.7136847329453,175.993898583381));
#91328=CARTESIAN_POINT('Ctrl Pts',(176.807983570011,54.4,175.993898583365));
#91329=CARTESIAN_POINT('Ctrl Pts',(175.705080835993,54.850181448236,176.761087998022));
#91330=CARTESIAN_POINT('Ctrl Pts',(175.908054306141,54.713684732986,176.957753246188));
#91331=CARTESIAN_POINT('Ctrl Pts',(175.908054306173,54.400000000018,176.957753246221));
#91332=CARTESIAN_POINT('Ctrl Pts',(173.820641754199,54.8501814482143,178.567587618226));
#91333=CARTESIAN_POINT('Ctrl Pts',(174.008563362028,54.7136847329387,178.778682191129));
#91334=CARTESIAN_POINT('Ctrl Pts',(174.008563361996,54.399999999982,178.778682191095));
#91335=CARTESIAN_POINT('Ctrl Pts',(172.828892835169,54.8501814482297,179.418025890271));
#91336=CARTESIAN_POINT('Ctrl Pts',(173.009030242955,54.7136847329708,179.635772395387));
#91337=CARTESIAN_POINT('Ctrl Pts',(173.009030242992,54.4,179.635772395448));
#91338=CARTESIAN_POINT('Ctrl Pts',(171.270964235975,54.8501814482229,180.618253074959));
#91339=CARTESIAN_POINT('Ctrl Pts',(171.43944285178,54.7136847329581,180.844981505819));
#91340=CARTESIAN_POINT('Ctrl Pts',(171.439442851761,54.4,180.844981505789));
#91341=CARTESIAN_POINT('Ctrl Pts',(170.739952716052,54.8501814482214,181.005775429243));
#91342=CARTESIAN_POINT('Ctrl Pts',(170.904547815832,54.7136847329552,181.235334021093));
#91343=CARTESIAN_POINT('Ctrl Pts',(170.904547815849,54.4,181.235334021119));
#91344=CARTESIAN_POINT('Ctrl Pts',(169.655345316385,54.850181448229,181.756533782417));
#91345=CARTESIAN_POINT('Ctrl Pts',(169.812238466112,54.7136847329695,181.991423615145));
#91346=CARTESIAN_POINT('Ctrl Pts',(169.812238466095,54.4,181.991423615119));
#91347=CARTESIAN_POINT('Ctrl Pts',(169.100565571154,54.8501814482237,182.120500287617));
#91348=CARTESIAN_POINT('Ctrl Pts',(169.253632525607,54.7136847329595,182.357896135585));
#91349=CARTESIAN_POINT('Ctrl Pts',(169.253632525641,54.4,182.357896135649));
#91350=CARTESIAN_POINT('Ctrl Pts',(166.286156024425,54.8501814482313,183.87344972053));
#91351=CARTESIAN_POINT('Ctrl Pts',(166.420470654194,54.7136847329738,184.122525416709));
#91352=CARTESIAN_POINT('Ctrl Pts',(166.420470654058,54.4,184.122525416454));
#91353=CARTESIAN_POINT('Ctrl Pts',(163.940300566172,54.8501814482033,185.044287598079));
#91354=CARTESIAN_POINT('Ctrl Pts',(164.06114669688,54.7136847329148,185.299869237578));
#91355=CARTESIAN_POINT('Ctrl Pts',(164.061146696941,54.3999999999638,185.299869237723));
#91356=CARTESIAN_POINT('Ctrl Pts',(159.119184755956,54.8501814482469,187.065920062995));
#91357=CARTESIAN_POINT('Ctrl Pts',(159.216773571118,54.7136847330098,187.331254163407));
#91358=CARTESIAN_POINT('Ctrl Pts',(159.216773571057,54.4000000000361,187.331254163262));
#91359=CARTESIAN_POINT('Ctrl Pts',(156.643629215511,54.850181448213,187.916140584353));
#91360=CARTESIAN_POINT('Ctrl Pts',(156.731364791414,54.7136847329395,188.184741416756));
#91361=CARTESIAN_POINT('Ctrl Pts',(156.731364791459,54.4,188.184741416887));
#91362=CARTESIAN_POINT('Ctrl Pts',(152.861957700333,54.8501814482313,189.022509905896));
#91363=CARTESIAN_POINT('Ctrl Pts',(152.937045612347,54.7136847329737,189.294810950442));
#91364=CARTESIAN_POINT('Ctrl Pts',(152.937045612325,54.4,189.294810950376));
#91365=CARTESIAN_POINT('Ctrl Pts',(151.588783040648,54.8501814482142,189.363028174597));
#91366=CARTESIAN_POINT('Ctrl Pts',(151.660004270742,54.7136847329384,189.636355189729));
#91367=CARTESIAN_POINT('Ctrl Pts',(151.660004270758,54.3999999999818,189.636355189793));
#91368=CARTESIAN_POINT('Ctrl Pts',(149.037627503664,54.8501814482361,189.99264387881));
#91369=CARTESIAN_POINT('Ctrl Pts',(149.10175078131,54.7136847329862,190.267722642176));
#91370=CARTESIAN_POINT('Ctrl Pts',(149.101750781294,54.4000000000181,190.267722642112));
#91371=CARTESIAN_POINT('Ctrl Pts',(147.757825267386,54.8501814482032,190.282313053568));
#91372=CARTESIAN_POINT('Ctrl Pts',(147.818710308861,54.7136847329145,190.558119250698));
#91373=CARTESIAN_POINT('Ctrl Pts',(147.818710308865,54.3999999999636,190.558119250731));
#91374=CARTESIAN_POINT('Ctrl Pts',(143.907886586798,54.8501814482689,191.088733427083));
#91375=CARTESIAN_POINT('Ctrl Pts',(143.959822853609,54.7136847330577,191.36641406294));
#91376=CARTESIAN_POINT('Ctrl Pts',(143.9598228536,54.4000000000726,191.366414062873));
#91377=CARTESIAN_POINT('Ctrl Pts',(141.327319087948,54.8501814482045,191.543506604474));
#91378=CARTESIAN_POINT('Ctrl Pts',(141.374302221674,54.7136847329135,191.822034897082));
#91379=CARTESIAN_POINT('Ctrl Pts',(141.374302221683,54.3999999999455,191.822034897143));
#91380=CARTESIAN_POINT('Ctrl Pts',(135.976046370232,54.8501814482472,192.362205111029));
#91381=CARTESIAN_POINT('Ctrl Pts',(136.014207098472,54.7136847330143,192.642083155408));
#91382=CARTESIAN_POINT('Ctrl Pts',(136.014207098463,54.400000000058,192.642083155343));
#91383=CARTESIAN_POINT('Ctrl Pts',(133.203932918804,54.8501814482507,192.717861291362));
#91384=CARTESIAN_POINT('Ctrl Pts',(133.238324066358,54.7136847330163,192.998208138289));
#91385=CARTESIAN_POINT('Ctrl Pts',(133.238324066359,54.4000000000337,192.998208138274));
#91386=CARTESIAN_POINT('Ctrl Pts',(130.423832944263,54.8501814482199,193.026279994343));
#91387=CARTESIAN_POINT('Ctrl Pts',(130.454964793654,54.713684732951,193.306989106035));
#91388=CARTESIAN_POINT('Ctrl Pts',(130.454964793654,54.3999999999926,193.306989106039));
#91389=CARTESIAN_POINT('',(130.970210996039,54.4,193.249273457296));
#91390=CARTESIAN_POINT('Origin',(130.914017984099,54.4,192.752441145644));
#91391=CARTESIAN_POINT('Ctrl Pts',(190.499797482064,54.4,102.3353360815));
#91392=CARTESIAN_POINT('Ctrl Pts',(190.262688257762,54.4,166.865108618385));
#91393=CARTESIAN_POINT('Ctrl Pts',(186.165595197882,54.4,187.00653358103));
#91394=CARTESIAN_POINT('Ctrl Pts',(130.970210995984,54.4,193.249273456807));
#91395=CARTESIAN_POINT('Origin',(-205.7,54.4,40.5));
#91396=CARTESIAN_POINT('',(-189.5,54.4,40.));
#91397=CARTESIAN_POINT('Origin',(-189.5,54.4,40.5));
#91398=CARTESIAN_POINT('',(189.5,54.4,40.));
#91399=CARTESIAN_POINT('Ctrl Pts',(127.255088949806,54.5666666666668,193.698954356396));
#91400=CARTESIAN_POINT('Ctrl Pts',(127.245376536202,54.7908851649001,193.620278369648));
#91401=CARTESIAN_POINT('Ctrl Pts',(127.217936735184,54.8708716449131,193.398000621877));
#91402=CARTESIAN_POINT('Ctrl Pts',(127.879084413169,54.5518028860853,193.627218234101));
#91403=CARTESIAN_POINT('Ctrl Pts',(127.874066995385,54.7851572329741,193.55278227821));
#91404=CARTESIAN_POINT('Ctrl Pts',(127.842033796868,54.8694502963056,193.324965268805));
#91405=CARTESIAN_POINT('Ctrl Pts',(128.500935272669,54.5302082089312,193.550095813408));
#91406=CARTESIAN_POINT('Ctrl Pts',(128.501328716631,54.7766711456716,193.482509467744));
#91407=CARTESIAN_POINT('Ctrl Pts',(128.464930906231,54.8673636527269,193.246434626864));
#91408=CARTESIAN_POINT('Ctrl Pts',(129.739491935211,54.4743280441491,193.395855537281));
#91409=CARTESIAN_POINT('Ctrl Pts',(129.743550596673,54.7536109502607,193.352491272635));
#91410=CARTESIAN_POINT('Ctrl Pts',(129.704532450547,54.8618212857288,193.094336154531));
#91411=CARTESIAN_POINT('Ctrl Pts',(130.356219027086,54.4400417824632,193.318717527232));
#91412=CARTESIAN_POINT('Ctrl Pts',(130.368680695371,54.7386547278232,193.292148787355));
#91413=CARTESIAN_POINT('Ctrl Pts',(130.326591494069,54.8583196432092,193.020261309429));
#91414=CARTESIAN_POINT('Ctrl Pts',(130.970210995984,54.4,193.249273456807));
#91415=CARTESIAN_POINT('Ctrl Pts',(130.970210995984,54.7201169082854,193.249273456807));
#91416=CARTESIAN_POINT('Ctrl Pts',(130.937537062709,54.85409895477,192.960385831121));
#91417=CARTESIAN_POINT('',(127.255088949811,54.5666666666664,193.698954356395));
#91418=CARTESIAN_POINT('Origin',(127.197333301155,54.4,193.231101273397));
#91419=CARTESIAN_POINT('Ctrl Pts',(130.970210995984,54.4,193.249273456807));
#91420=CARTESIAN_POINT('Ctrl Pts',(130.614606575102,54.4231909138639,193.289493231166));
#91421=CARTESIAN_POINT('Ctrl Pts',(130.259170754114,54.4443808577405,193.332166063808));
#91422=CARTESIAN_POINT('Ctrl Pts',(129.903752824151,54.4635009794963,193.375799905195));
#91423=CARTESIAN_POINT('Ctrl Pts',(129.642584059729,54.4775508575514,193.407862993411));
#91424=CARTESIAN_POINT('Ctrl Pts',(129.381424839028,54.4904830162573,193.440446446569));
#91425=CARTESIAN_POINT('Ctrl Pts',(129.12021360394,54.5022681265401,193.472975675345));
#91426=CARTESIAN_POINT('Ctrl Pts',(128.658090984803,54.5231177888026,193.530524855399));
#91427=CARTESIAN_POINT('Ctrl Pts',(128.19579463262,54.5403791895002,193.587914070895));
#91428=CARTESIAN_POINT('Ctrl Pts',(127.733073441423,54.5539583293988,193.642989461962));
#91429=CARTESIAN_POINT('Ctrl Pts',(127.573799286481,54.5586324313707,193.661947068696));
#91430=CARTESIAN_POINT('Ctrl Pts',(127.414474664831,54.5628700456414,193.680630964935));
#91431=CARTESIAN_POINT('Ctrl Pts',(127.255088949811,54.5666666666666,193.698954356395));
#91432=CARTESIAN_POINT('Ctrl Pts',(-190.217944947177,54.85,41.));
#91433=CARTESIAN_POINT('Ctrl Pts',(-190.217944947177,54.85,40.282055052823));
#91434=CARTESIAN_POINT('Ctrl Pts',(-189.5,54.85,40.282055052823));
#91435=CARTESIAN_POINT('Ctrl Pts',(-190.5,54.7133945031366,41.));
#91436=CARTESIAN_POINT('Ctrl Pts',(-190.5,54.7133945031366,40.));
#91437=CARTESIAN_POINT('Ctrl Pts',(-189.5,54.7133945031366,40.));
#91438=CARTESIAN_POINT('Ctrl Pts',(-190.5,54.4,41.));
#91439=CARTESIAN_POINT('Ctrl Pts',(-190.5,54.4,40.));
#91440=CARTESIAN_POINT('Ctrl Pts',(-189.5,54.4,40.));
#91441=CARTESIAN_POINT('',(-190.5,54.4,41.));
#91442=CARTESIAN_POINT('Origin',(-190.,54.4,41.));
#91443=CARTESIAN_POINT('Origin',(-189.5,54.4,41.));
#91444=CARTESIAN_POINT('Ctrl Pts',(123.160667751337,54.5666666666683,194.071736241466));
#91445=CARTESIAN_POINT('Ctrl Pts',(123.155832932771,54.798164012315,193.990032495164));
#91446=CARTESIAN_POINT('Ctrl Pts',(123.142055633115,54.8749333564381,193.757209488378));
#91447=CARTESIAN_POINT('Ctrl Pts',(123.844835624837,54.5829842777358,194.02547137401));
#91448=CARTESIAN_POINT('Ctrl Pts',(123.833025706398,54.8039632931889,193.938950966455));
#91449=CARTESIAN_POINT('Ctrl Pts',(123.819972220688,54.8762595151111,193.713054829141));
#91450=CARTESIAN_POINT('Ctrl Pts',(124.52750939263,54.5910529953054,193.97017604454));
#91451=CARTESIAN_POINT('Ctrl Pts',(124.520341811565,54.8067875878841,193.881257473471));
#91452=CARTESIAN_POINT('Ctrl Pts',(124.502450477311,54.8769102936331,193.659297116951));
#91453=CARTESIAN_POINT('Ctrl Pts',(125.891907678889,54.5910540215352,193.846078596068));
#91454=CARTESIAN_POINT('Ctrl Pts',(125.882915036185,54.8067879458432,193.757325735115));
#91455=CARTESIAN_POINT('Ctrl Pts',(125.860468063284,54.8769103762644,193.53578017915));
#91456=CARTESIAN_POINT('Ctrl Pts',(126.573706760202,54.5829737705273,193.777260604719));
#91457=CARTESIAN_POINT('Ctrl Pts',(126.56969460559,54.8039598662694,193.690031299387));
#91458=CARTESIAN_POINT('Ctrl Pts',(126.5417369025,54.8762586984535,193.465488140134));
#91459=CARTESIAN_POINT('Ctrl Pts',(127.255088949806,54.5666666666668,193.698954356396));
#91460=CARTESIAN_POINT('Ctrl Pts',(127.245061240287,54.7981640123145,193.617724296245));
#91461=CARTESIAN_POINT('Ctrl Pts',(127.216486277851,54.8749333564379,193.38625110558));
#91462=CARTESIAN_POINT('',(123.160667751337,54.5666666666683,194.071736241466));
#91463=CARTESIAN_POINT('Origin',(123.132821104816,54.4,193.601154913214));
#91464=CARTESIAN_POINT('Ctrl Pts',(127.255088949811,54.5666666666664,193.698954356395));
#91465=CARTESIAN_POINT('Ctrl Pts',(126.574306561438,54.5829594156373,193.777191674042));
#91466=CARTESIAN_POINT('Ctrl Pts',(125.892275665928,54.5910531277812,193.84604432789));
#91467=CARTESIAN_POINT('Ctrl Pts',(124.527367138449,54.5910538890815,193.970189781285));
#91468=CARTESIAN_POINT('Ctrl Pts',(123.844381692399,54.5829734511008,194.025502069948));
#91469=CARTESIAN_POINT('Ctrl Pts',(123.160667751337,54.5666666666683,194.071736241466));
#91470=CARTESIAN_POINT('Origin',(-190.,54.4,211.4));
#91471=CARTESIAN_POINT('',(-190.5,54.4,102.225104347671));
#91472=CARTESIAN_POINT('Origin',(-190.,54.4,102.225104347671));
#91473=CARTESIAN_POINT('',(-190.5,54.4,211.4));
#91474=CARTESIAN_POINT('Ctrl Pts',(119.431296799848,54.3999999999989,194.307271119568));
#91475=CARTESIAN_POINT('Ctrl Pts',(119.431296799848,54.7201173502107,194.307271119569));
#91476=CARTESIAN_POINT('Ctrl Pts',(119.4100538882,54.8540992171485,194.017318164862));
#91477=CARTESIAN_POINT('Ctrl Pts',(120.046537134136,54.4400570466082,194.262196579538));
#91478=CARTESIAN_POINT('Ctrl Pts',(120.029404725024,54.7386619686269,194.238375307498));
#91479=CARTESIAN_POINT('Ctrl Pts',(120.020823595006,54.8583214617764,193.963377414171));
#91480=CARTESIAN_POINT('Ctrl Pts',(120.665937074624,54.4743442642813,194.225052062148));
#91481=CARTESIAN_POINT('Ctrl Pts',(120.654018808206,54.7536182484867,194.18314784127));
#91482=CARTESIAN_POINT('Ctrl Pts',(120.645146597598,54.8618231409601,193.922220259519));
#91483=CARTESIAN_POINT('Ctrl Pts',(121.910047618945,54.5302211315643,194.150963131627));
#91484=CARTESIAN_POINT('Ctrl Pts',(121.897385648962,54.7766766101539,194.084574079458));
#91485=CARTESIAN_POINT('Ctrl Pts',(121.890278416236,54.8673650949516,193.845817355955));
#91486=CARTESIAN_POINT('Ctrl Pts',(122.534757882391,54.5518089947801,194.114036622563));
#91487=CARTESIAN_POINT('Ctrl Pts',(122.526207616594,54.7851599104661,194.039920256715));
#91488=CARTESIAN_POINT('Ctrl Pts',(122.516416141673,54.8694510563384,193.810074102007));
#91489=CARTESIAN_POINT('Ctrl Pts',(123.160667751337,54.5666666666683,194.071736241466));
#91490=CARTESIAN_POINT('Ctrl Pts',(123.155984945507,54.7908854465423,193.992601363026));
#91491=CARTESIAN_POINT('Ctrl Pts',(123.142754938,54.8708718087829,193.769027062935));
#91492=CARTESIAN_POINT('',(119.431296819576,54.4000000000025,194.307271388221));
#91493=CARTESIAN_POINT('Origin',(119.394763063948,54.4,193.80860761966));
#91494=CARTESIAN_POINT('Ctrl Pts',(123.160667751337,54.5666666666683,194.071736241466));
#91495=CARTESIAN_POINT('Ctrl Pts',(122.709671237679,54.5559610386616,194.102215588969));
#91496=CARTESIAN_POINT('Ctrl Pts',(122.258621784535,54.5417470109889,194.129947833764));
#91497=CARTESIAN_POINT('Ctrl Pts',(121.807669854806,54.5241144990764,194.157003923459));
#91498=CARTESIAN_POINT('Ctrl Pts',(121.634426284557,54.5173405635085,194.167398143478));
#91499=CARTESIAN_POINT('Ctrl Pts',(121.46119731046,54.5100618706114,194.177692942311));
#91500=CARTESIAN_POINT('Ctrl Pts',(121.287992346785,54.5022826979228,194.188007596887));
#91501=CARTESIAN_POINT('Ctrl Pts',(120.937031470456,54.486519955297,194.208907922908));
#91502=CARTESIAN_POINT('Ctrl Pts',(120.58616849523,54.4687032547822,194.229881013872));
#91503=CARTESIAN_POINT('Ctrl Pts',(120.23549875877,54.448899215471,194.252365264865));
#91504=CARTESIAN_POINT('Ctrl Pts',(119.967302221838,54.4337528420937,194.269561497174));
#91505=CARTESIAN_POINT('Ctrl Pts',(119.699218906683,54.4174438633529,194.287642260639));
#91506=CARTESIAN_POINT('Ctrl Pts',(119.431296799848,54.3999999999989,194.307271119568));
#91507=CARTESIAN_POINT('Origin',(-160.5,54.4,102.225104347671));
#91508=CARTESIAN_POINT('',(-190.499797482064,54.4,102.335336081498));
#91509=CARTESIAN_POINT('Origin',(-189.999800857363,54.4,102.333498885934));
#91510=CARTESIAN_POINT('Origin',(-160.5,54.4,102.225104347671));
#91511=CARTESIAN_POINT('Ctrl Pts',(119.509543988169,54.8500347278621,194.018642428937));
#91512=CARTESIAN_POINT('Ctrl Pts',(119.530234140646,54.7134500006186,194.300009508377));
#91513=CARTESIAN_POINT('Ctrl Pts',(119.530234140646,54.4000000000055,194.300009508373));
#91514=CARTESIAN_POINT('Ctrl Pts',(114.504744574281,54.850034727667,194.386640129845));
#91515=CARTESIAN_POINT('Ctrl Pts',(114.521587596702,54.7134500002014,194.668289990076));
#91516=CARTESIAN_POINT('Ctrl Pts',(114.521587596738,54.399999999722,194.668289990278));
#91517=CARTESIAN_POINT('Ctrl Pts',(109.498634847962,54.8500347277534,194.653631857555));
#91518=CARTESIAN_POINT('Ctrl Pts',(109.512638560261,54.7134500003821,194.935420030612));
#91519=CARTESIAN_POINT('Ctrl Pts',(109.512638560238,54.3999999998262,194.935420030681));
#91520=CARTESIAN_POINT('Ctrl Pts',(99.5180232912834,54.8500347279625,195.06907559322));
#91521=CARTESIAN_POINT('Ctrl Pts',(99.5275013045554,54.7134500008372,195.351052148972));
#91522=CARTESIAN_POINT('Ctrl Pts',(99.5275013045778,54.4000000001726,195.351052148903));
#91523=CARTESIAN_POINT('Ctrl Pts',(94.5434725844513,54.8500347278166,195.217450349044));
#91524=CARTESIAN_POINT('Ctrl Pts',(94.5512583514112,54.7134500005197,195.499472957335));
#91525=CARTESIAN_POINT('Ctrl Pts',(94.5512583514102,54.3999999999309,195.499472957289));
#91526=CARTESIAN_POINT('Ctrl Pts',(84.5934911422877,54.8500347278999,195.444079361659));
#91527=CARTESIAN_POINT('Ctrl Pts',(84.5985539486568,54.7134500007011,195.726163990358));
#91528=CARTESIAN_POINT('Ctrl Pts',(84.5985539486579,54.400000000069,195.726163990404));
#91529=CARTESIAN_POINT('Ctrl Pts',(79.6180568875425,54.8500347278166,195.521957077234));
#91530=CARTESIAN_POINT('Ctrl Pts',(79.6220940664667,54.7134500005197,195.804056143501));
#91531=CARTESIAN_POINT('Ctrl Pts',(79.622094066466,54.3999999999309,195.804056143444));
#91532=CARTESIAN_POINT('Ctrl Pts',(69.666675118241,54.8500347279,195.635564432718));
#91533=CARTESIAN_POINT('Ctrl Pts',(69.6690791730593,54.7134500007011,195.917682143204));
#91534=CARTESIAN_POINT('Ctrl Pts',(69.66907917306,54.400000000069,195.91768214326));
#91535=CARTESIAN_POINT('Ctrl Pts',(64.6907256720555,54.8500347278351,195.671107949031));
#91536=CARTESIAN_POINT('Ctrl Pts',(64.6925245012106,54.7134500005671,195.953229373737));
#91537=CARTESIAN_POINT('Ctrl Pts',(64.6925245012109,54.4,195.953229373792));
#91538=CARTESIAN_POINT('Ctrl Pts',(49.7624773894366,54.8500347279047,195.741536462924));
#91539=CARTESIAN_POINT('Ctrl Pts',(49.7628727410856,54.713450000697,196.023664508782));
#91540=CARTESIAN_POINT('Ctrl Pts',(49.7628727410851,54.4,196.023664508672));
#91541=CARTESIAN_POINT('Ctrl Pts',(39.8097639074172,54.850034728025,195.741812920426));
#91542=CARTESIAN_POINT('Ctrl Pts',(39.8097607474161,54.7134500009732,196.023939735264));
#91543=CARTESIAN_POINT('Ctrl Pts',(39.809760747416,54.4000000002762,196.023939735262));
#91544=CARTESIAN_POINT('Ctrl Pts',(19.8716555149193,54.850034727691,195.730534471012));
#91545=CARTESIAN_POINT('Ctrl Pts',(19.8713389735597,54.7134500002464,196.012661108492));
#91546=CARTESIAN_POINT('Ctrl Pts',(19.8713389735597,54.3999999997228,196.012661108494));
#91547=CARTESIAN_POINT('Ctrl Pts',(9.88631306985696,54.8500347271157,195.717789107939));
#91548=CARTESIAN_POINT('Ctrl Pts',(9.8860970633918,54.7134499989911,195.999915879995));
#91549=CARTESIAN_POINT('Ctrl Pts',(9.88609706339176,54.3999999987505,195.999915880082));
#91550=CARTESIAN_POINT('Ctrl Pts',(-0.0989467222038218,54.8500347278657,
195.717873647057));
#91551=CARTESIAN_POINT('Ctrl Pts',(-0.0989445642066252,54.7134500006265,
196.000000418499));
#91552=CARTESIAN_POINT('Ctrl Pts',(-0.0989445642066248,54.4000000000124,
196.000000418498));
#91553=CARTESIAN_POINT('',(1.2169238626783E-14,54.4,196.));
#91554=CARTESIAN_POINT('Origin',(1.20273620013996E-14,54.4,195.5));
#91555=CARTESIAN_POINT('Ctrl Pts',(119.431296799848,54.4,194.307271119568));
#91556=CARTESIAN_POINT('Ctrl Pts',(116.259838254169,54.4000000000022,194.539622653112));
#91557=CARTESIAN_POINT('Ctrl Pts',(113.087577822492,54.4000000000016,194.731577999437));
#91558=CARTESIAN_POINT('Ctrl Pts',(109.914729036557,54.4000000000232,194.893888974244));
#91559=CARTESIAN_POINT('Ctrl Pts',(108.111189387205,54.4000000000355,194.98615125913));
#91560=CARTESIAN_POINT('Ctrl Pts',(106.307459615187,54.4000000000549,195.068835854631));
#91561=CARTESIAN_POINT('Ctrl Pts',(104.503579022491,54.4000000000862,195.143922525206));
#91562=CARTESIAN_POINT('Ctrl Pts',(100.210957862777,54.4000000001608,195.322603216282));
#91563=CARTESIAN_POINT('Ctrl Pts',(95.9174700273534,54.4000000000422,195.457621859572));
#91564=CARTESIAN_POINT('Ctrl Pts',(91.6234160517253,54.4000000000305,195.564117476063));
#91565=CARTESIAN_POINT('Ctrl Pts',(90.9405933301759,54.4000000000286,195.581051968992));
#91566=CARTESIAN_POINT('Ctrl Pts',(90.2577562959791,54.4000000000294,195.597265313742));
#91567=CARTESIAN_POINT('Ctrl Pts',(89.574906150034,54.4000000000342,195.612818473846));
#91568=CARTESIAN_POINT('Ctrl Pts',(84.599074668863,54.4000000000691,195.726152130049));
#91569=CARTESIAN_POINT('Ctrl Pts',(79.622539877546,54.3999999999996,195.804051053958));
#91570=CARTESIAN_POINT('Ctrl Pts',(74.645586619763,54.4000000000343,195.860869143352));
#91571=CARTESIAN_POINT('Ctrl Pts',(69.6694102398991,54.400000000069,195.917678363722));
#91572=CARTESIAN_POINT('Ctrl Pts',(64.6928118455221,54.4,195.953228018159));
#91573=CARTESIAN_POINT('Ctrl Pts',(59.7159739145023,54.4000000000001,195.976707752086));
#91574=CARTESIAN_POINT('Ctrl Pts',(52.1214119494974,54.4000000000002,196.012537388634));
#91575=CARTESIAN_POINT('Ctrl Pts',(44.526289196523,54.400000000161,196.021189119254));
#91576=CARTESIAN_POINT('Ctrl Pts',(36.9310173515837,54.4000000001757,196.020774649485));
#91577=CARTESIAN_POINT('Ctrl Pts',(34.5730357339827,54.4000000001802,196.020645975737));
#91578=CARTESIAN_POINT('Ctrl Pts',(32.2150397510362,54.4000000001706,196.019643606687));
#91579=CARTESIAN_POINT('Ctrl Pts',(29.85704171195,54.400000000138,196.018309750873));
#91580=CARTESIAN_POINT('Ctrl Pts',(19.9046938155966,54.4000000000001,196.012679976427));
#91581=CARTESIAN_POINT('Ctrl Pts',(9.9523497061253,54.4,196.));
#91582=CARTESIAN_POINT('Ctrl Pts',(1.4210854715202E-14,54.4,196.));
#91583=CARTESIAN_POINT('Ctrl Pts',(0.108339742257026,54.8500380311149,195.717866914955));
#91584=CARTESIAN_POINT('Ctrl Pts',(0.108337388749144,54.713455280679,196.00000050967));
#91585=CARTESIAN_POINT('Ctrl Pts',(0.108337388749144,54.4,196.000000509671));
#91586=CARTESIAN_POINT('Ctrl Pts',(-10.6394131523854,54.8500380311152,195.717765695086));
#91587=CARTESIAN_POINT('Ctrl Pts',(-10.6391815802582,54.7134552806797,195.999899290541));
#91588=CARTESIAN_POINT('Ctrl Pts',(-10.6391815802582,54.400000000001,195.999899290448));
#91589=CARTESIAN_POINT('Ctrl Pts',(-21.3873590267281,54.850038031075,195.732769603628));
#91590=CARTESIAN_POINT('Ctrl Pts',(-21.3870266129879,54.7134552805766,196.014903083131));
#91591=CARTESIAN_POINT('Ctrl Pts',(-21.3870266129879,54.3999999998508,196.01490308311));
#91592=CARTESIAN_POINT('Ctrl Pts',(-42.8474989701256,54.8500380311547,195.741830949266));
#91593=CARTESIAN_POINT('Ctrl Pts',(-42.8475924106281,54.7134552807811,196.023964608597));
#91594=CARTESIAN_POINT('Ctrl Pts',(-42.8475924106281,54.4000000001486,196.023964608617));
#91595=CARTESIAN_POINT('Ctrl Pts',(-53.5596885725384,54.8500380310701,195.737760364647));
#91596=CARTESIAN_POINT('Ctrl Pts',(-53.5602852852272,54.7134552805814,196.019895896344));
#91597=CARTESIAN_POINT('Ctrl Pts',(-53.5602852852272,54.3999999999257,196.019895896344));
#91598=CARTESIAN_POINT('Ctrl Pts',(-69.6282502861437,54.8500380311374,195.635215850766));
#91599=CARTESIAN_POINT('Ctrl Pts',(-69.6306526067851,54.7134552807279,195.917339859647));
#91600=CARTESIAN_POINT('Ctrl Pts',(-69.6306526067851,54.4000000000371,195.917339859647));
#91601=CARTESIAN_POINT('Ctrl Pts',(-74.9844840288523,54.85003803109,195.584389730407));
#91602=CARTESIAN_POINT('Ctrl Pts',(-74.9876678043094,54.7134552806324,195.866507396244));
#91603=CARTESIAN_POINT('Ctrl Pts',(-74.9876678043095,54.4,195.866507396251));
#91604=CARTESIAN_POINT('Ctrl Pts',(-85.6970676947234,54.8500380311399,195.422795957478));
#91605=CARTESIAN_POINT('Ctrl Pts',(-85.7023946291779,54.7134552807256,195.704881294905));
#91606=CARTESIAN_POINT('Ctrl Pts',(-85.7023946291778,54.4,195.704881294898));
#91607=CARTESIAN_POINT('Ctrl Pts',(-91.0540074351636,54.8500380310899,195.312362346734));
#91608=CARTESIAN_POINT('Ctrl Pts',(-91.0606918126211,54.7134552806324,195.594422790046));
#91609=CARTESIAN_POINT('Ctrl Pts',(-91.0606918126185,54.4,195.594422789961));
#91610=CARTESIAN_POINT('Ctrl Pts',(-101.765528158601,54.8500380311399,194.988364284601));
#91611=CARTESIAN_POINT('Ctrl Pts',(-101.775903721038,54.7134552807256,195.270313078383));
#91612=CARTESIAN_POINT('Ctrl Pts',(-101.775903721041,54.4,195.270313078468));
#91613=CARTESIAN_POINT('Ctrl Pts',(-107.117526535979,54.85003803109,194.775617671763));
#91614=CARTESIAN_POINT('Ctrl Pts',(-107.130224336239,54.7134552806325,195.057483582586));
#91615=CARTESIAN_POINT('Ctrl Pts',(-107.130224336237,54.4,195.057483582537));
#91616=CARTESIAN_POINT('Ctrl Pts',(-117.808411473944,54.8500380311399,194.172315411311));
#91617=CARTESIAN_POINT('Ctrl Pts',(-117.827505515306,54.7134552807256,194.4538203729));
#91618=CARTESIAN_POINT('Ctrl Pts',(-117.827505515308,54.4,194.453820372949));
#91619=CARTESIAN_POINT('Ctrl Pts',(-123.147427885218,54.8500380310477,193.783642561154));
#91620=CARTESIAN_POINT('Ctrl Pts',(-123.170566875538,54.7134552805327,194.064885467444));
#91621=CARTESIAN_POINT('Ctrl Pts',(-123.170566875529,54.3999999998886,194.064885467356));
#91622=CARTESIAN_POINT('Ctrl Pts',(-131.13843404817,54.8500380311486,192.960571233706));
#91623=CARTESIAN_POINT('Ctrl Pts',(-131.170224675515,54.7134552807522,193.240923023929));
#91624=CARTESIAN_POINT('Ctrl Pts',(-131.170224675519,54.4000000000557,193.240923023973));
#91625=CARTESIAN_POINT('Ctrl Pts',(-133.799137053305,54.850038031115,192.64554864504));
#91626=CARTESIAN_POINT('Ctrl Pts',(-133.834251546657,54.7134552806791,192.925517262509));
#91627=CARTESIAN_POINT('Ctrl Pts',(-133.83425154665,54.4,192.925517262463));
#91628=CARTESIAN_POINT('Ctrl Pts',(-137.784045656388,54.850038031115,192.088101643795));
#91629=CARTESIAN_POINT('Ctrl Pts',(-137.825118822442,54.7134552806791,192.367236705357));
#91630=CARTESIAN_POINT('Ctrl Pts',(-137.825118822446,54.4,192.367236705381));
#91631=CARTESIAN_POINT('Ctrl Pts',(-139.111317684321,54.8500380311093,191.888039824932));
#91632=CARTESIAN_POINT('Ctrl Pts',(-139.154540611851,54.7134552806668,192.16685305033));
#91633=CARTESIAN_POINT('Ctrl Pts',(-139.154540611846,54.3999999999906,192.166853050303));
#91634=CARTESIAN_POINT('Ctrl Pts',(-141.763413284886,54.8500380311205,191.453946490174));
#91635=CARTESIAN_POINT('Ctrl Pts',(-141.811336381098,54.7134552806912,191.731990394955));
#91636=CARTESIAN_POINT('Ctrl Pts',(-141.811336381103,54.4000000000093,191.731990394983));
#91637=CARTESIAN_POINT('Ctrl Pts',(-143.089131113363,54.8500380311149,191.21973202617));
#91638=CARTESIAN_POINT('Ctrl Pts',(-143.13960666561,54.713455280679,191.497328231515));
#91639=CARTESIAN_POINT('Ctrl Pts',(-143.139606665603,54.3999999999999,191.497328231476));
#91640=CARTESIAN_POINT('Ctrl Pts',(-147.049213256429,54.8500380311149,190.458401104656));
#91641=CARTESIAN_POINT('Ctrl Pts',(-147.108057529445,54.713455280679,190.734388412647));
#91642=CARTESIAN_POINT('Ctrl Pts',(-147.10805752946,54.3999999999999,190.734388412724));
#91643=CARTESIAN_POINT('Ctrl Pts',(-149.669664355132,54.8500380311374,189.87321359446));
#91644=CARTESIAN_POINT('Ctrl Pts',(-149.735031156289,54.7134552807278,190.147792646779));
#91645=CARTESIAN_POINT('Ctrl Pts',(-149.735031156257,54.4000000000371,190.147792646636));
#91646=CARTESIAN_POINT('Ctrl Pts',(-153.558016900812,54.8500380311037,188.827413937642));
#91647=CARTESIAN_POINT('Ctrl Pts',(-153.63525005315,54.7134552806546,189.09880145176));
#91648=CARTESIAN_POINT('Ctrl Pts',(-153.635250053166,54.3999999999814,189.098801451831));
#91649=CARTESIAN_POINT('Ctrl Pts',(-154.847024685085,54.8500380311262,188.450588263097));
#91650=CARTESIAN_POINT('Ctrl Pts',(-154.928562946899,54.7134552807035,188.720727975034));
#91651=CARTESIAN_POINT('Ctrl Pts',(-154.928562946869,54.4000000000186,188.720727974942));
#91652=CARTESIAN_POINT('Ctrl Pts',(-157.4077546348,54.8500380311037,187.628297179058));
#91653=CARTESIAN_POINT('Ctrl Pts',(-157.49873505085,54.7134552806546,187.895404865313));
#91654=CARTESIAN_POINT('Ctrl Pts',(-157.49873505088,54.3999999999814,187.895404865405));
#91655=CARTESIAN_POINT('Ctrl Pts',(-158.680882160903,54.8500380311149,187.182323197846));
#91656=CARTESIAN_POINT('Ctrl Pts',(-158.777006808681,54.713455280679,187.447644908254));
#91657=CARTESIAN_POINT('Ctrl Pts',(-158.777006808645,54.3999999999999,187.447644908159));
#91658=CARTESIAN_POINT('Ctrl Pts',(-162.459478912646,54.8500380311149,185.7214999272));
#91659=CARTESIAN_POINT('Ctrl Pts',(-162.572437434655,54.713455280679,185.980313582809));
#91660=CARTESIAN_POINT('Ctrl Pts',(-162.572437434729,54.3999999999999,185.980313583));
#91661=CARTESIAN_POINT('Ctrl Pts',(-164.895955520428,54.850038031131,184.59598819763));
#91662=CARTESIAN_POINT('Ctrl Pts',(-165.021947502474,54.713455280716,184.848989685855));
#91663=CARTESIAN_POINT('Ctrl Pts',(-165.021947502338,54.4000000000369,184.848989685658));
#91664=CARTESIAN_POINT('Ctrl Pts',(-168.378946346957,54.8500380311069,182.593720138746));
#91665=CARTESIAN_POINT('Ctrl Pts',(-168.526867773834,54.7134552806605,182.834115040126));
#91666=CARTESIAN_POINT('Ctrl Pts',(-168.526867773903,54.3999999999815,182.834115040225));
#91667=CARTESIAN_POINT('Ctrl Pts',(-169.511164536588,54.8500380311165,181.873697436862));
#91668=CARTESIAN_POINT('Ctrl Pts',(-169.666776786271,54.7134552806819,182.10923579638));
#91669=CARTESIAN_POINT('Ctrl Pts',(-169.666776786166,54.3999999999999,182.109235796261));
#91670=CARTESIAN_POINT('Ctrl Pts',(-171.158953560921,54.8500380311141,180.701771054281));
#91671=CARTESIAN_POINT('Ctrl Pts',(-171.326425106144,54.7134552806775,180.928874947439));
#91672=CARTESIAN_POINT('Ctrl Pts',(-171.326425106196,54.3999999999999,180.928874947498));
#91673=CARTESIAN_POINT('Ctrl Pts',(-171.699784041561,54.8500380311085,180.29579974264));
#91674=CARTESIAN_POINT('Ctrl Pts',(-171.871260701899,54.7134552806652,180.519901406512));
#91675=CARTESIAN_POINT('Ctrl Pts',(-171.871260701859,54.3999999999906,180.519901406447));
#91676=CARTESIAN_POINT('Ctrl Pts',(-172.763252852148,54.8500380311214,179.450899492048));
#91677=CARTESIAN_POINT('Ctrl Pts',(-172.942780916033,54.7134552806928,179.668604510617));
#91678=CARTESIAN_POINT('Ctrl Pts',(-172.942780916073,54.4000000000093,179.668604510682));
#91679=CARTESIAN_POINT('Ctrl Pts',(-173.284583847363,54.8500380311172,179.01282876578));
#91680=CARTESIAN_POINT('Ctrl Pts',(-173.468148508317,54.7134552806834,179.227145347675));
#91681=CARTESIAN_POINT('Ctrl Pts',(-173.468148508316,54.3999999999999,179.227145347668));
#91682=CARTESIAN_POINT('Ctrl Pts',(-175.810760829173,54.8500380311055,176.765322607494));
#91683=CARTESIAN_POINT('Ctrl Pts',(-176.014168613311,54.7134552806614,176.9619850259));
#91684=CARTESIAN_POINT('Ctrl Pts',(-176.014168613314,54.3999999999999,176.961985025928));
#91685=CARTESIAN_POINT('Ctrl Pts',(-177.597158086212,54.8500380311261,174.763125936056));
#91686=CARTESIAN_POINT('Ctrl Pts',(-177.815415056901,54.7134552807034,174.943121919234));
#91687=CARTESIAN_POINT('Ctrl Pts',(-177.815415056962,54.4000000000186,174.943121919277));
#91688=CARTESIAN_POINT('Ctrl Pts',(-179.542670640116,54.8500380311121,172.013651556169));
#91689=CARTESIAN_POINT('Ctrl Pts',(-179.77599160756,54.7134552806729,172.172358510286));
#91690=CARTESIAN_POINT('Ctrl Pts',(-179.775991607544,54.3999999999953,172.172358510275));
#91691=CARTESIAN_POINT('Ctrl Pts',(-179.917528256893,54.8500380311093,171.451529957781));
#91692=CARTESIAN_POINT('Ctrl Pts',(-180.153696573202,54.7134552806667,171.605961658005));
#91693=CARTESIAN_POINT('Ctrl Pts',(-180.153696573215,54.3999999999906,171.605961658013));
#91694=CARTESIAN_POINT('Ctrl Pts',(-180.639398332045,54.8500380311206,170.303458800956));
#91695=CARTESIAN_POINT('Ctrl Pts',(-180.880916991954,54.7134552806913,170.449381248078));
#91696=CARTESIAN_POINT('Ctrl Pts',(-180.880916991941,54.4000000000093,170.44938124807));
#91697=CARTESIAN_POINT('Ctrl Pts',(-180.986399307621,54.8500380311124,169.717266069453));
#91698=CARTESIAN_POINT('Ctrl Pts',(-181.230420402746,54.7134552806726,169.858953973863));
#91699=CARTESIAN_POINT('Ctrl Pts',(-181.23042040281,54.3999999999906,169.858953973898));
#91700=CARTESIAN_POINT('Ctrl Pts',(-181.975711664719,54.8500380311199,167.9456619586));
#91701=CARTESIAN_POINT('Ctrl Pts',(-182.22665413232,54.7134552806918,168.074955463978));
#91702=CARTESIAN_POINT('Ctrl Pts',(-182.226654132192,54.4000000000186,168.074955463907));
#91703=CARTESIAN_POINT('Ctrl Pts',(-182.571021240997,54.8500380311088,166.740262383191));
#91704=CARTESIAN_POINT('Ctrl Pts',(-182.82582979671,54.7134552806674,166.861660004074));
#91705=CARTESIAN_POINT('Ctrl Pts',(-182.825829796822,54.4,166.861660004124));
#91706=CARTESIAN_POINT('Ctrl Pts',(-184.195262100537,54.8500380311274,163.063230859887));
#91707=CARTESIAN_POINT('Ctrl Pts',(-184.459874896115,54.7134552807022,163.162433189046));
#91708=CARTESIAN_POINT('Ctrl Pts',(-184.459874895891,54.4,163.162433188947));
#91709=CARTESIAN_POINT('Ctrl Pts',(-185.063862954418,54.8500380311274,160.531319247725));
#91710=CARTESIAN_POINT('Ctrl Pts',(-185.332658084472,54.7134552807023,160.617765878873));
#91711=CARTESIAN_POINT('Ctrl Pts',(-185.332658084675,54.4,160.61776587893));
#91712=CARTESIAN_POINT('Ctrl Pts',(-186.144761446821,54.8500380311087,156.650466794253));
#91713=CARTESIAN_POINT('Ctrl Pts',(-186.418046815866,54.7134552806674,156.720791693642));
#91714=CARTESIAN_POINT('Ctrl Pts',(-186.418046815765,54.4,156.720791693614));
#91715=CARTESIAN_POINT('Ctrl Pts',(-186.468386489537,54.850038031115,155.339660109173));
#91716=CARTESIAN_POINT('Ctrl Pts',(-186.74286676442,54.713455280679,155.405086705287));
#91717=CARTESIAN_POINT('Ctrl Pts',(-186.742866764511,54.4,155.405086705307));
#91718=CARTESIAN_POINT('Ctrl Pts',(-187.049982169092,54.850038031115,152.712642453476));
#91719=CARTESIAN_POINT('Ctrl Pts',(-187.326429131924,54.713455280679,152.769185688956));
#91720=CARTESIAN_POINT('Ctrl Pts',(-187.326429131834,54.4,152.769185688935));
#91721=CARTESIAN_POINT('Ctrl Pts',(-187.308038547416,54.8500380311205,151.397194165868));
#91722=CARTESIAN_POINT('Ctrl Pts',(-187.585258126222,54.7134552806912,151.449750314456));
#91723=CARTESIAN_POINT('Ctrl Pts',(-187.585258126313,54.4000000000092,151.449750314472));
#91724=CARTESIAN_POINT('Ctrl Pts',(-188.003945663939,54.8500380311037,147.446229609717));
#91725=CARTESIAN_POINT('Ctrl Pts',(-188.283075769649,54.7134552806547,147.48793887317));
#91726=CARTESIAN_POINT('Ctrl Pts',(-188.283075769467,54.3999999999814,147.487938873137));
#91727=CARTESIAN_POINT('Ctrl Pts',(-188.364534771007,54.8500380311496,144.806152648602));
#91728=CARTESIAN_POINT('Ctrl Pts',(-188.644410165692,54.7134552807506,144.842102846923));
#91729=CARTESIAN_POINT('Ctrl Pts',(-188.644410165763,54.4000000000368,144.842102846931));
#91730=CARTESIAN_POINT('Ctrl Pts',(-188.952047186871,54.8500380310803,139.518111180135));
#91731=CARTESIAN_POINT('Ctrl Pts',(-189.232988329538,54.7134552806075,139.544468866608));
#91732=CARTESIAN_POINT('Ctrl Pts',(-189.232988329467,54.3999999999631,139.5444688666));
#91733=CARTESIAN_POINT('Ctrl Pts',(-189.1784582655,54.8500380311149,136.870114362724));
#91734=CARTESIAN_POINT('Ctrl Pts',(-189.459709168722,54.713455280679,136.892642646065));
#91735=CARTESIAN_POINT('Ctrl Pts',(-189.45970916872,54.3999999999999,136.892642646065));
#91736=CARTESIAN_POINT('Ctrl Pts',(-189.542662973237,54.8500380311149,131.568886534478));
#91737=CARTESIAN_POINT('Ctrl Pts',(-189.824352296183,54.713455280679,131.585033344381));
#91738=CARTESIAN_POINT('Ctrl Pts',(-189.824352296185,54.3999999999999,131.585033344381));
#91739=CARTESIAN_POINT('Ctrl Pts',(-189.680191107803,54.8500380311248,128.915639981583));
#91740=CARTESIAN_POINT('Ctrl Pts',(-189.962004740436,54.7134552807043,128.92923846097));
#91741=CARTESIAN_POINT('Ctrl Pts',(-189.962004740445,54.4000000000368,128.929238460971));
#91742=CARTESIAN_POINT('Ctrl Pts',(-189.896513954462,54.8500380311051,123.605692278856));
#91743=CARTESIAN_POINT('Ctrl Pts',(-190.178499841913,54.7134552806537,123.615062522318));
#91744=CARTESIAN_POINT('Ctrl Pts',(-190.178499841904,54.3999999999631,123.615062522317));
#91745=CARTESIAN_POINT('Ctrl Pts',(-189.975161211412,54.8500380311372,120.948982719434));
#91746=CARTESIAN_POINT('Ctrl Pts',(-190.25719326379,54.7134552807275,120.956675467201));
#91747=CARTESIAN_POINT('Ctrl Pts',(-190.257193263797,54.4000000000369,120.956675467189));
#91748=CARTESIAN_POINT('Ctrl Pts',(-190.15455552149,54.8500380310701,112.939682823118));
#91749=CARTESIAN_POINT('Ctrl Pts',(-190.436680384205,54.7134552805815,112.943231928075));
#91750=CARTESIAN_POINT('Ctrl Pts',(-190.436680384191,54.3999999999257,112.943231928098));
#91751=CARTESIAN_POINT('Ctrl Pts',(-190.19870833527,54.850038030788,107.58375287472));
#91752=CARTESIAN_POINT('Ctrl Pts',(-190.480836465935,54.7134552799851,107.58575000634));
#91753=CARTESIAN_POINT('Ctrl Pts',(-190.480836465829,54.399999999552,107.585750006322));
#91754=CARTESIAN_POINT('Ctrl Pts',(-190.218057935276,54.8500380311216,102.226659873173));
#91755=CARTESIAN_POINT('Ctrl Pts',(-190.500189698379,54.7134552806931,102.227676769414));
#91756=CARTESIAN_POINT('Ctrl Pts',(-190.500189698381,54.4000000000091,102.227676769414));
#91757=CARTESIAN_POINT('Ctrl Pts',(1.21569421196455E-14,54.4,196.));
#91758=CARTESIAN_POINT('Ctrl Pts',(-10.7117531408873,54.4,196.));
#91759=CARTESIAN_POINT('Ctrl Pts',(-21.4235888453071,54.3999999999959,196.014918521175));
#91760=CARTESIAN_POINT('Ctrl Pts',(-32.1353671216415,54.4000000000734,196.019441470522));
#91761=CARTESIAN_POINT('Ctrl Pts',(-37.9435801512012,54.4000000001154,196.021893934778));
#91762=CARTESIAN_POINT('Ctrl Pts',(-43.7517791269623,54.4000000000876,196.021820074024));
#91763=CARTESIAN_POINT('Ctrl Pts',(-49.5599150077629,54.4000000000594,196.01034215732));
#91764=CARTESIAN_POINT('Ctrl Pts',(-54.4646195038332,54.4000000000355,196.000649582831));
#91765=CARTESIAN_POINT('Ctrl Pts',(-59.3692789259093,54.4000000000106,195.982824723479));
#91766=CARTESIAN_POINT('Ctrl Pts',(-64.2738634995991,54.400000000024,195.951525205213));
#91767=CARTESIAN_POINT('Ctrl Pts',(-69.6310359293998,54.4000000000387,195.917337413403));
#91768=CARTESIAN_POINT('Ctrl Pts',(-74.9881325496737,54.4,195.866500385808));
#91769=CARTESIAN_POINT('Ctrl Pts',(-80.3450312167437,54.4,195.785694345575));
#91770=CARTESIAN_POINT('Ctrl Pts',(-82.3276232645959,54.4,195.755787971991));
#91771=CARTESIAN_POINT('Ctrl Pts',(-84.3102773500987,54.4,195.721822553936));
#91772=CARTESIAN_POINT('Ctrl Pts',(-86.2928923209843,54.4,195.682687093389));
#91773=CARTESIAN_POINT('Ctrl Pts',(-89.6683134019806,54.4,195.616058594925));
#91774=CARTESIAN_POINT('Ctrl Pts',(-93.0436188031098,54.4,195.534443957971));
#91775=CARTESIAN_POINT('Ctrl Pts',(-96.4182977668297,54.4,195.432367934214));
#91776=CARTESIAN_POINT('Ctrl Pts',(-99.0028841103095,54.4,195.354190335743));
#91777=CARTESIAN_POINT('Ctrl Pts',(-101.586508773315,54.4,195.264201579288));
#91778=CARTESIAN_POINT('Ctrl Pts',(-104.168823808363,54.4000000000002,195.158121528418));
#91779=CARTESIAN_POINT('Ctrl Pts',(-106.940491118349,54.4000000000004,195.044262992474));
#91780=CARTESIAN_POINT('Ctrl Pts',(-109.71064886288,54.400000000001,194.911866455551));
#91781=CARTESIAN_POINT('Ctrl Pts',(-112.478864925773,54.400000000002,194.755651977743));
#91782=CARTESIAN_POINT('Ctrl Pts',(-114.594746353043,54.4000000000029,194.636249696723));
#91783=CARTESIAN_POINT('Ctrl Pts',(-116.709517996796,54.399999999997,194.503228627145));
#91784=CARTESIAN_POINT('Ctrl Pts',(-118.822814021222,54.3999999999952,194.352073476874));
#91785=CARTESIAN_POINT('Ctrl Pts',(-121.558134924859,54.3999999999929,194.156427510834));
#91786=CARTESIAN_POINT('Ctrl Pts',(-124.290982134953,54.3999999999953,193.93039917945));
#91787=CARTESIAN_POINT('Ctrl Pts',(-127.020559030863,54.400000000018,193.664236790067));
#91788=CARTESIAN_POINT('Ctrl Pts',(-127.515038935979,54.4000000000221,193.616019810635));
#91789=CARTESIAN_POINT('Ctrl Pts',(-128.009411525647,54.4000000000268,193.56648586568));
#91790=CARTESIAN_POINT('Ctrl Pts',(-128.503672075522,54.4000000000323,193.515577171767));
#91791=CARTESIAN_POINT('Ctrl Pts',(-130.44030260628,54.400000000054,193.316104786329));
#91792=CARTESIAN_POINT('Ctrl Pts',(-132.375187111056,54.4000000000251,193.095177265629));
#91793=CARTESIAN_POINT('Ctrl Pts',(-134.307827469057,54.4000000000103,192.846712461554));
#91794=CARTESIAN_POINT('Ctrl Pts',(-135.037156465656,54.4000000000048,192.752948205056));
#91795=CARTESIAN_POINT('Ctrl Pts',(-135.766166053061,54.4000000000007,192.655262645524));
#91796=CARTESIAN_POINT('Ctrl Pts',(-136.494829730514,54.4000000000009,192.553330224408));
#91797=CARTESIAN_POINT('Ctrl Pts',(-136.887919442628,54.400000000001,192.498341088389));
#91798=CARTESIAN_POINT('Ctrl Pts',(-137.28091003026,54.4000000000004,192.442107475666));
#91799=CARTESIAN_POINT('Ctrl Pts',(-137.6737996963,54.3999999999999,192.384558370491));
#91800=CARTESIAN_POINT('Ctrl Pts',(-138.610834530866,54.3999999999985,192.247304782757));
#91801=CARTESIAN_POINT('Ctrl Pts',(-139.547276781443,54.399999999997,192.102570241843));
#91802=CARTESIAN_POINT('Ctrl Pts',(-140.482938496475,54.4000000000026,191.949421722643));
#91803=CARTESIAN_POINT('Ctrl Pts',(-140.735750537609,54.4000000000041,191.908041607251));
#91804=CARTESIAN_POINT('Ctrl Pts',(-140.988534786983,54.4000000000047,191.866041232653));
#91805=CARTESIAN_POINT('Ctrl Pts',(-141.241276754107,54.400000000005,191.823400409481));
#91806=CARTESIAN_POINT('Ctrl Pts',(-142.316874391013,54.4000000000064,191.641933242939));
#91807=CARTESIAN_POINT('Ctrl Pts',(-143.391615355187,54.4000000000011,191.448879234487));
#91808=CARTESIAN_POINT('Ctrl Pts',(-144.462423620222,54.4000000000009,191.243014958559));
#91809=CARTESIAN_POINT('Ctrl Pts',(-144.849418259427,54.4000000000009,191.168614737913));
#91810=CARTESIAN_POINT('Ctrl Pts',(-145.235966560611,54.4000000000015,191.092555288149));
#91811=CARTESIAN_POINT('Ctrl Pts',(-145.622053844564,54.4000000000027,191.01472687048));
#91812=CARTESIAN_POINT('Ctrl Pts',(-147.026899899536,54.4000000000068,190.731534571558));
#91813=CARTESIAN_POINT('Ctrl Pts',(-148.425594625321,54.4000000000174,190.424926443793));
#91814=CARTESIAN_POINT('Ctrl Pts',(-149.816784865909,54.4000000000188,190.089768382214));
#91815=CARTESIAN_POINT('Ctrl Pts',(-150.659099159149,54.4000000000197,189.886842558322));
#91816=CARTESIAN_POINT('Ctrl Pts',(-151.498662621968,54.4000000000172,189.67345160904));
#91817=CARTESIAN_POINT('Ctrl Pts',(-152.33517708753,54.4000000000079,189.448465183433));
#91818=CARTESIAN_POINT('Ctrl Pts',(-152.632968467816,54.4000000000046,189.368372105566));
#91819=CARTESIAN_POINT('Ctrl Pts',(-152.930371223218,54.4000000000044,189.286797587327));
#91820=CARTESIAN_POINT('Ctrl Pts',(-153.227373996649,54.4000000000046,189.203666695846));
#91821=CARTESIAN_POINT('Ctrl Pts',(-154.162302082574,54.4000000000055,188.941980906329));
#91822=CARTESIAN_POINT('Ctrl Pts',(-155.093230768218,54.4000000000157,188.664878378805));
#91823=CARTESIAN_POINT('Ctrl Pts',(-156.019362358089,54.4000000000085,188.370172325145));
#91824=CARTESIAN_POINT('Ctrl Pts',(-156.084148131243,54.400000000008,188.34955672392));
#91825=CARTESIAN_POINT('Ctrl Pts',(-156.148910435088,54.4000000000074,188.328855001875));
#91826=CARTESIAN_POINT('Ctrl Pts',(-156.213648998875,54.4000000000067,188.308066420174));
#91827=CARTESIAN_POINT('Ctrl Pts',(-156.416564746016,54.4000000000046,188.24290694889));
#91828=CARTESIAN_POINT('Ctrl Pts',(-156.619277410847,54.4000000000042,188.176883120644));
#91829=CARTESIAN_POINT('Ctrl Pts',(-156.821789356633,54.4000000000037,188.109962015202));
#91830=CARTESIAN_POINT('Ctrl Pts',(-157.674439769922,54.4000000000014,187.828199336995));
#91831=CARTESIAN_POINT('Ctrl Pts',(-158.523442546846,54.4000000000024,187.530554236109));
#91832=CARTESIAN_POINT('Ctrl Pts',(-159.366711682169,54.4000000000019,187.215315777277));
#91833=CARTESIAN_POINT('Ctrl Pts',(-159.592281282814,54.4000000000018,187.130991318705));
#91834=CARTESIAN_POINT('Ctrl Pts',(-159.817440728344,54.4000000000015,187.045408262957));
#91835=CARTESIAN_POINT('Ctrl Pts',(-160.042150350673,54.4000000000011,186.958534466439));
#91836=CARTESIAN_POINT('Ctrl Pts',(-160.341043440676,54.4000000000005,186.842980992527));
#91837=CARTESIAN_POINT('Ctrl Pts',(-160.638745192439,54.4000000000012,186.725316022465));
#91838=CARTESIAN_POINT('Ctrl Pts',(-160.935217131209,54.400000000002,186.605440002852));
#91839=CARTESIAN_POINT('Ctrl Pts',(-162.043912972633,54.4000000000049,186.157147847507));
#91840=CARTESIAN_POINT('Ctrl Pts',(-163.135358589241,54.4000000000127,185.677949049057));
#91841=CARTESIAN_POINT('Ctrl Pts',(-164.206821641103,54.400000000017,185.162953209131));
#91842=CARTESIAN_POINT('Ctrl Pts',(-165.213812221236,54.400000000021,184.678945889688));
#91843=CARTESIAN_POINT('Ctrl Pts',(-166.203152821026,54.4000000000218,184.163320161186));
#91844=CARTESIAN_POINT('Ctrl Pts',(-167.172599949771,54.4000000000122,183.612061884605));
#91845=CARTESIAN_POINT('Ctrl Pts',(-167.234668705759,54.4000000000116,183.57676762828));
#91846=CARTESIAN_POINT('Ctrl Pts',(-167.296655923169,54.400000000011,183.541327323102));
#91847=CARTESIAN_POINT('Ctrl Pts',(-167.358561016714,54.4000000000103,183.505739922036));
#91848=CARTESIAN_POINT('Ctrl Pts',(-168.394803639309,54.3999999999987,182.910034791816));
#91849=CARTESIAN_POINT('Ctrl Pts',(-169.40790447556,54.4000000000016,182.27289323376));
#91850=CARTESIAN_POINT('Ctrl Pts',(-170.394537845123,54.4000000000013,181.588333408786));
#91851=CARTESIAN_POINT('Ctrl Pts',(-170.521200139063,54.4000000000013,181.500450796617));
#91852=CARTESIAN_POINT('Ctrl Pts',(-170.64742620343,54.4000000000013,181.411786725557));
#91853=CARTESIAN_POINT('Ctrl Pts',(-170.77320899952,54.4000000000012,181.322328563752));
#91854=CARTESIAN_POINT('Ctrl Pts',(-170.892813071244,54.4000000000011,181.237264781316));
#91855=CARTESIAN_POINT('Ctrl Pts',(-171.012017675547,54.4000000000009,181.151481008562));
#91856=CARTESIAN_POINT('Ctrl Pts',(-171.130802550739,54.4000000000005,181.064975846037));
#91857=CARTESIAN_POINT('Ctrl Pts',(-171.508826188153,54.3999999999992,180.789679886513));
#91858=CARTESIAN_POINT('Ctrl Pts',(-171.88264292564,54.3999999999966,180.50705177373));
#91859=CARTESIAN_POINT('Ctrl Pts',(-172.252308598498,54.4000000000004,180.216507814835));
#91860=CARTESIAN_POINT('Ctrl Pts',(-172.303960379812,54.4000000000009,180.175911367481));
#91861=CARTESIAN_POINT('Ctrl Pts',(-172.355531079046,54.4000000000015,180.135160303721));
#91862=CARTESIAN_POINT('Ctrl Pts',(-172.407020808966,54.4000000000023,180.094252958564));
#91863=CARTESIAN_POINT('Ctrl Pts',(-172.455054775837,54.400000000003,180.056091133574));
#91864=CARTESIAN_POINT('Ctrl Pts',(-172.50300769104,54.4000000000036,180.017800247102));
#91865=CARTESIAN_POINT('Ctrl Pts',(-172.550875974858,54.400000000004,179.979382823007));
#91866=CARTESIAN_POINT('Ctrl Pts',(-172.597530076281,54.4000000000044,179.941939859584));
#91867=CARTESIAN_POINT('Ctrl Pts',(-172.644097658006,54.4000000000046,179.904381602988));
#91868=CARTESIAN_POINT('Ctrl Pts',(-172.690571407175,54.4000000000048,179.866713791186));
#91869=CARTESIAN_POINT('Ctrl Pts',(-173.036090107705,54.4000000000061,179.586664653374));
#91870=CARTESIAN_POINT('Ctrl Pts',(-173.376498345685,54.4000000000024,179.300504241468));
#91871=CARTESIAN_POINT('Ctrl Pts',(-173.710509910594,54.4000000000008,179.009174034974));
#91872=CARTESIAN_POINT('Ctrl Pts',(-173.799924385604,54.4000000000004,178.931185305825));
#91873=CARTESIAN_POINT('Ctrl Pts',(-173.888880293489,54.4000000000001,178.852825858204));
#91874=CARTESIAN_POINT('Ctrl Pts',(-173.977352529316,54.4000000000001,178.77411328332));
#91875=CARTESIAN_POINT('Ctrl Pts',(-174.086885484671,54.4000000000001,178.676663265581));
#91876=CARTESIAN_POINT('Ctrl Pts',(-174.195746819395,54.4000000000001,178.578606690771));
#91877=CARTESIAN_POINT('Ctrl Pts',(-174.303919113315,54.4000000000002,178.479960989208));
#91878=CARTESIAN_POINT('Ctrl Pts',(-174.95858512167,54.4000000000008,177.882950559419));
#91879=CARTESIAN_POINT('Ctrl Pts',(-175.588161594654,54.400000000003,177.264237376583));
#91880=CARTESIAN_POINT('Ctrl Pts',(-176.192889081029,54.4000000000052,176.624027636066));
#91881=CARTESIAN_POINT('Ctrl Pts',(-176.801495076758,54.4000000000073,175.9797118155));
#91882=CARTESIAN_POINT('Ctrl Pts',(-177.384932334614,54.4000000000094,175.313622763741));
#91883=CARTESIAN_POINT('Ctrl Pts',(-177.943406073387,54.4000000000095,174.625935886316));
#91884=CARTESIAN_POINT('Ctrl Pts',(-178.443543971493,54.4000000000097,174.01008191584));
#91885=CARTESIAN_POINT('Ctrl Pts',(-178.923660601104,54.4000000000082,173.376906001319));
#91886=CARTESIAN_POINT('Ctrl Pts',(-179.383876297428,54.400000000004,172.726511192075));
#91887=CARTESIAN_POINT('Ctrl Pts',(-179.775881961457,54.4000000000004,172.172513466411));
#91888=CARTESIAN_POINT('Ctrl Pts',(-180.153586615473,54.3999999999974,171.606136536174));
#91889=CARTESIAN_POINT('Ctrl Pts',(-180.517306782578,54.4000000000037,171.027671453041));
#91890=CARTESIAN_POINT('Ctrl Pts',(-180.773257799144,54.4000000000081,170.620603768963));
#91891=CARTESIAN_POINT('Ctrl Pts',(-181.022282062403,54.4000000000033,170.207421858588));
#91892=CARTESIAN_POINT('Ctrl Pts',(-181.263216116216,54.4000000000031,169.790864332171));
#91893=CARTESIAN_POINT('Ctrl Pts',(-181.364433682584,54.400000000003,169.615866491854));
#91894=CARTESIAN_POINT('Ctrl Pts',(-181.464223290182,54.4000000000036,169.440273105744));
#91895=CARTESIAN_POINT('Ctrl Pts',(-181.562498312604,54.4000000000056,169.264287803901));
#91896=CARTESIAN_POINT('Ctrl Pts',(-181.963797855854,54.4000000000141,168.545663483017));
#91897=CARTESIAN_POINT('Ctrl Pts',(-182.341570248312,54.4000000000098,167.817937559455));
#91898=CARTESIAN_POINT('Ctrl Pts',(-182.698076436423,54.4000000000056,167.081983790314));
#91899=CARTESIAN_POINT('Ctrl Pts',(-182.931095611984,54.4000000000029,166.600950511637));
#91900=CARTESIAN_POINT('Ctrl Pts',(-183.155029566892,54.4,166.116402350166));
#91901=CARTESIAN_POINT('Ctrl Pts',(-183.370511496512,54.4,165.628584399065));
#91902=CARTESIAN_POINT('Ctrl Pts',(-183.755753296777,54.4,164.756456207084));
#91903=CARTESIAN_POINT('Ctrl Pts',(-184.114155896939,54.4,163.873944120111));
#91904=CARTESIAN_POINT('Ctrl Pts',(-184.448595887359,54.4,162.982161533304));
#91905=CARTESIAN_POINT('Ctrl Pts',(-184.791126771316,54.4,162.06880461874));
#91906=CARTESIAN_POINT('Ctrl Pts',(-185.10852159876,54.4,161.145723295192));
#91907=CARTESIAN_POINT('Ctrl Pts',(-185.403901993162,54.4,160.214125497789));
#91908=CARTESIAN_POINT('Ctrl Pts',(-185.613942467716,54.4,159.551680571965));
#91909=CARTESIAN_POINT('Ctrl Pts',(-185.812852196925,54.4,158.884929610429));
#91910=CARTESIAN_POINT('Ctrl Pts',(-186.001762645606,54.4,158.214310293893));
#91911=CARTESIAN_POINT('Ctrl Pts',(-186.020018321289,54.4,158.149503879878));
#91912=CARTESIAN_POINT('Ctrl Pts',(-186.038180629918,54.4,158.084661317201));
#91913=CARTESIAN_POINT('Ctrl Pts',(-186.056250572068,54.4,158.019783088719));
#91914=CARTESIAN_POINT('Ctrl Pts',(-186.248767714115,54.4,157.328570520082));
#91915=CARTESIAN_POINT('Ctrl Pts',(-186.430890122847,54.4,156.632354201029));
#91916=CARTESIAN_POINT('Ctrl Pts',(-186.603184662211,54.4,155.933322726759));
#91917=CARTESIAN_POINT('Ctrl Pts',(-186.726566778214,54.4,155.432738188409));
#91918=CARTESIAN_POINT('Ctrl Pts',(-186.844909102226,54.4,154.930710225721));
#91919=CARTESIAN_POINT('Ctrl Pts',(-186.958421160883,54.4,154.42804577865));
#91920=CARTESIAN_POINT('Ctrl Pts',(-186.98407601225,54.4,154.314438626865));
#91921=CARTESIAN_POINT('Ctrl Pts',(-187.009484169709,54.4,154.200798819904));
#91922=CARTESIAN_POINT('Ctrl Pts',(-187.034647948172,54.4,154.087136197121));
#91923=CARTESIAN_POINT('Ctrl Pts',(-187.249235148189,54.4,153.117864272993));
#91924=CARTESIAN_POINT('Ctrl Pts',(-187.446091441865,54.400000000005,152.147366918553));
#91925=CARTESIAN_POINT('Ctrl Pts',(-187.627848434952,54.4000000000063,151.175803321643));
#91926=CARTESIAN_POINT('Ctrl Pts',(-187.693091593958,54.4000000000068,150.827052623469));
#91927=CARTESIAN_POINT('Ctrl Pts',(-187.756389401055,54.4000000000069,150.478164329375));
#91928=CARTESIAN_POINT('Ctrl Pts',(-187.817864007364,54.4000000000059,150.129146500694));
#91929=CARTESIAN_POINT('Ctrl Pts',(-188.06963015802,54.4000000000017,148.699761580444));
#91930=CARTESIAN_POINT('Ctrl Pts',(-188.291104422212,54.4000000000111,147.268244123339));
#91931=CARTESIAN_POINT('Ctrl Pts',(-188.488029538762,54.4000000000176,145.834998333236));
#91932=CARTESIAN_POINT('Ctrl Pts',(-188.65465881123,54.400000000023,144.622249510451));
#91933=CARTESIAN_POINT('Ctrl Pts',(-188.803712723298,54.400000000027,143.408263309562));
#91934=CARTESIAN_POINT('Ctrl Pts',(-188.938699247615,54.4000000000176,142.193285856766));
#91935=CARTESIAN_POINT('Ctrl Pts',(-189.136760811129,54.4000000000038,140.410586915872));
#91936=CARTESIAN_POINT('Ctrl Pts',(-189.30429973454,54.4000000000006,138.625739732878));
#91937=CARTESIAN_POINT('Ctrl Pts',(-189.448306971578,54.4000000000001,136.839235864604));
#91938=CARTESIAN_POINT('Ctrl Pts',(-189.518148388495,54.3999999999998,135.972807454108));
#91939=CARTESIAN_POINT('Ctrl Pts',(-189.582455734489,54.4000000000004,135.105989435971));
#91940=CARTESIAN_POINT('Ctrl Pts',(-189.642030732453,54.4000000000003,134.238837995223));
#91941=CARTESIAN_POINT('Ctrl Pts',(-189.792507883552,54.4,132.048548732355));
#91942=CARTESIAN_POINT('Ctrl Pts',(-189.912606434434,54.4000000000252,129.856120468085));
#91943=CARTESIAN_POINT('Ctrl Pts',(-190.010855951794,54.4000000000233,127.662154066557));
#91944=CARTESIAN_POINT('Ctrl Pts',(-190.031601867449,54.4000000000229,127.198886224246));
#91945=CARTESIAN_POINT('Ctrl Pts',(-190.051373788504,54.4000000000214,126.735549820195));
#91946=CARTESIAN_POINT('Ctrl Pts',(-190.070252291175,54.4000000000179,126.272150491644));
#91947=CARTESIAN_POINT('Ctrl Pts',(-190.155978565131,54.4000000000021,124.167878850857));
#91948=CARTESIAN_POINT('Ctrl Pts',(-190.223187321394,54.4000000000231,122.062303121466));
#91949=CARTESIAN_POINT('Ctrl Pts',(-190.277034909484,54.4000000000263,119.95578683131));
#91950=CARTESIAN_POINT('Ctrl Pts',(-190.291163394482,54.4000000000271,119.403080853939));
#91951=CARTESIAN_POINT('Ctrl Pts',(-190.3043721644,54.4000000000267,118.850310089037));
#91952=CARTESIAN_POINT('Ctrl Pts',(-190.316754563799,54.4000000000241,118.297481238444));
#91953=CARTESIAN_POINT('Ctrl Pts',(-190.397155294802,54.4000000000074,114.707882625582));
#91954=CARTESIAN_POINT('Ctrl Pts',(-190.443516400857,54.4000000000024,111.11588653346));
#91955=CARTESIAN_POINT('Ctrl Pts',(-190.471166976935,54.4000000000008,107.522573212351));
#91956=CARTESIAN_POINT('Ctrl Pts',(-190.484470217798,54.4,105.793758866144));
#91957=CARTESIAN_POINT('Ctrl Pts',(-190.49344330146,54.4,104.064639655677));
#91958=CARTESIAN_POINT('Ctrl Pts',(-190.499797482064,54.4,102.335336081498));
#91959=CARTESIAN_POINT('Origin',(-189.5,59.,41.));
#91960=CARTESIAN_POINT('',(-190.5,51.8013867006572,41.));
#91961=CARTESIAN_POINT('',(-190.5,51.8013867006572,41.));
#91962=CARTESIAN_POINT('',(-189.5,51.8013867006572,40.));
#91963=CARTESIAN_POINT('',(-189.5,54.9,40.));
#91964=CARTESIAN_POINT('Origin',(-189.5,51.8013867006572,41.));
#91965=CARTESIAN_POINT('Ctrl Pts',(7.71069817591099E-15,-3.96262874552467,
41.));
#91966=CARTESIAN_POINT('Ctrl Pts',(7.71069817591099E-15,-3.96262874552467,
40.));
#91967=CARTESIAN_POINT('Ctrl Pts',(7.58040827681699E-15,-2.96262874552467,
40.));
#91968=CARTESIAN_POINT('Ctrl Pts',(-8.85050807869572,-3.96262874552467,
41.));
#91969=CARTESIAN_POINT('Ctrl Pts',(-8.85050807869562,-3.96262874563983,
40.));
#91970=CARTESIAN_POINT('Ctrl Pts',(-8.85149033058515,-2.96262874562831,
40.));
#91971=CARTESIAN_POINT('Ctrl Pts',(-17.7049033029141,-3.9725981542643,41.));
#91972=CARTESIAN_POINT('Ctrl Pts',(-17.7049033029142,-3.97259815428753,
40.));
#91973=CARTESIAN_POINT('Ctrl Pts',(-17.7032012684101,-2.97258723674239,
40.));
#91974=CARTESIAN_POINT('Ctrl Pts',(-35.4141298351867,-3.85438528439772,
41.));
#91975=CARTESIAN_POINT('Ctrl Pts',(-35.4141298351865,-3.85438528437448,
40.));
#91976=CARTESIAN_POINT('Ctrl Pts',(-35.4024817399098,-2.85444075890724,
40.));
#91977=CARTESIAN_POINT('Ctrl Pts',(-44.2690343362197,-3.7290091962045,41.));
#91978=CARTESIAN_POINT('Ctrl Pts',(-44.2690343362206,-3.72900919623712,
40.));
#91979=CARTESIAN_POINT('Ctrl Pts',(-44.2500950804588,-2.72914237565843,
40.));
#91980=CARTESIAN_POINT('Ctrl Pts',(-61.975684001311,-3.22335878785305,41.));
#91981=CARTESIAN_POINT('Ctrl Pts',(-61.9756840013101,-3.22335878782043,
40.));
#91982=CARTESIAN_POINT('Ctrl Pts',(-61.9375323490691,-2.22404061740319,
40.));
#91983=CARTESIAN_POINT('Ctrl Pts',(-70.8274773375622,-2.8447952216319,41.));
#91984=CARTESIAN_POINT('Ctrl Pts',(-70.8274773375648,-2.84479522167177,
40.));
#91985=CARTESIAN_POINT('Ctrl Pts',(-70.7774082065636,-1.84593393742596,
40.));
#91986=CARTESIAN_POINT('Ctrl Pts',(-84.1008785865341,-1.97714572979944,
41.));
#91987=CARTESIAN_POINT('Ctrl Pts',(-84.1008785865328,-1.97714572977952,
40.));
#91988=CARTESIAN_POINT('Ctrl Pts',(-84.0280706662548,-0.979770824085102,
40.));
#91989=CARTESIAN_POINT('Ctrl Pts',(-88.5246348023096,-1.63762966081861,
41.));
#91990=CARTESIAN_POINT('Ctrl Pts',(-88.5246348023124,-1.63762966084928,
40.0000000000001));
#91991=CARTESIAN_POINT('Ctrl Pts',(-88.4434228779164,-0.640887452776137,
40.0000000000001));
#91992=CARTESIAN_POINT('Ctrl Pts',(-97.3704217853518,-0.832166707467492,
41.));
#91993=CARTESIAN_POINT('Ctrl Pts',(-97.370421785349,-0.832166707436793,
40.0000000000001));
#91994=CARTESIAN_POINT('Ctrl Pts',(-97.2702717928855,0.162851073824349,
40.0000000000001));
#91995=CARTESIAN_POINT('Ctrl Pts',(-101.788182438523,-0.366638907835244,
41.));
#91996=CARTESIAN_POINT('Ctrl Pts',(-101.788182438527,-0.36663890786983,
40.));
#91997=CARTESIAN_POINT('Ctrl Pts',(-101.677510051103,0.627290636601703,
40.));
#91998=CARTESIAN_POINT('Ctrl Pts',(-110.595154903837,0.721257750102517,
41.));
#91999=CARTESIAN_POINT('Ctrl Pts',(-110.595154903833,0.721257750137102,
40.));
#92000=CARTESIAN_POINT('Ctrl Pts',(-110.460637374487,1.71224178179782,40.));
#92001=CARTESIAN_POINT('Ctrl Pts',(-114.986445334228,1.34357196524849,41.));
#92002=CARTESIAN_POINT('Ctrl Pts',(-114.986445334236,1.34357196519969,40.));
#92003=CARTESIAN_POINT('Ctrl Pts',(-114.838608995725,2.33270535868658,40.));
#92004=CARTESIAN_POINT('Ctrl Pts',(-123.73794201961,2.79063399912821,41.));
#92005=CARTESIAN_POINT('Ctrl Pts',(-123.737942019602,2.79063399917701,40.));
#92006=CARTESIAN_POINT('Ctrl Pts',(-123.559508040824,3.77470806565397,40.));
#92007=CARTESIAN_POINT('Ctrl Pts',(-128.098212002788,3.61490182217767,41.0000000001842));
#92008=CARTESIAN_POINT('Ctrl Pts',(-128.098212002812,3.61490182216112,40.0000000002763));
#92009=CARTESIAN_POINT('Ctrl Pts',(-127.902516032675,4.5957849159024,40.));
#92010=CARTESIAN_POINT('Ctrl Pts',(-134.607986242742,5.05437483435604,40.9999999999079));
#92011=CARTESIAN_POINT('Ctrl Pts',(-134.607986242731,5.05437483436432,39.9999999998619));
#92012=CARTESIAN_POINT('Ctrl Pts',(-134.381970283735,6.02855342450368,40.));
#92013=CARTESIAN_POINT('Ctrl Pts',(-136.772776373825,5.56826329016615,41.0000000000307));
#92014=CARTESIAN_POINT('Ctrl Pts',(-136.772776373836,5.56826329013963,40.0000000000461));
#92015=CARTESIAN_POINT('Ctrl Pts',(-136.535908314328,6.53988132256591,40.));
#92016=CARTESIAN_POINT('Ctrl Pts',(-141.090337531917,6.67665701106583,40.9999999999692));
#92017=CARTESIAN_POINT('Ctrl Pts',(-141.090337531907,6.67665701109232,39.9999999999538));
#92018=CARTESIAN_POINT('Ctrl Pts',(-140.829896351113,7.64222340961483,40.));
#92019=CARTESIAN_POINT('Ctrl Pts',(-143.245640919778,7.27188104593143,40.999999999815));
#92020=CARTESIAN_POINT('Ctrl Pts',(-143.245640919832,7.27188104576561,39.9999999997225));
#92021=CARTESIAN_POINT('Ctrl Pts',(-142.972463556223,8.23395393721191,40.));
#92022=CARTESIAN_POINT('Ctrl Pts',(-149.671568403027,9.19757481923777,41.00000000037));
#92023=CARTESIAN_POINT('Ctrl Pts',(-149.67156840292,9.19757481956941,40.000000000555));
#92024=CARTESIAN_POINT('Ctrl Pts',(-149.356734736723,10.1471643326025,40.));
#92025=CARTESIAN_POINT('Ctrl Pts',(-153.892282124603,10.6608124936544,41.));
#92026=CARTESIAN_POINT('Ctrl Pts',(-153.892282124687,10.660812493454,40.0000000000001));
#92027=CARTESIAN_POINT('Ctrl Pts',(-153.545256591485,11.5996387774958,40.0000000000001));
#92028=CARTESIAN_POINT('Ctrl Pts',(-160.084751714187,13.254997283011,41.));
#92029=CARTESIAN_POINT('Ctrl Pts',(-160.084751714145,13.2549972831112,40.0000000000001));
#92030=CARTESIAN_POINT('Ctrl Pts',(-159.678679400237,14.1690873519471,40.0000000000001));
#92031=CARTESIAN_POINT('Ctrl Pts',(-162.125908453503,14.187144173683,41.));
#92032=CARTESIAN_POINT('Ctrl Pts',(-162.125908453557,14.1871441735757,40.));
#92033=CARTESIAN_POINT('Ctrl Pts',(-161.69833306059,15.0915173718029,40.));
#92034=CARTESIAN_POINT('Ctrl Pts',(-166.147967957112,16.2216704183731,41.));
#92035=CARTESIAN_POINT('Ctrl Pts',(-166.147967957058,16.2216704184803,40.));
#92036=CARTESIAN_POINT('Ctrl Pts',(-165.672785207306,17.1019618206062,40.));
#92037=CARTESIAN_POINT('Ctrl Pts',(-168.107616958799,17.3133889676838,41.0000000000612));
#92038=CARTESIAN_POINT('Ctrl Pts',(-168.107616958864,17.3133889675427,40.0000000000764));
#92039=CARTESIAN_POINT('Ctrl Pts',(-167.606564886958,18.1794445808324,40.0000000000001));
#92040=CARTESIAN_POINT('Ctrl Pts',(-171.901224347846,19.6798162046833,40.9999999999389));
#92041=CARTESIAN_POINT('Ctrl Pts',(-171.901224347781,19.6798162048244,39.9999999999236));
#92042=CARTESIAN_POINT('Ctrl Pts',(-171.343751302672,20.5106767876529,40.0000000000001));
#92043=CARTESIAN_POINT('Ctrl Pts',(-173.735371451672,20.9542971278746,41.0000000000305));
#92044=CARTESIAN_POINT('Ctrl Pts',(-173.7353714518,20.9542971276705,40.0000000000305));
#92045=CARTESIAN_POINT('Ctrl Pts',(-173.147319647996,21.7642077357057,40.));
#92046=CARTESIAN_POINT('Ctrl Pts',(-177.244885717175,23.73437233231,40.9999999999695));
#92047=CARTESIAN_POINT('Ctrl Pts',(-177.244885717047,23.7343723325141,39.9999999999695));
#92048=CARTESIAN_POINT('Ctrl Pts',(-176.591062187867,24.4921816156992,40.));
#92049=CARTESIAN_POINT('Ctrl Pts',(-178.920625669167,25.2395538542272,40.9999999998762));
#92050=CARTESIAN_POINT('Ctrl Pts',(-178.920625669525,25.239553853915,39.9999999998375));
#92051=CARTESIAN_POINT('Ctrl Pts',(-178.231553296469,25.9661960735548,39.9999999999999));
#92052=CARTESIAN_POINT('Ctrl Pts',(-181.276582615106,27.724368039953,41.0000000000618));
#92053=CARTESIAN_POINT('Ctrl Pts',(-181.276582614927,27.724368040109,40.0000000000811));
#92054=CARTESIAN_POINT('Ctrl Pts',(-180.532610330637,28.3931076402081,39.9999999999999));
#92055=CARTESIAN_POINT('Ctrl Pts',(-182.038370134922,28.594995197168,41.000000000031));
#92056=CARTESIAN_POINT('Ctrl Pts',(-182.038370135018,28.5949951971027,40.0000000000465));
#92057=CARTESIAN_POINT('Ctrl Pts',(-181.275699297888,29.2424485691571,40.));
#92058=CARTESIAN_POINT('Ctrl Pts',(-183.470925423842,30.3865407544758,40.999999999969));
#92059=CARTESIAN_POINT('Ctrl Pts',(-183.470925423746,30.386540754541,39.9999999999534));
#92060=CARTESIAN_POINT('Ctrl Pts',(-182.671568980253,30.9881153143562,40.));
#92061=CARTESIAN_POINT('Ctrl Pts',(-184.144844526056,31.3102252938863,41.0000000000001));
#92062=CARTESIAN_POINT('Ctrl Pts',(-184.144844526143,31.3102252938285,40.0000000000001));
#92063=CARTESIAN_POINT('Ctrl Pts',(-183.327437398454,31.8871479480862,40.0000000000001));
#92064=CARTESIAN_POINT('Ctrl Pts',(-186.030824239729,34.1695586767068,41.0000000000001));
#92065=CARTESIAN_POINT('Ctrl Pts',(-186.030824239554,34.1695586768225,40.0000000000001));
#92066=CARTESIAN_POINT('Ctrl Pts',(-185.161335117964,34.6675198327877,40.0000000000001));
#92067=CARTESIAN_POINT('Ctrl Pts',(-187.108035248898,36.1953798490653,40.9999999997501));
#92068=CARTESIAN_POINT('Ctrl Pts',(-187.108035248771,36.1953798491075,39.999999999625));
#92069=CARTESIAN_POINT('Ctrl Pts',(-186.20661784616,36.6337883765426,40.));
#92070=CARTESIAN_POINT('Ctrl Pts',(-188.84587319312,40.4985477363864,41.00000000025));
#92071=CARTESIAN_POINT('Ctrl Pts',(-188.845873193246,40.4985477363443,40.0000000003749));
#92072=CARTESIAN_POINT('Ctrl Pts',(-187.89280993586,40.8090727718468,40.));
#92073=CARTESIAN_POINT('Ctrl Pts',(-189.476816493,42.70183971556,41.));
#92074=CARTESIAN_POINT('Ctrl Pts',(-189.476816492796,42.7018397155975,40.));
#92075=CARTESIAN_POINT('Ctrl Pts',(-188.505057255412,42.9465120076084,40.));
#92076=CARTESIAN_POINT('Ctrl Pts',(-190.097254322749,46.0714373593176,41.));
#92077=CARTESIAN_POINT('Ctrl Pts',(-190.09725432285,46.0714373592989,40.));
#92078=CARTESIAN_POINT('Ctrl Pts',(-189.107932516311,46.2207273442081,40.));
#92079=CARTESIAN_POINT('Ctrl Pts',(-190.249747513175,47.205433603925,41.));
#92080=CARTESIAN_POINT('Ctrl Pts',(-190.249747513114,47.2054336039303,40.));
#92081=CARTESIAN_POINT('Ctrl Pts',(-189.256273490598,47.3234827160453,40.));
#92082=CARTESIAN_POINT('Ctrl Pts',(-190.451241426909,49.4932627877844,41.));
#92083=CARTESIAN_POINT('Ctrl Pts',(-190.451241426969,49.4932627877791,40.));
#92084=CARTESIAN_POINT('Ctrl Pts',(-189.452427308737,49.5506786699904,40.));
#92085=CARTESIAN_POINT('Ctrl Pts',(-190.5,50.6495849457038,40.9999999998129));
#92086=CARTESIAN_POINT('Ctrl Pts',(-190.500000000406,50.6495849457076,39.9999999997193));
#92087=CARTESIAN_POINT('Ctrl Pts',(-189.500000000281,50.6775460919873,40.));
#92088=CARTESIAN_POINT('Ctrl Pts',(-190.5,51.8013867006572,41.));
#92089=CARTESIAN_POINT('Ctrl Pts',(-190.5,51.8013867006572,40.));
#92090=CARTESIAN_POINT('Ctrl Pts',(-189.5,51.8013867006572,40.));
#92091=CARTESIAN_POINT('',(7.58040827681699E-15,-2.96262874552467,40.));
#92092=CARTESIAN_POINT('',(7.71069817591099E-15,-3.96262874552467,41.));
#92093=CARTESIAN_POINT('Origin',(7.58040827681699E-15,-2.96262874552467,
41.));
#92094=CARTESIAN_POINT('Ctrl Pts',(-190.5,51.8013867006571,41.));
#92095=CARTESIAN_POINT('Ctrl Pts',(-190.5,51.1173208557555,40.9999999998888));
#92096=CARTESIAN_POINT('Ctrl Pts',(-190.482804508878,50.4323861127385,40.9999999999097));
#92097=CARTESIAN_POINT('Ctrl Pts',(-190.447827838384,49.749902987648,40.9999999999442));
#92098=CARTESIAN_POINT('Ctrl Pts',(-190.423824777408,49.2815426824526,40.9999999999678));
#92099=CARTESIAN_POINT('Ctrl Pts',(-190.391446880902,48.8143355445067,40.9999999999977));
#92100=CARTESIAN_POINT('Ctrl Pts',(-190.350494470042,48.3493481958547,40.9999999999965));
#92101=CARTESIAN_POINT('Ctrl Pts',(-190.291195016811,47.6760424012827,40.9999999999947));
#92102=CARTESIAN_POINT('Ctrl Pts',(-190.214000398395,47.0065391729747,40.9999999999964));
#92103=CARTESIAN_POINT('Ctrl Pts',(-190.11844385301,46.3409947367191,40.9999999999979));
#92104=CARTESIAN_POINT('Ctrl Pts',(-190.055206160698,45.9005487776227,40.999999999999));
#92105=CARTESIAN_POINT('Ctrl Pts',(-189.983926901072,45.4618373621409,41.0000000000006));
#92106=CARTESIAN_POINT('Ctrl Pts',(-189.904470540969,45.0249032275489,40.9999999999998));
#92107=CARTESIAN_POINT('Ctrl Pts',(-189.899822264666,44.9993421449489,40.9999999999998));
#92108=CARTESIAN_POINT('Ctrl Pts',(-189.89514599803,44.9737871160482,40.9999999999997));
#92109=CARTESIAN_POINT('Ctrl Pts',(-189.890441712832,44.9482381447317,40.9999999999996));
#92110=CARTESIAN_POINT('Ctrl Pts',(-189.738971319567,44.1256024900784,40.9999999999961));
#92111=CARTESIAN_POINT('Ctrl Pts',(-189.558451814601,43.309235270496,40.9999999999954));
#92112=CARTESIAN_POINT('Ctrl Pts',(-189.347911931431,42.4993478242337,40.9999999999948));
#92113=CARTESIAN_POINT('Ctrl Pts',(-189.165422479056,41.7973624600857,40.9999999999943));
#92114=CARTESIAN_POINT('Ctrl Pts',(-188.960378432237,41.1002453485348,40.9999999999939));
#92115=CARTESIAN_POINT('Ctrl Pts',(-188.732115344505,40.4081401060491,40.999999999992));
#92116=CARTESIAN_POINT('Ctrl Pts',(-188.617983800639,40.0620874848063,40.9999999999911));
#92117=CARTESIAN_POINT('Ctrl Pts',(-188.498047016744,39.7172879245513,40.9999999999898));
#92118=CARTESIAN_POINT('Ctrl Pts',(-188.3722189604,39.3737599806281,40.9999999999879));
#92119=CARTESIAN_POINT('Ctrl Pts',(-188.295438183618,39.1641378729073,40.9999999999868));
#92120=CARTESIAN_POINT('Ctrl Pts',(-188.216463758887,38.9549892582146,40.9999999999854));
#92121=CARTESIAN_POINT('Ctrl Pts',(-188.135275760166,38.7463184326317,40.9999999999838));
#92122=CARTESIAN_POINT('Ctrl Pts',(-188.101465942341,38.6594198428209,40.9999999999831));
#92123=CARTESIAN_POINT('Ctrl Pts',(-188.067273383454,38.5726068818537,40.9999999999828));
#92124=CARTESIAN_POINT('Ctrl Pts',(-188.032688393693,38.485859497833,40.99999999998));
#92125=CARTESIAN_POINT('Ctrl Pts',(-188.014221711024,38.4395406634451,40.9999999999785));
#92126=CARTESIAN_POINT('Ctrl Pts',(-187.99564365788,38.3932418618882,40.9999999999765));
#92127=CARTESIAN_POINT('Ctrl Pts',(-187.976954221009,38.3469637927259,40.9999999999739));
#92128=CARTESIAN_POINT('Ctrl Pts',(-187.868393712879,38.0781504123006,40.9999999999589));
#92129=CARTESIAN_POINT('Ctrl Pts',(-187.7565374796,37.8111930698997,40.9999999999416));
#92130=CARTESIAN_POINT('Ctrl Pts',(-187.641486166773,37.5461991512206,40.9999999999268));
#92131=CARTESIAN_POINT('Ctrl Pts',(-187.571160560859,37.3842204876452,40.9999999999178));
#92132=CARTESIAN_POINT('Ctrl Pts',(-187.499641397824,37.2229752862343,40.9999999999097));
#92133=CARTESIAN_POINT('Ctrl Pts',(-187.426953737642,37.0624868083052,40.9999999999037));
#92134=CARTESIAN_POINT('Ctrl Pts',(-187.379481793659,36.957672593416,40.9999999998998));
#92135=CARTESIAN_POINT('Ctrl Pts',(-187.331507172533,36.8531715415705,40.9999999998967));
#92136=CARTESIAN_POINT('Ctrl Pts',(-187.283032855265,36.7489815473987,40.9999999998944));
#92137=CARTESIAN_POINT('Ctrl Pts',(-187.00428820088,36.1498518318543,40.9999999998812));
#92138=CARTESIAN_POINT('Ctrl Pts',(-186.70902499862,35.5610077961926,40.9999999998937));
#92139=CARTESIAN_POINT('Ctrl Pts',(-186.397799748604,34.9821024060981,40.9999999999139));
#92140=CARTESIAN_POINT('Ctrl Pts',(-186.147394527304,34.5163274334359,40.9999999999302));
#92141=CARTESIAN_POINT('Ctrl Pts',(-185.886655271096,34.0569865721678,40.9999999999514));
#92142=CARTESIAN_POINT('Ctrl Pts',(-185.615851289347,33.6039114545961,40.9999999999676));
#92143=CARTESIAN_POINT('Ctrl Pts',(-185.43368915347,33.2991407101028,40.9999999999785));
#92144=CARTESIAN_POINT('Ctrl Pts',(-185.246972491802,32.9972053740416,40.9999999999872));
#92145=CARTESIAN_POINT('Ctrl Pts',(-185.055779072472,32.6980570974861,40.9999999999907));
#92146=CARTESIAN_POINT('Ctrl Pts',(-184.962742517282,32.5524886713373,40.9999999999924));
#92147=CARTESIAN_POINT('Ctrl Pts',(-184.868646723106,32.4075816278813,40.9999999999931));
#92148=CARTESIAN_POINT('Ctrl Pts',(-184.773504430614,32.2633364214931,40.9999999999929));
#92149=CARTESIAN_POINT('Ctrl Pts',(-184.458585155278,31.7858873851478,40.999999999992));
#92150=CARTESIAN_POINT('Ctrl Pts',(-184.132137181499,31.3155633445286,40.9999999999869));
#92151=CARTESIAN_POINT('Ctrl Pts',(-183.794494884448,30.8522043465452,40.9999999999853));
#92152=CARTESIAN_POINT('Ctrl Pts',(-183.591224917035,30.5732494607284,40.9999999999844));
#92153=CARTESIAN_POINT('Ctrl Pts',(-183.383897782516,30.2968189244016,40.9999999999847));
#92154=CARTESIAN_POINT('Ctrl Pts',(-183.172587081022,30.0228774709136,40.9999999999881));
#92155=CARTESIAN_POINT('Ctrl Pts',(-183.108845303359,29.9402431551997,40.9999999999891));
#92156=CARTESIAN_POINT('Ctrl Pts',(-183.044739012704,29.857832773681,40.9999999999905));
#92157=CARTESIAN_POINT('Ctrl Pts',(-182.980283594838,29.7756622281338,40.9999999999917));
#92158=CARTESIAN_POINT('Ctrl Pts',(-182.905546559319,29.6803842331343,40.999999999993));
#92159=CARTESIAN_POINT('Ctrl Pts',(-182.830335932828,29.5854231532485,40.9999999999942));
#92160=CARTESIAN_POINT('Ctrl Pts',(-182.754647779382,29.4907679758219,40.9999999999957));
#92161=CARTESIAN_POINT('Ctrl Pts',(-182.575856472569,29.2671725768292,40.9999999999991));
#92162=CARTESIAN_POINT('Ctrl Pts',(-182.394204884809,29.0451111870287,40.9999999999999));
#92163=CARTESIAN_POINT('Ctrl Pts',(-182.209929929983,28.8247353866391,41.0000000000001));
#92164=CARTESIAN_POINT('Ctrl Pts',(-182.12072133944,28.7180501642158,41.0000000000002));
#92165=CARTESIAN_POINT('Ctrl Pts',(-182.030898854479,28.6117613402199,41.0000000000002));
#92166=CARTESIAN_POINT('Ctrl Pts',(-181.940484260319,28.5058818454224,41.0000000000001));
#92167=CARTESIAN_POINT('Ctrl Pts',(-181.717534007252,28.2447972231964,41.0000000000001));
#92168=CARTESIAN_POINT('Ctrl Pts',(-181.491000481348,27.9862289912591,40.9999999999999));
#92169=CARTESIAN_POINT('Ctrl Pts',(-181.261802368934,27.7310307756614,40.9999999999976));
#92170=CARTESIAN_POINT('Ctrl Pts',(-181.198338976531,27.6603681322122,40.999999999997));
#92171=CARTESIAN_POINT('Ctrl Pts',(-181.134671516089,27.5899636589942,40.9999999999962));
#92172=CARTESIAN_POINT('Ctrl Pts',(-181.070819954649,27.5198349571244,40.9999999999952));
#92173=CARTESIAN_POINT('Ctrl Pts',(-181.018712159623,27.4626045317426,40.9999999999944));
#92174=CARTESIAN_POINT('Ctrl Pts',(-180.966481760453,27.4055577608882,40.9999999999934));
#92175=CARTESIAN_POINT('Ctrl Pts',(-180.914139683862,27.3487040801191,40.9999999999924));
#92176=CARTESIAN_POINT('Ctrl Pts',(-180.883283615482,27.315188385371,40.9999999999917));
#92177=CARTESIAN_POINT('Ctrl Pts',(-180.852387969248,27.2817389335116,40.999999999991));
#92178=CARTESIAN_POINT('Ctrl Pts',(-180.821445495686,27.2483474710294,40.9999999999902));
#92179=CARTESIAN_POINT('Ctrl Pts',(-180.711921869605,27.1301554317317,40.9999999999871));
#92180=CARTESIAN_POINT('Ctrl Pts',(-180.601840652286,27.0127215882594,40.9999999999823));
#92181=CARTESIAN_POINT('Ctrl Pts',(-180.491263633126,26.8960966447111,40.9999999999755));
#92182=CARTESIAN_POINT('Ctrl Pts',(-179.98837410592,26.3657019644473,40.9999999999445));
#92183=CARTESIAN_POINT('Ctrl Pts',(-179.474102428684,25.8501900736901,40.9999999999326));
#92184=CARTESIAN_POINT('Ctrl Pts',(-178.949364837618,25.3485900212007,40.9999999999311));
#92185=CARTESIAN_POINT('Ctrl Pts',(-178.394722254172,24.8184035933437,40.9999999999295));
#92186=CARTESIAN_POINT('Ctrl Pts',(-177.828386861868,24.3037598681548,40.9999999999397));
#92187=CARTESIAN_POINT('Ctrl Pts',(-177.251475858342,23.8034620495015,40.9999999999514));
#92188=CARTESIAN_POINT('Ctrl Pts',(-176.940781259065,23.5340273718199,40.9999999999577));
#92189=CARTESIAN_POINT('Ctrl Pts',(-176.62701995777,23.268752659544,40.9999999999644));
#92190=CARTESIAN_POINT('Ctrl Pts',(-176.310370263142,23.007445530886,40.99999999997));
#92191=CARTESIAN_POINT('Ctrl Pts',(-176.09830532097,22.8324443163949,40.9999999999737));
#92192=CARTESIAN_POINT('Ctrl Pts',(-175.884949396412,22.6592259929049,40.9999999999767));
#92193=CARTESIAN_POINT('Ctrl Pts',(-175.670328039924,22.4877094396632,40.9999999999798));
#92194=CARTESIAN_POINT('Ctrl Pts',(-175.610359698279,22.4397852096096,40.9999999999807));
#92195=CARTESIAN_POINT('Ctrl Pts',(-175.550292866756,22.3919940974155,40.9999999999815));
#92196=CARTESIAN_POINT('Ctrl Pts',(-175.490128584424,22.3443347300923,40.9999999999823));
#92197=CARTESIAN_POINT('Ctrl Pts',(-174.688956926142,21.7096835239187,40.9999999999932));
#92198=CARTESIAN_POINT('Ctrl Pts',(-173.870424468313,21.0984838183586,40.9999999999862));
#92199=CARTESIAN_POINT('Ctrl Pts',(-173.036110998015,20.5086051060234,40.9999999999796));
#92200=CARTESIAN_POINT('Ctrl Pts',(-172.184479498597,19.9064821508693,40.9999999999728));
#92201=CARTESIAN_POINT('Ctrl Pts',(-171.316405856158,19.326574818821,40.9999999999649));
#92202=CARTESIAN_POINT('Ctrl Pts',(-170.433598454822,18.7665715747235,40.9999999999801));
#92203=CARTESIAN_POINT('Ctrl Pts',(-170.290921642194,18.6760654486893,40.9999999999825));
#92204=CARTESIAN_POINT('Ctrl Pts',(-170.147859942551,18.5860790675574,40.9999999999858));
#92205=CARTESIAN_POINT('Ctrl Pts',(-170.004420653322,18.4966025861836,40.99999999999));
#92206=CARTESIAN_POINT('Ctrl Pts',(-169.057564734203,17.9059601166997,41.0000000000176));
#92207=CARTESIAN_POINT('Ctrl Pts',(-168.094206320727,17.3375962595065,41.0000000000171));
#92208=CARTESIAN_POINT('Ctrl Pts',(-167.115805421991,16.7895568522908,41.0000000000111));
#92209=CARTESIAN_POINT('Ctrl Pts',(-166.424537246453,16.4023513605147,41.0000000000068));
#92210=CARTESIAN_POINT('Ctrl Pts',(-165.725760727533,16.025290592085,40.9999999999997));
#92211=CARTESIAN_POINT('Ctrl Pts',(-165.019998607327,15.6576738469852,40.9999999999979));
#92212=CARTESIAN_POINT('Ctrl Pts',(-164.796837319539,15.541433793998,40.9999999999973));
#92213=CARTESIAN_POINT('Ctrl Pts',(-164.572975928768,15.4261369848494,40.9999999999972));
#92214=CARTESIAN_POINT('Ctrl Pts',(-164.348424175168,15.3117577010838,40.9999999999975));
#92215=CARTESIAN_POINT('Ctrl Pts',(-164.277996273564,15.2758840425021,40.9999999999976));
#92216=CARTESIAN_POINT('Ctrl Pts',(-164.207500742519,15.2401007843316,40.9999999999977));
#92217=CARTESIAN_POINT('Ctrl Pts',(-164.136938205308,15.204407296028,40.9999999999979));
#92218=CARTESIAN_POINT('Ctrl Pts',(-163.634767706658,14.9503884139369,40.9999999999993));
#92219=CARTESIAN_POINT('Ctrl Pts',(-163.130528643012,14.701581308456,40.9999999999997));
#92220=CARTESIAN_POINT('Ctrl Pts',(-162.624382406767,14.4577468036969,40.9999999999999));
#92221=CARTESIAN_POINT('Ctrl Pts',(-162.333101907192,14.3174232543474,40.9999999999999));
#92222=CARTESIAN_POINT('Ctrl Pts',(-162.041191333437,14.1787471618155,40.9999999999999));
#92223=CARTESIAN_POINT('Ctrl Pts',(-161.748676951111,14.0416699123734,40.9999999999999));
#92224=CARTESIAN_POINT('Ctrl Pts',(-161.024703460289,13.7024035351041,40.9999999999999));
#92225=CARTESIAN_POINT('Ctrl Pts',(-160.296989156764,13.3729114062466,41.));
#92226=CARTESIAN_POINT('Ctrl Pts',(-159.565837204964,13.0524114796293,41.));
#92227=CARTESIAN_POINT('Ctrl Pts',(-159.052413363196,12.8273525117845,41.));
#92228=CARTESIAN_POINT('Ctrl Pts',(-158.537289951449,12.6067257478939,41.0000000000012));
#92229=CARTESIAN_POINT('Ctrl Pts',(-158.020595184326,12.3902690198921,40.9999999999964));
#92230=CARTESIAN_POINT('Ctrl Pts',(-156.620459513298,11.803716174009,40.9999999999833));
#92231=CARTESIAN_POINT('Ctrl Pts',(-155.208729326418,11.2473855688854,40.9999999999796));
#92232=CARTESIAN_POINT('Ctrl Pts',(-153.786660840674,10.7180565395898,40.9999999999779));
#92233=CARTESIAN_POINT('Ctrl Pts',(-152.404789951638,10.2036900490597,40.9999999999763));
#92234=CARTESIAN_POINT('Ctrl Pts',(-151.01315718763,9.71481955399222,40.9999999999766));
#92235=CARTESIAN_POINT('Ctrl Pts',(-149.612929914259,9.24844692736709,40.9999999999717));
#92236=CARTESIAN_POINT('Ctrl Pts',(-148.892028742829,9.00833692576161,40.9999999999693));
#92237=CARTESIAN_POINT('Ctrl Pts',(-148.168849678895,8.77418970238386,40.9999999999654));
#92238=CARTESIAN_POINT('Ctrl Pts',(-147.443553337577,8.54559230069181,40.9999999999593));
#92239=CARTESIAN_POINT('Ctrl Pts',(-147.074239559723,8.42919274754762,40.9999999999562));
#92240=CARTESIAN_POINT('Ctrl Pts',(-146.704376838914,8.3142320835025,40.9999999999524));
#92241=CARTESIAN_POINT('Ctrl Pts',(-146.333986459289,8.20065555828211,40.999999999948));
#92242=CARTESIAN_POINT('Ctrl Pts',(-146.076894129919,8.12182075306847,40.9999999999449));
#92243=CARTESIAN_POINT('Ctrl Pts',(-145.819544077849,8.04365172394714,40.9999999999402));
#92244=CARTESIAN_POINT('Ctrl Pts',(-145.561936540897,7.96612814281965,40.9999999999303));
#92245=CARTESIAN_POINT('Ctrl Pts',(-145.503842861038,7.94864561821321,40.9999999999281));
#92246=CARTESIAN_POINT('Ctrl Pts',(-145.445736226424,7.93119596097413,40.9999999999257));
#92247=CARTESIAN_POINT('Ctrl Pts',(-145.387616747528,7.91377897036687,40.999999999923));
#92248=CARTESIAN_POINT('Ctrl Pts',(-144.317135170216,7.59298174487044,40.9999999998743));
#92249=CARTESIAN_POINT('Ctrl Pts',(-143.242915326353,7.28372140949535,40.9999999998847));
#92250=CARTESIAN_POINT('Ctrl Pts',(-142.16642871014,6.9853813390909,40.9999999999084));
#92251=CARTESIAN_POINT('Ctrl Pts',(-141.628185402034,6.83621130388867,40.9999999999202));
#92252=CARTESIAN_POINT('Ctrl Pts',(-141.089375548839,6.68977097174617,40.9999999999353));
#92253=CARTESIAN_POINT('Ctrl Pts',(-140.550183738394,6.54598122051974,40.9999999999481));
#92254=CARTESIAN_POINT('Ctrl Pts',(-140.301162777883,6.47957319786708,40.9999999999539));
#92255=CARTESIAN_POINT('Ctrl Pts',(-140.052060351194,6.41373051878849,40.9999999999593));
#92256=CARTESIAN_POINT('Ctrl Pts',(-139.802894658828,6.34844529911264,40.9999999999636));
#92257=CARTESIAN_POINT('Ctrl Pts',(-139.654849521108,6.30965521029164,40.9999999999661));
#92258=CARTESIAN_POINT('Ctrl Pts',(-139.506778229424,6.27106091261389,40.9999999999684));
#92259=CARTESIAN_POINT('Ctrl Pts',(-139.358676711506,6.23265874940007,40.9999999999706));
#92260=CARTESIAN_POINT('Ctrl Pts',(-139.216328160858,6.19574830883112,40.9999999999728));
#92261=CARTESIAN_POINT('Ctrl Pts',(-139.073953826219,6.15901592701736,40.9999999999747));
#92262=CARTESIAN_POINT('Ctrl Pts',(-138.931556952871,6.122460150616,40.9999999999763));
#92263=CARTESIAN_POINT('Ctrl Pts',(-137.852774493575,5.84551776107746,40.9999999999883));
#92264=CARTESIAN_POINT('Ctrl Pts',(-136.772065878145,5.57853332011435,40.9999999999726));
#92265=CARTESIAN_POINT('Ctrl Pts',(-135.68972235984,5.32079043385352,40.9999999999605));
#92266=CARTESIAN_POINT('Ctrl Pts',(-135.07155026317,5.17358258559918,40.9999999999537));
#92267=CARTESIAN_POINT('Ctrl Pts',(-134.45284490054,5.02938905934688,40.999999999948));
#92268=CARTESIAN_POINT('Ctrl Pts',(-133.833660863296,4.888074170245,40.9999999999494));
#92269=CARTESIAN_POINT('Ctrl Pts',(-133.368729598412,4.78196402175094,40.9999999999505));
#92270=CARTESIAN_POINT('Ctrl Pts',(-132.903533275812,4.67747788586212,40.9999999999548));
#92271=CARTESIAN_POINT('Ctrl Pts',(-132.438061496091,4.57455049696325,40.9999999999709));
#92272=CARTESIAN_POINT('Ctrl Pts',(-129.978499200868,4.03068009297673,41.0000000000562));
#92273=CARTESIAN_POINT('Ctrl Pts',(-127.511390385521,3.53007933571102,41.0000000000492));
#92274=CARTESIAN_POINT('Ctrl Pts',(-125.037816464169,3.06656201112882,41.0000000000282));
#92275=CARTESIAN_POINT('Ctrl Pts',(-123.149548259225,2.71272377775557,41.0000000000122));
#92276=CARTESIAN_POINT('Ctrl Pts',(-121.257513320784,2.38049453077747,40.999999999987));
#92277=CARTESIAN_POINT('Ctrl Pts',(-119.362193676919,2.06710298218835,40.9999999999911));
#92278=CARTESIAN_POINT('Ctrl Pts',(-117.175237669972,1.70548929241751,40.9999999999958));
#92279=CARTESIAN_POINT('Ctrl Pts',(-114.983887583549,1.36907516990482,40.999999999998));
#92280=CARTESIAN_POINT('Ctrl Pts',(-112.788634863691,1.05504893658129,40.9999999999991));
#92281=CARTESIAN_POINT('Ctrl Pts',(-111.65029988351,0.89221253836014,40.9999999999996));
#92282=CARTESIAN_POINT('Ctrl Pts',(-110.510915568272,0.735395733931361,
40.9999999999999));
#92283=CARTESIAN_POINT('Ctrl Pts',(-109.370550654786,0.584205063488431,
40.9999999999999));
#92284=CARTESIAN_POINT('Ctrl Pts',(-108.698866089248,0.495152481644728,
41.));
#92285=CARTESIAN_POINT('Ctrl Pts',(-108.02684132648,0.408051762178606,41.));
#92286=CARTESIAN_POINT('Ctrl Pts',(-107.354490434212,0.322822359446492,
41.));
#92287=CARTESIAN_POINT('Ctrl Pts',(-106.96698848389,0.273701342187092,41.));
#92288=CARTESIAN_POINT('Ctrl Pts',(-106.579377911394,0.225201882287813,
41.));
#92289=CARTESIAN_POINT('Ctrl Pts',(-106.19166867118,0.177309421133637,41.));
#92290=CARTESIAN_POINT('Ctrl Pts',(-103.990648852084,-0.0945753967966797,
41.));
#92291=CARTESIAN_POINT('Ctrl Pts',(-101.78586236742,-0.346893843387375,
41.));
#92292=CARTESIAN_POINT('Ctrl Pts',(-99.5782059295342,-0.581609328457616,
41.));
#92293=CARTESIAN_POINT('Ctrl Pts',(-98.4707994783828,-0.699347504512224,
41.));
#92294=CARTESIAN_POINT('Ctrl Pts',(-97.3626708656601,-0.812656151974744,
41.));
#92295=CARTESIAN_POINT('Ctrl Pts',(-96.2539332971608,-0.921782003691591,
41.));
#92296=CARTESIAN_POINT('Ctrl Pts',(-95.4162205862063,-1.00423263554009,
41.));
#92297=CARTESIAN_POINT('Ctrl Pts',(-94.5781602445548,-1.08429544478856,
41.));
#92298=CARTESIAN_POINT('Ctrl Pts',(-93.7398011429836,-1.16207664008724,
41.));
#92299=CARTESIAN_POINT('Ctrl Pts',(-93.4757377541879,-1.18657588626546,
41.));
#92300=CARTESIAN_POINT('Ctrl Pts',(-93.2116456158809,-1.21084868819005,
41.));
#92301=CARTESIAN_POINT('Ctrl Pts',(-92.9475282938307,-1.23489818414305,
41.));
#92302=CARTESIAN_POINT('Ctrl Pts',(-90.7372300593495,-1.43615934351134,
41.));
#92303=CARTESIAN_POINT('Ctrl Pts',(-88.5261974020728,-1.62168029502631,
41.));
#92304=CARTESIAN_POINT('Ctrl Pts',(-86.3143658196803,-1.79305840637293,
41.));
#92305=CARTESIAN_POINT('Ctrl Pts',(-84.9944564499124,-1.89532820699439,
41.));
#92306=CARTESIAN_POINT('Ctrl Pts',(-83.6742625748037,-1.99256160295836,
41.));
#92307=CARTESIAN_POINT('Ctrl Pts',(-82.3537704872285,-2.08509819210469,
41.));
#92308=CARTESIAN_POINT('Ctrl Pts',(-81.5348603298117,-2.14248524765592,
41.));
#92309=CARTESIAN_POINT('Ctrl Pts',(-80.7158331792441,-2.19806609943898,
41.));
#92310=CARTESIAN_POINT('Ctrl Pts',(-79.8966933309586,-2.25192128951806,
41.));
#92311=CARTESIAN_POINT('Ctrl Pts',(-79.8232669179519,-2.25674878440502,
41.));
#92312=CARTESIAN_POINT('Ctrl Pts',(-79.7498396409215,-2.26156241089664,
41.));
#92313=CARTESIAN_POINT('Ctrl Pts',(-79.6764115035435,-2.26636222707692,
41.));
#92314=CARTESIAN_POINT('Ctrl Pts',(-75.9717789993547,-2.50852491389651,
41.));
#92315=CARTESIAN_POINT('Ctrl Pts',(-72.264953695338,-2.7157624742687,41.));
#92316=CARTESIAN_POINT('Ctrl Pts',(-68.5564163959988,-2.89342107889025,
41.));
#92317=CARTESIAN_POINT('Ctrl Pts',(-65.9855045365144,-3.0165813916212,41.));
#92318=CARTESIAN_POINT('Ctrl Pts',(-63.4137699397649,-3.1255277688436,41.));
#92319=CARTESIAN_POINT('Ctrl Pts',(-60.8413730070096,-3.22205506124308,
41.));
#92320=CARTESIAN_POINT('Ctrl Pts',(-59.5551745406319,-3.27031870744282,
41.));
#92321=CARTESIAN_POINT('Ctrl Pts',(-58.2688104927504,-3.31547774299482,
41.));
#92322=CARTESIAN_POINT('Ctrl Pts',(-56.9823009271456,-3.35775741157833,
41.));
#92323=CARTESIAN_POINT('Ctrl Pts',(-56.240043581815,-3.38215085209619,41.));
#92324=CARTESIAN_POINT('Ctrl Pts',(-55.4977377972299,-3.40558582972323,
41.));
#92325=CARTESIAN_POINT('Ctrl Pts',(-54.7553874279252,-3.42810568308979,
41.));
#92326=CARTESIAN_POINT('Ctrl Pts',(-54.3016290330985,-3.44187084430996,
41.));
#92327=CARTESIAN_POINT('Ctrl Pts',(-53.8478518097628,-3.45529415926112,
41.));
#92328=CARTESIAN_POINT('Ctrl Pts',(-53.3940635403805,-3.4683853368097,41.));
#92329=CARTESIAN_POINT('Ctrl Pts',(-53.3034955436783,-3.47099810096656,
41.));
#92330=CARTESIAN_POINT('Ctrl Pts',(-53.2129274197839,-3.47359762622963,
41.));
#92331=CARTESIAN_POINT('Ctrl Pts',(-53.1223591687654,-3.47618399202878,
41.));
#92332=CARTESIAN_POINT('Ctrl Pts',(-47.2953401631429,-3.64258670487363,
41.));
#92333=CARTESIAN_POINT('Ctrl Pts',(-41.4677740863017,-3.7537775757723,41.));
#92334=CARTESIAN_POINT('Ctrl Pts',(-35.639833792225,-3.8272049942722,41.));
#92335=CARTESIAN_POINT('Ctrl Pts',(-32.6131542432301,-3.86533875246033,
41.));
#92336=CARTESIAN_POINT('Ctrl Pts',(-29.5863734940691,-3.89328680280741,
41.));
#92337=CARTESIAN_POINT('Ctrl Pts',(-26.5595165690504,-3.91349171933101,
41.));
#92338=CARTESIAN_POINT('Ctrl Pts',(-20.0200301960568,-3.95714418773194,
41.));
#92339=CARTESIAN_POINT('Ctrl Pts',(-13.4801699608071,-3.96312141411588,
41.));
#92340=CARTESIAN_POINT('Ctrl Pts',(-6.94025147230322,-3.96326053282878,
41.));
#92341=CARTESIAN_POINT('Ctrl Pts',(-4.62683685123245,-3.96330974433885,
41.));
#92342=CARTESIAN_POINT('Ctrl Pts',(-2.31341497974243,-3.96262874552467,
41.));
#92343=CARTESIAN_POINT('Ctrl Pts',(7.71069805227384E-15,-3.96262874552467,
41.));
#92344=CARTESIAN_POINT('Ctrl Pts',(7.58040827681699E-15,-2.96262874552467,
40.));
#92345=CARTESIAN_POINT('Ctrl Pts',(-8.85144823879692,-2.96262874562831,
40.));
#92346=CARTESIAN_POINT('Ctrl Pts',(-17.7032012684452,-2.97258723674216,
40.));
#92347=CARTESIAN_POINT('Ctrl Pts',(-26.5528415041601,-2.91351399783701,
40.));
#92348=CARTESIAN_POINT('Ctrl Pts',(-35.402481739875,-2.85444075893186,40.));
#92349=CARTESIAN_POINT('Ctrl Pts',(-44.2500950803765,-2.72914237566079,
40.));
#92350=CARTESIAN_POINT('Ctrl Pts',(-53.0938137147646,-2.4765914965461,40.));
#92351=CARTESIAN_POINT('Ctrl Pts',(-61.9375323491527,-2.22404061743142,
40.));
#92352=CARTESIAN_POINT('Ctrl Pts',(-70.7774082066898,-1.84593393741772,
40.));
#92353=CARTESIAN_POINT('Ctrl Pts',(-79.6111831796923,-1.26849186187931,
40.));
#92354=CARTESIAN_POINT('Ctrl Pts',(-84.0280706661936,-0.979770824110103,
40.));
#92355=CARTESIAN_POINT('Ctrl Pts',(-88.4434228779194,-0.640887452775866,
40.0000000000001));
#92356=CARTESIAN_POINT('Ctrl Pts',(-92.8568473354026,-0.239018189490933,
40.0000000000001));
#92357=CARTESIAN_POINT('Ctrl Pts',(-97.2702717928858,0.162851073794002,
40.0000000000001));
#92358=CARTESIAN_POINT('Ctrl Pts',(-101.677510051147,0.627290636607177,
40.));
#92359=CARTESIAN_POINT('Ctrl Pts',(-106.069073712797,1.16976620918298,40.));
#92360=CARTESIAN_POINT('Ctrl Pts',(-110.460637374447,1.71224178175879,40.));
#92361=CARTESIAN_POINT('Ctrl Pts',(-114.838608995747,2.33270535869012,40.));
#92362=CARTESIAN_POINT('Ctrl Pts',(-119.199058518279,3.05370671214597,40.));
#92363=CARTESIAN_POINT('Ctrl Pts',(-123.559508040812,3.77470806560183,40.));
#92364=CARTESIAN_POINT('Ctrl Pts',(-127.902516032416,4.59578491584501,40.));
#92365=CARTESIAN_POINT('Ctrl Pts',(-132.222152200056,5.55096392160199,40.));
#92366=CARTESIAN_POINT('Ctrl Pts',(-134.381970283877,6.02855342448048,40.));
#92367=CARTESIAN_POINT('Ctrl Pts',(-136.535908314317,6.53988132256321,40.));
#92368=CARTESIAN_POINT('Ctrl Pts',(-138.682902332726,7.09105236606981,40.));
#92369=CARTESIAN_POINT('Ctrl Pts',(-140.829896351135,7.6422234095764,40.));
#92370=CARTESIAN_POINT('Ctrl Pts',(-142.97246355619,8.23395393720208,40.));
#92371=CARTESIAN_POINT('Ctrl Pts',(-145.100553949739,8.87169073562511,40.));
#92372=CARTESIAN_POINT('Ctrl Pts',(-149.356734736836,10.1471643324712,40.));
#92373=CARTESIAN_POINT('Ctrl Pts',(-153.545256591528,11.5996387775139,40.0000000000001));
#92374=CARTESIAN_POINT('Ctrl Pts',(-157.634205130681,13.3126044937319,40.0000000000001));
#92375=CARTESIAN_POINT('Ctrl Pts',(-159.678679400257,14.1690873518408,40.0000000000001));
#92376=CARTESIAN_POINT('Ctrl Pts',(-161.698333060539,15.0915173717773,40.));
#92377=CARTESIAN_POINT('Ctrl Pts',(-163.685559133974,16.0967395961537,40.));
#92378=CARTESIAN_POINT('Ctrl Pts',(-165.672785207409,17.1019618205302,40.));
#92379=CARTESIAN_POINT('Ctrl Pts',(-167.606564886913,18.179444580804,40.0000000000001));
#92380=CARTESIAN_POINT('Ctrl Pts',(-169.475158094859,19.3450606841723,40.0000000000001));
#92381=CARTESIAN_POINT('Ctrl Pts',(-171.343751302806,20.5106767875407,40.0000000000001));
#92382=CARTESIAN_POINT('Ctrl Pts',(-173.147319648035,21.7642077357359,40.));
#92383=CARTESIAN_POINT('Ctrl Pts',(-174.869190918009,23.1281946756062,40.));
#92384=CARTESIAN_POINT('Ctrl Pts',(-176.591062187983,24.4921816154764,40.));
#92385=CARTESIAN_POINT('Ctrl Pts',(-178.23155329653,25.966196073619,39.9999999999999));
#92386=CARTESIAN_POINT('Ctrl Pts',(-179.765591319341,27.5841371179025,39.9999999999999));
#92387=CARTESIAN_POINT('Ctrl Pts',(-180.532610330747,28.3931076400442,39.9999999999999));
#92388=CARTESIAN_POINT('Ctrl Pts',(-181.275699297867,29.2424485691303,40.));
#92389=CARTESIAN_POINT('Ctrl Pts',(-181.973634139114,30.1152819417224,40.));
#92390=CARTESIAN_POINT('Ctrl Pts',(-182.671568980361,30.9881153143144,40.));
#92391=CARTESIAN_POINT('Ctrl Pts',(-183.327437398447,31.8871479480752,40.0000000000001));
#92392=CARTESIAN_POINT('Ctrl Pts',(-183.938736638342,32.8139385762865,40.0000000000001));
#92393=CARTESIAN_POINT('Ctrl Pts',(-185.161335118131,34.6675198327091,40.0000000000001));
#92394=CARTESIAN_POINT('Ctrl Pts',(-186.206617846403,36.6337883765178,40.));
#92395=CARTESIAN_POINT('Ctrl Pts',(-187.049713891119,38.7214305741511,40.));
#92396=CARTESIAN_POINT('Ctrl Pts',(-187.892809935835,40.8090727717843,40.));
#92397=CARTESIAN_POINT('Ctrl Pts',(-188.505057255607,42.9465120075526,40.));
#92398=CARTESIAN_POINT('Ctrl Pts',(-188.906974096078,45.129322231996,40.));
#92399=CARTESIAN_POINT('Ctrl Pts',(-189.107932516313,46.2207273442177,40.));
#92400=CARTESIAN_POINT('Ctrl Pts',(-189.256273490652,47.3234827160355,40.));
#92401=CARTESIAN_POINT('Ctrl Pts',(-189.354350399695,48.4370806930155,40.));
#92402=CARTESIAN_POINT('Ctrl Pts',(-189.405887616132,49.0222514587305,40.));
#92403=CARTESIAN_POINT('Ctrl Pts',(-189.443467838815,49.6109038488981,40.));
#92404=CARTESIAN_POINT('Ctrl Pts',(-189.467540106621,50.2009603371434,40.));
#92405=CARTESIAN_POINT('Ctrl Pts',(-189.489278105322,50.7337995062214,40.));
#92406=CARTESIAN_POINT('Ctrl Pts',(-189.500000000133,51.2677847576647,40.));
#92407=CARTESIAN_POINT('Ctrl Pts',(-189.5,51.8013867006571,40.));
#92408=CARTESIAN_POINT('Ctrl Pts',(7.59225281309826E-15,-2.96262874552467,
40.));
#92409=CARTESIAN_POINT('Ctrl Pts',(7.71069817591099E-15,-3.96262874552467,
40.));
#92410=CARTESIAN_POINT('Ctrl Pts',(7.71069817591099E-15,-3.96262874552467,
41.));
#92411=CARTESIAN_POINT('Ctrl Pts',(9.22286794822226,-2.96262874561266,40.));
#92412=CARTESIAN_POINT('Ctrl Pts',(9.22185412936952,-3.96262874542067,40.000000000576));
#92413=CARTESIAN_POINT('Ctrl Pts',(9.22185412936967,-3.96262874552467,41.000000000384));
#92414=CARTESIAN_POINT('Ctrl Pts',(18.4459311592863,-2.97316630718802,40.0000000000001));
#92415=CARTESIAN_POINT('Ctrl Pts',(18.4478537919059,-3.97317899216111,39.9999999998081));
#92416=CARTESIAN_POINT('Ctrl Pts',(18.4478537919057,-3.97317899207265,40.9999999998721));
#92417=CARTESIAN_POINT('Ctrl Pts',(36.888025186236,-2.83828047197706,40.0000000000001));
#92418=CARTESIAN_POINT('Ctrl Pts',(36.9007302013505,-3.83821429426901,40.000000000192));
#92419=CARTESIAN_POINT('Ctrl Pts',(36.9007302013507,-3.8382142943575,41.000000000128));
#92420=CARTESIAN_POINT('Ctrl Pts',(46.1071023205165,-2.69618114038663,40.));
#92421=CARTESIAN_POINT('Ctrl Pts',(46.127686373253,-3.69602375409421,40.0000000001919));
#92422=CARTESIAN_POINT('Ctrl Pts',(46.127686373252,-3.69602375412447,41.0000000001279));
#92423=CARTESIAN_POINT('Ctrl Pts',(64.5376642708818,-2.12424138803454,40.));
#92424=CARTESIAN_POINT('Ctrl Pts',(64.5791146330909,-3.12343647566289,39.999999999808));
#92425=CARTESIAN_POINT('Ctrl Pts',(64.579114633092,-3.12343647563261,40.999999999872));
#92426=CARTESIAN_POINT('Ctrl Pts',(73.7492053716307,-1.69653408055239,40.));
#92427=CARTESIAN_POINT('Ctrl Pts',(73.8036313518568,-2.69519228857308,40.0000000003842));
#92428=CARTESIAN_POINT('Ctrl Pts',(73.8036313518527,-2.69519228864398,41.0000000002562));
#92429=CARTESIAN_POINT('Ctrl Pts',(87.5574640501196,-0.711874711538739,
40.));
#92430=CARTESIAN_POINT('Ctrl Pts',(87.6369443133912,-1.70874631254166,39.9999999998079));
#92431=CARTESIAN_POINT('Ctrl Pts',(87.6369443133933,-1.70874631250621,40.9999999998719));
#92432=CARTESIAN_POINT('Ctrl Pts',(92.1597820946751,-0.325827219991832,
40.));
#92433=CARTESIAN_POINT('Ctrl Pts',(92.2485669610653,-1.32193429002331,40.));
#92434=CARTESIAN_POINT('Ctrl Pts',(92.2485669610628,-1.32193428999809,41.));
#92435=CARTESIAN_POINT('Ctrl Pts',(101.336839995159,0.590146567660638,40.));
#92436=CARTESIAN_POINT('Ctrl Pts',(101.446690684835,-0.403857895832186,
40.));
#92437=CARTESIAN_POINT('Ctrl Pts',(101.446690684837,-0.403857895857384,
41.));
#92438=CARTESIAN_POINT('Ctrl Pts',(105.914098473304,1.12003310600361,40.));
#92439=CARTESIAN_POINT('Ctrl Pts',(106.035715901227,0.127363203503316,40.000000000671));
#92440=CARTESIAN_POINT('Ctrl Pts',(106.035715901271,0.127363203184816,41.0000000004473));
#92441=CARTESIAN_POINT('Ctrl Pts',(110.476932254378,1.74203503103179,40.));
#92442=CARTESIAN_POINT('Ctrl Pts',(110.612002249462,0.751198971722283,40.));
#92443=CARTESIAN_POINT('Ctrl Pts',(110.612002249462,0.751198971722297,41.));
#92444=CARTESIAN_POINT('',(110.476932254378,1.74203503103179,40.));
#92445=CARTESIAN_POINT('',(110.612002249462,0.751198971722297,41.));
#92446=CARTESIAN_POINT('Origin',(110.476932254378,1.74203503103178,41.));
#92447=CARTESIAN_POINT('Ctrl Pts',(7.71069817591099E-15,-3.96262874552467,
41.));
#92448=CARTESIAN_POINT('Ctrl Pts',(5.82930178377565,-3.96262874552467,41.));
#92449=CARTESIAN_POINT('Ctrl Pts',(11.6587149026642,-3.96683913664252,40.9999999999486));
#92450=CARTESIAN_POINT('Ctrl Pts',(17.4876489527825,-3.95291174806464,40.9999999999272));
#92451=CARTESIAN_POINT('Ctrl Pts',(20.8833979233155,-3.94479810069465,40.9999999999147));
#92452=CARTESIAN_POINT('Ctrl Pts',(24.2789843696462,-3.93052998937519,40.9999999999123));
#92453=CARTESIAN_POINT('Ctrl Pts',(27.6742919966282,-3.90569664321507,40.9999999999361));
#92454=CARTESIAN_POINT('Ctrl Pts',(33.9894118154414,-3.8595077337752,40.9999999999802));
#92455=CARTESIAN_POINT('Ctrl Pts',(40.3036077491836,-3.77832350323118,40.9999999999941));
#92456=CARTESIAN_POINT('Ctrl Pts',(46.61629413806,-3.63995619654589,40.9999999999781));
#92457=CARTESIAN_POINT('Ctrl Pts',(49.5290034318352,-3.57611273667641,40.9999999999707));
#92458=CARTESIAN_POINT('Ctrl Pts',(52.4413913669821,-3.50009598589696,40.9999999999568));
#92459=CARTESIAN_POINT('Ctrl Pts',(55.353400503172,-3.40973011487854,40.9999999999364));
#92460=CARTESIAN_POINT('Ctrl Pts',(60.455282861202,-3.25140779459896,40.9999999999007));
#92461=CARTESIAN_POINT('Ctrl Pts',(65.5560203048567,-3.04969502865525,40.9999999999245));
#92462=CARTESIAN_POINT('Ctrl Pts',(70.6552234068538,-2.78987297547265,40.999999999938));
#92463=CARTESIAN_POINT('Ctrl Pts',(74.779834762682,-2.57970974611788,40.999999999949));
#92464=CARTESIAN_POINT('Ctrl Pts',(78.9034422335561,-2.33152756586165,40.9999999999533));
#92465=CARTESIAN_POINT('Ctrl Pts',(83.0258399928798,-2.03756163788547,40.9999999999148));
#92466=CARTESIAN_POINT('Ctrl Pts',(83.702952471426,-1.98927711763268,40.9999999999085));
#92467=CARTESIAN_POINT('Ctrl Pts',(84.3800458281722,-1.9397441896904,40.9999999999059));
#92468=CARTESIAN_POINT('Ctrl Pts',(85.0570974588133,-1.8889166619343,40.999999999906));
#92469=CARTESIAN_POINT('Ctrl Pts',(87.0236209542901,-1.74128607805296,40.9999999999064));
#92470=CARTESIAN_POINT('Ctrl Pts',(88.9897932279612,-1.58273540574224,40.9999999999299));
#92471=CARTESIAN_POINT('Ctrl Pts',(90.9550653787228,-1.4121181790945,40.9999999999533));
#92472=CARTESIAN_POINT('Ctrl Pts',(91.9377014541036,-1.32680956577063,40.999999999965));
#92473=CARTESIAN_POINT('Ctrl Pts',(92.9201124704526,-1.23848396737367,40.9999999999766));
#92474=CARTESIAN_POINT('Ctrl Pts',(93.9022294421414,-1.14699577506546,40.9999999999854));
#92475=CARTESIAN_POINT('Ctrl Pts',(94.3953787582656,-1.10105690956286,40.9999999999898));
#92476=CARTESIAN_POINT('Ctrl Pts',(94.8884539303434,-1.05432062249788,40.9999999999934));
#92477=CARTESIAN_POINT('Ctrl Pts',(95.381446184432,-1.00676831544679,40.999999999996));
#92478=CARTESIAN_POINT('Ctrl Pts',(95.7294863070638,-0.973197583573767,
40.9999999999978));
#92479=CARTESIAN_POINT('Ctrl Pts',(96.0774851027509,-0.939220144658271,
40.9999999999991));
#92480=CARTESIAN_POINT('Ctrl Pts',(96.4254394745113,-0.904829419904913,
40.9999999999996));
#92481=CARTESIAN_POINT('Ctrl Pts',(96.5661765935577,-0.890919402050511,
40.9999999999999));
#92482=CARTESIAN_POINT('Ctrl Pts',(96.7069064798408,-0.876941768460753,
41.));
#92483=CARTESIAN_POINT('Ctrl Pts',(96.84762882295,-0.862896092927736,41.));
#92484=CARTESIAN_POINT('Ctrl Pts',(100.443648508519,-0.503972807556701,
40.9999999999998));
#92485=CARTESIAN_POINT('Ctrl Pts',(104.034503830642,-0.100826113757949,
40.9999999999999));
#92486=CARTESIAN_POINT('Ctrl Pts',(107.619039731541,0.356421973888414,41.));
#92487=CARTESIAN_POINT('Ctrl Pts',(108.61719230131,0.483747621147737,41.));
#92488=CARTESIAN_POINT('Ctrl Pts',(109.61485481989,0.615268615590165,41.));
#92489=CARTESIAN_POINT('Ctrl Pts',(110.612002249462,0.751198971722297,41.));
#92490=CARTESIAN_POINT('Ctrl Pts',(110.476932254378,1.74203503103179,40.));
#92491=CARTESIAN_POINT('Ctrl Pts',(107.65673548948,1.35758801823668,40.));
#92492=CARTESIAN_POINT('Ctrl Pts',(104.832744534644,1.0085602200593,40.));
#92493=CARTESIAN_POINT('Ctrl Pts',(102.005490363231,0.690046765893749,40.0000000000001));
#92494=CARTESIAN_POINT('Ctrl Pts',(100.25430781925,0.492761637942585,40.0000000000001));
#92495=CARTESIAN_POINT('Ctrl Pts',(98.5018731756585,0.307184392575044,40.0000000000001));
#92496=CARTESIAN_POINT('Ctrl Pts',(96.74831108378,0.132159284469113,40.));
#92497=CARTESIAN_POINT('Ctrl Pts',(96.7415197154669,0.13148142995875,40.));
#92498=CARTESIAN_POINT('Ctrl Pts',(96.7347283247242,0.130803733819283,40.));
#92499=CARTESIAN_POINT('Ctrl Pts',(96.7279369115921,0.13012619600356,40.));
#92500=CARTESIAN_POINT('Ctrl Pts',(94.2757194146321,-0.114516568948024,
40.));
#92501=CARTESIAN_POINT('Ctrl Pts',(91.8208450764136,-0.338497674584954,
40.0000000000002));
#92502=CARTESIAN_POINT('Ctrl Pts',(89.364611533855,-0.544078641455991,40.0000000000008));
#92503=CARTESIAN_POINT('Ctrl Pts',(87.2287242584436,-0.722847379688103,
40.0000000000013));
#92504=CARTESIAN_POINT('Ctrl Pts',(85.0918085318741,-0.88770123381528,40.0000000000019));
#92505=CARTESIAN_POINT('Ctrl Pts',(82.9547112714115,-1.04009610158038,40.0000000000013));
#92506=CARTESIAN_POINT('Ctrl Pts',(82.9478289630004,-1.04058687404059,40.0000000000013));
#92507=CARTESIAN_POINT('Ctrl Pts',(82.9409466503039,-1.04107751870878,40.0000000000013));
#92508=CARTESIAN_POINT('Ctrl Pts',(82.9340643333063,-1.04156803562236,40.0000000000013));
#92509=CARTESIAN_POINT('Ctrl Pts',(73.7354319150329,-1.69717352205083,39.9999999999987));
#92510=CARTESIAN_POINT('Ctrl Pts',(64.5307746673837,-2.12445562062589,40.));
#92511=CARTESIAN_POINT('Ctrl Pts',(55.322383302435,-2.41021148127205,40.));
#92512=CARTESIAN_POINT('Ctrl Pts',(55.3177902240801,-2.41035401420819,40.));
#92513=CARTESIAN_POINT('Ctrl Pts',(55.3131971447822,-2.41049651140351,40.));
#92514=CARTESIAN_POINT('Ctrl Pts',(55.3086040645415,-2.41063897286659,40.));
#92515=CARTESIAN_POINT('Ctrl Pts',(46.0979123788003,-2.69632277214192,39.9999999999999));
#92516=CARTESIAN_POINT('Ctrl Pts',(36.8834292267035,-2.83831408691453,39.9999999999997));
#92517=CARTESIAN_POINT('Ctrl Pts',(27.6669781789878,-2.90572424091316,40.0000000000004));
#92518=CARTESIAN_POINT('Ctrl Pts',(27.6646802028605,-2.90574104856763,40.0000000000004));
#92519=CARTESIAN_POINT('Ctrl Pts',(27.6623822266079,-2.90575785137913,40.0000000000004));
#92520=CARTESIAN_POINT('Ctrl Pts',(27.6600842502302,-2.90577464934903,40.0000000000004));
#92521=CARTESIAN_POINT('Ctrl Pts',(18.4413342218722,-2.97316275959541,40.0000000000011));
#92522=CARTESIAN_POINT('Ctrl Pts',(9.22052813832371,-2.96262874561264,40.));
#92523=CARTESIAN_POINT('Ctrl Pts',(7.59225281309826E-15,-2.96262874552467,
40.));
#92524=CARTESIAN_POINT('Origin',(110.747072244546,-0.239637087587196,41.));
#92525=CARTESIAN_POINT('',(111.732514372547,1.50073753081004,40.));
#92526=CARTESIAN_POINT('Origin',(111.732514372547,1.50073753081004,41.));
#92527=CARTESIAN_POINT('Origin',(110.747072244546,-0.239637087587196,41.));
#92528=CARTESIAN_POINT('Origin',(110.747072244546,-0.239637087587196,40.));
#92529=CARTESIAN_POINT('Origin',(125.29348064571,25.4505574462982,41.));
#92530=CARTESIAN_POINT('',(147.519501177935,9.21794547079491,40.));
#92531=CARTESIAN_POINT('Origin',(147.519501177935,9.21794547079491,41.));
#92532=CARTESIAN_POINT('Origin',(125.29348064571,25.4505574462982,40.));
#92533=CARTESIAN_POINT('Origin',(110.747072244546,-0.239637087587196,150.608250755187));
#92534=CARTESIAN_POINT('',(110.612002249461,0.751198971722164,150.608250755189));
#92535=CARTESIAN_POINT('Origin',(110.747072244546,-0.239637087587191,150.608250755187));
#92536=CARTESIAN_POINT('',(110.612002249462,0.751198971722297,41.));
#92537=CARTESIAN_POINT('Origin',(149.134611526938,8.03836140827812,41.));
#92538=CARTESIAN_POINT('',(148.513697082188,9.93953611153414,40.));
#92539=CARTESIAN_POINT('',(148.824154304563,8.98894875990614,41.));
#92540=CARTESIAN_POINT('Origin',(148.513697082188,9.93953611153414,41.));
#92541=CARTESIAN_POINT('Origin',(149.134611526938,8.03836140827812,41.));
#92542=CARTESIAN_POINT('Origin',(149.134611526938,8.03836140827812,40.));
#92543=CARTESIAN_POINT('Ctrl Pts',(110.612002249462,0.751198971722294,150.608250755187));
#92544=CARTESIAN_POINT('Ctrl Pts',(110.946247390914,0.796763007456252,150.608250755187));
#92545=CARTESIAN_POINT('Ctrl Pts',(111.239793308547,0.630550221611425,150.608250755187));
#92546=CARTESIAN_POINT('Ctrl Pts',(110.612002230967,0.751198969201009,150.693639752826));
#92547=CARTESIAN_POINT('Ctrl Pts',(110.946247372074,0.796763018434683,150.731492884106));
#92548=CARTESIAN_POINT('Ctrl Pts',(111.23979328877,0.630550232809205,150.779028752436));
#92549=CARTESIAN_POINT('Ctrl Pts',(110.582396971373,0.758074598003006,150.775891503277));
#92550=CARTESIAN_POINT('Ctrl Pts',(110.917292843193,0.81358059931356,150.85066217237));
#92551=CARTESIAN_POINT('Ctrl Pts',(111.209697548339,0.647533917538457,150.943532248718));
#92552=CARTESIAN_POINT('Ctrl Pts',(110.473864498357,0.783673855713148,150.933269838702));
#92553=CARTESIAN_POINT('Ctrl Pts',(110.812459489596,0.875126003979084,151.073781688751));
#92554=CARTESIAN_POINT('Ctrl Pts',(111.099346993048,0.710519201534495,151.258288924866));
#92555=CARTESIAN_POINT('Ctrl Pts',(110.398057036428,0.801688169240552,151.004328255835));
#92556=CARTESIAN_POINT('Ctrl Pts',(110.738903039506,0.918545320463253,151.172655401108));
#92557=CARTESIAN_POINT('Ctrl Pts',(111.022262845842,0.754759056919205,151.400405752383));
#92558=CARTESIAN_POINT('Ctrl Pts',(110.218030599701,0.845370947931939,151.134168853203));
#92559=CARTESIAN_POINT('Ctrl Pts',(110.566311747443,1.02190104841371,151.346871626469));
#92560=CARTESIAN_POINT('Ctrl Pts',(110.839158587949,0.861480818033809,151.660086955321));
#92561=CARTESIAN_POINT('Ctrl Pts',(110.116756966979,0.870327544773072,151.190904988883));
#92562=CARTESIAN_POINT('Ctrl Pts',(110.469279013687,1.0806646106112,151.419609649809));
#92563=CARTESIAN_POINT('Ctrl Pts',(110.736134030468,0.922221916391551,151.773559220278));
#92564=CARTESIAN_POINT('Ctrl Pts',(109.898938544125,0.925233080786458,151.292822817772));
#92565=CARTESIAN_POINT('Ctrl Pts',(110.262975165541,1.20755085870014,151.542883455069));
#92566=CARTESIAN_POINT('Ctrl Pts',(110.514486881992,1.05512902874504,151.977394882657));
#92567=CARTESIAN_POINT('Ctrl Pts',(109.78151096426,0.955417648896434,151.338065123121));
#92568=CARTESIAN_POINT('Ctrl Pts',(110.152251323704,1.27662677766495,151.593100193495));
#92569=CARTESIAN_POINT('Ctrl Pts',(110.394965311842,1.12785792027832,152.067879488634));
#92570=CARTESIAN_POINT('Ctrl Pts',(109.422128673717,1.0500087684249,151.455574585986));
#92571=CARTESIAN_POINT('Ctrl Pts',(109.813360261285,1.49144507563439,151.711420401226));
#92572=CARTESIAN_POINT('Ctrl Pts',(110.029060664743,1.35452646652739,152.302898421626));
#92573=CARTESIAN_POINT('Ctrl Pts',(109.169114092848,1.1194514186453,151.51211819045));
#92574=CARTESIAN_POINT('Ctrl Pts',(109.580757706994,1.6437216273512,151.744418133447));
#92575=CARTESIAN_POINT('Ctrl Pts',(109.771307831859,1.51936475733935,152.415985623633));
#92576=CARTESIAN_POINT('Ctrl Pts',(108.649983750045,1.26921788090281,151.588936256037));
#92577=CARTESIAN_POINT('Ctrl Pts',(109.124609723565,1.95156485229409,151.736067979281));
#92578=CARTESIAN_POINT('Ctrl Pts',(109.242075229445,1.87107024784917,152.569621758969));
#92579=CARTESIAN_POINT('Ctrl Pts',(108.389788066051,1.34778888692035,151.608250755187));
#92580=CARTESIAN_POINT('Ctrl Pts',(108.904821123451,2.10515872248547,151.689264229384));
#92581=CARTESIAN_POINT('Ctrl Pts',(108.976632768029,2.05384440757191,152.608250750215));
#92582=CARTESIAN_POINT('Ctrl Pts',(108.12932364768,1.43023673425741,151.608250755187));
#92583=CARTESIAN_POINT('Ctrl Pts',(108.710714013295,2.24386148976203,151.608250755187));
#92584=CARTESIAN_POINT('Ctrl Pts',(108.710714013295,2.24386148976203,152.608250755187));
#92585=CARTESIAN_POINT('',(108.129344917475,1.43023000148885,151.608250755144));
#92586=CARTESIAN_POINT('Origin',(108.12932364768,1.43023673425741,152.608250755187));
#92587=CARTESIAN_POINT('Ctrl Pts',(110.612002249462,0.751198971722294,150.608250755189));
#92588=CARTESIAN_POINT('Ctrl Pts',(110.612002249452,0.751198971720885,150.629522166779));
#92589=CARTESIAN_POINT('Ctrl Pts',(110.610161909816,0.75162639831703,150.650481814028));
#92590=CARTESIAN_POINT('Ctrl Pts',(110.606637178143,0.752447951651463,150.671066183928));
#92591=CARTESIAN_POINT('Ctrl Pts',(110.603124557815,0.753266682043145,150.691579823791));
#92592=CARTESIAN_POINT('Ctrl Pts',(110.597938087509,0.754477085709687,150.711719134966));
#92593=CARTESIAN_POINT('Ctrl Pts',(110.591282043221,0.756034195684844,150.73139543502));
#92594=CARTESIAN_POINT('Ctrl Pts',(110.586707521022,0.757104355954006,150.744918432687));
#92595=CARTESIAN_POINT('Ctrl Pts',(110.581439972465,0.758338012708028,150.758222724358));
#92596=CARTESIAN_POINT('Ctrl Pts',(110.575559656037,0.759717155612428,150.771279454307));
#92597=CARTESIAN_POINT('Ctrl Pts',(110.570108513205,0.760995642076692,150.783383241706));
#92598=CARTESIAN_POINT('Ctrl Pts',(110.564129055894,0.762399560426148,150.795277264634));
#92599=CARTESIAN_POINT('Ctrl Pts',(110.557702779899,0.763910315589563,150.80692281406));
#92600=CARTESIAN_POINT('Ctrl Pts',(110.548682698323,0.766030849290375,150.823268798254));
#92601=CARTESIAN_POINT('Ctrl Pts',(110.538777594462,0.768362981190624,150.839142111502));
#92602=CARTESIAN_POINT('Ctrl Pts',(110.528130734865,0.770874226858077,150.854580670989));
#92603=CARTESIAN_POINT('Ctrl Pts',(110.522606361851,0.77217724561878,150.862591329967));
#92604=CARTESIAN_POINT('Ctrl Pts',(110.516916289504,0.773520734835112,150.87044028587));
#92605=CARTESIAN_POINT('Ctrl Pts',(110.511065300135,0.774903837338248,150.8781534036));
#92606=CARTESIAN_POINT('Ctrl Pts',(110.49675000416,0.778287798655982,150.897024667283));
#92607=CARTESIAN_POINT('Ctrl Pts',(110.481490408537,0.781904580009331,150.91504702297));
#92608=CARTESIAN_POINT('Ctrl Pts',(110.465697924213,0.785659761757801,150.932146675738));
#92609=CARTESIAN_POINT('Ctrl Pts',(110.462737064113,0.786363803476632,150.935352610825));
#92610=CARTESIAN_POINT('Ctrl Pts',(110.459756910977,0.787072836516795,150.938527001465));
#92611=CARTESIAN_POINT('Ctrl Pts',(110.456750103519,0.787788631045777,150.94167972859));
#92612=CARTESIAN_POINT('Ctrl Pts',(110.439536415148,0.791886487037215,150.959728793256));
#92613=CARTESIAN_POINT('Ctrl Pts',(110.42152783605,0.796187304544596,150.976987704495));
#92614=CARTESIAN_POINT('Ctrl Pts',(110.40290188466,0.800652170714823,150.993568951696));
#92615=CARTESIAN_POINT('Ctrl Pts',(110.383199066548,0.805375174882903,151.011108850242));
#92616=CARTESIAN_POINT('Ctrl Pts',(110.362805198615,0.810281780069283,151.027890437271));
#92617=CARTESIAN_POINT('Ctrl Pts',(110.341874993262,0.815338382011048,151.044029963927));
#92618=CARTESIAN_POINT('Ctrl Pts',(110.330744571933,0.81802741965561,151.052612762266));
#92619=CARTESIAN_POINT('Ctrl Pts',(110.319461583996,0.820759078031207,151.061013710925));
#92620=CARTESIAN_POINT('Ctrl Pts',(110.308043818064,0.823529558586245,151.069248554519));
#92621=CARTESIAN_POINT('Ctrl Pts',(110.282997151361,0.829607043751403,151.087312980089));
#92622=CARTESIAN_POINT('Ctrl Pts',(110.25753240075,0.835815613704716,151.104421923017));
#92623=CARTESIAN_POINT('Ctrl Pts',(110.231691500055,0.842147539981722,151.120755955339));
#92624=CARTESIAN_POINT('Ctrl Pts',(110.213993989033,0.846484050399732,151.131942551365));
#92625=CARTESIAN_POINT('Ctrl Pts',(110.196119026854,0.850878666513219,151.142764962505));
#92626=CARTESIAN_POINT('Ctrl Pts',(110.178068985415,0.855331688375319,151.15327329781));
#92627=CARTESIAN_POINT('Ctrl Pts',(110.144029566785,0.863729357479973,151.173090295226));
#92628=CARTESIAN_POINT('Ctrl Pts',(110.109390729821,0.872329659079962,151.191779430376));
#92629=CARTESIAN_POINT('Ctrl Pts',(110.074302136121,0.881101259647679,151.209539849258));
#92630=CARTESIAN_POINT('Ctrl Pts',(110.052320079445,0.886596430598848,151.220666272213));
#92631=CARTESIAN_POINT('Ctrl Pts',(110.030160566118,0.892159045199865,151.231427543411));
#92632=CARTESIAN_POINT('Ctrl Pts',(110.007852155919,0.89778332038,151.241866826161));
#92633=CARTESIAN_POINT('Ctrl Pts',(109.970500956097,0.907200101953821,151.259345424256));
#92634=CARTESIAN_POINT('Ctrl Pts',(109.932631685714,0.916816594981333,151.275928634357));
#92635=CARTESIAN_POINT('Ctrl Pts',(109.894447290657,0.926582979000112,151.291691334144));
#92636=CARTESIAN_POINT('Ctrl Pts',(109.852384741436,0.937341274578199,151.309054954405));
#92637=CARTESIAN_POINT('Ctrl Pts',(109.809939438207,0.948281505647227,151.325423210272));
#92638=CARTESIAN_POINT('Ctrl Pts',(109.767319628914,0.959353905644784,151.3408783142));
#92639=CARTESIAN_POINT('Ctrl Pts',(109.732213376733,0.968474323427329,151.35360879763));
#92640=CARTESIAN_POINT('Ctrl Pts',(109.696987178204,0.977684816576761,151.365719377932));
#92641=CARTESIAN_POINT('Ctrl Pts',(109.661733986723,0.986964195335185,151.377246386361));
#92642=CARTESIAN_POINT('Ctrl Pts',(109.614572865747,0.99937799067772,151.392667022513));
#92643=CARTESIAN_POINT('Ctrl Pts',(109.567209175688,1.01195382312556,151.407140915232));
#92644=CARTESIAN_POINT('Ctrl Pts',(109.519520623797,1.02472635764171,151.420776182521));
#92645=CARTESIAN_POINT('Ctrl Pts',(109.446484320137,1.0442878388033,151.441658962196));
#92646=CARTESIAN_POINT('Ctrl Pts',(109.37301201643,1.0642323371024,151.460485446871));
#92647=CARTESIAN_POINT('Ctrl Pts',(109.299170657915,1.08455251676184,151.477473436277));
#92648=CARTESIAN_POINT('Ctrl Pts',(109.220851198854,1.10610501133885,151.495491660314));
#92649=CARTESIAN_POINT('Ctrl Pts',(109.142116222202,1.12808011914536,151.511441624991));
#92650=CARTESIAN_POINT('Ctrl Pts',(109.063009522562,1.1504815767125,151.525536766875));
#92651=CARTESIAN_POINT('Ctrl Pts',(109.012011299796,1.16492326785228,151.534623572278));
#92652=CARTESIAN_POINT('Ctrl Pts',(108.960857865818,1.17954240781536,151.542938554077));
#92653=CARTESIAN_POINT('Ctrl Pts',(108.909554859704,1.1943425298468,151.550529724418));
#92654=CARTESIAN_POINT('Ctrl Pts',(108.882458423677,1.20215943162696,151.554539112505));
#92655=CARTESIAN_POINT('Ctrl Pts',(108.855384688227,1.21000775512804,151.558336010665));
#92656=CARTESIAN_POINT('Ctrl Pts',(108.828326358283,1.21788960972175,151.561922431859));
#92657=CARTESIAN_POINT('Ctrl Pts',(108.625188701118,1.2770618306088,151.588847123828));
#92658=CARTESIAN_POINT('Ctrl Pts',(108.421787066927,1.33847795579103,151.604069000832));
#92659=CARTESIAN_POINT('Ctrl Pts',(108.21817335316,1.40225878138333,151.607501729799));
#92660=CARTESIAN_POINT('Ctrl Pts',(108.188568310647,1.41153239079901,151.608000841991));
#92661=CARTESIAN_POINT('Ctrl Pts',(108.158958780341,1.4208560027417,151.608250635593));
#92662=CARTESIAN_POINT('Ctrl Pts',(108.129344917475,1.43023000148885,151.608250755144));
#92663=CARTESIAN_POINT('Ctrl Pts',(190.5,51.8013867006572,41.));
#92664=CARTESIAN_POINT('Ctrl Pts',(190.5,51.8013867006572,40.));
#92665=CARTESIAN_POINT('Ctrl Pts',(189.5,51.8013867006572,40.));
#92666=CARTESIAN_POINT('Ctrl Pts',(190.5,49.0776276471086,41.));
#92667=CARTESIAN_POINT('Ctrl Pts',(190.500000000443,49.077627647157,40.));
#92668=CARTESIAN_POINT('Ctrl Pts',(189.500000000443,49.1436388962432,40.));
#92669=CARTESIAN_POINT('Ctrl Pts',(190.230148217333,46.3947031958517,41.));
#92670=CARTESIAN_POINT('Ctrl Pts',(190.230148217548,46.3947031957874,40.));
#92671=CARTESIAN_POINT('Ctrl Pts',(189.236843327146,46.5338535505999,40.));
#92672=CARTESIAN_POINT('Ctrl Pts',(189.361745789355,42.4483454229149,41.));
#92673=CARTESIAN_POINT('Ctrl Pts',(189.361745789248,42.4483454229471,40.));
#92674=CARTESIAN_POINT('Ctrl Pts',(188.393447405239,42.7011350513066,40.));
#92675=CARTESIAN_POINT('Ctrl Pts',(188.994929796133,41.145948626321,41.));
#92676=CARTESIAN_POINT('Ctrl Pts',(188.994929796263,41.1459486262754,40.));
#92677=CARTESIAN_POINT('Ctrl Pts',(188.03743539513,41.4372314385205,40.));
#92678=CARTESIAN_POINT('Ctrl Pts',(188.320848581514,39.2146325226266,41.));
#92679=CARTESIAN_POINT('Ctrl Pts',(188.320848581448,39.2146325226495,40.));
#92680=CARTESIAN_POINT('Ctrl Pts',(187.383379063071,39.5632888051564,40.));
#92681=CARTESIAN_POINT('Ctrl Pts',(188.07440016264,38.5721075764589,41.0000000000092));
#92682=CARTESIAN_POINT('Ctrl Pts',(188.07440016258,38.5721075764866,40.0000000000138));
#92683=CARTESIAN_POINT('Ctrl Pts',(187.144269963878,38.939897855964,40.));
#92684=CARTESIAN_POINT('Ctrl Pts',(187.545929721486,37.3110698530063,40.9999999999908));
#92685=CARTESIAN_POINT('Ctrl Pts',(187.545929721547,37.3110698529785,39.9999999999862));
#92686=CARTESIAN_POINT('Ctrl Pts',(186.631487670084,37.7162952356469,40.));
#92687=CARTESIAN_POINT('Ctrl Pts',(187.263906551726,36.6919462209565,41.));
#92688=CARTESIAN_POINT('Ctrl Pts',(187.263906551658,36.6919462209899,40.));
#92689=CARTESIAN_POINT('Ctrl Pts',(186.357812851989,37.1154901542486,40.));
#92690=CARTESIAN_POINT('Ctrl Pts',(185.76842343351,33.6516773356634,41.));
#92691=CARTESIAN_POINT('Ctrl Pts',(185.768423433782,33.6516773355295,40.));
#92692=CARTESIAN_POINT('Ctrl Pts',(184.906205569059,34.1644194244269,40.));
#92693=CARTESIAN_POINT('Ctrl Pts',(184.299478625402,31.3966159998617,41.0000000000366));
#92694=CARTESIAN_POINT('Ctrl Pts',(184.299478625217,31.3966160000255,40.0000000000549));
#92695=CARTESIAN_POINT('Ctrl Pts',(183.479162611529,31.9726430192458,40.0000000000001));
#92696=CARTESIAN_POINT('Ctrl Pts',(182.174203530724,28.7729657639328,40.9999999999909));
#92697=CARTESIAN_POINT('Ctrl Pts',(182.174203530771,28.7729657638918,39.9999999999864));
#92698=CARTESIAN_POINT('Ctrl Pts',(181.407974125944,29.4157626542651,40.0000000000001));
#92699=CARTESIAN_POINT('Ctrl Pts',(181.734653162829,28.2579931028748,41.));
#92700=CARTESIAN_POINT('Ctrl Pts',(181.734653162795,28.2579931029011,39.9999999999931));
#92701=CARTESIAN_POINT('Ctrl Pts',(180.979331279132,28.9135514351784,40.0000000000001));
#92702=CARTESIAN_POINT('Ctrl Pts',(180.827681669059,27.246908681366,41.));
#92703=CARTESIAN_POINT('Ctrl Pts',(180.827681669093,27.2469086813396,40.0000000000069));
#92704=CARTESIAN_POINT('Ctrl Pts',(180.094217491189,27.9268338056749,40.0000000000001));
#92705=CARTESIAN_POINT('Ctrl Pts',(180.360725912636,26.7514671965533,40.9999999999908));
#92706=CARTESIAN_POINT('Ctrl Pts',(180.36072591255,26.7514671966354,39.9999999999862));
#92707=CARTESIAN_POINT('Ctrl Pts',(179.63819831998,27.4429796616177,40.));
#92708=CARTESIAN_POINT('Ctrl Pts',(178.935911835944,25.3077730343987,41.0000000000183));
#92709=CARTESIAN_POINT('Ctrl Pts',(178.935911836115,25.3077730342345,40.0000000000275));
#92710=CARTESIAN_POINT('Ctrl Pts',(178.245730718942,26.0320605949285,40.));
#92711=CARTESIAN_POINT('Ctrl Pts',(177.949212299624,24.3963507756892,41.0000000000183));
#92712=CARTESIAN_POINT('Ctrl Pts',(177.949212299508,24.3963507758324,40.0000000000274));
#92713=CARTESIAN_POINT('Ctrl Pts',(177.280088553843,25.1399810127014,40.0000000000001));
#92714=CARTESIAN_POINT('Ctrl Pts',(174.895556188476,21.7926966511935,40.9999999999637));
#92715=CARTESIAN_POINT('Ctrl Pts',(174.895556188708,21.7926966509072,39.9999999999455));
#92716=CARTESIAN_POINT('Ctrl Pts',(174.287368474715,22.5882830821278,40.0000000000001));
#92717=CARTESIAN_POINT('Ctrl Pts',(172.735872865175,20.2300058704473,41.));
#92718=CARTESIAN_POINT('Ctrl Pts',(172.735872865024,20.2300058706094,39.9999999999818));
#92719=CARTESIAN_POINT('Ctrl Pts',(172.165255517355,21.0522193748322,40.0000000000001));
#92720=CARTESIAN_POINT('Ctrl Pts',(169.356441294098,18.0818577291379,41.));
#92721=CARTESIAN_POINT('Ctrl Pts',(169.356441294173,18.0818577290568,40.0000000000092));
#92722=CARTESIAN_POINT('Ctrl Pts',(168.837076511978,18.9366501155665,40.0000000000001));
#92723=CARTESIAN_POINT('Ctrl Pts',(168.204655946576,17.3977933717527,41.));
#92724=CARTESIAN_POINT('Ctrl Pts',(168.204655946514,17.3977933718631,40.));
#92725=CARTESIAN_POINT('Ctrl Pts',(167.701570963275,18.2622113948054,40.));
#92726=CARTESIAN_POINT('Ctrl Pts',(165.867055390467,16.0921286981499,41.));
#92727=CARTESIAN_POINT('Ctrl Pts',(165.867055390528,16.0921286980395,40.));
#92728=CARTESIAN_POINT('Ctrl Pts',(165.394862835991,16.973801659069,40.));
#92729=CARTESIAN_POINT('Ctrl Pts',(164.686884180974,15.473505799436,40.9999999999817));
#92730=CARTESIAN_POINT('Ctrl Pts',(164.686884180934,15.4735057995083,39.9999999999726));
#92731=CARTESIAN_POINT('Ctrl Pts',(164.229235699794,16.3627715090405,39.9999999999999));
#92732=CARTESIAN_POINT('Ctrl Pts',(161.117211964886,13.7051879643896,41.0000000000364));
#92733=CARTESIAN_POINT('Ctrl Pts',(161.117211964965,13.705187964245,40.0000000000546));
#92734=CARTESIAN_POINT('Ctrl Pts',(160.700828996284,14.6148954782875,39.9999999999999));
#92735=CARTESIAN_POINT('Ctrl Pts',(158.698784431002,12.6423350514952,40.9999999998913));
#92736=CARTESIAN_POINT('Ctrl Pts',(158.698784430949,12.6423350515778,39.999999999837));
#92737=CARTESIAN_POINT('Ctrl Pts',(158.306770084267,13.5625992022113,40.0000000000001));
#92738=CARTESIAN_POINT('Ctrl Pts',(153.802915982434,10.6924687335121,41.0000000001088));
#92739=CARTESIAN_POINT('Ctrl Pts',(153.802915982487,10.6924687334295,40.0000000001631));
#92740=CARTESIAN_POINT('Ctrl Pts',(153.454924546975,11.6302657880098,40.0000000000001));
#92741=CARTESIAN_POINT('Ctrl Pts',(151.325348981608,9.80582682032301,40.9999999999275));
#92742=CARTESIAN_POINT('Ctrl Pts',(151.32534898167,9.80582682007378,39.9999999998913));
#92743=CARTESIAN_POINT('Ctrl Pts',(150.997001969331,10.7505714530412,40.0000000000001));
#92744=CARTESIAN_POINT('Ctrl Pts',(148.824154304563,8.98894875990613,41.));
#92745=CARTESIAN_POINT('Ctrl Pts',(148.824154304563,8.98894875990614,40.0000000000001));
#92746=CARTESIAN_POINT('Ctrl Pts',(148.513697082188,9.93953611153414,40.0000000000001));
#92747=CARTESIAN_POINT('',(189.5,51.8013867006572,40.));
#92748=CARTESIAN_POINT('',(190.5,51.8013867006572,41.));
#92749=CARTESIAN_POINT('Origin',(189.5,51.8013867006572,41.));
#92750=CARTESIAN_POINT('Ctrl Pts',(148.824154304563,8.98894875990614,41.));
#92751=CARTESIAN_POINT('Ctrl Pts',(151.374396929587,9.82184564245748,41.));
#92752=CARTESIAN_POINT('Ctrl Pts',(153.894322991189,10.7254588349369,41.));
#92753=CARTESIAN_POINT('Ctrl Pts',(158.858378723721,12.7094876159781,41.));
#92754=CARTESIAN_POINT('Ctrl Pts',(161.302641161874,13.7895935121803,41.));
#92755=CARTESIAN_POINT('Ctrl Pts',(164.895576805134,15.5811002632408,41.));
#92756=CARTESIAN_POINT('Ctrl Pts',(166.080912343717,16.2069826871151,41.));
#92757=CARTESIAN_POINT('Ctrl Pts',(168.423049908267,17.5253047067075,41.));
#92758=CARTESIAN_POINT('Ctrl Pts',(169.573365929323,18.214181934056,41.));
#92759=CARTESIAN_POINT('Ctrl Pts',(172.947104141466,20.3771647370291,41.));
#92760=CARTESIAN_POINT('Ctrl Pts',(175.097030815196,21.948091086913,41.));
#92761=CARTESIAN_POINT('Ctrl Pts',(178.127203245858,24.5574879603648,41.));
#92762=CARTESIAN_POINT('Ctrl Pts',(179.104620116965,25.4696986671831,41.));
#92763=CARTESIAN_POINT('Ctrl Pts',(180.513665800821,26.9121814463635,41.));
#92764=CARTESIAN_POINT('Ctrl Pts',(180.975042758687,27.4068420809117,41.));
#92765=CARTESIAN_POINT('Ctrl Pts',(181.868856334096,28.4135619078113,41.));
#92766=CARTESIAN_POINT('Ctrl Pts',(182.301682749673,28.9258761071667,41.));
#92767=CARTESIAN_POINT('Ctrl Pts',(184.393047680122,31.533722716317,41.));
#92768=CARTESIAN_POINT('Ctrl Pts',(185.833875349279,33.7677063786469,41.));
#92769=CARTESIAN_POINT('Ctrl Pts',(187.301196170355,36.77240822161,41.));
#92770=CARTESIAN_POINT('Ctrl Pts',(187.577936119931,37.3839842039535,41.));
#92771=CARTESIAN_POINT('Ctrl Pts',(188.096717650489,38.629202283799,41.));
#92772=CARTESIAN_POINT('Ctrl Pts',(188.338665411654,39.2629767077245,41.));
#92773=CARTESIAN_POINT('Ctrl Pts',(189.004582545503,41.1792956133264,41.));
#92774=CARTESIAN_POINT('Ctrl Pts',(189.371588131973,42.4864580865601,41.));
#92775=CARTESIAN_POINT('Ctrl Pts',(190.234410487385,46.4275807179081,41.));
#92776=CARTESIAN_POINT('Ctrl Pts',(190.5,49.0966280990945,41.));
#92777=CARTESIAN_POINT('Ctrl Pts',(190.5,51.8013867006572,41.));
#92778=CARTESIAN_POINT('Ctrl Pts',(189.5,51.8013867006572,40.));
#92779=CARTESIAN_POINT('Ctrl Pts',(189.500000000381,49.5150063958733,40.));
#92780=CARTESIAN_POINT('Ctrl Pts',(189.305251220874,47.2641771162462,39.9999999999999));
#92781=CARTESIAN_POINT('Ctrl Pts',(188.892871196549,45.0530760686969,40.0000000000001));
#92782=CARTESIAN_POINT('Ctrl Pts',(188.826741633494,44.6985022835477,40.0000000000001));
#92783=CARTESIAN_POINT('Ctrl Pts',(188.755015452642,44.3449501511665,40.0000000000002));
#92784=CARTESIAN_POINT('Ctrl Pts',(188.677598163273,43.9924369200007,40.0000000000002));
#92785=CARTESIAN_POINT('Ctrl Pts',(188.676593078966,43.9878603516488,40.0000000000002));
#92786=CARTESIAN_POINT('Ctrl Pts',(188.675587035428,43.9832839585214,40.0000000000002));
#92787=CARTESIAN_POINT('Ctrl Pts',(188.674580032453,43.9787077406567,40.0000000000002));
#92788=CARTESIAN_POINT('Ctrl Pts',(188.394958895188,42.7079992378199,40.0000000000004));
#92789=CARTESIAN_POINT('Ctrl Pts',(188.041258879596,41.4508135433267,40.));
#92790=CARTESIAN_POINT('Ctrl Pts',(187.60841945111,40.2080747459915,40.));
#92791=CARTESIAN_POINT('Ctrl Pts',(187.60608126682,40.2013615120737,40.));
#92792=CARTESIAN_POINT('Ctrl Pts',(187.603740773219,40.1946486981984,40.));
#92793=CARTESIAN_POINT('Ctrl Pts',(187.601397969504,40.1879363045588,40.));
#92794=CARTESIAN_POINT('Ctrl Pts',(187.386112555457,39.5711196097217,40.));
#92795=CARTESIAN_POINT('Ctrl Pts',(187.150262439701,38.9555155944513,40.0000000000113));
#92796=CARTESIAN_POINT('Ctrl Pts',(186.897516139808,38.3511109250051,40.0000000000038));
#92797=CARTESIAN_POINT('Ctrl Pts',(186.894307237426,38.3434373187688,40.0000000000037));
#92798=CARTESIAN_POINT('Ctrl Pts',(186.891095610294,38.3357655101271,40.0000000000036));
#92799=CARTESIAN_POINT('Ctrl Pts',(186.887881265928,38.328095519511,40.0000000000035));
#92800=CARTESIAN_POINT('Ctrl Pts',(186.635165548002,37.7250713987454,39.9999999999965));
#92801=CARTESIAN_POINT('Ctrl Pts',(186.365651623061,37.1327088502353,40.));
#92802=CARTESIAN_POINT('Ctrl Pts',(186.079960250839,36.5506519989377,40.));
#92803=CARTESIAN_POINT('Ctrl Pts',(186.07580740624,36.5421911496209,40.));
#92804=CARTESIAN_POINT('Ctrl Pts',(186.071651142412,36.5337324756742,40.));
#92805=CARTESIAN_POINT('Ctrl Pts',(186.067491461228,36.5252759759054,40.));
#92806=CARTESIAN_POINT('Ctrl Pts',(184.912445383137,34.1771039736579,40.));
#92807=CARTESIAN_POINT('Ctrl Pts',(183.494489308755,31.9961998873436,39.999999999999));
#92808=CARTESIAN_POINT('Ctrl Pts',(181.848901150115,29.9601216086773,40.0000000000012));
#92809=CARTESIAN_POINT('Ctrl Pts',(181.840011734412,29.9491227775739,40.0000000000012));
#92810=CARTESIAN_POINT('Ctrl Pts',(181.831115675126,29.9381281731419,40.0000000000012));
#92811=CARTESIAN_POINT('Ctrl Pts',(181.822212977855,29.9271377918265,40.0000000000012));
#92812=CARTESIAN_POINT('Ctrl Pts',(181.417620189473,29.4276679248657,40.0000000000016));
#92813=CARTESIAN_POINT('Ctrl Pts',(180.999283430905,28.9369421095781,40.0000000000001));
#92814=CARTESIAN_POINT('Ctrl Pts',(180.567663620525,28.4546672424251,40.0000000000001));
#92815=CARTESIAN_POINT('Ctrl Pts',(180.557374801756,28.4431709241716,40.0000000000001));
#92816=CARTESIAN_POINT('Ctrl Pts',(180.547078402794,28.4316793699371,40.0000000000001));
#92817=CARTESIAN_POINT('Ctrl Pts',(180.536774431889,28.4201925785101,40.0000000000001));
#92818=CARTESIAN_POINT('Ctrl Pts',(180.105311565568,27.9392009298139,40.0000000000001));
#92819=CARTESIAN_POINT('Ctrl Pts',(179.660998793274,27.4671830454874,40.0000000000089));
#92820=CARTESIAN_POINT('Ctrl Pts',(179.208941172121,27.0080712980567,40.0000000000045));
#92821=CARTESIAN_POINT('Ctrl Pts',(179.19731416185,26.9962628542807,40.0000000000044));
#92822=CARTESIAN_POINT('Ctrl Pts',(179.185681914772,26.9844628235726,40.0000000000043));
#92823=CARTESIAN_POINT('Ctrl Pts',(179.174044515442,26.9726712705521,40.0000000000042));
#92824=CARTESIAN_POINT('Ctrl Pts',(178.499085028626,26.2887709978425,39.999999999998));
#92825=CARTESIAN_POINT('Ctrl Pts',(177.804262150814,25.6304014524943,39.9999999999994));
#92826=CARTESIAN_POINT('Ctrl Pts',(177.091787308052,24.9950133496928,40.0000000000011));
#92827=CARTESIAN_POINT('Ctrl Pts',(176.838514100436,24.7691432231717,40.0000000000016));
#92828=CARTESIAN_POINT('Ctrl Pts',(176.583010542457,24.5461768349467,40.0000000000027));
#92829=CARTESIAN_POINT('Ctrl Pts',(176.325376910205,24.325998452793,40.0000000000056));
#92830=CARTESIAN_POINT('Ctrl Pts',(176.311096984169,24.3137945686019,40.0000000000057));
#92831=CARTESIAN_POINT('Ctrl Pts',(176.296810486525,24.3015992278323,40.0000000000059));
#92832=CARTESIAN_POINT('Ctrl Pts',(176.282517433164,24.2894124098309,40.0000000000061));
#92833=CARTESIAN_POINT('Ctrl Pts',(174.305240624492,22.6035086356279,40.0000000000279));
#92834=CARTESIAN_POINT('Ctrl Pts',(172.203250088958,21.0797419335985,39.9999999999525));
#92835=CARTESIAN_POINT('Ctrl Pts',(170.006058541585,19.6797512754289,40.0000000000483));
#92836=CARTESIAN_POINT('Ctrl Pts',(169.98620495979,19.6671011134178,40.0000000000492));
#92837=CARTESIAN_POINT('Ctrl Pts',(169.96634374653,19.6544611562793,40.00000000005));
#92838=CARTESIAN_POINT('Ctrl Pts',(169.946474915949,19.6418313700356,40.0000000000508));
#92839=CARTESIAN_POINT('Ctrl Pts',(169.265312398142,19.2088447902787,40.0000000000772));
#92840=CARTESIAN_POINT('Ctrl Pts',(168.57446714291,18.7875560756054,40.0000000000313));
#92841=CARTESIAN_POINT('Ctrl Pts',(167.875526707261,18.3776388152218,40.0000000000131));
#92842=CARTESIAN_POINT('Ctrl Pts',(167.458565391396,18.1330977476744,40.0000000000022));
#92843=CARTESIAN_POINT('Ctrl Pts',(167.038722359307,17.8926044574574,40.0000000000005));
#92844=CARTESIAN_POINT('Ctrl Pts',(166.616329946493,17.6560969384847,40.0000000000003));
#92845=CARTESIAN_POINT('Ctrl Pts',(166.593633120015,17.6433884476215,40.0000000000002));
#92846=CARTESIAN_POINT('Ctrl Pts',(166.570928868342,17.6306914358825,40.0000000000002));
#92847=CARTESIAN_POINT('Ctrl Pts',(166.54821725046,17.6180058988327,40.0000000000002));
#92848=CARTESIAN_POINT('Ctrl Pts',(165.41908891768,16.9873331139122,39.9999999999997));
#92849=CARTESIAN_POINT('Ctrl Pts',(164.277098272627,16.3878383790561,39.9999999999967));
#92850=CARTESIAN_POINT('Ctrl Pts',(163.123421206771,15.8150185333796,40.0000000000032));
#92851=CARTESIAN_POINT('Ctrl Pts',(163.099985980906,15.8033825540742,40.0000000000034));
#92852=CARTESIAN_POINT('Ctrl Pts',(163.076546021088,15.7917576290974,40.0000000000035));
#92853=CARTESIAN_POINT('Ctrl Pts',(163.053101341965,15.7801437228353,40.0000000000036));
#92854=CARTESIAN_POINT('Ctrl Pts',(161.986099857154,15.2515779377907,40.0000000000097));
#92855=CARTESIAN_POINT('Ctrl Pts',(160.909372419548,14.7457024936771,40.0000000000103));
#92856=CARTESIAN_POINT('Ctrl Pts',(159.823918020749,14.2601912942237,40.0000000000086));
#92857=CARTESIAN_POINT('Ctrl Pts',(158.70516141636,13.7597844033452,40.0000000000068));
#92858=CARTESIAN_POINT('Ctrl Pts',(157.577134187948,13.2810103531194,40.0000000000028));
#92859=CARTESIAN_POINT('Ctrl Pts',(156.440948827796,12.8212705536111,40.0000000000148));
#92860=CARTESIAN_POINT('Ctrl Pts',(156.270965230959,12.7524893252391,40.0000000000166));
#92861=CARTESIAN_POINT('Ctrl Pts',(156.100799064079,12.6841340486979,40.0000000000189));
#92862=CARTESIAN_POINT('Ctrl Pts',(155.930454085978,12.6161959298486,40.000000000022));
#92863=CARTESIAN_POINT('Ctrl Pts',(155.913921012608,12.6096020993987,40.0000000000223));
#92864=CARTESIAN_POINT('Ctrl Pts',(155.897386254016,12.6030121998952,40.0000000000226));
#92865=CARTESIAN_POINT('Ctrl Pts',(155.880849813508,12.5964262232311,40.0000000000228));
#92866=CARTESIAN_POINT('Ctrl Pts',(154.560886364425,12.0707237016309,40.0000000000461));
#92867=CARTESIAN_POINT('Ctrl Pts',(153.23016485382,11.5701212714179,40.0000000000271));
#92868=CARTESIAN_POINT('Ctrl Pts',(151.889842870709,11.0919212256656,40.0000000000128));
#92869=CARTESIAN_POINT('Ctrl Pts',(150.770923688729,10.6927132661168,40.0000000000009));
#92870=CARTESIAN_POINT('Ctrl Pts',(149.645314177788,10.3091167708951,40.0000000000001));
#92871=CARTESIAN_POINT('Ctrl Pts',(148.513697082188,9.9395361115339,40.0000000000001));
#92872=CARTESIAN_POINT('Origin',(149.134611526938,8.03836140827812,150.608250755187));
#92873=CARTESIAN_POINT('',(148.824154304613,8.98894875992246,150.608250755187));
#92874=CARTESIAN_POINT('Origin',(149.134611526927,8.03836140827455,150.608250755186));
#92875=CARTESIAN_POINT('',(148.824154304563,8.98894875990614,150.608250755187));
#92876=CARTESIAN_POINT('Origin',(125.29348064571,25.4505574462982,152.608250755187));
#92877=CARTESIAN_POINT('',(95.8129088738133,23.8757620423259,151.608250755187));
#92878=CARTESIAN_POINT('Origin',(95.8129088738133,23.8757620423259,152.608250755187));
#92879=CARTESIAN_POINT('Origin',(125.29348064571,25.4505574462982,151.608250755187));
#92880=CARTESIAN_POINT('Origin',(189.5,59.,41.));
#92881=CARTESIAN_POINT('',(189.5,51.8013867006572,40.));
#92882=CARTESIAN_POINT('',(190.5,54.9,41.));
#92883=CARTESIAN_POINT('Ctrl Pts',(150.890053008323,10.740031424167,151.608250755187));
#92884=CARTESIAN_POINT('Ctrl Pts',(150.023036902254,11.238311537975,151.608250755187));
#92885=CARTESIAN_POINT('Ctrl Pts',(150.023036902254,11.238311537975,152.608250755187));
#92886=CARTESIAN_POINT('Ctrl Pts',(150.679848671071,10.5466203837958,151.608250755187));
#92887=CARTESIAN_POINT('Ctrl Pts',(149.898373926292,11.0213957787624,151.690671913218));
#92888=CARTESIAN_POINT('Ctrl Pts',(149.856007771352,10.9476779311712,152.608250750006));
#92889=CARTESIAN_POINT('Ctrl Pts',(150.469500865012,10.3582448836075,151.58941017031));
#92890=CARTESIAN_POINT('Ctrl Pts',(149.756882065769,10.7815385921042,151.738129573559));
#92891=CARTESIAN_POINT('Ctrl Pts',(149.686939041021,10.6653465091927,152.570569586968));
#92892=CARTESIAN_POINT('Ctrl Pts',(150.049234791875,9.99119406960843,151.515506211375));
#92893=CARTESIAN_POINT('Ctrl Pts',(149.461299151908,10.2989599789586,151.749878235574));
#92894=CARTESIAN_POINT('Ctrl Pts',(149.345761369004,10.1165733930159,152.422761666028));
#92895=CARTESIAN_POINT('Ctrl Pts',(149.836710770193,9.81044310313042,151.459547614775));
#92896=CARTESIAN_POINT('Ctrl Pts',(149.304412653593,10.0509204841014,151.718712252751));
#92897=CARTESIAN_POINT('Ctrl Pts',(149.17146532147,9.8470577724018,152.310844478137));
#92898=CARTESIAN_POINT('Ctrl Pts',(149.43689869125,9.477996755743,151.305510205471));
#92899=CARTESIAN_POINT('Ctrl Pts',(149.002736057782,9.5899170411257,151.566756275077));
#92900=CARTESIAN_POINT('Ctrl Pts',(148.840879579051,9.35250297616965,152.002769651981));
#92901=CARTESIAN_POINT('Ctrl Pts',(149.244022866828,9.32177597503067,151.206172324202));
#92902=CARTESIAN_POINT('Ctrl Pts',(148.851344778941,9.36640628955775,151.448241697994));
#92903=CARTESIAN_POINT('Ctrl Pts',(148.679929727225,9.12075031956211,151.80409390049));
#92904=CARTESIAN_POINT('Ctrl Pts',(149.013179253012,9.13764052726729,151.012654819751));
#92905=CARTESIAN_POINT('Ctrl Pts',(148.668260894911,9.10226279678571,151.186102695064));
#92906=CARTESIAN_POINT('Ctrl Pts',(148.486316262615,8.84803681808999,151.41705888068));
#92907=CARTESIAN_POINT('Ctrl Pts',(148.946252751058,9.08480391731076,150.940166521214));
#92908=CARTESIAN_POINT('Ctrl Pts',(148.614853057507,9.02629227892066,151.085099511553));
#92909=CARTESIAN_POINT('Ctrl Pts',(148.429993799101,8.76987161641128,151.272082289649));
#92910=CARTESIAN_POINT('Ctrl Pts',(148.851443947787,9.01024718564305,150.781805962456));
#92911=CARTESIAN_POINT('Ctrl Pts',(148.539419389592,8.91959726288131,150.860017320521));
#92912=CARTESIAN_POINT('Ctrl Pts',(148.350106592124,8.65962177792194,150.955361167317));
#92913=CARTESIAN_POINT('Ctrl Pts',(148.824154321238,8.98894876535212,150.695048022002));
#92914=CARTESIAN_POINT('Ctrl Pts',(148.517388962888,8.88876069858572,150.733964227236));
#92915=CARTESIAN_POINT('Ctrl Pts',(148.327056364841,8.62815345652074,150.78184529078));
#92916=CARTESIAN_POINT('Ctrl Pts',(148.824154304563,8.98894875990614,150.608250755186));
#92917=CARTESIAN_POINT('Ctrl Pts',(148.517388951131,8.88876068209877,150.608250755186));
#92918=CARTESIAN_POINT('Ctrl Pts',(148.327056352437,8.62815343953653,150.608250755186));
#92919=CARTESIAN_POINT('',(150.890034276198,10.7400141885713,151.608250755137));
#92920=CARTESIAN_POINT('Origin',(150.890053008323,10.740031424167,152.608250755187));
#92921=CARTESIAN_POINT('Ctrl Pts',(150.890034276198,10.7400141885713,151.608250755137));
#92922=CARTESIAN_POINT('Ctrl Pts',(150.702220874324,10.5672055383393,151.60824975506));
#92923=CARTESIAN_POINT('Ctrl Pts',(150.513515802512,10.3977022423503,151.593212219756));
#92924=CARTESIAN_POINT('Ctrl Pts',(150.32404987297,10.2313684559334,151.563261500175));
#92925=CARTESIAN_POINT('Ctrl Pts',(150.302482255713,10.2124340572738,151.55985209745));
#92926=CARTESIAN_POINT('Ctrl Pts',(150.28092156319,10.1935549579782,151.556251950677));
#92927=CARTESIAN_POINT('Ctrl Pts',(150.259359907948,10.1747237977009,151.552460508724));
#92928=CARTESIAN_POINT('Ctrl Pts',(150.196877948972,10.1201543423087,151.541473563708));
#92929=CARTESIAN_POINT('Ctrl Pts',(150.134156936491,10.0658027349855,151.528804384371));
#92930=CARTESIAN_POINT('Ctrl Pts',(150.07139188021,10.0118119412705,151.51433719755));
#92931=CARTESIAN_POINT('Ctrl Pts',(150.015325641343,9.96358350149239,151.501414071211));
#92932=CARTESIAN_POINT('Ctrl Pts',(149.959223383041,9.9156424153212,151.487055826325));
#92933=CARTESIAN_POINT('Ctrl Pts',(149.903238759799,9.86810887537708,151.471148343347));
#92934=CARTESIAN_POINT('Ctrl Pts',(149.85352379096,9.82589856261102,151.457022321329));
#92935=CARTESIAN_POINT('Ctrl Pts',(149.803901299349,9.7840094868303,151.441674307829));
#92936=CARTESIAN_POINT('Ctrl Pts',(149.754498021731,9.74254510422443,151.425002834105));
#92937=CARTESIAN_POINT('Ctrl Pts',(149.715112765934,9.70948889026117,151.411712010322));
#92938=CARTESIAN_POINT('Ctrl Pts',(149.675856770622,9.67669314558932,151.397575569593));
#92939=CARTESIAN_POINT('Ctrl Pts',(149.636803961062,9.6442201983715,151.382529318118));
#92940=CARTESIAN_POINT('Ctrl Pts',(149.594993458305,9.60945419140713,151.366420583668));
#92941=CARTESIAN_POINT('Ctrl Pts',(149.553169819802,9.57485906888988,151.349214625101));
#92942=CARTESIAN_POINT('Ctrl Pts',(149.51159298729,9.54063089633836,151.330765820964));
#92943=CARTESIAN_POINT('Ctrl Pts',(149.498919450395,9.53019739331577,151.325142217968));
#92944=CARTESIAN_POINT('Ctrl Pts',(149.48626910023,9.51979819119965,151.319402992941));
#92945=CARTESIAN_POINT('Ctrl Pts',(149.473650016671,9.50943941894691,151.313543636607));
#92946=CARTESIAN_POINT('Ctrl Pts',(149.440007168315,9.48182262709181,151.297922420085));
#92947=CARTESIAN_POINT('Ctrl Pts',(149.406484061281,9.45440888248824,151.281402363808));
#92948=CARTESIAN_POINT('Ctrl Pts',(149.373220289311,9.42730489399397,151.263853428368));
#92949=CARTESIAN_POINT('Ctrl Pts',(149.342132586372,9.401974010187,151.247452519526));
#92950=CARTESIAN_POINT('Ctrl Pts',(149.311271225832,9.3769135727762,151.23015290458));
#92951=CARTESIAN_POINT('Ctrl Pts',(149.280781733949,9.352236209495,151.211831178815));
#92952=CARTESIAN_POINT('Ctrl Pts',(149.254017698261,9.33057412886442,151.19574815178));
#92953=CARTESIAN_POINT('Ctrl Pts',(149.227540417594,9.30920741102851,151.178877360186));
#92954=CARTESIAN_POINT('Ctrl Pts',(149.201472558853,9.28823154460514,151.161123285777));
#92955=CARTESIAN_POINT('Ctrl Pts',(149.178745519636,9.26994391524619,151.145644548172));
#92956=CARTESIAN_POINT('Ctrl Pts',(149.156284165708,9.25191801548321,151.129467025821));
#92957=CARTESIAN_POINT('Ctrl Pts',(149.134140819759,9.23419340628573,151.112465523864));
#92958=CARTESIAN_POINT('Ctrl Pts',(149.119315419052,9.2223264357599,151.101082687697));
#92959=CARTESIAN_POINT('Ctrl Pts',(149.10463318418,9.21059503744752,151.089330111665));
#92960=CARTESIAN_POINT('Ctrl Pts',(149.090119188631,9.19901878583329,151.077164926928));
#92961=CARTESIAN_POINT('Ctrl Pts',(149.072065293653,9.18461913756459,151.062032707349));
#92962=CARTESIAN_POINT('Ctrl Pts',(149.054284809231,9.1704676159025,151.04623098932));
#92963=CARTESIAN_POINT('Ctrl Pts',(149.036925482486,9.15667686664026,151.029695222165));
#92964=CARTESIAN_POINT('Ctrl Pts',(149.020628290217,9.14372990760409,151.014171199799));
#92965=CARTESIAN_POINT('Ctrl Pts',(149.004702141776,9.1311008202778,150.998000123864));
#92966=CARTESIAN_POINT('Ctrl Pts',(148.989304616076,9.11891023333167,150.981123519122));
#92967=CARTESIAN_POINT('Ctrl Pts',(148.978126890576,9.11006056246756,150.968872066593));
#92968=CARTESIAN_POINT('Ctrl Pts',(148.967228418988,9.10144250223408,150.956248701183));
#92969=CARTESIAN_POINT('Ctrl Pts',(148.956683203421,9.09311277673819,150.943229559169));
#92970=CARTESIAN_POINT('Ctrl Pts',(148.94495349998,9.08384741756284,150.928748046306));
#92971=CARTESIAN_POINT('Ctrl Pts',(148.933584378101,9.07489430584278,150.913728163051));
#92972=CARTESIAN_POINT('Ctrl Pts',(148.922730874631,9.06635281780613,150.898085641888));
#92973=CARTESIAN_POINT('Ctrl Pts',(148.917030133927,9.06186645000287,150.889869496995));
#92974=CARTESIAN_POINT('Ctrl Pts',(148.911472216629,9.05749419673198,150.881481585143));
#92975=CARTESIAN_POINT('Ctrl Pts',(148.906083889309,9.05325444445017,150.872909874024));
#92976=CARTESIAN_POINT('Ctrl Pts',(148.903614104637,9.05131111870578,150.868980958893));
#92977=CARTESIAN_POINT('Ctrl Pts',(148.901179323965,9.04939580803512,150.865014674827));
#92978=CARTESIAN_POINT('Ctrl Pts',(148.898781146499,9.04750992291207,150.86100941786));
#92979=CARTESIAN_POINT('Ctrl Pts',(148.890200772378,9.04076246567011,150.846679117571));
#92980=CARTESIAN_POINT('Ctrl Pts',(148.882105340252,9.03440329935373,150.831820967099));
#92981=CARTESIAN_POINT('Ctrl Pts',(148.874581296409,9.02850640119304,150.816392770031));
#92982=CARTESIAN_POINT('Ctrl Pts',(148.870885359862,9.02560974589988,150.808814180834));
#92983=CARTESIAN_POINT('Ctrl Pts',(148.867327896282,9.02282506859138,150.801098019324));
#92984=CARTESIAN_POINT('Ctrl Pts',(148.863922930779,9.02016392556131,150.793239294057));
#92985=CARTESIAN_POINT('Ctrl Pts',(148.8577859103,9.015367551189,150.779074933838));
#92986=CARTESIAN_POINT('Ctrl Pts',(148.852233457605,9.01101353123725,150.764504006908));
#92987=CARTESIAN_POINT('Ctrl Pts',(148.847355686723,9.00718402694656,150.749595709683));
#92988=CARTESIAN_POINT('Ctrl Pts',(148.839939029894,9.00136126080139,150.726927624791));
#92989=CARTESIAN_POINT('Ctrl Pts',(148.834072242688,8.99674936577631,150.703484221276));
#92990=CARTESIAN_POINT('Ctrl Pts',(148.830097384467,8.99362376040685,150.679507686099));
#92991=CARTESIAN_POINT('Ctrl Pts',(148.82622971412,8.99058244156457,150.656177713313));
#92992=CARTESIAN_POINT('Ctrl Pts',(148.824154304567,8.98894875990739,150.63234387459));
#92993=CARTESIAN_POINT('Ctrl Pts',(148.824154304563,8.98894875990613,150.608250755187));
#92994=CARTESIAN_POINT('Origin',(95.8129088738133,23.8757620423259,152.608250755187));
#92995=CARTESIAN_POINT('',(95.8129088738133,24.8757620423259,152.608250755187));
#92996=CARTESIAN_POINT('Origin',(95.8129088738133,23.8757620423259,152.608250755187));
#92997=CARTESIAN_POINT('Origin',(95.8129088738133,23.8757620423259,152.608250755187));
#92998=CARTESIAN_POINT('Origin',(125.29348064571,25.4505574462982,152.608250755187));
#92999=CARTESIAN_POINT('',(154.774052417606,23.8757620423259,151.608250755187));
#93000=CARTESIAN_POINT('Origin',(154.774052417606,23.8757620423259,152.608250755187));
#93001=CARTESIAN_POINT('Origin',(125.29348064571,25.4505574462982,151.608250755187));
#93002=CARTESIAN_POINT('Origin',(95.8129088738133,23.8757620423259,200.));
#93003=CARTESIAN_POINT('',(95.8129088734846,24.8757620423263,194.272015611497));
#93004=CARTESIAN_POINT('Origin',(95.8129088738133,23.8757620423259,194.272013743528));
#93005=CARTESIAN_POINT('',(95.8129088738133,24.8757620423259,209.282162333937));
#93006=CARTESIAN_POINT('Origin',(154.774052417606,23.8757620423259,152.608250755187));
#93007=CARTESIAN_POINT('',(154.774052417606,24.8757620423259,152.608250755187));
#93008=CARTESIAN_POINT('Origin',(154.774052417606,23.8757620423259,152.608250755187));
#93009=CARTESIAN_POINT('Origin',(154.774052417606,23.8757620423259,152.608250755187));
#93010=CARTESIAN_POINT('Ctrl Pts',(95.8129088738133,24.8757620423259,194.272013743528));
#93011=CARTESIAN_POINT('Ctrl Pts',(96.7609165275083,24.8757620423259,194.272013743528));
#93012=CARTESIAN_POINT('Ctrl Pts',(96.8114851745877,23.9291040663932,194.272013743528));
#93013=CARTESIAN_POINT('Ctrl Pts',(95.8079727953211,24.8757620423259,194.394449674887));
#93014=CARTESIAN_POINT('Ctrl Pts',(96.7606658729216,24.8804543649553,194.400983611462));
#93015=CARTESIAN_POINT('Ctrl Pts',(96.8114851740455,23.9291040765447,194.51649042457));
#93016=CARTESIAN_POINT('Ctrl Pts',(95.8006244305256,24.8980341121937,194.515591412477));
#93017=CARTESIAN_POINT('Ctrl Pts',(96.760522851172,24.910116493455,194.526658900505));
#93018=CARTESIAN_POINT('Ctrl Pts',(96.8090937438902,23.9721393953228,194.758275720961));
#93019=CARTESIAN_POINT('Ctrl Pts',(95.7873179138766,24.9635088171672,194.687547735987));
#93020=CARTESIAN_POINT('Ctrl Pts',(96.7608130482612,24.986259065464,194.698633486749));
#93021=CARTESIAN_POINT('Ctrl Pts',(96.8029028333402,24.098653234827,195.101372403818));
#93022=CARTESIAN_POINT('Ctrl Pts',(95.7826072263359,24.9902403040083,194.74214852889));
#93023=CARTESIAN_POINT('Ctrl Pts',(96.7609969780626,25.0165323795395,194.752374177845));
#93024=CARTESIAN_POINT('Ctrl Pts',(96.8004649444392,24.1503052933488,195.210295541072));
#93025=CARTESIAN_POINT('Ctrl Pts',(95.7729687455057,25.0532515622315,194.846058360888));
#93026=CARTESIAN_POINT('Ctrl Pts',(96.7615918607211,25.0855066901878,194.852621305907));
#93027=CARTESIAN_POINT('Ctrl Pts',(96.7951694477337,24.2720591317408,195.417558574747));
#93028=CARTESIAN_POINT('Ctrl Pts',(95.7679900091412,25.0899771867542,194.895826418653));
#93029=CARTESIAN_POINT('Ctrl Pts',(96.7620107784742,25.1247157442461,194.899520222782));
#93030=CARTESIAN_POINT('Ctrl Pts',(96.7922803023377,24.3430224150016,195.516813717754));
#93031=CARTESIAN_POINT('Ctrl Pts',(95.7584833321546,25.1712173600468,194.987060242779));
#93032=CARTESIAN_POINT('Ctrl Pts',(96.7630842785473,25.2087962452066,194.983645143531));
#93033=CARTESIAN_POINT('Ctrl Pts',(96.7866131605335,24.4999991676107,195.698751372675));
#93034=CARTESIAN_POINT('Ctrl Pts',(95.7539645643008,25.2155346348072,195.028519785351));
#93035=CARTESIAN_POINT('Ctrl Pts',(96.7637357976572,25.2535048092381,195.020845409791));
#93036=CARTESIAN_POINT('Ctrl Pts',(96.7838438654193,24.5856314571151,195.781421806259));
#93037=CARTESIAN_POINT('Ctrl Pts',(95.7457923218438,25.3114864345674,195.10320966763));
#93038=CARTESIAN_POINT('Ctrl Pts',(96.7652338888118,25.3476725061538,195.086601753473));
#93039=CARTESIAN_POINT('Ctrl Pts',(96.7788223919801,24.7710348316154,195.930352581545));
#93040=CARTESIAN_POINT('Ctrl Pts',(95.7421172576637,25.3636687358292,195.136650236237));
#93041=CARTESIAN_POINT('Ctrl Pts',(96.7660895466707,25.3976087993447,195.115261771168));
#93042=CARTESIAN_POINT('Ctrl Pts',(96.7765574337878,24.8718643595615,195.997032176725));
#93043=CARTESIAN_POINT('Ctrl Pts',(95.7333832975172,25.5258065749971,195.22061596659));
#93044=CARTESIAN_POINT('Ctrl Pts',(96.7687559909472,25.5496067281877,195.186532790236));
#93045=CARTESIAN_POINT('Ctrl Pts',(96.7713474235503,25.1851560562777,196.164477575663));
#93046=CARTESIAN_POINT('Ctrl Pts',(95.7304688922887,25.6430766735032,195.256533916462));
#93047=CARTESIAN_POINT('Ctrl Pts',(96.7706567312437,25.6544438350804,195.215613536792));
#93048=CARTESIAN_POINT('Ctrl Pts',(96.7699131986613,25.4117499178439,196.23613851731));
#93049=CARTESIAN_POINT('Ctrl Pts',(95.7316383541684,25.7661094150365,195.270070553806));
#93050=CARTESIAN_POINT('Ctrl Pts',(96.7723664237184,25.763493773239,195.227911042172));
#93051=CARTESIAN_POINT('Ctrl Pts',(96.7715712560824,25.6494824928011,196.263237066376));
#93052=CARTESIAN_POINT('',(95.731638354191,25.7661094150387,195.270070553806));
#93053=CARTESIAN_POINT('Origin',(95.7715955767732,25.6564567877472,196.263237066376));
#93054=CARTESIAN_POINT('Ctrl Pts',(95.8129087986265,24.8757620423276,194.272015608479));
#93055=CARTESIAN_POINT('Ctrl Pts',(95.8111599846757,24.8757621224561,194.315393480133));
#93056=CARTESIAN_POINT('Ctrl Pts',(95.8091170484719,24.8785534558019,194.358408096338));
#93057=CARTESIAN_POINT('Ctrl Pts',(95.8068203772479,24.8840451859619,194.400933950253));
#93058=CARTESIAN_POINT('Ctrl Pts',(95.8045026574643,24.8895872467953,194.443849545618));
#93059=CARTESIAN_POINT('Ctrl Pts',(95.8019264129473,24.8978795127077,194.486268093549));
#93060=CARTESIAN_POINT('Ctrl Pts',(95.7991270967733,24.9088812271481,194.528059904604));
#93061=CARTESIAN_POINT('Ctrl Pts',(95.79682015952,24.9179478217431,194.562500846539));
#93062=CARTESIAN_POINT('Ctrl Pts',(95.7943615808282,24.9288555341911,194.596516310934));
#93063=CARTESIAN_POINT('Ctrl Pts',(95.7917690076823,24.9416074763769,194.630028143149));
#93064=CARTESIAN_POINT('Ctrl Pts',(95.7917638288634,24.941632949139,194.630095085025));
#93065=CARTESIAN_POINT('Ctrl Pts',(95.7917586495273,24.9416584291797,194.630162024657));
#93066=CARTESIAN_POINT('Ctrl Pts',(95.7917534696742,24.9416839164987,194.630228962045));
#93067=CARTESIAN_POINT('Ctrl Pts',(95.787316972302,24.9635135747863,194.687560229433));
#93068=CARTESIAN_POINT('Ctrl Pts',(95.7826068075667,24.9902431242573,194.74215317923));
#93069=CARTESIAN_POINT('Ctrl Pts',(95.7777879962155,25.0217459334254,194.794103444976));
#93070=CARTESIAN_POINT('Ctrl Pts',(95.7729914787601,25.0531029970358,194.845813366426));
#93071=CARTESIAN_POINT('Ctrl Pts',(95.7680367191655,25.0896312250587,194.895360130286));
#93072=CARTESIAN_POINT('Ctrl Pts',(95.7633016033217,25.1300430217835,194.940820367825));
#93073=CARTESIAN_POINT('Ctrl Pts',(95.7632799654491,25.1302276899813,194.941028105684));
#93074=CARTESIAN_POINT('Ctrl Pts',(95.7632583319708,25.1304124409499,194.941235760046));
#93075=CARTESIAN_POINT('Ctrl Pts',(95.7632367029239,25.1305972745647,194.941443330717));
#93076=CARTESIAN_POINT('Ctrl Pts',(95.7584926044537,25.1711385372072,194.986971721539));
#93077=CARTESIAN_POINT('Ctrl Pts',(95.7539707476346,25.2154626761908,195.028463770006));
#93078=CARTESIAN_POINT('Ctrl Pts',(95.7498784975762,25.263510536673,195.065864725834));
#93079=CARTESIAN_POINT('Ctrl Pts',(95.7457948977628,25.3114568330366,195.103186623092));
#93080=CARTESIAN_POINT('Ctrl Pts',(95.7421178281146,25.3636590503685,195.136645218593));
#93081=CARTESIAN_POINT('Ctrl Pts',(95.7392059782138,25.4177146834181,195.164638812005));
#93082=CARTESIAN_POINT('Ctrl Pts',(95.7362880075347,25.4718839427025,195.192691248621));
#93083=CARTESIAN_POINT('Ctrl Pts',(95.7341019804868,25.5283457376407,195.215693951352));
#93084=CARTESIAN_POINT('Ctrl Pts',(95.7327939124058,25.5865853949566,195.233353660436));
#93085=CARTESIAN_POINT('Ctrl Pts',(95.7315641209546,25.6413399094394,195.249956587743));
#93086=CARTESIAN_POINT('Ctrl Pts',(95.7311104577768,25.6976651602042,195.261836989884));
#93087=CARTESIAN_POINT('Ctrl Pts',(95.7315446396439,25.7551239438692,195.268800596824));
#93088=CARTESIAN_POINT('Ctrl Pts',(95.7315722754624,25.7587812143241,195.269243832693));
#93089=CARTESIAN_POINT('Ctrl Pts',(95.7316035045552,25.7624430757672,195.269667166021));
#93090=CARTESIAN_POINT('Ctrl Pts',(95.731638354173,25.7661094150365,195.270070553806));
#93091=CARTESIAN_POINT('Origin',(154.774052417606,23.8757620423259,200.));
#93092=CARTESIAN_POINT('',(154.774052417606,24.8757620428585,184.081718857687));
#93093=CARTESIAN_POINT('Origin',(154.774052417606,23.8757620423259,184.081718857688));
#93094=CARTESIAN_POINT('',(154.774052417606,24.8757620423259,209.282162333937));
#93095=CARTESIAN_POINT('Ctrl Pts',(95.7316383541684,25.7661094150367,195.270070553806));
#93096=CARTESIAN_POINT('Ctrl Pts',(96.7723664237184,25.7634937732391,195.227911042172));
#93097=CARTESIAN_POINT('Ctrl Pts',(96.7715712560824,25.6494824928014,196.263237066376));
#93098=CARTESIAN_POINT('Ctrl Pts',(95.7431185671264,26.8818810097605,195.392797778142));
#93099=CARTESIAN_POINT('Ctrl Pts',(96.7843087616111,26.8373701392618,195.349876958745));
#93100=CARTESIAN_POINT('Ctrl Pts',(96.779337565007,26.7630172805684,196.390166135436));
#93101=CARTESIAN_POINT('Ctrl Pts',(95.8218441751224,27.9971373813779,195.450206233717));
#93102=CARTESIAN_POINT('Ctrl Pts',(96.8559141943711,27.9051069966177,195.411323729247));
#93103=CARTESIAN_POINT('Ctrl Pts',(96.8521036068265,27.8758205758653,196.449663888928));
#93104=CARTESIAN_POINT('Ctrl Pts',(95.9690444983148,29.1114187506901,195.445834017246));
#93105=CARTESIAN_POINT('Ctrl Pts',(96.9905454909872,28.9836527494144,195.415492891841));
#93106=CARTESIAN_POINT('Ctrl Pts',(96.9910158671794,28.9874167683923,196.445393189885));
#93107=CARTESIAN_POINT('',(95.9690447990561,29.111418071869,195.445834751564));
#93108=CARTESIAN_POINT('Origin',(95.9987338969782,29.1114187506901,196.445393189885));
#93109=CARTESIAN_POINT('Ctrl Pts',(95.7316383541731,25.7661094150388,195.270070553806));
#93110=CARTESIAN_POINT('Ctrl Pts',(95.7406061566686,26.6376977150264,195.365939290139));
#93111=CARTESIAN_POINT('Ctrl Pts',(95.790599427845,27.508471439827,195.421899098602));
#93112=CARTESIAN_POINT('Ctrl Pts',(95.882078879369,28.3783025745837,195.439761788028));
#93113=CARTESIAN_POINT('Ctrl Pts',(95.9077872007393,28.6227498026515,195.444781710564));
#93114=CARTESIAN_POINT('Ctrl Pts',(95.9367721585806,28.8671225938835,195.446792581224));
#93115=CARTESIAN_POINT('Ctrl Pts',(95.9690444149639,29.1114181197373,195.445834019721));
#93116=CARTESIAN_POINT('Ctrl Pts',(154.442742286491,25.4284918940124,185.219477651476));
#93117=CARTESIAN_POINT('Ctrl Pts',(153.817575691237,25.3176612644957,185.442322230393));
#93118=CARTESIAN_POINT('Ctrl Pts',(153.812479229217,24.9971192497071,186.033932954978));
#93119=CARTESIAN_POINT('Ctrl Pts',(154.472026398247,25.2558401938721,185.111373906101));
#93120=CARTESIAN_POINT('Ctrl Pts',(153.818074697533,25.110693010453,185.299575711385));
#93121=CARTESIAN_POINT('Ctrl Pts',(153.807172637763,24.6633611425982,185.846711293107));
#93122=CARTESIAN_POINT('Ctrl Pts',(154.516058475459,25.1137033968244,184.943001574196));
#93123=CARTESIAN_POINT('Ctrl Pts',(153.817447383613,24.9564514213952,185.077611618409));
#93124=CARTESIAN_POINT('Ctrl Pts',(153.796905931419,24.388867509514,185.554961769222));
#93125=CARTESIAN_POINT('Ctrl Pts',(154.600746940777,24.9716430335893,184.644296030959));
#93126=CARTESIAN_POINT('Ctrl Pts',(153.818898801799,24.8420834669797,184.714743312115));
#93127=CARTESIAN_POINT('Ctrl Pts',(153.784915835979,24.1143706192211,185.041138096643));
#93128=CARTESIAN_POINT('Ctrl Pts',(154.632378374674,24.9354624397147,184.535985737446));
#93129=CARTESIAN_POINT('Ctrl Pts',(153.819796875227,24.8226658090599,184.584352025953));
#93130=CARTESIAN_POINT('Ctrl Pts',(153.781441235691,24.0444604764696,184.855381098777));
#93131=CARTESIAN_POINT('Ctrl Pts',(154.699685066687,24.8878568443247,184.31420127492));
#93132=CARTESIAN_POINT('Ctrl Pts',(153.822398663114,24.8213877551996,184.328869994504));
#93133=CARTESIAN_POINT('Ctrl Pts',(153.776752125358,23.9524743105778,184.476529617814));
#93134=CARTESIAN_POINT('Ctrl Pts',(154.735994047269,24.8757620423259,184.1985843258));
#93135=CARTESIAN_POINT('Ctrl Pts',(153.824151134487,24.8403128253378,184.200581623196));
#93136=CARTESIAN_POINT('Ctrl Pts',(153.775476116835,23.9291040664471,184.279754424779));
#93137=CARTESIAN_POINT('Ctrl Pts',(154.774052417606,24.8757620423259,184.081718857687));
#93138=CARTESIAN_POINT('Ctrl Pts',(153.826044763911,24.8757620423257,184.081718857687));
#93139=CARTESIAN_POINT('Ctrl Pts',(153.775476116832,23.9291040663932,184.081718857688));
#93140=CARTESIAN_POINT('',(154.442742286966,25.4284918937499,185.219477651102));
#93141=CARTESIAN_POINT('Origin',(154.812352855916,24.9812217457127,186.033932954964));
#93142=CARTESIAN_POINT('Ctrl Pts',(154.44274228656,25.4284918936062,185.219477651221));
#93143=CARTESIAN_POINT('Ctrl Pts',(154.448284212903,25.3958180921978,185.19901935167));
#93144=CARTESIAN_POINT('Ctrl Pts',(154.454281299807,25.364663906821,185.176674057838));
#93145=CARTESIAN_POINT('Ctrl Pts',(154.460687448475,25.3350161332536,185.152758299799));
#93146=CARTESIAN_POINT('Ctrl Pts',(154.467312158215,25.3043568550406,185.128026598523));
#93147=CARTESIAN_POINT('Ctrl Pts',(154.474374329022,25.2753083237004,185.101615189071));
#93148=CARTESIAN_POINT('Ctrl Pts',(154.481831864672,25.2478538641296,185.073818892769));
#93149=CARTESIAN_POINT('Ctrl Pts',(154.489693131172,25.2189130942252,185.044517780015));
#93150=CARTESIAN_POINT('Ctrl Pts',(154.497993712757,25.1917434060434,185.013677634679));
#93151=CARTESIAN_POINT('Ctrl Pts',(154.506694089653,25.1663266839483,184.981586326707));
#93152=CARTESIAN_POINT('Ctrl Pts',(154.5156826416,25.1400681057713,184.948432086124));
#93153=CARTESIAN_POINT('Ctrl Pts',(154.525097929767,25.1156802398802,184.913942042753));
#93154=CARTESIAN_POINT('Ctrl Pts',(154.534906494078,25.0931489773896,184.878378268025));
#93155=CARTESIAN_POINT('Ctrl Pts',(154.545184815804,25.0695386346909,184.841111252502));
#93156=CARTESIAN_POINT('Ctrl Pts',(154.555894981686,25.047966594657,184.802664857134));
#93157=CARTESIAN_POINT('Ctrl Pts',(154.567009342758,25.0284284402446,184.763286335916));
#93158=CARTESIAN_POINT('Ctrl Pts',(154.56882939591,25.0252289329324,184.756837831931));
#93159=CARTESIAN_POINT('Ctrl Pts',(154.570660310709,25.0220839992451,184.750364225634));
#93160=CARTESIAN_POINT('Ctrl Pts',(154.572501991839,25.0189936596592,184.743866482733));
#93161=CARTESIAN_POINT('Ctrl Pts',(154.575023733311,25.0147621793188,184.73496937917));
#93162=CARTESIAN_POINT('Ctrl Pts',(154.577568015069,25.0106275870193,184.726018641299));
#93163=CARTESIAN_POINT('Ctrl Pts',(154.580133819563,25.0065893890237,184.717018488867));
#93164=CARTESIAN_POINT('Ctrl Pts',(154.591777703693,24.9882636320624,184.676174873404));
#93165=CARTESIAN_POINT('Ctrl Pts',(154.603854224587,24.9719426858168,184.634361233353));
#93166=CARTESIAN_POINT('Ctrl Pts',(154.616261722143,24.9575932362401,184.591988610101));
#93167=CARTESIAN_POINT('Ctrl Pts',(154.62935435389,24.9424514191077,184.547276197316));
#93168=CARTESIAN_POINT('Ctrl Pts',(154.642815578117,24.9295046365609,184.501941061476));
#93169=CARTESIAN_POINT('Ctrl Pts',(154.656540518755,24.9187250131128,184.456411390074));
#93170=CARTESIAN_POINT('Ctrl Pts',(154.659684720487,24.9162555444567,184.445981146663));
#93171=CARTESIAN_POINT('Ctrl Pts',(154.662842817589,24.9138998617083,184.435540489566));
#93172=CARTESIAN_POINT('Ctrl Pts',(154.666013643873,24.9116577244602,184.425094219679));
#93173=CARTESIAN_POINT('Ctrl Pts',(154.681690213016,24.9005725950782,184.373447848185));
#93174=CARTESIAN_POINT('Ctrl Pts',(154.697814213832,24.8921152784088,184.321202826052));
#93175=CARTESIAN_POINT('Ctrl Pts',(154.714295347124,24.8861977637108,184.268661979121));
#93176=CARTESIAN_POINT('Ctrl Pts',(154.731628586706,24.8799743021214,184.213404669348));
#93177=CARTESIAN_POINT('Ctrl Pts',(154.749356958483,24.8765597521334,184.157819589899));
#93178=CARTESIAN_POINT('Ctrl Pts',(154.767390788052,24.8758861536974,184.102216495425));
#93179=CARTESIAN_POINT('Ctrl Pts',(154.769606753279,24.8758033831076,184.095384085071));
#93180=CARTESIAN_POINT('Ctrl Pts',(154.771827347406,24.8757620423259,184.088551359106));
#93181=CARTESIAN_POINT('Ctrl Pts',(154.774052417606,24.8757620423259,184.081718857687));
#93182=CARTESIAN_POINT('Ctrl Pts',(95.9690444983151,29.1114187506925,195.445834017246));
#93183=CARTESIAN_POINT('Ctrl Pts',(96.9905454909875,28.9836527494168,195.415492891841));
#93184=CARTESIAN_POINT('Ctrl Pts',(96.9910158671796,28.9874167683946,196.445393189885));
#93185=CARTESIAN_POINT('Ctrl Pts',(96.1808469360716,30.8083310983659,195.439542956962));
#93186=CARTESIAN_POINT('Ctrl Pts',(97.1949838327504,30.6213702247017,195.409160016061));
#93187=CARTESIAN_POINT('Ctrl Pts',(97.1958901734581,30.6268508847717,196.43909456317));
#93188=CARTESIAN_POINT('Ctrl Pts',(96.5357039062144,32.4621522990289,195.428958375868));
#93189=CARTESIAN_POINT('Ctrl Pts',(97.5375062160773,32.2174773037551,195.398506678642));
#93190=CARTESIAN_POINT('Ctrl Pts',(97.5391410311521,32.2246530909199,196.428497216997));
#93191=CARTESIAN_POINT('Ctrl Pts',(97.2734769439721,34.8806495075041,195.406087214197));
#93192=CARTESIAN_POINT('Ctrl Pts',(98.2495553841758,34.5514785375348,195.375526283764));
#93193=CARTESIAN_POINT('Ctrl Pts',(98.2528123253432,34.5612301109138,196.405597550267));
#93194=CARTESIAN_POINT('Ctrl Pts',(97.5538509175081,35.6764000718443,195.397285235172));
#93195=CARTESIAN_POINT('Ctrl Pts',(98.5201541771945,35.3194365450969,195.366686752647));
#93196=CARTESIAN_POINT('Ctrl Pts',(98.5240305654619,35.3300267321143,196.396784487269));
#93197=CARTESIAN_POINT('Ctrl Pts',(98.18431282738,37.2468200580182,195.377069023014));
#93198=CARTESIAN_POINT('Ctrl Pts',(99.12861500334,36.8350067634597,195.346402562534));
#93199=CARTESIAN_POINT('Ctrl Pts',(99.1339182696851,36.8472528999435,196.376542353047));
#93200=CARTESIAN_POINT('Ctrl Pts',(98.5352221250904,38.0231116098076,195.365628086643));
#93201=CARTESIAN_POINT('Ctrl Pts',(99.467269260868,37.584178042332,195.334931117862));
#93202=CARTESIAN_POINT('Ctrl Pts',(99.4733823025719,37.5972496311567,196.365086544997));
#93203=CARTESIAN_POINT('Ctrl Pts',(99.6908456903027,40.308852455946,195.326983759774));
#93204=CARTESIAN_POINT('Ctrl Pts',(100.58251136751,39.7901098462954,195.296224400173));
#93205=CARTESIAN_POINT('Ctrl Pts',(100.591345561039,39.8055670589042,196.326390874288));
#93206=CARTESIAN_POINT('Ctrl Pts',(100.581425535931,41.7447648678172,195.296060783275));
#93207=CARTESIAN_POINT('Ctrl Pts',(101.441852730532,41.1757850798975,195.265300953242));
#93208=CARTESIAN_POINT('Ctrl Pts',(101.452939744803,41.1928417403813,196.295425589375));
#93209=CARTESIAN_POINT('Ctrl Pts',(102.090446775052,43.7718345514203,195.239992129605));
#93210=CARTESIAN_POINT('Ctrl Pts',(102.897968356158,43.1322235416134,195.209383242826));
#93211=CARTESIAN_POINT('Ctrl Pts',(102.912967222459,43.1512498063651,196.239275391062));
#93212=CARTESIAN_POINT('Ctrl Pts',(102.622478624349,44.4262693750096,195.219675251719));
#93213=CARTESIAN_POINT('Ctrl Pts',(103.411299657064,43.7638416825715,195.189144427864));
#93214=CARTESIAN_POINT('Ctrl Pts',(103.427743450085,43.7835173833033,196.218928280365));
#93215=CARTESIAN_POINT('Ctrl Pts',(103.464637936624,45.3755996946146,195.186370350926));
#93216=CARTESIAN_POINT('Ctrl Pts',(104.223880926985,44.680177009279,195.15601221913));
#93217=CARTESIAN_POINT('Ctrl Pts',(104.242626300959,44.7006916523046,196.185572234913));
#93218=CARTESIAN_POINT('Ctrl Pts',(103.752719651255,45.6866487784825,195.174795965706));
#93219=CARTESIAN_POINT('Ctrl Pts',(104.501829185358,44.9804130395041,195.144505518144));
#93220=CARTESIAN_POINT('Ctrl Pts',(104.521383391689,45.0012047721157,196.173979831597));
#93221=CARTESIAN_POINT('Ctrl Pts',(104.343828694018,46.2977922800091,195.150621120664));
#93222=CARTESIAN_POINT('Ctrl Pts',(105.072143291029,45.5703390039032,195.120488733774));
#93223=CARTESIAN_POINT('Ctrl Pts',(105.093373457231,45.5916474059541,196.149766749665));
#93224=CARTESIAN_POINT('Ctrl Pts',(104.647630621959,46.5986011658697,195.137987528073));
#93225=CARTESIAN_POINT('Ctrl Pts',(105.365249074382,45.8607130300027,195.107946133969));
#93226=CARTESIAN_POINT('Ctrl Pts',(105.387356025942,45.8822671873913,196.13711288398));
#93227=CARTESIAN_POINT('Ctrl Pts',(106.193340539684,48.0640285060236,195.072510066659));
#93228=CARTESIAN_POINT('Ctrl Pts',(106.856313491502,47.2751774604217,195.042996477193));
#93229=CARTESIAN_POINT('Ctrl Pts',(106.88314578035,47.2980570568634,196.071528584548));
#93230=CARTESIAN_POINT('Ctrl Pts',(107.513689725659,49.1139724683082,195.012882323802));
#93231=CARTESIAN_POINT('Ctrl Pts',(108.129721803209,48.2887968792928,194.984003591972));
#93232=CARTESIAN_POINT('Ctrl Pts',(108.160975010984,48.3124369479142,196.011798414246));
#93233=CARTESIAN_POINT('Ctrl Pts',(109.615125126087,50.511791610423,194.909278340031));
#93234=CARTESIAN_POINT('Ctrl Pts',(110.157489415393,49.6394299207645,194.881793166221));
#93235=CARTESIAN_POINT('Ctrl Pts',(110.195027611433,49.6629086681952,195.908000630588));
#93236=CARTESIAN_POINT('Ctrl Pts',(110.335870143622,50.9480470823175,194.872368331763));
#93237=CARTESIAN_POINT('Ctrl Pts',(110.85272962471,50.0609555896405,194.845443682159));
#93238=CARTESIAN_POINT('Ctrl Pts',(110.89270788553,50.0843871411745,195.871019251302));
#93239=CARTESIAN_POINT('Ctrl Pts',(111.447804523715,51.5572270341353,194.812857830125));
#93240=CARTESIAN_POINT('Ctrl Pts',(111.925622387835,50.6499225755847,194.786916511041));
#93241=CARTESIAN_POINT('Ctrl Pts',(111.969145579328,50.6729327353859,195.811388698003));
#93242=CARTESIAN_POINT('Ctrl Pts',(111.823592422802,51.7527428674394,194.792328697466));
#93243=CARTESIAN_POINT('Ctrl Pts',(112.288148478452,50.8389588738988,194.766745695778));
#93244=CARTESIAN_POINT('Ctrl Pts',(112.332951136671,50.861825987525,195.790817373735));
#93245=CARTESIAN_POINT('Ctrl Pts',(112.585611671513,52.1284437551186,194.749769711206));
#93246=CARTESIAN_POINT('Ctrl Pts',(113.023310517829,51.2023071262054,194.724961663351));
#93247=CARTESIAN_POINT('Ctrl Pts',(113.070704237323,51.2248010026007,195.748169059864));
#93248=CARTESIAN_POINT('Ctrl Pts',(112.972600874585,52.3089265662353,194.727693914219));
#93249=CARTESIAN_POINT('Ctrl Pts',(113.396653199089,51.3769027979713,194.703305191536));
#93250=CARTESIAN_POINT('Ctrl Pts',(113.445385623426,51.3991704364259,195.726046023214));
#93251=CARTESIAN_POINT('Ctrl Pts',(114.916147013965,53.1645838313077,194.614306433195));
#93252=CARTESIAN_POINT('Ctrl Pts',(115.270541301213,52.2043876372251,194.592229587412));
#93253=CARTESIAN_POINT('Ctrl Pts',(115.327204948124,52.2258445773799,195.612410617938));
#93254=CARTESIAN_POINT('Ctrl Pts',(116.508960581184,53.7063929000131,194.51347209248));
#93255=CARTESIAN_POINT('Ctrl Pts',(116.806433549694,52.7296177887198,194.493744543161));
#93256=CARTESIAN_POINT('Ctrl Pts',(116.869699925243,52.7493012987645,195.511340071764));
#93257=CARTESIAN_POINT('Ctrl Pts',(118.952752804013,54.3121536802558,194.342894831349));
#93258=CARTESIAN_POINT('Ctrl Pts',(119.166670826541,53.3192109895653,194.327446358241));
#93259=CARTESIAN_POINT('Ctrl Pts',(119.236843055431,53.3345435367134,195.340320085676));
#93260=CARTESIAN_POINT('Ctrl Pts',(119.776496894014,54.479388232144,194.282800692507));
#93261=CARTESIAN_POINT('Ctrl Pts',(119.961612355366,53.4823273585296,194.269002235245));
#93262=CARTESIAN_POINT('Ctrl Pts',(120.034841083494,53.4961134609636,195.280063484756));
#93263=CARTESIAN_POINT('Ctrl Pts',(121.442484198752,54.7433756911386,194.155240928781));
#93264=CARTESIAN_POINT('Ctrl Pts',(121.569977744677,53.7408888473484,194.145104510391));
#93265=CARTESIAN_POINT('Ctrl Pts',(121.648970880559,53.7511590439454,195.152141272117));
#93266=CARTESIAN_POINT('Ctrl Pts',(122.287131939476,54.8401884933555,194.087563676381));
#93267=CARTESIAN_POINT('Ctrl Pts',(122.385374501015,53.8364730184404,194.079483650773));
#93268=CARTESIAN_POINT('Ctrl Pts',(122.467432995904,53.8446925471786,195.084263387053));
#93269=CARTESIAN_POINT('Ctrl Pts',(123.132502129594,54.900000000005,194.016421260282));
#93270=CARTESIAN_POINT('Ctrl Pts',(123.202778920349,53.8965577541562,194.010507093035));
#93271=CARTESIAN_POINT('Ctrl Pts',(123.286717970418,53.9024781190629,195.01289889797));
#93272=CARTESIAN_POINT('Origin',(123.216361044378,54.900000000005,195.01289889797));
#93273=CARTESIAN_POINT('Ctrl Pts',(95.9690444983151,29.1114187506925,195.445834017246));
#93274=CARTESIAN_POINT('Ctrl Pts',(96.0972458594227,30.1385385277655,195.4420261173));
#93275=CARTESIAN_POINT('Ctrl Pts',(96.2779248487746,31.1498429318702,195.436643202798));
#93276=CARTESIAN_POINT('Ctrl Pts',(96.5096309404584,32.1457528185718,195.429606506193));
#93277=CARTESIAN_POINT('Ctrl Pts',(96.6251548158192,32.6422929344827,195.426098154489));
#93278=CARTESIAN_POINT('Ctrl Pts',(96.7533634969236,33.1350069337616,195.422178692833));
#93279=CARTESIAN_POINT('Ctrl Pts',(96.8940801655196,33.6239508552454,195.417838302303));
#93280=CARTESIAN_POINT('Ctrl Pts',(96.9374041579526,33.7744874119013,195.41650197841));
#93281=CARTESIAN_POINT('Ctrl Pts',(96.9819149598591,33.9246585378549,195.415125718949));
#93282=CARTESIAN_POINT('Ctrl Pts',(97.0276077670339,34.0744669046563,195.413709226167));
#93283=CARTESIAN_POINT('Ctrl Pts',(97.2531653090372,34.813979512362,195.406716864573));
#93284=CARTESIAN_POINT('Ctrl Pts',(97.5076915903295,35.5446174058597,195.398733680154));
#93285=CARTESIAN_POINT('Ctrl Pts',(97.7915382531106,36.2664435551117,195.389659814951));
#93286=CARTESIAN_POINT('Ctrl Pts',(97.817148339291,36.3315703729101,195.38884112479));
#93287=CARTESIAN_POINT('Ctrl Pts',(97.8429971441018,36.3966254500846,195.388013554678));
#93288=CARTESIAN_POINT('Ctrl Pts',(97.869084946264,36.4616088280606,195.387177030534));
#93289=CARTESIAN_POINT('Ctrl Pts',(98.0671074803695,36.9548728102672,195.380827295525));
#93290=CARTESIAN_POINT('Ctrl Pts',(98.2792236607968,37.4446461484459,195.373951152163));
#93291=CARTESIAN_POINT('Ctrl Pts',(98.5051187984374,37.9296227062782,195.366520946132));
#93292=CARTESIAN_POINT('Ctrl Pts',(98.6387261442667,38.2164656696027,195.362126295954));
#93293=CARTESIAN_POINT('Ctrl Pts',(98.7772051355907,38.5017229381189,195.357536120521));
#93294=CARTESIAN_POINT('Ctrl Pts',(98.920447684268,38.7850162524432,195.352746052521));
#93295=CARTESIAN_POINT('Ctrl Pts',(99.1268822676556,39.193285568083,195.345842826482));
#93296=CARTESIAN_POINT('Ctrl Pts',(99.3419895912592,39.595291259492,195.338567559063));
#93297=CARTESIAN_POINT('Ctrl Pts',(99.5655235788531,39.9908276271668,195.330900660422));
#93298=CARTESIAN_POINT('Ctrl Pts',(99.9441651921826,40.6608220651446,195.317913790274));
#93299=CARTESIAN_POINT('Ctrl Pts',(100.347228042345,41.3130031012681,195.303795012562));
#93300=CARTESIAN_POINT('Ctrl Pts',(100.774291075539,41.9476732328044,195.288422771642));
#93301=CARTESIAN_POINT('Ctrl Pts',(101.036318534828,42.3370794541982,195.27899102757));
#93302=CARTESIAN_POINT('Ctrl Pts',(101.307415862361,42.71986864212,195.269086164844));
#93303=CARTESIAN_POINT('Ctrl Pts',(101.587479545813,43.0961149066845,195.258680201397));
#93304=CARTESIAN_POINT('Ctrl Pts',(102.0904180901,43.7717781924818,195.239993165493));
#93305=CARTESIAN_POINT('Ctrl Pts',(102.6224379013,44.4262190589009,195.219676863045));
#93306=CARTESIAN_POINT('Ctrl Pts',(103.183919146169,45.0591553824135,195.197471945756));
#93307=CARTESIAN_POINT('Ctrl Pts',(103.328957744289,45.2226518444957,195.191736099538));
#93308=CARTESIAN_POINT('Ctrl Pts',(103.475964910566,45.3847114464566,195.185873922911));
#93309=CARTESIAN_POINT('Ctrl Pts',(103.624955980477,45.5453229777685,195.17987985077));
#93310=CARTESIAN_POINT('Ctrl Pts',(103.76432206781,45.6955588322588,195.174273002105));
#93311=CARTESIAN_POINT('Ctrl Pts',(103.905424036428,45.8445277145151,195.168550747912));
#93312=CARTESIAN_POINT('Ctrl Pts',(104.048275195727,45.9922195364714,195.162708501344));
#93313=CARTESIAN_POINT('Ctrl Pts',(104.34381814322,46.2977772694011,195.150621551688));
#93314=CARTESIAN_POINT('Ctrl Pts',(104.647622860237,46.5985833927272,195.137987864661));
#93315=CARTESIAN_POINT('Ctrl Pts',(104.9567881871,46.8916701423301,195.124891376));
#93316=CARTESIAN_POINT('Ctrl Pts',(105.059488272285,46.9890291652721,195.120540918868));
#93317=CARTESIAN_POINT('Ctrl Pts',(105.162768415866,47.0855444753236,195.116140391019));
#93318=CARTESIAN_POINT('Ctrl Pts',(105.266626989144,47.1812182581203,195.111688523098));
#93319=CARTESIAN_POINT('Ctrl Pts',(105.7772405543,47.651591861224,195.089801219247));
#93320=CARTESIAN_POINT('Ctrl Pts',(106.301870403894,48.1015964351509,195.066671393992));
#93321=CARTESIAN_POINT('Ctrl Pts',(106.840200252243,48.5316682118175,195.042153591274));
#93322=CARTESIAN_POINT('Ctrl Pts',(106.900314316541,48.5796933445769,195.039415744258));
#93323=CARTESIAN_POINT('Ctrl Pts',(106.960599259229,48.6274699524295,195.036660588573));
#93324=CARTESIAN_POINT('Ctrl Pts',(107.021054673501,48.6749986650904,195.033887920901));
#93325=CARTESIAN_POINT('Ctrl Pts',(107.634725807791,49.1574533692965,195.005743111454));
#93326=CARTESIAN_POINT('Ctrl Pts',(108.266032185147,49.6142467316366,194.975790759413));
#93327=CARTESIAN_POINT('Ctrl Pts',(108.914698173805,50.0457741179989,194.943810465903));
#93328=CARTESIAN_POINT('Ctrl Pts',(109.538356981193,50.46066538691,194.913063067305));
#93329=CARTESIAN_POINT('Ctrl Pts',(110.178153551123,50.8520678887675,194.880429223269));
#93330=CARTESIAN_POINT('Ctrl Pts',(110.834313273343,51.2196253302198,194.845632352756));
#93331=CARTESIAN_POINT('Ctrl Pts',(110.91501763279,51.2648330546013,194.841352511964));
#93332=CARTESIAN_POINT('Ctrl Pts',(110.995966727058,51.3096789160716,194.837040097392));
#93333=CARTESIAN_POINT('Ctrl Pts',(111.077161966758,51.3541629481376,194.832694544323));
#93334=CARTESIAN_POINT('Ctrl Pts',(111.447779236129,51.5572111878583,194.812859181829));
#93335=CARTESIAN_POINT('Ctrl Pts',(111.823530943453,51.7527118271191,194.792332131191));
#93336=CARTESIAN_POINT('Ctrl Pts',(112.204602154873,51.9405930916626,194.77104919832));
#93337=CARTESIAN_POINT('Ctrl Pts',(112.432425524418,52.0529178789464,194.75832519993));
#93338=CARTESIAN_POINT('Ctrl Pts',(112.662421583518,52.1626255365207,194.745314563013));
#93339=CARTESIAN_POINT('Ctrl Pts',(112.893703680816,52.2692992869394,194.732057324778));
#93340=CARTESIAN_POINT('Ctrl Pts',(113.049130625069,52.3409865262605,194.723148152592));
#93341=CARTESIAN_POINT('Ctrl Pts',(113.20509063946,52.4112759157413,194.714130343679));
#93342=CARTESIAN_POINT('Ctrl Pts',(113.361315636869,52.4800453780003,194.705016095229));
#93343=CARTESIAN_POINT('Ctrl Pts',(113.815260557361,52.6798696608935,194.678532710005));
#93344=CARTESIAN_POINT('Ctrl Pts',(114.272332766094,52.867453125254,194.65119297123));
#93345=CARTESIAN_POINT('Ctrl Pts',(114.732715972104,53.0430471260378,194.622914824101));
#93346=CARTESIAN_POINT('Ctrl Pts',(114.830412899452,53.0803095502821,194.61691397948));
#93347=CARTESIAN_POINT('Ctrl Pts',(114.928259001973,53.11703189196,194.610870861698));
#93348=CARTESIAN_POINT('Ctrl Pts',(115.026256154282,53.1532162768944,194.604784662144));
#93349=CARTESIAN_POINT('Ctrl Pts',(115.870603102918,53.4649822240463,194.552345750391));
#93350=CARTESIAN_POINT('Ctrl Pts',(116.72569566523,53.736734200438,194.496737807013));
#93351=CARTESIAN_POINT('Ctrl Pts',(117.591372418923,53.9690295322985,194.437533206228));
#93352=CARTESIAN_POINT('Ctrl Pts',(117.773172849744,54.0178137825741,194.425099671558));
#93353=CARTESIAN_POINT('Ctrl Pts',(117.955439915971,54.0648577672854,194.412507512248));
#93354=CARTESIAN_POINT('Ctrl Pts',(118.138171848527,54.1101665523461,194.399752772408));
#93355=CARTESIAN_POINT('Ctrl Pts',(118.566636924481,54.2164054114275,194.369845790647));
#93356=CARTESIAN_POINT('Ctrl Pts',(118.997672232339,54.3130506966135,194.339041040927));
#93357=CARTESIAN_POINT('Ctrl Pts',(119.431296878576,54.4000000000098,194.307272194192));
#93358=CARTESIAN_POINT('Ctrl Pts',(151.26536469753,39.0180386085744,189.729482705023));
#93359=CARTESIAN_POINT('Ctrl Pts',(150.582709291195,38.6415601415749,189.904601964429));
#93360=CARTESIAN_POINT('Ctrl Pts',(150.625700340104,38.5584761124776,190.698119455572));
#93361=CARTESIAN_POINT('Ctrl Pts',(151.840447122378,37.9152978809689,189.581958775083));
#93362=CARTESIAN_POINT('Ctrl Pts',(151.144695308609,37.5643261489478,189.757074220131));
#93363=CARTESIAN_POINT('Ctrl Pts',(151.196085224642,37.4561565472252,190.546670641828));
#93364=CARTESIAN_POINT('Ctrl Pts',(152.330726510846,36.7970892201137,189.376750805581));
#93365=CARTESIAN_POINT('Ctrl Pts',(151.62608674106,36.4755683238397,189.554480961614));
#93366=CARTESIAN_POINT('Ctrl Pts',(151.683367009845,36.3389829613473,190.335210178467));
#93367=CARTESIAN_POINT('Ctrl Pts',(153.15652020628,34.534931176203,188.851579727408));
#93368=CARTESIAN_POINT('Ctrl Pts',(152.445883342067,34.2654524607601,189.035735458266));
#93369=CARTESIAN_POINT('Ctrl Pts',(152.505948245037,34.0798980737316,189.793027255753));
#93370=CARTESIAN_POINT('Ctrl Pts',(153.491958385796,33.390916814621,188.531634280545));
#93371=CARTESIAN_POINT('Ctrl Pts',(152.782958948242,33.1498009792059,188.721591199022));
#93372=CARTESIAN_POINT('Ctrl Pts',(152.8411749936,32.9379252989499,189.462322785582));
#93373=CARTESIAN_POINT('Ctrl Pts',(153.884219724291,31.6583920225304,187.961341908996));
#93374=CARTESIAN_POINT('Ctrl Pts',(153.185398652578,31.4484371283528,188.157455545538));
#93375=CARTESIAN_POINT('Ctrl Pts',(153.234974567374,31.209126499478,188.872431610084));
#93376=CARTESIAN_POINT('Ctrl Pts',(153.996584103503,31.0765387279129,187.75544157011));
#93377=CARTESIAN_POINT('Ctrl Pts',(153.301912221398,30.8783831037092,187.954448638106));
#93378=CARTESIAN_POINT('Ctrl Pts',(153.348167691184,30.628630919208,188.659395307684));
#93379=CARTESIAN_POINT('Ctrl Pts',(154.182311310232,29.9244074378833,187.318655130299));
#93380=CARTESIAN_POINT('Ctrl Pts',(153.497581663401,29.7478870574723,187.523076488269));
#93381=CARTESIAN_POINT('Ctrl Pts',(153.536116366461,29.4793832870787,188.20737331349));
#93382=CARTESIAN_POINT('Ctrl Pts',(154.25617142518,29.3523851374075,187.087274026207));
#93383=CARTESIAN_POINT('Ctrl Pts',(153.577375107994,29.1862055274963,187.294578964887));
#93384=CARTESIAN_POINT('Ctrl Pts',(153.611369186077,28.9088901426605,187.967875908774));
#93385=CARTESIAN_POINT('Ctrl Pts',(154.424359066069,27.6487610028378,186.35421696411));
#93386=CARTESIAN_POINT('Ctrl Pts',(153.764597828238,27.5167379078432,186.571890016881));
#93387=CARTESIAN_POINT('Ctrl Pts',(153.784512596554,27.2100871723594,187.20899762199));
#93388=CARTESIAN_POINT('Ctrl Pts',(154.465433528124,26.5295110347379,185.813820974581));
#93389=CARTESIAN_POINT('Ctrl Pts',(153.822578759736,26.4144864228749,186.037727647489));
#93390=CARTESIAN_POINT('Ctrl Pts',(153.829924819726,26.0943597881929,186.649430085873));
#93391=CARTESIAN_POINT('Ctrl Pts',(154.442742286491,25.4284918940196,185.219477651461));
#93392=CARTESIAN_POINT('Ctrl Pts',(153.817575691237,25.3176612645029,185.442322230379));
#93393=CARTESIAN_POINT('Ctrl Pts',(153.812479229218,24.9971192497146,186.033932954963));
#93394=CARTESIAN_POINT('',(151.265364697496,39.0180386085597,189.729482705031));
#93395=CARTESIAN_POINT('Origin',(151.513845774243,39.0180386085744,190.698119455572));
#93396=CARTESIAN_POINT('Ctrl Pts',(151.26536469753,39.0180386085743,189.729482705023));
#93397=CARTESIAN_POINT('Ctrl Pts',(151.840421242892,37.9153475049247,189.58196541386));
#93398=CARTESIAN_POINT('Ctrl Pts',(152.330699670202,36.797162746522,189.376767875129));
#93399=CARTESIAN_POINT('Ctrl Pts',(152.743623347839,35.6660101936194,189.114165269229));
#93400=CARTESIAN_POINT('Ctrl Pts',(152.743647418205,35.6659442558763,189.114149961459));
#93401=CARTESIAN_POINT('Ctrl Pts',(152.743671488307,35.6658783180889,189.114134653494));
#93402=CARTESIAN_POINT('Ctrl Pts',(152.743695558146,35.6658123802572,189.114119345334));
#93403=CARTESIAN_POINT('Ctrl Pts',(153.156535386619,34.5348632769377,188.851557634363));
#93404=CARTESIAN_POINT('Ctrl Pts',(153.491959356164,33.3909113019664,188.531632564244));
#93405=CARTESIAN_POINT('Ctrl Pts',(153.753465858556,32.2359002590937,188.15143938991));
#93406=CARTESIAN_POINT('Ctrl Pts',(153.75352849967,32.2356235884284,188.151348318661));
#93407=CARTESIAN_POINT('Ctrl Pts',(153.753591136563,32.2353469167625,188.151257243784));
#93408=CARTESIAN_POINT('Ctrl Pts',(153.753653769237,32.2350702440973,188.151166165279));
#93409=CARTESIAN_POINT('Ctrl Pts',(153.884328977272,31.6578274745046,187.961142302926));
#93410=CARTESIAN_POINT('Ctrl Pts',(153.996637480094,31.0762076137486,187.755316040867));
#93411=CARTESIAN_POINT('Ctrl Pts',(154.089447697742,30.5004730803946,187.537048352865));
#93412=CARTESIAN_POINT('Ctrl Pts',(154.08951285666,30.5000688766304,187.536895114496));
#93413=CARTESIAN_POINT('Ctrl Pts',(154.089578006214,30.4996646749078,187.536741869751));
#93414=CARTESIAN_POINT('Ctrl Pts',(154.089643146404,30.4992604752267,187.536588618632));
#93415=CARTESIAN_POINT('Ctrl Pts',(154.182426783275,29.9235311698206,187.318302546945));
#93416=CARTESIAN_POINT('Ctrl Pts',(154.256217688442,29.3519165206558,187.087072383857));
#93417=CARTESIAN_POINT('Ctrl Pts',(154.312233949315,28.7845104204925,186.842921679277));
#93418=CARTESIAN_POINT('Ctrl Pts',(154.312273219189,28.7841126437454,186.842750518845));
#93419=CARTESIAN_POINT('Ctrl Pts',(154.312312480344,28.7837148690555,186.842579352087));
#93420=CARTESIAN_POINT('Ctrl Pts',(154.312351732781,28.7833170964228,186.842408179003));
#93421=CARTESIAN_POINT('Ctrl Pts',(154.417517426384,27.7175989418325,186.383798791121));
#93422=CARTESIAN_POINT('Ctrl Pts',(154.460104713933,26.6666603032434,185.879784621214));
#93423=CARTESIAN_POINT('Ctrl Pts',(154.44620363346,25.6318394819492,185.328524043399));
#93424=CARTESIAN_POINT('Ctrl Pts',(154.445292156395,25.56398752995,185.292378552803));
#93425=CARTESIAN_POINT('Ctrl Pts',(154.444137804104,25.4962048746116,185.256029929632));
#93426=CARTESIAN_POINT('Ctrl Pts',(154.44274228649,25.4284918940197,185.219477651461));
#93427=CARTESIAN_POINT('Ctrl Pts',(123.159109278332,54.5824004318885,194.066403916675));
#93428=CARTESIAN_POINT('Ctrl Pts',(123.226343764611,53.8982198229655,194.291916124396));
#93429=CARTESIAN_POINT('Ctrl Pts',(123.286717970418,53.9024781190629,195.01289889797));
#93430=CARTESIAN_POINT('Ctrl Pts',(123.83865733674,54.5931791852171,194.021690234304));
#93431=CARTESIAN_POINT('Ctrl Pts',(123.882504759287,53.9459026464787,194.265746571195));
#93432=CARTESIAN_POINT('Ctrl Pts',(123.956385232616,53.9497108975491,194.954566980795));
#93433=CARTESIAN_POINT('Ctrl Pts',(124.527075444545,54.599519113683,193.966755721732));
#93434=CARTESIAN_POINT('Ctrl Pts',(124.564090549894,53.9717473179622,194.217325738079));
#93435=CARTESIAN_POINT('Ctrl Pts',(124.625450088238,53.9731815252606,194.891331888951));
#93436=CARTESIAN_POINT('Ctrl Pts',(125.893284906873,54.6002480378726,193.842179627404));
#93437=CARTESIAN_POINT('Ctrl Pts',(125.901328293953,53.974575540568,194.09392865322));
#93438=CARTESIAN_POINT('Ctrl Pts',(125.96330325035,53.9731394972598,194.76538052756));
#93439=CARTESIAN_POINT('Ctrl Pts',(126.579778542857,54.5946481384655,193.771745245381));
#93440=CARTESIAN_POINT('Ctrl Pts',(126.579855830591,53.9516703754874,194.016863354465));
#93441=CARTESIAN_POINT('Ctrl Pts',(126.632097249348,53.9496036053775,194.702657351989));
#93442=CARTESIAN_POINT('Ctrl Pts',(127.255737937252,54.5846303501899,193.69266867861));
#93443=CARTESIAN_POINT('Ctrl Pts',(127.230565840969,53.907392591019,193.922470625941));
#93444=CARTESIAN_POINT('Ctrl Pts',(127.30024332108,53.9024781190574,194.634660522391));
#93445=CARTESIAN_POINT('Origin',(127.370600247112,54.9,194.634660522392));
#93446=CARTESIAN_POINT('Ctrl Pts',(127.272749841876,54.9000000000005,193.639459387849));
#93447=CARTESIAN_POINT('Ctrl Pts',(127.203543013627,53.909298557295,193.646263958256));
#93448=CARTESIAN_POINT('Ctrl Pts',(127.300243321063,53.9024781190585,194.634660522393));
#93449=CARTESIAN_POINT('Ctrl Pts',(128.52064511939,54.8116621740965,193.516763528339));
#93450=CARTESIAN_POINT('Ctrl Pts',(128.407405166125,53.8285119696612,193.528217006398));
#93451=CARTESIAN_POINT('Ctrl Pts',(128.510275384961,53.8171324859908,194.511516273623));
#93452=CARTESIAN_POINT('Ctrl Pts',(129.761927633803,54.643802091986,193.386070821232));
#93453=CARTESIAN_POINT('Ctrl Pts',(129.607546967154,53.6716622950793,193.402533723092));
#93454=CARTESIAN_POINT('Ctrl Pts',(129.714213057453,53.654958236656,194.380313990587));
#93455=CARTESIAN_POINT('Ctrl Pts',(131.6135224599,54.2702144010371,193.176442368403));
#93456=CARTESIAN_POINT('Ctrl Pts',(131.402782100654,53.3180517456064,193.200806873799));
#93457=CARTESIAN_POINT('Ctrl Pts',(131.510655492351,53.2940248395543,194.169798981518));
#93458=CARTESIAN_POINT('Ctrl Pts',(132.231120343818,54.1246783068022,193.104032183627));
#93459=CARTESIAN_POINT('Ctrl Pts',(132.000898867169,53.180233463908,193.13129396691));
#93460=CARTESIAN_POINT('Ctrl Pts',(132.109951292528,53.1534183951113,194.097071569746));
#93461=CARTESIAN_POINT('Ctrl Pts',(133.447960060778,53.795964138965,192.9562191062));
#93462=CARTESIAN_POINT('Ctrl Pts',(133.180061609208,52.8681545503538,192.989463215145));
#93463=CARTESIAN_POINT('Ctrl Pts',(133.290927472371,52.8358385491633,193.94858536401));
#93464=CARTESIAN_POINT('Ctrl Pts',(134.048018207581,53.6127861473261,192.880743397387));
#93465=CARTESIAN_POINT('Ctrl Pts',(133.761754639131,52.6940588112552,192.917106754388));
#93466=CARTESIAN_POINT('Ctrl Pts',(133.873399111762,52.6588652269854,193.87275353291));
#93467=CARTESIAN_POINT('Ctrl Pts',(135.823659132771,53.0080952690701,192.649586867277));
#93468=CARTESIAN_POINT('Ctrl Pts',(135.481197371613,52.11925883683,192.695966104266));
#93469=CARTESIAN_POINT('Ctrl Pts',(135.597302025426,52.0746566508346,193.640464175031));
#93470=CARTESIAN_POINT('Ctrl Pts',(136.97479908392,52.5316454904866,192.489156404314));
#93471=CARTESIAN_POINT('Ctrl Pts',(136.598560535411,51.6654276097848,192.542536330489));
#93472=CARTESIAN_POINT('Ctrl Pts',(136.715309703076,51.61434534683,193.479192548667));
#93473=CARTESIAN_POINT('Ctrl Pts',(138.6530486123,51.708035457433,192.239238024318));
#93474=CARTESIAN_POINT('Ctrl Pts',(138.233427443137,50.8764420724432,192.303042588419));
#93475=CARTESIAN_POINT('Ctrl Pts',(138.34589059586,50.818632922698,193.22785955661));
#93476=CARTESIAN_POINT('Ctrl Pts',(139.204365456023,51.415287483946,192.154391036192));
#93477=CARTESIAN_POINT('Ctrl Pts',(138.769728386523,50.596440619094,192.221944439597));
#93478=CARTESIAN_POINT('Ctrl Pts',(138.881656790172,50.5358010115302,193.142515545859));
#93479=CARTESIAN_POINT('Ctrl Pts',(140.290599308088,50.7928635888825,191.981721248658));
#93480=CARTESIAN_POINT('Ctrl Pts',(139.827189305459,50.0003680989601,192.056916645887));
#93481=CARTESIAN_POINT('Ctrl Pts',(139.937472164248,49.9344600777195,192.968796877316));
#93482=CARTESIAN_POINT('Ctrl Pts',(140.826728790772,50.4623774384289,191.89369145042));
#93483=CARTESIAN_POINT('Ctrl Pts',(140.34944784855,49.683754112497,191.972823987069));
#93484=CARTESIAN_POINT('Ctrl Pts',(140.458700441158,49.6151682704711,192.880213859559));
#93485=CARTESIAN_POINT('Ctrl Pts',(142.40172585476,49.4195194736428,191.626786341652));
#93486=CARTESIAN_POINT('Ctrl Pts',(141.881508560285,48.6857028891425,191.71841976379));
#93487=CARTESIAN_POINT('Ctrl Pts',(141.99025759904,48.6076343574705,192.611570669029));
#93488=CARTESIAN_POINT('Ctrl Pts',(143.395944403539,48.6640076534003,191.447054061697));
#93489=CARTESIAN_POINT('Ctrl Pts',(142.852474782588,47.9607749353619,191.546847984491));
#93490=CARTESIAN_POINT('Ctrl Pts',(142.957509894915,47.8777134995743,192.430587787633));
#93491=CARTESIAN_POINT('Ctrl Pts',(145.277446438577,47.0366597202735,191.087194166438));
#93492=CARTESIAN_POINT('Ctrl Pts',(144.692442366913,46.3952555402769,191.203195444119));
#93493=CARTESIAN_POINT('Ctrl Pts',(144.788791450931,46.3054876682523,192.068053266175));
#93494=CARTESIAN_POINT('Ctrl Pts',(146.164719382506,46.1648158566818,190.907052451028));
#93495=CARTESIAN_POINT('Ctrl Pts',(145.561937070811,45.5561147238115,191.031184857471));
#93496=CARTESIAN_POINT('Ctrl Pts',(145.652811102842,45.4631752067736,191.886487140678));
#93497=CARTESIAN_POINT('Ctrl Pts',(147.414929837981,44.7683638583841,190.640018592768));
#93498=CARTESIAN_POINT('Ctrl Pts',(146.791471289491,44.2057341261571,190.775475427974));
#93499=CARTESIAN_POINT('Ctrl Pts',(146.870806025728,44.1140243219997,191.617213295931));
#93500=CARTESIAN_POINT('Ctrl Pts',(147.81817715783,44.2880522144313,190.551549748198));
#93501=CARTESIAN_POINT('Ctrl Pts',(147.187487035208,43.7421608701101,190.690946555037));
#93502=CARTESIAN_POINT('Ctrl Pts',(147.263759692939,43.6499819630162,191.527980798402));
#93503=CARTESIAN_POINT('Ctrl Pts',(148.597101747504,43.2969309377458,190.376458300977));
#93504=CARTESIAN_POINT('Ctrl Pts',(147.952932529004,42.7847732161162,190.523620828458));
#93505=CARTESIAN_POINT('Ctrl Pts',(148.022976149422,42.6924322950368,191.351336094742));
#93506=CARTESIAN_POINT('Ctrl Pts',(148.97143365954,42.7876744441135,190.290130240647));
#93507=CARTESIAN_POINT('Ctrl Pts',(148.321195890274,42.2925616418689,190.441090549207));
#93508=CARTESIAN_POINT('Ctrl Pts',(148.387927948605,42.2004255165281,191.26422094652));
#93509=CARTESIAN_POINT('Ctrl Pts',(150.041310637799,41.2296646117753,190.037839922795));
#93510=CARTESIAN_POINT('Ctrl Pts',(149.371815095918,40.7891354956777,190.200429995867));
#93511=CARTESIAN_POINT('Ctrl Pts',(149.431228089319,40.6951891414559,191.009572227123));
#93512=CARTESIAN_POINT('Ctrl Pts',(150.687324774653,40.1465975881037,189.877765311828));
#93513=CARTESIAN_POINT('Ctrl Pts',(150.009650721621,39.7402487175424,190.04713963159));
#93514=CARTESIAN_POINT('Ctrl Pts',(150.061517666962,39.6488093520851,190.847921455656));
#93515=CARTESIAN_POINT('Ctrl Pts',(151.26536469753,39.0180386085743,189.729482705023));
#93516=CARTESIAN_POINT('Ctrl Pts',(150.582709291195,38.6415601415748,189.904601964429));
#93517=CARTESIAN_POINT('Ctrl Pts',(150.625700340104,38.5584761124775,190.698119455572));
#93518=CARTESIAN_POINT('Ctrl Pts',(130.970210996205,54.4,193.249273458763));
#93519=CARTESIAN_POINT('Ctrl Pts',(130.978915699594,54.3982519051478,193.248288933116));
#93520=CARTESIAN_POINT('Ctrl Pts',(130.987620092955,54.3964997672191,193.247303953753));
#93521=CARTESIAN_POINT('Ctrl Pts',(130.996324175466,54.394743585639,193.246318520373));
#93522=CARTESIAN_POINT('Ctrl Pts',(131.528258652909,54.2874176808117,193.18609551699));
#93523=CARTESIAN_POINT('Ctrl Pts',(132.060608026504,54.1644608290906,193.123976504334));
#93524=CARTESIAN_POINT('Ctrl Pts',(132.587072882371,54.0272948310328,193.060644636876));
#93525=CARTESIAN_POINT('Ctrl Pts',(132.671384407187,54.0053281711119,193.050502257465));
#93526=CARTESIAN_POINT('Ctrl Pts',(132.755547483063,53.9829974301109,193.040328484779));
#93527=CARTESIAN_POINT('Ctrl Pts',(132.839536755994,53.9603082180556,193.030126063637));
#93528=CARTESIAN_POINT('Ctrl Pts',(133.288581764007,53.8390013290499,192.97557926113));
#93529=CARTESIAN_POINT('Ctrl Pts',(133.733103527571,53.7074473366379,192.920173817067));
#93530=CARTESIAN_POINT('Ctrl Pts',(134.173150208173,53.5658027576502,192.863909643738));
#93531=CARTESIAN_POINT('Ctrl Pts',(134.329294379496,53.5155422367028,192.843945119276));
#93532=CARTESIAN_POINT('Ctrl Pts',(134.484875189166,53.4640102364994,192.823872469304));
#93533=CARTESIAN_POINT('Ctrl Pts',(134.639896091017,53.4112152443031,192.803691536399));
#93534=CARTESIAN_POINT('Ctrl Pts',(135.52206560457,53.1107774837966,192.688848934204));
#93535=CARTESIAN_POINT('Ctrl Pts',(136.386150108309,52.7695638810176,192.570489258043));
#93536=CARTESIAN_POINT('Ctrl Pts',(137.232334271804,52.3879729388403,192.448662213503));
#93537=CARTESIAN_POINT('Ctrl Pts',(137.521497146559,52.2575735073922,192.407030781551));
#93538=CARTESIAN_POINT('Ctrl Pts',(137.808605915557,52.1224240283374,192.364989126719));
#93539=CARTESIAN_POINT('Ctrl Pts',(138.093623908729,51.9825549712515,192.322545371402));
#93540=CARTESIAN_POINT('Ctrl Pts',(138.582860279063,51.742468269885,192.249690220878));
#93541=CARTESIAN_POINT('Ctrl Pts',(139.065917548896,51.4884308348136,192.175653643355));
#93542=CARTESIAN_POINT('Ctrl Pts',(139.54253534821,51.2204058123117,192.100502844523));
#93543=CARTESIAN_POINT('Ctrl Pts',(139.610982501645,51.1819146987483,192.089710427064));
#93544=CARTESIAN_POINT('Ctrl Pts',(139.67929688751,51.1431351852349,192.078895035667));
#93545=CARTESIAN_POINT('Ctrl Pts',(139.74747777422,51.1040672416763,192.068056874941));
#93546=CARTESIAN_POINT('Ctrl Pts',(139.879558530241,51.0283843960807,192.047061071988));
#93547=CARTESIAN_POINT('Ctrl Pts',(140.011209984247,50.9515712029546,192.025967578531));
#93548=CARTESIAN_POINT('Ctrl Pts',(140.142368765457,50.8736620979774,192.004788014758));
#93549=CARTESIAN_POINT('Ctrl Pts',(140.433548249307,50.7006997330856,191.957768254505));
#93550=CARTESIAN_POINT('Ctrl Pts',(140.722715780357,50.5220779847515,191.910256482707));
#93551=CARTESIAN_POINT('Ctrl Pts',(141.008893216184,50.3383113755541,191.862422646825));
#93552=CARTESIAN_POINT('Ctrl Pts',(141.123671784854,50.2646072125688,191.843237698855));
#93553=CARTESIAN_POINT('Ctrl Pts',(141.237969574942,50.1900759905089,191.824000990223));
#93554=CARTESIAN_POINT('Ctrl Pts',(141.351724540188,50.1147530003429,191.804723635321));
#93555=CARTESIAN_POINT('Ctrl Pts',(141.414571048868,50.073139107313,191.794073423705));
#93556=CARTESIAN_POINT('Ctrl Pts',(141.477211554499,50.031313156935,191.783417824362));
#93557=CARTESIAN_POINT('Ctrl Pts',(141.539643328611,49.9892780028454,191.772757758386));
#93558=CARTESIAN_POINT('Ctrl Pts',(141.996832974707,49.6814533815665,191.694693794001));
#93559=CARTESIAN_POINT('Ctrl Pts',(142.443279186456,49.3620733715139,191.61631369272));
#93560=CARTESIAN_POINT('Ctrl Pts',(142.879234659791,49.031386758862,191.537742560243));
#93561=CARTESIAN_POINT('Ctrl Pts',(143.378755062999,48.6524840493176,191.447715284119));
#93562=CARTESIAN_POINT('Ctrl Pts',(143.864466586805,48.2586932138852,191.357443433954));
#93563=CARTESIAN_POINT('Ctrl Pts',(144.336661238865,47.8502924156543,191.267130653307));
#93564=CARTESIAN_POINT('Ctrl Pts',(145.277629212541,47.0364499253106,191.087159461698));
#93565=CARTESIAN_POINT('Ctrl Pts',(146.164908890879,46.1645799402394,190.907011931677));
#93566=CARTESIAN_POINT('Ctrl Pts',(146.998187380399,45.2338425346647,190.729031083346));
#93567=CARTESIAN_POINT('Ctrl Pts',(147.2065276244,45.0011351497774,190.684531466669));
#93568=CARTESIAN_POINT('Ctrl Pts',(147.411482299837,44.764736358989,190.640170437272));
#93569=CARTESIAN_POINT('Ctrl Pts',(147.613014815304,44.5245956946798,190.59599572238));
#93570=CARTESIAN_POINT('Ctrl Pts',(147.814604235587,44.28438722414,190.551808534294));
#93571=CARTESIAN_POINT('Ctrl Pts',(148.012855510647,44.0403342210074,190.507788751385));
#93572=CARTESIAN_POINT('Ctrl Pts',(148.207638105612,43.792490454076,190.464004327389));
#93573=CARTESIAN_POINT('Ctrl Pts',(148.353953896311,43.6063164443546,190.431114568329));
#93574=CARTESIAN_POINT('Ctrl Pts',(148.498122737652,43.4182230180028,190.398399194814));
#93575=CARTESIAN_POINT('Ctrl Pts',(148.639973419214,43.2284516503636,190.365920168262));
#93576=CARTESIAN_POINT('Ctrl Pts',(148.861528696448,42.9320494934958,190.315191474874));
#93577=CARTESIAN_POINT('Ctrl Pts',(149.077359267845,42.6316595878099,190.265055846598));
#93578=CARTESIAN_POINT('Ctrl Pts',(149.287156197482,42.3277350997865,190.215670418501));
#93579=CARTESIAN_POINT('Ctrl Pts',(149.300814102149,42.3079494351891,190.212455397813));
#93580=CARTESIAN_POINT('Ctrl Pts',(149.314446420857,42.2881487801072,190.209243558129));
#93581=CARTESIAN_POINT('Ctrl Pts',(149.32805306199,42.268333255379,190.206034943533));
#93582=CARTESIAN_POINT('Ctrl Pts',(149.417400435735,42.1382155373879,190.184965725587));
#93583=CARTESIAN_POINT('Ctrl Pts',(149.505697057769,42.0073928187187,190.164022900144));
#93584=CARTESIAN_POINT('Ctrl Pts',(149.59295522357,41.8758397422702,190.143210337197));
#93585=CARTESIAN_POINT('Ctrl Pts',(150.13058284509,41.0652959158561,190.014976966573));
#93586=CARTESIAN_POINT('Ctrl Pts',(150.62797127562,40.2285141913915,189.891883007592));
#93587=CARTESIAN_POINT('Ctrl Pts',(151.084752919722,39.3649994489525,189.775631285513));
#93588=CARTESIAN_POINT('Ctrl Pts',(151.145679577168,39.2498217320022,189.760125345333));
#93589=CARTESIAN_POINT('Ctrl Pts',(151.205883795788,39.1341684866594,189.744741137557));
#93590=CARTESIAN_POINT('Ctrl Pts',(151.265364697529,39.0180386085774,189.729482705023));
#93591=CARTESIAN_POINT('Origin',(125.29348064571,25.4505574462982,200.));
#93592=CARTESIAN_POINT('Ctrl Pts',(1.55981000190379E-14,25.8701893108725,
195.999534166346));
#93593=CARTESIAN_POINT('Ctrl Pts',(1.55970277531197E-14,24.8757620423259,
195.993992404177));
#93594=CARTESIAN_POINT('Ctrl Pts',(1.54046147636829E-14,24.8757620423259,
194.999549694134));
#93595=CARTESIAN_POINT('Ctrl Pts',(-8.21740721796392,25.8701893108446,195.999534166345));
#93596=CARTESIAN_POINT('Ctrl Pts',(-8.21741052170387,24.8757620423259,195.993992404063));
#93597=CARTESIAN_POINT('Ctrl Pts',(-8.21804707909509,24.8757620423259,194.999549694362));
#93598=CARTESIAN_POINT('Ctrl Pts',(-16.4351123294179,25.8705045195437,196.008014433201));
#93599=CARTESIAN_POINT('Ctrl Pts',(-16.4284754963483,24.8757620422117,196.002778286315));
#93600=CARTESIAN_POINT('Ctrl Pts',(-16.4360935882987,24.8757620423259,195.008027382868));
#93601=CARTESIAN_POINT('Ctrl Pts',(-32.8716902536231,25.8672519270132,196.020072042458));
#93602=CARTESIAN_POINT('Ctrl Pts',(-32.8650631301397,24.8757620424398,196.011627858086));
#93603=CARTESIAN_POINT('Ctrl Pts',(-32.8721788518652,24.8757620423259,195.02010702045));
#93604=CARTESIAN_POINT('Ctrl Pts',(-41.0905284509966,25.8637497700185,196.024420502657));
#93605=CARTESIAN_POINT('Ctrl Pts',(-41.061781966308,24.8757620424403,196.012595535246));
#93606=CARTESIAN_POINT('Ctrl Pts',(-41.0902164350087,24.8757620423259,195.024465281298));
#93607=CARTESIAN_POINT('Ctrl Pts',(-57.530618958565,25.8495382670329,195.984820115083));
#93608=CARTESIAN_POINT('Ctrl Pts',(-57.5019615256235,24.8757620422122,195.959319017969));
#93609=CARTESIAN_POINT('Ctrl Pts',(-57.5261473827835,24.8757620423259,194.985146590421));
#93610=CARTESIAN_POINT('Ctrl Pts',(-65.752229349423,25.8388537616774,195.942570987272));
#93611=CARTESIAN_POINT('Ctrl Pts',(-65.6887149097543,24.8757620425557,195.907765994157));
#93612=CARTESIAN_POINT('Ctrl Pts',(-65.7444507976842,24.8757620423259,194.943132932891));
#93613=CARTESIAN_POINT('Ctrl Pts',(-78.0874808464977,25.8147115657548,195.767826780906));
#93614=CARTESIAN_POINT('Ctrl Pts',(-78.0708636749413,24.8757620422123,195.710593550958));
#93615=CARTESIAN_POINT('Ctrl Pts',(-78.0703083245555,24.8757620423259,194.769802366593));
#93616=CARTESIAN_POINT('Ctrl Pts',(-82.1988777916636,25.8053087434596,195.69044692859));
#93617=CARTESIAN_POINT('Ctrl Pts',(-82.1765025713025,24.875762042376,195.625301040975));
#93618=CARTESIAN_POINT('Ctrl Pts',(-82.1778160289154,24.8757620423259,194.693080125928));
#93619=CARTESIAN_POINT('Ctrl Pts',(-90.4203625136221,25.7832828451603,195.47321942372));
#93620=CARTESIAN_POINT('Ctrl Pts',(-90.3969486708277,24.8757620422763,195.389459554287));
#93621=CARTESIAN_POINT('Ctrl Pts',(-90.3892106396611,24.8757620423259,194.477917980567));
#93622=CARTESIAN_POINT('Ctrl Pts',(-94.5304565710492,25.770658639565,195.33357508742));
#93623=CARTESIAN_POINT('Ctrl Pts',(-94.5002180268611,24.8757620423259,195.240180499821));
#93624=CARTESIAN_POINT('Ctrl Pts',(-94.4931091307174,24.8757620423259,194.339675539885));
#93625=CARTESIAN_POINT('Ctrl Pts',(-102.748391728739,25.7416579173973,194.954772731233));
#93626=CARTESIAN_POINT('Ctrl Pts',(-102.715751986094,24.8757620423259,194.838866884368));
#93627=CARTESIAN_POINT('Ctrl Pts',(-102.695151200076,24.8757620423259,193.96509632142));
#93628=CARTESIAN_POINT('Ctrl Pts',(-106.856246027343,25.725278146861,194.715964350451));
#93629=CARTESIAN_POINT('Ctrl Pts',(-106.81543638418,24.875762042369,194.589246043723));
#93630=CARTESIAN_POINT('Ctrl Pts',(-106.793314622248,24.8757620423259,193.729097788723));
#93631=CARTESIAN_POINT('Ctrl Pts',(-115.068137297811,25.6882726032458,194.080718037657));
#93632=CARTESIAN_POINT('Ctrl Pts',(-115.022239145157,24.8757620422835,193.928538627727));
#93633=CARTESIAN_POINT('Ctrl Pts',(-114.980548200328,24.8757620423259,193.102103079899));
#93634=CARTESIAN_POINT('Ctrl Pts',(-119.172205639421,25.6676398016414,193.684925703402));
#93635=CARTESIAN_POINT('Ctrl Pts',(-119.116329484592,24.8757620423259,193.521895669482));
#93636=CARTESIAN_POINT('Ctrl Pts',(-119.069654868258,24.8757620423259,192.711729260958));
#93637=CARTESIAN_POINT('Ctrl Pts',(-125.323347744084,25.6332752863461,192.902977900697));
#93638=CARTESIAN_POINT('Ctrl Pts',(-125.288387595195,24.8757620423259,192.716487359207));
#93639=CARTESIAN_POINT('Ctrl Pts',(-125.192484832993,24.8757620423259,191.941567071429));
#93640=CARTESIAN_POINT('Ctrl Pts',(-127.374905650878,25.6212405876043,192.61026813322));
#93641=CARTESIAN_POINT('Ctrl Pts',(-127.336151672754,24.8757620423474,192.417706213037));
#93642=CARTESIAN_POINT('Ctrl Pts',(-127.233608145136,24.8757620423259,191.653411387743));
#93643=CARTESIAN_POINT('Ctrl Pts',(-131.463610310007,25.5961158342195,191.946252068015));
#93644=CARTESIAN_POINT('Ctrl Pts',(-131.417681393358,24.8757620423046,191.741054985749));
#93645=CARTESIAN_POINT('Ctrl Pts',(-131.299148124053,24.8757620423259,191.000170054907));
#93646=CARTESIAN_POINT('Ctrl Pts',(-133.500663498608,25.5830272913609,191.575072827975));
#93647=CARTESIAN_POINT('Ctrl Pts',(-133.450072443569,24.8757620423438,191.364331943371));
#93648=CARTESIAN_POINT('Ctrl Pts',(-133.323473052073,24.8757620423259,190.635208210175));
#93649=CARTESIAN_POINT('Ctrl Pts',(-137.556266128696,25.5558831018172,190.734424603672));
#93650=CARTESIAN_POINT('Ctrl Pts',(-137.49615141237,24.8757620423081,190.51226943187));
#93651=CARTESIAN_POINT('Ctrl Pts',(-137.350968148536,24.8757620423259,189.809240410191));
#93652=CARTESIAN_POINT('Ctrl Pts',(-139.574830376325,25.5418271597114,190.265017746423));
#93653=CARTESIAN_POINT('Ctrl Pts',(-139.50891157162,24.8757620423438,190.038258843073));
#93654=CARTESIAN_POINT('Ctrl Pts',(-139.354151496503,24.8757620423259,189.348294290982));
#93655=CARTESIAN_POINT('Ctrl Pts',(-142.584968697329,25.5201265620969,189.468074534053));
#93656=CARTESIAN_POINT('Ctrl Pts',(-142.517789134679,24.875762042317,189.232187304688));
#93657=CARTESIAN_POINT('Ctrl Pts',(-142.338980713026,24.8757620423259,188.56631973987));
#93658=CARTESIAN_POINT('Ctrl Pts',(-143.585385950339,25.5127907503976,189.186905273307));
#93659=CARTESIAN_POINT('Ctrl Pts',(-143.514862987652,24.8757620423259,188.948964700898));
#93660=CARTESIAN_POINT('Ctrl Pts',(-143.330589015116,24.8757620423259,188.290521463128));
#93661=CARTESIAN_POINT('Ctrl Pts',(-145.579494487103,25.4979389111357,188.589605422417));
#93662=CARTESIAN_POINT('Ctrl Pts',(-145.501925955778,24.8757620423259,188.347761030563));
#93663=CARTESIAN_POINT('Ctrl Pts',(-145.306300715501,24.8757620423259,187.704852113735));
#93664=CARTESIAN_POINT('Ctrl Pts',(-146.574200692161,25.49041488071,188.273089407368));
#93665=CARTESIAN_POINT('Ctrl Pts',(-146.492901158935,24.8757620423259,188.029599291115));
#93666=CARTESIAN_POINT('Ctrl Pts',(-146.291407749267,24.8757620423259,187.394603605153));
#93667=CARTESIAN_POINT('Ctrl Pts',(-149.530965389848,25.4677381713212,187.269955276074));
#93668=CARTESIAN_POINT('Ctrl Pts',(-149.429901591881,24.8757620423259,187.024697733763));
#93669=CARTESIAN_POINT('Ctrl Pts',(-149.218333471988,24.8757620423259,186.411710463469));
#93670=CARTESIAN_POINT('Ctrl Pts',(-151.469919324602,25.4524496338339,186.528895379912));
#93671=CARTESIAN_POINT('Ctrl Pts',(-151.360643558434,24.8757620423259,186.282461960026));
#93672=CARTESIAN_POINT('Ctrl Pts',(-151.135962079037,24.8757620423259,185.686074351676));
#93673=CARTESIAN_POINT('Ctrl Pts',(-155.268552533548,25.421878992293,184.870449086661));
#93674=CARTESIAN_POINT('Ctrl Pts',(-155.140301022575,24.8757620423259,184.622711642346));
#93675=CARTESIAN_POINT('Ctrl Pts',(-154.889283187975,24.8757620423259,184.063471352248));
#93676=CARTESIAN_POINT('Ctrl Pts',(-157.128318393194,25.4065973813273,183.953242115242));
#93677=CARTESIAN_POINT('Ctrl Pts',(-156.990494177067,24.8757620423259,183.707070687992));
#93678=CARTESIAN_POINT('Ctrl Pts',(-156.725059327294,24.8757620423259,183.166679353191));
#93679=CARTESIAN_POINT('Ctrl Pts',(-159.843877846741,25.3839693077877,182.4143228812));
#93680=CARTESIAN_POINT('Ctrl Pts',(-159.696302120373,24.8757620423259,182.167954674856));
#93681=CARTESIAN_POINT('Ctrl Pts',(-159.403034456653,24.8757620423259,181.663223290672));
#93682=CARTESIAN_POINT('Ctrl Pts',(-160.736671906421,25.3764758830308,181.874075657354));
#93683=CARTESIAN_POINT('Ctrl Pts',(-160.58348509393,24.8757620423331,181.629500993224));
#93684=CARTESIAN_POINT('Ctrl Pts',(-160.283036640086,24.8757620423259,181.135606802703));
#93685=CARTESIAN_POINT('Ctrl Pts',(-162.054867926021,25.3653482837207,181.017753243736));
#93686=CARTESIAN_POINT('Ctrl Pts',(-161.894451982614,24.8757620423223,180.775409581153));
#93687=CARTESIAN_POINT('Ctrl Pts',(-161.581727876928,24.8757620423259,180.299617979711));
#93688=CARTESIAN_POINT('Ctrl Pts',(-162.490762640011,25.361657861326,180.724643998008));
#93689=CARTESIAN_POINT('Ctrl Pts',(-162.32737504632,24.8757620423286,180.483534423218));
#93690=CARTESIAN_POINT('Ctrl Pts',(-162.011068383027,24.8757620423259,180.01351814156));
#93691=CARTESIAN_POINT('Ctrl Pts',(-163.355074229889,25.354321385116,180.122105972292));
#93692=CARTESIAN_POINT('Ctrl Pts',(-163.185636865372,24.8757620423232,179.883705522239));
#93693=CARTESIAN_POINT('Ctrl Pts',(-162.862182136119,24.8757620423259,179.42549510677));
#93694=CARTESIAN_POINT('Ctrl Pts',(-163.784024035092,25.3506707582467,179.812243966753));
#93695=CARTESIAN_POINT('Ctrl Pts',(-163.611544779999,24.8757620423259,179.575344130263));
#93696=CARTESIAN_POINT('Ctrl Pts',(-163.284479634629,24.8757620423259,179.123149423031));
#93697=CARTESIAN_POINT('Ctrl Pts',(-165.893924132154,25.3326733753055,178.230844182634));
#93698=CARTESIAN_POINT('Ctrl Pts',(-165.698702838315,24.8757620423259,178.007586069906));
#93699=CARTESIAN_POINT('Ctrl Pts',(-165.361175322346,24.8757620423259,177.580381667324));
#93700=CARTESIAN_POINT('Ctrl Pts',(-167.481106685865,25.3190005603972,176.856948482142));
#93701=CARTESIAN_POINT('Ctrl Pts',(-167.275278221452,24.8757620423152,176.642444583454));
#93702=CARTESIAN_POINT('Ctrl Pts',(-166.921818221905,24.8757620423259,176.240893842191));
#93703=CARTESIAN_POINT('Ctrl Pts',(-169.684665227087,25.2999653906393,174.605906246088));
#93704=CARTESIAN_POINT('Ctrl Pts',(-169.464760847503,24.8757620423312,174.403386973429));
#93705=CARTESIAN_POINT('Ctrl Pts',(-169.086795032884,24.8757620423259,174.047706451662));
#93706=CARTESIAN_POINT('Ctrl Pts',(-170.389548700331,25.2938670470603,173.823752953021));
#93707=CARTESIAN_POINT('Ctrl Pts',(-170.163773376106,24.8757620423223,173.627328010298));
#93708=CARTESIAN_POINT('Ctrl Pts',(-169.779023946969,24.8757620423259,173.285881474387));
#93709=CARTESIAN_POINT('Ctrl Pts',(-171.733708831765,25.2822654981617,172.189187311864));
#93710=CARTESIAN_POINT('Ctrl Pts',(-171.495932116079,24.8757620423295,172.006291779375));
#93711=CARTESIAN_POINT('Ctrl Pts',(-171.098494081107,24.8757620423259,171.694301405067));
#93712=CARTESIAN_POINT('Ctrl Pts',(-172.374791488579,25.2767480891279,171.333293369278));
#93713=CARTESIAN_POINT('Ctrl Pts',(-172.131402736303,24.8757620423313,171.157743137787));
#93714=CARTESIAN_POINT('Ctrl Pts',(-171.727502211852,24.8757620423259,170.861160982562));
#93715=CARTESIAN_POINT('Ctrl Pts',(-174.149962214451,25.2616143901389,168.706265498992));
#93716=CARTESIAN_POINT('Ctrl Pts',(-173.887056783482,24.8757620423152,168.558753202255));
#93717=CARTESIAN_POINT('Ctrl Pts',(-173.46844284384,24.8757620423259,168.304775190926));
#93718=CARTESIAN_POINT('Ctrl Pts',(-175.149896364286,25.2536804395812,166.860854093189));
#93719=CARTESIAN_POINT('Ctrl Pts',(-174.87876760015,24.8757620423401,166.730672448768));
#93720=CARTESIAN_POINT('Ctrl Pts',(-174.447418189425,24.8757620423259,166.510636295168));
#93721=CARTESIAN_POINT('Ctrl Pts',(-176.347229631101,25.2428388848927,163.944275786663));
#93722=CARTESIAN_POINT('Ctrl Pts',(-176.065432586062,24.8757620423188,163.840418898352));
#93723=CARTESIAN_POINT('Ctrl Pts',(-175.621308989244,24.8757620423259,163.673672937929));
#93724=CARTESIAN_POINT('Ctrl Pts',(-176.69550116753,25.239240468917,162.947498775422));
#93725=CARTESIAN_POINT('Ctrl Pts',(-176.410357889342,24.8757620423187,162.853899660982));
#93726=CARTESIAN_POINT('Ctrl Pts',(-175.96335024238,24.8757620423259,162.703646661311));
#93727=CARTESIAN_POINT('Ctrl Pts',(-177.143858779535,25.2329712637093,161.419747762863));
#93728=CARTESIAN_POINT('Ctrl Pts',(-176.85502728246,24.8757620423295,161.339448567081));
#93729=CARTESIAN_POINT('Ctrl Pts',(-176.405926433472,24.8757620423259,161.213730765013));
#93730=CARTESIAN_POINT('Ctrl Pts',(-177.281257913445,25.2307372146378,160.904114441399));
#93731=CARTESIAN_POINT('Ctrl Pts',(-176.991292739235,24.8757620423295,160.828489480191));
#93732=CARTESIAN_POINT('Ctrl Pts',(-176.54197824777,24.8757620423259,160.710339939802));
#93733=CARTESIAN_POINT('Ctrl Pts',(-177.530501036989,25.2260187908126,159.875002150419));
#93734=CARTESIAN_POINT('Ctrl Pts',(-177.238632774441,24.8757620423223,159.808152124321));
#93735=CARTESIAN_POINT('Ctrl Pts',(-176.789652532962,24.8757620423259,159.704364492039));
#93736=CARTESIAN_POINT('Ctrl Pts',(-177.642808421522,25.2235311200789,159.360184292277));
#93737=CARTESIAN_POINT('Ctrl Pts',(-177.350180560588,24.8757620423268,159.297529645419));
#93738=CARTESIAN_POINT('Ctrl Pts',(-176.901727564712,24.8757620423259,159.200477903653));
#93739=CARTESIAN_POINT('Ctrl Pts',(-178.150698495911,25.2105673597152,156.785499624353));
#93740=CARTESIAN_POINT('Ctrl Pts',(-177.853818377308,24.8757620423223,156.748431812088));
#93741=CARTESIAN_POINT('Ctrl Pts',(-177.410722924974,24.8757620423259,156.677118500037));
#93742=CARTESIAN_POINT('Ctrl Pts',(-178.38892700326,25.1986131825788,154.724292736304));
#93743=CARTESIAN_POINT('Ctrl Pts',(-178.092734343343,24.8757620423793,154.699739042078));
#93744=CARTESIAN_POINT('Ctrl Pts',(-177.656737843813,24.8757620423259,154.646113775664));
#93745=CARTESIAN_POINT('Ctrl Pts',(-178.535788240059,25.1869009068823,152.663678496546));
#93746=CARTESIAN_POINT('Ctrl Pts',(-178.240980734254,24.8757620423259,152.641070351893));
#93747=CARTESIAN_POINT('Ctrl Pts',(-177.813017113378,24.8757620423259,152.608250755187));
#93748=CARTESIAN_POINT('',(1.54046147636829E-14,24.8757620423259,194.999549694134));
#93749=CARTESIAN_POINT('',(1.58047048864619E-14,25.8701893108725,195.999534166346));
#93750=CARTESIAN_POINT('Origin',(1.54046147636829E-14,25.8757620423259,
194.999549694134));
#93751=CARTESIAN_POINT('',(-178.53578824005,25.1869009068724,152.663678496545));
#93752=CARTESIAN_POINT('Ctrl Pts',(-178.535788240059,25.1869009068823,152.663678496546));
#93753=CARTESIAN_POINT('Ctrl Pts',(-178.497300169629,25.1899703544864,153.203705718586));
#93754=CARTESIAN_POINT('Ctrl Pts',(-178.452605703909,25.1930505432942,153.74275174592));
#93755=CARTESIAN_POINT('Ctrl Pts',(-178.400429730265,25.1961079530536,154.280627961182));
#93756=CARTESIAN_POINT('Ctrl Pts',(-178.349499261461,25.1990923786713,154.805664407814));
#93757=CARTESIAN_POINT('Ctrl Pts',(-178.291439967185,25.202055092476,155.329586217056));
#93758=CARTESIAN_POINT('Ctrl Pts',(-178.225113983825,25.204965729571,155.85221882764));
#93759=CARTESIAN_POINT('Ctrl Pts',(-178.160952607745,25.2077813754435,156.357794859552));
#93760=CARTESIAN_POINT('Ctrl Pts',(-178.0890552258,25.2105482841908,156.862164463122));
#93761=CARTESIAN_POINT('Ctrl Pts',(-178.008439607117,25.2132398164984,157.365170531856));
#93762=CARTESIAN_POINT('Ctrl Pts',(-177.929150781168,25.21588705087,157.859897996418));
#93763=CARTESIAN_POINT('Ctrl Pts',(-177.841428154854,25.2184613643469,158.353306433683));
#93764=CARTESIAN_POINT('Ctrl Pts',(-177.744386392921,25.2209383168131,158.845247349922));
#93765=CARTESIAN_POINT('Ctrl Pts',(-177.743350247437,25.2209647640154,158.850499958162));
#93766=CARTESIAN_POINT('Ctrl Pts',(-177.742313016692,25.220991199489,158.855752396207));
#93767=CARTESIAN_POINT('Ctrl Pts',(-177.741274699235,25.2210176232105,158.861004663759));
#93768=CARTESIAN_POINT('Ctrl Pts',(-177.646352097481,25.2234332701475,159.341165039959));
#93769=CARTESIAN_POINT('Ctrl Pts',(-177.542342526488,25.2257507195669,159.819902563843));
#93770=CARTESIAN_POINT('Ctrl Pts',(-177.428152198495,25.2279524716699,160.297046148221));
#93771=CARTESIAN_POINT('Ctrl Pts',(-177.420819639305,25.2280938538508,160.327685201773));
#93772=CARTESIAN_POINT('Ctrl Pts',(-177.413445118906,25.228234759215,160.358317684296));
#93773=CARTESIAN_POINT('Ctrl Pts',(-177.406028355073,25.228375183231,160.388943551061));
#93774=CARTESIAN_POINT('Ctrl Pts',(-177.405978730098,25.2283761227969,160.38914846629));
#93775=CARTESIAN_POINT('Ctrl Pts',(-177.405929103243,25.228377062341,160.389353381181));
#93776=CARTESIAN_POINT('Ctrl Pts',(-177.405879474506,25.2283780018634,160.389558295734));
#93777=CARTESIAN_POINT('Ctrl Pts',(-177.327469296974,25.2298623861984,160.713309967531));
#93778=CARTESIAN_POINT('Ctrl Pts',(-177.244183872507,25.2312938639448,161.03674586819));
#93779=CARTESIAN_POINT('Ctrl Pts',(-177.156159366085,25.232669467775,161.358388065109));
#93780=CARTESIAN_POINT('Ctrl Pts',(-177.106238966282,25.2334495993085,161.540797574875));
#93781=CARTESIAN_POINT('Ctrl Pts',(-177.054793463084,25.2342117537668,161.722630946496));
#93782=CARTESIAN_POINT('Ctrl Pts',(-177.001840977559,25.2349553293434,161.903621195652));
#93783=CARTESIAN_POINT('Ctrl Pts',(-176.999365614225,25.2349900891795,161.912081924589));
#93784=CARTESIAN_POINT('Ctrl Pts',(-176.996886965513,25.2350248092209,161.920540784291));
#93785=CARTESIAN_POINT('Ctrl Pts',(-176.994405034784,25.2350594893758,161.928997741723));
#93786=CARTESIAN_POINT('Ctrl Pts',(-176.837547755075,25.2372512647935,162.463474921929));
#93787=CARTESIAN_POINT('Ctrl Pts',(-176.667267889636,25.2392828103483,162.991404312881));
#93788=CARTESIAN_POINT('Ctrl Pts',(-176.483342251063,25.2412384685856,163.512642511656));
#93789=CARTESIAN_POINT('Ctrl Pts',(-176.325980687731,25.242911674344,163.958599140999));
#93790=CARTESIAN_POINT('Ctrl Pts',(-176.158629659706,25.2445292808119,164.399657606776));
#93791=CARTESIAN_POINT('Ctrl Pts',(-175.981121483524,25.2461434645031,164.835716213452));
#93792=CARTESIAN_POINT('Ctrl Pts',(-175.970156859221,25.2462431721229,164.862651416659));
#93793=CARTESIAN_POINT('Ctrl Pts',(-175.959153364956,25.2463428834581,164.889567836151));
#93794=CARTESIAN_POINT('Ctrl Pts',(-175.94811096596,25.2464426111523,164.916465420591));
#93795=CARTESIAN_POINT('Ctrl Pts',(-175.659320785773,25.2490507743609,165.61991385235));
#93796=CARTESIAN_POINT('Ctrl Pts',(-175.344140309045,25.2517544614552,166.310398234908));
#93797=CARTESIAN_POINT('Ctrl Pts',(-175.003342450806,25.2546225778795,166.988304176856));
#93798=CARTESIAN_POINT('Ctrl Pts',(-174.654435203123,25.2575589420128,167.682341098376));
#93799=CARTESIAN_POINT('Ctrl Pts',(-174.278676824774,25.2606676279253,168.363193861084));
#93800=CARTESIAN_POINT('Ctrl Pts',(-173.87684769516,25.2640230810151,169.03125108838));
#93801=CARTESIAN_POINT('Ctrl Pts',(-173.623321907699,25.2661401348179,169.452747993748));
#93802=CARTESIAN_POINT('Ctrl Pts',(-173.359417112121,25.2683554311092,169.869150852764));
#93803=CARTESIAN_POINT('Ctrl Pts',(-173.085319953511,25.2706878379522,170.280552263732));
#93804=CARTESIAN_POINT('Ctrl Pts',(-173.04591944413,25.271023113291,170.339689779912));
#93805=CARTESIAN_POINT('Ctrl Pts',(-173.006317841426,25.271360622038,170.398709526143));
#93806=CARTESIAN_POINT('Ctrl Pts',(-172.966513141016,25.2717004535672,170.457616103021));
#93807=CARTESIAN_POINT('Ctrl Pts',(-172.789438023641,25.2732122274859,170.719667793079));
#93808=CARTESIAN_POINT('Ctrl Pts',(-172.608035715689,25.2747640234387,170.979815978787));
#93809=CARTESIAN_POINT('Ctrl Pts',(-172.422531449036,25.2763541171347,171.23792999103));
#93810=CARTESIAN_POINT('Ctrl Pts',(-172.345699804947,25.2770126977437,171.34483493872));
#93811=CARTESIAN_POINT('Ctrl Pts',(-172.268163938986,25.2776778538747,171.451390649919));
#93812=CARTESIAN_POINT('Ctrl Pts',(-172.18993771799,25.2783494853052,171.557586363661));
#93813=CARTESIAN_POINT('Ctrl Pts',(-171.979411745319,25.2801570104337,171.84338511048));
#93814=CARTESIAN_POINT('Ctrl Pts',(-171.764071045959,25.2820098626848,172.126315848985));
#93815=CARTESIAN_POINT('Ctrl Pts',(-171.544848096176,25.2838950226329,172.405334618166));
#93816=CARTESIAN_POINT('Ctrl Pts',(-171.441729184068,25.2847817712293,172.536580511737));
#93817=CARTESIAN_POINT('Ctrl Pts',(-171.337751912468,25.2856756597066,172.666961263959));
#93818=CARTESIAN_POINT('Ctrl Pts',(-171.233016183297,25.2865752923589,172.796371004303));
#93819=CARTESIAN_POINT('Ctrl Pts',(-171.17612444317,25.2870639667345,172.866665500515));
#93820=CARTESIAN_POINT('Ctrl Pts',(-171.118988187389,25.2875552733446,172.936700069534));
#93821=CARTESIAN_POINT('Ctrl Pts',(-171.061619131872,25.2880490444023,173.006462145406));
#93822=CARTESIAN_POINT('Ctrl Pts',(-170.680368993122,25.2913304350851,173.470070982369));
#93823=CARTESIAN_POINT('Ctrl Pts',(-170.288253320335,25.2947253627475,173.922762685443));
#93824=CARTESIAN_POINT('Ctrl Pts',(-169.885958968133,25.2982089938393,174.364917953415));
#93825=CARTESIAN_POINT('Ctrl Pts',(-169.652057198546,25.3002344447871,174.621995635577));
#93826=CARTESIAN_POINT('Ctrl Pts',(-169.414715275907,25.3022898525701,174.875512212633));
#93827=CARTESIAN_POINT('Ctrl Pts',(-169.174073915602,25.3043700857121,175.125548134129));
#93828=CARTESIAN_POINT('Ctrl Pts',(-169.099746717454,25.3050126099263,175.202777042149));
#93829=CARTESIAN_POINT('Ctrl Pts',(-169.02510205045,25.3056576781881,175.279676910402));
#93830=CARTESIAN_POINT('Ctrl Pts',(-168.950143152317,25.3063052525107,175.356251130019));
#93831=CARTESIAN_POINT('Ctrl Pts',(-168.078449890391,25.3138358617872,176.246728884361));
#93832=CARTESIAN_POINT('Ctrl Pts',(-167.164400855462,25.3217035673909,177.09331430014));
#93833=CARTESIAN_POINT('Ctrl Pts',(-166.211448824813,25.3298819796683,177.8995754802));
#93834=CARTESIAN_POINT('Ctrl Pts',(-165.665772060563,25.3345650795566,178.361254534051));
#93835=CARTESIAN_POINT('Ctrl Pts',(-165.107339947121,25.3393501326907,178.809712437871));
#93836=CARTESIAN_POINT('Ctrl Pts',(-164.536805415267,25.344232845357,179.245625184694));
#93837=CARTESIAN_POINT('Ctrl Pts',(-164.426984425153,25.345172708432,179.329533111009));
#93838=CARTESIAN_POINT('Ctrl Pts',(-164.31671449233,25.3461155817281,179.412976159758));
#93839=CARTESIAN_POINT('Ctrl Pts',(-164.206000395446,25.3470614307091,179.495959084527));
#93840=CARTESIAN_POINT('Ctrl Pts',(-163.784175350291,25.3506651523702,179.812127277856));
#93841=CARTESIAN_POINT('Ctrl Pts',(-163.35522805828,25.3543178969937,180.121997119112));
#93842=CARTESIAN_POINT('Ctrl Pts',(-162.922917985055,25.3579883154489,180.423374333965));
#93843=CARTESIAN_POINT('Ctrl Pts',(-162.614980433254,25.360602780721,180.638047475903));
#93844=CARTESIAN_POINT('Ctrl Pts',(-162.305066748929,25.3632285329527,180.848631163179));
#93845=CARTESIAN_POINT('Ctrl Pts',(-161.993261623921,25.3658651734537,181.05529624663));
#93846=CARTESIAN_POINT('Ctrl Pts',(-161.867636169548,25.3669274688888,181.1385610583));
#93847=CARTESIAN_POINT('Ctrl Pts',(-161.74170349846,25.3679913696006,181.221189795947));
#93848=CARTESIAN_POINT('Ctrl Pts',(-161.615469046877,25.3690568361265,181.303193728346));
#93849=CARTESIAN_POINT('Ctrl Pts',(-160.873076979922,25.3753229060188,181.785463569176));
#93850=CARTESIAN_POINT('Ctrl Pts',(-160.120260430856,25.3816429921167,182.246150230608));
#93851=CARTESIAN_POINT('Ctrl Pts',(-159.357962893647,25.3880105482161,182.68721140722));
#93852=CARTESIAN_POINT('Ctrl Pts',(-159.218520766211,25.3891753238131,182.767891857824));
#93853=CARTESIAN_POINT('Ctrl Pts',(-159.07876131923,25.3903412827711,182.847915451902));
#93854=CARTESIAN_POINT('Ctrl Pts',(-158.938690377899,25.391508366095,182.927294205919));
#93855=CARTESIAN_POINT('Ctrl Pts',(-157.86068685648,25.400490385642,183.538203046421));
#93856=CARTESIAN_POINT('Ctrl Pts',(-156.764294467523,25.4095384825695,184.111040501086));
#93857=CARTESIAN_POINT('Ctrl Pts',(-155.651548955509,25.418630158697,184.650020168367));
#93858=CARTESIAN_POINT('Ctrl Pts',(-155.059253323969,25.4234695042576,184.936909936937));
#93859=CARTESIAN_POINT('Ctrl Pts',(-154.462324779835,25.4283212431225,185.214207771741));
#93860=CARTESIAN_POINT('Ctrl Pts',(-153.861072648507,25.4331822909263,185.482554638578));
#93861=CARTESIAN_POINT('Ctrl Pts',(-153.697444572822,25.4345052033228,185.555584036977));
#93862=CARTESIAN_POINT('Ctrl Pts',(-153.533496042194,25.4358281612412,185.627950279612));
#93863=CARTESIAN_POINT('Ctrl Pts',(-153.369233365809,25.4371510777225,185.699666304073));
#93864=CARTESIAN_POINT('Ctrl Pts',(-152.168980557043,25.446817511129,186.223688934702));
#93865=CARTESIAN_POINT('Ctrl Pts',(-150.951918946651,25.4564813415511,186.712920141648));
#93866=CARTESIAN_POINT('Ctrl Pts',(-149.71990938609,25.4661146840139,187.171200413097));
#93867=CARTESIAN_POINT('Ctrl Pts',(-149.185779282653,25.4702911598878,187.369884982298));
#93868=CARTESIAN_POINT('Ctrl Pts',(-148.648839821616,25.4744619353068,187.562752628899));
#93869=CARTESIAN_POINT('Ctrl Pts',(-148.109243829216,25.4786248717976,187.750119081111));
#93870=CARTESIAN_POINT('Ctrl Pts',(-147.926402504759,25.4800354768286,187.813607933445));
#93871=CARTESIAN_POINT('Ctrl Pts',(-147.743247228578,25.4814447522696,187.876468024315));
#93872=CARTESIAN_POINT('Ctrl Pts',(-147.55978845866,25.4828525510777,187.938709975727));
#93873=CARTESIAN_POINT('Ctrl Pts',(-146.762673408406,25.4889693348008,188.209146740617));
#93874=CARTESIAN_POINT('Ctrl Pts',(-145.959131280017,25.4950633304527,188.468050410514));
#93875=CARTESIAN_POINT('Ctrl Pts',(-145.153130048878,25.5011006913591,188.715270729109));
#93876=CARTESIAN_POINT('Ctrl Pts',(-144.963043743523,25.5025245348775,188.773574854655));
#93877=CARTESIAN_POINT('Ctrl Pts',(-144.772797182542,25.5039455064929,188.831236637802));
#93878=CARTESIAN_POINT('Ctrl Pts',(-144.582440026613,25.5053631356726,188.888254699799));
#93879=CARTESIAN_POINT('Ctrl Pts',(-143.779879218403,25.5113399722913,189.128647353786));
#93880=CARTESIAN_POINT('Ctrl Pts',(-142.974694653033,25.5172625782225,189.357845213595));
#93881=CARTESIAN_POINT('Ctrl Pts',(-142.167290172813,25.5231223320602,189.576786264052));
#93882=CARTESIAN_POINT('Ctrl Pts',(-141.972188592948,25.5245382855994,189.629691277447));
#93883=CARTESIAN_POINT('Ctrl Pts',(-141.776953866285,25.5259504483271,189.681998426253));
#93884=CARTESIAN_POINT('Ctrl Pts',(-141.581589130899,25.5273587560137,189.733721790199));
#93885=CARTESIAN_POINT('Ctrl Pts',(-140.130979976262,25.5378156279707,190.117774649593));
#93886=CARTESIAN_POINT('Ctrl Pts',(-138.673224992468,25.5480587714908,190.469740822773));
#93887=CARTESIAN_POINT('Ctrl Pts',(-137.209373498613,25.5580722003362,190.794332526983));
#93888=CARTESIAN_POINT('Ctrl Pts',(-136.851595170103,25.5605195714322,190.873665627279));
#93889=CARTESIAN_POINT('Ctrl Pts',(-136.493452706413,25.5629532282201,190.951363735793));
#93890=CARTESIAN_POINT('Ctrl Pts',(-136.134961511771,25.5653729519654,191.027496107107));
#93891=CARTESIAN_POINT('Ctrl Pts',(-135.932905732926,25.5667367767211,191.070406465329));
#93892=CARTESIAN_POINT('Ctrl Pts',(-135.730739135609,25.5680958253213,191.112819318821));
#93893=CARTESIAN_POINT('Ctrl Pts',(-135.528464480754,25.5694500469772,191.154747092583));
#93894=CARTESIAN_POINT('Ctrl Pts',(-133.923642813523,25.5801942712463,191.487396775465));
#93895=CARTESIAN_POINT('Ctrl Pts',(-132.31200926945,25.590634688285,191.789469250514));
#93896=CARTESIAN_POINT('Ctrl Pts',(-130.694643085842,25.6007619388848,192.065796528307));
#93897=CARTESIAN_POINT('Ctrl Pts',(-130.475044601821,25.6021369700321,192.103314965327));
#93898=CARTESIAN_POINT('Ctrl Pts',(-130.2553404509,25.6035062306849,192.140358867938));
#93899=CARTESIAN_POINT('Ctrl Pts',(-130.035533347416,25.6048696998908,192.176940401655));
#93900=CARTESIAN_POINT('Ctrl Pts',(-129.830200894786,25.6061433824594,192.211112982614));
#93901=CARTESIAN_POINT('Ctrl Pts',(-129.624774577578,25.6074118350481,192.244882695885));
#93902=CARTESIAN_POINT('Ctrl Pts',(-129.419257839823,25.6086750127158,192.278259225451));
#93903=CARTESIAN_POINT('Ctrl Pts',(-128.048159852991,25.6171022599372,192.50092961714));
#93904=CARTESIAN_POINT('Ctrl Pts',(-126.673077985888,25.6252939765782,192.706038470115));
#93905=CARTESIAN_POINT('Ctrl Pts',(-125.296985611204,25.6332344356778,192.895668467366));
#93906=CARTESIAN_POINT('Ctrl Pts',(-124.827303057514,25.6359446426202,192.960392248272));
#93907=CARTESIAN_POINT('Ctrl Pts',(-124.357502920292,25.6386255864969,193.023313241805));
#93908=CARTESIAN_POINT('Ctrl Pts',(-123.887703735145,25.6412766658778,193.084515551574));
#93909=CARTESIAN_POINT('Ctrl Pts',(-123.682798716099,25.6424329460251,193.111209213133));
#93910=CARTESIAN_POINT('Ctrl Pts',(-123.47788354471,25.6435834960832,193.137577256653));
#93911=CARTESIAN_POINT('Ctrl Pts',(-123.272966987477,25.6447282671046,193.163626730597));
#93912=CARTESIAN_POINT('Ctrl Pts',(-121.444120246373,25.6549451611424,193.396114022849));
#93913=CARTESIAN_POINT('Ctrl Pts',(-119.613568752739,25.6647100991143,193.603766112159));
#93914=CARTESIAN_POINT('Ctrl Pts',(-117.7817201061,25.6740390861231,193.790689645519));
#93915=CARTESIAN_POINT('Ctrl Pts',(-115.810748231209,25.6840765807868,193.991809442007));
#93916=CARTESIAN_POINT('Ctrl Pts',(-113.838274697661,25.6936093935951,194.168932989191));
#93917=CARTESIAN_POINT('Ctrl Pts',(-111.864808666113,25.7026589407586,194.327234715607));
#93918=CARTESIAN_POINT('Ctrl Pts',(-111.760681072972,25.7031364293752,194.335587318337));
#93919=CARTESIAN_POINT('Ctrl Pts',(-111.656550716993,25.7036125728839,194.343887532483));
#93920=CARTESIAN_POINT('Ctrl Pts',(-111.552417673064,25.704087374533,194.352136121901));
#93921=CARTESIAN_POINT('Ctrl Pts',(-111.355686433126,25.7049843839128,194.367719602061));
#93922=CARTESIAN_POINT('Ctrl Pts',(-111.158944291909,25.7058764632696,194.383118901624));
#93923=CARTESIAN_POINT('Ctrl Pts',(-110.962191508823,25.7067636312559,194.398339186358));
#93924=CARTESIAN_POINT('Ctrl Pts',(-108.331895633658,25.7186237648639,194.601812049752));
#93925=CARTESIAN_POINT('Ctrl Pts',(-105.699684895831,25.7296088578491,194.77302215994));
#93926=CARTESIAN_POINT('Ctrl Pts',(-103.066012980214,25.7397901020854,194.919629802492));
#93927=CARTESIAN_POINT('Ctrl Pts',(-101.77346531473,25.744786830566,194.991581576364));
#93928=CARTESIAN_POINT('Ctrl Pts',(-100.480565724247,25.7495899739133,195.057608395254));
#93929=CARTESIAN_POINT('Ctrl Pts',(-99.1873679390386,25.7542081099002,195.118620245283));
#93930=CARTESIAN_POINT('Ctrl Pts',(-99.004725899309,25.7548603425176,195.127237124205));
#93931=CARTESIAN_POINT('Ctrl Pts',(-98.8220779192055,25.7555088353306,195.135753968689));
#93932=CARTESIAN_POINT('Ctrl Pts',(-98.6394241242379,25.7561536103568,195.144173347539));
#93933=CARTESIAN_POINT('Ctrl Pts',(-95.380241384999,25.7676586526498,195.294404522465));
#93934=CARTESIAN_POINT('Ctrl Pts',(-92.1191988411839,25.7779818585862,195.41337897528));
#93935=CARTESIAN_POINT('Ctrl Pts',(-88.8568519213988,25.787260115861,195.510390948637));
#93936=CARTESIAN_POINT('Ctrl Pts',(-88.1724603633154,25.7892065553749,195.530742608725));
#93937=CARTESIAN_POINT('Ctrl Pts',(-87.4880114041535,25.7911070139255,195.550127889636));
#93938=CARTESIAN_POINT('Ctrl Pts',(-86.8035101782839,25.7929627657666,195.568632876457));
#93939=CARTESIAN_POINT('Ctrl Pts',(-86.6388831801868,25.7934090861577,195.573083446179));
#93940=CARTESIAN_POINT('Ctrl Pts',(-86.4742531510357,25.7938528048312,195.577483095995));
#93941=CARTESIAN_POINT('Ctrl Pts',(-86.3096201486703,25.7942939388959,195.581833024548));
#93942=CARTESIAN_POINT('Ctrl Pts',(-82.3438711834279,25.8049201616776,195.686615932032));
#93943=CARTESIAN_POINT('Ctrl Pts',(-78.3763910652539,25.81404753251,195.762354575598));
#93944=CARTESIAN_POINT('Ctrl Pts',(-74.4078298020737,25.821907197684,195.819882597081));
#93945=CARTESIAN_POINT('Ctrl Pts',(-74.263798022696,25.8221924500678,195.821970472951));
#93946=CARTESIAN_POINT('Ctrl Pts',(-74.1197648633499,25.8224760292359,195.824034366091));
#93947=CARTESIAN_POINT('Ctrl Pts',(-73.9757303467128,25.8227579460834,195.82607479565));
#93948=CARTESIAN_POINT('Ctrl Pts',(-68.3928699838828,25.8336852045642,195.90516301405));
#93949=CARTESIAN_POINT('Ctrl Pts',(-62.8094936979019,25.8421199931682,195.950045641758));
#93950=CARTESIAN_POINT('Ctrl Pts',(-57.2260685167664,25.8486341168402,195.976904270453));
#93951=CARTESIAN_POINT('Ctrl Pts',(-54.6859273035473,25.8515976729854,195.98912342043));
#93952=CARTESIAN_POINT('Ctrl Pts',(-52.1457759576179,25.8541637485837,195.997612920801));
#93953=CARTESIAN_POINT('Ctrl Pts',(-49.605658395478,25.8563863803193,196.003899767975));
#93954=CARTESIAN_POINT('Ctrl Pts',(-49.5072967943702,25.8564724478381,196.004143215114));
#93955=CARTESIAN_POINT('Ctrl Pts',(-49.4089352305451,25.8565579998157,196.004383359602));
#93956=CARTESIAN_POINT('Ctrl Pts',(-49.310573704736,25.8566430393848,196.004620290147));
#93957=CARTESIAN_POINT('Ctrl Pts',(-41.1414030558168,25.8637057882182,196.024297964312));
#93958=CARTESIAN_POINT('Ctrl Pts',(-32.9721411092781,25.8672091692298,196.020124461517));
#93959=CARTESIAN_POINT('Ctrl Pts',(-24.8028804680956,25.8688484080511,196.014152702805));
#93960=CARTESIAN_POINT('Ctrl Pts',(-24.7530540772718,25.8688584061841,196.014116279535));
#93961=CARTESIAN_POINT('Ctrl Pts',(-24.7032276851075,25.868868334986,196.014079789476));
#93962=CARTESIAN_POINT('Ctrl Pts',(-24.6534012915206,25.8688781948416,196.014043237634));
#93963=CARTESIAN_POINT('Ctrl Pts',(-16.435603976083,25.8705043670193,196.008014793532));
#93964=CARTESIAN_POINT('Ctrl Pts',(-8.21780260152389,25.8701893108446,195.999534166345));
#93965=CARTESIAN_POINT('Ctrl Pts',(1.55981000190379E-14,25.8701893108725,
195.999534166346));
#93966=CARTESIAN_POINT('',(-177.813017113379,24.8757620423259,152.608250755187));
#93967=CARTESIAN_POINT('Origin',(-177.813017113379,25.8757620423259,152.608250755187));
#93968=CARTESIAN_POINT('Ctrl Pts',(1.54046147636829E-14,24.8757620423259,
194.999549694134));
#93969=CARTESIAN_POINT('Ctrl Pts',(-8.21488588608219,24.8757620423259,194.999549694362));
#93970=CARTESIAN_POINT('Ctrl Pts',(-16.4297691665589,24.8757620423259,195.008020860107));
#93971=CARTESIAN_POINT('Ctrl Pts',(-24.6446497557777,24.8757620423259,195.01406045846));
#93972=CARTESIAN_POINT('Ctrl Pts',(-24.64781191049,24.8757620423259,195.014062783283));
#93973=CARTESIAN_POINT('Ctrl Pts',(-24.6509740652016,24.8757620423259,195.014065107746));
#93974=CARTESIAN_POINT('Ctrl Pts',(-24.6541362199128,24.8757620423259,195.014067431847));
#93975=CARTESIAN_POINT('Ctrl Pts',(-32.8658546514293,24.875762042326,195.020102831808));
#93976=CARTESIAN_POINT('Ctrl Pts',(-41.0775680296323,24.8757620423251,195.024458577496));
#93977=CARTESIAN_POINT('Ctrl Pts',(-49.2892094763632,24.8757620423267,195.004852527973));
#93978=CARTESIAN_POINT('Ctrl Pts',(-49.2955336215858,24.8757620423267,195.004837428495));
#93979=CARTESIAN_POINT('Ctrl Pts',(-49.301857766761,24.8757620423267,195.004822314801));
#93980=CARTESIAN_POINT('Ctrl Pts',(-49.3081819118888,24.8757620423267,195.004807186881));
#93981=CARTESIAN_POINT('Ctrl Pts',(-57.5166612154801,24.8757620423282,194.985171771549));
#93982=CARTESIAN_POINT('Ctrl Pts',(-65.7254697695311,24.8757620423215,194.943230036326));
#93983=CARTESIAN_POINT('Ctrl Pts',(-73.9332331952951,24.8757620423304,194.827982077321));
#93984=CARTESIAN_POINT('Ctrl Pts',(-73.9427185287022,24.8757620423304,194.827848890574));
#93985=CARTESIAN_POINT('Ctrl Pts',(-73.9522038606495,24.8757620423304,194.827715605884));
#93986=CARTESIAN_POINT('Ctrl Pts',(-73.961689191135,24.8757620423304,194.827582223175));
#93987=CARTESIAN_POINT('Ctrl Pts',(-78.059246105284,24.8757620423347,194.769962381229));
#93988=CARTESIAN_POINT('Ctrl Pts',(-82.1556895284227,24.8757620423252,194.693493289495));
#93989=CARTESIAN_POINT('Ctrl Pts',(-86.2503383467373,24.8757620423266,194.58636884538));
#93990=CARTESIAN_POINT('Ctrl Pts',(-86.2613966994682,24.8757620423266,194.586079536104));
#93991=CARTESIAN_POINT('Ctrl Pts',(-86.2724550390773,24.8757620423266,194.585790003169));
#93992=CARTESIAN_POINT('Ctrl Pts',(-86.2835133655508,24.8757620423266,194.585500246345));
#93993=CARTESIAN_POINT('Ctrl Pts',(-90.3765727109929,24.875762042328,194.478251479603));
#93994=CARTESIAN_POINT('Ctrl Pts',(-94.4678439707547,24.8757620423236,194.340526346086));
#93995=CARTESIAN_POINT('Ctrl Pts',(-98.5562591476545,24.8757620423282,194.154116211922));
#93996=CARTESIAN_POINT('Ctrl Pts',(-98.5688828803835,24.8757620423282,194.153540636397));
#93997=CARTESIAN_POINT('Ctrl Pts',(-98.5815065858776,24.8757620423282,194.152964596616));
#93998=CARTESIAN_POINT('Ctrl Pts',(-98.5941302641051,24.8757620423282,194.152388092042));
#93999=CARTESIAN_POINT('Ctrl Pts',(-102.680949843047,24.8757620423327,193.965749131845));
#94000=CARTESIAN_POINT('Ctrl Pts',(-106.764931224453,24.8757620423183,193.730731754961));
#94001=CARTESIAN_POINT('Ctrl Pts',(-110.84440359735,24.8757620423337,193.418858454368));
#94002=CARTESIAN_POINT('Ctrl Pts',(-110.858579691179,24.8757620423337,193.417774700204));
#94003=CARTESIAN_POINT('Ctrl Pts',(-110.872755730562,24.8757620423338,193.416690017724));
#94004=CARTESIAN_POINT('Ctrl Pts',(-110.886931715427,24.8757620423338,193.415604405734));
#94005=CARTESIAN_POINT('Ctrl Pts',(-114.96479763357,24.875762042349,193.103317098939));
#94006=CARTESIAN_POINT('Ctrl Pts',(-119.03818825583,24.8757620423139,192.714732197115));
#94007=CARTESIAN_POINT('Ctrl Pts',(-123.104423976305,24.8757620423383,192.204214021647));
#94008=CARTESIAN_POINT('Ctrl Pts',(-123.120130138159,24.8757620423384,192.202242104217));
#94009=CARTESIAN_POINT('Ctrl Pts',(-123.135836193123,24.8757620423385,192.20026836683));
#94010=CARTESIAN_POINT('Ctrl Pts',(-123.151542141045,24.8757620423386,192.198292806863));
#94011=CARTESIAN_POINT('Ctrl Pts',(-125.175994041311,24.8757620423502,191.943648760649));
#94012=CARTESIAN_POINT('Ctrl Pts',(-127.200620383331,24.8757620423257,191.658066442003));
#94013=CARTESIAN_POINT('Ctrl Pts',(-129.217100987035,24.8757620423261,191.334701322639));
#94014=CARTESIAN_POINT('Ctrl Pts',(-129.233527280793,24.8757620423261,191.332067183519));
#94015=CARTESIAN_POINT('Ctrl Pts',(-129.249953033335,24.8757620423261,191.329430536661));
#94016=CARTESIAN_POINT('Ctrl Pts',(-129.266378240165,24.8757620423261,191.326791378358));
#94017=CARTESIAN_POINT('Ctrl Pts',(-131.281943276968,24.8757620423265,191.00293577899));
#94018=CARTESIAN_POINT('Ctrl Pts',(-133.289200652704,24.8757620423246,190.641384293948));
#94019=CARTESIAN_POINT('Ctrl Pts',(-135.286079698496,24.8757620423273,190.232703307421));
#94020=CARTESIAN_POINT('Ctrl Pts',(-135.303127536398,24.8757620423273,190.229214299298));
#94021=CARTESIAN_POINT('Ctrl Pts',(-135.320174617604,24.8757620423273,190.225721855634));
#94022=CARTESIAN_POINT('Ctrl Pts',(-135.337220940819,24.8757620423273,190.222225970564));
#94023=CARTESIAN_POINT('Ctrl Pts',(-137.333147727731,24.8757620423299,189.812898365584));
#94024=CARTESIAN_POINT('Ctrl Pts',(-139.31869551455,24.8757620423247,189.356449033943));
#94025=CARTESIAN_POINT('Ctrl Pts',(-141.291204979638,24.8757620423271,188.840805830176));
#94026=CARTESIAN_POINT('Ctrl Pts',(-141.308817044353,24.8757620423272,188.836201775475));
#94027=CARTESIAN_POINT('Ctrl Pts',(-141.326428069381,24.8757620423272,188.831593000313));
#94028=CARTESIAN_POINT('Ctrl Pts',(-141.344038052832,24.8757620423272,188.826979496123));
#94029=CARTESIAN_POINT('Ctrl Pts',(-142.320988421435,24.8757620423283,188.571035779219));
#94030=CARTESIAN_POINT('Ctrl Pts',(-143.294722983287,24.8757620423258,188.300491718125));
#94031=CARTESIAN_POINT('Ctrl Pts',(-144.264847386162,24.875762042326,188.013557547871));
#94032=CARTESIAN_POINT('Ctrl Pts',(-144.282714465166,24.875762042326,188.008272993154));
#94033=CARTESIAN_POINT('Ctrl Pts',(-144.300580331459,24.875762042326,188.002982874821));
#94034=CARTESIAN_POINT('Ctrl Pts',(-144.318444981918,24.875762042326,187.997687181806));
#94035=CARTESIAN_POINT('Ctrl Pts',(-145.288057437586,24.8757620423261,187.710260908361));
#94036=CARTESIAN_POINT('Ctrl Pts',(-146.255054777119,24.8757620423277,187.406047757954));
#94037=CARTESIAN_POINT('Ctrl Pts',(-147.212983965987,24.8757620423268,187.085108796902));
#94038=CARTESIAN_POINT('Ctrl Pts',(-147.23100919069,24.8757620423268,187.079069731639));
#94039=CARTESIAN_POINT('Ctrl Pts',(-147.249031241071,24.8757620423268,187.073024733291));
#94040=CARTESIAN_POINT('Ctrl Pts',(-147.267050074644,24.8757620423268,187.066973802089));
#94041=CARTESIAN_POINT('Ctrl Pts',(-149.083477336966,24.8757620423251,186.456996671566));
#94042=CARTESIAN_POINT('Ctrl Pts',(-150.870857453158,24.8757620423225,185.785994488404));
#94043=CARTESIAN_POINT('Ctrl Pts',(-152.623123968799,24.8757620423294,185.041686563971));
#94044=CARTESIAN_POINT('Ctrl Pts',(-152.73504513073,24.8757620423299,184.994145960419));
#94045=CARTESIAN_POINT('Ctrl Pts',(-152.846823049118,24.8757620423304,184.946306310615));
#94046=CARTESIAN_POINT('Ctrl Pts',(-152.958456146666,24.875762042331,184.898164421556));
#94047=CARTESIAN_POINT('Ctrl Pts',(-152.976515861628,24.8757620423311,184.890376150755));
#94048=CARTESIAN_POINT('Ctrl Pts',(-152.994571791993,24.8757620423311,184.882579966051));
#94049=CARTESIAN_POINT('Ctrl Pts',(-153.012623931258,24.8757620423312,184.874775853854));
#94050=CARTESIAN_POINT('Ctrl Pts',(-154.870511769106,24.8757620423408,184.071593199207));
#94051=CARTESIAN_POINT('Ctrl Pts',(-156.688325422377,24.8757620423189,183.1846136828));
#94052=CARTESIAN_POINT('Ctrl Pts',(-158.456781621831,24.8757620423332,182.194428286473));
#94053=CARTESIAN_POINT('Ctrl Pts',(-158.47465212741,24.8757620423334,182.184422319882));
#94054=CARTESIAN_POINT('Ctrl Pts',(-158.492517591448,24.8757620423335,182.174405810671));
#94055=CARTESIAN_POINT('Ctrl Pts',(-158.510378004392,24.8757620423336,182.164378738907));
#94056=CARTESIAN_POINT('Ctrl Pts',(-159.384833046953,24.8757620423397,181.673448126429));
#94057=CARTESIAN_POINT('Ctrl Pts',(-160.247140085049,24.8757620423256,181.157114890314));
#94058=CARTESIAN_POINT('Ctrl Pts',(-161.095845403919,24.8757620423262,180.612340916905));
#94059=CARTESIAN_POINT('Ctrl Pts',(-161.113513241408,24.8757620423262,180.601000139586));
#94060=CARTESIAN_POINT('Ctrl Pts',(-161.131175182557,24.8757620423262,180.589647032195));
#94061=CARTESIAN_POINT('Ctrl Pts',(-161.148831214264,24.8757620423262,180.578281567396));
#94062=CARTESIAN_POINT('Ctrl Pts',(-161.563905737138,24.8757620423264,180.311091580601));
#94063=CARTESIAN_POINT('Ctrl Pts',(-161.975710072057,24.8757620423259,180.037063261309));
#94064=CARTESIAN_POINT('Ctrl Pts',(-162.384044953281,24.8757620423259,179.755780375325));
#94065=CARTESIAN_POINT('Ctrl Pts',(-162.401578082186,24.8757620423259,179.743702619234));
#94066=CARTESIAN_POINT('Ctrl Pts',(-162.419104898429,24.8757620423259,179.731611433976));
#94067=CARTESIAN_POINT('Ctrl Pts',(-162.436625375847,24.8757620423259,179.719506792461));
#94068=CARTESIAN_POINT('Ctrl Pts',(-162.844501949097,24.875762042326,179.437710835434));
#94069=CARTESIAN_POINT('Ctrl Pts',(-163.249423819711,24.8757620423319,179.148232630283));
#94070=CARTESIAN_POINT('Ctrl Pts',(-163.64800894658,24.8757620423299,178.85302979587));
#94071=CARTESIAN_POINT('Ctrl Pts',(-163.665291233915,24.8757620423298,178.840230070385));
#94072=CARTESIAN_POINT('Ctrl Pts',(-163.682561810057,24.8757620423297,178.827419445818));
#94073=CARTESIAN_POINT('Ctrl Pts',(-163.699820408872,24.8757620423297,178.814598075025));
#94074=CARTESIAN_POINT('Ctrl Pts',(-164.709308917564,24.875762042325,178.064651534152));
#94075=CARTESIAN_POINT('Ctrl Pts',(-165.681737714684,24.8757620423251,177.275740093117));
#94076=CARTESIAN_POINT('Ctrl Pts',(-166.613250849857,24.8757620423274,176.444043333016));
#94077=CARTESIAN_POINT('Ctrl Pts',(-167.198094243251,24.8757620423289,175.921868886853));
#94078=CARTESIAN_POINT('Ctrl Pts',(-167.766809867722,24.8757620423314,175.382829696395));
#94079=CARTESIAN_POINT('Ctrl Pts',(-168.318450873044,24.8757620423482,174.825987926454));
#94080=CARTESIAN_POINT('Ctrl Pts',(-168.334027852459,24.8757620423487,174.810264090293));
#94081=CARTESIAN_POINT('Ctrl Pts',(-168.349591230718,24.8757620423491,174.794526036491));
#94082=CARTESIAN_POINT('Ctrl Pts',(-168.365140987195,24.8757620423495,174.77877374356));
#94083=CARTESIAN_POINT('Ctrl Pts',(-169.070974410657,24.8757620423678,174.063746800061));
#94084=CARTESIAN_POINT('Ctrl Pts',(-169.748646290608,24.8757620423234,173.319282963081));
#94085=CARTESIAN_POINT('Ctrl Pts',(-170.395306107718,24.8757620423285,172.542403589941));
#94086=CARTESIAN_POINT('Ctrl Pts',(-170.409806583172,24.8757620423286,172.524983116328));
#94087=CARTESIAN_POINT('Ctrl Pts',(-170.424291533727,24.8757620423288,172.507546270103));
#94088=CARTESIAN_POINT('Ctrl Pts',(-170.43876092208,24.875762042329,172.490093021554));
#94089=CARTESIAN_POINT('Ctrl Pts',(-170.88928987737,24.8757620423346,171.946656516614));
#94090=CARTESIAN_POINT('Ctrl Pts',(-171.325552583136,24.8757620424712,171.385736098847));
#94091=CARTESIAN_POINT('Ctrl Pts',(-171.741692841451,24.8757620425566,170.813322812391));
#94092=CARTESIAN_POINT('Ctrl Pts',(-171.921338161584,24.8757620425934,170.566215338314));
#94093=CARTESIAN_POINT('Ctrl Pts',(-172.09723391366,24.8757620425925,170.316966519992));
#94094=CARTESIAN_POINT('Ctrl Pts',(-172.268911669619,24.8757620425312,170.066059798355));
#94095=CARTESIAN_POINT('Ctrl Pts',(-172.28190915054,24.8757620425265,170.047064004118));
#94096=CARTESIAN_POINT('Ctrl Pts',(-172.294882644394,24.8757620425221,170.028058474253));
#94097=CARTESIAN_POINT('Ctrl Pts',(-172.307831949918,24.8757620425178,170.009043413777));
#94098=CARTESIAN_POINT('Ctrl Pts',(-172.881333308836,24.8757620423296,169.166900721047));
#94099=CARTESIAN_POINT('Ctrl Pts',(-173.410591971626,24.8757620423975,168.302660920235));
#94100=CARTESIAN_POINT('Ctrl Pts',(-173.893716192591,24.8757620424271,167.415541053399));
#94101=CARTESIAN_POINT('Ctrl Pts',(-174.376840413556,24.8757620424566,166.528421186564));
#94102=CARTESIAN_POINT('Ctrl Pts',(-174.813829816887,24.875762042452,165.618421053482));
#94103=CARTESIAN_POINT('Ctrl Pts',(-175.202841307782,24.8757620423681,164.684786982141));
#94104=CARTESIAN_POINT('Ctrl Pts',(-175.211927010215,24.8757620423662,164.662981144647));
#94105=CARTESIAN_POINT('Ctrl Pts',(-175.220986583199,24.8757620423644,164.641162380823));
#94106=CARTESIAN_POINT('Ctrl Pts',(-175.230020003396,24.8757620423629,164.619330678862));
#94107=CARTESIAN_POINT('Ctrl Pts',(-175.612126116306,24.8757620422975,163.695867960076));
#94108=CARTESIAN_POINT('Ctrl Pts',(-175.947287153428,24.8757620424648,162.749178442011));
#94109=CARTESIAN_POINT('Ctrl Pts',(-176.237555075868,24.8757620423541,161.780272945005));
#94110=CARTESIAN_POINT('Ctrl Pts',(-176.244531782355,24.8757620423515,161.756984910939));
#94111=CARTESIAN_POINT('Ctrl Pts',(-176.251482514742,24.8757620423493,161.733684386156));
#94112=CARTESIAN_POINT('Ctrl Pts',(-176.258407335464,24.8757620423475,161.710371268223));
#94113=CARTESIAN_POINT('Ctrl Pts',(-176.360806953651,24.8757620423206,161.365632469767));
#94114=CARTESIAN_POINT('Ctrl Pts',(-176.457676806858,24.8757620423462,161.017688127655));
#94115=CARTESIAN_POINT('Ctrl Pts',(-176.548849501517,24.8757620423492,160.668545469221));
#94116=CARTESIAN_POINT('Ctrl Pts',(-176.582804133289,24.8757620423503,160.538517389574));
#94117=CARTESIAN_POINT('Ctrl Pts',(-176.615968076816,24.8757620423472,160.408323068285));
#94118=CARTESIAN_POINT('Ctrl Pts',(-176.648330823726,24.8757620423399,160.278066605508));
#94119=CARTESIAN_POINT('Ctrl Pts',(-176.654186619902,24.8757620423386,160.254497676123));
#94120=CARTESIAN_POINT('Ctrl Pts',(-176.660016327933,24.8757620423374,160.230926318362));
#94121=CARTESIAN_POINT('Ctrl Pts',(-176.665819842891,24.8757620423364,160.207353312146));
#94122=CARTESIAN_POINT('Ctrl Pts',(-176.768995240264,24.875762042318,159.788270342399));
#94123=CARTESIAN_POINT('Ctrl Pts',(-176.86420175272,24.8757620423259,159.367762185166));
#94124=CARTESIAN_POINT('Ctrl Pts',(-176.952169714707,24.8757620423259,158.946132895978));
#94125=CARTESIAN_POINT('Ctrl Pts',(-176.964994102294,24.875762042326,158.884665774307));
#94126=CARTESIAN_POINT('Ctrl Pts',(-176.977664737325,24.875762042326,158.823174832625));
#94127=CARTESIAN_POINT('Ctrl Pts',(-176.990183971956,24.875762042326,158.761661020592));
#94128=CARTESIAN_POINT('Ctrl Pts',(-176.99465092232,24.875762042326,158.739712462785));
#94129=CARTESIAN_POINT('Ctrl Pts',(-176.999098629657,24.875762042326,158.717760829857));
#94130=CARTESIAN_POINT('Ctrl Pts',(-177.003527206417,24.8757620423261,158.695806137836));
#94131=CARTESIAN_POINT('Ctrl Pts',(-177.118219982101,24.8757620423264,158.127216113678));
#94132=CARTESIAN_POINT('Ctrl Pts',(-177.220333395014,24.8757620423267,157.556593568297));
#94133=CARTESIAN_POINT('Ctrl Pts',(-177.311324060744,24.8757620423267,156.984178905084));
#94134=CARTESIAN_POINT('Ctrl Pts',(-177.404696611944,24.8757620423267,156.396779999712));
#94135=CARTESIAN_POINT('Ctrl Pts',(-177.486356724851,24.8757620423264,155.807493942056));
#94136=CARTESIAN_POINT('Ctrl Pts',(-177.557934404858,24.8757620423262,155.216584754304));
#94137=CARTESIAN_POINT('Ctrl Pts',(-177.632922386434,24.875762042326,154.597521838599));
#94138=CARTESIAN_POINT('Ctrl Pts',(-177.69684448066,24.8757620423259,153.976677454172));
#94139=CARTESIAN_POINT('Ctrl Pts',(-177.751632462613,24.8757620423259,153.354359553465));
#94140=CARTESIAN_POINT('Ctrl Pts',(-177.77350781823,24.8757620423259,153.105884889862));
#94141=CARTESIAN_POINT('Ctrl Pts',(-177.793927627997,24.8757620423259,152.857175365898));
#94142=CARTESIAN_POINT('Ctrl Pts',(-177.813017113379,24.8757620423259,152.608250755187));
#94143=CARTESIAN_POINT('Ctrl Pts',(-175.73950529146,23.8567983454203,151.608424919145));
#94144=CARTESIAN_POINT('Ctrl Pts',(-176.388687107557,23.0874449616485,151.623023103975));
#94145=CARTESIAN_POINT('Ctrl Pts',(-176.384335038167,23.0735478218188,150.616361820745));
#94146=CARTESIAN_POINT('Ctrl Pts',(-176.003304916941,23.9680637154176,151.606384577597));
#94147=CARTESIAN_POINT('Ctrl Pts',(-176.593854313756,23.2639762965151,151.537709600337));
#94148=CARTESIAN_POINT('Ctrl Pts',(-176.656254705308,23.3029629324784,150.615565005799));
#94149=CARTESIAN_POINT('Ctrl Pts',(-176.258810630189,24.0795828100808,151.622206832873));
#94150=CARTESIAN_POINT('Ctrl Pts',(-176.815150128392,23.4580026124915,151.487215027469));
#94151=CARTESIAN_POINT('Ctrl Pts',(-176.919885733397,23.5331341645717,150.650684462557));
#94152=CARTESIAN_POINT('Ctrl Pts',(-176.736237334262,24.2964053110708,151.694271183075));
#94153=CARTESIAN_POINT('Ctrl Pts',(-177.237181962352,23.8405921073048,151.47948246492));
#94154=CARTESIAN_POINT('Ctrl Pts',(-177.413116931558,23.9811970433833,150.802131799252));
#94155=CARTESIAN_POINT('Ctrl Pts',(-176.962392794808,24.4033211362568,151.749272834437));
#94156=CARTESIAN_POINT('Ctrl Pts',(-177.443743421448,24.0332847294644,151.513241822621));
#94157=CARTESIAN_POINT('Ctrl Pts',(-177.647053524624,24.2023887513038,150.91600535664));
#94158=CARTESIAN_POINT('Ctrl Pts',(-177.261937401879,24.5519309185043,151.868767106029));
#94159=CARTESIAN_POINT('Ctrl Pts',(-177.721629599937,24.3032107970142,151.639069912478));
#94160=CARTESIAN_POINT('Ctrl Pts',(-177.957529153403,24.5103483072772,151.161146031839));
#94161=CARTESIAN_POINT('Ctrl Pts',(-177.356706714869,24.6002596109534,151.9155000569));
#94162=CARTESIAN_POINT('Ctrl Pts',(-177.809527175111,24.3904184950665,151.692946627691));
#94163=CARTESIAN_POINT('Ctrl Pts',(-178.055876609326,24.6105915832425,151.256755643874));
#94164=CARTESIAN_POINT('Ctrl Pts',(-177.525039051065,24.6888716230439,152.02203145606));
#94165=CARTESIAN_POINT('Ctrl Pts',(-177.965962925957,24.5495763065596,151.825376775102));
#94166=CARTESIAN_POINT('Ctrl Pts',(-178.230880519265,24.7946312006147,151.474169337755));
#94167=CARTESIAN_POINT('Ctrl Pts',(-177.598939664808,24.7292916556483,152.081679209295));
#94168=CARTESIAN_POINT('Ctrl Pts',(-178.035464730705,24.6223780008855,151.90353429491));
#94169=CARTESIAN_POINT('Ctrl Pts',(-178.307882838118,24.8787077221551,151.595672377231));
#94170=CARTESIAN_POINT('Ctrl Pts',(-177.720286934346,24.7991411953602,152.216892436631));
#94171=CARTESIAN_POINT('Ctrl Pts',(-178.149684748747,24.7467279407185,152.086964131903));
#94172=CARTESIAN_POINT('Ctrl Pts',(-178.434830427082,25.0243673086006,151.870608949261));
#94173=CARTESIAN_POINT('Ctrl Pts',(-177.765084499851,24.8270347155314,152.289484845931));
#94174=CARTESIAN_POINT('Ctrl Pts',(-178.192532655266,24.7961598874315,152.188512755172));
#94175=CARTESIAN_POINT('Ctrl Pts',(-178.482003941885,25.0827471702104,152.017997656931));
#94176=CARTESIAN_POINT('Ctrl Pts',(-177.821660312508,24.8682175857358,152.455831581551));
#94177=CARTESIAN_POINT('Ctrl Pts',(-178.247166957742,24.8667382439783,152.423392974383));
#94178=CARTESIAN_POINT('Ctrl Pts',(-178.542611941005,25.1696189974259,152.355268021077));
#94179=CARTESIAN_POINT('Ctrl Pts',(-177.826854605526,24.8780047222983,152.546670848957));
#94180=CARTESIAN_POINT('Ctrl Pts',(-178.253157647747,24.8819396453427,152.553901526939));
#94181=CARTESIAN_POINT('Ctrl Pts',(-178.549220219017,25.1908520618554,152.539188683824));
#94182=CARTESIAN_POINT('Ctrl Pts',(-177.807677777613,24.8753312313243,152.637557271751));
#94183=CARTESIAN_POINT('Ctrl Pts',(-178.236377845671,24.87399890951,152.682737783154));
#94184=CARTESIAN_POINT('Ctrl Pts',(-178.53072563814,25.1863823136132,152.722941452113));
#94185=CARTESIAN_POINT('',(-176.430593086108,23.1126512166031,150.616656461876));
#94186=CARTESIAN_POINT('',(-175.784380109018,23.8757620423259,151.608250755187));
#94187=CARTESIAN_POINT('Origin',(-175.784380109018,23.8757620423259,150.608250755187));
#94188=CARTESIAN_POINT('Ctrl Pts',(-175.784380109018,23.8757620423259,151.608250755187));
#94189=CARTESIAN_POINT('Ctrl Pts',(-175.888159349634,23.9197029023221,151.608250755187));
#94190=CARTESIAN_POINT('Ctrl Pts',(-175.991448416971,23.9640264362152,151.611061269963));
#94191=CARTESIAN_POINT('Ctrl Pts',(-176.094195590625,24.008769736127,151.617048131169));
#94192=CARTESIAN_POINT('Ctrl Pts',(-176.19694276428,24.0535130360388,151.623034992374));
#94193=CARTESIAN_POINT('Ctrl Pts',(-176.299148251002,24.098676111631,151.6321977244));
#94194=CARTESIAN_POINT('Ctrl Pts',(-176.400736032712,24.1442953670243,151.644955074084));
#94195=CARTESIAN_POINT('Ctrl Pts',(-176.435432451251,24.1598762247998,151.649312235315));
#94196=CARTESIAN_POINT('Ctrl Pts',(-176.470014453398,24.1754907487728,151.654083487016));
#94197=CARTESIAN_POINT('Ctrl Pts',(-176.504510507143,24.1911550184597,151.659289601702));
#94198=CARTESIAN_POINT('Ctrl Pts',(-176.560530785521,24.2165931962569,151.667744133809));
#94199=CARTESIAN_POINT('Ctrl Pts',(-176.616510806086,24.242257960854,151.677408353266));
#94200=CARTESIAN_POINT('Ctrl Pts',(-176.672282380912,24.2680844183909,151.688422405043));
#94201=CARTESIAN_POINT('Ctrl Pts',(-176.724797335908,24.2924028146258,151.698793323118));
#94202=CARTESIAN_POINT('Ctrl Pts',(-176.777128105327,24.3168648944967,151.710361068092));
#94203=CARTESIAN_POINT('Ctrl Pts',(-176.82910008493,24.3414050138239,151.723270748686));
#94204=CARTESIAN_POINT('Ctrl Pts',(-176.877613351544,24.364311998718,151.735321295565));
#94205=CARTESIAN_POINT('Ctrl Pts',(-176.925814331434,24.3872871657492,151.748541188469));
#94206=CARTESIAN_POINT('Ctrl Pts',(-176.973523867365,24.410263427155,151.76307286238));
#94207=CARTESIAN_POINT('Ctrl Pts',(-176.982726986036,24.4146955235108,151.765876006801));
#94208=CARTESIAN_POINT('Ctrl Pts',(-176.991911691641,24.4191276124988,151.768728038266));
#94209=CARTESIAN_POINT('Ctrl Pts',(-177.001076508298,24.4235591398025,151.771630090036));
#94210=CARTESIAN_POINT('Ctrl Pts',(-177.042173845054,24.4434312198195,151.784643618111));
#94211=CARTESIAN_POINT('Ctrl Pts',(-177.082911866297,24.4633059029067,151.79866930332));
#94212=CARTESIAN_POINT('Ctrl Pts',(-177.123173784831,24.4831461072352,151.813841057898));
#94213=CARTESIAN_POINT('Ctrl Pts',(-177.13619974057,24.4895650170348,151.818749582151));
#94214=CARTESIAN_POINT('Ctrl Pts',(-177.149175539937,24.4959801962463,151.823778263238));
#94215=CARTESIAN_POINT('Ctrl Pts',(-177.162096243315,24.5023900130613,151.828932215432));
#94216=CARTESIAN_POINT('Ctrl Pts',(-177.196296802062,24.519356528747,151.842574510253));
#94217=CARTESIAN_POINT('Ctrl Pts',(-177.230294880457,24.5363753306636,151.857180131003));
#94218=CARTESIAN_POINT('Ctrl Pts',(-177.263867635009,24.5533452343922,151.872819968914));
#94219=CARTESIAN_POINT('Ctrl Pts',(-177.27137398005,24.5571394405689,151.876316793089));
#94220=CARTESIAN_POINT('Ctrl Pts',(-177.278858881439,24.5609311195225,151.879865361306));
#94221=CARTESIAN_POINT('Ctrl Pts',(-177.286319519695,24.5647189898801,151.883466541106));
#94222=CARTESIAN_POINT('Ctrl Pts',(-177.314373267698,24.5789622699892,151.897007820972));
#94223=CARTESIAN_POINT('Ctrl Pts',(-177.342131087439,24.5931782747943,151.911315989472));
#94224=CARTESIAN_POINT('Ctrl Pts',(-177.369451368433,24.6073035761847,151.926466315716));
#94225=CARTESIAN_POINT('Ctrl Pts',(-177.393647488778,24.6198136046291,151.939884154176));
#94226=CARTESIAN_POINT('Ctrl Pts',(-177.417500241383,24.6322524359504,151.953962709686));
#94227=CARTESIAN_POINT('Ctrl Pts',(-177.440880693276,24.6445625833218,151.968762109259));
#94228=CARTESIAN_POINT('Ctrl Pts',(-177.466603695553,24.6581061174811,151.985044300496));
#94229=CARTESIAN_POINT('Ctrl Pts',(-177.491786560729,24.6715066684446,152.002183768001));
#94230=CARTESIAN_POINT('Ctrl Pts',(-177.516292176977,24.6847047655833,152.020331144545));
#94231=CARTESIAN_POINT('Ctrl Pts',(-177.527198432,24.6905785951475,152.028407657071));
#94232=CARTESIAN_POINT('Ctrl Pts',(-177.537970014763,24.6964120880033,152.036684115516));
#94233=CARTESIAN_POINT('Ctrl Pts',(-177.548592113994,24.7021987720431,152.045175385715));
#94234=CARTESIAN_POINT('Ctrl Pts',(-177.568202820616,24.7128822500032,152.060852118261));
#94235=CARTESIAN_POINT('Ctrl Pts',(-177.587313346476,24.7234120143457,152.077266089796));
#94236=CARTESIAN_POINT('Ctrl Pts',(-177.605849017592,24.7337606599818,152.094564516487));
#94237=CARTESIAN_POINT('Ctrl Pts',(-177.624384688707,24.744109305618,152.111862943177));
#94238=CARTESIAN_POINT('Ctrl Pts',(-177.642346062884,24.7542771121623,152.130045515296));
#94239=CARTESIAN_POINT('Ctrl Pts',(-177.659613299577,24.7642164255042,152.149285822963));
#94240=CARTESIAN_POINT('Ctrl Pts',(-177.675506713529,24.7733649432519,152.166995325632));
#94241=CARTESIAN_POINT('Ctrl Pts',(-177.690630352488,24.782214663373,152.18539780105));
#94242=CARTESIAN_POINT('Ctrl Pts',(-177.704840532489,24.7906991998897,152.204610352547));
#94243=CARTESIAN_POINT('Ctrl Pts',(-177.718477366732,24.798841406259,152.22304772492));
#94244=CARTESIAN_POINT('Ctrl Pts',(-177.731273086947,24.8066473872866,152.242231073656));
#94245=CARTESIAN_POINT('Ctrl Pts',(-177.743059463349,24.8140378964531,152.26227770449));
#94246=CARTESIAN_POINT('Ctrl Pts',(-177.747198803758,24.8166334213367,152.269318021739));
#94247=CARTESIAN_POINT('Ctrl Pts',(-177.751213259865,24.8191775046934,152.276464947716));
#94248=CARTESIAN_POINT('Ctrl Pts',(-177.755094216052,24.8216660422822,152.283724011869));
#94249=CARTESIAN_POINT('Ctrl Pts',(-177.766667220852,24.8290868571729,152.305370528925));
#94250=CARTESIAN_POINT('Ctrl Pts',(-177.776998408874,24.8359795863142,152.32792109276));
#94251=CARTESIAN_POINT('Ctrl Pts',(-177.785818285655,24.8421983688494,152.351336130936));
#94252=CARTESIAN_POINT('Ctrl Pts',(-177.787884465384,24.8436552058024,152.356821431744));
#94253=CARTESIAN_POINT('Ctrl Pts',(-177.789867903047,24.8450751394032,152.362354114282));
#94254=CARTESIAN_POINT('Ctrl Pts',(-177.791765513594,24.8464564548674,152.367933553429));
#94255=CARTESIAN_POINT('Ctrl Pts',(-177.799045366706,24.8517556316108,152.38933810216));
#94256=CARTESIAN_POINT('Ctrl Pts',(-177.804942413803,24.8564054048408,152.41117000322));
#94257=CARTESIAN_POINT('Ctrl Pts',(-177.809351695265,24.8603379619669,152.433309469188));
#94258=CARTESIAN_POINT('Ctrl Pts',(-177.813741723205,24.8642533472315,152.455352261202));
#94259=CARTESIAN_POINT('Ctrl Pts',(-177.816656889232,24.8674576873292,152.477699726678));
#94260=CARTESIAN_POINT('Ctrl Pts',(-177.818039597892,24.8699057546573,152.500225529015));
#94261=CARTESIAN_POINT('Ctrl Pts',(-177.819419519771,24.8723488880258,152.522705931702));
#94262=CARTESIAN_POINT('Ctrl Pts',(-177.819273139007,24.8740387349888,152.545363729093));
#94263=CARTESIAN_POINT('Ctrl Pts',(-177.817589716999,24.8749530460444,152.568068511054));
#94264=CARTESIAN_POINT('Ctrl Pts',(-177.816597164382,24.8754921276451,152.581455344921));
#94265=CARTESIAN_POINT('Ctrl Pts',(-177.815071168718,24.8757620423259,152.59485843705));
#94266=CARTESIAN_POINT('Ctrl Pts',(-177.813017113379,24.8757620423259,152.608250755187));
#94267=CARTESIAN_POINT('Ctrl Pts',(-178.535788240059,25.1869009068823,152.663678496546));
#94268=CARTESIAN_POINT('Ctrl Pts',(-178.547796223577,25.1859432627129,152.495194134801));
#94269=CARTESIAN_POINT('Ctrl Pts',(-178.538609818861,25.163582676433,152.329284557108));
#94270=CARTESIAN_POINT('Ctrl Pts',(-178.479567260233,25.0795971521013,152.008723248302));
#94271=CARTESIAN_POINT('Ctrl Pts',(-178.431254315525,25.0200759880067,151.860897232914));
#94272=CARTESIAN_POINT('Ctrl Pts',(-178.302546191152,24.8727975366848,151.586410602999));
#94273=CARTESIAN_POINT('Ctrl Pts',(-178.225101795571,24.7884206874165,151.465908921215));
#94274=CARTESIAN_POINT('Ctrl Pts',(-178.049596269999,24.604137587983,151.250262654017));
#94275=CARTESIAN_POINT('Ctrl Pts',(-177.951438762234,24.5042156002709,151.15576939922));
#94276=CARTESIAN_POINT('Ctrl Pts',(-177.641856056835,24.1974334944718,150.913299742263));
#94277=CARTESIAN_POINT('Ctrl Pts',(-177.409356901872,23.9777223770421,150.800741214681));
#94278=CARTESIAN_POINT('Ctrl Pts',(-176.932746614676,23.5448805316748,150.655018674087));
#94279=CARTESIAN_POINT('Ctrl Pts',(-176.685562735176,23.3285973273397,150.61976374185));
#94280=CARTESIAN_POINT('Ctrl Pts',(-176.430593086108,23.1126512166033,150.616656461907));
#94281=CARTESIAN_POINT('Ctrl Pts',(1.55202975899355E-14,24.8757620423259,
194.999549694134));
#94282=CARTESIAN_POINT('Ctrl Pts',(1.58565405550443E-14,24.8757620423259,
195.993992404177));
#94283=CARTESIAN_POINT('Ctrl Pts',(1.58584143467919E-14,25.8701893108725,
195.999534166346));
#94284=CARTESIAN_POINT('Ctrl Pts',(8.03327402494744,24.8757620423259,194.999549693465));
#94285=CARTESIAN_POINT('Ctrl Pts',(8.03265114999351,24.8757620423259,195.993992403173));
#94286=CARTESIAN_POINT('Ctrl Pts',(8.0326478760129,25.870189310896,195.999534166346));
#94287=CARTESIAN_POINT('Ctrl Pts',(16.0665519263718,24.8757620423259,195.007625218402));
#94288=CARTESIAN_POINT('Ctrl Pts',(16.05956801298,24.8757620423259,196.002365960777));
#94289=CARTESIAN_POINT('Ctrl Pts',(16.0655869046176,25.8704939364008,196.007612037979));
#94290=CARTESIAN_POINT('Ctrl Pts',(32.1331056843908,24.8757620423259,195.019685540921));
#94291=CARTESIAN_POINT('Ctrl Pts',(32.1265589240983,24.8757620423259,196.011429209992));
#94292=CARTESIAN_POINT('Ctrl Pts',(32.1325694456472,25.8674762936769,196.019652230615));
#94293=CARTESIAN_POINT('Ctrl Pts',(40.1663819277293,24.8757620423259,195.02433275779));
#94294=CARTESIAN_POINT('Ctrl Pts',(40.1403350532895,24.8757620423259,196.012908330767));
#94295=CARTESIAN_POINT('Ctrl Pts',(40.166583673479,25.8642139458239,196.024289902376));
#94296=CARTESIAN_POINT('Ctrl Pts',(56.2329144880606,24.8757620423259,194.990277721149));
#94297=CARTESIAN_POINT('Ctrl Pts',(56.2107775732178,24.8757620423259,195.965813387242));
#94298=CARTESIAN_POINT('Ctrl Pts',(56.2369512836255,25.8509477599953,195.989985501537));
#94299=CARTESIAN_POINT('Ctrl Pts',(64.2664422769928,24.8757620423259,194.952999205055));
#94300=CARTESIAN_POINT('Ctrl Pts',(64.2154476695745,24.8757620423259,195.919527238438));
#94301=CARTESIAN_POINT('Ctrl Pts',(64.2735317794456,25.8409667594794,195.952498173634));
#94302=CARTESIAN_POINT('Ctrl Pts',(76.314252180968,24.8757620423259,194.798403354012));
#94303=CARTESIAN_POINT('Ctrl Pts',(76.3147727001544,24.8757620423259,195.742698385788));
#94304=CARTESIAN_POINT('Ctrl Pts',(76.3299297419014,25.8184315808282,195.796667959559));
#94305=CARTESIAN_POINT('Ctrl Pts',(80.3298095531146,24.8757620423259,194.729928811641));
#94306=CARTESIAN_POINT('Ctrl Pts',(80.3286011897685,24.8757620423259,195.666169004327));
#94307=CARTESIAN_POINT('Ctrl Pts',(80.3490350159167,25.8096555448394,195.727620035734));
#94308=CARTESIAN_POINT('Ctrl Pts',(88.3596963527688,24.8757620423259,194.538124415895));
#94309=CARTESIAN_POINT('Ctrl Pts',(88.3667666841118,24.8757620423259,195.455007000289));
#94310=CARTESIAN_POINT('Ctrl Pts',(88.3880903624907,25.7890987455482,195.534021357848));
#94311=CARTESIAN_POINT('Ctrl Pts',(92.3740336964655,24.8757620423259,194.41496224834));
#94312=CARTESIAN_POINT('Ctrl Pts',(92.3804567159732,24.8757620423259,195.321439749224));
#94313=CARTESIAN_POINT('Ctrl Pts',(92.4080506792306,25.7773172405769,195.40964281312));
#94314=CARTESIAN_POINT('Ctrl Pts',(96.3873930174844,24.8757620423259,194.248481295077));
#94315=CARTESIAN_POINT('Ctrl Pts',(96.4244308304192,24.8757620423259,195.141352513976));
#94316=CARTESIAN_POINT('Ctrl Pts',(96.4285783862348,25.7637803812362,195.241337716207));
#94317=CARTESIAN_POINT('Ctrl Pts',(95.8129090247637,24.8757620423259,194.272017475705));
#94318=CARTESIAN_POINT('Ctrl Pts',(91.9909515239712,24.8757620423259,194.42665335126));
#94319=CARTESIAN_POINT('Ctrl Pts',(88.1681288624907,24.8757620425647,194.542724031316));
#94320=CARTESIAN_POINT('Ctrl Pts',(84.3447532974164,24.8757620424299,194.634041035195));
#94321=CARTESIAN_POINT('Ctrl Pts',(84.1771313987723,24.875762042424,194.638044494785));
#94322=CARTESIAN_POINT('Ctrl Pts',(84.0095084240956,24.8757620424174,194.64200008328));
#94323=CARTESIAN_POINT('Ctrl Pts',(83.8418843898354,24.8757620424104,194.645908558742));
#94324=CARTESIAN_POINT('Ctrl Pts',(79.9945138556477,24.8757620422484,194.735617372831));
#94325=CARTESIAN_POINT('Ctrl Pts',(76.1465874264899,24.8757620434871,194.800604548745));
#94326=CARTESIAN_POINT('Ctrl Pts',(72.2983160265908,24.8757620430265,194.849972733157));
#94327=CARTESIAN_POINT('Ctrl Pts',(72.1546046067635,24.8757620430093,194.851816358811));
#94328=CARTESIAN_POINT('Ctrl Pts',(72.0108926622784,24.8757620429891,194.853638836942));
#94329=CARTESIAN_POINT('Ctrl Pts',(71.8671802044666,24.8757620429662,194.855440421815));
#94330=CARTESIAN_POINT('Ctrl Pts',(63.9789651784272,24.8757620417107,194.954327387389));
#94331=CARTESIAN_POINT('Ctrl Pts',(56.0891782843935,24.8757620427095,194.990613753671));
#94332=CARTESIAN_POINT('Ctrl Pts',(48.1996482431872,24.8757620424645,195.007321889678));
#94333=CARTESIAN_POINT('Ctrl Pts',(48.1038239921383,24.8757620424615,195.007524822503));
#94334=CARTESIAN_POINT('Ctrl Pts',(48.0079997403916,24.8757620424585,195.007724664509));
#94335=CARTESIAN_POINT('Ctrl Pts',(47.912175487993,24.8757620424554,195.007921449932));
#94336=CARTESIAN_POINT('Ctrl Pts',(39.9747332096749,24.8757620421988,195.024221842576));
#94337=CARTESIAN_POINT('Ctrl Pts',(32.0372813112697,24.8757620423402,195.019619730156));
#94338=CARTESIAN_POINT('Ctrl Pts',(24.0998288030149,24.8757620423309,195.013658532168));
#94339=CARTESIAN_POINT('Ctrl Pts',(24.0519166148576,24.8757620423308,195.013622549081));
#94340=CARTESIAN_POINT('Ctrl Pts',(24.0040044266648,24.8757620423307,195.013586492909));
#94341=CARTESIAN_POINT('Ctrl Pts',(23.9560922384375,24.8757620423307,195.013550365792));
#94342=CARTESIAN_POINT('Ctrl Pts',(15.9707275303564,24.8757620423211,195.007529179632));
#94343=CARTESIAN_POINT('Ctrl Pts',(7.98536193554124,24.8757620423259,194.999549694134));
#94344=CARTESIAN_POINT('Ctrl Pts',(1.55202975899355E-14,24.8757620423259,
194.999549694134));
#94345=CARTESIAN_POINT('Ctrl Pts',(1.58047048864619E-14,25.8701893108725,
195.999534166346));
#94346=CARTESIAN_POINT('Ctrl Pts',(7.9786085072197,25.8701893108725,195.999534166346));
#94347=CARTESIAN_POINT('Ctrl Pts',(15.9572208444829,25.8704907335884,196.007496139866));
#94348=CARTESIAN_POINT('Ctrl Pts',(31.9144423244155,25.8675403396453,196.019522756113));
#94349=CARTESIAN_POINT('Ctrl Pts',(39.8930517912443,25.8643466712877,196.024234148174));
#94350=CARTESIAN_POINT('Ctrl Pts',(55.8502484700875,25.8513562852167,195.991424613018));
#94351=CARTESIAN_POINT('Ctrl Pts',(63.8291245674269,25.8415812736672,195.955278690271));
#94352=CARTESIAN_POINT('Ctrl Pts',(75.7949891858004,25.8195295821858,195.804927091771));
#94353=CARTESIAN_POINT('Ctrl Pts',(79.7832351076495,25.8109441238302,195.738304913061));
#94354=CARTESIAN_POINT('Ctrl Pts',(87.7585153676325,25.7908447875607,195.55171229018));
#94355=CARTESIAN_POINT('Ctrl Pts',(91.7455532525854,25.779330193458,195.431898989199));
#94356=CARTESIAN_POINT('Ctrl Pts',(95.731638354173,25.7661094150367,195.270070553806));
#94357=CARTESIAN_POINT('Ctrl Pts',(-175.118478031602,23.3269112215416,151.608250755187));
#94358=CARTESIAN_POINT('Ctrl Pts',(-175.744203657372,22.5468679911663,151.608250755187));
#94359=CARTESIAN_POINT('Ctrl Pts',(-175.744203657372,22.5468679911663,150.608250755187));
#94360=CARTESIAN_POINT('Ctrl Pts',(-175.343333626061,23.5072831574842,151.608250755187));
#94361=CARTESIAN_POINT('Ctrl Pts',(-175.973848539976,22.7347343216712,151.608250755187));
#94362=CARTESIAN_POINT('Ctrl Pts',(-175.975961504203,22.7327766922334,150.611103991362));
#94363=CARTESIAN_POINT('Ctrl Pts',(-175.565295636808,23.6902382307512,151.608250755187));
#94364=CARTESIAN_POINT('Ctrl Pts',(-176.200866106771,22.9254561683507,151.608250755183));
#94365=CARTESIAN_POINT('Ctrl Pts',(-176.20475353061,22.9213767890848,150.613904186401));
#94366=CARTESIAN_POINT('Ctrl Pts',(-175.784380109018,23.8757620423259,151.608250755187));
#94367=CARTESIAN_POINT('Ctrl Pts',(-176.425206487511,23.1190122335564,151.608250755187));
#94368=CARTESIAN_POINT('Ctrl Pts',(-176.430593086108,23.1126512166033,150.616656461907));
#94369=CARTESIAN_POINT('',(-175.744203657372,22.5468679911664,150.608250755186));
#94370=CARTESIAN_POINT('',(-175.118478031602,23.3269112215416,151.608250755187));
#94371=CARTESIAN_POINT('Origin',(-175.118478031602,23.3269112215417,150.608250755187));
#94372=CARTESIAN_POINT('Origin',(-154.804630390602,48.6513968890273,151.608250754885));
#94373=CARTESIAN_POINT('Origin',(-154.870164447103,48.5744178866766,150.300300299738));
#94374=CARTESIAN_POINT('Ctrl Pts',(177.813017113378,24.8757620423259,152.608250755187));
#94375=CARTESIAN_POINT('Ctrl Pts',(178.240980734254,24.8757620423259,152.641070351893));
#94376=CARTESIAN_POINT('Ctrl Pts',(178.535788240059,25.1869009068823,152.663678496546));
#94377=CARTESIAN_POINT('Ctrl Pts',(177.825566679641,24.8757620423259,152.526428293251));
#94378=CARTESIAN_POINT('Ctrl Pts',(178.251679320414,24.8784434436938,152.524853998483));
#94379=CARTESIAN_POINT('Ctrl Pts',(178.54758409262,25.1859601727659,152.498170456853));
#94380=CARTESIAN_POINT('Ctrl Pts',(177.818423466009,24.865861047641,152.446309988772));
#94381=CARTESIAN_POINT('Ctrl Pts',(178.244029236806,24.8627191690581,152.410014683625));
#94382=CARTESIAN_POINT('Ctrl Pts',(178.539112920021,25.1646159030061,152.335970744568));
#94383=CARTESIAN_POINT('Ctrl Pts',(177.765101637553,24.8270475515925,152.289539707351));
#94384=CARTESIAN_POINT('Ctrl Pts',(178.192522347297,24.7961838564161,152.188597127195));
#94385=CARTESIAN_POINT('Ctrl Pts',(178.48199168857,25.0827439046829,152.018126940536));
#94386=CARTESIAN_POINT('Ctrl Pts',(177.720007588841,24.7989783444832,152.216559013661));
#94387=CARTESIAN_POINT('Ctrl Pts',(178.149396328714,24.7464442378946,152.086521065475));
#94388=CARTESIAN_POINT('Ctrl Pts',(178.434507805055,25.0239982148635,151.86995404495));
#94389=CARTESIAN_POINT('Ctrl Pts',(177.599043397733,24.7293534239432,152.081816985205));
#94390=CARTESIAN_POINT('Ctrl Pts',(178.035536927632,24.6224967346167,151.903739043874));
#94391=CARTESIAN_POINT('Ctrl Pts',(178.307963263112,24.878810018743,151.595984391803));
#94392=CARTESIAN_POINT('Ctrl Pts',(177.524708125271,24.6886957305656,152.021807528286));
#94393=CARTESIAN_POINT('Ctrl Pts',(177.965629460751,24.5492727794077,151.82510958591));
#94394=CARTESIAN_POINT('Ctrl Pts',(178.230508883466,24.7942404010545,151.473748939335));
#94395=CARTESIAN_POINT('Ctrl Pts',(177.356757151249,24.6002878535161,151.915546497388));
#94396=CARTESIAN_POINT('Ctrl Pts',(177.809547956828,24.3904862015032,151.693026376618));
#94397=CARTESIAN_POINT('Ctrl Pts',(178.055904211603,24.6106280179359,151.256894473064));
#94398=CARTESIAN_POINT('Ctrl Pts',(177.261863754394,24.5518950929903,151.868742623834));
#94399=CARTESIAN_POINT('Ctrl Pts',(177.721535105475,24.3031663131539,151.639064057359));
#94400=CARTESIAN_POINT('Ctrl Pts',(177.957429169392,24.5102532970104,151.161143710607));
#94401=CARTESIAN_POINT('Ctrl Pts',(177.06248138814,24.452976281066,151.789195261869));
#94402=CARTESIAN_POINT('Ctrl Pts',(177.538716234914,24.1255898483891,151.556268560496));
#94403=CARTESIAN_POINT('Ctrl Pts',(177.750773427807,24.3052696647133,150.997960420331));
#94404=CARTESIAN_POINT('Ctrl Pts',(176.957127456991,24.4019796098267,151.755840098305));
#94405=CARTESIAN_POINT('Ctrl Pts',(177.442509904882,24.0339937760569,151.526995608583));
#94406=CARTESIAN_POINT('Ctrl Pts',(177.641692710208,24.1996827677703,150.929280961348));
#94407=CARTESIAN_POINT('Ctrl Pts',(176.736712019782,24.2976666717929,151.699677511058));
#94408=CARTESIAN_POINT('Ctrl Pts',(177.243766764194,23.8479909141434,151.489142631931));
#94409=CARTESIAN_POINT('Ctrl Pts',(177.413666278864,23.9838543743893,150.813119343421));
#94410=CARTESIAN_POINT('Ctrl Pts',(176.621429091326,24.2442684005504,151.676957335305));
#94411=CARTESIAN_POINT('Ctrl Pts',(177.140590331384,23.7531010317192,151.481294705877));
#94412=CARTESIAN_POINT('Ctrl Pts',(177.294493508481,23.8734448220722,150.765810854267));
#94413=CARTESIAN_POINT('Ctrl Pts',(176.272211171489,24.0856625592316,151.624198290699));
#94414=CARTESIAN_POINT('Ctrl Pts',(176.827686158777,23.4694432056994,151.486934169814));
#94415=CARTESIAN_POINT('Ctrl Pts',(176.93371995992,23.5456907356619,150.654945935944));
#94416=CARTESIAN_POINT('Ctrl Pts',(176.031572249751,23.9804249323003,151.608250755187));
#94417=CARTESIAN_POINT('Ctrl Pts',(176.619316842118,23.2864267698944,151.532148617704));
#94418=CARTESIAN_POINT('Ctrl Pts',(176.685418012928,23.3284747550706,150.61976197741));
#94419=CARTESIAN_POINT('Ctrl Pts',(175.784380109018,23.8757620423259,151.608250755187));
#94420=CARTESIAN_POINT('Ctrl Pts',(176.425206487511,23.1190122335564,151.608250755187));
#94421=CARTESIAN_POINT('Ctrl Pts',(176.430593086108,23.1126512166033,150.616656461907));
#94422=CARTESIAN_POINT('',(177.813017113379,24.8757620423259,152.608250755187));
#94423=CARTESIAN_POINT('',(178.535788240059,25.1869009068823,152.663678496546));
#94424=CARTESIAN_POINT('Origin',(177.813017113378,25.8757620423259,152.608250755187));
#94425=CARTESIAN_POINT('',(175.784380109018,23.8757620423259,151.608250755187));
#94426=CARTESIAN_POINT('Ctrl Pts',(175.784380109018,23.8757620423259,151.608250755187));
#94427=CARTESIAN_POINT('Ctrl Pts',(175.888180218743,23.9197117384257,151.608250755187));
#94428=CARTESIAN_POINT('Ctrl Pts',(175.991532071282,23.9640615485664,151.611059044171));
#94429=CARTESIAN_POINT('Ctrl Pts',(176.094384782567,24.0088514257039,151.617055154659));
#94430=CARTESIAN_POINT('Ctrl Pts',(176.197237493852,24.0536413028414,151.623051265146));
#94431=CARTESIAN_POINT('Ctrl Pts',(176.299591232898,24.0988712414086,151.632234747727));
#94432=CARTESIAN_POINT('Ctrl Pts',(176.401375438295,24.1445818688343,151.645033982858));
#94433=CARTESIAN_POINT('Ctrl Pts',(176.436027334069,24.1601438107991,151.649391414937));
#94434=CARTESIAN_POINT('Ctrl Pts',(176.470564826423,24.1757406050875,151.654162192433));
#94435=CARTESIAN_POINT('Ctrl Pts',(176.505029440578,24.1913935197761,151.659368902388));
#94436=CARTESIAN_POINT('Ctrl Pts',(176.558262537659,24.2155705821821,151.667411043676));
#94437=CARTESIAN_POINT('Ctrl Pts',(176.611498776826,24.2399670802618,151.676560125858));
#94438=CARTESIAN_POINT('Ctrl Pts',(176.664512322343,24.2644906804516,151.686907893715));
#94439=CARTESIAN_POINT('Ctrl Pts',(176.712038321724,24.286475790032,151.696184541862));
#94440=CARTESIAN_POINT('Ctrl Pts',(176.759385912566,24.3085633732731,151.706424858618));
#94441=CARTESIAN_POINT('Ctrl Pts',(176.806356876171,24.3306751310717,151.717716698402));
#94442=CARTESIAN_POINT('Ctrl Pts',(176.81991182181,24.3370561727181,151.720975313143));
#94443=CARTESIAN_POINT('Ctrl Pts',(176.833435128408,24.3434391303508,151.72432163475));
#94444=CARTESIAN_POINT('Ctrl Pts',(176.846921303972,24.349821858476,151.727758114264));
#94445=CARTESIAN_POINT('Ctrl Pts',(176.895195965378,24.3726692578471,151.740059220992));
#94446=CARTESIAN_POINT('Ctrl Pts',(176.943039615744,24.3955301215035,151.753495797282));
#94447=CARTESIAN_POINT('Ctrl Pts',(176.990442789502,24.4184161773618,151.76827863874));
#94448=CARTESIAN_POINT('Ctrl Pts',(176.994268160631,24.4202630506911,151.769471593778));
#94449=CARTESIAN_POINT('Ctrl Pts',(176.998090645382,24.4221100825407,151.770673337412));
#94450=CARTESIAN_POINT('Ctrl Pts',(177.001910229157,24.4239572760715,151.771883991953));
#94451=CARTESIAN_POINT('Ctrl Pts',(177.0444989963,24.4445536812752,151.785382919412));
#94452=CARTESIAN_POINT('Ctrl Pts',(177.08665352189,24.4651324708619,151.79996132566));
#94453=CARTESIAN_POINT('Ctrl Pts',(177.12839171876,24.4857188059926,151.815813193461));
#94454=CARTESIAN_POINT('Ctrl Pts',(177.13968511927,24.491288996971,151.820102345973));
#94455=CARTESIAN_POINT('Ctrl Pts',(177.150947856937,24.4968596820121,151.824484949505));
#94456=CARTESIAN_POINT('Ctrl Pts',(177.162179864868,24.5024312232115,151.828965353137));
#94457=CARTESIAN_POINT('Ctrl Pts',(177.195487427009,24.5189531537376,151.84225160821));
#94458=CARTESIAN_POINT('Ctrl Pts',(177.228624808266,24.5355367352923,151.856465474584));
#94459=CARTESIAN_POINT('Ctrl Pts',(177.261374704995,24.5520821064625,151.871664050034));
#94460=CARTESIAN_POINT('Ctrl Pts',(177.26991614724,24.5563972752534,151.875627963431));
#94461=CARTESIAN_POINT('Ctrl Pts',(177.27843099085,24.560709735723,151.879658911046));
#94462=CARTESIAN_POINT('Ctrl Pts',(177.28691483948,24.5650174701844,151.883758017371));
#94463=CARTESIAN_POINT('Ctrl Pts',(177.314410277666,24.5789784744137,151.8970428754));
#94464=CARTESIAN_POINT('Ctrl Pts',(177.341592500569,24.5928993205188,151.911050511792));
#94465=CARTESIAN_POINT('Ctrl Pts',(177.368326940738,24.6067183609374,151.925844650535));
#94466=CARTESIAN_POINT('Ctrl Pts',(177.392890006516,24.6194150172597,151.93943720758));
#94467=CARTESIAN_POINT('Ctrl Pts',(177.417075156271,24.6320258038282,151.953693827921));
#94468=CARTESIAN_POINT('Ctrl Pts',(177.440743155166,24.6444877057936,151.968672101291));
#94469=CARTESIAN_POINT('Ctrl Pts',(177.465429074447,24.6574855729723,151.984294564731));
#94470=CARTESIAN_POINT('Ctrl Pts',(177.489662827417,24.6703770455339,152.00074916361));
#94471=CARTESIAN_POINT('Ctrl Pts',(177.513302330664,24.683097490483,152.018148254101));
#94472=CARTESIAN_POINT('Ctrl Pts',(177.525339790684,24.6895748621053,152.027008036558));
#94473=CARTESIAN_POINT('Ctrl Pts',(177.537222502338,24.6960075867644,152.036112982289));
#94474=CARTESIAN_POINT('Ctrl Pts',(177.548927160266,24.7023850415595,152.045479650782));
#94475=CARTESIAN_POINT('Ctrl Pts',(177.570211034337,24.7139818729737,152.062512100076));
#94476=CARTESIAN_POINT('Ctrl Pts',(177.590992424048,24.725444492759,152.080478691788));
#94477=CARTESIAN_POINT('Ctrl Pts',(177.611061345678,24.7366768879423,152.099491146059));
#94478=CARTESIAN_POINT('Ctrl Pts',(177.627758076354,24.7460218981362,152.115308928116));
#94479=CARTESIAN_POINT('Ctrl Pts',(177.643961093387,24.7552072817013,152.131850812328));
#94480=CARTESIAN_POINT('Ctrl Pts',(177.659525493287,24.7641658842132,152.149187999433));
#94481=CARTESIAN_POINT('Ctrl Pts',(177.677793426276,24.7746805941549,152.169536652404));
#94482=CARTESIAN_POINT('Ctrl Pts',(177.695042493007,24.7848015699428,152.190821330371));
#94483=CARTESIAN_POINT('Ctrl Pts',(177.711012304548,24.7943992985756,152.213126541485));
#94484=CARTESIAN_POINT('Ctrl Pts',(177.719375281163,24.7994253804369,152.224807202742));
#94485=CARTESIAN_POINT('Ctrl Pts',(177.727386726949,24.8043075848329,152.23676782866));
#94486=CARTESIAN_POINT('Ctrl Pts',(177.735004212646,24.809024585629,152.249021220301));
#94487=CARTESIAN_POINT('Ctrl Pts',(177.741978345054,24.8133432006452,152.260239721936));
#94488=CARTESIAN_POINT('Ctrl Pts',(177.748622222903,24.8175233231468,152.27170363004));
#94489=CARTESIAN_POINT('Ctrl Pts',(177.754900516826,24.8215470776803,152.283423111307));
#94490=CARTESIAN_POINT('Ctrl Pts',(177.758407711195,24.8237948362933,152.289969873725));
#94491=CARTESIAN_POINT('Ctrl Pts',(177.761805375059,24.8259967232679,152.29660500088));
#94492=CARTESIAN_POINT('Ctrl Pts',(177.765085505741,24.8281486580691,152.303329793373));
#94493=CARTESIAN_POINT('Ctrl Pts',(177.77517402172,24.8347672445639,152.324012864603));
#94494=CARTESIAN_POINT('Ctrl Pts',(177.784149435374,24.8409126354964,152.345541699617));
#94495=CARTESIAN_POINT('Ctrl Pts',(177.791762551781,24.8464542996167,152.367924848061));
#94496=CARTESIAN_POINT('Ctrl Pts',(177.799661503614,24.8522040262227,152.391148374666));
#94497=CARTESIAN_POINT('Ctrl Pts',(177.805997059918,24.8572289222201,152.414969007613));
#94498=CARTESIAN_POINT('Ctrl Pts',(177.810561932378,24.861415583222,152.439360104592));
#94499=CARTESIAN_POINT('Ctrl Pts',(177.814618969591,24.8651364844365,152.461037728438));
#94500=CARTESIAN_POINT('Ctrl Pts',(177.81722943523,24.8681523378528,152.482924377057));
#94501=CARTESIAN_POINT('Ctrl Pts',(177.818364411308,24.8704356907676,152.504933805796));
#94502=CARTESIAN_POINT('Ctrl Pts',(177.819498002199,24.8727162569556,152.526916373043));
#94503=CARTESIAN_POINT('Ctrl Pts',(177.819159697831,24.8742660736894,152.549021416549));
#94504=CARTESIAN_POINT('Ctrl Pts',(177.817367217729,24.8750808954348,152.571158938715));
#94505=CARTESIAN_POINT('Ctrl Pts',(177.816366483363,24.8755358071082,152.583518227493));
#94506=CARTESIAN_POINT('Ctrl Pts',(177.814913325236,24.8757620423259,152.59588756713));
#94507=CARTESIAN_POINT('Ctrl Pts',(177.813017113379,24.8757620423259,152.608250755187));
#94508=CARTESIAN_POINT('',(176.430596903941,23.1126467080106,150.616656511736));
#94509=CARTESIAN_POINT('Origin',(175.784380109018,23.8757620423259,150.608250755187));
#94510=CARTESIAN_POINT('Ctrl Pts',(176.430593086108,23.1126512166033,150.616656461907));
#94511=CARTESIAN_POINT('Ctrl Pts',(176.620942243517,23.273867111808,150.618976220831));
#94512=CARTESIAN_POINT('Ctrl Pts',(176.807287751197,23.4355523540411,150.639197828199));
#94513=CARTESIAN_POINT('Ctrl Pts',(176.989159692478,23.5976629315714,150.679854720897));
#94514=CARTESIAN_POINT('Ctrl Pts',(177.050901364054,23.6526960387475,150.693656874756));
#94515=CARTESIAN_POINT('Ctrl Pts',(177.11212758244,23.707778192619,150.709813675416));
#94516=CARTESIAN_POINT('Ctrl Pts',(177.172820282514,23.7629077585044,150.728422933407));
#94517=CARTESIAN_POINT('Ctrl Pts',(177.173292023554,23.7633362594394,150.728567576019));
#94518=CARTESIAN_POINT('Ctrl Pts',(177.173763731008,23.7637647620101,150.728712366428));
#94519=CARTESIAN_POINT('Ctrl Pts',(177.174235404887,23.7641932662315,150.728857304682));
#94520=CARTESIAN_POINT('Ctrl Pts',(177.259960857398,23.8420727502167,150.755199440557));
#94521=CARTESIAN_POINT('Ctrl Pts',(177.345014579002,23.9204305734928,150.786762479351));
#94522=CARTESIAN_POINT('Ctrl Pts',(177.428034382514,23.998042726141,150.8237109945));
#94523=CARTESIAN_POINT('Ctrl Pts',(177.460499505064,24.028393171944,150.838159812994));
#94524=CARTESIAN_POINT('Ctrl Pts',(177.492653610754,24.0586297153941,150.85343273917));
#94525=CARTESIAN_POINT('Ctrl Pts',(177.524414819681,24.0886792232459,150.869541775791));
#94526=CARTESIAN_POINT('Ctrl Pts',(177.525503416018,24.0897091520578,150.870093903334));
#94527=CARTESIAN_POINT('Ctrl Pts',(177.526591550734,24.0907388611171,150.870647013372));
#94528=CARTESIAN_POINT('Ctrl Pts',(177.527679220282,24.0917683472481,150.871201106284));
#94529=CARTESIAN_POINT('Ctrl Pts',(177.639922830175,24.1980076365004,150.928381514429));
#94530=CARTESIAN_POINT('Ctrl Pts',(177.747432873769,24.3020358637303,150.995859328735));
#94531=CARTESIAN_POINT('Ctrl Pts',(177.849416010482,24.403116055102,151.075868335985));
#94532=CARTESIAN_POINT('Ctrl Pts',(177.850978666586,24.4046648756532,151.07709428929));
#94533=CARTESIAN_POINT('Ctrl Pts',(177.852540009189,24.4062129884345,151.078323175045));
#94534=CARTESIAN_POINT('Ctrl Pts',(177.854100036342,24.4077603916609,151.079555001813));
#94535=CARTESIAN_POINT('Ctrl Pts',(177.916984382241,24.4701358698746,151.129209663512));
#94536=CARTESIAN_POINT('Ctrl Pts',(177.978066376459,24.5317217937356,151.184101986091));
#94537=CARTESIAN_POINT('Ctrl Pts',(178.035969220689,24.591114122828,151.24395542159));
#94538=CARTESIAN_POINT('Ctrl Pts',(178.073149186829,24.6292505013424,151.282387880907));
#94539=CARTESIAN_POINT('Ctrl Pts',(178.10901808617,24.6664823060443,151.322866578078));
#94540=CARTESIAN_POINT('Ctrl Pts',(178.14320414749,24.7024320267223,151.365325418936));
#94541=CARTESIAN_POINT('Ctrl Pts',(178.189881763411,24.7515177414698,151.423298680247));
#94542=CARTESIAN_POINT('Ctrl Pts',(178.233801900382,24.7985951004967,151.485285816535));
#94543=CARTESIAN_POINT('Ctrl Pts',(178.274300365435,24.8429464492918,151.551510019952));
#94544=CARTESIAN_POINT('Ctrl Pts',(178.307825929647,24.8796615196029,151.606331944218));
#94545=CARTESIAN_POINT('Ctrl Pts',(178.339006378201,24.9145082772951,151.664057880399));
#94546=CARTESIAN_POINT('Ctrl Pts',(178.367447537254,24.9470634889582,151.724827914402));
#94547=CARTESIAN_POINT('Ctrl Pts',(178.368715166528,24.9485144825435,151.72753644938));
#94548=CARTESIAN_POINT('Ctrl Pts',(178.369977231717,24.9499607849485,151.730250787971));
#94549=CARTESIAN_POINT('Ctrl Pts',(178.371233703054,24.9514023638144,151.732970946095));
#94550=CARTESIAN_POINT('Ctrl Pts',(178.397594887464,24.9816471654459,151.790040763632));
#94551=CARTESIAN_POINT('Ctrl Pts',(178.421217785221,25.0094902291248,151.849052198428));
#94552=CARTESIAN_POINT('Ctrl Pts',(178.441897120666,25.0346736294332,151.910064285732));
#94553=CARTESIAN_POINT('Ctrl Pts',(178.461639263896,25.0587157122757,151.968311291274));
#94554=CARTESIAN_POINT('Ctrl Pts',(178.478698736833,25.0803339837904,152.02838190416));
#94555=CARTESIAN_POINT('Ctrl Pts',(178.492865080253,25.0992740523429,152.09034605596));
#94556=CARTESIAN_POINT('Ctrl Pts',(178.498894652275,25.1073354485726,152.116719644752));
#94557=CARTESIAN_POINT('Ctrl Pts',(178.504399693808,25.1149112646649,152.143436484153));
#94558=CARTESIAN_POINT('Ctrl Pts',(178.509362013848,25.1219799614452,152.170502939887));
#94559=CARTESIAN_POINT('Ctrl Pts',(178.50976172314,25.1225493370133,152.172683112426));
#94560=CARTESIAN_POINT('Ctrl Pts',(178.510157869719,25.1231153641414,152.174865339501));
#94561=CARTESIAN_POINT('Ctrl Pts',(178.510550445545,25.1236780327978,152.177049621895));
#94562=CARTESIAN_POINT('Ctrl Pts',(178.524799466834,25.1441007820793,152.256330831494));
#94563=CARTESIAN_POINT('Ctrl Pts',(178.53405773826,25.1596591700609,152.336459756157));
#94564=CARTESIAN_POINT('Ctrl Pts',(178.53828485658,25.170241131487,152.41753159637));
#94565=CARTESIAN_POINT('Ctrl Pts',(178.542284907349,25.1802546630996,152.494248511332));
#94566=CARTESIAN_POINT('Ctrl Pts',(178.54177950378,25.1858118327628,152.571809812277));
#94567=CARTESIAN_POINT('Ctrl Pts',(178.536697911727,25.186780381516,152.650302317055));
#94568=CARTESIAN_POINT('Ctrl Pts',(178.536409449221,25.1868353623168,152.654758035734));
#94569=CARTESIAN_POINT('Ctrl Pts',(178.536106230804,25.1868755467193,152.659216756742));
#94570=CARTESIAN_POINT('Ctrl Pts',(178.535788240059,25.1869009068823,152.663678496546));
#94571=CARTESIAN_POINT('Ctrl Pts',(7.58040827681699E-15,-2.96262874552467,
151.608250755187));
#94572=CARTESIAN_POINT('Ctrl Pts',(7.71069817591099E-15,-3.96262874552467,
151.608250755187));
#94573=CARTESIAN_POINT('Ctrl Pts',(7.71069817591099E-15,-3.96262874552467,
150.608250755187));
#94574=CARTESIAN_POINT('Ctrl Pts',(-7.48001477234627,-2.96262874562523,
151.608250755187));
#94575=CARTESIAN_POINT('Ctrl Pts',(-7.47915914848108,-3.96262874562523,
151.608250755187));
#94576=CARTESIAN_POINT('Ctrl Pts',(-7.47915914848117,-3.96262874552467,
150.608250755187));
#94577=CARTESIAN_POINT('Ctrl Pts',(-14.9601902827936,-2.9704066144946,151.608250755187));
#94578=CARTESIAN_POINT('Ctrl Pts',(-14.9611695836601,-3.97041247107443,
151.608250755187));
#94579=CARTESIAN_POINT('Ctrl Pts',(-14.96116958366,-3.97041247104644,150.608250755187));
#94580=CARTESIAN_POINT('Ctrl Pts',(-29.9184179910251,-2.90250945369316,
151.608250755187));
#94581=CARTESIAN_POINT('Ctrl Pts',(-29.9265168326519,-3.90248299383942,
151.608250755187));
#94582=CARTESIAN_POINT('Ctrl Pts',(-29.926516832652,-3.90248299386741,150.608250755187));
#94583=CARTESIAN_POINT('Ctrl Pts',(-37.3964862791675,-2.82824484200836,
151.608250755187));
#94584=CARTESIAN_POINT('Ctrl Pts',(-37.4098860289911,-3.82817884079897,
151.608250755083));
#94585=CARTESIAN_POINT('Ctrl Pts',(-37.4098860290166,-3.82817884077274,
150.608250755083));
#94586=CARTESIAN_POINT('Ctrl Pts',(-52.3486036457515,-2.52473868654688,
151.608250755187));
#94587=CARTESIAN_POINT('Ctrl Pts',(-52.3757926152852,-3.52439278430538,
151.60825075529));
#94588=CARTESIAN_POINT('Ctrl Pts',(-52.3757926152598,-3.52439278433161,
150.60825075529));
#94589=CARTESIAN_POINT('Ctrl Pts',(-59.8226717303696,-2.29623000265189,
151.608250755187));
#94590=CARTESIAN_POINT('Ctrl Pts',(-59.8583568649177,-3.29564767497403,
151.60825075529));
#94591=CARTESIAN_POINT('Ctrl Pts',(-59.8583568649164,-3.29564767494582,
150.60825075529));
#94592=CARTESIAN_POINT('Ctrl Pts',(-71.0292449211431,-1.77883547863047,
151.608250755187));
#94593=CARTESIAN_POINT('Ctrl Pts',(-71.0805819281094,-2.7775305221053,151.608250755135));
#94594=CARTESIAN_POINT('Ctrl Pts',(-71.0805819281101,-2.77753052211941,
150.608250755135));
#94595=CARTESIAN_POINT('Ctrl Pts',(-74.7640118647851,-1.57716395400885,
151.608250755187));
#94596=CARTESIAN_POINT('Ctrl Pts',(-74.8210574168792,-2.57555542360394,
151.608250755135));
#94597=CARTESIAN_POINT('Ctrl Pts',(-74.821057416878,-2.57555542358512,150.608250755135));
#94598=CARTESIAN_POINT('Ctrl Pts',(-82.2317153529343,-1.10324244350201,
151.608250755187));
#94599=CARTESIAN_POINT('Ctrl Pts',(-82.3013406088045,-2.10083556964149,
151.608250755239));
#94600=CARTESIAN_POINT('Ctrl Pts',(-82.3013406088056,-2.10083556966032,
150.608250755239));
#94601=CARTESIAN_POINT('Ctrl Pts',(-85.9661068731236,-0.830903349436501,
151.608250755187));
#94602=CARTESIAN_POINT('Ctrl Pts',(-86.0426053104115,-1.82800207668471,
151.608250755135));
#94603=CARTESIAN_POINT('Ctrl Pts',(-86.04260531041,-1.8280020766666,150.608250755135));
#94604=CARTESIAN_POINT('Ctrl Pts',(-97.1555011499729,0.113239291570469,
151.608250755187));
#94605=CARTESIAN_POINT('Ctrl Pts',(-97.2547429890782,-0.881940384928872,
151.60825075529));
#94606=CARTESIAN_POINT('Ctrl Pts',(-97.2547429890811,-0.881940384965111,
150.60825075529));
#94607=CARTESIAN_POINT('Ctrl Pts',(-104.589500516371,0.908590385417737,
151.608250755187));
#94608=CARTESIAN_POINT('Ctrl Pts',(-104.706623983818,-0.0847860000410842,
151.608250755187));
#94609=CARTESIAN_POINT('Ctrl Pts',(-104.70662398386,-0.0847859999660353,
150.608250755187));
#94610=CARTESIAN_POINT('Ctrl Pts',(-115.6832946476,2.47242844681118,151.608250755187));
#94611=CARTESIAN_POINT('Ctrl Pts',(-115.834110543524,1.48380151869801,151.608250755187));
#94612=CARTESIAN_POINT('Ctrl Pts',(-115.834110543502,1.48380151866048,150.608250755187));
#94613=CARTESIAN_POINT('Ctrl Pts',(-119.371604706226,3.0560747245114,151.608250755187));
#94614=CARTESIAN_POINT('Ctrl Pts',(-119.534815140111,2.06938108833564,151.608250755031));
#94615=CARTESIAN_POINT('Ctrl Pts',(-119.534815140076,2.06938108832628,150.608250755083));
#94616=CARTESIAN_POINT('Ctrl Pts',(-126.724082256959,4.37986325499499,151.608250755187));
#94617=CARTESIAN_POINT('Ctrl Pts',(-126.915266651803,3.39820623507059,151.608250755342));
#94618=CARTESIAN_POINT('Ctrl Pts',(-126.915266651838,3.39820623507995,150.60825075529));
#94619=CARTESIAN_POINT('Ctrl Pts',(-130.3882896118,5.11974710981558,151.608250755187));
#94620=CARTESIAN_POINT('Ctrl Pts',(-130.595044169067,4.14118311580342,151.608250755135));
#94621=CARTESIAN_POINT('Ctrl Pts',(-130.595044169049,4.14118311588002,150.608250755135));
#94622=CARTESIAN_POINT('Ctrl Pts',(-135.861220457415,6.38112699928991,151.608250755187));
#94623=CARTESIAN_POINT('Ctrl Pts',(-136.094725659691,5.4087283902617,151.608250755213));
#94624=CARTESIAN_POINT('Ctrl Pts',(-136.0947256597,5.4087283902234,150.608250755213));
#94625=CARTESIAN_POINT('Ctrl Pts',(-137.681613722953,6.82697768764861,151.608250755187));
#94626=CARTESIAN_POINT('Ctrl Pts',(-137.924606380511,5.85689247239123,151.608250755161));
#94627=CARTESIAN_POINT('Ctrl Pts',(-137.924606380501,5.85689247242799,150.608250755161));
#94628=CARTESIAN_POINT('Ctrl Pts',(-141.313341356547,7.77740028733485,151.608250755187));
#94629=CARTESIAN_POINT('Ctrl Pts',(-141.576696462501,6.81264392189733,151.608250755213));
#94630=CARTESIAN_POINT('Ctrl Pts',(-141.576696462511,6.81264392186057,150.608250755213));
#94631=CARTESIAN_POINT('Ctrl Pts',(-143.1189853136,8.28050120342763,151.608250755187));
#94632=CARTESIAN_POINT('Ctrl Pts',(-143.39318392604,7.31875148009332,151.608250755135));
#94633=CARTESIAN_POINT('Ctrl Pts',(-143.393183926052,7.31875148011453,150.608250755161));
#94634=CARTESIAN_POINT('Ctrl Pts',(-148.49688844256,9.88460944395078,151.608250755187));
#94635=CARTESIAN_POINT('Ctrl Pts',(-148.805991124598,8.93327082393873,151.60825075529));
#94636=CARTESIAN_POINT('Ctrl Pts',(-148.805991124574,8.93327082389632,150.608250755239));
#94637=CARTESIAN_POINT('Ctrl Pts',(-152.032276636241,11.0793251114952,151.608250755187));
#94638=CARTESIAN_POINT('Ctrl Pts',(-152.367777204989,10.1366936288938,151.608250755031));
#94639=CARTESIAN_POINT('Ctrl Pts',(-152.367777204931,10.1366936289926,150.608250755083));
#94640=CARTESIAN_POINT('Ctrl Pts',(-158.966663136563,13.8113957628694,151.608250755187));
#94641=CARTESIAN_POINT('Ctrl Pts',(-159.364291195684,12.8932418158741,151.608250755342));
#94642=CARTESIAN_POINT('Ctrl Pts',(-159.364291195742,12.8932418157753,150.60825075529));
#94643=CARTESIAN_POINT('Ctrl Pts',(-162.366411372621,15.3468667695571,151.608250755187));
#94644=CARTESIAN_POINT('Ctrl Pts',(-162.799768640706,14.4443390394639,151.60825075503));
#94645=CARTESIAN_POINT('Ctrl Pts',(-162.799768640555,14.4443390396976,150.608250755083));
#94646=CARTESIAN_POINT('Ctrl Pts',(-166.491318743796,17.5796732143735,151.608250755187));
#94647=CARTESIAN_POINT('Ctrl Pts',(-166.97802048339,16.7060207701578,151.608250755226));
#94648=CARTESIAN_POINT('Ctrl Pts',(-166.978020483428,16.7060207700994,150.608250755213));
#94649=CARTESIAN_POINT('Ctrl Pts',(-167.309955007446,18.0421749712842,151.608250755187));
#94650=CARTESIAN_POINT('Ctrl Pts',(-167.807762984048,17.1747832534819,151.608250755173));
#94651=CARTESIAN_POINT('Ctrl Pts',(-167.807762983994,17.1747832535731,150.608250755173));
#94652=CARTESIAN_POINT('Ctrl Pts',(-168.93299683872,19.0029289063352,151.608250755187));
#94653=CARTESIAN_POINT('Ctrl Pts',(-169.453970557405,18.1492500685391,151.6082507552));
#94654=CARTESIAN_POINT('Ctrl Pts',(-169.453970557459,18.1492500684478,150.6082507552));
#94655=CARTESIAN_POINT('Ctrl Pts',(-169.737204958192,19.5011635886747,151.608250755187));
#94656=CARTESIAN_POINT('Ctrl Pts',(-170.270238326363,18.6549382700629,151.608250755187));
#94657=CARTESIAN_POINT('Ctrl Pts',(-170.27023832632,18.6549382701294,150.608250755187));
#94658=CARTESIAN_POINT('Ctrl Pts',(-172.109848566929,21.0455107820461,151.608250755187));
#94659=CARTESIAN_POINT('Ctrl Pts',(-172.680332460927,20.22366190761,151.608250755187));
#94660=CARTESIAN_POINT('Ctrl Pts',(-172.680332461013,20.2236619074771,150.608250755187));
#94661=CARTESIAN_POINT('Ctrl Pts',(-173.643681898189,22.1438771319804,151.608250755187));
#94662=CARTESIAN_POINT('Ctrl Pts',(-174.24092113324,21.3409830339438,151.608250755108));
#94663=CARTESIAN_POINT('Ctrl Pts',(-174.240921133641,21.3409830334629,150.608250755029));
#94664=CARTESIAN_POINT('Ctrl Pts',(-175.118478031529,23.3269112214833,151.608250755187));
#94665=CARTESIAN_POINT('Ctrl Pts',(-175.744203657298,22.5468679911069,151.608250755187));
#94666=CARTESIAN_POINT('Ctrl Pts',(-175.744203657298,22.5468679911069,150.608250755187));
#94667=CARTESIAN_POINT('',(7.71069817591099E-15,-3.96262874552467,150.608250755187));
#94668=CARTESIAN_POINT('',(7.59225281309826E-15,-2.96262874552467,151.608250755187));
#94669=CARTESIAN_POINT('Origin',(7.59225281309826E-15,-2.96262874552467,
150.608250755187));
#94670=CARTESIAN_POINT('Ctrl Pts',(-175.118478031529,23.3269112214833,151.608250755187));
#94671=CARTESIAN_POINT('Ctrl Pts',(-173.643670919279,22.1438683242896,151.608250755187));
#94672=CARTESIAN_POINT('Ctrl Pts',(-172.109848567067,21.0455107819602,151.608250755187));
#94673=CARTESIAN_POINT('Ctrl Pts',(-170.528086161207,20.0159459864725,151.608250755187));
#94674=CARTESIAN_POINT('Ctrl Pts',(-169.737204958277,19.5011635887287,151.608250755187));
#94675=CARTESIAN_POINT('Ctrl Pts',(-168.932996838842,19.0029289062917,151.608250755187));
#94676=CARTESIAN_POINT('Ctrl Pts',(-168.121475923185,18.5225519388115,151.608250755187));
#94677=CARTESIAN_POINT('Ctrl Pts',(-167.309955007528,18.0421749713315,151.608250755187));
#94678=CARTESIAN_POINT('Ctrl Pts',(-166.491318743916,17.5796732143511,151.608250755187));
#94679=CARTESIAN_POINT('Ctrl Pts',(-165.666337269668,17.133111925397,151.608250755187));
#94680=CARTESIAN_POINT('Ctrl Pts',(-162.366411372674,15.3468667695806,151.608250755187));
#94681=CARTESIAN_POINT('Ctrl Pts',(-158.966663136623,13.8113957627309,151.608250755187));
#94682=CARTESIAN_POINT('Ctrl Pts',(-155.499469886505,12.4453604371405,151.608250755187));
#94683=CARTESIAN_POINT('Ctrl Pts',(-152.032276636387,11.07932511155,151.608250755187));
#94684=CARTESIAN_POINT('Ctrl Pts',(-148.496888442587,9.8846094438595,151.608250755187));
#94685=CARTESIAN_POINT('Ctrl Pts',(-144.911619690001,8.81520395025918,151.608250755187));
#94686=CARTESIAN_POINT('Ctrl Pts',(-143.118985313708,8.28050120345901,151.608250755187));
#94687=CARTESIAN_POINT('Ctrl Pts',(-141.313341356563,7.77740028730139,151.608250755187));
#94688=CARTESIAN_POINT('Ctrl Pts',(-139.497477539825,7.30218898749211,151.608250755187));
#94689=CARTESIAN_POINT('Ctrl Pts',(-137.681613723086,6.82697768768278,151.608250755187));
#94690=CARTESIAN_POINT('Ctrl Pts',(-135.861220457474,6.38112699926441,151.608250755187));
#94691=CARTESIAN_POINT('Ctrl Pts',(-134.036910175617,5.96066703612229,151.608250755187));
#94692=CARTESIAN_POINT('Ctrl Pts',(-130.388289611904,5.11974710983809,151.608250755187));
#94693=CARTESIAN_POINT('Ctrl Pts',(-126.724082256978,4.37986325495167,151.608250755187));
#94694=CARTESIAN_POINT('Ctrl Pts',(-123.047843481659,3.71796898974137,151.608250755187));
#94695=CARTESIAN_POINT('Ctrl Pts',(-119.37160470634,3.05607472453107,151.608250755187));
#94696=CARTESIAN_POINT('Ctrl Pts',(-115.683294647706,2.47242844679211,151.608250755187));
#94697=CARTESIAN_POINT('Ctrl Pts',(-111.985363270584,1.95114909299883,151.608250755187));
#94698=CARTESIAN_POINT('Ctrl Pts',(-104.589500516342,0.908590385412271,
151.608250755187));
#94699=CARTESIAN_POINT('Ctrl Pts',(-97.1555011500406,0.113239291541015,
151.608250755187));
#94700=CARTESIAN_POINT('Ctrl Pts',(-89.6959049654537,-0.516189135775493,
151.608250755187));
#94701=CARTESIAN_POINT('Ctrl Pts',(-85.9661068731603,-0.830903349433756,
151.608250755187));
#94702=CARTESIAN_POINT('Ctrl Pts',(-82.2317153529779,-1.10324244351832,
151.608250755187));
#94703=CARTESIAN_POINT('Ctrl Pts',(-78.4978636089007,-1.3402031987625,151.608250755187));
#94704=CARTESIAN_POINT('Ctrl Pts',(-74.7640118648235,-1.57716395400667,
151.608250755187));
#94705=CARTESIAN_POINT('Ctrl Pts',(-71.0292449211827,-1.77883547864296,
151.608250755187));
#94706=CARTESIAN_POINT('Ctrl Pts',(-67.2937205242537,-1.95130031997899,
151.608250755187));
#94707=CARTESIAN_POINT('Ctrl Pts',(-59.8226717303959,-2.29623000265104,
151.608250755187));
#94708=CARTESIAN_POINT('Ctrl Pts',(-52.3486036457986,-2.52473868657067,
151.608250755187));
#94709=CARTESIAN_POINT('Ctrl Pts',(-44.8725449624828,-2.6764917642896,151.608250755187));
#94710=CARTESIAN_POINT('Ctrl Pts',(-37.3964862791671,-2.82824484200852,
151.608250755187));
#94711=CARTESIAN_POINT('Ctrl Pts',(-29.9184179909671,-2.90250945372239,
151.608250755187));
#94712=CARTESIAN_POINT('Ctrl Pts',(-22.4393041369209,-2.93645803410833,
151.608250755187));
#94713=CARTESIAN_POINT('Ctrl Pts',(-14.9601902828747,-2.97040661449427,
151.608250755187));
#94714=CARTESIAN_POINT('Ctrl Pts',(-7.47999428485685,-2.96262874562523,
151.608250755187));
#94715=CARTESIAN_POINT('Ctrl Pts',(7.58040827681699E-15,-2.96262874552467,
151.608250755187));
#94716=CARTESIAN_POINT('Ctrl Pts',(7.71069817591099E-15,-3.96262874552467,
150.608250755187));
#94717=CARTESIAN_POINT('Ctrl Pts',(-7.50819538729109,-3.96262874552467,
150.608250755187));
#94718=CARTESIAN_POINT('Ctrl Pts',(-15.016593604005,-3.97044580329555,150.608250755187));
#94719=CARTESIAN_POINT('Ctrl Pts',(-30.0312011445192,-3.90171985843133,
150.608250755187));
#94720=CARTESIAN_POINT('Ctrl Pts',(-37.5374476689956,-3.82661057201559,
150.608250755187));
#94721=CARTESIAN_POINT('Ctrl Pts',(-52.5458801835575,-3.51989876720754,
150.608250755187));
#94722=CARTESIAN_POINT('Ctrl Pts',(-60.0480854211127,-3.28903804741979,
150.608250755187));
#94723=CARTESIAN_POINT('Ctrl Pts',(-71.2968182978101,-2.76642698606123,
150.608250755187));
#94724=CARTESIAN_POINT('Ctrl Pts',(-75.0456307554615,-2.56273368294278,
150.608250755187));
#94725=CARTESIAN_POINT('Ctrl Pts',(-82.541406464583,-2.08407856275224,150.608250755187));
#94726=CARTESIAN_POINT('Ctrl Pts',(-86.2899316135277,-1.80901706075654,
150.608250755187));
#94727=CARTESIAN_POINT('Ctrl Pts',(-97.5206070789962,-0.855541349070317,
150.608250755187));
#94728=CARTESIAN_POINT('Ctrl Pts',(-104.981869714816,-0.0523559943782628,
150.608250755187));
#94729=CARTESIAN_POINT('Ctrl Pts',(-116.115973027981,1.52690259340425,150.608250755187));
#94730=CARTESIAN_POINT('Ctrl Pts',(-119.817620868547,2.11630680211849,150.608250755187));
#94731=CARTESIAN_POINT('Ctrl Pts',(-127.196527399596,3.45315573247565,150.608250755187));
#94732=CARTESIAN_POINT('Ctrl Pts',(-130.873826011882,4.20034176276589,150.608250755187));
#94733=CARTESIAN_POINT('Ctrl Pts',(-138.196939381026,5.89872768376561,150.608250755187));
#94734=CARTESIAN_POINT('Ctrl Pts',(-141.849976625069,6.85208769613199,150.608250755187));
#94735=CARTESIAN_POINT('Ctrl Pts',(-149.04273478531,9.01070097414105,150.608250755187));
#94736=CARTESIAN_POINT('Ctrl Pts',(-152.588815574637,10.2162896078986,150.608250755187));
#94737=CARTESIAN_POINT('Ctrl Pts',(-159.543790312038,12.9718966302658,150.608250755187));
#94738=CARTESIAN_POINT('Ctrl Pts',(-162.953403385689,14.5201095377957,150.608250755187));
#94739=CARTESIAN_POINT('Ctrl Pts',(-167.090526771118,16.7689396411949,150.608250755187));
#94740=CARTESIAN_POINT('Ctrl Pts',(-167.911603711878,17.2346426806634,150.608250755187));
#94741=CARTESIAN_POINT('Ctrl Pts',(-169.539551113397,18.2017164255323,150.608250755187));
#94742=CARTESIAN_POINT('Ctrl Pts',(-170.345912390848,18.7028771029668,150.608250755186));
#94743=CARTESIAN_POINT('Ctrl Pts',(-172.725350664097,20.2557684708299,150.608250755186));
#94744=CARTESIAN_POINT('Ctrl Pts',(-174.26395189805,21.3594575729593,150.608250755187));
#94745=CARTESIAN_POINT('Ctrl Pts',(-175.744203657372,22.5468679911664,150.608250755186));
#94746=CARTESIAN_POINT('Ctrl Pts',(175.744203657372,22.5468679911664,150.608250755187));
#94747=CARTESIAN_POINT('Ctrl Pts',(175.744203657372,22.5468679911664,151.608250755187));
#94748=CARTESIAN_POINT('Ctrl Pts',(175.118478031602,23.3269112215417,151.608250755187));
#94749=CARTESIAN_POINT('Ctrl Pts',(175.975959514274,22.7327750959766,150.611103966871));
#94750=CARTESIAN_POINT('Ctrl Pts',(175.973846570991,22.7347327109198,151.608250755179));
#94751=CARTESIAN_POINT('Ctrl Pts',(175.343331695395,23.5072816087761,151.608250755187));
#94752=CARTESIAN_POINT('Ctrl Pts',(176.204751595057,22.9213751497708,150.613904162808));
#94753=CARTESIAN_POINT('Ctrl Pts',(176.200864181503,22.9254545071624,151.608250755187));
#94754=CARTESIAN_POINT('Ctrl Pts',(175.565293759208,23.6902366406671,151.608250755187));
#94755=CARTESIAN_POINT('Ctrl Pts',(176.430593086108,23.1126512166033,150.616656461907));
#94756=CARTESIAN_POINT('Ctrl Pts',(176.425206487511,23.1190122335564,151.608250755187));
#94757=CARTESIAN_POINT('Ctrl Pts',(175.784380109018,23.8757620423259,151.608250755187));
#94758=CARTESIAN_POINT('',(175.118478031602,23.3269112215418,151.608250755187));
#94759=CARTESIAN_POINT('',(175.744216329386,22.5468739627075,150.608257703203));
#94760=CARTESIAN_POINT('Origin',(175.118478031602,23.3269112215418,150.608250755187));
#94761=CARTESIAN_POINT('Origin',(154.866194135799,48.5801870238026,150.281756698687));
#94762=CARTESIAN_POINT('Origin',(154.804630199197,48.6513971212518,151.608250754784));
#94763=CARTESIAN_POINT('Ctrl Pts',(175.118478031529,23.3269112214834,151.608250755187));
#94764=CARTESIAN_POINT('Ctrl Pts',(175.744203657298,22.546867991107,151.608250755187));
#94765=CARTESIAN_POINT('Ctrl Pts',(175.744203657298,22.546867991107,150.608250755187));
#94766=CARTESIAN_POINT('Ctrl Pts',(173.120080073127,21.7238605655503,151.608250755187));
#94767=CARTESIAN_POINT('Ctrl Pts',(173.707215155453,20.9128612407145,151.608250755436));
#94768=CARTESIAN_POINT('Ctrl Pts',(173.707215156076,20.9128612399726,150.608250755435));
#94769=CARTESIAN_POINT('Ctrl Pts',(171.037782482163,20.2938924020537,151.608250755187));
#94770=CARTESIAN_POINT('Ctrl Pts',(171.589969109119,19.4593526556396,151.608250755187));
#94771=CARTESIAN_POINT('Ctrl Pts',(171.589969109234,19.4593526554507,150.608250755187));
#94772=CARTESIAN_POINT('Ctrl Pts',(166.754172906568,17.6818243599797,151.608250755187));
#94773=CARTESIAN_POINT('Ctrl Pts',(167.243233378372,16.8087914199981,151.608250755187));
#94774=CARTESIAN_POINT('Ctrl Pts',(167.243233378257,16.8087914201871,150.608250755187));
#94775=CARTESIAN_POINT('Ctrl Pts',(164.55225250787,16.5005018421618,151.608250755187));
#94776=CARTESIAN_POINT('Ctrl Pts',(165.013075266338,15.6125556413792,151.608250755187));
#94777=CARTESIAN_POINT('Ctrl Pts',(165.013075266415,15.6125556412203,150.608250755187));
#94778=CARTESIAN_POINT('Ctrl Pts',(160.0571058438,14.3272733601118,151.608250755187));
#94779=CARTESIAN_POINT('Ctrl Pts',(160.466806870505,13.414611791432,151.608250755187));
#94780=CARTESIAN_POINT('Ctrl Pts',(160.466806870428,13.4146117915908,150.608250755187));
#94781=CARTESIAN_POINT('Ctrl Pts',(157.763687679101,13.3357654966317,151.608250755187));
#94782=CARTESIAN_POINT('Ctrl Pts',(158.150493359254,12.4133327114123,151.608250755152));
#94783=CARTESIAN_POINT('Ctrl Pts',(158.150493359297,12.4133327113047,150.608250755152));
#94784=CARTESIAN_POINT('Ctrl Pts',(153.104239295307,11.5033854913725,151.608250755187));
#94785=CARTESIAN_POINT('Ctrl Pts',(153.449389725816,10.5645713149919,151.608250755221));
#94786=CARTESIAN_POINT('Ctrl Pts',(153.449389725773,10.5645713150995,150.608250755221));
#94787=CARTESIAN_POINT('Ctrl Pts',(150.738093671782,10.6627043727942,151.608250755187));
#94788=CARTESIAN_POINT('Ctrl Pts',(151.064489900424,9.71729891062486,151.608250755222));
#94789=CARTESIAN_POINT('Ctrl Pts',(151.064489900386,9.71729891075825,150.608250755222));
#94790=CARTESIAN_POINT('Ctrl Pts',(148.342276748097,9.8836739626675,151.608250755187));
#94791=CARTESIAN_POINT('Ctrl Pts',(148.651502801043,8.93268539902455,151.608250755187));
#94792=CARTESIAN_POINT('Ctrl Pts',(148.651502801043,8.93268539902455,150.608250755187));
#94793=CARTESIAN_POINT('Ctrl Pts',(150.890074370997,10.7399699375689,151.608250755187));
#94794=CARTESIAN_POINT('Ctrl Pts',(152.418601106946,11.2709967454126,151.608250755187));
#94795=CARTESIAN_POINT('Ctrl Pts',(153.933840147718,11.829615202147,151.608250755022));
#94796=CARTESIAN_POINT('Ctrl Pts',(155.433971914984,12.4195540635097,151.608250754921));
#94797=CARTESIAN_POINT('Ctrl Pts',(156.056167411372,12.664237437793,151.60825075488));
#94798=CARTESIAN_POINT('Ctrl Pts',(156.675772237677,12.9142950898713,151.60825075491));
#94799=CARTESIAN_POINT('Ctrl Pts',(157.292603196614,13.1701058677585,151.608250755012));
#94800=CARTESIAN_POINT('Ctrl Pts',(158.98541137872,13.8721435518337,151.608250755293));
#94801=CARTESIAN_POINT('Ctrl Pts',(160.657393444049,14.6173931442985,151.60825075146));
#94802=CARTESIAN_POINT('Ctrl Pts',(162.304716085384,15.4138112567312,151.608250751591));
#94803=CARTESIAN_POINT('Ctrl Pts',(162.70488712863,15.6072788015308,151.608250751623));
#94804=CARTESIAN_POINT('Ctrl Pts',(163.103608897851,15.803753154363,151.608250752144));
#94805=CARTESIAN_POINT('Ctrl Pts',(163.500798283409,16.003405836179,151.608250752999));
#94806=CARTESIAN_POINT('Ctrl Pts',(164.887524176526,16.7004625893846,151.608250755985));
#94807=CARTESIAN_POINT('Ctrl Pts',(166.255673442885,17.4360498920816,151.608250748576));
#94808=CARTESIAN_POINT('Ctrl Pts',(167.601685487584,18.2175677714455,151.608250744422));
#94809=CARTESIAN_POINT('Ctrl Pts',(168.035481204944,18.4694370696759,151.608250743083));
#94810=CARTESIAN_POINT('Ctrl Pts',(168.466977276069,18.7260768217338,151.608250742812));
#94811=CARTESIAN_POINT('Ctrl Pts',(168.896053436859,18.9877341686053,151.608250744604));
#94812=CARTESIAN_POINT('Ctrl Pts',(169.086720473706,19.1040059067164,151.6082507454));
#94813=CARTESIAN_POINT('Ctrl Pts',(169.276914485451,19.2212622613973,151.60825074658));
#94814=CARTESIAN_POINT('Ctrl Pts',(169.466617875306,19.3395384011703,151.608250747987));
#94815=CARTESIAN_POINT('Ctrl Pts',(170.713449384169,20.1169120576391,151.608250757236));
#94816=CARTESIAN_POINT('Ctrl Pts',(171.939119545222,20.9381212638537,151.608250755117));
#94817=CARTESIAN_POINT('Ctrl Pts',(173.138860719752,21.8131269850015,151.608250755171));
#94818=CARTESIAN_POINT('Ctrl Pts',(173.807052403966,22.3004583852424,151.608250755202));
#94819=CARTESIAN_POINT('Ctrl Pts',(174.467200766754,22.8044775175799,151.608250755187));
#94820=CARTESIAN_POINT('Ctrl Pts',(175.118478031529,23.3269112214834,151.608250755187));
#94821=CARTESIAN_POINT('Ctrl Pts',(175.744203657372,22.5468679911664,150.608250755187));
#94822=CARTESIAN_POINT('Ctrl Pts',(173.733839581004,20.9342184982058,150.608250755187));
#94823=CARTESIAN_POINT('Ctrl Pts',(171.640407580167,19.493722137766,150.608250755187));
#94824=CARTESIAN_POINT('Ctrl Pts',(167.333937892112,16.8606047997096,150.608250755187));
#94825=CARTESIAN_POINT('Ctrl Pts',(165.12049074122,15.6688324102149,150.608250755187));
#94826=CARTESIAN_POINT('Ctrl Pts',(160.601711271341,13.4757139554807,150.608250755187));
#94827=CARTESIAN_POINT('Ctrl Pts',(158.296197081565,12.4747448061917,150.608250755187));
#94828=CARTESIAN_POINT('Ctrl Pts',(153.611908863468,10.6246329890705,150.608250755187));
#94829=CARTESIAN_POINT('Ctrl Pts',(151.233043212517,9.77568020346336,150.608250755187));
#94830=CARTESIAN_POINT('Ctrl Pts',(148.824154304563,8.98894875990614,150.608250755187));
#94831=CARTESIAN_POINT('Origin',(-205.7,-9.35236728728476,151.608250755187));
#94832=CARTESIAN_POINT('',(-178.303739692644,23.8757620423259,151.608250755187));
#94833=CARTESIAN_POINT('',(-178.303739692644,23.8757620423259,151.608250755187));
#94834=CARTESIAN_POINT('Ctrl Pts',(7.105427357601E-15,-2.96262874552467,
151.608250755187));
#94835=CARTESIAN_POINT('Ctrl Pts',(9.02624649977933,-2.9626287456421,151.608250755187));
#94836=CARTESIAN_POINT('Ctrl Pts',(18.0527444291047,-2.9728621931889,151.60825074306));
#94837=CARTESIAN_POINT('Ctrl Pts',(27.0774432067146,-2.91001683511451,151.608250751144));
#94838=CARTESIAN_POINT('Ctrl Pts',(27.3305429265962,-2.9082543228228,151.608250751371));
#94839=CARTESIAN_POINT('Ctrl Pts',(27.5836412653319,-2.90643461439096,151.608250751582));
#94840=CARTESIAN_POINT('Ctrl Pts',(27.8367381802904,-2.90455588038999,151.608250751779));
#94841=CARTESIAN_POINT('Ctrl Pts',(36.6082400286613,-2.83944517461597,151.608250758593));
#94842=CARTESIAN_POINT('Ctrl Pts',(45.3780717103661,-2.70648749187338,151.608250755332));
#94843=CARTESIAN_POINT('Ctrl Pts',(54.1447641976466,-2.44599594155881,151.608250755033));
#94844=CARTESIAN_POINT('Ctrl Pts',(54.6506804038063,-2.43096325995591,151.608250755016));
#94845=CARTESIAN_POINT('Ctrl Pts',(55.1565862129384,-2.41550562764502,151.608250755));
#94846=CARTESIAN_POINT('Ctrl Pts',(55.6624813336477,-2.39961161868985,151.608250754986));
#94847=CARTESIAN_POINT('Ctrl Pts',(64.1758609249135,-2.13214169078735,151.608250754755));
#94848=CARTESIAN_POINT('Ctrl Pts',(72.6862574775868,-1.74295631081683,151.608250759293));
#94849=CARTESIAN_POINT('Ctrl Pts',(81.1919376197577,-1.16313723768181,151.608250750562));
#94850=CARTESIAN_POINT('Ctrl Pts',(81.9500796395524,-1.11145586760035,151.608250749784));
#94851=CARTESIAN_POINT('Ctrl Pts',(82.7082017514622,-1.05825235857909,151.608250749472));
#94852=CARTESIAN_POINT('Ctrl Pts',(83.4662947054053,-1.00347988218016,151.60825074959));
#94853=CARTESIAN_POINT('Ctrl Pts',(86.6559785797055,-0.773024126304283,
151.608250750086));
#94854=CARTESIAN_POINT('Ctrl Pts',(89.8432471884515,-0.514663737175523,
151.608250754812));
#94855=CARTESIAN_POINT('Ctrl Pts',(93.024774958763,-0.223757922142914,151.608250755027));
#94856=CARTESIAN_POINT('Ctrl Pts',(93.5808398870228,-0.172913631963855,
151.608250755064));
#94857=CARTESIAN_POINT('Ctrl Pts',(94.1367294898188,-0.121075272080125,
151.608250755069));
#94858=CARTESIAN_POINT('Ctrl Pts',(94.6924260755016,-0.068218227171274,
151.60825075503));
#94859=CARTESIAN_POINT('Ctrl Pts',(95.5740503470334,0.0156405815990452,
151.608250754969));
#94860=CARTESIAN_POINT('Ctrl Pts',(96.4552583878779,0.102078414550722,151.608250754932));
#94861=CARTESIAN_POINT('Ctrl Pts',(97.3359839441123,0.19119707264984,151.608250754931));
#94862=CARTESIAN_POINT('Ctrl Pts',(100.941451049396,0.556026261457694,151.608250754926));
#94863=CARTESIAN_POINT('Ctrl Pts',(104.539950590689,0.965744460923742,151.608250755187));
#94864=CARTESIAN_POINT('Ctrl Pts',(108.129330685163,1.43018233510906,151.608250755187));
#94865=CARTESIAN_POINT('',(-178.303739692644,23.8757620423259,151.608250755187));
#94866=CARTESIAN_POINT('',(-178.303739692644,23.8757620423259,151.608250755187));
#94867=CARTESIAN_POINT('Origin',(-160.5,51.8013867006571,102.225104347671));
#94868=CARTESIAN_POINT('',(-190.499797482064,51.8013867006572,102.335336081498));
#94869=CARTESIAN_POINT('',(-190.499797482064,59.,102.335336081498));
#94870=CARTESIAN_POINT('',(-190.5,51.8013867006572,102.225104347682));
#94871=CARTESIAN_POINT('',(-190.5,59.,102.225104347671));
#94872=CARTESIAN_POINT('Origin',(-160.5,51.8013867006572,102.225104347682));
#94873=CARTESIAN_POINT('Ctrl Pts',(-190.491663305814,52.7378649121229,102.843638895579));
#94874=CARTESIAN_POINT('Ctrl Pts',(-190.497736632342,52.3999363590591,102.904908304561));
#94875=CARTESIAN_POINT('Ctrl Pts',(-190.497486577525,52.0619530244292,102.966101522029));
#94876=CARTESIAN_POINT('Ctrl Pts',(-190.500794397929,52.1777803689832,102.165012668779));
#94877=CARTESIAN_POINT('Ctrl Pts',(-190.500218467073,52.0402913792871,102.219565731378));
#94878=CARTESIAN_POINT('Ctrl Pts',(-190.500020296148,51.9028032385845,102.274119986721));
#94879=CARTESIAN_POINT('Ctrl Pts',(-190.500380950584,51.8120846909133,102.197587822659));
#94880=CARTESIAN_POINT('Ctrl Pts',(-190.500101610712,51.8080280356141,102.252459235273));
#94881=CARTESIAN_POINT('Ctrl Pts',(-190.499901046205,51.8039712376326,102.307330335762));
#94882=CARTESIAN_POINT('Ctrl Pts',(-190.499485036411,51.5910001868266,102.262672212471));
#94883=CARTESIAN_POINT('Ctrl Pts',(-190.499861738055,51.6678861088951,102.318186867608));
#94884=CARTESIAN_POINT('Ctrl Pts',(-190.499656096965,51.7447735126223,102.373700417183));
#94885=CARTESIAN_POINT('Ctrl Pts',(-190.499276641726,51.5555442395852,102.277696646539));
#94886=CARTESIAN_POINT('Ctrl Pts',(-190.499806182338,51.6454376861142,102.333360080156));
#94887=CARTESIAN_POINT('Ctrl Pts',(-190.499599365699,51.7353333285508,102.389022107829));
#94888=CARTESIAN_POINT('Ctrl Pts',(-190.498637284839,51.4609849811862,102.323405682444));
#94889=CARTESIAN_POINT('Ctrl Pts',(-190.49963641837,51.5856027243035,102.379522755427));
#94890=CARTESIAN_POINT('Ctrl Pts',(-190.499425997259,51.7102254535205,102.435637407256));
#94891=CARTESIAN_POINT('Ctrl Pts',(-190.498179537645,51.4122959822613,102.355661727505));
#94892=CARTESIAN_POINT('Ctrl Pts',(-190.499515675854,51.5548458240518,102.412100111793));
#94893=CARTESIAN_POINT('Ctrl Pts',(-190.49930268195,51.6974029923146,102.468535392115));
#94894=CARTESIAN_POINT('Ctrl Pts',(-190.496764137211,51.2786905629959,102.453983419634));
#94895=CARTESIAN_POINT('Ctrl Pts',(-190.49914429648,51.4705106049134,102.511405737649));
#94896=CARTESIAN_POINT('Ctrl Pts',(-190.498923349085,51.6623471528931,102.568822318432));
#94897=CARTESIAN_POINT('Ctrl Pts',(-190.495771571132,51.209415072178,102.521125183006));
#94898=CARTESIAN_POINT('Ctrl Pts',(-190.498886347067,51.4268861937162,102.579224820903));
#94899=CARTESIAN_POINT('Ctrl Pts',(-190.498659830336,51.6443814238632,102.63731713971));
#94900=CARTESIAN_POINT('Ctrl Pts',(-190.492708303722,51.0187369204825,102.723145628418));
#94901=CARTESIAN_POINT('Ctrl Pts',(-190.498096192236,51.3069405894523,102.783302214059));
#94902=CARTESIAN_POINT('Ctrl Pts',(-190.497852468908,51.5951979523677,102.843444114641));
#94903=CARTESIAN_POINT('Ctrl Pts',(-190.490539813272,50.917161842527,102.85947607439));
#94904=CARTESIAN_POINT('Ctrl Pts',(-190.497544477131,51.2432568804925,102.921043654985));
#94905=CARTESIAN_POINT('Ctrl Pts',(-190.497288537386,51.569430449523,102.982592460488));
#94906=CARTESIAN_POINT('Ctrl Pts',(-190.483704239377,50.6334868253324,103.269643650079));
#94907=CARTESIAN_POINT('Ctrl Pts',(-190.49582522282,51.0656966540016,103.335535923897));
#94908=CARTESIAN_POINT('Ctrl Pts',(-190.495530565148,51.4980839253095,103.401385430389));
#94909=CARTESIAN_POINT('Ctrl Pts',(-190.478715221144,50.4768968387938,103.544270661594));
#94910=CARTESIAN_POINT('Ctrl Pts',(-190.494595543656,50.9681482986425,103.61315472568));
#94911=CARTESIAN_POINT('Ctrl Pts',(-190.494272325443,51.4596635555447,103.681982740741));
#94912=CARTESIAN_POINT('Ctrl Pts',(-190.462385362509,50.029883727716,104.369079428756));
#94913=CARTESIAN_POINT('Ctrl Pts',(-190.490647214857,50.6904232796527,104.447283745944));
#94914=CARTESIAN_POINT('Ctrl Pts',(-190.490229110897,51.3515886158552,104.525337933961));
#94915=CARTESIAN_POINT('Ctrl Pts',(-190.449683809442,49.7677262399101,104.92040760936));
#94916=CARTESIAN_POINT('Ctrl Pts',(-190.487668736046,50.5286860699985,105.005251885913));
#94917=CARTESIAN_POINT('Ctrl Pts',(-190.487175061528,51.2906141049957,105.089881803614));
#94918=CARTESIAN_POINT('Ctrl Pts',(-190.419875471187,49.2494562758818,106.023570052378));
#94919=CARTESIAN_POINT('Ctrl Pts',(-190.48093224589,50.2104897205784,106.122573675973));
#94920=CARTESIAN_POINT('Ctrl Pts',(-190.480254718442,51.1734947861719,106.22126805386));
#94921=CARTESIAN_POINT('Ctrl Pts',(-190.402769507585,48.9964283476031,106.575456298919));
#94922=CARTESIAN_POINT('Ctrl Pts',(-190.477173973333,50.0559837220552,106.682014500456));
#94923=CARTESIAN_POINT('Ctrl Pts',(-190.476388550459,51.1181863857103,106.788162672421));
#94924=CARTESIAN_POINT('Ctrl Pts',(-190.363099295219,48.4854361039805,107.679453599572));
#94925=CARTESIAN_POINT('Ctrl Pts',(-190.46877721616,49.7454964240051,107.802071096718));
#94926=CARTESIAN_POINT('Ctrl Pts',(-190.467733478659,51.0100384384107,107.924109474718));
#94927=CARTESIAN_POINT('Ctrl Pts',(-190.340537373167,48.2278592407325,108.231574631801));
#94928=CARTESIAN_POINT('Ctrl Pts',(-190.464138162999,49.5897493763273,108.36274109052));
#94929=CARTESIAN_POINT('Ctrl Pts',(-190.462944593205,50.9573036985215,108.493171689549));
#94930=CARTESIAN_POINT('Ctrl Pts',(-190.262632780692,47.4366289996939,109.888091607918));
#94931=CARTESIAN_POINT('Ctrl Pts',(-190.448733141734,49.1135245761933,110.046748125528));
#94932=CARTESIAN_POINT('Ctrl Pts',(-190.447010747744,50.8008981564959,110.203650811467));
#94933=CARTESIAN_POINT('Ctrl Pts',(-190.197333416625,46.8843769038143,110.992633024223));
#94934=CARTESIAN_POINT('Ctrl Pts',(-190.436483465423,48.7840526999304,111.171862472543));
#94935=CARTESIAN_POINT('Ctrl Pts',(-190.434305733042,50.6989369523421,111.34834113016));
#94936=CARTESIAN_POINT('Ctrl Pts',(-190.024035203772,45.6901117243083,113.201763481001));
#94937=CARTESIAN_POINT('Ctrl Pts',(-190.40704122806,48.0776487632177,113.426803183689));
#94938=CARTESIAN_POINT('Ctrl Pts',(-190.403599601366,50.4961283561593,113.647636636137));
#94939=CARTESIAN_POINT('Ctrl Pts',(-189.916118308262,45.0481787304179,114.306444419514));
#94940=CARTESIAN_POINT('Ctrl Pts',(-190.389831561577,47.7005628031284,114.557490865841));
#94941=CARTESIAN_POINT('Ctrl Pts',(-190.385599241613,50.3954125375369,114.802333478777));
#94942=CARTESIAN_POINT('Ctrl Pts',(-189.632120997169,43.6438029112513,116.515418563294));
#94943=CARTESIAN_POINT('Ctrl Pts',(-190.349296245468,46.8797597830052,116.824076695157));
#94944=CARTESIAN_POINT('Ctrl Pts',(-190.342926802733,50.1951730686192,117.12309103697));
#94945=CARTESIAN_POINT('Ctrl Pts',(-189.455515647208,42.8796590900541,117.619682593116));
#94946=CARTESIAN_POINT('Ctrl Pts',(-190.325937170929,46.4346322736547,117.961190795854));
#94947=CARTESIAN_POINT('Ctrl Pts',(-190.318259073436,50.0957162763353,118.289113661344));
#94948=CARTESIAN_POINT('Ctrl Pts',(-189.002145676919,41.2276412744401,119.827671012508));
#94949=CARTESIAN_POINT('Ctrl Pts',(-190.271688789567,45.4690939131192,120.241849554135));
#94950=CARTESIAN_POINT('Ctrl Pts',(-190.260543746634,49.8985024053798,120.634770552665));
#94951=CARTESIAN_POINT('Ctrl Pts',(-188.723384078107,40.3379738271532,120.931404423614));
#94952=CARTESIAN_POINT('Ctrl Pts',(-190.240733969511,44.9465217448158,121.387150250019));
#94953=CARTESIAN_POINT('Ctrl Pts',(-190.227500694656,49.800817210661,121.814404993884));
#94954=CARTESIAN_POINT('Ctrl Pts',(-188.06484104112,38.5294426245587,123.138051727137));
#94955=CARTESIAN_POINT('Ctrl Pts',(-190.169533062177,43.8657138954457,123.686077965342));
#94956=CARTESIAN_POINT('Ctrl Pts',(-190.150875780102,49.6062079663902,124.190105192337));
#94957=CARTESIAN_POINT('Ctrl Pts',(-187.68678109675,37.6174522484167,124.240963108104));
#94958=CARTESIAN_POINT('Ctrl Pts',(-190.129193199196,43.3099745219927,124.841340387957));
#94959=CARTESIAN_POINT('Ctrl Pts',(-190.10730109644,49.5092579859229,125.38615523586));
#94960=CARTESIAN_POINT('Ctrl Pts',(-186.887860552158,35.8988473048903,126.445328122734));
#94961=CARTESIAN_POINT('Ctrl Pts',(-190.036990023442,42.2318697577437,127.162839519027));
#94962=CARTESIAN_POINT('Ctrl Pts',(-190.006839455965,49.312572598589,127.798107978239));
#94963=CARTESIAN_POINT('Ctrl Pts',(-186.468827260737,35.0921688914378,127.546773447421));
#94964=CARTESIAN_POINT('Ctrl Pts',(-189.985031715257,41.709649458652,128.329913067888));
#94965=CARTESIAN_POINT('Ctrl Pts',(-189.94996479732,49.2127662094606,129.013981648704));
#94966=CARTESIAN_POINT('Ctrl Pts',(-185.622971106415,33.5951852320465,129.74743532292));
#94967=CARTESIAN_POINT('Ctrl Pts',(-189.866769695801,40.7086313682495,130.678624682498));
#94968=CARTESIAN_POINT('Ctrl Pts',(-189.819235897465,49.0062073327181,131.470286553815));
#94969=CARTESIAN_POINT('Ctrl Pts',(-185.195344088968,32.9022054207578,130.846652192156));
#94970=CARTESIAN_POINT('Ctrl Pts',(-189.800375510914,40.2286538411534,131.860497562516));
#94971=CARTESIAN_POINT('Ctrl Pts',(-189.745402573328,48.8994524120374,132.710684641086));
#94972=CARTESIAN_POINT('Ctrl Pts',(-184.332316899999,31.5951495873319,133.042097933749));
#94973=CARTESIAN_POINT('Ctrl Pts',(-189.649582724457,39.2936837439378,134.243547879917));
#94974=CARTESIAN_POINT('Ctrl Pts',(-189.575717682786,48.6755045049199,135.222940428359));
#94975=CARTESIAN_POINT('Ctrl Pts',(-183.896498248529,30.9805270643031,134.138330157969));
#94976=CARTESIAN_POINT('Ctrl Pts',(-189.56508157479,38.8385274591103,135.444827376579));
#94977=CARTESIAN_POINT('Ctrl Pts',(-189.479904579247,48.5583284722341,136.494741229239));
#94978=CARTESIAN_POINT('Ctrl Pts',(-183.007879854772,29.7992916323161,136.326983635148));
#94979=CARTESIAN_POINT('Ctrl Pts',(-189.373108647856,37.9355866103639,137.873607563424));
#94980=CARTESIAN_POINT('Ctrl Pts',(-189.259006538894,48.3103221431259,139.080158339632));
#94981=CARTESIAN_POINT('Ctrl Pts',(-182.555006195201,29.2327350916608,137.419409487353));
#94982=CARTESIAN_POINT('Ctrl Pts',(-189.265506543082,37.4878383145516,139.101327514706));
#94983=CARTESIAN_POINT('Ctrl Pts',(-189.13399969732,48.1795106830979,140.393659401794));
#94984=CARTESIAN_POINT('Ctrl Pts',(-181.620484012305,28.1255995839538,139.599441768215));
#94985=CARTESIAN_POINT('Ctrl Pts',(-189.02019842515,36.5848378699127,141.594013188396));
#94986=CARTESIAN_POINT('Ctrl Pts',(-188.843611611567,47.9007227666897,143.078697426969));
#94987=CARTESIAN_POINT('Ctrl Pts',(-181.138886935942,27.5851446107169,140.687055901723));
#94988=CARTESIAN_POINT('Ctrl Pts',(-188.882324844217,36.1295124585929,142.859405486123));
#94989=CARTESIAN_POINT('Ctrl Pts',(-188.678410370255,47.7527728507809,144.449973724618));
#94990=CARTESIAN_POINT('Ctrl Pts',(-180.132246584594,26.5129406317024,142.856096076585));
#94991=CARTESIAN_POINT('Ctrl Pts',(-188.565410200897,35.1965622431075,145.446412027918));
#94992=CARTESIAN_POINT('Ctrl Pts',(-188.289138096809,47.4352589096868,147.277825831555));
#94993=CARTESIAN_POINT('Ctrl Pts',(-179.607362760168,25.9813342957967,143.937538719537));
#94994=CARTESIAN_POINT('Ctrl Pts',(-188.386181827197,34.7187059931883,146.768668767197));
#94995=CARTESIAN_POINT('Ctrl Pts',(-188.06556355209,47.2657487316501,148.733707236845));
#94996=CARTESIAN_POINT('Ctrl Pts',(-178.771977332917,25.1780519636145,145.553513839897));
#94997=CARTESIAN_POINT('Ctrl Pts',(-188.072685289982,33.9724700260299,148.817294700524));
#94998=CARTESIAN_POINT('Ctrl Pts',(-187.659901468284,46.9904063042588,151.019801324971));
#94999=CARTESIAN_POINT('Ctrl Pts',(-178.485447212846,24.909306929138,146.091134114406));
#95000=CARTESIAN_POINT('Ctrl Pts',(-187.960223656828,33.717865232546,149.513668849716));
#95001=CARTESIAN_POINT('Ctrl Pts',(-187.512808021989,46.8950932019447,151.799103801632));
#95002=CARTESIAN_POINT('Ctrl Pts',(-177.89247216804,24.3673914569808,147.163909925698));
#95003=CARTESIAN_POINT('Ctrl Pts',(-187.7158093276,33.1945722270689,150.938584532678));
#95004=CARTESIAN_POINT('Ctrl Pts',(-187.186802763605,46.69618951942,153.40385117349));
#95005=CARTESIAN_POINT('Ctrl Pts',(-177.586052240338,24.0942352060037,147.69906801671));
#95006=CARTESIAN_POINT('Ctrl Pts',(-187.583772753384,32.9257648233002,151.667406988934));
#95007=CARTESIAN_POINT('Ctrl Pts',(-187.008003041589,46.5926072881889,154.229151155406));
#95008=CARTESIAN_POINT('Ctrl Pts',(-176.948143217813,23.5404470288426,148.766384943322));
#95009=CARTESIAN_POINT('Ctrl Pts',(-187.293812193883,32.3688904562231,153.170780717094));
#95010=CARTESIAN_POINT('Ctrl Pts',(-186.605647008022,46.3754949682409,155.944107159623));
#95011=CARTESIAN_POINT('Ctrl Pts',(-176.616706877241,23.2598444410281,149.298549155497));
#95012=CARTESIAN_POINT('Ctrl Pts',(-187.135798229102,32.0806671907642,153.945676070019));
#95013=CARTESIAN_POINT('Ctrl Pts',(-186.382371628933,46.2619825739634,156.833415590026));
#95014=CARTESIAN_POINT('Ctrl Pts',(-175.921123207185,22.68689689322,150.359084407924));
#95015=CARTESIAN_POINT('Ctrl Pts',(-186.78295328971,31.4765317295405,155.56522059985));
#95016=CARTESIAN_POINT('Ctrl Pts',(-185.86783817509,46.0225121039273,158.708068090631));
#95017=CARTESIAN_POINT('Ctrl Pts',(-175.556345307998,22.3940330134238,150.888497532651));
#95018=CARTESIAN_POINT('Ctrl Pts',(-186.58766639389,31.1597913758803,156.411907710318));
#95019=CARTESIAN_POINT('Ctrl Pts',(-185.576751299258,45.8963336811167,159.694503161785));
#95020=CARTESIAN_POINT('Ctrl Pts',(-174.977689406787,21.9427305260402,151.675396018314));
#95021=CARTESIAN_POINT('Ctrl Pts',(-186.252891316275,30.6548993698614,157.762856154212));
#95022=CARTESIAN_POINT('Ctrl Pts',(-185.055116025266,45.6954835717082,161.286489264472));
#95023=CARTESIAN_POINT('Ctrl Pts',(-174.780131262563,21.7907501675503,151.935659078575));
#95024=CARTESIAN_POINT('Ctrl Pts',(-186.134203124744,30.4815764712039,158.226875047));
#95025=CARTESIAN_POINT('Ctrl Pts',(-184.86739764927,45.6268041466984,161.834467135961));
#95026=CARTESIAN_POINT('Ctrl Pts',(-174.373917956148,21.4827711935778,152.451438547147));
#95027=CARTESIAN_POINT('Ctrl Pts',(-185.878705051747,30.122557034981,159.190342309378));
#95028=CARTESIAN_POINT('Ctrl Pts',(-184.453669466243,45.4854241746709,162.977435749436));
#95029=CARTESIAN_POINT('Ctrl Pts',(-174.165275538502,21.3267796903352,152.706959670213));
#95030=CARTESIAN_POINT('Ctrl Pts',(-185.741837597343,29.9367780900454,159.689993905649));
#95031=CARTESIAN_POINT('Ctrl Pts',(-184.227834488115,45.4127279366936,163.57226076685));
#95032=CARTESIAN_POINT('Ctrl Pts',(-173.734439484061,21.0094771153743,153.212317702731));
#95033=CARTESIAN_POINT('Ctrl Pts',(-185.442647757005,29.5479163706511,160.741061501243));
#95034=CARTESIAN_POINT('Ctrl Pts',(-183.720111579081,45.2625191728524,164.828753901589));
#95035=CARTESIAN_POINT('Ctrl Pts',(-173.512272690491,20.8481811116799,153.462164515318));
#95036=CARTESIAN_POINT('Ctrl Pts',(-185.280285255813,29.3447366612225,161.292714722918));
#95037=CARTESIAN_POINT('Ctrl Pts',(-183.438667186176,45.1850157200236,165.490044607484));
#95038=CARTESIAN_POINT('Ctrl Pts',(-173.050663888627,20.5182754311735,153.954763169577));
#95039=CARTESIAN_POINT('Ctrl Pts',(-184.916469656588,28.912060268967,162.477578251216));
#95040=CARTESIAN_POINT('Ctrl Pts',(-182.786281071338,45.0239741908854,166.914420710284));
#95041=CARTESIAN_POINT('Ctrl Pts',(-172.811285296472,20.3497013053525,154.197538421658));
#95042=CARTESIAN_POINT('Ctrl Pts',(-184.715109947839,28.6824943845155,163.111019415201));
#95043=CARTESIAN_POINT('Ctrl Pts',(-182.416611477759,44.9404575123914,167.676642584149));
#95044=CARTESIAN_POINT('Ctrl Pts',(-172.309018538915,20.0018559561541,154.673652378991));
#95045=CARTESIAN_POINT('Ctrl Pts',(-184.243978355941,28.1780553452027,164.520194582625));
#95046=CARTESIAN_POINT('Ctrl Pts',(-181.515829713772,44.7653314719405,169.370362068887));
#95047=CARTESIAN_POINT('Ctrl Pts',(-172.045925480568,19.8224282462785,154.907331215004));
#95048=CARTESIAN_POINT('Ctrl Pts',(-183.974169315528,27.9027184380179,165.298511579777));
#95049=CARTESIAN_POINT('Ctrl Pts',(-180.986839328195,44.6736488797049,170.303040533204));
#95050=CARTESIAN_POINT('Ctrl Pts',(-171.625945202672,19.5411769387697,155.246607689634));
#95051=CARTESIAN_POINT('Ctrl Pts',(-183.465863550883,27.423666236785,166.663047270596));
#95052=CARTESIAN_POINT('Ctrl Pts',(-179.945305056306,44.5275110953375,171.919856198926));
#95053=CARTESIAN_POINT('Ctrl Pts',(-171.482771006779,19.4461136400241,155.356899985026));
#95054=CARTESIAN_POINT('Ctrl Pts',(-183.278745110663,27.2528822960182,167.15099067036));
#95055=CARTESIAN_POINT('Ctrl Pts',(-179.557764749393,44.4777268164602,172.491992949612));
#95056=CARTESIAN_POINT('Ctrl Pts',(-171.188847173927,19.2527442241094,155.570893173036));
#95057=CARTESIAN_POINT('Ctrl Pts',(-182.858413959778,26.8834361487309,168.198730392038));
#95058=CARTESIAN_POINT('Ctrl Pts',(-178.678365949149,44.3756234802552,173.702488528128));
#95059=CARTESIAN_POINT('Ctrl Pts',(-171.038069041094,19.154419880975,155.674573264278));
#95060=CARTESIAN_POINT('Ctrl Pts',(-182.623941443772,26.6839205445033,168.761056756381));
#95061=CARTESIAN_POINT('Ctrl Pts',(-178.184545903382,44.3232947364561,174.342353684468));
#95062=CARTESIAN_POINT('Ctrl Pts',(-170.727951753196,18.9541141206573,155.874480212679));
#95063=CARTESIAN_POINT('Ctrl Pts',(-182.106163264014,26.2568588794142,169.929834066643));
#95064=CARTESIAN_POINT('Ctrl Pts',(-177.102347209724,44.2157955625374,175.639812340165));
#95065=CARTESIAN_POINT('Ctrl Pts',(-170.568582074872,18.8521156515048,155.970683147523));
#95066=CARTESIAN_POINT('Ctrl Pts',(-181.82239246479,26.0290489673764,170.535242403614));
#95067=CARTESIAN_POINT('Ctrl Pts',(-176.51488906461,44.1606146875356,176.294574849227));
#95068=CARTESIAN_POINT('Ctrl Pts',(-170.241606120522,18.6449123730739,156.155713131299));
#95069=CARTESIAN_POINT('Ctrl Pts',(-181.232293959555,25.5638692026676,171.70630221824));
#95070=CARTESIAN_POINT('Ctrl Pts',(-175.330183039519,44.0475587900912,177.520910260544));
#95071=CARTESIAN_POINT('Ctrl Pts',(-170.07403552873,18.5397328103892,156.244564605491));
#95072=CARTESIAN_POINT('Ctrl Pts',(-180.927197004254,25.3273242564655,172.269015371745));
#95073=CARTESIAN_POINT('Ctrl Pts',(-174.736536607708,43.9896960337974,178.090041787821));
#95074=CARTESIAN_POINT('Ctrl Pts',(-169.732361483832,18.3274378186121,156.416018514887));
#95075=CARTESIAN_POINT('Ctrl Pts',(-180.322025264393,24.8627580474761,173.309162198402));
#95076=CARTESIAN_POINT('Ctrl Pts',(-173.607575117574,43.8719040042023,179.109193252876));
#95077=CARTESIAN_POINT('Ctrl Pts',(-169.558289763168,18.2203422570752,156.49864439362));
#95078=CARTESIAN_POINT('Ctrl Pts',(-180.021949930072,24.6347745292575,173.787216467402));
#95079=CARTESIAN_POINT('Ctrl Pts',(-173.071167892211,43.8119858594125,179.561393389303));
#95080=CARTESIAN_POINT('Ctrl Pts',(-169.20537587151,18.0054276813585,156.658881832012));
#95081=CARTESIAN_POINT('Ctrl Pts',(-179.433143561921,24.1912128908626,174.668691448684));
#95082=CARTESIAN_POINT('Ctrl Pts',(-172.061207809833,43.6907330173011,180.372779053295));
#95083=CARTESIAN_POINT('Ctrl Pts',(-169.026537105077,17.8976098204552,156.736496564402));
#95084=CARTESIAN_POINT('Ctrl Pts',(-179.144397687481,23.9756821774116,175.072075935675));
#95085=CARTESIAN_POINT('Ctrl Pts',(-171.586680536841,43.6293995460746,180.732834377098));
#95086=CARTESIAN_POINT('Ctrl Pts',(-168.48479752681,17.5743365828396,156.96321970107));
#95087=CARTESIAN_POINT('Ctrl Pts',(-178.29068744621,23.344281769509,176.201380676567));
#95088=CARTESIAN_POINT('Ctrl Pts',(-170.238369313117,43.4439993478709,181.715166341082));
#95089=CARTESIAN_POINT('Ctrl Pts',(-168.119950530228,17.3610377067902,157.104986914531));
#95090=CARTESIAN_POINT('Ctrl Pts',(-177.749090613288,22.951799353339,176.832994154249));
#95091=CARTESIAN_POINT('Ctrl Pts',(-169.445239878046,43.3196577793825,182.237721038455));
#95092=CARTESIAN_POINT('Ctrl Pts',(-167.391270115551,16.9433709217743,157.374360062321));
#95093=CARTESIAN_POINT('Ctrl Pts',(-176.699191958229,22.206366498613,177.96534356467));
#95094=CARTESIAN_POINT('Ctrl Pts',(-167.986743550946,43.0725588756287,183.147764868599));
#95095=CARTESIAN_POINT('Ctrl Pts',(-167.026606688627,16.7384994826158,157.502198040807));
#95096=CARTESIAN_POINT('Ctrl Pts',(-176.191279038635,21.8538198757381,178.463340366889));
#95097=CARTESIAN_POINT('Ctrl Pts',(-167.320397138975,42.9495163323862,183.534097905677));
#95098=CARTESIAN_POINT('Ctrl Pts',(-166.298120791151,16.3369438280935,157.747661911419));
#95099=CARTESIAN_POINT('Ctrl Pts',(-175.195015680742,21.1770552515635,179.377764246932));
#95100=CARTESIAN_POINT('Ctrl Pts',(-166.064733590356,42.7050918843688,184.228282962997));
#95101=CARTESIAN_POINT('Ctrl Pts',(-165.934275361887,16.1402438203051,157.865253806892));
#95102=CARTESIAN_POINT('Ctrl Pts',(-174.707713182136,20.8536655692418,179.792126024603));
#95103=CARTESIAN_POINT('Ctrl Pts',(-165.475999358049,42.5837015136963,184.535227655678));
#95104=CARTESIAN_POINT('Ctrl Pts',(-165.208022298475,15.7547762879034,158.092246123888));
#95105=CARTESIAN_POINT('Ctrl Pts',(-173.746828237938,20.229692948097,180.563630707583));
#95106=CARTESIAN_POINT('Ctrl Pts',(-164.350718159951,42.3428835648365,185.097515905741));
#95107=CARTESIAN_POINT('Ctrl Pts',(-164.845605266082,15.5660026353619,158.201632183931));
#95108=CARTESIAN_POINT('Ctrl Pts',(-173.273911339772,19.9296328625437,180.919710822024));
#95109=CARTESIAN_POINT('Ctrl Pts',(-163.81441996652,42.2234523785788,185.352529880529));
#95110=CARTESIAN_POINT('Ctrl Pts',(-163.760868033552,15.0109620114243,158.519528866614));
#95111=CARTESIAN_POINT('Ctrl Pts',(-171.867024170727,19.0559076974448,181.926432993042));
#95112=CARTESIAN_POINT('Ctrl Pts',(-162.261759601125,41.8683318500525,186.062918065107));
#95113=CARTESIAN_POINT('Ctrl Pts',(-163.041094616692,14.6559663241023,158.717878535442));
#95114=CARTESIAN_POINT('Ctrl Pts',(-170.954197690537,18.5147147268493,182.508909839269));
#95115=CARTESIAN_POINT('Ctrl Pts',(-161.300437601311,41.6358321593886,186.464837080218));
#95116=CARTESIAN_POINT('Ctrl Pts',(-161.608449841267,13.9724013655304,159.09418397859));
#95117=CARTESIAN_POINT('Ctrl Pts',(-169.153718088121,17.4887166685363,183.570253534368));
#95118=CARTESIAN_POINT('Ctrl Pts',(-159.461971844518,41.1797152854594,187.187814858497));
#95119=CARTESIAN_POINT('Ctrl Pts',(-160.895540391279,13.6438160922004,159.272068429678));
#95120=CARTESIAN_POINT('Ctrl Pts',(-168.268459650413,17.0057013714701,184.04599417238));
#95121=CARTESIAN_POINT('Ctrl Pts',(-158.585843562126,40.9560813261876,187.507754562274));
#95122=CARTESIAN_POINT('Ctrl Pts',(-159.475832904077,13.009713555937,159.61133763757));
#95123=CARTESIAN_POINT('Ctrl Pts',(-166.517450272312,16.0855401228304,184.923294929289));
#95124=CARTESIAN_POINT('Ctrl Pts',(-156.888768072043,40.5175628988981,188.093656406087));
#95125=CARTESIAN_POINT('Ctrl Pts',(-158.768161459745,12.7038561024453,159.772867963314));
#95126=CARTESIAN_POINT('Ctrl Pts',(-165.652176896289,15.6489979847093,185.323724854997));
#95127=CARTESIAN_POINT('Ctrl Pts',(-156.067224181849,40.30242287474,188.359519533784));
#95128=CARTESIAN_POINT('Ctrl Pts',(-157.366637414052,12.1159235889831,160.080243562044));
#95129=CARTESIAN_POINT('Ctrl Pts',(-163.948110086599,14.8191886550039,186.064138967974));
#95130=CARTESIAN_POINT('Ctrl Pts',(-154.472181220503,39.8831463972658,188.849648065907));
#95131=CARTESIAN_POINT('Ctrl Pts',(-156.671806181714,11.8333912668499,160.226325665881));
#95132=CARTESIAN_POINT('Ctrl Pts',(-163.109179654483,14.4259531767049,186.40392320471));
#95133=CARTESIAN_POINT('Ctrl Pts',(-153.697617035838,39.6786970852446,189.074223406174));
#95134=CARTESIAN_POINT('Ctrl Pts',(-154.602353948334,11.0153977851208,160.645385145478));
#95135=CARTESIAN_POINT('Ctrl Pts',(-160.617480990202,13.2962599683315,187.356762363426));
#95136=CARTESIAN_POINT('Ctrl Pts',(-151.424212839044,39.079703876623,189.702420218299));
#95137=CARTESIAN_POINT('Ctrl Pts',(-153.242645750871,10.5093218873485,160.899346226424));
#95138=CARTESIAN_POINT('Ctrl Pts',(-159.004438990581,12.616621750998,187.897831581203));
#95139=CARTESIAN_POINT('Ctrl Pts',(-149.974679379033,38.6994698247911,190.061332929028));
#95140=CARTESIAN_POINT('Ctrl Pts',(-150.552367945823,9.55775821321174,161.369122024951));
#95141=CARTESIAN_POINT('Ctrl Pts',(-155.83710947237,11.3572417479211,188.864442741271));
#95142=CARTESIAN_POINT('Ctrl Pts',(-147.153418928472,37.9718709822992,190.705208506625));
#95143=CARTESIAN_POINT('Ctrl Pts',(-149.221854956537,9.11237711894784,161.584828734122));
#95144=CARTESIAN_POINT('Ctrl Pts',(-154.286803188465,10.7798696037116,189.287290737056));
#95145=CARTESIAN_POINT('Ctrl Pts',(-145.782463563151,37.6245184723861,190.989493670861));
#95146=CARTESIAN_POINT('Ctrl Pts',(-146.582857115906,8.27040425016005,161.985922311379));
#95147=CARTESIAN_POINT('Ctrl Pts',(-151.233794084843,9.7025332564364,190.050527735751));
#95148=CARTESIAN_POINT('Ctrl Pts',(-143.091958400352,36.9585685878482,191.506211581955));
#95149=CARTESIAN_POINT('Ctrl Pts',(-145.274405011894,7.87386890592969,162.171263429212));
#95150=CARTESIAN_POINT('Ctrl Pts',(-149.733537694999,9.2038575210509,190.389647349539));
#95151=CARTESIAN_POINT('Ctrl Pts',(-141.77268701756,36.6399800572188,191.738407898794));
#95152=CARTESIAN_POINT('Ctrl Pts',(-142.67454674327,7.12121869547241,162.517120670501));
#95153=CARTESIAN_POINT('Ctrl Pts',(-146.772252351223,8.26827178830752,191.00646086707));
#95154=CARTESIAN_POINT('Ctrl Pts',(-139.169890034152,36.0282859548994,192.16423420799));
#95155=CARTESIAN_POINT('Ctrl Pts',(-141.383159986701,6.76513568801358,162.677614078792));
#95156=CARTESIAN_POINT('Ctrl Pts',(-145.312838364958,7.83212105280727,191.283481494081));
#95157=CARTESIAN_POINT('Ctrl Pts',(-137.886484698437,35.7351864115571,192.357764299665));
#95158=CARTESIAN_POINT('Ctrl Pts',(-137.52916857534,5.74824757347732,163.127966083129));
#95159=CARTESIAN_POINT('Ctrl Pts',(-140.977953290624,6.59772745373911,192.044692926872));
#95160=CARTESIAN_POINT('Ctrl Pts',(-134.074948396479,34.8901222694588,192.893480588533));
#95161=CARTESIAN_POINT('Ctrl Pts',(-134.986444518518,5.1383515380875,163.386981976694));
#95162=CARTESIAN_POINT('Ctrl Pts',(-138.162497251024,5.87806901503397,192.456640771667));
#95163=CARTESIAN_POINT('Ctrl Pts',(-131.584657294362,34.3722288222929,193.191471577095));
#95164=CARTESIAN_POINT('Ctrl Pts',(-129.935383900544,4.02085867614368,163.845181682642));
#95165=CARTESIAN_POINT('Ctrl Pts',(-132.620396885526,4.57771828187325,193.164571707407));
#95166=CARTESIAN_POINT('Ctrl Pts',(-126.659823795758,33.4111402621432,193.710740918262));
#95167=CARTESIAN_POINT('Ctrl Pts',(-127.424374444051,3.51309267049032,164.044346664358));
#95168=CARTESIAN_POINT('Ctrl Pts',(-129.895918979684,3.99874755408819,193.458855240834));
#95169=CARTESIAN_POINT('Ctrl Pts',(-124.223164579543,32.9676271892553,193.931671784718));
#95170=CARTESIAN_POINT('Ctrl Pts',(-122.457511674559,2.58424517009923,164.395361452057));
#95171=CARTESIAN_POINT('Ctrl Pts',(-124.546807846014,2.95145956830643,193.965517338237));
#95172=CARTESIAN_POINT('Ctrl Pts',(-119.413835209996,32.1484825663496,194.31696041224));
#95173=CARTESIAN_POINT('Ctrl Pts',(-119.997764986607,2.16231324461259,164.547549718778));
#95174=CARTESIAN_POINT('Ctrl Pts',(-121.920684619804,2.48302644750518,194.177754122744));
#95175=CARTESIAN_POINT('Ctrl Pts',(-117.037520550194,31.7720605896045,194.481596153228));
#95176=CARTESIAN_POINT('Ctrl Pts',(-115.113796886312,1.38623409901235,164.816743346736));
#95177=CARTESIAN_POINT('Ctrl Pts',(-116.737508908147,1.62907241709631,194.546134226495));
#95178=CARTESIAN_POINT('Ctrl Pts',(-112.323537492297,31.07452765352,194.770608310854));
#95179=CARTESIAN_POINT('Ctrl Pts',(-112.689642445873,1.03217190481425,164.933695702807));
#95180=CARTESIAN_POINT('Ctrl Pts',(-114.182223627302,1.24409699109422,194.701890597857));
#95181=CARTESIAN_POINT('Ctrl Pts',(-109.986006545736,30.7534547062723,194.89488035781));
#95182=CARTESIAN_POINT('Ctrl Pts',(-105.458748863613,0.0537109949632699,
165.243789332008));
#95183=CARTESIAN_POINT('Ctrl Pts',(-106.593713186433,0.187356491350593,
195.108680154073));
#95184=CARTESIAN_POINT('Ctrl Pts',(-103.014954688006,29.8608768518165,195.222527902486));
#95185=CARTESIAN_POINT('Ctrl Pts',(-100.692926996796,-0.487837340122015,
165.396788055826));
#95186=CARTESIAN_POINT('Ctrl Pts',(-101.648242750641,-0.385696025224757,
195.2997496196));
#95187=CARTESIAN_POINT('Ctrl Pts',(-98.4220441742718,29.3594587157306,195.381539694843));
#95188=CARTESIAN_POINT('Ctrl Pts',(-91.2328687780407,-1.41275722738798,
165.637152647262));
#95189=CARTESIAN_POINT('Ctrl Pts',(-91.8896160224937,-1.35729231567298,
195.595521040211));
#95190=CARTESIAN_POINT('Ctrl Pts',(-89.2957519395693,28.4971764608672,195.630229860082));
#95191=CARTESIAN_POINT('Ctrl Pts',(-86.5390573445431,-1.79556727823837,
165.724146017721));
#95192=CARTESIAN_POINT('Ctrl Pts',(-87.0809543903837,-1.7543127179252,195.699017410214));
#95193=CARTESIAN_POINT('Ctrl Pts',(-84.7630722941598,28.1366238331763,195.719348296838));
#95194=CARTESIAN_POINT('Ctrl Pts',(-77.2034000845379,-2.44180831978024,
165.856868653474));
#95195=CARTESIAN_POINT('Ctrl Pts',(-77.5561948922658,-2.42113102767928,
195.855280888841));
#95196=CARTESIAN_POINT('Ctrl Pts',(-75.7339440753839,27.524859474872,195.854930954148));
#95197=CARTESIAN_POINT('Ctrl Pts',(-72.5617270997191,-2.70499078515223,
165.902429251621));
#95198=CARTESIAN_POINT('Ctrl Pts',(-72.8420539091534,-2.69036081274705,
195.90761787253));
#95199=CARTESIAN_POINT('Ctrl Pts',(-71.2377602240549,27.2738023676749,195.901170564023));
#95200=CARTESIAN_POINT('Ctrl Pts',(-63.3192368021652,-3.13951331323087,
165.968086174843));
#95201=CARTESIAN_POINT('Ctrl Pts',(-63.4824566004367,-3.13329077685642,
195.982573684347));
#95202=CARTESIAN_POINT('Ctrl Pts',(-62.2685467898851,26.8576621150016,195.967694278259));
#95203=CARTESIAN_POINT('Ctrl Pts',(-58.7184924969416,-3.31072222891366,
165.988096029799));
#95204=CARTESIAN_POINT('Ctrl Pts',(-58.8378802767016,-3.30674675640559,
196.005013040848));
#95205=CARTESIAN_POINT('Ctrl Pts',(-57.7956329921226,26.6926696350143,195.987872556486));
#95206=CARTESIAN_POINT('Ctrl Pts',(-44.9687962503876,-3.71864843947255,
166.025958285563));
#95207=CARTESIAN_POINT('Ctrl Pts',(-44.9856197745133,-3.71901632940911,
196.04750598918));
#95208=CARTESIAN_POINT('Ctrl Pts',(-44.4000239059869,26.2982864331341,196.026023260468));
#95209=CARTESIAN_POINT('Ctrl Pts',(-35.8704264307398,-3.84988321153493,
166.022565415402));
#95210=CARTESIAN_POINT('Ctrl Pts',(-35.8586554592819,-3.85007352565092,
196.043873063051));
#95211=CARTESIAN_POINT('Ctrl Pts',(-35.4996912577566,26.1694752614148,196.022557099425));
#95212=CARTESIAN_POINT('Ctrl Pts',(-17.7576320506981,-3.97366628546334,
166.00984699518));
#95213=CARTESIAN_POINT('Ctrl Pts',(-17.7264703415601,-3.97376872241134,
196.031052872576));
#95214=CARTESIAN_POINT('Ctrl Pts',(-17.6760420909501,26.0478005878471,196.009824900738));
#95215=CARTESIAN_POINT('Ctrl Pts',(-8.74333296613901,-3.96249962263878,
165.999882631878));
#95216=CARTESIAN_POINT('Ctrl Pts',(-8.72284852848699,-3.96249840284406,
196.020999546301));
#95217=CARTESIAN_POINT('Ctrl Pts',(-8.75350004691697,26.0586067043184,195.999875379291));
#95218=CARTESIAN_POINT('Ctrl Pts',(0.15743830809244,-3.96262988886149,166.00000104579));
#95219=CARTESIAN_POINT('Ctrl Pts',(0.157070562002837,-3.96262989972655,
196.021119017258));
#95220=CARTESIAN_POINT('Ctrl Pts',(0.157610541791236,26.0584806777796,195.999993616651));
#95221=CARTESIAN_POINT('',(1.578508351368E-14,26.0373712544753,196.));
#95222=CARTESIAN_POINT('Origin',(4.15733729152917E-15,26.0373712544753,
166.));
#95223=CARTESIAN_POINT('Ctrl Pts',(-190.499797482064,51.8013867006572,102.335336081498));
#95224=CARTESIAN_POINT('Ctrl Pts',(-190.499797482064,51.7796732650764,102.335336081498));
#95225=CARTESIAN_POINT('Ctrl Pts',(-190.499735682025,51.7624009619146,102.352155239618));
#95226=CARTESIAN_POINT('Ctrl Pts',(-190.499673388249,51.7493947125939,102.369009004064));
#95227=CARTESIAN_POINT('Ctrl Pts',(-190.499611094472,51.7363884632733,102.38586276851));
#95228=CARTESIAN_POINT('Ctrl Pts',(-190.499541046104,51.7261944008059,102.404734768362));
#95229=CARTESIAN_POINT('Ctrl Pts',(-190.499469961948,51.7170974306138,102.423784057877));
#95230=CARTESIAN_POINT('Ctrl Pts',(-190.499327793636,51.6989034902297,102.461882636908));
#95231=CARTESIAN_POINT('Ctrl Pts',(-190.499176806309,51.684877084871,102.50195510353));
#95232=CARTESIAN_POINT('Ctrl Pts',(-190.499023050416,51.6721578498453,102.542322989557));
#95233=CARTESIAN_POINT('Ctrl Pts',(-190.498715538629,51.6467193797941,102.62305876161));
#95234=CARTESIAN_POINT('Ctrl Pts',(-190.498396552736,51.627122398088,102.70511271305));
#95235=CARTESIAN_POINT('Ctrl Pts',(-190.498069248062,51.6091555610353,102.78753449951));
#95236=CARTESIAN_POINT('Ctrl Pts',(-190.497414638714,51.5732218869298,102.95237807243));
#95237=CARTESIAN_POINT('Ctrl Pts',(-190.496725517573,51.5447751841326,103.119010291625));
#95238=CARTESIAN_POINT('Ctrl Pts',(-190.496006633022,51.5184793922393,103.285777971499));
#95239=CARTESIAN_POINT('Ctrl Pts',(-190.49456886392,51.4658878084526,103.619313331245));
#95240=CARTESIAN_POINT('Ctrl Pts',(-190.493009667524,51.4229821624655,103.954070779999));
#95241=CARTESIAN_POINT('Ctrl Pts',(-190.491322220494,51.3825621856073,104.2891413603));
#95242=CARTESIAN_POINT('Ctrl Pts',(-190.488159741497,51.30681028015,104.917103989015));
#95243=CARTESIAN_POINT('Ctrl Pts',(-190.484546269356,51.2411823737622,105.546379733642));
#95244=CARTESIAN_POINT('Ctrl Pts',(-190.480418712091,51.178146335177,106.175836802634));
#95245=CARTESIAN_POINT('Ctrl Pts',(-190.480141475362,51.1739123769095,106.218115711987));
#95246=CARTESIAN_POINT('Ctrl Pts',(-190.479861919642,51.1696901117017,106.260395458915));
#95247=CARTESIAN_POINT('Ctrl Pts',(-190.479580025962,51.1654772571583,106.302675708929));
#95248=CARTESIAN_POINT('Ctrl Pts',(-190.47255445146,51.0604812053327,107.356417127231));
#95249=CARTESIAN_POINT('Ctrl Pts',(-190.46407790808,50.9625995955066,108.41079436899));
#95250=CARTESIAN_POINT('Ctrl Pts',(-190.453802680175,50.8668358069772,109.465349178475));
#95251=CARTESIAN_POINT('Ctrl Pts',(-190.450977048573,50.8405012877136,109.755345996389));
#95252=CARTESIAN_POINT('Ctrl Pts',(-190.44801515712,50.8143269223293,110.045356058084));
#95253=CARTESIAN_POINT('Ctrl Pts',(-190.444909217821,50.7882088029142,110.335369415777));
#95254=CARTESIAN_POINT('Ctrl Pts',(-190.435051162092,50.7053115367744,111.255853548446));
#95255=CARTESIAN_POINT('Ctrl Pts',(-190.423743516833,50.6233182006791,112.176446285769));
#95256=CARTESIAN_POINT('Ctrl Pts',(-190.410714850994,50.5421480526697,113.097071442683));
#95257=CARTESIAN_POINT('Ctrl Pts',(-190.397868218425,50.4621119937211,114.004833854546));
#95258=CARTESIAN_POINT('Ctrl Pts',(-190.383348467128,50.3828762807955,114.912627713187));
#95259=CARTESIAN_POINT('Ctrl Pts',(-190.366864774591,50.304363509189,115.820340176612));
#95260=CARTESIAN_POINT('Ctrl Pts',(-190.351225118062,50.2298709294274,116.681573854888));
#95261=CARTESIAN_POINT('Ctrl Pts',(-190.333817436516,50.1560291510364,117.542733975473));
#95262=CARTESIAN_POINT('Ctrl Pts',(-190.314365284359,50.0827720612279,118.403691037767));
#95263=CARTESIAN_POINT('Ctrl Pts',(-190.295448100247,50.0115296689136,119.240970282112));
#95264=CARTESIAN_POINT('Ctrl Pts',(-190.274596728903,49.9411985013373,120.078097715621));
#95265=CARTESIAN_POINT('Ctrl Pts',(-190.251524715879,49.8714851641544,120.91505355053));
#95266=CARTESIAN_POINT('Ctrl Pts',(-190.228651418363,49.8023722566437,121.744800820508));
#95267=CARTESIAN_POINT('Ctrl Pts',(-190.203595741332,49.7338665828117,122.574379401192));
#95268=CARTESIAN_POINT('Ctrl Pts',(-190.176046929657,49.665682264082,123.403729980441));
#95269=CARTESIAN_POINT('Ctrl Pts',(-190.148846990024,49.598361416445,124.222577847862));
#95270=CARTESIAN_POINT('Ctrl Pts',(-190.119216815711,49.5313538363069,125.041203389024));
#95271=CARTESIAN_POINT('Ctrl Pts',(-190.086823927838,49.4643843690408,125.859511081624));
#95272=CARTESIAN_POINT('Ctrl Pts',(-190.078849634445,49.4478982137334,126.060957326609));
#95273=CARTESIAN_POINT('Ctrl Pts',(-190.070707749289,49.4314143681323,126.262384127506));
#95274=CARTESIAN_POINT('Ctrl Pts',(-190.062392979207,49.4149287273199,126.463789702368));
#95275=CARTESIAN_POINT('Ctrl Pts',(-190.030547811375,49.3517895192197,127.235163326751));
#95276=CARTESIAN_POINT('Ctrl Pts',(-189.996170659515,49.2883645194752,128.006194734142));
#95277=CARTESIAN_POINT('Ctrl Pts',(-189.958940677373,49.2243050437096,128.776856652747));
#95278=CARTESIAN_POINT('Ctrl Pts',(-189.922052547442,49.1608337732603,129.540442218756));
#95279=CARTESIAN_POINT('Ctrl Pts',(-189.882363909103,49.0967396250354,130.303665012026));
#95280=CARTESIAN_POINT('Ctrl Pts',(-189.839528747592,49.031683431776,131.066460714902));
#95281=CARTESIAN_POINT('Ctrl Pts',(-189.797307015648,48.9675588888477,131.818332648131));
#95282=CARTESIAN_POINT('Ctrl Pts',(-189.752028378616,48.902499657906,132.569789563874));
#95283=CARTESIAN_POINT('Ctrl Pts',(-189.703326084319,48.8361809353554,133.320733846737));
#95284=CARTESIAN_POINT('Ctrl Pts',(-189.677789514313,48.8014073640976,133.714484111013));
#95285=CARTESIAN_POINT('Ctrl Pts',(-189.651311065098,48.7662875174997,134.108092840235));
#95286=CARTESIAN_POINT('Ctrl Pts',(-189.623833678354,48.7307745724516,134.50154201427));
#95287=CARTESIAN_POINT('Ctrl Pts',(-189.575579238559,48.6684084790239,135.19249816881));
#95288=CARTESIAN_POINT('Ctrl Pts',(-189.524246833971,48.6048542762143,135.882953961284));
#95289=CARTESIAN_POINT('Ctrl Pts',(-189.46949371259,48.540048518188,136.572913023358));
#95290=CARTESIAN_POINT('Ctrl Pts',(-189.415263393029,48.4758615480475,137.256284116672));
#95291=CARTESIAN_POINT('Ctrl Pts',(-189.357677536326,48.4104468091526,137.939167882345));
#95292=CARTESIAN_POINT('Ctrl Pts',(-189.2963680754,48.3437426557793,138.62153151236));
#95293=CARTESIAN_POINT('Ctrl Pts',(-189.236051587727,48.2781188485588,139.29284352287));
#95294=CARTESIAN_POINT('Ctrl Pts',(-189.172131261117,48.211247055563,139.963652031237));
#95295=CARTESIAN_POINT('Ctrl Pts',(-189.104220443876,48.1430685780765,140.633891378944));
#95296=CARTESIAN_POINT('Ctrl Pts',(-189.041196215209,48.0797959489164,141.255903005771));
#95297=CARTESIAN_POINT('Ctrl Pts',(-188.974734906569,48.01539791719,141.877424101301));
#95298=CARTESIAN_POINT('Ctrl Pts',(-188.90449721651,47.9498275654531,142.498375722798));
#95299=CARTESIAN_POINT('Ctrl Pts',(-188.834812474735,47.8847734182416,143.114438884366));
#95300=CARTESIAN_POINT('Ctrl Pts',(-188.761413027888,47.8185580207201,143.729925662549));
#95301=CARTESIAN_POINT('Ctrl Pts',(-188.683920571469,47.7512472696655,144.344853949472));
#95302=CARTESIAN_POINT('Ctrl Pts',(-188.607758227294,47.6850918678956,144.949227355559));
#95303=CARTESIAN_POINT('Ctrl Pts',(-188.527642294694,47.6178783920758,145.553061198004));
#95304=CARTESIAN_POINT('Ctrl Pts',(-188.443176958487,47.5496694036548,146.156338077234));
#95305=CARTESIAN_POINT('Ctrl Pts',(-188.359576961453,47.4821592097015,146.753434443376));
#95306=CARTESIAN_POINT('Ctrl Pts',(-188.271716386634,47.41367379652,147.349985158678));
#95307=CARTESIAN_POINT('Ctrl Pts',(-188.179173084183,47.3442738223829,147.945940209406));
#95308=CARTESIAN_POINT('Ctrl Pts',(-188.088056539572,47.275943800955,148.532707306839));
#95309=CARTESIAN_POINT('Ctrl Pts',(-187.992400672799,47.206727201113,149.118896894521));
#95310=CARTESIAN_POINT('Ctrl Pts',(-187.891763054282,47.1366819186201,149.704429809714));
#95311=CARTESIAN_POINT('Ctrl Pts',(-187.849814782888,47.1074852964908,149.948494544136));
#95312=CARTESIAN_POINT('Ctrl Pts',(-187.807000477934,47.078144696512,150.192444812282));
#95313=CARTESIAN_POINT('Ctrl Pts',(-187.763285937964,47.0486643115202,150.436273275158));
#95314=CARTESIAN_POINT('Ctrl Pts',(-187.667271248349,46.9839135440019,150.971818523922));
#95315=CARTESIAN_POINT('Ctrl Pts',(-187.566920476803,46.9184686150377,151.506755633221));
#95316=CARTESIAN_POINT('Ctrl Pts',(-187.461823165435,46.8524910947455,152.041113281851));
#95317=CARTESIAN_POINT('Ctrl Pts',(-187.358729974763,46.7877717123848,152.565281162455));
#95318=CARTESIAN_POINT('Ctrl Pts',(-187.251069644819,46.7225398571991,153.08889138662));
#95319=CARTESIAN_POINT('Ctrl Pts',(-187.138416624462,46.6569480314088,153.611939038436));
#95320=CARTESIAN_POINT('Ctrl Pts',(-187.026967315194,46.5920570621758,154.129397863105));
#95321=CARTESIAN_POINT('Ctrl Pts',(-186.910631597444,46.5268137738982,154.646306033395));
#95322=CARTESIAN_POINT('Ctrl Pts',(-186.788957749885,46.4613658323308,155.162628032045));
#95323=CARTESIAN_POINT('Ctrl Pts',(-186.665654696768,46.3950415467317,155.685863551444));
#95324=CARTESIAN_POINT('Ctrl Pts',(-186.536869956916,46.3285070905597,156.208497179867));
#95325=CARTESIAN_POINT('Ctrl Pts',(-186.402088378624,46.2619161410564,156.730459690725));
#95326=CARTESIAN_POINT('Ctrl Pts',(-186.267306800331,46.1953251915531,157.252422201583));
#95327=CARTESIAN_POINT('Ctrl Pts',(-186.126528666188,46.1286777487184,157.773713602935));
#95328=CARTESIAN_POINT('Ctrl Pts',(-185.979189427949,46.0621274897938,158.294232035195));
#95329=CARTESIAN_POINT('Ctrl Pts',(-185.8628900334,46.0095973225925,158.705093250761));
#95330=CARTESIAN_POINT('Ctrl Pts',(-185.742356438997,45.957106091155,159.115969231144));
#95331=CARTESIAN_POINT('Ctrl Pts',(-185.617482356425,45.9048666497495,159.526097415001));
#95332=CARTESIAN_POINT('Ctrl Pts',(-185.493615974712,45.8530487668366,159.932915972755));
#95333=CARTESIAN_POINT('Ctrl Pts',(-185.365478696385,45.8014786265943,160.338998741735));
#95334=CARTESIAN_POINT('Ctrl Pts',(-185.232986637722,45.7503639717296,160.743648602471));
#95335=CARTESIAN_POINT('Ctrl Pts',(-185.101749884476,45.6997336062917,161.14446457937));
#95336=CARTESIAN_POINT('Ctrl Pts',(-184.966240317941,45.649550136062,161.54387469968));
#95337=CARTESIAN_POINT('Ctrl Pts',(-184.826398490639,45.6000154546973,161.941247763602));
#95338=CARTESIAN_POINT('Ctrl Pts',(-184.79886466275,45.5902624400408,162.019487599001));
#95339=CARTESIAN_POINT('Ctrl Pts',(-184.771162960822,45.5805345767976,162.097648608569));
#95340=CARTESIAN_POINT('Ctrl Pts',(-184.743293041545,45.5708334059981,162.175726186804));
#95341=CARTESIAN_POINT('Ctrl Pts',(-184.536768932763,45.4989449432585,162.754303472959));
#95342=CARTESIAN_POINT('Ctrl Pts',(-184.320853286713,45.4284747155974,163.32874495722));
#95343=CARTESIAN_POINT('Ctrl Pts',(-184.094786606929,45.3598039129179,163.898733974326));
#95344=CARTESIAN_POINT('Ctrl Pts',(-183.872083263143,45.2921547689052,164.460242906788));
#95345=CARTESIAN_POINT('Ctrl Pts',(-183.639528757453,45.2262519058143,165.017430797686));
#95346=CARTESIAN_POINT('Ctrl Pts',(-183.39634647974,45.1624597518103,165.569990148998));
#95347=CARTESIAN_POINT('Ctrl Pts',(-183.340871979055,45.1479075487293,165.696039441739));
#95348=CARTESIAN_POINT('Ctrl Pts',(-183.28484421427,45.1334651833255,165.821847855984));
#95349=CARTESIAN_POINT('Ctrl Pts',(-183.228253584138,45.119136981697,165.947411712232));
#95350=CARTESIAN_POINT('Ctrl Pts',(-182.974553425451,45.0549025489239,166.510324162243));
#95351=CARTESIAN_POINT('Ctrl Pts',(-182.709541404531,44.9930065159401,167.068328533397));
#95352=CARTESIAN_POINT('Ctrl Pts',(-182.432350626818,44.9336063856646,167.621026623286));
#95353=CARTESIAN_POINT('Ctrl Pts',(-182.158590221301,44.8749413612142,168.166884802498));
#95354=CARTESIAN_POINT('Ctrl Pts',(-181.872950676918,44.8187108456795,168.707567162311));
#95355=CARTESIAN_POINT('Ctrl Pts',(-181.57454641481,44.7650665665191,169.242697316412));
#95356=CARTESIAN_POINT('Ctrl Pts',(-181.512347374015,44.7538850147397,169.354239229556));
#95357=CARTESIAN_POINT('Ctrl Pts',(-181.449593569415,44.7428158265347,169.465539944495));
#95358=CARTESIAN_POINT('Ctrl Pts',(-181.386276697259,44.7318603759468,169.576596096675));
#95359=CARTESIAN_POINT('Ctrl Pts',(-181.227234179103,44.7043419217072,169.855552550111));
#95360=CARTESIAN_POINT('Ctrl Pts',(-181.064463358344,44.6775394846246,170.133265862419));
#95361=CARTESIAN_POINT('Ctrl Pts',(-180.898096995233,44.6514228089558,170.409215846077));
#95362=CARTESIAN_POINT('Ctrl Pts',(-180.733096332856,44.6255205249614,170.682900557546));
#95363=CARTESIAN_POINT('Ctrl Pts',(-180.56455880916,44.6002927897678,170.954850835475));
#95364=CARTESIAN_POINT('Ctrl Pts',(-180.392647465491,44.5757100866394,171.224598059603));
#95365=CARTESIAN_POINT('Ctrl Pts',(-180.221339873901,44.5512137178845,171.493397932356));
#95366=CARTESIAN_POINT('Ctrl Pts',(-180.046682003667,44.5273578584496,171.760010253265));
#95367=CARTESIAN_POINT('Ctrl Pts',(-179.868870312727,44.5041133014966,172.024009230221));
#95368=CARTESIAN_POINT('Ctrl Pts',(-179.691626830169,44.4809430239796,172.287164581929));
#95369=CARTESIAN_POINT('Ctrl Pts',(-179.511249554796,44.4583801482762,172.547723337867));
#95370=CARTESIAN_POINT('Ctrl Pts',(-179.327969613584,44.4363957466509,172.805300555097));
#95371=CARTESIAN_POINT('Ctrl Pts',(-179.276482988262,44.4302199336191,172.877658618873));
#95372=CARTESIAN_POINT('Ctrl Pts',(-179.224767526064,44.4240897708081,172.949781614421));
#95373=CARTESIAN_POINT('Ctrl Pts',(-179.172828887012,44.4180046169303,173.021661519505));
#95374=CARTESIAN_POINT('Ctrl Pts',(-178.870046992592,44.3825305565271,173.440693173579));
#95375=CARTESIAN_POINT('Ctrl Pts',(-178.559161603634,44.3484774483554,173.852176021675));
#95376=CARTESIAN_POINT('Ctrl Pts',(-178.240147844902,44.315127964356,174.256013723285));
#95377=CARTESIAN_POINT('Ctrl Pts',(-177.922397125579,44.2819105176478,174.658252550493));
#95378=CARTESIAN_POINT('Ctrl Pts',(-177.596582140635,44.249391134563,175.052906781522));
#95379=CARTESIAN_POINT('Ctrl Pts',(-177.262717453059,44.2168609734906,175.439914913192));
#95380=CARTESIAN_POINT('Ctrl Pts',(-177.050436010064,44.1961772959701,175.685986593424));
#95381=CARTESIAN_POINT('Ctrl Pts',(-176.83490101927,44.1754892611164,175.928967772909));
#95382=CARTESIAN_POINT('Ctrl Pts',(-176.616124869558,44.154614658246,176.168849396935));
#95383=CARTESIAN_POINT('Ctrl Pts',(-176.272384001883,44.1218165030885,176.545751164748));
#95384=CARTESIAN_POINT('Ctrl Pts',(-175.920645070288,44.0884963485789,176.914993814555));
#95385=CARTESIAN_POINT('Ctrl Pts',(-175.560988485832,44.0537660832848,177.276571067712));
#95386=CARTESIAN_POINT('Ctrl Pts',(-175.202561092196,44.0191545148952,177.636912565821));
#95387=CARTESIAN_POINT('Ctrl Pts',(-174.836269971456,43.9831424578628,177.98964110849));
#95388=CARTESIAN_POINT('Ctrl Pts',(-174.462238176354,43.9448508755096,178.334778513058));
#95389=CARTESIAN_POINT('Ctrl Pts',(-174.219851918052,43.9200365322034,178.558440151425));
#95390=CARTESIAN_POINT('Ctrl Pts',(-173.97421583996,43.8942648992402,178.778914445244));
#95391=CARTESIAN_POINT('Ctrl Pts',(-173.725373524941,43.8672967522522,178.996213246504));
#95392=CARTESIAN_POINT('Ctrl Pts',(-173.33157436528,43.8246189881401,179.340094010213));
#95393=CARTESIAN_POINT('Ctrl Pts',(-172.929740164485,43.77893904078,179.676023922631));
#95394=CARTESIAN_POINT('Ctrl Pts',(-172.520054883594,43.7294367759111,180.004094210126));
#95395=CARTESIAN_POINT('Ctrl Pts',(-172.400129907369,43.7149462432647,180.100128466817));
#95396=CARTESIAN_POINT('Ctrl Pts',(-172.279532495907,43.7001281849663,180.195489398804));
#95397=CARTESIAN_POINT('Ctrl Pts',(-172.158268028556,43.6849620296658,180.290179656169));
#95398=CARTESIAN_POINT('Ctrl Pts',(-171.937519087759,43.6573536725623,180.462553101367));
#95399=CARTESIAN_POINT('Ctrl Pts',(-171.714272716709,43.6285444230998,180.632922956221));
#95400=CARTESIAN_POINT('Ctrl Pts',(-171.48897075388,43.5985086299391,180.800987948655));
#95401=CARTESIAN_POINT('Ctrl Pts',(-171.263429988966,43.5684410012367,180.969231076556));
#95402=CARTESIAN_POINT('Ctrl Pts',(-171.035829220323,43.5371442273815,181.135164528807));
#95403=CARTESIAN_POINT('Ctrl Pts',(-170.806655279466,43.5045925753827,181.29851498135));
#95404=CARTESIAN_POINT('Ctrl Pts',(-170.709384854195,43.4907763752452,181.367847331824));
#95405=CARTESIAN_POINT('Ctrl Pts',(-170.611831564477,43.4767341104252,181.436714707051));
#95406=CARTESIAN_POINT('Ctrl Pts',(-170.514035031329,43.462463813322,181.505097724209));
#95407=CARTESIAN_POINT('Ctrl Pts',(-170.078760309056,43.3989492959011,181.809458194294));
#95408=CARTESIAN_POINT('Ctrl Pts',(-169.639517762154,43.3309925285366,182.103636987488));
#95409=CARTESIAN_POINT('Ctrl Pts',(-169.196641938417,43.2586019347472,182.388337219161));
#95410=CARTESIAN_POINT('Ctrl Pts',(-168.747439482107,43.1851772165732,182.677104490991));
#95411=CARTESIAN_POINT('Ctrl Pts',(-168.294499348488,43.1071910897059,182.956120347362));
#95412=CARTESIAN_POINT('Ctrl Pts',(-167.838152191216,43.024652343844,183.226067938466));
#95413=CARTESIAN_POINT('Ctrl Pts',(-167.590085918936,42.9797850127379,183.372809057742));
#95414=CARTESIAN_POINT('Ctrl Pts',(-167.341012569015,42.9335724221927,183.51686972133));
#95415=CARTESIAN_POINT('Ctrl Pts',(-167.090982792996,42.8860159840665,183.658353716968));
#95416=CARTESIAN_POINT('Ctrl Pts',(-166.642612966349,42.8007346537463,183.912072116462));
#95417=CARTESIAN_POINT('Ctrl Pts',(-166.191155107318,42.7111080633194,184.157515138959));
#95418=CARTESIAN_POINT('Ctrl Pts',(-165.736825918976,42.6175507757671,184.39527710363));
#95419=CARTESIAN_POINT('Ctrl Pts',(-165.260941198057,42.5195546865456,184.644319624132));
#95420=CARTESIAN_POINT('Ctrl Pts',(-164.781906536675,42.4172460703372,184.884935082214));
#95421=CARTESIAN_POINT('Ctrl Pts',(-164.299938036989,42.3111013404516,185.117755861939));
#95422=CARTESIAN_POINT('Ctrl Pts',(-163.829408878122,42.207475915753,185.345050728144));
#95423=CARTESIAN_POINT('Ctrl Pts',(-163.356083415661,42.1001943137969,185.564916129514));
#95424=CARTESIAN_POINT('Ctrl Pts',(-162.880130934807,41.9896998241888,185.777896291562));
#95425=CARTESIAN_POINT('Ctrl Pts',(-162.386821667856,41.8751758793343,185.998643302748));
#95426=CARTESIAN_POINT('Ctrl Pts',(-161.890690542258,41.7572004422704,186.211993785727));
#95427=CARTESIAN_POINT('Ctrl Pts',(-161.391889708809,41.6362670896229,186.418507804901));
#95428=CARTESIAN_POINT('Ctrl Pts',(-160.893088875361,41.5153337369753,186.625021824075));
#95429=CARTESIAN_POINT('Ctrl Pts',(-160.391618367242,41.3914424687442,186.824699157984));
#95430=CARTESIAN_POINT('Ctrl Pts',(-159.887592775519,41.2650868615552,187.018056568477));
#95431=CARTESIAN_POINT('Ctrl Pts',(-159.229965927336,41.1002245191058,187.270339441655));
#95432=CARTESIAN_POINT('Ctrl Pts',(-158.567639773076,40.9312012789215,187.511993851814));
#95433=CARTESIAN_POINT('Ctrl Pts',(-157.901479365142,40.7592717923683,187.743807501735));
#95434=CARTESIAN_POINT('Ctrl Pts',(-157.317622400269,40.6085840195801,187.946980810216));
#95435=CARTESIAN_POINT('Ctrl Pts',(-156.730820322625,40.4556637660405,188.142593890958));
#95436=CARTESIAN_POINT('Ctrl Pts',(-156.141659320346,40.3013557385819,188.331144415625));
#95437=CARTESIAN_POINT('Ctrl Pts',(-155.654196713949,40.173683688052,188.487148173234));
#95438=CARTESIAN_POINT('Ctrl Pts',(-155.165963645099,40.0452972553808,188.638049161514));
#95439=CARTESIAN_POINT('Ctrl Pts',(-154.676990185282,39.9164969873809,188.784249754084));
#95440=CARTESIAN_POINT('Ctrl Pts',(-154.183078283921,39.7863958868276,188.93192691571));
#95441=CARTESIAN_POINT('Ctrl Pts',(-153.68841100885,39.6558725495822,189.074808137655));
#95442=CARTESIAN_POINT('Ctrl Pts',(-153.192977621197,39.5252367209535,189.213274927384));
#95443=CARTESIAN_POINT('Ctrl Pts',(-152.909710400687,39.4505448471376,189.29244420349));
#95444=CARTESIAN_POINT('Ctrl Pts',(-152.626191966415,39.3758161992806,189.370169781213));
#95445=CARTESIAN_POINT('Ctrl Pts',(-152.342414195266,39.3011086719599,189.446518398969));
#95446=CARTESIAN_POINT('Ctrl Pts',(-151.795151060383,39.1570358101738,189.593756090377));
#95447=CARTESIAN_POINT('Ctrl Pts',(-151.246876778824,39.0130961115111,189.735887647354));
#95448=CARTESIAN_POINT('Ctrl Pts',(-150.697673775629,38.8695161945702,189.873312967304));
#95449=CARTESIAN_POINT('Ctrl Pts',(-150.142368814188,38.7243410229547,190.012265160849));
#95450=CARTESIAN_POINT('Ctrl Pts',(-149.58611444304,38.5795336722339,190.146405843213));
#95451=CARTESIAN_POINT('Ctrl Pts',(-149.028954080029,38.4353283988271,190.276115113943));
#95452=CARTESIAN_POINT('Ctrl Pts',(-148.4684247408,38.290251160778,190.406608696474));
#95453=CARTESIAN_POINT('Ctrl Pts',(-147.906978444276,38.1457833032065,190.532616977839));
#95454=CARTESIAN_POINT('Ctrl Pts',(-147.344616727764,38.0021633577065,190.654495450789));
#95455=CARTESIAN_POINT('Ctrl Pts',(-146.777274095274,37.8572713503638,190.777453418333));
#95456=CARTESIAN_POINT('Ctrl Pts',(-146.208999795835,37.713242341761,190.896207979983));
#95457=CARTESIAN_POINT('Ctrl Pts',(-145.639751585534,37.5703212579178,191.011094050046));
#95458=CARTESIAN_POINT('Ctrl Pts',(-145.311331144991,37.4878647750177,191.077376091973));
#95459=CARTESIAN_POINT('Ctrl Pts',(-144.982585719152,37.4057770720487,191.142369935152));
#95460=CARTESIAN_POINT('Ctrl Pts',(-144.653500579793,37.3241051839344,191.206135628088));
#95461=CARTESIAN_POINT('Ctrl Pts',(-144.007827757714,37.1638630089583,191.331245424873));
#95462=CARTESIAN_POINT('Ctrl Pts',(-143.360891396152,37.0051772754077,191.451621044132));
#95463=CARTESIAN_POINT('Ctrl Pts',(-142.712787463218,36.8481764161634,191.567642104075));
#95464=CARTESIAN_POINT('Ctrl Pts',(-142.066595888332,36.6916388188152,191.683320821074));
#95465=CARTESIAN_POINT('Ctrl Pts',(-141.419243589998,36.5367761673373,191.79467045464));
#95466=CARTESIAN_POINT('Ctrl Pts',(-140.770782326781,36.3837157610625,191.902036140484));
#95467=CARTESIAN_POINT('Ctrl Pts',(-140.116576423578,36.2292994111407,192.010352965966));
#95468=CARTESIAN_POINT('Ctrl Pts',(-139.461241868626,36.0767173796067,192.114614827941));
#95469=CARTESIAN_POINT('Ctrl Pts',(-138.804787361359,35.9261003790415,192.215146561305));
#95470=CARTESIAN_POINT('Ctrl Pts',(-138.154084610909,35.7768030622473,192.314797450565));
#95471=CARTESIAN_POINT('Ctrl Pts',(-137.502281364437,35.6294364926588,192.410783106841));
#95472=CARTESIAN_POINT('Ctrl Pts',(-136.849343077584,35.4841279770207,192.50339336493));
#95473=CARTESIAN_POINT('Ctrl Pts',(-136.122601282649,35.3223948184655,192.606471629062));
#95474=CARTESIAN_POINT('Ctrl Pts',(-135.394479734399,35.1631836595734,192.705364347868));
#95475=CARTESIAN_POINT('Ctrl Pts',(-134.665082037698,35.0065278137277,192.800411184564));
#95476=CARTESIAN_POINT('Ctrl Pts',(-133.932046814869,34.8490907209231,192.895932022416));
#95477=CARTESIAN_POINT('Ctrl Pts',(-133.197722710275,34.6942344915477,192.987568389549));
#95478=CARTESIAN_POINT('Ctrl Pts',(-132.462170600657,34.5419929398785,193.075636120954));
#95479=CARTESIAN_POINT('Ctrl Pts',(-131.721209520432,34.3886318617104,193.164351468979));
#95480=CARTESIAN_POINT('Ctrl Pts',(-130.979002347912,34.2379240573311,193.249445386225));
#95481=CARTESIAN_POINT('Ctrl Pts',(-130.235565957058,34.0899040924884,193.331213319885));
#95482=CARTESIAN_POINT('Ctrl Pts',(-129.804514902801,34.0040807958603,193.378623097564));
#95483=CARTESIAN_POINT('Ctrl Pts',(-129.373049766394,33.9191610927974,193.424914252193));
#95484=CARTESIAN_POINT('Ctrl Pts',(-128.941166863061,33.8351517208289,193.470140433642));
#95485=CARTESIAN_POINT('Ctrl Pts',(-127.87729664587,33.6282088941676,193.581547454177));
#95486=CARTESIAN_POINT('Ctrl Pts',(-126.81071701587,33.4267339205888,193.686513206178));
#95487=CARTESIAN_POINT('Ctrl Pts',(-125.74260208096,33.2307969580634,193.785653161339));
#95488=CARTESIAN_POINT('Ctrl Pts',(-124.660791933785,33.0323477206837,193.886064274393));
#95489=CARTESIAN_POINT('Ctrl Pts',(-123.577407119073,32.8395794199289,193.980499117476));
#95490=CARTESIAN_POINT('Ctrl Pts',(-122.493654425769,32.652564947185,194.069545230172));
#95491=CARTESIAN_POINT('Ctrl Pts',(-121.980126210895,32.5639495195721,194.111739073451));
#95492=CARTESIAN_POINT('Ctrl Pts',(-121.466515184603,32.4766259807107,194.152722265915));
#95493=CARTESIAN_POINT('Ctrl Pts',(-120.952948478995,32.390602085543,194.192553446946));
#95494=CARTESIAN_POINT('Ctrl Pts',(-120.11885150105,32.250888451059,194.257244298909));
#95495=CARTESIAN_POINT('Ctrl Pts',(-119.284476123138,32.1145190215308,194.318928831136));
#95496=CARTESIAN_POINT('Ctrl Pts',(-118.449883143624,31.9813930461442,194.377867732749));
#95497=CARTESIAN_POINT('Ctrl Pts',(-117.611441106354,31.847653107328,194.437078454568));
#95498=CARTESIAN_POINT('Ctrl Pts',(-116.772779462249,31.7171866086003,194.493518045015));
#95499=CARTESIAN_POINT('Ctrl Pts',(-115.933912635633,31.5898913987512,194.54742738932));
#95500=CARTESIAN_POINT('Ctrl Pts',(-115.089760445711,31.461794152858,194.601676394775));
#95501=CARTESIAN_POINT('Ctrl Pts',(-114.245400495456,31.3369082837734,194.653363064254));
#95502=CARTESIAN_POINT('Ctrl Pts',(-113.40079958965,31.2151296972551,194.702710866655));
#95503=CARTESIAN_POINT('Ctrl Pts',(-113.248301152461,31.193141745313,194.711620947964));
#95504=CARTESIAN_POINT('Ctrl Pts',(-113.095794734474,31.1712550931384,194.720454725358));
#95505=CARTESIAN_POINT('Ctrl Pts',(-112.943279974745,31.1494691280026,194.729213442506));
#95506=CARTESIAN_POINT('Ctrl Pts',(-112.012917484241,31.0165715329257,194.782642906736));
#95507=CARTESIAN_POINT('Ctrl Pts',(-111.082171549081,30.8874107776426,194.833285574614));
#95508=CARTESIAN_POINT('Ctrl Pts',(-110.151163017163,30.7618507587285,194.881394610227));
#95509=CARTESIAN_POINT('Ctrl Pts',(-109.215546186852,30.6356692438631,194.929741775549));
#95510=CARTESIAN_POINT('Ctrl Pts',(-108.279664169512,30.513124199377,194.975530049119));
#95511=CARTESIAN_POINT('Ctrl Pts',(-107.343592216217,30.394077490774,195.018993347157));
#95512=CARTESIAN_POINT('Ctrl Pts',(-106.400548423923,30.2741441254533,195.062780358682));
#95513=CARTESIAN_POINT('Ctrl Pts',(-105.457311886688,30.1577614011017,195.104207531364));
#95514=CARTESIAN_POINT('Ctrl Pts',(-104.513911178532,30.0447880737119,195.143492362419));
#95515=CARTESIAN_POINT('Ctrl Pts',(-103.56665038208,29.9313524962783,195.182937934203));
#95516=CARTESIAN_POINT('Ctrl Pts',(-102.619224068339,29.8213542731688,195.220223489191));
#95517=CARTESIAN_POINT('Ctrl Pts',(-101.67161238576,29.7146504194992,195.255549022673));
#95518=CARTESIAN_POINT('Ctrl Pts',(-100.718092149116,29.6072812453192,195.291094818134));
#95519=CARTESIAN_POINT('Ctrl Pts',(-99.7643842389313,29.5032476508013,195.324655977918));
#95520=CARTESIAN_POINT('Ctrl Pts',(-98.8104190123668,29.4024039597289,195.356417394037));
#95521=CARTESIAN_POINT('Ctrl Pts',(-98.1692983922634,29.3346310808509,195.377762929734));
#95522=CARTESIAN_POINT('Ctrl Pts',(-97.5280605291925,29.2682989629573,195.398295200154));
#95523=CARTESIAN_POINT('Ctrl Pts',(-96.8866718339058,29.2033633869119,195.418065909768));
#95524=CARTESIAN_POINT('Ctrl Pts',(-95.8194851598921,29.0953191043508,195.450961777735));
#95525=CARTESIAN_POINT('Ctrl Pts',(-94.7519462915874,28.9911386886706,195.481748272047));
#95526=CARTESIAN_POINT('Ctrl Pts',(-93.6841635390857,28.8906537330632,195.51063659134));
#95527=CARTESIAN_POINT('Ctrl Pts',(-92.6091431308992,28.7894876693292,195.539720721727));
#95528=CARTESIAN_POINT('Ctrl Pts',(-91.5338755508916,28.6920673326612,195.566880757599));
#95529=CARTESIAN_POINT('Ctrl Pts',(-90.4584222720733,28.5982208684964,195.592312201723));
#95530=CARTESIAN_POINT('Ctrl Pts',(-89.3790508310761,28.5040324967158,195.617836299358));
#95531=CARTESIAN_POINT('Ctrl Pts',(-88.299492335566,28.413444086011,195.641619082449));
#95532=CARTESIAN_POINT('Ctrl Pts',(-87.2197595020423,28.3262818966322,195.663839656897));
#95533=CARTESIAN_POINT('Ctrl Pts',(-86.1335962252375,28.2386006052147,195.68619256792));
#95534=CARTESIAN_POINT('Ctrl Pts',(-85.0472565430152,28.1543864669692,195.70696451454));
#95535=CARTESIAN_POINT('Ctrl Pts',(-83.9607033276884,28.0734626194551,195.726320569441));
#95536=CARTESIAN_POINT('Ctrl Pts',(-82.9042804153475,27.9947828038117,195.745139877692));
#95537=CARTESIAN_POINT('Ctrl Pts',(-81.8476554011058,27.9192133283808,195.762620570897));
#95538=CARTESIAN_POINT('Ctrl Pts',(-80.7907491207154,27.8465916397671,195.778900114941));
#95539=CARTESIAN_POINT('Ctrl Pts',(-79.5927899892482,27.7642779884704,195.797352298267));
#95540=CARTESIAN_POINT('Ctrl Pts',(-78.3945110935997,27.6857558821897,195.814260762512));
#95541=CARTESIAN_POINT('Ctrl Pts',(-77.1960106267694,27.6108328461224,195.829803207285));
#95542=CARTESIAN_POINT('Ctrl Pts',(-75.9906334010089,27.5354799164742,195.845434831536));
#95543=CARTESIAN_POINT('Ctrl Pts',(-74.7850320750889,27.4637674770372,195.859684620514));
#95544=CARTESIAN_POINT('Ctrl Pts',(-73.5792566986783,27.3954997208146,195.872716012439));
#95545=CARTESIAN_POINT('Ctrl Pts',(-72.3695516951773,27.3270094796836,195.885789873725));
#95546=CARTESIAN_POINT('Ctrl Pts',(-71.1596715013674,27.2619864108281,195.89763728701));
#95547=CARTESIAN_POINT('Ctrl Pts',(-69.9496165320275,27.200232786598,195.90840734607));
#95548=CARTESIAN_POINT('Ctrl Pts',(-68.7337633573345,27.1381832582945,195.919229011888));
#95549=CARTESIAN_POINT('Ctrl Pts',(-67.5177337342398,27.0794345819982,195.928962886438));
#95550=CARTESIAN_POINT('Ctrl Pts',(-66.301477520774,27.0237861740703,195.937745524306));
#95551=CARTESIAN_POINT('Ctrl Pts',(-65.756109234319,26.9988334736939,195.941683651907));
#95552=CARTESIAN_POINT('Ctrl Pts',(-65.2106947138561,26.9745041189272,195.945430334053));
#95553=CARTESIAN_POINT('Ctrl Pts',(-64.6652261582808,26.9507800259604,195.948996999556));
#95554=CARTESIAN_POINT('Ctrl Pts',(-63.2921914866837,26.8910625557916,195.957974887188));
#95555=CARTESIAN_POINT('Ctrl Pts',(-61.9186754281437,26.8351713374488,195.965814281803));
#95556=CARTESIAN_POINT('Ctrl Pts',(-60.5448604722267,26.7828678234138,195.972681482714));
#95557=CARTESIAN_POINT('Ctrl Pts',(-59.1665103016465,26.7303916459041,195.979571353513));
#95558=CARTESIAN_POINT('Ctrl Pts',(-57.7878592656561,26.6815268991377,195.98548249961));
#95559=CARTESIAN_POINT('Ctrl Pts',(-56.4090416718605,26.6360326653217,195.990566152296));
#95560=CARTESIAN_POINT('Ctrl Pts',(-55.0256419341819,26.5903872431786,195.995666699189));
#95561=CARTESIAN_POINT('Ctrl Pts',(-53.6420745337509,26.5481347732668,195.999934147721));
#95562=CARTESIAN_POINT('Ctrl Pts',(-52.2584247821025,26.5090319279185,196.00350592515));
#95563=CARTESIAN_POINT('Ctrl Pts',(-50.8701549846142,26.4697985170583,196.007089628846));
#95564=CARTESIAN_POINT('Ctrl Pts',(-49.4818022848805,26.4337357992488,196.009972917482));
#95565=CARTESIAN_POINT('Ctrl Pts',(-48.0934022317709,26.4005980012406,196.012280609137));
#95566=CARTESIAN_POINT('Ctrl Pts',(-46.6978527766565,26.3672895640575,196.014600183977));
#95567=CARTESIAN_POINT('Ctrl Pts',(-45.3022554908575,26.3369362472909,196.016338136559));
#95568=CARTESIAN_POINT('Ctrl Pts',(-43.906595309167,26.3092884613659,196.017608406848));
#95569=CARTESIAN_POINT('Ctrl Pts',(-42.5069578153343,26.2815618855778,196.018882297116));
#95570=CARTESIAN_POINT('Ctrl Pts',(-41.1072570559494,26.256556282891,196.019685753621));
#95571=CARTESIAN_POINT('Ctrl Pts',(-39.7074265331523,26.2340199238245,196.020122080962));
#95572=CARTESIAN_POINT('Ctrl Pts',(-38.3013563474903,26.2113831102526,196.020560353207));
#95573=CARTESIAN_POINT('Ctrl Pts',(-36.8951552400075,26.1912376023804,196.020628141197));
#95574=CARTESIAN_POINT('Ctrl Pts',(-35.4887041846105,26.1733282894916,196.020419616074));
#95575=CARTESIAN_POINT('Ctrl Pts',(-34.4438796836606,26.1600238173384,196.02026470691));
#95576=CARTESIAN_POINT('Ctrl Pts',(-33.3989161740766,26.1479534359963,196.019957085882));
#95577=CARTESIAN_POINT('Ctrl Pts',(-32.3537465564776,26.1370125567383,196.019531990655));
#95578=CARTESIAN_POINT('Ctrl Pts',(-30.7854770717214,26.1205958461988,196.018894138328));
#95579=CARTESIAN_POINT('Ctrl Pts',(-29.2170110079495,26.1067517878668,196.017992423837));
#95580=CARTESIAN_POINT('Ctrl Pts',(-27.6484330828428,26.095104898452,196.016935586552));
#95581=CARTESIAN_POINT('Ctrl Pts',(-26.0759263950899,26.0834288374779,196.015876102243));
#95582=CARTESIAN_POINT('Ctrl Pts',(-24.5033072786384,26.0739609655501,196.014660632531));
#95583=CARTESIAN_POINT('Ctrl Pts',(-22.9306098968377,26.0663229709262,196.013387146679));
#95584=CARTESIAN_POINT('Ctrl Pts',(-21.352039330109,26.0586564524708,196.012108905038));
#95585=CARTESIAN_POINT('Ctrl Pts',(-19.7733899133043,26.0528335040686,196.01077213539));
#95586=CARTESIAN_POINT('Ctrl Pts',(-18.1946447084382,26.0484715597521,196.009465466002));
#95587=CARTESIAN_POINT('Ctrl Pts',(-17.5228889540512,26.0466155533579,196.00890947845));
#95588=CARTESIAN_POINT('Ctrl Pts',(-16.8511152226401,26.0450240618587,196.008358818673));
#95589=CARTESIAN_POINT('Ctrl Pts',(-16.1793193989419,26.0436676136088,196.007819795871));
#95590=CARTESIAN_POINT('Ctrl Pts',(-14.4910806772245,26.0402588272205,196.00646521888));
#95591=CARTESIAN_POINT('Ctrl Pts',(-12.8027179439815,26.0383672764135,196.005184901619));
#95592=CARTESIAN_POINT('Ctrl Pts',(-11.1143235409627,26.037377069714,196.004071270348));
#95593=CARTESIAN_POINT('Ctrl Pts',(-9.42199598084912,26.0363845563031,196.002955044845));
#95594=CARTESIAN_POINT('Ctrl Pts',(-7.72963659586614,26.0362975912985,196.002006202154));
#95595=CARTESIAN_POINT('Ctrl Pts',(-6.03728696792206,26.0364959689877,196.001307542158));
#95596=CARTESIAN_POINT('Ctrl Pts',(-4.33934640493638,26.0366950020479,196.000606574032));
#95597=CARTESIAN_POINT('Ctrl Pts',(-2.6414156613371,26.0371812662625,196.000157369753));
#95598=CARTESIAN_POINT('Ctrl Pts',(-0.94348510617516,26.0373283887573,196.000034389117));
#95599=CARTESIAN_POINT('Ctrl Pts',(-0.628990291197994,26.0373556391426,
196.000011610345));
#95600=CARTESIAN_POINT('Ctrl Pts',(-0.314495340669711,26.0373712544753,
196.));
#95601=CARTESIAN_POINT('Ctrl Pts',(2.8421709430404E-14,26.0373712544753,
196.));
#95602=CARTESIAN_POINT('Ctrl Pts',(-175.744237881275,22.546886555333,150.608265410388));
#95603=CARTESIAN_POINT('Ctrl Pts',(-175.908702878622,22.6788155043369,150.370416902681));
#95604=CARTESIAN_POINT('Ctrl Pts',(-176.070305087181,22.8100740741211,150.130584015011));
#95605=CARTESIAN_POINT('Ctrl Pts',(-176.229190935516,22.9406832143353,149.889269308473));
#95606=CARTESIAN_POINT('Ctrl Pts',(-176.242451717849,22.9515839924555,149.869128925734));
#95607=CARTESIAN_POINT('Ctrl Pts',(-176.255693602711,22.9624802562284,149.848978236114));
#95608=CARTESIAN_POINT('Ctrl Pts',(-176.268916688211,22.9733720229219,149.828817539881));
#95609=CARTESIAN_POINT('Ctrl Pts',(-176.44103106749,23.1151414808645,149.566401803559));
#95610=CARTESIAN_POINT('Ctrl Pts',(-176.610110587624,23.2562741012296,149.302035066109));
#95611=CARTESIAN_POINT('Ctrl Pts',(-176.776388927648,23.3968919164516,149.035943859508));
#95612=CARTESIAN_POINT('Ctrl Pts',(-176.942667267672,23.5375097316736,148.769852652907));
#95613=CARTESIAN_POINT('Ctrl Pts',(-177.106144812233,23.6776129639275,148.502037017761));
#95614=CARTESIAN_POINT('Ctrl Pts',(-177.267103401469,23.817346041801,148.232728813506));
#95615=CARTESIAN_POINT('Ctrl Pts',(-177.363999318881,23.9014643534589,148.070607204205));
#95616=CARTESIAN_POINT('Ctrl Pts',(-177.459978494646,23.9854462723562,147.907944307097));
#95617=CARTESIAN_POINT('Ctrl Pts',(-177.555073691723,24.0693089296899,147.744787763983));
#95618=CARTESIAN_POINT('Ctrl Pts',(-177.742739096476,24.2348075039171,147.422806847571));
#95619=CARTESIAN_POINT('Ctrl Pts',(-177.926980239791,24.3998589145364,147.098876637803));
#95620=CARTESIAN_POINT('Ctrl Pts',(-178.108158130897,24.5646751337556,146.773242494141));
#95621=CARTESIAN_POINT('Ctrl Pts',(-178.135162221033,24.5892405595513,146.724707577914));
#95622=CARTESIAN_POINT('Ctrl Pts',(-178.162098345943,24.6138007991985,146.676134818599));
#95623=CARTESIAN_POINT('Ctrl Pts',(-178.188967788788,24.6383565940794,146.627525038914));
#95624=CARTESIAN_POINT('Ctrl Pts',(-178.387133584952,24.819458921767,146.269021301122));
#95625=CARTESIAN_POINT('Ctrl Pts',(-178.581657096816,25.0003113926081,145.90850229487));
#95626=CARTESIAN_POINT('Ctrl Pts',(-178.772869825489,25.1811314130801,145.546279049829));
#95627=CARTESIAN_POINT('Ctrl Pts',(-178.86617158637,25.2693620786306,145.369533145784));
#95628=CARTESIAN_POINT('Ctrl Pts',(-178.958685835325,25.3575853437931,145.192381566129));
#95629=CARTESIAN_POINT('Ctrl Pts',(-179.050455154588,25.4458281382592,145.014860934436));
#95630=CARTESIAN_POINT('Ctrl Pts',(-179.092385660168,25.4861473322497,144.933749622971));
#95631=CARTESIAN_POINT('Ctrl Pts',(-179.134162006972,25.5264707409745,144.852561419544));
#95632=CARTESIAN_POINT('Ctrl Pts',(-179.17578644388,25.5668003915238,144.771299621934));
#95633=CARTESIAN_POINT('Ctrl Pts',(-179.39260672159,25.7768761710768,144.34800967897));
#95634=CARTESIAN_POINT('Ctrl Pts',(-179.605309522255,25.9871277930927,143.922719571555));
#95635=CARTESIAN_POINT('Ctrl Pts',(-179.814294542222,26.1979040977535,143.495807476513));
#95636=CARTESIAN_POINT('Ctrl Pts',(-180.037734528063,26.4232592669264,143.03936695036));
#95637=CARTESIAN_POINT('Ctrl Pts',(-180.256924825074,26.6492146536794,142.581072304569));
#95638=CARTESIAN_POINT('Ctrl Pts',(-180.47241005792,26.8762157659472,142.121392484689));
#95639=CARTESIAN_POINT('Ctrl Pts',(-180.527030915697,26.9337556507213,142.004873567206));
#95640=CARTESIAN_POINT('Ctrl Pts',(-180.581413973102,26.9913627943564,141.888265681818));
#95641=CARTESIAN_POINT('Ctrl Pts',(-180.635568590654,27.0490445708111,141.771576526924));
#95642=CARTESIAN_POINT('Ctrl Pts',(-180.886093230566,27.3158861981584,141.231760905778));
#95643=CARTESIAN_POINT('Ctrl Pts',(-181.131684690975,27.5842894890372,140.690201281687));
#95644=CARTESIAN_POINT('Ctrl Pts',(-181.372929297185,27.8550313552204,140.147621216792));
#95645=CARTESIAN_POINT('Ctrl Pts',(-181.594737305059,28.1039600874706,139.648755749095));
#95646=CARTESIAN_POINT('Ctrl Pts',(-181.812872298084,28.3548669042706,139.149027826144));
#95647=CARTESIAN_POINT('Ctrl Pts',(-182.02782728574,28.6083467745418,138.649005217546));
#95648=CARTESIAN_POINT('Ctrl Pts',(-182.04782703148,28.631930935164,138.602482337826));
#95649=CARTESIAN_POINT('Ctrl Pts',(-182.067799817512,28.6555380045141,138.555955681339));
#95650=CARTESIAN_POINT('Ctrl Pts',(-182.087745982222,28.6791683785366,138.509425856118));
#95651=CARTESIAN_POINT('Ctrl Pts',(-182.299276287944,28.9297699510136,138.015974192752));
#95652=CARTESIAN_POINT('Ctrl Pts',(-182.507800014602,29.182970670716,137.522164174549));
#95653=CARTESIAN_POINT('Ctrl Pts',(-182.713589982161,29.4394358963928,137.028706746927));
#95654=CARTESIAN_POINT('Ctrl Pts',(-182.901130257844,29.6731574898079,136.579009693605));
#95655=CARTESIAN_POINT('Ctrl Pts',(-183.086401030652,29.9095908775968,136.129605579487));
#95656=CARTESIAN_POINT('Ctrl Pts',(-183.269620366698,30.1491974649295,135.681035410223));
#95657=CARTESIAN_POINT('Ctrl Pts',(-183.330707454486,30.2290846043046,135.531477804022));
#95658=CARTESIAN_POINT('Ctrl Pts',(-183.391566549221,30.3093240737019,135.382012919852));
#95659=CARTESIAN_POINT('Ctrl Pts',(-183.452205819528,30.3899316377764,135.232660860471));
#95660=CARTESIAN_POINT('Ctrl Pts',(-183.614088692094,30.605121958454,134.833949921601));
#95661=CARTESIAN_POINT('Ctrl Pts',(-183.774414717316,30.822931855176,134.436042377523));
#95662=CARTESIAN_POINT('Ctrl Pts',(-183.933260187282,31.0438149196179,134.039316900741));
#95663=CARTESIAN_POINT('Ctrl Pts',(-184.083805069754,31.2531555761914,133.663322607113));
#95664=CARTESIAN_POINT('Ctrl Pts',(-184.233020269242,31.4652568189183,133.288390095977));
#95665=CARTESIAN_POINT('Ctrl Pts',(-184.380969182443,31.6804576051001,132.914842397316));
#95666=CARTESIAN_POINT('Ctrl Pts',(-184.435603688472,31.7599268515842,132.776898876452));
#95667=CARTESIAN_POINT('Ctrl Pts',(-184.49006548564,31.8398182782547,132.639144203768));
#95668=CARTESIAN_POINT('Ctrl Pts',(-184.544357638816,31.9201471237056,132.501594660764));
#95669=CARTESIAN_POINT('Ctrl Pts',(-184.617819762747,32.0288392137119,132.315477865177));
#95670=CARTESIAN_POINT('Ctrl Pts',(-184.690974787393,32.1383373743561,132.12972991714));
#95671=CARTESIAN_POINT('Ctrl Pts',(-184.763835795633,32.2486855326466,131.944376242217));
#95672=CARTESIAN_POINT('Ctrl Pts',(-184.908108059022,32.4671861949611,131.577356970119));
#95673=CARTESIAN_POINT('Ctrl Pts',(-185.051273897465,32.6890839232354,131.211883205961));
#95674=CARTESIAN_POINT('Ctrl Pts',(-185.193246738383,32.9147242786968,130.848150885959));
#95675=CARTESIAN_POINT('Ctrl Pts',(-185.332338778526,33.1357861182467,130.491799134966));
#95676=CARTESIAN_POINT('Ctrl Pts',(-185.470285743725,33.3604403311696,130.137118880231));
#95677=CARTESIAN_POINT('Ctrl Pts',(-185.607009479458,33.5889617133876,129.784294086801));
#95678=CARTESIAN_POINT('Ctrl Pts',(-185.643105683007,33.6492932592125,129.691145406418));
#95679=CARTESIAN_POINT('Ctrl Pts',(-185.679116644919,33.7098940684669,129.598126050538));
#95680=CARTESIAN_POINT('Ctrl Pts',(-185.715040966049,33.770768586648,129.505239400064));
#95681=CARTESIAN_POINT('Ctrl Pts',(-185.826219135776,33.9591623349881,129.21777487835));
#95682=CARTESIAN_POINT('Ctrl Pts',(-185.936515312922,34.15009092431,128.931710214066));
#95683=CARTESIAN_POINT('Ctrl Pts',(-186.045906297122,34.3436896511963,128.647105949505));
#95684=CARTESIAN_POINT('Ctrl Pts',(-186.187963906724,34.5951013426148,128.277512405741));
#95685=CARTESIAN_POINT('Ctrl Pts',(-186.328581615584,34.8513141937532,127.910381712665));
#95686=CARTESIAN_POINT('Ctrl Pts',(-186.467167928252,35.1117711144459,127.545845380182));
#95687=CARTESIAN_POINT('Ctrl Pts',(-186.587608752915,35.3381256924236,127.22903879475));
#95688=CARTESIAN_POINT('Ctrl Pts',(-186.706516042193,35.5676857771387,126.914191656203));
#95689=CARTESIAN_POINT('Ctrl Pts',(-186.823533306774,35.8000896127479,126.601389596021));
#95690=CARTESIAN_POINT('Ctrl Pts',(-186.935264325339,36.0219946227828,126.302718345085));
#95691=CARTESIAN_POINT('Ctrl Pts',(-187.045298175341,36.2465364855314,126.005843786788));
#95692=CARTESIAN_POINT('Ctrl Pts',(-187.153519980204,36.4737898819313,125.710359064098));
#95693=CARTESIAN_POINT('Ctrl Pts',(-187.198434955774,36.5681061868602,125.587724913636));
#95694=CARTESIAN_POINT('Ctrl Pts',(-187.243037899464,36.6628901737859,125.465330144598));
#95695=CARTESIAN_POINT('Ctrl Pts',(-187.287320824454,36.7581497766535,125.343145615419));
#95696=CARTESIAN_POINT('Ctrl Pts',(-187.38529512183,36.9689080466076,125.072816963927));
#95697=CARTESIAN_POINT('Ctrl Pts',(-187.481592779837,37.1819935292495,124.80351797177));
#95698=CARTESIAN_POINT('Ctrl Pts',(-187.575959132587,37.3967240017217,124.53493166223));
#95699=CARTESIAN_POINT('Ctrl Pts',(-187.663018946538,37.5948284577938,124.287141285079));
#95700=CARTESIAN_POINT('Ctrl Pts',(-187.748435398913,37.7943346717978,124.039957489253));
#95701=CARTESIAN_POINT('Ctrl Pts',(-187.832006518938,37.9947459637195,123.793130970979));
#95702=CARTESIAN_POINT('Ctrl Pts',(-187.931222863557,38.2326759543536,123.500096428773));
#95703=CARTESIAN_POINT('Ctrl Pts',(-188.027871329892,38.4719542366046,123.207477462073));
#95704=CARTESIAN_POINT('Ctrl Pts',(-188.121669748411,38.71200239098,122.914628621077));
#95705=CARTESIAN_POINT('Ctrl Pts',(-188.206651476469,38.9294869424027,122.649306444432));
#95706=CARTESIAN_POINT('Ctrl Pts',(-188.289294089793,39.1476058176956,122.383795546001));
#95707=CARTESIAN_POINT('Ctrl Pts',(-188.369345374146,39.3659272509012,122.117615059027));
#95708=CARTESIAN_POINT('Ctrl Pts',(-188.377650540578,39.3885776787255,122.089999346635));
#95709=CARTESIAN_POINT('Ctrl Pts',(-188.385927771447,39.4112302682003,122.062376426411));
#95710=CARTESIAN_POINT('Ctrl Pts',(-188.394176753812,39.4338845216231,122.034745760962));
#95711=CARTESIAN_POINT('Ctrl Pts',(-188.467578797548,39.6354692052961,121.78887939537));
#95712=CARTESIAN_POINT('Ctrl Pts',(-188.538661405825,39.8368471399804,121.542399924329));
#95713=CARTESIAN_POINT('Ctrl Pts',(-188.607469504649,40.037770592676,121.294926617));
#95714=CARTESIAN_POINT('Ctrl Pts',(-188.634278299083,40.1160537545741,121.198506847565));
#95715=CARTESIAN_POINT('Ctrl Pts',(-188.660741457239,40.1942675384835,121.101936207836));
#95716=CARTESIAN_POINT('Ctrl Pts',(-188.686860236094,40.2723955794952,121.005192162795));
#95717=CARTESIAN_POINT('Ctrl Pts',(-188.747793540263,40.4546628942767,120.779494998471));
#95718=CARTESIAN_POINT('Ctrl Pts',(-188.806812883497,40.6363432015775,120.552805785747));
#95719=CARTESIAN_POINT('Ctrl Pts',(-188.863919259891,40.8171855501551,120.32493878908));
#95720=CARTESIAN_POINT('Ctrl Pts',(-188.9195764212,40.9934385783092,120.10285447921));
#95721=CARTESIAN_POINT('Ctrl Pts',(-188.973416356601,41.1688959671253,119.87965139287));
#95722=CARTESIAN_POINT('Ctrl Pts',(-189.025418324791,41.3432817233448,119.655156510801));
#95723=CARTESIAN_POINT('Ctrl Pts',(-189.075659196967,41.5117617404008,119.438264361006));
#95724=CARTESIAN_POINT('Ctrl Pts',(-189.124184353139,41.6792416727984,119.220166418816));
#95725=CARTESIAN_POINT('Ctrl Pts',(-189.170956450069,41.8454277028942,119.000705813639));
#95726=CARTESIAN_POINT('Ctrl Pts',(-189.190583026184,41.9151629293015,118.90861543167));
#95727=CARTESIAN_POINT('Ctrl Pts',(-189.209900700109,41.9846697503341,118.816285099538));
#95728=CARTESIAN_POINT('Ctrl Pts',(-189.228905765118,42.0539238525625,118.723703186652));
#95729=CARTESIAN_POINT('Ctrl Pts',(-189.269701749122,42.2025836569575,118.524968258072));
#95730=CARTESIAN_POINT('Ctrl Pts',(-189.309122104735,42.3501377294883,118.325073829805));
#95731=CARTESIAN_POINT('Ctrl Pts',(-189.347227030635,42.496617577999,118.123903895185));
#95732=CARTESIAN_POINT('Ctrl Pts',(-189.41133846046,42.7430695079501,117.785436050364));
#95733=CARTESIAN_POINT('Ctrl Pts',(-189.471642745778,42.9861722585085,117.443390482533));
#95734=CARTESIAN_POINT('Ctrl Pts',(-189.528369432274,43.2256914913882,117.097684460107));
#95735=CARTESIAN_POINT('Ctrl Pts',(-189.583560824824,43.4587281945992,116.761334886931));
#95736=CARTESIAN_POINT('Ctrl Pts',(-189.635365277565,43.6883725336104,116.421520292599));
#95737=CARTESIAN_POINT('Ctrl Pts',(-189.684025408118,43.9143710383731,116.078162647865));
#95738=CARTESIAN_POINT('Ctrl Pts',(-189.71533602662,44.0597909721935,115.857227354393));
#95739=CARTESIAN_POINT('Ctrl Pts',(-189.745345430984,44.2037006513986,115.634825079113));
#95740=CARTESIAN_POINT('Ctrl Pts',(-189.774126467365,44.3460245195935,115.410934680711));
#95741=CARTESIAN_POINT('Ctrl Pts',(-189.788646208236,44.4178254672295,115.297984246074));
#95742=CARTESIAN_POINT('Ctrl Pts',(-189.80285892525,44.4892404437514,115.184655369196));
#95743=CARTESIAN_POINT('Ctrl Pts',(-189.816771882395,44.5602764703106,115.070945604173));
#95744=CARTESIAN_POINT('Ctrl Pts',(-189.845878495638,44.7088874470996,114.833058998333));
#95745=CARTESIAN_POINT('Ctrl Pts',(-189.873666771693,44.8558147467008,114.593508547228));
#95746=CARTESIAN_POINT('Ctrl Pts',(-189.900169411116,45.0008888701078,114.352652858109));
#95747=CARTESIAN_POINT('Ctrl Pts',(-189.927395037922,45.1499205903126,114.105226667775));
#95748=CARTESIAN_POINT('Ctrl Pts',(-189.953264055466,45.2969967153742,113.856423060368));
#95749=CARTESIAN_POINT('Ctrl Pts',(-189.977840198345,45.4419804406038,113.606631315635));
#95750=CARTESIAN_POINT('Ctrl Pts',(-189.982109404138,45.4671660591443,113.563239137737));
#95751=CARTESIAN_POINT('Ctrl Pts',(-189.986339659915,45.4922886464614,113.51981714256));
#95752=CARTESIAN_POINT('Ctrl Pts',(-189.990531378616,45.5173476214414,113.476367372042));
#95753=CARTESIAN_POINT('Ctrl Pts',(-190.024309750992,45.7192818275872,113.126233540803));
#95754=CARTESIAN_POINT('Ctrl Pts',(-190.055618148429,45.9172926050588,112.773946819036));
#95755=CARTESIAN_POINT('Ctrl Pts',(-190.084773825985,46.1116429059189,112.419679369385));
#95756=CARTESIAN_POINT('Ctrl Pts',(-190.093605530925,46.1705146131193,112.312366288447));
#95757=CARTESIAN_POINT('Ctrl Pts',(-190.102239941155,46.2290507217143,112.204871457883));
#95758=CARTESIAN_POINT('Ctrl Pts',(-190.110686478729,46.2872592582712,112.097199656883));
#95759=CARTESIAN_POINT('Ctrl Pts',(-190.117126005374,46.3316366636664,112.015112123932));
#95760=CARTESIAN_POINT('Ctrl Pts',(-190.123455889712,46.3758232353185,111.932921222337));
#95761=CARTESIAN_POINT('Ctrl Pts',(-190.129678414464,46.419824581143,111.850629008613));
#95762=CARTESIAN_POINT('Ctrl Pts',(-190.155150488636,46.5999452860367,111.513763595398));
#95763=CARTESIAN_POINT('Ctrl Pts',(-190.178819063545,46.7769386360979,111.175174863812));
#95764=CARTESIAN_POINT('Ctrl Pts',(-190.200847352509,46.9511673688017,110.835089165966));
#95765=CARTESIAN_POINT('Ctrl Pts',(-190.223891565535,47.1334313675208,110.479319034172));
#95766=CARTESIAN_POINT('Ctrl Pts',(-190.245140712285,47.31266995987,110.121910676907));
#95767=CARTESIAN_POINT('Ctrl Pts',(-190.264805352682,47.4893524414545,109.763123230192));
#95768=CARTESIAN_POINT('Ctrl Pts',(-190.282639426873,47.6495876871243,109.437735030117));
#95769=CARTESIAN_POINT('Ctrl Pts',(-190.299170675221,47.8077215438186,109.11121254813));
#95770=CARTESIAN_POINT('Ctrl Pts',(-190.31457133704,47.9641377788197,108.783749054156));
#95771=CARTESIAN_POINT('Ctrl Pts',(-190.3186324918,48.0053847424114,108.697396925725));
#95772=CARTESIAN_POINT('Ctrl Pts',(-190.322613497865,48.0465130238487,108.610979412536));
#95773=CARTESIAN_POINT('Ctrl Pts',(-190.326516429816,48.0875360219424,108.524500248369));
#95774=CARTESIAN_POINT('Ctrl Pts',(-190.347470973244,48.3077853641662,108.060200223779));
#95775=CARTESIAN_POINT('Ctrl Pts',(-190.366165850257,48.5249327446489,107.594151454416));
#95776=CARTESIAN_POINT('Ctrl Pts',(-190.382938268006,48.7409820320843,107.127459866807));
#95777=CARTESIAN_POINT('Ctrl Pts',(-190.386425985993,48.7859081123401,107.030414308507));
#95778=CARTESIAN_POINT('Ctrl Pts',(-190.389830635255,48.8307748699332,106.933340624158));
#95779=CARTESIAN_POINT('Ctrl Pts',(-190.3931546158,48.875624857867,106.836249384426));
#95780=CARTESIAN_POINT('Ctrl Pts',(-190.401482760198,48.9879953036755,106.592989878786));
#95781=CARTESIAN_POINT('Ctrl Pts',(-190.409300674852,49.1002112103535,106.349587462763));
#95782=CARTESIAN_POINT('Ctrl Pts',(-190.416648501021,49.2129329835915,106.106403549491));
#95783=CARTESIAN_POINT('Ctrl Pts',(-190.423045207733,49.3110637921878,105.894697919234));
#95784=CARTESIAN_POINT('Ctrl Pts',(-190.429085626652,49.4095780398654,105.683157832093));
#95785=CARTESIAN_POINT('Ctrl Pts',(-190.434796191365,49.5088790511891,105.472019538342));
#95786=CARTESIAN_POINT('Ctrl Pts',(-190.437734685736,49.5599765305866,105.363373770578));
#95787=CARTESIAN_POINT('Ctrl Pts',(-190.440585807973,49.611162274679,105.254832348517));
#95788=CARTESIAN_POINT('Ctrl Pts',(-190.443352111172,49.6626721329211,105.146434935855));
#95789=CARTESIAN_POINT('Ctrl Pts',(-190.447571428625,49.7412377955184,104.981101253329));
#95790=CARTESIAN_POINT('Ctrl Pts',(-190.451593258618,49.8205686724301,104.816139230826));
#95791=CARTESIAN_POINT('Ctrl Pts',(-190.455414205516,49.9011704353188,104.651848944708));
#95792=CARTESIAN_POINT('Ctrl Pts',(-190.458076115421,49.9573226501258,104.537394085334));
#95793=CARTESIAN_POINT('Ctrl Pts',(-190.460640829764,50.0140930954728,104.423265371995));
#95794=CARTESIAN_POINT('Ctrl Pts',(-190.463110495386,50.0716668432943,104.309565487542));
#95795=CARTESIAN_POINT('Ctrl Pts',(-190.465509387058,50.1275906829144,104.199123934862));
#95796=CARTESIAN_POINT('Ctrl Pts',(-190.46782537944,50.184430059915,104.089064186709));
#95797=CARTESIAN_POINT('Ctrl Pts',(-190.470059472272,50.242337358968,103.979614063443));
#95798=CARTESIAN_POINT('Ctrl Pts',(-190.471153763902,50.2707012084011,103.926003778254));
#95799=CARTESIAN_POINT('Ctrl Pts',(-190.472228401696,50.2993205360378,103.872539719887));
#95800=CARTESIAN_POINT('Ctrl Pts',(-190.473283481554,50.3282085918218,103.819248459061));
#95801=CARTESIAN_POINT('Ctrl Pts',(-190.474860709149,50.3713930374174,103.739583923273));
#95802=CARTESIAN_POINT('Ctrl Pts',(-190.476394184613,50.4150658005626,103.660301066565));
#95803=CARTESIAN_POINT('Ctrl Pts',(-190.47788357534,50.4597519396773,103.58150526024));
#95804=CARTESIAN_POINT('Ctrl Pts',(-190.478463762675,50.4771592804534,103.550810609066));
#95805=CARTESIAN_POINT('Ctrl Pts',(-190.479037260371,50.4947198656172,103.520189846983));
#95806=CARTESIAN_POINT('Ctrl Pts',(-190.479604049555,50.5124625282476,103.489649124445));
#95807=CARTESIAN_POINT('Ctrl Pts',(-190.480619357872,50.54424554994,103.434940512376));
#95808=CARTESIAN_POINT('Ctrl Pts',(-190.481609405472,50.5764981037343,103.38048925242));
#95809=CARTESIAN_POINT('Ctrl Pts',(-190.482573587812,50.6093230551895,103.326508708962));
#95810=CARTESIAN_POINT('Ctrl Pts',(-190.483480289518,50.6401911164417,103.275746266125));
#95811=CARTESIAN_POINT('Ctrl Pts',(-190.484364110455,50.67156559899,103.225400089796));
#95812=CARTESIAN_POINT('Ctrl Pts',(-190.485224213747,50.7034859716933,103.175645783279));
#95813=CARTESIAN_POINT('Ctrl Pts',(-190.485693564421,50.7209046336072,103.148495303176));
#95814=CARTESIAN_POINT('Ctrl Pts',(-190.486155847173,50.738485007477,103.121521036496));
#95815=CARTESIAN_POINT('Ctrl Pts',(-190.486610891693,50.7562268616243,103.094751266519));
#95816=CARTESIAN_POINT('Ctrl Pts',(-190.487171560686,50.7780869369309,103.061767724732));
#95817=CARTESIAN_POINT('Ctrl Pts',(-190.487724180922,50.8003067802776,103.028929310287));
#95818=CARTESIAN_POINT('Ctrl Pts',(-190.488268410957,50.8228991405886,102.996250130195));
#95819=CARTESIAN_POINT('Ctrl Pts',(-190.489052241381,50.8554379168998,102.949183753932));
#95820=CARTESIAN_POINT('Ctrl Pts',(-190.489818400132,50.8886218581293,102.902459464589));
#95821=CARTESIAN_POINT('Ctrl Pts',(-190.490565574978,50.9230915750538,102.856163776289));
#95822=CARTESIAN_POINT('Ctrl Pts',(-190.491265949113,50.9554022160489,102.812767906007));
#95823=CARTESIAN_POINT('Ctrl Pts',(-190.491949650515,50.9888425049264,102.76974862589));
#95824=CARTESIAN_POINT('Ctrl Pts',(-190.492616032225,51.0238897102706,102.727173554288));
#95825=CARTESIAN_POINT('Ctrl Pts',(-190.492660561478,51.0262316501122,102.724328584041));
#95826=CARTESIAN_POINT('Ctrl Pts',(-190.492705013542,51.0285807458312,102.721485595865));
#95827=CARTESIAN_POINT('Ctrl Pts',(-190.492749388285,51.0309371314078,102.718644609311));
#95828=CARTESIAN_POINT('Ctrl Pts',(-190.493173137558,51.0534390456138,102.691515078253));
#95829=CARTESIAN_POINT('Ctrl Pts',(-190.493585842178,51.0763984440354,102.664839908867));
#95830=CARTESIAN_POINT('Ctrl Pts',(-190.493986293241,51.0997856641685,102.638721920427));
#95831=CARTESIAN_POINT('Ctrl Pts',(-190.494246786517,51.1149990426479,102.621732178124));
#95832=CARTESIAN_POINT('Ctrl Pts',(-190.494502098002,51.1303924656902,102.604978141484));
#95833=CARTESIAN_POINT('Ctrl Pts',(-190.49475193048,51.1459458605707,102.588487321706));
#95834=CARTESIAN_POINT('Ctrl Pts',(-190.495025958524,51.1630055574701,102.570399412976));
#95835=CARTESIAN_POINT('Ctrl Pts',(-190.495293609111,51.1802133663293,102.552613124357));
#95836=CARTESIAN_POINT('Ctrl Pts',(-190.495554183348,51.1977393721181,102.535187035469));
#95837=CARTESIAN_POINT('Ctrl Pts',(-190.495800955596,51.214337067625,102.518683964506));
#95838=CARTESIAN_POINT('Ctrl Pts',(-190.496041381906,51.2312198938965,102.502503925468));
#95839=CARTESIAN_POINT('Ctrl Pts',(-190.49627495862,51.2484810562372,102.486691839988));
#95840=CARTESIAN_POINT('Ctrl Pts',(-190.496507440142,51.2656612846284,102.470953894041));
#95841=CARTESIAN_POINT('Ctrl Pts',(-190.4967331362,51.2832163684952,102.455580467278));
#95842=CARTESIAN_POINT('Ctrl Pts',(-190.496951637893,51.3011868238247,102.440610966142));
#95843=CARTESIAN_POINT('Ctrl Pts',(-190.497170421921,51.319180499469,102.42562212234));
#95844=CARTESIAN_POINT('Ctrl Pts',(-190.49738199311,51.3375906224577,102.411038251086));
#95845=CARTESIAN_POINT('Ctrl Pts',(-190.497586027925,51.3564056935099,102.396893915589));
#95846=CARTESIAN_POINT('Ctrl Pts',(-190.497622036443,51.3597262191685,102.394397691748));
#95847=CARTESIAN_POINT('Ctrl Pts',(-190.497657810449,51.3630592267632,102.391915145125));
#95848=CARTESIAN_POINT('Ctrl Pts',(-190.497693348437,51.3664044859326,102.389446449618));
#95849=CARTESIAN_POINT('Ctrl Pts',(-190.497698185796,51.3668598358445,102.389110415779));
#95850=CARTESIAN_POINT('Ctrl Pts',(-190.497703018127,51.3673153510038,102.388774686009));
#95851=CARTESIAN_POINT('Ctrl Pts',(-190.497707845407,51.3677710284501,102.388439262075));
#95852=CARTESIAN_POINT('Ctrl Pts',(-190.497829956126,51.3792978295723,102.379954389689));
#95853=CARTESIAN_POINT('Ctrl Pts',(-190.49794870553,51.3908794562608,102.371673743334));
#95854=CARTESIAN_POINT('Ctrl Pts',(-190.49806353266,51.4025952328269,102.363640762749));
#95855=CARTESIAN_POINT('Ctrl Pts',(-190.498176084254,51.4140788371052,102.35576697225));
#95856=CARTESIAN_POINT('Ctrl Pts',(-190.49828486745,51.4256914109588,102.348131139072));
#95857=CARTESIAN_POINT('Ctrl Pts',(-190.498389448386,51.4374575098775,102.340767949979));
#95858=CARTESIAN_POINT('Ctrl Pts',(-190.498493937874,51.4492133202251,102.333411199444));
#95859=CARTESIAN_POINT('Ctrl Pts',(-190.498594232461,51.4611224309089,102.326326621791));
#95860=CARTESIAN_POINT('Ctrl Pts',(-190.498689995252,51.473157593797,102.31954239481));
#95861=CARTESIAN_POINT('Ctrl Pts',(-190.498787203883,51.4853744653403,102.312655738574));
#95862=CARTESIAN_POINT('Ctrl Pts',(-190.498879742976,51.4977211980772,102.306078567821));
#95863=CARTESIAN_POINT('Ctrl Pts',(-190.498967358278,51.5101155779645,102.299833692461));
#95864=CARTESIAN_POINT('Ctrl Pts',(-190.499000191867,51.5147603370296,102.297493442952));
#95865=CARTESIAN_POINT('Ctrl Pts',(-190.499032334942,51.5194112573811,102.295199793732));
#95866=CARTESIAN_POINT('Ctrl Pts',(-190.499063777468,51.5240621615258,102.292953715569));
#95867=CARTESIAN_POINT('Ctrl Pts',(-190.499127550844,51.5334953684055,102.288398102442));
#95868=CARTESIAN_POINT('Ctrl Pts',(-190.499188701791,51.5429635346423,102.284018903747));
#95869=CARTESIAN_POINT('Ctrl Pts',(-190.49924660439,51.5524660168867,102.279864143773));
#95870=CARTESIAN_POINT('Ctrl Pts',(-190.499275923368,51.5572775982511,102.277760381287));
#95871=CARTESIAN_POINT('Ctrl Pts',(-190.499304413945,51.5620971811844,102.27571383855));
#95872=CARTESIAN_POINT('Ctrl Pts',(-190.49933202114,51.5669200122158,102.273728831663));
#95873=CARTESIAN_POINT('Ctrl Pts',(-190.499401179922,51.5790016855048,102.26875619121));
#95874=CARTESIAN_POINT('Ctrl Pts',(-190.499466261876,51.5913660796301,102.264061108971));
#95875=CARTESIAN_POINT('Ctrl Pts',(-190.499526819669,51.6040357712666,102.259679993778));
#95876=CARTESIAN_POINT('Ctrl Pts',(-190.499575160619,51.6141494972118,102.256182718575));
#95877=CARTESIAN_POINT('Ctrl Pts',(-190.499620626327,51.6244565361271,102.252884943998));
#95878=CARTESIAN_POINT('Ctrl Pts',(-190.499663124803,51.6349470309206,102.249795087218));
#95879=CARTESIAN_POINT('Ctrl Pts',(-190.499707459708,51.6458908374787,102.246571712576));
#95880=CARTESIAN_POINT('Ctrl Pts',(-190.499749250184,51.6572266217615,102.243522398947));
#95881=CARTESIAN_POINT('Ctrl Pts',(-190.499786904165,51.6688350796959,102.24076878861));
#95882=CARTESIAN_POINT('Ctrl Pts',(-190.499797766025,51.6721837149382,102.239974468066));
#95883=CARTESIAN_POINT('Ctrl Pts',(-190.499808288085,51.6755550949733,102.239204421804));
#95884=CARTESIAN_POINT('Ctrl Pts',(-190.499818442416,51.6789464892751,102.238460794519));
#95885=CARTESIAN_POINT('Ctrl Pts',(-190.49985255672,51.6903401557494,102.235962517845));
#95886=CARTESIAN_POINT('Ctrl Pts',(-190.4998824689,51.7019610574954,102.23376631126));
#95887=CARTESIAN_POINT('Ctrl Pts',(-190.499907362821,51.7136418981571,102.231935917858));
#95888=CARTESIAN_POINT('Ctrl Pts',(-190.499932499582,51.7254366852798,102.230087668989));
#95889=CARTESIAN_POINT('Ctrl Pts',(-190.499952519172,51.7372923374136,102.228612429663));
#95890=CARTESIAN_POINT('Ctrl Pts',(-190.499967274851,51.7490230427039,102.227523777426));
#95891=CARTESIAN_POINT('Ctrl Pts',(-190.499982652175,51.7612479527539,102.226389261185));
#95892=CARTESIAN_POINT('Ctrl Pts',(-190.499992312906,51.7733368621914,102.225674559321));
#95893=CARTESIAN_POINT('Ctrl Pts',(-190.499996850844,51.7850689572221,102.225338275583));
#95894=CARTESIAN_POINT('Ctrl Pts',(-190.499998988428,51.7905953287186,102.225179870041));
#95895=CARTESIAN_POINT('Ctrl Pts',(-190.5,51.7960424097962,102.225104635364));
#95896=CARTESIAN_POINT('Ctrl Pts',(-190.5,51.8013867006572,102.225104347682));
#95897=CARTESIAN_POINT('Ctrl Pts',(190.469429429736,54.1262777440014,110.636021302185));
#95898=CARTESIAN_POINT('Ctrl Pts',(190.470286237567,57.114886044131,110.505619326269));
#95899=CARTESIAN_POINT('Ctrl Pts',(190.390488824897,60.0974355462687,110.365455132863));
#95900=CARTESIAN_POINT('Ctrl Pts',(190.500739017087,52.1710967193735,102.073694012035));
#95901=CARTESIAN_POINT('Ctrl Pts',(190.500921335563,52.6730706221047,102.021024092992));
#95902=CARTESIAN_POINT('Ctrl Pts',(190.503306943774,53.175064208621,101.968360125277));
#95903=CARTESIAN_POINT('Ctrl Pts',(190.500187664912,51.8514724777866,102.229958216589));
#95904=CARTESIAN_POINT('Ctrl Pts',(190.500381911772,51.9211334344651,102.175808890008));
#95905=CARTESIAN_POINT('Ctrl Pts',(190.501435020995,51.9907954565713,102.121657812393));
#95906=CARTESIAN_POINT('Ctrl Pts',(190.499591926775,51.7334252320839,102.391035770384));
#95907=CARTESIAN_POINT('Ctrl Pts',(190.499799430221,51.6407334755141,102.335323750815));
#95908=CARTESIAN_POINT('Ctrl Pts',(190.499250292471,51.5480440363441,102.279610270829));
#95909=CARTESIAN_POINT('Ctrl Pts',(190.499515970613,51.7229179106605,102.411478309401));
#95910=CARTESIAN_POINT('Ctrl Pts',(190.49972516959,51.6156442577851,102.355567759317));
#95911=CARTESIAN_POINT('Ctrl Pts',(190.498970307289,51.5083740319849,102.299655341424));
#95912=CARTESIAN_POINT('Ctrl Pts',(190.499284059707,51.6946440831874,102.473535673214));
#95913=CARTESIAN_POINT('Ctrl Pts',(190.499498450219,51.5479726767401,102.417020913844));
#95914=CARTESIAN_POINT('Ctrl Pts',(190.498111784629,51.4013090294031,102.360502853894));
#95915=CARTESIAN_POINT('Ctrl Pts',(190.499119727676,51.6800791470945,102.517049663537));
#95916=CARTESIAN_POINT('Ctrl Pts',(190.499337816664,51.5128530332642,102.460109100771));
#95917=CARTESIAN_POINT('Ctrl Pts',(190.497498869166,51.345638318955,102.403164303197));
#95918=CARTESIAN_POINT('Ctrl Pts',(190.498618713093,51.6405359775216,102.648172265196));
#95919=CARTESIAN_POINT('Ctrl Pts',(190.498848143968,51.4171792202356,102.589942012296));
#95920=CARTESIAN_POINT('Ctrl Pts',(190.495619236823,51.1938479864711,102.531703725));
#95921=CARTESIAN_POINT('Ctrl Pts',(190.498271656209,51.6201726452936,102.737019270818));
#95922=CARTESIAN_POINT('Ctrl Pts',(190.498509029016,51.367385337178,102.677905732386));
#95923=CARTESIAN_POINT('Ctrl Pts',(190.49430319548,51.1146352450511,102.618781959713));
#95924=CARTESIAN_POINT('Ctrl Pts',(190.497201308041,51.5641115179798,103.004804782485));
#95925=CARTESIAN_POINT('Ctrl Pts',(190.497463445055,51.2295980868092,102.943002008983));
#95926=CARTESIAN_POINT('Ctrl Pts',(190.49021003554,50.8951677024927,102.881177837155));
#95927=CARTESIAN_POINT('Ctrl Pts',(190.496447643867,51.5344336039414,103.185292559695));
#95928=CARTESIAN_POINT('Ctrl Pts',(190.496727574125,51.1555210265605,103.121637703458));
#95929=CARTESIAN_POINT('Ctrl Pts',(190.487283349245,50.7767304584846,103.057955343393));
#95930=CARTESIAN_POINT('Ctrl Pts',(190.494081221756,51.4520056115398,103.727228609739));
#95931=CARTESIAN_POINT('Ctrl Pts',(190.494418228543,50.9480361132095,103.657900955732));
#95932=CARTESIAN_POINT('Ctrl Pts',(190.477971438738,50.444345763347,103.588507032427));
#95933=CARTESIAN_POINT('Ctrl Pts',(190.49235932922,51.4069351392841,104.090155717021));
#95934=CARTESIAN_POINT('Ctrl Pts',(190.492739427804,50.8318828452958,104.016865737875));
#95935=CARTESIAN_POINT('Ctrl Pts',(190.471040957409,50.2572502899628,103.943486936546));
#95936=CARTESIAN_POINT('Ctrl Pts',(190.486730141455,51.2791586543925,105.180968843957));
#95937=CARTESIAN_POINT('Ctrl Pts',(190.487257204149,50.4975091671849,105.095304416781));
#95938=CARTESIAN_POINT('Ctrl Pts',(190.447858717668,49.7168874252647,105.009386390733));
#95939=CARTESIAN_POINT('Ctrl Pts',(190.482359180188,51.2055248140897,105.911119065978));
#95940=CARTESIAN_POINT('Ctrl Pts',(190.483007695422,50.2972530200621,105.816498140453));
#95941=CARTESIAN_POINT('Ctrl Pts',(190.429230323806,49.3906083817691,105.721494395297));
#95942=CARTESIAN_POINT('Ctrl Pts',(190.472162308371,51.0626181516781,107.374691782782));
#95943=CARTESIAN_POINT('Ctrl Pts',(190.473121121834,49.8957928625997,107.260560352614));
#95944=CARTESIAN_POINT('Ctrl Pts',(190.383701752993,48.7324581795214,107.145873015116));
#95945=CARTESIAN_POINT('Ctrl Pts',(190.466335782918,50.9942518830845,108.108322244973));
#95946=CARTESIAN_POINT('Ctrl Pts',(190.467482361322,49.6966919813105,107.983721772173));
#95947=CARTESIAN_POINT('Ctrl Pts',(190.356804914099,48.4039286397594,107.858347999142));
#95948=CARTESIAN_POINT('Ctrl Pts',(190.452970899325,50.8595431134232,109.579204958687));
#95949=CARTESIAN_POINT('Ctrl Pts',(190.454586628089,49.2890216722974,109.431896793475));
#95950=CARTESIAN_POINT('Ctrl Pts',(190.292017249808,47.727047424533,109.283470480434));
#95951=CARTESIAN_POINT('Ctrl Pts',(190.445432703546,50.7933151759563,110.316467760936));
#95952=CARTESIAN_POINT('Ctrl Pts',(190.447327931139,49.0806876989918,110.15703956062));
#95953=CARTESIAN_POINT('Ctrl Pts',(190.254138221714,47.3791214038583,109.996128900898));
#95954=CARTESIAN_POINT('Ctrl Pts',(190.419816456401,50.5959796189513,112.534099894033));
#95955=CARTESIAN_POINT('Ctrl Pts',(190.422734650417,48.4315676710545,112.3360534236));
#95956=CARTESIAN_POINT('Ctrl Pts',(190.118372626102,46.2890691893423,112.134196728001));
#95957=CARTESIAN_POINT('Ctrl Pts',(190.398759656664,50.4661184136419,114.020346541584));
#95958=CARTESIAN_POINT('Ctrl Pts',(190.402589209194,47.966636367364,113.793361990212));
#95959=CARTESIAN_POINT('Ctrl Pts',(189.999306492312,45.5003667299309,113.559765336211));
#95960=CARTESIAN_POINT('Ctrl Pts',(190.359096412405,50.2726331003764,116.263830002808));
#95961=CARTESIAN_POINT('Ctrl Pts',(190.365014333285,47.1893016369557,115.984297698539));
#95962=CARTESIAN_POINT('Ctrl Pts',(189.741113284684,44.1704053032068,115.697893892108));
#95963=CARTESIAN_POINT('Ctrl Pts',(190.34452459809,50.2084149184493,117.013959238553));
#95964=CARTESIAN_POINT('Ctrl Pts',(190.351237949028,46.9164429231363,116.71648393922));
#95965=CARTESIAN_POINT('Ctrl Pts',(189.641525718368,43.7026480635995,116.410512021392));
#95966=CARTESIAN_POINT('Ctrl Pts',(190.31224902198,50.0806483650631,118.519403304998));
#95967=CARTESIAN_POINT('Ctrl Pts',(190.320859208328,46.3399940246239,118.183416722279));
#95968=CARTESIAN_POINT('Ctrl Pts',(189.406807784642,42.7138690255277,117.835543719062));
#95969=CARTESIAN_POINT('Ctrl Pts',(190.294545716396,50.0171081032886,119.274717542161));
#95970=CARTESIAN_POINT('Ctrl Pts',(190.304243560584,46.0360189897018,118.918579936746));
#95971=CARTESIAN_POINT('Ctrl Pts',(189.271522379414,42.1925277014723,118.547958266628));
#95972=CARTESIAN_POINT('Ctrl Pts',(190.255510033889,49.8907533419771,120.791203382157));
#95973=CARTESIAN_POINT('Ctrl Pts',(190.267779575357,45.3981681971246,120.391919060921));
#95974=CARTESIAN_POINT('Ctrl Pts',(188.957866276243,41.1027212910509,119.972550354973));
#95975=CARTESIAN_POINT('Ctrl Pts',(190.234178228885,49.8279470556339,121.552374076106));
#95976=CARTESIAN_POINT('Ctrl Pts',(190.247911663905,45.0638991441457,121.130595534004));
#95977=CARTESIAN_POINT('Ctrl Pts',(188.779250264425,40.5341155190546,120.684728907705));
#95978=CARTESIAN_POINT('Ctrl Pts',(190.187306873929,49.7027878508555,123.081327471884));
#95979=CARTESIAN_POINT('Ctrl Pts',(190.204468021955,44.3763011076148,122.611515499938));
#95980=CARTESIAN_POINT('Ctrl Pts',(188.378856035911,39.3756582923654,122.108773106394));
#95981=CARTESIAN_POINT('Ctrl Pts',(190.161768087685,49.6404349854971,123.84910806775));
#95982=CARTESIAN_POINT('Ctrl Pts',(190.180866911108,44.023010216783,123.3542529677));
#95983=CARTESIAN_POINT('Ctrl Pts',(188.157139850915,38.7864955565338,122.820638866055));
#95984=CARTESIAN_POINT('Ctrl Pts',(190.105804470716,49.5154258447559,125.392126822043));
#95985=CARTESIAN_POINT('Ctrl Pts',(190.129396822592,43.3164757243997,124.843934539981));
#95986=CARTESIAN_POINT('Ctrl Pts',(187.682431381576,37.6261436339848,124.243917236916));
#95987=CARTESIAN_POINT('Ctrl Pts',(190.075380715705,49.4527600253111,126.167361462351));
#95988=CARTESIAN_POINT('Ctrl Pts',(190.101500176494,42.9634678383499,125.591245111377));
#95989=CARTESIAN_POINT('Ctrl Pts',(187.429845353543,37.0556750039611,124.955328797435));
#95990=CARTESIAN_POINT('Ctrl Pts',(190.008843987008,49.3260415780364,127.726281125232));
#95991=CARTESIAN_POINT('Ctrl Pts',(190.040788198983,42.2719768330555,127.090804150198));
#95992=CARTESIAN_POINT('Ctrl Pts',(186.909282058273,35.9593595880391,126.377509295516));
#95993=CARTESIAN_POINT('Ctrl Pts',(189.972732501654,49.2619815486278,128.509962500036));
#95994=CARTESIAN_POINT('Ctrl Pts',(190.007946445721,41.9334210799763,127.84325017495));
#95995=CARTESIAN_POINT('Ctrl Pts',(186.64145632905,35.4333468604082,127.08827735133));
#95996=CARTESIAN_POINT('Ctrl Pts',(189.854418466984,49.0660570573506,130.875521988522));
#95997=CARTESIAN_POINT('Ctrl Pts',(189.900690411698,40.9424772204947,130.114102894018));
#95998=CARTESIAN_POINT('Ctrl Pts',(185.829257275597,33.9285810406561,129.219310893706));
#95999=CARTESIAN_POINT('Ctrl Pts',(189.762383383776,48.9303940639483,132.471700290503));
#96000=CARTESIAN_POINT('Ctrl Pts',(189.817923043442,40.3196344184964,131.636603424624));
#96001=CARTESIAN_POINT('Ctrl Pts',(185.277674642686,33.0230795598244,130.638306254556));
#96002=CARTESIAN_POINT('Ctrl Pts',(189.541450758005,48.6413779255017,135.716703876259));
#96003=CARTESIAN_POINT('Ctrl Pts',(189.622302528065,39.1154704613994,134.713814310541));
#96004=CARTESIAN_POINT('Ctrl Pts',(184.16314166873,31.343059040108,133.471278688383));
#96005=CARTESIAN_POINT('Ctrl Pts',(189.412696565286,48.4880858492789,137.365316901128));
#96006=CARTESIAN_POINT('Ctrl Pts',(189.509253756171,38.5332826287984,136.268745748172));
#96007=CARTESIAN_POINT('Ctrl Pts',(183.598718362169,30.5665275759884,134.885267769976));
#96008=CARTESIAN_POINT('Ctrl Pts',(189.101617591595,48.15693255634,140.73916716681));
#96009=CARTESIAN_POINT('Ctrl Pts',(189.241776478868,37.3725240109737,139.426916956348));
#96010=CARTESIAN_POINT('Ctrl Pts',(182.436006440891,29.0794895646531,137.706412840331));
#96011=CARTESIAN_POINT('Ctrl Pts',(188.91966300801,47.9791445996723,142.463861098625));
#96012=CARTESIAN_POINT('Ctrl Pts',(189.087110147823,36.7940512823183,141.030628638056));
#96013=CARTESIAN_POINT('Ctrl Pts',(181.837626822499,28.3693117365578,139.113588019648));
#96014=CARTESIAN_POINT('Ctrl Pts',(188.47229553167,47.5907621638428,146.033790251501));
#96015=CARTESIAN_POINT('Ctrl Pts',(188.717853953436,35.6098041142205,144.31641474328));
#96016=CARTESIAN_POINT('Ctrl Pts',(180.578988811759,26.9735714770137,141.918640354836));
#96017=CARTESIAN_POINT('Ctrl Pts',(188.208103854505,47.3803127607776,147.87729610845));
#96018=CARTESIAN_POINT('Ctrl Pts',(188.503079327534,35.0038658683449,145.999240295164));
#96019=CARTESIAN_POINT('Ctrl Pts',(179.919133224523,26.2884818917448,143.316561676331));
#96020=CARTESIAN_POINT('Ctrl Pts',(187.701708797589,47.0306444895355,150.802754104872));
#96021=CARTESIAN_POINT('Ctrl Pts',(188.110337479306,34.0490845545101,148.624600476526));
#96022=CARTESIAN_POINT('Ctrl Pts',(178.852766970947,25.2531568776001,145.403494991665));
#96023=CARTESIAN_POINT('Ctrl Pts',(187.5142585255,46.9083821641599,151.805049241076));
#96024=CARTESIAN_POINT('Ctrl Pts',(187.966748913229,33.721575883887,149.521043140327));
#96025=CARTESIAN_POINT('Ctrl Pts',(178.484425597357,24.9067806771726,146.097467019026));
#96026=CARTESIAN_POINT('Ctrl Pts',(187.084961282489,46.6498692416155,153.888493688112));
#96027=CARTESIAN_POINT('Ctrl Pts',(187.646445162211,33.0425327417734,151.368871051823));
#96028=CARTESIAN_POINT('Ctrl Pts',(177.713935688162,24.2062418677873,147.481240380467));
#96029=CARTESIAN_POINT('Ctrl Pts',(186.84356384104,46.5136513094283,154.969065472559));
#96030=CARTESIAN_POINT('Ctrl Pts',(187.469619298187,32.6907847434722,152.320710176512));
#96031=CARTESIAN_POINT('Ctrl Pts',(177.311884861241,23.8521344999142,148.171051695706));
#96032=CARTESIAN_POINT('Ctrl Pts',(186.274665703984,46.2233074742099,157.253389244316));
#96033=CARTESIAN_POINT('Ctrl Pts',(187.067385185671,31.9509244222017,154.312403060988));
#96034=CARTESIAN_POINT('Ctrl Pts',(176.461891719931,23.1291070452778,149.545249180182));
#96035=CARTESIAN_POINT('Ctrl Pts',(185.948755193325,46.0692730647339,158.455223543716));
#96036=CARTESIAN_POINT('Ctrl Pts',(186.842064169064,31.5626244001255,155.352420003862));
#96037=CARTESIAN_POINT('Ctrl Pts',(176.014221907291,22.7603385409926,150.229663071457));
#96038=CARTESIAN_POINT('Ctrl Pts',(185.341105577039,45.8195993055715,160.422578369751));
#96039=CARTESIAN_POINT('Ctrl Pts',(186.443675283611,30.9354856298111,157.030413584589));
#96040=CARTESIAN_POINT('Ctrl Pts',(175.292466123159,22.1873888600896,151.25057226375));
#96041=CARTESIAN_POINT('Ctrl Pts',(185.11820009744,45.7332168496864,161.106542537928));
#96042=CARTESIAN_POINT('Ctrl Pts',(186.29997071828,30.7179737283957,157.612199178184));
#96043=CARTESIAN_POINT('Ctrl Pts',(175.043347033158,21.9930297124899,151.589912581918));
#96044=CARTESIAN_POINT('Ctrl Pts',(184.616759767744,45.5544782741863,162.541567503122));
#96045=CARTESIAN_POINT('Ctrl Pts',(185.986027899374,30.2653381771069,158.825495053442));
#96046=CARTESIAN_POINT('Ctrl Pts',(174.528782445827,21.5990339634757,152.259669539456));
#96047=CARTESIAN_POINT('Ctrl Pts',(184.338298824303,45.4619607004085,163.293528615471));
#96048=CARTESIAN_POINT('Ctrl Pts',(185.815468705345,30.0296558164555,159.45843675178));
#96049=CARTESIAN_POINT('Ctrl Pts',(174.262870297413,21.3990136510515,152.590829373774));
#96050=CARTESIAN_POINT('Ctrl Pts',(183.690939071064,45.2690280167149,164.905619500582));
#96051=CARTESIAN_POINT('Ctrl Pts',(185.433213803636,29.5303219098013,160.807765819904));
#96052=CARTESIAN_POINT('Ctrl Pts',(173.708825716552,20.9902993513571,153.24381452559));
#96053=CARTESIAN_POINT('Ctrl Pts',(183.323597110923,45.1686445967153,165.764429148084));
#96054=CARTESIAN_POINT('Ctrl Pts',(185.22166924195,29.2666120232491,161.524194287642));
#96055=CARTESIAN_POINT('Ctrl Pts',(173.420787378789,20.7816581703162,153.565674560105));
#96056=CARTESIAN_POINT('Ctrl Pts',(182.647456403272,45.0101079286491,167.193151066404));
#96057=CARTESIAN_POINT('Ctrl Pts',(184.850837725503,28.8354472440965,162.71011232814));
#96058=CARTESIAN_POINT('Ctrl Pts',(172.965820078663,20.4588438804909,154.039099832331));
#96059=CARTESIAN_POINT('Ctrl Pts',(182.4008106133,44.9559247402993,167.693223955363));
#96060=CARTESIAN_POINT('Ctrl Pts',(184.717658151634,28.6851618676557,163.125789683885));
#96061=CARTESIAN_POINT('Ctrl Pts',(172.810312765267,20.3495787812123,154.195335097582));
#96062=CARTESIAN_POINT('Ctrl Pts',(181.844224354564,44.8443052620572,168.760246115741));
#96063=CARTESIAN_POINT('Ctrl Pts',(184.424357870275,28.3667030054888,164.013312964699));
#96064=CARTESIAN_POINT('Ctrl Pts',(172.489839921108,20.1267742123925,154.504000559469));
#96065=CARTESIAN_POINT('Ctrl Pts',(181.534618839301,44.7868741449486,169.327084815468));
#96066=CARTESIAN_POINT('Ctrl Pts',(184.26415365177,28.1984160514982,164.485572835663));
#96067=CARTESIAN_POINT('Ctrl Pts',(172.324889664599,20.0132431244623,154.656436448801));
#96068=CARTESIAN_POINT('Ctrl Pts',(180.816015283947,44.6679012328639,170.557089813402));
#96069=CARTESIAN_POINT('Ctrl Pts',(183.901791939756,27.8344037889279,165.514854559176));
#96070=CARTESIAN_POINT('Ctrl Pts',(171.982933620113,19.7804856361125,154.956532274931));
#96071=CARTESIAN_POINT('Ctrl Pts',(180.404978491179,44.606095409884,171.22402034852));
#96072=CARTESIAN_POINT('Ctrl Pts',(183.698284469547,27.6374346411265,166.075913204549));
#96073=CARTESIAN_POINT('Ctrl Pts',(171.805167736614,19.660753182185,155.104786004147));
#96074=CARTESIAN_POINT('Ctrl Pts',(179.676788347291,44.5104783181643,172.310866493804));
#96075=CARTESIAN_POINT('Ctrl Pts',(183.346182791328,27.3133423187831,166.999982185387));
#96076=CARTESIAN_POINT('Ctrl Pts',(171.529838730185,19.4774729604571,155.319896659783));
#96077=CARTESIAN_POINT('Ctrl Pts',(179.41543002632,44.4781344195113,172.68732829295));
#96078=CARTESIAN_POINT('Ctrl Pts',(183.220557062346,27.2001673966544,167.322714587353));
#96079=CARTESIAN_POINT('Ctrl Pts',(171.436652942884,19.4157890822098,155.390365310602));
#96080=CARTESIAN_POINT('Ctrl Pts',(178.849564583556,44.4123980422603,173.467349740303));
#96081=CARTESIAN_POINT('Ctrl Pts',(182.950138463494,26.9622256484572,167.997886625965));
#96082=CARTESIAN_POINT('Ctrl Pts',(171.247132785599,19.291074681691,155.528562264384));
#96083=CARTESIAN_POINT('Ctrl Pts',(178.544828026528,44.379004547457,173.871097732987));
#96084=CARTESIAN_POINT('Ctrl Pts',(182.805119762423,26.8373005774686,168.350789186519));
#96085=CARTESIAN_POINT('Ctrl Pts',(171.150795263472,19.228042132856,155.596288273887));
#96086=CARTESIAN_POINT('Ctrl Pts',(177.891978896762,44.311076287452,174.695871921722));
#96087=CARTESIAN_POINT('Ctrl Pts',(182.494224696965,26.5751718520979,169.081599863043));
#96088=CARTESIAN_POINT('Ctrl Pts',(170.954677195547,19.1004973565966,155.728748553708));
#96089=CARTESIAN_POINT('Ctrl Pts',(177.54370604816,44.2765399816905,175.116859637631));
#96090=CARTESIAN_POINT('Ctrl Pts',(182.328105345844,26.4378064245884,169.459826151321));
#96091=CARTESIAN_POINT('Ctrl Pts',(170.854891970795,19.0359822946474,155.793479304452));
#96092=CARTESIAN_POINT('Ctrl Pts',(176.816454914454,44.2062878499871,175.953808795454));
#96093=CARTESIAN_POINT('Ctrl Pts',(181.977837333457,26.1530991582133,170.225223838092));
#96094=CARTESIAN_POINT('Ctrl Pts',(170.651744296242,18.9054504576405,155.919809151524));
#96095=CARTESIAN_POINT('Ctrl Pts',(176.437805815838,44.1705713626272,176.369252899516));
#96096=CARTESIAN_POINT('Ctrl Pts',(181.79364300311,26.0057327649136,170.612157232357));
#96097=CARTESIAN_POINT('Ctrl Pts',(170.548379957486,18.8394328302813,155.981406632915));
#96098=CARTESIAN_POINT('Ctrl Pts',(175.67416196717,44.0980156569334,177.168406531664));
#96099=CARTESIAN_POINT('Ctrl Pts',(181.415109475414,25.7064830072658,171.371918912357));
#96100=CARTESIAN_POINT('Ctrl Pts',(170.338218421151,18.7060526535118,156.101533098092));
#96101=CARTESIAN_POINT('Ctrl Pts',(175.289646799165,44.0611777276179,177.551758007294));
#96102=CARTESIAN_POINT('Ctrl Pts',(181.220896603426,25.5546901009831,171.744319900801));
#96103=CARTESIAN_POINT('Ctrl Pts',(170.231425117911,18.6386929030414,156.160064719042));
#96104=CARTESIAN_POINT('Ctrl Pts',(174.535877481548,43.9865237830416,178.271798574629));
#96105=CARTESIAN_POINT('Ctrl Pts',(180.830591057864,25.2520703105088,172.458763603975));
#96106=CARTESIAN_POINT('Ctrl Pts',(170.014802174258,18.5029361223571,156.274313806325));
#96107=CARTESIAN_POINT('Ctrl Pts',(174.166661263537,43.9487095499583,178.608658923048));
#96108=CARTESIAN_POINT('Ctrl Pts',(180.634570310566,25.1013021558804,172.800659261218));
#96109=CARTESIAN_POINT('Ctrl Pts',(169.904977694101,18.4345424558401,156.330034996734));
#96110=CARTESIAN_POINT('Ctrl Pts',(173.096395080678,43.8340694277073,179.549104938071));
#96111=CARTESIAN_POINT('Ctrl Pts',(180.049380177025,24.6539596786527,173.776866319289));
#96112=CARTESIAN_POINT('Ctrl Pts',(169.571687500788,18.2283337795665,156.493479970059));
#96113=CARTESIAN_POINT('Ctrl Pts',(172.433943023058,43.7560611973564,180.082861701901));
#96114=CARTESIAN_POINT('Ctrl Pts',(179.666916997985,24.3652485690659,174.355239609894));
#96115=CARTESIAN_POINT('Ctrl Pts',(169.344451316501,18.089526387521,156.597515025505));
#96116=CARTESIAN_POINT('Ctrl Pts',(171.205786180245,43.5981266073985,181.019825600731));
#96117=CARTESIAN_POINT('Ctrl Pts',(178.920970523949,23.8083509956536,175.403059117497));
#96118=CARTESIAN_POINT('Ctrl Pts',(168.883249062146,17.8115169098302,156.798103910025));
#96119=CARTESIAN_POINT('Ctrl Pts',(170.637157103811,43.518029497162,181.424897130365));
#96120=CARTESIAN_POINT('Ctrl Pts',(178.556708868383,23.5397308935891,175.873065324021));
#96121=CARTESIAN_POINT('Ctrl Pts',(168.648778846346,17.6720218607262,156.89483965041));
#96122=CARTESIAN_POINT('Ctrl Pts',(169.577125502554,43.3582879379689,182.146828667796));
#96123=CARTESIAN_POINT('Ctrl Pts',(177.848422670943,23.0239393013448,176.731949074881));
#96124=CARTESIAN_POINT('Ctrl Pts',(168.179817243338,17.3966478726328,157.080712120593));
#96125=CARTESIAN_POINT('Ctrl Pts',(169.084091674877,43.2784719370058,182.46462633532));
#96126=CARTESIAN_POINT('Ctrl Pts',(177.503993626021,22.776498051728,177.121003860235));
#96127=CARTESIAN_POINT('Ctrl Pts',(167.944828417653,17.2604584461382,157.170067976753));
#96128=CARTESIAN_POINT('Ctrl Pts',(168.149706837097,43.11926457637,183.044103788451));
#96129=CARTESIAN_POINT('Ctrl Pts',(176.828250555667,22.2975347205762,177.844722410507));
#96130=CARTESIAN_POINT('Ctrl Pts',(167.474607120963,16.9913843688579,157.343134967837));
#96131=CARTESIAN_POINT('Ctrl Pts',(167.708474202632,43.0398707539592,183.305509411467));
#96132=CARTESIAN_POINT('Ctrl Pts',(176.497339532542,22.0663379064465,178.178536418142));
#96133=CARTESIAN_POINT('Ctrl Pts',(167.239368096194,16.8584950715248,157.426836570331));
#96134=CARTESIAN_POINT('Ctrl Pts',(166.441269532885,42.8026077754189,184.030870841384));
#96135=CARTESIAN_POINT('Ctrl Pts',(175.516740453347,21.3907448714663,179.122298645269));
#96136=CARTESIAN_POINT('Ctrl Pts',(166.533930460771,16.4649162452889,157.6709545235));
#96137=CARTESIAN_POINT('Ctrl Pts',(165.67057063508,42.645672122449,184.437373448117));
#96138=CARTESIAN_POINT('Ctrl Pts',(174.88514165464,20.9686022770523,179.668954321226));
#96139=CARTESIAN_POINT('Ctrl Pts',(166.064053906251,16.2093368164217,157.824459871347));
#96140=CARTESIAN_POINT('Ctrl Pts',(164.215189634904,42.3350660712107,185.165802042391));
#96141=CARTESIAN_POINT('Ctrl Pts',(173.644088953391,20.1618031972738,180.668647973063));
#96142=CARTESIAN_POINT('Ctrl Pts',(165.126741222935,15.7114345690758,158.117870390187));
#96143=CARTESIAN_POINT('Ctrl Pts',(163.531436677291,42.1813820193468,185.486483517213));
#96144=CARTESIAN_POINT('Ctrl Pts',(173.03620986103,19.7783760162525,181.118882320385));
#96145=CARTESIAN_POINT('Ctrl Pts',(164.659269936658,15.469088732046,158.257721966292));
#96146=CARTESIAN_POINT('Ctrl Pts',(162.220881816397,41.8775725051339,186.072809112622));
#96147=CARTESIAN_POINT('Ctrl Pts',(171.836140271617,19.0417666288641,181.953923628036));
#96148=CARTESIAN_POINT('Ctrl Pts',(163.727189231406,14.9967277807032,158.526558693323));
#96149=CARTESIAN_POINT('Ctrl Pts',(161.594416787495,41.7274416157552,186.338050141004));
#96150=CARTESIAN_POINT('Ctrl Pts',(171.244906300323,18.6893215198367,182.337382834772));
#96151=CARTESIAN_POINT('Ctrl Pts',(163.262566911235,14.7667051884807,158.65552280578));
#96152=CARTESIAN_POINT('Ctrl Pts',(160.381684956782,41.4308406296666,186.829865947347));
#96153=CARTESIAN_POINT('Ctrl Pts',(170.074501642088,18.0098120898375,183.055472768792));
#96154=CARTESIAN_POINT('Ctrl Pts',(162.336204079231,14.3179948881814,158.904394050565));
#96155=CARTESIAN_POINT('Ctrl Pts',(159.795558975426,41.2843680069152,187.056283248367));
#96156=CARTESIAN_POINT('Ctrl Pts',(169.495983674241,17.6832380393579,183.389338243258));
#96157=CARTESIAN_POINT('Ctrl Pts',(161.874458194339,14.0993047060754,159.024291458785));
#96158=CARTESIAN_POINT('Ctrl Pts',(158.081766525943,40.850451543292,187.692431197991));
#96159=CARTESIAN_POINT('Ctrl Pts',(167.771142741458,16.734066698008,184.335884123339));
#96160=CARTESIAN_POINT('Ctrl Pts',(160.493316742373,13.4588151165262,159.372323641613));
#96161=CARTESIAN_POINT('Ctrl Pts',(156.996151795608,40.5680775459283,188.060383044538));
#96162=CARTESIAN_POINT('Ctrl Pts',(166.644152309164,16.1471188061287,184.888549532335));
#96163=CARTESIAN_POINT('Ctrl Pts',(159.576564432943,13.0519322694405,159.589213106444));
#96164=CARTESIAN_POINT('Ctrl Pts',(154.902062387963,40.0195872766128,188.724538486421));
#96165=CARTESIAN_POINT('Ctrl Pts',(164.425531251345,15.0434942821473,185.891220463642));
#96166=CARTESIAN_POINT('Ctrl Pts',(157.758927004785,12.2759631210897,159.997426329598));
#96167=CARTESIAN_POINT('Ctrl Pts',(153.896877076874,39.7541702385511,189.019386070661));
#96168=CARTESIAN_POINT('Ctrl Pts',(163.339462148368,14.5299347015406,186.337660838382));
#96169=CARTESIAN_POINT('Ctrl Pts',(156.860464559164,11.9078480940796,160.188200885041));
#96170=CARTESIAN_POINT('Ctrl Pts',(151.941670484102,39.2392317495092,189.559159111861));
#96171=CARTESIAN_POINT('Ctrl Pts',(161.20045577941,13.560445138601,187.1554296739));
#96172=CARTESIAN_POINT('Ctrl Pts',(155.080186035148,11.2043865044206,160.548546057543));
#96173=CARTESIAN_POINT('Ctrl Pts',(150.992079329702,38.9897469154245,189.803781241461));
#96174=CARTESIAN_POINT('Ctrl Pts',(160.149374965747,13.1056749038428,187.525391586376));
#96175=CARTESIAN_POINT('Ctrl Pts',(154.198401648731,10.8690713312607,160.71807822485));
#96176=CARTESIAN_POINT('Ctrl Pts',(150.061838982486,38.7473935021229,190.030202679682));
#96177=CARTESIAN_POINT('Ctrl Pts',(159.114345837254,12.6753117645545,187.866263775242));
#96178=CARTESIAN_POINT('Ctrl Pts',(153.323364948845,10.5475610359161,160.878837531617));
#96179=CARTESIAN_POINT('',(190.499797482064,51.8013867006573,102.335336081514));
#96180=CARTESIAN_POINT('Ctrl Pts',(151.26536469753,39.0180386085743,189.729482705023));
#96181=CARTESIAN_POINT('Ctrl Pts',(152.311979458206,39.2925615430878,189.460998195749));
#96182=CARTESIAN_POINT('Ctrl Pts',(153.355186189874,39.5681010168028,189.174926079119));
#96183=CARTESIAN_POINT('Ctrl Pts',(155.434778870331,40.1162070651496,188.561125057896));
#96184=CARTESIAN_POINT('Ctrl Pts',(156.473210242748,40.3893067764282,188.232684087622));
#96185=CARTESIAN_POINT('Ctrl Pts',(159.560122787503,41.1893291647367,187.178921311955));
#96186=CARTESIAN_POINT('Ctrl Pts',(161.580064916327,41.6970588940589,186.386530151768));
#96187=CARTESIAN_POINT('Ctrl Pts',(165.526821722319,42.5922403987276,184.555727820473));
#96188=CARTESIAN_POINT('Ctrl Pts',(167.454218150135,42.9769238346723,183.517277705224));
#96189=CARTESIAN_POINT('Ctrl Pts',(170.249726424738,43.4291995534616,181.706506578626));
#96190=CARTESIAN_POINT('Ctrl Pts',(171.170073214828,43.5601865679599,181.056506878982));
#96191=CARTESIAN_POINT('Ctrl Pts',(172.935023625514,43.7831597459461,179.688354836545));
#96192=CARTESIAN_POINT('Ctrl Pts',(173.782417537072,43.8759288508816,178.968977104368));
#96193=CARTESIAN_POINT('Ctrl Pts',(176.214153740203,44.1226926454971,176.702601166982));
#96194=CARTESIAN_POINT('Ctrl Pts',(177.687043857519,44.247660840443,175.046670319815));
#96195=CARTESIAN_POINT('Ctrl Pts',(179.337557075668,44.4366493823772,172.799184311615));
#96196=CARTESIAN_POINT('Ctrl Pts',(179.658204132338,44.4759149514855,172.340861046938));
#96197=CARTESIAN_POINT('Ctrl Pts',(180.280752658175,44.5585643046451,171.406844757758));
#96198=CARTESIAN_POINT('Ctrl Pts',(180.582966807554,44.602014713882,170.930523914811));
#96199=CARTESIAN_POINT('Ctrl Pts',(181.45383672706,44.7382868762494,169.49003443454));
#96200=CARTESIAN_POINT('Ctrl Pts',(181.989702502981,44.8375345369766,168.51017247428));
#96201=CARTESIAN_POINT('Ctrl Pts',(183.479269028008,45.160389197305,165.519349529815));
#96202=CARTESIAN_POINT('Ctrl Pts',(184.315468338622,45.4093716649899,163.457423617314));
#96203=CARTESIAN_POINT('Ctrl Pts',(185.391987364775,45.807605610716,160.285891280647));
#96204=CARTESIAN_POINT('Ctrl Pts',(185.720583246987,45.9442010673929,159.21642893812));
#96205=CARTESIAN_POINT('Ctrl Pts',(186.320700873814,46.2176663718146,157.077876486429));
#96206=CARTESIAN_POINT('Ctrl Pts',(186.593330143435,46.3549283352379,156.005610616448));
#96207=CARTESIAN_POINT('Ctrl Pts',(187.34307110056,46.763277222671,152.78090583539));
#96208=CARTESIAN_POINT('Ctrl Pts',(187.752691172238,47.0305111914563,150.620590465638));
#96209=CARTESIAN_POINT('Ctrl Pts',(188.446157287329,47.5399101689615,146.283476114733));
#96210=CARTESIAN_POINT('Ctrl Pts',(188.729706086305,47.7822397640886,144.106660767897));
#96211=CARTESIAN_POINT('Ctrl Pts',(189.207183080785,48.2381611353919,139.74018708407));
#96212=CARTESIAN_POINT('Ctrl Pts',(189.400945395645,48.4517916420194,137.550514252977));
#96213=CARTESIAN_POINT('Ctrl Pts',(189.724147979183,48.8542816387485,133.161532602988));
#96214=CARTESIAN_POINT('Ctrl Pts',(189.853490061688,49.0429920619039,130.962197846555));
#96215=CARTESIAN_POINT('Ctrl Pts',(190.066046457663,49.40875100006,126.557233882612));
#96216=CARTESIAN_POINT('Ctrl Pts',(190.149197206518,49.5864981643842,124.35166813467));
#96217=CARTESIAN_POINT('Ctrl Pts',(190.282774616374,49.9515269587546,119.937868461153));
#96218=CARTESIAN_POINT('Ctrl Pts',(190.333166891757,50.1388961726539,117.729639560238));
#96219=CARTESIAN_POINT('Ctrl Pts',(190.411306967085,50.5223284935433,113.311546989386));
#96220=CARTESIAN_POINT('Ctrl Pts',(190.439016042554,50.7163027287905,111.102262196733));
#96221=CARTESIAN_POINT('Ctrl Pts',(190.469287350292,51.0207096976079,107.789673661224));
#96222=CARTESIAN_POINT('Ctrl Pts',(190.477479042423,51.1237807501464,106.685603953041));
#96223=CARTESIAN_POINT('Ctrl Pts',(190.487498953076,51.2962699272586,105.031116633254));
#96224=CARTESIAN_POINT('Ctrl Pts',(190.4904598684,51.3562576700685,104.47989406235));
#96225=CARTESIAN_POINT('Ctrl Pts',(190.494393761014,51.4628762247885,103.65518540443));
#96226=CARTESIAN_POINT('Ctrl Pts',(190.495620626626,51.5008184630458,103.380585399644));
#96227=CARTESIAN_POINT('Ctrl Pts',(190.497338199613,51.5713767347022,102.970407234778));
#96228=CARTESIAN_POINT('Ctrl Pts',(190.497889660856,51.5968666250794,102.834097086841));
#96229=CARTESIAN_POINT('Ctrl Pts',(190.498680294458,51.6455604475564,102.63201300199));
#96230=CARTESIAN_POINT('Ctrl Pts',(190.498938602068,51.6633593134969,102.564820245953));
#96231=CARTESIAN_POINT('Ctrl Pts',(190.499310561813,51.6980708668151,102.466436119011));
#96232=CARTESIAN_POINT('Ctrl Pts',(190.499431569571,51.7107691530297,102.434144296921));
#96233=CARTESIAN_POINT('Ctrl Pts',(190.499602005233,51.7356544621898,102.388309768035));
#96234=CARTESIAN_POINT('Ctrl Pts',(190.499657802637,51.7450073320729,102.373238940239));
#96235=CARTESIAN_POINT('Ctrl Pts',(190.499753774817,51.7683402146372,102.34723353356));
#96236=CARTESIAN_POINT('Ctrl Pts',(190.499797482064,51.7835531522669,102.3353360815));
#96237=CARTESIAN_POINT('Ctrl Pts',(190.499797482064,51.8013867006573,102.335336081514));
#96238=CARTESIAN_POINT('Ctrl Pts',(154.442742286491,25.4284918940193,185.219477651462));
#96239=CARTESIAN_POINT('Ctrl Pts',(155.25456339184,25.4219089188872,184.847447378001));
#96240=CARTESIAN_POINT('Ctrl Pts',(156.059626688009,25.4153258334577,184.457936844013));
#96241=CARTESIAN_POINT('Ctrl Pts',(157.654842582912,25.4021882974927,183.640346053175));
#96242=CARTESIAN_POINT('Ctrl Pts',(158.443529931846,25.3956457653571,183.21290121233));
#96243=CARTESIAN_POINT('Ctrl Pts',(160.764687787038,25.3762759136631,181.879229353496));
#96244=CARTESIAN_POINT('Ctrl Pts',(162.258407229187,25.3636567477705,180.918818281769));
#96245=CARTESIAN_POINT('Ctrl Pts',(165.122650460426,25.3392714587578,178.834487770115));
#96246=CARTESIAN_POINT('Ctrl Pts',(166.493313761037,25.3275024335347,177.710753515211));
#96247=CARTESIAN_POINT('Ctrl Pts',(168.440743116212,25.3107129547371,175.881059878429));
#96248=CARTESIAN_POINT('Ctrl Pts',(169.071734366144,25.3052609475703,175.247070171405));
#96249=CARTESIAN_POINT('Ctrl Pts',(170.293644774771,25.2946997332868,173.92590533392));
#96250=CARTESIAN_POINT('Ctrl Pts',(170.880307363561,25.2896272886514,173.242999300009));
#96251=CARTESIAN_POINT('Ctrl Pts',(172.548007721856,25.2752507069752,171.142925705269));
#96252=CARTESIAN_POINT('Ctrl Pts',(173.54407194752,25.2667550967002,169.667567264653));
#96253=CARTESIAN_POINT('Ctrl Pts',(174.844336948799,25.2558838450969,167.328403359915));
#96254=CARTESIAN_POINT('Ctrl Pts',(175.24527787866,25.2525778363154,166.527546788028));
#96255=CARTESIAN_POINT('Ctrl Pts',(175.794514753496,25.2478415600948,165.29231347852));
#96256=CARTESIAN_POINT('Ctrl Pts',(175.968732185778,25.2462958959865,164.87510964052));
#96257=CARTESIAN_POINT('Ctrl Pts',(176.296234803807,25.2432032648891,164.037870148976));
#96258=CARTESIAN_POINT('Ctrl Pts',(176.449996680554,25.2416509109389,163.616789191854));
#96259=CARTESIAN_POINT('Ctrl Pts',(177.170688179857,25.2336053720658,161.499530229832));
#96260=CARTESIAN_POINT('Ctrl Pts',(177.591573404014,25.2258451067606,159.767375049538));
#96261=CARTESIAN_POINT('Ctrl Pts',(178.209179105645,25.2074249258181,156.247847451973));
#96262=CARTESIAN_POINT('Ctrl Pts',(178.407949493929,25.1970961265605,154.457387616557));
#96263=CARTESIAN_POINT('Ctrl Pts',(178.535788240059,25.1869009068823,152.663678496546));
#96264=CARTESIAN_POINT('',(190.5,51.8013867006572,102.225104347683));
#96265=CARTESIAN_POINT('Ctrl Pts',(190.5,51.8013867006572,102.225104347683));
#96266=CARTESIAN_POINT('Ctrl Pts',(190.5,51.7819061888801,102.225107030451));
#96267=CARTESIAN_POINT('Ctrl Pts',(190.499987805158,51.7635986709013,102.226005968592));
#96268=CARTESIAN_POINT('Ctrl Pts',(190.499965895733,51.7462663363356,102.227616117064));
#96269=CARTESIAN_POINT('Ctrl Pts',(190.499940589854,51.7262470993417,102.229475874832));
#96270=CARTESIAN_POINT('Ctrl Pts',(190.499902299865,51.7075287120045,102.232286246869));
#96271=CARTESIAN_POINT('Ctrl Pts',(190.49985447553,51.6898704822393,102.235789048991));
#96272=CARTESIAN_POINT('Ctrl Pts',(190.499808728661,51.6729793172492,102.239139691118));
#96273=CARTESIAN_POINT('Ctrl Pts',(190.499754222189,51.6570599065149,102.243126566931));
#96274=CARTESIAN_POINT('Ctrl Pts',(190.499694135448,51.6419407404168,102.247511091656));
#96275=CARTESIAN_POINT('Ctrl Pts',(190.499639836321,51.6282778672001,102.251473294667));
#96276=CARTESIAN_POINT('Ctrl Pts',(190.499580960819,51.6152697582099,102.255761680282));
#96277=CARTESIAN_POINT('Ctrl Pts',(190.49952034789,51.6028024249967,102.260162820708));
#96278=CARTESIAN_POINT('Ctrl Pts',(190.499513887304,51.6014735618565,102.260631927708));
#96279=CARTESIAN_POINT('Ctrl Pts',(190.499507407636,51.6001508455561,102.261102265943));
#96280=CARTESIAN_POINT('Ctrl Pts',(190.499500912834,51.5988341389355,102.2615735385));
#96281=CARTESIAN_POINT('Ctrl Pts',(190.499435796719,51.5856329951794,102.266298461019));
#96282=CARTESIAN_POINT('Ctrl Pts',(190.499367209565,51.5728858133411,102.271265386069));
#96283=CARTESIAN_POINT('Ctrl Pts',(190.499294966487,51.5604980579874,102.276487402146));
#96284=CARTESIAN_POINT('Ctrl Pts',(190.499245073007,51.5519426609412,102.280093900632));
#96285=CARTESIAN_POINT('Ctrl Pts',(190.49919088718,51.5431272533784,102.284000583904));
#96286=CARTESIAN_POINT('Ctrl Pts',(190.499132702827,51.5341865318516,102.288183180012));
#96287=CARTESIAN_POINT('Ctrl Pts',(190.499075807096,51.5254438225133,102.292273143214));
#96288=CARTESIAN_POINT('Ctrl Pts',(190.499015087286,51.5165815564384,102.296626970431));
#96289=CARTESIAN_POINT('Ctrl Pts',(190.498950971254,51.5076773758461,102.301210936651));
#96290=CARTESIAN_POINT('Ctrl Pts',(190.498887080431,51.4988044714745,102.305778801541));
#96291=CARTESIAN_POINT('Ctrl Pts',(190.498819817172,51.489890005652,102.310575180582));
#96292=CARTESIAN_POINT('Ctrl Pts',(190.498749764597,51.4809597062609,102.31555539242));
#96293=CARTESIAN_POINT('Ctrl Pts',(190.498728849729,51.4782934797706,102.317042282405));
#96294=CARTESIAN_POINT('Ctrl Pts',(190.498707687303,51.4756254949432,102.31854548342));
#96295=CARTESIAN_POINT('Ctrl Pts',(190.498686295542,51.472955560573,102.320063617662));
#96296=CARTESIAN_POINT('Ctrl Pts',(190.49858999832,51.4609365752182,102.326897655768));
#96297=CARTESIAN_POINT('Ctrl Pts',(190.498488595803,51.4488755337678,102.334067398576));
#96298=CARTESIAN_POINT('Ctrl Pts',(190.498382995867,51.4369286075406,102.341503710545));
#96299=CARTESIAN_POINT('Ctrl Pts',(190.49827545108,51.4247616529285,102.349076978219));
#96300=CARTESIAN_POINT('Ctrl Pts',(190.498163552905,51.4127129205985,102.356926676939));
#96301=CARTESIAN_POINT('Ctrl Pts',(190.498048409372,51.4008932928763,102.364971649728));
#96302=CARTESIAN_POINT('Ctrl Pts',(190.497920233672,51.387735896961,102.373927168007));
#96303=CARTESIAN_POINT('Ctrl Pts',(190.49778803536,51.3748625721735,102.383124630778));
#96304=CARTESIAN_POINT('Ctrl Pts',(190.49765353826,51.3623579799668,102.392442509208));
#96305=CARTESIAN_POINT('Ctrl Pts',(190.497499626757,51.348048373481,102.403105405798));
#96306=CARTESIAN_POINT('Ctrl Pts',(190.497340595809,51.3340223984724,102.414076149627));
#96307=CARTESIAN_POINT('Ctrl Pts',(190.497177021594,51.3201942330095,102.425308352082));
#96308=CARTESIAN_POINT('Ctrl Pts',(190.497077659119,51.3117943716334,102.432131306568));
#96309=CARTESIAN_POINT('Ctrl Pts',(190.496976622798,51.3034664870513,102.439050563475));
#96310=CARTESIAN_POINT('Ctrl Pts',(190.496874065214,51.2951820979778,102.4460541533));
#96311=CARTESIAN_POINT('Ctrl Pts',(190.496632990611,51.2757085913373,102.462516978955));
#96312=CARTESIAN_POINT('Ctrl Pts',(190.49638320033,51.2565388519805,102.479469354575));
#96313=CARTESIAN_POINT('Ctrl Pts',(190.496125351658,51.2377329006417,102.496851940838));
#96314=CARTESIAN_POINT('Ctrl Pts',(190.495861249209,51.2184708358817,102.51465611869));
#96315=CARTESIAN_POINT('Ctrl Pts',(190.495588692412,51.1995904330682,102.532911629592));
#96316=CARTESIAN_POINT('Ctrl Pts',(190.495308471908,51.1811007324381,102.551551257997));
#96317=CARTESIAN_POINT('Ctrl Pts',(190.49502123726,51.1621482198251,102.570657451197));
#96318=CARTESIAN_POINT('Ctrl Pts',(190.494725950315,51.143606007776,102.590167219544));
#96319=CARTESIAN_POINT('Ctrl Pts',(190.494423553778,51.1254276671506,102.610004672516));
#96320=CARTESIAN_POINT('Ctrl Pts',(190.49410167335,51.1060780671041,102.631120284159));
#96321=CARTESIAN_POINT('Ctrl Pts',(190.493771737142,51.0871405553085,102.652607156205));
#96322=CARTESIAN_POINT('Ctrl Pts',(190.493434990178,51.0684986842281,102.674369990984));
#96323=CARTESIAN_POINT('Ctrl Pts',(190.49327146515,51.0594461527773,102.684938068912));
#96324=CARTESIAN_POINT('Ctrl Pts',(190.493106335701,51.0504624770422,102.69557116779));
#96325=CARTESIAN_POINT('Ctrl Pts',(190.492939753098,51.0415300296156,102.706258106843));
#96326=CARTESIAN_POINT('Ctrl Pts',(190.492873196198,51.037961133462,102.710527997709));
#96327=CARTESIAN_POINT('Ctrl Pts',(190.492806404688,51.0344025574796,102.7148066594));
#96328=CARTESIAN_POINT('Ctrl Pts',(190.492739387011,51.0308546706283,102.719093465428));
#96329=CARTESIAN_POINT('Ctrl Pts',(190.492217277783,51.00321443393,102.752490340321));
#96330=CARTESIAN_POINT('Ctrl Pts',(190.491680105235,50.9761560277177,102.78649716168));
#96331=CARTESIAN_POINT('Ctrl Pts',(190.491128747327,50.9496781884247,102.821001634167));
#96332=CARTESIAN_POINT('Ctrl Pts',(190.490561797783,50.9224515926376,102.856481845178));
#96333=CARTESIAN_POINT('Ctrl Pts',(190.489979853435,50.8958386079739,102.892488229329));
#96334=CARTESIAN_POINT('Ctrl Pts',(190.489383684826,50.8697813267168,102.928894775142));
#96335=CARTESIAN_POINT('Ctrl Pts',(190.488750358062,50.8420999403357,102.96757047778));
#96336=CARTESIAN_POINT('Ctrl Pts',(190.488100985496,50.8150454753715,103.006697754866));
#96337=CARTESIAN_POINT('Ctrl Pts',(190.48743619729,50.7884887641956,103.046121498537));
#96338=CARTESIAN_POINT('Ctrl Pts',(190.487145966101,50.7768947169831,103.063332995186));
#96339=CARTESIAN_POINT('Ctrl Pts',(190.486852792435,50.765394825828,103.080600950831));
#96340=CARTESIAN_POINT('Ctrl Pts',(190.486556707587,50.7539753280591,103.097912264592));
#96341=CARTESIAN_POINT('Ctrl Pts',(190.485781475642,50.724075927493,103.143238067439));
#96342=CARTESIAN_POINT('Ctrl Pts',(190.484990248106,50.6948833065813,103.188902737648));
#96343=CARTESIAN_POINT('Ctrl Pts',(190.484183841959,50.6660948762953,103.23483075695));
#96344=CARTESIAN_POINT('Ctrl Pts',(190.483057216169,50.6258747116616,103.298996551309));
#96345=CARTESIAN_POINT('Ctrl Pts',(190.481900571853,50.5865712041433,103.363708602892));
#96346=CARTESIAN_POINT('Ctrl Pts',(190.480713977185,50.5480908227822,103.428837031643));
#96347=CARTESIAN_POINT('Ctrl Pts',(190.48030288073,50.5347592709413,103.451400815927));
#96348=CARTESIAN_POINT('Ctrl Pts',(190.479888180932,50.5215260489788,103.474014558782));
#96349=CARTESIAN_POINT('Ctrl Pts',(190.479469852368,50.5083858374461,103.496672801637));
#96350=CARTESIAN_POINT('Ctrl Pts',(190.476436358211,50.4131000779096,103.66097821444));
#96351=CARTESIAN_POINT('Ctrl Pts',(190.473188613689,50.3220653991955,103.827547153392));
#96352=CARTESIAN_POINT('Ctrl Pts',(190.46973453625,50.2336378965589,103.995526950525));
#96353=CARTESIAN_POINT('Ctrl Pts',(190.467665095073,50.1806583330469,104.096168674713));
#96354=CARTESIAN_POINT('Ctrl Pts',(190.465522226543,50.128613102748,104.197316875812));
#96355=CARTESIAN_POINT('Ctrl Pts',(190.463314699951,50.0771562760488,104.298790001184));
#96356=CARTESIAN_POINT('Ctrl Pts',(190.463157784645,50.0734986241936,104.306002909346));
#96357=CARTESIAN_POINT('Ctrl Pts',(190.463000546636,50.0698445782581,104.313217483716));
#96358=CARTESIAN_POINT('Ctrl Pts',(190.462842989874,50.0661942109542,104.3204336661));
#96359=CARTESIAN_POINT('Ctrl Pts',(190.460234376599,50.0057563310984,104.439909523633));
#96360=CARTESIAN_POINT('Ctrl Pts',(190.4575319713,49.946177244841,104.559852577398));
#96361=CARTESIAN_POINT('Ctrl Pts',(190.454729245207,49.8872683438416,104.680145857249));
#96362=CARTESIAN_POINT('Ctrl Pts',(190.451857501286,49.82690879648,104.803401389083));
#96363=CARTESIAN_POINT('Ctrl Pts',(190.448880494172,49.7672527304977,104.927024628702));
#96364=CARTESIAN_POINT('Ctrl Pts',(190.445787762928,49.7080428432841,105.050886546628));
#96365=CARTESIAN_POINT('Ctrl Pts',(190.444871046973,49.6904924504486,105.08760043715));
#96366=CARTESIAN_POINT('Ctrl Pts',(190.443944137777,49.6729809089871,105.124335275583));
#96367=CARTESIAN_POINT('Ctrl Pts',(190.443006694391,49.655500653764,105.161087645489));
#96368=CARTESIAN_POINT('Ctrl Pts',(190.437604122775,49.5547603507539,105.372894900784));
#96369=CARTESIAN_POINT('Ctrl Pts',(190.43186467886,49.4553128650949,105.585253901174));
#96370=CARTESIAN_POINT('Ctrl Pts',(190.425767977364,49.3563958270275,105.797898094705));
#96371=CARTESIAN_POINT('Ctrl Pts',(190.419697186698,49.2578991839181,106.009638555689));
#96372=CARTESIAN_POINT('Ctrl Pts',(190.41327196394,49.1599272263073,106.221661693927));
#96373=CARTESIAN_POINT('Ctrl Pts',(190.406482906553,49.0617771372373,106.433708381924));
#96374=CARTESIAN_POINT('Ctrl Pts',(190.401950664083,48.996254049606,106.575266620446));
#96375=CARTESIAN_POINT('Ctrl Pts',(190.3972566273,48.9307847293818,106.716843520304));
#96376=CARTESIAN_POINT('Ctrl Pts',(190.392398235184,48.865383382616,106.858372934206));
#96377=CARTESIAN_POINT('Ctrl Pts',(190.38241104125,48.7309405632426,107.149309044396));
#96378=CARTESIAN_POINT('Ctrl Pts',(190.371691438842,48.5962741276876,107.440080064837));
#96379=CARTESIAN_POINT('Ctrl Pts',(190.360163745888,48.4608401849474,107.730416452946));
#96380=CARTESIAN_POINT('Ctrl Pts',(190.349247469066,48.3325895092942,108.005353718954));
#96381=CARTESIAN_POINT('Ctrl Pts',(190.337606452941,48.203650213339,108.279901220201));
#96382=CARTESIAN_POINT('Ctrl Pts',(190.325186866745,48.0736022962362,108.553832171948));
#96383=CARTESIAN_POINT('Ctrl Pts',(190.324928765199,48.0708996644553,108.559524954366));
#96384=CARTESIAN_POINT('Ctrl Pts',(190.324670326008,48.0681965365245,108.565217466365));
#96385=CARTESIAN_POINT('Ctrl Pts',(190.324411548623,48.0654929077705,108.570909706858));
#96386=CARTESIAN_POINT('Ctrl Pts',(190.30809950033,47.8950695038768,108.929720434545));
#96387=CARTESIAN_POINT('Ctrl Pts',(190.290445173734,47.7227602459063,109.287455099581));
#96388=CARTESIAN_POINT('Ctrl Pts',(190.271252865212,47.5479923029685,109.643858481022));
#96389=CARTESIAN_POINT('Ctrl Pts',(190.252060556691,47.3732243600308,110.000261862464));
#96390=CARTESIAN_POINT('Ctrl Pts',(190.231330066105,47.19599710458,110.355333952089));
#96391=CARTESIAN_POINT('Ctrl Pts',(190.208885317062,47.0157890831752,110.708819911125));
#96392=CARTESIAN_POINT('Ctrl Pts',(190.187535799278,46.8443746311556,111.045056897095));
#96393=CARTESIAN_POINT('Ctrl Pts',(190.164687494095,46.6702470477431,111.379862490087));
#96394=CARTESIAN_POINT('Ctrl Pts',(190.140086540729,46.4931565230915,111.713020121159));
#96395=CARTESIAN_POINT('Ctrl Pts',(190.135640195587,46.4611494060373,111.773234609293));
#96396=CARTESIAN_POINT('Ctrl Pts',(190.131136667723,46.4290456179944,111.833395265089));
#96397=CARTESIAN_POINT('Ctrl Pts',(190.126574553226,46.3968438430142,111.893500810988));
#96398=CARTESIAN_POINT('Ctrl Pts',(190.103520003164,46.234112847576,112.197242928358));
#96399=CARTESIAN_POINT('Ctrl Pts',(190.078949349961,46.0687489493423,112.499768106126));
#96400=CARTESIAN_POINT('Ctrl Pts',(190.05269520814,45.9006448211917,112.800818213231));
#96401=CARTESIAN_POINT('Ctrl Pts',(190.026979163907,45.7359861084927,113.09569808108));
#96402=CARTESIAN_POINT('Ctrl Pts',(189.999647793594,45.5686981823395,113.389162719898));
#96403=CARTESIAN_POINT('Ctrl Pts',(189.970568077575,45.3987230083238,113.6809699866));
#96404=CARTESIAN_POINT('Ctrl Pts',(189.942216363998,45.2330031145719,113.965471941159));
#96405=CARTESIAN_POINT('Ctrl Pts',(189.912202667965,45.0647287721212,114.248398465848));
#96406=CARTESIAN_POINT('Ctrl Pts',(189.880428588463,44.8938888954231,114.52952562181));
#96407=CARTESIAN_POINT('Ctrl Pts',(189.86320062523,44.8012592060418,114.681953272992));
#96408=CARTESIAN_POINT('Ctrl Pts',(189.845455581042,44.7078760453384,114.833851949159));
#96409=CARTESIAN_POINT('Ctrl Pts',(189.827181068214,44.6137431943845,114.98518601914));
#96410=CARTESIAN_POINT('Ctrl Pts',(189.821506870443,44.5845151422847,115.032174929357));
#96411=CARTESIAN_POINT('Ctrl Pts',(189.815780524983,44.5552150513257,115.07910917213));
#96412=CARTESIAN_POINT('Ctrl Pts',(189.810001379507,44.5258437663493,115.125987692428));
#96413=CARTESIAN_POINT('Ctrl Pts',(189.765174624184,44.2980212602981,115.489607533465));
#96414=CARTESIAN_POINT('Ctrl Pts',(189.717207375984,44.0661209111254,115.849506313826));
#96415=CARTESIAN_POINT('Ctrl Pts',(189.665770468423,43.830187225881,116.205776137928));
#96416=CARTESIAN_POINT('Ctrl Pts',(189.621237067927,43.6259189330552,116.514229882798));
#96417=CARTESIAN_POINT('Ctrl Pts',(189.574103889631,43.4186275748335,116.819963409595));
#96418=CARTESIAN_POINT('Ctrl Pts',(189.524188097192,43.2083484666004,117.123036448682));
#96419=CARTESIAN_POINT('Ctrl Pts',(189.471931048151,42.9882064006407,117.440324863695));
#96420=CARTESIAN_POINT('Ctrl Pts',(189.416593974544,42.7647307895591,117.754697553232));
#96421=CARTESIAN_POINT('Ctrl Pts',(189.358051649801,42.5384379229682,118.066222446577));
#96422=CARTESIAN_POINT('Ctrl Pts',(189.34997393449,42.5072138579641,118.109206892648));
#96423=CARTESIAN_POINT('Ctrl Pts',(189.341835231097,42.4759360834058,118.152137120363));
#96424=CARTESIAN_POINT('Ctrl Pts',(189.333635244335,42.4446058864512,118.195013308131));
#96425=CARTESIAN_POINT('Ctrl Pts',(189.281169294919,42.2441459861673,118.469347884994));
#96426=CARTESIAN_POINT('Ctrl Pts',(189.226201434868,42.0415675978545,118.74145480887));
#96427=CARTESIAN_POINT('Ctrl Pts',(189.168605458159,41.837000994173,119.011626542698));
#96428=CARTESIAN_POINT('Ctrl Pts',(189.150898374159,41.7741098298585,119.094687094124));
#96429=CARTESIAN_POINT('Ctrl Pts',(189.132942815417,41.7110303772408,119.177564735845));
#96430=CARTESIAN_POINT('Ctrl Pts',(189.114734900347,41.6477654678563,119.260267962345));
#96431=CARTESIAN_POINT('Ctrl Pts',(189.062359779652,41.4657837718707,119.498164034092));
#96432=CARTESIAN_POINT('Ctrl Pts',(189.007870691134,41.2822558358634,119.734617066258));
#96433=CARTESIAN_POINT('Ctrl Pts',(188.951308014775,41.0975794254857,119.969828354958));
#96434=CARTESIAN_POINT('Ctrl Pts',(188.891670312216,40.9028630941394,120.217826889982));
#96435=CARTESIAN_POINT('Ctrl Pts',(188.829727582339,40.7068697456579,120.464445000665));
#96436=CARTESIAN_POINT('Ctrl Pts',(188.765505290305,40.5100109306358,120.709918499324));
#96437=CARTESIAN_POINT('Ctrl Pts',(188.731311904526,40.4051988911872,120.840614084493));
#96438=CARTESIAN_POINT('Ctrl Pts',(188.696471946879,40.3001406356658,120.97098519985));
#96439=CARTESIAN_POINT('Ctrl Pts',(188.660986721352,40.194892939968,121.101067416233));
#96440=CARTESIAN_POINT('Ctrl Pts',(188.634061070125,40.1150325838717,121.199771830171));
#96441=CARTESIAN_POINT('Ctrl Pts',(188.606759755875,40.0350508878436,121.298330966865));
#96442=CARTESIAN_POINT('Ctrl Pts',(188.579082594393,39.9549720968558,121.396759465166));
#96443=CARTESIAN_POINT('Ctrl Pts',(188.505122801803,39.7409830005985,121.65978323385));
#96444=CARTESIAN_POINT('Ctrl Pts',(188.428490328119,39.5263977759299,121.921874171461));
#96445=CARTESIAN_POINT('Ctrl Pts',(188.349443899174,39.3119399066477,122.183309854839));
#96446=CARTESIAN_POINT('Ctrl Pts',(188.25931230754,39.0674073027749,122.48140825811));
#96447=CARTESIAN_POINT('Ctrl Pts',(188.166042607857,38.8230391186135,122.778654761601));
#96448=CARTESIAN_POINT('Ctrl Pts',(188.06996723637,38.5798577704378,123.075460334885));
#96449=CARTESIAN_POINT('Ctrl Pts',(188.020644387728,38.4550141539823,123.227833374309));
#96450=CARTESIAN_POINT('Ctrl Pts',(187.97058127727,38.3304826937849,123.380090193964));
#96451=CARTESIAN_POINT('Ctrl Pts',(187.919818326087,38.2063995497728,123.532286325396));
#96452=CARTESIAN_POINT('Ctrl Pts',(187.876714762721,38.1010387396561,123.661518283791));
#96453=CARTESIAN_POINT('Ctrl Pts',(187.833119954047,37.9960248692047,123.790706450871));
#96454=CARTESIAN_POINT('Ctrl Pts',(187.789067088822,37.8914036208365,123.91988464976));
#96455=CARTESIAN_POINT('Ctrl Pts',(187.688880417279,37.6534700700169,124.213666534698));
#96456=CARTESIAN_POINT('Ctrl Pts',(187.586266219707,37.4174238641642,124.507604623262));
#96457=CARTESIAN_POINT('Ctrl Pts',(187.481605512553,37.1838645680724,124.8020774362));
#96458=CARTESIAN_POINT('Ctrl Pts',(187.379427626148,36.9558458982757,125.089564597795));
#96459=CARTESIAN_POINT('Ctrl Pts',(187.275298297069,36.7301962684332,125.377561423478));
#96460=CARTESIAN_POINT('Ctrl Pts',(187.169565526471,36.5075211301387,125.666419468782));
#96461=CARTESIAN_POINT('Ctrl Pts',(187.060011656538,36.2767986871335,125.965716617105));
#96462=CARTESIAN_POINT('Ctrl Pts',(186.948763090548,36.0492413463077,126.265938222591));
#96463=CARTESIAN_POINT('Ctrl Pts',(186.835993331848,35.8248118979545,126.567473823342));
#96464=CARTESIAN_POINT('Ctrl Pts',(186.81435442702,35.7817470946811,126.62533419515));
#96465=CARTESIAN_POINT('Ctrl Pts',(186.792659524023,35.7387976140255,126.683242945147));
#96466=CARTESIAN_POINT('Ctrl Pts',(186.770909873261,35.6959634156462,126.741202820671));
#96467=CARTESIAN_POINT('Ctrl Pts',(186.639338192594,35.4368435091902,127.091823541781));
#96468=CARTESIAN_POINT('Ctrl Pts',(186.505773556998,35.1819666145873,127.444279414045));
#96469=CARTESIAN_POINT('Ctrl Pts',(186.370723311232,34.9317582538241,127.798621865455));
#96470=CARTESIAN_POINT('Ctrl Pts',(186.20804502502,34.6303632649153,128.225454281794));
#96471=CARTESIAN_POINT('Ctrl Pts',(186.043351381547,34.335748183931,128.655024244082));
#96472=CARTESIAN_POINT('Ctrl Pts',(185.876684597081,34.0472913013621,129.087419480968));
#96473=CARTESIAN_POINT('Ctrl Pts',(185.806771876844,33.9262905548952,129.26879891614));
#96474=CARTESIAN_POINT('Ctrl Pts',(185.736512055574,33.8063728032299,129.450675459093));
#96475=CARTESIAN_POINT('Ctrl Pts',(185.665908670656,33.6874894197892,129.633055460434));
#96476=CARTESIAN_POINT('Ctrl Pts',(185.527287154577,33.4540757545885,129.991137333107));
#96477=CARTESIAN_POINT('Ctrl Pts',(185.387363065923,33.2246908054913,130.351102371684));
#96478=CARTESIAN_POINT('Ctrl Pts',(185.246262498078,32.999087553421,130.712756874191));
#96479=CARTESIAN_POINT('Ctrl Pts',(185.10220568057,32.7687576050079,131.081988532605));
#96480=CARTESIAN_POINT('Ctrl Pts',(184.956922586553,32.5423693847545,131.452981180414));
#96481=CARTESIAN_POINT('Ctrl Pts',(184.810554291019,32.319606258196,131.825528446831));
#96482=CARTESIAN_POINT('Ctrl Pts',(184.780554568769,32.2739486115059,131.901885929007));
#96483=CARTESIAN_POINT('Ctrl Pts',(184.75050928061,32.2284430769014,131.978308718369));
#96484=CARTESIAN_POINT('Ctrl Pts',(184.720419674804,32.1830866635913,132.054795037419));
#96485=CARTESIAN_POINT('Ctrl Pts',(184.648336307881,32.0744297737673,132.238027461138));
#96486=CARTESIAN_POINT('Ctrl Pts',(184.575973994326,31.9665951990179,132.42162468394));
#96487=CARTESIAN_POINT('Ctrl Pts',(184.503318676827,31.8595431559822,132.605562041294));
#96488=CARTESIAN_POINT('Ctrl Pts',(184.348768662941,31.6318255530998,132.996827568877));
#96489=CARTESIAN_POINT('Ctrl Pts',(184.192900936543,31.4076637868292,133.38959457567));
#96490=CARTESIAN_POINT('Ctrl Pts',(184.035599174924,31.186668157996,133.783560786267));
#96491=CARTESIAN_POINT('Ctrl Pts',(183.868593799099,30.9520397745063,134.201829942223));
#96492=CARTESIAN_POINT('Ctrl Pts',(183.699971816693,30.7209801122015,134.621450788687));
#96493=CARTESIAN_POINT('Ctrl Pts',(183.52958893264,30.4929612354519,135.04206209289));
#96494=CARTESIAN_POINT('Ctrl Pts',(183.36063949118,30.2668606967534,135.459134766077));
#96495=CARTESIAN_POINT('Ctrl Pts',(183.189958389329,30.0437491561647,135.877181275877));
#96496=CARTESIAN_POINT('Ctrl Pts',(183.017403636412,29.823061307358,136.295850324503));
#96497=CARTESIAN_POINT('Ctrl Pts',(182.810366744021,29.5582727365807,136.798183278554));
#96498=CARTESIAN_POINT('Ctrl Pts',(182.600620696084,29.2970147069744,137.301414781572));
#96499=CARTESIAN_POINT('Ctrl Pts',(182.387736218738,29.0386703876795,137.804925385732));
#96500=CARTESIAN_POINT('Ctrl Pts',(182.262081339166,28.8861828755141,138.102122086581));
#96501=CARTESIAN_POINT('Ctrl Pts',(182.135333110065,28.7347093094155,138.399416072433));
#96502=CARTESIAN_POINT('Ctrl Pts',(182.007405205727,28.5841147979743,138.696680511829));
#96503=CARTESIAN_POINT('Ctrl Pts',(181.768065544775,28.3023682978958,139.252831028844));
#96504=CARTESIAN_POINT('Ctrl Pts',(181.524579784592,28.0236833319436,139.80891000626));
#96505=CARTESIAN_POINT('Ctrl Pts',(181.276383640261,27.7471156056873,140.36413417791));
#96506=CARTESIAN_POINT('Ctrl Pts',(181.253733983975,27.7218768415782,140.414802316545));
#96507=CARTESIAN_POINT('Ctrl Pts',(181.231045128986,27.6966556886218,140.465463341053));
#96508=CARTESIAN_POINT('Ctrl Pts',(181.208316664928,27.6714514183718,140.51611665903));
#96509=CARTESIAN_POINT('Ctrl Pts',(180.980534297709,27.4188567719832,141.023759086915));
#96510=CARTESIAN_POINT('Ctrl Pts',(180.748822648448,27.1680200449666,141.530632755925));
#96511=CARTESIAN_POINT('Ctrl Pts',(180.512479092602,26.9183528177257,142.036107824096));
#96512=CARTESIAN_POINT('Ctrl Pts',(180.299672774679,26.6935497206205,142.491243093911));
#96513=CARTESIAN_POINT('Ctrl Pts',(180.083110983336,26.4696940369098,142.945244465906));
#96514=CARTESIAN_POINT('Ctrl Pts',(179.862320517908,26.2463607446773,143.397657233819));
#96515=CARTESIAN_POINT('Ctrl Pts',(179.648388584287,26.0299649734357,143.836016462994));
#96516=CARTESIAN_POINT('Ctrl Pts',(179.430486159255,25.8140590945568,144.27288421347));
#96517=CARTESIAN_POINT('Ctrl Pts',(179.208227260175,25.5982699452165,144.707852190921));
#96518=CARTESIAN_POINT('Ctrl Pts',(179.195518563554,25.585931186928,144.732723528305));
#96519=CARTESIAN_POINT('Ctrl Pts',(179.182795480721,25.5735928331242,144.757588637647));
#96520=CARTESIAN_POINT('Ctrl Pts',(179.170057878368,25.5612547983027,144.78244743594));
#96521=CARTESIAN_POINT('Ctrl Pts',(178.979847025161,25.3770106944807,145.153664333906));
#96522=CARTESIAN_POINT('Ctrl Pts',(178.786394805049,25.1928363963962,145.523476609339));
#96523=CARTESIAN_POINT('Ctrl Pts',(178.589310654333,25.0084853544995,145.891550971731));
#96524=CARTESIAN_POINT('Ctrl Pts',(178.428416829498,24.8579864730049,146.192036281046));
#96525=CARTESIAN_POINT('Ctrl Pts',(178.265103079925,24.7073699745978,146.49136341204));
#96526=CARTESIAN_POINT('Ctrl Pts',(178.099180810728,24.5565114251989,146.789353762951));
#96527=CARTESIAN_POINT('Ctrl Pts',(177.920514420468,24.3940657656058,147.110232091021));
#96528=CARTESIAN_POINT('Ctrl Pts',(177.73884300383,24.2313506353695,147.429562397532));
#96529=CARTESIAN_POINT('Ctrl Pts',(177.553755639537,24.0681325678661,147.747103367846));
#96530=CARTESIAN_POINT('Ctrl Pts',(177.382332626396,23.9169643180119,148.041201401682));
#96531=CARTESIAN_POINT('Ctrl Pts',(177.207966406531,23.7653534854513,148.333785835995));
#96532=CARTESIAN_POINT('Ctrl Pts',(177.030419553461,23.6131761028683,148.624584498751));
#96533=CARTESIAN_POINT('Ctrl Pts',(176.982805614263,23.572365665981,148.702569940949));
#96534=CARTESIAN_POINT('Ctrl Pts',(176.934963189111,23.5315145984672,148.780426981826));
#96535=CARTESIAN_POINT('Ctrl Pts',(176.886888290586,23.490620772596,148.858150437944));
#96536=CARTESIAN_POINT('Ctrl Pts',(176.728507612646,23.3558978285284,149.114207009035));
#96537=CARTESIAN_POINT('Ctrl Pts',(176.56763806299,23.2207301604003,149.368817187247));
#96538=CARTESIAN_POINT('Ctrl Pts',(176.403920824963,23.084931065456,149.621773376208));
#96539=CARTESIAN_POINT('Ctrl Pts',(176.245282158161,22.9533445102802,149.866882767617));
#96540=CARTESIAN_POINT('Ctrl Pts',(176.083969629685,22.8211650153288,150.110439183361));
#96541=CARTESIAN_POINT('Ctrl Pts',(175.919700886915,22.6882438794319,150.35225852202));
#96542=CARTESIAN_POINT('Ctrl Pts',(175.861583564823,22.6412171576257,150.43781279215));
#96543=CARTESIAN_POINT('Ctrl Pts',(175.803096631979,22.5940978076811,150.523149677045));
#96544=CARTESIAN_POINT('Ctrl Pts',(175.744229001408,22.5468799342391,150.608261176452));
#96545=CARTESIAN_POINT('Origin',(160.5,51.8013867006572,102.225104347672));
#96546=CARTESIAN_POINT('Origin',(160.5,51.8013867006572,102.225104347672));
#96547=CARTESIAN_POINT('',(190.5,51.8013867006572,102.225104347672));
#96548=CARTESIAN_POINT('',(190.499797482064,51.8013867006573,102.335336081499));
#96549=CARTESIAN_POINT('Ctrl Pts',(-190.499797482064,25.5156816663762,102.335336081498));
#96550=CARTESIAN_POINT('Ctrl Pts',(-190.499797482064,60.1768636667247,102.335336081498));
#96551=CARTESIAN_POINT('Ctrl Pts',(-190.141509581597,25.5156816663762,199.844139409912));
#96552=CARTESIAN_POINT('Ctrl Pts',(-190.141509581597,60.1768636667247,199.844139409912));
#96553=CARTESIAN_POINT('Ctrl Pts',(-180.969631132311,25.5156816663762,196.));
#96554=CARTESIAN_POINT('Ctrl Pts',(-180.969631132311,60.1768636667247,196.));
#96555=CARTESIAN_POINT('Ctrl Pts',(1.58515917575596E-14,25.5156816663763,
196.));
#96556=CARTESIAN_POINT('Ctrl Pts',(1.58515917575596E-14,60.1768636667247,
196.));
#96557=CARTESIAN_POINT('',(3.34339434094657E-14,-112.4,196.));
#96558=CARTESIAN_POINT('Ctrl Pts',(129.971165261432,38.9257468402258,193.360148302349));
#96559=CARTESIAN_POINT('Ctrl Pts',(129.971165261432,57.4948506319549,193.360148302349));
#96560=CARTESIAN_POINT('Ctrl Pts',(186.116291121746,38.9257468402258,187.246632700069));
#96561=CARTESIAN_POINT('Ctrl Pts',(186.116291121746,57.4948506319549,187.246632700069));
#96562=CARTESIAN_POINT('Ctrl Pts',(190.261265602416,38.9257468402258,167.252287253607));
#96563=CARTESIAN_POINT('Ctrl Pts',(190.261265602416,57.4948506319549,167.252287253607));
#96564=CARTESIAN_POINT('Ctrl Pts',(190.499797482064,38.9257468402258,102.3353360815));
#96565=CARTESIAN_POINT('Ctrl Pts',(190.499797482064,57.4948506319549,102.3353360815));
#96566=CARTESIAN_POINT('Origin',(-122.710817715584,2.64173312008429,40.));
#96567=CARTESIAN_POINT('Origin',(-190.5,59.,211.4));
#96568=CARTESIAN_POINT('',(-190.5,51.8013867006572,211.4));
#96569=CARTESIAN_POINT('Origin',(190.5,59.,211.4));
#96570=CARTESIAN_POINT('',(190.5,51.8013867006572,211.4));
#96571=CARTESIAN_POINT('Ctrl Pts',(148.824154305368,8.98894876016889,150.608250755187));
#96572=CARTESIAN_POINT('Ctrl Pts',(148.824154305368,8.98894876016889,19.0783498489626));
#96573=CARTESIAN_POINT('Ctrl Pts',(173.689807552334,17.1099506086912,150.608250755187));
#96574=CARTESIAN_POINT('Ctrl Pts',(173.689807552334,17.1099506086912,19.0783498489626));
#96575=CARTESIAN_POINT('Ctrl Pts',(190.5,30.3189740729563,150.608250755187));
#96576=CARTESIAN_POINT('Ctrl Pts',(190.5,30.3189740729563,19.0783498489626));
#96577=CARTESIAN_POINT('Ctrl Pts',(190.5,51.8013867006572,150.608250755187));
#96578=CARTESIAN_POINT('Ctrl Pts',(190.5,51.8013867006572,19.0783498489626));
#96579=CARTESIAN_POINT('Ctrl Pts',(-190.5,51.8013867006572,150.608250755187));
#96580=CARTESIAN_POINT('Ctrl Pts',(-190.5,51.8013867006572,19.0783498489627));
#96581=CARTESIAN_POINT('Ctrl Pts',(-190.5,-4.93900225262807,150.608250755187));
#96582=CARTESIAN_POINT('Ctrl Pts',(-190.5,-4.93900225262807,19.0783498489627));
#96583=CARTESIAN_POINT('Ctrl Pts',(-73.2288472415572,-3.96262874552467,
150.608250755187));
#96584=CARTESIAN_POINT('Ctrl Pts',(-73.2288472415572,-3.96262874552467,
19.0783498489627));
#96585=CARTESIAN_POINT('Ctrl Pts',(7.71069817591099E-15,-3.96262874552467,
150.608250755187));
#96586=CARTESIAN_POINT('Ctrl Pts',(7.71069817591099E-15,-3.96262874552467,
19.0783498489627));
#96587=CARTESIAN_POINT('',(7.71069817591099E-15,-3.96262874552467,211.4));
#96588=CARTESIAN_POINT('Ctrl Pts',(153.843438675571,24.8757620423259,184.508710490748));
#96589=CARTESIAN_POINT('Ctrl Pts',(154.097189311659,24.8757620423259,185.073807734126));
#96590=CARTESIAN_POINT('Ctrl Pts',(154.210203413018,25.4303873898659,185.325487722502));
#96591=CARTESIAN_POINT('Ctrl Pts',(155.446182926033,24.8757620423259,183.789015999753));
#96592=CARTESIAN_POINT('Ctrl Pts',(155.704024681242,24.8757620423411,184.341199300067));
#96593=CARTESIAN_POINT('Ctrl Pts',(155.832745509897,25.4172512189876,184.589740299172));
#96594=CARTESIAN_POINT('Ctrl Pts',(157.036128954789,24.8757620423259,182.994575738328));
#96595=CARTESIAN_POINT('Ctrl Pts',(157.306394375555,24.8757620423136,183.529968721434));
#96596=CARTESIAN_POINT('Ctrl Pts',(157.443723445175,25.4039841842481,183.777098085943));
#96597=CARTESIAN_POINT('Ctrl Pts',(160.10416844211,24.8757620423259,181.266959679052));
#96598=CARTESIAN_POINT('Ctrl Pts',(160.398490808051,24.8757620423381,181.765887812577));
#96599=CARTESIAN_POINT('Ctrl Pts',(160.554889697529,25.3780508928129,182.00870277573));
#96600=CARTESIAN_POINT('Ctrl Pts',(161.585909292923,24.8757620423259,180.333133950633));
#96601=CARTESIAN_POINT('Ctrl Pts',(161.893267982881,24.8757620423381,180.813291368863));
#96602=CARTESIAN_POINT('Ctrl Pts',(162.058767051137,25.3653573201704,181.052285081176));
#96603=CARTESIAN_POINT('Ctrl Pts',(164.429011149336,24.8757620423259,178.304256437065));
#96604=CARTESIAN_POINT('Ctrl Pts',(164.76052871889,24.8757620423138,178.743922175154));
#96605=CARTESIAN_POINT('Ctrl Pts',(164.946574599667,25.3407885877743,178.972999501815));
#96606=CARTESIAN_POINT('Ctrl Pts',(165.790512137565,24.8757620423259,177.209392132235));
#96607=CARTESIAN_POINT('Ctrl Pts',(166.135033875418,24.8757620423076,177.627992122806));
#96608=CARTESIAN_POINT('Ctrl Pts',(166.330643962048,25.3289106297604,177.850325403001));
#96609=CARTESIAN_POINT('Ctrl Pts',(167.7262630848,24.8757620423259,175.424458331705));
#96610=CARTESIAN_POINT('Ctrl Pts',(168.091916053128,24.875762042335,175.805683882935));
#96611=CARTESIAN_POINT('Ctrl Pts',(168.299891924294,25.3119382317935,176.018973888766));
#96612=CARTESIAN_POINT('Ctrl Pts',(168.35370579661,24.8757620423259,174.805630477488));
#96613=CARTESIAN_POINT('Ctrl Pts',(168.725280353603,24.8757620423259,175.175178634881));
#96614=CARTESIAN_POINT('Ctrl Pts',(168.938439625813,25.3064219914066,175.38388734878));
#96615=CARTESIAN_POINT('Ctrl Pts',(169.265322202836,24.8757620423259,173.837815186678));
#96616=CARTESIAN_POINT('Ctrl Pts',(169.646212598391,24.8757620423259,174.188387298614));
#96617=CARTESIAN_POINT('Ctrl Pts',(169.866526829743,25.2984005760092,174.390370544029));
#96618=CARTESIAN_POINT('Ctrl Pts',(169.564467812621,24.8757620423259,173.508308943463));
#96619=CARTESIAN_POINT('Ctrl Pts',(169.948201978296,24.875762042322,173.852727851945));
#96620=CARTESIAN_POINT('Ctrl Pts',(170.171135592209,25.295767253308,174.052069713981));
#96621=CARTESIAN_POINT('Ctrl Pts',(170.147287755393,24.8757620423259,172.841326470637));
#96622=CARTESIAN_POINT('Ctrl Pts',(170.536563854742,24.8757620423297,173.173343282725));
#96623=CARTESIAN_POINT('Ctrl Pts',(170.764708940666,25.2906383278187,173.367194177139));
#96624=CARTESIAN_POINT('Ctrl Pts',(170.431610309457,24.8757620423259,172.503187193767));
#96625=CARTESIAN_POINT('Ctrl Pts',(170.823635650814,24.8757620423236,172.828932302436));
#96626=CARTESIAN_POINT('Ctrl Pts',(171.054333341806,25.2881370228471,173.019938913282));
#96627=CARTESIAN_POINT('Ctrl Pts',(171.817076225877,24.8757620423259,170.788785130436));
#96628=CARTESIAN_POINT('Ctrl Pts',(172.219289850269,24.875762042335,171.086871061764));
#96629=CARTESIAN_POINT('Ctrl Pts',(172.465898368354,25.2759637810014,171.259086668886));
#96630=CARTESIAN_POINT('Ctrl Pts',(172.810442504972,24.8757620423259,169.341840426858));
#96631=CARTESIAN_POINT('Ctrl Pts',(173.224067477814,24.8757620423259,169.612833465978));
#96632=CARTESIAN_POINT('Ctrl Pts',(173.478886091858,25.267312726279,169.772183826282));
#96633=CARTESIAN_POINT('Ctrl Pts',(174.107069219023,24.8757620423259,167.044573700205));
#96634=CARTESIAN_POINT('Ctrl Pts',(174.535707663812,24.8757620423259,167.271257953513));
#96635=CARTESIAN_POINT('Ctrl Pts',(174.802046949673,25.2562438193643,167.410304255125));
#96636=CARTESIAN_POINT('Ctrl Pts',(174.506855867878,24.8757620423259,166.257555096081));
#96637=CARTESIAN_POINT('Ctrl Pts',(174.939890357575,24.8757620423321,166.469932193093));
#96638=CARTESIAN_POINT('Ctrl Pts',(175.210198426796,25.2528791783321,166.600945447381));
#96639=CARTESIAN_POINT('Ctrl Pts',(175.054500634198,24.8757620423259,165.042901677538));
#96640=CARTESIAN_POINT('Ctrl Pts',(175.493435316943,24.8757620423228,165.23296575935));
#96641=CARTESIAN_POINT('Ctrl Pts',(175.769094570506,25.2480730731251,165.351948198845));
#96642=CARTESIAN_POINT('Ctrl Pts',(175.228346721299,24.8757620423259,164.632216279467));
#96643=CARTESIAN_POINT('Ctrl Pts',(175.669034332558,24.8757620423282,164.814988071584));
#96644=CARTESIAN_POINT('Ctrl Pts',(175.946466324372,25.2465059135025,164.929681619307));
#96645=CARTESIAN_POINT('Ctrl Pts',(175.555134756084,24.8757620423259,163.807963820627));
#96646=CARTESIAN_POINT('Ctrl Pts',(175.998882222778,24.8757620423236,163.976305634484));
#96647=CARTESIAN_POINT('Ctrl Pts',(176.279628859577,25.2433755556989,164.082445685088));
#96648=CARTESIAN_POINT('Ctrl Pts',(175.708568670929,24.8757620423259,163.393346553788));
#96649=CARTESIAN_POINT('Ctrl Pts',(176.153645063015,24.8757620423251,163.554541064828));
#96650=CARTESIAN_POINT('Ctrl Pts',(176.435919583728,25.2418067111356,163.656398290152));
#96651=CARTESIAN_POINT('Ctrl Pts',(176.427992501896,24.8757620423259,161.308318933633));
#96652=CARTESIAN_POINT('Ctrl Pts',(176.87730024609,24.8757620423289,161.437555001007));
#96653=CARTESIAN_POINT('Ctrl Pts',(177.16765157546,25.2336828542469,161.515194813592));
#96654=CARTESIAN_POINT('Ctrl Pts',(176.849355140085,24.8757620423259,159.601737069089));
#96655=CARTESIAN_POINT('Ctrl Pts',(177.298473156492,24.875762042329,159.707111376069));
#96656=CARTESIAN_POINT('Ctrl Pts',(177.591814447343,25.2258569061289,159.767692273689));
#96657=CARTESIAN_POINT('Ctrl Pts',(177.474201675422,24.8757620423259,156.129938446047));
#96658=CARTESIAN_POINT('Ctrl Pts',(177.915514314354,24.8757620423228,156.194887636441));
#96659=CARTESIAN_POINT('Ctrl Pts',(178.211970156958,25.2073379577766,156.230317176798));
#96660=CARTESIAN_POINT('Ctrl Pts',(177.679073669645,24.8757620423259,154.358973529501));
#96661=CARTESIAN_POINT('Ctrl Pts',(178.114003744645,24.8757620423629,154.40887674537));
#96662=CARTESIAN_POINT('Ctrl Pts',(178.409947754537,25.1969691506768,154.433928342043));
#96663=CARTESIAN_POINT('Ctrl Pts',(177.81394122412,24.8757620423259,152.596186324432));
#96664=CARTESIAN_POINT('Ctrl Pts',(178.241859855773,24.8757620423256,152.628925287436));
#96665=CARTESIAN_POINT('Ctrl Pts',(178.536663099516,25.1868384529694,152.651479916099));
#96666=CARTESIAN_POINT('Ctrl Pts',(177.813017113379,24.8757620423259,152.608250755187));
#96667=CARTESIAN_POINT('Ctrl Pts',(177.765987296558,24.8757620423259,153.221513948998));
#96668=CARTESIAN_POINT('Ctrl Pts',(177.710582914372,24.8757620423259,153.834376894056));
#96669=CARTESIAN_POINT('Ctrl Pts',(177.645263460167,24.8757620423259,154.44568556563));
#96670=CARTESIAN_POINT('Ctrl Pts',(177.586074917099,24.875762042326,154.999616551044));
#96671=CARTESIAN_POINT('Ctrl Pts',(177.51874600106,24.8757620423259,155.552273151529));
#96672=CARTESIAN_POINT('Ctrl Pts',(177.442095277715,24.8757620423273,156.102812608023));
#96673=CARTESIAN_POINT('Ctrl Pts',(177.36544455437,24.8757620423287,156.653352064516));
#96674=CARTESIAN_POINT('Ctrl Pts',(177.279473222263,24.8757620423312,157.201775687774));
#96675=CARTESIAN_POINT('Ctrl Pts',(177.182947814112,24.8757620423413,157.747235454427));
#96676=CARTESIAN_POINT('Ctrl Pts',(177.17583178297,24.875762042342,157.787447754595));
#96677=CARTESIAN_POINT('Ctrl Pts',(177.168658563601,24.8757620423432,157.827643161308));
#96678=CARTESIAN_POINT('Ctrl Pts',(177.161427682835,24.8757620423448,157.867821154608));
#96679=CARTESIAN_POINT('Ctrl Pts',(176.979848702746,24.8757620423849,158.87675482138));
#96680=CARTESIAN_POINT('Ctrl Pts',(176.761269560344,24.8757620439143,159.876604034587));
#96681=CARTESIAN_POINT('Ctrl Pts',(176.496786965883,24.8757620450215,160.864992501382));
#96682=CARTESIAN_POINT('Ctrl Pts',(176.328407801087,24.8757620457263,161.494236270229));
#96683=CARTESIAN_POINT('Ctrl Pts',(176.141424196877,24.8757620449383,162.118834667825));
#96684=CARTESIAN_POINT('Ctrl Pts',(175.933549890014,24.8757620433657,162.738171134661));
#96685=CARTESIAN_POINT('Ctrl Pts',(175.906871882401,24.8757620431639,162.817655046003));
#96686=CARTESIAN_POINT('Ctrl Pts',(175.879852392006,24.8757620430266,162.89704875974));
#96687=CARTESIAN_POINT('Ctrl Pts',(175.852486142522,24.8757620429244,162.976352314521));
#96688=CARTESIAN_POINT('Ctrl Pts',(175.708576843098,24.8757620423867,163.393381290935));
#96689=CARTESIAN_POINT('Ctrl Pts',(175.555168053394,24.8757620425669,163.807939748437));
#96690=CARTESIAN_POINT('Ctrl Pts',(175.391763439743,24.8757620426241,164.22009905024));
#96691=CARTESIAN_POINT('Ctrl Pts',(175.267447937342,24.8757620426675,164.533662966999));
#96692=CARTESIAN_POINT('Ctrl Pts',(175.137061255448,24.8757620426762,164.846446523615));
#96693=CARTESIAN_POINT('Ctrl Pts',(175.001324262928,24.8757620425231,165.156599195375));
#96694=CARTESIAN_POINT('Ctrl Pts',(174.958712271164,24.875762042475,165.253965601166));
#96695=CARTESIAN_POINT('Ctrl Pts',(174.915584685987,24.8757620424422,165.351048867319));
#96696=CARTESIAN_POINT('Ctrl Pts',(174.871964753249,24.875762042418,165.447791729611));
#96697=CARTESIAN_POINT('Ctrl Pts',(174.663058628572,24.875762042302,165.911116067434));
#96698=CARTESIAN_POINT('Ctrl Pts',(174.442901928491,24.875762042331,166.366783640181));
#96699=CARTESIAN_POINT('Ctrl Pts',(174.211821876959,24.8757620423295,166.815301616639));
#96700=CARTESIAN_POINT('Ctrl Pts',(174.097014960134,24.8757620423288,167.038137667074));
#96701=CARTESIAN_POINT('Ctrl Pts',(173.979511062044,24.875762042329,167.259208456611));
#96702=CARTESIAN_POINT('Ctrl Pts',(173.859346408156,24.8757620423283,167.478573498444));
#96703=CARTESIAN_POINT('Ctrl Pts',(173.798526854331,24.8757620423279,167.589601854432));
#96704=CARTESIAN_POINT('Ctrl Pts',(173.737029744405,24.8757620423276,167.700185927368));
#96705=CARTESIAN_POINT('Ctrl Pts',(173.674861839331,24.8757620423274,167.810330136494));
#96706=CARTESIAN_POINT('Ctrl Pts',(172.89367803685,24.8757620423246,169.194370213202));
#96707=CARTESIAN_POINT('Ctrl Pts',(172.007181861288,24.8757620420351,170.509352277933));
#96708=CARTESIAN_POINT('Ctrl Pts',(171.025691357068,24.8757620426587,171.762020930194));
#96709=CARTESIAN_POINT('Ctrl Pts',(170.92109883156,24.8757620427251,171.895511552264));
#96710=CARTESIAN_POINT('Ctrl Pts',(170.815442443059,24.8757620427619,172.028272940729));
#96711=CARTESIAN_POINT('Ctrl Pts',(170.708726570032,24.8757620427661,172.160325430636));
#96712=CARTESIAN_POINT('Ctrl Pts',(170.431637643182,24.8757620427769,172.503201159225));
#96713=CARTESIAN_POINT('Ctrl Pts',(170.147366737827,24.8757620425845,172.841271863791));
#96714=CARTESIAN_POINT('Ctrl Pts',(169.855890926735,24.8757620424782,173.174829191376));
#96715=CARTESIAN_POINT('Ctrl Pts',(169.691001898707,24.8757620424181,173.363523901001));
#96716=CARTESIAN_POINT('Ctrl Pts',(169.523598843296,24.8757620423814,173.550986300062));
#96717=CARTESIAN_POINT('Ctrl Pts',(169.354192863934,24.8757620423652,173.73672056851));
#96718=CARTESIAN_POINT('Ctrl Pts',(169.224305057717,24.8757620423528,173.879127682821));
#96719=CARTESIAN_POINT('Ctrl Pts',(169.093313104621,24.875762042345,174.020437340781));
#96720=CARTESIAN_POINT('Ctrl Pts',(168.96145390585,24.8757620423398,174.160423899149));
#96721=CARTESIAN_POINT('Ctrl Pts',(168.603675690039,24.8757620423257,174.540254366473));
#96722=CARTESIAN_POINT('Ctrl Pts',(168.239240001171,24.8757620423256,174.910770992204));
#96723=CARTESIAN_POINT('Ctrl Pts',(167.86832608009,24.875762042332,175.272717283235));
#96724=CARTESIAN_POINT('Ctrl Pts',(167.76110110206,24.8757620423338,175.377349870198));
#96725=CARTESIAN_POINT('Ctrl Pts',(167.653334541672,24.8757620423368,175.481265972554));
#96726=CARTESIAN_POINT('Ctrl Pts',(167.545030251731,24.8757620423426,175.584482916587));
#96727=CARTESIAN_POINT('Ctrl Pts',(167.391414817332,24.875762042351,175.73088261787));
#96728=CARTESIAN_POINT('Ctrl Pts',(167.236735452103,24.8757620423595,175.875857359385));
#96729=CARTESIAN_POINT('Ctrl Pts',(167.081018835541,24.8757620423659,176.019442844285));
#96730=CARTESIAN_POINT('Ctrl Pts',(165.977690059272,24.8757620424114,177.036816589251));
#96731=CARTESIAN_POINT('Ctrl Pts',(164.822456353684,24.8757620418276,177.984667554233));
#96732=CARTESIAN_POINT('Ctrl Pts',(163.622189357779,24.8757620429691,178.872211607));
#96733=CARTESIAN_POINT('Ctrl Pts',(163.418575347589,24.8757620431627,179.022775110304));
#96734=CARTESIAN_POINT('Ctrl Pts',(163.213663170986,24.8757620433069,179.171600306124));
#96735=CARTESIAN_POINT('Ctrl Pts',(163.007486724642,24.8757620433668,179.318732333689));
#96736=CARTESIAN_POINT('Ctrl Pts',(161.826761409925,24.8757620437098,180.161323777245));
#96737=CARTESIAN_POINT('Ctrl Pts',(160.604478799181,24.8757620422148,180.948253563706));
#96738=CARTESIAN_POINT('Ctrl Pts',(159.345247936767,24.8757620424794,181.685692517432));
#96739=CARTESIAN_POINT('Ctrl Pts',(159.088411572373,24.8757620425333,181.836102696765));
#96740=CARTESIAN_POINT('Ctrl Pts',(158.830038252835,24.8757620426851,181.984456843645));
#96741=CARTESIAN_POINT('Ctrl Pts',(158.570168232156,24.8757620431183,182.130802398217));
#96742=CARTESIAN_POINT('Ctrl Pts',(157.463233311892,24.8757620449639,182.754171744003));
#96743=CARTESIAN_POINT('Ctrl Pts',(156.32723882416,24.8757620554769,183.341433737248));
#96744=CARTESIAN_POINT('Ctrl Pts',(155.17857190235,24.8757620474239,183.890265373549));
#96745=CARTESIAN_POINT('Ctrl Pts',(155.043897412595,24.8757620464797,183.954612678392));
#96746=CARTESIAN_POINT('Ctrl Pts',(154.909048771853,24.8757620454079,184.018431744722));
#96747=CARTESIAN_POINT('Ctrl Pts',(154.774052417606,24.8757620444565,184.081718857687));
#96748=CARTESIAN_POINT('Origin',(-205.7,23.8757620423259,152.608250755187));
#96749=CARTESIAN_POINT('',(178.303739692644,24.8757620423259,152.608250755187));
#96750=CARTESIAN_POINT('',(-178.303739692644,23.8757620423259,151.608250755187));
#96751=CARTESIAN_POINT('Ctrl Pts',(111.133322854733,1.83216991269566,151.608250755187));
#96752=CARTESIAN_POINT('Ctrl Pts',(111.270341463106,0.841601439060684,151.608250755187));
#96753=CARTESIAN_POINT('Ctrl Pts',(111.270341463106,0.841601439060711,150.608250755187));
#96754=CARTESIAN_POINT('Ctrl Pts',(106.548434494274,1.19797344937741,151.608250755187));
#96755=CARTESIAN_POINT('Ctrl Pts',(106.671764202407,0.205511483093893,151.608250755379));
#96756=CARTESIAN_POINT('Ctrl Pts',(106.671764202405,0.205511483112742,150.608250755315));
#96757=CARTESIAN_POINT('Ctrl Pts',(101.948195700743,0.65791952309158,151.608250755187));
#96758=CARTESIAN_POINT('Ctrl Pts',(102.059566500144,-0.335917557920184,
151.608250755122));
#96759=CARTESIAN_POINT('Ctrl Pts',(102.059566500147,-0.335917557951168,
150.608250755122));
#96760=CARTESIAN_POINT('Ctrl Pts',(92.723767631763,-0.275480355398272,151.608250755187));
#96761=CARTESIAN_POINT('Ctrl Pts',(92.8137443254523,-1.27148225958765,151.608250755251));
#96762=CARTESIAN_POINT('Ctrl Pts',(92.8137443254492,-1.27148225955667,150.608250755251));
#96763=CARTESIAN_POINT('Ctrl Pts',(88.0977465730908,-0.668756637725884,
151.608250755187));
#96764=CARTESIAN_POINT('Ctrl Pts',(88.1782833145606,-1.66554450169544,151.608250755187));
#96765=CARTESIAN_POINT('Ctrl Pts',(88.1782833146266,-1.66554450171365,150.608250755187));
#96766=CARTESIAN_POINT('Ctrl Pts',(74.2033680985811,-1.6726098062369,151.608250755187));
#96767=CARTESIAN_POINT('Ctrl Pts',(74.2584777381936,-2.67123474963045,151.608250755187));
#96768=CARTESIAN_POINT('Ctrl Pts',(74.2584777380615,-2.67123474959403,150.608250755187));
#96769=CARTESIAN_POINT('Ctrl Pts',(64.9347005236076,-2.10826818027943,151.608250755187));
#96770=CARTESIAN_POINT('Ctrl Pts',(64.9766672764937,-3.10744308241369,151.608250755187));
#96771=CARTESIAN_POINT('Ctrl Pts',(64.9766672764947,-3.10744308244679,150.608250755187));
#96772=CARTESIAN_POINT('Ctrl Pts',(46.3902608861325,-2.69091503172259,151.608250755187));
#96773=CARTESIAN_POINT('Ctrl Pts',(46.411101044151,-3.69075370931775,151.608250755187));
#96774=CARTESIAN_POINT('Ctrl Pts',(46.41110104415,-3.69075370928465,150.608250755187));
#96775=CARTESIAN_POINT('Ctrl Pts',(37.1144344070604,-2.83569245393131,151.608250755187));
#96776=CARTESIAN_POINT('Ctrl Pts',(37.1273040291325,-3.83562452408217,151.6082507548));
#96777=CARTESIAN_POINT('Ctrl Pts',(37.1273040291327,-3.83562452423629,150.608250754929));
#96778=CARTESIAN_POINT('Ctrl Pts',(18.5590407294506,-2.97325419480569,151.608250755187));
#96779=CARTESIAN_POINT('Ctrl Pts',(18.5609978432699,-3.97326716587542,151.608250755573));
#96780=CARTESIAN_POINT('Ctrl Pts',(18.5609978432698,-3.9732671657213,150.608250755444));
#96781=CARTESIAN_POINT('Ctrl Pts',(9.27942897160271,-2.96262874564539,151.608250755187));
#96782=CARTESIAN_POINT('Ctrl Pts',(9.27841046030881,-3.9626287456454,151.608250755187));
#96783=CARTESIAN_POINT('Ctrl Pts',(9.27841046030894,-3.96262874552467,150.608250755187));
#96784=CARTESIAN_POINT('Ctrl Pts',(7.59225281309826E-15,-2.96262874552467,
151.608250755187));
#96785=CARTESIAN_POINT('Ctrl Pts',(7.71069817591099E-15,-3.96262874552467,
151.608250755187));
#96786=CARTESIAN_POINT('Ctrl Pts',(7.71069817591099E-15,-3.96262874552467,
150.608250755187));
#96787=CARTESIAN_POINT('Ctrl Pts',(110.612002249452,0.751198971720865,150.608250755187));
#96788=CARTESIAN_POINT('Ctrl Pts',(106.050488567514,0.129377001469773,150.608250755187));
#96789=CARTESIAN_POINT('Ctrl Pts',(101.47400078582,-0.400723078925373,150.608250755187));
#96790=CARTESIAN_POINT('Ctrl Pts',(92.2976017204801,-1.31744564164295,150.608250755187));
#96791=CARTESIAN_POINT('Ctrl Pts',(87.6963246266761,-1.70397824638163,150.608250755187));
#96792=CARTESIAN_POINT('Ctrl Pts',(73.8738846253088,-2.69123907257862,150.608250755187));
#96793=CARTESIAN_POINT('Ctrl Pts',(64.6442699267499,-3.12078579779498,150.608250755187));
#96794=CARTESIAN_POINT('Ctrl Pts',(46.1823666336506,-3.69495161107092,150.608250755187));
#96795=CARTESIAN_POINT('Ctrl Pts',(36.9474605582068,-3.83767561637138,150.608250755187));
#96796=CARTESIAN_POINT('Ctrl Pts',(18.4738883141652,-3.97318469247364,150.608250755187));
#96797=CARTESIAN_POINT('Ctrl Pts',(9.23693273607507,-3.96262874552467,150.608250755187));
#96798=CARTESIAN_POINT('Ctrl Pts',(7.71069817591099E-15,-3.96262874552467,
150.608250755187));
#96799=CARTESIAN_POINT('Origin',(-205.7,-9.35236728728476,151.608250755187));
#96800=CARTESIAN_POINT('Origin',(-205.7,24.8757620423259,209.282162333937));
#96801=CARTESIAN_POINT('Ctrl Pts',(96.5581428144939,29.1702255611255,195.428125979215));
#96802=CARTESIAN_POINT('Ctrl Pts',(96.7311023279802,27.510923329495,195.422864721506));
#96803=CARTESIAN_POINT('Ctrl Pts',(96.8973711956851,25.8618521564905,195.232745022291));
#96804=CARTESIAN_POINT('Ctrl Pts',(92.4415169449766,28.7565333888699,195.553349675513));
#96805=CARTESIAN_POINT('Ctrl Pts',(92.5976675800192,27.0947339894513,195.549474400368));
#96806=CARTESIAN_POINT('Ctrl Pts',(92.7481683291537,25.4431914874834,195.360541294257));
#96807=CARTESIAN_POINT('Ctrl Pts',(88.3520507412781,28.4030914565636,195.64700268798));
#96808=CARTESIAN_POINT('Ctrl Pts',(88.4934425831405,26.7395278446426,195.64402437791));
#96809=CARTESIAN_POINT('Ctrl Pts',(88.6300070463228,25.0862367508384,195.455861695539));
#96810=CARTESIAN_POINT('Ctrl Pts',(80.2076413227381,27.7915957659344,195.794185887528));
#96811=CARTESIAN_POINT('Ctrl Pts',(80.3223216239699,26.125270179941,195.792536551935));
#96812=CARTESIAN_POINT('Ctrl Pts',(80.4335599248988,24.4692428089101,195.605516960837));
#96813=CARTESIAN_POINT('Ctrl Pts',(76.1526889733453,27.5336304760513,195.847553658596));
#96814=CARTESIAN_POINT('Ctrl Pts',(76.2554887724622,25.8663249070321,195.846327241293));
#96815=CARTESIAN_POINT('Ctrl Pts',(76.3554012815499,24.2093261329018,195.659672537072));
#96816=CARTESIAN_POINT('Ctrl Pts',(68.0652206896679,27.0943461905063,195.928468679087));
#96817=CARTESIAN_POINT('Ctrl Pts',(68.1465044178566,25.4255294368387,195.927853344985));
#96818=CARTESIAN_POINT('Ctrl Pts',(68.2258303093629,23.7670327953681,195.741726502934));
#96819=CARTESIAN_POINT('Ctrl Pts',(64.03279795575,26.9130916763118,195.955933585121));
#96820=CARTESIAN_POINT('Ctrl Pts',(64.1044855996088,25.2437500578336,195.955502808343));
#96821=CARTESIAN_POINT('Ctrl Pts',(64.1745855046219,23.5847329161387,195.769535871164));
#96822=CARTESIAN_POINT('Ctrl Pts',(55.9832533396131,26.6122137200978,195.994697701943));
#96823=CARTESIAN_POINT('Ctrl Pts',(56.0376446038494,24.9420845379358,195.994521322064));
#96824=CARTESIAN_POINT('Ctrl Pts',(56.0910584623061,23.282286359139,195.808775043));
#96825=CARTESIAN_POINT('Ctrl Pts',(51.9661782517966,26.4926340937108,196.005952434106));
#96826=CARTESIAN_POINT('Ctrl Pts',(52.0128883060383,24.8222448356165,196.005844390051));
#96827=CARTESIAN_POINT('Ctrl Pts',(52.0588588944913,23.1621886081543,195.820157585625));
#96828=CARTESIAN_POINT('Ctrl Pts',(39.9311373606373,26.2070303356449,196.025623827227));
#96829=CARTESIAN_POINT('Ctrl Pts',(39.9573441152576,24.5360837036126,196.025644384184));
#96830=CARTESIAN_POINT('Ctrl Pts',(39.9833816094678,22.8754744091628,195.840069630165));
#96831=CARTESIAN_POINT('Ctrl Pts',(31.9288875819601,26.1142952297546,196.020515138928));
#96832=CARTESIAN_POINT('Ctrl Pts',(31.9447866062045,24.4432653675089,196.020526192105));
#96833=CARTESIAN_POINT('Ctrl Pts',(31.9607025010364,22.7825732665138,195.834943371232));
#96834=CARTESIAN_POINT('Ctrl Pts',(15.947733524435,26.0285644344409,196.007873194612));
#96835=CARTESIAN_POINT('Ctrl Pts',(15.9497758197389,24.3574643678052,196.007876333974));
#96836=CARTESIAN_POINT('Ctrl Pts',(15.9519837644084,22.6967024452114,195.822286623132));
#96837=CARTESIAN_POINT('Ctrl Pts',(7.96912902423969,26.0373712549187,196.));
#96838=CARTESIAN_POINT('Ctrl Pts',(7.96761387059107,24.3662859578773,196.000000000019));
#96839=CARTESIAN_POINT('Ctrl Pts',(7.96622304565945,22.7055386933791,195.814407453179));
#96840=CARTESIAN_POINT('Ctrl Pts',(1.578508351368E-14,26.0373712544753,
196.));
#96841=CARTESIAN_POINT('Ctrl Pts',(1.58962544981566E-14,24.3662859574616,
196.));
#96842=CARTESIAN_POINT('Ctrl Pts',(1.59444394375923E-14,22.7055386929907,
195.814407453146));
#96843=CARTESIAN_POINT('Ctrl Pts',(1.4210854715202E-14,26.0373712544753,
196.));
#96844=CARTESIAN_POINT('Ctrl Pts',(3.98999039555811,26.0373712544753,196.));
#96845=CARTESIAN_POINT('Ctrl Pts',(7.98016079670639,26.0351684189602,196.001973114377));
#96846=CARTESIAN_POINT('Ctrl Pts',(11.9700380568879,26.0383329718934,196.004732891428));
#96847=CARTESIAN_POINT('Ctrl Pts',(15.4357914559827,26.0410818183792,196.00713013477));
#96848=CARTESIAN_POINT('Ctrl Pts',(18.9013236137276,26.0478805596461,196.010120892553));
#96849=CARTESIAN_POINT('Ctrl Pts',(22.3663201987643,26.0636449968344,196.012933146671));
#96850=CARTESIAN_POINT('Ctrl Pts',(22.8903296073034,26.0660290434573,196.013358442218));
#96851=CARTESIAN_POINT('Ctrl Pts',(23.414326759107,26.0686180422282,196.013779667672));
#96852=CARTESIAN_POINT('Ctrl Pts',(23.9383105582663,26.071428887833,196.014194166774));
#96853=CARTESIAN_POINT('Ctrl Pts',(23.9724687182037,26.071612125013,196.014221187698));
#96854=CARTESIAN_POINT('Ctrl Pts',(24.0066268159181,26.0717962720147,196.014248186252));
#96855=CARTESIAN_POINT('Ctrl Pts',(24.0407848516479,26.0719813325248,196.014275161106));
#96856=CARTESIAN_POINT('Ctrl Pts',(27.1918482515225,26.0890530811696,196.016763579223));
#96857=CARTESIAN_POINT('Ctrl Pts',(30.3424154561325,26.1139030681914,196.019049376945));
#96858=CARTESIAN_POINT('Ctrl Pts',(33.492298128033,26.1494014787918,196.020095240139));
#96859=CARTESIAN_POINT('Ctrl Pts',(36.4310110091503,26.1825200572776,196.021070988114));
#96860=CARTESIAN_POINT('Ctrl Pts',(39.369128099848,26.2249073749037,196.020967358996));
#96861=CARTESIAN_POINT('Ctrl Pts',(42.3064876248667,26.2788516104082,196.018953311004));
#96862=CARTESIAN_POINT('Ctrl Pts',(44.1894841856694,26.3134326036659,196.017662204004));
#96863=CARTESIAN_POINT('Ctrl Pts',(46.0721692493293,26.3527620049448,196.015586250003));
#96864=CARTESIAN_POINT('Ctrl Pts',(47.9544979792259,26.3974318154924,196.012509565106));
#96865=CARTESIAN_POINT('Ctrl Pts',(47.9907577661141,26.3982923016472,196.012450298127));
#96866=CARTESIAN_POINT('Ctrl Pts',(48.0270174302833,26.3991547660561,196.012390648295));
#96867=CARTESIAN_POINT('Ctrl Pts',(48.0632769722344,26.4000192132909,196.012330613117));
#96868=CARTESIAN_POINT('Ctrl Pts',(50.5137145742306,26.4584389807552,196.008273406405));
#96869=CARTESIAN_POINT('Ctrl Pts',(52.963664586409,26.5259196423555,196.002454852829));
#96870=CARTESIAN_POINT('Ctrl Pts',(55.4128930506474,26.6038431345442,195.994113042992));
#96871=CARTESIAN_POINT('Ctrl Pts',(56.944906486256,26.6525849480279,195.988895169309));
#96872=CARTESIAN_POINT('Ctrl Pts',(58.4766373725112,26.7054118064935,195.982690335751));
#96873=CARTESIAN_POINT('Ctrl Pts',(60.0080256579301,26.7626524267857,195.975315643483));
#96874=CARTESIAN_POINT('Ctrl Pts',(62.218848643179,26.8452891298589,195.964669003875));
#96875=CARTESIAN_POINT('Ctrl Pts',(64.4289443566986,26.9371137869464,195.951596468763));
#96876=CARTESIAN_POINT('Ctrl Pts',(66.6383460860964,27.0392640263435,195.935316684546));
#96877=CARTESIAN_POINT('Ctrl Pts',(68.4417010588521,27.1226409603496,195.92202882049));
#96878=CARTESIAN_POINT('Ctrl Pts',(70.2445934657614,27.2128963010836,195.906604522875));
#96879=CARTESIAN_POINT('Ctrl Pts',(72.0470329001817,27.3106267279901,195.888629690922));
#96880=CARTESIAN_POINT('Ctrl Pts',(72.0676736114691,27.3117458921002,195.888423851375));
#96881=CARTESIAN_POINT('Ctrl Pts',(72.0883142769542,27.3128660370197,195.888217677336));
#96882=CARTESIAN_POINT('Ctrl Pts',(72.1089548960627,27.3139871636003,195.888011168196));
#96883=CARTESIAN_POINT('Ctrl Pts',(73.9322669317684,27.4130231264906,195.86976895369));
#96884=CARTESIAN_POINT('Ctrl Pts',(75.7551996644265,27.5197096363461,195.848926770467));
#96885=CARTESIAN_POINT('Ctrl Pts',(77.577565779252,27.6347862725935,195.824854974109));
#96886=CARTESIAN_POINT('Ctrl Pts',(79.326413066646,27.7452204282258,195.801754294493));
#96887=CARTESIAN_POINT('Ctrl Pts',(81.0747386415879,27.8633814946748,195.775679190743));
#96888=CARTESIAN_POINT('Ctrl Pts',(82.8223589117719,27.9898836032052,195.746094692498));
#96889=CARTESIAN_POINT('Ctrl Pts',(83.3082440207675,28.0250545678822,195.737869411869));
#96890=CARTESIAN_POINT('Ctrl Pts',(83.7940744942396,28.060870038313,195.729372997879));
#96891=CARTESIAN_POINT('Ctrl Pts',(84.2798461077883,28.0973426261767,195.720594286385));
#96892=CARTESIAN_POINT('Ctrl Pts',(85.8745187030419,28.2170734517788,195.691775865854));
#96893=CARTESIAN_POINT('Ctrl Pts',(87.4685601335887,28.343875044827,195.659938145996));
#96894=CARTESIAN_POINT('Ctrl Pts',(89.0620397243112,28.4783563924592,195.624449393539));
#96895=CARTESIAN_POINT('Ctrl Pts',(90.6059337456486,28.608652977241,195.590064972765));
#96896=CARTESIAN_POINT('Ctrl Pts',(92.149300428614,28.7461588482606,195.552253116234));
#96897=CARTESIAN_POINT('Ctrl Pts',(93.6921811470376,28.8913921093023,195.510464455059));
#96898=CARTESIAN_POINT('Ctrl Pts',(94.4512527163619,28.9628444504072,195.489905131037));
#96899=CARTESIAN_POINT('Ctrl Pts',(95.2102063150246,29.0361666270266,195.468383631185));
#96900=CARTESIAN_POINT('Ctrl Pts',(95.969044764986,29.1114169499324,195.445836982328));
#96901=CARTESIAN_POINT('Ctrl Pts',(7.71069817591099E-15,-3.96262874552467,
150.608250755187));
#96902=CARTESIAN_POINT('Ctrl Pts',(7.71069817591099E-15,-3.96262874552467,
19.0783498489627));
#96903=CARTESIAN_POINT('Ctrl Pts',(32.8608169036053,-3.96262874552466,150.608250755187));
#96904=CARTESIAN_POINT('Ctrl Pts',(32.8608169036053,-3.96262874552466,19.0783498489627));
#96905=CARTESIAN_POINT('Ctrl Pts',(74.5903827540722,-4.15923996764941,150.608250755187));
#96906=CARTESIAN_POINT('Ctrl Pts',(74.5903827540722,-4.15923996764941,19.0783498489627));
#96907=CARTESIAN_POINT('Ctrl Pts',(110.612002249464,0.751198971722513,150.608250755187));
#96908=CARTESIAN_POINT('Ctrl Pts',(110.612002249464,0.751198971722513,19.0783498489627));
#96909=CARTESIAN_POINT('Ctrl Pts',(1.58070730646102E-14,25.8648855730305,
196.));
#96910=CARTESIAN_POINT('Ctrl Pts',(1.14416717392176E-14,60.1070228853939,
196.));
#96911=CARTESIAN_POINT('Ctrl Pts',(53.668246544272,25.8648855730305,196.));
#96912=CARTESIAN_POINT('Ctrl Pts',(53.668246544272,60.1070228853939,196.));
#96913=CARTESIAN_POINT('Ctrl Pts',(92.2273133188686,25.8648855730305,196.338082381737));
#96914=CARTESIAN_POINT('Ctrl Pts',(92.2273133188686,60.1070228853939,196.338082381737));
#96915=CARTESIAN_POINT('Ctrl Pts',(119.928096709094,25.8648855730305,194.270533336501));
#96916=CARTESIAN_POINT('Ctrl Pts',(119.928096709094,60.1070228853939,194.270533336501));
#96917=CARTESIAN_POINT('Origin',(-205.7,23.8757620423259,152.608250755187));
#96918=CARTESIAN_POINT('',(178.303739692644,24.8757620423259,152.608250755187));
#96919=CARTESIAN_POINT('Origin',(-205.7,23.8757620423259,152.608250755187));
#96920=CARTESIAN_POINT('',(178.303739692644,24.8757620423259,152.608250755187));
#96921=CARTESIAN_POINT('Origin',(-205.7,23.8757620423259,152.608250755187));
#96922=CARTESIAN_POINT('',(178.303739692644,24.8757620423259,152.608250755187));
#96923=CARTESIAN_POINT('Origin',(-205.7,23.8757620423259,152.608250755187));
#96924=CARTESIAN_POINT('',(178.303739692644,24.8757620423259,152.608250755187));
#96925=CARTESIAN_POINT('Origin',(-205.7,24.8757620423259,209.282162333937));
#96926=CARTESIAN_POINT('',(0.,0.,0.));
#96927=CARTESIAN_POINT('Origin',(0.,799.524274233158,64.2994740882088));
#96928=CARTESIAN_POINT('',(-1.46957615897682E-15,819.591294394281,52.2994740882088));
#96929=CARTESIAN_POINT('Origin',(0.,819.591294394281,64.2994740882088));
#96930=CARTESIAN_POINT('',(-1.46957615897682E-15,842.524274233158,52.2994740882088));
#96931=CARTESIAN_POINT('',(-1.46957615897682E-15,799.524274233158,52.2994740882088));
#96932=CARTESIAN_POINT('Origin',(0.,842.524274233158,64.2994740882088));
#96933=CARTESIAN_POINT('Origin',(0.,0.,48.));
#96934=CARTESIAN_POINT('',(44.0626743494,846.77801102117,48.));
#96935=CARTESIAN_POINT('',(37.0626743494,853.77801102117,48.));
#96936=CARTESIAN_POINT('Origin',(37.0626743494,846.77801102117,48.));
#96937=CARTESIAN_POINT('',(-37.0626743494,853.77801102117,48.));
#96938=CARTESIAN_POINT('',(-37.0626743494,853.77801102117,48.));
#96939=CARTESIAN_POINT('',(-44.0626743494,846.77801102117,48.));
#96940=CARTESIAN_POINT('Origin',(-37.0626743494,846.77801102117,48.));
#96941=CARTESIAN_POINT('',(-44.0626743494,816.144821069057,48.));
#96942=CARTESIAN_POINT('',(-44.0626743494,816.144821069057,48.));
#96943=CARTESIAN_POINT('',(-37.0626743494,809.144821069057,48.));
#96944=CARTESIAN_POINT('Origin',(-37.0626743494,816.144821069057,48.));
#96945=CARTESIAN_POINT('',(37.0626743494,809.144821069057,48.));
#96946=CARTESIAN_POINT('',(37.0626743494,809.144821069057,48.));
#96947=CARTESIAN_POINT('',(44.0626743494,816.144821069057,48.));
#96948=CARTESIAN_POINT('Origin',(37.0626743494,816.144821069057,48.));
#96949=CARTESIAN_POINT('',(44.0626743494,846.77801102117,48.));
#96950=CARTESIAN_POINT('',(-34.9669957384604,825.005507956654,48.));
#96951=CARTESIAN_POINT('',(-34.9669957384604,837.110060670785,48.));
#96952=CARTESIAN_POINT('',(-34.9669957384604,837.110060670785,48.));
#96953=CARTESIAN_POINT('',(-34.08831608202,839.231381014344,48.));
#96954=CARTESIAN_POINT('Origin',(-31.9669957384604,837.110060670785,48.));
#96955=CARTESIAN_POINT('',(-29.674102519647,843.645594576717,48.));
#96956=CARTESIAN_POINT('',(-436.659848548182,436.659848548186,48.));
#96957=CARTESIAN_POINT('',(-27.5527821760873,844.524274233158,48.));
#96958=CARTESIAN_POINT('Origin',(-27.5527821760873,841.524274233158,48.));
#96959=CARTESIAN_POINT('',(27.5527821760873,844.524274233158,48.));
#96960=CARTESIAN_POINT('',(27.5527821760873,844.524274233158,48.));
#96961=CARTESIAN_POINT('',(29.674102519647,843.645594576717,48.));
#96962=CARTESIAN_POINT('Origin',(27.5527821760873,841.524274233158,48.));
#96963=CARTESIAN_POINT('',(34.0883160820201,839.231381014345,48.));
#96964=CARTESIAN_POINT('',(436.659848548182,436.659848548186,48.));
#96965=CARTESIAN_POINT('',(34.9669957384604,837.110060670785,48.));
#96966=CARTESIAN_POINT('Origin',(31.9669957384604,837.110060670785,48.));
#96967=CARTESIAN_POINT('',(34.9669957384604,825.005507956654,48.));
#96968=CARTESIAN_POINT('',(34.9669957384604,825.005507956654,48.));
#96969=CARTESIAN_POINT('',(34.08831608202,822.884187613094,48.));
#96970=CARTESIAN_POINT('Origin',(31.9669957384604,825.005507956654,48.));
#96971=CARTESIAN_POINT('',(29.6741025196469,818.469974050721,48.));
#96972=CARTESIAN_POINT('',(-394.397935765537,394.397935765538,48.));
#96973=CARTESIAN_POINT('',(27.5527821760872,817.591294394281,48.));
#96974=CARTESIAN_POINT('Origin',(27.5527821760872,820.591294394281,48.));
#96975=CARTESIAN_POINT('',(-27.5527821760872,817.591294394281,48.));
#96976=CARTESIAN_POINT('',(-27.5527821760872,817.591294394281,48.));
#96977=CARTESIAN_POINT('',(-29.6741025196469,818.469974050721,48.));
#96978=CARTESIAN_POINT('Origin',(-27.5527821760872,820.591294394281,48.));
#96979=CARTESIAN_POINT('',(-34.08831608202,822.884187613094,48.));
#96980=CARTESIAN_POINT('',(394.397935765537,394.397935765538,48.));
#96981=CARTESIAN_POINT('Origin',(-31.9669957384604,825.005507956654,48.));
#96982=CARTESIAN_POINT('Origin',(-45.0626743494,854.77801102117,48.));
#96983=CARTESIAN_POINT('',(-45.0626743494,846.77801102117,47.));
#96984=CARTESIAN_POINT('',(-45.0626743494,846.77801102117,41.));
#96985=CARTESIAN_POINT('',(-45.0626743494,846.77801102117,48.));
#96986=CARTESIAN_POINT('',(-45.0626743494,816.144821069057,41.));
#96987=CARTESIAN_POINT('',(-45.0626743494,854.77801102117,41.));
#96988=CARTESIAN_POINT('',(-45.0626743494,816.144821069057,47.));
#96989=CARTESIAN_POINT('',(-45.0626743494,816.144821069057,48.));
#96990=CARTESIAN_POINT('',(-45.0626743494,846.77801102117,47.));
#96991=CARTESIAN_POINT('Origin',(45.0626743494,808.144821069057,48.));
#96992=CARTESIAN_POINT('',(-37.0626743494,808.144821069057,47.));
#96993=CARTESIAN_POINT('',(-37.0626743494,808.144821069057,41.));
#96994=CARTESIAN_POINT('',(-37.0626743494,808.144821069057,48.));
#96995=CARTESIAN_POINT('',(37.0626743494,808.144821069057,41.));
#96996=CARTESIAN_POINT('',(45.0626743494,808.144821069057,41.));
#96997=CARTESIAN_POINT('',(37.0626743494,808.144821069057,47.));
#96998=CARTESIAN_POINT('',(37.0626743494,808.144821069057,48.));
#96999=CARTESIAN_POINT('',(-37.0626743494,808.144821069057,47.));
#97000=CARTESIAN_POINT('Origin',(45.0626743494,854.77801102117,48.));
#97001=CARTESIAN_POINT('',(45.0626743494,816.144821069057,47.));
#97002=CARTESIAN_POINT('',(45.0626743494,816.144821069057,41.));
#97003=CARTESIAN_POINT('',(45.0626743494,816.144821069057,48.));
#97004=CARTESIAN_POINT('',(45.0626743494,846.77801102117,41.));
#97005=CARTESIAN_POINT('',(45.0626743494,854.77801102117,41.));
#97006=CARTESIAN_POINT('',(45.0626743494,846.77801102117,47.));
#97007=CARTESIAN_POINT('',(45.0626743494,846.77801102117,48.));
#97008=CARTESIAN_POINT('',(45.0626743494,816.144821069057,47.));
#97009=CARTESIAN_POINT('Origin',(45.0626743494,854.77801102117,48.));
#97010=CARTESIAN_POINT('',(37.0626743494,854.77801102117,47.));
#97011=CARTESIAN_POINT('',(37.0626743494,854.77801102117,41.));
#97012=CARTESIAN_POINT('',(37.0626743494,854.77801102117,48.));
#97013=CARTESIAN_POINT('',(-37.0626743494,854.77801102117,41.));
#97014=CARTESIAN_POINT('',(45.0626743494,854.77801102117,41.));
#97015=CARTESIAN_POINT('',(-37.0626743494,854.77801102117,47.));
#97016=CARTESIAN_POINT('',(-37.0626743494,854.77801102117,48.));
#97017=CARTESIAN_POINT('',(37.0626743494,854.77801102117,47.));
#97018=CARTESIAN_POINT('Origin',(0.,0.,40.));
#97019=CARTESIAN_POINT('',(-37.0626743494,809.144821069057,40.));
#97020=CARTESIAN_POINT('',(-44.0626743494,816.144821069057,40.));
#97021=CARTESIAN_POINT('Origin',(-37.0626743494,816.144821069057,40.));
#97022=CARTESIAN_POINT('',(-44.0626743494,846.77801102117,40.));
#97023=CARTESIAN_POINT('',(-44.0626743494,0.,40.));
#97024=CARTESIAN_POINT('',(-37.0626743494,853.77801102117,40.));
#97025=CARTESIAN_POINT('Origin',(-37.0626743494,846.77801102117,40.));
#97026=CARTESIAN_POINT('',(37.0626743494,853.77801102117,40.));
#97027=CARTESIAN_POINT('',(0.,853.77801102117,40.));
#97028=CARTESIAN_POINT('',(44.0626743494,846.77801102117,40.));
#97029=CARTESIAN_POINT('Origin',(37.0626743494,846.77801102117,40.));
#97030=CARTESIAN_POINT('',(44.0626743494,816.144821069057,40.));
#97031=CARTESIAN_POINT('',(44.0626743494,0.,40.));
#97032=CARTESIAN_POINT('',(37.0626743494,809.144821069057,40.));
#97033=CARTESIAN_POINT('Origin',(37.0626743494,816.144821069057,40.));
#97034=CARTESIAN_POINT('',(0.,809.144821069057,40.));
#97035=CARTESIAN_POINT('Origin',(-32.9669957384604,842.524274233158,91.));
#97036=CARTESIAN_POINT('',(-32.9669957384604,837.110060670785,83.));
#97037=CARTESIAN_POINT('',(-32.9669957384604,837.110060670785,50.));
#97038=CARTESIAN_POINT('',(-32.9669957384604,837.110060670785,48.));
#97039=CARTESIAN_POINT('',(-32.9669957384604,825.005507956654,50.));
#97040=CARTESIAN_POINT('',(-32.9669957384604,825.005507956654,50.));
#97041=CARTESIAN_POINT('',(-32.9669957384604,825.005507956654,83.));
#97042=CARTESIAN_POINT('',(-32.9669957384604,825.005507956654,83.));
#97043=CARTESIAN_POINT('',(-32.9669957384604,842.524274233158,83.));
#97044=CARTESIAN_POINT('Origin',(32.9669957384604,819.591294394281,91.));
#97045=CARTESIAN_POINT('',(-27.5527821760872,819.591294394281,83.));
#97046=CARTESIAN_POINT('',(-27.5527821760872,819.591294394281,50.));
#97047=CARTESIAN_POINT('',(-27.5527821760872,819.591294394281,48.));
#97048=CARTESIAN_POINT('',(27.5527821760872,819.591294394281,50.));
#97049=CARTESIAN_POINT('',(27.5527821760872,819.591294394281,50.));
#97050=CARTESIAN_POINT('',(27.5527821760872,819.591294394281,83.));
#97051=CARTESIAN_POINT('',(27.5527821760872,819.591294394281,83.));
#97052=CARTESIAN_POINT('',(24.9669957384604,819.591294394281,85.5857864376269));
#97053=CARTESIAN_POINT('Origin',(24.9669957384604,819.591294394281,83.));
#97054=CARTESIAN_POINT('',(-24.9669957384604,819.591294394281,85.5857864376269));
#97055=CARTESIAN_POINT('',(-24.9669957384604,819.591294394281,85.5857864376269));
#97056=CARTESIAN_POINT('Origin',(-24.9669957384604,819.591294394281,83.));
#97057=CARTESIAN_POINT('Origin',(32.9669957384604,842.524274233158,91.));
#97058=CARTESIAN_POINT('',(32.9669957384604,825.005507956654,83.));
#97059=CARTESIAN_POINT('',(32.9669957384604,825.005507956654,50.));
#97060=CARTESIAN_POINT('',(32.9669957384604,825.005507956654,48.));
#97061=CARTESIAN_POINT('',(32.9669957384604,837.110060670785,50.));
#97062=CARTESIAN_POINT('',(32.9669957384604,837.110060670785,50.));
#97063=CARTESIAN_POINT('',(32.9669957384604,837.110060670785,83.));
#97064=CARTESIAN_POINT('',(32.9669957384604,837.110060670785,83.));
#97065=CARTESIAN_POINT('',(32.9669957384604,842.524274233158,83.));
#97066=CARTESIAN_POINT('Origin',(32.9669957384604,842.524274233158,91.));
#97067=CARTESIAN_POINT('',(27.5527821760873,842.524274233158,83.));
#97068=CARTESIAN_POINT('',(27.5527821760873,842.524274233158,50.));
#97069=CARTESIAN_POINT('',(27.5527821760873,842.524274233158,48.));
#97070=CARTESIAN_POINT('',(-27.5527821760873,842.524274233158,50.));
#97071=CARTESIAN_POINT('',(-27.5527821760873,842.524274233158,50.));
#97072=CARTESIAN_POINT('',(-27.5527821760873,842.524274233158,83.));
#97073=CARTESIAN_POINT('',(-27.5527821760873,842.524274233158,83.));
#97074=CARTESIAN_POINT('',(-24.9669957384604,842.524274233158,85.585786437627));
#97075=CARTESIAN_POINT('Origin',(-24.9669957384604,842.524274233158,83.));
#97076=CARTESIAN_POINT('',(24.9669957384604,842.524274233158,85.585786437627));
#97077=CARTESIAN_POINT('',(24.9669957384604,842.524274233158,85.585786437627));
#97078=CARTESIAN_POINT('Origin',(24.9669957384604,842.524274233158,83.));
#97079=CARTESIAN_POINT('Origin',(0.,0.,91.));
#97080=CARTESIAN_POINT('',(-24.9669957384604,837.110060670785,91.));
#97081=CARTESIAN_POINT('',(-24.9669957384604,825.005507956654,91.));
#97082=CARTESIAN_POINT('',(-24.9669957384604,0.,91.));
#97083=CARTESIAN_POINT('',(24.9669957384604,825.005507956654,91.));
#97084=CARTESIAN_POINT('',(24.9669957384604,825.005507956654,91.));
#97085=CARTESIAN_POINT('',(24.9669957384604,837.110060670785,91.));
#97086=CARTESIAN_POINT('',(24.9669957384604,0.,91.));
#97087=CARTESIAN_POINT('',(-24.9669957384604,837.110060670785,91.));
#97088=CARTESIAN_POINT('Origin',(24.9669957384604,0.,83.));
#97089=CARTESIAN_POINT('Origin',(24.9669957384604,825.005507956654,83.));
#97090=CARTESIAN_POINT('Origin',(24.9669957384604,837.110060670785,83.));
#97091=CARTESIAN_POINT('Origin',(-24.9669957384604,0.,83.));
#97092=CARTESIAN_POINT('Origin',(-24.9669957384604,825.005507956654,83.));
#97093=CARTESIAN_POINT('Origin',(-24.9669957384604,837.110060670785,83.));
#97094=CARTESIAN_POINT('Origin',(37.0626743494,846.77801102117,48.));
#97095=CARTESIAN_POINT('Origin',(37.0626743494,846.77801102117,41.));
#97096=CARTESIAN_POINT('Origin',(37.0626743494,846.77801102117,47.));
#97097=CARTESIAN_POINT('Origin',(37.0626743494,816.144821069057,48.));
#97098=CARTESIAN_POINT('Origin',(37.0626743494,816.144821069057,41.));
#97099=CARTESIAN_POINT('Origin',(37.0626743494,816.144821069057,47.));
#97100=CARTESIAN_POINT('Origin',(-37.0626743494,816.144821069057,48.));
#97101=CARTESIAN_POINT('Origin',(-37.0626743494,816.144821069057,41.));
#97102=CARTESIAN_POINT('Origin',(-37.0626743494,816.144821069057,47.));
#97103=CARTESIAN_POINT('Origin',(-37.0626743494,846.77801102117,48.));
#97104=CARTESIAN_POINT('Origin',(-37.0626743494,846.77801102117,41.));
#97105=CARTESIAN_POINT('Origin',(-37.0626743494,846.77801102117,47.));
#97106=CARTESIAN_POINT('Origin',(-27.9669957384604,819.591294394281,91.));
#97107=CARTESIAN_POINT('',(-32.6741025196469,824.298401175467,83.));
#97108=CARTESIAN_POINT('',(-32.6741025196469,824.298401175467,50.));
#97109=CARTESIAN_POINT('',(-32.6741025196469,824.298401175467,48.));
#97110=CARTESIAN_POINT('',(-28.2598889572738,819.884187613094,50.));
#97111=CARTESIAN_POINT('',(-27.9669957384604,819.591294394281,50.));
#97112=CARTESIAN_POINT('',(-28.2598889572738,819.884187613094,83.));
#97113=CARTESIAN_POINT('',(-28.2598889572738,819.884187613094,83.));
#97114=CARTESIAN_POINT('',(-32.9669957384604,824.591294394281,83.));
#97115=CARTESIAN_POINT('Origin',(-24.9669957384604,819.591294394281,83.));
#97116=CARTESIAN_POINT('',(-24.9669957384604,824.298401175467,90.7071067811866));
#97117=CARTESIAN_POINT('',(-24.9669957384604,819.884187613094,86.2928932188134));
#97118=CARTESIAN_POINT('',(-24.9669957384604,824.591294394281,91.));
#97119=CARTESIAN_POINT('Origin',(-24.9669957384604,824.298401175467,83.));
#97120=CARTESIAN_POINT('Origin',(-24.9669957384604,819.884187613094,83.));
#97121=CARTESIAN_POINT('Origin',(0.,824.591294394281,91.));
#97122=CARTESIAN_POINT('',(24.9669957384604,824.298401175467,90.7071067811866));
#97123=CARTESIAN_POINT('',(24.9669957384604,819.884187613094,86.2928932188134));
#97124=CARTESIAN_POINT('',(24.9669957384604,824.591294394281,91.));
#97125=CARTESIAN_POINT('',(-24.9669957384604,824.298401175467,90.7071067811866));
#97126=CARTESIAN_POINT('',(24.9669957384604,819.884187613094,86.2928932188134));
#97127=CARTESIAN_POINT('Origin',(24.9669957384604,819.591294394281,83.));
#97128=CARTESIAN_POINT('',(32.6741025196469,824.298401175467,83.));
#97129=CARTESIAN_POINT('',(28.2598889572738,819.884187613094,83.));
#97130=CARTESIAN_POINT('',(32.9669957384604,824.591294394281,83.));
#97131=CARTESIAN_POINT('Origin',(24.9669957384604,824.298401175467,83.));
#97132=CARTESIAN_POINT('Origin',(24.9669957384604,819.884187613094,83.));
#97133=CARTESIAN_POINT('Origin',(32.9669957384604,824.591294394281,91.));
#97134=CARTESIAN_POINT('',(28.2598889572738,819.884187613094,50.));
#97135=CARTESIAN_POINT('',(28.2598889572738,819.884187613094,48.));
#97136=CARTESIAN_POINT('',(32.6741025196469,824.298401175467,50.));
#97137=CARTESIAN_POINT('',(32.9669957384604,824.591294394281,50.));
#97138=CARTESIAN_POINT('',(32.6741025196469,824.298401175467,83.));
#97139=CARTESIAN_POINT('Origin',(-32.9669957384604,837.524274233158,91.));
#97140=CARTESIAN_POINT('',(-28.2598889572739,842.231381014344,83.));
#97141=CARTESIAN_POINT('',(-28.2598889572739,842.231381014344,50.));
#97142=CARTESIAN_POINT('',(-28.2598889572739,842.231381014344,48.));
#97143=CARTESIAN_POINT('',(-32.6741025196469,837.817167451971,50.));
#97144=CARTESIAN_POINT('',(-32.9669957384604,837.524274233158,50.));
#97145=CARTESIAN_POINT('',(-32.6741025196469,837.817167451971,83.));
#97146=CARTESIAN_POINT('',(-32.6741025196469,837.817167451971,83.));
#97147=CARTESIAN_POINT('',(-27.9669957384604,842.524274233158,83.));
#97148=CARTESIAN_POINT('Origin',(-24.9669957384604,842.524274233158,83.));
#97149=CARTESIAN_POINT('',(-24.9669957384604,842.231381014344,86.2928932188135));
#97150=CARTESIAN_POINT('',(-24.9669957384604,837.817167451971,90.7071067811866));
#97151=CARTESIAN_POINT('',(-24.9669957384604,842.524274233158,86.0000000000001));
#97152=CARTESIAN_POINT('Origin',(-24.9669957384604,842.231381014344,83.));
#97153=CARTESIAN_POINT('Origin',(-24.9669957384604,837.817167451971,83.));
#97154=CARTESIAN_POINT('Origin',(0.,837.524274233158,91.));
#97155=CARTESIAN_POINT('',(24.9669957384604,842.231381014344,86.2928932188135));
#97156=CARTESIAN_POINT('',(24.9669957384604,837.817167451971,90.7071067811866));
#97157=CARTESIAN_POINT('',(24.9669957384604,842.524274233158,86.0000000000001));
#97158=CARTESIAN_POINT('',(-24.9669957384604,842.231381014344,86.2928932188135));
#97159=CARTESIAN_POINT('',(24.9669957384604,837.817167451971,90.7071067811866));
#97160=CARTESIAN_POINT('Origin',(24.9669957384604,842.524274233158,83.));
#97161=CARTESIAN_POINT('',(28.2598889572739,842.231381014344,83.));
#97162=CARTESIAN_POINT('',(32.6741025196469,837.817167451971,83.));
#97163=CARTESIAN_POINT('',(27.9669957384604,842.524274233158,83.));
#97164=CARTESIAN_POINT('Origin',(24.9669957384604,842.231381014344,83.));
#97165=CARTESIAN_POINT('Origin',(24.9669957384604,837.817167451971,83.));
#97166=CARTESIAN_POINT('Origin',(27.9669957384604,842.524274233158,91.));
#97167=CARTESIAN_POINT('',(32.6741025196469,837.817167451971,50.));
#97168=CARTESIAN_POINT('',(32.6741025196469,837.817167451971,48.));
#97169=CARTESIAN_POINT('',(28.2598889572739,842.231381014344,50.));
#97170=CARTESIAN_POINT('',(27.9669957384604,842.524274233158,50.));
#97171=CARTESIAN_POINT('',(28.2598889572739,842.231381014344,83.));
#97172=CARTESIAN_POINT('Origin',(44.0626743494,0.,41.));
#97173=CARTESIAN_POINT('Origin',(44.0626743494,846.77801102117,41.));
#97174=CARTESIAN_POINT('Origin',(44.0626743494,816.144821069057,41.));
#97175=CARTESIAN_POINT('Origin',(37.0626743494,816.144821069057,41.));
#97176=CARTESIAN_POINT('Origin',(37.0626743494,809.144821069057,41.));
#97177=CARTESIAN_POINT('Origin',(37.0626743494,846.77801102117,41.));
#97178=CARTESIAN_POINT('Origin',(37.0626743494,853.77801102117,41.));
#97179=CARTESIAN_POINT('Origin',(0.,809.144821069057,41.));
#97180=CARTESIAN_POINT('Origin',(-37.0626743494,809.144821069057,41.));
#97181=CARTESIAN_POINT('Origin',(0.,853.77801102117,41.));
#97182=CARTESIAN_POINT('Origin',(-37.0626743494,853.77801102117,41.));
#97183=CARTESIAN_POINT('Origin',(-37.0626743494,816.144821069057,41.));
#97184=CARTESIAN_POINT('Origin',(-44.0626743494,816.144821069057,41.));
#97185=CARTESIAN_POINT('Origin',(-37.0626743494,846.77801102117,41.));
#97186=CARTESIAN_POINT('Origin',(-44.0626743494,846.77801102117,41.));
#97187=CARTESIAN_POINT('Origin',(-44.0626743494,0.,41.));
#97188=CARTESIAN_POINT('Origin',(45.0626743494,809.144821069057,47.));
#97189=CARTESIAN_POINT('Origin',(37.0626743494,809.144821069057,47.));
#97190=CARTESIAN_POINT('Origin',(-37.0626743494,809.144821069057,47.));
#97191=CARTESIAN_POINT('Origin',(-37.0626743494,816.144821069057,47.));
#97192=CARTESIAN_POINT('Origin',(-44.0626743494,816.144821069057,47.));
#97193=CARTESIAN_POINT('Origin',(37.0626743494,816.144821069057,47.));
#97194=CARTESIAN_POINT('Origin',(44.0626743494,816.144821069057,47.));
#97195=CARTESIAN_POINT('Origin',(-44.0626743494,854.77801102117,47.));
#97196=CARTESIAN_POINT('Origin',(-44.0626743494,846.77801102117,47.));
#97197=CARTESIAN_POINT('Origin',(44.0626743494,854.77801102117,47.));
#97198=CARTESIAN_POINT('Origin',(44.0626743494,846.77801102117,47.));
#97199=CARTESIAN_POINT('Origin',(-37.0626743494,846.77801102117,47.));
#97200=CARTESIAN_POINT('Origin',(-37.0626743494,853.77801102117,47.));
#97201=CARTESIAN_POINT('Origin',(37.0626743494,846.77801102117,47.));
#97202=CARTESIAN_POINT('Origin',(37.0626743494,853.77801102117,47.));
#97203=CARTESIAN_POINT('Origin',(45.0626743494,853.77801102117,47.));
#97204=CARTESIAN_POINT('Origin',(31.9669957384604,825.005507956654,91.));
#97205=CARTESIAN_POINT('Origin',(31.9669957384604,825.005507956654,50.));
#97206=CARTESIAN_POINT('Origin',(31.9669957384604,825.005507956654,83.));
#97207=CARTESIAN_POINT('Origin',(24.9669957384604,825.005507956654,83.));
#97208=CARTESIAN_POINT('Origin',(24.9669957384604,825.005507956654,90.0000000000001));
#97209=CARTESIAN_POINT('Origin',(0.,825.005507956654,90.));
#97210=CARTESIAN_POINT('Origin',(-24.9669957384604,825.005507956654,90.0000000000001));
#97211=CARTESIAN_POINT('Origin',(-24.9669957384604,825.005507956654,83.));
#97212=CARTESIAN_POINT('Origin',(-31.9669957384604,825.005507956654,83.));
#97213=CARTESIAN_POINT('Origin',(-31.9669957384604,825.005507956654,91.));
#97214=CARTESIAN_POINT('Origin',(-31.9669957384604,825.005507956654,50.));
#97215=CARTESIAN_POINT('Origin',(-27.5527821760872,820.591294394281,91.));
#97216=CARTESIAN_POINT('Origin',(-27.5527821760872,820.591294394281,50.));
#97217=CARTESIAN_POINT('Origin',(-27.5527821760873,820.591294394281,83.));
#97218=CARTESIAN_POINT('Origin',(-24.9669957384604,820.591294394281,83.));
#97219=CARTESIAN_POINT('Origin',(-24.9669957384604,820.591294394281,85.5857864376269));
#97220=CARTESIAN_POINT('Origin',(32.9669957384604,820.591294394281,85.5857864376269));
#97221=CARTESIAN_POINT('Origin',(24.9669957384604,820.591294394281,85.5857864376269));
#97222=CARTESIAN_POINT('Origin',(24.9669957384604,820.591294394281,83.));
#97223=CARTESIAN_POINT('Origin',(27.5527821760872,820.591294394281,83.));
#97224=CARTESIAN_POINT('Origin',(27.5527821760872,820.591294394281,91.));
#97225=CARTESIAN_POINT('Origin',(27.5527821760872,820.591294394281,50.));
#97226=CARTESIAN_POINT('Origin',(27.5527821760873,841.524274233158,91.));
#97227=CARTESIAN_POINT('Origin',(27.5527821760873,841.524274233158,50.));
#97228=CARTESIAN_POINT('Origin',(27.5527821760873,841.524274233158,83.));
#97229=CARTESIAN_POINT('Origin',(24.9669957384604,841.524274233158,83.));
#97230=CARTESIAN_POINT('Origin',(24.9669957384604,841.524274233158,85.585786437627));
#97231=CARTESIAN_POINT('Origin',(32.9669957384604,841.524274233158,85.585786437627));
#97232=CARTESIAN_POINT('Origin',(-24.9669957384604,841.524274233158,85.585786437627));
#97233=CARTESIAN_POINT('Origin',(-24.9669957384604,841.524274233158,83.));
#97234=CARTESIAN_POINT('Origin',(-27.5527821760873,841.524274233158,83.));
#97235=CARTESIAN_POINT('Origin',(-27.5527821760873,841.524274233158,91.));
#97236=CARTESIAN_POINT('Origin',(-27.5527821760873,841.524274233158,50.));
#97237=CARTESIAN_POINT('Origin',(-31.9669957384604,837.110060670785,91.));
#97238=CARTESIAN_POINT('Origin',(-31.9669957384604,837.110060670785,50.));
#97239=CARTESIAN_POINT('Origin',(-31.9669957384604,837.110060670785,83.));
#97240=CARTESIAN_POINT('Origin',(-24.9669957384604,837.110060670785,83.));
#97241=CARTESIAN_POINT('Origin',(-24.9669957384604,837.110060670785,90.0000000000001));
#97242=CARTESIAN_POINT('Origin',(0.,837.110060670785,90.));
#97243=CARTESIAN_POINT('Origin',(24.9669957384604,837.110060670785,90.0000000000001));
#97244=CARTESIAN_POINT('Origin',(24.9669957384604,837.110060670785,83.));
#97245=CARTESIAN_POINT('Origin',(31.9669957384604,837.110060670785,83.));
#97246=CARTESIAN_POINT('Origin',(31.9669957384604,837.110060670785,91.));
#97247=CARTESIAN_POINT('Origin',(31.9669957384604,837.110060670785,50.));
#97248=CARTESIAN_POINT('Origin',(31.9669957384604,825.005507956654,50.));
#97249=CARTESIAN_POINT('Origin',(34.9669957384604,825.005507956654,50.));
#97250=CARTESIAN_POINT('Origin',(34.08831608202,822.884187613094,50.));
#97251=CARTESIAN_POINT('Origin',(-394.397935765537,394.397935765538,50.));
#97252=CARTESIAN_POINT('Origin',(29.6741025196469,818.469974050721,50.));
#97253=CARTESIAN_POINT('Origin',(34.9669957384604,842.524274233158,50.));
#97254=CARTESIAN_POINT('Origin',(34.9669957384604,837.110060670785,50.));
#97255=CARTESIAN_POINT('Origin',(27.5527821760872,820.591294394281,50.));
#97256=CARTESIAN_POINT('Origin',(27.5527821760872,817.591294394281,50.));
#97257=CARTESIAN_POINT('Origin',(31.9669957384604,837.110060670785,50.));
#97258=CARTESIAN_POINT('Origin',(34.08831608202,839.231381014344,50.));
#97259=CARTESIAN_POINT('Origin',(32.9669957384604,817.591294394281,50.));
#97260=CARTESIAN_POINT('Origin',(-27.5527821760872,817.591294394281,50.));
#97261=CARTESIAN_POINT('Origin',(436.659848548182,436.659848548186,50.));
#97262=CARTESIAN_POINT('Origin',(29.674102519647,843.645594576717,50.));
#97263=CARTESIAN_POINT('Origin',(-27.5527821760872,820.591294394281,50.));
#97264=CARTESIAN_POINT('Origin',(-29.6741025196469,818.469974050721,50.));
#97265=CARTESIAN_POINT('Origin',(27.5527821760873,841.524274233158,50.));
#97266=CARTESIAN_POINT('Origin',(27.5527821760873,844.524274233158,50.));
#97267=CARTESIAN_POINT('Origin',(394.397935765537,394.397935765538,50.));
#97268=CARTESIAN_POINT('Origin',(-34.08831608202,822.884187613094,50.));
#97269=CARTESIAN_POINT('Origin',(32.9669957384604,844.524274233158,50.));
#97270=CARTESIAN_POINT('Origin',(-27.5527821760873,844.524274233158,50.));
#97271=CARTESIAN_POINT('Origin',(-31.9669957384604,825.005507956654,50.));
#97272=CARTESIAN_POINT('Origin',(-34.9669957384604,825.005507956654,50.));
#97273=CARTESIAN_POINT('Origin',(-27.5527821760873,841.524274233158,50.));
#97274=CARTESIAN_POINT('Origin',(-29.6741025196469,843.645594576717,50.));
#97275=CARTESIAN_POINT('Origin',(-34.9669957384604,842.524274233158,50.));
#97276=CARTESIAN_POINT('Origin',(-34.9669957384604,837.110060670785,50.));
#97277=CARTESIAN_POINT('Origin',(-436.659848548182,436.659848548186,50.));
#97278=CARTESIAN_POINT('Origin',(-34.08831608202,839.231381014344,50.));
#97279=CARTESIAN_POINT('Origin',(-31.9669957384604,837.110060670785,50.));
#97280=CARTESIAN_POINT('',(0.,0.,0.));
#97281=CARTESIAN_POINT('Origin',(24.5,620.675373764374,64.2994740882088));
#97282=CARTESIAN_POINT('',(24.5,620.675373764374,44.8494740882089));
#97283=CARTESIAN_POINT('',(24.5,620.675373764374,83.7494740882087));
#97284=CARTESIAN_POINT('Origin',(24.5,620.675373764374,64.2994740882088));
#97285=CARTESIAN_POINT('Origin',(24.5,620.675373764374,64.2994740882088));
#97286=CARTESIAN_POINT('',(24.,620.675373764374,83.2494740882088));
#97287=CARTESIAN_POINT('Origin',(24.5,620.675373764374,83.2494740882087));
#97288=CARTESIAN_POINT('Origin',(24.,620.675373764374,64.2994740882088));
#97289=CARTESIAN_POINT('Origin',(52.8776183915471,639.625373764374,90.6087118617898));
#97290=CARTESIAN_POINT('',(61.9796230824862,639.625373764374,98.7473601281983));
#97291=CARTESIAN_POINT('',(43.775613700608,639.625373764374,98.7473601281983));
#97292=CARTESIAN_POINT('Origin',(52.8776183915471,639.625373764374,90.6087118617898));
#97293=CARTESIAN_POINT('',(62.3523505660608,640.125373764374,99.080638124754));
#97294=CARTESIAN_POINT('Origin',(62.3523505660608,639.625373764374,99.080638124754));
#97295=CARTESIAN_POINT('',(43.4028862170334,640.125373764374,99.080638124754));
#97296=CARTESIAN_POINT('Origin',(52.8776183915471,640.125373764374,90.6087118617898));
#97297=CARTESIAN_POINT('Origin',(43.4028862170334,639.625373764374,99.080638124754));
#97298=CARTESIAN_POINT('Origin',(52.8776183915471,601.725373764374,90.6087118617898));
#97299=CARTESIAN_POINT('',(62.3523505660608,601.225373764374,99.080638124754));
#97300=CARTESIAN_POINT('',(43.4028862170334,601.225373764374,99.080638124754));
#97301=CARTESIAN_POINT('Origin',(52.8776183915471,601.225373764374,90.6087118617898));
#97302=CARTESIAN_POINT('',(61.9796230824862,601.725373764374,98.7473601281983));
#97303=CARTESIAN_POINT('Origin',(62.3523505660608,601.725373764374,99.080638124754));
#97304=CARTESIAN_POINT('',(43.775613700608,601.725373764374,98.7473601281983));
#97305=CARTESIAN_POINT('Origin',(52.8776183915471,601.725373764374,90.6087118617898));
#97306=CARTESIAN_POINT('Origin',(43.4028862170334,601.725373764374,99.080638124754));
#97307=CARTESIAN_POINT('Origin',(70.,620.675373764374,64.2994740882088));
#97308=CARTESIAN_POINT('',(70.,640.125373764374,64.2994740882088));
#97309=CARTESIAN_POINT('',(70.,620.675373764374,44.8494740882089));
#97310=CARTESIAN_POINT('Origin',(70.,620.675373764374,64.2994740882088));
#97311=CARTESIAN_POINT('',(71.,639.125373764374,64.2994740882088));
#97312=CARTESIAN_POINT('Origin',(70.,639.125373764374,64.2994740882088));
#97313=CARTESIAN_POINT('',(71.,602.225373764374,64.2994740882088));
#97314=CARTESIAN_POINT('Origin',(71.,620.675373764374,64.2994740882088));
#97315=CARTESIAN_POINT('',(70.,601.225373764374,64.2994740882088));
#97316=CARTESIAN_POINT('Origin',(70.,602.225373764374,64.2994740882088));
#97317=CARTESIAN_POINT('Origin',(70.,620.675373764374,64.2994740882088));
#97318=CARTESIAN_POINT('Origin',(71.,620.675373764374,64.2994740882088));
#97319=CARTESIAN_POINT('',(71.,620.675373764374,44.8494740882089));
#97320=CARTESIAN_POINT('',(35.7552367830941,601.225373764374,64.2994740882088));
#97321=CARTESIAN_POINT('',(71.,601.225373764374,64.2994740882088));
#97322=CARTESIAN_POINT('',(33.7552367830941,603.127574253371,72.6885880057606));
#97323=CARTESIAN_POINT('Ctrl Pts',(35.7552367830941,601.225373764374,64.2994740882088));
#97324=CARTESIAN_POINT('Ctrl Pts',(35.6257365591854,601.225373764374,64.6933227733964));
#97325=CARTESIAN_POINT('Ctrl Pts',(35.4961078469376,601.237366261793,65.0875125516637));
#97326=CARTESIAN_POINT('Ctrl Pts',(35.3683280852255,601.261325958332,65.4811925716977));
#97327=CARTESIAN_POINT('Ctrl Pts',(35.2659632064297,601.280520167174,65.7965712122205));
#97328=CARTESIAN_POINT('Ctrl Pts',(35.164784366186,601.307395533574,66.1116230291669));
#97329=CARTESIAN_POINT('Ctrl Pts',(35.0658114313479,601.341963007925,66.425909717438));
#97330=CARTESIAN_POINT('Ctrl Pts',(35.0654326493907,601.342095302027,66.4271125324004));
#97331=CARTESIAN_POINT('Ctrl Pts',(35.0650539000296,601.342227708726,66.4283153352887));
#97332=CARTESIAN_POINT('Ctrl Pts',(35.0646751833233,601.342360228022,66.4295181260736));
#97333=CARTESIAN_POINT('Ctrl Pts',(34.9032152398727,601.39885775679,66.9423091618597));
#97334=CARTESIAN_POINT('Ctrl Pts',(34.7473679169488,601.47569378957,67.4534199949505));
#97335=CARTESIAN_POINT('Ctrl Pts',(34.6015663494618,601.573679242807,67.9640147041513));
#97336=CARTESIAN_POINT('Ctrl Pts',(34.5468057526337,601.610480917798,68.1557854203037));
#97337=CARTESIAN_POINT('Ctrl Pts',(34.4934625501783,601.650266373644,68.347483350911));
#97338=CARTESIAN_POINT('Ctrl Pts',(34.441772953152,601.693080009916,68.539170305048));
#97339=CARTESIAN_POINT('Ctrl Pts',(34.4412715863034,601.693495283765,68.5410295860184));
#97340=CARTESIAN_POINT('Ctrl Pts',(34.4407703749893,601.693910842595,68.5428888663075));
#97341=CARTESIAN_POINT('Ctrl Pts',(34.4402693194284,601.694326686444,68.544748145963));
#97342=CARTESIAN_POINT('Ctrl Pts',(34.2998573245699,601.810859600235,69.0657785182523));
#97343=CARTESIAN_POINT('Ctrl Pts',(34.1716160470563,601.950101647865,69.5868210918051));
#97344=CARTESIAN_POINT('Ctrl Pts',(34.064487473247,602.111405838435,70.1029417803957));
#97345=CARTESIAN_POINT('Ctrl Pts',(34.0274026664021,602.167244673377,70.2816078016488));
#97346=CARTESIAN_POINT('Ctrl Pts',(33.9928482010104,602.225727031641,70.4596837544423));
#97347=CARTESIAN_POINT('Ctrl Pts',(33.9611958099703,602.286825206801,70.6369642677272));
#97348=CARTESIAN_POINT('Ctrl Pts',(33.9609301528875,602.287338001015,70.638452175037));
#97349=CARTESIAN_POINT('Ctrl Pts',(33.9606647001835,602.287850979633,70.6399400267307));
#97350=CARTESIAN_POINT('Ctrl Pts',(33.9603994520774,602.288364142641,70.6414278226942));
#97351=CARTESIAN_POINT('Ctrl Pts',(33.8988854931898,602.407372299352,70.986464102381));
#97352=CARTESIAN_POINT('Ctrl Pts',(33.8482365019429,602.536496470251,71.3293804030283));
#97353=CARTESIAN_POINT('Ctrl Pts',(33.8123513013975,602.676232077861,71.6705933077606));
#97354=CARTESIAN_POINT('Ctrl Pts',(33.7806037130973,602.799855980581,71.9724639022542));
#97355=CARTESIAN_POINT('Ctrl Pts',(33.7602910819696,602.931779777438,72.2730015582567));
#97356=CARTESIAN_POINT('Ctrl Pts',(33.7560607839295,603.072602503069,72.57262184915));
#97357=CARTESIAN_POINT('Ctrl Pts',(33.7555148022906,603.090777728977,72.611292216089));
#97358=CARTESIAN_POINT('Ctrl Pts',(33.7552367835934,603.109101210383,72.6499473033098));
#97359=CARTESIAN_POINT('Ctrl Pts',(33.7552367830941,603.127574253371,72.6885880057606));
#97360=CARTESIAN_POINT('',(33.7552367830941,638.223173275376,72.6885880057604));
#97361=CARTESIAN_POINT('Origin',(33.7552367830941,620.675373764374,64.2994740882088));
#97362=CARTESIAN_POINT('',(35.7552367830941,640.125373764374,64.2994740882088));
#97363=CARTESIAN_POINT('Ctrl Pts',(33.7552367830941,638.223173275376,72.6885880057604));
#97364=CARTESIAN_POINT('Ctrl Pts',(33.7552367869584,638.366316942016,72.3891694511719));
#97365=CARTESIAN_POINT('Ctrl Pts',(33.7719257417031,638.500481620589,72.0888870509365));
#97366=CARTESIAN_POINT('Ctrl Pts',(33.8006485106675,638.626268389842,71.7873250236769));
#97367=CARTESIAN_POINT('Ctrl Pts',(33.8043525567342,638.642489666713,71.7484360279008));
#97368=CARTESIAN_POINT('Ctrl Pts',(33.808256796361,638.658571596475,71.7095257528911));
#97369=CARTESIAN_POINT('Ctrl Pts',(33.8123513034981,638.674515450813,71.6705933079404));
#97370=CARTESIAN_POINT('Ctrl Pts',(33.8482365102383,638.814251074653,71.3293803635857));
#97371=CARTESIAN_POINT('Ctrl Pts',(33.8988855120037,638.943375249915,70.9864640427555));
#97372=CARTESIAN_POINT('Ctrl Pts',(33.9603994665039,639.062383385352,70.6414278248801));
#97373=CARTESIAN_POINT('Ctrl Pts',(33.960667679382,639.062902284109,70.6399233994569));
#97374=CARTESIAN_POINT('Ctrl Pts',(33.9609361014569,639.06342099433,70.6384189170522));
#97375=CARTESIAN_POINT('Ctrl Pts',(33.9612047325023,639.063939516001,70.6369143777839));
#97376=CARTESIAN_POINT('Ctrl Pts',(34.0526561269075,639.240462411137,70.1247166389886));
#97377=CARTESIAN_POINT('Ctrl Pts',(34.168330227834,639.395147745896,69.6058806834539));
#97378=CARTESIAN_POINT('Ctrl Pts',(34.2992699048925,639.527337269571,69.0853523891265));
#97379=CARTESIAN_POINT('Ctrl Pts',(34.3445659440352,639.573065668885,68.9052857315297));
#97380=CARTESIAN_POINT('Ctrl Pts',(34.3916890276511,639.616102313696,68.7250163402484));
#97381=CARTESIAN_POINT('Ctrl Pts',(34.440269340592,639.656420841148,68.5447481511289));
#97382=CARTESIAN_POINT('Ctrl Pts',(34.4407795157771,639.656844253658,68.5428550312376));
#97383=CARTESIAN_POINT('Ctrl Pts',(34.4412898524366,639.657267370677,68.5409619106906));
#97384=CARTESIAN_POINT('Ctrl Pts',(34.4418003503396,639.657690192248,68.5390687894377));
#97385=CARTESIAN_POINT('Ctrl Pts',(34.5794751777585,639.771719821878,68.0285179325883));
#97386=CARTESIAN_POINT('Ctrl Pts',(34.7288776165414,639.864270380756,67.5178887275615));
#97387=CARTESIAN_POINT('Ctrl Pts',(34.8855569182322,639.93616826794,67.006014915324));
#97388=CARTESIAN_POINT('Ctrl Pts',(34.9443169906728,639.96313242347,66.8140448084693));
#97389=CARTESIAN_POINT('Ctrl Pts',(35.0041009383194,639.987191371054,66.6218996870685));
#97390=CARTESIAN_POINT('Ctrl Pts',(35.0646751529483,640.008387301716,66.4295181170863));
#97391=CARTESIAN_POINT('Ctrl Pts',(35.0650699280554,640.008525440127,66.4282643252648));
#97392=CARTESIAN_POINT('Ctrl Pts',(35.0654647386451,640.008663456191,66.4270105202926));
#97393=CARTESIAN_POINT('Ctrl Pts',(35.0658595846507,640.008801349907,66.4257567022029));
#97394=CARTESIAN_POINT('Ctrl Pts',(35.1771223453717,640.047658107464,66.0724461454543));
#97395=CARTESIAN_POINT('Ctrl Pts',(35.2912445666128,640.076808508222,65.7179802822932));
#97396=CARTESIAN_POINT('Ctrl Pts',(35.4066366929697,640.09623524223,65.3633493527697));
#97397=CARTESIAN_POINT('Ctrl Pts',(35.4643327561481,640.105948609234,65.186033888008));
#97398=CARTESIAN_POINT('Ctrl Pts',(35.5223291503942,640.113230342378,65.0087318398257));
#97399=CARTESIAN_POINT('Ctrl Pts',(35.5804869830593,640.118087133712,64.831397796837));
#97400=CARTESIAN_POINT('Ctrl Pts',(35.6150978613504,640.120977506445,64.7258627949723));
#97401=CARTESIAN_POINT('Ctrl Pts',(35.6499102657678,640.123016256969,64.6198773927215));
#97402=CARTESIAN_POINT('Ctrl Pts',(35.6846226908027,640.124185031716,64.5142623497308));
#97403=CARTESIAN_POINT('Ctrl Pts',(35.7082387308706,640.124980188817,64.4424088539142));
#97404=CARTESIAN_POINT('Ctrl Pts',(35.7318083908217,640.125373764374,64.3707267948586));
#97405=CARTESIAN_POINT('Ctrl Pts',(35.7552367830941,640.125373764374,64.2994740882088));
#97406=CARTESIAN_POINT('',(71.,640.125373764374,64.2994740882088));
#97407=CARTESIAN_POINT('Origin',(23.5,620.675373764374,64.2994740882088));
#97408=CARTESIAN_POINT('',(23.5,620.675373764374,83.7494740882088));
#97409=CARTESIAN_POINT('Origin',(23.5,620.675373764374,83.2494740882088));
#97410=CARTESIAN_POINT('',(23.5,620.675373764374,44.8494740882088));
#97411=CARTESIAN_POINT('Origin',(23.5,620.675373764374,64.2994740882088));
#97412=CARTESIAN_POINT('Origin',(23.5,620.675373764374,64.2994740882088));
#97413=CARTESIAN_POINT('Origin',(22.5,620.675373764374,64.2994740882088));
#97414=CARTESIAN_POINT('',(22.,620.675373764374,45.3494740882088));
#97415=CARTESIAN_POINT('Origin',(22.,620.675373764374,64.2994740882088));
#97416=CARTESIAN_POINT('',(22.5,620.675373764374,44.8494740882088));
#97417=CARTESIAN_POINT('Origin',(22.5,620.675373764374,45.3494740882088));
#97418=CARTESIAN_POINT('Origin',(22.5,620.675373764374,64.2994740882088));
#97419=CARTESIAN_POINT('Origin',(22.,620.675373764374,64.2994740882088));
#97420=CARTESIAN_POINT('',(22.,620.675373764374,44.8494740882088));
#97421=CARTESIAN_POINT('Ctrl Pts',(-4.46675582290381,607.708350351965,79.3699798038647));
#97422=CARTESIAN_POINT('Ctrl Pts',(-4.65179838528775,608.301384168068,79.3159462734029));
#97423=CARTESIAN_POINT('Ctrl Pts',(-4.39560350684042,607.872719845594,78.941911814982));
#97424=CARTESIAN_POINT('Ctrl Pts',(-3.27436645786458,608.106096967698,79.722255531378));
#97425=CARTESIAN_POINT('Ctrl Pts',(-3.35828013221585,608.779842649617,79.710778768012));
#97426=CARTESIAN_POINT('Ctrl Pts',(-3.22222729142889,608.265397557493,79.2841755866817));
#97427=CARTESIAN_POINT('Ctrl Pts',(-2.0401534841229,608.377157746436,79.9382527125226));
#97428=CARTESIAN_POINT('Ctrl Pts',(-2.13704517638702,609.079904904266,79.9301149240667));
#97429=CARTESIAN_POINT('Ctrl Pts',(-2.00765458360655,608.533014332571,79.4940431330354));
#97430=CARTESIAN_POINT('Ctrl Pts',(-0.477078115453726,608.470043666149,
80.0129132419871));
#97431=CARTESIAN_POINT('Ctrl Pts',(-0.504033715610802,609.190797807749,
80.0123807664004));
#97432=CARTESIAN_POINT('Ctrl Pts',(-0.46947699470708,608.624717782472,79.5665829488807));
#97433=CARTESIAN_POINT('Ctrl Pts',(-0.201739610759609,608.477464067233,
80.018847964929));
#97434=CARTESIAN_POINT('Ctrl Pts',(-0.213567627251543,609.199734125483,
80.0189726826106));
#97435=CARTESIAN_POINT('Ctrl Pts',(-0.198525207359669,608.632043701841,
79.5723490852243));
#97436=CARTESIAN_POINT('Ctrl Pts',(0.343267231354877,608.474402475761,80.016394319429));
#97437=CARTESIAN_POINT('Ctrl Pts',(0.363172475404081,609.19602915895,80.0162332785399));
#97438=CARTESIAN_POINT('Ctrl Pts',(0.337797886426132,608.629021099499,79.569965145871));
#97439=CARTESIAN_POINT('Ctrl Pts',(0.614288243293599,608.464030193296,80.0080931677934));
#97440=CARTESIAN_POINT('Ctrl Pts',(0.648999446052346,609.183542498368,80.0070154560597));
#97441=CARTESIAN_POINT('Ctrl Pts',(0.604500980807282,608.618780884095,79.5618998035947));
#97442=CARTESIAN_POINT('Ctrl Pts',(1.42305709514243,608.407424943048,79.9625420908729));
#97443=CARTESIAN_POINT('Ctrl Pts',(1.49988036818683,609.115508961494,79.9564789876385));
#97444=CARTESIAN_POINT('Ctrl Pts',(1.40038494278016,608.562896395885,79.5176427201739));
#97445=CARTESIAN_POINT('Ctrl Pts',(1.95650990903739,608.335644777334,79.9047081360849));
#97446=CARTESIAN_POINT('Ctrl Pts',(2.05434637538844,609.030990740555,79.8936395733644));
#97447=CARTESIAN_POINT('Ctrl Pts',(1.92534113326012,608.492029675597,79.4614512450883));
#97448=CARTESIAN_POINT('Ctrl Pts',(2.74875593427252,608.182424012343,79.777879100916));
#97449=CARTESIAN_POINT('Ctrl Pts',(2.8863399589135,608.8483829158,79.7536174784857));
#97450=CARTESIAN_POINT('Ctrl Pts',(2.70496406063899,608.340760187158,79.3382254829299));
#97451=CARTESIAN_POINT('Ctrl Pts',(3.01256338076222,608.12349345016,79.7286663835033));
#97452=CARTESIAN_POINT('Ctrl Pts',(3.15905718679442,608.779515695899,79.700294762995));
#97453=CARTESIAN_POINT('Ctrl Pts',(2.96456958631009,608.282579746035,79.290410633663));
#97454=CARTESIAN_POINT('Ctrl Pts',(3.53144620093892,607.993176826927,79.6182338532211));
#97455=CARTESIAN_POINT('Ctrl Pts',(3.69386701621685,608.627862943539,79.5809202469059));
#97456=CARTESIAN_POINT('Ctrl Pts',(3.47518780032947,608.153921993654,79.1831150315862));
#97457=CARTESIAN_POINT('Ctrl Pts',(3.78653130909377,607.921879230461,79.5570911547537));
#97458=CARTESIAN_POINT('Ctrl Pts',(3.95514895647901,608.545755658182,79.5154433630724));
#97459=CARTESIAN_POINT('Ctrl Pts',(3.72621041294374,608.083531812044,79.1237090131227));
#97460=CARTESIAN_POINT('Ctrl Pts',(4.54004264997885,607.69222741958,79.3568092233317));
#97461=CARTESIAN_POINT('Ctrl Pts',(4.71519034053281,608.285724795436,79.3041392307202));
#97462=CARTESIAN_POINT('Ctrl Pts',(4.46772555015823,607.856801716605,78.9291150218727));
#97463=CARTESIAN_POINT('Ctrl Pts',(5.02678739774566,607.518206712822,79.2008962492214));
#97464=CARTESIAN_POINT('Ctrl Pts',(5.20619063282509,608.090787346965,79.1411907055206));
#97465=CARTESIAN_POINT('Ctrl Pts',(4.94672040811002,607.684994790463,78.7776297759102));
#97466=CARTESIAN_POINT('Ctrl Pts',(5.97439705300667,607.139979558517,78.8468983899839));
#97467=CARTESIAN_POINT('Ctrl Pts',(6.15788846175844,607.669560635868,78.7714177057809));
#97468=CARTESIAN_POINT('Ctrl Pts',(5.87924293219311,607.311580055514,78.4336864380197));
#97469=CARTESIAN_POINT('Ctrl Pts',(6.43524462113633,606.935745723925,78.6487931851204));
#97470=CARTESIAN_POINT('Ctrl Pts',(6.6170133392223,607.446118460456,78.5679319403425));
#97471=CARTESIAN_POINT('Ctrl Pts',(6.33275437617335,607.109943925485,78.241207083469));
#97472=CARTESIAN_POINT('Ctrl Pts',(7.33453041364423,606.506055797746,78.2106205359385));
#97473=CARTESIAN_POINT('Ctrl Pts',(7.50949169824814,606.978742271419,78.1180713169069));
#97474=CARTESIAN_POINT('Ctrl Pts',(7.21772555207048,606.685719938611,77.8154792735));
#97475=CARTESIAN_POINT('Ctrl Pts',(7.76940426542435,606.282236687675,77.9721240183561));
#97476=CARTESIAN_POINT('Ctrl Pts',(7.93961757498883,606.73810424419,77.8759092393284));
#97477=CARTESIAN_POINT('Ctrl Pts',(7.64567757896694,606.464747461961,77.5837558363346));
#97478=CARTESIAN_POINT('Ctrl Pts',(9.0235661087087,605.602041993258,77.2068280660124));
#97479=CARTESIAN_POINT('Ctrl Pts',(9.14486309090703,606.028967316258,77.1186234238837));
#97480=CARTESIAN_POINT('Ctrl Pts',(8.87989624832361,605.793194699699,76.8401851017735));
#97481=CARTESIAN_POINT('Ctrl Pts',(9.79898624522685,605.134564116264,76.6280570123386));
#97482=CARTESIAN_POINT('Ctrl Pts',(9.91195517002788,605.535098232726,76.5412806704512));
#97483=CARTESIAN_POINT('Ctrl Pts',(9.6429736636773,605.331661990879,76.277848672361));
#97484=CARTESIAN_POINT('Ctrl Pts',(10.8844475000821,604.443294288982,75.6498569210074));
#97485=CARTESIAN_POINT('Ctrl Pts',(10.996929204677,604.796890866984,75.5414473133398));
#97486=CARTESIAN_POINT('Ctrl Pts',(10.7111493226909,604.649191799515,75.3274439525344));
#97487=CARTESIAN_POINT('Ctrl Pts',(11.2331134421883,604.214386386114,75.3052878963191));
#97488=CARTESIAN_POINT('Ctrl Pts',(11.3383050337577,604.558413915678,75.1981903967951));
#97489=CARTESIAN_POINT('Ctrl Pts',(11.0542671299848,604.423194954832,74.9926611496337));
#97490=CARTESIAN_POINT('Ctrl Pts',(11.9041426976532,603.763841215211,74.5757653364059));
#97491=CARTESIAN_POINT('Ctrl Pts',(11.9934013858358,604.091098654978,74.4717373421274));
#97492=CARTESIAN_POINT('Ctrl Pts',(11.7146199608134,603.978379024213,74.2838589448406));
#97493=CARTESIAN_POINT('Ctrl Pts',(12.2226419987782,603.544786801835,74.1948314957367));
#97494=CARTESIAN_POINT('Ctrl Pts',(12.3052838069643,603.86393368874,74.0929439227344));
#97495=CARTESIAN_POINT('Ctrl Pts',(12.0280511690333,603.762110554936,73.9137447966116));
#97496=CARTESIAN_POINT('Ctrl Pts',(13.1218292556881,602.915923230929,73.0096082212392));
#97497=CARTESIAN_POINT('Ctrl Pts',(13.1682069587253,603.225589567109,72.9350760877258));
#97498=CARTESIAN_POINT('Ctrl Pts',(12.9129429279531,603.141236478736,72.7621724811206));
#97499=CARTESIAN_POINT('Ctrl Pts',(13.6498656696272,602.532207939341,72.1603061192183));
#97500=CARTESIAN_POINT('Ctrl Pts',(13.691058719412,602.826004591238,72.0905203676822));
#97501=CARTESIAN_POINT('Ctrl Pts',(13.4325731745126,602.762404239833,71.9369957714403));
#97502=CARTESIAN_POINT('Ctrl Pts',(14.3276327741606,602.031260936065,70.7837383555535));
#97503=CARTESIAN_POINT('Ctrl Pts',(14.3599543505595,602.306311131027,70.7113989853479));
#97504=CARTESIAN_POINT('Ctrl Pts',(14.0995518794942,602.267831951347,70.5995413985153));
#97505=CARTESIAN_POINT('Ctrl Pts',(14.5343332153866,601.876752255328,70.3076585181821));
#97506=CARTESIAN_POINT('Ctrl Pts',(14.5622961369223,602.147552358501,70.2399143740041));
#97507=CARTESIAN_POINT('Ctrl Pts',(14.3029634008898,602.115288534774,70.136985137629));
#97508=CARTESIAN_POINT('Ctrl Pts',(14.9054756223491,601.597383091018,69.3166364965849));
#97509=CARTESIAN_POINT('Ctrl Pts',(14.9241336165254,601.861845857833,69.2600256603411));
#97510=CARTESIAN_POINT('Ctrl Pts',(14.6682015611194,601.839471988102,69.174113632982));
#97511=CARTESIAN_POINT('Ctrl Pts',(15.0666029583495,601.475024328722,68.8100615928647));
#97512=CARTESIAN_POINT('Ctrl Pts',(15.0820212400289,601.736215094156,68.7582297164531));
#97513=CARTESIAN_POINT('Ctrl Pts',(14.8267650211877,601.718669700196,68.6819292751414));
#97514=CARTESIAN_POINT('Ctrl Pts',(15.3369981776382,601.268803317671,67.781486615588));
#97515=CARTESIAN_POINT('Ctrl Pts',(15.345642317407,601.525631362788,67.7418790685988));
#97516=CARTESIAN_POINT('Ctrl Pts',(15.0928587745384,601.51507115203,67.6825720627153));
#97517=CARTESIAN_POINT('Ctrl Pts',(15.4467037685615,601.184606480853,67.2583447276789));
#97518=CARTESIAN_POINT('Ctrl Pts',(15.4531593768323,601.439270686425,67.2238371821344));
#97519=CARTESIAN_POINT('Ctrl Pts',(15.2008187183865,601.431945381811,67.1742916843792));
#97520=CARTESIAN_POINT('Ctrl Pts',(15.5714893985198,601.088632207677,66.4596770533946));
#97521=CARTESIAN_POINT('Ctrl Pts',(15.5750769362233,601.341153963858,66.4333318182824));
#97522=CARTESIAN_POINT('Ctrl Pts',(15.3236190583423,601.337191765776,66.3983126284387));
#97523=CARTESIAN_POINT('Ctrl Pts',(15.6064418001331,601.06170107286,66.191124442761));
#97524=CARTESIAN_POINT('Ctrl Pts',(15.6092008209444,601.313647862235,66.1679286147603));
#97525=CARTESIAN_POINT('Ctrl Pts',(15.3580154032569,601.310603141948,66.1373887935008));
#97526=CARTESIAN_POINT('Ctrl Pts',(15.6626190527797,601.018381804667,65.649189292362));
#97527=CARTESIAN_POINT('Ctrl Pts',(15.6639728424716,601.269466973693,65.6327189571251));
#97528=CARTESIAN_POINT('Ctrl Pts',(15.4132989948751,601.267834762569,65.6108481462777));
#97529=CARTESIAN_POINT('Ctrl Pts',(15.6838311981551,601.002003491397,65.37513074784));
#97530=CARTESIAN_POINT('Ctrl Pts',(15.6846836179855,601.252741847092,65.361885527254));
#97531=CARTESIAN_POINT('Ctrl Pts',(15.4341736765461,601.251664750571,65.3445748221907));
#97532=CARTESIAN_POINT('Ctrl Pts',(15.7535397227803,600.948166401941,64.0126917270571));
#97533=CARTESIAN_POINT('Ctrl Pts',(15.7525074770034,601.197957730567,64.019253662881));
#97534=CARTESIAN_POINT('Ctrl Pts',(15.5027734069943,601.198512215226,64.0208357993163));
#97535=CARTESIAN_POINT('Ctrl Pts',(15.6961577000033,600.992752129991,62.9336548017417));
#97536=CARTESIAN_POINT('Ctrl Pts',(15.6953430710373,601.244369811282,62.9419553492361));
#97537=CARTESIAN_POINT('Ctrl Pts',(15.4463052101678,601.242530165078,62.972460326068));
#97538=CARTESIAN_POINT('Ctrl Pts',(15.4449172446521,601.185978519767,61.3309552205203));
#97539=CARTESIAN_POINT('Ctrl Pts',(15.4514130025606,601.440674321061,61.3655583025674));
#97540=CARTESIAN_POINT('Ctrl Pts',(15.1990606178882,601.433299969603,61.4152823525307));
#97541=CARTESIAN_POINT('Ctrl Pts',(15.3326315846512,601.272148638439,60.7979635436387));
#97542=CARTESIAN_POINT('Ctrl Pts',(15.3413681900166,601.529059099786,60.8377615984788));
#97543=CARTESIAN_POINT('Ctrl Pts',(15.0885616588025,601.5183739204,60.897431997035));
#97544=CARTESIAN_POINT('Ctrl Pts',(15.0597162431557,601.480260879463,59.7656992724498));
#97545=CARTESIAN_POINT('Ctrl Pts',(15.0752901365765,601.741577703714,59.8177577361634));
#97546=CARTESIAN_POINT('Ctrl Pts',(14.8199878745666,601.723839648942,59.894490282593));
#97547=CARTESIAN_POINT('Ctrl Pts',(14.8986984980326,601.602505699219,59.2627428795189));
#97548=CARTESIAN_POINT('Ctrl Pts',(14.9175497152663,601.867063568807,59.3196546068316));
#97549=CARTESIAN_POINT('Ctrl Pts',(14.6615322304544,601.844529468462,59.405821548259));
#97550=CARTESIAN_POINT('Ctrl Pts',(14.5300665302068,601.879941981165,58.2814141988727));
#97551=CARTESIAN_POINT('Ctrl Pts',(14.5581603558448,602.150797938548,58.3493442354962));
#97552=CARTESIAN_POINT('Ctrl Pts',(14.2987645730368,602.118437712548,58.452368034267));
#97553=CARTESIAN_POINT('Ctrl Pts',(14.3223620118629,602.035207147482,57.8028805682137));
#97554=CARTESIAN_POINT('Ctrl Pts',(14.3547106916411,602.310430445876,57.8751573631045));
#97555=CARTESIAN_POINT('Ctrl Pts',(14.0943650477467,602.271727921001,57.987427888935));
#97556=CARTESIAN_POINT('Ctrl Pts',(13.8614639308801,602.375760037317,56.870100046218));
#97557=CARTESIAN_POINT('Ctrl Pts',(13.905352230957,602.6594624201,56.9519457897139));
#97558=CARTESIAN_POINT('Ctrl Pts',(13.6407992303396,602.607950213347,57.0811428907972));
#97559=CARTESIAN_POINT('Ctrl Pts',(13.611788274916,602.558441818736,56.4228707819826));
#97560=CARTESIAN_POINT('Ctrl Pts',(13.660997958786,602.847564244315,56.5087094937084));
#97561=CARTESIAN_POINT('Ctrl Pts',(13.3950963108816,602.788308498489,56.6466171892939));
#97562=CARTESIAN_POINT('Ctrl Pts',(13.0764921418282,602.944386245562,55.5629408541681));
#97563=CARTESIAN_POINT('Ctrl Pts',(13.1390236076535,603.244280565436,55.6564090278324));
#97564=CARTESIAN_POINT('Ctrl Pts',(12.8683162606274,603.169345173769,55.8111128357767));
#97565=CARTESIAN_POINT('Ctrl Pts',(12.7908624053289,603.147665803391,55.1502548367754));
#97566=CARTESIAN_POINT('Ctrl Pts',(12.8594650095397,603.454227818642,55.2468622237164));
#97567=CARTESIAN_POINT('Ctrl Pts',(12.5872314290769,603.370039355094,55.4101487566788));
#97568=CARTESIAN_POINT('Ctrl Pts',(12.1845042755668,603.571151168872,54.3570282351227));
#97569=CARTESIAN_POINT('Ctrl Pts',(12.2679641743712,603.891253550521,54.4591095196187));
#97570=CARTESIAN_POINT('Ctrl Pts',(11.9905202907966,603.788139618472,54.6394524585066));
#97571=CARTESIAN_POINT('Ctrl Pts',(11.8627313233714,603.792069253919,53.9753888666545));
#97572=CARTESIAN_POINT('Ctrl Pts',(11.9529310376215,604.120352293626,54.0796602679055));
#97573=CARTESIAN_POINT('Ctrl Pts',(11.6738674877948,604.006248090623,54.2686527469967));
#97574=CARTESIAN_POINT('Ctrl Pts',(10.8510402072694,604.469985948396,52.8843970456025));
#97575=CARTESIAN_POINT('Ctrl Pts',(10.945265328937,604.837892193095,52.9711566209328));
#97576=CARTESIAN_POINT('Ctrl Pts',(10.6782856421904,604.675535692234,53.2086614405224));
#97577=CARTESIAN_POINT('Ctrl Pts',(10.1231644802855,604.937352782708,52.2355170621796));
#97578=CARTESIAN_POINT('Ctrl Pts',(10.2261851601175,605.328623293813,52.325672618392));
#97579=CARTESIAN_POINT('Ctrl Pts',(9.9619956407393,605.13695811471,52.5782081758289));
#97580=CARTESIAN_POINT('Ctrl Pts',(8.94566114499843,605.634568642711,51.3658592810726));
#97581=CARTESIAN_POINT('Ctrl Pts',(9.09775647626564,606.047668837203,51.4706442472986));
#97582=CARTESIAN_POINT('Ctrl Pts',(8.80321427157987,605.825316635566,51.7332383677212));
#97583=CARTESIAN_POINT('Ctrl Pts',(8.53871075522488,605.866292458671,51.0934261046552));
#97584=CARTESIAN_POINT('Ctrl Pts',(8.69719315797,606.293588447686,51.1963055952873));
#97585=CARTESIAN_POINT('Ctrl Pts',(8.40274055580763,606.054093444861,51.468542205798));
#97586=CARTESIAN_POINT('Ctrl Pts',(7.69242405624649,606.322458739373,50.5832101346318));
#97587=CARTESIAN_POINT('Ctrl Pts',(7.86343028959298,606.781403923533,50.6785875112157));
#97588=CARTESIAN_POINT('Ctrl Pts',(7.56992268932879,606.504457879526,50.9728170395581));
#97589=CARTESIAN_POINT('Ctrl Pts',(7.25341144010781,606.546582345598,50.3459105384044));
#97590=CARTESIAN_POINT('Ctrl Pts',(7.42930129741494,607.022466301498,50.4376325390388));
#97591=CARTESIAN_POINT('Ctrl Pts',(7.13789769244056,606.725731037077,50.7422564476865));
#97592=CARTESIAN_POINT('Ctrl Pts',(5.74078325584115,607.262802253728,49.6195861520783));
#97593=CARTESIAN_POINT('Ctrl Pts',(5.86838675370132,607.833044383481,49.6620231583292));
#97594=CARTESIAN_POINT('Ctrl Pts',(5.64937448274724,607.432827203209,50.036573743915));
#97595=CARTESIAN_POINT('Ctrl Pts',(4.61020627219875,607.711095870914,49.2207424753209));
#97596=CARTESIAN_POINT('Ctrl Pts',(4.73821803523183,608.319969502878,49.262455296545));
#97597=CARTESIAN_POINT('Ctrl Pts',(4.53678997843925,607.875425333392,49.6490480272317));
#97598=CARTESIAN_POINT('Ctrl Pts',(3.37684626304299,608.03198826415,48.9478721491));
#97599=CARTESIAN_POINT('Ctrl Pts',(3.53826781775195,608.671892366682,48.9831770877157));
#97600=CARTESIAN_POINT('Ctrl Pts',(3.32305067588146,608.192239283157,49.3839240770586));
#97601=CARTESIAN_POINT('',(3.445572367957E-11,608.476132031989,80.0177796115133));
#97602=CARTESIAN_POINT('',(3.93978362444746,607.874843764614,49.082928510463));
#97603=CARTESIAN_POINT('Ctrl Pts',(6.891144735914E-11,608.476132031982,
80.0177787907144));
#97604=CARTESIAN_POINT('Ctrl Pts',(0.023608644378443,608.476133391052,80.0177797817517));
#97605=CARTESIAN_POINT('Ctrl Pts',(0.0471977207100223,608.476067912617,
80.0177272377913));
#97606=CARTESIAN_POINT('Ctrl Pts',(0.0707638231545097,608.475935523855,
80.017621142111));
#97607=CARTESIAN_POINT('Ctrl Pts',(0.343491007326588,608.474403407364,80.0163933117468));
#97608=CARTESIAN_POINT('Ctrl Pts',(0.614496441609094,608.464020952774,80.0080814531982));
#97609=CARTESIAN_POINT('Ctrl Pts',(0.883878526644414,608.445171171727,79.992909437795));
#97610=CARTESIAN_POINT('Ctrl Pts',(1.24943310899289,608.419591802421,79.9723208386927));
#97611=CARTESIAN_POINT('Ctrl Pts',(1.61199825335794,608.378394662748,79.9391295369998));
#97612=CARTESIAN_POINT('Ctrl Pts',(1.97182100459186,608.322782114007,79.8936222931225));
#97613=CARTESIAN_POINT('Ctrl Pts',(2.14338863407167,608.296265410646,79.8719239154367));
#97614=CARTESIAN_POINT('Ctrl Pts',(2.31433265226537,608.266470720811,79.8474250872981));
#97615=CARTESIAN_POINT('Ctrl Pts',(2.48467918176857,608.233525031413,79.8201546029834));
#97616=CARTESIAN_POINT('Ctrl Pts',(2.64668359998501,608.202192739179,79.7942195929848));
#97617=CARTESIAN_POINT('Ctrl Pts',(2.80854164377701,608.167910736366,79.7656811760263));
#97618=CARTESIAN_POINT('Ctrl Pts',(2.96931905952992,608.131056409394,79.7347565578901));
#97619=CARTESIAN_POINT('Ctrl Pts',(3.07072240523472,608.107812149364,79.7152522031959));
#97620=CARTESIAN_POINT('Ctrl Pts',(3.17169670908154,608.083545727609,79.6947984620929));
#97621=CARTESIAN_POINT('Ctrl Pts',(3.2720087069542,608.05835117884,79.6734492843488));
#97622=CARTESIAN_POINT('Ctrl Pts',(3.53149735464349,607.993177525359,79.6182228968817));
#97623=CARTESIAN_POINT('Ctrl Pts',(3.78656458821257,607.921882403724,79.5570823750604));
#97624=CARTESIAN_POINT('Ctrl Pts',(4.03770549440548,607.845341550768,79.4903295169232));
#97625=CARTESIAN_POINT('Ctrl Pts',(4.40729347692822,607.732701280996,79.3920936120658));
#97626=CARTESIAN_POINT('Ctrl Pts',(4.76841289982341,607.608751209855,79.2817479196197));
#97627=CARTESIAN_POINT('Ctrl Pts',(5.12226678865739,607.475746685772,79.1597571080133));
#97628=CARTESIAN_POINT('Ctrl Pts',(5.24929534886865,607.427999935689,79.1159641255244));
#97629=CARTESIAN_POINT('Ctrl Pts',(5.37538735229175,607.379086051863,79.0706700669591));
#97630=CARTESIAN_POINT('Ctrl Pts',(5.50059773443485,607.32910861461,79.0238952610022));
#97631=CARTESIAN_POINT('Ctrl Pts',(5.57281046246083,607.300285069613,78.9969187732444));
#97632=CARTESIAN_POINT('Ctrl Pts',(5.64472953797074,607.271107125461,78.9694492784864));
#97633=CARTESIAN_POINT('Ctrl Pts',(5.71636225209787,607.241589948643,78.9414864057523));
#97634=CARTESIAN_POINT('Ctrl Pts',(6.1145430789441,607.077514441875,78.7860507235792));
#97635=CARTESIAN_POINT('Ctrl Pts',(6.50370968196559,606.903036652875,78.6154339417837));
#97636=CARTESIAN_POINT('Ctrl Pts',(6.8848883010362,606.720902758003,78.4297064786912));
#97637=CARTESIAN_POINT('Ctrl Pts',(7.33445681558759,606.506090959885,78.210656365394));
#97638=CARTESIAN_POINT('Ctrl Pts',(7.76935072835595,606.282265744325,77.9721566871374));
#97639=CARTESIAN_POINT('Ctrl Pts',(8.187458217611,606.055505133889,77.7170253648745));
#97640=CARTESIAN_POINT('Ctrl Pts',(8.18746947767835,606.055499026991,77.717018493924));
#97641=CARTESIAN_POINT('Ctrl Pts',(8.18748073773472,606.05549292009,77.7170116229611));
#97642=CARTESIAN_POINT('Ctrl Pts',(8.18749199778011,606.055486813187,77.7170047519856));
#97643=CARTESIAN_POINT('Ctrl Pts',(8.77466513832359,605.737032553591,77.3587067095187));
#97644=CARTESIAN_POINT('Ctrl Pts',(9.33198432025338,605.411622763145,76.9665375838635));
#97645=CARTESIAN_POINT('Ctrl Pts',(9.86244451672601,605.086463613717,76.5388820034507));
#97646=CARTESIAN_POINT('Ctrl Pts',(10.0299804484333,604.983768177915,76.4038149869418));
#97647=CARTESIAN_POINT('Ctrl Pts',(10.1948374650659,604.881097800488,76.2652085139033));
#97648=CARTESIAN_POINT('Ctrl Pts',(10.3571105681779,604.778679548307,76.1230125476067));
#97649=CARTESIAN_POINT('Ctrl Pts',(10.4125855674164,604.743666645041,76.0744011574826));
#97650=CARTESIAN_POINT('Ctrl Pts',(10.4677585361306,604.708682049518,76.0253703145274));
#97651=CARTESIAN_POINT('Ctrl Pts',(10.5226333425913,604.673735097822,75.9759179749725));
#97652=CARTESIAN_POINT('Ctrl Pts',(10.8021362240136,604.495734038209,75.7240342365111));
#97653=CARTESIAN_POINT('Ctrl Pts',(11.0737787493323,604.318624837962,75.4611186031081));
#97654=CARTESIAN_POINT('Ctrl Pts',(11.3375596732538,604.143426989905,75.1864000604821));
#97655=CARTESIAN_POINT('Ctrl Pts',(11.4152479295857,604.091828052703,75.105490477479));
#97656=CARTESIAN_POINT('Ctrl Pts',(11.4922757377262,604.040378802491,75.023534546417));
#97657=CARTESIAN_POINT('Ctrl Pts',(11.5686281331514,603.989114002876,74.9405265476199));
#97658=CARTESIAN_POINT('Ctrl Pts',(11.7428614430267,603.872129648067,74.7511053998486));
#97659=CARTESIAN_POINT('Ctrl Pts',(11.9125329809615,603.756803523413,74.5572877444752));
#97660=CARTESIAN_POINT('Ctrl Pts',(12.0772418647187,603.643694083311,74.3595533209466));
#97661=CARTESIAN_POINT('Ctrl Pts',(12.1335432671765,603.60503059435,74.2919630058106));
#97662=CARTESIAN_POINT('Ctrl Pts',(12.1892651384275,603.566625966915,74.2239153125446));
#97663=CARTESIAN_POINT('Ctrl Pts',(12.2443925060635,603.528501994852,74.1554302041702));
#97664=CARTESIAN_POINT('Ctrl Pts',(12.3387364620062,603.463257335169,74.0382260581302));
#97665=CARTESIAN_POINT('Ctrl Pts',(12.4314151262027,603.398784198907,73.9196466444437));
#97666=CARTESIAN_POINT('Ctrl Pts',(12.5223735539976,603.335175124649,73.7997538153799));
#97667=CARTESIAN_POINT('Ctrl Pts',(12.7691297819514,603.162613487337,73.474503006019));
#97668=CARTESIAN_POINT('Ctrl Pts',(13.003843124458,602.996038420695,73.1391451429734));
#97669=CARTESIAN_POINT('Ctrl Pts',(13.2260892248692,602.836485522975,72.7931543849762));
#97670=CARTESIAN_POINT('Ctrl Pts',(13.4204829916168,602.696928119152,72.4905238930013));
#97671=CARTESIAN_POINT('Ctrl Pts',(13.6053390538352,602.562743113451,72.1797589167256));
#97672=CARTESIAN_POINT('Ctrl Pts',(13.7803977512332,602.434610850826,71.8605255759729));
#97673=CARTESIAN_POINT('Ctrl Pts',(13.8914471872944,602.353329453687,71.6580181713741));
#97674=CARTESIAN_POINT('Ctrl Pts',(13.9985704807448,602.274488846586,71.4520750410271));
#97675=CARTESIAN_POINT('Ctrl Pts',(14.1017118649645,602.198253227673,71.2425913130359));
#97676=CARTESIAN_POINT('Ctrl Pts',(14.2070716057042,602.120377939255,71.0286020260264));
#97677=CARTESIAN_POINT('Ctrl Pts',(14.3082384476158,602.04522874082,70.81089177479));
#97678=CARTESIAN_POINT('Ctrl Pts',(14.4050208561385,601.97303833151,70.5892424956487));
#97679=CARTESIAN_POINT('Ctrl Pts',(14.5157812425591,601.890421689158,70.3355811104625));
#97680=CARTESIAN_POINT('Ctrl Pts',(14.6208678960898,601.811623873729,70.0765942455147));
#97681=CARTESIAN_POINT('Ctrl Pts',(14.7199048617496,601.737072380968,69.8121463246681));
#97682=CARTESIAN_POINT('Ctrl Pts',(14.7921227929364,601.682709300089,69.6193104312928));
#97683=CARTESIAN_POINT('Ctrl Pts',(14.8606224440704,601.630982676328,69.4248390807865));
#97684=CARTESIAN_POINT('Ctrl Pts',(14.9252970870176,601.582022741331,69.2290149637919));
#97685=CARTESIAN_POINT('Ctrl Pts',(15.0269343231625,601.505081420156,68.9212742308732));
#97686=CARTESIAN_POINT('Ctrl Pts',(15.1192104490316,601.434902446505,68.6099443406549));
#97687=CARTESIAN_POINT('Ctrl Pts',(15.2018005707495,601.371913878203,68.2957740937441));
#97688=CARTESIAN_POINT('Ctrl Pts',(15.3370175067359,601.268788697724,67.781413086861));
#97689=CARTESIAN_POINT('Ctrl Pts',(15.4467112583919,601.184600964787,67.2582968021332));
#97690=CARTESIAN_POINT('Ctrl Pts',(15.5298941967001,601.120624070575,66.7258995592193));
#97691=CARTESIAN_POINT('Ctrl Pts',(15.5492380442097,601.105746509011,66.6020927871707));
#97692=CARTESIAN_POINT('Ctrl Pts',(15.567145084157,601.091963469233,66.4777831582835));
#97693=CARTESIAN_POINT('Ctrl Pts',(15.5835932838998,601.079296047254,66.3529610769457));
#97694=CARTESIAN_POINT('Ctrl Pts',(15.6025152015847,601.064723515323,66.2093664474261));
#97695=CARTESIAN_POINT('Ctrl Pts',(15.6195051466467,601.051628333843,66.0651039293665));
#97696=CARTESIAN_POINT('Ctrl Pts',(15.6345304353988,601.040042512501,65.9201567812727));
#97697=CARTESIAN_POINT('Ctrl Pts',(15.6626204963928,601.018382600765,65.6491753513615));
#97698=CARTESIAN_POINT('Ctrl Pts',(15.6838314901426,601.002007634833,65.3751252063361));
#97699=CARTESIAN_POINT('Ctrl Pts',(15.6977729274255,600.991248095703,65.1026424621912));
#97700=CARTESIAN_POINT('Ctrl Pts',(15.7020662908531,600.987934620136,65.0187294893299));
#97701=CARTESIAN_POINT('Ctrl Pts',(15.7056890266772,600.985141168189,64.934880886641));
#97702=CARTESIAN_POINT('Ctrl Pts',(15.7086425189985,600.982866284406,64.8510957582209));
#97703=CARTESIAN_POINT('Ctrl Pts',(15.7263165930932,600.969253090209,64.3497148820873));
#97704=CARTESIAN_POINT('Ctrl Pts',(15.7200248924218,600.974244879535,63.8506118554521));
#97705=CARTESIAN_POINT('Ctrl Pts',(15.690054723568,600.997369844198,63.3537494689464));
#97706=CARTESIAN_POINT('Ctrl Pts',(15.6600845547142,601.020494808862,62.8568870824407));
#97707=CARTESIAN_POINT('Ctrl Pts',(15.6064372952925,601.061755283394,62.3622858632638));
#97708=CARTESIAN_POINT('Ctrl Pts',(15.5294020172295,601.121002544319,61.8699005539026));
#97709=CARTESIAN_POINT('Ctrl Pts',(15.5291562735781,601.121191543938,61.8683298376431));
#97710=CARTESIAN_POINT('Ctrl Pts',(15.5289102911643,601.121380726214,61.8667591390815));
#97711=CARTESIAN_POINT('Ctrl Pts',(15.5286640699994,601.121570091134,61.8651884582589));
#97712=CARTESIAN_POINT('Ctrl Pts',(15.4868770628324,601.153707837259,61.5986230278064));
#97713=CARTESIAN_POINT('Ctrl Pts',(15.4379580369834,601.19128412897,61.3322197252209));
#97714=CARTESIAN_POINT('Ctrl Pts',(15.3824805581734,601.233797688178,61.0681260116062));
#97715=CARTESIAN_POINT('Ctrl Pts',(15.3358122267525,601.269560612406,60.8459671605279));
#97716=CARTESIAN_POINT('Ctrl Pts',(15.2845038713035,601.308816554583,60.625443469707));
#97717=CARTESIAN_POINT('Ctrl Pts',(15.2289186178845,601.351251028551,60.4078240107633));
#97718=CARTESIAN_POINT('Ctrl Pts',(15.2181659569586,601.35945974367,60.3657267258007));
#97719=CARTESIAN_POINT('Ctrl Pts',(15.2072508201014,601.367788808569,60.3237283373609));
#97720=CARTESIAN_POINT('Ctrl Pts',(15.196175503333,601.376236194403,60.2818374278755));
#97721=CARTESIAN_POINT('Ctrl Pts',(15.096781692569,601.452046023291,59.9058935865223));
#97722=CARTESIAN_POINT('Ctrl Pts',(14.9842779945814,601.53754841251,59.536653111409));
#97723=CARTESIAN_POINT('Ctrl Pts',(14.859145984944,601.63209461805,59.1739255762946));
#97724=CARTESIAN_POINT('Ctrl Pts',(14.8126284390042,601.667241959425,59.0390824228346));
#97725=CARTESIAN_POINT('Ctrl Pts',(14.7643660978949,601.703638825262,58.9051391515248));
#97726=CARTESIAN_POINT('Ctrl Pts',(14.7143850694044,601.741250875155,58.7720853460319));
#97727=CARTESIAN_POINT('Ctrl Pts',(14.5736911865015,601.84712675453,58.3975461039397));
#97728=CARTESIAN_POINT('Ctrl Pts',(14.4193228109465,601.962676680985,58.0299622878074));
#97729=CARTESIAN_POINT('Ctrl Pts',(14.2516172400983,602.087194168844,57.6694867820627));
#97730=CARTESIAN_POINT('Ctrl Pts',(14.1996634649568,602.125768639165,57.5578145026341));
#97731=CARTESIAN_POINT('Ctrl Pts',(14.1464260882526,602.165206051972,57.4468157386464));
#97732=CARTESIAN_POINT('Ctrl Pts',(14.0919132979964,602.205485809269,57.3364909682744));
#97733=CARTESIAN_POINT('Ctrl Pts',(13.9337411446871,602.322359957823,57.0163769838124));
#97734=CARTESIAN_POINT('Ctrl Pts',(13.7664884987757,602.445098355549,56.7052436349986));
#97735=CARTESIAN_POINT('Ctrl Pts',(13.5905541920496,602.573008005882,56.4024860662583));
#97736=CARTESIAN_POINT('Ctrl Pts',(13.5102146755005,602.631417304562,56.2642333447919));
#97737=CARTESIAN_POINT('Ctrl Pts',(13.4280641419558,602.690908584722,56.1277259803299));
#97738=CARTESIAN_POINT('Ctrl Pts',(13.3441406912912,602.751416392403,55.9929065938881));
#97739=CARTESIAN_POINT('Ctrl Pts',(13.18094216384,602.869080585599,55.7307352321897));
#97740=CARTESIAN_POINT('Ctrl Pts',(13.0110358717025,602.990595148795,55.474952500565));
#97741=CARTESIAN_POINT('Ctrl Pts',(12.834515971694,603.115539209283,55.2252918717908));
#97742=CARTESIAN_POINT('Ctrl Pts',(12.7215730554199,603.195482301036,55.065551244863));
#97743=CARTESIAN_POINT('Ctrl Pts',(12.6059608809529,603.276803544364,54.9083700535969));
#97744=CARTESIAN_POINT('Ctrl Pts',(12.4876834913282,603.359409062561,54.7536417333293));
#97745=CARTESIAN_POINT('Ctrl Pts',(12.3260424195162,603.472299992445,54.5421858362463));
#97746=CARTESIAN_POINT('Ctrl Pts',(12.1591272633341,603.587791808995,54.3349982249624));
#97747=CARTESIAN_POINT('Ctrl Pts',(11.9873446890175,603.705306278801,54.132457025428));
#97748=CARTESIAN_POINT('Ctrl Pts',(11.8370887041423,603.808094658053,53.9552968708842));
#97749=CARTESIAN_POINT('Ctrl Pts',(11.682992340067,603.912509879882,53.7815611779533));
#97750=CARTESIAN_POINT('Ctrl Pts',(11.5255012613246,604.018042470088,53.6117252605926));
#97751=CARTESIAN_POINT('Ctrl Pts',(11.3711873179765,604.121446105878,53.445315516375));
#97752=CARTESIAN_POINT('Ctrl Pts',(11.2140552717419,604.225670952781,53.2829927429756));
#97753=CARTESIAN_POINT('Ctrl Pts',(11.0542019754069,604.330409538232,53.1247785161059));
#97754=CARTESIAN_POINT('Ctrl Pts',(10.5698058925877,604.647794050629,52.6453492300101));
#97755=CARTESIAN_POINT('Ctrl Pts',(10.0592926797871,604.97065899169,52.2024986105179));
#97756=CARTESIAN_POINT('Ctrl Pts',(9.5214912839734,605.292961601669,51.7931946721202));
#97757=CARTESIAN_POINT('Ctrl Pts',(9.46073141911627,605.329374789098,51.7469522261613));
#97758=CARTESIAN_POINT('Ctrl Pts',(9.39962327601398,605.365780791358,51.7011379286063));
#97759=CARTESIAN_POINT('Ctrl Pts',(9.3381651900171,605.40217089056,51.6557473746705));
#97760=CARTESIAN_POINT('Ctrl Pts',(9.21814549218713,605.473236050488,51.5671054900537));
#97761=CARTESIAN_POINT('Ctrl Pts',(9.09677553395676,605.544236595435,51.4800960735065));
#97762=CARTESIAN_POINT('Ctrl Pts',(8.97400639050295,605.615087250737,51.3947159850713));
#97763=CARTESIAN_POINT('Ctrl Pts',(8.69526626352681,605.775949500807,51.200865510741));
#97764=CARTESIAN_POINT('Ctrl Pts',(8.40931705214077,605.936070716091,51.0154168364813));
#97765=CARTESIAN_POINT('Ctrl Pts',(8.11558835298554,606.094427751649,50.8383307562355));
#97766=CARTESIAN_POINT('Ctrl Pts',(7.69239174854488,606.322584414344,50.5831897772666));
#97767=CARTESIAN_POINT('Ctrl Pts',(7.25336993337879,606.546758860276,50.3458922881572));
#97768=CARTESIAN_POINT('Ctrl Pts',(6.8038425239994,606.759577373996,50.1300393648259));
#97769=CARTESIAN_POINT('Ctrl Pts',(6.73473828265154,606.792293203172,50.0968570667095));
#97770=CARTESIAN_POINT('Ctrl Pts',(6.66535065282465,606.82477352714,50.0641473617017));
#97771=CARTESIAN_POINT('Ctrl Pts',(6.59567017408018,606.856998130578,50.0319141884441));
#97772=CARTESIAN_POINT('Ctrl Pts',(6.03292698896474,607.117245710745,49.7715973979719));
#97773=CARTESIAN_POINT('Ctrl Pts',(5.45113667966419,607.360978280686,49.542387508329));
#97774=CARTESIAN_POINT('Ctrl Pts',(4.8452572739386,607.577752733781,49.3462933887054));
#97775=CARTESIAN_POINT('Ctrl Pts',(4.54937241788851,607.683615843243,49.2505296446191));
#97776=CARTESIAN_POINT('Ctrl Pts',(4.24774282917826,607.783050325799,49.1626636005067));
#97777=CARTESIAN_POINT('Ctrl Pts',(3.93978362444746,607.874843764614,49.082928510463));
#97778=CARTESIAN_POINT('',(3.87712128125394,608.037287038731,49.5149800517143));
#97779=CARTESIAN_POINT('Origin',(3.87712128127698,607.874843764616,49.3249479946959));
#97780=CARTESIAN_POINT('',(-3.85030552837329,608.045280920111,79.0907977188138));
#97781=CARTESIAN_POINT('Ctrl Pts',(3.87712128125394,608.037287038731,49.5149800517143));
#97782=CARTESIAN_POINT('Ctrl Pts',(4.87153021748849,607.739915203809,49.7691795549397));
#97783=CARTESIAN_POINT('Ctrl Pts',(5.79934294385505,607.361106997409,50.1085862160764));
#97784=CARTESIAN_POINT('Ctrl Pts',(7.12166692125997,606.734009856725,50.7337821806858));
#97785=CARTESIAN_POINT('Ctrl Pts',(7.55227759129253,606.513849499917,50.9628773512951));
#97786=CARTESIAN_POINT('Ctrl Pts',(8.38321347944639,606.065233520004,51.4559004400492));
#97787=CARTESIAN_POINT('Ctrl Pts',(8.78304187688083,605.837184142117,51.7192666405192));
#97788=CARTESIAN_POINT('Ctrl Pts',(9.94055760102618,605.150556485895,52.5603722809289));
#97789=CARTESIAN_POINT('Ctrl Pts',(10.6569237854819,604.689665531714,53.1884290403189));
#97790=CARTESIAN_POINT('Ctrl Pts',(11.6536196238761,604.020275142643,54.2454145926918));
#97791=CARTESIAN_POINT('Ctrl Pts',(11.9710603883753,603.801813085304,54.6156007098022));
#97792=CARTESIAN_POINT('Ctrl Pts',(12.5694073935915,603.382876923177,55.385215476498));
#97793=CARTESIAN_POINT('Ctrl Pts',(12.8514309701718,603.181641349324,55.7857953218243));
#97794=CARTESIAN_POINT('Ctrl Pts',(13.3802712808598,602.79932278676,56.6209194460713));
#97795=CARTESIAN_POINT('Ctrl Pts',(13.6270976333542,602.618222784044,57.0554488359468));
#97796=CARTESIAN_POINT('Ctrl Pts',(14.0830317948412,602.280372513136,57.9622402793));
#97797=CARTESIAN_POINT('Ctrl Pts',(14.288866825385,602.126052058398,58.4281588815737));
#97798=CARTESIAN_POINT('Ctrl Pts',(14.6541428180436,601.850313463799,59.3835018865815));
#97799=CARTESIAN_POINT('Ctrl Pts',(14.813802564089,601.728726306764,59.8733378707772));
#97800=CARTESIAN_POINT('Ctrl Pts',(15.0845904681104,601.521591068862,60.8791319779345));
#97801=CARTESIAN_POINT('Ctrl Pts',(15.1961319187924,601.435719945448,61.3988026843396));
#97802=CARTESIAN_POINT('Ctrl Pts',(15.445895886564,601.243012879202,62.9621091081608));
#97803=CARTESIAN_POINT('Ctrl Pts',(15.5031899681929,601.198348388516,64.0148308425101));
#97804=CARTESIAN_POINT('Ctrl Pts',(15.4344186449233,601.251635259198,65.3443173476824));
#97805=CARTESIAN_POINT('Ctrl Pts',(15.4134449473779,601.267882404695,65.6117770146501));
#97806=CARTESIAN_POINT('Ctrl Pts',(15.3578567110548,601.310887267439,66.1405396918101));
#97807=CARTESIAN_POINT('Ctrl Pts',(15.3232550273986,601.337635013737,66.4025181324823));
#97808=CARTESIAN_POINT('Ctrl Pts',(15.1997028143738,601.432969072053,67.1815043824831));
#97809=CARTESIAN_POINT('Ctrl Pts',(15.0910612840211,601.516618757114,67.6915802539796));
#97810=CARTESIAN_POINT('Ctrl Pts',(14.8233372862475,601.721454107234,68.694153518926));
#97811=CARTESIAN_POINT('Ctrl Pts',(14.6637788819681,601.843004162358,69.1878707203431));
#97812=CARTESIAN_POINT('Ctrl Pts',(14.2965526740649,602.120283814448,70.1529519783302));
#97813=CARTESIAN_POINT('Ctrl Pts',(14.0918748017888,602.273750570818,70.6169548967642));
#97814=CARTESIAN_POINT('Ctrl Pts',(13.4200658305586,602.771767364609,71.9594073502309));
#97815=CARTESIAN_POINT('Ctrl Pts',(12.8958575906797,603.153805305363,72.7887618167445));
#97816=CARTESIAN_POINT('Ctrl Pts',(12.0012587128913,603.78090420349,73.9468631187593));
#97817=CARTESIAN_POINT('Ctrl Pts',(11.683780665072,603.999674377738,74.3193541873481));
#97818=CARTESIAN_POINT('Ctrl Pts',(11.0214171690138,604.445181629234,75.0259744723523));
#97819=CARTESIAN_POINT('Ctrl Pts',(10.6774393735486,604.671360763517,75.3595543546866));
#97820=CARTESIAN_POINT('Ctrl Pts',(9.60714722132492,605.353866408868,76.3061032107106));
#97821=CARTESIAN_POINT('Ctrl Pts',(8.84327964705721,605.814723142904,76.865511939863));
#97822=CARTESIAN_POINT('Ctrl Pts',(7.60921202386664,606.484073904586,77.6043583167633));
#97823=CARTESIAN_POINT('Ctrl Pts',(7.1813427653491,606.704199580113,77.8345316034363));
#97824=CARTESIAN_POINT('Ctrl Pts',(6.29818432438025,607.125857945281,78.2566267740411));
#97825=CARTESIAN_POINT('Ctrl Pts',(5.84582286264931,607.326074990086,78.4473366643001));
#97826=CARTESIAN_POINT('Ctrl Pts',(4.91622538701958,607.696478903184,78.7878860584469));
#97827=CARTESIAN_POINT('Ctrl Pts',(4.43900471573538,607.86669051722,78.9377439866561));
#97828=CARTESIAN_POINT('Ctrl Pts',(3.45473183503186,608.165828521108,79.1941909352119));
#97829=CARTESIAN_POINT('Ctrl Pts',(2.94362350959894,608.295390945239,79.3013079500641));
#97830=CARTESIAN_POINT('Ctrl Pts',(1.90950562370682,608.494575880372,79.4634826852088));
#97831=CARTESIAN_POINT('Ctrl Pts',(1.38650131959488,608.564625822707,79.5190163918644));
#97832=CARTESIAN_POINT('Ctrl Pts',(0.592249243454403,608.619578731141,79.5625292223074));
#97833=CARTESIAN_POINT('Ctrl Pts',(0.325874264894089,608.629555363385,79.5703863596371));
#97834=CARTESIAN_POINT('Ctrl Pts',(-0.21025693007535,608.632063664679,79.5723645937365));
#97835=CARTESIAN_POINT('Ctrl Pts',(-0.48111240188688,608.624461420681,79.5663806670725));
#97836=CARTESIAN_POINT('Ctrl Pts',(-1.81787718546613,608.543639087743,79.5024445409065));
#97837=CARTESIAN_POINT('Ctrl Pts',(-2.84910806661434,608.342800223654,79.3448450590357));
#97838=CARTESIAN_POINT('Ctrl Pts',(-3.85030552837329,608.045280920111,79.0907977188138));
#97839=CARTESIAN_POINT('',(-3.91253447320281,607.88294039512,79.5230488432747));
#97840=CARTESIAN_POINT('Origin',(-3.85030552837329,607.88294039512,79.2809175598242));
#97841=CARTESIAN_POINT('Ctrl Pts',(-3.91253447320281,607.88294039512,79.5230488432747));
#97842=CARTESIAN_POINT('Ctrl Pts',(-3.28597810505974,608.068523823524,79.6840769479877));
#97843=CARTESIAN_POINT('Ctrl Pts',(-2.64771851246926,608.217057906509,79.807103090937));
#97844=CARTESIAN_POINT('Ctrl Pts',(-1.67000646568519,608.37000307792,79.9322661229594));
#97845=CARTESIAN_POINT('Ctrl Pts',(-1.34070899812117,608.409338421479,79.9640509087433));
#97846=CARTESIAN_POINT('Ctrl Pts',(-0.674809016948164,608.462436221459,
80.0068322484697));
#97847=CARTESIAN_POINT('Ctrl Pts',(-0.336249102370441,608.476132031997,
80.0177804323122));
#97848=CARTESIAN_POINT('Ctrl Pts',(0.,608.476132031997,80.0177804323122));
#97849=CARTESIAN_POINT('Ctrl Pts',(1.89318255568148,606.702491294468,79.9033522554387));
#97850=CARTESIAN_POINT('Ctrl Pts',(1.88043236474459,606.605433408562,79.9049255377571));
#97851=CARTESIAN_POINT('Ctrl Pts',(1.86306288877797,606.534169754924,79.840079036097));
#97852=CARTESIAN_POINT('Ctrl Pts',(0.820646498012525,606.843220307922,80.0334805824724));
#97853=CARTESIAN_POINT('Ctrl Pts',(0.818743950698483,606.747324662366,80.0328500715449));
#97854=CARTESIAN_POINT('Ctrl Pts',(0.807589904959771,606.67659431856,79.9696785476399));
#97855=CARTESIAN_POINT('Ctrl Pts',(-0.249753392942154,606.864684633585,
80.0523236519829));
#97856=CARTESIAN_POINT('Ctrl Pts',(-0.250591804105095,606.769288903197,
80.0516667261813));
#97857=CARTESIAN_POINT('Ctrl Pts',(-0.24578162409436,606.698317026832,79.9884448322078));
#97858=CARTESIAN_POINT('Ctrl Pts',(-1.85230285694165,606.71760788908,79.9174605062688));
#97859=CARTESIAN_POINT('Ctrl Pts',(-1.84045202787124,606.620669616219,79.9187905906115));
#97860=CARTESIAN_POINT('Ctrl Pts',(-1.82283398292192,606.549468432993,79.8541299127167));
#97861=CARTESIAN_POINT('Ctrl Pts',(-2.38933484362825,606.638031596339,79.8441641306276));
#97862=CARTESIAN_POINT('Ctrl Pts',(-2.37466264357767,606.539938200002,79.8462807686187));
#97863=CARTESIAN_POINT('Ctrl Pts',(-2.35132258925576,606.468933259531,79.7811312873554));
#97864=CARTESIAN_POINT('Ctrl Pts',(-3.43147735551065,606.430320367494,79.6478052879441));
#97865=CARTESIAN_POINT('Ctrl Pts',(-3.4101627228699,606.329716176394,79.6525292086393));
#97866=CARTESIAN_POINT('Ctrl Pts',(-3.37688542676327,606.258719512165,79.5855704382192));
#97867=CARTESIAN_POINT('Ctrl Pts',(-3.93983799323764,606.302315894287,79.524834163758));
#97868=CARTESIAN_POINT('Ctrl Pts',(-3.91596185111129,606.19983418155,79.5308660063145));
#97869=CARTESIAN_POINT('Ctrl Pts',(-3.87715892282217,606.12917261973,79.4630988338053));
#97870=CARTESIAN_POINT('Ctrl Pts',(-4.93450429122366,606.007958107776,79.2321422141563));
#97871=CARTESIAN_POINT('Ctrl Pts',(-4.9048700052628,605.901729272729,79.2419298822336));
#97872=CARTESIAN_POINT('Ctrl Pts',(-4.85600136127738,605.831268332999,79.1715962336162));
#97873=CARTESIAN_POINT('Ctrl Pts',(-5.42323859046886,605.840637330157,79.0613640029475));
#97874=CARTESIAN_POINT('Ctrl Pts',(-5.3913805012487,605.731886424723,79.0729171785271));
#97875=CARTESIAN_POINT('Ctrl Pts',(-5.33696096117466,605.661931391049,79.0015116750124));
#97876=CARTESIAN_POINT('Ctrl Pts',(-6.36814164931806,605.481318537322,78.6790317667906));
#97877=CARTESIAN_POINT('Ctrl Pts',(-6.33161473347315,605.367659836615,78.6952414948338));
#97878=CARTESIAN_POINT('Ctrl Pts',(-6.26683249734681,605.298283329195,78.6207327915938));
#97879=CARTESIAN_POINT('Ctrl Pts',(-6.8234072526896,605.289965981239,78.4682119648795));
#97880=CARTESIAN_POINT('Ctrl Pts',(-6.78508370064266,605.17331911893,78.4865227570079));
#97881=CARTESIAN_POINT('Ctrl Pts',(-6.71485606394656,605.104625043036,78.4107691833072));
#97882=CARTESIAN_POINT('Ctrl Pts',(-8.14524394474732,604.693296470928,77.7793700065673));
#97883=CARTESIAN_POINT('Ctrl Pts',(-8.10998737994438,604.564036856332,77.80127117446));
#97884=CARTESIAN_POINT('Ctrl Pts',(-8.01567130514643,604.500763916929,77.7247225905372));
#97885=CARTESIAN_POINT('Ctrl Pts',(-8.96853196172094,604.265846804672,77.2457034968301));
#97886=CARTESIAN_POINT('Ctrl Pts',(-8.93226681233894,604.127883129672,77.269520633413));
#97887=CARTESIAN_POINT('Ctrl Pts',(-8.82586458852353,604.068162696145,77.1932211322336));
#97888=CARTESIAN_POINT('Ctrl Pts',(-10.1303565945194,603.615007657105,76.327964798955));
#97889=CARTESIAN_POINT('Ctrl Pts',(-10.0844043143262,603.470213448972,76.3668461206142));
#97890=CARTESIAN_POINT('Ctrl Pts',(-9.96920498164766,603.409484218181,76.2792128579425));
#97891=CARTESIAN_POINT('Ctrl Pts',(-10.5047617063463,603.396503758538,76.0023613348043));
#97892=CARTESIAN_POINT('Ctrl Pts',(-10.4588442149254,603.247407263905,76.0434598022962));
#97893=CARTESIAN_POINT('Ctrl Pts',(-10.3376554216138,603.18834726738,75.9549308895933));
#97894=CARTESIAN_POINT('Ctrl Pts',(-11.2166306018809,602.968484050211,75.3219412047775));
#97895=CARTESIAN_POINT('Ctrl Pts',(-11.1717706789499,602.810553673284,75.3678438460831));
#97896=CARTESIAN_POINT('Ctrl Pts',(-11.0382031181792,602.755169692434,75.2772723636161));
#97897=CARTESIAN_POINT('Ctrl Pts',(-11.5558920129996,602.757959408171,74.96577030963));
#97898=CARTESIAN_POINT('Ctrl Pts',(-11.5117299914059,602.595452945654,75.0135259579074));
#97899=CARTESIAN_POINT('Ctrl Pts',(-11.3720692100036,602.542108069546,74.9225466233422));
#97900=CARTESIAN_POINT('Ctrl Pts',(-12.5250601941573,602.142743928326,73.8473239435239));
#97901=CARTESIAN_POINT('Ctrl Pts',(-12.4934838485426,601.960237519276,73.890709901465));
#97902=CARTESIAN_POINT('Ctrl Pts',(-12.3258306637108,601.91947521679,73.8086323110397));
#97903=CARTESIAN_POINT('Ctrl Pts',(-13.1077845770232,601.753730803073,73.0346961932179));
#97904=CARTESIAN_POINT('Ctrl Pts',(-13.077744970774,601.562117682642,73.078286707878));
#97905=CARTESIAN_POINT('Ctrl Pts',(-12.8992879967844,601.525774448587,72.9992994563982));
#97906=CARTESIAN_POINT('Ctrl Pts',(-14.1322077025265,601.0526083829,71.2563976137341));
#97907=CARTESIAN_POINT('Ctrl Pts',(-14.1129332121865,600.839741480705,71.2991153875746));
#97908=CARTESIAN_POINT('Ctrl Pts',(-13.9074241048782,600.816201428823,71.2282105920088));
#97909=CARTESIAN_POINT('Ctrl Pts',(-14.5579479788688,600.751472223843,70.3184194820127));
#97910=CARTESIAN_POINT('Ctrl Pts',(-14.540191874148,600.531314919786,70.3605898861845));
#97911=CARTESIAN_POINT('Ctrl Pts',(-14.3263939594619,600.511437089383,70.2940353094581));
#97912=CARTESIAN_POINT('Ctrl Pts',(-15.0602487335032,600.392181562599,68.8302748068456));
#97913=CARTESIAN_POINT('Ctrl Pts',(-15.0476696916696,600.161090211342,68.873414318539));
#97914=CARTESIAN_POINT('Ctrl Pts',(-14.8207085214835,600.147816634657,68.8119251561665));
#97915=CARTESIAN_POINT('Ctrl Pts',(-15.2051396204071,600.287604348783,68.318981400867));
#97916=CARTESIAN_POINT('Ctrl Pts',(-15.1947954692115,600.052766952685,68.3589101018559));
#97917=CARTESIAN_POINT('Ctrl Pts',(-14.9632961223424,600.041978928605,68.3027032249751));
#97918=CARTESIAN_POINT('Ctrl Pts',(-15.443724690614,600.114666560778,67.273372933676));
#97919=CARTESIAN_POINT('Ctrl Pts',(-15.438260005894,599.87275398679,67.3038920930527));
#97920=CARTESIAN_POINT('Ctrl Pts',(-15.1980890660801,599.866956287625,67.2613296018157));
#97921=CARTESIAN_POINT('Ctrl Pts',(-15.535710856414,600.047555866634,66.7472152886528));
#97922=CARTESIAN_POINT('Ctrl Pts',(-15.5318361040902,599.803106749797,66.7735722504368));
#97923=CARTESIAN_POINT('Ctrl Pts',(-15.2886130183545,599.799036681608,66.7373033136078));
#97924=CARTESIAN_POINT('Ctrl Pts',(-15.6659206532499,599.95240616771,65.6882422743292));
#97925=CARTESIAN_POINT('Ctrl Pts',(-15.6650029770329,599.703836396114,65.702986948441));
#97926=CARTESIAN_POINT('Ctrl Pts',(-15.416753347311,599.702739853292,65.6826183891459));
#97927=CARTESIAN_POINT('Ctrl Pts',(-15.7041440786651,599.924364187608,65.1554257032332));
#97928=CARTESIAN_POINT('Ctrl Pts',(-15.7039435893066,599.674691055738,65.1652840040138));
#97929=CARTESIAN_POINT('Ctrl Pts',(-15.4543691947642,599.674359863803,65.1519598739898));
#97930=CARTESIAN_POINT('Ctrl Pts',(-15.725963719193,599.908367606241,64.0830042219837));
#97931=CARTESIAN_POINT('Ctrl Pts',(-15.7262805762302,599.657984756203,64.0801660974849));
#97932=CARTESIAN_POINT('Ctrl Pts',(-15.4758420566949,599.658170422961,64.0838805525614));
#97933=CARTESIAN_POINT('Ctrl Pts',(-15.7093838004202,599.920543415892,63.5413158590829));
#97934=CARTESIAN_POINT('Ctrl Pts',(-15.7093899474743,599.670639481593,63.533432145575));
#97935=CARTESIAN_POINT('Ctrl Pts',(-15.4595256835684,599.67049299479,63.5443861522047));
#97936=CARTESIAN_POINT('Ctrl Pts',(-15.5748761636817,600.019013261713,61.9191477303746));
#97937=CARTESIAN_POINT('Ctrl Pts',(-15.5720423635036,599.773215559694,61.8961392504176));
#97938=CARTESIAN_POINT('Ctrl Pts',(-15.3271559384047,599.770149902152,61.9287880982582));
#97939=CARTESIAN_POINT('Ctrl Pts',(-15.3766850183768,600.164210165805,60.8731529828927));
#97940=CARTESIAN_POINT('Ctrl Pts',(-15.3728291173236,599.922150618853,60.8481294183498));
#97941=CARTESIAN_POINT('Ctrl Pts',(-15.1321164848615,599.917095981418,60.8870337307209));
#97942=CARTESIAN_POINT('Ctrl Pts',(-14.9288646952281,600.486393343205,59.3524144284031));
#97943=CARTESIAN_POINT('Ctrl Pts',(-14.9137106754242,600.259060007561,59.3061798598269));
#97944=CARTESIAN_POINT('Ctrl Pts',(-14.6914127541727,600.24316421183,59.3724502436072));
#97945=CARTESIAN_POINT('Ctrl Pts',(-14.7530559724391,600.612143493662,58.8510846321664));
#97946=CARTESIAN_POINT('Ctrl Pts',(-14.735492592348,600.389087069143,58.8024640384097));
#97947=CARTESIAN_POINT('Ctrl Pts',(-14.5183989336226,600.370430015253,58.8731518928978));
#97948=CARTESIAN_POINT('Ctrl Pts',(-14.359091214726,600.890882373311,57.8843269848985));
#97949=CARTESIAN_POINT('Ctrl Pts',(-14.3355486906423,600.677666788424,57.831412861111));
#97950=CARTESIAN_POINT('Ctrl Pts',(-14.1306968197733,600.652528873856,57.9103117242868));
#97951=CARTESIAN_POINT('Ctrl Pts',(-14.1407177531074,601.044041513339,57.4171203625588));
#97952=CARTESIAN_POINT('Ctrl Pts',(-14.1147768511432,600.835594442267,57.3630755463199));
#97953=CARTESIAN_POINT('Ctrl Pts',(-13.9157951809153,600.807533961072,57.4449987770471));
#97954=CARTESIAN_POINT('Ctrl Pts',(-13.6634366702206,601.374137201052,56.5124852728989));
#97955=CARTESIAN_POINT('Ctrl Pts',(-13.6319576862835,601.176086556912,56.4571863827656));
#97956=CARTESIAN_POINT('Ctrl Pts',(-13.4461019523439,601.141608393448,56.5440307949745));
#97957=CARTESIAN_POINT('Ctrl Pts',(-13.4045217018066,601.551087874668,56.0750652474453));
#97958=CARTESIAN_POINT('Ctrl Pts',(-13.3709792891119,601.357985213843,56.0198511196711));
#97959=CARTESIAN_POINT('Ctrl Pts',(-13.1913037235795,601.320691655312,56.1083842943529));
#97960=CARTESIAN_POINT('Ctrl Pts',(-12.8467572513285,601.925479899478,55.2284798584221));
#97961=CARTESIAN_POINT('Ctrl Pts',(-12.8086534652092,601.742797603221,55.1745452490493));
#97962=CARTESIAN_POINT('Ctrl Pts',(-12.64240759359,601.699596004276,55.2652320085852));
#97963=CARTESIAN_POINT('Ctrl Pts',(-12.5479044351808,602.122879885018,54.8198060554334));
#97964=CARTESIAN_POINT('Ctrl Pts',(-12.5081763747874,601.945188305703,54.7668256888035));
#97965=CARTESIAN_POINT('Ctrl Pts',(-12.3483069071172,601.899374950781,54.8582156625017));
#97966=CARTESIAN_POINT('Ctrl Pts',(-11.6083463397431,602.729536752221,53.6549020913345));
#97967=CARTESIAN_POINT('Ctrl Pts',(-11.5721545818985,602.561244927479,53.6169046527624));
#97968=CARTESIAN_POINT('Ctrl Pts',(-11.4236939741492,602.513339744895,53.6980435355989));
#97969=CARTESIAN_POINT('Ctrl Pts',(-10.9203783533487,603.156822706136,52.9511800330592));
#97970=CARTESIAN_POINT('Ctrl Pts',(-10.8838506687482,602.997717916532,52.9147405141667));
#97971=CARTESIAN_POINT('Ctrl Pts',(-10.7466675601512,602.945774750955,52.9971756449448));
#97972=CARTESIAN_POINT('Ctrl Pts',(-9.79188180091539,603.807239137665,51.9938845551591));
#97973=CARTESIAN_POINT('Ctrl Pts',(-9.74600809350948,603.666006770914,51.9575122012219));
#97974=CARTESIAN_POINT('Ctrl Pts',(-9.63611348815389,603.604032067193,52.043761533861));
#97975=CARTESIAN_POINT('Ctrl Pts',(-9.39789698724152,604.026363466371,51.6904175829392));
#97976=CARTESIAN_POINT('Ctrl Pts',(-9.35238143885824,603.889218513118,51.6563518525185));
#97977=CARTESIAN_POINT('Ctrl Pts',(-9.24839501364177,603.825796888994,51.7415264001437));
#97978=CARTESIAN_POINT('Ctrl Pts',(-8.5882707639602,604.455409354432,51.1256218197328));
#97979=CARTESIAN_POINT('Ctrl Pts',(-8.54421880589914,604.325589629118,51.0970442175137));
#97980=CARTESIAN_POINT('Ctrl Pts',(-8.45164641908639,604.260012585311,51.1790240815796));
#97981=CARTESIAN_POINT('Ctrl Pts',(-8.17152248677756,604.666045668114,50.863137499133));
#97982=CARTESIAN_POINT('Ctrl Pts',(-8.12841996224356,604.539860982956,50.8368346325361));
#97983=CARTESIAN_POINT('Ctrl Pts',(-8.04152694278709,604.473187063978,50.9176054756285));
#97984=CARTESIAN_POINT('Ctrl Pts',(-6.8824505977745,605.277521007612,50.1335953878553));
#97985=CARTESIAN_POINT('Ctrl Pts',(-6.85180078127635,605.15681962248,50.1198420410442));
#97986=CARTESIAN_POINT('Ctrl Pts',(-6.77296527985932,605.092027537154,50.1910295542293));
#97987=CARTESIAN_POINT('Ctrl Pts',(-5.97236940852388,605.659075019653,49.7234080275098));
#97988=CARTESIAN_POINT('Ctrl Pts',(-5.94378154267043,605.545965583367,49.7114424968018));
#97989=CARTESIAN_POINT('Ctrl Pts',(-5.87736007948177,605.478180238876,49.7825065974709));
#97990=CARTESIAN_POINT('Ctrl Pts',(-4.50406198106329,606.142293047406,49.2314609330919));
#97991=CARTESIAN_POINT('Ctrl Pts',(-4.47704379275699,606.03766895215,49.2235345335548));
#97992=CARTESIAN_POINT('Ctrl Pts',(-4.43240690450128,605.967221696673,49.2925569652473));
#97993=CARTESIAN_POINT('Ctrl Pts',(-3.99670954179865,606.287879162115,49.088694597554));
#97994=CARTESIAN_POINT('Ctrl Pts',(-3.97216443006434,606.185409069474,49.0822732722215));
#97995=CARTESIAN_POINT('Ctrl Pts',(-3.93312549027658,606.114562082292,49.1503705419181));
#97996=CARTESIAN_POINT('Ctrl Pts',(-2.85259747095036,606.558470894243,48.8286226638388));
#97997=CARTESIAN_POINT('Ctrl Pts',(-2.83595961871912,606.459127596936,48.8258047037337));
#97998=CARTESIAN_POINT('Ctrl Pts',(-2.80721571937531,606.388413802999,48.8913556172026));
#97999=CARTESIAN_POINT('Ctrl Pts',(-2.20802541233332,606.672670497811,48.7229986861156));
#98000=CARTESIAN_POINT('Ctrl Pts',(-2.19436435103283,606.575165993762,48.7211342965073));
#98001=CARTESIAN_POINT('Ctrl Pts',(-2.17289772765275,606.50398958997,48.7861606117232));
#98002=CARTESIAN_POINT('Ctrl Pts',(-1.548495767235,606.743661819472,48.6576047836375));
#98003=CARTESIAN_POINT('Ctrl Pts',(-1.53802701918798,606.647079799347,48.6565547220104));
#98004=CARTESIAN_POINT('Ctrl Pts',(-1.52385975718171,606.575836310594,48.7210323974217));
#98005=CARTESIAN_POINT('',(1.49247642388117E-9,606.827127123144,80.0178253754844));
#98006=CARTESIAN_POINT('',(-1.91941230150446,606.698958856847,48.698800681464));
#98007=CARTESIAN_POINT('Ctrl Pts',(0.,606.827186486861,80.0177804323122));
#98008=CARTESIAN_POINT('Ctrl Pts',(-0.523838402099614,606.827186486861,
80.0177804323122));
#98009=CARTESIAN_POINT('Ctrl Pts',(-1.04370866617181,606.798326811839,79.9916639229812));
#98010=CARTESIAN_POINT('Ctrl Pts',(-2.07588373512256,606.686421518492,79.8887286024128));
#98011=CARTESIAN_POINT('Ctrl Pts',(-2.58884491618879,606.602944672362,79.8114551737427));
#98012=CARTESIAN_POINT('Ctrl Pts',(-3.58593453053115,606.392664702315,79.6117158816492));
#98013=CARTESIAN_POINT('Ctrl Pts',(-4.0730770151066,606.265685908356,79.4890655970438));
#98014=CARTESIAN_POINT('Ctrl Pts',(-5.02736864376844,605.97675047939,79.2004542940851));
#98015=CARTESIAN_POINT('Ctrl Pts',(-5.49684127598253,605.813849430916,79.0334559601684));
#98016=CARTESIAN_POINT('Ctrl Pts',(-6.85808462896243,605.292109959681,78.4766795782573));
#98017=CARTESIAN_POINT('Ctrl Pts',(-7.70355359238228,604.902197691963,78.0333468553696));
#98018=CARTESIAN_POINT('Ctrl Pts',(-8.89973254356871,604.293516577598,77.2642195998673));
#98019=CARTESIAN_POINT('Ctrl Pts',(-9.28623993692406,604.086441118006,76.9902938266832));
#98020=CARTESIAN_POINT('Ctrl Pts',(-10.0362291980326,603.668698110008,76.4058881437883));
#98021=CARTESIAN_POINT('Ctrl Pts',(-10.4000435824971,603.457751878295,76.0948005375614));
#98022=CARTESIAN_POINT('Ctrl Pts',(-11.4396209671232,602.83682855148,75.1208482803277));
#98023=CARTESIAN_POINT('Ctrl Pts',(-12.0708675035256,602.435159887223,74.4129443846916));
#98024=CARTESIAN_POINT('Ctrl Pts',(-12.9272407039081,601.871954972911,73.2539335615611));
#98025=CARTESIAN_POINT('Ctrl Pts',(-13.1974645163444,601.690741457398,72.8512918153461));
#98026=CARTESIAN_POINT('Ctrl Pts',(-13.705907162251,601.344998141025,72.0101656887144));
#98027=CARTESIAN_POINT('Ctrl Pts',(-13.9424367491172,601.181602019743,71.5740025956755));
#98028=CARTESIAN_POINT('Ctrl Pts',(-14.5877396657579,600.731202865487,70.2361076880824));
#98029=CARTESIAN_POINT('Ctrl Pts',(-14.9374786600809,600.48060273398,69.2981314957323));
#98030=CARTESIAN_POINT('Ctrl Pts',(-15.2640367599687,600.244791441604,68.0597854794833));
#98031=CARTESIAN_POINT('Ctrl Pts',(-15.3238781708752,600.201438975219,67.8080648198323));
#98032=CARTESIAN_POINT('Ctrl Pts',(-15.4305740793169,600.123978935667,67.3042760285323));
#98033=CARTESIAN_POINT('Ctrl Pts',(-15.4776212824142,600.089732808377,67.0516154405275));
#98034=CARTESIAN_POINT('Ctrl Pts',(-15.6000369014761,600.0004912733,66.2913465819385));
#98035=CARTESIAN_POINT('Ctrl Pts',(-15.6567243462522,599.958974605742,65.7814558786312));
#98036=CARTESIAN_POINT('Ctrl Pts',(-15.7200921410461,599.912552918423,64.7555336881403));
#98037=CARTESIAN_POINT('Ctrl Pts',(-15.7267764511932,599.907644658805,64.2395027071171));
#98038=CARTESIAN_POINT('Ctrl Pts',(-15.6884879697056,599.935709166568,63.2010937639321));
#98039=CARTESIAN_POINT('Ctrl Pts',(-15.6429785458214,599.969074428584,62.6781815568624));
#98040=CARTESIAN_POINT('Ctrl Pts',(-15.4329805623442,600.122406036859,61.1446179884831));
#98041=CARTESIAN_POINT('Ctrl Pts',(-15.1957463219534,600.295330691334,60.1535682172885));
#98042=CARTESIAN_POINT('Ctrl Pts',(-14.7000874693409,600.64956243217,58.7109944575794));
#98043=CARTESIAN_POINT('Ctrl Pts',(-14.5127468230508,600.782527387899,58.242003763886));
#98044=CARTESIAN_POINT('Ctrl Pts',(-14.1005377299408,601.071729059695,57.3361700731209));
#98045=CARTESIAN_POINT('Ctrl Pts',(-13.8750752636248,601.228396330728,56.8975962595972));
#98046=CARTESIAN_POINT('Ctrl Pts',(-13.1426912261625,601.729855835972,55.6221334704683));
#98047=CARTESIAN_POINT('Ctrl Pts',(-12.5757171471258,602.108922153606,54.8214953487566));
#98048=CARTESIAN_POINT('Ctrl Pts',(-11.3331559325469,602.900605352485,53.3660245246631));
#98049=CARTESIAN_POINT('Ctrl Pts',(-10.6547752361309,603.31564013608,52.7042730339687));
#98050=CARTESIAN_POINT('Ctrl Pts',(-9.54585906942516,603.944213997349,51.8027276685537));
#98051=CARTESIAN_POINT('Ctrl Pts',(-9.16098839272779,604.154506913516,51.5179512580578));
#98052=CARTESIAN_POINT('Ctrl Pts',(-8.37201911995265,604.565048924592,50.9878126575492));
#98053=CARTESIAN_POINT('Ctrl Pts',(-7.96635410967427,604.766222133218,50.7411093620899));
#98054=CARTESIAN_POINT('Ctrl Pts',(-6.71291294709257,605.349307836359,50.0548419703803));
#98055=CARTESIAN_POINT('Ctrl Pts',(-5.82961165971477,605.711811288536,49.6681929464691));
#98056=CARTESIAN_POINT('Ctrl Pts',(-4.40836677555933,606.170246586049,49.2037840375558));
#98057=CARTESIAN_POINT('Ctrl Pts',(-3.91938654325121,606.30783645178,49.0692534214259));
#98058=CARTESIAN_POINT('Ctrl Pts',(-2.93166846065344,606.537737419501,48.8486963579089));
#98059=CARTESIAN_POINT('Ctrl Pts',(-2.42992069874045,606.63106204052,48.7616105405085));
#98060=CARTESIAN_POINT('Ctrl Pts',(-1.91941230150446,606.698958856847,48.698800681464));
#98061=CARTESIAN_POINT('',(-1.8888840075986,606.53066176659,48.7620619651123));
#98062=CARTESIAN_POINT('Origin',(-1.88888400761935,606.698958856848,48.9469297270682));
#98063=CARTESIAN_POINT('',(1.86306288877797,606.534169754924,79.840079036097));
#98064=CARTESIAN_POINT('Ctrl Pts',(-1.8888840075986,606.53066176659,48.7620619651123));
#98065=CARTESIAN_POINT('Ctrl Pts',(-2.41149695900853,606.45918119815,48.8271353535257));
#98066=CARTESIAN_POINT('Ctrl Pts',(-2.9244450266129,606.359900440675,48.9183242031726));
#98067=CARTESIAN_POINT('Ctrl Pts',(-3.42867105811377,606.237260990053,49.0343192413469));
#98068=CARTESIAN_POINT('Ctrl Pts',(-3.43116315307001,606.236654854834,49.0348925371141));
#98069=CARTESIAN_POINT('Ctrl Pts',(-3.43365511556903,606.236048119746,49.0354664692823));
#98070=CARTESIAN_POINT('Ctrl Pts',(-3.43614694410228,606.235440785882,49.0360410372358));
#98071=CARTESIAN_POINT('Ctrl Pts',(-3.82123395676472,606.141583451774,49.1248347298391));
#98072=CARTESIAN_POINT('Ctrl Pts',(-4.20323008343107,606.033396925328,49.2288408126609));
#98073=CARTESIAN_POINT('Ctrl Pts',(-4.57646776406636,605.914924717136,49.3457763159031));
#98074=CARTESIAN_POINT('Ctrl Pts',(-4.68985979718866,605.878932090313,49.381302081775));
#98075=CARTESIAN_POINT('Ctrl Pts',(-4.80244368080559,605.841990257397,49.4180209911653));
#98076=CARTESIAN_POINT('Ctrl Pts',(-4.91406129959471,605.804212857108,49.4558685205457));
#98077=CARTESIAN_POINT('Ctrl Pts',(-4.91843568064348,605.802732331492,49.4573517945759));
#98078=CARTESIAN_POINT('Ctrl Pts',(-4.92280863589928,605.801250575485,49.4588367478035));
#98079=CARTESIAN_POINT('Ctrl Pts',(-4.92718016685644,605.799767592365,49.4603233795273));
#98080=CARTESIAN_POINT('Ctrl Pts',(-5.42040916321487,605.632446284766,49.6280563500277));
#98081=CARTESIAN_POINT('Ctrl Pts',(-5.89557048330097,605.449497266521,49.8171650183942));
#98082=CARTESIAN_POINT('Ctrl Pts',(-6.35515504475826,605.255478405036,50.0267811577471));
#98083=CARTESIAN_POINT('Ctrl Pts',(-6.78955134201509,605.072093056409,50.2249089505768));
#98084=CARTESIAN_POINT('Ctrl Pts',(-7.21003104626367,604.878817257618,50.4413581653025));
#98085=CARTESIAN_POINT('Ctrl Pts',(-7.61867416252443,604.679468187595,50.6754123677936));
#98086=CARTESIAN_POINT('Ctrl Pts',(-7.62456670988117,604.676593616144,50.6787873799187));
#98087=CARTESIAN_POINT('Ctrl Pts',(-7.63045674519379,604.673717724625,50.682166103682));
#98088=CARTESIAN_POINT('Ctrl Pts',(-7.63634427132602,604.670840521053,50.6855485406359));
#98089=CARTESIAN_POINT('Ctrl Pts',(-8.05314726616496,604.467151053103,50.9250056267778));
#98090=CARTESIAN_POINT('Ctrl Pts',(-8.45740792076493,604.256872635283,51.1830917656922));
#98091=CARTESIAN_POINT('Ctrl Pts',(-8.85002243750457,604.042905930577,51.4602736948679));
#98092=CARTESIAN_POINT('Ctrl Pts',(-8.85593145106616,604.039685641704,51.4644453994501));
#98093=CARTESIAN_POINT('Ctrl Pts',(-8.86183806655528,604.036464358004,51.4686216821428));
#98094=CARTESIAN_POINT('Ctrl Pts',(-8.8677422613673,604.033242102544,51.4728025248131));
#98095=CARTESIAN_POINT('Ctrl Pts',(-9.23018926554603,603.835434124481,51.7294563021764));
#98096=CARTESIAN_POINT('Ctrl Pts',(-9.58363022322654,603.633898543708,52.0033825468461));
#98097=CARTESIAN_POINT('Ctrl Pts',(-9.92280720323148,603.433969241314,52.2903964742726));
#98098=CARTESIAN_POINT('Ctrl Pts',(-9.95073667621177,603.417506095587,52.3140305892144));
#98099=CARTESIAN_POINT('Ctrl Pts',(-9.97856945642496,603.401053828896,52.3377534407258));
#98100=CARTESIAN_POINT('Ctrl Pts',(-10.0063026234584,603.384615411585,52.3615626894153));
#98101=CARTESIAN_POINT('Ctrl Pts',(-10.0117904989737,603.381362555978,52.3662740948153));
#98102=CARTESIAN_POINT('Ctrl Pts',(-10.0172748471287,603.378110078954,52.3709890470135));
#98103=CARTESIAN_POINT('Ctrl Pts',(-10.0227556688064,603.374857987524,52.3757075484961));
#98104=CARTESIAN_POINT('Ctrl Pts',(-10.4844704326174,603.10089566681,52.7732030200994));
#98105=CARTESIAN_POINT('Ctrl Pts',(-10.9212653118694,602.829618351376,53.1959678505452));
#98106=CARTESIAN_POINT('Ctrl Pts',(-11.3338346746107,602.565105027701,53.6456472273239));
#98107=CARTESIAN_POINT('Ctrl Pts',(-11.5776710652414,602.408772590193,53.911416346597));
#98108=CARTESIAN_POINT('Ctrl Pts',(-11.8130457209473,602.254802291871,54.1865861674907));
#98109=CARTESIAN_POINT('Ctrl Pts',(-12.040104661015,602.104030570697,54.4714903191273));
#98110=CARTESIAN_POINT('Ctrl Pts',(-12.0438323006949,602.101555342677,54.4761676069729));
#98111=CARTESIAN_POINT('Ctrl Pts',(-12.0475578528827,602.099080844204,54.4808478324097));
#98112=CARTESIAN_POINT('Ctrl Pts',(-12.0512813078029,602.096607084918,54.4855309851298));
#98113=CARTESIAN_POINT('Ctrl Pts',(-12.3319606431896,601.910131586404,54.8385537076184));
#98114=CARTESIAN_POINT('Ctrl Pts',(-12.6007933233764,601.727806201388,55.2083103080585));
#98115=CARTESIAN_POINT('Ctrl Pts',(-12.8535510646359,601.553786258449,55.5903491042369));
#98116=CARTESIAN_POINT('Ctrl Pts',(-12.8747668387784,601.539179513716,55.6224163666401));
#98117=CARTESIAN_POINT('Ctrl Pts',(-12.8958693833388,601.524631267288,55.6545701590746));
#98118=CARTESIAN_POINT('Ctrl Pts',(-12.9168562126465,601.510143966277,55.6868078477631));
#98119=CARTESIAN_POINT('Ctrl Pts',(-12.9194398545994,601.50836046682,55.6907765580309));
#98120=CARTESIAN_POINT('Ctrl Pts',(-12.922021743077,601.506577894755,55.6947464964152));
#98121=CARTESIAN_POINT('Ctrl Pts',(-12.9246018778219,601.504796251497,55.6987176634258));
#98122=CARTESIAN_POINT('Ctrl Pts',(-13.1962036721651,601.31724887374,56.1167485774522));
#98123=CARTESIAN_POINT('Ctrl Pts',(-13.4484034732778,601.139972120339,56.5484436861926));
#98124=CARTESIAN_POINT('Ctrl Pts',(-13.680948979807,600.974571248321,56.9945145943681));
#98125=CARTESIAN_POINT('Ctrl Pts',(-13.6823423951751,600.97358016438,56.9971874564155));
#98126=CARTESIAN_POINT('Ctrl Pts',(-13.6837351051094,600.972589506321,56.9998608343006));
#98127=CARTESIAN_POINT('Ctrl Pts',(-13.6851271093878,600.97159927454,57.0025347282826));
#98128=CARTESIAN_POINT('Ctrl Pts',(-13.9184371521736,600.805629224882,57.4506988101028));
#98129=CARTESIAN_POINT('Ctrl Pts',(-14.1319267819666,600.651633932193,57.9133662944617));
#98130=CARTESIAN_POINT('Ctrl Pts',(-14.3245484115035,600.511479503361,58.3917316078811));
#98131=CARTESIAN_POINT('Ctrl Pts',(-14.3248720257519,600.51124403671,58.3925352862205));
#98132=CARTESIAN_POINT('Ctrl Pts',(-14.3251955816966,600.511008608642,58.393339013801));
#98133=CARTESIAN_POINT('Ctrl Pts',(-14.3255190793133,600.51077321918,58.3941427905652));
#98134=CARTESIAN_POINT('Ctrl Pts',(-14.5183947849969,600.37042934596,58.8733704651744));
#98135=CARTESIAN_POINT('Ctrl Pts',(-14.6905438911395,600.243803913954,59.3700945593781));
#98136=CARTESIAN_POINT('Ctrl Pts',(-14.8368369280143,600.135568860125,59.8722326143599));
#98137=CARTESIAN_POINT('Ctrl Pts',(-14.8373300871407,600.135203995838,59.8739253399318));
#98138=CARTESIAN_POINT('Ctrl Pts',(-14.8378229525661,600.134839340462,59.8756181274375));
#98139=CARTESIAN_POINT('Ctrl Pts',(-14.8383155240927,600.134474894177,59.8773109764116));
#98140=CARTESIAN_POINT('Ctrl Pts',(-15.0414396046863,599.984186433293,60.5753992192415));
#98141=CARTESIAN_POINT('Ctrl Pts',(-15.1973006598741,599.867605992967,61.2886164434837));
#98142=CARTESIAN_POINT('Ctrl Pts',(-15.3033244732793,599.788005372271,62.0179657611667));
#98143=CARTESIAN_POINT('Ctrl Pts',(-15.3495814983162,599.753276495935,62.3361728560179));
#98144=CARTESIAN_POINT('Ctrl Pts',(-15.3863525773886,599.725586246286,62.6574505117789));
#98145=CARTESIAN_POINT('Ctrl Pts',(-15.4134262294948,599.705204325428,62.9818812830931));
#98146=CARTESIAN_POINT('Ctrl Pts',(-15.4140928759569,599.704702452412,62.989869884891));
#98147=CARTESIAN_POINT('Ctrl Pts',(-15.4147536449623,599.704205007555,62.997860444859));
#98148=CARTESIAN_POINT('Ctrl Pts',(-15.4154085331436,599.703711995057,63.0058529638405));
#98149=CARTESIAN_POINT('Ctrl Pts',(-15.4549862599016,599.673917116299,63.4888754727571));
#98150=CARTESIAN_POINT('Ctrl Pts',(-15.4721900515042,599.660932130311,63.9727246693828));
#98151=CARTESIAN_POINT('Ctrl Pts',(-15.4675657250193,599.664413653428,64.4526573526759));
#98152=CARTESIAN_POINT('Ctrl Pts',(-15.4671428394911,599.664732031844,64.496546249141));
#98153=CARTESIAN_POINT('Ctrl Pts',(-15.4665374395127,599.665188093949,64.5404023977502));
#98154=CARTESIAN_POINT('Ctrl Pts',(-15.465749959502,599.665781564301,64.5842221752744));
#98155=CARTESIAN_POINT('Ctrl Pts',(-15.4655480571059,599.665933724463,64.5954571500792));
#98156=CARTESIAN_POINT('Ctrl Pts',(-15.4653341842431,599.666094919118,64.6066898685709));
#98157=CARTESIAN_POINT('Ctrl Pts',(-15.4651083473515,599.666265144236,64.6179202686375));
#98158=CARTESIAN_POINT('Ctrl Pts',(-15.4565102683663,599.672745967626,65.0454848978372));
#98159=CARTESIAN_POINT('Ctrl Pts',(-15.4306782059201,599.692234295056,65.4710177591388));
#98160=CARTESIAN_POINT('Ctrl Pts',(-15.3878202693317,599.724471888615,65.8944225395669));
#98161=CARTESIAN_POINT('Ctrl Pts',(-15.3786070250364,599.731402059515,65.9854425929899));
#98162=CARTESIAN_POINT('Ctrl Pts',(-15.3686071189849,599.738921295213,66.0763643200901));
#98163=CARTESIAN_POINT('Ctrl Pts',(-15.3578228674146,599.747026843009,66.1671867939494));
#98164=CARTESIAN_POINT('Ctrl Pts',(-15.3561295795732,599.74829953453,66.1814472727328));
#98165=CARTESIAN_POINT('Ctrl Pts',(-15.3544169428895,599.749586685959,66.1957053639419));
#98166=CARTESIAN_POINT('Ctrl Pts',(-15.3526849656753,599.750888287307,66.209961068781));
#98167=CARTESIAN_POINT('Ctrl Pts',(-15.2907263898706,599.797450889354,66.7199349654947));
#98168=CARTESIAN_POINT('Ctrl Pts',(-15.2040176992693,599.862508071703,67.2268545417177));
#98169=CARTESIAN_POINT('Ctrl Pts',(-15.0921759771049,599.945907616897,67.7306968564119));
#98170=CARTESIAN_POINT('Ctrl Pts',(-15.0883779410082,599.948739784329,67.7478068513332));
#98171=CARTESIAN_POINT('Ctrl Pts',(-15.0845508622971,599.951593143233,67.7649135318261));
#98172=CARTESIAN_POINT('Ctrl Pts',(-15.0806947254962,599.954467687614,67.7820168863499));
#98173=CARTESIAN_POINT('Ctrl Pts',(-14.9906512622063,600.0215902885,68.18139205241));
#98174=CARTESIAN_POINT('Ctrl Pts',(-14.8857494405989,600.099522550423,68.5741722445984));
#98175=CARTESIAN_POINT('Ctrl Pts',(-14.7673626316929,600.186916360206,68.9585381212224));
#98176=CARTESIAN_POINT('Ctrl Pts',(-14.7373499494797,600.209071891423,69.0559801505778));
#98177=CARTESIAN_POINT('Ctrl Pts',(-14.7064707999309,600.231835360312,69.152881479814));
#98178=CARTESIAN_POINT('Ctrl Pts',(-14.6747479525069,600.255184517968,69.2492126559159));
#98179=CARTESIAN_POINT('Ctrl Pts',(-14.6685113493146,600.259774882422,69.2681510353232));
#98180=CARTESIAN_POINT('Ctrl Pts',(-14.6622419924248,600.264387994604,69.2870678366535));
#98181=CARTESIAN_POINT('Ctrl Pts',(-14.6559400474473,600.269023690891,69.3059628438942));
#98182=CARTESIAN_POINT('Ctrl Pts',(-14.4881365257408,600.392459577008,69.8090850972572));
#98183=CARTESIAN_POINT('Ctrl Pts',(-14.2970453980955,600.532137247967,70.2985271979679));
#98184=CARTESIAN_POINT('Ctrl Pts',(-14.0832076583593,600.686446678114,70.7748546652877));
#98185=CARTESIAN_POINT('Ctrl Pts',(-13.8873140841882,600.827807252899,71.2112111763704));
#98186=CARTESIAN_POINT('Ctrl Pts',(-13.672331791668,600.981446349243,71.6365621257633));
#98187=CARTESIAN_POINT('Ctrl Pts',(-13.4387032223677,601.146104556008,72.0513594656846));
#98188=CARTESIAN_POINT('Ctrl Pts',(-13.4269732670318,601.154371667418,72.0721854900244));
#98189=CARTESIAN_POINT('Ctrl Pts',(-13.4151954394702,601.162667108948,72.0929863162258));
#98190=CARTESIAN_POINT('Ctrl Pts',(-13.4033698516022,601.170990683808,72.1137618746436));
#98191=CARTESIAN_POINT('Ctrl Pts',(-13.2658603218258,601.267778334276,72.3553428683983));
#98192=CARTESIAN_POINT('Ctrl Pts',(-13.1230592827393,601.367544932225,72.5914514645205));
#98193=CARTESIAN_POINT('Ctrl Pts',(-12.9752216473718,601.469860105797,72.8220741360305));
#98194=CARTESIAN_POINT('Ctrl Pts',(-12.8657608690502,601.545615501272,72.9928299591965));
#98195=CARTESIAN_POINT('Ctrl Pts',(-12.7535396983437,601.622767571966,73.1605791986362));
#98196=CARTESIAN_POINT('Ctrl Pts',(-12.6386729408157,601.701135811342,73.3253295048864));
#98197=CARTESIAN_POINT('Ctrl Pts',(-12.4290296027772,601.844165697905,73.6260153158943));
#98198=CARTESIAN_POINT('Ctrl Pts',(-12.2103932272426,601.991362007103,73.9169651025679));
#98199=CARTESIAN_POINT('Ctrl Pts',(-11.9829905178613,602.141928579844,74.1987899101));
#98200=CARTESIAN_POINT('Ctrl Pts',(-11.9030428234133,602.194863087019,74.2978707155211));
#98201=CARTESIAN_POINT('Ctrl Pts',(-11.8220112796174,602.24821427354,74.3958233320019));
#98202=CARTESIAN_POINT('Ctrl Pts',(-11.7399047075142,602.301947835157,74.4926732578091));
#98203=CARTESIAN_POINT('Ctrl Pts',(-11.723313317863,602.312805850968,74.512243857526));
#98204=CARTESIAN_POINT('Ctrl Pts',(-11.7066783200462,602.323679189369,74.5317689045803));
#98205=CARTESIAN_POINT('Ctrl Pts',(-11.6899998492773,602.3345675332,74.5512485570586));
#98206=CARTESIAN_POINT('Ctrl Pts',(-11.3893716288856,602.530829137398,74.9023678736653));
#98207=CARTESIAN_POINT('Ctrl Pts',(-11.0743064696377,602.732118822314,75.2388277121095));
#98208=CARTESIAN_POINT('Ctrl Pts',(-10.7444640677328,602.936745911554,75.5611408646035));
#98209=CARTESIAN_POINT('Ctrl Pts',(-10.7256680559147,602.94840655059,75.5795078234554));
#98210=CARTESIAN_POINT('Ctrl Pts',(-10.706824102173,602.960077953694,75.5978287367274));
#98211=CARTESIAN_POINT('Ctrl Pts',(-10.687932101418,602.97175982427,75.6161037296602));
#98212=CARTESIAN_POINT('Ctrl Pts',(-10.391643904776,603.154969660612,75.9027152310002));
#98213=CARTESIAN_POINT('Ctrl Pts',(-10.0822730964368,603.341485904188,76.1790010607769));
#98214=CARTESIAN_POINT('Ctrl Pts',(-9.76302160159852,603.527656477313,76.4419445958769));
#98215=CARTESIAN_POINT('Ctrl Pts',(-9.72558983078315,603.549484704708,76.472774340772));
#98216=CARTESIAN_POINT('Ctrl Pts',(-9.68802222053652,603.571308158203,76.503420611066));
#98217=CARTESIAN_POINT('Ctrl Pts',(-9.65032392871191,603.593120930745,76.5338784979795));
#98218=CARTESIAN_POINT('Ctrl Pts',(-9.62962043291993,603.605100270462,76.5506056413864));
#98219=CARTESIAN_POINT('Ctrl Pts',(-9.60887807747269,603.617076106053,76.5672755719517));
#98220=CARTESIAN_POINT('Ctrl Pts',(-9.58809774349921,603.629047449649,76.5838874705586));
#98221=CARTESIAN_POINT('Ctrl Pts',(-9.17209645664058,603.868701650953,76.9164408937348));
#98222=CARTESIAN_POINT('Ctrl Pts',(-8.74167731913442,604.106495599033,77.2259224192872));
#98223=CARTESIAN_POINT('Ctrl Pts',(-8.29525516685564,604.338636728732,77.5129331902665));
#98224=CARTESIAN_POINT('Ctrl Pts',(-7.94596840716844,604.520267103858,77.7374943185145));
#98225=CARTESIAN_POINT('Ctrl Pts',(-7.58688458985845,604.698436781484,77.9482988748373));
#98226=CARTESIAN_POINT('Ctrl Pts',(-7.21723077844874,604.871316351623,78.1456225473664));
#98227=CARTESIAN_POINT('Ctrl Pts',(-7.19435330607696,604.882015680204,78.1578346948602));
#98228=CARTESIAN_POINT('Ctrl Pts',(-7.17143531739344,604.89269462405,78.1699950695054));
#98229=CARTESIAN_POINT('Ctrl Pts',(-7.1484766436231,604.903352752914,78.1821037431292));
#98230=CARTESIAN_POINT('Ctrl Pts',(-6.75967649946682,605.083845845844,78.3871614959228));
#98231=CARTESIAN_POINT('Ctrl Pts',(-6.35908010474382,605.258272755171,78.5772453811039));
#98232=CARTESIAN_POINT('Ctrl Pts',(-5.94486173928286,605.423622180316,78.7517442440193));
#98233=CARTESIAN_POINT('Ctrl Pts',(-5.92075101065575,605.433246802136,78.7619014342366));
#98234=CARTESIAN_POINT('Ctrl Pts',(-5.89659411591536,605.442840663064,78.7720058150056));
#98235=CARTESIAN_POINT('Ctrl Pts',(-5.87239069016909,605.452403167251,78.7820572638862));
#98236=CARTESIAN_POINT('Ctrl Pts',(-5.8489383682211,605.461668918686,78.7917967866158));
#98237=CARTESIAN_POINT('Ctrl Pts',(-5.82544172188546,605.470905403857,78.801486795087));
#98238=CARTESIAN_POINT('Ctrl Pts',(-5.8019005095584,605.480112026635,78.8111271194742));
#98239=CARTESIAN_POINT('Ctrl Pts',(-5.52092170778195,605.589998713896,78.9261903013284));
#98240=CARTESIAN_POINT('Ctrl Pts',(-5.23391572238947,605.695391403333,79.0339059074638));
#98241=CARTESIAN_POINT('Ctrl Pts',(-4.9427116750574,605.794468591044,79.1333013998922));
#98242=CARTESIAN_POINT('Ctrl Pts',(-4.77501441594139,605.851524710189,79.1905408229065));
#98243=CARTESIAN_POINT('Ctrl Pts',(-4.60592561275599,605.906486672614,79.2450216198832));
#98244=CARTESIAN_POINT('Ctrl Pts',(-4.43579829675243,605.959010640085,79.296563818299));
#98245=CARTESIAN_POINT('Ctrl Pts',(-4.41274763656984,605.966127146441,79.3035473041298));
#98246=CARTESIAN_POINT('Ctrl Pts',(-4.38967592729236,605.973199574385,79.3104775101188));
#98247=CARTESIAN_POINT('Ctrl Pts',(-4.36658401678448,605.980227058812,79.3173539744283));
#98248=CARTESIAN_POINT('Ctrl Pts',(-4.04882336544269,606.076930102417,79.4119788768226));
#98249=CARTESIAN_POINT('Ctrl Pts',(-3.72622839314485,606.165533628874,79.4968684248683));
#98250=CARTESIAN_POINT('Ctrl Pts',(-3.39848998478872,606.244581226598,79.5715572830011));
#98251=CARTESIAN_POINT('Ctrl Pts',(-3.24344222817048,606.281977370537,79.6068913775186));
#98252=CARTESIAN_POINT('Ctrl Pts',(-3.0872435683354,606.317235184592,79.6399430181275));
#98253=CARTESIAN_POINT('Ctrl Pts',(-2.92986272136945,606.350202891215,79.670666001624));
#98254=CARTESIAN_POINT('Ctrl Pts',(-2.90796583102345,606.354789791533,79.6749405865795));
#98255=CARTESIAN_POINT('Ctrl Pts',(-2.8860468670402,606.359332262393,79.6791700030137));
#98256=CARTESIAN_POINT('Ctrl Pts',(-2.86410536448453,606.36382997616,79.6833542027662));
#98257=CARTESIAN_POINT('Ctrl Pts',(-2.67077137140168,606.403460851943,79.7202226006324));
#98258=CARTESIAN_POINT('Ctrl Pts',(-2.47523365108864,606.439601026273,79.7535703438643));
#98259=CARTESIAN_POINT('Ctrl Pts',(-2.27824761486158,606.471936730464,79.7832366450388));
#98260=CARTESIAN_POINT('Ctrl Pts',(-2.09244054750841,606.502437381585,79.811219381917));
#98261=CARTESIAN_POINT('Ctrl Pts',(-1.9053436242915,606.529553234617,79.8359266171057));
#98262=CARTESIAN_POINT('Ctrl Pts',(-1.71759256271035,606.552987944339,79.857193117338));
#98263=CARTESIAN_POINT('Ctrl Pts',(-1.59648021957914,606.568104943312,79.8709114721193));
#98264=CARTESIAN_POINT('Ctrl Pts',(-1.47509576548736,606.581689501849,79.8831974849582));
#98265=CARTESIAN_POINT('Ctrl Pts',(-1.35361376683637,606.593653739294,79.8939995839849));
#98266=CARTESIAN_POINT('Ctrl Pts',(-1.3347974152013,606.595506880511,79.8956727215357));
#98267=CARTESIAN_POINT('Ctrl Pts',(-1.31597645205385,606.597321531768,79.8973106052341));
#98268=CARTESIAN_POINT('Ctrl Pts',(-1.29715200364571,606.599097281125,79.8989129667661));
#98269=CARTESIAN_POINT('Ctrl Pts',(-1.11523121238239,606.616258247602,79.9143983011279));
#98270=CARTESIAN_POINT('Ctrl Pts',(-0.932588982072346,606.629864250476,
79.9267009011115));
#98271=CARTESIAN_POINT('Ctrl Pts',(-0.749467854777604,606.639830437194,
79.9357300191261));
#98272=CARTESIAN_POINT('Ctrl Pts',(-0.683607177593734,606.643414839584,
79.9389773988009));
#98273=CARTESIAN_POINT('Ctrl Pts',(-0.617684568111035,606.646528786564,
79.9418016685007));
#98274=CARTESIAN_POINT('Ctrl Pts',(-0.551711358599842,606.649169564796,
79.9441997051945));
#98275=CARTESIAN_POINT('Ctrl Pts',(-0.345342966588009,606.657430086932,
79.9517009163702));
#98276=CARTESIAN_POINT('Ctrl Pts',(-0.138423353440868,606.661078221085,
79.9550471976344));
#98277=CARTESIAN_POINT('Ctrl Pts',(0.0688418019391206,606.660027049308,
79.9541394471178));
#98278=CARTESIAN_POINT('Ctrl Pts',(0.131131170307284,606.6597111408,79.953866640981));
#98279=CARTESIAN_POINT('Ctrl Pts',(0.193451665010783,606.658971058177,79.9532098508916));
#98280=CARTESIAN_POINT('Ctrl Pts',(0.255797490386203,606.657805108831,79.9521669823773));
#98281=CARTESIAN_POINT('Ctrl Pts',(0.666136198923766,606.650131232575,79.945303181686));
#98282=CARTESIAN_POINT('Ctrl Pts',(1.07421972549342,606.624141270417,79.921831977901));
#98283=CARTESIAN_POINT('Ctrl Pts',(1.48012296273393,606.580564567151,79.8822570048524));
#98284=CARTESIAN_POINT('Ctrl Pts',(1.60798473410058,606.566837663893,79.8697906688108));
#98285=CARTESIAN_POINT('Ctrl Pts',(1.73563038646646,606.551365380786,79.8557262296395));
#98286=CARTESIAN_POINT('Ctrl Pts',(1.86306288877797,606.534169754924,79.840079036097));
#98287=CARTESIAN_POINT('',(1.89317385967765,606.70242510632,79.9033533194805));
#98288=CARTESIAN_POINT('Origin',(1.86306288877797,606.70242510632,79.6551732851678));
#98289=CARTESIAN_POINT('Ctrl Pts',(1.89317385967764,606.70242510632,79.9033533194805));
#98290=CARTESIAN_POINT('Ctrl Pts',(1.58012448505219,606.743501216302,79.9413347011642));
#98291=CARTESIAN_POINT('Ctrl Pts',(1.26585353386947,606.774601642493,79.9700061023909));
#98292=CARTESIAN_POINT('Ctrl Pts',(0.950335111694906,606.795445530877,79.9891761306859));
#98293=CARTESIAN_POINT('Ctrl Pts',(0.78817740514306,606.806158050014,79.9990283852751));
#98294=CARTESIAN_POINT('Ctrl Pts',(0.625503300952601,606.814170420382,80.0063792748621));
#98295=CARTESIAN_POINT('Ctrl Pts',(0.462595958335336,606.819424912887,80.0111851918326));
#98296=CARTESIAN_POINT('Ctrl Pts',(0.308526274104866,606.824394351269,80.0157303897235));
#98297=CARTESIAN_POINT('Ctrl Pts',(0.154247965606297,606.826897303316,80.0179995314596));
#98298=CARTESIAN_POINT('Ctrl Pts',(6.79067047038018E-9,606.826916385848,
80.0179849207937));
#98299=CARTESIAN_POINT('Ctrl Pts',(-0.247612686332898,604.134451125088,
76.5969814761947));
#98300=CARTESIAN_POINT('Ctrl Pts',(-0.239928764978578,603.631174020018,
76.5971361934352));
#98301=CARTESIAN_POINT('Ctrl Pts',(-0.252645464510396,603.935273498433,
76.9980210944396));
#98302=CARTESIAN_POINT('Ctrl Pts',(0.587407127222549,604.147464416195,76.613794761412));
#98303=CARTESIAN_POINT('Ctrl Pts',(0.570806075610003,603.642504151856,76.6129375177081));
#98304=CARTESIAN_POINT('Ctrl Pts',(0.599346104179961,603.948443486134,77.0153826803362));
#98305=CARTESIAN_POINT('Ctrl Pts',(1.40663729476956,604.094168032195,76.5461272140149));
#98306=CARTESIAN_POINT('Ctrl Pts',(1.3489476199593,603.598226411249,76.5522413898123));
#98307=CARTESIAN_POINT('Ctrl Pts',(1.43522748368769,603.894505336773,76.9455084004709));
#98308=CARTESIAN_POINT('Ctrl Pts',(2.61366069407739,603.927699846335,76.3255317586155));
#98309=CARTESIAN_POINT('Ctrl Pts',(2.53731328870643,603.450528037425,76.3416431735781));
#98310=CARTESIAN_POINT('Ctrl Pts',(2.66678387891633,603.726032622645,76.7177190065359));
#98311=CARTESIAN_POINT('Ctrl Pts',(3.01445595206078,603.857371670206,76.2313414391483));
#98312=CARTESIAN_POINT('Ctrl Pts',(2.92857212557764,603.388846213913,76.2529152101653));
#98313=CARTESIAN_POINT('Ctrl Pts',(3.07572538189221,603.654857589732,76.6204570030234));
#98314=CARTESIAN_POINT('Ctrl Pts',(3.7983954194345,603.69287182511,76.0053954703534));
#98315=CARTESIAN_POINT('Ctrl Pts',(3.70006557576271,603.242083137045,76.0368396544836));
#98316=CARTESIAN_POINT('Ctrl Pts',(3.8755985784546,603.488376918241,76.3871426082101));
#98317=CARTESIAN_POINT('Ctrl Pts',(4.17984986817795,603.599268233769,75.874409667253));
#98318=CARTESIAN_POINT('Ctrl Pts',(4.07641784659729,603.158465786143,75.9117507781356));
#98319=CARTESIAN_POINT('Ctrl Pts',(4.26480616625281,603.393646199154,76.2518851665813));
#98320=CARTESIAN_POINT('Ctrl Pts',(4.92370189566428,603.394079103706,75.5781015854782));
#98321=CARTESIAN_POINT('Ctrl Pts',(4.81486847221986,602.972538673971,75.6252072189681));
#98322=CARTESIAN_POINT('Ctrl Pts',(5.02377713750492,603.185986282303,75.9459140475635));
#98323=CARTESIAN_POINT('Ctrl Pts',(5.28609505655054,603.282487531454,75.4127725629522));
#98324=CARTESIAN_POINT('Ctrl Pts',(5.17578544904304,602.871110243873,75.4653304964425));
#98325=CARTESIAN_POINT('Ctrl Pts',(5.39353601298289,603.073050979998,75.7751934044062));
#98326=CARTESIAN_POINT('Ctrl Pts',(5.99304821798366,603.045463077024,75.0480357125633));
#98327=CARTESIAN_POINT('Ctrl Pts',(5.88314832657038,602.653172554016,75.1089592769933));
#98328=CARTESIAN_POINT('Ctrl Pts',(6.11485814111501,602.833172393456,75.398561954746));
#98329=CARTESIAN_POINT('Ctrl Pts',(6.33872452185387,602.919536364403,74.8477580011569));
#98330=CARTESIAN_POINT('Ctrl Pts',(6.23031283838703,602.536883703424,74.9130743719703));
#98331=CARTESIAN_POINT('Ctrl Pts',(6.46756038601705,602.705729334106,75.1917528950879));
#98332=CARTESIAN_POINT('Ctrl Pts',(7.33337757366972,602.533334747895,74.2057580358069));
#98333=CARTESIAN_POINT('Ctrl Pts',(7.21704842590842,602.182602812065,74.2897410752272));
#98334=CARTESIAN_POINT('Ctrl Pts',(7.48242996358273,602.314877267486,74.5288163772505));
#98335=CARTESIAN_POINT('Ctrl Pts',(7.94559727067024,602.263368546861,73.721359506763));
#98336=CARTESIAN_POINT('Ctrl Pts',(7.84051708959433,601.928604105213,73.8120742692735));
#98337=CARTESIAN_POINT('Ctrl Pts',(8.10709315029709,602.041660267919,74.028620906189));
#98338=CARTESIAN_POINT('Ctrl Pts',(8.79441170737145,601.860736855362,72.9077220474778));
#98339=CARTESIAN_POINT('Ctrl Pts',(8.71531793774959,601.540974637517,72.9883352789045));
#98340=CARTESIAN_POINT('Ctrl Pts',(8.97315991273498,601.634180283339,73.188449545123));
#98341=CARTESIAN_POINT('Ctrl Pts',(9.06684564649771,601.726233572703,72.6204124471552));
#98342=CARTESIAN_POINT('Ctrl Pts',(8.99305377021651,601.412739404795,72.7011730151351));
#98343=CARTESIAN_POINT('Ctrl Pts',(9.25113112703224,601.498057379104,72.8917703602215));
#98344=CARTESIAN_POINT('Ctrl Pts',(9.58153921876773,601.464380717656,72.0221557047211));
#98345=CARTESIAN_POINT('Ctrl Pts',(9.51738335439514,601.162565769111,72.1016116954675));
#98346=CARTESIAN_POINT('Ctrl Pts',(9.77628595094184,601.233051420721,72.2740035948496));
#98347=CARTESIAN_POINT('Ctrl Pts',(9.82332486871901,601.337330579973,71.7120858574342));
#98348=CARTESIAN_POINT('Ctrl Pts',(9.76463235697413,601.040586840631,71.7902694724233));
#98349=CARTESIAN_POINT('Ctrl Pts',(10.0229859433045,601.104471408494,71.9538219181877));
#98350=CARTESIAN_POINT('Ctrl Pts',(10.5032304581882,600.971778124982,70.7485243138466));
#98351=CARTESIAN_POINT('Ctrl Pts',(10.4508934408169,600.693428016039,70.8323532494638));
#98352=CARTESIAN_POINT('Ctrl Pts',(10.7167107520177,600.734517150472,70.9588372302021));
#98353=CARTESIAN_POINT('Ctrl Pts',(10.8964735613622,600.748744139839,70.0620801831889));
#98354=CARTESIAN_POINT('Ctrl Pts',(10.8576198832383,600.476090849664,70.138628472291));
#98355=CARTESIAN_POINT('Ctrl Pts',(11.1179466017888,600.508797501419,70.250007157043));
#98356=CARTESIAN_POINT('Ctrl Pts',(11.390954790485,600.461487996467,68.957675482628));
#98357=CARTESIAN_POINT('Ctrl Pts',(11.3677587268443,600.195940392519,69.014472786789));
#98358=CARTESIAN_POINT('Ctrl Pts',(11.6224782615555,600.218082360239,69.109586211324));
#98359=CARTESIAN_POINT('Ctrl Pts',(11.5400169509314,600.373465765884,68.5753485881025));
#98360=CARTESIAN_POINT('Ctrl Pts',(11.520855565674,600.110410221362,68.6277463485386));
#98361=CARTESIAN_POINT('Ctrl Pts',(11.7745701409246,600.129000209871,68.714791080186));
#98362=CARTESIAN_POINT('Ctrl Pts',(11.7970486078528,600.220248563911,67.804433162233));
#98363=CARTESIAN_POINT('Ctrl Pts',(11.7840009883711,599.961885843497,67.8485756225846));
#98364=CARTESIAN_POINT('Ctrl Pts',(12.036826018648,599.973938041764,67.9187349800865));
#98365=CARTESIAN_POINT('Ctrl Pts',(11.906165321538,600.154392365188,67.4136688048127));
#98366=CARTESIAN_POINT('Ctrl Pts',(11.8961680044815,599.897744992462,67.4527537325953));
#98367=CARTESIAN_POINT('Ctrl Pts',(12.1481605517107,599.907288835447,67.5152272280643));
#98368=CARTESIAN_POINT('Ctrl Pts',(12.0856804087928,600.045433573986,66.6213936503897));
#98369=CARTESIAN_POINT('Ctrl Pts',(12.0800305729695,599.791959022311,66.6513216880366));
#98370=CARTESIAN_POINT('Ctrl Pts',(12.3313243194805,599.79701801597,66.6971148274926));
#98371=CARTESIAN_POINT('Ctrl Pts',(12.1560806850811,600.002326913111,66.2198837351635));
#98372=CARTESIAN_POINT('Ctrl Pts',(12.1524261846195,599.749918292424,66.2443008543885));
#98373=CARTESIAN_POINT('Ctrl Pts',(12.4031554959512,599.753392286295,66.2825110894363));
#98374=CARTESIAN_POINT('Ctrl Pts',(12.257019799162,599.940372122965,65.405700320617));
#98375=CARTESIAN_POINT('Ctrl Pts',(12.2558350970482,599.689710423845,65.4202915379704));
#98376=CARTESIAN_POINT('Ctrl Pts',(12.5061462176465,599.690691466762,65.4417759684511));
#98377=CARTESIAN_POINT('Ctrl Pts',(12.2875921822733,599.921503557896,64.9916064252471));
#98378=CARTESIAN_POINT('Ctrl Pts',(12.2872829443278,599.671293324974,65.0003000739761));
#98379=CARTESIAN_POINT('Ctrl Pts',(12.5373399906064,599.671595695793,65.0141778683388));
#98380=CARTESIAN_POINT('Ctrl Pts',(12.3155824582831,599.904242740066,63.7406324714832));
#98381=CARTESIAN_POINT('Ctrl Pts',(12.3159477798069,599.654520254612,63.7345453497792));
#98382=CARTESIAN_POINT('Ctrl Pts',(12.5658991754142,599.654127032142,63.7224078328247));
#98383=CARTESIAN_POINT('Ctrl Pts',(12.2499433960128,599.945028255623,62.9203303339275));
#98384=CARTESIAN_POINT('Ctrl Pts',(12.2476351021315,599.694804185309,62.8975114326958));
#98385=CARTESIAN_POINT('Ctrl Pts',(12.4989259854136,599.695403666325,62.8753544483646));
#98386=CARTESIAN_POINT('Ctrl Pts',(12.0311680098947,600.078586517253,61.7092455282533));
#98387=CARTESIAN_POINT('Ctrl Pts',(12.02433270669,599.824074107251,61.6764817660471));
#98388=CARTESIAN_POINT('Ctrl Pts',(12.2757039450297,599.83057017083,61.6247744041512));
#98389=CARTESIAN_POINT('Ctrl Pts',(11.9376414045012,600.135444418401,61.3074767223547));
#98390=CARTESIAN_POINT('Ctrl Pts',(11.9281609256542,599.879495717932,61.269319855613));
#98391=CARTESIAN_POINT('Ctrl Pts',(12.1802763920905,599.888112726373,61.2099033326353));
#98392=CARTESIAN_POINT('Ctrl Pts',(11.710977576111,600.271739313276,60.5163094405145));
#98393=CARTESIAN_POINT('Ctrl Pts',(11.6960573690714,600.011715656205,60.4693531862596));
#98394=CARTESIAN_POINT('Ctrl Pts',(11.9490055759325,600.026048817743,60.3929349339052));
#98395=CARTESIAN_POINT('Ctrl Pts',(11.5792520747703,600.35032371235,60.1312636317803));
#98396=CARTESIAN_POINT('Ctrl Pts',(11.5607302358161,600.088147945631,60.0796799798351));
#98397=CARTESIAN_POINT('Ctrl Pts',(11.8146027265403,600.105579490779,59.9953322208473));
#98398=CARTESIAN_POINT('Ctrl Pts',(11.280933108072,600.525733694853,59.3807745414427));
#98399=CARTESIAN_POINT('Ctrl Pts',(11.2554200175323,600.257981891559,59.3216529465386));
#98400=CARTESIAN_POINT('Ctrl Pts',(11.5102203665223,600.283101674251,59.220368588735));
#98401=CARTESIAN_POINT('Ctrl Pts',(11.1143334927416,600.622567061909,59.0153358225178));
#98402=CARTESIAN_POINT('Ctrl Pts',(11.0844074462808,600.351921242835,58.9523736714234));
#98403=CARTESIAN_POINT('Ctrl Pts',(11.340234579966,600.381101060427,58.8430123811434));
#98404=CARTESIAN_POINT('Ctrl Pts',(10.7468891809611,600.832177942095,58.3032336718348));
#98405=CARTESIAN_POINT('Ctrl Pts',(10.7086606118733,600.554322751232,58.2342052329224));
#98406=CARTESIAN_POINT('Ctrl Pts',(10.9653218879177,600.593235971834,58.1076875427682));
#98407=CARTESIAN_POINT('Ctrl Pts',(10.5450918351581,600.945481422084,57.9551454984287));
#98408=CARTESIAN_POINT('Ctrl Pts',(10.5017718495429,600.663853925032,57.8832035358986));
#98409=CARTESIAN_POINT('Ctrl Pts',(10.7594229698032,600.707903795814,57.748247707264));
#98410=CARTESIAN_POINT('Ctrl Pts',(9.89450525281217,601.302185996578,56.9491928643266));
#98411=CARTESIAN_POINT('Ctrl Pts',(9.82988413289725,601.010868747812,56.8595245434182));
#98412=CARTESIAN_POINT('Ctrl Pts',(10.0956130835857,601.068903631842,56.7094894932663));
#98413=CARTESIAN_POINT('Ctrl Pts',(9.40533537943261,601.560087977633,56.3342751495656));
#98414=CARTESIAN_POINT('Ctrl Pts',(9.32615145971497,601.259629550472,56.2424874391652));
#98415=CARTESIAN_POINT('Ctrl Pts',(9.5965007327143,601.329911139954,56.0745184163995));
#98416=CARTESIAN_POINT('Ctrl Pts',(8.31786154047716,602.092338504356,55.2045355438743));
#98417=CARTESIAN_POINT('Ctrl Pts',(8.21935109391615,601.766545930577,55.1122541884108));
#98418=CARTESIAN_POINT('Ctrl Pts',(8.48692376686844,601.868570765985,54.9079363581114));
#98419=CARTESIAN_POINT('Ctrl Pts',(7.71423400494031,602.368763849128,54.687263637379));
#98420=CARTESIAN_POINT('Ctrl Pts',(7.60328278950778,602.027967838335,54.6002522073219));
#98421=CARTESIAN_POINT('Ctrl Pts',(7.87102737898878,602.148324687105,54.3737954611148));
#98422=CARTESIAN_POINT('Ctrl Pts',(6.43211894031247,602.891956348124,53.786061608348));
#98423=CARTESIAN_POINT('Ctrl Pts',(6.30828894600969,602.517777832124,53.7086110751252));
#98424=CARTESIAN_POINT('Ctrl Pts',(6.56285306515126,602.677817213243,53.4432039225965));
#98425=CARTESIAN_POINT('Ctrl Pts',(5.75022841332413,603.140946661166,53.3970489773778));
#98426=CARTESIAN_POINT('Ctrl Pts',(5.62291561811055,602.745988465143,53.3322766970217));
#98427=CARTESIAN_POINT('Ctrl Pts',(5.86710297479519,602.929805743566,53.0415050222643));
#98428=CARTESIAN_POINT('Ctrl Pts',(4.65647911755443,603.471153411197,52.9079552143514));
#98429=CARTESIAN_POINT('Ctrl Pts',(4.54890972975399,603.042807841159,52.8639499834371));
#98430=CARTESIAN_POINT('Ctrl Pts',(4.75112300194525,603.263988681109,52.5364612008833));
#98431=CARTESIAN_POINT('Ctrl Pts',(4.27753470189083,603.574456560643,52.760103963041));
#98432=CARTESIAN_POINT('Ctrl Pts',(4.17347758256706,603.135790146889,52.7219730108443));
#98433=CARTESIAN_POINT('Ctrl Pts',(4.36447646411708,603.368535755551,52.3837883044384));
#98434=CARTESIAN_POINT('Ctrl Pts',(3.5083765892915,603.757724414251,52.503472235072));
#98435=CARTESIAN_POINT('Ctrl Pts',(3.41373149403426,603.300363485533,52.4753963396111));
#98436=CARTESIAN_POINT('Ctrl Pts',(3.57968505656083,603.554010430754,52.118787442565));
#98437=CARTESIAN_POINT('Ctrl Pts',(3.11779861057926,603.837956243184,52.3942248829386));
#98438=CARTESIAN_POINT('Ctrl Pts',(3.0308328190885,603.37125022269,52.3719224428149));
#98439=CARTESIAN_POINT('Ctrl Pts',(3.18116850106493,603.635208371282,52.005977374802));
#98440=CARTESIAN_POINT('Ctrl Pts',(1.92712773112881,604.03906916062,52.1241430466814));
#98441=CARTESIAN_POINT('Ctrl Pts',(1.85276789715343,603.550990732668,52.1125876973074));
#98442=CARTESIAN_POINT('Ctrl Pts',(1.96629699390316,603.838742991852,51.7270877774893));
#98443=CARTESIAN_POINT('Ctrl Pts',(1.10486896435858,604.120172016418,52.0204162706371));
#98444=CARTESIAN_POINT('Ctrl Pts',(1.06865977295132,603.618795371852,52.0190762779579));
#98445=CARTESIAN_POINT('Ctrl Pts',(1.12732576421391,603.920822446017,51.6199783226107));
#98446=CARTESIAN_POINT('Ctrl Pts',(0.264827872760487,604.134173512545,52.0023253862613));
#98447=CARTESIAN_POINT('Ctrl Pts',(0.256610940649088,603.630932780795,52.0021484287645));
#98448=CARTESIAN_POINT('Ctrl Pts',(0.270210553101147,603.934992543017,51.6012974652903));
#98449=CARTESIAN_POINT('',(-3.86212964915782E-9,604.136374737192,76.5994959777072));
#98450=CARTESIAN_POINT('',(0.264827872760508,604.134173512545,52.0023253862613));
#98451=CARTESIAN_POINT('Ctrl Pts',(-3.25135887657702E-9,604.136374737192,
76.5994959777073));
#98452=CARTESIAN_POINT('Ctrl Pts',(0.310528165472252,604.136361525075,76.5995448311342));
#98453=CARTESIAN_POINT('Ctrl Pts',(0.618777498407439,604.127218112862,76.5878893241729));
#98454=CARTESIAN_POINT('Ctrl Pts',(0.924673649407594,604.109433246351,76.5648366833291));
#98455=CARTESIAN_POINT('Ctrl Pts',(1.23978245630647,604.09111275409,76.5410897674937));
#98456=CARTESIAN_POINT('Ctrl Pts',(1.55239421536116,604.063622646471,76.5052488949338));
#98457=CARTESIAN_POINT('Ctrl Pts',(1.8624376689848,604.027528506644,76.4576945787578));
#98458=CARTESIAN_POINT('Ctrl Pts',(1.97909517691912,604.013947660624,76.4398017061562));
#98459=CARTESIAN_POINT('Ctrl Pts',(2.09538918047889,603.999149011819,76.4202509684407));
#98460=CARTESIAN_POINT('Ctrl Pts',(2.21131621964626,603.983163694485,76.3990641890932));
#98461=CARTESIAN_POINT('Ctrl Pts',(2.28847278600611,603.972524483767,76.3849630858612));
#98462=CARTESIAN_POINT('Ctrl Pts',(2.36554368200416,603.961344248248,76.3701075120779));
#98463=CARTESIAN_POINT('Ctrl Pts',(2.44247543406213,603.949645260512,76.354512897056));
#98464=CARTESIAN_POINT('Ctrl Pts',(2.64351074550446,603.919073882892,76.3137616051136));
#98465=CARTESIAN_POINT('Ctrl Pts',(2.84402605786525,603.884881770879,76.2678728545117));
#98466=CARTESIAN_POINT('Ctrl Pts',(3.04288942631138,603.847462527482,76.2171146986224));
#98467=CARTESIAN_POINT('Ctrl Pts',(3.16477478015113,603.824527897753,76.18600451559));
#98468=CARTESIAN_POINT('Ctrl Pts',(3.28603954227911,603.800381622635,76.153065981003));
#98469=CARTESIAN_POINT('Ctrl Pts',(3.40642527297712,603.775119573837,76.1183685737292));
#98470=CARTESIAN_POINT('Ctrl Pts',(3.47943076865768,603.759799914409,76.0973270316614));
#98471=CARTESIAN_POINT('Ctrl Pts',(3.55205443377298,603.744089700583,76.0756654689925));
#98472=CARTESIAN_POINT('Ctrl Pts',(3.62429267927299,603.728007283723,76.0533936492377));
#98473=CARTESIAN_POINT('Ctrl Pts',(3.94018000276088,603.657681217773,75.9560022261365));
#98474=CARTESIAN_POINT('Ctrl Pts',(4.24915881614502,603.580147082534,75.8468009339012));
#98475=CARTESIAN_POINT('Ctrl Pts',(4.55177540581521,603.496671628223,75.7262558160285));
#98476=CARTESIAN_POINT('Ctrl Pts',(4.61866590223142,603.478220179201,75.6996104732076));
#98477=CARTESIAN_POINT('Ctrl Pts',(4.68524538832333,603.459478235103,75.6724106564061));
#98478=CARTESIAN_POINT('Ctrl Pts',(4.75151758316339,603.440457788941,75.6446572600295));
#98479=CARTESIAN_POINT('Ctrl Pts',(5.00694798018935,603.367148007569,75.5376884011832));
#98480=CARTESIAN_POINT('Ctrl Pts',(5.25788462122224,603.289684311589,75.4224616809191));
#98481=CARTESIAN_POINT('Ctrl Pts',(5.50437127899814,603.208814644317,75.2991083225829));
#98482=CARTESIAN_POINT('Ctrl Pts',(5.54958725705096,603.193979759811,75.2764801495467));
#98483=CARTESIAN_POINT('Ctrl Pts',(5.59465355084976,603.179030309245,75.2535786253423));
#98484=CARTESIAN_POINT('Ctrl Pts',(5.63957051211805,603.163970968637,75.2304047182994));
#98485=CARTESIAN_POINT('Ctrl Pts',(5.70073378556493,603.143464715732,75.1988488878676));
#98486=CARTESIAN_POINT('Ctrl Pts',(5.76165357779712,603.122739917901,75.1667619524567));
#98487=CARTESIAN_POINT('Ctrl Pts',(5.82229488838826,603.101821536855,75.1341674982548));
#98488=CARTESIAN_POINT('Ctrl Pts',(6.03771053820998,603.027513336684,75.0183824754042));
#98489=CARTESIAN_POINT('Ctrl Pts',(6.24993868384465,602.950644480758,74.8960130814168));
#98490=CARTESIAN_POINT('Ctrl Pts',(6.45731962017304,602.872343202487,74.768123123783));
#98491=CARTESIAN_POINT('Ctrl Pts',(6.5289039751283,602.845314939444,74.7239776961243));
#98492=CARTESIAN_POINT('Ctrl Pts',(6.5999109723249,602.818116157948,74.6791748810223));
#98493=CARTESIAN_POINT('Ctrl Pts',(6.67027315473924,602.790793615782,74.6337595519187));
#98494=CARTESIAN_POINT('Ctrl Pts',(6.72531600416887,602.769419768029,74.598232099019));
#98495=CARTESIAN_POINT('Ctrl Pts',(6.78000298293603,602.747961435351,74.5623194192597));
#98496=CARTESIAN_POINT('Ctrl Pts',(6.83433353593322,602.726427989239,74.526023120994));
#98497=CARTESIAN_POINT('Ctrl Pts',(7.10822454753838,602.617873648939,74.3430463371938));
#98498=CARTESIAN_POINT('Ctrl Pts',(7.37336538639597,602.507313778295,74.1501101955184));
#98499=CARTESIAN_POINT('Ctrl Pts',(7.6299541645097,602.395819428982,73.9471842046893));
#98500=CARTESIAN_POINT('Ctrl Pts',(7.88844352073621,602.283499230146,73.7427551212483));
#98501=CARTESIAN_POINT('Ctrl Pts',(8.1382537825677,602.170231334259,73.5281875575888));
#98502=CARTESIAN_POINT('Ctrl Pts',(8.37962080004122,602.057113267395,73.3034909566141));
#98503=CARTESIAN_POINT('Ctrl Pts',(8.42385440908689,602.036382927359,73.2623124157122));
#98504=CARTESIAN_POINT('Ctrl Pts',(8.46780453567475,602.015657609979,73.2207937995259));
#98505=CARTESIAN_POINT('Ctrl Pts',(8.51147274583541,601.994944051262,73.1789353160944));
#98506=CARTESIAN_POINT('Ctrl Pts',(8.55430052500405,601.974629142196,73.1378824339602));
#98507=CARTESIAN_POINT('Ctrl Pts',(8.59688191547822,601.954309987454,73.0964662008015));
#98508=CARTESIAN_POINT('Ctrl Pts',(8.63920055811426,601.934000270583,73.0547024182158));
#98509=CARTESIAN_POINT('Ctrl Pts',(8.79391013170848,601.8597514894,72.9020213161517));
#98510=CARTESIAN_POINT('Ctrl Pts',(8.94539579189053,601.785495853092,72.744405309215));
#98511=CARTESIAN_POINT('Ctrl Pts',(9.09269306746393,601.711972387154,72.582736303401));
#98512=CARTESIAN_POINT('Ctrl Pts',(9.17109278887552,601.672839149798,72.4966871557344));
#98513=CARTESIAN_POINT('Ctrl Pts',(9.24830637545171,601.633913409097,72.4094906238459));
#98514=CARTESIAN_POINT('Ctrl Pts',(9.32419224683953,601.595306269131,72.3212842918984));
#98515=CARTESIAN_POINT('Ctrl Pts',(9.36129694465004,601.576429154912,72.2781554560291));
#98516=CARTESIAN_POINT('Ctrl Pts',(9.39807441423151,601.557634424496,72.2348034790566));
#98517=CARTESIAN_POINT('Ctrl Pts',(9.43452337359977,601.538927353083,72.1912312995811));
#98518=CARTESIAN_POINT('Ctrl Pts',(9.65091478739477,601.427866579296,71.9325505119194));
#98519=CARTESIAN_POINT('Ctrl Pts',(9.85597586740214,601.319771443215,71.665812843898));
#98520=CARTESIAN_POINT('Ctrl Pts',(10.0499594594973,601.215476303349,71.3908995346974));
#98521=CARTESIAN_POINT('Ctrl Pts',(10.0810275633506,601.198772559482,71.3468698559567));
#98522=CARTESIAN_POINT('Ctrl Pts',(10.1118142187007,601.18216568156,71.3026323420182));
#98523=CARTESIAN_POINT('Ctrl Pts',(10.1423182570292,601.165659189488,71.2581851032761));
#98524=CARTESIAN_POINT('Ctrl Pts',(10.3686972363495,601.043159906367,70.9283297434156));
#98525=CARTESIAN_POINT('Ctrl Pts',(10.579559455429,600.926156659991,70.5868461102067));
#98526=CARTESIAN_POINT('Ctrl Pts',(10.7743498376453,600.81612193495,70.2330686262663));
#98527=CARTESIAN_POINT('Ctrl Pts',(10.9361257815845,600.724736665785,69.9392518281387));
#98528=CARTESIAN_POINT('Ctrl Pts',(11.0868167655327,600.638157980438,69.6369556978456));
#98529=CARTESIAN_POINT('Ctrl Pts',(11.2261259025389,600.557220983097,69.325814430765));
#98530=CARTESIAN_POINT('Ctrl Pts',(11.2465333475455,600.545364493582,69.2802352359348));
#98531=CARTESIAN_POINT('Ctrl Pts',(11.2666986076393,600.533626714025,69.2344396511952));
#98532=CARTESIAN_POINT('Ctrl Pts',(11.2866125566538,600.522014665127,69.1884489145415));
#98533=CARTESIAN_POINT('Ctrl Pts',(11.3880924823089,600.462840572735,68.9540837199202));
#98534=CARTESIAN_POINT('Ctrl Pts',(11.4831444008088,600.406895471585,68.7144140723634));
#98535=CARTESIAN_POINT('Ctrl Pts',(11.5704748159017,600.355136620185,68.4723906692956));
#98536=CARTESIAN_POINT('Ctrl Pts',(11.6043465274097,600.335061588128,68.3785202018511));
#98537=CARTESIAN_POINT('Ctrl Pts',(11.6370570637982,600.315616134507,68.2842960263233));
#98538=CARTESIAN_POINT('Ctrl Pts',(11.6685326694549,600.296855283816,68.1898912049256));
#98539=CARTESIAN_POINT('Ctrl Pts',(11.683669793509,600.287832889541,68.1444904107873));
#98540=CARTESIAN_POINT('Ctrl Pts',(11.698537234685,600.278959648324,68.0990176527924));
#98541=CARTESIAN_POINT('Ctrl Pts',(11.7131347554859,600.270236634273,68.0534740137289));
#98542=CARTESIAN_POINT('Ctrl Pts',(11.8224706417622,600.204900986847,67.7123507360731));
#98543=CARTESIAN_POINT('Ctrl Pts',(11.9167276342155,600.147980114719,67.3670528841897));
#98544=CARTESIAN_POINT('Ctrl Pts',(11.9959228357299,600.099911956208,67.0175313575219));
#98545=CARTESIAN_POINT('Ctrl Pts',(12.0059728443566,600.093812023403,66.973176468702));
#98546=CARTESIAN_POINT('Ctrl Pts',(12.0157803206307,600.087854604843,66.9287535733242));
#98547=CARTESIAN_POINT('Ctrl Pts',(12.0253444381024,600.082040781623,66.8842623710702));
#98548=CARTESIAN_POINT('Ctrl Pts',(12.0802141521759,600.048686651592,66.6290146125931));
#98549=CARTESIAN_POINT('Ctrl Pts',(12.1270883150595,600.020048631873,66.3714346350682));
#98550=CARTESIAN_POINT('Ctrl Pts',(12.1657799000495,599.996347167062,66.111637861221));
#98551=CARTESIAN_POINT('Ctrl Pts',(12.1805677414246,599.987288517692,66.0123440875899));
#98552=CARTESIAN_POINT('Ctrl Pts',(12.1941607596469,599.978950710257,65.9127266173918));
#98553=CARTESIAN_POINT('Ctrl Pts',(12.2065502013075,599.971345031511,65.8127923574291));
#98554=CARTESIAN_POINT('Ctrl Pts',(12.2119202405116,599.968048450909,65.769477177574));
#98555=CARTESIAN_POINT('Ctrl Pts',(12.2170645586533,599.964889174657,65.7260864061383));
#98556=CARTESIAN_POINT('Ctrl Pts',(12.2219815693876,599.961868387845,65.6826258242829));
#98557=CARTESIAN_POINT('Ctrl Pts',(12.2489552484082,599.945296991469,65.4442102811103));
#98558=CARTESIAN_POINT('Ctrl Pts',(12.2691246111535,599.932876901693,65.2033421763265));
#98559=CARTESIAN_POINT('Ctrl Pts',(12.28218480039,599.92482856721,64.9610218376272));
#98560=CARTESIAN_POINT('Ctrl Pts',(12.2891074986876,599.920562458166,64.8325772518866));
#98561=CARTESIAN_POINT('Ctrl Pts',(12.2940334684439,599.917524237441,64.7037249406715));
#98562=CARTESIAN_POINT('Ctrl Pts',(12.2969222724657,599.915743706266,64.5746151917459));
#98563=CARTESIAN_POINT('Ctrl Pts',(12.297866127023,599.915161956016,64.5324313592704));
#98564=CARTESIAN_POINT('Ctrl Pts',(12.2985942535798,599.914714020858,64.490284702133));
#98565=CARTESIAN_POINT('Ctrl Pts',(12.2991072457852,599.914399324768,64.4481760965921));
#98566=CARTESIAN_POINT('Ctrl Pts',(12.3039230418204,599.911445065093,64.0528748551926));
#98567=CARTESIAN_POINT('Ctrl Pts',(12.2897795816084,599.92023327766,63.6605870250526));
#98568=CARTESIAN_POINT('Ctrl Pts',(12.2571208090154,599.94032743659,63.2713649049953));
#98569=CARTESIAN_POINT('Ctrl Pts',(12.2244620364223,599.96042159552,62.8821427849379));
#98570=CARTESIAN_POINT('Ctrl Pts',(12.1732881572924,599.991821500362,62.4959863338011));
#98571=CARTESIAN_POINT('Ctrl Pts',(12.1040930127778,600.034060437411,62.1129397664499));
#98572=CARTESIAN_POINT('Ctrl Pts',(12.097501651259,600.038084016033,62.076451680159));
#98573=CARTESIAN_POINT('Ctrl Pts',(12.0907423182806,600.042208174621,62.0399811711845));
#98574=CARTESIAN_POINT('Ctrl Pts',(12.083815675173,600.046432094228,62.0035314922614));
#98575=CARTESIAN_POINT('Ctrl Pts',(12.036394081548,600.075350142405,61.7539875451004));
#98576=CARTESIAN_POINT('Ctrl Pts',(11.9810777244824,600.108982138256,61.5051624948093));
#98577=CARTESIAN_POINT('Ctrl Pts',(11.9180804827827,600.14705872784,61.2582463139844));
#98578=CARTESIAN_POINT('Ctrl Pts',(11.8885070001017,600.164933436831,61.1423337565412));
#98579=CARTESIAN_POINT('Ctrl Pts',(11.857241490088,600.18378723064,61.0268418090815));
#98580=CARTESIAN_POINT('Ctrl Pts',(11.824309419125,600.203590273384,60.9118928329591));
#98581=CARTESIAN_POINT('Ctrl Pts',(11.8147012792869,600.209367936263,60.8783557426836));
#98582=CARTESIAN_POINT('Ctrl Pts',(11.8049614391109,600.215220265117,60.8448961507762));
#98583=CARTESIAN_POINT('Ctrl Pts',(11.7950906598908,600.2211463396,60.8115140280204));
#98584=CARTESIAN_POINT('Ctrl Pts',(11.6884979670894,600.285140906071,60.4510267476747));
#98585=CARTESIAN_POINT('Ctrl Pts',(11.5665815949929,600.357772992541,60.0993881528898));
#98586=CARTESIAN_POINT('Ctrl Pts',(11.4300925444937,600.438028106791,59.7560189685528));
#98587=CARTESIAN_POINT('Ctrl Pts',(11.4183382568568,600.444939589388,59.7264483902274));
#98588=CARTESIAN_POINT('Ctrl Pts',(11.4064758513312,600.451907658307,59.6969391717302));
#98589=CARTESIAN_POINT('Ctrl Pts',(11.3945054923629,600.458931745061,59.6674910998064));
#98590=CARTESIAN_POINT('Ctrl Pts',(11.2921850121051,600.518972378091,59.4157742657605));
#98591=CARTESIAN_POINT('Ctrl Pts',(11.1819396276912,600.583126551534,59.1684441712597));
#98592=CARTESIAN_POINT('Ctrl Pts',(11.0639479787222,600.650992808033,58.9255372139082));
#98593=CARTESIAN_POINT('Ctrl Pts',(11.0205465320782,600.675956385847,58.8361875570378));
#98594=CARTESIAN_POINT('Ctrl Pts',(10.9760974098984,600.701422015914,58.7474361314692));
#98595=CARTESIAN_POINT('Ctrl Pts',(10.9306109324387,600.727369061768,58.6592839633751));
#98596=CARTESIAN_POINT('Ctrl Pts',(10.9173036742458,600.734959977966,58.6334946799086));
#98597=CARTESIAN_POINT('Ctrl Pts',(10.9039026380964,600.742594854799,58.6077492085215));
#98598=CARTESIAN_POINT('Ctrl Pts',(10.8904091198926,600.75027250686,58.5820495569516));
#98599=CARTESIAN_POINT('Ctrl Pts',(10.7698070167273,600.81889367533,58.3523517136518));
#98600=CARTESIAN_POINT('Ctrl Pts',(10.6416424932073,600.891037826986,58.1259903442765));
#98601=CARTESIAN_POINT('Ctrl Pts',(10.5068163412964,600.965864459736,57.9044450450971));
#98602=CARTESIAN_POINT('Ctrl Pts',(10.4485076621509,600.998224962937,57.808632670547));
#98603=CARTESIAN_POINT('Ctrl Pts',(10.388953607307,601.031086906189,57.713720804032));
#98604=CARTESIAN_POINT('Ctrl Pts',(10.3282293807528,601.064381304421,57.6198275512506));
#98605=CARTESIAN_POINT('Ctrl Pts',(10.3139692496735,601.072199971037,57.5977781952009));
#98606=CARTESIAN_POINT('Ctrl Pts',(10.2996497960813,601.08004000547,57.5757900176145));
#98607=CARTESIAN_POINT('Ctrl Pts',(10.2852711775002,601.087900914242,57.5538629682177));
#98608=CARTESIAN_POINT('Ctrl Pts',(10.0352430737208,601.224593330348,57.1725760906757));
#98609=CARTESIAN_POINT('Ctrl Pts',(9.7670951332938,601.367730358321,56.8094299412247));
#98610=CARTESIAN_POINT('Ctrl Pts',(9.48107593711002,601.51505087391,56.4634525360561));
#98611=CARTESIAN_POINT('Ctrl Pts',(9.28311236320542,601.617016392884,56.2239898547702));
#98612=CARTESIAN_POINT('Ctrl Pts',(9.07658839347743,601.720985696932,55.9927510172806));
#98613=CARTESIAN_POINT('Ctrl Pts',(8.86159725045973,601.826207998157,55.7694040901285));
#98614=CARTESIAN_POINT('Ctrl Pts',(8.84757081570353,601.833072903019,55.75483250798));
#98615=CARTESIAN_POINT('Ctrl Pts',(8.83350480090613,601.839944523442,55.7402928849304));
#98616=CARTESIAN_POINT('Ctrl Pts',(8.81939960411073,601.846822423391,55.7257855526291));
#98617=CARTESIAN_POINT('Ctrl Pts',(8.49324152367174,602.005861866595,55.3903287898257));
#98618=CARTESIAN_POINT('Ctrl Pts',(8.14587360451403,602.168394192616,55.071876469928));
#98619=CARTESIAN_POINT('Ctrl Pts',(7.78212530167639,602.329037592453,54.7745772655493));
#98620=CARTESIAN_POINT('Ctrl Pts',(7.55195563853653,602.430688203432,54.5864547171009));
#98621=CARTESIAN_POINT('Ctrl Pts',(7.31522835413509,602.53158201021,54.406801468053));
#98622=CARTESIAN_POINT('Ctrl Pts',(7.07317494872266,602.630354405577,54.2366615516199));
#98623=CARTESIAN_POINT('Ctrl Pts',(7.06129788050289,602.635200966095,54.2283131320183));
#98624=CARTESIAN_POINT('Ctrl Pts',(7.04940682153739,602.640043182324,54.219985871321));
#98625=CARTESIAN_POINT('Ctrl Pts',(7.03750173377691,602.644880949622,54.2116797798133));
#98626=CARTESIAN_POINT('Ctrl Pts',(6.64028634981823,602.806293921402,53.9345455499968));
#98627=CARTESIAN_POINT('Ctrl Pts',(6.22730832302605,602.962823386694,53.6808812320354));
#98628=CARTESIAN_POINT('Ctrl Pts',(5.79712163891057,603.110586537824,53.451089758777));
#98629=CARTESIAN_POINT('Ctrl Pts',(5.54446643552948,603.197370091056,53.3161297203678));
#98630=CARTESIAN_POINT('Ctrl Pts',(5.28587575785619,603.281129805348,53.1894035722773));
#98631=CARTESIAN_POINT('Ctrl Pts',(5.02106131531314,603.361080841205,53.0709860658359));
#98632=CARTESIAN_POINT('Ctrl Pts',(5.01259930724037,603.363635635061,53.0672020958763));
#98633=CARTESIAN_POINT('Ctrl Pts',(5.00412957485699,603.366186781108,53.0634263089924));
#98634=CARTESIAN_POINT('Ctrl Pts',(4.99565222801652,603.36873421786,53.0596587598676));
#98635=CARTESIAN_POINT('Ctrl Pts',(4.72092237011719,603.451290346567,52.9375618048699));
#98636=CARTESIAN_POINT('Ctrl Pts',(4.43801237496684,603.530001065124,52.8240393805438));
#98637=CARTESIAN_POINT('Ctrl Pts',(4.15077506050142,603.602727805415,52.7210258524162));
#98638=CARTESIAN_POINT('Ctrl Pts',(4.06518506620748,603.624398671187,52.6903302330081));
#98639=CARTESIAN_POINT('Ctrl Pts',(3.9792111112585,603.645538308539,52.6605674732759));
#98640=CARTESIAN_POINT('Ctrl Pts',(3.89295563852526,603.666090453821,52.631788096699));
#98641=CARTESIAN_POINT('Ctrl Pts',(3.88647932075825,603.667633570094,52.6296272553988));
#98642=CARTESIAN_POINT('Ctrl Pts',(3.88000131269559,603.66917345026,52.6274718253079));
#98643=CARTESIAN_POINT('Ctrl Pts',(3.87352161455216,603.670710085412,52.6253218076544));
#98644=CARTESIAN_POINT('Ctrl Pts',(3.49528738953934,603.760406857197,52.4998205508172));
#98645=CARTESIAN_POINT('Ctrl Pts',(3.11117130680275,603.839071965887,52.3927215905075));
#98646=CARTESIAN_POINT('Ctrl Pts',(2.72090801980655,603.904991991953,52.3041975366685));
#98647=CARTESIAN_POINT('Ctrl Pts',(2.71660777482109,603.905718353543,52.3032221051296));
#98648=CARTESIAN_POINT('Ctrl Pts',(2.71230668873312,603.906443162019,52.3022489124891));
#98649=CARTESIAN_POINT('Ctrl Pts',(2.70800476328749,603.907166415128,52.3012779602549));
#98650=CARTESIAN_POINT('Ctrl Pts',(2.51064590304966,603.9403470016,52.2567337140315));
#98651=CARTESIAN_POINT('Ctrl Pts',(2.31170028173491,603.970224507093,52.2169417014671));
#98652=CARTESIAN_POINT('Ctrl Pts',(2.11111770838935,603.996621239467,52.1819925296957));
#98653=CARTESIAN_POINT('Ctrl Pts',(1.91053513504379,604.023017971842,52.1470433579242));
#98654=CARTESIAN_POINT('Ctrl Pts',(1.70831537286292,604.045934249502,52.116936815071));
#98655=CARTESIAN_POINT('Ctrl Pts',(1.50439479076097,604.0651612546,52.0918063490636));
#98656=CARTESIAN_POINT('Ctrl Pts',(1.36067001764632,604.07871259364,52.0740942059933));
#98657=CARTESIAN_POINT('Ctrl Pts',(1.21594950307107,604.09044149521,52.0588407343315));
#98658=CARTESIAN_POINT('Ctrl Pts',(1.07058065254979,604.10023689204,52.0461417320882));
#98659=CARTESIAN_POINT('Ctrl Pts',(0.927490453078763,604.109878746408,52.0336417862087));
#98660=CARTESIAN_POINT('Ctrl Pts',(0.783772258610783,604.117647119529,52.0236168794799));
#98661=CARTESIAN_POINT('Ctrl Pts',(0.639767420115063,604.12346573865,52.0161192211438));
#98662=CARTESIAN_POINT('Ctrl Pts',(0.514927066399052,604.128510002973,52.0096193678855));
#98663=CARTESIAN_POINT('Ctrl Pts',(0.389871499267707,604.132089331343,52.0050182899915));
#98664=CARTESIAN_POINT('Ctrl Pts',(0.264827872760508,604.134173512545,52.0023253862613));
#98665=CARTESIAN_POINT('',(0.270210553101167,603.934992543017,51.6012974652903));
#98666=CARTESIAN_POINT('Origin',(0.270210553101161,604.134173512545,51.7523833394738));
#98667=CARTESIAN_POINT('',(-0.252645464510396,603.935273498433,76.9980210944396));
#98668=CARTESIAN_POINT('Ctrl Pts',(0.270210553101167,603.934992543017,51.6012974652903));
#98669=CARTESIAN_POINT('Ctrl Pts',(0.416188845712395,603.932579184183,51.6044790675076));
#98670=CARTESIAN_POINT('Ctrl Pts',(0.562179672062878,603.928184368032,51.6102408737133));
#98671=CARTESIAN_POINT('Ctrl Pts',(0.707836668903442,603.921856159795,51.6185654510171));
#98672=CARTESIAN_POINT('Ctrl Pts',(0.855734314323341,603.915430604426,51.6270180856934));
#98673=CARTESIAN_POINT('Ctrl Pts',(1.00328760572363,603.907011809844,51.6381129450356));
#98674=CARTESIAN_POINT('Ctrl Pts',(1.15014230608927,603.896682910039,51.651789297983));
#98675=CARTESIAN_POINT('Ctrl Pts',(1.28385901362533,603.887278059729,51.6642421298138));
#98676=CARTESIAN_POINT('Ctrl Pts',(1.41699655037471,603.876290085905,51.678834639128));
#98677=CARTESIAN_POINT('Ctrl Pts',(1.54929519817638,603.863803587702,51.6954914009046));
#98678=CARTESIAN_POINT('Ctrl Pts',(1.75719362309163,603.844181895777,51.7216663814889));
#98679=CARTESIAN_POINT('Ctrl Pts',(1.96334804814265,603.82083589846,51.7529703760962));
#98680=CARTESIAN_POINT('Ctrl Pts',(2.16781670603911,603.793978432753,51.7892635905837));
#98681=CARTESIAN_POINT('Ctrl Pts',(2.37228536393557,603.767120967045,51.8255568050712));
#98682=CARTESIAN_POINT('Ctrl Pts',(2.57506848853287,603.736751721069,51.8668394514028));
#98683=CARTESIAN_POINT('Ctrl Pts',(2.77621117828721,603.703052922097,51.913014617884));
#98684=CARTESIAN_POINT('Ctrl Pts',(2.78094727797299,603.702259451197,51.9141018569566));
#98685=CARTESIAN_POINT('Ctrl Pts',(2.78568258013029,603.701464139836,51.9151918299073));
#98686=CARTESIAN_POINT('Ctrl Pts',(2.79041708794954,603.700666990254,51.9162845374166));
#98687=CARTESIAN_POINT('Ctrl Pts',(3.19062783311622,603.633283464828,52.0086517492297));
#98688=CARTESIAN_POINT('Ctrl Pts',(3.58441626783843,603.552886400077,52.120393363137));
#98689=CARTESIAN_POINT('Ctrl Pts',(3.97207884850313,603.461270401369,52.2512917195333));
#98690=CARTESIAN_POINT('Ctrl Pts',(3.97854352352209,603.459742609708,52.2534745851923));
#98691=CARTESIAN_POINT('Ctrl Pts',(3.98500659612942,603.458211624714,52.2556629087787));
#98692=CARTESIAN_POINT('Ctrl Pts',(3.99146802647606,603.456677468783,52.2578566698448));
#98693=CARTESIAN_POINT('Ctrl Pts',(4.32723754948626,603.376954748337,52.3718559033388));
#98694=CARTESIAN_POINT('Ctrl Pts',(4.65860664857762,603.288651568303,52.5005649822081));
#98695=CARTESIAN_POINT('Ctrl Pts',(4.97989942382872,603.194923456042,52.6410924029741));
#98696=CARTESIAN_POINT('Ctrl Pts',(5.02786800045472,603.180929975698,52.6620729567566));
#98697=CARTESIAN_POINT('Ctrl Pts',(5.0756120622286,603.166815578228,52.6833169044434));
#98698=CARTESIAN_POINT('Ctrl Pts',(5.12311282356784,603.15259076398,52.7048145891233));
#98699=CARTESIAN_POINT('Ctrl Pts',(5.13072165517588,603.150312185422,52.708258160512));
#98700=CARTESIAN_POINT('Ctrl Pts',(5.1383253293963,603.148030584285,52.7117084833211));
#98701=CARTESIAN_POINT('Ctrl Pts',(5.14592385222659,603.145745978856,52.7151655548058));
#98702=CARTESIAN_POINT('Ctrl Pts',(5.65405453740944,602.992969163174,52.9463478703011));
#98703=CARTESIAN_POINT('Ctrl Pts',(6.13932327105491,602.826720053408,53.2077731233885));
#98704=CARTESIAN_POINT('Ctrl Pts',(6.60384272748034,602.652322803614,53.4988133236704));
#98705=CARTESIAN_POINT('Ctrl Pts',(6.81232117442907,602.574052523895,53.6294334906302));
#98706=CARTESIAN_POINT('Ctrl Pts',(7.01662033266161,602.494140574613,53.7660183722793));
#98707=CARTESIAN_POINT('Ctrl Pts',(7.21693171141822,602.413065746167,53.9085088387218));
#98708=CARTESIAN_POINT('Ctrl Pts',(7.22513947055266,602.409743704913,53.9143473858616));
#98709=CARTESIAN_POINT('Ctrl Pts',(7.2333410811538,602.40641935671,53.9201966743798));
#98710=CARTESIAN_POINT('Ctrl Pts',(7.24153649808195,602.403092752226,53.92605666394));
#98711=CARTESIAN_POINT('Ctrl Pts',(7.6043313178296,602.255830583023,54.1854667555637));
#98712=CARTESIAN_POINT('Ctrl Pts',(7.95512168434254,602.104087311807,54.4659556720524));
#98713=CARTESIAN_POINT('Ctrl Pts',(8.28995998189607,601.952249122013,54.7640522820103));
#98714=CARTESIAN_POINT('Ctrl Pts',(8.55084003074742,601.833948573179,54.996306055657));
#98715=CARTESIAN_POINT('Ctrl Pts',(8.80203719276935,601.715590317356,55.23924784128));
#98716=CARTESIAN_POINT('Ctrl Pts',(9.04170368382727,601.599237814998,55.4912341838177));
#98717=CARTESIAN_POINT('Ctrl Pts',(9.04882604992429,601.595780072055,55.4987226690669));
#98718=CARTESIAN_POINT('Ctrl Pts',(9.05593912941172,601.592323753148,55.5062195590408));
#98719=CARTESIAN_POINT('Ctrl Pts',(9.06304292057171,601.588868883909,55.51372486464));
#98720=CARTESIAN_POINT('Ctrl Pts',(9.41782794432331,601.416322163805,55.8885627456103));
#98721=CARTESIAN_POINT('Ctrl Pts',(9.74946630680735,601.247393456694,56.2843874741021));
#98722=CARTESIAN_POINT('Ctrl Pts',(10.0578808158284,601.085182977549,56.7027531625713));
#98723=CARTESIAN_POINT('Ctrl Pts',(10.2247778709415,600.997403542776,56.9291497792141));
#98724=CARTESIAN_POINT('Ctrl Pts',(10.3848733586417,600.911591214942,57.1621477031375));
#98725=CARTESIAN_POINT('Ctrl Pts',(10.5381498361278,600.828236438483,57.4019967994255));
#98726=CARTESIAN_POINT('Ctrl Pts',(10.5430825010644,600.825553957845,57.4097154999511));
#98727=CARTESIAN_POINT('Ctrl Pts',(10.5480074933753,600.822874310698,57.4174407015241));
#98728=CARTESIAN_POINT('Ctrl Pts',(10.5529247796569,600.820197529248,57.4251723494432));
#98729=CARTESIAN_POINT('Ctrl Pts',(10.7311538823448,600.723176463412,57.7054091695081));
#98730=CARTESIAN_POINT('Ctrl Pts',(10.8991800315513,600.629963227712,57.9939850694789));
#98731=CARTESIAN_POINT('Ctrl Pts',(11.0554949410961,600.542048163169,58.2883985366065));
#98732=CARTESIAN_POINT('Ctrl Pts',(11.0884477683713,600.523514742747,58.3504639925379));
#98733=CARTESIAN_POINT('Ctrl Pts',(11.1208800201954,600.505216810882,58.412789017351));
#98734=CARTESIAN_POINT('Ctrl Pts',(11.1527773651985,600.487168396746,58.4753503757855));
#98735=CARTESIAN_POINT('Ctrl Pts',(11.1563744083562,600.485133088649,58.4824053800899));
#98736=CARTESIAN_POINT('Ctrl Pts',(11.1599650069621,600.483100757688,58.4894639315986));
#98737=CARTESIAN_POINT('Ctrl Pts',(11.1635491598044,600.481071411546,58.4965260351482));
#98738=CARTESIAN_POINT('Ctrl Pts',(11.3468191789593,600.377303987905,58.8576355943088));
#98739=CARTESIAN_POINT('Ctrl Pts',(11.5131975113051,600.281365293344,59.2279486399778));
#98740=CARTESIAN_POINT('Ctrl Pts',(11.6624107054815,600.194340509752,59.6078507224401));
#98741=CARTESIAN_POINT('Ctrl Pts',(11.6647417380394,600.192980994563,59.613785613975));
#98742=CARTESIAN_POINT('Ctrl Pts',(11.6670685829227,600.191623652892,59.6197228445413));
#98743=CARTESIAN_POINT('Ctrl Pts',(11.6693912367388,600.19026848945,59.6256624167821));
#98744=CARTESIAN_POINT('Ctrl Pts',(11.7914614847136,600.119046021278,59.9378247593849));
#98745=CARTESIAN_POINT('Ctrl Pts',(11.9019377577438,600.053852316669,60.2563928913557));
#98746=CARTESIAN_POINT('Ctrl Pts',(12.0003794520661,599.995341549017,60.5818958373324));
#98747=CARTESIAN_POINT('Ctrl Pts',(12.022403961461,599.982250846336,60.6547211045231));
#98748=CARTESIAN_POINT('Ctrl Pts',(12.0438259072257,599.969494746759,60.7278935918928));
#98749=CARTESIAN_POINT('Ctrl Pts',(12.0646400666275,599.957080728915,60.80141938881));
#98750=CARTESIAN_POINT('Ctrl Pts',(12.0658734024639,599.956345140569,60.8057761345467));
#98751=CARTESIAN_POINT('Ctrl Pts',(12.0671044404052,599.955610851485,60.8101336095226));
#98752=CARTESIAN_POINT('Ctrl Pts',(12.0683331795544,599.954877862898,60.8144918087508));
#98753=CARTESIAN_POINT('Ctrl Pts',(12.1541174147216,599.903704377145,61.1187588191434));
#98754=CARTESIAN_POINT('Ctrl Pts',(12.2286492071889,599.858897740509,61.4263757001235));
#98755=CARTESIAN_POINT('Ctrl Pts',(12.2916497337276,599.820862373119,61.7356739632439));
#98756=CARTESIAN_POINT('Ctrl Pts',(12.3123901833266,599.808340721893,61.8374982715437));
#98757=CARTESIAN_POINT('Ctrl Pts',(12.3318805284037,599.796553133965,61.9395049355604));
#98758=CARTESIAN_POINT('Ctrl Pts',(12.3501097718202,599.785514639999,62.0416346902988));
#98759=CARTESIAN_POINT('Ctrl Pts',(12.3505132822593,599.785270299219,62.0438953667977));
#98760=CARTESIAN_POINT('Ctrl Pts',(12.3509161912353,599.785026317299,62.0461561431484));
#98761=CARTESIAN_POINT('Ctrl Pts',(12.3513184986724,599.784782694315,62.048417019426));
#98762=CARTESIAN_POINT('Ctrl Pts',(12.4988878701167,599.695419964955,62.8777233171341));
#98763=CARTESIAN_POINT('Ctrl Pts',(12.5654436335101,599.654404252705,63.719998294979));
#98764=CARTESIAN_POINT('Ctrl Pts',(12.547023784357,599.665671383483,64.5759864683422));
#98765=CARTESIAN_POINT('Ctrl Pts',(12.5469692630458,599.665704733307,64.5785201263098));
#98766=CARTESIAN_POINT('Ctrl Pts',(12.5469139970635,599.665738541241,64.5810539094377));
#98767=CARTESIAN_POINT('Ctrl Pts',(12.5468579862992,599.665772807391,64.5835878177418));
#98768=CARTESIAN_POINT('Ctrl Pts',(12.5374524690111,599.67152689537,65.0090902838063));
#98769=CARTESIAN_POINT('Ctrl Pts',(12.5068775203495,599.690243814354,65.4317526596763));
#98770=CARTESIAN_POINT('Ctrl Pts',(12.4564407748525,599.720951539445,65.8474537330173));
#98771=CARTESIAN_POINT('Ctrl Pts',(12.4558465628446,599.721313317328,65.8523512450805));
#98772=CARTESIAN_POINT('Ctrl Pts',(12.4552495926927,599.721676760513,65.8572478053186));
#98773=CARTESIAN_POINT('Ctrl Pts',(12.4546498665094,599.722041867425,65.8621434068506));
#98774=CARTESIAN_POINT('Ctrl Pts',(12.4040416607679,599.752851604014,66.2752612870232));
#98775=CARTESIAN_POINT('Ctrl Pts',(12.3337717584624,599.795530575477,66.6829679693347));
#98776=CARTESIAN_POINT('Ctrl Pts',(12.2443814590765,599.849359697038,67.0853656096814));
#98777=CARTESIAN_POINT('Ctrl Pts',(12.2428405235091,599.850287618843,67.0923022553853));
#98778=CARTESIAN_POINT('Ctrl Pts',(12.2412939039662,599.851218854629,67.0992373326653));
#98779=CARTESIAN_POINT('Ctrl Pts',(12.2397416031979,599.852153400742,67.1061708425376));
#98780=CARTESIAN_POINT('Ctrl Pts',(12.150177183183,599.90607470408,67.5062194691017));
#98781=CARTESIAN_POINT('Ctrl Pts',(12.0416978792334,599.971020248024,67.9010490570525));
#98782=CARTESIAN_POINT('Ctrl Pts',(11.914246482633,600.046412925267,68.2907180385381));
#98783=CARTESIAN_POINT('Ctrl Pts',(11.9114061210395,600.048093114505,68.2994021396051));
#98784=CARTESIAN_POINT('Ctrl Pts',(11.9085563276577,600.049778496453,68.3080836988315));
#98785=CARTESIAN_POINT('Ctrl Pts',(11.9056971018176,600.051469064628,68.3167627159898));
#98786=CARTESIAN_POINT('Ctrl Pts',(11.7780348473212,600.12695164511,68.7042742170754));
#98787=CARTESIAN_POINT('Ctrl Pts',(11.63045559295,600.213409708628,69.0888496165626));
#98788=CARTESIAN_POINT('Ctrl Pts',(11.4674585767456,600.30739636449,69.4598550915683));
#98789=CARTESIAN_POINT('Ctrl Pts',(11.4630803893133,600.309920896565,69.4698204979655));
#98790=CARTESIAN_POINT('Ctrl Pts',(11.458691033693,600.312450893269,69.4797762480409));
#98791=CARTESIAN_POINT('Ctrl Pts',(11.4542905965529,600.314986288131,69.4897221352274));
#98792=CARTESIAN_POINT('Ctrl Pts',(11.2649214349098,600.424094902628,69.9177351390182));
#98793=CARTESIAN_POINT('Ctrl Pts',(11.0548558466121,600.543398885326,70.3297521124981));
#98794=CARTESIAN_POINT('Ctrl Pts',(10.8247037222242,600.670946153262,70.726699225892));
#98795=CARTESIAN_POINT('Ctrl Pts',(10.6530709448023,600.766062771919,71.0227170694926));
#98796=CARTESIAN_POINT('Ctrl Pts',(10.4702683526939,600.86576296356,71.3103549097454));
#98797=CARTESIAN_POINT('Ctrl Pts',(10.2765612833766,600.969227847842,71.5900073533418));
#98798=CARTESIAN_POINT('Ctrl Pts',(10.26913038327,600.973196919402,71.6007352497487));
#98799=CARTESIAN_POINT('Ctrl Pts',(10.2616833989456,600.97717153958,71.6114514209664));
#98800=CARTESIAN_POINT('Ctrl Pts',(10.2542203448061,600.981151662732,71.6221558912206));
#98801=CARTESIAN_POINT('Ctrl Pts',(10.0309413485718,601.100228636524,71.9424112891989));
#98802=CARTESIAN_POINT('Ctrl Pts',(9.79314227964304,601.224262012816,72.252096789745));
#98803=CARTESIAN_POINT('Ctrl Pts',(9.54042013959494,601.352059769454,72.5513581119672));
#98804=CARTESIAN_POINT('Ctrl Pts',(9.53153439293212,601.356553156893,72.561880182945));
#98805=CARTESIAN_POINT('Ctrl Pts',(9.52263008694161,601.36105124802,72.5723894853929));
#98806=CARTESIAN_POINT('Ctrl Pts',(9.51370721162863,601.365553986183,72.5828860130588));
#98807=CARTESIAN_POINT('Ctrl Pts',(9.31151806381215,601.467584414717,72.8207335576388));
#98808=CARTESIAN_POINT('Ctrl Pts',(9.10007725190372,601.571822437062,73.0514824786637));
#98809=CARTESIAN_POINT('Ctrl Pts',(8.88162082266105,601.676422980297,73.27297063567));
#98810=CARTESIAN_POINT('Ctrl Pts',(8.82635703934914,601.702884191695,73.3290013670949));
#98811=CARTESIAN_POINT('Ctrl Pts',(8.77064449620276,601.729368546238,73.3844395960069));
#98812=CARTESIAN_POINT('Ctrl Pts',(8.71451977111148,601.7558461,73.4392506659581));
#98813=CARTESIAN_POINT('Ctrl Pts',(8.70451527424168,601.760565848797,73.4490209976055));
#98814=CARTESIAN_POINT('Ctrl Pts',(8.69449736220669,601.765285535632,73.4587717209558));
#98815=CARTESIAN_POINT('Ctrl Pts',(8.68446623164617,601.770004995063,73.4685026450421));
#98816=CARTESIAN_POINT('Ctrl Pts',(8.35856609473877,601.923334917907,73.784649411633));
#98817=CARTESIAN_POINT('Ctrl Pts',(8.0173051312327,602.077302264897,74.0819867967456));
#98818=CARTESIAN_POINT('Ctrl Pts',(7.65987184783966,602.229304213188,74.3606572775429));
#98819=CARTESIAN_POINT('Ctrl Pts',(7.39538696002535,602.341778960531,74.566861160268));
#98820=CARTESIAN_POINT('Ctrl Pts',(7.12204759188462,602.453176967428,74.7628452062661));
#98821=CARTESIAN_POINT('Ctrl Pts',(6.83953361923856,602.562438676942,74.9486824712655));
#98822=CARTESIAN_POINT('Ctrl Pts',(6.8283183754523,602.566776149872,74.9560598417085));
#98823=CARTESIAN_POINT('Ctrl Pts',(6.81708850557562,602.571110306088,74.963421308603));
#98824=CARTESIAN_POINT('Ctrl Pts',(6.80584399584163,602.575441076129,74.9707668709572));
#98825=CARTESIAN_POINT('Ctrl Pts',(6.53600531050979,602.679368176726,75.1470410648162));
#98826=CARTESIAN_POINT('Ctrl Pts',(6.25682003402361,602.781549749761,75.3144018558047));
#98827=CARTESIAN_POINT('Ctrl Pts',(5.97168962523098,602.879560274357,75.4705491677736));
#98828=CARTESIAN_POINT('Ctrl Pts',(5.91058146394901,602.900565550398,75.5040141186497));
#98829=CARTESIAN_POINT('Ctrl Pts',(5.84920038486591,602.921379256117,75.5369641331808));
#98830=CARTESIAN_POINT('Ctrl Pts',(5.78758008341291,602.94197756147,75.5693767842874));
#98831=CARTESIAN_POINT('Ctrl Pts',(5.77645936187983,602.94569497298,75.5752263510472));
#98832=CARTESIAN_POINT('Ctrl Pts',(5.76533057667263,602.949405471281,75.5810585770746));
#98833=CARTESIAN_POINT('Ctrl Pts',(5.75419392195764,602.953108915887,75.5868733289663));
#98834=CARTESIAN_POINT('Ctrl Pts',(5.43563539121675,603.059044127368,75.7532014469371));
#98835=CARTESIAN_POINT('Ctrl Pts',(5.10974723271856,603.159597121675,75.9059290152303));
#98836=CARTESIAN_POINT('Ctrl Pts',(4.77620299473305,603.25324969582,76.0448419303691));
#98837=CARTESIAN_POINT('Ctrl Pts',(4.74275640446179,603.262640831743,76.0587716069364));
#98838=CARTESIAN_POINT('Ctrl Pts',(4.70923285127606,603.271962590153,76.0725624092105));
#98839=CARTESIAN_POINT('Ctrl Pts',(4.67563202082693,603.281213446915,76.0862141459992));
#98840=CARTESIAN_POINT('Ctrl Pts',(4.66519251392581,603.284087613468,76.0904556304658));
#98841=CARTESIAN_POINT('Ctrl Pts',(4.65474549323412,603.286954951213,76.0946837135968));
#98842=CARTESIAN_POINT('Ctrl Pts',(4.64429094472362,603.28981541585,76.0988983916672));
#98843=CARTESIAN_POINT('Ctrl Pts',(4.27379986217436,603.391185325689,76.248259278874));
#98844=CARTESIAN_POINT('Ctrl Pts',(3.89386018446255,603.483930593988,76.3807926409729));
#98845=CARTESIAN_POINT('Ctrl Pts',(3.50348924748349,603.565802211847,76.4956462456033));
#98846=CARTESIAN_POINT('Ctrl Pts',(3.49421925398875,603.567746386715,76.4983736314481));
#98847=CARTESIAN_POINT('Ctrl Pts',(3.48494331671118,603.569684439582,76.5010910617607));
#98848=CARTESIAN_POINT('Ctrl Pts',(3.47566142285345,603.571616339724,76.5037985243144));
#98849=CARTESIAN_POINT('Ctrl Pts',(3.11357967530811,603.646978737772,76.6094151999532));
#98850=CARTESIAN_POINT('Ctrl Pts',(2.7438424302204,603.712508108099,76.6992121831753));
#98851=CARTESIAN_POINT('Ctrl Pts',(2.37198166188092,603.765955496843,76.7716691688606));
#98852=CARTESIAN_POINT('Ctrl Pts',(2.34061880025861,603.770463267493,76.7777802152766));
#98853=CARTESIAN_POINT('Ctrl Pts',(2.30924086295087,603.774885088492,76.7837679159742));
#98854=CARTESIAN_POINT('Ctrl Pts',(2.27785118480887,603.779219606907,76.7896313582786));
#98855=CARTESIAN_POINT('Ctrl Pts',(2.27065610270344,603.780213156944,76.7909753653311));
#98856=CARTESIAN_POINT('Ctrl Pts',(2.26346025582309,603.781202142936,76.7923128747317));
#98857=CARTESIAN_POINT('Ctrl Pts',(2.2562636865822,603.7821865477,76.7936438742462));
#98858=CARTESIAN_POINT('Ctrl Pts',(1.9692581637581,603.821445477121,76.8467253077395));
#98859=CARTESIAN_POINT('Ctrl Pts',(1.68006019104971,603.853622624926,76.8898579427872));
#98860=CARTESIAN_POINT('Ctrl Pts',(1.38876410941509,603.878279106643,76.9227278834569));
#98861=CARTESIAN_POINT('Ctrl Pts',(1.10512361179407,603.902287588681,76.9547339656398));
#98862=CARTESIAN_POINT('Ctrl Pts',(0.819493826352742,603.919165365058,76.9770097040741));
#98863=CARTESIAN_POINT('Ctrl Pts',(0.531969592127929,603.928534477404,76.9893049833241));
#98864=CARTESIAN_POINT('Ctrl Pts',(0.271955131239933,603.937007170853,77.0004238735779));
#98865=CARTESIAN_POINT('Ctrl Pts',(0.0103914694479063,603.939339493112,
77.0033811689881));
#98866=CARTESIAN_POINT('Ctrl Pts',(-0.252645464510395,603.935273498433,
76.9980210944396));
#98867=CARTESIAN_POINT('',(-0.247612686332903,604.134451125088,76.5969814761947));
#98868=CARTESIAN_POINT('Origin',(-0.252645464510396,604.134451125088,76.8469308133488));
#98869=CARTESIAN_POINT('Origin',(0.00102225664455322,598.119834463972,68.9078455093001));
#98870=CARTESIAN_POINT('Origin',(0.,1218.57245358804,64.2994740882088));
#98871=CARTESIAN_POINT('',(5.49793566439933E-15,605.608439769695,76.5994740882088));
#98872=CARTESIAN_POINT('',(1.50631556295125E-15,605.608439769695,51.9994740882088));
#98873=CARTESIAN_POINT('Ctrl Pts',(-5.41233724504764E-15,605.608439769695,
76.5994740882088));
#98874=CARTESIAN_POINT('Ctrl Pts',(0.803517342471626,605.608439769695,76.5994740882088));
#98875=CARTESIAN_POINT('Ctrl Pts',(1.62216512710203,605.542186255804,76.5196085118227));
#98876=CARTESIAN_POINT('Ctrl Pts',(3.23077935439455,605.286420618322,76.195909276783));
#98877=CARTESIAN_POINT('Ctrl Pts',(4.02089381669516,605.097608851242,75.952258243854));
#98878=CARTESIAN_POINT('Ctrl Pts',(6.27564182199435,604.41675711289,75.0030400468755));
#98879=CARTESIAN_POINT('Ctrl Pts',(7.62604171070065,603.813936675359,74.0682591946972));
#98880=CARTESIAN_POINT('Ctrl Pts',(9.75980156458901,602.747193352477,71.9344993408089));
#98881=CARTESIAN_POINT('Ctrl Pts',(10.7006947361121,602.202165792572,70.5818572288996));
#98882=CARTESIAN_POINT('Ctrl Pts',(11.654095320228,601.628958177762,68.317292844778));
#98883=CARTESIAN_POINT('Ctrl Pts',(11.8983125166469,601.477289438537,67.5235508793709));
#98884=CARTESIAN_POINT('Ctrl Pts',(12.2213288811781,601.275438695951,65.9130515674887));
#98885=CARTESIAN_POINT('Ctrl Pts',(12.3,601.225373764374,65.0962538701053));
#98886=CARTESIAN_POINT('Ctrl Pts',(12.3,601.225373764374,63.5026943063123));
#98887=CARTESIAN_POINT('Ctrl Pts',(12.2213288811781,601.275438695951,62.6858966089289));
#98888=CARTESIAN_POINT('Ctrl Pts',(11.8983125166469,601.477289438537,61.0753972970467));
#98889=CARTESIAN_POINT('Ctrl Pts',(11.654095320228,601.628958177762,60.2816553316396));
#98890=CARTESIAN_POINT('Ctrl Pts',(10.7006947361121,602.202165792572,58.017090947518));
#98891=CARTESIAN_POINT('Ctrl Pts',(9.75980156458901,602.747193352477,56.6644488356087));
#98892=CARTESIAN_POINT('Ctrl Pts',(7.62604171070065,603.813936675359,54.5306889817204));
#98893=CARTESIAN_POINT('Ctrl Pts',(6.27564182199435,604.41675711289,53.5959081295421));
#98894=CARTESIAN_POINT('Ctrl Pts',(4.02089381669516,605.097608851242,52.6466899325635));
#98895=CARTESIAN_POINT('Ctrl Pts',(3.23077935439454,605.286420618322,52.4030388996346));
#98896=CARTESIAN_POINT('Ctrl Pts',(1.62216512710202,605.542186255804,52.0793396645949));
#98897=CARTESIAN_POINT('Ctrl Pts',(0.803517342471629,605.608439769695,51.9994740882088));
#98898=CARTESIAN_POINT('Ctrl Pts',(-1.66533453693773E-15,605.608439769695,
51.9994740882088));
#98899=CARTESIAN_POINT('',(2.22564887778133E-9,604.13637726519,51.9994620213434));
#98900=CARTESIAN_POINT('',(1.50631556295125E-15,1218.57245358804,51.9994740882088));
#98901=CARTESIAN_POINT('Origin',(-0.00103899058863242,598.122522219325,
59.6908665380107));
#98902=CARTESIAN_POINT('Ctrl Pts',(-1.17513814323332E-13,604.136380686556,
51.9994740882088));
#98903=CARTESIAN_POINT('Ctrl Pts',(-0.830412355315779,604.136380686556,
51.9994740882088));
#98904=CARTESIAN_POINT('Ctrl Pts',(-1.64231938507752,604.071082960544,52.0826407378975));
#98905=CARTESIAN_POINT('Ctrl Pts',(-2.83515367981027,603.890097069807,52.323812890186));
#98906=CARTESIAN_POINT('Ctrl Pts',(-3.22987045740506,603.81567035152,52.424181909713));
#98907=CARTESIAN_POINT('Ctrl Pts',(-4.00546366491676,603.643294902985,52.6628556650889));
#98908=CARTESIAN_POINT('Ctrl Pts',(-4.38197303754884,603.546457604273,52.7996457417166));
#98909=CARTESIAN_POINT('Ctrl Pts',(-5.11472586370269,603.336277713785,53.1062922778494));
#98910=CARTESIAN_POINT('Ctrl Pts',(-5.47096314710355,603.222927458667,53.2761570602037));
#98911=CARTESIAN_POINT('Ctrl Pts',(-6.16461781176576,602.983839522965,53.6485378245871));
#98912=CARTESIAN_POINT('Ctrl Pts',(-6.50301550231245,602.857701739012,53.851722530015));
#98913=CARTESIAN_POINT('Ctrl Pts',(-7.48440400049397,602.468880926984,54.5069979081194));
#98914=CARTESIAN_POINT('Ctrl Pts',(-8.08540127789581,602.199757460366,54.9978561404269));
#98915=CARTESIAN_POINT('Ctrl Pts',(-8.91512989826463,601.801595070901,55.8164668699611));
#98916=CARTESIAN_POINT('Ctrl Pts',(-9.17960981988056,601.669736473115,56.1031778705516));
#98917=CARTESIAN_POINT('Ctrl Pts',(-9.68420831858871,601.410800771055,56.7060152337074));
#98918=CARTESIAN_POINT('Ctrl Pts',(-9.92291043224852,601.284425051111,57.020747596285));
#98919=CARTESIAN_POINT('Ctrl Pts',(-10.5886307482388,600.924068655943,57.9917849677706));
#98920=CARTESIAN_POINT('Ctrl Pts',(-10.9702548417479,600.706496345919,58.6797638067076));
#98921=CARTESIAN_POINT('Ctrl Pts',(-11.4461458407884,600.429020734492,59.778948219836));
#98922=CARTESIAN_POINT('Ctrl Pts',(-11.5888532985442,600.344508512903,60.1575729830521));
#98923=CARTESIAN_POINT('Ctrl Pts',(-11.8381254652903,600.195540415103,60.9355996838764));
#98924=CARTESIAN_POINT('Ctrl Pts',(-11.942724253673,600.132274080171,61.3285943265156));
#98925=CARTESIAN_POINT('Ctrl Pts',(-12.1975694083951,599.977328667355,62.5194580326036));
#98926=CARTESIAN_POINT('Ctrl Pts',(-12.289485607334,599.920336544294,63.3290997708905));
#98927=CARTESIAN_POINT('Ctrl Pts',(-12.3039937693074,599.911388735899,64.5687472338976));
#98928=CARTESIAN_POINT('Ctrl Pts',(-12.2877001556324,599.921457064597,64.9861606719559));
#98929=CARTESIAN_POINT('Ctrl Pts',(-12.2143945388426,599.966555320586,65.8053557663365));
#98930=CARTESIAN_POINT('Ctrl Pts',(-12.157513719035,600.001503621978,66.2102226898584));
#98931=CARTESIAN_POINT('Ctrl Pts',(-12.0043633846711,600.094884079366,67.0108131994228));
#98932=CARTESIAN_POINT('Ctrl Pts',(-11.9080923355525,600.153319701732,67.4065361653133));
#98933=CARTESIAN_POINT('Ctrl Pts',(-11.6759895729646,600.292636128654,68.1889168908538));
#98934=CARTESIAN_POINT('Ctrl Pts',(-11.5401719162743,600.373491958218,68.574557701102));
#98935=CARTESIAN_POINT('Ctrl Pts',(-11.0840493285825,600.641030827664,69.6921989559469));
#98936=CARTESIAN_POINT('Ctrl Pts',(-10.7131207478732,600.854147781253,70.3944487585354));
#98937=CARTESIAN_POINT('Ctrl Pts',(-10.0591458219388,601.211445845161,71.3889736072566));
#98938=CARTESIAN_POINT('Ctrl Pts',(-9.82548367484483,601.336394134174,71.709149064036));
#98939=CARTESIAN_POINT('Ctrl Pts',(-9.33415010121997,601.59145909223,72.3192655181611));
#98940=CARTESIAN_POINT('Ctrl Pts',(-9.07556749241062,601.722084359554,72.6106271901342));
#98941=CARTESIAN_POINT('Ctrl Pts',(-8.53249912601977,601.986550095139,73.1672612900657));
#98942=CARTESIAN_POINT('Ctrl Pts',(-8.24801593828978,602.120399261203,73.4325321421858));
#98943=CARTESIAN_POINT('Ctrl Pts',(-7.65202535438249,602.388174013953,73.9373693102728));
#98944=CARTESIAN_POINT('Ctrl Pts',(-7.33917816046283,602.522602244775,74.1777117225767));
#98945=CARTESIAN_POINT('Ctrl Pts',(-6.37510403592012,602.913420537684,74.8474837516201));
#98946=CARTESIAN_POINT('Ctrl Pts',(-5.69483978904818,603.159546862301,75.230310456561));
#98947=CARTESIAN_POINT('Ctrl Pts',(-4.61072722039349,603.483928244513,75.7094386141298));
#98948=CARTESIAN_POINT('Ctrl Pts',(-4.2386453508364,603.58453418778,75.8531520209646));
#98949=CARTESIAN_POINT('Ctrl Pts',(-3.47047139790995,603.76585931445,76.1066505694978));
#98950=CARTESIAN_POINT('Ctrl Pts',(-3.07637753452551,603.845878534603,76.215460838861));
#98951=CARTESIAN_POINT('Ctrl Pts',(-1.88763310249759,604.04373748117,76.4808614138366));
#98952=CARTESIAN_POINT('Ctrl Pts',(-1.07745358387034,604.121518543566,76.5802724694517));
#98953=CARTESIAN_POINT('Ctrl Pts',(-0.247612686332903,604.134451125088,
76.5969814761947));
#98954=CARTESIAN_POINT('Ctrl Pts',(1.87350135405495E-15,605.608439769695,
51.9994740882088));
#98955=CARTESIAN_POINT('Ctrl Pts',(-0.803517342471629,605.608439769695,
51.9994740882088));
#98956=CARTESIAN_POINT('Ctrl Pts',(-1.62216512710202,605.542186255804,52.0793396645949));
#98957=CARTESIAN_POINT('Ctrl Pts',(-3.23077935439454,605.286420618322,52.4030388996346));
#98958=CARTESIAN_POINT('Ctrl Pts',(-4.02089381669516,605.097608851242,52.6466899325635));
#98959=CARTESIAN_POINT('Ctrl Pts',(-6.27564182199435,604.41675711289,53.5959081295421));
#98960=CARTESIAN_POINT('Ctrl Pts',(-7.62604171070064,603.813936675359,54.5306889817204));
#98961=CARTESIAN_POINT('Ctrl Pts',(-9.75980156458901,602.747193352477,56.6644488356087));
#98962=CARTESIAN_POINT('Ctrl Pts',(-10.7006947361121,602.202165792572,58.017090947518));
#98963=CARTESIAN_POINT('Ctrl Pts',(-11.654095320228,601.628958177762,60.2816553316396));
#98964=CARTESIAN_POINT('Ctrl Pts',(-11.8983125166469,601.477289438537,61.0753972970467));
#98965=CARTESIAN_POINT('Ctrl Pts',(-12.2213288811781,601.275438695951,62.6858966089289));
#98966=CARTESIAN_POINT('Ctrl Pts',(-12.3,601.225373764374,63.5026943063123));
#98967=CARTESIAN_POINT('Ctrl Pts',(-12.3,601.225373764374,65.0962538701053));
#98968=CARTESIAN_POINT('Ctrl Pts',(-12.2213288811781,601.275438695951,65.9130515674887));
#98969=CARTESIAN_POINT('Ctrl Pts',(-11.8983125166469,601.477289438537,67.5235508793709));
#98970=CARTESIAN_POINT('Ctrl Pts',(-11.654095320228,601.628958177762,68.317292844778));
#98971=CARTESIAN_POINT('Ctrl Pts',(-10.7006947361121,602.202165792572,70.5818572288996));
#98972=CARTESIAN_POINT('Ctrl Pts',(-9.75980156458901,602.747193352477,71.9344993408089));
#98973=CARTESIAN_POINT('Ctrl Pts',(-7.62604171070064,603.813936675359,74.0682591946972));
#98974=CARTESIAN_POINT('Ctrl Pts',(-6.27564182199435,604.41675711289,75.0030400468755));
#98975=CARTESIAN_POINT('Ctrl Pts',(-4.02089381669516,605.097608851242,75.952258243854));
#98976=CARTESIAN_POINT('Ctrl Pts',(-3.23077935439458,605.286420618322,76.195909276783));
#98977=CARTESIAN_POINT('Ctrl Pts',(-1.62216512710205,605.542186255804,76.5196085118227));
#98978=CARTESIAN_POINT('Ctrl Pts',(-0.803517342471629,605.608439769695,
76.5994740882088));
#98979=CARTESIAN_POINT('Ctrl Pts',(2.63677968348475E-15,605.608439769695,
76.5994740882088));
#98980=CARTESIAN_POINT('Origin',(0.,1218.57245358804,64.2994740882088));
#98981=CARTESIAN_POINT('',(-1.09932974876048E-8,606.827140852494,48.5811983853019));
#98982=CARTESIAN_POINT('Ctrl Pts',(-6.34270402866122E-9,606.827140852493,
48.5811983853026));
#98983=CARTESIAN_POINT('Ctrl Pts',(0.131183067920692,606.827109872663,48.5812192224713));
#98984=CARTESIAN_POINT('Ctrl Pts',(0.262263850660884,606.825270297635,48.5828845405628));
#98985=CARTESIAN_POINT('Ctrl Pts',(0.393087042492152,606.82166339004,48.5861654542112));
#98986=CARTESIAN_POINT('Ctrl Pts',(0.625956739931848,606.815242972769,48.5920055912538));
#98987=CARTESIAN_POINT('Ctrl Pts',(0.858266994442126,606.803210550177,48.6029757350671));
#98988=CARTESIAN_POINT('Ctrl Pts',(1.08860828168967,606.78577822036,48.618932133042));
#98989=CARTESIAN_POINT('Ctrl Pts',(1.16869635359817,606.779717119892,48.62448006222));
#98990=CARTESIAN_POINT('Ctrl Pts',(1.24854641186113,606.773003566343,48.6306304686977));
#98991=CARTESIAN_POINT('Ctrl Pts',(1.32809942293837,606.765647546756,48.637376328015));
#98992=CARTESIAN_POINT('Ctrl Pts',(1.40535872090964,606.758503619687,48.6439276872661));
#98993=CARTESIAN_POINT('Ctrl Pts',(1.48241468364269,606.750760481874,48.6510297053401));
#98994=CARTESIAN_POINT('Ctrl Pts',(1.55926269747948,606.742431721439,48.6586783314213));
#98995=CARTESIAN_POINT('Ctrl Pts',(2.07067858640153,606.687004649108,48.7095791772737));
#98996=CARTESIAN_POINT('Ctrl Pts',(2.57353940461455,606.60556357932,48.7847527919497));
#98997=CARTESIAN_POINT('Ctrl Pts',(3.06861266584221,606.501763789166,48.8833382201712));
#98998=CARTESIAN_POINT('Ctrl Pts',(3.5280360180697,606.405438555533,48.9748245747402));
#98999=CARTESIAN_POINT('Ctrl Pts',(3.98077413585813,606.2898469916,49.0864791016381));
#99000=CARTESIAN_POINT('Ctrl Pts',(4.42735940791135,606.157954728535,49.2175762302821));
#99001=CARTESIAN_POINT('Ctrl Pts',(4.46201311942236,606.147720274511,49.2277489842));
#99002=CARTESIAN_POINT('Ctrl Pts',(4.49663613259049,606.137384633688,49.2380436267645));
#99003=CARTESIAN_POINT('Ctrl Pts',(4.53121896438333,606.12695270202,49.2484565026335));
#99004=CARTESIAN_POINT('Ctrl Pts',(4.74601947947585,606.062157999576,49.3131328459027));
#99005=CARTESIAN_POINT('Ctrl Pts',(4.95932213084444,605.993629202336,49.3823865525655));
#99006=CARTESIAN_POINT('Ctrl Pts',(5.16884411272973,605.92253759955,49.4553437713038));
#99007=CARTESIAN_POINT('Ctrl Pts',(5.41200740793915,605.840031371614,49.5400151626208));
#99008=CARTESIAN_POINT('Ctrl Pts',(5.65093526308688,605.753840160942,49.6299024007825));
#99009=CARTESIAN_POINT('Ctrl Pts',(5.8859656787125,605.664587255718,49.7248192945151));
#99010=CARTESIAN_POINT('Ctrl Pts',(5.9012058732883,605.658799785026,49.7309740380412));
#99011=CARTESIAN_POINT('Ctrl Pts',(5.91642974293557,605.652999506951,49.7371498648016));
#99012=CARTESIAN_POINT('Ctrl Pts',(5.93163735194618,605.647186561106,49.7433467521698));
#99013=CARTESIAN_POINT('Ctrl Pts',(6.38532277407425,605.47377016229,49.9282171982447));
#99014=CARTESIAN_POINT('Ctrl Pts',(6.82458941528544,605.289065018589,50.1318546390623));
#99015=CARTESIAN_POINT('Ctrl Pts',(7.25129724309775,605.096716462177,50.3537276895692));
#99016=CARTESIAN_POINT('Ctrl Pts',(7.67449000072657,604.905952406051,50.5737730273099));
#99017=CARTESIAN_POINT('Ctrl Pts',(8.08531522162717,604.707648175585,50.8117642540156));
#99018=CARTESIAN_POINT('Ctrl Pts',(8.48485213004562,604.504622243655,51.0679794092165));
#99019=CARTESIAN_POINT('Ctrl Pts',(8.50152150271616,604.496151649701,51.0786691498034));
#99020=CARTESIAN_POINT('Ctrl Pts',(8.51817133864071,604.487672771725,51.0893906828856));
#99021=CARTESIAN_POINT('Ctrl Pts',(8.53480170293739,604.479185821683,51.1001440211828));
#99022=CARTESIAN_POINT('Ctrl Pts',(8.88265589538547,604.301665888822,51.3250695695815));
#99023=CARTESIAN_POINT('Ctrl Pts',(9.22310591837765,604.119945955855,51.564885383951));
#99024=CARTESIAN_POINT('Ctrl Pts',(9.55213627055251,603.938098784817,51.8166263297717));
#99025=CARTESIAN_POINT('Ctrl Pts',(9.58597325041618,603.919397898944,51.8425149849012));
#99026=CARTESIAN_POINT('Ctrl Pts',(9.61968948708153,603.900695672363,51.8685297222792));
#99027=CARTESIAN_POINT('Ctrl Pts',(9.65328063531735,603.881996535394,51.8946672948334));
#99028=CARTESIAN_POINT('Ctrl Pts',(9.68287665471879,603.865521361142,51.917696221948));
#99029=CARTESIAN_POINT('Ctrl Pts',(9.71237647083121,603.849047630201,51.940821203202));
#99030=CARTESIAN_POINT('Ctrl Pts',(9.74177715342261,603.832578395773,51.9640400780151));
#99031=CARTESIAN_POINT('Ctrl Pts',(10.085743018819,603.63990074433,52.2356834435658));
#99032=CARTESIAN_POINT('Ctrl Pts',(10.4168996980707,603.447637351623,52.5202505899506));
#99033=CARTESIAN_POINT('Ctrl Pts',(10.7356021263374,603.25742169904,52.8182111751762));
#99034=CARTESIAN_POINT('Ctrl Pts',(11.1345671134278,603.019301814638,53.191210658376));
#99035=CARTESIAN_POINT('Ctrl Pts',(11.5140262355694,602.784321821904,53.5852075140256));
#99036=CARTESIAN_POINT('Ctrl Pts',(11.8747642121883,602.555396734084,54.0011669855163));
#99037=CARTESIAN_POINT('Ctrl Pts',(12.1396201387599,602.387318599316,54.3065668557228));
#99038=CARTESIAN_POINT('Ctrl Pts',(12.3942600538462,602.222458556566,54.6238994674662));
#99039=CARTESIAN_POINT('Ctrl Pts',(12.6384027128533,602.061913537245,54.9540941874028));
#99040=CARTESIAN_POINT('Ctrl Pts',(12.6934199989364,602.025734889511,55.0285032130265));
#99041=CARTESIAN_POINT('Ctrl Pts',(12.7479128130092,601.989770157807,55.1035770627712));
#99042=CARTESIAN_POINT('Ctrl Pts',(12.8018733060317,601.954035169909,55.1793208996343));
#99043=CARTESIAN_POINT('Ctrl Pts',(12.9672617185302,601.844507762207,55.4114750597183));
#99044=CARTESIAN_POINT('Ctrl Pts',(13.1265971638445,601.737833525833,55.6485181832555));
#99045=CARTESIAN_POINT('Ctrl Pts',(13.2794577936644,601.634588593285,55.8898965896893));
#99046=CARTESIAN_POINT('Ctrl Pts',(13.338098902136,601.594981290242,55.9824953008883));
#99047=CARTESIAN_POINT('Ctrl Pts',(13.3957875297173,601.555878461061,56.0757317394338));
#99048=CARTESIAN_POINT('Ctrl Pts',(13.4525014240595,601.517311758678,56.1695736395204));
#99049=CARTESIAN_POINT('Ctrl Pts',(13.5103276838369,601.477988623198,56.265256120072));
#99050=CARTESIAN_POINT('Ctrl Pts',(13.5671707966639,601.439201248967,56.3616179364094));
#99051=CARTESIAN_POINT('Ctrl Pts',(13.6230077720489,601.400982219844,56.4586314313638));
#99052=CARTESIAN_POINT('Ctrl Pts',(13.7869220361003,601.288786958761,56.7434229251517));
#99053=CARTESIAN_POINT('Ctrl Pts',(13.9424991854398,601.181288965271,57.034114638469));
#99054=CARTESIAN_POINT('Ctrl Pts',(14.0893519141326,601.079054705159,57.3308706561203));
#99055=CARTESIAN_POINT('Ctrl Pts',(14.1111562362249,601.063875220541,57.3749322397849));
#99056=CARTESIAN_POINT('Ctrl Pts',(14.132768292625,601.048811737215,57.4191274655816));
#99057=CARTESIAN_POINT('Ctrl Pts',(14.1541868887825,601.033866065188,57.4634568184053));
#99058=CARTESIAN_POINT('Ctrl Pts',(14.3690003859214,600.883971457167,57.9080491360308));
#99059=CARTESIAN_POINT('Ctrl Pts',(14.5644206321617,600.74588107374,58.3662732287448));
#99060=CARTESIAN_POINT('Ctrl Pts',(14.7394736989775,600.62123961036,58.8391490276349));
#99061=CARTESIAN_POINT('Ctrl Pts',(14.7930222736766,600.583111899524,58.9838013065173));
#99062=CARTESIAN_POINT('Ctrl Pts',(14.844665954123,600.546245890809,59.129826700604));
#99063=CARTESIAN_POINT('Ctrl Pts',(14.8943779224113,600.510686681454,59.2772573842497));
#99064=CARTESIAN_POINT('Ctrl Pts',(14.9788181415358,600.450286187705,59.5276815710471));
#99065=CARTESIAN_POINT('Ctrl Pts',(15.0576110594056,600.393686811632,59.7824113765591));
#99066=CARTESIAN_POINT('Ctrl Pts',(15.1295263785222,600.341868479667,60.0377155440763));
#99067=CARTESIAN_POINT('Ctrl Pts',(15.1536787692919,600.324465558871,60.1234581382101));
#99068=CARTESIAN_POINT('Ctrl Pts',(15.1770912859024,600.307576293993,60.2093651695768));
#99069=CARTESIAN_POINT('Ctrl Pts',(15.1997652434983,600.291202752349,60.2954371488871));
#99070=CARTESIAN_POINT('Ctrl Pts',(15.2446133607517,600.258816588073,60.4656838384653));
#99071=CARTESIAN_POINT('Ctrl Pts',(15.2865717155591,600.22845079911,60.636574808298));
#99072=CARTESIAN_POINT('Ctrl Pts',(15.325649598072,600.200124194892,60.8081106404716));
#99073=CARTESIAN_POINT('Ctrl Pts',(15.4433396652835,600.114813534744,61.3247216316376));
#99074=CARTESIAN_POINT('Ctrl Pts',(15.5349555636936,600.047977681829,61.8471715921895));
#99075=CARTESIAN_POINT('Ctrl Pts',(15.600123128367,600.000357873918,62.3755944903987));
#99076=CARTESIAN_POINT('Ctrl Pts',(15.6386979344604,599.972170157137,62.6883852312509));
#99077=CARTESIAN_POINT('Ctrl Pts',(15.6680084809615,599.950712943742,63.00326810169));
#99078=CARTESIAN_POINT('Ctrl Pts',(15.6877925284557,599.936218732362,63.3203069204358));
#99079=CARTESIAN_POINT('Ctrl Pts',(15.7005815679487,599.926849211701,63.5252509277185));
#99080=CARTESIAN_POINT('Ctrl Pts',(15.7093924335227,599.920387366526,63.731194673896));
#99081=CARTESIAN_POINT('Ctrl Pts',(15.7141470311175,599.916898340084,63.9378910949099));
#99082=CARTESIAN_POINT('Ctrl Pts',(15.7144659003351,599.916664346962,63.9517532829757));
#99083=CARTESIAN_POINT('Ctrl Pts',(15.7147665408604,599.916443713548,63.9656188529851));
#99084=CARTESIAN_POINT('Ctrl Pts',(15.7150489358492,599.916236454561,63.9794877289295));
#99085=CARTESIAN_POINT('Ctrl Pts',(15.7158488065306,599.915649403114,64.0187706754704));
#99086=CARTESIAN_POINT('Ctrl Pts',(15.7165007988266,599.915170663659,64.0581033421356));
#99087=CARTESIAN_POINT('Ctrl Pts',(15.7170049051664,599.914800215272,64.0974701301083));
#99088=CARTESIAN_POINT('Ctrl Pts',(15.7194694294047,599.912989131069,64.2899303224863));
#99089=CARTESIAN_POINT('Ctrl Pts',(15.7184018336157,599.913777206096,64.4836683248951));
#99090=CARTESIAN_POINT('Ctrl Pts',(15.7137735335997,599.917173057418,64.6767950132617));
#99091=CARTESIAN_POINT('Ctrl Pts',(15.712833394712,599.917862851051,64.716024516398));
#99092=CARTESIAN_POINT('Ctrl Pts',(15.7117464743577,599.918660143879,64.7552287682158));
#99093=CARTESIAN_POINT('Ctrl Pts',(15.7105127430939,599.919564854116,64.7943919360785));
#99094=CARTESIAN_POINT('Ctrl Pts',(15.7095991882977,599.92023477503,64.8233915252814));
#99095=CARTESIAN_POINT('Ctrl Pts',(15.708605979292,599.92096297442,64.8523701843884));
#99096=CARTESIAN_POINT('Ctrl Pts',(15.7075334205578,599.921749165278,64.8813270198615));
#99097=CARTESIAN_POINT('Ctrl Pts',(15.6985693797753,599.928319851522,65.1233373134135));
#99098=CARTESIAN_POINT('Ctrl Pts',(15.6840546075089,599.938957018774,65.3640472137197));
#99099=CARTESIAN_POINT('Ctrl Pts',(15.6641212610662,599.953549632281,65.6034907467274));
#99100=CARTESIAN_POINT('Ctrl Pts',(15.6411292069346,599.970381435241,65.8796761172172));
#99101=CARTESIAN_POINT('Ctrl Pts',(15.6110000935115,599.992447069947,66.1541909485691));
#99102=CARTESIAN_POINT('Ctrl Pts',(15.5737798644399,600.019643054132,66.4270558219922));
#99103=CARTESIAN_POINT('Ctrl Pts',(15.5042909343416,600.070417052335,66.9364854678731));
#99104=CARTESIAN_POINT('Ctrl Pts',(15.4100832406381,600.13907485609,67.4401695893287));
#99105=CARTESIAN_POINT('Ctrl Pts',(15.2914680739337,600.224933399288,67.9381923855767));
#99106=CARTESIAN_POINT('Ctrl Pts',(15.2270223963164,600.271581835144,68.2087768096833));
#99107=CARTESIAN_POINT('Ctrl Pts',(15.1553484481903,600.323324701704,68.4777850319379));
#99108=CARTESIAN_POINT('Ctrl Pts',(15.0765013223764,600.380048388059,68.7451756305374));
#99109=CARTESIAN_POINT('Ctrl Pts',(15.0102267686864,600.42772719636,68.969929448767));
#99110=CARTESIAN_POINT('Ctrl Pts',(14.9393986310139,600.478551665265,69.1917973879912));
#99111=CARTESIAN_POINT('Ctrl Pts',(14.8641408406389,600.532348321835,69.4108007082289));
#99112=CARTESIAN_POINT('Ctrl Pts',(14.6384917767306,600.693649432805,70.0674489297383));
#99113=CARTESIAN_POINT('Ctrl Pts',(14.3730295175932,600.881663250137,70.6983179949));
#99114=CARTESIAN_POINT('Ctrl Pts',(14.0709202551345,601.091836979959,71.3048669688541));
#99115=CARTESIAN_POINT('Ctrl Pts',(14.0153823306542,601.130474036763,71.4163712333539));
#99116=CARTESIAN_POINT('Ctrl Pts',(13.9586060318343,601.169859933587,71.5270536792301));
#99117=CARTESIAN_POINT('Ctrl Pts',(13.9006111685527,601.209966324507,71.6369234719541));
#99118=CARTESIAN_POINT('Ctrl Pts',(13.8132963508808,601.270348951737,71.8023391721821));
#99119=CARTESIAN_POINT('Ctrl Pts',(13.722999297798,601.332505688626,71.9661929969353));
#99120=CARTESIAN_POINT('Ctrl Pts',(13.6299592468021,601.396203040114,72.1281591912608));
#99121=CARTESIAN_POINT('Ctrl Pts',(13.5153701108117,601.474653389117,72.3276385130017));
#99122=CARTESIAN_POINT('Ctrl Pts',(13.3964238457257,601.555586127919,72.524588512448));
#99123=CARTESIAN_POINT('Ctrl Pts',(13.2736785048461,601.638477345278,72.7181535822209));
#99124=CARTESIAN_POINT('Ctrl Pts',(13.2230467223124,601.67266951959,72.7979981160226));
#99125=CARTESIAN_POINT('Ctrl Pts',(13.1717690142467,601.707194642083,72.877266958708));
#99126=CARTESIAN_POINT('Ctrl Pts',(13.119886458028,601.742014888341,72.9559013911626));
#99127=CARTESIAN_POINT('Ctrl Pts',(13.028077430013,601.803631223334,73.0950493310163));
#99128=CARTESIAN_POINT('Ctrl Pts',(12.9344479627768,601.866125360828,73.232156163104));
#99129=CARTESIAN_POINT('Ctrl Pts',(12.8390792114001,601.929383398044,73.367197238578));
#99130=CARTESIAN_POINT('Ctrl Pts',(12.6440223006845,602.058764533259,73.643395622445));
#99131=CARTESIAN_POINT('Ctrl Pts',(12.4414058536515,602.191546620317,73.9113615973352));
#99132=CARTESIAN_POINT('Ctrl Pts',(12.2313971791557,602.327125324242,74.1715598542876));
#99133=CARTESIAN_POINT('Ctrl Pts',(12.1400319511015,602.386109455412,74.2847602882354));
#99134=CARTESIAN_POINT('Ctrl Pts',(12.0472674516941,602.445624173488,74.3964896998921));
#99135=CARTESIAN_POINT('Ctrl Pts',(11.9530990206169,602.50562051508,74.506770281284));
#99136=CARTESIAN_POINT('Ctrl Pts',(11.7624766227194,602.627069352749,74.7300080333202));
#99137=CARTESIAN_POINT('Ctrl Pts',(11.5660389794749,602.750532246518,74.9473754835045));
#99138=CARTESIAN_POINT('Ctrl Pts',(11.3639002900369,602.875504933021,75.158894069929));
#99139=CARTESIAN_POINT('Ctrl Pts',(11.3241855659211,602.900058647999,75.2004516872687));
#99140=CARTESIAN_POINT('Ctrl Pts',(11.2842508843427,602.924670611825,75.2417836420512));
#99141=CARTESIAN_POINT('Ctrl Pts',(11.244097275529,602.949336959137,75.2828902591882));
#99142=CARTESIAN_POINT('Ctrl Pts',(11.1555970541534,603.003702612987,75.373490950486));
#99143=CARTESIAN_POINT('Ctrl Pts',(11.0659447322039,603.058384308477,75.463070243372));
#99144=CARTESIAN_POINT('Ctrl Pts',(10.9752166475744,603.113292912197,75.5515588294562));
#99145=CARTESIAN_POINT('Ctrl Pts',(10.7995114119639,603.21962965669,75.7229270218991));
#99146=CARTESIAN_POINT('Ctrl Pts',(10.6193973010466,603.327051486015,75.8905643475695));
#99147=CARTESIAN_POINT('Ctrl Pts',(10.4355011010676,603.434846331506,76.0538402392495));
#99148=CARTESIAN_POINT('Ctrl Pts',(10.3437034279004,603.488655578226,76.1353446256493));
#99149=CARTESIAN_POINT('Ctrl Pts',(10.2509639608671,603.54255759095,76.215762720377));
#99150=CARTESIAN_POINT('Ctrl Pts',(10.1573640686073,603.596463254928,76.2950194899588));
#99151=CARTESIAN_POINT('Ctrl Pts',(10.0741297969101,603.644399193455,76.3654990528508));
#99152=CARTESIAN_POINT('Ctrl Pts',(9.99030988510561,603.692296630999,76.4350092280443));
#99153=CARTESIAN_POINT('Ctrl Pts',(9.90591360420889,603.740115162276,76.5035433110902));
#99154=CARTESIAN_POINT('Ctrl Pts',(9.4063955163693,604.023139734598,76.9091774664249));
#99155=CARTESIAN_POINT('Ctrl Pts',(8.88565058296727,604.304165011645,77.281463795644));
#99156=CARTESIAN_POINT('Ctrl Pts',(8.34163289819202,604.577037261729,77.621886832962));
#99157=CARTESIAN_POINT('Ctrl Pts',(8.14290238271327,604.676717923657,77.746243903661));
#99158=CARTESIAN_POINT('Ctrl Pts',(7.94106647154317,604.775310977399,77.866349108996));
#99159=CARTESIAN_POINT('Ctrl Pts',(7.73602658782701,604.87251780605,77.982275225029));
#99160=CARTESIAN_POINT('Ctrl Pts',(7.67213350385386,604.902808713132,78.0183993045599));
#99161=CARTESIAN_POINT('Ctrl Pts',(7.607925744799,604.932962822967,78.0541135135407));
#99162=CARTESIAN_POINT('Ctrl Pts',(7.54339610210028,604.962967574738,78.0894159789354));
#99163=CARTESIAN_POINT('Ctrl Pts',(7.29105366481601,605.080300816876,78.2274658702299));
#99164=CARTESIAN_POINT('Ctrl Pts',(7.03370074023305,605.195402283494,78.3592633252969));
#99165=CARTESIAN_POINT('Ctrl Pts',(6.77108651639008,605.307447272327,78.4846057105468));
#99166=CARTESIAN_POINT('Ctrl Pts',(6.64811138532239,605.359914907116,78.543300156068));
#99167=CARTESIAN_POINT('Ctrl Pts',(6.52398298359675,605.411712539362,78.6005796581665));
#99168=CARTESIAN_POINT('Ctrl Pts',(6.39867799322463,605.462756977176,78.6564262110446));
#99169=CARTESIAN_POINT('Ctrl Pts',(6.34699373997078,605.483811155812,78.6794611067318));
#99170=CARTESIAN_POINT('Ctrl Pts',(6.29507802198154,605.504745800373,78.7022602318609));
#99171=CARTESIAN_POINT('Ctrl Pts',(6.24294708348502,605.525547606992,78.7248152334023));
#99172=CARTESIAN_POINT('Ctrl Pts',(5.9934113591915,605.625119838586,78.8327795019997));
#99173=CARTESIAN_POINT('Ctrl Pts',(5.73853110389339,605.721805612182,78.9353252138375));
#99174=CARTESIAN_POINT('Ctrl Pts',(5.48010053992522,605.814107611896,79.0314825681166));
#99175=CARTESIAN_POINT('Ctrl Pts',(5.31038406680991,605.874724164414,79.0946310083854));
#99176=CARTESIAN_POINT('Ctrl Pts',(5.13913733644966,605.933450239989,79.1550248358518));
#99177=CARTESIAN_POINT('Ctrl Pts',(4.96687438959262,605.989867757648,79.2123984530303));
#99178=CARTESIAN_POINT('Ctrl Pts',(4.93007196624935,606.001920850938,79.2246558083506));
#99179=CARTESIAN_POINT('Ctrl Pts',(4.89321390536558,606.013874408525,79.2367829629027));
#99180=CARTESIAN_POINT('Ctrl Pts',(4.85630009928057,606.02572615544,79.2487791179175));
#99181=CARTESIAN_POINT('Ctrl Pts',(4.25499476199429,606.218784510348,79.4441898003244));
#99182=CARTESIAN_POINT('Ctrl Pts',(3.63825269281664,606.385103343078,79.6050498204426));
#99183=CARTESIAN_POINT('Ctrl Pts',(3.00303825816605,606.515495744393,79.7285331847965));
#99184=CARTESIAN_POINT('Ctrl Pts',(2.6393277264934,606.590155712778,79.7992371827726));
#99185=CARTESIAN_POINT('Ctrl Pts',(2.26956149135921,606.6530382001,79.8576872889477));
#99186=CARTESIAN_POINT('Ctrl Pts',(1.89317385967764,606.70242510632,79.9033533194805));
#99187=CARTESIAN_POINT('',(-7.31873414160669E-15,608.476132031997,48.5811677441054));
#99188=CARTESIAN_POINT('',(1.92493735523237E-15,1218.57245358804,48.5811677441054));
#99189=CARTESIAN_POINT('Ctrl Pts',(3.93978362444746,607.874843764614,49.082928510463));
#99190=CARTESIAN_POINT('Ctrl Pts',(3.62591964374305,607.968397240746,49.0016645885587));
#99191=CARTESIAN_POINT('Ctrl Pts',(3.30579924060091,608.053570299406,48.9292260493855));
#99192=CARTESIAN_POINT('Ctrl Pts',(2.66144129984969,608.201953140762,48.8046503202028));
#99193=CARTESIAN_POINT('Ctrl Pts',(2.3359974548026,608.265536826742,48.7521822712622));
#99194=CARTESIAN_POINT('Ctrl Pts',(1.67806442767431,608.369017250152,48.6674791187011));
#99195=CARTESIAN_POINT('Ctrl Pts',(1.34557472886657,608.408910004209,48.6352427984729));
#99196=CARTESIAN_POINT('Ctrl Pts',(0.672995467599795,608.462621079598,48.5919666363597));
#99197=CARTESIAN_POINT('Ctrl Pts',(0.334567964264235,608.476132031997,48.5811677441054));
#99198=CARTESIAN_POINT('Ctrl Pts',(-7.31873414160669E-15,608.476132031997,
48.5811677441054));
#99199=CARTESIAN_POINT('Ctrl Pts',(-7.31873414160669E-15,608.476132031997,
48.5811677441054));
#99200=CARTESIAN_POINT('Ctrl Pts',(-1.00038541833525,608.476132031997,48.5811677441054));
#99201=CARTESIAN_POINT('Ctrl Pts',(-1.98186107540155,608.355804039834,48.6756960232106));
#99202=CARTESIAN_POINT('Ctrl Pts',(-3.18805636841628,608.0812830782,48.9059115645402));
#99203=CARTESIAN_POINT('Ctrl Pts',(-3.42854858272458,608.0201047022,48.9577280742447));
#99204=CARTESIAN_POINT('Ctrl Pts',(-3.9008061116148,607.88835111953,49.0709538770827));
#99205=CARTESIAN_POINT('Ctrl Pts',(-4.13345843873349,607.817596758595,49.1325121211066));
#99206=CARTESIAN_POINT('Ctrl Pts',(-4.82191402968074,607.59267130225,49.3314235132617));
#99207=CARTESIAN_POINT('Ctrl Pts',(-5.26825798195031,607.4259010746,49.4829579943547));
#99208=CARTESIAN_POINT('Ctrl Pts',(-6.13948585279377,607.067521867576,49.8222366173663));
#99209=CARTESIAN_POINT('Ctrl Pts',(-6.56545659234339,606.875360414686,50.0105449985554));
#99210=CARTESIAN_POINT('Ctrl Pts',(-7.39359379433368,606.47552949295,50.4209480281591));
#99211=CARTESIAN_POINT('Ctrl Pts',(-7.79284032142572,606.269378077533,50.6414529752954));
#99212=CARTESIAN_POINT('Ctrl Pts',(-8.95204291419482,605.641124055901,51.3478306146848));
#99213=CARTESIAN_POINT('Ctrl Pts',(-9.6739937385886,605.209537903166,51.8780902826517));
#99214=CARTESIAN_POINT('Ctrl Pts',(-10.6909797044834,604.568043191503,52.7681666459264));
#99215=CARTESIAN_POINT('Ctrl Pts',(-11.018834746685,604.355085789127,53.0807607042935));
#99216=CARTESIAN_POINT('Ctrl Pts',(-11.6523858512663,603.934348995513,53.7403002029845));
#99217=CARTESIAN_POINT('Ctrl Pts',(-11.9552766171641,603.728415571992,54.0845026139995));
#99218=CARTESIAN_POINT('Ctrl Pts',(-12.8157642528714,603.133398024851,55.1530076404017));
#99219=CARTESIAN_POINT('Ctrl Pts',(-13.3290592983858,602.764738088077,55.9162808887406));
#99220=CARTESIAN_POINT('Ctrl Pts',(-14.004746121757,602.270400060673,57.1474541420456));
#99221=CARTESIAN_POINT('Ctrl Pts',(-14.2141395881851,602.115412268844,57.5723098240839));
#99222=CARTESIAN_POINT('Ctrl Pts',(-14.5988681163382,601.828423328471,58.4540012253265));
#99223=CARTESIAN_POINT('Ctrl Pts',(-14.774314469106,601.696323764207,58.9121779826557));
#99224=CARTESIAN_POINT('Ctrl Pts',(-15.2329469259702,601.34910589721,60.3025784912361));
#99225=CARTESIAN_POINT('Ctrl Pts',(-15.4543798168271,601.178811145537,61.2611681259982));
#99226=CARTESIAN_POINT('Ctrl Pts',(-15.6499076381601,601.02822212081,62.7513958204655));
#99227=CARTESIAN_POINT('Ctrl Pts',(-15.6916676668363,600.995953718117,63.2567226635694));
#99228=CARTESIAN_POINT('Ctrl Pts',(-15.7262198238666,600.969261205682,64.2573462892223));
#99229=CARTESIAN_POINT('Ctrl Pts',(-15.7195678789232,600.974407590695,64.7561248933746));
#99230=CARTESIAN_POINT('Ctrl Pts',(-15.6590995589811,601.021098663315,65.7506616225585));
#99231=CARTESIAN_POINT('Ctrl Pts',(-15.6052831790191,601.062644377796,66.2464197156399));
#99232=CARTESIAN_POINT('Ctrl Pts',(-15.4498800061554,601.182160079324,67.2348902714699));
#99233=CARTESIAN_POINT('Ctrl Pts',(-15.3482435235833,601.260162049379,67.7257307925787));
#99234=CARTESIAN_POINT('Ctrl Pts',(-14.9812478047689,601.540233943488,69.1572522104259));
#99235=CARTESIAN_POINT('Ctrl Pts',(-14.6526793160863,601.789458207514,70.0696014607015));
#99236=CARTESIAN_POINT('Ctrl Pts',(-13.8372960983329,602.394765535271,71.8177596455625));
#99237=CARTESIAN_POINT('Ctrl Pts',(-13.3616578586644,602.742527172046,72.6296038086577));
#99238=CARTESIAN_POINT('Ctrl Pts',(-12.2895634342419,603.50114039407,74.1428267938299));
#99239=CARTESIAN_POINT('Ctrl Pts',(-11.6877930740782,603.915615183279,74.8486713035806));
#99240=CARTESIAN_POINT('Ctrl Pts',(-10.3949373649157,604.761836407664,76.1246737064291));
#99241=CARTESIAN_POINT('Ctrl Pts',(-9.70188800092167,605.195554364056,76.6994753988773));
#99242=CARTESIAN_POINT('Ctrl Pts',(-8.58467388731213,605.839463452404,77.4742190882292));
#99243=CARTESIAN_POINT('Ctrl Pts',(-8.19773601749983,606.05368580674,77.7185803584321));
#99244=CARTESIAN_POINT('Ctrl Pts',(-7.40176600282271,606.47083721012,78.1735199632814));
#99245=CARTESIAN_POINT('Ctrl Pts',(-6.99390219741844,606.673234514064,78.3836222033658));
#99246=CARTESIAN_POINT('Ctrl Pts',(-5.73705816174997,607.252779638758,78.9624303035971));
#99247=CARTESIAN_POINT('Ctrl Pts',(-4.8557807881079,607.603554702388,79.2806298462149));
#99248=CARTESIAN_POINT('Ctrl Pts',(-3.91253447320281,607.88294039512,79.5230488432747));
#99249=CARTESIAN_POINT('Ctrl Pts',(-1.91941230150446,606.698958856847,48.698800681464));
#99250=CARTESIAN_POINT('Ctrl Pts',(-1.77856148952992,606.717691793978,48.6814712512444));
#99251=CARTESIAN_POINT('Ctrl Pts',(-1.63703421267371,606.734446862159,48.6660258498612));
#99252=CARTESIAN_POINT('Ctrl Pts',(-1.49482298761707,606.749197548788,48.6524629893762));
#99253=CARTESIAN_POINT('Ctrl Pts',(-1.47848330594896,606.750892362428,48.6509046537192));
#99254=CARTESIAN_POINT('Ctrl Pts',(-1.4621345691852,606.752560679373,48.6493712049886));
#99255=CARTESIAN_POINT('Ctrl Pts',(-1.44577674730114,606.754202430862,48.647862668289));
#99256=CARTESIAN_POINT('Ctrl Pts',(-1.30269956743955,606.76856236061,48.6346679301252));
#99257=CARTESIAN_POINT('Ctrl Pts',(-1.15892868452667,606.780892900214,48.6233762927986));
#99258=CARTESIAN_POINT('Ctrl Pts',(-1.01444129745525,606.791127273198,48.6140239791455));
#99259=CARTESIAN_POINT('Ctrl Pts',(-0.998637300191364,606.792246706568,
48.6130010252228));
#99260=CARTESIAN_POINT('Ctrl Pts',(-0.98282472172319,606.79334102437,48.6120013076366));
#99261=CARTESIAN_POINT('Ctrl Pts',(-0.967003526926913,606.79441011141,48.6110248994056));
#99262=CARTESIAN_POINT('Ctrl Pts',(-0.806537717335273,606.805253282208,
48.6011217195697));
#99263=CARTESIAN_POINT('Ctrl Pts',(-0.645476066513777,606.813481813266,
48.5936338603989));
#99264=CARTESIAN_POINT('Ctrl Pts',(-0.484183920938916,606.818964448633,
48.588641220104));
#99265=CARTESIAN_POINT('Ctrl Pts',(-0.422615490343729,606.82105727996,48.586735429674));
#99266=CARTESIAN_POINT('Ctrl Pts',(-0.361005641426017,606.822749448665,
48.58519312428));
#99267=CARTESIAN_POINT('Ctrl Pts',(-0.29939725843297,606.824040854733,48.5840194145379));
#99268=CARTESIAN_POINT('Ctrl Pts',(-0.280307236559404,606.82444101083,48.5836557279167));
#99269=CARTESIAN_POINT('Ctrl Pts',(-0.261214851172684,606.824802746722,
48.5833273536881));
#99270=CARTESIAN_POINT('Ctrl Pts',(-0.242121350637935,606.825126404318,
48.5830342121591));
#99271=CARTESIAN_POINT('Ctrl Pts',(-0.161408243682281,606.826494587699,
48.5817950279905));
#99272=CARTESIAN_POINT('Ctrl Pts',(-0.0806852921308739,606.827159906852,
48.5811855692694));
#99273=CARTESIAN_POINT('Ctrl Pts',(-1.56438910714485E-8,606.827140852495,
48.5811983853012));
#99274=CARTESIAN_POINT('Ctrl Pts',(-19.6604693917099,639.614613618721,62.5660159449655));
#99275=CARTESIAN_POINT('Ctrl Pts',(-19.6043473940929,640.042864396936,62.5045768852686));
#99276=CARTESIAN_POINT('Ctrl Pts',(-19.1902534503917,640.029230307342,62.3679625261942));
#99277=CARTESIAN_POINT('Ctrl Pts',(-19.5362970273361,639.656420566866,62.9361067570152));
#99278=CARTESIAN_POINT('Ctrl Pts',(-19.4739947450425,640.077793049794,62.8838115245112));
#99279=CARTESIAN_POINT('Ctrl Pts',(-19.0563824034601,640.070385553537,62.780340451598));
#99280=CARTESIAN_POINT('Ctrl Pts',(-19.4529721346903,639.685402500002,63.3126278577785));
#99281=CARTESIAN_POINT('Ctrl Pts',(-19.3848517001577,640.102600286318,63.2753840449119));
#99282=CARTESIAN_POINT('Ctrl Pts',(-18.9665644890546,640.098956603779,63.199877359281));
#99283=CARTESIAN_POINT('Ctrl Pts',(-19.3883804561941,639.707874785332,63.8868784008059));
#99284=CARTESIAN_POINT('Ctrl Pts',(-19.3163013556422,640.121692201212,63.8713399627084));
#99285=CARTESIAN_POINT('Ctrl Pts',(-18.8969388964883,640.121110791056,63.8397379568555));
#99286=CARTESIAN_POINT('Ctrl Pts',(-19.3769841736612,639.711863719473,64.0798899164937));
#99287=CARTESIAN_POINT('Ctrl Pts',(-19.3041878248497,640.12508992708,64.0717390566854));
#99288=CARTESIAN_POINT('Ctrl Pts',(-18.8846548024122,640.125044298213,64.0548016868818));
#99289=CARTESIAN_POINT('Ctrl Pts',(-19.375186673142,639.71249178762,64.4692203034188));
#99290=CARTESIAN_POINT('Ctrl Pts',(-19.3022819370354,640.125623427249,64.4755024746936));
#99291=CARTESIAN_POINT('Ctrl Pts',(-18.8827172550505,640.125663592786,64.4886143790017));
#99292=CARTESIAN_POINT('Ctrl Pts',(-19.3849840685433,639.709061256727,64.6658272951823));
#99293=CARTESIAN_POINT('Ctrl Pts',(-19.3126965606472,640.12270098294,64.6796458141313));
#99294=CARTESIAN_POINT('Ctrl Pts',(-18.8932778841669,640.122280676192,64.707684380311));
#99295=CARTESIAN_POINT('Ctrl Pts',(-19.4452767686435,639.688071722563,65.2450126378428));
#99296=CARTESIAN_POINT('Ctrl Pts',(-19.3766820633375,640.104867502093,65.2807205567288));
#99297=CARTESIAN_POINT('Ctrl Pts',(-18.9582692702832,640.101587693298,65.3530435950167));
#99298=CARTESIAN_POINT('Ctrl Pts',(-19.526131319747,639.65992314981,65.6222918010434));
#99299=CARTESIAN_POINT('Ctrl Pts',(-19.4631745914249,640.080771137981,65.6731048965284));
#99300=CARTESIAN_POINT('Ctrl Pts',(-19.0454249069794,640.073836781612,65.7734281706718));
#99301=CARTESIAN_POINT('Ctrl Pts',(-19.7068251736695,639.59897289078,66.1753917003921));
#99302=CARTESIAN_POINT('Ctrl Pts',(-19.6535908638706,640.029636059382,66.2421063751751));
#99303=CARTESIAN_POINT('Ctrl Pts',(-19.2402290736399,640.013832011843,66.3897215922081));
#99304=CARTESIAN_POINT('Ctrl Pts',(-19.7773500518966,639.575429358817,66.3580430271829));
#99305=CARTESIAN_POINT('Ctrl Pts',(-19.7282627805238,640.009830550918,66.4305066259489));
#99306=CARTESIAN_POINT('Ctrl Pts',(-19.3162648045463,639.990664629944,66.5932414468988));
#99307=CARTESIAN_POINT('Ctrl Pts',(-19.9349482970738,639.523774305166,66.7110781169987));
#99308=CARTESIAN_POINT('Ctrl Pts',(-19.8945480523043,639.966662205344,66.7935682190135));
#99309=CARTESIAN_POINT('Ctrl Pts',(-19.4861918640954,639.939877906828,66.9866119824641));
#99310=CARTESIAN_POINT('Ctrl Pts',(-20.0222946068357,639.495568525969,66.8824893749696));
#99311=CARTESIAN_POINT('Ctrl Pts',(-19.9867696521186,639.943145147396,66.969541097156));
#99312=CARTESIAN_POINT('Ctrl Pts',(-19.5803774190672,639.912165675139,67.1776075526048));
#99313=CARTESIAN_POINT('Ctrl Pts',(-20.2134165147897,639.435245715633,67.2155869499658));
#99314=CARTESIAN_POINT('Ctrl Pts',(-20.1878269004917,639.893224462444,67.3103559506421));
#99315=CARTESIAN_POINT('Ctrl Pts',(-19.7864846440742,639.852963266996,67.5487626450847));
#99316=CARTESIAN_POINT('Ctrl Pts',(-20.3171936898167,639.403126937874,67.3772721460263));
#99317=CARTESIAN_POINT('Ctrl Pts',(-20.2970154844049,639.866746775558,67.47535656416));
#99318=CARTESIAN_POINT('Ctrl Pts',(-19.8984079972179,639.821471319271,67.7289209182822));
#99319=CARTESIAN_POINT('Ctrl Pts',(-20.5410431146462,639.33577623417,67.6911018289748));
#99320=CARTESIAN_POINT('Ctrl Pts',(-20.5315995437245,639.811706987032,67.7943468231785));
#99321=CARTESIAN_POINT('Ctrl Pts',(-20.1398571470931,639.755528739292,68.078606697025));
#99322=CARTESIAN_POINT('Ctrl Pts',(-20.66161879079,639.300409001074,67.8437149881379));
#99323=CARTESIAN_POINT('Ctrl Pts',(-20.6578743308502,639.782976975004,67.9488690872092));
#99324=CARTESIAN_POINT('Ctrl Pts',(-20.2699261878463,639.720946438105,68.2486564224931));
#99325=CARTESIAN_POINT('Ctrl Pts',(-21.0408663871178,639.192912656625,68.2791535667018));
#99326=CARTESIAN_POINT('Ctrl Pts',(-21.0562413302891,639.695892337362,68.3909401809132));
#99327=CARTESIAN_POINT('Ctrl Pts',(-20.6790881543741,639.616027662147,68.7338453225555));
#99328=CARTESIAN_POINT('Ctrl Pts',(-21.3184472555098,639.118885613595,68.5424636157139));
#99329=CARTESIAN_POINT('Ctrl Pts',(-21.345483233491,639.637322639742,68.6531058695304));
#99330=CARTESIAN_POINT('Ctrl Pts',(-20.9786322139011,639.544022285944,69.0272394297093));
#99331=CARTESIAN_POINT('Ctrl Pts',(-21.921761724668,638.973297071061,69.0180659887194));
#99332=CARTESIAN_POINT('Ctrl Pts',(-21.9667100270014,639.525213923758,69.1216530518533));
#99333=CARTESIAN_POINT('Ctrl Pts',(-21.6299071797506,639.403272217871,69.5571809714726));
#99334=CARTESIAN_POINT('Ctrl Pts',(-22.2494126434192,638.901508308394,69.2305907102972));
#99335=CARTESIAN_POINT('Ctrl Pts',(-22.3020685690074,639.471693284507,69.3264745684198));
#99336=CARTESIAN_POINT('Ctrl Pts',(-21.9837112677507,639.334322479089,69.7939873572225));
#99337=CARTESIAN_POINT('Ctrl Pts',(-22.9292469963058,638.772850945573,69.5887280397824));
#99338=CARTESIAN_POINT('Ctrl Pts',(-22.9897008093125,639.379125595584,69.667121205382));
#99339=CARTESIAN_POINT('Ctrl Pts',(-22.7181072739011,639.212144997237,70.1930430801067));
#99340=CARTESIAN_POINT('Ctrl Pts',(-23.2840893761466,638.715229200386,69.7368588847111));
#99341=CARTESIAN_POINT('Ctrl Pts',(-23.3447311905104,639.340004169329,69.8029639541895));
#99342=CARTESIAN_POINT('Ctrl Pts',(-23.1015678781488,639.158182199808,70.3580983729776));
#99343=CARTESIAN_POINT('Ctrl Pts',(-23.8400397081407,638.643801346691,69.9110832725672));
#99344=CARTESIAN_POINT('Ctrl Pts',(-23.8907379099241,639.294626550114,69.958336958928));
#99345=CARTESIAN_POINT('Ctrl Pts',(-23.7026318796329,639.093034350673,70.5522284812034));
#99346=CARTESIAN_POINT('Ctrl Pts',(-24.0301388274256,638.622452400188,69.9611880307775));
#99347=CARTESIAN_POINT('Ctrl Pts',(-24.0776195734464,639.281653485817,70.002165703523));
#99348=CARTESIAN_POINT('Ctrl Pts',(-23.9082019757128,639.073922036048,70.6080578768363));
#99349=CARTESIAN_POINT('Ctrl Pts',(-24.410372221457,638.58639745276,70.0426866143446));
#99350=CARTESIAN_POINT('Ctrl Pts',(-24.4496351039123,639.2609913659,70.0718111149744));
#99351=CARTESIAN_POINT('Ctrl Pts',(-24.3194774954357,639.042533755913,70.6988679476676));
#99352=CARTESIAN_POINT('Ctrl Pts',(-24.601335407632,638.571560050251,70.074414171567));
#99353=CARTESIAN_POINT('Ctrl Pts',(-24.6352021221028,639.253302178315,70.0976274626793));
#99354=CARTESIAN_POINT('Ctrl Pts',(-24.526078729531,639.030135030137,70.7342204849604));
#99355=CARTESIAN_POINT('Ctrl Pts',(-25.1767601479727,638.537133522905,70.1426665970483));
#99356=CARTESIAN_POINT('Ctrl Pts',(-25.1955539595057,639.23785273376,70.1500812974023));
#99357=CARTESIAN_POINT('Ctrl Pts',(-25.1487757592767,639.003355461779,70.8102709790819));
#99358=CARTESIAN_POINT('Ctrl Pts',(-25.563731151051,638.527630622351,70.1525518511399));
#99359=CARTESIAN_POINT('Ctrl Pts',(-25.5643966079534,639.238200260492,70.1503052553348));
#99360=CARTESIAN_POINT('Ctrl Pts',(-25.5677370210007,638.999391403185,70.8212856580984));
#99361=CARTESIAN_POINT('Ctrl Pts',(-26.3449430775709,638.538201511733,70.0952068196612));
#99362=CARTESIAN_POINT('Ctrl Pts',(-26.3101215344426,639.259956556377,70.0813790172625));
#99363=CARTESIAN_POINT('Ctrl Pts',(-26.4139660749482,639.022007969339,70.7573887616778));
#99364=CARTESIAN_POINT('Ctrl Pts',(-26.7282279181265,638.55827679445,70.0283683140306));
#99365=CARTESIAN_POINT('Ctrl Pts',(-26.6721307562498,639.281238556969,70.0125473081986));
#99366=CARTESIAN_POINT('Ctrl Pts',(-26.8293681462139,639.048425499655,70.6829137334035));
#99367=CARTESIAN_POINT('Ctrl Pts',(-27.2841361653692,638.607369964634,69.8731681263508));
#99368=CARTESIAN_POINT('Ctrl Pts',(-27.2028933885728,639.326706258709,69.8587349175253));
#99369=CARTESIAN_POINT('Ctrl Pts',(-27.4321510026923,639.107297343891,70.5099814025619));
#99370=CARTESIAN_POINT('Ctrl Pts',(-27.4667215187653,638.626901856262,69.8121804983067));
#99371=CARTESIAN_POINT('Ctrl Pts',(-27.3772534188525,639.344086126414,69.7991077552769));
#99372=CARTESIAN_POINT('Ctrl Pts',(-27.63018197883,639.130139927938,70.4420257333318));
#99373=CARTESIAN_POINT('Ctrl Pts',(-27.8263762321758,638.671746207838,69.6711847249545));
#99374=CARTESIAN_POINT('Ctrl Pts',(-27.7224215060154,639.383169440062,69.6618289971831));
#99375=CARTESIAN_POINT('Ctrl Pts',(-28.0203545837303,639.181690618376,70.2849207185056));
#99376=CARTESIAN_POINT('Ctrl Pts',(-28.0042122567427,638.697208341129,69.5906848480275));
#99377=CARTESIAN_POINT('Ctrl Pts',(-27.8935367666387,639.404934118318,69.5839425890701));
#99378=CARTESIAN_POINT('Ctrl Pts',(-28.2133287232379,639.210564262153,70.1952234599579));
#99379=CARTESIAN_POINT('Ctrl Pts',(-28.517678386789,638.779374195469,69.3254946573024));
#99380=CARTESIAN_POINT('Ctrl Pts',(-28.3889976863558,639.474465198322,69.3278776694702));
#99381=CARTESIAN_POINT('Ctrl Pts',(-28.7706297699789,639.302831299308,69.8997343998282));
#99382=CARTESIAN_POINT('Ctrl Pts',(-28.8368019609363,638.842144825035,69.1164244028433));
#99383=CARTESIAN_POINT('Ctrl Pts',(-28.7004074914826,639.526813318195,69.1267051815092));
#99384=CARTESIAN_POINT('Ctrl Pts',(-29.1171684630673,639.372219716366,69.6667771654812));
#99385=CARTESIAN_POINT('Ctrl Pts',(-29.2821652331234,638.942012522508,68.754787226998));
#99386=CARTESIAN_POINT('Ctrl Pts',(-29.1426111606792,639.611228165578,68.7725889580942));
#99387=CARTESIAN_POINT('Ctrl Pts',(-29.6009713712576,639.481679229375,69.2638217267234));
#99388=CARTESIAN_POINT('Ctrl Pts',(-29.4257458324037,638.976445684631,68.6254237801236));
#99389=CARTESIAN_POINT('Ctrl Pts',(-29.2853375079637,639.640235865451,68.6462428574156));
#99390=CARTESIAN_POINT('Ctrl Pts',(-29.7569772664138,639.519269640047,69.1196780709533));
#99391=CARTESIAN_POINT('Ctrl Pts',(-29.6975535013539,639.045172134778,68.3539257857801));
#99392=CARTESIAN_POINT('Ctrl Pts',(-29.5569080178443,639.698370750662,68.3797876371925));
#99393=CARTESIAN_POINT('Ctrl Pts',(-30.0523587091175,639.594075821366,68.8171605190338));
#99394=CARTESIAN_POINT('Ctrl Pts',(-29.8255815043549,639.079383885521,68.2121761101742));
#99395=CARTESIAN_POINT('Ctrl Pts',(-29.6856009206759,639.727412866963,68.2402497616682));
#99396=CARTESIAN_POINT('Ctrl Pts',(-30.1915174672224,639.631204693504,68.6592154660613));
#99397=CARTESIAN_POINT('Ctrl Pts',(-30.1870135856361,639.180024049103,67.7693531242958));
#99398=CARTESIAN_POINT('Ctrl Pts',(-30.0486031852443,639.812777163191,67.804557648681));
#99399=CARTESIAN_POINT('Ctrl Pts',(-30.5844318653539,639.740197922646,68.1657984662501));
#99400=CARTESIAN_POINT('Ctrl Pts',(-30.3980015252607,639.244468011042,67.4508867391265));
#99401=CARTESIAN_POINT('Ctrl Pts',(-30.2645436408508,639.868308369816,67.4876764108793));
#99402=CARTESIAN_POINT('Ctrl Pts',(-30.8138811498187,639.809683374485,67.8109462262171));
#99403=CARTESIAN_POINT('Ctrl Pts',(-30.7593869387953,639.360204041504,66.7653665317526));
#99404=CARTESIAN_POINT('Ctrl Pts',(-30.6352574879512,639.968523506671,66.8008921937396));
#99405=CARTESIAN_POINT('Ctrl Pts',(-31.206966008069,639.934210074654,67.047103030666));
#99406=CARTESIAN_POINT('Ctrl Pts',(-30.9041015064952,639.409625712735,66.4088790927884));
#99407=CARTESIAN_POINT('Ctrl Pts',(-30.7858111889449,640.01191089884,66.4409608338525));
#99408=CARTESIAN_POINT('Ctrl Pts',(-31.3644198481214,639.987241357622,66.6498843590981));
#99409=CARTESIAN_POINT('Ctrl Pts',(-31.0141476947143,639.44800149248,66.0405185693756));
#99410=CARTESIAN_POINT('Ctrl Pts',(-30.9005396207576,640.045728745606,66.0664164809275));
#99411=CARTESIAN_POINT('Ctrl Pts',(-31.484164369445,640.02838482468,66.2394387527513));
#99412=CARTESIAN_POINT('',(-31.0141476947143,639.44800149248,66.0405185693756));
#99413=CARTESIAN_POINT('',(-19.3760282912166,639.712197922296,64.2994740881845));
#99414=CARTESIAN_POINT('Ctrl Pts',(-31.0141476947143,639.44800149248,66.0405185693756));
#99415=CARTESIAN_POINT('Ctrl Pts',(-30.964172162317,639.430573810473,66.2078029936897));
#99416=CARTESIAN_POINT('Ctrl Pts',(-30.9070963674012,639.410889044142,66.3724853570777));
#99417=CARTESIAN_POINT('Ctrl Pts',(-30.8427717435498,639.389175714363,66.5345397812563));
#99418=CARTESIAN_POINT('Ctrl Pts',(-30.7784471196983,639.367462384584,66.6965942054349));
#99419=CARTESIAN_POINT('Ctrl Pts',(-30.7068738047457,639.343720218765,66.8560208760923));
#99420=CARTESIAN_POINT('Ctrl Pts',(-30.6278540796739,639.318163608302,67.0127761790815));
#99421=CARTESIAN_POINT('Ctrl Pts',(-30.6117724312023,639.312962471178,67.0446781336433));
#99422=CARTESIAN_POINT('Ctrl Pts',(-30.5953858009309,639.307687752954,67.0764620783354));
#99423=CARTESIAN_POINT('Ctrl Pts',(-30.5786931148851,639.302341438801,67.1081269277583));
#99424=CARTESIAN_POINT('Ctrl Pts',(-30.4687474822263,639.267128178916,67.3166860472013));
#99425=CARTESIAN_POINT('Ctrl Pts',(-30.3476320077173,639.229502304161,67.5161693060764));
#99426=CARTESIAN_POINT('Ctrl Pts',(-30.2153800827863,639.190321630889,67.7069108282264));
#99427=CARTESIAN_POINT('Ctrl Pts',(-30.1703849865028,639.17699147961,67.771805408467));
#99428=CARTESIAN_POINT('Ctrl Pts',(-30.1241004869899,639.163481279123,67.8356878427701));
#99429=CARTESIAN_POINT('Ctrl Pts',(-30.0765268382153,639.149824622943,67.8985704517844));
#99430=CARTESIAN_POINT('Ctrl Pts',(-30.0340673542078,639.137636056591,67.9546931836028));
#99431=CARTESIAN_POINT('Ctrl Pts',(-29.9905766274731,639.125330676828,68.0100248730267));
#99432=CARTESIAN_POINT('Ctrl Pts',(-29.9460581899746,639.112933745349,68.0645685899863));
#99433=CARTESIAN_POINT('Ctrl Pts',(-29.825600346812,639.079390168538,68.2121528016568));
#99434=CARTESIAN_POINT('Ctrl Pts',(-29.6975577157899,639.045173518059,68.3539215227992));
#99435=CARTESIAN_POINT('Ctrl Pts',(-29.5616496471025,639.010809002831,68.4896747861607));
#99436=CARTESIAN_POINT('Ctrl Pts',(-29.5009767263279,638.995467783358,68.550278597784));
#99437=CARTESIAN_POINT('Ctrl Pts',(-29.4387762621089,638.980113378838,68.6096070566503));
#99438=CARTESIAN_POINT('Ctrl Pts',(-29.3753030064446,638.964854823256,68.6674399705206));
#99439=CARTESIAN_POINT('Ctrl Pts',(-29.2965613930307,638.945925854318,68.7391844698206));
#99440=CARTESIAN_POINT('Ctrl Pts',(-29.2158764789106,638.927149530007,68.8086138167981));
#99441=CARTESIAN_POINT('Ctrl Pts',(-29.1337101377013,638.908726592018,68.875333021914));
#99442=CARTESIAN_POINT('Ctrl Pts',(-28.9858011108829,638.875563148338,68.9954353966035));
#99443=CARTESIAN_POINT('Ctrl Pts',(-28.8324181716989,638.84335373522,69.1075648843374));
#99444=CARTESIAN_POINT('Ctrl Pts',(-28.6733382516838,638.812589007746,69.2117599847112));
#99445=CARTESIAN_POINT('Ctrl Pts',(-28.6310104190001,638.804403158539,69.2394841171767));
#99446=CARTESIAN_POINT('Ctrl Pts',(-28.5882790861707,638.796319628859,69.2666462816184));
#99447=CARTESIAN_POINT('Ctrl Pts',(-28.5451396868815,638.788347763513,69.2932467040797));
#99448=CARTESIAN_POINT('Ctrl Pts',(-28.4250134433244,638.766149256951,69.3673184083678));
#99449=CARTESIAN_POINT('Ctrl Pts',(-28.3017294042537,638.744824138075,69.4370253915424));
#99450=CARTESIAN_POINT('Ctrl Pts',(-28.1753668997168,638.72460142226,69.5022880910652));
#99451=CARTESIAN_POINT('Ctrl Pts',(-28.1463954434268,638.719964908213,69.5172510379736));
#99452=CARTESIAN_POINT('Ctrl Pts',(-28.1172369493377,638.715384248088,69.5319854519995));
#99453=CARTESIAN_POINT('Ctrl Pts',(-28.0879158996004,638.710864993133,69.54648058979));
#99454=CARTESIAN_POINT('Ctrl Pts',(-27.9760916405646,638.693629514143,69.6017619681025));
#99455=CARTESIAN_POINT('Ctrl Pts',(-27.861674530411,638.677255876872,69.6536712213467));
#99456=CARTESIAN_POINT('Ctrl Pts',(-27.7460960223066,638.662070518278,69.7015521321279));
#99457=CARTESIAN_POINT('Ctrl Pts',(-27.7129974149808,638.657721835902,69.7152639500977));
#99458=CARTESIAN_POINT('Ctrl Pts',(-27.6798037327096,638.653470532345,69.7286456758798));
#99459=CARTESIAN_POINT('Ctrl Pts',(-27.6465488703812,638.649324069762,69.7416826110321));
#99460=CARTESIAN_POINT('Ctrl Pts',(-27.6326745277465,638.647594113943,69.7471217827063));
#99461=CARTESIAN_POINT('Ctrl Pts',(-27.6187849721134,638.645881515037,69.7525038695469));
#99462=CARTESIAN_POINT('Ctrl Pts',(-27.6048805343477,638.644186425559,69.7578289051375));
#99463=CARTESIAN_POINT('Ctrl Pts',(-27.4384561734201,638.623897638069,69.8215650777181));
#99464=CARTESIAN_POINT('Ctrl Pts',(-27.2697521412095,638.606099695926,69.8771839024021));
#99465=CARTESIAN_POINT('Ctrl Pts',(-27.0988334158908,638.591005578511,69.9249015221625));
#99466=CARTESIAN_POINT('Ctrl Pts',(-26.9337006291902,638.576422426976,69.971003805637));
#99467=CARTESIAN_POINT('Ctrl Pts',(-26.7661415228627,638.564359870537,70.0098078169358));
#99468=CARTESIAN_POINT('Ctrl Pts',(-26.5966620479512,638.554998549506,70.041199579679));
#99469=CARTESIAN_POINT('Ctrl Pts',(-26.461079942878,638.547509574145,70.0663127166939));
#99470=CARTESIAN_POINT('Ctrl Pts',(-26.3239827419714,638.541734850019,70.0867314754902));
#99471=CARTESIAN_POINT('Ctrl Pts',(-26.1857776575908,638.537787923926,70.1023345303239));
#99472=CARTESIAN_POINT('Ctrl Pts',(-26.1089490305539,638.535593815699,70.1110083159942));
#99473=CARTESIAN_POINT('Ctrl Pts',(-26.0317783136576,638.533964259481,70.1181947427061));
#99474=CARTESIAN_POINT('Ctrl Pts',(-25.9543371050814,638.532916410857,70.1238793316371));
#99475=CARTESIAN_POINT('Ctrl Pts',(-25.8167125789174,638.531054228265,70.133981690219));
#99476=CARTESIAN_POINT('Ctrl Pts',(-25.6795944555712,638.531029990121,70.1392897137754));
#99477=CARTESIAN_POINT('Ctrl Pts',(-25.5431350324273,638.532774282377,70.139953710851));
#99478=CARTESIAN_POINT('Ctrl Pts',(-25.2914954588901,638.535990864635,70.1411781623186));
#99479=CARTESIAN_POINT('Ctrl Pts',(-25.0415283182023,638.54522420148,70.1266264453647));
#99480=CARTESIAN_POINT('Ctrl Pts',(-24.7931436546858,638.560084548181,70.0971649802425));
#99481=CARTESIAN_POINT('Ctrl Pts',(-24.6947005333332,638.565974198906,70.0854884195998));
#99482=CARTESIAN_POINT('Ctrl Pts',(-24.5965076945556,638.57274775555,70.0714505616851));
#99483=CARTESIAN_POINT('Ctrl Pts',(-24.4985645019917,638.580380570782,70.0550492251778));
#99484=CARTESIAN_POINT('Ctrl Pts',(-24.4055700369588,638.587627726511,70.0394765909354));
#99485=CARTESIAN_POINT('Ctrl Pts',(-24.3128009675369,638.595649471429,70.0217733564026));
#99486=CARTESIAN_POINT('Ctrl Pts',(-24.2202555268896,638.604424965257,70.0019373245855));
#99487=CARTESIAN_POINT('Ctrl Pts',(-24.0300461694498,638.622461305359,69.961168175509));
#99488=CARTESIAN_POINT('Ctrl Pts',(-23.8399539788754,638.643812726827,69.9110564175541));
#99489=CARTESIAN_POINT('Ctrl Pts',(-23.6547230176572,638.667611720096,69.8530085660251));
#99490=CARTESIAN_POINT('Ctrl Pts',(-23.5956647900816,638.675199686769,69.83450084354));
#99491=CARTESIAN_POINT('Ctrl Pts',(-23.5370157634051,638.683040624755,69.815183697452));
#99492=CARTESIAN_POINT('Ctrl Pts',(-23.4787716692218,638.691121070468,69.7950618652513));
#99493=CARTESIAN_POINT('Ctrl Pts',(-23.2954816375586,638.716549659775,69.7317398870677));
#99494=CARTESIAN_POINT('Ctrl Pts',(-23.1161090862269,638.744363790947,69.6604122975168));
#99495=CARTESIAN_POINT('Ctrl Pts',(-22.9406726614924,638.77412321845,69.5812766910076));
#99496=CARTESIAN_POINT('Ctrl Pts',(-22.8217503042241,638.794296117407,69.5276333675976));
#99497=CARTESIAN_POINT('Ctrl Pts',(-22.7046361153286,638.81536258406,69.4704032346877));
#99498=CARTESIAN_POINT('Ctrl Pts',(-22.5893301219767,638.837183127349,69.4096598760731));
#99499=CARTESIAN_POINT('Ctrl Pts',(-22.5686659162834,638.841093628284,69.398773943604));
#99500=CARTESIAN_POINT('Ctrl Pts',(-22.5480499464903,638.845031127836,69.3877658954824));
#99501=CARTESIAN_POINT('Ctrl Pts',(-22.5274854821768,638.848994107946,69.3766377974433));
#99502=CARTESIAN_POINT('Ctrl Pts',(-22.367532149233,638.879818731788,69.2900818656407));
#99503=CARTESIAN_POINT('Ctrl Pts',(-22.210359426731,638.912253152739,69.1960767963424));
#99504=CARTESIAN_POINT('Ctrl Pts',(-22.0575602488078,638.945591200531,69.0955440329588));
#99505=CARTESIAN_POINT('Ctrl Pts',(-21.9193885106254,638.975737802585,69.0046352541957));
#99506=CARTESIAN_POINT('Ctrl Pts',(-21.7847938371326,639.006622687079,68.9083899705106));
#99507=CARTESIAN_POINT('Ctrl Pts',(-21.6549354488148,639.037718739692,68.8075207260076));
#99508=CARTESIAN_POINT('Ctrl Pts',(-21.643287802225,639.040507899759,68.7984732603261));
#99509=CARTESIAN_POINT('Ctrl Pts',(-21.6316772250658,639.043298999767,68.7893878199803));
#99510=CARTESIAN_POINT('Ctrl Pts',(-21.6201045092409,639.046091673901,68.7802648661229));
#99511=CARTESIAN_POINT('Ctrl Pts',(-21.3855062639945,639.102703834884,68.5953273805063));
#99512=CARTESIAN_POINT('Ctrl Pts',(-21.1653101456083,639.160101323533,68.3948305812084));
#99513=CARTESIAN_POINT('Ctrl Pts',(-20.9599503527233,639.216574790309,68.1780943251773));
#99514=CARTESIAN_POINT('Ctrl Pts',(-20.9375987588717,639.222721426781,68.1545045041142));
#99515=CARTESIAN_POINT('Ctrl Pts',(-20.9154228865181,639.228857107169,68.1307223393094));
#99516=CARTESIAN_POINT('Ctrl Pts',(-20.8934232692971,639.234979621408,68.1067469800065));
#99517=CARTESIAN_POINT('Ctrl Pts',(-20.8578334961279,639.244884288876,68.0679609597466));
#99518=CARTESIAN_POINT('Ctrl Pts',(-20.8227033851914,639.254754601208,68.0286675090153));
#99519=CARTESIAN_POINT('Ctrl Pts',(-20.7880346630825,639.264581421708,67.9888621558238));
#99520=CARTESIAN_POINT('Ctrl Pts',(-20.6616762743501,639.300397602092,67.8437820955777));
#99521=CARTESIAN_POINT('Ctrl Pts',(-20.5410984570128,639.335762387801,67.6911801290186));
#99522=CARTESIAN_POINT('Ctrl Pts',(-20.4291183567793,639.369452958869,67.534187278599));
#99523=CARTESIAN_POINT('Ctrl Pts',(-20.3697325502214,639.387319898906,67.4509301014172));
#99524=CARTESIAN_POINT('Ctrl Pts',(-20.3126235691871,639.40475389604,67.366306414107));
#99525=CARTESIAN_POINT('Ctrl Pts',(-20.2578038594729,639.421695203221,67.2802970661521));
#99526=CARTESIAN_POINT('Ctrl Pts',(-20.2093649909189,639.436664595726,67.2042989347917));
#99527=CARTESIAN_POINT('Ctrl Pts',(-20.1627111642279,639.451249581901,67.1272149272915));
#99528=CARTESIAN_POINT('Ctrl Pts',(-20.1178555439554,639.465407366224,67.0490382112228));
#99529=CARTESIAN_POINT('Ctrl Pts',(-20.0223407470047,639.495554712012,66.8825700380885));
#99530=CARTESIAN_POINT('Ctrl Pts',(-19.9349790005985,639.523766588609,66.7111477600417));
#99531=CARTESIAN_POINT('Ctrl Pts',(-19.8561484137327,639.549609228609,66.5345618643413));
#99532=CARTESIAN_POINT('Ctrl Pts',(-19.8294237927332,639.558370228458,66.4746968890304));
#99533=CARTESIAN_POINT('Ctrl Pts',(-19.8036481144562,639.566869796379,66.414120338036));
#99534=CARTESIAN_POINT('Ctrl Pts',(-19.7789014749039,639.575070818021,66.3530062062367));
#99535=CARTESIAN_POINT('Ctrl Pts',(-19.7307143056419,639.591040017278,66.2340035025727));
#99536=CARTESIAN_POINT('Ctrl Pts',(-19.6864044881282,639.605878387103,66.1128942179124));
#99537=CARTESIAN_POINT('Ctrl Pts',(-19.646591826502,639.619305133542,65.9910272445652));
#99538=CARTESIAN_POINT('Ctrl Pts',(-19.5982725234243,639.635600729064,65.8431213528264));
#99539=CARTESIAN_POINT('Ctrl Pts',(-19.5563270690099,639.64988432506,65.6938288756537));
#99540=CARTESIAN_POINT('Ctrl Pts',(-19.5208462578372,639.662045684834,65.5432736384627));
#99541=CARTESIAN_POINT('Ctrl Pts',(-19.505465144989,639.667317696405,65.4780071742364));
#99542=CARTESIAN_POINT('Ctrl Pts',(-19.4912982950981,639.672191081517,65.4125035254526));
#99543=CARTESIAN_POINT('Ctrl Pts',(-19.4783502595523,639.676657814842,65.3467733418589));
#99544=CARTESIAN_POINT('Ctrl Pts',(-19.460100437904,639.682953525589,65.2541288535699));
#99545=CARTESIAN_POINT('Ctrl Pts',(-19.4443099666198,639.688427265665,65.1612494229568));
#99546=CARTESIAN_POINT('Ctrl Pts',(-19.4309280055641,639.693076648407,65.0679022967298));
#99547=CARTESIAN_POINT('Ctrl Pts',(-19.420981995495,639.696532256099,64.9985229693267));
#99548=CARTESIAN_POINT('Ctrl Pts',(-19.4123674445347,639.699532175518,64.9288850734574));
#99549=CARTESIAN_POINT('Ctrl Pts',(-19.4050808070072,639.702069575624,64.8588893165577));
#99550=CARTESIAN_POINT('Ctrl Pts',(-19.3955152473809,639.70540055674,64.767002134893));
#99551=CARTESIAN_POINT('Ctrl Pts',(-19.3882670280903,639.707928940124,64.6741951541139));
#99552=CARTESIAN_POINT('Ctrl Pts',(-19.3833968487432,639.709628527129,64.5808344913998));
#99553=CARTESIAN_POINT('Ctrl Pts',(-19.3787769857904,639.711240759139,64.4922723592536));
#99554=CARTESIAN_POINT('Ctrl Pts',(-19.3762971925334,639.71210714373,64.4032105488006));
#99555=CARTESIAN_POINT('Ctrl Pts',(-19.3760492768828,639.712191230638,64.3139797755864));
#99556=CARTESIAN_POINT('Ctrl Pts',(-19.3760358441571,639.712195786689,64.3091450162767));
#99557=CARTESIAN_POINT('Ctrl Pts',(-19.3760289735364,639.712198042607,64.3043097686405));
#99558=CARTESIAN_POINT('Ctrl Pts',(-19.3760286830353,639.712197991384,64.2994740881603));
#99559=CARTESIAN_POINT('',(-31.4841643694399,640.028384824678,66.2394387527688));
#99560=CARTESIAN_POINT('Origin',(-31.4841643694399,639.530878113616,66.1895681958392));
#99561=CARTESIAN_POINT('',(-19.1902534503917,640.029230307342,62.3679625261942));
#99562=CARTESIAN_POINT('Ctrl Pts',(-19.1902534503917,640.029230307342,62.3679625261942));
#99563=CARTESIAN_POINT('Ctrl Pts',(-19.0661541944461,640.067381465102,62.7502393133262));
#99564=CARTESIAN_POINT('Ctrl Pts',(-18.9797925330106,640.094758237498,63.1390436335595));
#99565=CARTESIAN_POINT('Ctrl Pts',(-18.9308583517509,640.110319951076,63.5343769526662));
#99566=CARTESIAN_POINT('Ctrl Pts',(-18.9275335472574,640.111377282656,63.5612376451706));
#99567=CARTESIAN_POINT('Ctrl Pts',(-18.9243815405164,640.112380060573,63.5881284854448));
#99568=CARTESIAN_POINT('Ctrl Pts',(-18.9214022412361,640.113327953849,63.615049477024));
#99569=CARTESIAN_POINT('Ctrl Pts',(-18.9209816912288,640.113461755957,63.6188495729999));
#99570=CARTESIAN_POINT('Ctrl Pts',(-18.920564586754,640.113594463482,63.6226502418285));
#99571=CARTESIAN_POINT('Ctrl Pts',(-18.9201509276431,640.113726075471,63.6264514814598));
#99572=CARTESIAN_POINT('Ctrl Pts',(-18.902553802402,640.119324870691,63.7881568279721));
#99573=CARTESIAN_POINT('Ctrl Pts',(-18.8912383129095,640.122939359055,63.9509059522893));
#99574=CARTESIAN_POINT('Ctrl Pts',(-18.8863728855358,640.12449505208,64.1145722906471));
#99575=CARTESIAN_POINT('Ctrl Pts',(-18.8848185279603,640.124992049168,64.1668587586874));
#99576=CARTESIAN_POINT('Ctrl Pts',(-18.8839220986039,640.125279042398,64.219238776882));
#99577=CARTESIAN_POINT('Ctrl Pts',(-18.8836880253474,640.125353945508,64.2717080420946));
#99578=CARTESIAN_POINT('Ctrl Pts',(-18.88301708418,640.125568645732,64.4221045058983));
#99579=CARTESIAN_POINT('Ctrl Pts',(-18.8878933700143,640.124007040391,64.5733859358451));
#99580=CARTESIAN_POINT('Ctrl Pts',(-18.8981256828954,640.120744141073,64.7234029230822));
#99581=CARTESIAN_POINT('Ctrl Pts',(-18.9021353453646,640.119465532308,64.7821889952511));
#99582=CARTESIAN_POINT('Ctrl Pts',(-18.906967113598,640.117925787138,64.8407812737556));
#99583=CARTESIAN_POINT('Ctrl Pts',(-18.9126081755515,640.116129824278,64.8990522739188));
#99584=CARTESIAN_POINT('Ctrl Pts',(-18.9133750559051,640.115885670138,64.9069739889396));
#99585=CARTESIAN_POINT('Ctrl Pts',(-18.9141569982845,640.115636744668,64.9148909499626));
#99586=CARTESIAN_POINT('Ctrl Pts',(-18.9149539843053,640.115383055814,64.9228028479913));
#99587=CARTESIAN_POINT('Ctrl Pts',(-18.9390529021059,640.107712122208,65.1620393907661));
#99588=CARTESIAN_POINT('Ctrl Pts',(-18.9767296895114,640.095716478747,65.3984843576705));
#99589=CARTESIAN_POINT('Ctrl Pts',(-19.0278441371165,640.0796734569,65.6320777987911));
#99590=CARTESIAN_POINT('Ctrl Pts',(-19.0657431118152,640.067778305773,65.8052764212864));
#99591=CARTESIAN_POINT('Ctrl Pts',(-19.1110284495377,640.053658493531,65.9769076528193));
#99592=CARTESIAN_POINT('Ctrl Pts',(-19.1636259297164,640.037432831445,66.1469510602767));
#99593=CARTESIAN_POINT('Ctrl Pts',(-19.1674780851709,640.036244489865,66.1594047678937));
#99594=CARTESIAN_POINT('Ctrl Pts',(-19.1713696911087,640.035044796896,66.1718505666322));
#99595=CARTESIAN_POINT('Ctrl Pts',(-19.1753007143207,640.033833800824,66.1842884067607));
#99596=CARTESIAN_POINT('Ctrl Pts',(-19.2285496458958,640.017429866411,66.3527691463099));
#99597=CARTESIAN_POINT('Ctrl Pts',(-19.289319827394,639.998881530564,66.5201053281933));
#99598=CARTESIAN_POINT('Ctrl Pts',(-19.3563790031072,639.978718302077,66.6834337378297));
#99599=CARTESIAN_POINT('Ctrl Pts',(-19.3652569531254,639.976048896544,66.7050567512635));
#99600=CARTESIAN_POINT('Ctrl Pts',(-19.3742450600393,639.97335120706,66.7266095305223));
#99601=CARTESIAN_POINT('Ctrl Pts',(-19.3833404036078,639.970626479297,66.7480854497941));
#99602=CARTESIAN_POINT('Ctrl Pts',(-19.389259711703,639.968853208943,66.7620621161881));
#99603=CARTESIAN_POINT('Ctrl Pts',(-19.3952253226528,639.967068178453,66.7760086572856));
#99604=CARTESIAN_POINT('Ctrl Pts',(-19.4012364653116,639.965271726116,66.7899231687001));
#99605=CARTESIAN_POINT('Ctrl Pts',(-19.4648946971272,639.94624722681,66.9372783794339));
#99606=CARTESIAN_POINT('Ctrl Pts',(-19.5338281275451,639.925888517147,67.0816821104859));
#99607=CARTESIAN_POINT('Ctrl Pts',(-19.6078620284061,639.904390307426,67.2230749934025));
#99608=CARTESIAN_POINT('Ctrl Pts',(-19.6247075204097,639.899498657578,67.2552471827756));
#99609=CARTESIAN_POINT('Ctrl Pts',(-19.6418168977857,639.894548065483,67.2872635875361));
#99610=CARTESIAN_POINT('Ctrl Pts',(-19.6591877821883,639.889540914653,67.3191236770128));
#99611=CARTESIAN_POINT('Ctrl Pts',(-19.6672132267431,639.887227583309,67.3338432143535));
#99612=CARTESIAN_POINT('Ctrl Pts',(-19.6752948262461,639.884902074872,67.3485300567643));
#99613=CARTESIAN_POINT('Ctrl Pts',(-19.6834324285052,639.882564594915,67.3631843223957));
#99614=CARTESIAN_POINT('Ctrl Pts',(-19.7776280083814,639.855507450449,67.5328125500803));
#99615=CARTESIAN_POINT('Ctrl Pts',(-19.8793287143073,639.826844553833,67.6980744824025));
#99616=CARTESIAN_POINT('Ctrl Pts',(-19.9885164512294,639.796882111454,67.8590274942721));
#99617=CARTESIAN_POINT('Ctrl Pts',(-19.998657149862,639.794099380472,67.8739758395112));
#99618=CARTESIAN_POINT('Ctrl Pts',(-20.0088629640138,639.791305313846,67.8888877085587));
#99619=CARTESIAN_POINT('Ctrl Pts',(-20.0191337952575,639.788500187125,67.9037629706155));
#99620=CARTESIAN_POINT('Ctrl Pts',(-20.1143609759211,639.762492135519,68.0416806555319));
#99621=CARTESIAN_POINT('Ctrl Pts',(-20.2155196510365,639.735450423221,68.1767756433179));
#99622=CARTESIAN_POINT('Ctrl Pts',(-20.3210516911105,639.707998172089,68.3071685062823));
#99623=CARTESIAN_POINT('Ctrl Pts',(-20.3372811768278,639.703776364974,68.3272212704061));
#99624=CARTESIAN_POINT('Ctrl Pts',(-20.3536140016895,639.69954486717,68.3471628573523));
#99625=CARTESIAN_POINT('Ctrl Pts',(-20.3700444059045,639.695305961865,68.3669864753928));
#99626=CARTESIAN_POINT('Ctrl Pts',(-20.3820839732001,639.692199855343,68.3815124590702));
#99627=CARTESIAN_POINT('Ctrl Pts',(-20.3941775547018,639.689089316829,68.3959772275318));
#99628=CARTESIAN_POINT('Ctrl Pts',(-20.4063230234607,639.685975213723,68.4103781892567));
#99629=CARTESIAN_POINT('Ctrl Pts',(-20.5574363591296,639.647229693296,68.5895542594672));
#99630=CARTESIAN_POINT('Ctrl Pts',(-20.717043795479,639.607778714808,68.7598361525156));
#99631=CARTESIAN_POINT('Ctrl Pts',(-20.8850330097057,639.568267584666,68.9213365607569));
#99632=CARTESIAN_POINT('Ctrl Pts',(-21.0058686124506,639.539847002738,69.0375047282385));
#99633=CARTESIAN_POINT('Ctrl Pts',(-21.1310402565699,639.511395652052,69.1491302172699));
#99634=CARTESIAN_POINT('Ctrl Pts',(-21.2604957797351,639.483157142327,69.2562674885842));
#99635=CARTESIAN_POINT('Ctrl Pts',(-21.2750353916501,639.479985574499,69.2683004579659));
#99636=CARTESIAN_POINT('Ctrl Pts',(-21.289629990286,639.476816511724,69.2802775120789));
#99637=CARTESIAN_POINT('Ctrl Pts',(-21.3042794741003,639.4736503114,69.2921986802951));
#99638=CARTESIAN_POINT('Ctrl Pts',(-21.4607808919954,639.43982558103,69.4195533197106));
#99639=CARTESIAN_POINT('Ctrl Pts',(-21.6240297334742,639.406279563647,69.5405878515707));
#99640=CARTESIAN_POINT('Ctrl Pts',(-21.7923110743027,639.373756834287,69.6541564729845));
#99641=CARTESIAN_POINT('Ctrl Pts',(-21.9591823739661,639.341506615159,69.766773494949));
#99642=CARTESIAN_POINT('Ctrl Pts',(-22.1310007280687,639.310263231699,69.8720483495535));
#99643=CARTESIAN_POINT('Ctrl Pts',(-22.3060525550972,639.280754274564,69.9688928418353));
#99644=CARTESIAN_POINT('Ctrl Pts',(-22.3209841823156,639.278237210018,69.9771535145827));
#99645=CARTESIAN_POINT('Ctrl Pts',(-22.3359409831016,639.275732443914,69.9853539171062));
#99646=CARTESIAN_POINT('Ctrl Pts',(-22.3509219295449,639.273240430825,69.9934933567789));
#99647=CARTESIAN_POINT('Ctrl Pts',(-22.5575543226994,639.238868061217,70.1057607562306));
#99648=CARTESIAN_POINT('Ctrl Pts',(-22.7696906147764,639.206689097186,70.207314951391));
#99649=CARTESIAN_POINT('Ctrl Pts',(-22.9874368158415,639.177355225063,70.2977872106618));
#99650=CARTESIAN_POINT('Ctrl Pts',(-23.1430911565897,639.156386112837,70.3624606690456));
#99651=CARTESIAN_POINT('Ctrl Pts',(-23.3016117153739,639.136870942413,70.4214721408255));
#99652=CARTESIAN_POINT('Ctrl Pts',(-23.4630294903487,639.119046867783,70.4747013867516));
#99653=CARTESIAN_POINT('Ctrl Pts',(-23.4760929938243,639.117604369514,70.4790092174058));
#99654=CARTESIAN_POINT('Ctrl Pts',(-23.4891763555709,639.11617285942,70.4832794429651));
#99655=CARTESIAN_POINT('Ctrl Pts',(-23.5022794848633,639.114752478456,70.4875119546639));
#99656=CARTESIAN_POINT('Ctrl Pts',(-23.6447432912411,639.099309382824,70.5335299488156));
#99657=CARTESIAN_POINT('Ctrl Pts',(-23.7900031744777,639.085168169529,70.5751004640745));
#99658=CARTESIAN_POINT('Ctrl Pts',(-23.9360313149344,639.072643530069,70.6116036338563));
#99659=CARTESIAN_POINT('Ctrl Pts',(-23.984047368707,639.068525256975,70.6236063763252));
#99660=CARTESIAN_POINT('Ctrl Pts',(-24.0321462796011,639.064581660107,70.6350616021584));
#99661=CARTESIAN_POINT('Ctrl Pts',(-24.0802556359924,639.060823572796,70.6459484087714));
#99662=CARTESIAN_POINT('Ctrl Pts',(-24.0914495259928,639.059949156277,70.6484815067969));
#99663=CARTESIAN_POINT('Ctrl Pts',(-24.1026450649215,639.059084673775,70.6509841478699));
#99664=CARTESIAN_POINT('Ctrl Pts',(-24.1138413856779,639.05823026425,70.6534560603949));
#99665=CARTESIAN_POINT('Ctrl Pts',(-24.2901636767411,639.044774822211,70.6923843198837));
#99666=CARTESIAN_POINT('Ctrl Pts',(-24.4673393093431,639.033728544892,70.7239610465782));
#99667=CARTESIAN_POINT('Ctrl Pts',(-24.6452243354155,639.025223969683,70.7481570845842));
#99668=CARTESIAN_POINT('Ctrl Pts',(-24.6658100213957,639.024239780521,70.7509571631032));
#99669=CARTESIAN_POINT('Ctrl Pts',(-24.6864051962316,639.0232896132,70.7536584516014));
#99670=CARTESIAN_POINT('Ctrl Pts',(-24.7070096277252,639.022373659332,70.7562609470984));
#99671=CARTESIAN_POINT('Ctrl Pts',(-24.7158860784374,639.021979063666,70.7573821099421));
#99672=CARTESIAN_POINT('Ctrl Pts',(-24.7247643877193,639.021590806335,70.7584849700153));
#99673=CARTESIAN_POINT('Ctrl Pts',(-24.7336445558265,639.021208901519,70.7595695302754));
#99674=CARTESIAN_POINT('Ctrl Pts',(-25.1448548055267,639.003524194108,70.8097918109785));
#99675=CARTESIAN_POINT('Ctrl Pts',(-25.5600221154403,638.999460434065,70.8210939230077));
#99676=CARTESIAN_POINT('Ctrl Pts',(-25.9794873808982,639.010400866811,70.7901814866191));
#99677=CARTESIAN_POINT('Ctrl Pts',(-25.9832750388911,639.010499655962,70.7899023556722));
#99678=CARTESIAN_POINT('Ctrl Pts',(-25.9870629997303,639.010599667727,70.7896197849193));
#99679=CARTESIAN_POINT('Ctrl Pts',(-25.9908512633906,639.010700903034,70.7893337721921));
#99680=CARTESIAN_POINT('Ctrl Pts',(-26.2663020200481,639.018061885379,70.7685373257971));
#99681=CARTESIAN_POINT('Ctrl Pts',(-26.5383229063629,639.03182351378,70.7297246005164));
#99682=CARTESIAN_POINT('Ctrl Pts',(-26.8052344292236,639.051326252545,70.6734607796385));
#99683=CARTESIAN_POINT('Ctrl Pts',(-26.9487943211451,639.061815912336,70.6431989611986));
#99684=CARTESIAN_POINT('Ctrl Pts',(-27.0908765464588,639.073966216304,70.6078894896557));
#99685=CARTESIAN_POINT('Ctrl Pts',(-27.2312233323724,639.087673452015,70.56762534775));
#99686=CARTESIAN_POINT('Ctrl Pts',(-27.2323605203673,639.087784517643,70.5672990994608));
#99687=CARTESIAN_POINT('Ctrl Pts',(-27.2334976101377,639.087895685839,70.5669725224296));
#99688=CARTESIAN_POINT('Ctrl Pts',(-27.2346346016704,639.08800695655,70.5666456166163));
#99689=CARTESIAN_POINT('Ctrl Pts',(-27.4345340242248,639.107569943678,70.5091708848989));
#99690=CARTESIAN_POINT('Ctrl Pts',(-27.6314474761934,639.130308814554,70.4415110705284));
#99691=CARTESIAN_POINT('Ctrl Pts',(-27.8252672673916,639.15591603875,70.3634708926868));
#99692=CARTESIAN_POINT('Ctrl Pts',(-27.8282445068165,639.156309387835,70.3622721281398));
#99693=CARTESIAN_POINT('Ctrl Pts',(-27.8312212104409,639.156703452167,70.3610707873401));
#99694=CARTESIAN_POINT('Ctrl Pts',(-27.834197359946,639.157098227311,70.3598668790042));
#99695=CARTESIAN_POINT('Ctrl Pts',(-27.9894491330569,639.177691796646,70.2970646227717));
#99696=CARTESIAN_POINT('Ctrl Pts',(-28.1432703577507,639.20023292809,70.2272339023149));
#99697=CARTESIAN_POINT('Ctrl Pts',(-28.2929815772957,639.224084541252,70.1516373994087));
#99698=CARTESIAN_POINT('Ctrl Pts',(-28.3285967893406,639.229758666832,70.1336535402895));
#99699=CARTESIAN_POINT('Ctrl Pts',(-28.3639795834936,639.235506933618,70.1153435164027));
#99700=CARTESIAN_POINT('Ctrl Pts',(-28.3990942913099,639.241320738419,70.096724553437));
#99701=CARTESIAN_POINT('Ctrl Pts',(-28.4034106922287,639.242035388033,70.0944358569377));
#99702=CARTESIAN_POINT('Ctrl Pts',(-28.4077235599911,639.242751075026,70.0921423887562));
#99703=CARTESIAN_POINT('Ctrl Pts',(-28.4120328939071,639.243467791937,70.0898441520015));
#99704=CARTESIAN_POINT('Ctrl Pts',(-28.658158288822,639.284402710433,69.9585815392916));
#99705=CARTESIAN_POINT('Ctrl Pts',(-28.8929149867157,639.328720256045,69.8116819089959));
#99706=CARTESIAN_POINT('Ctrl Pts',(-29.116618808618,639.375128618273,69.6494399515747));
#99707=CARTESIAN_POINT('Ctrl Pts',(-29.2269895260826,639.398025519149,69.5693932134762));
#99708=CARTESIAN_POINT('Ctrl Pts',(-29.334670118163,639.421431631444,69.4856124469673));
#99709=CARTESIAN_POINT('Ctrl Pts',(-29.4397007152155,639.44519366648,69.3981367404782));
#99710=CARTESIAN_POINT('Ctrl Pts',(-29.4448089218575,639.446349342908,69.3938823232185));
#99711=CARTESIAN_POINT('Ctrl Pts',(-29.4499116020077,639.447506069964,69.3896182581848));
#99712=CARTESIAN_POINT('Ctrl Pts',(-29.4550086592013,639.448663806067,69.3853446352532));
#99713=CARTESIAN_POINT('Ctrl Pts',(-29.5908506819648,639.47951871078,69.2714480157898));
#99714=CARTESIAN_POINT('Ctrl Pts',(-29.7228031442344,639.511116227394,69.1506637347806));
#99715=CARTESIAN_POINT('Ctrl Pts',(-29.8489633040033,639.54265629442,69.0247387156344));
#99716=CARTESIAN_POINT('Ctrl Pts',(-29.8676605002224,639.547330597488,69.0060763677411));
#99717=CARTESIAN_POINT('Ctrl Pts',(-29.8862305633637,639.55200365133,68.9873011389271));
#99718=CARTESIAN_POINT('Ctrl Pts',(-29.9046673995305,639.55667286808,68.9684187394493));
#99719=CARTESIAN_POINT('Ctrl Pts',(-29.9094138856866,639.557874938352,68.9635575448873));
#99720=CARTESIAN_POINT('Ctrl Pts',(-29.9141513180268,639.559076664587,68.9586896901739));
#99721=CARTESIAN_POINT('Ctrl Pts',(-29.9188797057288,639.560278028195,68.953815187973));
#99722=CARTESIAN_POINT('Ctrl Pts',(-30.0614635141599,639.596504964179,68.8068253191634));
#99723=CARTESIAN_POINT('Ctrl Pts',(-30.195875970295,639.632413788924,68.6537419339198));
#99724=CARTESIAN_POINT('Ctrl Pts',(-30.3224858870252,639.667536294259,68.4947407588566));
#99725=CARTESIAN_POINT('Ctrl Pts',(-30.3264285834488,639.668630026722,68.4897893823731));
#99726=CARTESIAN_POINT('Ctrl Pts',(-30.3303637706444,639.669723000392,68.4848323127038));
#99727=CARTESIAN_POINT('Ctrl Pts',(-30.3342914487826,639.670815201699,68.4798695468125));
#99728=CARTESIAN_POINT('Ctrl Pts',(-30.4782769420951,639.710854415335,68.2979385764189));
#99729=CARTESIAN_POINT('Ctrl Pts',(-30.6121413968524,639.749841074717,68.1084191608539));
#99730=CARTESIAN_POINT('Ctrl Pts',(-30.7359639883784,639.787131213705,67.9110767494707));
#99731=CARTESIAN_POINT('Ctrl Pts',(-30.8337001870814,639.816565232077,67.7553095595437));
#99732=CARTESIAN_POINT('Ctrl Pts',(-30.9251791288008,639.844942498338,67.5946678504991));
#99733=CARTESIAN_POINT('Ctrl Pts',(-31.0104208812647,639.871946950842,67.4290232404352));
#99734=CARTESIAN_POINT('Ctrl Pts',(-31.0122763604105,639.872534763704,67.4254176116124));
#99735=CARTESIAN_POINT('Ctrl Pts',(-31.0141283326744,639.87312174693,67.421810661113));
#99736=CARTESIAN_POINT('Ctrl Pts',(-31.0159767997225,639.873707898436,67.4182023901961));
#99737=CARTESIAN_POINT('Ctrl Pts',(-31.1033885579826,639.901426290174,67.2475716475735));
#99738=CARTESIAN_POINT('Ctrl Pts',(-31.1828892592656,639.927259372726,67.0741503956703));
#99739=CARTESIAN_POINT('Ctrl Pts',(-31.2547101808772,639.95100397125,66.8980122231744));
#99740=CARTESIAN_POINT('Ctrl Pts',(-31.3273357480885,639.975014592351,66.7199006868974));
#99741=CARTESIAN_POINT('Ctrl Pts',(-31.3921084363252,639.996889925891,66.5390108510075));
#99742=CARTESIAN_POINT('Ctrl Pts',(-31.4492188957602,640.016409086981,66.3553999762133));
#99743=CARTESIAN_POINT('Ctrl Pts',(-31.4612045326073,640.020505527085,66.3168659968294));
#99744=CARTESIAN_POINT('Ctrl Pts',(-31.4728525242766,640.024498145574,66.2782121103769));
#99745=CARTESIAN_POINT('Ctrl Pts',(-31.4841643694399,640.028384824678,66.2394387527688));
#99746=CARTESIAN_POINT('',(-19.6604693917099,639.614613618721,62.5660159449655));
#99747=CARTESIAN_POINT('Origin',(-19.1902534503917,639.531701861507,62.4176157797164));
#99748=CARTESIAN_POINT('Ctrl Pts',(-19.376027899398,639.712197853207,64.2994740882088));
#99749=CARTESIAN_POINT('Ctrl Pts',(-19.376027899398,639.712197853207,64.0018698655157));
#99750=CARTESIAN_POINT('Ctrl Pts',(-19.4004974737455,639.703610742277,63.7087642394116));
#99751=CARTESIAN_POINT('Ctrl Pts',(-19.4956764044269,639.670658245073,63.1310286597025));
#99752=CARTESIAN_POINT('Ctrl Pts',(-19.5663951239896,639.646286994885,62.8464005726073));
#99753=CARTESIAN_POINT('Ctrl Pts',(-19.6604693917099,639.614613618721,62.5660159449655));
#99754=CARTESIAN_POINT('Ctrl Pts',(-2.24785136021961,606.490049520156,76.3728616211989));
#99755=CARTESIAN_POINT('Ctrl Pts',(-2.07645831249209,605.414627084222,76.4046723372956));
#99756=CARTESIAN_POINT('Ctrl Pts',(-2.33937824014887,606.115760787361,77.1959965376399));
#99757=CARTESIAN_POINT('Ctrl Pts',(-1.40572798238319,606.634621533619,76.5295902130151));
#99758=CARTESIAN_POINT('Ctrl Pts',(-1.2654170129743,605.520243681078,76.5426302087965));
#99759=CARTESIAN_POINT('Ctrl Pts',(-1.46297067363917,606.264147629094,77.3634086157539));
#99760=CARTESIAN_POINT('Ctrl Pts',(-0.558874392673838,606.700257805871,
76.5971497221964));
#99761=CARTESIAN_POINT('Ctrl Pts',(-0.514725151067144,605.560838546424,
76.5942633105063));
#99762=CARTESIAN_POINT('Ctrl Pts',(-0.581630402706062,606.331517016794,
77.4355745853251));
#99763=CARTESIAN_POINT('Ctrl Pts',(0.706100277663303,606.671595580696,76.5669850049637));
#99764=CARTESIAN_POINT('Ctrl Pts',(0.646113299414241,605.541339525764,76.5691293178837));
#99765=CARTESIAN_POINT('Ctrl Pts',(0.734851049714794,606.302098310751,77.4033535057652));
#99766=CARTESIAN_POINT('Ctrl Pts',(1.12182523736722,606.642185791387,76.5361105303261));
#99767=CARTESIAN_POINT('Ctrl Pts',(1.0251340776358,605.521722692831,76.543880399892));
#99768=CARTESIAN_POINT('Ctrl Pts',(1.16750341452896,606.271912301717,77.3703742754705));
#99769=CARTESIAN_POINT('Ctrl Pts',(1.95026027616442,606.544314852399,76.4316729163024));
#99770=CARTESIAN_POINT('Ctrl Pts',(1.79327421445325,605.453614337091,76.455582544209));
#99771=CARTESIAN_POINT('Ctrl Pts',(2.0296703980175,606.171458263482,77.2588170101284));
#99772=CARTESIAN_POINT('Ctrl Pts',(2.35571831397261,606.47689240761,76.3591800393728));
#99773=CARTESIAN_POINT('Ctrl Pts',(2.1710193365545,605.406592564273,76.3944710230157));
#99774=CARTESIAN_POINT('Ctrl Pts',(2.45163778157805,606.102256333507,77.1813821711447));
#99775=CARTESIAN_POINT('Ctrl Pts',(3.15092750039858,606.310847716552,76.1762401766097));
#99776=CARTESIAN_POINT('Ctrl Pts',(2.92564597397687,605.285471359352,76.234853866594));
#99777=CARTESIAN_POINT('Ctrl Pts',(3.27922604287808,605.931829263743,76.9859709699879));
#99778=CARTESIAN_POINT('Ctrl Pts',(3.54067700376135,606.212227570323,76.0657839944311));
#99779=CARTESIAN_POINT('Ctrl Pts',(3.29897216237761,605.212582988352,76.1380212205389));
#99780=CARTESIAN_POINT('Ctrl Pts',(3.68484527501558,605.830606250497,76.8679847444035));
#99781=CARTESIAN_POINT('Ctrl Pts',(4.30578941666232,605.989162728325,75.8078458454146));
#99782=CARTESIAN_POINT('Ctrl Pts',(4.04402710457102,605.040948311733,75.904820336075));
#99783=CARTESIAN_POINT('Ctrl Pts',(4.48111132932754,605.601654146907,76.5924623214939));
#99784=CARTESIAN_POINT('Ctrl Pts',(4.68185936719368,605.864313109311,75.6597967341437));
#99785=CARTESIAN_POINT('Ctrl Pts',(4.41428255177422,604.943151687818,75.7698350030808));
#99786=CARTESIAN_POINT('Ctrl Pts',(4.87249402091235,605.473509417797,76.4343202707809));
#99787=CARTESIAN_POINT('Ctrl Pts',(5.76664965320662,605.467770079489,75.1711954372518));
#99788=CARTESIAN_POINT('Ctrl Pts',(5.47578346481391,604.628428677137,75.3217454446971));
#99789=CARTESIAN_POINT('Ctrl Pts',(6.00145504788499,605.066500484564,75.9124092474764));
#99790=CARTESIAN_POINT('Ctrl Pts',(6.44125011399598,605.172267934022,74.784314430178));
#99791=CARTESIAN_POINT('Ctrl Pts',(6.16307079581374,604.382188597855,74.9571009510351));
#99792=CARTESIAN_POINT('Ctrl Pts',(6.70352384989602,604.763199285767,75.4991529048738));
#99793=CARTESIAN_POINT('Ctrl Pts',(7.39260369019905,604.71114788997,74.1137189387619));
#99794=CARTESIAN_POINT('Ctrl Pts',(7.15897786590069,603.974427505579,74.2892807227976));
#99795=CARTESIAN_POINT('Ctrl Pts',(7.69361438062187,604.289909408297,74.7828399123804));
#99796=CARTESIAN_POINT('Ctrl Pts',(7.69999421515557,604.554074189567,73.8745480813111));
#99797=CARTESIAN_POINT('Ctrl Pts',(7.47684208610668,603.836400663942,74.0542734601015));
#99798=CARTESIAN_POINT('Ctrl Pts',(8.01352130722828,604.128690167082,74.5273634858685));
#99799=CARTESIAN_POINT('Ctrl Pts',(8.29275501798807,604.238713379567,73.3660152009349));
#99800=CARTESIAN_POINT('Ctrl Pts',(8.09137141934386,603.556059847339,73.5499197260923));
#99801=CARTESIAN_POINT('Ctrl Pts',(8.63041836958312,603.805006249089,73.9841609752444));
#99802=CARTESIAN_POINT('Ctrl Pts',(8.57500490891436,604.082124761452,73.0994134185156));
#99803=CARTESIAN_POINT('Ctrl Pts',(8.38578298933409,603.415273016501,73.2841816609331));
#99804=CARTESIAN_POINT('Ctrl Pts',(8.92416103428722,603.644284895453,73.6993832924709));
#99805=CARTESIAN_POINT('Ctrl Pts',(9.38165373201386,603.620751618402,72.2621847580793));
#99806=CARTESIAN_POINT('Ctrl Pts',(9.21438704392936,603.003986413452,72.4577134501767));
#99807=CARTESIAN_POINT('Ctrl Pts',(9.76365581150127,603.170734829699,72.8050748647865));
#99808=CARTESIAN_POINT('Ctrl Pts',(9.86648097776603,603.324313826912,71.654602795079));
#99809=CARTESIAN_POINT('Ctrl Pts',(9.72827362326639,602.72931292187,71.8438171025923));
#99810=CARTESIAN_POINT('Ctrl Pts',(10.2682245291729,602.866473387679,72.1560695767886));
#99811=CARTESIAN_POINT('Ctrl Pts',(10.5131125646575,602.91509695399,70.659537110542));
#99812=CARTESIAN_POINT('Ctrl Pts',(10.4161108402933,602.345015132654,70.8199643162105));
#99813=CARTESIAN_POINT('Ctrl Pts',(10.941186104955,602.446456401338,71.0931626340489));
#99814=CARTESIAN_POINT('Ctrl Pts',(10.7157975268766,602.784113279091,70.3120817185628));
#99815=CARTESIAN_POINT('Ctrl Pts',(10.6299402839473,602.222643594815,70.4658892792959));
#99816=CARTESIAN_POINT('Ctrl Pts',(11.1521242095173,602.312015745438,70.7220183137493));
#99817=CARTESIAN_POINT('Ctrl Pts',(11.084674691934,602.542335927575,69.6013374038105));
#99818=CARTESIAN_POINT('Ctrl Pts',(11.0180928131922,601.996679307108,69.7407948866327));
#99819=CARTESIAN_POINT('Ctrl Pts',(11.536021775298,602.063857265052,69.962816417792));
#99820=CARTESIAN_POINT('Ctrl Pts',(11.2518487421506,602.430935708244,69.2368447373392));
#99821=CARTESIAN_POINT('Ctrl Pts',(11.1947990337114,601.891830607767,69.3678350652564));
#99822=CARTESIAN_POINT('Ctrl Pts',(11.7100030252517,601.949516913845,69.5734730530018));
#99823=CARTESIAN_POINT('Ctrl Pts',(11.551217309919,602.229419141143,68.4888783550685));
#99824=CARTESIAN_POINT('Ctrl Pts',(11.5101732026518,601.702409110986,68.6025385409749));
#99825=CARTESIAN_POINT('Ctrl Pts',(12.0215617073792,601.742681788853,68.7745109630704));
#99826=CARTESIAN_POINT('Ctrl Pts',(11.6834165707129,602.139294354524,68.1054086939741));
#99827=CARTESIAN_POINT('Ctrl Pts',(11.6500527589341,601.617151454847,68.2091225258212));
#99828=CARTESIAN_POINT('Ctrl Pts',(12.1591440413972,601.650178377243,68.3648966030017));
#99829=CARTESIAN_POINT('Ctrl Pts',(11.9111236037373,601.982987992257,67.3181651639017));
#99830=CARTESIAN_POINT('Ctrl Pts',(11.890105925035,601.469623640317,67.4020108101631));
#99831=CARTESIAN_POINT('Ctrl Pts',(12.3961232041752,601.489746664308,67.5239791695796));
#99832=CARTESIAN_POINT('Ctrl Pts',(12.0069667791483,601.916568786804,66.911668961761));
#99833=CARTESIAN_POINT('Ctrl Pts',(11.9916079185944,601.406550775875,66.9841120694481));
#99834=CARTESIAN_POINT('Ctrl Pts',(12.4958690656147,601.421574482202,67.089768199197));
#99835=CARTESIAN_POINT('Ctrl Pts',(12.2299344763514,601.761466322693,65.690004883469));
#99836=CARTESIAN_POINT('Ctrl Pts',(12.2258063111644,601.260358021303,65.7350813999208));
#99837=CARTESIAN_POINT('Ctrl Pts',(12.7279159619352,601.262378414473,65.7848111091887));
#99838=CARTESIAN_POINT('Ctrl Pts',(12.2958567378873,601.714886434859,64.8673118420714));
#99839=CARTESIAN_POINT('Ctrl Pts',(12.2966228016023,601.215349916125,64.8820610902705));
#99840=CARTESIAN_POINT('Ctrl Pts',(12.7965225255397,601.214569178336,64.906027061425));
#99841=CARTESIAN_POINT('Ctrl Pts',(12.2691242107389,601.733648040287,63.6206371830607));
#99842=CARTESIAN_POINT('Ctrl Pts',(12.2684356679878,601.233129138177,63.6017923894247));
#99843=CARTESIAN_POINT('Ctrl Pts',(12.7687014560782,601.233825955092,63.5743540715745));
#99844=CARTESIAN_POINT('Ctrl Pts',(12.2386272268548,601.755068763332,63.199960706747));
#99845=CARTESIAN_POINT('Ctrl Pts',(12.2361148149086,601.253534283818,63.1686064467318));
#99846=CARTESIAN_POINT('Ctrl Pts',(12.7369626473578,601.25581202788,63.1249959000212));
#99847=CARTESIAN_POINT('Ctrl Pts',(12.1360150250495,601.826793186119,62.3733211263854));
#99848=CARTESIAN_POINT('Ctrl Pts',(12.1278783154331,601.321481049692,62.3196016812068));
#99849=CARTESIAN_POINT('Ctrl Pts',(12.6301721078754,601.329429458576,62.2419960871396));
#99850=CARTESIAN_POINT('Ctrl Pts',(12.0642627442628,601.876841506454,61.966781870534));
#99851=CARTESIAN_POINT('Ctrl Pts',(12.0518668066587,601.369077315824,61.9013451715682));
#99852=CARTESIAN_POINT('Ctrl Pts',(12.5554981065861,601.380798685877,61.8077390713353));
#99853=CARTESIAN_POINT('Ctrl Pts',(11.8816140310333,602.003262763878,61.166562295788));
#99854=CARTESIAN_POINT('Ctrl Pts',(11.8592631718102,601.488601905001,61.0802544646279));
#99855=CARTESIAN_POINT('Ctrl Pts',(12.3654120067484,601.510556548268,60.9529607510218));
#99856=CARTESIAN_POINT('Ctrl Pts',(11.7707128919438,602.079641820668,60.772884098279));
#99857=CARTESIAN_POINT('Ctrl Pts',(11.7418361923576,601.561038683665,60.6757975217571));
#99858=CARTESIAN_POINT('Ctrl Pts',(12.24999503422,601.588951446709,60.5324417644507));
#99859=CARTESIAN_POINT('Ctrl Pts',(11.5101835598806,602.257123807651,59.9980565322959));
#99860=CARTESIAN_POINT('Ctrl Pts',(11.4672537822116,601.728288580003,59.8820278090674));
#99861=CARTESIAN_POINT('Ctrl Pts',(11.9788570767703,601.771117661675,59.7047869321897));
#99862=CARTESIAN_POINT('Ctrl Pts',(11.3599469816121,602.358621283629,59.6161284319979));
#99863=CARTESIAN_POINT('Ctrl Pts',(11.3083541540513,601.824109992935,59.4906070974741));
#99864=CARTESIAN_POINT('Ctrl Pts',(11.8225029661159,601.875293914858,59.2968193042848));
#99865=CARTESIAN_POINT('Ctrl Pts',(10.8623141995672,602.690011075352,58.5132634066806));
#99866=CARTESIAN_POINT('Ctrl Pts',(10.7793394197783,602.137864461831,58.3527219119798));
#99867=CARTESIAN_POINT('Ctrl Pts',(11.3046070446312,602.215429860194,58.1187624395528));
#99868=CARTESIAN_POINT('Ctrl Pts',(10.4661234341584,602.948411668527,57.826102858912));
#99869=CARTESIAN_POINT('Ctrl Pts',(10.356765890555,602.381898559536,57.6501409533267));
#99870=CARTESIAN_POINT('Ctrl Pts',(10.8922838620022,602.480650216832,57.38475245639));
#99871=CARTESIAN_POINT('Ctrl Pts',(9.77894881027317,603.375457962377,56.8598623147943));
#99872=CARTESIAN_POINT('Ctrl Pts',(9.64506765475245,602.77115804364,56.6833001238243));
#99873=CARTESIAN_POINT('Ctrl Pts',(10.1771279455515,602.918967477386,56.3526354312712));
#99874=CARTESIAN_POINT('Ctrl Pts',(9.53441356862628,603.524266415077,56.5491977096818));
#99875=CARTESIAN_POINT('Ctrl Pts',(9.3881532972667,602.908133560702,56.3693702079608));
#99876=CARTESIAN_POINT('Ctrl Pts',(9.92263552743373,603.071703338872,56.0207905222547));
#99877=CARTESIAN_POINT('Ctrl Pts',(9.02298980808865,603.826597991785,55.9593613574983));
#99878=CARTESIAN_POINT('Ctrl Pts',(8.85332952510663,603.18403735001,55.7753564682485));
#99879=CARTESIAN_POINT('Ctrl Pts',(9.39038724050548,603.382014172498,55.3907408801181));
#99880=CARTESIAN_POINT('Ctrl Pts',(8.75507913189959,603.980773157895,55.6786872175428));
#99881=CARTESIAN_POINT('Ctrl Pts',(8.57309886107225,603.323937574205,55.4940908270661));
#99882=CARTESIAN_POINT('Ctrl Pts',(9.11156762612114,603.540258381175,55.090931316096));
#99883=CARTESIAN_POINT('Ctrl Pts',(8.19463976841416,604.291810284563,55.1442976661868));
#99884=CARTESIAN_POINT('Ctrl Pts',(7.98991581692825,603.603406408195,54.9607215721971));
#99885=CARTESIAN_POINT('Ctrl Pts',(8.52830801024527,603.859504509158,54.5201090911092));
#99886=CARTESIAN_POINT('Ctrl Pts',(7.90211495074044,604.44868351391,54.8905842355243));
#99887=CARTESIAN_POINT('Ctrl Pts',(7.68581591431249,603.743146615829,54.7092695072828));
#99888=CARTESIAN_POINT('Ctrl Pts',(8.2238720660799,604.020517985683,54.249098530159));
#99889=CARTESIAN_POINT('Ctrl Pts',(7.29112855786425,604.761500763142,54.4095765831193));
#99890=CARTESIAN_POINT('Ctrl Pts',(7.05467644855106,604.018499588404,54.235046571121));
#99891=CARTESIAN_POINT('Ctrl Pts',(7.58800735659369,604.341591210503,53.7352979823133));
#99892=CARTESIAN_POINT('Ctrl Pts',(6.97101558534139,604.918182407445,54.1813147654603));
#99893=CARTESIAN_POINT('Ctrl Pts',(6.72505953251661,604.154601600561,54.0123480361725));
#99894=CARTESIAN_POINT('Ctrl Pts',(7.25485997662567,604.502408049335,53.4914744107168));
#99895=CARTESIAN_POINT('Ctrl Pts',(5.98483237209617,605.372809378709,53.5471616990657));
#99896=CARTESIAN_POINT('Ctrl Pts',(5.69764408550192,604.551590711133,53.3856625261571));
#99897=CARTESIAN_POINT('Ctrl Pts',(6.2285217108747,604.969033495642,52.8140885319357));
#99898=CARTESIAN_POINT('Ctrl Pts',(5.291763389905,605.656883943073,53.1889683039969));
#99899=CARTESIAN_POINT('Ctrl Pts',(4.99883657181497,604.782956995844,53.0534099549068));
#99900=CARTESIAN_POINT('Ctrl Pts',(5.50723239645897,605.260605545413,52.4314756793782));
#99901=CARTESIAN_POINT('Ctrl Pts',(4.18911713925861,606.025248782652,52.7483954928647));
#99902=CARTESIAN_POINT('Ctrl Pts',(3.92944127969241,605.069509242206,52.6545633889695));
#99903=CARTESIAN_POINT('Ctrl Pts',(4.35968842339054,605.638692597612,51.9608675862803));
#99904=CARTESIAN_POINT('Ctrl Pts',(3.81096175995496,606.138324284714,52.6178133054263));
#99905=CARTESIAN_POINT('Ctrl Pts',(3.56120429928033,605.155992497434,52.5373866738974));
#99906=CARTESIAN_POINT('Ctrl Pts',(3.9661354003342,605.754752469228,51.8213832724702));
#99907=CARTESIAN_POINT('Ctrl Pts',(3.00672598670703,606.344708975615,52.3845762519713));
#99908=CARTESIAN_POINT('Ctrl Pts',(2.78594596552362,605.311313687175,52.3295333561008));
#99909=CARTESIAN_POINT('Ctrl Pts',(3.12915300807807,605.966584199717,51.5722459548577));
#99910=CARTESIAN_POINT('Ctrl Pts',(2.57673878094782,606.43650711821,52.283993642024));
#99911=CARTESIAN_POINT('Ctrl Pts',(2.37958814121467,605.377182855783,52.2431427434406));
#99912=CARTESIAN_POINT('Ctrl Pts',(2.68165673811207,606.060805327666,51.464806254603));
#99913=CARTESIAN_POINT('Ctrl Pts',(2.14707264243295,606.506964973997,52.2077657609361));
#99914=CARTESIAN_POINT('Ctrl Pts',(1.98191615594632,605.426670682687,52.1785498499702));
#99915=CARTESIAN_POINT('Ctrl Pts',(2.23449661093605,606.133122595151,51.3833819921005));
#99916=CARTESIAN_POINT('',(2.22051577456844,606.494663641934,52.2210317180765));
#99917=CARTESIAN_POINT('',(4.22249409534898E-10,606.684224932409,76.580334695687));
#99918=CARTESIAN_POINT('Ctrl Pts',(2.22051577456844,606.494663641934,52.2210317180765));
#99919=CARTESIAN_POINT('Ctrl Pts',(2.60483303074393,606.429484540379,52.2916850774771));
#99920=CARTESIAN_POINT('Ctrl Pts',(2.98704755411254,606.347911981023,52.381202132682));
#99921=CARTESIAN_POINT('Ctrl Pts',(3.72765041168058,606.161164801006,52.5916868547165));
#99922=CARTESIAN_POINT('Ctrl Pts',(4.08671405697885,606.056144140749,52.7124754929602));
#99923=CARTESIAN_POINT('Ctrl Pts',(5.1345743018316,605.714430404768,53.1183811864826));
#99924=CARTESIAN_POINT('Ctrl Pts',(5.79438301248105,605.451397101099,53.4465291776656));
#99925=CARTESIAN_POINT('Ctrl Pts',(6.7355315478591,605.029219853622,54.0238946887425));
#99926=CARTESIAN_POINT('Ctrl Pts',(7.04239893277636,604.883107748655,54.2317409141202));
#99927=CARTESIAN_POINT('Ctrl Pts',(7.63205469932197,604.589122876331,54.6710591065219));
#99928=CARTESIAN_POINT('Ctrl Pts',(7.91508088583165,604.441230479337,54.9024484325785));
#99929=CARTESIAN_POINT('Ctrl Pts',(8.73098867449171,603.999577513356,55.6321883543658));
#99930=CARTESIAN_POINT('Ctrl Pts',(9.23111241966252,603.707850689127,56.1656879276833));
#99931=CARTESIAN_POINT('Ctrl Pts',(9.91630154576906,603.290954132867,57.0451969084296));
#99932=CARTESIAN_POINT('Ctrl Pts',(10.1324915118317,603.156183694246,57.3502753776917));
#99933=CARTESIAN_POINT('Ctrl Pts',(10.5357713613976,602.900401551024,57.9783769701487));
#99934=CARTESIAN_POINT('Ctrl Pts',(10.7236262872103,602.778919608739,58.3023594003029));
#99935=CARTESIAN_POINT('Ctrl Pts',(11.0712376013219,602.551117160149,58.9713183751389));
#99936=CARTESIAN_POINT('Ctrl Pts',(11.2309988089124,602.444788739996,59.3162894189298));
#99937=CARTESIAN_POINT('Ctrl Pts',(11.5208797326646,602.249914737681,60.0290181547742));
#99938=CARTESIAN_POINT('Ctrl Pts',(11.6501690769847,602.161922525909,60.3953019668914));
#99939=CARTESIAN_POINT('Ctrl Pts',(11.9839910541968,601.933170100156,61.5063440997196));
#99940=CARTESIAN_POINT('Ctrl Pts',(12.1379146213264,601.825487893945,62.2699324426638));
#99941=CARTESIAN_POINT('Ctrl Pts',(12.2580662787846,601.741388185839,63.4530645764399));
#99942=CARTESIAN_POINT('Ctrl Pts',(12.2789163285454,601.726736270966,63.8499267607108));
#99943=CARTESIAN_POINT('Ctrl Pts',(12.2825378585981,601.724194293723,64.6358410829958));
#99944=CARTESIAN_POINT('Ctrl Pts',(12.2655225913637,601.736153568246,65.0268582260156));
#99945=CARTESIAN_POINT('Ctrl Pts',(12.1944767448526,601.785908540228,65.8050866022495));
#99946=CARTESIAN_POINT('Ctrl Pts',(12.1404459138046,601.82370562741,66.1922977510875));
#99947=CARTESIAN_POINT('Ctrl Pts',(11.9949724860648,601.92483744177,66.9629011030374));
#99948=CARTESIAN_POINT('Ctrl Pts',(11.903019104308,601.988518090871,67.3470686022024));
#99949=CARTESIAN_POINT('Ctrl Pts',(11.5792106607343,602.210767543754,68.4638808611085));
#99950=CARTESIAN_POINT('Ctrl Pts',(11.2984041214378,602.401449237337,69.1715940183495));
#99951=CARTESIAN_POINT('Ctrl Pts',(10.7859893300428,602.73835379426,70.1837668701614));
#99952=CARTESIAN_POINT('Ctrl Pts',(10.5987639460202,602.859865399784,70.5144589620626));
#99953=CARTESIAN_POINT('Ctrl Pts',(10.2001915144139,603.113663105627,71.1489943075356));
#99954=CARTESIAN_POINT('Ctrl Pts',(9.98878898534629,603.246010799224,71.4534198335247));
#99955=CARTESIAN_POINT('Ctrl Pts',(9.31947230013895,603.655393049318,72.3311884350087));
#99956=CARTESIAN_POINT('Ctrl Pts',(8.82689483618176,603.944863634538,72.8693491319149));
#99957=CARTESIAN_POINT('Ctrl Pts',(8.01529581017258,604.388031905717,73.6112320344375));
#99958=CARTESIAN_POINT('Ctrl Pts',(7.73182881330978,604.537533259381,73.8478989536329));
#99959=CARTESIAN_POINT('Ctrl Pts',(7.14908314421362,604.831207252798,74.2916812721146));
#99960=CARTESIAN_POINT('Ctrl Pts',(6.84872810477117,604.976001626505,74.4998846147026));
#99961=CARTESIAN_POINT('Ctrl Pts',(5.91918799038042,605.399129104306,75.0845859838612));
#99962=CARTESIAN_POINT('Ctrl Pts',(5.26207272556291,605.666687613147,75.4217452738926));
#99963=CARTESIAN_POINT('Ctrl Pts',(4.20600812444231,606.019585586432,75.8438524767));
#99964=CARTESIAN_POINT('Ctrl Pts',(3.84458489423226,606.128056920297,75.9693060886928));
#99965=CARTESIAN_POINT('Ctrl Pts',(3.11078512019224,606.319311478279,76.185971800507));
#99966=CARTESIAN_POINT('Ctrl Pts',(2.73707032232845,606.402551374238,76.2777372174655));
#99967=CARTESIAN_POINT('Ctrl Pts',(1.97462989968799,606.539511783188,76.4267647296646));
#99968=CARTESIAN_POINT('Ctrl Pts',(1.58407504305315,606.593371762541,76.4841860202651));
#99969=CARTESIAN_POINT('Ctrl Pts',(0.795241544847691,606.665735849296,76.5609621502088));
#99970=CARTESIAN_POINT('Ctrl Pts',(0.400287481815783,606.684227202053,76.5803315661586));
#99971=CARTESIAN_POINT('Ctrl Pts',(5.83190623966335E-15,606.684227202053,
76.5803315661586));
#99972=CARTESIAN_POINT('',(2.31092134190293,606.120502424978,51.3976052199539));
#99973=CARTESIAN_POINT('Origin',(2.31092134187393,606.494663641934,51.7292728001094));
#99974=CARTESIAN_POINT('',(-2.26224148372674,606.128561192588,77.2104285068931));
#99975=CARTESIAN_POINT('Ctrl Pts',(-2.26224148372674,606.128561192588,77.2104285068931));
#99976=CARTESIAN_POINT('Ctrl Pts',(-1.83032423084503,606.199321946877,77.2901548692284));
#99977=CARTESIAN_POINT('Ctrl Pts',(-1.39473620312201,606.250907869188,77.3470551071421));
#99978=CARTESIAN_POINT('Ctrl Pts',(-0.515891315837579,606.31235552653,77.4146673352173));
#99979=CARTESIAN_POINT('Ctrl Pts',(-0.0702880625902517,606.322061908389,
77.4252220449457));
#99980=CARTESIAN_POINT('Ctrl Pts',(0.814508254993039,606.297917403733,77.3987706058388));
#99981=CARTESIAN_POINT('Ctrl Pts',(1.25591590129853,606.264149217592,77.3618450733092));
#99982=CARTESIAN_POINT('Ctrl Pts',(2.12632669303214,606.156946302591,77.2425878065961));
#99983=CARTESIAN_POINT('Ctrl Pts',(2.55179819911838,606.084174367916,77.1609561180698));
#99984=CARTESIAN_POINT('Ctrl Pts',(3.38538928239685,605.906592410097,76.9566426950186));
#99985=CARTESIAN_POINT('Ctrl Pts',(3.79350628097141,605.801783546111,76.833949796622));
#99986=CARTESIAN_POINT('Ctrl Pts',(4.5939136248181,605.565907235288,76.5485878713385));
#99987=CARTESIAN_POINT('Ctrl Pts',(4.98575248625829,605.434795373065,76.3857550747386));
#99988=CARTESIAN_POINT('Ctrl Pts',(6.11412644163187,605.020347147677,75.850504898419));
#99989=CARTESIAN_POINT('Ctrl Pts',(6.81399404095514,604.713607705726,75.4287590544389));
#99990=CARTESIAN_POINT('Ctrl Pts',(7.79889285265662,604.237467754231,74.7005250396438));
#99991=CARTESIAN_POINT('Ctrl Pts',(8.11734298004477,604.075354707554,74.4406405058552));
#99992=CARTESIAN_POINT('Ctrl Pts',(8.72762915407622,603.75229671606,73.8918331418519));
#99993=CARTESIAN_POINT('Ctrl Pts',(9.01787207664488,603.592262947776,73.6045582479782));
#99994=CARTESIAN_POINT('Ctrl Pts',(9.84637516857155,603.121737222959,72.7037235931987));
#99995=CARTESIAN_POINT('Ctrl Pts',(10.3429614399288,602.820770001216,72.0516283531007));
#99996=CARTESIAN_POINT('Ctrl Pts',(11.0032431948168,602.407067467609,70.9865177450937));
#99997=CARTESIAN_POINT('Ctrl Pts',(11.2093789343219,602.275251835416,70.6157898317709));
#99998=CARTESIAN_POINT('Ctrl Pts',(11.5836014028183,602.032675897713,69.8591636321725));
#99999=CARTESIAN_POINT('Ctrl Pts',(11.7528969072206,601.921164391175,69.4715259668061));
#100000=CARTESIAN_POINT('Ctrl Pts',(12.0554510123091,601.719930759937,68.6768786107822));
#100001=CARTESIAN_POINT('Ctrl Pts',(12.1887140449545,601.630200580394,68.2698726655556));
#100002=CARTESIAN_POINT('Ctrl Pts',(12.4175304640208,601.475114177481,67.4351906357858));
#100003=CARTESIAN_POINT('Ctrl Pts',(12.5132629458602,601.409630372534,67.0052234510874));
#100004=CARTESIAN_POINT('Ctrl Pts',(12.7346497723208,601.257655920815,65.7152869175487));
#100005=CARTESIAN_POINT('Ctrl Pts',(12.7982740854582,601.213319476748,64.8470309669364));
#100006=CARTESIAN_POINT('Ctrl Pts',(12.766112503726,601.235579417349,63.5319360416885));
#100007=CARTESIAN_POINT('Ctrl Pts',(12.7334707525218,601.258186828756,63.0884936792983));
#100008=CARTESIAN_POINT('Ctrl Pts',(12.6260778331749,601.332207022654,62.2172823473981));
#100009=CARTESIAN_POINT('Ctrl Pts',(12.551632369959,601.383407841326,61.788489253183));
#100010=CARTESIAN_POINT('Ctrl Pts',(12.3628457782987,601.51225949665,60.9438749494673));
#100011=CARTESIAN_POINT('Ctrl Pts',(12.2485007430305,601.589915970709,60.5280554739999));
#100012=CARTESIAN_POINT('Ctrl Pts',(11.9802058693947,601.770170646653,59.7090936426398));
#100013=CARTESIAN_POINT('Ctrl Pts',(11.8256357552361,601.873166560103,59.3051045068694));
#100014=CARTESIAN_POINT('Ctrl Pts',(11.3133789750381,602.209683025684,58.1368724774906));
#100015=CARTESIAN_POINT('Ctrl Pts',(10.9053335034014,602.472295759362,57.4071299613224));
#100016=CARTESIAN_POINT('Ctrl Pts',(10.1963986672724,602.907259896225,56.3789236860282));
#100017=CARTESIAN_POINT('Ctrl Pts',(9.94375223192614,603.059090221129,56.0476855370183));
#100018=CARTESIAN_POINT('Ctrl Pts',(9.41478615234259,603.367978324838,55.4180596023799));
#100019=CARTESIAN_POINT('Ctrl Pts',(9.13741954079915,603.525697149408,55.1180679858199));
#100020=CARTESIAN_POINT('Ctrl Pts',(8.55656002383599,603.844325765871,54.5462464538821));
#100021=CARTESIAN_POINT('Ctrl Pts',(8.25307216483238,604.005247212705,54.2744178365614));
#100022=CARTESIAN_POINT('Ctrl Pts',(7.61843493119114,604.326614811804,53.7584611953167));
#100023=CARTESIAN_POINT('Ctrl Pts',(7.28550391450078,604.487856905221,53.513234090336));
#100024=CARTESIAN_POINT('Ctrl Pts',(6.25785460882906,604.956716882825,52.8307763736279));
#100025=CARTESIAN_POINT('Ctrl Pts',(5.53420093242913,605.250586826674,52.4443472052227));
#100026=CARTESIAN_POINT('Ctrl Pts',(4.37964798732873,605.632586367383,51.9682761050355));
#100027=CARTESIAN_POINT('Ctrl Pts',(3.98317189683697,605.750021198994,51.8270164181643));
#100028=CARTESIAN_POINT('Ctrl Pts',(3.16332124464332,605.958246731221,51.5819852864849));
#100029=CARTESIAN_POINT('Ctrl Pts',(2.73846394280183,606.048990746731,51.478279057735));
#100030=CARTESIAN_POINT('Ctrl Pts',(2.31092134190293,606.120502424978,51.3976052199539));
#100031=CARTESIAN_POINT('',(-2.17374032143659,606.502515243277,76.3864221483552));
#100032=CARTESIAN_POINT('Origin',(-2.26224148372674,606.502515243277,76.8785273650246));
#100033=CARTESIAN_POINT('Ctrl Pts',(3.771343681791E-9,606.684206930352,
76.5803595180565));
#100034=CARTESIAN_POINT('Ctrl Pts',(-0.346198564393155,606.684165521778,
76.5804168433102));
#100035=CARTESIAN_POINT('Ctrl Pts',(-0.689932235512485,606.670170944619,
76.5658934870616));
#100036=CARTESIAN_POINT('Ctrl Pts',(-1.03129404442789,606.643008160357,
76.5371136743068));
#100037=CARTESIAN_POINT('Ctrl Pts',(-1.05249997323572,606.641320765768,
76.5353258273818));
#100038=CARTESIAN_POINT('Ctrl Pts',(-1.07369674828705,606.639582538745,
76.5334829566656));
#100039=CARTESIAN_POINT('Ctrl Pts',(-1.09488439167535,606.637793661485,
76.5315851371587));
#100040=CARTESIAN_POINT('Ctrl Pts',(-1.43870745097142,606.6087646071,76.5007882194979));
#100041=CARTESIAN_POINT('Ctrl Pts',(-1.78012200264755,606.566401949312,
76.4555237331009));
#100042=CARTESIAN_POINT('Ctrl Pts',(-2.11922347843876,606.51145981661,76.3961009878374));
#100043=CARTESIAN_POINT('Ctrl Pts',(-2.13740240261687,606.508514418445,
76.3929153880753));
#100044=CARTESIAN_POINT('Ctrl Pts',(-2.1555746787607,606.505532856527,76.3896890929762));
#100045=CARTESIAN_POINT('Ctrl Pts',(-2.17374032143659,606.502515243277,
76.3864221483552));
#100046=CARTESIAN_POINT('Ctrl Pts',(2.24785136038932,634.860698008622,76.3728616211674));
#100047=CARTESIAN_POINT('Ctrl Pts',(2.07645831265176,635.936120444547,76.4046723372692));
#100048=CARTESIAN_POINT('Ctrl Pts',(2.33937824032558,635.234986741416,77.1959965376062));
#100049=CARTESIAN_POINT('Ctrl Pts',(1.40572798249692,634.716125995138,76.529590213006));
#100050=CARTESIAN_POINT('Ctrl Pts',(1.26541701307411,635.830503847675,76.5426302087904));
#100051=CARTESIAN_POINT('Ctrl Pts',(1.4629706737577,635.086599899663,77.3634086157443));
#100052=CARTESIAN_POINT('Ctrl Pts',(0.558874392731051,634.650489722876,
76.5971497221977));
#100053=CARTESIAN_POINT('Ctrl Pts',(0.514725151119972,635.789908982322,
76.5942633105082));
#100054=CARTESIAN_POINT('Ctrl Pts',(0.581630402765628,635.019230511953,
77.4355745853267));
#100055=CARTESIAN_POINT('Ctrl Pts',(-0.706100277663284,634.679151948051,
76.5669850049637));
#100056=CARTESIAN_POINT('Ctrl Pts',(-0.646113299414298,635.809408002983,
76.5691293178845));
#100057=CARTESIAN_POINT('Ctrl Pts',(-0.734851049714807,635.048649217997,
77.4033535057653));
#100058=CARTESIAN_POINT('Ctrl Pts',(-1.12182523736719,634.708561737361,
76.536110530326));
#100059=CARTESIAN_POINT('Ctrl Pts',(-1.02513407763589,635.829024835917,
76.5438803998928));
#100060=CARTESIAN_POINT('Ctrl Pts',(-1.16750341452898,635.078835227031,
77.3703742754706));
#100061=CARTESIAN_POINT('Ctrl Pts',(-1.95026027616437,634.806432676349,
76.4316729163024));
#100062=CARTESIAN_POINT('Ctrl Pts',(-1.7932742144534,635.897133191657,76.4555825442098));
#100063=CARTESIAN_POINT('Ctrl Pts',(-2.02967039801753,635.179289265266,
77.2588170101285));
#100064=CARTESIAN_POINT('Ctrl Pts',(-2.35571831397255,634.873855121138,
76.3591800393728));
#100065=CARTESIAN_POINT('Ctrl Pts',(-2.17101933655468,635.944154964474,
76.3944710230165));
#100066=CARTESIAN_POINT('Ctrl Pts',(-2.45163778157809,635.24849119524,77.1813821711449));
#100067=CARTESIAN_POINT('Ctrl Pts',(-3.1509275003985,635.039899812196,76.1762401766097));
#100068=CARTESIAN_POINT('Ctrl Pts',(-2.92564597397709,636.065276169395,
76.2348538665947));
#100069=CARTESIAN_POINT('Ctrl Pts',(-3.27922604287813,635.418918265005,
76.9859709699881));
#100070=CARTESIAN_POINT('Ctrl Pts',(-3.54067700376127,635.138519958425,
76.0657839944311));
#100071=CARTESIAN_POINT('Ctrl Pts',(-3.29897216237785,636.138164540395,
76.1380212205395));
#100072=CARTESIAN_POINT('Ctrl Pts',(-3.68484527501564,635.52014127825,76.8679847444036));
#100073=CARTESIAN_POINT('Ctrl Pts',(-4.30578941666223,635.361584800423,
75.8078458454146));
#100074=CARTESIAN_POINT('Ctrl Pts',(-4.04402710457129,636.309799217015,
75.9048203360756));
#100075=CARTESIAN_POINT('Ctrl Pts',(-4.48111132932761,635.74909338184,76.592462321494));
#100076=CARTESIAN_POINT('Ctrl Pts',(-4.68185936719358,635.486434419437,
75.6597967341437));
#100077=CARTESIAN_POINT('Ctrl Pts',(-4.4142825517745,636.407595840929,75.7698350030814));
#100078=CARTESIAN_POINT('Ctrl Pts',(-4.87249402091242,635.87723811095,76.434320270781));
#100079=CARTESIAN_POINT('Ctrl Pts',(-5.76664965320651,635.882977449259,
75.1711954372518));
#100080=CARTESIAN_POINT('Ctrl Pts',(-5.47578346481422,636.72231885161,75.3217454446976));
#100081=CARTESIAN_POINT('Ctrl Pts',(-6.00145504788508,636.284247044183,
75.9124092474765));
#100082=CARTESIAN_POINT('Ctrl Pts',(-6.44125011399587,636.178479594726,
74.7843144301781));
#100083=CARTESIAN_POINT('Ctrl Pts',(-6.16307079581405,636.968558930894,
74.9571009510356));
#100084=CARTESIAN_POINT('Ctrl Pts',(-6.70352384989611,636.58754824298,75.4991529048738));
#100085=CARTESIAN_POINT('Ctrl Pts',(-7.39260369019896,636.639599638778,
74.113718938762));
#100086=CARTESIAN_POINT('Ctrl Pts',(-7.158977865901,637.376320023169,74.2892807227981));
#100087=CARTESIAN_POINT('Ctrl Pts',(-7.69361438062197,637.060838120451,
74.7828399123805));
#100088=CARTESIAN_POINT('Ctrl Pts',(-7.69999421515548,636.79667333918,73.8745480813112));
#100089=CARTESIAN_POINT('Ctrl Pts',(-7.47684208610699,637.514346864805,
74.0542734601019));
#100090=CARTESIAN_POINT('Ctrl Pts',(-8.01352130722838,637.222057361665,
74.5273634858686));
#100091=CARTESIAN_POINT('Ctrl Pts',(-8.29275501798799,637.112034149181,
73.366015200935));
#100092=CARTESIAN_POINT('Ctrl Pts',(-8.09137141934416,637.794687681408,
73.5499197260926));
#100093=CARTESIAN_POINT('Ctrl Pts',(-8.63041836958322,637.545741279659,
73.9841609752445));
#100094=CARTESIAN_POINT('Ctrl Pts',(-8.57500490891427,637.268622767296,
73.0994134185157));
#100095=CARTESIAN_POINT('Ctrl Pts',(-8.38578298933439,637.935474512246,
73.2841816609334));
#100096=CARTESIAN_POINT('Ctrl Pts',(-8.92416103428733,637.706462633295,
73.699383292471));
#100097=CARTESIAN_POINT('Ctrl Pts',(-9.38165373201378,637.729995910346,
72.2621847580794));
#100098=CARTESIAN_POINT('Ctrl Pts',(-9.21438704392967,638.346761115296,
72.457713450177));
#100099=CARTESIAN_POINT('Ctrl Pts',(-9.76365581150139,638.180012699049,
72.8050748647866));
#100100=CARTESIAN_POINT('Ctrl Pts',(-9.86648097776597,638.026433701836,
71.6546027950791));
#100101=CARTESIAN_POINT('Ctrl Pts',(-9.72827362326668,638.621434606878,
71.8438171025925));
#100102=CARTESIAN_POINT('Ctrl Pts',(-10.268224529173,638.484274141068,72.1560695767887));
#100103=CARTESIAN_POINT('Ctrl Pts',(-10.5131125646575,638.435650574758,
70.6595371105421));
#100104=CARTESIAN_POINT('Ctrl Pts',(-10.4161108402936,639.005732396094,
70.8199643162107));
#100105=CARTESIAN_POINT('Ctrl Pts',(-10.9411861049551,638.904291127409,
71.093162634049));
#100106=CARTESIAN_POINT('Ctrl Pts',(-10.7157975268765,638.566634249657,
70.3120817185629));
#100107=CARTESIAN_POINT('Ctrl Pts',(-10.6299402839476,639.128103933932,
70.4658892792961));
#100108=CARTESIAN_POINT('Ctrl Pts',(-11.1521242095175,639.038731783309,
70.7220183137494));
#100109=CARTESIAN_POINT('Ctrl Pts',(-11.084674691934,638.808411601172,69.6013374038106));
#100110=CARTESIAN_POINT('Ctrl Pts',(-11.0180928131925,639.354068221639,
69.7407948866329));
#100111=CARTESIAN_POINT('Ctrl Pts',(-11.5360217752982,639.286890263696,
69.9628164177921));
#100112=CARTESIAN_POINT('Ctrl Pts',(-11.2518487421506,638.919811820504,
69.2368447373392));
#100113=CARTESIAN_POINT('Ctrl Pts',(-11.1947990337117,639.458916920981,
69.3678350652566));
#100114=CARTESIAN_POINT('Ctrl Pts',(-11.7100030252518,639.401230614902,
69.5734730530018));
#100115=CARTESIAN_POINT('Ctrl Pts',(-11.5512173099189,639.121328387605,
68.4888783550686));
#100116=CARTESIAN_POINT('Ctrl Pts',(-11.5101732026521,639.648338417762,
68.602538540975));
#100117=CARTESIAN_POINT('Ctrl Pts',(-12.0215617073794,639.608065739894,
68.7745109630704));
#100118=CARTESIAN_POINT('Ctrl Pts',(-11.6834165707129,639.211453174224,
68.1054086939742));
#100119=CARTESIAN_POINT('Ctrl Pts',(-11.6500527589344,639.733596073901,
68.2091225258213));
#100120=CARTESIAN_POINT('Ctrl Pts',(-12.1591440413973,639.700569151504,
68.3648966030017));
#100121=CARTESIAN_POINT('Ctrl Pts',(-11.9111236037372,639.36775953649,67.3181651639018));
#100122=CARTESIAN_POINT('Ctrl Pts',(-11.8901059250353,639.88112388843,67.4020108101632));
#100123=CARTESIAN_POINT('Ctrl Pts',(-12.3961232041754,639.861000864439,
67.5239791695796));
#100124=CARTESIAN_POINT('Ctrl Pts',(-12.0069667791483,639.434178741944,
66.911668961761));
#100125=CARTESIAN_POINT('Ctrl Pts',(-11.9916079185947,639.944196752873,
66.9841120694482));
#100126=CARTESIAN_POINT('Ctrl Pts',(-12.4958690656149,639.929173046546,
67.089768199197));
#100127=CARTESIAN_POINT('Ctrl Pts',(-12.2299344763514,639.589281206055,
65.690004883469));
#100128=CARTESIAN_POINT('Ctrl Pts',(-12.2258063111646,640.090389507445,
65.7350813999209));
#100129=CARTESIAN_POINT('Ctrl Pts',(-12.7279159619353,640.088369114275,
65.7848111091887));
#100130=CARTESIAN_POINT('Ctrl Pts',(-12.2958567378873,639.635861093889,
64.8673118420714));
#100131=CARTESIAN_POINT('Ctrl Pts',(-12.2966228016026,640.135397612622,
64.8820610902705));
#100132=CARTESIAN_POINT('Ctrl Pts',(-12.7965225255398,640.136178350411,
64.9060270614251));
#100133=CARTESIAN_POINT('Ctrl Pts',(-12.2691242107389,639.617099488461,
63.6206371830607));
#100134=CARTESIAN_POINT('Ctrl Pts',(-12.2684356679881,640.117618390571,
63.6017923894247));
#100135=CARTESIAN_POINT('Ctrl Pts',(-12.7687014560783,640.116921573656,
63.5743540715744));
#100136=CARTESIAN_POINT('Ctrl Pts',(-12.2386272268548,639.595678765416,
63.199960706747));
#100137=CARTESIAN_POINT('Ctrl Pts',(-12.2361148149089,640.097213244929,
63.1686064467318));
#100138=CARTESIAN_POINT('Ctrl Pts',(-12.7369626473579,640.094935500868,
63.1249959000212));
#100139=CARTESIAN_POINT('Ctrl Pts',(-12.1360150250495,639.523954342629,
62.3733211263854));
#100140=CARTESIAN_POINT('Ctrl Pts',(-12.1278783154334,640.029266479055,
62.3196016812068));
#100141=CARTESIAN_POINT('Ctrl Pts',(-12.6301721078756,640.021318070172,
62.2419960871396));
#100142=CARTESIAN_POINT('Ctrl Pts',(-12.0642627442628,639.473906022293,
61.966781870534));
#100143=CARTESIAN_POINT('Ctrl Pts',(-12.051866806659,639.981670212924,61.9013451715682));
#100144=CARTESIAN_POINT('Ctrl Pts',(-12.5554981065862,639.96994884287,61.8077390713353));
#100145=CARTESIAN_POINT('Ctrl Pts',(-11.8816140310333,639.34748476487,61.1665622957879));
#100146=CARTESIAN_POINT('Ctrl Pts',(-11.8592631718105,639.862145623747,
61.0802544646277));
#100147=CARTESIAN_POINT('Ctrl Pts',(-12.3654120067485,639.840190980479,
60.9529607510217));
#100148=CARTESIAN_POINT('Ctrl Pts',(-11.7707128919438,639.271105708079,
60.772884098279));
#100149=CARTESIAN_POINT('Ctrl Pts',(-11.7418361923579,639.789708845082,
60.675797521757));
#100150=CARTESIAN_POINT('Ctrl Pts',(-12.2499950342201,639.761796082038,
60.5324417644507));
#100151=CARTESIAN_POINT('Ctrl Pts',(-11.5101835598806,639.093623721097,
59.9980565322958));
#100152=CARTESIAN_POINT('Ctrl Pts',(-11.4672537822119,639.622458948745,
59.8820278090672));
#100153=CARTESIAN_POINT('Ctrl Pts',(-11.9788570767705,639.579629867072,
59.7047869321897));
#100154=CARTESIAN_POINT('Ctrl Pts',(-11.3599469816121,638.992126245118,
59.6161284319978));
#100155=CARTESIAN_POINT('Ctrl Pts',(-11.3083541540516,639.526637535813,
59.490607097474));
#100156=CARTESIAN_POINT('Ctrl Pts',(-11.822502966116,639.47545361389,59.2968193042847));
#100157=CARTESIAN_POINT('Ctrl Pts',(-10.8623141995672,638.660736453396,
58.5132634066805));
#100158=CARTESIAN_POINT('Ctrl Pts',(-10.7793394197786,639.212883066916,
58.3527219119796));
#100159=CARTESIAN_POINT('Ctrl Pts',(-11.3046070446313,639.135317668554,
58.1187624395527));
#100160=CARTESIAN_POINT('Ctrl Pts',(-10.4661234341583,638.402335860221,
57.8261028589119));
#100161=CARTESIAN_POINT('Ctrl Pts',(-10.3567658905553,638.968848969211,
57.6501409533265));
#100162=CARTESIAN_POINT('Ctrl Pts',(-10.8922838620024,638.870097311915,
57.3847524563899));
#100163=CARTESIAN_POINT('Ctrl Pts',(-9.77894881027311,637.975289566371,
56.8598623147942));
#100164=CARTESIAN_POINT('Ctrl Pts',(-9.64506765475275,638.579589485108,
56.6833001238241));
#100165=CARTESIAN_POINT('Ctrl Pts',(-10.1771279455516,638.431780051362,
56.3526354312712));
#100166=CARTESIAN_POINT('Ctrl Pts',(-9.53441356862621,637.826481113671,
56.5491977096817));
#100167=CARTESIAN_POINT('Ctrl Pts',(-9.38815329726699,638.442613968045,
56.3693702079605));
#100168=CARTESIAN_POINT('Ctrl Pts',(-9.92263552743384,638.279044189875,
56.0207905222546));
#100169=CARTESIAN_POINT('Ctrl Pts',(-9.02298980808857,637.524149536963,
55.9593613574982));
#100170=CARTESIAN_POINT('Ctrl Pts',(-8.85332952510693,638.166710178738,
55.7753564682482));
#100171=CARTESIAN_POINT('Ctrl Pts',(-9.39038724050559,637.96873335625,55.390740880118));
#100172=CARTESIAN_POINT('Ctrl Pts',(-8.75507913189951,637.369974370853,
55.6786872175427));
#100173=CARTESIAN_POINT('Ctrl Pts',(-8.57309886107255,638.026809954543,
55.4940908270658));
#100174=CARTESIAN_POINT('Ctrl Pts',(-9.11156762612125,637.810489147573,
55.0909313160959));
#100175=CARTESIAN_POINT('Ctrl Pts',(-8.19463976841408,637.058937244184,
55.1442976661868));
#100176=CARTESIAN_POINT('Ctrl Pts',(-7.98991581692855,637.747341120553,
54.9607215721967));
#100177=CARTESIAN_POINT('Ctrl Pts',(-8.52830801024537,637.491243019589,
54.5201090911091));
#100178=CARTESIAN_POINT('Ctrl Pts',(-7.90211495074035,636.902064014837,
54.8905842355242));
#100179=CARTESIAN_POINT('Ctrl Pts',(-7.6858159143128,637.607600912918,54.7092695072824));
#100180=CARTESIAN_POINT('Ctrl Pts',(-8.22387206608,637.330229543065,54.2490985301589));
#100181=CARTESIAN_POINT('Ctrl Pts',(-7.29112855786415,636.589246765606,
54.4095765831192));
#100182=CARTESIAN_POINT('Ctrl Pts',(-7.05467644855137,637.332247940343,
54.2350465711206));
#100183=CARTESIAN_POINT('Ctrl Pts',(-7.58800735659379,637.009156318244,
53.7352979823133));
#100184=CARTESIAN_POINT('Ctrl Pts',(-6.97101558534129,636.432565121303,
54.1813147654602));
#100185=CARTESIAN_POINT('Ctrl Pts',(-6.72505953251691,637.196145928187,
54.012348036172));
#100186=CARTESIAN_POINT('Ctrl Pts',(-7.25485997662576,636.848339479412,
53.4914744107167));
#100187=CARTESIAN_POINT('Ctrl Pts',(-5.98483237209606,635.977938150039,
53.5471616990657));
#100188=CARTESIAN_POINT('Ctrl Pts',(-5.69764408550223,636.799156817614,
53.3856625261566));
#100189=CARTESIAN_POINT('Ctrl Pts',(-6.22852171087479,636.381714033105,
52.8140885319356));
#100190=CARTESIAN_POINT('Ctrl Pts',(-5.29176338990489,635.693863585674,
53.1889683039969));
#100191=CARTESIAN_POINT('Ctrl Pts',(-4.99883657181527,636.567790532904,
53.0534099549063));
#100192=CARTESIAN_POINT('Ctrl Pts',(-5.50723239645906,636.090141983335,
52.4314756793781));
#100193=CARTESIAN_POINT('Ctrl Pts',(-4.18911713925852,635.325498746096,
52.7483954928647));
#100194=CARTESIAN_POINT('Ctrl Pts',(-3.92944127969268,636.281238286542,
52.6545633889689));
#100195=CARTESIAN_POINT('Ctrl Pts',(-4.35968842339061,635.712054931135,
51.9608675862802));
#100196=CARTESIAN_POINT('Ctrl Pts',(-3.81096175995487,635.212423244034,
52.6178133054263));
#100197=CARTESIAN_POINT('Ctrl Pts',(-3.56120429928059,636.194755031314,
52.5373866738968));
#100198=CARTESIAN_POINT('Ctrl Pts',(-3.96613540033426,635.59599505952,51.8213832724701));
#100199=CARTESIAN_POINT('Ctrl Pts',(-3.0067259866529,635.006038553119,52.3845762519556));
#100200=CARTESIAN_POINT('Ctrl Pts',(-2.78594596547,636.039433841561,52.3295333560857));
#100201=CARTESIAN_POINT('Ctrl Pts',(-3.12915300802187,635.384163329016,
51.5722459548408));
#100202=CARTESIAN_POINT('Ctrl Pts',(-2.57673878083549,634.914240410514,
52.2839936419978));
#100203=CARTESIAN_POINT('Ctrl Pts',(-2.37958814110711,635.973564672946,
52.243142743417));
#100204=CARTESIAN_POINT('Ctrl Pts',(-2.68165673799516,635.289942201056,
51.4648062545748));
#100205=CARTESIAN_POINT('Ctrl Pts',(-2.14707264226455,634.843782554723,
52.2077657609063));
#100206=CARTESIAN_POINT('Ctrl Pts',(-1.98191615578883,635.924076846041,
52.1785498499438));
#100207=CARTESIAN_POINT('Ctrl Pts',(-2.23449661076091,635.217624933568,
51.3833819920685));
#100208=CARTESIAN_POINT('',(-2.22051577456844,634.856083886813,52.2210317180765));
#100209=CARTESIAN_POINT('',(-4.22249464140995E-10,634.666522596339,76.5803346956872));
#100210=CARTESIAN_POINT('Ctrl Pts',(-2.22051577456844,634.856083886813,
52.2210317180765));
#100211=CARTESIAN_POINT('Ctrl Pts',(-2.60483303074393,634.921262988369,
52.2916850774771));
#100212=CARTESIAN_POINT('Ctrl Pts',(-2.98704755411254,635.002835547725,
52.381202132682));
#100213=CARTESIAN_POINT('Ctrl Pts',(-3.72765041168058,635.189582727741,
52.5916868547165));
#100214=CARTESIAN_POINT('Ctrl Pts',(-4.08671405697885,635.294603387999,
52.7124754929602));
#100215=CARTESIAN_POINT('Ctrl Pts',(-5.1345743018316,635.63631712398,53.1183811864826));
#100216=CARTESIAN_POINT('Ctrl Pts',(-5.79438301248105,635.899350427649,
53.4465291776656));
#100217=CARTESIAN_POINT('Ctrl Pts',(-6.7355315478591,636.321527675125,54.0238946887425));
#100218=CARTESIAN_POINT('Ctrl Pts',(-7.04239893277636,636.467639780093,
54.2317409141202));
#100219=CARTESIAN_POINT('Ctrl Pts',(-7.63205469932197,636.761624652416,
54.6710591065219));
#100220=CARTESIAN_POINT('Ctrl Pts',(-7.91508088583165,636.909517049411,
54.9024484325785));
#100221=CARTESIAN_POINT('Ctrl Pts',(-8.73098867449171,637.351170015392,
55.6321883543658));
#100222=CARTESIAN_POINT('Ctrl Pts',(-9.23111241966252,637.64289683962,56.1656879276833));
#100223=CARTESIAN_POINT('Ctrl Pts',(-9.91630154576906,638.059793395881,
57.0451969084296));
#100224=CARTESIAN_POINT('Ctrl Pts',(-10.1324915118317,638.194563834501,
57.3502753776917));
#100225=CARTESIAN_POINT('Ctrl Pts',(-10.5357713613976,638.450345977724,
57.9783769701487));
#100226=CARTESIAN_POINT('Ctrl Pts',(-10.7236262872103,638.571827920009,
58.3023594003029));
#100227=CARTESIAN_POINT('Ctrl Pts',(-11.0712376013219,638.799630368598,
58.9713183751389));
#100228=CARTESIAN_POINT('Ctrl Pts',(-11.2309988089124,638.905958788751,
59.3162894189298));
#100229=CARTESIAN_POINT('Ctrl Pts',(-11.5208797326646,639.100832791066,
60.0290181547742));
#100230=CARTESIAN_POINT('Ctrl Pts',(-11.6501690769847,639.188825002839,
60.3953019668914));
#100231=CARTESIAN_POINT('Ctrl Pts',(-11.9839910541968,639.417577428592,
61.5063440997196));
#100232=CARTESIAN_POINT('Ctrl Pts',(-12.1379146213264,639.525259634802,
62.2699324426638));
#100233=CARTESIAN_POINT('Ctrl Pts',(-12.2580662787846,639.609359342908,
63.4530645764399));
#100234=CARTESIAN_POINT('Ctrl Pts',(-12.2789163285454,639.624011257781,
63.8499267607108));
#100235=CARTESIAN_POINT('Ctrl Pts',(-12.2825378585981,639.626553235025,
64.6358410829958));
#100236=CARTESIAN_POINT('Ctrl Pts',(-12.2655225913637,639.614593960502,
65.0268582260156));
#100237=CARTESIAN_POINT('Ctrl Pts',(-12.1944767448526,639.56483898852,65.8050866022495));
#100238=CARTESIAN_POINT('Ctrl Pts',(-12.1404459138046,639.527041901337,
66.1922977510875));
#100239=CARTESIAN_POINT('Ctrl Pts',(-11.9949724860648,639.425910086977,
66.9629011030374));
#100240=CARTESIAN_POINT('Ctrl Pts',(-11.903019104308,639.362229437876,67.3470686022024));
#100241=CARTESIAN_POINT('Ctrl Pts',(-11.5792106607343,639.139979984994,
68.4638808611085));
#100242=CARTESIAN_POINT('Ctrl Pts',(-11.2984041214378,638.949298291411,
69.1715940183495));
#100243=CARTESIAN_POINT('Ctrl Pts',(-10.7859893300428,638.612393734488,
70.1837668701614));
#100244=CARTESIAN_POINT('Ctrl Pts',(-10.5987639460202,638.490882128964,
70.5144589620626));
#100245=CARTESIAN_POINT('Ctrl Pts',(-10.2001915144139,638.237084423121,
71.1489943075356));
#100246=CARTESIAN_POINT('Ctrl Pts',(-9.98878898534629,638.104736729523,
71.4534198335247));
#100247=CARTESIAN_POINT('Ctrl Pts',(-9.31947230013895,637.695354479429,
72.3311884350087));
#100248=CARTESIAN_POINT('Ctrl Pts',(-8.82689483618176,637.405883894209,
72.8693491319149));
#100249=CARTESIAN_POINT('Ctrl Pts',(-8.01529581017258,636.96271562303,73.6112320344375));
#100250=CARTESIAN_POINT('Ctrl Pts',(-7.73182881330978,636.813214269367,
73.8478989536329));
#100251=CARTESIAN_POINT('Ctrl Pts',(-7.14908314421362,636.51954027595,74.2916812721146));
#100252=CARTESIAN_POINT('Ctrl Pts',(-6.84872810477117,636.374745902242,
74.4998846147026));
#100253=CARTESIAN_POINT('Ctrl Pts',(-5.91918799038042,635.951618424442,
75.0845859838612));
#100254=CARTESIAN_POINT('Ctrl Pts',(-5.26207272556291,635.684059915601,
75.4217452738926));
#100255=CARTESIAN_POINT('Ctrl Pts',(-4.20600812444231,635.331161942316,
75.8438524767));
#100256=CARTESIAN_POINT('Ctrl Pts',(-3.84458489423226,635.22269060845,75.9693060886928));
#100257=CARTESIAN_POINT('Ctrl Pts',(-3.11078512019224,635.031436050469,
76.185971800507));
#100258=CARTESIAN_POINT('Ctrl Pts',(-2.73707032232845,634.94819615451,76.2777372174655));
#100259=CARTESIAN_POINT('Ctrl Pts',(-1.97462989968799,634.81123574556,76.4267647296646));
#100260=CARTESIAN_POINT('Ctrl Pts',(-1.58407504305315,634.757375766206,
76.4841860202651));
#100261=CARTESIAN_POINT('Ctrl Pts',(-0.795241544847691,634.685011679452,
76.5609621502088));
#100262=CARTESIAN_POINT('Ctrl Pts',(-0.400287481815783,634.666520326694,
76.5803315661586));
#100263=CARTESIAN_POINT('Ctrl Pts',(-5.83190623966335E-15,634.666520326694,
76.5803315661586));
#100264=CARTESIAN_POINT('',(-2.31092134190293,635.230245103769,51.3976052199539));
#100265=CARTESIAN_POINT('Origin',(-2.31092134187393,634.856083886813,51.7292728001094));
#100266=CARTESIAN_POINT('',(2.26224148372674,635.222186336159,77.2104285068931));
#100267=CARTESIAN_POINT('Ctrl Pts',(2.26224148372674,635.222186336159,77.2104285068931));
#100268=CARTESIAN_POINT('Ctrl Pts',(1.83032423084503,635.151425581871,77.2901548692284));
#100269=CARTESIAN_POINT('Ctrl Pts',(1.39473620312201,635.099839659559,77.3470551071421));
#100270=CARTESIAN_POINT('Ctrl Pts',(0.515891315837579,635.038392002217,
77.4146673352173));
#100271=CARTESIAN_POINT('Ctrl Pts',(0.0702880625902517,635.028685620358,
77.4252220449457));
#100272=CARTESIAN_POINT('Ctrl Pts',(-0.814508254993039,635.052830125015,
77.3987706058388));
#100273=CARTESIAN_POINT('Ctrl Pts',(-1.25591590129853,635.086598311156,
77.3618450733092));
#100274=CARTESIAN_POINT('Ctrl Pts',(-2.12632669303214,635.193801226157,
77.2425878065961));
#100275=CARTESIAN_POINT('Ctrl Pts',(-2.55179819911838,635.266573160832,
77.1609561180698));
#100276=CARTESIAN_POINT('Ctrl Pts',(-3.38538928239685,635.444155118651,
76.9566426950186));
#100277=CARTESIAN_POINT('Ctrl Pts',(-3.79350628097141,635.548963982637,
76.833949796622));
#100278=CARTESIAN_POINT('Ctrl Pts',(-4.5939136248181,635.784840293459,76.5485878713385));
#100279=CARTESIAN_POINT('Ctrl Pts',(-4.98575248625829,635.915952155682,
76.3857550747386));
#100280=CARTESIAN_POINT('Ctrl Pts',(-6.11412644163187,636.33040038107,75.850504898419));
#100281=CARTESIAN_POINT('Ctrl Pts',(-6.81399404095514,636.637139823021,
75.4287590544389));
#100282=CARTESIAN_POINT('Ctrl Pts',(-7.79889285265662,637.113279774517,
74.7005250396438));
#100283=CARTESIAN_POINT('Ctrl Pts',(-8.11734298004477,637.275392821193,
74.4406405058552));
#100284=CARTESIAN_POINT('Ctrl Pts',(-8.72762915407622,637.598450812687,
73.8918331418519));
#100285=CARTESIAN_POINT('Ctrl Pts',(-9.01787207664488,637.758484580972,
73.6045582479782));
#100286=CARTESIAN_POINT('Ctrl Pts',(-9.84637516857155,638.229010305788,
72.7037235931987));
#100287=CARTESIAN_POINT('Ctrl Pts',(-10.3429614399288,638.529977527531,
72.0516283531007));
#100288=CARTESIAN_POINT('Ctrl Pts',(-11.0032431948168,638.943680061139,
70.9865177450937));
#100289=CARTESIAN_POINT('Ctrl Pts',(-11.2093789343219,639.075495693331,
70.6157898317709));
#100290=CARTESIAN_POINT('Ctrl Pts',(-11.5836014028183,639.318071631035,
69.8591636321725));
#100291=CARTESIAN_POINT('Ctrl Pts',(-11.7528969072206,639.429583137573,
69.4715259668061));
#100292=CARTESIAN_POINT('Ctrl Pts',(-12.0554510123091,639.630816768811,
68.6768786107822));
#100293=CARTESIAN_POINT('Ctrl Pts',(-12.1887140449545,639.720546948354,
68.2698726655556));
#100294=CARTESIAN_POINT('Ctrl Pts',(-12.4175304640208,639.875633351266,
67.4351906357858));
#100295=CARTESIAN_POINT('Ctrl Pts',(-12.5132629458602,639.941117156214,
67.0052234510874));
#100296=CARTESIAN_POINT('Ctrl Pts',(-12.7346497723208,640.093091607933,
65.7152869175487));
#100297=CARTESIAN_POINT('Ctrl Pts',(-12.7982740854582,640.137428052,64.8470309669364));
#100298=CARTESIAN_POINT('Ctrl Pts',(-12.766112503726,640.115168111399,63.5319360416885));
#100299=CARTESIAN_POINT('Ctrl Pts',(-12.7334707525218,640.092560699991,
63.0884936792983));
#100300=CARTESIAN_POINT('Ctrl Pts',(-12.6260778331749,640.018540506094,
62.2172823473981));
#100301=CARTESIAN_POINT('Ctrl Pts',(-12.551632369959,639.967339687422,61.788489253183));
#100302=CARTESIAN_POINT('Ctrl Pts',(-12.3628457782987,639.838488032098,
60.9438749494673));
#100303=CARTESIAN_POINT('Ctrl Pts',(-12.2485007430305,639.760831558039,
60.5280554739999));
#100304=CARTESIAN_POINT('Ctrl Pts',(-11.9802058693947,639.580576882095,
59.7090936426398));
#100305=CARTESIAN_POINT('Ctrl Pts',(-11.8256357552361,639.477580968645,
59.3051045068694));
#100306=CARTESIAN_POINT('Ctrl Pts',(-11.3133789750381,639.141064503064,
58.1368724774906));
#100307=CARTESIAN_POINT('Ctrl Pts',(-10.9053335034014,638.878451769385,
57.4071299613224));
#100308=CARTESIAN_POINT('Ctrl Pts',(-10.1963986672724,638.443487632523,
56.3789236860282));
#100309=CARTESIAN_POINT('Ctrl Pts',(-9.94375223192614,638.291657307618,
56.0476855370183));
#100310=CARTESIAN_POINT('Ctrl Pts',(-9.41478615234259,637.982769203909,
55.4180596023799));
#100311=CARTESIAN_POINT('Ctrl Pts',(-9.13741954079915,637.82505037934,55.1180679858199));
#100312=CARTESIAN_POINT('Ctrl Pts',(-8.55656002383599,637.506421762877,
54.5462464538821));
#100313=CARTESIAN_POINT('Ctrl Pts',(-8.25307216483238,637.345500316042,
54.2744178365614));
#100314=CARTESIAN_POINT('Ctrl Pts',(-7.61843493119114,637.024132716943,
53.7584611953167));
#100315=CARTESIAN_POINT('Ctrl Pts',(-7.28550391450078,636.862890623527,
53.513234090336));
#100316=CARTESIAN_POINT('Ctrl Pts',(-6.25785460882906,636.394030645923,
52.8307763736279));
#100317=CARTESIAN_POINT('Ctrl Pts',(-5.53420093242913,636.100160702073,
52.4443472052227));
#100318=CARTESIAN_POINT('Ctrl Pts',(-4.37964798732873,635.718161161364,
51.9682761050355));
#100319=CARTESIAN_POINT('Ctrl Pts',(-3.98317189683697,635.600726329753,
51.8270164181643));
#100320=CARTESIAN_POINT('Ctrl Pts',(-3.16332124464332,635.392500797527,
51.5819852864849));
#100321=CARTESIAN_POINT('Ctrl Pts',(-2.73846394280183,635.301756782016,
51.478279057735));
#100322=CARTESIAN_POINT('Ctrl Pts',(-2.31092134190293,635.230245103769,
51.3976052199539));
#100323=CARTESIAN_POINT('',(2.17374032143659,634.848232285471,76.3864221483552));
#100324=CARTESIAN_POINT('Origin',(2.26224148372674,634.848232285471,76.8785273650246));
#100325=CARTESIAN_POINT('Ctrl Pts',(-3.77134412588021E-9,634.666540598395,
76.5803595180565));
#100326=CARTESIAN_POINT('Ctrl Pts',(0.346198564424135,634.66658200697,76.5804168433102));
#100327=CARTESIAN_POINT('Ctrl Pts',(0.689932235574015,634.680576584132,
76.565893487059));
#100328=CARTESIAN_POINT('Ctrl Pts',(1.03129404451953,634.707739368398,76.5371136742991));
#100329=CARTESIAN_POINT('Ctrl Pts',(1.05249997329679,634.709426762985,76.5353258273765));
#100330=CARTESIAN_POINT('Ctrl Pts',(1.07369674831757,634.711164990005,76.5334829566629));
#100331=CARTESIAN_POINT('Ctrl Pts',(1.09488439167535,634.712953867263,76.5315851371587));
#100332=CARTESIAN_POINT('Ctrl Pts',(1.43870745103581,634.741982921654,76.5007882194922));
#100333=CARTESIAN_POINT('Ctrl Pts',(1.78012200277545,634.784345579451,76.455523733084));
#100334=CARTESIAN_POINT('Ctrl Pts',(2.11922347862932,634.839287712169,76.396100987804));
#100335=CARTESIAN_POINT('Ctrl Pts',(2.13740240274387,634.842233110324,76.3929153880528));
#100336=CARTESIAN_POINT('Ctrl Pts',(2.15557467882417,634.845214672232,76.3896890929648));
#100337=CARTESIAN_POINT('Ctrl Pts',(2.17374032143659,634.848232285471,76.3864221483552));
#100338=CARTESIAN_POINT('Origin',(21.5,620.675373764374,64.2994740882088));
#100339=CARTESIAN_POINT('',(21.5,620.675373764374,44.8494740882088));
#100340=CARTESIAN_POINT('Origin',(21.5,620.675373764374,64.2994740882088));
#100341=CARTESIAN_POINT('Origin',(21.5,620.675373764374,45.3494740882088));
#100342=CARTESIAN_POINT('Origin',(-47.,620.675373764374,64.2994740882088));
#100343=CARTESIAN_POINT('',(-47.,620.675373764374,44.8494740882088));
#100344=CARTESIAN_POINT('',(-47.,620.675373764374,83.7494740882088));
#100345=CARTESIAN_POINT('Origin',(-47.,620.675373764374,64.2994740882088));
#100346=CARTESIAN_POINT('Origin',(-47.,620.675373764374,64.2994740882088));
#100347=CARTESIAN_POINT('',(-48.,620.675373764374,82.7494740882088));
#100348=CARTESIAN_POINT('Origin',(-47.,620.675373764374,82.7494740882088));
#100349=CARTESIAN_POINT('Origin',(-48.,620.675373764374,64.2994740882088));
#100350=CARTESIAN_POINT('Origin',(0.,646.549217610995,64.2994740882088));
#100351=CARTESIAN_POINT('',(-1.07343961497457E-8,606.684183939705,52.0186534989093));
#100352=CARTESIAN_POINT('Ctrl Pts',(-2.17374032143659,606.502515243277,
76.3864221483552));
#100353=CARTESIAN_POINT('Ctrl Pts',(-2.46707185687862,606.453788029884,
76.3336688327153));
#100354=CARTESIAN_POINT('Ctrl Pts',(-2.75429831334365,606.396546320481,
76.2711602395621));
#100355=CARTESIAN_POINT('Ctrl Pts',(-3.03595174524071,606.33200370037,76.1993630371087));
#100356=CARTESIAN_POINT('Ctrl Pts',(-3.32677393225283,606.265360003505,
76.1252285971402));
#100357=CARTESIAN_POINT('Ctrl Pts',(-3.61165436076205,606.190932157165,
76.0411909881563));
#100358=CARTESIAN_POINT('Ctrl Pts',(-3.89115974378405,606.110012377849,
75.9477342140385));
#100359=CARTESIAN_POINT('Ctrl Pts',(-4.05802307910513,606.061703668643,
75.8919409807596));
#100360=CARTESIAN_POINT('Ctrl Pts',(-4.22297037084448,606.011080391334,
75.8327901578527));
#100361=CARTESIAN_POINT('Ctrl Pts',(-4.38611911179911,605.958410855426,
75.7703798975853));
#100362=CARTESIAN_POINT('Ctrl Pts',(-4.42882625023245,605.944623650278,
75.7540428813797));
#100363=CARTESIAN_POINT('Ctrl Pts',(-4.4713977435419,605.93069957899,75.7374872585257));
#100364=CARTESIAN_POINT('Ctrl Pts',(-4.51383960644833,605.916642373094,
75.7207136183459));
#100365=CARTESIAN_POINT('Ctrl Pts',(-4.68077779163335,605.861350633278,
75.6547372247853));
#100366=CARTESIAN_POINT('Ctrl Pts',(-4.84590667786203,605.803892065816,
75.5852360338964));
#100367=CARTESIAN_POINT('Ctrl Pts',(-5.00922883921225,605.744546045644,
75.5122717295713));
#100368=CARTESIAN_POINT('Ctrl Pts',(-5.1452103593152,605.695134735088,75.4515218782752));
#100369=CARTESIAN_POINT('Ctrl Pts',(-5.27993934023756,605.644414219227,
75.3883704451901));
#100370=CARTESIAN_POINT('Ctrl Pts',(-5.41340686872785,605.592533100018,
75.3228309779361));
#100371=CARTESIAN_POINT('Ctrl Pts',(-5.4767325267563,605.567917329798,75.2917348009286));
#100372=CARTESIAN_POINT('Ctrl Pts',(-5.53988672272686,605.542995856186,
75.2600451580777));
#100373=CARTESIAN_POINT('Ctrl Pts',(-5.60282655347565,605.517797003193,
75.2277765641491));
#100374=CARTESIAN_POINT('Ctrl Pts',(-5.74446489104482,605.461090087969,
75.1551600676419));
#100375=CARTESIAN_POINT('Ctrl Pts',(-5.88451794386309,605.403194028895,
75.0798887530446));
#100376=CARTESIAN_POINT('Ctrl Pts',(-6.02277650795407,605.344367506919,
75.00208867691));
#100377=CARTESIAN_POINT('Ctrl Pts',(-6.14763311325176,605.291243276361,
74.9318300751233));
#100378=CARTESIAN_POINT('Ctrl Pts',(-6.27102683838747,605.237360714913,
74.8595096788036));
#100379=CARTESIAN_POINT('Ctrl Pts',(-6.39282729924325,605.18292181379,74.7852455842724));
#100380=CARTESIAN_POINT('Ctrl Pts',(-6.47083494811976,605.148056176549,
74.7376828134124));
#100381=CARTESIAN_POINT('Ctrl Pts',(-6.54814400546939,605.112980745157,
74.6893515147672));
#100382=CARTESIAN_POINT('Ctrl Pts',(-6.62477499791199,605.07772814186,74.6402582278617));
#100383=CARTESIAN_POINT('Ctrl Pts',(-6.96478303205049,604.921314033637,
74.4224336710075));
#100384=CARTESIAN_POINT('Ctrl Pts',(-7.29157363628114,604.761467878279,
74.1897538732292));
#100385=CARTESIAN_POINT('Ctrl Pts',(-7.60591158708235,604.600369471168,
73.9417908300559));
#100386=CARTESIAN_POINT('Ctrl Pts',(-7.79580795695568,604.503047456359,
73.7919925583507));
#100387=CARTESIAN_POINT('Ctrl Pts',(-7.98115910169857,604.405267574512,
73.6366162396827));
#100388=CARTESIAN_POINT('Ctrl Pts',(-8.16212832796301,604.307503591966,
73.4755645439775));
#100389=CARTESIAN_POINT('Ctrl Pts',(-8.26136891658198,604.253891409531,
73.3872464060831));
#100390=CARTESIAN_POINT('Ctrl Pts',(-8.35931409671926,604.200262850107,
73.2972012703487));
#100391=CARTESIAN_POINT('Ctrl Pts',(-8.45597459854735,604.146704981741,
73.2054245700201));
#100392=CARTESIAN_POINT('Ctrl Pts',(-8.62621244832271,604.052379210854,
73.0437880398146));
#100393=CARTESIAN_POINT('Ctrl Pts',(-8.79257116956151,603.95814323677,72.8764594849325));
#100394=CARTESIAN_POINT('Ctrl Pts',(-8.95390631633433,603.865073190674,
72.704606310153));
#100395=CARTESIAN_POINT('Ctrl Pts',(-9.06095118698477,603.803321791521,
72.5905827930637));
#100396=CARTESIAN_POINT('Ctrl Pts',(-9.16584077110249,603.742048678356,
72.4745092679943));
#100397=CARTESIAN_POINT('Ctrl Pts',(-9.26827482729216,603.681541731399,
72.3566784495144));
#100398=CARTESIAN_POINT('Ctrl Pts',(-9.40788641074879,603.599074327598,
72.1960819861906));
#100399=CARTESIAN_POINT('Ctrl Pts',(-9.54330408966463,603.517830454451,
72.0319079775284));
#100400=CARTESIAN_POINT('Ctrl Pts',(-9.67458462015739,603.438025868564,
71.8640057896189));
#100401=CARTESIAN_POINT('Ctrl Pts',(-9.78480582545456,603.371023110335,
71.7230375786134));
#100402=CARTESIAN_POINT('Ctrl Pts',(-9.89203337317964,603.305082450115,
71.5795402257765));
#100403=CARTESIAN_POINT('Ctrl Pts',(-9.99631546020291,603.240324463723,
71.4334167298244));
#100404=CARTESIAN_POINT('Ctrl Pts',(-10.1466411918896,603.146973899259,
71.2227753620435));
#100405=CARTESIAN_POINT('Ctrl Pts',(-10.2908485193802,603.056075593346,
71.0066806945939));
#100406=CARTESIAN_POINT('Ctrl Pts',(-10.4288865117607,602.968017132758,
70.784690190237));
#100407=CARTESIAN_POINT('Ctrl Pts',(-10.5005094876998,602.922326747849,
70.6695072592333));
#100408=CARTESIAN_POINT('Ctrl Pts',(-10.5704709864211,602.877401174178,
70.5527365289386));
#100409=CARTESIAN_POINT('Ctrl Pts',(-10.6387601151285,602.83329660101,70.4343126036391));
#100410=CARTESIAN_POINT('Ctrl Pts',(-10.724621663596,602.777842870403,70.2854153809878));
#100411=CARTESIAN_POINT('Ctrl Pts',(-10.8079009366217,602.723642207191,
70.1336854355193));
#100412=CARTESIAN_POINT('Ctrl Pts',(-10.888241259658,602.671014635769,69.9796674430985));
#100413=CARTESIAN_POINT('Ctrl Pts',(-10.9945530515871,602.601374245846,
69.7758603367196));
#100414=CARTESIAN_POINT('Ctrl Pts',(-11.0954755518842,602.534655054501,
69.5685147915909));
#100415=CARTESIAN_POINT('Ctrl Pts',(-11.1902371419611,602.471566104083,
69.3589259475648));
#100416=CARTESIAN_POINT('Ctrl Pts',(-11.300099218997,602.3984237779,69.1159386178927));
#100417=CARTESIAN_POINT('Ctrl Pts',(-11.4021973889724,602.329852464716,
68.869301471737));
#100418=CARTESIAN_POINT('Ctrl Pts',(-11.4964066628775,602.266152746647,
68.6186837688837));
#100419=CARTESIAN_POINT('Ctrl Pts',(-11.5906159367827,602.202453028578,
68.3680660660304));
#100420=CARTESIAN_POINT('Ctrl Pts',(-11.6769365272855,602.143624555107,
68.1134679693462));
#100421=CARTESIAN_POINT('Ctrl Pts',(-11.7551965015822,602.089998067109,
67.8545346302323));
#100422=CARTESIAN_POINT('Ctrl Pts',(-11.8169098336505,602.047709920566,
67.6503480165271));
#100423=CARTESIAN_POINT('Ctrl Pts',(-11.8735597973911,602.008694644865,
67.4436368914992));
#100424=CARTESIAN_POINT('Ctrl Pts',(-11.9250862572614,601.973096443384,
67.2341237558232));
#100425=CARTESIAN_POINT('Ctrl Pts',(-11.9407583946926,601.962268998469,
67.1703988528467));
#100426=CARTESIAN_POINT('Ctrl Pts',(-11.9559562743235,601.951757858935,
67.1064145882828));
#100427=CARTESIAN_POINT('Ctrl Pts',(-11.9706774739931,601.941567587219,
67.0421627707268));
#100428=CARTESIAN_POINT('Ctrl Pts',(-11.9954037307114,601.924451640141,
66.9342431058105));
#100429=CARTESIAN_POINT('Ctrl Pts',(-12.018712244929,601.908287348004,66.8257413548535));
#100430=CARTESIAN_POINT('Ctrl Pts',(-12.0405781026576,601.893099709119,
66.716775352046));
#100431=CARTESIAN_POINT('Ctrl Pts',(-12.0731127727702,601.870501701438,
66.5546425421266));
#100432=CARTESIAN_POINT('Ctrl Pts',(-12.1023388533522,601.850161851815,
66.3920691391728));
#100433=CARTESIAN_POINT('Ctrl Pts',(-12.1282540008843,601.832100855068,
66.2292774714516));
#100434=CARTESIAN_POINT('Ctrl Pts',(-12.1502877690817,601.816744900979,
66.0908675370076));
#100435=CARTESIAN_POINT('Ctrl Pts',(-12.1699275035384,601.803036685216,
65.9522990545189));
#100436=CARTESIAN_POINT('Ctrl Pts',(-12.1871477917995,601.79100539956,65.8137029664605));
#100437=CARTESIAN_POINT('Ctrl Pts',(-12.1980348631784,601.783398937709,
65.7260792588519));
#100438=CARTESIAN_POINT('Ctrl Pts',(-12.2079791265231,601.776445852263,
65.6383428164895));
#100439=CARTESIAN_POINT('Ctrl Pts',(-12.2169811144402,601.770146217632,
65.5504516908381));
#100440=CARTESIAN_POINT('Ctrl Pts',(-12.2439507747706,601.751272719049,
65.2871327632072));
#100441=CARTESIAN_POINT('Ctrl Pts',(-12.262381938816,601.738341021169,65.0232227696719));
#100442=CARTESIAN_POINT('Ctrl Pts',(-12.2722764759267,601.731396026852,
64.758554127766));
#100443=CARTESIAN_POINT('Ctrl Pts',(-12.2745803436584,601.729778937733,
64.6969280469448));
#100444=CARTESIAN_POINT('Ctrl Pts',(-12.2764212110178,601.72848654818,64.6352608197646));
#100445=CARTESIAN_POINT('Ctrl Pts',(-12.2777987694388,601.727519657373,
64.5735503018836));
#100446=CARTESIAN_POINT('Ctrl Pts',(-12.2836252561778,601.723430120131,
64.3125410346233));
#100447=CARTESIAN_POINT('Ctrl Pts',(-12.2811683166638,601.725160388178,
64.0507577357569));
#100448=CARTESIAN_POINT('Ctrl Pts',(-12.2702125553129,601.732843354971,
63.7880240573192));
#100449=CARTESIAN_POINT('Ctrl Pts',(-12.2637572833743,601.737370255326,
63.6332180801329));
#100450=CARTESIAN_POINT('Ctrl Pts',(-12.254350682346,601.743964308948,63.4780820905828));
#100451=CARTESIAN_POINT('Ctrl Pts',(-12.2419417245922,601.752657551092,
63.322579412737));
#100452=CARTESIAN_POINT('Ctrl Pts',(-12.2383613410484,601.755165831137,
63.27771188721));
#100453=CARTESIAN_POINT('Ctrl Pts',(-12.2345355379089,601.757845659036,
63.2328883365077));
#100454=CARTESIAN_POINT('Ctrl Pts',(-12.2304658136691,601.760695594299,
63.1881120965528));
#100455=CARTESIAN_POINT('Ctrl Pts',(-12.20802985293,601.77640698699,62.9412654056049));
#100456=CARTESIAN_POINT('Ctrl Pts',(-12.1782497081193,601.797243520989,
62.6965771340082));
#100457=CARTESIAN_POINT('Ctrl Pts',(-12.1414782088463,601.822892192644,
62.4545441951047));
#100458=CARTESIAN_POINT('Ctrl Pts',(-12.1225673535514,601.836082797536,
62.3300714383586));
#100459=CARTESIAN_POINT('Ctrl Pts',(-12.1018066819712,601.850546650797,
62.2063009544923));
#100460=CARTESIAN_POINT('Ctrl Pts',(-12.0792398615636,601.866244252266,
62.083300637742));
#100461=CARTESIAN_POINT('Ctrl Pts',(-12.0338392047362,601.897825192977,
61.8358446350983));
#100462=CARTESIAN_POINT('Ctrl Pts',(-11.9810913904904,601.934449474634,
61.5908900513811));
#100463=CARTESIAN_POINT('Ctrl Pts',(-11.9210791903706,601.975905237726,
61.3483598142781));
#100464=CARTESIAN_POINT('Ctrl Pts',(-11.8825771448038,602.002502024319,
61.1927596159579));
#100465=CARTESIAN_POINT('Ctrl Pts',(-11.8410841234437,602.031088120635,
61.0381575576643));
#100466=CARTESIAN_POINT('Ctrl Pts',(-11.7966129422133,602.061613620413,
60.8845362018886));
#100467=CARTESIAN_POINT('Ctrl Pts',(-11.7145024730305,602.117975134532,
60.6008935989656));
#100468=CARTESIAN_POINT('Ctrl Pts',(-11.622240048691,602.180950916266,60.3206183352987));
#100469=CARTESIAN_POINT('Ctrl Pts',(-11.5200358747597,602.250140176206,
60.0440321693328));
#100470=CARTESIAN_POINT('Ctrl Pts',(-11.4804847370665,602.27691514871,59.9369984043372));
#100471=CARTESIAN_POINT('Ctrl Pts',(-11.4394452245149,602.304620325316,
59.8305169440055));
#100472=CARTESIAN_POINT('Ctrl Pts',(-11.3969311992182,602.333231415316,
59.7246058240927));
#100473=CARTESIAN_POINT('Ctrl Pts',(-11.2825177403899,602.410229388217,
59.4395785307927));
#100474=CARTESIAN_POINT('Ctrl Pts',(-11.158988431834,602.492725506564,59.1623611802148));
#100475=CARTESIAN_POINT('Ctrl Pts',(-11.0267821846615,602.579993779557,
58.8926332895343));
#100476=CARTESIAN_POINT('Ctrl Pts',(-11.0022967669809,602.596156405455,
58.8426780097752));
#100477=CARTESIAN_POINT('Ctrl Pts',(-10.9775138237409,602.612482671629,
58.7929795440708));
#100478=CARTESIAN_POINT('Ctrl Pts',(-10.9524362839605,602.628967901316,
58.7435357446885));
#100479=CARTESIAN_POINT('Ctrl Pts',(-10.7519969306551,602.760730777836,
58.3483421467532));
#100480=CARTESIAN_POINT('Ctrl Pts',(-10.5325668032455,602.902760978284,
57.9690756449635));
#100481=CARTESIAN_POINT('Ctrl Pts',(-10.2952739748061,603.052908390917,
57.6041926021618));
#100482=CARTESIAN_POINT('Ctrl Pts',(-10.1290947826627,603.15805853767,57.3486603567147));
#100483=CARTESIAN_POINT('Ctrl Pts',(-9.95405618215907,603.267227434755,
57.1002579207061));
#100484=CARTESIAN_POINT('Ctrl Pts',(-9.77011972363466,603.379759886329,
56.8587519976395));
#100485=CARTESIAN_POINT('Ctrl Pts',(-9.71724352583042,603.412109580438,
56.7893263108485));
#100486=CARTESIAN_POINT('Ctrl Pts',(-9.66363239874421,603.444736981392,
56.720471086118));
#100487=CARTESIAN_POINT('Ctrl Pts',(-9.60928507234348,603.477626699899,
56.6521803974868));
#100488=CARTESIAN_POINT('Ctrl Pts',(-9.36573391882352,603.625018106469,
56.3461437054854));
#100489=CARTESIAN_POINT('Ctrl Pts',(-9.10609991920284,603.778422086477,
56.0501477801115));
#100490=CARTESIAN_POINT('Ctrl Pts',(-8.83441059956637,603.93369250988,55.7687853847948));
#100491=CARTESIAN_POINT('Ctrl Pts',(-8.65468490819934,604.036405727434,
55.5826608397055));
#100492=CARTESIAN_POINT('Ctrl Pts',(-8.47006004966758,604.139793805599,
55.4030725521529));
#100493=CARTESIAN_POINT('Ctrl Pts',(-8.28039538035885,604.243327157586,
55.2298442866972));
#100494=CARTESIAN_POINT('Ctrl Pts',(-7.9890388931648,604.402371611421,54.9637368504001));
#100495=CARTESIAN_POINT('Ctrl Pts',(-7.68586832487023,604.561762715034,
54.7127055606849));
#100496=CARTESIAN_POINT('Ctrl Pts',(-7.37033208730518,604.71958124259,54.4760819004763));
#100497=CARTESIAN_POINT('Ctrl Pts',(-7.2700391143498,604.769743751461,54.4008712351751));
#100498=CARTESIAN_POINT('Ctrl Pts',(-7.16849659991518,604.819747365336,
54.3271164420992));
#100499=CARTESIAN_POINT('Ctrl Pts',(-7.06568610310642,604.869530328493,
54.25479687612));
#100500=CARTESIAN_POINT('Ctrl Pts',(-6.89206181747092,604.953602788829,
54.1326650571874));
#100501=CARTESIAN_POINT('Ctrl Pts',(-6.71445450113538,605.037163623483,
54.014541313487));
#100502=CARTESIAN_POINT('Ctrl Pts',(-6.53323952933694,605.119585952013,
53.9007405871998));
#100503=CARTESIAN_POINT('Ctrl Pts',(-6.39148708172352,605.184059470349,
53.8117218304641));
#100504=CARTESIAN_POINT('Ctrl Pts',(-6.24726996399549,605.247955635443,
53.7251920165717));
#100505=CARTESIAN_POINT('Ctrl Pts',(-6.1010333037784,605.310847708287,53.6414835032615));
#100506=CARTESIAN_POINT('Ctrl Pts',(-5.9575052790118,605.372574876943,53.5593254619487));
#100507=CARTESIAN_POINT('Ctrl Pts',(-5.81203236066972,605.433334144939,
53.4798854136267));
#100508=CARTESIAN_POINT('Ctrl Pts',(-5.66506348803577,605.492735683132,
53.4034385207339));
#100509=CARTESIAN_POINT('Ctrl Pts',(-5.63106986886025,605.506475145316,
53.3857565006055));
#100510=CARTESIAN_POINT('Ctrl Pts',(-5.59699631957295,605.520142052501,
53.3682344347307));
#100511=CARTESIAN_POINT('Ctrl Pts',(-5.56284856908302,605.533731743956,
53.3508754028169));
#100512=CARTESIAN_POINT('Ctrl Pts',(-5.38268096900712,605.6054325752,53.2592870822194));
#100513=CARTESIAN_POINT('Ctrl Pts',(-5.19987034695042,605.675213610825,
53.1719434243341));
#100514=CARTESIAN_POINT('Ctrl Pts',(-5.01474362923014,605.742546333116,
53.0891303500769));
#100515=CARTESIAN_POINT('Ctrl Pts',(-4.85852202040101,605.799365933943,
53.0192474512071));
#100516=CARTESIAN_POINT('Ctrl Pts',(-4.70043407277484,605.854543653029,
52.9524335003881));
#100517=CARTESIAN_POINT('Ctrl Pts',(-4.54038793193478,605.90783958427,52.8887479043086));
#100518=CARTESIAN_POINT('Ctrl Pts',(-4.32988395211606,605.977938154442,
52.8049841136825));
#100519=CARTESIAN_POINT('Ctrl Pts',(-4.11606910507959,606.044759266673,
52.7266642081674));
#100520=CARTESIAN_POINT('Ctrl Pts',(-3.89880804431973,606.107740093685,
52.6539274618112));
#100521=CARTESIAN_POINT('Ctrl Pts',(-3.75513870481496,606.149387749213,
52.6058284593017));
#100522=CARTESIAN_POINT('Ctrl Pts',(-3.60957076508887,606.189429699183,
52.5600901866311));
#100523=CARTESIAN_POINT('Ctrl Pts',(-3.46260051940716,606.227568994084,
52.5169114539341));
#100524=CARTESIAN_POINT('Ctrl Pts',(-3.30083889264099,606.269546704321,
52.4693871267455));
#100525=CARTESIAN_POINT('Ctrl Pts',(-3.13696220030451,606.309325226518,
52.4248444109981));
#100526=CARTESIAN_POINT('Ctrl Pts',(-2.97184384013739,606.346433279838,
52.3836415514574));
#100527=CARTESIAN_POINT('Ctrl Pts',(-2.88817958080778,606.365235657679,
52.3627643654059));
#100528=CARTESIAN_POINT('Ctrl Pts',(-2.8041970333705,606.383352786247,52.3427440958518));
#100529=CARTESIAN_POINT('Ctrl Pts',(-2.72001197855735,606.400726128442,
52.3236235868221));
#100530=CARTESIAN_POINT('Ctrl Pts',(-2.59111236083403,606.427327253457,
52.2943472941348));
#100531=CARTESIAN_POINT('Ctrl Pts',(-2.46182005847151,606.452184037893,
52.2671471808491));
#100532=CARTESIAN_POINT('Ctrl Pts',(-2.33225003338043,606.475224241091,
52.2420568539227));
#100533=CARTESIAN_POINT('Ctrl Pts',(-2.02166802222565,606.530452081339,
52.181914824994));
#100534=CARTESIAN_POINT('Ctrl Pts',(-1.70858199877496,606.575372497744,
52.1337147382732));
#100535=CARTESIAN_POINT('Ctrl Pts',(-1.39302211019354,606.609207737378,
52.0977046786308));
#100536=CARTESIAN_POINT('Ctrl Pts',(-1.08056553839342,606.642710230454,
52.0620487534219));
#100537=CARTESIAN_POINT('Ctrl Pts',(-0.765683584542685,606.665344269887,
52.0383441545844));
#100538=CARTESIAN_POINT('Ctrl Pts',(-0.448405337689409,606.676388629552,
52.0267929415551));
#100539=CARTESIAN_POINT('Ctrl Pts',(-0.388670115536972,606.678467994541,
52.0246181492923));
#100540=CARTESIAN_POINT('Ctrl Pts',(-0.328849950036206,606.680136641758,
52.0228740510578));
#100541=CARTESIAN_POINT('Ctrl Pts',(-0.268945032176679,606.681389902202,
52.021561847169));
#100542=CARTESIAN_POINT('Ctrl Pts',(-0.17955506691534,606.683260014231,
52.0196037798813));
#100543=CARTESIAN_POINT('Ctrl Pts',(-0.0898586837202595,606.684188838802,
52.0186356114588));
#100544=CARTESIAN_POINT('Ctrl Pts',(-1.0734396260768E-8,606.684183939704,
52.0186534989093));
#100545=CARTESIAN_POINT('',(1.07518174918924E-8,634.666563589043,52.0186534989093));
#100546=CARTESIAN_POINT('',(-1.50397128011561E-15,646.549217610995,52.018616610259));
#100547=CARTESIAN_POINT('Ctrl Pts',(2.24521812585737E-14,634.666520326694,
52.018616610259));
#100548=CARTESIAN_POINT('Ctrl Pts',(-0.373817003726286,634.666520326694,
52.018616610259));
#100549=CARTESIAN_POINT('Ctrl Pts',(-0.751201067837897,634.68307764615,
52.0359697011552));
#100550=CARTESIAN_POINT('Ctrl Pts',(-1.49208745862324,634.747185279649,
52.1039208858558));
#100551=CARTESIAN_POINT('Ctrl Pts',(-1.8582948677369,634.794652262569,52.1544405788509));
#100552=CARTESIAN_POINT('Ctrl Pts',(-2.22051577456844,634.856083886813,
52.2210317180765));
#100553=CARTESIAN_POINT('Ctrl Pts',(2.17374032143659,634.848232285471,76.3864221483552));
#100554=CARTESIAN_POINT('Ctrl Pts',(2.46707185688744,634.896959498865,76.3336688327137));
#100555=CARTESIAN_POINT('Ctrl Pts',(2.75429831336094,634.95420120827,76.2711602395584));
#100556=CARTESIAN_POINT('Ctrl Pts',(3.03595174526615,635.018743828384,76.1993630371022));
#100557=CARTESIAN_POINT('Ctrl Pts',(3.32677393228709,635.085387525251,76.1252285971308));
#100558=CARTESIAN_POINT('Ctrl Pts',(3.61165436080482,635.159815371594,76.0411909881434));
#100559=CARTESIAN_POINT('Ctrl Pts',(3.89115974383501,635.240735150913,75.9477342140214));
#100560=CARTESIAN_POINT('Ctrl Pts',(4.05802307913842,635.289043860115,75.8919409807476));
#100561=CARTESIAN_POINT('Ctrl Pts',(4.22297037086047,635.339667137419,75.8327901578465));
#100562=CARTESIAN_POINT('Ctrl Pts',(4.3861191117982,635.392336673321,75.7703798975857));
#100563=CARTESIAN_POINT('Ctrl Pts',(4.42882625023184,635.40612387847,75.7540428813799));
#100564=CARTESIAN_POINT('Ctrl Pts',(4.47139774354158,635.420047949757,75.7374872585258));
#100565=CARTESIAN_POINT('Ctrl Pts',(4.5138396064483,635.434105155654,75.7207136183459));
#100566=CARTESIAN_POINT('Ctrl Pts',(4.68077779162843,635.489396895468,75.6547372247873));
#100567=CARTESIAN_POINT('Ctrl Pts',(4.84590667785229,635.546855462928,75.5852360339005));
#100568=CARTESIAN_POINT('Ctrl Pts',(5.00922883919779,635.606201483099,75.5122717295777));
#100569=CARTESIAN_POINT('Ctrl Pts',(5.14521035930517,635.655612793656,75.4515218782799));
#100570=CARTESIAN_POINT('Ctrl Pts',(5.27993934023189,635.706333309519,75.3883704451929));
#100571=CARTESIAN_POINT('Ctrl Pts',(5.41340686872647,635.758214428729,75.3228309779368));
#100572=CARTESIAN_POINT('Ctrl Pts',(5.47673252675539,635.782830198949,75.2917348009291));
#100573=CARTESIAN_POINT('Ctrl Pts',(5.53988672272641,635.807751672561,75.2600451580779));
#100574=CARTESIAN_POINT('Ctrl Pts',(5.60282655347567,635.832950525554,75.2277765641491));
#100575=CARTESIAN_POINT('Ctrl Pts',(5.74446489104563,635.889657440779,75.1551600676415));
#100576=CARTESIAN_POINT('Ctrl Pts',(5.88451794386466,635.947553499853,75.0798887530437));
#100577=CARTESIAN_POINT('Ctrl Pts',(6.02277650795639,636.00638002183,75.0020886769087));
#100578=CARTESIAN_POINT('Ctrl Pts',(6.1476331132527,636.059504252387,74.9318300751227));
#100579=CARTESIAN_POINT('Ctrl Pts',(6.27102683838704,636.113386813834,74.8595096788039));
#100580=CARTESIAN_POINT('Ctrl Pts',(6.39282729924149,636.167825714957,74.7852455842735));
#100581=CARTESIAN_POINT('Ctrl Pts',(6.4708349481186,636.202691352198,74.7376828134132));
#100582=CARTESIAN_POINT('Ctrl Pts',(6.54814400546881,636.23776678359,74.6893515147675));
#100583=CARTESIAN_POINT('Ctrl Pts',(6.62477499791198,636.273019386888,74.6402582278617));
#100584=CARTESIAN_POINT('Ctrl Pts',(6.96478303207395,636.429433495122,74.4224336709924));
#100585=CARTESIAN_POINT('Ctrl Pts',(7.29157363632626,636.589279650491,74.1897538731971));
#100586=CARTESIAN_POINT('Ctrl Pts',(7.60591158714745,636.750378057613,73.9417908300045));
#100587=CARTESIAN_POINT('Ctrl Pts',(7.79580795699725,636.84770007241,73.7919925583159));
#100588=CARTESIAN_POINT('Ctrl Pts',(7.98115910171771,636.945479954246,73.6366162396656));
#100589=CARTESIAN_POINT('Ctrl Pts',(8.16212832796075,637.04324393678,73.4755645439795));
#100590=CARTESIAN_POINT('Ctrl Pts',(8.26136891658048,637.096856119215,73.3872464060845));
#100591=CARTESIAN_POINT('Ctrl Pts',(8.35931409671852,637.15048467864,73.2972012703495));
#100592=CARTESIAN_POINT('Ctrl Pts',(8.45597459854733,637.204042547007,73.2054245700202));
#100593=CARTESIAN_POINT('Ctrl Pts',(8.62621244832184,637.298368317893,73.0437880398154));
#100594=CARTESIAN_POINT('Ctrl Pts',(8.79257116955984,637.392604291977,72.8764594849342));
#100595=CARTESIAN_POINT('Ctrl Pts',(8.95390631633191,637.485674338072,72.7046063101555));
#100596=CARTESIAN_POINT('Ctrl Pts',(9.06095118698319,637.547425737225,72.5905827930654));
#100597=CARTESIAN_POINT('Ctrl Pts',(9.16584077110172,637.608698850392,72.4745092679952));
#100598=CARTESIAN_POINT('Ctrl Pts',(9.26827482729214,637.669205797348,72.3566784495144));
#100599=CARTESIAN_POINT('Ctrl Pts',(9.4078864107479,637.751673201148,72.1960819861916));
#100600=CARTESIAN_POINT('Ctrl Pts',(9.5433040896629,637.832917074295,72.0319079775306));
#100601=CARTESIAN_POINT('Ctrl Pts',(9.67458462015488,637.912721660182,71.8640057896221));
#100602=CARTESIAN_POINT('Ctrl Pts',(9.78480582545293,637.979724418411,71.7230375786156));
#100603=CARTESIAN_POINT('Ctrl Pts',(9.89203337317883,638.045665078632,71.5795402257776));
#100604=CARTESIAN_POINT('Ctrl Pts',(9.99631546020288,638.110423065025,71.4334167298244));
#100605=CARTESIAN_POINT('Ctrl Pts',(10.1466411918942,638.203773629491,71.2227753620371));
#100606=CARTESIAN_POINT('Ctrl Pts',(10.290848519389,638.294671935407,71.0066806945808));
#100607=CARTESIAN_POINT('Ctrl Pts',(10.4288865117733,638.382730395997,70.7846901902168));
#100608=CARTESIAN_POINT('Ctrl Pts',(10.500509487708,638.428420780904,70.6695072592196));
#100609=CARTESIAN_POINT('Ctrl Pts',(10.570470986425,638.473346354573,70.5527365289317));
#100610=CARTESIAN_POINT('Ctrl Pts',(10.6387601151285,638.517450927738,70.4343126036392));
#100611=CARTESIAN_POINT('Ctrl Pts',(10.7246216635952,638.572904658344,70.2854153809893));
#100612=CARTESIAN_POINT('Ctrl Pts',(10.80790093662,638.627105321556,70.1336854355224));
#100613=CARTESIAN_POINT('Ctrl Pts',(10.8882412596556,638.679732892978,69.9796674431032));
#100614=CARTESIAN_POINT('Ctrl Pts',(10.9945530515856,638.749373282901,69.7758603367227));
#100615=CARTESIAN_POINT('Ctrl Pts',(11.0954755518835,638.816092474246,69.5685147915925));
#100616=CARTESIAN_POINT('Ctrl Pts',(11.1902371419611,638.879181424665,69.3589259475647));
#100617=CARTESIAN_POINT('Ctrl Pts',(11.3000992189965,638.952323750847,69.1159386178936));
#100618=CARTESIAN_POINT('Ctrl Pts',(11.4021973889716,639.020895064031,68.869301471739));
#100619=CARTESIAN_POINT('Ctrl Pts',(11.4964066628764,639.0845947821,68.6186837688867));
#100620=CARTESIAN_POINT('Ctrl Pts',(11.5906159367812,639.148294500168,68.3680660660344));
#100621=CARTESIAN_POINT('Ctrl Pts',(11.6769365272838,639.207122973639,68.1134679693512));
#100622=CARTESIAN_POINT('Ctrl Pts',(11.7551965015803,639.260749461637,67.8545346302384));
#100623=CARTESIAN_POINT('Ctrl Pts',(11.8169098336493,639.30303760818,67.6503480165316));
#100624=CARTESIAN_POINT('Ctrl Pts',(11.8735597973904,639.342052883881,67.443636891502));
#100625=CARTESIAN_POINT('Ctrl Pts',(11.9250862572612,639.377651085363,67.2341237558242));
#100626=CARTESIAN_POINT('Ctrl Pts',(11.9407583946925,639.388478530278,67.1703988528473));
#100627=CARTESIAN_POINT('Ctrl Pts',(11.9559562743234,639.398989669813,67.1064145882831));
#100628=CARTESIAN_POINT('Ctrl Pts',(11.9706774739931,639.409179941528,67.0421627707268));
#100629=CARTESIAN_POINT('Ctrl Pts',(11.9954037307109,639.426295888606,66.9342431058128));
#100630=CARTESIAN_POINT('Ctrl Pts',(12.018712244928,639.442460180743,66.8257413548581));
#100631=CARTESIAN_POINT('Ctrl Pts',(12.0405781026562,639.457647819627,66.7167753520528));
#100632=CARTESIAN_POINT('Ctrl Pts',(12.0731127727685,639.480245827309,66.5546425421351));
#100633=CARTESIAN_POINT('Ctrl Pts',(12.1023388533504,639.500585676932,66.3920691391829));
#100634=CARTESIAN_POINT('Ctrl Pts',(12.1282540008825,639.518646673678,66.2292774714633));
#100635=CARTESIAN_POINT('Ctrl Pts',(12.1502877690806,639.534002627768,66.0908675370154));
#100636=CARTESIAN_POINT('Ctrl Pts',(12.169927503538,639.547710843531,65.9522990545228));
#100637=CARTESIAN_POINT('Ctrl Pts',(12.1871477917995,639.559742129188,65.8137029664605));
#100638=CARTESIAN_POINT('Ctrl Pts',(12.1980348631781,639.567348591038,65.7260792588543));
#100639=CARTESIAN_POINT('Ctrl Pts',(12.2079791265226,639.574301676484,65.6383428164945));
#100640=CARTESIAN_POINT('Ctrl Pts',(12.2169811144395,639.580601311115,65.5504516908455));
#100641=CARTESIAN_POINT('Ctrl Pts',(12.2439507747694,639.599474809698,65.2871327632205));
#100642=CARTESIAN_POINT('Ctrl Pts',(12.2623819388147,639.612406507578,65.023222769691));
#100643=CARTESIAN_POINT('Ctrl Pts',(12.2722764759257,639.619351501895,64.758554127791));
#100644=CARTESIAN_POINT('Ctrl Pts',(12.2745803436579,639.620968591014,64.6969280469615));
#100645=CARTESIAN_POINT('Ctrl Pts',(12.2764212110176,639.622260980568,64.6352608197729));
#100646=CARTESIAN_POINT('Ctrl Pts',(12.2777987694388,639.623227871375,64.5735503018836));
#100647=CARTESIAN_POINT('Ctrl Pts',(12.2836252561777,639.627317408616,64.3125410346274));
#100648=CARTESIAN_POINT('Ctrl Pts',(12.2811683166639,639.625587140569,64.0507577357652));
#100649=CARTESIAN_POINT('Ctrl Pts',(12.2702125553135,639.617904173777,63.7880240573317));
#100650=CARTESIAN_POINT('Ctrl Pts',(12.2637572833749,639.613377273422,63.6332180801413));
#100651=CARTESIAN_POINT('Ctrl Pts',(12.2543506823463,639.6067832198,63.478082090587));
#100652=CARTESIAN_POINT('Ctrl Pts',(12.2419417245922,639.598089977656,63.322579412737));
#100653=CARTESIAN_POINT('Ctrl Pts',(12.2383613410486,639.595581697611,63.2777118872129));
#100654=CARTESIAN_POINT('Ctrl Pts',(12.2345355379094,639.592901869712,63.2328883365136));
#100655=CARTESIAN_POINT('Ctrl Pts',(12.2304658136699,639.590051934449,63.1881120965615));
#100656=CARTESIAN_POINT('Ctrl Pts',(12.2080298529311,639.574340541758,62.9412654056156));
#100657=CARTESIAN_POINT('Ctrl Pts',(12.1782497081209,639.55350400776,62.6965771340207));
#100658=CARTESIAN_POINT('Ctrl Pts',(12.1414782088484,639.527855336105,62.454544195119));
#100659=CARTESIAN_POINT('Ctrl Pts',(12.122567353553,639.514664731212,62.3300714383681));
#100660=CARTESIAN_POINT('Ctrl Pts',(12.1018066819721,639.500200877951,62.206300954497));
#100661=CARTESIAN_POINT('Ctrl Pts',(12.0792398615636,639.484503276481,62.0833006377421));
#100662=CARTESIAN_POINT('Ctrl Pts',(12.0338392047365,639.452922335771,61.8358446351003));
#100663=CARTESIAN_POINT('Ctrl Pts',(11.9810913904912,639.416298054115,61.590890051385));
#100664=CARTESIAN_POINT('Ctrl Pts',(11.921079190372,639.374842291023,61.3483598142839));
#100665=CARTESIAN_POINT('Ctrl Pts',(11.8825771448056,639.34824550443,61.1927596159649));
#100666=CARTESIAN_POINT('Ctrl Pts',(11.8410841234459,639.319659408115,61.0381575576725));
#100667=CARTESIAN_POINT('Ctrl Pts',(11.796612942216,639.289133908337,60.8845362018978));
#100668=CARTESIAN_POINT('Ctrl Pts',(11.7145024730303,639.232772394216,60.600893598964));
#100669=CARTESIAN_POINT('Ctrl Pts',(11.6222400486871,639.169796612479,60.3206183352867));
#100670=CARTESIAN_POINT('Ctrl Pts',(11.5200358747514,639.100607352536,60.0440321693105));
#100671=CARTESIAN_POINT('Ctrl Pts',(11.4804847370608,639.073832380033,59.9369984043224));
#100672=CARTESIAN_POINT('Ctrl Pts',(11.439445224512,639.046127203429,59.8305169439982));
#100673=CARTESIAN_POINT('Ctrl Pts',(11.3969311992182,639.017516113431,59.7246058240927));
#100674=CARTESIAN_POINT('Ctrl Pts',(11.2825177403853,638.940518140527,59.4395785307811));
#100675=CARTESIAN_POINT('Ctrl Pts',(11.158988431824,638.858022022176,59.1623611801923));
#100676=CARTESIAN_POINT('Ctrl Pts',(11.0267821846454,638.77075374918,58.8926332895015));
#100677=CARTESIAN_POINT('Ctrl Pts',(11.0022967669716,638.754591123286,58.8426780097566));
#100678=CARTESIAN_POINT('Ctrl Pts',(10.9775138237385,638.738264857117,58.7929795440662));
#100679=CARTESIAN_POINT('Ctrl Pts',(10.9524362839652,638.721779627435,58.7435357446977));
#100680=CARTESIAN_POINT('Ctrl Pts',(10.7519969306585,638.590016750914,58.3483421467591));
#100681=CARTESIAN_POINT('Ctrl Pts',(10.5325668032473,638.447986550465,57.9690756449664));
#100682=CARTESIAN_POINT('Ctrl Pts',(10.2952739748061,638.29783913783,57.6041926021619));
#100683=CARTESIAN_POINT('Ctrl Pts',(10.1290947826648,638.192688991078,57.3486603567179));
#100684=CARTESIAN_POINT('Ctrl Pts',(9.95405618216335,638.083520093995,57.1002579207122));
#100685=CARTESIAN_POINT('Ctrl Pts',(9.77011972364139,637.970987642423,56.8587519976483));
#100686=CARTESIAN_POINT('Ctrl Pts',(9.71724352583497,637.938637948312,56.7893263108543));
#100687=CARTESIAN_POINT('Ctrl Pts',(9.66363239874653,637.906010547357,56.7204710861209));
#100688=CARTESIAN_POINT('Ctrl Pts',(9.60928507234349,637.873120828848,56.6521803974868));
#100689=CARTESIAN_POINT('Ctrl Pts',(9.36573391882352,637.725729422279,56.3461437054853));
#100690=CARTESIAN_POINT('Ctrl Pts',(9.10609991920284,637.572325442271,56.0501477801115));
#100691=CARTESIAN_POINT('Ctrl Pts',(8.83441059956637,637.417055018867,55.7687853847949));
#100692=CARTESIAN_POINT('Ctrl Pts',(8.65468490820217,637.314341801315,55.5826608397085));
#100693=CARTESIAN_POINT('Ctrl Pts',(8.47006004967338,637.210953723151,55.4030725521586));
#100694=CARTESIAN_POINT('Ctrl Pts',(8.28039538036778,637.107420371167,55.2298442867054));
#100695=CARTESIAN_POINT('Ctrl Pts',(7.98903889316609,636.948375917327,54.9637368504007));
#100696=CARTESIAN_POINT('Ctrl Pts',(7.68586832486323,636.78898481371,54.7127055606788));
#100697=CARTESIAN_POINT('Ctrl Pts',(7.37033208728924,636.63116628615,54.4760819004643));
#100698=CARTESIAN_POINT('Ctrl Pts',(7.27003911433903,636.581003777281,54.4008712351672));
#100699=CARTESIAN_POINT('Ctrl Pts',(7.16849659990973,636.531000163409,54.3271164420954));
#100700=CARTESIAN_POINT('Ctrl Pts',(7.06568610310641,636.481217200254,54.25479687612));
#100701=CARTESIAN_POINT('Ctrl Pts',(6.89206181747449,636.39714473992,54.1326650571899));
#100702=CARTESIAN_POINT('Ctrl Pts',(6.7144545011427,636.313583905268,54.0145413134919));
#100703=CARTESIAN_POINT('Ctrl Pts',(6.53323952934815,636.23116157674,53.9007405872068));
#100704=CARTESIAN_POINT('Ctrl Pts',(6.39148708173227,636.166688058402,53.8117218304693));
#100705=CARTESIAN_POINT('Ctrl Pts',(6.2472699640017,636.102791893307,53.7251920165753));
#100706=CARTESIAN_POINT('Ctrl Pts',(6.10103330378201,636.039899820462,53.6414835032635));
#100707=CARTESIAN_POINT('Ctrl Pts',(5.95750527901565,635.978172651807,53.5593254619508));
#100708=CARTESIAN_POINT('Ctrl Pts',(5.81203236067384,635.91741338381,53.4798854136289));
#100709=CARTESIAN_POINT('Ctrl Pts',(5.66506348804016,635.858011845617,53.4034385207361));
#100710=CARTESIAN_POINT('Ctrl Pts',(5.63106986886731,635.844272383434,53.3857565006092));
#100711=CARTESIAN_POINT('Ctrl Pts',(5.5969963195827,635.83060547625,53.3682344347357));
#100712=CARTESIAN_POINT('Ctrl Pts',(5.56284856909546,635.817015784796,53.3508754028232));
#100713=CARTESIAN_POINT('Ctrl Pts',(5.38268096901558,635.745314953551,53.2592870822234));
#100714=CARTESIAN_POINT('Ctrl Pts',(5.19987034695471,635.675533917924,53.171943424336));
#100715=CARTESIAN_POINT('Ctrl Pts',(5.01474362923015,635.608201195631,53.0891303500769));
#100716=CARTESIAN_POINT('Ctrl Pts',(4.85852202040539,635.551381594805,53.019247451209));
#100717=CARTESIAN_POINT('Ctrl Pts',(4.70043407278366,635.496203875722,52.9524335003918));
#100718=CARTESIAN_POINT('Ctrl Pts',(4.54038793194821,635.442907944482,52.888747904314));
#100719=CARTESIAN_POINT('Ctrl Pts',(4.32988395212515,635.372809374309,52.8049841136858));
#100720=CARTESIAN_POINT('Ctrl Pts',(4.11606910508421,635.305988262076,52.7266642081689));
#100721=CARTESIAN_POINT('Ctrl Pts',(3.89880804431974,635.243007435063,52.6539274618112));
#100722=CARTESIAN_POINT('Ctrl Pts',(3.75513870481975,635.201359779536,52.6058284593033));
#100723=CARTESIAN_POINT('Ctrl Pts',(3.6095707650986,635.161317829567,52.5600901866341));
#100724=CARTESIAN_POINT('Ctrl Pts',(3.46260051942188,635.123178534668,52.5169114539384));
#100725=CARTESIAN_POINT('Ctrl Pts',(3.30083889265518,635.08120082443,52.4693871267495));
#100726=CARTESIAN_POINT('Ctrl Pts',(3.13696220031812,635.041422302233,52.4248444110017));
#100727=CARTESIAN_POINT('Ctrl Pts',(2.97184384015041,635.004314248912,52.3836415514606));
#100728=CARTESIAN_POINT('Ctrl Pts',(2.8881795808165,634.985511871071,52.3627643654079));
#100729=CARTESIAN_POINT('Ctrl Pts',(2.80419703337489,634.967394742501,52.3427440958528));
#100730=CARTESIAN_POINT('Ctrl Pts',(2.72001197855739,634.950021400306,52.3236235868221));
#100731=CARTESIAN_POINT('Ctrl Pts',(2.59111236083927,634.923420275291,52.294347294136));
#100732=CARTESIAN_POINT('Ctrl Pts',(2.46182005848197,634.898563490856,52.2671471808513));
#100733=CARTESIAN_POINT('Ctrl Pts',(2.33225003339614,634.875523287659,52.2420568539257));
#100734=CARTESIAN_POINT('Ctrl Pts',(2.0216680222383,634.820295447411,52.181914824996));
#100735=CARTESIAN_POINT('Ctrl Pts',(1.70858199878448,634.775375031004,52.1337147382744));
#100736=CARTESIAN_POINT('Ctrl Pts',(1.39302211019991,634.74153979137,52.0977046786315));
#100737=CARTESIAN_POINT('Ctrl Pts',(1.08056553841527,634.708037298296,52.0620487534243));
#100738=CARTESIAN_POINT('Ctrl Pts',(0.765683584580269,634.685403258863,
52.0383441545871));
#100739=CARTESIAN_POINT('Ctrl Pts',(0.448405337742959,634.674358899197,
52.0267929415571));
#100740=CARTESIAN_POINT('Ctrl Pts',(0.388670115572721,634.672279534207,
52.0246181492933));
#100741=CARTESIAN_POINT('Ctrl Pts',(0.328849950054106,634.67061088699,52.0228740510582));
#100742=CARTESIAN_POINT('Ctrl Pts',(0.26894503217668,634.669357626546,52.0215618471691));
#100743=CARTESIAN_POINT('Ctrl Pts',(0.179555066921117,634.667487514516,
52.0196037798815));
#100744=CARTESIAN_POINT('Ctrl Pts',(0.0898586837318516,634.666558689946,
52.0186356114589));
#100745=CARTESIAN_POINT('Ctrl Pts',(1.07518175474036E-8,634.666563589043,
52.0186534989093));
#100746=CARTESIAN_POINT('Ctrl Pts',(1.7398767070424E-11,606.684227202053,
52.018616610259));
#100747=CARTESIAN_POINT('Ctrl Pts',(0.373817003740921,606.684227202053,
52.0186166102595));
#100748=CARTESIAN_POINT('Ctrl Pts',(0.75120106784948,606.667669882597,52.035969701156));
#100749=CARTESIAN_POINT('Ctrl Pts',(1.49208745862893,606.603562249098,52.1039208858566));
#100750=CARTESIAN_POINT('Ctrl Pts',(1.85829486773971,606.556095266178,52.1544405788514));
#100751=CARTESIAN_POINT('Ctrl Pts',(2.22051577456844,606.494663641934,52.2210317180765));
#100752=CARTESIAN_POINT('Origin',(-48.,620.675373764374,64.2994740882088));
#100753=CARTESIAN_POINT('',(-48.,620.675373764374,44.8494740882088));
#100754=CARTESIAN_POINT('Ctrl Pts',(-3.85030552837329,608.045280920111,
79.0907977188138));
#100755=CARTESIAN_POINT('Ctrl Pts',(-4.23115754611984,607.932105616136,
78.99415899786));
#100756=CARTESIAN_POINT('Ctrl Pts',(-4.60131346252692,607.807253127989,
78.8852799373076));
#100757=CARTESIAN_POINT('Ctrl Pts',(-4.96211414895984,607.673156473991,
78.7647299399134));
#100758=CARTESIAN_POINT('Ctrl Pts',(-5.34276158691742,607.531683495412,
78.6375487859429));
#100759=CARTESIAN_POINT('Ctrl Pts',(-5.71299620598676,607.379921133396,
78.4973774780135));
#100760=CARTESIAN_POINT('Ctrl Pts',(-6.07436314690284,607.220681681377,
78.3448595458295));
#100761=CARTESIAN_POINT('Ctrl Pts',(-6.27213868897694,607.133530186936,
78.2613867283182));
#100762=CARTESIAN_POINT('Ctrl Pts',(-6.46725754698847,607.044138294261,
78.1742152209262));
#100763=CARTESIAN_POINT('Ctrl Pts',(-6.65996976734686,606.952962317827,
78.0834474967339));
#100764=CARTESIAN_POINT('Ctrl Pts',(-6.66518312762042,606.950495773606,
78.080991996784));
#100765=CARTESIAN_POINT('Ctrl Pts',(-6.67039454639831,606.948028009746,
78.0785339506688));
#100766=CARTESIAN_POINT('Ctrl Pts',(-6.67560403513433,606.945559032559,
78.0760733579906));
#100767=CARTESIAN_POINT('Ctrl Pts',(-6.8578343467733,606.859193075165,77.9900006945705));
#100768=CARTESIAN_POINT('Ctrl Pts',(-7.03785733736652,606.771178203692,
77.9006116068874));
#100769=CARTESIAN_POINT('Ctrl Pts',(-7.215789858865,606.6817674534,77.8079341656738));
#100770=CARTESIAN_POINT('Ctrl Pts',(-7.39804086769688,606.590186671518,
77.7130074090872));
#100771=CARTESIAN_POINT('Ctrl Pts',(-7.5780991625022,606.497140675157,77.614630588693));
#100772=CARTESIAN_POINT('Ctrl Pts',(-7.75606262292596,606.402883414968,
77.5127908409613));
#100773=CARTESIAN_POINT('Ctrl Pts',(-7.8179153405013,606.370123500769,77.4773955685869));
#100774=CARTESIAN_POINT('Ctrl Pts',(-7.87951473545424,606.337217167687,
77.4415816227428));
#100775=CARTESIAN_POINT('Ctrl Pts',(-7.94086400011092,606.304174852542,
77.4053473424493));
#100776=CARTESIAN_POINT('Ctrl Pts',(-8.121437580548,606.206919095931,77.2986964516231));
#100777=CARTESIAN_POINT('Ctrl Pts',(-8.30015667393309,606.108308982384,
77.1882091735264));
#100778=CARTESIAN_POINT('Ctrl Pts',(-8.47654659987535,606.008907743947,
77.0741437637344));
#100779=CARTESIAN_POINT('Ctrl Pts',(-8.65758128459169,605.906889038713,
76.9570747452605));
#100780=CARTESIAN_POINT('Ctrl Pts',(-8.83616203701266,605.804037747601,
76.8362367877207));
#100781=CARTESIAN_POINT('Ctrl Pts',(-9.01180166947103,605.700983120861,
76.7119523503828));
#100782=CARTESIAN_POINT('Ctrl Pts',(-9.05844940407669,605.67361307453,76.6789439264445));
#100783=CARTESIAN_POINT('Ctrl Pts',(-9.10488984292617,605.646228758214,
76.6456926236426));
#100784=CARTESIAN_POINT('Ctrl Pts',(-9.15111422548108,605.618842082703,
76.612204957696));
#100785=CARTESIAN_POINT('Ctrl Pts',(-9.15898657611739,605.614177931438,
76.6065017631101));
#100786=CARTESIAN_POINT('Ctrl Pts',(-9.1668522498693,605.609513942502,76.6007919954538));
#100787=CARTESIAN_POINT('Ctrl Pts',(-9.17471122726756,605.60485016159,76.5950756732529));
#100788=CARTESIAN_POINT('Ctrl Pts',(-9.60207382531122,605.351238854893,
76.2842283220931));
#100789=CARTESIAN_POINT('Ctrl Pts',(-10.0116117983045,605.097205235008,
75.953330317504));
#100790=CARTESIAN_POINT('Ctrl Pts',(-10.4040324386218,604.845763559111,
75.6011406067169));
#100791=CARTESIAN_POINT('Ctrl Pts',(-10.7191297461544,604.64386644429,75.3183470474384));
#100792=CARTESIAN_POINT('Ctrl Pts',(-11.0231911890468,604.44364022255,75.0218264745212));
#100793=CARTESIAN_POINT('Ctrl Pts',(-11.3165906288581,604.246631862434,
74.7109552956669));
#100794=CARTESIAN_POINT('Ctrl Pts',(-11.3211660968142,604.243559581725,
74.7061073616756));
#100795=CARTESIAN_POINT('Ctrl Pts',(-11.3257389714887,604.240488082105,
74.701255936195));
#100796=CARTESIAN_POINT('Ctrl Pts',(-11.330309255645,604.23741736854,74.6964010155038));
#100797=CARTESIAN_POINT('Ctrl Pts',(-11.5510374470401,604.089113011908,
74.4619259091729));
#100798=CARTESIAN_POINT('Ctrl Pts',(-11.7657533239914,603.942514229819,
74.2189269147374));
#100799=CARTESIAN_POINT('Ctrl Pts',(-11.9729190514427,603.799244900531,
73.9689066228666));
#100800=CARTESIAN_POINT('Ctrl Pts',(-12.0734225150265,603.729739852587,
73.8476128856814));
#100801=CARTESIAN_POINT('Ctrl Pts',(-12.1721485958898,603.661018499151,
73.7246659781166));
#100802=CARTESIAN_POINT('Ctrl Pts',(-12.2689186597508,603.593267506438,
73.6002344485137));
#100803=CARTESIAN_POINT('Ctrl Pts',(-12.2725876177275,603.590698782855,
73.5955167286437));
#100804=CARTESIAN_POINT('Ctrl Pts',(-12.2762537641056,603.588131453901,
73.5907968737177));
#100805=CARTESIAN_POINT('Ctrl Pts',(-12.2799170881477,603.585565530419,
73.5860748940442));
#100806=CARTESIAN_POINT('Ctrl Pts',(-12.5761628621236,603.378064370561,
73.2042177318029));
#100807=CARTESIAN_POINT('Ctrl Pts',(-12.8553373541657,603.178825518264,
72.8071138322945));
#100808=CARTESIAN_POINT('Ctrl Pts',(-13.1169859722107,602.989662224037,
72.3937997341821));
#100809=CARTESIAN_POINT('Ctrl Pts',(-13.1196323729917,602.987748963828,
72.3896193385041));
#100810=CARTESIAN_POINT('Ctrl Pts',(-13.1222769834676,602.985836732372,
72.3854372806603));
#100811=CARTESIAN_POINT('Ctrl Pts',(-13.124919803262,602.983925531487,72.3812535595345));
#100812=CARTESIAN_POINT('Ctrl Pts',(-13.3868026742264,602.794540399873,
71.9666793603881));
#100813=CARTESIAN_POINT('Ctrl Pts',(-13.631110707103,602.615257919091,71.5357863466911));
#100814=CARTESIAN_POINT('Ctrl Pts',(-13.856691485181,602.448092654014,71.0868685526235));
#100815=CARTESIAN_POINT('Ctrl Pts',(-13.8582610272093,602.446929554429,
71.0837450801759));
#100816=CARTESIAN_POINT('Ctrl Pts',(-13.859829662386,602.445767041551,71.0806207352235));
#100817=CARTESIAN_POINT('Ctrl Pts',(-13.8613973903024,602.444605116074,
71.0774955172258));
#100818=CARTESIAN_POINT('Ctrl Pts',(-14.0874235511567,602.277085260077,
70.6269192287555));
#100819=CARTESIAN_POINT('Ctrl Pts',(-14.2932373615726,602.12276713293,70.1602556258246));
#100820=CARTESIAN_POINT('Ctrl Pts',(-14.4749373298438,601.985591928934,
69.6841332957598));
#100821=CARTESIAN_POINT('Ctrl Pts',(-14.475477179548,601.985184366985,69.6827186862722));
#100822=CARTESIAN_POINT('Ctrl Pts',(-14.476016816648,601.984776956179,69.6813039927107));
#100823=CARTESIAN_POINT('Ctrl Pts',(-14.476556241042,601.984369696621,69.6798892152476));
#100824=CARTESIAN_POINT('Ctrl Pts',(-14.6585293164953,601.846982001182,
69.2026186118272));
#100825=CARTESIAN_POINT('Ctrl Pts',(-14.8173572004353,601.726014684511,
68.7137722568826));
#100826=CARTESIAN_POINT('Ctrl Pts',(-14.9519074395826,601.623084951773,
68.2126302314325));
#100827=CARTESIAN_POINT('Ctrl Pts',(-14.9521319248731,601.622913222528,
68.2117941198516));
#100828=CARTESIAN_POINT('Ctrl Pts',(-14.9523563424351,601.622741543562,
68.2109579739804));
#100829=CARTESIAN_POINT('Ctrl Pts',(-14.95258069226,601.622569914884,68.210121793814));
#100830=CARTESIAN_POINT('Ctrl Pts',(-15.0195558479621,601.571333603616,
67.9604969194963));
#100831=CARTESIAN_POINT('Ctrl Pts',(-15.0804980243008,601.524576095695,
67.7077995412209));
#100832=CARTESIAN_POINT('Ctrl Pts',(-15.1351710050067,601.48254956767,67.4519333432102));
#100833=CARTESIAN_POINT('Ctrl Pts',(-15.135636996097,601.482191365367,67.4497525334749));
#100834=CARTESIAN_POINT('Ctrl Pts',(-15.1361025388452,601.481833501261,
67.4475714348023));
#100835=CARTESIAN_POINT('Ctrl Pts',(-15.1365676327062,601.48147597581,67.4453900497329));
#100836=CARTESIAN_POINT('Ctrl Pts',(-15.1908350502443,601.439759701831,
67.1908647929737));
#100837=CARTESIAN_POINT('Ctrl Pts',(-15.2390028207857,601.402644801267,
66.9323762776556));
#100838=CARTESIAN_POINT('Ctrl Pts',(-15.2801892173651,601.370866225702,
66.6740242960524));
#100839=CARTESIAN_POINT('Ctrl Pts',(-15.2807701109302,601.370418020188,
66.6703804957663));
#100840=CARTESIAN_POINT('Ctrl Pts',(-15.2813496618532,601.369970844881,
66.666736612685));
#100841=CARTESIAN_POINT('Ctrl Pts',(-15.2819278700575,601.369524699882,
66.6630926470816));
#100842=CARTESIAN_POINT('Ctrl Pts',(-15.3731745585429,601.299118826362,
66.0880406298869));
#100843=CARTESIAN_POINT('Ctrl Pts',(-15.4310118252878,601.254354048509,
65.5107688555495));
#100844=CARTESIAN_POINT('Ctrl Pts',(-15.4552801915147,601.235537263915,
64.9313506760282));
#100845=CARTESIAN_POINT('Ctrl Pts',(-15.4748377843986,601.220373036994,
64.4644043328481));
#100846=CARTESIAN_POINT('Ctrl Pts',(-15.4725946351504,601.222060296525,
63.9960640263858));
#100847=CARTESIAN_POINT('Ctrl Pts',(-15.4484868316277,601.240744657969,
63.526368979289));
#100848=CARTESIAN_POINT('Ctrl Pts',(-15.4479899849941,601.24112973088,63.5166888604538));
#100849=CARTESIAN_POINT('Ctrl Pts',(-15.4474835199924,601.241522257243,
63.5070072900479));
#100850=CARTESIAN_POINT('Ctrl Pts',(-15.4469674516523,601.241922223809,
63.4973243783675));
#100851=CARTESIAN_POINT('Ctrl Pts',(-15.4286622195785,601.25610926116,63.1538660964509));
#100852=CARTESIAN_POINT('Ctrl Pts',(-15.3982529686908,601.279665380914,
62.8085899300613));
#100853=CARTESIAN_POINT('Ctrl Pts',(-15.3564213514686,601.311998214373,
62.4665526792109));
#100854=CARTESIAN_POINT('Ctrl Pts',(-15.3350964847613,601.328480803609,
62.2921893801648));
#100855=CARTESIAN_POINT('Ctrl Pts',(-15.3108039221149,601.347243706909,
62.1186678639537));
#100856=CARTESIAN_POINT('Ctrl Pts',(-15.283637958771,601.368205423024,61.9466564924111));
#100857=CARTESIAN_POINT('Ctrl Pts',(-15.2816660309461,601.369726995837,
61.9341705000882));
#100858=CARTESIAN_POINT('Ctrl Pts',(-15.2796790199361,601.371260110549,
61.9216904451658));
#100859=CARTESIAN_POINT('Ctrl Pts',(-15.2776769461705,601.372804744798,
61.9092163265372));
#100860=CARTESIAN_POINT('Ctrl Pts',(-15.1964258864429,601.43549133098,61.4029735620699));
#100861=CARTESIAN_POINT('Ctrl Pts',(-15.0903354122302,601.517167712133,
60.906367091332));
#100862=CARTESIAN_POINT('Ctrl Pts',(-14.9606030100877,601.616433700872,
60.4188422252059));
#100863=CARTESIAN_POINT('Ctrl Pts',(-14.9567124177469,601.619410624826,
60.4042216641215));
#100864=CARTESIAN_POINT('Ctrl Pts',(-14.9528005558405,601.622403377454,
60.3896092743672));
#100865=CARTESIAN_POINT('Ctrl Pts',(-14.9488674344808,601.625411931282,
60.3750050482591));
#100866=CARTESIAN_POINT('Ctrl Pts',(-14.8183427926634,601.725253857031,
59.8903489170524));
#100867=CARTESIAN_POINT('Ctrl Pts',(-14.6644248370208,601.842487872357,
59.4147167113827));
#100868=CARTESIAN_POINT('Ctrl Pts',(-14.4874575536325,601.976141950479,
58.9477239471356));
#100869=CARTESIAN_POINT('Ctrl Pts',(-14.4812763675599,601.980810275101,
58.9314126317608));
#100870=CARTESIAN_POINT('Ctrl Pts',(-14.4750668043185,601.98549878938,58.9151121429094));
#100871=CARTESIAN_POINT('Ctrl Pts',(-14.4688293500762,601.990207092219,
58.898823461902));
#100872=CARTESIAN_POINT('Ctrl Pts',(-14.3830461531583,602.054959995219,
58.6748065671682));
#100873=CARTESIAN_POINT('Ctrl Pts',(-14.292004696505,602.123442202462,58.4530694500958));
#100874=CARTESIAN_POINT('Ctrl Pts',(-14.1969736437625,602.194605881907,
58.2361648853124));
#100875=CARTESIAN_POINT('Ctrl Pts',(-14.094982172067,602.270981847324,58.0033734435543));
#100876=CARTESIAN_POINT('Ctrl Pts',(-13.9880772628478,602.350687445523,
57.7752684237754));
#100877=CARTESIAN_POINT('Ctrl Pts',(-13.8764789934297,602.433436002756,
57.5515702123706));
#100878=CARTESIAN_POINT('Ctrl Pts',(-13.8680348690463,602.439697202983,
57.5346440043631));
#100879=CARTESIAN_POINT('Ctrl Pts',(-13.8595642190567,602.445975710707,
57.5177427581886));
#100880=CARTESIAN_POINT('Ctrl Pts',(-13.851067080703,602.452271426782,57.5008664006862));
#100881=CARTESIAN_POINT('Ctrl Pts',(-13.5414068385151,602.681705488394,
56.8858432324252));
#100882=CARTESIAN_POINT('Ctrl Pts',(-13.1966130805123,602.933991273143,
56.3038699396781));
#100883=CARTESIAN_POINT('Ctrl Pts',(-12.818575692922,603.204311674987,55.7515264358009));
#100884=CARTESIAN_POINT('Ctrl Pts',(-12.6579969944005,603.319135498601,
55.516907840125));
#100885=CARTESIAN_POINT('Ctrl Pts',(-12.4914199381588,603.437213717574,
55.2876357592081));
#100886=CARTESIAN_POINT('Ctrl Pts',(-12.3189883302193,603.558178954703,
55.0634499517658));
#100887=CARTESIAN_POINT('Ctrl Pts',(-12.3063145884526,603.567069912668,
55.046972270758));
#100888=CARTESIAN_POINT('Ctrl Pts',(-12.293608875228,603.575976591379,55.0305223394531));
#100889=CARTESIAN_POINT('Ctrl Pts',(-12.2808711596615,603.584898854644,
55.0141001141053));
#100890=CARTESIAN_POINT('Ctrl Pts',(-12.1059805186862,603.70740279448,54.788620631358));
#100891=CARTESIAN_POINT('Ctrl Pts',(-11.9251378242665,603.832790898451,
54.5684575845009));
#100892=CARTESIAN_POINT('Ctrl Pts',(-11.7381263933771,603.960807456315,
54.3533266754511));
#100893=CARTESIAN_POINT('Ctrl Pts',(-11.621570829978,604.040594247718,54.2192455436742));
#100894=CARTESIAN_POINT('Ctrl Pts',(-11.5026183161173,604.121402448223,
54.0871197659894));
#100895=CARTESIAN_POINT('Ctrl Pts',(-11.3812089157723,604.203173369559,
53.9568866869203));
#100896=CARTESIAN_POINT('Ctrl Pts',(-11.3665916244721,604.213018318744,
53.9412070538089));
#100897=CARTESIAN_POINT('Ctrl Pts',(-11.3519440806364,604.222873520687,
53.9255610169989));
#100898=CARTESIAN_POINT('Ctrl Pts',(-11.3372665071724,604.23273864033,53.909948683445));
#100899=CARTESIAN_POINT('Ctrl Pts',(-11.1445926511092,604.362238972701,
53.7050041457561));
#100900=CARTESIAN_POINT('Ctrl Pts',(-10.9471021948111,604.493214313288,
53.5062326251606));
#100901=CARTESIAN_POINT('Ctrl Pts',(-10.745312746339,604.624903460212,53.313822665779));
#100902=CARTESIAN_POINT('Ctrl Pts',(-10.6147258174735,604.71012536548,53.1893056215578));
#100903=CARTESIAN_POINT('Ctrl Pts',(-10.4823376624323,604.795646602209,
53.0674534899227));
#100904=CARTESIAN_POINT('Ctrl Pts',(-10.3482814114362,604.881262749726,
52.9483262480232));
#100905=CARTESIAN_POINT('Ctrl Pts',(-10.3323385786133,604.891444773441,
52.9341588691196));
#100906=CARTESIAN_POINT('Ctrl Pts',(-10.316370473426,604.901629819377,52.9200274595625));
#100907=CARTESIAN_POINT('Ctrl Pts',(-10.3003769198535,604.911817706811,
52.9059318994444));
#100908=CARTESIAN_POINT('Ctrl Pts',(-9.82420777102504,605.215137270266,
52.4862708883196));
#100909=CARTESIAN_POINT('Ctrl Pts',(-9.32605084326132,605.520676590294,
52.0987968357783));
#100910=CARTESIAN_POINT('Ctrl Pts',(-8.80356011337631,605.822413129915,
51.7419140852932));
#100911=CARTESIAN_POINT('Ctrl Pts',(-8.55658179181229,605.965042232878,
51.5732176899919));
#100912=CARTESIAN_POINT('Ctrl Pts',(-8.30416681543672,606.10682215787,51.4113565816857));
#100913=CARTESIAN_POINT('Ctrl Pts',(-8.04607025545264,606.247119801894,
51.256162100614));
#100914=CARTESIAN_POINT('Ctrl Pts',(-8.02850322970694,606.25666898893,51.2455989786384));
#100915=CARTESIAN_POINT('Ctrl Pts',(-8.01090956281672,606.266211131474,
51.2350670302149));
#100916=CARTESIAN_POINT('Ctrl Pts',(-7.9932890588355,606.275745937602,51.2245662881426));
#100917=CARTESIAN_POINT('Ctrl Pts',(-7.59780332812586,606.48975115405,50.9888809946957));
#100918=CARTESIAN_POINT('Ctrl Pts',(-7.18882425917877,606.700057952479,
50.7689174218948));
#100919=CARTESIAN_POINT('Ctrl Pts',(-6.76412222102934,606.903391967464,
50.5650277071314));
#100920=CARTESIAN_POINT('Ctrl Pts',(-6.32001855033077,607.116014875577,
50.3518237132475));
#100921=CARTESIAN_POINT('Ctrl Pts',(-5.8641859945191,607.318324825404,50.1588849102787));
#100922=CARTESIAN_POINT('Ctrl Pts',(-5.39617905494641,607.50523847829,49.9868909337918));
#100923=CARTESIAN_POINT('Ctrl Pts',(-5.37904744986577,607.512080536847,
49.9805950167182));
#100924=CARTESIAN_POINT('Ctrl Pts',(-5.36189899496725,607.518902273776,
49.9743268675902));
#100925=CARTESIAN_POINT('Ctrl Pts',(-5.34473356176528,607.525703405737,
49.9680865467441));
#100926=CARTESIAN_POINT('Ctrl Pts',(-5.05505639185856,607.640476661693,
49.8627773208862));
#100927=CARTESIAN_POINT('Ctrl Pts',(-4.7604858066973,607.749407504922,49.7653700783089));
#100928=CARTESIAN_POINT('Ctrl Pts',(-4.46054827631106,607.851090892826,
49.6761957671012));
#100929=CARTESIAN_POINT('Ctrl Pts',(-4.29218546500682,607.90816844837,49.6261398847589));
#100930=CARTESIAN_POINT('Ctrl Pts',(-4.12213195856964,607.96296293255,49.5786775358458));
#100931=CARTESIAN_POINT('Ctrl Pts',(-3.95030718844,608.015230706238,49.5338627639009));
#100932=CARTESIAN_POINT('Ctrl Pts',(-3.93446701216018,608.020049166047,
49.5297313811729));
#100933=CARTESIAN_POINT('Ctrl Pts',(-3.918608077318,608.024846507359,49.5256222106105));
#100934=CARTESIAN_POINT('Ctrl Pts',(-3.90273095451652,608.029622392916,
49.5215354186));
#100935=CARTESIAN_POINT('Ctrl Pts',(-3.55379715979371,608.13458271168,49.4317194070769));
#100936=CARTESIAN_POINT('Ctrl Pts',(-3.19571883730709,608.229248742951,
49.3526530596434));
#100937=CARTESIAN_POINT('Ctrl Pts',(-2.83439734133167,608.310054485557,
49.2860999619015));
#100938=CARTESIAN_POINT('Ctrl Pts',(-2.69666016753091,608.340857952102,
49.260729659573));
#100939=CARTESIAN_POINT('Ctrl Pts',(-2.55845161164899,608.369647675702,
49.2371774467656));
#100940=CARTESIAN_POINT('Ctrl Pts',(-2.4200977988402,608.396227713108,49.2155398450576));
#100941=CARTESIAN_POINT('Ctrl Pts',(-2.40660419108442,608.398820056548,
49.2134295359574));
#100942=CARTESIAN_POINT('Ctrl Pts',(-2.39310738388888,608.401392124616,
49.2113367450485));
#100943=CARTESIAN_POINT('Ctrl Pts',(-2.37960737536317,608.40394385778,49.209261482295));
#100944=CARTESIAN_POINT('Ctrl Pts',(-1.98661162622564,608.478226795045,
49.1488489693005));
#100945=CARTESIAN_POINT('Ctrl Pts',(-1.59091824851033,608.535255871218,
49.1033073919222));
#100946=CARTESIAN_POINT('Ctrl Pts',(-1.19224235498086,608.573554311811,
49.072890147475));
#100947=CARTESIAN_POINT('Ctrl Pts',(-1.07867395166442,608.584464158176,
49.0642253700424));
#100948=CARTESIAN_POINT('Ctrl Pts',(-0.964863484237993,608.593853827031,
49.0567881087316));
#100949=CARTESIAN_POINT('Ctrl Pts',(-0.850804267018435,608.601688592408,
49.0505847395293));
#100950=CARTESIAN_POINT('Ctrl Pts',(-0.467771498280798,608.627999240051,
49.0297526337251));
#100951=CARTESIAN_POINT('Ctrl Pts',(-0.0819322950985286,608.636758310879,
49.0228304603039));
#100952=CARTESIAN_POINT('Ctrl Pts',(0.306952880974604,608.627117381494,
49.0304624743328));
#100953=CARTESIAN_POINT('Ctrl Pts',(0.454443680653595,608.623460907881,
49.0333570353024));
#100954=CARTESIAN_POINT('Ctrl Pts',(0.602372687010726,608.617157325412,
49.038345428801));
#100955=CARTESIAN_POINT('Ctrl Pts',(0.750753219933458,608.608158800935,
49.0454640244197));
#100956=CARTESIAN_POINT('Ctrl Pts',(0.757600042190903,608.607743575996,
49.0457925025426));
#100957=CARTESIAN_POINT('Ctrl Pts',(0.764445410940781,608.607322738532,
49.0461253700537));
#100958=CARTESIAN_POINT('Ctrl Pts',(0.77128932685212,608.60689629941,49.0464626238936));
#100959=CARTESIAN_POINT('Ctrl Pts',(1.0999295210194,608.586418982362,49.0626573242459));
#100960=CARTESIAN_POINT('Ctrl Pts',(1.42500065461206,608.553042141358,49.0889528591604));
#100961=CARTESIAN_POINT('Ctrl Pts',(1.74665485822711,608.507994127727,49.1249902270901));
#100962=CARTESIAN_POINT('Ctrl Pts',(1.94934880633034,608.479606624518,49.1476995724145));
#100963=CARTESIAN_POINT('Ctrl Pts',(2.15068565983306,608.446583546877,49.1742781049698));
#100964=CARTESIAN_POINT('Ctrl Pts',(2.35070124101387,608.409224348695,49.2046424827418));
#100965=CARTESIAN_POINT('Ctrl Pts',(2.5214420972517,608.377333125781,49.2305626627063));
#100966=CARTESIAN_POINT('Ctrl Pts',(2.69150512765591,608.342225093235,49.2592881187915));
#100967=CARTESIAN_POINT('Ctrl Pts',(2.86062884454046,608.304125672787,49.2907367311987));
#100968=CARTESIAN_POINT('Ctrl Pts',(3.03567001919357,608.264693194413,49.3232856968811));
#100969=CARTESIAN_POINT('Ctrl Pts',(3.20970492776411,608.222056535811,49.3587517991215));
#100970=CARTESIAN_POINT('Ctrl Pts',(3.38245717567461,608.176507008384,49.3970067274567));
#100971=CARTESIAN_POINT('Ctrl Pts',(3.54860965817915,608.132697638895,49.4338001781227));
#100972=CARTESIAN_POINT('Ctrl Pts',(3.71357570183652,608.0861943321,49.4731731008924));
#100973=CARTESIAN_POINT('Ctrl Pts',(3.87712128125395,608.037287038732,49.5149800517143));
#100974=CARTESIAN_POINT('',(-3.85030552837329,633.305466608637,79.0907977188138));
#100975=CARTESIAN_POINT('',(3.87712128125394,633.313460490016,49.5149800517143));
#100976=CARTESIAN_POINT('Ctrl Pts',(-3.85030552837329,633.305466608637,
79.0907977188139));
#100977=CARTESIAN_POINT('Ctrl Pts',(-4.23115754609872,633.418641912605,
78.9941589978653));
#100978=CARTESIAN_POINT('Ctrl Pts',(-4.60131346248585,633.543494400745,
78.8852799373196));
#100979=CARTESIAN_POINT('Ctrl Pts',(-4.96211414889978,633.677591054735,
78.7647299399334));
#100980=CARTESIAN_POINT('Ctrl Pts',(-5.34276158684725,633.819064033309,
78.637548785968));
#100981=CARTESIAN_POINT('Ctrl Pts',(-5.71299620590704,633.970826395318,
78.4973774780445));
#100982=CARTESIAN_POINT('Ctrl Pts',(-6.07436314681395,634.130065847331,
78.344859545867));
#100983=CARTESIAN_POINT('Ctrl Pts',(-6.27213868891848,634.217217341785,
78.2613867283443));
#100984=CARTESIAN_POINT('Ctrl Pts',(-6.46725754695957,634.306609234473,
78.1742152209399));
#100985=CARTESIAN_POINT('Ctrl Pts',(-6.65996976734683,634.39778521092,78.083447496734));
#100986=CARTESIAN_POINT('Ctrl Pts',(-6.66518312762043,634.400251755141,
78.0809919967841));
#100987=CARTESIAN_POINT('Ctrl Pts',(-6.67039454639835,634.402719519002,
78.0785339506688));
#100988=CARTESIAN_POINT('Ctrl Pts',(-6.67560403513441,634.405188496189,
78.0760733579906));
#100989=CARTESIAN_POINT('Ctrl Pts',(-6.85783434677776,634.491554453585,
77.9900006945685));
#100990=CARTESIAN_POINT('Ctrl Pts',(-7.03785733737531,634.57956932506,77.9006116068831));
#100991=CARTESIAN_POINT('Ctrl Pts',(-7.21578985887797,634.668980075354,
77.8079341656671));
#100992=CARTESIAN_POINT('Ctrl Pts',(-7.39804086771728,634.76056085724,77.7130074090763));
#100993=CARTESIAN_POINT('Ctrl Pts',(-7.57809916252988,634.853606853605,
77.6146305886777));
#100994=CARTESIAN_POINT('Ctrl Pts',(-7.75606262296074,634.947864113798,
77.5127908409413));
#100995=CARTESIAN_POINT('Ctrl Pts',(-7.81791534052439,634.980624027991,
77.4773955685734));
#100996=CARTESIAN_POINT('Ctrl Pts',(-7.87951473546575,635.013530361067,
77.441581622736));
#100997=CARTESIAN_POINT('Ctrl Pts',(-7.94086400011093,635.046572676206,
77.4053473424492));
#100998=CARTESIAN_POINT('Ctrl Pts',(-8.12143758056441,635.143828432826,
77.2986964516133));
#100999=CARTESIAN_POINT('Ctrl Pts',(-8.30015667396553,635.242438546382,
77.1882091735063));
#101000=CARTESIAN_POINT('Ctrl Pts',(-8.47654659992338,635.341839784828,
77.0741437637033));
#101001=CARTESIAN_POINT('Ctrl Pts',(-8.65758128464239,635.443858490064,
76.9570747452268));
#101002=CARTESIAN_POINT('Ctrl Pts',(-8.83616203706591,635.546709781178,
76.8362367876842));
#101003=CARTESIAN_POINT('Ctrl Pts',(-9.01180166952668,635.649764407919,
76.7119523503434));
#101004=CARTESIAN_POINT('Ctrl Pts',(-9.05844940411363,635.677134454239,
76.6789439264181));
#101005=CARTESIAN_POINT('Ctrl Pts',(-9.10488984294456,635.704518770545,
76.6456926236292));
#101006=CARTESIAN_POINT('Ctrl Pts',(-9.15111422548109,635.731905446044,
76.6122049576959));
#101007=CARTESIAN_POINT('Ctrl Pts',(-9.1589865761174,635.73656959731,76.60650176311));
#101008=CARTESIAN_POINT('Ctrl Pts',(-9.1668522498693,635.741233586245,76.6007919954539));
#101009=CARTESIAN_POINT('Ctrl Pts',(-9.17471122726756,635.745897367157,
76.5950756732529));
#101010=CARTESIAN_POINT('Ctrl Pts',(-9.60207382528573,635.99950867384,76.2842283221116));
#101011=CARTESIAN_POINT('Ctrl Pts',(-10.0116117982556,636.253542293709,
75.9533303175435));
#101012=CARTESIAN_POINT('Ctrl Pts',(-10.4040324385516,636.504983969591,
75.6011406067799));
#101013=CARTESIAN_POINT('Ctrl Pts',(-10.7191297461092,636.706881084428,
75.3183470474824));
#101014=CARTESIAN_POINT('Ctrl Pts',(-11.023191189025,636.907107306183,75.0218264745442));
#101015=CARTESIAN_POINT('Ctrl Pts',(-11.316590628858,637.104115666314,74.7109552956668));
#101016=CARTESIAN_POINT('Ctrl Pts',(-11.321166096814,637.107187947022,74.7061073616755));
#101017=CARTESIAN_POINT('Ctrl Pts',(-11.3257389714886,637.110259446643,
74.7012559361948));
#101018=CARTESIAN_POINT('Ctrl Pts',(-11.3303092556449,637.113330160208,
74.6964010155037));
#101019=CARTESIAN_POINT('Ctrl Pts',(-11.5510374470378,637.261634516839,
74.4619259091749));
#101020=CARTESIAN_POINT('Ctrl Pts',(-11.7657533239874,637.408233298925,
74.2189269147418));
#101021=CARTESIAN_POINT('Ctrl Pts',(-11.972919051437,637.551502628213,73.9689066228734));
#101022=CARTESIAN_POINT('Ctrl Pts',(-12.0734225150228,637.621007676158,
73.847612885686));
#101023=CARTESIAN_POINT('Ctrl Pts',(-12.1721485958881,637.689729029595,
73.724665978119));
#101024=CARTESIAN_POINT('Ctrl Pts',(-12.2689186597508,637.757480022309,
73.6002344485137));
#101025=CARTESIAN_POINT('Ctrl Pts',(-12.2725876177276,637.760048745892,
73.5955167286437));
#101026=CARTESIAN_POINT('Ctrl Pts',(-12.2762537641056,637.762616074847,
73.5907968737177));
#101027=CARTESIAN_POINT('Ctrl Pts',(-12.2799170881477,637.765181998328,
73.5860748940442));
#101028=CARTESIAN_POINT('Ctrl Pts',(-12.5761628621236,637.972683158187,
73.2042177318029));
#101029=CARTESIAN_POINT('Ctrl Pts',(-12.8553373541657,638.171922010484,
72.8071138322945));
#101030=CARTESIAN_POINT('Ctrl Pts',(-13.1169859722108,638.361085304711,
72.393799734182));
#101031=CARTESIAN_POINT('Ctrl Pts',(-13.1196323729917,638.36299856492,72.3896193385041));
#101032=CARTESIAN_POINT('Ctrl Pts',(-13.1222769834676,638.364910796376,
72.3854372806603));
#101033=CARTESIAN_POINT('Ctrl Pts',(-13.124919803262,638.36682199726,72.3812535595345));
#101034=CARTESIAN_POINT('Ctrl Pts',(-13.3868026742264,638.556207128875,
71.966679360388));
#101035=CARTESIAN_POINT('Ctrl Pts',(-13.631110707103,638.735489609657,71.5357863466911));
#101036=CARTESIAN_POINT('Ctrl Pts',(-13.8566914851811,638.902654874734,
71.0868685526236));
#101037=CARTESIAN_POINT('Ctrl Pts',(-13.8582610272094,638.903817974319,
71.0837450801759));
#101038=CARTESIAN_POINT('Ctrl Pts',(-13.8598296623861,638.904980487196,
71.0806207352236));
#101039=CARTESIAN_POINT('Ctrl Pts',(-13.8613973903024,638.906142412673,
71.0774955172259));
#101040=CARTESIAN_POINT('Ctrl Pts',(-14.0874235511568,639.073662268671,
70.6269192287556));
#101041=CARTESIAN_POINT('Ctrl Pts',(-14.2932373615726,639.227980395818,
70.1602556258246));
#101042=CARTESIAN_POINT('Ctrl Pts',(-14.4749373298438,639.365155599813,
69.6841332957598));
#101043=CARTESIAN_POINT('Ctrl Pts',(-14.475477179548,639.365563161763,69.6827186862722));
#101044=CARTESIAN_POINT('Ctrl Pts',(-14.476016816648,639.365970572568,69.6813039927107));
#101045=CARTESIAN_POINT('Ctrl Pts',(-14.476556241042,639.366377832127,69.6798892152477));
#101046=CARTESIAN_POINT('Ctrl Pts',(-14.6585293164953,639.503765527566,
69.2026186118272));
#101047=CARTESIAN_POINT('Ctrl Pts',(-14.8173572004353,639.624732844237,
68.7137722568825));
#101048=CARTESIAN_POINT('Ctrl Pts',(-14.9519074395826,639.727662576974,
68.2126302314325));
#101049=CARTESIAN_POINT('Ctrl Pts',(-14.9521319248731,639.727834306219,
68.2117941198516));
#101050=CARTESIAN_POINT('Ctrl Pts',(-14.9523563424351,639.728005985186,
68.2109579739804));
#101051=CARTESIAN_POINT('Ctrl Pts',(-14.95258069226,639.728177613864,68.210121793814));
#101052=CARTESIAN_POINT('Ctrl Pts',(-15.0195558479621,639.779413925132,
67.9604969194963));
#101053=CARTESIAN_POINT('Ctrl Pts',(-15.0804980243008,639.826171433052,
67.7077995412209));
#101054=CARTESIAN_POINT('Ctrl Pts',(-15.1351710050066,639.868197961077,
67.4519333432102));
#101055=CARTESIAN_POINT('Ctrl Pts',(-15.135636996097,639.868556163381,67.4497525334749));
#101056=CARTESIAN_POINT('Ctrl Pts',(-15.1361025388452,639.868914027486,
67.4475714348023));
#101057=CARTESIAN_POINT('Ctrl Pts',(-15.1365676327062,639.869271552937,
67.4453900497329));
#101058=CARTESIAN_POINT('Ctrl Pts',(-15.1908350502443,639.910987826917,
67.1908647929736));
#101059=CARTESIAN_POINT('Ctrl Pts',(-15.2390028207857,639.94810272748,66.9323762776555));
#101060=CARTESIAN_POINT('Ctrl Pts',(-15.2801892173651,639.979881303045,
66.6740242960524));
#101061=CARTESIAN_POINT('Ctrl Pts',(-15.2807701109302,639.980329508559,
66.6703804957663));
#101062=CARTESIAN_POINT('Ctrl Pts',(-15.2813496618532,639.980776683867,
66.6667366126849));
#101063=CARTESIAN_POINT('Ctrl Pts',(-15.2819278700575,639.981222828865,
66.6630926470815));
#101064=CARTESIAN_POINT('Ctrl Pts',(-15.3731745585433,640.051628702386,
66.0880406298841));
#101065=CARTESIAN_POINT('Ctrl Pts',(-15.4310118252884,640.096393480239,
65.5107688555439));
#101066=CARTESIAN_POINT('Ctrl Pts',(-15.4552801915151,640.115210264833,
64.9313506760199));
#101067=CARTESIAN_POINT('Ctrl Pts',(-15.4748377843986,640.130374491754,
64.4644043328425));
#101068=CARTESIAN_POINT('Ctrl Pts',(-15.4725946351503,640.128687232222,
63.9960640263831));
#101069=CARTESIAN_POINT('Ctrl Pts',(-15.4484868316277,640.110002870779,
63.5263689792891));
#101070=CARTESIAN_POINT('Ctrl Pts',(-15.4479899849941,640.109617797867,
63.5166888604539));
#101071=CARTESIAN_POINT('Ctrl Pts',(-15.4474835199924,640.109225271504,
63.5070072900479));
#101072=CARTESIAN_POINT('Ctrl Pts',(-15.4469674516523,640.108825304938,
63.4973243783675));
#101073=CARTESIAN_POINT('Ctrl Pts',(-15.4286622195784,640.094638267587,
63.1538660964489));
#101074=CARTESIAN_POINT('Ctrl Pts',(-15.3982529686904,640.071082147833,
62.8085899300572));
#101075=CARTESIAN_POINT('Ctrl Pts',(-15.3564213514678,640.038749314374,
62.4665526792047));
#101076=CARTESIAN_POINT('Ctrl Pts',(-15.3350964847608,640.022266725138,
62.2921893801607));
#101077=CARTESIAN_POINT('Ctrl Pts',(-15.3108039221145,640.003503821838,
62.1186678639517));
#101078=CARTESIAN_POINT('Ctrl Pts',(-15.283637958771,639.982542105723,61.9466564924111));
#101079=CARTESIAN_POINT('Ctrl Pts',(-15.2816660309461,639.98102053291,61.9341705000882));
#101080=CARTESIAN_POINT('Ctrl Pts',(-15.2796790199361,639.979487418199,
61.9216904451658));
#101081=CARTESIAN_POINT('Ctrl Pts',(-15.2776769461705,639.977942783949,
61.9092163265373));
#101082=CARTESIAN_POINT('Ctrl Pts',(-15.1964258864429,639.915256197767,
61.40297356207));
#101083=CARTESIAN_POINT('Ctrl Pts',(-15.0903354122302,639.833579816615,
60.9063670913321));
#101084=CARTESIAN_POINT('Ctrl Pts',(-14.9606030100877,639.734313827876,
60.4188422252059));
#101085=CARTESIAN_POINT('Ctrl Pts',(-14.9567124177469,639.731336903922,
60.4042216641216));
#101086=CARTESIAN_POINT('Ctrl Pts',(-14.9528005558405,639.728344151294,
60.3896092743672));
#101087=CARTESIAN_POINT('Ctrl Pts',(-14.9488674344808,639.725335597466,
60.3750050482591));
#101088=CARTESIAN_POINT('Ctrl Pts',(-14.8183427926634,639.625493671717,
59.8903489170524));
#101089=CARTESIAN_POINT('Ctrl Pts',(-14.6644248370209,639.508259656391,
59.4147167113827));
#101090=CARTESIAN_POINT('Ctrl Pts',(-14.4874575536325,639.374605578268,
58.9477239471356));
#101091=CARTESIAN_POINT('Ctrl Pts',(-14.4812763675599,639.369937253647,
58.9314126317608));
#101092=CARTESIAN_POINT('Ctrl Pts',(-14.4750668043185,639.365248739367,
58.9151121429094));
#101093=CARTESIAN_POINT('Ctrl Pts',(-14.4688293500763,639.360540436529,
58.898823461902));
#101094=CARTESIAN_POINT('Ctrl Pts',(-14.3830461531583,639.295787533528,
58.6748065671682));
#101095=CARTESIAN_POINT('Ctrl Pts',(-14.292004696505,639.227305326286,58.4530694500958));
#101096=CARTESIAN_POINT('Ctrl Pts',(-14.1969736437625,639.156141646841,
58.2361648853124));
#101097=CARTESIAN_POINT('Ctrl Pts',(-14.094982172067,639.079765681423,58.0033734435543));
#101098=CARTESIAN_POINT('Ctrl Pts',(-13.9880772628478,639.000060083224,
57.7752684237754));
#101099=CARTESIAN_POINT('Ctrl Pts',(-13.8764789934297,638.917311525991,
57.5515702123706));
#101100=CARTESIAN_POINT('Ctrl Pts',(-13.8680348690463,638.911050325764,
57.5346440043631));
#101101=CARTESIAN_POINT('Ctrl Pts',(-13.8595642190568,638.904771818041,
57.5177427581885));
#101102=CARTESIAN_POINT('Ctrl Pts',(-13.851067080703,638.898476101966,57.5008664006861));
#101103=CARTESIAN_POINT('Ctrl Pts',(-13.5414068385364,638.66904204037,56.8858432324675));
#101104=CARTESIAN_POINT('Ctrl Pts',(-13.1966130805598,638.416756255639,
56.3038699397583));
#101105=CARTESIAN_POINT('Ctrl Pts',(-12.818575693,638.146435853816,55.751526435915));
#101106=CARTESIAN_POINT('Ctrl Pts',(-12.6579969944544,638.031612030185,
55.5169078401994));
#101107=CARTESIAN_POINT('Ctrl Pts',(-12.4914199381867,637.913533811193,
55.2876357592445));
#101108=CARTESIAN_POINT('Ctrl Pts',(-12.3189883302193,637.792568574045,
55.0634499517658));
#101109=CARTESIAN_POINT('Ctrl Pts',(-12.3063145884526,637.783677616079,
55.046972270758));
#101110=CARTESIAN_POINT('Ctrl Pts',(-12.2936088752279,637.774770937369,
55.0305223394531));
#101111=CARTESIAN_POINT('Ctrl Pts',(-12.2808711596615,637.765848674103,
55.0141001141053));
#101112=CARTESIAN_POINT('Ctrl Pts',(-12.1059805186987,637.643344734276,
54.7886206313742));
#101113=CARTESIAN_POINT('Ctrl Pts',(-11.9251378242925,637.517956630315,
54.5684575845326));
#101114=CARTESIAN_POINT('Ctrl Pts',(-11.7381263934176,637.38994007246,54.3533266754976));
#101115=CARTESIAN_POINT('Ctrl Pts',(-11.6215708300055,637.310153281049,
54.2192455437048));
#101116=CARTESIAN_POINT('Ctrl Pts',(-11.5026183161313,637.229345080535,
54.0871197660045));
#101117=CARTESIAN_POINT('Ctrl Pts',(-11.3812089157723,637.147574159189,
53.9568866869203));
#101118=CARTESIAN_POINT('Ctrl Pts',(-11.3665916244721,637.137729210003,
53.941207053809));
#101119=CARTESIAN_POINT('Ctrl Pts',(-11.3519440806364,637.12787400806,53.9255610169989));
#101120=CARTESIAN_POINT('Ctrl Pts',(-11.3372665071724,637.118008888418,
53.9099486834451));
#101121=CARTESIAN_POINT('Ctrl Pts',(-11.1445926511122,636.988508556048,
53.7050041457592));
#101122=CARTESIAN_POINT('Ctrl Pts',(-10.9471021948171,636.857533215464,
53.5062326251667));
#101123=CARTESIAN_POINT('Ctrl Pts',(-10.7453127463482,636.725844068542,
53.3138226657878));
#101124=CARTESIAN_POINT('Ctrl Pts',(-10.6147258174797,636.640622163272,
53.1893056215636));
#101125=CARTESIAN_POINT('Ctrl Pts',(-10.4823376624354,636.55510092654,53.0674534899255));
#101126=CARTESIAN_POINT('Ctrl Pts',(-10.3482814114362,636.469484779022,
52.9483262480233));
#101127=CARTESIAN_POINT('Ctrl Pts',(-10.3323385786133,636.459302755307,
52.9341588691196));
#101128=CARTESIAN_POINT('Ctrl Pts',(-10.316370473426,636.449117709371,52.9200274595626));
#101129=CARTESIAN_POINT('Ctrl Pts',(-10.3003769198535,636.438929821937,
52.9059318994444));
#101130=CARTESIAN_POINT('Ctrl Pts',(-9.82420777099613,636.135610258463,
52.4862708882941));
#101131=CARTESIAN_POINT('Ctrl Pts',(-9.32605084320083,635.830070938416,
52.0987968357312));
#101132=CARTESIAN_POINT('Ctrl Pts',(-8.80356011328112,635.528334398778,
51.741914085228));
#101133=CARTESIAN_POINT('Ctrl Pts',(-8.55658179174747,635.385705295833,
51.5732176899501));
#101134=CARTESIAN_POINT('Ctrl Pts',(-8.3041668154036,635.24392537086,51.4113565816656));
#101135=CARTESIAN_POINT('Ctrl Pts',(-8.04607025545269,635.103627726854,
51.2561621006139));
#101136=CARTESIAN_POINT('Ctrl Pts',(-8.028503229707,635.094078539818,51.2455989786384));
#101137=CARTESIAN_POINT('Ctrl Pts',(-8.01090956281682,635.084536397273,
51.2350670302149));
#101138=CARTESIAN_POINT('Ctrl Pts',(-7.99328905883562,635.075001591146,
51.2245662881425));
#101139=CARTESIAN_POINT('Ctrl Pts',(-7.59780332812596,634.860996374697,
50.9888809946957));
#101140=CARTESIAN_POINT('Ctrl Pts',(-7.18882425917893,634.650689576269,
50.7689174218947));
#101141=CARTESIAN_POINT('Ctrl Pts',(-6.76412222102952,634.447355561283,
50.5650277071313));
#101142=CARTESIAN_POINT('Ctrl Pts',(-6.32001855033099,634.23473265317,50.3518237132473));
#101143=CARTESIAN_POINT('Ctrl Pts',(-5.86418599451931,634.032422703343,
50.1588849102784));
#101144=CARTESIAN_POINT('Ctrl Pts',(-5.39617905494653,633.845509050457,
49.9868909337916));
#101145=CARTESIAN_POINT('Ctrl Pts',(-5.37904744986588,633.838666991901,
49.980595016718));
#101146=CARTESIAN_POINT('Ctrl Pts',(-5.36189899496736,633.831845254971,
49.97432686759));
#101147=CARTESIAN_POINT('Ctrl Pts',(-5.34473356176537,633.82504412301,49.9680865467439));
#101148=CARTESIAN_POINT('Ctrl Pts',(-5.055056391868,633.710270867058,49.8627773208895));
#101149=CARTESIAN_POINT('Ctrl Pts',(-4.76048580671642,633.601340023833,
49.7653700783152));
#101150=CARTESIAN_POINT('Ctrl Pts',(-4.46054827634026,633.499656635932,
49.6761957671099));
#101151=CARTESIAN_POINT('Ctrl Pts',(-4.29218546502649,633.442579080384,
49.6261398847644));
#101152=CARTESIAN_POINT('Ctrl Pts',(-4.12213195857958,633.387784596201,
49.5786775358484));
#101153=CARTESIAN_POINT('Ctrl Pts',(-3.95030718844002,633.335516822509,
49.5338627639008));
#101154=CARTESIAN_POINT('Ctrl Pts',(-3.93446701216019,633.3306983627,49.5297313811729));
#101155=CARTESIAN_POINT('Ctrl Pts',(-3.91860807731799,633.325901021388,
49.5256222106105));
#101156=CARTESIAN_POINT('Ctrl Pts',(-3.90273095451649,633.321125135832,
49.5215354185999));
#101157=CARTESIAN_POINT('Ctrl Pts',(-3.55379715982543,633.216164817077,
49.431719407085));
#101158=CARTESIAN_POINT('Ctrl Pts',(-3.19571883737219,633.121498785814,
49.3526530596577));
#101159=CARTESIAN_POINT('Ctrl Pts',(-2.8343973414302,633.040693043213,49.2860999619196));
#101160=CARTESIAN_POINT('Ctrl Pts',(-2.69666016759681,633.009889576659,
49.2607296595842));
#101161=CARTESIAN_POINT('Ctrl Pts',(-2.55845161168197,632.981099853051,
49.2371774467707));
#101162=CARTESIAN_POINT('Ctrl Pts',(-2.42009779884018,632.954519815639,
49.2155398450577));
#101163=CARTESIAN_POINT('Ctrl Pts',(-2.40660419108441,632.9519274722,49.2134295359574));
#101164=CARTESIAN_POINT('Ctrl Pts',(-2.39310738388887,632.949355404132,
49.2113367450486));
#101165=CARTESIAN_POINT('Ctrl Pts',(-2.37960737536316,632.946803670967,
49.209261482295));
#101166=CARTESIAN_POINT('Ctrl Pts',(-1.98661162623389,632.872520733704,
49.1488489693019));
#101167=CARTESIAN_POINT('Ctrl Pts',(-1.59091824852693,632.815491657532,
49.1033073919242));
#101168=CARTESIAN_POINT('Ctrl Pts',(-1.19224235500595,632.777193216939,
49.0728901474769));
#101169=CARTESIAN_POINT('Ctrl Pts',(-1.07867395168118,632.766283370573,
49.0642253700436));
#101170=CARTESIAN_POINT('Ctrl Pts',(-0.964863484246403,632.756893701717,
49.0567881087321));
#101171=CARTESIAN_POINT('Ctrl Pts',(-0.850804267018436,632.74905893634,
49.0505847395294));
#101172=CARTESIAN_POINT('Ctrl Pts',(-0.467771498273324,632.722748288696,
49.0297526337247));
#101173=CARTESIAN_POINT('Ctrl Pts',(-0.0819322950834558,632.713989217867,
49.0228304603037));
#101174=CARTESIAN_POINT('Ctrl Pts',(0.306952880997389,632.723630147254,
49.0304624743333));
#101175=CARTESIAN_POINT('Ctrl Pts',(0.454443680668833,632.727286620868,
49.0333570353029));
#101176=CARTESIAN_POINT('Ctrl Pts',(0.602372687018365,632.733590203336,
49.0383454288014));
#101177=CARTESIAN_POINT('Ctrl Pts',(0.750753219933457,632.742588727813,
49.0454640244198));
#101178=CARTESIAN_POINT('Ctrl Pts',(0.757600042190907,632.743003952751,
49.0457925025427));
#101179=CARTESIAN_POINT('Ctrl Pts',(0.764445410940789,632.743424790216,
49.0461253700538));
#101180=CARTESIAN_POINT('Ctrl Pts',(0.771289326852132,632.743851229338,
49.0464626238936));
#101181=CARTESIAN_POINT('Ctrl Pts',(1.09992952098518,632.764328546383,49.0626573242443));
#101182=CARTESIAN_POINT('Ctrl Pts',(1.42500065454434,632.797705387382,49.0889528591549));
#101183=CARTESIAN_POINT('Ctrl Pts',(1.74665485812661,632.842753401007,49.1249902270789));
#101184=CARTESIAN_POINT('Ctrl Pts',(1.9493488062638,632.871140904219,49.1476995724057));
#101185=CARTESIAN_POINT('Ctrl Pts',(2.1506856598,632.904163981864,49.1742781049647));
#101186=CARTESIAN_POINT('Ctrl Pts',(2.35070124101388,632.941523180052,49.2046424827418));
#101187=CARTESIAN_POINT('Ctrl Pts',(2.52144209724989,632.973414402967,49.2305626627061));
#101188=CARTESIAN_POINT('Ctrl Pts',(2.6915051276523,633.008522435512,49.2592881187909));
#101189=CARTESIAN_POINT('Ctrl Pts',(2.86062884453507,633.046621855959,49.2907367311976));
#101190=CARTESIAN_POINT('Ctrl Pts',(3.03567001918768,633.086054334334,49.3232856968799));
#101191=CARTESIAN_POINT('Ctrl Pts',(3.20970492775773,633.128690992935,49.3587517991202));
#101192=CARTESIAN_POINT('Ctrl Pts',(3.38245717566776,633.174240520362,49.3970067274552));
#101193=CARTESIAN_POINT('Ctrl Pts',(3.54860965817462,633.218049889852,49.4338001781216));
#101194=CARTESIAN_POINT('Ctrl Pts',(3.71357570183427,633.264553196647,49.4731731008918));
#101195=CARTESIAN_POINT('Ctrl Pts',(3.87712128125395,633.313460490017,49.5149800517143));
#101196=CARTESIAN_POINT('Ctrl Pts',(3.87712128125394,633.313460490016,49.5149800517143));
#101197=CARTESIAN_POINT('Ctrl Pts',(4.87153021748849,633.610832324939,49.7691795549397));
#101198=CARTESIAN_POINT('Ctrl Pts',(5.79934294385505,633.989640531339,50.1085862160764));
#101199=CARTESIAN_POINT('Ctrl Pts',(7.12166692125997,634.616737672023,50.7337821806858));
#101200=CARTESIAN_POINT('Ctrl Pts',(7.55227759129253,634.836898028831,50.9628773512951));
#101201=CARTESIAN_POINT('Ctrl Pts',(8.38321347944639,635.285514008744,51.4559004400492));
#101202=CARTESIAN_POINT('Ctrl Pts',(8.78304187688083,635.513563386631,51.7192666405192));
#101203=CARTESIAN_POINT('Ctrl Pts',(9.94055760102618,636.200191042852,52.5603722809289));
#101204=CARTESIAN_POINT('Ctrl Pts',(10.6569237854819,636.661081997033,53.1884290403189));
#101205=CARTESIAN_POINT('Ctrl Pts',(11.6536196238761,637.330472386105,54.2454145926918));
#101206=CARTESIAN_POINT('Ctrl Pts',(11.9710603883753,637.548934443444,54.6156007098022));
#101207=CARTESIAN_POINT('Ctrl Pts',(12.5694073935915,637.967870605571,55.385215476498));
#101208=CARTESIAN_POINT('Ctrl Pts',(12.8514309701718,638.169106179423,55.7857953218243));
#101209=CARTESIAN_POINT('Ctrl Pts',(13.3802712808598,638.551424741988,56.6209194460713));
#101210=CARTESIAN_POINT('Ctrl Pts',(13.6270976333542,638.732524744703,57.0554488359468));
#101211=CARTESIAN_POINT('Ctrl Pts',(14.0830317948412,639.070375015612,57.9622402793));
#101212=CARTESIAN_POINT('Ctrl Pts',(14.288866825385,639.22469547035,58.4281588815737));
#101213=CARTESIAN_POINT('Ctrl Pts',(14.6541428180436,639.500434064949,59.3835018865815));
#101214=CARTESIAN_POINT('Ctrl Pts',(14.813802564089,639.622021221983,59.8733378707772));
#101215=CARTESIAN_POINT('Ctrl Pts',(15.0845904681104,639.829156459885,60.8791319779345));
#101216=CARTESIAN_POINT('Ctrl Pts',(15.1961319187924,639.9150275833,61.3988026843396));
#101217=CARTESIAN_POINT('Ctrl Pts',(15.445895886564,640.107734649545,62.9621091081608));
#101218=CARTESIAN_POINT('Ctrl Pts',(15.5031899681929,640.152399140232,64.0148308425101));
#101219=CARTESIAN_POINT('Ctrl Pts',(15.4344186449233,640.09911226955,65.3443173476824));
#101220=CARTESIAN_POINT('Ctrl Pts',(15.4134449473779,640.082865124052,65.6117770146501));
#101221=CARTESIAN_POINT('Ctrl Pts',(15.3578567110548,640.039860261308,66.1405396918101));
#101222=CARTESIAN_POINT('Ctrl Pts',(15.3232550273986,640.013112515011,66.4025181324823));
#101223=CARTESIAN_POINT('Ctrl Pts',(15.1997028143738,639.917778456694,67.1815043824831));
#101224=CARTESIAN_POINT('Ctrl Pts',(15.0910612840211,639.834128771633,67.6915802539796));
#101225=CARTESIAN_POINT('Ctrl Pts',(14.8233372862475,639.629293421513,68.694153518926));
#101226=CARTESIAN_POINT('Ctrl Pts',(14.6637788819681,639.50774336639,69.1878707203431));
#101227=CARTESIAN_POINT('Ctrl Pts',(14.2965526740649,639.2304637143,70.1529519783302));
#101228=CARTESIAN_POINT('Ctrl Pts',(14.0918748017888,639.07699695793,70.6169548967642));
#101229=CARTESIAN_POINT('Ctrl Pts',(13.4200658305586,638.578980164138,71.9594073502309));
#101230=CARTESIAN_POINT('Ctrl Pts',(12.8958575906797,638.196942223385,72.7887618167445));
#101231=CARTESIAN_POINT('Ctrl Pts',(12.0012587128913,637.569843325258,73.9468631187593));
#101232=CARTESIAN_POINT('Ctrl Pts',(11.683780665072,637.35107315101,74.3193541873481));
#101233=CARTESIAN_POINT('Ctrl Pts',(11.0214171690138,636.905565899513,75.0259744723523));
#101234=CARTESIAN_POINT('Ctrl Pts',(10.6774393735486,636.67938676523,75.3595543546866));
#101235=CARTESIAN_POINT('Ctrl Pts',(9.60714722132492,635.996881119879,76.3061032107106));
#101236=CARTESIAN_POINT('Ctrl Pts',(8.84327964705721,635.536024385843,76.865511939863));
#101237=CARTESIAN_POINT('Ctrl Pts',(7.60921202386664,634.866673624162,77.6043583167633));
#101238=CARTESIAN_POINT('Ctrl Pts',(7.1813427653491,634.646547948635,77.8345316034363));
#101239=CARTESIAN_POINT('Ctrl Pts',(6.29818432438025,634.224889583467,78.2566267740411));
#101240=CARTESIAN_POINT('Ctrl Pts',(5.84582286264931,634.024672538662,78.4473366643001));
#101241=CARTESIAN_POINT('Ctrl Pts',(4.91622538701958,633.654268625565,78.7878860584469));
#101242=CARTESIAN_POINT('Ctrl Pts',(4.43900471573538,633.484057011527,78.9377439866561));
#101243=CARTESIAN_POINT('Ctrl Pts',(3.45473183503186,633.184919007639,79.1941909352119));
#101244=CARTESIAN_POINT('Ctrl Pts',(2.94362350959894,633.055356583509,79.3013079500641));
#101245=CARTESIAN_POINT('Ctrl Pts',(1.90950562370682,632.856171648375,79.4634826852088));
#101246=CARTESIAN_POINT('Ctrl Pts',(1.38650131959488,632.786121706041,79.5190163918644));
#101247=CARTESIAN_POINT('Ctrl Pts',(0.592249243454403,632.731168797606,
79.5625292223074));
#101248=CARTESIAN_POINT('Ctrl Pts',(0.325874264894089,632.721192165362,
79.5703863596371));
#101249=CARTESIAN_POINT('Ctrl Pts',(-0.21025693007535,632.718683864069,
79.5723645937365));
#101250=CARTESIAN_POINT('Ctrl Pts',(-0.48111240188688,632.726286108066,
79.5663806670725));
#101251=CARTESIAN_POINT('Ctrl Pts',(-1.81787718546613,632.807108441004,
79.5024445409065));
#101252=CARTESIAN_POINT('Ctrl Pts',(-2.84910806661434,633.007947305093,
79.3448450590357));
#101253=CARTESIAN_POINT('Ctrl Pts',(-3.85030552837329,633.305466608637,
79.0907977188138));
#101254=CARTESIAN_POINT('Ctrl Pts',(-31.4841643694399,640.028384824678,
66.2394387527688));
#101255=CARTESIAN_POINT('Ctrl Pts',(-31.5102422866113,640.037345033595,
66.1500520616432));
#101256=CARTESIAN_POINT('Ctrl Pts',(-31.5344697491162,640.045722080512,
66.0600041335432));
#101257=CARTESIAN_POINT('Ctrl Pts',(-31.5568948002686,640.053514660279,
65.9693158656704));
#101258=CARTESIAN_POINT('Ctrl Pts',(-31.5799157801734,640.061514321951,
65.8762176257544));
#101259=CARTESIAN_POINT('Ctrl Pts',(-31.6010376935118,640.068898248738,
65.7824435675418));
#101260=CARTESIAN_POINT('Ctrl Pts',(-31.6202693727863,640.075651611604,
65.6879866773397));
#101261=CARTESIAN_POINT('Ctrl Pts',(-31.6248896050321,640.07727404428,65.6652942871582));
#101262=CARTESIAN_POINT('Ctrl Pts',(-31.6294005338969,640.078860015917,
65.6425623950765));
#101263=CARTESIAN_POINT('Ctrl Pts',(-31.6338018813918,640.080409188182,
65.6197907592958));
#101264=CARTESIAN_POINT('Ctrl Pts',(-31.654946100996,640.087851463219,65.5103950643971));
#101265=CARTESIAN_POINT('Ctrl Pts',(-31.6735752186302,640.094449440729,
65.3999871588139));
#101266=CARTESIAN_POINT('Ctrl Pts',(-31.6895226485726,640.100117970976,
65.2892446570257));
#101267=CARTESIAN_POINT('Ctrl Pts',(-31.7041726680797,640.105325335361,
65.1875116619713));
#101268=CARTESIAN_POINT('Ctrl Pts',(-31.7165598903944,640.109748371004,
65.085497360404));
#101269=CARTESIAN_POINT('Ctrl Pts',(-31.7265914867054,640.113333580631,
64.9837326301969));
#101270=CARTESIAN_POINT('Ctrl Pts',(-31.7270906099686,640.11351196316,64.9786693139858));
#101271=CARTESIAN_POINT('Ctrl Pts',(-31.7275839622651,640.113688290221,
64.9736061633852));
#101272=CARTESIAN_POINT('Ctrl Pts',(-31.7280715338081,640.113862555796,
64.9685432194279));
#101273=CARTESIAN_POINT('Ctrl Pts',(-31.764504511737,640.126884263006,64.5902230978285));
#101274=CARTESIAN_POINT('Ctrl Pts',(-31.7700166160656,640.128859737276,
64.2118862669711));
#101275=CARTESIAN_POINT('Ctrl Pts',(-31.7446624416281,640.119794168933,
63.8336029368517));
#101276=CARTESIAN_POINT('Ctrl Pts',(-31.7418698618535,640.118795661848,
63.7919377515238));
#101277=CARTESIAN_POINT('Ctrl Pts',(-31.7387028782001,640.117663227655,
63.7502732253699));
#101278=CARTESIAN_POINT('Ctrl Pts',(-31.7351615999219,640.116396885934,
63.7086094597171));
#101279=CARTESIAN_POINT('Ctrl Pts',(-31.7342761400163,640.11608025032,63.6981918672244));
#101280=CARTESIAN_POINT('Ctrl Pts',(-31.7333672691212,640.115755243257,
63.6877743355871));
#101281=CARTESIAN_POINT('Ctrl Pts',(-31.7324349885411,640.11542186466,63.6773568521116));
#101282=CARTESIAN_POINT('Ctrl Pts',(-31.7131811671587,640.108536800135,
63.4622109289096));
#101283=CARTESIAN_POINT('Ctrl Pts',(-31.683622095357,640.097991917248,63.245890825627));
#101284=CARTESIAN_POINT('Ctrl Pts',(-31.6441613654705,640.084079144946,
63.0327241328211));
#101285=CARTESIAN_POINT('Ctrl Pts',(-31.6075834037094,640.071182757711,
62.8351301410067));
#101286=CARTESIAN_POINT('Ctrl Pts',(-31.5626857917352,640.055459282476,
62.6406026984657));
#101287=CARTESIAN_POINT('Ctrl Pts',(-31.5096017754345,640.037144233563,
62.4489753179586));
#101288=CARTESIAN_POINT('Ctrl Pts',(-31.5054732129836,640.035719796821,
62.4340716678045));
#101289=CARTESIAN_POINT('Ctrl Pts',(-31.5012951264941,640.034279706936,
62.4191858432772));
#101290=CARTESIAN_POINT('Ctrl Pts',(-31.4970675917481,640.032824078575,
62.4043178063035));
#101291=CARTESIAN_POINT('Ctrl Pts',(-31.3960489687264,639.998041260346,
62.0490401534014));
#101292=CARTESIAN_POINT('Ctrl Pts',(-31.2670264883458,639.954378011182,
61.7038445239479));
#101293=CARTESIAN_POINT('Ctrl Pts',(-31.1086646817577,639.903345001752,
61.3690067539261));
#101294=CARTESIAN_POINT('Ctrl Pts',(-31.0920627526296,639.89799493393,61.3339038901288));
#101295=CARTESIAN_POINT('Ctrl Pts',(-31.0751383343455,639.892563878665,
61.2989148348993));
#101296=CARTESIAN_POINT('Ctrl Pts',(-31.0578898612242,639.887053582625,
61.2640398858555));
#101297=CARTESIAN_POINT('Ctrl Pts',(-31.0492646062338,639.884298109251,
61.246600352155));
#101298=CARTESIAN_POINT('Ctrl Pts',(-31.0405577742687,639.881522719423,
61.2291887088941));
#101299=CARTESIAN_POINT('Ctrl Pts',(-31.0317691561598,639.878727630602,
61.2118050194646));
#101300=CARTESIAN_POINT('Ctrl Pts',(-30.8901561041094,639.833689712945,
60.9316975798752));
#101301=CARTESIAN_POINT('Ctrl Pts',(-30.7301960856141,639.784493060366,
60.6647961351979));
#101302=CARTESIAN_POINT('Ctrl Pts',(-30.552570698745,639.732879161611,60.4117938284315));
#101303=CARTESIAN_POINT('Ctrl Pts',(-30.5000976258482,639.717631679708,
60.3370533382344));
#101304=CARTESIAN_POINT('Ctrl Pts',(-30.4460831214046,639.702173469663,
60.2635256557381));
#101305=CARTESIAN_POINT('Ctrl Pts',(-30.390545271495,639.686549959976,60.1912282413397));
#101306=CARTESIAN_POINT('Ctrl Pts',(-30.3775068190579,639.682882076032,
60.1742551968214));
#101307=CARTESIAN_POINT('Ctrl Pts',(-30.3643834596268,639.679204897354,
60.1573491022777));
#101308=CARTESIAN_POINT('Ctrl Pts',(-30.3511754754658,639.675519029086,
60.1405102847351));
#101309=CARTESIAN_POINT('Ctrl Pts',(-30.235121732026,639.643132647847,59.9925537315534));
#101310=CARTESIAN_POINT('Ctrl Pts',(-30.1123925773292,639.610042934629,
59.849656540082));
#101311=CARTESIAN_POINT('Ctrl Pts',(-29.9827850448132,639.57663347586,59.7120039038443));
#101312=CARTESIAN_POINT('Ctrl Pts',(-29.9677860070962,639.572767113138,
59.696073833711));
#101313=CARTESIAN_POINT('Ctrl Pts',(-29.9526930083797,639.568896032035,
59.6802121620136));
#101314=CARTESIAN_POINT('Ctrl Pts',(-29.9375060153829,639.565020925164,
59.6644195965418));
#101315=CARTESIAN_POINT('Ctrl Pts',(-29.8373419011642,639.539463091078,
59.5602614967747));
#101316=CARTESIAN_POINT('Ctrl Pts',(-29.7327995153621,639.513674609795,
59.458939882618));
#101317=CARTESIAN_POINT('Ctrl Pts',(-29.6252314154097,639.48817571714,59.3617773359258));
#101318=CARTESIAN_POINT('Ctrl Pts',(-29.5921376179513,639.480330871045,
59.3318848525389));
#101319=CARTESIAN_POINT('Ctrl Pts',(-29.5587577612501,639.47251345882,59.3023858391177));
#101320=CARTESIAN_POINT('Ctrl Pts',(-29.5251319616347,639.464738635874,
59.273318160203));
#101321=CARTESIAN_POINT('Ctrl Pts',(-29.5086752766871,639.460933586976,
59.2590922491607));
#101322=CARTESIAN_POINT('Ctrl Pts',(-29.4921556791454,639.457137728834,
59.244965869578));
#101323=CARTESIAN_POINT('Ctrl Pts',(-29.4755774290304,639.453352761744,
59.2309432594684));
#101324=CARTESIAN_POINT('Ctrl Pts',(-29.3099773946231,639.415544749685,
59.0908714967353));
#101325=CARTESIAN_POINT('Ctrl Pts',(-29.1378119106167,639.378613173181,
58.9601884052983));
#101326=CARTESIAN_POINT('Ctrl Pts',(-28.9590308976962,639.343172368862,
58.8390285950504));
#101327=CARTESIAN_POINT('Ctrl Pts',(-28.8087859082244,639.313388427128,
58.7372076347721));
#101328=CARTESIAN_POINT('Ctrl Pts',(-28.6538691499679,639.284657645377,
58.6421117181841));
#101329=CARTESIAN_POINT('Ctrl Pts',(-28.4942662542453,639.257346611503,
58.5537968335703));
#101330=CARTESIAN_POINT('Ctrl Pts',(-28.4769007957699,639.254375057494,
58.5441878070262));
#101331=CARTESIAN_POINT('Ctrl Pts',(-28.459478271223,639.251420060263,58.5346582250449));
#101332=CARTESIAN_POINT('Ctrl Pts',(-28.4419987306746,639.248482115936,
58.5252082343139));
#101333=CARTESIAN_POINT('Ctrl Pts',(-28.2888749865063,639.222745224608,
58.4424247103949));
#101334=CARTESIAN_POINT('Ctrl Pts',(-28.1308888550333,639.198321952111,
58.3657956999464));
#101335=CARTESIAN_POINT('Ctrl Pts',(-27.9696009617568,639.175673567212,
58.2959953699951));
#101336=CARTESIAN_POINT('Ctrl Pts',(-27.8035137347293,639.152351249782,
58.2241180392686));
#101337=CARTESIAN_POINT('Ctrl Pts',(-27.6339267596476,639.130911539138,
58.1594826664216));
#101338=CARTESIAN_POINT('Ctrl Pts',(-27.4625791838735,639.111850435863,
58.1027857638719));
#101339=CARTESIAN_POINT('Ctrl Pts',(-27.4162113318999,639.106692368051,
58.087443185648));
#101340=CARTESIAN_POINT('Ctrl Pts',(-27.3697146769788,639.101708413567,
58.0726816677735));
#101341=CARTESIAN_POINT('Ctrl Pts',(-27.3231238847891,639.096908229404,
58.0585144074595));
#101342=CARTESIAN_POINT('Ctrl Pts',(-27.3077052706593,639.095319671153,
58.0538259377042));
#101343=CARTESIAN_POINT('Ctrl Pts',(-27.2922743593198,639.093750967214,
58.0492017474521));
#101344=CARTESIAN_POINT('Ctrl Pts',(-27.2768323473444,639.092202478353,
58.0446423518745));
#101345=CARTESIAN_POINT('Ctrl Pts',(-27.0730982847699,639.071772502834,
57.9844880024676));
#101346=CARTESIAN_POINT('Ctrl Pts',(-26.8663796549633,639.054639627356,
57.9348961994572));
#101347=CARTESIAN_POINT('Ctrl Pts',(-26.6567340260135,639.041091703772,
57.8960408616036));
#101348=CARTESIAN_POINT('Ctrl Pts',(-26.4648399672041,639.028690939406,
57.8604755673283));
#101349=CARTESIAN_POINT('Ctrl Pts',(-26.270493782847,639.019293785622,57.8339051264844));
#101350=CARTESIAN_POINT('Ctrl Pts',(-26.0737540205691,639.013111701195,
57.8164286107964));
#101351=CARTESIAN_POINT('Ctrl Pts',(-26.0625619002153,639.01276001513,57.8154344077707));
#101352=CARTESIAN_POINT('Ctrl Pts',(-26.0513595866431,639.012418650729,
57.8144693989542));
#101353=CARTESIAN_POINT('Ctrl Pts',(-26.0401473720418,639.012087666317,
57.8135336570049));
#101354=CARTESIAN_POINT('Ctrl Pts',(-25.9356392028654,639.009002586677,
57.8048116799985));
#101355=CARTESIAN_POINT('Ctrl Pts',(-25.8309402583624,639.006848581643,
57.7987137325091));
#101356=CARTESIAN_POINT('Ctrl Pts',(-25.7263828388109,639.005616381943,
57.7952202807389));
#101357=CARTESIAN_POINT('Ctrl Pts',(-25.6276871999166,639.004453262796,
57.7919226816218));
#101358=CARTESIAN_POINT('Ctrl Pts',(-25.5291178586403,639.004111297681,
57.7909452136726));
#101359=CARTESIAN_POINT('Ctrl Pts',(-25.4309523482839,639.004568492207,
57.7922313210019));
#101360=CARTESIAN_POINT('Ctrl Pts',(-25.294918478184,639.005202054245,57.7940135575199));
#101361=CARTESIAN_POINT('Ctrl Pts',(-25.1593220246081,639.007368336825,
57.8001370969469));
#101362=CARTESIAN_POINT('Ctrl Pts',(-25.0241528026831,639.011027220461,
57.8105033392556));
#101363=CARTESIAN_POINT('Ctrl Pts',(-24.9473593427915,639.01310593579,57.8163926948472));
#101364=CARTESIAN_POINT('Ctrl Pts',(-24.8707038305026,639.015666741267,
57.8236523823281));
#101365=CARTESIAN_POINT('Ctrl Pts',(-24.7941852298226,639.01870474031,57.8322713177254));
#101366=CARTESIAN_POINT('Ctrl Pts',(-24.7886039418909,639.018926332802,
57.832899985261));
#101367=CARTESIAN_POINT('Ctrl Pts',(-24.783023664907,639.019150453516,57.8335358543738));
#101368=CARTESIAN_POINT('Ctrl Pts',(-24.7774444134025,639.019377099508,
57.8341789177943));
#101369=CARTESIAN_POINT('Ctrl Pts',(-24.5718967014472,639.02772706634,57.8578703062588));
#101370=CARTESIAN_POINT('Ctrl Pts',(-24.3672912611834,639.039490474857,
57.8913676774045));
#101371=CARTESIAN_POINT('Ctrl Pts',(-24.1636900166142,639.054489501827,
57.9346799113559));
#101372=CARTESIAN_POINT('Ctrl Pts',(-24.1607192710785,639.054708352613,
57.9353118801138));
#101373=CARTESIAN_POINT('Ctrl Pts',(-24.157748731861,639.054927892726,57.9359459397558));
#101374=CARTESIAN_POINT('Ctrl Pts',(-24.1547783995907,639.055148121579,
57.9365820902092));
#101375=CARTESIAN_POINT('Ctrl Pts',(-23.9761114704639,639.068394994095,
57.9748468490423));
#101376=CARTESIAN_POINT('Ctrl Pts',(-23.7981202073762,639.084173694413,
58.020803853977));
#101377=CARTESIAN_POINT('Ctrl Pts',(-23.6236786700018,639.101975805995,
58.073492891561));
#101378=CARTESIAN_POINT('Ctrl Pts',(-23.5968668085346,639.104712010667,
58.0815912561925));
#101379=CARTESIAN_POINT('Ctrl Pts',(-23.5701387392797,639.107495996677,
58.0898485859262));
#101380=CARTESIAN_POINT('Ctrl Pts',(-23.5435048114214,639.110325898878,
58.0982613196408));
#101381=CARTESIAN_POINT('Ctrl Pts',(-23.5429448698536,639.110385393666,
58.0984381857543));
#101382=CARTESIAN_POINT('Ctrl Pts',(-23.5423849693564,639.110444908808,
58.0986151207343));
#101383=CARTESIAN_POINT('Ctrl Pts',(-23.5418251100215,639.110504444289,
58.0987921245494));
#101384=CARTESIAN_POINT('Ctrl Pts',(-23.1762012421074,639.149384911802,
58.2143869097244));
#101385=CARTESIAN_POINT('Ctrl Pts',(-22.8243998969131,639.197144672671,
58.3597501602455));
#101386=CARTESIAN_POINT('Ctrl Pts',(-22.485780010064,639.251242388907,58.534088114487));
#101387=CARTESIAN_POINT('Ctrl Pts',(-22.4521163261309,639.256620479479,
58.5514198129993));
#101388=CARTESIAN_POINT('Ctrl Pts',(-22.4185829180421,639.262061250877,
58.5690378848413));
#101389=CARTESIAN_POINT('Ctrl Pts',(-22.3851791566599,639.267562233714,
58.5869415569959));
#101390=CARTESIAN_POINT('Ctrl Pts',(-22.3824169167542,639.268017123633,
58.5884220560666));
#101391=CARTESIAN_POINT('Ctrl Pts',(-22.3796555707751,639.268472436214,
58.5899045687243));
#101392=CARTESIAN_POINT('Ctrl Pts',(-22.3768951241845,639.268928168783,
58.5913890909715));
#101393=CARTESIAN_POINT('Ctrl Pts',(-22.2816916837795,639.284645664844,
58.6425879171943));
#101394=CARTESIAN_POINT('Ctrl Pts',(-22.1873305987372,639.300901973426,
58.6963061579081));
#101395=CARTESIAN_POINT('Ctrl Pts',(-22.0942798727876,639.317549730656,
58.7522616622872));
#101396=CARTESIAN_POINT('Ctrl Pts',(-22.0053194489196,639.333465689661,
58.8057574876718));
#101397=CARTESIAN_POINT('Ctrl Pts',(-21.9175571859603,639.349739080634,
58.8612974640396));
#101398=CARTESIAN_POINT('Ctrl Pts',(-21.8313793586397,639.366234879066,
58.9185972031316));
#101399=CARTESIAN_POINT('Ctrl Pts',(-21.7404851365708,639.383633470009,
58.9790328786581));
#101400=CARTESIAN_POINT('Ctrl Pts',(-21.6513542120641,639.401277476804,
59.0414157758743));
#101401=CARTESIAN_POINT('Ctrl Pts',(-21.5639768145986,639.419098754486,
59.1057211509867));
#101402=CARTESIAN_POINT('Ctrl Pts',(-21.4860588850607,639.434990702506,
59.1630648329029));
#101403=CARTESIAN_POINT('Ctrl Pts',(-21.4095352908753,639.451023925407,
59.2219381824051));
#101404=CARTESIAN_POINT('Ctrl Pts',(-21.3344208389071,639.467153202096,
59.2823508523678));
#101405=CARTESIAN_POINT('Ctrl Pts',(-21.3303712812063,639.468022760948,
59.2856078100699));
#101406=CARTESIAN_POINT('Ctrl Pts',(-21.3263252327256,639.468892694763,
59.2888695173619));
#101407=CARTESIAN_POINT('Ctrl Pts',(-21.3222826740452,639.469763001685,
59.2921359995237));
#101408=CARTESIAN_POINT('Ctrl Pts',(-21.0528504262188,639.52776803483,59.509843570628));
#101409=CARTESIAN_POINT('Ctrl Pts',(-20.8009946645294,639.586975366306,
59.7470704016645));
#101410=CARTESIAN_POINT('Ctrl Pts',(-20.5670888588777,639.645312005445,
60.004810465092));
#101411=CARTESIAN_POINT('Ctrl Pts',(-20.5213856139102,639.656710498533,
60.0551707253855));
#101412=CARTESIAN_POINT('Ctrl Pts',(-20.4763676412837,639.66807589812,60.1063140803729));
#101413=CARTESIAN_POINT('Ctrl Pts',(-20.432037699356,639.679392953574,60.1582478620834));
#101414=CARTESIAN_POINT('Ctrl Pts',(-20.4285403996402,639.680285784313,
60.1623450476902));
#101415=CARTESIAN_POINT('Ctrl Pts',(-20.4250475423573,639.68117828926,60.1664471954375));
#101416=CARTESIAN_POINT('Ctrl Pts',(-20.4215591732656,639.682070449002,
60.1705542466145));
#101417=CARTESIAN_POINT('Ctrl Pts',(-20.287610486405,639.716328184557,60.3282594944146));
#101418=CARTESIAN_POINT('Ctrl Pts',(-20.1603042570768,639.75007161128,60.4931698430411));
#101419=CARTESIAN_POINT('Ctrl Pts',(-20.0421702953158,639.782219628577,
60.6620380239489));
#101420=CARTESIAN_POINT('Ctrl Pts',(-20.039477867816,639.782952323938,60.6658867506599));
#101421=CARTESIAN_POINT('Ctrl Pts',(-20.0367898122911,639.783684290105,
60.6697379704284));
#101422=CARTESIAN_POINT('Ctrl Pts',(-20.0341061280847,639.784415522889,
60.6735916845282));
#101423=CARTESIAN_POINT('Ctrl Pts',(-19.9157181298536,639.816673113164,
60.8435943610537));
#101424=CARTESIAN_POINT('Ctrl Pts',(-19.8058462866112,639.847499911429,
61.0184341585709));
#101425=CARTESIAN_POINT('Ctrl Pts',(-19.7044789025187,639.876528688321,
61.1981599173521));
#101426=CARTESIAN_POINT('Ctrl Pts',(-19.7027270351528,639.877030374019,
61.2012660021588));
#101427=CARTESIAN_POINT('Ctrl Pts',(-19.7009776841107,639.87753152646,61.2043735352324));
#101428=CARTESIAN_POINT('Ctrl Pts',(-19.6992308514509,639.87803214358,61.2074825179746));
#101429=CARTESIAN_POINT('Ctrl Pts',(-19.5329119435344,639.925696750844,
61.5034940514717));
#101430=CARTESIAN_POINT('Ctrl Pts',(-19.3894177738832,639.968502028101,
61.8126262806501));
#101431=CARTESIAN_POINT('Ctrl Pts',(-19.2704812976807,640.004691234995,
62.1360898569805));
#101432=CARTESIAN_POINT('Ctrl Pts',(-19.2423582110331,640.013248342399,
62.2125743340303));
#101433=CARTESIAN_POINT('Ctrl Pts',(-19.2156080374183,640.021435685137,
62.2898599650054));
#101434=CARTESIAN_POINT('Ctrl Pts',(-19.1902534503917,640.029230307342,
62.3679625261942));
#101435=CARTESIAN_POINT('Ctrl Pts',(-4.39560350684949,633.478027683157,
78.9419118149793));
#101436=CARTESIAN_POINT('Ctrl Pts',(-4.65179838529719,633.049363360682,
79.3159462734001));
#101437=CARTESIAN_POINT('Ctrl Pts',(-4.46675582291307,633.642397176786,
79.3699798038619));
#101438=CARTESIAN_POINT('Ctrl Pts',(-3.22222729143504,633.085349971256,
79.2841755866806));
#101439=CARTESIAN_POINT('Ctrl Pts',(-3.35828013222165,632.570904879132,
79.710778768011));
#101440=CARTESIAN_POINT('Ctrl Pts',(-3.27436645787075,633.244650561051,
79.722255531377));
#101441=CARTESIAN_POINT('Ctrl Pts',(-2.00765458360981,632.817733196177,
79.4940431330352));
#101442=CARTESIAN_POINT('Ctrl Pts',(-2.13704517639042,632.270842624481,
79.9301149240665));
#101443=CARTESIAN_POINT('Ctrl Pts',(-2.04015348412621,632.973589782311,
79.9382527125224));
#101444=CARTESIAN_POINT('Ctrl Pts',(-0.46947699470708,632.726029746276,
79.5665829488807));
#101445=CARTESIAN_POINT('Ctrl Pts',(-0.504033715610802,632.159949720998,
80.0123807664003));
#101446=CARTESIAN_POINT('Ctrl Pts',(-0.477078115453726,632.880703862599,
80.0129132419871));
#101447=CARTESIAN_POINT('Ctrl Pts',(-0.198525207359669,632.718703826906,
79.5723490852243));
#101448=CARTESIAN_POINT('Ctrl Pts',(-0.213567627251543,632.151013403264,
80.0189726826106));
#101449=CARTESIAN_POINT('Ctrl Pts',(-0.201739610759609,632.873283461515,
80.018847964929));
#101450=CARTESIAN_POINT('Ctrl Pts',(0.337797886426132,632.721726429248,
79.569965145871));
#101451=CARTESIAN_POINT('Ctrl Pts',(0.363172475404082,632.154718369797,
80.01623327854));
#101452=CARTESIAN_POINT('Ctrl Pts',(0.343267231354877,632.876345052986,
80.016394319429));
#101453=CARTESIAN_POINT('Ctrl Pts',(0.604500980807282,632.731966644653,
79.5618998035946));
#101454=CARTESIAN_POINT('Ctrl Pts',(0.648999446052346,632.16720503038,80.0070154560596));
#101455=CARTESIAN_POINT('Ctrl Pts',(0.614288243293599,632.886717335452,
80.0080931677934));
#101456=CARTESIAN_POINT('Ctrl Pts',(1.40038494278016,632.787851132862,79.517642720174));
#101457=CARTESIAN_POINT('Ctrl Pts',(1.49988036818683,632.235238567253,79.9564789876384));
#101458=CARTESIAN_POINT('Ctrl Pts',(1.42305709514243,632.9433225857,79.9625420908729));
#101459=CARTESIAN_POINT('Ctrl Pts',(1.92534113326012,632.858717853151,79.4614512450883));
#101460=CARTESIAN_POINT('Ctrl Pts',(2.05434637538845,632.319756788193,79.8936395733644));
#101461=CARTESIAN_POINT('Ctrl Pts',(1.95650990903739,633.015102751413,79.9047081360849));
#101462=CARTESIAN_POINT('Ctrl Pts',(2.70496406063899,633.00998734159,79.3382254829299));
#101463=CARTESIAN_POINT('Ctrl Pts',(2.88633995891351,632.502364612948,79.7536174784857));
#101464=CARTESIAN_POINT('Ctrl Pts',(2.74875593427252,633.168323516404,79.777879100916));
#101465=CARTESIAN_POINT('Ctrl Pts',(2.96456958631008,633.068167782713,79.290410633663));
#101466=CARTESIAN_POINT('Ctrl Pts',(3.15905718679442,632.571231832849,79.7002947629951));
#101467=CARTESIAN_POINT('Ctrl Pts',(3.01256338076222,633.227254078587,79.7286663835033));
#101468=CARTESIAN_POINT('Ctrl Pts',(3.47518780032947,633.196825535093,79.1831150315862));
#101469=CARTESIAN_POINT('Ctrl Pts',(3.69386701621685,632.722884585209,79.5809202469059));
#101470=CARTESIAN_POINT('Ctrl Pts',(3.53144620093892,633.35757070182,79.6182338532211));
#101471=CARTESIAN_POINT('Ctrl Pts',(3.72621041294374,633.267215716703,79.1237090131227));
#101472=CARTESIAN_POINT('Ctrl Pts',(3.95514895647901,632.804991870565,79.5154433630724));
#101473=CARTESIAN_POINT('Ctrl Pts',(3.78653130909377,633.428868298287,79.5570911547537));
#101474=CARTESIAN_POINT('Ctrl Pts',(4.46772555015823,633.493945812143,78.9291150218726));
#101475=CARTESIAN_POINT('Ctrl Pts',(4.71519034053282,633.065022733312,79.3041392307203));
#101476=CARTESIAN_POINT('Ctrl Pts',(4.54004264997885,633.658520109168,79.3568092233317));
#101477=CARTESIAN_POINT('Ctrl Pts',(4.94672040811002,633.665752738284,78.7776297759102));
#101478=CARTESIAN_POINT('Ctrl Pts',(5.20619063282509,633.259960181782,79.1411907055206));
#101479=CARTESIAN_POINT('Ctrl Pts',(5.02678739774566,633.832540815926,79.2008962492214));
#101480=CARTESIAN_POINT('Ctrl Pts',(5.8792429321931,634.039167473233,78.4336864380197));
#101481=CARTESIAN_POINT('Ctrl Pts',(6.15788846175844,633.681186892879,78.7714177057809));
#101482=CARTESIAN_POINT('Ctrl Pts',(5.97439705300667,634.210767970231,78.8468983899839));
#101483=CARTESIAN_POINT('Ctrl Pts',(6.33275437617335,634.240803603263,78.241207083469));
#101484=CARTESIAN_POINT('Ctrl Pts',(6.61701333922231,633.904629068291,78.5679319403425));
#101485=CARTESIAN_POINT('Ctrl Pts',(6.43524462113633,634.415001804823,78.6487931851204));
#101486=CARTESIAN_POINT('Ctrl Pts',(7.21772555207048,634.665027590137,77.8154792735));
#101487=CARTESIAN_POINT('Ctrl Pts',(7.50949169824814,634.372005257329,78.1180713169069));
#101488=CARTESIAN_POINT('Ctrl Pts',(7.33453041364423,634.844691731002,78.2106205359385));
#101489=CARTESIAN_POINT('Ctrl Pts',(7.64567757896693,634.886000066787,77.5837558363346));
#101490=CARTESIAN_POINT('Ctrl Pts',(7.93961757498883,634.612643284557,77.8759092393284));
#101491=CARTESIAN_POINT('Ctrl Pts',(7.76940426542435,635.068510841072,77.9721240183561));
#101492=CARTESIAN_POINT('Ctrl Pts',(8.87989624832361,635.557552829048,76.8401851017735));
#101493=CARTESIAN_POINT('Ctrl Pts',(9.14486309090704,635.321780212489,77.1186234238837));
#101494=CARTESIAN_POINT('Ctrl Pts',(9.0235661087087,635.74870553549,77.2068280660124));
#101495=CARTESIAN_POINT('Ctrl Pts',(9.64297366367729,636.019085537869,76.277848672361));
#101496=CARTESIAN_POINT('Ctrl Pts',(9.91195517002788,635.815649296021,76.5412806704512));
#101497=CARTESIAN_POINT('Ctrl Pts',(9.79898624522685,636.216183412484,76.6280570123386));
#101498=CARTESIAN_POINT('Ctrl Pts',(10.7111493226909,636.701555729233,75.3274439525344));
#101499=CARTESIAN_POINT('Ctrl Pts',(10.996929204677,636.553856661763,75.5414473133398));
#101500=CARTESIAN_POINT('Ctrl Pts',(10.8844475000821,636.907453239766,75.6498569210074));
#101501=CARTESIAN_POINT('Ctrl Pts',(11.0542671299848,636.927552573915,74.9926611496337));
#101502=CARTESIAN_POINT('Ctrl Pts',(11.3383050337577,636.792333613069,75.1981903967951));
#101503=CARTESIAN_POINT('Ctrl Pts',(11.2331134421883,637.136361142634,75.3052878963191));
#101504=CARTESIAN_POINT('Ctrl Pts',(11.7146199608134,637.372368504535,74.2838589448406));
#101505=CARTESIAN_POINT('Ctrl Pts',(11.9934013858358,637.259648873769,74.4717373421274));
#101506=CARTESIAN_POINT('Ctrl Pts',(11.9041426976532,637.586906313537,74.5757653364059));
#101507=CARTESIAN_POINT('Ctrl Pts',(12.0280511690333,637.588636973812,73.9137447966116));
#101508=CARTESIAN_POINT('Ctrl Pts',(12.3052838069643,637.486813840008,74.0929439227344));
#101509=CARTESIAN_POINT('Ctrl Pts',(12.2226419987782,637.805960726912,74.1948314957367));
#101510=CARTESIAN_POINT('Ctrl Pts',(12.9129429279531,638.209511050012,72.7621724811206));
#101511=CARTESIAN_POINT('Ctrl Pts',(13.1682069587253,638.125157961639,72.9350760877257));
#101512=CARTESIAN_POINT('Ctrl Pts',(13.1218292556881,638.434824297819,73.0096082212392));
#101513=CARTESIAN_POINT('Ctrl Pts',(13.4325731745126,638.588343288914,71.9369957714403));
#101514=CARTESIAN_POINT('Ctrl Pts',(13.691058719412,638.52474293751,72.0905203676822));
#101515=CARTESIAN_POINT('Ctrl Pts',(13.6498656696272,638.818539589406,72.1603061192183));
#101516=CARTESIAN_POINT('Ctrl Pts',(14.0995518794942,639.0829155774,70.5995413985153));
#101517=CARTESIAN_POINT('Ctrl Pts',(14.3599543505595,639.04443639772,70.7113989853479));
#101518=CARTESIAN_POINT('Ctrl Pts',(14.3276327741606,639.319486592683,70.7837383555535));
#101519=CARTESIAN_POINT('Ctrl Pts',(14.3029634008898,639.235458993974,70.136985137629));
#101520=CARTESIAN_POINT('Ctrl Pts',(14.5622961369223,639.203195170246,70.2399143740041));
#101521=CARTESIAN_POINT('Ctrl Pts',(14.5343332153866,639.47399527342,70.3076585181821));
#101522=CARTESIAN_POINT('Ctrl Pts',(14.6682015611194,639.511275540645,69.174113632982));
#101523=CARTESIAN_POINT('Ctrl Pts',(14.9241336165254,639.488901670915,69.2600256603411));
#101524=CARTESIAN_POINT('Ctrl Pts',(14.9054756223491,639.753364437729,69.3166364965849));
#101525=CARTESIAN_POINT('Ctrl Pts',(14.8267650211877,639.632077828551,68.6819292751415));
#101526=CARTESIAN_POINT('Ctrl Pts',(15.0820212400289,639.614532434591,68.7582297164531));
#101527=CARTESIAN_POINT('Ctrl Pts',(15.0666029583495,639.875723200025,68.8100615928647));
#101528=CARTESIAN_POINT('Ctrl Pts',(15.0928587745384,639.835676376718,67.6825720627153));
#101529=CARTESIAN_POINT('Ctrl Pts',(15.345642317407,639.82511616596,67.7418790685988));
#101530=CARTESIAN_POINT('Ctrl Pts',(15.3369981776382,640.081944211076,67.781486615588));
#101531=CARTESIAN_POINT('Ctrl Pts',(15.2008187183865,639.918802146937,67.1742916843792));
#101532=CARTESIAN_POINT('Ctrl Pts',(15.4531593768323,639.911476842323,67.2238371821344));
#101533=CARTESIAN_POINT('Ctrl Pts',(15.4467037685615,640.166141047895,67.2583447276789));
#101534=CARTESIAN_POINT('Ctrl Pts',(15.3236190583423,640.013555762971,66.3983126284387));
#101535=CARTESIAN_POINT('Ctrl Pts',(15.5750769362233,640.009593564889,66.4333318182824));
#101536=CARTESIAN_POINT('Ctrl Pts',(15.5714893985198,640.262115321071,66.4596770533946));
#101537=CARTESIAN_POINT('Ctrl Pts',(15.3580154032569,640.0401443868,66.1373887935008));
#101538=CARTESIAN_POINT('Ctrl Pts',(15.6092008209444,640.037099666513,66.1679286147603));
#101539=CARTESIAN_POINT('Ctrl Pts',(15.6064418001331,640.289046455888,66.191124442761));
#101540=CARTESIAN_POINT('Ctrl Pts',(15.4132989948751,640.082912766178,65.6108481462777));
#101541=CARTESIAN_POINT('Ctrl Pts',(15.6639728424716,640.081280555054,65.6327189571251));
#101542=CARTESIAN_POINT('Ctrl Pts',(15.6626190527797,640.332365724081,65.649189292362));
#101543=CARTESIAN_POINT('Ctrl Pts',(15.4341736765461,640.099082778176,65.3445748221907));
#101544=CARTESIAN_POINT('Ctrl Pts',(15.6846836179855,640.098005681656,65.361885527254));
#101545=CARTESIAN_POINT('Ctrl Pts',(15.6838311981551,640.34874403735,65.37513074784));
#101546=CARTESIAN_POINT('Ctrl Pts',(15.5027734069943,640.152235313522,64.0208357993163));
#101547=CARTESIAN_POINT('Ctrl Pts',(15.7525074770034,640.152789798181,64.019253662881));
#101548=CARTESIAN_POINT('Ctrl Pts',(15.7535397227803,640.402581126806,64.0126917270571));
#101549=CARTESIAN_POINT('Ctrl Pts',(15.4463052101678,640.10821736367,62.972460326068));
#101550=CARTESIAN_POINT('Ctrl Pts',(15.6953430710373,640.106377717465,62.9419553492361));
#101551=CARTESIAN_POINT('Ctrl Pts',(15.6961577000033,640.357995398756,62.9336548017417));
#101552=CARTESIAN_POINT('Ctrl Pts',(15.1990606178882,639.917447559145,61.4152823525307));
#101553=CARTESIAN_POINT('Ctrl Pts',(15.4514130025606,639.910073207687,61.3655583025674));
#101554=CARTESIAN_POINT('Ctrl Pts',(15.4449172446521,640.164769008981,61.3309552205203));
#101555=CARTESIAN_POINT('Ctrl Pts',(15.0885616588025,639.832373608348,60.897431997035));
#101556=CARTESIAN_POINT('Ctrl Pts',(15.3413681900166,639.821688428962,60.8377615984788));
#101557=CARTESIAN_POINT('Ctrl Pts',(15.3326315846512,640.078598890309,60.7979635436387));
#101558=CARTESIAN_POINT('Ctrl Pts',(14.8199878745666,639.626907879806,59.894490282593));
#101559=CARTESIAN_POINT('Ctrl Pts',(15.0752901365765,639.609169825034,59.8177577361634));
#101560=CARTESIAN_POINT('Ctrl Pts',(15.0597162431557,639.870486649284,59.7656992724498));
#101561=CARTESIAN_POINT('Ctrl Pts',(14.6615322304544,639.506218060285,59.405821548259));
#101562=CARTESIAN_POINT('Ctrl Pts',(14.9175497152663,639.48368395994,59.3196546068316));
#101563=CARTESIAN_POINT('Ctrl Pts',(14.8986984980326,639.748241829529,59.2627428795189));
#101564=CARTESIAN_POINT('Ctrl Pts',(14.2987645730368,639.2323098162,58.452368034267));
#101565=CARTESIAN_POINT('Ctrl Pts',(14.5581603558448,639.199949590199,58.3493442354962));
#101566=CARTESIAN_POINT('Ctrl Pts',(14.5300665302068,639.470805547583,58.2814141988727));
#101567=CARTESIAN_POINT('Ctrl Pts',(14.0943650477466,639.079019607747,57.987427888935));
#101568=CARTESIAN_POINT('Ctrl Pts',(14.3547106916411,639.040317082871,57.8751573631045));
#101569=CARTESIAN_POINT('Ctrl Pts',(14.3223620118629,639.315540381266,57.8028805682137));
#101570=CARTESIAN_POINT('Ctrl Pts',(13.6407992303396,638.7427973154,57.0811428907972));
#101571=CARTESIAN_POINT('Ctrl Pts',(13.905352230957,638.691285108647,56.9519457897139));
#101572=CARTESIAN_POINT('Ctrl Pts',(13.8614639308801,638.97498749143,56.870100046218));
#101573=CARTESIAN_POINT('Ctrl Pts',(13.3950963108816,638.562439030259,56.6466171892939));
#101574=CARTESIAN_POINT('Ctrl Pts',(13.660997958786,638.503183284432,56.5087094937084));
#101575=CARTESIAN_POINT('Ctrl Pts',(13.611788274916,638.792305710012,56.4228707819826));
#101576=CARTESIAN_POINT('Ctrl Pts',(12.8683162606274,638.181402354979,55.8111128357767));
#101577=CARTESIAN_POINT('Ctrl Pts',(13.1390236076535,638.106466963312,55.6564090278324));
#101578=CARTESIAN_POINT('Ctrl Pts',(13.0764921418282,638.406361283186,55.5629408541681));
#101579=CARTESIAN_POINT('Ctrl Pts',(12.5872314290769,637.980708173654,55.4101487566788));
#101580=CARTESIAN_POINT('Ctrl Pts',(12.8594650095397,637.896519710106,55.2468622237164));
#101581=CARTESIAN_POINT('Ctrl Pts',(12.7908624053289,638.203081725356,55.1502548367754));
#101582=CARTESIAN_POINT('Ctrl Pts',(11.9905202907966,637.562607910276,54.6394524585066));
#101583=CARTESIAN_POINT('Ctrl Pts',(12.2679641743712,637.459493978226,54.4591095196187));
#101584=CARTESIAN_POINT('Ctrl Pts',(12.1845042755668,637.779596359876,54.3570282351227));
#101585=CARTESIAN_POINT('Ctrl Pts',(11.6738674877948,637.344499438125,54.2686527469967));
#101586=CARTESIAN_POINT('Ctrl Pts',(11.9529310376215,637.230395235121,54.0796602679055));
#101587=CARTESIAN_POINT('Ctrl Pts',(11.8627313233714,637.558678274829,53.9753888666545));
#101588=CARTESIAN_POINT('Ctrl Pts',(10.6782856421904,636.675211836513,53.2086614405224));
#101589=CARTESIAN_POINT('Ctrl Pts',(10.945265328937,636.512855335653,52.9711566209328));
#101590=CARTESIAN_POINT('Ctrl Pts',(10.8510402072694,636.880761580352,52.8843970456025));
#101591=CARTESIAN_POINT('Ctrl Pts',(9.9619956407393,636.213789414038,52.5782081758289));
#101592=CARTESIAN_POINT('Ctrl Pts',(10.2261851601175,636.022124234935,52.325672618392));
#101593=CARTESIAN_POINT('Ctrl Pts',(10.1231644802855,636.41339474604,52.2355170621796));
#101594=CARTESIAN_POINT('Ctrl Pts',(8.80321427157986,635.525430893182,51.7332383677212));
#101595=CARTESIAN_POINT('Ctrl Pts',(9.09775647626564,635.303078691545,51.4706442472987));
#101596=CARTESIAN_POINT('Ctrl Pts',(8.94566114499843,635.716178886036,51.3658592810726));
#101597=CARTESIAN_POINT('Ctrl Pts',(8.40274055580763,635.296654083887,51.468542205798));
#101598=CARTESIAN_POINT('Ctrl Pts',(8.69719315797,635.057159081061,51.1963055952873));
#101599=CARTESIAN_POINT('Ctrl Pts',(8.53871075522488,635.484455070077,51.0934261046552));
#101600=CARTESIAN_POINT('Ctrl Pts',(7.56992268932879,634.846289649222,50.9728170395581));
#101601=CARTESIAN_POINT('Ctrl Pts',(7.86343028959298,634.569343605214,50.6785875112157));
#101602=CARTESIAN_POINT('Ctrl Pts',(7.69242405624649,635.028288789374,50.5832101346318));
#101603=CARTESIAN_POINT('Ctrl Pts',(7.13789769244056,634.625016491671,50.7422564476865));
#101604=CARTESIAN_POINT('Ctrl Pts',(7.42930129741495,634.32828122725,50.4376325390388));
#101605=CARTESIAN_POINT('Ctrl Pts',(7.25341144010781,634.804165183149,50.3459105384044));
#101606=CARTESIAN_POINT('Ctrl Pts',(5.64937448274455,633.917920325537,50.0365737439137));
#101607=CARTESIAN_POINT('Ctrl Pts',(5.86838675369824,633.517703145266,49.6620231583277));
#101608=CARTESIAN_POINT('Ctrl Pts',(5.74078325583842,634.087945275018,49.619586152077));
#101609=CARTESIAN_POINT('Ctrl Pts',(4.53678997843346,633.475322195353,49.6490480272297));
#101610=CARTESIAN_POINT('Ctrl Pts',(4.73821803522549,633.030778025867,49.2624552965428));
#101611=CARTESIAN_POINT('Ctrl Pts',(4.6102062721931,633.639651657831,49.2207424753189));
#101612=CARTESIAN_POINT('Ctrl Pts',(3.32305067587215,633.158508245587,49.3839240770566));
#101613=CARTESIAN_POINT('Ctrl Pts',(3.5382678177423,632.678855162063,48.9831770877134));
#101614=CARTESIAN_POINT('Ctrl Pts',(3.3768462630334,633.318759264595,48.9478721490979));
#101615=CARTESIAN_POINT('',(3.93978362444746,633.475903764133,49.082928510463));
#101616=CARTESIAN_POINT('Origin',(3.87712128127698,633.475903764132,49.3249479946959));
#101617=CARTESIAN_POINT('',(3.44556542901615E-11,632.874615496758,80.0177796115133));
#101618=CARTESIAN_POINT('Ctrl Pts',(6.89110032669561E-11,632.874615496766,
80.0177787907144));
#101619=CARTESIAN_POINT('Ctrl Pts',(0.0236086443784427,632.874614137695,
80.0177797817517));
#101620=CARTESIAN_POINT('Ctrl Pts',(0.0471977207100217,632.874679616131,
80.0177272377913));
#101621=CARTESIAN_POINT('Ctrl Pts',(0.0707638231545093,632.874812004893,
80.017621142111));
#101622=CARTESIAN_POINT('Ctrl Pts',(0.343491007326591,632.876344121384,
80.0163933117468));
#101623=CARTESIAN_POINT('Ctrl Pts',(0.614496441609097,632.886726575974,
80.0080814531982));
#101624=CARTESIAN_POINT('Ctrl Pts',(0.883878526644417,632.90557635702,79.992909437795));
#101625=CARTESIAN_POINT('Ctrl Pts',(1.24943310899451,632.931155726327,79.9723208386927));
#101626=CARTESIAN_POINT('Ctrl Pts',(1.61199825336115,632.972352866,79.9391295369995));
#101627=CARTESIAN_POINT('Ctrl Pts',(1.97182100459663,633.027965414741,79.8936222931219));
#101628=CARTESIAN_POINT('Ctrl Pts',(2.14338863407486,633.054482118102,79.8719239154363));
#101629=CARTESIAN_POINT('Ctrl Pts',(2.31433265226697,633.084276807937,79.8474250872979));
#101630=CARTESIAN_POINT('Ctrl Pts',(2.48467918176861,633.117222497334,79.8201546029834));
#101631=CARTESIAN_POINT('Ctrl Pts',(2.64668359998503,633.148554789569,79.7942195929849));
#101632=CARTESIAN_POINT('Ctrl Pts',(2.80854164377702,633.182836792382,79.7656811760263));
#101633=CARTESIAN_POINT('Ctrl Pts',(2.96931905952992,633.219691119353,79.7347565578901));
#101634=CARTESIAN_POINT('Ctrl Pts',(3.07072240523473,633.242935379383,79.7152522031959));
#101635=CARTESIAN_POINT('Ctrl Pts',(3.17169670908156,633.267201801138,79.6947984620929));
#101636=CARTESIAN_POINT('Ctrl Pts',(3.27200870695423,633.292396349908,79.6734492843488));
#101637=CARTESIAN_POINT('Ctrl Pts',(3.53149735464351,633.357570003389,79.6182228968818));
#101638=CARTESIAN_POINT('Ctrl Pts',(3.78656458821259,633.428865125024,79.5570823750604));
#101639=CARTESIAN_POINT('Ctrl Pts',(4.0377054944055,633.50540597798,79.4903295169232));
#101640=CARTESIAN_POINT('Ctrl Pts',(4.40729347692622,633.618046247752,79.3920936120663));
#101641=CARTESIAN_POINT('Ctrl Pts',(4.76841289981949,633.741996318891,79.2817479196209));
#101642=CARTESIAN_POINT('Ctrl Pts',(5.12226678865164,633.875000842973,79.1597571080153));
#101643=CARTESIAN_POINT('Ctrl Pts',(5.24929534886485,633.922747593057,79.1159641255257));
#101644=CARTESIAN_POINT('Ctrl Pts',(5.37538735228987,633.971661476884,79.0706700669597));
#101645=CARTESIAN_POINT('Ctrl Pts',(5.50059773443487,634.021638914138,79.0238952610022));
#101646=CARTESIAN_POINT('Ctrl Pts',(5.57281046246084,634.050462459135,78.9969187732444));
#101647=CARTESIAN_POINT('Ctrl Pts',(5.64472953797076,634.079640403287,78.9694492784864));
#101648=CARTESIAN_POINT('Ctrl Pts',(5.71636225209789,634.109157580105,78.9414864057523));
#101649=CARTESIAN_POINT('Ctrl Pts',(6.11454307894412,634.273233086873,78.7860507235792));
#101650=CARTESIAN_POINT('Ctrl Pts',(6.5037096819656,634.447710875873,78.6154339417837));
#101651=CARTESIAN_POINT('Ctrl Pts',(6.8848883010362,634.629844770744,78.4297064786912));
#101652=CARTESIAN_POINT('Ctrl Pts',(7.33445681558759,634.844656568862,78.2106563653939));
#101653=CARTESIAN_POINT('Ctrl Pts',(7.76935072835594,635.068481784423,77.9721566871374));
#101654=CARTESIAN_POINT('Ctrl Pts',(8.187458217611,635.295242394859,77.7170253648745));
#101655=CARTESIAN_POINT('Ctrl Pts',(8.18746947767835,635.295248501757,77.717018493924));
#101656=CARTESIAN_POINT('Ctrl Pts',(8.18748073773472,635.295254608657,77.717011622961));
#101657=CARTESIAN_POINT('Ctrl Pts',(8.18749199778011,635.29526071556,77.7170047519856));
#101658=CARTESIAN_POINT('Ctrl Pts',(8.77466513792119,635.613714974938,77.3587067097642));
#101659=CARTESIAN_POINT('Ctrl Pts',(9.33198431948961,635.939124765157,76.966537584401));
#101660=CARTESIAN_POINT('Ctrl Pts',(9.86244451563549,636.264283914362,76.5388820043299));
#101661=CARTESIAN_POINT('Ctrl Pts',(10.0299804477179,636.366979350387,76.4038149875433));
#101662=CARTESIAN_POINT('Ctrl Pts',(10.1948374647139,636.469649728038,76.2652085142118));
#101663=CARTESIAN_POINT('Ctrl Pts',(10.357110568178,636.572067980441,76.1230125476066));
#101664=CARTESIAN_POINT('Ctrl Pts',(10.4125855674164,636.607080883706,76.0744011574826));
#101665=CARTESIAN_POINT('Ctrl Pts',(10.4677585361306,636.642065479229,76.0253703145275));
#101666=CARTESIAN_POINT('Ctrl Pts',(10.5226333425913,636.677012430926,75.9759179749726));
#101667=CARTESIAN_POINT('Ctrl Pts',(10.8021362240136,636.855013490539,75.7240342365111));
#101668=CARTESIAN_POINT('Ctrl Pts',(11.0737787493323,637.032122690786,75.4611186031081));
#101669=CARTESIAN_POINT('Ctrl Pts',(11.3375596732538,637.207320538843,75.1864000604822));
#101670=CARTESIAN_POINT('Ctrl Pts',(11.4152479295857,637.258919476045,75.1054904774791));
#101671=CARTESIAN_POINT('Ctrl Pts',(11.4922757377262,637.310368726257,75.023534546417));
#101672=CARTESIAN_POINT('Ctrl Pts',(11.5686281331514,637.361633525872,74.9405265476199));
#101673=CARTESIAN_POINT('Ctrl Pts',(11.7428614430288,637.478617880682,74.7511053998464));
#101674=CARTESIAN_POINT('Ctrl Pts',(11.9125329809655,637.593944005337,74.5572877444706));
#101675=CARTESIAN_POINT('Ctrl Pts',(12.0772418647245,637.707053445441,74.3595533209396));
#101676=CARTESIAN_POINT('Ctrl Pts',(12.1335432671804,637.745716934401,74.2919630058059));
#101677=CARTESIAN_POINT('Ctrl Pts',(12.1892651384294,637.784121561834,74.2239153125423));
#101678=CARTESIAN_POINT('Ctrl Pts',(12.2443925060635,637.822245533895,74.1554302041703));
#101679=CARTESIAN_POINT('Ctrl Pts',(12.3387364620062,637.887490193579,74.0382260581302));
#101680=CARTESIAN_POINT('Ctrl Pts',(12.4314151262027,637.951963329841,73.9196466444437));
#101681=CARTESIAN_POINT('Ctrl Pts',(12.5223735539977,638.015572404099,73.7997538153798));
#101682=CARTESIAN_POINT('Ctrl Pts',(12.7691297819456,638.188134041407,73.4745030060267));
#101683=CARTESIAN_POINT('Ctrl Pts',(13.0038431244469,638.354709108044,73.1391451429892));
#101684=CARTESIAN_POINT('Ctrl Pts',(13.2260892248535,638.514262005761,72.7931543850006));
#101685=CARTESIAN_POINT('Ctrl Pts',(13.4204829916068,638.653819409589,72.490523893018));
#101686=CARTESIAN_POINT('Ctrl Pts',(13.6053390538305,638.788004415294,72.1797589167343));
#101687=CARTESIAN_POINT('Ctrl Pts',(13.7803977512332,638.916136677922,71.8605255759729));
#101688=CARTESIAN_POINT('Ctrl Pts',(13.8914471872943,638.997418075061,71.6580181713742));
#101689=CARTESIAN_POINT('Ctrl Pts',(13.9985704807448,639.076258682161,71.4520750410272));
#101690=CARTESIAN_POINT('Ctrl Pts',(14.1017118649645,639.152494301075,71.242591313036));
#101691=CARTESIAN_POINT('Ctrl Pts',(14.2070716057042,639.230369589492,71.0286020260264));
#101692=CARTESIAN_POINT('Ctrl Pts',(14.3082384476158,639.305518787928,70.81089177479));
#101693=CARTESIAN_POINT('Ctrl Pts',(14.4050208561385,639.377709197237,70.5892424956487));
#101694=CARTESIAN_POINT('Ctrl Pts',(14.5157812425591,639.46032583959,70.3355811104624));
#101695=CARTESIAN_POINT('Ctrl Pts',(14.6208678960897,639.539123655019,70.0765942455148));
#101696=CARTESIAN_POINT('Ctrl Pts',(14.7199048617496,639.61367514778,69.8121463246681));
#101697=CARTESIAN_POINT('Ctrl Pts',(14.7921227929364,639.668038228658,69.6193104312928));
#101698=CARTESIAN_POINT('Ctrl Pts',(14.8606224440704,639.71976485242,69.4248390807865));
#101699=CARTESIAN_POINT('Ctrl Pts',(14.9252970870176,639.768724787416,69.2290149637919));
#101700=CARTESIAN_POINT('Ctrl Pts',(15.0269343231625,639.845666108592,68.9212742308732));
#101701=CARTESIAN_POINT('Ctrl Pts',(15.1192104490316,639.915845082243,68.6099443406549));
#101702=CARTESIAN_POINT('Ctrl Pts',(15.2018005707495,639.978833650544,68.2957740937441));
#101703=CARTESIAN_POINT('Ctrl Pts',(15.3370175067359,640.081958831023,67.781413086861));
#101704=CARTESIAN_POINT('Ctrl Pts',(15.446711258392,640.16614656396,67.2582968021332));
#101705=CARTESIAN_POINT('Ctrl Pts',(15.5298941967001,640.230123458173,66.7258995592192));
#101706=CARTESIAN_POINT('Ctrl Pts',(15.5492380442097,640.245001019737,66.6020927871707));
#101707=CARTESIAN_POINT('Ctrl Pts',(15.567145084157,640.258784059514,66.4777831582835));
#101708=CARTESIAN_POINT('Ctrl Pts',(15.5835932838998,640.271451481493,66.3529610769457));
#101709=CARTESIAN_POINT('Ctrl Pts',(15.6025152015847,640.286024013424,66.2093664474262));
#101710=CARTESIAN_POINT('Ctrl Pts',(15.6195051466467,640.299119194904,66.0651039293665));
#101711=CARTESIAN_POINT('Ctrl Pts',(15.6345304353988,640.310705016247,65.9201567812727));
#101712=CARTESIAN_POINT('Ctrl Pts',(15.6626204963928,640.332364927982,65.6491753513615));
#101713=CARTESIAN_POINT('Ctrl Pts',(15.6838314901426,640.348739893915,65.3751252063361));
#101714=CARTESIAN_POINT('Ctrl Pts',(15.6977729274255,640.359499433045,65.1026424621912));
#101715=CARTESIAN_POINT('Ctrl Pts',(15.7020662908531,640.362812908611,65.0187294893299));
#101716=CARTESIAN_POINT('Ctrl Pts',(15.7056890266772,640.365606360559,64.934880886641));
#101717=CARTESIAN_POINT('Ctrl Pts',(15.7086425189985,640.367881244341,64.8510957582209));
#101718=CARTESIAN_POINT('Ctrl Pts',(15.7263165930932,640.381494438539,64.3497148820873));
#101719=CARTESIAN_POINT('Ctrl Pts',(15.7200248924218,640.376502649213,63.8506118554521));
#101720=CARTESIAN_POINT('Ctrl Pts',(15.690054723568,640.35337768455,63.3537494689463));
#101721=CARTESIAN_POINT('Ctrl Pts',(15.6600845547142,640.330252719886,62.8568870824406));
#101722=CARTESIAN_POINT('Ctrl Pts',(15.6064372952925,640.288992245354,62.3622858632638));
#101723=CARTESIAN_POINT('Ctrl Pts',(15.5294020172295,640.229744984429,61.8699005539026));
#101724=CARTESIAN_POINT('Ctrl Pts',(15.5291562735781,640.229555984809,61.8683298376432));
#101725=CARTESIAN_POINT('Ctrl Pts',(15.5289102911643,640.229366802534,61.8667591390815));
#101726=CARTESIAN_POINT('Ctrl Pts',(15.5286640699994,640.229177437613,61.8651884582589));
#101727=CARTESIAN_POINT('Ctrl Pts',(15.4868770628328,640.197039691489,61.5986230278086));
#101728=CARTESIAN_POINT('Ctrl Pts',(15.4379580369842,640.159463399778,61.3322197252253));
#101729=CARTESIAN_POINT('Ctrl Pts',(15.3824805581748,640.11694984057,61.0681260116128));
#101730=CARTESIAN_POINT('Ctrl Pts',(15.3358122267536,640.081186916342,60.8459671605322));
#101731=CARTESIAN_POINT('Ctrl Pts',(15.2845038713041,640.041930974165,60.6254434697092));
#101732=CARTESIAN_POINT('Ctrl Pts',(15.2289186178845,639.999496500196,60.4078240107633));
#101733=CARTESIAN_POINT('Ctrl Pts',(15.2181659569586,639.991287785077,60.3657267258008));
#101734=CARTESIAN_POINT('Ctrl Pts',(15.2072508201014,639.982958720179,60.3237283373609));
#101735=CARTESIAN_POINT('Ctrl Pts',(15.196175503333,639.974511334344,60.2818374278755));
#101736=CARTESIAN_POINT('Ctrl Pts',(15.0967816925709,639.898701505458,59.9058935865296));
#101737=CARTESIAN_POINT('Ctrl Pts',(14.9842779945857,639.813199116241,59.5366531114232));
#101738=CARTESIAN_POINT('Ctrl Pts',(14.8591459849512,639.718652910703,59.1739255763155));
#101739=CARTESIAN_POINT('Ctrl Pts',(14.8126284390092,639.683505569327,59.0390824228484));
#101740=CARTESIAN_POINT('Ctrl Pts',(14.7643660978975,639.647108703488,58.9051391515317));
#101741=CARTESIAN_POINT('Ctrl Pts',(14.7143850694044,639.609496653593,58.7720853460318));
#101742=CARTESIAN_POINT('Ctrl Pts',(14.5736911865015,639.503620774218,58.3975461039397));
#101743=CARTESIAN_POINT('Ctrl Pts',(14.4193228109465,639.388070847762,58.0299622878074));
#101744=CARTESIAN_POINT('Ctrl Pts',(14.2516172400983,639.263553359904,57.6694867820626));
#101745=CARTESIAN_POINT('Ctrl Pts',(14.1996634649568,639.224978889583,57.5578145026341));
#101746=CARTESIAN_POINT('Ctrl Pts',(14.1464260882526,639.185541476775,57.4468157386464));
#101747=CARTESIAN_POINT('Ctrl Pts',(14.0919132979964,639.145261719478,57.3364909682744));
#101748=CARTESIAN_POINT('Ctrl Pts',(13.9337411446871,639.028387570924,57.0163769838124));
#101749=CARTESIAN_POINT('Ctrl Pts',(13.7664884987757,638.905649173198,56.7052436349986));
#101750=CARTESIAN_POINT('Ctrl Pts',(13.5905541920495,638.777739522865,56.4024860662582));
#101751=CARTESIAN_POINT('Ctrl Pts',(13.5102146755004,638.719330224185,56.2642333447919));
#101752=CARTESIAN_POINT('Ctrl Pts',(13.4280641419558,638.659838944025,56.1277259803299));
#101753=CARTESIAN_POINT('Ctrl Pts',(13.3441406912912,638.599331136345,55.9929065938881));
#101754=CARTESIAN_POINT('Ctrl Pts',(13.18094216384,638.481666943148,55.7307352321897));
#101755=CARTESIAN_POINT('Ctrl Pts',(13.0110358717025,638.360152379953,55.4749525005651));
#101756=CARTESIAN_POINT('Ctrl Pts',(12.834515971694,638.235208319465,55.2252918717908));
#101757=CARTESIAN_POINT('Ctrl Pts',(12.72157305542,638.155265227711,55.065551244863));
#101758=CARTESIAN_POINT('Ctrl Pts',(12.605960880953,638.073943984384,54.908370053597));
#101759=CARTESIAN_POINT('Ctrl Pts',(12.4876834913283,637.991338466186,54.7536417333294));
#101760=CARTESIAN_POINT('Ctrl Pts',(12.3260424195162,637.878447536303,54.5421858362462));
#101761=CARTESIAN_POINT('Ctrl Pts',(12.1591272633341,637.762955719753,54.3349982249623));
#101762=CARTESIAN_POINT('Ctrl Pts',(11.9873446890174,637.645441249947,54.1324570254279));
#101763=CARTESIAN_POINT('Ctrl Pts',(11.8370887041422,637.542652870694,53.9552968708841));
#101764=CARTESIAN_POINT('Ctrl Pts',(11.6829923400669,637.438237648866,53.7815611779533));
#101765=CARTESIAN_POINT('Ctrl Pts',(11.5255012613247,637.332705058659,53.6117252605926));
#101766=CARTESIAN_POINT('Ctrl Pts',(11.3711873179765,637.229301422869,53.445315516375));
#101767=CARTESIAN_POINT('Ctrl Pts',(11.2140552717419,637.125076575966,53.2829927429756));
#101768=CARTESIAN_POINT('Ctrl Pts',(11.0542019754068,637.020337990515,53.1247785161058));
#101769=CARTESIAN_POINT('Ctrl Pts',(10.5698058923565,636.702953477967,52.6453492297812));
#101770=CARTESIAN_POINT('Ctrl Pts',(10.0592926792999,636.38008853675,52.2024986100953));
#101771=CARTESIAN_POINT('Ctrl Pts',(9.52149128320355,636.057785926617,51.7931946715343));
#101772=CARTESIAN_POINT('Ctrl Pts',(9.4607314186001,636.021372739342,51.7469522257744));
#101773=CARTESIAN_POINT('Ctrl Pts',(9.39962327575445,635.984966737236,51.7011379284146));
#101774=CARTESIAN_POINT('Ctrl Pts',(9.33816519001716,635.948576638187,51.6557473746706));
#101775=CARTESIAN_POINT('Ctrl Pts',(9.21814549218717,635.877511478259,51.5671054900537));
#101776=CARTESIAN_POINT('Ctrl Pts',(9.09677553395677,635.806510933312,51.4800960735065));
#101777=CARTESIAN_POINT('Ctrl Pts',(8.97400639050294,635.735660278011,51.3947159850713));
#101778=CARTESIAN_POINT('Ctrl Pts',(8.6952662635268,635.57479802794,51.200865510741));
#101779=CARTESIAN_POINT('Ctrl Pts',(8.40931705214077,635.414676812656,51.0154168364813));
#101780=CARTESIAN_POINT('Ctrl Pts',(8.11558835298555,635.256319777099,50.8383307562355));
#101781=CARTESIAN_POINT('Ctrl Pts',(7.6923917485449,635.028163114403,50.5831897772666));
#101782=CARTESIAN_POINT('Ctrl Pts',(7.2533699333788,634.803988668472,50.3458922881572));
#101783=CARTESIAN_POINT('Ctrl Pts',(6.8038425239994,634.591170154752,50.1300393648259));
#101784=CARTESIAN_POINT('Ctrl Pts',(6.73473828265152,634.558454325575,50.0968570667095));
#101785=CARTESIAN_POINT('Ctrl Pts',(6.66535065282463,634.525974001608,50.0641473617017));
#101786=CARTESIAN_POINT('Ctrl Pts',(6.59567017408014,634.493749398169,50.0319141884441));
#101787=CARTESIAN_POINT('Ctrl Pts',(6.0329269890491,634.233501818042,49.7715973980109));
#101788=CARTESIAN_POINT('Ctrl Pts',(5.45113667983874,633.989769248135,49.5423875083977));
#101789=CARTESIAN_POINT('Ctrl Pts',(4.84525727421132,633.772994795064,49.3462933887937));
#101790=CARTESIAN_POINT('Ctrl Pts',(4.54937241807388,633.667131685566,49.2505296446731));
#101791=CARTESIAN_POINT('Ctrl Pts',(4.24774282927289,633.567697202977,49.1626636005312));
#101792=CARTESIAN_POINT('Ctrl Pts',(3.93978362444749,633.475903764133,49.082928510463));
#101793=CARTESIAN_POINT('',(-3.91253447320281,633.467807133627,79.5230488432747));
#101794=CARTESIAN_POINT('Ctrl Pts',(-3.91253447320281,633.467807133627,
79.5230488432747));
#101795=CARTESIAN_POINT('Ctrl Pts',(-3.28597810505974,633.282223705224,
79.6840769479877));
#101796=CARTESIAN_POINT('Ctrl Pts',(-2.64771851246926,633.133689622239,
79.807103090937));
#101797=CARTESIAN_POINT('Ctrl Pts',(-1.67000646568519,632.980744450827,
79.9322661229594));
#101798=CARTESIAN_POINT('Ctrl Pts',(-1.34070899812117,632.941409107268,
79.9640509087433));
#101799=CARTESIAN_POINT('Ctrl Pts',(-0.674809016948164,632.888311307288,
80.0068322484697));
#101800=CARTESIAN_POINT('Ctrl Pts',(-0.336249102370441,632.874615496751,
80.0177804323122));
#101801=CARTESIAN_POINT('Ctrl Pts',(0.,632.874615496751,80.0177804323122));
#101802=CARTESIAN_POINT('Origin',(-3.85030552837329,633.467807133627,79.2809175598242));
#101803=CARTESIAN_POINT('Ctrl Pts',(1.86306288877797,634.816577773823,79.840079036097));
#101804=CARTESIAN_POINT('Ctrl Pts',(1.88043236474458,634.745314120185,79.9049255377571));
#101805=CARTESIAN_POINT('Ctrl Pts',(1.89318255568148,634.648256234279,79.9033522554387));
#101806=CARTESIAN_POINT('Ctrl Pts',(0.807589904959711,634.674153210188,
79.96967854764));
#101807=CARTESIAN_POINT('Ctrl Pts',(0.818743950698479,634.603422866382,
80.0328500715449));
#101808=CARTESIAN_POINT('Ctrl Pts',(0.820646498012554,634.507527220826,
80.0334805824724));
#101809=CARTESIAN_POINT('Ctrl Pts',(-0.24578162409436,634.652430501916,
79.9884448322078));
#101810=CARTESIAN_POINT('Ctrl Pts',(-0.250591804105093,634.58145862555,
80.0516667261813));
#101811=CARTESIAN_POINT('Ctrl Pts',(-0.249753392942155,634.486062895163,
80.0523236519829));
#101812=CARTESIAN_POINT('Ctrl Pts',(-1.82283398292192,634.801279095755,
79.8541299127167));
#101813=CARTESIAN_POINT('Ctrl Pts',(-1.84045202787124,634.730077912528,
79.9187905906115));
#101814=CARTESIAN_POINT('Ctrl Pts',(-1.85230285694165,634.633139639668,
79.9174605062689));
#101815=CARTESIAN_POINT('Ctrl Pts',(-2.35132258925576,634.881814269216,
79.7811312873554));
#101816=CARTESIAN_POINT('Ctrl Pts',(-2.37466264357766,634.810809328746,
79.8462807686186));
#101817=CARTESIAN_POINT('Ctrl Pts',(-2.38933484362825,634.712715932409,
79.8441641306276));
#101818=CARTESIAN_POINT('Ctrl Pts',(-3.37688542676327,635.092028016582,
79.5855704382192));
#101819=CARTESIAN_POINT('Ctrl Pts',(-3.41016272286989,635.021031352354,
79.6525292086393));
#101820=CARTESIAN_POINT('Ctrl Pts',(-3.43147735551063,634.920427161253,
79.6478052879441));
#101821=CARTESIAN_POINT('Ctrl Pts',(-3.87715892282217,635.221574909017,
79.4630988338053));
#101822=CARTESIAN_POINT('Ctrl Pts',(-3.91596185111128,635.150913347198,
79.5308660063145));
#101823=CARTESIAN_POINT('Ctrl Pts',(-3.93983799323763,635.048431634461,
79.524834163758));
#101824=CARTESIAN_POINT('Ctrl Pts',(-4.85600136127738,635.519479195749,
79.1715962336162));
#101825=CARTESIAN_POINT('Ctrl Pts',(-4.90487000526279,635.449018256018,
79.2419298822336));
#101826=CARTESIAN_POINT('Ctrl Pts',(-4.93450429122365,635.342789420971,
79.2321422141563));
#101827=CARTESIAN_POINT('Ctrl Pts',(-5.33696096117466,635.688816137699,
79.0015116750124));
#101828=CARTESIAN_POINT('Ctrl Pts',(-5.39138050124868,635.618861104025,
79.0729171785271));
#101829=CARTESIAN_POINT('Ctrl Pts',(-5.42323859046884,635.51011019859,79.0613640029475));
#101830=CARTESIAN_POINT('Ctrl Pts',(-6.26683249734681,636.052464199552,
78.6207327915938));
#101831=CARTESIAN_POINT('Ctrl Pts',(-6.33161473347313,635.983087692133,
78.6952414948338));
#101832=CARTESIAN_POINT('Ctrl Pts',(-6.36814164931804,635.869428991425,
78.6790317667906));
#101833=CARTESIAN_POINT('Ctrl Pts',(-6.71485606394656,636.246122485711,
78.4107691833072));
#101834=CARTESIAN_POINT('Ctrl Pts',(-6.78508370064264,636.177428409817,
78.4865227570079));
#101835=CARTESIAN_POINT('Ctrl Pts',(-6.82340725268958,636.060781547509,
78.4682119648795));
#101836=CARTESIAN_POINT('Ctrl Pts',(-8.01567130514643,636.849983611819,
77.7247225905372));
#101837=CARTESIAN_POINT('Ctrl Pts',(-8.10998737994435,636.786710672416,
77.80127117446));
#101838=CARTESIAN_POINT('Ctrl Pts',(-8.1452439447473,636.65745105782,77.7793700065673));
#101839=CARTESIAN_POINT('Ctrl Pts',(-8.82586458852353,637.282584832603,
77.1932211322336));
#101840=CARTESIAN_POINT('Ctrl Pts',(-8.9322668123389,637.222864399076,77.2695206334129));
#101841=CARTESIAN_POINT('Ctrl Pts',(-8.96853196172092,637.084900724076,
77.2457034968301));
#101842=CARTESIAN_POINT('Ctrl Pts',(-9.96920498164766,637.941263310567,
76.2792128579425));
#101843=CARTESIAN_POINT('Ctrl Pts',(-10.0844043143261,637.880534079776,
76.3668461206141));
#101844=CARTESIAN_POINT('Ctrl Pts',(-10.1303565945194,637.735739871643,
76.3279647989551));
#101845=CARTESIAN_POINT('Ctrl Pts',(-10.3376554216138,638.162400261368,
75.9549308895933));
#101846=CARTESIAN_POINT('Ctrl Pts',(-10.4588442149254,638.103340264843,
76.0434598022962));
#101847=CARTESIAN_POINT('Ctrl Pts',(-10.5047617063462,637.95424377021,76.0023613348043));
#101848=CARTESIAN_POINT('Ctrl Pts',(-11.0382031181792,638.595577836314,
75.2772723636161));
#101849=CARTESIAN_POINT('Ctrl Pts',(-11.1717706789499,638.540193855464,
75.367843846083));
#101850=CARTESIAN_POINT('Ctrl Pts',(-11.2166306018809,638.382263478537,
75.3219412047776));
#101851=CARTESIAN_POINT('Ctrl Pts',(-11.3720692100036,638.808639459202,
74.9225466233422));
#101852=CARTESIAN_POINT('Ctrl Pts',(-11.5117299914058,638.755294583093,
75.0135259579074));
#101853=CARTESIAN_POINT('Ctrl Pts',(-11.5558920129995,638.592788120577,
74.9657703096301));
#101854=CARTESIAN_POINT('Ctrl Pts',(-12.3258306637108,639.431272311957,
73.8086323110397));
#101855=CARTESIAN_POINT('Ctrl Pts',(-12.4934838485425,639.390510009471,
73.890709901465));
#101856=CARTESIAN_POINT('Ctrl Pts',(-12.5250601941573,639.208003600421,
73.8473239435239));
#101857=CARTESIAN_POINT('Ctrl Pts',(-12.8992879967844,639.824973080161,
72.9992994563982));
#101858=CARTESIAN_POINT('Ctrl Pts',(-13.077744970774,639.788629846106,73.078286707878));
#101859=CARTESIAN_POINT('Ctrl Pts',(-13.1077845770232,639.597016725675,
73.0346961932179));
#101860=CARTESIAN_POINT('Ctrl Pts',(-13.9074241048782,640.534546099924,
71.2282105920088));
#101861=CARTESIAN_POINT('Ctrl Pts',(-14.1129332121864,640.511006048043,
71.2991153875746));
#101862=CARTESIAN_POINT('Ctrl Pts',(-14.1322077025265,640.298139145848,
71.2563976137341));
#101863=CARTESIAN_POINT('Ctrl Pts',(-14.3263939594619,640.839310439365,
70.2940353094581));
#101864=CARTESIAN_POINT('Ctrl Pts',(-14.5401918741479,640.819432608961,
70.3605898861845));
#101865=CARTESIAN_POINT('Ctrl Pts',(-14.5579479788688,640.599275304904,
70.3184194820128));
#101866=CARTESIAN_POINT('Ctrl Pts',(-14.8207085214835,641.20293089409,68.8119251561665));
#101867=CARTESIAN_POINT('Ctrl Pts',(-15.0476696916695,641.189657317405,
68.873414318539));
#101868=CARTESIAN_POINT('Ctrl Pts',(-15.0602487335032,640.958565966149,
68.8302748068456));
#101869=CARTESIAN_POINT('Ctrl Pts',(-14.9632961223424,641.308768600142,
68.3027032249751));
#101870=CARTESIAN_POINT('Ctrl Pts',(-15.1947954692114,641.297980576062,
68.3589101018559));
#101871=CARTESIAN_POINT('Ctrl Pts',(-15.2051396204071,641.063143179964,
68.3189814008671));
#101872=CARTESIAN_POINT('Ctrl Pts',(-15.1980890660801,641.483791241123,
67.2613296018157));
#101873=CARTESIAN_POINT('Ctrl Pts',(-15.4382600058939,641.477993541957,
67.3038920930527));
#101874=CARTESIAN_POINT('Ctrl Pts',(-15.443724690614,641.23608096797,67.273372933676));
#101875=CARTESIAN_POINT('Ctrl Pts',(-15.2886130183545,641.551710847139,
66.7373033136078));
#101876=CARTESIAN_POINT('Ctrl Pts',(-15.5318361040901,641.54764077895,66.7735722504368));
#101877=CARTESIAN_POINT('Ctrl Pts',(-15.535710856414,641.303191662114,66.7472152886529));
#101878=CARTESIAN_POINT('Ctrl Pts',(-15.416753347311,641.648007675455,65.6826183891459));
#101879=CARTESIAN_POINT('Ctrl Pts',(-15.6650029770328,641.646911132633,
65.702986948441));
#101880=CARTESIAN_POINT('Ctrl Pts',(-15.6659206532499,641.398341361037,
65.6882422743292));
#101881=CARTESIAN_POINT('Ctrl Pts',(-15.4543691947642,641.676387664944,
65.1519598739898));
#101882=CARTESIAN_POINT('Ctrl Pts',(-15.7039435893065,641.67605647301,65.1652840040138));
#101883=CARTESIAN_POINT('Ctrl Pts',(-15.7041440786651,641.426383341139,
65.1554257032332));
#101884=CARTESIAN_POINT('Ctrl Pts',(-15.4758420566949,641.692577105787,
64.0838805525614));
#101885=CARTESIAN_POINT('Ctrl Pts',(-15.7262805762301,641.692762772545,
64.0801660974848));
#101886=CARTESIAN_POINT('Ctrl Pts',(-15.725963719193,641.442379922507,64.0830042219837));
#101887=CARTESIAN_POINT('Ctrl Pts',(-15.4595256835684,641.680254533958,
63.5443861522047));
#101888=CARTESIAN_POINT('Ctrl Pts',(-15.7093899474742,641.680108047155,
63.533432145575));
#101889=CARTESIAN_POINT('Ctrl Pts',(-15.7093838004202,641.430204112855,
63.5413158590829));
#101890=CARTESIAN_POINT('Ctrl Pts',(-15.3271559384047,641.580597626596,
61.9287880982582));
#101891=CARTESIAN_POINT('Ctrl Pts',(-15.5720423635035,641.577531969054,
61.8961392504176));
#101892=CARTESIAN_POINT('Ctrl Pts',(-15.5748761636817,641.331734267035,
61.9191477303746));
#101893=CARTESIAN_POINT('Ctrl Pts',(-15.1321164848615,641.43365154733,60.8870337307209));
#101894=CARTESIAN_POINT('Ctrl Pts',(-15.3728291173235,641.428596909895,
60.8481294183498));
#101895=CARTESIAN_POINT('Ctrl Pts',(-15.3766850183768,641.186537362943,
60.8731529828927));
#101896=CARTESIAN_POINT('Ctrl Pts',(-14.6914127541727,641.107583316918,
59.3724502436072));
#101897=CARTESIAN_POINT('Ctrl Pts',(-14.9137106754241,641.091687521186,
59.3061798598269));
#101898=CARTESIAN_POINT('Ctrl Pts',(-14.9288646952281,640.864354185543,
59.352414428403));
#101899=CARTESIAN_POINT('Ctrl Pts',(-14.5183989336226,640.980317513494,
58.8731518928978));
#101900=CARTESIAN_POINT('Ctrl Pts',(-14.7354925923479,640.961660459604,
58.8024640384097));
#101901=CARTESIAN_POINT('Ctrl Pts',(-14.7530559724391,640.738604035086,
58.8510846321663));
#101902=CARTESIAN_POINT('Ctrl Pts',(-14.1306968197733,640.698218654891,
57.9103117242868));
#101903=CARTESIAN_POINT('Ctrl Pts',(-14.3355486906423,640.673080740323,
57.831412861111));
#101904=CARTESIAN_POINT('Ctrl Pts',(-14.359091214726,640.459865155437,57.8843269848985));
#101905=CARTESIAN_POINT('Ctrl Pts',(-13.9157951809153,640.543213567675,
57.4449987770471));
#101906=CARTESIAN_POINT('Ctrl Pts',(-14.1147768511431,640.515153086481,
57.36307554632));
#101907=CARTESIAN_POINT('Ctrl Pts',(-14.1407177531073,640.306706015409,
57.4171203625588));
#101908=CARTESIAN_POINT('Ctrl Pts',(-13.4461019523439,640.2091391353,56.5440307949745));
#101909=CARTESIAN_POINT('Ctrl Pts',(-13.6319576862834,640.174660971835,
56.4571863827656));
#101910=CARTESIAN_POINT('Ctrl Pts',(-13.6634366702206,639.976610327696,
56.5124852728988));
#101911=CARTESIAN_POINT('Ctrl Pts',(-13.1913037235795,640.030055873436,
56.1083842943529));
#101912=CARTESIAN_POINT('Ctrl Pts',(-13.3709792891118,639.992762314905,
56.0198511196711));
#101913=CARTESIAN_POINT('Ctrl Pts',(-13.4045217018065,639.79965965408,56.0750652474453));
#101914=CARTESIAN_POINT('Ctrl Pts',(-12.64240759359,639.651151524472,55.2652320085852));
#101915=CARTESIAN_POINT('Ctrl Pts',(-12.8086534652092,639.607949925527,
55.1745452490493));
#101916=CARTESIAN_POINT('Ctrl Pts',(-12.8467572513285,639.42526762927,55.228479858422));
#101917=CARTESIAN_POINT('Ctrl Pts',(-12.3483069071172,639.451372577967,
54.8582156625017));
#101918=CARTESIAN_POINT('Ctrl Pts',(-12.5081763747874,639.405559223045,
54.7668256888036));
#101919=CARTESIAN_POINT('Ctrl Pts',(-12.5479044351808,639.22786764373,54.8198060554334));
#101920=CARTESIAN_POINT('Ctrl Pts',(-11.4236939741492,638.837407783853,
53.6980435355989));
#101921=CARTESIAN_POINT('Ctrl Pts',(-11.5721545818984,638.789502601269,
53.6169046527624));
#101922=CARTESIAN_POINT('Ctrl Pts',(-11.6083463397431,638.621210776527,
53.6549020913344));
#101923=CARTESIAN_POINT('Ctrl Pts',(-10.7466675601512,638.404972777793,
52.9971756449448));
#101924=CARTESIAN_POINT('Ctrl Pts',(-10.8838506687482,638.353029612216,
52.9147405141668));
#101925=CARTESIAN_POINT('Ctrl Pts',(-10.9203783533487,638.193924822611,
52.9511800330592));
#101926=CARTESIAN_POINT('Ctrl Pts',(-9.63611348815389,637.746715461555,
52.043761533861));
#101927=CARTESIAN_POINT('Ctrl Pts',(-9.74600809350944,637.684740757834,
51.957512201222));
#101928=CARTESIAN_POINT('Ctrl Pts',(-9.79188180091537,637.543508391082,
51.9938845551591));
#101929=CARTESIAN_POINT('Ctrl Pts',(-9.24839501364177,637.524950639754,
51.7415264001437));
#101930=CARTESIAN_POINT('Ctrl Pts',(-9.3523814388582,637.46152901563,51.6563518525185));
#101931=CARTESIAN_POINT('Ctrl Pts',(-9.39789698724149,637.324384062376,
51.6904175829392));
#101932=CARTESIAN_POINT('Ctrl Pts',(-8.45164641908639,637.090734943436,
51.1790240815796));
#101933=CARTESIAN_POINT('Ctrl Pts',(-8.5442188058991,637.02515789963,51.0970442175137));
#101934=CARTESIAN_POINT('Ctrl Pts',(-8.58827076396017,636.895338174316,
51.1256218197328));
#101935=CARTESIAN_POINT('Ctrl Pts',(-8.04152694278709,636.87756046477,50.9176054756285));
#101936=CARTESIAN_POINT('Ctrl Pts',(-8.12841996224353,636.810886545792,
50.8368346325361));
#101937=CARTESIAN_POINT('Ctrl Pts',(-8.17152248677754,636.684701860634,
50.863137499133));
#101938=CARTESIAN_POINT('Ctrl Pts',(-6.77296527985932,636.258719991593,
50.1910295542293));
#101939=CARTESIAN_POINT('Ctrl Pts',(-6.85180078127632,636.193927906267,
50.1198420410442));
#101940=CARTESIAN_POINT('Ctrl Pts',(-6.88245059777448,636.073226521136,
50.1335953878553));
#101941=CARTESIAN_POINT('Ctrl Pts',(-5.87736007948177,635.872567289871,
49.7825065974709));
#101942=CARTESIAN_POINT('Ctrl Pts',(-5.9437815426704,635.804781945381,49.7114424968018));
#101943=CARTESIAN_POINT('Ctrl Pts',(-5.97236940852386,635.691672509095,
49.7234080275098));
#101944=CARTESIAN_POINT('Ctrl Pts',(-4.43240690450128,635.383525832075,
49.2925569652473));
#101945=CARTESIAN_POINT('Ctrl Pts',(-4.47704379275697,635.313078576597,
49.2235345335549));
#101946=CARTESIAN_POINT('Ctrl Pts',(-4.50406198106327,635.208454481341,
49.2314609330919));
#101947=CARTESIAN_POINT('Ctrl Pts',(-3.93312549027658,635.236185446456,
49.1503705419181));
#101948=CARTESIAN_POINT('Ctrl Pts',(-3.97216443006433,635.165338459273,
49.0822732722215));
#101949=CARTESIAN_POINT('Ctrl Pts',(-3.99670954179863,635.062868366633,
49.088694597554));
#101950=CARTESIAN_POINT('Ctrl Pts',(-2.80721571948024,634.962333725774,
48.8913556172268));
#101951=CARTESIAN_POINT('Ctrl Pts',(-2.83595961882426,634.891619931837,
48.8258047037574));
#101952=CARTESIAN_POINT('Ctrl Pts',(-2.85259747105698,634.79227663453,48.828622663863));
#101953=CARTESIAN_POINT('Ctrl Pts',(-2.17289772786691,634.846757938817,
48.7861606117588));
#101954=CARTESIAN_POINT('Ctrl Pts',(-2.19436435124887,634.775581535024,
48.7211342965425));
#101955=CARTESIAN_POINT('Ctrl Pts',(-2.20802541255103,634.678077030975,
48.7229986861513));
#101956=CARTESIAN_POINT('Ctrl Pts',(-1.52385975751051,634.77491121819,48.7210323974546));
#101957=CARTESIAN_POINT('Ctrl Pts',(-1.53802701951984,634.703667729437,
48.6565547220431));
#101958=CARTESIAN_POINT('Ctrl Pts',(-1.54849576756905,634.607085709312,
48.6576047836707));
#101959=CARTESIAN_POINT('',(-1.8888840075986,634.820085762158,48.7620619651123));
#101960=CARTESIAN_POINT('',(1.86306288877797,634.816577773823,79.840079036097));
#101961=CARTESIAN_POINT('Ctrl Pts',(-1.88888400759861,634.820085762158,
48.7620619651124));
#101962=CARTESIAN_POINT('Ctrl Pts',(-2.41149695900854,634.891566330598,
48.8271353535257));
#101963=CARTESIAN_POINT('Ctrl Pts',(-2.92444502661294,634.990847088073,
48.9183242031726));
#101964=CARTESIAN_POINT('Ctrl Pts',(-3.42867105811381,635.113486538694,
49.0343192413469));
#101965=CARTESIAN_POINT('Ctrl Pts',(-3.43116315307004,635.114092673914,
49.0348925371141));
#101966=CARTESIAN_POINT('Ctrl Pts',(-3.43365511556905,635.114699409002,
49.0354664692822));
#101967=CARTESIAN_POINT('Ctrl Pts',(-3.43614694410229,635.115306742866,
49.0360410372357));
#101968=CARTESIAN_POINT('Ctrl Pts',(-3.82123395661622,635.209164076938,
49.1248347298047));
#101969=CARTESIAN_POINT('Ctrl Pts',(-4.20323008313647,635.317350603336,
49.2288408125806));
#101970=CARTESIAN_POINT('Ctrl Pts',(-4.57646776363458,635.435822811474,
49.3457763157678));
#101971=CARTESIAN_POINT('Ctrl Pts',(-4.68985979690286,635.471815438341,
49.3813020816818));
#101972=CARTESIAN_POINT('Ctrl Pts',(-4.80244368066391,635.508757271302,
49.4180209911173));
#101973=CARTESIAN_POINT('Ctrl Pts',(-4.91406129959471,635.546534671639,
49.4558685205457));
#101974=CARTESIAN_POINT('Ctrl Pts',(-4.91843568064348,635.548015197256,
49.4573517945759));
#101975=CARTESIAN_POINT('Ctrl Pts',(-4.92280863589928,635.549496953263,
49.4588367478035));
#101976=CARTESIAN_POINT('Ctrl Pts',(-4.92718016685644,635.550979936383,
49.4603233795273));
#101977=CARTESIAN_POINT('Ctrl Pts',(-5.42040916316384,635.718301243964,
49.6280563500103));
#101978=CARTESIAN_POINT('Ctrl Pts',(-5.89557048320261,635.901250262189,
49.8171650183551));
#101979=CARTESIAN_POINT('Ctrl Pts',(-6.35515504461554,636.095269123651,
50.026781157682));
#101980=CARTESIAN_POINT('Ctrl Pts',(-6.78955134192294,636.278654472296,
50.2249089505294));
#101981=CARTESIAN_POINT('Ctrl Pts',(-7.21003104621884,636.471930271108,
50.4413581652769));
#101982=CARTESIAN_POINT('Ctrl Pts',(-7.61867416252441,636.671279341153,
50.6754123677936));
#101983=CARTESIAN_POINT('Ctrl Pts',(-7.62456670988115,636.674153912604,
50.6787873799187));
#101984=CARTESIAN_POINT('Ctrl Pts',(-7.63045674519379,636.677029804123,
50.682166103682));
#101985=CARTESIAN_POINT('Ctrl Pts',(-7.63634427132602,636.679907007694,
50.6855485406359));
#101986=CARTESIAN_POINT('Ctrl Pts',(-8.05314726616503,636.883596475645,
50.9250056267778));
#101987=CARTESIAN_POINT('Ctrl Pts',(-8.45740792076498,637.093874893464,
51.1830917656922));
#101988=CARTESIAN_POINT('Ctrl Pts',(-8.85002243750459,637.30784159817,51.4602736948679));
#101989=CARTESIAN_POINT('Ctrl Pts',(-8.85593145106618,637.311061887044,
51.4644453994501));
#101990=CARTESIAN_POINT('Ctrl Pts',(-8.8618380665553,637.314283170744,51.4686216821428));
#101991=CARTESIAN_POINT('Ctrl Pts',(-8.86774226136733,637.317505426203,
51.4728025248131));
#101992=CARTESIAN_POINT('Ctrl Pts',(-9.23018926555088,637.515313404269,
51.7294563021797));
#101993=CARTESIAN_POINT('Ctrl Pts',(-9.583630223236,637.716848985045,52.0033825468534));
#101994=CARTESIAN_POINT('Ctrl Pts',(-9.92280720324511,637.916778287441,
52.2903964742841));
#101995=CARTESIAN_POINT('Ctrl Pts',(-9.95073667622084,637.933241433166,
52.314030589222));
#101996=CARTESIAN_POINT('Ctrl Pts',(-9.9785694564295,637.949693699854,52.3377534407296));
#101997=CARTESIAN_POINT('Ctrl Pts',(-10.0063026234585,637.966132117163,
52.3615626894152));
#101998=CARTESIAN_POINT('Ctrl Pts',(-10.0117904989738,637.969384972769,
52.3662740948152));
#101999=CARTESIAN_POINT('Ctrl Pts',(-10.0172748471287,637.972637449793,
52.3709890470134));
#102000=CARTESIAN_POINT('Ctrl Pts',(-10.0227556688065,637.975889541223,
52.375707548496));
#102001=CARTESIAN_POINT('Ctrl Pts',(-10.4844704327222,638.249851862,52.7732030201896));
#102002=CARTESIAN_POINT('Ctrl Pts',(-10.9212653120677,638.521129177495,
53.1959678507371));
#102003=CARTESIAN_POINT('Ctrl Pts',(-11.3338346748915,638.785642501227,
53.64564722763));
#102004=CARTESIAN_POINT('Ctrl Pts',(-11.5776710654221,638.941974938673,
53.9114163468082));
#102005=CARTESIAN_POINT('Ctrl Pts',(-11.8130457210345,639.095945236935,
54.1865861676));
#102006=CARTESIAN_POINT('Ctrl Pts',(-12.0401046610149,639.246716958051,
54.4714903191273));
#102007=CARTESIAN_POINT('Ctrl Pts',(-12.0438323006949,639.24919218607,54.476167606973));
#102008=CARTESIAN_POINT('Ctrl Pts',(-12.0475578528826,639.251666684543,
54.4808478324097));
#102009=CARTESIAN_POINT('Ctrl Pts',(-12.0512813078029,639.25414044383,54.4855309851298));
#102010=CARTESIAN_POINT('Ctrl Pts',(-12.3319606432928,639.440615942412,
54.8385537077483));
#102011=CARTESIAN_POINT('Ctrl Pts',(-12.6007933235743,639.622941327494,
55.2083103083306));
#102012=CARTESIAN_POINT('Ctrl Pts',(-12.853551064915,639.796961270491,55.5903491046588));
#102013=CARTESIAN_POINT('Ctrl Pts',(-12.8747668389634,639.811568015159,
55.622416366922));
#102014=CARTESIAN_POINT('Ctrl Pts',(-12.8958693834308,639.826116261523,
55.654570159216));
#102015=CARTESIAN_POINT('Ctrl Pts',(-12.9168562126465,639.840603562471,
55.6868078477632));
#102016=CARTESIAN_POINT('Ctrl Pts',(-12.9194398545994,639.842387061928,
55.6907765580309));
#102017=CARTESIAN_POINT('Ctrl Pts',(-12.922021743077,639.844169633993,55.6947464964152));
#102018=CARTESIAN_POINT('Ctrl Pts',(-12.9246018778219,639.845951277251,
55.6987176634258));
#102019=CARTESIAN_POINT('Ctrl Pts',(-13.1962036721651,640.033498655008,
56.1167485774522));
#102020=CARTESIAN_POINT('Ctrl Pts',(-13.4484034732778,640.210775408409,
56.5484436861926));
#102021=CARTESIAN_POINT('Ctrl Pts',(-13.680948979807,640.376176280427,56.9945145943681));
#102022=CARTESIAN_POINT('Ctrl Pts',(-13.6823423951751,640.377167364368,
56.9971874564156));
#102023=CARTESIAN_POINT('Ctrl Pts',(-13.6837351051094,640.378158022426,
56.9998608343006));
#102024=CARTESIAN_POINT('Ctrl Pts',(-13.6851271093879,640.379148254207,
57.0025347282827));
#102025=CARTESIAN_POINT('Ctrl Pts',(-13.9184371521736,640.545118303866,
57.4506988101028));
#102026=CARTESIAN_POINT('Ctrl Pts',(-14.1319267819666,640.699113596555,
57.9133662944617));
#102027=CARTESIAN_POINT('Ctrl Pts',(-14.3245484115035,640.839268025387,
58.3917316078811));
#102028=CARTESIAN_POINT('Ctrl Pts',(-14.3248720257519,640.839503492038,
58.3925352862205));
#102029=CARTESIAN_POINT('Ctrl Pts',(-14.3251955816966,640.839738920106,
58.3933390138011));
#102030=CARTESIAN_POINT('Ctrl Pts',(-14.3255190793133,640.839974309567,
58.3941427905653));
#102031=CARTESIAN_POINT('Ctrl Pts',(-14.5183947849969,640.980318182788,
58.8733704651745));
#102032=CARTESIAN_POINT('Ctrl Pts',(-14.6905438911395,641.106943614794,
59.370094559378));
#102033=CARTESIAN_POINT('Ctrl Pts',(-14.8368369280143,641.215178668622,
59.8722326143598));
#102034=CARTESIAN_POINT('Ctrl Pts',(-14.8373300871407,641.215543532909,
59.8739253399318));
#102035=CARTESIAN_POINT('Ctrl Pts',(-14.8378229525661,641.215908188285,
59.8756181274374));
#102036=CARTESIAN_POINT('Ctrl Pts',(-14.8383155240927,641.21627263457,59.8773109764116));
#102037=CARTESIAN_POINT('Ctrl Pts',(-15.0414396045849,641.366561095379,
60.575399218893));
#102038=CARTESIAN_POINT('Ctrl Pts',(-15.1973006597185,641.483141535664,
61.2886164427717));
#102039=CARTESIAN_POINT('Ctrl Pts',(-15.3033244731206,641.562742156357,
62.0179657600747));
#102040=CARTESIAN_POINT('Ctrl Pts',(-15.3495814982321,641.597471032749,
62.3361728552828));
#102041=CARTESIAN_POINT('Ctrl Pts',(-15.3863525773576,641.625161282438,
62.6574505114078));
#102042=CARTESIAN_POINT('Ctrl Pts',(-15.4134262294948,641.64554320332,62.9818812830931));
#102043=CARTESIAN_POINT('Ctrl Pts',(-15.4140928759569,641.646045076336,
62.989869884891));
#102044=CARTESIAN_POINT('Ctrl Pts',(-15.4147536449624,641.646542521192,
62.997860444859));
#102045=CARTESIAN_POINT('Ctrl Pts',(-15.4154085331436,641.647035533691,
63.0058529638405));
#102046=CARTESIAN_POINT('Ctrl Pts',(-15.4549862599015,641.676830412449,
63.4888754727554));
#102047=CARTESIAN_POINT('Ctrl Pts',(-15.4721900515041,641.689815398436,
63.9727246693793));
#102048=CARTESIAN_POINT('Ctrl Pts',(-15.4675657250194,641.68633387532,64.4526573526707));
#102049=CARTESIAN_POINT('Ctrl Pts',(-15.4671428394911,641.686015496904,
64.4965462491376));
#102050=CARTESIAN_POINT('Ctrl Pts',(-15.4665374395128,641.685559434798,
64.5404023977485));
#102051=CARTESIAN_POINT('Ctrl Pts',(-15.465749959502,641.684965964447,64.5842221752744));
#102052=CARTESIAN_POINT('Ctrl Pts',(-15.4655480571059,641.684813804285,
64.5954571500793));
#102053=CARTESIAN_POINT('Ctrl Pts',(-15.4653341842431,641.68465260963,64.6066898685709));
#102054=CARTESIAN_POINT('Ctrl Pts',(-15.4651083473515,641.684482384512,
64.6179202686375));
#102055=CARTESIAN_POINT('Ctrl Pts',(-15.4565102683661,641.678001561122,
65.0454848978451));
#102056=CARTESIAN_POINT('Ctrl Pts',(-15.4306782059191,641.658513233691,
65.4710177591547));
#102057=CARTESIAN_POINT('Ctrl Pts',(-15.3878202693293,641.62627564013,65.8944225395906));
#102058=CARTESIAN_POINT('Ctrl Pts',(-15.3786070250346,641.619345469231,
65.9854425930057));
#102059=CARTESIAN_POINT('Ctrl Pts',(-15.368607118984,641.611826233534,66.076364320098));
#102060=CARTESIAN_POINT('Ctrl Pts',(-15.3578228674146,641.603720685738,
66.1671867939494));
#102061=CARTESIAN_POINT('Ctrl Pts',(-15.3561295795732,641.602447994218,
66.1814472727328));
#102062=CARTESIAN_POINT('Ctrl Pts',(-15.3544169428895,641.601160842789,
66.1957053639419));
#102063=CARTESIAN_POINT('Ctrl Pts',(-15.3526849656753,641.599859241441,
66.209961068781));
#102064=CARTESIAN_POINT('Ctrl Pts',(-15.2907263898706,641.553296639394,
66.7199349654947));
#102065=CARTESIAN_POINT('Ctrl Pts',(-15.2040176992693,641.488239457045,
67.2268545417177));
#102066=CARTESIAN_POINT('Ctrl Pts',(-15.0921759771049,641.404839911851,
67.7306968564118));
#102067=CARTESIAN_POINT('Ctrl Pts',(-15.0883779410082,641.402007744419,
67.7478068513332));
#102068=CARTESIAN_POINT('Ctrl Pts',(-15.0845508622971,641.399154385515,
67.7649135318261));
#102069=CARTESIAN_POINT('Ctrl Pts',(-15.0806947254962,641.396279841134,
67.7820168863499));
#102070=CARTESIAN_POINT('Ctrl Pts',(-14.9906512622138,641.329157240253,
68.181392052377));
#102071=CARTESIAN_POINT('Ctrl Pts',(-14.8857494406163,641.251224978338,
68.5741722445334));
#102072=CARTESIAN_POINT('Ctrl Pts',(-14.7673626317222,641.163831168564,
68.9585381211271));
#102073=CARTESIAN_POINT('Ctrl Pts',(-14.7373499494998,641.14167563734,69.0559801505146));
#102074=CARTESIAN_POINT('Ctrl Pts',(-14.7064707999412,641.118912168443,
69.1528814797826));
#102075=CARTESIAN_POINT('Ctrl Pts',(-14.6747479525069,641.095563010779,
69.249212655916));
#102076=CARTESIAN_POINT('Ctrl Pts',(-14.6685113493146,641.090972646326,
69.2681510353233));
#102077=CARTESIAN_POINT('Ctrl Pts',(-14.6622419924248,641.086359534144,
69.2870678366535));
#102078=CARTESIAN_POINT('Ctrl Pts',(-14.6559400474473,641.081723837857,
69.3059628438942));
#102079=CARTESIAN_POINT('Ctrl Pts',(-14.4881365257321,640.958287951733,
69.8090850972834));
#102080=CARTESIAN_POINT('Ctrl Pts',(-14.2970453980756,640.818610280766,
70.2985271980189));
#102081=CARTESIAN_POINT('Ctrl Pts',(-14.0832076583259,640.664300850609,
70.774854665362));
#102082=CARTESIAN_POINT('Ctrl Pts',(-13.8873140841637,640.522940275832,
71.2112111764187));
#102083=CARTESIAN_POINT('Ctrl Pts',(-13.6723317916547,640.369301179495,
71.6365621257869));
#102084=CARTESIAN_POINT('Ctrl Pts',(-13.4387032223677,640.204642972739,
72.0513594656846));
#102085=CARTESIAN_POINT('Ctrl Pts',(-13.4269732670318,640.196375861329,
72.0721854900244));
#102086=CARTESIAN_POINT('Ctrl Pts',(-13.4151954394702,640.1880804198,72.0929863162258));
#102087=CARTESIAN_POINT('Ctrl Pts',(-13.4033698516022,640.179756844939,
72.1137618746436));
#102088=CARTESIAN_POINT('Ctrl Pts',(-13.2658603218293,640.082969194474,
72.3553428683921));
#102089=CARTESIAN_POINT('Ctrl Pts',(-13.1230592827466,639.983202596528,
72.5914514645084));
#102090=CARTESIAN_POINT('Ctrl Pts',(-12.9752216473832,639.880887422958,
72.8220741360128));
#102091=CARTESIAN_POINT('Ctrl Pts',(-12.865760869058,639.805132027481,72.9928299591849));
#102092=CARTESIAN_POINT('Ctrl Pts',(-12.7535396983477,639.727979956785,
73.1605791986305));
#102093=CARTESIAN_POINT('Ctrl Pts',(-12.6386729408158,639.649611717406,
73.3253295048863));
#102094=CARTESIAN_POINT('Ctrl Pts',(-12.4290296027194,639.506581830803,
73.6260153159772));
#102095=CARTESIAN_POINT('Ctrl Pts',(-12.2103932271219,639.359385521563,
73.9169651027286));
#102096=CARTESIAN_POINT('Ctrl Pts',(-11.9829905176729,639.208818948779,
74.1987899103335));
#102097=CARTESIAN_POINT('Ctrl Pts',(-11.903042823286,639.155884441644,74.2978707156751));
#102098=CARTESIAN_POINT('Ctrl Pts',(-11.8220112795529,639.102533255166,
74.3958233320781));
#102099=CARTESIAN_POINT('Ctrl Pts',(-11.7399047075142,639.048799693591,
74.4926732578092));
#102100=CARTESIAN_POINT('Ctrl Pts',(-11.723313317863,639.03794167778,74.512243857526));
#102101=CARTESIAN_POINT('Ctrl Pts',(-11.7066783200462,639.027068339378,
74.5317689045803));
#102102=CARTESIAN_POINT('Ctrl Pts',(-11.6899998492774,639.016179995548,
74.5512485570587));
#102103=CARTESIAN_POINT('Ctrl Pts',(-11.3893716288856,638.81991839135,74.9023678736655));
#102104=CARTESIAN_POINT('Ctrl Pts',(-11.0743064696377,638.618628706434,
75.2388277121095));
#102105=CARTESIAN_POINT('Ctrl Pts',(-10.7444640677327,638.414001617194,
75.5611408646034));
#102106=CARTESIAN_POINT('Ctrl Pts',(-10.7256680559147,638.402340978157,
75.5795078234553));
#102107=CARTESIAN_POINT('Ctrl Pts',(-10.706824102173,638.390669575054,75.5978287367273));
#102108=CARTESIAN_POINT('Ctrl Pts',(-10.687932101418,638.378987704478,75.6161037296601));
#102109=CARTESIAN_POINT('Ctrl Pts',(-10.3916439046371,638.195777868049,
75.9027152311344));
#102110=CARTESIAN_POINT('Ctrl Pts',(-10.0822730961469,638.009261624385,
76.1790010610358));
#102111=CARTESIAN_POINT('Ctrl Pts',(-9.76302160114976,637.823091051173,
76.4419445962466));
#102112=CARTESIAN_POINT('Ctrl Pts',(-9.72558983048289,637.801262823865,
76.472774341017));
#102113=CARTESIAN_POINT('Ctrl Pts',(-9.68802222038585,637.779439370458,
76.5034206111878));
#102114=CARTESIAN_POINT('Ctrl Pts',(-9.65032392871187,637.757626598003,
76.5338784979796));
#102115=CARTESIAN_POINT('Ctrl Pts',(-9.62962043291992,637.745647258285,
76.5506056413865));
#102116=CARTESIAN_POINT('Ctrl Pts',(-9.60887807747271,637.733671422695,
76.5672755719518));
#102117=CARTESIAN_POINT('Ctrl Pts',(-9.58809774349925,637.721700079099,
76.5838874705586));
#102118=CARTESIAN_POINT('Ctrl Pts',(-9.17209645664792,637.482045877798,
76.916440893729));
#102119=CARTESIAN_POINT('Ctrl Pts',(-8.7416773191496,637.244251929722,77.2259224192763));
#102120=CARTESIAN_POINT('Ctrl Pts',(-8.29525516687926,637.012110800027,
77.5129331902512));
#102121=CARTESIAN_POINT('Ctrl Pts',(-7.94596840718463,636.830480424898,
77.7374943185049));
#102122=CARTESIAN_POINT('Ctrl Pts',(-7.58688458986681,636.652310747268,
77.9482988748328));
#102123=CARTESIAN_POINT('Ctrl Pts',(-7.21723077844875,636.479431177125,
78.1456225473662));
#102124=CARTESIAN_POINT('Ctrl Pts',(-7.19435330607693,636.468731848544,
78.15783469486));
#102125=CARTESIAN_POINT('Ctrl Pts',(-7.17143531739337,636.458052904697,
78.1699950695052));
#102126=CARTESIAN_POINT('Ctrl Pts',(-7.14847664362299,636.447394775834,
78.182103743129));
#102127=CARTESIAN_POINT('Ctrl Pts',(-6.75967649899132,636.266901682683,
78.3871614961733));
#102128=CARTESIAN_POINT('Ctrl Pts',(-6.35908010376408,636.09247477315,78.5772453815688));
#102129=CARTESIAN_POINT('Ctrl Pts',(-5.94486173776335,635.927125347824,
78.7517442446595));
#102130=CARTESIAN_POINT('Ctrl Pts',(-5.9207510096408,635.917500726208,78.7619014346612));
#102131=CARTESIAN_POINT('Ctrl Pts',(-5.8965941154069,635.907906865483,78.7720058152168));
#102132=CARTESIAN_POINT('Ctrl Pts',(-5.87239069016908,635.898344361496,
78.7820572638862));
#102133=CARTESIAN_POINT('Ctrl Pts',(-5.8489383682211,635.889078610061,78.7917967866158));
#102134=CARTESIAN_POINT('Ctrl Pts',(-5.82544172188548,635.879842124891,
78.8014867950871));
#102135=CARTESIAN_POINT('Ctrl Pts',(-5.80190050955843,635.870635502112,
78.8111271194743));
#102136=CARTESIAN_POINT('Ctrl Pts',(-5.52092170777908,635.76074881485,78.9261903013297));
#102137=CARTESIAN_POINT('Ctrl Pts',(-5.23391572238355,635.655356125412,
79.033905907466));
#102138=CARTESIAN_POINT('Ctrl Pts',(-4.94271167504838,635.5562789377,79.1333013998953));
#102139=CARTESIAN_POINT('Ctrl Pts',(-4.77501441593533,635.499222818557,
79.1905408229085));
#102140=CARTESIAN_POINT('Ctrl Pts',(-4.60592561275295,635.444260856133,
79.2450216198842));
#102141=CARTESIAN_POINT('Ctrl Pts',(-4.43579829675245,635.391736888662,
79.296563818299));
#102142=CARTESIAN_POINT('Ctrl Pts',(-4.41274763656986,635.384620382307,
79.3035473041298));
#102143=CARTESIAN_POINT('Ctrl Pts',(-4.38967592729238,635.377547954362,
79.3104775101188));
#102144=CARTESIAN_POINT('Ctrl Pts',(-4.3665840167845,635.370520469936,79.3173539744283));
#102145=CARTESIAN_POINT('Ctrl Pts',(-4.04882336542099,635.273817426323,
79.4119788768291));
#102146=CARTESIAN_POINT('Ctrl Pts',(-3.72622839310077,635.185213899862,
79.4968684248799));
#102147=CARTESIAN_POINT('Ctrl Pts',(-3.39848998472152,635.106166302133,
79.5715572830165));
#102148=CARTESIAN_POINT('Ctrl Pts',(-3.24344222812536,635.0687701582,79.6068913775282));
#102149=CARTESIAN_POINT('Ctrl Pts',(-3.0872435683127,635.033512344151,79.639943018132));
#102150=CARTESIAN_POINT('Ctrl Pts',(-2.92986272136949,635.000544637532,
79.6706660016241));
#102151=CARTESIAN_POINT('Ctrl Pts',(-2.90796583102349,634.995957737215,
79.6749405865796));
#102152=CARTESIAN_POINT('Ctrl Pts',(-2.88604686704024,634.991415266355,
79.6791700030138));
#102153=CARTESIAN_POINT('Ctrl Pts',(-2.86410536448456,634.986917552588,
79.6833542027662));
#102154=CARTESIAN_POINT('Ctrl Pts',(-2.67077137140562,634.947286676806,
79.7202226006317));
#102155=CARTESIAN_POINT('Ctrl Pts',(-2.47523365109657,634.911146502476,
79.7535703438631));
#102156=CARTESIAN_POINT('Ctrl Pts',(-2.27824761487356,634.878810798285,
79.783236645037));
#102157=CARTESIAN_POINT('Ctrl Pts',(-2.09244054752051,634.848310147165,
79.8112193819154));
#102158=CARTESIAN_POINT('Ctrl Pts',(-1.90534362430371,634.821194294132,
79.8359266171042));
#102159=CARTESIAN_POINT('Ctrl Pts',(-1.71759256272266,634.79775958441,79.8571931173366));
#102160=CARTESIAN_POINT('Ctrl Pts',(-1.59648021958737,634.782642585437,
79.8709114721185));
#102161=CARTESIAN_POINT('Ctrl Pts',(-1.47509576549149,634.769058026899,
79.8831974849578));
#102162=CARTESIAN_POINT('Ctrl Pts',(-1.35361376683639,634.757093789453,
79.8939995839849));
#102163=CARTESIAN_POINT('Ctrl Pts',(-1.33479741520131,634.755240648236,
79.8956727215356));
#102164=CARTESIAN_POINT('Ctrl Pts',(-1.31597645205385,634.753425996979,
79.8973106052341));
#102165=CARTESIAN_POINT('Ctrl Pts',(-1.29715200364572,634.751650247623,
79.8989129667661));
#102166=CARTESIAN_POINT('Ctrl Pts',(-1.11523121238339,634.734489281146,
79.9143983011279));
#102167=CARTESIAN_POINT('Ctrl Pts',(-0.932588982074347,634.720883278272,
79.9267009011113));
#102168=CARTESIAN_POINT('Ctrl Pts',(-0.749467854780609,634.710917091553,
79.9357300191259));
#102169=CARTESIAN_POINT('Ctrl Pts',(-0.68360717759574,634.707332689164,
79.9389773988008));
#102170=CARTESIAN_POINT('Ctrl Pts',(-0.617684568112042,634.704218742184,
79.9418016685007));
#102171=CARTESIAN_POINT('Ctrl Pts',(-0.551711358599846,634.701577963951,
79.9441997051945));
#102172=CARTESIAN_POINT('Ctrl Pts',(-0.345342966588289,634.693317441815,
79.9517009163701));
#102173=CARTESIAN_POINT('Ctrl Pts',(-0.13842335344143,634.689669307663,
79.9550471976343));
#102174=CARTESIAN_POINT('Ctrl Pts',(0.0688418019382751,634.69072047944,
79.9541394471176));
#102175=CARTESIAN_POINT('Ctrl Pts',(0.131131170306721,634.691036387948,
79.9538666409809));
#102176=CARTESIAN_POINT('Ctrl Pts',(0.193451665010501,634.69177647057,79.9532098508914));
#102177=CARTESIAN_POINT('Ctrl Pts',(0.255797490386204,634.692942419917,
79.9521669823772));
#102178=CARTESIAN_POINT('Ctrl Pts',(0.666136199024486,634.700616296175,
79.9453031816842));
#102179=CARTESIAN_POINT('Ctrl Pts',(1.07421972569375,634.726606258343,79.9218319778895));
#102180=CARTESIAN_POINT('Ctrl Pts',(1.48012296303281,634.770182961628,79.8822570048232));
#102181=CARTESIAN_POINT('Ctrl Pts',(1.6079847342995,634.783909864879,79.8697906687889));
#102182=CARTESIAN_POINT('Ctrl Pts',(1.73563038656575,634.799382147975,79.8557262296273));
#102183=CARTESIAN_POINT('Ctrl Pts',(1.86306288877797,634.816577773823,79.840079036097));
#102184=CARTESIAN_POINT('',(-1.91941230150446,634.6517886719,48.698800681464));
#102185=CARTESIAN_POINT('Origin',(-1.88888400761935,634.651788671899,48.9469297270682));
#102186=CARTESIAN_POINT('',(1.49247666926852E-9,634.523620405604,80.0178253754844));
#102187=CARTESIAN_POINT('Ctrl Pts',(0.,634.523561041887,80.0177804323122));
#102188=CARTESIAN_POINT('Ctrl Pts',(-0.523838402099614,634.523561041886,
80.0177804323122));
#102189=CARTESIAN_POINT('Ctrl Pts',(-1.04370866617181,634.552420716909,
79.9916639229812));
#102190=CARTESIAN_POINT('Ctrl Pts',(-2.07588373512256,634.664326010256,
79.8887286024128));
#102191=CARTESIAN_POINT('Ctrl Pts',(-2.58884491618879,634.747802856386,
79.8114551737427));
#102192=CARTESIAN_POINT('Ctrl Pts',(-3.58593453053115,634.958082826433,
79.6117158816492));
#102193=CARTESIAN_POINT('Ctrl Pts',(-4.0730770151066,635.085061620392,79.4890655970438));
#102194=CARTESIAN_POINT('Ctrl Pts',(-5.02736864376844,635.373997049357,
79.2004542940851));
#102195=CARTESIAN_POINT('Ctrl Pts',(-5.49684127598253,635.536898097831,
79.0334559601684));
#102196=CARTESIAN_POINT('Ctrl Pts',(-6.85808462896243,636.058637569066,
78.4766795782573));
#102197=CARTESIAN_POINT('Ctrl Pts',(-7.70355359238228,636.448549836785,
78.0333468553696));
#102198=CARTESIAN_POINT('Ctrl Pts',(-8.89973254356871,637.057230951149,
77.2642195998673));
#102199=CARTESIAN_POINT('Ctrl Pts',(-9.28623993692406,637.264306410741,
76.9902938266832));
#102200=CARTESIAN_POINT('Ctrl Pts',(-10.0362291980326,637.68204941874,76.4058881437883));
#102201=CARTESIAN_POINT('Ctrl Pts',(-10.4000435824971,637.892995650452,
76.0948005375614));
#102202=CARTESIAN_POINT('Ctrl Pts',(-11.4396209671232,638.513918977268,
75.1208482803277));
#102203=CARTESIAN_POINT('Ctrl Pts',(-12.0708675035256,638.915587641525,
74.4129443846916));
#102204=CARTESIAN_POINT('Ctrl Pts',(-12.9272407039081,639.478792555837,
73.2539335615611));
#102205=CARTESIAN_POINT('Ctrl Pts',(-13.1974645163444,639.660006071349,
72.8512918153461));
#102206=CARTESIAN_POINT('Ctrl Pts',(-13.705907162251,640.005749387722,72.0101656887144));
#102207=CARTESIAN_POINT('Ctrl Pts',(-13.9424367491172,640.169145509004,
71.5740025956755));
#102208=CARTESIAN_POINT('Ctrl Pts',(-14.5877396657579,640.61954466326,70.2361076880824));
#102209=CARTESIAN_POINT('Ctrl Pts',(-14.9374786600809,640.870144794768,
69.2981314957323));
#102210=CARTESIAN_POINT('Ctrl Pts',(-15.2640367599687,641.105956087144,
68.0597854794833));
#102211=CARTESIAN_POINT('Ctrl Pts',(-15.3238781708752,641.149308553529,
67.8080648198323));
#102212=CARTESIAN_POINT('Ctrl Pts',(-15.4305740793169,641.22676859308,67.3042760285323));
#102213=CARTESIAN_POINT('Ctrl Pts',(-15.4776212824142,641.26101472037,67.0516154405275));
#102214=CARTESIAN_POINT('Ctrl Pts',(-15.6000369014761,641.350256255448,
66.2913465819385));
#102215=CARTESIAN_POINT('Ctrl Pts',(-15.6567243462522,641.391772923005,
65.7814558786312));
#102216=CARTESIAN_POINT('Ctrl Pts',(-15.7200921410461,641.438194610325,
64.7555336881403));
#102217=CARTESIAN_POINT('Ctrl Pts',(-15.7267764511932,641.443102869943,
64.2395027071171));
#102218=CARTESIAN_POINT('Ctrl Pts',(-15.6884879697056,641.41503836218,63.2010937639321));
#102219=CARTESIAN_POINT('Ctrl Pts',(-15.6429785458214,641.381673100163,
62.6781815568624));
#102220=CARTESIAN_POINT('Ctrl Pts',(-15.4329805623442,641.228341491889,
61.1446179884831));
#102221=CARTESIAN_POINT('Ctrl Pts',(-15.1957463219534,641.055416837413,
60.1535682172885));
#102222=CARTESIAN_POINT('Ctrl Pts',(-14.7000874693409,640.701185096577,
58.7109944575794));
#102223=CARTESIAN_POINT('Ctrl Pts',(-14.5127468230508,640.568220140849,
58.242003763886));
#102224=CARTESIAN_POINT('Ctrl Pts',(-14.1005377299408,640.279018469053,
57.3361700731209));
#102225=CARTESIAN_POINT('Ctrl Pts',(-13.8750752636248,640.122351198019,
56.8975962595972));
#102226=CARTESIAN_POINT('Ctrl Pts',(-13.1426912261625,639.620891692776,
55.6221334704683));
#102227=CARTESIAN_POINT('Ctrl Pts',(-12.5757171471258,639.241825375141,
54.8214953487566));
#102228=CARTESIAN_POINT('Ctrl Pts',(-11.3331559325469,638.450142176263,
53.3660245246631));
#102229=CARTESIAN_POINT('Ctrl Pts',(-10.6547752361309,638.035107392668,
52.7042730339687));
#102230=CARTESIAN_POINT('Ctrl Pts',(-9.54585906942516,637.406533531398,
51.8027276685537));
#102231=CARTESIAN_POINT('Ctrl Pts',(-9.16098839272779,637.196240615232,
51.5179512580578));
#102232=CARTESIAN_POINT('Ctrl Pts',(-8.37201911995265,636.785698604155,
50.9878126575492));
#102233=CARTESIAN_POINT('Ctrl Pts',(-7.96635410967427,636.58452539553,50.7411093620899));
#102234=CARTESIAN_POINT('Ctrl Pts',(-6.71291294709257,636.001439692389,
50.0548419703803));
#102235=CARTESIAN_POINT('Ctrl Pts',(-5.82961165971477,635.638936240212,
49.6681929464691));
#102236=CARTESIAN_POINT('Ctrl Pts',(-4.40836677555933,635.180500942699,
49.2037840375558));
#102237=CARTESIAN_POINT('Ctrl Pts',(-3.91938654325121,635.042911076968,
49.0692534214259));
#102238=CARTESIAN_POINT('Ctrl Pts',(-2.93166846065344,634.813010109247,
48.8486963579089));
#102239=CARTESIAN_POINT('Ctrl Pts',(-2.42992069874045,634.719685488227,
48.7616105405085));
#102240=CARTESIAN_POINT('Ctrl Pts',(-1.91941230150446,634.6517886719,48.698800681464));
#102241=CARTESIAN_POINT('',(1.89317385967765,634.648322422428,79.9033533194805));
#102242=CARTESIAN_POINT('Ctrl Pts',(1.89317385967764,634.648322422428,79.9033533194805));
#102243=CARTESIAN_POINT('Ctrl Pts',(1.58012448505219,634.607246312445,79.9413347011642));
#102244=CARTESIAN_POINT('Ctrl Pts',(1.26585353386948,634.576145886255,79.9700061023909));
#102245=CARTESIAN_POINT('Ctrl Pts',(0.950335111694906,634.555301997871,
79.9891761306859));
#102246=CARTESIAN_POINT('Ctrl Pts',(0.788177405142235,634.544589478733,
79.9990283852752));
#102247=CARTESIAN_POINT('Ctrl Pts',(0.625503300950952,634.536577108366,
80.0063792748622));
#102248=CARTESIAN_POINT('Ctrl Pts',(0.462595958332864,634.531322615861,
80.0111851918327));
#102249=CARTESIAN_POINT('Ctrl Pts',(0.308526274103216,634.526353177478,
80.0157303897235));
#102250=CARTESIAN_POINT('Ctrl Pts',(0.154247965605474,634.523850225432,
80.0179995314596));
#102251=CARTESIAN_POINT('Ctrl Pts',(6.79067047038018E-9,634.5238311429,
80.0179849207937));
#102252=CARTESIAN_POINT('Origin',(1.86306288877797,634.648322422428,79.6551732851678));
#102253=CARTESIAN_POINT('Ctrl Pts',(-0.252645464510396,637.415474030314,
76.9980210944396));
#102254=CARTESIAN_POINT('Ctrl Pts',(-0.239928764978578,637.71957350873,
76.5971361934352));
#102255=CARTESIAN_POINT('Ctrl Pts',(-0.247612686332898,637.216296403659,
76.5969814761947));
#102256=CARTESIAN_POINT('Ctrl Pts',(0.599346104179954,637.402304042614,
77.0153826803362));
#102257=CARTESIAN_POINT('Ctrl Pts',(0.570806075610007,637.708243376892,
76.6129375177081));
#102258=CARTESIAN_POINT('Ctrl Pts',(0.587407127222553,637.203283112552,
76.613794761412));
#102259=CARTESIAN_POINT('Ctrl Pts',(1.43522748368769,637.456242191975,76.9455084004709));
#102260=CARTESIAN_POINT('Ctrl Pts',(1.3489476199593,637.752521117499,76.5522413898123));
#102261=CARTESIAN_POINT('Ctrl Pts',(1.40663729476956,637.256579496553,76.5461272140149));
#102262=CARTESIAN_POINT('Ctrl Pts',(2.66678387891633,637.624714906102,76.7177190065359));
#102263=CARTESIAN_POINT('Ctrl Pts',(2.53731328870643,637.900219491323,76.3416431735781));
#102264=CARTESIAN_POINT('Ctrl Pts',(2.61366069407739,637.423047682413,76.3255317586155));
#102265=CARTESIAN_POINT('Ctrl Pts',(3.07572538189221,637.695889939016,76.6204570030234));
#102266=CARTESIAN_POINT('Ctrl Pts',(2.92857212557764,637.961901314834,76.2529152101653));
#102267=CARTESIAN_POINT('Ctrl Pts',(3.01445595206078,637.493375858542,76.2313414391483));
#102268=CARTESIAN_POINT('Ctrl Pts',(3.8755985784546,637.862370610506,76.3871426082101));
#102269=CARTESIAN_POINT('Ctrl Pts',(3.70006557576271,638.108664391703,76.0368396544836));
#102270=CARTESIAN_POINT('Ctrl Pts',(3.7983954194345,637.657875703638,76.0053954703534));
#102271=CARTESIAN_POINT('Ctrl Pts',(4.26480616625281,637.957101329594,76.2518851665813));
#102272=CARTESIAN_POINT('Ctrl Pts',(4.07641784659729,638.192281742605,75.9117507781356));
#102273=CARTESIAN_POINT('Ctrl Pts',(4.17984986817795,637.751479294978,75.874409667253));
#102274=CARTESIAN_POINT('Ctrl Pts',(5.02377713750492,638.164761246445,75.9459140475635));
#102275=CARTESIAN_POINT('Ctrl Pts',(4.81486847221986,638.378208854777,75.6252072189681));
#102276=CARTESIAN_POINT('Ctrl Pts',(4.92370189566428,637.956668425041,75.5781015854782));
#102277=CARTESIAN_POINT('Ctrl Pts',(5.39353601298289,638.277696548749,75.7751934044062));
#102278=CARTESIAN_POINT('Ctrl Pts',(5.17578544904304,638.479637284875,75.4653304964425));
#102279=CARTESIAN_POINT('Ctrl Pts',(5.28609505655054,638.068259997294,75.4127725629522));
#102280=CARTESIAN_POINT('Ctrl Pts',(6.11485814111501,638.517575135291,75.398561954746));
#102281=CARTESIAN_POINT('Ctrl Pts',(5.88314832657038,638.697574974731,75.1089592769933));
#102282=CARTESIAN_POINT('Ctrl Pts',(5.99304821798366,638.305284451723,75.0480357125633));
#102283=CARTESIAN_POINT('Ctrl Pts',(6.46756038601705,638.645018194642,75.1917528950879));
#102284=CARTESIAN_POINT('Ctrl Pts',(6.23031283838703,638.813863825324,74.9130743719703));
#102285=CARTESIAN_POINT('Ctrl Pts',(6.33872452185387,638.431211164344,74.8477580011569));
#102286=CARTESIAN_POINT('Ctrl Pts',(7.48242996358273,639.035870261262,74.5288163772505));
#102287=CARTESIAN_POINT('Ctrl Pts',(7.21704842590842,639.168144716683,74.2897410752272));
#102288=CARTESIAN_POINT('Ctrl Pts',(7.33337757366972,638.817412780853,74.2057580358069));
#102289=CARTESIAN_POINT('Ctrl Pts',(8.10709315029709,639.309087260829,74.028620906189));
#102290=CARTESIAN_POINT('Ctrl Pts',(7.84051708959433,639.422143423535,73.8120742692735));
#102291=CARTESIAN_POINT('Ctrl Pts',(7.94559727067024,639.087378981886,73.721359506763));
#102292=CARTESIAN_POINT('Ctrl Pts',(8.97315991273498,639.716567245409,73.188449545123));
#102293=CARTESIAN_POINT('Ctrl Pts',(8.71531793774959,639.809772891231,72.9883352789045));
#102294=CARTESIAN_POINT('Ctrl Pts',(8.79441170737145,639.490010673385,72.9077220474778));
#102295=CARTESIAN_POINT('Ctrl Pts',(9.25113112703224,639.852690149644,72.8917703602215));
#102296=CARTESIAN_POINT('Ctrl Pts',(8.99305377021651,639.938008123952,72.7011730151351));
#102297=CARTESIAN_POINT('Ctrl Pts',(9.06684564649771,639.624513956044,72.6204124471552));
#102298=CARTESIAN_POINT('Ctrl Pts',(9.77628595094184,640.117696108027,72.2740035948496));
#102299=CARTESIAN_POINT('Ctrl Pts',(9.51738335439514,640.188181759637,72.1016116954675));
#102300=CARTESIAN_POINT('Ctrl Pts',(9.58153921876773,639.886366811092,72.0221557047211));
#102301=CARTESIAN_POINT('Ctrl Pts',(10.0229859433045,640.246276120254,71.9538219181877));
#102302=CARTESIAN_POINT('Ctrl Pts',(9.76463235697413,640.310160688117,71.7902694724233));
#102303=CARTESIAN_POINT('Ctrl Pts',(9.82332486871901,640.013416948774,71.7120858574342));
#102304=CARTESIAN_POINT('Ctrl Pts',(10.7167107520177,640.616230378276,70.9588372302021));
#102305=CARTESIAN_POINT('Ctrl Pts',(10.4508934408169,640.657319512709,70.8323532494638));
#102306=CARTESIAN_POINT('Ctrl Pts',(10.5032304581882,640.378969403766,70.7485243138466));
#102307=CARTESIAN_POINT('Ctrl Pts',(11.1179466017888,640.841950027329,70.250007157043));
#102308=CARTESIAN_POINT('Ctrl Pts',(10.8576198832383,640.874656679083,70.138628472291));
#102309=CARTESIAN_POINT('Ctrl Pts',(10.8964735613622,640.602003388908,70.0620801831889));
#102310=CARTESIAN_POINT('Ctrl Pts',(11.6224782615555,641.132665168508,69.109586211324));
#102311=CARTESIAN_POINT('Ctrl Pts',(11.3677587268443,641.154807136228,69.014472786789));
#102312=CARTESIAN_POINT('Ctrl Pts',(11.390954790485,640.88925953228,68.957675482628));
#102313=CARTESIAN_POINT('Ctrl Pts',(11.7745701409246,641.221747318877,68.714791080186));
#102314=CARTESIAN_POINT('Ctrl Pts',(11.520855565674,641.240337307385,68.6277463485386));
#102315=CARTESIAN_POINT('Ctrl Pts',(11.5400169509314,640.977281762863,68.5753485881025));
#102316=CARTESIAN_POINT('Ctrl Pts',(12.036826018648,641.376809486983,67.9187349800865));
#102317=CARTESIAN_POINT('Ctrl Pts',(11.7840009883711,641.38886168525,67.8485756225846));
#102318=CARTESIAN_POINT('Ctrl Pts',(11.7970486078528,641.130498964837,67.804433162233));
#102319=CARTESIAN_POINT('Ctrl Pts',(12.1481605517107,641.4434586933,67.5152272280643));
#102320=CARTESIAN_POINT('Ctrl Pts',(11.8961680044815,641.453002536285,67.4527537325953));
#102321=CARTESIAN_POINT('Ctrl Pts',(11.906165321538,641.19635516356,67.4136688048127));
#102322=CARTESIAN_POINT('Ctrl Pts',(12.3313243194805,641.553729512778,66.6971148274926));
#102323=CARTESIAN_POINT('Ctrl Pts',(12.0800305729695,641.558788506436,66.6513216880366));
#102324=CARTESIAN_POINT('Ctrl Pts',(12.0856804087928,641.305313954761,66.6213936503897));
#102325=CARTESIAN_POINT('Ctrl Pts',(12.4031554959512,641.597355242453,66.2825110894363));
#102326=CARTESIAN_POINT('Ctrl Pts',(12.1524261846195,641.600829236324,66.2443008543885));
#102327=CARTESIAN_POINT('Ctrl Pts',(12.1560806850811,641.348420615636,66.2198837351635));
#102328=CARTESIAN_POINT('Ctrl Pts',(12.5061462176465,641.660056061986,65.4417759684511));
#102329=CARTESIAN_POINT('Ctrl Pts',(12.2558350970482,641.661037104903,65.4202915379704));
#102330=CARTESIAN_POINT('Ctrl Pts',(12.257019799162,641.410375405783,65.405700320617));
#102331=CARTESIAN_POINT('Ctrl Pts',(12.5373399906064,641.679151832955,65.0141778683388));
#102332=CARTESIAN_POINT('Ctrl Pts',(12.2872829443278,641.679454203773,65.0003000739761));
#102333=CARTESIAN_POINT('Ctrl Pts',(12.2875921822733,641.429243970851,64.9916064252471));
#102334=CARTESIAN_POINT('Ctrl Pts',(12.5658991754142,641.696620496606,63.7224078328247));
#102335=CARTESIAN_POINT('Ctrl Pts',(12.3159477798069,641.696227274136,63.7345453497792));
#102336=CARTESIAN_POINT('Ctrl Pts',(12.3155824582831,641.446504788682,63.7406324714832));
#102337=CARTESIAN_POINT('Ctrl Pts',(12.4989259854136,641.655343862422,62.8753544483646));
#102338=CARTESIAN_POINT('Ctrl Pts',(12.2476351021315,641.655943343438,62.8975114326958));
#102339=CARTESIAN_POINT('Ctrl Pts',(12.2499433960128,641.405719273125,62.9203303339275));
#102340=CARTESIAN_POINT('Ctrl Pts',(12.2757039450297,641.520177357917,61.6247744041512));
#102341=CARTESIAN_POINT('Ctrl Pts',(12.02433270669,641.526673421497,61.6764817660471));
#102342=CARTESIAN_POINT('Ctrl Pts',(12.0311680098947,641.272161011494,61.7092455282533));
#102343=CARTESIAN_POINT('Ctrl Pts',(12.1802763920905,641.462634802374,61.2099033326353));
#102344=CARTESIAN_POINT('Ctrl Pts',(11.9281609256542,641.471251810815,61.269319855613));
#102345=CARTESIAN_POINT('Ctrl Pts',(11.9376414045012,641.215303110347,61.3074767223547));
#102346=CARTESIAN_POINT('Ctrl Pts',(11.9490055759325,641.324698711005,60.3929349339052));
#102347=CARTESIAN_POINT('Ctrl Pts',(11.6960573690714,641.339031872542,60.4693531862596));
#102348=CARTESIAN_POINT('Ctrl Pts',(11.710977576111,641.079008215471,60.5163094405145));
#102349=CARTESIAN_POINT('Ctrl Pts',(11.8146027265403,641.245168037968,59.9953322208473));
#102350=CARTESIAN_POINT('Ctrl Pts',(11.5607302358161,641.262599583117,60.0796799798351));
#102351=CARTESIAN_POINT('Ctrl Pts',(11.5792520747703,641.000423816397,60.1312636317803));
#102352=CARTESIAN_POINT('Ctrl Pts',(11.5102203665223,641.067645854497,59.220368588735));
#102353=CARTESIAN_POINT('Ctrl Pts',(11.2554200175323,641.092765637189,59.3216529465386));
#102354=CARTESIAN_POINT('Ctrl Pts',(11.280933108072,640.825013833895,59.3807745414427));
#102355=CARTESIAN_POINT('Ctrl Pts',(11.340234579966,640.969646468321,58.8430123811434));
#102356=CARTESIAN_POINT('Ctrl Pts',(11.0844074462808,640.998826285913,58.9523736714234));
#102357=CARTESIAN_POINT('Ctrl Pts',(11.1143334927416,640.728180466839,59.0153358225178));
#102358=CARTESIAN_POINT('Ctrl Pts',(10.9653218879177,640.757511556913,58.1076875427682));
#102359=CARTESIAN_POINT('Ctrl Pts',(10.7086606118733,640.796424777516,58.2342052329224));
#102360=CARTESIAN_POINT('Ctrl Pts',(10.7468891809611,640.518569586652,58.3032336718348));
#102361=CARTESIAN_POINT('Ctrl Pts',(10.7594229698032,640.642843732934,57.748247707264));
#102362=CARTESIAN_POINT('Ctrl Pts',(10.5017718495429,640.686893603715,57.8832035358986));
#102363=CARTESIAN_POINT('Ctrl Pts',(10.5450918351581,640.405266106664,57.9551454984287));
#102364=CARTESIAN_POINT('Ctrl Pts',(10.0956130835857,640.281843896905,56.7094894932663));
#102365=CARTESIAN_POINT('Ctrl Pts',(9.82988413289725,640.339878780936,56.8595245434182));
#102366=CARTESIAN_POINT('Ctrl Pts',(9.89450525281217,640.04856153217,56.9491928643266));
#102367=CARTESIAN_POINT('Ctrl Pts',(9.5965007327143,640.020836388794,56.0745184163995));
#102368=CARTESIAN_POINT('Ctrl Pts',(9.32615145971497,640.091117978275,56.2424874391652));
#102369=CARTESIAN_POINT('Ctrl Pts',(9.40533537943261,639.790659551114,56.3342751495656));
#102370=CARTESIAN_POINT('Ctrl Pts',(8.48692376686844,639.482176762763,54.9079363581114));
#102371=CARTESIAN_POINT('Ctrl Pts',(8.21935109391615,639.584201598171,55.1122541884108));
#102372=CARTESIAN_POINT('Ctrl Pts',(8.31786154047716,639.258409024392,55.2045355438743));
#102373=CARTESIAN_POINT('Ctrl Pts',(7.87102737898878,639.202422841643,54.3737954611148));
#102374=CARTESIAN_POINT('Ctrl Pts',(7.60328278950778,639.322779690413,54.6002522073219));
#102375=CARTESIAN_POINT('Ctrl Pts',(7.71423400494031,638.98198367962,54.687263637379));
#102376=CARTESIAN_POINT('Ctrl Pts',(6.56285306515126,638.672930315504,53.4432039225965));
#102377=CARTESIAN_POINT('Ctrl Pts',(6.30828894600969,638.832969696623,53.7086110751252));
#102378=CARTESIAN_POINT('Ctrl Pts',(6.43211894031247,638.458791180624,53.786061608348));
#102379=CARTESIAN_POINT('Ctrl Pts',(5.86710297479519,638.420941785181,53.0415050222643));
#102380=CARTESIAN_POINT('Ctrl Pts',(5.62291561811055,638.604759063604,53.3322766970217));
#102381=CARTESIAN_POINT('Ctrl Pts',(5.75022841332413,638.209800867581,53.3970489773778));
#102382=CARTESIAN_POINT('Ctrl Pts',(4.75112300194525,638.086758847639,52.5364612008833));
#102383=CARTESIAN_POINT('Ctrl Pts',(4.54890972975399,638.307939687588,52.8639499834371));
#102384=CARTESIAN_POINT('Ctrl Pts',(4.65647911755443,637.87959411755,52.9079552143514));
#102385=CARTESIAN_POINT('Ctrl Pts',(4.36447646411708,637.982211773197,52.3837883044384));
#102386=CARTESIAN_POINT('Ctrl Pts',(4.17347758256706,638.214957381859,52.7219730108443));
#102387=CARTESIAN_POINT('Ctrl Pts',(4.27753470189083,637.776290968105,52.760103963041));
#102388=CARTESIAN_POINT('Ctrl Pts',(3.57968505656083,637.796737097994,52.118787442565));
#102389=CARTESIAN_POINT('Ctrl Pts',(3.41373149403426,638.050384043215,52.4753963396111));
#102390=CARTESIAN_POINT('Ctrl Pts',(3.5083765892915,637.593023114497,52.503472235072));
#102391=CARTESIAN_POINT('Ctrl Pts',(3.18116850106493,637.715539157465,52.005977374802));
#102392=CARTESIAN_POINT('Ctrl Pts',(3.0308328190885,637.979497306057,52.3719224428149));
#102393=CARTESIAN_POINT('Ctrl Pts',(3.11779861057926,637.512791285563,52.3942248829386));
#102394=CARTESIAN_POINT('Ctrl Pts',(1.96629699390316,637.512004536896,51.7270877774893));
#102395=CARTESIAN_POINT('Ctrl Pts',(1.85276789715343,637.799756796079,52.1125876973074));
#102396=CARTESIAN_POINT('Ctrl Pts',(1.92712773112881,637.311678368128,52.1241430466814));
#102397=CARTESIAN_POINT('Ctrl Pts',(1.1273257642139,637.429925082731,51.6199783226107));
#102398=CARTESIAN_POINT('Ctrl Pts',(1.06865977295132,637.731952156895,52.0190762779579));
#102399=CARTESIAN_POINT('Ctrl Pts',(1.10486896435859,637.23057551233,52.0204162706371));
#102400=CARTESIAN_POINT('Ctrl Pts',(0.270210553101147,637.415754985731,
51.6012974652903));
#102401=CARTESIAN_POINT('Ctrl Pts',(0.256610940649088,637.719814747952,
52.0021484287645));
#102402=CARTESIAN_POINT('Ctrl Pts',(0.264827872760487,637.216574016203,
52.0023253862613));
#102403=CARTESIAN_POINT('',(0.270210553101167,637.415754985731,51.6012974652903));
#102404=CARTESIAN_POINT('',(-0.252645464510396,637.415474030314,76.9980210944396));
#102405=CARTESIAN_POINT('Ctrl Pts',(0.270210553101167,637.415754985731,
51.6012974652903));
#102406=CARTESIAN_POINT('Ctrl Pts',(0.416188845712236,637.418168344564,
51.6044790675076));
#102407=CARTESIAN_POINT('Ctrl Pts',(0.562179672062563,637.422563160715,
51.6102408737133));
#102408=CARTESIAN_POINT('Ctrl Pts',(0.707836668902967,637.428891368953,
51.6185654510171));
#102409=CARTESIAN_POINT('Ctrl Pts',(0.855734314323139,637.435316924322,
51.6270180856934));
#102410=CARTESIAN_POINT('Ctrl Pts',(1.00328760572369,637.443735718904,51.6381129450356));
#102411=CARTESIAN_POINT('Ctrl Pts',(1.1501423060896,637.454064618708,51.651789297983));
#102412=CARTESIAN_POINT('Ctrl Pts',(1.28385901362555,637.463469469019,51.6642421298138));
#102413=CARTESIAN_POINT('Ctrl Pts',(1.4169965503748,637.474457442842,51.678834639128));
#102414=CARTESIAN_POINT('Ctrl Pts',(1.54929519817636,637.486943941046,51.6954914009046));
#102415=CARTESIAN_POINT('Ctrl Pts',(1.75719362309161,637.506565632971,51.7216663814889));
#102416=CARTESIAN_POINT('Ctrl Pts',(1.96334804814262,637.529911630287,51.7529703760962));
#102417=CARTESIAN_POINT('Ctrl Pts',(2.1678167060391,637.556769095995,51.7892635905837));
#102418=CARTESIAN_POINT('Ctrl Pts',(2.37228536393557,637.583626561702,51.8255568050713));
#102419=CARTESIAN_POINT('Ctrl Pts',(2.57506848853288,637.613995807679,51.8668394514028));
#102420=CARTESIAN_POINT('Ctrl Pts',(2.77621117828721,637.64769460665,51.913014617884));
#102421=CARTESIAN_POINT('Ctrl Pts',(2.780947277973,637.648488077551,51.9141018569566));
#102422=CARTESIAN_POINT('Ctrl Pts',(2.78568258013031,637.649283388912,51.9151918299073));
#102423=CARTESIAN_POINT('Ctrl Pts',(2.79041708794957,637.650080538493,51.9162845374166));
#102424=CARTESIAN_POINT('Ctrl Pts',(3.19062783311624,637.71746406392,52.0086517492298));
#102425=CARTESIAN_POINT('Ctrl Pts',(3.58441626783845,637.79786112867,52.1203933631369));
#102426=CARTESIAN_POINT('Ctrl Pts',(3.97207884850314,637.889477127378,52.2512917195333));
#102427=CARTESIAN_POINT('Ctrl Pts',(3.9785435235221,637.89100491904,52.2534745851923));
#102428=CARTESIAN_POINT('Ctrl Pts',(3.98500659612944,637.892535904034,52.2556629087786));
#102429=CARTESIAN_POINT('Ctrl Pts',(3.99146802647607,637.894070059965,52.2578566698448));
#102430=CARTESIAN_POINT('Ctrl Pts',(4.32723754954278,637.973792780423,52.371855903358));
#102431=CARTESIAN_POINT('Ctrl Pts',(4.65860664868912,638.062095960474,52.5005649822514));
#102432=CARTESIAN_POINT('Ctrl Pts',(4.97989942399088,638.155824072753,52.6410924030451));
#102433=CARTESIAN_POINT('Ctrl Pts',(5.02786800056233,638.169817553081,52.6620729568045));
#102434=CARTESIAN_POINT('Ctrl Pts',(5.07561206228213,638.183931950536,52.6833169044677));
#102435=CARTESIAN_POINT('Ctrl Pts',(5.12311282356784,638.198156764768,52.7048145891233));
#102436=CARTESIAN_POINT('Ctrl Pts',(5.13072165517588,638.200435343325,52.708258160512));
#102437=CARTESIAN_POINT('Ctrl Pts',(5.13832532939628,638.202716944462,52.7117084833211));
#102438=CARTESIAN_POINT('Ctrl Pts',(5.14592385222657,638.205001549891,52.7151655548058));
#102439=CARTESIAN_POINT('Ctrl Pts',(5.6540545374847,638.357778365596,52.9463478703353));
#102440=CARTESIAN_POINT('Ctrl Pts',(6.13932327119867,638.524027475389,53.2077731234659));
#102441=CARTESIAN_POINT('Ctrl Pts',(6.60384272768677,638.698424725211,53.4988133237996));
#102442=CARTESIAN_POINT('Ctrl Pts',(6.81232117456394,638.776695004905,53.6294334907203));
#102443=CARTESIAN_POINT('Ctrl Pts',(7.01662033272776,638.856606954161,53.7660183723263));
#102444=CARTESIAN_POINT('Ctrl Pts',(7.21693171141826,638.937681782581,53.9085088387218));
#102445=CARTESIAN_POINT('Ctrl Pts',(7.22513947055269,638.941003823834,53.9143473858616));
#102446=CARTESIAN_POINT('Ctrl Pts',(7.23334108115382,638.944328172037,53.9201966743797));
#102447=CARTESIAN_POINT('Ctrl Pts',(7.24153649808195,638.947654776522,53.92605666394));
#102448=CARTESIAN_POINT('Ctrl Pts',(7.60433131784438,639.09491694573,54.1854667555743));
#102449=CARTESIAN_POINT('Ctrl Pts',(7.95512168437114,639.246660216953,54.4659556720753));
#102450=CARTESIAN_POINT('Ctrl Pts',(8.28995998193701,639.398498406753,54.7640522820467));
#102451=CARTESIAN_POINT('Ctrl Pts',(8.55084003077369,639.51679895558,54.9963060556824));
#102452=CARTESIAN_POINT('Ctrl Pts',(8.80203719278185,639.635157211398,55.2392478412932));
#102453=CARTESIAN_POINT('Ctrl Pts',(9.04170368382722,639.75150971375,55.4912341838178));
#102454=CARTESIAN_POINT('Ctrl Pts',(9.04882604992424,639.754967456693,55.4987226690669));
#102455=CARTESIAN_POINT('Ctrl Pts',(9.05593912941169,639.7584237756,55.5062195590408));
#102456=CARTESIAN_POINT('Ctrl Pts',(9.06304292057168,639.761878644838,55.51372486464));
#102457=CARTESIAN_POINT('Ctrl Pts',(9.41782794429989,639.934425364931,55.8885627455857));
#102458=CARTESIAN_POINT('Ctrl Pts',(9.74946630676366,640.103354072031,56.2843874740499));
#102459=CARTESIAN_POINT('Ctrl Pts',(10.0578808157674,640.265564551166,56.7027531624886));
#102460=CARTESIAN_POINT('Ctrl Pts',(10.2247778709026,640.353343985951,56.9291497791573));
#102461=CARTESIAN_POINT('Ctrl Pts',(10.3848733586231,640.439156313795,57.1621477031083));
#102462=CARTESIAN_POINT('Ctrl Pts',(10.5381498361278,640.522511090264,57.4019967994255));
#102463=CARTESIAN_POINT('Ctrl Pts',(10.5430825010644,640.525193570903,57.4097154999511));
#102464=CARTESIAN_POINT('Ctrl Pts',(10.5480074933753,640.527873218049,57.4174407015242));
#102465=CARTESIAN_POINT('Ctrl Pts',(10.552924779657,640.5305499995,57.4251723494433));
#102466=CARTESIAN_POINT('Ctrl Pts',(10.7311538823148,640.627571065319,57.7054091694609));
#102467=CARTESIAN_POINT('Ctrl Pts',(10.8991800314946,640.720784301005,57.9939850693816));
#102468=CARTESIAN_POINT('Ctrl Pts',(11.055494941017,640.808699365534,58.2883985364575));
#102469=CARTESIAN_POINT('Ctrl Pts',(11.0884477683194,640.827232785971,58.3504639924381));
#102470=CARTESIAN_POINT('Ctrl Pts',(11.1208800201698,640.845530717851,58.412789017301));
#102471=CARTESIAN_POINT('Ctrl Pts',(11.1527773651984,640.863579132001,58.4753503757855));
#102472=CARTESIAN_POINT('Ctrl Pts',(11.1563744083562,640.865614440099,58.48240538009));
#102473=CARTESIAN_POINT('Ctrl Pts',(11.1599650069621,640.86764677106,58.4894639315986));
#102474=CARTESIAN_POINT('Ctrl Pts',(11.1635491598044,640.869676117202,58.4965260351483));
#102475=CARTESIAN_POINT('Ctrl Pts',(11.3468191789592,640.973443540843,58.8576355943088));
#102476=CARTESIAN_POINT('Ctrl Pts',(11.5131975113051,641.069382235403,59.2279486399778));
#102477=CARTESIAN_POINT('Ctrl Pts',(11.6624107054815,641.156407018995,59.6078507224401));
#102478=CARTESIAN_POINT('Ctrl Pts',(11.6647417380394,641.157766534184,59.613785613975));
#102479=CARTESIAN_POINT('Ctrl Pts',(11.6670685829227,641.159123875855,59.6197228445413));
#102480=CARTESIAN_POINT('Ctrl Pts',(11.6693912367388,641.160479039298,59.6256624167821));
#102481=CARTESIAN_POINT('Ctrl Pts',(11.791461484725,641.231701507476,59.9378247594141));
#102482=CARTESIAN_POINT('Ctrl Pts',(11.9019377577645,641.296895212091,60.2563928914153));
#102483=CARTESIAN_POINT('Ctrl Pts',(12.0003794520937,641.355405979746,60.5818958374238));
#102484=CARTESIAN_POINT('Ctrl Pts',(12.0224039614789,641.368496682422,60.6547211045843));
#102485=CARTESIAN_POINT('Ctrl Pts',(12.0438259072343,641.381252781993,60.7278935919235));
#102486=CARTESIAN_POINT('Ctrl Pts',(12.0646400666275,641.393666799833,60.80141938881));
#102487=CARTESIAN_POINT('Ctrl Pts',(12.0658734024639,641.394402388178,60.8057761345467));
#102488=CARTESIAN_POINT('Ctrl Pts',(12.0671044404052,641.395136677262,60.8101336095226));
#102489=CARTESIAN_POINT('Ctrl Pts',(12.0683331795544,641.395869665849,60.8144918087508));
#102490=CARTESIAN_POINT('Ctrl Pts',(12.1541174147233,641.447043151603,61.1187588191497));
#102491=CARTESIAN_POINT('Ctrl Pts',(12.228649207192,641.49184978824,61.4263757001361));
#102492=CARTESIAN_POINT('Ctrl Pts',(12.2916497337314,641.529885155632,61.7356739632629));
#102493=CARTESIAN_POINT('Ctrl Pts',(12.312390183329,641.542406806856,61.8374982715564));
#102494=CARTESIAN_POINT('Ctrl Pts',(12.3318805284049,641.554194394784,61.9395049355668));
#102495=CARTESIAN_POINT('Ctrl Pts',(12.3501097718202,641.565232888749,62.0416346902988));
#102496=CARTESIAN_POINT('Ctrl Pts',(12.3505132822593,641.565477229528,62.0438953667977));
#102497=CARTESIAN_POINT('Ctrl Pts',(12.3509161912353,641.565721211449,62.0461561431484));
#102498=CARTESIAN_POINT('Ctrl Pts',(12.3513184986724,641.565964834433,62.048417019426));
#102499=CARTESIAN_POINT('Ctrl Pts',(12.4988878701167,641.655327563793,62.8777233171341));
#102500=CARTESIAN_POINT('Ctrl Pts',(12.5654436335101,641.696343276042,63.719998294979));
#102501=CARTESIAN_POINT('Ctrl Pts',(12.547023784357,641.685076145265,64.5759864683422));
#102502=CARTESIAN_POINT('Ctrl Pts',(12.5469692630458,641.68504279544,64.5785201263097));
#102503=CARTESIAN_POINT('Ctrl Pts',(12.5469139970635,641.685008987506,64.5810539094377));
#102504=CARTESIAN_POINT('Ctrl Pts',(12.5468579862992,641.684974721356,64.5835878177417));
#102505=CARTESIAN_POINT('Ctrl Pts',(12.5374524690111,641.679220633378,65.0090902838063));
#102506=CARTESIAN_POINT('Ctrl Pts',(12.5068775203495,641.660503714393,65.4317526596763));
#102507=CARTESIAN_POINT('Ctrl Pts',(12.4564407748525,641.629795989302,65.8474537330173));
#102508=CARTESIAN_POINT('Ctrl Pts',(12.4558465628446,641.62943421142,65.8523512450805));
#102509=CARTESIAN_POINT('Ctrl Pts',(12.4552495926927,641.629070768235,65.8572478053186));
#102510=CARTESIAN_POINT('Ctrl Pts',(12.4546498665094,641.628705661322,65.8621434068506));
#102511=CARTESIAN_POINT('Ctrl Pts',(12.4040416607679,641.597895924734,66.2752612870232));
#102512=CARTESIAN_POINT('Ctrl Pts',(12.3337717584624,641.55521695327,66.6829679693347));
#102513=CARTESIAN_POINT('Ctrl Pts',(12.2443814590765,641.50138783171,67.0853656096814));
#102514=CARTESIAN_POINT('Ctrl Pts',(12.2428405235091,641.500459909904,67.0923022553853));
#102515=CARTESIAN_POINT('Ctrl Pts',(12.2412939039662,641.499528674119,67.0992373326653));
#102516=CARTESIAN_POINT('Ctrl Pts',(12.2397416031979,641.498594128006,67.1061708425375));
#102517=CARTESIAN_POINT('Ctrl Pts',(12.150177183183,641.444672824668,67.5062194691017));
#102518=CARTESIAN_POINT('Ctrl Pts',(12.0416978792334,641.379727280723,67.9010490570524));
#102519=CARTESIAN_POINT('Ctrl Pts',(11.914246482633,641.30433460348,68.2907180385381));
#102520=CARTESIAN_POINT('Ctrl Pts',(11.9114061210395,641.302654414243,68.2994021396051));
#102521=CARTESIAN_POINT('Ctrl Pts',(11.9085563276577,641.300969032295,68.3080836988315));
#102522=CARTESIAN_POINT('Ctrl Pts',(11.9056971018176,641.29927846412,68.3167627159898));
#102523=CARTESIAN_POINT('Ctrl Pts',(11.7780348473212,641.223795883638,68.7042742170754));
#102524=CARTESIAN_POINT('Ctrl Pts',(11.63045559295,641.13733782012,69.0888496165626));
#102525=CARTESIAN_POINT('Ctrl Pts',(11.4674585767456,641.043351164257,69.4598550915683));
#102526=CARTESIAN_POINT('Ctrl Pts',(11.4630803893133,641.040826632183,69.4698204979656));
#102527=CARTESIAN_POINT('Ctrl Pts',(11.458691033693,641.038296635479,69.4797762480409));
#102528=CARTESIAN_POINT('Ctrl Pts',(11.4542905965529,641.035761240617,69.4897221352274));
#102529=CARTESIAN_POINT('Ctrl Pts',(11.2649214349003,640.926652626114,69.9177351390396));
#102530=CARTESIAN_POINT('Ctrl Pts',(11.0548558465911,640.807348643409,70.3297521125393));
#102531=CARTESIAN_POINT('Ctrl Pts',(10.8247037221897,640.679801375466,70.7266992259515));
#102532=CARTESIAN_POINT('Ctrl Pts',(10.6530709447778,640.584684756816,71.0227170695312));
#102533=CARTESIAN_POINT('Ctrl Pts',(10.470268352681,640.484984565181,71.3103549097642));
#102534=CARTESIAN_POINT('Ctrl Pts',(10.2765612833766,640.381519680905,71.5900073533417));
#102535=CARTESIAN_POINT('Ctrl Pts',(10.26913038327,640.377550609346,71.6007352497487));
#102536=CARTESIAN_POINT('Ctrl Pts',(10.2616833989456,640.373575989167,71.6114514209664));
#102537=CARTESIAN_POINT('Ctrl Pts',(10.2542203448061,640.369595866016,71.6221558912206));
#102538=CARTESIAN_POINT('Ctrl Pts',(10.0309413485718,640.250518892223,71.9424112891989));
#102539=CARTESIAN_POINT('Ctrl Pts',(9.79314227964304,640.126485515932,72.2520967897448));
#102540=CARTESIAN_POINT('Ctrl Pts',(9.54042013959494,639.998687759293,72.5513581119671));
#102541=CARTESIAN_POINT('Ctrl Pts',(9.53153439293211,639.994194371855,72.5618801829449));
#102542=CARTESIAN_POINT('Ctrl Pts',(9.52263008694159,639.989696280727,72.5723894853929));
#102543=CARTESIAN_POINT('Ctrl Pts',(9.51370721162859,639.985193542565,72.5828860130588));
#102544=CARTESIAN_POINT('Ctrl Pts',(9.3115180637735,639.883163114011,72.8207335576842));
#102545=CARTESIAN_POINT('Ctrl Pts',(9.10007725182296,639.778925091646,73.0514824787519));
#102546=CARTESIAN_POINT('Ctrl Pts',(8.8816208225359,639.674324548391,73.2729706357969));
#102547=CARTESIAN_POINT('Ctrl Pts',(8.82635703926505,639.647863337012,73.3290013671786));
#102548=CARTESIAN_POINT('Ctrl Pts',(8.77064449616043,639.621378982489,73.3844395960483));
#102549=CARTESIAN_POINT('Ctrl Pts',(8.71451977111152,639.594901428748,73.4392506659581));
#102550=CARTESIAN_POINT('Ctrl Pts',(8.70451527424171,639.590181679951,73.4490209976055));
#102551=CARTESIAN_POINT('Ctrl Pts',(8.69449736220672,639.585461993116,73.4587717209558));
#102552=CARTESIAN_POINT('Ctrl Pts',(8.68446623164618,639.580742533684,73.4685026450421));
#102553=CARTESIAN_POINT('Ctrl Pts',(8.35856609470834,639.427412610826,73.7846494116626));
#102554=CARTESIAN_POINT('Ctrl Pts',(8.01730513116886,639.273445263822,74.081986796801));
#102555=CARTESIAN_POINT('Ctrl Pts',(7.65987184773939,639.121443315517,74.3606572776207));
#102556=CARTESIAN_POINT('Ctrl Pts',(7.39538695995618,639.008968568188,74.5668611603172));
#102557=CARTESIAN_POINT('Ctrl Pts',(7.12204759184878,638.897570561306,74.7628452062894));
#102558=CARTESIAN_POINT('Ctrl Pts',(6.83953361923845,638.788308851806,74.9486824712654));
#102559=CARTESIAN_POINT('Ctrl Pts',(6.8283183754522,638.783971378876,74.9560598417084));
#102560=CARTESIAN_POINT('Ctrl Pts',(6.81708850557552,638.77963722266,74.9634213086029));
#102561=CARTESIAN_POINT('Ctrl Pts',(6.80584399584154,638.775306452619,74.9707668709571));
#102562=CARTESIAN_POINT('Ctrl Pts',(6.53600531050182,638.671379352018,75.1470410648213));
#102563=CARTESIAN_POINT('Ctrl Pts',(6.25682003400716,638.569197778981,75.3144018558145));
#102564=CARTESIAN_POINT('Ctrl Pts',(5.97168962520577,638.471187254382,75.4705491677874));
#102565=CARTESIAN_POINT('Ctrl Pts',(5.91058146393213,638.450181978343,75.5040141186588));
#102566=CARTESIAN_POINT('Ctrl Pts',(5.84920038485744,638.429368272628,75.5369641331853));
#102567=CARTESIAN_POINT('Ctrl Pts',(5.78758008341291,638.408769967278,75.5693767842875));
#102568=CARTESIAN_POINT('Ctrl Pts',(5.77645936187983,638.405052555768,75.5752263510472));
#102569=CARTESIAN_POINT('Ctrl Pts',(5.76533057667264,638.401342057466,75.5810585770746));
#102570=CARTESIAN_POINT('Ctrl Pts',(5.75419392195765,638.39763861286,75.5868733289663));
#102571=CARTESIAN_POINT('Ctrl Pts',(5.43563539119555,638.291703401373,75.7532014469483));
#102572=CARTESIAN_POINT('Ctrl Pts',(5.10974723267518,638.191150407059,75.9059290152506));
#102573=CARTESIAN_POINT('Ctrl Pts',(4.77620299466647,638.097497832909,76.0448419303968));
#102574=CARTESIAN_POINT('Ctrl Pts',(4.74275640441732,638.088106696992,76.0587716069547));
#102575=CARTESIAN_POINT('Ctrl Pts',(4.70923285125379,638.078784938588,76.0725624092196));
#102576=CARTESIAN_POINT('Ctrl Pts',(4.67563202082697,638.069534081832,76.0862141459991));
#102577=CARTESIAN_POINT('Ctrl Pts',(4.66519251392584,638.06665991528,76.0904556304658));
#102578=CARTESIAN_POINT('Ctrl Pts',(4.65474549323414,638.063792577535,76.0946837135968));
#102579=CARTESIAN_POINT('Ctrl Pts',(4.64429094472362,638.060932112898,76.0988983916671));
#102580=CARTESIAN_POINT('Ctrl Pts',(4.27379986217441,637.959562203058,76.2482592788739));
#102581=CARTESIAN_POINT('Ctrl Pts',(3.89386018446253,637.86681693476,76.3807926409731));
#102582=CARTESIAN_POINT('Ctrl Pts',(3.50348924748349,637.784945316901,76.4956462456033));
#102583=CARTESIAN_POINT('Ctrl Pts',(3.49421925398876,637.783001142033,76.4983736314482));
#102584=CARTESIAN_POINT('Ctrl Pts',(3.4849433167112,637.781063089165,76.5010910617607));
#102585=CARTESIAN_POINT('Ctrl Pts',(3.47566142285349,637.779131189023,76.5037985243145));
#102586=CARTESIAN_POINT('Ctrl Pts',(3.1135796752967,637.703768790973,76.6094151999565));
#102587=CARTESIAN_POINT('Ctrl Pts',(2.74384243019707,637.638239420645,76.6992121831809));
#102588=CARTESIAN_POINT('Ctrl Pts',(2.3719816618457,637.5847920319,76.7716691688675));
#102589=CARTESIAN_POINT('Ctrl Pts',(2.34061880023512,637.580284261252,76.7777802152811));
#102590=CARTESIAN_POINT('Ctrl Pts',(2.30924086293913,637.575862440254,76.7837679159765));
#102591=CARTESIAN_POINT('Ctrl Pts',(2.27785118480889,637.571527921841,76.7896313582787));
#102592=CARTESIAN_POINT('Ctrl Pts',(2.27065610270346,637.570534371804,76.7909753653312));
#102593=CARTESIAN_POINT('Ctrl Pts',(2.26346025582311,637.569545385811,76.7923128747317));
#102594=CARTESIAN_POINT('Ctrl Pts',(2.25626368658222,637.568560981047,76.7936438742463));
#102595=CARTESIAN_POINT('Ctrl Pts',(1.96925816375727,637.529302051626,76.8467253077398));
#102596=CARTESIAN_POINT('Ctrl Pts',(1.68006019104803,637.497124903821,76.8898579427876));
#102597=CARTESIAN_POINT('Ctrl Pts',(1.38876410941254,637.472468422105,76.9227278834574));
#102598=CARTESIAN_POINT('Ctrl Pts',(1.10512361178556,637.448459940066,76.9547339656408));
#102599=CARTESIAN_POINT('Ctrl Pts',(0.819493826338199,637.431582163689,
76.9770097040753));
#102600=CARTESIAN_POINT('Ctrl Pts',(0.531969592107279,637.422213051343,
76.989304983325));
#102601=CARTESIAN_POINT('Ctrl Pts',(0.271955131226084,637.413740357895,
77.000423873578));
#102602=CARTESIAN_POINT('Ctrl Pts',(0.0103914694409467,637.411408035635,
77.003381168988));
#102603=CARTESIAN_POINT('Ctrl Pts',(-0.252645464510395,637.415474030314,
76.9980210944396));
#102604=CARTESIAN_POINT('',(0.264827872760508,637.216574016203,52.0023253862613));
#102605=CARTESIAN_POINT('Origin',(0.270210553101161,637.216574016203,51.7523833394738));
#102606=CARTESIAN_POINT('',(-3.86212967253593E-9,637.214372791556,76.5994959777072));
#102607=CARTESIAN_POINT('Ctrl Pts',(-3.25135893208817E-9,637.214372791556,
76.5994959777073));
#102608=CARTESIAN_POINT('Ctrl Pts',(0.310528165472536,637.214386003673,
76.5995448311342));
#102609=CARTESIAN_POINT('Ctrl Pts',(0.618777498408002,637.223529415885,
76.5878893241728));
#102610=CARTESIAN_POINT('Ctrl Pts',(0.92467364940843,637.241314282396,76.564836683329));
#102611=CARTESIAN_POINT('Ctrl Pts',(1.23978245630703,637.259634774658,76.5410897674936));
#102612=CARTESIAN_POINT('Ctrl Pts',(1.55239421536144,637.287124882276,76.5052488949338));
#102613=CARTESIAN_POINT('Ctrl Pts',(1.86243766898481,637.323219022104,76.4576945787577));
#102614=CARTESIAN_POINT('Ctrl Pts',(1.97909517691913,637.336799868124,76.4398017061562));
#102615=CARTESIAN_POINT('Ctrl Pts',(2.09538918047889,637.351598516929,76.4202509684407));
#102616=CARTESIAN_POINT('Ctrl Pts',(2.21131621964626,637.367583834262,76.3990641890932));
#102617=CARTESIAN_POINT('Ctrl Pts',(2.28847278600611,637.37822304498,76.3849630858612));
#102618=CARTESIAN_POINT('Ctrl Pts',(2.36554368200416,637.389403280499,76.3701075120779));
#102619=CARTESIAN_POINT('Ctrl Pts',(2.44247543406213,637.401102268236,76.354512897056));
#102620=CARTESIAN_POINT('Ctrl Pts',(2.64351074550122,637.431673645855,76.3137616051143));
#102621=CARTESIAN_POINT('Ctrl Pts',(2.8440260578588,637.465865757867,76.2678728545131));
#102622=CARTESIAN_POINT('Ctrl Pts',(3.04288942630178,637.503285001264,76.2171146986249));
#102623=CARTESIAN_POINT('Ctrl Pts',(3.16477478014477,637.526219630993,76.1860045155917));
#102624=CARTESIAN_POINT('Ctrl Pts',(3.28603954227595,637.550365906112,76.1530659810039));
#102625=CARTESIAN_POINT('Ctrl Pts',(3.40642527297713,637.57562795491,76.1183685737292));
#102626=CARTESIAN_POINT('Ctrl Pts',(3.47943076865769,637.590947614339,76.0973270316614));
#102627=CARTESIAN_POINT('Ctrl Pts',(3.55205443377299,637.606657828165,76.0756654689925));
#102628=CARTESIAN_POINT('Ctrl Pts',(3.624292679273,637.622740245025,76.0533936492376));
#102629=CARTESIAN_POINT('Ctrl Pts',(3.94018000276088,637.693066310974,75.9560022261365));
#102630=CARTESIAN_POINT('Ctrl Pts',(4.24915881614502,637.770600446213,75.8468009339012));
#102631=CARTESIAN_POINT('Ctrl Pts',(4.55177540581521,637.854075900525,75.7262558160285));
#102632=CARTESIAN_POINT('Ctrl Pts',(4.61866590223142,637.872527349547,75.6996104732076));
#102633=CARTESIAN_POINT('Ctrl Pts',(4.68524538832333,637.891269293644,75.6724106564061));
#102634=CARTESIAN_POINT('Ctrl Pts',(4.75151758316339,637.910289739806,75.6446572600295));
#102635=CARTESIAN_POINT('Ctrl Pts',(5.00694798017803,637.983599521175,75.537688401188));
#102636=CARTESIAN_POINT('Ctrl Pts',(5.25788462119999,638.061063217152,75.4224616809293));
#102637=CARTESIAN_POINT('Ctrl Pts',(5.50437127896534,638.141932884419,75.2991083225993));
#102638=CARTESIAN_POINT('Ctrl Pts',(5.54958725702918,638.156767768929,75.2764801495578));
#102639=CARTESIAN_POINT('Ctrl Pts',(5.59465355083892,638.171717219499,75.2535786253479));
#102640=CARTESIAN_POINT('Ctrl Pts',(5.63957051211808,638.18677656011,75.2304047182994));
#102641=CARTESIAN_POINT('Ctrl Pts',(5.70073378556493,638.207282813015,75.1988488878676));
#102642=CARTESIAN_POINT('Ctrl Pts',(5.76165357779709,638.228007610847,75.1667619524568));
#102643=CARTESIAN_POINT('Ctrl Pts',(5.82229488838819,638.248925991892,75.1341674982549));
#102644=CARTESIAN_POINT('Ctrl Pts',(6.03771053817337,638.323234192051,75.0183824754239));
#102645=CARTESIAN_POINT('Ctrl Pts',(6.24993868377269,638.400103047963,74.8960130814583));
#102646=CARTESIAN_POINT('Ctrl Pts',(6.45731962006765,638.478404326221,74.768123123848));
#102647=CARTESIAN_POINT('Ctrl Pts',(6.52890397505861,638.505432589277,74.7239776961683));
#102648=CARTESIAN_POINT('Ctrl Pts',(6.59991097229038,638.532631370786,74.6791748810446));
#102649=CARTESIAN_POINT('Ctrl Pts',(6.67027315473924,638.559953912966,74.6337595519187));
#102650=CARTESIAN_POINT('Ctrl Pts',(6.72531600416889,638.581327760719,74.598232099019));
#102651=CARTESIAN_POINT('Ctrl Pts',(6.78000298293607,638.602786093397,74.5623194192597));
#102652=CARTESIAN_POINT('Ctrl Pts',(6.83433353593326,638.624319539508,74.526023120994));
#102653=CARTESIAN_POINT('Ctrl Pts',(7.10822454753777,638.732873879809,74.3430463371942));
#102654=CARTESIAN_POINT('Ctrl Pts',(7.37336538639476,638.843433750453,74.1501101955193));
#102655=CARTESIAN_POINT('Ctrl Pts',(7.62995416450792,638.954928099765,73.9471842046907));
#102656=CARTESIAN_POINT('Ctrl Pts',(7.8884435207344,639.0672482986,73.7427551212498));
#102657=CARTESIAN_POINT('Ctrl Pts',(8.13825378256586,639.180516194487,73.5281875575904));
#102658=CARTESIAN_POINT('Ctrl Pts',(8.37962080003936,639.293634261351,73.3034909566159));
#102659=CARTESIAN_POINT('Ctrl Pts',(8.42385440908566,639.314364601387,73.2623124157134));
#102660=CARTESIAN_POINT('Ctrl Pts',(8.46780453567413,639.335089918768,73.2207937995264));
#102661=CARTESIAN_POINT('Ctrl Pts',(8.5114727458354,639.355803477485,73.1789353160944));
#102662=CARTESIAN_POINT('Ctrl Pts',(8.55430052500404,639.376118386551,73.1378824339602));
#102663=CARTESIAN_POINT('Ctrl Pts',(8.59688191547822,639.396437541293,73.0964662008016));
#102664=CARTESIAN_POINT('Ctrl Pts',(8.63920055811426,639.416747258165,73.0547024182158));
#102665=CARTESIAN_POINT('Ctrl Pts',(8.79391013170621,639.490996039346,72.902021316154));
#102666=CARTESIAN_POINT('Ctrl Pts',(8.94539579188608,639.565251675653,72.7444053092197));
#102667=CARTESIAN_POINT('Ctrl Pts',(9.09269306745744,639.638775141591,72.5827363034081));
#102668=CARTESIAN_POINT('Ctrl Pts',(9.17109278887125,639.677908378947,72.4966871557392));
#102669=CARTESIAN_POINT('Ctrl Pts',(9.24830637544962,639.716834119649,72.4094906238483));
#102670=CARTESIAN_POINT('Ctrl Pts',(9.32419224683953,639.755441259617,72.3212842918984));
#102671=CARTESIAN_POINT('Ctrl Pts',(9.36129694465004,639.774318373836,72.2781554560291));
#102672=CARTESIAN_POINT('Ctrl Pts',(9.39807441423151,639.793113104251,72.2348034790566));
#102673=CARTESIAN_POINT('Ctrl Pts',(9.43452337359978,639.811820175665,72.1912312995811));
#102674=CARTESIAN_POINT('Ctrl Pts',(9.65091478739477,639.922880949451,71.9325505119194));
#102675=CARTESIAN_POINT('Ctrl Pts',(9.85597586740215,640.030976085533,71.665812843898));
#102676=CARTESIAN_POINT('Ctrl Pts',(10.0499594594973,640.135271225398,71.3908995346973));
#102677=CARTESIAN_POINT('Ctrl Pts',(10.0810275633506,640.151974969265,71.3468698559567));
#102678=CARTESIAN_POINT('Ctrl Pts',(10.1118142187007,640.168581847187,71.3026323420182));
#102679=CARTESIAN_POINT('Ctrl Pts',(10.1423182570292,640.18508833926,71.2581851032761));
#102680=CARTESIAN_POINT('Ctrl Pts',(10.368697236347,640.307587622379,70.9283297434193));
#102681=CARTESIAN_POINT('Ctrl Pts',(10.5795594554243,640.424590868755,70.5868461102142));
#102682=CARTESIAN_POINT('Ctrl Pts',(10.7743498376389,640.534625593794,70.233068626278));
#102683=CARTESIAN_POINT('Ctrl Pts',(10.9361257815805,640.62601086296,69.9392518281467));
#102684=CARTESIAN_POINT('Ctrl Pts',(11.0868167655308,640.712589548309,69.6369556978497));
#102685=CARTESIAN_POINT('Ctrl Pts',(11.2261259025389,640.793526545651,69.325814430765));
#102686=CARTESIAN_POINT('Ctrl Pts',(11.2465333475455,640.805383035166,69.2802352359348));
#102687=CARTESIAN_POINT('Ctrl Pts',(11.2666986076393,640.817120814722,69.2344396511952));
#102688=CARTESIAN_POINT('Ctrl Pts',(11.2866125566538,640.82873286362,69.1884489145415));
#102689=CARTESIAN_POINT('Ctrl Pts',(11.3880924823146,640.887906956016,68.954083719907));
#102690=CARTESIAN_POINT('Ctrl Pts',(11.4831444008195,640.943852057169,68.7144140723365));
#102691=CARTESIAN_POINT('Ctrl Pts',(11.5704748159164,640.995610908571,68.4723906692549));
#102692=CARTESIAN_POINT('Ctrl Pts',(11.6043465274191,641.015685940625,68.3785202018239));
#102693=CARTESIAN_POINT('Ctrl Pts',(11.6370570638028,641.035131394244,68.2842960263096));
#102694=CARTESIAN_POINT('Ctrl Pts',(11.668532669455,641.053892244932,68.1898912049256));
#102695=CARTESIAN_POINT('Ctrl Pts',(11.683669793509,641.062914639206,68.1444904107873));
#102696=CARTESIAN_POINT('Ctrl Pts',(11.698537234685,641.071787880423,68.0990176527924));
#102697=CARTESIAN_POINT('Ctrl Pts',(11.7131347554859,641.080510894475,68.0534740137289));
#102698=CARTESIAN_POINT('Ctrl Pts',(11.8224706417623,641.1458465419,67.7123507360731));
#102699=CARTESIAN_POINT('Ctrl Pts',(11.9167276342155,641.202767414028,67.3670528841897));
#102700=CARTESIAN_POINT('Ctrl Pts',(11.9959228357299,641.25083557254,67.0175313575219));
#102701=CARTESIAN_POINT('Ctrl Pts',(12.0059728443566,641.256935505345,66.973176468702));
#102702=CARTESIAN_POINT('Ctrl Pts',(12.0157803206307,641.262892923904,66.9287535733242));
#102703=CARTESIAN_POINT('Ctrl Pts',(12.0253444381023,641.268706747125,66.8842623710702));
#102704=CARTESIAN_POINT('Ctrl Pts',(12.0802141521749,641.302060877155,66.6290146125976));
#102705=CARTESIAN_POINT('Ctrl Pts',(12.1270883150579,641.330698896874,66.3714346350773));
#102706=CARTESIAN_POINT('Ctrl Pts',(12.1657799000475,641.354400361684,66.1116378612346));
#102707=CARTESIAN_POINT('Ctrl Pts',(12.1805677414234,641.363459011054,66.012344087599));
#102708=CARTESIAN_POINT('Ctrl Pts',(12.1941607596463,641.37179681849,65.9127266173964));
#102709=CARTESIAN_POINT('Ctrl Pts',(12.2065502013075,641.379402497237,65.812792357429));
#102710=CARTESIAN_POINT('Ctrl Pts',(12.2119202405116,641.382699077838,65.769477177574));
#102711=CARTESIAN_POINT('Ctrl Pts',(12.2170645586533,641.385858354091,65.7260864061383));
#102712=CARTESIAN_POINT('Ctrl Pts',(12.2219815693876,641.388879140903,65.6826258242829));
#102713=CARTESIAN_POINT('Ctrl Pts',(12.2489552484072,641.405450537277,65.4442102811187));
#102714=CARTESIAN_POINT('Ctrl Pts',(12.2691246111521,641.417870627053,65.2033421763435));
#102715=CARTESIAN_POINT('Ctrl Pts',(12.2821848003886,641.425918961536,64.9610218376528));
#102716=CARTESIAN_POINT('Ctrl Pts',(12.2891074986869,641.430185070581,64.8325772519037));
#102717=CARTESIAN_POINT('Ctrl Pts',(12.2940334684438,641.433223291306,64.7037249406801));
#102718=CARTESIAN_POINT('Ctrl Pts',(12.2969222724657,641.435003822481,64.5746151917459));
#102719=CARTESIAN_POINT('Ctrl Pts',(12.297866127023,641.435585572732,64.5324313592704));
#102720=CARTESIAN_POINT('Ctrl Pts',(12.2985942535798,641.436033507889,64.4902847021331));
#102721=CARTESIAN_POINT('Ctrl Pts',(12.2991072457852,641.43634820398,64.4481760965921));
#102722=CARTESIAN_POINT('Ctrl Pts',(12.3039230418204,641.439302463655,64.0528748551926));
#102723=CARTESIAN_POINT('Ctrl Pts',(12.2897795816084,641.430514251088,63.6605870250526));
#102724=CARTESIAN_POINT('Ctrl Pts',(12.2571208090154,641.410420092158,63.2713649049953));
#102725=CARTESIAN_POINT('Ctrl Pts',(12.2244620364223,641.390325933228,62.8821427849379));
#102726=CARTESIAN_POINT('Ctrl Pts',(12.1732881572924,641.358926028386,62.4959863338011));
#102727=CARTESIAN_POINT('Ctrl Pts',(12.1040930127778,641.316687091337,62.1129397664499));
#102728=CARTESIAN_POINT('Ctrl Pts',(12.097501651259,641.312663512714,62.076451680159));
#102729=CARTESIAN_POINT('Ctrl Pts',(12.0907423182806,641.308539354126,62.0399811711845));
#102730=CARTESIAN_POINT('Ctrl Pts',(12.083815675173,641.304315434519,62.0035314922614));
#102731=CARTESIAN_POINT('Ctrl Pts',(12.0363940815464,641.275397386341,61.7539875450918));
#102732=CARTESIAN_POINT('Ctrl Pts',(11.9810777244786,641.241765390489,61.5051624947921));
#102733=CARTESIAN_POINT('Ctrl Pts',(11.9180804827761,641.203688800903,61.2582463139588));
#102734=CARTESIAN_POINT('Ctrl Pts',(11.8885070000971,641.185814091913,61.1423337565242));
#102735=CARTESIAN_POINT('Ctrl Pts',(11.8572414900855,641.166960298106,61.0268418090731));
#102736=CARTESIAN_POINT('Ctrl Pts',(11.824309419125,641.147157255363,60.9118928329591));
#102737=CARTESIAN_POINT('Ctrl Pts',(11.8147012792868,641.141379592485,60.8783557426836));
#102738=CARTESIAN_POINT('Ctrl Pts',(11.8049614391109,641.135527263631,60.8448961507762));
#102739=CARTESIAN_POINT('Ctrl Pts',(11.7950906598908,641.129601189148,60.8115140280203));
#102740=CARTESIAN_POINT('Ctrl Pts',(11.6884979670894,641.065606622677,60.4510267476747));
#102741=CARTESIAN_POINT('Ctrl Pts',(11.5665815949929,640.992974536206,60.0993881528899));
#102742=CARTESIAN_POINT('Ctrl Pts',(11.4300925444937,640.912719421956,59.7560189685529));
#102743=CARTESIAN_POINT('Ctrl Pts',(11.4183382568568,640.905807939359,59.7264483902275));
#102744=CARTESIAN_POINT('Ctrl Pts',(11.4064758513312,640.89883987044,59.6969391717302));
#102745=CARTESIAN_POINT('Ctrl Pts',(11.3945054923629,640.891815783686,59.6674910998064));
#102746=CARTESIAN_POINT('Ctrl Pts',(11.2921850121202,640.831775150665,59.4157742657978));
#102747=CARTESIAN_POINT('Ctrl Pts',(11.1819396277238,640.767620977233,59.1684441713329));
#102748=CARTESIAN_POINT('Ctrl Pts',(11.0639479787746,640.699754720745,58.9255372140161));
#102749=CARTESIAN_POINT('Ctrl Pts',(11.020546532114,640.674791142921,58.8361875571092));
#102750=CARTESIAN_POINT('Ctrl Pts',(10.9760974099167,640.649325512844,58.7474361315046));
#102751=CARTESIAN_POINT('Ctrl Pts',(10.9306109324387,640.623378466979,58.6592839633751));
#102752=CARTESIAN_POINT('Ctrl Pts',(10.9173036742458,640.615787550781,58.6334946799086));
#102753=CARTESIAN_POINT('Ctrl Pts',(10.9039026380964,640.608152673949,58.6077492085214));
#102754=CARTESIAN_POINT('Ctrl Pts',(10.8904091198925,640.600475021888,58.5820495569515));
#102755=CARTESIAN_POINT('Ctrl Pts',(10.7698070167312,640.53185385342,58.3523517136592));
#102756=CARTESIAN_POINT('Ctrl Pts',(10.6416424932156,640.459709701766,58.1259903442911));
#102757=CARTESIAN_POINT('Ctrl Pts',(10.5068163413095,640.384883069019,57.9044450451186));
#102758=CARTESIAN_POINT('Ctrl Pts',(10.4485076621598,640.352522565815,57.8086326705612));
#102759=CARTESIAN_POINT('Ctrl Pts',(10.3889536073115,640.319660622561,57.713720804039));
#102760=CARTESIAN_POINT('Ctrl Pts',(10.3282293807528,640.286366224327,57.6198275512506));
#102761=CARTESIAN_POINT('Ctrl Pts',(10.3139692496735,640.27854755771,57.597778195201));
#102762=CARTESIAN_POINT('Ctrl Pts',(10.2996497960813,640.270707523277,57.5757900176145));
#102763=CARTESIAN_POINT('Ctrl Pts',(10.2852711775002,640.262846614506,57.5538629682177));
#102764=CARTESIAN_POINT('Ctrl Pts',(10.0352430737247,640.126154198402,57.1725760906817));
#102765=CARTESIAN_POINT('Ctrl Pts',(9.76709513330229,639.983017170431,56.8094299412362));
#102766=CARTESIAN_POINT('Ctrl Pts',(9.48107593712361,639.835696654845,56.4634525360726));
#102767=CARTESIAN_POINT('Ctrl Pts',(9.28311236321487,639.733731135868,56.2239898547808));
#102768=CARTESIAN_POINT('Ctrl Pts',(9.07658839348234,639.629761831818,55.9927510172857));
#102769=CARTESIAN_POINT('Ctrl Pts',(8.86159725045972,639.524539530591,55.7694040901285));
#102770=CARTESIAN_POINT('Ctrl Pts',(8.84757081570353,639.517674625729,55.75483250798));
#102771=CARTESIAN_POINT('Ctrl Pts',(8.83350480090612,639.510803005305,55.7402928849304));
#102772=CARTESIAN_POINT('Ctrl Pts',(8.81939960411072,639.503925105357,55.7257855526291));
#102773=CARTESIAN_POINT('Ctrl Pts',(8.49324152366855,639.344885662151,55.3903287898225));
#102774=CARTESIAN_POINT('Ctrl Pts',(8.14587360450725,639.182353336129,55.0718764699218));
#102775=CARTESIAN_POINT('Ctrl Pts',(7.78212530166576,639.02170993629,54.7745772655406));
#102776=CARTESIAN_POINT('Ctrl Pts',(7.55195563852923,638.920059325312,54.5864547170954));
#102777=CARTESIAN_POINT('Ctrl Pts',(7.31522835413135,638.819165518536,54.4068014680504));
#102778=CARTESIAN_POINT('Ctrl Pts',(7.07317494872264,638.720393123171,54.2366615516199));
#102779=CARTESIAN_POINT('Ctrl Pts',(7.06129788050288,638.715546562653,54.2283131320183));
#102780=CARTESIAN_POINT('Ctrl Pts',(7.04940682153739,638.710704346424,54.219985871321));
#102781=CARTESIAN_POINT('Ctrl Pts',(7.03750173377691,638.705866579126,54.2116797798133));
#102782=CARTESIAN_POINT('Ctrl Pts',(6.64028634979692,638.544453607337,53.9345455499819));
#102783=CARTESIAN_POINT('Ctrl Pts',(6.22730832298175,638.387924142036,53.6808812320082));
#102784=CARTESIAN_POINT('Ctrl Pts',(5.79712163884134,638.2401609909,53.45108975874));
#102785=CARTESIAN_POINT('Ctrl Pts',(5.54446643548225,638.153377437676,53.3161297203447));
#102786=CARTESIAN_POINT('Ctrl Pts',(5.28587575783202,638.069617723393,53.1894035722665));
#102787=CARTESIAN_POINT('Ctrl Pts',(5.02106131531316,637.989666687543,53.0709860658359));
#102788=CARTESIAN_POINT('Ctrl Pts',(5.01259930724038,637.987111893687,53.0672020958763));
#102789=CARTESIAN_POINT('Ctrl Pts',(5.00412957485698,637.984560747639,53.0634263089924));
#102790=CARTESIAN_POINT('Ctrl Pts',(4.9956522280165,637.982013310887,53.0596587598676));
#102791=CARTESIAN_POINT('Ctrl Pts',(4.72092237015458,637.899457182191,52.9375618048865));
#102792=CARTESIAN_POINT('Ctrl Pts',(4.43801237504386,637.820746463645,52.8240393805747));
#102793=CARTESIAN_POINT('Ctrl Pts',(4.15077506061875,637.748019723362,52.7210258524583));
#102794=CARTESIAN_POINT('Ctrl Pts',(4.06518506628605,637.726348857579,52.6903302330353));
#102795=CARTESIAN_POINT('Ctrl Pts',(3.97921111129791,637.705209220218,52.660567473289));
#102796=CARTESIAN_POINT('Ctrl Pts',(3.89295563852527,637.684657074927,52.631788096699));
#102797=CARTESIAN_POINT('Ctrl Pts',(3.88647932075825,637.683113958654,52.6296272553988));
#102798=CARTESIAN_POINT('Ctrl Pts',(3.88000131269557,637.681574078487,52.6274718253079));
#102799=CARTESIAN_POINT('Ctrl Pts',(3.87352161455212,637.680037443336,52.6253218076544));
#102800=CARTESIAN_POINT('Ctrl Pts',(3.49528738953933,637.590340671551,52.4998205508172));
#102801=CARTESIAN_POINT('Ctrl Pts',(3.11117130680274,637.511675562861,52.3927215905075));
#102802=CARTESIAN_POINT('Ctrl Pts',(2.72090801980653,637.445755536795,52.3041975366685));
#102803=CARTESIAN_POINT('Ctrl Pts',(2.71660777482107,637.445029175205,52.3032221051296));
#102804=CARTESIAN_POINT('Ctrl Pts',(2.71230668873312,637.444304366729,52.3022489124891));
#102805=CARTESIAN_POINT('Ctrl Pts',(2.70800476328749,637.44358111362,52.3012779602549));
#102806=CARTESIAN_POINT('Ctrl Pts',(2.51064590304966,637.410400527148,52.2567337140315));
#102807=CARTESIAN_POINT('Ctrl Pts',(2.31170028173491,637.380523021655,52.2169417014671));
#102808=CARTESIAN_POINT('Ctrl Pts',(2.11111770838934,637.35412628928,52.1819925296957));
#102809=CARTESIAN_POINT('Ctrl Pts',(1.91053513504378,637.327729556906,52.1470433579242));
#102810=CARTESIAN_POINT('Ctrl Pts',(1.70831537286292,637.304813279245,52.116936815071));
#102811=CARTESIAN_POINT('Ctrl Pts',(1.50439479076096,637.285586274148,52.0918063490636));
#102812=CARTESIAN_POINT('Ctrl Pts',(1.36067001764642,637.272034935108,52.0740942059933));
#102813=CARTESIAN_POINT('Ctrl Pts',(1.21594950307129,637.260306033537,52.0588407343316));
#102814=CARTESIAN_POINT('Ctrl Pts',(1.07058065255011,637.250510636707,52.0461417320882));
#102815=CARTESIAN_POINT('Ctrl Pts',(0.927490453078941,637.24086878234,52.0336417862087));
#102816=CARTESIAN_POINT('Ctrl Pts',(0.783772258610834,637.233100409219,
52.0236168794799));
#102817=CARTESIAN_POINT('Ctrl Pts',(0.639767420114975,637.227281790098,
52.0161192211438));
#102818=CARTESIAN_POINT('Ctrl Pts',(0.514927066398998,637.222237525774,
52.0096193678855));
#102819=CARTESIAN_POINT('Ctrl Pts',(0.389871499267673,637.218658197405,
52.0050182899915));
#102820=CARTESIAN_POINT('Ctrl Pts',(0.264827872760508,637.216574016203,
52.0023253862613));
#102821=CARTESIAN_POINT('',(-0.247612686332903,637.216296403659,76.5969814761947));
#102822=CARTESIAN_POINT('Origin',(0.00102225664371531,643.230913064776,
68.9078455093003));
#102823=CARTESIAN_POINT('Origin',(-0.252645464510396,637.216296403659,76.8469308133488));
#102824=CARTESIAN_POINT('Origin',(0.,22.7782939407039,64.2994740882088));
#102825=CARTESIAN_POINT('',(-3.417213350044E-14,635.742307759052,51.9994740882088));
#102826=CARTESIAN_POINT('Ctrl Pts',(-4.02455846426619E-15,635.742307759052,
51.9994740882088));
#102827=CARTESIAN_POINT('Ctrl Pts',(-0.803517342471636,635.742307759052,
51.9994740882088));
#102828=CARTESIAN_POINT('Ctrl Pts',(-1.62216512710203,635.808561272943,
52.0793396645949));
#102829=CARTESIAN_POINT('Ctrl Pts',(-3.23077935439454,636.064326910425,
52.4030388996346));
#102830=CARTESIAN_POINT('Ctrl Pts',(-4.02089381669516,636.253138677506,
52.6466899325635));
#102831=CARTESIAN_POINT('Ctrl Pts',(-6.27564182199435,636.933990415857,
53.5959081295421));
#102832=CARTESIAN_POINT('Ctrl Pts',(-7.62604171070064,637.536810853389,
54.5306889817204));
#102833=CARTESIAN_POINT('Ctrl Pts',(-9.75980156458901,638.60355417627,56.6644488356087));
#102834=CARTESIAN_POINT('Ctrl Pts',(-10.7006947361121,639.148581736175,
58.017090947518));
#102835=CARTESIAN_POINT('Ctrl Pts',(-11.654095320228,639.721789350985,60.2816553316396));
#102836=CARTESIAN_POINT('Ctrl Pts',(-11.8983125166469,639.873458090211,
61.0753972970467));
#102837=CARTESIAN_POINT('Ctrl Pts',(-12.2213288811781,640.075308832797,
62.6858966089289));
#102838=CARTESIAN_POINT('Ctrl Pts',(-12.3,640.125373764374,63.5026943063123));
#102839=CARTESIAN_POINT('Ctrl Pts',(-12.3,640.125373764374,65.0962538701053));
#102840=CARTESIAN_POINT('Ctrl Pts',(-12.2213288811781,640.075308832797,
65.9130515674887));
#102841=CARTESIAN_POINT('Ctrl Pts',(-11.8983125166469,639.873458090211,
67.5235508793709));
#102842=CARTESIAN_POINT('Ctrl Pts',(-11.654095320228,639.721789350985,68.317292844778));
#102843=CARTESIAN_POINT('Ctrl Pts',(-10.7006947361121,639.148581736175,
70.5818572288996));
#102844=CARTESIAN_POINT('Ctrl Pts',(-9.75980156458901,638.60355417627,71.9344993408089));
#102845=CARTESIAN_POINT('Ctrl Pts',(-7.62604171070064,637.536810853389,
74.0682591946972));
#102846=CARTESIAN_POINT('Ctrl Pts',(-6.27564182199435,636.933990415857,
75.0030400468755));
#102847=CARTESIAN_POINT('Ctrl Pts',(-4.02089381669516,636.253138677506,
75.952258243854));
#102848=CARTESIAN_POINT('Ctrl Pts',(-3.23077935439454,636.064326910425,
76.195909276783));
#102849=CARTESIAN_POINT('Ctrl Pts',(-1.62216512710202,635.808561272943,
76.5196085118227));
#102850=CARTESIAN_POINT('Ctrl Pts',(-0.80351734247163,635.742307759052,
76.5994740882088));
#102851=CARTESIAN_POINT('Ctrl Pts',(0.803517342471631,635.742307759052,
76.5994740882088));
#102852=CARTESIAN_POINT('Ctrl Pts',(1.62216512710202,635.808561272943,76.5196085118227));
#102853=CARTESIAN_POINT('Ctrl Pts',(3.23077935439454,636.064326910425,76.195909276783));
#102854=CARTESIAN_POINT('Ctrl Pts',(4.02089381669516,636.253138677506,75.952258243854));
#102855=CARTESIAN_POINT('Ctrl Pts',(6.27564182199435,636.933990415857,75.0030400468755));
#102856=CARTESIAN_POINT('Ctrl Pts',(7.62604171070065,637.536810853389,74.0682591946972));
#102857=CARTESIAN_POINT('Ctrl Pts',(9.75980156458901,638.60355417627,71.9344993408089));
#102858=CARTESIAN_POINT('Ctrl Pts',(10.7006947361121,639.148581736175,70.5818572288996));
#102859=CARTESIAN_POINT('Ctrl Pts',(11.654095320228,639.721789350985,68.317292844778));
#102860=CARTESIAN_POINT('Ctrl Pts',(11.8983125166469,639.873458090211,67.5235508793709));
#102861=CARTESIAN_POINT('Ctrl Pts',(12.2213288811781,640.075308832797,65.9130515674887));
#102862=CARTESIAN_POINT('Ctrl Pts',(12.3,640.125373764374,65.0962538701053));
#102863=CARTESIAN_POINT('Ctrl Pts',(12.3,640.125373764374,63.5026943063123));
#102864=CARTESIAN_POINT('Ctrl Pts',(12.2213288811781,640.075308832797,62.6858966089289));
#102865=CARTESIAN_POINT('Ctrl Pts',(11.8983125166469,639.873458090211,61.0753972970467));
#102866=CARTESIAN_POINT('Ctrl Pts',(11.654095320228,639.721789350985,60.2816553316396));
#102867=CARTESIAN_POINT('Ctrl Pts',(10.7006947361121,639.148581736175,58.017090947518));
#102868=CARTESIAN_POINT('Ctrl Pts',(9.75980156458901,638.60355417627,56.6644488356087));
#102869=CARTESIAN_POINT('Ctrl Pts',(7.62604171070065,637.536810853389,54.5306889817204));
#102870=CARTESIAN_POINT('Ctrl Pts',(6.27564182199435,636.933990415857,53.5959081295421));
#102871=CARTESIAN_POINT('Ctrl Pts',(4.02089381669516,636.253138677506,52.6466899325635));
#102872=CARTESIAN_POINT('Ctrl Pts',(3.23077935439455,636.064326910425,52.4030388996346));
#102873=CARTESIAN_POINT('Ctrl Pts',(1.62216512710203,635.808561272943,52.0793396645949));
#102874=CARTESIAN_POINT('Ctrl Pts',(0.803517342471631,635.742307759052,
51.9994740882088));
#102875=CARTESIAN_POINT('Ctrl Pts',(-1.11022302462516E-15,635.742307759052,
51.9994740882088));
#102876=CARTESIAN_POINT('',(3.02331010654657E-11,637.214366842191,51.9994740882088));
#102877=CARTESIAN_POINT('',(-1.50631556295125E-15,22.7782939407039,51.9994740882088));
#102878=CARTESIAN_POINT('Ctrl Pts',(3.02331010654653E-11,637.214366842191,
51.9994740882088));
#102879=CARTESIAN_POINT('Ctrl Pts',(-0.830412355286513,637.21436684219,
51.9994740882068));
#102880=CARTESIAN_POINT('Ctrl Pts',(-1.64231938504929,637.2796645682,52.0826407378937));
#102881=CARTESIAN_POINT('Ctrl Pts',(-2.83515367978352,637.460650458936,
52.3238128901797));
#102882=CARTESIAN_POINT('Ctrl Pts',(-3.22987045737859,637.535077177222,
52.4241819097058));
#102883=CARTESIAN_POINT('Ctrl Pts',(-4.00546366489188,637.707452625756,
52.6628556650804));
#102884=CARTESIAN_POINT('Ctrl Pts',(-4.3819730375247,637.804289924468,52.7996457417074));
#102885=CARTESIAN_POINT('Ctrl Pts',(-5.11472586367998,638.014469814955,
53.106292277839));
#102886=CARTESIAN_POINT('Ctrl Pts',(-5.4709631470815,638.127820070073,53.2761570601927));
#102887=CARTESIAN_POINT('Ctrl Pts',(-6.16461781174502,638.366908005775,
53.648537824575));
#102888=CARTESIAN_POINT('Ctrl Pts',(-6.50301550229225,638.493045789728,
53.8517225300024));
#102889=CARTESIAN_POINT('Ctrl Pts',(-7.48440400047611,638.881866601756,
54.5069979081057));
#102890=CARTESIAN_POINT('Ctrl Pts',(-8.08540127787933,639.150990068374,
54.9978561404126));
#102891=CARTESIAN_POINT('Ctrl Pts',(-8.91512989825012,639.549152457839,
55.8164668699459));
#102892=CARTESIAN_POINT('Ctrl Pts',(-9.17960981986667,639.681011055625,
56.1031778705361));
#102893=CARTESIAN_POINT('Ctrl Pts',(-9.68420831857607,639.939946757686,
56.7060152336913));
#102894=CARTESIAN_POINT('Ctrl Pts',(-9.92291043223669,640.06632247763,57.0207475962688));
#102895=CARTESIAN_POINT('Ctrl Pts',(-10.588630748229,640.426678872799,57.9917849677541));
#102896=CARTESIAN_POINT('Ctrl Pts',(-10.9702548417394,640.644251182824,
58.6797638066909));
#102897=CARTESIAN_POINT('Ctrl Pts',(-11.4461458407818,640.921726794252,
59.7789482198191));
#102898=CARTESIAN_POINT('Ctrl Pts',(-11.5888532985381,641.006239015841,
60.157572983035));
#102899=CARTESIAN_POINT('Ctrl Pts',(-11.8381254652856,641.155207113641,
60.9355996838596));
#102900=CARTESIAN_POINT('Ctrl Pts',(-11.9427242536689,641.218473448575,
61.328594326499));
#102901=CARTESIAN_POINT('Ctrl Pts',(-12.1975694083928,641.373418861391,
62.5194580325877));
#102902=CARTESIAN_POINT('Ctrl Pts',(-12.2894856073328,641.430410984453,
63.329099770875));
#102903=CARTESIAN_POINT('Ctrl Pts',(-12.3039937693077,641.439358792849,
64.5687472338827));
#102904=CARTESIAN_POINT('Ctrl Pts',(-12.2877001556332,641.429290464151,
64.9861606719414));
#102905=CARTESIAN_POINT('Ctrl Pts',(-12.2143945388442,641.384192208162,
65.8053557663228));
#102906=CARTESIAN_POINT('Ctrl Pts',(-12.1575137190371,641.349243906771,
66.2102226898452));
#102907=CARTESIAN_POINT('Ctrl Pts',(-12.0043633846739,641.255863449383,
67.0108131994104));
#102908=CARTESIAN_POINT('Ctrl Pts',(-11.9080923355556,641.197427827018,
67.4065361653013));
#102909=CARTESIAN_POINT('Ctrl Pts',(-11.6759895729683,641.058111400096,
68.1889168908426));
#102910=CARTESIAN_POINT('Ctrl Pts',(-11.5401719162782,640.977255570532,
68.5745577010913));
#102911=CARTESIAN_POINT('Ctrl Pts',(-11.084049328587,640.709716701086,69.6921989559377));
#102912=CARTESIAN_POINT('Ctrl Pts',(-10.713120747878,640.496599747497,70.394448758527));
#102913=CARTESIAN_POINT('Ctrl Pts',(-10.0591458219439,640.13930168359,71.3889736072495));
#102914=CARTESIAN_POINT('Ctrl Pts',(-9.82548367484988,640.014353394576,
71.7091490640292));
#102915=CARTESIAN_POINT('Ctrl Pts',(-9.33415010122502,639.75928843652,72.3192655181552));
#102916=CARTESIAN_POINT('Ctrl Pts',(-9.07556749241562,639.628663169196,
72.6106271901288));
#102917=CARTESIAN_POINT('Ctrl Pts',(-8.53249912602467,639.364197433611,
73.167261290061));
#102918=CARTESIAN_POINT('Ctrl Pts',(-8.24801593829463,639.230348267547,
73.4325321421815));
#102919=CARTESIAN_POINT('Ctrl Pts',(-7.65202535438717,638.962573514797,
73.9373693102691));
#102920=CARTESIAN_POINT('Ctrl Pts',(-7.33917816046739,638.828145283974,
74.1777117225733));
#102921=CARTESIAN_POINT('Ctrl Pts',(-6.37510403592419,638.437326991065,
74.8474837516176));
#102922=CARTESIAN_POINT('Ctrl Pts',(-5.69483978905192,638.191200666448,
75.2303104565591));
#102923=CARTESIAN_POINT('Ctrl Pts',(-4.61072722039661,637.866819284235,
75.7094386141286));
#102924=CARTESIAN_POINT('Ctrl Pts',(-4.23864535083926,637.766213340969,
75.8531520209636));
#102925=CARTESIAN_POINT('Ctrl Pts',(-3.47047139791234,637.584888214298,
76.1066505694972));
#102926=CARTESIAN_POINT('Ctrl Pts',(-3.0763775345276,637.504868994145,76.2154608388605));
#102927=CARTESIAN_POINT('Ctrl Pts',(-1.88763310249882,637.307010047577,
76.4808614138365));
#102928=CARTESIAN_POINT('Ctrl Pts',(-1.07745358387097,637.229228985181,
76.5802724694516));
#102929=CARTESIAN_POINT('Ctrl Pts',(-0.247612686332903,637.216296403659,
76.5969814761947));
#102930=CARTESIAN_POINT('Origin',(-0.00103899059614113,643.228225309358,
59.690866538563));
#102931=CARTESIAN_POINT('Origin',(0.,22.7782939407039,64.2994740882088));
#102932=CARTESIAN_POINT('',(-1.09932974876048E-8,634.523606676254,48.5811983853019));
#102933=CARTESIAN_POINT('Ctrl Pts',(-1.91941230150446,634.6517886719,48.698800681464));
#102934=CARTESIAN_POINT('Ctrl Pts',(-1.77856148953381,634.63305573477,48.6814712512449));
#102935=CARTESIAN_POINT('Ctrl Pts',(-1.63703421268158,634.61630066659,48.6660258498621));
#102936=CARTESIAN_POINT('Ctrl Pts',(-1.49482298762889,634.601549979961,
48.6524629893774));
#102937=CARTESIAN_POINT('Ctrl Pts',(-1.47848330595685,634.599855166321,
48.65090465372));
#102938=CARTESIAN_POINT('Ctrl Pts',(-1.46213456918917,634.598186849375,
48.649371204989));
#102939=CARTESIAN_POINT('Ctrl Pts',(-1.44577674730117,634.596545097886,
48.6478626682891));
#102940=CARTESIAN_POINT('Ctrl Pts',(-1.30269956743721,634.582185168137,
48.634667930125));
#102941=CARTESIAN_POINT('Ctrl Pts',(-1.15892868452191,634.569854628533,
48.6233762927982));
#102942=CARTESIAN_POINT('Ctrl Pts',(-1.01444129744806,634.559620255549,
48.614023979145));
#102943=CARTESIAN_POINT('Ctrl Pts',(-0.998637300186558,634.558500822179,
48.6130010252225));
#102944=CARTESIAN_POINT('Ctrl Pts',(-0.982824721720789,634.557406504378,
48.6120013076365));
#102945=CARTESIAN_POINT('Ctrl Pts',(-0.967003526926908,634.556337417338,
48.6110248994056));
#102946=CARTESIAN_POINT('Ctrl Pts',(-0.806537717335257,634.545494246539,
48.6011217195698));
#102947=CARTESIAN_POINT('Ctrl Pts',(-0.645476066513774,634.537265715482,
48.5936338603989));
#102948=CARTESIAN_POINT('Ctrl Pts',(-0.484183920938914,634.531783080114,
48.588641220104));
#102949=CARTESIAN_POINT('Ctrl Pts',(-0.42261549034373,634.529690248787,
48.586735429674));
#102950=CARTESIAN_POINT('Ctrl Pts',(-0.361005641426023,634.527998080083,
48.58519312428));
#102951=CARTESIAN_POINT('Ctrl Pts',(-0.299397258432974,634.526706674014,
48.5840194145379));
#102952=CARTESIAN_POINT('Ctrl Pts',(-0.280307236559402,634.526306517917,
48.5836557279166));
#102953=CARTESIAN_POINT('Ctrl Pts',(-0.261214851172683,634.525944782025,
48.5833273536881));
#102954=CARTESIAN_POINT('Ctrl Pts',(-0.242121350637931,634.52562112443,
48.5830342121591));
#102955=CARTESIAN_POINT('Ctrl Pts',(-0.161408243682273,634.524252941048,
48.5817950279905));
#102956=CARTESIAN_POINT('Ctrl Pts',(-0.0806852921308739,634.523587621895,
48.5811855692694));
#102957=CARTESIAN_POINT('Ctrl Pts',(-1.56438910714485E-8,634.523606676253,
48.5811983853012));
#102958=CARTESIAN_POINT('',(-4.88526835490447E-16,632.874615496751,48.5811677441054));
#102959=CARTESIAN_POINT('',(-1.92493735523237E-15,22.7782939407039,48.5811677441054));
#102960=CARTESIAN_POINT('Ctrl Pts',(-4.88526835490447E-16,632.874615496751,
48.5811677441054));
#102961=CARTESIAN_POINT('Ctrl Pts',(-1.00038541833524,632.874615496751,
48.5811677441054));
#102962=CARTESIAN_POINT('Ctrl Pts',(-1.98186107540154,632.994943488914,
48.6756960232106));
#102963=CARTESIAN_POINT('Ctrl Pts',(-3.18805636841627,633.269464450547,
48.9059115645402));
#102964=CARTESIAN_POINT('Ctrl Pts',(-3.42854858272457,633.330642826548,
48.9577280742447));
#102965=CARTESIAN_POINT('Ctrl Pts',(-3.90080611161479,633.462396409217,
49.0709538770827));
#102966=CARTESIAN_POINT('Ctrl Pts',(-4.13345843873348,633.533150770153,
49.1325121211066));
#102967=CARTESIAN_POINT('Ctrl Pts',(-4.82191402968073,633.758076226497,
49.3314235132617));
#102968=CARTESIAN_POINT('Ctrl Pts',(-5.2682579819503,633.924846454147,49.4829579943546));
#102969=CARTESIAN_POINT('Ctrl Pts',(-6.13948585279376,634.283225661171,
49.8222366173663));
#102970=CARTESIAN_POINT('Ctrl Pts',(-6.56545659234337,634.475387114061,
50.0105449985554));
#102971=CARTESIAN_POINT('Ctrl Pts',(-7.39359379433367,634.875218035797,
50.4209480281591));
#102972=CARTESIAN_POINT('Ctrl Pts',(-7.79284032142571,635.081369451215,
50.6414529752954));
#102973=CARTESIAN_POINT('Ctrl Pts',(-8.95204291419481,635.709623472847,
51.3478306146848));
#102974=CARTESIAN_POINT('Ctrl Pts',(-9.6739937385886,636.141209625582,51.8780902826517));
#102975=CARTESIAN_POINT('Ctrl Pts',(-10.6909797044834,636.782704337244,
52.7681666459264));
#102976=CARTESIAN_POINT('Ctrl Pts',(-11.018834746685,636.99566173962,53.0807607042935));
#102977=CARTESIAN_POINT('Ctrl Pts',(-11.6523858512663,637.416398533235,
53.7403002029845));
#102978=CARTESIAN_POINT('Ctrl Pts',(-11.9552766171641,637.622331956755,
54.0845026139995));
#102979=CARTESIAN_POINT('Ctrl Pts',(-12.8157642528714,638.217349503897,
55.1530076404017));
#102980=CARTESIAN_POINT('Ctrl Pts',(-13.3290592983858,638.586009440671,
55.9162808887405));
#102981=CARTESIAN_POINT('Ctrl Pts',(-14.004746121757,639.080347468074,57.1474541420455));
#102982=CARTESIAN_POINT('Ctrl Pts',(-14.2141395881851,639.235335259904,
57.5723098240839));
#102983=CARTESIAN_POINT('Ctrl Pts',(-14.5988681163382,639.522324200276,
58.4540012253265));
#102984=CARTESIAN_POINT('Ctrl Pts',(-14.774314469106,639.654423764541,58.9121779826557));
#102985=CARTESIAN_POINT('Ctrl Pts',(-15.2329469259702,640.001641631537,
60.3025784912361));
#102986=CARTESIAN_POINT('Ctrl Pts',(-15.4543798168271,640.171936383211,
61.2611681259983));
#102987=CARTESIAN_POINT('Ctrl Pts',(-15.6499076381601,640.322525407937,
62.7513958204655));
#102988=CARTESIAN_POINT('Ctrl Pts',(-15.6916676668363,640.354793810631,
63.2567226635694));
#102989=CARTESIAN_POINT('Ctrl Pts',(-15.7262198238666,640.381486323066,
64.2573462892223));
#102990=CARTESIAN_POINT('Ctrl Pts',(-15.7195678789232,640.376339938052,
64.7561248933746));
#102991=CARTESIAN_POINT('Ctrl Pts',(-15.6590995589811,640.329648865433,
65.7506616225585));
#102992=CARTESIAN_POINT('Ctrl Pts',(-15.6052831790191,640.288103150951,
66.2464197156399));
#102993=CARTESIAN_POINT('Ctrl Pts',(-15.4498800061554,640.168587449424,
67.2348902714699));
#102994=CARTESIAN_POINT('Ctrl Pts',(-15.3482435235833,640.090585479368,
67.7257307925787));
#102995=CARTESIAN_POINT('Ctrl Pts',(-14.9812478047689,639.81051358526,69.1572522104259));
#102996=CARTESIAN_POINT('Ctrl Pts',(-14.6526793160863,639.561289321234,
70.0696014607015));
#102997=CARTESIAN_POINT('Ctrl Pts',(-13.8372960983329,638.955981993477,
71.8177596455625));
#102998=CARTESIAN_POINT('Ctrl Pts',(-13.3616578586644,638.608220356701,
72.6296038086576));
#102999=CARTESIAN_POINT('Ctrl Pts',(-12.2895634342419,637.849607134678,
74.1428267938299));
#103000=CARTESIAN_POINT('Ctrl Pts',(-11.6877930740782,637.435132345469,
74.8486713035806));
#103001=CARTESIAN_POINT('Ctrl Pts',(-10.3949373649157,636.588911121083,
76.1246737064291));
#103002=CARTESIAN_POINT('Ctrl Pts',(-9.70188800092167,636.155193164691,
76.6994753988773));
#103003=CARTESIAN_POINT('Ctrl Pts',(-8.58467388731213,635.511284076344,
77.4742190882293));
#103004=CARTESIAN_POINT('Ctrl Pts',(-8.19773601749983,635.297061722008,
77.7185803584321));
#103005=CARTESIAN_POINT('Ctrl Pts',(-7.40176600282271,634.879910318627,
78.1735199632814));
#103006=CARTESIAN_POINT('Ctrl Pts',(-6.99390219741844,634.677513014684,
78.3836222033658));
#103007=CARTESIAN_POINT('Ctrl Pts',(-5.73705816174996,634.097967889989,
78.9624303035972));
#103008=CARTESIAN_POINT('Ctrl Pts',(-4.8557807881079,633.747192826359,79.2806298462149));
#103009=CARTESIAN_POINT('Ctrl Pts',(-3.91253447320281,633.467807133627,
79.5230488432747));
#103010=CARTESIAN_POINT('Ctrl Pts',(3.93978362444746,633.475903764133,49.082928510463));
#103011=CARTESIAN_POINT('Ctrl Pts',(3.62591964374305,633.382350288002,49.0016645885587));
#103012=CARTESIAN_POINT('Ctrl Pts',(3.3057992406009,633.297177229342,48.9292260493855));
#103013=CARTESIAN_POINT('Ctrl Pts',(2.66144129984969,633.148794387986,48.8046503202028));
#103014=CARTESIAN_POINT('Ctrl Pts',(2.3359974548026,633.085210702006,48.7521822712622));
#103015=CARTESIAN_POINT('Ctrl Pts',(1.67806442767431,632.981730278595,48.6674791187011));
#103016=CARTESIAN_POINT('Ctrl Pts',(1.34557472886657,632.941837524538,48.6352427984729));
#103017=CARTESIAN_POINT('Ctrl Pts',(0.672995467599795,632.88812644915,48.5919666363597));
#103018=CARTESIAN_POINT('Ctrl Pts',(0.334567964264241,632.874615496751,
48.5811677441054));
#103019=CARTESIAN_POINT('Ctrl Pts',(-4.88526835490447E-16,632.874615496751,
48.5811677441054));
#103020=CARTESIAN_POINT('Ctrl Pts',(-6.34270402866122E-9,634.523606676255,
48.5811983853026));
#103021=CARTESIAN_POINT('Ctrl Pts',(0.131183067920692,634.523637656084,
48.5812192224713));
#103022=CARTESIAN_POINT('Ctrl Pts',(0.262263850660877,634.525477231112,
48.5828845405628));
#103023=CARTESIAN_POINT('Ctrl Pts',(0.393087042492144,634.529084138707,
48.5861654542112));
#103024=CARTESIAN_POINT('Ctrl Pts',(0.62595673992944,634.535504555978,48.5920055912538));
#103025=CARTESIAN_POINT('Ctrl Pts',(0.858266994437316,634.547536978571,
48.6029757350669));
#103026=CARTESIAN_POINT('Ctrl Pts',(1.08860828168253,634.564969308388,48.6189321330415));
#103027=CARTESIAN_POINT('Ctrl Pts',(1.16869635359341,634.571030408856,48.6244800622196));
#103028=CARTESIAN_POINT('Ctrl Pts',(1.24854641185876,634.577743962404,48.6306304686975));
#103029=CARTESIAN_POINT('Ctrl Pts',(1.32809942293835,634.585099981992,48.637376328015));
#103030=CARTESIAN_POINT('Ctrl Pts',(1.40535872090963,634.592243909061,48.6439276872661));
#103031=CARTESIAN_POINT('Ctrl Pts',(1.48241468364269,634.599987046874,48.6510297053401));
#103032=CARTESIAN_POINT('Ctrl Pts',(1.55926269747949,634.608315807309,48.6586783314213));
#103033=CARTESIAN_POINT('Ctrl Pts',(2.07067858640156,634.66374287964,48.7095791772737));
#103034=CARTESIAN_POINT('Ctrl Pts',(2.57353940461454,634.745183949427,48.7847527919497));
#103035=CARTESIAN_POINT('Ctrl Pts',(3.0686126658422,634.848983739582,48.8833382201712));
#103036=CARTESIAN_POINT('Ctrl Pts',(3.5280360180697,634.945308973214,48.9748245747402));
#103037=CARTESIAN_POINT('Ctrl Pts',(3.98077413585814,635.060900537147,49.0864791016381));
#103038=CARTESIAN_POINT('Ctrl Pts',(4.42735940791138,635.192792800213,49.2175762302821));
#103039=CARTESIAN_POINT('Ctrl Pts',(4.46201311942238,635.203027254237,49.2277489842));
#103040=CARTESIAN_POINT('Ctrl Pts',(4.49663613259052,635.213362895059,49.2380436267645));
#103041=CARTESIAN_POINT('Ctrl Pts',(4.53121896438336,635.223794826727,49.2484565026335));
#103042=CARTESIAN_POINT('Ctrl Pts',(4.74601947947587,635.288589529171,49.3131328459027));
#103043=CARTESIAN_POINT('Ctrl Pts',(4.95932213084446,635.357118326411,49.3823865525656));
#103044=CARTESIAN_POINT('Ctrl Pts',(5.16884411272974,635.428209929197,49.4553437713038));
#103045=CARTESIAN_POINT('Ctrl Pts',(5.41200740793916,635.510716157134,49.5400151626208));
#103046=CARTESIAN_POINT('Ctrl Pts',(5.65093526308688,635.596907367806,49.6299024007825));
#103047=CARTESIAN_POINT('Ctrl Pts',(5.88596567871249,635.68616027303,49.7248192945151));
#103048=CARTESIAN_POINT('Ctrl Pts',(5.9012058732883,635.691947743721,49.7309740380412));
#103049=CARTESIAN_POINT('Ctrl Pts',(5.91642974293561,635.697748021797,49.7371498648016));
#103050=CARTESIAN_POINT('Ctrl Pts',(5.93163735194624,635.703560967641,49.7433467521698));
#103051=CARTESIAN_POINT('Ctrl Pts',(6.38532277407427,635.876977366458,49.9282171982447));
#103052=CARTESIAN_POINT('Ctrl Pts',(6.82458941528542,636.061682510158,50.1318546390623));
#103053=CARTESIAN_POINT('Ctrl Pts',(7.25129724309772,636.254031066571,50.3537276895692));
#103054=CARTESIAN_POINT('Ctrl Pts',(7.67449000072657,636.444795122697,50.5737730273099));
#103055=CARTESIAN_POINT('Ctrl Pts',(8.08531522162718,636.643099353163,50.8117642540156));
#103056=CARTESIAN_POINT('Ctrl Pts',(8.48485213004565,636.846125285092,51.0679794092165));
#103057=CARTESIAN_POINT('Ctrl Pts',(8.50152150271618,636.854595879047,51.0786691498034));
#103058=CARTESIAN_POINT('Ctrl Pts',(8.51817133864072,636.863074757022,51.0893906828856));
#103059=CARTESIAN_POINT('Ctrl Pts',(8.53480170293738,636.871561707065,51.1001440211828));
#103060=CARTESIAN_POINT('Ctrl Pts',(8.88265589543402,637.04908163995,51.3250695696129));
#103061=CARTESIAN_POINT('Ctrl Pts',(9.22310591847262,637.230801572943,51.5648853840179));
#103062=CARTESIAN_POINT('Ctrl Pts',(9.55213627069025,637.412648744007,51.8166263298771));
#103063=CARTESIAN_POINT('Ctrl Pts',(9.58597325050769,637.431349629854,51.8425149849719));
#103064=CARTESIAN_POINT('Ctrl Pts',(9.61968948712715,637.45005185641,51.8685297223147));
#103065=CARTESIAN_POINT('Ctrl Pts',(9.65328063531741,637.468750993354,51.8946672948334));
#103066=CARTESIAN_POINT('Ctrl Pts',(9.68287665471881,637.485226167606,51.917696221948));
#103067=CARTESIAN_POINT('Ctrl Pts',(9.71237647083123,637.501699898547,51.940821203202));
#103068=CARTESIAN_POINT('Ctrl Pts',(9.74177715342259,637.518169132975,51.9640400780151));
#103069=CARTESIAN_POINT('Ctrl Pts',(10.0857430188191,637.710846784418,52.2356834435658));
#103070=CARTESIAN_POINT('Ctrl Pts',(10.4168996980707,637.903110177124,52.5202505899506));
#103071=CARTESIAN_POINT('Ctrl Pts',(10.7356021263374,638.093325829708,52.8182111751762));
#103072=CARTESIAN_POINT('Ctrl Pts',(11.1345671134278,638.331445714109,53.1912106583761));
#103073=CARTESIAN_POINT('Ctrl Pts',(11.5140262355694,638.566425706844,53.5852075140256));
#103074=CARTESIAN_POINT('Ctrl Pts',(11.8747642121883,638.795350794663,54.0011669855164));
#103075=CARTESIAN_POINT('Ctrl Pts',(12.1396201387599,638.963428929431,54.3065668557228));
#103076=CARTESIAN_POINT('Ctrl Pts',(12.3942600538462,639.128288972181,54.6238994674662));
#103077=CARTESIAN_POINT('Ctrl Pts',(12.6384027128533,639.288833991502,54.9540941874028));
#103078=CARTESIAN_POINT('Ctrl Pts',(12.6934199989364,639.325012639237,55.0285032130264));
#103079=CARTESIAN_POINT('Ctrl Pts',(12.7479128130092,639.360977370941,55.1035770627711));
#103080=CARTESIAN_POINT('Ctrl Pts',(12.8018733060316,639.396712358839,55.1793208996343));
#103081=CARTESIAN_POINT('Ctrl Pts',(12.9672617185343,639.506239766544,55.4114750597241));
#103082=CARTESIAN_POINT('Ctrl Pts',(13.1265971638525,639.61291400292,55.6485181832674));
#103083=CARTESIAN_POINT('Ctrl Pts',(13.2794577936759,639.71615893547,55.8898965897075));
#103084=CARTESIAN_POINT('Ctrl Pts',(13.3380989021436,639.755766238511,55.9824953009005));
#103085=CARTESIAN_POINT('Ctrl Pts',(13.395787529721,639.794869067689,56.0757317394399));
#103086=CARTESIAN_POINT('Ctrl Pts',(13.4525014240595,639.83343577007,56.1695736395204));
#103087=CARTESIAN_POINT('Ctrl Pts',(13.5103276838369,639.87275890555,56.265256120072));
#103088=CARTESIAN_POINT('Ctrl Pts',(13.5671707966639,639.911546279781,56.3616179364094));
#103089=CARTESIAN_POINT('Ctrl Pts',(13.6230077720489,639.949765308903,56.4586314313637));
#103090=CARTESIAN_POINT('Ctrl Pts',(13.7869220361162,640.061960569997,56.7434229251792));
#103091=CARTESIAN_POINT('Ctrl Pts',(13.9424991854698,640.169458563498,57.0341146385251));
#103092=CARTESIAN_POINT('Ctrl Pts',(14.0893519141752,640.271692823618,57.3308706562064));
#103093=CARTESIAN_POINT('Ctrl Pts',(14.111156236253,640.286872308227,57.3749322398425));
#103094=CARTESIAN_POINT('Ctrl Pts',(14.1327682926389,640.301935791542,57.4191274656104));
#103095=CARTESIAN_POINT('Ctrl Pts',(14.1541868887825,640.31688146356,57.4634568184052));
#103096=CARTESIAN_POINT('Ctrl Pts',(14.3690003859214,640.46677607158,57.9080491360309));
#103097=CARTESIAN_POINT('Ctrl Pts',(14.5644206321617,640.604866455008,58.3662732287448));
#103098=CARTESIAN_POINT('Ctrl Pts',(14.7394736989775,640.729507918388,58.8391490276349));
#103099=CARTESIAN_POINT('Ctrl Pts',(14.7930222736766,640.767635629223,58.9838013065174));
#103100=CARTESIAN_POINT('Ctrl Pts',(14.844665954123,640.804501637939,59.1298267006041));
#103101=CARTESIAN_POINT('Ctrl Pts',(14.8943779224113,640.840060847293,59.2772573842497));
#103102=CARTESIAN_POINT('Ctrl Pts',(14.9788181415358,640.900461341042,59.5276815710471));
#103103=CARTESIAN_POINT('Ctrl Pts',(15.0576110594056,640.957060717116,59.7824113765591));
#103104=CARTESIAN_POINT('Ctrl Pts',(15.1295263785222,641.008879049081,60.0377155440764));
#103105=CARTESIAN_POINT('Ctrl Pts',(15.1536787692919,641.026281969877,60.1234581382101));
#103106=CARTESIAN_POINT('Ctrl Pts',(15.1770912859024,641.043171234754,60.2093651695768));
#103107=CARTESIAN_POINT('Ctrl Pts',(15.1997652434983,641.059544776398,60.2954371488871));
#103108=CARTESIAN_POINT('Ctrl Pts',(15.2446133607517,641.091930940674,60.4656838384653));
#103109=CARTESIAN_POINT('Ctrl Pts',(15.2865717155591,641.122296729638,60.636574808298));
#103110=CARTESIAN_POINT('Ctrl Pts',(15.325649598072,641.150623333856,60.8081106404716));
#103111=CARTESIAN_POINT('Ctrl Pts',(15.4433396652835,641.235933994003,61.3247216316376));
#103112=CARTESIAN_POINT('Ctrl Pts',(15.5349555636936,641.302769846919,61.8471715921895));
#103113=CARTESIAN_POINT('Ctrl Pts',(15.600123128367,641.350389654829,62.3755944903987));
#103114=CARTESIAN_POINT('Ctrl Pts',(15.6386979344604,641.378577371611,62.688385231251));
#103115=CARTESIAN_POINT('Ctrl Pts',(15.6680084809615,641.400034585006,63.00326810169));
#103116=CARTESIAN_POINT('Ctrl Pts',(15.6877925284557,641.414528796385,63.3203069204358));
#103117=CARTESIAN_POINT('Ctrl Pts',(15.7005815679481,641.423898317046,63.525250927709));
#103118=CARTESIAN_POINT('Ctrl Pts',(15.7093924335219,641.430360162221,63.7311946738769));
#103119=CARTESIAN_POINT('Ctrl Pts',(15.7141470311169,641.433849188663,63.9378910948812));
#103120=CARTESIAN_POINT('Ctrl Pts',(15.7144659003347,641.434083181785,63.9517532829566));
#103121=CARTESIAN_POINT('Ctrl Pts',(15.7147665408602,641.434303815199,63.9656188529755));
#103122=CARTESIAN_POINT('Ctrl Pts',(15.7150489358492,641.434511074186,63.9794877289295));
#103123=CARTESIAN_POINT('Ctrl Pts',(15.7158488065306,641.435098125634,64.0187706754704));
#103124=CARTESIAN_POINT('Ctrl Pts',(15.7165007988266,641.435576865089,64.0581033421356));
#103125=CARTESIAN_POINT('Ctrl Pts',(15.7170049051664,641.435947313476,64.0974701301083));
#103126=CARTESIAN_POINT('Ctrl Pts',(15.7194694294045,641.437758397678,64.2899303224724));
#103127=CARTESIAN_POINT('Ctrl Pts',(15.7184018336159,641.436970322652,64.4836683248673));
#103128=CARTESIAN_POINT('Ctrl Pts',(15.7137735336007,641.433574471331,64.6767950132201));
#103129=CARTESIAN_POINT('Ctrl Pts',(15.7128333947127,641.432884677698,64.7160245163702));
#103130=CARTESIAN_POINT('Ctrl Pts',(15.7117464743582,641.432087384869,64.7552287682019));
#103131=CARTESIAN_POINT('Ctrl Pts',(15.7105127430939,641.431182674632,64.7943919360785));
#103132=CARTESIAN_POINT('Ctrl Pts',(15.7095991882977,641.430512753718,64.8233915252814));
#103133=CARTESIAN_POINT('Ctrl Pts',(15.708605979292,641.429784554329,64.8523701843884));
#103134=CARTESIAN_POINT('Ctrl Pts',(15.7075334205578,641.42899836347,64.8813270198615));
#103135=CARTESIAN_POINT('Ctrl Pts',(15.6985693797753,641.422427677226,65.1233373134135));
#103136=CARTESIAN_POINT('Ctrl Pts',(15.6840546075089,641.411790509973,65.3640472137197));
#103137=CARTESIAN_POINT('Ctrl Pts',(15.6641212610662,641.397197896467,65.6034907467274));
#103138=CARTESIAN_POINT('Ctrl Pts',(15.6411292069346,641.380366093507,65.8796761172173));
#103139=CARTESIAN_POINT('Ctrl Pts',(15.6110000935115,641.3583004588,66.1541909485691));
#103140=CARTESIAN_POINT('Ctrl Pts',(15.5737798644399,641.331104474615,66.4270558219922));
#103141=CARTESIAN_POINT('Ctrl Pts',(15.5042909343416,641.280330476413,66.9364854678731));
#103142=CARTESIAN_POINT('Ctrl Pts',(15.4100832406381,641.211672672658,67.4401695893287));
#103143=CARTESIAN_POINT('Ctrl Pts',(15.2914680739336,641.12581412946,67.9381923855767));
#103144=CARTESIAN_POINT('Ctrl Pts',(15.2270223963164,641.079165693603,68.2087768096833));
#103145=CARTESIAN_POINT('Ctrl Pts',(15.1553484481903,641.027422827044,68.4777850319379));
#103146=CARTESIAN_POINT('Ctrl Pts',(15.0765013223764,640.970699140689,68.7451756305374));
#103147=CARTESIAN_POINT('Ctrl Pts',(15.0102267686864,640.923020332387,68.969929448767));
#103148=CARTESIAN_POINT('Ctrl Pts',(14.9393986310139,640.872195863483,69.1917973879912));
#103149=CARTESIAN_POINT('Ctrl Pts',(14.8641408406389,640.818399206912,69.4108007082289));
#103150=CARTESIAN_POINT('Ctrl Pts',(14.638491776709,640.657098095927,70.0674489298011));
#103151=CARTESIAN_POINT('Ctrl Pts',(14.3730295175424,640.469084278575,70.6983179950207));
#103152=CARTESIAN_POINT('Ctrl Pts',(14.0709202550478,640.258910548728,71.3048669690282));
#103153=CARTESIAN_POINT('Ctrl Pts',(14.0153823305951,640.220273491944,71.4163712334691));
#103154=CARTESIAN_POINT('Ctrl Pts',(13.9586060318041,640.18088759514,71.5270536792873));
#103155=CARTESIAN_POINT('Ctrl Pts',(13.9006111685527,640.14078120424,71.6369234719542));
#103156=CARTESIAN_POINT('Ctrl Pts',(13.8132963508808,640.080398577011,71.8023391721822));
#103157=CARTESIAN_POINT('Ctrl Pts',(13.722999297798,640.018241840122,71.9661929969353));
#103158=CARTESIAN_POINT('Ctrl Pts',(13.6299592468021,639.954544488634,72.1281591912608));
#103159=CARTESIAN_POINT('Ctrl Pts',(13.5153701108086,639.876094139629,72.3276385130071));
#103160=CARTESIAN_POINT('Ctrl Pts',(13.3964238457193,639.795161400824,72.5245885124587));
#103161=CARTESIAN_POINT('Ctrl Pts',(13.2736785048361,639.712270183463,72.7181535822366));
#103162=CARTESIAN_POINT('Ctrl Pts',(13.2230467223056,639.678078009153,72.797998116033));
#103163=CARTESIAN_POINT('Ctrl Pts',(13.1717690142433,639.643552886662,72.8772669587132));
#103164=CARTESIAN_POINT('Ctrl Pts',(13.119886458028,639.608732640406,72.9559013911626));
#103165=CARTESIAN_POINT('Ctrl Pts',(13.028077430013,639.547116305414,73.0950493310163));
#103166=CARTESIAN_POINT('Ctrl Pts',(12.9344479627768,639.48462216792,73.232156163104));
#103167=CARTESIAN_POINT('Ctrl Pts',(12.8390792114001,639.421364130704,73.367197238578));
#103168=CARTESIAN_POINT('Ctrl Pts',(12.6440223006845,639.291982995488,73.643395622445));
#103169=CARTESIAN_POINT('Ctrl Pts',(12.4414058536515,639.15920090843,73.9113615973352));
#103170=CARTESIAN_POINT('Ctrl Pts',(12.2313971791556,639.023622204506,74.1715598542876));
#103171=CARTESIAN_POINT('Ctrl Pts',(12.1400319511015,638.964638073335,74.2847602882354));
#103172=CARTESIAN_POINT('Ctrl Pts',(12.0472674516941,638.90512335526,74.3964896998921));
#103173=CARTESIAN_POINT('Ctrl Pts',(11.9530990206169,638.845127013667,74.506770281284));
#103174=CARTESIAN_POINT('Ctrl Pts',(11.7624766227016,638.723678175987,74.7300080333411));
#103175=CARTESIAN_POINT('Ctrl Pts',(11.5660389794382,638.600215282207,74.9473754835452));
#103176=CARTESIAN_POINT('Ctrl Pts',(11.3639002899801,638.475242595692,75.1588940699884));
#103177=CARTESIAN_POINT('Ctrl Pts',(11.324185565883,638.450688880725,75.2004516873081));
#103178=CARTESIAN_POINT('Ctrl Pts',(11.2842508843236,638.42607691691,75.2417836420707));
#103179=CARTESIAN_POINT('Ctrl Pts',(11.244097275529,638.401410569611,75.2828902591882));
#103180=CARTESIAN_POINT('Ctrl Pts',(11.1555970541534,638.347044915761,75.373490950486));
#103181=CARTESIAN_POINT('Ctrl Pts',(11.0659447322039,638.292363220271,75.463070243372));
#103182=CARTESIAN_POINT('Ctrl Pts',(10.9752166475745,638.237454616551,75.5515588294561));
#103183=CARTESIAN_POINT('Ctrl Pts',(10.7995114119609,638.131117872056,75.722927021902));
#103184=CARTESIAN_POINT('Ctrl Pts',(10.6193973010404,638.023696042729,75.8905643475752));
#103185=CARTESIAN_POINT('Ctrl Pts',(10.4355011010581,637.915901197236,76.053840239258));
#103186=CARTESIAN_POINT('Ctrl Pts',(10.343703427894,637.862091950518,76.1353446256548));
#103187=CARTESIAN_POINT('Ctrl Pts',(10.2509639608639,637.808189937796,76.2157627203798));
#103188=CARTESIAN_POINT('Ctrl Pts',(10.1573640686073,637.75428427382,76.2950194899588));
#103189=CARTESIAN_POINT('Ctrl Pts',(10.0741297969102,637.706348335293,76.3654990528508));
#103190=CARTESIAN_POINT('Ctrl Pts',(9.99030988510562,637.658450897748,76.4350092280443));
#103191=CARTESIAN_POINT('Ctrl Pts',(9.90591360420892,637.610632366472,76.5035433110902));
#103192=CARTESIAN_POINT('Ctrl Pts',(9.40639551616552,637.327607794034,76.9091774665904));
#103193=CARTESIAN_POINT('Ctrl Pts',(8.88565058254247,637.046582516874,77.2814637959477));
#103194=CARTESIAN_POINT('Ctrl Pts',(8.34163289752633,636.773710266685,77.6218868333786));
#103195=CARTESIAN_POINT('Ctrl Pts',(8.14290238226259,636.674029604871,77.7462439039291));
#103196=CARTESIAN_POINT('Ctrl Pts',(7.94106647131428,636.57543655124,77.8663491091254));
#103197=CARTESIAN_POINT('Ctrl Pts',(7.73602658782707,636.478229722697,77.982275225029));
#103198=CARTESIAN_POINT('Ctrl Pts',(7.67213350385392,636.447938815615,78.0183993045599));
#103199=CARTESIAN_POINT('Ctrl Pts',(7.60792574479906,636.41778470578,78.0541135135407));
#103200=CARTESIAN_POINT('Ctrl Pts',(7.54339610210034,636.387779954009,78.0894159789354));
#103201=CARTESIAN_POINT('Ctrl Pts',(7.29105366480304,636.270446711865,78.227465870237));
#103202=CARTESIAN_POINT('Ctrl Pts',(7.03370074020654,636.155345245241,78.3592633253105));
#103203=CARTESIAN_POINT('Ctrl Pts',(6.77108651634947,636.043300256403,78.4846057105662));
#103204=CARTESIAN_POINT('Ctrl Pts',(6.64811138529507,635.99083262162,78.5433001560806));
#103205=CARTESIAN_POINT('Ctrl Pts',(6.52398298358298,635.93903498938,78.6005796581726));
#103206=CARTESIAN_POINT('Ctrl Pts',(6.39867799322467,635.887990551571,78.6564262110446));
#103207=CARTESIAN_POINT('Ctrl Pts',(6.3469937399708,635.866936372936,78.6794611067318));
#103208=CARTESIAN_POINT('Ctrl Pts',(6.29507802198154,635.846001728375,78.7022602318609));
#103209=CARTESIAN_POINT('Ctrl Pts',(6.242947083485,635.825199921756,78.7248152334023));
#103210=CARTESIAN_POINT('Ctrl Pts',(5.9934113591813,635.725627690158,78.8327795020041));
#103211=CARTESIAN_POINT('Ctrl Pts',(5.73853110387259,635.628941916558,78.9353252138458));
#103212=CARTESIAN_POINT('Ctrl Pts',(5.48010053989362,635.53663991684,79.0314825681284));
#103213=CARTESIAN_POINT('Ctrl Pts',(5.31038406678866,635.476023364326,79.0946310083929));
#103214=CARTESIAN_POINT('Ctrl Pts',(5.13913733643898,635.417297288755,79.1550248358553));
#103215=CARTESIAN_POINT('Ctrl Pts',(4.96687438959262,635.360879771099,79.2123984530303));
#103216=CARTESIAN_POINT('Ctrl Pts',(4.93007196624935,635.348826677809,79.2246558083506));
#103217=CARTESIAN_POINT('Ctrl Pts',(4.89321390536558,635.336873120223,79.2367829629027));
#103218=CARTESIAN_POINT('Ctrl Pts',(4.85630009928058,635.325021373308,79.2487791179174));
#103219=CARTESIAN_POINT('Ctrl Pts',(4.25499476163656,635.131963018284,79.4441898004406));
#103220=CARTESIAN_POINT('Ctrl Pts',(3.63825269208279,634.965644185472,79.605049820634));
#103221=CARTESIAN_POINT('Ctrl Pts',(3.00303825703234,634.835251784121,79.7285331850169));
#103222=CARTESIAN_POINT('Ctrl Pts',(2.63932772572501,634.760591815839,79.799237182894));
#103223=CARTESIAN_POINT('Ctrl Pts',(2.26956149096814,634.697709328596,79.8576872889952));
#103224=CARTESIAN_POINT('Ctrl Pts',(1.89317385967765,634.648322422428,79.9033533194805));
#103225=CARTESIAN_POINT('Ctrl Pts',(-29.2194381818547,646.39670912511,64.2994740882088));
#103226=CARTESIAN_POINT('Ctrl Pts',(-30.058537813032,646.39670912511,64.2994740882088));
#103227=CARTESIAN_POINT('Ctrl Pts',(-30.204245934867,645.570357302777,64.2994740882088));
#103228=CARTESIAN_POINT('Ctrl Pts',(-29.2194381818525,646.39670912511,63.6657417300129));
#103229=CARTESIAN_POINT('Ctrl Pts',(-30.058537813076,646.39670912511,63.5542259178429));
#103230=CARTESIAN_POINT('Ctrl Pts',(-30.2042459348789,645.570357302709,
63.5348184358982));
#103231=CARTESIAN_POINT('Ctrl Pts',(-29.0915097686744,646.39670912511,63.0324871423586));
#103232=CARTESIAN_POINT('Ctrl Pts',(-29.9111456379662,646.39670912511,62.8068138256533));
#103233=CARTESIAN_POINT('Ctrl Pts',(-30.0506856115286,645.565837705453,
62.7707392571429));
#103234=CARTESIAN_POINT('Ctrl Pts',(-28.5990783166314,646.39670912511,61.8617135225403));
#103235=CARTESIAN_POINT('Ctrl Pts',(-29.3454369712421,646.39670912511,61.4226444395839));
#103236=CARTESIAN_POINT('Ctrl Pts',(-29.45958992671,645.548440539176,61.3580945430258));
#103237=CARTESIAN_POINT('Ctrl Pts',(-28.234769018359,646.39670912511,61.3247693565845));
#103238=CARTESIAN_POINT('Ctrl Pts',(-28.9235388845874,646.39670912511,60.7826106946149));
#103239=CARTESIAN_POINT('Ctrl Pts',(-29.0222871239381,645.535569814948,
60.7102226359645));
#103240=CARTESIAN_POINT('Ctrl Pts',(-27.3248743388726,646.39670912511,60.4286980218046));
#103241=CARTESIAN_POINT('Ctrl Pts',(-27.8689763870026,646.39670912511,59.7035779132664));
#103242=CARTESIAN_POINT('Ctrl Pts',(-27.9300847139336,645.50342404321,59.6290311800515));
#103243=CARTESIAN_POINT('Ctrl Pts',(-26.7796469437582,646.39670912511,60.0699234004071));
#103244=CARTESIAN_POINT('Ctrl Pts',(-27.2309350653715,646.39670912511,59.2646547208034));
#103245=CARTESIAN_POINT('Ctrl Pts',(-27.275614819367,645.484161643149,59.1961370117062));
#103246=CARTESIAN_POINT('Ctrl Pts',(-25.590812253516,646.39670912511,59.584973088534));
#103247=CARTESIAN_POINT('Ctrl Pts',(-25.8325282144725,646.39670912511,58.6515832061606));
#103248=CARTESIAN_POINT('Ctrl Pts',(-25.8485836001921,645.442161168378,
58.6110004122124));
#103249=CARTESIAN_POINT('Ctrl Pts',(-24.9476726899769,646.39670912511,59.4589881954405));
#103250=CARTESIAN_POINT('Ctrl Pts',(-25.0679049368893,646.39670912511,58.4814632535357));
#103251=CARTESIAN_POINT('Ctrl Pts',(-25.0765837225069,645.419439618224,
58.4589881954405));
#103252=CARTESIAN_POINT('Ctrl Pts',(-23.6608872937837,646.39670912511,59.4589881954405));
#103253=CARTESIAN_POINT('Ctrl Pts',(-23.5230979344025,646.39670912511,58.4359963952912));
#103254=CARTESIAN_POINT('Ctrl Pts',(-23.5319762612537,645.373978631996,
58.4589881954405));
#103255=CARTESIAN_POINT('Ctrl Pts',(-23.0177477302446,646.39670912511,59.584973088534));
#103256=CARTESIAN_POINT('Ctrl Pts',(-22.7425774139614,646.39670912511,58.566978825107));
#103257=CARTESIAN_POINT('Ctrl Pts',(-22.7599763835685,645.351257081842,
58.6110004122124));
#103258=CARTESIAN_POINT('Ctrl Pts',(-21.8289130400024,646.39670912511,60.0699234004071));
#103259=CARTESIAN_POINT('Ctrl Pts',(-21.280243410082,646.39670912511,59.1147920019372));
#103260=CARTESIAN_POINT('Ctrl Pts',(-21.3329451643936,645.309256607071,
59.1961370117062));
#103261=CARTESIAN_POINT('Ctrl Pts',(-21.2836856448871,646.39670912511,60.4286980218043));
#103262=CARTESIAN_POINT('Ctrl Pts',(-20.6031006941262,646.39670912511,59.5367585763147));
#103263=CARTESIAN_POINT('Ctrl Pts',(-20.6784752698267,645.28999420701,59.6290311800517));
#103264=CARTESIAN_POINT('Ctrl Pts',(-20.3737909654025,646.39670912511,61.3247693565847));
#103265=CARTESIAN_POINT('Ctrl Pts',(-19.4561930076906,646.39670912511,60.6144134200796));
#103266=CARTESIAN_POINT('Ctrl Pts',(-19.5862728598228,645.257848435272,
60.7102226359643));
#103267=CARTESIAN_POINT('Ctrl Pts',(-20.0094816671295,646.39670912511,61.8617135225397));
#103268=CARTESIAN_POINT('Ctrl Pts',(-18.9941367827483,646.39670912511,61.2703174980295));
#103269=CARTESIAN_POINT('Ctrl Pts',(-19.1489700570509,645.244977711044,
61.358094543025));
#103270=CARTESIAN_POINT('Ctrl Pts',(-19.517050215086,646.39670912511,63.0324871423592));
#103271=CARTESIAN_POINT('Ctrl Pts',(-18.3617148294141,646.39670912511,62.7197742154602));
#103272=CARTESIAN_POINT('Ctrl Pts',(-18.5578743722317,645.227580544767,
62.7707392571437));
#103273=CARTESIAN_POINT('Ctrl Pts',(-19.3891218019081,646.39670912511,63.6657417300125));
#103274=CARTESIAN_POINT('Ctrl Pts',(-18.1973682094106,646.39670912511,63.5071737129916));
#103275=CARTESIAN_POINT('Ctrl Pts',(-18.4043140488817,645.223060947511,
63.5348184358976));
#103276=CARTESIAN_POINT('Ctrl Pts',(-19.3891218019059,646.39670912511,64.2994740882088));
#103277=CARTESIAN_POINT('Ctrl Pts',(-18.1973682093116,646.39670912511,64.2994740882088));
#103278=CARTESIAN_POINT('Ctrl Pts',(-18.4043140488937,645.223060947443,
64.2994740882088));
#103279=CARTESIAN_POINT('',(-19.3891218019059,646.39670912511,64.2994740882088));
#103280=CARTESIAN_POINT('',(-29.2194381818547,646.39670912511,64.2994740882088));
#103281=CARTESIAN_POINT('Ctrl Pts',(-19.3891218019059,646.39670912511,64.2994740882088));
#103282=CARTESIAN_POINT('Ctrl Pts',(-19.3891218019081,646.39670912511,63.6657417300125));
#103283=CARTESIAN_POINT('Ctrl Pts',(-19.517050215086,646.39670912511,63.0324871423592));
#103284=CARTESIAN_POINT('Ctrl Pts',(-19.7632659411077,646.39670912511,62.4471003324495));
#103285=CARTESIAN_POINT('Ctrl Pts',(-20.0094816671295,646.39670912511,61.8617135225397));
#103286=CARTESIAN_POINT('Ctrl Pts',(-20.3737909654025,646.39670912511,61.3247693565847));
#103287=CARTESIAN_POINT('Ctrl Pts',(-20.8287383051448,646.39670912511,60.8767336891945));
#103288=CARTESIAN_POINT('Ctrl Pts',(-21.2836856448871,646.39670912511,60.4286980218043));
#103289=CARTESIAN_POINT('Ctrl Pts',(-21.8289130400025,646.39670912511,60.0699234004071));
#103290=CARTESIAN_POINT('Ctrl Pts',(-22.4233303851235,646.39670912511,59.8274482444706));
#103291=CARTESIAN_POINT('Ctrl Pts',(-23.0177477302446,646.39670912511,59.584973088534));
#103292=CARTESIAN_POINT('Ctrl Pts',(-23.6608872937837,646.39670912511,59.4589881954405));
#103293=CARTESIAN_POINT('Ctrl Pts',(-24.3042799918803,646.39670912511,59.4589881954405));
#103294=CARTESIAN_POINT('Ctrl Pts',(-24.9476726899769,646.39670912511,59.4589881954405));
#103295=CARTESIAN_POINT('Ctrl Pts',(-25.590812253516,646.39670912511,59.584973088534));
#103296=CARTESIAN_POINT('Ctrl Pts',(-26.1852295986371,646.39670912511,59.8274482444706));
#103297=CARTESIAN_POINT('Ctrl Pts',(-26.7796469437582,646.39670912511,60.0699234004071));
#103298=CARTESIAN_POINT('Ctrl Pts',(-27.3248743388726,646.39670912511,60.4286980218046));
#103299=CARTESIAN_POINT('Ctrl Pts',(-27.7798216786158,646.39670912511,60.8767336891945));
#103300=CARTESIAN_POINT('Ctrl Pts',(-28.234769018359,646.39670912511,61.3247693565845));
#103301=CARTESIAN_POINT('Ctrl Pts',(-28.5990783166314,646.39670912511,61.8617135225403));
#103302=CARTESIAN_POINT('Ctrl Pts',(-28.8452940426529,646.39670912511,62.4471003324495));
#103303=CARTESIAN_POINT('Ctrl Pts',(-29.0915097686744,646.39670912511,63.0324871423586));
#103304=CARTESIAN_POINT('Ctrl Pts',(-29.2194381818525,646.39670912511,63.6657417300129));
#103305=CARTESIAN_POINT('Ctrl Pts',(-29.2194381818548,646.39670912511,64.2994740882088));
#103306=CARTESIAN_POINT('',(-18.4043140488937,645.223060947443,64.2994740882088));
#103307=CARTESIAN_POINT('Origin',(-19.3891218019059,645.39670912511,64.2994740882088));
#103308=CARTESIAN_POINT('',(-30.204245934867,645.570357302777,64.2994740882088));
#103309=CARTESIAN_POINT('Ctrl Pts',(-30.204245934867,645.570357302777,64.2994740882088));
#103310=CARTESIAN_POINT('Ctrl Pts',(-30.2042459348789,645.570357302709,
63.5348184358982));
#103311=CARTESIAN_POINT('Ctrl Pts',(-30.0506856115286,645.565837705453,
62.7707392571429));
#103312=CARTESIAN_POINT('Ctrl Pts',(-29.45958992671,645.548440539176,61.3580945430258));
#103313=CARTESIAN_POINT('Ctrl Pts',(-29.0222871239381,645.535569814948,
60.7102226359645));
#103314=CARTESIAN_POINT('Ctrl Pts',(-27.9300847139336,645.50342404321,59.6290311800515));
#103315=CARTESIAN_POINT('Ctrl Pts',(-27.275614819367,645.484161643149,59.1961370117062));
#103316=CARTESIAN_POINT('Ctrl Pts',(-25.8485836001921,645.442161168378,
58.6110004122124));
#103317=CARTESIAN_POINT('Ctrl Pts',(-25.0765837225069,645.419439618224,
58.4589881954405));
#103318=CARTESIAN_POINT('Ctrl Pts',(-23.5319762612537,645.373978631996,
58.4589881954405));
#103319=CARTESIAN_POINT('Ctrl Pts',(-22.7599763835685,645.351257081842,
58.6110004122124));
#103320=CARTESIAN_POINT('Ctrl Pts',(-21.3329451643936,645.309256607071,
59.1961370117062));
#103321=CARTESIAN_POINT('Ctrl Pts',(-20.6784752698267,645.28999420701,59.6290311800517));
#103322=CARTESIAN_POINT('Ctrl Pts',(-19.5862728598228,645.257848435272,
60.7102226359643));
#103323=CARTESIAN_POINT('Ctrl Pts',(-19.1489700570509,645.244977711044,
61.358094543025));
#103324=CARTESIAN_POINT('Ctrl Pts',(-18.5578743722317,645.227580544767,
62.7707392571437));
#103325=CARTESIAN_POINT('Ctrl Pts',(-18.4043140488817,645.223060947511,
63.5348184358976));
#103326=CARTESIAN_POINT('Ctrl Pts',(-18.4043140488937,645.223060947443,
64.2994740882088));
#103327=CARTESIAN_POINT('Origin',(-29.2194381818547,645.39670912511,64.2994740882088));
#103328=CARTESIAN_POINT('Origin',(-26.4620031331058,633.159653102509,64.2994740882088));
#103329=CARTESIAN_POINT('',(-31.2678407122057,639.538553970656,64.2994740877864));
#103330=CARTESIAN_POINT('Ctrl Pts',(-19.6604693917099,639.614613618721,
62.5660159449655));
#103331=CARTESIAN_POINT('Ctrl Pts',(-19.7556504099892,639.582567616465,
62.282332691133));
#103332=CARTESIAN_POINT('Ctrl Pts',(-19.8718432110569,639.544021407052,
62.0111775190741));
#103333=CARTESIAN_POINT('Ctrl Pts',(-20.0074654347315,639.500530839039,
61.7514240468761));
#103334=CARTESIAN_POINT('Ctrl Pts',(-20.032231644244,639.492588950976,61.7039900147554));
#103335=CARTESIAN_POINT('Ctrl Pts',(-20.057645885894,639.484482149599,61.6569362630971));
#103336=CARTESIAN_POINT('Ctrl Pts',(-20.0836986773465,639.476219869507,
61.6102560203614));
#103337=CARTESIAN_POINT('Ctrl Pts',(-20.101297793179,639.470638554942,61.5787227007747));
#103338=CARTESIAN_POINT('Ctrl Pts',(-20.1191895721033,639.464985737746,
61.5473576036808));
#103339=CARTESIAN_POINT('Ctrl Pts',(-20.1373704921135,639.459264520637,
61.516159925298));
#103340=CARTESIAN_POINT('Ctrl Pts',(-20.2253501924973,639.43157884979,61.3651905356716));
#103341=CARTESIAN_POINT('Ctrl Pts',(-20.3201686033712,639.402279383082,
61.2181734019715));
#103342=CARTESIAN_POINT('Ctrl Pts',(-20.4217102305742,639.371692235151,
61.0751674764617));
#103343=CARTESIAN_POINT('Ctrl Pts',(-20.4312396758219,639.368821702547,
61.0617467033779));
#103344=CARTESIAN_POINT('Ctrl Pts',(-20.4408283027393,639.365939834986,
61.0483612397612));
#103345=CARTESIAN_POINT('Ctrl Pts',(-20.4504759958362,639.363046905543,
61.0350111227245));
#103346=CARTESIAN_POINT('Ctrl Pts',(-20.5204449471276,639.342066217495,
60.9381907036576));
#103347=CARTESIAN_POINT('Ctrl Pts',(-20.5938065024781,639.320423943129,
60.8429238161653));
#103348=CARTESIAN_POINT('Ctrl Pts',(-20.6698874971932,639.298416870665,
60.7499994453728));
#103349=CARTESIAN_POINT('Ctrl Pts',(-20.7162781708621,639.284997975173,
60.6933384595712));
#103350=CARTESIAN_POINT('Ctrl Pts',(-20.7636535181521,639.271451210823,
60.6375798052197));
#103351=CARTESIAN_POINT('Ctrl Pts',(-20.8118752315682,639.257838908372,
60.5828777103897));
#103352=CARTESIAN_POINT('Ctrl Pts',(-20.9167303497794,639.228239802877,
60.4639314056347));
#103353=CARTESIAN_POINT('Ctrl Pts',(-21.0254306336414,639.198358602934,
60.3499372916202));
#103354=CARTESIAN_POINT('Ctrl Pts',(-21.1379837166309,639.168414488515,
60.2406077607254));
#103355=CARTESIAN_POINT('Ctrl Pts',(-21.252662669507,639.137904798375,60.129213245458));
#103356=CARTESIAN_POINT('Ctrl Pts',(-21.3713413391399,639.107329448174,
60.0226612620548));
#103357=CARTESIAN_POINT('Ctrl Pts',(-21.494062811382,639.076916809791,59.9206887222358));
#103358=CARTESIAN_POINT('Ctrl Pts',(-21.5446960815533,639.064368954002,
59.8786161894965));
#103359=CARTESIAN_POINT('Ctrl Pts',(-21.5960179561576,639.051848786154,
59.8373236768977));
#103360=CARTESIAN_POINT('Ctrl Pts',(-21.6480331481804,639.03937239533,59.7967946409827));
#103361=CARTESIAN_POINT('Ctrl Pts',(-21.7727113592165,639.009467015235,
59.6996482593893));
#103362=CARTESIAN_POINT('Ctrl Pts',(-21.9019771385064,638.979701094277,
59.6066175164186));
#103363=CARTESIAN_POINT('Ctrl Pts',(-22.0351170267143,638.950494813038,
59.5182198819255));
#103364=CARTESIAN_POINT('Ctrl Pts',(-22.0990564322483,638.936468721493,
59.4757675990208));
#103365=CARTESIAN_POINT('Ctrl Pts',(-22.163889678691,638.922571825977,59.4343845095441));
#103366=CARTESIAN_POINT('Ctrl Pts',(-22.2295390374144,638.908851679777,
59.3941319438193));
#103367=CARTESIAN_POINT('Ctrl Pts',(-22.3576108890827,638.882085774319,
59.3156053484799));
#103368=CARTESIAN_POINT('Ctrl Pts',(-22.4883155563332,638.856091013215,
59.2416680648132));
#103369=CARTESIAN_POINT('Ctrl Pts',(-22.6210518826277,638.831204223815,
59.1726911130992));
#103370=CARTESIAN_POINT('Ctrl Pts',(-22.7582179760615,638.805486895519,
59.1014122155458));
#103371=CARTESIAN_POINT('Ctrl Pts',(-22.8975352876073,638.780921855692,
59.0352728308619));
#103372=CARTESIAN_POINT('Ctrl Pts',(-23.0391982842766,638.757684060641,
58.974232786797));
#103373=CARTESIAN_POINT('Ctrl Pts',(-23.07924643566,638.751114732335,58.9569767567635));
#103374=CARTESIAN_POINT('Ctrl Pts',(-23.1194821783114,638.744651545692,
58.9401285470228));
#103375=CARTESIAN_POINT('Ctrl Pts',(-23.159910205694,638.738298632261,58.9236879248849));
#103376=CARTESIAN_POINT('Ctrl Pts',(-23.3335921112647,638.711006029033,
58.8530577515488));
#103377=CARTESIAN_POINT('Ctrl Pts',(-23.5106709624866,638.685770612436,
58.7900097568909));
#103378=CARTESIAN_POINT('Ctrl Pts',(-23.6913019668401,638.662951844834,
58.7345974353322));
#103379=CARTESIAN_POINT('Ctrl Pts',(-23.8453703780755,638.643488678566,
58.6873337422804));
#103380=CARTESIAN_POINT('Ctrl Pts',(-24.0027408049985,638.625730877479,
58.6455484140267));
#103381=CARTESIAN_POINT('Ctrl Pts',(-24.1612188560548,638.610135581286,
58.6099678299653));
#103382=CARTESIAN_POINT('Ctrl Pts',(-24.1934780298083,638.606961063639,
58.6027251850954));
#103383=CARTESIAN_POINT('Ctrl Pts',(-24.2257795091491,638.603876337104,
58.5957405138027));
#103384=CARTESIAN_POINT('Ctrl Pts',(-24.2581039558078,638.600885318481,
58.5890200208385));
#103385=CARTESIAN_POINT('Ctrl Pts',(-24.4490665789934,638.583215324987,
58.5493174706578));
#103386=CARTESIAN_POINT('Ctrl Pts',(-24.6409245786182,638.568764510727,
58.5186878559351));
#103387=CARTESIAN_POINT('Ctrl Pts',(-24.8336179601762,638.557716475292,
58.4971174009262));
#103388=CARTESIAN_POINT('Ctrl Pts',(-24.956409356204,638.550676255833,58.4833719040021));
#103389=CARTESIAN_POINT('Ctrl Pts',(-25.0797134668603,638.545021125185,
58.4732899575493));
#103390=CARTESIAN_POINT('Ctrl Pts',(-25.2033487449366,638.540792331728,
58.4669566006054));
#103391=CARTESIAN_POINT('Ctrl Pts',(-25.3294688219745,638.536478548761,
58.4604959570246));
#103392=CARTESIAN_POINT('Ctrl Pts',(-25.4559981094795,638.533643884368,
58.457928470776));
#103393=CARTESIAN_POINT('Ctrl Pts',(-25.582949758537,638.532336794653,58.4593676132319));
#103394=CARTESIAN_POINT('Ctrl Pts',(-25.6324008606534,638.531827647844,
58.4599281981559));
#103395=CARTESIAN_POINT('Ctrl Pts',(-25.681916058785,638.531550479522,58.4610972295894));
#103396=CARTESIAN_POINT('Ctrl Pts',(-25.7314961026847,638.531508928283,
58.4628834273625));
#103397=CARTESIAN_POINT('Ctrl Pts',(-25.8208733205009,638.531434024473,
58.4661033798851));
#103398=CARTESIAN_POINT('Ctrl Pts',(-25.9103675409668,638.532125410603,
58.4713269333322));
#103399=CARTESIAN_POINT('Ctrl Pts',(-25.9998450012477,638.533598565417,
58.4785846158281));
#103400=CARTESIAN_POINT('Ctrl Pts',(-26.0874286185417,638.535040540045,
58.4856886852124));
#103401=CARTESIAN_POINT('Ctrl Pts',(-26.1744866897434,638.537216683504,
58.4946845281867));
#103402=CARTESIAN_POINT('Ctrl Pts',(-26.260956425424,638.54010194845,58.5055543459801));
#103403=CARTESIAN_POINT('Ctrl Pts',(-26.4140421982678,638.545210013261,
58.5247982403261));
#103404=CARTESIAN_POINT('Ctrl Pts',(-26.5656810056143,638.552564467409,
58.5499668723704));
#103405=CARTESIAN_POINT('Ctrl Pts',(-26.7157330220559,638.562036190887,
58.5810246871823));
#103406=CARTESIAN_POINT('Ctrl Pts',(-26.858938066883,638.571075713429,58.6106653135986));
#103407=CARTESIAN_POINT('Ctrl Pts',(-27.0006979484278,638.582043429483,
58.6456695550396));
#103408=CARTESIAN_POINT('Ctrl Pts',(-27.1409029558934,638.594812782266,
58.6859663162781));
#103409=CARTESIAN_POINT('Ctrl Pts',(-27.1893002543444,638.599220628953,
58.699876335724));
#103410=CARTESIAN_POINT('Ctrl Pts',(-27.2375765636139,638.603856450057,
58.7144595173002));
#103411=CARTESIAN_POINT('Ctrl Pts',(-27.2856852257159,638.608706436981,
58.7296967699079));
#103412=CARTESIAN_POINT('Ctrl Pts',(-27.415223027167,638.621765553902,58.7707247286313));
#103413=CARTESIAN_POINT('Ctrl Pts',(-27.5439630743014,638.636437015089,
58.8166317822243));
#103414=CARTESIAN_POINT('Ctrl Pts',(-27.6709204151557,638.652471757745,
58.8670909282801));
#103415=CARTESIAN_POINT('Ctrl Pts',(-27.7999621376017,638.668769758297,
58.9183785109941));
#103416=CARTESIAN_POINT('Ctrl Pts',(-27.9271607180627,638.686475807047,
58.974368497831));
#103417=CARTESIAN_POINT('Ctrl Pts',(-28.0514926947167,638.705312224822,
59.0346686070573));
#103418=CARTESIAN_POINT('Ctrl Pts',(-28.106553485054,638.713653989167,59.0613726920464));
#103419=CARTESIAN_POINT('Ctrl Pts',(-28.1610523512498,638.722217263826,
59.0889214729824));
#103420=CARTESIAN_POINT('Ctrl Pts',(-28.2149021938079,638.730977240033,
59.1172782101099));
#103421=CARTESIAN_POINT('Ctrl Pts',(-28.2278313024328,638.733080471511,
59.1240865370642));
#103422=CARTESIAN_POINT('Ctrl Pts',(-28.2407267529919,638.735194947273,
59.1309410998825));
#103423=CARTESIAN_POINT('Ctrl Pts',(-28.2535884192766,638.737320402262,
59.1378417863349));
#103424=CARTESIAN_POINT('Ctrl Pts',(-28.5599916610745,638.787955077793,
59.3022367140878));
#103425=CARTESIAN_POINT('Ctrl Pts',(-28.8480542326587,638.844955355957,
59.4932554983916));
#103426=CARTESIAN_POINT('Ctrl Pts',(-29.1182177859427,638.905258731902,
59.7110768906355));
#103427=CARTESIAN_POINT('Ctrl Pts',(-29.1344578639101,638.908883689877,
59.7241705753683));
#103428=CARTESIAN_POINT('Ctrl Pts',(-29.1506332937596,638.912520616295,
59.7373611342055));
#103429=CARTESIAN_POINT('Ctrl Pts',(-29.1667441676304,638.916168843431,
59.7506486031058));
#103430=CARTESIAN_POINT('Ctrl Pts',(-29.3144417784627,638.949614231696,
59.8724624430206));
#103431=CARTESIAN_POINT('Ctrl Pts',(-29.4573274362203,638.984191717442,
60.0032376747088));
#103432=CARTESIAN_POINT('Ctrl Pts',(-29.5918674028682,639.018481680813,
60.1396878642134));
#103433=CARTESIAN_POINT('Ctrl Pts',(-29.6867899181019,639.042674414403,
60.2359581065406));
#103434=CARTESIAN_POINT('Ctrl Pts',(-29.7778370811571,639.066776771326,
60.3352163695295));
#103435=CARTESIAN_POINT('Ctrl Pts',(-29.8651104143972,639.09060876673,60.4374188246835));
#103436=CARTESIAN_POINT('Ctrl Pts',(-29.9015533966364,639.100560363088,
60.4800958042338));
#103437=CARTESIAN_POINT('Ctrl Pts',(-29.9373294444809,639.110462869717,
60.5232757287555));
#103438=CARTESIAN_POINT('Ctrl Pts',(-29.9724503412504,639.120304145742,
60.5669591429136));
#103439=CARTESIAN_POINT('Ctrl Pts',(-30.0771776841521,639.149649942222,
60.6972191395098));
#103440=CARTESIAN_POINT('Ctrl Pts',(-30.1762070237057,639.178479714589,
60.8320715218747));
#103441=CARTESIAN_POINT('Ctrl Pts',(-30.2694728974752,639.206447349291,
60.9715318367259));
#103442=CARTESIAN_POINT('Ctrl Pts',(-30.3375768093777,639.22686966726,61.0733675094394));
#103443=CARTESIAN_POINT('Ctrl Pts',(-30.4026067951602,639.246832284511,
61.1776608748026));
#103444=CARTESIAN_POINT('Ctrl Pts',(-30.4645235373007,639.266198028526,
61.284428590957));
#103445=CARTESIAN_POINT('Ctrl Pts',(-30.5108974286489,639.280702423908,
61.3643945952601));
#103446=CARTESIAN_POINT('Ctrl Pts',(-30.5555184235738,639.294872545955,
61.4457413550946));
#103447=CARTESIAN_POINT('Ctrl Pts',(-30.598331303557,639.308639388708,61.5284018708633));
#103448=CARTESIAN_POINT('Ctrl Pts',(-30.636366414163,639.320869899411,61.6018377588772));
#103449=CARTESIAN_POINT('Ctrl Pts',(-30.6727477715507,639.332705897609,
61.6758548871431));
#103450=CARTESIAN_POINT('Ctrl Pts',(-30.7074777887601,639.344119541394,
61.7504116450392));
#103451=CARTESIAN_POINT('Ctrl Pts',(-30.7813004242086,639.368380550517,
61.9088905863311));
#103452=CARTESIAN_POINT('Ctrl Pts',(-30.8477744207413,639.390757120824,
62.0700388044301));
#103453=CARTESIAN_POINT('Ctrl Pts',(-30.9070565975758,639.411020592166,
62.2338230900162));
#103454=CARTESIAN_POINT('Ctrl Pts',(-30.9505698013699,639.425894009526,
62.3540409932298));
#103455=CARTESIAN_POINT('Ctrl Pts',(-30.9901926242488,639.439629706583,
62.4756348854126));
#103456=CARTESIAN_POINT('Ctrl Pts',(-31.0260078756452,639.452145446073,
62.598642517993));
#103457=CARTESIAN_POINT('Ctrl Pts',(-31.0749693290293,639.469255162511,
62.7668008369673));
#103458=CARTESIAN_POINT('Ctrl Pts',(-31.116758386068,639.484088469113,62.9376198059619));
#103459=CARTESIAN_POINT('Ctrl Pts',(-31.1512286201053,639.496418452856,
63.1113174708579));
#103460=CARTESIAN_POINT('Ctrl Pts',(-31.1546163045033,639.497630225701,
63.128388224387));
#103461=CARTESIAN_POINT('Ctrl Pts',(-31.157933261746,639.498817806503,63.1454867960826));
#103462=CARTESIAN_POINT('Ctrl Pts',(-31.1611793284332,639.499980970938,
63.1626134020239));
#103463=CARTESIAN_POINT('Ctrl Pts',(-31.1665764304226,639.501914916752,
63.1910891075168));
#103464=CARTESIAN_POINT('Ctrl Pts',(-31.1717730915779,639.503779752154,
63.2196340647483));
#103465=CARTESIAN_POINT('Ctrl Pts',(-31.1767679222504,639.505574492154,
63.2482357712307));
#103466=CARTESIAN_POINT('Ctrl Pts',(-31.205332312064,639.515838234079,63.4118029363383));
#103467=CARTESIAN_POINT('Ctrl Pts',(-31.2272400925891,639.523787147066,
63.5768839956324));
#103468=CARTESIAN_POINT('Ctrl Pts',(-31.2422935239496,639.529260134671,
63.741146664961));
#103469=CARTESIAN_POINT('Ctrl Pts',(-31.2580716979021,639.534996617496,
63.913317707462));
#103470=CARTESIAN_POINT('Ctrl Pts',(-31.2665570468194,639.538079648504,
64.0854433189719));
#103471=CARTESIAN_POINT('Ctrl Pts',(-31.2677422818647,639.538509777967,
64.2576679511823));
#103472=CARTESIAN_POINT('Ctrl Pts',(-31.2678381792997,639.538544579767,
64.2716026559762));
#103473=CARTESIAN_POINT('Ctrl Pts',(-31.2678862604399,639.538562004858,
64.2855380090525));
#103474=CARTESIAN_POINT('Ctrl Pts',(-31.2678865073884,639.538562048433,
64.2994740869496));
#103475=CARTESIAN_POINT('',(-32.2137589216624,634.173842834478,64.2994740882088));
#103476=CARTESIAN_POINT('Ctrl Pts',(-18.4043140488937,645.223060947443,
64.2994740882088));
#103477=CARTESIAN_POINT('Ctrl Pts',(-18.4043140488817,645.223060947511,
65.0641297405231));
#103478=CARTESIAN_POINT('Ctrl Pts',(-18.55787437223,645.227580544767,65.8282089192698));
#103479=CARTESIAN_POINT('Ctrl Pts',(-19.1489700570526,645.244977711044,
67.2408536333967));
#103480=CARTESIAN_POINT('Ctrl Pts',(-19.5862728598217,645.257848435272,
67.8887255404523));
#103481=CARTESIAN_POINT('Ctrl Pts',(-20.6784752698278,645.28999420701,68.969916996367));
#103482=CARTESIAN_POINT('Ctrl Pts',(-21.3329451643959,645.309256607072,
69.4028111647124));
#103483=CARTESIAN_POINT('Ctrl Pts',(-22.7599763835661,645.351257081842,
69.9879477642043));
#103484=CARTESIAN_POINT('Ctrl Pts',(-23.5319762612528,645.373978631996,
70.1399599809771));
#103485=CARTESIAN_POINT('Ctrl Pts',(-25.0765837225078,645.419439618224,
70.1399599809771));
#103486=CARTESIAN_POINT('Ctrl Pts',(-25.8485836001935,645.442161168379,
69.9879477642046));
#103487=CARTESIAN_POINT('Ctrl Pts',(-27.2756148193656,645.484161643148,
69.402811164712));
#103488=CARTESIAN_POINT('Ctrl Pts',(-27.9300847139356,645.50342404321,68.9699169963641));
#103489=CARTESIAN_POINT('Ctrl Pts',(-29.0222871239361,645.535569814948,
67.8887255404551));
#103490=CARTESIAN_POINT('Ctrl Pts',(-29.4595899267082,645.548440539176,
67.2408536333963));
#103491=CARTESIAN_POINT('Ctrl Pts',(-30.0506856115305,645.565837705453,
65.8282089192702));
#103492=CARTESIAN_POINT('Ctrl Pts',(-30.2042459348789,645.570357302709,
65.0641297405228));
#103493=CARTESIAN_POINT('Ctrl Pts',(-30.204245934867,645.570357302777,64.2994740882088));
#103494=CARTESIAN_POINT('Ctrl Pts',(-31.2678163619919,639.53854967554,64.2994740882313));
#103495=CARTESIAN_POINT('Ctrl Pts',(-31.2678163619908,639.53854967554,64.5926872821248));
#103496=CARTESIAN_POINT('Ctrl Pts',(-31.2468826932858,639.530860720871,
64.885924677304));
#103497=CARTESIAN_POINT('Ctrl Pts',(-31.1615715333149,639.500058690408,
65.4724494968625));
#103498=CARTESIAN_POINT('Ctrl Pts',(-31.0977211744434,639.477145594786,
65.7607708453645));
#103499=CARTESIAN_POINT('Ctrl Pts',(-31.0141476947143,639.44800149248,66.0405185693756));
#103500=CARTESIAN_POINT('Origin',(-33.3604437899019,646.39670912511,26.2994740882088));
#103501=CARTESIAN_POINT('Ctrl Pts',(-29.2194381818547,646.39670912511,64.2994740882088));
#103502=CARTESIAN_POINT('Ctrl Pts',(-29.2194381818525,646.39670912511,64.9332064464068));
#103503=CARTESIAN_POINT('Ctrl Pts',(-29.0915097686747,646.39670912511,65.5664610340562));
#103504=CARTESIAN_POINT('Ctrl Pts',(-28.8452940426529,646.39670912511,66.1518478439682));
#103505=CARTESIAN_POINT('Ctrl Pts',(-28.5990783166312,646.39670912511,66.7372346538801));
#103506=CARTESIAN_POINT('Ctrl Pts',(-28.2347690183583,646.39670912511,67.2741788198361));
#103507=CARTESIAN_POINT('Ctrl Pts',(-27.7798216786158,646.39670912511,67.7222144872231));
#103508=CARTESIAN_POINT('Ctrl Pts',(-27.3248743388734,646.39670912511,68.1702501546101));
#103509=CARTESIAN_POINT('Ctrl Pts',(-26.779646943758,646.39670912511,68.529024776011));
#103510=CARTESIAN_POINT('Ctrl Pts',(-26.1852295986371,646.39670912511,68.7714999319471));
#103511=CARTESIAN_POINT('Ctrl Pts',(-25.5908122535162,646.39670912511,69.0139750878831));
#103512=CARTESIAN_POINT('Ctrl Pts',(-24.9476726899776,646.39670912511,69.1399599809771));
#103513=CARTESIAN_POINT('Ctrl Pts',(-24.3042799918803,646.39670912511,69.1399599809771));
#103514=CARTESIAN_POINT('Ctrl Pts',(-23.660887293783,646.39670912511,69.1399599809771));
#103515=CARTESIAN_POINT('Ctrl Pts',(-23.0177477302444,646.39670912511,69.0139750878831));
#103516=CARTESIAN_POINT('Ctrl Pts',(-22.4233303851235,646.39670912511,68.771499931947));
#103517=CARTESIAN_POINT('Ctrl Pts',(-21.8289130400026,646.39670912511,68.529024776011));
#103518=CARTESIAN_POINT('Ctrl Pts',(-21.2836856448871,646.39670912511,68.1702501546155));
#103519=CARTESIAN_POINT('Ctrl Pts',(-20.8287383051448,646.39670912511,67.7222144872231));
#103520=CARTESIAN_POINT('Ctrl Pts',(-20.3737909654025,646.39670912511,67.2741788198307));
#103521=CARTESIAN_POINT('Ctrl Pts',(-20.0094816671294,646.39670912511,66.7372346538801));
#103522=CARTESIAN_POINT('Ctrl Pts',(-19.7632659411077,646.39670912511,66.1518478439682));
#103523=CARTESIAN_POINT('Ctrl Pts',(-19.517050215086,646.39670912511,65.5664610340562));
#103524=CARTESIAN_POINT('Ctrl Pts',(-19.3891218019081,646.39670912511,64.9332064464068));
#103525=CARTESIAN_POINT('Ctrl Pts',(-19.3891218019059,646.39670912511,64.2994740882088));
#103526=CARTESIAN_POINT('Ctrl Pts',(-19.3891218019059,646.39670912511,64.2994740882088));
#103527=CARTESIAN_POINT('Ctrl Pts',(-18.1973682093116,646.39670912511,64.2994740882088));
#103528=CARTESIAN_POINT('Ctrl Pts',(-18.4043140488937,645.223060947443,
64.2994740882088));
#103529=CARTESIAN_POINT('Ctrl Pts',(-19.3891218019081,646.39670912511,64.9332064464068));
#103530=CARTESIAN_POINT('Ctrl Pts',(-18.1973682094106,646.39670912511,65.0917744634339));
#103531=CARTESIAN_POINT('Ctrl Pts',(-18.4043140488817,645.223060947511,
65.0641297405231));
#103532=CARTESIAN_POINT('Ctrl Pts',(-19.517050215086,646.39670912511,65.5664610340562));
#103533=CARTESIAN_POINT('Ctrl Pts',(-18.3617148294095,646.39670912511,65.8791739609459));
#103534=CARTESIAN_POINT('Ctrl Pts',(-18.55787437223,645.227580544767,65.8282089192698));
#103535=CARTESIAN_POINT('Ctrl Pts',(-20.0094816671294,646.39670912511,66.7372346538801));
#103536=CARTESIAN_POINT('Ctrl Pts',(-18.9941367827525,646.39670912511,67.3286306783986));
#103537=CARTESIAN_POINT('Ctrl Pts',(-19.1489700570526,645.244977711044,
67.2408536333967));
#103538=CARTESIAN_POINT('Ctrl Pts',(-20.3737909654025,646.39670912511,67.2741788198307));
#103539=CARTESIAN_POINT('Ctrl Pts',(-19.4561930076916,646.39670912511,67.984534756338));
#103540=CARTESIAN_POINT('Ctrl Pts',(-19.5862728598217,645.257848435272,
67.8887255404523));
#103541=CARTESIAN_POINT('Ctrl Pts',(-21.2836856448871,646.39670912511,68.1702501546155));
#103542=CARTESIAN_POINT('Ctrl Pts',(-20.6031006941251,646.39670912511,69.0621896001028));
#103543=CARTESIAN_POINT('Ctrl Pts',(-20.6784752698278,645.28999420701,68.969916996367));
#103544=CARTESIAN_POINT('Ctrl Pts',(-21.8289130400026,646.39670912511,68.529024776011));
#103545=CARTESIAN_POINT('Ctrl Pts',(-21.2802434100837,646.39670912511,69.4841561744855));
#103546=CARTESIAN_POINT('Ctrl Pts',(-21.3329451643959,645.309256607072,
69.4028111647124));
#103547=CARTESIAN_POINT('Ctrl Pts',(-23.0177477302444,646.39670912511,69.0139750878831));
#103548=CARTESIAN_POINT('Ctrl Pts',(-22.7425774139599,646.39670912511,70.0319693513056));
#103549=CARTESIAN_POINT('Ctrl Pts',(-22.7599763835661,645.351257081842,
69.9879477642043));
#103550=CARTESIAN_POINT('Ctrl Pts',(-23.660887293783,646.39670912511,69.1399599809771));
#103551=CARTESIAN_POINT('Ctrl Pts',(-23.5230979344017,646.39670912511,70.1629517811265));
#103552=CARTESIAN_POINT('Ctrl Pts',(-23.5319762612528,645.373978631996,
70.1399599809771));
#103553=CARTESIAN_POINT('Ctrl Pts',(-24.9476726899776,646.39670912511,69.1399599809771));
#103554=CARTESIAN_POINT('Ctrl Pts',(-25.0679049368901,646.39670912511,70.1174849228819));
#103555=CARTESIAN_POINT('Ctrl Pts',(-25.0765837225078,645.419439618224,
70.1399599809771));
#103556=CARTESIAN_POINT('Ctrl Pts',(-25.5908122535162,646.39670912511,69.0139750878831));
#103557=CARTESIAN_POINT('Ctrl Pts',(-25.832528214473,646.39670912511,69.9473649702541));
#103558=CARTESIAN_POINT('Ctrl Pts',(-25.8485836001935,645.442161168379,
69.9879477642046));
#103559=CARTESIAN_POINT('Ctrl Pts',(-26.779646943758,646.39670912511,68.529024776011));
#103560=CARTESIAN_POINT('Ctrl Pts',(-27.2309350653711,646.39670912511,69.3342934556171));
#103561=CARTESIAN_POINT('Ctrl Pts',(-27.2756148193656,645.484161643148,
69.402811164712));
#103562=CARTESIAN_POINT('Ctrl Pts',(-27.3248743388734,646.39670912511,68.1702501546101));
#103563=CARTESIAN_POINT('Ctrl Pts',(-27.8689763870033,646.39670912511,68.8953702631505));
#103564=CARTESIAN_POINT('Ctrl Pts',(-27.9300847139356,645.50342404321,68.9699169963641));
#103565=CARTESIAN_POINT('Ctrl Pts',(-28.2347690183583,646.39670912511,67.2741788198361));
#103566=CARTESIAN_POINT('Ctrl Pts',(-28.9235388845863,646.39670912511,67.8163374818037));
#103567=CARTESIAN_POINT('Ctrl Pts',(-29.0222871239361,645.535569814948,
67.8887255404551));
#103568=CARTESIAN_POINT('Ctrl Pts',(-28.5990783166312,646.39670912511,66.7372346538801));
#103569=CARTESIAN_POINT('Ctrl Pts',(-29.3454369712419,646.39670912511,67.1763037368409));
#103570=CARTESIAN_POINT('Ctrl Pts',(-29.4595899267082,645.548440539176,
67.2408536333963));
#103571=CARTESIAN_POINT('Ctrl Pts',(-29.0915097686747,646.39670912511,65.5664610340562));
#103572=CARTESIAN_POINT('Ctrl Pts',(-29.9111456379665,646.39670912511,65.7921343507568));
#103573=CARTESIAN_POINT('Ctrl Pts',(-30.0506856115305,645.565837705453,
65.8282089192702));
#103574=CARTESIAN_POINT('Ctrl Pts',(-29.2194381818525,646.39670912511,64.9332064464067));
#103575=CARTESIAN_POINT('Ctrl Pts',(-30.058537813076,646.39670912511,65.04472225858));
#103576=CARTESIAN_POINT('Ctrl Pts',(-30.2042459348789,645.570357302709,
65.0641297405228));
#103577=CARTESIAN_POINT('Ctrl Pts',(-29.2194381818547,646.39670912511,64.2994740882088));
#103578=CARTESIAN_POINT('Ctrl Pts',(-30.058537813032,646.39670912511,64.2994740882088));
#103579=CARTESIAN_POINT('Ctrl Pts',(-30.204245934867,645.570357302777,64.2994740882088));
#103580=CARTESIAN_POINT('Origin',(-48.,620.675373764374,64.2994740882088));
#103581=CARTESIAN_POINT('Ctrl Pts',(-2.31092134190293,635.230245103769,
51.3976052199539));
#103582=CARTESIAN_POINT('Ctrl Pts',(-1.92439042612671,635.165593126578,
51.3246699561202));
#103583=CARTESIAN_POINT('Ctrl Pts',(-1.53337526906528,635.116006409181,
51.2697641942075));
#103584=CARTESIAN_POINT('Ctrl Pts',(-1.1377271716918,635.083088344485,51.2334761581173));
#103585=CARTESIAN_POINT('Ctrl Pts',(-1.10108396587682,635.080039616517,
51.2301153180579));
#103586=CARTESIAN_POINT('Ctrl Pts',(-1.06440101541229,635.077133844473,
51.2269141451115));
#103587=CARTESIAN_POINT('Ctrl Pts',(-1.02767819909564,635.074372288393,
51.223873088555));
#103588=CARTESIAN_POINT('Ctrl Pts',(-1.02189271947806,635.07393722028,51.2233939866645));
#103589=CARTESIAN_POINT('Ctrl Pts',(-1.0161058148073,635.073505788182,51.2229189177151));
#103590=CARTESIAN_POINT('Ctrl Pts',(-1.01031752097321,635.07307799376,51.2224478826357));
#103591=CARTESIAN_POINT('Ctrl Pts',(-0.769279298802908,635.055263623935,
51.2028328697539));
#103592=CARTESIAN_POINT('Ctrl Pts',(-0.525719603099018,635.043759102955,
51.1902149545465));
#103593=CARTESIAN_POINT('Ctrl Pts',(-0.282374958370322,635.038699233314,
51.1846774469337));
#103594=CARTESIAN_POINT('Ctrl Pts',(-0.0944016631441944,635.034790701155,
51.180399959938));
#103595=CARTESIAN_POINT('Ctrl Pts',(0.093442328449993,635.034726965756,
51.1803465302695));
#103596=CARTESIAN_POINT('Ctrl Pts',(0.279895468563292,635.038555816393,
51.1845398016811));
#103597=CARTESIAN_POINT('Ctrl Pts',(0.291911936050454,635.038802576835,
51.1848100481867));
#103598=CARTESIAN_POINT('Ctrl Pts',(0.303924672822358,635.039065220646,
51.1850974258479));
#103599=CARTESIAN_POINT('Ctrl Pts',(0.315933663727289,635.039343708228,
51.1854019212719));
#103600=CARTESIAN_POINT('Ctrl Pts',(0.743857359011281,635.049267226064,
51.1962521923799));
#103601=CARTESIAN_POINT('Ctrl Pts',(1.16718217071826,635.079312657792,51.2288431932868));
#103602=CARTESIAN_POINT('Ctrl Pts',(1.58621543213723,635.127765019396,51.2826473556403));
#103603=CARTESIAN_POINT('Ctrl Pts',(2.0052486935562,635.176217381,51.3364515179938));
#103604=CARTESIAN_POINT('Ctrl Pts',(2.41999047219474,635.243076943181,51.4114688925647));
#103605=CARTESIAN_POINT('Ctrl Pts',(2.83074822463683,635.326669258824,51.5072092257538));
#103606=CARTESIAN_POINT('Ctrl Pts',(2.8531115207118,635.331220359061,51.5124217126873));
#103607=CARTESIAN_POINT('Ctrl Pts',(2.8754606313574,635.335821069522,51.5176966435968));
#103608=CARTESIAN_POINT('Ctrl Pts',(2.89779414296658,635.340470518694,51.5230334110954));
#103609=CARTESIAN_POINT('Ctrl Pts',(3.2059760252613,635.404628633299,51.5966758853225));
#103610=CARTESIAN_POINT('Ctrl Pts',(3.51096003017398,635.478035219308,51.682057065885));
#103611=CARTESIAN_POINT('Ctrl Pts',(3.80902312884625,635.558364152402,51.7775305592728));
#103612=CARTESIAN_POINT('Ctrl Pts',(3.89243156637124,635.580842986002,51.804247368378));
#103613=CARTESIAN_POINT('Ctrl Pts',(3.9752983018007,635.603864039638,51.8317545824764));
#103614=CARTESIAN_POINT('Ctrl Pts',(4.05754235020458,635.627376688186,51.8600163602557));
#103615=CARTESIAN_POINT('Ctrl Pts',(4.08324888549469,635.634725897538,51.8688499768146));
#103616=CARTESIAN_POINT('Ctrl Pts',(4.10890664396029,635.642125363381,51.8777598513787));
#103617=CARTESIAN_POINT('Ctrl Pts',(4.13451596947741,635.649574255906,51.8867457715323));
#103618=CARTESIAN_POINT('Ctrl Pts',(4.42402771911023,635.733783498605,51.9883310110177));
#103619=CARTESIAN_POINT('Ctrl Pts',(4.70743818545356,635.824338401075,52.099671909975));
#103620=CARTESIAN_POINT('Ctrl Pts',(4.98507049296477,635.919988661691,52.2203911200408));
#103621=CARTESIAN_POINT('Ctrl Pts',(5.06347338651508,635.947000133333,52.2544820205599));
#103622=CARTESIAN_POINT('Ctrl Pts',(5.14141563710596,635.974417869963,52.2893205600875));
#103623=CARTESIAN_POINT('Ctrl Pts',(5.21890487245677,636.002213564635,52.3248976144886));
#103624=CARTESIAN_POINT('Ctrl Pts',(5.24645122189637,636.01209454894,52.3375447643556));
#103625=CARTESIAN_POINT('Ctrl Pts',(5.27394681459041,636.022026291278,52.3502900634043));
#103626=CARTESIAN_POINT('Ctrl Pts',(5.30139053208206,636.032007124586,52.3631325099365));
#103627=CARTESIAN_POINT('Ctrl Pts',(5.66366362029753,636.163759949502,52.5326602995614));
#103628=CARTESIAN_POINT('Ctrl Pts',(6.01738163217709,636.304261509107,52.7193702986017));
#103629=CARTESIAN_POINT('Ctrl Pts',(6.36015875743509,636.449853171429,52.9212117806643));
#103630=CARTESIAN_POINT('Ctrl Pts',(6.6668495712861,636.58011748056,53.1018041359916));
#103631=CARTESIAN_POINT('Ctrl Pts',(6.96478180978636,636.714455521892,53.294508596502));
#103632=CARTESIAN_POINT('Ctrl Pts',(7.252286828916,636.850261023332,53.4978360667219));
#103633=CARTESIAN_POINT('Ctrl Pts',(7.286115672764,636.866240372548,53.5217602864134));
#103634=CARTESIAN_POINT('Ctrl Pts',(7.31980020593987,636.882240065713,53.5458315632047));
#103635=CARTESIAN_POINT('Ctrl Pts',(7.3533377524904,636.89825588133,53.5700474603553));
#103636=CARTESIAN_POINT('Ctrl Pts',(7.38103000654088,636.911480284439,53.5900427445943));
#103637=CARTESIAN_POINT('Ctrl Pts',(7.40863101404073,636.924718513479,53.6101387611507));
#103638=CARTESIAN_POINT('Ctrl Pts',(7.43614101292839,636.937969405349,53.6303357171611));
#103639=CARTESIAN_POINT('Ctrl Pts',(7.75229632205443,637.090253665066,53.8624467723794));
#103640=CARTESIAN_POINT('Ctrl Pts',(8.05648904258589,637.244211023545,54.1078905944875));
#103641=CARTESIAN_POINT('Ctrl Pts',(8.34929453939061,637.398218046919,54.367192659054));
#103642=CARTESIAN_POINT('Ctrl Pts',(8.64210003619533,637.552225070293,54.6264947236205));
#103643=CARTESIAN_POINT('Ctrl Pts',(8.92351801894892,637.706282566528,54.8996548343145));
#103644=CARTESIAN_POINT('Ctrl Pts',(9.19408464066941,637.858782543927,55.1872316250658));
#103645=CARTESIAN_POINT('Ctrl Pts',(9.21816683588506,637.872356037223,55.2128278363439));
#103646=CARTESIAN_POINT('Ctrl Pts',(9.24215653499201,637.885914773942,55.2385359314635));
#103647=CARTESIAN_POINT('Ctrl Pts',(9.26605121704551,637.899456160225,55.264352878163));
#103648=CARTESIAN_POINT('Ctrl Pts',(9.44919177119536,638.003243981389,55.4622266106705));
#103649=CARTESIAN_POINT('Ctrl Pts',(9.62656991923521,638.105909953643,55.6662959234571));
#103650=CARTESIAN_POINT('Ctrl Pts',(9.79718029221805,638.206352078217,55.875291238877));
#103651=CARTESIAN_POINT('Ctrl Pts',(9.86608440420505,638.246917462835,55.9596978102167));
#103652=CARTESIAN_POINT('Ctrl Pts',(9.93388438713161,638.287120177701,56.0449084297527));
#103653=CARTESIAN_POINT('Ctrl Pts',(10.0005127777516,638.326887615128,56.1308414745918));
#103654=CARTESIAN_POINT('Ctrl Pts',(10.0215035613001,638.339416053284,56.1579140472159));
#103655=CARTESIAN_POINT('Ctrl Pts',(10.042387340134,638.351906539481,56.1850678260703));
#103656=CARTESIAN_POINT('Ctrl Pts',(10.0631644425131,638.3643584128,56.2123033808313));
#103657=CARTESIAN_POINT('Ctrl Pts',(10.2934195924269,638.502352051449,56.5141321262486));
#103658=CARTESIAN_POINT('Ctrl Pts',(10.5104654401652,638.635528067867,56.8258408735637));
#103659=CARTESIAN_POINT('Ctrl Pts',(10.7144165406335,638.762815059803,57.1477632880394));
#103660=CARTESIAN_POINT('Ctrl Pts',(10.7319264752442,638.773743105302,57.1754014837356));
#103661=CARTESIAN_POINT('Ctrl Pts',(10.7493409367416,638.78462813815,57.2031141332604));
#103662=CARTESIAN_POINT('Ctrl Pts',(10.7666595412329,638.795469398194,57.230901767464));
#103663=CARTESIAN_POINT('Ctrl Pts',(10.9204731636551,638.891755070628,57.477695132226));
#103664=CARTESIAN_POINT('Ctrl Pts',(11.0666558808102,638.984520457955,57.7302247072842));
#103665=CARTESIAN_POINT('Ctrl Pts',(11.2050607147562,639.073307885872,57.9890220210292));
#103666=CARTESIAN_POINT('Ctrl Pts',(11.3377551216451,639.158432044838,58.2371416500389));
#103667=CARTESIAN_POINT('Ctrl Pts',(11.4633001687123,639.239900016211,58.4910223940965));
#103668=CARTESIAN_POINT('Ctrl Pts',(11.5815311313975,639.317292073406,58.75115916475));
#103669=CARTESIAN_POINT('Ctrl Pts',(11.6797499746333,639.381584524053,58.9672644227669));
#103670=CARTESIAN_POINT('Ctrl Pts',(11.772920633671,639.443063906455,59.1876875040297));
#103671=CARTESIAN_POINT('Ctrl Pts',(11.8609291144948,639.501478257648,59.4127277678694));
#103672=CARTESIAN_POINT('Ctrl Pts',(11.8711982768748,639.508294265061,59.4389863169294));
#103673=CARTESIAN_POINT('Ctrl Pts',(11.8813850119675,639.515060403206,59.4652785322609));
#103674=CARTESIAN_POINT('Ctrl Pts',(11.8914892131512,639.52177641536,59.4916044497248));
#103675=CARTESIAN_POINT('Ctrl Pts',(11.9959186669105,639.59118808561,59.763689410277));
#103676=CARTESIAN_POINT('Ctrl Pts',(12.0913107765294,639.655087543383,60.0387465906077));
#103677=CARTESIAN_POINT('Ctrl Pts',(12.1776505788846,639.713252624643,60.3167757884058));
#103678=CARTESIAN_POINT('Ctrl Pts',(12.2628096616696,639.770622283075,60.5910028635912));
#103679=CARTESIAN_POINT('Ctrl Pts',(12.3391623321398,639.822413503614,60.8681213879122));
#103680=CARTESIAN_POINT('Ctrl Pts',(12.4066531860897,639.868389472887,61.1481479683271));
#103681=CARTESIAN_POINT('Ctrl Pts',(12.4690433776627,639.91089078029,61.407011369442));
#103682=CARTESIAN_POINT('Ctrl Pts',(12.5238602515816,639.948422497839,61.6683601245959));
#103683=CARTESIAN_POINT('Ctrl Pts',(12.5710279567737,639.980777202583,61.9322186969404));
#103684=CARTESIAN_POINT('Ctrl Pts',(12.5745024304964,639.983160519113,61.9516550819074));
#103685=CARTESIAN_POINT('Ctrl Pts',(12.5779356066442,639.985516021405,61.9711086414617));
#103686=CARTESIAN_POINT('Ctrl Pts',(12.5813273486773,639.987843586439,61.9905791155502));
#103687=CARTESIAN_POINT('Ctrl Pts',(12.6482309907011,640.033755856973,62.3746430024116));
#103688=CARTESIAN_POINT('Ctrl Pts',(12.6989827550157,640.068776619721,62.7651309615334));
#103689=CARTESIAN_POINT('Ctrl Pts',(12.7325045718648,640.091936878102,63.1594985618337));
#103690=CARTESIAN_POINT('Ctrl Pts',(12.7352361632803,640.093824137473,63.1916343841963));
#103691=CARTESIAN_POINT('Ctrl Pts',(12.7378533692285,640.095632658281,63.2237959670548));
#103692=CARTESIAN_POINT('Ctrl Pts',(12.7403556191587,640.097361925308,63.2559819337451));
#103693=CARTESIAN_POINT('Ctrl Pts',(12.7415108518539,640.098160289125,63.2708414729934));
#103694=CARTESIAN_POINT('Ctrl Pts',(12.7426411255945,640.098941441112,63.2856985588883));
#103695=CARTESIAN_POINT('Ctrl Pts',(12.7437464711904,640.099705399842,63.3005531880157));
#103696=CARTESIAN_POINT('Ctrl Pts',(12.7759162994634,640.121939551085,63.7328802989446));
#103697=CARTESIAN_POINT('Ctrl Pts',(12.7870003318299,640.129625522797,64.1634229287959));
#103698=CARTESIAN_POINT('Ctrl Pts',(12.7776731523991,640.123170325736,64.5922349254529));
#103699=CARTESIAN_POINT('Ctrl Pts',(12.7774670029556,640.123027652885,64.6017125338895));
#103700=CARTESIAN_POINT('Ctrl Pts',(12.7772508808923,640.122878071158,64.6111892966089));
#103701=CARTESIAN_POINT('Ctrl Pts',(12.7770247866986,640.122721582759,64.6206652136733));
#103702=CARTESIAN_POINT('Ctrl Pts',(12.7666730268079,640.115556735669,65.0545216369199));
#103703=CARTESIAN_POINT('Ctrl Pts',(12.7354157605725,640.093909778564,65.4866513230427));
#103704=CARTESIAN_POINT('Ctrl Pts',(12.6833305290434,640.05800335744,65.9169319880768));
#103705=CARTESIAN_POINT('Ctrl Pts',(12.6828077078149,640.057642935903,65.9212510600921));
#103706=CARTESIAN_POINT('Ctrl Pts',(12.6822827336681,640.057281040276,65.9255701772016));
#103707=CARTESIAN_POINT('Ctrl Pts',(12.6817556078935,640.056917671866,65.9298893314512));
#103708=CARTESIAN_POINT('Ctrl Pts',(12.6329480531516,640.023272715739,66.3298078474232));
#103709=CARTESIAN_POINT('Ctrl Pts',(12.5656816350177,639.976995913131,66.7301336276553));
#103710=CARTESIAN_POINT('Ctrl Pts',(12.4809092885621,639.91907782816,67.1247607525797));
#103711=CARTESIAN_POINT('Ctrl Pts',(12.4735560157396,639.914053931831,67.158991265643));
#103712=CARTESIAN_POINT('Ctrl Pts',(12.4660710046806,639.908942431424,67.1931788821358));
#103713=CARTESIAN_POINT('Ctrl Pts',(12.4584548648209,639.903743965574,67.2273196043471));
#103714=CARTESIAN_POINT('Ctrl Pts',(12.4583195473824,639.90365160342,67.2279261892));
#103715=CARTESIAN_POINT('Ctrl Pts',(12.4581841884965,639.903559213782,67.228532759456));
#103716=CARTESIAN_POINT('Ctrl Pts',(12.4580487881665,639.903466796663,67.2291393150922));
#103717=CARTESIAN_POINT('Ctrl Pts',(12.3287543193047,639.815217216541,67.8083423998278));
#103718=CARTESIAN_POINT('Ctrl Pts',(12.1635881082219,639.703112683783,68.3695526413109));
#103719=CARTESIAN_POINT('Ctrl Pts',(11.9641361655058,639.570100576874,68.9140157869479));
#103720=CARTESIAN_POINT('Ctrl Pts',(11.8692267001007,639.506806593435,69.1730992803526));
#103721=CARTESIAN_POINT('Ctrl Pts',(11.76655415419,639.438778971279,69.4283910409158));
#103722=CARTESIAN_POINT('Ctrl Pts',(11.6562914846914,639.36633818961,69.6800273323468));
#103723=CARTESIAN_POINT('Ctrl Pts',(11.6528123180315,639.364052433665,69.6879673232751));
#103724=CARTESIAN_POINT('Ctrl Pts',(11.6493255850376,639.361762281841,69.6959036824858));
#103725=CARTESIAN_POINT('Ctrl Pts',(11.6458312910723,639.359467744224,69.7038364142171));
#103726=CARTESIAN_POINT('Ctrl Pts',(11.4971366810822,639.261827024956,70.0414023038092));
#103727=CARTESIAN_POINT('Ctrl Pts',(11.3338413940789,639.155709421531,70.3735482476988));
#103728=CARTESIAN_POINT('Ctrl Pts',(11.1589239953535,639.043766058966,70.6951271369094));
#103729=CARTESIAN_POINT('Ctrl Pts',(11.1357897462097,639.028960638474,70.7376585614365));
#103730=CARTESIAN_POINT('Ctrl Pts',(11.1124522364092,639.014053343863,70.7800050873094));
#103731=CARTESIAN_POINT('Ctrl Pts',(11.08891838951,638.999050337027,70.8221547543116));
#103732=CARTESIAN_POINT('Ctrl Pts',(11.0832572973831,638.995441347632,70.8322939019418));
#103733=CARTESIAN_POINT('Ctrl Pts',(11.0775847776858,638.991826767618,70.8424218051789));
#103734=CARTESIAN_POINT('Ctrl Pts',(11.0719009273916,638.988206683529,70.8525382931254));
#103735=CARTESIAN_POINT('Ctrl Pts',(10.8933793466194,638.874505037529,71.170282661222));
#103736=CARTESIAN_POINT('Ctrl Pts',(10.7034240270576,638.755189205572,71.4776963878882));
#103737=CARTESIAN_POINT('Ctrl Pts',(10.5023371609787,638.631287386234,71.7752823633198));
#103738=CARTESIAN_POINT('Ctrl Pts',(10.477246088299,638.61582725393,71.8124143326205));
#103739=CARTESIAN_POINT('Ctrl Pts',(10.4519817462916,638.60029575369,71.8493933295574));
#103740=CARTESIAN_POINT('Ctrl Pts',(10.4265447575929,638.584694910286,71.8862203643523));
#103741=CARTESIAN_POINT('Ctrl Pts',(10.4188131204951,638.579952994446,71.89741403479));
#103742=CARTESIAN_POINT('Ctrl Pts',(10.4110654988077,638.57520465167,71.9085937144694));
#103743=CARTESIAN_POINT('Ctrl Pts',(10.4033019069229,638.570449936256,71.9197594373552));
#103744=CARTESIAN_POINT('Ctrl Pts',(10.1743043134857,638.430203204648,72.249107464377));
#103745=CARTESIAN_POINT('Ctrl Pts',(9.9314107080512,638.28440118465,72.5663065584188));
#103746=CARTESIAN_POINT('Ctrl Pts',(9.67444603037878,638.134398646701,72.8718105219762));
#103747=CARTESIAN_POINT('Ctrl Pts',(9.66485722564937,638.128801204055,72.8832106018516));
#103748=CARTESIAN_POINT('Ctrl Pts',(9.65524877276325,638.12319788993,72.894594446214));
#103749=CARTESIAN_POINT('Ctrl Pts',(9.64562066556107,638.117588777634,72.9059620729246));
#103750=CARTESIAN_POINT('Ctrl Pts',(9.42731586112809,637.990409453907,73.1637082190586));
#103751=CARTESIAN_POINT('Ctrl Pts',(9.19804063693805,637.859784539816,73.4138743235853));
#103752=CARTESIAN_POINT('Ctrl Pts',(8.96066185930502,637.728380992124,73.6534663850734));
#103753=CARTESIAN_POINT('Ctrl Pts',(8.91843648227902,637.70500668546,73.6960854651346));
#103754=CARTESIAN_POINT('Ctrl Pts',(8.87595480168801,637.681607813329,73.738369934181));
#103755=CARTESIAN_POINT('Ctrl Pts',(8.83323308819527,637.658199473966,73.7803029115011));
#103756=CARTESIAN_POINT('Ctrl Pts',(8.82225322068705,637.652183318626,73.7910800666655));
#103757=CARTESIAN_POINT('Ctrl Pts',(8.8112573568705,637.646166453333,73.8018341562657));
#103758=CARTESIAN_POINT('Ctrl Pts',(8.80024576806366,637.640149131977,73.8125648963688));
#103759=CARTESIAN_POINT('Ctrl Pts',(8.45642397146976,637.452266504349,74.1476175763908));
#103760=CARTESIAN_POINT('Ctrl Pts',(8.09685247539544,637.263431908529,74.461195042532));
#103761=CARTESIAN_POINT('Ctrl Pts',(7.72053287787403,637.07685274923,74.75389752882));
#103762=CARTESIAN_POINT('Ctrl Pts',(7.4646028508242,636.949962707891,74.9529606542237));
#103763=CARTESIAN_POINT('Ctrl Pts',(7.20092632659578,636.824116856345,75.1423691924486));
#103764=CARTESIAN_POINT('Ctrl Pts',(6.92918660057919,636.700336265871,75.3223177033396));
#103765=CARTESIAN_POINT('Ctrl Pts',(6.91763580200828,636.695074743426,75.3299667469039));
#103766=CARTESIAN_POINT('Ctrl Pts',(6.90607038322277,636.689816954487,75.3375986977512));
#103767=CARTESIAN_POINT('Ctrl Pts',(6.89449031796739,636.684562976726,75.3452135726443));
#103768=CARTESIAN_POINT('Ctrl Pts',(6.56315230202816,636.534231995945,75.5630964155352));
#103769=CARTESIAN_POINT('Ctrl Pts',(6.21970864445252,636.387065880779,75.7668655454909));
#103770=CARTESIAN_POINT('Ctrl Pts',(5.8626639024424,636.245440217798,75.9560400598351));
#103771=CARTESIAN_POINT('Ctrl Pts',(5.85210062245606,636.241250178413,75.9616368468093));
#103772=CARTESIAN_POINT('Ctrl Pts',(5.84152543830141,636.237064998961,75.9672208471966));
#103773=CARTESIAN_POINT('Ctrl Pts',(5.83093831658855,636.232884744127,75.9727920447534));
#103774=CARTESIAN_POINT('Ctrl Pts',(5.51616734454452,636.108599512216,76.1384320853574));
#103775=CARTESIAN_POINT('Ctrl Pts',(5.19319897983501,635.989681238602,76.2913913409048));
#103776=CARTESIAN_POINT('Ctrl Pts',(4.863933133145,635.878703176547,76.4304781402202));
#103777=CARTESIAN_POINT('Ctrl Pts',(4.81686179178898,635.862837922697,76.4503617761166));
#103778=CARTESIAN_POINT('Ctrl Pts',(4.76966181406017,635.847134946092,76.4699619551446));
#103779=CARTESIAN_POINT('Ctrl Pts',(4.72233881323827,635.831601761893,76.4892752541631));
#103780=CARTESIAN_POINT('Ctrl Pts',(4.71410218547924,635.828898191664,76.4926367581263));
#103781=CARTESIAN_POINT('Ctrl Pts',(4.7058617639725,635.826199741836,76.495989600344));
#103782=CARTESIAN_POINT('Ctrl Pts',(4.69761757561058,635.823506451461,76.4993337633957));
#103783=CARTESIAN_POINT('Ctrl Pts',(4.33883025531642,635.706294375029,76.6448718378883));
#103784=CARTESIAN_POINT('Ctrl Pts',(3.97204499540476,635.598372180541,76.7746808977565));
#103785=CARTESIAN_POINT('Ctrl Pts',(3.59624449099713,635.502338704144,76.8878059230238));
#103786=CARTESIAN_POINT('Ctrl Pts',(3.23104131737279,635.40901330957,76.9977408958602));
#103787=CARTESIAN_POINT('Ctrl Pts',(2.85732420826786,635.326915434987,77.0919195272795));
#103788=CARTESIAN_POINT('Ctrl Pts',(2.4741421477009,635.258470242481,77.169441631003));
#103789=CARTESIAN_POINT('Ctrl Pts',(2.40382931954546,635.245910742562,77.1836667185483));
#103790=CARTESIAN_POINT('Ctrl Pts',(2.33319774590726,635.233811059836,77.1973308945058));
#103791=CARTESIAN_POINT('Ctrl Pts',(2.26224148372674,635.222186336159,77.2104285068931));
#103792=CARTESIAN_POINT('Origin',(28.,620.675373764374,64.2994740882088));
#103793=CARTESIAN_POINT('Ctrl Pts',(1.86306288877798,634.816577773823,79.840079036097));
#103794=CARTESIAN_POINT('Ctrl Pts',(2.1402114497942,634.853975948363,79.8060484936876));
#103795=CARTESIAN_POINT('Ctrl Pts',(2.41337614608207,634.898916808426,79.7649147909196));
#103796=CARTESIAN_POINT('Ctrl Pts',(2.68283184001296,634.950697211643,79.7169704303209));
#103797=CARTESIAN_POINT('Ctrl Pts',(2.97414735926638,635.006678344683,79.6651365421617));
#103798=CARTESIAN_POINT('Ctrl Pts',(3.26112767369113,635.070653432778,79.605341209851));
#103799=CARTESIAN_POINT('Ctrl Pts',(3.54412011469586,635.141683071731,79.5379106224164));
#103800=CARTESIAN_POINT('Ctrl Pts',(3.88187814635018,635.22645859067,79.457430654809));
#103801=CARTESIAN_POINT('Ctrl Pts',(4.21395546218051,635.321283246751,79.3660724895557));
#103802=CARTESIAN_POINT('Ctrl Pts',(4.54094258490074,635.424491558278,79.2643522128287));
#103803=CARTESIAN_POINT('Ctrl Pts',(4.66022073584993,635.462139819345,79.2272467561333));
#103804=CARTESIAN_POINT('Ctrl Pts',(4.7788215654647,635.500903092017,79.1887623167328));
#103805=CARTESIAN_POINT('Ctrl Pts',(4.89677373712177,635.540698981156,79.1489238821404));
#103806=CARTESIAN_POINT('Ctrl Pts',(5.16043615149924,635.62965605643,79.0598717036));
#103807=CARTESIAN_POINT('Ctrl Pts',(5.42147464015965,635.724158708811,78.9636635925424));
#103808=CARTESIAN_POINT('Ctrl Pts',(5.67881724162163,635.822969674527,78.8608748149905));
#103809=CARTESIAN_POINT('Ctrl Pts',(5.89134528490862,635.904573346361,78.7759860416554));
#103810=CARTESIAN_POINT('Ctrl Pts',(6.1013525895396,635.98911515618,78.686609180123));
#103811=CARTESIAN_POINT('Ctrl Pts',(6.30823535587315,636.075909817726,78.5930930229847));
#103812=CARTESIAN_POINT('Ctrl Pts',(6.60818034578659,636.201747384303,78.4575104256195));
#103813=CARTESIAN_POINT('Ctrl Pts',(6.90074477300754,636.33186003416,78.3137274985375));
#103814=CARTESIAN_POINT('Ctrl Pts',(7.1866141870702,636.465136951872,78.1619208948133));
#103815=CARTESIAN_POINT('Ctrl Pts',(7.33667046294903,636.535095600641,78.0822357921472));
#103816=CARTESIAN_POINT('Ctrl Pts',(7.48488204463925,636.605925993923,78.0003406744232));
#103817=CARTESIAN_POINT('Ctrl Pts',(7.63134808340531,636.677467493344,77.9162670025646));
#103818=CARTESIAN_POINT('Ctrl Pts',(7.91723728696255,636.817110392566,77.7521623726431));
#103819=CARTESIAN_POINT('Ctrl Pts',(8.19655198249425,636.959386851472,77.5798506235794));
#103820=CARTESIAN_POINT('Ctrl Pts',(8.46960770405218,637.103497273499,77.399123356496));
#103821=CARTESIAN_POINT('Ctrl Pts',(8.73947522321689,637.245925060239,77.2205062634905));
#103822=CARTESIAN_POINT('Ctrl Pts',(9.00322907486019,637.390143982264,77.0336684769876));
#103823=CARTESIAN_POINT('Ctrl Pts',(9.26117386904128,637.535339977012,76.8384370553729));
#103824=CARTESIAN_POINT('Ctrl Pts',(9.51911866322236,637.680535971759,76.6432056337581));
#103825=CARTESIAN_POINT('Ctrl Pts',(9.77125439994123,637.826708823744,76.4395799971643));
#103826=CARTESIAN_POINT('Ctrl Pts',(10.0178856892571,637.973005429087,76.2274241122122));
#103827=CARTESIAN_POINT('Ctrl Pts',(10.203587578906,638.083159968426,76.0676805985443));
#103828=CARTESIAN_POINT('Ctrl Pts',(10.3856411221024,638.193166844564,75.9034085015197));
#103829=CARTESIAN_POINT('Ctrl Pts',(10.5636740062097,638.302444690353,75.7349637390155));
#103830=CARTESIAN_POINT('Ctrl Pts',(10.7417068903169,638.411722536141,75.5665189765113));
#103831=CARTESIAN_POINT('Ctrl Pts',(10.9157191153351,638.520270922481,75.3939015342056));
#103832=CARTESIAN_POINT('Ctrl Pts',(11.0853383686276,638.627547204778,75.2175106217998));
#103833=CARTESIAN_POINT('Ctrl Pts',(11.2982866914253,638.762227106663,74.9960608263053));
#103834=CARTESIAN_POINT('Ctrl Pts',(11.5047763502784,638.895162465455,74.7682551816796));
#103835=CARTESIAN_POINT('Ctrl Pts',(11.7048608093241,639.02588366622,74.5338690056148));
#103836=CARTESIAN_POINT('Ctrl Pts',(11.823522007374,639.103408599278,74.3948649840589));
#103837=CARTESIAN_POINT('Ctrl Pts',(11.9399304013403,639.180153876557,74.2535467954849));
#103838=CARTESIAN_POINT('Ctrl Pts',(12.0540971431182,639.256013429961,74.1098707468977));
#103839=CARTESIAN_POINT('Ctrl Pts',(12.2247846330212,639.369428918167,73.8950647209866));
#103840=CARTESIAN_POINT('Ctrl Pts',(12.3904618758828,639.480866713069,73.6749899684775));
#103841=CARTESIAN_POINT('Ctrl Pts',(12.5510400004964,639.590004181669,73.449381692131));
#103842=CARTESIAN_POINT('Ctrl Pts',(12.6789711937418,639.676953052317,73.2696415434122));
#103843=CARTESIAN_POINT('Ctrl Pts',(12.8036658898911,639.76244096806,73.0863892069992));
#103844=CARTESIAN_POINT('Ctrl Pts',(12.9250791491289,639.846281360739,72.8994947227659));
#103845=CARTESIAN_POINT('Ctrl Pts',(13.0388387824086,639.924836638681,72.7243816575058));
#103846=CARTESIAN_POINT('Ctrl Pts',(13.149577296258,640.001877851171,72.5462085445932));
#103847=CARTESIAN_POINT('Ctrl Pts',(13.2569702277696,640.077040702749,72.3654131529155));
#103848=CARTESIAN_POINT('Ctrl Pts',(13.3632468260264,640.15142224787,72.1864971019469));
#103849=CARTESIAN_POINT('Ctrl Pts',(13.4662470340887,640.223964114305,72.0050131874289));
#103850=CARTESIAN_POINT('Ctrl Pts',(13.5656564024644,640.294356943015,71.821412137635));
#103851=CARTESIAN_POINT('Ctrl Pts',(13.6075769852428,640.324041352554,71.7439882174165));
#103852=CARTESIAN_POINT('Ctrl Pts',(13.6488590164015,640.353344153431,71.6661881202239));
#103853=CARTESIAN_POINT('Ctrl Pts',(13.6894789155558,640.382244612178,71.5880469506538));
#103854=CARTESIAN_POINT('Ctrl Pts',(13.8286010750807,640.481227975402,71.3204153591252));
#103855=CARTESIAN_POINT('Ctrl Pts',(13.960518022757,640.575774225862,71.0480331379661));
#103856=CARTESIAN_POINT('Ctrl Pts',(14.0849573496661,640.66553284446,70.7707639855962));
#103857=CARTESIAN_POINT('Ctrl Pts',(14.2077624538306,640.754112691205,70.4971361222502));
#103858=CARTESIAN_POINT('Ctrl Pts',(14.3232850500893,640.838029842505,70.2187485294791));
#103859=CARTESIAN_POINT('Ctrl Pts',(14.4312633215793,640.916900373456,69.9354880623769));
#103860=CARTESIAN_POINT('Ctrl Pts',(14.5371375665815,640.994234061078,69.6577471087608));
#103861=CARTESIAN_POINT('Ctrl Pts',(14.6357586344064,641.066715828707,69.3753210477021));
#103862=CARTESIAN_POINT('Ctrl Pts',(14.7268797169126,641.133938640373,69.0881248582813));
#103863=CARTESIAN_POINT('Ctrl Pts',(14.765817850058,641.162664493042,68.9653993247939));
#103864=CARTESIAN_POINT('Ctrl Pts',(14.8033864488709,641.190429470735,68.8418030398912));
#103865=CARTESIAN_POINT('Ctrl Pts',(14.8395662545944,641.217199266066,68.7173308130521));
#103866=CARTESIAN_POINT('Ctrl Pts',(14.9306676469202,641.28460608537,68.4039075388212));
#103867=CARTESIAN_POINT('Ctrl Pts',(15.0120041807898,641.344996930947,68.0882301956662));
#103868=CARTESIAN_POINT('Ctrl Pts',(15.0834994605392,641.398252513301,67.7702592069465));
#103869=CARTESIAN_POINT('Ctrl Pts',(15.1544872250653,641.45113005645,67.4545453618861));
#103870=CARTESIAN_POINT('Ctrl Pts',(15.2157729575024,641.496973294811,67.1365698743781));
#103871=CARTESIAN_POINT('Ctrl Pts',(15.2672818775681,641.535614532624,66.8162990868602));
#103872=CARTESIAN_POINT('Ctrl Pts',(15.3181640307078,641.573785579064,66.4999253939952));
#103873=CARTESIAN_POINT('Ctrl Pts',(15.3595058548198,641.604928781656,66.1813114971206));
#103874=CARTESIAN_POINT('Ctrl Pts',(15.391235266347,641.628832901803,65.860436342483));
#103875=CARTESIAN_POINT('Ctrl Pts',(15.399680349928,641.635195209922,65.7750323791085));
#103876=CARTESIAN_POINT('Ctrl Pts',(15.407444481865,641.641044422465,65.6894683089283));
#103877=CARTESIAN_POINT('Ctrl Pts',(15.414526303025,641.6463759616,65.6037439326523));
#103878=CARTESIAN_POINT('Ctrl Pts',(15.4364643525561,641.662891991443,65.3381871542066));
#103879=CARTESIAN_POINT('Ctrl Pts',(15.4517893452765,641.674443724131,65.0710724250625));
#103880=CARTESIAN_POINT('Ctrl Pts',(15.4603232031337,641.680876931242,64.8023554757184));
#103881=CARTESIAN_POINT('Ctrl Pts',(15.4648538948456,641.684292371084,64.6596915509598));
#103882=CARTESIAN_POINT('Ctrl Pts',(15.4674510190573,641.68626151627,64.5165142301015));
#103883=CARTESIAN_POINT('Ctrl Pts',(15.4681203454456,641.686765325652,64.3734851808154));
#103884=CARTESIAN_POINT('Ctrl Pts',(15.4687117396317,641.687210474604,64.2471095445317));
#103885=CARTESIAN_POINT('Ctrl Pts',(15.4677981227552,641.686512405933,64.1208497755977));
#103886=CARTESIAN_POINT('Ctrl Pts',(15.465383474685,641.684691870118,63.9951622171671));
#103887=CARTESIAN_POINT('Ctrl Pts',(15.4594523424331,641.680220063719,63.6864341914555));
#103888=CARTESIAN_POINT('Ctrl Pts',(15.444557626696,641.6689755171,63.3797508309682));
#103889=CARTESIAN_POINT('Ctrl Pts',(15.4209342345179,641.65118995091,63.0750606401239));
#103890=CARTESIAN_POINT('Ctrl Pts',(15.4035532438903,641.638104160481,62.8508838025451));
#103891=CARTESIAN_POINT('Ctrl Pts',(15.381447132351,641.621476462837,62.6277854531146));
#103892=CARTESIAN_POINT('Ctrl Pts',(15.3547094604652,641.60138204407,62.4057395605387));
#103893=CARTESIAN_POINT('Ctrl Pts',(15.3159115020446,641.572223842595,62.083537711986));
#103894=CARTESIAN_POINT('Ctrl Pts',(15.2673586125668,641.535768218365,61.7635549646432));
#103895=CARTESIAN_POINT('Ctrl Pts',(15.209136597126,641.49220316936,61.4457630820078));
#103896=CARTESIAN_POINT('Ctrl Pts',(15.1727005295007,641.464939615193,61.2468849353337));
#103897=CARTESIAN_POINT('Ctrl Pts',(15.1324776324191,641.434890687182,61.0488645460175));
#103898=CARTESIAN_POINT('Ctrl Pts',(15.0884889362004,641.402092265999,60.8516931877507));
#103899=CARTESIAN_POINT('Ctrl Pts',(15.0441618970615,641.36904157288,60.6530052686653));
#103900=CARTESIAN_POINT('Ctrl Pts',(14.9958796103505,641.333129102149,60.454790109615));
#103901=CARTESIAN_POINT('Ctrl Pts',(14.9437846854314,641.294465026022,60.2575526977022));
#103902=CARTESIAN_POINT('Ctrl Pts',(14.8915150909167,641.255671312726,60.0596539664951));
#103903=CARTESIAN_POINT('Ctrl Pts',(14.8354072484664,641.214107571676,59.8627397875055));
#103904=CARTESIAN_POINT('Ctrl Pts',(14.7756052067288,641.169936228604,59.667308030848));
#103905=CARTESIAN_POINT('Ctrl Pts',(14.7413494348752,641.144634024753,59.5553609221125));
#103906=CARTESIAN_POINT('Ctrl Pts',(14.7058815145681,641.118477144786,59.4438999846865));
#103907=CARTESIAN_POINT('Ctrl Pts',(14.6692285204308,641.091503479503,59.3330165540888));
#103908=CARTESIAN_POINT('Ctrl Pts',(14.5803938226745,641.026128263667,59.0642719051131));
#103909=CARTESIAN_POINT('Ctrl Pts',(14.4851858741749,640.956266144212,58.8001708828617));
#103910=CARTESIAN_POINT('Ctrl Pts',(14.3837715170968,640.882274341514,58.5405486633777));
#103911=CARTESIAN_POINT('Ctrl Pts',(14.2810607054585,640.807336647004,58.2776075014868));
#103912=CARTESIAN_POINT('Ctrl Pts',(14.1719837887646,640.728162967591,58.0192600662555));
#103913=CARTESIAN_POINT('Ctrl Pts',(14.0567140899262,640.645072609331,57.7653191294626));
#103914=CARTESIAN_POINT('Ctrl Pts',(13.9392204614165,640.560379166175,57.506478841064));
#103915=CARTESIAN_POINT('Ctrl Pts',(13.8152927875581,640.471616451942,57.2522164161331));
#103916=CARTESIAN_POINT('Ctrl Pts',(13.685114617953,640.379069406133,57.0023218326963));
#103917=CARTESIAN_POINT('Ctrl Pts',(13.602335492943,640.320219573649,56.8434161189011));
#103918=CARTESIAN_POINT('Ctrl Pts',(13.5170289340378,640.259838448468,56.6862763549364));
#103919=CARTESIAN_POINT('Ctrl Pts',(13.4292421368317,640.197988495442,56.5308469864962));
#103920=CARTESIAN_POINT('Ctrl Pts',(13.2697747250469,640.085636157255,56.248504767742));
#103921=CARTESIAN_POINT('Ctrl Pts',(13.1018986617114,639.968380260892,55.9716775249343));
#103922=CARTESIAN_POINT('Ctrl Pts',(12.9258526145704,639.846811878008,55.7006361644966));
#103923=CARTESIAN_POINT('Ctrl Pts',(12.828662025543,639.779697035435,55.55100105539));
#103924=CARTESIAN_POINT('Ctrl Pts',(12.7289813349122,639.711268159354,55.403128539522));
#103925=CARTESIAN_POINT('Ctrl Pts',(12.6268507021078,639.64162697107,55.2570578025761));
#103926=CARTESIAN_POINT('Ctrl Pts',(12.4693452509776,639.534226610603,55.0317880995707));
#103927=CARTESIAN_POINT('Ctrl Pts',(12.3071295901739,639.424692655522,54.8123661471315));
#103928=CARTESIAN_POINT('Ctrl Pts',(12.1402844332092,639.31338341686,54.5985128380537));
#103929=CARTESIAN_POINT('Ctrl Pts',(12.002978936203,639.221781295386,54.4225219047624));
#103930=CARTESIAN_POINT('Ctrl Pts',(11.8625381156246,639.128975808109,54.2503020731748));
#103931=CARTESIAN_POINT('Ctrl Pts',(11.7190069566274,639.035140454571,54.0816944827995));
#103932=CARTESIAN_POINT('Ctrl Pts',(11.5129986901229,638.900459883089,53.8396943648085));
#103933=CARTESIAN_POINT('Ctrl Pts',(11.3007022404411,638.763614383175,53.6050605705702));
#103934=CARTESIAN_POINT('Ctrl Pts',(11.0819551471624,638.625229473852,53.3776274956168));
#103935=CARTESIAN_POINT('Ctrl Pts',(10.8537269626186,638.480846587891,53.1403368554358));
#103936=CARTESIAN_POINT('Ctrl Pts',(10.6184768396454,638.33478826757,52.9108844662543));
#103937=CARTESIAN_POINT('Ctrl Pts',(10.3760202645821,638.187715079138,52.6890496920728));
#103938=CARTESIAN_POINT('Ctrl Pts',(10.1335636895188,638.040641890706,52.4672149178913));
#103939=CARTESIAN_POINT('Ctrl Pts',(9.88390066236547,637.892553766813,52.2529973474516));
#103940=CARTESIAN_POINT('Ctrl Pts',(9.62684666946167,637.744061124887,52.046149446617));
#103941=CARTESIAN_POINT('Ctrl Pts',(9.46346234490038,637.649678735689,51.9146762717287));
#103942=CARTESIAN_POINT('Ctrl Pts',(9.29686479133905,637.555081299247,51.7861174760067));
#103943=CARTESIAN_POINT('Ctrl Pts',(9.1275807697391,637.460801611946,51.6609035615571));
#103944=CARTESIAN_POINT('Ctrl Pts',(8.95353419623788,637.363869507129,51.5321669415345));
#103945=CARTESIAN_POINT('Ctrl Pts',(8.77664786888201,637.267273530126,51.406966138181));
#103946=CARTESIAN_POINT('Ctrl Pts',(8.59749427003405,637.171630477508,51.2857287611495));
#103947=CARTESIAN_POINT('Ctrl Pts',(8.54536693178636,637.143801744025,51.250452987727));
#103948=CARTESIAN_POINT('Ctrl Pts',(8.49304764555581,637.116053909166,51.2155125022222));
#103949=CARTESIAN_POINT('Ctrl Pts',(8.44055051338909,637.088402691147,51.1809172151339));
#103950=CARTESIAN_POINT('Ctrl Pts',(8.16409659561434,636.942789259763,50.9987357843133));
#103951=CARTESIAN_POINT('Ctrl Pts',(7.88203506759558,636.79939500734,50.8255502039267));
#103952=CARTESIAN_POINT('Ctrl Pts',(7.59396676190408,636.659228030904,50.6612756819119));
#103953=CARTESIAN_POINT('Ctrl Pts',(7.45646787272285,636.592324441793,50.5828652360158));
#103954=CARTESIAN_POINT('Ctrl Pts',(7.31760047037385,636.526155614565,50.5064843721738));
#103955=CARTESIAN_POINT('Ctrl Pts',(7.1773211472115,636.460828180361,50.4321209931152));
#103956=CARTESIAN_POINT('Ctrl Pts',(6.88018284129507,636.322452240901,50.274605202637));
#103957=CARTESIAN_POINT('Ctrl Pts',(6.57671769730352,636.187844122741,50.1261374141606));
#103958=CARTESIAN_POINT('Ctrl Pts',(6.26623698972816,636.058320110097,49.9869266312468));
#103959=CARTESIAN_POINT('Ctrl Pts',(6.12304923299931,635.998586115809,49.9227252840084));
#103960=CARTESIAN_POINT('Ctrl Pts',(5.97836935164948,635.939933327015,49.8604919927752));
#103961=CARTESIAN_POINT('Ctrl Pts',(5.83212979029488,635.882489700749,49.8002438368877));
#103962=CARTESIAN_POINT('Ctrl Pts',(5.60046097050222,635.791489037329,49.7048003123048));
#103963=CARTESIAN_POINT('Ctrl Pts',(5.36486309244537,635.70354017929,49.6143579168887));
#103964=CARTESIAN_POINT('Ctrl Pts',(5.12496004470658,635.619272900355,49.5291006468632));
#103965=CARTESIAN_POINT('Ctrl Pts',(4.92336015566138,635.548459818806,49.4574556371836));
#103966=CARTESIAN_POINT('Ctrl Pts',(4.71807804535173,635.480062142841,49.3892915169399));
#103967=CARTESIAN_POINT('Ctrl Pts',(4.51111271500933,635.415177638747,49.3254220404758));
#103968=CARTESIAN_POINT('Ctrl Pts',(4.47179014429899,635.402849846957,49.3132870998056));
#103969=CARTESIAN_POINT('Ctrl Pts',(4.43240681194781,635.390648970691,49.3013070706534));
#103970=CARTESIAN_POINT('Ctrl Pts',(4.39297642822443,635.378582662943,49.2894873770812));
#103971=CARTESIAN_POINT('Ctrl Pts',(4.12486075126194,635.29653511573,49.2091167378853));
#103972=CARTESIAN_POINT('Ctrl Pts',(3.85444033265441,635.220537807346,49.1359860390466));
#103973=CARTESIAN_POINT('Ctrl Pts',(3.58156371892505,635.151343123417,49.0702139584702));
#103974=CARTESIAN_POINT('Ctrl Pts',(3.32312890924843,635.08581051977,49.0079228192864));
#103975=CARTESIAN_POINT('Ctrl Pts',(3.06249100951263,635.026379694471,48.9522313546328));
#103976=CARTESIAN_POINT('Ctrl Pts',(2.79952136274532,634.973653473136,48.90326512778));
#103977=CARTESIAN_POINT('Ctrl Pts',(2.55448969638528,634.924523871932,48.8576390400981));
#103978=CARTESIAN_POINT('Ctrl Pts',(2.30743354479113,634.881215358141,48.8178516695863));
#103979=CARTESIAN_POINT('Ctrl Pts',(2.0582488241727,634.844182631359,48.7840331252826));
#103980=CARTESIAN_POINT('Ctrl Pts',(1.81685586891611,634.808307882149,48.7512720541715));
#103981=CARTESIAN_POINT('Ctrl Pts',(1.57346538001366,634.778322729849,48.7241119998909));
#103982=CARTESIAN_POINT('Ctrl Pts',(1.32798273535137,634.754607307784,48.7027040439557));
#103983=CARTESIAN_POINT('Ctrl Pts',(1.093192418537,634.731924842929,48.6822285404296));
#103984=CARTESIAN_POINT('Ctrl Pts',(0.855738997651462,634.715070446946,
48.6670981287459));
#103985=CARTESIAN_POINT('Ctrl Pts',(0.616984794805639,634.704331439349,
48.6574665592196));
#103986=CARTESIAN_POINT('Ctrl Pts',(0.386532831300444,634.693965861037,
48.6481699098516));
#103987=CARTESIAN_POINT('Ctrl Pts',(0.154868977576536,634.689297832698,
48.6439961961591));
#103988=CARTESIAN_POINT('Ctrl Pts',(-0.076781676442522,634.690552953027,
48.645119892231));
#103989=CARTESIAN_POINT('Ctrl Pts',(-0.145864683307238,634.690927255818,
48.6454550015954));
#103990=CARTESIAN_POINT('Ctrl Pts',(-0.21494651624892,634.691828105029,
48.6462614978511));
#103991=CARTESIAN_POINT('Ctrl Pts',(-0.283994682921353,634.693260874937,
48.6475446883329));
#103992=CARTESIAN_POINT('Ctrl Pts',(-0.520075952304442,634.698159631196,
48.6519320204288));
#103993=CARTESIAN_POINT('Ctrl Pts',(-0.755839055281249,634.709248379301,
48.6618612476738));
#103994=CARTESIAN_POINT('Ctrl Pts',(-0.990327191986353,634.726188034766,
48.67709682602));
#103995=CARTESIAN_POINT('Ctrl Pts',(-1.23740315666479,634.744037047402,
48.6931502830104));
#103996=CARTESIAN_POINT('Ctrl Pts',(-1.48306359503919,634.768381892692,
48.7150953295273));
#103997=CARTESIAN_POINT('Ctrl Pts',(-1.72618919815624,634.798786848871,
48.7426988494953));
#103998=CARTESIAN_POINT('Ctrl Pts',(-1.7805517045467,634.805585349742,48.7488709535905));
#103999=CARTESIAN_POINT('Ctrl Pts',(-1.83478747864479,634.81268669057,48.7553261113014));
#104000=CARTESIAN_POINT('Ctrl Pts',(-1.8888840075986,634.820085762158,48.7620619651124));
#104001=CARTESIAN_POINT('Ctrl Pts',(-0.252645464510396,637.415474030314,
76.9980210944396));
#104002=CARTESIAN_POINT('Ctrl Pts',(-1.11302381605652,637.42877366079,76.980488604498));
#104003=CARTESIAN_POINT('Ctrl Pts',(-1.94758251680077,637.509665462313,
76.8749778358584));
#104004=CARTESIAN_POINT('Ctrl Pts',(-3.16572559796507,637.712565815082,
76.5970874596841));
#104005=CARTESIAN_POINT('Ctrl Pts',(-3.56612249316459,637.793779472012,
76.4843247054231));
#104006=CARTESIAN_POINT('Ctrl Pts',(-4.35605342916383,637.979980203759,
76.2184083741727));
#104007=CARTESIAN_POINT('Ctrl Pts',(-4.74439125163809,638.08483946683,76.0653418396745));
#104008=CARTESIAN_POINT('Ctrl Pts',(-5.86615041872897,638.420465470767,
75.5582538330123));
#104009=CARTESIAN_POINT('Ctrl Pts',(-6.56690401319744,638.674272442424,
75.153793775975));
#104010=CARTESIAN_POINT('Ctrl Pts',(-7.55642794248227,639.075238610304,
74.4484723523538));
#104011=CARTESIAN_POINT('Ctrl Pts',(-7.87639888507424,639.212635032722,
74.1960774136137));
#104012=CARTESIAN_POINT('Ctrl Pts',(-8.48513868812207,639.485777362373,
73.6665189366011));
#104013=CARTESIAN_POINT('Ctrl Pts',(-8.77540631388641,639.622107542019,
73.3883947993268));
#104014=CARTESIAN_POINT('Ctrl Pts',(-9.32889245043522,639.891043814546,
72.8050737176796));
#104015=CARTESIAN_POINT('Ctrl Pts',(-9.59210827130408,640.023658956193,
72.4998783443379));
#104016=CARTESIAN_POINT('Ctrl Pts',(-10.0915350771624,640.28212906445,71.8610821467425));
#104017=CARTESIAN_POINT('Ctrl Pts',(-10.3287739497107,640.408558271658,
71.525776856965));
#104018=CARTESIAN_POINT('Ctrl Pts',(-10.9894725080146,640.768129166215,
70.4882632613146));
#104019=CARTESIAN_POINT('Ctrl Pts',(-11.3625914305347,640.981504678687,
69.7564109606946));
#104020=CARTESIAN_POINT('Ctrl Pts',(-11.818404938002,641.247406419786,68.5929331071031));
#104021=CARTESIAN_POINT('Ctrl Pts',(-11.9534576443998,641.327342492746,
68.1916750120165));
#104022=CARTESIAN_POINT('Ctrl Pts',(-12.182174157639,641.463778556434,67.3809131335881));
#104023=CARTESIAN_POINT('Ctrl Pts',(-12.276307508626,641.520542453502,66.9709644805429));
#104024=CARTESIAN_POINT('Ctrl Pts',(-12.4242394369779,641.610119675406,
66.1418454500847));
#104025=CARTESIAN_POINT('Ctrl Pts',(-12.4780399075043,641.642936469747,
65.7226757432849));
#104026=CARTESIAN_POINT('Ctrl Pts',(-12.5441585218638,641.683305659608,
64.8747881241364));
#104027=CARTESIAN_POINT('Ctrl Pts',(-12.5562467120334,641.690716433489,
64.4432644779558));
#104028=CARTESIAN_POINT('Ctrl Pts',(-12.5282315834883,641.673580507606,
63.1661747786782));
#104029=CARTESIAN_POINT('Ctrl Pts',(-12.4261421803805,641.610839125609,
62.3315318096105));
#104030=CARTESIAN_POINT('Ctrl Pts',(-12.1532157238051,641.446489533143,
61.1033176255798));
#104031=CARTESIAN_POINT('Ctrl Pts',(-12.0418922330986,641.379825623817,
60.6972107540752));
#104032=CARTESIAN_POINT('Ctrl Pts',(-11.7789498235242,641.224316920002,
59.8958888312612));
#104033=CARTESIAN_POINT('Ctrl Pts',(-11.6297082784345,641.136886271958,
59.5076325746472));
#104034=CARTESIAN_POINT('Ctrl Pts',(-11.1319937919119,640.849938512318,
58.3769969850098));
#104035=CARTESIAN_POINT('Ctrl Pts',(-10.7340829199422,640.625798126202,
57.6684452447755));
#104036=CARTESIAN_POINT('Ctrl Pts',(-10.040023576069,640.255218646015,56.6679468437341));
#104037=CARTESIAN_POINT('Ctrl Pts',(-9.79091798691913,640.125241864666,
56.3433436698442));
#104038=CARTESIAN_POINT('Ctrl Pts',(-9.26667744604236,639.860382199086,
55.7243454178727));
#104039=CARTESIAN_POINT('Ctrl Pts',(-8.99185892776024,639.725615805067,
55.4299091303579));
#104040=CARTESIAN_POINT('Ctrl Pts',(-8.1292937094432,639.319056101314,54.5894500217195));
#104041=CARTESIAN_POINT('Ctrl Pts',(-7.5038764230366,639.044668394762,54.0856572853192));
#104042=CARTESIAN_POINT('Ctrl Pts',(-6.14010017594243,638.518378987584,
53.1918099095666));
#104043=CARTESIAN_POINT('Ctrl Pts',(-5.42038031899213,638.273835975921,
52.8139552665562));
#104044=CARTESIAN_POINT('Ctrl Pts',(-4.27629107737484,637.959970371973,
52.3511891253608));
#104045=CARTESIAN_POINT('Ctrl Pts',(-3.88308899204296,637.864026388571,
52.2141438459509));
#104046=CARTESIAN_POINT('Ctrl Pts',(-3.07656099875632,637.695968083433,
51.9785830844804));
#104047=CARTESIAN_POINT('Ctrl Pts',(-2.66897700762064,637.625031584555,
51.8816585325753));
#104048=CARTESIAN_POINT('Ctrl Pts',(-1.84491113503772,637.512268879597,
51.7291914233704));
#104049=CARTESIAN_POINT('Ctrl Pts',(-1.42842899531872,637.470445472889,
51.67364863131));
#104050=CARTESIAN_POINT('Ctrl Pts',(-0.586133086793797,637.418625085894,
51.6050092571627));
#104051=CARTESIAN_POINT('Ctrl Pts',(-0.159088542674411,637.408657678832,
51.5919408760206));
#104052=CARTESIAN_POINT('Ctrl Pts',(0.270210553101167,637.415754985731,
51.6012974652903));
#104053=CARTESIAN_POINT('Ctrl Pts',(0.422698892023407,637.418949661958,
51.6054949190759));
#104054=CARTESIAN_POINT('Ctrl Pts',(0.401375821438588,637.722772699625,
52.0060233138173));
#104055=CARTESIAN_POINT('Ctrl Pts',(0.414276434700987,637.21974803095,52.0064418924399));
#104056=CARTESIAN_POINT('Ctrl Pts',(-0.485687802890622,637.395421830215,
51.5746539347076));
#104057=CARTESIAN_POINT('Ctrl Pts',(-0.464187114878885,637.702785894513,
51.9782978993784));
#104058=CARTESIAN_POINT('Ctrl Pts',(-0.476010708084271,637.196500386218,
51.9765750164005));
#104059=CARTESIAN_POINT('Ctrl Pts',(-1.37343881346729,637.448508508017,
51.6430377951267));
#104060=CARTESIAN_POINT('Ctrl Pts',(-1.28833508012202,637.745869850797,
52.037024971321));
#104061=CARTESIAN_POINT('Ctrl Pts',(-1.3460709313523,637.248954683656,52.0427987467284));
#104062=CARTESIAN_POINT('Ctrl Pts',(-2.65150548283939,637.622235142896,
51.8778512479119));
#104063=CARTESIAN_POINT('Ctrl Pts',(-2.52264148011033,637.898282658345,
52.2542948909666));
#104064=CARTESIAN_POINT('Ctrl Pts',(-2.59867283526968,637.420612734044,
52.2701959516384));
#104065=CARTESIAN_POINT('Ctrl Pts',(-3.05701248764582,637.692361961531,
51.9736219146518));
#104066=CARTESIAN_POINT('Ctrl Pts',(-2.9104992780375,637.959022674606,52.3416256351175));
#104067=CARTESIAN_POINT('Ctrl Pts',(-2.99609991422878,637.489904443202,
52.3629416887653));
#104068=CARTESIAN_POINT('Ctrl Pts',(-3.85966274491754,637.858622815906,
52.2064814361353));
#104069=CARTESIAN_POINT('Ctrl Pts',(-3.68456306759803,638.105545872289,
52.5572384796229));
#104070=CARTESIAN_POINT('Ctrl Pts',(-3.78275735662804,637.654185523528,
52.5884464824649));
#104071=CARTESIAN_POINT('Ctrl Pts',(-4.2516957080172,637.953733553696,52.342197416409));
#104072=CARTESIAN_POINT('Ctrl Pts',(-4.06360822860176,638.189474882183,
52.6827304516184));
#104073=CARTESIAN_POINT('Ctrl Pts',(-4.166979050703,637.748163685361,52.7198758782938));
#104074=CARTESIAN_POINT('Ctrl Pts',(-5.39252319671764,638.265104382238,
52.8006937061185));
#104075=CARTESIAN_POINT('Ctrl Pts',(-5.15820380454856,638.464354488508,
53.106143986478));
#104076=CARTESIAN_POINT('Ctrl Pts',(-5.28507434996358,638.055826516981,
53.1638902156519));
#104077=CARTESIAN_POINT('Ctrl Pts',(-6.11111639604367,638.508142463439,
53.1755283868842));
#104078=CARTESIAN_POINT('Ctrl Pts',(-5.8622172477199,638.682290229399,53.4546201335385));
#104079=CARTESIAN_POINT('Ctrl Pts',(-5.98934985904857,638.295970472941,
53.5268853366489));
#104080=CARTESIAN_POINT('Ctrl Pts',(-7.47414788157404,639.032208675362,
54.0634384892155));
#104081=CARTESIAN_POINT('Ctrl Pts',(-7.20845486530066,639.164782335859,
54.3026771532069));
#104082=CARTESIAN_POINT('Ctrl Pts',(-7.32522403708878,638.813796828574,
54.3867510931747));
#104083=CARTESIAN_POINT('Ctrl Pts',(-8.10110508190111,639.306397424697,
54.5652847276252));
#104084=CARTESIAN_POINT('Ctrl Pts',(-7.83452284189272,639.419779216059,
54.7821223431411));
#104085=CARTESIAN_POINT('Ctrl Pts',(-7.93969011684976,639.084720971824,
54.8727462625326));
#104086=CARTESIAN_POINT('Ctrl Pts',(-8.96598822614474,639.713072351722,
55.4030453263832));
#104087=CARTESIAN_POINT('Ctrl Pts',(-8.70809531403378,639.8065991219,55.6034482729444));
#104088=CARTESIAN_POINT('Ctrl Pts',(-8.78734281065214,639.486554596994,
55.6840474437807));
#104089=CARTESIAN_POINT('Ctrl Pts',(-9.24171805717354,639.847996124981,
55.6967061098111));
#104090=CARTESIAN_POINT('Ctrl Pts',(-8.98356312241736,639.933680039658,
55.887647513816));
#104091=CARTESIAN_POINT('Ctrl Pts',(-9.05757910582421,639.619871964218,
55.9684328676933));
#104092=CARTESIAN_POINT('Ctrl Pts',(-9.76801292518633,640.113392489719,
56.3144572329125));
#104093=CARTESIAN_POINT('Ctrl Pts',(-9.50901929974678,640.184197151179,
56.4871657754348));
#104094=CARTESIAN_POINT('Ctrl Pts',(-9.57338818638589,639.882108498261,
56.5666721248706));
#104095=CARTESIAN_POINT('Ctrl Pts',(-10.0185033275,640.243874592087,56.6388958448344));
#104096=CARTESIAN_POINT('Ctrl Pts',(-9.7600322735385,640.307954662928,56.8025965430298));
#104097=CARTESIAN_POINT('Ctrl Pts',(-9.8188879556435,640.011037106482,56.8808632052432));
#104098=CARTESIAN_POINT('Ctrl Pts',(-10.716727326934,640.616151015162,57.6394451240119));
#104099=CARTESIAN_POINT('Ctrl Pts',(-10.4506899105479,640.65724880266,57.7657813921744));
#104100=CARTESIAN_POINT('Ctrl Pts',(-10.5031997469232,640.378880679238,
57.8498081873022));
#104101=CARTESIAN_POINT('Ctrl Pts',(-11.1175203099313,640.841694041044,
58.3487305133394));
#104102=CARTESIAN_POINT('Ctrl Pts',(-10.8571731765776,640.874517949965,
58.4602774988305));
#104103=CARTESIAN_POINT('Ctrl Pts',(-10.8960080548356,640.601738696694,
58.5366905083561));
#104104=CARTESIAN_POINT('Ctrl Pts',(-11.619394535175,641.130841438184,59.4818150157709));
#104105=CARTESIAN_POINT('Ctrl Pts',(-11.3646047806954,641.153135988497,
59.5771443494444));
#104106=CARTESIAN_POINT('Ctrl Pts',(-11.3878836354649,640.887443837893,
59.6339866130622));
#104107=CARTESIAN_POINT('Ctrl Pts',(-11.7699948379489,641.219020908331,
59.8711153341678));
#104108=CARTESIAN_POINT('Ctrl Pts',(-11.5161693648167,641.237777958691,
59.9583961633857));
#104109=CARTESIAN_POINT('Ctrl Pts',(-11.5354834909803,640.974573487447,
60.0109905179452));
#104110=CARTESIAN_POINT('Ctrl Pts',(-12.0355183921279,641.375990158675,
60.6750733074951));
#104111=CARTESIAN_POINT('Ctrl Pts',(-11.7825939140218,641.388123439216,
60.7452930450769));
#104112=CARTESIAN_POINT('Ctrl Pts',(-11.7957168424692,641.129673875916,
60.7895545484208));
#104113=CARTESIAN_POINT('Ctrl Pts',(-12.1481703593011,641.443430005107,
61.0832468504235));
#104114=CARTESIAN_POINT('Ctrl Pts',(-11.8961009417762,641.453030580109,
61.145720101883));
#104115=CARTESIAN_POINT('Ctrl Pts',(-11.9061244276539,641.196310824918,
61.1848355228865));
#104116=CARTESIAN_POINT('Ctrl Pts',(-12.4242303319733,641.609632067201,
62.3171054077186));
#104117=CARTESIAN_POINT('Ctrl Pts',(-12.1719915811263,641.611765497776,
62.3490805674734));
#104118=CARTESIAN_POINT('Ctrl Pts',(-12.1766841067953,641.360534000301,
62.3797203320405));
#104119=CARTESIAN_POINT('Ctrl Pts',(-12.5276874182953,641.673215309511,
63.1559355922065));
#104120=CARTESIAN_POINT('Ctrl Pts',(-12.2775058411409,641.673796783702,
63.1776792731061));
#104121=CARTESIAN_POINT('Ctrl Pts',(-12.2780801673297,641.423360360423,
63.1920557640221));
#104122=CARTESIAN_POINT('Ctrl Pts',(-12.5564129571305,641.690785777535,
64.4400267385226));
#104123=CARTESIAN_POINT('Ctrl Pts',(-12.3063643128568,641.69068276132,64.4370638410256));
#104124=CARTESIAN_POINT('Ctrl Pts',(-12.3062333905587,641.440721636806,
64.4355871579955));
#104125=CARTESIAN_POINT('Ctrl Pts',(-12.5443205872794,641.683372183581,
64.8740772469317));
#104126=CARTESIAN_POINT('Ctrl Pts',(-12.2941718209377,641.68353116687,64.8634434416355));
#104127=CARTESIAN_POINT('Ctrl Pts',(-12.2943819383328,641.433396304253,
64.8559276849426));
#104128=CARTESIAN_POINT('Ctrl Pts',(-12.4777330003823,641.64271664739,65.7266035670265));
#104129=CARTESIAN_POINT('Ctrl Pts',(-12.2273094971991,641.644483451026,
65.6991136324248));
#104130=CARTESIAN_POINT('Ctrl Pts',(-12.2291210200655,641.393224809202,
65.6815257693198));
#104131=CARTESIAN_POINT('Ctrl Pts',(-12.4234779559463,641.609622661129,
66.1479562446186));
#104132=CARTESIAN_POINT('Ctrl Pts',(-12.1726163502219,641.612576505469,
66.1128812981191));
#104133=CARTESIAN_POINT('Ctrl Pts',(-12.1759469061432,641.360524818572,
66.0895695514284));
#104134=CARTESIAN_POINT('Ctrl Pts',(-12.2742573339491,641.519271348643,
66.9811892328191));
#104135=CARTESIAN_POINT('Ctrl Pts',(-12.0228067561347,641.525859578493,
66.9293351464561));
#104136=CARTESIAN_POINT('Ctrl Pts',(-12.0296993061205,641.271249220213,
66.896483765114));
#104137=CARTESIAN_POINT('Ctrl Pts',(-12.1792897304192,641.462010453369,
67.393068477219));
#104138=CARTESIAN_POINT('Ctrl Pts',(-11.9271007354986,641.470712297851,
67.3335484589464));
#104139=CARTESIAN_POINT('Ctrl Pts',(-11.9366237554634,641.214670037509,
67.2953533735953));
#104140=CARTESIAN_POINT('Ctrl Pts',(-11.9485583932798,641.324400942808,
68.20744886739));
#104141=CARTESIAN_POINT('Ctrl Pts',(-11.6955378132595,641.338808940148,
68.130976713246));
#104142=CARTESIAN_POINT('Ctrl Pts',(-11.7104894329877,641.078698892736,
68.0840105657425));
#104143=CARTESIAN_POINT('Ctrl Pts',(-11.8123667673948,641.243813984238,
68.6102326743059));
#104144=CARTESIAN_POINT('Ctrl Pts',(-11.5583984649845,641.261357597934,
68.5257596552219));
#104145=CARTESIAN_POINT('Ctrl Pts',(-11.5770111802493,640.999071358111,
68.474072058525));
#104146=CARTESIAN_POINT('Ctrl Pts',(-11.3530417450549,640.975973416792,
69.7773368489012));
#104147=CARTESIAN_POINT('Ctrl Pts',(-11.094177851908,641.003183187458,69.6760041353329));
#104148=CARTESIAN_POINT('Ctrl Pts',(-11.1268371472754,640.734419412521,
69.6043131395056));
#104149=CARTESIAN_POINT('Ctrl Pts',(-10.9773436374481,640.761257671499,
70.5106549236237));
#104150=CARTESIAN_POINT('Ctrl Pts',(-10.7127265394219,640.795865883309,
70.3951256963504));
#104151=CARTESIAN_POINT('Ctrl Pts',(-10.7586237260962,640.522259749011,
70.3144690681693));
#104152=CARTESIAN_POINT('Ctrl Pts',(-10.3128000119404,640.399951370545,
71.5492638109213));
#104153=CARTESIAN_POINT('Ctrl Pts',(-10.0546064812974,640.45606535248,71.3965629016389));
#104154=CARTESIAN_POINT('Ctrl Pts',(-10.1073211782066,640.165255645638,
71.3202714227271));
#104155=CARTESIAN_POINT('Ctrl Pts',(-10.0744570782856,640.273083587572,
71.8844906020682));
#104156=CARTESIAN_POINT('Ctrl Pts',(-9.81559960598111,640.335484419032,
71.722883385682));
#104157=CARTESIAN_POINT('Ctrl Pts',(-9.87372685329524,640.039898320491,
71.6449099002616));
#104158=CARTESIAN_POINT('Ctrl Pts',(-9.5730180198315,640.013923785954,72.5228060041743));
#104159=CARTESIAN_POINT('Ctrl Pts',(-9.31451031820139,640.090283649802,
72.3432405042314));
#104160=CARTESIAN_POINT('Ctrl Pts',(-9.38227834633797,639.783824086546,
72.2630638437438));
#104161=CARTESIAN_POINT('Ctrl Pts',(-9.30888880145443,639.881056246463,
72.827584871394));
#104162=CARTESIAN_POINT('Ctrl Pts',(-9.05028270509328,639.96475736298,72.6387917490736));
#104163=CARTESIAN_POINT('Ctrl Pts',(-9.12341151926098,639.652538458904,
72.5582161648588));
#104164=CARTESIAN_POINT('Ctrl Pts',(-8.75381487614663,639.611825072234,
73.40978275451));
#104165=CARTESIAN_POINT('Ctrl Pts',(-8.49692150109578,639.711562811131,
73.2025036527718));
#104166=CARTESIAN_POINT('Ctrl Pts',(-8.57939679683925,639.386512790825,
73.1220252238533));
#104167=CARTESIAN_POINT('Ctrl Pts',(-8.46287263080748,639.475452444918,
73.6871999316855));
#104168=CARTESIAN_POINT('Ctrl Pts',(-8.2067446500672,639.583671139382,73.4702530911214));
#104169=CARTESIAN_POINT('Ctrl Pts',(-8.29425119061942,639.251763833223,
73.3906801363316));
#104170=CARTESIAN_POINT('Ctrl Pts',(-7.85308898859091,639.202454098524,
74.2151005589185));
#104171=CARTESIAN_POINT('Ctrl Pts',(-7.60084562786785,639.328898689758,
73.978892784628));
#104172=CARTESIAN_POINT('Ctrl Pts',(-7.69661684926344,638.982015887313,
73.9019070495361));
#104173=CARTESIAN_POINT('Ctrl Pts',(-7.53269227808987,639.065231345536,
74.4665545912258));
#104174=CARTESIAN_POINT('Ctrl Pts',(-7.28274092847238,639.201467950777,
74.2199817961026));
#104175=CARTESIAN_POINT('Ctrl Pts',(-7.3826036898993,638.84642696737,74.1454188990161));
#104176=CARTESIAN_POINT('Ctrl Pts',(-6.54436688094676,638.665837118865,
75.1676209958109));
#104177=CARTESIAN_POINT('Ctrl Pts',(-6.28966522125244,638.826499839077,
74.9017755309047));
#104178=CARTESIAN_POINT('Ctrl Pts',(-6.41396819947268,638.45178748053,74.8243434255003));
#104179=CARTESIAN_POINT('Ctrl Pts',(-5.84677300034356,638.414131609539,
75.5680603372253));
#104180=CARTESIAN_POINT('Ctrl Pts',(-5.60308614276541,638.598811561366,
75.2765310704285));
#104181=CARTESIAN_POINT('Ctrl Pts',(-5.73027341984355,638.20307921196,75.2121345157478));
#104182=CARTESIAN_POINT('Ctrl Pts',(-4.735123634144,638.082280084104,76.0690872002211));
#104183=CARTESIAN_POINT('Ctrl Pts',(-4.53330991520824,638.304130947767,
75.7410809439269));
#104184=CARTESIAN_POINT('Ctrl Pts',(-4.64077478504796,637.875179554541,
75.6973360141623));
#104185=CARTESIAN_POINT('Ctrl Pts',(-4.35360434329439,637.979334203798,
76.2193388306527));
#104186=CARTESIAN_POINT('Ctrl Pts',(-4.16281829720205,638.212579524345,
75.8808099165903));
#104187=CARTESIAN_POINT('Ctrl Pts',(-4.26685720707408,637.773459525923,
75.8428419591479));
#104188=CARTESIAN_POINT('Ctrl Pts',(-3.56604570114688,637.793748701365,
76.4843606975452));
#104189=CARTESIAN_POINT('Ctrl Pts',(-3.40047115190969,638.047948850038,
76.127370335997));
#104190=CARTESIAN_POINT('Ctrl Pts',(-3.49499057985149,637.590083879434,
76.0994932686235));
#104191=CARTESIAN_POINT('Ctrl Pts',(-3.16152317445562,637.71170299198,76.5982831453345));
#104192=CARTESIAN_POINT('Ctrl Pts',(-3.01184896420212,637.976344024389,
76.2318455359098));
#104193=CARTESIAN_POINT('Ctrl Pts',(-3.09852828926658,637.509015197064,
76.2098174680871));
#104194=CARTESIAN_POINT('Ctrl Pts',(-1.89224989733331,637.500669633967,
76.887268497963));
#104195=CARTESIAN_POINT('Ctrl Pts',(-1.77973073550203,637.789819969329,
76.5008366075363));
#104196=CARTESIAN_POINT('Ctrl Pts',(-1.85454421885567,637.300494574968,
76.4896756819702));
#104197=CARTESIAN_POINT('Ctrl Pts',(-1.0083393223673,637.41933676935,76.9927644491279));
#104198=CARTESIAN_POINT('Ctrl Pts',(-0.956219519798643,637.723350752829,
76.5919508447244));
#104199=CARTESIAN_POINT('Ctrl Pts',(-0.988247314567113,637.220130545011,
76.5918392124773));
#104200=CARTESIAN_POINT('Ctrl Pts',(-0.100242643464739,637.413790050648,
77.0002550481953));
#104201=CARTESIAN_POINT('Ctrl Pts',(-0.0952647791071383,637.71834699738,
76.5990988612787));
#104202=CARTESIAN_POINT('Ctrl Pts',(-0.098245300777777,637.214649861766,
76.5990932436941));
#104203=CARTESIAN_POINT('Ctrl Pts',(-3.14894350550333,635.052705176108,
48.9762189006802));
#104204=CARTESIAN_POINT('Ctrl Pts',(-3.17805581581006,634.981774591649,
48.9095429264701));
#104205=CARTESIAN_POINT('Ctrl Pts',(-3.19988829483125,634.881466988651,
48.9136642378198));
#104206=CARTESIAN_POINT('Ctrl Pts',(-2.26217542759882,634.844413884159,
48.7825198376226));
#104207=CARTESIAN_POINT('Ctrl Pts',(-2.28874499765809,634.773843548207,
48.7179545738432));
#104208=CARTESIAN_POINT('Ctrl Pts',(-2.2988111695793,634.675657800926,48.7191843934846));
#104209=CARTESIAN_POINT('Ctrl Pts',(-1.27865210597201,634.714844669714,
48.6668762937005));
#104210=CARTESIAN_POINT('Ctrl Pts',(-1.29103235742706,634.643610831895,
48.6027815718824));
#104211=CARTESIAN_POINT('Ctrl Pts',(-1.29934864835061,634.547626991756,
48.6030696395671));
#104212=CARTESIAN_POINT('Ctrl Pts',(0.242130489444798,634.682105481683,
48.6375535275712));
#104213=CARTESIAN_POINT('Ctrl Pts',(0.244224674588167,634.610876552288,
48.5737334451187));
#104214=CARTESIAN_POINT('Ctrl Pts',(0.24604904762521,634.515277216675,48.5736280341214));
#104215=CARTESIAN_POINT('Ctrl Pts',(0.781040459010377,634.702757772588,
48.6559104137994));
#104216=CARTESIAN_POINT('Ctrl Pts',(0.788931574693899,634.631577480282,
48.5919652205538));
#104217=CARTESIAN_POINT('Ctrl Pts',(0.793683375382584,634.535683985946,
48.5920594319863));
#104218=CARTESIAN_POINT('Ctrl Pts',(2.35874810817493,634.852789214134,48.791311990248));
#104219=CARTESIAN_POINT('Ctrl Pts',(2.38338099377123,634.781749974576,48.7262413336859));
#104220=CARTESIAN_POINT('Ctrl Pts',(2.39693158170349,634.683931291769,48.7280101254697));
#104221=CARTESIAN_POINT('Ctrl Pts',(3.37298184661552,635.068933230022,48.9865958531244));
#104222=CARTESIAN_POINT('Ctrl Pts',(3.41253860309941,634.999941019321,48.9217203889832));
#104223=CARTESIAN_POINT('Ctrl Pts',(3.42759398731837,634.897509402095,48.9240904248496));
#104224=CARTESIAN_POINT('Ctrl Pts',(4.60280256700872,635.442476264948,49.351977573634));
#104225=CARTESIAN_POINT('Ctrl Pts',(4.64765158093338,635.37152943939,49.2817265518851));
#104226=CARTESIAN_POINT('Ctrl Pts',(4.67730317816144,635.266604909258,49.2909483904667));
#104227=CARTESIAN_POINT('Ctrl Pts',(4.84718746008067,635.522512124264,49.4313666860681));
#104228=CARTESIAN_POINT('Ctrl Pts',(4.89464885506356,635.451676187017,49.3604691881232));
#104229=CARTESIAN_POINT('Ctrl Pts',(4.92564398215479,635.345689107181,49.3706595461052));
#104230=CARTESIAN_POINT('Ctrl Pts',(5.32584062015199,635.689537216775,49.6000512954552));
#104231=CARTESIAN_POINT('Ctrl Pts',(5.37840998526045,635.618886104377,49.5277111330022));
#104232=CARTESIAN_POINT('Ctrl Pts',(5.41204506061927,635.510728093336,49.5400282810896));
#104233=CARTESIAN_POINT('Ctrl Pts',(5.56095277341081,635.776762458102,49.6895734166027));
#104234=CARTESIAN_POINT('Ctrl Pts',(5.61612178002954,635.706265107494,49.6165277399625));
#104235=CARTESIAN_POINT('Ctrl Pts',(5.65096311005464,635.596916271685,49.6299136263926));
#104236=CARTESIAN_POINT('Ctrl Pts',(6.25472898600255,636.04770447283,49.973139660512));
#104237=CARTESIAN_POINT('Ctrl Pts',(6.31941936621702,635.978335899727,49.8984892971421));
#104238=CARTESIAN_POINT('Ctrl Pts',(6.35597407519104,635.864638452226,49.914631946893));
#104239=CARTESIAN_POINT('Ctrl Pts',(6.70189742601776,636.240627504047,50.1821258540263));
#104240=CARTESIAN_POINT('Ctrl Pts',(6.77205222396553,636.171955285493,50.1062416227097));
#104241=CARTESIAN_POINT('Ctrl Pts',(6.81038188975856,636.05526856269,50.1244671165347));
#104242=CARTESIAN_POINT('Ctrl Pts',(7.56968515550765,636.642919469563,50.6387960920349));
#104243=CARTESIAN_POINT('Ctrl Pts',(7.65049736475119,636.575382508907,50.5595723308578));
#104244=CARTESIAN_POINT('Ctrl Pts',(7.69221803306948,636.452778493096,50.5829910891641));
#104245=CARTESIAN_POINT('Ctrl Pts',(7.99028738530131,636.852312016469,50.8864885495721));
#104246=CARTESIAN_POINT('Ctrl Pts',(8.07671976444589,636.785759599221,50.8060183026103));
#104247=CARTESIAN_POINT('Ctrl Pts',(8.11963001506569,636.659682895894,50.831690360471));
#104248=CARTESIAN_POINT('Ctrl Pts',(8.80740286369044,637.281161742136,51.4212246124972));
#104249=CARTESIAN_POINT('Ctrl Pts',(8.90504619960573,637.216475096936,51.3374439703381));
#104250=CARTESIAN_POINT('Ctrl Pts',(8.94997490797288,637.083436369467,51.3685986628816));
#104251=CARTESIAN_POINT('Ctrl Pts',(9.20548162083383,637.501580052554,51.7096442401456));
#104252=CARTESIAN_POINT('Ctrl Pts',(9.30897039084119,637.438216925406,51.6247044118637));
#104253=CARTESIAN_POINT('Ctrl Pts',(9.35449918700437,637.301236129998,51.658191408593));
#104254=CARTESIAN_POINT('Ctrl Pts',(10.3487844505047,638.160185666631,52.6234603889831));
#104255=CARTESIAN_POINT('Ctrl Pts',(10.4792441450531,638.106209094922,52.541391505325));
#104256=CARTESIAN_POINT('Ctrl Pts',(10.5163351536716,637.952029241467,52.575739049541));
#104257=CARTESIAN_POINT('Ctrl Pts',(11.0469172883128,638.596769704622,53.2977962975319));
#104258=CARTESIAN_POINT('Ctrl Pts',(11.1886816147118,638.54672121981,53.2166715576217));
#104259=CARTESIAN_POINT('Ctrl Pts',(11.2257713012345,638.383429089509,53.2528256613287));
#104260=CARTESIAN_POINT('Ctrl Pts',(12.004918884179,639.222046706336,54.4157870888981));
#104261=CARTESIAN_POINT('Ctrl Pts',(12.1575997879902,639.173534897356,54.3239043685374));
#104262=CARTESIAN_POINT('Ctrl Pts',(12.1992715391054,639.001272383721,54.3753501795627));
#104263=CARTESIAN_POINT('Ctrl Pts',(12.3091950227284,639.425602760796,54.8063260024279));
#104264=CARTESIAN_POINT('Ctrl Pts',(12.4682176936469,639.379586655534,54.7148446167707));
#104265=CARTESIAN_POINT('Ctrl Pts',(12.5084759793438,639.202412549241,54.7674817836186));
#104266=CARTESIAN_POINT('Ctrl Pts',(12.8866359918317,639.818864013947,55.6266595150129));
#104267=CARTESIAN_POINT('Ctrl Pts',(13.0590920906577,639.778506365938,55.5364326108684));
#104268=CARTESIAN_POINT('Ctrl Pts',(13.0952716020131,639.591007890039,55.5911613762021));
#104269=CARTESIAN_POINT('Ctrl Pts',(13.156552724659,640.006361596555,56.0520433785381));
#104270=CARTESIAN_POINT('Ctrl Pts',(13.335263436409,639.968754189557,55.9630634399455));
#104271=CARTESIAN_POINT('Ctrl Pts',(13.3695604686926,639.776280855815,56.0182814407224));
#104272=CARTESIAN_POINT('Ctrl Pts',(13.9047588183327,640.533044717664,57.36769888129));
#104273=CARTESIAN_POINT('Ctrl Pts',(14.1102991866389,640.509684718848,57.296294905319));
#104274=CARTESIAN_POINT('Ctrl Pts',(14.1299035774209,640.29672728974,57.3393334951756));
#104275=CARTESIAN_POINT('Ctrl Pts',(14.3247076934248,640.838404048473,58.3002140367118));
#104276=CARTESIAN_POINT('Ctrl Pts',(14.5388220217874,640.818919962782,58.233681282548));
#104277=CARTESIAN_POINT('Ctrl Pts',(14.5566498549489,640.598461612561,58.2756573376281));
#104278=CARTESIAN_POINT('Ctrl Pts',(14.7401433929705,641.144014898982,59.5471387316695));
#104279=CARTESIAN_POINT('Ctrl Pts',(14.9637997646997,641.128994182546,59.4803694808451));
#104280=CARTESIAN_POINT('Ctrl Pts',(14.9788110762547,640.900445339403,59.5276607666015));
#104281=CARTESIAN_POINT('Ctrl Pts',(14.8176813623333,641.201300483029,59.8008321998988));
#104282=CARTESIAN_POINT('Ctrl Pts',(15.0439529783747,641.187731406209,59.7367889937231));
#104283=CARTESIAN_POINT('Ctrl Pts',(15.0576058396701,640.957052162534,59.7823928247067));
#104284=CARTESIAN_POINT('Ctrl Pts',(14.9592279732976,641.306193352759,60.3093954217731));
#104285=CARTESIAN_POINT('Ctrl Pts',(15.1905205855739,641.295464675235,60.2513664040229));
#104286=CARTESIAN_POINT('Ctrl Pts',(15.2014471033479,641.060702480953,60.2930389236187));
#104287=CARTESIAN_POINT('Ctrl Pts',(15.0235498579237,641.354030625955,60.5651452400211));
#104288=CARTESIAN_POINT('Ctrl Pts',(15.2571084270983,641.344588327562,60.5101927719222));
#104289=CARTESIAN_POINT('Ctrl Pts',(15.2668116417703,641.107973039748,60.5498362104747));
#104290=CARTESIAN_POINT('Ctrl Pts',(15.1972467822455,641.483514247277,61.3368028828921));
#104291=CARTESIAN_POINT('Ctrl Pts',(15.4377062255518,641.478133269179,61.2940470335773));
#104292=CARTESIAN_POINT('Ctrl Pts',(15.4433255182961,641.23592371238,61.3246595339165));
#104293=CARTESIAN_POINT('Ctrl Pts',(15.2874077780666,641.551156104484,61.8571195614639));
#104294=CARTESIAN_POINT('Ctrl Pts',(15.5309261439817,641.547515205012,61.8206844364525));
#104295=CARTESIAN_POINT('Ctrl Pts',(15.5349475887123,641.302764009413,61.8471069255291));
#104296=CARTESIAN_POINT('Ctrl Pts',(15.4156790030771,641.647548755422,62.9097786108428));
#104297=CARTESIAN_POINT('Ctrl Pts',(15.6642372322958,641.646898393203,62.8892513959473));
#104298=CARTESIAN_POINT('Ctrl Pts',(15.6652986681034,641.398015292898,62.9040820559312));
#104299=CARTESIAN_POINT('Ctrl Pts',(15.4537982322333,641.67630751549,63.4421236247392));
#104300=CARTESIAN_POINT('Ctrl Pts',(15.7037030786927,641.676438218184,63.4286901969925));
#104301=CARTESIAN_POINT('Ctrl Pts',(15.7040356606937,641.426433309297,63.4386078350693));
#104302=CARTESIAN_POINT('Ctrl Pts',(15.4700545523021,641.68856386249,64.2501300119848));
#104303=CARTESIAN_POINT('Ctrl Pts',(15.720610340671,641.689084457603,64.2494068634906));
#104304=CARTESIAN_POINT('Ctrl Pts',(15.720555575138,641.438544541415,64.2499277579685));
#104305=CARTESIAN_POINT('Ctrl Pts',(15.4685832963044,641.687454020083,64.5221427161502));
#104306=CARTESIAN_POINT('Ctrl Pts',(15.7190815934227,641.687940364418,64.5256053426526));
#104307=CARTESIAN_POINT('Ctrl Pts',(15.7190604657519,641.437447841463,64.5230557734976));
#104308=CARTESIAN_POINT('Ctrl Pts',(15.4517606369933,641.67477231473,65.0625984317746));
#104309=CARTESIAN_POINT('Ctrl Pts',(15.7015814327667,641.674852353065,65.0746869533344));
#104310=CARTESIAN_POINT('Ctrl Pts',(15.7019650213429,641.424916281739,65.0657280699177));
#104311=CARTESIAN_POINT('Ctrl Pts',(15.4364817742608,641.663255235677,65.3311812375999));
#104312=CARTESIAN_POINT('Ctrl Pts',(15.685708149129,641.662981907014,65.3473542470335));
#104313=CARTESIAN_POINT('Ctrl Pts',(15.6864384446807,641.413535586959,65.3354120618728));
#104314=CARTESIAN_POINT('Ctrl Pts',(15.3266757045973,641.580587358346,66.6661082158761));
#104315=CARTESIAN_POINT('Ctrl Pts',(15.5718851336501,641.577969541552,66.6988378773207));
#104316=CARTESIAN_POINT('Ctrl Pts',(15.574852527381,641.331846983568,66.675805476863));
#104317=CARTESIAN_POINT('Ctrl Pts',(15.1329768512553,641.434622754534,67.7086964322208));
#104318=CARTESIAN_POINT('Ctrl Pts',(15.3741355634771,641.430085435439,67.7474289072551));
#104319=CARTESIAN_POINT('Ctrl Pts',(15.3780196332794,641.18761548309,67.7226505757277));
#104320=CARTESIAN_POINT('Ctrl Pts',(14.5395600793765,640.995589078133,69.7454059551597));
#104321=CARTESIAN_POINT('Ctrl Pts',(14.7598045961286,640.979270094842,69.8078650818198));
#104322=CARTESIAN_POINT('Ctrl Pts',(14.7749830115725,640.753782796594,69.7677006850111));
#104323=CARTESIAN_POINT('Ctrl Pts',(14.1502976929651,640.710325139517,70.7036228750289));
#104324=CARTESIAN_POINT('Ctrl Pts',(14.3625245593818,640.690337599714,70.7712664447536));
#104325=CARTESIAN_POINT('Ctrl Pts',(14.3794203054433,640.471905369692,70.7298312303411));
#104326=CARTESIAN_POINT('Ctrl Pts',(13.4435515701974,640.207670726134,72.0586962144293));
#104327=CARTESIAN_POINT('Ctrl Pts',(13.6295943491114,640.173459148157,72.1457661580742));
#104328=CARTESIAN_POINT('Ctrl Pts',(13.6612091794102,639.975202281057,72.0904647072316));
#104329=CARTESIAN_POINT('Ctrl Pts',(13.185856425802,640.026580539771,72.4987899104209));
#104330=CARTESIAN_POINT('Ctrl Pts',(13.3656347598372,639.989501793385,72.5875774487109));
#104331=CARTESIAN_POINT('Ctrl Pts',(13.3993396267296,639.796260366034,72.5323553744969));
#104332=CARTESIAN_POINT('Ctrl Pts',(12.6358638843126,639.647007028405,73.342434424191));
#104333=CARTESIAN_POINT('Ctrl Pts',(12.8021776094238,639.603984080128,73.4333645836815));
#104334=CARTESIAN_POINT('Ctrl Pts',(12.8404364611288,639.421189580259,73.3794426010547));
#104335=CARTESIAN_POINT('Ctrl Pts',(12.3442395607504,639.448958868854,73.745486468069));
#104336=CARTESIAN_POINT('Ctrl Pts',(12.5042121997375,639.403324003737,73.8371312504688));
#104337=CARTESIAN_POINT('Ctrl Pts',(12.5440885772941,639.225491647343,73.7841389135551));
#104338=CARTESIAN_POINT('Ctrl Pts',(11.7288256021103,639.040370142431,74.5171827762023));
#104339=CARTESIAN_POINT('Ctrl Pts',(11.875674081091,638.989684606096,74.6087740523791));
#104340=CARTESIAN_POINT('Ctrl Pts',(11.9187059559954,638.821752085494,74.5589805782249));
#104341=CARTESIAN_POINT('Ctrl Pts',(11.405033028947,638.829813906688,74.8858160421478));
#104342=CARTESIAN_POINT('Ctrl Pts',(11.5456832679028,638.776912022865,74.9772519297627));
#104343=CARTESIAN_POINT('Ctrl Pts',(11.5896694934917,638.613695450973,74.929116152772));
#104344=CARTESIAN_POINT('Ctrl Pts',(10.7249053554299,638.400136864158,75.5904935058696));
#104345=CARTESIAN_POINT('Ctrl Pts',(10.8529135843585,638.3431579851,75.6803058137442));
#104346=CARTESIAN_POINT('Ctrl Pts',(10.8985267731535,638.189120059749,75.6366626093528));
#104347=CARTESIAN_POINT('Ctrl Pts',(10.3672411512523,638.180215772508,75.9276498830203));
#104348=CARTESIAN_POINT('Ctrl Pts',(10.4891833026195,638.121410763412,76.0167162365072));
#104349=CARTESIAN_POINT('Ctrl Pts',(10.5350707806408,637.971810624902,75.9751917541415));
#104350=CARTESIAN_POINT('Ctrl Pts',(9.25217348404458,637.519731600676,76.8832498458298));
#104351=CARTESIAN_POINT('Ctrl Pts',(9.36501835682016,637.461581119493,76.9607377506827));
#104352=CARTESIAN_POINT('Ctrl Pts',(9.40196706845938,637.319183392587,76.9346610568732));
#104353=CARTESIAN_POINT('Ctrl Pts',(8.46041324950306,637.081923907435,77.4415886133237));
#104354=CARTESIAN_POINT('Ctrl Pts',(8.56117701294616,637.020060912213,77.5194907589741));
#104355=CARTESIAN_POINT('Ctrl Pts',(8.59738601729796,636.886574518512,77.495276682365));
#104356=CARTESIAN_POINT('Ctrl Pts',(7.18898333288859,636.462030730398,78.1691179476835));
#104357=CARTESIAN_POINT('Ctrl Pts',(7.26509469234156,636.394030650501,78.2466972418932));
#104358=CARTESIAN_POINT('Ctrl Pts',(7.30535316787382,636.274040082039,78.2257709379294));
#104359=CARTESIAN_POINT('Ctrl Pts',(6.75104020321683,636.261633925678,78.3931160864462));
#104360=CARTESIAN_POINT('Ctrl Pts',(6.82166576422308,636.192852698254,78.4694208274702));
#104361=CARTESIAN_POINT('Ctrl Pts',(6.86031993687873,636.076024891079,78.4506791819244));
#104362=CARTESIAN_POINT('Ctrl Pts',(5.84247174669281,635.881018125929,78.8029438408063));
#104363=CARTESIAN_POINT('Ctrl Pts',(5.902618394964,635.811465969196,78.8760152018326));
#104364=CARTESIAN_POINT('Ctrl Pts',(5.93704365902223,635.699934177541,78.8621698493515));
#104365=CARTESIAN_POINT('Ctrl Pts',(5.36938928293472,635.700106636653,78.9894068856547));
#104366=CARTESIAN_POINT('Ctrl Pts',(5.42397848879053,635.629978355184,79.0613189453554));
#104367=CARTESIAN_POINT('Ctrl Pts',(5.45630243005711,635.521173033899,79.0493901878842));
#104368=CARTESIAN_POINT('Ctrl Pts',(3.52314404173299,635.078196936271,79.6117444884673));
#104369=CARTESIAN_POINT('Ctrl Pts',(3.57309729308637,635.012413171809,79.6733677987882));
#104370=CARTESIAN_POINT('Ctrl Pts',(3.58020877289446,634.90667060112,79.6742394975195));
#104371=CARTESIAN_POINT('Ctrl Pts',(2.0770701544568,634.760124060554,79.8888901784769));
#104372=CARTESIAN_POINT('Ctrl Pts',(2.10064307445653,634.687981505965,79.9545722316598));
#104373=CARTESIAN_POINT('Ctrl Pts',(2.11068986848203,634.592364494609,79.9525257971374));
#104374=CARTESIAN_POINT('Ctrl Pts',(0.512173773971106,634.699225564137,
79.9473100410624));
#104375=CARTESIAN_POINT('Ctrl Pts',(0.516051947899616,634.628452832944,
80.0106401135641));
#104376=CARTESIAN_POINT('Ctrl Pts',(0.520472179553334,634.532196202332,
80.0111755920238));
#104377=CARTESIAN_POINT('Ctrl Pts',(3.90492814027074,633.321803177584,49.5221152197639));
#104378=CARTESIAN_POINT('Ctrl Pts',(4.14330398493611,632.870375197478,49.135784443326));
#104379=CARTESIAN_POINT('Ctrl Pts',(3.96801791400367,633.484430412185,49.0902664690196));
#104380=CARTESIAN_POINT('Ctrl Pts',(2.89083941488624,633.016561541034,49.2609200704197));
#104381=CARTESIAN_POINT('Ctrl Pts',(3.03742703509678,632.497931245809,48.8340694352976));
#104382=CARTESIAN_POINT('Ctrl Pts',(2.93755241694889,633.17526999398,48.8214432993564));
#104383=CARTESIAN_POINT('Ctrl Pts',(1.83964868594593,632.808625463471,49.0977046826038));
#104384=CARTESIAN_POINT('Ctrl Pts',(1.96126338863992,632.261216236514,48.6607567236519));
#104385=CARTESIAN_POINT('Ctrl Pts',(1.86937071959366,632.964660360168,48.6534581338935));
#104386=CARTESIAN_POINT('Ctrl Pts',(0.211280116816066,632.709872623992,
49.0195828117931));
#104387=CARTESIAN_POINT('Ctrl Pts',(0.224160992892843,632.141263789567,
48.5717336255604));
#104388=CARTESIAN_POINT('Ctrl Pts',(0.214693779414581,632.864638970137,
48.5730542692393));
#104389=CARTESIAN_POINT('Ctrl Pts',(-0.32245537920764,632.712766771114,
49.0218495189568));
#104390=CARTESIAN_POINT('Ctrl Pts',(-0.343446449653068,632.144773325884,
48.574308500153));
#104391=CARTESIAN_POINT('Ctrl Pts',(-0.327665155014434,632.867570296855,
48.5753871894563));
#104392=CARTESIAN_POINT('Ctrl Pts',(-1.37915307127922,632.785351839707,
49.0793205445456));
#104393=CARTESIAN_POINT('Ctrl Pts',(-1.47715237700549,632.233425912244,
48.6401671207799));
#104394=CARTESIAN_POINT('Ctrl Pts',(-1.40143442624709,632.941087722613,
48.6345369452367));
#104395=CARTESIAN_POINT('Ctrl Pts',(-1.90211842335103,632.855006180268,
49.1345303092449));
#104396=CARTESIAN_POINT('Ctrl Pts',(-2.02961823976853,632.316499577614,
48.701927360293));
#104397=CARTESIAN_POINT('Ctrl Pts',(-1.93284944505609,633.01163696098,48.6913595421491));
#104398=CARTESIAN_POINT('Ctrl Pts',(-2.93807698482498,633.054034036731,
49.2965498576802));
#104399=CARTESIAN_POINT('Ctrl Pts',(-3.12573547424563,632.554675921558,
48.8844736999008));
#104400=CARTESIAN_POINT('Ctrl Pts',(-2.98554566101708,633.213221513822,
48.858111903559));
#104401=CARTESIAN_POINT('Ctrl Pts',(-3.45374791090643,633.184501638302,
49.4043809868049));
#104402=CARTESIAN_POINT('Ctrl Pts',(-3.66252614078188,632.706685205911,
49.002867092975));
#104403=CARTESIAN_POINT('Ctrl Pts',(-3.50954896370792,633.345365412611,
48.969093235558));
#104404=CARTESIAN_POINT('Ctrl Pts',(-4.4468510663278,633.486560814703,49.6633692434331));
#104405=CARTESIAN_POINT('Ctrl Pts',(-4.69335204058051,633.057479661184,
49.2876872236508));
#104406=CARTESIAN_POINT('Ctrl Pts',(-4.51869902314396,633.651305216357,
49.2356474341197));
#104407=CARTESIAN_POINT('Ctrl Pts',(-4.92792605251174,633.658498481233,
49.8148076425706));
#104408=CARTESIAN_POINT('Ctrl Pts',(-5.18656612683332,633.252577971486,
49.4506178691368));
#104409=CARTESIAN_POINT('Ctrl Pts',(-5.00754801428307,633.825452135949,
49.3915102529955));
#104410=CARTESIAN_POINT('Ctrl Pts',(-5.86442374504572,634.032530746289,
50.1589844638927));
#104411=CARTESIAN_POINT('Ctrl Pts',(-6.14248615971892,633.674547007798,
49.8207309756671));
#104412=CARTESIAN_POINT('Ctrl Pts',(-5.95917956692151,634.204290165079,
49.7457424205663));
#104413=CARTESIAN_POINT('Ctrl Pts',(-6.32024772390201,634.234853771403,
50.351944968455));
#104414=CARTESIAN_POINT('Ctrl Pts',(-6.60402168968756,633.898761420426,
50.024761085077));
#104415=CARTESIAN_POINT('Ctrl Pts',(-6.4223701414918,634.409213025463,49.9443408012826));
#104416=CARTESIAN_POINT('Ctrl Pts',(-7.20798452548951,634.659869888413,
50.7781230179888));
#104417=CARTESIAN_POINT('Ctrl Pts',(-7.49937336947295,634.367016492284,
50.4751585816832));
#104418=CARTESIAN_POINT('Ctrl Pts',(-7.32445419098542,634.839690427277,
50.382970765863));
#104419=CARTESIAN_POINT('Ctrl Pts',(-7.63444059270741,634.879877998268,
51.0086543329385));
#104420=CARTESIAN_POINT('Ctrl Pts',(-7.92808282222852,634.606627980339,
50.7161247240279));
#104421=CARTESIAN_POINT('Ctrl Pts',(-7.75780268783223,635.062525716147,
50.6202380193044));
#104422=CARTESIAN_POINT('Ctrl Pts',(-8.86930646895302,635.551146061136,
51.7511985187908));
#104423=CARTESIAN_POINT('Ctrl Pts',(-9.13407034427917,635.315485808938,
51.4724609662051));
#104424=CARTESIAN_POINT('Ctrl Pts',(-9.01263265026787,635.742422596475,
51.3844819472612));
#104425=CARTESIAN_POINT('Ctrl Pts',(-9.63391884695173,636.013257995688,
52.3135263786952));
#104426=CARTESIAN_POINT('Ctrl Pts',(-9.90255020916195,635.809844851862,
52.0496752501994));
#104427=CARTESIAN_POINT('Ctrl Pts',(-9.78960325654475,636.21047313013,51.9632424341007));
#104428=CARTESIAN_POINT('Ctrl Pts',(-10.705439897833,636.697610172111,53.2657428837752));
#104429=CARTESIAN_POINT('Ctrl Pts',(-10.9910069155268,636.550097791243,
53.0515055379338));
#104430=CARTESIAN_POINT('Ctrl Pts',(-10.878441060838,636.903617518938,52.9432807545543));
#104431=CARTESIAN_POINT('Ctrl Pts',(-11.0508876799252,636.925101298073,
53.6025635511897));
#104432=CARTESIAN_POINT('Ctrl Pts',(-11.3347418937743,636.79016171467,53.3968965258403));
#104433=CARTESIAN_POINT('Ctrl Pts',(-11.229472953103,637.134032223376,53.2899442539113));
#104434=CARTESIAN_POINT('Ctrl Pts',(-11.7115273981156,637.370048161634,
54.31121164042));
#104435=CARTESIAN_POINT('Ctrl Pts',(-11.9901371105211,637.257589819536,
54.1232083059766));
#104436=CARTESIAN_POINT('Ctrl Pts',(-11.900792348141,637.58469745544,54.0193011734408));
#104437=CARTESIAN_POINT('Ctrl Pts',(-12.0239781544445,637.585612042381,
54.679895712359));
#104438=CARTESIAN_POINT('Ctrl Pts',(-12.3010560005085,637.484007381368,
54.5005517772709));
#104439=CARTESIAN_POINT('Ctrl Pts',(-12.218293964521,637.803031627762,54.3987594591597));
#104440=CARTESIAN_POINT('Ctrl Pts',(-12.9089989609887,638.206484722157,
55.8305641478284));
#104441=CARTESIAN_POINT('Ctrl Pts',(-13.1641372034306,638.122333337238,
55.657554710526));
#104442=CARTESIAN_POINT('Ctrl Pts',(-13.1176253793484,638.431885953125,
55.5830589493271));
#104443=CARTESIAN_POINT('Ctrl Pts',(-13.4299816943561,638.586242973041,
56.6565755853746));
#104444=CARTESIAN_POINT('Ctrl Pts',(-13.6882441199943,638.522792922679,
56.502781818501));
#104445=CARTESIAN_POINT('Ctrl Pts',(-13.6470291437565,638.81652388569,56.4332097702866));
#104446=CARTESIAN_POINT('Ctrl Pts',(-13.9880869203314,639.000081291731,
57.7753259736852));
#104447=CARTESIAN_POINT('Ctrl Pts',(-14.2513227291178,638.960240306637,
57.6633206048862));
#104448=CARTESIAN_POINT('Ctrl Pts',(-14.2141551453113,639.235679320329,
57.5846512128922));
#104449=CARTESIAN_POINT('Ctrl Pts',(-14.0949913651594,639.079785918328,
58.0034349097068));
#104450=CARTESIAN_POINT('Ctrl Pts',(-14.3573300164066,639.042991451251,
57.895659279968));
#104451=CARTESIAN_POINT('Ctrl Pts',(-14.3227879338756,639.316408326257,
57.8194266921124));
#104452=CARTESIAN_POINT('Ctrl Pts',(-14.2989297883243,639.23250072315,58.4689050674605));
#104453=CARTESIAN_POINT('Ctrl Pts',(-14.5593558255444,639.201314374317,
58.3695243760315));
#104454=CARTESIAN_POINT('Ctrl Pts',(-14.5300235323771,639.471085886935,
58.298500421927));
#104455=CARTESIAN_POINT('Ctrl Pts',(-14.3962813329383,639.305751532961,
58.707145038779));
#104456=CARTESIAN_POINT('Ctrl Pts',(-14.655901579792,639.277294876988,58.6120969468063));
#104457=CARTESIAN_POINT('Ctrl Pts',(-14.628948992512,639.545278131669,58.5437030695108));
#104458=CARTESIAN_POINT('Ctrl Pts',(-14.6697948864641,639.512315164104,
59.4288869888394));
#104459=CARTESIAN_POINT('Ctrl Pts',(-14.9255658148712,639.490221334045,
59.3430538394069));
#104460=CARTESIAN_POINT('Ctrl Pts',(-14.9068849327433,639.754496848634,
59.2865392357633));
#104461=CARTESIAN_POINT('Ctrl Pts',(-14.8276358084694,639.632573093502,
59.919163080231));
#104462=CARTESIAN_POINT('Ctrl Pts',(-15.0827345831201,639.615278031787,
59.8429002079945));
#104463=CARTESIAN_POINT('Ctrl Pts',(-15.0672776140326,639.876300254906,
59.7911438168927));
#104464=CARTESIAN_POINT('Ctrl Pts',(-15.0935663577189,639.836054760192,
60.9185223424128));
#104465=CARTESIAN_POINT('Ctrl Pts',(-15.3461975432606,639.825729960273,
60.8592543910126));
#104466=CARTESIAN_POINT('Ctrl Pts',(-15.3375077166812,640.082397178936,
60.8197103861867));
#104467=CARTESIAN_POINT('Ctrl Pts',(-15.2016635310883,639.919288867215,
61.427601771592));
#104468=CARTESIAN_POINT('Ctrl Pts',(-15.4538492122169,639.91219607755,61.3780952510847));
#104469=CARTESIAN_POINT('Ctrl Pts',(-15.4473524788766,640.166700956264,
61.3436679646832));
#104470=CARTESIAN_POINT('Ctrl Pts',(-15.3656085202112,640.045795416604,
62.4657118072439));
#104471=CARTESIAN_POINT('Ctrl Pts',(-15.6162781423566,640.042912732702,
62.4334323880538));
#104472=CARTESIAN_POINT('Ctrl Pts',(-15.6139481543257,640.29483344227,62.4121180900535));
#104473=CARTESIAN_POINT('Ctrl Pts',(-15.4213599206253,640.088993672632,
62.9982308158159));
#104474=CARTESIAN_POINT('Ctrl Pts',(-15.6718168191366,640.087770818522,
62.9761672199096));
#104475=CARTESIAN_POINT('Ctrl Pts',(-15.6706008816092,640.338586851437,
62.9602003371774));
#104476=CARTESIAN_POINT('Ctrl Pts',(-15.5027019825929,640.152021343924,
64.5826472633091));
#104477=CARTESIAN_POINT('Ctrl Pts',(-15.7522976417821,640.152776608118,
64.5843508815025));
#104478=CARTESIAN_POINT('Ctrl Pts',(-15.7532581285021,640.40242461464,64.5909241146122));
#104479=CARTESIAN_POINT('Ctrl Pts',(-15.4463343132364,640.108075542961,
65.6318366328334));
#104480=CARTESIAN_POINT('Ctrl Pts',(-15.6952083223957,640.10642266285,65.6625224224092));
#104481=CARTESIAN_POINT('Ctrl Pts',(-15.6959793937825,640.357914230718,
65.6707746519288));
#104482=CARTESIAN_POINT('Ctrl Pts',(-15.2386509518819,639.947832781043,
66.9345709030678));
#104483=CARTESIAN_POINT('Ctrl Pts',(-15.4907481596751,639.941893637217,
66.9784967286438));
#104484=CARTESIAN_POINT('Ctrl Pts',(-15.4849378554675,640.195611685116,
67.011585045083));
#104485=CARTESIAN_POINT('Ctrl Pts',(-15.1900189384783,639.910359834832,
67.1952431231479));
#104486=CARTESIAN_POINT('Ctrl Pts',(-15.442502106951,639.903116285289,67.2436796227911));
#104487=CARTESIAN_POINT('Ctrl Pts',(-15.4355195703926,640.15765712674,67.2798756894921));
#104488=CARTESIAN_POINT('Ctrl Pts',(-15.0803219964504,639.826036123596,
67.7086233424261));
#104489=CARTESIAN_POINT('Ctrl Pts',(-15.3338238879868,639.81595115727,67.7656619175894));
#104490=CARTESIAN_POINT('Ctrl Pts',(-15.3240490417368,640.072249639251,
67.8082600435595));
#104491=CARTESIAN_POINT('Ctrl Pts',(-15.0191594320567,639.779109751635,
67.9621453552883));
#104492=CARTESIAN_POINT('Ctrl Pts',(-15.2731532452162,639.767372623407,
68.0236001703991));
#104493=CARTESIAN_POINT('Ctrl Pts',(-15.2618976191312,640.024720157075,
68.0691914822997));
#104494=CARTESIAN_POINT('Ctrl Pts',(-14.8174033801442,639.624768231545,
68.7135999647743));
#104495=CARTESIAN_POINT('Ctrl Pts',(-15.0725761726714,639.607186299064,
68.7904931957739));
#104496=CARTESIAN_POINT('Ctrl Pts',(-15.0568797539538,639.86839508466,68.8426074874175));
#104497=CARTESIAN_POINT('Ctrl Pts',(-14.6585957360926,639.50381566693,69.202444416695));
#104498=CARTESIAN_POINT('Ctrl Pts',(-14.9144766233915,639.481427523697,
69.2887981194115));
#104499=CARTESIAN_POINT('Ctrl Pts',(-14.8955047156438,639.745888110387,
69.3457386057789));
#104500=CARTESIAN_POINT('Ctrl Pts',(-14.2945157770192,639.228940094288,
70.1573336769515));
#104501=CARTESIAN_POINT('Ctrl Pts',(-14.55378196445,639.196702300566,70.2605787665661));
#104502=CARTESIAN_POINT('Ctrl Pts',(-14.5255384316863,639.467479706879,
70.3285351375797));
#104503=CARTESIAN_POINT('Ctrl Pts',(-14.0881807313278,639.074224407355,
70.6254072326268));
#104504=CARTESIAN_POINT('Ctrl Pts',(-14.3484256804248,639.035608179291,
70.7379242119137));
#104505=CARTESIAN_POINT('Ctrl Pts',(-14.3158676780004,639.310775702103,
70.8102881691105));
#104506=CARTESIAN_POINT('Ctrl Pts',(-13.6346129612246,638.738060594009,
71.5295833283864));
#104507=CARTESIAN_POINT('Ctrl Pts',(-13.8990584488247,638.686648055336,
71.6590019112753));
#104508=CARTESIAN_POINT('Ctrl Pts',(-13.8549669417811,638.970291387194,
71.740888971284));
#104509=CARTESIAN_POINT('Ctrl Pts',(-13.3887414345827,638.557610315938,
71.9636076884644));
#104510=CARTESIAN_POINT('Ctrl Pts',(-13.6545221187428,638.498448696131,
72.1017559982509));
#104511=CARTESIAN_POINT('Ctrl Pts',(-13.6051205939733,638.787522044506,
72.1875975711325));
#104512=CARTESIAN_POINT('Ctrl Pts',(-12.8610969146662,638.176033974939,
72.7988987818575));
#104513=CARTESIAN_POINT('Ctrl Pts',(-13.1316816038927,638.101182146061,
72.9538576019717));
#104514=CARTESIAN_POINT('Ctrl Pts',(-13.0689457304277,638.401041596807,
73.0472996885173));
#104515=CARTESIAN_POINT('Ctrl Pts',(-12.5793162792295,637.974891871437,
73.2001530637705));
#104516=CARTESIAN_POINT('Ctrl Pts',(-12.851407762716,637.890759692315,73.3637342809632));
#104517=CARTESIAN_POINT('Ctrl Pts',(-12.7826098802753,638.197314518502,
73.4602802768307));
#104518=CARTESIAN_POINT('Ctrl Pts',(-11.9805147599271,637.55547313329,73.9719948691702));
#104519=CARTESIAN_POINT('Ctrl Pts',(-12.2578204673371,637.452363532576,
74.1526852709296));
#104520=CARTESIAN_POINT('Ctrl Pts',(-12.1741279655269,637.772505393729,
74.2546782628821));
#104521=CARTESIAN_POINT('Ctrl Pts',(-11.6620754094574,637.336246875743,
74.3439606423759));
#104522=CARTESIAN_POINT('Ctrl Pts',(-11.9410485726769,637.222125276071,
74.5332916257023));
#104523=CARTESIAN_POINT('Ctrl Pts',(-11.8505409335869,637.550461763023,
74.6375141662316));
#104524=CARTESIAN_POINT('Ctrl Pts',(-10.6667627124656,636.667502706153,
75.4012723114464));
#104525=CARTESIAN_POINT('Ctrl Pts',(-10.9336515194875,636.505188339921,
75.6390199582536));
#104526=CARTESIAN_POINT('Ctrl Pts',(-10.8391421878638,636.873125582928,
75.7257195228643));
#104527=CARTESIAN_POINT('Ctrl Pts',(-9.94964215326505,636.205767320931,
76.0314203061157));
#104528=CARTESIAN_POINT('Ctrl Pts',(-10.2135091666313,636.014005317852,
76.284404155343));
#104529=CARTESIAN_POINT('Ctrl Pts',(-10.1104306891926,636.405456574106,
76.3742823947935));
#104530=CARTESIAN_POINT('Ctrl Pts',(-8.39977812395367,635.286028861029,
77.1587292660183));
#104531=CARTESIAN_POINT('Ctrl Pts',(-8.66654368556743,635.029291056602,
77.453673623364));
#104532=CARTESIAN_POINT('Ctrl Pts',(-8.53551476998558,635.473898567317,
77.5345321156382));
#104533=CARTESIAN_POINT('Ctrl Pts',(-7.56052958968753,634.824608154755,
77.6580776200298));
#104534=CARTESIAN_POINT('Ctrl Pts',(-7.82150334606982,634.531572945309,
77.9681106439715));
#104535=CARTESIAN_POINT('Ctrl Pts',(-7.68270213057854,635.006547965821,
78.0484723196597));
#104536=CARTESIAN_POINT('Ctrl Pts',(-5.74312393564903,633.963249742456,
78.5165117385326));
#104537=CARTESIAN_POINT('Ctrl Pts',(-5.97772848586131,633.57629741229,78.8809740559797));
#104538=CARTESIAN_POINT('Ctrl Pts',(-5.83592524213799,634.134121869069,
78.9319873742495));
#104539=CARTESIAN_POINT('Ctrl Pts',(-4.75593424029188,633.563595057341,
78.8719595177936));
#104540=CARTESIAN_POINT('Ctrl Pts',(-4.97553001272719,633.135378140081,
79.2506052240653));
#104541=CARTESIAN_POINT('Ctrl Pts',(-4.83278432840491,633.729331434717,
79.2978208896897));
#104542=CARTESIAN_POINT('Ctrl Pts',(-3.68751695697931,633.257997703468,
79.1311980167567));
#104543=CARTESIAN_POINT('Ctrl Pts',(-3.91740045113657,632.79611528243,79.5230579121953));
#104544=CARTESIAN_POINT('Ctrl Pts',(-3.74709337805201,633.419805103089,
79.5646350435076));
#104545=CARTESIAN_POINT('Origin',(-48.,640.125373764374,64.2994740882088));
#104546=CARTESIAN_POINT('Ctrl Pts',(-2.24460771689896,634.860167926555,
52.2254855816307));
#104547=CARTESIAN_POINT('Ctrl Pts',(-2.07343281068578,635.935476877995,
52.1937144269263));
#104548=CARTESIAN_POINT('Ctrl Pts',(-2.33599035692052,635.234460352332,
51.4023619931513));
#104549=CARTESIAN_POINT('Ctrl Pts',(-1.83071110480402,634.789230599513,
52.1485430639701));
#104550=CARTESIAN_POINT('Ctrl Pts',(-1.68007361159745,635.884219683812,
52.1267455450006));
#104551=CARTESIAN_POINT('Ctrl Pts',(-1.90524322638816,635.161651519204,
51.3201743394719));
#104552=CARTESIAN_POINT('Ctrl Pts',(-1.41178093416776,634.736536724958,
52.0926096107395));
#104553=CARTESIAN_POINT('Ctrl Pts',(-1.29419848643582,635.848311670572,
52.0803434838513));
#104554=CARTESIAN_POINT('Ctrl Pts',(-1.46925731177574,635.107567404497,
51.2604278885429));
#104555=CARTESIAN_POINT('Ctrl Pts',(-0.57140262553684,634.672468556966,
52.0248171104673));
#104556=CARTESIAN_POINT('Ctrl Pts',(-0.520642208727863,635.80436668002,
52.0235847625471));
#104557=CARTESIAN_POINT('Ctrl Pts',(-0.594665493514755,635.041808942665,
51.1880140002959));
#104558=CARTESIAN_POINT('Ctrl Pts',(-0.147816545353252,634.660621292595,
52.0124327336182));
#104559=CARTESIAN_POINT('Ctrl Pts',(-0.136056956437475,635.796530340598,
52.0135137672583));
#104560=CARTESIAN_POINT('Ctrl Pts',(-0.153834462869262,635.029649119754,
51.1747853911568));
#104561=CARTESIAN_POINT('Ctrl Pts',(1.1024719364547,634.686646709549,52.0398201590788));
#104562=CARTESIAN_POINT('Ctrl Pts',(1.00747162781077,635.814178115524,52.0362579003524));
#104563=CARTESIAN_POINT('Ctrl Pts',(1.1473556856947,635.05636115653,51.2040398030431));
#104564=CARTESIAN_POINT('Ctrl Pts',(1.91894009807576,634.784664642294,52.1416799438264));
#104565=CARTESIAN_POINT('Ctrl Pts',(1.74120896424278,635.876480206933,52.1156863094179));
#104566=CARTESIAN_POINT('Ctrl Pts',(1.99706350164218,635.156964960755,51.3128431956377));
#104567=CARTESIAN_POINT('Ctrl Pts',(3.12055673201111,635.032654985143,52.414597409285));
#104568=CARTESIAN_POINT('Ctrl Pts',(2.89662070513935,636.059663351124,52.3569131035477));
#104569=CARTESIAN_POINT('Ctrl Pts',(3.24760126429163,635.411498116049,51.6043655628081));
#104570=CARTESIAN_POINT('Ctrl Pts',(3.51645511552271,635.132146568009,52.5259194378218));
#104571=CARTESIAN_POINT('Ctrl Pts',(3.27570850901759,636.133135826386,52.4544566039408));
#104572=CARTESIAN_POINT('Ctrl Pts',(3.65961769328675,635.513614580972,51.7232764264806));
#104573=CARTESIAN_POINT('Ctrl Pts',(4.28117411180073,635.353817098604,52.7819398834267));
#104574=CARTESIAN_POINT('Ctrl Pts',(4.01998858621208,636.303527595311,52.6857610821952));
#104575=CARTESIAN_POINT('Ctrl Pts',(4.45547060211493,635.741133515995,51.9967499482209));
#104576=CARTESIAN_POINT('Ctrl Pts',(4.6527703895603,635.476516292076,52.9272079191087));
#104577=CARTESIAN_POINT('Ctrl Pts',(4.38560256268007,636.399515892701,52.8180868283054));
#104578=CARTESIAN_POINT('Ctrl Pts',(4.84219570557192,635.867069920958,52.151921010376));
#104579=CARTESIAN_POINT('Ctrl Pts',(5.73871252059237,635.87149768931,53.412985235997));
#104580=CARTESIAN_POINT('Ctrl Pts',(5.44769236904264,636.712667166468,53.2632683827815));
#104581=CARTESIAN_POINT('Ctrl Pts',(5.97234965215429,636.27247217119,52.6708141112791));
#104582=CARTESIAN_POINT('Ctrl Pts',(6.42887593638936,636.172846954948,53.8068469880404));
#104583=CARTESIAN_POINT('Ctrl Pts',(6.15032378335572,636.963514950924,53.6342198283953));
#104584=CARTESIAN_POINT('Ctrl Pts',(6.69061225764372,636.581772120217,53.0915259083752));
#104585=CARTESIAN_POINT('Ctrl Pts',(7.70252122853822,636.789511859623,54.7027643205653));
#104586=CARTESIAN_POINT('Ctrl Pts',(7.45997458021479,637.499093628627,54.5105690457221));
#104587=CARTESIAN_POINT('Ctrl Pts',(8.01611292013624,637.214707153726,54.0485198842105));
#104588=CARTESIAN_POINT('Ctrl Pts',(8.29093833512778,637.106408722947,55.2059626243289));
#104589=CARTESIAN_POINT('Ctrl Pts',(8.07548401458602,637.781573825439,55.0065471941012));
#104590=CARTESIAN_POINT('Ctrl Pts',(8.62848726547417,637.539965112437,54.5860224232522));
#104591=CARTESIAN_POINT('Ctrl Pts',(9.10615860494565,637.572335029063,56.0502090602173));
#104592=CARTESIAN_POINT('Ctrl Pts',(8.93980322327443,638.210231222331,55.8666947129737));
#104593=CARTESIAN_POINT('Ctrl Pts',(9.47689944401278,638.018184818951,55.4878240797596));
#104594=CARTESIAN_POINT('Ctrl Pts',(9.36580248126735,637.725748496083,56.3462294979682));
#104595=CARTESIAN_POINT('Ctrl Pts',(9.21205942946594,638.350440979971,56.164626520581));
#104596=CARTESIAN_POINT('Ctrl Pts',(9.74711472218158,638.17564602195,55.8040251608737));
#104597=CARTESIAN_POINT('Ctrl Pts',(9.85277663850557,638.020454436639,56.9581425734282));
#104598=CARTESIAN_POINT('Ctrl Pts',(9.72214071534082,638.620905078637,56.782813652941));
#104599=CARTESIAN_POINT('Ctrl Pts',(10.2539160475817,638.478127626706,56.4576543706004));
#104600=CARTESIAN_POINT('Ctrl Pts',(10.0814069885408,638.162492524898,57.2753308908016));
#104601=CARTESIAN_POINT('Ctrl Pts',(9.96275939343532,638.752361475952,57.1043691500725));
#104602=CARTESIAN_POINT('Ctrl Pts',(10.4918551409475,638.62391333402,56.7964665120035));
#104603=CARTESIAN_POINT('Ctrl Pts',(10.7230189007579,638.568474894698,58.2619328657198));
#104604=CARTESIAN_POINT('Ctrl Pts',(10.6285633925527,639.124299658112,58.0946841395296));
#104605=CARTESIAN_POINT('Ctrl Pts',(11.1595901762937,639.040607207916,57.8503282493184));
#104606=CARTESIAN_POINT('Ctrl Pts',(11.0923717675951,638.812533808457,58.9658852559509));
#104607=CARTESIAN_POINT('Ctrl Pts',(11.0225929845114,639.355453995367,58.8154970554682));
#104608=CARTESIAN_POINT('Ctrl Pts',(11.543981587863,639.291105624835,58.6022718329819));
#104609=CARTESIAN_POINT('Ctrl Pts',(11.7014944118088,639.222460518805,60.4833358094967));
#104610=CARTESIAN_POINT('Ctrl Pts',(11.6644122825579,639.740850111134,60.3684103254258));
#104611=CARTESIAN_POINT('Ctrl Pts',(12.1779050110386,639.71184812148,60.223173033479));
#104612=CARTESIAN_POINT('Ctrl Pts',(11.9301672368271,639.380786781681,61.2707799874375));
#104613=CARTESIAN_POINT('Ctrl Pts',(11.9096549681383,639.892977017353,61.182086329466));
#104614=CARTESIAN_POINT('Ctrl Pts',(12.4158885617532,639.874351870955,61.0643007636695));
#104615=CARTESIAN_POINT('Ctrl Pts',(12.1537770914997,639.536320911666,62.4895659620246));
#104616=CARTESIAN_POINT('Ctrl Pts',(12.1464642268629,640.040786570914,62.4384492041064));
#104617=CARTESIAN_POINT('Ctrl Pts',(12.6486028978816,640.033989752196,62.3661767157842));
#104618=CARTESIAN_POINT('Ctrl Pts',(12.2085200304299,639.574645413003,62.9037553260946));
#104619=CARTESIAN_POINT('Ctrl Pts',(12.2044669680803,640.077264694283,62.864765245725));
#104620=CARTESIAN_POINT('Ctrl Pts',(12.7055747490575,640.073325442003,62.808603167802));
#104621=CARTESIAN_POINT('Ctrl Pts',(12.2753636450861,639.621482578138,63.7414063290601));
#104622=CARTESIAN_POINT('Ctrl Pts',(12.274978483213,640.121657485856,63.7252770410462));
#104623=CARTESIAN_POINT('Ctrl Pts',(12.7751399565671,640.121398393795,63.7033604237967));
#104624=CARTESIAN_POINT('Ctrl Pts',(12.2870666679087,639.629713325934,64.1583756132804));
#104625=CARTESIAN_POINT('Ctrl Pts',(12.2873846747713,640.129502073405,64.1547225574821));
#104626=CARTESIAN_POINT('Ctrl Pts',(12.787319479616,640.129846309535,64.148756333092));
#104627=CARTESIAN_POINT('Ctrl Pts',(12.268530884661,639.616704590037,64.9887244061268));
#104628=CARTESIAN_POINT('Ctrl Pts',(12.2678309313977,640.117168305939,65.0078610328854));
#104629=CARTESIAN_POINT('Ctrl Pts',(12.7680289967845,640.11649434121,65.0357135662794));
#104630=CARTESIAN_POINT('Ctrl Pts',(12.238288133047,639.595462971966,65.4021035317435));
#104631=CARTESIAN_POINT('Ctrl Pts',(12.235780004542,640.096933666824,65.4335305959216));
#104632=CARTESIAN_POINT('Ctrl Pts',(12.7365548811428,640.094692264775,65.4772745550034));
#104633=CARTESIAN_POINT('Ctrl Pts',(12.1360079708598,639.523971401827,66.2252982180572));
#104634=CARTESIAN_POINT('Ctrl Pts',(12.1278948320545,640.029206587871,66.2789946000502));
#104635=CARTESIAN_POINT('Ctrl Pts',(12.6301103000015,640.021314407659,66.3565899298897));
#104636=CARTESIAN_POINT('Ctrl Pts',(12.0634251058667,639.473341425651,66.6373579383003));
#104637=CARTESIAN_POINT('Ctrl Pts',(12.0509917691496,639.981048358942,66.7029848588286));
#104638=CARTESIAN_POINT('Ctrl Pts',(12.5545721539083,639.969348564671,66.7967415398965));
#104639=CARTESIAN_POINT('Ctrl Pts',(11.7851849710258,639.280776882324,67.8517603894219));
#104640=CARTESIAN_POINT('Ctrl Pts',(11.7560671806613,639.798044599605,67.9555151604994));
#104641=CARTESIAN_POINT('Ctrl Pts',(12.265003213869,639.771703221168,68.0939351245997));
#104642=CARTESIAN_POINT('Ctrl Pts',(11.5231511655743,639.100787569077,68.6226018819362));
#104643=CARTESIAN_POINT('Ctrl Pts',(11.4753688142236,639.625565690201,68.7506469944195));
#104644=CARTESIAN_POINT('Ctrl Pts',(11.9923003685254,639.586964845123,68.9173282151888));
#104645=CARTESIAN_POINT('Ctrl Pts',(11.0237873908383,638.768313052576,69.7270719203858));
#104646=CARTESIAN_POINT('Ctrl Pts',(10.9544028777391,639.316649953524,69.8689551387737));
#104647=CARTESIAN_POINT('Ctrl Pts',(11.4726049050073,639.245718209948,70.0970939152249));
#104648=CARTESIAN_POINT('Ctrl Pts',(10.8384310991565,638.646368112428,70.0880515743831));
#104649=CARTESIAN_POINT('Ctrl Pts',(10.7586359325232,639.202227930314,70.237687260735));
#104650=CARTESIAN_POINT('Ctrl Pts',(11.2797017252308,639.120555783983,70.4826829420179));
#104651=CARTESIAN_POINT('Ctrl Pts',(10.4390987804155,638.388472497937,70.7805569003536));
#104652=CARTESIAN_POINT('Ctrl Pts',(10.3387444088613,638.961980514628,70.9429750385828));
#104653=CARTESIAN_POINT('Ctrl Pts',(10.8641104504998,638.855855695182,71.2223989202368));
#104654=CARTESIAN_POINT('Ctrl Pts',(10.2247929217345,638.252281349441,71.1132662015513));
#104655=CARTESIAN_POINT('Ctrl Pts',(10.1129153329541,638.835266089697,71.2812239398438));
#104656=CARTESIAN_POINT('Ctrl Pts',(10.6410790491553,638.716071190731,71.5777902117513));
#104657=CARTESIAN_POINT('Ctrl Pts',(9.76784625223806,637.968524861273,71.7535556942923));
#104658=CARTESIAN_POINT('Ctrl Pts',(9.63349659380944,638.573272816231,71.9302320108111));
#104659=CARTESIAN_POINT('Ctrl Pts',(10.1655277254286,638.424827920137,72.261730451579));
#104660=CARTESIAN_POINT('Ctrl Pts',(9.5252037421373,637.820949216077,72.0611303923611));
#104661=CARTESIAN_POINT('Ctrl Pts',(9.37852363969348,638.437416201048,72.2410837179652));
#104662=CARTESIAN_POINT('Ctrl Pts',(9.91300599012881,638.273358557248,72.5902735372759));
#104663=CARTESIAN_POINT('Ctrl Pts',(9.01135722475072,637.517417174847,72.6522134952531));
#104664=CARTESIAN_POINT('Ctrl Pts',(8.84120033390604,638.160459112116,72.836293304798));
#104665=CARTESIAN_POINT('Ctrl Pts',(9.37823825283678,637.961817993545,73.2216526442934));
#104666=CARTESIAN_POINT('Ctrl Pts',(8.73891002500459,637.360785169889,72.9367840692432));
#104667=CARTESIAN_POINT('Ctrl Pts',(8.55620892724539,638.018341471135,73.1214587846384));
#104668=CARTESIAN_POINT('Ctrl Pts',(9.09469840048593,637.801053343874,73.5256232407945));
#104669=CARTESIAN_POINT('Ctrl Pts',(7.89012810647255,636.890473661098,73.7426824430362));
#104670=CARTESIAN_POINT('Ctrl Pts',(7.65796125292149,637.588671243196,73.939427215562));
#104671=CARTESIAN_POINT('Ctrl Pts',(8.21135820442717,637.318332755003,74.3864623908746));
#104672=CARTESIAN_POINT('Ctrl Pts',(7.28116846417886,636.574939347645,74.219742003199));
#104673=CARTESIAN_POINT('Ctrl Pts',(7.02391120497905,637.310866383018,74.4058463661051));
#104674=CARTESIAN_POINT('Ctrl Pts',(7.57760505325563,636.99447333735,74.8960441316923));
#104675=CARTESIAN_POINT('Ctrl Pts',(6.2965924934778,636.122015748582,74.8505072253373));
#104676=CARTESIAN_POINT('Ctrl Pts',(6.03600513843958,636.930051586802,75.0061312303154));
#104677=CARTESIAN_POINT('Ctrl Pts',(6.55294358412831,636.529600037755,75.5698095385058));
#104678=CARTESIAN_POINT('Ctrl Pts',(5.95642441709212,635.974486587073,75.0464903317535));
#104679=CARTESIAN_POINT('Ctrl Pts',(5.69039769264687,636.806083719561,75.193320382361));
#104680=CARTESIAN_POINT('Ctrl Pts',(6.19892597176367,636.378178494287,75.7791531330914));
#104681=CARTESIAN_POINT('Ctrl Pts',(5.24924375098351,635.691366240682,75.4090550759564));
#104682=CARTESIAN_POINT('Ctrl Pts',(4.97872636614066,636.572134933507,75.5368081438878));
#104683=CARTESIAN_POINT('Ctrl Pts',(5.46295346090092,636.087588372664,76.166434449957));
#104684=CARTESIAN_POINT('Ctrl Pts',(4.88532837447766,635.557125517645,75.5738955184618));
#104685=CARTESIAN_POINT('Ctrl Pts',(4.61623378897083,636.464208081758,75.6897044857469));
#104686=CARTESIAN_POINT('Ctrl Pts',(5.084221879631,635.9498059108,76.3425122362357));
#104687=CARTESIAN_POINT('Ctrl Pts',(3.7708907749372,635.18796386149,76.0143384748105));
#104688=CARTESIAN_POINT('Ctrl Pts',(3.4968238391205,636.167052993904,76.1025288496455));
#104689=CARTESIAN_POINT('Ctrl Pts',(3.92441156002437,635.570904328349,76.812980796566));
#104690=CARTESIAN_POINT('Ctrl Pts',(2.99381238346123,634.984436447013,76.238938541679));
#104691=CARTESIAN_POINT('Ctrl Pts',(2.75796680224509,636.02168241599,76.2927147804116));
#104692=CARTESIAN_POINT('Ctrl Pts',(3.11569968988111,635.362007903861,77.0528911109046));
#104693=CARTESIAN_POINT('Ctrl Pts',(2.17374385871217,634.848209408432,76.3864215127495));
#104694=CARTESIAN_POINT('Ctrl Pts',(2.00694303543428,635.926951046402,76.4163679119409));
#104695=CARTESIAN_POINT('Ctrl Pts',(2.26224148372674,635.222186336159,77.2104285068931));
#104696=CARTESIAN_POINT('Ctrl Pts',(2.24460771693217,606.490579602187,52.2254855816369));
#104697=CARTESIAN_POINT('Ctrl Pts',(2.07343281071693,605.415270650748,52.1937144269317));
#104698=CARTESIAN_POINT('Ctrl Pts',(2.33599035695507,606.116287176409,51.4023619931579));
#104699=CARTESIAN_POINT('Ctrl Pts',(1.83071110482637,606.561516929231,52.1485430639731));
#104700=CARTESIAN_POINT('Ctrl Pts',(1.68007361161791,605.466527844934,52.1267455450031));
#104701=CARTESIAN_POINT('Ctrl Pts',(1.90524322641147,606.18909600954,51.3201743394751));
#104702=CARTESIAN_POINT('Ctrl Pts',(1.4117809341791,606.614210803789,52.0926096107404));
#104703=CARTESIAN_POINT('Ctrl Pts',(1.29419848644613,605.502435858175,52.0803434838521));
#104704=CARTESIAN_POINT('Ctrl Pts',(1.46925731178754,606.24318012425,51.2604278885439));
#104705=CARTESIAN_POINT('Ctrl Pts',(0.571402625536841,606.678278971782,
52.0248171104673));
#104706=CARTESIAN_POINT('Ctrl Pts',(0.520642208727856,605.546380848727,
52.0235847625472));
#104707=CARTESIAN_POINT('Ctrl Pts',(0.594665493514755,606.308938586082,
51.1880140002959));
#104708=CARTESIAN_POINT('Ctrl Pts',(0.147816545353252,606.690126236152,
52.0124327336182));
#104709=CARTESIAN_POINT('Ctrl Pts',(0.136056956437473,605.554217188149,
52.0135137672583));
#104710=CARTESIAN_POINT('Ctrl Pts',(0.153834462869262,606.321098408993,
51.1747853911568));
#104711=CARTESIAN_POINT('Ctrl Pts',(-1.10247193645471,606.664100819198,
52.0398201590788));
#104712=CARTESIAN_POINT('Ctrl Pts',(-1.00747162781075,605.536569413224,
52.0362579003525));
#104713=CARTESIAN_POINT('Ctrl Pts',(-1.1473556856947,606.294386372217,51.2040398030431));
#104714=CARTESIAN_POINT('Ctrl Pts',(-1.91894009807577,606.566082886454,
52.1416799438264));
#104715=CARTESIAN_POINT('Ctrl Pts',(-1.74120896424276,605.474267321815,
52.1156863094179));
#104716=CARTESIAN_POINT('Ctrl Pts',(-1.99706350164218,606.193782567993,
51.3128431956377));
#104717=CARTESIAN_POINT('Ctrl Pts',(-3.12055673201112,606.318092543604,
52.414597409285));
#104718=CARTESIAN_POINT('Ctrl Pts',(-2.89662070513932,605.291084177624,
52.3569131035478));
#104719=CARTESIAN_POINT('Ctrl Pts',(-3.24760126429163,605.939249412698,
51.6043655628081));
#104720=CARTESIAN_POINT('Ctrl Pts',(-3.51645511552272,606.218600960739,
52.5259194378218));
#104721=CARTESIAN_POINT('Ctrl Pts',(-3.27570850901756,605.217611702361,
52.4544566039408));
#104722=CARTESIAN_POINT('Ctrl Pts',(-3.65961769328675,605.837132947776,
51.7232764264806));
#104723=CARTESIAN_POINT('Ctrl Pts',(-4.28117411180073,605.996930430144,
52.7819398834267));
#104724=CARTESIAN_POINT('Ctrl Pts',(-4.01998858621205,605.047219933437,
52.6857610821952));
#104725=CARTESIAN_POINT('Ctrl Pts',(-4.45547060211493,605.609614012752,
51.9967499482209));
#104726=CARTESIAN_POINT('Ctrl Pts',(-4.6527703895603,605.874231236671,52.9272079191087));
#104727=CARTESIAN_POINT('Ctrl Pts',(-4.38560256268003,604.951231636046,
52.8180868283054));
#104728=CARTESIAN_POINT('Ctrl Pts',(-4.84219570557192,605.48367760779,52.151921010376));
#104729=CARTESIAN_POINT('Ctrl Pts',(-5.73871252059238,605.479249839438,
53.412985235997));
#104730=CARTESIAN_POINT('Ctrl Pts',(-5.4476923690426,604.63808036228,53.2632683827815));
#104731=CARTESIAN_POINT('Ctrl Pts',(-5.97234965215429,605.078275357558,
52.6708141112791));
#104732=CARTESIAN_POINT('Ctrl Pts',(-6.42887593638937,605.1779005738,53.8068469880404));
#104733=CARTESIAN_POINT('Ctrl Pts',(-6.15032378335568,604.387232577824,
53.6342198283954));
#104734=CARTESIAN_POINT('Ctrl Pts',(-6.69061225764372,604.76897540853,53.0915259083752));
#104735=CARTESIAN_POINT('Ctrl Pts',(-7.70252122853823,604.561235669124,
54.7027643205653));
#104736=CARTESIAN_POINT('Ctrl Pts',(-7.45997458021475,603.85165390012,54.5105690457221));
#104737=CARTESIAN_POINT('Ctrl Pts',(-8.01611292013624,604.136040375022,
54.0485198842105));
#104738=CARTESIAN_POINT('Ctrl Pts',(-8.29093833512779,604.244338805801,
55.2059626243289));
#104739=CARTESIAN_POINT('Ctrl Pts',(-8.07548401458598,603.569173703309,
55.0065471941012));
#104740=CARTESIAN_POINT('Ctrl Pts',(-8.62848726547417,603.810782416311,
54.5860224232522));
#104741=CARTESIAN_POINT('Ctrl Pts',(-9.10615860494566,603.778412499685,
56.0502090602173));
#104742=CARTESIAN_POINT('Ctrl Pts',(-8.9398032232744,603.140516306416,55.8666947129738));
#104743=CARTESIAN_POINT('Ctrl Pts',(-9.47689944401278,603.332562709797,
55.4878240797596));
#104744=CARTESIAN_POINT('Ctrl Pts',(-9.36580248126736,603.624999032665,
56.3462294979683));
#104745=CARTESIAN_POINT('Ctrl Pts',(-9.21205942946592,603.000306548777,
56.164626520581));
#104746=CARTESIAN_POINT('Ctrl Pts',(-9.74711472218158,603.175101506797,
55.8040251608737));
#104747=CARTESIAN_POINT('Ctrl Pts',(-9.85277663850557,603.330293092108,
56.9581425734283));
#104748=CARTESIAN_POINT('Ctrl Pts',(-9.72214071534079,602.729842450111,
56.7828136529411));
#104749=CARTESIAN_POINT('Ctrl Pts',(-10.2539160475817,602.872619902042,
56.4576543706004));
#104750=CARTESIAN_POINT('Ctrl Pts',(-10.0814069885409,603.188255003849,
57.2753308908016));
#104751=CARTESIAN_POINT('Ctrl Pts',(-9.96275939343529,602.598386052796,
57.1043691500725));
#104752=CARTESIAN_POINT('Ctrl Pts',(-10.4918551409475,602.726834194727,
56.7964665120035));
#104753=CARTESIAN_POINT('Ctrl Pts',(-10.7230189007579,602.782272634049,
58.2619328657199));
#104754=CARTESIAN_POINT('Ctrl Pts',(-10.6285633925526,602.226447870635,
58.0946841395296));
#104755=CARTESIAN_POINT('Ctrl Pts',(-11.1595901762937,602.310140320832,
57.8503282493184));
#104756=CARTESIAN_POINT('Ctrl Pts',(-11.0923717675951,602.53821372029,58.9658852559509));
#104757=CARTESIAN_POINT('Ctrl Pts',(-11.0225929845114,601.995293533381,
58.8154970554682));
#104758=CARTESIAN_POINT('Ctrl Pts',(-11.543981587863,602.059641903912,58.6022718329819));
#104759=CARTESIAN_POINT('Ctrl Pts',(-11.7014944118088,602.128287009942,
60.4833358094967));
#104760=CARTESIAN_POINT('Ctrl Pts',(-11.6644122825579,601.609897417614,
60.3684103254258));
#104761=CARTESIAN_POINT('Ctrl Pts',(-12.1779050110386,601.638899407267,
60.223173033479));
#104762=CARTESIAN_POINT('Ctrl Pts',(-11.9301672368271,601.969960747067,
61.2707799874375));
#104763=CARTESIAN_POINT('Ctrl Pts',(-11.9096549681383,601.457770511395,
61.182086329466));
#104764=CARTESIAN_POINT('Ctrl Pts',(-12.4158885617532,601.476395657792,
61.0643007636695));
#104765=CARTESIAN_POINT('Ctrl Pts',(-12.1537770914997,601.814426617082,
62.4895659620246));
#104766=CARTESIAN_POINT('Ctrl Pts',(-12.1464642268629,601.309960957834,
62.4384492041064));
#104767=CARTESIAN_POINT('Ctrl Pts',(-12.6486028978816,601.316757776551,
62.3661767157842));
#104768=CARTESIAN_POINT('Ctrl Pts',(-12.2085200304299,601.776102115745,
62.9037553260946));
#104769=CARTESIAN_POINT('Ctrl Pts',(-12.2044669680803,601.273482834465,
62.864765245725));
#104770=CARTESIAN_POINT('Ctrl Pts',(-12.7055747490575,601.277422086745,
62.808603167802));
#104771=CARTESIAN_POINT('Ctrl Pts',(-12.2753636450861,601.729264950609,
63.7414063290601));
#104772=CARTESIAN_POINT('Ctrl Pts',(-12.274978483213,601.229090042892,63.7252770410462));
#104773=CARTESIAN_POINT('Ctrl Pts',(-12.7751399565671,601.229349134952,
63.7033604237967));
#104774=CARTESIAN_POINT('Ctrl Pts',(-12.2870666679087,601.721034202814,
64.1583756132804));
#104775=CARTESIAN_POINT('Ctrl Pts',(-12.2873846747713,601.221245455343,
64.1547225574821));
#104776=CARTESIAN_POINT('Ctrl Pts',(-12.787319479616,601.220901219213,64.148756333092));
#104777=CARTESIAN_POINT('Ctrl Pts',(-12.268530884661,601.734042938711,64.9887244061267));
#104778=CARTESIAN_POINT('Ctrl Pts',(-12.2678309313976,601.233579222809,
65.0078610328854));
#104779=CARTESIAN_POINT('Ctrl Pts',(-12.7680289967845,601.234253187538,
65.0357135662794));
#104780=CARTESIAN_POINT('Ctrl Pts',(-12.238288133047,601.755284556781,65.4021035317435));
#104781=CARTESIAN_POINT('Ctrl Pts',(-12.235780004542,601.253813861924,65.4335305959216));
#104782=CARTESIAN_POINT('Ctrl Pts',(-12.7365548811428,601.256055263972,
65.4772745550034));
#104783=CARTESIAN_POINT('Ctrl Pts',(-12.1360079708598,601.82677612692,66.2252982180572));
#104784=CARTESIAN_POINT('Ctrl Pts',(-12.1278948320545,601.321540940876,
66.2789946000502));
#104785=CARTESIAN_POINT('Ctrl Pts',(-12.6301103000015,601.329433121089,
66.3565899298897));
#104786=CARTESIAN_POINT('Ctrl Pts',(-12.0634251058667,601.877406103097,
66.6373579383003));
#104787=CARTESIAN_POINT('Ctrl Pts',(-12.0509917691496,601.369699169805,
66.7029848588286));
#104788=CARTESIAN_POINT('Ctrl Pts',(-12.5545721539083,601.381398964076,
66.7967415398965));
#104789=CARTESIAN_POINT('Ctrl Pts',(-11.7851849710258,602.069970646424,
67.8517603894219));
#104790=CARTESIAN_POINT('Ctrl Pts',(-11.7560671806612,601.552702929143,
67.9555151604994));
#104791=CARTESIAN_POINT('Ctrl Pts',(-12.265003213869,601.57904430758,68.0939351245997));
#104792=CARTESIAN_POINT('Ctrl Pts',(-11.5231511655743,602.249959959671,
68.6226018819362));
#104793=CARTESIAN_POINT('Ctrl Pts',(-11.4753688142236,601.725181838547,
68.7506469944195));
#104794=CARTESIAN_POINT('Ctrl Pts',(-11.9923003685254,601.763782683624,
68.9173282151888));
#104795=CARTESIAN_POINT('Ctrl Pts',(-11.0237873908383,602.582434476172,
69.7270719203858));
#104796=CARTESIAN_POINT('Ctrl Pts',(-10.9544028777391,602.034097575223,
69.8689551387738));
#104797=CARTESIAN_POINT('Ctrl Pts',(-11.4726049050073,602.105029318799,
70.0970939152249));
#104798=CARTESIAN_POINT('Ctrl Pts',(-10.8384310991565,602.704379416319,
70.0880515743831));
#104799=CARTESIAN_POINT('Ctrl Pts',(-10.7586359325232,602.148519598434,
70.237687260735));
#104800=CARTESIAN_POINT('Ctrl Pts',(-11.2797017252308,602.230191744764,
70.4826829420179));
#104801=CARTESIAN_POINT('Ctrl Pts',(-10.4390987804155,602.96227503081,70.7805569003536));
#104802=CARTESIAN_POINT('Ctrl Pts',(-10.3387444088613,602.388767014119,
70.9429750385828));
#104803=CARTESIAN_POINT('Ctrl Pts',(-10.8641104504998,602.494891833565,
71.2223989202368));
#104804=CARTESIAN_POINT('Ctrl Pts',(-10.2247929217345,603.098466179307,
71.1132662015513));
#104805=CARTESIAN_POINT('Ctrl Pts',(-10.112915332954,602.51548143905,71.2812239398437));
#104806=CARTESIAN_POINT('Ctrl Pts',(-10.6410790491553,602.634676338017,
71.5777902117513));
#104807=CARTESIAN_POINT('Ctrl Pts',(-9.76784625223807,603.382222667475,
71.7535556942923));
#104808=CARTESIAN_POINT('Ctrl Pts',(-9.63349659380942,602.777474712516,
71.9302320108111));
#104809=CARTESIAN_POINT('Ctrl Pts',(-10.1655277254286,602.92591960861,72.261730451579));
#104810=CARTESIAN_POINT('Ctrl Pts',(-9.52520374213731,603.529798312671,
72.0611303923611));
#104811=CARTESIAN_POINT('Ctrl Pts',(-9.37852363969346,602.9133313277,72.2410837179652));
#104812=CARTESIAN_POINT('Ctrl Pts',(-9.91300599012881,603.077388971499,
72.5902735372759));
#104813=CARTESIAN_POINT('Ctrl Pts',(-9.01135722475072,603.833330353901,
72.6522134952531));
#104814=CARTESIAN_POINT('Ctrl Pts',(-8.84120033390601,603.190288416632,
72.836293304798));
#104815=CARTESIAN_POINT('Ctrl Pts',(-9.37823825283678,603.388929535203,
73.2216526442934));
#104816=CARTESIAN_POINT('Ctrl Pts',(-8.7389100250046,603.989962358859,72.9367840692432));
#104817=CARTESIAN_POINT('Ctrl Pts',(-8.55620892724536,603.332406057612,
73.1214587846384));
#104818=CARTESIAN_POINT('Ctrl Pts',(-9.09469840048593,603.549694184874,
73.5256232407945));
#104819=CARTESIAN_POINT('Ctrl Pts',(-7.89012810647256,604.46027386765,73.7426824430362));
#104820=CARTESIAN_POINT('Ctrl Pts',(-7.65796125292146,603.762076285552,
73.9394272155619));
#104821=CARTESIAN_POINT('Ctrl Pts',(-8.21135820442717,604.032414773745,
74.3864623908746));
#104822=CARTESIAN_POINT('Ctrl Pts',(-7.28116846417887,604.775808181103,
74.219742003199));
#104823=CARTESIAN_POINT('Ctrl Pts',(-7.02391120497901,604.039881145729,
74.4058463661051));
#104824=CARTESIAN_POINT('Ctrl Pts',(-7.57760505325563,604.356274191398,
74.8960441316923));
#104825=CARTESIAN_POINT('Ctrl Pts',(-6.29659249347781,605.228731780166,
74.8505072253373));
#104826=CARTESIAN_POINT('Ctrl Pts',(-6.03600513843954,604.420695941946,
75.0061312303154));
#104827=CARTESIAN_POINT('Ctrl Pts',(-6.55294358412831,604.821147490993,
75.5698095385058));
#104828=CARTESIAN_POINT('Ctrl Pts',(-5.95642441709213,605.376260941674,
75.0464903317535));
#104829=CARTESIAN_POINT('Ctrl Pts',(-5.69039769264683,604.544663809187,
75.1933203823609));
#104830=CARTESIAN_POINT('Ctrl Pts',(-6.19892597176367,604.972569034461,
75.7791531330914));
#104831=CARTESIAN_POINT('Ctrl Pts',(-5.24924375098352,605.659381288065,
75.4090550759564));
#104832=CARTESIAN_POINT('Ctrl Pts',(-4.97872636614062,604.778612595241,
75.5368081438878));
#104833=CARTESIAN_POINT('Ctrl Pts',(-5.46295346090092,605.263159156084,
76.166434449957));
#104834=CARTESIAN_POINT('Ctrl Pts',(-4.88532837447767,605.793622011102,
75.5738955184618));
#104835=CARTESIAN_POINT('Ctrl Pts',(-4.61623378897079,604.886539446989,
75.6897044857469));
#104836=CARTESIAN_POINT('Ctrl Pts',(-5.084221879631,605.400941617948,76.3425122362357));
#104837=CARTESIAN_POINT('Ctrl Pts',(-3.77089077493721,606.162783667258,
76.0143384748105));
#104838=CARTESIAN_POINT('Ctrl Pts',(-3.49682383912046,605.183694534843,
76.1025288496454));
#104839=CARTESIAN_POINT('Ctrl Pts',(-3.92441156002437,605.779843200399,
76.812980796566));
#104840=CARTESIAN_POINT('Ctrl Pts',(-2.99381238346118,606.366311081735,
76.238938541679));
#104841=CARTESIAN_POINT('Ctrl Pts',(-2.75796680224509,605.329065112758,
76.2927147804116));
#104842=CARTESIAN_POINT('Ctrl Pts',(-3.11569968988111,605.988739624887,
77.0528911109046));
#104843=CARTESIAN_POINT('Ctrl Pts',(-2.17374385871217,606.502538120315,
76.3864215127495));
#104844=CARTESIAN_POINT('Ctrl Pts',(-2.00694303543426,605.423796482346,
76.4163679119408));
#104845=CARTESIAN_POINT('Ctrl Pts',(-2.26224148372674,606.128561192588,
77.2104285068931));
#104846=CARTESIAN_POINT('Ctrl Pts',(2.31092134190292,606.120502424978,51.3976052199539));
#104847=CARTESIAN_POINT('Ctrl Pts',(1.9243904261614,606.185154402164,51.3246699561266));
#104848=CARTESIAN_POINT('Ctrl Pts',(1.53337526913546,606.234741119557,51.2697641942173));
#104849=CARTESIAN_POINT('Ctrl Pts',(1.13772717179832,606.267659184254,51.2334761581271));
#104850=CARTESIAN_POINT('Ctrl Pts',(1.10108396594791,606.270707912225,51.2301153180641));
#104851=CARTESIAN_POINT('Ctrl Pts',(1.06440101544787,606.273613684272,51.2269141451144));
#104852=CARTESIAN_POINT('Ctrl Pts',(1.02767819909564,606.276375240354,51.223873088555));
#104853=CARTESIAN_POINT('Ctrl Pts',(1.02189271947807,606.276810308468,51.2233939866645));
#104854=CARTESIAN_POINT('Ctrl Pts',(1.01610581480731,606.277241740565,51.2229189177151));
#104855=CARTESIAN_POINT('Ctrl Pts',(1.01031752097323,606.277669534987,51.2224478826357));
#104856=CARTESIAN_POINT('Ctrl Pts',(0.769279298806018,606.295483904812,
51.2028328697541));
#104857=CARTESIAN_POINT('Ctrl Pts',(0.525719603105276,606.306988425792,
51.1902149545468));
#104858=CARTESIAN_POINT('Ctrl Pts',(0.282374958379684,606.312048295433,
51.1846774469339));
#104859=CARTESIAN_POINT('Ctrl Pts',(0.0944016631504275,606.315956827592,
51.180399959938));
#104860=CARTESIAN_POINT('Ctrl Pts',(-0.0934423284468907,606.316020562991,
51.1803465302694));
#104861=CARTESIAN_POINT('Ctrl Pts',(-0.279895468563284,606.312191712354,
51.1845398016811));
#104862=CARTESIAN_POINT('Ctrl Pts',(-0.291911936050446,606.311944951913,
51.1848100481868));
#104863=CARTESIAN_POINT('Ctrl Pts',(-0.303924672822357,606.311682308102,
51.1850974258479));
#104864=CARTESIAN_POINT('Ctrl Pts',(-0.315933663727288,606.311403820519,
51.1854019212719));
#104865=CARTESIAN_POINT('Ctrl Pts',(-0.743857359011278,606.301480302683,
51.19625219238));
#104866=CARTESIAN_POINT('Ctrl Pts',(-1.16718217071824,606.271434870956,
51.2288431932868));
#104867=CARTESIAN_POINT('Ctrl Pts',(-1.58621543213723,606.222982509351,
51.2826473556403));
#104868=CARTESIAN_POINT('Ctrl Pts',(-2.00524869355621,606.174530147747,
51.3364515179938));
#104869=CARTESIAN_POINT('Ctrl Pts',(-2.41999047219477,606.107670585567,
51.4114688925646));
#104870=CARTESIAN_POINT('Ctrl Pts',(-2.83074822463685,606.024078269923,
51.5072092257538));
#104871=CARTESIAN_POINT('Ctrl Pts',(-2.85311152071182,606.019527169687,
51.5124217126872));
#104872=CARTESIAN_POINT('Ctrl Pts',(-2.87546063135743,606.014926459225,
51.5176966435968));
#104873=CARTESIAN_POINT('Ctrl Pts',(-2.89779414296661,606.010277010054,
51.5230334110954));
#104874=CARTESIAN_POINT('Ctrl Pts',(-3.2059760252563,605.94611889545,51.5966758853213));
#104875=CARTESIAN_POINT('Ctrl Pts',(-3.51096003016406,605.872712309442,
51.6820570658823));
#104876=CARTESIAN_POINT('Ctrl Pts',(-3.80902312883169,605.79238337635,51.7775305592681));
#104877=CARTESIAN_POINT('Ctrl Pts',(-3.8924315663616,605.769904542748,51.8042473683747));
#104878=CARTESIAN_POINT('Ctrl Pts',(-3.97529830179592,605.746883489111,
51.8317545824747));
#104879=CARTESIAN_POINT('Ctrl Pts',(-4.0575423502046,605.723370840561,51.8600163602557));
#104880=CARTESIAN_POINT('Ctrl Pts',(-4.0832488854947,605.716021631209,51.8688499768145));
#104881=CARTESIAN_POINT('Ctrl Pts',(-4.10890664396029,605.708622165367,
51.8777598513787));
#104882=CARTESIAN_POINT('Ctrl Pts',(-4.1345159694774,605.701173272842,51.8867457715322));
#104883=CARTESIAN_POINT('Ctrl Pts',(-4.42402771904677,605.616964030161,
51.9883310109953));
#104884=CARTESIAN_POINT('Ctrl Pts',(-4.70743818532932,605.526409127712,
52.0996719099263));
#104885=CARTESIAN_POINT('Ctrl Pts',(-4.9850704927822,605.430758867119,52.2203911199615));
#104886=CARTESIAN_POINT('Ctrl Pts',(-5.06347338639407,605.403747395457,
52.2544820205059));
#104887=CARTESIAN_POINT('Ctrl Pts',(-5.14141563704577,605.376329658806,
52.2893205600599));
#104888=CARTESIAN_POINT('Ctrl Pts',(-5.21890487245671,605.348533964113,
52.3248976144887));
#104889=CARTESIAN_POINT('Ctrl Pts',(-5.24645122189632,605.338652979808,
52.3375447643557));
#104890=CARTESIAN_POINT('Ctrl Pts',(-5.27394681459037,605.32872123747,52.3502900634044));
#104891=CARTESIAN_POINT('Ctrl Pts',(-5.30139053208202,605.318740404161,
52.3631325099366));
#104892=CARTESIAN_POINT('Ctrl Pts',(-5.66366362029746,605.186987579246,
52.5326602995615));
#104893=CARTESIAN_POINT('Ctrl Pts',(-6.01738163217701,605.04648601964,52.7193702986017));
#104894=CARTESIAN_POINT('Ctrl Pts',(-6.36015875743499,604.900894357318,
52.9212117806643));
#104895=CARTESIAN_POINT('Ctrl Pts',(-6.66684957126459,604.770630048196,
53.101804135979));
#104896=CARTESIAN_POINT('Ctrl Pts',(-6.96478180974465,604.636292006874,
53.2945085964751));
#104897=CARTESIAN_POINT('Ctrl Pts',(-7.25228682885563,604.500486505444,
53.4978360666795));
#104898=CARTESIAN_POINT('Ctrl Pts',(-7.28611567272387,604.484507156219,
53.521760286385));
#104899=CARTESIAN_POINT('Ctrl Pts',(-7.3198002059198,604.468507463044,53.5458315631905));
#104900=CARTESIAN_POINT('Ctrl Pts',(-7.35333775249021,604.452491647418,
53.5700474603555));
#104901=CARTESIAN_POINT('Ctrl Pts',(-7.38103000654065,604.439267244309,
53.5900427445945));
#104902=CARTESIAN_POINT('Ctrl Pts',(-7.40863101404046,604.426029015268,
53.6101387611508));
#104903=CARTESIAN_POINT('Ctrl Pts',(-7.43614101292809,604.412778123398,
53.6303357171612));
#104904=CARTESIAN_POINT('Ctrl Pts',(-7.75229632205407,604.260493863682,
53.8624467723796));
#104905=CARTESIAN_POINT('Ctrl Pts',(-8.05648904258559,604.106536505203,
54.1078905944877));
#104906=CARTESIAN_POINT('Ctrl Pts',(-8.3492945393904,603.952529481828,54.3671926590542));
#104907=CARTESIAN_POINT('Ctrl Pts',(-8.64210003619521,603.798522458454,
54.6264947236207));
#104908=CARTESIAN_POINT('Ctrl Pts',(-8.9235180189489,603.644464962219,54.8996548343146));
#104909=CARTESIAN_POINT('Ctrl Pts',(-9.1940846406694,603.491964984821,55.1872316250658));
#104910=CARTESIAN_POINT('Ctrl Pts',(-9.21816683588502,603.478391491525,
55.2128278363438));
#104911=CARTESIAN_POINT('Ctrl Pts',(-9.24215653499197,603.464832754806,
55.2385359314634));
#104912=CARTESIAN_POINT('Ctrl Pts',(-9.26605121704545,603.451291368523,
55.2643528781629));
#104913=CARTESIAN_POINT('Ctrl Pts',(-9.44919177121111,603.34750354735,55.4622266106876));
#104914=CARTESIAN_POINT('Ctrl Pts',(-9.62656991926582,603.244837575087,
55.6662959234923));
#104915=CARTESIAN_POINT('Ctrl Pts',(-9.79718029226227,603.144395450504,
55.8752912389312));
#104916=CARTESIAN_POINT('Ctrl Pts',(-9.86608440423407,603.103830065895,
55.9596978102531));
#104917=CARTESIAN_POINT('Ctrl Pts',(-9.93388438714588,603.063627351038,
56.0449084297711));
#104918=CARTESIAN_POINT('Ctrl Pts',(-10.0005127777516,603.02385991362,56.1308414745918));
#104919=CARTESIAN_POINT('Ctrl Pts',(-10.0215035613001,603.011331475464,
56.1579140472159));
#104920=CARTESIAN_POINT('Ctrl Pts',(-10.042387340134,602.998840989267,56.1850678260703));
#104921=CARTESIAN_POINT('Ctrl Pts',(-10.0631644425131,602.986389115948,
56.2123033808313));
#104922=CARTESIAN_POINT('Ctrl Pts',(-10.293419592427,602.848395477299,56.5141321262486));
#104923=CARTESIAN_POINT('Ctrl Pts',(-10.5104654401652,602.71521946088,56.8258408735637));
#104924=CARTESIAN_POINT('Ctrl Pts',(-10.7144165406335,602.587932468945,
57.1477632880394));
#104925=CARTESIAN_POINT('Ctrl Pts',(-10.7319264752442,602.577004423445,
57.1754014837356));
#104926=CARTESIAN_POINT('Ctrl Pts',(-10.7493409367415,602.566119390598,
57.2031141332603));
#104927=CARTESIAN_POINT('Ctrl Pts',(-10.7666595412328,602.555278130554,
57.2309017674638));
#104928=CARTESIAN_POINT('Ctrl Pts',(-10.9204731636543,602.458992458119,
57.4776951322247));
#104929=CARTESIAN_POINT('Ctrl Pts',(-11.0666558808087,602.366227070793,
57.7302247072817));
#104930=CARTESIAN_POINT('Ctrl Pts',(-11.2050607147541,602.277439642877,
57.9890220210254));
#104931=CARTESIAN_POINT('Ctrl Pts',(-11.3377551216428,602.192315483911,
58.2371416500344));
#104932=CARTESIAN_POINT('Ctrl Pts',(-11.4633001687098,602.110847512538,
58.4910223940912));
#104933=CARTESIAN_POINT('Ctrl Pts',(-11.5815311313948,602.033455455343,
58.7511591647439));
#104934=CARTESIAN_POINT('Ctrl Pts',(-11.6797499746316,601.969163004696,
58.9672644227628));
#104935=CARTESIAN_POINT('Ctrl Pts',(-11.7729206336702,601.907683622293,
59.1876875040276));
#104936=CARTESIAN_POINT('Ctrl Pts',(-11.8609291144948,601.8492692711,59.4127277678694));
#104937=CARTESIAN_POINT('Ctrl Pts',(-11.8711982768748,601.842453263687,
59.4389863169294));
#104938=CARTESIAN_POINT('Ctrl Pts',(-11.8813850119675,601.835687125542,
59.4652785322609));
#104939=CARTESIAN_POINT('Ctrl Pts',(-11.8914892131512,601.828971113388,
59.4916044497248));
#104940=CARTESIAN_POINT('Ctrl Pts',(-11.9959186669114,601.759559443137,
59.7636894102792));
#104941=CARTESIAN_POINT('Ctrl Pts',(-12.091310776531,601.695659985364,60.0387465906123));
#104942=CARTESIAN_POINT('Ctrl Pts',(-12.1776505788867,601.637494904103,
60.3167757884128));
#104943=CARTESIAN_POINT('Ctrl Pts',(-12.2628096616721,601.580125245671,
60.5910028635999));
#104944=CARTESIAN_POINT('Ctrl Pts',(-12.3391623321425,601.528334025132,
60.8681213879226));
#104945=CARTESIAN_POINT('Ctrl Pts',(-12.4066531860926,601.482358055859,
61.1481479683393));
#104946=CARTESIAN_POINT('Ctrl Pts',(-12.4690433776644,601.439856748456,
61.4070113694502));
#104947=CARTESIAN_POINT('Ctrl Pts',(-12.5238602515823,601.402325030908,
61.6683601246001));
#104948=CARTESIAN_POINT('Ctrl Pts',(-12.5710279567737,601.369970326165,
61.9322186969404));
#104949=CARTESIAN_POINT('Ctrl Pts',(-12.5745024304964,601.367587009635,
61.9516550819074));
#104950=CARTESIAN_POINT('Ctrl Pts',(-12.5779356066442,601.365231507343,
61.9711086414617));
#104951=CARTESIAN_POINT('Ctrl Pts',(-12.5813273486773,601.362903942309,
61.9905791155502));
#104952=CARTESIAN_POINT('Ctrl Pts',(-12.6482309907147,601.316991671765,
62.3746430024895));
#104953=CARTESIAN_POINT('Ctrl Pts',(-12.6989827550363,601.281970909012,
62.7651309616918));
#104954=CARTESIAN_POINT('Ctrl Pts',(-12.7325045718852,601.258810650632,
63.1594985620737));
#104955=CARTESIAN_POINT('Ctrl Pts',(-12.7352361632934,601.256923391266,
63.1916343843564));
#104956=CARTESIAN_POINT('Ctrl Pts',(-12.7378533692347,601.255114870462,
63.2237959671349));
#104957=CARTESIAN_POINT('Ctrl Pts',(-12.7403556191587,601.25338560344,63.2559819337451));
#104958=CARTESIAN_POINT('Ctrl Pts',(-12.7415108518539,601.252587239622,
63.2708414729934));
#104959=CARTESIAN_POINT('Ctrl Pts',(-12.7426411255945,601.251806087635,
63.2856985588883));
#104960=CARTESIAN_POINT('Ctrl Pts',(-12.7437464711904,601.251042128905,
63.3005531880157));
#104961=CARTESIAN_POINT('Ctrl Pts',(-12.7759162994634,601.228807977662,
63.7328802989446));
#104962=CARTESIAN_POINT('Ctrl Pts',(-12.7870003318299,601.221122005951,
64.1634229287959));
#104963=CARTESIAN_POINT('Ctrl Pts',(-12.7776731523991,601.227577203012,
64.5922349254529));
#104964=CARTESIAN_POINT('Ctrl Pts',(-12.7774670029556,601.227719875863,
64.6017125338895));
#104965=CARTESIAN_POINT('Ctrl Pts',(-12.7772508808923,601.22786945759,64.611189296609));
#104966=CARTESIAN_POINT('Ctrl Pts',(-12.7770247866986,601.228025945988,
64.6206652136733));
#104967=CARTESIAN_POINT('Ctrl Pts',(-12.7666730268079,601.235190793079,
65.0545216369199));
#104968=CARTESIAN_POINT('Ctrl Pts',(-12.7354157605725,601.256837750184,
65.4866513230427));
#104969=CARTESIAN_POINT('Ctrl Pts',(-12.6833305290434,601.292744171308,
65.9169319880768));
#104970=CARTESIAN_POINT('Ctrl Pts',(-12.6828077078149,601.293104592845,
65.9212510600921));
#104971=CARTESIAN_POINT('Ctrl Pts',(-12.6822827336681,601.293466488472,
65.9255701772016));
#104972=CARTESIAN_POINT('Ctrl Pts',(-12.6817556078935,601.293829856882,
65.9298893314513));
#104973=CARTESIAN_POINT('Ctrl Pts',(-12.6329480531499,601.32747481301,66.3298078474378));
#104974=CARTESIAN_POINT('Ctrl Pts',(-12.5656816350128,601.37375161562,66.7301336276845));
#104975=CARTESIAN_POINT('Ctrl Pts',(-12.4809092885528,601.431669700594,
67.1247607526229));
#104976=CARTESIAN_POINT('Ctrl Pts',(-12.4735560157333,601.436693596921,
67.1589912656718));
#104977=CARTESIAN_POINT('Ctrl Pts',(-12.4660710046774,601.441805097326,
67.1931788821502));
#104978=CARTESIAN_POINT('Ctrl Pts',(-12.4584548648209,601.447003563173,
67.2273196043471));
#104979=CARTESIAN_POINT('Ctrl Pts',(-12.4583195473824,601.447095925327,
67.2279261892));
#104980=CARTESIAN_POINT('Ctrl Pts',(-12.4581841884965,601.447188314965,
67.228532759456));
#104981=CARTESIAN_POINT('Ctrl Pts',(-12.4580487881665,601.447280732084,
67.2291393150922));
#104982=CARTESIAN_POINT('Ctrl Pts',(-12.3287543192927,601.535530312215,
67.8083423998814));
#104983=CARTESIAN_POINT('Ctrl Pts',(-12.1635881081911,601.647634844985,
68.3695526414148));
#104984=CARTESIAN_POINT('Ctrl Pts',(-11.9641361654503,601.780646951911,
68.914015787099));
#104985=CARTESIAN_POINT('Ctrl Pts',(-11.8692267000605,601.843940935339,
69.1730992804518));
#104986=CARTESIAN_POINT('Ctrl Pts',(-11.7665541541683,601.911968557483,
69.4283910409647));
#104987=CARTESIAN_POINT('Ctrl Pts',(-11.6562914846912,601.984409339138,
69.6800273323468));
#104988=CARTESIAN_POINT('Ctrl Pts',(-11.6528123180314,601.986695095083,
69.6879673232751));
#104989=CARTESIAN_POINT('Ctrl Pts',(-11.6493255850375,601.988985246907,
69.6959036824858));
#104990=CARTESIAN_POINT('Ctrl Pts',(-11.6458312910721,601.991279784524,
69.703836414217));
#104991=CARTESIAN_POINT('Ctrl Pts',(-11.4971366810285,602.088920503827,
70.0414023039313));
#104992=CARTESIAN_POINT('Ctrl Pts',(-11.3338413939608,602.195038107293,
70.3735482479391));
#104993=CARTESIAN_POINT('Ctrl Pts',(-11.1589239951637,602.306981469902,
70.6951271372583));
#104994=CARTESIAN_POINT('Ctrl Pts',(-11.1357897460821,602.321786890355,
70.7376585616681));
#104995=CARTESIAN_POINT('Ctrl Pts',(-11.1124522363448,602.336694184926,
70.7800050874247));
#104996=CARTESIAN_POINT('Ctrl Pts',(-11.08891838951,602.351697191721,70.8221547543116));
#104997=CARTESIAN_POINT('Ctrl Pts',(-11.0832572973831,602.355306181115,
70.8322939019419));
#104998=CARTESIAN_POINT('Ctrl Pts',(-11.0775847776858,602.358920761129,
70.8424218051789));
#104999=CARTESIAN_POINT('Ctrl Pts',(-11.0719009273916,602.362540845218,
70.8525382931254));
#105000=CARTESIAN_POINT('Ctrl Pts',(-10.8933793466742,602.476242491184,
71.1702826611247));
#105001=CARTESIAN_POINT('Ctrl Pts',(-10.703424027174,602.595558323103,71.4776963876999));
#105002=CARTESIAN_POINT('Ctrl Pts',(-10.5023371611635,602.719460142399,
71.7752823630464));
#105003=CARTESIAN_POINT('Ctrl Pts',(-10.477246088423,602.734920274741,71.812414332439));
#105004=CARTESIAN_POINT('Ctrl Pts',(-10.451981746354,602.750451775019,71.849393329467));
#105005=CARTESIAN_POINT('Ctrl Pts',(-10.4265447575929,602.766052618462,
71.8862203643523));
#105006=CARTESIAN_POINT('Ctrl Pts',(-10.4188131204951,602.770794534301,
71.89741403479));
#105007=CARTESIAN_POINT('Ctrl Pts',(-10.4110654988077,602.775542877077,
71.9085937144694));
#105008=CARTESIAN_POINT('Ctrl Pts',(-10.403301906923,602.780297592492,71.9197594373552));
#105009=CARTESIAN_POINT('Ctrl Pts',(-10.1743043134857,602.9205443241,72.249107464377));
#105010=CARTESIAN_POINT('Ctrl Pts',(-9.9314107080512,603.066346344098,72.5663065584189));
#105011=CARTESIAN_POINT('Ctrl Pts',(-9.67444603037874,603.216348882047,
72.8718105219763));
#105012=CARTESIAN_POINT('Ctrl Pts',(-9.66485722564934,603.221946324693,
72.8832106018516));
#105013=CARTESIAN_POINT('Ctrl Pts',(-9.65524877276323,603.227549638817,
72.894594446214));
#105014=CARTESIAN_POINT('Ctrl Pts',(-9.64562066556107,603.233158751113,
72.9059620729246));
#105015=CARTESIAN_POINT('Ctrl Pts',(-9.42731586110791,603.360338074853,
73.1637082190824));
#105016=CARTESIAN_POINT('Ctrl Pts',(-9.19804063689573,603.490962988956,
73.4138743236315));
#105017=CARTESIAN_POINT('Ctrl Pts',(-8.9606618592393,603.62236653666,73.6534663851397));
#105018=CARTESIAN_POINT('Ctrl Pts',(-8.91843648223493,603.645740843312,
73.6960854651785));
#105019=CARTESIAN_POINT('Ctrl Pts',(-8.87595480166585,603.669139715431,
73.7383699342028));
#105020=CARTESIAN_POINT('Ctrl Pts',(-8.83323308819527,603.692548054781,
73.7803029115011));
#105021=CARTESIAN_POINT('Ctrl Pts',(-8.82225322068705,603.698564210122,
73.7910800666655));
#105022=CARTESIAN_POINT('Ctrl Pts',(-8.8112573568705,603.704581075414,73.8018341562657));
#105023=CARTESIAN_POINT('Ctrl Pts',(-8.80024576806367,603.710598396771,
73.8125648963688));
#105024=CARTESIAN_POINT('Ctrl Pts',(-8.45642397178709,603.898481024225,
74.1476175760816));
#105025=CARTESIAN_POINT('Ctrl Pts',(-8.09685247605963,604.087315619871,
74.4611950419538));
#105026=CARTESIAN_POINT('Ctrl Pts',(-7.72053287891659,604.273894779001,
74.7538975280105));
#105027=CARTESIAN_POINT('Ctrl Pts',(-7.46460285154065,604.400784820516,
74.9529606537106));
#105028=CARTESIAN_POINT('Ctrl Pts',(-7.20092632696537,604.526630672235,
75.1423691922054));
#105029=CARTESIAN_POINT('Ctrl Pts',(-6.92918660057972,604.650411262877,
75.3223177033401));
#105030=CARTESIAN_POINT('Ctrl Pts',(-6.91763580200879,604.655672785322,
75.3299667469043));
#105031=CARTESIAN_POINT('Ctrl Pts',(-6.90607038322324,604.660930574261,
75.3375986977517));
#105032=CARTESIAN_POINT('Ctrl Pts',(-6.89449031796784,604.666184552022,
75.3452135726448));
#105033=CARTESIAN_POINT('Ctrl Pts',(-6.56315230202821,604.816515532802,
75.5630964155351));
#105034=CARTESIAN_POINT('Ctrl Pts',(-6.21970864445251,604.963681647969,
75.7668655454909));
#105035=CARTESIAN_POINT('Ctrl Pts',(-5.86266390244237,605.105307310949,
75.9560400598351));
#105036=CARTESIAN_POINT('Ctrl Pts',(-5.85210062245604,605.109497350335,
75.9616368468093));
#105037=CARTESIAN_POINT('Ctrl Pts',(-5.84152543830141,605.113682529787,
75.9672208471966));
#105038=CARTESIAN_POINT('Ctrl Pts',(-5.83093831658856,605.11786278462,75.9727920447534));
#105039=CARTESIAN_POINT('Ctrl Pts',(-5.5161673445808,605.242148016517,76.1384320853383));
#105040=CARTESIAN_POINT('Ctrl Pts',(-5.19319897990937,605.361066290119,
76.2913913408696));
#105041=CARTESIAN_POINT('Ctrl Pts',(-4.86393313325879,605.472044352162,
76.4304781401722));
#105042=CARTESIAN_POINT('Ctrl Pts',(-4.81686179186501,605.487909606025,
76.4503617760851));
#105043=CARTESIAN_POINT('Ctrl Pts',(-4.76966181409826,605.503612582643,
76.4699619551291));
#105044=CARTESIAN_POINT('Ctrl Pts',(-4.72233881323819,605.519145766855,
76.4892752541632));
#105045=CARTESIAN_POINT('Ctrl Pts',(-4.71410218547921,605.521849337084,
76.4926367581264));
#105046=CARTESIAN_POINT('Ctrl Pts',(-4.70586176397251,605.524547786911,
76.4959896003441));
#105047=CARTESIAN_POINT('Ctrl Pts',(-4.69761757561064,605.527241077286,
76.4993337633958));
#105048=CARTESIAN_POINT('Ctrl Pts',(-4.3388302553356,605.644453153712,76.6448718378807));
#105049=CARTESIAN_POINT('Ctrl Pts',(-3.9720449954439,605.752375348195,76.7746808977428));
#105050=CARTESIAN_POINT('Ctrl Pts',(-3.59624449105719,605.848408824589,
76.8878059230058));
#105051=CARTESIAN_POINT('Ctrl Pts',(-3.23104131746731,605.941734219155,
76.9977408958338));
#105052=CARTESIAN_POINT('Ctrl Pts',(-2.85732420839845,606.023832093733,
77.0919195272477));
#105053=CARTESIAN_POINT('Ctrl Pts',(-2.47414214786944,606.092277286236,
77.1694416309688));
#105054=CARTESIAN_POINT('Ctrl Pts',(-2.40382931965833,606.104836786166,
77.1836667185264));
#105055=CARTESIAN_POINT('Ctrl Pts',(-2.33319774596395,606.116936468902,
77.1973308944953));
#105056=CARTESIAN_POINT('Ctrl Pts',(-2.26224148372675,606.128561192588,
77.2104285068931));
#105057=CARTESIAN_POINT('Ctrl Pts',(-31.0097671277257,639.446460969661,
66.0551195689836));
#105058=CARTESIAN_POINT('Ctrl Pts',(-30.8959801896217,640.044390291998,
66.0811757608045));
#105059=CARTESIAN_POINT('Ctrl Pts',(-31.4793952064496,640.026746757976,
66.2557082786456));
#105060=CARTESIAN_POINT('Ctrl Pts',(-31.1216215713103,639.485438110803,
65.6842493861687));
#105061=CARTESIAN_POINT('Ctrl Pts',(-31.011297302018,640.078355022162,65.7082942948574));
#105062=CARTESIAN_POINT('Ctrl Pts',(-31.6011050878646,640.068535529554,
65.8424727426508));
#105063=CARTESIAN_POINT('Ctrl Pts',(-31.199678803567,639.513756569195,65.2913781212572));
#105064=CARTESIAN_POINT('Ctrl Pts',(-31.0932130181999,640.10348882227,65.308332916704));
#105065=CARTESIAN_POINT('Ctrl Pts',(-31.6860601122613,640.098849863563,
65.4047068941051));
#105066=CARTESIAN_POINT('Ctrl Pts',(-31.2763918246953,639.541623224254,
64.5136325787294));
#105067=CARTESIAN_POINT('Ctrl Pts',(-31.173175859161,640.12806781138,64.5180893199653));
#105068=CARTESIAN_POINT('Ctrl Pts',(-31.7695504886776,640.128678316087,
64.5381010125616));
#105069=CARTESIAN_POINT('Ctrl Pts',(-31.2776919379551,639.542105193104,
64.127368726076));
#105070=CARTESIAN_POINT('Ctrl Pts',(-31.174545243998,640.128497521662,64.1236757188328));
#105071=CARTESIAN_POINT('Ctrl Pts',(-31.7709656050263,640.129193814483,
64.1077050217475));
#105072=CARTESIAN_POINT('Ctrl Pts',(-31.224600053557,639.522805357793,63.5480361507529));
#105073=CARTESIAN_POINT('Ctrl Pts',(-31.1192510473443,640.111488697363,
63.5355366548963));
#105074=CARTESIAN_POINT('Ctrl Pts',(-31.7131830184482,640.108535850692,
63.4621815431067));
#105075=CARTESIAN_POINT('Ctrl Pts',(-31.1974309863985,639.512951461025,
63.3538641004119));
#105076=CARTESIAN_POINT('Ctrl Pts',(-31.0908849094541,640.102784037384,
63.3381669310628));
#105077=CARTESIAN_POINT('Ctrl Pts',(-31.6836138753777,640.097987603797,
63.2458246077949));
#105078=CARTESIAN_POINT('Ctrl Pts',(-31.1249336139912,639.486977930442,
62.9713637144933));
#105079=CARTESIAN_POINT('Ctrl Pts',(-31.0154542096272,640.079925697966,
62.9501636895933));
#105080=CARTESIAN_POINT('Ctrl Pts',(-31.6047168885246,640.070170586937,
62.8196221380521));
#105081=CARTESIAN_POINT('Ctrl Pts',(-31.0798069669301,639.470931087843,
62.7834074755949));
#105082=CARTESIAN_POINT('Ctrl Pts',(-30.9684675402991,640.065797566145,
62.7595873868922));
#105083=CARTESIAN_POINT('Ctrl Pts',(-31.5556085077068,640.052979751955,
62.6101912064094));
#105084=CARTESIAN_POINT('Ctrl Pts',(-30.9184187369807,639.414526541786,
62.2291146946095));
#105085=CARTESIAN_POINT('Ctrl Pts',(-30.8006348715585,640.016214778984,
62.1974227483927));
#105086=CARTESIAN_POINT('Ctrl Pts',(-31.379994664234,639.992512479841,61.9925684320935));
#105087=CARTESIAN_POINT('Ctrl Pts',(-30.7764312493032,639.365891441069,
61.8722609501814));
#105088=CARTESIAN_POINT('Ctrl Pts',(-30.6528555145984,639.973496030507,
61.8369829267743));
#105089=CARTESIAN_POINT('Ctrl Pts',(-31.2255061246491,639.940331754255,
61.5949428691868));
#105090=CARTESIAN_POINT('Ctrl Pts',(-30.4202373697957,639.251358448989,
61.1845444688204));
#105091=CARTESIAN_POINT('Ctrl Pts',(-30.2872866136104,639.874270624505,
61.1477102937615));
#105092=CARTESIAN_POINT('Ctrl Pts',(-30.8380612906271,639.817121140284,
60.8286524472484));
#105093=CARTESIAN_POINT('Ctrl Pts',(-30.2110021753699,639.187131253443,
60.8636665662452));
#105094=CARTESIAN_POINT('Ctrl Pts',(-30.0729968186835,639.818885980513,
60.8282389397767));
#105095=CARTESIAN_POINT('Ctrl Pts',(-30.6105133697495,639.747885147849,
60.4711132048704));
#105096=CARTESIAN_POINT('Ctrl Pts',(-29.8531791687691,639.086868693642,
60.4186064777946));
#105097=CARTESIAN_POINT('Ctrl Pts',(-29.7133672861232,639.733791481457,
60.3901096029334));
#105098=CARTESIAN_POINT('Ctrl Pts',(-30.2215132342272,639.639334841987,
59.9752036724944));
#105099=CARTESIAN_POINT('Ctrl Pts',(-29.7264149308112,639.052757750992,
60.2761430493737));
#105100=CARTESIAN_POINT('Ctrl Pts',(-29.5858497865698,639.70481779123,60.2497909596439));
#105101=CARTESIAN_POINT('Ctrl Pts',(-30.0837246437525,639.602328735179,
59.8164633689678));
#105102=CARTESIAN_POINT('Ctrl Pts',(-29.4573261779289,638.984176116224,
60.0032337484715));
#105103=CARTESIAN_POINT('Ctrl Pts',(-29.3167867305768,639.646776340438,
59.9818071084143));
#105104=CARTESIAN_POINT('Ctrl Pts',(-29.7912900142244,639.52771251499,59.5123733782039));
#105105=CARTESIAN_POINT('Ctrl Pts',(-29.3144414166823,638.949599478752,
59.8724601150719));
#105106=CARTESIAN_POINT('Ctrl Pts',(-29.1746256162575,639.617633014463,
59.854007428715));
#105107=CARTESIAN_POINT('Ctrl Pts',(-29.6360356611041,639.489984964564,
59.3666584849922));
#105108=CARTESIAN_POINT('Ctrl Pts',(-28.8713588165294,638.849263193194,
59.5070266266901));
#105109=CARTESIAN_POINT('Ctrl Pts',(-28.7343122010769,639.53279745443,59.4959957724646));
#105110=CARTESIAN_POINT('Ctrl Pts',(-29.1546960250352,639.380077654759,
58.959473158275));
#105111=CARTESIAN_POINT('Ctrl Pts',(-28.5542773646734,638.786167723086,
59.2959879030435));
#105112=CARTESIAN_POINT('Ctrl Pts',(-28.4246322286205,639.480180811518,
59.2928614504489));
#105113=CARTESIAN_POINT('Ctrl Pts',(-28.8103644308171,639.310385750122,
58.724322722433));
#105114=CARTESIAN_POINT('Ctrl Pts',(-27.8755320887359,638.675756812919,
58.9385684071363));
#105115=CARTESIAN_POINT('Ctrl Pts',(-27.7672168563168,639.3865757007,58.9467223246297));
#105116=CARTESIAN_POINT('Ctrl Pts',(-28.0736484273117,639.186570194773,
58.3260670892298));
#105117=CARTESIAN_POINT('Ctrl Pts',(-27.5112853189433,638.62850564541,58.7924168303215));
#105118=CARTESIAN_POINT('Ctrl Pts',(-27.4195305018196,639.346056019806,
58.8059538597408));
#105119=CARTESIAN_POINT('Ctrl Pts',(-27.6784676113671,639.132473886899,
58.1632173161809));
#105120=CARTESIAN_POINT('Ctrl Pts',(-26.7705302994941,638.561026384799,
58.5795138846031));
#105121=CARTESIAN_POINT('Ctrl Pts',(-26.7123185573368,639.283986825685,
58.5954396179378));
#105122=CARTESIAN_POINT('Ctrl Pts',(-26.8752220660644,639.051904635401,
57.9259895427364));
#105123=CARTESIAN_POINT('Ctrl Pts',(-26.390262231729,638.540012680231,58.5102517531126));
#105124=CARTESIAN_POINT('Ctrl Pts',(-26.3531632859189,639.262102841207,
58.5245086708497));
#105125=CARTESIAN_POINT('Ctrl Pts',(-26.4630739366364,639.024566786374,
57.8488139449765));
#105126=CARTESIAN_POINT('Ctrl Pts',(-25.6094285011568,638.527157113703,
58.4469171473938));
#105127=CARTESIAN_POINT('Ctrl Pts',(-25.6080269458141,639.238702551721,
58.4501065549983));
#105128=CARTESIAN_POINT('Ctrl Pts',(-25.6172217634613,638.999604848902,
57.778242915881));
#105129=CARTESIAN_POINT('Ctrl Pts',(-25.2189809711016,638.535609798989,
58.453979164517));
#105130=CARTESIAN_POINT('Ctrl Pts',(-25.2361374307006,639.23752462347,58.4476660614292));
#105131=CARTESIAN_POINT('Ctrl Pts',(-25.194480338516,639.002435896301,57.7861115876274));
#105132=CARTESIAN_POINT('Ctrl Pts',(-24.6409354929901,638.568745456371,
58.5186871133032));
#105133=CARTESIAN_POINT('Ctrl Pts',(-24.6736512904528,639.251920802327,
58.4966619148348));
#105134=CARTESIAN_POINT('Ctrl Pts',(-24.5689264138619,639.027847597861,
57.8582122899254));
#105135=CARTESIAN_POINT('Ctrl Pts',(-24.4490972732004,638.583191576161,
58.5493117143284));
#105136=CARTESIAN_POINT('Ctrl Pts',(-24.4873728312289,639.259283169087,
58.5213924422961));
#105137=CARTESIAN_POINT('Ctrl Pts',(-24.3613718882865,639.039830475442,
57.8923357215899));
#105138=CARTESIAN_POINT('Ctrl Pts',(-24.0671081959017,638.618540338843,
58.6287302863804));
#105139=CARTESIAN_POINT('Ctrl Pts',(-24.1139136994163,639.279335311201,
58.5889529536862));
#105140=CARTESIAN_POINT('Ctrl Pts',(-23.9481847707517,639.070465560091,
57.9808278590847));
#105141=CARTESIAN_POINT('Ctrl Pts',(-23.8768636638465,638.639494936042,
58.6776732346629));
#105142=CARTESIAN_POINT('Ctrl Pts',(-23.9270215097293,639.291978429298,
58.6316256560464));
#105143=CARTESIAN_POINT('Ctrl Pts',(-23.7424514950666,639.089169818811,
58.0353625563298));
#105144=CARTESIAN_POINT('Ctrl Pts',(-23.3201749292324,638.709821703261,
58.8484494113552));
#105145=CARTESIAN_POINT('Ctrl Pts',(-23.3806749026967,639.336411072855,
58.7835372517324));
#105146=CARTESIAN_POINT('Ctrl Pts',(-23.1405719163352,639.15317327971,58.2256500255681));
#105147=CARTESIAN_POINT('Ctrl Pts',(-22.9636204205607,638.766962613931,
58.9946750187081));
#105148=CARTESIAN_POINT('Ctrl Pts',(-23.0243053306422,639.375032265077,
58.9173052658177));
#105149=CARTESIAN_POINT('Ctrl Pts',(-22.7552500131854,639.206615373746,
58.3885820845647));
#105150=CARTESIAN_POINT('Ctrl Pts',(-22.27848089945,638.895420482319,59.3507109235853));
#105151=CARTESIAN_POINT('Ctrl Pts',(-22.3317399785605,639.467210290523,
59.2554960516949));
#105152=CARTESIAN_POINT('Ctrl Pts',(-22.0151053084073,639.328507485308,
58.7852957947004));
#105153=CARTESIAN_POINT('Ctrl Pts',(-21.9500159216726,638.966926375171,
59.5614980956268));
#105154=CARTESIAN_POINT('Ctrl Pts',(-21.995648509837,639.520426082359,59.4584719479871));
#105155=CARTESIAN_POINT('Ctrl Pts',(-21.6604152666523,639.397153710713,
59.0201658778045));
#105156=CARTESIAN_POINT('Ctrl Pts',(-21.3460486897185,639.111793677402,
60.0320961056729));
#105157=CARTESIAN_POINT('Ctrl Pts',(-21.374045693413,639.631792692931,59.9216812301887));
#105158=CARTESIAN_POINT('Ctrl Pts',(-21.0084223762403,639.537151410169,
59.5445310201806));
#105159=CARTESIAN_POINT('Ctrl Pts',(-21.0669931238233,639.185808726979,
60.2934777106252));
#105160=CARTESIAN_POINT('Ctrl Pts',(-21.0834671017477,639.690247737726,
60.1816491447995));
#105161=CARTESIAN_POINT('Ctrl Pts',(-20.7072807213335,639.609122100779,
59.8357762715668));
#105162=CARTESIAN_POINT('Ctrl Pts',(-20.6843161289542,639.293828358263,
60.7275832942433));
#105163=CARTESIAN_POINT('Ctrl Pts',(-20.6816094426164,639.777663387302,
60.6221327845261));
#105164=CARTESIAN_POINT('Ctrl Pts',(-20.2944117951707,639.714527579313,
60.3194799830296));
#105165=CARTESIAN_POINT('Ctrl Pts',(-20.5629709963199,639.329293550566,
60.879349817338));
#105166=CARTESIAN_POINT('Ctrl Pts',(-20.554558284157,639.806446454198,60.7757280451264));
#105167=CARTESIAN_POINT('Ctrl Pts',(-20.1635106966246,639.749199037125,
60.4885863707933));
#105168=CARTESIAN_POINT('Ctrl Pts',(-20.3379823034572,639.396756759074,
61.1906817235449));
#105169=CARTESIAN_POINT('Ctrl Pts',(-20.3188450962156,639.861528013512,
61.0920285161997));
#105170=CARTESIAN_POINT('Ctrl Pts',(-19.9208290490855,639.815240108573,
60.8354890916476));
#105171=CARTESIAN_POINT('Ctrl Pts',(-20.2336008003601,639.428961041436,
61.3510394361652));
#105172=CARTESIAN_POINT('Ctrl Pts',(-20.2090499310174,639.888053434363,
61.2556019061011));
#105173=CARTESIAN_POINT('Ctrl Pts',(-19.8082522970898,639.846810887964,
61.0141682831509));
#105174=CARTESIAN_POINT('Ctrl Pts',(-19.9449136033705,639.519814097585,
61.8464125125788));
#105175=CARTESIAN_POINT('Ctrl Pts',(-19.9070847959734,639.962771595516,
61.7594811413053));
#105176=CARTESIAN_POINT('Ctrl Pts',(-19.4969257393655,639.935963708212,
61.5661395895971));
#105177=CARTESIAN_POINT('Ctrl Pts',(-19.7847575698374,639.57275723913,62.1955854246443));
#105178=CARTESIAN_POINT('Ctrl Pts',(-19.7367196925424,640.007397463489,
62.1194969013774));
#105179=CARTESIAN_POINT('Ctrl Pts',(-19.3242457747715,639.988037778914,
61.9552110306678));
#105180=CARTESIAN_POINT('Ctrl Pts',(-19.6604708015409,639.614602859825,
62.5660174884535));
#105181=CARTESIAN_POINT('Ctrl Pts',(-19.6043565557346,640.042864698584,
62.5045799077997));
#105182=CARTESIAN_POINT('Ctrl Pts',(-19.1902534503917,640.029230307342,
62.3679625261942));
#105183=CARTESIAN_POINT('Origin',(-48.,620.675373764374,64.2994740882088));
#105184=CARTESIAN_POINT('Origin',(28.,620.675373764374,64.2994740882088));
#105185=CARTESIAN_POINT('Ctrl Pts',(1.86306288877798,606.534169754924,79.840079036097));
#105186=CARTESIAN_POINT('Ctrl Pts',(2.14021144979533,606.496771580384,79.8060484936875));
#105187=CARTESIAN_POINT('Ctrl Pts',(2.4133761460843,606.451830720321,79.7649147909193));
#105188=CARTESIAN_POINT('Ctrl Pts',(2.68283184001625,606.400050317104,79.7169704303203));
#105189=CARTESIAN_POINT('Ctrl Pts',(2.97414735927081,606.344069184063,79.6651365421608));
#105190=CARTESIAN_POINT('Ctrl Pts',(3.26112767369667,606.280094095968,79.6053412098497));
#105191=CARTESIAN_POINT('Ctrl Pts',(3.54412011470249,606.209064457015,79.5379106224147));
#105192=CARTESIAN_POINT('Ctrl Pts',(3.88187814635567,606.124288938076,79.4574306548075));
#105193=CARTESIAN_POINT('Ctrl Pts',(4.21395546218491,606.029464281995,79.3660724895544));
#105194=CARTESIAN_POINT('Ctrl Pts',(4.54094258490408,605.926255970468,79.2643522128276));
#105195=CARTESIAN_POINT('Ctrl Pts',(4.66022073585215,605.888607709402,79.2272467561326));
#105196=CARTESIAN_POINT('Ctrl Pts',(4.7788215654658,605.84984443673,79.1887623167325));
#105197=CARTESIAN_POINT('Ctrl Pts',(4.89677373712177,605.810048547591,79.1489238821405));
#105198=CARTESIAN_POINT('Ctrl Pts',(5.16043615150262,605.721091472317,79.0598717035989));
#105199=CARTESIAN_POINT('Ctrl Pts',(5.42147464016636,605.626588819934,78.9636635925401));
#105200=CARTESIAN_POINT('Ctrl Pts',(5.67881724163154,605.527777854217,78.8608748149868));
#105201=CARTESIAN_POINT('Ctrl Pts',(5.89134528491515,605.446174182384,78.7759860416529));
#105202=CARTESIAN_POINT('Ctrl Pts',(6.10135258954282,605.361632372566,78.6866091801219));
#105203=CARTESIAN_POINT('Ctrl Pts',(6.30823535587315,605.274837711021,78.593093022985));
#105204=CARTESIAN_POINT('Ctrl Pts',(6.6081803457824,605.149000144447,78.4575104256217));
#105205=CARTESIAN_POINT('Ctrl Pts',(6.90074477299936,605.018887494591,78.3137274985418));
#105206=CARTESIAN_POINT('Ctrl Pts',(7.18661418705821,604.885610576882,78.1619208948199));
#105207=CARTESIAN_POINT('Ctrl Pts',(7.33667046294114,604.81565192811,78.0822357921518));
#105208=CARTESIAN_POINT('Ctrl Pts',(7.48488204463535,604.744821534827,78.0003406744257));
#105209=CARTESIAN_POINT('Ctrl Pts',(7.63134808340531,604.673280035404,77.9162670025649));
#105210=CARTESIAN_POINT('Ctrl Pts',(7.91723728695995,604.533637136183,77.7521623726448));
#105211=CARTESIAN_POINT('Ctrl Pts',(8.19655198248917,604.391360677278,77.5798506235828));
#105212=CARTESIAN_POINT('Ctrl Pts',(8.46960770404473,604.247250255253,77.3991233565012));
#105213=CARTESIAN_POINT('Ctrl Pts',(8.73947522321079,604.104822468513,77.220506263495));
#105214=CARTESIAN_POINT('Ctrl Pts',(9.00322907485539,603.960603546486,77.0336684769913));
#105215=CARTESIAN_POINT('Ctrl Pts',(9.26117386903771,603.815407551738,76.8384370553757));
#105216=CARTESIAN_POINT('Ctrl Pts',(9.51911866322004,603.67021155699,76.6432056337602));
#105217=CARTESIAN_POINT('Ctrl Pts',(9.7712543999401,603.524038705004,76.4395799971655));
#105218=CARTESIAN_POINT('Ctrl Pts',(10.0178856892571,603.377742099661,76.2274241122124));
#105219=CARTESIAN_POINT('Ctrl Pts',(10.203587578906,603.267587560322,76.0676805985445));
#105220=CARTESIAN_POINT('Ctrl Pts',(10.3856411221024,603.157580684183,75.9034085015199));
#105221=CARTESIAN_POINT('Ctrl Pts',(10.5636740062097,603.048302838395,75.7349637390157));
#105222=CARTESIAN_POINT('Ctrl Pts',(10.7417068903169,602.939024992607,75.5665189765115));
#105223=CARTESIAN_POINT('Ctrl Pts',(10.9157191153351,602.830476606266,75.3939015342058));
#105224=CARTESIAN_POINT('Ctrl Pts',(11.0853383686276,602.723200323969,75.2175106218));
#105225=CARTESIAN_POINT('Ctrl Pts',(11.2982866914204,602.588520422088,74.9960608263106));
#105226=CARTESIAN_POINT('Ctrl Pts',(11.5047763502688,602.455585063299,74.7682551816903));
#105227=CARTESIAN_POINT('Ctrl Pts',(11.7048608093102,602.324863862536,74.5338690056311));
#105228=CARTESIAN_POINT('Ctrl Pts',(11.8235220073649,602.247338929476,74.39486498407));
#105229=CARTESIAN_POINT('Ctrl Pts',(11.9399304013359,602.170593652194,74.2535467954905));
#105230=CARTESIAN_POINT('Ctrl Pts',(12.0540971431182,602.094734098787,74.1098707468977));
#105231=CARTESIAN_POINT('Ctrl Pts',(12.2247846330108,601.981318610587,73.8950647209996));
#105232=CARTESIAN_POINT('Ctrl Pts',(12.3904618758627,601.869880815692,73.6749899685042));
#105233=CARTESIAN_POINT('Ctrl Pts',(12.5510400004671,601.760743347098,73.4493816921722));
#105234=CARTESIAN_POINT('Ctrl Pts',(12.6789711937227,601.673794476444,73.2696415434402));
#105235=CARTESIAN_POINT('Ctrl Pts',(12.8036658898818,601.588306560693,73.0863892070135));
#105236=CARTESIAN_POINT('Ctrl Pts',(12.9250791491289,601.504466168008,72.899494722766));
#105237=CARTESIAN_POINT('Ctrl Pts',(13.0388387824065,601.425910890068,72.724381657509));
#105238=CARTESIAN_POINT('Ctrl Pts',(13.1495772962539,601.348869677579,72.5462085445997));
#105239=CARTESIAN_POINT('Ctrl Pts',(13.2569702277637,601.273706826003,72.3654131529255));
#105240=CARTESIAN_POINT('Ctrl Pts',(13.3632468260221,601.19932528088,72.1864971019544));
#105241=CARTESIAN_POINT('Ctrl Pts',(13.466247034086,601.126783414445,72.0050131874339));
#105242=CARTESIAN_POINT('Ctrl Pts',(13.565656402463,601.056390585734,71.8214121376375));
#105243=CARTESIAN_POINT('Ctrl Pts',(13.6075769852419,601.026706176194,71.7439882174182));
#105244=CARTESIAN_POINT('Ctrl Pts',(13.6488590164011,600.997403375317,71.6661881202247));
#105245=CARTESIAN_POINT('Ctrl Pts',(13.6894789155558,600.96850291657,71.5880469506538));
#105246=CARTESIAN_POINT('Ctrl Pts',(13.8286010750813,600.869519553345,71.320415359124));
#105247=CARTESIAN_POINT('Ctrl Pts',(13.9605180227581,600.774973302884,71.0480331379636));
#105248=CARTESIAN_POINT('Ctrl Pts',(14.0849573496678,600.685214684286,70.7707639855925));
#105249=CARTESIAN_POINT('Ctrl Pts',(14.2077624538311,600.596634837542,70.4971361222487));
#105250=CARTESIAN_POINT('Ctrl Pts',(14.3232850500889,600.512717686243,70.21874852948));
#105251=CARTESIAN_POINT('Ctrl Pts',(14.431263321578,600.433847155292,69.9354880623801));
#105252=CARTESIAN_POINT('Ctrl Pts',(14.53713756658,600.356513467671,69.6577471087649));
#105253=CARTESIAN_POINT('Ctrl Pts',(14.6357586344046,600.284031700042,69.3753210477071));
#105254=CARTESIAN_POINT('Ctrl Pts',(14.7268797169107,600.216808888376,69.0881248582872));
#105255=CARTESIAN_POINT('Ctrl Pts',(14.7658178500568,600.188083035706,68.9653993247979));
#105256=CARTESIAN_POINT('Ctrl Pts',(14.8033864488703,600.160318058013,68.8418030398932));
#105257=CARTESIAN_POINT('Ctrl Pts',(14.8395662545944,600.133548262682,68.7173308130521));
#105258=CARTESIAN_POINT('Ctrl Pts',(14.9306676469207,600.066141443377,68.4039075388196));
#105259=CARTESIAN_POINT('Ctrl Pts',(15.0120041807907,600.0057505978,68.0882301956629));
#105260=CARTESIAN_POINT('Ctrl Pts',(15.0834994605404,599.952495015445,67.7702592069415));
#105261=CARTESIAN_POINT('Ctrl Pts',(15.1544872250668,599.899617472296,67.4545453618789));
#105262=CARTESIAN_POINT('Ctrl Pts',(15.2157729575042,599.853774233935,67.1365698743685));
#105263=CARTESIAN_POINT('Ctrl Pts',(15.26728187757,599.815132996122,66.8162990868483));
#105264=CARTESIAN_POINT('Ctrl Pts',(15.3181640307096,599.776961949682,66.4999253939824));
#105265=CARTESIAN_POINT('Ctrl Pts',(15.3595058548215,599.74581874709,66.1813114971069));
#105266=CARTESIAN_POINT('Ctrl Pts',(15.3912352663485,599.721914626943,65.8604363424684));
#105267=CARTESIAN_POINT('Ctrl Pts',(15.3996803499289,599.715552318824,65.7750323790987));
#105268=CARTESIAN_POINT('Ctrl Pts',(15.4074444818654,599.709703106282,65.6894683089235));
#105269=CARTESIAN_POINT('Ctrl Pts',(15.414526303025,599.704371567147,65.6037439326523));
#105270=CARTESIAN_POINT('Ctrl Pts',(15.4364643525561,599.687855537305,65.3381871542066));
#105271=CARTESIAN_POINT('Ctrl Pts',(15.4517893452765,599.676303804616,65.0710724250625));
#105272=CARTESIAN_POINT('Ctrl Pts',(15.4603232031337,599.669870597506,64.8023554757184));
#105273=CARTESIAN_POINT('Ctrl Pts',(15.4648538948456,599.666455157663,64.6596915509595));
#105274=CARTESIAN_POINT('Ctrl Pts',(15.4674510190573,599.664486012478,64.5165142301009));
#105275=CARTESIAN_POINT('Ctrl Pts',(15.4681203454456,599.663982203095,64.3734851808145));
#105276=CARTESIAN_POINT('Ctrl Pts',(15.4687117396317,599.663537054144,64.2471095445311));
#105277=CARTESIAN_POINT('Ctrl Pts',(15.4677981227552,599.664235122814,64.1208497755974));
#105278=CARTESIAN_POINT('Ctrl Pts',(15.465383474685,599.66605565863,63.9951622171671));
#105279=CARTESIAN_POINT('Ctrl Pts',(15.459452342433,599.670527465029,63.6864341914551));
#105280=CARTESIAN_POINT('Ctrl Pts',(15.4445576266959,599.681772011648,63.3797508309674));
#105281=CARTESIAN_POINT('Ctrl Pts',(15.4209342345178,599.699557577838,63.0750606401227));
#105282=CARTESIAN_POINT('Ctrl Pts',(15.4035532438902,599.712643368266,62.8508838025442));
#105283=CARTESIAN_POINT('Ctrl Pts',(15.381447132351,599.72927106591,62.6277854531142));
#105284=CARTESIAN_POINT('Ctrl Pts',(15.3547094604652,599.749365484678,62.4057395605387));
#105285=CARTESIAN_POINT('Ctrl Pts',(15.3159115020454,599.778523686152,62.0835377119923));
#105286=CARTESIAN_POINT('Ctrl Pts',(15.2673586125687,599.814979310381,61.7635549646558));
#105287=CARTESIAN_POINT('Ctrl Pts',(15.2091365971295,599.858544359385,61.4457630820266));
#105288=CARTESIAN_POINT('Ctrl Pts',(15.1727005295032,599.885807913552,61.2468849353461));
#105289=CARTESIAN_POINT('Ctrl Pts',(15.1324776324204,599.915856841564,61.0488645460237));
#105290=CARTESIAN_POINT('Ctrl Pts',(15.0884889362004,599.948655262748,60.8516931877506));
#105291=CARTESIAN_POINT('Ctrl Pts',(15.0441618970613,599.981705955868,60.6530052686642));
#105292=CARTESIAN_POINT('Ctrl Pts',(14.99587961035,600.017618426599,60.4547901096127));
#105293=CARTESIAN_POINT('Ctrl Pts',(14.9437846854305,600.056282502727,60.2575526976988));
#105294=CARTESIAN_POINT('Ctrl Pts',(14.891515090916,600.095076216022,60.0596539664928));
#105295=CARTESIAN_POINT('Ctrl Pts',(14.8354072484661,600.136639957072,59.8627397875043));
#105296=CARTESIAN_POINT('Ctrl Pts',(14.7756052067288,600.180811300144,59.6673080308479));
#105297=CARTESIAN_POINT('Ctrl Pts',(14.7413494348752,600.206113503994,59.5553609221124));
#105298=CARTESIAN_POINT('Ctrl Pts',(14.7058815145681,600.232270383962,59.4438999846864));
#105299=CARTESIAN_POINT('Ctrl Pts',(14.6692285204308,600.259244049245,59.3330165540887));
#105300=CARTESIAN_POINT('Ctrl Pts',(14.5803938226727,600.324619265082,59.0642719051074));
#105301=CARTESIAN_POINT('Ctrl Pts',(14.4851858741709,600.394481384538,58.8001708828506));
#105302=CARTESIAN_POINT('Ctrl Pts',(14.3837715170904,600.468473187238,58.5405486633614));
#105303=CARTESIAN_POINT('Ctrl Pts',(14.2810607054499,600.54341088175,58.2776075014656));
#105304=CARTESIAN_POINT('Ctrl Pts',(14.1719837887536,600.622584561164,58.0192600662296));
#105305=CARTESIAN_POINT('Ctrl Pts',(14.0567140899125,600.705674919426,57.7653191294322));
#105306=CARTESIAN_POINT('Ctrl Pts',(13.9392204614059,600.79036836258,57.5064788410421));
#105307=CARTESIAN_POINT('Ctrl Pts',(13.8152927875511,600.879131076811,57.2522164161193));
#105308=CARTESIAN_POINT('Ctrl Pts',(13.6851146179499,600.971678122617,57.0023218326902));
#105309=CARTESIAN_POINT('Ctrl Pts',(13.6023354929409,601.0305279551,56.8434161188971));
#105310=CARTESIAN_POINT('Ctrl Pts',(13.5170289340367,601.09090908028,56.6862763549344));
#105311=CARTESIAN_POINT('Ctrl Pts',(13.4292421368317,601.152759033305,56.5308469864961));
#105312=CARTESIAN_POINT('Ctrl Pts',(13.2697747250477,601.265111371492,56.2485047677433));
#105313=CARTESIAN_POINT('Ctrl Pts',(13.101898661713,601.382367267854,55.9716775249368));
#105314=CARTESIAN_POINT('Ctrl Pts',(12.9258526145729,601.503935650737,55.7006361645003));
#105315=CARTESIAN_POINT('Ctrl Pts',(12.8286620255447,601.571050493311,55.5510010553925));
#105316=CARTESIAN_POINT('Ctrl Pts',(12.728981334913,601.639479369392,55.4031285395231));
#105317=CARTESIAN_POINT('Ctrl Pts',(12.6268507021078,601.709120557677,55.257057802576));
#105318=CARTESIAN_POINT('Ctrl Pts',(12.469345250969,601.81652091815,55.0317880995584));
#105319=CARTESIAN_POINT('Ctrl Pts',(12.3071295901563,601.926054873237,54.8123661471076));
#105320=CARTESIAN_POINT('Ctrl Pts',(12.140284433182,602.037364111905,54.5985128380187));
#105321=CARTESIAN_POINT('Ctrl Pts',(12.0029789361845,602.128966233374,54.4225219047395));
#105322=CARTESIAN_POINT('Ctrl Pts',(11.8625381156151,602.221771720644,54.2503020731634));
#105323=CARTESIAN_POINT('Ctrl Pts',(11.7190069566274,602.315607074176,54.0816944827994));
#105324=CARTESIAN_POINT('Ctrl Pts',(11.5129986901234,602.450287645658,53.8396943648089));
#105325=CARTESIAN_POINT('Ctrl Pts',(11.300702240442,602.587133145572,53.6050605705711));
#105326=CARTESIAN_POINT('Ctrl Pts',(11.0819551471639,602.725518054895,53.3776274956182));
#105327=CARTESIAN_POINT('Ctrl Pts',(10.8537269626199,602.869900940856,53.140336855437));
#105328=CARTESIAN_POINT('Ctrl Pts',(10.6184768396464,603.015959261177,52.9108844662551));
#105329=CARTESIAN_POINT('Ctrl Pts',(10.3760202645829,603.163032449609,52.6890496920733));
#105330=CARTESIAN_POINT('Ctrl Pts',(10.1335636895193,603.310105638041,52.4672149178915));
#105331=CARTESIAN_POINT('Ctrl Pts',(9.88390066236575,603.458193761935,52.2529973474516));
#105332=CARTESIAN_POINT('Ctrl Pts',(9.62684666946167,603.60668640386,52.0461494466168));
#105333=CARTESIAN_POINT('Ctrl Pts',(9.46346234489243,603.701068793063,51.914676271722));
#105334=CARTESIAN_POINT('Ctrl Pts',(9.29686479132284,603.79566622951,51.7861174759939));
#105335=CARTESIAN_POINT('Ctrl Pts',(9.1275807697144,603.889945916815,51.6609035615386));
#105336=CARTESIAN_POINT('Ctrl Pts',(8.95353419621665,603.98687802163,51.5321669415191));
#105337=CARTESIAN_POINT('Ctrl Pts',(8.77664786886439,604.083473998631,51.4069661381686));
#105338=CARTESIAN_POINT('Ctrl Pts',(8.59749427002016,604.179117051247,51.28572876114));
#105339=CARTESIAN_POINT('Ctrl Pts',(8.54536693177707,604.206945784727,51.2504529877208));
#105340=CARTESIAN_POINT('Ctrl Pts',(8.49304764555114,604.234693619584,51.2155125022191));
#105341=CARTESIAN_POINT('Ctrl Pts',(8.44055051338909,604.2623448376,51.1809172151338));
#105342=CARTESIAN_POINT('Ctrl Pts',(8.16409659561211,604.407958268986,50.9987357843119));
#105343=CARTESIAN_POINT('Ctrl Pts',(7.88203506759103,604.551352521409,50.8255502039239));
#105344=CARTESIAN_POINT('Ctrl Pts',(7.59396676189712,604.691519497847,50.661275681908));
#105345=CARTESIAN_POINT('Ctrl Pts',(7.45646787271816,604.758423086957,50.5828652360132));
#105346=CARTESIAN_POINT('Ctrl Pts',(7.31760047037148,604.824591914183,50.5064843721725));
#105347=CARTESIAN_POINT('Ctrl Pts',(7.1773211472115,604.889919348387,50.4321209931153));
#105348=CARTESIAN_POINT('Ctrl Pts',(6.8801828412943,605.028295287847,50.2746052026366));
#105349=CARTESIAN_POINT('Ctrl Pts',(6.57671769730194,605.162903406008,50.1261374141598));
#105350=CARTESIAN_POINT('Ctrl Pts',(6.26623698972573,605.292427418651,49.9869266312457));
#105351=CARTESIAN_POINT('Ctrl Pts',(6.12304923299768,605.352161412939,49.9227252840077));
#105352=CARTESIAN_POINT('Ctrl Pts',(5.97836935164866,605.410814201732,49.8604919927748));
#105353=CARTESIAN_POINT('Ctrl Pts',(5.83212979029488,605.468257827998,49.8002438368876));
#105354=CARTESIAN_POINT('Ctrl Pts',(5.60046097050222,605.559258491419,49.7048003123046));
#105355=CARTESIAN_POINT('Ctrl Pts',(5.36486309244537,605.647207349457,49.6143579168885));
#105356=CARTESIAN_POINT('Ctrl Pts',(5.12496004470658,605.731474628392,49.5291006468632));
#105357=CARTESIAN_POINT('Ctrl Pts',(4.92336015567768,605.802287709935,49.4574556371894));
#105358=CARTESIAN_POINT('Ctrl Pts',(4.71807804538495,605.870685385895,49.3892915169508));
#105359=CARTESIAN_POINT('Ctrl Pts',(4.51111271505955,605.935569889985,49.3254220404912));
#105360=CARTESIAN_POINT('Ctrl Pts',(4.47179014433253,605.947897681781,49.3132870998157));
#105361=CARTESIAN_POINT('Ctrl Pts',(4.4324068119646,605.960098558052,49.3013070706584));
#105362=CARTESIAN_POINT('Ctrl Pts',(4.39297642822443,605.972164865804,49.2894873770812));
#105363=CARTESIAN_POINT('Ctrl Pts',(4.12486075126134,606.054212413018,49.209116737885));
#105364=CARTESIAN_POINT('Ctrl Pts',(3.8544403326532,606.130209721402,49.1359860390462));
#105365=CARTESIAN_POINT('Ctrl Pts',(3.58156371892322,606.199404405331,49.0702139584696));
#105366=CARTESIAN_POINT('Ctrl Pts',(3.32312890924601,606.264937008978,49.0079228192858));
#105367=CARTESIAN_POINT('Ctrl Pts',(3.06249100950961,606.324367834277,48.9522313546321));
#105368=CARTESIAN_POINT('Ctrl Pts',(2.7995213627417,606.377094055612,48.9032651277793));
#105369=CARTESIAN_POINT('Ctrl Pts',(2.55448969638108,606.426223656816,48.8576390400973));
#105370=CARTESIAN_POINT('Ctrl Pts',(2.30743354478633,606.469532170608,48.8178516695855));
#105371=CARTESIAN_POINT('Ctrl Pts',(2.0582488241673,606.50656489739,48.7840331252817));
#105372=CARTESIAN_POINT('Ctrl Pts',(1.81685586891249,606.542439646599,48.7512720541711));
#105373=CARTESIAN_POINT('Ctrl Pts',(1.57346538001183,606.572424798898,48.7241119998907));
#105374=CARTESIAN_POINT('Ctrl Pts',(1.32798273535137,606.596140220963,48.7027040439557));
#105375=CARTESIAN_POINT('Ctrl Pts',(1.09319241853544,606.618822685819,48.6822285404295));
#105376=CARTESIAN_POINT('Ctrl Pts',(0.855738997648291,606.635677081802,
48.6670981287456));
#105377=CARTESIAN_POINT('Ctrl Pts',(0.616984794800867,606.646416089399,
48.6574665592193));
#105378=CARTESIAN_POINT('Ctrl Pts',(0.386532831296134,606.65678166771,48.6481699098514));
#105379=CARTESIAN_POINT('Ctrl Pts',(0.154868977572705,606.661449696049,
48.6439961961589));
#105380=CARTESIAN_POINT('Ctrl Pts',(-0.0767816764458722,606.66019457572,
48.6451198922309));
#105381=CARTESIAN_POINT('Ctrl Pts',(-0.145864683309471,606.659820272929,
48.6454550015954));
#105382=CARTESIAN_POINT('Ctrl Pts',(-0.214946516250035,606.658919423718,
48.6462614978511));
#105383=CARTESIAN_POINT('Ctrl Pts',(-0.283994682921353,606.65748665381,
48.6475446883329));
#105384=CARTESIAN_POINT('Ctrl Pts',(-0.520075952304776,606.652587897551,
48.6519320204289));
#105385=CARTESIAN_POINT('Ctrl Pts',(-0.755839055281912,606.641499149446,
48.6618612476739));
#105386=CARTESIAN_POINT('Ctrl Pts',(-0.990327191987344,606.624559493982,
48.6770968260201));
#105387=CARTESIAN_POINT('Ctrl Pts',(-1.23740315666562,606.606710481345,
48.6931502830105));
#105388=CARTESIAN_POINT('Ctrl Pts',(-1.48306359503986,606.582365636056,
48.7150953295273));
#105389=CARTESIAN_POINT('Ctrl Pts',(-1.72618919815674,606.551960679876,
48.7426988494953));
#105390=CARTESIAN_POINT('Ctrl Pts',(-1.78055170454703,606.545162179005,
48.7488709535905));
#105391=CARTESIAN_POINT('Ctrl Pts',(-1.83478747864495,606.538060838178,
48.7553261113013));
#105392=CARTESIAN_POINT('Ctrl Pts',(-1.8888840075986,606.53066176659,48.7620619651123));
#105393=CARTESIAN_POINT('Ctrl Pts',(-0.252645464510396,603.935273498433,
76.9980210944396));
#105394=CARTESIAN_POINT('Ctrl Pts',(-1.11302381605652,603.921973867958,
76.980488604498));
#105395=CARTESIAN_POINT('Ctrl Pts',(-1.94758251680077,603.841082066435,
76.8749778358584));
#105396=CARTESIAN_POINT('Ctrl Pts',(-3.16572559796507,603.638181713665,
76.5970874596841));
#105397=CARTESIAN_POINT('Ctrl Pts',(-3.56612249316459,603.556968056736,
76.4843247054231));
#105398=CARTESIAN_POINT('Ctrl Pts',(-4.35605342916383,603.370767324989,
76.2184083741727));
#105399=CARTESIAN_POINT('Ctrl Pts',(-4.74439125163809,603.265908061918,
76.0653418396745));
#105400=CARTESIAN_POINT('Ctrl Pts',(-5.86615041872897,602.93028205798,75.5582538330123));
#105401=CARTESIAN_POINT('Ctrl Pts',(-6.56690401319744,602.676475086324,
75.153793775975));
#105402=CARTESIAN_POINT('Ctrl Pts',(-7.55642794248227,602.275508918443,
74.4484723523538));
#105403=CARTESIAN_POINT('Ctrl Pts',(-7.87639888507424,602.138112496026,
74.1960774136137));
#105404=CARTESIAN_POINT('Ctrl Pts',(-8.48513868812207,601.864970166375,
73.6665189366011));
#105405=CARTESIAN_POINT('Ctrl Pts',(-8.77540631388641,601.728639986729,
73.3883947993268));
#105406=CARTESIAN_POINT('Ctrl Pts',(-9.32889245043522,601.459703714202,
72.8050737176796));
#105407=CARTESIAN_POINT('Ctrl Pts',(-9.59210827130408,601.327088572554,
72.4998783443379));
#105408=CARTESIAN_POINT('Ctrl Pts',(-10.0915350771624,601.068618464298,
71.8610821467425));
#105409=CARTESIAN_POINT('Ctrl Pts',(-10.3287739497107,600.94218925709,71.525776856965));
#105410=CARTESIAN_POINT('Ctrl Pts',(-10.9894725080146,600.582618362532,
70.4882632613146));
#105411=CARTESIAN_POINT('Ctrl Pts',(-11.3625914305347,600.369242850061,
69.7564109606946));
#105412=CARTESIAN_POINT('Ctrl Pts',(-11.818404938002,600.103341108961,68.5929331071031));
#105413=CARTESIAN_POINT('Ctrl Pts',(-11.9534576443998,600.023405036002,
68.1916750120165));
#105414=CARTESIAN_POINT('Ctrl Pts',(-12.182174157639,599.886968972313,67.3809131335881));
#105415=CARTESIAN_POINT('Ctrl Pts',(-12.276307508626,599.830205075246,66.9709644805429));
#105416=CARTESIAN_POINT('Ctrl Pts',(-12.4242394369779,599.740627853341,
66.1418454500847));
#105417=CARTESIAN_POINT('Ctrl Pts',(-12.4780399075043,599.707811059001,
65.7226757432849));
#105418=CARTESIAN_POINT('Ctrl Pts',(-12.5441585218638,599.667441869139,
64.8747881241364));
#105419=CARTESIAN_POINT('Ctrl Pts',(-12.5562467120334,599.660031095258,
64.4432644779558));
#105420=CARTESIAN_POINT('Ctrl Pts',(-12.5282315834883,599.677167021141,
63.1661747786782));
#105421=CARTESIAN_POINT('Ctrl Pts',(-12.4261421803805,599.739908403138,
62.3315318096105));
#105422=CARTESIAN_POINT('Ctrl Pts',(-12.1532157238051,599.904257995604,
61.1033176255798));
#105423=CARTESIAN_POINT('Ctrl Pts',(-12.0418922330986,599.970921904931,
60.6972107540752));
#105424=CARTESIAN_POINT('Ctrl Pts',(-11.7789498235242,600.126430608746,
59.8958888312612));
#105425=CARTESIAN_POINT('Ctrl Pts',(-11.6297082784345,600.213861256789,
59.5076325746472));
#105426=CARTESIAN_POINT('Ctrl Pts',(-11.1319937919119,600.50080901643,58.3769969850098));
#105427=CARTESIAN_POINT('Ctrl Pts',(-10.7340829199422,600.724949402545,
57.6684452447755));
#105428=CARTESIAN_POINT('Ctrl Pts',(-10.040023576069,601.095528882733,56.6679468437341));
#105429=CARTESIAN_POINT('Ctrl Pts',(-9.79091798691913,601.225505664081,
56.3433436698442));
#105430=CARTESIAN_POINT('Ctrl Pts',(-9.26667744604236,601.490365329661,
55.7243454178727));
#105431=CARTESIAN_POINT('Ctrl Pts',(-8.99185892776024,601.62513172368,55.4299091303579));
#105432=CARTESIAN_POINT('Ctrl Pts',(-8.1292937094432,602.031691427434,54.5894500217195));
#105433=CARTESIAN_POINT('Ctrl Pts',(-7.5038764230366,602.306079133985,54.0856572853192));
#105434=CARTESIAN_POINT('Ctrl Pts',(-6.14010017594243,602.832368541163,
53.1918099095666));
#105435=CARTESIAN_POINT('Ctrl Pts',(-5.42038031899213,603.076911552827,
52.8139552665562));
#105436=CARTESIAN_POINT('Ctrl Pts',(-4.27629107737484,603.390777156775,
52.3511891253608));
#105437=CARTESIAN_POINT('Ctrl Pts',(-3.88308899204296,603.486721140176,
52.2141438459509));
#105438=CARTESIAN_POINT('Ctrl Pts',(-3.07656099875632,603.654779445314,
51.9785830844804));
#105439=CARTESIAN_POINT('Ctrl Pts',(-2.66897700762064,603.725715944193,
51.8816585325753));
#105440=CARTESIAN_POINT('Ctrl Pts',(-1.84491113503772,603.838478649151,
51.7291914233704));
#105441=CARTESIAN_POINT('Ctrl Pts',(-1.42842899531872,603.880302055858,
51.67364863131));
#105442=CARTESIAN_POINT('Ctrl Pts',(-0.586133086793797,603.932122442854,
51.6050092571627));
#105443=CARTESIAN_POINT('Ctrl Pts',(-0.159088542674411,603.942089849916,
51.5919408760206));
#105444=CARTESIAN_POINT('Ctrl Pts',(0.270210553101167,603.934992543017,
51.6012974652903));
#105445=CARTESIAN_POINT('Ctrl Pts',(0.414276434602871,604.1309994978,52.0064418924366));
#105446=CARTESIAN_POINT('Ctrl Pts',(0.401375821343561,603.627974829126,
52.0060233138142));
#105447=CARTESIAN_POINT('Ctrl Pts',(0.422698891923292,603.931797866792,
51.6054949190725));
#105448=CARTESIAN_POINT('Ctrl Pts',(-0.476010708148196,604.154247142527,
51.9765750164054));
#105449=CARTESIAN_POINT('Ctrl Pts',(-0.464187114939955,603.647961634232,
51.9782978993827));
#105450=CARTESIAN_POINT('Ctrl Pts',(-0.485687802955836,603.955325698529,
51.5746539347127));
#105451=CARTESIAN_POINT('Ctrl Pts',(-1.34607093138357,604.101792845088,
52.0427987467341));
#105452=CARTESIAN_POINT('Ctrl Pts',(-1.28833508015367,603.604877677947,
52.0370249713265));
#105453=CARTESIAN_POINT('Ctrl Pts',(-1.37343881349918,603.902239020726,
51.6430377951326));
#105454=CARTESIAN_POINT('Ctrl Pts',(-2.59867283526968,603.930134794704,
52.2701959516384));
#105455=CARTESIAN_POINT('Ctrl Pts',(-2.52264148011035,603.452464870403,
52.2542948909666));
#105456=CARTESIAN_POINT('Ctrl Pts',(-2.65150548283938,603.728512385852,
51.877851247912));
#105457=CARTESIAN_POINT('Ctrl Pts',(-2.99609991422878,603.860843085546,
52.3629416887653));
#105458=CARTESIAN_POINT('Ctrl Pts',(-2.91049927803752,603.391724854142,
52.3416256351175));
#105459=CARTESIAN_POINT('Ctrl Pts',(-3.0570124876458,603.658385567216,51.9736219146518));
#105460=CARTESIAN_POINT('Ctrl Pts',(-3.78275735662804,603.69656200522,52.5884464824649));
#105461=CARTESIAN_POINT('Ctrl Pts',(-3.68456306759805,603.245201656458,
52.5572384796229));
#105462=CARTESIAN_POINT('Ctrl Pts',(-3.85966274491753,603.492124712842,
52.2064814361353));
#105463=CARTESIAN_POINT('Ctrl Pts',(-4.166979050703,603.602583843386,52.7198758782938));
#105464=CARTESIAN_POINT('Ctrl Pts',(-4.06360822860178,603.161272646565,
52.6827304516184));
#105465=CARTESIAN_POINT('Ctrl Pts',(-4.25169570801719,603.397013975051,
52.3421974164091));
#105466=CARTESIAN_POINT('Ctrl Pts',(-5.28507434996358,603.294921011766,
53.1638902156519));
#105467=CARTESIAN_POINT('Ctrl Pts',(-5.15820380454859,602.88639304024,53.1061439864781));
#105468=CARTESIAN_POINT('Ctrl Pts',(-5.39252319671762,603.085643146509,
52.8006937061186));
#105469=CARTESIAN_POINT('Ctrl Pts',(-5.98934985904857,603.054777055807,
53.5268853366489));
#105470=CARTESIAN_POINT('Ctrl Pts',(-5.86221724771992,602.668457299349,
53.4546201335385));
#105471=CARTESIAN_POINT('Ctrl Pts',(-6.11111639604364,602.842605065308,
53.1755283868843));
#105472=CARTESIAN_POINT('Ctrl Pts',(-7.32522403708878,602.536950700174,
54.3867510931747));
#105473=CARTESIAN_POINT('Ctrl Pts',(-7.20845486530068,602.185965192888,
54.3026771532069));
#105474=CARTESIAN_POINT('Ctrl Pts',(-7.47414788157401,602.318538853386,
54.0634384892156));
#105475=CARTESIAN_POINT('Ctrl Pts',(-7.93969011684976,602.266026556923,
54.8727462625326));
#105476=CARTESIAN_POINT('Ctrl Pts',(-7.83452284189274,601.930968312689,
54.7821223431411));
#105477=CARTESIAN_POINT('Ctrl Pts',(-8.10110508190108,602.044350104051,
54.5652847276252));
#105478=CARTESIAN_POINT('Ctrl Pts',(-8.78734281065214,601.864192931754,
55.6840474437808));
#105479=CARTESIAN_POINT('Ctrl Pts',(-8.70809531403379,601.544148406847,
55.6034482729444));
#105480=CARTESIAN_POINT('Ctrl Pts',(-8.96598822614471,601.637675177026,
55.4030453263832));
#105481=CARTESIAN_POINT('Ctrl Pts',(-9.05757910582421,601.730875564529,
55.9684328676932));
#105482=CARTESIAN_POINT('Ctrl Pts',(-8.98356312241737,601.41706748909,55.887647513816));
#105483=CARTESIAN_POINT('Ctrl Pts',(-9.24171805717351,601.502751403766,
55.6967061098111));
#105484=CARTESIAN_POINT('Ctrl Pts',(-9.57338818638589,601.468639030487,
56.5666721248706));
#105485=CARTESIAN_POINT('Ctrl Pts',(-9.50901929974679,601.166550377569,
56.4871657754348));
#105486=CARTESIAN_POINT('Ctrl Pts',(-9.7680129251863,601.237355039028,56.3144572329125));
#105487=CARTESIAN_POINT('Ctrl Pts',(-9.8188879556435,601.339710422266,56.8808632052432));
#105488=CARTESIAN_POINT('Ctrl Pts',(-9.7600322735385,601.042792865819,56.8025965430298));
#105489=CARTESIAN_POINT('Ctrl Pts',(-10.0185033274999,601.106872936661,
56.6388958448344));
#105490=CARTESIAN_POINT('Ctrl Pts',(-10.5031997469232,600.97186684951,57.8498081873022));
#105491=CARTESIAN_POINT('Ctrl Pts',(-10.4506899105479,600.693498726088,
57.7657813921744));
#105492=CARTESIAN_POINT('Ctrl Pts',(-10.716727326934,600.734596513586,57.6394451240119));
#105493=CARTESIAN_POINT('Ctrl Pts',(-10.8960080548356,600.749008832054,
58.5366905083561));
#105494=CARTESIAN_POINT('Ctrl Pts',(-10.8571731765776,600.476229578782,
58.4602774988305));
#105495=CARTESIAN_POINT('Ctrl Pts',(-11.1175203099313,600.509053487703,
58.3487305133394));
#105496=CARTESIAN_POINT('Ctrl Pts',(-11.3878836354649,600.463303690855,
59.6339866130622));
#105497=CARTESIAN_POINT('Ctrl Pts',(-11.3646047806954,600.197611540251,
59.5771443494444));
#105498=CARTESIAN_POINT('Ctrl Pts',(-11.619394535175,600.219906090563,59.481815015771));
#105499=CARTESIAN_POINT('Ctrl Pts',(-11.5354834909803,600.376174041301,
60.0109905179452));
#105500=CARTESIAN_POINT('Ctrl Pts',(-11.5161693648167,600.112969570056,
59.9583961633857));
#105501=CARTESIAN_POINT('Ctrl Pts',(-11.7699948379489,600.131726620416,
59.8711153341678));
#105502=CARTESIAN_POINT('Ctrl Pts',(-11.7957168424692,600.221073652832,
60.7895545484208));
#105503=CARTESIAN_POINT('Ctrl Pts',(-11.7825939140218,599.962624089532,
60.7452930450769));
#105504=CARTESIAN_POINT('Ctrl Pts',(-12.0355183921278,599.974757370073,
60.6750733074951));
#105505=CARTESIAN_POINT('Ctrl Pts',(-11.9061244276539,600.15443670383,61.1848355228865));
#105506=CARTESIAN_POINT('Ctrl Pts',(-11.8961009417762,599.897716948639,
61.145720101883));
#105507=CARTESIAN_POINT('Ctrl Pts',(-12.1481703593011,599.90731752364,61.0832468504235));
#105508=CARTESIAN_POINT('Ctrl Pts',(-12.1766841067953,599.990213528446,
62.3797203320405));
#105509=CARTESIAN_POINT('Ctrl Pts',(-12.1719915811263,599.738982030972,
62.3490805674734));
#105510=CARTESIAN_POINT('Ctrl Pts',(-12.4242303319733,599.741115461546,
62.3171054077186));
#105511=CARTESIAN_POINT('Ctrl Pts',(-12.2780801673297,599.927387168324,
63.1920557640221));
#105512=CARTESIAN_POINT('Ctrl Pts',(-12.2775058411409,599.676950745045,
63.1776792731061));
#105513=CARTESIAN_POINT('Ctrl Pts',(-12.5276874182952,599.677532219236,
63.1559355922065));
#105514=CARTESIAN_POINT('Ctrl Pts',(-12.3062333905587,599.910025891942,
64.4355871579955));
#105515=CARTESIAN_POINT('Ctrl Pts',(-12.3063643128568,599.660064767427,
64.4370638410256));
#105516=CARTESIAN_POINT('Ctrl Pts',(-12.5564129571305,599.659961751212,
64.4400267385226));
#105517=CARTESIAN_POINT('Ctrl Pts',(-12.2943819383328,599.917351224494,
64.8559276849426));
#105518=CARTESIAN_POINT('Ctrl Pts',(-12.2941718209377,599.667216361877,
64.8634434416355));
#105519=CARTESIAN_POINT('Ctrl Pts',(-12.5443205872794,599.667375345166,
64.8740772469317));
#105520=CARTESIAN_POINT('Ctrl Pts',(-12.2291210200655,599.957522719545,
65.6815257693199));
#105521=CARTESIAN_POINT('Ctrl Pts',(-12.2273094971991,599.706264077721,
65.6991136324248));
#105522=CARTESIAN_POINT('Ctrl Pts',(-12.4777330003822,599.708030881358,
65.7266035670265));
#105523=CARTESIAN_POINT('Ctrl Pts',(-12.1759469061432,599.990222710175,
66.0895695514285));
#105524=CARTESIAN_POINT('Ctrl Pts',(-12.1726163502219,599.738171023279,
66.1128812981191));
#105525=CARTESIAN_POINT('Ctrl Pts',(-12.4234779559463,599.741124867619,
66.1479562446186));
#105526=CARTESIAN_POINT('Ctrl Pts',(-12.0296993061205,600.079498308535,
66.896483765114));
#105527=CARTESIAN_POINT('Ctrl Pts',(-12.0228067561347,599.824887950255,
66.9293351464561));
#105528=CARTESIAN_POINT('Ctrl Pts',(-12.2742573339491,599.831476180105,
66.9811892328191));
#105529=CARTESIAN_POINT('Ctrl Pts',(-11.9366237554634,600.136077491239,
67.2953533735953));
#105530=CARTESIAN_POINT('Ctrl Pts',(-11.9271007354986,599.880035230897,
67.3335484589463));
#105531=CARTESIAN_POINT('Ctrl Pts',(-12.1792897304192,599.888737075378,
67.393068477219));
#105532=CARTESIAN_POINT('Ctrl Pts',(-11.7104894329877,600.272048636011,
68.0840105657425));
#105533=CARTESIAN_POINT('Ctrl Pts',(-11.6955378132595,600.0119385886,68.130976713246));
#105534=CARTESIAN_POINT('Ctrl Pts',(-11.9485583932798,600.02634658594,68.20744886739));
#105535=CARTESIAN_POINT('Ctrl Pts',(-11.5770111802493,600.351676170637,
68.474072058525));
#105536=CARTESIAN_POINT('Ctrl Pts',(-11.5583984649845,600.089389930813,
68.5257596552219));
#105537=CARTESIAN_POINT('Ctrl Pts',(-11.8123667673947,600.10693354451,68.6102326743058));
#105538=CARTESIAN_POINT('Ctrl Pts',(-11.1268371472754,600.616328116227,
69.6043131395056));
#105539=CARTESIAN_POINT('Ctrl Pts',(-11.094177851908,600.347564341289,69.6760041353329));
#105540=CARTESIAN_POINT('Ctrl Pts',(-11.3530417450548,600.374774111955,
69.7773368489012));
#105541=CARTESIAN_POINT('Ctrl Pts',(-10.7586237260962,600.828487779737,
70.3144690681693));
#105542=CARTESIAN_POINT('Ctrl Pts',(-10.7127265394219,600.554881645438,
70.3951256963503));
#105543=CARTESIAN_POINT('Ctrl Pts',(-10.977343637448,600.589489857249,70.5106549236237));
#105544=CARTESIAN_POINT('Ctrl Pts',(-10.1073211782066,601.185491883109,
71.3202714227271));
#105545=CARTESIAN_POINT('Ctrl Pts',(-10.0546064812974,600.894682176268,
71.3965629016389));
#105546=CARTESIAN_POINT('Ctrl Pts',(-10.3128000119404,600.950796158203,
71.5492638109212));
#105547=CARTESIAN_POINT('Ctrl Pts',(-9.87372685329524,601.310849208256,
71.6449099002616));
#105548=CARTESIAN_POINT('Ctrl Pts',(-9.81559960598111,601.015263109716,
71.7228833856819));
#105549=CARTESIAN_POINT('Ctrl Pts',(-10.0744570782856,601.077663941176,
71.8844906020682));
#105550=CARTESIAN_POINT('Ctrl Pts',(-9.38227834633797,601.566923442202,
72.2630638437438));
#105551=CARTESIAN_POINT('Ctrl Pts',(-9.3145103182014,601.260463878945,72.3432405042314));
#105552=CARTESIAN_POINT('Ctrl Pts',(-9.57301801983148,601.336823742793,
72.5228060041743));
#105553=CARTESIAN_POINT('Ctrl Pts',(-9.12341151926098,601.698209069844,
72.5582161648588));
#105554=CARTESIAN_POINT('Ctrl Pts',(-9.05028270509329,601.385990165768,
72.6387917490736));
#105555=CARTESIAN_POINT('Ctrl Pts',(-9.3088888014544,601.469691282284,72.827584871394));
#105556=CARTESIAN_POINT('Ctrl Pts',(-8.57939679683925,601.964234737923,
73.1220252238533));
#105557=CARTESIAN_POINT('Ctrl Pts',(-8.49692150109579,601.639184717617,
73.2025036527718));
#105558=CARTESIAN_POINT('Ctrl Pts',(-8.7538148761466,601.738922456514,73.4097827545099));
#105559=CARTESIAN_POINT('Ctrl Pts',(-8.29425119061942,602.098983695525,
73.3906801363316));
#105560=CARTESIAN_POINT('Ctrl Pts',(-8.20674465006721,601.767076389366,
73.4702530911213));
#105561=CARTESIAN_POINT('Ctrl Pts',(-8.46287263080745,601.87529508383,73.6871999316855));
#105562=CARTESIAN_POINT('Ctrl Pts',(-7.69661684926344,602.368731641435,
73.9019070495361));
#105563=CARTESIAN_POINT('Ctrl Pts',(-7.60084562786787,602.021848838989,
73.978892784628));
#105564=CARTESIAN_POINT('Ctrl Pts',(-7.85308898859088,602.148293430223,
74.2151005589185));
#105565=CARTESIAN_POINT('Ctrl Pts',(-7.3826036898993,602.504320561377,74.1454188990161));
#105566=CARTESIAN_POINT('Ctrl Pts',(-7.2827409284724,602.14927957797,74.2199817961026));
#105567=CARTESIAN_POINT('Ctrl Pts',(-7.53269227808984,602.285516183211,
74.4665545912257));
#105568=CARTESIAN_POINT('Ctrl Pts',(-6.41396819947268,602.898960048218,
74.8243434255003));
#105569=CARTESIAN_POINT('Ctrl Pts',(-6.28966522125246,602.524247689671,
74.9017755309047));
#105570=CARTESIAN_POINT('Ctrl Pts',(-6.54436688094673,602.684910409883,
75.1676209958109));
#105571=CARTESIAN_POINT('Ctrl Pts',(-5.73027341984355,603.147668316788,
75.2121345157478));
#105572=CARTESIAN_POINT('Ctrl Pts',(-5.60308614276544,602.751935967381,
75.2765310704285));
#105573=CARTESIAN_POINT('Ctrl Pts',(-5.84677300034353,602.936615919209,
75.5680603372252));
#105574=CARTESIAN_POINT('Ctrl Pts',(-4.64077478504796,603.475567974207,
75.6973360141623));
#105575=CARTESIAN_POINT('Ctrl Pts',(-4.53330991520826,603.046616580981,
75.7410809439269));
#105576=CARTESIAN_POINT('Ctrl Pts',(-4.73512363414398,603.268467444644,
76.0690872002211));
#105577=CARTESIAN_POINT('Ctrl Pts',(-4.26685720707408,603.577288002825,
75.8428419591479));
#105578=CARTESIAN_POINT('Ctrl Pts',(-4.16281829720207,603.138168004403,
75.8808099165903));
#105579=CARTESIAN_POINT('Ctrl Pts',(-4.35360434329437,603.371413324949,
76.2193388306527));
#105580=CARTESIAN_POINT('Ctrl Pts',(-3.49499057985149,603.760663649314,
76.0994932686235));
#105581=CARTESIAN_POINT('Ctrl Pts',(-3.40047115190971,603.302798678709,
76.127370335997));
#105582=CARTESIAN_POINT('Ctrl Pts',(-3.56604570114687,603.556998827382,
76.4843606975452));
#105583=CARTESIAN_POINT('Ctrl Pts',(-3.09852828926658,603.841732331683,
76.209817468087));
#105584=CARTESIAN_POINT('Ctrl Pts',(-3.01184896420214,603.374403504358,
76.2318455359098));
#105585=CARTESIAN_POINT('Ctrl Pts',(-3.16152317445561,603.639044536767,
76.5982831453344));
#105586=CARTESIAN_POINT('Ctrl Pts',(-1.85454421888672,604.050252953775,
76.4896756819632));
#105587=CARTESIAN_POINT('Ctrl Pts',(-1.77973073553379,603.560927559414,
76.5008366075293));
#105588=CARTESIAN_POINT('Ctrl Pts',(-1.89224989736498,603.850077894776,
76.8872684979557));
#105589=CARTESIAN_POINT('Ctrl Pts',(-0.988247314630766,604.13061698373,
76.5918392124698));
#105590=CARTESIAN_POINT('Ctrl Pts',(-0.956219519859947,603.627396775914,
76.5919508447176));
#105591=CARTESIAN_POINT('Ctrl Pts',(-1.00833932243225,603.931410759391,
76.9927644491201));
#105592=CARTESIAN_POINT('Ctrl Pts',(-0.0982453008758767,604.136097666981,
76.5990932436933));
#105593=CARTESIAN_POINT('Ctrl Pts',(-0.0952647792021157,603.632400531367,
76.599098861278));
#105594=CARTESIAN_POINT('Ctrl Pts',(-0.100242643564831,603.936957478099,
77.0002550481944));
#105595=CARTESIAN_POINT('Ctrl Pts',(-3.19988829303768,606.469280540506,
48.9136642374327));
#105596=CARTESIAN_POINT('Ctrl Pts',(-3.17805581403023,606.368972937512,
48.9095429260867));
#105597=CARTESIAN_POINT('Ctrl Pts',(-3.14894350373811,606.298042353055,
48.9762189002942));
#105598=CARTESIAN_POINT('Ctrl Pts',(-2.29881116825274,606.675089727992,
48.7191843933304));
#105599=CARTESIAN_POINT('Ctrl Pts',(-2.2887449963298,606.576903980715,48.7179545736899));
#105600=CARTESIAN_POINT('Ctrl Pts',(-2.26217542629362,606.506333644761,
48.7825198374689));
#105601=CARTESIAN_POINT('Ctrl Pts',(-1.29934864768706,606.803120537005,
48.6030696395544));
#105602=CARTESIAN_POINT('Ctrl Pts',(-1.29103235676735,606.707136696867,
48.60278157187));
#105603=CARTESIAN_POINT('Ctrl Pts',(-1.27865210531907,606.635902859048,
48.6668762936877));
#105604=CARTESIAN_POINT('Ctrl Pts',(0.24604904762521,606.835470312073,48.5736280341214));
#105605=CARTESIAN_POINT('Ctrl Pts',(0.244224674588171,606.73987097646,48.5737334451187));
#105606=CARTESIAN_POINT('Ctrl Pts',(0.242130489444806,606.668642047065,
48.6375535275709));
#105607=CARTESIAN_POINT('Ctrl Pts',(0.793683375382584,606.815063542801,
48.5920594319863));
#105608=CARTESIAN_POINT('Ctrl Pts',(0.788931574693909,606.719170048466,
48.5919652205538));
#105609=CARTESIAN_POINT('Ctrl Pts',(0.781040459010405,606.64798975616,48.6559104137992));
#105610=CARTESIAN_POINT('Ctrl Pts',(2.39693158170349,606.666816236979,48.7280101254697));
#105611=CARTESIAN_POINT('Ctrl Pts',(2.38338099377126,606.568997554172,48.7262413336859));
#105612=CARTESIAN_POINT('Ctrl Pts',(2.35874810817502,606.497958314614,48.7913119902478));
#105613=CARTESIAN_POINT('Ctrl Pts',(3.42759398731837,606.453238126653,48.9240904248496));
#105614=CARTESIAN_POINT('Ctrl Pts',(3.41253860309944,606.350806509426,48.9217203889832));
#105615=CARTESIAN_POINT('Ctrl Pts',(3.37298184661566,606.281814298726,48.9865958531241));
#105616=CARTESIAN_POINT('Ctrl Pts',(4.67730317816144,606.08414261949,49.2909483904667));
#105617=CARTESIAN_POINT('Ctrl Pts',(4.64765158093344,605.979218089358,49.2817265518851));
#105618=CARTESIAN_POINT('Ctrl Pts',(4.60280256700888,605.908271263799,49.3519775736338));
#105619=CARTESIAN_POINT('Ctrl Pts',(4.92564398215479,606.005058421566,49.3706595461052));
#105620=CARTESIAN_POINT('Ctrl Pts',(4.89464885506363,605.899071341731,49.3604691881233));
#105621=CARTESIAN_POINT('Ctrl Pts',(4.84718746008084,605.828235404484,49.4313666860679));
#105622=CARTESIAN_POINT('Ctrl Pts',(5.41204506061927,605.840019435411,49.5400282810896));
#105623=CARTESIAN_POINT('Ctrl Pts',(5.37840998526052,605.731861424371,49.5277111330022));
#105624=CARTESIAN_POINT('Ctrl Pts',(5.32584062015217,605.661210311973,49.6000512954549));
#105625=CARTESIAN_POINT('Ctrl Pts',(5.65096311005464,605.753831257063,49.6299136263926));
#105626=CARTESIAN_POINT('Ctrl Pts',(5.61612178002961,605.644482421254,49.6165277399625));
#105627=CARTESIAN_POINT('Ctrl Pts',(5.560952773411,605.573985070646,49.6895734166024));
#105628=CARTESIAN_POINT('Ctrl Pts',(6.35597407519104,605.486109076522,49.914631946893));
#105629=CARTESIAN_POINT('Ctrl Pts',(6.3194193662171,605.37241162902,49.8984892971421));
#105630=CARTESIAN_POINT('Ctrl Pts',(6.25472898600277,605.303043055918,49.9731396605117));
#105631=CARTESIAN_POINT('Ctrl Pts',(6.81038188975856,605.295478966058,50.1244671165347));
#105632=CARTESIAN_POINT('Ctrl Pts',(6.77205222396561,605.178792243254,50.1062416227097));
#105633=CARTESIAN_POINT('Ctrl Pts',(6.701897426018,605.110120024701,50.182125854026));
#105634=CARTESIAN_POINT('Ctrl Pts',(7.69221803306948,604.897969035652,50.5829910891641));
#105635=CARTESIAN_POINT('Ctrl Pts',(7.65049736475128,604.775365019841,50.5595723308578));
#105636=CARTESIAN_POINT('Ctrl Pts',(7.56968515550792,604.707828059185,50.6387960920346));
#105637=CARTESIAN_POINT('Ctrl Pts',(8.11963001506569,604.691064632854,50.831690360471));
#105638=CARTESIAN_POINT('Ctrl Pts',(8.07671976444598,604.564987929527,50.8060183026104));
#105639=CARTESIAN_POINT('Ctrl Pts',(7.99028738530161,604.498435512279,50.8864885495719));
#105640=CARTESIAN_POINT('Ctrl Pts',(8.94997490797288,604.267311159281,51.3685986628816));
#105641=CARTESIAN_POINT('Ctrl Pts',(8.90504619960583,604.134272431812,51.3374439703381));
#105642=CARTESIAN_POINT('Ctrl Pts',(8.80740286369077,604.069585786612,51.421224612497));
#105643=CARTESIAN_POINT('Ctrl Pts',(9.35449918700437,604.049511398749,51.658191408593));
#105644=CARTESIAN_POINT('Ctrl Pts',(9.30897039084129,603.912530603342,51.6247044118638));
#105645=CARTESIAN_POINT('Ctrl Pts',(9.20548162083417,603.849167476194,51.7096442401454));
#105646=CARTESIAN_POINT('Ctrl Pts',(10.5163351536716,603.398718287281,52.575739049541));
#105647=CARTESIAN_POINT('Ctrl Pts',(10.4792441450532,603.244538433826,52.5413915053251));
#105648=CARTESIAN_POINT('Ctrl Pts',(10.3487844505051,603.190561862117,52.6234603889828));
#105649=CARTESIAN_POINT('Ctrl Pts',(11.2257713012345,602.967318439238,53.2528256613287));
#105650=CARTESIAN_POINT('Ctrl Pts',(11.1886816147119,602.804026308938,53.2166715576217));
#105651=CARTESIAN_POINT('Ctrl Pts',(11.0469172883132,602.753977824126,53.2977962975316));
#105652=CARTESIAN_POINT('Ctrl Pts',(12.1992715391054,602.349475145027,54.3753501795627));
#105653=CARTESIAN_POINT('Ctrl Pts',(12.1575997879903,602.177212631392,54.3239043685375));
#105654=CARTESIAN_POINT('Ctrl Pts',(12.0049188841794,602.128700822412,54.4157870888978));
#105655=CARTESIAN_POINT('Ctrl Pts',(12.5084759793438,602.148334979507,54.7674817836186));
#105656=CARTESIAN_POINT('Ctrl Pts',(12.468217693647,601.971160873214,54.7148446167709));
#105657=CARTESIAN_POINT('Ctrl Pts',(12.3091950227289,601.925144767952,54.8063260024276));
#105658=CARTESIAN_POINT('Ctrl Pts',(13.0952716020131,601.759739638709,55.5911613762021));
#105659=CARTESIAN_POINT('Ctrl Pts',(13.0590920906578,601.57224116281,55.5364326108686));
#105660=CARTESIAN_POINT('Ctrl Pts',(12.8866359918322,601.531883514801,55.6266595150127));
#105661=CARTESIAN_POINT('Ctrl Pts',(13.3695604686926,601.574466672933,56.0182814407224));
#105662=CARTESIAN_POINT('Ctrl Pts',(13.3352634364091,601.381993339191,55.9630634399456));
#105663=CARTESIAN_POINT('Ctrl Pts',(13.1565527246595,601.344385932193,56.0520433785379));
#105664=CARTESIAN_POINT('Ctrl Pts',(14.1299035774209,601.054020239008,57.3393334951756));
#105665=CARTESIAN_POINT('Ctrl Pts',(14.1102991866389,600.8410628099,57.2962949053191));
#105666=CARTESIAN_POINT('Ctrl Pts',(13.9047588183333,600.817702811084,57.3676988812898));
#105667=CARTESIAN_POINT('Ctrl Pts',(14.5566498549489,600.752285916186,58.2756573376281));
#105668=CARTESIAN_POINT('Ctrl Pts',(14.5388220217875,600.531827565967,58.2336812825481));
#105669=CARTESIAN_POINT('Ctrl Pts',(14.3247076934254,600.512343480275,58.3002140367116));
#105670=CARTESIAN_POINT('Ctrl Pts',(14.9788110762547,600.450302189345,59.5276607666015));
#105671=CARTESIAN_POINT('Ctrl Pts',(14.9637997646997,600.221753346202,59.4803694808452));
#105672=CARTESIAN_POINT('Ctrl Pts',(14.7401433929711,600.206732629765,59.5471387316693));
#105673=CARTESIAN_POINT('Ctrl Pts',(15.0576058396701,600.393695366213,59.7823928247067));
#105674=CARTESIAN_POINT('Ctrl Pts',(15.0439529783748,600.163016122539,59.7367889937232));
#105675=CARTESIAN_POINT('Ctrl Pts',(14.817681362334,600.149447045719,59.8008321998986));
#105676=CARTESIAN_POINT('Ctrl Pts',(15.2014471033479,600.290045047794,60.2930389236187));
#105677=CARTESIAN_POINT('Ctrl Pts',(15.1905205855739,600.055282853514,60.251366404023));
#105678=CARTESIAN_POINT('Ctrl Pts',(14.9592279732983,600.044554175989,60.3093954217729));
#105679=CARTESIAN_POINT('Ctrl Pts',(15.2668116417703,600.242774489,60.5498362104747));
#105680=CARTESIAN_POINT('Ctrl Pts',(15.2571084270983,600.006159201186,60.5101927719224));
#105681=CARTESIAN_POINT('Ctrl Pts',(15.0235498579243,599.996716902792,60.565145240021));
#105682=CARTESIAN_POINT('Ctrl Pts',(15.4433255182961,600.114823816367,61.3246595339165));
#105683=CARTESIAN_POINT('Ctrl Pts',(15.4377062255518,599.87261425957,61.2940470335774));
#105684=CARTESIAN_POINT('Ctrl Pts',(15.1972467822461,599.867233281471,61.336802882892));
#105685=CARTESIAN_POINT('Ctrl Pts',(15.5349475887123,600.047983519335,61.8471069255291));
#105686=CARTESIAN_POINT('Ctrl Pts',(15.5309261439817,599.803232323736,61.8206844364526));
#105687=CARTESIAN_POINT('Ctrl Pts',(15.2874077780673,599.799591424263,61.8571195614638));
#105688=CARTESIAN_POINT('Ctrl Pts',(15.6652986681034,599.95273223585,62.9040820559312));
#105689=CARTESIAN_POINT('Ctrl Pts',(15.6642372322958,599.703849135545,62.8892513959474));
#105690=CARTESIAN_POINT('Ctrl Pts',(15.4156790030778,599.703198773326,62.9097786108428));
#105691=CARTESIAN_POINT('Ctrl Pts',(15.7040356606937,599.92431421945,63.4386078350693));
#105692=CARTESIAN_POINT('Ctrl Pts',(15.7037030786927,599.674309310564,63.4286901969925));
#105693=CARTESIAN_POINT('Ctrl Pts',(15.4537982322339,599.674440013257,63.4421236247391));
#105694=CARTESIAN_POINT('Ctrl Pts',(15.720555575138,599.912202987333,64.2499277579685));
#105695=CARTESIAN_POINT('Ctrl Pts',(15.720610340671,599.661663071146,64.2494068634906));
#105696=CARTESIAN_POINT('Ctrl Pts',(15.4700545523028,599.662183666258,64.2501300119848));
#105697=CARTESIAN_POINT('Ctrl Pts',(15.7190604657519,599.913299687284,64.5230557734976));
#105698=CARTESIAN_POINT('Ctrl Pts',(15.7190815934227,599.66280716433,64.5256053426526));
#105699=CARTESIAN_POINT('Ctrl Pts',(15.4685832963051,599.663293508665,64.5221427161502));
#105700=CARTESIAN_POINT('Ctrl Pts',(15.7019650213429,599.925831247008,65.0657280699177));
#105701=CARTESIAN_POINT('Ctrl Pts',(15.7015814327667,599.675895175684,65.0746869533344));
#105702=CARTESIAN_POINT('Ctrl Pts',(15.451760636994,599.675975214018,65.0625984317746));
#105703=CARTESIAN_POINT('Ctrl Pts',(15.6864384446807,599.937211941789,65.3354120618728));
#105704=CARTESIAN_POINT('Ctrl Pts',(15.685708149129,599.687765621734,65.3473542470335));
#105705=CARTESIAN_POINT('Ctrl Pts',(15.4364817742615,599.68749229307,65.3311812375999));
#105706=CARTESIAN_POINT('Ctrl Pts',(15.574852527381,600.01890054518,66.675805476863));
#105707=CARTESIAN_POINT('Ctrl Pts',(15.5718851336501,599.772777987196,66.6988378773207));
#105708=CARTESIAN_POINT('Ctrl Pts',(15.326675704598,599.770160170402,66.6661082158762));
#105709=CARTESIAN_POINT('Ctrl Pts',(15.3780196332794,600.163132045658,67.7226505757277));
#105710=CARTESIAN_POINT('Ctrl Pts',(15.3741355634771,599.920662093309,67.747428907255));
#105711=CARTESIAN_POINT('Ctrl Pts',(15.132976851256,599.916124774213,67.7086964322209));
#105712=CARTESIAN_POINT('Ctrl Pts',(14.7749830115725,600.596964732154,69.7677006850111));
#105713=CARTESIAN_POINT('Ctrl Pts',(14.7598045961286,600.371477433906,69.8078650818197));
#105714=CARTESIAN_POINT('Ctrl Pts',(14.5395600793771,600.355158450615,69.7454059551599));
#105715=CARTESIAN_POINT('Ctrl Pts',(14.3794203054433,600.878842159056,70.7298312303411));
#105716=CARTESIAN_POINT('Ctrl Pts',(14.3625245593818,600.660409929034,70.7712664447535));
#105717=CARTESIAN_POINT('Ctrl Pts',(14.1502976929657,600.640422389231,70.7036228750291));
#105718=CARTESIAN_POINT('Ctrl Pts',(13.6612091794102,601.375545247691,72.0904647072316));
#105719=CARTESIAN_POINT('Ctrl Pts',(13.6295943491115,601.177288380591,72.1457661580741));
#105720=CARTESIAN_POINT('Ctrl Pts',(13.443551570198,601.143076802614,72.0586962144295));
#105721=CARTESIAN_POINT('Ctrl Pts',(13.3993396267296,601.554487162714,72.5323553744969));
#105722=CARTESIAN_POINT('Ctrl Pts',(13.3656347598373,601.361245735362,72.5875774487108));
#105723=CARTESIAN_POINT('Ctrl Pts',(13.1858564258026,601.324166988977,72.4987899104211));
#105724=CARTESIAN_POINT('Ctrl Pts',(12.8404364611288,601.929557948488,73.3794426010547));
#105725=CARTESIAN_POINT('Ctrl Pts',(12.8021776094239,601.74676344862,73.4333645836814));
#105726=CARTESIAN_POINT('Ctrl Pts',(12.6358638843131,601.703740500343,73.3424344241913));
#105727=CARTESIAN_POINT('Ctrl Pts',(12.5440885772941,602.125255881405,73.7841389135551));
#105728=CARTESIAN_POINT('Ctrl Pts',(12.5042121997376,601.947423525011,73.8371312504687));
#105729=CARTESIAN_POINT('Ctrl Pts',(12.3442395607509,601.901788659894,73.7454864680693));
#105730=CARTESIAN_POINT('Ctrl Pts',(11.9187059559954,602.528995443253,74.5589805782249));
#105731=CARTESIAN_POINT('Ctrl Pts',(11.8756740810911,602.361062922652,74.608774052379));
#105732=CARTESIAN_POINT('Ctrl Pts',(11.7288256021108,602.310377386317,74.5171827762026));
#105733=CARTESIAN_POINT('Ctrl Pts',(11.5896694934917,602.737052077775,74.929116152772));
#105734=CARTESIAN_POINT('Ctrl Pts',(11.5456832679029,602.573835505882,74.9772519297626));
#105735=CARTESIAN_POINT('Ctrl Pts',(11.4050330289474,602.52093362206,74.8858160421481));
#105736=CARTESIAN_POINT('Ctrl Pts',(10.8985267731535,603.161627468999,75.6366626093528));
#105737=CARTESIAN_POINT('Ctrl Pts',(10.8529135843586,603.007589543647,75.6803058137441));
#105738=CARTESIAN_POINT('Ctrl Pts',(10.7249053554303,602.950610664589,75.5904935058699));
#105739=CARTESIAN_POINT('Ctrl Pts',(10.5350707806408,603.378936903845,75.9751917541415));
#105740=CARTESIAN_POINT('Ctrl Pts',(10.4891833026196,603.229336765336,76.0167162365071));
#105741=CARTESIAN_POINT('Ctrl Pts',(10.3672411512527,603.17053175624,75.9276498830206));
#105742=CARTESIAN_POINT('Ctrl Pts',(9.40196706845938,604.031564136161,76.9346610568732));
#105743=CARTESIAN_POINT('Ctrl Pts',(9.36501835682024,603.889166409255,76.9607377506827));
#105744=CARTESIAN_POINT('Ctrl Pts',(9.25217348404495,603.831015928072,76.88324984583));
#105745=CARTESIAN_POINT('Ctrl Pts',(8.59738601729796,604.464173010235,77.495276682365));
#105746=CARTESIAN_POINT('Ctrl Pts',(8.56117701294624,604.330686616535,77.5194907589741));
#105747=CARTESIAN_POINT('Ctrl Pts',(8.4604132495034,604.268823621313,77.441588613324));
#105748=CARTESIAN_POINT('Ctrl Pts',(7.30535316787382,605.076707446709,78.2257709379294));
#105749=CARTESIAN_POINT('Ctrl Pts',(7.26509469234165,604.956716878247,78.2466972418932));
#105750=CARTESIAN_POINT('Ctrl Pts',(7.18898333288885,604.88871679835,78.1691179476838));
#105751=CARTESIAN_POINT('Ctrl Pts',(6.86031993687873,605.274722637669,78.4506791819244));
#105752=CARTESIAN_POINT('Ctrl Pts',(6.82166576422317,605.157894830494,78.4694208274701));
#105753=CARTESIAN_POINT('Ctrl Pts',(6.75104020321707,605.08911360307,78.3931160864464));
#105754=CARTESIAN_POINT('Ctrl Pts',(5.93704365902223,605.650813351207,78.8621698493515));
#105755=CARTESIAN_POINT('Ctrl Pts',(5.90261839496408,605.539281559552,78.8760152018326));
#105756=CARTESIAN_POINT('Ctrl Pts',(5.84247174669302,605.469729402818,78.8029438408065));
#105757=CARTESIAN_POINT('Ctrl Pts',(5.45630243005711,605.829574494848,79.0493901878842));
#105758=CARTESIAN_POINT('Ctrl Pts',(5.4239784887906,605.720769173563,79.0613189453554));
#105759=CARTESIAN_POINT('Ctrl Pts',(5.3693892829349,605.650640892095,78.9894068856549));
#105760=CARTESIAN_POINT('Ctrl Pts',(3.58020877348986,606.444076927432,79.6742394973212));
#105761=CARTESIAN_POINT('Ctrl Pts',(3.57309729366402,606.338334356746,79.6733677985972));
#105762=CARTESIAN_POINT('Ctrl Pts',(3.52314404231912,606.27255059228,79.6117444882699));
#105763=CARTESIAN_POINT('Ctrl Pts',(2.11068986974404,606.758383033869,79.9525257968984));
#105764=CARTESIAN_POINT('Ctrl Pts',(2.10064307571136,606.662766022507,79.9545722314202));
#105765=CARTESIAN_POINT('Ctrl Pts',(2.07707015569879,606.59062346792,79.8888901782391));
#105766=CARTESIAN_POINT('Ctrl Pts',(0.520472181601657,606.818551326338,
80.0111755919482));
#105767=CARTESIAN_POINT('Ctrl Pts',(0.516051949937491,606.722294695726,
80.010640113492));
#105768=CARTESIAN_POINT('Ctrl Pts',(0.512173775986833,606.651521964532,
79.9473100409873));
#105769=CARTESIAN_POINT('Ctrl Pts',(3.96801791420419,607.866317116503,49.0902664690719));
#105770=CARTESIAN_POINT('Ctrl Pts',(4.14330398514067,608.4803723312,49.135784443382));
#105771=CARTESIAN_POINT('Ctrl Pts',(3.90492814046806,608.028944351104,49.5221152198147));
#105772=CARTESIAN_POINT('Ctrl Pts',(2.93755241708741,608.17547753474,48.8214432993782));
#105773=CARTESIAN_POINT('Ctrl Pts',(3.03742703523094,608.85281628291,48.8340694353193));
#105774=CARTESIAN_POINT('Ctrl Pts',(2.89083941502255,608.334185987686,49.2609200704409));
#105775=CARTESIAN_POINT('Ctrl Pts',(1.86937071966544,608.386087168575,48.6534581338969));
#105776=CARTESIAN_POINT('Ctrl Pts',(1.96126338871385,609.089531292228,48.6607567236558));
#105777=CARTESIAN_POINT('Ctrl Pts',(1.83964868601656,608.542122065273,49.0977046826072));
#105778=CARTESIAN_POINT('Ctrl Pts',(0.214693779414581,608.48610855861,48.5730542692393));
#105779=CARTESIAN_POINT('Ctrl Pts',(0.22416099289284,609.20948373918,48.5717336255605));
#105780=CARTESIAN_POINT('Ctrl Pts',(0.211280116816066,608.640874904755,
49.0195828117931));
#105781=CARTESIAN_POINT('Ctrl Pts',(-0.327665155014435,608.483177231892,
48.5753871894563));
#105782=CARTESIAN_POINT('Ctrl Pts',(-0.343446449653063,609.205974202863,
48.5743085001531));
#105783=CARTESIAN_POINT('Ctrl Pts',(-0.32245537920764,608.637980757633,
49.0218495189568));
#105784=CARTESIAN_POINT('Ctrl Pts',(-1.4014344262471,608.409659806134,48.6345369452367));
#105785=CARTESIAN_POINT('Ctrl Pts',(-1.47715237700547,609.117321616503,
48.64016712078));
#105786=CARTESIAN_POINT('Ctrl Pts',(-1.37915307127922,608.56539568904,49.0793205445456));
#105787=CARTESIAN_POINT('Ctrl Pts',(-1.93284944505609,608.339110567767,
48.6913595421491));
#105788=CARTESIAN_POINT('Ctrl Pts',(-2.0296182397685,609.034247951133,48.7019273602932));
#105789=CARTESIAN_POINT('Ctrl Pts',(-1.90211842335103,608.49574134848,49.1345303092449));
#105790=CARTESIAN_POINT('Ctrl Pts',(-2.98554566101708,608.137526014925,
48.858111903559));
#105791=CARTESIAN_POINT('Ctrl Pts',(-3.12573547424559,608.796071607189,
48.8844736999009));
#105792=CARTESIAN_POINT('Ctrl Pts',(-2.93807698482498,608.296713492016,
49.2965498576802));
#105793=CARTESIAN_POINT('Ctrl Pts',(-3.50954896370793,608.005382116136,
48.969093235558));
#105794=CARTESIAN_POINT('Ctrl Pts',(-3.66252614078184,608.644062322836,
49.0028670929732));
#105795=CARTESIAN_POINT('Ctrl Pts',(-3.45374791090643,608.166245890445,
49.4043809868049));
#105796=CARTESIAN_POINT('Ctrl Pts',(-4.51869902314397,607.699442312391,
49.2356474341197));
#105797=CARTESIAN_POINT('Ctrl Pts',(-4.69335204058046,608.293267867564,
49.2876872236527));
#105798=CARTESIAN_POINT('Ctrl Pts',(-4.4468510663278,607.864186714045,49.6633692434331));
#105799=CARTESIAN_POINT('Ctrl Pts',(-5.00754801428308,607.525295392799,
49.3915102529955));
#105800=CARTESIAN_POINT('Ctrl Pts',(-5.18656612683327,608.098169557262,
49.4506178691369));
#105801=CARTESIAN_POINT('Ctrl Pts',(-4.92792605251174,607.692249047515,
49.8148076425706));
#105802=CARTESIAN_POINT('Ctrl Pts',(-5.95917956692152,607.146457363669,
49.7457424205663));
#105803=CARTESIAN_POINT('Ctrl Pts',(-6.14248615971886,607.676200520949,
49.8207309756671));
#105804=CARTESIAN_POINT('Ctrl Pts',(-5.86442374504572,607.318216782459,
50.1589844638927));
#105805=CARTESIAN_POINT('Ctrl Pts',(-6.42237014149181,606.941534503285,
49.9443408012826));
#105806=CARTESIAN_POINT('Ctrl Pts',(-6.60402168968751,607.451986108322,
50.0247610850771));
#105807=CARTESIAN_POINT('Ctrl Pts',(-6.32024772390201,607.115893757345,
50.351944968455));
#105808=CARTESIAN_POINT('Ctrl Pts',(-7.32445419098543,606.511057101471,
50.382970765863));
#105809=CARTESIAN_POINT('Ctrl Pts',(-7.49937336947291,606.983731036464,
50.4751585816833));
#105810=CARTESIAN_POINT('Ctrl Pts',(-7.20798452548951,606.690877640335,
50.7781230179888));
#105811=CARTESIAN_POINT('Ctrl Pts',(-7.75780268783224,606.2882218126,50.6202380193044));
#105812=CARTESIAN_POINT('Ctrl Pts',(-7.92808282222848,606.744119548409,
50.7161247240279));
#105813=CARTESIAN_POINT('Ctrl Pts',(-7.63444059270741,606.47086953048,51.0086543329385));
#105814=CARTESIAN_POINT('Ctrl Pts',(-9.01263265026788,605.608324932273,
51.3844819472612));
#105815=CARTESIAN_POINT('Ctrl Pts',(-9.13407034427913,606.035261719809,
51.4724609662051));
#105816=CARTESIAN_POINT('Ctrl Pts',(-8.86930646895302,605.799601467611,
51.7511985187908));
#105817=CARTESIAN_POINT('Ctrl Pts',(-9.78960325654476,605.140274398618,
51.9632424341007));
#105818=CARTESIAN_POINT('Ctrl Pts',(-9.90255020916191,605.540902676885,
52.0496752501994));
#105819=CARTESIAN_POINT('Ctrl Pts',(-9.63391884695173,605.337489533059,
52.3135263786952));
#105820=CARTESIAN_POINT('Ctrl Pts',(-10.878441060838,604.447130009809,52.9432807545543));
#105821=CARTESIAN_POINT('Ctrl Pts',(-10.9910069155268,604.800649737504,
53.0515055379338));
#105822=CARTESIAN_POINT('Ctrl Pts',(-10.705439897833,604.653137356637,53.2657428837752));
#105823=CARTESIAN_POINT('Ctrl Pts',(-11.229472953103,604.216715305371,53.2899442539113));
#105824=CARTESIAN_POINT('Ctrl Pts',(-11.3347418937742,604.560585814078,
53.3968965258403));
#105825=CARTESIAN_POINT('Ctrl Pts',(-11.0508876799252,604.425646230675,
53.6025635511897));
#105826=CARTESIAN_POINT('Ctrl Pts',(-11.900792348141,603.766050073307,54.0193011734408));
#105827=CARTESIAN_POINT('Ctrl Pts',(-11.9901371105211,604.093157709212,
54.1232083059766));
#105828=CARTESIAN_POINT('Ctrl Pts',(-11.7115273981156,603.980699367114,
54.31121164042));
#105829=CARTESIAN_POINT('Ctrl Pts',(-12.218293964521,603.547715900985,54.3987594591597));
#105830=CARTESIAN_POINT('Ctrl Pts',(-12.3010560005085,603.866740147379,
54.5005517772709));
#105831=CARTESIAN_POINT('Ctrl Pts',(-12.0239781544445,603.765135486367,
54.679895712359));
#105832=CARTESIAN_POINT('Ctrl Pts',(-13.1176253793484,602.918861575623,
55.5830589493271));
#105833=CARTESIAN_POINT('Ctrl Pts',(-13.1641372034305,603.22841419151,55.657554710526));
#105834=CARTESIAN_POINT('Ctrl Pts',(-12.9089989609887,603.14426280659,55.8305641478284));
#105835=CARTESIAN_POINT('Ctrl Pts',(-13.6470291437565,602.534223643058,
56.4332097702865));
#105836=CARTESIAN_POINT('Ctrl Pts',(-13.6882441199942,602.827954606069,
56.502781818501));
#105837=CARTESIAN_POINT('Ctrl Pts',(-13.4299816943561,602.764504555706,
56.6565755853746));
#105838=CARTESIAN_POINT('Ctrl Pts',(-14.2141551453113,602.115068208418,
57.5846512128922));
#105839=CARTESIAN_POINT('Ctrl Pts',(-14.2513227291177,602.390507222111,
57.6633206048862));
#105840=CARTESIAN_POINT('Ctrl Pts',(-13.9880869203314,602.350666237017,
57.7753259736852));
#105841=CARTESIAN_POINT('Ctrl Pts',(-14.3227879338756,602.03433920249,57.8194266921124));
#105842=CARTESIAN_POINT('Ctrl Pts',(-14.3573300164066,602.307756077497,
57.895659279968));
#105843=CARTESIAN_POINT('Ctrl Pts',(-14.0949913651594,602.27096161042,58.0034349097068));
#105844=CARTESIAN_POINT('Ctrl Pts',(-14.5300235323771,601.879661641812,
58.298500421927));
#105845=CARTESIAN_POINT('Ctrl Pts',(-14.5593558255444,602.14943315443,58.3695243760315));
#105846=CARTESIAN_POINT('Ctrl Pts',(-14.2989297883243,602.118246805598,
58.4689050674605));
#105847=CARTESIAN_POINT('Ctrl Pts',(-14.628948992512,601.805469397078,58.5437030695108));
#105848=CARTESIAN_POINT('Ctrl Pts',(-14.655901579792,602.07345265176,58.6120969468063));
#105849=CARTESIAN_POINT('Ctrl Pts',(-14.3962813329383,602.044995995787,
58.707145038779));
#105850=CARTESIAN_POINT('Ctrl Pts',(-14.9068849327433,601.596250680114,
59.2865392357633));
#105851=CARTESIAN_POINT('Ctrl Pts',(-14.9255658148712,601.860526194702,
59.3430538394069));
#105852=CARTESIAN_POINT('Ctrl Pts',(-14.6697948864641,601.838432364643,
59.4288869888394));
#105853=CARTESIAN_POINT('Ctrl Pts',(-15.0672776140326,601.474447273842,
59.7911438168927));
#105854=CARTESIAN_POINT('Ctrl Pts',(-15.08273458312,601.73546949696,59.8429002079945));
#105855=CARTESIAN_POINT('Ctrl Pts',(-14.8276358084694,601.718174435246,
59.919163080231));
#105856=CARTESIAN_POINT('Ctrl Pts',(-15.3375077166812,601.268350349811,
60.8197103861867));
#105857=CARTESIAN_POINT('Ctrl Pts',(-15.3461975432605,601.525017568474,
60.8592543910126));
#105858=CARTESIAN_POINT('Ctrl Pts',(-15.0935663577189,601.514692768556,
60.9185223424128));
#105859=CARTESIAN_POINT('Ctrl Pts',(-15.4473524788766,601.184046572484,
61.3436679646832));
#105860=CARTESIAN_POINT('Ctrl Pts',(-15.4538492122169,601.438551451198,
61.3780952510847));
#105861=CARTESIAN_POINT('Ctrl Pts',(-15.2016635310883,601.431458661533,
61.427601771592));
#105862=CARTESIAN_POINT('Ctrl Pts',(-15.6139481543257,601.055914086478,
62.4121180900535));
#105863=CARTESIAN_POINT('Ctrl Pts',(-15.6162781423566,601.307834796045,
62.4334323880538));
#105864=CARTESIAN_POINT('Ctrl Pts',(-15.3656085202112,601.304952112143,
62.4657118072439));
#105865=CARTESIAN_POINT('Ctrl Pts',(-15.6706008816092,601.01216067731,62.9602003371774));
#105866=CARTESIAN_POINT('Ctrl Pts',(-15.6718168191366,601.262976710226,
62.9761672199096));
#105867=CARTESIAN_POINT('Ctrl Pts',(-15.4213599206253,601.261753856115,
62.9982308158159));
#105868=CARTESIAN_POINT('Ctrl Pts',(-15.7532581285021,600.948322914108,
64.5909241146122));
#105869=CARTESIAN_POINT('Ctrl Pts',(-15.7522976417821,601.19797092063,64.5843508815025));
#105870=CARTESIAN_POINT('Ctrl Pts',(-15.5027019825929,601.198726184824,
64.5826472633091));
#105871=CARTESIAN_POINT('Ctrl Pts',(-15.6959793937825,600.992833298029,
65.6707746519288));
#105872=CARTESIAN_POINT('Ctrl Pts',(-15.6952083223957,601.244324865898,
65.6625224224092));
#105873=CARTESIAN_POINT('Ctrl Pts',(-15.4463343132364,601.242671985787,
65.6318366328334));
#105874=CARTESIAN_POINT('Ctrl Pts',(-15.4849378554675,601.155135843631,
67.011585045083));
#105875=CARTESIAN_POINT('Ctrl Pts',(-15.490748159675,601.40885389153,66.9784967286438));
#105876=CARTESIAN_POINT('Ctrl Pts',(-15.2386509518819,601.402914747705,
66.9345709030678));
#105877=CARTESIAN_POINT('Ctrl Pts',(-15.4355195703926,601.193090402008,
67.2798756894921));
#105878=CARTESIAN_POINT('Ctrl Pts',(-15.442502106951,601.447631243458,67.2436796227911));
#105879=CARTESIAN_POINT('Ctrl Pts',(-15.1900189384783,601.440387693915,
67.1952431231479));
#105880=CARTESIAN_POINT('Ctrl Pts',(-15.3240490417368,601.278497889497,
67.8082600435595));
#105881=CARTESIAN_POINT('Ctrl Pts',(-15.3338238879868,601.534796371477,
67.7656619175894));
#105882=CARTESIAN_POINT('Ctrl Pts',(-15.0803219964504,601.524711405152,
67.7086233424261));
#105883=CARTESIAN_POINT('Ctrl Pts',(-15.2618976191312,601.326027371672,
68.0691914822996));
#105884=CARTESIAN_POINT('Ctrl Pts',(-15.2731532452161,601.58337490534,68.0236001703991));
#105885=CARTESIAN_POINT('Ctrl Pts',(-15.0191594320567,601.571637777113,
67.9621453552883));
#105886=CARTESIAN_POINT('Ctrl Pts',(-15.0568797539538,601.482352444088,
68.8426074874175));
#105887=CARTESIAN_POINT('Ctrl Pts',(-15.0725761726714,601.743561229684,
68.7904931957739));
#105888=CARTESIAN_POINT('Ctrl Pts',(-14.8174033801442,601.725979297202,
68.7135999647743));
#105889=CARTESIAN_POINT('Ctrl Pts',(-14.8955047156438,601.60485941836,69.3457386057789));
#105890=CARTESIAN_POINT('Ctrl Pts',(-14.9144766233915,601.86932000505,69.2887981194078));
#105891=CARTESIAN_POINT('Ctrl Pts',(-14.6585957360926,601.846931861818,
69.202444416695));
#105892=CARTESIAN_POINT('Ctrl Pts',(-14.5255384316863,601.883267821869,
70.3285351375797));
#105893=CARTESIAN_POINT('Ctrl Pts',(-14.5537819644499,602.154045228181,
70.2605787665699));
#105894=CARTESIAN_POINT('Ctrl Pts',(-14.2945157770192,602.12180743446,70.1573336769515));
#105895=CARTESIAN_POINT('Ctrl Pts',(-14.3158676780004,602.039971826645,
70.8102881691105));
#105896=CARTESIAN_POINT('Ctrl Pts',(-14.3484256804248,602.315139349457,
70.7379242119137));
#105897=CARTESIAN_POINT('Ctrl Pts',(-14.0881807313278,602.276523121392,
70.6254072326268));
#105898=CARTESIAN_POINT('Ctrl Pts',(-13.8549669417811,602.380456141554,
71.740888971284));
#105899=CARTESIAN_POINT('Ctrl Pts',(-13.8990584488247,602.664099473411,
71.6590019112753));
#105900=CARTESIAN_POINT('Ctrl Pts',(-13.6346129612246,602.612686934738,
71.5295833283864));
#105901=CARTESIAN_POINT('Ctrl Pts',(-13.6051205939733,602.563225484241,
72.1875975711325));
#105902=CARTESIAN_POINT('Ctrl Pts',(-13.6545221187428,602.852298832617,
72.1017559982508));
#105903=CARTESIAN_POINT('Ctrl Pts',(-13.3887414345827,602.793137212809,
71.9636076884644));
#105904=CARTESIAN_POINT('Ctrl Pts',(-13.0689457304277,602.94970593194,73.0472996885173));
#105905=CARTESIAN_POINT('Ctrl Pts',(-13.1316816038927,603.249565382686,
72.9538576019717));
#105906=CARTESIAN_POINT('Ctrl Pts',(-12.8610969146662,603.174713553808,
72.7988987818575));
#105907=CARTESIAN_POINT('Ctrl Pts',(-12.7826098802753,603.153433010245,
73.4602802768307));
#105908=CARTESIAN_POINT('Ctrl Pts',(-12.851407762716,603.459987836432,73.3637342809632));
#105909=CARTESIAN_POINT('Ctrl Pts',(-12.5793162792295,603.37585565731,73.2001530637705));
#105910=CARTESIAN_POINT('Ctrl Pts',(-12.1741279655269,603.578242135018,
74.2546782628821));
#105911=CARTESIAN_POINT('Ctrl Pts',(-12.2578204673371,603.898383996172,
74.1526852709296));
#105912=CARTESIAN_POINT('Ctrl Pts',(-11.9805147599271,603.795274395457,
73.9719948691702));
#105913=CARTESIAN_POINT('Ctrl Pts',(-11.850540933587,603.800285765725,74.6375141662316));
#105914=CARTESIAN_POINT('Ctrl Pts',(-11.9410485726768,604.128622252677,
74.5332916257023));
#105915=CARTESIAN_POINT('Ctrl Pts',(-11.6620754094574,604.014500653005,
74.3439606423759));
#105916=CARTESIAN_POINT('Ctrl Pts',(-10.8391421878638,604.47762194582,75.7257195228643));
#105917=CARTESIAN_POINT('Ctrl Pts',(-10.9336515194875,604.845559188827,
75.6390199582536));
#105918=CARTESIAN_POINT('Ctrl Pts',(-10.6667627124656,604.683244822595,
75.4012723114464));
#105919=CARTESIAN_POINT('Ctrl Pts',(-10.1104306891926,604.945290954641,
76.3742823947935));
#105920=CARTESIAN_POINT('Ctrl Pts',(-10.2135091666312,605.336742210894,
76.284404155343));
#105921=CARTESIAN_POINT('Ctrl Pts',(-9.94964215326505,605.144980207816,
76.0314203061157));
#105922=CARTESIAN_POINT('Ctrl Pts',(-8.53551476998559,605.87684896143,77.5345321156382));
#105923=CARTESIAN_POINT('Ctrl Pts',(-8.66654368556738,606.321456472146,
77.4536736233639));
#105924=CARTESIAN_POINT('Ctrl Pts',(-8.39977812395367,606.064718667719,
77.1587292660183));
#105925=CARTESIAN_POINT('Ctrl Pts',(-7.68270213057855,606.344199562926,
78.0484723196597));
#105926=CARTESIAN_POINT('Ctrl Pts',(-7.82150334606978,606.819174583438,
77.9681106439715));
#105927=CARTESIAN_POINT('Ctrl Pts',(-7.56052958968753,606.526139373993,
77.6580776200298));
#105928=CARTESIAN_POINT('Ctrl Pts',(-5.83592524215899,607.216625659669,
78.9319873742395));
#105929=CARTESIAN_POINT('Ctrl Pts',(-5.97772848588468,607.774450116446,
78.880974055968));
#105930=CARTESIAN_POINT('Ctrl Pts',(-5.7431239356697,607.387497786281,78.5165117385228));
#105931=CARTESIAN_POINT('Ctrl Pts',(-4.83278432844931,607.621416094013,
79.2978208896735));
#105932=CARTESIAN_POINT('Ctrl Pts',(-4.97553001277422,608.215369388646,
79.2506052240478));
#105933=CARTESIAN_POINT('Ctrl Pts',(-4.75593424033569,607.787152471388,
78.8719595177779));
#105934=CARTESIAN_POINT('Ctrl Pts',(-3.74709337812421,607.930942425638,
79.5646350434898));
#105935=CARTESIAN_POINT('Ctrl Pts',(-3.9174004512104,608.554632246293,79.5230579121762));
#105936=CARTESIAN_POINT('Ctrl Pts',(-3.68751695705033,608.09274982526,79.1311980167394));
#105937=CARTESIAN_POINT('Origin',(52.8776183915471,601.225373764374,90.6087118617898));
#105938=CARTESIAN_POINT('',(71.,639.125373764374,90.6087118617898));
#105939=CARTESIAN_POINT('',(62.6211772316338,639.125373764374,105.888887786568));
#105940=CARTESIAN_POINT('Origin',(52.8776183915471,639.125373764374,90.6087118617898));
#105941=CARTESIAN_POINT('',(62.6211772316338,602.225373764374,105.888887786568));
#105942=CARTESIAN_POINT('',(62.6211772316338,601.225373764374,105.888887786568));
#105943=CARTESIAN_POINT('',(71.,602.225373764374,90.6087118617898));
#105944=CARTESIAN_POINT('Origin',(52.8776183915471,602.225373764374,90.6087118617898));
#105945=CARTESIAN_POINT('',(71.,601.225373764374,90.6087118617898));
#105946=CARTESIAN_POINT('Origin',(0.,640.125373764374,0.));
#105947=CARTESIAN_POINT('',(62.3523505660608,640.125373764374,104.870738441723));
#105948=CARTESIAN_POINT('',(62.3523505660608,640.125373764374,105.190554486823));
#105949=CARTESIAN_POINT('',(70.,640.125373764374,90.6087118617898));
#105950=CARTESIAN_POINT('Origin',(52.8776183915471,640.125373764374,90.6087118617898));
#105951=CARTESIAN_POINT('',(70.,640.125373764374,64.2994740882088));
#105952=CARTESIAN_POINT('',(35.7552367830941,640.125373764374,90.6087118617898));
#105953=CARTESIAN_POINT('',(35.7552367830941,640.125373764374,-5.58390168977932E-15));
#105954=CARTESIAN_POINT('',(43.4028862170334,640.125373764374,104.870738441723));
#105955=CARTESIAN_POINT('Origin',(52.8776183915471,640.125373764374,90.6087118617898));
#105956=CARTESIAN_POINT('',(43.4028862170334,640.125373764374,0.));
#105957=CARTESIAN_POINT('Origin',(0.,601.225373764374,0.));
#105958=CARTESIAN_POINT('',(70.,601.225373764374,90.6087118617898));
#105959=CARTESIAN_POINT('',(62.3523505660608,601.225373764374,104.870738441723));
#105960=CARTESIAN_POINT('Origin',(52.8776183915471,601.225373764374,90.6087118617898));
#105961=CARTESIAN_POINT('',(62.3523505660608,601.225373764374,0.));
#105962=CARTESIAN_POINT('',(43.4028862170334,601.225373764374,104.870738441723));
#105963=CARTESIAN_POINT('',(43.4028862170334,601.225373764374,105.190554486823));
#105964=CARTESIAN_POINT('',(35.7552367830941,601.225373764374,90.6087118617898));
#105965=CARTESIAN_POINT('Origin',(52.8776183915471,601.225373764374,90.6087118617898));
#105966=CARTESIAN_POINT('',(35.7552367830941,601.225373764374,64.2994740882088));
#105967=CARTESIAN_POINT('',(70.,601.225373764374,0.));
#105968=CARTESIAN_POINT('Origin',(52.8776183915471,601.225373764374,90.6087118617898));
#105969=CARTESIAN_POINT('',(34.7552367830941,602.225373764374,90.6087118617898));
#105970=CARTESIAN_POINT('',(43.1340595514603,602.225373764374,105.888887786568));
#105971=CARTESIAN_POINT('Origin',(52.8776183915471,602.225373764374,90.6087118617898));
#105972=CARTESIAN_POINT('',(43.1340595514603,639.125373764374,105.888887786568));
#105973=CARTESIAN_POINT('',(43.1340595514603,601.225373764374,105.888887786568));
#105974=CARTESIAN_POINT('',(34.7552367830941,639.125373764374,90.6087118617898));
#105975=CARTESIAN_POINT('Origin',(52.8776183915471,639.125373764374,90.6087118617898));
#105976=CARTESIAN_POINT('',(34.7552367830941,640.125373764374,90.6087118617898));
#105977=CARTESIAN_POINT('Origin',(71.,620.675373764374,64.2994740882088));
#105978=CARTESIAN_POINT('',(71.,602.225373764374,64.2994740882088));
#105979=CARTESIAN_POINT('',(71.,639.125373764374,90.6087118617898));
#105980=CARTESIAN_POINT('Origin',(34.7552367830941,640.125373764374,64.2994740882088));
#105981=CARTESIAN_POINT('',(34.7552367830941,639.125373764374,73.1199049166885));
#105982=CARTESIAN_POINT('',(34.7552367830941,602.225373764374,73.1199049166887));
#105983=CARTESIAN_POINT('Origin',(34.7552367830941,620.675373764374,64.2994740882088));
#105984=CARTESIAN_POINT('',(34.7552367830941,602.225373764374,90.6087118617898));
#105985=CARTESIAN_POINT('',(34.7552367830941,639.125373764374,64.2994740882088));
#105986=CARTESIAN_POINT('Origin',(52.8776183915471,601.125373764374,90.6087118617898));
#105987=CARTESIAN_POINT('',(43.775613700608,601.125373764374,98.7473601281983));
#105988=CARTESIAN_POINT('',(61.9796230824862,601.125373764374,98.7473601281983));
#105989=CARTESIAN_POINT('Origin',(61.8523505660607,601.125373764374,0.));
#105990=CARTESIAN_POINT('',(61.8523505660607,639.125373764374,105.467304788954));
#105991=CARTESIAN_POINT('',(61.8523505660607,639.625373764374,104.870738441723));
#105992=CARTESIAN_POINT('Ctrl Pts',(61.8523505660607,639.125373764374,105.467304788954));
#105993=CARTESIAN_POINT('Ctrl Pts',(61.8523505660608,639.270789691535,105.467304788954));
#105994=CARTESIAN_POINT('Ctrl Pts',(61.8523505660608,639.406718012507,105.388349047246));
#105995=CARTESIAN_POINT('Ctrl Pts',(61.8523505660607,639.582389805433,105.159369804922));
#105996=CARTESIAN_POINT('Ctrl Pts',(61.8523505660608,639.625373764374,105.015531405683));
#105997=CARTESIAN_POINT('Ctrl Pts',(61.8523505660607,639.625373764374,104.870738441723));
#105998=CARTESIAN_POINT('',(61.8523505660607,639.625373764374,99.080638124754));
#105999=CARTESIAN_POINT('',(61.8523505660607,639.625373764374,98.8874960354436));
#106000=CARTESIAN_POINT('',(61.8523505660607,601.725373764374,99.080638124754));
#106001=CARTESIAN_POINT('',(61.8523505660607,601.225373764374,99.080638124754));
#106002=CARTESIAN_POINT('',(61.8523505660607,601.725373764374,104.870738441723));
#106003=CARTESIAN_POINT('',(61.8523505660607,601.725373764374,0.));
#106004=CARTESIAN_POINT('',(61.8523505660607,602.225373764374,105.467304788954));
#106005=CARTESIAN_POINT('Ctrl Pts',(61.8523505660607,601.725373764374,104.870738441723));
#106006=CARTESIAN_POINT('Ctrl Pts',(61.8523505660607,601.725373764374,104.934462686335));
#106007=CARTESIAN_POINT('Ctrl Pts',(61.8523505660607,601.733555001666,104.996692081853));
#106008=CARTESIAN_POINT('Ctrl Pts',(61.8523505660607,601.75024142028,105.057367425609));
#106009=CARTESIAN_POINT('Ctrl Pts',(61.8523505660607,601.752544915752,105.065743421852));
#106010=CARTESIAN_POINT('Ctrl Pts',(61.8523505660607,601.755010572306,105.074089788599));
#106011=CARTESIAN_POINT('Ctrl Pts',(61.8523505660607,601.757639320276,105.082406355946));
#106012=CARTESIAN_POINT('Ctrl Pts',(61.8523505660607,601.779310601466,105.150967766776));
#106013=CARTESIAN_POINT('Ctrl Pts',(61.8523505660608,601.811992484867,105.215987728384));
#106014=CARTESIAN_POINT('Ctrl Pts',(61.8523505660608,601.855441859262,105.272877360388));
#106015=CARTESIAN_POINT('Ctrl Pts',(61.8523505660607,601.898891233656,105.329766992393));
#106016=CARTESIAN_POINT('Ctrl Pts',(61.8523505660607,601.953782542618,105.379045945291));
#106017=CARTESIAN_POINT('Ctrl Pts',(61.8523505660607,602.017642969564,105.41367565036));
#106018=CARTESIAN_POINT('Ctrl Pts',(61.8523505660608,602.041337088189,105.426524301381));
#106019=CARTESIAN_POINT('Ctrl Pts',(61.8523505660608,602.065992574575,105.437249174374));
#106020=CARTESIAN_POINT('Ctrl Pts',(61.8523505660608,602.091368457776,105.445633434612));
#106021=CARTESIAN_POINT('Ctrl Pts',(61.8523505660608,602.115878069975,105.453731476576));
#106022=CARTESIAN_POINT('Ctrl Pts',(61.8523505660608,602.141059071268,105.459645696455));
#106023=CARTESIAN_POINT('Ctrl Pts',(61.8523505660608,602.166680666438,105.463226524911));
#106024=CARTESIAN_POINT('Ctrl Pts',(61.8523505660608,602.186027969902,105.465930469547));
#106025=CARTESIAN_POINT('Ctrl Pts',(61.8523505660608,602.205626172223,105.467304788954));
#106026=CARTESIAN_POINT('Ctrl Pts',(61.8523505660608,602.225373764374,105.467304788954));
#106027=CARTESIAN_POINT('',(61.8523505660607,601.125373764374,105.467304788954));
#106028=CARTESIAN_POINT('Origin',(43.9028862170334,601.125373764374,0.));
#106029=CARTESIAN_POINT('',(43.9028862170334,602.225373764374,105.467304788954));
#106030=CARTESIAN_POINT('',(43.9028862170334,601.725373764374,104.870738441723));
#106031=CARTESIAN_POINT('Ctrl Pts',(43.9028862170334,602.225373764374,105.467304788954));
#106032=CARTESIAN_POINT('Ctrl Pts',(43.9028862170334,602.199366036638,105.467304788954));
#106033=CARTESIAN_POINT('Ctrl Pts',(43.9028862170334,602.173617536014,105.464919144673));
#106034=CARTESIAN_POINT('Ctrl Pts',(43.9028862170334,602.148359776795,105.460256351402));
#106035=CARTESIAN_POINT('Ctrl Pts',(43.9028862170334,602.122200630188,105.455427154493));
#106036=CARTESIAN_POINT('Ctrl Pts',(43.9028862170334,602.096568531369,105.448155596141));
#106037=CARTESIAN_POINT('Ctrl Pts',(43.9028862170334,602.071712802132,105.438618445843));
#106038=CARTESIAN_POINT('Ctrl Pts',(43.9028862170334,602.053228082178,105.431525853598));
#106039=CARTESIAN_POINT('Ctrl Pts',(43.9028862170334,602.035172629463,105.423181489599));
#106040=CARTESIAN_POINT('Ctrl Pts',(43.9028862170334,602.017642969564,105.41367565036));
#106041=CARTESIAN_POINT('Ctrl Pts',(43.9028862170334,601.953782542618,105.37904594529));
#106042=CARTESIAN_POINT('Ctrl Pts',(43.9028862170334,601.898891233656,105.329766992393));
#106043=CARTESIAN_POINT('Ctrl Pts',(43.9028862170334,601.855441859261,105.272877360388));
#106044=CARTESIAN_POINT('Ctrl Pts',(43.9028862170334,601.811992484867,105.215987728384));
#106045=CARTESIAN_POINT('Ctrl Pts',(43.9028862170334,601.779310601467,105.150967766776));
#106046=CARTESIAN_POINT('Ctrl Pts',(43.9028862170334,601.757639320276,105.082406355946));
#106047=CARTESIAN_POINT('Ctrl Pts',(43.9028862170334,601.738596787043,105.022161512427));
#106048=CARTESIAN_POINT('Ctrl Pts',(43.9028862170334,601.72810819572,104.960353720503));
#106049=CARTESIAN_POINT('Ctrl Pts',(43.9028862170334,601.725842518628,104.897043449009));
#106050=CARTESIAN_POINT('Ctrl Pts',(43.9028862170334,601.725529750681,104.888303711238));
#106051=CARTESIAN_POINT('Ctrl Pts',(43.9028862170334,601.725373764374,104.879535326884));
#106052=CARTESIAN_POINT('Ctrl Pts',(43.9028862170334,601.725373764374,104.870738441723));
#106053=CARTESIAN_POINT('',(43.9028862170334,601.725373764374,99.080638124754));
#106054=CARTESIAN_POINT('',(43.9028862170334,601.725373764374,98.8874960354436));
#106055=CARTESIAN_POINT('',(43.9028862170334,639.625373764374,99.080638124754));
#106056=CARTESIAN_POINT('',(43.9028862170334,601.125373764374,99.080638124754));
#106057=CARTESIAN_POINT('',(43.9028862170334,639.625373764374,104.870738441723));
#106058=CARTESIAN_POINT('',(43.9028862170334,639.625373764374,0.));
#106059=CARTESIAN_POINT('',(43.9028862170334,639.125373764374,105.467304788954));
#106060=CARTESIAN_POINT('Ctrl Pts',(43.9028862170334,639.625373764374,104.870738441723));
#106061=CARTESIAN_POINT('Ctrl Pts',(43.9028862170334,639.625373764374,105.015531405683));
#106062=CARTESIAN_POINT('Ctrl Pts',(43.9028862170334,639.582389805433,105.159369804922));
#106063=CARTESIAN_POINT('Ctrl Pts',(43.9028862170334,639.406718012507,105.388349047246));
#106064=CARTESIAN_POINT('Ctrl Pts',(43.9028862170334,639.270789691535,105.467304788954));
#106065=CARTESIAN_POINT('Ctrl Pts',(43.9028862170334,639.125373764374,105.467304788954));
#106066=CARTESIAN_POINT('',(43.9028862170334,602.225373764374,105.467304788954));
#106067=CARTESIAN_POINT('Origin',(52.8776183915471,639.125373764374,90.6087118617898));
#106068=CARTESIAN_POINT('Ctrl Pts',(43.1340595514603,639.125373764374,105.888887786568));
#106069=CARTESIAN_POINT('Ctrl Pts',(43.1340595514603,639.183634335595,105.888887786568));
#106070=CARTESIAN_POINT('Ctrl Pts',(43.1353749199127,639.241023457001,105.883765013252));
#106071=CARTESIAN_POINT('Ctrl Pts',(43.1379705232213,639.297646653191,105.873657394149));
#106072=CARTESIAN_POINT('Ctrl Pts',(43.1385991820447,639.311360872069,105.871209314385));
#106073=CARTESIAN_POINT('Ctrl Pts',(43.139303000641,639.325030102463,105.868468588626));
#106074=CARTESIAN_POINT('Ctrl Pts',(43.1400815900552,639.338655734907,105.865436756047));
#106075=CARTESIAN_POINT('Ctrl Pts',(43.1425184881117,639.381302445243,105.855947458114));
#106076=CARTESIAN_POINT('Ctrl Pts',(43.1457204641877,639.423585630974,105.843480262565));
#106077=CARTESIAN_POINT('Ctrl Pts',(43.149600304955,639.464673649675,105.82838734085));
#106078=CARTESIAN_POINT('Ctrl Pts',(43.1512777614199,639.482438131966,105.821861887712));
#106079=CARTESIAN_POINT('Ctrl Pts',(43.1530819274064,639.499978593913,105.814845638027));
#106080=CARTESIAN_POINT('Ctrl Pts',(43.1550057044128,639.51722471474,105.807367331575));
#106081=CARTESIAN_POINT('Ctrl Pts',(43.155836125878,639.524669210063,105.804139230719));
#106082=CARTESIAN_POINT('Ctrl Pts',(43.1566894887349,639.532063578086,105.800823057735));
#106083=CARTESIAN_POINT('Ctrl Pts',(43.1575652792992,639.539401572236,105.797420942698));
#106084=CARTESIAN_POINT('Ctrl Pts',(43.1620564698277,639.577031950051,105.779974366481));
#106085=CARTESIAN_POINT('Ctrl Pts',(43.1671922663579,639.613728245051,105.760055341059));
#106086=CARTESIAN_POINT('Ctrl Pts',(43.1729063844078,639.649034910278,105.737944045788));
#106087=CARTESIAN_POINT('Ctrl Pts',(43.1766524913453,639.672181534551,105.723448147052));
#106088=CARTESIAN_POINT('Ctrl Pts',(43.1806469908836,639.694730149313,105.708010711998));
#106089=CARTESIAN_POINT('Ctrl Pts',(43.184869232144,639.716543554195,105.69171884283));
#106090=CARTESIAN_POINT('Ctrl Pts',(43.193616403455,639.761734147912,105.657967154616));
#106091=CARTESIAN_POINT('Ctrl Pts',(43.2032702988599,639.803594208621,105.620819562242));
#106092=CARTESIAN_POINT('Ctrl Pts',(43.213825446355,639.842208965498,105.580362184908));
#106093=CARTESIAN_POINT('Ctrl Pts',(43.2158189162106,639.849501838843,105.572721309952));
#106094=CARTESIAN_POINT('Ctrl Pts',(43.2178438267247,639.856676746876,105.564964855412));
#106095=CARTESIAN_POINT('Ctrl Pts',(43.2199001658011,639.86373494426,105.557093372208));
#106096=CARTESIAN_POINT('Ctrl Pts',(43.2306831409574,639.900746528542,105.515817101766));
#106097=CARTESIAN_POINT('Ctrl Pts',(43.2422060359435,639.934106550084,105.47185885015));
#106098=CARTESIAN_POINT('Ctrl Pts',(43.2543899245646,639.963675367698,105.425575864041));
#106099=CARTESIAN_POINT('Ctrl Pts',(43.2659229308836,639.991664573032,105.381765387119));
#106100=CARTESIAN_POINT('Ctrl Pts',(43.2780483172813,640.016256574864,105.33587144162));
#106101=CARTESIAN_POINT('Ctrl Pts',(43.2906914506057,640.03730213598,105.288231896121));
#106102=CARTESIAN_POINT('Ctrl Pts',(43.294007829138,640.042822527586,105.275735724332));
#106103=CARTESIAN_POINT('Ctrl Pts',(43.2973597827178,640.048098745172,105.263119663155));
#106104=CARTESIAN_POINT('Ctrl Pts',(43.3007458539078,640.053127748537,105.250390301448));
#106105=CARTESIAN_POINT('Ctrl Pts',(43.3024790201449,640.055701852373,105.243874756236));
#106106=CARTESIAN_POINT('Ctrl Pts',(43.3042190431903,640.058208132244,105.237337246198));
#106107=CARTESIAN_POINT('Ctrl Pts',(43.3059656934663,640.060646673368,105.23077875602));
#106108=CARTESIAN_POINT('Ctrl Pts',(43.3194716366484,640.079502650615,105.180065343653));
#106109=CARTESIAN_POINT('Ctrl Pts',(43.3331997567824,640.094186237523,105.128744628145));
#106110=CARTESIAN_POINT('Ctrl Pts',(43.3471728225631,640.104775540729,105.076754341906));
#106111=CARTESIAN_POINT('Ctrl Pts',(43.3613724966737,640.115536576062,105.023920902695));
#106112=CARTESIAN_POINT('Ctrl Pts',(43.3758251265072,640.122069386147,104.970395944298));
#106113=CARTESIAN_POINT('Ctrl Pts',(43.3905572354151,640.124402582393,104.916108237801));
#106114=CARTESIAN_POINT('Ctrl Pts',(43.3946451609367,640.125050007181,104.901044264117));
#106115=CARTESIAN_POINT('Ctrl Pts',(43.3987546209328,640.125373764374,104.885921529213));
#106116=CARTESIAN_POINT('Ctrl Pts',(43.4028862170334,640.125373764374,104.870738441723));
#106117=CARTESIAN_POINT('Origin',(35.7552367830941,639.125373764374,90.6087118617898));
#106118=CARTESIAN_POINT('Origin',(35.7552367830941,639.125373764374,-5.58390168977932E-15));
#106119=CARTESIAN_POINT('Ctrl Pts',(34.7552367830941,639.125373764374,73.1199049166885));
#106120=CARTESIAN_POINT('Ctrl Pts',(34.7552367830941,639.200884802411,72.8040068203705));
#106121=CARTESIAN_POINT('Ctrl Pts',(34.7636376301548,639.271491652081,72.4878072684));
#106122=CARTESIAN_POINT('Ctrl Pts',(34.7779932599735,639.337516912742,72.1711663955806));
#106123=CARTESIAN_POINT('Ctrl Pts',(34.7798305566038,639.345967115935,72.1306413043105));
#106124=CARTESIAN_POINT('Ctrl Pts',(34.7817654544466,639.354342292342,72.090109013267));
#106125=CARTESIAN_POINT('Ctrl Pts',(34.7837928855838,639.362643134571,72.0495692558948));
#106126=CARTESIAN_POINT('Ctrl Pts',(34.8004726967557,639.43093471716,71.7160459684573));
#106127=CARTESIAN_POINT('Ctrl Pts',(34.8234784568466,639.494189531026,71.3820173166586));
#106128=CARTESIAN_POINT('Ctrl Pts',(34.851116807566,639.552654661099,71.0475114120635));
#106129=CARTESIAN_POINT('Ctrl Pts',(34.8533204597638,639.557316184273,71.0208406935639));
#106130=CARTESIAN_POINT('Ctrl Pts',(34.8555535843187,639.56194726855,70.9941669549191));
#106131=CARTESIAN_POINT('Ctrl Pts',(34.8578153353241,639.566548044146,70.967490217716));
#106132=CARTESIAN_POINT('Ctrl Pts',(34.8588927099961,639.568739602406,70.954782876843));
#106133=CARTESIAN_POINT('Ctrl Pts',(34.8599766633094,639.570924412863,70.9420737239539));
#106134=CARTESIAN_POINT('Ctrl Pts',(34.8610671285686,639.573102474715,70.9293628456683));
#106135=CARTESIAN_POINT('Ctrl Pts',(34.8816001688782,639.614114539466,70.6900219093161));
#106136=CARTESIAN_POINT('Ctrl Pts',(34.9044201141224,639.652698786736,70.4502744546756));
#106137=CARTESIAN_POINT('Ctrl Pts',(34.9291259895506,639.688922550039,70.2102707123723));
#106138=CARTESIAN_POINT('Ctrl Pts',(34.956169125434,639.728573205448,69.9475617938197));
#106139=CARTESIAN_POINT('Ctrl Pts',(34.9854722230115,639.765396145449,69.6845451902924));
#106140=CARTESIAN_POINT('Ctrl Pts',(35.0165561203898,639.799447393656,69.4213836553411));
#106141=CARTESIAN_POINT('Ctrl Pts',(35.0424690442426,639.827834033566,69.2020004572428));
#106142=CARTESIAN_POINT('Ctrl Pts',(35.0696207330031,639.85429387261,68.9825155527574));
#106143=CARTESIAN_POINT('Ctrl Pts',(35.0977513325307,639.878841004738,68.7630133520805));
#106144=CARTESIAN_POINT('Ctrl Pts',(35.0994093669033,639.880287827398,68.7500757609986));
#106145=CARTESIAN_POINT('Ctrl Pts',(35.1010708214122,639.881728095368,68.7371380738301));
#106146=CARTESIAN_POINT('Ctrl Pts',(35.1027356711041,639.883161820044,68.7242002248716));
#106147=CARTESIAN_POINT('Ctrl Pts',(35.1578246869571,639.930603028578,68.2960934895558));
#106148=CARTESIAN_POINT('Ctrl Pts',(35.2166172729909,639.970862604241,67.8679097403797));
#106149=CARTESIAN_POINT('Ctrl Pts',(35.2779103319681,640.004140516552,67.4395068625554));
#106150=CARTESIAN_POINT('Ctrl Pts',(35.3208375199838,640.027447025027,67.1394707542299));
#106151=CARTESIAN_POINT('Ctrl Pts',(35.36499069794,640.047330100565,66.8393272423455));
#106152=CARTESIAN_POINT('Ctrl Pts',(35.4099554169091,640.063872980232,66.5390317516864));
#106153=CARTESIAN_POINT('Ctrl Pts',(35.4112107944409,640.064334843664,66.5306477515076));
#106154=CARTESIAN_POINT('Ctrl Pts',(35.4124668432853,640.06479408847,66.5222635016681));
#106155=CARTESIAN_POINT('Ctrl Pts',(35.4137235541889,640.065250715059,66.5138790148404));
#106156=CARTESIAN_POINT('Ctrl Pts',(35.4873122291016,640.091989200063,66.0229122589214));
#106157=CARTESIAN_POINT('Ctrl Pts',(35.563215136994,640.109769754558,65.5307970571815));
#106158=CARTESIAN_POINT('Ctrl Pts',(35.6397290728435,640.118672316601,65.0392629090769));
#106159=CARTESIAN_POINT('Ctrl Pts',(35.6781489588635,640.123142553495,64.7924492308175));
#106160=CARTESIAN_POINT('Ctrl Pts',(35.7167231407543,640.125373764374,64.5457813055128));
#106161=CARTESIAN_POINT('Ctrl Pts',(35.7552367830941,640.125373764374,64.2994740882088));
#106162=CARTESIAN_POINT('Ctrl Pts',(33.7552367830941,638.223173275376,72.6885880057604));
#106163=CARTESIAN_POINT('Ctrl Pts',(34.7552367830941,638.223173275376,72.6885880057604));
#106164=CARTESIAN_POINT('Ctrl Pts',(34.7552367830941,639.125373764374,73.1199049166885));
#106165=CARTESIAN_POINT('Ctrl Pts',(33.7552367874537,638.384664659928,72.3507908955142));
#106166=CARTESIAN_POINT('Ctrl Pts',(34.6814263287167,638.363575572785,72.3949036703327));
#106167=CARTESIAN_POINT('Ctrl Pts',(34.7552367830941,639.210271619968,72.7647373589289));
#106168=CARTESIAN_POINT('Ctrl Pts',(33.7764837682833,638.534848672552,72.0116381428428));
#106169=CARTESIAN_POINT('Ctrl Pts',(34.6339372270254,638.50739702657,72.0748761014097));
#106170=CARTESIAN_POINT('Ctrl Pts',(34.7658602751036,639.289223684062,72.4081504335284));
#106171=CARTESIAN_POINT('Ctrl Pts',(33.8482184555667,638.814182242514,71.3295484402176));
#106172=CARTESIAN_POINT('Ctrl Pts',(34.5852404580364,638.77802067215,71.4214334883314));
#106173=CARTESIAN_POINT('Ctrl Pts',(34.8017276199155,639.436071280424,71.690991851673));
#106174=CARTESIAN_POINT('Ctrl Pts',(33.8988585801114,638.943324593884,70.9866109201948));
#106175=CARTESIAN_POINT('Ctrl Pts',(34.5812439461558,638.907206976171,71.085350352821));
#106176=CARTESIAN_POINT('Ctrl Pts',(34.8270476812808,639.503962311126,71.3304225824941));
#106177=CARTESIAN_POINT('Ctrl Pts',(34.0834772923341,639.30050117458,69.9510610361466));
#106178=CARTESIAN_POINT('Ctrl Pts',(34.6170246837339,639.258114901121,70.0851505103093));
#106179=CARTESIAN_POINT('Ctrl Pts',(34.919357038358,639.691732518317,70.2416310592042));
#106180=CARTESIAN_POINT('Ctrl Pts',(34.2506966542608,639.499087923712,69.2481994911169));
#106181=CARTESIAN_POINT('Ctrl Pts',(34.7001850449893,639.468602714415,69.3679973198037));
#106182=CARTESIAN_POINT('Ctrl Pts',(35.0029667184136,639.796130951156,69.5026326737362));
#106183=CARTESIAN_POINT('Ctrl Pts',(34.6298396352898,639.813753889154,67.841296227345));
#106184=CARTESIAN_POINT('Ctrl Pts',(34.9323200255037,639.794711368262,67.9421363496405));
#106185=CARTESIAN_POINT('Ctrl Pts',(35.1925382094558,639.961553032868,68.0233950520287));
#106186=CARTESIAN_POINT('Ctrl Pts',(34.8418678006974,639.930423294367,67.1371463181171));
#106187=CARTESIAN_POINT('Ctrl Pts',(35.0803796729177,639.919899379557,67.2146858539356));
#106188=CARTESIAN_POINT('Ctrl Pts',(35.2985522918458,640.022886949265,67.2830420625807));
#106189=CARTESIAN_POINT('Ctrl Pts',(35.2874823657224,640.086351313611,65.7218898747875));
#106190=CARTESIAN_POINT('Ctrl Pts',(35.4025374070644,640.083346941915,65.7667284931679));
#106191=CARTESIAN_POINT('Ctrl Pts',(35.5213595744583,640.104859391058,65.79502179184));
#106192=CARTESIAN_POINT('Ctrl Pts',(35.5216787611567,640.125373764374,65.0097934141342));
#106193=CARTESIAN_POINT('Ctrl Pts',(35.5800722057109,640.125373764374,65.0280371672288));
#106194=CARTESIAN_POINT('Ctrl Pts',(35.6384569650295,640.125373764374,65.0463188496307));
#106195=CARTESIAN_POINT('Ctrl Pts',(35.7552367830941,640.125373764374,64.2994740882088));
#106196=CARTESIAN_POINT('Ctrl Pts',(35.7552367830941,640.125373764374,64.2994740882088));
#106197=CARTESIAN_POINT('Ctrl Pts',(35.7552367830941,640.125373764374,64.2994740882088));
#106198=CARTESIAN_POINT('Origin',(33.7552367830941,639.125373764374,73.1199049166885));
#106199=CARTESIAN_POINT('Origin',(33.7552367830941,620.675373764374,64.2994740882088));
#106200=CARTESIAN_POINT('Origin',(33.7552367830941,602.225373764374,73.1199049166887));
#106201=CARTESIAN_POINT('Ctrl Pts',(34.7552367830941,602.225373764374,73.1199049166888));
#106202=CARTESIAN_POINT('Ctrl Pts',(34.7552367830941,603.127574253371,72.6885880057606));
#106203=CARTESIAN_POINT('Ctrl Pts',(33.7552367830941,603.127574253371,72.6885880057606));
#106204=CARTESIAN_POINT('Ctrl Pts',(34.7552367830941,602.140475908865,72.764737358909));
#106205=CARTESIAN_POINT('Ctrl Pts',(34.6814263286416,602.98717195596,72.3949036703512));
#106206=CARTESIAN_POINT('Ctrl Pts',(33.7552367874592,602.966082868819,72.3507908955145));
#106207=CARTESIAN_POINT('Ctrl Pts',(34.7658602751036,602.061523844686,72.4081504335286));
#106208=CARTESIAN_POINT('Ctrl Pts',(34.6339372270254,602.843350502178,72.0748761014127));
#106209=CARTESIAN_POINT('Ctrl Pts',(33.7764837682833,602.815898856196,72.011638142843));
#106210=CARTESIAN_POINT('Ctrl Pts',(34.8017276199155,601.914676248324,71.6909918516732));
#106211=CARTESIAN_POINT('Ctrl Pts',(34.5852404580363,602.572726856598,71.4214334883289));
#106212=CARTESIAN_POINT('Ctrl Pts',(33.8482184555667,602.536565286233,71.3295484402178));
#106213=CARTESIAN_POINT('Ctrl Pts',(34.8270476812803,601.846785217622,71.3304225825078));
#106214=CARTESIAN_POINT('Ctrl Pts',(34.5812439461531,602.443540552576,71.0853503528376));
#106215=CARTESIAN_POINT('Ctrl Pts',(33.8988585801101,602.407422934868,70.9866109202095));
#106216=CARTESIAN_POINT('Ctrl Pts',(34.919357038359,601.659015010429,70.2416310591774));
#106217=CARTESIAN_POINT('Ctrl Pts',(34.6170246837392,602.092632627626,70.0851505102782));
#106218=CARTESIAN_POINT('Ctrl Pts',(34.0834772923369,602.050246354158,69.9510610361178));
#106219=CARTESIAN_POINT('Ctrl Pts',(35.0029667184137,601.554616577592,69.5026326737309));
#106220=CARTESIAN_POINT('Ctrl Pts',(34.7001850449893,601.882144814288,69.3679973197988));
#106221=CARTESIAN_POINT('Ctrl Pts',(34.2506966542582,601.851659605033,69.2481994911067));
#106222=CARTESIAN_POINT('Ctrl Pts',(35.1925382094559,601.38919449588,68.0233950520342));
#106223=CARTESIAN_POINT('Ctrl Pts',(34.9323200255037,601.556036160528,67.9421363496463));
#106224=CARTESIAN_POINT('Ctrl Pts',(34.6298396352926,601.536993639596,67.8412962273554));
#106225=CARTESIAN_POINT('Ctrl Pts',(35.2985522918459,601.327860579483,67.2830420625863));
#106226=CARTESIAN_POINT('Ctrl Pts',(35.0803796729178,601.43084814919,67.2146858539412));
#106227=CARTESIAN_POINT('Ctrl Pts',(34.8418678006976,601.420324234381,67.1371463181226));
#106228=CARTESIAN_POINT('Ctrl Pts',(35.5213595744584,601.24588813769,65.7950217918347));
#106229=CARTESIAN_POINT('Ctrl Pts',(35.4025374070644,601.267400586833,65.7667284931627));
#106230=CARTESIAN_POINT('Ctrl Pts',(35.2874823657227,601.264396215136,65.7218898747823));
#106231=CARTESIAN_POINT('Ctrl Pts',(35.6384569653697,601.225373764374,65.0463188496885));
#106232=CARTESIAN_POINT('Ctrl Pts',(35.580072206224,601.225373764374,65.0280371673566));
#106233=CARTESIAN_POINT('Ctrl Pts',(35.5216787617927,601.225373764374,65.0097934143472));
#106234=CARTESIAN_POINT('Ctrl Pts',(35.7552367830941,601.225373764374,64.2994740882088));
#106235=CARTESIAN_POINT('Ctrl Pts',(35.7552367830941,601.225373764374,64.2994740882088));
#106236=CARTESIAN_POINT('Ctrl Pts',(35.7552367830941,601.225373764374,64.2994740882088));
#106237=CARTESIAN_POINT('Ctrl Pts',(34.7552367830941,602.225373764374,73.1199049166888));
#106238=CARTESIAN_POINT('Ctrl Pts',(34.7552367830941,602.149862727759,72.8040068259897));
#106239=CARTESIAN_POINT('Ctrl Pts',(34.7636376298549,602.079255879206,72.4878072796902));
#106240=CARTESIAN_POINT('Ctrl Pts',(34.7779932592036,602.013230619549,72.1711664125558));
#106241=CARTESIAN_POINT('Ctrl Pts',(34.7798305560632,602.004780415154,72.1306413156293));
#106242=CARTESIAN_POINT('Ctrl Pts',(34.7817654541633,601.996405237566,72.0901090189274));
#106243=CARTESIAN_POINT('Ctrl Pts',(34.7837928855835,601.988104394178,72.0495692558945));
#106244=CARTESIAN_POINT('Ctrl Pts',(34.8004726966809,601.919812811894,71.7160459699422));
#106245=CARTESIAN_POINT('Ctrl Pts',(34.8234784566402,601.85655799829,71.3820173196514));
#106246=CARTESIAN_POINT('Ctrl Pts',(34.8511168071947,601.798092868435,71.0475114165508));
#106247=CARTESIAN_POINT('Ctrl Pts',(34.8533204595128,601.793431344995,71.0208406965558));
#106248=CARTESIAN_POINT('Ctrl Pts',(34.8555535841913,601.788800260457,70.9941669564151));
#106249=CARTESIAN_POINT('Ctrl Pts',(34.8578153353235,601.784199484603,70.9674902177157));
#106250=CARTESIAN_POINT('Ctrl Pts',(34.8588927099955,601.782007926342,70.9547828768427));
#106251=CARTESIAN_POINT('Ctrl Pts',(34.8599766633088,601.779823115886,70.9420737239535));
#106252=CARTESIAN_POINT('Ctrl Pts',(34.861067128568,601.777645054033,70.9293628456679));
#106253=CARTESIAN_POINT('Ctrl Pts',(34.8816001689142,601.73663298921,70.6900219088858));
#106254=CARTESIAN_POINT('Ctrl Pts',(34.9044201142034,601.698048741874,70.4502744538141));
#106255=CARTESIAN_POINT('Ctrl Pts',(34.9291259896828,601.661824978515,70.210270711079));
#106256=CARTESIAN_POINT('Ctrl Pts',(34.9561691256169,601.622174323051,69.9475617921052));
#106257=CARTESIAN_POINT('Ctrl Pts',(34.9854722232518,601.585351383005,69.6845451881559));
#106258=CARTESIAN_POINT('Ctrl Pts',(35.0165561206916,601.551300134761,69.4213836527824));
#106259=CARTESIAN_POINT('Ctrl Pts',(35.0424690444536,601.522913494976,69.2020004555364));
#106260=CARTESIAN_POINT('Ctrl Pts',(35.0696207331126,601.496453656042,68.9825155519043));
#106261=CARTESIAN_POINT('Ctrl Pts',(35.097751332531,601.471906524009,68.7630133520807));
#106262=CARTESIAN_POINT('Ctrl Pts',(35.0994093669035,601.47045970135,68.7500757609988));
#106263=CARTESIAN_POINT('Ctrl Pts',(35.1010708214125,601.46901943338,68.7371380738303));
#106264=CARTESIAN_POINT('Ctrl Pts',(35.1027356711043,601.467585708703,68.7242002248718));
#106265=CARTESIAN_POINT('Ctrl Pts',(35.1578246853299,601.420144501571,68.296093502205));
#106266=CARTESIAN_POINT('Ctrl Pts',(35.2166172695204,601.379884926883,67.8679097656832));
#106267=CARTESIAN_POINT('Ctrl Pts',(35.2779103265398,601.346607015144,67.4395069005296));
#106268=CARTESIAN_POINT('Ctrl Pts',(35.3208375162637,601.323300505397,67.1394707795558));
#106269=CARTESIAN_POINT('Ctrl Pts',(35.364990696048,601.303417428879,66.8393272550155));
#106270=CARTESIAN_POINT('Ctrl Pts',(35.4099554169122,601.286874548515,66.5390317516875));
#106271=CARTESIAN_POINT('Ctrl Pts',(35.411210794444,601.286412685082,66.5306477515087));
#106272=CARTESIAN_POINT('Ctrl Pts',(35.4124668432884,601.285953440277,66.5222635016692));
#106273=CARTESIAN_POINT('Ctrl Pts',(35.413723554192,601.285496813687,66.5138790148415));
#106274=CARTESIAN_POINT('Ctrl Pts',(35.4873122167619,601.258758333171,66.0229123412839));
#106275=CARTESIAN_POINT('Ctrl Pts',(35.5632151116575,601.24097778016,65.5307972223043));
#106276=CARTESIAN_POINT('Ctrl Pts',(35.6397290344742,601.232075216629,65.0392631564647));
#106277=CARTESIAN_POINT('Ctrl Pts',(35.6781489332305,601.227604976743,64.7924493956532));
#106278=CARTESIAN_POINT('Ctrl Pts',(35.716723128,601.225373764374,64.5457813878173));
#106279=CARTESIAN_POINT('Ctrl Pts',(35.7552367830941,601.225373764374,64.2994740882088));
#106280=CARTESIAN_POINT('Origin',(52.8776183915471,602.225373764374,90.6087118617898));
#106281=CARTESIAN_POINT('Ctrl Pts',(43.4028862170334,601.225373764374,104.870738441723));
#106282=CARTESIAN_POINT('Ctrl Pts',(43.3929635135731,601.225373764374,104.907203108541));
#106283=CARTESIAN_POINT('Ctrl Pts',(43.3830997768354,601.227246441777,104.943571896842));
#106284=CARTESIAN_POINT('Ctrl Pts',(43.3733309369751,601.231039696142,104.979707661265));
#106285=CARTESIAN_POINT('Ctrl Pts',(43.3636271064666,601.234807707283,105.015602950601));
#106286=CARTESIAN_POINT('Ctrl Pts',(43.3540169147645,601.24047088985,105.051268273045));
#106287=CARTESIAN_POINT('Ctrl Pts',(43.3445328457605,601.248025482688,105.086576105327));
#106288=CARTESIAN_POINT('Ctrl Pts',(43.3350946628853,601.25554352465,105.121713110115));
#106289=CARTESIAN_POINT('Ctrl Pts',(43.3257813836885,601.264934744555,105.156496049068));
#106290=CARTESIAN_POINT('Ctrl Pts',(43.3166223112608,601.276144301285,105.190806555502));
#106291=CARTESIAN_POINT('Ctrl Pts',(43.3130932278474,601.280463457078,105.204026741293));
#106292=CARTESIAN_POINT('Ctrl Pts',(43.3095870100482,601.285052028013,105.217176867284));
#106293=CARTESIAN_POINT('Ctrl Pts',(43.3061052272023,601.28990483431,105.23025046543));
#106294=CARTESIAN_POINT('Ctrl Pts',(43.304133024549,601.292653632233,105.237655805192));
#106295=CARTESIAN_POINT('Ctrl Pts',(43.3021714197628,601.295486654525,105.245026401512));
#106296=CARTESIAN_POINT('Ctrl Pts',(43.3002211472687,601.298402436799,105.252359276489));
#106297=CARTESIAN_POINT('Ctrl Pts',(43.2895700950561,601.314326441949,105.292406415793));
#106298=CARTESIAN_POINT('Ctrl Pts',(43.2792549047321,601.332717916753,105.33133652796));
#106299=CARTESIAN_POINT('Ctrl Pts',(43.2693167278587,601.353472222818,105.368963065964));
#106300=CARTESIAN_POINT('Ctrl Pts',(43.259184556759,601.374631655054,105.407324077827));
#106301=CARTESIAN_POINT('Ctrl Pts',(43.2494440091227,601.398247078674,105.444331157281));
#106302=CARTESIAN_POINT('Ctrl Pts',(43.2401379297371,601.424261011787,105.479794260594));
#106303=CARTESIAN_POINT('Ctrl Pts',(43.2332977787152,601.443381763264,105.505860337652));
#106304=CARTESIAN_POINT('Ctrl Pts',(43.2266923194162,601.46379943899,105.531092498743));
#106305=CARTESIAN_POINT('Ctrl Pts',(43.2203395080143,601.485508985179,105.555412940236));
#106306=CARTESIAN_POINT('Ctrl Pts',(43.2180660612489,601.493278064795,105.564116367042));
#106307=CARTESIAN_POINT('Ctrl Pts',(43.2158231146049,601.501223507163,105.572710082201));
#106308=CARTESIAN_POINT('Ctrl Pts',(43.2136122722059,601.509342317478,105.581187290618));
#106309=CARTESIAN_POINT('Ctrl Pts',(43.2064137894534,601.535777090056,105.608789004159));
#106310=CARTESIAN_POINT('Ctrl Pts',(43.1996287034623,601.563766590648,105.634860742575));
#106311=CARTESIAN_POINT('Ctrl Pts',(43.1932901049922,601.593131983422,105.659265244783));
#106312=CARTESIAN_POINT('Ctrl Pts',(43.1895319638322,601.610542660528,105.67373462073));
#106313=CARTESIAN_POINT('Ctrl Pts',(43.185930708089,601.628438044517,105.687618274192));
#106314=CARTESIAN_POINT('Ctrl Pts',(43.1824929871301,601.646789202091,105.700889266621));
#106315=CARTESIAN_POINT('Ctrl Pts',(43.1777050796575,601.672347892144,105.719372524738));
#106316=CARTESIAN_POINT('Ctrl Pts',(43.1732335162674,601.698788718341,105.736663826652));
#106317=CARTESIAN_POINT('Ctrl Pts',(43.1690998968992,601.726006943104,105.752668960234));
#106318=CARTESIAN_POINT('Ctrl Pts',(43.1665477254134,601.742811968179,105.76255081967));
#106319=CARTESIAN_POINT('Ctrl Pts',(43.1641243233116,601.759913496151,105.771942622967));
#106320=CARTESIAN_POINT('Ctrl Pts',(43.1618342559007,601.777288313322,105.780824375912));
#106321=CARTESIAN_POINT('Ctrl Pts',(43.1604152202763,601.788054583525,105.786327936101));
#106322=CARTESIAN_POINT('Ctrl Pts',(43.1590471800471,601.798926909346,105.791636433213));
#106323=CARTESIAN_POINT('Ctrl Pts',(43.157729864875,601.809912196874,105.796750406581));
#106324=CARTESIAN_POINT('Ctrl Pts',(43.1548317951143,601.83407963248,105.808001056302));
#106325=CARTESIAN_POINT('Ctrl Pts',(43.1521935219777,601.85861883404,105.818251934007));
#106326=CARTESIAN_POINT('Ctrl Pts',(43.1498084920379,601.88360920051,105.827525146265));
#106327=CARTESIAN_POINT('Ctrl Pts',(43.1459272965156,601.924276404232,105.842615585714));
#106328=CARTESIAN_POINT('Ctrl Pts',(43.1427359349044,601.965977548306,105.855042406237));
#106329=CARTESIAN_POINT('Ctrl Pts',(43.1402686261021,602.008411386523,105.864658408952));
#106330=CARTESIAN_POINT('Ctrl Pts',(43.1378679784102,602.049698758287,105.874014608995));
#106331=CARTESIAN_POINT('Ctrl Pts',(43.1361528128068,602.091679257314,105.880709694516));
#106332=CARTESIAN_POINT('Ctrl Pts',(43.1351426655521,602.134070837637,105.884655190318));
#106333=CARTESIAN_POINT('Ctrl Pts',(43.1344216259734,602.164329799462,105.887471471427));
#106334=CARTESIAN_POINT('Ctrl Pts',(43.1340595514603,602.194798103695,105.888887786568));
#106335=CARTESIAN_POINT('Ctrl Pts',(43.1340595514603,602.225373764374,105.888887786568));
#106336=CARTESIAN_POINT('Origin',(35.7552367830941,602.225373764374,90.6087118617898));
#106337=CARTESIAN_POINT('Origin',(35.7552367830941,602.225373764374,64.2994740882088));
#106338=CARTESIAN_POINT('Origin',(52.8776183915471,639.125373764374,90.6087118617898));
#106339=CARTESIAN_POINT('Ctrl Pts',(62.3523505660607,640.125373764374,104.870738441723));
#106340=CARTESIAN_POINT('Ctrl Pts',(62.3672566615477,640.125373764374,104.925516437054));
#106341=CARTESIAN_POINT('Ctrl Pts',(62.3818748211232,640.12116355199,104.979509244738));
#106342=CARTESIAN_POINT('Ctrl Pts',(62.3962323728286,640.112728812014,105.032789790483));
#106343=CARTESIAN_POINT('Ctrl Pts',(62.4103590117932,640.104429728099,105.085213424333));
#106344=CARTESIAN_POINT('Ctrl Pts',(62.4242333587675,640.092040971772,105.136947576151));
#106345=CARTESIAN_POINT('Ctrl Pts',(62.4378789602574,640.075498690852,105.18805636452));
#106346=CARTESIAN_POINT('Ctrl Pts',(62.4416940728365,640.07087370865,105.202345641658));
#106347=CARTESIAN_POINT('Ctrl Pts',(62.445491289658,640.065923744451,105.216586000138));
#106348=CARTESIAN_POINT('Ctrl Pts',(62.4492710896279,640.060646673367,105.23077875602));
#106349=CARTESIAN_POINT('Ctrl Pts',(62.4510177399038,640.058208132244,105.237337246198));
#106350=CARTESIAN_POINT('Ctrl Pts',(62.4527577629492,640.055701852373,105.243874756236));
#106351=CARTESIAN_POINT('Ctrl Pts',(62.4544909291863,640.053127748537,105.250390301448));
#106352=CARTESIAN_POINT('Ctrl Pts',(62.4673673952944,640.034003581395,105.29879719705));
#106353=CARTESIAN_POINT('Ctrl Pts',(62.4797497248421,640.01130676641,105.34556227519));
#106354=CARTESIAN_POINT('Ctrl Pts',(62.4915614193837,639.985193361949,105.390339388072));
#106355=CARTESIAN_POINT('Ctrl Pts',(62.5040208719223,639.957647888065,105.437572095522));
#106356=CARTESIAN_POINT('Ctrl Pts',(62.5158455201389,639.926301077701,105.482593345719));
#106357=CARTESIAN_POINT('Ctrl Pts',(62.5269553724346,639.891300137618,105.525040935468));
#106358=CARTESIAN_POINT('Ctrl Pts',(62.5297962366821,639.882350160907,105.535895070779));
#106359=CARTESIAN_POINT('Ctrl Pts',(62.5325904047578,639.873161069724,105.546581114723));
#106360=CARTESIAN_POINT('Ctrl Pts',(62.5353366172931,639.86373494426,105.557093372208));
#106361=CARTESIAN_POINT('Ctrl Pts',(62.5373929563694,639.856676746876,105.564964855412));
#106362=CARTESIAN_POINT('Ctrl Pts',(62.5394178668836,639.849501838843,105.572721309952));
#106363=CARTESIAN_POINT('Ctrl Pts',(62.5414113367392,639.842208965498,105.580362184908));
#106364=CARTESIAN_POINT('Ctrl Pts',(62.5519664842342,639.803594208621,105.620819562242));
#106365=CARTESIAN_POINT('Ctrl Pts',(62.5616203796391,639.761734147913,105.657967154616));
#106366=CARTESIAN_POINT('Ctrl Pts',(62.5703675509501,639.716543554195,105.69171884283));
#106367=CARTESIAN_POINT('Ctrl Pts',(62.5768079397057,639.683270512969,105.716569618644));
#106368=CARTESIAN_POINT('Ctrl Pts',(62.5827180384413,639.648288685124,105.739430714702));
#106369=CARTESIAN_POINT('Ctrl Pts',(62.588026029441,639.612078409095,105.759999089233));
#106370=CARTESIAN_POINT('Ctrl Pts',(62.5915058843782,639.588339388471,105.773483467722));
#106371=CARTESIAN_POINT('Ctrl Pts',(62.594727133404,639.564071594478,105.785983177564));
#106372=CARTESIAN_POINT('Ctrl Pts',(62.5976715037949,639.539401572236,105.797420942698));
#106373=CARTESIAN_POINT('Ctrl Pts',(62.5985472943592,639.532063578086,105.800823057735));
#106374=CARTESIAN_POINT('Ctrl Pts',(62.599400657216,639.524669210063,105.804139230719));
#106375=CARTESIAN_POINT('Ctrl Pts',(62.6002310786813,639.51722471474,105.807367331575));
#106376=CARTESIAN_POINT('Ctrl Pts',(62.6046806418219,639.477335630251,105.824664137095));
#106377=CARTESIAN_POINT('Ctrl Pts',(62.6084902505575,639.435875719075,105.839488697653));
#106378=CARTESIAN_POINT('Ctrl Pts',(62.6115724087117,639.393699090601,105.851487144451));
#106379=CARTESIAN_POINT('Ctrl Pts',(62.6129049855962,639.375463945823,105.856674695529));
#106380=CARTESIAN_POINT('Ctrl Pts',(62.6141015955733,639.357094120464,105.861334040209));
#106381=CARTESIAN_POINT('Ctrl Pts',(62.615155193039,639.338655734907,105.865436756047));
#106382=CARTESIAN_POINT('Ctrl Pts',(62.6183698289984,639.282398293922,105.877954570768));
#106383=CARTESIAN_POINT('Ctrl Pts',(62.6203108230594,639.225398602282,105.885513606456));
#106384=CARTESIAN_POINT('Ctrl Pts',(62.6209461358816,639.167554174569,105.887987792193));
#106385=CARTESIAN_POINT('Ctrl Pts',(62.6211000095532,639.153544171681,105.888587043507));
#106386=CARTESIAN_POINT('Ctrl Pts',(62.6211772316339,639.139484557814,105.888887786568));
#106387=CARTESIAN_POINT('Ctrl Pts',(62.6211772316339,639.125373764374,105.888887786568));
#106388=CARTESIAN_POINT('Origin',(70.,639.125373764374,90.6087118617898));
#106389=CARTESIAN_POINT('Origin',(70.,639.125373764374,0.));
#106390=CARTESIAN_POINT('Origin',(70.,602.225373764374,64.2994740882088));
#106391=CARTESIAN_POINT('Origin',(70.,602.225373764374,90.6087118617898));
#106392=CARTESIAN_POINT('Origin',(52.8776183915471,602.225373764374,90.6087118617898));
#106393=CARTESIAN_POINT('Ctrl Pts',(62.6211772316338,602.225373764374,105.888887786568));
#106394=CARTESIAN_POINT('Ctrl Pts',(62.6211772316338,602.089770025929,105.888887786568));
#106395=CARTESIAN_POINT('Ctrl Pts',(62.6140693717759,601.957352722376,105.861084706529));
#106396=CARTESIAN_POINT('Ctrl Pts',(62.5864687826938,601.710190425818,105.753868890961));
#106397=CARTESIAN_POINT('Ctrl Pts',(62.5663210244106,601.599765986676,105.675841090715));
#106398=CARTESIAN_POINT('Ctrl Pts',(62.5166193069308,601.417736746075,105.485314668297));
#106399=CARTESIAN_POINT('Ctrl Pts',(62.4870014923168,601.346042473617,105.372610356784));
#106400=CARTESIAN_POINT('Ctrl Pts',(62.4224093356835,601.249834603749,105.129772481131));
#106401=CARTESIAN_POINT('Ctrl Pts',(62.3879065652659,601.225373764374,105.001402189963));
#106402=CARTESIAN_POINT('Ctrl Pts',(62.3523505660608,601.225373764374,104.870738441723));
#106403=CARTESIAN_POINT('Ctrl Pts',(43.9028862170334,601.725373764374,104.870738441723));
#106404=CARTESIAN_POINT('Ctrl Pts',(43.9028862170334,601.225373764374,104.870738441723));
#106405=CARTESIAN_POINT('Ctrl Pts',(43.4028862170334,601.225373764374,104.870738441723));
#106406=CARTESIAN_POINT('Ctrl Pts',(43.9028862170334,601.72537378749,104.943235299706));
#106407=CARTESIAN_POINT('Ctrl Pts',(43.9028862170334,601.190801415598,104.997787302213));
#106408=CARTESIAN_POINT('Ctrl Pts',(43.3694713913988,601.225373764374,104.993533654581));
#106409=CARTESIAN_POINT('Ctrl Pts',(43.9028862170334,601.73596803839,105.013844943794));
#106410=CARTESIAN_POINT('Ctrl Pts',(43.9028862170334,601.173966762123,105.128551144522));
#106411=CARTESIAN_POINT('Ctrl Pts',(43.3372020726836,601.246562349658,105.113484360187));
#106412=CARTESIAN_POINT('Ctrl Pts',(43.9028862170334,601.779310621476,105.150967761993));
#106413=CARTESIAN_POINT('Ctrl Pts',(43.9028862170334,601.181604534533,105.413925765979));
#106414=CARTESIAN_POINT('Ctrl Pts',(43.2750077312619,601.333247441326,105.347016531996));
#106415=CARTESIAN_POINT('Ctrl Pts',(43.9028862170334,601.811992484093,105.215987727826));
#106416=CARTESIAN_POINT('Ctrl Pts',(43.9028862170332,601.21008627854,105.567638910342));
#106417=CARTESIAN_POINT('Ctrl Pts',(43.2457683931895,601.398611244944,105.45806492406));
#106418=CARTESIAN_POINT('Ctrl Pts',(43.9028862170334,601.898891258024,105.32976697493));
#106419=CARTESIAN_POINT('Ctrl Pts',(43.9028862170337,601.340706749462,105.880668070497));
#106420=CARTESIAN_POINT('Ctrl Pts',(43.194904253426,601.572408710543,105.652759440274));
#106421=CARTESIAN_POINT('Ctrl Pts',(43.9028862170334,601.953782539583,105.379045943916));
#106422=CARTESIAN_POINT('Ctrl Pts',(43.9028862170334,601.450221684901,106.040501254842));
#106423=CARTESIAN_POINT('Ctrl Pts',(43.1730456780328,601.68219134858,105.737292607677));
#106424=CARTESIAN_POINT('Ctrl Pts',(43.9028862170334,602.081503421665,105.448305316015));
#106425=CARTESIAN_POINT('Ctrl Pts',(43.9028862170334,601.779838730324,106.297756031046));
#106426=CARTESIAN_POINT('Ctrl Pts',(43.1424140517172,601.937633045168,105.856208205485));
#106427=CARTESIAN_POINT('Ctrl Pts',(43.9028862170334,602.151908862397,105.467304770256));
#106428=CARTESIAN_POINT('Ctrl Pts',(43.9028862170334,601.99123573158,106.379137803783));
#106429=CARTESIAN_POINT('Ctrl Pts',(43.1340595427293,602.078443985827,105.888887781));
#106430=CARTESIAN_POINT('Ctrl Pts',(43.9028862170334,602.225373764374,105.467304788954));
#106431=CARTESIAN_POINT('Ctrl Pts',(43.9028862170334,602.225373764374,106.379137891718));
#106432=CARTESIAN_POINT('Ctrl Pts',(43.1340595514603,602.225373764374,105.888887786568));
#106433=CARTESIAN_POINT('Origin',(43.4028862170334,602.225373764374,105.467304788954));
#106434=CARTESIAN_POINT('Origin',(43.4028862170334,601.725373764374,104.870738441723));
#106435=CARTESIAN_POINT('Origin',(43.4028862170334,601.725373764374,0.));
#106436=CARTESIAN_POINT('Origin',(43.4028862170334,601.725373764374,99.080638124754));
#106437=CARTESIAN_POINT('Origin',(43.4028862170334,601.225373764374,105.467304788954));
#106438=CARTESIAN_POINT('Origin',(43.4028862170334,639.125373764374,105.467304788954));
#106439=CARTESIAN_POINT('Origin',(43.4028862170334,601.725373764374,99.080638124754));
#106440=CARTESIAN_POINT('Origin',(43.4028862170334,601.725373764374,99.080638124754));
#106441=CARTESIAN_POINT('Ctrl Pts',(43.9028849796099,639.036778038132,105.45715096646));
#106442=CARTESIAN_POINT('Ctrl Pts',(43.9048962221699,638.846637779719,106.341172765461));
#106443=CARTESIAN_POINT('Ctrl Pts',(43.1380480521351,638.94771437284,105.873295625316));
#106444=CARTESIAN_POINT('Ctrl Pts',(43.9028849698754,639.104429949246,105.470819015702));
#106445=CARTESIAN_POINT('Ctrl Pts',(43.9049389572813,639.057960777493,106.401099978679));
#106446=CARTESIAN_POINT('Ctrl Pts',(43.1320188140359,639.083373273735,105.896877360038));
#106447=CARTESIAN_POINT('Ctrl Pts',(43.9028849713453,639.169333962302,105.468738411503));
#106448=CARTESIAN_POINT('Ctrl Pts',(43.9049320498006,639.266412765078,106.390924409249));
#106449=CARTESIAN_POINT('Ctrl Pts',(43.1329294306683,639.213530456068,105.893276648178));
#106450=CARTESIAN_POINT('Ctrl Pts',(43.9028849892889,639.266404183712,105.443607670973));
#106451=CARTESIAN_POINT('Ctrl Pts',(43.9048555577325,639.560609042325,106.285968855676));
#106452=CARTESIAN_POINT('Ctrl Pts',(43.1440423040929,639.40816781027,105.84996254853));
#106453=CARTESIAN_POINT('Ctrl Pts',(43.902884998944,639.300380640497,105.430093200578));
#106454=CARTESIAN_POINT('Ctrl Pts',(43.9048160471508,639.656569714094,106.231993523399));
#106455=CARTESIAN_POINT('Ctrl Pts',(43.1500216005741,639.476286250348,105.826675971902));
#106456=CARTESIAN_POINT('Ctrl Pts',(43.9028850232857,639.363350391771,105.396101801474));
#106457=CARTESIAN_POINT('Ctrl Pts',(43.904722123573,639.819653222097,106.105164437961));
#106458=CARTESIAN_POINT('Ctrl Pts',(43.1650945293205,639.602513033697,105.768158764631));
#106459=CARTESIAN_POINT('Ctrl Pts',(43.9028850382186,639.393109422988,105.375281527712));
#106460=CARTESIAN_POINT('Ctrl Pts',(43.9046677648458,639.888724247457,106.032369901576));
#106461=CARTESIAN_POINT('Ctrl Pts',(43.1743404473524,639.662155988573,105.732338549014));
#106462=CARTESIAN_POINT('Ctrl Pts',(43.9028850722291,639.447392783658,105.328007499781));
#106463=CARTESIAN_POINT('Ctrl Pts',(43.9045527207096,640.00043915945,105.879788807098));
#106464=CARTESIAN_POINT('Ctrl Pts',(43.1953957620866,639.770930402132,105.651098312915));
#106465=CARTESIAN_POINT('Ctrl Pts',(43.9028850911418,639.471794258301,105.301782188552));
#106466=CARTESIAN_POINT('Ctrl Pts',(43.9044931551193,640.043577922308,105.801414716341));
#106467=CARTESIAN_POINT('Ctrl Pts',(43.2071028495104,639.819816105116,105.606071364224));
#106468=CARTESIAN_POINT('Ctrl Pts',(43.9028851531601,639.537574714346,105.216089189308));
#106469=CARTESIAN_POINT('Ctrl Pts',(43.9043159644082,640.14086522548,105.569416826768));
#106470=CARTESIAN_POINT('Ctrl Pts',(43.2454862343439,639.951569950465,105.459135338167));
#106471=CARTESIAN_POINT('Ctrl Pts',(43.9028852004078,639.570271688884,105.151191462665));
#106472=CARTESIAN_POINT('Ctrl Pts',(43.9041973830617,640.169349769983,105.41549399436));
#106473=CARTESIAN_POINT('Ctrl Pts',(43.2747212509798,640.01702622273,105.348095923453));
#106474=CARTESIAN_POINT('Ctrl Pts',(43.9028853216263,639.622599458369,104.986125028804));
#106475=CARTESIAN_POINT('Ctrl Pts',(43.9039388064658,640.178380909355,105.076238171418));
#106476=CARTESIAN_POINT('Ctrl Pts',(43.3497043955024,640.121714641666,105.066534511823));
#106477=CARTESIAN_POINT('Ctrl Pts',(43.9028853957751,639.631100186342,104.886222171346));
#106478=CARTESIAN_POINT('Ctrl Pts',(43.9038057069545,640.143976851776,104.898778370354));
#106479=CARTESIAN_POINT('Ctrl Pts',(43.3955564977506,640.138657441274,104.896768194163));
#106480=CARTESIAN_POINT('Ctrl Pts',(43.9028854731814,639.619496306592,104.783210498779));
#106481=CARTESIAN_POINT('Ctrl Pts',(43.9036820200741,640.078232214502,104.726934492466));
#106482=CARTESIAN_POINT('Ctrl Pts',(43.4434121618144,640.115332282487,104.722478050627));
#106483=CARTESIAN_POINT('Origin',(43.4028862170334,639.625373764374,104.870738441723));
#106484=CARTESIAN_POINT('Origin',(43.4028862170334,601.125373764374,99.080638124754));
#106485=CARTESIAN_POINT('Origin',(43.4028862170334,639.625373764374,99.080638124754));
#106486=CARTESIAN_POINT('Origin',(43.4028862170334,639.625373764374,0.));
#106487=CARTESIAN_POINT('Origin',(43.4028862170334,639.625373764374,99.080638124754));
#106488=CARTESIAN_POINT('Origin',(62.3523505660608,601.725373764374,0.));
#106489=CARTESIAN_POINT('Origin',(62.3523505660608,601.725373764374,99.080638124754));
#106490=CARTESIAN_POINT('Origin',(62.3523505660608,601.725373764374,104.870738441723));
#106491=CARTESIAN_POINT('Origin',(62.3523505660608,601.725373764374,99.080638124754));
#106492=CARTESIAN_POINT('Origin',(62.3523505660608,601.725373764374,99.080638124754));
#106493=CARTESIAN_POINT('Origin',(43.4028862170334,639.625373764374,99.080638124754));
#106494=CARTESIAN_POINT('Ctrl Pts',(62.3523505660608,601.225373764374,104.870738441723));
#106495=CARTESIAN_POINT('Ctrl Pts',(61.8523505660607,601.225373764374,104.870738441723));
#106496=CARTESIAN_POINT('Ctrl Pts',(61.8523505660607,601.725373764374,104.870738441723));
#106497=CARTESIAN_POINT('Ctrl Pts',(62.3857653916954,601.225373764374,104.993533654581));
#106498=CARTESIAN_POINT('Ctrl Pts',(61.8523505660607,601.190801415598,104.997787302213));
#106499=CARTESIAN_POINT('Ctrl Pts',(61.8523505660607,601.72537378749,104.943235299706));
#106500=CARTESIAN_POINT('Ctrl Pts',(62.4180347104105,601.246562349658,105.113484360187));
#106501=CARTESIAN_POINT('Ctrl Pts',(61.8523505660608,601.173966762123,105.128551144522));
#106502=CARTESIAN_POINT('Ctrl Pts',(61.8523505660607,601.73596803839,105.013844943794));
#106503=CARTESIAN_POINT('Ctrl Pts',(62.4802290518323,601.333247441326,105.347016531996));
#106504=CARTESIAN_POINT('Ctrl Pts',(61.8523505660608,601.181604534533,105.413925765979));
#106505=CARTESIAN_POINT('Ctrl Pts',(61.8523505660607,601.779310621476,105.150967761993));
#106506=CARTESIAN_POINT('Ctrl Pts',(62.5094683899049,601.398611244944,105.45806492406));
#106507=CARTESIAN_POINT('Ctrl Pts',(61.8523505660608,601.21008627854,105.567638910342));
#106508=CARTESIAN_POINT('Ctrl Pts',(61.8523505660607,601.811992484093,105.215987727826));
#106509=CARTESIAN_POINT('Ctrl Pts',(62.560332529668,601.572408710543,105.652759440274));
#106510=CARTESIAN_POINT('Ctrl Pts',(61.8523505660607,601.340706749462,105.880668070497));
#106511=CARTESIAN_POINT('Ctrl Pts',(61.8523505660607,601.898891258024,105.32976697493));
#106512=CARTESIAN_POINT('Ctrl Pts',(62.582191105061,601.68219134858,105.737292607677));
#106513=CARTESIAN_POINT('Ctrl Pts',(61.8523505660607,601.450221684905,106.040501254842));
#106514=CARTESIAN_POINT('Ctrl Pts',(61.8523505660607,601.953782539583,105.379045943916));
#106515=CARTESIAN_POINT('Ctrl Pts',(62.6128227313773,601.937633045168,105.856208205485));
#106516=CARTESIAN_POINT('Ctrl Pts',(61.8523505660607,601.779838730321,106.297756031047));
#106517=CARTESIAN_POINT('Ctrl Pts',(61.8523505660607,602.081503421665,105.448305316015));
#106518=CARTESIAN_POINT('Ctrl Pts',(62.6211772403636,602.078443985827,105.888887781001));
#106519=CARTESIAN_POINT('Ctrl Pts',(61.8523505660605,601.991235731583,106.37913780378));
#106520=CARTESIAN_POINT('Ctrl Pts',(61.8523505660607,602.151908862397,105.467304770256));
#106521=CARTESIAN_POINT('Ctrl Pts',(62.6211772316338,602.225373764374,105.888887786568));
#106522=CARTESIAN_POINT('Ctrl Pts',(61.8523505660608,602.225373764374,106.379137891718));
#106523=CARTESIAN_POINT('Ctrl Pts',(61.8523505660607,602.225373764374,105.467304788954));
#106524=CARTESIAN_POINT('Origin',(62.3523505660608,602.225373764374,105.467304788954));
#106525=CARTESIAN_POINT('Origin',(62.3523505660608,601.125373764374,99.080638124754));
#106526=CARTESIAN_POINT('Origin',(62.3523505660608,639.625373764374,99.080638124754));
#106527=CARTESIAN_POINT('Origin',(62.3523505660608,601.225373764374,105.467304788954));
#106528=CARTESIAN_POINT('Origin',(62.3523505660608,639.125373764374,105.467304788954));
#106529=CARTESIAN_POINT('Origin',(62.3523505660608,639.625373764374,99.080638124754));
#106530=CARTESIAN_POINT('Origin',(62.3523505660608,639.625373764374,99.080638124754));
#106531=CARTESIAN_POINT('Ctrl Pts',(62.6171887309608,638.947714372838,105.873295625315));
#106532=CARTESIAN_POINT('Ctrl Pts',(61.8503235888569,638.846635542666,106.34118312063));
#106533=CARTESIAN_POINT('Ctrl Pts',(61.8523518244269,639.036780009716,105.457141799944));
#106534=CARTESIAN_POINT('Ctrl Pts',(62.6232179690577,639.083373273735,105.896877360039));
#106535=CARTESIAN_POINT('Ctrl Pts',(61.8502804923024,639.057960207594,106.401111286378));
#106536=CARTESIAN_POINT('Ctrl Pts',(61.852351834326,639.10443042477,105.470809496035));
#106537=CARTESIAN_POINT('Ctrl Pts',(62.6223073524257,639.213530456068,105.893276648178));
#106538=CARTESIAN_POINT('Ctrl Pts',(61.8502874582075,639.266413948424,106.390935545101));
#106539=CARTESIAN_POINT('Ctrl Pts',(61.8523518328312,639.169332966705,105.46872895397));
#106540=CARTESIAN_POINT('Ctrl Pts',(62.6111944790013,639.40816781027,105.84996254853));
#106541=CARTESIAN_POINT('Ctrl Pts',(61.8503645972132,639.560612374044,106.285978384924));
#106542=CARTESIAN_POINT('Ctrl Pts',(61.8523518145843,639.266401094432,105.443598825812));
#106543=CARTESIAN_POINT('Ctrl Pts',(62.6052151825202,639.476286250348,105.826675971902));
#106544=CARTESIAN_POINT('Ctrl Pts',(61.8504044419249,639.656573605937,106.232002273134));
#106545=CARTESIAN_POINT('Ctrl Pts',(61.852351804766,639.300376853797,105.430084675454));
#106546=CARTESIAN_POINT('Ctrl Pts',(62.5901422537736,639.602513033697,105.768158764631));
#106547=CARTESIAN_POINT('Ctrl Pts',(61.8504991596906,639.819657772544,106.10517150034));
#106548=CARTESIAN_POINT('Ctrl Pts',(61.8523517800127,639.36334539447,105.396094036019));
#106549=CARTESIAN_POINT('Ctrl Pts',(62.5808963357417,639.662155988573,105.732338549014));
#106550=CARTESIAN_POINT('Ctrl Pts',(61.850553977998,639.88872891337,106.032376080376));
#106551=CARTESIAN_POINT('Ctrl Pts',(61.8523517648272,639.393103899509,105.375274204658));
#106552=CARTESIAN_POINT('Ctrl Pts',(62.5598410210075,639.770930402132,105.651098312915));
#106553=CARTESIAN_POINT('Ctrl Pts',(61.8506699946354,640.00044371228,105.879793343696));
#106554=CARTESIAN_POINT('Ctrl Pts',(61.8523517302416,639.447386384734,105.328001115495));
#106555=CARTESIAN_POINT('Ctrl Pts',(62.5481339335838,639.819816105116,105.606071364224));
#106556=CARTESIAN_POINT('Ctrl Pts',(61.8507300636749,640.043582274495,105.801418515785));
#106557=CARTESIAN_POINT('Ctrl Pts',(61.8523517110091,639.471787510695,105.301776292401));
#106558=CARTESIAN_POINT('Ctrl Pts',(62.5097505487502,639.951569950465,105.459135338167));
#106559=CARTESIAN_POINT('Ctrl Pts',(61.8509087517028,640.140868692571,105.56941884666));
#106560=CARTESIAN_POINT('Ctrl Pts',(61.8523516479419,639.537567153372,105.216084761092));
#106561=CARTESIAN_POINT('Ctrl Pts',(62.4805155321142,640.01702622273,105.348095923452));
#106562=CARTESIAN_POINT('Ctrl Pts',(61.8510283348443,640.169352447589,105.41549517911));
#106563=CARTESIAN_POINT('Ctrl Pts',(61.852351599895,639.570263865268,105.151188011025));
#106564=CARTESIAN_POINT('Ctrl Pts',(62.4055323875921,640.121714641665,105.066534511825));
#106565=CARTESIAN_POINT('Ctrl Pts',(61.8512890952677,640.178381817406,105.076238326916));
#106566=CARTESIAN_POINT('Ctrl Pts',(61.8523514766257,639.622591495187,104.986123737673));
#106567=CARTESIAN_POINT('Ctrl Pts',(62.3596802853423,640.138657441275,104.896768194161));
#106568=CARTESIAN_POINT('Ctrl Pts',(61.8514233185298,640.143976932967,104.898778401034));
#106569=CARTESIAN_POINT('Ctrl Pts',(61.8523514012223,639.631092470791,104.886221982453));
#106570=CARTESIAN_POINT('Ctrl Pts',(62.311824621281,640.115332282486,104.722478050629));
#106571=CARTESIAN_POINT('Ctrl Pts',(61.8515480494827,640.078231673359,104.72693455747));
#106572=CARTESIAN_POINT('Ctrl Pts',(61.852351322506,639.619489084467,104.783211384763));
#106573=CARTESIAN_POINT('Origin',(62.3523505660608,639.625373764374,104.870738441723));
#106574=CARTESIAN_POINT('Origin',(62.3523505660608,639.625373764374,0.));
#106575=CARTESIAN_POINT('',(0.,0.,0.));
#106576=CARTESIAN_POINT('Origin',(0.,59.,64.2994740882088));
#106577=CARTESIAN_POINT('',(-1.40834381901946E-15,60.,52.7994740882088));
#106578=CARTESIAN_POINT('Origin',(0.,60.,64.2994740882088));
#106579=CARTESIAN_POINT('',(-1.40834381901946E-15,829.165008980169,52.7994740882088));
#106580=CARTESIAN_POINT('',(-1.40834381901946E-15,59.,52.7994740882088));
#106581=CARTESIAN_POINT('Origin',(0.,829.165008980169,64.2994740882095));
#106582=CARTESIAN_POINT('Origin',(0.,59.,64.2994740882088));
#106583=CARTESIAN_POINT('',(-1.53080849893419E-15,829.165008980169,51.7994740882088));
#106584=CARTESIAN_POINT('Origin',(0.,829.165008980169,64.2994740882088));
#106585=CARTESIAN_POINT('',(-1.53080849893419E-15,49.,51.7994740882088));
#106586=CARTESIAN_POINT('',(-1.53080849893419E-15,59.,51.7994740882088));
#106587=CARTESIAN_POINT('Origin',(0.,49.,64.2994740882088));
#106588=CARTESIAN_POINT('Origin',(0.,49.,64.2994740882088));
#106589=CARTESIAN_POINT('Origin',(0.,829.165008980169,76.7994740882088));
#106590=CARTESIAN_POINT('Origin',(0.,60.,64.2994740882088));
#106591=CARTESIAN_POINT('',(0.,0.,0.));
#106592=CARTESIAN_POINT('Ctrl Pts',(0.,1078.73142393294,339.50750164799));
#106593=CARTESIAN_POINT('Ctrl Pts',(-170.225481863728,1078.73142393294,
339.50750164799));
#106594=CARTESIAN_POINT('Ctrl Pts',(-170.225481863728,1078.73142393294,
509.732983511718));
#106595=CARTESIAN_POINT('Ctrl Pts',(-1.04233045748865E-14,1078.73142393294,
509.732983511718));
#106596=CARTESIAN_POINT('Ctrl Pts',(0.,1078.73142393294,320.460533783102));
#106597=CARTESIAN_POINT('Ctrl Pts',(-208.319417593505,1078.73142393294,
320.460533783101));
#106598=CARTESIAN_POINT('Ctrl Pts',(-208.319417593505,1078.73142393294,
528.779951376607));
#106599=CARTESIAN_POINT('Ctrl Pts',(-1.27558853978063E-14,1078.73142393294,
528.779951376607));
#106600=CARTESIAN_POINT('Ctrl Pts',(0.,1074.39201604106,297.79821279751));
#106601=CARTESIAN_POINT('Ctrl Pts',(-253.644059564688,1074.39201604106,
297.79821279751));
#106602=CARTESIAN_POINT('Ctrl Pts',(-253.644059564688,1074.39201604106,
551.442272362198));
#106603=CARTESIAN_POINT('Ctrl Pts',(-1.55312192834318E-14,1074.39201604106,
551.442272362198));
#106604=CARTESIAN_POINT('',(0.,1078.73142393294,339.50750164799));
#106605=CARTESIAN_POINT('',(-1.29772619291592E-14,1078.73142393294,509.732983511718));
#106606=CARTESIAN_POINT('Origin',(0.,1078.73142393294,424.620242579854));
#106607=CARTESIAN_POINT('',(1.55675932686082E-14,1074.39201604106,551.442272362198));
#106608=CARTESIAN_POINT('Ctrl Pts',(-1.29772619291592E-14,1078.73142393294,
509.732983511718));
#106609=CARTESIAN_POINT('Ctrl Pts',(-1.27558853978063E-14,1078.73142393294,
528.779951376607));
#106610=CARTESIAN_POINT('Ctrl Pts',(1.55675932686082E-14,1074.39201604106,
551.442272362198));
#106611=CARTESIAN_POINT('',(0.,1074.39201604106,297.79821279751));
#106612=CARTESIAN_POINT('Origin',(0.,1074.39201604106,424.620242579854));
#106613=CARTESIAN_POINT('Ctrl Pts',(0.,1078.73142393294,339.50750164799));
#106614=CARTESIAN_POINT('Ctrl Pts',(0.,1078.73142393294,320.460533783102));
#106615=CARTESIAN_POINT('Ctrl Pts',(0.,1074.39201604106,297.79821279751));
#106616=CARTESIAN_POINT('',(-80.0774492048026,1076.71653899679,503.992543977749));
#106617=CARTESIAN_POINT('',(-80.0774492048019,1076.92126679813,501.811462480293));
#106618=CARTESIAN_POINT('Ctrl Pts',(-80.0774492048026,1076.71653899679,
503.99254397775));
#106619=CARTESIAN_POINT('Ctrl Pts',(-80.0744534615737,1076.71683147352,
503.99254397775));
#106620=CARTESIAN_POINT('Ctrl Pts',(-80.0714573718756,1076.71712514229,
503.992531633677));
#106621=CARTESIAN_POINT('Ctrl Pts',(-79.943955331041,1076.72967184833,503.991480731246));
#106622=CARTESIAN_POINT('Ctrl Pts',(-79.8207166503327,1076.74379814044,
503.969143227292));
#106623=CARTESIAN_POINT('Ctrl Pts',(-79.577533957504,1076.77578352609,503.88051966644));
#106624=CARTESIAN_POINT('Ctrl Pts',(-79.4607372426172,1076.79359323853,
503.81141461075));
#106625=CARTESIAN_POINT('Ctrl Pts',(-79.2503459058597,1076.83112034606,
503.627408466814));
#106626=CARTESIAN_POINT('Ctrl Pts',(-79.1612532432344,1076.85052705261,
503.511054337047));
#106627=CARTESIAN_POINT('Ctrl Pts',(-79.034986449722,1076.88662226974,503.252524728555));
#106628=CARTESIAN_POINT('Ctrl Pts',(-78.9980549007521,1076.90302340953,
503.113237675));
#106629=CARTESIAN_POINT('Ctrl Pts',(-78.981158028069,1076.92937865835,502.845054518431));
#106630=CARTESIAN_POINT('Ctrl Pts',(-78.9950123084823,1076.9396744246,502.718929500932));
#106631=CARTESIAN_POINT('Ctrl Pts',(-79.0631424379183,1076.95481257403,
502.48437207685));
#106632=CARTESIAN_POINT('Ctrl Pts',(-79.114335267768,1076.95985546338,502.376940166403));
#106633=CARTESIAN_POINT('Ctrl Pts',(-79.2009077894259,1076.96315646626,
502.252333982574));
#106634=CARTESIAN_POINT('Ctrl Pts',(-79.2212198095973,1076.96368450051,
502.225788297461));
#106635=CARTESIAN_POINT('Ctrl Pts',(-79.2551483758368,1076.96420163092,
502.18543262218));
#106636=CARTESIAN_POINT('Ctrl Pts',(-79.2679670347454,1076.96432402283,
502.17098288737));
#106637=CARTESIAN_POINT('Ctrl Pts',(-79.2912378146408,1076.96442142972,
502.146114217026));
#106638=CARTESIAN_POINT('Ctrl Pts',(-79.3015300358806,1076.96442444417,
502.135552973688));
#106639=CARTESIAN_POINT('Ctrl Pts',(-79.325475365329,1076.96434204115,502.11195855146));
#106640=CARTESIAN_POINT('Ctrl Pts',(-79.3392587639923,1076.9642316591,502.099064815849));
#106641=CARTESIAN_POINT('Ctrl Pts',(-79.3775703970506,1076.9637581534,502.0650467013));
#106642=CARTESIAN_POINT('Ctrl Pts',(-79.4027138542756,1076.96327099962,
502.044647745071));
#106643=CARTESIAN_POINT('Ctrl Pts',(-79.5260338693428,1076.96007640994,
501.953385719726));
#106644=CARTESIAN_POINT('Ctrl Pts',(-79.6345730508686,1076.95496834037,
501.898137388195));
#106645=CARTESIAN_POINT('Ctrl Pts',(-79.8559752282958,1076.9405751612,501.82840729055));
#106646=CARTESIAN_POINT('Ctrl Pts',(-79.966456771482,1076.93174117589,501.811462480293));
#106647=CARTESIAN_POINT('Ctrl Pts',(-80.0774492048019,1076.92126679813,
501.811462480293));
#106648=CARTESIAN_POINT('Ctrl Pts',(-80.0774492048018,1076.92126679813,
501.811462480293));
#106649=CARTESIAN_POINT('Ctrl Pts',(-80.0774629292238,1076.92126550295,
501.811462480293));
#106650=CARTESIAN_POINT('Ctrl Pts',(-80.0774766536537,1076.92126420775,
501.811462480552));
#106651=CARTESIAN_POINT('Ctrl Pts',(-80.0774903780913,1076.92126291252,
501.81146248107));
#106652=CARTESIAN_POINT('Ctrl Pts',(-80.2021265314636,1076.90950053199,
501.811467186699));
#106653=CARTESIAN_POINT('Ctrl Pts',(-80.3256648570161,1076.89583323305,
501.83283599449));
#106654=CARTESIAN_POINT('Ctrl Pts',(-80.5700028028231,1076.86453989815,
501.919709426156));
#106655=CARTESIAN_POINT('Ctrl Pts',(-80.6876152646318,1076.84693308657,
501.988137880998));
#106656=CARTESIAN_POINT('Ctrl Pts',(-80.9000017320625,1076.80939942596,
502.1713164524));
#106657=CARTESIAN_POINT('Ctrl Pts',(-80.9901753298772,1076.78975278149,
502.28762664943));
#106658=CARTESIAN_POINT('Ctrl Pts',(-81.1180209332028,1076.75293615633,
502.545939183293));
#106659=CARTESIAN_POINT('Ctrl Pts',(-81.1556746375667,1076.73605729288,
502.684941916594));
#106660=CARTESIAN_POINT('Ctrl Pts',(-81.1740308668573,1076.70871614022,
502.952856609623));
#106661=CARTESIAN_POINT('Ctrl Pts',(-81.1608916991995,1076.69793149323,
503.078985121758));
#106662=CARTESIAN_POINT('Ctrl Pts',(-81.0937095185396,1076.68187189764,
503.315280887528));
#106663=CARTESIAN_POINT('Ctrl Pts',(-81.0422687355384,1076.67645734701,
503.424266348347));
#106664=CARTESIAN_POINT('Ctrl Pts',(-80.9548714480136,1076.67291908737,
503.550498510701));
#106665=CARTESIAN_POINT('Ctrl Pts',(-80.9344015515705,1076.67235413421,
503.577317294338));
#106666=CARTESIAN_POINT('Ctrl Pts',(-80.9001937579785,1076.67180071199,
503.618068925671));
#106667=CARTESIAN_POINT('Ctrl Pts',(-80.8872700626789,1076.67166965064,
503.632652871637));
#106668=CARTESIAN_POINT('Ctrl Pts',(-80.8638039277403,1076.67156506224,
503.657745619015));
#106669=CARTESIAN_POINT('Ctrl Pts',(-80.8534244163316,1076.6715616049,503.668399199569));
#106670=CARTESIAN_POINT('Ctrl Pts',(-80.8292723903451,1076.67164906506,
503.692195150688));
#106671=CARTESIAN_POINT('Ctrl Pts',(-80.8153674388274,1076.67176663838,
503.705195625592));
#106672=CARTESIAN_POINT('Ctrl Pts',(-80.7767073202748,1076.6722714466,503.739489346514));
#106673=CARTESIAN_POINT('Ctrl Pts',(-80.7513267907336,1076.672791148,503.760043730673));
#106674=CARTESIAN_POINT('Ctrl Pts',(-80.6266644716121,1076.67620269702,
503.852055507836));
#106675=CARTESIAN_POINT('Ctrl Pts',(-80.5168403634148,1076.68166443625,
503.907546730497));
#106676=CARTESIAN_POINT('Ctrl Pts',(-80.2955490543128,1076.69678724743,
503.976117862873));
#106677=CARTESIAN_POINT('Ctrl Pts',(-80.1867296369359,1076.70586986388,
503.99254397775));
#106678=CARTESIAN_POINT('Ctrl Pts',(-80.0774492048026,1076.71653899679,
503.99254397775));
#106679=CARTESIAN_POINT('',(-94.6032580293202,1076.74090351967,485.632861828239));
#106680=CARTESIAN_POINT('',(-94.6032580293197,1076.89762188922,483.451780330783));
#106681=CARTESIAN_POINT('Ctrl Pts',(-94.6032580293202,1076.74090351967,
485.63286182824));
#106682=CARTESIAN_POINT('Ctrl Pts',(-94.4934032622873,1076.75352605296,
485.63286182824));
#106683=CARTESIAN_POINT('Ctrl Pts',(-94.3841704543758,1076.76724681555,
485.616262376579));
#106684=CARTESIAN_POINT('Ctrl Pts',(-94.1464351966987,1076.79973481212,
485.542293254238));
#106685=CARTESIAN_POINT('Ctrl Pts',(-94.0227520764538,1076.81856962477,
485.475933789659));
#106686=CARTESIAN_POINT('Ctrl Pts',(-93.8025697775747,1076.8563159382,485.296740373648));
#106687=CARTESIAN_POINT('Ctrl Pts',(-93.7094593202231,1076.87484627511,
485.183773120545));
#106688=CARTESIAN_POINT('Ctrl Pts',(-93.5758671374664,1076.90758888432,
484.933433266239));
#106689=CARTESIAN_POINT('Ctrl Pts',(-93.534411712552,1076.92166811443,484.79959274449));
#106690=CARTESIAN_POINT('Ctrl Pts',(-93.5055131017688,1076.94342992723,
484.536401468821));
#106691=CARTESIAN_POINT('Ctrl Pts',(-93.5134824327387,1076.95143233486,
484.409867704565));
#106692=CARTESIAN_POINT('Ctrl Pts',(-93.5600329759078,1076.95985956288,
484.216275065995));
#106693=CARTESIAN_POINT('Ctrl Pts',(-93.5842379368745,1076.96203239778,
484.147060908851));
#106694=CARTESIAN_POINT('Ctrl Pts',(-93.6263115269911,1076.96368945428,
484.056992980237));
#106695=CARTESIAN_POINT('Ctrl Pts',(-93.6382737929135,1076.96400366827,
484.033623314572));
#106696=CARTESIAN_POINT('Ctrl Pts',(-93.6591896714621,1076.96431490958,
483.996160281757));
#106697=CARTESIAN_POINT('Ctrl Pts',(-93.6676434573539,1076.96438582567,
483.981801614756));
#106698=CARTESIAN_POINT('Ctrl Pts',(-93.6845453285145,1076.96442611176,
483.954542490863));
#106699=CARTESIAN_POINT('Ctrl Pts',(-93.6929444419125,1076.96440268101,
483.941616604474));
#106700=CARTESIAN_POINT('Ctrl Pts',(-93.7129292816478,1076.96425007526,
483.912242966635));
#106701=CARTESIAN_POINT('Ctrl Pts',(-93.724701520582,1076.96409086024,483.895929460495));
#106702=CARTESIAN_POINT('Ctrl Pts',(-93.7624748523549,1076.963373952,483.846524192872));
#106703=CARTESIAN_POINT('Ctrl Pts',(-93.7899415522706,1076.96257163799,
483.81460892862));
#106704=CARTESIAN_POINT('Ctrl Pts',(-93.9196445930091,1076.95762210125,
483.680435726889));
#106705=CARTESIAN_POINT('Ctrl Pts',(-94.0396516800389,1076.95014256301,
483.597637961895));
#106706=CARTESIAN_POINT('Ctrl Pts',(-94.246520508683,1076.93342095431,483.508600621991));
#106707=CARTESIAN_POINT('Ctrl Pts',(-94.3241836294889,1076.92644211135,
483.484997789265));
#106708=CARTESIAN_POINT('Ctrl Pts',(-94.4695396532436,1076.91214081338,
483.457937088357));
#106709=CARTESIAN_POINT('Ctrl Pts',(-94.5363541198077,1076.9051120287,483.451780330783));
#106710=CARTESIAN_POINT('Ctrl Pts',(-94.6032580293197,1076.89762188922,
483.451780330783));
#106711=CARTESIAN_POINT('Ctrl Pts',(-94.6032580293197,1076.89762188922,
483.451780330783));
#106712=CARTESIAN_POINT('Ctrl Pts',(-94.6033088295668,1076.89761620195,
483.451780330783));
#106713=CARTESIAN_POINT('Ctrl Pts',(-94.6033596298654,1076.8976105144,483.451780334333));
#106714=CARTESIAN_POINT('Ctrl Pts',(-94.6034104302152,1076.8976048266,483.451780341432));
#106715=CARTESIAN_POINT('Ctrl Pts',(-94.7345782155871,1076.88291876555,
483.451798671868));
#106716=CARTESIAN_POINT('Ctrl Pts',(-94.8645199165171,1076.86663371627,
483.475479152504));
#106717=CARTESIAN_POINT('Ctrl Pts',(-95.1194516259798,1076.83100336629,
483.571323081755));
#106718=CARTESIAN_POINT('Ctrl Pts',(-95.24091267592,1076.81183445465,483.646396699055));
#106719=CARTESIAN_POINT('Ctrl Pts',(-95.4504511381765,1076.77393950236,
483.840637335467));
#106720=CARTESIAN_POINT('Ctrl Pts',(-95.5358689623058,1076.75558168784,
483.958862417053));
#106721=CARTESIAN_POINT('Ctrl Pts',(-95.6520833276736,1076.72364111572,
484.21413129241));
#106722=CARTESIAN_POINT('Ctrl Pts',(-95.6848687531977,1076.71011140889,
484.347438871334));
#106723=CARTESIAN_POINT('Ctrl Pts',(-95.6993860135574,1076.68872679539,
484.616451385736));
#106724=CARTESIAN_POINT('Ctrl Pts',(-95.6821786999132,1076.68093128049,
484.749708287279));
#106725=CARTESIAN_POINT('Ctrl Pts',(-95.6250071691597,1076.67452004241,
484.927186355404));
#106726=CARTESIAN_POINT('Ctrl Pts',(-95.6050779052817,1076.67321222476,
484.97643194779));
#106727=CARTESIAN_POINT('Ctrl Pts',(-95.5715286428288,1076.67209627377,
485.044570774938));
#106728=CARTESIAN_POINT('Ctrl Pts',(-95.5607766979455,1076.67185853078,
485.064777617924));
#106729=CARTESIAN_POINT('Ctrl Pts',(-95.5422279124747,1076.67163220854,
485.097138602302));
#106730=CARTESIAN_POINT('Ctrl Pts',(-95.5348120391529,1076.67158400241,
485.109501880515));
#106731=CARTESIAN_POINT('Ctrl Pts',(-95.518779683349,1076.67156534638,485.135066913996));
#106732=CARTESIAN_POINT('Ctrl Pts',(-95.5101177694239,1076.67160257376,
485.148236032317));
#106733=CARTESIAN_POINT('Ctrl Pts',(-95.4889316728475,1076.67180194277,
485.178973763344));
#106734=CARTESIAN_POINT('Ctrl Pts',(-95.476165970251,1076.672005032,485.19636702731));
#106735=CARTESIAN_POINT('Ctrl Pts',(-95.4326636719739,1076.67295772295,
485.252094906878));
#106736=CARTESIAN_POINT('Ctrl Pts',(-95.3998579760909,1076.67407291771,
485.288725236744));
#106737=CARTESIAN_POINT('Ctrl Pts',(-95.261000092873,1076.68023290497,485.424159775002));
#106738=CARTESIAN_POINT('Ctrl Pts',(-95.1383265104726,1076.68863623939,
485.503495528396));
#106739=CARTESIAN_POINT('Ctrl Pts',(-94.8940061951528,1076.70981789088,
485.600016013295));
#106740=CARTESIAN_POINT('Ctrl Pts',(-94.7778927388487,1076.72137705126,
485.625223525282));
#106741=CARTESIAN_POINT('Ctrl Pts',(-94.6411952947611,1076.7365793124,485.632367414648));
#106742=CARTESIAN_POINT('Ctrl Pts',(-94.6222173980957,1076.73872505013,
485.63286182824));
#106743=CARTESIAN_POINT('Ctrl Pts',(-94.6032580293201,1076.74090351967,
485.63286182824));
#106744=CARTESIAN_POINT('',(-93.6720377362212,1077.61442735558,472.874586465029));
#106745=CARTESIAN_POINT('',(-93.6720377362213,1077.7163862265,470.676924193044));
#106746=CARTESIAN_POINT('Ctrl Pts',(-93.6720377362213,1077.61442735558,
472.874586465029));
#106747=CARTESIAN_POINT('Ctrl Pts',(-93.5677573540383,1077.62420150145,
472.874586465029));
#106748=CARTESIAN_POINT('Ctrl Pts',(-93.4639081817383,1077.63458923107,
472.859741243044));
#106749=CARTESIAN_POINT('Ctrl Pts',(-93.2274100948857,1077.65976663472,
472.790586039158));
#106750=CARTESIAN_POINT('Ctrl Pts',(-93.1001671010855,1077.67454354204,
472.724726821711));
#106751=CARTESIAN_POINT('Ctrl Pts',(-92.8753830609211,1077.70331191389,
472.546338198103));
#106752=CARTESIAN_POINT('Ctrl Pts',(-92.7806725594652,1077.71700728856,
472.43453227919));
#106753=CARTESIAN_POINT('Ctrl Pts',(-92.6442782205473,1077.74049969227,
472.187843968462));
#106754=CARTESIAN_POINT('Ctrl Pts',(-92.6009800357877,1077.75027798954,
472.056842117196));
#106755=CARTESIAN_POINT('Ctrl Pts',(-92.5645514630971,1077.76578299318,
471.783922622182));
#106756=CARTESIAN_POINT('Ctrl Pts',(-92.5723175270602,1077.77132437777,
471.644386886577));
#106757=CARTESIAN_POINT('Ctrl Pts',(-92.6171461547586,1077.77537343022,
471.464608895946));
#106758=CARTESIAN_POINT('Ctrl Pts',(-92.6313139919142,1077.77610402404,
471.420082301668));
#106759=CARTESIAN_POINT('Ctrl Pts',(-92.6552158608447,1077.77672038478,
471.358779940149));
#106760=CARTESIAN_POINT('Ctrl Pts',(-92.6626228297686,1077.77685015463,
471.341155770395));
#106761=CARTESIAN_POINT('Ctrl Pts',(-92.6770340275328,1077.77699746164,
471.309224656014));
#106762=CARTESIAN_POINT('Ctrl Pts',(-92.6838967055807,1077.77703011986,
471.294859748602));
#106763=CARTESIAN_POINT('Ctrl Pts',(-92.6983844259794,1077.7770268126,471.266154808273));
#106764=CARTESIAN_POINT('Ctrl Pts',(-92.7060200917941,1077.77698946655,
471.251824640119));
#106765=CARTESIAN_POINT('Ctrl Pts',(-92.7254310449002,1077.77681123887,
471.217263273819));
#106766=CARTESIAN_POINT('Ctrl Pts',(-92.7375404027597,1077.77663197313,
471.197229366688));
#106767=CARTESIAN_POINT('Ctrl Pts',(-92.7822999176905,1077.77574284715,
471.128255162783));
#106768=CARTESIAN_POINT('Ctrl Pts',(-92.8182257847877,1077.77464215865,
471.081570174133));
#106769=CARTESIAN_POINT('Ctrl Pts',(-92.9554883524616,1077.76923248309,
470.930062508393));
#106770=CARTESIAN_POINT('Ctrl Pts',(-93.0736767060949,1077.76264360369,
470.842727633437));
#106771=CARTESIAN_POINT('Ctrl Pts',(-93.284470346795,1077.74825807343,470.743833021938));
#106772=CARTESIAN_POINT('Ctrl Pts',(-93.367713387491,1077.74204260413,470.71630235684));
#106773=CARTESIAN_POINT('Ctrl Pts',(-93.5253158985138,1077.72931495661,
470.684285821923));
#106774=CARTESIAN_POINT('Ctrl Pts',(-93.5986020744376,1077.72303707031,
470.676924193044));
#106775=CARTESIAN_POINT('Ctrl Pts',(-93.6720377362213,1077.7163862265,470.676924193044));
#106776=CARTESIAN_POINT('Ctrl Pts',(-93.6720377362213,1077.7163862265,470.676924193044));
#106777=CARTESIAN_POINT('Ctrl Pts',(-93.6720989375535,1077.71638068368,
470.676924193044));
#106778=CARTESIAN_POINT('Ctrl Pts',(-93.6721601389895,1077.71637514061,
470.676924198158));
#106779=CARTESIAN_POINT('Ctrl Pts',(-93.6722213405288,1077.71636959727,
470.676924208384));
#106780=CARTESIAN_POINT('Ctrl Pts',(-93.8069747497468,1077.70416429332,
470.676946724406));
#106781=CARTESIAN_POINT('Ctrl Pts',(-93.9405034286092,1077.69085743869,
470.701755567198));
#106782=CARTESIAN_POINT('Ctrl Pts',(-94.2016506327738,1077.66224222225,
470.802097597682));
#106783=CARTESIAN_POINT('Ctrl Pts',(-94.3255124721466,1077.64712899308,
470.880501190131));
#106784=CARTESIAN_POINT('Ctrl Pts',(-94.5347300985438,1077.61827007746,
471.08011089913));
#106785=CARTESIAN_POINT('Ctrl Pts',(-94.6184413026895,1077.60478566402,
471.199088474615));
#106786=CARTESIAN_POINT('Ctrl Pts',(-94.729661473487,1077.58235596944,471.450324393789));
#106787=CARTESIAN_POINT('Ctrl Pts',(-94.7608620275231,1077.57328087477,
471.578278060553));
#106788=CARTESIAN_POINT('Ctrl Pts',(-94.7768576812629,1077.55920485216,
471.840396296642));
#106789=CARTESIAN_POINT('Ctrl Pts',(-94.7611515141652,1077.55435498801,
471.972426858902));
#106790=CARTESIAN_POINT('Ctrl Pts',(-94.7132899750522,1077.55143783682,
472.128147618054));
#106791=CARTESIAN_POINT('Ctrl Pts',(-94.7029580846465,1077.55102179974,
472.15731793579));
#106792=CARTESIAN_POINT('Ctrl Pts',(-94.683983093621,1077.55056687217,472.204465013655));
#106793=CARTESIAN_POINT('Ctrl Pts',(-94.676058017025,1077.5504464427,472.222710256017));
#106794=CARTESIAN_POINT('Ctrl Pts',(-94.6609819777631,1077.55033416925,
472.25499103914));
#106795=CARTESIAN_POINT('Ctrl Pts',(-94.6540163463915,1077.55032075153,
472.269106716838));
#106796=CARTESIAN_POINT('Ctrl Pts',(-94.6386592725339,1077.55036888241,
472.298612639016));
#106797=CARTESIAN_POINT('Ctrl Pts',(-94.6301980232085,1077.55043909918,
472.313961437729));
#106798=CARTESIAN_POINT('Ctrl Pts',(-94.6069026241503,1077.5507426939,472.353927678301));
#106799=CARTESIAN_POINT('Ctrl Pts',(-94.5914641541615,1077.55105160265,
472.378175900708));
#106800=CARTESIAN_POINT('Ctrl Pts',(-94.5201589573807,1077.55291755194,
472.481033754357));
#106801=CARTESIAN_POINT('Ctrl Pts',(-94.4550534889925,1077.55569273445,
472.552672163626));
#106802=CARTESIAN_POINT('Ctrl Pts',(-94.2985309346692,1077.56426334619,
472.685004076036));
#106803=CARTESIAN_POINT('Ctrl Pts',(-94.2057085098637,1077.57034929027,
472.742393452037));
#106804=CARTESIAN_POINT('Ctrl Pts',(-93.9942646670983,1077.58605709614,
472.833304396527));
#106805=CARTESIAN_POINT('Ctrl Pts',(-93.8753492459016,1077.59590949919,
472.862427008106));
#106806=CARTESIAN_POINT('Ctrl Pts',(-93.7268170147061,1077.60933804293,
472.873563519947));
#106807=CARTESIAN_POINT('Ctrl Pts',(-93.6994125152431,1077.61186153181,
472.874586465029));
#106808=CARTESIAN_POINT('Ctrl Pts',(-93.6720377362213,1077.61442735558,
472.874586465029));
#106809=CARTESIAN_POINT('',(-90.2477595453604,1078.31906551735,460.717880652247));
#106810=CARTESIAN_POINT('',(-90.2477595453604,1078.37785269114,458.166992409975));
#106811=CARTESIAN_POINT('Ctrl Pts',(-90.2477595453603,1078.31906551735,
460.717880652247));
#106812=CARTESIAN_POINT('Ctrl Pts',(-90.2327982517213,1078.31998718321,
460.717880652247));
#106813=CARTESIAN_POINT('Ctrl Pts',(-90.2178282660456,1078.32091437956,
460.717617403605));
#106814=CARTESIAN_POINT('Ctrl Pts',(-90.043575120828,1078.33176482721,460.71147887043));
#106815=CARTESIAN_POINT('Ctrl Pts',(-89.886755391279,1078.34208576221,460.676061788484));
#106816=CARTESIAN_POINT('Ctrl Pts',(-89.5854872611562,1078.36301604073,
460.545481693515));
#106817=CARTESIAN_POINT('Ctrl Pts',(-89.4452959445034,1078.37340027169,
460.448116084544));
#106818=CARTESIAN_POINT('Ctrl Pts',(-89.2139758478804,1078.39203625929,
460.207419305018));
#106819=CARTESIAN_POINT('Ctrl Pts',(-89.1238577528026,1078.40016459373,
460.067568688696));
#106820=CARTESIAN_POINT('Ctrl Pts',(-89.0106452747436,1078.41260133485,
459.783327773387));
#106821=CARTESIAN_POINT('Ctrl Pts',(-88.980534811914,1078.41720851565,459.64447860233));
#106822=CARTESIAN_POINT('Ctrl Pts',(-88.9683367981648,1078.42325841417,
459.389970877563));
#106823=CARTESIAN_POINT('Ctrl Pts',(-88.9780938758569,1078.42511565521,
459.276212343589));
#106824=CARTESIAN_POINT('Ctrl Pts',(-89.0105033541495,1078.42640768501,
459.130649493654));
#106825=CARTESIAN_POINT('Ctrl Pts',(-89.0196454756031,1078.42662929176,
459.09638747785));
#106826=CARTESIAN_POINT('Ctrl Pts',(-89.036460872709,1078.42684554272,459.042493179283));
#106827=CARTESIAN_POINT('Ctrl Pts',(-89.0432135336209,1078.42689582627,
459.022593618969));
#106828=CARTESIAN_POINT('Ctrl Pts',(-89.0567634716925,1078.42693336289,
458.985685888084));
#106829=CARTESIAN_POINT('Ctrl Pts',(-89.063441455711,1078.42692789351,458.968639676382));
#106830=CARTESIAN_POINT('Ctrl Pts',(-89.0792381930181,1078.42686416129,
458.93074001787));
#106831=CARTESIAN_POINT('Ctrl Pts',(-89.0885528277506,1078.42679340298,
458.90997503149));
#106832=CARTESIAN_POINT('Ctrl Pts',(-89.117169212609,1078.42648547986,458.850495787964));
#106833=CARTESIAN_POINT('Ctrl Pts',(-89.1378904705034,1078.42615605814,
458.812500967417));
#106834=CARTESIAN_POINT('Ctrl Pts',(-89.2494795984902,1078.42390412161,
458.630548929456));
#106835=CARTESIAN_POINT('Ctrl Pts',(-89.3665830069868,1078.42017199183,
458.504765896987));
#106836=CARTESIAN_POINT('Ctrl Pts',(-89.6158695020872,1078.41020970943,
458.326138649693));
#106837=CARTESIAN_POINT('Ctrl Pts',(-89.7388956965627,1078.4046794168,458.264963799376));
#106838=CARTESIAN_POINT('Ctrl Pts',(-89.9918262523886,1078.39212139507,
458.18635595696));
#106839=CARTESIAN_POINT('Ctrl Pts',(-90.1194443891827,1078.38527238758,
458.166992409975));
#106840=CARTESIAN_POINT('Ctrl Pts',(-90.2477595453605,1078.37785269114,
458.166992409975));
#106841=CARTESIAN_POINT('Ctrl Pts',(-90.2477595453605,1078.37785269114,
458.166992409974));
#106842=CARTESIAN_POINT('Ctrl Pts',(-90.2478324244995,1078.37784847698,
458.166992409974));
#106843=CARTESIAN_POINT('Ctrl Pts',(-90.2479053038633,1078.37784426263,
458.166992416221));
#106844=CARTESIAN_POINT('Ctrl Pts',(-90.2479781834512,1078.3778400481,458.166992428714));
#106845=CARTESIAN_POINT('Ctrl Pts',(-90.4072919887955,1078.36862713961,
458.167019738469));
#106846=CARTESIAN_POINT('Ctrl Pts',(-90.5651677819751,1078.35867654221,
458.196895678002));
#106847=CARTESIAN_POINT('Ctrl Pts',(-90.8708241345389,1078.33764553449,
458.316767158458));
#106848=CARTESIAN_POINT('Ctrl Pts',(-91.0144005994746,1078.3267382461,458.409182948326));
#106849=CARTESIAN_POINT('Ctrl Pts',(-91.2543332497696,1078.30637298371,
458.641908303166));
#106850=CARTESIAN_POINT('Ctrl Pts',(-91.3494706778114,1078.29708088055,
458.778881164629));
#106851=CARTESIAN_POINT('Ctrl Pts',(-91.4710865323649,1078.28258952335,
459.056231867705));
#106852=CARTESIAN_POINT('Ctrl Pts',(-91.5056040365209,1078.27706244958,
459.190374667953));
#106853=CARTESIAN_POINT('Ctrl Pts',(-91.5295395049849,1078.26895951083,
459.454844678659));
#106854=CARTESIAN_POINT('Ctrl Pts',(-91.5218465515413,1078.26624929941,
459.583252359866));
#106855=CARTESIAN_POINT('Ctrl Pts',(-91.4874400031134,1078.26444461224,
459.744635337777));
#106856=CARTESIAN_POINT('Ctrl Pts',(-91.4781338890357,1078.26414997498,
459.780535424518));
#106857=CARTESIAN_POINT('Ctrl Pts',(-91.4609077268045,1078.26386000067,
459.836774160456));
#106858=CARTESIAN_POINT('Ctrl Pts',(-91.4540075142604,1078.26379133509,
459.857402221682));
#106859=CARTESIAN_POINT('Ctrl Pts',(-91.4402753088666,1078.2637358018,459.89521162881));
#106860=CARTESIAN_POINT('Ctrl Pts',(-91.4335907385148,1078.26373819291,
459.912440272066));
#106861=CARTESIAN_POINT('Ctrl Pts',(-91.4179825895442,1078.26380518905,
459.95021322715));
#106862=CARTESIAN_POINT('Ctrl Pts',(-91.4088874623377,1078.2638828574,459.970679935325));
#106863=CARTESIAN_POINT('Ctrl Pts',(-91.3816603578278,1078.26421798958,
460.027843598228));
#106864=CARTESIAN_POINT('Ctrl Pts',(-91.3622948627012,1078.26457087229,
460.06392130448));
#106865=CARTESIAN_POINT('Ctrl Pts',(-91.2535722720426,1078.26708713234,
460.244991450979));
#106866=CARTESIAN_POINT('Ctrl Pts',(-91.1375908418323,1078.27142677595,
460.371909259997));
#106867=CARTESIAN_POINT('Ctrl Pts',(-90.89063281603,1078.28278378677,460.552335975317));
#106868=CARTESIAN_POINT('Ctrl Pts',(-90.7690567174844,1078.28900377703,
460.614352732602));
#106869=CARTESIAN_POINT('Ctrl Pts',(-90.513202878717,1078.30310708823,460.697055991285));
#106870=CARTESIAN_POINT('Ctrl Pts',(-90.380825036293,1078.31086823689,460.717880652247));
#106871=CARTESIAN_POINT('Ctrl Pts',(-90.2477595453603,1078.31906551735,
460.717880652247));
#106872=CARTESIAN_POINT('',(-86.3230601853152,1078.66271960918,449.952384165744));
#106873=CARTESIAN_POINT('',(-86.3230601853153,1078.68303149632,446.995777901357));
#106874=CARTESIAN_POINT('Ctrl Pts',(-86.3230601853152,1078.66271960918,
449.952384165744));
#106875=CARTESIAN_POINT('Ctrl Pts',(-86.3219893136851,1078.66274837852,
449.952384165744));
#106876=CARTESIAN_POINT('Ctrl Pts',(-86.3209183914346,1078.66277714952,
449.952383002147));
#106877=CARTESIAN_POINT('Ctrl Pts',(-86.1332083697891,1078.66782014887,
449.951975054968));
#106878=CARTESIAN_POINT('Ctrl Pts',(-85.9483182623366,1078.6727868702,449.916227592599));
#106879=CARTESIAN_POINT('Ctrl Pts',(-85.5935530569033,1078.6822529705,449.774602911678));
#106880=CARTESIAN_POINT('Ctrl Pts',(-85.4282654883527,1078.68662678793,
449.666930277804));
#106881=CARTESIAN_POINT('Ctrl Pts',(-85.1536649443362,1078.69400200111,
449.397993711266));
#106882=CARTESIAN_POINT('Ctrl Pts',(-85.0452361752256,1078.69698175616,
449.241070641324));
#106883=CARTESIAN_POINT('Ctrl Pts',(-84.8998827329711,1078.70144206657,
448.909744723854));
#106884=CARTESIAN_POINT('Ctrl Pts',(-84.8587403413835,1078.70300008527,
448.74055367043));
#106885=CARTESIAN_POINT('Ctrl Pts',(-84.8414343770874,1078.70461263675,
448.46900283252));
#106886=CARTESIAN_POINT('Ctrl Pts',(-84.8451198713728,1078.70502007381,
448.369517451852));
#106887=CARTESIAN_POINT('Ctrl Pts',(-84.8638170256399,1078.70533761927,
448.234599199511));
#106888=CARTESIAN_POINT('Ctrl Pts',(-84.870250125856,1078.70539915702,448.198245783733));
#106889=CARTESIAN_POINT('Ctrl Pts',(-84.8830601167758,1078.70546027829,
448.138899337221));
#106890=CARTESIAN_POINT('Ctrl Pts',(-84.8886448447503,1078.7054740855,448.115752136688));
#106891=CARTESIAN_POINT('Ctrl Pts',(-84.9005336739799,1078.70548116606,
448.071222576539));
#106892=CARTESIAN_POINT('Ctrl Pts',(-84.9067671709716,1078.70547569801,
448.049827914266));
#106893=CARTESIAN_POINT('Ctrl Pts',(-84.9223509492737,1078.70544236374,
448.000520122945));
#106894=CARTESIAN_POINT('Ctrl Pts',(-84.9320560671682,1078.70540788418,
447.972729020238));
#106895=CARTESIAN_POINT('Ctrl Pts',(-84.9650283518623,1078.70525120061,
447.886657824034));
#106896=CARTESIAN_POINT('Ctrl Pts',(-84.9911794707813,1078.70507413603,
447.829557798599));
#106897=CARTESIAN_POINT('Ctrl Pts',(-85.1138785811796,1078.70404784773,
447.601236637608));
#106898=CARTESIAN_POINT('Ctrl Pts',(-85.2404477033097,1078.70258807734,
447.448447719624));
#106899=CARTESIAN_POINT('Ctrl Pts',(-85.5180168122914,1078.69859589733,
447.223849449712));
#106900=CARTESIAN_POINT('Ctrl Pts',(-85.6584950184123,1078.69632926921,
447.143846921644));
#106901=CARTESIAN_POINT('Ctrl Pts',(-85.973574281774,1078.69057592466,447.027006745919));
#106902=CARTESIAN_POINT('Ctrl Pts',(-86.1476258600309,1078.68703696195,
446.995777901357));
#106903=CARTESIAN_POINT('Ctrl Pts',(-86.3230601853154,1078.68303149632,
446.995777901357));
#106904=CARTESIAN_POINT('Ctrl Pts',(-86.3230601853153,1078.68303149632,
446.995777901357));
#106905=CARTESIAN_POINT('Ctrl Pts',(-86.3231037532579,1078.68303050158,
446.995777901357));
#106906=CARTESIAN_POINT('Ctrl Pts',(-86.3231473212856,1078.68302950683,
446.995777903283));
#106907=CARTESIAN_POINT('Ctrl Pts',(-86.3231908893986,1078.68302851204,
446.995777907135));
#106908=CARTESIAN_POINT('Ctrl Pts',(-86.5113795548305,1078.67873161425,
446.995794545825));
#106909=CARTESIAN_POINT('Ctrl Pts',(-86.6978364457682,1078.67397007578,
447.031745567121));
#106910=CARTESIAN_POINT('Ctrl Pts',(-87.0537013248571,1078.66381058891,
447.174223629047));
#106911=CARTESIAN_POINT('Ctrl Pts',(-87.2187323359064,1078.65849680364,
447.281924061899));
#106912=CARTESIAN_POINT('Ctrl Pts',(-87.4924716008461,1078.64859012056,
447.550346108494));
#106913=CARTESIAN_POINT('Ctrl Pts',(-87.6004774446379,1078.64407484309,
447.70660239725));
#106914=CARTESIAN_POINT('Ctrl Pts',(-87.7457840386515,1078.6368402648,448.036984561462));
#106915=CARTESIAN_POINT('Ctrl Pts',(-87.7870783246366,1078.63406305431,
448.20602200215));
#106916=CARTESIAN_POINT('Ctrl Pts',(-87.8046993616625,1078.63111784649,
448.477581050921));
#106917=CARTESIAN_POINT('Ctrl Pts',(-87.8011107850664,1078.6303496369,448.577203692244));
#106918=CARTESIAN_POINT('Ctrl Pts',(-87.7824753157512,1078.62974695066,
448.712557434865));
#106919=CARTESIAN_POINT('Ctrl Pts',(-87.7760135969678,1078.62962913423,
448.749199048912));
#106920=CARTESIAN_POINT('Ctrl Pts',(-87.7631010239068,1078.6295119873,448.809107730244));
#106921=CARTESIAN_POINT('Ctrl Pts',(-87.7574502758618,1078.62948555117,
448.832529878704));
#106922=CARTESIAN_POINT('Ctrl Pts',(-87.7453884064107,1078.62947240845,
448.877657941451));
#106923=CARTESIAN_POINT('Ctrl Pts',(-87.7390462559079,1078.62948337909,
448.899375444873));
#106924=CARTESIAN_POINT('Ctrl Pts',(-87.7231398310093,1078.62954918598,
448.949535715553));
#106925=CARTESIAN_POINT('Ctrl Pts',(-87.7132030298227,1078.62961715035,
448.977849862148));
#106926=CARTESIAN_POINT('Ctrl Pts',(-87.679228711486,1078.62992641947,449.065976923457));
#106927=CARTESIAN_POINT('Ctrl Pts',(-87.6521383269708,1078.63027691846,
449.124530815579));
#106928=CARTESIAN_POINT('Ctrl Pts',(-87.5272729774475,1078.63224471684,
449.35380373895));
#106929=CARTESIAN_POINT('Ctrl Pts',(-87.3997279375185,1078.6349729785,449.505980258295));
#106930=CARTESIAN_POINT('Ctrl Pts',(-87.1210580936803,1078.64166558737,
449.728767677051));
#106931=CARTESIAN_POINT('Ctrl Pts',(-86.9805207319876,1078.64525869543,
449.807789584479));
#106932=CARTESIAN_POINT('Ctrl Pts',(-86.6676033718544,1078.65346701037,
449.922039748485));
#106933=CARTESIAN_POINT('Ctrl Pts',(-86.4959918761742,1078.65807373949,
449.952384165744));
#106934=CARTESIAN_POINT('Ctrl Pts',(-86.3230601853152,1078.66271960918,
449.952384165744));
#106935=CARTESIAN_POINT('',(-69.1578093449745,1078.64674583663,483.000863198568));
#106936=CARTESIAN_POINT('',(-69.1578093449747,1078.69514019783,480.044256934181));
#106937=CARTESIAN_POINT('Ctrl Pts',(-69.1578093449745,1078.64674583663,
483.000863198568));
#106938=CARTESIAN_POINT('Ctrl Pts',(-69.1220937668084,1078.64759196713,
483.000863198568));
#106939=CARTESIAN_POINT('Ctrl Pts',(-69.0863498276105,1078.64845820303,
482.99956888825));
#106940=CARTESIAN_POINT('Ctrl Pts',(-68.8768662085712,1078.6536434673,482.984343449551));
#106941=CARTESIAN_POINT('Ctrl Pts',(-68.7066832936626,1078.65829077859,
482.941088098396));
#106942=CARTESIAN_POINT('Ctrl Pts',(-68.3777949600251,1078.66799062584,
482.792148860044));
#106943=CARTESIAN_POINT('Ctrl Pts',(-68.2237562448034,1078.67295694628,
482.683519495698));
#106944=CARTESIAN_POINT('Ctrl Pts',(-67.9583997108454,1078.68240848418,
482.408532395796));
#106945=CARTESIAN_POINT('Ctrl Pts',(-67.8519529437903,1078.68676874044,
482.242475741192));
#106946=CARTESIAN_POINT('Ctrl Pts',(-67.7121084334976,1078.69411350738,
481.884538077247));
#106947=CARTESIAN_POINT('Ctrl Pts',(-67.6777201905111,1078.69707705634,
481.696980993371));
#106948=CARTESIAN_POINT('Ctrl Pts',(-67.6813191949551,1078.70156116495,
481.330864883684));
#106949=CARTESIAN_POINT('Ctrl Pts',(-67.7148960065625,1078.70312947517,
481.155443117896));
#106950=CARTESIAN_POINT('Ctrl Pts',(-67.8118699942329,1078.70466121946,
480.904251222763));
#106951=CARTESIAN_POINT('Ctrl Pts',(-67.8529853071337,1078.70502962209,
480.821637090225));
#106952=CARTESIAN_POINT('Ctrl Pts',(-67.921526960054,1078.7053360895,480.711124816198));
#106953=CARTESIAN_POINT('Ctrl Pts',(-67.942771262791,1078.70539962805,480.679646211886));
#106954=CARTESIAN_POINT('Ctrl Pts',(-67.9788928060586,1078.70546039652,
480.63033104458));
#106955=CARTESIAN_POINT('Ctrl Pts',(-67.9930194307043,1078.70547380595,
480.611966145203));
#106956=CARTESIAN_POINT('Ctrl Pts',(-68.0230900753445,1078.70548165651,
480.574719032977));
#106957=CARTESIAN_POINT('Ctrl Pts',(-68.0390877603405,1078.70547477867,
480.555889253051));
#106958=CARTESIAN_POINT('Ctrl Pts',(-68.0773204176942,1078.70543340838,
480.51310912399));
#106959=CARTESIAN_POINT('Ctrl Pts',(-68.0998926254822,1078.70539074163,
480.489477427577));
#106960=CARTESIAN_POINT('Ctrl Pts',(-68.1729193002667,1078.70519722749,
480.417928429381));
#106961=CARTESIAN_POINT('Ctrl Pts',(-68.2259837965977,1078.7049790155,480.372812039255));
#106962=CARTESIAN_POINT('Ctrl Pts',(-68.4405702555798,1078.7038067604,480.215014037646));
#106963=CARTESIAN_POINT('Ctrl Pts',(-68.6208052854813,1078.70225534419,
480.131254604214));
#106964=CARTESIAN_POINT('Ctrl Pts',(-68.9253462279713,1078.69860635502,
480.05801257821));
#106965=CARTESIAN_POINT('Ctrl Pts',(-69.0413762084877,1078.69700068759,
480.044256934181));
#106966=CARTESIAN_POINT('Ctrl Pts',(-69.1578093449746,1078.69514019783,
480.044256934181));
#106967=CARTESIAN_POINT('Ctrl Pts',(-69.1578093449747,1078.69514019783,
480.044256934181));
#106968=CARTESIAN_POINT('Ctrl Pts',(-69.1578255873479,1078.69513993829,
480.044256934181));
#106969=CARTESIAN_POINT('Ctrl Pts',(-69.1578418297291,1078.69513967875,
480.044256934449));
#106970=CARTESIAN_POINT('Ctrl Pts',(-69.157858072118,1078.6951394192,480.044256934984));
#106971=CARTESIAN_POINT('Ctrl Pts',(-69.3304172925023,1078.69238198582,
480.044262622801));
#106972=CARTESIAN_POINT('Ctrl Pts',(-69.5016402651383,1078.68909651496,
480.074481766387));
#106973=CARTESIAN_POINT('Ctrl Pts',(-69.8382050392031,1078.68127504934,
480.197075232476));
#106974=CARTESIAN_POINT('Ctrl Pts',(-69.9991185706044,1078.67672836683,
480.292909581556));
#106975=CARTESIAN_POINT('Ctrl Pts',(-70.2844405337472,1078.66679166732,
480.545668199062));
#106976=CARTESIAN_POINT('Ctrl Pts',(-70.4036363608493,1078.66146765396,
480.70309082141));
#106977=CARTESIAN_POINT('Ctrl Pts',(-70.5717345936668,1078.65128240561,
481.050804271054));
#106978=CARTESIAN_POINT('Ctrl Pts',(-70.6207385150725,1078.64651419783,
481.236929995868));
#106979=CARTESIAN_POINT('Ctrl Pts',(-70.643809200598,1078.63883572837,481.593955476461));
#106980=CARTESIAN_POINT('Ctrl Pts',(-70.6262425150681,1078.6358277134,481.761316621795));
#106981=CARTESIAN_POINT('Ctrl Pts',(-70.5469147492507,1078.63195396571,
482.043838842373));
#106982=CARTESIAN_POINT('Ctrl Pts',(-70.4973005612334,1078.63076075498,
482.160612556531));
#106983=CARTESIAN_POINT('Ctrl Pts',(-70.4112452026124,1078.62986506717,
482.307548963095));
#106984=CARTESIAN_POINT('Ctrl Pts',(-70.3873719454327,1078.62969817139,
482.344438933343));
#106985=CARTESIAN_POINT('Ctrl Pts',(-70.3460392107666,1078.62953296329,
482.40246719796));
#106986=CARTESIAN_POINT('Ctrl Pts',(-70.3295726739802,1078.62949480491,
482.424279246017));
#106987=CARTESIAN_POINT('Ctrl Pts',(-70.2969879577151,1078.62947022325,
482.465040988458));
#106988=CARTESIAN_POINT('Ctrl Pts',(-70.2809774640063,1078.62947944854,
482.48406491604));
#106989=CARTESIAN_POINT('Ctrl Pts',(-70.2434089302868,1078.62954815663,
482.526484950677));
#106990=CARTESIAN_POINT('Ctrl Pts',(-70.2215602004611,1078.62962094107,
482.549607163961));
#106991=CARTESIAN_POINT('Ctrl Pts',(-70.1534914889801,1078.62994290845,
482.617139272593));
#106992=CARTESIAN_POINT('Ctrl Pts',(-70.1051142213755,1078.630295898,482.659265768164));
#106993=CARTESIAN_POINT('Ctrl Pts',(-69.8972925153034,1078.63228055406,
482.817726952498));
#106994=CARTESIAN_POINT('Ctrl Pts',(-69.7180755427923,1078.63503192318,
482.904726208679));
#106995=CARTESIAN_POINT('Ctrl Pts',(-69.4063231087205,1078.64109433978,
482.9851528028));
#106996=CARTESIAN_POINT('Ctrl Pts',(-69.2822383408889,1078.64379801457,
483.000863198568));
#106997=CARTESIAN_POINT('Ctrl Pts',(-69.1578093449745,1078.64674583663,
483.000863198568));
#106998=CARTESIAN_POINT('',(-68.281968522817,1078.28930526318,494.414414572902));
#106999=CARTESIAN_POINT('',(-68.2819685228173,1078.40494192759,491.86352633063));
#107000=CARTESIAN_POINT('Ctrl Pts',(-68.2819685228169,1078.28930526318,
494.414414572903));
#107001=CARTESIAN_POINT('Ctrl Pts',(-68.2268299973128,1078.29194915715,
494.414414572903));
#107002=CARTESIAN_POINT('Ctrl Pts',(-68.1716716781174,1078.2947564259,494.410839066877));
#107003=CARTESIAN_POINT('Ctrl Pts',(-67.9689152532529,1078.30566708968,
494.384366341749));
#107004=CARTESIAN_POINT('Ctrl Pts',(-67.8255576261282,1078.3145504416,494.339253502769));
#107005=CARTESIAN_POINT('Ctrl Pts',(-67.5511678987433,1078.33392330302,
494.196492245403));
#107006=CARTESIAN_POINT('Ctrl Pts',(-67.4242506988773,1078.34431070701,
494.096435629777));
#107007=CARTESIAN_POINT('Ctrl Pts',(-67.2084150268444,1078.36520475051,
493.848027835637));
#107008=CARTESIAN_POINT('Ctrl Pts',(-67.1240358591932,1078.37548319379,
493.699772664207));
#107009=CARTESIAN_POINT('Ctrl Pts',(-67.0194581552401,1078.393793904,493.383468981787));
#107010=CARTESIAN_POINT('Ctrl Pts',(-66.9984816421114,1078.40171502936,
493.219040849127));
#107011=CARTESIAN_POINT('Ctrl Pts',(-67.0189661114801,1078.41399807541,
492.908188050846));
#107012=CARTESIAN_POINT('Ctrl Pts',(-67.0540168145405,1078.41855449535,
492.764013049827));
#107013=CARTESIAN_POINT('Ctrl Pts',(-67.1516743758756,1078.42381114958,
492.540148623869));
#107014=CARTESIAN_POINT('Ctrl Pts',(-67.2004349724833,1078.42527980687,
492.45600542429));
#107015=CARTESIAN_POINT('Ctrl Pts',(-67.2795034245054,1078.42641946076,
492.349610104343));
#107016=CARTESIAN_POINT('Ctrl Pts',(-67.3019344077776,1078.42663933247,
492.321927465234));
#107017=CARTESIAN_POINT('Ctrl Pts',(-67.3405658070389,1078.42685775428,
492.278135013906));
#107018=CARTESIAN_POINT('Ctrl Pts',(-67.3560919764303,1078.42690746162,
492.261457287901));
#107019=CARTESIAN_POINT('Ctrl Pts',(-67.3868845947875,1078.42693479384,
492.23010840154));
#107020=CARTESIAN_POINT('Ctrl Pts',(-67.4020860214614,1078.42691729369,
492.215383830676));
#107021=CARTESIAN_POINT('Ctrl Pts',(-67.4380043830343,1078.4268061449,492.182284184333));
#107022=CARTESIAN_POINT('Ctrl Pts',(-67.4589673129964,1078.42669071656,
492.164191980125));
#107023=CARTESIAN_POINT('Ctrl Pts',(-67.5255311999959,1078.42617220555,
492.110422463409));
#107024=CARTESIAN_POINT('Ctrl Pts',(-67.572982585475,1078.42559337072,492.077157468938));
#107025=CARTESIAN_POINT('Ctrl Pts',(-67.6866117922098,1078.42374835658,
492.008522129749));
#107026=CARTESIAN_POINT('Ctrl Pts',(-67.7539752922965,1078.42233399342,
491.975534101653));
#107027=CARTESIAN_POINT('Ctrl Pts',(-67.9700643467163,1078.41683480429,
491.892365402126));
#107028=CARTESIAN_POINT('Ctrl Pts',(-68.1253745050975,1078.4115692788,491.86352633063));
#107029=CARTESIAN_POINT('Ctrl Pts',(-68.2819685228173,1078.40494192759,
491.86352633063));
#107030=CARTESIAN_POINT('Ctrl Pts',(-68.2819685228173,1078.40494192759,
491.86352633063));
#107031=CARTESIAN_POINT('Ctrl Pts',(-68.2819829283623,1078.40494131792,
491.86352633063));
#107032=CARTESIAN_POINT('Ctrl Pts',(-68.2819973339181,1078.40494070824,
491.863526330874));
#107033=CARTESIAN_POINT('Ctrl Pts',(-68.2820117394848,1078.40494009854,
491.863526331362));
#107034=CARTESIAN_POINT('Ctrl Pts',(-68.4272840304119,1078.39879168051,
491.863531253714));
#107035=CARTESIAN_POINT('Ctrl Pts',(-68.5714448488071,1078.39156228246,
491.888355050204));
#107036=CARTESIAN_POINT('Ctrl Pts',(-68.856114368212,1078.37478838096,491.989310049922));
#107037=CARTESIAN_POINT('Ctrl Pts',(-68.9929838731265,1078.36524384175,
492.06855112643));
#107038=CARTESIAN_POINT('Ctrl Pts',(-69.2401818060572,1078.34460579562,
492.280439104039));
#107039=CARTESIAN_POINT('Ctrl Pts',(-69.3452689297273,1078.33364938682,
492.414647381526));
#107040=CARTESIAN_POINT('Ctrl Pts',(-69.4961255434096,1078.31268815387,
492.714283929801));
#107041=CARTESIAN_POINT('Ctrl Pts',(-69.5411959190575,1078.30287512033,
492.876452206662));
#107042=CARTESIAN_POINT('Ctrl Pts',(-69.5651285669973,1078.28658287664,
493.192770983976));
#107043=CARTESIAN_POINT('Ctrl Pts',(-69.5498486225684,1078.28000195096,
493.343683187072));
#107044=CARTESIAN_POINT('Ctrl Pts',(-69.4699801429818,1078.27021897769,
493.62398246855));
#107045=CARTESIAN_POINT('Ctrl Pts',(-69.4091759352283,1078.26689649371,
493.752183733321));
#107046=CARTESIAN_POINT('Ctrl Pts',(-69.3047151517117,1078.26463987754,
493.902185344627));
#107047=CARTESIAN_POINT('Ctrl Pts',(-69.2791339195289,1078.26426398191,
493.935317753207));
#107048=CARTESIAN_POINT('Ctrl Pts',(-69.2359818467912,1078.2638929568,493.985860400982));
#107049=CARTESIAN_POINT('Ctrl Pts',(-69.2194546082755,1078.26380487283,
494.004120072329));
#107050=CARTESIAN_POINT('Ctrl Pts',(-69.1879156040516,1078.26373353815,
494.036999374624));
#107051=CARTESIAN_POINT('Ctrl Pts',(-69.1730522981399,1078.26373657664,
494.051749595717));
#107052=CARTESIAN_POINT('Ctrl Pts',(-69.1393976081116,1078.2638224945,494.083542423332));
#107053=CARTESIAN_POINT('Ctrl Pts',(-69.1204473950492,1078.26392208766,
494.100403760098));
#107054=CARTESIAN_POINT('Ctrl Pts',(-69.0655984514433,1078.26435079716,
494.146350951707));
#107055=CARTESIAN_POINT('Ctrl Pts',(-69.0286056692421,1078.26480095416,
494.174066583747));
#107056=CARTESIAN_POINT('Ctrl Pts',(-68.8491702885579,1078.26770143216,
494.293869834285));
#107057=CARTESIAN_POINT('Ctrl Pts',(-68.6908257250236,1078.27225785884,
494.358933903536));
#107058=CARTESIAN_POINT('Ctrl Pts',(-68.4444135365115,1078.2818687177,494.40665186068));
#107059=CARTESIAN_POINT('Ctrl Pts',(-68.3632125148549,1078.28540961131,
494.414414572903));
#107060=CARTESIAN_POINT('Ctrl Pts',(-68.2819685228169,1078.28930526318,
494.414414572903));
#107061=CARTESIAN_POINT('',(-66.3937896239303,1077.5767973048,506.897628369571));
#107062=CARTESIAN_POINT('',(-66.3937896239306,1077.7522985528,504.699966097586));
#107063=CARTESIAN_POINT('Ctrl Pts',(-66.3937896239303,1077.5767973048,506.897628369571));
#107064=CARTESIAN_POINT('Ctrl Pts',(-66.3853559678242,1077.57736420966,
506.897628369571));
#107065=CARTESIAN_POINT('Ctrl Pts',(-66.3769184655453,1077.57793920547,
506.8975312759));
#107066=CARTESIAN_POINT('Ctrl Pts',(-66.2463058532424,1077.586961466,506.894521901349));
#107067=CARTESIAN_POINT('Ctrl Pts',(-66.1255620075913,1077.59694399031,
506.871349468675));
#107068=CARTESIAN_POINT('Ctrl Pts',(-65.8870614803648,1077.62003119709,
506.782764275726));
#107069=CARTESIAN_POINT('Ctrl Pts',(-65.7723496933046,1077.63314310058,
506.714624527884));
#107070=CARTESIAN_POINT('Ctrl Pts',(-65.5651978050541,1077.66124918253,
506.534401986959));
#107071=CARTESIAN_POINT('Ctrl Pts',(-65.4769865219931,1077.67605382795,
506.421019613032));
#107072=CARTESIAN_POINT('Ctrl Pts',(-65.3475489881898,1077.70475069346,
506.164595790279));
#107073=CARTESIAN_POINT('Ctrl Pts',(-65.3084300766143,1077.71835008719,
506.023488598657));
#107074=CARTESIAN_POINT('Ctrl Pts',(-65.2879564868442,1077.74157487067,
505.742844215521));
#107075=CARTESIAN_POINT('Ctrl Pts',(-65.3033985549367,1077.75119462358,
505.606152551454));
#107076=CARTESIAN_POINT('Ctrl Pts',(-65.3860865330705,1077.7667390475,505.33738744492));
#107077=CARTESIAN_POINT('Ctrl Pts',(-65.4555593111009,1077.77225545012,
505.208761274875));
#107078=CARTESIAN_POINT('Ctrl Pts',(-65.5706518389485,1077.77568246524,
505.070012687636));
#107079=CARTESIAN_POINT('Ctrl Pts',(-65.5945547767765,1077.77618820348,
505.043875559786));
#107080=CARTESIAN_POINT('Ctrl Pts',(-65.6358852820681,1077.77674264264,
505.002849821875));
#107081=CARTESIAN_POINT('Ctrl Pts',(-65.6525891034229,1077.77688971025,
504.987272060215));
#107082=CARTESIAN_POINT('Ctrl Pts',(-65.6833669877132,1077.7770268665,504.96031262419));
#107083=CARTESIAN_POINT('Ctrl Pts',(-65.6972595005272,1077.77704324399,
504.948736909486));
#107084=CARTESIAN_POINT('Ctrl Pts',(-65.7271925313,1077.77698438522,504.925022366546));
#107085=CARTESIAN_POINT('Ctrl Pts',(-65.7432933581614,1077.77689868045,
504.912970617086));
#107086=CARTESIAN_POINT('Ctrl Pts',(-65.7865327726175,1077.77652918517,
504.882420045287));
#107087=CARTESIAN_POINT('Ctrl Pts',(-65.814184471588,1077.77615454949,504.864684984899));
#107088=CARTESIAN_POINT('Ctrl Pts',(-65.9355076578786,1077.77393708599,
504.794334767766));
#107089=CARTESIAN_POINT('Ctrl Pts',(-66.0357896988928,1077.77070569018,
504.754390776742));
#107090=CARTESIAN_POINT('Ctrl Pts',(-66.2233464398009,1077.76231141693,
504.709908902157));
#107091=CARTESIAN_POINT('Ctrl Pts',(-66.3084454335179,1077.75770593228,
504.699966097586));
#107092=CARTESIAN_POINT('Ctrl Pts',(-66.3937896239306,1077.7522985528,504.699966097586));
#107093=CARTESIAN_POINT('Ctrl Pts',(-66.3937896239306,1077.7522985528,504.699966097586));
#107094=CARTESIAN_POINT('Ctrl Pts',(-66.3938084673047,1077.75229735889,
504.699966097586));
#107095=CARTESIAN_POINT('Ctrl Pts',(-66.3938273106907,1077.75229616494,
504.699966098071));
#107096=CARTESIAN_POINT('Ctrl Pts',(-66.3938461540887,1077.75229497095,
504.69996609904));
#107097=CARTESIAN_POINT('Ctrl Pts',(-66.5156065443393,1077.74457977763,
504.699972363091));
#107098=CARTESIAN_POINT('Ctrl Pts',(-66.6364182768944,1077.73532348152,
504.720215429604));
#107099=CARTESIAN_POINT('Ctrl Pts',(-66.8764665702453,1077.71349650879,
504.802826892518));
#107100=CARTESIAN_POINT('Ctrl Pts',(-66.992684073827,1077.70087981196,504.86809095845));
#107101=CARTESIAN_POINT('Ctrl Pts',(-67.2041756848766,1077.67328580985,
505.043160212084));
#107102=CARTESIAN_POINT('Ctrl Pts',(-67.2951805003475,1077.65845238968,
505.154435897107));
#107103=CARTESIAN_POINT('Ctrl Pts',(-67.4308921457612,1077.62913719015,
505.40779887864));
#107104=CARTESIAN_POINT('Ctrl Pts',(-67.4734317282079,1077.61494517145,
505.548020848206));
#107105=CARTESIAN_POINT('Ctrl Pts',(-67.500710521595,1077.59022855711,505.828823720037));
#107106=CARTESIAN_POINT('Ctrl Pts',(-67.4883762012569,1077.57975598967,
505.966508905856));
#107107=CARTESIAN_POINT('Ctrl Pts',(-67.4125473874403,1077.56284062142,
506.234002406126));
#107108=CARTESIAN_POINT('Ctrl Pts',(-67.3484000506283,1077.55667530757,
506.360980143391));
#107109=CARTESIAN_POINT('Ctrl Pts',(-67.2363282566319,1077.55230743023,
506.505409444125));
#107110=CARTESIAN_POINT('Ctrl Pts',(-67.208878139826,1077.55155830391,506.536905377716));
#107111=CARTESIAN_POINT('Ctrl Pts',(-67.16403020963,1077.55079497178,506.582801028961));
#107112=CARTESIAN_POINT('Ctrl Pts',(-67.1478735815684,1077.55060126855,
506.59835333289));
#107113=CARTESIAN_POINT('Ctrl Pts',(-67.1174308896334,1077.55038077494,
506.625913165198));
#107114=CARTESIAN_POINT('Ctrl Pts',(-67.1032934568024,1077.55033139792,
506.638071783022));
#107115=CARTESIAN_POINT('Ctrl Pts',(-67.0741656131291,1077.55033423883,
506.661860383956));
#107116=CARTESIAN_POINT('Ctrl Pts',(-67.0591698389931,1077.55038821396,
506.673473544454));
#107117=CARTESIAN_POINT('Ctrl Pts',(-67.021952643986,1077.55064735473,506.700784421853));
#107118=CARTESIAN_POINT('Ctrl Pts',(-66.9994350087688,1077.5509079106,506.716055773345));
#107119=CARTESIAN_POINT('Ctrl Pts',(-66.9193343639818,1077.55218544493,
506.766143298981));
#107120=CARTESIAN_POINT('Ctrl Pts',(-66.8591513321462,1077.55374861682,
506.796489695749));
#107121=CARTESIAN_POINT('Ctrl Pts',(-66.6681341490792,1077.56044538203,
506.871749450635));
#107122=CARTESIAN_POINT('Ctrl Pts',(-66.5314743793487,1077.56754222529,
506.897628369571));
#107123=CARTESIAN_POINT('Ctrl Pts',(-66.3937896239304,1077.5767973048,506.897628369571));
#107124=CARTESIAN_POINT('',(-62.0518715958015,1076.69664647652,518.930937549326));
#107125=CARTESIAN_POINT('',(-62.0518715958009,1076.94043266168,516.749856051871));
#107126=CARTESIAN_POINT('Ctrl Pts',(-62.0518715958021,1076.69664647652,
518.930937549327));
#107127=CARTESIAN_POINT('Ctrl Pts',(-62.0309428736203,1076.69823468214,
518.930937549327));
#107128=CARTESIAN_POINT('Ctrl Pts',(-62.0099972381441,1076.69989227498,
518.93033508609));
#107129=CARTESIAN_POINT('Ctrl Pts',(-61.8702596372939,1076.71140673666,
518.922273344549));
#107130=CARTESIAN_POINT('Ctrl Pts',(-61.7535543466491,1076.72322347486,
518.896032706119));
#107131=CARTESIAN_POINT('Ctrl Pts',(-61.5232595973848,1076.75112850709,
518.803033990147));
#107132=CARTESIAN_POINT('Ctrl Pts',(-61.4127569856185,1076.76729365557,
518.733459504443));
#107133=CARTESIAN_POINT('Ctrl Pts',(-61.2139218145621,1076.80255979482,
518.552171175206));
#107134=CARTESIAN_POINT('Ctrl Pts',(-61.1297606841958,1076.82148425931,
518.439134765405));
#107135=CARTESIAN_POINT('Ctrl Pts',(-61.0064647608932,1076.85917061545,
518.182943057433));
#107136=CARTESIAN_POINT('Ctrl Pts',(-60.9702209374447,1076.87755055723,
518.041234693432));
#107137=CARTESIAN_POINT('Ctrl Pts',(-60.9556737561427,1076.90983262079,
517.75846838187));
#107138=CARTESIAN_POINT('Ctrl Pts',(-60.9748424773294,1076.92362217153,
517.62019281886));
#107139=CARTESIAN_POINT('Ctrl Pts',(-61.0621948369667,1076.94537645386,
517.363549963148));
#107140=CARTESIAN_POINT('Ctrl Pts',(-61.1274639683931,1076.95338497051,
517.246765259848));
#107141=CARTESIAN_POINT('Ctrl Pts',(-61.2509713977901,1076.96067484561,
517.097751600319));
#107142=CARTESIAN_POINT('Ctrl Pts',(-61.2935481798764,1076.96232004537,
517.054322467613));
#107143=CARTESIAN_POINT('Ctrl Pts',(-61.3597302000752,1076.96374168155,
516.997229572262));
#107144=CARTESIAN_POINT('Ctrl Pts',(-61.3805619022868,1076.96404818309,
516.980551382795));
#107145=CARTESIAN_POINT('Ctrl Pts',(-61.4155780365264,1076.96433999714,
516.954566038484));
#107146=CARTESIAN_POINT('Ctrl Pts',(-61.4294038456974,1076.96440171807,
516.944796696053));
#107147=CARTESIAN_POINT('Ctrl Pts',(-61.4588678731883,1076.96442293565,
516.924989363265));
#107148=CARTESIAN_POINT('Ctrl Pts',(-61.4745463073216,1076.96437188453,
516.91502136754));
#107149=CARTESIAN_POINT('Ctrl Pts',(-61.5123304531631,1076.96410341071,
516.892333209576));
#107150=CARTESIAN_POINT('Ctrl Pts',(-61.5346419319995,1076.96383117584,
516.879978886678));
#107151=CARTESIAN_POINT('Ctrl Pts',(-61.6090510508618,1076.96255842063,
516.842122262473));
#107152=CARTESIAN_POINT('Ctrl Pts',(-61.6627392432878,1076.96107413403,
516.819997545311));
#107153=CARTESIAN_POINT('Ctrl Pts',(-61.8259400467811,1076.95494888004,
516.76749847443));
#107154=CARTESIAN_POINT('Ctrl Pts',(-61.9386176641616,1076.9486863086,516.749856051871));
#107155=CARTESIAN_POINT('Ctrl Pts',(-62.0518715958011,1076.94043266168,
516.749856051871));
#107156=CARTESIAN_POINT('Ctrl Pts',(-62.0518715958011,1076.94043266168,
516.749856051871));
#107157=CARTESIAN_POINT('Ctrl Pts',(-62.0518860945413,1076.94043160505,
516.749856051871));
#107158=CARTESIAN_POINT('Ctrl Pts',(-62.0519005932904,1076.94043054838,
516.749856052221));
#107159=CARTESIAN_POINT('Ctrl Pts',(-62.0519150920495,1076.94042949168,
516.749856052799));
#107160=CARTESIAN_POINT('Ctrl Pts',(-62.1689455307399,1076.93190010702,
516.74986072057));
#107161=CARTESIAN_POINT('Ctrl Pts',(-62.285050312318,1076.92135637129,516.768701950391));
#107162=CARTESIAN_POINT('Ctrl Pts',(-62.5175394541443,1076.89581215433,
516.845968825757));
#107163=CARTESIAN_POINT('Ctrl Pts',(-62.6310190020822,1076.88066991008,
516.907530197521));
#107164=CARTESIAN_POINT('Ctrl Pts',(-62.8394594150589,1076.84686333787,
517.07348046616));
#107165=CARTESIAN_POINT('Ctrl Pts',(-62.9303300689801,1076.82830263051,
517.179540249254));
#107166=CARTESIAN_POINT('Ctrl Pts',(-63.0708671223406,1076.7902651475,517.425692916797));
#107167=CARTESIAN_POINT('Ctrl Pts',(-63.1169984188379,1076.77114306749,
517.564894100113));
#107168=CARTESIAN_POINT('Ctrl Pts',(-63.1513190562355,1076.7365705027,517.848010775854));
#107169=CARTESIAN_POINT('Ctrl Pts',(-63.1413083435132,1076.72131909065,
517.989032987736));
#107170=CARTESIAN_POINT('Ctrl Pts',(-63.0720823829983,1076.69736849267,
518.245588451812));
#107171=CARTESIAN_POINT('Ctrl Pts',(-63.0187168505342,1076.68832791401,
518.360306003776));
#107172=CARTESIAN_POINT('Ctrl Pts',(-62.899836155743,1076.67786005376,518.531054132045));
#107173=CARTESIAN_POINT('Ctrl Pts',(-62.8452960169199,1076.67491672067,
518.59308750105));
#107174=CARTESIAN_POINT('Ctrl Pts',(-62.7615126542785,1076.67260893543,
518.669028856576));
#107175=CARTESIAN_POINT('Ctrl Pts',(-62.7379049398262,1076.67215874285,
518.68867746773));
#107176=CARTESIAN_POINT('Ctrl Pts',(-62.6977606012892,1076.67171059659,
518.71931569315));
#107177=CARTESIAN_POINT('Ctrl Pts',(-62.6816992167771,1076.67160888965,
518.730895664975));
#107178=CARTESIAN_POINT('Ctrl Pts',(-62.6500338078085,1076.6715554871,518.75244034779));
#107179=CARTESIAN_POINT('Ctrl Pts',(-62.6344741045533,1076.67159442363,
518.762457412867));
#107180=CARTESIAN_POINT('Ctrl Pts',(-62.5978415909017,1076.67183458187,
518.784743194191));
#107181=CARTESIAN_POINT('Ctrl Pts',(-62.5765979847648,1076.67208333266,
518.796710272157));
#107182=CARTESIAN_POINT('Ctrl Pts',(-62.5091961101175,1076.67320687118,
518.831757187203));
#107183=CARTESIAN_POINT('Ctrl Pts',(-62.4617991714205,1076.67446907833,
518.852275281));
#107184=CARTESIAN_POINT('Ctrl Pts',(-62.2967790475951,1076.68040509685,
518.910213838104));
#107185=CARTESIAN_POINT('Ctrl Pts',(-62.174616158295,1076.68733183217,518.930937549327));
#107186=CARTESIAN_POINT('Ctrl Pts',(-62.0518715958021,1076.69664647652,
518.930937549327));
#107187=CARTESIAN_POINT('',(-79.4772023228642,1078.65448750233,467.378693963514));
#107188=CARTESIAN_POINT('',(-79.4772023228643,1078.68962000954,464.422087699128));
#107189=CARTESIAN_POINT('Ctrl Pts',(-79.4772023228642,1078.65448750233,
467.378693963514));
#107190=CARTESIAN_POINT('Ctrl Pts',(-79.4699089493478,1078.65467754156,
467.378693963514));
#107191=CARTESIAN_POINT('Ctrl Pts',(-79.4626135119311,1078.65486804194,
467.37863998956));
#107192=CARTESIAN_POINT('Ctrl Pts',(-79.2756436512785,1078.6597605043,467.375871667671));
#107193=CARTESIAN_POINT('Ctrl Pts',(-79.0979527863087,1078.66464638793,
467.340473831258));
#107194=CARTESIAN_POINT('Ctrl Pts',(-78.7518256378851,1078.67449916672,
467.202841918134));
#107195=CARTESIAN_POINT('Ctrl Pts',(-78.5883194849916,1078.67934854359,
467.097238535432));
#107196=CARTESIAN_POINT('Ctrl Pts',(-78.3103484198939,1078.68806921248,
466.828506201587));
#107197=CARTESIAN_POINT('Ctrl Pts',(-78.1988374302271,1078.69185430098,
466.667683721362));
#107198=CARTESIAN_POINT('Ctrl Pts',(-78.0504298588254,1078.69784732802,
466.326410125835));
#107199=CARTESIAN_POINT('Ctrl Pts',(-78.0094872349183,1078.7001144017,466.151368340374));
#107200=CARTESIAN_POINT('Ctrl Pts',(-77.9921230780727,1078.70345252511,
465.799565326274));
#107201=CARTESIAN_POINT('Ctrl Pts',(-78.0142689356406,1078.70453002986,
465.625701199463));
#107202=CARTESIAN_POINT('Ctrl Pts',(-78.0791044252518,1078.70520849538,
465.418104226389));
#107203=CARTESIAN_POINT('Ctrl Pts',(-78.0939238002015,1078.70531014839,
465.377113998268));
#107204=CARTESIAN_POINT('Ctrl Pts',(-78.1214134034484,1078.70542214597,
465.310449007007));
#107205=CARTESIAN_POINT('Ctrl Pts',(-78.1330571459278,1078.70545185736,
465.28438052663));
#107206=CARTESIAN_POINT('Ctrl Pts',(-78.1553956241902,1078.70547912026,
465.23802212617));
#107207=CARTESIAN_POINT('Ctrl Pts',(-78.1658215987045,1078.70548185375,
465.217612795024));
#107208=CARTESIAN_POINT('Ctrl Pts',(-78.1890012309822,1078.70546766202,
465.174728774328));
#107209=CARTESIAN_POINT('Ctrl Pts',(-78.2018782554098,1078.70544819281,
465.152329338921));
#107210=CARTESIAN_POINT('Ctrl Pts',(-78.2377454740045,1078.70536440738,
465.093559117774));
#107211=CARTESIAN_POINT('Ctrl Pts',(-78.2617474687001,1078.70527893133,
465.057835087687));
#107212=CARTESIAN_POINT('Ctrl Pts',(-78.3753394022478,1078.7047501631,464.903743500304));
#107213=CARTESIAN_POINT('Ctrl Pts',(-78.4808956004949,1078.70394945296,
464.798220491965));
#107214=CARTESIAN_POINT('Ctrl Pts',(-78.7219583311996,1078.70150402876,
464.620629726257));
#107215=CARTESIAN_POINT('Ctrl Pts',(-78.8565367240314,1078.6998573544,464.550222893131));
#107216=CARTESIAN_POINT('Ctrl Pts',(-79.1532470397934,1078.69553189093,
464.448890448833));
#107217=CARTESIAN_POINT('Ctrl Pts',(-79.314675118167,1078.69281018161,464.422087699128));
#107218=CARTESIAN_POINT('Ctrl Pts',(-79.4772023228643,1078.68962000954,
464.422087699128));
#107219=CARTESIAN_POINT('Ctrl Pts',(-79.4772023228643,1078.68962000954,
464.422087699128));
#107220=CARTESIAN_POINT('Ctrl Pts',(-79.4772374221895,1078.68961932059,
464.422087699128));
#107221=CARTESIAN_POINT('Ctrl Pts',(-79.4772725215661,1078.68961863162,
464.422087700378));
#107222=CARTESIAN_POINT('Ctrl Pts',(-79.4773076209938,1078.68961794263,
464.422087702878));
#107223=CARTESIAN_POINT('Ctrl Pts',(-79.6578351445778,1078.68607423721,
464.422100561682));
#107224=CARTESIAN_POINT('Ctrl Pts',(-79.8368317539902,1078.68200453645,
464.455181557539));
#107225=CARTESIAN_POINT('Ctrl Pts',(-80.1867070141573,1078.67273506018,
464.589033850225));
#107226=CARTESIAN_POINT('Ctrl Pts',(-80.3525644969555,1078.66756098388,
464.693414859106));
#107227=CARTESIAN_POINT('Ctrl Pts',(-80.6340883428405,1078.65714770488,
464.959929228747));
#107228=CARTESIAN_POINT('Ctrl Pts',(-80.747171545548,1078.65201361478,465.119342388313));
#107229=CARTESIAN_POINT('Ctrl Pts',(-80.8991659411406,1078.64310800614,
465.458632852703));
#107230=CARTESIAN_POINT('Ctrl Pts',(-80.9420213988041,1078.63933891585,
465.633099070356));
#107231=CARTESIAN_POINT('Ctrl Pts',(-80.9635642652209,1078.6334210861,465.98865397077));
#107232=CARTESIAN_POINT('Ctrl Pts',(-80.9421536870177,1078.63132275593,
466.16682496811));
#107233=CARTESIAN_POINT('Ctrl Pts',(-80.8765123219844,1078.63000398886,
466.379215479463));
#107234=CARTESIAN_POINT('Ctrl Pts',(-80.8615403073948,1078.62980609902,
466.420919326469));
#107235=CARTESIAN_POINT('Ctrl Pts',(-80.8337123344805,1078.62958784544,
466.488693830072));
#107236=CARTESIAN_POINT('Ctrl Pts',(-80.821920249749,1078.62952980067,466.515170087636));
#107237=CARTESIAN_POINT('Ctrl Pts',(-80.7992810929771,1078.62947641098,
466.562227751899));
#107238=CARTESIAN_POINT('Ctrl Pts',(-80.7887119724455,1078.62947093756,
466.582932275856));
#107239=CARTESIAN_POINT('Ctrl Pts',(-80.7652055309049,1078.6294982132,466.626416808503));
#107240=CARTESIAN_POINT('Ctrl Pts',(-80.7521420032339,1078.62953588985,
466.64911961512));
#107241=CARTESIAN_POINT('Ctrl Pts',(-80.7157427964114,1078.62969797923,
466.708659528841));
#107242=CARTESIAN_POINT('Ctrl Pts',(-80.6913690895156,1078.6298633371,466.744831364274));
#107243=CARTESIAN_POINT('Ctrl Pts',(-80.5758345934766,1078.63088139912,
466.900925063529));
#107244=CARTESIAN_POINT('Ctrl Pts',(-80.4682664607717,1078.63242197353,
467.007571660406));
#107245=CARTESIAN_POINT('Ctrl Pts',(-80.2243697756869,1078.63681484799,
467.184877133115));
#107246=CARTESIAN_POINT('Ctrl Pts',(-80.0894097608931,1078.6396428075,467.254407262539));
#107247=CARTESIAN_POINT('Ctrl Pts',(-79.795016720375,1078.646399601,467.352912073684));
#107248=CARTESIAN_POINT('Ctrl Pts',(-79.6366024626598,1078.6503341046,467.378693963515));
#107249=CARTESIAN_POINT('Ctrl Pts',(-79.4772023228642,1078.65448750233,
467.378693963515));
#107250=CARTESIAN_POINT('',(-81.0356882485059,1078.30327084026,478.72049644629));
#107251=CARTESIAN_POINT('',(-81.035688248506,1078.39243716831,476.169608204017));
#107252=CARTESIAN_POINT('Ctrl Pts',(-81.0356882485058,1078.30327084026,
478.72049644629));
#107253=CARTESIAN_POINT('Ctrl Pts',(-81.0246146286944,1078.30389283659,
478.72049644629));
#107254=CARTESIAN_POINT('Ctrl Pts',(-81.013536285703,1078.30451982721,478.720352232097));
#107255=CARTESIAN_POINT('Ctrl Pts',(-80.849922124026,1078.31384932016,478.716087747516));
#107256=CARTESIAN_POINT('Ctrl Pts',(-80.6993645438354,1078.32332388982,
478.684773255856));
#107257=CARTESIAN_POINT('Ctrl Pts',(-80.406120054577,1078.34352880323,478.566307789147));
#107258=CARTESIAN_POINT('Ctrl Pts',(-80.2675087598995,1078.35411307893,
478.476302582562));
#107259=CARTESIAN_POINT('Ctrl Pts',(-80.0287142245288,1078.37463495229,
478.245708296621));
#107260=CARTESIAN_POINT('Ctrl Pts',(-79.9319852644289,1078.38434954179,
478.106051722543));
#107261=CARTESIAN_POINT('Ctrl Pts',(-79.8016771481059,1078.40100347093,
477.804932762459));
#107262=CARTESIAN_POINT('Ctrl Pts',(-79.7663133135025,1078.40791484644,
477.647584775361));
#107263=CARTESIAN_POINT('Ctrl Pts',(-79.7555600297393,1078.41884496892,
477.326581155275));
#107264=CARTESIAN_POINT('Ctrl Pts',(-79.7807759131022,1078.42274366209,
477.165797839069));
#107265=CARTESIAN_POINT('Ctrl Pts',(-79.8544214029996,1078.42568001192,
476.960734248989));
#107266=CARTESIAN_POINT('Ctrl Pts',(-79.8770533837945,1078.42622650527,
476.908842398745));
#107267=CARTESIAN_POINT('Ctrl Pts',(-79.9149852322163,1078.42670603233,
476.835580661151));
#107268=CARTESIAN_POINT('Ctrl Pts',(-79.9276157778859,1078.4268108751,476.81290805346));
#107269=CARTESIAN_POINT('Ctrl Pts',(-79.9510641285986,1078.42691440006,
476.773681786644));
#107270=CARTESIAN_POINT('Ctrl Pts',(-79.9615916111564,1078.42693243605,
476.756964905051));
#107271=CARTESIAN_POINT('Ctrl Pts',(-79.9840377208164,1078.4269145742,476.723093261105));
#107272=CARTESIAN_POINT('Ctrl Pts',(-79.995998033311,1078.42687554031,476.705973185222));
#107273=CARTESIAN_POINT('Ctrl Pts',(-80.0272864672442,1078.42670142049,
476.663450137169));
#107274=CARTESIAN_POINT('Ctrl Pts',(-80.047157582036,1078.42652655107,476.638464941525));
#107275=CARTESIAN_POINT('Ctrl Pts',(-80.1267336508165,1078.42559146828,
476.5457721397));
#107276=CARTESIAN_POINT('Ctrl Pts',(-80.1926209575092,1078.42434875834,
476.483731250177));
#107277=CARTESIAN_POINT('Ctrl Pts',(-80.3621838379226,1078.42014554662,
476.355010072729));
#107278=CARTESIAN_POINT('Ctrl Pts',(-80.4700396685857,1078.41675072151,
476.2953437933));
#107279=CARTESIAN_POINT('Ctrl Pts',(-80.7288782737061,1078.40704842616,
476.197504052671));
#107280=CARTESIAN_POINT('Ctrl Pts',(-80.8816760726839,1078.4002949488,476.169608204017));
#107281=CARTESIAN_POINT('Ctrl Pts',(-81.035688248506,1078.39243716831,476.169608204017));
#107282=CARTESIAN_POINT('Ctrl Pts',(-81.035688248506,1078.39243716831,476.169608204017));
#107283=CARTESIAN_POINT('Ctrl Pts',(-81.0357370854227,1078.39243467663,
476.169608204017));
#107284=CARTESIAN_POINT('Ctrl Pts',(-81.0357859224614,1078.39243218483,
476.169608206822));
#107285=CARTESIAN_POINT('Ctrl Pts',(-81.0358347596221,1078.39242969293,
476.169608212432));
#107286=CARTESIAN_POINT('Ctrl Pts',(-81.1884097858379,1078.38464458215,
476.169625738827));
#107287=CARTESIAN_POINT('Ctrl Pts',(-81.339705315759,1078.37589900606,476.197020008355));
#107288=CARTESIAN_POINT('Ctrl Pts',(-81.6362043920957,1078.35649949467,
476.307925396765));
#107289=CARTESIAN_POINT('Ctrl Pts',(-81.7773384188491,1078.34592786177,
476.394517607236));
#107290=CARTESIAN_POINT('Ctrl Pts',(-82.0221363012155,1078.32463965672,
476.619227519744));
#107291=CARTESIAN_POINT('Ctrl Pts',(-82.1223813506698,1078.31413352335,
476.756439070523));
#107292=CARTESIAN_POINT('Ctrl Pts',(-82.260471498279,1078.29547961063,477.054697824724));
#107293=CARTESIAN_POINT('Ctrl Pts',(-82.2998260628927,1078.28741236139,
477.211674781804));
#107294=CARTESIAN_POINT('Ctrl Pts',(-82.3180260970581,1078.27452931816,
477.528409403417));
#107295=CARTESIAN_POINT('Ctrl Pts',(-82.2980854407609,1078.26975642285,
477.685309053818));
#107296=CARTESIAN_POINT('Ctrl Pts',(-82.2302887610955,1078.26569519593,
477.896624925614));
#107297=CARTESIAN_POINT('Ctrl Pts',(-82.2057090814756,1078.26483744237,
477.956951338812));
#107298=CARTESIAN_POINT('Ctrl Pts',(-82.1637895291425,1078.26409446277,
478.040846633512));
#107299=CARTESIAN_POINT('Ctrl Pts',(-82.1500809942766,1078.26393382971,
478.066109657378));
#107300=CARTESIAN_POINT('Ctrl Pts',(-82.1253253740612,1078.26377514787,
478.108267852636));
#107301=CARTESIAN_POINT('Ctrl Pts',(-82.1147094808373,1078.26374289417,
478.125403033569));
#107302=CARTESIAN_POINT('Ctrl Pts',(-82.092485377571,1078.26374479904,478.159445633166));
#107303=CARTESIAN_POINT('Ctrl Pts',(-82.080866558139,1078.26378010682,478.176339045595));
#107304=CARTESIAN_POINT('Ctrl Pts',(-82.0515873176963,1078.26394966612,
478.21678611052));
#107305=CARTESIAN_POINT('Ctrl Pts',(-82.0335091520795,1078.26412027579,
478.240022357411));
#107306=CARTESIAN_POINT('Ctrl Pts',(-81.9677280412465,1078.26496015125,
478.318789414217));
#107307=CARTESIAN_POINT('Ctrl Pts',(-81.9160676781231,1078.26599227478,
478.370819582238));
#107308=CARTESIAN_POINT('Ctrl Pts',(-81.730506780143,1078.27081218889,478.528056937085));
#107309=CARTESIAN_POINT('Ctrl Pts',(-81.5801458160651,1078.27639325169,
478.610898179553));
#107310=CARTESIAN_POINT('Ctrl Pts',(-81.2942153277187,1078.28939691917,
478.700746590495));
#107311=CARTESIAN_POINT('Ctrl Pts',(-81.1652752015319,1078.2959920452,478.72049644629));
#107312=CARTESIAN_POINT('Ctrl Pts',(-81.0356882485059,1078.30327084026,
478.72049644629));
#107313=CARTESIAN_POINT('',(-81.8208965804703,1077.59408165985,491.319637120915));
#107314=CARTESIAN_POINT('',(-81.8208965804704,1077.73591376921,489.12197484893));
#107315=CARTESIAN_POINT('Ctrl Pts',(-81.8208965804702,1077.59408165985,
491.319637120915));
#107316=CARTESIAN_POINT('Ctrl Pts',(-81.8118915361856,1077.59482365131,
491.319637120915));
#107317=CARTESIAN_POINT('Ctrl Pts',(-81.8028833073338,1077.59557296073,
491.319526425073));
#107318=CARTESIAN_POINT('Ctrl Pts',(-81.6650299504941,1077.60714761654,
491.316135283922));
#107319=CARTESIAN_POINT('Ctrl Pts',(-81.5378374876298,1077.61926824562,
491.29032572045));
#107320=CARTESIAN_POINT('Ctrl Pts',(-81.2890739137649,1077.64591676414,
491.192312092427));
#107321=CARTESIAN_POINT('Ctrl Pts',(-81.1708563653607,1077.66032580353,
491.117520350974));
#107322=CARTESIAN_POINT('Ctrl Pts',(-80.9632826475642,1077.68950111704,
490.923075558048));
#107323=CARTESIAN_POINT('Ctrl Pts',(-80.8777154171757,1077.70396840503,
490.803164881407));
#107324=CARTESIAN_POINT('Ctrl Pts',(-80.7603977399351,1077.7298560879,490.541226072427));
#107325=CARTESIAN_POINT('Ctrl Pts',(-80.7280107668011,1077.74112818323,
490.402466783174));
#107326=CARTESIAN_POINT('Ctrl Pts',(-80.7182084710857,1077.75856843853,
490.136304571665));
#107327=CARTESIAN_POINT('Ctrl Pts',(-80.7349615340522,1077.76504817312,
490.011397952834));
#107328=CARTESIAN_POINT('Ctrl Pts',(-80.7976636227379,1077.77261702441,
489.811502576923));
#107329=CARTESIAN_POINT('Ctrl Pts',(-80.832069735605,1077.77474978174,489.734221745625));
#107330=CARTESIAN_POINT('Ctrl Pts',(-80.8898798419136,1077.77634356121,
489.636431121329));
#107331=CARTESIAN_POINT('Ctrl Pts',(-80.9057720620957,1077.77663908756,
489.611845063301));
#107332=CARTESIAN_POINT('Ctrl Pts',(-80.9331333362566,1077.77693110706,
489.573010483975));
#107333=CARTESIAN_POINT('Ctrl Pts',(-80.9440090522601,1077.77699826122,
489.558362881511));
#107334=CARTESIAN_POINT('Ctrl Pts',(-80.9654901296214,1077.77704056502,
489.530888332557));
#107335=CARTESIAN_POINT('Ctrl Pts',(-80.976032040185,1077.77702329235,489.518018342442));
#107336=CARTESIAN_POINT('Ctrl Pts',(-81.0007633359159,1077.77689835396,
489.48918640079));
#107337=CARTESIAN_POINT('Ctrl Pts',(-81.0151338254733,1077.77676647083,
489.473389028346));
#107338=CARTESIAN_POINT('Ctrl Pts',(-81.0600520314457,1077.77618036466,
489.42681279229));
#107339=CARTESIAN_POINT('Ctrl Pts',(-81.0919670543924,1077.77553457296,
489.397416206979));
#107340=CARTESIAN_POINT('Ctrl Pts',(-81.1684314400932,1077.77349358948,
489.334922941254));
#107341=CARTESIAN_POINT('Ctrl Pts',(-81.2139127955276,1077.77194298042,
489.303163477479));
#107342=CARTESIAN_POINT('Ctrl Pts',(-81.3532708389864,1077.76625856801,
489.220754906984));
#107343=CARTESIAN_POINT('Ctrl Pts',(-81.4522991486972,1077.7610929863,489.180188351247));
#107344=CARTESIAN_POINT('Ctrl Pts',(-81.642393652247,1077.74922189726,489.132882805429));
#107345=CARTESIAN_POINT('Ctrl Pts',(-81.7315060347125,1077.74293575321,
489.12197484893));
#107346=CARTESIAN_POINT('Ctrl Pts',(-81.8208965804703,1077.73591376921,
489.12197484893));
#107347=CARTESIAN_POINT('Ctrl Pts',(-81.8208965804703,1077.73591376921,
489.12197484893));
#107348=CARTESIAN_POINT('Ctrl Pts',(-81.8209326256086,1077.73591093772,
489.12197484893));
#107349=CARTESIAN_POINT('Ctrl Pts',(-81.8209686707924,1077.73590810611,
489.121974850652));
#107350=CARTESIAN_POINT('Ctrl Pts',(-81.821004716021,1077.73590527439,489.121974854199));
#107351=CARTESIAN_POINT('Ctrl Pts',(-81.9496463542983,1077.72579913187,
489.121987513779));
#107352=CARTESIAN_POINT('Ctrl Pts',(-82.0771879486502,1077.71429939178,
489.144588824965));
#107353=CARTESIAN_POINT('Ctrl Pts',(-82.3281263519596,1077.68850371663,
489.236232017209));
#107354=CARTESIAN_POINT('Ctrl Pts',(-82.4481876460914,1077.67428167137,
489.308035833405));
#107355=CARTESIAN_POINT('Ctrl Pts',(-82.6606397964049,1077.64490782975,
489.497244059042));
#107356=CARTESIAN_POINT('Ctrl Pts',(-82.749220716077,1077.63002708413,489.61503396911));
#107357=CARTESIAN_POINT('Ctrl Pts',(-82.8731942416252,1077.60287597756,
489.874276442954));
#107358=CARTESIAN_POINT('Ctrl Pts',(-82.9090585203821,1077.59078683123,
490.012502904669));
#107359=CARTESIAN_POINT('Ctrl Pts',(-82.9251666420322,1077.57194715739,
490.276411796771));
#107360=CARTESIAN_POINT('Ctrl Pts',(-82.91206039424,1077.56483498601,490.399452575105));
#107361=CARTESIAN_POINT('Ctrl Pts',(-82.8537628365387,1077.55582790869,
490.607078570887));
#107362=CARTESIAN_POINT('Ctrl Pts',(-82.8175118277962,1077.55311660244,
490.692812219282));
#107363=CARTESIAN_POINT('Ctrl Pts',(-82.755506224016,1077.55115312648,490.799488581695));
#107364=CARTESIAN_POINT('Ctrl Pts',(-82.7390062251826,1077.55080121714,
490.825325305712));
#107365=CARTESIAN_POINT('Ctrl Pts',(-82.7107542610172,1077.5504550759,490.865733425717));
#107366=CARTESIAN_POINT('Ctrl Pts',(-82.699673504174,1077.55037484557,490.880752370421));
#107367=CARTESIAN_POINT('Ctrl Pts',(-82.6779419108619,1077.5503191592,490.908689071181));
#107368=CARTESIAN_POINT('Ctrl Pts',(-82.6673679989646,1077.55033373751,
490.921659732327));
#107369=CARTESIAN_POINT('Ctrl Pts',(-82.6428036944148,1077.55045913459,
490.950424732042));
#107370=CARTESIAN_POINT('Ctrl Pts',(-82.6286465420175,1077.550594023,490.966067540874));
#107371=CARTESIAN_POINT('Ctrl Pts',(-82.5852589271665,1077.55118740396,
491.011318758765));
#107372=CARTESIAN_POINT('Ctrl Pts',(-82.5547905059292,1077.55183252429,
491.039682847927));
#107373=CARTESIAN_POINT('Ctrl Pts',(-82.4106545990951,1077.55585409507,
491.159345734858));
#107374=CARTESIAN_POINT('Ctrl Pts',(-82.2812024659983,1077.56198577209,
491.229134551155));
#107375=CARTESIAN_POINT('Ctrl Pts',(-82.0378234752273,1077.57723552437,
491.303508793025));
#107376=CARTESIAN_POINT('Ctrl Pts',(-81.9295920155049,1077.58512544789,
491.319637120915));
#107377=CARTESIAN_POINT('Ctrl Pts',(-81.8208965804703,1077.59408165985,
491.319637120915));
#107378=CARTESIAN_POINT('',(-88.5622696992322,1078.67883079978,412.779359758956));
#107379=CARTESIAN_POINT('',(-88.5622696999027,1078.6674873026,409.822753494571));
#107380=CARTESIAN_POINT('Ctrl Pts',(-88.5622696992322,1078.67883079978,
412.779359758958));
#107381=CARTESIAN_POINT('Ctrl Pts',(-88.3720465431456,1078.68346300856,
412.779359758958));
#107382=CARTESIAN_POINT('Ctrl Pts',(-88.1835393752714,1078.68762476377,
412.742643006163));
#107383=CARTESIAN_POINT('Ctrl Pts',(-87.8330299621801,1078.69469627254,
412.600624952613));
#107384=CARTESIAN_POINT('Ctrl Pts',(-87.6739489247432,1078.69756238392,
412.497535482797));
#107385=CARTESIAN_POINT('Ctrl Pts',(-87.4110242733929,1078.70187707695,
412.245095658751));
#107386=CARTESIAN_POINT('Ctrl Pts',(-87.3065626456926,1078.70337092014,
412.100918382936));
#107387=CARTESIAN_POINT('Ctrl Pts',(-87.1922830720543,1078.70477103525,
411.863280437301));
#107388=CARTESIAN_POINT('Ctrl Pts',(-87.1615575513009,1078.70509473567,
411.781644408685));
#107389=CARTESIAN_POINT('Ctrl Pts',(-87.1288978711513,1078.70535802001,
411.664409618201));
#107390=CARTESIAN_POINT('Ctrl Pts',(-87.1207771437061,1078.70541138917,
411.630722228774));
#107391=CARTESIAN_POINT('Ctrl Pts',(-87.1092252263883,1078.70546453852,
411.574142281458));
#107392=CARTESIAN_POINT('Ctrl Pts',(-87.1051345194932,1078.70547623568,
411.551398557956));
#107393=CARTESIAN_POINT('Ctrl Pts',(-87.0981626334012,1078.7054804261,411.50663702773));
#107394=CARTESIAN_POINT('Ctrl Pts',(-87.0952410569726,1078.70547365665,
411.484631579642));
#107395=CARTESIAN_POINT('Ctrl Pts',(-87.0895162870177,1078.70543683694,
411.432547037356));
#107396=CARTESIAN_POINT('Ctrl Pts',(-87.0871373275958,1078.70539928134,
411.402431296504));
#107397=CARTESIAN_POINT('Ctrl Pts',(-87.082411904188,1078.70522408831,411.304442748419));
#107398=CARTESIAN_POINT('Ctrl Pts',(-87.0838178213005,1078.70502038877,
411.236476986767));
#107399=CARTESIAN_POINT('Ctrl Pts',(-87.1075152500637,1078.70389881578,
410.972560504793));
#107400=CARTESIAN_POINT('Ctrl Pts',(-87.1642153990549,1078.70237783114,
410.781768540865));
#107401=CARTESIAN_POINT('Ctrl Pts',(-87.3323601198773,1078.69825985756,
410.465134173314));
#107402=CARTESIAN_POINT('Ctrl Pts',(-87.4309231016497,1078.69592960438,
410.335917043225));
#107403=CARTESIAN_POINT('Ctrl Pts',(-87.6762789245318,1078.69004880737,
410.104698021033));
#107404=CARTESIAN_POINT('Ctrl Pts',(-87.8246111859352,1078.68645095964,
410.007957014957));
#107405=CARTESIAN_POINT('Ctrl Pts',(-88.1603822288219,1078.67803437732,
409.865946290356));
#107406=CARTESIAN_POINT('Ctrl Pts',(-88.3468328146265,1078.67321809151,
409.826391913944));
#107407=CARTESIAN_POINT('Ctrl Pts',(-88.5445356951068,1078.66795983999,
409.822833239939));
#107408=CARTESIAN_POINT('Ctrl Pts',(-88.5534044842976,1078.66772366684,
409.822753494563));
#107409=CARTESIAN_POINT('Ctrl Pts',(-88.5622697005729,1078.6674873026,409.822753494571));
#107410=CARTESIAN_POINT('Ctrl Pts',(-88.5622697005729,1078.6674873026,409.822753494571));
#107411=CARTESIAN_POINT('Ctrl Pts',(-88.7482632788002,1078.66252834504,
409.82275349474));
#107412=CARTESIAN_POINT('Ctrl Pts',(-88.9326839838793,1078.65747797831,
409.857856290321));
#107413=CARTESIAN_POINT('Ctrl Pts',(-89.2800864525725,1078.64789049099,
409.995207055741));
#107414=CARTESIAN_POINT('Ctrl Pts',(-89.4397013581415,1078.64345127623,
410.096636922239));
#107415=CARTESIAN_POINT('Ctrl Pts',(-89.7035541722497,1078.6363283406,410.345277781389));
#107416=CARTESIAN_POINT('Ctrl Pts',(-89.8086570987339,1078.63360899343,
410.487072400501));
#107417=CARTESIAN_POINT('Ctrl Pts',(-89.9270742879669,1078.63091347673,
410.725713827499));
#107418=CARTESIAN_POINT('Ctrl Pts',(-89.959986675958,1078.63025236458,410.811057805764));
#107419=CARTESIAN_POINT('Ctrl Pts',(-89.994507635958,1078.62971995358,410.933166340795));
#107420=CARTESIAN_POINT('Ctrl Pts',(-90.0029554151524,1078.62961297761,
410.967779783559));
#107421=CARTESIAN_POINT('Ctrl Pts',(-90.0148960647361,1078.62950648655,
411.025718890385));
#107422=CARTESIAN_POINT('Ctrl Pts',(-90.0190960092562,1078.62948284379,
411.048883412025));
#107423=CARTESIAN_POINT('Ctrl Pts',(-90.0262181507212,1078.62947332018,
411.094321821039));
#107424=CARTESIAN_POINT('Ctrl Pts',(-90.0291893723829,1078.62948575078,
411.116581643447));
#107425=CARTESIAN_POINT('Ctrl Pts',(-90.0349780532876,1078.62955506483,
411.169035941086));
#107426=CARTESIAN_POINT('Ctrl Pts',(-90.0373758374848,1078.62962597853,
411.199266507595));
#107427=CARTESIAN_POINT('Ctrl Pts',(-90.0396300006932,1078.62978247808,
411.245813272079));
#107428=CARTESIAN_POINT('Ctrl Pts',(-90.0401488707183,1078.6298460624,411.262089135427));
#107429=CARTESIAN_POINT('Ctrl Pts',(-90.040398755281,1078.62991850175,411.278370581859));
#107430=CARTESIAN_POINT('Ctrl Pts',(-90.0421089956495,1078.63041428546,
411.389802783379));
#107431=CARTESIAN_POINT('Ctrl Pts',(-90.0312128827685,1078.63132398269,
411.501068368572));
#107432=CARTESIAN_POINT('Ctrl Pts',(-89.9779962522632,1078.63427467906,
411.750050090782));
#107433=CARTESIAN_POINT('Ctrl Pts',(-89.9278941082664,1078.63654858306,
411.884958985214));
#107434=CARTESIAN_POINT('Ctrl Pts',(-89.7817738647771,1078.64242142456,
412.152062147659));
#107435=CARTESIAN_POINT('Ctrl Pts',(-89.6817174915438,1078.64611047156,
412.279949410848));
#107436=CARTESIAN_POINT('Ctrl Pts',(-89.4342242384996,1078.65449935178,
412.507575555964));
#107437=CARTESIAN_POINT('Ctrl Pts',(-89.2854378955564,1078.65918827646,
412.602216692662));
#107438=CARTESIAN_POINT('Ctrl Pts',(-88.9500209872393,1078.66892647233,
412.739885380551));
#107439=CARTESIAN_POINT('Ctrl Pts',(-88.7644669161036,1078.67388501125,
412.777437263733));
#107440=CARTESIAN_POINT('Ctrl Pts',(-88.5719892200386,1078.67859384164,
412.779335800596));
#107441=CARTESIAN_POINT('Ctrl Pts',(-88.5671288996929,1078.67871247122,
412.779359758958));
#107442=CARTESIAN_POINT('Ctrl Pts',(-88.5622696992322,1078.67883079978,
412.779359758958));
#107443=CARTESIAN_POINT('',(-96.6088930673541,1078.35304757369,421.000273047718));
#107444=CARTESIAN_POINT('',(-96.6088930673544,1078.34478217746,418.449384805446));
#107445=CARTESIAN_POINT('Ctrl Pts',(-96.608893067354,1078.35304757369,421.000273047718));
#107446=CARTESIAN_POINT('Ctrl Pts',(-96.4411564053785,1078.36372558668,
421.000273047718));
#107447=CARTESIAN_POINT('Ctrl Pts',(-96.2750044101523,1078.37400306029,
420.967183692732));
#107448=CARTESIAN_POINT('Ctrl Pts',(-95.9679692011027,1078.39248845416,
420.839756898053));
#107449=CARTESIAN_POINT('Ctrl Pts',(-95.8295373430025,1078.40056280147,
420.747810081579));
#107450=CARTESIAN_POINT('Ctrl Pts',(-95.6123829417737,1078.412878806,420.53321688905));
#107451=CARTESIAN_POINT('Ctrl Pts',(-95.5293799427867,1078.41742648329,
420.418511532374));
#107452=CARTESIAN_POINT('Ctrl Pts',(-95.4165609832057,1078.42336871561,
420.191545765542));
#107453=CARTESIAN_POINT('Ctrl Pts',(-95.3799678353809,1078.4251832957,420.084313466252));
#107454=CARTESIAN_POINT('Ctrl Pts',(-95.3512046396373,1078.42643124959,
419.939713717261));
#107455=CARTESIAN_POINT('Ctrl Pts',(-95.3458366620551,1078.42664268365,
419.90550609858));
#107456=CARTESIAN_POINT('Ctrl Pts',(-95.3395277148658,1078.42684860335,
419.850865132454));
#107457=CARTESIAN_POINT('Ctrl Pts',(-95.3376749296248,1078.4268965,419.830554869784));
#107458=CARTESIAN_POINT('Ctrl Pts',(-95.3351138846986,1078.42693294963,
419.792382646171));
#107459=CARTESIAN_POINT('Ctrl Pts',(-95.3342925845398,1078.42692811306,
419.774533252375));
#107460=CARTESIAN_POINT('Ctrl Pts',(-95.3332974444016,1078.4268685624,419.73468693578));
#107461=CARTESIAN_POINT('Ctrl Pts',(-95.3333171057799,1078.42680259814,
419.71269091993));
#107462=CARTESIAN_POINT('Ctrl Pts',(-95.3350236084832,1078.42651536784,
419.648927201414));
#107463=CARTESIAN_POINT('Ctrl Pts',(-95.3381946140514,1078.4262079424,419.607228903325));
#107464=CARTESIAN_POINT('Ctrl Pts',(-95.3646195983356,1078.4240482944,419.396999232236));
#107465=CARTESIAN_POINT('Ctrl Pts',(-95.419373153071,1078.42037839787,419.234211423141));
#107466=CARTESIAN_POINT('Ctrl Pts',(-95.5725099644199,1078.41053271886,
418.969039496746));
#107467=CARTESIAN_POINT('Ctrl Pts',(-95.6590553100129,1078.4050613179,418.862799618694));
#107468=CARTESIAN_POINT('Ctrl Pts',(-95.8721100587869,1078.39162143158,
418.673089397293));
#107469=CARTESIAN_POINT('Ctrl Pts',(-96.0000096685498,1078.38356507368,
418.594236415888));
#107470=CARTESIAN_POINT('Ctrl Pts',(-96.2882865967761,1078.36529676825,
418.479874465366));
#107471=CARTESIAN_POINT('Ctrl Pts',(-96.4478799282913,1078.35512374414,
418.449384805446));
#107472=CARTESIAN_POINT('Ctrl Pts',(-96.6088930673548,1078.34478217746,
418.449384805446));
#107473=CARTESIAN_POINT('Ctrl Pts',(-96.6088930673548,1078.34478217746,
418.449384805446));
#107474=CARTESIAN_POINT('Ctrl Pts',(-96.6090238328897,1078.34477377864,
418.449384805446));
#107475=CARTESIAN_POINT('Ctrl Pts',(-96.6091545993613,1078.34476537971,
418.449384825556));
#107476=CARTESIAN_POINT('Ctrl Pts',(-96.6092853667651,1078.34475698068,
418.449384865777));
#107477=CARTESIAN_POINT('Ctrl Pts',(-96.7781840641058,1078.33390881808,
418.449436815417));
#107478=CARTESIAN_POINT('Ctrl Pts',(-96.9454236811818,1078.32308238173,
418.483037464539));
#107479=CARTESIAN_POINT('Ctrl Pts',(-97.2526487103228,1078.30313265084,
418.611605927842));
#107480=CARTESIAN_POINT('Ctrl Pts',(-97.3904437732686,1078.29415721113,
418.703602447287));
#107481=CARTESIAN_POINT('Ctrl Pts',(-97.6069684432521,1078.28017173905,
418.918348363267));
#107482=CARTESIAN_POINT('Ctrl Pts',(-97.689839152874,1078.2748765614,419.033347266563));
#107483=CARTESIAN_POINT('Ctrl Pts',(-97.8017923212791,1078.26794721432,
419.259806506448));
#107484=CARTESIAN_POINT('Ctrl Pts',(-97.8379520527778,1078.26581376158,
419.366113891067));
#107485=CARTESIAN_POINT('Ctrl Pts',(-97.8665581381454,1078.26433496545,
419.50979672806));
#107486=CARTESIAN_POINT('Ctrl Pts',(-97.8719396195343,1078.26408207387,
419.54407002045));
#107487=CARTESIAN_POINT('Ctrl Pts',(-97.8782748555643,1078.26383537897,
419.598932935124));
#107488=CARTESIAN_POINT('Ctrl Pts',(-97.8801383359718,1078.26377802594,
419.619399329966));
#107489=CARTESIAN_POINT('Ctrl Pts',(-97.8826989434441,1078.26373525483,
419.657769482161));
#107490=CARTESIAN_POINT('Ctrl Pts',(-97.8835148994611,1078.26374154366,
419.675660201531));
#107491=CARTESIAN_POINT('Ctrl Pts',(-97.8844999904487,1078.26381444934,
419.715832257367));
#107492=CARTESIAN_POINT('Ctrl Pts',(-97.8844625442838,1078.2638954001,419.738112705142));
#107493=CARTESIAN_POINT('Ctrl Pts',(-97.8826586561125,1078.26424800808,
419.802803525369));
#107494=CARTESIAN_POINT('Ctrl Pts',(-97.8793590894313,1078.26462575466,
419.845139695908));
#107495=CARTESIAN_POINT('Ctrl Pts',(-97.8522819676114,1078.26724351246,
420.056062005821));
#107496=CARTESIAN_POINT('Ctrl Pts',(-97.7970373399257,1078.27164432092,
420.218802382153));
#107497=CARTESIAN_POINT('Ctrl Pts',(-97.643243576394,1078.28310383072,420.483340876153));
#107498=CARTESIAN_POINT('Ctrl Pts',(-97.5566384047077,1078.28937278886,
420.589106385314));
#107499=CARTESIAN_POINT('Ctrl Pts',(-97.3439211599217,1078.30435189313,
420.777701893593));
#107500=CARTESIAN_POINT('Ctrl Pts',(-97.2164873800139,1078.31311945353,
420.856028921133));
#107501=CARTESIAN_POINT('Ctrl Pts',(-96.9301325538843,1078.33231895252,
420.969428425943));
#107502=CARTESIAN_POINT('Ctrl Pts',(-96.7720542839807,1078.34265680146,
420.99981801351));
#107503=CARTESIAN_POINT('Ctrl Pts',(-96.6112907641862,1078.35289492281,
421.000271357194));
#107504=CARTESIAN_POINT('Ctrl Pts',(-96.6100918752876,1078.35297125831,
421.000273047718));
#107505=CARTESIAN_POINT('Ctrl Pts',(-96.608893067354,1078.35304757369,421.000273047718));
#107506=CARTESIAN_POINT('',(-104.753539540172,1077.66045630879,430.69792801177));
#107507=CARTESIAN_POINT('',(-104.753539540172,1077.67122217491,428.500265739785));
#107508=CARTESIAN_POINT('Ctrl Pts',(-104.753539540173,1077.66045630879,
430.69792801177));
#107509=CARTESIAN_POINT('Ctrl Pts',(-104.665620762378,1077.66953439425,
430.69792801177));
#107510=CARTESIAN_POINT('Ctrl Pts',(-104.577820809394,1077.67861004491,
430.687375893461));
#107511=CARTESIAN_POINT('Ctrl Pts',(-104.351123445455,1077.70207399203,
430.63183273988));
#107512=CARTESIAN_POINT('Ctrl Pts',(-104.218319609593,1077.71585004638,
430.569706428685));
#107513=CARTESIAN_POINT('Ctrl Pts',(-103.991013504431,1077.73957922168,
430.402083048091));
#107514=CARTESIAN_POINT('Ctrl Pts',(-103.896754594879,1077.74949975389,
430.300681307374));
#107515=CARTESIAN_POINT('Ctrl Pts',(-103.751674047223,1077.76506878071,
430.070177655793));
#107516=CARTESIAN_POINT('Ctrl Pts',(-103.701384955506,1077.77065556777,
429.943581637273));
#107517=CARTESIAN_POINT('Ctrl Pts',(-103.665470205862,1077.77507824458,
429.760799175423));
#107518=CARTESIAN_POINT('Ctrl Pts',(-103.659125711864,1077.77594593367,
429.710011696374));
#107519=CARTESIAN_POINT('Ctrl Pts',(-103.655144653883,1077.776683831,429.637047095014));
#107520=CARTESIAN_POINT('Ctrl Pts',(-103.654605759401,1077.77684051502,
429.615101075762));
#107521=CARTESIAN_POINT('Ctrl Pts',(-103.654799106998,1077.77698962827,
429.579356677061));
#107522=CARTESIAN_POINT('Ctrl Pts',(-103.655133568426,1077.77702143461,
429.565562705391));
#107523=CARTESIAN_POINT('Ctrl Pts',(-103.656376372779,1077.77703407627,
429.536728899218));
#107524=CARTESIAN_POINT('Ctrl Pts',(-103.657334452703,1077.77700996203,
429.521694130414));
#107525=CARTESIAN_POINT('Ctrl Pts',(-103.660332586206,1077.77688024178,
429.486171312399));
#107526=CARTESIAN_POINT('Ctrl Pts',(-103.662639901655,1077.77674803136,
429.465711801408));
#107527=CARTESIAN_POINT('Ctrl Pts',(-103.672067549693,1077.77612822872,
429.399004127164));
#107528=CARTESIAN_POINT('Ctrl Pts',(-103.68156597282,1077.77540318433,429.353148475303));
#107529=CARTESIAN_POINT('Ctrl Pts',(-103.732641877495,1077.77121575433,
429.16720675395));
#107530=CARTESIAN_POINT('Ctrl Pts',(-103.798990576823,1077.7652556671,429.035590811263));
#107531=CARTESIAN_POINT('Ctrl Pts',(-103.962445650476,1077.74993136629,
428.827247625019));
#107532=CARTESIAN_POINT('Ctrl Pts',(-104.050523213927,1077.74149890571,
428.746275707446));
#107533=CARTESIAN_POINT('Ctrl Pts',(-104.24332608149,1077.72268663222,428.619477357485));
#107534=CARTESIAN_POINT('Ctrl Pts',(-104.345692450359,1077.71255409562,
428.572646466051));
#107535=CARTESIAN_POINT('Ctrl Pts',(-104.550985544958,1077.6919361633,428.51433065816));
#107536=CARTESIAN_POINT('Ctrl Pts',(-104.652034278672,1077.6816652382,428.500265739785));
#107537=CARTESIAN_POINT('Ctrl Pts',(-104.753539540172,1077.67122217491,
428.500265739785));
#107538=CARTESIAN_POINT('Ctrl Pts',(-104.753539540172,1077.67122217491,
428.500265739785));
#107539=CARTESIAN_POINT('Ctrl Pts',(-104.753621771129,1077.67121371483,
428.500265739785));
#107540=CARTESIAN_POINT('Ctrl Pts',(-104.753704002386,1077.67120525463,
428.500265749015));
#107541=CARTESIAN_POINT('Ctrl Pts',(-104.75378623394,1077.67119679432,428.500265767477));
#107542=CARTESIAN_POINT('Ctrl Pts',(-104.900517796687,1077.65610046838,
428.500298709538));
#107543=CARTESIAN_POINT('Ctrl Pts',(-105.045800523816,1077.64088944,428.529721821319));
#107544=CARTESIAN_POINT('Ctrl Pts',(-105.312932914101,1077.61243730724,
428.642535747821));
#107545=CARTESIAN_POINT('Ctrl Pts',(-105.432794474776,1077.5994227841,428.723532962091));
#107546=CARTESIAN_POINT('Ctrl Pts',(-105.621654555545,1077.57850681184,
428.913983809731));
#107547=CARTESIAN_POINT('Ctrl Pts',(-105.693868838685,1077.57031405657,
429.016998651975));
#107548=CARTESIAN_POINT('Ctrl Pts',(-105.799176783322,1077.55797322637,
429.240096076958));
#107549=CARTESIAN_POINT('Ctrl Pts',(-105.832510274906,1077.55381211552,
429.358071980582));
#107550=CARTESIAN_POINT('Ctrl Pts',(-105.848955940181,1077.55129397634,
429.507852615428));
#107551=CARTESIAN_POINT('Ctrl Pts',(-105.850974463313,1077.55093190504,
429.5366519147));
#107552=CARTESIAN_POINT('Ctrl Pts',(-105.852428428032,1077.55053499933,
429.584181780693));
#107553=CARTESIAN_POINT('Ctrl Pts',(-105.852523154506,1077.55042988131,
429.602876669696));
#107554=CARTESIAN_POINT('Ctrl Pts',(-105.851836458914,1077.55033268639,
429.636453088896));
#107555=CARTESIAN_POINT('Ctrl Pts',(-105.851229370754,1077.55032197857,
429.651333327891));
#107556=CARTESIAN_POINT('Ctrl Pts',(-105.849300796291,1077.55036797892,
429.682856867601));
#107557=CARTESIAN_POINT('Ctrl Pts',(-105.847902079528,1077.55043298755,
429.699491547961));
#107558=CARTESIAN_POINT('Ctrl Pts',(-105.843181715915,1077.55071361145,
429.743575329433));
#107559=CARTESIAN_POINT('Ctrl Pts',(-105.839202285154,1077.55099996445,
429.770940923325));
#107560=CARTESIAN_POINT('Ctrl Pts',(-105.816884053324,1077.5527696387,429.892120706807));
#107561=CARTESIAN_POINT('Ctrl Pts',(-105.787389925437,1077.55545785379,
429.983420553608));
#107562=CARTESIAN_POINT('Ctrl Pts',(-105.700209827115,1077.56382072101,
430.167356278329));
#107563=CARTESIAN_POINT('Ctrl Pts',(-105.639821682493,1077.56979383656,
430.257560864994));
#107564=CARTESIAN_POINT('Ctrl Pts',(-105.485794488914,1077.58527230502,
430.427319683297));
#107565=CARTESIAN_POINT('Ctrl Pts',(-105.390018630039,1077.59501673188,
430.502974946802));
#107566=CARTESIAN_POINT('Ctrl Pts',(-105.168565812765,1077.6176822067,430.62502929099));
#107567=CARTESIAN_POINT('Ctrl Pts',(-105.042763154243,1077.63062515425,
430.667317225829));
#107568=CARTESIAN_POINT('Ctrl Pts',(-104.859791132155,1077.64948899038,
430.694078487688));
#107569=CARTESIAN_POINT('Ctrl Pts',(-104.806643653434,1077.65497302422,
430.69792801177));
#107570=CARTESIAN_POINT('Ctrl Pts',(-104.753539540173,1077.66045630879,
430.69792801177));
#107571=CARTESIAN_POINT('',(-110.796881705951,1076.79846644782,441.973714359567));
#107572=CARTESIAN_POINT('',(-110.796881705952,1076.84100217604,439.792632862112));
#107573=CARTESIAN_POINT('Ctrl Pts',(-110.796881705951,1076.79846644782,
441.973714359568));
#107574=CARTESIAN_POINT('Ctrl Pts',(-110.692273774677,1076.81241408223,
441.973714359568));
#107575=CARTESIAN_POINT('Ctrl Pts',(-110.588028811789,1076.82655918924,
441.958661837672));
#107576=CARTESIAN_POINT('Ctrl Pts',(-110.348684785172,1076.85962684279,
441.887824330035));
#107577=CARTESIAN_POINT('Ctrl Pts',(-110.219371784325,1076.877980297,441.819537372388));
#107578=CARTESIAN_POINT('Ctrl Pts',(-110.000351151244,1076.91015763524,
441.640675412221));
#107579=CARTESIAN_POINT('Ctrl Pts',(-109.910929629034,1076.923879414,441.533925201476));
#107580=CARTESIAN_POINT('Ctrl Pts',(-109.782461101245,1076.94503069519,
441.302864272028));
#107581=CARTESIAN_POINT('Ctrl Pts',(-109.74068377013,1076.9527437549,441.182689327982));
#107582=CARTESIAN_POINT('Ctrl Pts',(-109.709471388927,1076.96045410788,
440.990387616337));
#107583=CARTESIAN_POINT('Ctrl Pts',(-109.704885215509,1076.96234971779,
440.921979321037));
#107584=CARTESIAN_POINT('Ctrl Pts',(-109.70740490224,1076.96378815122,440.829188651065));
#107585=CARTESIAN_POINT('Ctrl Pts',(-109.708884892985,1076.96405957878,
440.804833727284));
#107586=CARTESIAN_POINT('Ctrl Pts',(-109.712635154749,1076.96432820452,
440.765158889882));
#107587=CARTESIAN_POINT('Ctrl Pts',(-109.71441682864,1076.96438940442,440.749802474235));
#107588=CARTESIAN_POINT('Ctrl Pts',(-109.718472879028,1076.96442436584,
440.72033081604));
#107589=CARTESIAN_POINT('Ctrl Pts',(-109.720699520378,1076.96440437256,
440.706212383326));
#107590=CARTESIAN_POINT('Ctrl Pts',(-109.726469843612,1076.96427351887,
440.673780747735));
#107591=CARTESIAN_POINT('Ctrl Pts',(-109.7302070774,1076.96413683291,440.655506898849));
#107592=CARTESIAN_POINT('Ctrl Pts',(-109.743219717341,1076.96352035238,
440.599267826861));
#107593=CARTESIAN_POINT('Ctrl Pts',(-109.754067283443,1076.96282921733,
440.561702889637));
#107594=CARTESIAN_POINT('Ctrl Pts',(-109.814439595316,1076.95830494407,
440.388188327854));
#107595=CARTESIAN_POINT('Ctrl Pts',(-109.888623562675,1076.95107882451,
440.262547084959));
#107596=CARTESIAN_POINT('Ctrl Pts',(-110.062839703741,1076.93211989836,
440.068274204388));
#107597=CARTESIAN_POINT('Ctrl Pts',(-110.154010601421,1076.9216439643,439.994622440335));
#107598=CARTESIAN_POINT('Ctrl Pts',(-110.341671486236,1076.89915372656,
439.887155452571));
#107599=CARTESIAN_POINT('Ctrl Pts',(-110.434726911207,1076.88766844724,
439.849698395017));
#107600=CARTESIAN_POINT('Ctrl Pts',(-110.618310048536,1076.86439463511,
439.803633080794));
#107601=CARTESIAN_POINT('Ctrl Pts',(-110.707453167309,1076.85284210735,
439.792632862112));
#107602=CARTESIAN_POINT('Ctrl Pts',(-110.796881705953,1076.84100217604,
439.792632862112));
#107603=CARTESIAN_POINT('Ctrl Pts',(-110.796881705953,1076.84100217604,
439.792632862112));
#107604=CARTESIAN_POINT('Ctrl Pts',(-110.797144710037,1076.8409673555,439.792632862112));
#107605=CARTESIAN_POINT('Ctrl Pts',(-110.797407716591,1076.84093253247,
439.792632957254));
#107606=CARTESIAN_POINT('Ctrl Pts',(-110.797670725563,1076.84089770697,
439.792633147545));
#107607=CARTESIAN_POINT('Ctrl Pts',(-110.940875143062,1076.82193574766,
439.792736757725));
#107608=CARTESIAN_POINT('Ctrl Pts',(-111.082679377719,1076.80251686205,
439.821046646856));
#107609=CARTESIAN_POINT('Ctrl Pts',(-111.347617338863,1076.76494997321,
439.931019391774));
#107610=CARTESIAN_POINT('Ctrl Pts',(-111.468259603526,1076.74715260503,
440.011817417049));
#107611=CARTESIAN_POINT('Ctrl Pts',(-111.663219862428,1076.7170028084,440.207700701182));
#107612=CARTESIAN_POINT('Ctrl Pts',(-111.73889487444,1076.70457505583,440.317907003865));
#107613=CARTESIAN_POINT('Ctrl Pts',(-111.850563178268,1076.68445565207,
440.568443064145));
#107614=CARTESIAN_POINT('Ctrl Pts',(-111.882534220777,1076.67732722463,
440.70781449107));
#107615=CARTESIAN_POINT('Ctrl Pts',(-111.887907283963,1076.67311846043,
440.882092345228));
#107616=CARTESIAN_POINT('Ctrl Pts',(-111.887453915195,1076.67253021244,
440.914649172624));
#107617=CARTESIAN_POINT('Ctrl Pts',(-111.884518469112,1076.67193211686,
440.96460803008));
#107618=CARTESIAN_POINT('Ctrl Pts',(-111.883071842286,1076.6717806839,440.982048878092));
#107619=CARTESIAN_POINT('Ctrl Pts',(-111.879649247935,1076.67160898888,
441.013966538923));
#107620=CARTESIAN_POINT('Ctrl Pts',(-111.877800927294,1076.67157118055,
441.028452600474));
#107621=CARTESIAN_POINT('Ctrl Pts',(-111.873474867749,1076.67157625955,
441.057670989545));
#107622=CARTESIAN_POINT('Ctrl Pts',(-111.870984243651,1076.67162100385,
441.072398091426));
#107623=CARTESIAN_POINT('Ctrl Pts',(-111.864148755149,1076.67183370564,
441.108313168006));
#107624=CARTESIAN_POINT('Ctrl Pts',(-111.859474700419,1076.67204783228,
441.12943126288));
#107625=CARTESIAN_POINT('Ctrl Pts',(-111.840686961053,1076.67311905997,
441.203767105688));
#107626=CARTESIAN_POINT('Ctrl Pts',(-111.823179257166,1076.67445681808,
441.256027453616));
#107627=CARTESIAN_POINT('Ctrl Pts',(-111.745741740518,1076.68131660462,
441.439754842337));
#107628=CARTESIAN_POINT('Ctrl Pts',(-111.663902326627,1076.6900350907,441.560138537338));
#107629=CARTESIAN_POINT('Ctrl Pts',(-111.476430942617,1076.71175599412,
441.744346762287));
#107630=CARTESIAN_POINT('Ctrl Pts',(-111.378726898161,1076.72359527886,
441.813110961287));
#107631=CARTESIAN_POINT('Ctrl Pts',(-111.155314698242,1076.75154113672,
441.921260149142));
#107632=CARTESIAN_POINT('Ctrl Pts',(-111.029570986107,1076.76772622122,
441.956431059971));
#107633=CARTESIAN_POINT('Ctrl Pts',(-110.866165924499,1076.78925564003,
441.972065634675));
#107634=CARTESIAN_POINT('Ctrl Pts',(-110.831503928816,1076.79385018115,
441.973714359568));
#107635=CARTESIAN_POINT('Ctrl Pts',(-110.796881705951,1076.79846644782,
441.973714359568));
#107636=CARTESIAN_POINT('',(-89.3961860936676,1078.67097321562,431.48354716413));
#107637=CARTESIAN_POINT('',(-89.3961860936676,1078.67555974723,428.526940899744));
#107638=CARTESIAN_POINT('Ctrl Pts',(-89.3961860936678,1078.67097321562,
431.48354716413));
#107639=CARTESIAN_POINT('Ctrl Pts',(-89.3503684205628,1078.6721747184,431.48354716413));
#107640=CARTESIAN_POINT('Ctrl Pts',(-89.3045016225727,1078.67336423892,
431.481417139091));
#107641=CARTESIAN_POINT('Ctrl Pts',(-89.0639230639002,1078.67953217154,
431.458950921387));
#107642=CARTESIAN_POINT('Ctrl Pts',(-88.8746373636803,1078.68412818373,
431.402261580626));
#107643=CARTESIAN_POINT('Ctrl Pts',(-88.5330027004404,1078.69204156997,
431.220516060359));
#107644=CARTESIAN_POINT('Ctrl Pts',(-88.3831469945233,1078.69531624797,
431.098739153579));
#107645=CARTESIAN_POINT('Ctrl Pts',(-88.1541705001929,1078.70019971376,
430.824044466892));
#107646=CARTESIAN_POINT('Ctrl Pts',(-88.0699999443497,1078.70194023454,
430.679240083613));
#107647=CARTESIAN_POINT('Ctrl Pts',(-87.9653316907437,1078.70416949295,
430.3996148194));
#107648=CARTESIAN_POINT('Ctrl Pts',(-87.9357979108968,1078.70483203888,
430.270083290523));
#107649=CARTESIAN_POINT('Ctrl Pts',(-87.9201609749338,1078.70529363399,
430.097132364434));
#107650=CARTESIAN_POINT('Ctrl Pts',(-87.9181668276158,1078.70537280154,
430.055768046747));
#107651=CARTESIAN_POINT('Ctrl Pts',(-87.9177594245223,1078.7054500744,429.989808453584));
#107652=CARTESIAN_POINT('Ctrl Pts',(-87.918220082033,1078.70546803225,429.965242250974));
#107653=CARTESIAN_POINT('Ctrl Pts',(-87.9202278753444,1078.7054814182,429.919300758652));
#107654=CARTESIAN_POINT('Ctrl Pts',(-87.9216279836036,1078.70547943631,
429.897925401036));
#107655=CARTESIAN_POINT('Ctrl Pts',(-87.9258105131604,1078.70545655004,
429.850048997176));
#107656=CARTESIAN_POINT('Ctrl Pts',(-87.9288459451285,1078.70543115622,
429.823577485973));
#107657=CARTESIAN_POINT('Ctrl Pts',(-87.9397257026432,1078.70532051322,
429.747037398998));
#107658=CARTESIAN_POINT('Ctrl Pts',(-87.9494308166955,1078.70520204839,
429.697272144726));
#107659=CARTESIAN_POINT('Ctrl Pts',(-88.009378559838,1078.7043948384,429.456481844696));
#107660=CARTESIAN_POINT('Ctrl Pts',(-88.0949993889729,1078.70306520414,
429.276351340573));
#107661=CARTESIAN_POINT('Ctrl Pts',(-88.3085838548858,1078.69933176898,
428.991517520783));
#107662=CARTESIAN_POINT('Ctrl Pts',(-88.4234937228195,1078.69721031364,
428.880794932558));
#107663=CARTESIAN_POINT('Ctrl Pts',(-88.6833406166949,1078.69203232056,
428.700602039454));
#107664=CARTESIAN_POINT('Ctrl Pts',(-88.8264409007805,1078.68901143704,
428.632063451516));
#107665=CARTESIAN_POINT('Ctrl Pts',(-89.1135426005729,1078.6825108496,428.547310221386));
#107666=CARTESIAN_POINT('Ctrl Pts',(-89.2545008260199,1078.67914164015,
428.526940899744));
#107667=CARTESIAN_POINT('Ctrl Pts',(-89.3961860936677,1078.67555974723,
428.526940899744));
#107668=CARTESIAN_POINT('Ctrl Pts',(-89.3961860936677,1078.67555974723,
428.526940899743));
#107669=CARTESIAN_POINT('Ctrl Pts',(-89.3962427801943,1078.67555831416,
428.526940899743));
#107670=CARTESIAN_POINT('Ctrl Pts',(-89.3962994668373,1078.67555688106,
428.526940902775));
#107671=CARTESIAN_POINT('Ctrl Pts',(-89.3963561535964,1078.67555544792,
428.526940909296));
#107672=CARTESIAN_POINT('Ctrl Pts',(-89.592592917535,1078.67059424695,428.526963483905));
#107673=CARTESIAN_POINT('Ctrl Pts',(-89.7868711403322,1078.66530455267,
428.566059828392));
#107674=CARTESIAN_POINT('Ctrl Pts',(-90.1455237677059,1078.65489299863,
428.716447037405));
#107675=CARTESIAN_POINT('Ctrl Pts',(-90.3069516447766,1078.64987461811,
428.824982534491));
#107676=CARTESIAN_POINT('Ctrl Pts',(-90.5639852988258,1078.64146856408,
429.082758398322));
#107677=CARTESIAN_POINT('Ctrl Pts',(-90.6629613753267,1078.63803012931,
429.224204035469));
#107678=CARTESIAN_POINT('Ctrl Pts',(-90.8046827979466,1078.6328410931,429.527513504186));
#107679=CARTESIAN_POINT('Ctrl Pts',(-90.8488395845207,1078.63105794091,
429.686037599397));
#107680=CARTESIAN_POINT('Ctrl Pts',(-90.8709485547003,1078.62990838013,
429.893463944237));
#107681=CARTESIAN_POINT('Ctrl Pts',(-90.8736746522949,1078.62972718908,
429.938560351527));
#107682=CARTESIAN_POINT('Ctrl Pts',(-90.8747098084299,1078.62955017559,
430.009618815121));
#107683=CARTESIAN_POINT('Ctrl Pts',(-90.874406017504,1078.62950828611,430.035532223773));
#107684=CARTESIAN_POINT('Ctrl Pts',(-90.8725898400971,1078.62947295051,
430.083287837502));
#107685=CARTESIAN_POINT('Ctrl Pts',(-90.8712730739436,1078.62947298496,
430.105130261123));
#107686=CARTESIAN_POINT('Ctrl Pts',(-90.8673373367039,1078.62950848658,
430.152779217494));
#107687=CARTESIAN_POINT('Ctrl Pts',(-90.8645230313847,1078.62955051016,
430.178562364891));
#107688=CARTESIAN_POINT('Ctrl Pts',(-90.8547741527985,1078.62973121606,
430.250319136657));
#107689=CARTESIAN_POINT('Ctrl Pts',(-90.8463472804366,1078.62992003172,
430.296059113835));
#107690=CARTESIAN_POINT('Ctrl Pts',(-90.7911388502875,1078.63128071601,
430.532542485652));
#107691=CARTESIAN_POINT('Ctrl Pts',(-90.7088479183431,1078.63365390632,
430.712948633658));
#107692=CARTESIAN_POINT('Ctrl Pts',(-90.5017020705458,1078.63976408734,
430.999152287797));
#107693=CARTESIAN_POINT('Ctrl Pts',(-90.3900075983879,1078.64308907709,
431.110835136399));
#107694=CARTESIAN_POINT('Ctrl Pts',(-90.1239594440925,1078.65087851801,
431.303367194158));
#107695=CARTESIAN_POINT('Ctrl Pts',(-89.9686290285824,1078.65535737901,
431.378955271829));
#107696=CARTESIAN_POINT('Ctrl Pts',(-89.6710761276956,1078.66364245453,
431.464315639791));
#107697=CARTESIAN_POINT('Ctrl Pts',(-89.5338528917158,1078.66736310127,
431.48354716413));
#107698=CARTESIAN_POINT('Ctrl Pts',(-89.3961860936678,1078.67097321562,
431.48354716413));
#107699=CARTESIAN_POINT('',(-104.994450521159,1076.76862933859,464.654297310259));
#107700=CARTESIAN_POINT('',(-104.994450521158,1076.8704842326,462.473215812804));
#107701=CARTESIAN_POINT('Ctrl Pts',(-104.994450521159,1076.76862933859,
464.65429731026));
#107702=CARTESIAN_POINT('Ctrl Pts',(-104.858658359836,1076.78586976643,
464.65429731026));
#107703=CARTESIAN_POINT('Ctrl Pts',(-104.724111967629,1076.8040722823,464.628935472442));
#107704=CARTESIAN_POINT('Ctrl Pts',(-104.462350706126,1076.84178842186,
464.526705426959));
#107705=CARTESIAN_POINT('Ctrl Pts',(-104.338796665719,1076.86094842948,
464.447262771309));
#107706=CARTESIAN_POINT('Ctrl Pts',(-104.133160632069,1076.89582341618,
464.24741888124));
#107707=CARTESIAN_POINT('Ctrl Pts',(-104.051818760982,1076.91130880812,
464.130132324092));
#107708=CARTESIAN_POINT('Ctrl Pts',(-103.949391403289,1076.93472987125,
463.895686030557));
#107709=CARTESIAN_POINT('Ctrl Pts',(-103.920333066717,1076.9434016353,463.78435057897));
#107710=CARTESIAN_POINT('Ctrl Pts',(-103.898342221727,1076.95632754564,
463.560541570395));
#107711=CARTESIAN_POINT('Ctrl Pts',(-103.904282010018,1076.96065179248,
463.449602661549));
#107712=CARTESIAN_POINT('Ctrl Pts',(-103.932945385877,1076.9634002689,463.311987610233));
#107713=CARTESIAN_POINT('Ctrl Pts',(-103.940280223014,1076.96382645952,
463.282854404866));
#107714=CARTESIAN_POINT('Ctrl Pts',(-103.953690373367,1076.96424190995,
463.237577294334));
#107715=CARTESIAN_POINT('Ctrl Pts',(-103.958961004619,1076.9643400147,463.221213010892));
#107716=CARTESIAN_POINT('Ctrl Pts',(-103.96891034016,1076.96441900298,463.192654396277));
#107717=CARTESIAN_POINT('Ctrl Pts',(-103.973425261387,1076.96442241245,
463.180406981277));
#107718=CARTESIAN_POINT('Ctrl Pts',(-103.984192399116,1076.96436037745,
463.152740253009));
#107719=CARTESIAN_POINT('Ctrl Pts',(-103.990579735707,1076.96427577895,
463.137377257781));
#107720=CARTESIAN_POINT('Ctrl Pts',(-104.008815295691,1076.96391201987,
463.096200351771));
#107721=CARTESIAN_POINT('Ctrl Pts',(-104.021323831314,1076.96353773417,
463.070694857799));
#107722=CARTESIAN_POINT('Ctrl Pts',(-104.085329266719,1076.96107805047,
462.952130525259));
#107723=CARTESIAN_POINT('Ctrl Pts',(-104.149228396746,1076.95713089861,
462.866506244061));
#107724=CARTESIAN_POINT('Ctrl Pts',(-104.301841385759,1076.94529522403,
462.714332647535));
#107725=CARTESIAN_POINT('Ctrl Pts',(-104.390321610185,1076.93736453761,
462.649315741908));
#107726=CARTESIAN_POINT('Ctrl Pts',(-104.571126005816,1076.91937744636,
462.554230757962));
#107727=CARTESIAN_POINT('Ctrl Pts',(-104.660748401951,1076.90979666082,
462.521188143708));
#107728=CARTESIAN_POINT('Ctrl Pts',(-104.83256621036,1076.89024834434,462.482248176407));
#107729=CARTESIAN_POINT('Ctrl Pts',(-104.913414836135,1076.88060035961,
462.473215812804));
#107730=CARTESIAN_POINT('Ctrl Pts',(-104.994450521158,1076.8704842326,462.473215812804));
#107731=CARTESIAN_POINT('Ctrl Pts',(-104.994450521158,1076.8704842326,462.473215812804));
#107732=CARTESIAN_POINT('Ctrl Pts',(-104.994528833149,1076.87047445649,
462.473215812804));
#107733=CARTESIAN_POINT('Ctrl Pts',(-104.994607145314,1076.87046467994,
462.473215821239));
#107734=CARTESIAN_POINT('Ctrl Pts',(-104.994685457652,1076.87045490295,
462.47321583811));
#107735=CARTESIAN_POINT('Ctrl Pts',(-105.131886787753,1076.85332585709,
462.473245395557));
#107736=CARTESIAN_POINT('Ctrl Pts',(-105.267772173138,1076.83508401853,
462.499165114115));
#107737=CARTESIAN_POINT('Ctrl Pts',(-105.530374457735,1076.79715501205,
462.602932847247));
#107738=CARTESIAN_POINT('Ctrl Pts',(-105.653583153228,1076.77780211827,
462.682850918198));
#107739=CARTESIAN_POINT('Ctrl Pts',(-105.858177340716,1076.74233967145,
462.883240741875));
#107740=CARTESIAN_POINT('Ctrl Pts',(-105.938927628521,1076.72646720446,
463.000542870787));
#107741=CARTESIAN_POINT('Ctrl Pts',(-106.043399555415,1076.70163199974,
463.241666955628));
#107742=CARTESIAN_POINT('Ctrl Pts',(-106.072798134984,1076.69218792766,
463.360574308658));
#107743=CARTESIAN_POINT('Ctrl Pts',(-106.089666298165,1076.67930832872,
463.58505686271));
#107744=CARTESIAN_POINT('Ctrl Pts',(-106.082735619161,1076.67524669101,
463.688724171103));
#107745=CARTESIAN_POINT('Ctrl Pts',(-106.055199289107,1076.67258694552,
463.818611382102));
#107746=CARTESIAN_POINT('Ctrl Pts',(-106.047963104158,1076.67216048016,
463.847041661286));
#107747=CARTESIAN_POINT('Ctrl Pts',(-106.034703928088,1076.67174195216,
463.891544105304));
#107748=CARTESIAN_POINT('Ctrl Pts',(-106.029433539461,1076.67164299098,
463.90782341647));
#107749=CARTESIAN_POINT('Ctrl Pts',(-106.018995802968,1076.6715624156,463.93764968879));
#107750=CARTESIAN_POINT('Ctrl Pts',(-106.01393724764,1076.67156516842,463.951230329643));
#107751=CARTESIAN_POINT('Ctrl Pts',(-106.002168856373,1076.67165894452,
463.980997215355));
#107752=CARTESIAN_POINT('Ctrl Pts',(-105.995336666991,1076.67176827397,
463.997130426362));
#107753=CARTESIAN_POINT('Ctrl Pts',(-105.974958748641,1076.6722404088,464.042194545623));
#107754=CARTESIAN_POINT('Ctrl Pts',(-105.960527522606,1076.67273755706,
464.070702461631));
#107755=CARTESIAN_POINT('Ctrl Pts',(-105.874190085076,1076.67652915516,
464.224143244695));
#107756=CARTESIAN_POINT('Ctrl Pts',(-105.779397311726,1076.68347705017,
464.334352387907));
#107757=CARTESIAN_POINT('Ctrl Pts',(-105.575552107716,1076.70206999252,
464.493708257795));
#107758=CARTESIAN_POINT('Ctrl Pts',(-105.474509528114,1076.7123695875,464.549637315668));
#107759=CARTESIAN_POINT('Ctrl Pts',(-105.24793524325,1076.73743542702,464.63193754997));
#107760=CARTESIAN_POINT('Ctrl Pts',(-105.122649946795,1076.75236364489,
464.654054595566));
#107761=CARTESIAN_POINT('Ctrl Pts',(-104.995838203487,1076.76845318515,
464.654296648121));
#107762=CARTESIAN_POINT('Ctrl Pts',(-104.995144346057,1076.76854124928,
464.65429731026));
#107763=CARTESIAN_POINT('Ctrl Pts',(-104.994450521159,1076.76862933859,
464.65429731026));
#107764=CARTESIAN_POINT('',(-101.429261354592,1077.63689261564,452.368613624749));
#107765=CARTESIAN_POINT('',(-101.429261354592,1077.69451627758,450.170951352764));
#107766=CARTESIAN_POINT('Ctrl Pts',(-101.429261354592,1077.63689261564,
452.368613624749));
#107767=CARTESIAN_POINT('Ctrl Pts',(-101.307605703774,1077.64915059475,
452.368613624749));
#107768=CARTESIAN_POINT('Ctrl Pts',(-101.18668444173,1077.66179391028,452.348409001666));
#107769=CARTESIAN_POINT('Ctrl Pts',(-100.933618173617,1077.6892560253,452.261258318599));
#107770=CARTESIAN_POINT('Ctrl Pts',(-100.80650567583,1077.7037342887,452.186793901045));
#107771=CARTESIAN_POINT('Ctrl Pts',(-100.592363567915,1077.72965390654,
451.995681680799));
#107772=CARTESIAN_POINT('Ctrl Pts',(-100.506087865567,1077.7409464009,451.882278538947));
#107773=CARTESIAN_POINT('Ctrl Pts',(-100.389540214887,1077.75825533559,
451.645782492565));
#107774=CARTESIAN_POINT('Ctrl Pts',(-100.354126513678,1077.76465606984,
451.52770444186));
#107775=CARTESIAN_POINT('Ctrl Pts',(-100.327844344213,1077.7724947649,451.317549332329));
#107776=CARTESIAN_POINT('Ctrl Pts',(-100.327600274001,1077.77477784652,
451.227910410291));
#107777=CARTESIAN_POINT('Ctrl Pts',(-100.341573462965,1077.77638028958,
451.111152839007));
#107778=CARTESIAN_POINT('Ctrl Pts',(-100.346012308605,1077.77665806041,
451.083235064126));
#107779=CARTESIAN_POINT('Ctrl Pts',(-100.354818929977,1077.77692965332,
451.038938135266));
#107780=CARTESIAN_POINT('Ctrl Pts',(-100.358497462294,1077.77699268214,
451.022435895688));
#107781=CARTESIAN_POINT('Ctrl Pts',(-100.365790889745,1077.77703645925,
450.992939322167));
#107782=CARTESIAN_POINT('Ctrl Pts',(-100.369267007333,1077.77703128793,
450.979914324867));
#107783=CARTESIAN_POINT('Ctrl Pts',(-100.377936166874,1077.7769618355,450.949675645639));
#107784=CARTESIAN_POINT('Ctrl Pts',(-100.383313741584,1077.77687842007,
450.932519062293));
#107785=CARTESIAN_POINT('Ctrl Pts',(-100.399756472976,1077.7765179199,450.884243895061));
#107786=CARTESIAN_POINT('Ctrl Pts',(-100.41180635154,1077.77613737507,450.853482828614));
#107787=CARTESIAN_POINT('Ctrl Pts',(-100.484498524452,1077.77328377933,
450.690009776044));
#107788=CARTESIAN_POINT('Ctrl Pts',(-100.569692629977,1077.76813739926,
450.569922918353));
#107789=CARTESIAN_POINT('Ctrl Pts',(-100.760536161183,1077.75427975263,
450.390119661033));
#107790=CARTESIAN_POINT('Ctrl Pts',(-100.857420541936,1077.7465783772,450.324289715235));
#107791=CARTESIAN_POINT('Ctrl Pts',(-101.039523498113,1077.73103967016,
450.238895285109));
#107792=CARTESIAN_POINT('Ctrl Pts',(-101.120185883533,1077.72385572255,
450.211916445114));
#107793=CARTESIAN_POINT('Ctrl Pts',(-101.277497005792,1077.7092800982,450.178829841757));
#107794=CARTESIAN_POINT('Ctrl Pts',(-101.353291460102,1077.70202396362,
450.170951352764));
#107795=CARTESIAN_POINT('Ctrl Pts',(-101.429261354593,1077.69451627758,
450.170951352764));
#107796=CARTESIAN_POINT('Ctrl Pts',(-101.429261354593,1077.69451627758,
450.170951352764));
#107797=CARTESIAN_POINT('Ctrl Pts',(-101.429339798802,1077.69450852537,
450.170951352764));
#107798=CARTESIAN_POINT('Ctrl Pts',(-101.429418243198,1077.69450077289,
450.170951361164));
#107799=CARTESIAN_POINT('Ctrl Pts',(-101.429496687781,1077.69449302015,
450.170951377965));
#107800=CARTESIAN_POINT('Ctrl Pts',(-101.570117366432,1077.6805953591,450.170981494251));
#107801=CARTESIAN_POINT('Ctrl Pts',(-101.709404414697,1077.66602412535,
450.198004259033));
#107802=CARTESIAN_POINT('Ctrl Pts',(-101.974748435885,1077.63660106094,
450.304877484262));
#107803=CARTESIAN_POINT('Ctrl Pts',(-102.097648397907,1077.6220376026,450.385530117599));
#107804=CARTESIAN_POINT('Ctrl Pts',(-102.300392047101,1077.59607630245,
450.585709210324));
#107805=CARTESIAN_POINT('Ctrl Pts',(-102.380088023211,1077.58480026738,
450.701603731434));
#107806=CARTESIAN_POINT('Ctrl Pts',(-102.486864493364,1077.56724237183,
450.945723512633));
#107807=CARTESIAN_POINT('Ctrl Pts',(-102.517236113633,1077.56073632167,
451.070034462404));
#107808=CARTESIAN_POINT('Ctrl Pts',(-102.530485864684,1077.55395826846,
451.269276335541));
#107809=CARTESIAN_POINT('Ctrl Pts',(-102.528117831316,1077.55222618741,
451.341998907716));
#107810=CARTESIAN_POINT('Ctrl Pts',(-102.515183211102,1077.5509077679,451.439717906269));
#107811=CARTESIAN_POINT('Ctrl Pts',(-102.510863569694,1077.55065819379,
451.465335737234));
#107812=CARTESIAN_POINT('Ctrl Pts',(-102.502325869235,1077.55041101153,
451.506919510223));
#107813=CARTESIAN_POINT('Ctrl Pts',(-102.498648933293,1077.5503546808,451.522985245446));
#107814=CARTESIAN_POINT('Ctrl Pts',(-102.490877143383,1077.55032261067,
451.553744166218));
#107815=CARTESIAN_POINT('Ctrl Pts',(-102.486835014044,1077.55034116096,
451.568446632));
#107816=CARTESIAN_POINT('Ctrl Pts',(-102.476813400386,1077.55046219859,
451.602138890561));
#107817=CARTESIAN_POINT('Ctrl Pts',(-102.470621270859,1077.55058857809,
451.621059535528));
#107818=CARTESIAN_POINT('Ctrl Pts',(-102.44987370328,1077.55115831956,451.679074506687));
#107819=CARTESIAN_POINT('Ctrl Pts',(-102.433605206687,1077.5517968029,451.717512673844));
#107820=CARTESIAN_POINT('Ctrl Pts',(-102.350769277051,1077.55579025146,
451.885854571335));
#107821=CARTESIAN_POINT('Ctrl Pts',(-102.260962116599,1077.561907593,452.00253898184));
#107822=CARTESIAN_POINT('Ctrl Pts',(-102.062285427086,1077.57766885212,
452.175646847466));
#107823=CARTESIAN_POINT('Ctrl Pts',(-101.961667307769,1077.58630783823,
452.23818708051));
#107824=CARTESIAN_POINT('Ctrl Pts',(-101.734338897954,1077.60696361097,
452.333240482375));
#107825=CARTESIAN_POINT('Ctrl Pts',(-101.607797366091,1077.61906373766,
452.361613190581));
#107826=CARTESIAN_POINT('Ctrl Pts',(-101.462631740008,1077.63353889845,
452.368233908657));
#107827=CARTESIAN_POINT('Ctrl Pts',(-101.445939644068,1077.63521211726,
452.368613624749));
#107828=CARTESIAN_POINT('Ctrl Pts',(-101.429261354592,1077.63689261564,
452.368613624749));
#107829=CARTESIAN_POINT('',(-95.5155706932853,1078.335920315,441.193367887108));
#107830=CARTESIAN_POINT('',(-95.5155706932855,1078.36174835417,438.642479644836));
#107831=CARTESIAN_POINT('Ctrl Pts',(-95.5155706932858,1078.335920315,441.193367887108));
#107832=CARTESIAN_POINT('Ctrl Pts',(-95.4111650117638,1078.34261218989,
441.193367887108));
#107833=CARTESIAN_POINT('Ctrl Pts',(-95.3069403455621,1078.34935333886,
441.180547621747));
#107834=CARTESIAN_POINT('Ctrl Pts',(-95.0415379989269,1078.36667274019,
441.113977418461));
#107835=CARTESIAN_POINT('Ctrl Pts',(-94.8875378294586,1078.37687478399,
441.040801713221));
#107836=CARTESIAN_POINT('Ctrl Pts',(-94.6211947967623,1078.39494797311,
440.841831258262));
#107837=CARTESIAN_POINT('Ctrl Pts',(-94.5101532264005,1078.40271926822,
440.719601144812));
#107838=CARTESIAN_POINT('Ctrl Pts',(-94.3502012312986,1078.41462450173,
440.45605199741));
#107839=CARTESIAN_POINT('Ctrl Pts',(-94.2967225248972,1078.41899296749,
440.32053829704));
#107840=CARTESIAN_POINT('Ctrl Pts',(-94.2472215401051,1078.4240533987,440.083756446023));
#107841=CARTESIAN_POINT('Ctrl Pts',(-94.2382709359166,1078.42546434301,
439.986617993523));
#107842=CARTESIAN_POINT('Ctrl Pts',(-94.2411740814405,1078.42649355455,
439.856831077137));
#107843=CARTESIAN_POINT('Ctrl Pts',(-94.243150250138,1078.42667954197,439.824300513367));
#107844=CARTESIAN_POINT('Ctrl Pts',(-94.2483461187777,1078.42686262727,
439.771980174333));
#107845=CARTESIAN_POINT('Ctrl Pts',(-94.2507902387295,1078.4269049037,439.752128525486));
#107846=CARTESIAN_POINT('Ctrl Pts',(-94.2563257391841,1078.42693323349,
439.714489567494));
#107847=CARTESIAN_POINT('Ctrl Pts',(-94.259329922922,1078.42692437279,439.696694349757));
#107848=CARTESIAN_POINT('Ctrl Pts',(-94.2670033721579,1078.42685365778,
439.656461826716));
#107849=CARTESIAN_POINT('Ctrl Pts',(-94.2719017829188,1078.42677816682,
439.634074627876));
#107850=CARTESIAN_POINT('Ctrl Pts',(-94.2883841190779,1078.42644433089,
439.567402091362));
#107851=CARTESIAN_POINT('Ctrl Pts',(-94.3017509040923,1078.42607897945,
439.523596933438));
#107852=CARTESIAN_POINT('Ctrl Pts',(-94.3755538628997,1078.42369309505,
439.321397383178));
#107853=CARTESIAN_POINT('Ctrl Pts',(-94.4648057222744,1078.41989727353,
439.175395008897));
#107854=CARTESIAN_POINT('Ctrl Pts',(-94.6729613332543,1078.40982820227,
438.95070920374));
#107855=CARTESIAN_POINT('Ctrl Pts',(-94.7815198966757,1078.40423331603,
438.865953113181));
#107856=CARTESIAN_POINT('Ctrl Pts',(-95.0000296449497,1078.39232693233,
438.745902276943));
#107857=CARTESIAN_POINT('Ctrl Pts',(-95.1053525005845,1078.38637056336,
438.705023934537));
#107858=CARTESIAN_POINT('Ctrl Pts',(-95.3131762615605,1078.37417675069,
438.654564547404));
#107859=CARTESIAN_POINT('Ctrl Pts',(-95.4142012927564,1078.36806750606,
438.642479644836));
#107860=CARTESIAN_POINT('Ctrl Pts',(-95.5155706932855,1078.36174835417,
438.642479644836));
#107861=CARTESIAN_POINT('Ctrl Pts',(-95.5155706932855,1078.36174835417,
438.642479644836));
#107862=CARTESIAN_POINT('Ctrl Pts',(-95.5156721781734,1078.36174202782,
438.642479644836));
#107863=CARTESIAN_POINT('Ctrl Pts',(-95.5157736634065,1078.36173570126,
438.642479656949));
#107864=CARTESIAN_POINT('Ctrl Pts',(-95.5158751489827,1078.36172937449,
438.642479681174));
#107865=CARTESIAN_POINT('Ctrl Pts',(-95.6819526409652,1078.3513758431,438.642519324808));
#107866=CARTESIAN_POINT('Ctrl Pts',(-95.8464280210779,1078.34061188616,
438.674996311814));
#107867=CARTESIAN_POINT('Ctrl Pts',(-96.1551547787413,1078.31939507363,
438.801767312496));
#107868=CARTESIAN_POINT('Ctrl Pts',(-96.2962316659722,1078.30915212528,
438.895441517433));
#107869=CARTESIAN_POINT('Ctrl Pts',(-96.526298600044,1078.2914383833,439.124345093502));
#107870=CARTESIAN_POINT('Ctrl Pts',(-96.6161466462865,1078.28398359501,
439.254517570002));
#107871=CARTESIAN_POINT('Ctrl Pts',(-96.7479248536023,1078.27185279146,
439.549557216462));
#107872=CARTESIAN_POINT('Ctrl Pts',(-96.7854148901343,1078.26748934377,
439.713181488898));
#107873=CARTESIAN_POINT('Ctrl Pts',(-96.7916602299975,1078.26479107824,
439.920054866255));
#107874=CARTESIAN_POINT('Ctrl Pts',(-96.790944607503,1078.26439360767,439.960709768068));
#107875=CARTESIAN_POINT('Ctrl Pts',(-96.7867037236683,1078.26397300568,
440.025475162709));
#107876=CARTESIAN_POINT('Ctrl Pts',(-96.7844275958912,1078.26386365463,
440.049638105698));
#107877=CARTESIAN_POINT('Ctrl Pts',(-96.7792072515004,1078.2637557252,440.092054590898));
#107878=CARTESIAN_POINT('Ctrl Pts',(-96.7765529539311,1078.26373694388,
440.110336439396));
#107879=CARTESIAN_POINT('Ctrl Pts',(-96.7702751038564,1078.26375567953,
440.147829154859));
#107880=CARTESIAN_POINT('Ctrl Pts',(-96.7666050904893,1078.26379652429,
440.167027316342));
#107881=CARTESIAN_POINT('Ctrl Pts',(-96.7561993855903,1078.2639788657,440.215404124046));
#107882=CARTESIAN_POINT('Ctrl Pts',(-96.7488747468521,1078.26416229516,
440.244443560783));
#107883=CARTESIAN_POINT('Ctrl Pts',(-96.7166902878999,1078.26515057891,
440.355413706194));
#107884=CARTESIAN_POINT('Ctrl Pts',(-96.6846313263266,1078.26647454538,
440.43501175105));
#107885=CARTESIAN_POINT('Ctrl Pts',(-96.588797529577,1078.27102595418,440.617553685033));
#107886=CARTESIAN_POINT('Ctrl Pts',(-96.5179040708547,1078.27478743375,
440.715802746704));
#107887=CARTESIAN_POINT('Ctrl Pts',(-96.3390656351305,1078.28487699519,
440.901522687317));
#107888=CARTESIAN_POINT('Ctrl Pts',(-96.2285097408588,1078.29142226283,
440.98436808755));
#107889=CARTESIAN_POINT('Ctrl Pts',(-95.974354769648,1078.30690338705,441.117367802158));
#107890=CARTESIAN_POINT('Ctrl Pts',(-95.8306287246488,1078.31588032969,
441.162859488262));
#107891=CARTESIAN_POINT('Ctrl Pts',(-95.6269453490775,1078.32879928642,
441.189724286364));
#107892=CARTESIAN_POINT('Ctrl Pts',(-95.571232289585,1078.33235268885,441.193367887108));
#107893=CARTESIAN_POINT('Ctrl Pts',(-95.5155706932857,1078.33592031499,
441.193367887108));
#107894=CARTESIAN_POINT('',(-5.99814689883682,1077.55052528867,530.41919439426));
#107895=CARTESIAN_POINT('',(-5.99814689883688,1077.77685018773,528.221532122276));
#107896=CARTESIAN_POINT('Ctrl Pts',(-5.99814689883686,1077.55052528867,
530.419194394261));
#107897=CARTESIAN_POINT('Ctrl Pts',(-5.99625157451302,1077.55053689014,
530.419194394261));
#107898=CARTESIAN_POINT('Ctrl Pts',(-5.99435621017774,1077.55054901575,
530.419189490521));
#107899=CARTESIAN_POINT('Ctrl Pts',(-5.95516251023783,1077.55081059178,
530.418986673861));
#107900=CARTESIAN_POINT('Ctrl Pts',(-5.91790066207507,1077.55126217839,
530.416894720419));
#107901=CARTESIAN_POINT('Ctrl Pts',(-5.80468871392544,1077.5532533346,530.404737083079));
#107902=CARTESIAN_POINT('Ctrl Pts',(-5.72964359113455,1077.55543236532,
530.388628980098));
#107903=CARTESIAN_POINT('Ctrl Pts',(-5.51807109371232,1077.56409236501,
530.319507345083));
#107904=CARTESIAN_POINT('Ctrl Pts',(-5.38980568816756,1077.57259502735,
530.246971516507));
#107905=CARTESIAN_POINT('Ctrl Pts',(-5.18501442972,1077.59256506602,530.069931278608));
#107906=CARTESIAN_POINT('Ctrl Pts',(-5.10520905667489,1077.60328642072,
529.972780228673));
#107907=CARTESIAN_POINT('Ctrl Pts',(-4.97682800013577,1077.62765370819,
529.747500600443));
#107908=CARTESIAN_POINT('Ctrl Pts',(-4.93227056529072,1077.6412613617,529.619387270914));
#107909=CARTESIAN_POINT('Ctrl Pts',(-4.89011014567468,1077.67001268881,
529.34370690663));
#107910=CARTESIAN_POINT('Ctrl Pts',(-4.89663170480415,1077.68492512121,
529.197982555071));
#107911=CARTESIAN_POINT('Ctrl Pts',(-4.96566336731164,1077.71307903982,
528.917606861634));
#107912=CARTESIAN_POINT('Ctrl Pts',(-5.0274178409016,1077.72605912643,528.785583485956));
#107913=CARTESIAN_POINT('Ctrl Pts',(-5.19233601030598,1077.74763244216,
528.561412409395));
#107914=CARTESIAN_POINT('Ctrl Pts',(-5.29073346742357,1077.75630078835,
528.468914039881));
#107915=CARTESIAN_POINT('Ctrl Pts',(-5.49533693715638,1077.7682395786,528.337229939953));
#107916=CARTESIAN_POINT('Ctrl Pts',(-5.5955710041969,1077.77214423415,528.292100479986));
#107917=CARTESIAN_POINT('Ctrl Pts',(-5.74421572185004,1077.7754395239,528.250327385468));
#107918=CARTESIAN_POINT('Ctrl Pts',(-5.78828107617766,1077.77613099263,
528.240819421478));
#107919=CARTESIAN_POINT('Ctrl Pts',(-5.86233038665581,1077.77682681411,
528.229549148356));
#107920=CARTESIAN_POINT('Ctrl Pts',(-5.89202299874192,1077.77698389145,
528.226261187363));
#107921=CARTESIAN_POINT('Ctrl Pts',(-5.94721628748892,1077.77705135184,
528.222417728899));
#107922=CARTESIAN_POINT('Ctrl Pts',(-5.97267302793693,1077.77699463516,
528.22153234558));
#107923=CARTESIAN_POINT('Ctrl Pts',(-5.99813726465766,1077.77685024236,
528.221532122318));
#107924=CARTESIAN_POINT('Ctrl Pts',(-5.99814689883633,1077.77685018773,
528.221532122276));
#107925=CARTESIAN_POINT('Ctrl Pts',(-6.03403752468953,1077.77664664181,
528.221532122276));
#107926=CARTESIAN_POINT('Ctrl Pts',(-6.06989519952883,1077.77626926427,
528.223289913179));
#107927=CARTESIAN_POINT('Ctrl Pts',(-6.17620342407288,1077.774631476,528.233736703841));
#107928=CARTESIAN_POINT('Ctrl Pts',(-6.24594319565952,1077.77287310659,
528.24749148978));
#107929=CARTESIAN_POINT('Ctrl Pts',(-6.45376854617888,1077.76550530709,
528.309830747198));
#107930=CARTESIAN_POINT('Ctrl Pts',(-6.58379450417654,1077.75786641588,
528.379239756435));
#107931=CARTESIAN_POINT('Ctrl Pts',(-6.79255995050972,1077.73947563506,
528.551046657383));
#107932=CARTESIAN_POINT('Ctrl Pts',(-6.8744895962233,1077.72947377155,528.645890896189));
#107933=CARTESIAN_POINT('Ctrl Pts',(-7.00828360006629,1077.70628653847,
528.867441368));
#107934=CARTESIAN_POINT('Ctrl Pts',(-7.0560413653166,1077.69309881595,528.994276264719));
#107935=CARTESIAN_POINT('Ctrl Pts',(-7.1052442529102,1077.6646610266,529.268780480461));
#107936=CARTESIAN_POINT('Ctrl Pts',(-7.10242420913194,1077.64959680605,
529.414720044921));
#107937=CARTESIAN_POINT('Ctrl Pts',(-7.0404778165884,1077.62059389268,529.696955104784));
#107938=CARTESIAN_POINT('Ctrl Pts',(-6.98200917043208,1077.6069278055,529.830611541411));
#107939=CARTESIAN_POINT('Ctrl Pts',(-6.82220676816419,1077.58375419136,
530.059609284421));
#107940=CARTESIAN_POINT('Ctrl Pts',(-6.72543730811032,1077.57422170571,
530.155034572304));
#107941=CARTESIAN_POINT('Ctrl Pts',(-6.51859958642837,1077.56060987426,
530.29490747696));
#107942=CARTESIAN_POINT('Ctrl Pts',(-6.41396045197862,1077.55601586345,
530.343953694494));
#107943=CARTESIAN_POINT('Ctrl Pts',(-6.25908219165767,1077.55217890304,
530.388767037483));
#107944=CARTESIAN_POINT('Ctrl Pts',(-6.21382930607271,1077.55138257418,
530.398813970393));
#107945=CARTESIAN_POINT('Ctrl Pts',(-6.1381096864318,1077.55057980532,530.41066599318));
#107946=CARTESIAN_POINT('Ctrl Pts',(-6.10796468216702,1077.55039594603,
530.414113590531));
#107947=CARTESIAN_POINT('Ctrl Pts',(-6.05123494798002,1077.55030312154,
530.418232290127));
#107948=CARTESIAN_POINT('Ctrl Pts',(-6.024694848476,1077.55036278595,530.419194394261));
#107949=CARTESIAN_POINT('Ctrl Pts',(-5.99814689883686,1077.55052528867,
530.419194394261));
#107950=CARTESIAN_POINT('',(-14.9669751953828,1078.26481065249,521.463636077531));
#107951=CARTESIAN_POINT('',(-14.9669751953831,1078.42603095152,518.912747835258));
#107952=CARTESIAN_POINT('Ctrl Pts',(-14.9669751953828,1078.26481065249,
521.463636077531));
#107953=CARTESIAN_POINT('Ctrl Pts',(-14.8840637748006,1078.26570128176,
521.463636077531));
#107954=CARTESIAN_POINT('Ctrl Pts',(-14.8013579449129,1078.26714355705,
521.455551522256));
#107955=CARTESIAN_POINT('Ctrl Pts',(-14.5537465604665,1078.27313268402,
521.406685807278));
#107956=CARTESIAN_POINT('Ctrl Pts',(-14.3957277923221,1078.27929036862,
521.34106585285));
#107957=CARTESIAN_POINT('Ctrl Pts',(-14.1357242669877,1078.29378715813,
521.166203806205));
#107958=CARTESIAN_POINT('Ctrl Pts',(-14.0307601869211,1078.30155359426,
521.066235321447));
#107959=CARTESIAN_POINT('Ctrl Pts',(-13.8520520489992,1078.31915918547,
520.826719033803));
#107960=CARTESIAN_POINT('Ctrl Pts',(-13.7828050194282,1078.32896433589,
520.686686188885));
#107961=CARTESIAN_POINT('Ctrl Pts',(-13.6948414272472,1078.34958104434,
520.377975725675));
#107962=CARTESIAN_POINT('Ctrl Pts',(-13.6809576326698,1078.36021810875,
520.210865778312));
#107963=CARTESIAN_POINT('Ctrl Pts',(-13.7182217730068,1078.38034555768,
519.879215693371));
#107964=CARTESIAN_POINT('Ctrl Pts',(-13.7695938782063,1078.38963277858,
519.717909230261));
#107965=CARTESIAN_POINT('Ctrl Pts',(-13.9268469953116,1078.40516638536,
519.433448029209));
#107966=CARTESIAN_POINT('Ctrl Pts',(-14.0277996544593,1078.41143642874,
519.310988082309));
#107967=CARTESIAN_POINT('Ctrl Pts',(-14.2531230341966,1078.42038035336,
519.122466835079));
#107968=CARTESIAN_POINT('Ctrl Pts',(-14.3710958524674,1078.42336647845,
519.052279763025));
#107969=CARTESIAN_POINT('Ctrl Pts',(-14.5470792565021,1078.42579035591,
518.982689924465));
#107970=CARTESIAN_POINT('Ctrl Pts',(-14.5973600212422,1078.42627852434,
518.96633568821));
#107971=CARTESIAN_POINT('Ctrl Pts',(-14.6812535315019,1078.42676739158,
518.944703244199));
#107972=CARTESIAN_POINT('Ctrl Pts',(-14.7143189158074,1078.42688008554,
518.937565758563));
#107973=CARTESIAN_POINT('Ctrl Pts',(-14.7783386230042,1078.42694625596,
518.926389366863));
#107974=CARTESIAN_POINT('Ctrl Pts',(-14.8092344514433,1078.42691145112,
518.922155866722));
#107975=CARTESIAN_POINT('Ctrl Pts',(-14.8801991700964,1078.42667968432,
518.915070148516));
#107976=CARTESIAN_POINT('Ctrl Pts',(-14.9203095720602,1078.42643908678,
518.912969845802));
#107977=CARTESIAN_POINT('Ctrl Pts',(-14.9626259596285,1078.42606986321,
518.912753396805));
#107978=CARTESIAN_POINT('Ctrl Pts',(-14.9648005775582,1078.42605056793,
518.912747835258));
#107979=CARTESIAN_POINT('Ctrl Pts',(-14.9669751953831,1078.42603095152,
518.912747835258));
#107980=CARTESIAN_POINT('Ctrl Pts',(-14.9669751953831,1078.42603095152,
518.912747835258));
#107981=CARTESIAN_POINT('Ctrl Pts',(-14.9669963294508,1078.42603076088,
518.912747835258));
#107982=CARTESIAN_POINT('Ctrl Pts',(-14.9670174635184,1078.42603057021,
518.912747835782));
#107983=CARTESIAN_POINT('Ctrl Pts',(-14.9670385975861,1078.42603037951,
518.912747836833));
#107984=CARTESIAN_POINT('Ctrl Pts',(-15.0508711366131,1078.42527391702,
518.91275200414));
#107985=CARTESIAN_POINT('Ctrl Pts',(-15.1344926621712,1078.42404252594,
518.921021396378));
#107986=CARTESIAN_POINT('Ctrl Pts',(-15.3828314393348,1078.41892080874,
518.970602243735));
#107987=CARTESIAN_POINT('Ctrl Pts',(-15.5406578597173,1078.41365282696,
519.036534404558));
#107988=CARTESIAN_POINT('Ctrl Pts',(-15.8007897652478,1078.40085990006,
519.212270378563));
#107989=CARTESIAN_POINT('Ctrl Pts',(-15.9059426375644,1078.39386650394,
519.312987051048));
#107990=CARTESIAN_POINT('Ctrl Pts',(-16.084764132545,1078.37752517669,519.554451961017));
#107991=CARTESIAN_POINT('Ctrl Pts',(-16.1537850219646,1078.36816898871,
519.695711086767));
#107992=CARTESIAN_POINT('Ctrl Pts',(-16.2405780395232,1078.34781501935,
520.007222418239));
#107993=CARTESIAN_POINT('Ctrl Pts',(-16.2533116890618,1078.33694060142,
520.175863473803));
#107994=CARTESIAN_POINT('Ctrl Pts',(-16.2128993166143,1078.31582637112,
520.508233024411));
#107995=CARTESIAN_POINT('Ctrl Pts',(-16.1602105279201,1078.30579044325,
520.66878949279));
#107996=CARTESIAN_POINT('Ctrl Pts',(-16.0013218645856,1078.28866975536,
520.950589724364));
#107997=CARTESIAN_POINT('Ctrl Pts',(-15.900313741323,1078.28157880434,521.071390335792));
#107998=CARTESIAN_POINT('Ctrl Pts',(-15.6764206193954,1078.27138154275,
521.256600438396));
#107999=CARTESIAN_POINT('Ctrl Pts',(-15.5599847466809,1078.26792207522,
521.32536687353));
#108000=CARTESIAN_POINT('Ctrl Pts',(-15.3859927535195,1078.26508682437,
521.393990512086));
#108001=CARTESIAN_POINT('Ctrl Pts',(-15.3358988461925,1078.26450957978,
521.410248306169));
#108002=CARTESIAN_POINT('Ctrl Pts',(-15.2520147660141,1078.26392919726,
521.431842308626));
#108003=CARTESIAN_POINT('Ctrl Pts',(-15.2187614326536,1078.2637954148,521.438998694873));
#108004=CARTESIAN_POINT('Ctrl Pts',(-15.1541290539122,1078.26371955013,
521.450225879352));
#108005=CARTESIAN_POINT('Ctrl Pts',(-15.1228063827288,1078.26376461504,
521.454475027578));
#108006=CARTESIAN_POINT('Ctrl Pts',(-15.0504852084235,1078.26405564199,
521.46156167709));
#108007=CARTESIAN_POINT('Ctrl Pts',(-15.0094433975959,1078.26435760333,
521.463590190717));
#108008=CARTESIAN_POINT('Ctrl Pts',(-14.9679093429678,1078.2648006355,521.46363582097));
#108009=CARTESIAN_POINT('Ctrl Pts',(-14.9674422659131,1078.26480563524,
521.463636077531));
#108010=CARTESIAN_POINT('Ctrl Pts',(-14.9669751953828,1078.26481065249,
521.463636077531));
#108011=CARTESIAN_POINT('',(-22.5035000139861,1078.63105472707,512.783427991792));
#108012=CARTESIAN_POINT('',(-22.5035000139863,1078.70463504016,509.826821727405));
#108013=CARTESIAN_POINT('Ctrl Pts',(-22.503500013986,1078.63105472707,512.783427991792));
#108014=CARTESIAN_POINT('Ctrl Pts',(-22.4866131393249,1078.63119537603,
512.783427991792));
#108015=CARTESIAN_POINT('Ctrl Pts',(-22.4697230374544,1078.63134520182,
512.783138640098));
#108016=CARTESIAN_POINT('Ctrl Pts',(-22.2564438309899,1078.63335213982,
512.775825059762));
#108017=CARTESIAN_POINT('Ctrl Pts',(-22.0633670060187,1078.63640805523,
512.729999251495));
#108018=CARTESIAN_POINT('Ctrl Pts',(-21.73593348499,1078.64364815094,512.579145630744));
#108019=CARTESIAN_POINT('Ctrl Pts',(-21.5994177766968,1078.64750787693,
512.486190611309));
#108020=CARTESIAN_POINT('Ctrl Pts',(-21.3532336058568,1078.65616653841,
512.250402802075));
#108021=CARTESIAN_POINT('Ctrl Pts',(-21.2484882435221,1078.66094147988,
512.106128332391));
#108022=CARTESIAN_POINT('Ctrl Pts',(-21.0895328385584,1078.6707535532,511.776217186613));
#108023=CARTESIAN_POINT('Ctrl Pts',(-21.0408755713378,1078.67569105934,
511.591422106885));
#108024=CARTESIAN_POINT('Ctrl Pts',(-21.0155711088123,1078.68487174283,
511.208000152065));
#108025=CARTESIAN_POINT('Ctrl Pts',(-21.041320678264,1078.68900204053,511.012881063472));
#108026=CARTESIAN_POINT('Ctrl Pts',(-21.1643993578183,1078.69582055692,
510.651631738279));
#108027=CARTESIAN_POINT('Ctrl Pts',(-21.2575622877129,1078.69850743778,
510.487879708474));
#108028=CARTESIAN_POINT('Ctrl Pts',(-21.4986248017531,1078.70259043296,
510.20524567757));
#108029=CARTESIAN_POINT('Ctrl Pts',(-21.6438032309659,1078.70397036822,
510.088394310602));
#108030=CARTESIAN_POINT('Ctrl Pts',(-21.8639162363545,1078.70501767972,
509.970765468915));
#108031=CARTESIAN_POINT('Ctrl Pts',(-21.9230371623637,1078.70521343827,
509.944005713321));
#108032=CARTESIAN_POINT('Ctrl Pts',(-22.0203370579845,1078.70540677582,
509.907461311816));
#108033=CARTESIAN_POINT('Ctrl Pts',(-22.0574823032989,1078.70545205536,
509.895168107777));
#108034=CARTESIAN_POINT('Ctrl Pts',(-22.1279356992911,1078.7054856114,509.874914760205));
#108035=CARTESIAN_POINT('Ctrl Pts',(-22.1611181117293,1078.70548032343,
509.866610307785));
#108036=CARTESIAN_POINT('Ctrl Pts',(-22.2359581713495,1078.70542160338,
509.850616793126));
#108037=CARTESIAN_POINT('Ctrl Pts',(-22.2777187020305,1078.70535704858,
509.843552027201));
#108038=CARTESIAN_POINT('Ctrl Pts',(-22.3806344301835,1078.70511991512,
509.830658027611));
#108039=CARTESIAN_POINT('Ctrl Pts',(-22.4419602626397,1078.70491208442,
509.826828139419));
#108040=CARTESIAN_POINT('Ctrl Pts',(-22.5033457918472,1078.70463573459,
509.82682173545));
#108041=CARTESIAN_POINT('Ctrl Pts',(-22.503397199361,1078.70463550316,509.826821730087));
#108042=CARTESIAN_POINT('Ctrl Pts',(-22.5034486067408,1078.70463527168,
509.826821727406));
#108043=CARTESIAN_POINT('Ctrl Pts',(-22.5035000139863,1078.70463504016,
509.826821727406));
#108044=CARTESIAN_POINT('Ctrl Pts',(-22.5035000139863,1078.70463504015,
509.826821727406));
#108045=CARTESIAN_POINT('Ctrl Pts',(-22.6999431535576,1078.70375031174,
509.826821727406));
#108046=CARTESIAN_POINT('Ctrl Pts',(-22.8944252605779,1078.70218239496,
509.86597802692));
#108047=CARTESIAN_POINT('Ctrl Pts',(-23.2260476523347,1078.69795920695,
510.005147255519));
#108048=CARTESIAN_POINT('Ctrl Pts',(-23.3650410264147,1078.69555650679,
510.092788524152));
#108049=CARTESIAN_POINT('Ctrl Pts',(-23.618871788352,1078.68952227114,510.318934274039));
#108050=CARTESIAN_POINT('Ctrl Pts',(-23.7286918856681,1078.68584927833,
510.459238343909));
#108051=CARTESIAN_POINT('Ctrl Pts',(-23.8996148619197,1078.67729450252,
510.78337132357));
#108052=CARTESIAN_POINT('Ctrl Pts',(-23.9549745129172,1078.67241982118,
510.966629185851));
#108053=CARTESIAN_POINT('Ctrl Pts',(-23.9939459883892,1078.66216114497,
511.349253265408));
#108054=CARTESIAN_POINT('Ctrl Pts',(-23.9751487448127,1078.65686949352,
511.545184600554));
#108055=CARTESIAN_POINT('Ctrl Pts',(-23.8647850039104,1078.64713354384,
511.91127044371));
#108056=CARTESIAN_POINT('Ctrl Pts',(-23.777045119279,1078.64275876997,512.078818369425));
#108057=CARTESIAN_POINT('Ctrl Pts',(-23.5377300378039,1078.63538886956,
512.379615425074));
#108058=CARTESIAN_POINT('Ctrl Pts',(-23.3855469346556,1078.6325554677,512.507691403558));
#108059=CARTESIAN_POINT('Ctrl Pts',(-23.1537877386577,1078.63041905963,
512.634417826553));
#108060=CARTESIAN_POINT('Ctrl Pts',(-23.0927105917142,1078.63002172931,
512.662594950278));
#108061=CARTESIAN_POINT('Ctrl Pts',(-22.992561123175,1078.62962914044,512.700760374292));
#108062=CARTESIAN_POINT('Ctrl Pts',(-22.9546311509793,1078.62953636008,
512.713478499856));
#108063=CARTESIAN_POINT('Ctrl Pts',(-22.8826389400606,1078.62946389858,
512.73441060299));
#108064=CARTESIAN_POINT('Ctrl Pts',(-22.8487095354434,1078.62947153576,
512.742982448831));
#108065=CARTESIAN_POINT('Ctrl Pts',(-22.7727869887952,1078.62958044117,
512.759320835298));
#108066=CARTESIAN_POINT('Ctrl Pts',(-22.7306968491649,1078.62970188294,
512.766488257087));
#108067=CARTESIAN_POINT('Ctrl Pts',(-22.6270231116153,1078.63014849078,
512.779554805226));
#108068=CARTESIAN_POINT('Ctrl Pts',(-22.5652831616516,1078.63054014191,
512.783427991792));
#108069=CARTESIAN_POINT('Ctrl Pts',(-22.503500013986,1078.63105472707,512.783427991792));
#108070=CARTESIAN_POINT('',(-3.9889441036734,1078.62952598896,515.567896071097));
#108071=CARTESIAN_POINT('',(-3.98894410367367,1078.70545282671,512.611289806711));
#108072=CARTESIAN_POINT('Ctrl Pts',(-3.98894410367339,1078.62952598896,
515.567896071097));
#108073=CARTESIAN_POINT('Ctrl Pts',(-3.97557954633002,1078.62954585557,
515.567896071097));
#108074=CARTESIAN_POINT('Ctrl Pts',(-3.96221426603179,1078.62957176346,
515.567714838267));
#108075=CARTESIAN_POINT('Ctrl Pts',(-3.8925818337087,1078.62973820289,515.565825684791));
#108076=CARTESIAN_POINT('Ctrl Pts',(-3.83644530112953,1078.62997953828,
515.561086337221));
#108077=CARTESIAN_POINT('Ctrl Pts',(-3.66587032856376,1078.63103846207,
515.536817915507));
#108078=CARTESIAN_POINT('Ctrl Pts',(-3.55334980457449,1078.63219293344,
515.507017548996));
#108079=CARTESIAN_POINT('Ctrl Pts',(-3.2618459890488,1078.63638717737,515.391782908239));
#108080=CARTESIAN_POINT('Ctrl Pts',(-3.09462218266161,1078.6401407127,515.283136431196));
#108081=CARTESIAN_POINT('Ctrl Pts',(-2.8322928991613,1078.64848047957,515.025786265432));
#108082=CARTESIAN_POINT('Ctrl Pts',(-2.73235785647567,1078.65281227588,
514.886641081079));
#108083=CARTESIAN_POINT('Ctrl Pts',(-2.57893237056587,1078.66214960547,
514.569620538358));
#108084=CARTESIAN_POINT('Ctrl Pts',(-2.53056467850437,1078.66709701536,
514.392396344916));
#108085=CARTESIAN_POINT('Ctrl Pts',(-2.49961058230914,1078.67693702634,
514.016309205842));
#108086=CARTESIAN_POINT('Ctrl Pts',(-2.52228850411433,1078.68170124812,
513.820494124643));
#108087=CARTESIAN_POINT('Ctrl Pts',(-2.64179113186497,1078.69007640222,
513.450943900934));
#108088=CARTESIAN_POINT('Ctrl Pts',(-2.73668149203204,1078.6936230876,513.280556001807));
#108089=CARTESIAN_POINT('Ctrl Pts',(-2.97657675542087,1078.6991469545,512.99778433898));
#108090=CARTESIAN_POINT('Ctrl Pts',(-3.11497587303917,1078.70118866009,
512.884139562166));
#108091=CARTESIAN_POINT('Ctrl Pts',(-3.38118250318559,1078.70371200763,
512.736030196637));
#108092=CARTESIAN_POINT('Ctrl Pts',(-3.49964810861994,1078.70446243519,
512.68884436575));
#108093=CARTESIAN_POINT('Ctrl Pts',(-3.68054142585995,1078.70514282573,
512.64258404416));
#108094=CARTESIAN_POINT('Ctrl Pts',(-3.7392458118229,1078.70529591639,512.631307042471));
#108095=CARTESIAN_POINT('Ctrl Pts',(-3.84050239514498,1078.70544857754,
512.618150902082));
#108096=CARTESIAN_POINT('Ctrl Pts',(-3.882749205525,1078.70547971775,512.614499973586));
#108097=CARTESIAN_POINT('Ctrl Pts',(-3.94635948868066,1078.70547820009,
512.611749999776));
#108098=CARTESIAN_POINT('Ctrl Pts',(-3.96764200581816,1078.70546957949,
512.611290052986));
#108099=CARTESIAN_POINT('Ctrl Pts',(-3.98892700603221,1078.70545284015,
512.61128980681));
#108100=CARTESIAN_POINT('Ctrl Pts',(-3.98893270524644,1078.70545283567,
512.611289806744));
#108101=CARTESIAN_POINT('Ctrl Pts',(-3.98893840446025,1078.70545283119,
512.611289806711));
#108102=CARTESIAN_POINT('Ctrl Pts',(-3.98894410367366,1078.70545282671,
512.611289806711));
#108103=CARTESIAN_POINT('Ctrl Pts',(-3.98894410367366,1078.70545282671,
512.611289806711));
#108104=CARTESIAN_POINT('Ctrl Pts',(-4.03787639450469,1078.7054143345,512.611289806711));
#108105=CARTESIAN_POINT('Ctrl Pts',(-4.08677847020839,1078.70533300906,
512.613719318494));
#108106=CARTESIAN_POINT('Ctrl Pts',(-4.22075193636127,1078.70499064457,
512.627064134004));
#108107=CARTESIAN_POINT('Ctrl Pts',(-4.30513368183501,1078.7046414018,512.642959141823));
#108108=CARTESIAN_POINT('Ctrl Pts',(-4.57794119745513,1078.70304202139,
512.719370449642));
#108109=CARTESIAN_POINT('Ctrl Pts',(-4.75561195822102,1078.70123179215,
512.810279607493));
#108110=CARTESIAN_POINT('Ctrl Pts',(-5.04059969034957,1078.69650907921,
513.037346969308));
#108111=CARTESIAN_POINT('Ctrl Pts',(-5.1525179032029,1078.69384088833,513.162612966679));
#108112=CARTESIAN_POINT('Ctrl Pts',(-5.3366551908863,1078.68725408687,513.456080988321));
#108113=CARTESIAN_POINT('Ctrl Pts',(-5.40360259185759,1078.68330499974,
513.624408312825));
#108114=CARTESIAN_POINT('Ctrl Pts',(-5.47638507738358,1078.67425140327,
513.989526988659));
#108115=CARTESIAN_POINT('Ctrl Pts',(-5.47675302990086,1078.6691679112,514.184005102085));
#108116=CARTESIAN_POINT('Ctrl Pts',(-5.40256299088101,1078.65877709986,
514.563722667025));
#108117=CARTESIAN_POINT('Ctrl Pts',(-5.32809344979178,1078.65357300242,
514.745184755656));
#108118=CARTESIAN_POINT('Ctrl Pts',(-5.11867735485001,1078.64429362908,
515.06072666782));
#108119=CARTESIAN_POINT('Ctrl Pts',(-4.98881577998556,1078.64026196557,
515.193977130005));
#108120=CARTESIAN_POINT('Ctrl Pts',(-4.70670876744872,1078.63429634077,
515.391832795471));
#108121=CARTESIAN_POINT('Ctrl Pts',(-4.56154984555295,1078.63219753844,
515.461869640279));
#108122=CARTESIAN_POINT('Ctrl Pts',(-4.34326753126651,1078.63038212659,
515.526391544756));
#108123=CARTESIAN_POINT('Ctrl Pts',(-4.27730879521058,1078.6299914462,515.541068519988));
#108124=CARTESIAN_POINT('Ctrl Pts',(-4.16613656476757,1078.6295950361,515.557926493658));
#108125=CARTESIAN_POINT('Ctrl Pts',(-4.12141087466975,1078.62950448441,
515.562635088888));
#108126=CARTESIAN_POINT('Ctrl Pts',(-4.04737063402253,1078.62946800522,
515.567030028428));
#108127=CARTESIAN_POINT('Ctrl Pts',(-4.0181590962076,1078.62948256043,515.567896071097));
#108128=CARTESIAN_POINT('Ctrl Pts',(-3.98894410367339,1078.62952598896,
515.567896071097));
#108129=CARTESIAN_POINT('',(-41.3143294401482,1076.68214102845,529.795163061528));
#108130=CARTESIAN_POINT('',(-41.3143294401472,1076.95433007119,527.614081564072));
#108131=CARTESIAN_POINT('Ctrl Pts',(-41.3143294401484,1076.68214102845,
529.795163061529));
#108132=CARTESIAN_POINT('Ctrl Pts',(-41.2773532062123,1076.68401340828,
529.795163061529));
#108133=CARTESIAN_POINT('Ctrl Pts',(-41.2403641585233,1076.68612555935,
529.793282476709));
#108134=CARTESIAN_POINT('Ctrl Pts',(-41.0916802738423,1076.69558300308,
529.778094241651));
#108135=CARTESIAN_POINT('Ctrl Pts',(-40.982442325362,1076.70474658777,529.74946695222));
#108136=CARTESIAN_POINT('Ctrl Pts',(-40.7657520329234,1076.72761663204,
529.655283541194));
#108137=CARTESIAN_POINT('Ctrl Pts',(-40.661332177464,1076.74153707759,529.586781886565));
#108138=CARTESIAN_POINT('Ctrl Pts',(-40.472571066346,1076.77317219352,529.410836213898));
#108139=CARTESIAN_POINT('Ctrl Pts',(-40.3921931906226,1076.79084766685,
529.302041545776));
#108140=CARTESIAN_POINT('Ctrl Pts',(-40.2704123107375,1076.82820945122,
529.051586041641));
#108141=CARTESIAN_POINT('Ctrl Pts',(-40.2336512592061,1076.84759879574,
528.910344328474));
#108142=CARTESIAN_POINT('Ctrl Pts',(-40.2174768337832,1076.88394278164,
528.623315243353));
#108143=CARTESIAN_POINT('Ctrl Pts',(-40.237542682625,1076.90058944192,528.480248851961));
#108144=CARTESIAN_POINT('Ctrl Pts',(-40.3273254919708,1076.92777386773,
528.223240517014));
#108145=CARTESIAN_POINT('Ctrl Pts',(-40.3911653338904,1076.93854435829,
528.109837635294));
#108146=CARTESIAN_POINT('Ctrl Pts',(-40.5462307588409,1076.95395240713,
527.92209964645));
#108147=CARTESIAN_POINT('Ctrl Pts',(-40.6323854102545,1076.95906150556,
527.84595306808));
#108148=CARTESIAN_POINT('Ctrl Pts',(-40.7612077031207,1076.96281651451,
527.763982304864));
#108149=CARTESIAN_POINT('Ctrl Pts',(-40.794600371696,1076.96349818409,527.745127807664));
#108150=CARTESIAN_POINT('Ctrl Pts',(-40.8496698516572,1076.96416939454,
527.717754792231));
#108151=CARTESIAN_POINT('Ctrl Pts',(-40.8707433593247,1076.96432584668,
527.708104629852));
#108152=CARTESIAN_POINT('Ctrl Pts',(-40.9091996231162,1076.9644334277,527.691956251063));
#108153=CARTESIAN_POINT('Ctrl Pts',(-40.9264705446296,1076.96441935555,
527.685216505806));
#108154=CARTESIAN_POINT('Ctrl Pts',(-40.9671508477464,1076.96424215317,
527.67052511976));
#108155=CARTESIAN_POINT('Ctrl Pts',(-40.990674735862,1076.96403095435,527.662922966839));
#108156=CARTESIAN_POINT('Ctrl Pts',(-41.0577495325793,1076.96312540197,
527.643738036847));
#108157=CARTESIAN_POINT('Ctrl Pts',(-41.1017823575711,1076.96217742873,
527.634047185999));
#108158=CARTESIAN_POINT('Ctrl Pts',(-41.2018975214531,1076.95923923163,
527.618433245831));
#108159=CARTESIAN_POINT('Ctrl Pts',(-41.258081909659,1076.95705246719,527.614081564072));
#108160=CARTESIAN_POINT('Ctrl Pts',(-41.3143294401472,1076.95433007119,
527.614081564072));
#108161=CARTESIAN_POINT('Ctrl Pts',(-41.3143294401472,1076.95433007119,
527.614081564072));
#108162=CARTESIAN_POINT('Ctrl Pts',(-41.3143342582443,1076.954329838,527.614081564072));
#108163=CARTESIAN_POINT('Ctrl Pts',(-41.3143390763419,1076.9543296048,527.614081564095));
#108164=CARTESIAN_POINT('Ctrl Pts',(-41.3143438944399,1076.95432937159,
527.614081564159));
#108165=CARTESIAN_POINT('Ctrl Pts',(-41.4218177571127,1076.94912743262,
527.61408298865));
#108166=CARTESIAN_POINT('Ctrl Pts',(-41.5285839269821,1076.94201581872,
527.629970842879));
#108167=CARTESIAN_POINT('Ctrl Pts',(-41.7465398764455,1076.92332522854,
527.696156819038));
#108168=CARTESIAN_POINT('Ctrl Pts',(-41.8551083744335,1076.91143242287,
527.750008868671));
#108169=CARTESIAN_POINT('Ctrl Pts',(-42.0589640033117,1076.8833436954,527.897149040317));
#108170=CARTESIAN_POINT('Ctrl Pts',(-42.1505015252907,1076.8670766189,527.992418056515));
#108171=CARTESIAN_POINT('Ctrl Pts',(-42.3011123191613,1076.83147634675,
528.219303416123));
#108172=CARTESIAN_POINT('Ctrl Pts',(-42.3556523794505,1076.81231881471,
528.351193817558));
#108173=CARTESIAN_POINT('Ctrl Pts',(-42.4119343242816,1076.7744051732,528.631303749692));
#108174=CARTESIAN_POINT('Ctrl Pts',(-42.4120238714279,1076.75601786499,
528.777213302029));
#108175=CARTESIAN_POINT('Ctrl Pts',(-42.3567499892214,1076.72393871357,
529.052853298823));
#108176=CARTESIAN_POINT('Ctrl Pts',(-42.3049903317031,1076.71031796148,
529.18066405343));
#108177=CARTESIAN_POINT('Ctrl Pts',(-42.1543372528411,1076.68820744054,
529.414238842814));
#108178=CARTESIAN_POINT('Ctrl Pts',(-42.0555282974927,1076.68010067045,
529.516961357787));
#108179=CARTESIAN_POINT('Ctrl Pts',(-41.9049993341205,1076.67427558416,
529.622326933881));
#108180=CARTESIAN_POINT('Ctrl Pts',(-41.8689120808022,1076.6732632532,529.644575584759));
#108181=CARTESIAN_POINT('Ctrl Pts',(-41.8079907982816,1076.67215898277,
529.677400659774));
#108182=CARTESIAN_POINT('Ctrl Pts',(-41.7839035379483,1076.67186607917,
529.689254012106));
#108183=CARTESIAN_POINT('Ctrl Pts',(-41.7403344899076,1076.67158708777,
529.708731399799));
#108184=CARTESIAN_POINT('Ctrl Pts',(-41.7210256829323,1076.67154742352,
529.716706077007));
#108185=CARTESIAN_POINT('Ctrl Pts',(-41.6801628030987,1076.67163705262,
529.732224372033));
#108186=CARTESIAN_POINT('Ctrl Pts',(-41.6585774119473,1076.67178233153,
529.739655319584));
#108187=CARTESIAN_POINT('Ctrl Pts',(-41.6020983112158,1076.67241315148,
529.757136396111));
#108188=CARTESIAN_POINT('Ctrl Pts',(-41.5669110503444,1076.67304855044,
529.766130080952));
#108189=CARTESIAN_POINT('Ctrl Pts',(-41.4597866241902,1076.67570131867,
529.787882716096));
#108190=CARTESIAN_POINT('Ctrl Pts',(-41.387082831868,1076.67845698686,529.795163061529));
#108191=CARTESIAN_POINT('Ctrl Pts',(-41.3143294401484,1076.68214102845,
529.795163061529));
#108192=CARTESIAN_POINT('',(-48.0649554680748,1077.56338652908,518.927727241935));
#108193=CARTESIAN_POINT('',(-48.064955468075,1077.76488388158,516.73006496995));
#108194=CARTESIAN_POINT('Ctrl Pts',(-48.0649554680755,1077.56338652908,
518.927727241935));
#108195=CARTESIAN_POINT('Ctrl Pts',(-48.0145010273267,1077.56585180285,
518.927727241935));
#108196=CARTESIAN_POINT('Ctrl Pts',(-47.9640080026722,1077.56864550973,
518.924252272737));
#108197=CARTESIAN_POINT('Ctrl Pts',(-47.796039599905,1077.57903610607,518.900930551175));
#108198=CARTESIAN_POINT('Ctrl Pts',(-47.6817794730932,1077.58792237194,
518.865574638573));
#108199=CARTESIAN_POINT('Ctrl Pts',(-47.4595039067031,1077.60903595514,
518.754983962953));
#108200=CARTESIAN_POINT('Ctrl Pts',(-47.3547210668178,1077.62132914573,
518.677266611072));
#108201=CARTESIAN_POINT('Ctrl Pts',(-47.170326116537,1077.64824277595,518.481934787316));
#108202=CARTESIAN_POINT('Ctrl Pts',(-47.0948596323801,1077.66273265577,
518.363431087428));
#108203=CARTESIAN_POINT('Ctrl Pts',(-46.9898154918473,1077.69187953984,
518.098582349962));
#108204=CARTESIAN_POINT('Ctrl Pts',(-46.9635362291813,1077.7062346296,517.953729404063));
#108205=CARTESIAN_POINT('Ctrl Pts',(-46.9690145884228,1077.73177117505,
517.667251220634));
#108206=CARTESIAN_POINT('Ctrl Pts',(-46.9986857143744,1077.74281759757,
517.528301087755));
#108207=CARTESIAN_POINT('Ctrl Pts',(-47.1056804118959,1077.76027751622,
517.276870741214));
#108208=CARTESIAN_POINT('Ctrl Pts',(-47.1791052670855,1077.76678989412,
517.165374239164));
#108209=CARTESIAN_POINT('Ctrl Pts',(-47.3189758623651,1077.77334205686,
517.019063429134));
#108210=CARTESIAN_POINT('Ctrl Pts',(-47.3719917744344,1077.77497057583,
516.973255993722));
#108211=CARTESIAN_POINT('Ctrl Pts',(-47.4536554849855,1077.776367297,516.915301368854));
#108212=CARTESIAN_POINT('Ctrl Pts',(-47.479010752856,1077.77666610845,516.898835917402));
#108213=CARTESIAN_POINT('Ctrl Pts',(-47.5213219030368,1077.77695163645,
516.873777440269));
#108214=CARTESIAN_POINT('Ctrl Pts',(-47.5378776790546,1077.7770131232,516.864542365627));
#108215=CARTESIAN_POINT('Ctrl Pts',(-47.5729058783718,1077.77703996874,
516.846174719934));
#108216=CARTESIAN_POINT('Ctrl Pts',(-47.5914128481066,1077.77699652695,
516.837124206612));
#108217=CARTESIAN_POINT('Ctrl Pts',(-47.6355330724613,1077.7767592945,516.817064621247));
#108218=CARTESIAN_POINT('Ctrl Pts',(-47.6613318700247,1077.77651793062,
516.806499685223));
#108219=CARTESIAN_POINT('Ctrl Pts',(-47.7452557410909,1077.77540887468,
516.775803766469));
#108220=CARTESIAN_POINT('Ctrl Pts',(-47.8046698637717,1077.7741389845,516.759569074191));
#108221=CARTESIAN_POINT('Ctrl Pts',(-47.9310529949326,1077.77044907064,
516.73619484361));
#108222=CARTESIAN_POINT('Ctrl Pts',(-47.9979446125574,1077.76794311597,
516.73006496995));
#108223=CARTESIAN_POINT('Ctrl Pts',(-48.0649554680748,1077.76488388158,
516.73006496995));
#108224=CARTESIAN_POINT('Ctrl Pts',(-48.0649554680748,1077.76488388158,
516.73006496995));
#108225=CARTESIAN_POINT('Ctrl Pts',(-48.0649598430732,1077.76488368185,
516.73006496995));
#108226=CARTESIAN_POINT('Ctrl Pts',(-48.0649642180723,1077.76488348212,
516.730064969925));
#108227=CARTESIAN_POINT('Ctrl Pts',(-48.0649685930717,1077.76488328238,
516.730064969977));
#108228=CARTESIAN_POINT('Ctrl Pts',(-48.1783489980554,1077.75970702632,
516.730066324253));
#108229=CARTESIAN_POINT('Ctrl Pts',(-48.2909640961249,1077.75299756761,
516.747615160064));
#108230=CARTESIAN_POINT('Ctrl Pts',(-48.518206698586,1077.73608207952,516.820088184502));
#108231=CARTESIAN_POINT('Ctrl Pts',(-48.630094046204,1077.72570265682,516.878265831029));
#108232=CARTESIAN_POINT('Ctrl Pts',(-48.8375422331832,1077.70184037015,
517.035875863945));
#108233=CARTESIAN_POINT('Ctrl Pts',(-48.9292511454738,1077.68837061489,
517.13699504206));
#108234=CARTESIAN_POINT('Ctrl Pts',(-49.076806488182,1077.65953151255,517.376286722553));
#108235=CARTESIAN_POINT('Ctrl Pts',(-49.1278911292269,1077.64437086784,
517.51444485906));
#108236=CARTESIAN_POINT('Ctrl Pts',(-49.1727820385911,1077.61567177391,
517.80054201422));
#108237=CARTESIAN_POINT('Ctrl Pts',(-49.1670092371341,1077.60238215247,
517.945636395291));
#108238=CARTESIAN_POINT('Ctrl Pts',(-49.1030894837639,1077.58048233853,
518.211675364131));
#108239=CARTESIAN_POINT('Ctrl Pts',(-49.0506933432679,1077.57171147817,
518.331513012622));
#108240=CARTESIAN_POINT('Ctrl Pts',(-48.9137484537884,1077.5589952769,518.536400788778));
#108241=CARTESIAN_POINT('Ctrl Pts',(-48.8339457995117,1077.55472998722,
518.622430126506));
#108242=CARTESIAN_POINT('Ctrl Pts',(-48.7118559167702,1077.55163430139,
518.717951772243));
#108243=CARTESIAN_POINT('Ctrl Pts',(-48.6804376729709,1077.55107969025,
518.739984630358));
#108244=CARTESIAN_POINT('Ctrl Pts',(-48.628410105786,1077.55053427899,518.772548047195));
#108245=CARTESIAN_POINT('Ctrl Pts',(-48.608511334067,1077.55040688114,518.784148521431));
#108246=CARTESIAN_POINT('Ctrl Pts',(-48.5721331343716,1077.55031714445,
518.803851051258));
#108247=CARTESIAN_POINT('Ctrl Pts',(-48.5557876574196,1077.55032651165,
518.812181462383));
#108248=CARTESIAN_POINT('Ctrl Pts',(-48.5172563691362,1077.55046276701,
518.830618504336));
#108249=CARTESIAN_POINT('Ctrl Pts',(-48.4949280004348,1077.55062723332,
518.840403612521));
#108250=CARTESIAN_POINT('Ctrl Pts',(-48.431225361482,1077.55133326594,518.865829806309));
#108251=CARTESIAN_POINT('Ctrl Pts',(-48.3892097524541,1077.55207220881,
518.879726004704));
#108252=CARTESIAN_POINT('Ctrl Pts',(-48.2543653682687,1077.55528433236,
518.915466015449));
#108253=CARTESIAN_POINT('Ctrl Pts',(-48.1597284755232,1077.55875578884,
518.927727241935));
#108254=CARTESIAN_POINT('Ctrl Pts',(-48.0649554680755,1077.56338652908,
518.927727241935));
#108255=CARTESIAN_POINT('',(-52.5439991194435,1078.27787179661,507.113735502178));
#108256=CARTESIAN_POINT('',(-52.5439991194437,1078.41491649088,504.562847259905));
#108257=CARTESIAN_POINT('Ctrl Pts',(-52.5439991194441,1078.27787179661,
507.113735502178));
#108258=CARTESIAN_POINT('Ctrl Pts',(-52.4986442771421,1078.27956269921,
507.113735502178));
#108259=CARTESIAN_POINT('Ctrl Pts',(-52.4532386218892,1078.28139109926,
507.111316334615));
#108260=CARTESIAN_POINT('Ctrl Pts',(-52.2679433665825,1078.28940503941,
507.091441651501));
#108261=CARTESIAN_POINT('Ctrl Pts',(-52.1314099928142,1078.29660548746,
507.05333718123));
#108262=CARTESIAN_POINT('Ctrl Pts',(-51.8658116666798,1078.31324672697,
506.929188792383));
#108263=CARTESIAN_POINT('Ctrl Pts',(-51.7404285211826,1078.32268861784,
506.840414518152));
#108264=CARTESIAN_POINT('Ctrl Pts',(-51.5191679411933,1078.34285032232,
506.614960460239));
#108265=CARTESIAN_POINT('Ctrl Pts',(-51.4281340532332,1078.35342681473,
506.477310289254));
#108266=CARTESIAN_POINT('Ctrl Pts',(-51.3012013249814,1078.37398778512,
506.170747028407));
#108267=CARTESIAN_POINT('Ctrl Pts',(-51.2682084167509,1078.38374779276,
506.004016022769));
#108268=CARTESIAN_POINT('Ctrl Pts',(-51.2688907632724,1078.40054457389,
505.675133975294));
#108269=CARTESIAN_POINT('Ctrl Pts',(-51.2995208059245,1078.40754151525,
505.516063695471));
#108270=CARTESIAN_POINT('Ctrl Pts',(-51.4200773886815,1078.41875122293,
505.213029763869));
#108271=CARTESIAN_POINT('Ctrl Pts',(-51.5106296082965,1078.42276998262,
505.072572155123));
#108272=CARTESIAN_POINT('Ctrl Pts',(-51.6633428479768,1078.4256964583,504.914076643506));
#108273=CARTESIAN_POINT('Ctrl Pts',(-51.7036385084434,1078.426220819,504.87729043587));
#108274=CARTESIAN_POINT('Ctrl Pts',(-51.7685152953052,1078.4267121243,504.825274505618));
#108275=CARTESIAN_POINT('Ctrl Pts',(-51.7914630822053,1078.42682534233,
504.808112808865));
#108276=CARTESIAN_POINT('Ctrl Pts',(-51.8339693610143,1078.42692852969,
504.778502901022));
#108277=CARTESIAN_POINT('Ctrl Pts',(-51.85332625225,1078.426937945,504.765787361048));
#108278=CARTESIAN_POINT('Ctrl Pts',(-51.8953202222838,1078.42687972818,
504.739810120037));
#108279=CARTESIAN_POINT('Ctrl Pts',(-51.9180419639268,1078.42680173631,
504.726705568707));
#108280=CARTESIAN_POINT('Ctrl Pts',(-51.9797576465656,1078.42646791388,
504.69360431753));
#108281=CARTESIAN_POINT('Ctrl Pts',(-52.01940431159,1078.42612814473,504.674901065275));
#108282=CARTESIAN_POINT('Ctrl Pts',(-52.1980810234138,1078.42405657482,
504.601604395505));
#108283=CARTESIAN_POINT('Ctrl Pts',(-52.3450857331372,1078.4209624869,504.569642288513));
#108284=CARTESIAN_POINT('Ctrl Pts',(-52.5108155057554,1078.41596659625,
504.563171036046));
#108285=CARTESIAN_POINT('Ctrl Pts',(-52.5274067847652,1078.4154498872,504.562847259905));
#108286=CARTESIAN_POINT('Ctrl Pts',(-52.5439991194437,1078.41491649088,
504.562847259905));
#108287=CARTESIAN_POINT('Ctrl Pts',(-52.5439991194437,1078.41491649088,
504.562847259905));
#108288=CARTESIAN_POINT('Ctrl Pts',(-52.544008079654,1078.41491620283,504.562847259905));
#108289=CARTESIAN_POINT('Ctrl Pts',(-52.5440170398646,1078.41491591478,
504.56284726));
#108290=CARTESIAN_POINT('Ctrl Pts',(-52.5440260000755,1078.41491562673,
504.562847260189));
#108291=CARTESIAN_POINT('Ctrl Pts',(-52.6807106207702,1078.41052145713,
504.562850140886));
#108292=CARTESIAN_POINT('Ctrl Pts',(-52.8164686631165,1078.40502727986,
504.584824495826));
#108293=CARTESIAN_POINT('Ctrl Pts',(-53.0878585470118,1078.39154213021,
504.674983409868));
#108294=CARTESIAN_POINT('Ctrl Pts',(-53.220195364015,1078.3834675677,504.74659532574));
#108295=CARTESIAN_POINT('Ctrl Pts',(-53.4629705438839,1078.36519532637,
504.939358940828));
#108296=CARTESIAN_POINT('Ctrl Pts',(-53.5688001439053,1078.35504191809,
505.062176281989));
#108297=CARTESIAN_POINT('Ctrl Pts',(-53.7333772667468,1078.33387359429,
505.347714228365));
#108298=CARTESIAN_POINT('Ctrl Pts',(-53.7878303959066,1078.32304757444,
505.509377161157));
#108299=CARTESIAN_POINT('Ctrl Pts',(-53.829975549002,1078.30309169221,505.839904830851));
#108300=CARTESIAN_POINT('Ctrl Pts',(-53.8190890232239,1078.29411126856,
506.005390567118));
#108301=CARTESIAN_POINT('Ctrl Pts',(-53.7391564514496,1078.27978192806,
506.307719020495));
#108302=CARTESIAN_POINT('Ctrl Pts',(-53.6764949059545,1078.2742763811,506.443474578826));
#108303=CARTESIAN_POINT('Ctrl Pts',(-53.5356430599943,1078.26778775998,
506.646453133765));
#108304=CARTESIAN_POINT('Ctrl Pts',(-53.470205072877,1078.26592891012,506.720692161054));
#108305=CARTESIAN_POINT('Ctrl Pts',(-53.3684007172843,1078.26443147481,
506.812244325751));
#108306=CARTESIAN_POINT('Ctrl Pts',(-53.3388064915731,1078.26413099571,
506.836541709559));
#108307=CARTESIAN_POINT('Ctrl Pts',(-53.2880420463172,1078.26383082245,
506.874529502126));
#108308=CARTESIAN_POINT('Ctrl Pts',(-53.2674794631115,1078.26376334058,
506.88898901963));
#108309=CARTESIAN_POINT('Ctrl Pts',(-53.2266443211653,1078.2637324558,506.915936658567));
#108310=CARTESIAN_POINT('Ctrl Pts',(-53.2064228488732,1078.26376370447,
506.928483388593));
#108311=CARTESIAN_POINT('Ctrl Pts',(-53.1584150395403,1078.26394458987,
506.956441477233));
#108312=CARTESIAN_POINT('Ctrl Pts',(-53.1303806368008,1078.26413031448,
506.971394737863));
#108313=CARTESIAN_POINT('Ctrl Pts',(-53.0401906655634,1078.26497503102,
507.015256899258));
#108314=CARTESIAN_POINT('Ctrl Pts',(-52.9762529287781,1078.26593173545,
507.040210314352));
#108315=CARTESIAN_POINT('Ctrl Pts',(-52.7914285797817,1078.2696604641,507.095679226291));
#108316=CARTESIAN_POINT('Ctrl Pts',(-52.667903440952,1078.27325244113,507.113735502178));
#108317=CARTESIAN_POINT('Ctrl Pts',(-52.5439991194441,1078.27787179661,
507.113735502178));
#108318=CARTESIAN_POINT('',(-55.8158882427213,1078.63997504936,496.136128111847));
#108319=CARTESIAN_POINT('',(-55.8158882427217,1078.69949549139,493.17952184746));
#108320=CARTESIAN_POINT('Ctrl Pts',(-55.8158882427213,1078.63997504936,
496.136128111847));
#108321=CARTESIAN_POINT('Ctrl Pts',(-55.7381761621697,1078.64151398949,
496.136128111847));
#108322=CARTESIAN_POINT('Ctrl Pts',(-55.6604683092864,1078.64318748345,
496.130000302946));
#108323=CARTESIAN_POINT('Ctrl Pts',(-55.416052423721,1078.64884766251,496.091093319474));
#108324=CARTESIAN_POINT('Ctrl Pts',(-55.2544465367711,1078.65318431832,
496.035832602985));
#108325=CARTESIAN_POINT('Ctrl Pts',(-54.94601132426,1078.66252338863,495.866901885036));
#108326=CARTESIAN_POINT('Ctrl Pts',(-54.803802738849,1078.66746722632,495.750636405023));
#108327=CARTESIAN_POINT('Ctrl Pts',(-54.5601086818315,1078.67729340092,
495.461982382799));
#108328=CARTESIAN_POINT('Ctrl Pts',(-54.4648213922992,1078.68204475838,
495.288917633588));
#108329=CARTESIAN_POINT('Ctrl Pts',(-54.3480562560232,1078.69035884261,
494.918549985383));
#108330=CARTESIAN_POINT('Ctrl Pts',(-54.3266007807071,1078.69386378003,
494.725202486329));
#108331=CARTESIAN_POINT('Ctrl Pts',(-54.3571894053235,1078.69920699931,
494.363710454937));
#108332=CARTESIAN_POINT('Ctrl Pts',(-54.4006686152582,1078.70115814677,
494.197973752867));
#108333=CARTESIAN_POINT('Ctrl Pts',(-54.5313053539874,1078.70379577326,
493.912164267285));
#108334=CARTESIAN_POINT('Ctrl Pts',(-54.6100947628516,1078.70461690227,
493.790515106427));
#108335=CARTESIAN_POINT('Ctrl Pts',(-54.7374721507079,1078.705221843,493.645508700875));
#108336=CARTESIAN_POINT('Ctrl Pts',(-54.7715034960503,1078.70533186944,
493.610434872485));
#108337=CARTESIAN_POINT('Ctrl Pts',(-54.8289920197998,1078.70544028254,
493.556778248848));
#108338=CARTESIAN_POINT('Ctrl Pts',(-54.8513854833553,1078.70546543502,
493.537109811828));
#108339=CARTESIAN_POINT('Ctrl Pts',(-54.8949247678817,1078.70548297794,
493.501140880741));
#108340=CARTESIAN_POINT('Ctrl Pts',(-54.9159476721064,1078.70547851921,
493.484709982686));
#108341=CARTESIAN_POINT('Ctrl Pts',(-54.9643394375763,1078.70543970664,
493.448955091846));
#108342=CARTESIAN_POINT('Ctrl Pts',(-54.9919437658391,1078.70539802359,
493.429974309028));
#108343=CARTESIAN_POINT('Ctrl Pts',(-55.0751380384177,1078.70521578472,
493.376839631339));
#108344=CARTESIAN_POINT('Ctrl Pts',(-55.132370378762,1078.70501927599,493.345408277861));
#108345=CARTESIAN_POINT('Ctrl Pts',(-55.2658228272856,1078.70440139534,
493.283222039045));
#108346=CARTESIAN_POINT('Ctrl Pts',(-55.3429080832118,1078.70393632846,
493.254830058092));
#108347=CARTESIAN_POINT('Ctrl Pts',(-55.5502578875137,1078.7023895069,493.197502204148));
#108348=CARTESIAN_POINT('Ctrl Pts',(-55.6827707839958,1078.70111160033,
493.17952184746));
#108349=CARTESIAN_POINT('Ctrl Pts',(-55.8158882427217,1078.69949549139,
493.17952184746));
#108350=CARTESIAN_POINT('Ctrl Pts',(-55.8158882427217,1078.69949549139,
493.17952184746));
#108351=CARTESIAN_POINT('Ctrl Pts',(-55.8159000830156,1078.69949534765,
493.17952184746));
#108352=CARTESIAN_POINT('Ctrl Pts',(-55.8159119233143,1078.6994952039,493.179521847602));
#108353=CARTESIAN_POINT('Ctrl Pts',(-55.8159237636178,1078.69949506015,
493.179521847887));
#108354=CARTESIAN_POINT('Ctrl Pts',(-55.9794669437012,1078.697509496,493.179525777528));
#108355=CARTESIAN_POINT('Ctrl Pts',(-56.1418739339458,1078.69503594291,
493.206668486392));
#108356=CARTESIAN_POINT('Ctrl Pts',(-56.4642283140259,1078.68885330115,
493.317494273381));
#108357=CARTESIAN_POINT('Ctrl Pts',(-56.620191844934,1078.68510311682,493.404860507457));
#108358=CARTESIAN_POINT('Ctrl Pts',(-56.9038669012547,1078.67640524987,
493.639014332784));
#108359=CARTESIAN_POINT('Ctrl Pts',(-57.0259632007142,1078.67146741882,
493.787545880715));
#108360=CARTESIAN_POINT('Ctrl Pts',(-57.2090528540562,1078.66116333372,
494.126432935689));
#108361=CARTESIAN_POINT('Ctrl Pts',(-57.2668540772811,1078.65589337403,
494.314333985789));
#108362=CARTESIAN_POINT('Ctrl Pts',(-57.3053909479616,1078.64630679125,
494.692693485502));
#108363=CARTESIAN_POINT('Ctrl Pts',(-57.2892537050925,1078.64204836896,
494.879269873133));
#108364=CARTESIAN_POINT('Ctrl Pts',(-57.1873539376165,1078.63501285798,
495.241664465276));
#108365=CARTESIAN_POINT('Ctrl Pts',(-57.1006254796562,1078.63235236716,
495.413633894357));
#108366=CARTESIAN_POINT('Ctrl Pts',(-56.9434526347171,1078.63034957464,
495.61608640209));
#108367=CARTESIAN_POINT('Ctrl Pts',(-56.8999128617944,1078.62997713082,
495.665077305353));
#108368=CARTESIAN_POINT('Ctrl Pts',(-56.8291832737198,1078.62963033988,
495.734744787117));
#108369=CARTESIAN_POINT('Ctrl Pts',(-56.8042908779995,1078.62955065203,
495.757635570108));
#108370=CARTESIAN_POINT('Ctrl Pts',(-56.7581163548514,1078.6294768266,495.797262327063));
#108371=CARTESIAN_POINT('Ctrl Pts',(-56.7371178441088,1078.62946876772,
495.814305548708));
#108372=CARTESIAN_POINT('Ctrl Pts',(-56.6915994559401,1078.62950421266,
495.849223269005));
#108373=CARTESIAN_POINT('Ctrl Pts',(-56.6669728114318,1078.62955410197,
495.866938317575));
#108374=CARTESIAN_POINT('Ctrl Pts',(-56.6003281284012,1078.62976846143,
495.911833311335));
#108375=CARTESIAN_POINT('Ctrl Pts',(-56.5574457528482,1078.6299861943,495.937659038498));
#108376=CARTESIAN_POINT('Ctrl Pts',(-56.3671092090801,1078.63128264162,
496.039505266986));
#108377=CARTESIAN_POINT('Ctrl Pts',(-56.2087602522833,1078.63318248535,
496.092583017586));
#108378=CARTESIAN_POINT('Ctrl Pts',(-55.9690462876418,1078.63707281428,
496.130178026875));
#108379=CARTESIAN_POINT('Ctrl Pts',(-55.8924652122921,1078.63845858794,
496.136128111847));
#108380=CARTESIAN_POINT('Ctrl Pts',(-55.8158882427213,1078.63997504936,
496.136128111847));
#108381=CARTESIAN_POINT('',(-40.0345449899137,1078.63462185218,506.210414596646));
#108382=CARTESIAN_POINT('',(-40.034544989914,1078.7026568498,503.25380833226));
#108383=CARTESIAN_POINT('Ctrl Pts',(-40.0345449899137,1078.63462185218,
506.210414596647));
#108384=CARTESIAN_POINT('Ctrl Pts',(-39.933258250339,1078.63609822354,506.210414596647));
#108385=CARTESIAN_POINT('Ctrl Pts',(-39.831992934802,1078.63786301688,506.200004964856));
#108386=CARTESIAN_POINT('Ctrl Pts',(-39.5729316752126,1078.64308303955,
506.145908031524));
#108387=CARTESIAN_POINT('Ctrl Pts',(-39.4201008036855,1078.64686749493,
506.08649678629));
#108388=CARTESIAN_POINT('Ctrl Pts',(-39.1286730549577,1078.65540843741,
505.913536323377));
#108389=CARTESIAN_POINT('Ctrl Pts',(-38.9945519874464,1078.66014658622,
505.797372361076));
#108390=CARTESIAN_POINT('Ctrl Pts',(-38.765611758857,1078.66992924473,505.513614639003));
#108391=CARTESIAN_POINT('Ctrl Pts',(-38.6763669008811,1078.67487807669,
505.34554104547));
#108392=CARTESIAN_POINT('Ctrl Pts',(-38.5639735921682,1078.68414476881,
504.978762411192));
#108393=CARTESIAN_POINT('Ctrl Pts',(-38.5442911297931,1078.68834555087,
504.782802219003));
#108394=CARTESIAN_POINT('Ctrl Pts',(-38.5813873444244,1078.69532057629,
504.402296862145));
#108395=CARTESIAN_POINT('Ctrl Pts',(-38.634805018151,1078.69808856571,504.22105406683));
#108396=CARTESIAN_POINT('Ctrl Pts',(-38.8090985689076,1078.70241361652,
503.883040137149));
#108397=CARTESIAN_POINT('Ctrl Pts',(-38.9303202102076,1078.70389690259,
503.730446529508));
#108398=CARTESIAN_POINT('Ctrl Pts',(-39.1226275039791,1078.70497374679,
503.567078410624));
#108399=CARTESIAN_POINT('Ctrl Pts',(-39.1700827343216,1078.70516294172,
503.531444743352));
#108400=CARTESIAN_POINT('Ctrl Pts',(-39.2513682316366,1078.70537039634,
503.477731603099));
#108401=CARTESIAN_POINT('Ctrl Pts',(-39.2839888419741,1078.70542545713,
503.457945012923));
#108402=CARTESIAN_POINT('Ctrl Pts',(-39.3435670224156,1078.70547731193,
503.424889471978));
#108403=CARTESIAN_POINT('Ctrl Pts',(-39.3702329000793,1078.70548401992,
503.4111385892));
#108404=CARTESIAN_POINT('Ctrl Pts',(-39.4271171972576,1078.70546425462,
503.383963214299));
#108405=CARTESIAN_POINT('Ctrl Pts',(-39.4574050806584,1078.70543434434,
503.37072182486));
#108406=CARTESIAN_POINT('Ctrl Pts',(-39.5373714213134,1078.70530541979,
503.338910410266));
#108407=CARTESIAN_POINT('Ctrl Pts',(-39.5876500715567,1078.70517570366,
503.321978264619));
#108408=CARTESIAN_POINT('Ctrl Pts',(-39.7676132958365,1078.70453972674,
503.271967097767));
#108409=CARTESIAN_POINT('Ctrl Pts',(-39.900762934436,1078.70376561848,503.253809917498));
#108410=CARTESIAN_POINT('Ctrl Pts',(-40.0345274717492,1078.70265699499,
503.253808332364));
#108411=CARTESIAN_POINT('Ctrl Pts',(-40.0345333111388,1078.70265694659,
503.253808332295));
#108412=CARTESIAN_POINT('Ctrl Pts',(-40.0345391505271,1078.7026568982,503.25380833226));
#108413=CARTESIAN_POINT('Ctrl Pts',(-40.034544989914,1078.7026568498,503.25380833226));
#108414=CARTESIAN_POINT('Ctrl Pts',(-40.034544989914,1078.7026568498,503.25380833226));
#108415=CARTESIAN_POINT('Ctrl Pts',(-40.1870861698988,1078.70139257487,
503.25380833226));
#108416=CARTESIAN_POINT('Ctrl Pts',(-40.3387075824845,1078.69970632408,
503.277418627439));
#108417=CARTESIAN_POINT('Ctrl Pts',(-40.644307575697,1078.69522353048,503.374952849358));
#108418=CARTESIAN_POINT('Ctrl Pts',(-40.7946844730414,1078.69235962397,
503.453099222605));
#108419=CARTESIAN_POINT('Ctrl Pts',(-41.0731515358608,1078.68537363958,
503.664592747099));
#108420=CARTESIAN_POINT('Ctrl Pts',(-41.1962022846745,1078.68122526846,
503.799992955703));
#108421=CARTESIAN_POINT('Ctrl Pts',(-41.3942613937534,1078.67182122879,
504.120086316256));
#108422=CARTESIAN_POINT('Ctrl Pts',(-41.4630451756302,1078.66659606366,
504.304575468052));
#108423=CARTESIAN_POINT('Ctrl Pts',(-41.5247800067169,1078.65617525521,
504.687939704521));
#108424=CARTESIAN_POINT('Ctrl Pts',(-41.5177819598931,1078.65108481618,
504.882993551684));
#108425=CARTESIAN_POINT('Ctrl Pts',(-41.4327461327301,1078.6423370141,505.243866559487));
#108426=CARTESIAN_POINT('Ctrl Pts',(-41.3612897767765,1078.63867254317,
505.407845986762));
#108427=CARTESIAN_POINT('Ctrl Pts',(-41.1751706699865,1078.63331759805,
505.685496222142));
#108428=CARTESIAN_POINT('Ctrl Pts',(-41.0676822154739,1078.63148297625,
505.801037120108));
#108429=CARTESIAN_POINT('Ctrl Pts',(-40.9008382405138,1078.63009065515,
505.931244722696));
#108430=CARTESIAN_POINT('Ctrl Pts',(-40.8557846356255,1078.62982884185,
505.962538266879));
#108431=CARTESIAN_POINT('Ctrl Pts',(-40.7803490443768,1078.62956909803,
506.008941776923));
#108432=CARTESIAN_POINT('Ctrl Pts',(-40.7510036608353,1078.62950848841,
506.025636229184));
#108433=CARTESIAN_POINT('Ctrl Pts',(-40.6942131746564,1078.62946662967,
506.05541815989));
#108434=CARTESIAN_POINT('Ctrl Pts',(-40.6668853893315,1078.62947805342,
506.068692304597));
#108435=CARTESIAN_POINT('Ctrl Pts',(-40.6042329065985,1078.62957444609,
506.096773133909));
#108436=CARTESIAN_POINT('Ctrl Pts',(-40.56870272132,1078.629677762,506.111068060059));
#108437=CARTESIAN_POINT('Ctrl Pts',(-40.4622717437087,1078.63012789064,
506.149157232906));
#108438=CARTESIAN_POINT('Ctrl Pts',(-40.3900772345219,1078.63061242184,
506.168971012288));
#108439=CARTESIAN_POINT('Ctrl Pts',(-40.2235011822194,1078.63211880381,
506.201359340723));
#108440=CARTESIAN_POINT('Ctrl Pts',(-40.1290137673779,1078.6332448605,506.210414596647));
#108441=CARTESIAN_POINT('Ctrl Pts',(-40.0345449899137,1078.63462185218,
506.210414596647));
#108442=CARTESIAN_POINT('',(-34.5096048204685,1078.26956110846,516.263437971404));
#108443=CARTESIAN_POINT('',(-34.5096048204688,1078.42202250585,513.712549729131));
#108444=CARTESIAN_POINT('Ctrl Pts',(-34.5096048204687,1078.26956110846,
516.263437971403));
#108445=CARTESIAN_POINT('Ctrl Pts',(-34.3781595851867,1078.27280332059,
516.263437971403));
#108446=CARTESIAN_POINT('Ctrl Pts',(-34.2473014668533,1078.27733135701,
516.243116621277));
#108447=CARTESIAN_POINT('Ctrl Pts',(-33.9875836940846,1078.28895388381,
516.160204287482));
#108448=CARTESIAN_POINT('Ctrl Pts',(-33.8615086191089,1078.29610910236,
516.095481226303));
#108449=CARTESIAN_POINT('Ctrl Pts',(-33.6263664264477,1078.31267233544,
515.920648540955));
#108450=CARTESIAN_POINT('Ctrl Pts',(-33.5214294590781,1078.322082882,515.808630798506));
#108451=CARTESIAN_POINT('Ctrl Pts',(-33.3500319054978,1078.34220282634,
515.543703624841));
#108452=CARTESIAN_POINT('Ctrl Pts',(-33.2884764078526,1078.35277147479,
515.390825895484));
#108453=CARTESIAN_POINT('Ctrl Pts',(-33.2254191302722,1078.37336835185,
515.065221580362));
#108454=CARTESIAN_POINT('Ctrl Pts',(-33.226437950399,1078.38317090214,514.895188092461));
#108455=CARTESIAN_POINT('Ctrl Pts',(-33.2930447262667,1078.40010065184,
514.572420400151));
#108456=CARTESIAN_POINT('Ctrl Pts',(-33.3552301369026,1078.4071775404,514.422154131845));
#108457=CARTESIAN_POINT('Ctrl Pts',(-33.5370928998336,1078.41866703871,
514.145480475725));
#108458=CARTESIAN_POINT('Ctrl Pts',(-33.657834487675,1078.42280636536,514.023564507335));
#108459=CARTESIAN_POINT('Ctrl Pts',(-33.842737444783,1078.42572190575,513.899496597316));
#108460=CARTESIAN_POINT('Ctrl Pts',(-33.8883070778172,1078.42622474724,
513.872858046193));
#108461=CARTESIAN_POINT('Ctrl Pts',(-33.9629561338825,1078.42672167601,
513.835220862287));
#108462=CARTESIAN_POINT('Ctrl Pts',(-33.9910117688328,1078.42684008775,
513.822330250798));
#108463=CARTESIAN_POINT('Ctrl Pts',(-34.0413321025789,1078.42693406492,
513.801386421076));
#108464=CARTESIAN_POINT('Ctrl Pts',(-34.0634049962602,1078.42693656199,
513.792911322874));
#108465=CARTESIAN_POINT('Ctrl Pts',(-34.1142066783052,1078.4268550657,513.775009300899));
#108466=CARTESIAN_POINT('Ctrl Pts',(-34.1430605880461,1078.42674681602,
513.765980549334));
#108467=CARTESIAN_POINT('Ctrl Pts',(-34.2217440415278,1078.42628615213,
513.744397306075));
#108468=CARTESIAN_POINT('Ctrl Pts',(-34.2720545294198,1078.42581637524,
513.733814548442));
#108469=CARTESIAN_POINT('Ctrl Pts',(-34.3846943410285,1078.42437988848,
513.717143026564));
#108470=CARTESIAN_POINT('Ctrl Pts',(-34.4471095633331,1078.42332948689,
513.712549729131));
#108471=CARTESIAN_POINT('Ctrl Pts',(-34.5096048204688,1078.42202250585,
513.712549729131));
#108472=CARTESIAN_POINT('Ctrl Pts',(-34.5096048204688,1078.42202250585,
513.712549729131));
#108473=CARTESIAN_POINT('Ctrl Pts',(-34.5096083249495,1078.42202243256,
513.712549729131));
#108474=CARTESIAN_POINT('Ctrl Pts',(-34.5096118294305,1078.42202235927,
513.712549729145));
#108475=CARTESIAN_POINT('Ctrl Pts',(-34.5096153339117,1078.42202228598,
513.712549729174));
#108476=CARTESIAN_POINT('Ctrl Pts',(-34.6788906624206,1078.41848210556,
513.712551124505));
#108477=CARTESIAN_POINT('Ctrl Pts',(-34.8464290549155,1078.41311075097,
513.746250451062));
#108478=CARTESIAN_POINT('Ctrl Pts',(-35.1359553121413,1078.40014343692,
513.867551311148));
#108479=CARTESIAN_POINT('Ctrl Pts',(-35.2589159630341,1078.39307230121,
513.945778393466));
#108480=CARTESIAN_POINT('Ctrl Pts',(-35.4818547242167,1078.37658781807,
514.14781922937));
#108481=CARTESIAN_POINT('Ctrl Pts',(-35.5773306722079,1078.36716819326,
514.273080049463));
#108482=CARTESIAN_POINT('Ctrl Pts',(-35.7235800354469,1078.34671685574,
514.562289401582));
#108483=CARTESIAN_POINT('Ctrl Pts',(-35.7690251798978,1078.33581292178,
514.72565620032));
#108484=CARTESIAN_POINT('Ctrl Pts',(-35.7939442369292,1078.31474727396,
515.059759364467));
#108485=CARTESIAN_POINT('Ctrl Pts',(-35.7735106256755,1078.30478586434,
515.227268355529));
#108486=CARTESIAN_POINT('Ctrl Pts',(-35.6732220271771,1078.2879504767,515.532513944678));
#108487=CARTESIAN_POINT('Ctrl Pts',(-35.5989618694391,1078.28103729642,
515.669054685904));
#108488=CARTESIAN_POINT('Ctrl Pts',(-35.4155787819824,1078.27094006414,
515.896258729525));
#108489=CARTESIAN_POINT('Ctrl Pts',(-35.3122410260585,1078.26750497277,
515.98875731029));
#108490=CARTESIAN_POINT('Ctrl Pts',(-35.1553933362622,1078.26489491808,
516.088923488741));
#108491=CARTESIAN_POINT('Ctrl Pts',(-35.1132567881329,1078.2644040275,516.112579795059));
#108492=CARTESIAN_POINT('Ctrl Pts',(-35.0431913200874,1078.26391702542,
516.146840553654));
#108493=CARTESIAN_POINT('Ctrl Pts',(-35.0160556257707,1078.26380335526,
516.158954075922));
#108494=CARTESIAN_POINT('Ctrl Pts',(-34.9637699410496,1078.26372442065,
516.180136855707));
#108495=CARTESIAN_POINT('Ctrl Pts',(-34.9387095644595,1078.26374533838,
516.189384717918));
#108496=CARTESIAN_POINT('Ctrl Pts',(-34.8814984340421,1078.26392412015,
516.208478307941));
#108497=CARTESIAN_POINT('Ctrl Pts',(-34.849211869092,1078.26411591235,516.217853254797));
#108498=CARTESIAN_POINT('Ctrl Pts',(-34.753114777645,1078.26495074676,516.241683577449));
#108499=CARTESIAN_POINT('Ctrl Pts',(-34.688523965642,1078.26584788725,516.252518175395));
#108500=CARTESIAN_POINT('Ctrl Pts',(-34.5854895384334,1078.26779742569,
516.261747118207));
#108501=CARTESIAN_POINT('Ctrl Pts',(-34.5475227526251,1078.26862582937,
516.263437971403));
#108502=CARTESIAN_POINT('Ctrl Pts',(-34.5096048204687,1078.26956110846,
516.263437971403));
#108503=CARTESIAN_POINT('',(-27.6354521170187,1077.55448697719,526.884160690467));
#108504=CARTESIAN_POINT('',(-27.6354521170191,1077.7731748795,524.686498418482));
#108505=CARTESIAN_POINT('Ctrl Pts',(-27.6354521170187,1077.55448697719,
526.884160690467));
#108506=CARTESIAN_POINT('Ctrl Pts',(-27.4944194254515,1077.55845967166,
526.884160690467));
#108507=CARTESIAN_POINT('Ctrl Pts',(-27.3547655994155,1077.5651885524,526.857010205863));
#108508=CARTESIAN_POINT('Ctrl Pts',(-27.1123084716077,1077.58201060038,
526.759129373448));
#108509=CARTESIAN_POINT('Ctrl Pts',(-27.0087974110687,1077.59135802978,
526.695944893038));
#108510=CARTESIAN_POINT('Ctrl Pts',(-26.8186154364285,1077.61331290848,
526.531868835868));
#108511=CARTESIAN_POINT('Ctrl Pts',(-26.7356817152725,1077.62595899111,
526.429467635875));
#108512=CARTESIAN_POINT('Ctrl Pts',(-26.6049852710548,1077.65340079863,
526.191905641563));
#108513=CARTESIAN_POINT('Ctrl Pts',(-26.5614978708921,1077.66804164051,
526.056967889487));
#108514=CARTESIAN_POINT('Ctrl Pts',(-26.5271042387479,1077.69706818465,
525.773116606164));
#108515=CARTESIAN_POINT('Ctrl Pts',(-26.5384377884101,1077.71115024743,
525.626583722595));
#108516=CARTESIAN_POINT('Ctrl Pts',(-26.6160007339918,1077.73585153354,
525.352188612712));
#108517=CARTESIAN_POINT('Ctrl Pts',(-26.6792045143013,1077.74637215479,
525.226263733483));
#108518=CARTESIAN_POINT('Ctrl Pts',(-26.8506200369833,1077.76335471662,
525.003364520485));
#108519=CARTESIAN_POINT('Ctrl Pts',(-26.9577338924268,1077.76960835039,
524.908867437982));
#108520=CARTESIAN_POINT('Ctrl Pts',(-27.126159928436,1077.77465432355,524.810176943307));
#108521=CARTESIAN_POINT('Ctrl Pts',(-27.1743180298784,1077.77566097145,
524.786501222173));
#108522=CARTESIAN_POINT('Ctrl Pts',(-27.2505560510525,1077.7766137893,524.755716031541));
#108523=CARTESIAN_POINT('Ctrl Pts',(-27.277503781822,1077.77683515238,524.746040336496));
#108524=CARTESIAN_POINT('Ctrl Pts',(-27.3270077544142,1077.77703575551,
524.730419954695));
#108525=CARTESIAN_POINT('Ctrl Pts',(-27.3494334710484,1077.77705237691,
524.724120088884));
#108526=CARTESIAN_POINT('Ctrl Pts',(-27.3977437097661,1077.77693106318,
524.712191442753));
#108527=CARTESIAN_POINT('Ctrl Pts',(-27.4236654094531,1077.77677172016,
524.706776344388));
#108528=CARTESIAN_POINT('Ctrl Pts',(-27.4933862554123,1077.77609332008,
524.694822034415));
#108529=CARTESIAN_POINT('Ctrl Pts',(-27.5374240335677,1077.77540513217,
524.6899852492));
#108530=CARTESIAN_POINT('Ctrl Pts',(-27.5995589824073,1077.77407182594,
524.686938093064));
#108531=CARTESIAN_POINT('Ctrl Pts',(-27.6175026981217,1077.77364454734,
524.686498418482));
#108532=CARTESIAN_POINT('Ctrl Pts',(-27.6354521170191,1077.7731748795,524.686498418482));
#108533=CARTESIAN_POINT('Ctrl Pts',(-27.6354561400331,1077.77317477423,
524.686498418489));
#108534=CARTESIAN_POINT('Ctrl Pts',(-27.7820956642943,1077.76933772555,
524.686498955362));
#108535=CARTESIAN_POINT('Ctrl Pts',(-27.9271441422489,1077.76272533786,
524.715850776585));
#108536=CARTESIAN_POINT('Ctrl Pts',(-28.1739877151007,1077.7461839246,524.81984742957));
#108537=CARTESIAN_POINT('Ctrl Pts',(-28.2772144729253,1077.73712729329,
524.885179807013));
#108538=CARTESIAN_POINT('Ctrl Pts',(-28.465932537063,1077.71567113954,525.053813521592));
#108539=CARTESIAN_POINT('Ctrl Pts',(-28.54756760258,1077.70321909422,525.158582208306));
#108540=CARTESIAN_POINT('Ctrl Pts',(-28.6745327676321,1077.67588233529,
525.400812310426));
#108541=CARTESIAN_POINT('Ctrl Pts',(-28.7154274784568,1077.66113102755,
525.537971543861));
#108542=CARTESIAN_POINT('Ctrl Pts',(-28.7431770550444,1077.63175362073,
525.823645092682));
#108543=CARTESIAN_POINT('Ctrl Pts',(-28.7284302767064,1077.61741865038,
525.969646916927));
#108544=CARTESIAN_POINT('Ctrl Pts',(-28.6449441352305,1077.59219522922,
526.240846925399));
#108545=CARTESIAN_POINT('Ctrl Pts',(-28.5795927763327,1077.58139702623,
526.364330327838));
#108546=CARTESIAN_POINT('Ctrl Pts',(-28.4015536566291,1077.56360198954,
526.586490696771));
#108547=CARTESIAN_POINT('Ctrl Pts',(-28.2883033202278,1077.55702438246,
526.681222253459));
#108548=CARTESIAN_POINT('Ctrl Pts',(-28.118571025877,1077.55230238546,526.773366796316));
#108549=CARTESIAN_POINT('Ctrl Pts',(-28.0760380383956,1077.55146969774,
526.793053012111));
#108550=CARTESIAN_POINT('Ctrl Pts',(-28.0069991874668,1077.5506558012,526.819797117005));
#108551=CARTESIAN_POINT('Ctrl Pts',(-27.9812673491887,1077.55046431516,
526.828681016945));
#108552=CARTESIAN_POINT('Ctrl Pts',(-27.9327825569301,1077.55030907861,
526.843429295737));
#108553=CARTESIAN_POINT('Ctrl Pts',(-27.9101205994786,1077.55031762927,
526.849537089353));
#108554=CARTESIAN_POINT('Ctrl Pts',(-27.8597731253211,1077.55051373359,
526.861391147864));
#108555=CARTESIAN_POINT('Ctrl Pts',(-27.8320269931328,1077.55073743459,
526.86680386544));
#108556=CARTESIAN_POINT('Ctrl Pts',(-27.7533535565146,1077.55169446046,
526.879023691287));
#108557=CARTESIAN_POINT('Ctrl Pts',(-27.7021200903622,1077.5526937158,526.883337529065));
#108558=CARTESIAN_POINT('Ctrl Pts',(-27.6456694783558,1077.55420283149,
526.884125076254));
#108559=CARTESIAN_POINT('Ctrl Pts',(-27.6405598934223,1077.55434309824,
526.884160690467));
#108560=CARTESIAN_POINT('Ctrl Pts',(-27.6354521170187,1077.55448697719,
526.884160690467));
#108561=CARTESIAN_POINT('',(-18.7711528398125,1076.67369445817,536.110401727133));
#108562=CARTESIAN_POINT('',(-18.7711528398114,1076.96239239593,533.929320229677));
#108563=CARTESIAN_POINT('Ctrl Pts',(-18.7711528398125,1076.67369445817,
536.110401727133));
#108564=CARTESIAN_POINT('Ctrl Pts',(-18.7378804569628,1076.67446093905,
536.110401727133));
#108565=CARTESIAN_POINT('Ctrl Pts',(-18.7046206626837,1076.67543331161,
536.108879017021));
#108566=CARTESIAN_POINT('Ctrl Pts',(-18.5272337525884,1076.68172279721,
536.092597788566));
#108567=CARTESIAN_POINT('Ctrl Pts',(-18.3872766379643,1076.69060559347,
536.050775989781));
#108568=CARTESIAN_POINT('Ctrl Pts',(-18.1537505337702,1076.7126886191,535.926769037891));
#108569=CARTESIAN_POINT('Ctrl Pts',(-18.0579697079482,1076.72474508379,
535.853501593805));
#108570=CARTESIAN_POINT('Ctrl Pts',(-17.886902156147,1076.75308894105,535.671291466018));
#108571=CARTESIAN_POINT('Ctrl Pts',(-17.8155522268604,1076.76943501427,
535.561171622241));
#108572=CARTESIAN_POINT('Ctrl Pts',(-17.7111553573034,1076.80497018818,
535.311966774057));
#108573=CARTESIAN_POINT('Ctrl Pts',(-17.6824284223714,1076.82396971125,
535.173473734423));
#108574=CARTESIAN_POINT('Ctrl Pts',(-17.6789074975495,1076.86159765628,
534.88876956391));
#108575=CARTESIAN_POINT('Ctrl Pts',(-17.7058880366738,1076.87984471399,
534.745107066));
#108576=CARTESIAN_POINT('Ctrl Pts',(-17.8120177685867,1076.91175883886,
534.482845643484));
#108577=CARTESIAN_POINT('Ctrl Pts',(-17.8876864205616,1076.92532263287,
534.365695713357));
#108578=CARTESIAN_POINT('Ctrl Pts',(-18.0817082999133,1076.94733838705,
534.163039433835));
#108579=CARTESIAN_POINT('Ctrl Pts',(-18.199238741333,1076.9554303907,534.080451454268));
#108580=CARTESIAN_POINT('Ctrl Pts',(-18.3746955392613,1076.9616169263,534.002735542328));
#108581=CARTESIAN_POINT('Ctrl Pts',(-18.4212096783747,1076.96278143829,
533.985808584999));
#108582=CARTESIAN_POINT('Ctrl Pts',(-18.4961774846045,1076.96392959738,
533.964169585458));
#108583=CARTESIAN_POINT('Ctrl Pts',(-18.523935830246,1076.96420372957,533.957326422666));
#108584=CARTESIAN_POINT('Ctrl Pts',(-18.5755035674115,1076.96443793394,
533.946744260779));
#108585=CARTESIAN_POINT('Ctrl Pts',(-18.5992285780617,1076.96444072849,
533.942688669616));
#108586=CARTESIAN_POINT('Ctrl Pts',(-18.6510674633464,1076.96422008411,
533.935583658997));
#108587=CARTESIAN_POINT('Ctrl Pts',(-18.6792039575024,1076.96395717902,
533.932836110281));
#108588=CARTESIAN_POINT('Ctrl Pts',(-18.7286390493162,1076.96324559583,
533.929941831058));
#108589=CARTESIAN_POINT('Ctrl Pts',(-18.7498944078045,1076.96285919691,
533.929320229677));
#108590=CARTESIAN_POINT('Ctrl Pts',(-18.7711528398114,1076.96239239593,
533.929320229677));
#108591=CARTESIAN_POINT('Ctrl Pts',(-18.7711528398114,1076.96239239593,
533.929320229677));
#108592=CARTESIAN_POINT('Ctrl Pts',(-18.7711593766065,1076.96239225239,
533.929320229677));
#108593=CARTESIAN_POINT('Ctrl Pts',(-18.7711659134019,1076.96239210885,
533.929320229734));
#108594=CARTESIAN_POINT('Ctrl Pts',(-18.7711724501977,1076.96239196529,
533.929320229852));
#108595=CARTESIAN_POINT('Ctrl Pts',(-18.8565470695821,1076.96051707751,
533.92932176508));
#108596=CARTESIAN_POINT('Ctrl Pts',(-18.9415806054822,1076.95735439006,
533.939348641314));
#108597=CARTESIAN_POINT('Ctrl Pts',(-19.1311778469061,1076.94732487712,
533.984639419983));
#108598=CARTESIAN_POINT('Ctrl Pts',(-19.2332505207632,1076.93971791319,
534.026023063032));
#108599=CARTESIAN_POINT('Ctrl Pts',(-19.4322264027534,1076.91999849037,
534.144003844772));
#108600=CARTESIAN_POINT('Ctrl Pts',(-19.5257787844361,1076.90761052154,
534.223242102698));
#108601=CARTESIAN_POINT('Ctrl Pts',(-19.6896244258647,1076.87861076925,
534.417202776863));
#108602=CARTESIAN_POINT('Ctrl Pts',(-19.7558130643799,1076.86195584331,
534.532870669917));
#108603=CARTESIAN_POINT('Ctrl Pts',(-19.8470606724238,1076.82577138095,
534.791809293444));
#108604=CARTESIAN_POINT('Ctrl Pts',(-19.8676232339308,1076.80644511075,
534.934197365998));
#108605=CARTESIAN_POINT('Ctrl Pts',(-19.8527423631478,1076.76870475962,
535.220301377621));
#108606=CARTESIAN_POINT('Ctrl Pts',(-19.8168486234442,1076.75065191003,
535.361373301155));
#108607=CARTESIAN_POINT('Ctrl Pts',(-19.6959630684685,1076.71958458469,
535.61339210574));
#108608=CARTESIAN_POINT('Ctrl Pts',(-19.6152485022439,1076.70658854724,
535.723545725683));
#108609=CARTESIAN_POINT('Ctrl Pts',(-19.4206961725884,1076.68647771366,
535.905572984115));
#108610=CARTESIAN_POINT('Ctrl Pts',(-19.3097538384437,1076.67934105716,
535.977138375156));
#108611=CARTESIAN_POINT('Ctrl Pts',(-19.1467569215491,1076.67394631301,
536.04468022157));
#108612=CARTESIAN_POINT('Ctrl Pts',(-19.1038417330316,1076.67293972572,
536.059405377297));
#108613=CARTESIAN_POINT('Ctrl Pts',(-19.033663976462,1076.67194329584,536.078690605452));
#108614=CARTESIAN_POINT('Ctrl Pts',(-19.0069350927697,1076.6717093418,536.084961511477));
#108615=CARTESIAN_POINT('Ctrl Pts',(-18.9584943858724,1076.67154464201,
536.094413085446));
#108616=CARTESIAN_POINT('Ctrl Pts',(-18.9368703335593,1076.67156227912,
536.09795967355));
#108617=CARTESIAN_POINT('Ctrl Pts',(-18.8863234875917,1076.67181449225,
536.104693134127));
#108618=CARTESIAN_POINT('Ctrl Pts',(-18.8573522663231,1076.6721181415,536.107378591539));
#108619=CARTESIAN_POINT('Ctrl Pts',(-18.8092665804636,1076.67288406952,
536.109902316604));
#108620=CARTESIAN_POINT('Ctrl Pts',(-18.7902076457917,1076.6732555012,536.110401727133));
#108621=CARTESIAN_POINT('Ctrl Pts',(-18.7711528398125,1076.67369445817,
536.110401727133));
#108622=CARTESIAN_POINT('',(-83.8577571500211,1078.68595559847,394.657284692478));
#108623=CARTESIAN_POINT('',(-83.8577571699087,1078.65918801557,391.700678428093));
#108624=CARTESIAN_POINT('Ctrl Pts',(-83.857757150021,1078.68595559847,394.657284692479));
#108625=CARTESIAN_POINT('Ctrl Pts',(-83.7830020049961,1078.68756601077,
394.657284692479));
#108626=CARTESIAN_POINT('Ctrl Pts',(-83.7081818716811,1078.68909176713,
394.65161448755));
#108627=CARTESIAN_POINT('Ctrl Pts',(-83.4473097045803,1078.69413214015,
394.611658438446));
#108628=CARTESIAN_POINT('Ctrl Pts',(-83.2678576875645,1078.69709119872,
394.5475779628));
#108629=CARTESIAN_POINT('Ctrl Pts',(-82.9555074237683,1078.70153146215,
394.362880050757));
#108630=CARTESIAN_POINT('Ctrl Pts',(-82.8225076238217,1078.70308077374,
394.248529135822));
#108631=CARTESIAN_POINT('Ctrl Pts',(-82.6516281007895,1078.70464604701,
394.039149515351));
#108632=CARTESIAN_POINT('Ctrl Pts',(-82.5982181108242,1078.70503348135,
393.958851975401));
#108633=CARTESIAN_POINT('Ctrl Pts',(-82.535740029746,1078.70534048075,393.841550260136));
#108634=CARTESIAN_POINT('Ctrl Pts',(-82.5197021499793,1078.70540102225,
393.808533282827));
#108635=CARTESIAN_POINT('Ctrl Pts',(-82.4952411485322,1078.7054612726,393.753007193096));
#108636=CARTESIAN_POINT('Ctrl Pts',(-82.4861084175877,1078.70547477707,
393.730828492865));
#108637=CARTESIAN_POINT('Ctrl Pts',(-82.4694008190376,1078.70548101321,
393.68727347696));
#108638=CARTESIAN_POINT('Ctrl Pts',(-82.4617702176421,1078.70547484159,
393.665925560053));
#108639=CARTESIAN_POINT('Ctrl Pts',(-82.445102997834,1078.70543892756,393.615679087994));
#108640=CARTESIAN_POINT('Ctrl Pts',(-82.4364572227992,1078.70540198493,
393.586661580845));
#108641=CARTESIAN_POINT('Ctrl Pts',(-82.4118776292392,1078.7052326084,393.493839697126));
#108642=CARTESIAN_POINT('Ctrl Pts',(-82.3993059989355,1078.70503931191,
393.429228270991));
#108643=CARTESIAN_POINT('Ctrl Pts',(-82.3664518067997,1078.70395439044,
393.168779889638));
#108644=CARTESIAN_POINT('Ctrl Pts',(-82.3810479627093,1078.70245681784,
392.970603162102));
#108645=CARTESIAN_POINT('Ctrl Pts',(-82.477378225941,1078.69838679515,392.62589133012));
#108646=CARTESIAN_POINT('Ctrl Pts',(-82.5458454370355,1078.69607986296,
392.478811472983));
#108647=CARTESIAN_POINT('Ctrl Pts',(-82.7355870232928,1078.69024848228,
392.200768214227));
#108648=CARTESIAN_POINT('Ctrl Pts',(-82.8595022990829,1078.68667601281,
392.074604992627));
#108649=CARTESIAN_POINT('Ctrl Pts',(-83.1564653130985,1078.67830698645,
391.864012121185));
#108650=CARTESIAN_POINT('Ctrl Pts',(-83.3297793584802,1078.67351179497,
391.785357451956));
#108651=CARTESIAN_POINT('Ctrl Pts',(-83.6263047866715,1078.66541325289,
391.714282887937));
#108652=CARTESIAN_POINT('Ctrl Pts',(-83.7419675128545,1078.66228048325,
391.700678426534));
#108653=CARTESIAN_POINT('Ctrl Pts',(-83.8577571699228,1078.6591880161,391.700678428093));
#108654=CARTESIAN_POINT('Ctrl Pts',(-83.8577571699228,1078.6591880161,391.700678428093));
#108655=CARTESIAN_POINT('Ctrl Pts',(-83.9361428063095,1078.65709452164,
391.700678429148));
#108656=CARTESIAN_POINT('Ctrl Pts',(-84.0145866217131,1078.65501982623,
391.706912780499));
#108657=CARTESIAN_POINT('Ctrl Pts',(-84.2777277500826,1078.64816109357,
391.749204980039));
#108658=CARTESIAN_POINT('Ctrl Pts',(-84.4557642993797,1078.64369124269,
391.814051899594));
#108659=CARTESIAN_POINT('Ctrl Pts',(-84.767012057516,1078.6365087334,392.000321846345));
#108660=CARTESIAN_POINT('Ctrl Pts',(-84.9000006834767,1078.63375775461,
392.116098628436));
#108661=CARTESIAN_POINT('Ctrl Pts',(-85.0681332592125,1078.63098308652,
392.32512370263));
#108662=CARTESIAN_POINT('Ctrl Pts',(-85.1195945401495,1078.63029128167,
392.403191166495));
#108663=CARTESIAN_POINT('Ctrl Pts',(-85.1804949501597,1078.6297326019,392.517861140866));
#108664=CARTESIAN_POINT('Ctrl Pts',(-85.1964325685189,1078.62962003544,
392.550758955335));
#108665=CARTESIAN_POINT('Ctrl Pts',(-85.2208593784637,1078.62950795544,
392.606341466739));
#108666=CARTESIAN_POINT('Ctrl Pts',(-85.2300397724008,1078.62948308274,
392.628704567858));
#108667=CARTESIAN_POINT('Ctrl Pts',(-85.2469014151216,1078.62947314879,
392.672829015174));
#108668=CARTESIAN_POINT('Ctrl Pts',(-85.2546296799325,1078.6294863213,392.694565083902));
#108669=CARTESIAN_POINT('Ctrl Pts',(-85.2715916654432,1078.62955959754,
392.74605848812));
#108670=CARTESIAN_POINT('Ctrl Pts',(-85.2803995957563,1078.62963451504,
392.775944483141));
#108671=CARTESIAN_POINT('Ctrl Pts',(-85.3056802704074,1078.62998047341,
392.872926123062));
#108672=CARTESIAN_POINT('Ctrl Pts',(-85.3183974782786,1078.63037894675,
392.940904097667));
#108673=CARTESIAN_POINT('Ctrl Pts',(-85.3319452307445,1078.6313252237,393.058309575461));
#108674=CARTESIAN_POINT('Ctrl Pts',(-85.3351402243465,1078.63179597117,
393.107348224157));
#108675=CARTESIAN_POINT('Ctrl Pts',(-85.3358886250479,1078.63234098491,
393.156453950822));
#108676=CARTESIAN_POINT('Ctrl Pts',(-85.3380512724778,1078.63391590668,
393.298354370417));
#108677=CARTESIAN_POINT('Ctrl Pts',(-85.319769042644,1078.63610153108,393.439820960922));
#108678=CARTESIAN_POINT('Ctrl Pts',(-85.2384769594119,1078.64180196812,
393.73100120205));
#108679=CARTESIAN_POINT('Ctrl Pts',(-85.1704821986696,1078.6454133185,393.877450934156));
#108680=CARTESIAN_POINT('Ctrl Pts',(-84.9823652816383,1078.65367758615,
394.154166395819));
#108681=CARTESIAN_POINT('Ctrl Pts',(-84.8597262402881,1078.65832495621,
394.279792018397));
#108682=CARTESIAN_POINT('Ctrl Pts',(-84.566136971883,1078.66802426645,394.489889677009));
#108683=CARTESIAN_POINT('Ctrl Pts',(-84.3949648404668,1078.67298987461,
394.568835447));
#108684=CARTESIAN_POINT('Ctrl Pts',(-84.0969449776526,1078.68058133679,
394.642751299174));
#108685=CARTESIAN_POINT('Ctrl Pts',(-83.9774343555987,1078.68337745292,
394.657284692479));
#108686=CARTESIAN_POINT('Ctrl Pts',(-83.857757150021,1078.68595559847,394.657284692479));
#108687=CARTESIAN_POINT('',(-93.479943233477,1078.36968470723,401.021131275777));
#108688=CARTESIAN_POINT('',(-93.4799432334773,1078.32768892479,398.470243033506));
#108689=CARTESIAN_POINT('Ctrl Pts',(-93.4799432334771,1078.36968470723,
401.021131275778));
#108690=CARTESIAN_POINT('Ctrl Pts',(-93.3443468026236,1078.37788346231,
401.021131275778));
#108691=CARTESIAN_POINT('Ctrl Pts',(-93.2093682722063,1078.38557917959,
400.999506151711));
#108692=CARTESIAN_POINT('Ctrl Pts',(-92.928228749206,1078.40067097742,400.906706245128));
#108693=CARTESIAN_POINT('Ctrl Pts',(-92.7870338447336,1078.40763059762,
400.828399373262));
#108694=CARTESIAN_POINT('Ctrl Pts',(-92.5426108389938,1078.41853931467,
400.624950294691));
#108695=CARTESIAN_POINT('Ctrl Pts',(-92.4410200677746,1078.42243681255,
400.502230414303));
#108696=CARTESIAN_POINT('Ctrl Pts',(-92.3353783834339,1078.42553732989,
400.311653448111));
#108697=CARTESIAN_POINT('Ctrl Pts',(-92.3100605755805,1078.42614825743,
400.257274590558));
#108698=CARTESIAN_POINT('Ctrl Pts',(-92.2791932132023,1078.42667705383,
400.176568920504));
#108699=CARTESIAN_POINT('Ctrl Pts',(-92.2705015924285,1078.42679127773,
400.151532750479));
#108700=CARTESIAN_POINT('Ctrl Pts',(-92.2570434538043,1078.42690397468,
400.108482066834));
#108701=CARTESIAN_POINT('Ctrl Pts',(-92.2518802888594,1078.42692676604,
400.090600805307));
#108702=CARTESIAN_POINT('Ctrl Pts',(-92.2422505638834,1078.42692490132,
400.054287235839));
#108703=CARTESIAN_POINT('Ctrl Pts',(-92.2378001219983,1078.42689934626,
400.035855456433));
#108704=CARTESIAN_POINT('Ctrl Pts',(-92.2279503806879,1078.42677699572,
399.99066928959));
#108705=CARTESIAN_POINT('Ctrl Pts',(-92.2229957402848,1078.42665386976,
399.963827764946));
#108706=CARTESIAN_POINT('Ctrl Pts',(-92.2086630231361,1078.42604428688,
399.869278765671));
#108707=CARTESIAN_POINT('Ctrl Pts',(-92.2038680061345,1078.4252910569,399.80099849208));
#108708=CARTESIAN_POINT('Ctrl Pts',(-92.2063023970707,1078.42156961972,
399.562532434339));
#108709=CARTESIAN_POINT('Ctrl Pts',(-92.2420643603704,1078.41701476496,
399.394500946095));
#108710=CARTESIAN_POINT('Ctrl Pts',(-92.3655777692062,1078.40555107239,
399.109529049789));
#108711=CARTESIAN_POINT('Ctrl Pts',(-92.4423752417591,1078.39926392785,
398.990746016807));
#108712=CARTESIAN_POINT('Ctrl Pts',(-92.6397786825266,1078.38424410647,
398.773983516468));
#108713=CARTESIAN_POINT('Ctrl Pts',(-92.7620361835586,1078.37546399791,
398.680479090426));
#108714=CARTESIAN_POINT('Ctrl Pts',(-92.9872004074533,1078.35992808373,
398.564990802216));
#108715=CARTESIAN_POINT('Ctrl Pts',(-93.0816331847033,1078.3535622419,398.529880805453));
#108716=CARTESIAN_POINT('Ctrl Pts',(-93.2776558908996,1078.34062563531,
398.482317337839));
#108717=CARTESIAN_POINT('Ctrl Pts',(-93.3786182744213,1078.33409880642,
398.470243033506));
#108718=CARTESIAN_POINT('Ctrl Pts',(-93.4799432334774,1078.32768892479,
398.470243033506));
#108719=CARTESIAN_POINT('Ctrl Pts',(-93.4799432334774,1078.32768892479,
398.470243033506));
#108720=CARTESIAN_POINT('Ctrl Pts',(-93.4800221521823,1078.32768393234,
398.470243033506));
#108721=CARTESIAN_POINT('Ctrl Pts',(-93.4801010711071,1078.32767893996,
398.47024304083));
#108722=CARTESIAN_POINT('Ctrl Pts',(-93.4801799902509,1078.32767394766,
398.47024305548));
#108723=CARTESIAN_POINT('Ctrl Pts',(-93.6475450953458,1078.31708668642,
398.470274122951));
#108724=CARTESIAN_POINT('Ctrl Pts',(-93.813324821803,1078.30697958876,398.503247682793));
#108725=CARTESIAN_POINT('Ctrl Pts',(-94.1110507908088,1078.2897294135,398.626569583309));
#108726=CARTESIAN_POINT('Ctrl Pts',(-94.2421493192321,1078.28256603449,
398.711376395216));
#108727=CARTESIAN_POINT('Ctrl Pts',(-94.4731405686298,1078.27107926861,
398.929147344998));
#108728=CARTESIAN_POINT('Ctrl Pts',(-94.569046186137,1078.26702254175,399.06226731877));
#108729=CARTESIAN_POINT('Ctrl Pts',(-94.6529473653915,1078.26462949997,
399.243498387251));
#108730=CARTESIAN_POINT('Ctrl Pts',(-94.667049114324,1078.26429572699,399.277806795964));
#108731=CARTESIAN_POINT('Ctrl Pts',(-94.6876349454864,1078.26393260091,
399.334842287549));
#108732=CARTESIAN_POINT('Ctrl Pts',(-94.695017900571,1078.26383669524,399.35722049196));
#108733=CARTESIAN_POINT('Ctrl Pts',(-94.7070735842507,1078.26374648541,
399.397477868595));
#108734=CARTESIAN_POINT('Ctrl Pts',(-94.7119856526584,1078.2637347001,399.415278189755));
#108735=CARTESIAN_POINT('Ctrl Pts',(-94.7215007570535,1078.26376851016,
399.452928577923));
#108736=CARTESIAN_POINT('Ctrl Pts',(-94.7260180708382,1078.26382015356,
399.472794937436));
#108737=CARTESIAN_POINT('Ctrl Pts',(-94.7365988302227,1078.26404408383,
399.52509143752));
#108738=CARTESIAN_POINT('Ctrl Pts',(-94.7418832482197,1078.26427119764,
399.55766300504));
#108739=CARTESIAN_POINT('Ctrl Pts',(-94.7589552501901,1078.26561079107,
399.696841893122));
#108740=CARTESIAN_POINT('Ctrl Pts',(-94.7585335945485,1078.26756087739,
399.804488076565));
#108741=CARTESIAN_POINT('Ctrl Pts',(-94.7284222724645,1078.2736692602,400.035142288318));
#108742=CARTESIAN_POINT('Ctrl Pts',(-94.6939426921799,1078.278112298,400.156383552612));
#108743=CARTESIAN_POINT('Ctrl Pts',(-94.5844842414275,1078.28959199805,
400.39877399275));
#108744=CARTESIAN_POINT('Ctrl Pts',(-94.5058292701608,1078.29679870896,
400.516443260722));
#108745=CARTESIAN_POINT('Ctrl Pts',(-94.3052864300364,1078.31345013503,
400.729958641151));
#108746=CARTESIAN_POINT('Ctrl Pts',(-94.1819085725339,1078.32289706299,
400.821423045078));
#108747=CARTESIAN_POINT('Ctrl Pts',(-93.8987493745196,1078.34306541874,
400.961463479716));
#108748=CARTESIAN_POINT('Ctrl Pts',(-93.7395389413744,1078.35364300685,
401.00510255998));
#108749=CARTESIAN_POINT('Ctrl Pts',(-93.5442751715031,1078.36576886695,
401.019915801626));
#108750=CARTESIAN_POINT('Ctrl Pts',(-93.5120918319992,1078.36774086193,
401.021131275778));
#108751=CARTESIAN_POINT('Ctrl Pts',(-93.4799432334771,1078.36968470723,
401.021131275778));
#108752=CARTESIAN_POINT('',(-103.499585384594,1077.68406953396,408.809642574865));
#108753=CARTESIAN_POINT('',(-103.499585384594,1077.64750623718,406.61198030288));
#108754=CARTESIAN_POINT('Ctrl Pts',(-103.499585384593,1077.68406953396,
408.809642574865));
#108755=CARTESIAN_POINT('Ctrl Pts',(-103.387195904803,1077.69544404394,
408.809642574865));
#108756=CARTESIAN_POINT('Ctrl Pts',(-103.275219790437,1077.70642353688,
408.79239857909));
#108757=CARTESIAN_POINT('Ctrl Pts',(-103.033088326383,1077.72939676398,
408.715662964053));
#108758=CARTESIAN_POINT('Ctrl Pts',(-102.907898540638,1077.74071996647,
408.647468219755));
#108759=CARTESIAN_POINT('Ctrl Pts',(-102.705108256707,1077.75805576399,
408.479631245935));
#108760=CARTESIAN_POINT('Ctrl Pts',(-102.624742911153,1077.76446604495,
408.386807518368));
#108761=CARTESIAN_POINT('Ctrl Pts',(-102.51405891374,1077.77241716349,408.205169765255));
#108762=CARTESIAN_POINT('Ctrl Pts',(-102.476624646068,1077.77475445129,
408.122167372458));
#108763=CARTESIAN_POINT('Ctrl Pts',(-102.441461890835,1077.77637828966,
408.00847543288));
#108764=CARTESIAN_POINT('Ctrl Pts',(-102.434153463183,1077.77665665802,
407.981152193012));
#108765=CARTESIAN_POINT('Ctrl Pts',(-102.424194390188,1077.77692835504,
407.937188192762));
#108766=CARTESIAN_POINT('Ctrl Pts',(-102.42085834713,1077.77699146811,407.920716689828));
#108767=CARTESIAN_POINT('Ctrl Pts',(-102.415318214654,1077.77703812476,
407.889724956683));
#108768=CARTESIAN_POINT('Ctrl Pts',(-102.413024910849,1077.7770307153,407.875224574348));
#108769=CARTESIAN_POINT('Ctrl Pts',(-102.408525549262,1077.77694853326,
407.842544264892));
#108770=CARTESIAN_POINT('Ctrl Pts',(-102.406482064689,1077.77685756785,
407.824346534452));
#108771=CARTESIAN_POINT('Ctrl Pts',(-102.401855056095,1077.7764605486,407.771194294265));
#108772=CARTESIAN_POINT('Ctrl Pts',(-102.400487934671,1077.77603414094,
407.736158649954));
#108773=CARTESIAN_POINT('Ctrl Pts',(-102.402087814159,1077.77297595205,
407.554773456108));
#108774=CARTESIAN_POINT('Ctrl Pts',(-102.432600529893,1077.76767653332,
407.410246970002));
#108775=CARTESIAN_POINT('Ctrl Pts',(-102.536710677082,1077.75353423174,
407.168615955267));
#108776=CARTESIAN_POINT('Ctrl Pts',(-102.599789875725,1077.74570258254,
407.069383771022));
#108777=CARTESIAN_POINT('Ctrl Pts',(-102.762352772215,1077.72657605154,
406.885953758826));
#108778=CARTESIAN_POINT('Ctrl Pts',(-102.86358111237,1077.71515978003,406.805631539784));
#108779=CARTESIAN_POINT('Ctrl Pts',(-103.057064140004,1077.6939836464,406.700836816488));
#108780=CARTESIAN_POINT('Ctrl Pts',(-103.143010528088,1077.68475060885,
406.667394956358));
#108781=CARTESIAN_POINT('Ctrl Pts',(-103.319555893004,1077.66609486489,
406.623083169243));
#108782=CARTESIAN_POINT('Ctrl Pts',(-103.409399714469,1077.65674657888,
406.61198030288));
#108783=CARTESIAN_POINT('Ctrl Pts',(-103.499585384594,1077.64750623718,
406.61198030288));
#108784=CARTESIAN_POINT('Ctrl Pts',(-103.499585384594,1077.64750623718,
406.61198030288));
#108785=CARTESIAN_POINT('Ctrl Pts',(-103.499677903439,1077.64749675779,
406.61198030288));
#108786=CARTESIAN_POINT('Ctrl Pts',(-103.499770422644,1077.6474872785,406.611980314598));
#108787=CARTESIAN_POINT('Ctrl Pts',(-103.499862942206,1077.64747779934,
406.611980337968));
#108788=CARTESIAN_POINT('Ctrl Pts',(-103.645113351412,1077.63259604917,
406.612017027284));
#108789=CARTESIAN_POINT('Ctrl Pts',(-103.78901276622,1077.61822198197,406.640853589671));
#108790=CARTESIAN_POINT('Ctrl Pts',(-104.050499855146,1077.5929165144,406.750104219455));
#108791=CARTESIAN_POINT('Ctrl Pts',(-104.166776622412,1077.58206955235,
406.826846821377));
#108792=CARTESIAN_POINT('Ctrl Pts',(-104.359585229407,1077.56505932727,
407.014439894671));
#108793=CARTESIAN_POINT('Ctrl Pts',(-104.436360211142,1077.55881456015,
407.121712524817));
#108794=CARTESIAN_POINT('Ctrl Pts',(-104.518664583071,1077.55312449566,
407.295305133208));
#108795=CARTESIAN_POINT('Ctrl Pts',(-104.540205719576,1077.55183917524,
407.352649557091));
#108796=CARTESIAN_POINT('Ctrl Pts',(-104.563392490146,1077.55080367557,
407.434553513139));
#108797=CARTESIAN_POINT('Ctrl Pts',(-104.569163649531,1077.55059554773,
407.457816567282));
#108798=CARTESIAN_POINT('Ctrl Pts',(-104.577163530036,1077.55039678801,
407.495264322674));
#108799=CARTESIAN_POINT('Ctrl Pts',(-104.57988289321,1077.55035237737,407.509335590598));
#108800=CARTESIAN_POINT('Ctrl Pts',(-104.584899660064,1077.55032279116,
407.538327872764));
#108801=CARTESIAN_POINT('Ctrl Pts',(-104.587166359717,1077.55034089609,
407.553251045044));
#108802=CARTESIAN_POINT('Ctrl Pts',(-104.591680568707,1077.55045930185,
407.587743127609));
#108803=CARTESIAN_POINT('Ctrl Pts',(-104.593710738872,1077.55058295483,
407.607334956696));
#108804=CARTESIAN_POINT('Ctrl Pts',(-104.59835973683,1077.55114023486,407.668087676534));
#108805=CARTESIAN_POINT('Ctrl Pts',(-104.599188787289,1077.55176454043,
407.709345782444));
#108806=CARTESIAN_POINT('Ctrl Pts',(-104.592420320313,1077.55570454201,
407.896386519467));
#108807=CARTESIAN_POINT('Ctrl Pts',(-104.558149962599,1077.56179066911,
408.03960335307));
#108808=CARTESIAN_POINT('Ctrl Pts',(-104.447617840476,1077.5774967984,408.278720181223));
#108809=CARTESIAN_POINT('Ctrl Pts',(-104.381421926256,1077.58610752184,
408.376847563264));
#108810=CARTESIAN_POINT('Ctrl Pts',(-104.212973558089,1077.60671077601,
408.55643095952));
#108811=CARTESIAN_POINT('Ctrl Pts',(-104.109175869781,1077.61878832806,
408.63403867532));
#108812=CARTESIAN_POINT('Ctrl Pts',(-103.870733798094,1077.64537003777,
408.754299904278));
#108813=CARTESIAN_POINT('Ctrl Pts',(-103.736380651267,1077.65975831344,
408.792724592087));
#108814=CARTESIAN_POINT('Ctrl Pts',(-103.565530808957,1077.67736519591,
408.808160083521));
#108815=CARTESIAN_POINT('Ctrl Pts',(-103.532540320879,1077.68073429073,
408.809642574865));
#108816=CARTESIAN_POINT('Ctrl Pts',(-103.499585384593,1077.68406953396,
408.809642574865));
#108817=CARTESIAN_POINT('',(-111.756957497768,1076.82908683399,418.58236328462));
#108818=CARTESIAN_POINT('',(-111.75695749777,1076.81044237657,416.401281787164));
#108819=CARTESIAN_POINT('Ctrl Pts',(-111.756957497768,1076.82908683399,
418.582363284621));
#108820=CARTESIAN_POINT('Ctrl Pts',(-111.628259262186,1076.8463078706,418.582363284621));
#108821=CARTESIAN_POINT('Ctrl Pts',(-111.500348586371,1076.86315267952,
418.559579819116));
#108822=CARTESIAN_POINT('Ctrl Pts',(-111.246798174954,1076.89600265962,
418.465958371192));
#108823=CARTESIAN_POINT('Ctrl Pts',(-111.124924534418,1076.911467731,418.391744289392));
#108824=CARTESIAN_POINT('Ctrl Pts',(-110.930262576408,1076.93559468084,
418.21350468216));
#108825=CARTESIAN_POINT('Ctrl Pts',(-110.854450678783,1076.94472378238,
418.11616918541));
#108826=CARTESIAN_POINT('Ctrl Pts',(-110.747079300555,1076.95711960265,
417.916401071468));
#108827=CARTESIAN_POINT('Ctrl Pts',(-110.711140439506,1076.96099751614,
417.818036534783));
#108828=CARTESIAN_POINT('Ctrl Pts',(-110.683801095832,1076.96348609575,
417.687884112442));
#108829=CARTESIAN_POINT('Ctrl Pts',(-110.679007433349,1076.96387630448,
417.659538662239));
#108830=CARTESIAN_POINT('Ctrl Pts',(-110.673222765968,1076.96425764857,
417.614594389605));
#108831=CARTESIAN_POINT('Ctrl Pts',(-110.671481815592,1076.96434773263,
417.598107341844));
#108832=CARTESIAN_POINT('Ctrl Pts',(-110.669075432751,1076.96441934202,
417.568971525337));
#108833=CARTESIAN_POINT('Ctrl Pts',(-110.668253236375,1076.96442148999,
417.556339095609));
#108834=CARTESIAN_POINT('Ctrl Pts',(-110.666879590667,1076.96436055169,
417.527493054449));
#108835=CARTESIAN_POINT('Ctrl Pts',(-110.666469633752,1076.96427894538,
417.511275920127));
#108836=CARTESIAN_POINT('Ctrl Pts',(-110.666338713738,1076.9639279657,417.467119864967));
#108837=CARTESIAN_POINT('Ctrl Pts',(-110.66732936936,1076.96356568417,417.439192707383));
#108838=CARTESIAN_POINT('Ctrl Pts',(-110.677327174604,1076.96113241606,
417.304097911965));
#108839=CARTESIAN_POINT('Ctrl Pts',(-110.701075157017,1076.95714930044,
417.198694067498));
#108840=CARTESIAN_POINT('Ctrl Pts',(-110.779225135746,1076.94522297492,
416.996578366205));
#108841=CARTESIAN_POINT('Ctrl Pts',(-110.833702655736,1076.93728064874,
416.901252350489));
#108842=CARTESIAN_POINT('Ctrl Pts',(-110.977153046549,1076.91688585791,
416.719718413115));
#108843=CARTESIAN_POINT('Ctrl Pts',(-111.068482638917,1076.90414816897,
416.637328507757));
#108844=CARTESIAN_POINT('Ctrl Pts',(-111.26119942533,1076.8775905672,416.514664442732));
#108845=CARTESIAN_POINT('Ctrl Pts',(-111.358823174717,1076.8642527306,416.471006946803));
#108846=CARTESIAN_POINT('Ctrl Pts',(-111.557414731369,1076.83729812384,
416.415035320248));
#108847=CARTESIAN_POINT('Ctrl Pts',(-111.656961589264,1076.82386419738,
416.401281787164));
#108848=CARTESIAN_POINT('Ctrl Pts',(-111.756957497771,1076.81044237657,
416.401281787164));
#108849=CARTESIAN_POINT('Ctrl Pts',(-111.756957497771,1076.81044237657,
416.401281787165));
#108850=CARTESIAN_POINT('Ctrl Pts',(-111.757267709608,1076.81040073879,
416.401281787165));
#108851=CARTESIAN_POINT('Ctrl Pts',(-111.757577925767,1076.81035910114,
416.401281919527));
#108852=CARTESIAN_POINT('Ctrl Pts',(-111.757888146164,1076.81031746362,
416.401282184264));
#108853=CARTESIAN_POINT('Ctrl Pts',(-111.902996520501,1076.79084114005,
416.401406017257));
#108854=CARTESIAN_POINT('Ctrl Pts',(-112.046743521567,1076.77169855101,
416.430491124244));
#108855=CARTESIAN_POINT('Ctrl Pts',(-112.309506872607,1076.73706338498,
416.54128472119));
#108856=CARTESIAN_POINT('Ctrl Pts',(-112.426914414638,1076.72177026875,
416.619978092971));
#108857=CARTESIAN_POINT('Ctrl Pts',(-112.610593742355,1076.69830509568,
416.802822001851));
#108858=CARTESIAN_POINT('Ctrl Pts',(-112.680687760257,1076.68956305877,
416.90003483103));
#108859=CARTESIAN_POINT('Ctrl Pts',(-112.775652343149,1076.67822796178,
417.091279122111));
#108860=CARTESIAN_POINT('Ctrl Pts',(-112.806488667435,1076.67478243055,
417.180888335835));
#108861=CARTESIAN_POINT('Ctrl Pts',(-112.830946879632,1076.67247436043,
417.300530613086));
#108862=CARTESIAN_POINT('Ctrl Pts',(-112.835457774785,1076.67209468439,
417.327861662961));
#108863=CARTESIAN_POINT('Ctrl Pts',(-112.840977616086,1076.67172032577,
417.371619185811));
#108864=CARTESIAN_POINT('Ctrl Pts',(-112.842663810689,1076.67163186579,
417.387946243501));
#108865=CARTESIAN_POINT('Ctrl Pts',(-112.84512027116,1076.67156185247,417.418457189968));
#108866=CARTESIAN_POINT('Ctrl Pts',(-112.845983174103,1076.6715674915,417.432629866402));
#108867=CARTESIAN_POINT('Ctrl Pts',(-112.847281541207,1076.6716644326,417.464062975881));
#108868=CARTESIAN_POINT('Ctrl Pts',(-112.847584329845,1076.67177394905,
417.481324757331));
#108869=CARTESIAN_POINT('Ctrl Pts',(-112.847277345293,1076.67224918448,
417.530821221527));
#108870=CARTESIAN_POINT('Ctrl Pts',(-112.8456482608,1076.67275449419,417.563028604543));
#108871=CARTESIAN_POINT('Ctrl Pts',(-112.828942160006,1076.67658199652,
417.73861788006));
#108872=CARTESIAN_POINT('Ctrl Pts',(-112.786990441977,1076.68355429553,
417.877825079406));
#108873=CARTESIAN_POINT('Ctrl Pts',(-112.665274248443,1076.7021883218,418.106195316027));
#108874=CARTESIAN_POINT('Ctrl Pts',(-112.595585198562,1076.71250485626,
418.198310352126));
#108875=CARTESIAN_POINT('Ctrl Pts',(-112.421820259228,1076.7376028886,418.365452664304));
#108876=CARTESIAN_POINT('Ctrl Pts',(-112.316242023973,1076.75254589309,
418.436487945748));
#108877=CARTESIAN_POINT('Ctrl Pts',(-112.076327646254,1076.78589013309,
418.543451279366));
#108878=CARTESIAN_POINT('Ctrl Pts',(-111.942348722303,1076.8041941881,418.575112552085));
#108879=CARTESIAN_POINT('Ctrl Pts',(-111.789698540157,1076.82470143,418.581994958318));
#108880=CARTESIAN_POINT('Ctrl Pts',(-111.773321650249,1076.82689715619,
418.582363284621));
#108881=CARTESIAN_POINT('Ctrl Pts',(-111.756957497768,1076.82908683399,
418.582363284621));
#108882=CARTESIAN_POINT('',(-4.59241321360755,1076.96429318502,313.820919344588));
#108883=CARTESIAN_POINT('',(-4.59241321360898,1076.67169969354,311.639837847132));
#108884=CARTESIAN_POINT('Ctrl Pts',(-4.59241321360756,1076.96429318502,
313.820919344589));
#108885=CARTESIAN_POINT('Ctrl Pts',(-4.58729141192633,1076.96432069071,
313.820919344589));
#108886=CARTESIAN_POINT('Ctrl Pts',(-4.58216931622271,1076.96434347666,
313.820883262235));
#108887=CARTESIAN_POINT('Ctrl Pts',(-4.55268786777427,1076.96444744273,
313.820467822336));
#108888=CARTESIAN_POINT('Ctrl Pts',(-4.52834681763773,1076.9644264611,313.819308398949));
#108889=CARTESIAN_POINT('Ctrl Pts',(-4.47186306088004,1076.96412909633,
313.81471738548));
#108890=CARTESIAN_POINT('Ctrl Pts',(-4.43979518576418,1076.96377179711,
313.81067042068));
#108891=CARTESIAN_POINT('Ctrl Pts',(-4.35106200456937,1076.96225555879,
313.795442454999));
#108892=CARTESIAN_POINT('Ctrl Pts',(-4.29504813396338,1076.96068964902,
313.781179160654));
#108893=CARTESIAN_POINT('Ctrl Pts',(-4.10334820036271,1076.95315811824,
313.715809651604));
#108894=CARTESIAN_POINT('Ctrl Pts',(-3.97712765537905,1076.94420059741,
313.64228441493));
#108895=CARTESIAN_POINT('Ctrl Pts',(-3.77807475162618,1076.92205481482,
313.465839559047));
#108896=CARTESIAN_POINT('Ctrl Pts',(-3.70137252335428,1076.90992091133,
313.370702534953));
#108897=CARTESIAN_POINT('Ctrl Pts',(-3.57730558465704,1076.88138648815,
313.150162388361));
#108898=CARTESIAN_POINT('Ctrl Pts',(-3.53410540296603,1076.86493319215,
313.024610501353));
#108899=CARTESIAN_POINT('Ctrl Pts',(-3.49293822453981,1076.829053337,312.754261159156));
#108900=CARTESIAN_POINT('Ctrl Pts',(-3.49916309745467,1076.80981604943,
312.61115533408));
#108901=CARTESIAN_POINT('Ctrl Pts',(-3.56661826077018,1076.771958454,312.333104019716));
#108902=CARTESIAN_POINT('Ctrl Pts',(-3.62813357417901,1076.75370491763,
312.200906315366));
#108903=CARTESIAN_POINT('Ctrl Pts',(-3.79463761831558,1076.72197916882,
311.974416325197));
#108904=CARTESIAN_POINT('Ctrl Pts',(-3.89559692218598,1076.7085736548,311.880383538161));
#108905=CARTESIAN_POINT('Ctrl Pts',(-4.12289809990298,1076.68772609551,
311.737328147627));
#108906=CARTESIAN_POINT('Ctrl Pts',(-4.24616683617815,1076.68024738659,
311.687886528618));
#108907=CARTESIAN_POINT('Ctrl Pts',(-4.42333628054291,1076.6743115547,311.651915824879));
#108908=CARTESIAN_POINT('Ctrl Pts',(-4.47185491688664,1076.67314588412,
311.6454192786));
#108909=CARTESIAN_POINT('Ctrl Pts',(-4.54453812250696,1076.6720779021,311.640626358958));
#108910=CARTESIAN_POINT('Ctrl Pts',(-4.56846673687735,1076.6718347264,311.639838072435));
#108911=CARTESIAN_POINT('Ctrl Pts',(-4.59240295092762,1076.6716997514,311.63983784718));
#108912=CARTESIAN_POINT('Ctrl Pts',(-4.59240637182156,1076.67169973211,
311.639837847148));
#108913=CARTESIAN_POINT('Ctrl Pts',(-4.59240979271534,1076.67169971282,
311.639837847132));
#108914=CARTESIAN_POINT('Ctrl Pts',(-4.59241321360898,1076.67169969354,
311.639837847132));
#108915=CARTESIAN_POINT('Ctrl Pts',(-4.59241321360898,1076.67169969354,
311.639837847132));
#108916=CARTESIAN_POINT('Ctrl Pts',(-4.61963976148801,1076.67154619972,
311.639837847132));
#108917=CARTESIAN_POINT('Ctrl Pts',(-4.64685685878174,1076.67153280805,
311.640857457555));
#108918=CARTESIAN_POINT('Ctrl Pts',(-4.70549373046377,1076.67180653836,
311.645256991049));
#108919=CARTESIAN_POINT('Ctrl Pts',(-4.73686073894702,1076.67214185729,
311.648985620302));
#108920=CARTESIAN_POINT('Ctrl Pts',(-4.82129447019147,1076.67355784612,
311.662761510641));
#108921=CARTESIAN_POINT('Ctrl Pts',(-4.87383616757046,1076.67499655887,
311.675394736954));
#108922=CARTESIAN_POINT('Ctrl Pts',(-5.06278685633759,1076.68224252415,
311.735945191482));
#108923=CARTESIAN_POINT('Ctrl Pts',(-5.19003318628404,1076.6912545598,311.806860980777));
#108924=CARTESIAN_POINT('Ctrl Pts',(-5.39141937328519,1076.71358036343,
311.978453906474));
#108925=CARTESIAN_POINT('Ctrl Pts',(-5.46942446138266,1076.72579093342,
312.071158674187));
#108926=CARTESIAN_POINT('Ctrl Pts',(-5.59728194242799,1076.75441450228,
312.286985756856));
#108927=CARTESIAN_POINT('Ctrl Pts',(-5.64306900721297,1076.77087528038,
312.410362266729));
#108928=CARTESIAN_POINT('Ctrl Pts',(-5.69066760956401,1076.80657872611,
312.67702863095));
#108929=CARTESIAN_POINT('Ctrl Pts',(-5.68840316010873,1076.82562354149,
312.818780749043));
#108930=CARTESIAN_POINT('Ctrl Pts',(-5.62939171111655,1076.86320394024,
313.097584341478));
#108931=CARTESIAN_POINT('Ctrl Pts',(-5.57162369771359,1076.88135917392,
313.231783869726));
#108932=CARTESIAN_POINT('Ctrl Pts',(-5.41074762692253,1076.91301948294,
313.464285973936));
#108933=CARTESIAN_POINT('Ctrl Pts',(-5.31137024183056,1076.92642847705,
313.561950175355));
#108934=CARTESIAN_POINT('Ctrl Pts',(-5.08104710013323,1076.94780601059,
313.715078109525));
#108935=CARTESIAN_POINT('Ctrl Pts',(-4.95225472506798,1076.95557912384,
313.769128268537));
#108936=CARTESIAN_POINT('Ctrl Pts',(-4.76774811052037,1076.96164639615,
313.807890106027));
#108937=CARTESIAN_POINT('Ctrl Pts',(-4.71821465098195,1076.96281554133,
313.814790621794));
#108938=CARTESIAN_POINT('Ctrl Pts',(-4.64309093629956,1076.96390544454,
313.820035965356));
#108939=CARTESIAN_POINT('Ctrl Pts',(-4.61775567411502,1076.96415708804,
313.820919344589));
#108940=CARTESIAN_POINT('Ctrl Pts',(-4.59241321360756,1076.96429318502,
313.820919344589));
#108941=CARTESIAN_POINT('',(-27.7552687727498,1076.95995571924,317.220797722382));
#108942=CARTESIAN_POINT('',(-27.7552687727512,1076.67624971362,315.039716224926));
#108943=CARTESIAN_POINT('Ctrl Pts',(-27.7552687727499,1076.95995571924,
317.220797722383));
#108944=CARTESIAN_POINT('Ctrl Pts',(-27.7283065932649,1076.9608315155,317.220797722383));
#108945=CARTESIAN_POINT('Ctrl Pts',(-27.7013269466995,1076.96158071917,
317.219797825468));
#108946=CARTESIAN_POINT('Ctrl Pts',(-27.6380375280953,1076.96303827534,
317.215090801021));
#108947=CARTESIAN_POINT('Ctrl Pts',(-27.6018441062499,1076.96363908436,
317.210566671319));
#108948=CARTESIAN_POINT('Ctrl Pts',(-27.5421598760239,1076.96424144341,
317.200045209562));
#108949=CARTESIAN_POINT('Ctrl Pts',(-27.5185233406895,1076.96437664644,
317.195063966051));
#108950=CARTESIAN_POINT('Ctrl Pts',(-27.4727725357422,1076.96443551049,
317.183823413574));
#108951=CARTESIAN_POINT('Ctrl Pts',(-27.4506527530679,1076.96436923397,
317.177642015045));
#108952=CARTESIAN_POINT('Ctrl Pts',(-27.3994333479822,1076.96399247892,
317.1615687837));
#108953=CARTESIAN_POINT('Ctrl Pts',(-27.370525558967,1076.96360722564,317.151136644694));
#108954=CARTESIAN_POINT('Ctrl Pts',(-27.2809741631887,1076.96186228721,
317.114475514941));
#108955=CARTESIAN_POINT('Ctrl Pts',(-27.2222700454178,1076.95989543648,
317.083959217189));
#108956=CARTESIAN_POINT('Ctrl Pts',(-27.0445564264891,1076.9511983321,316.970030246813));
#108957=CARTESIAN_POINT('Ctrl Pts',(-26.9394359176285,1076.94167740887,
316.868248954268));
#108958=CARTESIAN_POINT('Ctrl Pts',(-26.7879377872872,1076.91856026459,
316.648428107375));
#108959=CARTESIAN_POINT('Ctrl Pts',(-26.7360743008871,1076.90598960822,
316.536939532749));
#108960=CARTESIAN_POINT('Ctrl Pts',(-26.6685714347086,1076.87665653534,
316.291422777216));
#108961=CARTESIAN_POINT('Ctrl Pts',(-26.6570743801922,1076.85985904197,
316.15826683924));
#108962=CARTESIAN_POINT('Ctrl Pts',(-26.683286842315,1076.82346318484,315.884160849458));
#108963=CARTESIAN_POINT('Ctrl Pts',(-26.7247343598561,1076.80407850786,
315.74592401004));
#108964=CARTESIAN_POINT('Ctrl Pts',(-26.8590086649868,1076.76643261199,
315.492542911362));
#108965=CARTESIAN_POINT('Ctrl Pts',(-26.9509072428477,1076.74852722254,
315.379880588055));
#108966=CARTESIAN_POINT('Ctrl Pts',(-27.165830693425,1076.71793190902,315.202974765251));
#108967=CARTESIAN_POINT('Ctrl Pts',(-27.2844707606106,1076.70522514792,
315.137406121238));
#108968=CARTESIAN_POINT('Ctrl Pts',(-27.5227910213039,1076.68665485675,
315.058440623339));
#108969=CARTESIAN_POINT('Ctrl Pts',(-27.6385873640558,1076.68022264015,
315.039716557163));
#108970=CARTESIAN_POINT('Ctrl Pts',(-27.755265667519,1076.67624981935,315.03971622493));
#108971=CARTESIAN_POINT('Ctrl Pts',(-27.7552687727511,1076.67624971362,
315.039716224926));
#108972=CARTESIAN_POINT('Ctrl Pts',(-27.8007518713627,1076.67470106072,
315.039716224926));
#108973=CARTESIAN_POINT('Ctrl Pts',(-27.8461971406638,1076.67353185038,
315.042561401899));
#108974=CARTESIAN_POINT('Ctrl Pts',(-27.9202855407047,1076.67224860099,
315.051878823282));
#108975=CARTESIAN_POINT('Ctrl Pts',(-27.9490710048065,1076.67190703763,
315.056678431789));
#108976=CARTESIAN_POINT('Ctrl Pts',(-28.0000313111751,1076.67158427596,
315.067292271787));
#108977=CARTESIAN_POINT('Ctrl Pts',(-28.0222792846111,1076.67154132652,
315.072661557919));
#108978=CARTESIAN_POINT('Ctrl Pts',(-28.0685876243102,1076.67165897077,
315.085392056044));
#108979=CARTESIAN_POINT('Ctrl Pts',(-28.0925946139439,1076.67184008542,
315.092893685262));
#108980=CARTESIAN_POINT('Ctrl Pts',(-28.1542559773114,1076.67262044032,
315.11452835087));
#108981=CARTESIAN_POINT('Ctrl Pts',(-28.191421324654,1076.67340451482,315.129924308094));
#108982=CARTESIAN_POINT('Ctrl Pts',(-28.33763630249,1076.67777933126,315.200192997297));
#108983=CARTESIAN_POINT('Ctrl Pts',(-28.4378615576082,1076.68380215683,
315.271083493085));
#108984=CARTESIAN_POINT('Ctrl Pts',(-28.6057533053263,1076.70026477736,
315.438032105936));
#108985=CARTESIAN_POINT('Ctrl Pts',(-28.6738365810709,1076.71033062527,
315.531373911654));
#108986=CARTESIAN_POINT('Ctrl Pts',(-28.7835382230844,1076.7349519754,315.745741443132));
#108987=CARTESIAN_POINT('Ctrl Pts',(-28.8210098270542,1076.74967060233,
315.866999484348));
#108988=CARTESIAN_POINT('Ctrl Pts',(-28.854256696121,1076.78264601847,316.126738212153));
#108989=CARTESIAN_POINT('Ctrl Pts',(-28.8461190155926,1076.80081702579,
316.263653738805));
#108990=CARTESIAN_POINT('Ctrl Pts',(-28.7774318909521,1076.83874830462,
316.537604021781));
#108991=CARTESIAN_POINT('Ctrl Pts',(-28.7134896140636,1076.85815994421,
316.671203027659));
#108992=CARTESIAN_POINT('Ctrl Pts',(-28.5394420059432,1076.89354415798,
316.901257682134));
#108993=CARTESIAN_POINT('Ctrl Pts',(-28.4325714020263,1076.90928919192,
316.996716669842));
#108994=CARTESIAN_POINT('Ctrl Pts',(-28.1982878041784,1076.93465221454,
317.135199002589));
#108995=CARTESIAN_POINT('Ctrl Pts',(-28.0753080562897,1076.94447665053,
317.18089597302));
#108996=CARTESIAN_POINT('Ctrl Pts',(-27.8836893492438,1076.95506208686,
317.215117900989));
#108997=CARTESIAN_POINT('Ctrl Pts',(-27.8195286686761,1076.95786840369,
317.220797722383));
#108998=CARTESIAN_POINT('Ctrl Pts',(-27.7552687727499,1076.95995571924,
317.220797722383));
#108999=CARTESIAN_POINT('',(-15.901306121126,1077.7757685569,322.059817014206));
#109000=CARTESIAN_POINT('',(-15.9013061211259,1077.55169226467,319.862154742221));
#109001=CARTESIAN_POINT('Ctrl Pts',(-15.901306121126,1077.7757685569,322.059817014206));
#109002=CARTESIAN_POINT('Ctrl Pts',(-15.8763153185509,1077.77614444359,
322.059817014206));
#109003=CARTESIAN_POINT('Ctrl Pts',(-15.8513260666884,1077.77643663632,
322.058964462218));
#109004=CARTESIAN_POINT('Ctrl Pts',(-15.7992118709224,1077.77687111121,
322.055402752679));
#109005=CARTESIAN_POINT('Ctrl Pts',(-15.7721196426239,1077.77699748596,
322.052536352266));
#109006=CARTESIAN_POINT('Ctrl Pts',(-15.7193773953242,1077.77704836048,
322.044964810555));
#109007=CARTESIAN_POINT('Ctrl Pts',(-15.693733258665,1077.77698139505,322.040347667022));
#109008=CARTESIAN_POINT('Ctrl Pts',(-15.6340889654077,1077.77660956875,
322.027404544378));
#109009=CARTESIAN_POINT('Ctrl Pts',(-15.6002757202476,1077.7762312001,322.018357257053));
#109010=CARTESIAN_POINT('Ctrl Pts',(-15.4954092673977,1077.77452401565,
321.984860110433));
#109011=CARTESIAN_POINT('Ctrl Pts',(-15.4264140583218,1077.77260769411,
321.954737703618));
#109012=CARTESIAN_POINT('Ctrl Pts',(-15.2338516749138,1077.76482613741,
321.846011556185));
#109013=CARTESIAN_POINT('Ctrl Pts',(-15.1223597126749,1077.75702121677,
321.749615662955));
#109014=CARTESIAN_POINT('Ctrl Pts',(-14.9565068695404,1077.73834570816,
321.535756964948));
#109015=CARTESIAN_POINT('Ctrl Pts',(-14.8974444185682,1077.72821424148,
321.424902304248));
#109016=CARTESIAN_POINT('Ctrl Pts',(-14.815846395992,1077.70479394902,321.178655454585));
#109017=CARTESIAN_POINT('Ctrl Pts',(-14.7973751725187,1077.69150802529,
321.044049350579));
#109018=CARTESIAN_POINT('Ctrl Pts',(-14.8104680840599,1077.66292909833,
320.764718967026));
#109019=CARTESIAN_POINT('Ctrl Pts',(-14.8458506578202,1077.64782959948,
320.622650324851));
#109020=CARTESIAN_POINT('Ctrl Pts',(-14.9693979142027,1077.61891985513,
320.361181895259));
#109021=CARTESIAN_POINT('Ctrl Pts',(-15.0561021188595,1077.60537548996,
320.244108958898));
#109022=CARTESIAN_POINT('Ctrl Pts',(-15.261793050972,1077.58260156969,320.057536280435));
#109023=CARTESIAN_POINT('Ctrl Pts',(-15.3760943816234,1077.57330979647,
319.986605614853));
#109024=CARTESIAN_POINT('Ctrl Pts',(-15.6070919418772,1077.56004935432,
319.896096315778));
#109025=CARTESIAN_POINT('Ctrl Pts',(-15.719690296169,1077.55559535068,319.871216440949));
#109026=CARTESIAN_POINT('Ctrl Pts',(-15.8565128661309,1077.55249125783,
319.862839684625));
#109027=CARTESIAN_POINT('Ctrl Pts',(-15.8789061743036,1077.55205562809,
319.862154742221));
#109028=CARTESIAN_POINT('Ctrl Pts',(-15.901306121126,1077.55169226467,319.862154742221));
#109029=CARTESIAN_POINT('Ctrl Pts',(-15.901306121126,1077.55169226467,319.862154742221));
#109030=CARTESIAN_POINT('Ctrl Pts',(-15.9013154729183,1077.55169211297,
319.862154742221));
#109031=CARTESIAN_POINT('Ctrl Pts',(-15.9013248247117,1077.55169196128,
319.862154742341));
#109032=CARTESIAN_POINT('Ctrl Pts',(-15.9013341765063,1077.5516918096,319.86215474258));
#109033=CARTESIAN_POINT('Ctrl Pts',(-15.9354270010144,1077.55113886074,
319.862155613039));
#109034=CARTESIAN_POINT('Ctrl Pts',(-15.969503221363,1077.55075384282,319.863743150515));
#109035=CARTESIAN_POINT('Ctrl Pts',(-16.0295162085435,1077.55037270648,
319.869346152583));
#109036=CARTESIAN_POINT('Ctrl Pts',(-16.05548515086,1077.55030715598,319.872710190745));
#109037=CARTESIAN_POINT('Ctrl Pts',(-16.1086477485862,1077.55037833879,
319.881538190335));
#109038=CARTESIAN_POINT('Ctrl Pts',(-16.1358040189333,1077.55052713191,
319.887110404563));
#109039=CARTESIAN_POINT('Ctrl Pts',(-16.2035721971005,1077.55118327113,
319.903709135491));
#109040=CARTESIAN_POINT('Ctrl Pts',(-16.2438123836615,1077.55183582535,
319.916051576552));
#109041=CARTESIAN_POINT('Ctrl Pts',(-16.3891197145259,1077.55517374827,
319.96991664901));
#109042=CARTESIAN_POINT('Ctrl Pts',(-16.4882562820175,1077.55941189024,
320.025228405409));
#109043=CARTESIAN_POINT('Ctrl Pts',(-16.6682470308535,1077.57129210572,
320.165643791508));
#109044=CARTESIAN_POINT('Ctrl Pts',(-16.7474617131533,1077.57893653912,
320.250531662784));
#109045=CARTESIAN_POINT('Ctrl Pts',(-16.8827297744749,1077.59771946772,
320.450867575481));
#109046=CARTESIAN_POINT('Ctrl Pts',(-16.9348080994281,1077.60898296415,
320.566984549141));
#109047=CARTESIAN_POINT('Ctrl Pts',(-16.999661876788,1077.63425790322,320.821134373471));
#109048=CARTESIAN_POINT('Ctrl Pts',(-17.0085147851678,1077.64820141357,
320.958038324616));
#109049=CARTESIAN_POINT('Ctrl Pts',(-16.9745994864718,1077.67734414832,
321.238225219221));
#109050=CARTESIAN_POINT('Ctrl Pts',(-16.928204810578,1077.69227788608,321.378517652842));
#109051=CARTESIAN_POINT('Ctrl Pts',(-16.7845999240235,1077.71980366842,
321.630143207751));
#109052=CARTESIAN_POINT('Ctrl Pts',(-16.6898009891721,1077.73218168076,
321.739656395799));
#109053=CARTESIAN_POINT('Ctrl Pts',(-16.4752118164617,1077.75204183279,
321.906790796576));
#109054=CARTESIAN_POINT('Ctrl Pts',(-16.3607870364596,1077.7597522867,321.967387962371));
#109055=CARTESIAN_POINT('Ctrl Pts',(-16.1444952563454,1077.76988030395,
322.037099431661));
#109056=CARTESIAN_POINT('Ctrl Pts',(-16.0469166395223,1077.77306540288,
322.054591994785));
#109057=CARTESIAN_POINT('Ctrl Pts',(-15.9326289447255,1077.77526457008,
322.059482198915));
#109058=CARTESIAN_POINT('Ctrl Pts',(-15.9169672284338,1077.77553299816,
322.059817014206));
#109059=CARTESIAN_POINT('Ctrl Pts',(-15.901306121126,1077.7757685569,322.059817014206));
#109060=CARTESIAN_POINT('',(-5.22978306525612,1078.42681724135,329.304317191978));
#109061=CARTESIAN_POINT('',(-5.22978306525612,1078.26387343671,326.753428949706));
#109062=CARTESIAN_POINT('Ctrl Pts',(-5.22978306525612,1078.42681724135,
329.304317191978));
#109063=CARTESIAN_POINT('Ctrl Pts',(-5.21817028911033,1078.42685380516,
329.304317191978));
#109064=CARTESIAN_POINT('Ctrl Pts',(-5.20655679442347,1078.42688114565,
329.304158592439));
#109065=CARTESIAN_POINT('Ctrl Pts',(-5.16100430481912,1078.42695218218,
329.302913916183));
#109066=CARTESIAN_POINT('Ctrl Pts',(-5.12711338286783,1078.42692617242,
329.300631508059));
#109067=CARTESIAN_POINT('Ctrl Pts',(-5.05124102899184,1078.42669038787,
329.292468925888));
#109068=CARTESIAN_POINT('Ctrl Pts',(-5.00938046874832,1078.42643689142,
329.285843363698));
#109069=CARTESIAN_POINT('Ctrl Pts',(-4.88956556139944,1078.42535139762,
329.260709366201));
#109070=CARTESIAN_POINT('Ctrl Pts',(-4.81293064865789,1078.42420795463,
329.236929669119));
#109071=CARTESIAN_POINT('Ctrl Pts',(-4.58266992306639,1078.41932324785,
329.140944099275));
#109072=CARTESIAN_POINT('Ctrl Pts',(-4.44089376022422,1078.41415833089,
329.045277202033));
#109073=CARTESIAN_POINT('Ctrl Pts',(-4.22049158176406,1078.40154118619,
328.821942320666));
#109074=CARTESIAN_POINT('Ctrl Pts',(-4.13725339237452,1078.39462432085,
328.702654126653));
#109075=CARTESIAN_POINT('Ctrl Pts',(-4.00946950365154,1078.37842387353,
328.431156616306));
#109076=CARTESIAN_POINT('Ctrl Pts',(-3.96953530824098,1078.36912992539,
328.279370354261));
#109077=CARTESIAN_POINT('Ctrl Pts',(-3.94541827194013,1078.34887201492,
327.957567159541));
#109078=CARTESIAN_POINT('Ctrl Pts',(-3.96579539791426,1078.33802728437,
327.790103478902));
#109079=CARTESIAN_POINT('Ctrl Pts',(-4.07008338707345,1078.31687148192,
327.472173835751));
#109080=CARTESIAN_POINT('Ctrl Pts',(-4.1531559897116,1078.30676709278,327.324797726721));
#109081=CARTESIAN_POINT('Ctrl Pts',(-4.36504731564363,1078.2893987037,327.078184844938));
#109082=CARTESIAN_POINT('Ctrl Pts',(-4.4890086736669,1078.28215286931,326.978698259012));
#109083=CARTESIAN_POINT('Ctrl Pts',(-4.74619433616403,1078.27175416546,
326.841074725353));
#109084=CARTESIAN_POINT('Ctrl Pts',(-4.87363484038006,1078.2682171669,326.796842524499));
#109085=CARTESIAN_POINT('Ctrl Pts',(-5.06037098935054,1078.26520873547,
326.763508636248));
#109086=CARTESIAN_POINT('Ctrl Pts',(-5.11567564599099,1078.26457242965,
326.75732766106));
#109087=CARTESIAN_POINT('Ctrl Pts',(-5.19071540936995,1078.26405133643,
326.753877890726));
#109088=CARTESIAN_POINT('Ctrl Pts',(-5.21023951006827,1078.26394686982,
326.753429205568));
#109089=CARTESIAN_POINT('Ctrl Pts',(-5.22976636012611,1078.26387349947,
326.753428949815));
#109090=CARTESIAN_POINT('Ctrl Pts',(-5.22977192850314,1078.26387347855,
326.753428949742));
#109091=CARTESIAN_POINT('Ctrl Pts',(-5.22977749687982,1078.26387345763,
326.753428949706));
#109092=CARTESIAN_POINT('Ctrl Pts',(-5.22978306525612,1078.26387343671,
326.753428949706));
#109093=CARTESIAN_POINT('Ctrl Pts',(-5.22978306525612,1078.26387343671,
326.753428949706));
#109094=CARTESIAN_POINT('Ctrl Pts',(-5.26413051380193,1078.26374441052,
326.753428949706));
#109095=CARTESIAN_POINT('Ctrl Pts',(-5.29846403555081,1078.2637116895,326.754816403494));
#109096=CARTESIAN_POINT('Ctrl Pts',(-5.37080486946607,1078.26384626869,
326.76067274049));
#109097=CARTESIAN_POINT('Ctrl Pts',(-5.40875149683686,1078.26403652857,
326.765469161249));
#109098=CARTESIAN_POINT('Ctrl Pts',(-5.50662085947742,1078.26483892336,
326.782337964163));
#109099=CARTESIAN_POINT('Ctrl Pts',(-5.56599011321287,1078.26563428291,
326.797023720027));
#109100=CARTESIAN_POINT('Ctrl Pts',(-5.78523386914472,1078.26974517431,
326.868291820281));
#109101=CARTESIAN_POINT('Ctrl Pts',(-5.9342881382041,1078.27499041673,326.952254384132));
#109102=CARTESIAN_POINT('Ctrl Pts',(-6.16926264670932,1078.28795185216,
327.154811053109));
#109103=CARTESIAN_POINT('Ctrl Pts',(-6.2599594072838,1078.29501218834,327.263813377943));
#109104=CARTESIAN_POINT('Ctrl Pts',(-6.40771546101825,1078.31141118208,
327.516664664636));
#109105=CARTESIAN_POINT('Ctrl Pts',(-6.4603254996497,1078.32075416327,327.660596885459));
#109106=CARTESIAN_POINT('Ctrl Pts',(-6.51426724469931,1078.34078303726,
327.970781555767));
#109107=CARTESIAN_POINT('Ctrl Pts',(-6.51118729517371,1078.35133351777,
328.135087825742));
#109108=CARTESIAN_POINT('Ctrl Pts',(-6.44221485146335,1078.37200493712,
328.459169753573));
#109109=CARTESIAN_POINT('Ctrl Pts',(-6.37482210851326,1078.38189816543,
328.615442749315));
#109110=CARTESIAN_POINT('Ctrl Pts',(-6.18661499244605,1078.39911311341,
328.887712488775));
#109111=CARTESIAN_POINT('Ctrl Pts',(-6.06956520407042,1078.40636287919,
329.00249266118));
#109112=CARTESIAN_POINT('Ctrl Pts',(-5.79905642962203,1078.41785859816,
329.18165742599));
#109113=CARTESIAN_POINT('Ctrl Pts',(-5.64820140192462,1078.42201395796,
329.24457695622));
#109114=CARTESIAN_POINT('Ctrl Pts',(-5.42983885156224,1078.42535425019,
329.29000668505));
#109115=CARTESIAN_POINT('Ctrl Pts',(-5.36928719555942,1078.42601802146,
329.298132529575));
#109116=CARTESIAN_POINT('Ctrl Pts',(-5.28221266556542,1078.42660514664,
329.303508871083));
#109117=CARTESIAN_POINT('Ctrl Pts',(-5.25599969646798,1078.42673469605,
329.304317191978));
#109118=CARTESIAN_POINT('Ctrl Pts',(-5.22978306525612,1078.42681724135,
329.304317191978));
#109119=CARTESIAN_POINT('',(-63.8195601713291,1078.69713855509,363.267501886));
#109120=CARTESIAN_POINT('',(-63.8195601713292,1078.64371919106,360.310895621613));
#109121=CARTESIAN_POINT('Ctrl Pts',(-63.8195601713295,1078.69713855509,
363.267501886));
#109122=CARTESIAN_POINT('Ctrl Pts',(-63.7654276633616,1078.69791571789,
363.267501886));
#109123=CARTESIAN_POINT('Ctrl Pts',(-63.7112348515189,1078.69863923751,
363.264528627404));
#109124=CARTESIAN_POINT('Ctrl Pts',(-63.4806174827022,1078.70150018512,
363.239050330233));
#109125=CARTESIAN_POINT('Ctrl Pts',(-63.3089585971147,1078.70308592287,
363.187855743175));
#109126=CARTESIAN_POINT('Ctrl Pts',(-63.0679262643324,1078.70464054456,
363.065522553551));
#109127=CARTESIAN_POINT('Ctrl Pts',(-62.9894676807408,1078.70501590417,
363.015943494998));
#109128=CARTESIAN_POINT('Ctrl Pts',(-62.8854962694621,1078.70533108872,
362.93567418569));
#109129=CARTESIAN_POINT('Ctrl Pts',(-62.8557706289723,1078.70539704784,
362.910800739169));
#109130=CARTESIAN_POINT('Ctrl Pts',(-62.8093656128901,1078.70546021498,
362.868762052048));
#109131=CARTESIAN_POINT('Ctrl Pts',(-62.7920654939823,1078.70547408166,
362.852309589674));
#109132=CARTESIAN_POINT('Ctrl Pts',(-62.75703720122,1078.70548167737,362.817343499119));
#109133=CARTESIAN_POINT('Ctrl Pts',(-62.7393767376307,1078.7054738528,362.798773133657));
#109134=CARTESIAN_POINT('Ctrl Pts',(-62.6993218465886,1078.70542815254,
362.754399674498));
#109135=CARTESIAN_POINT('Ctrl Pts',(-62.6773213699519,1078.70538115641,
362.728260646393));
#109136=CARTESIAN_POINT('Ctrl Pts',(-62.6108179918521,1078.70516671703,
362.643448501102));
#109137=CARTESIAN_POINT('Ctrl Pts',(-62.5697813447945,1078.7049233308,362.582201324117));
#109138=CARTESIAN_POINT('Ctrl Pts',(-62.4364456959654,1078.7036670757,362.346959598677));
#109139=CARTESIAN_POINT('Ctrl Pts',(-62.3745670561911,1078.70206695397,
362.15810698534));
#109140=CARTESIAN_POINT('Ctrl Pts',(-62.3323635444361,1078.69778702226,
361.800995099826));
#109141=CARTESIAN_POINT('Ctrl Pts',(-62.3401009842014,1078.69536514556,
361.637248430636));
#109142=CARTESIAN_POINT('Ctrl Pts',(-62.4115686960024,1078.68929087543,
361.305268495352));
#109143=CARTESIAN_POINT('Ctrl Pts',(-62.4794658479006,1078.68559525106,
361.140531861869));
#109144=CARTESIAN_POINT('Ctrl Pts',(-62.6772734345405,1078.67699749055,
360.831790216029));
#109145=CARTESIAN_POINT('Ctrl Pts',(-62.8095880196696,1078.67210256283,
360.693114562129));
#109146=CARTESIAN_POINT('Ctrl Pts',(-63.0788830265797,1078.66328791611,
360.502172178049));
#109147=CARTESIAN_POINT('Ctrl Pts',(-63.2042216726988,1078.65949595976,
360.437755469273));
#109148=CARTESIAN_POINT('Ctrl Pts',(-63.4920519938876,1078.65148884259,
360.338296316964));
#109149=CARTESIAN_POINT('Ctrl Pts',(-63.655229864875,1078.64736986489,360.310895621613));
#109150=CARTESIAN_POINT('Ctrl Pts',(-63.8195601713292,1078.64371919106,
360.310895621613));
#109151=CARTESIAN_POINT('Ctrl Pts',(-63.8195601713292,1078.64371919106,
360.310895621613));
#109152=CARTESIAN_POINT('Ctrl Pts',(-63.8195692561662,1078.64371898923,
360.310895621613));
#109153=CARTESIAN_POINT('Ctrl Pts',(-63.8195783410068,1078.64371878741,
360.310895621697));
#109154=CARTESIAN_POINT('Ctrl Pts',(-63.8195874258508,1078.64371858559,
360.310895621865));
#109155=CARTESIAN_POINT('Ctrl Pts',(-63.9840880711053,1078.64006418243,
360.310898654657));
#109156=CARTESIAN_POINT('Ctrl Pts',(-64.1474517009238,1078.63693314233,
360.338359260013));
#109157=CARTESIAN_POINT('Ctrl Pts',(-64.4375133454174,1078.63248761909,
360.438719377146));
#109158=CARTESIAN_POINT('Ctrl Pts',(-64.5646686302155,1078.63100970962,
360.504489606167));
#109159=CARTESIAN_POINT('Ctrl Pts',(-64.7189171915552,1078.629931692,360.61498571193));
#109160=CARTESIAN_POINT('Ctrl Pts',(-64.7560402577428,1078.62973704016,
360.644373691614));
#109161=CARTESIAN_POINT('Ctrl Pts',(-64.8133214071306,1078.62954551884,
360.694373110903));
#109162=CARTESIAN_POINT('Ctrl Pts',(-64.834398153059,1078.62950100695,360.713880913424));
#109163=CARTESIAN_POINT('Ctrl Pts',(-64.8731921848538,1078.62946960111,
360.751944240303));
#109164=CARTESIAN_POINT('Ctrl Pts',(-64.8910208318981,1078.62947704798,
360.77037129156));
#109165=CARTESIAN_POINT('Ctrl Pts',(-64.9300915095018,1078.6295439517,360.812913778697));
#109166=CARTESIAN_POINT('Ctrl Pts',(-64.95104463411,1078.62961608288,360.83727695762));
#109167=CARTESIAN_POINT('Ctrl Pts',(-65.0104012958941,1078.62993090917,
360.911025018266));
#109168=CARTESIAN_POINT('Ctrl Pts',(-65.046483463865,1078.63027019649,360.962185601849));
#109169=CARTESIAN_POINT('Ctrl Pts',(-65.1824629782876,1078.63220921242,
361.183566658344));
#109170=CARTESIAN_POINT('Ctrl Pts',(-65.251019535922,1078.63493719135,361.370621080719));
#109171=CARTESIAN_POINT('Ctrl Pts',(-65.3051133582954,1078.64163702058,
361.724127004683));
#109172=CARTESIAN_POINT('Ctrl Pts',(-65.3034107922253,1078.64523224278,
361.885549877209));
#109173=CARTESIAN_POINT('Ctrl Pts',(-65.2458716339885,1078.65347084342,
362.215021809456));
#109174=CARTESIAN_POINT('Ctrl Pts',(-65.1858599118924,1078.65810944785,
362.379885969386));
#109175=CARTESIAN_POINT('Ctrl Pts',(-65.0049667573119,1078.6678008815,362.691988432195));
#109176=CARTESIAN_POINT('Ctrl Pts',(-64.8816256635728,1078.67276841009,
362.834300953678));
#109177=CARTESIAN_POINT('Ctrl Pts',(-64.581690312079,1078.68223685099,363.070876817612));
#109178=CARTESIAN_POINT('Ctrl Pts',(-64.4058332189708,1078.68661220443,
363.16026913069));
#109179=CARTESIAN_POINT('Ctrl Pts',(-64.0878422058905,1078.69295053254,
363.249192272456));
#109180=CARTESIAN_POINT('Ctrl Pts',(-63.9538868561519,1078.69521007057,
363.267501886));
#109181=CARTESIAN_POINT('Ctrl Pts',(-63.8195601713295,1078.69713855509,
363.267501886));
#109182=CARTESIAN_POINT('',(-75.2807843499775,1078.39877300636,365.149931275707));
#109183=CARTESIAN_POINT('',(-75.2807843499774,1078.29624496504,362.599043033435));
#109184=CARTESIAN_POINT('Ctrl Pts',(-75.2807843499775,1078.39877300636,
365.149931275707));
#109185=CARTESIAN_POINT('Ctrl Pts',(-75.2161334842683,1078.40181327285,
365.149931275707));
#109186=CARTESIAN_POINT('Ctrl Pts',(-75.1514247503078,1078.4046523139,365.145015809985));
#109187=CARTESIAN_POINT('Ctrl Pts',(-74.9448585872546,1078.41307129843,
365.113299692974));
#109188=CARTESIAN_POINT('Ctrl Pts',(-74.8071834118907,1078.41769218236,
365.067477827383));
#109189=CARTESIAN_POINT('Ctrl Pts',(-74.5863101850922,1078.42343536425,
364.949549063762));
#109190=CARTESIAN_POINT('Ctrl Pts',(-74.499171623296,1078.42513500621,364.887965809381));
#109191=CARTESIAN_POINT('Ctrl Pts',(-74.3939533568889,1078.42639080928,
364.791873924468));
#109192=CARTESIAN_POINT('Ctrl Pts',(-74.3682783039198,1078.42662066959,
364.766339436608));
#109193=CARTESIAN_POINT('Ctrl Pts',(-74.3285856758789,1078.4268475706,364.723353057851));
#109194=CARTESIAN_POINT('Ctrl Pts',(-74.3138804217284,1078.42690004791,
364.706564336766));
#109195=CARTESIAN_POINT('Ctrl Pts',(-74.2867342554265,1078.42693505528,
364.67388008605));
#109196=CARTESIAN_POINT('Ctrl Pts',(-74.2742153451122,1078.42692380994,
364.658058138182));
#109197=CARTESIAN_POINT('Ctrl Pts',(-74.2466507018341,1078.42683500453,
364.621469458007));
#109198=CARTESIAN_POINT('Ctrl Pts',(-74.2318453978593,1078.42674032876,
364.600532622343));
#109199=CARTESIAN_POINT('Ctrl Pts',(-74.1894275609345,1078.42632234112,
364.536539413027));
#109200=CARTESIAN_POINT('Ctrl Pts',(-74.1637638132263,1078.42586570789,
364.492255420951));
#109201=CARTESIAN_POINT('Ctrl Pts',(-74.0648826593169,1078.4231351608,364.295214661423));
#109202=CARTESIAN_POINT('Ctrl Pts',(-74.0198471130781,1078.41913258796,
364.130296520653));
#109203=CARTESIAN_POINT('Ctrl Pts',(-73.99889279747,1078.40868075344,363.823672373705));
#109204=CARTESIAN_POINT('Ctrl Pts',(-74.0119178471483,1078.40288387041,
363.685322336896));
#109205=CARTESIAN_POINT('Ctrl Pts',(-74.0849456862005,1078.38880697799,
363.40606661576));
#109206=CARTESIAN_POINT('Ctrl Pts',(-74.148560344525,1078.38045633396,363.268277557071));
#109207=CARTESIAN_POINT('Ctrl Pts',(-74.3273946189254,1078.36171230716,
363.011895031162));
#109208=CARTESIAN_POINT('Ctrl Pts',(-74.4445747218407,1078.3513780663,362.897882325637));
#109209=CARTESIAN_POINT('Ctrl Pts',(-74.6771585021235,1078.33348783158,
362.744913697328));
#109210=CARTESIAN_POINT('Ctrl Pts',(-74.7826914890141,1078.32605355494,
362.694568377246));
#109211=CARTESIAN_POINT('Ctrl Pts',(-75.0187524433123,1078.31080177787,
362.619356602734));
#109212=CARTESIAN_POINT('Ctrl Pts',(-75.1493582059871,1078.3031483309,362.599043033435));
#109213=CARTESIAN_POINT('Ctrl Pts',(-75.2807843499774,1078.29624496504,
362.599043033435));
#109214=CARTESIAN_POINT('Ctrl Pts',(-75.2807843499774,1078.29624496504,
362.599043033435));
#109215=CARTESIAN_POINT('Ctrl Pts',(-75.2808246059088,1078.29624285053,
362.599043033435));
#109216=CARTESIAN_POINT('Ctrl Pts',(-75.2808648619172,1078.29624073609,
362.599043035341));
#109217=CARTESIAN_POINT('Ctrl Pts',(-75.2809051180025,1078.29623862173,
362.599043039152));
#109218=CARTESIAN_POINT('Ctrl Pts',(-75.4339110658859,1078.28820230906,
362.599057526832));
#109219=CARTESIAN_POINT('Ctrl Pts',(-75.585730203367,1078.28130554178,362.626604428352));
#109220=CARTESIAN_POINT('Ctrl Pts',(-75.8700236650462,1078.2707025985,362.733338630975));
#109221=CARTESIAN_POINT('Ctrl Pts',(-76.0005275537089,1078.26703110392,
362.810806746118));
#109222=CARTESIAN_POINT('Ctrl Pts',(-76.1462977818729,1078.26464543997,
362.936719743162));
#109223=CARTESIAN_POINT('Ctrl Pts',(-76.1767035716881,1078.26426694338,
362.965724159803));
#109224=CARTESIAN_POINT('Ctrl Pts',(-76.2221910149657,1078.26389723162,
363.013621316875));
#109225=CARTESIAN_POINT('Ctrl Pts',(-76.2382614055876,1078.26380971888,
363.031531518975));
#109226=CARTESIAN_POINT('Ctrl Pts',(-76.266922221215,1078.26373558589,363.06535133532));
#109227=CARTESIAN_POINT('Ctrl Pts',(-76.279658143114,1078.2637352656,363.081127324293));
#109228=CARTESIAN_POINT('Ctrl Pts',(-76.3066136828094,1078.26380783499,
363.116195714162));
#109229=CARTESIAN_POINT('Ctrl Pts',(-76.3206765016514,1078.26389403413,
363.13559878332));
#109230=CARTESIAN_POINT('Ctrl Pts',(-76.3582619672818,1078.26426397588,
363.190657162071));
#109231=CARTESIAN_POINT('Ctrl Pts',(-76.3805521556505,1078.264649296,363.227113984603));
#109232=CARTESIAN_POINT('Ctrl Pts',(-76.4819965114546,1078.26729100623,
363.413443730654));
#109233=CARTESIAN_POINT('Ctrl Pts',(-76.5325310959413,1078.27168449831,
363.576884398006));
#109234=CARTESIAN_POINT('Ctrl Pts',(-76.5634527382886,1078.28312828969,
363.880752998088));
#109235=CARTESIAN_POINT('Ctrl Pts',(-76.5554686847615,1078.28941049513,
364.017429732933));
#109236=CARTESIAN_POINT('Ctrl Pts',(-76.4939475753043,1078.30441417504,
364.295285570309));
#109237=CARTESIAN_POINT('Ctrl Pts',(-76.4367295223015,1078.31319122092,
364.433596763608));
#109238=CARTESIAN_POINT('Ctrl Pts',(-76.2713754352099,1078.33240509299,
364.693614326351));
#109239=CARTESIAN_POINT('Ctrl Pts',(-76.1611860349923,1078.34274708112,
364.811038803311));
#109240=CARTESIAN_POINT('Ctrl Pts',(-75.8956883837525,1078.36366889432,
365.004618549399));
#109241=CARTESIAN_POINT('Ctrl Pts',(-75.7407077768385,1078.37402253982,
365.076069801023));
#109242=CARTESIAN_POINT('Ctrl Pts',(-75.4792733932657,1078.38895729896,
365.138331357763));
#109243=CARTESIAN_POINT('Ctrl Pts',(-75.3800971557428,1078.39410273021,
365.149931275707));
#109244=CARTESIAN_POINT('Ctrl Pts',(-75.2807843499775,1078.39877300636,
365.149931275707));
#109245=CARTESIAN_POINT('',(-87.6738908373843,1077.72740193357,368.174465786616));
#109246=CARTESIAN_POINT('',(-87.6738908373841,1077.60298376124,365.976803514632));
#109247=CARTESIAN_POINT('Ctrl Pts',(-87.6738908373845,1077.72740193357,
368.174465786616));
#109248=CARTESIAN_POINT('Ctrl Pts',(-87.5573652041762,1077.73724060115,
368.174465786616));
#109249=CARTESIAN_POINT('Ctrl Pts',(-87.4413379559943,1077.74595717174,
368.155929576178));
#109250=CARTESIAN_POINT('Ctrl Pts',(-87.2081865583119,1077.76124290941,
368.079155469716));
#109251=CARTESIAN_POINT('Ctrl Pts',(-87.0940626911965,1077.76738850911,
368.017855331126));
#109252=CARTESIAN_POINT('Ctrl Pts',(-86.937335696392,1077.77366264064,367.894145559585));
#109253=CARTESIAN_POINT('Ctrl Pts',(-86.8859755761865,1077.77523785621,
367.844833744352));
#109254=CARTESIAN_POINT('Ctrl Pts',(-86.8223756947841,1077.77647476621,
367.770661603692));
#109255=CARTESIAN_POINT('Ctrl Pts',(-86.8057648978473,1077.77671665045,
367.749799280664));
#109256=CARTESIAN_POINT('Ctrl Pts',(-86.7796558363558,1077.77695715498,
367.714440349409));
#109257=CARTESIAN_POINT('Ctrl Pts',(-86.7697126380652,1077.7770113458,367.700287154191));
#109258=CARTESIAN_POINT('Ctrl Pts',(-86.7510769658923,1077.77703794975,
367.672383188798));
#109259=CARTESIAN_POINT('Ctrl Pts',(-86.7423476385495,1077.77701505646,
367.658662543958));
#109260=CARTESIAN_POINT('Ctrl Pts',(-86.7227413944098,1077.7768784821,367.626280580748));
#109261=CARTESIAN_POINT('Ctrl Pts',(-86.7121039478821,1077.77673751051,
367.607482510928));
#109262=CARTESIAN_POINT('Ctrl Pts',(-86.6803229937885,1077.77609450137,
367.54724495784));
#109263=CARTESIAN_POINT('Ctrl Pts',(-86.6612545546933,1077.77536423692,
367.504773625786));
#109264=CARTESIAN_POINT('Ctrl Pts',(-86.5937762745918,1077.77115672216,
367.324707375812));
#109265=CARTESIAN_POINT('Ctrl Pts',(-86.5703302700837,1077.76518941578,
367.179463664682));
#109266=CARTESIAN_POINT('Ctrl Pts',(-86.5803643398938,1077.74985083539,
366.914971971357));
#109267=CARTESIAN_POINT('Ctrl Pts',(-86.6041910643592,1077.74139850213,
366.797588014984));
#109268=CARTESIAN_POINT('Ctrl Pts',(-86.6923877389255,1077.7210800103,366.564750883201));
#109269=CARTESIAN_POINT('Ctrl Pts',(-86.7596651934525,1077.70912548192,
366.452342304681));
#109270=CARTESIAN_POINT('Ctrl Pts',(-86.9369203232877,1077.68257914247,
366.24862501908));
#109271=CARTESIAN_POINT('Ctrl Pts',(-87.0482725867131,1077.66808828252,
366.161493284213));
#109272=CARTESIAN_POINT('Ctrl Pts',(-87.2468460860523,1077.64510635443,
366.05978237616));
#109273=CARTESIAN_POINT('Ctrl Pts',(-87.3248097970308,1077.63664740925,
366.030421117856));
#109274=CARTESIAN_POINT('Ctrl Pts',(-87.4931076423008,1077.61951793621,
365.988005314607));
#109275=CARTESIAN_POINT('Ctrl Pts',(-87.5833033350967,1077.61095961518,
365.976803514632));
#109276=CARTESIAN_POINT('Ctrl Pts',(-87.6738908373841,1077.60298376124,
365.976803514632));
#109277=CARTESIAN_POINT('Ctrl Pts',(-87.6738908373841,1077.60298376124,
365.976803514632));
#109278=CARTESIAN_POINT('Ctrl Pts',(-87.6739295858868,1077.60298034959,
365.976803514632));
#109279=CARTESIAN_POINT('Ctrl Pts',(-87.6739683344612,1077.60297693806,
365.976803516681));
#109280=CARTESIAN_POINT('Ctrl Pts',(-87.674007083107,1077.60297352662,365.97680352078));
#109281=CARTESIAN_POINT('Ctrl Pts',(-87.8110948853574,1077.59090431333,
365.976818023346));
#109282=CARTESIAN_POINT('Ctrl Pts',(-87.9471081365583,1077.58034330989,
366.00248659144));
#109283=CARTESIAN_POINT('Ctrl Pts',(-88.2018405975823,1077.56352565653,
366.102358515398));
#109284=CARTESIAN_POINT('Ctrl Pts',(-88.3184445103972,1077.55738583551,
366.175299484557));
#109285=CARTESIAN_POINT('Ctrl Pts',(-88.4570236364598,1077.55249567817,
366.303080205187));
#109286=CARTESIAN_POINT('Ctrl Pts',(-88.4927285909642,1077.55152990991,
366.341030288748));
#109287=CARTESIAN_POINT('Ctrl Pts',(-88.5385533914332,1077.55073137724,
366.397248335192));
#109288=CARTESIAN_POINT('Ctrl Pts',(-88.5510474224014,1077.55056685126,
366.413482333986));
#109289=CARTESIAN_POINT('Ctrl Pts',(-88.5720144121306,1077.55038680279,
366.442361303932));
#109290=CARTESIAN_POINT('Ctrl Pts',(-88.580691801958,1077.55034383564,366.454850385869));
#109291=CARTESIAN_POINT('Ctrl Pts',(-88.5982445402759,1077.55032467677,
366.481267177206));
#109292=CARTESIAN_POINT('Ctrl Pts',(-88.607070691021,1077.55035453155,366.495222885357));
#109293=CARTESIAN_POINT('Ctrl Pts',(-88.6271147213411,1077.5505186285,366.528555878046));
#109294=CARTESIAN_POINT('Ctrl Pts',(-88.638061263345,1077.550686195,366.548087215086));
#109295=CARTESIAN_POINT('Ctrl Pts',(-88.671527076778,1077.55146414451,366.612324198192));
#109296=CARTESIAN_POINT('Ctrl Pts',(-88.691588364216,1077.55236494906,366.658231848467));
#109297=CARTESIAN_POINT('Ctrl Pts',(-88.7575613918226,1077.55728181453,
366.842552617564));
#109298=CARTESIAN_POINT('Ctrl Pts',(-88.7788484232324,1077.56391245768,
366.98805397235));
#109299=CARTESIAN_POINT('Ctrl Pts',(-88.7649366627409,1077.58057374157,
367.252513441476));
#109300=CARTESIAN_POINT('Ctrl Pts',(-88.7393088371827,1077.58966347007,
367.369749958813));
#109301=CARTESIAN_POINT('Ctrl Pts',(-88.6475228088464,1077.61114894308,
367.601344363622));
#109302=CARTESIAN_POINT('Ctrl Pts',(-88.5785904850142,1077.62360235186,
367.712662757938));
#109303=CARTESIAN_POINT('Ctrl Pts',(-88.3985567348636,1077.65075882583,
367.913390194743));
#109304=CARTESIAN_POINT('Ctrl Pts',(-88.2862066369907,1077.66532082558,
367.998694712242));
#109305=CARTESIAN_POINT('Ctrl Pts',(-88.0304113322889,1077.6944116005,368.125164019262));
#109306=CARTESIAN_POINT('Ctrl Pts',(-87.8883136821735,1077.70863675563,
368.163152580909));
#109307=CARTESIAN_POINT('Ctrl Pts',(-87.7198685969776,1077.72347788553,
368.173744969849));
#109308=CARTESIAN_POINT('Ctrl Pts',(-87.6968700256675,1077.72546172017,
368.174465786616));
#109309=CARTESIAN_POINT('Ctrl Pts',(-87.6738908373845,1077.72740193357,
368.174465786616));
#109310=CARTESIAN_POINT('',(-99.195671242928,1076.88734730071,373.742997844246));
#109311=CARTESIAN_POINT('',(-99.1956712429287,1076.75143050179,371.56191634679));
#109312=CARTESIAN_POINT('Ctrl Pts',(-99.1956712429275,1076.88734730071,
373.742997844247));
#109313=CARTESIAN_POINT('Ctrl Pts',(-99.0736283223645,1076.90169935678,
373.742997844247));
#109314=CARTESIAN_POINT('Ctrl Pts',(-98.9521493125783,1076.91466858142,
373.722510530752));
#109315=CARTESIAN_POINT('Ctrl Pts',(-98.722881029104,1076.93655311003,373.642505437814));
#109316=CARTESIAN_POINT('Ctrl Pts',(-98.6165758032035,1076.94538160664,
373.584362543656));
#109317=CARTESIAN_POINT('Ctrl Pts',(-98.4429100659212,1076.9572595498,373.447884683702));
#109318=CARTESIAN_POINT('Ctrl Pts',(-98.3728788279871,1076.96096862298,
373.375223966441));
#109319=CARTESIAN_POINT('Ctrl Pts',(-98.2965085693078,1076.9634476614,373.270232018967));
#109320=CARTESIAN_POINT('Ctrl Pts',(-98.2802183338221,1076.96385410401,
373.245825099279));
#109321=CARTESIAN_POINT('Ctrl Pts',(-98.2559131695869,1076.96425457554,
373.20602127878));
#109322=CARTESIAN_POINT('Ctrl Pts',(-98.2472480318087,1076.96434931847,
373.191040397767));
#109323=CARTESIAN_POINT('Ctrl Pts',(-98.231787152459,1076.96442531798,373.162779421882));
#109324=CARTESIAN_POINT('Ctrl Pts',(-98.2249003947043,1076.96442045692,
373.149554043209));
#109325=CARTESIAN_POINT('Ctrl Pts',(-98.2102834705255,1076.96432123289,
373.120020590978));
#109326=CARTESIAN_POINT('Ctrl Pts',(-98.2026826917412,1076.96420828855,
373.103653720111));
#109327=CARTESIAN_POINT('Ctrl Pts',(-98.1821750046192,1076.9637193216,373.056463076137));
#109328=CARTESIAN_POINT('Ctrl Pts',(-98.1702749096861,1076.96320143812,
373.025227000313));
#109329=CARTESIAN_POINT('Ctrl Pts',(-98.1147448066343,1076.95939190168,
372.856565076093));
#109330=CARTESIAN_POINT('Ctrl Pts',(-98.0973062481845,1076.95263957393,
372.712199361141));
#109331=CARTESIAN_POINT('Ctrl Pts',(-98.1172160193176,1076.93453988868,
372.453536329503));
#109332=CARTESIAN_POINT('Ctrl Pts',(-98.1443316171273,1076.9244749459,372.340607577463));
#109333=CARTESIAN_POINT('Ctrl Pts',(-98.2373238720896,1076.89985498333,
372.116712072768));
#109334=CARTESIAN_POINT('Ctrl Pts',(-98.3062049072568,1076.88513007261,
372.008858521594));
#109335=CARTESIAN_POINT('Ctrl Pts',(-98.4848473774606,1076.85201772236,
371.814063640996));
#109336=CARTESIAN_POINT('Ctrl Pts',(-98.5960196878507,1076.83370852677,
371.7312893177));
#109337=CARTESIAN_POINT('Ctrl Pts',(-98.7912365215574,1076.80456118302,
371.6365529696));
#109338=CARTESIAN_POINT('Ctrl Pts',(-98.8665380857841,1076.79389477705,
371.609717639631));
#109339=CARTESIAN_POINT('Ctrl Pts',(-99.0264816047437,1076.77237825944,
371.571799441588));
#109340=CARTESIAN_POINT('Ctrl Pts',(-99.1109041596281,1076.76162623678,
371.56191634679));
#109341=CARTESIAN_POINT('Ctrl Pts',(-99.1956712429287,1076.75143050179,
371.56191634679));
#109342=CARTESIAN_POINT('Ctrl Pts',(-99.1956712429287,1076.75143050179,
371.56191634679));
#109343=CARTESIAN_POINT('Ctrl Pts',(-99.1957283200062,1076.75142363659,
371.56191634679));
#109344=CARTESIAN_POINT('Ctrl Pts',(-99.19578539724,1076.75141677165,371.561916351271));
#109345=CARTESIAN_POINT('Ctrl Pts',(-99.1958424746294,1076.75140990695,
371.561916360233));
#109346=CARTESIAN_POINT('Ctrl Pts',(-99.3351577757383,1076.73465446801,
371.561938234883));
#109347=CARTESIAN_POINT('Ctrl Pts',(-99.4734071019285,1076.71964185485,
371.588656038097));
#109348=CARTESIAN_POINT('Ctrl Pts',(-99.7161381234471,1076.6964459697,371.686404254856));
#109349=CARTESIAN_POINT('Ctrl Pts',(-99.82094661711,1076.68780253686,371.750652243197));
#109350=CARTESIAN_POINT('Ctrl Pts',(-99.9771424816468,1076.6775001339,371.887061624022));
#109351=CARTESIAN_POINT('Ctrl Pts',(-100.034523423316,1076.67455483639,
371.950410338995));
#109352=CARTESIAN_POINT('Ctrl Pts',(-100.1000822094,1076.67244457439,372.042463658499));
#109353=CARTESIAN_POINT('Ctrl Pts',(-100.115331214849,1076.67207043337,
372.065705922058));
#109354=CARTESIAN_POINT('Ctrl Pts',(-100.138383581076,1076.67170327283,
372.103952707521));
#109355=CARTESIAN_POINT('Ctrl Pts',(-100.146754284508,1076.67161830542,
372.118598798295));
#109356=CARTESIAN_POINT('Ctrl Pts',(-100.161250809849,1076.6715620031,372.145387118025));
#109357=CARTESIAN_POINT('Ctrl Pts',(-100.167495537484,1076.6715718107,372.157460731202));
#109358=CARTESIAN_POINT('Ctrl Pts',(-100.181620096997,1076.67167681144,
372.186067440803));
#109359=CARTESIAN_POINT('Ctrl Pts',(-100.189312206167,1076.67180045741,
372.202688202966));
#109360=CARTESIAN_POINT('Ctrl Pts',(-100.210170193117,1076.67233665881,
372.250907092201));
#109361=CARTESIAN_POINT('Ctrl Pts',(-100.222270579505,1076.67290660126,
372.282938726163));
#109362=CARTESIAN_POINT('Ctrl Pts',(-100.27746691294,1076.67702211819,372.452827331005));
#109363=CARTESIAN_POINT('Ctrl Pts',(-100.294314900092,1076.68419817679,
372.597502874207));
#109364=CARTESIAN_POINT('Ctrl Pts',(-100.273215784234,1076.70320477396,
372.856203967397));
#109365=CARTESIAN_POINT('Ctrl Pts',(-100.245620991406,1076.71370265287,
372.968918041803));
#109366=CARTESIAN_POINT('Ctrl Pts',(-100.151825362005,1076.73914601096,
373.192033923503));
#109367=CARTESIAN_POINT('Ctrl Pts',(-100.082694943572,1076.75424225081,
373.299359770525));
#109368=CARTESIAN_POINT('Ctrl Pts',(-99.9039546807303,1076.78783535912,
373.492907388989));
#109369=CARTESIAN_POINT('Ctrl Pts',(-99.7929994064649,1076.80622551015,
373.575057070781));
#109370=CARTESIAN_POINT('Ctrl Pts',(-99.5389909591353,1076.84405296943,
373.697690927404));
#109371=CARTESIAN_POINT('Ctrl Pts',(-99.3967539688833,1076.8631299079,373.734129799356));
#109372=CARTESIAN_POINT('Ctrl Pts',(-99.2328506581823,1076.88294455326,
373.742522852492));
#109373=CARTESIAN_POINT('Ctrl Pts',(-99.2142544122992,1076.88516194913,
373.742997844247));
#109374=CARTESIAN_POINT('Ctrl Pts',(-99.1956712429275,1076.88734730071,
373.742997844247));
#109375=CARTESIAN_POINT('',(-75.4882582191906,1078.69210669589,377.909343604465));
#109376=CARTESIAN_POINT('',(-75.4882582209909,1078.65110559495,374.952737340079));
#109377=CARTESIAN_POINT('Ctrl Pts',(-75.4882582191907,1078.69210669589,
377.909343604465));
#109378=CARTESIAN_POINT('Ctrl Pts',(-75.3723553642364,1078.69420613881,
377.909343604465));
#109379=CARTESIAN_POINT('Ctrl Pts',(-75.256587670448,1078.69606590151,377.895712558815));
#109380=CARTESIAN_POINT('Ctrl Pts',(-74.9775322007986,1078.70004877863,
377.828761931101));
#109381=CARTESIAN_POINT('Ctrl Pts',(-74.8198153044357,1078.70185771599,
377.760572053417));
#109382=CARTESIAN_POINT('Ctrl Pts',(-74.5678748243461,1078.70412727041,
377.595247777887));
#109383=CARTESIAN_POINT('Ctrl Pts',(-74.4685339332241,1078.70479436216,
377.509301780905));
#109384=CARTESIAN_POINT('Ctrl Pts',(-74.3531109587763,1078.70527726789,
377.379034307612));
#109385=CARTESIAN_POINT('Ctrl Pts',(-74.3258568093545,1078.70536357389,
377.345411616369));
#109386=CARTESIAN_POINT('Ctrl Pts',(-74.2844809867876,1078.70544845401,
377.289522297816));
#109387=CARTESIAN_POINT('Ctrl Pts',(-74.269411432456,1078.7054681463,377.267989205266));
#109388=CARTESIAN_POINT('Ctrl Pts',(-74.2419697761637,1078.70548202747,
377.226463216105));
#109389=CARTESIAN_POINT('Ctrl Pts',(-74.2294848941881,1078.70547869262,
377.206554457254));
#109390=CARTESIAN_POINT('Ctrl Pts',(-74.2024030982817,1078.7054488587,377.160990807056));
#109391=CARTESIAN_POINT('Ctrl Pts',(-74.1880892206401,1078.70541666008,
377.135179277233));
#109392=CARTESIAN_POINT('Ctrl Pts',(-74.1480880766633,1078.70527527731,
377.057663016202));
#109393=CARTESIAN_POINT('Ctrl Pts',(-74.1246456264381,1078.70512211053,
377.004863166626));
#109394=CARTESIAN_POINT('Ctrl Pts',(-74.0349484347774,1078.70417865361,
376.766049210628));
#109395=CARTESIAN_POINT('Ctrl Pts',(-74.0032534078389,1078.70276108278,
376.569232269852));
#109396=CARTESIAN_POINT('Ctrl Pts',(-74.0175242273733,1078.69884917058,
376.212092296399));
#109397=CARTESIAN_POINT('Ctrl Pts',(-74.0498438928602,1078.69662979895,
376.054268760415));
#109398=CARTESIAN_POINT('Ctrl Pts',(-74.1689539178824,1078.69098482109,
375.741642429826));
#109399=CARTESIAN_POINT('Ctrl Pts',(-74.259468349416,1078.68750830159,375.590860557683));
#109400=CARTESIAN_POINT('Ctrl Pts',(-74.497478193385,1078.67932032412,375.31796608691));
#109401=CARTESIAN_POINT('Ctrl Pts',(-74.6465874232387,1078.67460612919,
375.201339900436));
#109402=CARTESIAN_POINT('Ctrl Pts',(-74.9872371740712,1078.66449165679,
375.026588823309));
#109403=CARTESIAN_POINT('Ctrl Pts',(-75.1769197320241,1078.65917180238,
374.972762191345));
#109404=CARTESIAN_POINT('Ctrl Pts',(-75.4104491222578,1078.65308609293,
374.954271430745));
#109405=CARTESIAN_POINT('Ctrl Pts',(-75.4493746762025,1078.65208707672,
374.952737339984));
#109406=CARTESIAN_POINT('Ctrl Pts',(-75.4882582227912,1078.65110559495,
374.952737340079));
#109407=CARTESIAN_POINT('Ctrl Pts',(-75.4882582227911,1078.65110559495,
374.952737340079));
#109408=CARTESIAN_POINT('Ctrl Pts',(-75.6377283020281,1078.64733273544,
374.952737340443));
#109409=CARTESIAN_POINT('Ctrl Pts',(-75.7865776407321,1078.64381852535,
374.975408230683));
#109410=CARTESIAN_POINT('Ctrl Pts',(-76.0944769116894,1078.63724511373,
375.071739479389));
#109411=CARTESIAN_POINT('Ctrl Pts',(-76.2489933327613,1078.63439627033,
375.151786494705));
#109412=CARTESIAN_POINT('Ctrl Pts',(-76.4684122859027,1078.63127796722,
375.319559165766));
#109413=CARTESIAN_POINT('Ctrl Pts',(-76.543805534904,1078.63044039654,375.390889675293));
#109414=CARTESIAN_POINT('Ctrl Pts',(-76.6366811080338,1078.62977669572,
375.499349378235));
#109415=CARTESIAN_POINT('Ctrl Pts',(-76.6610334217237,1078.62964561687,
375.530195436815));
#109416=CARTESIAN_POINT('Ctrl Pts',(-76.6991779067036,1078.62951517723,
375.582683817286));
#109417=CARTESIAN_POINT('Ctrl Pts',(-76.7136871158323,1078.62948585624,
375.603780219566));
#109418=CARTESIAN_POINT('Ctrl Pts',(-76.7407966396375,1078.62947201969,
375.645476889364));
#109419=CARTESIAN_POINT('Ctrl Pts',(-76.753454593751,1078.6294850376,375.666030164883));
#109420=CARTESIAN_POINT('Ctrl Pts',(-76.7817762502066,1078.62956133302,
375.714644326584));
#109421=CARTESIAN_POINT('Ctrl Pts',(-76.7970395231866,1078.62963981064,
375.742924332503));
#109422=CARTESIAN_POINT('Ctrl Pts',(-76.8422978146681,1078.62999718961,
375.833742113927));
#109423=CARTESIAN_POINT('Ctrl Pts',(-76.8688209305646,1078.63040263772,
375.897903621101));
#109424=CARTESIAN_POINT('Ctrl Pts',(-76.9385947214267,1078.63218843821,
376.107288762677));
#109425=CARTESIAN_POINT('Ctrl Pts',(-76.9641067637324,1078.63414625799,
376.257382120507));
#109426=CARTESIAN_POINT('Ctrl Pts',(-76.9663927178114,1078.63671295251,
376.408712135129));
#109427=CARTESIAN_POINT('Ctrl Pts',(-76.9687550474511,1078.63936540235,
376.565098207013));
#109428=CARTESIAN_POINT('Ctrl Pts',(-76.9462840670978,1078.64263324409,
376.720862236921));
#109429=CARTESIAN_POINT('Ctrl Pts',(-76.849045006429,1078.65032555411,377.033422833942));
#109430=CARTESIAN_POINT('Ctrl Pts',(-76.7703310052505,1078.65476804806,
377.186613134866));
#109431=CARTESIAN_POINT('Ctrl Pts',(-76.556457741345,1078.66423994707,377.469318337356));
#109432=CARTESIAN_POINT('Ctrl Pts',(-76.4194148317565,1078.66920200388,
377.59380461101));
#109433=CARTESIAN_POINT('Ctrl Pts',(-76.09490818475,1078.67898216859,377.793521966059));
#109434=CARTESIAN_POINT('Ctrl Pts',(-75.9076663876631,1078.6836606122,377.862293621273));
#109435=CARTESIAN_POINT('Ctrl Pts',(-75.638094200845,1078.68929363306,377.903652929645));
#109436=CARTESIAN_POINT('Ctrl Pts',(-75.563147994354,1078.69075015633,377.909343604465));
#109437=CARTESIAN_POINT('Ctrl Pts',(-75.4882582191907,1078.69210669589,
377.909343604465));
#109438=CARTESIAN_POINT('',(-86.2654713137622,1078.38513071259,382.129126937278));
#109439=CARTESIAN_POINT('',(-86.2654713137623,1078.31124838463,379.578238695006));
#109440=CARTESIAN_POINT('Ctrl Pts',(-86.2654713137622,1078.38513071259,
382.129126937278));
#109441=CARTESIAN_POINT('Ctrl Pts',(-86.2621547182598,1078.38531245274,
382.129126937278));
#109442=CARTESIAN_POINT('Ctrl Pts',(-86.2588374878412,1078.38549380858,
382.129114000842));
#109443=CARTESIAN_POINT('Ctrl Pts',(-86.0917677461627,1078.39460656414,
382.127810404116));
#109444=CARTESIAN_POINT('Ctrl Pts',(-85.9297263566369,1078.40242275905,
382.095007511258));
#109445=CARTESIAN_POINT('Ctrl Pts',(-85.6438360470429,1078.41444363147,
381.97684376163));
#109446=CARTESIAN_POINT('Ctrl Pts',(-85.5198491960599,1078.41886952219,
381.898666233538));
#109447=CARTESIAN_POINT('Ctrl Pts',(-85.3396895129841,1078.42398312223,
381.736340881773));
#109448=CARTESIAN_POINT('Ctrl Pts',(-85.2752894839162,1078.42540855029,
381.663436266356));
#109449=CARTESIAN_POINT('Ctrl Pts',(-85.2005866677153,1078.42647054059,
381.556463735536));
#109450=CARTESIAN_POINT('Ctrl Pts',(-85.1824928029337,1078.42666681157,
381.52824781302));
#109451=CARTESIAN_POINT('Ctrl Pts',(-85.1549758939361,1078.42686075099,
381.481370915634));
#109452=CARTESIAN_POINT('Ctrl Pts',(-85.14486345472,1078.42690540145,381.463133765222));
#109453=CARTESIAN_POINT('Ctrl Pts',(-85.1264023958257,1078.42693384648,
381.427826028171));
#109454=CARTESIAN_POINT('Ctrl Pts',(-85.1179792315186,1078.4269227042,381.410800710198));
#109455=CARTESIAN_POINT('Ctrl Pts',(-85.0996305820789,1078.42684091163,
381.371530432162));
#109456=CARTESIAN_POINT('Ctrl Pts',(-85.0899558203568,1078.42675437259,
381.349176585955));
#109457=CARTESIAN_POINT('Ctrl Pts',(-85.0626207109228,1078.42636969245,
381.280702840654));
#109458=CARTESIAN_POINT('Ctrl Pts',(-85.04699321582,1078.42594586249,381.233822948609));
#109459=CARTESIAN_POINT('Ctrl Pts',(-84.9899689914733,1078.42333734463,
381.022628530569));
#109460=CARTESIAN_POINT('Ctrl Pts',(-84.9788404704694,1078.41940782916,
380.851971940393));
#109461=CARTESIAN_POINT('Ctrl Pts',(-85.0196343822102,1078.40909248357,
380.547756161376));
#109462=CARTESIAN_POINT('Ctrl Pts',(-85.0598810465616,1078.4033688104,380.41524168594));
#109463=CARTESIAN_POINT('Ctrl Pts',(-85.1866963815276,1078.38943448825,
380.156840420775));
#109464=CARTESIAN_POINT('Ctrl Pts',(-85.2762164577842,1078.38114900333,
380.034724433226));
#109465=CARTESIAN_POINT('Ctrl Pts',(-85.5018643349163,1078.36251506329,
379.819363290741));
#109466=CARTESIAN_POINT('Ctrl Pts',(-85.6390156033082,1078.35222191958,
379.730984498714));
#109467=CARTESIAN_POINT('Ctrl Pts',(-85.940418487836,1078.33133882896,379.609597495995));
#109468=CARTESIAN_POINT('Ctrl Pts',(-86.1021781226936,1078.32093787104,
379.578238695006));
#109469=CARTESIAN_POINT('Ctrl Pts',(-86.2654713137625,1078.31124838463,
379.578238695006));
#109470=CARTESIAN_POINT('Ctrl Pts',(-86.2654713137625,1078.31124838463,
379.578238695006));
#109471=CARTESIAN_POINT('Ctrl Pts',(-86.265575958347,1078.31124217524,379.578238695006));
#109472=CARTESIAN_POINT('Ctrl Pts',(-86.2656806035614,1078.31123596613,
379.578238707884));
#109473=CARTESIAN_POINT('Ctrl Pts',(-86.2657852494035,1078.31122975733,
379.578238733642));
#109474=CARTESIAN_POINT('Ctrl Pts',(-86.4293026049154,1078.30152800581,
379.578278981526));
#109475=CARTESIAN_POINT('Ctrl Pts',(-86.5913564860174,1078.29272124311,
379.609764341875));
#109476=CARTESIAN_POINT('Ctrl Pts',(-86.8771103923418,1078.27890818754,
379.725167162856));
#109477=CARTESIAN_POINT('Ctrl Pts',(-87.0010080157548,1078.27368093378,
379.801702207554));
#109478=CARTESIAN_POINT('Ctrl Pts',(-87.1845084879564,1078.26743513804,
379.963654487604));
#109479=CARTESIAN_POINT('Ctrl Pts',(-87.2515171654767,1078.26563813562,
380.038514857939));
#109480=CARTESIAN_POINT('Ctrl Pts',(-87.3287326688149,1078.26430944615,
380.148416128401));
#109481=CARTESIAN_POINT('Ctrl Pts',(-87.3472491551574,1078.2640657592,380.177160382035));
#109482=CARTESIAN_POINT('Ctrl Pts',(-87.3753205099728,1078.26382535787,
380.224842683963));
#109483=CARTESIAN_POINT('Ctrl Pts',(-87.3855968713634,1078.26376994913,
380.243335461318));
#109484=CARTESIAN_POINT('Ctrl Pts',(-87.4043122307246,1078.2637340015,380.279080752547));
#109485=CARTESIAN_POINT('Ctrl Pts',(-87.4128308211753,1078.26374701227,
380.2962850005));
#109486=CARTESIAN_POINT('Ctrl Pts',(-87.4313377721645,1078.26384518278,
380.335885408117));
#109487=CARTESIAN_POINT('Ctrl Pts',(-87.4410750434965,1078.26394932319,
380.358390372272));
#109488=CARTESIAN_POINT('Ctrl Pts',(-87.4684632283201,1078.26441083775,
380.427056954226));
#109489=CARTESIAN_POINT('Ctrl Pts',(-87.4840856639928,1078.26491761527,
380.473975241045));
#109490=CARTESIAN_POINT('Ctrl Pts',(-87.5410400556552,1078.26802511368,
380.685231750097));
#109491=CARTESIAN_POINT('Ctrl Pts',(-87.5520988849694,1078.27269527575,
380.855884335518));
#109492=CARTESIAN_POINT('Ctrl Pts',(-87.5112581275218,1078.28461173595,
381.159604267135));
#109493=CARTESIAN_POINT('Ctrl Pts',(-87.4711738678357,1078.29112017793,
381.291665561591));
#109494=CARTESIAN_POINT('Ctrl Pts',(-87.3451063310103,1078.30653492256,
381.549021443521));
#109495=CARTESIAN_POINT('Ctrl Pts',(-87.2562627295294,1078.31548411379,
381.670638991274));
#109496=CARTESIAN_POINT('Ctrl Pts',(-87.0325714922947,1078.33495405235,
381.885231964823));
#109497=CARTESIAN_POINT('Ctrl Pts',(-86.8967577762174,1078.3453682177,381.973509683456));
#109498=CARTESIAN_POINT('Ctrl Pts',(-86.5949453282657,1078.36602661873,
382.096903707261));
#109499=CARTESIAN_POINT('Ctrl Pts',(-86.4309992401525,1078.37606024535,
382.129126937278));
#109500=CARTESIAN_POINT('Ctrl Pts',(-86.2654713137622,1078.38513071259,
382.129126937278));
#109501=CARTESIAN_POINT('',(-97.7222027015963,1077.70670509264,387.660380419275));
#109502=CARTESIAN_POINT('',(-97.7222027015963,1077.62441341004,385.46271814729));
#109503=CARTESIAN_POINT('Ctrl Pts',(-97.7222027015964,1077.70670509264,
387.660380419275));
#109504=CARTESIAN_POINT('Ctrl Pts',(-97.7124019766386,1077.70763427451,
387.660380419275));
#109505=CARTESIAN_POINT('Ctrl Pts',(-97.7025952568283,1077.70855872694,
387.660249297581));
#109506=CARTESIAN_POINT('Ctrl Pts',(-97.5502098697314,1077.72284132834,
387.656168217868));
#109507=CARTESIAN_POINT('Ctrl Pts',(-97.4096043505871,1077.73489851245,
387.624623763402));
#109508=CARTESIAN_POINT('Ctrl Pts',(-97.169800320246,1077.75347129077,387.518884174392));
#109509=CARTESIAN_POINT('Ctrl Pts',(-97.0691998068531,1077.76045188173,
387.453327295383));
#109510=CARTESIAN_POINT('Ctrl Pts',(-96.8984417573925,1077.77065894042,
387.29732888491));
#109511=CARTESIAN_POINT('Ctrl Pts',(-96.8277980615754,1077.77403230899,
387.209634913951));
#109512=CARTESIAN_POINT('Ctrl Pts',(-96.7560163049699,1077.77621092385,
387.085839992693));
#109513=CARTESIAN_POINT('Ctrl Pts',(-96.7415657066971,1077.77655464824,
387.058286804692));
#109514=CARTESIAN_POINT('Ctrl Pts',(-96.7206548707728,1077.77689079151,
387.013935641314));
#109515=CARTESIAN_POINT('Ctrl Pts',(-96.7134051313894,1077.77697027794,
386.997529731309));
#109516=CARTESIAN_POINT('Ctrl Pts',(-96.7013379606228,1077.77703368949,
386.968307491944));
#109517=CARTESIAN_POINT('Ctrl Pts',(-96.6963524665975,1077.77703579725,
386.955564962614));
#109518=CARTESIAN_POINT('Ctrl Pts',(-96.6855323263409,1077.77698284554,
386.926310805474));
#109519=CARTESIAN_POINT('Ctrl Pts',(-96.6798518570805,1077.7769116381,386.909746268716));
#109520=CARTESIAN_POINT('Ctrl Pts',(-96.6655000873494,1077.77660560169,
386.864391191729));
#109521=CARTESIAN_POINT('Ctrl Pts',(-96.6576109506054,1077.77629020174,
386.8353701896));
#109522=CARTESIAN_POINT('Ctrl Pts',(-96.6255902928541,1077.77419968886,
386.695079361964));
#109523=CARTESIAN_POINT('Ctrl Pts',(-96.6176693844983,1077.77082064868,
386.580878045216));
#109524=CARTESIAN_POINT('Ctrl Pts',(-96.6369579713206,1077.76091279066,
386.356221646851));
#109525=CARTESIAN_POINT('Ctrl Pts',(-96.6634347193482,1077.75449907891,
386.247079266533));
#109526=CARTESIAN_POINT('Ctrl Pts',(-96.7530886076295,1077.73818158454,
386.028921411652));
#109527=CARTESIAN_POINT('Ctrl Pts',(-96.8194458346927,1077.728081044,385.922914334021));
#109528=CARTESIAN_POINT('Ctrl Pts',(-96.9915923964205,1077.70471525454,
385.729829840551));
#109529=CARTESIAN_POINT('Ctrl Pts',(-97.0988197627813,1077.69144658987,
385.646725366817));
#109530=CARTESIAN_POINT('Ctrl Pts',(-97.294594857691,1077.66893024175,385.545699458093));
#109531=CARTESIAN_POINT('Ctrl Pts',(-97.3752307887054,1077.66003850054,
385.515409278508));
#109532=CARTESIAN_POINT('Ctrl Pts',(-97.5448000331111,1077.64207747447,
385.473500987036));
#109533=CARTESIAN_POINT('Ctrl Pts',(-97.6333258257655,1077.63307625427,
385.46271814729));
#109534=CARTESIAN_POINT('Ctrl Pts',(-97.7222027015963,1077.62441341004,
385.46271814729));
#109535=CARTESIAN_POINT('Ctrl Pts',(-97.7222027015963,1077.62441341004,
385.46271814729));
#109536=CARTESIAN_POINT('Ctrl Pts',(-97.722261074218,1077.62440772045,385.46271814729));
#109537=CARTESIAN_POINT('Ctrl Pts',(-97.7223194469913,1077.624402031,385.462718151941));
#109538=CARTESIAN_POINT('Ctrl Pts',(-97.7223778199155,1077.62439634171,
385.462718161244));
#109539=CARTESIAN_POINT('Ctrl Pts',(-97.8652491765215,1077.61047143409,
385.46274093034));
#109540=CARTESIAN_POINT('Ctrl Pts',(-98.0068781946763,1077.59763002745,
385.490628024508));
#109541=CARTESIAN_POINT('Ctrl Pts',(-98.2526251510877,1077.57726326324,
385.591451297604));
#109542=CARTESIAN_POINT('Ctrl Pts',(-98.3574907158762,1077.56938264513,
385.656619489785));
#109543=CARTESIAN_POINT('Ctrl Pts',(-98.5370654765183,1077.5576776994,385.815171509941));
#109544=CARTESIAN_POINT('Ctrl Pts',(-98.6118031717629,1077.55375460098,
385.906018887543));
#109545=CARTESIAN_POINT('Ctrl Pts',(-98.6868907005084,1077.55125604196,
386.03446325289));
#109546=CARTESIAN_POINT('Ctrl Pts',(-98.7017513784915,1077.55086778311,
386.062623199424));
#109547=CARTESIAN_POINT('Ctrl Pts',(-98.723157013672,1077.55048929991,386.107840569333));
#109548=CARTESIAN_POINT('Ctrl Pts',(-98.7305347775942,1077.55039988931,
386.124482269751));
#109549=CARTESIAN_POINT('Ctrl Pts',(-98.743363360559,1077.55032428065,386.155475219288));
#109550=CARTESIAN_POINT('Ctrl Pts',(-98.7489333442791,1077.55032408311,
386.169772019185));
#109551=CARTESIAN_POINT('Ctrl Pts',(-98.7604385844994,1077.55039873531,
386.201235696041));
#109552=CARTESIAN_POINT('Ctrl Pts',(-98.7662512061097,1077.55048736267,
386.218442399869));
#109553=CARTESIAN_POINT('Ctrl Pts',(-98.7812747190916,1077.55086882648,
386.266839833452));
#109554=CARTESIAN_POINT('Ctrl Pts',(-98.7895309779033,1077.5512675288,386.298305466541));
#109555=CARTESIAN_POINT('Ctrl Pts',(-98.8256759340566,1077.55417681907,
386.466049416065));
#109556=CARTESIAN_POINT('Ctrl Pts',(-98.8288759317787,1077.55930119417,
386.60624802771));
#109557=CARTESIAN_POINT('Ctrl Pts',(-98.7868430036914,1077.57316200743,
386.856958875455));
#109558=CARTESIAN_POINT('Ctrl Pts',(-98.7500125751257,1077.58104749303,
386.96687578604));
#109559=CARTESIAN_POINT('Ctrl Pts',(-98.6383089138675,1077.60028660184,
387.1814278163));
#109560=CARTESIAN_POINT('Ctrl Pts',(-98.5607974191268,1077.61176563041,
387.282805400229));
#109561=CARTESIAN_POINT('Ctrl Pts',(-98.3674509235807,1077.63739387053,
387.46141342537));
#109562=CARTESIAN_POINT('Ctrl Pts',(-98.2506919031589,1077.65146471467,
387.534575124751));
#109563=CARTESIAN_POINT('Ctrl Pts',(-97.9956721116306,1077.67973475138,
387.63463744473));
#109564=CARTESIAN_POINT('Ctrl Pts',(-97.8595260274799,1077.69368581638,
387.660380419275));
#109565=CARTESIAN_POINT('Ctrl Pts',(-97.7222027015963,1077.70670509264,
387.660380419275));
#109566=CARTESIAN_POINT('',(-107.832717977552,1076.85914687694,395.502558371549));
#109567=CARTESIAN_POINT('',(-107.832717977553,1076.78013798525,393.321476874093));
#109568=CARTESIAN_POINT('Ctrl Pts',(-107.832717977554,1076.85914687694,
395.502558371549));
#109569=CARTESIAN_POINT('Ctrl Pts',(-107.743834231058,1076.87056475884,
395.502558371549));
#109570=CARTESIAN_POINT('Ctrl Pts',(-107.655018492996,1076.88154915174,
395.491691901226));
#109571=CARTESIAN_POINT('Ctrl Pts',(-107.43387654173,1076.90781939257,395.436417944525));
#109572=CARTESIAN_POINT('Ctrl Pts',(-107.306890784662,1076.92186348896,
395.377469040284));
#109573=CARTESIAN_POINT('Ctrl Pts',(-107.093476636667,1076.94345094462,
395.223342404524));
#109574=CARTESIAN_POINT('Ctrl Pts',(-107.005777038169,1076.95136409676,
395.133798552405));
#109575=CARTESIAN_POINT('Ctrl Pts',(-106.89253177196,1076.95985669707,394.969631173146));
#109576=CARTESIAN_POINT('Ctrl Pts',(-106.856466274116,1076.96207863835,
394.903773857406));
#109577=CARTESIAN_POINT('Ctrl Pts',(-106.817521811368,1076.96371792518,
394.811153097107));
#109578=CARTESIAN_POINT('Ctrl Pts',(-106.80844590849,1076.96401800765,394.787249893623));
#109579=CARTESIAN_POINT('Ctrl Pts',(-106.795113727036,1076.96431392295,
394.748035464688));
#109580=CARTESIAN_POINT('Ctrl Pts',(-106.790337528235,1076.96438197428,
394.732912596409));
#109581=CARTESIAN_POINT('Ctrl Pts',(-106.781848225682,1076.96442545441,
394.703839658075));
#109582=CARTESIAN_POINT('Ctrl Pts',(-106.778079011649,1076.96440866751,
394.689909663929));
#109583=CARTESIAN_POINT('Ctrl Pts',(-106.770110157312,1076.96428478801,
394.657956786525));
#109584=CARTESIAN_POINT('Ctrl Pts',(-106.766090668207,1076.96415356652,
394.639893917074));
#109585=CARTESIAN_POINT('Ctrl Pts',(-106.755297954521,1076.96356896599,
394.584819605243));
#109586=CARTESIAN_POINT('Ctrl Pts',(-106.749979223518,1076.96292323385,
394.547555752335));
#109587=CARTESIAN_POINT('Ctrl Pts',(-106.733593452344,1076.95857768857,
394.366099626876));
#109588=CARTESIAN_POINT('Ctrl Pts',(-106.749367551661,1076.95146361364,
394.221115678595));
#109589=CARTESIAN_POINT('Ctrl Pts',(-106.827870156943,1076.93270635441,
393.972584113405));
#109590=CARTESIAN_POINT('Ctrl Pts',(-106.880405833519,1076.92232831509,
393.868095912839));
#109591=CARTESIAN_POINT('Ctrl Pts',(-107.023109630229,1076.89710299884,
393.670291014135));
#109592=CARTESIAN_POINT('Ctrl Pts',(-107.115459687654,1076.88210154595,
393.580703815282));
#109593=CARTESIAN_POINT('Ctrl Pts',(-107.311016879167,1076.85224750454,
393.448212750265));
#109594=CARTESIAN_POINT('Ctrl Pts',(-107.409560626406,1076.83785959358,
393.401074093128));
#109595=CARTESIAN_POINT('Ctrl Pts',(-107.616839334652,1076.80877365399,
393.337595562981));
#109596=CARTESIAN_POINT('Ctrl Pts',(-107.72446400748,1076.79422752107,393.321476874092));
#109597=CARTESIAN_POINT('Ctrl Pts',(-107.832717977553,1076.78013798525,
393.321476874092));
#109598=CARTESIAN_POINT('Ctrl Pts',(-107.832717977553,1076.78013798525,
393.321476874092));
#109599=CARTESIAN_POINT('Ctrl Pts',(-107.832801593366,1076.78012710243,
393.321476874092));
#109600=CARTESIAN_POINT('Ctrl Pts',(-107.832885209555,1076.78011621989,
393.321476883709));
#109601=CARTESIAN_POINT('Ctrl Pts',(-107.832968826119,1076.78010533762,
393.321476902943));
#109602=CARTESIAN_POINT('Ctrl Pts',(-107.976290564888,1076.76145274409,
393.321509870123));
#109603=CARTESIAN_POINT('Ctrl Pts',(-108.118396783563,1076.74390205806,
393.349796213408));
#109604=CARTESIAN_POINT('Ctrl Pts',(-108.371790543568,1076.71452021206,
393.455063317854));
#109605=CARTESIAN_POINT('Ctrl Pts',(-108.48268278115,1076.70255142369,393.526573111447));
#109606=CARTESIAN_POINT('Ctrl Pts',(-108.679563846868,1076.68339274454,
393.711040992627));
#109607=CARTESIAN_POINT('Ctrl Pts',(-108.761872786949,1076.67670331073,
393.824419531492));
#109608=CARTESIAN_POINT('Ctrl Pts',(-108.833425645152,1076.67291107488,
393.977547250601));
#109609=CARTESIAN_POINT('Ctrl Pts',(-108.845007144768,1076.67240572431,
394.005260532755));
#109610=CARTESIAN_POINT('Ctrl Pts',(-108.861958279561,1076.67185991099,
394.051050854009));
#109611=CARTESIAN_POINT('Ctrl Pts',(-108.868028528609,1076.67171637715,
394.068848988473));
#109612=CARTESIAN_POINT('Ctrl Pts',(-108.877981436976,1076.67158017808,
394.100704645584));
#109613=CARTESIAN_POINT('Ctrl Pts',(-108.882047932659,1076.67156084976,
394.114699410081));
#109614=CARTESIAN_POINT('Ctrl Pts',(-108.889968783515,1076.67160443275,
394.144149296745));
#109615=CARTESIAN_POINT('Ctrl Pts',(-108.893767425531,1076.67167513526,
394.159615633152));
#109616=CARTESIAN_POINT('Ctrl Pts',(-108.902759865924,1076.67198347169,
394.200030212478));
#109617=CARTESIAN_POINT('Ctrl Pts',(-108.907420116095,1076.67229571535,
394.225085892644));
#109618=CARTESIAN_POINT('Ctrl Pts',(-108.92319796496,1076.67410833811,394.330294146571));
#109619=CARTESIAN_POINT('Ctrl Pts',(-108.926250240401,1076.67670988062,
394.41135717249));
#109620=CARTESIAN_POINT('Ctrl Pts',(-108.912699057437,1076.68532792927,
394.595688063361));
#109621=CARTESIAN_POINT('Ctrl Pts',(-108.890287560378,1076.69206260374,
394.697665693222));
#109622=CARTESIAN_POINT('Ctrl Pts',(-108.812358953408,1076.71000823363,
394.905534729815));
#109623=CARTESIAN_POINT('Ctrl Pts',(-108.7531963639,1076.72158961181,395.008588695904));
#109624=CARTESIAN_POINT('Ctrl Pts',(-108.597337520389,1076.74906138808,
395.200252715122));
#109625=CARTESIAN_POINT('Ctrl Pts',(-108.498801915667,1076.76504418789,
395.285067420751));
#109626=CARTESIAN_POINT('Ctrl Pts',(-108.268111950518,1076.80003416511,
395.421511062668));
#109627=CARTESIAN_POINT('Ctrl Pts',(-108.135891714292,1076.81887756447,
395.468767126857));
#109628=CARTESIAN_POINT('Ctrl Pts',(-107.943459073455,1076.84475656851,
395.498343392934));
#109629=CARTESIAN_POINT('Ctrl Pts',(-107.888075329727,1076.85203574881,
395.502558371549));
#109630=CARTESIAN_POINT('Ctrl Pts',(-107.832717977554,1076.85914687694,
395.502558371549));
#109631=CARTESIAN_POINT('',(-69.482552265803,1076.93351373127,337.889334626622));
#109632=CARTESIAN_POINT('',(-69.4825522658041,1076.7038426352,335.708253129166));
#109633=CARTESIAN_POINT('Ctrl Pts',(-69.482552265803,1076.93351373127,337.889334626623));
#109634=CARTESIAN_POINT('Ctrl Pts',(-69.4806455417213,1076.93366952156,
337.889334626623));
#109635=CARTESIAN_POINT('Ctrl Pts',(-69.4787385413302,1076.93382481149,
337.88932962599));
#109636=CARTESIAN_POINT('Ctrl Pts',(-69.346539373702,1076.94455372551,337.888636098955));
#109637=CARTESIAN_POINT('Ctrl Pts',(-69.2172598274196,1076.95260563072,
337.864606939716));
#109638=CARTESIAN_POINT('Ctrl Pts',(-69.0345323697271,1076.96033080558,
337.795169885668));
#109639=CARTESIAN_POINT('Ctrl Pts',(-68.9760522862653,1076.96216490022,
337.766755690126));
#109640=CARTESIAN_POINT('Ctrl Pts',(-68.8973961547121,1076.96369723422,
337.719442570328));
#109641=CARTESIAN_POINT('Ctrl Pts',(-68.8748805788767,1076.96401668702,
337.704739224455));
#109642=CARTESIAN_POINT('Ctrl Pts',(-68.8394767011401,1076.9643223835,337.679705018433));
#109643=CARTESIAN_POINT('Ctrl Pts',(-68.8262403690781,1076.96438970002,
337.669888204085));
#109644=CARTESIAN_POINT('Ctrl Pts',(-68.7993083603979,1076.96442783121,
337.64895144849));
#109645=CARTESIAN_POINT('Ctrl Pts',(-68.7856499918525,1076.96439152641,
337.637791696533));
#109646=CARTESIAN_POINT('Ctrl Pts',(-68.7544788172581,1076.96417654368,
337.611036330553));
#109647=CARTESIAN_POINT('Ctrl Pts',(-68.7371870016368,1076.96395496774,
337.595197846194));
#109648=CARTESIAN_POINT('Ctrl Pts',(-68.6843380719293,1076.96294595699,
337.543560937507));
#109649=CARTESIAN_POINT('Ctrl Pts',(-68.6507533009033,1076.96180204728,
337.505852781911));
#109650=CARTESIAN_POINT('Ctrl Pts',(-68.5315759500406,1076.95565567046,
337.351757260213));
#109651=CARTESIAN_POINT('Ctrl Pts',(-68.466915680369,1076.94750167682,337.221291751667));
#109652=CARTESIAN_POINT('Ctrl Pts',(-68.3985533178926,1076.92686613888,
336.967288790625));
#109653=CARTESIAN_POINT('Ctrl Pts',(-68.3866862445795,1076.91552301861,
336.848236154612));
#109654=CARTESIAN_POINT('Ctrl Pts',(-68.4024228070353,1076.88846032279,
336.600061187796));
#109655=CARTESIAN_POINT('Ctrl Pts',(-68.4337617413244,1076.87263894941,
336.473011315067));
#109656=CARTESIAN_POINT('Ctrl Pts',(-68.54369542598,1076.83773329672,336.22653119835));
#109657=CARTESIAN_POINT('Ctrl Pts',(-68.6249506262102,1076.81879473621,
336.110727338302));
#109658=CARTESIAN_POINT('Ctrl Pts',(-68.8156040935837,1076.78344761007,
335.927019151369));
#109659=CARTESIAN_POINT('Ctrl Pts',(-68.9195814222719,1076.76723515419,
335.856497108887));
#109660=CARTESIAN_POINT('Ctrl Pts',(-69.0976118141404,1076.74366830961,
335.776014237312));
#109661=CARTESIAN_POINT('Ctrl Pts',(-69.1646226245242,1076.73558050823,
335.753234972091));
#109662=CARTESIAN_POINT('Ctrl Pts',(-69.3149948320073,1076.71909341971,
335.717949458206));
#109663=CARTESIAN_POINT('Ctrl Pts',(-69.3985893007012,1076.71096940083,
335.708253129166));
#109664=CARTESIAN_POINT('Ctrl Pts',(-69.4825522658041,1076.7038426352,335.708253129166));
#109665=CARTESIAN_POINT('Ctrl Pts',(-69.4825522658041,1076.7038426352,335.708253129166));
#109666=CARTESIAN_POINT('Ctrl Pts',(-69.4825705531623,1076.70384108297,
335.708253129166));
#109667=CARTESIAN_POINT('Ctrl Pts',(-69.4825888405381,1076.70383953079,
335.708253129627));
#109668=CARTESIAN_POINT('Ctrl Pts',(-69.4826071279312,1076.70383797866,
335.708253130547));
#109669=CARTESIAN_POINT('Ctrl Pts',(-69.6122661348406,1076.6928332308,335.708259653337));
#109670=CARTESIAN_POINT('Ctrl Pts',(-69.7410600097854,1076.68435586556,
335.731389570645));
#109671=CARTESIAN_POINT('Ctrl Pts',(-69.9252515962546,1076.67604353777,
335.799932842917));
#109672=CARTESIAN_POINT('Ctrl Pts',(-69.9853773394517,1076.6740281655,335.828804479751));
#109673=CARTESIAN_POINT('Ctrl Pts',(-70.065966362588,1076.67235332251,335.877027030626));
#109674=CARTESIAN_POINT('Ctrl Pts',(-70.0888852300184,1076.67200602789,
335.891938511393));
#109675=CARTESIAN_POINT('Ctrl Pts',(-70.1248349067323,1076.67167395913,
335.917300983904));
#109676=CARTESIAN_POINT('Ctrl Pts',(-70.1382271237482,1076.67160062707,
335.927216453134));
#109677=CARTESIAN_POINT('Ctrl Pts',(-70.1654173135824,1076.67155755917,
335.948329307373));
#109678=CARTESIAN_POINT('Ctrl Pts',(-70.1791791775886,1076.67159500239,
335.959564711252));
#109679=CARTESIAN_POINT('Ctrl Pts',(-70.2104970271546,1076.67182050406,
335.986434420972));
#109680=CARTESIAN_POINT('Ctrl Pts',(-70.2278335388946,1076.67205325274,
336.002309611403));
#109681=CARTESIAN_POINT('Ctrl Pts',(-70.2805374697881,1076.673108753,336.053799314351));
#109682=CARTESIAN_POINT('Ctrl Pts',(-70.3139607991339,1076.67430003511,
336.091294821934));
#109683=CARTESIAN_POINT('Ctrl Pts',(-70.4330963815764,1076.6807143756,336.24508761985));
#109684=CARTESIAN_POINT('Ctrl Pts',(-70.49784937384,1076.68924147617,336.375489895875));
#109685=CARTESIAN_POINT('Ctrl Pts',(-70.5663202198497,1076.7106436688,336.629068129207));
#109686=CARTESIAN_POINT('Ctrl Pts',(-70.5783051280181,1076.72234154244,
336.747740675396));
#109687=CARTESIAN_POINT('Ctrl Pts',(-70.5630714656046,1076.75002812789,
336.995035830317));
#109688=CARTESIAN_POINT('Ctrl Pts',(-70.5321877705488,1076.76610070584,
337.121631978629));
#109689=CARTESIAN_POINT('Ctrl Pts',(-70.423597839457,1076.80122695084,337.367252835835));
#109690=CARTESIAN_POINT('Ctrl Pts',(-70.3433102000216,1076.82011050786,
337.482752026317));
#109691=CARTESIAN_POINT('Ctrl Pts',(-70.1397833686064,1076.8578278015,337.680994956384));
#109692=CARTESIAN_POINT('Ctrl Pts',(-70.0169048613728,1076.87627974686,
337.760452494493));
#109693=CARTESIAN_POINT('Ctrl Pts',(-69.7549067552893,1076.90856542224,
337.863563967587));
#109694=CARTESIAN_POINT('Ctrl Pts',(-69.619441594183,1076.92232908849,337.889334626623));
#109695=CARTESIAN_POINT('Ctrl Pts',(-69.482552265803,1076.93351373127,337.889334626623));
#109696=CARTESIAN_POINT('',(-56.6885840720973,1077.75968243012,337.489274485682));
#109697=CARTESIAN_POINT('',(-56.6885840720974,1077.56894342885,335.291612213697));
#109698=CARTESIAN_POINT('Ctrl Pts',(-56.6885840720972,1077.75968243012,
337.489274485682));
#109699=CARTESIAN_POINT('Ctrl Pts',(-56.613442812984,1077.76373623307,337.489274485682));
#109700=CARTESIAN_POINT('Ctrl Pts',(-56.5383276565235,1077.7671323857,337.481566998586));
#109701=CARTESIAN_POINT('Ctrl Pts',(-56.3865521884614,1077.77264390424,
337.449940841078));
#109702=CARTESIAN_POINT('Ctrl Pts',(-56.3106458623279,1077.77465802433,
337.425299584034));
#109703=CARTESIAN_POINT('Ctrl Pts',(-56.2097428198071,1077.77628305086,
337.379940323458));
#109704=CARTESIAN_POINT('Ctrl Pts',(-56.1819845595998,1077.77660965807,
337.366020258967));
#109705=CARTESIAN_POINT('Ctrl Pts',(-56.1369653440164,1077.77693575642,
337.341003898954));
#109706=CARTESIAN_POINT('Ctrl Pts',(-56.1193598203174,1077.77700872447,
337.330566929611));
#109707=CARTESIAN_POINT('Ctrl Pts',(-56.0856173841726,1077.7770405101,337.309268104186));
#109708=CARTESIAN_POINT('Ctrl Pts',(-56.0694572267866,1077.77700484843,
337.298457500082));
#109709=CARTESIAN_POINT('Ctrl Pts',(-56.0323218691688,1077.77680172933,
337.272162730304));
#109710=CARTESIAN_POINT('Ctrl Pts',(-56.0115944661511,1077.77659357258,
337.256349892332));
#109711=CARTESIAN_POINT('Ctrl Pts',(-55.9476021541347,1077.77564178804,
337.203827277157));
#109712=CARTESIAN_POINT('Ctrl Pts',(-55.9066136065438,1077.77455785302,
337.164502756248));
#109713=CARTESIAN_POINT('Ctrl Pts',(-55.7718866054966,1077.76918085393,
337.01357711742));
#109714=CARTESIAN_POINT('Ctrl Pts',(-55.6975501542133,1077.76257803684,
336.886849074861));
#109715=CARTESIAN_POINT('Ctrl Pts',(-55.6104673649987,1077.74608591605,
336.634930365164));
#109716=CARTESIAN_POINT('Ctrl Pts',(-55.5901268619979,1077.73704060687,
336.514756146664));
#109717=CARTESIAN_POINT('Ctrl Pts',(-55.589356343351,1077.71560543996,336.26204679572));
#109718=CARTESIAN_POINT('Ctrl Pts',(-55.6126508740519,1077.70315950819,
336.131390238009));
#109719=CARTESIAN_POINT('Ctrl Pts',(-55.7077875383169,1077.67583059169,
335.875101844607));
#109720=CARTESIAN_POINT('Ctrl Pts',(-55.7824013406094,1077.66108014764,
335.752977937319));
#109721=CARTESIAN_POINT('Ctrl Pts',(-55.9672709205554,1077.63306107873,
335.551063375541));
#109722=CARTESIAN_POINT('Ctrl Pts',(-56.0732663837531,1077.61998074431,
335.470512491792));
#109723=CARTESIAN_POINT('Ctrl Pts',(-56.2594731817596,1077.60103232,335.375959466957));
#109724=CARTESIAN_POINT('Ctrl Pts',(-56.3313515194324,1077.59449180072,
335.348468860971));
#109725=CARTESIAN_POINT('Ctrl Pts',(-56.4978156201092,1077.58102251536,
335.304093553933));
#109726=CARTESIAN_POINT('Ctrl Pts',(-56.5929620084085,1077.57444466517,
335.291612213697));
#109727=CARTESIAN_POINT('Ctrl Pts',(-56.6885840720975,1077.56894342885,
335.291612213697));
#109728=CARTESIAN_POINT('Ctrl Pts',(-56.6885840720975,1077.56894342885,
335.291612213697));
#109729=CARTESIAN_POINT('Ctrl Pts',(-56.6886054837368,1077.56894219702,
335.291612213697));
#109730=CARTESIAN_POINT('Ctrl Pts',(-56.6886268953997,1077.56894096524,
335.291612214276));
#109731=CARTESIAN_POINT('Ctrl Pts',(-56.6886483070866,1077.56893973351,
335.291612215528));
#109732=CARTESIAN_POINT('Ctrl Pts',(-56.8261524989056,1077.56102968588,
335.291620253694));
#109733=CARTESIAN_POINT('Ctrl Pts',(-56.9625358482213,1077.55546902066,
335.317438268971));
#109734=CARTESIAN_POINT('Ctrl Pts',(-57.1275010395179,1077.55176827106,
335.382302884576));
#109735=CARTESIAN_POINT('Ctrl Pts',(-57.1635167452176,1077.55116664873,
335.398760540504));
#109736=CARTESIAN_POINT('Ctrl Pts',(-57.2187492407822,1077.55057716798,
335.427700492683));
#109737=CARTESIAN_POINT('Ctrl Pts',(-57.2385961998946,1077.55043734646,
335.438899543604));
#109738=CARTESIAN_POINT('Ctrl Pts',(-57.274532934087,1077.55031926313,335.460677859578));
#109739=CARTESIAN_POINT('Ctrl Pts',(-57.2907201865981,1077.55031926237,
335.471078332917));
#109740=CARTESIAN_POINT('Ctrl Pts',(-57.3254407128916,1077.55043726238,
335.49469713275));
#109741=CARTESIAN_POINT('Ctrl Pts',(-57.3438528839117,1077.55057681396,
335.508076981979));
#109742=CARTESIAN_POINT('Ctrl Pts',(-57.3938617433937,1077.55117448315,
335.546846668709));
#109743=CARTESIAN_POINT('Ctrl Pts',(-57.4244866662291,1077.55179580614,
335.573425151543));
#109744=CARTESIAN_POINT('Ctrl Pts',(-57.5580740842792,1077.55572990302,
335.702977760875));
#109745=CARTESIAN_POINT('Ctrl Pts',(-57.6413195462532,1077.56180608728,
335.824003580477));
#109746=CARTESIAN_POINT('Ctrl Pts',(-57.7450845616833,1077.57750963289,
336.066133436293));
#109747=CARTESIAN_POINT('Ctrl Pts',(-57.7737586136471,1077.58615022061,
336.181350369018));
#109748=CARTESIAN_POINT('Ctrl Pts',(-57.7943339688813,1077.606809626,336.427227303112));
#109749=CARTESIAN_POINT('Ctrl Pts',(-57.7824003765923,1077.61890859438,
336.556442315922));
#109750=CARTESIAN_POINT('Ctrl Pts',(-57.7118296547517,1077.64552330391,
336.814246723941));
#109751=CARTESIAN_POINT('Ctrl Pts',(-57.6502753482028,1077.65992134601,
336.939788007474));
#109752=CARTESIAN_POINT('Ctrl Pts',(-57.4794403334006,1077.68910347425,
337.167126248791));
#109753=CARTESIAN_POINT('Ctrl Pts',(-57.36946577095,1077.70358920761,337.2651649272));
#109754=CARTESIAN_POINT('Ctrl Pts',(-57.1215703856538,1077.72954462121,
337.410197946034));
#109755=CARTESIAN_POINT('Ctrl Pts',(-56.9869411183763,1077.74086153681,
337.457417069255));
#109756=CARTESIAN_POINT('Ctrl Pts',(-56.7944096421122,1077.75364784999,
337.485453510447));
#109757=CARTESIAN_POINT('Ctrl Pts',(-56.7414903885327,1077.75682818221,
337.489274485682));
#109758=CARTESIAN_POINT('Ctrl Pts',(-56.6885840720972,1077.75968243012,
337.489274485682));
#109759=CARTESIAN_POINT('',(-44.0648939479108,1078.41872688014,339.782224246531));
#109760=CARTESIAN_POINT('',(-44.0648939479107,1078.2734328653,337.231336004259));
#109761=CARTESIAN_POINT('Ctrl Pts',(-44.0648939479108,1078.41872688014,
339.782224246531));
#109762=CARTESIAN_POINT('Ctrl Pts',(-43.9698585685592,1078.42127600878,
339.782224246531));
#109763=CARTESIAN_POINT('Ctrl Pts',(-43.8748911966279,1078.42325397626,
339.771602237811));
#109764=CARTESIAN_POINT('Ctrl Pts',(-43.7242121194281,1078.42547969287,
339.737300270294));
#109765=CARTESIAN_POINT('Ctrl Pts',(-43.667617845379,1078.42609562414,339.720211708276));
#109766=CARTESIAN_POINT('Ctrl Pts',(-43.5837314112947,1078.42667110235,
339.688381229543));
#109767=CARTESIAN_POINT('Ctrl Pts',(-43.5554548940477,1078.4268036277,339.676468305807));
#109768=CARTESIAN_POINT('Ctrl Pts',(-43.5053435987973,1078.42692639709,
339.653194195071));
#109769=CARTESIAN_POINT('Ctrl Pts',(-43.4833559077857,1078.42693965325,
339.642198692177));
#109770=CARTESIAN_POINT('Ctrl Pts',(-43.4373976527315,1078.42687999769,
339.617530701329));
#109771=CARTESIAN_POINT('Ctrl Pts',(-43.4135252695797,1078.42679637772,
339.603701849644));
#109772=CARTESIAN_POINT('Ctrl Pts',(-43.3515726057863,1078.42643740777,
339.565077738407));
#109773=CARTESIAN_POINT('Ctrl Pts',(-43.31433734979,1078.4260732985,339.539003823256));
#109774=CARTESIAN_POINT('Ctrl Pts',(-43.1618656252936,1078.42392496087,
339.419615998369));
#109775=CARTESIAN_POINT('Ctrl Pts',(-43.0620000515213,1078.42081136629,
339.308600827055));
#109776=CARTESIAN_POINT('Ctrl Pts',(-42.9117761736833,1078.41221921664,
339.068342403409));
#109777=CARTESIAN_POINT('Ctrl Pts',(-42.8588046707743,1078.40702463369,
338.943083927874));
#109778=CARTESIAN_POINT('Ctrl Pts',(-42.7910566805472,1078.39413187769,
338.668107998734));
#109779=CARTESIAN_POINT('Ctrl Pts',(-42.7809529005184,1078.38633677174,
338.519289117061));
#109780=CARTESIAN_POINT('Ctrl Pts',(-42.8134108370878,1078.36855139611,
338.213583100402));
#109781=CARTESIAN_POINT('Ctrl Pts',(-42.8598155164218,1078.35859085684,
338.059631555308));
#109782=CARTESIAN_POINT('Ctrl Pts',(-43.0113674875638,1078.33755056151,
337.768252159249));
#109783=CARTESIAN_POINT('Ctrl Pts',(-43.1184390201791,1078.32664465516,
337.635244041802));
#109784=CARTESIAN_POINT('Ctrl Pts',(-43.3444784264674,1078.30872444725,
337.446864562296));
#109785=CARTESIAN_POINT('Ctrl Pts',(-43.4519113159758,1078.30153381717,
337.381308044457));
#109786=CARTESIAN_POINT('Ctrl Pts',(-43.6363565982265,1078.29115440135,
337.303137310967));
#109787=CARTESIAN_POINT('Ctrl Pts',(-43.7079861960549,1078.28753594555,
337.279986987218));
#109788=CARTESIAN_POINT('Ctrl Pts',(-43.874283065922,1078.28006182476,337.242054582449));
#109789=CARTESIAN_POINT('Ctrl Pts',(-43.9694259521163,1078.2764294892,337.231336100891));
#109790=CARTESIAN_POINT('Ctrl Pts',(-44.0648926569059,1078.27343290582,
337.23133600426));
#109791=CARTESIAN_POINT('Ctrl Pts',(-44.0648939479107,1078.2734328653,337.231336004259));
#109792=CARTESIAN_POINT('Ctrl Pts',(-44.1880047205763,1078.26956857586,
337.231336004259));
#109793=CARTESIAN_POINT('Ctrl Pts',(-44.3104925612769,1078.26679899349,
337.249160351226));
#109794=CARTESIAN_POINT('Ctrl Pts',(-44.4706067741549,1078.26467963642,
337.296788011882));
#109795=CARTESIAN_POINT('Ctrl Pts',(-44.5120000439969,1078.26427737102,
337.311464184729));
#109796=CARTESIAN_POINT('Ctrl Pts',(-44.5778875498776,1078.26387835467,
337.338727532798));
#109797=CARTESIAN_POINT('Ctrl Pts',(-44.6028752707143,1078.2637861645,337.350023706425));
#109798=CARTESIAN_POINT('Ctrl Pts',(-44.6498772982532,1078.26372736808,
337.373124526043));
#109799=CARTESIAN_POINT('Ctrl Pts',(-44.6719469510812,1078.263750252,337.384787619108));
#109800=CARTESIAN_POINT('Ctrl Pts',(-44.7213912479415,1078.26391818437,
337.412803476177));
#109801=CARTESIAN_POINT('Ctrl Pts',(-44.7485231994662,1078.26409527662,
337.429550065953));
#109802=CARTESIAN_POINT('Ctrl Pts',(-44.8279209712877,1078.26487350374,
337.482765306169));
#109803=CARTESIAN_POINT('Ctrl Pts',(-44.8781074114896,1078.26572049452,
337.522148538001));
#109804=CARTESIAN_POINT('Ctrl Pts',(-45.0507228634677,1078.26999963111,
337.679838407417));
#109805=CARTESIAN_POINT('Ctrl Pts',(-45.1520505367577,1078.27534679267,
337.818491183739));
#109806=CARTESIAN_POINT('Ctrl Pts',(-45.2819458029642,1078.28844897224,
338.100293223211));
#109807=CARTESIAN_POINT('Ctrl Pts',(-45.3192348827645,1078.29552830067,
338.236503697566));
#109808=CARTESIAN_POINT('Ctrl Pts',(-45.3491963327816,1078.31195866523,
338.527139642762));
#109809=CARTESIAN_POINT('Ctrl Pts',(-45.3376392626775,1078.32131730675,
338.679831390756));
#109810=CARTESIAN_POINT('Ctrl Pts',(-45.2586250696309,1078.34136719712,
338.984611036105));
#109811=CARTESIAN_POINT('Ctrl Pts',(-45.1878669986355,1078.35192173704,
339.133080819982));
#109812=CARTESIAN_POINT('Ctrl Pts',(-44.9910710420895,1078.37255856159,
339.399704198003));
#109813=CARTESIAN_POINT('Ctrl Pts',(-44.8651833819723,1078.38241385252,
339.514096763639));
#109814=CARTESIAN_POINT('Ctrl Pts',(-44.5822473190854,1078.39948632042,
339.683702256633));
#109815=CARTESIAN_POINT('Ctrl Pts',(-44.4292884205347,1078.40664767814,
339.739684338288));
#109816=CARTESIAN_POINT('Ctrl Pts',(-44.201977036801,1078.41475375434,339.776702094143));
#109817=CARTESIAN_POINT('Ctrl Pts',(-44.1334178162447,1078.41688886827,
339.782224246531));
#109818=CARTESIAN_POINT('Ctrl Pts',(-44.0648939479108,1078.41872688014,
339.782224246531));
#109819=CARTESIAN_POINT('',(-14.6999478050468,1078.7051236444,337.754967205958));
#109820=CARTESIAN_POINT('',(-14.6999478050467,1078.63014532468,334.798360941572));
#109821=CARTESIAN_POINT('Ctrl Pts',(-14.6999478050468,1078.7051236444,337.754967205958));
#109822=CARTESIAN_POINT('Ctrl Pts',(-14.6589123536955,1078.7052433175,337.754967205958));
#109823=CARTESIAN_POINT('Ctrl Pts',(-14.6178921577028,1078.7053326354,337.753258582307));
#109824=CARTESIAN_POINT('Ctrl Pts',(-14.5422341208689,1078.70544207271,
337.74694404751));
#109825=CARTESIAN_POINT('Ctrl Pts',(-14.5075879085124,1078.70547052478,
337.742813616038));
#109826=CARTESIAN_POINT('Ctrl Pts',(-14.4357656202781,1078.70548443118,
337.731661304056));
#109827=CARTESIAN_POINT('Ctrl Pts',(-14.3986471606966,1078.70546608187,
337.72443031423));
#109828=CARTESIAN_POINT('Ctrl Pts',(-14.3125881117328,1078.70536326053,
337.704211958564));
#109829=CARTESIAN_POINT('Ctrl Pts',(-14.2639561299985,1078.70525859826,
337.690117906049));
#109830=CARTESIAN_POINT('Ctrl Pts',(-14.1147826631352,1078.70478798948,
337.638452680117));
#109831=CARTESIAN_POINT('Ctrl Pts',(-14.0175446031057,1078.70426283054,
337.592419327622));
#109832=CARTESIAN_POINT('Ctrl Pts',(-13.758249841205,1078.70216932428,337.433129884863));
#109833=CARTESIAN_POINT('Ctrl Pts',(-13.6126630540636,1078.70011869856,
337.29745514565));
#109834=CARTESIAN_POINT('Ctrl Pts',(-13.399413227183,1078.69491773742,336.999607363213));
#109835=CARTESIAN_POINT('Ctrl Pts',(-13.325241670197,1078.69199617544,336.846062448113));
#109836=CARTESIAN_POINT('Ctrl Pts',(-13.2285735283737,1078.6848939826,336.508210561569));
#109837=CARTESIAN_POINT('Ctrl Pts',(-13.2112641298419,1078.68069073918,
336.325344224527));
#109838=CARTESIAN_POINT('Ctrl Pts',(-13.2451714983133,1078.67119546056,
335.949155420977));
#109839=CARTESIAN_POINT('Ctrl Pts',(-13.3012165217026,1078.66593770448,
335.75976615305));
#109840=CARTESIAN_POINT('Ctrl Pts',(-13.4826519806559,1078.65551499784,
335.415908764833));
#109841=CARTESIAN_POINT('Ctrl Pts',(-13.605449867651,1078.65045491218,335.264345333663));
#109842=CARTESIAN_POINT('Ctrl Pts',(-13.8908387664958,1078.64178807057,
335.026676995523));
#109843=CARTESIAN_POINT('Ctrl Pts',(-14.0472523841235,1078.6381751293,334.938335581696));
#109844=CARTESIAN_POINT('Ctrl Pts',(-14.3495679685873,1078.63320356144,
334.833502505654));
#109845=CARTESIAN_POINT('Ctrl Pts',(-14.4895158833743,1078.6315618089,334.806560824859));
#109846=CARTESIAN_POINT('Ctrl Pts',(-14.6540516932643,1078.6304135091,334.798895782795));
#109847=CARTESIAN_POINT('Ctrl Pts',(-14.6769708122268,1078.63027087472,
334.798361789893));
#109848=CARTESIAN_POINT('Ctrl Pts',(-14.6998931606234,1078.63014562323,
334.798360942585));
#109849=CARTESIAN_POINT('Ctrl Pts',(-14.6999113754354,1078.6301455237,334.798360941911));
#109850=CARTESIAN_POINT('Ctrl Pts',(-14.6999295902432,1078.63014542419,
334.798360941572));
#109851=CARTESIAN_POINT('Ctrl Pts',(-14.6999478050467,1078.63014532468,
334.798360941572));
#109852=CARTESIAN_POINT('Ctrl Pts',(-14.6999478050467,1078.63014532468,
334.798360941572));
#109853=CARTESIAN_POINT('Ctrl Pts',(-14.7496366904929,1078.62987387635,
334.798360941572));
#109854=CARTESIAN_POINT('Ctrl Pts',(-14.7992942996238,1078.62968439931,
334.800866162424));
#109855=CARTESIAN_POINT('Ctrl Pts',(-14.8867403145353,1078.62949663331,
334.809712077419));
#109856=CARTESIAN_POINT('Ctrl Pts',(-14.9245858035539,1078.62946433312,
334.815028901272));
#109857=CARTESIAN_POINT('Ctrl Pts',(-15.0019471554124,1078.62949962106,
334.828973111974));
#109858=CARTESIAN_POINT('Ctrl Pts',(-15.0414008598778,1078.6295730621,334.837767787017));
#109859=CARTESIAN_POINT('Ctrl Pts',(-15.1394814709311,1078.62989560303,
334.863892701655));
#109860=CARTESIAN_POINT('Ctrl Pts',(-15.1974861911861,1078.63021513983,
334.883262411773));
#109861=CARTESIAN_POINT('Ctrl Pts',(-15.4035650497694,1078.63182149038,
334.966592792844));
#109862=CARTESIAN_POINT('Ctrl Pts',(-15.5421111064959,1078.63382773723,
335.051054370372));
#109863=CARTESIAN_POINT('Ctrl Pts',(-15.7838671273692,1078.63917763711,
335.259120231833));
#109864=CARTESIAN_POINT('Ctrl Pts',(-15.88620544731,1078.64245551688,335.380526314563));
#109865=CARTESIAN_POINT('Ctrl Pts',(-16.0556344970397,1078.65016819128,
335.662760107197));
#109866=CARTESIAN_POINT('Ctrl Pts',(-16.1176273394778,1078.65461665645,
335.823955988844));
#109867=CARTESIAN_POINT('Ctrl Pts',(-16.185959543564,1078.66409952728,336.172373481196));
#109868=CARTESIAN_POINT('Ctrl Pts',(-16.1874143971128,1078.66906641868,
336.35761110391));
#109869=CARTESIAN_POINT('Ctrl Pts',(-16.1199834112205,1078.67885370572,
336.73250043513));
#109870=CARTESIAN_POINT('Ctrl Pts',(-16.0465580177525,1078.68353601572,
336.917708199298));
#109871=CARTESIAN_POINT('Ctrl Pts',(-15.8341720149533,1078.69160169471,
337.244037831854));
#109872=CARTESIAN_POINT('Ctrl Pts',(-15.6990081640736,1078.69494485142,
337.383083186043));
#109873=CARTESIAN_POINT('Ctrl Pts',(-15.3933037326129,1078.70012415692,
337.594580624634));
#109874=CARTESIAN_POINT('Ctrl Pts',(-15.2281790413487,1078.7020071838,337.669008364265));
#109875=CARTESIAN_POINT('Ctrl Pts',(-14.9434874709919,1078.70413372867,
337.73918496718));
#109876=CARTESIAN_POINT('Ctrl Pts',(-14.8304481116973,1078.70471821139,
337.753569334503));
#109877=CARTESIAN_POINT('Ctrl Pts',(-14.711236065491,1078.70509015022,337.754934883857));
#109878=CARTESIAN_POINT('Ctrl Pts',(-14.7055917909763,1078.70510718465,
337.754967205958));
#109879=CARTESIAN_POINT('Ctrl Pts',(-14.6999478050468,1078.7051236444,337.754967205958));
#109880=CARTESIAN_POINT('',(-25.1979747106604,1078.42435733551,332.502403403865));
#109881=CARTESIAN_POINT('',(-25.1979747106603,1078.26679962567,329.951515161593));
#109882=CARTESIAN_POINT('Ctrl Pts',(-25.1979747106604,1078.42435733551,
332.502403403865));
#109883=CARTESIAN_POINT('Ctrl Pts',(-25.152160999578,1078.42505470245,332.502403403865));
#109884=CARTESIAN_POINT('Ctrl Pts',(-25.1063479654105,1078.42561183531,
332.499934973706));
#109885=CARTESIAN_POINT('Ctrl Pts',(-25.0252461736709,1078.42634944539,
332.491157371042));
#109886=CARTESIAN_POINT('Ctrl Pts',(-24.9899331133854,1078.42658556673,
332.485828112392));
#109887=CARTESIAN_POINT('Ctrl Pts',(-24.9287492539622,1078.42684587456,
332.473949434464));
#109888=CARTESIAN_POINT('Ctrl Pts',(-24.9027740417738,1078.42690859574,
332.468056927039));
#109889=CARTESIAN_POINT('Ctrl Pts',(-24.849042837633,1078.426938142,332.45408553475));
#109890=CARTESIAN_POINT('Ctrl Pts',(-24.8213385508615,1078.42689636731,
332.445867599421));
#109891=CARTESIAN_POINT('Ctrl Pts',(-24.7570850203332,1078.42666450101,
332.424408058209));
#109892=CARTESIAN_POINT('Ctrl Pts',(-24.7208148879577,1078.42642835409,
332.410422715425));
#109893=CARTESIAN_POINT('Ctrl Pts',(-24.6084599785012,1078.42535813259,
332.361094055936));
#109894=CARTESIAN_POINT('Ctrl Pts',(-24.5351968034651,1078.42415126337,
332.319896847511));
#109895=CARTESIAN_POINT('Ctrl Pts',(-24.3276760062992,1078.4191009773,332.174619777398));
#109896=CARTESIAN_POINT('Ctrl Pts',(-24.2096372996228,1078.4138765529,332.050752574564));
#109897=CARTESIAN_POINT('Ctrl Pts',(-24.0422923077211,1078.40116943319,
331.785497718849));
#109898=CARTESIAN_POINT('Ctrl Pts',(-23.9866003231676,1078.39422554416,
331.651356599257));
#109899=CARTESIAN_POINT('Ctrl Pts',(-23.9198638252662,1078.37797500119,
331.359003512358));
#109900=CARTESIAN_POINT('Ctrl Pts',(-23.9133094359033,1078.36865673574,
331.20216901896));
#109901=CARTESIAN_POINT('Ctrl Pts',(-23.9585998767981,1078.34835887168,
330.882441906846));
#109902=CARTESIAN_POINT('Ctrl Pts',(-24.0144206331024,1078.33749981153,
330.723033929454));
#109903=CARTESIAN_POINT('Ctrl Pts',(-24.1844442927444,1078.31636709739,
330.434794148616));
#109904=CARTESIAN_POINT('Ctrl Pts',(-24.2970507612122,1078.30629851345,
330.308734657781));
#109905=CARTESIAN_POINT('Ctrl Pts',(-24.5554661786938,1078.28909552609,
330.114179678535));
#109906=CARTESIAN_POINT('Ctrl Pts',(-24.6963108177312,1078.28195547514,
330.043969101914));
#109907=CARTESIAN_POINT('Ctrl Pts',(-24.9606785236178,1078.2721924645,329.968156166984));
#109908=CARTESIAN_POINT('Ctrl Pts',(-25.0790207575768,1078.26894718679,
329.951515180457));
#109909=CARTESIAN_POINT('Ctrl Pts',(-25.1979745084014,1078.26679962932,
329.951515161593));
#109910=CARTESIAN_POINT('Ctrl Pts',(-25.1979747106603,1078.26679962567,
329.951515161593));
#109911=CARTESIAN_POINT('Ctrl Pts',(-25.2538390162154,1078.26579106784,
329.951515161593));
#109912=CARTESIAN_POINT('Ctrl Pts',(-25.3096461383107,1078.2650278866,329.955185413986));
#109913=CARTESIAN_POINT('Ctrl Pts',(-25.4010408522882,1078.26418420401,
329.967260573507));
#109914=CARTESIAN_POINT('Ctrl Pts',(-25.4368269000737,1078.26395863441,
329.973553353014));
#109915=CARTESIAN_POINT('Ctrl Pts',(-25.5003875254845,1078.26374726159,
329.987551522511));
#109916=CARTESIAN_POINT('Ctrl Pts',(-25.528261637163,1078.26372140329,329.994686723473));
#109917=CARTESIAN_POINT('Ctrl Pts',(-25.5864441219895,1078.26380940912,
330.01169641011));
#109918=CARTESIAN_POINT('Ctrl Pts',(-25.6166716843358,1078.26393854366,
330.0217766678));
#109919=CARTESIAN_POINT('Ctrl Pts',(-25.6945523141232,1078.26449138128,
330.05103226143));
#109920=CARTESIAN_POINT('Ctrl Pts',(-25.7414786658446,1078.26504649419,
330.07197155084));
#109921=CARTESIAN_POINT('Ctrl Pts',(-25.9260906165669,1078.26814828127,
330.168095987952));
#109922=CARTESIAN_POINT('Ctrl Pts',(-26.0505853878352,1078.2724199097,330.265517330287));
#109923=CARTESIAN_POINT('Ctrl Pts',(-26.2451111638944,1078.28354380179,
330.485941438791));
#109924=CARTESIAN_POINT('Ctrl Pts',(-26.3187027191012,1078.28993492838,
330.602823386777));
#109925=CARTESIAN_POINT('Ctrl Pts',(-26.430495652749,1078.30513901016,330.866516436001));
#109926=CARTESIAN_POINT('Ctrl Pts',(-26.4641653372882,1078.31399636629,
331.013031980771));
#109927=CARTESIAN_POINT('Ctrl Pts',(-26.47991708103,1078.33333093322,331.321855554161));
#109928=CARTESIAN_POINT('Ctrl Pts',(-26.4579025795552,1078.34370740875,
331.481832355953));
#109929=CARTESIAN_POINT('Ctrl Pts',(-26.353027678289,1078.36461949114,331.793655948564));
#109930=CARTESIAN_POINT('Ctrl Pts',(-26.2678904931126,1078.37492771218,
331.941522037978));
#109931=CARTESIAN_POINT('Ctrl Pts',(-26.0477585667338,1078.39334303653,
332.192218928031));
#109932=CARTESIAN_POINT('Ctrl Pts',(-25.9161694794889,1078.40133180787,
332.293773788076));
#109933=CARTESIAN_POINT('Ctrl Pts',(-25.6296807223542,1078.41405867805,
332.437169584067));
#109934=CARTESIAN_POINT('Ctrl Pts',(-25.4788877391697,1078.41884847287,
332.480790853491));
#109935=CARTESIAN_POINT('Ctrl Pts',(-25.2820480479779,1078.42295952733,
332.500325235152));
#109936=CARTESIAN_POINT('Ctrl Pts',(-25.2400110944244,1078.42371746628,
332.502403403865));
#109937=CARTESIAN_POINT('Ctrl Pts',(-25.1979747106604,1078.42435733551,
332.502403403865));
#109938=CARTESIAN_POINT('',(-37.1057957606637,1077.76997147869,327.631087921141));
#109939=CARTESIAN_POINT('',(-37.1057957606635,1077.5579316459,325.433425649156));
#109940=CARTESIAN_POINT('Ctrl Pts',(-37.1057957606639,1077.76997147869,
327.631087921141));
#109941=CARTESIAN_POINT('Ctrl Pts',(-37.0507987318168,1077.77190604638,
327.631087921141));
#109942=CARTESIAN_POINT('Ctrl Pts',(-36.9957541821996,1077.77345630688,
327.626959114939));
#109943=CARTESIAN_POINT('Ctrl Pts',(-36.8986799269302,1077.77549923108,
327.61224576858));
#109944=CARTESIAN_POINT('Ctrl Pts',(-36.8566408676037,1077.77614728382,
327.603328977249));
#109945=CARTESIAN_POINT('Ctrl Pts',(-36.7910552112728,1077.77678054052,
327.585345823688));
#109946=CARTESIAN_POINT('Ctrl Pts',(-36.7671154963525,1077.77692917547,
327.577892411466));
#109947=CARTESIAN_POINT('Ctrl Pts',(-36.7229587698778,1077.77704792786,
327.562468841074));
#109948=CARTESIAN_POINT('Ctrl Pts',(-36.7026829298606,1077.77703927445,
327.554705357602));
#109949=CARTESIAN_POINT('Ctrl Pts',(-36.6583938295681,1077.77687919098,
327.536225013625));
#109950=CARTESIAN_POINT('Ctrl Pts',(-36.6345088005065,1077.77669809455,
327.525236756178));
#109951=CARTESIAN_POINT('Ctrl Pts',(-36.5679569453334,1077.77592045116,
327.491677211778));
#109952=CARTESIAN_POINT('Ctrl Pts',(-36.5263549901042,1077.77510407512,
327.467139411149));
#109953=CARTESIAN_POINT('Ctrl Pts',(-36.3656673256076,1077.77056904092,
327.357507276023));
#109954=CARTESIAN_POINT('Ctrl Pts',(-36.2625920360524,1077.76437350324,
327.251822883907));
#109955=CARTESIAN_POINT('Ctrl Pts',(-36.1179450963914,1077.74858962957,
327.028268383998));
#109956=CARTESIAN_POINT('Ctrl Pts',(-36.0697037120012,1077.73990347443,
326.917410247792));
#109957=CARTESIAN_POINT('Ctrl Pts',(-36.0083464949823,1077.71914166221,
326.674206792521));
#109958=CARTESIAN_POINT('Ctrl Pts',(-35.999275836045,1077.70699389374,326.542752524337));
#109959=CARTESIAN_POINT('Ctrl Pts',(-36.0287616005446,1077.68013760776,
326.272935955355));
#109960=CARTESIAN_POINT('Ctrl Pts',(-36.0708062327943,1077.66554285194,
326.13724840386));
#109961=CARTESIAN_POINT('Ctrl Pts',(-36.2060056656884,1077.63611503389,
325.884974465073));
#109962=CARTESIAN_POINT('Ctrl Pts',(-36.2995550386854,1077.62157098013,
325.77158691681));
#109963=CARTESIAN_POINT('Ctrl Pts',(-36.4915776751045,1077.59907323847,
325.615447952087));
#109964=CARTESIAN_POINT('Ctrl Pts',(-36.5792024850074,1077.59056064311,
325.562447192936));
#109965=CARTESIAN_POINT('Ctrl Pts',(-36.7310998545457,1077.57841283068,
325.49734794043));
#109966=CARTESIAN_POINT('Ctrl Pts',(-36.7913278422833,1077.57417553721,
325.477481637902));
#109967=CARTESIAN_POINT('Ctrl Pts',(-36.935768174724,1077.56534061361,325.443330204206));
#109968=CARTESIAN_POINT('Ctrl Pts',(-37.0206145131777,1077.56115002462,
325.43342572128));
#109969=CARTESIAN_POINT('Ctrl Pts',(-37.1057948302677,1077.55793168106,
325.433425649157));
#109970=CARTESIAN_POINT('Ctrl Pts',(-37.1057957606634,1077.5579316459,325.433425649156));
#109971=CARTESIAN_POINT('Ctrl Pts',(-37.1819018986778,1077.55505615586,
325.433425649156));
#109972=CARTESIAN_POINT('Ctrl Pts',(-37.2578231472279,1077.55297389363,
325.441332273578));
#109973=CARTESIAN_POINT('Ctrl Pts',(-37.3645574303048,1077.55118391002,
325.463820301091));
#109974=CARTESIAN_POINT('Ctrl Pts',(-37.3964584062127,1077.55080015102,
325.472054170212));
#109975=CARTESIAN_POINT('Ctrl Pts',(-37.4476616454257,1077.55043295362,
325.487755483657));
#109976=CARTESIAN_POINT('Ctrl Pts',(-37.4672063328431,1077.55035358104,
325.494356178952));
#109977=CARTESIAN_POINT('Ctrl Pts',(-37.5075396586184,1077.55031767442,
325.509255218331));
#109978=CARTESIAN_POINT('Ctrl Pts',(-37.5282836445334,1077.55037212035,
325.517646349847));
#109979=CARTESIAN_POINT('Ctrl Pts',(-37.5763639693276,1077.55067151027,
325.538825625678));
#109980=CARTESIAN_POINT('Ctrl Pts',(-37.6034573646397,1077.55097609398,
325.552117676913));
#109981=CARTESIAN_POINT('Ctrl Pts',(-37.6879494814917,1077.55236674982,
325.597976802609));
#109982=CARTESIAN_POINT('Ctrl Pts',(-37.7429657864938,1077.553948481,325.63459730327));
#109983=CARTESIAN_POINT('Ctrl Pts',(-37.9084491018374,1077.56098962291,
325.767658168065));
#109984=CARTESIAN_POINT('Ctrl Pts',(-38.0029572944813,1077.56875408708,
325.881189615137));
#109985=CARTESIAN_POINT('Ctrl Pts',(-38.1307558457615,1077.58742051731,
326.117621726534));
#109986=CARTESIAN_POINT('Ctrl Pts',(-38.1705470485416,1077.59748227609,
326.234397852002));
#109987=CARTESIAN_POINT('Ctrl Pts',(-38.2116478433377,1077.62070890731,
326.48615956015));
#109988=CARTESIAN_POINT('Ctrl Pts',(-38.2091217001448,1077.63387487959,
326.619827418889));
#109989=CARTESIAN_POINT('Ctrl Pts',(-38.1546825940271,1077.662054189,326.889432100301));
#109990=CARTESIAN_POINT('Ctrl Pts',(-38.0995667696273,1077.67687374602,
327.022325921047));
#109991=CARTESIAN_POINT('Ctrl Pts',(-37.9403437576909,1077.70553168252,
327.261603277977));
#109992=CARTESIAN_POINT('Ctrl Pts',(-37.8369629836312,1077.71907910922,
327.365248436876));
#109993=CARTESIAN_POINT('Ctrl Pts',(-37.602967274512,1077.74218215927,327.521620702492));
#109994=CARTESIAN_POINT('Ctrl Pts',(-37.4763845891422,1077.75173219943,
327.575689200392));
#109995=CARTESIAN_POINT('Ctrl Pts',(-37.2649855750143,1077.76356243156,
327.62242852211));
#109996=CARTESIAN_POINT('Ctrl Pts',(-37.185440496621,1077.76716990674,327.631087921141));
#109997=CARTESIAN_POINT('Ctrl Pts',(-37.1057957606639,1077.76997147869,
327.631087921141));
#109998=CARTESIAN_POINT('',(-49.7050859019669,1076.94955520377,325.362209063876));
#109999=CARTESIAN_POINT('',(-49.7050859019678,1076.68713253746,323.18112756642));
#110000=CARTESIAN_POINT('Ctrl Pts',(-49.7050859019669,1076.94955520377,
325.362209063877));
#110001=CARTESIAN_POINT('Ctrl Pts',(-49.6460399786472,1076.95299643431,
325.362209063877));
#110002=CARTESIAN_POINT('Ctrl Pts',(-49.58693856471,1076.95587354174,325.357413855934));
#110003=CARTESIAN_POINT('Ctrl Pts',(-49.4669163176567,1076.96054214956,
325.337704192653));
#110004=CARTESIAN_POINT('Ctrl Pts',(-49.4064236017617,1076.96225869733,
325.322364600977));
#110005=CARTESIAN_POINT('Ctrl Pts',(-49.3242057966663,1076.96368973578,
325.2938328615));
#110006=CARTESIAN_POINT('Ctrl Pts',(-49.3011366422712,1076.96398683401,
325.284937843907));
#110007=CARTESIAN_POINT('Ctrl Pts',(-49.2615021139303,1076.96431313749,
325.268086523608));
#110008=CARTESIAN_POINT('Ctrl Pts',(-49.2447993283327,1076.96439158963,
325.260481801689));
#110009=CARTESIAN_POINT('Ctrl Pts',(-49.2104143436567,1076.96442869618,
325.24376630412));
#110010=CARTESIAN_POINT('Ctrl Pts',(-49.1927737557973,1076.96437678777,
325.234586120349));
#110011=CARTESIAN_POINT('Ctrl Pts',(-49.1519567431063,1076.96408777922,
325.211905614821));
#110012=CARTESIAN_POINT('Ctrl Pts',(-49.1290088083054,1076.96379254135,
325.198023038725));
#110013=CARTESIAN_POINT('Ctrl Pts',(-49.0573709533917,1076.9624374318,325.150993082848));
#110014=CARTESIAN_POINT('Ctrl Pts',(-49.0108565895208,1076.9608877905,325.114751116459));
#110015=CARTESIAN_POINT('Ctrl Pts',(-48.861222714599,1076.95345472606,324.977355147536));
#110016=CARTESIAN_POINT('Ctrl Pts',(-48.7755054433334,1076.94462512839,
324.859775958759));
#110017=CARTESIAN_POINT('Ctrl Pts',(-48.6645186776712,1076.92276836248,
324.61960299161));
#110018=CARTESIAN_POINT('Ctrl Pts',(-48.6325024177503,1076.91080296668,
324.502586298824));
#110019=CARTESIAN_POINT('Ctrl Pts',(-48.6068359393774,1076.8825796473,324.252221412734));
#110020=CARTESIAN_POINT('Ctrl Pts',(-48.6171694112931,1076.86625340712,
324.120360301));
#110021=CARTESIAN_POINT('Ctrl Pts',(-48.6866796476855,1076.83056196565,
323.856732994555));
#110022=CARTESIAN_POINT('Ctrl Pts',(-48.7490856498951,1076.81137638158,
323.728181714423));
#110023=CARTESIAN_POINT('Ctrl Pts',(-48.9188284544825,1076.77399917669,
323.50303606543));
#110024=CARTESIAN_POINT('Ctrl Pts',(-49.0243157812746,1076.75612934328,
323.408168544092));
#110025=CARTESIAN_POINT('Ctrl Pts',(-49.2171405867449,1076.73041995546,
323.292768333095));
#110026=CARTESIAN_POINT('Ctrl Pts',(-49.2940375705273,1076.7215242049,323.258059331199));
#110027=CARTESIAN_POINT('Ctrl Pts',(-49.4810832272676,1076.70289454892,
323.19850750249));
#110028=CARTESIAN_POINT('Ctrl Pts',(-49.5926721239983,1076.6939757664,323.18112756642));
#110029=CARTESIAN_POINT('Ctrl Pts',(-49.7050859019677,1076.68713253746,
323.18112756642));
#110030=CARTESIAN_POINT('Ctrl Pts',(-49.7050859019677,1076.68713253746,
323.18112756642));
#110031=CARTESIAN_POINT('Ctrl Pts',(-49.7050914492263,1076.68713219976,
323.18112756642));
#110032=CARTESIAN_POINT('Ctrl Pts',(-49.7050969964872,1076.68713186208,
323.1811275665));
#110033=CARTESIAN_POINT('Ctrl Pts',(-49.7051025437499,1076.6871315244,323.181127566585));
#110034=CARTESIAN_POINT('Ctrl Pts',(-49.8088206851785,1076.68081783899,
323.181129149337));
#110035=CARTESIAN_POINT('Ctrl Pts',(-49.9120892726801,1076.67634161631,
323.195927130838));
#110036=CARTESIAN_POINT('Ctrl Pts',(-50.0459484580094,1076.67300727247,
323.235154900677));
#110037=CARTESIAN_POINT('Ctrl Pts',(-50.0796160366933,1076.67239233504,
323.246839014162));
#110038=CARTESIAN_POINT('Ctrl Pts',(-50.1329751701086,1076.67178502818,
323.268338935774));
#110039=CARTESIAN_POINT('Ctrl Pts',(-50.153044503504,1076.67164427003,323.27713716433));
#110040=CARTESIAN_POINT('Ctrl Pts',(-50.19066912511,1076.67154917843,323.295001643121));
#110041=CARTESIAN_POINT('Ctrl Pts',(-50.2082692535228,1076.67157780006,
323.303951745155));
#110042=CARTESIAN_POINT('Ctrl Pts',(-50.2475561875321,1076.67180943091,
323.325291815224));
#110043=CARTESIAN_POINT('Ctrl Pts',(-50.2690789873096,1076.67205652613,
323.33795841797));
#110044=CARTESIAN_POINT('Ctrl Pts',(-50.3317134774138,1076.67313965593,
323.377776251054));
#110045=CARTESIAN_POINT('Ctrl Pts',(-50.3714327852864,1076.67431348698,
323.406980586524));
#110046=CARTESIAN_POINT('Ctrl Pts',(-50.5193156694129,1076.68068270556,
323.53196688866));
#110047=CARTESIAN_POINT('Ctrl Pts',(-50.6098383556455,1076.68920039534,
323.646015709891));
#110048=CARTESIAN_POINT('Ctrl Pts',(-50.7297360052905,1076.71060001064,
323.879894089432));
#110049=CARTESIAN_POINT('Ctrl Pts',(-50.766217518536,1076.72230878929,323.993612070658));
#110050=CARTESIAN_POINT('Ctrl Pts',(-50.8027981187008,1076.75001568232,
324.238868941098));
#110051=CARTESIAN_POINT('Ctrl Pts',(-50.7989166745544,1076.7660952531,324.36918024798));
#110052=CARTESIAN_POINT('Ctrl Pts',(-50.7437470917788,1076.80123169195,
324.632085196037));
#110053=CARTESIAN_POINT('Ctrl Pts',(-50.6892150515513,1076.82011778402,
324.761768185158));
#110054=CARTESIAN_POINT('Ctrl Pts',(-50.5313241389388,1076.85783783144,
324.998003904691));
#110055=CARTESIAN_POINT('Ctrl Pts',(-50.4276394566757,1076.8762899973,325.101269412309));
#110056=CARTESIAN_POINT('Ctrl Pts',(-50.1911036244038,1076.90880622727,
325.257697883359));
#110057=CARTESIAN_POINT('Ctrl Pts',(-50.0618732563135,1076.92274398555,
325.311519480018));
#110058=CARTESIAN_POINT('Ctrl Pts',(-49.8530821577486,1076.94003770994,
325.354668307415));
#110059=CARTESIAN_POINT('Ctrl Pts',(-49.779127659166,1076.94524000737,325.362209063877));
#110060=CARTESIAN_POINT('Ctrl Pts',(-49.7050859019669,1076.94955520377,
325.362209063877));
#110061=CARTESIAN_POINT('',(-86.2232976813461,1076.9124877279,354.254678911709));
#110062=CARTESIAN_POINT('',(-86.223297681347,1076.72560793676,352.073597414254));
#110063=CARTESIAN_POINT('Ctrl Pts',(-86.2232976813464,1076.9124877279,354.254678911711));
#110064=CARTESIAN_POINT('Ctrl Pts',(-86.1106700087104,1076.92394995339,
354.254678911711));
#110065=CARTESIAN_POINT('Ctrl Pts',(-85.9984479843176,1076.93386455963,
354.237230908178));
#110066=CARTESIAN_POINT('Ctrl Pts',(-85.7548899619962,1076.95197767004,
354.159227193133));
#110067=CARTESIAN_POINT('Ctrl Pts',(-85.6287945239059,1076.95886673878,
354.08948200948));
#110068=CARTESIAN_POINT('Ctrl Pts',(-85.4948783902631,1076.96291995683,
353.976378537235));
#110069=CARTESIAN_POINT('Ctrl Pts',(-85.4710647283615,1076.96348255733,
353.954375533283));
#110070=CARTESIAN_POINT('Ctrl Pts',(-85.4338411076001,1076.96409366365,
353.916772045896));
#110071=CARTESIAN_POINT('Ctrl Pts',(-85.4198313036292,1076.96425497713,
353.90179748482));
#110072=CARTESIAN_POINT('Ctrl Pts',(-85.3956531693964,1076.96440748106,
353.8744477722));
#110073=CARTESIAN_POINT('Ctrl Pts',(-85.3853198471695,1076.96442822542,
353.862227221899));
#110074=CARTESIAN_POINT('Ctrl Pts',(-85.3642048128736,1076.96437496735,
353.836111156062));
#110075=CARTESIAN_POINT('Ctrl Pts',(-85.3534829036369,1076.9642914137,353.822173493486));
#110076=CARTESIAN_POINT('Ctrl Pts',(-85.3263966080289,1076.96392829675,
353.785144040836));
#110077=CARTESIAN_POINT('Ctrl Pts',(-85.3105867383334,1076.96356046082,
353.761665037151));
#110078=CARTESIAN_POINT('Ctrl Pts',(-85.2481878537172,1076.96141770149,
353.66073317949));
#110079=CARTESIAN_POINT('Ctrl Pts',(-85.2104303172905,1076.95833556205,
353.578298258425));
#110080=CARTESIAN_POINT('Ctrl Pts',(-85.1510914289845,1076.94858128102,
353.39018380428));
#110081=CARTESIAN_POINT('Ctrl Pts',(-85.134130936169,1076.94140600827,353.284095820838));
#110082=CARTESIAN_POINT('Ctrl Pts',(-85.1313765667379,1076.92258949993,
353.056874669399));
#110083=CARTESIAN_POINT('Ctrl Pts',(-85.1498936083631,1076.91062347989,
352.937155489594));
#110084=CARTESIAN_POINT('Ctrl Pts',(-85.2285473991811,1076.88239895222,
352.698316308956));
#110085=CARTESIAN_POINT('Ctrl Pts',(-85.2917524177404,1076.86606956431,
352.582186930196));
#110086=CARTESIAN_POINT('Ctrl Pts',(-85.4627331970511,1076.8303715638,352.36986520423));
#110087=CARTESIAN_POINT('Ctrl Pts',(-85.5721656192275,1076.81118246124,
352.277940107348));
#110088=CARTESIAN_POINT('Ctrl Pts',(-85.7716420283623,1076.78098194181,
352.167777036374));
#110089=CARTESIAN_POINT('Ctrl Pts',(-85.8519240535133,1076.76980246967,
352.135145175158));
#110090=CARTESIAN_POINT('Ctrl Pts',(-86.0290190547706,1076.74711303435,
352.086648114149));
#110091=CARTESIAN_POINT('Ctrl Pts',(-86.1258876281242,1076.73583360847,
352.073597414254));
#110092=CARTESIAN_POINT('Ctrl Pts',(-86.2232976813471,1076.72560793676,
352.073597414254));
#110093=CARTESIAN_POINT('Ctrl Pts',(-86.2232976813471,1076.72560793676,
352.073597414254));
#110094=CARTESIAN_POINT('Ctrl Pts',(-86.2233382977044,1076.72560367304,
352.073597414254));
#110095=CARTESIAN_POINT('Ctrl Pts',(-86.2233789141559,1076.7255994095,352.073597416523));
#110096=CARTESIAN_POINT('Ctrl Pts',(-86.2234195307013,1076.72559514614,
352.073597421061));
#110097=CARTESIAN_POINT('Ctrl Pts',(-86.352409189064,1076.71205561553,352.073611833463));
#110098=CARTESIAN_POINT('Ctrl Pts',(-86.480575631451,1076.70055082089,352.096511565282));
#110099=CARTESIAN_POINT('Ctrl Pts',(-86.7226974278544,1076.68283928162,
352.186146101408));
#110100=CARTESIAN_POINT('Ctrl Pts',(-86.8347358248615,1076.67675513596,
352.251954646566));
#110101=CARTESIAN_POINT('Ctrl Pts',(-86.9563727615988,1076.6730211201,352.35614840662));
#110102=CARTESIAN_POINT('Ctrl Pts',(-86.9791202646848,1076.67247634619,
352.377385887761));
#110103=CARTESIAN_POINT('Ctrl Pts',(-87.015077807269,1076.67187843216,352.413957831622));
#110104=CARTESIAN_POINT('Ctrl Pts',(-87.0288231641388,1076.67171992704,
352.428736881043));
#110105=CARTESIAN_POINT('Ctrl Pts',(-87.0527719437454,1076.67157337991,
352.455964324506));
#110106=CARTESIAN_POINT('Ctrl Pts',(-87.0631246088755,1076.67155727495,
352.468272892784));
#110107=CARTESIAN_POINT('Ctrl Pts',(-87.0844920994205,1076.67162681896,
352.494848997105));
#110108=CARTESIAN_POINT('Ctrl Pts',(-87.0954328916507,1076.67172494973,
352.509169487017));
#110109=CARTESIAN_POINT('Ctrl Pts',(-87.1235095361551,1076.67214795035,
352.547870804807));
#110110=CARTESIAN_POINT('Ctrl Pts',(-87.1400083324327,1076.67257890375,
352.572692356219));
#110111=CARTESIAN_POINT('Ctrl Pts',(-87.2083307388048,1076.67521734954,
352.685219225984));
#110112=CARTESIAN_POINT('Ctrl Pts',(-87.2486979470708,1076.67918720723,
352.779197400646));
#110113=CARTESIAN_POINT('Ctrl Pts',(-87.3041124358866,1076.69113007012,
352.982485843146));
#110114=CARTESIAN_POINT('Ctrl Pts',(-87.3168160143593,1076.69929810105,
353.091211016504));
#110115=CARTESIAN_POINT('Ctrl Pts',(-87.3092618540888,1076.72018562122,
353.321578436446));
#110116=CARTESIAN_POINT('Ctrl Pts',(-87.2849250164885,1076.73318438117,
353.44157419653));
#110117=CARTESIAN_POINT('Ctrl Pts',(-87.1940484156991,1076.76321716278,
353.678327874337));
#110118=CARTESIAN_POINT('Ctrl Pts',(-87.1246917993476,1076.78026540416,
353.791971853215));
#110119=CARTESIAN_POINT('Ctrl Pts',(-86.9420713038994,1076.81680851671,
353.99653735009));
#110120=CARTESIAN_POINT('Ctrl Pts',(-86.8274306336196,1076.83606112735,
354.08314068069));
#110121=CARTESIAN_POINT('Ctrl Pts',(-86.5699763667257,1076.87316862321,
354.208060979568));
#110122=CARTESIAN_POINT('Ctrl Pts',(-86.429273298908,1076.89066372331,354.244713132033));
#110123=CARTESIAN_POINT('Ctrl Pts',(-86.2646505302865,1076.90822847593,
354.254091272874));
#110124=CARTESIAN_POINT('Ctrl Pts',(-86.2439672746539,1076.9103841637,354.254678911711));
#110125=CARTESIAN_POINT('Ctrl Pts',(-86.2232976813464,1076.9124877279,354.254678911711));
#110126=CARTESIAN_POINT('',(-73.7938092375735,1077.74530255756,351.20352665013));
#110127=CARTESIAN_POINT('',(-73.7938092375734,1077.58420144585,349.005864378145));
#110128=CARTESIAN_POINT('Ctrl Pts',(-73.7938092375746,1077.74530255756,
351.20352665013));
#110129=CARTESIAN_POINT('Ctrl Pts',(-73.769883441808,1077.74699181584,351.20352665013));
#110130=CARTESIAN_POINT('Ctrl Pts',(-73.7459292397079,1077.74862579125,
351.202745233119));
#110131=CARTESIAN_POINT('Ctrl Pts',(-73.5963574879468,1077.75846980289,
351.192947562019));
#110132=CARTESIAN_POINT('Ctrl Pts',(-73.4729823801501,1077.76500962047,
351.163183030474));
#110133=CARTESIAN_POINT('Ctrl Pts',(-73.2807897034584,1077.77257859337,
351.079984154165));
#110134=CARTESIAN_POINT('Ctrl Pts',(-73.2082940154623,1077.77469879822,
351.038267379108));
#110135=CARTESIAN_POINT('Ctrl Pts',(-73.1171602315749,1077.77631811397,
350.970991583833));
#110136=CARTESIAN_POINT('Ctrl Pts',(-73.0938527327019,1077.77662537864,
350.952270758455));
#110137=CARTESIAN_POINT('Ctrl Pts',(-73.0570920529911,1077.77693018526,
350.920192336047));
#110138=CARTESIAN_POINT('Ctrl Pts',(-73.0431706502578,1077.77699998685,
350.907396579794));
#110139=CARTESIAN_POINT('Ctrl Pts',(-73.0170663687754,1077.77704117237,
350.882129741572));
#110140=CARTESIAN_POINT('Ctrl Pts',(-73.0048365783284,1077.77701983436,
350.869715514687));
#110141=CARTESIAN_POINT('Ctrl Pts',(-72.9774240804161,1077.77687641546,
350.84053283029));
#110142=CARTESIAN_POINT('Ctrl Pts',(-72.9624538003779,1077.77672625347,
350.823576154841));
#110143=CARTESIAN_POINT('Ctrl Pts',(-72.9181926212019,1077.77605439756,
350.770208957175));
#110144=CARTESIAN_POINT('Ctrl Pts',(-72.8906943116465,1077.77530803227,
350.732385855732));
#110145=CARTESIAN_POINT('Ctrl Pts',(-72.7876613244233,1077.77103915678,
350.569820296116));
#110146=CARTESIAN_POINT('Ctrl Pts',(-72.7349599947952,1077.76503247187,
350.432497846024));
#110147=CARTESIAN_POINT('Ctrl Pts',(-72.6905343650455,1077.74961804802,
350.171390094682));
#110148=CARTESIAN_POINT('Ctrl Pts',(-72.6898266910601,1077.7411215929,350.051397067388));
#110149=CARTESIAN_POINT('Ctrl Pts',(-72.7286199156512,1077.72071917826,
349.805097050745));
#110150=CARTESIAN_POINT('Ctrl Pts',(-72.7715697705636,1077.7087279905,349.681179983827));
#110151=CARTESIAN_POINT('Ctrl Pts',(-72.9036577589566,1077.68212249008,
349.44535140389));
#110152=CARTESIAN_POINT('Ctrl Pts',(-72.9949871466016,1077.66761155408,
349.337251524034));
#110153=CARTESIAN_POINT('Ctrl Pts',(-73.1930475153763,1077.64141300526,
349.177571599089));
#110154=CARTESIAN_POINT('Ctrl Pts',(-73.2926249391797,1077.62985505809,
349.120162029067));
#110155=CARTESIAN_POINT('Ctrl Pts',(-73.5249284601887,1077.60607322753,
349.030799462205));
#110156=CARTESIAN_POINT('Ctrl Pts',(-73.6584887580826,1077.59429279595,
349.005923538466));
#110157=CARTESIAN_POINT('Ctrl Pts',(-73.7933279877136,1077.58423732673,
349.005864483564));
#110158=CARTESIAN_POINT('Ctrl Pts',(-73.7934884055767,1077.58422536376,
349.005864413307));
#110159=CARTESIAN_POINT('Ctrl Pts',(-73.7936488222002,1077.58421340347,
349.005864378145));
#110160=CARTESIAN_POINT('Ctrl Pts',(-73.7938092375731,1077.58420144585,
349.005864378145));
#110161=CARTESIAN_POINT('Ctrl Pts',(-73.7938092375731,1077.58420144585,
349.005864378145));
#110162=CARTESIAN_POINT('Ctrl Pts',(-73.9127579711805,1077.57533481387,
349.005864378145));
#110163=CARTESIAN_POINT('Ctrl Pts',(-74.0310190634156,1077.56793745143,
349.025178687888));
#110164=CARTESIAN_POINT('Ctrl Pts',(-74.2455312164974,1077.55730474254,
349.097292143534));
#110165=CARTESIAN_POINT('Ctrl Pts',(-74.3416174673074,1077.55378482318,
349.146133172946));
#110166=CARTESIAN_POINT('Ctrl Pts',(-74.4565104103741,1077.55132490339,
349.227550874274));
#110167=CARTESIAN_POINT('Ctrl Pts',(-74.4829840495733,1077.55090110641,
349.248194541628));
#110168=CARTESIAN_POINT('Ctrl Pts',(-74.5235557610025,1077.5504874011,349.282932687793));
#110169=CARTESIAN_POINT('Ctrl Pts',(-74.5382859532575,1077.55039106719,
349.296253449057));
#110170=CARTESIAN_POINT('Ctrl Pts',(-74.5651350068478,1077.55031863291,
349.321889955745));
#110171=CARTESIAN_POINT('Ctrl Pts',(-74.5773399300205,1077.55032849654,
349.334106365208));
#110172=CARTESIAN_POINT('Ctrl Pts',(-74.6040201376241,1077.55044811707,
349.362101151894));
#110173=CARTESIAN_POINT('Ctrl Pts',(-74.6183321234707,1077.55058123348,
349.378024980907));
#110174=CARTESIAN_POINT('Ctrl Pts',(-74.6583278629841,1077.55115878459,
349.425228967539));
#110175=CARTESIAN_POINT('Ctrl Pts',(-74.6827584932905,1077.55177443679,
349.457520204184));
#110176=CARTESIAN_POINT('Ctrl Pts',(-74.7871426080836,1077.5557028426,349.612585944698));
#110177=CARTESIAN_POINT('Ctrl Pts',(-74.8437562329453,1077.56181743687,
349.74912510091));
#110178=CARTESIAN_POINT('Ctrl Pts',(-74.8947463291063,1077.57759525021,
350.008361242852));
#110179=CARTESIAN_POINT('Ctrl Pts',(-74.8987087697233,1077.58623671196,
350.126908186342));
#110180=CARTESIAN_POINT('Ctrl Pts',(-74.8675109748959,1077.60689739488,
350.371513308744));
#110181=CARTESIAN_POINT('Ctrl Pts',(-74.8288765795316,1077.6189981894,350.495357450571));
#110182=CARTESIAN_POINT('Ctrl Pts',(-74.7060680826829,1077.64561586336,
350.732728466384));
#110183=CARTESIAN_POINT('Ctrl Pts',(-74.619665487082,1077.66001512009,350.842660302186));
#110184=CARTESIAN_POINT('Ctrl Pts',(-74.4051459038507,1077.68919424678,
351.029333606172));
#110185=CARTESIAN_POINT('Ctrl Pts',(-74.2771371650477,1077.70367560779,
351.10225761206));
#110186=CARTESIAN_POINT('Ctrl Pts',(-74.0272615767765,1077.72744772394,
351.184818012273));
#110187=CARTESIAN_POINT('Ctrl Pts',(-73.9108754585647,1077.73703720726,
351.20352665013));
#110188=CARTESIAN_POINT('Ctrl Pts',(-73.7938092375746,1077.74530255756,
351.20352665013));
#110189=CARTESIAN_POINT('',(-61.0059658728168,1078.41010379242,350.825616616696));
#110190=CARTESIAN_POINT('',(-61.0059658728168,1078.28342170814,348.274728374424));
#110191=CARTESIAN_POINT('Ctrl Pts',(-61.0059658728173,1078.41010379242,
350.825616616696));
#110192=CARTESIAN_POINT('Ctrl Pts',(-60.9835823540215,1078.4109445386,350.825616616696));
#110193=CARTESIAN_POINT('Ctrl Pts',(-60.9611778050674,1078.41175745992,
350.82502739226));
#110194=CARTESIAN_POINT('Ctrl Pts',(-60.7774291209768,1078.4181906595,350.815334014705));
#110195=CARTESIAN_POINT('Ctrl Pts',(-60.6191200404424,1078.42225757925,
350.776238705868));
#110196=CARTESIAN_POINT('Ctrl Pts',(-60.417522270934,1078.42547434699,350.683366845324));
#110197=CARTESIAN_POINT('Ctrl Pts',(-60.3645995731918,1078.42610381919,
350.654276292849));
#110198=CARTESIAN_POINT('Ctrl Pts',(-60.2898907365497,1078.42666702699,
350.606019679417));
#110199=CARTESIAN_POINT('Ctrl Pts',(-60.2663782038122,1078.42679236091,
350.589685355149));
#110200=CARTESIAN_POINT('Ctrl Pts',(-60.2256708122253,1078.42691530777,
350.559324824838));
#110201=CARTESIAN_POINT('Ctrl Pts',(-60.2082549415685,1078.42693534259,
350.54561515021));
#110202=CARTESIAN_POINT('Ctrl Pts',(-60.1729253108439,1078.42690717166,
350.516280999461));
#110203=CARTESIAN_POINT('Ctrl Pts',(-60.1550732490697,1078.42685394484,
350.500595535313));
#110204=CARTESIAN_POINT('Ctrl Pts',(-60.1106345171936,1078.42661943572,
350.4592939022));
#110205=CARTESIAN_POINT('Ctrl Pts',(-60.0847030480664,1078.42638370712,
350.433005826605));
#110206=CARTESIAN_POINT('Ctrl Pts',(-59.9880853087506,1078.42510201004,
350.326160112222));
#110207=CARTESIAN_POINT('Ctrl Pts',(-59.9265296506684,1078.42337392092,
350.237958763876));
#110208=CARTESIAN_POINT('Ctrl Pts',(-59.8175059324121,1078.4179504817,350.030328345937));
#110209=CARTESIAN_POINT('Ctrl Pts',(-59.7755270796808,1078.41397518225,
349.909327053499));
#110210=CARTESIAN_POINT('Ctrl Pts',(-59.7260766921979,1078.40357100613,
349.644345582651));
#110211=CARTESIAN_POINT('Ctrl Pts',(-59.7235613141722,1078.39698103055,
349.501198818696));
#110212=CARTESIAN_POINT('Ctrl Pts',(-59.767580262996,1078.38138883551,349.208261623922));
#110213=CARTESIAN_POINT('Ctrl Pts',(-59.8178971668436,1078.37235536533,
349.061327112453));
#110214=CARTESIAN_POINT('Ctrl Pts',(-59.9740915904031,1078.35249506362,
348.782427503392));
#110215=CARTESIAN_POINT('Ctrl Pts',(-60.0824132468098,1078.34176895436,
348.655051228122));
#110216=CARTESIAN_POINT('Ctrl Pts',(-60.3125778170563,1078.32303443442,
348.471993008598));
#110217=CARTESIAN_POINT('Ctrl Pts',(-60.4246332309683,1078.31506405064,
348.407665841913));
#110218=CARTESIAN_POINT('Ctrl Pts',(-60.6915389098853,1078.29845566072,
348.304059259342));
#110219=CARTESIAN_POINT('Ctrl Pts',(-60.8480392077451,1078.29022370571,
348.274728374424));
#110220=CARTESIAN_POINT('Ctrl Pts',(-61.0059658728168,1078.28342170814,
348.274728374424));
#110221=CARTESIAN_POINT('Ctrl Pts',(-61.0059658728168,1078.28342170814,
348.274728374424));
#110222=CARTESIAN_POINT('Ctrl Pts',(-61.0059827805808,1078.28342097991,
348.274728374424));
#110223=CARTESIAN_POINT('Ctrl Pts',(-61.005999688361,1078.2834202517,348.27472837476));
#110224=CARTESIAN_POINT('Ctrl Pts',(-61.0060165961576,1078.2834195235,348.274728375433));
#110225=CARTESIAN_POINT('Ctrl Pts',(-61.1593590601562,1078.27681528043,
348.274734473733));
#110226=CARTESIAN_POINT('Ctrl Pts',(-61.3115017102687,1078.27167170399,
348.3023941924));
#110227=CARTESIAN_POINT('Ctrl Pts',(-61.5294609256413,1078.26656243912,
348.384402300238));
#110228=CARTESIAN_POINT('Ctrl Pts',(-61.6010368702449,1078.26530680575,
348.419261274088));
#110229=CARTESIAN_POINT('Ctrl Pts',(-61.6976455193526,1078.26424351022,
348.478039852353));
#110230=CARTESIAN_POINT('Ctrl Pts',(-61.7256791657564,1078.26401878458,
348.496653631182));
#110231=CARTESIAN_POINT('Ctrl Pts',(-61.7698763406202,1078.26380403625,
348.528588013559));
#110232=CARTESIAN_POINT('Ctrl Pts',(-61.786505005854,1078.26375737109,348.541236062661));
#110233=CARTESIAN_POINT('Ctrl Pts',(-61.8204282979527,1078.26373448169,
348.568379505588));
#110234=CARTESIAN_POINT('Ctrl Pts',(-61.837664018575,1078.26376418286,348.582936894935));
#110235=CARTESIAN_POINT('Ctrl Pts',(-61.8771322488985,1078.26393115545,
348.618107348569));
#110236=CARTESIAN_POINT('Ctrl Pts',(-61.8990337049147,1078.2641018342,348.63907091478));
#110237=CARTESIAN_POINT('Ctrl Pts',(-61.9663995201969,1078.26488343763,
348.708316966918));
#110238=CARTESIAN_POINT('Ctrl Pts',(-62.0088525833007,1078.26577538336,
348.75936876583));
#110239=CARTESIAN_POINT('Ctrl Pts',(-62.1453593331114,1078.27018473839,
348.952296518979));
#110240=CARTESIAN_POINT('Ctrl Pts',(-62.2147952713521,1078.27558502052,
349.109304819584));
#110241=CARTESIAN_POINT('Ctrl Pts',(-62.2816741097721,1078.28876876373,
349.412265919201));
#110242=CARTESIAN_POINT('Ctrl Pts',(-62.289092421718,1078.29588005414,349.553304160252));
#110243=CARTESIAN_POINT('Ctrl Pts',(-62.2564400197717,1078.31236588406,
349.843752420324));
#110244=CARTESIAN_POINT('Ctrl Pts',(-62.2125777372731,1078.32174712249,
349.990562260382));
#110245=CARTESIAN_POINT('Ctrl Pts',(-62.0702790979688,1078.34182755987,
350.271701058825));
#110246=CARTESIAN_POINT('Ctrl Pts',(-61.9693691942809,1078.35238824387,
350.401774119559));
#110247=CARTESIAN_POINT('Ctrl Pts',(-61.7200869783476,1078.37300097648,
350.620281009542));
#110248=CARTESIAN_POINT('Ctrl Pts',(-61.572718682285,1078.38282673004,350.705129347727));
#110249=CARTESIAN_POINT('Ctrl Pts',(-61.2817936853834,1078.39865035328,
350.803115988936));
#110250=CARTESIAN_POINT('Ctrl Pts',(-61.1442812981844,1078.40490853391,
350.825616616696));
#110251=CARTESIAN_POINT('Ctrl Pts',(-61.0059658728173,1078.41010379242,
350.825616616696));
#110252=CARTESIAN_POINT('',(-49.361641103754,1078.70098643656,351.371678279531));
#110253=CARTESIAN_POINT('',(-49.3616411037539,1078.63750051791,348.415072015145));
#110254=CARTESIAN_POINT('Ctrl Pts',(-49.361641103754,1078.70098643656,351.371678279532));
#110255=CARTESIAN_POINT('Ctrl Pts',(-49.2474022975557,1078.70218551221,
351.371678279532));
#110256=CARTESIAN_POINT('Ctrl Pts',(-49.1333327929675,1078.70313956229,
351.358435789987));
#110257=CARTESIAN_POINT('Ctrl Pts',(-48.9242447656558,1078.70448454113,
351.309037947563));
#110258=CARTESIAN_POINT('Ctrl Pts',(-48.8293388095697,1078.70492697835,
351.276151812854));
#110259=CARTESIAN_POINT('Ctrl Pts',(-48.6999965585767,1078.70530180718,
351.216027256903));
#110260=CARTESIAN_POINT('Ctrl Pts',(-48.6622913268644,1078.7053809091,351.196483740757));
#110261=CARTESIAN_POINT('Ctrl Pts',(-48.6026699313023,1078.70545678433,
351.162246594364));
#110262=CARTESIAN_POINT('Ctrl Pts',(-48.5802140089712,1078.70547340844,
351.148541943398));
#110263=CARTESIAN_POINT('Ctrl Pts',(-48.534367693116,1078.70548220577,351.118854907875));
#110264=CARTESIAN_POINT('Ctrl Pts',(-48.5110467815598,1078.7054724093,351.10278460562));
#110265=CARTESIAN_POINT('Ctrl Pts',(-48.4576823902483,1078.70541596183,
351.063704064073));
#110266=CARTESIAN_POINT('Ctrl Pts',(-48.4280320949426,1078.70535806403,
351.040190451367));
#110267=CARTESIAN_POINT('Ctrl Pts',(-48.3374601039413,1078.7050942927,350.962521228007));
#110268=CARTESIAN_POINT('Ctrl Pts',(-48.2800956207935,1078.70479548163,
350.904453426482));
#110269=CARTESIAN_POINT('Ctrl Pts',(-48.1016976331506,1078.70336224855,
350.69121564366));
#110270=CARTESIAN_POINT('Ctrl Pts',(-48.0069076523202,1078.70166332956,
350.516832914347));
#110271=CARTESIAN_POINT('Ctrl Pts',(-47.900552771282,1078.69718193973,350.171972083686));
#110272=CARTESIAN_POINT('Ctrl Pts',(-47.8786484309515,1078.69464832435,
350.007931932167));
#110273=CARTESIAN_POINT('Ctrl Pts',(-47.8901581205458,1078.68834019769,
349.665765819091));
#110274=CARTESIAN_POINT('Ctrl Pts',(-47.9282280257163,1078.68452704653,
349.490401141928));
#110275=CARTESIAN_POINT('Ctrl Pts',(-48.0699098465574,1078.67571466901,
349.149491228314));
#110276=CARTESIAN_POINT('Ctrl Pts',(-48.1768371093475,1078.67072843342,
348.988849273787));
#110277=CARTESIAN_POINT('Ctrl Pts',(-48.4308943937773,1078.66105421524,
348.732369328139));
#110278=CARTESIAN_POINT('Ctrl Pts',(-48.5703201797615,1078.6564704628,348.633201775985));
#110279=CARTESIAN_POINT('Ctrl Pts',(-48.8124860674955,1078.64961844272,
348.517317059492));
#110280=CARTESIAN_POINT('Ctrl Pts',(-48.9054902156945,1078.64720357858,
348.483752957437));
#110281=CARTESIAN_POINT('Ctrl Pts',(-49.1189409154863,1078.642172311,348.430080862271));
#110282=CARTESIAN_POINT('Ctrl Pts',(-49.2399464028628,1078.63965826912,
348.415090001983));
#110283=CARTESIAN_POINT('Ctrl Pts',(-49.3614224096618,1078.63750439515,
348.415072031322));
#110284=CARTESIAN_POINT('Ctrl Pts',(-49.3614953079448,1078.6375031026,348.415072020537));
#110285=CARTESIAN_POINT('Ctrl Pts',(-49.3615682059758,1078.63750181019,
348.415072015145));
#110286=CARTESIAN_POINT('Ctrl Pts',(-49.3616411037539,1078.63750051791,
348.415072015145));
#110287=CARTESIAN_POINT('Ctrl Pts',(-49.3616411037539,1078.63750051791,
348.415072015145));
#110288=CARTESIAN_POINT('Ctrl Pts',(-49.5473794481685,1078.63420789306,
348.415072015145));
#110289=CARTESIAN_POINT('Ctrl Pts',(-49.7314770144804,1078.63181126302,
348.450076940995));
#110290=CARTESIAN_POINT('Ctrl Pts',(-49.9566522384781,1078.63015111076,
348.53893333064));
#110291=CARTESIAN_POINT('Ctrl Pts',(-50.0078076303818,1078.62986890781,
348.562578460187));
#110292=CARTESIAN_POINT('Ctrl Pts',(-50.086610561338,1078.62959029906,348.604620384083));
#110293=CARTESIAN_POINT('Ctrl Pts',(-50.1152030772046,1078.62952401153,
348.621127562959));
#110294=CARTESIAN_POINT('Ctrl Pts',(-50.1647507719704,1078.62947200173,
348.651989432685));
#110295=CARTESIAN_POINT('Ctrl Pts',(-50.1859336821702,1078.62947119004,
348.665952898537));
#110296=CARTESIAN_POINT('Ctrl Pts',(-50.233484907002,1078.62951912204,348.69908434006));
#110297=CARTESIAN_POINT('Ctrl Pts',(-50.2595996327525,1078.62958202898,
348.718593201347));
#110298=CARTESIAN_POINT('Ctrl Pts',(-50.3287621158506,1078.62985018255,
348.773915172431));
#110299=CARTESIAN_POINT('Ctrl Pts',(-50.3704543160287,1078.630125015,348.811335648915));
#110300=CARTESIAN_POINT('Ctrl Pts',(-50.5483957383052,1078.63182779745,
348.990290557874));
#110301=CARTESIAN_POINT('Ctrl Pts',(-50.6577288698742,1078.63440940937,
349.155747720034));
#110302=CARTESIAN_POINT('Ctrl Pts',(-50.7914599112017,1078.64087156722,
349.485437812721));
#110303=CARTESIAN_POINT('Ctrl Pts',(-50.8270896083253,1078.64436959382,
349.641881746109));
#110304=CARTESIAN_POINT('Ctrl Pts',(-50.847880572619,1078.65244966803,349.973843595793));
#110305=CARTESIAN_POINT('Ctrl Pts',(-50.8282401499088,1078.6570331927,350.147277574448));
#110306=CARTESIAN_POINT('Ctrl Pts',(-50.7262824892511,1078.66666845342,
350.491384812048));
#110307=CARTESIAN_POINT('Ctrl Pts',(-50.6404515340994,1078.67164038373,
350.657906846764));
#110308=CARTESIAN_POINT('Ctrl Pts',(-50.4055947837767,1078.68120425931,
350.958155708281));
#110309=CARTESIAN_POINT('Ctrl Pts',(-50.2557877467823,1078.68566765131,
351.086734958728));
#110310=CARTESIAN_POINT('Ctrl Pts',(-49.9194397133287,1078.69326155037,
351.275554836402));
#110311=CARTESIAN_POINT('Ctrl Pts',(-49.7371470374138,1078.69636009907,
351.335790823846));
#110312=CARTESIAN_POINT('Ctrl Pts',(-49.4863747495536,1078.69960458914,
351.367734830859));
#110313=CARTESIAN_POINT('Ctrl Pts',(-49.4239827183277,1078.70033208525,
351.371678279532));
#110314=CARTESIAN_POINT('Ctrl Pts',(-49.361641103754,1078.70098643656,351.371678279532));
#110315=CARTESIAN_POINT('',(-32.7463814565112,1078.70364178837,342.741777359158));
#110316=CARTESIAN_POINT('',(-32.7463814565112,1078.63286818763,339.785171094771));
#110317=CARTESIAN_POINT('Ctrl Pts',(-32.7463814565111,1078.70364178837,
342.741777359158));
#110318=CARTESIAN_POINT('Ctrl Pts',(-32.6713741841051,1078.70414194159,
342.741777359158));
#110319=CARTESIAN_POINT('Ctrl Pts',(-32.5963229919856,1078.70453928808,
342.736068777415));
#110320=CARTESIAN_POINT('Ctrl Pts',(-32.4619676045483,1078.70507352558,
342.715425854039));
#110321=CARTESIAN_POINT('Ctrl Pts',(-32.4026747646749,1078.70524517308,
342.702543552129));
#110322=CARTESIAN_POINT('Ctrl Pts',(-32.3096229810331,1078.70541410201,
342.676245888326));
#110323=CARTESIAN_POINT('Ctrl Pts',(-32.2752761282601,1078.70545376002,
342.665166599314));
#110324=CARTESIAN_POINT('Ctrl Pts',(-32.2116579431705,1078.70548445708,
342.642042431627));
#110325=CARTESIAN_POINT('Ctrl Pts',(-32.182300878416,1078.70548089485,342.630292661137));
#110326=CARTESIAN_POINT('Ctrl Pts',(-32.1179106121875,1078.70543316383,
342.60209321987));
#110327=CARTESIAN_POINT('Ctrl Pts',(-32.0831007842742,1078.70538011837,
342.585190972261));
#110328=CARTESIAN_POINT('Ctrl Pts',(-31.9856063501934,1078.70515161973,
342.533029089356));
#110329=CARTESIAN_POINT('Ctrl Pts',(-31.924777075105,1078.70491063053,342.494536557997));
#110330=CARTESIAN_POINT('Ctrl Pts',(-31.7089434112895,1078.70365917325,
342.334810492918));
#110331=CARTESIAN_POINT('Ctrl Pts',(-31.5758117086972,1078.70205794374,
342.187487834967));
#110332=CARTESIAN_POINT('Ctrl Pts',(-31.391956447934,1078.69776982643,341.877974582164));
#110333=CARTESIAN_POINT('Ctrl Pts',(-31.3323784881597,1078.69533634405,
341.724634479672));
#110334=CARTESIAN_POINT('Ctrl Pts',(-31.2630177903554,1078.6892374063,341.391358707963));
#110335=CARTESIAN_POINT('Ctrl Pts',(-31.2583746289087,1078.68553075741,
341.21296768739));
#110336=CARTESIAN_POINT('Ctrl Pts',(-31.3143545559451,1078.67691354353,
340.850199183331));
#110337=CARTESIAN_POINT('Ctrl Pts',(-31.3792849734701,1078.67201134558,
340.669724489054));
#110338=CARTESIAN_POINT('Ctrl Pts',(-31.5763580872497,1078.66173191616,
340.339144076358));
#110339=CARTESIAN_POINT('Ctrl Pts',(-31.7082342479793,1078.65644880894,
340.193150117647));
#110340=CARTESIAN_POINT('Ctrl Pts',(-31.9687313552379,1078.64821972667,
339.999565526789));
#110341=CARTESIAN_POINT('Ctrl Pts',(-32.0825776364142,1078.64512142403,
339.936231817622));
#110342=CARTESIAN_POINT('Ctrl Pts',(-32.3761475540104,1078.63836207686,
339.820257205896));
#110343=CARTESIAN_POINT('Ctrl Pts',(-32.5604271771752,1078.63510338789,
339.785171133029));
#110344=CARTESIAN_POINT('Ctrl Pts',(-32.7463811523675,1078.63286819129,
339.785171094771));
#110345=CARTESIAN_POINT('Ctrl Pts',(-32.7463814565112,1078.63286818763,
339.785171094771));
#110346=CARTESIAN_POINT('Ctrl Pts',(-32.8530886027707,1078.63158555127,
339.785171094771));
#110347=CARTESIAN_POINT('Ctrl Pts',(-32.9594854136948,1078.63064964381,
339.796724557869));
#110348=CARTESIAN_POINT('Ctrl Pts',(-33.1088409688472,1078.6298487241,339.829550125131));
#110349=CARTESIAN_POINT('Ctrl Pts',(-33.1534811476541,1078.62967771178,
339.841579322797));
#110350=CARTESIAN_POINT('Ctrl Pts',(-33.2287139910778,1078.62950852057,
339.865686373331));
#110351=CARTESIAN_POINT('Ctrl Pts',(-33.2596017028888,1078.62947461875,
339.876729642869));
#110352=CARTESIAN_POINT('Ctrl Pts',(-33.3212695504499,1078.62947974259,
339.901120527232));
#110353=CARTESIAN_POINT('Ctrl Pts',(-33.3520140885504,1078.62952040567,
339.914506831955));
#110354=CARTESIAN_POINT('Ctrl Pts',(-33.4257326566979,1078.6297118798,339.949632817897));
#110355=CARTESIAN_POINT('Ctrl Pts',(-33.4681508808316,1078.62990288704,
339.972448998294));
#110356=CARTESIAN_POINT('Ctrl Pts',(-33.6098470881348,1078.63082348223,
340.057834916935));
#110357=CARTESIAN_POINT('Ctrl Pts',(-33.7027488075639,1078.63193031958,
340.130116966911));
#110358=CARTESIAN_POINT('Ctrl Pts',(-33.8919236819845,1078.63537423128,
340.317290290093));
#110359=CARTESIAN_POINT('Ctrl Pts',(-33.9813026029615,1078.63794233502,
340.437341501565));
#110360=CARTESIAN_POINT('Ctrl Pts',(-34.1286422639572,1078.64438118988,
340.714059363595));
#110361=CARTESIAN_POINT('Ctrl Pts',(-34.1812054568531,1078.64831415834,
340.871331955417));
#110362=CARTESIAN_POINT('Ctrl Pts',(-34.2343278454567,1078.65708324425,
341.209410210286));
#110363=CARTESIAN_POINT('Ctrl Pts',(-34.2300629536692,1078.66189057828,
341.388353896305));
#110364=CARTESIAN_POINT('Ctrl Pts',(-34.1557398972309,1078.67172127567,
341.748512799217));
#110365=CARTESIAN_POINT('Ctrl Pts',(-34.0817114907015,1078.67664045421,
341.92563206815));
#110366=CARTESIAN_POINT('Ctrl Pts',(-33.8681204439433,1078.68571166209,
342.245807905333));
#110367=CARTESIAN_POINT('Ctrl Pts',(-33.7291470577312,1078.68975641055,
342.384838922209));
#110368=CARTESIAN_POINT('Ctrl Pts',(-33.4132957289521,1078.69637206328,
342.595712884842));
#110369=CARTESIAN_POINT('Ctrl Pts',(-33.2414233519641,1078.69895403983,
342.668669691896));
#110370=CARTESIAN_POINT('Ctrl Pts',(-32.9571302673294,1078.70203309239,
342.730501098562));
#110371=CARTESIAN_POINT('Ctrl Pts',(-32.8517992372279,1078.70293885596,
342.741777359158));
#110372=CARTESIAN_POINT('Ctrl Pts',(-32.7463814565111,1078.70364178837,
342.741777359158));
#110373=CARTESIAN_POINT('Origin',(0.,1121.00270384563,424.620242579854));
#110374=CARTESIAN_POINT('',(0.,1120.6032985308,433.13766592946));
#110375=CARTESIAN_POINT('Origin',(0.,1120.6032985308,424.620242579854));
#110376=CARTESIAN_POINT('',(-1.07991983210742E-15,1121.50270384563,433.438457210059));
#110377=CARTESIAN_POINT('Origin',(-1.07991983210742E-15,1121.00270384563,
433.438457210059));
#110378=CARTESIAN_POINT('Origin',(0.,1121.50270384563,424.620242579854));
#110379=CARTESIAN_POINT('Origin',(-96.6088930673541,1067.7251047501,419.724828926582));
#110380=CARTESIAN_POINT('',(-96.6088930673714,1076.34045666952,418.449384805446));
#110381=CARTESIAN_POINT('',(-96.6088930673541,1067.7251047501,418.449384805446));
#110382=CARTESIAN_POINT('Ctrl Pts',(-96.6091111714779,1076.34879426825,
421.00027302907));
#110383=CARTESIAN_POINT('Ctrl Pts',(-96.6934658979017,1076.34336808336,
421.000258604201));
#110384=CARTESIAN_POINT('Ctrl Pts',(-96.7776101869679,1076.33788022423,
420.991875696778));
#110385=CARTESIAN_POINT('Ctrl Pts',(-97.0246046251495,1076.32155185089,
420.942214030049));
#110386=CARTESIAN_POINT('Ctrl Pts',(-97.1808249622019,1076.31092564066,
420.877113178739));
#110387=CARTESIAN_POINT('Ctrl Pts',(-97.4590385965904,1076.29151215733,
420.690261995754));
#110388=CARTESIAN_POINT('Ctrl Pts',(-97.578386193813,1076.28291423195,420.570367896947));
#110389=CARTESIAN_POINT('Ctrl Pts',(-97.7636848388148,1076.2691425121,420.291538056674));
#110390=CARTESIAN_POINT('Ctrl Pts',(-97.8279726351012,1076.26409798675,
420.135421129003));
#110391=CARTESIAN_POINT('Ctrl Pts',(-97.8925180619294,1076.25842139181,
419.807694921063));
#110392=CARTESIAN_POINT('Ctrl Pts',(-97.8923486646185,1076.25783277121,
419.639350332658));
#110393=CARTESIAN_POINT('Ctrl Pts',(-97.8272870029328,1076.26123041105,
419.312532654493));
#110394=CARTESIAN_POINT('Ctrl Pts',(-97.7631404829371,1076.26517449256,
419.157242625782));
#110395=CARTESIAN_POINT('Ctrl Pts',(-97.5788022868022,1076.27698529881,
418.879974273196));
#110396=CARTESIAN_POINT('Ctrl Pts',(-97.4603375294596,1076.28473799535,
418.760722871916));
#110397=CARTESIAN_POINT('Ctrl Pts',(-97.184031603033,1076.30287163333,418.574250135011));
#110398=CARTESIAN_POINT('Ctrl Pts',(-97.0287317697544,1076.31308155743,
418.50896656265));
#110399=CARTESIAN_POINT('Ctrl Pts',(-96.7835295820195,1076.32910110253,
418.458641213602));
#110400=CARTESIAN_POINT('Ctrl Pts',(-96.7002900684221,1076.33452396562,
418.449926958333));
#110401=CARTESIAN_POINT('Ctrl Pts',(-96.5334138301987,1076.34535623463,
418.448892315101));
#110402=CARTESIAN_POINT('Ctrl Pts',(-96.450172515565,1076.35073999321,418.456554280965));
#110403=CARTESIAN_POINT('Ctrl Pts',(-96.202237145488,1076.36671788244,418.504184046656));
#110404=CARTESIAN_POINT('Ctrl Pts',(-96.0441417310531,1076.3768219841,418.568787674226));
#110405=CARTESIAN_POINT('Ctrl Pts',(-95.7628312524325,1076.39475610547,
418.755631963734));
#110406=CARTESIAN_POINT('Ctrl Pts',(-95.6422513989531,1076.40242267967,
418.875824267539));
#110407=CARTESIAN_POINT('Ctrl Pts',(-95.4545203116411,1076.41453184978,
419.15667837884));
#110408=CARTESIAN_POINT('Ctrl Pts',(-95.389402564051,1076.41884917017,419.314653376189));
#110409=CARTESIAN_POINT('Ctrl Pts',(-95.3245375004729,1076.4236669704,419.647371493635));
#110410=CARTESIAN_POINT('Ctrl Pts',(-95.3256387503052,1076.42411022557,
419.81879984222));
#110411=CARTESIAN_POINT('Ctrl Pts',(-95.394816262567,1076.42102943628,420.150827440191));
#110412=CARTESIAN_POINT('Ctrl Pts',(-95.4620611281913,1076.41754260207,
420.308103464037));
#110413=CARTESIAN_POINT('Ctrl Pts',(-95.653643033737,1076.40695423484,420.586643512474));
#110414=CARTESIAN_POINT('Ctrl Pts',(-95.7758659371814,1076.39996626672,
420.705263612867));
#110415=CARTESIAN_POINT('Ctrl Pts',(-96.0595238157265,1076.3831610753,420.888225198292));
#110416=CARTESIAN_POINT('Ctrl Pts',(-96.2182291908095,1076.37349975092,
420.950652212279));
#110417=CARTESIAN_POINT('Ctrl Pts',(-96.4585900798052,1076.35841675149,
420.993624920888));
#110418=CARTESIAN_POINT('Ctrl Pts',(-96.5337802450701,1076.35363999001,
421.000285910846));
#110419=CARTESIAN_POINT('Ctrl Pts',(-96.6091111714779,1076.34879426825,
421.00027302907));
#110420=CARTESIAN_POINT('Origin',(-96.6088930673541,1067.7251047501,419.724828926582));
#110421=CARTESIAN_POINT('',(-96.6088930673541,1076.34724098047,420.400273047718));
#110422=CARTESIAN_POINT('',(-96.6088930673541,1076.34281999372,419.049384805446));
#110423=CARTESIAN_POINT('Ctrl Pts',(-96.6088930673539,1076.34724098048,
420.400273047718));
#110424=CARTESIAN_POINT('Ctrl Pts',(-96.6630013691699,1076.34375464799,
420.400273047718));
#110425=CARTESIAN_POINT('Ctrl Pts',(-96.7170432733172,1076.34023157328,
420.393771073853));
#110426=CARTESIAN_POINT('Ctrl Pts',(-96.8568536895203,1076.3310097968,420.359468532486));
#110427=CARTESIAN_POINT('Ctrl Pts',(-96.9387782122827,1076.32549269668,
420.321013241726));
#110428=CARTESIAN_POINT('Ctrl Pts',(-97.0820158891483,1076.31565002899,
420.21495872601));
#110429=CARTESIAN_POINT('Ctrl Pts',(-97.1421790804019,1076.31140735321,
420.148728473975));
#110430=CARTESIAN_POINT('Ctrl Pts',(-97.2333937131289,1076.30477649208,
419.996938823552));
#110431=CARTESIAN_POINT('Ctrl Pts',(-97.263630432367,1076.30244937286,419.912906040649));
#110432=CARTESIAN_POINT('Ctrl Pts',(-97.2899522751061,1076.30007551188,
419.738113677132));
#110433=CARTESIAN_POINT('Ctrl Pts',(-97.2858573195978,1076.30004731371,
419.64908162663));
#110434=CARTESIAN_POINT('Ctrl Pts',(-97.243660907243,1076.3023088206,419.47768620825));
#110435=CARTESIAN_POINT('Ctrl Pts',(-97.2059913611933,1076.30457463278,
419.396995971581));
#110436=CARTESIAN_POINT('Ctrl Pts',(-97.1017281190888,1076.31108244457,
419.254573937871));
#110437=CARTESIAN_POINT('Ctrl Pts',(-97.0361007336843,1076.31526324838,
419.194256128484));
#110438=CARTESIAN_POINT('Ctrl Pts',(-96.8852372927702,1076.32495029318,
419.10218282481));
#110439=CARTESIAN_POINT('Ctrl Pts',(-96.8014020866585,1076.33036553896,
419.071386849031));
#110440=CARTESIAN_POINT('Ctrl Pts',(-96.6792674609004,1076.33826497715,
419.052139225811));
#110441=CARTESIAN_POINT('Ctrl Pts',(-96.6441196379992,1076.34053956284,
419.049386150044));
#110442=CARTESIAN_POINT('Ctrl Pts',(-96.6089188583591,1076.34281832411,
419.049384805945));
#110443=CARTESIAN_POINT('Ctrl Pts',(-96.6089102613534,1076.34281888064,
419.049384805617));
#110444=CARTESIAN_POINT('Ctrl Pts',(-96.6089016643518,1076.34281943718,
419.049384805446));
#110445=CARTESIAN_POINT('Ctrl Pts',(-96.6088930673541,1076.34281999372,
419.049384805446));
#110446=CARTESIAN_POINT('',(-96.6088930673541,1082.7251047501,419.049384805446));
#110447=CARTESIAN_POINT('',(-96.6088930673541,1067.7251047501,419.049384805446));
#110448=CARTESIAN_POINT('Origin',(-96.6088930673541,1082.7251047501,419.724828926582));
#110449=CARTESIAN_POINT('Ctrl Pts',(-96.6088930673541,1076.34281999372,
419.049384805446));
#110450=CARTESIAN_POINT('Ctrl Pts',(-96.5647749711265,1076.34567602779,
419.049384805446));
#110451=CARTESIAN_POINT('Ctrl Pts',(-96.5207611365838,1076.3485264382,419.053707309114));
#110452=CARTESIAN_POINT('Ctrl Pts',(-96.3893344285309,1076.35704212704,
419.079774994987));
#110453=CARTESIAN_POINT('Ctrl Pts',(-96.3055315220453,1076.36247676985,
419.114680582747));
#110454=CARTESIAN_POINT('Ctrl Pts',(-96.1566135189695,1076.3721827834,419.215198003661));
#110455=CARTESIAN_POINT('Ctrl Pts',(-96.0929422216552,1076.37636121942,
419.279758926146));
#110456=CARTESIAN_POINT('Ctrl Pts',(-95.9944757732211,1076.38295249723,
419.430191596767));
#110457=CARTESIAN_POINT('Ctrl Pts',(-95.9607219633189,1076.38529735789,
419.51458425605));
#110458=CARTESIAN_POINT('Ctrl Pts',(-95.9282585263141,1076.3878511197,419.691815258127));
#110459=CARTESIAN_POINT('Ctrl Pts',(-95.9299334347195,1076.38803143259,
419.782862020509));
#110460=CARTESIAN_POINT('Ctrl Pts',(-95.9689054643075,1076.38618059823,
419.958818508899));
#110461=CARTESIAN_POINT('Ctrl Pts',(-96.0057648545025,1076.38417032814,
420.041946979932));
#110462=CARTESIAN_POINT('Ctrl Pts',(-96.1097622097469,1076.37818175468,
420.188687195005));
#110463=CARTESIAN_POINT('Ctrl Pts',(-96.1757946134576,1076.37426617928,
420.250861067473));
#110464=CARTESIAN_POINT('Ctrl Pts',(-96.3283172821437,1076.36498138409,
420.345778970902));
#110465=CARTESIAN_POINT('Ctrl Pts',(-96.4133104738226,1076.35970172009,
420.37754595798));
#110466=CARTESIAN_POINT('Ctrl Pts',(-96.5374317443997,1076.35182760772,
420.397440208269));
#110467=CARTESIAN_POINT('Ctrl Pts',(-96.5731768688769,1076.34954226399,
420.400273047718));
#110468=CARTESIAN_POINT('Ctrl Pts',(-96.6088930673539,1076.34724098048,
420.400273047718));
#110469=CARTESIAN_POINT('Origin',(-103.499585384594,1067.7251047501,407.710811438872));
#110470=CARTESIAN_POINT('',(-103.499585384625,1075.63641735374,406.61198030288));
#110471=CARTESIAN_POINT('',(-103.499585384594,1067.7251047501,406.61198030288));
#110472=CARTESIAN_POINT('Ctrl Pts',(-103.499237229524,1075.67335103125,
408.80964251971));
#110473=CARTESIAN_POINT('Ctrl Pts',(-103.570842938863,1075.66603801704,
408.809665207356));
#110474=CARTESIAN_POINT('Ctrl Pts',(-103.642272130286,1075.65859878446,
408.80268854293));
#110475=CARTESIAN_POINT('Ctrl Pts',(-103.857312099209,1075.63575788223,
408.760215201832));
#110476=CARTESIAN_POINT('Ctrl Pts',(-103.994938595762,1075.62050843749,
408.702716643784));
#110477=CARTESIAN_POINT('Ctrl Pts',(-104.236668660875,1075.59247150676,
408.538474848238));
#110478=CARTESIAN_POINT('Ctrl Pts',(-104.339136961286,1075.57990651222,
408.434379507201));
#110479=CARTESIAN_POINT('Ctrl Pts',(-104.497456465949,1075.55902288678,
408.192895957227));
#110480=CARTESIAN_POINT('Ctrl Pts',(-104.55203586182,1075.55088577264,408.058053343401));
#110481=CARTESIAN_POINT('Ctrl Pts',(-104.605830509118,1075.54025643221,
407.775581124673));
#110482=CARTESIAN_POINT('Ctrl Pts',(-104.604847733568,1075.53783727971,
407.630841402448));
#110483=CARTESIAN_POINT('Ctrl Pts',(-104.547371063327,1075.53907653389,
407.350209343589));
#110484=CARTESIAN_POINT('Ctrl Pts',(-104.491602637381,1075.5427058224,407.217099347191));
#110485=CARTESIAN_POINT('Ctrl Pts',(-104.332126057741,1075.55552449156,
406.979489664524));
#110486=CARTESIAN_POINT('Ctrl Pts',(-104.229872213046,1075.56459934331,
406.877410552782));
#110487=CARTESIAN_POINT('Ctrl Pts',(-103.991532047764,1075.58696970732,
406.71777712761));
#110488=CARTESIAN_POINT('Ctrl Pts',(-103.857541658741,1075.60007222497,
406.662038734679));
#110489=CARTESIAN_POINT('Ctrl Pts',(-103.646058401863,1075.62136958147,
406.619401133722));
#110490=CARTESIAN_POINT('Ctrl Pts',(-103.574148099986,1075.6287101144,406.612145678));
#110491=CARTESIAN_POINT('Ctrl Pts',(-103.430023932663,1075.64360756256,
406.61182061805));
#110492=CARTESIAN_POINT('Ctrl Pts',(-103.358144535959,1075.65112975667,
406.618742976178));
#110493=CARTESIAN_POINT('Ctrl Pts',(-103.144009500649,1075.6738153511,406.660872723149));
#110494=CARTESIAN_POINT('Ctrl Pts',(-103.007547154574,1075.68865114894,
406.717459821904));
#110495=CARTESIAN_POINT('Ctrl Pts',(-102.765411353305,1075.71582812797,
406.880396711323));
#110496=CARTESIAN_POINT('Ctrl Pts',(-102.661909954341,1075.72792217764,
406.984877355043));
#110497=CARTESIAN_POINT('Ctrl Pts',(-102.501633689167,1075.74789608371,
407.228361262746));
#110498=CARTESIAN_POINT('Ctrl Pts',(-102.446449642118,1075.75558042025,
407.364917638641));
#110499=CARTESIAN_POINT('Ctrl Pts',(-102.392620475075,1075.76555576074,
407.652125573174));
#110500=CARTESIAN_POINT('Ctrl Pts',(-102.394636540744,1075.76773602572,
407.799843881201));
#110501=CARTESIAN_POINT('Ctrl Pts',(-102.455810470833,1075.76626291771,
408.082988733887));
#110502=CARTESIAN_POINT('Ctrl Pts',(-102.513202388073,1075.76274081205,
408.215781884077));
#110503=CARTESIAN_POINT('Ctrl Pts',(-102.677110990787,1075.75034653712,
408.453944106876));
#110504=CARTESIAN_POINT('Ctrl Pts',(-102.782837580232,1075.74150132232,
408.556332158873));
#110505=CARTESIAN_POINT('Ctrl Pts',(-103.027985011516,1075.71953762433,
408.713951888631));
#110506=CARTESIAN_POINT('Ctrl Pts',(-103.165014956945,1075.70662837047,
408.767544630906));
#110507=CARTESIAN_POINT('Ctrl Pts',(-103.371398898217,1075.68629194353,
408.804015321739));
#110508=CARTESIAN_POINT('Ctrl Pts',(-103.435264134528,1075.67988453476,
408.809622250391));
#110509=CARTESIAN_POINT('Ctrl Pts',(-103.499237229524,1075.67335103125,
408.80964251971));
#110510=CARTESIAN_POINT('Origin',(-103.499585384594,1067.7251047501,407.710811438872));
#110511=CARTESIAN_POINT('',(-103.499585384594,1075.66376111901,408.209642574865));
#110512=CARTESIAN_POINT('',(-103.499585384594,1075.64701319545,407.21198030288));
#110513=CARTESIAN_POINT('Ctrl Pts',(-103.499585384594,1075.66376111901,
408.209642574865));
#110514=CARTESIAN_POINT('Ctrl Pts',(-103.502071362693,1075.66350639334,
408.209642574865));
#110515=CARTESIAN_POINT('Ctrl Pts',(-103.504557676489,1075.66325128953,
408.209623991148));
#110516=CARTESIAN_POINT('Ctrl Pts',(-103.539600239299,1075.65965095847,
408.209099961378));
#110517=CARTESIAN_POINT('Ctrl Pts',(-103.572028400505,1075.6562601718,408.205426810701));
#110518=CARTESIAN_POINT('Ctrl Pts',(-103.669219505184,1075.64591619944,
408.184650261159));
#110519=CARTESIAN_POINT('Ctrl Pts',(-103.731134995342,1075.63907092801,
408.157680344789));
#110520=CARTESIAN_POINT('Ctrl Pts',(-103.840052189201,1075.6265048167,408.081333398875));
#110521=CARTESIAN_POINT('Ctrl Pts',(-103.886164608578,1075.62089391449,
408.032956602154));
#110522=CARTESIAN_POINT('Ctrl Pts',(-103.956328176386,1075.61170073141,
407.921713108968));
#110523=CARTESIAN_POINT('Ctrl Pts',(-103.980008644332,1075.60818007301,
407.86015016588));
#110524=CARTESIAN_POINT('Ctrl Pts',(-104.002208409432,1075.60366971968,
407.731620100496));
#110525=CARTESIAN_POINT('Ctrl Pts',(-104.000640174725,1075.60271181179,
407.665959140142));
#110526=CARTESIAN_POINT('Ctrl Pts',(-103.972385499019,1075.6034971417,407.539015070644));
#110527=CARTESIAN_POINT('Ctrl Pts',(-103.946022142635,1075.6052280724,407.478992720413));
#110528=CARTESIAN_POINT('Ctrl Pts',(-103.871712953719,1075.61116235175,
407.37229473525));
#110529=CARTESIAN_POINT('Ctrl Pts',(-103.824434517262,1075.61531430681,
407.326716025527));
#110530=CARTESIAN_POINT('Ctrl Pts',(-103.714848323074,1075.62550452348,
407.25609274143));
#110531=CARTESIAN_POINT('Ctrl Pts',(-103.653511860268,1075.63145482351,
407.2318550433));
#110532=CARTESIAN_POINT('Ctrl Pts',(-103.559699774815,1075.64086023512,
407.214701920339));
#110533=CARTESIAN_POINT('Ctrl Pts',(-103.529670011463,1075.64391337157,
407.21198030288));
#110534=CARTESIAN_POINT('Ctrl Pts',(-103.499585384594,1075.64701319545,
407.21198030288));
#110535=CARTESIAN_POINT('',(-103.499585384594,1082.7251047501,407.21198030288));
#110536=CARTESIAN_POINT('',(-103.499585384594,1067.7251047501,407.21198030288));
#110537=CARTESIAN_POINT('Origin',(-103.499585384594,1082.7251047501,407.710811438872));
#110538=CARTESIAN_POINT('Ctrl Pts',(-103.499585384594,1075.64701319545,
407.21198030288));
#110539=CARTESIAN_POINT('Ctrl Pts',(-103.499513271807,1075.64702062572,
407.21198030288));
#110540=CARTESIAN_POINT('Ctrl Pts',(-103.499441158706,1075.64702805626,
407.211980318517));
#110541=CARTESIAN_POINT('Ctrl Pts',(-103.499369045294,1075.64703548707,
407.211980349792));
#110542=CARTESIAN_POINT('Ctrl Pts',(-103.466724572183,1075.65039928297,
407.211994507455));
#110543=CARTESIAN_POINT('Ctrl Pts',(-103.434161726441,1075.65380296785,
407.21521310209));
#110544=CARTESIAN_POINT('Ctrl Pts',(-103.33689583746,1075.664116205,407.23458513421));
#110545=CARTESIAN_POINT('Ctrl Pts',(-103.274865982197,1075.67089625435,
407.260512561931));
#110546=CARTESIAN_POINT('Ctrl Pts',(-103.164782694419,1075.68336832813,
407.335116923966));
#110547=CARTESIAN_POINT('Ctrl Pts',(-103.117760449514,1075.68894240784,
407.382991737611));
#110548=CARTESIAN_POINT('Ctrl Pts',(-103.045243081654,1075.69814449495,
407.494430475869));
#110549=CARTESIAN_POINT('Ctrl Pts',(-103.020460482078,1075.70168204059,
407.556856021544));
#110550=CARTESIAN_POINT('Ctrl Pts',(-102.997130157182,1075.70617793649,
407.686349243561));
#110551=CARTESIAN_POINT('Ctrl Pts',(-102.998218997141,1075.70715000442,
407.751994498134));
#110552=CARTESIAN_POINT('Ctrl Pts',(-103.025545812247,1075.70648900357,
407.879183199904));
#110553=CARTESIAN_POINT('Ctrl Pts',(-103.051505854999,1075.70486302484,
407.939459087447));
#110554=CARTESIAN_POINT('Ctrl Pts',(-103.125173240855,1075.69918689037,
408.046820779613));
#110555=CARTESIAN_POINT('Ctrl Pts',(-103.172230360576,1075.69518359488,
408.092792831827));
#110556=CARTESIAN_POINT('Ctrl Pts',(-103.282414929773,1075.68518922301,
408.164786984131));
#110557=CARTESIAN_POINT('Ctrl Pts',(-103.344761955394,1075.6792567197,408.189633794588));
#110558=CARTESIAN_POINT('Ctrl Pts',(-103.43962405692,1075.66985494325,408.206935319653));
#110559=CARTESIAN_POINT('Ctrl Pts',(-103.469580270733,1075.66683559205,
408.209642574865));
#110560=CARTESIAN_POINT('Ctrl Pts',(-103.499585384594,1075.66376111901,
408.209642574865));
#110561=CARTESIAN_POINT('Origin',(-107.832717977552,1067.7251047501,394.412017622821));
#110562=CARTESIAN_POINT('',(-107.832717977578,1074.76154318277,393.321476874093));
#110563=CARTESIAN_POINT('',(-107.832717977552,1067.7251047501,393.321476874093));
#110564=CARTESIAN_POINT('Ctrl Pts',(-107.832910139828,1074.84118131354,
395.502558354619));
#110565=CARTESIAN_POINT('Ctrl Pts',(-107.903854913976,1074.8319916062,395.502545853564));
#110566=CARTESIAN_POINT('Ctrl Pts',(-107.974605324901,1074.82255439571,
395.49561052102));
#110567=CARTESIAN_POINT('Ctrl Pts',(-108.113974483817,1074.80341334749,
395.468066248453));
#110568=CARTESIAN_POINT('Ctrl Pts',(-108.18227296561,1074.79375135477,395.447466853533));
#110569=CARTESIAN_POINT('Ctrl Pts',(-108.383552042772,1074.76439718822,
395.364555872695));
#110570=CARTESIAN_POINT('Ctrl Pts',(-108.506532479351,1074.7451943403,395.281961889542));
#110571=CARTESIAN_POINT('Ctrl Pts',(-108.710269160931,1074.71067322688,
395.075172153568));
#110572=CARTESIAN_POINT('Ctrl Pts',(-108.789989509366,1074.69560519737,
394.953902490361));
#110573=CARTESIAN_POINT('Ctrl Pts',(-108.897265991725,1074.67147159055,
394.688279698583));
#110574=CARTESIAN_POINT('Ctrl Pts',(-108.924291576163,1074.66258573781,
394.546786497073));
#110575=CARTESIAN_POINT('Ctrl Pts',(-108.922174602421,1074.65223823734,
394.262243588738));
#110576=CARTESIAN_POINT('Ctrl Pts',(-108.893527587802,1074.65082028394,
394.122102134176));
#110577=CARTESIAN_POINT('Ctrl Pts',(-108.784263529771,1074.65563152539,
393.86077721138));
#110578=CARTESIAN_POINT('Ctrl Pts',(-108.704843923112,1074.66179882768,
393.742226857959));
#110579=CARTESIAN_POINT('Ctrl Pts',(-108.504816332335,1074.68093510674,
393.541519893516));
#110580=CARTESIAN_POINT('Ctrl Pts',(-108.38594290611,1074.69375465292,393.461601719654));
#110581=CARTESIAN_POINT('Ctrl Pts',(-108.123388677827,1074.72440253584,
393.351225217733));
#110582=CARTESIAN_POINT('Ctrl Pts',(-107.981978401088,1074.74198570064,
393.322346248265));
#110583=CARTESIAN_POINT('Ctrl Pts',(-107.767590175171,1074.7700758924,393.321069769749));
#110584=CARTESIAN_POINT('Ctrl Pts',(-107.696120910827,1074.77967830712,
393.327700062632));
#110585=CARTESIAN_POINT('Ctrl Pts',(-107.555795427375,1074.79900268354,
393.354812807297));
#110586=CARTESIAN_POINT('Ctrl Pts',(-107.48724521197,1074.80868084317,393.375186810816));
#110587=CARTESIAN_POINT('Ctrl Pts',(-107.287030355667,1074.83768519115,
393.456775942496));
#110588=CARTESIAN_POINT('Ctrl Pts',(-107.164973574096,1074.85640529594,
393.537680045991));
#110589=CARTESIAN_POINT('Ctrl Pts',(-106.960070173757,1074.89018328405,
393.742234430188));
#110590=CARTESIAN_POINT('Ctrl Pts',(-106.878990434508,1074.90493716678,
393.863688363703));
#110591=CARTESIAN_POINT('Ctrl Pts',(-106.768955434767,1074.92860023213,
394.13158258457));
#110592=CARTESIAN_POINT('Ctrl Pts',(-106.741091560602,1074.93727445006,
394.275284544965));
#110593=CARTESIAN_POINT('Ctrl Pts',(-106.743300631791,1074.94721750422,
394.562049905487));
#110594=CARTESIAN_POINT('Ctrl Pts',(-106.771973979401,1074.9485604562,394.702155806973));
#110595=CARTESIAN_POINT('Ctrl Pts',(-106.881415658133,1074.94396263451,
394.963773820071));
#110596=CARTESIAN_POINT('Ctrl Pts',(-106.961137569745,1074.93805868516,
395.082601658698));
#110597=CARTESIAN_POINT('Ctrl Pts',(-107.163657499755,1074.91946644001,
395.285309568277));
#110598=CARTESIAN_POINT('Ctrl Pts',(-107.28531438269,1074.90681428368,395.366215762831));
#110599=CARTESIAN_POINT('Ctrl Pts',(-107.550499991754,1074.8766722165,395.474958483077));
#110600=CARTESIAN_POINT('Ctrl Pts',(-107.691128263104,1074.85954678119,
395.502583337756));
#110601=CARTESIAN_POINT('Ctrl Pts',(-107.832910139828,1074.84118131354,
395.502558354619));
#110602=CARTESIAN_POINT('Origin',(-107.832717977552,1067.7251047501,394.412017622821));
#110603=CARTESIAN_POINT('',(-107.832717977552,1074.8199670159,394.902558371549));
#110604=CARTESIAN_POINT('',(-107.832717977552,1074.78413642061,393.921476874093));
#110605=CARTESIAN_POINT('Ctrl Pts',(-107.832717977552,1074.8199670159,394.902558371549));
#110606=CARTESIAN_POINT('Ctrl Pts',(-107.83392382367,1074.81981027287,394.902558371549));
#110607=CARTESIAN_POINT('Ctrl Pts',(-107.835129853334,1074.81965333798,
394.902553925238));
#110608=CARTESIAN_POINT('Ctrl Pts',(-107.86832801063,1074.81532879109,394.90230906005));
#110609=CARTESIAN_POINT('Ctrl Pts',(-107.900210461572,1074.81105729803,
394.898944004619));
#110610=CARTESIAN_POINT('Ctrl Pts',(-107.962902415974,1074.80241994308,
394.886051563901));
#110611=CARTESIAN_POINT('Ctrl Pts',(-107.993569896714,1074.79807321681,
394.876542057167));
#110612=CARTESIAN_POINT('Ctrl Pts',(-108.0836376156,1074.7849281648,394.838615112471));
#110613=CARTESIAN_POINT('Ctrl Pts',(-108.138510467907,1074.77637628905,
394.801188906155));
#110614=CARTESIAN_POINT('Ctrl Pts',(-108.229681180665,1074.76098307302,
394.707430962913));
#110615=CARTESIAN_POINT('Ctrl Pts',(-108.265341803572,1074.75426851599,
394.652254555808));
#110616=CARTESIAN_POINT('Ctrl Pts',(-108.312644906129,1074.74361978502,
394.532021316516));
#110617=CARTESIAN_POINT('Ctrl Pts',(-108.324227019244,1074.7397446815,394.468334043055));
#110618=CARTESIAN_POINT('Ctrl Pts',(-108.322171678761,1074.73529550747,
394.340428915001));
#110619=CARTESIAN_POINT('Ctrl Pts',(-108.308745384814,1074.73474192927,
394.277513882568));
#110620=CARTESIAN_POINT('Ctrl Pts',(-108.258576734306,1074.73702777487,
394.160357857072));
#110621=CARTESIAN_POINT('Ctrl Pts',(-108.222360722634,1074.73984155129,
394.107304158825));
#110622=CARTESIAN_POINT('Ctrl Pts',(-108.131503147455,1074.74849574992,
394.017740314956));
#110623=CARTESIAN_POINT('Ctrl Pts',(-108.07764587156,1074.75426967849,393.982238014158));
#110624=CARTESIAN_POINT('Ctrl Pts',(-107.95954634089,1074.76799050231,393.933877526661));
#110625=CARTESIAN_POINT('Ctrl Pts',(-107.896413195801,1074.77580841974,
393.921482136063));
#110626=CARTESIAN_POINT('Ctrl Pts',(-107.832758514871,1074.78413112039,
393.921476875766));
#110627=CARTESIAN_POINT('Ctrl Pts',(-107.832745002416,1074.78413288711,
393.921476874649));
#110628=CARTESIAN_POINT('Ctrl Pts',(-107.832731489977,1074.78413465385,
393.921476874093));
#110629=CARTESIAN_POINT('Ctrl Pts',(-107.832717977552,1074.78413642061,
393.921476874093));
#110630=CARTESIAN_POINT('',(-107.832717977552,1082.7251047501,393.921476874092));
#110631=CARTESIAN_POINT('',(-107.832717977552,1067.7251047501,393.921476874092));
#110632=CARTESIAN_POINT('Origin',(-107.832717977552,1082.7251047501,394.412017622821));
#110633=CARTESIAN_POINT('Ctrl Pts',(-107.832717977552,1074.78413642061,
393.921476874093));
#110634=CARTESIAN_POINT('Ctrl Pts',(-107.800604272338,1074.78833530606,
393.921476874093));
#110635=CARTESIAN_POINT('Ctrl Pts',(-107.768577169475,1074.79263405602,
393.924630379442));
#110636=CARTESIAN_POINT('Ctrl Pts',(-107.705650853594,1074.80130169454,
393.937136487566));
#110637=CARTESIAN_POINT('Ctrl Pts',(-107.674891200817,1074.80565111403,
393.946454427611));
#110638=CARTESIAN_POINT('Ctrl Pts',(-107.584867137173,1074.81873019232,
393.983682233695));
#110639=CARTESIAN_POINT('Ctrl Pts',(-107.530007475898,1074.82719627437,
394.020501214459));
#110640=CARTESIAN_POINT('Ctrl Pts',(-107.438068603545,1074.84249388482,
394.113454207606));
#110641=CARTESIAN_POINT('Ctrl Pts',(-107.401819425782,1074.84918310533,
394.168618631387));
#110642=CARTESIAN_POINT('Ctrl Pts',(-107.353409780512,1074.85980829449,
394.289294474671));
#110643=CARTESIAN_POINT('Ctrl Pts',(-107.341405020451,1074.86367556168,
394.353444839142));
#110644=CARTESIAN_POINT('Ctrl Pts',(-107.343013754148,1074.86810855196,
394.481869409797));
#110645=CARTESIAN_POINT('Ctrl Pts',(-107.356216144261,1074.86868008251,
394.544829605904));
#110646=CARTESIAN_POINT('Ctrl Pts',(-107.405996004093,1074.86650196661,
394.662230000609));
#110647=CARTESIAN_POINT('Ctrl Pts',(-107.442079945846,1074.86377251483,
394.715471003849));
#110648=CARTESIAN_POINT('Ctrl Pts',(-107.532789046877,1074.85531420137,
394.805441835666));
#110649=CARTESIAN_POINT('Ctrl Pts',(-107.586634462912,1074.84964866483,
394.841152004075));
#110650=CARTESIAN_POINT('Ctrl Pts',(-107.705111949593,1074.83607933483,
394.890009008638));
#110651=CARTESIAN_POINT('Ctrl Pts',(-107.768655973974,1074.82829417471,
394.902558371549));
#110652=CARTESIAN_POINT('Ctrl Pts',(-107.832717977552,1074.8199670159,394.902558371549));
#110653=CARTESIAN_POINT('Origin',(-86.3230601853152,1067.7251047501,448.47408103355));
#110654=CARTESIAN_POINT('',(-86.3230601853431,1076.68243856932,446.995777901357));
#110655=CARTESIAN_POINT('',(-86.3230601853152,1067.7251047501,446.995777901357));
#110656=CARTESIAN_POINT('Ctrl Pts',(-86.323166507663,1076.66188309602,449.95238416192));
#110657=CARTESIAN_POINT('Ctrl Pts',(-86.5172614368491,1076.65660731882,
449.952370202247));
#110658=CARTESIAN_POINT('Ctrl Pts',(-86.7094736205971,1076.65138668446,
449.914130614729));
#110659=CARTESIAN_POINT('Ctrl Pts',(-87.0682048713522,1076.64193094744,
449.765532290042));
#110660=CARTESIAN_POINT('Ctrl Pts',(-87.2312315510664,1076.63779524223,
449.656588436172));
#110661=CARTESIAN_POINT('Ctrl Pts',(-87.5056709311274,1076.63151683903,
449.382064201945));
#110662=CARTESIAN_POINT('Ctrl Pts',(-87.6144815374425,1076.62943854855,
449.219226268801));
#110663=CARTESIAN_POINT('Ctrl Pts',(-87.762812829159,1076.6278327369,448.86128268278));
#110664=CARTESIAN_POINT('Ctrl Pts',(-87.8010755829468,1076.62831568124,
448.669736455142));
#110665=CARTESIAN_POINT('Ctrl Pts',(-87.8016472192217,1076.63174641416,
448.28320356723));
#110666=CARTESIAN_POINT('Ctrl Pts',(-87.7641097372451,1076.63465248883,
448.091956916499));
#110667=CARTESIAN_POINT('Ctrl Pts',(-87.6176832980475,1076.64226268814,
447.734770499957));
#110668=CARTESIAN_POINT('Ctrl Pts',(-87.5102148846989,1076.64688667322,
447.572259245402));
#110669=CARTESIAN_POINT('Ctrl Pts',(-87.2387777836349,1076.65692796677,
447.297574466114));
#110670=CARTESIAN_POINT('Ctrl Pts',(-87.0773491930349,1076.66224324643,
447.188097761844));
#110671=CARTESIAN_POINT('Ctrl Pts',(-86.8104892082658,1076.67004015432,
447.075108429827));
#110672=CARTESIAN_POINT('Ctrl Pts',(-86.7180562722278,1076.67259256297,
447.046253957327));
#110673=CARTESIAN_POINT('Ctrl Pts',(-86.431201397442,1076.6800734711,446.986719209002));
#110674=CARTESIAN_POINT('Ctrl Pts',(-86.2328838610349,1076.68465096512,
446.985518930173));
#110675=CARTESIAN_POINT('Ctrl Pts',(-85.8487964974497,1076.69253439563,
447.060414648582));
#110676=CARTESIAN_POINT('Ctrl Pts',(-85.6667126046689,1076.69577849607,
447.135202738786));
#110677=CARTESIAN_POINT('Ctrl Pts',(-85.341832830451,1076.70087449289,447.351279210184));
#110678=CARTESIAN_POINT('Ctrl Pts',(-85.2022904039396,1076.7026828969,447.490530755828));
#110679=CARTESIAN_POINT('Ctrl Pts',(-84.9849845958677,1076.7049304295,447.815802891922));
#110680=CARTESIAN_POINT('Ctrl Pts',(-84.9096054342876,1076.70534782308,
447.998767235241));
#110681=CARTESIAN_POINT('Ctrl Pts',(-84.8346263006418,1076.7048087597,448.383212003071));
#110682=CARTESIAN_POINT('Ctrl Pts',(-84.835684426703,1076.70385768645,448.580867548382));
#110683=CARTESIAN_POINT('Ctrl Pts',(-84.9145712714694,1076.70051169125,
448.963523477952));
#110684=CARTESIAN_POINT('Ctrl Pts',(-84.9913286135803,1076.69814784631,
449.144811578407));
#110685=CARTESIAN_POINT('Ctrl Pts',(-85.2109345071113,1076.69194406988,
449.467406514347));
#110686=CARTESIAN_POINT('Ctrl Pts',(-85.3517320431411,1076.68815444462,
449.605465730436));
#110687=CARTESIAN_POINT('Ctrl Pts',(-85.5955775481193,1076.68158862809,
449.764563096708));
#110688=CARTESIAN_POINT('Ctrl Pts',(-85.680790816734,1076.67929497928,449.809020704177));
#110689=CARTESIAN_POINT('Ctrl Pts',(-85.8569752279724,1076.6745385003,449.88014016367));
#110690=CARTESIAN_POINT('Ctrl Pts',(-85.9474096947825,1076.67209040593,
449.906953479439));
#110691=CARTESIAN_POINT('Ctrl Pts',(-86.133137971659,1076.66705026916,449.943216367105));
#110692=CARTESIAN_POINT('Ctrl Pts',(-86.2280420848667,1076.66446871359,
449.952391003448));
#110693=CARTESIAN_POINT('Ctrl Pts',(-86.323166507663,1076.66188309602,449.95238416192));
#110694=CARTESIAN_POINT('Origin',(-86.3230601853152,1067.7251047501,448.47408103355));
#110695=CARTESIAN_POINT('',(-86.3230601853152,1076.66654097421,449.352384165744));
#110696=CARTESIAN_POINT('',(-86.3230601853154,1076.67873408293,447.595777901357));
#110697=CARTESIAN_POINT('Ctrl Pts',(-86.3230601853151,1076.66654097421,
449.352384165744));
#110698=CARTESIAN_POINT('Ctrl Pts',(-86.3901181015092,1076.66477558714,
449.352384165744));
#110699=CARTESIAN_POINT('Ctrl Pts',(-86.4571142523758,1076.66303405489,
449.344704219338));
#110700=CARTESIAN_POINT('Ctrl Pts',(-86.6349456175339,1076.65849642279,
449.303191689395));
#110701=CARTESIAN_POINT('Ctrl Pts',(-86.7409318553903,1076.65588594487,
449.255159581536));
#110702=CARTESIAN_POINT('Ctrl Pts',(-86.9282672280694,1076.65158872148,
449.120929485844));
#110703=CARTESIAN_POINT('Ctrl Pts',(-87.0078094645969,1076.64994579721,
449.036051140019));
#110704=CARTESIAN_POINT('Ctrl Pts',(-87.1294979961342,1076.6479566119,448.840564835501));
#110705=CARTESIAN_POINT('Ctrl Pts',(-87.1705189077138,1076.64762908125,
448.731892701794));
#110706=CARTESIAN_POINT('Ctrl Pts',(-87.2082992243034,1076.64836457455,
448.505101618138));
#110707=CARTESIAN_POINT('Ctrl Pts',(-87.2047642788882,1076.64941770649,
448.389193820259));
#110708=CARTESIAN_POINT('Ctrl Pts',(-87.1533029894093,1076.65270906129,
448.165390564633));
#110709=CARTESIAN_POINT('Ctrl Pts',(-87.1058985607682,1076.65491274874,
448.059649853931));
#110710=CARTESIAN_POINT('Ctrl Pts',(-86.9730765281975,1076.66007334864,
447.872346414937));
#110711=CARTESIAN_POINT('Ctrl Pts',(-86.8889138097755,1076.66297848812,
447.792602368897));
#110712=CARTESIAN_POINT('Ctrl Pts',(-86.7432564855229,1076.66749935026,
447.700681787845));
#110713=CARTESIAN_POINT('Ctrl Pts',(-86.6918267176327,1076.66902275366,
447.674879842137));
#110714=CARTESIAN_POINT('Ctrl Pts',(-86.5882581317525,1076.67195158694,
447.635060818344));
#110715=CARTESIAN_POINT('Ctrl Pts',(-86.5366134513795,1076.67335198428,
447.620453481324));
#110716=CARTESIAN_POINT('Ctrl Pts',(-86.4308998346368,1076.67610124917,
447.600753944207));
#110717=CARTESIAN_POINT('Ctrl Pts',(-86.3770394159166,1076.67744380712,
447.595778081493));
#110718=CARTESIAN_POINT('Ctrl Pts',(-86.3230631164002,1076.67873401287,
447.595777901362));
#110719=CARTESIAN_POINT('',(-86.3230601853152,1082.7251047501,447.595777901357));
#110720=CARTESIAN_POINT('',(-86.3230601853152,1067.7251047501,447.595777901357));
#110721=CARTESIAN_POINT('Origin',(-86.3230601853152,1082.7251047501,448.47408103355));
#110722=CARTESIAN_POINT('Ctrl Pts',(-86.3230601853156,1076.67873408293,
447.595777901357));
#110723=CARTESIAN_POINT('Ctrl Pts',(-86.2063772042534,1076.68152317411,
447.595777901357));
#110724=CARTESIAN_POINT('Ctrl Pts',(-86.0908516781534,1076.68402501507,
447.619029177307));
#110725=CARTESIAN_POINT('Ctrl Pts',(-85.8758342807902,1076.68825831458,
447.709245703915));
#110726=CARTESIAN_POINT('Ctrl Pts',(-85.7784499291699,1076.68995199795,
447.775234437677));
#110727=CARTESIAN_POINT('Ctrl Pts',(-85.61494962158,1076.69242874122,447.94152348628));
#110728=CARTESIAN_POINT('Ctrl Pts',(-85.5505234694667,1076.69318803405,
448.040230224465));
#110729=CARTESIAN_POINT('Ctrl Pts',(-85.4639913045317,1076.69373323332,
448.257140974017));
#110730=CARTESIAN_POINT('Ctrl Pts',(-85.4427853611372,1076.69351357969,
448.373194189322));
#110731=CARTESIAN_POINT('Ctrl Pts',(-85.4470130157523,1076.69209332713,
448.606569592611));
#110732=CARTESIAN_POINT('Ctrl Pts',(-85.4723188227951,1076.69090693583,
448.72156616507));
#110733=CARTESIAN_POINT('Ctrl Pts',(-85.5663144925847,1076.68761288142,
448.934869113926));
#110734=CARTESIAN_POINT('Ctrl Pts',(-85.6340383967117,1076.68553563327,
449.031068942445));
#110735=CARTESIAN_POINT('Ctrl Pts',(-85.8034210616211,1076.68062678245,
449.191771366874));
#110736=CARTESIAN_POINT('Ctrl Pts',(-85.9035306249559,1076.67783864142,
449.254527326388));
#110737=CARTESIAN_POINT('Ctrl Pts',(-86.0672423860777,1076.67337214142,
449.316302607773));
#110738=CARTESIAN_POINT('Ctrl Pts',(-86.12339803899,1076.6718547263,449.331352751992));
#110739=CARTESIAN_POINT('Ctrl Pts',(-86.2278178847014,1076.66905962772,
449.348513775272));
#110740=CARTESIAN_POINT('Ctrl Pts',(-86.275454598382,1076.66779425334,449.352384165744));
#110741=CARTESIAN_POINT('Ctrl Pts',(-86.3230601853151,1076.66654097421,
449.352384165744));
#110742=CARTESIAN_POINT('Origin',(-95.5155706932854,1067.7251047501,439.917923765972));
#110743=CARTESIAN_POINT('',(-95.5155706933052,1076.35760005837,438.642479644836));
#110744=CARTESIAN_POINT('',(-95.5155706932854,1067.7251047501,438.642479644836));
#110745=CARTESIAN_POINT('Ctrl Pts',(-95.5152422626988,1076.33152383034,
441.193367844822));
#110746=CARTESIAN_POINT('Ctrl Pts',(-95.6828139562135,1076.32067145058,
441.193410995024));
#110747=CARTESIAN_POINT('Ctrl Pts',(-95.8487982401502,1076.31007821196,
441.160429595892));
#110748=CARTESIAN_POINT('Ctrl Pts',(-96.1583840432205,1076.29077894953,
441.032190098894));
#110749=CARTESIAN_POINT('Ctrl Pts',(-96.2990284046096,1076.28226094656,
440.938236132061));
#110750=CARTESIAN_POINT('Ctrl Pts',(-96.5356946515849,1076.26868427456,
440.701530519116));
#110751=CARTESIAN_POINT('Ctrl Pts',(-96.6295306238772,1076.26375277916,
440.561214321463));
#110752=CARTESIAN_POINT('Ctrl Pts',(-96.7575246336427,1076.25831659374,
440.252744110367));
#110753=CARTESIAN_POINT('Ctrl Pts',(-96.7906131552752,1076.25785331984,
440.08770265456));
#110754=CARTESIAN_POINT('Ctrl Pts',(-96.7914086114346,1076.26149407278,
439.754483068864));
#110755=CARTESIAN_POINT('Ctrl Pts',(-96.7592059937086,1076.26555428597,
439.589571774213));
#110756=CARTESIAN_POINT('Ctrl Pts',(-96.6332654975541,1076.27757075149,
439.281314097811));
#110757=CARTESIAN_POINT('Ctrl Pts',(-96.5406732396144,1076.28541145008,
439.140985420101));
#110758=CARTESIAN_POINT('Ctrl Pts',(-96.3065934397241,1076.30367981313,
438.903572082332));
#110759=CARTESIAN_POINT('Ctrl Pts',(-96.1672147526564,1076.31393506852,
438.808889499782));
#110760=CARTESIAN_POINT('Ctrl Pts',(-95.9367383909986,1076.32998643442,
438.71113138861));
#110761=CARTESIAN_POINT('Ctrl Pts',(-95.8568522290869,1076.33541341161,
438.686154180861));
#110762=CARTESIAN_POINT('Ctrl Pts',(-95.693549633131,1076.34623590983,438.652214737871));
#110763=CARTESIAN_POINT('Ctrl Pts',(-95.6105276802408,1076.35160590179,
438.643294187491));
#110764=CARTESIAN_POINT('Ctrl Pts',(-95.3582991611468,1076.3675300373,438.640989092166));
#110765=CARTESIAN_POINT('Ctrl Pts',(-95.1906877056548,1076.37757908158,
438.673021968305));
#110766=CARTESIAN_POINT('Ctrl Pts',(-94.8780934410209,1076.39538146742,
438.800434011967));
#110767=CARTESIAN_POINT('Ctrl Pts',(-94.7361152043874,1076.40297107354,
438.894375362848));
#110768=CARTESIAN_POINT('Ctrl Pts',(-94.4964315895821,1076.41491058555,
439.132580605632));
#110769=CARTESIAN_POINT('Ctrl Pts',(-94.401286817847,1076.41913438666,439.274643977476));
#110770=CARTESIAN_POINT('Ctrl Pts',(-94.2718273939629,1076.42375173698,
439.588198443855));
#110771=CARTESIAN_POINT('Ctrl Pts',(-94.2390147023854,1076.42408915898,
439.756605778015));
#110772=CARTESIAN_POINT('Ctrl Pts',(-94.2412932871994,1076.42079372705,
440.095973795517));
#110773=CARTESIAN_POINT('Ctrl Pts',(-94.2762030297749,1076.41720145592,
440.263506279824));
#110774=CARTESIAN_POINT('Ctrl Pts',(-94.409120985165,1076.40641719041,440.574425162885));
#110775=CARTESIAN_POINT('Ctrl Pts',(-94.5055462696883,1076.39934239347,
440.714814519768));
#110776=CARTESIAN_POINT('Ctrl Pts',(-94.7474950406095,1076.38239560869,
440.950074021745));
#110777=CARTESIAN_POINT('Ctrl Pts',(-94.8907053021309,1076.37268187305,
441.042548865023));
#110778=CARTESIAN_POINT('Ctrl Pts',(-95.1966006470039,1076.35230137259,
441.163168135794));
#110779=CARTESIAN_POINT('Ctrl Pts',(-95.3552144545814,1076.34188764842,
441.193326637193));
#110780=CARTESIAN_POINT('Ctrl Pts',(-95.5152422626988,1076.33152383034,
441.193367844822));
#110781=CARTESIAN_POINT('Origin',(-95.5155706932854,1067.7251047501,439.917923765972));
#110782=CARTESIAN_POINT('',(-95.5155706932854,1076.33810018128,440.593367887109));
#110783=CARTESIAN_POINT('',(-95.5155706932854,1076.35191524971,439.242479644836));
#110784=CARTESIAN_POINT('Ctrl Pts',(-95.5155706932854,1076.33810018128,
440.593367887109));
#110785=CARTESIAN_POINT('Ctrl Pts',(-95.5230299670075,1076.33762039049,
440.593367887109));
#110786=CARTESIAN_POINT('Ctrl Pts',(-95.5304943432052,1076.33714118425,
440.593244323034));
#110787=CARTESIAN_POINT('Ctrl Pts',(-95.627504268366,1076.33092522636,440.590026799769));
#110788=CARTESIAN_POINT('Ctrl Pts',(-95.7155911655218,1076.32541224372,
440.569269688472));
#110789=CARTESIAN_POINT('Ctrl Pts',(-95.8775875839268,1076.31558272049,
440.494997225786));
#110790=CARTESIAN_POINT('Ctrl Pts',(-95.950092136511,1076.31134871855,440.442588892107));
#110791=CARTESIAN_POINT('Ctrl Pts',(-96.0706049845411,1076.30473754511,
440.312866459206));
#110792=CARTESIAN_POINT('Ctrl Pts',(-96.1175013592039,1076.30242126744,
440.236877363948));
#110793=CARTESIAN_POINT('Ctrl Pts',(-96.1792732406646,1076.30006955532,
440.071274783904));
#110794=CARTESIAN_POINT('Ctrl Pts',(-96.1936134077525,1076.30005266803,
439.983313047932));
#110795=CARTESIAN_POINT('Ctrl Pts',(-96.1876450931037,1076.30233602738,
439.80689653668));
#110796=CARTESIAN_POINT('Ctrl Pts',(-96.1674102694078,1076.30461244013,
439.720168206024));
#110797=CARTESIAN_POINT('Ctrl Pts',(-96.0947228253676,1076.31113950101,
439.559299527691));
#110798=CARTESIAN_POINT('Ctrl Pts',(-96.0429223630463,1076.31532888567,
439.486743418212));
#110799=CARTESIAN_POINT('Ctrl Pts',(-95.9142430055404,1076.3250295308,439.36555000779));
#110800=CARTESIAN_POINT('Ctrl Pts',(-95.8385381801963,1076.330449611,439.31814014607));
#110801=CARTESIAN_POINT('Ctrl Pts',(-95.7177361820896,1076.33871064195,
439.272153569839));
#110802=CARTESIAN_POINT('Ctrl Pts',(-95.6783620139873,1076.34135172418,
439.261121781354));
#110803=CARTESIAN_POINT('Ctrl Pts',(-95.5977925667714,1076.34665438765,
439.246242525049));
#110804=CARTESIAN_POINT('Ctrl Pts',(-95.5567507615488,1076.34930508029,
439.242482714328));
#110805=CARTESIAN_POINT('Ctrl Pts',(-95.5156210705524,1076.35191205661,
439.242479646715));
#110806=CARTESIAN_POINT('Ctrl Pts',(-95.5156042780997,1076.35191312098,
439.242479645462));
#110807=CARTESIAN_POINT('Ctrl Pts',(-95.5155874856773,1076.35191418535,
439.242479644836));
#110808=CARTESIAN_POINT('Ctrl Pts',(-95.5155706932854,1076.35191524971,
439.242479644836));
#110809=CARTESIAN_POINT('',(-95.5155706932854,1082.7251047501,439.242479644836));
#110810=CARTESIAN_POINT('',(-95.5155706932854,1067.7251047501,439.242479644836));
#110811=CARTESIAN_POINT('Origin',(-95.5155706932854,1082.7251047501,439.917923765972));
#110812=CARTESIAN_POINT('Ctrl Pts',(-95.5155706932854,1076.35191524971,
439.242479644836));
#110813=CARTESIAN_POINT('Ctrl Pts',(-95.4257877829596,1076.35760598816,
439.242479644836));
#110814=CARTESIAN_POINT('Ctrl Pts',(-95.3368745387622,1076.36300547989,
439.260381116648));
#110815=CARTESIAN_POINT('Ctrl Pts',(-95.1712970043486,1076.37262315823,
439.329913689638));
#110816=CARTESIAN_POINT('Ctrl Pts',(-95.0962644496087,1076.37674825756,
439.380825446226));
#110817=CARTESIAN_POINT('Ctrl Pts',(-94.9703261473707,1076.3832185644,439.509220382696));
#110818=CARTESIAN_POINT('Ctrl Pts',(-94.9207483488372,1076.38549570174,
439.585470636753));
#110819=CARTESIAN_POINT('Ctrl Pts',(-94.8546980200677,1076.38789194751,
439.752250744966));
#110820=CARTESIAN_POINT('Ctrl Pts',(-94.8386058514874,1076.388006019,439.840986744035));
#110821=CARTESIAN_POINT('Ctrl Pts',(-94.8418568845122,1076.38607531259,
440.018673303983));
#110822=CARTESIAN_POINT('Ctrl Pts',(-94.8608123091726,1076.38407067916,
440.105872600748));
#110823=CARTESIAN_POINT('Ctrl Pts',(-94.9317859374777,1076.37811315774,
440.269337621984));
#110824=CARTESIAN_POINT('Ctrl Pts',(-94.9836365508097,1076.37418693194,
440.343752813501));
#110825=CARTESIAN_POINT('Ctrl Pts',(-95.1133703141433,1076.36488745776,
440.467949083075));
#110826=CARTESIAN_POINT('Ctrl Pts',(-95.1899764453381,1076.35960461803,
440.516481846211));
#110827=CARTESIAN_POINT('Ctrl Pts',(-95.3510319527794,1076.34879392822,
440.578221706843));
#110828=CARTESIAN_POINT('Ctrl Pts',(-95.4329886699305,1076.34341197116,
440.593367887109));
#110829=CARTESIAN_POINT('Ctrl Pts',(-95.5155706932854,1076.33810018128,
440.593367887109));
#110830=CARTESIAN_POINT('Origin',(-104.753539540172,1067.7251047501,429.599096875777));
#110831=CARTESIAN_POINT('',(-104.753539540193,1075.66035026279,428.500265739785));
#110832=CARTESIAN_POINT('',(-104.753539540172,1067.7251047501,428.500265739785));
#110833=CARTESIAN_POINT('Ctrl Pts',(-104.753203728027,1075.6495208014,430.697927960456));
#110834=CARTESIAN_POINT('Ctrl Pts',(-104.900480042956,1075.63417453868,
430.697972969353));
#110835=CARTESIAN_POINT('Ctrl Pts',(-105.046335055649,1075.61900230498,
430.668408371385));
#110836=CARTESIAN_POINT('Ctrl Pts',(-105.315072036072,1075.59116670263,
430.554594465636));
#110837=CARTESIAN_POINT('Ctrl Pts',(-105.435805338195,1075.57872574262,
430.472531235281));
#110838=CARTESIAN_POINT('Ctrl Pts',(-105.638083926395,1075.55814657647,
430.26670957947));
#110839=CARTESIAN_POINT('Ctrl Pts',(-105.717889540202,1075.55018619578,
430.145201466243));
#110840=CARTESIAN_POINT('Ctrl Pts',(-105.825786489787,1075.53993329877,
429.878820981651));
#110841=CARTESIAN_POINT('Ctrl Pts',(-105.853102821232,1075.53771168743,
429.736734886952));
#110842=CARTESIAN_POINT('Ctrl Pts',(-105.851610307087,1075.53934106797,
429.450316660049));
#110843=CARTESIAN_POINT('Ctrl Pts',(-105.822938025717,1075.5431623155,429.308853765669));
#110844=CARTESIAN_POINT('Ctrl Pts',(-105.712951594158,1075.55633717576,
429.044563420142));
#110845=CARTESIAN_POINT('Ctrl Pts',(-105.632566779557,1075.56557513932,
428.924404614211));
#110846=CARTESIAN_POINT('Ctrl Pts',(-105.429866042245,1075.58821951279,
428.721180042264));
#110847=CARTESIAN_POINT('Ctrl Pts',(-105.309248312879,1075.60143030756,
428.640309884849));
#110848=CARTESIAN_POINT('Ctrl Pts',(-105.110033232513,1075.62283344418,
428.557201513108));
#110849=CARTESIAN_POINT('Ctrl Pts',(-105.04089791964,1075.63019795806,428.536056719325));
#110850=CARTESIAN_POINT('Ctrl Pts',(-104.899789171971,1075.64509975411,
428.507675700065));
#110851=CARTESIAN_POINT('Ctrl Pts',(-104.828152980214,1075.65260188103,
428.500451494514));
#110852=CARTESIAN_POINT('Ctrl Pts',(-104.610523619321,1075.67520212854,
428.499899378922));
#110853=CARTESIAN_POINT('Ctrl Pts',(-104.466016769097,1075.68994652228,
428.528552975495));
#110854=CARTESIAN_POINT('Ctrl Pts',(-104.197056730414,1075.7169178972,428.640509340355));
#110855=CARTESIAN_POINT('Ctrl Pts',(-104.075129543157,1075.72889582137,
428.722510568931));
#110856=CARTESIAN_POINT('Ctrl Pts',(-103.869985002791,1075.74862465936,
428.929725118191));
#110857=CARTESIAN_POINT('Ctrl Pts',(-103.788907408865,1075.75617197411,
429.052943954296));
#110858=CARTESIAN_POINT('Ctrl Pts',(-103.68080558744,1075.76572489395,429.321315274353));
#110859=CARTESIAN_POINT('Ctrl Pts',(-103.653765135895,1075.76774947395,
429.463310635218));
#110860=CARTESIAN_POINT('Ctrl Pts',(-103.655703044621,1075.76619401393,
429.749910518335));
#110861=CARTESIAN_POINT('Ctrl Pts',(-103.684727106134,1075.76262263895,
429.89166100879));
#110862=CARTESIAN_POINT('Ctrl Pts',(-103.796520628938,1075.75013016158,
430.158433119729));
#110863=CARTESIAN_POINT('Ctrl Pts',(-103.879155940594,1075.74123414344,
430.280358639091));
#110864=CARTESIAN_POINT('Ctrl Pts',(-104.086884357666,1075.71920019498,
430.484653206964));
#110865=CARTESIAN_POINT('Ctrl Pts',(-104.209888346711,1075.7062805828,430.565020155921));
#110866=CARTESIAN_POINT('Ctrl Pts',(-104.409299093131,1075.68540947004,
430.644922448304));
#110867=CARTESIAN_POINT('Ctrl Pts',(-104.476049332423,1075.67843389929,
430.664576481816));
#110868=CARTESIAN_POINT('Ctrl Pts',(-104.613063503368,1075.66413004391,
430.691167789154));
#110869=CARTESIAN_POINT('Ctrl Pts',(-104.683055196913,1075.65683031202,
430.697906522467));
#110870=CARTESIAN_POINT('Ctrl Pts',(-104.753203728027,1075.6495208014,430.697927960456));
#110871=CARTESIAN_POINT('Origin',(-104.753539540172,1067.7251047501,429.599096875777));
#110872=CARTESIAN_POINT('',(-104.753539540172,1075.6529321444,430.09792801177));
#110873=CARTESIAN_POINT('',(-104.753539540172,1075.65786345153,429.100265739785));
#110874=CARTESIAN_POINT('Ctrl Pts',(-104.753539540172,1075.6529321444,430.09792801177));
#110875=CARTESIAN_POINT('Ctrl Pts',(-104.75491854207,1075.65278861588,430.09792801177));
#110876=CARTESIAN_POINT('Ctrl Pts',(-104.756297668151,1075.65264509248,
430.097922293444));
#110877=CARTESIAN_POINT('Ctrl Pts',(-104.824346678404,1075.64556423468,
430.097357870435));
#110878=CARTESIAN_POINT('Ctrl Pts',(-104.890265025792,1075.63874646745,
430.083443905758));
#110879=CARTESIAN_POINT('Ctrl Pts',(-105.012201501236,1075.62623228538,
430.030718819393));
#110880=CARTESIAN_POINT('Ctrl Pts',(-105.067126415725,1075.62064759498,
429.992649514473));
#110881=CARTESIAN_POINT('Ctrl Pts',(-105.158275187127,1075.61152075326,
429.897890801476));
#110882=CARTESIAN_POINT('Ctrl Pts',(-105.193882096471,1075.60803841156,
429.842411760024));
#110883=CARTESIAN_POINT('Ctrl Pts',(-105.241579526787,1075.60360730913,
429.721070879668));
#110884=CARTESIAN_POINT('Ctrl Pts',(-105.253313431322,1075.60269027868,
429.656466455001));
#110885=CARTESIAN_POINT('Ctrl Pts',(-105.2513107664,1075.6035557548,429.526438301903));
#110886=CARTESIAN_POINT('Ctrl Pts',(-105.237623854927,1075.60532639985,
429.46231451433));
#110887=CARTESIAN_POINT('Ctrl Pts',(-105.186398834638,1075.61133551359,
429.342757781232));
#110888=CARTESIAN_POINT('Ctrl Pts',(-105.14928447161,1075.61552267919,429.288538457274));
#110889=CARTESIAN_POINT('Ctrl Pts',(-105.056167703792,1075.62577355843,
429.197191130533));
#110890=CARTESIAN_POINT('Ctrl Pts',(-105.000953634881,1075.63174869342,
429.161051507176));
#110891=CARTESIAN_POINT('Ctrl Pts',(-104.910877121333,1075.64135040035,
429.124658888835));
#110892=CARTESIAN_POINT('Ctrl Pts',(-104.88028424772,1075.6445902119,429.115587402101));
#110893=CARTESIAN_POINT('Ctrl Pts',(-104.817578083212,1075.65118828267,
429.103355711211));
#110894=CARTESIAN_POINT('Ctrl Pts',(-104.785595469618,1075.65453248655,
429.100265739785));
#110895=CARTESIAN_POINT('Ctrl Pts',(-104.753539540172,1075.65786345153,
429.100265739785));
#110896=CARTESIAN_POINT('',(-104.753539540172,1082.7251047501,429.100265739785));
#110897=CARTESIAN_POINT('',(-104.753539540172,1067.7251047501,429.100265739785));
#110898=CARTESIAN_POINT('Origin',(-104.753539540172,1082.7251047501,429.599096875777));
#110899=CARTESIAN_POINT('Ctrl Pts',(-104.753539540172,1075.65786345153,
429.100265739785));
#110900=CARTESIAN_POINT('Ctrl Pts',(-104.75346795341,1075.65787089019,429.100265739785));
#110901=CARTESIAN_POINT('Ctrl Pts',(-104.753396366282,1075.65787832878,
429.100265755192));
#110902=CARTESIAN_POINT('Ctrl Pts',(-104.753324778794,1075.6578857673,429.100265786012));
#110903=CARTESIAN_POINT('Ctrl Pts',(-104.686962910483,1075.66478130571,
429.100294356738));
#110904=CARTESIAN_POINT('Ctrl Pts',(-104.621235645922,1075.67152088023,
429.113565303564));
#110905=CARTESIAN_POINT('Ctrl Pts',(-104.498876025575,1075.68389797613,
429.16507081349));
#110906=CARTESIAN_POINT('Ctrl Pts',(-104.443425001876,1075.68941674587,
429.202766209488));
#110907=CARTESIAN_POINT('Ctrl Pts',(-104.350901439487,1075.69845229737,
429.297348716436));
#110908=CARTESIAN_POINT('Ctrl Pts',(-104.314585719611,1075.70189765785,
429.353121936495));
#110909=CARTESIAN_POINT('Ctrl Pts',(-104.266094122455,1075.70626601641,
429.474780855182));
#110910=CARTESIAN_POINT('Ctrl Pts',(-104.254053192325,1075.70718226731,
429.539303262049));
#110911=CARTESIAN_POINT('Ctrl Pts',(-104.255418784207,1075.70641096511,
429.669382186887));
#110912=CARTESIAN_POINT('Ctrl Pts',(-104.268818673046,1075.70473032009,
429.733641276545));
#110913=CARTESIAN_POINT('Ctrl Pts',(-104.319579146063,1075.69895077073,
429.853595944209));
#110914=CARTESIAN_POINT('Ctrl Pts',(-104.356533450706,1075.69489891119,
429.908065835912));
#110915=CARTESIAN_POINT('Ctrl Pts',(-104.450100574957,1075.68482951885,
430.000556228394));
#110916=CARTESIAN_POINT('Ctrl Pts',(-104.506150165916,1075.67887495066,
430.037306690302));
#110917=CARTESIAN_POINT('Ctrl Pts',(-104.597798222821,1075.66921721702,
430.074102295117));
#110918=CARTESIAN_POINT('Ctrl Pts',(-104.629012220032,1075.66593954012,
430.083222283081));
#110919=CARTESIAN_POINT('Ctrl Pts',(-104.691434319411,1075.65940527056,
430.095022538473));
#110920=CARTESIAN_POINT('Ctrl Pts',(-104.722455383358,1075.65616742862,
430.09792801177));
#110921=CARTESIAN_POINT('Ctrl Pts',(-104.753539540172,1075.6529321444,430.09792801177));
#110922=CARTESIAN_POINT('Origin',(-111.756957497768,1067.7251047501,417.491822535893));
#110923=CARTESIAN_POINT('',(-111.756957497784,1074.79209786668,416.401281787164));
#110924=CARTESIAN_POINT('',(-111.756957497768,1067.7251047501,416.401281787164));
#110925=CARTESIAN_POINT('Ctrl Pts',(-111.757173944974,1074.8108674823,418.582363263141));
#110926=CARTESIAN_POINT('Ctrl Pts',(-111.828369018416,1074.80126179765,
418.58234913256));
#110927=CARTESIAN_POINT('Ctrl Pts',(-111.8993932438,1074.79159616308,418.575363169141));
#110928=CARTESIAN_POINT('Ctrl Pts',(-112.112986052677,1074.76227600642,
418.532977014325));
#110929=CARTESIAN_POINT('Ctrl Pts',(-112.249671521804,1074.74315514854,
418.475731697485));
#110930=CARTESIAN_POINT('Ctrl Pts',(-112.489587534351,1074.70891584145,
418.312258102391));
#110931=CARTESIAN_POINT('Ctrl Pts',(-112.591248920725,1074.69404104959,
418.208730976483));
#110932=CARTESIAN_POINT('Ctrl Pts',(-112.747877742657,1074.67036863216,
417.968949724906));
#110933=CARTESIAN_POINT('Ctrl Pts',(-112.801771032909,1074.66174547335,
417.835403348587));
#110934=CARTESIAN_POINT('Ctrl Pts',(-112.854790240717,1074.65195312084,
417.555899494077));
#110935=CARTESIAN_POINT('Ctrl Pts',(-112.853829509201,1074.65082295652,
417.41288999358));
#110936=CARTESIAN_POINT('Ctrl Pts',(-112.797269999421,1074.65619647349,
417.135371467911));
#110937=CARTESIAN_POINT('Ctrl Pts',(-112.742319431075,1074.66263476029,
417.003678538191));
#110938=CARTESIAN_POINT('Ctrl Pts',(-112.584948650193,1074.68226237821,
416.767997893567));
#110939=CARTESIAN_POINT('Ctrl Pts',(-112.483783333288,1074.69529886287,
416.666546296024));
#110940=CARTESIAN_POINT('Ctrl Pts',(-112.247521232048,1074.72629641018,
416.507380196275));
#110941=CARTESIAN_POINT('Ctrl Pts',(-112.114342126929,1074.74400864694,
416.451653992195));
#110942=CARTESIAN_POINT('Ctrl Pts',(-111.904225205491,1074.77220838194,
416.408900838912));
#110943=CARTESIAN_POINT('Ctrl Pts',(-111.832834138731,1074.781830748,416.401572610849));
#110944=CARTESIAN_POINT('Ctrl Pts',(-111.68993678724,1074.80116657414,416.401008927996));
#110945=CARTESIAN_POINT('Ctrl Pts',(-111.618751538001,1074.81083631535,
416.407725139025));
#110946=CARTESIAN_POINT('Ctrl Pts',(-111.406558891734,1074.83977480743,
416.449001080662));
#110947=CARTESIAN_POINT('Ctrl Pts',(-111.271160348732,1074.85839618931,
416.504732318284));
#110948=CARTESIAN_POINT('Ctrl Pts',(-111.030528495974,1074.89188335811,
416.665731890742));
#110949=CARTESIAN_POINT('Ctrl Pts',(-110.927461150854,1074.90644753492,
416.769189489503));
#110950=CARTESIAN_POINT('Ctrl Pts',(-110.767625296664,1074.92966250548,
417.010720055326));
#110951=CARTESIAN_POINT('Ctrl Pts',(-110.712462791914,1074.93808223461,
417.146314622044));
#110952=CARTESIAN_POINT('Ctrl Pts',(-110.659106724347,1074.94748972575,
417.428081571844));
#110953=CARTESIAN_POINT('Ctrl Pts',(-110.660111085797,1074.9485578929,417.571079281942));
#110954=CARTESIAN_POINT('Ctrl Pts',(-110.716821982437,1074.94341878076,
417.848942680033));
#110955=CARTESIAN_POINT('Ctrl Pts',(-110.772035119322,1074.93725198434,
417.980970676675));
#110956=CARTESIAN_POINT('Ctrl Pts',(-110.931477108568,1074.91817490145,
418.219049774777));
#110957=CARTESIAN_POINT('Ctrl Pts',(-111.035157534774,1074.90530748675,
418.321970429161));
#110958=CARTESIAN_POINT('Ctrl Pts',(-111.276600097951,1074.87451979485,
418.481546744203));
#110959=CARTESIAN_POINT('Ctrl Pts',(-111.412102704599,1074.85688261778,
418.536456478853));
#110960=CARTESIAN_POINT('Ctrl Pts',(-111.621114619278,1074.82914878572,
418.57601257562));
#110961=CARTESIAN_POINT('Ctrl Pts',(-111.689080214018,1074.82005473184,
418.582376778178));
#110962=CARTESIAN_POINT('Ctrl Pts',(-111.757173944974,1074.8108674823,418.582363263141));
#110963=CARTESIAN_POINT('Origin',(-111.756957497768,1067.7251047501,417.491822535893));
#110964=CARTESIAN_POINT('',(-111.756957497768,1074.80630411877,417.982363284621));
#110965=CARTESIAN_POINT('',(-111.756957497768,1074.79784893105,417.001281787164));
#110966=CARTESIAN_POINT('Ctrl Pts',(-111.756957497768,1074.80630411877,
417.982363284621));
#110967=CARTESIAN_POINT('Ctrl Pts',(-111.758122579226,1074.80614680927,
417.982363284621));
#110968=CARTESIAN_POINT('Ctrl Pts',(-111.759287742904,1074.80598944682,
417.982359133837));
#110969=CARTESIAN_POINT('Ctrl Pts',(-111.792489563395,1074.80150414604,
417.982122540079));
#110970=CARTESIAN_POINT('Ctrl Pts',(-111.824428613561,1074.79715774821,
417.978756301525));
#110971=CARTESIAN_POINT('Ctrl Pts',(-111.920169596025,1074.7840323223,417.959058285948));
#110972=CARTESIAN_POINT('Ctrl Pts',(-111.98128266174,1074.77551819495,417.933006813256));
#110973=CARTESIAN_POINT('Ctrl Pts',(-112.088934161954,1074.76024863573,
417.858753351402));
#110974=CARTESIAN_POINT('Ctrl Pts',(-112.134628157483,1074.75361762822,
417.811572467289));
#110975=CARTESIAN_POINT('Ctrl Pts',(-112.204388627454,1074.74316509674,
417.702854312296));
#110976=CARTESIAN_POINT('Ctrl Pts',(-112.228128074018,1074.73940039555,
417.642649452916));
#110977=CARTESIAN_POINT('Ctrl Pts',(-112.250986578072,1074.73518380817,
417.516810173952));
#110978=CARTESIAN_POINT('Ctrl Pts',(-112.250054978383,1074.73475053742,
417.452494232804));
#110979=CARTESIAN_POINT('Ctrl Pts',(-112.223640476455,1074.73727160334,
417.32782259427));
#110980=CARTESIAN_POINT('Ctrl Pts',(-112.19843628193,1074.74019878948,417.268734382283));
#110981=CARTESIAN_POINT('Ctrl Pts',(-112.126731015357,1074.7490590343,417.163194451443));
#110982=CARTESIAN_POINT('Ctrl Pts',(-112.080798213839,1074.75492408497,
417.117885404554));
#110983=CARTESIAN_POINT('Ctrl Pts',(-111.973815063771,1074.76885940437,
417.047122570625));
#110984=CARTESIAN_POINT('Ctrl Pts',(-111.913642204305,1074.77681732983,
417.02255301957));
#110985=CARTESIAN_POINT('Ctrl Pts',(-111.819690596518,1074.78938851283,
417.004296465626));
#110986=CARTESIAN_POINT('Ctrl Pts',(-111.788356249039,1074.79360359439,
417.001281787164));
#110987=CARTESIAN_POINT('Ctrl Pts',(-111.756957497768,1074.79784893105,
417.001281787164));
#110988=CARTESIAN_POINT('',(-111.756957497768,1082.7251047501,417.001281787164));
#110989=CARTESIAN_POINT('',(-111.756957497768,1067.7251047501,417.001281787164));
#110990=CARTESIAN_POINT('Origin',(-111.756957497768,1082.7251047501,417.491822535893));
#110991=CARTESIAN_POINT('Ctrl Pts',(-111.756957497768,1074.79784893105,
417.001281787164));
#110992=CARTESIAN_POINT('Ctrl Pts',(-111.75689461651,1074.79785743305,417.001281787164));
#110993=CARTESIAN_POINT('Ctrl Pts',(-111.756831734994,1074.79786593517,
417.001281799255));
#110994=CARTESIAN_POINT('Ctrl Pts',(-111.756768853224,1074.79787443741,
417.001281823437));
#110995=CARTESIAN_POINT('Ctrl Pts',(-111.724708510328,1074.80220931429,
417.001294152707));
#110996=CARTESIAN_POINT('Ctrl Pts',(-111.692723880739,1074.80655641454,
417.004449512646));
#110997=CARTESIAN_POINT('Ctrl Pts',(-111.597177519773,1074.81961098445,
417.023451445351));
#110998=CARTESIAN_POINT('Ctrl Pts',(-111.536201424335,1074.82803720812,
417.048893667185));
#110999=CARTESIAN_POINT('Ctrl Pts',(-111.42793105659,1074.84321316049,417.122187470758));
#111000=CARTESIAN_POINT('Ctrl Pts',(-111.381641165088,1074.84982169605,
417.16924757614));
#111001=CARTESIAN_POINT('Ctrl Pts',(-111.310685003306,1074.86025526917,
417.278194578269));
#111002=CARTESIAN_POINT('Ctrl Pts',(-111.286433231381,1074.8640143001,417.33877238344));
#111003=CARTESIAN_POINT('Ctrl Pts',(-111.263022506741,1074.86822032095,
417.465038755468));
#111004=CARTESIAN_POINT('Ctrl Pts',(-111.263720260096,1074.86867504262,
417.529358895175));
#111005=CARTESIAN_POINT('Ctrl Pts',(-111.289697643028,1074.86626754205,
417.654201766278));
#111006=CARTESIAN_POINT('Ctrl Pts',(-111.314732530891,1074.86342703873,
417.713451591914));
#111007=CARTESIAN_POINT('Ctrl Pts',(-111.386207212044,1074.85476542394,
417.819367731334));
#111008=CARTESIAN_POINT('Ctrl Pts',(-111.432084671134,1074.84900924268,
417.864880964565));
#111009=CARTESIAN_POINT('Ctrl Pts',(-111.539816795936,1074.83516303436,
417.936532211971));
#111010=CARTESIAN_POINT('Ctrl Pts',(-111.600963410419,1074.82715661552,
417.961460574622));
#111011=CARTESIAN_POINT('Ctrl Pts',(-111.695393552302,1074.81458719603,
417.979460462524));
#111012=CARTESIAN_POINT('Ctrl Pts',(-111.726146777071,1074.81046418773,
417.982363284621));
#111013=CARTESIAN_POINT('Ctrl Pts',(-111.756957497768,1074.80630411877,
417.982363284621));
#111014=CARTESIAN_POINT('Origin',(-79.4772023228643,1067.7251047501,465.900390831321));
#111015=CARTESIAN_POINT('',(-79.4772023228921,1076.68910595681,464.422087699128));
#111016=CARTESIAN_POINT('',(-79.4772023228643,1067.7251047501,464.422087699128));
#111017=CARTESIAN_POINT('Ctrl Pts',(-79.4773207736094,1076.6535541543,467.378693958769));
#111018=CARTESIAN_POINT('Ctrl Pts',(-79.6713773118498,1076.64843867231,
467.378678409765));
#111019=CARTESIAN_POINT('Ctrl Pts',(-79.86355791831,1076.64366238044,467.340452351834));
#111020=CARTESIAN_POINT('Ctrl Pts',(-80.2221051063023,1076.63566604264,
467.191954301431));
#111021=CARTESIAN_POINT('Ctrl Pts',(-80.385001689945,1076.63252997765,467.08315387701));
#111022=CARTESIAN_POINT('Ctrl Pts',(-80.6592225868108,1076.62861881595,
466.8090805442));
#111023=CARTESIAN_POINT('Ctrl Pts',(-80.7679781329324,1076.62788120595,
466.646574536193));
#111024=CARTESIAN_POINT('Ctrl Pts',(-80.9164782089922,1076.62899174161,
466.289257129839));
#111025=CARTESIAN_POINT('Ctrl Pts',(-80.9549317568238,1076.63082244591,
466.09797586385));
#111026=CARTESIAN_POINT('Ctrl Pts',(-80.9560659558716,1076.63665533535,
465.711641132296));
#111027=CARTESIAN_POINT('Ctrl Pts',(-80.9187967152726,1076.6405940468,465.520314950613));
#111028=CARTESIAN_POINT('Ctrl Pts',(-80.7727863600171,1076.64975813045,
465.162712325768));
#111029=CARTESIAN_POINT('Ctrl Pts',(-80.6653957651852,1076.65488926548,
464.999892180117));
#111030=CARTESIAN_POINT('Ctrl Pts',(-80.4619123520525,1076.6627531713,464.793567716721));
#111031=CARTESIAN_POINT('Ctrl Pts',(-80.3875042400959,1076.66538434143,
464.731604357531));
#111032=CARTESIAN_POINT('Ctrl Pts',(-80.2276586167916,1076.67057108426,
464.623077804526));
#111033=CARTESIAN_POINT('Ctrl Pts',(-80.142603097741,1076.67311413955,464.576776185806));
#111034=CARTESIAN_POINT('Ctrl Pts',(-79.8734027534427,1076.68054042448,
464.46278330814));
#111035=CARTESIAN_POINT('Ctrl Pts',(-79.6797801662227,1076.68506645828,
464.423007479017));
#111036=CARTESIAN_POINT('Ctrl Pts',(-79.2892719337877,1076.69285388908,
464.421204035365));
#111037=CARTESIAN_POINT('Ctrl Pts',(-79.0962322658128,1076.69605170485,
464.458800853409));
#111038=CARTESIAN_POINT('Ctrl Pts',(-78.7350849451112,1076.70106353305,
464.60698613581));
#111039=CARTESIAN_POINT('Ctrl Pts',(-78.5706534717544,1076.70283087364,
464.716411105573));
#111040=CARTESIAN_POINT('Ctrl Pts',(-78.2932219028221,1076.70499407301,
464.993626917563));
#111041=CARTESIAN_POINT('Ctrl Pts',(-78.1832587368082,1076.70536681328,
465.15894531095));
#111042=CARTESIAN_POINT('Ctrl Pts',(-78.0345830847091,1076.70472822829,
465.52257559874));
#111043=CARTESIAN_POINT('Ctrl Pts',(-77.997223574233,1076.70372393956,465.717211250815));
#111044=CARTESIAN_POINT('Ctrl Pts',(-78.0006798152531,1076.70026427114,
466.108516119396));
#111045=CARTESIAN_POINT('Ctrl Pts',(-78.0409973261513,1076.69784400125,
466.301319033678));
#111046=CARTESIAN_POINT('Ctrl Pts',(-78.194107701336,1076.69153551541,466.660035848239));
#111047=CARTESIAN_POINT('Ctrl Pts',(-78.3053623993841,1076.68770177684,
466.822439755124));
#111048=CARTESIAN_POINT('Ctrl Pts',(-78.5133820383168,1076.68108741469,
467.025371971186));
#111049=CARTESIAN_POINT('Ctrl Pts',(-78.5881813312674,1076.67878159535,
467.085368776092));
#111050=CARTESIAN_POINT('Ctrl Pts',(-78.7499337728941,1076.67391472848,
467.191121363255));
#111051=CARTESIAN_POINT('Ctrl Pts',(-78.8367059389319,1076.67136132967,
467.236305672403));
#111052=CARTESIAN_POINT('Ctrl Pts',(-79.1021950212922,1076.66371040272,
467.342699065507));
#111053=CARTESIAN_POINT('Ctrl Pts',(-79.2888959287506,1076.65852118045,
467.378709056527));
#111054=CARTESIAN_POINT('Ctrl Pts',(-79.4773207736094,1076.6535541543,467.378693958769));
#111055=CARTESIAN_POINT('Origin',(-79.4772023228643,1067.7251047501,465.900390831321));
#111056=CARTESIAN_POINT('',(-79.4772023228642,1076.66179580959,466.778693963515));
#111057=CARTESIAN_POINT('',(-79.4772023228643,1076.68289265596,465.022087699128));
#111058=CARTESIAN_POINT('Ctrl Pts',(-79.4772023228642,1076.66179580959,
466.778693963515));
#111059=CARTESIAN_POINT('Ctrl Pts',(-79.4857706943264,1076.661581251,466.778693963515));
#111060=CARTESIAN_POINT('Ctrl Pts',(-79.4943443628444,1076.66136773358,
466.778568579773));
#111061=CARTESIAN_POINT('Ctrl Pts',(-79.6180460225395,1076.65830438857,
466.774944817879));
#111062=CARTESIAN_POINT('Ctrl Pts',(-79.7313993347598,1076.65571272977,
466.74895960446));
#111063=CARTESIAN_POINT('Ctrl Pts',(-79.9415719837507,1076.6514631756,466.654734254006));
#111064=CARTESIAN_POINT('Ctrl Pts',(-80.0363613716195,1076.64984857097,
466.587426342055));
#111065=CARTESIAN_POINT('Ctrl Pts',(-80.1944790720495,1076.64791978271,
466.42015987799));
#111066=CARTESIAN_POINT('Ctrl Pts',(-80.2563099089907,1076.64762411971,
466.32186195923));
#111067=CARTESIAN_POINT('Ctrl Pts',(-80.3385198977434,1076.64842148663,
466.107148066569));
#111068=CARTESIAN_POINT('Ctrl Pts',(-80.3581498408944,1076.64950465016,
465.99283240926));
#111069=CARTESIAN_POINT('Ctrl Pts',(-80.3522902572622,1076.65284946089,
465.763171373147));
#111070=CARTESIAN_POINT('Ctrl Pts',(-80.3268675305151,1076.65507640488,
465.650044443106));
#111071=CARTESIAN_POINT('Ctrl Pts',(-80.2339095005646,1076.66027249429,
465.439939545758));
#111072=CARTESIAN_POINT('Ctrl Pts',(-80.1672433907226,1076.66318946683,
465.344997078396));
#111073=CARTESIAN_POINT('Ctrl Pts',(-80.042700892681,1076.66771807545,465.225910284604));
#111074=CARTESIAN_POINT('Ctrl Pts',(-79.9974144236322,1076.66924207577,
465.190396467831));
#111075=CARTESIAN_POINT('Ctrl Pts',(-79.900589286229,1076.67226968345,465.12873531195));
#111076=CARTESIAN_POINT('Ctrl Pts',(-79.8492862372823,1076.67376602991,
465.10273019738));
#111077=CARTESIAN_POINT('Ctrl Pts',(-79.6942576590158,1076.67799255003,
465.042381510243));
#111078=CARTESIAN_POINT('Ctrl Pts',(-79.5862197918597,1076.68058364682,
465.022091072706));
#111079=CARTESIAN_POINT('Ctrl Pts',(-79.4772294980396,1076.68289208039,
465.022087699549));
#111080=CARTESIAN_POINT('Ctrl Pts',(-79.4772204396409,1076.68289227225,
465.022087699268));
#111081=CARTESIAN_POINT('Ctrl Pts',(-79.4772113812491,1076.68289246411,
465.022087699128));
#111082=CARTESIAN_POINT('Ctrl Pts',(-79.4772023228643,1076.68289265596,
465.022087699128));
#111083=CARTESIAN_POINT('',(-79.4772023228643,1082.7251047501,465.022087699128));
#111084=CARTESIAN_POINT('',(-79.4772023228643,1067.7251047501,465.022087699128));
#111085=CARTESIAN_POINT('Origin',(-79.4772023228643,1082.7251047501,465.900390831321));
#111086=CARTESIAN_POINT('Ctrl Pts',(-79.4772023228643,1076.68289265596,
465.022087699128));
#111087=CARTESIAN_POINT('Ctrl Pts',(-79.3608033170153,1076.68535795407,
465.022087699128));
#111088=CARTESIAN_POINT('Ctrl Pts',(-79.2455503107277,1076.68745541836,
465.04522672191));
#111089=CARTESIAN_POINT('Ctrl Pts',(-79.0304199919175,1076.69079932101,
465.135248625558));
#111090=CARTESIAN_POINT('Ctrl Pts',(-78.9327419473629,1076.69201259101,
465.201375736584));
#111091=CARTESIAN_POINT('Ctrl Pts',(-78.768703890884,1076.69348580652,465.368243895008));
#111092=CARTESIAN_POINT('Ctrl Pts',(-78.7040989728584,1076.69372956816,
465.467421941505));
#111093=CARTESIAN_POINT('Ctrl Pts',(-78.6176794381873,1076.69322646309,
465.685133549991));
#111094=CARTESIAN_POINT('Ctrl Pts',(-78.596676188045,1076.69248526583,465.801458285212));
#111095=CARTESIAN_POINT('Ctrl Pts',(-78.6014845360777,1076.69004089533,
466.035003685674));
#111096=CARTESIAN_POINT('Ctrl Pts',(-78.6270572558308,1076.68836333028,
466.149896022123));
#111097=CARTESIAN_POINT('Ctrl Pts',(-78.7215121176519,1076.68416339597,
466.362895931512));
#111098=CARTESIAN_POINT('Ctrl Pts',(-78.789423853008,1076.68168045485,466.458903395041));
#111099=CARTESIAN_POINT('Ctrl Pts',(-78.9155353807194,1076.67754967797,
466.5780338605));
#111100=CARTESIAN_POINT('Ctrl Pts',(-78.9607154788485,1076.67613226927,
466.613069501702));
#111101=CARTESIAN_POINT('Ctrl Pts',(-79.0573836203829,1076.67320938354,
466.673981829001));
#111102=CARTESIAN_POINT('Ctrl Pts',(-79.1086612891547,1076.67171059189,
466.699683105052));
#111103=CARTESIAN_POINT('Ctrl Pts',(-79.2627029750366,1076.66735002856,
466.75889487307));
#111104=CARTESIAN_POINT('Ctrl Pts',(-79.3695344822519,1076.66449189475,
466.778693963515));
#111105=CARTESIAN_POINT('Ctrl Pts',(-79.4772023228642,1076.66179580959,
466.778693963515));
#111106=CARTESIAN_POINT('Origin',(-90.2477595453604,1067.7251047501,459.442436531111));
#111107=CARTESIAN_POINT('',(-90.2477595453866,1076.37387335857,458.166992409975));
#111108=CARTESIAN_POINT('',(-90.2477595453604,1067.7251047501,458.166992409975));
#111109=CARTESIAN_POINT('Ctrl Pts',(-90.2473951380049,1076.31449558095,
460.717880600189));
#111110=CARTESIAN_POINT('Ctrl Pts',(-90.4149925201918,1076.30406321819,
460.717928484468));
#111111=CARTESIAN_POINT('Ctrl Pts',(-90.5810244388579,1076.29435900911,
460.684941623415));
#111112=CARTESIAN_POINT('Ctrl Pts',(-90.8906028854361,1076.27773119679,
460.556675727967));
#111113=CARTESIAN_POINT('Ctrl Pts',(-91.0311902148397,1076.27096807621,
460.462758836199));
#111114=CARTESIAN_POINT('Ctrl Pts',(-91.2677010387952,1076.26151736905,
460.226242819948));
#111115=CARTESIAN_POINT('Ctrl Pts',(-91.3614573749476,1076.25891190801,
460.086122300387));
#111116=CARTESIAN_POINT('Ctrl Pts',(-91.4894636636373,1076.25831245208,
459.77809376442));
#111117=CARTESIAN_POINT('Ctrl Pts',(-91.5226275761762,1076.26031136127,
459.613287069429));
#111118=CARTESIAN_POINT('Ctrl Pts',(-91.5237646897207,1076.2686084767,459.28035364862));
#111119=CARTESIAN_POINT('Ctrl Pts',(-91.4917496119433,1076.27482153916,
459.115471286924));
#111120=CARTESIAN_POINT('Ctrl Pts',(-91.3661653991122,1076.29050641563,
458.807052313795));
#111121=CARTESIAN_POINT('Ctrl Pts',(-91.273666100747,1076.29983013518,458.666536713084));
#111122=CARTESIAN_POINT('Ctrl Pts',(-91.0396594316448,1076.32019392865,
458.428752379496));
#111123=CARTESIAN_POINT('Ctrl Pts',(-90.9002504266469,1076.33104061181,
458.333877082239));
#111124=CARTESIAN_POINT('Ctrl Pts',(-90.6697075900341,1076.34728440329,
458.235917758385));
#111125=CARTESIAN_POINT('Ctrl Pts',(-90.5898448415355,1076.35265663299,
458.210889928147));
#111126=CARTESIAN_POINT('Ctrl Pts',(-90.3424368776555,1076.36856070555,
458.159302263942));
#111127=CARTESIAN_POINT('Ctrl Pts',(-90.1714882801023,1076.37856592741,
458.158063609476));
#111128=CARTESIAN_POINT('Ctrl Pts',(-89.8397465957344,1076.39621679187,
458.222313455795));
#111129=CARTESIAN_POINT('Ctrl Pts',(-89.6821722332112,1076.40370379496,
458.286872878131));
#111130=CARTESIAN_POINT('Ctrl Pts',(-89.4009393614874,1076.4153989733,458.473821287724));
#111131=CARTESIAN_POINT('Ctrl Pts',(-89.2801489336416,1076.41948958617,
458.594452002963));
#111132=CARTESIAN_POINT('Ctrl Pts',(-89.0924232299604,1076.42383922101,
458.876162491902));
#111133=CARTESIAN_POINT('Ctrl Pts',(-89.0274934847933,1076.42404876803,
459.034489783154));
#111134=CARTESIAN_POINT('Ctrl Pts',(-88.9633643405313,1076.42052079141,
459.366955042704));
#111135=CARTESIAN_POINT('Ctrl Pts',(-88.9646919349542,1076.41682369359,
459.537726478374));
#111136=CARTESIAN_POINT('Ctrl Pts',(-89.0337562040218,1076.40585083862,
459.868364025985));
#111137=CARTESIAN_POINT('Ctrl Pts',(-89.100659739176,1076.39868710692,460.024964939687));
#111138=CARTESIAN_POINT('Ctrl Pts',(-89.2917513009851,1076.3815753021,460.303503544349));
#111139=CARTESIAN_POINT('Ctrl Pts',(-89.4142549940543,1076.3717819452,460.422550099397));
#111140=CARTESIAN_POINT('Ctrl Pts',(-89.6998581839638,1076.35063884563,
460.606792905232));
#111141=CARTESIAN_POINT('Ctrl Pts',(-89.8604942758898,1076.33948408229,
460.669603518788));
#111142=CARTESIAN_POINT('Ctrl Pts',(-90.1009177432434,1076.32373433747,
460.711518116806));
#111143=CARTESIAN_POINT('Ctrl Pts',(-90.1740847277611,1076.31905890279,
460.717859654659));
#111144=CARTESIAN_POINT('Ctrl Pts',(-90.2473951380049,1076.31449558095,
460.717880600189));
#111145=CARTESIAN_POINT('Origin',(-90.2477595453604,1067.7251047501,459.442436531111));
#111146=CARTESIAN_POINT('',(-90.2477595453604,1076.32917837425,460.117880652247));
#111147=CARTESIAN_POINT('',(-90.2477595453606,1076.3606248843,458.766992409975));
#111148=CARTESIAN_POINT('Ctrl Pts',(-90.2477595453603,1076.32917837425,
460.117880652247));
#111149=CARTESIAN_POINT('Ctrl Pts',(-90.2572965053981,1076.32859342499,
460.117880652247));
#111150=CARTESIAN_POINT('Ctrl Pts',(-90.266841445427,1076.32801224415,460.117678667997));
#111151=CARTESIAN_POINT('Ctrl Pts',(-90.3649713709435,1076.32208148596,
460.113515719287));
#111152=CARTESIAN_POINT('Ctrl Pts',(-90.4519859111912,1076.31719251032,
460.092350909843));
#111153=CARTESIAN_POINT('Ctrl Pts',(-90.6127328843783,1076.3089705214,460.01763878999));
#111154=CARTESIAN_POINT('Ctrl Pts',(-90.6849346217564,1076.30571522265,
459.964885283311));
#111155=CARTESIAN_POINT('Ctrl Pts',(-90.8047232882335,1076.30134150474,
459.834639139193));
#111156=CARTESIAN_POINT('Ctrl Pts',(-90.8512057910747,1076.30026087909,
459.758488254488));
#111157=CARTESIAN_POINT('Ctrl Pts',(-90.9121552741609,1076.3004507403,459.592727808095));
#111158=CARTESIAN_POINT('Ctrl Pts',(-90.9260802207466,1076.30171526864,
459.504765666679));
#111159=CARTESIAN_POINT('Ctrl Pts',(-90.9193391352392,1076.30641611299,
459.328451622158));
#111160=CARTESIAN_POINT('Ctrl Pts',(-90.8987220164565,1076.309806762,459.24181781014));
#111161=CARTESIAN_POINT('Ctrl Pts',(-90.8253166579501,1076.31823580457,
459.081237916383));
#111162=CARTESIAN_POINT('Ctrl Pts',(-90.7731619803815,1076.32319538349,
459.008872035341));
#111163=CARTESIAN_POINT('Ctrl Pts',(-90.6438585005819,1076.33398835859,
458.888208399147));
#111164=CARTESIAN_POINT('Ctrl Pts',(-90.5678881490822,1076.33971955767,
458.841123369004));
#111165=CARTESIAN_POINT('Ctrl Pts',(-90.409162252535,1076.35067725464,458.781575796335));
#111166=CARTESIAN_POINT('Ctrl Pts',(-90.3287961942446,1076.35581800331,
458.766992409975));
#111167=CARTESIAN_POINT('Ctrl Pts',(-90.2477595453608,1076.3606248843,458.766992409975));
#111168=CARTESIAN_POINT('',(-90.2477595453604,1082.7251047501,458.766992409975));
#111169=CARTESIAN_POINT('',(-90.2477595453604,1067.7251047501,458.766992409975));
#111170=CARTESIAN_POINT('Origin',(-90.2477595453604,1082.7251047501,459.442436531111));
#111171=CARTESIAN_POINT('Ctrl Pts',(-90.2477595453608,1076.3606248843,458.766992409975));
#111172=CARTESIAN_POINT('Ctrl Pts',(-90.2476740819054,1076.36062995377,
458.766992409975));
#111173=CARTESIAN_POINT('Ctrl Pts',(-90.2475886177041,1076.36063502286,
458.766992426301));
#111174=CARTESIAN_POINT('Ctrl Pts',(-90.2475031527616,1076.36064009159,
458.766992458742));
#111175=CARTESIAN_POINT('Ctrl Pts',(-90.1576841753495,1076.36596704673,
458.767026553234));
#111176=CARTESIAN_POINT('Ctrl Pts',(-90.0687357095448,1076.37078390744,
458.784976170086));
#111177=CARTESIAN_POINT('Ctrl Pts',(-89.9031079874359,1076.37888217561,
458.854640640584));
#111178=CARTESIAN_POINT('Ctrl Pts',(-89.8280721524695,1076.38208554669,
458.905629095858));
#111179=CARTESIAN_POINT('Ctrl Pts',(-89.7022535079224,1076.38648665427,
459.034098107516));
#111180=CARTESIAN_POINT('Ctrl Pts',(-89.6527700077903,1076.38763878941,
459.110308275996));
#111181=CARTESIAN_POINT('Ctrl Pts',(-89.5865703611777,1076.38773229927,
459.277660306333));
#111182=CARTESIAN_POINT('Ctrl Pts',(-89.5705276812917,1076.38667266553,
459.367103428081));
#111183=CARTESIAN_POINT('Ctrl Pts',(-89.5744170575338,1076.38244544676,
459.546889603371));
#111184=CARTESIAN_POINT('Ctrl Pts',(-89.594270106551,1076.37932178872,459.635416429416));
#111185=CARTESIAN_POINT('Ctrl Pts',(-89.6674262014148,1076.37136061123,
459.799529708689));
#111186=CARTESIAN_POINT('Ctrl Pts',(-89.7200223908945,1076.36660000202,
459.873463499818));
#111187=CARTESIAN_POINT('Ctrl Pts',(-89.8512791660716,1076.35600260715,
459.99666138276));
#111188=CARTESIAN_POINT('Ctrl Pts',(-89.9287443458786,1076.35026587117,
460.044587310458));
#111189=CARTESIAN_POINT('Ctrl Pts',(-90.0884175699086,1076.33924971808,
460.103684060641));
#111190=CARTESIAN_POINT('Ctrl Pts',(-90.1678081753738,1076.33408218995,
460.117880652247));
#111191=CARTESIAN_POINT('Ctrl Pts',(-90.2477595453603,1076.32917837425,
460.117880652247));
#111192=CARTESIAN_POINT('Origin',(-101.429261354592,1067.7251047501,451.269782488757));
#111193=CARTESIAN_POINT('',(-101.429261354619,1075.68385821193,450.170951352764));
#111194=CARTESIAN_POINT('',(-101.429261354592,1067.7251047501,450.170951352764));
#111195=CARTESIAN_POINT('Ctrl Pts',(-101.428824831104,1075.62575125877,
452.368613538042));
#111196=CARTESIAN_POINT('Ctrl Pts',(-101.573543970317,1075.61103511209,
452.368671029413));
#111197=CARTESIAN_POINT('Ctrl Pts',(-101.716968304491,1075.59710718154,
452.340138063898));
#111198=CARTESIAN_POINT('Ctrl Pts',(-101.98404922685,1075.57260139272,452.229186104905));
#111199=CARTESIAN_POINT('Ctrl Pts',(-102.105224112842,1075.56224700518,
452.148078505666));
#111200=CARTESIAN_POINT('Ctrl Pts',(-102.308724606694,1075.54666616046,
451.944023198637));
#111201=CARTESIAN_POINT('Ctrl Pts',(-102.389291852746,1075.54156266542,
451.823362835185));
#111202=CARTESIAN_POINT('Ctrl Pts',(-102.499149199234,1075.53736334671,
451.558313457678));
#111203=CARTESIAN_POINT('Ctrl Pts',(-102.527586606201,1075.53828136185,
451.416689367917));
#111204=CARTESIAN_POINT('Ctrl Pts',(-102.528585005851,1075.54602103374,
451.130541210698));
#111205=CARTESIAN_POINT('Ctrl Pts',(-102.501137546036,1075.55276429535,
450.988863241077));
#111206=CARTESIAN_POINT('Ctrl Pts',(-102.393426157324,1075.57116695209,
450.723503440223));
#111207=CARTESIAN_POINT('Ctrl Pts',(-102.313957484765,1075.58266800443,
450.602500278067));
#111208=CARTESIAN_POINT('Ctrl Pts',(-102.112659620965,1075.60886453958,
450.397324375233));
#111209=CARTESIAN_POINT('Ctrl Pts',(-101.992478980741,1075.62332820295,
450.315343042515));
#111210=CARTESIAN_POINT('Ctrl Pts',(-101.793664510477,1075.64571534432,
450.23062965139));
#111211=CARTESIAN_POINT('Ctrl Pts',(-101.724714463618,1075.65324654696,
450.208964154126));
#111212=CARTESIAN_POINT('Ctrl Pts',(-101.51092097434,1075.67591701036,450.164264299751));
#111213=CARTESIAN_POINT('Ctrl Pts',(-101.363073605718,1075.69068622292,
450.163209338025));
#111214=CARTESIAN_POINT('Ctrl Pts',(-101.076433525723,1075.71762090883,
450.219008594389));
#111215=CARTESIAN_POINT('Ctrl Pts',(-100.94037211969,1075.72954308128,450.274955108786));
#111216=CARTESIAN_POINT('Ctrl Pts',(-100.697957721304,1075.74909097304,
450.436810959434));
#111217=CARTESIAN_POINT('Ctrl Pts',(-100.594000675888,1075.75652868986,
450.541046538769));
#111218=CARTESIAN_POINT('Ctrl Pts',(-100.432679844794,1075.76597495695,
450.784404075123));
#111219=CARTESIAN_POINT('Ctrl Pts',(-100.377033325883,1075.76788171489,
450.921065603358));
#111220=CARTESIAN_POINT('Ctrl Pts',(-100.322475883854,1075.76586122839,
451.208157841083));
#111221=CARTESIAN_POINT('Ctrl Pts',(-100.324107852411,1075.76195662614,
451.355612832337));
#111222=CARTESIAN_POINT('Ctrl Pts',(-100.384802397907,1075.74876668641,
451.640992358975));
#111223=CARTESIAN_POINT('Ctrl Pts',(-100.443189323568,1075.73961841438,
451.776017968428));
#111224=CARTESIAN_POINT('Ctrl Pts',(-100.609221178158,1075.71713607322,
452.015616628179));
#111225=CARTESIAN_POINT('Ctrl Pts',(-100.715352191986,1075.70401092934,
452.117717880423));
#111226=CARTESIAN_POINT('Ctrl Pts',(-100.898457705771,1075.68273065259,
452.2345567985));
#111227=CARTESIAN_POINT('Ctrl Pts',(-100.962326366096,1075.67549874985,
452.267033044876));
#111228=CARTESIAN_POINT('Ctrl Pts',(-101.092160019658,1075.66114233945,
452.317833223314));
#111229=CARTESIAN_POINT('Ctrl Pts',(-101.157599505607,1075.65405970112,
452.33666879454));
#111230=CARTESIAN_POINT('Ctrl Pts',(-101.291751240266,1075.63983794698,
452.362131740878));
#111231=CARTESIAN_POINT('Ctrl Pts',(-101.360207120892,1075.63272883129,
452.368586278854));
#111232=CARTESIAN_POINT('Ctrl Pts',(-101.428824831104,1075.62575125877,
452.368613538042));
#111233=CARTESIAN_POINT('Origin',(-101.429261354592,1067.7251047501,451.269782488757));
#111234=CARTESIAN_POINT('',(-101.429261354592,1075.64217240143,451.768613624749));
#111235=CARTESIAN_POINT('',(-101.429261354593,1075.66856733728,450.770951352764));
#111236=CARTESIAN_POINT('Ctrl Pts',(-101.429261354592,1075.64217240143,
451.768613624749));
#111237=CARTESIAN_POINT('Ctrl Pts',(-101.466625322109,1075.63839354457,
451.768613624749));
#111238=CARTESIAN_POINT('Ctrl Pts',(-101.503974500602,1075.63472064406,
451.76441563379));
#111239=CARTESIAN_POINT('Ctrl Pts',(-101.604479016645,1075.6251333703,451.741403281128));
#111240=CARTESIAN_POINT('Ctrl Pts',(-101.664919483172,1075.61970292959,
451.71431521238));
#111241=CARTESIAN_POINT('Ctrl Pts',(-101.771609546742,1075.61085297973,
451.638415711296));
#111242=CARTESIAN_POINT('Ctrl Pts',(-101.816900766962,1075.6075086123,451.590473884824));
#111243=CARTESIAN_POINT('Ctrl Pts',(-101.886268944348,1075.60337917568,
451.480035129975));
#111244=CARTESIAN_POINT('Ctrl Pts',(-101.909766742443,1075.60262211248,
451.418713403683));
#111245=CARTESIAN_POINT('Ctrl Pts',(-101.931875986063,1075.60380581233,
451.29057206556));
#111246=CARTESIAN_POINT('Ctrl Pts',(-101.930302916489,1075.60573073487,
451.22503969026));
#111247=CARTESIAN_POINT('Ctrl Pts',(-101.902126735514,1075.61202024156,
451.098110585345));
#111248=CARTESIAN_POINT('Ctrl Pts',(-101.875718903519,1075.61633035449,
451.037980671676));
#111249=CARTESIAN_POINT('Ctrl Pts',(-101.801195055009,1075.62677977734,
450.931000457423));
#111250=CARTESIAN_POINT('Ctrl Pts',(-101.753667768507,1075.63282862234,
450.885264232718));
#111251=CARTESIAN_POINT('Ctrl Pts',(-101.671194895238,1075.64258551325,
450.832322134364));
#111252=CARTESIAN_POINT('Ctrl Pts',(-101.641988912993,1075.64593367939,
450.817400432505));
#111253=CARTESIAN_POINT('Ctrl Pts',(-101.582652265061,1075.65253818379,
450.794107385504));
#111254=CARTESIAN_POINT('Ctrl Pts',(-101.552769804416,1075.65577663001,
450.785487935513));
#111255=CARTESIAN_POINT('Ctrl Pts',(-101.491621722104,1075.66223332618,
450.773881744183));
#111256=CARTESIAN_POINT('Ctrl Pts',(-101.460478627276,1075.66543770614,
450.770951352764));
#111257=CARTESIAN_POINT('Ctrl Pts',(-101.429261354593,1075.66856733728,
450.770951352764));
#111258=CARTESIAN_POINT('',(-101.429261354592,1082.7251047501,450.770951352764));
#111259=CARTESIAN_POINT('',(-101.429261354592,1067.7251047501,450.770951352764));
#111260=CARTESIAN_POINT('Origin',(-101.429261354592,1082.7251047501,451.269782488757));
#111261=CARTESIAN_POINT('Ctrl Pts',(-101.429261354593,1075.66856733728,
450.770951352764));
#111262=CARTESIAN_POINT('Ctrl Pts',(-101.429175761062,1075.6685759183,450.770951352764));
#111263=CARTESIAN_POINT('Ctrl Pts',(-101.429090166973,1075.66858449877,
450.770951374888));
#111264=CARTESIAN_POINT('Ctrl Pts',(-101.429004572336,1075.66859307867,
450.770951418949));
#111265=CARTESIAN_POINT('Ctrl Pts',(-101.362529805005,1075.67525642691,
450.770985638031));
#111266=CARTESIAN_POINT('Ctrl Pts',(-101.296673859189,1075.68148464945,
450.784307273578));
#111267=CARTESIAN_POINT('Ctrl Pts',(-101.17416604199,1075.69233675057,450.836001435219));
#111268=CARTESIAN_POINT('Ctrl Pts',(-101.118705158814,1075.69685802441,
450.873787915152));
#111269=CARTESIAN_POINT('Ctrl Pts',(-101.026316089801,1075.70355338138,
450.968463479552));
#111270=CARTESIAN_POINT('Ctrl Pts',(-100.990115036859,1075.70568647433,
451.024184226064));
#111271=CARTESIAN_POINT('Ctrl Pts',(-100.941739472419,1075.70731242583,
451.14576370675));
#111272=CARTESIAN_POINT('Ctrl Pts',(-100.929746901932,1075.70682245188,
451.210274363339));
#111273=CARTESIAN_POINT('Ctrl Pts',(-100.931175069105,1075.70329699079,
451.340371816795));
#111274=CARTESIAN_POINT('Ctrl Pts',(-100.944631276456,1075.70029130348,
451.404665834681));
#111275=CARTESIAN_POINT('Ctrl Pts',(-100.995984741017,1075.69203156629,
451.525769431355));
#111276=CARTESIAN_POINT('Ctrl Pts',(-101.033917198477,1075.68681056514,
451.581140146956));
#111277=CARTESIAN_POINT('Ctrl Pts',(-101.12929508331,1075.67485578366,451.673878168055));
#111278=CARTESIAN_POINT('Ctrl Pts',(-101.185866774295,1075.66823437907,
451.710261001859));
#111279=CARTESIAN_POINT('Ctrl Pts',(-101.278243710066,1075.6579987126,451.746321634162));
#111280=CARTESIAN_POINT('Ctrl Pts',(-101.309709438091,1075.65459710411,
451.755172100283));
#111281=CARTESIAN_POINT('Ctrl Pts',(-101.37074274857,1075.64815481417,451.766040101891));
#111282=CARTESIAN_POINT('Ctrl Pts',(-101.400006584011,1075.64513112337,
451.768613624749));
#111283=CARTESIAN_POINT('Ctrl Pts',(-101.429261354592,1075.64217240143,
451.768613624749));
#111284=CARTESIAN_POINT('Origin',(-110.796881705951,1067.7251047501,440.88317361084));
#111285=CARTESIAN_POINT('',(-110.796881705974,1074.82291082631,439.792632862112));
#111286=CARTESIAN_POINT('',(-110.796881705951,1067.7251047501,439.792632862112));
#111287=CARTESIAN_POINT('Ctrl Pts',(-110.797105361067,1074.77999286998,
441.973714336634));
#111288=CARTESIAN_POINT('Ctrl Pts',(-110.94348355177,1074.76031515429,441.973684316452));
#111289=CARTESIAN_POINT('Ctrl Pts',(-111.088520200642,1074.74130263312,
441.944183028484));
#111290=CARTESIAN_POINT('Ctrl Pts',(-111.355468495658,1074.70735540124,
441.830707025445));
#111291=CARTESIAN_POINT('Ctrl Pts',(-111.47530196927,1074.69266196889,441.749039437982));
#111292=CARTESIAN_POINT('Ctrl Pts',(-111.675601131087,1074.66941281543,
441.544538841122));
#111293=CARTESIAN_POINT('Ctrl Pts',(-111.754483912226,1074.66102693366,
441.424151601835));
#111294=CARTESIAN_POINT('Ctrl Pts',(-111.86103748437,1074.65172829746,441.160494132515));
#111295=CARTESIAN_POINT('Ctrl Pts',(-111.888028253745,1074.65085210625,
441.020088872214));
#111296=CARTESIAN_POINT('Ctrl Pts',(-111.886796482441,1074.6567199401,440.736877025722));
#111297=CARTESIAN_POINT('Ctrl Pts',(-111.858630045261,1074.66339754126,
440.596957194216));
#111298=CARTESIAN_POINT('Ctrl Pts',(-111.750295413962,1074.6834619519,440.334980400228));
#111299=CARTESIAN_POINT('Ctrl Pts',(-111.670842497709,1074.69669386072,
440.21566274908));
#111300=CARTESIAN_POINT('Ctrl Pts',(-111.470078312828,1074.72800902203,
440.01334173779));
#111301=CARTESIAN_POINT('Ctrl Pts',(-111.350259188695,1074.74583983454,
439.932662373144));
#111302=CARTESIAN_POINT('Ctrl Pts',(-111.152549809805,1074.77412359308,
439.849786511264));
#111303=CARTESIAN_POINT('Ctrl Pts',(-111.084083513385,1074.78374592789,
439.828707263087));
#111304=CARTESIAN_POINT('Ctrl Pts',(-110.944321453409,1074.80305320118,
439.800304398657));
#111305=CARTESIAN_POINT('Ctrl Pts',(-110.873349194707,1074.81269472288,
439.792990457562));
#111306=CARTESIAN_POINT('Ctrl Pts',(-110.657571261627,1074.8415236111,439.791945286038));
#111307=CARTESIAN_POINT('Ctrl Pts',(-110.514112629573,1074.86003078403,
439.820008247311));
#111308=CARTESIAN_POINT('Ctrl Pts',(-110.246794346848,1074.89324742946,
439.930534675914));
#111309=CARTESIAN_POINT('Ctrl Pts',(-110.125441587613,1074.90765269428,
440.011724697301));
#111310=CARTESIAN_POINT('Ctrl Pts',(-109.922203971637,1074.93039849742,
440.216234446847));
#111311=CARTESIAN_POINT('Ctrl Pts',(-109.842005480321,1074.93856779183,
440.337112198895));
#111312=CARTESIAN_POINT('Ctrl Pts',(-109.733915731825,1074.94762980625,
440.601325409095));
#111313=CARTESIAN_POINT('Ctrl Pts',(-109.706326683477,1074.94854259667,
440.741620931826));
#111314=CARTESIAN_POINT('Ctrl Pts',(-109.706355270303,1074.94309864505,
441.025226449537));
#111315=CARTESIAN_POINT('Ctrl Pts',(-109.734079176414,1074.93678250172,
441.165657709974));
#111316=CARTESIAN_POINT('Ctrl Pts',(-109.842760866284,1074.9174281049,441.430838479501));
#111317=CARTESIAN_POINT('Ctrl Pts',(-109.923803895461,1074.90443647703,
441.552413102722));
#111318=CARTESIAN_POINT('Ctrl Pts',(-110.128406458997,1074.87346552783,
441.756895815543));
#111319=CARTESIAN_POINT('Ctrl Pts',(-110.250054594975,1074.85577660562,
441.837699186511));
#111320=CARTESIAN_POINT('Ctrl Pts',(-110.448836749423,1074.82771140611,
441.919076633296));
#111321=CARTESIAN_POINT('Ctrl Pts',(-110.516364905335,1074.81829981499,
441.939362542594));
#111322=CARTESIAN_POINT('Ctrl Pts',(-110.655091245718,1074.79919877588,
441.966791599466));
#111323=CARTESIAN_POINT('Ctrl Pts',(-110.726012464015,1074.78954993452,
441.973728916823));
#111324=CARTESIAN_POINT('Ctrl Pts',(-110.797105361067,1074.77999286998,
441.973714336634));
#111325=CARTESIAN_POINT('Origin',(-110.796881705951,1067.7251047501,440.88317361084));
#111326=CARTESIAN_POINT('',(-110.796881705951,1074.79242545665,441.373714359568));
#111327=CARTESIAN_POINT('',(-110.796881705951,1074.81171529132,440.392632862112));
#111328=CARTESIAN_POINT('Ctrl Pts',(-110.796881705951,1074.79242545665,
441.373714359568));
#111329=CARTESIAN_POINT('Ctrl Pts',(-110.797786191687,1074.79230410707,
441.373714359568));
#111330=CARTESIAN_POINT('Ctrl Pts',(-110.798690737079,1074.79218279516,
441.373711857939));
#111331=CARTESIAN_POINT('Ctrl Pts',(-110.865211266256,1074.78326484229,
441.37334386692));
#111332=CARTESIAN_POINT('Ctrl Pts',(-110.930162714815,1074.77479705536,
441.359818516996));
#111333=CARTESIAN_POINT('Ctrl Pts',(-111.050222236907,1074.75964388772,
441.308218999479));
#111334=CARTESIAN_POINT('Ctrl Pts',(-111.10429124951,1074.75308331224,441.270952994277));
#111335=CARTESIAN_POINT('Ctrl Pts',(-111.194042578868,1074.74279701432,
441.17811141175));
#111336=CARTESIAN_POINT('Ctrl Pts',(-111.229146768844,1074.73912533272,
441.123783231449));
#111337=CARTESIAN_POINT('Ctrl Pts',(-111.276317327878,1074.73510149318,
441.004949108279));
#111338=CARTESIAN_POINT('Ctrl Pts',(-111.288065990577,1074.73476714158,
440.941721814427));
#111339=CARTESIAN_POINT('Ctrl Pts',(-111.286724467102,1074.73748093841,
440.814289054747));
#111340=CARTESIAN_POINT('Ctrl Pts',(-111.27364581082,1074.7405016105,440.751380682394));
#111341=CARTESIAN_POINT('Ctrl Pts',(-111.224104855968,1074.74953313192,
440.633747223378));
#111342=CARTESIAN_POINT('Ctrl Pts',(-111.187966971081,1074.75547515032,
440.580257315185));
#111343=CARTESIAN_POINT('Ctrl Pts',(-111.096945747979,1074.76953619832,
440.489789711359));
#111344=CARTESIAN_POINT('Ctrl Pts',(-111.042749008856,1074.7775414189,440.453851251935));
#111345=CARTESIAN_POINT('Ctrl Pts',(-110.953841827618,1074.79020181952,
440.417336716221));
#111346=CARTESIAN_POINT('Ctrl Pts',(-110.923343030664,1074.79447471961,
440.408150353881));
#111347=CARTESIAN_POINT('Ctrl Pts',(-110.860796572288,1074.80310121376,
440.395763566507));
#111348=CARTESIAN_POINT('Ctrl Pts',(-110.828879020003,1074.80743593212,
440.392632862112));
#111349=CARTESIAN_POINT('Ctrl Pts',(-110.796881705951,1074.81171529132,
440.392632862112));
#111350=CARTESIAN_POINT('',(-110.796881705951,1082.7251047501,440.392632862112));
#111351=CARTESIAN_POINT('',(-110.796881705951,1067.7251047501,440.392632862112));
#111352=CARTESIAN_POINT('Origin',(-110.796881705951,1082.7251047501,440.88317361084));
#111353=CARTESIAN_POINT('Ctrl Pts',(-110.796881705951,1074.81171529132,
440.392632862112));
#111354=CARTESIAN_POINT('Ctrl Pts',(-110.796800433509,1074.8117261608,440.392632862112));
#111355=CARTESIAN_POINT('Ctrl Pts',(-110.796719160552,1074.81173702992,
440.392632882309));
#111356=CARTESIAN_POINT('Ctrl Pts',(-110.796637887089,1074.81174789867,
440.392632922706));
#111357=CARTESIAN_POINT('Ctrl Pts',(-110.731386270444,1074.82047404469,
440.392665355438));
#111358=CARTESIAN_POINT('Ctrl Pts',(-110.666720623711,1074.8288468084,440.405717121953));
#111359=CARTESIAN_POINT('Ctrl Pts',(-110.546326109029,1074.84389122311,
440.456431152121));
#111360=CARTESIAN_POINT('Ctrl Pts',(-110.491749163602,1074.8504206601,440.493545729109));
#111361=CARTESIAN_POINT('Ctrl Pts',(-110.400901860152,1074.86066985068,
440.586533917516));
#111362=CARTESIAN_POINT('Ctrl Pts',(-110.365295313079,1074.86432560277,
440.641204083187));
#111363=CARTESIAN_POINT('Ctrl Pts',(-110.317687268505,1074.86831513604,
440.760451244923));
#111364=CARTESIAN_POINT('Ctrl Pts',(-110.305813334118,1074.86865888794,
440.823658359471));
#111365=CARTESIAN_POINT('Ctrl Pts',(-110.30690528324,1074.86603420645,440.951175505274));
#111366=CARTESIAN_POINT('Ctrl Pts',(-110.31989222242,1074.86308803514,441.014189692276));
#111367=CARTESIAN_POINT('Ctrl Pts',(-110.369332767942,1074.85423162507,
441.132067233784));
#111368=CARTESIAN_POINT('Ctrl Pts',(-110.405467601649,1074.84838740974,
441.185686945772));
#111369=CARTESIAN_POINT('Ctrl Pts',(-110.497127501705,1074.83440666427,
441.276942815033));
#111370=CARTESIAN_POINT('Ctrl Pts',(-110.552165749063,1074.82635909903,
441.313288309164));
#111371=CARTESIAN_POINT('Ctrl Pts',(-110.642223161231,1074.81361095413,
441.349790887485));
#111372=CARTESIAN_POINT('Ctrl Pts',(-110.672926082968,1074.8093264257,441.358867733615));
#111373=CARTESIAN_POINT('Ctrl Pts',(-110.734800811584,1074.80080836035,
441.370761405948));
#111374=CARTESIAN_POINT('Ctrl Pts',(-110.76580605255,1074.79659469598,441.373714359568));
#111375=CARTESIAN_POINT('Ctrl Pts',(-110.796881705951,1074.79242545665,
441.373714359568));
#111376=CARTESIAN_POINT('Origin',(-69.1578093449747,1067.7251047501,481.522560066374));
#111377=CARTESIAN_POINT('',(-69.1578093449979,1076.6946925711,480.044256934181));
#111378=CARTESIAN_POINT('',(-69.1578093449747,1067.7251047501,480.044256934181));
#111379=CARTESIAN_POINT('Ctrl Pts',(-69.1578534910652,1076.64572415765,
483.000863197909));
#111380=CARTESIAN_POINT('Ctrl Pts',(-69.3520466123464,1076.64107006247,
483.000857398782));
#111381=CARTESIAN_POINT('Ctrl Pts',(-69.5443646856791,1076.63704453658,
482.96258724071));
#111382=CARTESIAN_POINT('Ctrl Pts',(-69.9029585790611,1076.63104156109,
482.813973068201));
#111383=CARTESIAN_POINT('Ctrl Pts',(-70.06578441007,1076.62912526241,482.705177728005));
#111384=CARTESIAN_POINT('Ctrl Pts',(-70.3397664037465,1076.62785868295,
482.43128278759));
#111385=CARTESIAN_POINT('Ctrl Pts',(-70.4484034651645,1076.6285149798,482.26899375864));
#111386=CARTESIAN_POINT('Ctrl Pts',(-70.5968530602563,1076.63226388891,
481.912171287804));
#111387=CARTESIAN_POINT('Ctrl Pts',(-70.635373255508,1076.63531162612,481.7211479596));
#111388=CARTESIAN_POINT('Ctrl Pts',(-70.6368305743748,1076.64314502678,
481.335148627493));
#111389=CARTESIAN_POINT('Ctrl Pts',(-70.5997593297441,1076.64784852514,
481.143881781424));
#111390=CARTESIAN_POINT('Ctrl Pts',(-70.4541500357107,1076.65797750975,
480.786211519797));
#111391=CARTESIAN_POINT('Ctrl Pts',(-70.3469225550915,1076.66330023062,
480.623272986609));
#111392=CARTESIAN_POINT('Ctrl Pts',(-70.1436357428308,1076.67106272851,
480.41673104042));
#111393=CARTESIAN_POINT('Ctrl Pts',(-70.069288050044,1076.67359620194,480.354690715285));
#111394=CARTESIAN_POINT('Ctrl Pts',(-69.8271376497734,1076.68099936237,
480.189928182539));
#111395=CARTESIAN_POINT('Ctrl Pts',(-69.644467384676,1076.68550062963,480.112921324492));
#111396=CARTESIAN_POINT('Ctrl Pts',(-69.2610670673237,1076.69321259593,
480.035041249039));
#111397=CARTESIAN_POINT('Ctrl Pts',(-69.0642350746438,1076.69636314841,
480.034397912974));
#111398=CARTESIAN_POINT('Ctrl Pts',(-68.6813723762028,1076.70127064601,
480.109583154842));
#111399=CARTESIAN_POINT('Ctrl Pts',(-68.4991289955559,1076.70298574406,
480.184785473457));
#111400=CARTESIAN_POINT('Ctrl Pts',(-68.1738614375616,1076.70504878505,
480.402023564848));
#111401=CARTESIAN_POINT('Ctrl Pts',(-68.0341946314356,1076.705376912,480.542128323284));
#111402=CARTESIAN_POINT('Ctrl Pts',(-67.8177661864602,1076.70465733861,
480.868393826114));
#111403=CARTESIAN_POINT('Ctrl Pts',(-67.7430559236265,1076.7036167256,481.051265004334));
#111404=CARTESIAN_POINT('Ctrl Pts',(-67.6692951014785,1076.70008714064,
481.434786315442));
#111405=CARTESIAN_POINT('Ctrl Pts',(-67.6707044431848,1076.69763031507,
481.631606673994));
#111406=CARTESIAN_POINT('Ctrl Pts',(-67.7498936363522,1076.69124335579,
482.013827147402));
#111407=CARTESIAN_POINT('Ctrl Pts',(-67.8270903594424,1076.68736423883,
482.195425233566));
#111408=CARTESIAN_POINT('Ctrl Pts',(-67.9915155812525,1076.68068561915,
482.435989318868));
#111409=CARTESIAN_POINT('Ctrl Pts',(-68.0532692814349,1076.67835803169,
482.50977044806));
#111410=CARTESIAN_POINT('Ctrl Pts',(-68.1913390059092,1076.67345969519,
482.645430029059));
#111411=CARTESIAN_POINT('Ctrl Pts',(-68.2675419814773,1076.6708974976,482.706758169247));
#111412=CARTESIAN_POINT('Ctrl Pts',(-68.5116665156276,1076.66307951883,
482.866260119487));
#111413=CARTESIAN_POINT('Ctrl Pts',(-68.6934238718275,1076.65773437225,
482.939379589634));
#111414=CARTESIAN_POINT('Ctrl Pts',(-68.9743622230062,1076.65025167938,
482.992309082317));
#111415=CARTESIAN_POINT('Ctrl Pts',(-69.066006941971,1076.64792538177,483.000865940693));
#111416=CARTESIAN_POINT('Ctrl Pts',(-69.1578534910652,1076.64572415765,
483.000863197909));
#111417=CARTESIAN_POINT('Origin',(-69.1578093449747,1067.7251047501,481.522560066374));
#111418=CARTESIAN_POINT('',(-69.1578093449746,1076.65741108281,482.400863198568));
#111419=CARTESIAN_POINT('',(-69.1578093449744,1076.68648464657,480.644256934181));
#111420=CARTESIAN_POINT('Ctrl Pts',(-69.1578093449746,1076.65741108281,
482.400863198568));
#111421=CARTESIAN_POINT('Ctrl Pts',(-69.2234418991496,1076.6559402335,482.400863198568));
#111422=CARTESIAN_POINT('Ctrl Pts',(-69.2890259697938,1076.65458596451,
482.393506311697));
#111423=CARTESIAN_POINT('Ctrl Pts',(-69.4656324118671,1076.65129261893,
482.353182614794));
#111424=CARTESIAN_POINT('Ctrl Pts',(-69.571819936465,1076.6497153178,482.305686807597));
#111425=CARTESIAN_POINT('Ctrl Pts',(-69.7596569569364,1076.64787071332,
482.172506146584));
#111426=CARTESIAN_POINT('Ctrl Pts',(-69.8395218595992,1076.64762051612,
482.088174007604));
#111427=CARTESIAN_POINT('Ctrl Pts',(-69.9620961476268,1076.64850686382,
481.893680683398));
#111428=CARTESIAN_POINT('Ctrl Pts',(-70.0036798545837,1076.64963192794,
481.785444498049));
#111429=CARTESIAN_POINT('Ctrl Pts',(-70.0428234626304,1076.65304808726,
481.55918185984));
#111430=CARTESIAN_POINT('Ctrl Pts',(-70.0400292849277,1076.65530344979,
481.443343021985));
#111431=CARTESIAN_POINT('Ctrl Pts',(-69.9900378964925,1076.66053930322,
481.219243524958));
#111432=CARTESIAN_POINT('Ctrl Pts',(-69.9432918137948,1076.66346733952,
481.113145343748));
#111433=CARTESIAN_POINT('Ctrl Pts',(-69.8445544662576,1076.66800051871,
480.972021712607));
#111434=CARTESIAN_POINT('Ctrl Pts',(-69.8071161421933,1076.66952437174,
480.928327771717));
#111435=CARTESIAN_POINT('Ctrl Pts',(-69.7242446613695,1076.67254902727,
480.848866227006));
#111436=CARTESIAN_POINT('Ctrl Pts',(-69.6790090045838,1076.67404255437,
480.813290409741));
#111437=CARTESIAN_POINT('Ctrl Pts',(-69.5320560412162,1076.67845657641,
480.719418444827));
#111438=CARTESIAN_POINT('Ctrl Pts',(-69.4218891224324,1076.68120355579,
480.676769441779));
#111439=CARTESIAN_POINT('Ctrl Pts',(-69.2574551311642,1076.68463859819,
480.648503983826));
#111440=CARTESIAN_POINT('Ctrl Pts',(-69.2076810999441,1076.68559798675,
480.644256934181));
#111441=CARTESIAN_POINT('Ctrl Pts',(-69.157809344974,1076.68648464657,480.644256934181));
#111442=CARTESIAN_POINT('',(-69.1578093449747,1082.7251047501,480.644256934181));
#111443=CARTESIAN_POINT('',(-69.1578093449747,1067.7251047501,480.644256934181));
#111444=CARTESIAN_POINT('Origin',(-69.1578093449747,1082.7251047501,481.522560066374));
#111445=CARTESIAN_POINT('Ctrl Pts',(-69.1578034448267,1076.68648475146,
480.644256934201));
#111446=CARTESIAN_POINT('Ctrl Pts',(-69.0413256637295,1076.68855557259,
480.64425771666));
#111447=CARTESIAN_POINT('Ctrl Pts',(-68.9259972394792,1076.69020053972,
480.667428872737));
#111448=CARTESIAN_POINT('Ctrl Pts',(-68.7109178618377,1076.6925746641,480.757497738844));
#111449=CARTESIAN_POINT('Ctrl Pts',(-68.613337610142,1076.69328117763,480.823572092937));
#111450=CARTESIAN_POINT('Ctrl Pts',(-68.4496593311885,1076.69371963535,
480.990043135918));
#111451=CARTESIAN_POINT('Ctrl Pts',(-68.3852149705645,1076.69344715755,
481.088799595298));
#111452=CARTESIAN_POINT('Ctrl Pts',(-68.2987971436756,1076.6919231308,481.305532099511));
#111453=CARTESIAN_POINT('Ctrl Pts',(-68.2776098766221,1076.69068659907,
481.421318711384));
#111454=CARTESIAN_POINT('Ctrl Pts',(-68.2816683989113,1076.68729786405,
481.654361485375));
#111455=CARTESIAN_POINT('Ctrl Pts',(-68.3068627986114,1076.6851765445,481.769301587661));
#111456=CARTESIAN_POINT('Ctrl Pts',(-68.4008529499654,1076.68019194474,
481.983147336794));
#111457=CARTESIAN_POINT('Ctrl Pts',(-68.4689181916272,1076.67737269356,
482.079830109188));
#111458=CARTESIAN_POINT('Ctrl Pts',(-68.5960343334076,1076.67287855751,
482.200194577173));
#111459=CARTESIAN_POINT('Ctrl Pts',(-68.641990916816,1076.67135580326,482.235799792611));
#111460=CARTESIAN_POINT('Ctrl Pts',(-68.7887122087969,1076.66677549102,
482.327827110654));
#111461=CARTESIAN_POINT('Ctrl Pts',(-68.8974035657164,1076.66372781536,
482.369246363832));
#111462=CARTESIAN_POINT('Ctrl Pts',(-69.0596088337739,1076.65967636945,
482.396748218617));
#111463=CARTESIAN_POINT('Ctrl Pts',(-69.1087226494482,1076.65851113343,
482.400863198568));
#111464=CARTESIAN_POINT('Ctrl Pts',(-69.1578093449746,1076.65741108281,
482.400863198568));
#111465=CARTESIAN_POINT('Origin',(-81.035688248506,1067.7251047501,477.445052325154));
#111466=CARTESIAN_POINT('',(-81.035688248534,1076.38861150411,476.169608204017));
#111467=CARTESIAN_POINT('',(-81.035688248506,1067.7251047501,476.169608204017));
#111468=CARTESIAN_POINT('Ctrl Pts',(-81.0350577987155,1076.29855081768,
478.720496290475));
#111469=CARTESIAN_POINT('Ctrl Pts',(-81.2025872754575,1076.28904104832,
478.720579100011));
#111470=CARTESIAN_POINT('Ctrl Pts',(-81.3685713429343,1076.28071251082,
478.687653651935));
#111471=CARTESIAN_POINT('Ctrl Pts',(-81.6779649861134,1076.26760505678,
478.55958789631));
#111472=CARTESIAN_POINT('Ctrl Pts',(-81.8184203241435,1076.26294804639,
478.46587303349));
#111473=CARTESIAN_POINT('Ctrl Pts',(-82.0547972518833,1076.25810168175,
478.229889358828));
#111474=CARTESIAN_POINT('Ctrl Pts',(-82.1485512834177,1076.25794630665,
478.090102318924));
#111475=CARTESIAN_POINT('Ctrl Pts',(-82.2768528229317,1076.26218228058,
477.782644138906));
#111476=CARTESIAN_POINT('Ctrl Pts',(-82.3102484857368,1076.26652278209,
477.618028368156));
#111477=CARTESIAN_POINT('Ctrl Pts',(-82.3119826647834,1076.2790267047,477.285168278088));
#111478=CARTESIAN_POINT('Ctrl Pts',(-82.2802282147205,1076.28706960511,
477.120143535699));
#111479=CARTESIAN_POINT('Ctrl Pts',(-82.1550323352381,1076.30563793529,
476.811272820305));
#111480=CARTESIAN_POINT('Ctrl Pts',(-82.0626112673567,1076.31598830964,
476.670449657923));
#111481=CARTESIAN_POINT('Ctrl Pts',(-81.8872474634401,1076.33209795959,
476.491859992467));
#111482=CARTESIAN_POINT('Ctrl Pts',(-81.8230420025745,1076.33753081149,
476.438174772569));
#111483=CARTESIAN_POINT('Ctrl Pts',(-81.6850684766686,1076.34835045727,
476.344128585188));
#111484=CARTESIAN_POINT('Ctrl Pts',(-81.6116280997105,1076.35371156829,
476.303990155284));
#111485=CARTESIAN_POINT('Ctrl Pts',(-81.3790489997821,1076.36956256003,
476.205092004347));
#111486=CARTESIAN_POINT('Ctrl Pts',(-81.2116281892164,1076.37950643801,
476.170502300506));
#111487=CARTESIAN_POINT('Ctrl Pts',(-80.8737184860208,1076.3969948398,476.168752249334));
#111488=CARTESIAN_POINT('Ctrl Pts',(-80.7065692166189,1076.4043825128,476.201308734276));
#111489=CARTESIAN_POINT('Ctrl Pts',(-80.394267683289,1076.41585345873,476.329752933126));
#111490=CARTESIAN_POINT('Ctrl Pts',(-80.252268303724,1076.41982178174,476.42446734997));
#111491=CARTESIAN_POINT('Ctrl Pts',(-80.0132049540281,1076.42391724823,
476.664042335541));
#111492=CARTESIAN_POINT('Ctrl Pts',(-79.9186337580982,1076.42399815458,
476.806586549861));
#111493=CARTESIAN_POINT('Ctrl Pts',(-79.7908232378988,1076.42021996792,
477.119999971423));
#111494=CARTESIAN_POINT('Ctrl Pts',(-79.7587569641805,1076.4164036502,477.287674129747));
#111495=CARTESIAN_POINT('Ctrl Pts',(-79.7618344059718,1076.4052118501,477.62536860419));
#111496=CARTESIAN_POINT('Ctrl Pts',(-79.7968236670402,1076.39794918094,
477.792026290804));
#111497=CARTESIAN_POINT('Ctrl Pts',(-79.9297897299973,1076.38066932286,
478.102626681248));
#111498=CARTESIAN_POINT('Ctrl Pts',(-80.0267102412019,1076.37080744361,
478.243390457155));
#111499=CARTESIAN_POINT('Ctrl Pts',(-80.2709610251275,1076.34957324633,
478.48001817901));
#111500=CARTESIAN_POINT('Ctrl Pts',(-80.4163480458686,1076.33839736225,
478.573047215329));
#111501=CARTESIAN_POINT('Ctrl Pts',(-80.7222066175661,1076.31726838241,
478.69130787995));
#111502=CARTESIAN_POINT('Ctrl Pts',(-80.8779342293022,1076.30746989828,
478.720418624561));
#111503=CARTESIAN_POINT('Ctrl Pts',(-81.0350577987155,1076.29855081768,
478.720496290475));
#111504=CARTESIAN_POINT('Origin',(-81.035688248506,1067.7251047501,477.445052325154));
#111505=CARTESIAN_POINT('',(-81.035688248506,1076.32087957987,478.12049644629));
#111506=CARTESIAN_POINT('',(-81.0356882485063,1076.36858155369,476.769608204017));
#111507=CARTESIAN_POINT('Ctrl Pts',(-81.0356882485058,1076.32087957987,
478.12049644629));
#111508=CARTESIAN_POINT('Ctrl Pts',(-81.0876899683255,1076.31799162062,
478.12049644629));
#111509=CARTESIAN_POINT('Ctrl Pts',(-81.1396509250425,1076.31531083151,
478.114491043542));
#111510=CARTESIAN_POINT('Ctrl Pts',(-81.2767049632162,1076.30881714018,
478.082213763299));
#111511=CARTESIAN_POINT('Ctrl Pts',(-81.3580914012869,1076.30558998787,
478.045161876903));
#111512=CARTESIAN_POINT('Ctrl Pts',(-81.5017615346713,1076.30127879455,
477.941849337013));
#111513=CARTESIAN_POINT('Ctrl Pts',(-81.5626924302093,1076.30023185449,
477.876680169358));
#111514=CARTESIAN_POINT('Ctrl Pts',(-81.6559233030925,1076.30048940395,
477.726685444176));
#111515=CARTESIAN_POINT('Ctrl Pts',(-81.687359818685,1076.30178720242,477.643363879025));
#111516=CARTESIAN_POINT('Ctrl Pts',(-81.7164386739801,1076.30654910395,
477.469340570339));
#111517=CARTESIAN_POINT('Ctrl Pts',(-81.7137814951616,1076.30996693042,
477.380330855999));
#111518=CARTESIAN_POINT('Ctrl Pts',(-81.6743968578101,1076.3184404379,477.208224530291));
#111519=CARTESIAN_POINT('Ctrl Pts',(-81.6379696361283,1076.32341688763,
477.126803176128));
#111520=CARTESIAN_POINT('Ctrl Pts',(-81.5357678564573,1076.33423131285,
476.982469018654));
#111521=CARTESIAN_POINT('Ctrl Pts',(-81.4709012897918,1076.33996689521,
476.920982383539));
#111522=CARTESIAN_POINT('Ctrl Pts',(-81.3197704532662,1076.35151253806,
476.82565555341));
#111523=CARTESIAN_POINT('Ctrl Pts',(-81.2346252268159,1076.35720761268,
476.793296719234));
#111524=CARTESIAN_POINT('Ctrl Pts',(-81.1093088234223,1076.36458502301,
476.77262422383));
#111525=CARTESIAN_POINT('Ctrl Pts',(-81.0725580361971,1076.36663518759,
476.769611028284));
#111526=CARTESIAN_POINT('Ctrl Pts',(-81.0357400173349,1076.36857882086,
476.76960820633));
#111527=CARTESIAN_POINT('Ctrl Pts',(-81.0357227610269,1076.36857973182,
476.769608205008));
#111528=CARTESIAN_POINT('Ctrl Pts',(-81.0357055047511,1076.36858064277,
476.769608204017));
#111529=CARTESIAN_POINT('Ctrl Pts',(-81.0356882485066,1076.36858155369,
476.769608204017));
#111530=CARTESIAN_POINT('',(-81.035688248506,1082.7251047501,476.769608204017));
#111531=CARTESIAN_POINT('',(-81.035688248506,1067.7251047501,476.769608204017));
#111532=CARTESIAN_POINT('Origin',(-81.035688248506,1082.7251047501,477.445052325154));
#111533=CARTESIAN_POINT('Ctrl Pts',(-81.0356882485066,1076.36858155369,
476.769608204017));
#111534=CARTESIAN_POINT('Ctrl Pts',(-80.9459376043467,1076.37331926323,
476.769608204017));
#111535=CARTESIAN_POINT('Ctrl Pts',(-80.8570465935824,1076.37735746331,
476.787496825715));
#111536=CARTESIAN_POINT('Ctrl Pts',(-80.6913756260759,1076.3836223215,476.857048565197));
#111537=CARTESIAN_POINT('Ctrl Pts',(-80.6162677526475,1076.38578648672,
476.908028783951));
#111538=CARTESIAN_POINT('Ctrl Pts',(-80.490354059149,1076.38796575458,477.036482166989));
#111539=CARTESIAN_POINT('Ctrl Pts',(-80.4408421981638,1076.38795784533,
477.112671384822));
#111540=CARTESIAN_POINT('Ctrl Pts',(-80.3746031318373,1076.38574772309,
477.2799034164));
#111541=CARTESIAN_POINT('Ctrl Pts',(-80.3585233940397,1076.38356883935,
477.369242298903));
#111542=CARTESIAN_POINT('Ctrl Pts',(-80.3622558168713,1076.37727679008,
477.548898300214));
#111543=CARTESIAN_POINT('Ctrl Pts',(-80.382020323534,1076.37322599853,477.63740972814));
#111544=CARTESIAN_POINT('Ctrl Pts',(-80.4550618199596,1076.36371555603,
477.801709096096));
#111545=CARTESIAN_POINT('Ctrl Pts',(-80.507708273909,1076.35834542562,477.875817963691));
#111546=CARTESIAN_POINT('Ctrl Pts',(-80.605452720709,1076.34987842304,477.967610853476));
#111547=CARTESIAN_POINT('Ctrl Pts',(-80.6404817164721,1076.34703887773,
477.994580700113));
#111548=CARTESIAN_POINT('Ctrl Pts',(-80.7539130304431,1076.33838431086,
478.065424897086));
#111549=CARTESIAN_POINT('Ctrl Pts',(-80.8386464989045,1076.33260746561,
478.097308551931));
#111550=CARTESIAN_POINT('Ctrl Pts',(-80.9631062455084,1076.32501022693,
478.117573261705));
#111551=CARTESIAN_POINT('Ctrl Pts',(-80.9994071681082,1076.32289448018,
478.12049644629));
#111552=CARTESIAN_POINT('Ctrl Pts',(-81.0356882485058,1076.32087957987,
478.12049644629));
#111553=CARTESIAN_POINT('Origin',(-93.6720377362213,1067.7251047501,471.775755329037));
#111554=CARTESIAN_POINT('',(-93.6720377362212,1075.70592960701,470.676924193044));
#111555=CARTESIAN_POINT('',(-93.6720377362213,1067.7251047501,470.676924193044));
#111556=CARTESIAN_POINT('Ctrl Pts',(-93.6724912621575,1075.60299418635,
472.874586371436));
#111557=CARTESIAN_POINT('Ctrl Pts',(-93.8169302540145,1075.58933558814,
472.874526756422));
#111558=CARTESIAN_POINT('Ctrl Pts',(-93.9600910334365,1075.57706485313,
472.845988318381));
#111559=CARTESIAN_POINT('Ctrl Pts',(-94.2265607311415,1075.55691151587,
472.735247792837));
#111560=CARTESIAN_POINT('Ctrl Pts',(-94.3473884187733,1075.54920204289,
472.654445900629));
#111561=CARTESIAN_POINT('Ctrl Pts',(-94.5505303134195,1075.53949431675,
472.451185501296));
#111562=CARTESIAN_POINT('Ctrl Pts',(-94.6310424305107,1075.53756147911,
472.330990881764));
#111563=CARTESIAN_POINT('Ctrl Pts',(-94.7412746804731,1075.53976384039,
472.066661254209));
#111564=CARTESIAN_POINT('Ctrl Pts',(-94.7699955975805,1075.54386435273,
471.925217352867));
#111565=CARTESIAN_POINT('Ctrl Pts',(-94.7717056673004,1075.55754939313,
471.638964047272));
#111566=CARTESIAN_POINT('Ctrl Pts',(-94.7445019646648,1075.56701403193,
471.496970713478));
#111567=CARTESIAN_POINT('Ctrl Pts',(-94.637016943371,1075.59002791232,471.230801805686));
#111568=CARTESIAN_POINT('Ctrl Pts',(-94.5574400275378,1075.60337795513,
471.109307337067));
#111569=CARTESIAN_POINT('Ctrl Pts',(-94.4063394473801,1075.62491014947,
470.955124244313));
#111570=CARTESIAN_POINT('Ctrl Pts',(-94.3509033093937,1075.63230386669,
470.908707578224));
#111571=CARTESIAN_POINT('Ctrl Pts',(-94.2319879551823,1075.64723723404,
470.827574452807));
#111572=CARTESIAN_POINT('Ctrl Pts',(-94.1688138660993,1075.65474178336,
470.79300164833));
#111573=CARTESIAN_POINT('Ctrl Pts',(-93.9685431431715,1075.67730907353,
470.707679880593));
#111574=CARTESIAN_POINT('Ctrl Pts',(-93.824244517943,1075.69197607329,470.677765702776));
#111575=CARTESIAN_POINT('Ctrl Pts',(-93.5328349810482,1075.71869264892,
470.676121075161));
#111576=CARTESIAN_POINT('Ctrl Pts',(-93.3885638460807,1075.73049592361,
470.704169315622));
#111577=CARTESIAN_POINT('Ctrl Pts',(-93.118898028987,1075.74979914152,470.815151093479));
#111578=CARTESIAN_POINT('Ctrl Pts',(-92.9962482006577,1075.75710075947,
470.897062055314));
#111579=CARTESIAN_POINT('Ctrl Pts',(-92.7921704384465,1075.76613296183,
471.102140540071));
#111580=CARTESIAN_POINT('Ctrl Pts',(-92.7119651934467,1075.76788731263,
471.222399927589));
#111581=CARTESIAN_POINT('Ctrl Pts',(-92.602133018938,1075.76579171759,471.487141717504));
#111582=CARTESIAN_POINT('Ctrl Pts',(-92.5736649139426,1075.76195513217,
471.629015406361));
#111583=CARTESIAN_POINT('Ctrl Pts',(-92.5727508400567,1075.7489670063,471.91821427215));
#111584=CARTESIAN_POINT('Ctrl Pts',(-92.6013627896465,1075.73984827547,
472.062639524665));
#111585=CARTESIAN_POINT('Ctrl Pts',(-92.7130987407103,1075.7174364238,472.33171554884));
#111586=CARTESIAN_POINT('Ctrl Pts',(-92.7951223488863,1075.70436191303,
472.453694586321));
#111587=CARTESIAN_POINT('Ctrl Pts',(-92.9490408166069,1075.68315553206,
472.606290889229));
#111588=CARTESIAN_POINT('Ctrl Pts',(-93.0044293445341,1075.67595097932,
472.65143098531));
#111589=CARTESIAN_POINT('Ctrl Pts',(-93.1233387940823,1075.66125814001,
472.730466514943));
#111590=CARTESIAN_POINT('Ctrl Pts',(-93.1866147717712,1075.65380259906,
472.764141522232));
#111591=CARTESIAN_POINT('Ctrl Pts',(-93.385771493417,1075.63136578552,472.846365209264));
#111592=CARTESIAN_POINT('Ctrl Pts',(-93.5284035649352,1075.61661956506,
472.87464584146));
#111593=CARTESIAN_POINT('Ctrl Pts',(-93.6724912621575,1075.60299418635,
472.874586371436));
#111594=CARTESIAN_POINT('Origin',(-93.6720377362213,1067.7251047501,471.775755329037));
#111595=CARTESIAN_POINT('',(-93.6720377362213,1075.63195590694,472.274586465029));
#111596=CARTESIAN_POINT('',(-93.6720377362213,1075.67866049267,471.276924193045));
#111597=CARTESIAN_POINT('Ctrl Pts',(-93.6720377362214,1075.63195590694,
472.274586465029));
#111598=CARTESIAN_POINT('Ctrl Pts',(-93.6737691348478,1075.63179365252,
472.274586465029));
#111599=CARTESIAN_POINT('Ctrl Pts',(-93.675500986709,1075.63163176809,472.274577450741));
#111600=CARTESIAN_POINT('Ctrl Pts',(-93.743328560288,1075.6253077827,472.273870966368));
#111601=CARTESIAN_POINT('Ctrl Pts',(-93.8086976309984,1075.61981426241,
472.260051449589));
#111602=CARTESIAN_POINT('Ctrl Pts',(-93.9294189604092,1075.61090887706,
472.208008495179));
#111603=CARTESIAN_POINT('Ctrl Pts',(-93.9837309733091,1075.60755437524,
472.170660119206));
#111604=CARTESIAN_POINT('Ctrl Pts',(-94.0747040602113,1075.60339910519,
472.077284693635));
#111605=CARTESIAN_POINT('Ctrl Pts',(-94.110547226867,1075.60262743349,472.022277883647));
#111606=CARTESIAN_POINT('Ctrl Pts',(-94.1590787287541,1075.60378121623,
471.901638891653));
#111607=CARTESIAN_POINT('Ctrl Pts',(-94.1713055789272,1075.60569234708,
471.837222228766));
#111608=CARTESIAN_POINT('Ctrl Pts',(-94.1704066890215,1075.61195888507,
471.707154680144));
#111609=CARTESIAN_POINT('Ctrl Pts',(-94.1571976209969,1075.6162607745,471.642785171551));
#111610=CARTESIAN_POINT('Ctrl Pts',(-94.1067412339385,1075.62669969183,
471.522485245883));
#111611=CARTESIAN_POINT('Ctrl Pts',(-94.0698363103155,1075.63274628175,
471.467769964241));
#111612=CARTESIAN_POINT('Ctrl Pts',(-94.0003209811604,1075.64249340348,
471.398756760698));
#111613=CARTESIAN_POINT('Ctrl Pts',(-93.9749618585148,1075.64583148274,
471.378094761762));
#111614=CARTESIAN_POINT('Ctrl Pts',(-93.9206384928281,1075.65258399093,
471.342061386539));
#111615=CARTESIAN_POINT('Ctrl Pts',(-93.8918063336955,1075.65598272677,
471.326762543099));
#111616=CARTESIAN_POINT('Ctrl Pts',(-93.8015629462923,1075.66609816722,
471.289667018385));
#111617=CARTESIAN_POINT('Ctrl Pts',(-93.7371481923161,1075.67265257079,
471.276928469069));
#111618=CARTESIAN_POINT('Ctrl Pts',(-93.6720705043938,1075.67865746911,
471.276924194121));
#111619=CARTESIAN_POINT('Ctrl Pts',(-93.6720595816534,1075.67865847699,
471.276924193404));
#111620=CARTESIAN_POINT('Ctrl Pts',(-93.6720486589293,1075.67865948484,
471.276924193045));
#111621=CARTESIAN_POINT('Ctrl Pts',(-93.6720377362213,1075.67866049267,
471.276924193045));
#111622=CARTESIAN_POINT('',(-93.6720377362213,1082.7251047501,471.276924193044));
#111623=CARTESIAN_POINT('',(-93.6720377362213,1067.7251047501,471.276924193044));
#111624=CARTESIAN_POINT('Origin',(-93.6720377362213,1082.7251047501,471.775755329037));
#111625=CARTESIAN_POINT('Ctrl Pts',(-93.6720377362213,1075.67866049267,
471.276924193045));
#111626=CARTESIAN_POINT('Ctrl Pts',(-93.6057021697443,1075.68478125021,
471.276924193045));
#111627=CARTESIAN_POINT('Ctrl Pts',(-93.5399634596612,1075.69021285038,
471.290156336786));
#111628=CARTESIAN_POINT('Ctrl Pts',(-93.4179970438533,1075.69903597252,
471.341438225336));
#111629=CARTESIAN_POINT('Ctrl Pts',(-93.3628981850123,1075.70235892845,
471.378747617469));
#111630=CARTESIAN_POINT('Ctrl Pts',(-93.2710109458655,1075.7064665635,471.472052912521));
#111631=CARTESIAN_POINT('Ctrl Pts',(-93.2348802972019,1075.70724676277,
471.526848205431));
#111632=CARTESIAN_POINT('Ctrl Pts',(-93.1856677095831,1075.70620435935,
471.647267394553));
#111633=CARTESIAN_POINT('Ctrl Pts',(-93.1730860586743,1075.70439100265,
471.711694413156));
#111634=CARTESIAN_POINT('Ctrl Pts',(-93.1733293925817,1075.69836557453,
471.841952972592));
#111635=CARTESIAN_POINT('Ctrl Pts',(-93.1862574974906,1075.69420280903,
471.906498430089));
#111636=CARTESIAN_POINT('Ctrl Pts',(-93.2366226107059,1075.68394572461,
472.0280667968));
#111637=CARTESIAN_POINT('Ctrl Pts',(-93.2740394554466,1075.67791644558,
472.0836995133));
#111638=CARTESIAN_POINT('Ctrl Pts',(-93.3442711117432,1075.66818445032,
472.153188397825));
#111639=CARTESIAN_POINT('Ctrl Pts',(-93.3695203473757,1075.66488807269,
472.173711286108));
#111640=CARTESIAN_POINT('Ctrl Pts',(-93.4236710698175,1075.6581869491,472.209578650767));
#111641=CARTESIAN_POINT('Ctrl Pts',(-93.452453444199,1075.65479742239,472.224833554217));
#111642=CARTESIAN_POINT('Ctrl Pts',(-93.5426317880684,1075.64466393579,
472.261873245006));
#111643=CARTESIAN_POINT('Ctrl Pts',(-93.6070151801627,1075.63804936053,
472.274586465029));
#111644=CARTESIAN_POINT('Ctrl Pts',(-93.6720377362214,1075.63195590694,
472.274586465029));
#111645=CARTESIAN_POINT('Origin',(-104.994450521158,1067.7251047501,463.563756561532));
#111646=CARTESIAN_POINT('',(-104.994450521158,1074.8526378468,462.473215812804));
#111647=CARTESIAN_POINT('',(-104.994450521158,1067.7251047501,462.473215812804));
#111648=CARTESIAN_POINT('Ctrl Pts',(-104.993489577313,1074.75006270401,
464.654296886886));
#111649=CARTESIAN_POINT('Ctrl Pts',(-105.137367767514,1074.73163951737,
464.654423667032));
#111650=CARTESIAN_POINT('Ctrl Pts',(-105.280072879011,1074.71463613285,
464.626075909733));
#111651=CARTESIAN_POINT('Ctrl Pts',(-105.545324057093,1074.68569695547,
464.515734326609));
#111652=CARTESIAN_POINT('Ctrl Pts',(-105.665476382385,1074.67399870599,
464.435296075217));
#111653=CARTESIAN_POINT('Ctrl Pts',(-105.867001838481,1074.65758776391,
464.233154467582));
#111654=CARTESIAN_POINT('Ctrl Pts',(-105.946730719867,1074.6529721013,464.113906624031));
#111655=CARTESIAN_POINT('Ctrl Pts',(-106.055683810394,1074.65143823157,
463.851986175433));
#111656=CARTESIAN_POINT('Ctrl Pts',(-106.084056288577,1074.65449593288,
463.712112038072));
#111657=CARTESIAN_POINT('Ctrl Pts',(-106.085883608058,1074.66788353223,
463.429046701911));
#111658=CARTESIAN_POINT('Ctrl Pts',(-106.059155506872,1074.67809875985,
463.288701813979));
#111659=CARTESIAN_POINT('Ctrl Pts',(-105.953374507423,1074.70439182409,
463.025150401418));
#111660=CARTESIAN_POINT('Ctrl Pts',(-105.874863628056,1074.72026544387,
462.904684537913));
#111661=CARTESIAN_POINT('Ctrl Pts',(-105.675433656561,1074.75558205367,
462.699949665295));
#111662=CARTESIAN_POINT('Ctrl Pts',(-105.555975816372,1074.77472591118,
462.617960354975));
#111663=CARTESIAN_POINT('Ctrl Pts',(-105.358517822884,1074.8038144677,462.533300937462));
#111664=CARTESIAN_POINT('Ctrl Pts',(-105.290235479964,1074.81349026178,
462.511664545201));
#111665=CARTESIAN_POINT('Ctrl Pts',(-105.078437171931,1074.84238669272,
462.466825187557));
#111666=CARTESIAN_POINT('Ctrl Pts',(-104.931817723056,1074.86090661222,
462.465356096695));
#111667=CARTESIAN_POINT('Ctrl Pts',(-104.647237696593,1074.8940390347,462.519928292812));
#111668=CARTESIAN_POINT('Ctrl Pts',(-104.511978138741,1074.90835773384,
462.57507423291));
#111669=CARTESIAN_POINT('Ctrl Pts',(-104.270797373955,1074.93097649917,
462.735194331009));
#111670=CARTESIAN_POINT('Ctrl Pts',(-104.167278755511,1074.93905994392,
462.838443218777));
#111671=CARTESIAN_POINT('Ctrl Pts',(-104.008363161499,1074.94778814809,
463.076956530643));
#111672=CARTESIAN_POINT('Ctrl Pts',(-103.953527163956,1074.94851122642,
463.209030175445));
#111673=CARTESIAN_POINT('Ctrl Pts',(-103.897397084343,1074.94269359972,
463.487006669484));
#111674=CARTESIAN_POINT('Ctrl Pts',(-103.89675656806,1074.93619993154,463.630106351421));
#111675=CARTESIAN_POINT('Ctrl Pts',(-103.950724284045,1074.91652422059,
463.911467977091));
#111676=CARTESIAN_POINT('Ctrl Pts',(-104.006041448505,1074.90339307649,
464.046641489684));
#111677=CARTESIAN_POINT('Ctrl Pts',(-104.166220633862,1074.87215504748,
464.287909340975));
#111678=CARTESIAN_POINT('Ctrl Pts',(-104.269769523854,1074.85432750344,
464.391457913392));
#111679=CARTESIAN_POINT('Ctrl Pts',(-104.449555246214,1074.82602986511,
464.511082923885));
#111680=CARTESIAN_POINT('Ctrl Pts',(-104.512467851101,1074.81649698506,
464.54458547443));
#111681=CARTESIAN_POINT('Ctrl Pts',(-104.643520285306,1074.79732832783,
464.598708574211));
#111682=CARTESIAN_POINT('Ctrl Pts',(-104.711341338543,1074.78773558188,
464.619279248892));
#111683=CARTESIAN_POINT('Ctrl Pts',(-104.850723767376,1074.76865710029,
464.647142030681));
#111684=CARTESIAN_POINT('Ctrl Pts',(-104.922002764286,1074.75921638392,
464.654233895348));
#111685=CARTESIAN_POINT('Ctrl Pts',(-104.993489577313,1074.75006270401,
464.654296886886));
#111686=CARTESIAN_POINT('Origin',(-104.994450521158,1067.7251047501,463.563756561532));
#111687=CARTESIAN_POINT('',(-104.994450521158,1074.77893852154,464.05429731026));
#111688=CARTESIAN_POINT('',(-104.994450521158,1074.82513013623,463.073215812804));
#111689=CARTESIAN_POINT('Ctrl Pts',(-104.994450521158,1074.77893852154,
464.05429731026));
#111690=CARTESIAN_POINT('Ctrl Pts',(-105.030095890685,1074.77439673021,
464.05429731026));
#111691=CARTESIAN_POINT('Ctrl Pts',(-105.065745517352,1074.77003297191,
464.050412186953));
#111692=CARTESIAN_POINT('Ctrl Pts',(-105.163681512993,1074.75855790272,
464.028670857344));
#111693=CARTESIAN_POINT('Ctrl Pts',(-105.223343682509,1074.75217048114,
464.002413949173));
#111694=CARTESIAN_POINT('Ctrl Pts',(-105.328667510103,1074.74219393818,
463.928484696109));
#111695=CARTESIAN_POINT('Ctrl Pts',(-105.373423586705,1074.73867624248,
463.881761777249));
#111696=CARTESIAN_POINT('Ctrl Pts',(-105.442219218817,1074.73497992791,
463.773974006962));
#111697=CARTESIAN_POINT('Ctrl Pts',(-105.465707864338,1074.73481509992,
463.714108546454));
#111698=CARTESIAN_POINT('Ctrl Pts',(-105.488479889226,1074.73785905108,
463.588739883212));
#111699=CARTESIAN_POINT('Ctrl Pts',(-105.487533259021,1074.74103652407,
463.524511433594));
#111700=CARTESIAN_POINT('Ctrl Pts',(-105.461148520179,1074.7503474454,463.399674225694));
#111701=CARTESIAN_POINT('Ctrl Pts',(-105.435795894582,1074.75640913827,
463.340335266017));
#111702=CARTESIAN_POINT('Ctrl Pts',(-105.363573412933,1074.77065743129,
463.234310312591));
#111703=CARTESIAN_POINT('Ctrl Pts',(-105.317177481959,1074.77872845181,
463.188771704626));
#111704=CARTESIAN_POINT('Ctrl Pts',(-105.236483829072,1074.79149302069,
463.135871837016));
#111705=CARTESIAN_POINT('Ctrl Pts',(-105.207910629415,1074.79582979228,
463.120925430747));
#111706=CARTESIAN_POINT('Ctrl Pts',(-105.149116860948,1074.80441314705,
463.097189721489));
#111707=CARTESIAN_POINT('Ctrl Pts',(-105.119091577843,1074.80864054609,
463.088286888806));
#111708=CARTESIAN_POINT('Ctrl Pts',(-105.057488876431,1074.81701159186,
463.076263403711));
#111709=CARTESIAN_POINT('Ctrl Pts',(-105.026034191749,1074.8211360572,463.073218466764));
#111710=CARTESIAN_POINT('Ctrl Pts',(-104.994491767958,1074.82512492024,
463.073215814539));
#111711=CARTESIAN_POINT('Ctrl Pts',(-104.994478019,1074.82512665893,463.073215813383));
#111712=CARTESIAN_POINT('Ctrl Pts',(-104.994464270067,1074.8251283976,463.073215812804));
#111713=CARTESIAN_POINT('Ctrl Pts',(-104.994450521158,1074.82513013623,
463.073215812804));
#111714=CARTESIAN_POINT('',(-104.994450521158,1082.7251047501,463.073215812804));
#111715=CARTESIAN_POINT('',(-104.994450521158,1067.7251047501,463.073215812804));
#111716=CARTESIAN_POINT('Origin',(-104.994450521158,1082.7251047501,463.563756561532));
#111717=CARTESIAN_POINT('Ctrl Pts',(-104.994450521158,1074.82513013623,
463.073215812804));
#111718=CARTESIAN_POINT('Ctrl Pts',(-104.929134780518,1074.83338971686,
463.073215812804));
#111719=CARTESIAN_POINT('Ctrl Pts',(-104.864372632066,1074.84095001567,
463.08626102952));
#111720=CARTESIAN_POINT('Ctrl Pts',(-104.743862011825,1074.85376020283,
463.137031952008));
#111721=CARTESIAN_POINT('Ctrl Pts',(-104.689285712492,1074.85889120532,
463.174154416784));
#111722=CARTESIAN_POINT('Ctrl Pts',(-104.598966777381,1074.86593142847,
463.266616183336));
#111723=CARTESIAN_POINT('Ctrl Pts',(-104.563685271589,1074.86784902223,
463.320543505307));
#111724=CARTESIAN_POINT('Ctrl Pts',(-104.515827292603,1074.86834965407,
463.438820828996));
#111725=CARTESIAN_POINT('Ctrl Pts',(-104.50367647131,1074.86693664149,463.501938919774));
#111726=CARTESIAN_POINT('Ctrl Pts',(-104.504150930195,1074.86093236406,
463.6295110763));
#111727=CARTESIAN_POINT('Ctrl Pts',(-104.516881728838,1074.85638733246,
463.692681254243));
#111728=CARTESIAN_POINT('Ctrl Pts',(-104.5663688629,1074.84457922523,463.812086803098));
#111729=CARTESIAN_POINT('Ctrl Pts',(-104.603275539818,1074.83736414877,
463.866868200142));
#111730=CARTESIAN_POINT('Ctrl Pts',(-104.696435940095,1074.82127878478,
463.958884685947));
#111731=CARTESIAN_POINT('Ctrl Pts',(-104.751884373655,1074.81255586224,
463.995135213247));
#111732=CARTESIAN_POINT('Ctrl Pts',(-104.842594637019,1074.79934181929,
464.0313047854));
#111733=CARTESIAN_POINT('Ctrl Pts',(-104.873524270356,1074.79499132664,
464.040242492033));
#111734=CARTESIAN_POINT('Ctrl Pts',(-104.934634235345,1074.78668581557,
464.05156178044));
#111735=CARTESIAN_POINT('Ctrl Pts',(-104.964540878907,1074.7827494893,464.05429731026));
#111736=CARTESIAN_POINT('Ctrl Pts',(-104.994450521158,1074.77893852154,
464.05429731026));
#111737=CARTESIAN_POINT('Origin',(-55.8158882427217,1067.7251047501,494.657824979653));
#111738=CARTESIAN_POINT('',(-55.8158882427496,1076.69910051006,493.17952184746));
#111739=CARTESIAN_POINT('',(-55.8158882427217,1067.7251047501,493.17952184746));
#111740=CARTESIAN_POINT('Ctrl Pts',(-57.2940029153359,1076.64571253121,
494.681429327873));
#111741=CARTESIAN_POINT('Ctrl Pts',(-57.2970861273448,1076.65033938597,
494.488357235108));
#111742=CARTESIAN_POINT('Ctrl Pts',(-57.2623109437452,1076.65549195305,
494.296546507661));
#111743=CARTESIAN_POINT('Ctrl Pts',(-57.1563128506684,1076.66335905769,
494.026976710274));
#111744=CARTESIAN_POINT('Ctrl Pts',(-57.1122476020844,1076.66598700711,
493.940775273864));
#111745=CARTESIAN_POINT('Ctrl Pts',(-57.0079236857122,1076.67115904959,
493.778186891722));
#111746=CARTESIAN_POINT('Ctrl Pts',(-56.9479117161991,1076.67369065833,
493.702191547212));
#111747=CARTESIAN_POINT('Ctrl Pts',(-56.7448274654058,1076.68108498756,
493.491224108044));
#111748=CARTESIAN_POINT('Ctrl Pts',(-56.581935758937,1076.68557793453,493.378346098784));
#111749=CARTESIAN_POINT('Ctrl Pts',(-56.2228054111147,1076.69327299039,
493.223325920551));
#111750=CARTESIAN_POINT('Ctrl Pts',(-56.0303254656401,1076.69641487917,
493.182225388176));
#111751=CARTESIAN_POINT('Ctrl Pts',(-55.640164985733,1076.70130569293,493.177071759869));
#111752=CARTESIAN_POINT('Ctrl Pts',(-55.4463199432541,1076.70301258711,
493.213202969801));
#111753=CARTESIAN_POINT('Ctrl Pts',(-55.0832621058866,1076.70505910468,
493.358965902032));
#111754=CARTESIAN_POINT('Ctrl Pts',(-54.9177371508854,1076.70537890105,
493.467404272984));
#111755=CARTESIAN_POINT('Ctrl Pts',(-54.6388244198768,1076.70464167866,
493.742300828558));
#111756=CARTESIAN_POINT('Ctrl Pts',(-54.5281179015418,1076.70359198019,
493.905955049508));
#111757=CARTESIAN_POINT('Ctrl Pts',(-54.3771381331761,1076.70004341043,
494.266188308545));
#111758=CARTESIAN_POINT('Ctrl Pts',(-54.3380906066545,1076.69757708303,
494.45910768757));
#111759=CARTESIAN_POINT('Ctrl Pts',(-54.3370881340296,1076.69117204073,
494.849428321895));
#111760=CARTESIAN_POINT('Ctrl Pts',(-54.3753325767836,1076.68728473173,
495.042989296045));
#111761=CARTESIAN_POINT('Ctrl Pts',(-54.48681820115,1076.68059650085,495.312167589186));
#111762=CARTESIAN_POINT('Ctrl Pts',(-54.5320900300352,1076.67826624934,
495.397049254801));
#111763=CARTESIAN_POINT('Ctrl Pts',(-54.6393344195377,1076.67336333136,
495.558171091746));
#111764=CARTESIAN_POINT('Ctrl Pts',(-54.7013118826123,1076.6707992158,495.633847942096));
#111765=CARTESIAN_POINT('Ctrl Pts',(-54.9074558971707,1076.6629777965,495.840102357091));
#111766=CARTESIAN_POINT('Ctrl Pts',(-55.0703097504237,1076.65763333709,
495.949003880213));
#111767=CARTESIAN_POINT('Ctrl Pts',(-55.4289045490332,1076.64748045596,
496.097730756909));
#111768=CARTESIAN_POINT('Ctrl Pts',(-55.6211913806661,1076.64277749116,
496.136063240489));
#111769=CARTESIAN_POINT('Ctrl Pts',(-56.0094935863397,1076.63499579872,
496.136192783591));
#111770=CARTESIAN_POINT('Ctrl Pts',(-56.2017324936643,1076.63199875157,
496.098029869471));
#111771=CARTESIAN_POINT('Ctrl Pts',(-56.5600799978547,1076.62840406014,
495.949751020717));
#111772=CARTESIAN_POINT('Ctrl Pts',(-56.7227652434645,1076.62783944081,
495.841239952424));
#111773=CARTESIAN_POINT('Ctrl Pts',(-56.9966772267137,1076.62928815504,
495.568012544925));
#111774=CARTESIAN_POINT('Ctrl Pts',(-57.1053849872915,1076.63127933247,
495.406085393848));
#111775=CARTESIAN_POINT('Ctrl Pts',(-57.2522748438085,1076.63730171277,
495.05460157633));
#111776=CARTESIAN_POINT('Ctrl Pts',(-57.2910052075554,1076.64121398928,
494.869147108234));
#111777=CARTESIAN_POINT('Ctrl Pts',(-57.2940029153359,1076.64571253121,
494.681429327873));
#111778=CARTESIAN_POINT('Origin',(-55.8158882427217,1067.7251047501,494.657824979653));
#111779=CARTESIAN_POINT('',(-55.8158882427216,1076.65362934538,495.536128111846));
#111780=CARTESIAN_POINT('',(-55.8158882427215,1076.68940454296,493.77952184746));
#111781=CARTESIAN_POINT('Ctrl Pts',(-55.8158882427216,1076.65362934538,
495.536128111847));
#111782=CARTESIAN_POINT('Ctrl Pts',(-55.9318099253898,1076.6514841644,495.536128111847));
#111783=CARTESIAN_POINT('Ctrl Pts',(-56.0465906650825,1076.64985449637,
495.513181130269));
#111784=CARTESIAN_POINT('Ctrl Pts',(-56.2597332812426,1076.64792005606,
495.424397387823));
#111785=CARTESIAN_POINT('Ctrl Pts',(-56.356150285274,1076.64762439934,495.359786049275));
#111786=CARTESIAN_POINT('Ctrl Pts',(-56.5187548885584,1076.64842144831,
495.196950801317));
#111787=CARTESIAN_POINT('Ctrl Pts',(-56.5833076956239,1076.64950824845,
495.100253495072));
#111788=CARTESIAN_POINT('Ctrl Pts',(-56.6714627049711,1076.65286727937,
494.887375877515));
#111789=CARTESIAN_POINT('Ctrl Pts',(-56.6941678581457,1076.65510581828,
494.773247505017));
#111790=CARTESIAN_POINT('Ctrl Pts',(-56.6942147740036,1076.66031704546,
494.543158682441));
#111791=CARTESIAN_POINT('Ctrl Pts',(-56.6717125907137,1076.66323443647,
494.4294211434));
#111792=CARTESIAN_POINT('Ctrl Pts',(-56.606100422734,1076.66776210203,494.270170403875));
#111793=CARTESIAN_POINT('Ctrl Pts',(-56.5790833909399,1076.6692858448,494.219368012302));
#111794=CARTESIAN_POINT('Ctrl Pts',(-56.5155193997886,1076.67231347924,
494.123757001964));
#111795=CARTESIAN_POINT('Ctrl Pts',(-56.4791234046984,1076.67381008737,
494.079178587676));
#111796=CARTESIAN_POINT('Ctrl Pts',(-56.3561618958448,1076.67823756045,
493.955542808976));
#111797=CARTESIAN_POINT('Ctrl Pts',(-56.2579414138775,1076.68099912889,
493.889913730455));
#111798=CARTESIAN_POINT('Ctrl Pts',(-56.0438306225788,1076.68580135196,
493.801920488004));
#111799=CARTESIAN_POINT('Ctrl Pts',(-55.9304168842139,1076.6878121255,493.77952184746));
#111800=CARTESIAN_POINT('Ctrl Pts',(-55.8158882427215,1076.68940454296,
493.77952184746));
#111801=CARTESIAN_POINT('',(-55.8158882427217,1082.7251047501,493.77952184746));
#111802=CARTESIAN_POINT('',(-55.8158882427217,1067.7251047501,493.77952184746));
#111803=CARTESIAN_POINT('Origin',(-55.8158882427217,1082.7251047501,494.657824979653));
#111804=CARTESIAN_POINT('Ctrl Pts',(-55.8158882427215,1076.68940454296,
493.77952184746));
#111805=CARTESIAN_POINT('Ctrl Pts',(-55.7821001946735,1076.68987433529,
493.77952184746));
#111806=CARTESIAN_POINT('Ctrl Pts',(-55.7482262561783,1076.6903067822,493.781475913434));
#111807=CARTESIAN_POINT('Ctrl Pts',(-55.7145493171291,1076.69070046539,
493.785387695844));
#111808=CARTESIAN_POINT('Ctrl Pts',(-55.6808922225021,1076.6910939166,493.789297173203));
#111809=CARTESIAN_POINT('Ctrl Pts',(-55.6474325946985,1076.69144864976,
493.795162012409));
#111810=CARTESIAN_POINT('Ctrl Pts',(-55.6144491808781,1076.69176324906,
493.802933936079));
#111811=CARTESIAN_POINT('Ctrl Pts',(-55.581442507272,1076.69207807021,493.810711340481));
#111812=CARTESIAN_POINT('Ctrl Pts',(-55.5489133962765,1076.69235270089,
493.820398332048));
#111813=CARTESIAN_POINT('Ctrl Pts',(-55.5171271742132,1076.69258572228,
493.831896280573));
#111814=CARTESIAN_POINT('Ctrl Pts',(-55.5046378310411,1076.69267728032,
493.836414018624));
#111815=CARTESIAN_POINT('Ctrl Pts',(-55.492262970637,1076.69276241456,493.841210808931));
#111816=CARTESIAN_POINT('Ctrl Pts',(-55.4800177556225,1076.69284103895,
493.846278672955));
#111817=CARTESIAN_POINT('Ctrl Pts',(-55.4493021409524,1076.69303825855,
493.858990786084));
#111818=CARTESIAN_POINT('Ctrl Pts',(-55.4192090869223,1076.69319580211,
493.87349241555));
#111819=CARTESIAN_POINT('Ctrl Pts',(-55.3899988367886,1076.69331340156,
493.889687878652));
#111820=CARTESIAN_POINT('Ctrl Pts',(-55.3608116220149,1076.69343090827,
493.905870569925));
#111821=CARTESIAN_POINT('Ctrl Pts',(-55.3325064623312,1076.69350853384,
493.923744129845));
#111822=CARTESIAN_POINT('Ctrl Pts',(-55.3053211225215,1076.69354601083,
493.943165894641));
#111823=CARTESIAN_POINT('Ctrl Pts',(-55.2781218566449,1076.69358350702,
493.962597608505));
#111824=CARTESIAN_POINT('Ctrl Pts',(-55.2520441293685,1076.69358081348,
493.983578693448));
#111825=CARTESIAN_POINT('Ctrl Pts',(-55.2272950298924,1076.69353766235,
494.005924356988));
#111826=CARTESIAN_POINT('Ctrl Pts',(-55.216333613823,1076.69351855065,494.015821287405));
#111827=CARTESIAN_POINT('Ctrl Pts',(-55.2056323644168,1076.69349150272,
494.025985384072));
#111828=CARTESIAN_POINT('Ctrl Pts',(-55.1952069125942,1076.69345649528,
494.036398331969));
#111829=CARTESIAN_POINT('Ctrl Pts',(-55.1691826970598,1076.69336910902,
494.062391334963));
#111830=CARTESIAN_POINT('Ctrl Pts',(-55.1447437569286,1076.69323205413,
494.090072711985));
#111831=CARTESIAN_POINT('Ctrl Pts',(-55.122118922625,1076.69304601473,494.119215174216));
#111832=CARTESIAN_POINT('Ctrl Pts',(-55.0995148656774,1076.69286014618,
494.148330873674));
#111833=CARTESIAN_POINT('Ctrl Pts',(-55.0787220094823,1076.69262538305,
494.178904513048));
#111834=CARTESIAN_POINT('Ctrl Pts',(-55.0599299770165,1076.69234240759,
494.210674565886));
#111835=CARTESIAN_POINT('Ctrl Pts',(-55.0411416141871,1076.69205948739,
494.242438414789));
#111836=CARTESIAN_POINT('Ctrl Pts',(-55.0243536261026,1076.69172837369,
494.275397675653));
#111837=CARTESIAN_POINT('Ctrl Pts',(-55.0097112425333,1076.69134974834,
494.309263598563));
#111838=CARTESIAN_POINT('Ctrl Pts',(-55.00801180533,1076.69130580399,494.313194175101));
#111839=CARTESIAN_POINT('Ctrl Pts',(-55.0063412185899,1076.69126121963,
494.317136939995));
#111840=CARTESIAN_POINT('Ctrl Pts',(-55.0046996678512,1076.69121599633,
494.321091423232));
#111841=CARTESIAN_POINT('Ctrl Pts',(-54.9799734517168,1076.69053481046,
494.380656689733));
#111842=CARTESIAN_POINT('Ctrl Pts',(-54.9619045291505,1076.68971277992,
494.44270380246));
#111843=CARTESIAN_POINT('Ctrl Pts',(-54.9507810139883,1076.68875358168,
494.506148103322));
#111844=CARTESIAN_POINT('Ctrl Pts',(-54.94206944209,1076.68800236911,494.555835596927));
#111845=CARTESIAN_POINT('Ctrl Pts',(-54.9376183128041,1076.68716702462,
494.606383269385));
#111846=CARTESIAN_POINT('Ctrl Pts',(-54.9375852955171,1076.68624931446,
494.657254933818));
#111847=CARTESIAN_POINT('Ctrl Pts',(-54.9375535676497,1076.68536744351,
494.70613991419));
#111848=CARTESIAN_POINT('Ctrl Pts',(-54.9415996313463,1076.6844205659,494.754701443179));
#111849=CARTESIAN_POINT('Ctrl Pts',(-54.9495839293193,1076.68341457731,
494.802508180478));
#111850=CARTESIAN_POINT('Ctrl Pts',(-54.9579461006785,1076.68236097824,
494.852577470324));
#111851=CARTESIAN_POINT('Ctrl Pts',(-54.9706280948863,1076.6812425407,494.901822277584));
#111852=CARTESIAN_POINT('Ctrl Pts',(-54.9875207779439,1076.68006603769,
494.949756025139));
#111853=CARTESIAN_POINT('Ctrl Pts',(-54.9927155722863,1076.67970424252,
494.964496487607));
#111854=CARTESIAN_POINT('Ctrl Pts',(-54.9983088980644,1076.67933695628,
494.979112820609));
#111855=CARTESIAN_POINT('Ctrl Pts',(-55.0042983918879,1076.67896437592,
494.993590234026));
#111856=CARTESIAN_POINT('Ctrl Pts',(-55.0200636920399,1076.67798368518,
495.031697088241));
#111857=CARTESIAN_POINT('Ctrl Pts',(-55.0384962901014,1076.67697084568,
495.068642297839));
#111858=CARTESIAN_POINT('Ctrl Pts',(-55.0594003527511,1076.67593566601,
495.104078791232));
#111859=CARTESIAN_POINT('Ctrl Pts',(-55.0803703395622,1076.67489722175,
495.139627039031));
#111860=CARTESIAN_POINT('Ctrl Pts',(-55.1038271479132,1076.6738362962,495.173656708332));
#111861=CARTESIAN_POINT('Ctrl Pts',(-55.1295307205056,1076.67276279107,
495.205848467944));
#111862=CARTESIAN_POINT('Ctrl Pts',(-55.1498187127608,1076.67191546668,
495.231257627209));
#111863=CARTESIAN_POINT('Ctrl Pts',(-55.1715055634551,1076.67106030516,
495.255522324595));
#111864=CARTESIAN_POINT('Ctrl Pts',(-55.1944563571628,1076.67020217557,
495.278501065572));
#111865=CARTESIAN_POINT('Ctrl Pts',(-55.2244257789509,1076.66908161966,
495.308506981239));
#111866=CARTESIAN_POINT('Ctrl Pts',(-55.2565645231671,1076.66795552721,
495.336332204534));
#111867=CARTESIAN_POINT('Ctrl Pts',(-55.2905527314867,1076.66683710651,
495.361699252983));
#111868=CARTESIAN_POINT('Ctrl Pts',(-55.3245065779363,1076.66571981652,
495.387040655502));
#111869=CARTESIAN_POINT('Ctrl Pts',(-55.3603058985636,1076.66461018279,
495.409928645985));
#111870=CARTESIAN_POINT('Ctrl Pts',(-55.3975995587667,1076.66352137361,
495.430127361429));
#111871=CARTESIAN_POINT('Ctrl Pts',(-55.4347481129749,1076.66243680088,
495.450247485641));
#111872=CARTESIAN_POINT('Ctrl Pts',(-55.4733791295403,1076.66137289095,
495.467699041941));
#111873=CARTESIAN_POINT('Ctrl Pts',(-55.5131174748948,1076.66034265901,
495.482292234412));
#111874=CARTESIAN_POINT('Ctrl Pts',(-55.5527151677933,1076.65931607353,
495.4968337748));
#111875=CARTESIAN_POINT('Ctrl Pts',(-55.5934120861939,1076.65832292806,
495.508536971963));
#111876=CARTESIAN_POINT('Ctrl Pts',(-55.6348132231612,1076.65737610005,
495.517259810988));
#111877=CARTESIAN_POINT('Ctrl Pts',(-55.6759343182162,1076.65643567649,
495.525923647756));
#111878=CARTESIAN_POINT('Ctrl Pts',(-55.7177498362673,1076.65554094593,
495.53164716325));
#111879=CARTESIAN_POINT('Ctrl Pts',(-55.759853498463,1076.65470452627,495.534338812662));
#111880=CARTESIAN_POINT('Ctrl Pts',(-55.7784875977145,1076.65433434643,
495.535530073937));
#111881=CARTESIAN_POINT('Ctrl Pts',(-55.79717791048,1076.65397558818,495.536128111847));
#111882=CARTESIAN_POINT('Ctrl Pts',(-55.8158882427216,1076.65362934538,
495.536128111847));
#111883=CARTESIAN_POINT('Origin',(-68.2819685228173,1067.7251047501,493.138970451766));
#111884=CARTESIAN_POINT('',(-68.2819685228347,1076.40124852519,491.86352633063));
#111885=CARTESIAN_POINT('',(-68.2819685228173,1067.7251047501,491.86352633063));
#111886=CARTESIAN_POINT('Ctrl Pts',(-68.28346036406,1076.28433347533,494.414413700426));
#111887=CARTESIAN_POINT('Ctrl Pts',(-68.4507247165836,1076.27623971056,
494.414218057178));
#111888=CARTESIAN_POINT('Ctrl Pts',(-68.6163941082646,1076.26973623853,
494.381121241454));
#111889=CARTESIAN_POINT('Ctrl Pts',(-68.9251148339525,1076.26086237681,
494.252957240118));
#111890=CARTESIAN_POINT('Ctrl Pts',(-69.0652141470784,1076.25856900424,
494.15933750728));
#111891=CARTESIAN_POINT('Ctrl Pts',(-69.3011533784143,1076.25859589523,
493.92367273988));
#111892=CARTESIAN_POINT('Ctrl Pts',(-69.3947797701972,1076.26090533003,
493.784050058676));
#111893=CARTESIAN_POINT('Ctrl Pts',(-69.5230973071309,1076.26977603473,
493.476742386807));
#111894=CARTESIAN_POINT('Ctrl Pts',(-69.5565242665948,1076.27624887419,
493.31204540069));
#111895=CARTESIAN_POINT('Ctrl Pts',(-69.5582682694181,1076.29236389343,
492.978828645352));
#111896=CARTESIAN_POINT('Ctrl Pts',(-69.5264060108366,1076.30185418939,
492.813512226457));
#111897=CARTESIAN_POINT('Ctrl Pts',(-69.4007987743507,1076.3224317955,492.504222142674));
#111898=CARTESIAN_POINT('Ctrl Pts',(-69.30810009183,1076.3333229227,492.363257618105));
#111899=CARTESIAN_POINT('Ctrl Pts',(-69.0720632380055,1076.35510063472,
492.123494272292));
#111900=CARTESIAN_POINT('Ctrl Pts',(-68.9303646132984,1076.36577121848,
492.027643532448));
#111901=CARTESIAN_POINT('Ctrl Pts',(-68.618627538777,1076.38529820527,491.897278417455));
#111902=CARTESIAN_POINT('Ctrl Pts',(-68.4518005764208,1076.3939771793,491.863691508352));
#111903=CARTESIAN_POINT('Ctrl Pts',(-68.1142574840619,1076.40842911541,
491.863362007998));
#111904=CARTESIAN_POINT('Ctrl Pts',(-67.9468862164521,1076.4140573458,491.896770805172));
#111905=CARTESIAN_POINT('Ctrl Pts',(-67.6341061620142,1076.42166822459,
492.027268821322));
#111906=CARTESIAN_POINT('Ctrl Pts',(-67.4919651124891,1076.42356086842,
492.123335356597));
#111907=CARTESIAN_POINT('Ctrl Pts',(-67.253679533919,1076.42336420323,492.365515393761));
#111908=CARTESIAN_POINT('Ctrl Pts',(-67.1599417634095,1076.42127739741,
492.509167522619));
#111909=CARTESIAN_POINT('Ctrl Pts',(-67.0345376360758,1076.41329897268,
492.823944335523));
#111910=CARTESIAN_POINT('Ctrl Pts',(-67.0038350587453,1076.40750105159,
492.991786039058));
#111911=CARTESIAN_POINT('Ctrl Pts',(-67.0095776549753,1076.3927512793,493.329242637938));
#111912=CARTESIAN_POINT('Ctrl Pts',(-67.0458392912545,1076.38394597266,
493.495517830332));
#111913=CARTESIAN_POINT('Ctrl Pts',(-67.146396932864,1076.3693004159,493.725528588682));
#111914=CARTESIAN_POINT('Ctrl Pts',(-67.1867291668689,1076.36427303905,
493.797772779109));
#111915=CARTESIAN_POINT('Ctrl Pts',(-67.2809487626751,1076.35390579143,
493.933690962128));
#111916=CARTESIAN_POINT('Ctrl Pts',(-67.3346658747061,1076.3485890675,493.997013071455));
#111917=CARTESIAN_POINT('Ctrl Pts',(-67.5156666153374,1076.3322570061,494.172504309097));
#111918=CARTESIAN_POINT('Ctrl Pts',(-67.6594579543074,1076.3212390108,494.264982563189));
#111919=CARTESIAN_POINT('Ctrl Pts',(-67.9656582728335,1076.30108565678,
494.384823070276));
#111920=CARTESIAN_POINT('Ctrl Pts',(-68.1238430822138,1076.29205720553,
494.414600399163));
#111921=CARTESIAN_POINT('Ctrl Pts',(-68.28346036406,1076.28433347533,494.414413700426));
#111922=CARTESIAN_POINT('Origin',(-68.2819685228173,1067.7251047501,493.138970451766));
#111923=CARTESIAN_POINT('',(-68.2819685228173,1076.31358867648,493.814414572903));
#111924=CARTESIAN_POINT('',(-68.2819685228168,1076.37545952532,492.46352633063));
#111925=CARTESIAN_POINT('Ctrl Pts',(-68.2819685228173,1076.31358867648,
493.814414572903));
#111926=CARTESIAN_POINT('Ctrl Pts',(-68.2864411550903,1076.31337786948,
493.814414572903));
#111927=CARTESIAN_POINT('Ctrl Pts',(-68.2909158340225,1076.31316900213,
493.814370147943));
#111928=CARTESIAN_POINT('Ctrl Pts',(-68.3838552239154,1076.3088732745,493.812522758853));
#111929=CARTESIAN_POINT('Ctrl Pts',(-68.4711496327909,1076.30563774319,
493.793398173427));
#111930=CARTESIAN_POINT('Ctrl Pts',(-68.6332391257118,1076.30130401655,
493.722610190779));
#111931=CARTESIAN_POINT('Ctrl Pts',(-68.7064803386932,1076.30024379268,
493.6717186001));
#111932=CARTESIAN_POINT('Ctrl Pts',(-68.8291498753305,1076.300473154,493.544684578535));
#111933=CARTESIAN_POINT('Ctrl Pts',(-68.8774057128442,1076.30175750292,
493.469818716931));
#111934=CARTESIAN_POINT('Ctrl Pts',(-68.9424310720892,1076.30649637888,
493.305731364767));
#111935=CARTESIAN_POINT('Ctrl Pts',(-68.9585386094659,1076.30990566649,
493.218098001518));
#111936=CARTESIAN_POINT('Ctrl Pts',(-68.9561614864957,1076.31836794158,
493.041450750661));
#111937=CARTESIAN_POINT('Ctrl Pts',(-68.9376160109658,1076.32334182643,
492.954141112806));
#111938=CARTESIAN_POINT('Ctrl Pts',(-68.867916727381,1076.33415469827,492.791503619692));
#111939=CARTESIAN_POINT('Ctrl Pts',(-68.8173619963439,1076.33989098519,
492.717759030771));
#111940=CARTESIAN_POINT('Ctrl Pts',(-68.6897538986778,1076.35142054282,
492.593065306653));
#111941=CARTESIAN_POINT('Ctrl Pts',(-68.6135705877628,1076.35709993303,
492.543699464199));
#111942=CARTESIAN_POINT('Ctrl Pts',(-68.4512493750913,1076.36725084899,
492.479632558453));
#111943=CARTESIAN_POINT('Ctrl Pts',(-68.3673872694444,1076.37168574005,
492.463621698737));
#111944=CARTESIAN_POINT('Ctrl Pts',(-68.2827260003963,1076.37542607939,
492.463526755188));
#111945=CARTESIAN_POINT('Ctrl Pts',(-68.2824735011445,1076.37543723482,
492.463526472023));
#111946=CARTESIAN_POINT('Ctrl Pts',(-68.2822210085788,1076.37544838346,
492.46352633063));
#111947=CARTESIAN_POINT('Ctrl Pts',(-68.2819685228162,1076.37545952532,
492.46352633063));
#111948=CARTESIAN_POINT('',(-68.2819685228173,1082.7251047501,492.46352633063));
#111949=CARTESIAN_POINT('',(-68.2819685228173,1067.7251047501,492.46352633063));
#111950=CARTESIAN_POINT('Origin',(-68.2819685228173,1082.7251047501,493.138970451766));
#111951=CARTESIAN_POINT('Ctrl Pts',(-68.2819685228162,1076.37545952532,
492.46352633063));
#111952=CARTESIAN_POINT('Ctrl Pts',(-68.1923058793769,1076.37941621885,
492.46352633063));
#111953=CARTESIAN_POINT('Ctrl Pts',(-68.1035011486521,1076.3825178246,492.481379977689));
#111954=CARTESIAN_POINT('Ctrl Pts',(-67.9383966698456,1076.38669236412,
492.550617802864));
#111955=CARTESIAN_POINT('Ctrl Pts',(-67.8636891351381,1076.38773405336,
492.601153607532));
#111956=CARTESIAN_POINT('Ctrl Pts',(-67.7389491901221,1076.38763727639,
492.727679936259));
#111957=CARTESIAN_POINT('Ctrl Pts',(-67.689875002397,1076.38652356686,492.802145822773));
#111958=CARTESIAN_POINT('Ctrl Pts',(-67.6225539748602,1076.38222927618,
492.967238976585));
#111959=CARTESIAN_POINT('Ctrl Pts',(-67.6055794948339,1076.37905299928,
493.056471144438));
#111960=CARTESIAN_POINT('Ctrl Pts',(-67.6075487900604,1076.37100669699,
493.236124391691));
#111961=CARTESIAN_POINT('Ctrl Pts',(-67.6264112580172,1076.36621842504,
493.3247501305));
#111962=CARTESIAN_POINT('Ctrl Pts',(-67.6794323987065,1076.35831982768,
493.447354940598));
#111963=CARTESIAN_POINT('Ctrl Pts',(-67.7007344862452,1076.35562021979,
493.485837650045));
#111964=CARTESIAN_POINT('Ctrl Pts',(-67.7505366092786,1076.35007996947,
493.558179967727));
#111965=CARTESIAN_POINT('Ctrl Pts',(-67.778931956496,1076.347252097,493.591861516285));
#111966=CARTESIAN_POINT('Ctrl Pts',(-67.8751166977207,1076.33855925955,
493.685659388942));
#111967=CARTESIAN_POINT('Ctrl Pts',(-67.9518640126957,1076.33272861279,
493.735152037157));
#111968=CARTESIAN_POINT('Ctrl Pts',(-68.1144526174297,1076.32220392407,
493.798699872179));
#111969=CARTESIAN_POINT('Ctrl Pts',(-68.1978485987653,1076.31755347115,
493.814414572903));
#111970=CARTESIAN_POINT('Ctrl Pts',(-68.2819685228173,1076.31358867648,
493.814414572903));
#111971=CARTESIAN_POINT('Origin',(-81.8208965804705,1067.7251047501,490.220805984922));
#111972=CARTESIAN_POINT('',(-81.8208965804703,1075.72563758024,489.12197484893));
#111973=CARTESIAN_POINT('',(-81.8208965804705,1067.7251047501,489.12197484893));
#111974=CARTESIAN_POINT('Ctrl Pts',(-81.8203373471217,1075.58255321203,
491.319636978608));
#111975=CARTESIAN_POINT('Ctrl Pts',(-81.9646166296934,1075.57055250947,
491.319710407358));
#111976=CARTESIAN_POINT('Ctrl Pts',(-82.1076543015382,1075.56048347303,
491.291366883468));
#111977=CARTESIAN_POINT('Ctrl Pts',(-82.3739159099637,1075.54556110887,
491.181130335127));
#111978=CARTESIAN_POINT('Ctrl Pts',(-82.494635113198,1075.54082336383,491.100680853538));
#111979=CARTESIAN_POINT('Ctrl Pts',(-82.6978507957194,1075.53738048746,
490.898195365247));
#111980=CARTESIAN_POINT('Ctrl Pts',(-82.7784964943414,1075.53868154857,
490.778383852575));
#111981=CARTESIAN_POINT('Ctrl Pts',(-82.8893387983906,1075.54714880989,
490.514622704056));
#111982=CARTESIAN_POINT('Ctrl Pts',(-82.9184286424565,1075.55423018492,
490.37329056519));
#111983=CARTESIAN_POINT('Ctrl Pts',(-82.9209480543768,1075.57321784832,
490.086938074674));
#111984=CARTESIAN_POINT('Ctrl Pts',(-82.8940753521044,1075.58496062669,
489.944689724177));
#111985=CARTESIAN_POINT('Ctrl Pts',(-82.7870675930831,1075.6115118452,489.677915064077));
#111986=CARTESIAN_POINT('Ctrl Pts',(-82.7076098244324,1075.62608482105,
489.556041063862));
#111987=CARTESIAN_POINT('Ctrl Pts',(-82.5565427608021,1075.64853464767,
489.401376995566));
#111988=CARTESIAN_POINT('Ctrl Pts',(-82.5011454202698,1075.65607337828,
489.354837736317));
#111989=CARTESIAN_POINT('Ctrl Pts',(-82.3207397628291,1075.67870862611,
489.231344855946));
#111990=CARTESIAN_POINT('Ctrl Pts',(-82.1844971094241,1075.69337870064,
489.173561564481));
#111991=CARTESIAN_POINT('Ctrl Pts',(-81.8982106477311,1075.71997194167,
489.11507227108));
#111992=CARTESIAN_POINT('Ctrl Pts',(-81.7510559619819,1075.73165729849,
489.114538175976));
#111993=CARTESIAN_POINT('Ctrl Pts',(-81.4651538278172,1075.75062697051,
489.17101295363));
#111994=CARTESIAN_POINT('Ctrl Pts',(-81.3292540072322,1075.7577332212,489.227340633631));
#111995=CARTESIAN_POINT('Ctrl Pts',(-81.0871420691125,1075.76647355093,
489.389957368954));
#111996=CARTESIAN_POINT('Ctrl Pts',(-80.9834303138446,1075.76801710112,
489.494602294134));
#111997=CARTESIAN_POINT('Ctrl Pts',(-80.8229474671619,1075.76529117916,
489.738303819777));
#111998=CARTESIAN_POINT('Ctrl Pts',(-80.7678188203122,1075.76105076667,
489.874837375416));
#111999=CARTESIAN_POINT('Ctrl Pts',(-80.7140371765568,1075.74724912962,
490.161323105469));
#112000=CARTESIAN_POINT('Ctrl Pts',(-80.7159396644293,1075.737824714,490.308363349736));
#112001=CARTESIAN_POINT('Ctrl Pts',(-80.7769326337171,1075.71486884397,
490.593530058177));
#112002=CARTESIAN_POINT('Ctrl Pts',(-80.8356659658541,1075.70154513099,
490.728774888186));
#112003=CARTESIAN_POINT('Ctrl Pts',(-80.9599158685222,1075.68005764875,
490.907298409197));
#112004=CARTESIAN_POINT('Ctrl Pts',(-81.0064703572462,1075.6727703422,490.961930090968));
#112005=CARTESIAN_POINT('Ctrl Pts',(-81.109749956188,1075.65794178802,491.061562738272));
#112006=CARTESIAN_POINT('Ctrl Pts',(-81.1662810764314,1075.65043384449,
491.106288507833));
#112007=CARTESIAN_POINT('Ctrl Pts',(-81.3497181808003,1075.62776190875,
491.224190695909));
#112008=CARTESIAN_POINT('Ctrl Pts',(-81.487266511086,1075.61291106123,491.277936473259));
#112009=CARTESIAN_POINT('Ctrl Pts',(-81.693743883515,1075.59343542508,491.314090566497));
#112010=CARTESIAN_POINT('Ctrl Pts',(-81.7569663426371,1075.58782421534,
491.319604726898));
#112011=CARTESIAN_POINT('Ctrl Pts',(-81.8203373471217,1075.58255321203,
491.319636978608));
#112012=CARTESIAN_POINT('Origin',(-81.8208965804705,1067.7251047501,490.220805984922));
#112013=CARTESIAN_POINT('',(-81.8208965804705,1075.62273721903,490.719637120915));
#112014=CARTESIAN_POINT('',(-81.820896580471,1075.68770968364,489.72197484893));
#112015=CARTESIAN_POINT('Ctrl Pts',(-81.8208965804704,1075.62273721903,
490.719637120915));
#112016=CARTESIAN_POINT('Ctrl Pts',(-81.8588780724229,1075.61961893,490.719637120915));
#112017=CARTESIAN_POINT('Ctrl Pts',(-81.8968463527419,1075.61678257443,
490.715299293843));
#112018=CARTESIAN_POINT('Ctrl Pts',(-81.9976197562922,1075.61003590419,
490.691827487908));
#112019=CARTESIAN_POINT('Ctrl Pts',(-82.0577185983606,1075.60687226465,
490.664677186573));
#112020=CARTESIAN_POINT('Ctrl Pts',(-82.1638192327644,1075.60313082568,
490.588862270848));
#112021=CARTESIAN_POINT('Ctrl Pts',(-82.2088376321711,1075.60257710667,
490.54106500921));
#112022=CARTESIAN_POINT('Ctrl Pts',(-82.2779498742101,1075.6041617528,490.430937922303));
#112023=CARTESIAN_POINT('Ctrl Pts',(-82.3013818132731,1075.60628063025,
490.369725899407));
#112024=CARTESIAN_POINT('Ctrl Pts',(-82.3235293872305,1075.61292268631,
490.241618157459));
#112025=CARTESIAN_POINT('Ctrl Pts',(-82.3219409959161,1075.61738828803,
490.175965021238));
#112026=CARTESIAN_POINT('Ctrl Pts',(-82.2936394865667,1075.62808942795,
490.048694371556));
#112027=CARTESIAN_POINT('Ctrl Pts',(-82.2670455329507,1075.63423207163,
489.988328440433));
#112028=CARTESIAN_POINT('Ctrl Pts',(-82.2108403700009,1075.64407656532,
489.907997267171));
#112029=CARTESIAN_POINT('Ctrl Pts',(-82.1894673926781,1075.64744644861,
489.883077890287));
#112030=CARTESIAN_POINT('Ctrl Pts',(-82.1421791932408,1075.65424552923,
489.837817587488));
#112031=CARTESIAN_POINT('Ctrl Pts',(-82.1163780874431,1075.65765889112,
489.817577227677));
#112032=CARTESIAN_POINT('Ctrl Pts',(-82.0325593384745,1075.66792326837,
489.764217231675));
#112033=CARTESIAN_POINT('Ctrl Pts',(-81.9696965176828,1075.67456753992,
489.740031918538));
#112034=CARTESIAN_POINT('Ctrl Pts',(-81.8764847473424,1075.68309081853,
489.724302826255));
#112035=CARTESIAN_POINT('Ctrl Pts',(-81.848720763783,1075.68547411165,489.72197484893));
#112036=CARTESIAN_POINT('Ctrl Pts',(-81.8208965804714,1075.68770968364,
489.72197484893));
#112037=CARTESIAN_POINT('',(-81.8208965804705,1082.7251047501,489.72197484893));
#112038=CARTESIAN_POINT('',(-81.8208965804705,1067.7251047501,489.72197484893));
#112039=CARTESIAN_POINT('Origin',(-81.8208965804705,1082.7251047501,490.220805984922));
#112040=CARTESIAN_POINT('Ctrl Pts',(-81.8208965804714,1075.68770968364,
489.72197484893));
#112041=CARTESIAN_POINT('Ctrl Pts',(-81.8207984790147,1075.68771756574,
489.72197484893));
#112042=CARTESIAN_POINT('Ctrl Pts',(-81.8207003768087,1075.68772544599,
489.721974878031));
#112043=CARTESIAN_POINT('Ctrl Pts',(-81.820602273868,1075.68773332441,489.721974935911));
#112044=CARTESIAN_POINT('Ctrl Pts',(-81.7542336351232,1075.69306323746,
489.722014092904));
#112045=CARTESIAN_POINT('Ctrl Pts',(-81.6884706566742,1075.69747669195,
489.73529825801));
#112046=CARTESIAN_POINT('Ctrl Pts',(-81.5660255278227,1075.70396160132,
489.786894832373));
#112047=CARTESIAN_POINT('Ctrl Pts',(-81.5105806699821,1075.70597139481,
489.824634589899));
#112048=CARTESIAN_POINT('Ctrl Pts',(-81.4187028763101,1075.70728846299,
489.918649282645));
#112049=CARTESIAN_POINT('Ctrl Pts',(-81.3827992951993,1075.70664027812,
489.973569025033));
#112050=CARTESIAN_POINT('Ctrl Pts',(-81.3335242572579,1075.70277203779,
490.095432948114));
#112051=CARTESIAN_POINT('Ctrl Pts',(-81.3211946552715,1075.6995335249,490.16135988493));
#112052=CARTESIAN_POINT('Ctrl Pts',(-81.3230344980214,1075.69084730567,
490.2942555415));
#112053=CARTESIAN_POINT('Ctrl Pts',(-81.3372608131545,1075.68548091103,
490.35987688527));
#112054=CARTESIAN_POINT('Ctrl Pts',(-81.390631021944,1075.67329905375,490.481878157933));
#112055=CARTESIAN_POINT('Ctrl Pts',(-81.4293656593663,1075.66659692712,
490.537003193671));
#112056=CARTESIAN_POINT('Ctrl Pts',(-81.5014678562907,1075.65630439878,
490.605338489547));
#112057=CARTESIAN_POINT('Ctrl Pts',(-81.527332271515,1075.65289408786,490.625429196208));
#112058=CARTESIAN_POINT('Ctrl Pts',(-81.6110935566909,1075.64263303744,
490.678206100116));
#112059=CARTESIAN_POINT('Ctrl Pts',(-81.6737373478057,1075.63595515846,
490.702039981009));
#112060=CARTESIAN_POINT('Ctrl Pts',(-81.7662844050241,1075.62736601428,
490.717395580663));
#112061=CARTESIAN_POINT('Ctrl Pts',(-81.793593906212,1075.62497877472,490.719637120915));
#112062=CARTESIAN_POINT('Ctrl Pts',(-81.8208965804704,1075.62273721903,
490.719637120915));
#112063=CARTESIAN_POINT('Origin',(-94.6032580293197,1067.7251047501,484.542321079512));
#112064=CARTESIAN_POINT('',(-94.6032580293197,1074.88000163213,483.451780330783));
#112065=CARTESIAN_POINT('',(-94.6032580293197,1067.7251047501,483.451780330783));
#112066=CARTESIAN_POINT('Ctrl Pts',(-94.6024687290833,1074.72207722087,
485.632861542604));
#112067=CARTESIAN_POINT('Ctrl Pts',(-94.745896664052,1074.7054542846,485.63296535141));
#112068=CARTESIAN_POINT('Ctrl Pts',(-94.8881904781405,1074.69097422865,
485.604772829182));
#112069=CARTESIAN_POINT('Ctrl Pts',(-95.15266120531,1074.66823897832,485.495062329079));
#112070=CARTESIAN_POINT('Ctrl Pts',(-95.2724181595792,1074.66014758065,
485.415183548233));
#112071=CARTESIAN_POINT('Ctrl Pts',(-95.4737463182846,1074.65147622274,
485.21432125542));
#112072=CARTESIAN_POINT('Ctrl Pts',(-95.5535724265119,1074.65092522316,
485.095714625435));
#112073=CARTESIAN_POINT('Ctrl Pts',(-95.66336567463,1074.65742595818,484.83469329457));
#112074=CARTESIAN_POINT('Ctrl Pts',(-95.6922583981725,1074.66440433594,
484.694954729699));
#112075=CARTESIAN_POINT('Ctrl Pts',(-95.6952297931477,1074.68500431369,
484.411552000752));
#112076=CARTESIAN_POINT('Ctrl Pts',(-95.6688934506936,1074.69846571525,
484.270680473507));
#112077=CARTESIAN_POINT('Ctrl Pts',(-95.5635056872982,1074.7301393527,484.005929220394));
#112078=CARTESIAN_POINT('Ctrl Pts',(-95.4849113886009,1074.74809568166,
483.884765536165));
#112079=CARTESIAN_POINT('Ctrl Pts',(-95.3354082583345,1074.77650113298,
483.730922002435));
#112080=CARTESIAN_POINT('Ctrl Pts',(-95.2805439144007,1074.78616535173,
483.684596042482));
#112081=CARTESIAN_POINT('Ctrl Pts',(-95.162760948298,1074.80552929484,483.603530038944));
#112082=CARTESIAN_POINT('Ctrl Pts',(-95.1001353917849,1074.81518538595,
483.568931131701));
#112083=CARTESIAN_POINT('Ctrl Pts',(-94.9014833492655,1074.8439957061,483.483389043402));
#112084=CARTESIAN_POINT('Ctrl Pts',(-94.7581467770505,1074.8624183042,483.453109785185));
#112085=CARTESIAN_POINT('Ctrl Pts',(-94.468525646668,1074.89530267907,483.450543856115));
#112086=CARTESIAN_POINT('Ctrl Pts',(-94.3250650326983,1074.90947031478,
483.477954009334));
#112087=CARTESIAN_POINT('Ctrl Pts',(-94.0569836323811,1074.93174628175,
483.587438277236));
#112088=CARTESIAN_POINT('Ctrl Pts',(-93.9350801038396,1074.9396364655,483.668332137648));
#112089=CARTESIAN_POINT('Ctrl Pts',(-93.7322722672411,1074.94794831263,
483.870961103211));
#112090=CARTESIAN_POINT('Ctrl Pts',(-93.6525214656037,1074.94845783271,
483.989648223678));
#112091=CARTESIAN_POINT('Ctrl Pts',(-93.5427663055076,1074.94222195788,
484.251147178559));
#112092=CARTESIAN_POINT('Ctrl Pts',(-93.5139706064368,1074.93552546865,
484.391347020229));
#112093=CARTESIAN_POINT('Ctrl Pts',(-93.5115161919005,1074.91547687092,
484.677855297207));
#112094=CARTESIAN_POINT('Ctrl Pts',(-93.5391549381978,1074.90218075921,
484.821277616227));
#112095=CARTESIAN_POINT('Ctrl Pts',(-93.6487067240138,1074.87068512212,
485.089289147712));
#112096=CARTESIAN_POINT('Ctrl Pts',(-93.7298082798916,1074.85276960261,
485.211140951457));
#112097=CARTESIAN_POINT('Ctrl Pts',(-93.9353946458708,1074.8145642406,485.416703002735));
#112098=CARTESIAN_POINT('Ctrl Pts',(-94.0582756150637,1074.79461906541,
485.498127843746));
#112099=CARTESIAN_POINT('Ctrl Pts',(-94.3232856728116,1074.75635740111,
485.605573678612));
#112100=CARTESIAN_POINT('Ctrl Pts',(-94.4621322209791,1074.73834186855,
485.63275997128));
#112101=CARTESIAN_POINT('Ctrl Pts',(-94.6024687290833,1074.72207722087,
485.632861542604));
#112102=CARTESIAN_POINT('Origin',(-94.6032580293197,1067.7251047501,484.542321079512));
#112103=CARTESIAN_POINT('',(-94.6032580293198,1074.76643751182,485.03286182824));
#112104=CARTESIAN_POINT('',(-94.60325802932,1074.83751173097,484.051780330783));
#112105=CARTESIAN_POINT('Ctrl Pts',(-94.6032580293198,1074.76643751182,
485.03286182824));
#112106=CARTESIAN_POINT('Ctrl Pts',(-94.6064097860182,1074.76607494461,
485.03286182824));
#112107=CARTESIAN_POINT('Ctrl Pts',(-94.6095631087125,1074.765714379,485.032831452973));
#112108=CARTESIAN_POINT('Ctrl Pts',(-94.6771372393172,1074.75803452305,
485.031528117375));
#112109=CARTESIAN_POINT('Ctrl Pts',(-94.7407944245279,1074.75171223875,
485.017603492421));
#112110=CARTESIAN_POINT('Ctrl Pts',(-94.8586327401454,1074.7418854872,484.966005962437));
#112111=CARTESIAN_POINT('Ctrl Pts',(-94.9117375447669,1074.73845089191,
484.929083822759));
#112112=CARTESIAN_POINT('Ctrl Pts',(-95.0005030181127,1074.73492674128,
484.837081653654));
#112113=CARTESIAN_POINT('Ctrl Pts',(-95.0353817940901,1074.7348499967,484.783063505805));
#112114=CARTESIAN_POINT('Ctrl Pts',(-95.0825445278263,1074.7380647946,484.664693286736));
#112115=CARTESIAN_POINT('Ctrl Pts',(-95.0943431949663,1074.74132438622,
484.601541527186));
#112116=CARTESIAN_POINT('Ctrl Pts',(-95.0932115512552,1074.75078405641,
484.473923114327));
#112117=CARTESIAN_POINT('Ctrl Pts',(-95.0801080805805,1074.7569114572,484.410717421114));
#112118=CARTESIAN_POINT('Ctrl Pts',(-95.0302899119064,1074.77126494828,
484.292455501764));
#112119=CARTESIAN_POINT('Ctrl Pts',(-94.9938128842482,1074.77937423418,
484.238617070232));
#112120=CARTESIAN_POINT('Ctrl Pts',(-94.9251845633391,1074.7921660622,484.170801255045));
#112121=CARTESIAN_POINT('Ctrl Pts',(-94.9001564002189,1074.79650407244,
484.150512099338));
#112122=CARTESIAN_POINT('Ctrl Pts',(-94.8465456064098,1074.80519900672,
484.115155060813));
#112123=CARTESIAN_POINT('Ctrl Pts',(-94.8180886671918,1074.80953642642,
484.100158106668));
#112124=CARTESIAN_POINT('Ctrl Pts',(-94.7296563935429,1074.82223691641,
484.064123506368));
#112125=CARTESIAN_POINT('Ctrl Pts',(-94.6667958248473,1074.83028711391,
484.051780330783));
#112126=CARTESIAN_POINT('Ctrl Pts',(-94.6032580293202,1074.83751173097,
484.051780330783));
#112127=CARTESIAN_POINT('',(-94.6032580293197,1082.7251047501,484.051780330783));
#112128=CARTESIAN_POINT('',(-94.6032580293197,1067.7251047501,484.051780330783));
#112129=CARTESIAN_POINT('Origin',(-94.6032580293197,1082.7251047501,484.542321079512));
#112130=CARTESIAN_POINT('Ctrl Pts',(-94.6032580293202,1074.83751173097,
484.051780330783));
#112131=CARTESIAN_POINT('Ctrl Pts',(-94.6031280517499,1074.83752651018,
484.051780330783));
#112132=CARTESIAN_POINT('Ctrl Pts',(-94.6029980713456,1074.83754128593,
484.051780382445));
#112133=CARTESIAN_POINT('Ctrl Pts',(-94.6028680881373,1074.83755605823,
484.051780485771));
#112134=CARTESIAN_POINT('Ctrl Pts',(-94.5376062273942,1074.84497292011,
484.051832363816));
#112135=CARTESIAN_POINT('Ctrl Pts',(-94.4728961004285,1074.85137516962,
484.064907529361));
#112136=CARTESIAN_POINT('Ctrl Pts',(-94.3531213898483,1074.86132287037,
484.115443377367));
#112137=CARTESIAN_POINT('Ctrl Pts',(-94.2991328186827,1074.86480920347,
484.152037997717));
#112138=CARTESIAN_POINT('Ctrl Pts',(-94.2090502874632,1074.86844628791,
484.243508428265));
#112139=CARTESIAN_POINT('Ctrl Pts',(-94.1736130737808,1074.8686093583,484.297178339696));
#112140=CARTESIAN_POINT('Ctrl Pts',(-94.1252124831204,1074.86563134578,
484.415148274704));
#112141=CARTESIAN_POINT('Ctrl Pts',(-94.1127692976782,1074.86251619174,
484.47826283707));
#112142=CARTESIAN_POINT('Ctrl Pts',(-94.1126651952564,1074.85335524365,
484.606063527551));
#112143=CARTESIAN_POINT('Ctrl Pts',(-94.1251918226818,1074.84737857733,
484.669483302672));
#112144=CARTESIAN_POINT('Ctrl Pts',(-94.1743606068894,1074.83316915046,
484.789244988087));
#112145=CARTESIAN_POINT('Ctrl Pts',(-94.2111091104492,1074.82502408753,
484.844185383084));
#112146=CARTESIAN_POINT('Ctrl Pts',(-94.3040475266962,1074.80774374707,
484.93654810885));
#112147=CARTESIAN_POINT('Ctrl Pts',(-94.3594406529071,1074.79876839697,
484.973010432572));
#112148=CARTESIAN_POINT('Ctrl Pts',(-94.4784676554407,1074.78165605926,
485.020839280529));
#112149=CARTESIAN_POINT('Ctrl Pts',(-94.5405529418956,1074.77365088853,
485.03286182824));
#112150=CARTESIAN_POINT('Ctrl Pts',(-94.6032580293198,1074.76643751182,
485.03286182824));
#112151=CARTESIAN_POINT('Origin',(-40.034544989914,1067.7251047501,504.732111464453));
#112152=CARTESIAN_POINT('',(-40.0345449899334,1076.70230022208,503.25380833226));
#112153=CARTESIAN_POINT('',(-40.034544989914,1067.7251047501,503.25380833226));
#112154=CARTESIAN_POINT('Ctrl Pts',(-41.5126544848484,1076.65353483496,
504.756037843979));
#112155=CARTESIAN_POINT('Ctrl Pts',(-41.5157829477054,1076.65862947213,
504.562769545764));
#112156=CARTESIAN_POINT('Ctrl Pts',(-41.4809754826117,1076.66395691137,
504.370751622908));
#112157=CARTESIAN_POINT('Ctrl Pts',(-41.3748386768931,1076.671697424,504.100980925426));
#112158=CARTESIAN_POINT('Ctrl Pts',(-41.3307415283915,1076.67421835813,
504.014763411445));
#112159=CARTESIAN_POINT('Ctrl Pts',(-41.1728328279325,1076.68155683822,
503.768798538432));
#112160=CARTESIAN_POINT('Ctrl Pts',(-41.035460762808,1076.68599837266,503.626739159453));
#112161=CARTESIAN_POINT('Ctrl Pts',(-40.7141068724518,1076.69359618941,
503.404889210497));
#112162=CARTESIAN_POINT('Ctrl Pts',(-40.5334941467736,1076.69669063987,
503.326984693202));
#112163=CARTESIAN_POINT('Ctrl Pts',(-40.1516574964021,1076.70149343388,
503.245527793793));
#112164=CARTESIAN_POINT('Ctrl Pts',(-39.9541267344701,1076.70315709624,
503.243090353066));
#112165=CARTESIAN_POINT('Ctrl Pts',(-39.5687072605579,1076.70511465722,
503.315426844983));
#112166=CARTESIAN_POINT('Ctrl Pts',(-39.3847114872663,1076.70538783021,
503.389830836801));
#112167=CARTESIAN_POINT('Ctrl Pts',(-39.0569614391553,1076.70454797393,
503.60598480715));
#112168=CARTESIAN_POINT('Ctrl Pts',(-38.9163742522714,1076.70344403643,
503.745439270994));
#112169=CARTESIAN_POINT('Ctrl Pts',(-38.6984245787826,1076.69978090374,
504.070154914735));
#112170=CARTESIAN_POINT('Ctrl Pts',(-38.6228580340899,1076.69725797628,
504.251968490841));
#112171=CARTESIAN_POINT('Ctrl Pts',(-38.5466193189783,1076.69074840334,
504.634528523447));
#112172=CARTESIAN_POINT('Ctrl Pts',(-38.5467436536565,1076.68681682594,
504.83152478639));
#112173=CARTESIAN_POINT('Ctrl Pts',(-38.6039355625039,1076.68008029063,
505.116702268898));
#112174=CARTESIAN_POINT('Ctrl Pts',(-38.6318496719947,1076.67773785312,
505.208554792672));
#112175=CARTESIAN_POINT('Ctrl Pts',(-38.7057448878917,1076.67281221251,
505.387240795265));
#112176=CARTESIAN_POINT('Ctrl Pts',(-38.7518781659053,1076.67023730474,
505.473508302114));
#112177=CARTESIAN_POINT('Ctrl Pts',(-38.9141030826265,1076.66239782396,
505.715789219588));
#112178=CARTESIAN_POINT('Ctrl Pts',(-39.0527146610104,1076.65705882752,
505.854173265541));
#112179=CARTESIAN_POINT('Ctrl Pts',(-39.375534020827,1076.64695840291,506.069553768881));
#112180=CARTESIAN_POINT('Ctrl Pts',(-39.556634319814,1076.64230177121,506.144435499386));
#112181=CARTESIAN_POINT('Ctrl Pts',(-39.9373270307768,1076.63464626945,
506.219916336102));
#112182=CARTESIAN_POINT('Ctrl Pts',(-40.1332117643458,1076.63172763579,
506.219824770339));
#112183=CARTESIAN_POINT('Ctrl Pts',(-40.5133943389907,1076.6283043857,506.144052600482));
#112184=CARTESIAN_POINT('Ctrl Pts',(-40.6940222587757,1076.62783155312,
506.069260076883));
#112185=CARTESIAN_POINT('Ctrl Pts',(-41.0158209134949,1076.62945747136,
505.854525767654));
#112186=CARTESIAN_POINT('Ctrl Pts',(-41.1539607251774,1076.63153330559,
505.716802225688));
#112187=CARTESIAN_POINT('Ctrl Pts',(-41.3693507204397,1076.63778327435,
505.396152827116));
#112188=CARTESIAN_POINT('Ctrl Pts',(-41.4445668953704,1076.64188997198,
505.216346606781));
#112189=CARTESIAN_POINT('Ctrl Pts',(-41.5012863953776,1076.64880143344,
504.937907114078));
#112190=CARTESIAN_POINT('Ctrl Pts',(-41.5111798515923,1076.65113342516,
504.847136851046));
#112191=CARTESIAN_POINT('Ctrl Pts',(-41.5126544848484,1076.65353483496,
504.756037843979));
#112192=CARTESIAN_POINT('Origin',(-40.034544989914,1067.7251047501,504.732111464453));
#112193=CARTESIAN_POINT('',(-40.034544989914,1076.65067043007,505.610414596646));
#112194=CARTESIAN_POINT('',(-40.0345449899148,1076.69158153387,503.85380833226));
#112195=CARTESIAN_POINT('Ctrl Pts',(-40.034544989914,1076.65067043007,505.610414596647));
#112196=CARTESIAN_POINT('Ctrl Pts',(-40.099230217787,1076.64979703943,505.610414596647));
#112197=CARTESIAN_POINT('Ctrl Pts',(-40.1638735490618,1076.64911108635,
505.603268574889));
#112198=CARTESIAN_POINT('Ctrl Pts',(-40.3394889650877,1076.64779221792,
505.563768045686));
#112199=CARTESIAN_POINT('Ctrl Pts',(-40.4456532701006,1076.64762563924,
505.51673487539));
#112200=CARTESIAN_POINT('Ctrl Pts',(-40.6337073127725,1076.64867381101,
505.384505414016));
#112201=CARTESIAN_POINT('Ctrl Pts',(-40.7138042450954,1076.64987607597,
505.300633618999));
#112202=CARTESIAN_POINT('Ctrl Pts',(-40.8371524395397,1076.65342653398,
505.106847831021));
#112203=CARTESIAN_POINT('Ctrl Pts',(-40.8792192419791,1076.65573802481,
504.998809249611));
#112204=CARTESIAN_POINT('Ctrl Pts',(-40.9194065315618,1076.66105587421,
504.772613146271));
#112205=CARTESIAN_POINT('Ctrl Pts',(-40.9171097966551,1076.66400893629,
504.656628413306));
#112206=CARTESIAN_POINT('Ctrl Pts',(-40.8802800239126,1076.66855499991,
504.488298378343));
#112207=CARTESIAN_POINT('Ctrl Pts',(-40.8625390204781,1076.67007872801,
504.433550794752));
#112208=CARTESIAN_POINT('Ctrl Pts',(-40.8166453557619,1076.67309430675,
504.328346280406));
#112209=CARTESIAN_POINT('Ctrl Pts',(-40.7886109472355,1076.67457894721,
504.278137862969));
#112210=CARTESIAN_POINT('Ctrl Pts',(-40.6893417422963,1076.6789503985,504.13523618805));
#112211=CARTESIAN_POINT('Ctrl Pts',(-40.6043812201753,1076.68165548887,
504.053651109645));
#112212=CARTESIAN_POINT('Ctrl Pts',(-40.4077164533096,1076.68637261445,
503.928545470762));
#112213=CARTESIAN_POINT('Ctrl Pts',(-40.2980076229507,1076.68834162645,
503.886200266871));
#112214=CARTESIAN_POINT('Ctrl Pts',(-40.1341230671946,1076.69052631114,
503.858049952025));
#112215=CARTESIAN_POINT('Ctrl Pts',(-40.0843834156782,1076.69109675782,
503.853808757965));
#112216=CARTESIAN_POINT('Ctrl Pts',(-40.0345524926856,1076.69158146089,
503.853808332292));
#112217=CARTESIAN_POINT('',(-40.034544989914,1082.7251047501,503.85380833226));
#112218=CARTESIAN_POINT('',(-40.034544989914,1067.7251047501,503.85380833226));
#112219=CARTESIAN_POINT('Origin',(-40.034544989914,1082.7251047501,504.732111464453));
#112220=CARTESIAN_POINT('Ctrl Pts',(-40.0345449899164,1076.69158153387,
503.85380833226));
#112221=CARTESIAN_POINT('Ctrl Pts',(-39.9175261494676,1076.69271975024,
503.85380833226));
#112222=CARTESIAN_POINT('Ctrl Pts',(-39.8016831027087,1076.69337219467,
503.877192551933));
#112223=CARTESIAN_POINT('Ctrl Pts',(-39.5858789949519,1076.69369562175,
503.968022865444));
#112224=CARTESIAN_POINT('Ctrl Pts',(-39.4881051958344,1076.69336295687,
504.034590504819));
#112225=CARTESIAN_POINT('Ctrl Pts',(-39.3247018721275,1076.69171549948,
504.201862509166));
#112226=CARTESIAN_POINT('Ctrl Pts',(-39.2605967479819,1076.69041841276,
504.300784393691));
#112227=CARTESIAN_POINT('Ctrl Pts',(-39.1749142126364,1076.68691720146,
504.517617169565));
#112228=CARTESIAN_POINT('Ctrl Pts',(-39.1540837692115,1076.68474700539,
504.633330225056));
#112229=CARTESIAN_POINT('Ctrl Pts',(-39.1587608620073,1076.67968679998,
504.86650153227));
#112230=CARTESIAN_POINT('Ctrl Pts',(-39.1843734758727,1076.6768426824,504.981639703758));
#112231=CARTESIAN_POINT('Ctrl Pts',(-39.2552755448874,1076.67232959844,
505.141403131959));
#112232=CARTESIAN_POINT('Ctrl Pts',(-39.28399682815,1076.67080152637,505.191956959883));
#112233=CARTESIAN_POINT('Ctrl Pts',(-39.3839984221867,1076.66621825487,
505.333335029321));
#112234=CARTESIAN_POINT('Ctrl Pts',(-39.4683574262096,1076.66318463493,
505.413370284416));
#112235=CARTESIAN_POINT('Ctrl Pts',(-39.6631621868751,1076.65757214213,
505.536324749776));
#112236=CARTESIAN_POINT('Ctrl Pts',(-39.7717249270997,1076.65505002948,
505.578050817571));
#112237=CARTESIAN_POINT('Ctrl Pts',(-39.9346746491659,1076.65213011358,
505.606158255156));
#112238=CARTESIAN_POINT('Ctrl Pts',(-39.9846222978553,1076.65134449451,
505.610414596647));
#112239=CARTESIAN_POINT('Ctrl Pts',(-40.034544989914,1076.65067043007,505.610414596647));
#112240=CARTESIAN_POINT('Origin',(-52.5439991194437,1067.7251047501,505.838291381042));
#112241=CARTESIAN_POINT('',(-52.5439991194708,1076.41132893179,504.562847259905));
#112242=CARTESIAN_POINT('',(-52.5439991194437,1067.7251047501,504.562847259905));
#112243=CARTESIAN_POINT('Ctrl Pts',(-52.5448754729142,1076.27282192338,
507.113735201108));
#112244=CARTESIAN_POINT('Ctrl Pts',(-52.7120708255886,1076.26653123827,
507.113620321703));
#112245=CARTESIAN_POINT('Ctrl Pts',(-52.8776731502766,1076.26216701088,
507.08063083869));
#112246=CARTESIAN_POINT('Ctrl Pts',(-53.1862263402415,1076.25794216686,
506.952781983516));
#112247=CARTESIAN_POINT('Ctrl Pts',(-53.3262292977647,1076.25810841153,
506.85939843974));
#112248=CARTESIAN_POINT('Ctrl Pts',(-53.5621686327428,1076.26296163143,
506.624279190074));
#112249=CARTESIAN_POINT('Ctrl Pts',(-53.6558776560769,1076.2675914453,506.484926632456));
#112250=CARTESIAN_POINT('Ctrl Pts',(-53.7845871745367,1076.28059635365,
506.178029184282));
#112251=CARTESIAN_POINT('Ctrl Pts',(-53.8182701685065,1076.2888463096,506.013417708415));
#112252=CARTESIAN_POINT('Ctrl Pts',(-53.8205595391109,1076.30771904487,
505.680191254166));
#112253=CARTESIAN_POINT('Ctrl Pts',(-53.7889494086595,1076.31816396595,
505.514755483463));
#112254=CARTESIAN_POINT('Ctrl Pts',(-53.6637610991126,1076.33972761712,
505.205183755935));
#112255=CARTESIAN_POINT('Ctrl Pts',(-53.5712476554929,1076.35064011546,
505.064042953511));
#112256=CARTESIAN_POINT('Ctrl Pts',(-53.3355031310887,1076.37159041586,
504.823916099185));
#112257=CARTESIAN_POINT('Ctrl Pts',(-53.1939404166316,1076.38141052102,
504.727864515446));
#112258=CARTESIAN_POINT('Ctrl Pts',(-52.8822616770613,1076.3985626049,504.597019981783));
#112259=CARTESIAN_POINT('Ctrl Pts',(-52.715362969147,1076.40574306297,504.56320249138));
#112260=CARTESIAN_POINT('Ctrl Pts',(-52.3778389214085,1076.41674546459,
504.562497332901));
#112261=CARTESIAN_POINT('Ctrl Pts',(-52.2105725882794,1076.42046023434,
504.595668260933));
#112262=CARTESIAN_POINT('Ctrl Pts',(-51.8984330780026,1076.42403563,504.725366919091));
#112263=CARTESIAN_POINT('Ctrl Pts',(-51.7567208113037,1076.42385755791,
504.820672643409));
#112264=CARTESIAN_POINT('Ctrl Pts',(-51.5189065640949,1076.41958346645,
505.060821615217));
#112265=CARTESIAN_POINT('Ctrl Pts',(-51.425118593829,1076.41553343089,505.203191024268));
#112266=CARTESIAN_POINT('Ctrl Pts',(-51.2984594434416,1076.40391402638,
505.51602663548));
#112267=CARTESIAN_POINT('Ctrl Pts',(-51.2668218078869,1076.3964565273,505.683371240081));
#112268=CARTESIAN_POINT('Ctrl Pts',(-51.2704451220595,1076.37884131952,
506.021523645012));
#112269=CARTESIAN_POINT('Ctrl Pts',(-51.3060590868485,1076.36883879867,
506.188982377302));
#112270=CARTESIAN_POINT('Ctrl Pts',(-51.4068094233405,1076.3528790641,506.421963701217));
#112271=CARTESIAN_POINT('Ctrl Pts',(-51.4478889292366,1076.34745324099,
506.49587366197));
#112272=CARTESIAN_POINT('Ctrl Pts',(-51.591489026787,1076.33111484934,506.702918265949));
#112273=CARTESIAN_POINT('Ctrl Pts',(-51.7132521954594,1076.32022615565,
506.820496694586));
#112274=CARTESIAN_POINT('Ctrl Pts',(-51.9952958290798,1076.29976031084,
507.001813900014));
#112275=CARTESIAN_POINT('Ctrl Pts',(-52.1528580501541,1076.29038355797,
507.063815480095));
#112276=CARTESIAN_POINT('Ctrl Pts',(-52.3928309469499,1076.27892838407,
507.107028210238));
#112277=CARTESIAN_POINT('Ctrl Pts',(-52.4687717021975,1076.27568530953,
507.113787491771));
#112278=CARTESIAN_POINT('Ctrl Pts',(-52.5448754729142,1076.27282192338,
507.113735201108));
#112279=CARTESIAN_POINT('Origin',(-52.5439991194437,1067.7251047501,505.838291381042));
#112280=CARTESIAN_POINT('',(-52.5439991194437,1076.3076507295,506.513735502178));
#112281=CARTESIAN_POINT('',(-52.543999119444,1076.38098512892,505.162847259905));
#112282=CARTESIAN_POINT('Ctrl Pts',(-52.5439991194437,1076.3076507295,506.513735502178));
#112283=CARTESIAN_POINT('Ctrl Pts',(-52.5941445622273,1076.30582150806,
506.513735502178));
#112284=CARTESIAN_POINT('Ctrl Pts',(-52.6442631377859,1076.30430342464,
506.508151231897));
#112285=CARTESIAN_POINT('Ctrl Pts',(-52.7795876422319,1076.30108395938,
506.477455207571));
#112286=CARTESIAN_POINT('Ctrl Pts',(-52.8611026658913,1076.30014727865,
506.441185788444));
#112287=CARTESIAN_POINT('Ctrl Pts',(-53.005413680361,1076.30062591086,506.339393634614));
#112288=CARTESIAN_POINT('Ctrl Pts',(-53.0668314323192,1076.30203198681,
506.274923252499));
#112289=CARTESIAN_POINT('Ctrl Pts',(-53.1614262452317,1076.30699175589,
506.126026444978));
#112290=CARTESIAN_POINT('Ctrl Pts',(-53.1936708617585,1076.31049710481,
506.043041214527));
#112291=CARTESIAN_POINT('Ctrl Pts',(-53.2244955888446,1076.31911280663,
505.869235450439));
#112292=CARTESIAN_POINT('Ctrl Pts',(-53.2226986656671,1076.32414260447,
505.780072386387));
#112293=CARTESIAN_POINT('Ctrl Pts',(-53.1943537621746,1076.33229664811,
505.650627069925));
#112294=CARTESIAN_POINT('Ctrl Pts',(-53.180681692702,1076.33509882485,505.608479093141));
#112295=CARTESIAN_POINT('Ctrl Pts',(-53.1452919845341,1076.34078421601,
505.527441243967));
#112296=CARTESIAN_POINT('Ctrl Pts',(-53.1236531670261,1076.34365396815,
505.488745897926));
#112297=CARTESIAN_POINT('Ctrl Pts',(-53.047789446097,1076.35222361264,505.379744018297));
#112298=CARTESIAN_POINT('Ctrl Pts',(-52.983370784426,1076.35779279807,505.317686780181));
#112299=CARTESIAN_POINT('Ctrl Pts',(-52.8331743764977,1076.36809886091,
505.221302044327));
#112300=CARTESIAN_POINT('Ctrl Pts',(-52.7485973774765,1076.37272189553,
505.188330179835));
#112301=CARTESIAN_POINT('Ctrl Pts',(-52.621857827715,1076.3781787059,505.166232553107));
#112302=CARTESIAN_POINT('Ctrl Pts',(-52.5831920692139,1076.37966146313,
505.162873039544));
#112303=CARTESIAN_POINT('Ctrl Pts',(-52.5444459373632,1076.38097004623,
505.162847408246));
#112304=CARTESIAN_POINT('Ctrl Pts',(-52.5442969956814,1076.38097507648,
505.162847309719));
#112305=CARTESIAN_POINT('Ctrl Pts',(-52.5441480563678,1076.38098010406,
505.162847259905));
#112306=CARTESIAN_POINT('Ctrl Pts',(-52.5439991194442,1076.38098512892,
505.162847259905));
#112307=CARTESIAN_POINT('',(-52.5439991194437,1082.7251047501,505.162847259905));
#112308=CARTESIAN_POINT('',(-52.5439991194437,1067.7251047501,505.162847259905));
#112309=CARTESIAN_POINT('Origin',(-52.5439991194437,1082.7251047501,505.838291381042));
#112310=CARTESIAN_POINT('Ctrl Pts',(-52.5439991194442,1076.38098512892,
505.162847259905));
#112311=CARTESIAN_POINT('Ctrl Pts',(-52.454389053301,1076.38400840739,505.162847259905));
#112312=CARTESIAN_POINT('Ctrl Pts',(-52.3656445614433,1076.38605774787,
505.180680000485));
#112313=CARTESIAN_POINT('Ctrl Pts',(-52.200111080427,1076.38801101988,505.250044928404));
#112314=CARTESIAN_POINT('Ctrl Pts',(-52.1250195665029,1076.38789171826,
505.300938128183));
#112315=CARTESIAN_POINT('Ctrl Pts',(-51.999162401815,1076.38547113493,505.429094455614));
#112316=CARTESIAN_POINT('Ctrl Pts',(-51.9496627855191,1076.38319411869,
505.505057357832));
#112317=CARTESIAN_POINT('Ctrl Pts',(-51.883228099544,1076.37672581559,505.671920978432));
#112318=CARTESIAN_POINT('Ctrl Pts',(-51.8669938531162,1076.37259614805,
505.76116031435));
#112319=CARTESIAN_POINT('Ctrl Pts',(-51.8703596771028,1076.36295358499,
505.941075171903));
#112320=CARTESIAN_POINT('Ctrl Pts',(-51.8900794118279,1076.35753006859,
506.029954351681));
#112321=CARTESIAN_POINT('Ctrl Pts',(-51.9447688812763,1076.34898179335,
506.153163881526));
#112322=CARTESIAN_POINT('Ctrl Pts',(-51.9669056362615,1076.34609765802,
506.19210538115));
#112323=CARTESIAN_POINT('Ctrl Pts',(-52.0439818174159,1076.33746234889,
506.300975951162));
#112324=CARTESIAN_POINT('Ctrl Pts',(-52.1090127195029,1076.33176781271,
506.362586846487));
#112325=CARTESIAN_POINT('Ctrl Pts',(-52.2591523583701,1076.32115888301,
506.457122883992));
#112326=CARTESIAN_POINT('Ctrl Pts',(-52.3428061494639,1076.31634712274,
506.489154634628));
#112327=CARTESIAN_POINT('Ctrl Pts',(-52.4679363166643,1076.31060366373,
506.510524761264));
#112328=CARTESIAN_POINT('Ctrl Pts',(-52.5059754427173,1076.3090377693,506.513735502178));
#112329=CARTESIAN_POINT('Ctrl Pts',(-52.5439991194437,1076.3076507295,506.513735502178));
#112330=CARTESIAN_POINT('Origin',(-66.3937896239306,1067.7251047501,505.798797233579));
#112331=CARTESIAN_POINT('',(-66.3937896239305,1075.74217416993,504.699966097586));
#112332=CARTESIAN_POINT('',(-66.3937896239306,1067.7251047501,504.699966097586));
#112333=CARTESIAN_POINT('Ctrl Pts',(-66.3938922946787,1075.56505891227,
506.897628364774));
#112334=CARTESIAN_POINT('Ctrl Pts',(-66.5377439329708,1075.5553029594,506.897614923805));
#112335=CARTESIAN_POINT('Ctrl Pts',(-66.6803277369447,1075.54793464586,
506.869353627706));
#112336=CARTESIAN_POINT('Ctrl Pts',(-66.9458979690475,1075.53896655866,
506.759593170502));
#112337=CARTESIAN_POINT('Ctrl Pts',(-67.0663498678771,1075.53742419525,
506.679497121772));
#112338=CARTESIAN_POINT('Ctrl Pts',(-67.2695429342651,1075.54039830516,
506.477727005766));
#112339=CARTESIAN_POINT('Ctrl Pts',(-67.3503282205808,1075.54487262748,
506.358150666703));
#112340=CARTESIAN_POINT('Ctrl Pts',(-67.4617465953587,1075.55923551352,
506.094509517608));
#112341=CARTESIAN_POINT('Ctrl Pts',(-67.4911177270138,1075.56899806553,
505.952963071634));
#112342=CARTESIAN_POINT('Ctrl Pts',(-67.4940205904077,1075.59249143215,
505.66594860695));
#112343=CARTESIAN_POINT('Ctrl Pts',(-67.4671709701334,1075.60601842522,
505.523219983919));
#112344=CARTESIAN_POINT('Ctrl Pts',(-67.3868194776427,1075.62770861649,
505.322849447008));
#112345=CARTESIAN_POINT('Ctrl Pts',(-67.3534429135765,1075.63513685526,
505.258707843303));
#112346=CARTESIAN_POINT('Ctrl Pts',(-67.2747200780839,1075.65011148731,
505.138065664204));
#112347=CARTESIAN_POINT('Ctrl Pts',(-67.2295862227784,1075.65762291195,
505.081824883924));
#112348=CARTESIAN_POINT('Ctrl Pts',(-67.0771670909457,1075.68015355567,
504.926015563009));
#112349=CARTESIAN_POINT('Ctrl Pts',(-66.9552034804363,1075.69471965159,
504.842963485428));
#112350=CARTESIAN_POINT('Ctrl Pts',(-66.6864183602497,1075.72108584257,
504.729703518017));
#112351=CARTESIAN_POINT('Ctrl Pts',(-66.5423355880472,1075.7326452051,504.700339722112));
#112352=CARTESIAN_POINT('Ctrl Pts',(-66.2507605417059,1075.75134979152,
504.699599396793));
#112353=CARTESIAN_POINT('Ctrl Pts',(-66.1062000943209,1075.75830783535,
504.72825892625));
#112354=CARTESIAN_POINT('Ctrl Pts',(-65.8376706292063,1075.76667319234,
504.840080292173));
#112355=CARTESIAN_POINT('Ctrl Pts',(-65.7162600264784,1075.76804302978,
504.921657187487));
#112356=CARTESIAN_POINT('Ctrl Pts',(-65.5130971587849,1075.76506869291,
505.126206457029));
#112357=CARTESIAN_POINT('Ctrl Pts',(-65.4329794682159,1075.76081132962,
505.246711156188));
#112358=CARTESIAN_POINT('Ctrl Pts',(-65.3225598718984,1075.74704172745,
505.513900695787));
#112359=CARTESIAN_POINT('Ctrl Pts',(-65.294299520288,1075.73757430082,505.658295646118));
#112360=CARTESIAN_POINT('Ctrl Pts',(-65.2956421914888,1075.71456780327,
505.949730301104));
#112361=CARTESIAN_POINT('Ctrl Pts',(-65.3253509701224,1075.70124560524,
506.093883541034));
#112362=CARTESIAN_POINT('Ctrl Pts',(-65.4101272555891,1075.67978247192,
506.293713601267));
#112363=CARTESIAN_POINT('Ctrl Pts',(-65.4443703142224,1075.67250956308,
506.356589596288));
#112364=CARTESIAN_POINT('Ctrl Pts',(-65.5247093080667,1075.65771823703,
506.475014049654));
#112365=CARTESIAN_POINT('Ctrl Pts',(-65.5706668421235,1075.65023296772,
506.530260184581));
#112366=CARTESIAN_POINT('Ctrl Pts',(-65.72565702693,1075.62758724997,506.683323175303));
#112367=CARTESIAN_POINT('Ctrl Pts',(-65.8491425729377,1075.6127436033,506.76429769867));
#112368=CARTESIAN_POINT('Ctrl Pts',(-66.1148498821844,1075.58616820431,
506.870811005097));
#112369=CARTESIAN_POINT('Ctrl Pts',(-66.2536558097413,1075.57456968708,
506.897641467957));
#112370=CARTESIAN_POINT('Ctrl Pts',(-66.3938922946787,1075.56505891227,
506.897628364774));
#112371=CARTESIAN_POINT('Origin',(-66.3937896239306,1067.7251047501,505.798797233579));
#112372=CARTESIAN_POINT('',(-66.3937896239306,1075.61493016275,506.297628369571));
#112373=CARTESIAN_POINT('',(-66.3937896239315,1075.69533039084,505.299966097586));
#112374=CARTESIAN_POINT('Ctrl Pts',(-66.3937896239305,1075.61493016275,
506.297628369571));
#112375=CARTESIAN_POINT('Ctrl Pts',(-66.3969872526643,1075.61471660334,
506.297628369571));
#112376=CARTESIAN_POINT('Ctrl Pts',(-66.4001864101225,1075.61450543078,
506.2975976233));
#112377=CARTESIAN_POINT('Ctrl Pts',(-66.4686082155845,1075.61004237143,
506.296281008526));
#112378=CARTESIAN_POINT('Ctrl Pts',(-66.5330083204022,1075.60687880481,
506.282243259306));
#112379=CARTESIAN_POINT('Ctrl Pts',(-66.6525296057925,1075.60313393998,
506.230205843174));
#112380=CARTESIAN_POINT('Ctrl Pts',(-66.7065062669411,1075.60257758674,
506.192841425143));
#112381=CARTESIAN_POINT('Ctrl Pts',(-66.7970476739618,1075.60415638336,
506.099526567021));
#112382=CARTESIAN_POINT('Ctrl Pts',(-66.8327242575731,1075.60627324959,
506.044524015442));
#112383=CARTESIAN_POINT('Ctrl Pts',(-66.8810824623255,1075.61291386197,
505.923789671765));
#112384=CARTESIAN_POINT('Ctrl Pts',(-66.8932004913451,1075.61738067694,
505.859208593282));
#112385=CARTESIAN_POINT('Ctrl Pts',(-66.8919947248666,1075.62808638916,
505.728765714233));
#112386=CARTESIAN_POINT('Ctrl Pts',(-66.8785272948644,1075.63423222768,
505.664154900985));
#112387=CARTESIAN_POINT('Ctrl Pts',(-66.8402623969173,1075.64407255818,
505.573936318237));
#112388=CARTESIAN_POINT('Ctrl Pts',(-66.8245795297104,1075.64743432094,
505.545183962969));
#112389=CARTESIAN_POINT('Ctrl Pts',(-66.7878564053252,1075.6542146777,505.49121405238));
#112390=CARTESIAN_POINT('Ctrl Pts',(-66.76690987515,1075.65761753216,505.466115040111));
#112391=CARTESIAN_POINT('Ctrl Pts',(-66.6962780648952,1075.6678554098,505.396612235028));
#112392=CARTESIAN_POINT('Ctrl Pts',(-66.6400176078294,1075.67448591137,
505.359895853247));
#112393=CARTESIAN_POINT('Ctrl Pts',(-66.5195556583078,1075.68618860093,
505.311975903565));
#112394=CARTESIAN_POINT('Ctrl Pts',(-66.4569901306746,1075.69122073777,
505.299966097586));
#112395=CARTESIAN_POINT('Ctrl Pts',(-66.3937896239324,1075.69533039084,
505.299966097586));
#112396=CARTESIAN_POINT('',(-66.3937896239306,1082.7251047501,505.299966097586));
#112397=CARTESIAN_POINT('',(-66.3937896239306,1067.7251047501,505.299966097586));
#112398=CARTESIAN_POINT('Origin',(-66.3937896239306,1082.7251047501,505.798797233579));
#112399=CARTESIAN_POINT('Ctrl Pts',(-66.3937896239324,1075.69533039084,
505.299966097586));
#112400=CARTESIAN_POINT('Ctrl Pts',(-66.393696991604,1075.69533641431,505.299966097586));
#112401=CARTESIAN_POINT('Ctrl Pts',(-66.3936043579098,1075.69534243578,
505.299966123717));
#112402=CARTESIAN_POINT('Ctrl Pts',(-66.3935117228637,1075.69534845529,
505.299966175325));
#112403=CARTESIAN_POINT('Ctrl Pts',(-66.3270385250359,1075.69966794578,
505.300003207775));
#112404=CARTESIAN_POINT('Ctrl Pts',(-66.2611841876149,1075.70288158026,
505.313327059998));
#112405=CARTESIAN_POINT('Ctrl Pts',(-66.1399497147479,1075.7066846604,505.36448891194));
#112406=CARTESIAN_POINT('Ctrl Pts',(-66.0855609170226,1075.70729683034,
505.401234133577));
#112407=CARTESIAN_POINT('Ctrl Pts',(-65.9939189543823,1075.70592073745,
505.493562152881));
#112408=CARTESIAN_POINT('Ctrl Pts',(-65.9575867145451,1075.70394500289,
505.548231953087));
#112409=CARTESIAN_POINT('Ctrl Pts',(-65.907358753142,1075.69755912678,505.669784714922));
#112410=CARTESIAN_POINT('Ctrl Pts',(-65.8945322385433,1075.69315748623,
505.735676699996));
#112411=CARTESIAN_POINT('Ctrl Pts',(-65.8954070785054,1075.68250522403,
505.868595325266));
#112412=CARTESIAN_POINT('Ctrl Pts',(-65.9091428791379,1075.67635739562,
505.934295742771));
#112413=CARTESIAN_POINT('Ctrl Pts',(-65.9481199830954,1075.66650768815,
506.025223447394));
#112414=CARTESIAN_POINT('Ctrl Pts',(-65.9638238820153,1075.6631813765,506.053785225724));
#112415=CARTESIAN_POINT('Ctrl Pts',(-66.0005904751435,1075.65644016903,
506.107484303071));
#112416=CARTESIAN_POINT('Ctrl Pts',(-66.0215782871409,1075.65304063377,
506.132491675586));
#112417=CARTESIAN_POINT('Ctrl Pts',(-66.0926231435377,1075.64273371705,
506.202033754521));
#112418=CARTESIAN_POINT('Ctrl Pts',(-66.1493354797772,1075.63599973081,
506.238743969495));
#112419=CARTESIAN_POINT('Ctrl Pts',(-66.2696390533603,1075.6241684572,506.285932949106));
#112420=CARTESIAN_POINT('Ctrl Pts',(-66.3314235794298,1075.61909539169,
506.297628369571));
#112421=CARTESIAN_POINT('Ctrl Pts',(-66.3937896239305,1075.61493016275,
506.297628369571));
#112422=CARTESIAN_POINT('Origin',(-80.0774492048019,1067.7251047501,502.902003229021));
#112423=CARTESIAN_POINT('',(-80.0774492048019,1074.90384407591,501.811462480293));
#112424=CARTESIAN_POINT('',(-80.0774492048019,1067.7251047501,501.811462480293));
#112425=CARTESIAN_POINT('Ctrl Pts',(-80.0775556651706,1074.69741082091,
503.992543972553));
#112426=CARTESIAN_POINT('Ctrl Pts',(-80.2203939055204,1074.68335242624,
503.992530028451));
#112427=CARTESIAN_POINT('Ctrl Pts',(-80.3620774576235,1074.67206368809,
503.964453024161));
#112428=CARTESIAN_POINT('Ctrl Pts',(-80.6255874212788,1074.65654223953,
503.855395313021));
#112429=CARTESIAN_POINT('Ctrl Pts',(-80.7449440196709,1074.6523996033,503.776028182163));
#112430=CARTESIAN_POINT('Ctrl Pts',(-80.9461808540607,1074.65181168185,
503.576243475235));
#112431=CARTESIAN_POINT('Ctrl Pts',(-81.0261661284762,1074.6553392513,503.458044660765));
#112432=CARTESIAN_POINT('Ctrl Pts',(-81.1367694022258,1074.66961052421,
503.197374581285));
#112433=CARTESIAN_POINT('Ctrl Pts',(-81.1660809474431,1074.68023672022,
503.057438861993));
#112434=CARTESIAN_POINT('Ctrl Pts',(-81.1697363998317,1074.70723981908,
502.773232310702));
#112435=CARTESIAN_POINT('Ctrl Pts',(-81.1435079619441,1074.72340672621,
502.631697216134));
#112436=CARTESIAN_POINT('Ctrl Pts',(-81.0368996889042,1074.75947744905,
502.363331420954));
#112437=CARTESIAN_POINT('Ctrl Pts',(-80.9560413553554,1074.77912227993,
502.239633765539));
#112438=CARTESIAN_POINT('Ctrl Pts',(-80.8032700801437,1074.80856466224,
502.084978808424));
#112439=CARTESIAN_POINT('Ctrl Pts',(-80.7484058314527,1074.81817637982,
502.039352859407));
#112440=CARTESIAN_POINT('Ctrl Pts',(-80.5697774790657,1074.84681222231,
501.918231233593));
#112441=CARTESIAN_POINT('Ctrl Pts',(-80.4349776991283,1074.86505126372,
501.861586297577));
#112442=CARTESIAN_POINT('Ctrl Pts',(-80.1513251869895,1074.89748746044,
501.804428811488));
#112443=CARTESIAN_POINT('Ctrl Pts',(-80.0052807514068,1074.91138774107,
501.804252305455));
#112444=CARTESIAN_POINT('Ctrl Pts',(-79.7225931968404,1074.93295007086,
501.86088327094));
#112445=CARTESIAN_POINT('Ctrl Pts',(-79.5887155205554,1074.94045724399,
501.916564990387));
#112446=CARTESIAN_POINT('Ctrl Pts',(-79.351804312291,1074.94814247841,502.075700378908));
#112447=CARTESIAN_POINT('Ctrl Pts',(-79.2507353332974,1074.94835107219,
502.176824798993));
#112448=CARTESIAN_POINT('Ctrl Pts',(-79.0927212169076,1074.94152693975,
502.412358619853));
#112449=CARTESIAN_POINT('Ctrl Pts',(-79.0374909897089,1074.93454479757,
502.54445607692));
#112450=CARTESIAN_POINT('Ctrl Pts',(-78.9800102013773,1074.91397284501,
502.825200418115));
#112451=CARTESIAN_POINT('Ctrl Pts',(-78.9795713602911,1074.90044714542,
502.971264433429));
#112452=CARTESIAN_POINT('Ctrl Pts',(-79.0355385610595,1074.86860672502,
503.255142309305));
#112453=CARTESIAN_POINT('Ctrl Pts',(-79.0915985444302,1074.8505849915,503.390141249739));
#112454=CARTESIAN_POINT('Ctrl Pts',(-79.2534617935822,1074.81229849349,
503.631076731761));
#112455=CARTESIAN_POINT('Ctrl Pts',(-79.3581097527856,1074.79237972676,
503.73449679173));
#112456=CARTESIAN_POINT('Ctrl Pts',(-79.602566463531,1074.75337675315,503.894598889858));
#112457=CARTESIAN_POINT('Ctrl Pts',(-79.7402559800462,1074.73467195852,
503.949457322082));
#112458=CARTESIAN_POINT('Ctrl Pts',(-79.9483999920536,1074.71066669124,
503.986804683043));
#112459=CARTESIAN_POINT('Ctrl Pts',(-80.0128883498499,1074.70377549355,
503.992550285482));
#112460=CARTESIAN_POINT('Ctrl Pts',(-80.0775556651706,1074.69741082091,
503.992543972553));
#112461=CARTESIAN_POINT('Origin',(-80.0774492048019,1067.7251047501,502.902003229021));
#112462=CARTESIAN_POINT('',(-80.077449204802,1074.75547652074,503.39254397775));
#112463=CARTESIAN_POINT('',(-80.0774492048019,1074.84832662855,502.411462480293));
#112464=CARTESIAN_POINT('Ctrl Pts',(-80.077449204802,1074.75547652074,503.39254397775));
#112465=CARTESIAN_POINT('Ctrl Pts',(-80.0804386977064,1074.75518491478,
503.39254397775));
#112466=CARTESIAN_POINT('Ctrl Pts',(-80.0834296668131,1074.75489575047,
503.392516649627));
#112467=CARTESIAN_POINT('Ctrl Pts',(-80.1505817358878,1074.74846175269,
503.391288156812));
#112468=CARTESIAN_POINT('Ctrl Pts',(-80.2139925467697,1074.74357852497,
503.377534158872));
#112469=CARTESIAN_POINT('Ctrl Pts',(-80.3315251714612,1074.73697045175,
503.326437741991));
#112470=CARTESIAN_POINT('Ctrl Pts',(-80.3845436293575,1074.73528448238,
503.289821015878));
#112471=CARTESIAN_POINT('Ctrl Pts',(-80.4734725583864,1074.73532796221,
503.198397642156));
#112472=CARTESIAN_POINT('Ctrl Pts',(-80.5085290514065,1074.73704629545,
503.144580661257));
#112473=CARTESIAN_POINT('Ctrl Pts',(-80.5562437403426,1074.74367979716,
503.026372118594));
#112474=CARTESIAN_POINT('Ctrl Pts',(-80.5683167302978,1074.74854254875,
502.963124043407));
#112475=CARTESIAN_POINT('Ctrl Pts',(-80.5676464698705,1074.76081522022,
502.83512323168));
#112476=CARTESIAN_POINT('Ctrl Pts',(-80.5546684257742,1074.76812935686,
502.771608449677));
#112477=CARTESIAN_POINT('Ctrl Pts',(-80.5045169611936,1074.78438363024,
502.65188725358));
#112478=CARTESIAN_POINT('Ctrl Pts',(-80.4672435467254,1074.79320189596,
502.597053187483));
#112479=CARTESIAN_POINT('Ctrl Pts',(-80.3735738883454,1074.81093511663,
502.505500458746));
#112480=CARTESIAN_POINT('Ctrl Pts',(-80.318121606227,1074.81968358517,502.469576653714));
#112481=CARTESIAN_POINT('Ctrl Pts',(-80.2000500020039,1074.83544850608,
502.423073813707));
#112482=CARTESIAN_POINT('Ctrl Pts',(-80.1390813375835,1074.84240529864,
502.411464629318));
#112483=CARTESIAN_POINT('Ctrl Pts',(-80.0774663116128,1074.84832498503,
502.411462480594));
#112484=CARTESIAN_POINT('Ctrl Pts',(-80.0774606093383,1074.84832553288,
502.411462480395));
#112485=CARTESIAN_POINT('Ctrl Pts',(-80.0774549070681,1074.84832608072,
502.411462480293));
#112486=CARTESIAN_POINT('Ctrl Pts',(-80.0774492048019,1074.84832662855,
502.411462480293));
#112487=CARTESIAN_POINT('',(-80.0774492048019,1082.7251047501,502.411462480293));
#112488=CARTESIAN_POINT('',(-80.0774492048019,1067.7251047501,502.411462480293));
#112489=CARTESIAN_POINT('Origin',(-80.0774492048019,1082.7251047501,502.902003229021));
#112490=CARTESIAN_POINT('Ctrl Pts',(-80.0774492048019,1074.84832662855,
502.411462480293));
#112491=CARTESIAN_POINT('Ctrl Pts',(-80.0127825915629,1074.8545392838,502.411462480293));
#112492=CARTESIAN_POINT('Ctrl Pts',(-79.9486491232316,1074.8594902095,502.424249728139));
#112493=CARTESIAN_POINT('Ctrl Pts',(-79.8299151493609,1074.86623401415,
502.473724313552));
#112494=CARTESIAN_POINT('Ctrl Pts',(-79.7763608843544,1074.86801171817,
502.509508066976));
#112495=CARTESIAN_POINT('Ctrl Pts',(-79.686013081107,1074.86823282458,502.599566153324));
#112496=CARTESIAN_POINT('Ctrl Pts',(-79.6501060045928,1074.86668059872,
502.652887070509));
#112497=CARTESIAN_POINT('Ctrl Pts',(-79.6005542127742,1074.86041180784,
502.770495814349));
#112498=CARTESIAN_POINT('Ctrl Pts',(-79.5875240977248,1074.85574220163,
502.833649874922));
#112499=CARTESIAN_POINT('Ctrl Pts',(-79.5863199589662,1074.84372459065,
502.962872637271));
#112500=CARTESIAN_POINT('Ctrl Pts',(-79.5988104681922,1074.83643155972,
503.027665799191));
#112501=CARTESIAN_POINT('Ctrl Pts',(-79.6483757697716,1074.82025748681,
503.148603427903));
#112502=CARTESIAN_POINT('Ctrl Pts',(-79.685057162547,1074.81152653033,503.203552594586));
#112503=CARTESIAN_POINT('Ctrl Pts',(-79.777881940359,1074.79379699465,503.295948849467));
#112504=CARTESIAN_POINT('Ctrl Pts',(-79.8332183009218,1074.78496473368,
503.332462500812));
#112505=CARTESIAN_POINT('Ctrl Pts',(-79.952341812871,1074.76882355205,503.380454685222));
#112506=CARTESIAN_POINT('Ctrl Pts',(-80.0145689753705,1074.76161008594,
503.39254397775));
#112507=CARTESIAN_POINT('Ctrl Pts',(-80.077449204802,1074.75547652074,503.39254397775));
#112508=CARTESIAN_POINT('Origin',(-22.5035000139863,1067.7251047501,511.305124859599));
#112509=CARTESIAN_POINT('',(-22.5035000140048,1076.70430247523,509.826821727406));
#112510=CARTESIAN_POINT('',(-22.5035000139863,1067.7251047501,509.826821727406));
#112511=CARTESIAN_POINT('Ctrl Pts',(-22.5035327361191,1076.6298518624,512.78342799143));
#112512=CARTESIAN_POINT('Ctrl Pts',(-22.697188336794,1076.62822043967,512.783423704877));
#112513=CARTESIAN_POINT('Ctrl Pts',(-22.8889703125145,1076.62783250898,
512.745366885901));
#112514=CARTESIAN_POINT('Ctrl Pts',(-23.2464818143271,1076.62962273074,
512.597668356197));
#112515=CARTESIAN_POINT('Ctrl Pts',(-23.4088197788964,1076.63177508635,
512.489640658617));
#112516=CARTESIAN_POINT('Ctrl Pts',(-23.6826202279391,1076.63815172445,
512.217423455911));
#112517=CARTESIAN_POINT('Ctrl Pts',(-23.7914950365478,1076.6423068606,512.055904652138));
#112518=CARTESIAN_POINT('Ctrl Pts',(-23.9411046906667,1076.65176378763,
511.700044378558));
#112519=CARTESIAN_POINT('Ctrl Pts',(-23.9803420008756,1076.65696882156,
511.509089417913));
#112520=CARTESIAN_POINT('Ctrl Pts',(-23.9824739336125,1076.66484283965,
511.219425695112));
#112521=CARTESIAN_POINT('Ctrl Pts',(-23.9737183561377,1076.6674612293,511.123008031829));
#112522=CARTESIAN_POINT('Ctrl Pts',(-23.9375214641077,1076.6725935507,510.933245449221));
#112523=CARTESIAN_POINT('Ctrl Pts',(-23.9101636017548,1076.67509510596,
510.840355902925));
#112524=CARTESIAN_POINT('Ctrl Pts',(-23.8004027713136,1076.68237077316,
510.568997838307));
#112525=CARTESIAN_POINT('Ctrl Pts',(-23.6914150010189,1076.68675194435,
510.403622117564));
#112526=CARTESIAN_POINT('Ctrl Pts',(-23.4161126676759,1076.69419979021,
510.12592921612));
#112527=CARTESIAN_POINT('Ctrl Pts',(-23.2528652196348,1076.69720855228,
510.016007307325));
#112528=CARTESIAN_POINT('Ctrl Pts',(-22.8927823991851,1076.70183240506,
509.865689241871));
#112529=CARTESIAN_POINT('Ctrl Pts',(-22.6994323131464,1076.70340777433,
509.826906152296));
#112530=CARTESIAN_POINT('Ctrl Pts',(-22.3082658034494,1076.70519399336,
509.826737328439));
#112531=CARTESIAN_POINT('Ctrl Pts',(-22.1143143021181,1076.70538769376,
509.865582884672));
#112532=CARTESIAN_POINT('Ctrl Pts',(-21.7531812058628,1076.70439475941,
510.016471427184));
#112533=CARTESIAN_POINT('Ctrl Pts',(-21.5895165689669,1076.70321779961,
510.126890158071));
#112534=CARTESIAN_POINT('Ctrl Pts',(-21.3150766651475,1076.69940842177,
510.404560234275));
#112535=CARTESIAN_POINT('Ctrl Pts',(-21.2068326793722,1076.69681002284,
510.568909243009));
#112536=CARTESIAN_POINT('Ctrl Pts',(-21.0600685816595,1076.69014662445,
510.930764109334));
#112537=CARTESIAN_POINT('Ctrl Pts',(-21.0232572846915,1076.68613413807,
511.12481342175));
#112538=CARTESIAN_POINT('Ctrl Pts',(-21.0272970997305,1076.67695082874,
511.516256004342));
#112539=CARTESIAN_POINT('Ctrl Pts',(-21.0682305948924,1076.67186587121,
511.709780751801));
#112540=CARTESIAN_POINT('Ctrl Pts',(-21.2224183718107,1076.66134236978,
512.067928084707));
#112541=CARTESIAN_POINT('Ctrl Pts',(-21.3335069705477,1076.65601271149,
512.229331198209));
#112542=CARTESIAN_POINT('Ctrl Pts',(-21.6117872969745,1076.64600420641,
512.500090524125));
#112543=CARTESIAN_POINT('Ctrl Pts',(-21.7763186727178,1076.64142975664,
512.606782500528));
#112544=CARTESIAN_POINT('Ctrl Pts',(-22.1307308239509,1076.63413695962,
512.747857579243));
#112545=CARTESIAN_POINT('Ctrl Pts',(-22.3162777347941,1076.63142936424,
512.783432136306));
#112546=CARTESIAN_POINT('Ctrl Pts',(-22.5035327361191,1076.6298518624,512.78342799143));
#112547=CARTESIAN_POINT('Origin',(-22.5035000139863,1067.7251047501,511.305124859599));
#112548=CARTESIAN_POINT('',(-22.5035000139863,1076.64871264505,512.183427991792));
#112549=CARTESIAN_POINT('',(-22.5035000139663,1076.69297254634,510.426821727406));
#112550=CARTESIAN_POINT('Ctrl Pts',(-22.5035000139863,1076.64871264505,
512.183427991792));
#112551=CARTESIAN_POINT('Ctrl Pts',(-22.6136921936282,1076.64786711526,
512.183427991792));
#112552=CARTESIAN_POINT('Ctrl Pts',(-22.7229531368515,1076.64763898538,
512.162690172106));
#112553=CARTESIAN_POINT('Ctrl Pts',(-22.9324051162973,1076.64847486863,
512.080139744173));
#112554=CARTESIAN_POINT('Ctrl Pts',(-23.0299618966429,1076.64958430376,
512.017475159969));
#112555=CARTESIAN_POINT('Ctrl Pts',(-23.195370245027,1076.65297330517,511.858212204119));
#112556=CARTESIAN_POINT('Ctrl Pts',(-23.2616434659143,1076.65521736704,
511.763169348596));
#112557=CARTESIAN_POINT('Ctrl Pts',(-23.3539103754164,1076.66043671566,
511.552927523711));
#112558=CARTESIAN_POINT('Ctrl Pts',(-23.3789889237328,1076.66335970471,
511.439738840843));
#112559=CARTESIAN_POINT('Ctrl Pts',(-23.3828746159423,1076.66789018712,
511.267554586315));
#112560=CARTESIAN_POINT('Ctrl Pts',(-23.3785409393564,1076.66941398011,
511.210179675387));
#112561=CARTESIAN_POINT('Ctrl Pts',(-23.3587389585038,1076.67244001584,
511.09708961534));
#112562=CARTESIAN_POINT('Ctrl Pts',(-23.3433162721398,1076.67393497921,
511.041645943522));
#112563=CARTESIAN_POINT('Ctrl Pts',(-23.2803642688379,1076.67835615271,
510.878995148548));
#112564=CARTESIAN_POINT('Ctrl Pts',(-23.216753876109,1076.6811106595,510.779409748454));
#112565=CARTESIAN_POINT('Ctrl Pts',(-23.0546047170834,1076.68593465301,
510.611387941601));
#112566=CARTESIAN_POINT('Ctrl Pts',(-22.9578292528528,1076.68796173538,
510.54448344382));
#112567=CARTESIAN_POINT('Ctrl Pts',(-22.7437560177297,1076.6911466657,510.452317512047));
#112568=CARTESIAN_POINT('Ctrl Pts',(-22.6285772038153,1076.69227539346,
510.427992582682));
#112569=CARTESIAN_POINT('Ctrl Pts',(-22.5091734568623,1076.69294175239,
510.426835467202));
#112570=CARTESIAN_POINT('Ctrl Pts',(-22.5063364099955,1076.69295729554,
510.426821727405));
#112571=CARTESIAN_POINT('Ctrl Pts',(-22.5035000139464,1076.69297254634,
510.426821727406));
#112572=CARTESIAN_POINT('',(-22.5035000139863,1082.7251047501,510.426821727406));
#112573=CARTESIAN_POINT('',(-22.5035000139863,1067.7251047501,510.426821727406));
#112574=CARTESIAN_POINT('Origin',(-22.5035000139863,1082.7251047501,511.305124859599));
#112575=CARTESIAN_POINT('Ctrl Pts',(-22.5035000139464,1076.69297254634,
510.426821727406));
#112576=CARTESIAN_POINT('Ctrl Pts',(-22.389645575796,1076.69358472169,510.426821727411));
#112577=CARTESIAN_POINT('Ctrl Pts',(-22.2768397969015,1076.69372982667,
510.448960806448));
#112578=CARTESIAN_POINT('Ctrl Pts',(-22.0634032383318,1076.69307529407,
510.536140253258));
#112579=CARTESIAN_POINT('Ctrl Pts',(-21.9652822146936,1076.69225884732,
510.601319054443));
#112580=CARTESIAN_POINT('Ctrl Pts',(-21.8003577505346,1076.68967204169,
510.766074764882));
#112581=CARTESIAN_POINT('Ctrl Pts',(-21.735149768211,1076.68792596669,510.863968325622));
#112582=CARTESIAN_POINT('Ctrl Pts',(-21.6493793336339,1076.68373279841,
511.073003965486));
#112583=CARTESIAN_POINT('Ctrl Pts',(-21.6271245598466,1076.68136863704,
511.181166429725));
#112584=CARTESIAN_POINT('Ctrl Pts',(-21.6253166699448,1076.6787531034,511.290619472025));
#112585=CARTESIAN_POINT('Ctrl Pts',(-21.6243587796215,1076.67736729205,
511.348611947101));
#112586=CARTESIAN_POINT('Ctrl Pts',(-21.6291477183368,1076.67592112488,
511.406555672307));
#112587=CARTESIAN_POINT('Ctrl Pts',(-21.6499798988723,1076.67295937525,
511.520115905184));
#112588=CARTESIAN_POINT('Ctrl Pts',(-21.6658677631083,1076.6714516809,511.57547613968));
#112589=CARTESIAN_POINT('Ctrl Pts',(-21.729513563702,1076.66688656265,511.735976408328));
#112590=CARTESIAN_POINT('Ctrl Pts',(-21.7926384809357,1076.66383645352,
511.833674838728));
#112591=CARTESIAN_POINT('Ctrl Pts',(-21.9530348133738,1076.65814954945,
511.999162481131));
#112592=CARTESIAN_POINT('Ctrl Pts',(-22.048766413592,1076.65557036805,512.065336018375));
#112593=CARTESIAN_POINT('Ctrl Pts',(-22.2602774764295,1076.65135643461,
512.156907125427));
#112594=CARTESIAN_POINT('Ctrl Pts',(-22.3739937884222,1076.64976462194,
512.181436332894));
#112595=CARTESIAN_POINT('Ctrl Pts',(-22.4939718080278,1076.64878689139,
512.183389243752));
#112596=CARTESIAN_POINT('Ctrl Pts',(-22.4987367810559,1076.64874919442,
512.183427991792));
#112597=CARTESIAN_POINT('Ctrl Pts',(-22.5035000139863,1076.64871264505,
512.183427991792));
#112598=CARTESIAN_POINT('Origin',(-34.5096048204688,1067.7251047501,514.987993850267));
#112599=CARTESIAN_POINT('',(-34.5096048204686,1076.41851054042,513.712549729131));
#112600=CARTESIAN_POINT('',(-34.5096048204688,1067.7251047501,513.712549729131));
#112601=CARTESIAN_POINT('Ctrl Pts',(-34.510210550676,1076.26444406336,516.263437827568));
#112602=CARTESIAN_POINT('Ctrl Pts',(-34.6770761418107,1076.26029120131,
516.263358580238));
#112603=CARTESIAN_POINT('Ctrl Pts',(-34.8423390931997,1076.25829883923,
516.230534091237));
#112604=CARTESIAN_POINT('Ctrl Pts',(-35.1505137202821,1076.25893043407,
516.103217369855));
#112605=CARTESIAN_POINT('Ctrl Pts',(-35.2904555944617,1076.26153711202,
516.010118411505));
#112606=CARTESIAN_POINT('Ctrl Pts',(-35.5266628802956,1076.27094966102,
515.775442346978));
#112607=CARTESIAN_POINT('Ctrl Pts',(-35.6206174798617,1076.27766188471,
515.636136749945));
#112608=CARTESIAN_POINT('Ctrl Pts',(-35.7498704340647,1076.29416258726,
515.329053401729));
#112609=CARTESIAN_POINT('Ctrl Pts',(-35.7837744926969,1076.30379557645,
515.164160424993));
#112610=CARTESIAN_POINT('Ctrl Pts',(-35.7862560111193,1076.32454585444,
514.830372499115));
#112611=CARTESIAN_POINT('Ctrl Pts',(-35.7546458658456,1076.33546533049,
514.664655541728));
#112612=CARTESIAN_POINT('Ctrl Pts',(-35.6284501149868,1076.3571975243,514.352646635918));
#112613=CARTESIAN_POINT('Ctrl Pts',(-35.534206291959,1076.36779288197,514.209727796389));
#112614=CARTESIAN_POINT('Ctrl Pts',(-35.2960069591467,1076.38707298587,
513.9697917652));
#112615=CARTESIAN_POINT('Ctrl Pts',(-35.1546820135756,1076.39558365587,
513.874853901345));
#112616=CARTESIAN_POINT('Ctrl Pts',(-34.8429315588452,1076.40962934384,
513.745341652921));
#112617=CARTESIAN_POINT('Ctrl Pts',(-34.6755586727011,1076.41502554586,
513.712146813909));
#112618=CARTESIAN_POINT('Ctrl Pts',(-34.3368750129064,1076.4221382511,513.712961563743));
#112619=CARTESIAN_POINT('Ctrl Pts',(-34.1689685251534,1076.42377274472,
513.74721915866));
#112620=CARTESIAN_POINT('Ctrl Pts',(-33.8564683098246,1076.42306559179,
513.879418325012));
#112621=CARTESIAN_POINT('Ctrl Pts',(-33.7150198072083,1076.42073260849,
513.975993466824));
#112622=CARTESIAN_POINT('Ctrl Pts',(-33.4786776417656,1076.412295967,514.218271328925));
#112623=CARTESIAN_POINT('Ctrl Pts',(-33.3859622956867,1076.40628728116,
514.361357255944));
#112624=CARTESIAN_POINT('Ctrl Pts',(-33.2616665770459,1076.39116443452,
514.675143622838));
#112625=CARTESIAN_POINT('Ctrl Pts',(-33.2312922293419,1076.38219590285,
514.842728733327));
#112626=CARTESIAN_POINT('Ctrl Pts',(-33.2358846722379,1076.36736587868,
515.093961251048));
#112627=CARTESIAN_POINT('Ctrl Pts',(-33.2454281379424,1076.36228606157,
515.176265123999));
#112628=CARTESIAN_POINT('Ctrl Pts',(-33.2803741619054,1076.35183445363,
515.338193358098));
#112629=CARTESIAN_POINT('Ctrl Pts',(-33.3057626507355,1076.34648603911,
515.417423922129));
#112630=CARTESIAN_POINT('Ctrl Pts',(-33.4057693169067,1076.33011967124,
515.649021362422));
#112631=CARTESIAN_POINT('Ctrl Pts',(-33.5031513467196,1076.31914258526,
515.789539701725));
#112632=CARTESIAN_POINT('Ctrl Pts',(-33.7458423042442,1076.29869782582,
516.023121450383));
#112633=CARTESIAN_POINT('Ctrl Pts',(-33.8883025592264,1076.28941582096,
516.114425004076));
#112634=CARTESIAN_POINT('Ctrl Pts',(-34.1927603496154,1076.27427812612,
516.233688459787));
#112635=CARTESIAN_POINT('Ctrl Pts',(-34.350758296486,1076.26841242621,516.263513554176));
#112636=CARTESIAN_POINT('Ctrl Pts',(-34.510210550676,1076.26444406336,516.263437827568));
#112637=CARTESIAN_POINT('Origin',(-34.5096048204688,1067.7251047501,514.987993850267));
#112638=CARTESIAN_POINT('',(-34.5096048204688,1076.30335139737,515.663437971403));
#112639=CARTESIAN_POINT('',(-34.5096048204687,1076.38494400861,514.312549729131));
#112640=CARTESIAN_POINT('Ctrl Pts',(-34.5096048204688,1076.30335139737,
515.663437971403));
#112641=CARTESIAN_POINT('Ctrl Pts',(-34.5147607200677,1076.3032273638,515.663437971403));
#112642=CARTESIAN_POINT('Ctrl Pts',(-34.5199192890106,1076.30310696305,
515.663378936453));
#112643=CARTESIAN_POINT('Ctrl Pts',(-34.6133832608504,1076.30099273748,
515.66123707454));
#112644=CARTESIAN_POINT('Ctrl Pts',(-34.700448866802,1076.30011145474,515.641911819858));
#112645=CARTESIAN_POINT('Ctrl Pts',(-34.8621113822095,1076.30069909558,
515.57087383221));
#112646=CARTESIAN_POINT('Ctrl Pts',(-34.9351405015941,1076.30215908264,
515.519899188168));
#112647=CARTESIAN_POINT('Ctrl Pts',(-35.0575110263185,1076.30721945871,
515.392736761286));
#112648=CARTESIAN_POINT('Ctrl Pts',(-35.1056388675218,1076.31077147118,
515.317765781211));
#112649=CARTESIAN_POINT('Ctrl Pts',(-35.170418690475,1076.31946619841,515.153431373832));
#112650=CARTESIAN_POINT('Ctrl Pts',(-35.1863680819962,1076.32452759051,
515.065619221493));
#112651=CARTESIAN_POINT('Ctrl Pts',(-35.1842608595915,1076.3327125846,514.933044487346));
#112652=CARTESIAN_POINT('Ctrl Pts',(-35.1792178233148,1076.33552155445,
514.889009034933));
#112653=CARTESIAN_POINT('Ctrl Pts',(-35.160605440651,1076.34121170766,514.802586854367));
#112654=CARTESIAN_POINT('Ctrl Pts',(-35.1470845835084,1076.34407935344,
514.760404110216));
#112655=CARTESIAN_POINT('Ctrl Pts',(-35.0938308440773,1076.35272825597,
514.637285988837));
#112656=CARTESIAN_POINT('Ctrl Pts',(-35.0419779334543,1076.3583648964,514.562668436976));
#112657=CARTESIAN_POINT('Ctrl Pts',(-34.9122336573852,1076.36866166981,
514.438295951173));
#112658=CARTESIAN_POINT('Ctrl Pts',(-34.8356972543447,1076.37322379078,
514.389701805251));
#112659=CARTESIAN_POINT('Ctrl Pts',(-34.6746757044643,1076.38041569092,
514.327831209519));
#112660=CARTESIAN_POINT('Ctrl Pts',(-34.5926654537101,1076.38310991803,
514.312588592663));
#112661=CARTESIAN_POINT('Ctrl Pts',(-34.509921460243,1076.38493702107,514.312549803324));
#112662=CARTESIAN_POINT('Ctrl Pts',(-34.5098159124342,1076.38493935172,
514.312549753845));
#112663=CARTESIAN_POINT('Ctrl Pts',(-34.5097103658399,1076.38494168089,
514.312549729131));
#112664=CARTESIAN_POINT('Ctrl Pts',(-34.5096048204686,1076.38494400861,
514.312549729131));
#112665=CARTESIAN_POINT('',(-34.5096048204688,1082.7251047501,514.312549729131));
#112666=CARTESIAN_POINT('',(-34.5096048204688,1067.7251047501,514.312549729131));
#112667=CARTESIAN_POINT('Origin',(-34.5096048204688,1082.7251047501,514.987993850267));
#112668=CARTESIAN_POINT('Ctrl Pts',(-34.5096048204686,1076.38494400861,
514.312549729131));
#112669=CARTESIAN_POINT('Ctrl Pts',(-34.4195797209484,1076.38692943473,
514.312549729131));
#112670=CARTESIAN_POINT('Ctrl Pts',(-34.3304444186114,1076.38785074114,
514.330548069844));
#112671=CARTESIAN_POINT('Ctrl Pts',(-34.1643896087766,1076.38747560109,
514.400478078721));
#112672=CARTESIAN_POINT('Ctrl Pts',(-34.0891738841783,1076.38618084193,
514.451728079472));
#112673=CARTESIAN_POINT('Ctrl Pts',(-33.963441665068,1076.38150815206,514.580546241006));
#112674=CARTESIAN_POINT('Ctrl Pts',(-33.9141407280796,1076.37818083265,
514.656755276528));
#112675=CARTESIAN_POINT('Ctrl Pts',(-33.848269512731,1076.36987453135,514.823899897506));
#112676=CARTESIAN_POINT('Ctrl Pts',(-33.832345532267,1076.36497759429,514.913161534974));
#112677=CARTESIAN_POINT('Ctrl Pts',(-33.8352940715305,1076.35696281089,
515.046819095554));
#112678=CARTESIAN_POINT('Ctrl Pts',(-33.8405471527631,1076.35423184587,
515.090543327369));
#112679=CARTESIAN_POINT('Ctrl Pts',(-33.8594872938482,1076.34864452046,
515.176435539951));
#112680=CARTESIAN_POINT('Ctrl Pts',(-33.8731482725201,1076.3458010522,515.218397487686));
#112681=CARTESIAN_POINT('Ctrl Pts',(-33.9267185940827,1076.33714899981,
515.340841430359));
#112682=CARTESIAN_POINT('Ctrl Pts',(-33.9786358918692,1076.33140337561,
515.415000511813));
#112683=CARTESIAN_POINT('Ctrl Pts',(-34.1076721876445,1076.32078808864,
515.538020849947));
#112684=CARTESIAN_POINT('Ctrl Pts',(-34.1832562655626,1076.31601221174,
515.585980243906));
#112685=CARTESIAN_POINT('Ctrl Pts',(-34.3437014148138,1076.30830828351,
515.648028036408));
#112686=CARTESIAN_POINT('Ctrl Pts',(-34.4263047253469,1076.30535531691,
515.663437971403));
#112687=CARTESIAN_POINT('Ctrl Pts',(-34.5096048204688,1076.30335139737,
515.663437971403));
#112688=CARTESIAN_POINT('Origin',(-48.0649554680751,1067.7251047501,517.828896105943));
#112689=CARTESIAN_POINT('',(-48.064955468075,1075.7548763624,516.73006496995));
#112690=CARTESIAN_POINT('',(-48.0649554680751,1067.7251047501,516.73006496995));
#112691=CARTESIAN_POINT('Ctrl Pts',(-48.0649893420775,1075.55153228081,
518.927727241413));
#112692=CARTESIAN_POINT('Ctrl Pts',(-48.2084938936629,1075.54445758504,
518.927722817555));
#112693=CARTESIAN_POINT('Ctrl Pts',(-48.3506973821094,1075.54011567547,
518.899606749943));
#112694=CARTESIAN_POINT('Ctrl Pts',(-48.6158197749301,1075.53747767521,
518.79037881918));
#112695=CARTESIAN_POINT('Ctrl Pts',(-48.7361648149422,1075.5391837126,518.710576143554));
#112696=CARTESIAN_POINT('Ctrl Pts',(-48.9395756994896,1075.54841917822,
518.509307741398));
#112697=CARTESIAN_POINT('Ctrl Pts',(-49.0205871483468,1075.55586065419,
518.389803671339));
#112698=CARTESIAN_POINT('Ctrl Pts',(-49.1325649150761,1075.5754767029,518.126018496399));
#112699=CARTESIAN_POINT('Ctrl Pts',(-49.1621703363378,1075.58748310855,
517.984173555892));
#112700=CARTESIAN_POINT('Ctrl Pts',(-49.1652837174281,1075.61442205228,
517.69652035456));
#112701=CARTESIAN_POINT('Ctrl Pts',(-49.1384171214939,1075.62911403942,
517.553423285889));
#112702=CARTESIAN_POINT('Ctrl Pts',(-49.0579586152795,1075.65158960913,
517.352929660374));
#112703=CARTESIAN_POINT('Ctrl Pts',(-49.0246954806973,1075.65909376488,
517.28898935585));
#112704=CARTESIAN_POINT('Ctrl Pts',(-48.9057044795966,1075.68157591868,
517.106486232892));
#112705=CARTESIAN_POINT('Ctrl Pts',(-48.8023667811879,1075.69607284841,
517.001241563726));
#112706=CARTESIAN_POINT('Ctrl Pts',(-48.5609641233725,1075.72224327897,
516.837651228932));
#112707=CARTESIAN_POINT('Ctrl Pts',(-48.4254097032791,1075.73367717674,
516.780685382225));
#112708=CARTESIAN_POINT('Ctrl Pts',(-48.1395762712534,1075.75208870326,
516.72294128722));
#112709=CARTESIAN_POINT('Ctrl Pts',(-47.9921652529731,1075.75888045524,
516.722789674877));
#112710=CARTESIAN_POINT('Ctrl Pts',(-47.7069256019333,1075.76688907848,
516.779981637933));
#112711=CARTESIAN_POINT('Ctrl Pts',(-47.5719153765225,1075.76807339262,
516.836257764457));
#112712=CARTESIAN_POINT('Ctrl Pts',(-47.3326842943825,1075.76473349722,
516.997162265414));
#112713=CARTESIAN_POINT('Ctrl Pts',(-47.2305532509364,1075.76029878756,
517.099697161617));
#112714=CARTESIAN_POINT('Ctrl Pts',(-47.0700490322263,1075.74619951358,
517.340164075618));
#112715=CARTESIAN_POINT('Ctrl Pts',(-47.0141195650448,1075.73658401839,
517.476247390196));
#112716=CARTESIAN_POINT('Ctrl Pts',(-46.9584863513016,1075.71333331429,
517.762313849099));
#112717=CARTESIAN_POINT('Ctrl Pts',(-46.9594505166007,1075.69991724618,
517.909490060293));
#112718=CARTESIAN_POINT('Ctrl Pts',(-47.0035391842712,1075.67836579534,
518.122033215604));
#112719=CARTESIAN_POINT('Ctrl Pts',(-47.0248343869156,1075.67107227863,
518.190389843968));
#112720=CARTESIAN_POINT('Ctrl Pts',(-47.0804823842841,1075.65625767349,
518.322234520378));
#112721=CARTESIAN_POINT('Ctrl Pts',(-47.1147586064389,1075.64876984785,
518.385399115621));
#112722=CARTESIAN_POINT('Ctrl Pts',(-47.2368435396587,1075.62614696949,
518.565790955365));
#112723=CARTESIAN_POINT('Ctrl Pts',(-47.3421142764355,1075.61135807081,
518.669330549812));
#112724=CARTESIAN_POINT('Ctrl Pts',(-47.5856008105526,1075.58455096299,
518.828148616589));
#112725=CARTESIAN_POINT('Ctrl Pts',(-47.7210591086514,1075.57275791273,
518.88251120031));
#112726=CARTESIAN_POINT('Ctrl Pts',(-47.9297854064988,1075.55879087764,
518.921476688485));
#112727=CARTESIAN_POINT('Ctrl Pts',(-47.9972990103319,1075.55486937707,
518.927729328124));
#112728=CARTESIAN_POINT('Ctrl Pts',(-48.0649893420775,1075.55153228081,
518.927727241413));
#112729=CARTESIAN_POINT('Origin',(-48.0649554680751,1067.7251047501,517.828896105943));
#112730=CARTESIAN_POINT('',(-48.0649554680751,1075.60888786087,518.327727241935));
#112731=CARTESIAN_POINT('',(-48.0649554680755,1075.70120171291,517.33006496995));
#112732=CARTESIAN_POINT('Ctrl Pts',(-48.0649554680751,1075.60888786087,
518.327727241935));
#112733=CARTESIAN_POINT('Ctrl Pts',(-48.0992071391453,1075.60722863437,
518.327727241935));
#112734=CARTESIAN_POINT('Ctrl Pts',(-48.1334637973026,1075.60589929547,
518.324199567418));
#112735=CARTESIAN_POINT('Ctrl Pts',(-48.2308120936188,1075.60309465836,
518.303818200272));
#112736=CARTESIAN_POINT('Ctrl Pts',(-48.2912423276458,1075.60257430731,
518.278180242568));
#112737=CARTESIAN_POINT('Ctrl Pts',(-48.3988286987254,1075.60422377285,
518.205172799759));
#112738=CARTESIAN_POINT('Ctrl Pts',(-48.4449216152782,1075.60637486178,
518.158549147097));
#112739=CARTESIAN_POINT('Ctrl Pts',(-48.5167682161754,1075.61307782021,
518.050127754965));
#112740=CARTESIAN_POINT('Ctrl Pts',(-48.5417351328201,1075.61757231021,
517.989341218083));
#112741=CARTESIAN_POINT('Ctrl Pts',(-48.5670113254588,1075.6283229294,517.861353012332));
#112742=CARTESIAN_POINT('Ctrl Pts',(-48.5669260928725,1075.63448554066,
517.795346963405));
#112743=CARTESIAN_POINT('Ctrl Pts',(-48.547749762996,1075.64433990826,517.699244525297));
#112744=CARTESIAN_POINT('Ctrl Pts',(-48.5382257162028,1075.64770385252,
517.667916543383));
#112745=CARTESIAN_POINT('Ctrl Pts',(-48.5132180523867,1075.65448488088,
517.607635886622));
#112746=CARTESIAN_POINT('Ctrl Pts',(-48.4978024745126,1075.65788623618,
517.578818041224));
#112747=CARTESIAN_POINT('Ctrl Pts',(-48.4427527368316,1075.66811484334,
517.496451774604));
#112748=CARTESIAN_POINT('Ctrl Pts',(-48.3951237054828,1075.67473242701,
517.449093957106));
#112749=CARTESIAN_POINT('Ctrl Pts',(-48.2841578640708,1075.68669618333,
517.375918605308));
#112750=CARTESIAN_POINT('Ctrl Pts',(-48.2219505162228,1075.69192852252,
517.350766227478));
#112751=CARTESIAN_POINT('Ctrl Pts',(-48.1263765506259,1075.69805613701,
517.332908445803));
#112752=CARTESIAN_POINT('Ctrl Pts',(-48.0957077644681,1075.69975700063,
517.330065222216));
#112753=CARTESIAN_POINT('Ctrl Pts',(-48.0649595603431,1075.70120152066,
517.330064969967));
#112754=CARTESIAN_POINT('',(-48.0649554680751,1082.7251047501,517.33006496995));
#112755=CARTESIAN_POINT('',(-48.0649554680751,1067.7251047501,517.33006496995));
#112756=CARTESIAN_POINT('Origin',(-48.0649554680751,1082.7251047501,517.828896105943));
#112757=CARTESIAN_POINT('Ctrl Pts',(-48.0649554680764,1075.70120171291,
517.33006496995));
#112758=CARTESIAN_POINT('Ctrl Pts',(-47.9999044611301,1075.70425769564,
517.33006496995));
#112759=CARTESIAN_POINT('Ctrl Pts',(-47.9354476847099,1075.70612243468,
517.342788618147));
#112760=CARTESIAN_POINT('Ctrl Pts',(-47.8151009740486,1075.70726495575,
517.392282464125));
#112761=CARTESIAN_POINT('Ctrl Pts',(-47.760399983833,1075.70653554622,517.428519769089));
#112762=CARTESIAN_POINT('Ctrl Pts',(-47.6678714445977,1075.70255080872,
517.520024927186));
#112763=CARTESIAN_POINT('Ctrl Pts',(-47.6310077010242,1075.69932836894,
517.574430432736));
#112764=CARTESIAN_POINT('Ctrl Pts',(-47.5796961761757,1075.69068537271,
517.695559617548));
#112765=CARTESIAN_POINT('Ctrl Pts',(-47.5662879622311,1075.68530429028,
517.761303506675));
#112766=CARTESIAN_POINT('Ctrl Pts',(-47.5659632347747,1075.67311728063,
517.89423329901));
#112767=CARTESIAN_POINT('Ctrl Pts',(-47.5791216868771,1075.66642707446,
517.960113186052));
#112768=CARTESIAN_POINT('Ctrl Pts',(-47.6173529427976,1075.65616205148,
518.051482856452));
#112769=CARTESIAN_POINT('Ctrl Pts',(-47.6328336540704,1075.65276309956,
518.08021984393));
#112770=CARTESIAN_POINT('Ctrl Pts',(-47.6882984438738,1075.64246312669,
518.162706048491));
#112771=CARTESIAN_POINT('Ctrl Pts',(-47.7363836679969,1075.63574105283,
518.210144475302));
#112772=CARTESIAN_POINT('Ctrl Pts',(-47.8472836194192,1075.62365372496,
518.282482986071));
#112773=CARTESIAN_POINT('Ctrl Pts',(-47.9087082971881,1075.61837852881,
518.307148991997));
#112774=CARTESIAN_POINT('Ctrl Pts',(-48.0035260426066,1075.61212913645,
518.324890046688));
#112775=CARTESIAN_POINT('Ctrl Pts',(-48.0342387500439,1075.61037584645,
518.327727241935));
#112776=CARTESIAN_POINT('Ctrl Pts',(-48.0649554680751,1075.60888786087,
518.327727241935));
#112777=CARTESIAN_POINT('Origin',(-62.0518715958007,1067.7251047501,517.840396800599));
#112778=CARTESIAN_POINT('',(-62.0518715958006,1074.92317040789,516.749856051871));
#112779=CARTESIAN_POINT('',(-62.0518715958007,1067.7251047501,516.749856051871));
#112780=CARTESIAN_POINT('Ctrl Pts',(-62.0518921470758,1074.67736430787,
518.930937549134));
#112781=CARTESIAN_POINT('Ctrl Pts',(-62.1942603310177,1074.6664724145,518.930934866201));
#112782=CARTESIAN_POINT('Ctrl Pts',(-62.3354342418161,1074.6588514615,518.903053580556));
#112783=CARTESIAN_POINT('Ctrl Pts',(-62.5982952366624,1074.65116544269,
518.794728005698));
#112784=CARTESIAN_POINT('Ctrl Pts',(-62.7174536596923,1074.65112062037,
518.715798377873));
#112785=CARTESIAN_POINT('Ctrl Pts',(-62.9188964488192,1074.65860121385,
518.516843327924));
#112786=CARTESIAN_POINT('Ctrl Pts',(-62.9991504226547,1074.66604642403,
518.398857898355));
#112787=CARTESIAN_POINT('Ctrl Pts',(-63.1105553117035,1074.68748139238,
518.138225299841));
#112788=CARTESIAN_POINT('Ctrl Pts',(-63.1402390812243,1074.70130458149,
517.997983712585));
#112789=CARTESIAN_POINT('Ctrl Pts',(-63.144377361419,1074.73354656551,517.712985785065));
#112790=CARTESIAN_POINT('Ctrl Pts',(-63.1182120614598,1074.75170339004,
517.570905749583));
#112791=CARTESIAN_POINT('Ctrl Pts',(-63.0390351988826,1074.78026899616,
517.37143452765));
#112792=CARTESIAN_POINT('Ctrl Pts',(-63.0060882392591,1074.7899634778,517.307588148536));
#112793=CARTESIAN_POINT('Ctrl Pts',(-62.9283002311598,1074.80933903494,
517.187518129765));
#112794=CARTESIAN_POINT('Ctrl Pts',(-62.8836767151113,1074.81897657058,
517.131537294117));
#112795=CARTESIAN_POINT('Ctrl Pts',(-62.7328609165993,1074.84765366419,
516.976368806949));
#112796=CARTESIAN_POINT('Ctrl Pts',(-62.6119908311008,1074.8658884934,516.893476149168));
#112797=CARTESIAN_POINT('Ctrl Pts',(-62.3453452480775,1074.89822042974,
516.780205972353));
#112798=CARTESIAN_POINT('Ctrl Pts',(-62.2023159366344,1074.91203054126,
516.750609636004));
#112799=CARTESIAN_POINT('Ctrl Pts',(-61.9128168598515,1074.93346996096,
516.749132190848));
#112800=CARTESIAN_POINT('Ctrl Pts',(-61.7693157896017,1074.94089276304,
516.777169066897));
#112801=CARTESIAN_POINT('Ctrl Pts',(-61.5044467524128,1074.94824448377,
516.886631823903));
#112802=CARTESIAN_POINT('Ctrl Pts',(-61.3853260643093,1074.94826687542,
516.965720359438));
#112803=CARTESIAN_POINT('Ctrl Pts',(-61.183773745132,1074.94107926119,517.165238963778));
#112804=CARTESIAN_POINT('Ctrl Pts',(-61.1034687898453,1074.93392550071,
517.283733177875));
#112805=CARTESIAN_POINT('Ctrl Pts',(-60.9914678374334,1074.91304234065,
517.547458667016));
#112806=CARTESIAN_POINT('Ctrl Pts',(-60.96206910612,1074.89937940805,517.690526211221));
#112807=CARTESIAN_POINT('Ctrl Pts',(-60.9606156081248,1074.86728232888,
517.980207661109));
#112808=CARTESIAN_POINT('Ctrl Pts',(-60.9889230114392,1074.84913335557,
518.123987149514));
#112809=CARTESIAN_POINT('Ctrl Pts',(-61.0716553509557,1074.82055740719,
518.323638730849));
#112810=CARTESIAN_POINT('Ctrl Pts',(-61.105274860867,1074.8109653838,518.386562580986));
#112811=CARTESIAN_POINT('Ctrl Pts',(-61.2261573621606,1074.7814783898,518.567700229877));
#112812=CARTESIAN_POINT('Ctrl Pts',(-61.3313523951008,1074.7617213709,518.672068189386));
#112813=CARTESIAN_POINT('Ctrl Pts',(-61.5743947133541,1074.72519418999,
518.83134188934));
#112814=CARTESIAN_POINT('Ctrl Pts',(-61.7092633476778,1074.70871466609,
518.885721882607));
#112815=CARTESIAN_POINT('Ctrl Pts',(-61.9172146951714,1074.68838082161,
518.924684432473));
#112816=CARTESIAN_POINT('Ctrl Pts',(-61.984452321395,1074.68252379905,518.930938820039));
#112817=CARTESIAN_POINT('Ctrl Pts',(-62.0518921470758,1074.67736430787,
518.930937549134));
#112818=CARTESIAN_POINT('Origin',(-62.0518715958007,1067.7251047501,517.840396800599));
#112819=CARTESIAN_POINT('',(-62.0518715958007,1074.74654397689,518.330937549327));
#112820=CARTESIAN_POINT('',(-62.0518715957997,1074.85711166046,517.34985605187));
#112821=CARTESIAN_POINT('Ctrl Pts',(-62.0518715958007,1074.74654397689,
518.330937549327));
#112822=CARTESIAN_POINT('Ctrl Pts',(-62.0866933977911,1074.7439081959,518.330937549327));
#112823=CARTESIAN_POINT('Ctrl Pts',(-62.1215275249672,1074.74169147073,
518.327229946954));
#112824=CARTESIAN_POINT('Ctrl Pts',(-62.2181304218292,1074.73675502954,
518.306292312785));
#112825=CARTESIAN_POINT('Ctrl Pts',(-62.277288270712,1074.73517998283,518.280734905449));
#112826=CARTESIAN_POINT('Ctrl Pts',(-62.3823615920401,1074.73544743233,
518.208445189124));
#112827=CARTESIAN_POINT('Ctrl Pts',(-62.4272491252186,1074.73727582866,
518.162520707078));
#112828=CARTESIAN_POINT('Ctrl Pts',(-62.4971238766243,1074.7441125856,518.055941661903));
#112829=CARTESIAN_POINT('Ctrl Pts',(-62.5213179376707,1074.74906609204,
517.996293967899));
#112830=CARTESIAN_POINT('Ctrl Pts',(-62.5456795632218,1074.76148918912,
517.870678112267));
#112831=CARTESIAN_POINT('Ctrl Pts',(-62.545375877548,1074.76886150459,517.805874706433));
#112832=CARTESIAN_POINT('Ctrl Pts',(-62.5195854725174,1074.7852194219,517.678491490727));
#112833=CARTESIAN_POINT('Ctrl Pts',(-62.4936505331052,1074.79408514107,
517.617258120011));
#112834=CARTESIAN_POINT('Ctrl Pts',(-62.4193661503622,1074.81186524658,
517.508920862243));
#112835=CARTESIAN_POINT('Ctrl Pts',(-62.3717968856127,1074.82061190484,
517.462787413382));
#112836=CARTESIAN_POINT('Ctrl Pts',(-62.2615240094876,1074.83677645864,
517.392131814308));
#112837=CARTESIAN_POINT('Ctrl Pts',(-62.1999590077581,1074.84404634731,
517.368175631442));
#112838=CARTESIAN_POINT('Ctrl Pts',(-62.1078295525999,1074.85268291733,
517.352255748845));
#112839=CARTESIAN_POINT('Ctrl Pts',(-62.0798907785677,1074.8550288411,517.34985605187));
#112840=CARTESIAN_POINT('Ctrl Pts',(-62.0518715957983,1074.85711166046,
517.34985605187));
#112841=CARTESIAN_POINT('',(-62.0518715958007,1082.7251047501,517.349856051871));
#112842=CARTESIAN_POINT('',(-62.0518715958007,1067.7251047501,517.349856051871));
#112843=CARTESIAN_POINT('Origin',(-62.0518715958007,1082.7251047501,517.840396800599));
#112844=CARTESIAN_POINT('Ctrl Pts',(-62.0518636614512,1074.85711225026,
517.349856051935));
#112845=CARTESIAN_POINT('Ctrl Pts',(-61.9873582813733,1074.86190717157,
517.34985709529));
#112846=CARTESIAN_POINT('Ctrl Pts',(-61.9234066217985,1074.86523466756,
517.362581724588));
#112847=CARTESIAN_POINT('Ctrl Pts',(-61.8048657531118,1074.86854214945,
517.411821523904));
#112848=CARTESIAN_POINT('Ctrl Pts',(-61.7513535549066,1074.8685370349,517.447487760785));
#112849=CARTESIAN_POINT('Ctrl Pts',(-61.6608927591218,1074.86523161019,
517.537351112991));
#112850=CARTESIAN_POINT('Ctrl Pts',(-61.624887274215,1074.8619598069,517.590663062806));
#112851=CARTESIAN_POINT('Ctrl Pts',(-61.574577695082,1074.85241793378,517.70959785811));
#112852=CARTESIAN_POINT('Ctrl Pts',(-61.561443420754,1074.84616349522,517.774295153346));
#112853=CARTESIAN_POINT('Ctrl Pts',(-61.5612191536718,1074.83152276947,
517.905144090354));
#112854=CARTESIAN_POINT('Ctrl Pts',(-61.5742603948211,1074.82327037349,
517.970007685616));
#112855=CARTESIAN_POINT('Ctrl Pts',(-61.6120158739641,1074.81033229964,
518.059910237568));
#112856=CARTESIAN_POINT('Ctrl Pts',(-61.6273052580951,1074.80600235113,
518.08819086711));
#112857=CARTESIAN_POINT('Ctrl Pts',(-61.6820460903651,1074.79275149702,
518.16931808239));
#112858=CARTESIAN_POINT('Ctrl Pts',(-61.7294769085497,1074.78391794939,
518.215940335845));
#112859=CARTESIAN_POINT('Ctrl Pts',(-61.8393283348014,1074.767568359,518.28726613734));
#112860=CARTESIAN_POINT('Ctrl Pts',(-61.9005188251533,1074.76019322307,
518.311550515567));
#112861=CARTESIAN_POINT('Ctrl Pts',(-61.9935655083327,1074.7512518364,518.328337882215));
#112862=CARTESIAN_POINT('Ctrl Pts',(-62.0227142309869,1074.7487509973,518.330937549327));
#112863=CARTESIAN_POINT('Ctrl Pts',(-62.0518715958007,1074.74654397689,
518.330937549327));
#112864=CARTESIAN_POINT('Origin',(-3.98894410367368,1067.7251047501,514.089592938904));
#112865=CARTESIAN_POINT('',(-3.98894410369425,1076.70513022417,512.611289806711));
#112866=CARTESIAN_POINT('',(-3.98894410367368,1067.7251047501,512.611289806711));
#112867=CARTESIAN_POINT('',(-3.98894410367368,1076.62830575618,515.567896071097));
#112868=CARTESIAN_POINT('Ctrl Pts',(-3.98894410367368,1076.62830575618,
515.567896071097));
#112869=CARTESIAN_POINT('Ctrl Pts',(-4.03382380580244,1076.62823827216,
515.567896071097));
#112870=CARTESIAN_POINT('Ctrl Pts',(-4.07835975006978,1076.62823966801,
515.565856602404));
#112871=CARTESIAN_POINT('Ctrl Pts',(-4.12255616830439,1076.62830843885,
515.561845623343));
#112872=CARTESIAN_POINT('Ctrl Pts',(-4.16719148972908,1076.62837789263,
515.557794812287));
#112873=CARTESIAN_POINT('Ctrl Pts',(-4.21148143877147,1076.62851606623,
515.551733139065));
#112874=CARTESIAN_POINT('Ctrl Pts',(-4.25543363066647,1076.6287214095,515.54367804049));
#112875=CARTESIAN_POINT('Ctrl Pts',(-4.26269409923196,1076.62875533018,
515.54234741766));
#112876=CARTESIAN_POINT('Ctrl Pts',(-4.2699453401395,1076.62879108377,515.540962283859));
#112877=CARTESIAN_POINT('Ctrl Pts',(-4.27718736869677,1076.62882866329,
515.539522582308));
#112878=CARTESIAN_POINT('Ctrl Pts',(-4.3152789658614,1076.6290263239,515.531950044988));
#112879=CARTESIAN_POINT('Ctrl Pts',(-4.3532804804579,1076.62927674603,515.522830609595));
#112880=CARTESIAN_POINT('Ctrl Pts',(-4.39093485348061,1076.62957750851,
515.512190418067));
#112881=CARTESIAN_POINT('Ctrl Pts',(-4.42855367177372,1076.62987798701,
515.501560273424));
#112882=CARTESIAN_POINT('Ctrl Pts',(-4.46582540448601,1076.63022871084,
515.489412364288));
#112883=CARTESIAN_POINT('Ctrl Pts',(-4.50250499970203,1076.63062726572,
515.475823567884));
#112884=CARTESIAN_POINT('Ctrl Pts',(-4.52018651723302,1076.63081939038,
515.469273044619));
#112885=CARTESIAN_POINT('Ctrl Pts',(-4.53773066102735,1076.63102262981,
515.462388439635));
#112886=CARTESIAN_POINT('Ctrl Pts',(-4.55511153485945,1076.63123671354,
515.455182405221));
#112887=CARTESIAN_POINT('Ctrl Pts',(-4.59683648483769,1076.63175064817,
515.437883423113));
#112888=CARTESIAN_POINT('Ctrl Pts',(-4.63755429334944,1076.63232447203,
515.418765655002));
#112889=CARTESIAN_POINT('Ctrl Pts',(-4.67728134605977,1076.6329563068,515.397863549824));
#112890=CARTESIAN_POINT('Ctrl Pts',(-4.71710436732038,1076.6335896679,515.376910951478));
#112891=CARTESIAN_POINT('Ctrl Pts',(-4.75593268733475,1076.63428132053,
515.354164962572));
#112892=CARTESIAN_POINT('Ctrl Pts',(-4.79376065554514,1076.63502937274,
515.329613288933));
#112893=CARTESIAN_POINT('Ctrl Pts',(-4.79916555013926,1076.63513625512,
515.326105323414));
#112894=CARTESIAN_POINT('Ctrl Pts',(-4.80454997336945,1076.6352442889,515.322560423272));
#112895=CARTESIAN_POINT('Ctrl Pts',(-4.8099138564203,1076.63535346856,515.318978482876));
#112896=CARTESIAN_POINT('Ctrl Pts',(-4.84006919053791,1076.63596726809,
515.298841092034));
#112897=CARTESIAN_POINT('Ctrl Pts',(-4.86963875872755,1076.63661969767,
515.277485372765));
#112898=CARTESIAN_POINT('Ctrl Pts',(-4.89840452092768,1076.63730478053,
515.255037875441));
#112899=CARTESIAN_POINT('Ctrl Pts',(-4.92717801125513,1076.63799004744,
515.232584347438));
#112900=CARTESIAN_POINT('Ctrl Pts',(-4.9551467821994,1076.6387079852,515.209038795042));
#112901=CARTESIAN_POINT('Ctrl Pts',(-4.9821237700803,1076.63945261223,515.18456978838));
#112902=CARTESIAN_POINT('Ctrl Pts',(-5.00004363908716,1076.63994724191,
515.168315883532));
#112903=CARTESIAN_POINT('Ctrl Pts',(-5.01752654789864,1076.64045364818,
515.151655371139));
#112904=CARTESIAN_POINT('Ctrl Pts',(-5.03452671334026,1076.64097007782,
515.13464660117));
#112905=CARTESIAN_POINT('Ctrl Pts',(-5.06961887939331,1076.64203610477,
515.099536673436));
#112906=CARTESIAN_POINT('Ctrl Pts',(-5.10302181777584,1076.64315559168,
515.062573790306));
#112907=CARTESIAN_POINT('Ctrl Pts',(-5.13450312720013,1076.64431787742,
515.023977588965));
#112908=CARTESIAN_POINT('Ctrl Pts',(-5.16596650616121,1076.64547950116,
514.985403370438));
#112909=CARTESIAN_POINT('Ctrl Pts',(-5.19551002466464,1076.64668387499,
514.945198147337));
#112910=CARTESIAN_POINT('Ctrl Pts',(-5.22294001512885,1076.64792035598,
514.903616428224));
#112911=CARTESIAN_POINT('Ctrl Pts',(-5.25039095889401,1076.64915778149,
514.862002945546));
#112912=CARTESIAN_POINT('Ctrl Pts',(-5.27572480832945,1076.65042736322,
514.819011384178));
#112913=CARTESIAN_POINT('Ctrl Pts',(-5.29879155836087,1076.65171843384,
514.774924826461));
#112914=CARTESIAN_POINT('Ctrl Pts',(-5.31922564937179,1076.65286215172,
514.735869964743));
#112915=CARTESIAN_POINT('Ctrl Pts',(-5.3378811359444,1076.65402273325,514.695956452106));
#112916=CARTESIAN_POINT('Ctrl Pts',(-5.35468532261741,1076.65519276256,
514.65539420572));
#112917=CARTESIAN_POINT('Ctrl Pts',(-5.37357582673536,1076.65650805641,
514.609795968965));
#112918=CARTESIAN_POINT('Ctrl Pts',(-5.39023224656117,1076.65784178247,
514.563120864991));
#112919=CARTESIAN_POINT('Ctrl Pts',(-5.40451833901832,1076.65918391593,
514.515656003345));
#112920=CARTESIAN_POINT('Ctrl Pts',(-5.41879401809223,1076.66052507109,
514.468225739669));
#112921=CARTESIAN_POINT('Ctrl Pts',(-5.43070259306572,1076.6618746214,514.420007443696));
#112922=CARTESIAN_POINT('Ctrl Pts',(-5.4401565240363,1076.66322256394,514.37130673274));
#112923=CARTESIAN_POINT('Ctrl Pts',(-5.44961550628525,1076.6645712267,514.322580000773));
#112924=CARTESIAN_POINT('Ctrl Pts',(-5.45661709319358,1076.66591827998,
514.27337094645));
#112925=CARTESIAN_POINT('Ctrl Pts',(-5.46112479268709,1076.66725370484,
514.223995950583));
#112926=CARTESIAN_POINT('Ctrl Pts',(-5.46519159746117,1076.66845851279,
514.179450286169));
#112927=CARTESIAN_POINT('Ctrl Pts',(-5.46722916015916,1076.66965385581,
514.134770005097));
#112928=CARTESIAN_POINT('Ctrl Pts',(-5.46724711596372,1076.67083237661,
514.090188343358));
#112929=CARTESIAN_POINT('Ctrl Pts',(-5.46726177561919,1076.67179455621,
514.053790542343));
#112930=CARTESIAN_POINT('Ctrl Pts',(-5.46592795458365,1076.67275310273,
514.017175204292));
#112931=CARTESIAN_POINT('Ctrl Pts',(-5.46322340498931,1076.67370161935,
513.980594350085));
#112932=CARTESIAN_POINT('Ctrl Pts',(-5.46052021283035,1076.6746496599,513.944031856106));
#112933=CARTESIAN_POINT('Ctrl Pts',(-5.45644767069605,1076.67558768062,
513.907504402001));
#112934=CARTESIAN_POINT('Ctrl Pts',(-5.4510356663401,1076.67650929431,513.871261967597));
#112935=CARTESIAN_POINT('Ctrl Pts',(-5.44752072436303,1076.67710785603,
513.847723543446));
#112936=CARTESIAN_POINT('Ctrl Pts',(-5.44344185186923,1076.67769949705,
513.824305287228));
#112937=CARTESIAN_POINT('Ctrl Pts',(-5.43881882267849,1076.67828246757,
513.801073529084));
#112938=CARTESIAN_POINT('Ctrl Pts',(-5.43000622466527,1076.67939374864,
513.756788248326));
#112939=CARTESIAN_POINT('Ctrl Pts',(-5.41920433510385,1076.68047665497,
513.713083925439));
#112940=CARTESIAN_POINT('Ctrl Pts',(-5.40643602623801,1076.68153210232,
513.669954046382));
#112941=CARTESIAN_POINT('Ctrl Pts',(-5.3936828518979,1076.68258629864,513.626875290013));
#112942=CARTESIAN_POINT('Ctrl Pts',(-5.37896763951009,1076.68361310103,
513.584368714443));
#112943=CARTESIAN_POINT('Ctrl Pts',(-5.36226378135259,1076.68461342204,
513.542442855698));
#112944=CARTESIAN_POINT('Ctrl Pts',(-5.35989519129212,1076.68475526654,
513.536497811663));
#112945=CARTESIAN_POINT('Ctrl Pts',(-5.35748653872257,1076.68489657858,
513.530564481821));
#112946=CARTESIAN_POINT('Ctrl Pts',(-5.3550376727605,1076.68503736076,513.524642931247));
#112947=CARTESIAN_POINT('Ctrl Pts',(-5.34042728288203,1076.68587729344,
513.489313858967));
#112948=CARTESIAN_POINT('Ctrl Pts',(-5.32439017493919,1076.6866972177,513.454426945205));
#112949=CARTESIAN_POINT('Ctrl Pts',(-5.30701842434866,1076.68749315242,
513.420219921948));
#112950=CARTESIAN_POINT('Ctrl Pts',(-5.28963199199989,1076.68828975983,
513.385983988579));
#112951=CARTESIAN_POINT('Ctrl Pts',(-5.27090892993038,1076.68906233713,
513.352429639599));
#112952=CARTESIAN_POINT('Ctrl Pts',(-5.25098810610052,1076.68980689311,
513.319771474803));
#112953=CARTESIAN_POINT('Ctrl Pts',(-5.24039444818967,1076.69020283915,
513.302404249994));
#112954=CARTESIAN_POINT('Ctrl Pts',(-5.22946282924075,1076.6905908608,513.285290012385));
#112955=CARTESIAN_POINT('Ctrl Pts',(-5.21821901558114,1076.69097035782,
513.268457541051));
#112956=CARTESIAN_POINT('Ctrl Pts',(-5.19335281033031,1076.69180963273,
513.231231765194));
#112957=CARTESIAN_POINT('Ctrl Pts',(-5.16683758555087,1076.69261257175,
513.195190469683));
#112958=CARTESIAN_POINT('Ctrl Pts',(-5.13866486638326,1076.69338071947,
513.160333923104));
#112959=CARTESIAN_POINT('Ctrl Pts',(-5.11073634250464,1076.69414220905,
513.125779505843));
#112960=CARTESIAN_POINT('Ctrl Pts',(-5.08117830263898,1076.69486950784,
513.092388723484));
#112961=CARTESIAN_POINT('Ctrl Pts',(-5.04994673371333,1076.69556412063,
513.06019817998));
#112962=CARTESIAN_POINT('Ctrl Pts',(-5.04488406308498,1076.6956767181,513.05498005855));
#112963=CARTESIAN_POINT('Ctrl Pts',(-5.03977735273785,1076.69578845669,
513.049793565901));
#112964=CARTESIAN_POINT('Ctrl Pts',(-5.03462634377255,1076.69589934281,
513.044638967002));
#112965=CARTESIAN_POINT('Ctrl Pts',(-4.98509132459662,1076.69696568653,
512.995069424986));
#112966=CARTESIAN_POINT('Ctrl Pts',(-4.93233611087355,1076.69793441364,
512.949321540321));
#112967=CARTESIAN_POINT('Ctrl Pts',(-4.87678398576265,1076.69880913241,
512.907594421805));
#112968=CARTESIAN_POINT('Ctrl Pts',(-4.81842086903492,1076.69972811281,
512.863755870467));
#112969=CARTESIAN_POINT('Ctrl Pts',(-4.7569688942424,1076.70054333035,512.824353182086));
#112970=CARTESIAN_POINT('Ctrl Pts',(-4.69286914438583,1076.70125896924,
512.789643059982));
#112971=CARTESIAN_POINT('Ctrl Pts',(-4.64805083877426,1076.70175934128,
512.765373872289));
#112972=CARTESIAN_POINT('Ctrl Pts',(-4.60193692810212,1076.70221103177,
512.743399379173));
#112973=CARTESIAN_POINT('Ctrl Pts',(-4.55467309415124,1076.70261547096,
512.723821779454));
#112974=CARTESIAN_POINT('Ctrl Pts',(-4.51294825012113,1076.7029725127,512.706538537143));
#112975=CARTESIAN_POINT('Ctrl Pts',(-4.47065903441898,1076.70328996082,
512.69125696259));
#112976=CARTESIAN_POINT('Ctrl Pts',(-4.42781932239519,1076.70356952053,
512.677938344804));
#112977=CARTESIAN_POINT('Ctrl Pts',(-4.38484404374123,1076.7038499649,512.66457758014));
#112978=CARTESIAN_POINT('Ctrl Pts',(-4.34131388393893,1076.7040922807,512.653191908722));
#112979=CARTESIAN_POINT('Ctrl Pts',(-4.29722472367035,1076.70429818939,
512.643791012641));
#112980=CARTESIAN_POINT('Ctrl Pts',(-4.29088399272208,1076.70432780237,
512.642439012458));
#112981=CARTESIAN_POINT('Ctrl Pts',(-4.28453168290618,1076.70435666234,
512.641128149906));
#112982=CARTESIAN_POINT('Ctrl Pts',(-4.27816776842535,1076.70438477442,
512.639858541713));
#112983=CARTESIAN_POINT('Ctrl Pts',(-4.2427823506189,1076.70454108667,512.632799110526));
#112984=CARTESIAN_POINT('Ctrl Pts',(-4.20694315657351,1076.704673918,512.627000670701));
#112985=CARTESIAN_POINT('Ctrl Pts',(-4.17089333556487,1076.70478300393,
512.622529672488));
#112986=CARTESIAN_POINT('Ctrl Pts',(-4.13483990415784,1076.70489210079,
512.618058226504));
#112987=CARTESIAN_POINT('Ctrl Pts',(-4.09857638220709,1076.70497744749,
512.614914591586));
#112988=CARTESIAN_POINT('Ctrl Pts',(-4.06235386956601,1076.7050387795,512.613113627527));
#112989=CARTESIAN_POINT('Ctrl Pts',(-4.03783906398118,1076.70508028799,
512.611894764435));
#112990=CARTESIAN_POINT('Ctrl Pts',(-4.01334319964393,1076.70511079689,
512.611289806711));
#112991=CARTESIAN_POINT('Ctrl Pts',(-3.98894410369425,1076.70513022417,
512.611289806711));
#112992=CARTESIAN_POINT('Ctrl Pts',(-3.98894410369425,1076.70513022417,
512.611289806711));
#112993=CARTESIAN_POINT('Ctrl Pts',(-3.89010227930185,1076.70520892495,
512.61128980671));
#112994=CARTESIAN_POINT('Ctrl Pts',(-3.7915191632709,1076.70511108275,512.621201580718));
#112995=CARTESIAN_POINT('Ctrl Pts',(-3.59467449494741,1076.70455073789,
512.661188086013));
#112996=CARTESIAN_POINT('Ctrl Pts',(-3.49706431916902,1076.704078049,512.691793644763));
#112997=CARTESIAN_POINT('Ctrl Pts',(-3.23483687727456,1076.702211287,512.804914607444));
#112998=CARTESIAN_POINT('Ctrl Pts',(-3.08130018423767,1076.70040097121,
512.908384151165));
#112999=CARTESIAN_POINT('Ctrl Pts',(-2.81189620632753,1076.69531749021,
513.1742069126));
#113000=CARTESIAN_POINT('Ctrl Pts',(-2.70159427009519,1076.69200279032,
513.33720003985));
#113001=CARTESIAN_POINT('Ctrl Pts',(-2.55003143068424,1076.68399367258,
513.697863740724));
#113002=CARTESIAN_POINT('Ctrl Pts',(-2.51078829823382,1076.67936288322,
513.892190254648));
#113003=CARTESIAN_POINT('Ctrl Pts',(-2.51049475856978,1076.66927561583,
514.284400974555));
#113004=CARTESIAN_POINT('Ctrl Pts',(-2.54929534796991,1076.66392059558,
514.47840051194));
#113005=CARTESIAN_POINT('Ctrl Pts',(-2.69956374535934,1076.65337255126,
514.838293157373));
#113006=CARTESIAN_POINT('Ctrl Pts',(-2.80890085393043,1076.64828624815,
515.000942899898));
#113007=CARTESIAN_POINT('Ctrl Pts',(-3.07721597011864,1076.639554502,515.26776677021));
#113008=CARTESIAN_POINT('Ctrl Pts',(-3.23105328591043,1076.63593165891,
515.372150493012));
#113009=CARTESIAN_POINT('Ctrl Pts',(-3.49427595121394,1076.6317746266,515.486454209748));
#113010=CARTESIAN_POINT('Ctrl Pts',(-3.59244187907109,1076.63059411286,
515.517425376927));
#113011=CARTESIAN_POINT('Ctrl Pts',(-3.79040983355065,1076.62894293207,
515.557872175624));
#113012=CARTESIAN_POINT('Ctrl Pts',(-3.88954463142303,1076.62845521963,
515.567896071097));
#113013=CARTESIAN_POINT('Ctrl Pts',(-3.98894410367368,1076.62830575618,
515.567896071097));
#113014=CARTESIAN_POINT('Origin',(-3.98894410367368,1067.7251047501,514.089592938904));
#113015=CARTESIAN_POINT('',(-3.98894410367369,1076.64787682225,514.967896071097));
#113016=CARTESIAN_POINT('',(-3.98894410328192,1076.69355479191,513.211289806711));
#113017=CARTESIAN_POINT('Ctrl Pts',(-3.98894410367369,1076.64787682225,
514.967896071097));
#113018=CARTESIAN_POINT('Ctrl Pts',(-4.04149225305876,1076.64780501974,
514.967896071097));
#113019=CARTESIAN_POINT('Ctrl Pts',(-4.09405915061969,1076.64787785117,
514.963180256518));
#113020=CARTESIAN_POINT('Ctrl Pts',(-4.25901867059246,1076.64857049626,
514.93319827929));
#113021=CARTESIAN_POINT('Ctrl Pts',(-4.36690585428157,1076.64972588111,
514.890687485131));
#113022=CARTESIAN_POINT('Ctrl Pts',(-4.56015184895358,1076.65319497187,
514.766585953667));
#113023=CARTESIAN_POINT('Ctrl Pts',(-4.6436542891775,1076.65547258593,514.686207246268));
#113024=CARTESIAN_POINT('Ctrl Pts',(-4.77504221070995,1076.66074118729,
514.497835356852));
#113025=CARTESIAN_POINT('Ctrl Pts',(-4.82163796085241,1076.66367938196,
514.391637552296));
#113026=CARTESIAN_POINT('Ctrl Pts',(-4.85888449665252,1076.66821809082,
514.223442198093));
#113027=CARTESIAN_POINT('Ctrl Pts',(-4.86577146008994,1076.66974202842,
514.166311287477));
#113028=CARTESIAN_POINT('Ctrl Pts',(-4.86829784916898,1076.67276384636,
514.051520487883));
#113029=CARTESIAN_POINT('Ctrl Pts',(-4.86393018775512,1076.67425446059,
513.994135845765));
#113030=CARTESIAN_POINT('Ctrl Pts',(-4.83377771086896,1076.67865188257,
513.822539379258));
#113031=CARTESIAN_POINT('Ctrl Pts',(-4.79081030033423,1076.68138199551,
513.712664687311));
#113032=CARTESIAN_POINT('Ctrl Pts',(-4.66459751953398,1076.6861530925,513.516467774466));
#113033=CARTESIAN_POINT('Ctrl Pts',(-4.58272850939619,1076.68815139934,
513.432019243722));
#113034=CARTESIAN_POINT('Ctrl Pts',(-4.39063234601568,1076.69127697328,
513.299858850111));
#113035=CARTESIAN_POINT('Ctrl Pts',(-4.28226733965402,1076.69237443015,
513.253532640986));
#113036=CARTESIAN_POINT('Ctrl Pts',(-4.10897180875891,1076.69331089348,
513.217441882773));
#113037=CARTESIAN_POINT('Ctrl Pts',(-4.04896272635834,1076.69349799811,
513.211289806658));
#113038=CARTESIAN_POINT('Ctrl Pts',(-3.98894410289016,1076.69355479191,
513.211289806711));
#113039=CARTESIAN_POINT('',(-3.98894410367368,1082.7251047501,513.211289806711));
#113040=CARTESIAN_POINT('',(-3.98894410367368,1067.7251047501,513.211289806711));
#113041=CARTESIAN_POINT('Origin',(-3.98894410367368,1082.7251047501,514.089592938904));
#113042=CARTESIAN_POINT('Ctrl Pts',(-3.98894410289016,1076.69355479191,
513.211289806711));
#113043=CARTESIAN_POINT('Ctrl Pts',(-3.93259196053329,1076.69360811622,
513.211289806761));
#113044=CARTESIAN_POINT('Ctrl Pts',(-3.87623140718768,1076.69354653842,
513.216713139767));
#113045=CARTESIAN_POINT('Ctrl Pts',(-3.70602832970331,1076.69300108805,
513.249941693398));
#113046=CARTESIAN_POINT('Ctrl Pts',(-3.59701492633745,1076.69214788553,
513.294957478828));
#113047=CARTESIAN_POINT('Ctrl Pts',(-3.40322866750269,1076.68948920037,
513.424818703465));
#113048=CARTESIAN_POINT('Ctrl Pts',(-3.32032214304025,1076.68770970805,
513.508276215716));
#113049=CARTESIAN_POINT('Ctrl Pts',(-3.19180681534375,1076.68332366884,
513.702810789303));
#113050=CARTESIAN_POINT('Ctrl Pts',(-3.14753761985142,1076.68075664216,
513.811995534928));
#113051=CARTESIAN_POINT('Ctrl Pts',(-3.11660159621135,1076.67670312101,
513.975829298708));
#113052=CARTESIAN_POINT('Ctrl Pts',(-3.1115356003055,1076.67544402827,514.025735618899));
#113053=CARTESIAN_POINT('Ctrl Pts',(-3.11074928295003,1076.67415562567,
514.07579986548));
#113054=CARTESIAN_POINT('Ctrl Pts',(-3.10983848239562,1076.67266325392,
514.133789865604));
#113055=CARTESIAN_POINT('Ctrl Pts',(-3.11467382062161,1076.67113829599,
514.191727200505));
#113056=CARTESIAN_POINT('Ctrl Pts',(-3.14605896703041,1076.66655651049,
514.362043412921));
#113057=CARTESIAN_POINT('Ctrl Pts',(-3.18901660653344,1076.6635141462,514.470121302242));
#113058=CARTESIAN_POINT('Ctrl Pts',(-3.31421419718697,1076.65786322126,
514.66355454975));
#113059=CARTESIAN_POINT('Ctrl Pts',(-3.39525158639593,1076.65531186279,
514.747031234788));
#113060=CARTESIAN_POINT('Ctrl Pts',(-3.58489355607944,1076.65116968365,
514.877898170841));
#113061=CARTESIAN_POINT('Ctrl Pts',(-3.69164387888887,1076.64962103285,
514.924037620655));
#113062=CARTESIAN_POINT('Ctrl Pts',(-3.8650972758057,1076.64824710587,514.961344519471));
#113063=CARTESIAN_POINT('Ctrl Pts',(-3.92700766681083,1076.64796145305,
514.967896071097));
#113064=CARTESIAN_POINT('Ctrl Pts',(-3.98894410367369,1076.64787682225,
514.967896071097));
#113065=CARTESIAN_POINT('Origin',(-14.9669751953831,1067.7251047501,520.188191956395));
#113066=CARTESIAN_POINT('',(-14.9669751954018,1076.42256169839,518.912747835258));
#113067=CARTESIAN_POINT('',(-14.9669751953831,1067.7251047501,518.912747835258));
#113068=CARTESIAN_POINT('Ctrl Pts',(-14.9670021241791,1076.25965984465,
521.463636077246));
#113069=CARTESIAN_POINT('Ctrl Pts',(-15.1336635644875,1076.25785153312,
521.463632558478));
#113070=CARTESIAN_POINT('Ctrl Pts',(-15.2987115911046,1076.25832656805,
521.430963338145));
#113071=CARTESIAN_POINT('Ctrl Pts',(-15.6066713015969,1076.26376895275,
521.304096002063));
#113072=CARTESIAN_POINT('Ctrl Pts',(-15.7466054890221,1076.26867493645,
521.21122325551));
#113073=CARTESIAN_POINT('Ctrl Pts',(-15.9830506727415,1076.28215836799,
520.976919933069));
#113074=CARTESIAN_POINT('Ctrl Pts',(-16.0772095673545,1076.29060690936,
520.837681537416));
#113075=CARTESIAN_POINT('Ctrl Pts',(-16.2068907476775,1076.30977042356,
520.530582611396));
#113076=CARTESIAN_POINT('Ctrl Pts',(-16.2409974736705,1076.32030446555,
520.365577861591));
#113077=CARTESIAN_POINT('Ctrl Pts',(-16.2437565496537,1076.34192696332,
520.03158437749));
#113078=CARTESIAN_POINT('Ctrl Pts',(-16.2122673467434,1076.35280840907,
519.865772543202));
#113079=CARTESIAN_POINT('Ctrl Pts',(-16.0863865872732,1076.37357572541,
519.553944418207));
#113080=CARTESIAN_POINT('Ctrl Pts',(-15.9925110914523,1076.38324688577,
519.411233388948));
#113081=CARTESIAN_POINT('Ctrl Pts',(-15.7548895327075,1076.40004536789,
519.171152346095));
#113082=CARTESIAN_POINT('Ctrl Pts',(-15.6136669424916,1076.40702126391,
519.075982913399));
#113083=CARTESIAN_POINT('Ctrl Pts',(-15.3019561978232,1076.41757526725,
518.945969105108));
#113084=CARTESIAN_POINT('Ctrl Pts',(-15.1345246872508,1076.42104616242,
518.912542548849));
#113085=CARTESIAN_POINT('Ctrl Pts',(-14.7960739890186,1076.42410766345,
518.912955312285));
#113086=CARTESIAN_POINT('Ctrl Pts',(-14.628456499764,1076.42366363939,518.946887187125));
#113087=CARTESIAN_POINT('Ctrl Pts',(-14.3166047174734,1076.41886072836,
519.078086691963));
#113088=CARTESIAN_POINT('Ctrl Pts',(-14.175446968428,1076.41455533409,519.173909391717));
#113089=CARTESIAN_POINT('Ctrl Pts',(-13.9388582324749,1076.40246837647,
519.414760269681));
#113090=CARTESIAN_POINT('Ctrl Pts',(-13.8457245853666,1076.39480575976,
519.557338223495));
#113091=CARTESIAN_POINT('Ctrl Pts',(-13.7199886720594,1076.37686140203,
519.871161458313));
#113092=CARTESIAN_POINT('Ctrl Pts',(-13.6889596529711,1076.36673965532,
520.039439402739));
#113093=CARTESIAN_POINT('Ctrl Pts',(-13.6930612725026,1076.3506808469,520.293154918816));
#113094=CARTESIAN_POINT('Ctrl Pts',(-13.7027893854653,1076.3452340051,520.377154043451));
#113095=CARTESIAN_POINT('Ctrl Pts',(-13.7564001201965,1076.32887787121,
520.62334720139));
#113096=CARTESIAN_POINT('Ctrl Pts',(-13.8240053407547,1076.31803638244,
520.778519821053));
#113097=CARTESIAN_POINT('Ctrl Pts',(-14.0153576593589,1076.29778936615,
521.053794890939));
#113098=CARTESIAN_POINT('Ctrl Pts',(-14.1372416223797,1076.28858188701,
521.171262865823));
#113099=CARTESIAN_POINT('Ctrl Pts',(-14.4192662617666,1076.27327573536,
521.352138307294));
#113100=CARTESIAN_POINT('Ctrl Pts',(-14.5765772173206,1076.26732318967,
521.413911181364));
#113101=CARTESIAN_POINT('Ctrl Pts',(-14.8158415454656,1076.26176583286,
521.456907181747));
#113102=CARTESIAN_POINT('Ctrl Pts',(-14.8913430558827,1076.26048076139,
521.463637674657));
#113103=CARTESIAN_POINT('Ctrl Pts',(-14.9670021241791,1076.25965984465,
521.463636077246));
#113104=CARTESIAN_POINT('Origin',(-14.9669751953831,1067.7251047501,520.188191956395));
#113105=CARTESIAN_POINT('',(-14.9669751953831,1076.30090002967,520.863636077531));
#113106=CARTESIAN_POINT('',(-14.9669751953831,1076.38718569293,519.512747835259));
#113107=CARTESIAN_POINT('Ctrl Pts',(-14.9669751953831,1076.30090002967,
520.863636077531));
#113108=CARTESIAN_POINT('Ctrl Pts',(-15.0159124905779,1076.30038825754,
520.863636077531));
#113109=CARTESIAN_POINT('Ctrl Pts',(-15.0648239295839,1076.30023170671,
520.858317612946));
#113110=CARTESIAN_POINT('Ctrl Pts',(-15.1989748452287,1076.30081025746,
520.828647733869));
#113111=CARTESIAN_POINT('Ctrl Pts',(-15.2805325350751,1076.30234596997,
520.79290915802));
#113112=CARTESIAN_POINT('Ctrl Pts',(-15.4253275056845,1076.30754318032,
520.692102076889));
#113113=CARTESIAN_POINT('Ctrl Pts',(-15.4871425503217,1076.31115458539,
520.627994392063));
#113114=CARTESIAN_POINT('Ctrl Pts',(-15.5827342408467,1076.31994379382,
520.479532668925));
#113115=CARTESIAN_POINT('Ctrl Pts',(-15.6155204543622,1076.32503940514,
520.396560635829));
#113116=CARTESIAN_POINT('Ctrl Pts',(-15.6393585190988,1076.33325478884,
520.266168602466));
#113117=CARTESIAN_POINT('Ctrl Pts',(-15.6430195310319,1076.33607071421,
520.222002421342));
#113118=CARTESIAN_POINT('Ctrl Pts',(-15.6416588370593,1076.34177054242,
520.133573441364));
#113119=CARTESIAN_POINT('Ctrl Pts',(-15.6366356806778,1076.34464093559,
520.089520542491));
#113120=CARTESIAN_POINT('Ctrl Pts',(-15.6084041255894,1076.35329360248,
519.95815266914));
#113121=CARTESIAN_POINT('Ctrl Pts',(-15.5720124726391,1076.35891932012,
519.874685772055));
#113122=CARTESIAN_POINT('Ctrl Pts',(-15.4687950299649,1076.36915635785,
519.72725219796));
#113123=CARTESIAN_POINT('Ctrl Pts',(-15.4031181994801,1076.37367156808,
519.664665599285));
#113124=CARTESIAN_POINT('Ctrl Pts',(-15.2511143303541,1076.38104185865,
519.568874191581));
#113125=CARTESIAN_POINT('Ctrl Pts',(-15.1663229962618,1076.38382570443,
519.536609231153));
#113126=CARTESIAN_POINT('Ctrl Pts',(-15.0410966181079,1076.38629232625,
519.515803738376));
#113127=CARTESIAN_POINT('Ctrl Pts',(-15.0040740883286,1076.38683176229,
519.512748425204));
#113128=CARTESIAN_POINT('Ctrl Pts',(-14.9669859361834,1076.38718559046,
519.512747835446));
#113129=CARTESIAN_POINT('Ctrl Pts',(-14.9669823559152,1076.38718562461,
519.512747835389));
#113130=CARTESIAN_POINT('Ctrl Pts',(-14.9669787756485,1076.38718565877,
519.512747835259));
#113131=CARTESIAN_POINT('Ctrl Pts',(-14.9669751953832,1076.38718569293,
519.512747835259));
#113132=CARTESIAN_POINT('',(-14.9669751953831,1082.7251047501,519.512747835259));
#113133=CARTESIAN_POINT('',(-14.9669751953831,1067.7251047501,519.512747835259));
#113134=CARTESIAN_POINT('Origin',(-14.9669751953831,1082.7251047501,520.188191956395));
#113135=CARTESIAN_POINT('Ctrl Pts',(-14.9669751953832,1076.38718569293,
519.512747835259));
#113136=CARTESIAN_POINT('Ctrl Pts',(-14.8770304130865,1076.38804369637,
519.512747835259));
#113137=CARTESIAN_POINT('Ctrl Pts',(-14.7879875438153,1076.38779961628,
519.530713998948));
#113138=CARTESIAN_POINT('Ctrl Pts',(-14.6222355938098,1076.38513168314,
519.600435473661));
#113139=CARTESIAN_POINT('Ctrl Pts',(-14.5471950195292,1076.38273558835,
519.651462301316));
#113140=CARTESIAN_POINT('Ctrl Pts',(-14.4214950009639,1076.37605308584,
519.779844122122));
#113141=CARTESIAN_POINT('Ctrl Pts',(-14.372100867259,1076.37183209441,519.855913435516));
#113142=CARTESIAN_POINT('Ctrl Pts',(-14.3058422523083,1076.36204990605,
520.023132686935));
#113143=CARTESIAN_POINT('Ctrl Pts',(-14.2897540825696,1076.35658048938,
520.112664605299));
#113144=CARTESIAN_POINT('Ctrl Pts',(-14.2926457301874,1076.34799942994,
520.247364448804));
#113145=CARTESIAN_POINT('Ctrl Pts',(-14.2980359096252,1076.34510915037,
520.291833557599));
#113146=CARTESIAN_POINT('Ctrl Pts',(-14.3271149076484,1076.33647555813,
520.422012246066));
#113147=CARTESIAN_POINT('Ctrl Pts',(-14.3633213046354,1076.33080807973,
520.503945350285));
#113148=CARTESIAN_POINT('Ctrl Pts',(-14.465315504119,1076.32030516021,520.649085801352));
#113149=CARTESIAN_POINT('Ctrl Pts',(-14.5300989395078,1076.3155711368,520.710912154196));
#113150=CARTESIAN_POINT('Ctrl Pts',(-14.6797494835211,1076.30774429653,
520.805899496244));
#113151=CARTESIAN_POINT('Ctrl Pts',(-14.7631174696826,1076.30472505357,
520.838202974895));
#113152=CARTESIAN_POINT('Ctrl Pts',(-14.8889629914079,1076.30194121674,
520.860258709262));
#113153=CARTESIAN_POINT('Ctrl Pts',(-14.9279773035416,1076.30130785838,
520.863636077531));
#113154=CARTESIAN_POINT('Ctrl Pts',(-14.9669751953831,1076.30090002967,
520.863636077531));
#113155=CARTESIAN_POINT('Origin',(-27.6354521170191,1067.7251047501,525.785329554474));
#113156=CARTESIAN_POINT('',(-27.6354521170396,1075.76324447263,524.686498418482));
#113157=CARTESIAN_POINT('',(-27.6354521170191,1067.7251047501,524.686498418482));
#113158=CARTESIAN_POINT('Ctrl Pts',(-27.6354652325881,1075.54255375362,
526.884160690388));
#113159=CARTESIAN_POINT('Ctrl Pts',(-27.7787046764732,1075.53848270391,
526.884158980693));
#113160=CARTESIAN_POINT('Ctrl Pts',(-27.9205917190107,1075.53736076137,
526.856149463651));
#113161=CARTESIAN_POINT('Ctrl Pts',(-28.1854094989536,1075.54116058917,
526.747323595548));
#113162=CARTESIAN_POINT('Ctrl Pts',(-28.3057312819153,1075.54603270978,
526.667690377292));
#113163=CARTESIAN_POINT('Ctrl Pts',(-28.5094053471864,1075.56111303089,
526.466639419499));
#113164=CARTESIAN_POINT('Ctrl Pts',(-28.5906269865123,1075.57118904213,
526.347055459459));
#113165=CARTESIAN_POINT('Ctrl Pts',(-28.7029706979218,1075.59518245946,
526.082924025914));
#113166=CARTESIAN_POINT('Ctrl Pts',(-28.7326929653438,1075.60889119952,
525.940755182517));
#113167=CARTESIAN_POINT('Ctrl Pts',(-28.7349881424606,1075.63073750512,
525.724867493293));
#113168=CARTESIAN_POINT('Ctrl Pts',(-28.728647938235,1075.63819784828,525.652834322231));
#113169=CARTESIAN_POINT('Ctrl Pts',(-28.7019715325416,1075.65320332144,
525.511192800037));
#113170=CARTESIAN_POINT('Ctrl Pts',(-28.6817206106976,1075.66071353583,
525.4419084292));
#113171=CARTESIAN_POINT('Ctrl Pts',(-28.6002762760136,1075.68317816295,
525.239525837309));
#113172=CARTESIAN_POINT('Ctrl Pts',(-28.5191792744387,1075.69761865733,
525.11609989725));
#113173=CARTESIAN_POINT('Ctrl Pts',(-28.3138232725783,1075.72358285087,
524.908736133025));
#113174=CARTESIAN_POINT('Ctrl Pts',(-28.1918083061117,1075.73487172659,
524.826604577536));
#113175=CARTESIAN_POINT('Ctrl Pts',(-27.9226159359435,1075.7529270516,524.714721275686));
#113176=CARTESIAN_POINT('Ctrl Pts',(-27.7781589010898,1075.7595168294,524.686073495363));
#113177=CARTESIAN_POINT('Ctrl Pts',(-27.486117459956,1075.76714618751,524.686933330395));
#113178=CARTESIAN_POINT('Ctrl Pts',(-27.3415408701877,1075.76810258596,
524.716497676236));
#113179=CARTESIAN_POINT('Ctrl Pts',(-27.0724953047898,1075.764197711,524.830428100375));
#113180=CARTESIAN_POINT('Ctrl Pts',(-26.9507918943143,1075.75937986775,
524.913579353033));
#113181=CARTESIAN_POINT('Ctrl Pts',(-26.7471198413149,1075.74451321898,
525.122343925765));
#113182=CARTESIAN_POINT('Ctrl Pts',(-26.6671944704052,1075.73461570059,
525.245811191617));
#113183=CARTESIAN_POINT('Ctrl Pts',(-26.5599362661046,1075.71088579724,
525.516943428423));
#113184=CARTESIAN_POINT('Ctrl Pts',(-26.5338673749122,1075.69727107743,
525.662008759801));
#113185=CARTESIAN_POINT('Ctrl Pts',(-26.5383155148456,1075.67551881133,
525.879379334709));
#113186=CARTESIAN_POINT('Ctrl Pts',(-26.5467697760468,1075.6681729337,525.950620268285));
#113187=CARTESIAN_POINT('Ctrl Pts',(-26.5774672516633,1075.65328667062,
526.090718627744));
#113188=CARTESIAN_POINT('Ctrl Pts',(-26.5996988288234,1075.6457799459,526.159241031157));
#113189=CARTESIAN_POINT('Ctrl Pts',(-26.6869345144187,1075.62319814399,
526.358993781912));
#113190=CARTESIAN_POINT('Ctrl Pts',(-26.7715637127726,1075.60852924894,
526.47996836697));
#113191=CARTESIAN_POINT('Ctrl Pts',(-26.9820307799952,1075.5821082306,526.68050016929));
#113192=CARTESIAN_POINT('Ctrl Pts',(-27.1053264362455,1075.57057670524,
526.758643785125));
#113193=CARTESIAN_POINT('Ctrl Pts',(-27.3663317956198,1075.55279443144,
526.859213399613));
#113194=CARTESIAN_POINT('Ctrl Pts',(-27.5002648809074,1075.54639632195,
526.88416230413));
#113195=CARTESIAN_POINT('Ctrl Pts',(-27.6354652325881,1075.54255375362,
526.884160690388));
#113196=CARTESIAN_POINT('Origin',(-27.6354521170191,1067.7251047501,525.785329554474));
#113197=CARTESIAN_POINT('',(-27.6354521170191,1075.60488526556,526.284160690467));
#113198=CARTESIAN_POINT('',(-27.6354521170191,1075.70507826342,525.286498418482));
#113199=CARTESIAN_POINT('Ctrl Pts',(-27.6354521170191,1075.60488526556,
526.284160690467));
#113200=CARTESIAN_POINT('Ctrl Pts',(-27.637581719016,1075.60482587619,526.284160690467));
#113201=CARTESIAN_POINT('Ctrl Pts',(-27.6397120058775,1075.60476785828,
526.28414705299));
#113202=CARTESIAN_POINT('Ctrl Pts',(-27.7068531308022,1075.60298317991,
526.283286809497));
#113203=CARTESIAN_POINT('Ctrl Pts',(-27.7710854290312,1075.60257302789,
526.269752069927));
#113204=CARTESIAN_POINT('Ctrl Pts',(-27.8906979085476,1075.60443883698,
526.218808743026));
#113205=CARTESIAN_POINT('Ctrl Pts',(-27.9448925263289,1075.60669375515,
526.181928547868));
#113206=CARTESIAN_POINT('Ctrl Pts',(-28.0362447104239,1075.61358359968,
526.089372519587));
#113207=CARTESIAN_POINT('Ctrl Pts',(-28.0724372738785,1075.61815928623,
526.034536383933));
#113208=CARTESIAN_POINT('Ctrl Pts',(-28.121868734487,1075.62903903416,525.913825428912));
#113209=CARTESIAN_POINT('Ctrl Pts',(-28.134490643121,1075.63524834314,525.849045650563));
#113210=CARTESIAN_POINT('Ctrl Pts',(-28.1341755161321,1075.64514708704,
525.75101151662));
#113211=CARTESIAN_POINT('Ctrl Pts',(-28.1308523712347,1075.64852408539,
525.718391545539));
#113212=CARTESIAN_POINT('Ctrl Pts',(-28.1178815982617,1075.65532165104,
525.654330654986));
#113213=CARTESIAN_POINT('Ctrl Pts',(-28.1082734017101,1075.65872643261,
525.623036102101));
#113214=CARTESIAN_POINT('Ctrl Pts',(-28.0700028005121,1075.66894646184,
525.531504301829));
#113215=CARTESIAN_POINT('Ctrl Pts',(-28.0322844342556,1075.67553482616,
525.47581880527));
#113216=CARTESIAN_POINT('Ctrl Pts',(-27.9373027258572,1075.68739031963,
525.38268004294));
#113217=CARTESIAN_POINT('Ctrl Pts',(-27.8810450351777,1075.69254604396,
525.346077979356));
#113218=CARTESIAN_POINT('Ctrl Pts',(-27.760754306957,1075.7005204626,525.298416886474));
#113219=CARTESIAN_POINT('Ctrl Pts',(-27.6984115041873,1075.70337998349,
525.286498576198));
#113220=CARTESIAN_POINT('Ctrl Pts',(-27.6354533666297,1075.70507822971,
525.286498418483));
#113221=CARTESIAN_POINT('',(-27.6354521170191,1082.7251047501,525.286498418482));
#113222=CARTESIAN_POINT('',(-27.6354521170191,1067.7251047501,525.286498418482));
#113223=CARTESIAN_POINT('Origin',(-27.6354521170191,1082.7251047501,525.785329554474));
#113224=CARTESIAN_POINT('Ctrl Pts',(-27.6354521170192,1075.70507826342,
525.286498418482));
#113225=CARTESIAN_POINT('Ctrl Pts',(-27.5704411122387,1075.70683186801,
525.286498418482));
#113226=CARTESIAN_POINT('Ctrl Pts',(-27.5060446831974,1075.70731322558,
525.299207181009));
#113227=CARTESIAN_POINT('Ctrl Pts',(-27.3857177316477,1075.70567854251,
525.348640197058));
#113228=CARTESIAN_POINT('Ctrl Pts',(-27.330991362886,1075.70357758552,525.384881156227));
#113229=CARTESIAN_POINT('Ctrl Pts',(-27.2374708795837,1075.6969610597,525.477323575225));
#113230=CARTESIAN_POINT('Ctrl Pts',(-27.2000417531703,1075.69245724965,
525.533025441205));
#113231=CARTESIAN_POINT('Ctrl Pts',(-27.1491348021389,1075.68163327302,
525.655863927699));
#113232=CARTESIAN_POINT('Ctrl Pts',(-27.1362363999838,1075.67541537829,
525.721805829603));
#113233=CARTESIAN_POINT('Ctrl Pts',(-27.1368224186861,1075.66549628098,
525.820850957811));
#113234=CARTESIAN_POINT('Ctrl Pts',(-27.1402045434783,1075.66215223877,
525.853317933819));
#113235=CARTESIAN_POINT('Ctrl Pts',(-27.1532576068827,1075.65538745492,
525.917183579509));
#113236=CARTESIAN_POINT('Ctrl Pts',(-27.1629115826284,1075.65198218319,
525.948432418141));
#113237=CARTESIAN_POINT('Ctrl Pts',(-27.2014706749091,1075.64168178599,
526.040227892965));
#113238=CARTESIAN_POINT('Ctrl Pts',(-27.2395677639214,1075.63498222398,
526.096133854981));
#113239=CARTESIAN_POINT('Ctrl Pts',(-27.3345534635558,1075.62299136117,
526.188546074565));
#113240=CARTESIAN_POINT('Ctrl Pts',(-27.3900931550745,1075.61778677211,
526.224578420605));
#113241=CARTESIAN_POINT('Ctrl Pts',(-27.5097210762046,1075.60961542773,
526.272163085955));
#113242=CARTESIAN_POINT('Ctrl Pts',(-27.5722853209087,1075.60664683237,
526.284160690467));
#113243=CARTESIAN_POINT('Ctrl Pts',(-27.6354521170191,1075.60488526556,
526.284160690467));
#113244=CARTESIAN_POINT('Origin',(-41.3143294401472,1067.7251047501,528.704622312801));
#113245=CARTESIAN_POINT('',(-41.314329440147,1074.93718437437,527.614081564072));
#113246=CARTESIAN_POINT('',(-41.3143294401472,1067.7251047501,527.614081564072));
#113247=CARTESIAN_POINT('Ctrl Pts',(-41.3147349368617,1074.66272114928,
529.795162986141));
#113248=CARTESIAN_POINT('Ctrl Pts',(-41.4565839003635,1074.65548636531,
529.795110242314));
#113249=CARTESIAN_POINT('Ctrl Pts',(-41.5971570089355,1074.65186733571,
529.767382442196));
#113250=CARTESIAN_POINT('Ctrl Pts',(-41.8594095745204,1074.6523287955,529.659704010895));
#113251=CARTESIAN_POINT('Ctrl Pts',(-41.9784831358845,1074.65637448485,
529.581057138748));
#113252=CARTESIAN_POINT('Ctrl Pts',(-42.1803317397281,1074.67161051664,
529.382452429747));
#113253=CARTESIAN_POINT('Ctrl Pts',(-42.2609179997288,1074.68267674667,
529.264316016156));
#113254=CARTESIAN_POINT('Ctrl Pts',(-42.3729390913502,1074.71042386179,
529.00300705716));
#113255=CARTESIAN_POINT('Ctrl Pts',(-42.4027939265198,1074.72688791419,
528.862132421517));
#113256=CARTESIAN_POINT('Ctrl Pts',(-42.4067926729944,1074.76336581939,
528.573317249071));
#113257=CARTESIAN_POINT('Ctrl Pts',(-42.3793156828108,1074.78311131342,
528.428083368655));
#113258=CARTESIAN_POINT('Ctrl Pts',(-42.26924765968,1074.822552856,528.158298115756));
#113259=CARTESIAN_POINT('Ctrl Pts',(-42.1881133129265,1074.84187982289,
528.036113619881));
#113260=CARTESIAN_POINT('Ctrl Pts',(-41.9832034495463,1074.87754647936,
527.831273672055));
#113261=CARTESIAN_POINT('Ctrl Pts',(-41.8616520587045,1074.89356728745,
527.75031640009));
#113262=CARTESIAN_POINT('Ctrl Pts',(-41.5937742418405,1074.9202727164,527.640618985392));
#113263=CARTESIAN_POINT('Ctrl Pts',(-41.4501718347894,1074.93070054373,
527.612897211704));
#113264=CARTESIAN_POINT('Ctrl Pts',(-41.1634517280726,1074.94439594919,
527.61531515592));
#113265=CARTESIAN_POINT('Ctrl Pts',(-41.0232724842316,1074.94768751226,
527.644111186203));
#113266=CARTESIAN_POINT('Ctrl Pts',(-40.7617525825489,1074.94696346259,
527.753815837843));
#113267=CARTESIAN_POINT('Ctrl Pts',(-40.6430599502034,1074.94295948973,
527.833577653202));
#113268=CARTESIAN_POINT('Ctrl Pts',(-40.4423049032428,1074.92805447489,
528.034446428386));
#113269=CARTESIAN_POINT('Ctrl Pts',(-40.3624894630061,1074.91726146972,
528.153766950873));
#113270=CARTESIAN_POINT('Ctrl Pts',(-40.2520633692188,1074.88993585858,
528.418517953024));
#113271=CARTESIAN_POINT('Ctrl Pts',(-40.2235815203424,1074.87356315,528.561774659589));
#113272=CARTESIAN_POINT('Ctrl Pts',(-40.2238920221908,1074.84669833597,
528.777049214715));
#113273=CARTESIAN_POINT('Ctrl Pts',(-40.2308990529131,1074.83752097588,
528.847689597252));
#113274=CARTESIAN_POINT('Ctrl Pts',(-40.2585333116757,1074.81871742584,
528.986791992705));
#113275=CARTESIAN_POINT('Ctrl Pts',(-40.2791468108806,1074.80913181389,
529.054934175923));
#113276=CARTESIAN_POINT('Ctrl Pts',(-40.3620343381846,1074.77970044653,
529.255819191466));
#113277=CARTESIAN_POINT('Ctrl Pts',(-40.4445223765027,1074.76002862967,
529.378546440448));
#113278=CARTESIAN_POINT('Ctrl Pts',(-40.6512227926117,1074.72372088479,
529.582245716887));
#113279=CARTESIAN_POINT('Ctrl Pts',(-40.7726856396383,1074.70737583042,
529.662059071412));
#113280=CARTESIAN_POINT('Ctrl Pts',(-41.0359626757278,1074.68040361457,
529.768254314931));
#113281=CARTESIAN_POINT('Ctrl Pts',(-41.1745848054429,1074.66986928699,
529.79521509829));
#113282=CARTESIAN_POINT('Ctrl Pts',(-41.3147349368616,1074.66272114928,
529.795162986141));
#113283=CARTESIAN_POINT('Origin',(-41.3143294401472,1067.7251047501,528.704622312801));
#113284=CARTESIAN_POINT('',(-41.3143294401472,1074.74003968768,529.195163061529));
#113285=CARTESIAN_POINT('',(-41.3143294401478,1074.86349252611,528.214081564072));
#113286=CARTESIAN_POINT('Ctrl Pts',(-41.3143294401473,1074.74003968768,
529.195163061529));
#113287=CARTESIAN_POINT('Ctrl Pts',(-41.3149650648345,1074.74000762129,
529.195163061529));
#113288=CARTESIAN_POINT('Ctrl Pts',(-41.315600759631,1074.73997570815,529.1951618261));
#113289=CARTESIAN_POINT('Ctrl Pts',(-41.3800205074441,1074.7367576039,529.194911378812));
#113290=CARTESIAN_POINT('Ctrl Pts',(-41.4431861274814,1074.73518157134,
529.18222505377));
#113291=CARTESIAN_POINT('Ctrl Pts',(-41.5609956021098,1074.735445482,529.133387891354));
#113292=CARTESIAN_POINT('Ctrl Pts',(-41.6144628987129,1074.73727251931,
529.097805368761));
#113293=CARTESIAN_POINT('Ctrl Pts',(-41.7050067635757,1074.74410843458,
529.008075075171));
#113294=CARTESIAN_POINT('Ctrl Pts',(-41.7410924447216,1074.74906329865,
528.954742912866));
#113295=CARTESIAN_POINT('Ctrl Pts',(-41.7910608480751,1074.76149153383,
528.836887829166));
#113296=CARTESIAN_POINT('Ctrl Pts',(-41.8042382686789,1074.76886763768,
528.773407019333));
#113297=CARTESIAN_POINT('Ctrl Pts',(-41.8054729513215,1074.78521111985,
528.643568446466));
#113298=CARTESIAN_POINT('Ctrl Pts',(-41.792884918473,1074.79405545382,528.578431307186));
#113299=CARTESIAN_POINT('Ctrl Pts',(-41.742954636749,1074.8117951711,528.457257189193));
#113300=CARTESIAN_POINT('Ctrl Pts',(-41.7061682231797,1074.82052396794,
528.402324735324));
#113301=CARTESIAN_POINT('Ctrl Pts',(-41.6132936582189,1074.83667516872,
528.310276378473));
#113302=CARTESIAN_POINT('Ctrl Pts',(-41.5581693039621,1074.84394813471,
528.273974587247));
#113303=CARTESIAN_POINT('Ctrl Pts',(-41.4393192886644,1074.85580739449,
528.226153185481));
#113304=CARTESIAN_POINT('Ctrl Pts',(-41.3771671640389,1074.86038580463,
528.214082208443));
#113305=CARTESIAN_POINT('Ctrl Pts',(-41.3143344706058,1074.8634922774,528.214081564098));
#113306=CARTESIAN_POINT('',(-41.3143294401472,1082.7251047501,528.214081564072));
#113307=CARTESIAN_POINT('',(-41.3143294401472,1067.7251047501,528.214081564072));
#113308=CARTESIAN_POINT('Origin',(-41.3143294401472,1082.7251047501,528.704622312801));
#113309=CARTESIAN_POINT('Ctrl Pts',(-41.3143294401492,1074.86349252611,
528.214081564072));
#113310=CARTESIAN_POINT('Ctrl Pts',(-41.2505739327455,1074.8666445416,528.214081564072));
#113311=CARTESIAN_POINT('Ctrl Pts',(-41.1873927330606,1074.86821828261,
528.22650978009));
#113312=CARTESIAN_POINT('Ctrl Pts',(-41.0693622129366,1074.86802962759,
528.274875616737));
#113313=CARTESIAN_POINT('Ctrl Pts',(-41.0157058632845,1074.86627445234,
528.310281568565));
#113314=CARTESIAN_POINT('Ctrl Pts',(-40.9247150070383,1074.85962435634,
528.399785349406));
#113315=CARTESIAN_POINT('Ctrl Pts',(-40.8883875279695,1074.85477936378,
528.453079629283));
#113316=CARTESIAN_POINT('Ctrl Pts',(-40.8375628576031,1074.84245873064,
528.571924129615));
#113317=CARTESIAN_POINT('Ctrl Pts',(-40.8241704833866,1074.83504196565,
528.636556360447));
#113318=CARTESIAN_POINT('Ctrl Pts',(-40.8236135986097,1074.82288413253,
528.733788934864));
#113319=CARTESIAN_POINT('Ctrl Pts',(-40.826557553515,1074.81873561267,528.765690725002));
#113320=CARTESIAN_POINT('Ctrl Pts',(-40.838608761746,1074.81024794443,528.828494391202));
#113321=CARTESIAN_POINT('Ctrl Pts',(-40.8477001013119,1074.80592749524,
528.859253514476));
#113322=CARTESIAN_POINT('Ctrl Pts',(-40.8843820828532,1074.79270684827,
528.949746165404));
#113323=CARTESIAN_POINT('Ctrl Pts',(-40.9210270111728,1074.78389469495,
529.005063318077));
#113324=CARTESIAN_POINT('Ctrl Pts',(-41.0135485047486,1074.76756439382,
529.097556825592));
#113325=CARTESIAN_POINT('Ctrl Pts',(-41.0683544996801,1074.7601897016,529.134028548398));
#113326=CARTESIAN_POINT('Ctrl Pts',(-41.187608901482,1074.74800778374,529.182752351033));
#113327=CARTESIAN_POINT('Ctrl Pts',(-41.2506169667632,1074.74325389345,
529.195163061529));
#113328=CARTESIAN_POINT('Ctrl Pts',(-41.3143294401473,1074.74003968768,
529.195163061529));
#113329=CARTESIAN_POINT('Origin',(14.699947805047,1067.7251047501,512.963821085944));
#113330=CARTESIAN_POINT('',(14.6999478050656,1078.7051236444,511.48551795375));
#113331=CARTESIAN_POINT('Ctrl Pts',(14.6998978962583,1078.63014559736,514.442124217295));
#113332=CARTESIAN_POINT('Ctrl Pts',(14.7496044544337,1078.62987399772,514.442125895431));
#113333=CARTESIAN_POINT('Ctrl Pts',(14.7992797757492,1078.62968442711,514.439620569293));
#113334=CARTESIAN_POINT('Ctrl Pts',(14.8867432338949,1078.62949662964,514.430772707963));
#113335=CARTESIAN_POINT('Ctrl Pts',(14.9245886139143,1078.62946433203,514.425455823912));
#113336=CARTESIAN_POINT('Ctrl Pts',(15.0019500580471,1078.62949962489,514.411511448347));
#113337=CARTESIAN_POINT('Ctrl Pts',(15.0414039587513,1078.62957306913,514.402716643483));
#113338=CARTESIAN_POINT('Ctrl Pts',(15.1394856411381,1078.62989562152,514.376591201779));
#113339=CARTESIAN_POINT('Ctrl Pts',(15.1974912031204,1078.63021516986,514.357221000039));
#113340=CARTESIAN_POINT('Ctrl Pts',(15.4035757752251,1078.63182159784,514.273887294396));
#113341=CARTESIAN_POINT('Ctrl Pts',(15.5421258678977,1078.6338279638,514.189421381273));
#113342=CARTESIAN_POINT('Ctrl Pts',(15.7838834832569,1078.63917809705,513.981347624014));
#113343=CARTESIAN_POINT('Ctrl Pts',(15.8862203321114,1078.64245604748,513.859939276477));
#113344=CARTESIAN_POINT('Ctrl Pts',(16.0556452944737,1078.65016884252,513.577701386725));
#113345=CARTESIAN_POINT('Ctrl Pts',(16.1176355195055,1078.65461735318,513.416503796587));
#113346=CARTESIAN_POINT('Ctrl Pts',(16.1859615775165,1078.6641002794,513.068083803391));
#113347=CARTESIAN_POINT('Ctrl Pts',(16.1874129211241,1078.66906717691,512.882845505973));
#113348=CARTESIAN_POINT('Ctrl Pts',(16.1199743296375,1078.67885443951,512.507956087882));
#113349=CARTESIAN_POINT('Ctrl Pts',(16.0465448510673,1078.6835367153,512.322749055966));
#113350=CARTESIAN_POINT('Ctrl Pts',(15.8341517173147,1078.69160227121,511.996423613929));
#113351=CARTESIAN_POINT('Ctrl Pts',(15.6989852787079,1078.69494534877,511.85738138296));
#113352=CARTESIAN_POINT('Ctrl Pts',(15.3932749645222,1078.7001245418,511.645889081803));
#113353=CARTESIAN_POINT('Ctrl Pts',(15.2281463969002,1078.70200751748,511.571464109408));
#113354=CARTESIAN_POINT('Ctrl Pts',(14.9434586716088,1078.70413388698,511.501296026986));
#113355=CARTESIAN_POINT('Ctrl Pts',(14.8304271962009,1078.70471829418,511.486914601018));
#113356=CARTESIAN_POINT('Ctrl Pts',(14.6701871029876,1078.70521821483,511.485080473285));
#113357=CARTESIAN_POINT('Ctrl Pts',(14.6235074471387,1078.70532451767,511.486757652073));
#113358=CARTESIAN_POINT('Ctrl Pts',(14.5422261995786,1078.7054420807,511.493541971162));
#113359=CARTESIAN_POINT('Ctrl Pts',(14.5075803961572,1078.70547052923,511.497672538586));
#113360=CARTESIAN_POINT('Ctrl Pts',(14.4357582627616,1078.70548442937,511.508825184092));
#113361=CARTESIAN_POINT('Ctrl Pts',(14.3986395576713,1078.70546607648,511.516056420283));
#113362=CARTESIAN_POINT('Ctrl Pts',(14.3125787790289,1078.70536324443,511.536275676784));
#113363=CARTESIAN_POINT('Ctrl Pts',(14.2639453551362,1078.70525857253,511.550370519949));
#113364=CARTESIAN_POINT('Ctrl Pts',(14.1147636199825,1078.70478791188,511.602040062133));
#113365=CARTESIAN_POINT('Ctrl Pts',(14.0175193639402,1078.70426268457,511.648078300942));
#113366=CARTESIAN_POINT('Ctrl Pts',(13.7582214073901,1078.7021689885,511.807378320523));
#113367=CARTESIAN_POINT('Ctrl Pts',(13.6126375009139,1078.70011826636,511.943057109904));
#113368=CARTESIAN_POINT('Ctrl Pts',(13.3993942633451,1078.69491711075,512.240911669003));
#113369=CARTESIAN_POINT('Ctrl Pts',(13.3252263044758,1078.69199545058,512.394459501776));
#113370=CARTESIAN_POINT('Ctrl Pts',(13.2285668949958,1078.68489306036,512.73231598474));
#113371=CARTESIAN_POINT('Ctrl Pts',(13.2112626086718,1078.68068972132,512.915183813181));
#113372=CARTESIAN_POINT('Ctrl Pts',(13.2451812497772,1078.67119428078,513.291373738735));
#113373=CARTESIAN_POINT('Ctrl Pts',(13.3012324075905,1078.66593646387,513.480762428237));
#113374=CARTESIAN_POINT('Ctrl Pts',(13.4826791150468,1078.6555137632,513.824614664237));
#113375=CARTESIAN_POINT('Ctrl Pts',(13.605481449819,1078.65045374298,513.976173883456));
#113376=CARTESIAN_POINT('Ctrl Pts',(13.8908753439773,1078.64178715355,514.213831471779));
#113377=CARTESIAN_POINT('Ctrl Pts',(14.0472891538332,1078.63817437732,514.302167165923));
#113378=CARTESIAN_POINT('Ctrl Pts',(14.3495968267505,1078.63320320409,514.406988811613));
#113379=CARTESIAN_POINT('Ctrl Pts',(14.4895365839382,1078.63156162662,514.433926464569));
#113380=CARTESIAN_POINT('Ctrl Pts',(14.6540613618039,1078.63041344773,514.441589638889));
#113381=CARTESIAN_POINT('Ctrl Pts',(14.6769780156839,1078.63027083297,514.4421234435));
#113382=CARTESIAN_POINT('Ctrl Pts',(14.6998978962583,1078.63014559736,514.442124217295));
#113383=CARTESIAN_POINT('',(14.6999478050287,1076.70479703066,511.48551795375));
#113384=CARTESIAN_POINT('',(14.699947805047,1067.7251047501,511.485517953751));
#113385=CARTESIAN_POINT('Ctrl Pts',(14.7001358865113,1076.6289311992,514.442124206172));
#113386=CARTESIAN_POINT('Ctrl Pts',(14.507008105989,1076.62999761294,514.442148777423));
#113387=CARTESIAN_POINT('Ctrl Pts',(14.3157483578776,1076.63231146501,514.404327824439));
#113388=CARTESIAN_POINT('Ctrl Pts',(13.9587634920547,1076.6389578427,514.25736482587));
#113389=CARTESIAN_POINT('Ctrl Pts',(13.7964514000899,1076.64321875908,514.149693054514));
#113390=CARTESIAN_POINT('Ctrl Pts',(13.5222436425071,1076.65281493507,513.87797884017));
#113391=CARTESIAN_POINT('Ctrl Pts',(13.4130296203176,1076.65805219814,513.716488948897));
#113392=CARTESIAN_POINT('Ctrl Pts',(13.3004013968247,1076.6659230134,513.449597277797));
#113393=CARTESIAN_POINT('Ctrl Pts',(13.2716601826682,1076.66853181555,513.35714476367));
#113394=CARTESIAN_POINT('Ctrl Pts',(13.2326215889435,1076.67363038448,513.167942887925));
#113395=CARTESIAN_POINT('Ctrl Pts',(13.2224206474366,1076.6761078662,513.071646428809));
#113396=CARTESIAN_POINT('Ctrl Pts',(13.2201992174956,1076.68329114308,512.779032057933));
#113397=CARTESIAN_POINT('Ctrl Pts',(13.2577112268904,1076.68758814285,512.584656160735));
#113398=CARTESIAN_POINT('Ctrl Pts',(13.4059486805338,1076.69485270936,512.222925245413));
#113399=CARTESIAN_POINT('Ctrl Pts',(13.5147872705394,1076.69776396805,512.058966000734));
#113400=CARTESIAN_POINT('Ctrl Pts',(13.7900865941845,1076.7021931983,511.782434420035));
#113401=CARTESIAN_POINT('Ctrl Pts',(13.9539504277458,1076.70367307539,511.672692175678));
#113402=CARTESIAN_POINT('Ctrl Pts',(14.3153297364348,1076.70527006636,511.523058786727));
#113403=CARTESIAN_POINT('Ctrl Pts',(14.5093533614346,1076.70537192508,511.48483457621));
#113404=CARTESIAN_POINT('Ctrl Pts',(14.9005962585822,1076.70419215139,511.486218398268));
#113405=CARTESIAN_POINT('Ctrl Pts',(15.0939490284075,1076.70292187599,511.525652441588));
#113406=CARTESIAN_POINT('Ctrl Pts',(15.4536207665189,1076.69892134873,511.677220962288));
#113407=CARTESIAN_POINT('Ctrl Pts',(15.6164807544368,1076.69622620615,511.78767363118));
#113408=CARTESIAN_POINT('Ctrl Pts',(15.8905787292192,1076.68937498994,512.065991252439));
#113409=CARTESIAN_POINT('Ctrl Pts',(15.9988665664837,1076.68527236375,512.231358863645));
#113410=CARTESIAN_POINT('Ctrl Pts',(16.1447883504337,1076.67594711465,512.594781835267));
#113411=CARTESIAN_POINT('Ctrl Pts',(16.1809202016486,1076.67081308396,512.789268333462));
#113412=CARTESIAN_POINT('Ctrl Pts',(16.1753005948981,1076.66025649441,513.179181144081));
#113413=CARTESIAN_POINT('Ctrl Pts',(16.1343164117519,1076.65494289453,513.370804310472));
#113414=CARTESIAN_POINT('Ctrl Pts',(15.9806014887991,1076.6450430403,513.727382427962));
#113415=CARTESIAN_POINT('Ctrl Pts',(15.8693138868247,1076.64056031446,513.888858337136));
#113416=CARTESIAN_POINT('Ctrl Pts',(15.5907757988116,1076.63338473419,514.159425483661));
#113417=CARTESIAN_POINT('Ctrl Pts',(15.4262833660638,1076.63076665523,514.265931546221));
#113418=CARTESIAN_POINT('Ctrl Pts',(15.0722278865958,1076.62805579513,514.406636173868));
#113419=CARTESIAN_POINT('Ctrl Pts',(14.8870272186761,1076.62789922191,514.442100428373));
#113420=CARTESIAN_POINT('Ctrl Pts',(14.7001358865113,1076.6289311992,514.442124206172));
#113421=CARTESIAN_POINT('Origin',(14.699947805047,1067.7251047501,512.963821085944));
#113422=CARTESIAN_POINT('',(14.699947805047,1076.64821521145,513.842124218137));
#113423=CARTESIAN_POINT('',(14.699947805044,1076.69331989119,512.085517953751));
#113424=CARTESIAN_POINT('Ctrl Pts',(14.699947805047,1076.64821521145,513.842124218137));
#113425=CARTESIAN_POINT('Ctrl Pts',(14.5902341892714,1076.64876664723,513.842124218137));
#113426=CARTESIAN_POINT('Ctrl Pts',(14.4814440862202,1076.6499345,513.821566166036));
#113427=CARTESIAN_POINT('Ctrl Pts',(14.2723884424619,1076.65339518764,513.739567009876));
#113428=CARTESIAN_POINT('Ctrl Pts',(14.1747942053337,1076.65570057739,513.677122346968));
#113429=CARTESIAN_POINT('Ctrl Pts',(14.0090981910953,1076.66100818296,513.518195556117));
#113430=CARTESIAN_POINT('Ctrl Pts',(13.9426126809805,1076.66395730214,513.423218232298));
#113431=CARTESIAN_POINT('Ctrl Pts',(13.8731309645065,1076.66850029281,513.265624382355));
#113432=CARTESIAN_POINT('Ctrl Pts',(13.8551785910615,1076.67002381275,513.2109573044));
#113433=CARTESIAN_POINT('Ctrl Pts',(13.8301966195557,1076.67304115965,513.098896023708));
#113434=CARTESIAN_POINT('Ctrl Pts',(13.8232286368745,1076.674527731,513.041770144096));
#113435=CARTESIAN_POINT('Ctrl Pts',(13.8191479878038,1076.67891209652,512.86743340148));
#113436=CARTESIAN_POINT('Ctrl Pts',(13.8397991282349,1076.68162769075,512.751109826172));
#113437=CARTESIAN_POINT('Ctrl Pts',(13.9252803318556,1076.68635655882,512.533848931459));
#113438=CARTESIAN_POINT('Ctrl Pts',(13.98907440702,1076.68832843462,512.435003694698));
#113439=CARTESIAN_POINT('Ctrl Pts',(14.1515572663527,1076.69139454872,512.26792630332));
#113440=CARTESIAN_POINT('Ctrl Pts',(14.2486471533298,1076.69246080991,512.201370193172));
#113441=CARTESIAN_POINT('Ctrl Pts',(14.4632835550863,1076.69363475109,512.109989242052));
#113442=CARTESIAN_POINT('Ctrl Pts',(14.5787157912715,1076.69373093964,512.086129931039));
#113443=CARTESIAN_POINT('Ctrl Pts',(14.696936129852,1076.69333034212,512.085521825869));
#113444=CARTESIAN_POINT('Ctrl Pts',(14.6984420617311,1076.69332515727,512.085517953751));
#113445=CARTESIAN_POINT('Ctrl Pts',(14.6999478050411,1076.69331989119,512.085517953751));
#113446=CARTESIAN_POINT('',(14.699947805047,1082.7251047501,512.085517953751));
#113447=CARTESIAN_POINT('',(14.699947805047,1067.7251047501,512.085517953751));
#113448=CARTESIAN_POINT('Origin',(14.699947805047,1082.7251047501,512.963821085944));
#113449=CARTESIAN_POINT('Ctrl Pts',(14.6999478050411,1076.69331989119,512.08551795375));
#113450=CARTESIAN_POINT('Ctrl Pts',(14.8150174298463,1076.69291745447,512.08551795375));
#113451=CARTESIAN_POINT('Ctrl Pts',(14.9289858052922,1076.69204383407,512.108131785945));
#113452=CARTESIAN_POINT('Ctrl Pts',(15.1430067031942,1076.68935404349,512.196564529957));
#113453=CARTESIAN_POINT('Ctrl Pts',(15.2407356916632,1076.68755084412,512.262016733255));
#113454=CARTESIAN_POINT('Ctrl Pts',(15.4052186375597,1076.68311950555,512.427480302874));
#113455=CARTESIAN_POINT('Ctrl Pts',(15.4702298040019,1076.68053016571,512.525950177848));
#113456=CARTESIAN_POINT('Ctrl Pts',(15.554784697244,1076.6750258843,512.734816095846));
#113457=CARTESIAN_POINT('Ctrl Pts',(15.5765117015373,1076.67219414545,512.842067512456));
#113458=CARTESIAN_POINT('Ctrl Pts',(15.5781507156001,1076.66932269893,512.950553082464));
#113459=CARTESIAN_POINT('Ctrl Pts',(15.5798911289057,1076.66627360751,513.065750220667));
#113460=CARTESIAN_POINT('Ctrl Pts',(15.5589484464421,1076.66323751492,513.180174989549));
#113461=CARTESIAN_POINT('Ctrl Pts',(15.474065251113,1076.65761621789,513.394453181141));
#113462=CARTESIAN_POINT('Ctrl Pts',(15.410929900768,1076.6550880753,513.492224212286));
#113463=CARTESIAN_POINT('Ctrl Pts',(15.2505387101093,1076.65100759029,513.657751439642));
#113464=CARTESIAN_POINT('Ctrl Pts',(15.1548601169707,1076.64949675587,513.723918305029));
#113465=CARTESIAN_POINT('Ctrl Pts',(14.9435839893325,1076.64779756826,513.815460695151));
#113466=CARTESIAN_POINT('Ctrl Pts',(14.8300703324198,1076.64762466531,513.840015801074));
#113467=CARTESIAN_POINT('Ctrl Pts',(14.7100170574461,1076.64816590382,513.842080945559));
#113468=CARTESIAN_POINT('Ctrl Pts',(14.7049814592775,1076.64818991161,513.842124218137));
#113469=CARTESIAN_POINT('Ctrl Pts',(14.699947805047,1076.64821521145,513.842124218137));
#113470=CARTESIAN_POINT('Origin',(5.22978306525629,1067.7251047501,521.211612088867));
#113471=CARTESIAN_POINT('',(5.22978306527375,1078.42681724135,519.93616796773));
#113472=CARTESIAN_POINT('Ctrl Pts',(5.22976567235167,1078.26387350206,522.487056209884));
#113473=CARTESIAN_POINT('Ctrl Pts',(5.26411870576279,1078.26374442239,522.487056678348));
#113474=CARTESIAN_POINT('Ctrl Pts',(5.29845782220942,1078.26371167916,522.485669241599));
#113475=CARTESIAN_POINT('Ctrl Pts',(5.37080415501917,1078.263846266,522.479812496659));
#113476=CARTESIAN_POINT('Ctrl Pts',(5.40875071914021,1078.26403652399,522.475016106612));
#113477=CARTESIAN_POINT('Ctrl Pts',(5.50661975544815,1078.26483891144,522.458147427206));
#113478=CARTESIAN_POINT('Ctrl Pts',(5.56598875477243,1078.26563426326,522.443461796757));
#113479=CARTESIAN_POINT('Ctrl Pts',(5.78523223648911,1078.26974512755,522.372194104605));
#113480=CARTESIAN_POINT('Ctrl Pts',(5.93428652750519,1078.27499035138,522.288231812167));
#113481=CARTESIAN_POINT('Ctrl Pts',(6.16926122574186,1078.28795175423,522.085675624277));
#113482=CARTESIAN_POINT('Ctrl Pts',(6.25995812646026,1078.29501207729,521.976673495429));
#113483=CARTESIAN_POINT('Ctrl Pts',(6.40771455656613,1078.31141104809,521.723822559312));
#113484=CARTESIAN_POINT('Ctrl Pts',(6.46032483203251,1078.32075402018,521.579890482998));
#113485=CARTESIAN_POINT('Ctrl Pts',(6.51426712829598,1078.34078288177,521.269706019815));
#113486=CARTESIAN_POINT('Ctrl Pts',(6.51118749253278,1078.35133335968,521.105399802076));
#113487=CARTESIAN_POINT('Ctrl Pts',(6.44221569650749,1078.37200478621,520.781317782674));
#113488=CARTESIAN_POINT('Ctrl Pts',(6.37482325455214,1078.38189802412,520.625044644336));
#113489=CARTESIAN_POINT('Ctrl Pts',(6.18661662569876,1078.39911299917,520.352774478781));
#113490=CARTESIAN_POINT('Ctrl Pts',(6.06956700635826,1078.4063627812,520.237994042669));
#113491=CARTESIAN_POINT('Ctrl Pts',(5.79905804478788,1078.41785855085,520.058828454279));
#113492=CARTESIAN_POINT('Ctrl Pts',(5.64820256977495,1078.42201393506,519.99590853225));
#113493=CARTESIAN_POINT('Ctrl Pts',(5.42983939844212,1078.42535424372,519.950478556129));
#113494=CARTESIAN_POINT('Ctrl Pts',(5.36928763696347,1078.42601801755,519.942352673398));
#113495=CARTESIAN_POINT('Ctrl Pts',(5.27062000758902,1078.42668331406,519.936260500062));
#113496=CARTESIAN_POINT('Ctrl Pts',(5.23276961374977,1078.4268402678,519.935610335759));
#113497=CARTESIAN_POINT('Ctrl Pts',(5.16100456457109,1078.42695218217,519.937571229624));
#113498=CARTESIAN_POINT('Ctrl Pts',(5.12711364669926,1078.42692617282,519.939853630472));
#113499=CARTESIAN_POINT('Ctrl Pts',(5.05124133802895,1078.42669038935,519.948016191585));
#113500=CARTESIAN_POINT('Ctrl Pts',(5.00938081825521,1078.4264368938,519.954641736164));
#113501=CARTESIAN_POINT('Ctrl Pts',(4.8895661263475,1078.42535140423,519.979775649532));
#113502=CARTESIAN_POINT('Ctrl Pts',(4.81293137931116,1078.4242079663,520.003555250756));
#113503=CARTESIAN_POINT('Ctrl Pts',(4.58267075101719,1078.41932327351,520.099540578291));
#113504=CARTESIAN_POINT('Ctrl Pts',(4.44089451496295,1078.41415836311,520.195207371471));
#113505=CARTESIAN_POINT('Ctrl Pts',(4.22049218825775,1078.40154123029,520.418542072107));
#113506=CARTESIAN_POINT('Ctrl Pts',(4.13725392248797,1078.39462437085,520.537830179254));
#113507=CARTESIAN_POINT('Ctrl Pts',(4.00946983763835,1078.37842393442,520.809327539929));
#113508=CARTESIAN_POINT('Ctrl Pts',(3.96953552233366,1078.369129991,520.961113743919));
#113509=CARTESIAN_POINT('Ctrl Pts',(3.94541821257091,1078.34887208769,521.28291686476));
#113510=CARTESIAN_POINT('Ctrl Pts',(3.96579518517392,1078.33802735926,521.450380534731));
#113511=CARTESIAN_POINT('Ctrl Pts',(4.07008287336911,1078.31687155432,521.768310256668));
#113512=CARTESIAN_POINT('Ctrl Pts',(4.15315534560916,1078.30676716075,521.915686450277));
#113513=CARTESIAN_POINT('Ctrl Pts',(4.36504648521359,1078.28939875751,522.16229956733));
#113514=CARTESIAN_POINT('Ctrl Pts',(4.48900779682275,1078.28215291433,522.261786289363));
#113515=CARTESIAN_POINT('Ctrl Pts',(4.74619359579404,1078.27175418726,522.399410159));
#113516=CARTESIAN_POINT('Ctrl Pts',(4.87363429925156,1078.26821717801,522.443642503963));
#113517=CARTESIAN_POINT('Ctrl Pts',(5.06037071587576,1078.26520873888,522.476976489007));
#113518=CARTESIAN_POINT('Ctrl Pts',(5.11567542033187,1078.26457243175,522.483157480549));
#113519=CARTESIAN_POINT('Ctrl Pts',(5.1907150622956,1078.26405133865,522.486607255741));
#113520=CARTESIAN_POINT('Ctrl Pts',(5.21023899255782,1078.2639468725,522.487055943604));
#113521=CARTESIAN_POINT('Ctrl Pts',(5.22976567235167,1078.26387350206,522.487056209884));
#113522=CARTESIAN_POINT('',(5.22978306523924,1076.42335637261,519.93616796773));
#113523=CARTESIAN_POINT('',(5.22978306525629,1067.7251047501,519.936167967731));
#113524=CARTESIAN_POINT('Ctrl Pts',(5.22980079484193,1076.2587132809,522.487056209879));
#113525=CARTESIAN_POINT('Ctrl Pts',(5.06334132967647,1076.25934481001,522.487058523785));
#113526=CARTESIAN_POINT('Ctrl Pts',(4.89851973416088,1076.26225948526,522.454474761201));
#113527=CARTESIAN_POINT('Ctrl Pts',(4.59076760731962,1076.27222559529,522.327899665305));
#113528=CARTESIAN_POINT('Ctrl Pts',(4.45082336662027,1076.27917657429,522.235143334438));
#113529=CARTESIAN_POINT('Ctrl Pts',(4.21418460098485,1076.29605216036,522.000976871181));
#113530=CARTESIAN_POINT('Ctrl Pts',(4.11987400053696,1076.30581788062,521.861691349361));
#113531=CARTESIAN_POINT('Ctrl Pts',(4.02251851690844,1076.32148184635,521.63141390347));
#113532=CARTESIAN_POINT('Ctrl Pts',(3.99764721524802,1076.32684141485,521.551554199838));
#113533=CARTESIAN_POINT('Ctrl Pts',(3.9638497969926,1076.33765889563,521.388082127266));
#113534=CARTESIAN_POINT('Ctrl Pts',(3.95501449308845,1076.34309116847,521.304854850028));
#113535=CARTESIAN_POINT('Ctrl Pts',(3.95309841160809,1076.35922309317,521.054214952404));
#113536=CARTESIAN_POINT('Ctrl Pts',(3.98469064664019,1076.36958810969,520.888396373723));
#113537=CARTESIAN_POINT('Ctrl Pts',(4.1106920745005,1076.38852965609,520.576876803706));
#113538=CARTESIAN_POINT('Ctrl Pts',(4.20445407101636,1076.39690587049,520.434440461867));
#113539=CARTESIAN_POINT('Ctrl Pts',(4.44186123868912,1076.41059644603,520.194584052986));
#113540=CARTESIAN_POINT('Ctrl Pts',(4.58304544841294,1076.41578739126,520.099437952901));
#113541=CARTESIAN_POINT('Ctrl Pts',(4.89450892846827,1076.42247147271,519.969495721745));
#113542=CARTESIAN_POINT('Ctrl Pts',(5.06170769696453,1076.42389732787,519.936064006097));
#113543=CARTESIAN_POINT('Ctrl Pts',(5.39938269945827,1076.42281054014,519.936272384284));
#113544=CARTESIAN_POINT('Ctrl Pts',(5.56647947264613,1076.42030932585,519.969890272096));
#113545=CARTESIAN_POINT('Ctrl Pts',(5.87772196664879,1076.41157710857,520.100139449533));
#113546=CARTESIAN_POINT('Ctrl Pts',(6.01878590088497,1076.40543149535,520.195426699665));
#113547=CARTESIAN_POINT('Ctrl Pts',(6.25611337178095,1076.39004924351,520.435704605549));
#113548=CARTESIAN_POINT('Ctrl Pts',(6.34983577046797,1076.38094815867,520.578502077093));
#113549=CARTESIAN_POINT('Ctrl Pts',(6.44397685863669,1076.36595130184,520.812380823332));
#113550=CARTESIAN_POINT('Ctrl Pts',(6.46738234656901,1076.36081768811,520.892242468003));
#113551=CARTESIAN_POINT('Ctrl Pts',(6.49858790273712,1076.35021220659,521.05667062681));
#113552=CARTESIAN_POINT('Ctrl Pts',(6.50605498115587,1076.34476192239,521.140893103485));
#113553=CARTESIAN_POINT('Ctrl Pts',(6.50336458026901,1076.32840192542,521.392865411299));
#113554=CARTESIAN_POINT('Ctrl Pts',(6.46854063521812,1076.317569398,521.558538406778));
#113555=CARTESIAN_POINT('Ctrl Pts',(6.33677561685729,1076.29736433717,521.866926855902));
#113556=CARTESIAN_POINT('Ctrl Pts',(6.24111209788622,1076.28819005243,522.00667543937));
#113557=CARTESIAN_POINT('Ctrl Pts',(6.00134838792477,1076.27297537825,522.240916764585));
#113558=CARTESIAN_POINT('Ctrl Pts',(5.85969373012418,1076.26708029017,522.333233951461));
#113559=CARTESIAN_POINT('Ctrl Pts',(5.55335213624406,1076.25966852185,522.4559852736));
#113560=CARTESIAN_POINT('Ctrl Pts',(5.39233178566741,1076.25809665599,522.487053950582));
#113561=CARTESIAN_POINT('Ctrl Pts',(5.22980079484193,1076.2587132809,522.487056209879));
#113562=CARTESIAN_POINT('Origin',(5.22978306525629,1067.7251047501,521.211612088867));
#113563=CARTESIAN_POINT('',(5.22978306525628,1076.30041692086,521.887056210003));
#113564=CARTESIAN_POINT('',(5.22978306525629,1076.38762615333,520.536167967731));
#113565=CARTESIAN_POINT('Ctrl Pts',(5.22978306525629,1076.30041692086,521.887056210003));
#113566=CARTESIAN_POINT('Ctrl Pts',(5.22636307154697,1076.30042942372,521.887056210003));
#113567=CARTESIAN_POINT('Ctrl Pts',(5.22294188876261,1076.30044368456,521.887030235228));
#113568=CARTESIAN_POINT('Ctrl Pts',(5.13132690531383,1076.30087259974,521.885638000346));
#113569=CARTESIAN_POINT('Ctrl Pts',(5.04426484962881,1076.30244826036,521.867036420831));
#113570=CARTESIAN_POINT('Ctrl Pts',(4.88220300795897,1076.30771664338,521.797439252864));
#113571=CARTESIAN_POINT('Ctrl Pts',(4.80878446062561,1076.31135809685,521.747105820346));
#113572=CARTESIAN_POINT('Ctrl Pts',(4.6853157352251,1076.3201938069,521.620985871368));
#113573=CARTESIAN_POINT('Ctrl Pts',(4.63651184212421,1076.32530547997,521.546351967946));
#113574=CARTESIAN_POINT('Ctrl Pts',(4.58690612046484,1076.33353431322,521.423480691079));
#113575=CARTESIAN_POINT('Ctrl Pts',(4.57442202372235,1076.33635337301,521.380964969194));
#113576=CARTESIAN_POINT('Ctrl Pts',(4.55793561504524,1076.34205598278,521.294085861446));
#113577=CARTESIAN_POINT('Ctrl Pts',(4.55397770763807,1076.34492602243,521.249927569434));
#113578=CARTESIAN_POINT('Ctrl Pts',(4.55514010358894,1076.35347245615,521.117123388698));
#113579=CARTESIAN_POINT('Ctrl Pts',(4.57333251787838,1076.35899405347,521.029538666631));
#113580=CARTESIAN_POINT('Ctrl Pts',(4.64300463506706,1076.36914822281,520.865213839047));
#113581=CARTESIAN_POINT('Ctrl Pts',(4.69425883575052,1076.37366755107,520.790273191389));
#113582=CARTESIAN_POINT('Ctrl Pts',(4.82297891891141,1076.38103583083,520.665006597796));
#113583=CARTESIAN_POINT('Ctrl Pts',(4.89908587152979,1076.3838173038,520.615863343598));
#113584=CARTESIAN_POINT('Ctrl Pts',(5.06132194296739,1076.38721072309,520.55206546916));
#113585=CARTESIAN_POINT('Ctrl Pts',(5.14517421313421,1076.38790802239,520.536167967731));
#113586=CARTESIAN_POINT('Ctrl Pts',(5.2297830652563,1076.38762615333,520.536167967731));
#113587=CARTESIAN_POINT('',(5.22978306525629,1082.7251047501,520.536167967731));
#113588=CARTESIAN_POINT('',(5.22978306525629,1067.7251047501,520.536167967731));
#113589=CARTESIAN_POINT('Origin',(5.22978306525629,1082.7251047501,521.211612088867));
#113590=CARTESIAN_POINT('Ctrl Pts',(5.22978353114544,1076.38762615178,520.536167967731));
#113591=CARTESIAN_POINT('Ctrl Pts',(5.31949312756942,1076.38732728611,520.536168029608));
#113592=CARTESIAN_POINT('Ctrl Pts',(5.40829400123085,1076.38593355036,520.554040101875));
#113593=CARTESIAN_POINT('Ctrl Pts',(5.57378252673664,1076.3810882742,520.623438541529));
#113594=CARTESIAN_POINT('Ctrl Pts',(5.64879219423385,1076.37768222906,520.674300510113));
#113595=CARTESIAN_POINT('Ctrl Pts',(5.77476330846205,1076.36923107347,520.802549715811));
#113596=CARTESIAN_POINT('Ctrl Pts',(5.82436604459513,1076.36426296791,520.878752565947));
#113597=CARTESIAN_POINT('Ctrl Pts',(5.87406002213901,1076.35612839439,521.003936693618));
#113598=CARTESIAN_POINT('Ctrl Pts',(5.88638390275323,1076.35333417558,521.047002303802));
#113599=CARTESIAN_POINT('Ctrl Pts',(5.90226938780586,1076.34766152172,521.134506038321));
#113600=CARTESIAN_POINT('Ctrl Pts',(5.90587551991134,1076.34479763704,521.17871891908));
#113601=CARTESIAN_POINT('Ctrl Pts',(5.90364065959751,1076.33619212936,521.311671849643));
#113602=CARTESIAN_POINT('Ctrl Pts',(5.88468608857278,1076.33053182074,521.399237546016));
#113603=CARTESIAN_POINT('Ctrl Pts',(5.81400676365003,1076.32005684067,521.562005230839));
#113604=CARTESIAN_POINT('Ctrl Pts',(5.76298003150811,1076.31534364291,521.635646812019));
#113605=CARTESIAN_POINT('Ctrl Pts',(5.63545941022927,1076.30757189409,521.758873402087));
#113606=CARTESIAN_POINT('Ctrl Pts',(5.56026352919896,1076.30458642456,521.807314975803));
#113607=CARTESIAN_POINT('Ctrl Pts',(5.3988307917615,1076.3008809691,521.871052324356));
#113608=CARTESIAN_POINT('Ctrl Pts',(5.31467323103817,1076.30010657814,521.887056210003));
#113609=CARTESIAN_POINT('Ctrl Pts',(5.22978306525629,1076.30041692086,521.887056210003));
#113610=CARTESIAN_POINT('Origin',(-5.99814689883715,1067.7251047501,529.320363258268));
#113611=CARTESIAN_POINT('',(-5.99814689886821,1075.76695399575,528.221532122276));
#113612=CARTESIAN_POINT('',(-5.99814689883715,1067.7251047501,528.221532122276));
#113613=CARTESIAN_POINT('Ctrl Pts',(-5.99814221872999,1075.53855676448,
530.419194394251));
#113614=CARTESIAN_POINT('Ctrl Pts',(-6.14120201009968,1075.53767312577,
530.419195003567));
#113615=CARTESIAN_POINT('Ctrl Pts',(-6.28284864094654,1075.53981354691,
530.391258873147));
#113616=CARTESIAN_POINT('Ctrl Pts',(-6.5475753084573,1075.54986582568,530.282678498626));
#113617=CARTESIAN_POINT('Ctrl Pts',(-6.66800732574684,1075.5576831081,530.203049841736));
#113618=CARTESIAN_POINT('Ctrl Pts',(-6.8720519362554,1075.5779410052,530.001808475949));
#113619=CARTESIAN_POINT('Ctrl Pts',(-6.95347628374648,1075.59020773967,
529.881918882545));
#113620=CARTESIAN_POINT('Ctrl Pts',(-7.06594680082405,1075.6175154686,529.61710135549));
#113621=CARTESIAN_POINT('Ctrl Pts',(-7.0956189940278,1075.63231181689,529.474535113313));
#113622=CARTESIAN_POINT('Ctrl Pts',(-7.09758769177086,1075.6548203051,529.258453798557));
#113623=CARTESIAN_POINT('Ctrl Pts',(-7.09118015406157,1075.66231536263,
529.18663729525));
#113624=CARTESIAN_POINT('Ctrl Pts',(-7.05063852966411,1075.68470750054,
528.972498566485));
#113625=CARTESIAN_POINT('Ctrl Pts',(-6.99513672767571,1075.69906109191,
528.835785138501));
#113626=CARTESIAN_POINT('Ctrl Pts',(-6.83413894957984,1075.72479847781,
528.592548127098));
#113627=CARTESIAN_POINT('Ctrl Pts',(-6.73045584163645,1075.73594775202,
528.488255337386));
#113628=CARTESIAN_POINT('Ctrl Pts',(-6.48813180567354,1075.75368495786,
528.326076586428));
#113629=CARTESIAN_POINT('Ctrl Pts',(-6.35192389613001,1075.76009563144,
528.269841643617));
#113630=CARTESIAN_POINT('Ctrl Pts',(-6.06508096297714,1075.76733907375,
528.21386801996));
#113631=CARTESIAN_POINT('Ctrl Pts',(-5.91738958264268,1075.76809081394,
528.214787290593));
#113632=CARTESIAN_POINT('Ctrl Pts',(-5.63115141807019,1075.76377400335,
528.274373072617));
#113633=CARTESIAN_POINT('Ctrl Pts',(-5.49555571288412,1075.75875452978,
528.332369224935));
#113634=CARTESIAN_POINT('Ctrl Pts',(-5.25520570932623,1075.74351803806,
528.497730718745));
#113635=CARTESIAN_POINT('Ctrl Pts',(-5.1528562515381,1075.73345837417,528.603363975249));
#113636=CARTESIAN_POINT('Ctrl Pts',(-4.99509660502515,1075.70946886991,
528.848516262205));
#113637=CARTESIAN_POINT('Ctrl Pts',(-4.94140800577116,1075.69576066359,
528.98572124902));
#113638=CARTESIAN_POINT('Ctrl Pts',(-4.90361508272451,1075.67392971182,
529.199742450141));
#113639=CARTESIAN_POINT('Ctrl Pts',(-4.89808675040854,1075.66656836557,
529.271236972101));
#113640=CARTESIAN_POINT('Ctrl Pts',(-4.9010069329658,1075.65167221851,529.414558490779));
#113641=CARTESIAN_POINT('Ctrl Pts',(-4.90950759888245,1075.64417115885,
529.486055197811));
#113642=CARTESIAN_POINT('Ctrl Pts',(-4.95627999852536,1075.6216317123,529.698892705372));
#113643=CARTESIAN_POINT('Ctrl Pts',(-5.01579579578355,1075.6070316305,529.833987059212));
#113644=CARTESIAN_POINT('Ctrl Pts',(-5.18327558174302,1075.58082906822,
530.071537681488));
#113645=CARTESIAN_POINT('Ctrl Pts',(-5.28901001441675,1075.56944370285,
530.172118720282));
#113646=CARTESIAN_POINT('Ctrl Pts',(-5.53287583850086,1075.5514482599,530.326156258603));
#113647=CARTESIAN_POINT('Ctrl Pts',(-5.66840793539604,1075.54498741651,
530.378396404296));
#113648=CARTESIAN_POINT('Ctrl Pts',(-5.87230887821545,1075.53991780616,
530.413779398576));
#113649=CARTESIAN_POINT('Ctrl Pts',(-5.93516279572556,1075.53894577005,
530.419194126011));
#113650=CARTESIAN_POINT('Ctrl Pts',(-5.99814221873,1075.53855676448,530.419194394251));
#113651=CARTESIAN_POINT('Origin',(-5.99814689883715,1067.7251047501,529.320363258268));
#113652=CARTESIAN_POINT('',(-5.99814689883715,1075.60310529676,529.819194394261));
#113653=CARTESIAN_POINT('',(-5.99814689883715,1075.70679891916,528.821532122276));
#113654=CARTESIAN_POINT('Ctrl Pts',(-5.99814689883716,1075.60310529676,
529.819194394261));
#113655=CARTESIAN_POINT('Ctrl Pts',(-6.03252410608921,1075.60289709975,
529.819194394261));
#113656=CARTESIAN_POINT('Ctrl Pts',(-6.0668923489677,1075.60306468037,529.815640697523));
#113657=CARTESIAN_POINT('Ctrl Pts',(-6.16429428135216,1075.60463756082,
529.79517970399));
#113658=CARTESIAN_POINT('Ctrl Pts',(-6.22462787047192,1075.60698346613,
529.769530387408));
#113659=CARTESIAN_POINT('Ctrl Pts',(-6.33224176667914,1075.61403827695,
529.696474753279));
#113660=CARTESIAN_POINT('Ctrl Pts',(-6.37840974236614,1075.61868677132,
529.649699848775));
#113661=CARTESIAN_POINT('Ctrl Pts',(-6.45036121560613,1075.6296835713,529.540855683966));
#113662=CARTESIAN_POINT('Ctrl Pts',(-6.47532694324519,1075.6359358906,529.479740397663));
#113663=CARTESIAN_POINT('Ctrl Pts',(-6.49404293736756,1075.6458684236,529.38351500831));
#113664=CARTESIAN_POINT('Ctrl Pts',(-6.49711397960339,1075.64924946972,
529.350896666296));
#113665=CARTESIAN_POINT('Ctrl Pts',(-6.49683309921706,1075.65604511042,
529.285593986273));
#113666=CARTESIAN_POINT('Ctrl Pts',(-6.49349267468341,1075.65944396227,
529.253060472506));
#113667=CARTESIAN_POINT('Ctrl Pts',(-6.47376400397003,1075.66963383704,
529.155915340796));
#113668=CARTESIAN_POINT('Ctrl Pts',(-6.44762122171576,1075.67618441246,
529.094002601275));
#113669=CARTESIAN_POINT('Ctrl Pts',(-6.37262348355696,1075.68793821837,
528.984198403479));
#113670=CARTESIAN_POINT('Ctrl Pts',(-6.32457509952072,1075.69303023553,
528.937346833578));
#113671=CARTESIAN_POINT('Ctrl Pts',(-6.21340227194694,1075.70103774583,
528.865579339296));
#113672=CARTESIAN_POINT('Ctrl Pts',(-6.15155160596148,1075.70389643969,
528.841152365395));
#113673=CARTESIAN_POINT('Ctrl Pts',(-6.05747564078982,1075.70618097767,
528.824183865406));
#113674=CARTESIAN_POINT('Ctrl Pts',(-6.02784296238916,1075.70662516651,
528.821532122276));
#113675=CARTESIAN_POINT('Ctrl Pts',(-5.99814689883715,1075.70679891916,
528.821532122276));
#113676=CARTESIAN_POINT('',(-5.99814689883715,1082.7251047501,528.821532122276));
#113677=CARTESIAN_POINT('',(-5.99814689883715,1067.7251047501,528.821532122276));
#113678=CARTESIAN_POINT('Origin',(-5.99814689883715,1082.7251047501,529.320363258268));
#113679=CARTESIAN_POINT('Ctrl Pts',(-5.99814673263117,1075.70679892014,
528.821532122276));
#113680=CARTESIAN_POINT('Ctrl Pts',(-5.93313362101752,1075.70717931179,
528.821532143938));
#113681=CARTESIAN_POINT('Ctrl Pts',(-5.86876118686279,1075.70625867822,
528.834241700176));
#113682=CARTESIAN_POINT('Ctrl Pts',(-5.74837980993453,1075.70190989668,
528.88367758071));
#113683=CARTESIAN_POINT('Ctrl Pts',(-5.69359049502711,1075.69851786768,
528.91997694178));
#113684=CARTESIAN_POINT('Ctrl Pts',(-5.60005316507632,1075.68957579206,
529.012501767536));
#113685=CARTESIAN_POINT('Ctrl Pts',(-5.56264141879102,1075.68406867106,
529.068221741975));
#113686=CARTESIAN_POINT('Ctrl Pts',(-5.51176420879098,1075.67169092605,
529.191122729049));
#113687=CARTESIAN_POINT('Ctrl Pts',(-5.49888335354078,1075.66493707847,
529.25713215309));
#113688=CARTESIAN_POINT('Ctrl Pts',(-5.49954408692235,1075.65463529819,
529.356290523305));
#113689=CARTESIAN_POINT('Ctrl Pts',(-5.5029573133427,1075.65123350083,529.388795264001));
#113690=CARTESIAN_POINT('Ctrl Pts',(-5.52297899150482,1075.64095736565,
529.486265039177));
#113691=CARTESIAN_POINT('Ctrl Pts',(-5.54949426896431,1075.63429345119,
529.548463741102));
#113692=CARTESIAN_POINT('Ctrl Pts',(-5.6247105130087,1075.6224060827,529.657507757935));
#113693=CARTESIAN_POINT('Ctrl Pts',(-5.67218601133138,1075.6172679483,529.703622592007));
#113694=CARTESIAN_POINT('Ctrl Pts',(-5.78205417802778,1075.60911836451,
529.774664701286));
#113695=CARTESIAN_POINT('Ctrl Pts',(-5.84327982710687,1075.60617454501,
529.799023140969));
#113696=CARTESIAN_POINT('Ctrl Pts',(-5.93747642234815,1075.60376521422,
529.816427903331));
#113697=CARTESIAN_POINT('Ctrl Pts',(-5.96781514998269,1075.60328899345,
529.819194394261));
#113698=CARTESIAN_POINT('Ctrl Pts',(-5.99814689883716,1075.60310529676,
529.819194394261));
#113699=CARTESIAN_POINT('Origin',(-18.7711528398113,1067.7251047501,535.019860978405));
#113700=CARTESIAN_POINT('',(-18.7711528398381,1074.94531439476,533.929320229677));
#113701=CARTESIAN_POINT('',(-18.7711528398113,1067.7251047501,533.929320229677));
#113702=CARTESIAN_POINT('Ctrl Pts',(-18.7711547684023,1074.65422624396,
536.110401727132));
#113703=CARTESIAN_POINT('Ctrl Pts',(-18.9127131527175,1074.65093863987,
536.11040147679));
#113704=CARTESIAN_POINT('Ctrl Pts',(-19.0529112739059,1074.65144815089,
536.082839303297));
#113705=CARTESIAN_POINT('Ctrl Pts',(-19.3149494445529,1074.65999650034,
535.975688086813));
#113706=CARTESIAN_POINT('Ctrl Pts',(-19.4341264139645,1074.6679489259,535.89717792505));
#113707=CARTESIAN_POINT('Ctrl Pts',(-19.636505420761,1074.69028812969,535.698608584391));
#113708=CARTESIAN_POINT('Ctrl Pts',(-19.7174230174435,1074.70450182111,
535.580191978784));
#113709=CARTESIAN_POINT('Ctrl Pts',(-19.8298594761071,1074.73735176127,
535.318125738536));
#113710=CARTESIAN_POINT('Ctrl Pts',(-19.8597900299775,1074.75571916076,
535.176709440408));
#113711=CARTESIAN_POINT('Ctrl Pts',(-19.8634602527513,1074.79438921212,
534.887640108292));
#113712=CARTESIAN_POINT('Ctrl Pts',(-19.8359479568745,1074.81435732531,
534.742657657127));
#113713=CARTESIAN_POINT('Ctrl Pts',(-19.7258905597185,1074.85260860472,
534.473289331668));
#113714=CARTESIAN_POINT('Ctrl Pts',(-19.6448535671405,1074.8705466394,534.351265782043));
#113715=CARTESIAN_POINT('Ctrl Pts',(-19.4400133171832,1074.90207526721,
534.146502177501));
#113716=CARTESIAN_POINT('Ctrl Pts',(-19.3184540089299,1074.91538485099,
534.065539747917));
#113717=CARTESIAN_POINT('Ctrl Pts',(-19.0505079984785,1074.93567743386,
533.955827468364));
#113718=CARTESIAN_POINT('Ctrl Pts',(-18.9069088925942,1074.94246286451,
533.92813471574));
#113719=CARTESIAN_POINT('Ctrl Pts',(-18.6203036704244,1074.94849365463,
533.930555427321));
#113720=CARTESIAN_POINT('Ctrl Pts',(-18.4802603852379,1074.94784777991,
533.959335194944));
#113721=CARTESIAN_POINT('Ctrl Pts',(-18.2186702056287,1074.93936104051,
534.068960620253));
#113722=CARTESIAN_POINT('Ctrl Pts',(-18.0998305093355,1074.9315850408,534.148839297154));
#113723=CARTESIAN_POINT('Ctrl Pts',(-17.897283572241,1074.90957296588,534.351561473377));
#113724=CARTESIAN_POINT('Ctrl Pts',(-17.8165022098086,1074.89541815361,
534.473257285375));
#113725=CARTESIAN_POINT('Ctrl Pts',(-17.7067821425449,1074.8625410088,534.741437244337));
#113726=CARTESIAN_POINT('Ctrl Pts',(-17.6792550977401,1074.84411004723,
534.885446175479));
#113727=CARTESIAN_POINT('Ctrl Pts',(-17.6813553440007,1074.81530924104,
535.101679459));
#113728=CARTESIAN_POINT('Ctrl Pts',(-17.6890237594445,1074.80567512096,
535.172656662161));
#113729=CARTESIAN_POINT('Ctrl Pts',(-17.7334786396821,1074.7761677942,535.385953587735));
#113730=CARTESIAN_POINT('Ctrl Pts',(-17.7920876144873,1074.75654137926,
535.522139528844));
#113731=CARTESIAN_POINT('Ctrl Pts',(-17.9580613663079,1074.72056985167,
535.760683714768));
#113732=CARTESIAN_POINT('Ctrl Pts',(-18.0627989601439,1074.70450255018,
535.861468498097));
#113733=CARTESIAN_POINT('Ctrl Pts',(-18.3046595839089,1074.67794315162,
536.015874947154));
#113734=CARTESIAN_POINT('Ctrl Pts',(-18.439095365224,1074.66765942824,536.068441902923));
#113735=CARTESIAN_POINT('Ctrl Pts',(-18.6431240172495,1074.65797102832,
536.104752084804));
#113736=CARTESIAN_POINT('Ctrl Pts',(-18.7070637566873,1074.65571471724,
536.110401840475));
#113737=CARTESIAN_POINT('Ctrl Pts',(-18.7711547684023,1074.65422624396,
536.110401727132));
#113738=CARTESIAN_POINT('Origin',(-18.7711528398113,1067.7251047501,535.019860978405));
#113739=CARTESIAN_POINT('',(-18.7711528398113,1074.73625576269,535.510401727133));
#113740=CARTESIAN_POINT('',(-18.7711528398123,1074.86719845859,534.529320229677));
#113741=CARTESIAN_POINT('Ctrl Pts',(-18.7711528398114,1074.73625576269,
535.510401727133));
#113742=CARTESIAN_POINT('Ctrl Pts',(-18.8052066733967,1074.73547473995,
535.510401727133));
#113743=CARTESIAN_POINT('Ctrl Pts',(-18.8392574174682,1074.73517201613,
535.506855701214));
#113744=CARTESIAN_POINT('Ctrl Pts',(-18.9350338741057,1074.73571041669,
535.486580018099));
#113745=CARTESIAN_POINT('Ctrl Pts',(-18.9941097748032,1074.73775213253,
535.461405442099));
#113746=CARTESIAN_POINT('Ctrl Pts',(-19.0995598509404,1074.74498546157,
535.389808231347));
#113747=CARTESIAN_POINT('Ctrl Pts',(-19.1448107129023,1074.75011964075,
535.344000007114));
#113748=CARTESIAN_POINT('Ctrl Pts',(-19.2155424766701,1074.76284773375,
535.237311807002));
#113749=CARTESIAN_POINT('Ctrl Pts',(-19.2401396458003,1074.77034151344,
535.177322032859));
#113750=CARTESIAN_POINT('Ctrl Pts',(-19.2587048565978,1074.78258398033,
535.082793576055));
#113751=CARTESIAN_POINT('Ctrl Pts',(-19.261781551059,1074.78681388689,535.050669961364));
#113752=CARTESIAN_POINT('Ctrl Pts',(-19.2616018415929,1074.79542137452,
534.98632695665));
#113753=CARTESIAN_POINT('Ctrl Pts',(-19.258348824959,1074.79977944901,534.954252870605));
#113754=CARTESIAN_POINT('Ctrl Pts',(-19.2390031904703,1074.81299654071,
534.858484243277));
#113755=CARTESIAN_POINT('Ctrl Pts',(-19.2132684912105,1074.82170607306,
534.797434470212));
#113756=CARTESIAN_POINT('Ctrl Pts',(-19.1394197922584,1074.83774227509,
534.689294666574));
#113757=CARTESIAN_POINT('Ctrl Pts',(-19.0921328220124,1074.84492216286,
534.643172922295));
#113758=CARTESIAN_POINT('Ctrl Pts',(-18.9822466284785,1074.8567815164,534.572280588167));
#113759=CARTESIAN_POINT('Ctrl Pts',(-18.9208165985547,1074.86135101369,
534.548146307163));
#113760=CARTESIAN_POINT('Ctrl Pts',(-18.8282424568846,1074.86558707483,
534.531817674485));
#113761=CARTESIAN_POINT('Ctrl Pts',(-18.7997335851328,1074.86655681678,
534.529320597696));
#113762=CARTESIAN_POINT('Ctrl Pts',(-18.7711591569468,1074.86719831677,
534.529320229717));
#113763=CARTESIAN_POINT('',(-18.7711528398113,1082.7251047501,534.529320229677));
#113764=CARTESIAN_POINT('',(-18.7711528398113,1067.7251047501,534.529320229677));
#113765=CARTESIAN_POINT('Origin',(-18.7711528398113,1082.7251047501,535.019860978405));
#113766=CARTESIAN_POINT('Ctrl Pts',(-18.7711528398145,1074.86719845859,
534.529320229677));
#113767=CARTESIAN_POINT('Ctrl Pts',(-18.7074504788267,1074.86862847736,
534.529320229676));
#113768=CARTESIAN_POINT('Ctrl Pts',(-18.6443653971043,1074.86840674218,
534.541727296054));
#113769=CARTESIAN_POINT('Ctrl Pts',(-18.5263471574557,1074.86468127263,
534.59000816825));
#113770=CARTESIAN_POINT('Ctrl Pts',(-18.4726342372528,1074.86120870885,
534.625436830946));
#113771=CARTESIAN_POINT('Ctrl Pts',(-18.3805410345879,1074.85130297252,
534.715984699392));
#113772=CARTESIAN_POINT('Ctrl Pts',(-18.3435923279513,1074.84489038946,
534.770698752533));
#113773=CARTESIAN_POINT('Ctrl Pts',(-18.2931913483521,1074.83000282662,
534.891464050108));
#113774=CARTESIAN_POINT('Ctrl Pts',(-18.2803538904494,1074.82166400125,
534.95638013702));
#113775=CARTESIAN_POINT('Ctrl Pts',(-18.280744529368,1074.80866099614,535.053908368051));
#113776=CARTESIAN_POINT('Ctrl Pts',(-18.2840201429532,1074.80432025391,
535.085896769819));
#113777=CARTESIAN_POINT('Ctrl Pts',(-18.3034686683672,1074.79107069298,
535.181823794996));
#113778=CARTESIAN_POINT('Ctrl Pts',(-18.3293979746482,1074.78228336716,
535.243077568395));
#113779=CARTESIAN_POINT('Ctrl Pts',(-18.4034963443633,1074.76611618187,
535.351058366833));
#113780=CARTESIAN_POINT('Ctrl Pts',(-18.4506742638047,1074.75887395473,
535.396933453209));
#113781=CARTESIAN_POINT('Ctrl Pts',(-18.5594922362588,1074.74695625201,
535.467015424092));
#113782=CARTESIAN_POINT('Ctrl Pts',(-18.6198148560792,1074.74235630109,
535.490890599223));
#113783=CARTESIAN_POINT('Ctrl Pts',(-18.7122310511654,1074.737965022,535.507747898848));
#113784=CARTESIAN_POINT('Ctrl Pts',(-18.741693101653,1074.73693142012,535.510401727133));
#113785=CARTESIAN_POINT('Ctrl Pts',(-18.7711528398114,1074.73625576269,
535.510401727133));
#113786=CARTESIAN_POINT('Origin',(32.7463814565115,1067.7251047501,507.977010932744));
#113787=CARTESIAN_POINT('',(32.7463814565274,1078.70364178837,506.498707800551));
#113788=CARTESIAN_POINT('Ctrl Pts',(32.746381249705,1078.63286819012,509.455314064938));
#113789=CARTESIAN_POINT('Ctrl Pts',(32.8530883738035,1078.63158555358,509.455314079865));
#113790=CARTESIAN_POINT('Ctrl Pts',(32.9594854661601,1078.63064964346,509.443760592605));
#113791=CARTESIAN_POINT('Ctrl Pts',(33.1088409948913,1078.62984872399,509.410935027859));
#113792=CARTESIAN_POINT('Ctrl Pts',(33.1534811694462,1078.62967771172,509.398905830537));
#113793=CARTESIAN_POINT('Ctrl Pts',(33.2287140077989,1078.62950852055,509.37479878059));
#113794=CARTESIAN_POINT('Ctrl Pts',(33.259601718698,1078.62947461873,509.363755510969));
#113795=CARTESIAN_POINT('Ctrl Pts',(33.3212695661467,1078.6294797426,509.339364625878));
#113796=CARTESIAN_POINT('Ctrl Pts',(33.3520141050007,1078.6295204057,509.325978320393));
#113797=CARTESIAN_POINT('Ctrl Pts',(33.425732677801,1078.62971187988,509.290852331071));
#113798=CARTESIAN_POINT('Ctrl Pts',(33.4681509056471,1078.62990288716,509.268036147716));
#113799=CARTESIAN_POINT('Ctrl Pts',(33.6098471373868,1078.63082348265,509.182650210039));
#113800=CARTESIAN_POINT('Ctrl Pts',(33.7027488741016,1078.63193032042,509.11036813935));
#113801=CARTESIAN_POINT('Ctrl Pts',(33.8919237564726,1078.6353742331,508.923194780199));
#113802=CARTESIAN_POINT('Ctrl Pts',(33.9813026708042,1078.63794233723,508.803143557609));
#113803=CARTESIAN_POINT('Ctrl Pts',(34.1286423123368,1078.64438119282,508.526425675508));
#113804=CARTESIAN_POINT('Ctrl Pts',(34.1812054924937,1078.6483141616,508.369153075442));
#113805=CARTESIAN_POINT('Ctrl Pts',(34.2343278509573,1078.65708324799,508.031074808779));
#113806=CARTESIAN_POINT('Ctrl Pts',(34.2300629419761,1078.66189058216,507.852131119818));
#113807=CARTESIAN_POINT('Ctrl Pts',(34.1557398485126,1078.67172127962,507.491972217516));
#113808=CARTESIAN_POINT('Ctrl Pts',(34.0817114223846,1078.67664045808,507.314852952749));
#113809=CARTESIAN_POINT('Ctrl Pts',(33.8681203401151,1078.6857116655,506.994677135991));
#113810=CARTESIAN_POINT('Ctrl Pts',(33.7291469399183,1078.68975641361,506.855646134404));
#113811=CARTESIAN_POINT('Ctrl Pts',(33.4132955946416,1078.69637206553,506.644772208427));
#113812=CARTESIAN_POINT('Ctrl Pts',(33.2414232158748,1078.69895404166,506.571815420625));
#113813=CARTESIAN_POINT('Ctrl Pts',(32.8835406774432,1078.70283010831,506.493978948077));
#113814=CARTESIAN_POINT('Ctrl Pts',(32.7009432313531,1078.70412328656,506.488342087204));
#113815=CARTESIAN_POINT('Ctrl Pts',(32.4619675773265,1078.70507352566,506.525059311246));
#113816=CARTESIAN_POINT('Ctrl Pts',(32.4026747434072,1078.70524517313,506.537941612906));
#113817=CARTESIAN_POINT('Ctrl Pts',(32.3096229670037,1078.70541410203,506.564239275755));
#113818=CARTESIAN_POINT('Ctrl Pts',(32.2752761156426,1078.70545376003,506.575318564671));
#113819=CARTESIAN_POINT('Ctrl Pts',(32.2116579319089,1078.70548445708,506.598442732447));
#113820=CARTESIAN_POINT('Ctrl Pts',(32.1823008671319,1078.70548089485,506.610192503226));
#113821=CARTESIAN_POINT('Ctrl Pts',(32.117910599325,1078.70543316381,506.638391945824));
#113822=CARTESIAN_POINT('Ctrl Pts',(32.0831007699214,1078.70538011835,506.655294194597));
#113823=CARTESIAN_POINT('Ctrl Pts',(31.985606327637,1078.70515161966,506.707456083407));
#113824=CARTESIAN_POINT('Ctrl Pts',(31.9247770463984,1078.70491063041,506.745948620394));
#113825=CARTESIAN_POINT('Ctrl Pts',(31.708943380727,1078.70365917296,506.905674696418));
#113826=CARTESIAN_POINT('Ctrl Pts',(31.5758116824482,1078.70205794334,507.052997358032));
#113827=CARTESIAN_POINT('Ctrl Pts',(31.3919564298537,1078.69776982583,507.362510617041));
#113828=CARTESIAN_POINT('Ctrl Pts',(31.3323784741342,1078.69533634334,507.51585072257));
#113829=CARTESIAN_POINT('Ctrl Pts',(31.2630177861554,1078.68923740537,507.849126498867));
#113830=CARTESIAN_POINT('Ctrl Pts',(31.2583746304162,1078.68553075635,508.027517520772));
#113831=CARTESIAN_POINT('Ctrl Pts',(31.3143545699072,1078.67691354226,508.390286025321));
#113832=CARTESIAN_POINT('Ctrl Pts',(31.3792849940979,1078.67201134422,508.570760718543));
#113833=CARTESIAN_POINT('Ctrl Pts',(31.5763581202034,1078.66173191473,508.901341125006));
#113834=CARTESIAN_POINT('Ctrl Pts',(31.7082342859328,1078.65644880754,509.047335078825));
#113835=CARTESIAN_POINT('Ctrl Pts',(31.9687314017846,1078.64821972533,509.240919661813));
#113836=CARTESIAN_POINT('Ctrl Pts',(32.0825776875407,1078.64512142271,509.304253367899));
#113837=CARTESIAN_POINT('Ctrl Pts',(32.3761476239361,1078.63836207545,509.42022797339));
#113838=CARTESIAN_POINT('Ctrl Pts',(32.5604272617905,1078.63510338651,509.455314038924));
#113839=CARTESIAN_POINT('Ctrl Pts',(32.746381249705,1078.63286819012,509.455314064938));
#113840=CARTESIAN_POINT('',(32.7463814564926,1076.70329713523,506.498707800551));
#113841=CARTESIAN_POINT('',(32.7463814565115,1067.7251047501,506.498707800551));
#113842=CARTESIAN_POINT('Ctrl Pts',(32.7473303221479,1076.6316750193,509.455313760417));
#113843=CARTESIAN_POINT('Ctrl Pts',(32.5543036171815,1076.63401833412,509.455437656823));
#113844=CARTESIAN_POINT('Ctrl Pts',(32.363125508151,1076.63747722987,509.417754613386));
#113845=CARTESIAN_POINT('Ctrl Pts',(32.0060300173876,1076.64594260234,509.271048238892));
#113846=CARTESIAN_POINT('Ctrl Pts',(31.843551984202,1076.65086126279,509.163410266948));
#113847=CARTESIAN_POINT('Ctrl Pts',(31.5690105217389,1076.6612031598,508.891632046527));
#113848=CARTESIAN_POINT('Ctrl Pts',(31.4596450000888,1076.6665218222,508.73003448844));
#113849=CARTESIAN_POINT('Ctrl Pts',(31.3469010632648,1076.67414465603,508.46298095179));
#113850=CARTESIAN_POINT('Ctrl Pts',(31.3181416154283,1076.67660949418,508.370513264503));
#113851=CARTESIAN_POINT('Ctrl Pts',(31.2590373252825,1076.68373889658,508.084222303228));
#113852=CARTESIAN_POINT('Ctrl Pts',(31.2579203683751,1076.68798848716,507.8865678999));
#113853=CARTESIAN_POINT('Ctrl Pts',(31.3325849906484,1076.6951592245,507.503164611125));
#113854=CARTESIAN_POINT('Ctrl Pts',(31.4072871625381,1076.69802331024,507.321126044623));
#113855=CARTESIAN_POINT('Ctrl Pts',(31.6233655336458,1076.70236155665,506.995967508178));
#113856=CARTESIAN_POINT('Ctrl Pts',(31.7628279883748,1076.70379658765,506.856190921005));
#113857=CARTESIAN_POINT('Ctrl Pts',(32.0885502051469,1076.70530205959,506.638689396146));
#113858=CARTESIAN_POINT('Ctrl Pts',(32.2717140624998,1076.70535737953,506.563314533295));
#113859=CARTESIAN_POINT('Ctrl Pts',(32.6562536171745,1076.70407841855,506.488548271379));
#113860=CARTESIAN_POINT('Ctrl Pts',(32.8537795626229,1076.70275703919,506.489695857962));
#113861=CARTESIAN_POINT('Ctrl Pts',(33.2362057872882,1076.69865085437,506.568666071004));
#113862=CARTESIAN_POINT('Ctrl Pts',(33.4173962178751,1076.6959035228,506.645434850156));
#113863=CARTESIAN_POINT('Ctrl Pts',(33.7401441385592,1076.68895573799,506.865221058208));
#113864=CARTESIAN_POINT('Ctrl Pts',(33.8783610276179,1076.68481087431,507.006313388783));
#113865=CARTESIAN_POINT('Ctrl Pts',(34.0920129432897,1076.67541942983,507.334338046798));
#113866=CARTESIAN_POINT('Ctrl Pts',(34.1652348325223,1076.67026148756,507.518097419006));
#113867=CARTESIAN_POINT('Ctrl Pts',(34.2354602451169,1076.65969232901,507.901645069903));
#113868=CARTESIAN_POINT('Ctrl Pts',(34.2324865839961,1076.65439006213,508.097553038576));
#113869=CARTESIAN_POINT('Ctrl Pts',(34.1510038145265,1076.6445529373,508.477125912479));
#113870=CARTESIAN_POINT('Ctrl Pts',(34.0732448440796,1076.64012091762,508.657101987969));
#113871=CARTESIAN_POINT('Ctrl Pts',(33.8526860802714,1076.63307811178,508.976566882754));
#113872=CARTESIAN_POINT('Ctrl Pts',(33.7120890361442,1076.63054061637,509.112986843496));
#113873=CARTESIAN_POINT('Ctrl Pts',(33.3866049505424,1076.62795519261,509.323474590133));
#113874=CARTESIAN_POINT('Ctrl Pts',(33.2049862459164,1076.62792892676,509.395648404247));
#113875=CARTESIAN_POINT('Ctrl Pts',(32.9264542257899,1076.62974528757,509.447042578769));
#113876=CARTESIAN_POINT('Ctrl Pts',(32.8369865558007,1076.63058660627,509.455256213535));
#113877=CARTESIAN_POINT('Ctrl Pts',(32.7473303221479,1076.6316750193,509.455313760417));
#113878=CARTESIAN_POINT('Origin',(32.7463814565115,1067.7251047501,507.977010932744));
#113879=CARTESIAN_POINT('',(32.7463814565115,1076.64970661189,508.855314064937));
#113880=CARTESIAN_POINT('',(32.7463814541604,1076.69227114044,507.098707800551));
#113881=CARTESIAN_POINT('Ctrl Pts',(32.7463814565115,1076.64970661189,508.855314064937));
#113882=CARTESIAN_POINT('Ctrl Pts',(32.6369671703856,1076.65092157723,508.855314064937));
#113883=CARTESIAN_POINT('Ctrl Pts',(32.5284680697616,1076.65269351219,508.834867999844));
#113884=CARTESIAN_POINT('Ctrl Pts',(32.3195549767455,1076.65718584503,508.753168717285));
#113885=CARTESIAN_POINT('Ctrl Pts',(32.2218529608895,1076.65990155956,508.690781557422));
#113886=CARTESIAN_POINT('Ctrl Pts',(32.0559289775466,1076.66574613851,508.531895820681));
#113887=CARTESIAN_POINT('Ctrl Pts',(31.9893304978876,1076.66881699953,508.4368970313));
#113888=CARTESIAN_POINT('Ctrl Pts',(31.919725082527,1076.67333812372,508.279255429859));
#113889=CARTESIAN_POINT('Ctrl Pts',(31.9017403200052,1076.67482018496,508.224587282085));
#113890=CARTESIAN_POINT('Ctrl Pts',(31.8637451809236,1076.67918147736,508.054559231728));
#113891=CARTESIAN_POINT('Ctrl Pts',(31.8612648616058,1076.68187406866,507.936611800604));
#113892=CARTESIAN_POINT('Ctrl Pts',(31.9025351075754,1076.6865534672,507.707002540313));
#113893=CARTESIAN_POINT('Ctrl Pts',(31.945736976525,1076.68849857901,507.597599996767));
#113894=CARTESIAN_POINT('Ctrl Pts',(32.0724188694461,1076.69150946777,507.401854109998));
#113895=CARTESIAN_POINT('Ctrl Pts',(32.1547058196195,1076.69254664494,507.317501460307));
#113896=CARTESIAN_POINT('Ctrl Pts',(32.3476041347743,1076.69365919543,507.185772822873));
#113897=CARTESIAN_POINT('Ctrl Pts',(32.4563357059021,1076.69372312936,507.139780570975));
#113898=CARTESIAN_POINT('Ctrl Pts',(32.6287768372029,1076.6930768903,507.104613294972));
#113899=CARTESIAN_POINT('Ctrl Pts',(32.687577791763,1076.6927351604,507.098707800866));
#113900=CARTESIAN_POINT('Ctrl Pts',(32.7463814518093,1076.69227114044,507.098707800551));
#113901=CARTESIAN_POINT('',(32.7463814565115,1082.7251047501,507.098707800551));
#113902=CARTESIAN_POINT('',(32.7463814565115,1067.7251047501,507.098707800551));
#113903=CARTESIAN_POINT('Origin',(32.7463814565115,1082.7251047501,507.977010932744));
#113904=CARTESIAN_POINT('Ctrl Pts',(32.7463814518093,1076.69227114044,507.098707800551));
#113905=CARTESIAN_POINT('Ctrl Pts',(32.8037342847657,1076.69181856897,507.098707800244));
#113906=CARTESIAN_POINT('Ctrl Pts',(32.8610896909645,1076.6912496181,507.104325473822));
#113907=CARTESIAN_POINT('Ctrl Pts',(33.0318664443822,1076.6891790374,507.138271654048));
#113908=CARTESIAN_POINT('Ctrl Pts',(33.1404587774664,1076.68734536723,507.183483765153));
#113909=CARTESIAN_POINT('Ctrl Pts',(33.3338825170799,1076.68286219988,507.313771296859));
#113910=CARTESIAN_POINT('Ctrl Pts',(33.4167316120568,1076.68025276808,507.397638929314));
#113911=CARTESIAN_POINT('Ctrl Pts',(33.5445984446936,1076.67452752786,507.592548806499));
#113912=CARTESIAN_POINT('Ctrl Pts',(33.5884622035893,1076.67146883894,507.701583623083));
#113913=CARTESIAN_POINT('Ctrl Pts',(33.6188854603855,1076.66707695697,507.864716278004));
#113914=CARTESIAN_POINT('Ctrl Pts',(33.6238316626777,1076.66576974659,507.914125891656));
#113915=CARTESIAN_POINT('Ctrl Pts',(33.6245835404832,1076.66448388031,507.963688330589));
#113916=CARTESIAN_POINT('Ctrl Pts',(33.6263312369102,1076.66149495858,508.078893350336));
#113917=CARTESIAN_POINT('Ctrl Pts',(33.6053926774398,1076.65866150851,508.193330375199));
#113918=CARTESIAN_POINT('Ctrl Pts',(33.5205254249345,1076.65373818431,508.407583827307));
#113919=CARTESIAN_POINT('Ctrl Pts',(33.457423506089,1076.65169860574,508.505324214213));
#113920=CARTESIAN_POINT('Ctrl Pts',(33.2971618619861,1076.64881045897,508.670773621486));
#113921=CARTESIAN_POINT('Ctrl Pts',(33.2015962164759,1076.64799048993,508.736910425619));
#113922=CARTESIAN_POINT('Ctrl Pts',(32.9905663110002,1076.64774301643,508.828479114546));
#113923=CARTESIAN_POINT('Ctrl Pts',(32.8771803110057,1076.64831579393,508.853090008474));
#113924=CARTESIAN_POINT('Ctrl Pts',(32.7569785132388,1076.64959026502,508.855266137898));
#113925=CARTESIAN_POINT('Ctrl Pts',(32.7516789122271,1076.64964778753,508.855314064937));
#113926=CARTESIAN_POINT('Ctrl Pts',(32.7463814565115,1076.64970661189,508.855314064937));
#113927=CARTESIAN_POINT('Origin',(25.1979747106606,1067.7251047501,518.01352587698));
#113928=CARTESIAN_POINT('',(25.1979747106869,1078.42435733551,516.738081755843));
#113929=CARTESIAN_POINT('Ctrl Pts',(25.1979750950576,1078.26679961873,519.288969998116));
#113930=CARTESIAN_POINT('Ctrl Pts',(25.2538393015146,1078.26579106381,519.288969981279));
#113931=CARTESIAN_POINT('Ctrl Pts',(25.3096465254065,1078.26502788217,519.285299707378));
#113932=CARTESIAN_POINT('Ctrl Pts',(25.4010411064822,1078.26418420223,519.273224544298));
#113933=CARTESIAN_POINT('Ctrl Pts',(25.4368271213489,1078.2639586333,519.266931763596));
#113934=CARTESIAN_POINT('Ctrl Pts',(25.5003877095324,1078.26374726128,519.252933592203));
#113935=CARTESIAN_POINT('Ctrl Pts',(25.5282618165064,1078.26372140327,519.245798388078));
#113936=CARTESIAN_POINT('Ctrl Pts',(25.586444312872,1078.26380940973,519.228788689061));
#113937=CARTESIAN_POINT('Ctrl Pts',(25.6166718909598,1078.2639385447,519.218708420609));
#113938=CARTESIAN_POINT('Ctrl Pts',(25.6945526056013,1078.26449138403,519.189452778603));
#113939=CARTESIAN_POINT('Ctrl Pts',(25.7414790230461,1078.26504649876,519.168513444252));
#113940=CARTESIAN_POINT('Ctrl Pts',(25.9260914974776,1078.26814830043,519.072388647803));
#113941=CARTESIAN_POINT('Ctrl Pts',(26.0505866156886,1078.27241995435,518.974966830462));
#113942=CARTESIAN_POINT('Ctrl Pts',(26.2451124389318,1078.2835438971,518.754541932419));
#113943=CARTESIAN_POINT('Ctrl Pts',(26.318703829592,1078.28993503851,518.637659794602));
#113944=CARTESIAN_POINT('Ctrl Pts',(26.4304963335197,1078.30513914723,518.373966420577));
#113945=CARTESIAN_POINT('Ctrl Pts',(26.4641657543368,1078.31399651465,518.227450752337));
#113946=CARTESIAN_POINT('Ctrl Pts',(26.4799168977178,1078.33333109839,517.918627028371));
#113947=CARTESIAN_POINT('Ctrl Pts',(26.4579020625722,1078.34370757868,517.758650210284));
#113948=CARTESIAN_POINT('Ctrl Pts',(26.3530264885736,1078.36461965783,517.446826788575));
#113949=CARTESIAN_POINT('Ctrl Pts',(26.2678889976152,1078.37492787065,517.298960884281));
#113950=CARTESIAN_POINT('Ctrl Pts',(26.0477565847437,1078.39334316983,517.04826449496));
#113951=CARTESIAN_POINT('Ctrl Pts',(25.9161673302562,1078.40133192517,516.946709932133));
#113952=CARTESIAN_POINT('Ctrl Pts',(25.6296781349704,1078.41405877237,516.803314624226));
#113953=CARTESIAN_POINT('Ctrl Pts',(25.4788848365716,1078.41884855583,516.75969362844));
#113954=CARTESIAN_POINT('Ctrl Pts',(25.2363989338142,1078.4239129098,516.73562992413));
#113955=CARTESIAN_POINT('Ctrl Pts',(25.1481978933723,1078.42523121994,516.736020716809));
#113956=CARTESIAN_POINT('Ctrl Pts',(25.0252452362049,1078.42634945222,516.749327920288));
#113957=CARTESIAN_POINT('Ctrl Pts',(24.9899323035213,1078.42658557129,516.754657184705));
#113958=CARTESIAN_POINT('Ctrl Pts',(24.9287486053121,1078.42684587648,516.766535865982));
#113959=CARTESIAN_POINT('Ctrl Pts',(24.9027734278071,1078.4269085968,516.772428379401));
#113960=CARTESIAN_POINT('Ctrl Pts',(24.8490422379368,1078.42693814154,516.786399794905));
#113961=CARTESIAN_POINT('Ctrl Pts',(24.8213379317463,1078.42689636598,516.79461775101));
#113962=CARTESIAN_POINT('Ctrl Pts',(24.7570842598639,1078.42666449705,516.81607737707));
#113963=CARTESIAN_POINT('Ctrl Pts',(24.7208140096023,1078.42642834775,516.830062793949));
#113964=CARTESIAN_POINT('Ctrl Pts',(24.608458401249,1078.42535811319,516.879391873892));
#113965=CARTESIAN_POINT('Ctrl Pts',(24.5351947032948,1078.42415122644,516.920589534214));
#113966=CARTESIAN_POINT('Ctrl Pts',(24.3276737151788,1078.41910089287,517.065867488017));
#113967=CARTESIAN_POINT('Ctrl Pts',(24.2096353141831,1078.41387644729,517.189734969079));
#113968=CARTESIAN_POINT('Ctrl Pts',(24.0422909167752,1078.40116928911,517.454990295583));
#113969=CARTESIAN_POINT('Ctrl Pts',(23.9865992335089,1078.39422538086,517.589131640078));
#113970=CARTESIAN_POINT('Ctrl Pts',(23.9198634616342,1078.37797480244,517.881485069862));
#113971=CARTESIAN_POINT('Ctrl Pts',(23.9133094938973,1078.36865652168,518.038319665684));
#113972=CARTESIAN_POINT('Ctrl Pts',(23.9586008571845,1078.34835863445,518.358046825016));
#113973=CARTESIAN_POINT('Ctrl Pts',(24.0144221101813,1078.33749956753,518.517454730633));
#113974=CARTESIAN_POINT('Ctrl Pts',(24.1844466729048,1078.316366862,518.805694049332));
#113975=CARTESIAN_POINT('Ctrl Pts',(24.2970534952695,1078.30629829287,518.931753178497));
#113976=CARTESIAN_POINT('Ctrl Pts',(24.5554693101356,1078.28909535356,519.126307262868));
#113977=CARTESIAN_POINT('Ctrl Pts',(24.6963139681842,1078.2819553323,519.196517368932));
#113978=CARTESIAN_POINT('Ctrl Pts',(24.9606808418641,1078.27219239906,519.272329347048));
#113979=CARTESIAN_POINT('Ctrl Pts',(25.0790222205508,1078.26894715674,519.288970033966));
#113980=CARTESIAN_POINT('Ctrl Pts',(25.1979750950576,1078.26679961873,519.288969998116));
#113981=CARTESIAN_POINT('',(25.197974710641,1076.42087024281,516.738081755844));
#113982=CARTESIAN_POINT('',(25.1979747106606,1067.7251047501,516.738081755843));
#113983=CARTESIAN_POINT('Ctrl Pts',(25.1980044361408,1076.26166889074,519.288969997769));
#113984=CARTESIAN_POINT('Ctrl Pts',(25.031537606726,1076.26470468843,519.288973877443));
#113985=CARTESIAN_POINT('Ctrl Pts',(24.8667318546538,1076.26990561849,519.256389121415));
#113986=CARTESIAN_POINT('Ctrl Pts',(24.5587436286835,1076.28389738122,519.129732630649));
#113987=CARTESIAN_POINT('Ctrl Pts',(24.4185795947314,1076.29255534022,519.036772507589));
#113988=CARTESIAN_POINT('Ctrl Pts',(24.1816428518619,1076.31202071232,518.802017551005));
#113989=CARTESIAN_POINT('Ctrl Pts',(24.087263209789,1076.32264379334,518.66233126658));
#113990=CARTESIAN_POINT('Ctrl Pts',(23.9900737635484,1076.33888785251,518.431504929377));
#113991=CARTESIAN_POINT('Ctrl Pts',(23.9653043796319,1076.34431759179,518.351543066889));
#113992=CARTESIAN_POINT('Ctrl Pts',(23.9145150247131,1076.36055618046,518.103859956947));
#113993=CARTESIAN_POINT('Ctrl Pts',(23.9138627054195,1076.37099485117,517.932819995292));
#113994=CARTESIAN_POINT('Ctrl Pts',(23.9792829582952,1076.38983033526,517.601276433598));
#113995=CARTESIAN_POINT('Ctrl Pts',(24.0443684741143,1076.39805683879,517.44397031636));
#113996=CARTESIAN_POINT('Ctrl Pts',(24.232245828346,1076.41144415945,517.163416124712));
#113997=CARTESIAN_POINT('Ctrl Pts',(24.3532884105665,1076.41647058397,517.043032546197));
#113998=CARTESIAN_POINT('Ctrl Pts',(24.6358632193602,1076.42279156108,516.856120911585));
#113999=CARTESIAN_POINT('Ctrl Pts',(24.7946853442826,1076.424012382,516.791673881075));
#114000=CARTESIAN_POINT('Ctrl Pts',(25.1280767874121,1076.42247563035,516.728761698703));
#114001=CARTESIAN_POINT('Ctrl Pts',(25.2992647614757,1076.41973682242,516.730862473475));
#114002=CARTESIAN_POINT('Ctrl Pts',(25.6300874785057,1076.4105383985,516.801692798854));
#114003=CARTESIAN_POINT('Ctrl Pts',(25.7864647294093,1076.40418066329,516.869453557925));
#114004=CARTESIAN_POINT('Ctrl Pts',(26.0637479056959,1076.38845202921,517.061852664176));
#114005=CARTESIAN_POINT('Ctrl Pts',(26.1818977119738,1076.37923043119,517.184609950215));
#114006=CARTESIAN_POINT('Ctrl Pts',(26.3172690778288,1076.36412954347,517.396450065671));
#114007=CARTESIAN_POINT('Ctrl Pts',(26.354924744394,1076.35897736963,517.470326050818));
#114008=CARTESIAN_POINT('Ctrl Pts',(26.4155329911697,1076.34841954437,517.624662810669));
#114009=CARTESIAN_POINT('Ctrl Pts',(26.438274306961,1076.34303766751,517.704789000514));
#114010=CARTESIAN_POINT('Ctrl Pts',(26.4831811410849,1076.32665049629,517.953108160057));
#114011=CARTESIAN_POINT('Ctrl Pts',(26.4798530782244,1076.31575718523,518.124032056819));
#114012=CARTESIAN_POINT('Ctrl Pts',(26.407016890058,1076.29567121162,518.452882314315));
#114013=CARTESIAN_POINT('Ctrl Pts',(26.3389131487456,1076.28665897991,518.607764461718));
#114014=CARTESIAN_POINT('Ctrl Pts',(26.1468440263256,1076.27184899657,518.882070442686));
#114015=CARTESIAN_POINT('Ctrl Pts',(26.0248815138126,1076.26619180919,518.998913384367));
#114016=CARTESIAN_POINT('Ctrl Pts',(25.7431482078447,1076.25919072888,519.17858641003));
#114017=CARTESIAN_POINT('Ctrl Pts',(25.5862626857221,1076.25790385133,519.239830662437));
#114018=CARTESIAN_POINT('Ctrl Pts',(25.3480749433583,1076.25937840023,519.282332473962));
#114019=CARTESIAN_POINT('Ctrl Pts',(25.2731103698183,1076.26029920995,519.288968247352));
#114020=CARTESIAN_POINT('Ctrl Pts',(25.1980044361408,1076.26166889074,519.288969997769));
#114021=CARTESIAN_POINT('Origin',(25.1979747106606,1067.7251047501,518.01352587698));
#114022=CARTESIAN_POINT('',(25.1979747106606,1076.3019258569,518.688969998116));
#114023=CARTESIAN_POINT('',(25.1979747106607,1076.38624898044,517.338081755843));
#114024=CARTESIAN_POINT('Ctrl Pts',(25.1979747106606,1076.3019258569,518.688969998116));
#114025=CARTESIAN_POINT('Ctrl Pts',(25.1506482879843,1076.30275829312,518.688969998116));
#114026=CARTESIAN_POINT('Ctrl Pts',(25.1033458087688,1076.30391372793,518.683995895215));
#114027=CARTESIAN_POINT('Ctrl Pts',(24.9705154872112,1076.30808645208,518.655617822141));
#114028=CARTESIAN_POINT('Ctrl Pts',(24.8886594604942,1076.31179806768,518.620429280826));
#114029=CARTESIAN_POINT('Ctrl Pts',(24.7429745164403,1076.32075060247,518.52049903454));
#114030=CARTESIAN_POINT('Ctrl Pts',(24.6805960922587,1076.3259077255,518.456647167304));
#114031=CARTESIAN_POINT('Ctrl Pts',(24.6081303200936,1076.33417911531,518.345586287252));
#114032=CARTESIAN_POINT('Ctrl Pts',(24.5876614884424,1076.33700701395,518.306267672777));
#114033=CARTESIAN_POINT('Ctrl Pts',(24.5547233750118,1076.34271386765,518.224247033879));
#114034=CARTESIAN_POINT('Ctrl Pts',(24.5423232870404,1076.3455792421,518.181742945173));
#114035=CARTESIAN_POINT('Ctrl Pts',(24.5175462711231,1076.35419315865,518.049961454994));
#114036=CARTESIAN_POINT('Ctrl Pts',(24.5187402570958,1076.3597677743,517.959134452175));
#114037=CARTESIAN_POINT('Ctrl Pts',(24.5566081677011,1076.36987625386,517.783466779294));
#114038=CARTESIAN_POINT('Ctrl Pts',(24.5928209289011,1076.37431376896,517.700349972542));
#114039=CARTESIAN_POINT('Ctrl Pts',(24.6957495694736,1076.38151050216,517.553002240948));
#114040=CARTESIAN_POINT('Ctrl Pts',(24.761473338734,1076.38419657027,517.490277855503));
#114041=CARTESIAN_POINT('Ctrl Pts',(24.913824288656,1076.38747633607,517.394162825976));
#114042=CARTESIAN_POINT('Ctrl Pts',(24.998940634694,1076.38803361555,517.361805249456));
#114043=CARTESIAN_POINT('Ctrl Pts',(25.1242863879005,1076.38725323819,517.34110121662));
#114044=CARTESIAN_POINT('Ctrl Pts',(25.1610987811129,1076.38684187574,517.338081755843));
#114045=CARTESIAN_POINT('Ctrl Pts',(25.1979747106609,1076.38624898044,517.338081755843));
#114046=CARTESIAN_POINT('',(25.1979747106606,1082.7251047501,517.338081755844));
#114047=CARTESIAN_POINT('',(25.1979747106606,1067.7251047501,517.338081755844));
#114048=CARTESIAN_POINT('Origin',(25.1979747106606,1082.7251047501,518.01352587698));
#114049=CARTESIAN_POINT('Ctrl Pts',(25.19797846324,1076.3862489201,517.338081755854));
#114050=CARTESIAN_POINT('Ctrl Pts',(25.2879847978612,1076.38480175833,517.338082255904));
#114051=CARTESIAN_POINT('Ctrl Pts',(25.3770617771146,1076.38229506456,517.356072898381));
#114052=CARTESIAN_POINT('Ctrl Pts',(25.5427548319197,1076.3754154159,517.425803272491));
#114053=CARTESIAN_POINT('Ctrl Pts',(25.6177287943988,1076.37111298612,517.476789791512));
#114054=CARTESIAN_POINT('Ctrl Pts',(25.7434527121999,1076.36121280296,517.605155566688));
#114055=CARTESIAN_POINT('Ctrl Pts',(25.7929021281417,1076.35570964023,517.681312341625));
#114056=CARTESIAN_POINT('Ctrl Pts',(25.842204694364,1076.34714948523,517.805841920776));
#114057=CARTESIAN_POINT('Ctrl Pts',(25.8543735968277,1076.34429679249,517.848282997687));
#114058=CARTESIAN_POINT('Ctrl Pts',(25.8785009286614,1076.33564934978,517.979752579884));
#114059=CARTESIAN_POINT('Ctrl Pts',(25.8769764775005,1076.32994791322,518.070261173533));
#114060=CARTESIAN_POINT('Ctrl Pts',(25.8388866316471,1076.31949889079,518.244415281066));
#114061=CARTESIAN_POINT('Ctrl Pts',(25.8030912747009,1076.31484265673,518.326453675911));
#114062=CARTESIAN_POINT('Ctrl Pts',(25.7019184575798,1076.30720792409,518.471885516939));
#114063=CARTESIAN_POINT('Ctrl Pts',(25.6375923832873,1076.30430091073,518.533910326504));
#114064=CARTESIAN_POINT('Ctrl Pts',(25.4888078416967,1076.30068727313,518.629513160756));
#114065=CARTESIAN_POINT('Ctrl Pts',(25.4058557840819,1076.30001124025,518.66222657909));
#114066=CARTESIAN_POINT('Ctrl Pts',(25.2789384875224,1076.3007382741,518.685332295366));
#114067=CARTESIAN_POINT('Ctrl Pts',(25.2384478437601,1076.30121396489,518.688969998116));
#114068=CARTESIAN_POINT('Ctrl Pts',(25.1979747106606,1076.3019258569,518.688969998116));
#114069=CARTESIAN_POINT('Origin',(15.9013061211262,1067.7251047501,528.279499281495));
#114070=CARTESIAN_POINT('',(15.9013061211524,1077.7757685569,527.180668145503));
#114071=CARTESIAN_POINT('Ctrl Pts',(15.9013326495842,1077.55169183437,529.378330417168));
#114072=CARTESIAN_POINT('Ctrl Pts',(15.9354256569584,1077.55113887753,529.37832959408));
#114073=CARTESIAN_POINT('Ctrl Pts',(15.9695020621221,1077.55075385341,529.376742086929));
#114074=CARTESIAN_POINT('Ctrl Pts',(16.029515268272,1077.55037270998,529.371139118324));
#114075=CARTESIAN_POINT('Ctrl Pts',(16.0554842451758,1077.55030715702,529.367775098043));
#114076=CARTESIAN_POINT('Ctrl Pts',(16.1086468112226,1077.55037833515,529.358947147593));
#114077=CARTESIAN_POINT('Ctrl Pts',(16.1358030166974,1077.55052712521,529.353374972161));
#114078=CARTESIAN_POINT('Ctrl Pts',(16.2035708404945,1077.55118325342,529.336776399701));
#114079=CARTESIAN_POINT('Ctrl Pts',(16.2438107469713,1077.55183579649,529.324434107133));
#114080=CARTESIAN_POINT('Ctrl Pts',(16.3891161115835,1077.55517364205,529.270570068469));
#114081=CARTESIAN_POINT('Ctrl Pts',(16.4882512437389,1077.55941166206,529.215259687026));
#114082=CARTESIAN_POINT('Ctrl Pts',(16.6682412594859,1077.57129161793,529.074846892129));
#114083=CARTESIAN_POINT('Ctrl Pts',(16.747456369472,1077.57893596218,528.989959815292));
#114084=CARTESIAN_POINT('Ctrl Pts',(16.8827256923866,1077.59771871991,528.789625379511));
#114085=CARTESIAN_POINT('Ctrl Pts',(16.9348048549741,1077.60898213919,528.673509045357));
#114086=CARTESIAN_POINT('Ctrl Pts',(16.999660649027,1077.63425695103,528.419360210446));
#114087=CARTESIAN_POINT('Ctrl Pts',(17.0085147312245,1077.64820041578,528.282456567556));
#114088=CARTESIAN_POINT('Ctrl Pts',(16.9746020120754,1077.6773431011,528.00226985882));
#114089=CARTESIAN_POINT('Ctrl Pts',(16.928208735083,1077.69227684009,527.861977254396));
#114090=CARTESIAN_POINT('Ctrl Pts',(16.7846063607034,1077.71980272233,527.61035041876));
#114091=CARTESIAN_POINT('Ctrl Pts',(16.6898083768046,1077.73218082522,527.500836219454));
#114092=CARTESIAN_POINT('Ctrl Pts',(16.4752200190605,1077.75204122725,527.333699230502));
#114093=CARTESIAN_POINT('Ctrl Pts',(16.3607950054836,1077.7597518177,527.273100731741));
#114094=CARTESIAN_POINT('Ctrl Pts',(16.1445012200799,1077.7698800982,527.203386909236));
#114095=CARTESIAN_POINT('Ctrl Pts',(16.0469208706027,1077.77306530005,527.185893563921));
#114096=CARTESIAN_POINT('Ctrl Pts',(15.9076554089286,1077.77574512915,527.179934289773));
#114097=CARTESIAN_POINT('Ctrl Pts',(15.8669595666641,1077.77630629531,527.180452286059));
#114098=CARTESIAN_POINT('Ctrl Pts',(15.7992131197838,1077.77687110405,527.185082288483));
#114099=CARTESIAN_POINT('Ctrl Pts',(15.7721208064804,1077.77699748216,527.187948667648));
#114100=CARTESIAN_POINT('Ctrl Pts',(15.7193785141611,1077.77704836196,527.19552016244));
#114101=CARTESIAN_POINT('Ctrl Pts',(15.6937344163041,1077.77698139936,527.20013727113));
#114102=CARTESIAN_POINT('Ctrl Pts',(15.6340903930987,1077.77660958155,527.213080265684));
#114103=CARTESIAN_POINT('Ctrl Pts',(15.6002773735579,1077.77623122058,527.222127440125));
#114104=CARTESIAN_POINT('Ctrl Pts',(15.495412242424,1077.7745240779,527.255623958176));
#114105=CARTESIAN_POINT('Ctrl Pts',(15.4264180411923,1077.77260781199,527.285745643577));
#114106=CARTESIAN_POINT('Ctrl Pts',(15.2338561401924,1077.76482640166,527.394470233332));
#114107=CARTESIAN_POINT('Ctrl Pts',(15.1223636790291,1077.75702154368,527.49086557591));
#114108=CARTESIAN_POINT('Ctrl Pts',(14.9565098520058,1077.73834614646,527.7047233275));
#114109=CARTESIAN_POINT('Ctrl Pts',(14.8974468985504,1077.72821473454,527.815577532673));
#114110=CARTESIAN_POINT('Ctrl Pts',(14.8158476309181,1077.70479454011,528.061823640231));
#114111=CARTESIAN_POINT('Ctrl Pts',(14.7973756669171,1077.69150865683,528.196429485797));
#114112=CARTESIAN_POINT('Ctrl Pts',(14.8104669248276,1077.66292978698,528.475759623976));
#114113=CARTESIAN_POINT('Ctrl Pts',(14.8458485901493,1077.64783030156,528.617828310167));
#114114=CARTESIAN_POINT('Ctrl Pts',(14.9693941473493,1077.61892051957,528.879297428913));
#114115=CARTESIAN_POINT('Ctrl Pts',(15.0560976649763,1077.60537610607,528.996370963454));
#114116=CARTESIAN_POINT('Ctrl Pts',(15.2617877721368,1077.58260204064,529.182945196387));
#114117=CARTESIAN_POINT('Ctrl Pts',(15.3760890202089,1077.5733101814,529.253876705106));
#114118=CARTESIAN_POINT('Ctrl Pts',(15.6070877152219,1077.56004953077,529.34438782175));
#114119=CARTESIAN_POINT('Ctrl Pts',(15.7196873345586,1077.55559543575,529.369268368028));
#114120=CARTESIAN_POINT('Ctrl Pts',(15.8565206111492,1077.55249107862,529.377645982359));
#114121=CARTESIAN_POINT('Ctrl Pts',(15.8789233143288,1077.55205529292,529.378330958184));
#114122=CARTESIAN_POINT('Ctrl Pts',(15.9013326495842,1077.55169183437,529.378330417168));
#114123=CARTESIAN_POINT('',(15.9013061211098,1075.76586229356,527.180668145503));
#114124=CARTESIAN_POINT('',(15.9013061211262,1067.7251047501,527.180668145503));
#114125=CARTESIAN_POINT('Ctrl Pts',(15.9013205982293,1075.53973398927,529.378330417393));
#114126=CARTESIAN_POINT('Ctrl Pts',(15.7583042502497,1075.54207465006,529.378332301633));
#114127=CARTESIAN_POINT('Ctrl Pts',(15.6167585256812,1075.54737091471,529.350415482922));
#114128=CARTESIAN_POINT('Ctrl Pts',(15.3519511202224,1075.56321196787,529.241887338351));
#114129=CARTESIAN_POINT('Ctrl Pts',(15.2313566414536,1075.57361833005,529.162146819059));
#114130=CARTESIAN_POINT('Ctrl Pts',(15.0270198064597,1075.5981335215,528.960519269506));
#114131=CARTESIAN_POINT('Ctrl Pts',(14.9454746476426,1075.61202853342,528.840293754353));
#114132=CARTESIAN_POINT('Ctrl Pts',(14.8612892957594,1075.63402729201,528.641439964089));
#114133=CARTESIAN_POINT('Ctrl Pts',(14.8397758507011,1075.64151639324,528.572393654757));
#114134=CARTESIAN_POINT('Ctrl Pts',(14.8106159174879,1075.65653838638,528.431201920474));
#114135=CARTESIAN_POINT('Ctrl Pts',(14.8030172675462,1075.66403638592,528.359388136089));
#114136=CARTESIAN_POINT('Ctrl Pts',(14.8014594959151,1075.68639799958,528.141163889383));
#114137=CARTESIAN_POINT('Ctrl Pts',(14.8295960057726,1075.70068345627,527.996135575297));
#114138=CARTESIAN_POINT('Ctrl Pts',(14.9408226164428,1075.7261872287,527.726257167342));
#114139=CARTESIAN_POINT('Ctrl Pts',(15.0225028353466,1075.73717649953,527.603930820679));
#114140=CARTESIAN_POINT('Ctrl Pts',(15.2289890933845,1075.75452775864,527.398229518589));
#114141=CARTESIAN_POINT('Ctrl Pts',(15.3516751352132,1075.76072223674,527.31689178922));
#114142=CARTESIAN_POINT('Ctrl Pts',(15.6219424740288,1075.76751920701,527.206796633006));
#114143=CARTESIAN_POINT('Ctrl Pts',(15.7667576394102,1075.76804937915,527.179209577086));
#114144=CARTESIAN_POINT('Ctrl Pts',(16.0586305848033,1075.7633177527,527.182244737854));
#114145=CARTESIAN_POINT('Ctrl Pts',(16.202679044292,1075.75810682931,527.212803301843));
#114146=CARTESIAN_POINT('Ctrl Pts',(16.4703467320378,1075.74252796372,527.328250825835));
#114147=CARTESIAN_POINT('Ctrl Pts',(16.5912471421057,1075.73231345017,527.411985403997));
#114148=CARTESIAN_POINT('Ctrl Pts',(16.793751260426,1075.70805565276,527.621964298198));
#114149=CARTESIAN_POINT('Ctrl Pts',(16.8731493277795,1075.69423139713,527.74633383078));
#114150=CARTESIAN_POINT('Ctrl Pts',(16.9791153025329,1075.66465804811,528.019792617817));
#114151=CARTESIAN_POINT('Ctrl Pts',(17.0041757197176,1075.64918170966,528.166409856263));
#114152=CARTESIAN_POINT('Ctrl Pts',(16.9951178013447,1075.6190763178,528.458291803031));
#114153=CARTESIAN_POINT('Ctrl Pts',(16.9620684160472,1075.60472218162,528.60079010185));
#114154=CARTESIAN_POINT('Ctrl Pts',(16.8426819748313,1075.57895916141,528.864388687406));
#114155=CARTESIAN_POINT('Ctrl Pts',(16.7576903529827,1075.56778863589,528.983043762542));
#114156=CARTESIAN_POINT('Ctrl Pts',(16.5470403842023,1075.55030847844,529.180124481898));
#114157=CARTESIAN_POINT('Ctrl Pts',(16.4237153657142,1075.54414224892,529.256868179455));
#114158=CARTESIAN_POINT('Ctrl Pts',(16.1650890549829,1075.53797233457,529.354386493475));
#114159=CARTESIAN_POINT('Ctrl Pts',(16.0337516693691,1075.53756657121,529.378328672613));
#114160=CARTESIAN_POINT('Ctrl Pts',(15.9013205982293,1075.53973398927,529.378330417393));
#114161=CARTESIAN_POINT('Origin',(15.9013061211262,1067.7251047501,528.279499281495));
#114162=CARTESIAN_POINT('',(15.9013061211262,1075.60362949862,528.778330417488));
#114163=CARTESIAN_POINT('',(15.9013061211261,1075.70629239322,527.780668145503));
#114164=CARTESIAN_POINT('Ctrl Pts',(15.9013061211262,1075.60362949862,528.778330417488));
#114165=CARTESIAN_POINT('Ctrl Pts',(15.8995926060343,1075.60365700516,528.778330417488));
#114166=CARTESIAN_POINT('Ctrl Pts',(15.8978786789049,1075.60368544188,528.778321588453));
#114167=CARTESIAN_POINT('Ctrl Pts',(15.8311908049592,1075.60482786782,528.777634164962));
#114168=CARTESIAN_POINT('Ctrl Pts',(15.7670166584918,1075.60725579324,528.764277247047));
#114169=CARTESIAN_POINT('Ctrl Pts',(15.647217236971,1075.61445686718,528.713683958102));
#114170=CARTESIAN_POINT('Ctrl Pts',(15.5928041508971,1075.61916809108,528.676849510168));
#114171=CARTESIAN_POINT('Ctrl Pts',(15.5009685292575,1075.63026307702,528.584200793289));
#114172=CARTESIAN_POINT('Ctrl Pts',(15.4645337217032,1075.636549945,528.529160128414));
#114173=CARTESIAN_POINT('Ctrl Pts',(15.4273353345171,1075.646515274,528.438420401918));
#114174=CARTESIAN_POINT('Ctrl Pts',(15.4179313081546,1075.64990696243,528.406984517297));
#114175=CARTESIAN_POINT('Ctrl Pts',(15.4054270487921,1075.65671629965,528.342780497876));
#114176=CARTESIAN_POINT('Ctrl Pts',(15.4023465654893,1075.66011814095,528.310162979115));
#114177=CARTESIAN_POINT('Ctrl Pts',(15.4027490443541,1075.67030039173,528.210890973561));
#114178=CARTESIAN_POINT('Ctrl Pts',(15.416348788394,1075.67682638207,528.144983077483));
#114179=CARTESIAN_POINT('Ctrl Pts',(15.4685914924221,1075.68848859448,528.02259721819));
#114180=CARTESIAN_POINT('Ctrl Pts',(15.5066139908239,1075.69351612248,527.967287481599));
#114181=CARTESIAN_POINT('Ctrl Pts',(15.602125880045,1075.7014060213,527.87486300747));
#114182=CARTESIAN_POINT('Ctrl Pts',(15.6586046110204,1075.70419329947,527.838650013437));
#114183=CARTESIAN_POINT('Ctrl Pts',(15.7781887853578,1075.70704013822,527.792163073099));
#114184=CARTESIAN_POINT('Ctrl Pts',(15.8394782944546,1075.70725159426,527.780668145503));
#114185=CARTESIAN_POINT('Ctrl Pts',(15.9013061211261,1075.70629239322,527.780668145503));
#114186=CARTESIAN_POINT('',(15.9013061211262,1082.7251047501,527.780668145503));
#114187=CARTESIAN_POINT('',(15.9013061211262,1067.7251047501,527.780668145503));
#114188=CARTESIAN_POINT('Origin',(15.9013061211262,1082.7251047501,528.279499281495));
#114189=CARTESIAN_POINT('Ctrl Pts',(15.9013061211261,1075.70629239322,527.780668145503));
#114190=CARTESIAN_POINT('Ctrl Pts',(15.9013960893017,1075.70629099745,527.780668145503));
#114191=CARTESIAN_POINT('Ctrl Pts',(15.9014860586171,1075.70628959919,527.78066816984));
#114192=CARTESIAN_POINT('Ctrl Pts',(15.9015760290626,1075.70628819846,527.780668218521));
#114193=CARTESIAN_POINT('Ctrl Pts',(15.9666371127217,1075.70527527467,527.78070342183));
#114194=CARTESIAN_POINT('Ctrl Pts',(16.0310242090725,1075.70298577075,527.793466033217));
#114195=CARTESIAN_POINT('Ctrl Pts',(16.1526245906639,1075.69602260248,527.843500270199));
#114196=CARTESIAN_POINT('Ctrl Pts',(16.208388263226,1075.69136503836,527.880827323484));
#114197=CARTESIAN_POINT('Ctrl Pts',(16.3021419088947,1075.6802886557,527.975190243344));
#114198=CARTESIAN_POINT('Ctrl Pts',(16.3391258504495,1075.67397312267,528.031359182079));
#114199=CARTESIAN_POINT('Ctrl Pts',(16.3761786504636,1075.66396426213,528.12332023625));
#114200=CARTESIAN_POINT('Ctrl Pts',(16.3853682646411,1075.66059943618,528.154683383715));
#114201=CARTESIAN_POINT('Ctrl Pts',(16.3975088511561,1075.65381222211,528.218813718927));
#114202=CARTESIAN_POINT('Ctrl Pts',(16.4004178469543,1075.6504054272,528.251435472857));
#114203=CARTESIAN_POINT('Ctrl Pts',(16.3995033647169,1075.64020624374,528.350409933561));
#114204=CARTESIAN_POINT('Ctrl Pts',(16.3856771876017,1075.6336357142,528.415971570707));
#114205=CARTESIAN_POINT('Ctrl Pts',(16.3334741559357,1075.62188942714,528.537091545518));
#114206=CARTESIAN_POINT('Ctrl Pts',(16.2959262991265,1075.61680913897,528.591613097222));
#114207=CARTESIAN_POINT('Ctrl Pts',(16.2020522544986,1075.60879854306,528.682784560787));
#114208=CARTESIAN_POINT('Ctrl Pts',(16.1467618635846,1075.60593434293,528.718648108494));
#114209=CARTESIAN_POINT('Ctrl Pts',(16.0272885556594,1075.60286717747,528.766292040893));
#114210=CARTESIAN_POINT('Ctrl Pts',(15.9645782347285,1075.60261381045,528.778330417488));
#114211=CARTESIAN_POINT('Ctrl Pts',(15.9013061211262,1075.60362949862,528.778330417488));
#114212=CARTESIAN_POINT('Origin',(4.59241321360915,1067.7251047501,536.510106563848));
#114213=CARTESIAN_POINT('',(4.59241321363791,1076.96429318502,535.41956581512));
#114214=CARTESIAN_POINT('Ctrl Pts',(4.59240250088817,1076.67169975394,537.600647312524));
#114215=CARTESIAN_POINT('Ctrl Pts',(4.61963247439736,1076.67154620407,537.600647580012));
#114216=CARTESIAN_POINT('Ctrl Pts',(4.64685300256101,1076.67153279158,537.599627980395));
#114217=CARTESIAN_POINT('Ctrl Pts',(4.70549323594633,1076.67180653428,537.595228218623));
#114218=CARTESIAN_POINT('Ctrl Pts',(4.73686019260232,1076.67214185057,537.591499610811));
#114219=CARTESIAN_POINT('Ctrl Pts',(4.8212936532487,1076.67355782825,537.57772381268));
#114220=CARTESIAN_POINT('Ctrl Pts',(4.87383513915931,1076.67499652859,537.565090685447));
#114221=CARTESIAN_POINT('Ctrl Pts',(5.06278565836851,1076.68224245367,537.504540531177));
#114222=CARTESIAN_POINT('Ctrl Pts',(5.19003205201556,1076.69125446614,537.433624909088));
#114223=CARTESIAN_POINT('Ctrl Pts',(5.39141840175913,1076.71358022889,537.262032278697));
#114224=CARTESIAN_POINT('Ctrl Pts',(5.46942358282502,1076.72579078015,537.169327646511));
#114225=CARTESIAN_POINT('Ctrl Pts',(5.59728131715015,1076.75441431509,536.953500808567));
#114226=CARTESIAN_POINT('Ctrl Pts',(5.64306854302756,1076.77087507896,536.830124400968));
#114227=CARTESIAN_POINT('Ctrl Pts',(5.69066752396957,1076.80657850383,536.56345818499));
#114228=CARTESIAN_POINT('Ctrl Pts',(5.68840329148452,1076.82562331359,536.421706105464));
#114229=CARTESIAN_POINT('Ctrl Pts',(5.62939229014925,1076.8632037199,536.142902448811));
#114230=CARTESIAN_POINT('Ctrl Pts',(5.57162448245924,1076.8813589666,536.008702819453));
#114231=CARTESIAN_POINT('Ctrl Pts',(5.41074873767791,1076.91301931469,535.776200414741));
#114232=CARTESIAN_POINT('Ctrl Pts',(5.31137146010354,1076.92642833287,535.67853602913));
#114233=CARTESIAN_POINT('Ctrl Pts',(5.08104817907621,1076.94780594154,535.525407532778));
#114234=CARTESIAN_POINT('Ctrl Pts',(4.952255495658,1076.95557909134,535.471357107651));
#114235=CARTESIAN_POINT('Ctrl Pts',(4.76774845647982,1076.96164638735,535.432595106691));
#114236=CARTESIAN_POINT('Ctrl Pts',(4.71821492839048,1076.96281553606,535.425694566824));
#114237=CARTESIAN_POINT('Ctrl Pts',(4.63798156785976,1076.96397957258,535.420092438433));
#114238=CARTESIAN_POINT('Ctrl Pts',(4.60751297418011,1076.96425410189,535.419244769929));
#114239=CARTESIAN_POINT('Ctrl Pts',(4.55268802689552,1076.96444744263,535.420017331621));
#114240=CARTESIAN_POINT('Ctrl Pts',(4.52834697868929,1076.96442646147,535.421176751332));
#114241=CARTESIAN_POINT('Ctrl Pts',(4.4718632457097,1076.96412909794,535.42576775435));
#114242=CARTESIAN_POINT('Ctrl Pts',(4.43979539215814,1076.96377179973,535.429814710541));
#114243=CARTESIAN_POINT('Ctrl Pts',(4.35106232444018,1076.96225556588,535.445042637426));
#114244=CARTESIAN_POINT('Ctrl Pts',(4.29504854230218,1076.96068966126,535.45930588876));
#114245=CARTESIAN_POINT('Ctrl Pts',(4.10334867623869,1076.95315814647,535.524675273155));
#114246=CARTESIAN_POINT('Ctrl Pts',(3.97712810276218,1076.94420063445,535.598200444191));
#114247=CARTESIAN_POINT('Ctrl Pts',(3.7780751300857,1076.92205486763,535.774645184438));
#114248=CARTESIAN_POINT('Ctrl Pts',(3.70137286321866,1076.90992097153,535.869782155043));
#114249=CARTESIAN_POINT('Ctrl Pts',(3.57730582055464,1076.88138656195,536.090322205786));
#114250=CARTESIAN_POINT('Ctrl Pts',(3.53410557316563,1076.86493327179,536.215874053228));
#114251=CARTESIAN_POINT('Ctrl Pts',(3.49293824102599,1076.82905342546,536.486223339413));
#114252=CARTESIAN_POINT('Ctrl Pts',(3.49916302609928,1076.80981614048,536.629329151069));
#114253=CARTESIAN_POINT('Ctrl Pts',(3.566618010933,1076.77195854236,536.907380496889));
#114254=CARTESIAN_POINT('Ctrl Pts',(3.62813324410225,1076.75370500083,537.039578244589));
#114255=CARTESIAN_POINT('Ctrl Pts',(3.79463716522226,1076.72197923598,537.266068360592));
#114256=CARTESIAN_POINT('Ctrl Pts',(3.8955964316538,1076.70857371197,537.360101223211));
#114257=CARTESIAN_POINT('Ctrl Pts',(4.12289767311567,1076.68772612295,537.503156829554));
#114258=CARTESIAN_POINT('Ctrl Pts',(4.24616653037819,1076.68024739971,537.55259854802));
#114259=CARTESIAN_POINT('Ctrl Pts',(4.42333613990684,1076.67431155834,537.588569314053));
#114260=CARTESIAN_POINT('Ctrl Pts',(4.47185480341855,1076.67314588631,537.595065869767));
#114261=CARTESIAN_POINT('Ctrl Pts',(4.5445379155475,1076.67207790489,537.599858788991));
#114262=CARTESIAN_POINT('Ctrl Pts',(4.56846640826851,1076.67183472961,537.600647077392));
#114263=CARTESIAN_POINT('Ctrl Pts',(4.59240250088817,1076.67169975394,537.600647312524));
#114264=CARTESIAN_POINT('',(4.59241321359178,1074.94723115222,535.41956581512));
#114265=CARTESIAN_POINT('',(4.59241321360915,1067.7251047501,535.41956581512));
#114266=CARTESIAN_POINT('Ctrl Pts',(4.59241350730773,1074.65221523953,537.600647312576));
#114267=CARTESIAN_POINT('Ctrl Pts',(4.45097247351488,1074.65301913803,537.600647350669));
#114268=CARTESIAN_POINT('Ctrl Pts',(4.31099418018631,1074.6576275787,537.573133182937));
#114269=CARTESIAN_POINT('Ctrl Pts',(4.04892093847275,1074.67389907727,537.466148598073));
#114270=CARTESIAN_POINT('Ctrl Pts',(3.92953334655367,1074.68542816297,537.387524090739));
#114271=CARTESIAN_POINT('Ctrl Pts',(3.7266755056389,1074.71394090407,537.18846756568));
#114272=CARTESIAN_POINT('Ctrl Pts',(3.64553305693232,1074.73070049125,537.069547156246));
#114273=CARTESIAN_POINT('Ctrl Pts',(3.56138277177411,1074.75804181118,536.872606487432));
#114274=CARTESIAN_POINT('Ctrl Pts',(3.53977837373126,1074.76750128965,536.804013876899));
#114275=CARTESIAN_POINT('Ctrl Pts',(3.51034273845369,1074.78673962673,536.66358020759));
#114276=CARTESIAN_POINT('Ctrl Pts',(3.50259049049914,1074.79647502727,536.592055365455));
#114277=CARTESIAN_POINT('Ctrl Pts',(3.50055916703735,1074.82587855887,536.374630470324));
#114278=CARTESIAN_POINT('Ctrl Pts',(3.52839677931706,1074.84517135384,536.230039212452));
#114279=CARTESIAN_POINT('Ctrl Pts',(3.63894992867444,1074.88053853766,535.961383359238));
#114280=CARTESIAN_POINT('Ctrl Pts',(3.72011828051353,1074.89630388714,535.839714909502));
#114281=CARTESIAN_POINT('Ctrl Pts',(3.92518913613577,1074.92231188485,535.635506876668));
#114282=CARTESIAN_POINT('Ctrl Pts',(4.04682534609737,1074.93232348045,535.554822731648));
#114283=CARTESIAN_POINT('Ctrl Pts',(4.31474911424055,1074.94529735909,535.445644685266));
#114284=CARTESIAN_POINT('Ctrl Pts',(4.45820555561252,1074.94813479584,535.418225528271));
#114285=CARTESIAN_POINT('Ctrl Pts',(4.74464142728425,1074.94622035816,535.420978564132));
#114286=CARTESIAN_POINT('Ctrl Pts',(4.88465939827589,1074.94164078346,535.449962376807));
#114287=CARTESIAN_POINT('Ctrl Pts',(5.14860256833081,1074.9255281304,535.560951332028));
#114288=CARTESIAN_POINT('Ctrl Pts',(5.26934107995339,1074.91400444726,535.642996236302));
#114289=CARTESIAN_POINT('Ctrl Pts',(5.47222927006135,1074.88540823187,535.849582890718));
#114290=CARTESIAN_POINT('Ctrl Pts',(5.55210927611159,1074.86858646151,535.972308997168));
#114291=CARTESIAN_POINT('Ctrl Pts',(5.63195595118891,1074.84122470969,536.172926716412));
#114292=CARTESIAN_POINT('Ctrl Pts',(5.65171985197724,1074.83190547949,536.24140586266));
#114293=CARTESIAN_POINT('Ctrl Pts',(5.67769575715397,1074.81287411049,536.381499008862));
#114294=CARTESIAN_POINT('Ctrl Pts',(5.68378522507747,1074.80320323547,536.45281027509));
#114295=CARTESIAN_POINT('Ctrl Pts',(5.68098327565191,1074.77384035403,536.669684489158));
#114296=CARTESIAN_POINT('Ctrl Pts',(5.65000381268211,1074.75443997486,536.813447584097));
#114297=CARTESIAN_POINT('Ctrl Pts',(5.53404430120954,1074.71883253648,537.078678969888));
#114298=CARTESIAN_POINT('Ctrl Pts',(5.45088611797357,1074.70292233435,537.197930594038));
#114299=CARTESIAN_POINT('Ctrl Pts',(5.24362006982905,1074.67675924409,537.396444401062));
#114300=CARTESIAN_POINT('Ctrl Pts',(5.12195193450283,1074.66671014128,537.474148409721));
#114301=CARTESIAN_POINT('Ctrl Pts',(4.86232331778747,1074.65418471931,537.575364659058));
#114302=CARTESIAN_POINT('Ctrl Pts',(4.72799470805854,1074.65144464615,537.600647276063));
#114303=CARTESIAN_POINT('Ctrl Pts',(4.59241350730772,1074.65221523953,537.600647312576));
#114304=CARTESIAN_POINT('Origin',(4.59241321360915,1067.7251047501,536.510106563848));
#114305=CARTESIAN_POINT('',(4.59241321360915,1074.73536251872,537.000647312576));
#114306=CARTESIAN_POINT('',(4.59241321360923,1074.8680726283,536.01956581512));
#114307=CARTESIAN_POINT('Ctrl Pts',(4.59241321360915,1074.73536251872,537.000647312576));
#114308=CARTESIAN_POINT('Ctrl Pts',(4.59111296646291,1074.73536981555,537.000647312576));
#114309=CARTESIAN_POINT('Ctrl Pts',(4.58981246310562,1074.73537782066,537.000642142847));
#114310=CARTESIAN_POINT('Ctrl Pts',(4.52485381758119,1074.73581300135,537.000125482655));
#114311=CARTESIAN_POINT('Ctrl Pts',(4.46195359926289,1074.73792920154,536.987233759357));
#114312=CARTESIAN_POINT('Ctrl Pts',(4.34436934018267,1074.74529884748,536.938107046314));
#114313=CARTESIAN_POINT('Ctrl Pts',(4.29090598636675,1074.75049324738,536.902251505426));
#114314=CARTESIAN_POINT('Ctrl Pts',(4.20033795354942,1074.76331991499,536.811838149889));
#114315=CARTESIAN_POINT('Ctrl Pts',(4.16427511206219,1074.77085110083,536.757974648325));
#114316=CARTESIAN_POINT('Ctrl Pts',(4.12720605980857,1074.78313632965,536.669018569248));
#114317=CARTESIAN_POINT('Ctrl Pts',(4.11777072189871,1074.78738233221,536.638104710596));
#114318=CARTESIAN_POINT('Ctrl Pts',(4.10510359199887,1074.79601709625,536.57490114595));
#114319=CARTESIAN_POINT('Ctrl Pts',(4.10190044694374,1074.80038628712,536.542754657397));
#114320=CARTESIAN_POINT('Ctrl Pts',(4.10181599721064,1074.81362343086,536.444861376876));
#114321=CARTESIAN_POINT('Ctrl Pts',(4.11494634489056,1074.82232886225,536.379791782595));
#114322=CARTESIAN_POINT('Ctrl Pts',(4.16597308217532,1074.83830918791,536.259011817999));
#114323=CARTESIAN_POINT('Ctrl Pts',(4.20321540052522,1074.84543949873,536.204406608515));
#114324=CARTESIAN_POINT('Ctrl Pts',(4.29688139158837,1074.85716195678,536.113192568182));
#114325=CARTESIAN_POINT('Ctrl Pts',(4.35225336206347,1074.86164989832,536.077408196333));
#114326=CARTESIAN_POINT('Ctrl Pts',(4.47020097331052,1074.86720243615,536.031090224403));
#114327=CARTESIAN_POINT('Ctrl Pts',(4.53102029027343,1074.86840975228,536.01956581512));
#114328=CARTESIAN_POINT('Ctrl Pts',(4.59241321360938,1074.8680726283,536.01956581512));
#114329=CARTESIAN_POINT('',(4.59241321360915,1082.7251047501,536.01956581512));
#114330=CARTESIAN_POINT('',(4.59241321360915,1067.7251047501,536.01956581512));
#114331=CARTESIAN_POINT('Origin',(4.59241321360915,1082.7251047501,536.510106563848));
#114332=CARTESIAN_POINT('Ctrl Pts',(4.59241494804499,1074.86807261878,536.019565815123));
#114333=CARTESIAN_POINT('Ctrl Pts',(4.65613540139557,1074.8677226836,536.019566040424));
#114334=CARTESIAN_POINT('Ctrl Pts',(4.71919903687055,1074.86571598349,536.031981090877));
#114335=CARTESIAN_POINT('Ctrl Pts',(4.83730193509805,1074.85859856745,536.080278813853));
#114336=CARTESIAN_POINT('Ctrl Pts',(4.89110933749994,1074.85354264986,536.115799904315));
#114337=CARTESIAN_POINT('Ctrl Pts',(4.98330162341501,1074.84084878979,536.206561222789));
#114338=CARTESIAN_POINT('Ctrl Pts',(5.02027070079791,1074.83326895952,536.261418717346));
#114339=CARTESIAN_POINT('Ctrl Pts',(5.05769302124054,1074.82093012762,536.351441427919));
#114340=CARTESIAN_POINT('Ctrl Pts',(5.06706788991385,1074.81672948397,536.382196172587));
#114341=CARTESIAN_POINT('Ctrl Pts',(5.0796970982866,1074.80815704409,536.445156596179));
#114342=CARTESIAN_POINT('Ctrl Pts',(5.08290513911219,1074.80380415207,536.477223963017));
#114343=CARTESIAN_POINT('Ctrl Pts',(5.083052418277,1074.7905296475,536.57530599089));
#114344=CARTESIAN_POINT('Ctrl Pts',(5.06985629252667,1074.78174088848,536.640640133447));
#114345=CARTESIAN_POINT('Ctrl Pts',(5.0187255712267,1074.76562260392,536.761342540552));
#114346=CARTESIAN_POINT('Ctrl Pts',(4.98164835173554,1074.75842705477,536.815696300057));
#114347=CARTESIAN_POINT('Ctrl Pts',(4.88898788677217,1074.74662133191,536.906077212551));
#114348=CARTESIAN_POINT('Ctrl Pts',(4.83462408568439,1074.74208631009,536.941508679684));
#114349=CARTESIAN_POINT('Ctrl Pts',(4.71686744409228,1074.73629900908,536.988694094649));
#114350=CARTESIAN_POINT('Ctrl Pts',(4.65493653762755,1074.73501164518,537.000647312576));
#114351=CARTESIAN_POINT('Ctrl Pts',(4.59241321360915,1074.73536251872,537.000647312576));
#114352=CARTESIAN_POINT('Origin',(49.3616411037544,1067.7251047501,499.347110012371));
#114353=CARTESIAN_POINT('',(49.3616411037703,1078.70098643656,497.868806880177));
#114354=CARTESIAN_POINT('Ctrl Pts',(50.8397772837836,1078.64997002067,499.369326761487));
#114355=CARTESIAN_POINT('Ctrl Pts',(50.8424068823753,1078.65432609598,499.194372955374));
#114356=CARTESIAN_POINT('Ctrl Pts',(50.8139541383063,1078.65901118556,499.020338179437));
#114357=CARTESIAN_POINT('Ctrl Pts',(50.6933755445324,1078.66874765754,498.678513848796));
#114358=CARTESIAN_POINT('Ctrl Pts',(50.5979231326937,1078.67370907481,498.515155430946));
#114359=CARTESIAN_POINT('Ctrl Pts',(50.3459846066139,1078.68309182049,498.227039440132));
#114360=CARTESIAN_POINT('Ctrl Pts',(50.1896261463433,1078.68739095086,498.106972871076));
#114361=CARTESIAN_POINT('Ctrl Pts',(49.8454398767191,1078.69459396784,497.937569631812));
#114362=CARTESIAN_POINT('Ctrl Pts',(49.6620657588907,1078.69748205776,497.887446512515));
#114363=CARTESIAN_POINT('Ctrl Pts',(49.2896157478694,1078.70192809518,497.859000632821));
#114364=CARTESIAN_POINT('Ctrl Pts',(49.1039909490667,1078.70347537265,497.879705027883));
#114365=CARTESIAN_POINT('Ctrl Pts',(48.8507729174781,1078.70481731323,497.957592848052));
#114366=CARTESIAN_POINT('Ctrl Pts',(48.7765461814908,1078.70510525467,497.98718048505));
#114367=CARTESIAN_POINT('Ctrl Pts',(48.6718521247516,1078.70536039302,498.039078707383));
#114368=CARTESIAN_POINT('Ctrl Pts',(48.6392653583714,1078.70541663073,498.05678911477));
#114369=CARTESIAN_POINT('Ctrl Pts',(48.583042040328,1078.70547240393,498.090143670295));
#114370=CARTESIAN_POINT('Ctrl Pts',(48.5591247209862,1078.70548219651,498.105277357441));
#114371=CARTESIAN_POINT('Ctrl Pts',(48.5108578570887,1078.70547284712,498.137795280551));
#114372=CARTESIAN_POINT('Ctrl Pts',(48.4865717984161,1078.70545203616,498.155250975752));
#114373=CARTESIAN_POINT('Ctrl Pts',(48.4267098417356,1078.70535912999,498.201093564839));
#114374=CARTESIAN_POINT('Ctrl Pts',(48.3918841440097,1078.70526601773,498.230408804135));
#114375=CARTESIAN_POINT('Ctrl Pts',(48.2664622690791,1078.70477650681,498.346283727692));
#114376=CARTESIAN_POINT('Ctrl Pts',(48.1856347557062,1078.70413810346,498.442633210835));
#114377=CARTESIAN_POINT('Ctrl Pts',(48.0373344179074,1078.70210163806,498.67344752563));
#114378=CARTESIAN_POINT('Ctrl Pts',(47.9761814572351,1078.70059316131,498.810352642049));
#114379=CARTESIAN_POINT('Ctrl Pts',(47.8924765415345,1078.6965091591,499.113855164203));
#114380=CARTESIAN_POINT('Ctrl Pts',(47.875595619189,1078.69385899944,499.279908399778));
#114381=CARTESIAN_POINT('Ctrl Pts',(47.898502127747,1078.68730940719,499.624106142555));
#114382=CARTESIAN_POINT('Ctrl Pts',(47.9428257315769,1078.68337551964,499.799280688149));
#114383=CARTESIAN_POINT('Ctrl Pts',(48.0975032165717,1078.67434615777,500.137299861922));
#114384=CARTESIAN_POINT('Ctrl Pts',(48.2110409173425,1078.66926963615,500.295033527205));
#114385=CARTESIAN_POINT('Ctrl Pts',(48.4933837520922,1078.65888588427,500.559218340279));
#114386=CARTESIAN_POINT('Ctrl Pts',(48.6599163753638,1078.65368157732,500.662657050314));
#114387=CARTESIAN_POINT('Ctrl Pts',(49.0124902482889,1078.64443898008,500.795132753));
#114388=CARTESIAN_POINT('Ctrl Pts',(49.1937308847251,1078.64043452576,500.827141052003));
#114389=CARTESIAN_POINT('Ctrl Pts',(49.5581299687267,1078.63406328938,500.823547169656));
#114390=CARTESIAN_POINT('Ctrl Pts',(49.7381667272288,1078.6317503759,500.788189944642));
#114391=CARTESIAN_POINT('Ctrl Pts',(49.9590648889496,1078.63013700081,500.700465722135));
#114392=CARTESIAN_POINT('Ctrl Pts',(50.0096629034765,1078.62986059048,500.676980200575));
#114393=CARTESIAN_POINT('Ctrl Pts',(50.0877975385495,1078.6295871773,500.635192812644));
#114394=CARTESIAN_POINT('Ctrl Pts',(50.1162560963385,1078.62952212581,500.618729723957));
#114395=CARTESIAN_POINT('Ctrl Pts',(50.167830319471,1078.62946945633,500.586552886558));
#114396=CARTESIAN_POINT('Ctrl Pts',(50.1910949554386,1078.6294716644,500.571105926506));
#114397=CARTESIAN_POINT('Ctrl Pts',(50.2414641234579,1078.62953481524,500.535566558212));
#114398=CARTESIAN_POINT('Ctrl Pts',(50.2683466198659,1078.62960785773,500.515186466865));
#114399=CARTESIAN_POINT('Ctrl Pts',(50.3417913497394,1078.62992029996,500.455442400916));
#114400=CARTESIAN_POINT('Ctrl Pts',(50.3866497236217,1078.63024616515,500.414092842344));
#114401=CARTESIAN_POINT('Ctrl Pts',(50.5651229817255,1078.63213805046,500.227907847569));
#114402=CARTESIAN_POINT('Ctrl Pts',(50.6716282390872,1078.63483689903,500.05991866479));
#114403=CARTESIAN_POINT('Ctrl Pts',(50.80410847851,1078.64173387056,499.714149024615));
#114404=CARTESIAN_POINT('Ctrl Pts',(50.8371724553628,1078.64565497852,499.542632545847));
#114405=CARTESIAN_POINT('Ctrl Pts',(50.8397772837836,1078.64997002067,499.369326761487));
#114406=CARTESIAN_POINT('',(49.3616411037368,1076.7006095282,497.868806880177));
#114407=CARTESIAN_POINT('',(49.3616411037544,1067.7251047501,497.868806880177));
#114408=CARTESIAN_POINT('Ctrl Pts',(49.3624292594544,1076.63635835644,500.825412934462));
#114409=CARTESIAN_POINT('Ctrl Pts',(49.169353872364,1076.63981814556,500.825515872408));
#114410=CARTESIAN_POINT('Ctrl Pts',(48.9781312245865,1076.64418702791,500.787792900627));
#114411=CARTESIAN_POINT('Ctrl Pts',(48.6208591844163,1076.65392418461,500.64092682057));
#114412=CARTESIAN_POINT('Ctrl Pts',(48.4582674877644,1076.65919298524,500.533125372586));
#114413=CARTESIAN_POINT('Ctrl Pts',(48.1836868704222,1076.66968175505,500.260998222324));
#114414=CARTESIAN_POINT('Ctrl Pts',(48.0743734531646,1076.67479716143,500.099250538524));
#114415=CARTESIAN_POINT('Ctrl Pts',(47.923449534576,1076.68421023618,499.741004657796));
#114416=CARTESIAN_POINT('Ctrl Pts',(47.8840332144445,1076.68840827999,499.547690141379));
#114417=CARTESIAN_POINT('Ctrl Pts',(47.8826628493512,1076.69547892568,499.157450850087));
#114418=CARTESIAN_POINT('Ctrl Pts',(47.920509380774,1076.69829323977,498.964364345255));
#114419=CARTESIAN_POINT('Ctrl Pts',(48.069289066609,1076.70253581002,498.60309569489));
#114420=CARTESIAN_POINT('Ctrl Pts',(48.1791084959194,1076.70392346639,498.438621398773));
#114421=CARTESIAN_POINT('Ctrl Pts',(48.4569428659271,1076.70533126823,498.161562221212));
#114422=CARTESIAN_POINT('Ctrl Pts',(48.622387596233,1076.70533637046,498.051924027819));
#114423=CARTESIAN_POINT('Ctrl Pts',(48.9858236698055,1076.70394944997,497.904023210739));
#114424=CARTESIAN_POINT('Ctrl Pts',(49.1801007082442,1076.70257225397,497.866982469837));
#114425=CARTESIAN_POINT('Ctrl Pts',(49.5707994477516,1076.69835099485,497.870760125806));
#114426=CARTESIAN_POINT('Ctrl Pts',(49.7633720973987,1076.69554737456,497.911157079714));
#114427=CARTESIAN_POINT('Ctrl Pts',(50.1222140806546,1076.68849710468,498.06450259862));
#114428=CARTESIAN_POINT('Ctrl Pts',(50.2848734023975,1076.68430861636,498.176133635553));
#114429=CARTESIAN_POINT('Ctrl Pts',(50.5589386098338,1076.67480716416,498.457775948561));
#114430=CARTESIAN_POINT('Ctrl Pts',(50.666967154968,1076.66957478604,498.625615433594));
#114431=CARTESIAN_POINT('Ctrl Pts',(50.8093329902586,1076.65894549525,498.990446072193));
#114432=CARTESIAN_POINT('Ctrl Pts',(50.8435982120277,1076.65366044596,499.183318187261));
#114433=CARTESIAN_POINT('Ctrl Pts',(50.8356722690318,1076.64391066459,499.571349616223));
#114434=CARTESIAN_POINT('Ctrl Pts',(50.7935307746048,1076.63954780243,499.762747796716));
#114435=CARTESIAN_POINT('Ctrl Pts',(50.6377522610623,1076.63268400824,500.118170230531));
#114436=CARTESIAN_POINT('Ctrl Pts',(50.5256942373236,1076.63025439825,500.278766550657));
#114437=CARTESIAN_POINT('Ctrl Pts',(50.2462547107407,1076.62789959202,500.54723333446));
#114438=CARTESIAN_POINT('Ctrl Pts',(50.0817088218061,1076.62799406049,500.65261346529));
#114439=CARTESIAN_POINT('Ctrl Pts',(49.7297753855395,1076.63064111655,500.790682492722));
#114440=CARTESIAN_POINT('Ctrl Pts',(49.5469155692401,1076.63305247816,500.825314575773));
#114441=CARTESIAN_POINT('Ctrl Pts',(49.3624292594544,1076.63635835644,500.825412934462));
#114442=CARTESIAN_POINT('Origin',(49.3616411037544,1067.7251047501,499.347110012371));
#114443=CARTESIAN_POINT('',(49.3616411037544,1076.65225835227,500.225413144564));
#114444=CARTESIAN_POINT('',(49.3616411037542,1076.69042463418,498.468806880177));
#114445=CARTESIAN_POINT('Ctrl Pts',(49.3616411037544,1076.65225835227,500.225413144564));
#114446=CARTESIAN_POINT('Ctrl Pts',(49.2526397446302,1076.65405656161,500.225413144564));
#114447=CARTESIAN_POINT('Ctrl Pts',(49.1445390094345,1076.656318982,500.205121031533));
#114448=CARTESIAN_POINT('Ctrl Pts',(48.9358138895393,1076.661577456,500.123828754696));
#114449=CARTESIAN_POINT('Ctrl Pts',(48.837959421548,1076.66455181297,500.06151639355));
#114450=CARTESIAN_POINT('Ctrl Pts',(48.7133726407549,1076.66910586258,499.942475946899));
#114451=CARTESIAN_POINT('Ctrl Pts',(48.6758510030616,1076.67062826025,499.898838728586));
#114452=CARTESIAN_POINT('Ctrl Pts',(48.6099016312046,1076.67363340817,499.804922924166));
#114453=CARTESIAN_POINT('Ctrl Pts',(48.5816210798479,1076.67510900197,499.754876943453));
#114454=CARTESIAN_POINT('Ctrl Pts',(48.5112459995488,1076.6794443307,499.59579115308));
#114455=CARTESIAN_POINT('Ctrl Pts',(48.4857749565104,1076.68211321505,499.480809663299));
#114456=CARTESIAN_POINT('Ctrl Pts',(48.4812371815133,1076.68674331669,499.247776609224));
#114457=CARTESIAN_POINT('Ctrl Pts',(48.5021492347113,1076.68866226052,499.132040380882));
#114458=CARTESIAN_POINT('Ctrl Pts',(48.5880483514483,1076.69161962061,498.91510906484));
#114459=CARTESIAN_POINT('Ctrl Pts',(48.6523218104215,1076.69262848295,498.816131172533));
#114460=CARTESIAN_POINT('Ctrl Pts',(48.8160266865626,1076.69368053487,498.648939949345));
#114461=CARTESIAN_POINT('Ctrl Pts',(48.9138959172231,1076.69371222786,498.582478836269));
#114462=CARTESIAN_POINT('Ctrl Pts',(49.1294936780044,1076.69278723447,498.49204620934));
#114463=CARTESIAN_POINT('Ctrl Pts',(49.2449904043857,1076.69184255343,498.468806880177));
#114464=CARTESIAN_POINT('Ctrl Pts',(49.361641103754,1076.69042463418,498.468806880177));
#114465=CARTESIAN_POINT('',(49.3616411037544,1082.7251047501,498.468806880177));
#114466=CARTESIAN_POINT('',(49.3616411037544,1067.7251047501,498.468806880177));
#114467=CARTESIAN_POINT('Origin',(49.3616411037544,1082.7251047501,499.347110012371));
#114468=CARTESIAN_POINT('Ctrl Pts',(49.361641103754,1076.69042463418,498.468806880177));
#114469=CARTESIAN_POINT('Ctrl Pts',(49.3618661819275,1076.6904218983,498.468806880177));
#114470=CARTESIAN_POINT('Ctrl Pts',(49.362091264397,1076.69041916064,498.468806966697));
#114471=CARTESIAN_POINT('Ctrl Pts',(49.478798580427,1076.68899876853,498.468896692359));
#114472=CARTESIAN_POINT('Ctrl Pts',(49.5941007023354,1076.68713463047,498.492157345844));
#114473=CARTESIAN_POINT('Ctrl Pts',(49.8090051354294,1076.68260080841,498.582338809127));
#114474=CARTESIAN_POINT('Ctrl Pts',(49.9064550787002,1076.67997265236,498.648408157275));
#114475=CARTESIAN_POINT('Ctrl Pts',(50.0704006515689,1076.67419715182,498.815275564623));
#114476=CARTESIAN_POINT('Ctrl Pts',(50.1350381480216,1076.67110351319,498.914624450601));
#114477=CARTESIAN_POINT('Ctrl Pts',(50.2172975299658,1076.66519369211,499.122345575253));
#114478=CARTESIAN_POINT('Ctrl Pts',(50.238166604033,1076.66242934611,499.227229665931));
#114479=CARTESIAN_POINT('Ctrl Pts',(50.2398355216052,1076.65987444592,499.333291312131));
#114480=CARTESIAN_POINT('Ctrl Pts',(50.2416478298962,1076.65710003281,499.448465604721));
#114481=CARTESIAN_POINT('Ctrl Pts',(50.2207851993397,1076.65462615942,499.562887367419));
#114482=CARTESIAN_POINT('Ctrl Pts',(50.1360989378208,1076.65068256021,499.777096010322));
#114483=CARTESIAN_POINT('Ctrl Pts',(50.0731216638255,1076.64925290657,499.874813993407));
#114484=CARTESIAN_POINT('Ctrl Pts',(49.9131483865159,1076.64772752428,500.040277564078));
#114485=CARTESIAN_POINT('Ctrl Pts',(49.817748553446,1076.64764590949,500.106456927186));
#114486=CARTESIAN_POINT('Ctrl Pts',(49.606992395841,1076.64885773552,500.198235456417));
#114487=CARTESIAN_POINT('Ctrl Pts',(49.4936990042523,1076.65013703494,500.22299217993));
#114488=CARTESIAN_POINT('Ctrl Pts',(49.3731201546009,1076.65207030756,500.225356909283));
#114489=CARTESIAN_POINT('Ctrl Pts',(49.3673793811915,1076.65216368718,500.225413144564));
#114490=CARTESIAN_POINT('Ctrl Pts',(49.3616411037544,1076.65225835227,500.225413144564));
#114491=CARTESIAN_POINT('Origin',(44.0648939479111,1067.7251047501,510.733705034314));
#114492=CARTESIAN_POINT('',(44.0648939479365,1078.41872688014,509.458260913177));
#114493=CARTESIAN_POINT('Ctrl Pts',(44.0649233283352,1078.2734319431,512.009149155111));
#114494=CARTESIAN_POINT('Ctrl Pts',(44.1880264249484,1078.26956806541,512.009146319377));
#114495=CARTESIAN_POINT('Ctrl Pts',(44.3105075695597,1078.26679874672,511.991321125002));
#114496=CARTESIAN_POINT('Ctrl Pts',(44.4706129032522,1078.26467957244,511.943695046355));
#114497=CARTESIAN_POINT('Ctrl Pts',(44.5120048987952,1078.2642773326,511.9290191121));
#114498=CARTESIAN_POINT('Ctrl Pts',(44.5778908661641,1078.26387834022,511.901756163488));
#114499=CARTESIAN_POINT('Ctrl Pts',(44.6028782862815,1078.26378615623,511.890460043791));
#114500=CARTESIAN_POINT('Ctrl Pts',(44.649880058208,1078.26372736872,511.867359211077));
#114501=CARTESIAN_POINT('Ctrl Pts',(44.6719497463567,1078.26375025698,511.855696029825));
#114502=CARTESIAN_POINT('Ctrl Pts',(44.7213945258687,1078.26391820128,511.82767973288));
#114503=CARTESIAN_POINT('Ctrl Pts',(44.7485269043753,1078.26409530375,511.810932759244));
#114504=CARTESIAN_POINT('Ctrl Pts',(44.8279271463046,1078.26487358262,511.757715417644));
#114505=CARTESIAN_POINT('Ctrl Pts',(44.8781154099761,1078.26572063921,511.718330187519));
#114506=CARTESIAN_POINT('Ctrl Pts',(45.0507311696377,1078.26999998016,511.560636833786));
#114507=CARTESIAN_POINT('Ctrl Pts',(45.1520574044804,1078.27534724355,511.421983108299));
#114508=CARTESIAN_POINT('Ctrl Pts',(45.2819500075955,1078.28844959601,511.140179486435));
#114509=CARTESIAN_POINT('Ctrl Pts',(45.3192377794129,1078.29552900789,511.003968227667));
#114510=CARTESIAN_POINT('Ctrl Pts',(45.3491961468539,1078.31195951831,510.713331211856));
#114511=CARTESIAN_POINT('Ctrl Pts',(45.3376373286404,1078.32131821746,510.560639240082));
#114512=CARTESIAN_POINT('Ctrl Pts',(45.2586193967198,1078.34136818601,510.255859826798));
#114513=CARTESIAN_POINT('Ctrl Pts',(45.1878593661594,1078.351922742,510.107390558694));
#114514=CARTESIAN_POINT('Ctrl Pts',(44.9910598959799,1078.372559519,509.840769415868));
#114515=CARTESIAN_POINT('Ctrl Pts',(44.8651708735293,1078.38241474774,509.726378471745));
#114516=CARTESIAN_POINT('Ctrl Pts',(44.5822331974789,1078.399487038,509.556776761719));
#114517=CARTESIAN_POINT('Ctrl Pts',(44.4292741045652,1078.4066482895,509.500796653613));
#114518=CARTESIAN_POINT('Ctrl Pts',(44.1077587594526,1078.41811353863,509.448441447054));
#114519=CARTESIAN_POINT('Ctrl Pts',(43.9420068574355,1078.42226273415,509.453601435726));
#114520=CARTESIAN_POINT('Ctrl Pts',(43.7241966059722,1078.42547987196,509.50318937737));
#114521=CARTESIAN_POINT('Ctrl Pts',(43.6676063820261,1078.42609572361,509.520277400153));
#114522=CARTESIAN_POINT('Ctrl Pts',(43.5837247291025,1078.42667113737,509.552106674066));
#114523=CARTESIAN_POINT('Ctrl Pts',(43.5554490856828,1078.42680364945,509.564019406702));
#114524=CARTESIAN_POINT('Ctrl Pts',(43.5053387657168,1078.42692640291,509.587293325476));
#114525=CARTESIAN_POINT('Ctrl Pts',(43.4833511983387,1078.42693965304,509.598288881504));
#114526=CARTESIAN_POINT('Ctrl Pts',(43.4373926283563,1078.42687998455,509.622957282948));
#114527=CARTESIAN_POINT('Ctrl Pts',(43.4135198271369,1078.42679635528,509.636786527848));
#114528=CARTESIAN_POINT('Ctrl Pts',(43.351564860165,1078.4264373479,509.675412539031));
#114529=CARTESIAN_POINT('Ctrl Pts',(43.3143278474008,1078.42607319779,509.7014881403));
#114530=CARTESIAN_POINT('Ctrl Pts',(43.1618407086329,1078.42392450151,509.820890749726));
#114531=CARTESIAN_POINT('Ctrl Pts',(43.0619659177488,1078.42081023532,509.93192354757));
#114532=CARTESIAN_POINT('Ctrl Pts',(42.9117438614676,1078.41221661889,510.172208468626));
#114533=CARTESIAN_POINT('Ctrl Pts',(42.8587785837881,1078.40702155248,510.297472526595));
#114534=CARTESIAN_POINT('Ctrl Pts',(42.7910462855203,1078.39412783417,510.572457283003));
#114535=CARTESIAN_POINT('Ctrl Pts',(42.7809518465782,1078.38633227265,510.721279006368));
#114536=CARTESIAN_POINT('Ctrl Pts',(42.81343049477,1078.36854609626,511.026987087462));
#114537=CARTESIAN_POINT('Ctrl Pts',(42.8598463718235,1078.35858523557,511.180937499236));
#114538=CARTESIAN_POINT('Ctrl Pts',(43.011419943816,1078.33754469861,511.472307774161));
#114539=CARTESIAN_POINT('Ctrl Pts',(43.1185007686512,1078.32663889876,511.605308130303));
#114540=CARTESIAN_POINT('Ctrl Pts',(43.3445464540617,1078.30871969167,511.793665775114));
#114541=CARTESIAN_POINT('Ctrl Pts',(43.4519755230289,1078.30152981722,511.859211086788));
#114542=CARTESIAN_POINT('Ctrl Pts',(43.6364119537953,1078.29115151849,511.937367251213));
#114543=CARTESIAN_POINT('Ctrl Pts',(43.708037897756,1078.28753344912,511.960512913644));
#114544=CARTESIAN_POINT('Ctrl Pts',(43.8743255501986,1078.28006013478,511.998436522319));
#114545=CARTESIAN_POINT('Ctrl Pts',(43.9694626892088,1078.27642819782,512.00915135409));
#114546=CARTESIAN_POINT('Ctrl Pts',(44.0649233283352,1078.2734319431,512.009149155111));
#114547=CARTESIAN_POINT('',(44.0648939478931,1076.41517983612,509.458260913177));
#114548=CARTESIAN_POINT('',(44.0648939479111,1067.7251047501,509.458260913177));
#114549=CARTESIAN_POINT('Ctrl Pts',(44.0649289142737,1076.26836941018,512.009149154971));
#114550=CARTESIAN_POINT('Ctrl Pts',(43.898466721868,1076.27364765281,512.00915371854));
#114551=CARTESIAN_POINT('Ctrl Pts',(43.7336757635041,1076.28085793182,511.976571532619));
#114552=CARTESIAN_POINT('Ctrl Pts',(43.4255980312565,1076.29814802138,511.849892034166));
#114553=CARTESIAN_POINT('Ctrl Pts',(43.2853292344771,1076.30806503659,511.756845973201));
#114554=CARTESIAN_POINT('Ctrl Pts',(43.1076795744347,1076.32385879801,511.580738504689));
#114555=CARTESIAN_POINT('Ctrl Pts',(43.0543151174143,1076.3292440124,511.516299408341));
#114556=CARTESIAN_POINT('Ctrl Pts',(42.9609252978987,1076.34007978619,511.377897182119));
#114557=CARTESIAN_POINT('Ctrl Pts',(42.92112790914,1076.34550463083,511.304257657007));
#114558=CARTESIAN_POINT('Ctrl Pts',(42.8231671228517,1076.36172686774,511.070827742348));
#114559=CARTESIAN_POINT('Ctrl Pts',(42.7893682881464,1076.37212929197,510.902822386907));
#114560=CARTESIAN_POINT('Ctrl Pts',(42.789531130527,1076.39082207213,510.564461885871));
#114561=CARTESIAN_POINT('Ctrl Pts',(42.8230537282854,1076.39894628175,510.397448781163));
#114562=CARTESIAN_POINT('Ctrl Pts',(42.9532536253702,1076.41208001526,510.086009985341));
#114563=CARTESIAN_POINT('Ctrl Pts',(43.0486587750672,1076.41696331781,509.944685561946));
#114564=CARTESIAN_POINT('Ctrl Pts',(43.2893362834614,1076.42298691131,509.707095303306));
#114565=CARTESIAN_POINT('Ctrl Pts',(43.4323053363089,1076.42406124075,509.613322596213));
#114566=CARTESIAN_POINT('Ctrl Pts',(43.7463888061328,1076.42225126093,509.487137638111));
#114567=CARTESIAN_POINT('Ctrl Pts',(43.9143232162407,1076.4193875216,509.455939848884));
#114568=CARTESIAN_POINT('Ctrl Pts',(44.2521255034383,1076.40996404624,509.460845403669));
#114569=CARTESIAN_POINT('Ctrl Pts',(44.4186228177448,1076.40350198033,509.496747470433));
#114570=CARTESIAN_POINT('Ctrl Pts',(44.7283047831834,1076.38758170073,509.631334097181));
#114571=CARTESIAN_POINT('Ctrl Pts',(44.8683568598277,1076.37826864388,509.728844772274));
#114572=CARTESIAN_POINT('Ctrl Pts',(45.0427133406882,1076.36305942859,509.910598795777));
#114573=CARTESIAN_POINT('Ctrl Pts',(45.0941421083455,1076.35787432204,509.975892416633));
#114574=CARTESIAN_POINT('Ctrl Pts',(45.1843665778088,1076.34719554529,510.116733352278));
#114575=CARTESIAN_POINT('Ctrl Pts',(45.2227080714411,1076.34172394529,510.1920977003));
#114576=CARTESIAN_POINT('Ctrl Pts',(45.314177609022,1076.32536347,510.426875244866));
#114577=CARTESIAN_POINT('Ctrl Pts',(45.3436560276373,1076.31461218309,510.593560774999));
#114578=CARTESIAN_POINT('Ctrl Pts',(45.3364295434161,1076.29473867435,510.928736467631));
#114579=CARTESIAN_POINT('Ctrl Pts',(45.2998322220975,1076.28581091494,511.093997874046));
#114580=CARTESIAN_POINT('Ctrl Pts',(45.1648858177163,1076.27122059476,511.400608487779));
#114581=CARTESIAN_POINT('Ctrl Pts',(45.0680041547839,1076.26569628253,511.539032561309));
#114582=CARTESIAN_POINT('Ctrl Pts',(44.8266311050491,1076.25898953484,511.770209463768));
#114583=CARTESIAN_POINT('Ctrl Pts',(44.6846746230433,1076.25785997188,511.860854687224));
#114584=CARTESIAN_POINT('Ctrl Pts',(44.3812706408253,1076.2601490384,511.979465613399));
#114585=CARTESIAN_POINT('Ctrl Pts',(44.223776818423,1076.26333260411,512.009144800148));
#114586=CARTESIAN_POINT('Ctrl Pts',(44.0649289142737,1076.26836941018,512.009149154971));
#114587=CARTESIAN_POINT('Origin',(44.0648939479111,1067.7251047501,510.733705034314));
#114588=CARTESIAN_POINT('',(44.0648939479111,1076.3053526307,511.40914915545));
#114589=CARTESIAN_POINT('',(44.0648939479122,1076.38310559156,510.058260913177));
#114590=CARTESIAN_POINT('Ctrl Pts',(44.0648939479111,1076.3053526307,511.40914915545));
#114591=CARTESIAN_POINT('Ctrl Pts',(44.0633527628547,1076.30539988211,511.40914915545));
#114592=CARTESIAN_POINT('Ctrl Pts',(44.0618113343601,1076.30544745384,511.409143880586));
#114593=CARTESIAN_POINT('Ctrl Pts',(43.9720188605801,1076.30823686737,511.408529124494));
#114594=CARTESIAN_POINT('Ctrl Pts',(43.884773315559,1076.31197309278,511.390635615152));
#114595=CARTESIAN_POINT('Ctrl Pts',(43.721946257568,1076.32096316671,511.322285843355));
#114596=CARTESIAN_POINT('Ctrl Pts',(43.6479630276562,1076.32613292064,511.272406572667));
#114597=CARTESIAN_POINT('Ctrl Pts',(43.5545347528908,1076.33441434733,511.17835484543));
#114598=CARTESIAN_POINT('Ctrl Pts',(43.5265300258902,1076.33724450606,511.144002164113));
#114599=CARTESIAN_POINT('Ctrl Pts',(43.4776284811296,1076.34295724576,511.070306507139));
#114600=CARTESIAN_POINT('Ctrl Pts',(43.4568510945842,1076.34582627713,511.031136155473));
#114601=CARTESIAN_POINT('Ctrl Pts',(43.4058321641746,1076.3544500931,510.906858046465));
#114602=CARTESIAN_POINT('Ctrl Pts',(43.3886279945003,1076.3600251194,510.817468897038));
#114603=CARTESIAN_POINT('Ctrl Pts',(43.3903285823292,1076.37010972279,510.637534695334));
#114604=CARTESIAN_POINT('Ctrl Pts',(43.4090728930029,1076.37452473097,510.548778109158));
#114605=CARTESIAN_POINT('Ctrl Pts',(43.480211565499,1076.38165860269,510.383795285743));
#114606=CARTESIAN_POINT('Ctrl Pts',(43.5318752711781,1076.38430833495,510.309215794991));
#114607=CARTESIAN_POINT('Ctrl Pts',(43.6614488871979,1076.38751506255,510.184574883999));
#114608=CARTESIAN_POINT('Ctrl Pts',(43.7380667818616,1076.38803887879,510.135793679277));
#114609=CARTESIAN_POINT('Ctrl Pts',(43.8995060293051,1076.38692014794,510.073574062566));
#114610=CARTESIAN_POINT('Ctrl Pts',(43.9818499782334,1076.38544930888,510.058260913177));
#114611=CARTESIAN_POINT('Ctrl Pts',(44.0648939479144,1076.38310559156,510.058260913177));
#114612=CARTESIAN_POINT('',(44.0648939479111,1082.7251047501,510.058260913177));
#114613=CARTESIAN_POINT('',(44.0648939479111,1067.7251047501,510.058260913177));
#114614=CARTESIAN_POINT('Origin',(44.0648939479111,1082.7251047501,510.733705034314));
#114615=CARTESIAN_POINT('Ctrl Pts',(44.0649019425061,1076.38310536593,510.058260913225));
#114616=CARTESIAN_POINT('Ctrl Pts',(44.1547346152825,1076.38056999439,510.058261976489));
#114617=CARTESIAN_POINT('Ctrl Pts',(44.2436360023306,1076.37706156818,510.076183629503));
#114618=CARTESIAN_POINT('Ctrl Pts',(44.4093391643003,1076.36844335467,510.145765016121));
#114619=CARTESIAN_POINT('Ctrl Pts',(44.4844585717707,1076.36341511981,510.19679661222));
#114620=CARTESIAN_POINT('Ctrl Pts',(44.5781912597982,1076.35526119709,510.292467494895));
#114621=CARTESIAN_POINT('Ctrl Pts',(44.6058611629681,1076.35249267579,510.326865469975));
#114622=CARTESIAN_POINT('Ctrl Pts',(44.6544610113736,1076.34681628114,510.40109094345));
#114623=CARTESIAN_POINT('Ctrl Pts',(44.6751678808445,1076.34392071567,510.440810837595));
#114624=CARTESIAN_POINT('Ctrl Pts',(44.7248188201033,1076.33529466325,510.564612268263));
#114625=CARTESIAN_POINT('Ctrl Pts',(44.7413041669408,1076.32966310519,510.652660939925));
#114626=CARTESIAN_POINT('Ctrl Pts',(44.7392854090862,1076.31929313078,510.830041948944));
#114627=CARTESIAN_POINT('Ctrl Pts',(44.7208320987569,1076.31465481247,510.917666177242));
#114628=CARTESIAN_POINT('Ctrl Pts',(44.6511545552143,1076.30706721385,511.080631198303));
#114629=CARTESIAN_POINT('Ctrl Pts',(44.6006845645422,1076.30418898174,511.154416852484));
#114630=CARTESIAN_POINT('Ctrl Pts',(44.4742704873603,1076.30064035351,511.278165817368));
#114631=CARTESIAN_POINT('Ctrl Pts',(44.3996341008144,1076.29999935545,511.326982776317));
#114632=CARTESIAN_POINT('Ctrl Pts',(44.2373389937831,1076.30105501513,511.392491591372));
#114633=CARTESIAN_POINT('Ctrl Pts',(44.1515008222423,1076.30269733816,511.40914915545));
#114634=CARTESIAN_POINT('Ctrl Pts',(44.0648939479111,1076.3053526307,511.40914915545));
#114635=CARTESIAN_POINT('Origin',(37.1057957606637,1067.7251047501,522.70822837456));
#114636=CARTESIAN_POINT('',(37.1057957606635,1077.76997147869,521.609397238568));
#114637=CARTESIAN_POINT('Ctrl Pts',(37.105796071773,1077.55793163415,523.807059510553));
#114638=CARTESIAN_POINT('Ctrl Pts',(37.1819019257861,1077.55505615697,523.807059489005));
#114639=CARTESIAN_POINT('Ctrl Pts',(37.2578238143658,1077.55297387967,523.799152773324));
#114640=CARTESIAN_POINT('Ctrl Pts',(37.3645577570114,1077.55118390574,523.776664777783));
#114641=CARTESIAN_POINT('Ctrl Pts',(37.396458676761,1077.55080014837,523.768430913599));
#114642=CARTESIAN_POINT('Ctrl Pts',(37.4476618495431,1077.5504329526,523.752729609035));
#114643=CARTESIAN_POINT('Ctrl Pts',(37.4672065256664,1077.55035358048,523.746128913403));
#114644=CARTESIAN_POINT('Ctrl Pts',(37.5075398463782,1077.55031767467,523.731229867817));
#114645=CARTESIAN_POINT('Ctrl Pts',(37.5282838381324,1077.55037212107,523.722838729423));
#114646=CARTESIAN_POINT('Ctrl Pts',(37.576364206958,1077.55067151241,523.701659422828));
#114647=CARTESIAN_POINT('Ctrl Pts',(37.6034576390165,1077.5509760974,523.688367344859));
#114648=CARTESIAN_POINT('Ctrl Pts',(37.6879499798836,1077.55236676043,523.64250806257));
#114649=CARTESIAN_POINT('Ctrl Pts',(37.7429664517361,1077.5539485014,523.605887400888));
#114650=CARTESIAN_POINT('Ctrl Pts',(37.9084498148921,1077.5609896708,523.472826242117));
#114651=CARTESIAN_POINT('Ctrl Pts',(38.002957898368,1077.56875414734,523.359294711216));
#114652=CARTESIAN_POINT('Ctrl Pts',(38.130756243618,1077.58742059887,523.122862458955));
#114653=CARTESIAN_POINT('Ctrl Pts',(38.1705473439029,1077.59748236801,523.006086264765));
#114654=CARTESIAN_POINT('Ctrl Pts',(38.2116478943223,1077.62070901741,522.754324456711));
#114655=CARTESIAN_POINT('Ctrl Pts',(38.2091216107585,1077.63387499693,522.620656571859));
#114656=CARTESIAN_POINT('Ctrl Pts',(38.1546822006451,1077.66205431621,522.351051892117));
#114657=CARTESIAN_POINT('Ctrl Pts',(38.0995662146793,1077.67687387527,522.218158104341));
#114658=CARTESIAN_POINT('Ctrl Pts',(37.9403429117606,1077.70553180493,521.978880915739));
#114659=CARTESIAN_POINT('Ctrl Pts',(37.8369620251451,1077.71907922308,521.875235883165));
#114660=CARTESIAN_POINT('Ctrl Pts',(37.6029661902064,1077.74218224825,521.718863919753));
#114661=CARTESIAN_POINT('Ctrl Pts',(37.4763834979393,1077.75173227366,521.664795578838));
#114662=CARTESIAN_POINT('Ctrl Pts',(37.2111042970911,1077.76657770235,521.6061438797));
#114663=CARTESIAN_POINT('Ctrl Pts',(37.0748600856621,1077.77179152888,521.601536093843));
#114664=CARTESIAN_POINT('Ctrl Pts',(36.8986797266645,1077.77549923438,521.628239431293));
#114665=CARTESIAN_POINT('Ctrl Pts',(36.8566407122039,1077.77614728576,521.637156220384));
#114666=CARTESIAN_POINT('Ctrl Pts',(36.7910551103268,1077.77678054124,521.655139366435));
#114667=CARTESIAN_POINT('Ctrl Pts',(36.7671154058867,1077.77692917591,521.662592777791));
#114668=CARTESIAN_POINT('Ctrl Pts',(36.7229586896977,1077.77704792792,521.678016348418));
#114669=CARTESIAN_POINT('Ctrl Pts',(36.7026828497048,1077.77703927433,521.685779833696));
#114670=CARTESIAN_POINT('Ctrl Pts',(36.6583937387185,1077.77687919045,521.704260186241));
#114671=CARTESIAN_POINT('Ctrl Pts',(36.6345086993071,1077.77669809368,521.71524845123));
#114672=CARTESIAN_POINT('Ctrl Pts',(36.5679567870713,1077.77592044874,521.748808033854));
#114673=CARTESIAN_POINT('Ctrl Pts',(36.5263547884368,1077.77510407087,521.773345870686));
#114674=CARTESIAN_POINT('Ctrl Pts',(36.3656670996843,1077.77056903018,521.882978084723));
#114675=CARTESIAN_POINT('Ctrl Pts',(36.2625918330275,1077.76437348841,521.988662511923));
#114676=CARTESIAN_POINT('Ctrl Pts',(36.1179449472872,1077.74858960728,522.212217070053));
#114677=CARTESIAN_POINT('Ctrl Pts',(36.0697035921556,1077.7399034487,522.323075230964));
#114678=CARTESIAN_POINT('Ctrl Pts',(36.0083464475759,1077.71914163,522.566278725154));
#114679=CARTESIAN_POINT('Ctrl Pts',(35.9992758314291,1077.70699385866,522.697733005839));
#114680=CARTESIAN_POINT('Ctrl Pts',(36.0287616905797,1077.68013756808,522.967549583484));
#114681=CARTESIAN_POINT('Ctrl Pts',(36.0708063740701,1077.66554281071,523.103237129484));
#114682=CARTESIAN_POINT('Ctrl Pts',(36.2060059036698,1077.63611499291,523.355511024951));
#114683=CARTESIAN_POINT('Ctrl Pts',(36.2995553167718,1077.62157094099,523.46889853725));
#114684=CARTESIAN_POINT('Ctrl Pts',(36.4915780543861,1077.59907319862,523.625037468314));
#114685=CARTESIAN_POINT('Ctrl Pts',(36.5792029394156,1077.59056060109,523.678038219772));
#114686=CARTESIAN_POINT('Ctrl Pts',(36.7311004545636,1077.57841278622,523.743137440291));
#114687=CARTESIAN_POINT('Ctrl Pts',(36.7913285133599,1077.57417549172,523.76300372559));
#114688=CARTESIAN_POINT('Ctrl Pts',(36.9357690856537,1077.56534056385,523.797155110267));
#114689=CARTESIAN_POINT('Ctrl Pts',(37.0206155941158,1077.56114997422,523.80705953467));
#114690=CARTESIAN_POINT('Ctrl Pts',(37.105796071773,1077.55793163415,523.807059510553));
#114691=CARTESIAN_POINT('',(37.1057957606431,1075.76001126608,521.609397238568));
#114692=CARTESIAN_POINT('',(37.1057957606637,1067.7251047501,521.609397238568));
#114693=CARTESIAN_POINT('Ctrl Pts',(37.1058085229615,1075.54602936729,523.807059510479));
#114694=CARTESIAN_POINT('Ctrl Pts',(36.962618776904,1075.55148807702,523.807061173546));
#114695=CARTESIAN_POINT('Ctrl Pts',(36.820944062981,1075.55969809754,523.779077062919));
#114696=CARTESIAN_POINT('Ctrl Pts',(36.5557180154681,1075.58062367947,523.670262608626));
#114697=CARTESIAN_POINT('Ctrl Pts',(36.4348455022318,1075.59315951082,523.590183173545));
#114698=CARTESIAN_POINT('Ctrl Pts',(36.2302689579569,1075.62084154858,523.387724464143));
#114699=CARTESIAN_POINT('Ctrl Pts',(36.1487230710439,1075.63573855628,523.267014954714));
#114700=CARTESIAN_POINT('Ctrl Pts',(36.0649907979957,1075.65825363871,523.067833724736));
#114701=CARTESIAN_POINT('Ctrl Pts',(36.0437090753994,1075.66572117715,522.999028954527));
#114702=CARTESIAN_POINT('Ctrl Pts',(36.0000341115014,1075.68797032344,522.785712403809));
#114703=CARTESIAN_POINT('Ctrl Pts',(35.9995046517734,1075.70214461371,522.638284032741));
#114704=CARTESIAN_POINT('Ctrl Pts',(36.0560928927073,1075.72739320482,522.352250426399));
#114705=CARTESIAN_POINT('Ctrl Pts',(36.1124217679349,1075.73823577623,522.216408218919));
#114706=CARTESIAN_POINT('Ctrl Pts',(36.275083603449,1075.75526553076,521.974312345321));
#114707=CARTESIAN_POINT('Ctrl Pts',(36.3798167189253,1075.76127923228,521.870535446229));
#114708=CARTESIAN_POINT('Ctrl Pts',(36.6228750045003,1075.76764624752,521.710633225511));
#114709=CARTESIAN_POINT('Ctrl Pts',(36.7584387976241,1075.7679844608,521.65572882712));
#114710=CARTESIAN_POINT('Ctrl Pts',(37.0443266705674,1075.76294126561,521.60142655478));
#114711=CARTESIAN_POINT('Ctrl Pts',(37.1918160398829,1075.75755997854,521.603088103954));
#114712=CARTESIAN_POINT('Ctrl Pts',(37.4771699604814,1075.7416667549,521.663831536216));
#114713=CARTESIAN_POINT('Ctrl Pts',(37.6121558493899,1075.73131925553,521.722225884631));
#114714=CARTESIAN_POINT('Ctrl Pts',(37.8517472187289,1075.70686501772,521.888286373147));
#114715=CARTESIAN_POINT('Ctrl Pts',(37.9538798086312,1075.69298431231,521.994479518879));
#114716=CARTESIAN_POINT('Ctrl Pts',(38.1112913603744,1075.66337753341,522.241314981971));
#114717=CARTESIAN_POINT('Ctrl Pts',(38.1646495489176,1075.6479250309,522.379822325483));
#114718=CARTESIAN_POINT('Ctrl Pts',(38.2135845009188,1075.61776955795,522.668693638895));
#114719=CARTESIAN_POINT('Ctrl Pts',(38.209043326696,1075.6033529045,522.816211823732));
#114720=CARTESIAN_POINT('Ctrl Pts',(38.142835677807,1075.57771197269,523.099136293412));
#114721=CARTESIAN_POINT('Ctrl Pts',(38.0825476903773,1075.56669678043,523.231966100617));
#114722=CARTESIAN_POINT('Ctrl Pts',(37.9143117441168,1075.5495760996,523.466106350132));
#114723=CARTESIAN_POINT('Ctrl Pts',(37.8083228233454,1075.54361032715,523.565312995936));
#114724=CARTESIAN_POINT('Ctrl Pts',(37.5645628638608,1075.53761517467,523.716918627914));
#114725=CARTESIAN_POINT('Ctrl Pts',(37.4293911130489,1075.53761606337,523.768044094385));
#114726=CARTESIAN_POINT('Ctrl Pts',(37.2279325124291,1075.54188513668,523.801960689426));
#114727=CARTESIAN_POINT('Ctrl Pts',(37.1669160619767,1075.54369981279,523.80705880075));
#114728=CARTESIAN_POINT('Ctrl Pts',(37.1058085229615,1075.54602936729,523.807059510479));
#114729=CARTESIAN_POINT('Origin',(37.1057957606637,1067.7251047501,522.70822837456));
#114730=CARTESIAN_POINT('',(37.1057957606637,1075.60643384366,523.207059510553));
#114731=CARTESIAN_POINT('',(37.1057957606638,1075.70357965628,522.209397238568));
#114732=CARTESIAN_POINT('Ctrl Pts',(37.1057957606637,1075.60643384366,523.207059510553));
#114733=CARTESIAN_POINT('Ctrl Pts',(37.0715278617885,1075.60771635452,523.207059510553));
#114734=CARTESIAN_POINT('Ctrl Pts',(37.0372821742987,1075.60934665592,523.203528331015));
#114735=CARTESIAN_POINT('Ctrl Pts',(36.9397986981363,1075.61500489314,523.183125618715));
#114736=CARTESIAN_POINT('Ctrl Pts',(36.8792909601871,1075.61980011443,523.157406655478));
#114737=CARTESIAN_POINT('Ctrl Pts',(36.7713261037424,1075.6310295087,523.084057867589));
#114738=CARTESIAN_POINT('Ctrl Pts',(36.7249865915008,1075.63736525146,523.036998776482));
#114739=CARTESIAN_POINT('Ctrl Pts',(36.6711059659364,1075.64736299764,522.95509753201));
#114740=CARTESIAN_POINT('Ctrl Pts',(36.6558783678005,1075.65075368797,522.926112470758));
#114741=CARTESIAN_POINT('Ctrl Pts',(36.6313332594527,1075.65754877975,522.86564658854));
#114742=CARTESIAN_POINT('Ctrl Pts',(36.6220612865006,1075.66093749477,522.834309770799));
#114743=CARTESIAN_POINT('Ctrl Pts',(36.6033808891434,1075.67106949781,522.737020463842));
#114744=CARTESIAN_POINT('Ctrl Pts',(36.6040095655807,1075.6775436533,522.669854002592));
#114745=CARTESIAN_POINT('Ctrl Pts',(36.6315873077625,1075.68908235576,522.539806990181));
#114746=CARTESIAN_POINT('Ctrl Pts',(36.6581982056893,1075.69403710896,522.478199419826));
#114747=CARTESIAN_POINT('Ctrl Pts',(36.7337017348081,1075.70172462878,522.36954278163));
#114748=CARTESIAN_POINT('Ctrl Pts',(36.7815977993668,1075.704404469,522.32343008279));
#114749=CARTESIAN_POINT('Ctrl Pts',(36.8918809489161,1075.70715944505,522.252928195246));
#114750=CARTESIAN_POINT('Ctrl Pts',(36.9529692099161,1075.70724196444,522.228955747049));
#114751=CARTESIAN_POINT('Ctrl Pts',(37.0462652018157,1075.70548062127,522.212066026661));
#114752=CARTESIAN_POINT('Ctrl Pts',(37.0760029825362,1075.70465924766,522.209397238568));
#114753=CARTESIAN_POINT('Ctrl Pts',(37.1057957606639,1075.70357965628,522.209397238568));
#114754=CARTESIAN_POINT('',(37.1057957606637,1082.7251047501,522.209397238568));
#114755=CARTESIAN_POINT('',(37.1057957606637,1067.7251047501,522.209397238568));
#114756=CARTESIAN_POINT('Origin',(37.1057957606637,1082.7251047501,522.70822837456));
#114757=CARTESIAN_POINT('Ctrl Pts',(37.1057981350553,1075.70357957024,522.209397238574));
#114758=CARTESIAN_POINT('Ctrl Pts',(37.1709760170612,1075.70121771037,522.209397548814));
#114759=CARTESIAN_POINT('Ctrl Pts',(37.2354654141579,1075.69765473122,522.22217096653));
#114760=CARTESIAN_POINT('Ctrl Pts',(37.3571418365381,1075.68841522189,522.272245048994));
#114761=CARTESIAN_POINT('Ctrl Pts',(37.4129068670046,1075.68278623442,522.309577632184));
#114762=CARTESIAN_POINT('Ctrl Pts',(37.5066358474258,1075.6702348421,522.403931631854));
#114763=CARTESIAN_POINT('Ctrl Pts',(37.5436188803242,1075.6634310619,522.460091045283));
#114764=CARTESIAN_POINT('Ctrl Pts',(37.5806691086318,1075.65311475641,522.552054126811));
#114765=CARTESIAN_POINT('Ctrl Pts',(37.5898582728438,1075.64971799561,522.583413152199));
#114766=CARTESIAN_POINT('Ctrl Pts',(37.6083628897596,1075.63948692928,522.681164147311));
#114767=CARTESIAN_POINT('Ctrl Pts',(37.6074680466773,1075.63289357422,522.74876246245));
#114768=CARTESIAN_POINT('Ctrl Pts',(37.5793307466939,1075.62121979839,522.878177227253));
#114769=CARTESIAN_POINT('Ctrl Pts',(37.552951258777,1075.61622087836,522.938851680759));
#114770=CARTESIAN_POINT('Ctrl Pts',(37.4783575255633,1075.60839855439,523.046282286457));
#114771=CARTESIAN_POINT('Ctrl Pts',(37.4310075752998,1075.60563935457,523.092067615194));
#114772=CARTESIAN_POINT('Ctrl Pts',(37.3215124375085,1075.60274958377,523.162676949381));
#114773=CARTESIAN_POINT('Ctrl Pts',(37.2605243187527,1075.60263640758,523.186889878728));
#114774=CARTESIAN_POINT('Ctrl Pts',(37.1665751422606,1075.60443311762,523.204284112385));
#114775=CARTESIAN_POINT('Ctrl Pts',(37.1361767225813,1075.60529680536,523.207059510553));
#114776=CARTESIAN_POINT('Ctrl Pts',(37.1057957606637,1075.60643384366,523.207059510553));
#114777=CARTESIAN_POINT('Origin',(27.7552687727514,1067.7251047501,533.110228186055));
#114778=CARTESIAN_POINT('',(27.7552687727512,1076.95995571924,532.019687437326));
#114779=CARTESIAN_POINT('Ctrl Pts',(27.7552666781061,1076.67624978494,534.200768934781));
#114780=CARTESIAN_POINT('Ctrl Pts',(27.800749602656,1076.67470112636,534.200769022142));
#114781=CARTESIAN_POINT('Ctrl Pts',(27.8461978020645,1076.67353183618,534.197923695252));
#114782=CARTESIAN_POINT('Ctrl Pts',(27.9202859703263,1076.67224859531,534.188606269179));
#114783=CARTESIAN_POINT('Ctrl Pts',(27.9490713776196,1076.67190703409,534.183806659105));
#114784=CARTESIAN_POINT('Ctrl Pts',(28.000031619331,1076.67158427493,534.173192816812));
#114785=CARTESIAN_POINT('Ctrl Pts',(28.022279584309,1076.6715413264,534.167823525971));
#114786=CARTESIAN_POINT('Ctrl Pts',(28.0685879420242,1076.67165897254,534.155093009102));
#114787=CARTESIAN_POINT('Ctrl Pts',(28.0925949574108,1076.67184008849,534.147591363473));
#114788=CARTESIAN_POINT('Ctrl Pts',(28.1542564602887,1076.67262044846,534.125956624133));
#114789=CARTESIAN_POINT('Ctrl Pts',(28.1914219166206,1076.67340452834,534.110560598595));
#114790=CARTESIAN_POINT('Ctrl Pts',(28.3376377751246,1076.67777938803,534.040291359133));
#114791=CARTESIAN_POINT('Ctrl Pts',(28.4378636452712,1076.68380228948,533.969400135769));
#114792=CARTESIAN_POINT('Ctrl Pts',(28.6057555957578,1076.70026506997,533.802450261603));
#114793=CARTESIAN_POINT('Ctrl Pts',(28.6738386372743,1076.71033096995,533.70910811931));
#114794=CARTESIAN_POINT('Ctrl Pts',(28.7835396313896,1076.73495241998,533.494739986341));
#114795=CARTESIAN_POINT('Ctrl Pts',(28.8210108220568,1076.74967109205,533.373481699937));
#114796=CARTESIAN_POINT('Ctrl Pts',(28.8542567229034,1076.78264658264,533.113742631473));
#114797=CARTESIAN_POINT('Ctrl Pts',(28.8461184918472,1076.8008176166,532.976827028232));
#114798=CARTESIAN_POINT('Ctrl Pts',(28.7774301812217,1076.83874892362,532.702876802798));
#114799=CARTESIAN_POINT('Ctrl Pts',(28.7134872748216,1076.85816056167,532.569277953425));
#114800=CARTESIAN_POINT('Ctrl Pts',(28.5394386091861,1076.89354471149,532.33922403747));
#114801=CARTESIAN_POINT('Ctrl Pts',(28.4325676500709,1076.90928968887,532.243765569968));
#114802=CARTESIAN_POINT('Ctrl Pts',(28.198283894545,1076.93465255479,532.105284488169));
#114803=CARTESIAN_POINT('Ctrl Pts',(28.0753043849492,1076.94447690571,532.059588121092));
#114804=CARTESIAN_POINT('Ctrl Pts',(27.8571232945171,1076.95652961713,532.020623011117));
#114805=CARTESIAN_POINT('Ctrl Pts',(27.7655359639275,1076.96010199512,532.015911833822));
#114806=CARTESIAN_POINT('Ctrl Pts',(27.6380366991379,1076.96303829024,532.025394453301));
#114807=CARTESIAN_POINT('Ctrl Pts',(27.6018434293981,1076.96363909349,532.029918589574));
#114808=CARTESIAN_POINT('Ctrl Pts',(27.5421593853192,1076.96424144684,532.040440048664));
#114809=CARTESIAN_POINT('Ctrl Pts',(27.5185228853992,1076.96437664828,532.045421295655));
#114810=CARTESIAN_POINT('Ctrl Pts',(27.4727721014839,1076.96443550985,532.056661862207));
#114811=CARTESIAN_POINT('Ctrl Pts',(27.4506523051707,1076.96436923202,532.062843274559));
#114812=CARTESIAN_POINT('Ctrl Pts',(27.3994327987842,1076.96399247307,532.078916562617));
#114813=CARTESIAN_POINT('Ctrl Pts',(27.3705249246315,1076.96360721627,532.089348751169));
#114814=CARTESIAN_POINT('Ctrl Pts',(27.2809730208945,1076.96186225852,532.126010163014));
#114815=CARTESIAN_POINT('Ctrl Pts',(27.2222685165802,1076.95989538189,532.156526763776));
#114816=CARTESIAN_POINT('Ctrl Pts',(27.044554732498,1076.95119820474,532.270456348092));
#114817=CARTESIAN_POINT('Ctrl Pts',(26.9394344356685,1076.94167724829,532.372237845655));
#114818=CARTESIAN_POINT('Ctrl Pts',(26.7879367113717,1076.91856004502,532.592059044527));
#114819=CARTESIAN_POINT('Ctrl Pts',(26.7360734287624,1076.90598935935,532.703547791886));
#114820=CARTESIAN_POINT('Ctrl Pts',(26.6685710651777,1076.87665623319,532.949064822446));
#114821=CARTESIAN_POINT('Ctrl Pts',(26.6570743079382,1076.85985871735,533.082220851289));
#114822=CARTESIAN_POINT('Ctrl Pts',(26.6832874301669,1076.82346282728,533.356326910267));
#114823=CARTESIAN_POINT('Ctrl Pts',(26.7247353072037,1076.80407814151,533.494563715906));
#114824=CARTESIAN_POINT('Ctrl Pts',(26.8590102789459,1076.76643226086,533.747944510667));
#114825=CARTESIAN_POINT('Ctrl Pts',(26.9509091231919,1076.7485268945,533.860606582479));
#114826=CARTESIAN_POINT('Ctrl Pts',(27.1658328961315,1076.71793165164,534.037511776423));
#114827=CARTESIAN_POINT('Ctrl Pts',(27.284473001473,1076.70522493337,534.103080083893));
#114828=CARTESIAN_POINT('Ctrl Pts',(27.5227928918663,1076.68665474553,534.182044894166));
#114829=CARTESIAN_POINT('Ctrl Pts',(27.638588818275,1076.68022257627,534.200768710673));
#114830=CARTESIAN_POINT('Ctrl Pts',(27.7552666781061,1076.67624978494,534.200768934781));
#114831=CARTESIAN_POINT('',(27.7552687727293,1074.94285725241,532.019687437326));
#114832=CARTESIAN_POINT('',(27.7552687727514,1067.7251047501,532.019687437326));
#114833=CARTESIAN_POINT('Ctrl Pts',(27.755275424151,1074.65680217842,534.200768934763));
#114834=CARTESIAN_POINT('Ctrl Pts',(27.6136253996526,1074.66166448356,534.200769798711));
#114835=CARTESIAN_POINT('Ctrl Pts',(27.4735280043461,1074.67017283515,534.173176636777));
#114836=CARTESIAN_POINT('Ctrl Pts',(27.2108671662123,1074.69350273941,534.065845243065));
#114837=CARTESIAN_POINT('Ctrl Pts',(27.0910484391902,1074.70814472328,533.986729086362));
#114838=CARTESIAN_POINT('Ctrl Pts',(26.8877068762176,1074.74165627613,533.786390102643));
#114839=CARTESIAN_POINT('Ctrl Pts',(26.8064892950006,1074.76024863888,533.666639584316));
#114840=CARTESIAN_POINT('Ctrl Pts',(26.7229560449997,1074.7890820409,533.468988528123));
#114841=CARTESIAN_POINT('Ctrl Pts',(26.7016858388308,1074.79877338609,533.400642763769));
#114842=CARTESIAN_POINT('Ctrl Pts',(26.6579396846555,1074.82800508257,533.188738752911));
#114843=CARTESIAN_POINT('Ctrl Pts',(26.6572064079259,1074.84713066521,533.042212086953));
#114844=CARTESIAN_POINT('Ctrl Pts',(26.7131036243726,1074.8821553278,532.758073590742));
#114845=CARTESIAN_POINT('Ctrl Pts',(26.7688679879507,1074.89774018205,532.623125712085));
#114846=CARTESIAN_POINT('Ctrl Pts',(26.9301219154371,1074.92339221948,532.382665414629));
#114847=CARTESIAN_POINT('Ctrl Pts',(27.033942798244,1074.9332082023,532.279551635639));
#114848=CARTESIAN_POINT('Ctrl Pts',(27.2733725151368,1074.94557923062,532.121733319789));
#114849=CARTESIAN_POINT('Ctrl Pts',(27.4057662935109,1074.94817794078,532.067525467788));
#114850=CARTESIAN_POINT('Ctrl Pts',(27.6840218614343,1074.94606974451,532.012817250953));
#114851=CARTESIAN_POINT('Ctrl Pts',(27.8270551253356,1074.94138305118,532.012880236067));
#114852=CARTESIAN_POINT('Ctrl Pts',(28.1082300688142,1074.92505604725,532.068249721328));
#114853=CARTESIAN_POINT('Ctrl Pts',(28.2432401627996,1074.91342028451,532.124300675689));
#114854=CARTESIAN_POINT('Ctrl Pts',(28.4834925723629,1074.88467231471,532.285634813647));
#114855=CARTESIAN_POINT('Ctrl Pts',(28.5862764841568,1074.86783197128,532.389418357372));
#114856=CARTESIAN_POINT('Ctrl Pts',(28.7047763799925,1074.84049411415,532.569176746184));
#114857=CARTESIAN_POINT('Ctrl Pts',(28.7379040672622,1074.83119757991,532.631980612322));
#114858=CARTESIAN_POINT('Ctrl Pts',(28.7915935595026,1074.81223324189,532.763298958413));
#114859=CARTESIAN_POINT('Ctrl Pts',(28.8119899361011,1074.80260655093,532.831539942821));
#114860=CARTESIAN_POINT('Ctrl Pts',(28.8536452009153,1074.77317887653,533.044908497349));
#114861=CARTESIAN_POINT('Ctrl Pts',(28.8525099084244,1074.75368525076,533.192844219449));
#114862=CARTESIAN_POINT('Ctrl Pts',(28.7923690303293,1074.7180903992,533.476735824113));
#114863=CARTESIAN_POINT('Ctrl Pts',(28.7350936718625,1074.70226461112,533.610210217195));
#114864=CARTESIAN_POINT('Ctrl Pts',(28.5724437477429,1074.67629286926,533.846332736054));
#114865=CARTESIAN_POINT('Ctrl Pts',(28.469141521979,1074.66634798717,533.946967242136));
#114866=CARTESIAN_POINT('Ctrl Pts',(28.2302627188289,1074.6537424931,534.10207169616));
#114867=CARTESIAN_POINT('Ctrl Pts',(28.0974024754569,1074.65114515647,534.155385465907));
#114868=CARTESIAN_POINT('Ctrl Pts',(27.8911442059687,1074.65299064074,534.194408051689));
#114869=CARTESIAN_POINT('Ctrl Pts',(27.8232750413236,1074.65446801089,534.200768520021));
#114870=CARTESIAN_POINT('Ctrl Pts',(27.755275424151,1074.65680217842,534.200768934763));
#114871=CARTESIAN_POINT('Origin',(27.7552687727514,1067.7251047501,533.110228186055));
#114872=CARTESIAN_POINT('',(27.7552687727514,1074.73740020174,533.600768934783));
#114873=CARTESIAN_POINT('',(27.7552687727514,1074.86607808781,532.619687437326));
#114874=CARTESIAN_POINT('Ctrl Pts',(27.7552687727514,1074.73740020174,533.600768934783));
#114875=CARTESIAN_POINT('Ctrl Pts',(27.7217220514107,1074.73853763052,533.600768934783));
#114876=CARTESIAN_POINT('Ctrl Pts',(27.6881995638384,1074.74013005689,533.597327622873));
#114877=CARTESIAN_POINT('Ctrl Pts',(27.5926310129866,1074.74600435434,533.577420134648));
#114878=CARTESIAN_POINT('Ctrl Pts',(27.5332872568249,1074.75133989622,533.552288455029));
#114879=CARTESIAN_POINT('Ctrl Pts',(27.427153033961,1074.76440786162,533.480519027331));
#114880=CARTESIAN_POINT('Ctrl Pts',(27.3815200989915,1074.7720368498,533.434363159037));
#114881=CARTESIAN_POINT('Ctrl Pts',(27.3283822682814,1074.78440280468,533.35401244561));
#114882=CARTESIAN_POINT('Ctrl Pts',(27.3133399123249,1074.7886527102,533.325542322099));
#114883=CARTESIAN_POINT('Ctrl Pts',(27.2890584726604,1074.79727255547,533.266133892481));
#114884=CARTESIAN_POINT('Ctrl Pts',(27.2798663335074,1074.80162300998,533.235331970339));
#114885=CARTESIAN_POINT('Ctrl Pts',(27.2612704923806,1074.81478286354,533.139694328085));
#114886=CARTESIAN_POINT('Ctrl Pts',(27.2617330322699,1074.82340768767,533.073626534165));
#114887=CARTESIAN_POINT('Ctrl Pts',(27.2885631672471,1074.83921156428,532.945689302679));
#114888=CARTESIAN_POINT('Ctrl Pts',(27.3145829076547,1074.84624380939,532.885037407387));
#114889=CARTESIAN_POINT('Ctrl Pts',(27.388561934187,1074.85769618983,532.778069288628));
#114890=CARTESIAN_POINT('Ctrl Pts',(27.4354966049048,1074.86203580859,532.7326397653));
#114891=CARTESIAN_POINT('Ctrl Pts',(27.5435969923283,1074.86746688699,532.663141308034));
#114892=CARTESIAN_POINT('Ctrl Pts',(27.603431634089,1074.86855547558,532.639437617623));
#114893=CARTESIAN_POINT('Ctrl Pts',(27.6955543522107,1074.86770593739,532.622418338912));
#114894=CARTESIAN_POINT('Ctrl Pts',(27.7253834821696,1074.86707024684,532.619687437326));
#114895=CARTESIAN_POINT('Ctrl Pts',(27.7552687727515,1074.86607808781,532.619687437326));
#114896=CARTESIAN_POINT('',(27.7552687727514,1082.7251047501,532.619687437326));
#114897=CARTESIAN_POINT('',(27.7552687727514,1067.7251047501,532.619687437326));
#114898=CARTESIAN_POINT('Origin',(27.7552687727514,1082.7251047501,533.110228186055));
#114899=CARTESIAN_POINT('Ctrl Pts',(27.7552701015566,1074.86607804369,532.619687437328));
#114900=CARTESIAN_POINT('Ctrl Pts',(27.8191337024483,1074.86395781937,532.619687610326));
#114901=CARTESIAN_POINT('Ctrl Pts',(27.8822994455548,1074.86024186908,532.63215767805));
#114902=CARTESIAN_POINT('Ctrl Pts',(28.0018273593798,1074.84989940556,532.681129971462));
#114903=CARTESIAN_POINT('Ctrl Pts',(28.0567224362022,1074.84330132016,532.717782421802));
#114904=CARTESIAN_POINT('Ctrl Pts',(28.1489781808369,1074.82814462366,532.81038119986));
#114905=CARTESIAN_POINT('Ctrl Pts',(28.1853811897379,1074.81972767506,532.865482372977));
#114906=CARTESIAN_POINT('Ctrl Pts',(28.2219278451578,1074.80668908636,532.955684646427));
#114907=CARTESIAN_POINT('Ctrl Pts',(28.2310129009365,1074.80235096542,532.986447773686));
#114908=CARTESIAN_POINT('Ctrl Pts',(28.2493971918684,1074.78914652732,533.082348995895));
#114909=CARTESIAN_POINT('Ctrl Pts',(28.2486991028959,1074.78044035288,533.148707651386));
#114910=CARTESIAN_POINT('Ctrl Pts',(28.2212979116833,1074.76451019408,533.276587597903));
#114911=CARTESIAN_POINT('Ctrl Pts',(28.1951436695123,1074.75742307522,533.336935756115));
#114912=CARTESIAN_POINT('Ctrl Pts',(28.1212511010678,1074.74588577366,533.443088602389));
#114913=CARTESIAN_POINT('Ctrl Pts',(28.0746167460702,1074.74150513762,533.488090561853));
#114914=CARTESIAN_POINT('Ctrl Pts',(27.9669175562519,1074.73598171402,533.557328621623));
#114915=CARTESIAN_POINT('Ctrl Pts',(27.907062940919,1074.73486832538,533.581035451629));
#114916=CARTESIAN_POINT('Ctrl Pts',(27.8148661819697,1074.7357389034,533.598055532107));
#114917=CARTESIAN_POINT('Ctrl Pts',(27.7850579233091,1074.73639017645,533.600768934783));
#114918=CARTESIAN_POINT('Ctrl Pts',(27.7552687727514,1074.73740020174,533.600768934783));
#114919=CARTESIAN_POINT('Origin',(63.8195601713296,1067.7251047501,487.451286405902));
#114920=CARTESIAN_POINT('',(63.8195601713476,1078.69713855509,485.972983273709));
#114921=CARTESIAN_POINT('Ctrl Pts',(63.8195894624746,1078.64371854035,488.929589537805));
#114922=CARTESIAN_POINT('Ctrl Pts',(63.9840898466471,1078.64006414708,488.929586278389));
#114923=CARTESIAN_POINT('Ctrl Pts',(64.147453182996,1078.63693311643,488.902125535132));
#114924=CARTESIAN_POINT('Ctrl Pts',(64.437514187406,1078.63248760894,488.801765362934));
#114925=CARTESIAN_POINT('Ctrl Pts',(64.5646691439413,1078.63100970525,488.73599521947));
#114926=CARTESIAN_POINT('Ctrl Pts',(64.7189173791907,1078.62993169095,488.625499302091));
#114927=CARTESIAN_POINT('Ctrl Pts',(64.7560404026802,1078.62973703954,488.596111347511));
#114928=CARTESIAN_POINT('Ctrl Pts',(64.8133215019525,1078.62954551861,488.546111962442));
#114929=CARTESIAN_POINT('Ctrl Pts',(64.8343982379717,1078.62950100682,488.526604165847));
#114930=CARTESIAN_POINT('Ctrl Pts',(64.8731922603131,1078.62946960111,488.488540842801));
#114931=CARTESIAN_POINT('Ctrl Pts',(64.8910209072986,1078.62947704804,488.470113788901));
#114932=CARTESIAN_POINT('Ctrl Pts',(64.9300915952786,1078.62954395193,488.427571284039));
#114933=CARTESIAN_POINT('Ctrl Pts',(64.951044729482,1078.62961608325,488.403208089341));
#114934=CARTESIAN_POINT('Ctrl Pts',(65.0104014475364,1078.62993091023,488.329459941845));
#114935=CARTESIAN_POINT('Ctrl Pts',(65.0464836543618,1078.63027019842,488.278299281655));
#114936=CARTESIAN_POINT('Ctrl Pts',(65.1824631487881,1078.63220921733,488.056918116752));
#114937=CARTESIAN_POINT('Ctrl Pts',(65.2510196528309,1078.63493719783,487.869863677846));
#114938=CARTESIAN_POINT('Ctrl Pts',(65.3051133784915,1078.64163702959,487.516357727991));
#114939=CARTESIAN_POINT('Ctrl Pts',(65.3034107651073,1078.64523225297,487.354934841883));
#114940=CARTESIAN_POINT('Ctrl Pts',(65.2458715016793,1078.65347085552,487.025462902417));
#114941=CARTESIAN_POINT('Ctrl Pts',(65.1858597232329,1078.6581094606,486.860598750576));
#114942=CARTESIAN_POINT('Ctrl Pts',(65.0049664543459,1078.6678008949,486.548496327283));
#114943=CARTESIAN_POINT('Ctrl Pts',(64.8816253042141,1078.67276842342,486.406183838743));
#114944=CARTESIAN_POINT('Ctrl Pts',(64.5816898614871,1078.68223686314,486.169608074433));
#114945=CARTESIAN_POINT('Ctrl Pts',(64.4058327386662,1078.68661221552,486.080215823895));
#114946=CARTESIAN_POINT('Ctrl Pts',(64.0355180964178,1078.69399347682,485.976661019645));
#114947=CARTESIAN_POINT('Ctrl Pts',(63.8452519507421,1078.69697667558,485.961150441436));
#114948=CARTESIAN_POINT('Ctrl Pts',(63.4806169621885,1078.70150019059,486.001434944975));
#114949=CARTESIAN_POINT('Ctrl Pts',(63.3089580462608,1078.70308592756,486.052629611219));
#114950=CARTESIAN_POINT('Ctrl Pts',(63.0679258473507,1078.70464054665,486.174962862035));
#114951=CARTESIAN_POINT('Ctrl Pts',(62.9894673987184,1078.70501590523,486.224541866277));
#114952=CARTESIAN_POINT('Ctrl Pts',(62.8854961345996,1078.70533108904,486.3048110849));
#114953=CARTESIAN_POINT('Ctrl Pts',(62.855770519636,1078.70539704804,486.32968451552));
#114954=CARTESIAN_POINT('Ctrl Pts',(62.8093655331422,1078.70546021506,486.371723182413));
#114955=CARTESIAN_POINT('Ctrl Pts',(62.7920654195967,1078.70547408171,486.388175642058));
#114956=CARTESIAN_POINT('Ctrl Pts',(62.7570371306505,1078.70548167735,486.423141733429));
#114957=CARTESIAN_POINT('Ctrl Pts',(62.7393766658493,1078.70547385276,486.441712102762));
#114958=CARTESIAN_POINT('Ctrl Pts',(62.6993217611342,1078.7054281524,486.486085583627));
#114959=CARTESIAN_POINT('Ctrl Pts',(62.6773212730456,1078.70538115618,486.512224630403));
#114960=CARTESIAN_POINT('Ctrl Pts',(62.6108178240106,1078.70516671632,486.597036886666));
#114961=CARTESIAN_POINT('Ctrl Pts',(62.5697811297559,1078.70492332943,486.658284164334));
#114962=CARTESIAN_POINT('Ctrl Pts',(62.4364455080255,1078.70366707218,486.893526027989));
#114963=CARTESIAN_POINT('Ctrl Pts',(62.3745669326555,1078.70206694927,487.082378659631));
#114964=CARTESIAN_POINT('Ctrl Pts',(62.3323635385775,1078.69778701519,487.439490572911));
#114965=CARTESIAN_POINT('Ctrl Pts',(62.3401010365273,1078.69536513719,487.603237256047));
#114966=CARTESIAN_POINT('Ctrl Pts',(62.4115688765271,1078.68929086434,487.935217194669));
#114967=CARTESIAN_POINT('Ctrl Pts',(62.479466096613,1078.6855952386,488.099953815447));
#114968=CARTESIAN_POINT('Ctrl Pts',(62.6772738206339,1078.67699747554,488.408695407246));
#114969=CARTESIAN_POINT('Ctrl Pts',(62.8095884730262,1078.67210254672,488.547371017869));
#114970=CARTESIAN_POINT('Ctrl Pts',(63.0788837150454,1078.66328789451,488.738313396836));
#114971=CARTESIAN_POINT('Ctrl Pts',(63.2042225570539,1078.65949593348,488.802730111167));
#114972=CARTESIAN_POINT('Ctrl Pts',(63.4920619879084,1078.65148856653,488.902192161214));
#114973=CARTESIAN_POINT('Ctrl Pts',(63.6552496452803,1078.6473693666,488.92959279404));
#114974=CARTESIAN_POINT('Ctrl Pts',(63.8195894624746,1078.64371854035,488.929589537805));
#114975=CARTESIAN_POINT('',(63.8195601713054,1076.69671505693,485.972983273709));
#114976=CARTESIAN_POINT('',(63.8195601713296,1067.7251047501,485.972983273709));
#114977=CARTESIAN_POINT('Ctrl Pts',(63.8196790295888,1076.64266067219,488.929589533317));
#114978=CARTESIAN_POINT('Ctrl Pts',(63.6266637061908,1076.64699817558,488.9296050521));
#114979=CARTESIAN_POINT('Ctrl Pts',(63.4355114909343,1076.65198209469,488.891818924218));
#114980=CARTESIAN_POINT('Ctrl Pts',(63.0783218190941,1076.66237653906,488.744844186407));
#114981=CARTESIAN_POINT('Ctrl Pts',(62.9157480424437,1076.6676822105,488.636972471792));
#114982=CARTESIAN_POINT('Ctrl Pts',(62.6412573598861,1076.67776335618,488.364723487194));
#114983=CARTESIAN_POINT('Ctrl Pts',(62.5320074252481,1076.6824408189,488.20293863512));
#114984=CARTESIAN_POINT('Ctrl Pts',(62.3813117723216,1076.69069166442,487.844855465753));
#114985=CARTESIAN_POINT('Ctrl Pts',(62.3419715931296,1076.69417867454,487.651775912808));
#114986=CARTESIAN_POINT('Ctrl Pts',(62.3405622868592,1076.69976087682,487.261618709333));
#114987=CARTESIAN_POINT('Ctrl Pts',(62.3784511593684,1076.70181077384,487.068377724351));
#114988=CARTESIAN_POINT('Ctrl Pts',(62.5273030519845,1076.70453642962,486.707150006348));
#114989=CARTESIAN_POINT('Ctrl Pts',(62.6370364788583,1076.70518710588,486.542822342158));
#114990=CARTESIAN_POINT('Ctrl Pts',(62.9141008093992,1076.70512360841,486.266464209322));
#114991=CARTESIAN_POINT('Ctrl Pts',(63.0786857269495,1076.70441004859,486.157159896911));
#114992=CARTESIAN_POINT('Ctrl Pts',(63.4402417057163,1076.70155480918,486.009231475747));
#114993=CARTESIAN_POINT('Ctrl Pts',(63.633551754434,1076.69943928384,485.971827051054));
#114994=CARTESIAN_POINT('Ctrl Pts',(64.0237269139951,1076.69372595064,485.974195249882));
#114995=CARTESIAN_POINT('Ctrl Pts',(64.2167544746152,1076.69017424572,486.014028607335));
#114996=CARTESIAN_POINT('Ctrl Pts',(64.4846573373595,1076.68391175077,486.127578245854));
#114997=CARTESIAN_POINT('Ctrl Pts',(64.5690151412844,1076.68170928521,486.173446959145));
#114998=CARTESIAN_POINT('Ctrl Pts',(64.8105570368171,1076.67463682357,486.336978368092));
#114999=CARTESIAN_POINT('Ctrl Pts',(64.9493321941796,1076.66944502775,486.477958746744));
#115000=CARTESIAN_POINT('Ctrl Pts',(65.1628585102578,1076.65885899044,486.804291013134));
#115001=CARTESIAN_POINT('Ctrl Pts',(65.2361140013734,1076.65357364652,486.986063387697));
#115002=CARTESIAN_POINT('Ctrl Pts',(65.3082193662151,1076.64382909709,487.367639770847));
#115003=CARTESIAN_POINT('Ctrl Pts',(65.3063239173843,1076.63947208179,487.563750204927));
#115004=CARTESIAN_POINT('Ctrl Pts',(65.2268400786758,1076.63262870979,487.943828373376));
#115005=CARTESIAN_POINT('Ctrl Pts',(65.150105079873,1076.6302132747,488.12411224945));
#115006=CARTESIAN_POINT('Ctrl Pts',(64.9316461160177,1076.62789251368,488.444316314171));
#115007=CARTESIAN_POINT('Ctrl Pts',(64.7922171890342,1076.6280053344,488.581233911691));
#115008=CARTESIAN_POINT('Ctrl Pts',(64.4689266284222,1076.63074726386,488.793293728351));
#115009=CARTESIAN_POINT('Ctrl Pts',(64.2882973189173,1076.633340972,488.86653745439));
#115010=CARTESIAN_POINT('Ctrl Pts',(64.0067526630902,1076.63861956661,488.920677163634));
#115011=CARTESIAN_POINT('Ctrl Pts',(63.9133200171384,1076.64055634134,488.929582004412));
#115012=CARTESIAN_POINT('Ctrl Pts',(63.8196790295888,1076.64266067219,488.929589533317));
#115013=CARTESIAN_POINT('Origin',(63.8195601713296,1067.7251047501,487.451286405902));
#115014=CARTESIAN_POINT('',(63.8195601713296,1076.65571487055,488.329589538096));
#115015=CARTESIAN_POINT('',(63.819560171333,1076.68781395203,486.572983273709));
#115016=CARTESIAN_POINT('Ctrl Pts',(63.8195601713296,1076.65571487055,488.329589538096));
#115017=CARTESIAN_POINT('Ctrl Pts',(63.7107697804043,1076.65798824794,488.329589538096));
#115018=CARTESIAN_POINT('Ctrl Pts',(63.6028716162922,1076.66061090128,488.309375843125));
#115019=CARTESIAN_POINT('Ctrl Pts',(63.39429164515,1076.66634768013,488.228309470195));
#115020=CARTESIAN_POINT('Ctrl Pts',(63.2963987561866,1076.66942216486,488.166073090089));
#115021=CARTESIAN_POINT('Ctrl Pts',(63.1300943178984,1076.6754291516,488.007405178066));
#115022=CARTESIAN_POINT('Ctrl Pts',(63.063300272878,1076.67830344724,487.912485291315));
#115023=CARTESIAN_POINT('Ctrl Pts',(62.9694049578448,1076.68354215884,487.700790544189));
#115024=CARTESIAN_POINT('Ctrl Pts',(62.9438210601612,1076.68584838576,487.58582423722));
#115025=CARTESIAN_POINT('Ctrl Pts',(62.9390622631114,1076.68964004189,487.352764181843));
#115026=CARTESIAN_POINT('Ctrl Pts',(62.9598730251725,1076.69109192874,487.23698824714));
#115027=CARTESIAN_POINT('Ctrl Pts',(63.045517073269,1076.69306253932,487.020145887916));
#115028=CARTESIAN_POINT('Ctrl Pts',(63.1095607462142,1076.69356254242,486.921261308762));
#115029=CARTESIAN_POINT('Ctrl Pts',(63.2725389825084,1076.69358373261,486.754296937428));
#115030=CARTESIAN_POINT('Ctrl Pts',(63.3698504694939,1076.69310471028,486.687881665862));
#115031=CARTESIAN_POINT('Ctrl Pts',(63.5845665079714,1076.69117522368,486.597024029905));
#115032=CARTESIAN_POINT('Ctrl Pts',(63.6998086185617,1076.6897431168,486.573423475287));
#115033=CARTESIAN_POINT('Ctrl Pts',(63.8173780549111,1076.68784921539,486.572985306547));
#115034=CARTESIAN_POINT('Ctrl Pts',(63.818469163189,1076.6878316016,486.572983273709));
#115035=CARTESIAN_POINT('Ctrl Pts',(63.8195601713365,1076.68781395203,486.572983273709));
#115036=CARTESIAN_POINT('',(63.8195601713296,1082.7251047501,486.572983273709));
#115037=CARTESIAN_POINT('',(63.8195601713296,1067.7251047501,486.572983273709));
#115038=CARTESIAN_POINT('Origin',(63.8195601713296,1082.7251047501,487.451286405902));
#115039=CARTESIAN_POINT('Ctrl Pts',(63.8195601713365,1076.68781395203,486.572983273709));
#115040=CARTESIAN_POINT('Ctrl Pts',(63.9350701010665,1076.68594531276,486.572983273709));
#115041=CARTESIAN_POINT('Ctrl Pts',(64.0494576024828,1076.68367400261,486.595770247173));
#115042=CARTESIAN_POINT('Ctrl Pts',(64.2645360000653,1076.67843271753,486.685008814363));
#115043=CARTESIAN_POINT('Ctrl Pts',(64.3628089626602,1076.67550321216,486.751241238968));
#115044=CARTESIAN_POINT('Ctrl Pts',(64.5260112993656,1076.66942713559,486.916859920746));
#115045=CARTESIAN_POINT('Ctrl Pts',(64.589937036861,1076.66634467399,487.014016877144));
#115046=CARTESIAN_POINT('Ctrl Pts',(64.6741808433638,1076.66060693963,487.221404317127));
#115047=CARTESIAN_POINT('Ctrl Pts',(64.6960422229002,1076.65798862615,487.328795694996));
#115048=CARTESIAN_POINT('Ctrl Pts',(64.6977542871803,1076.65571755183,487.437448526525));
#115049=CARTESIAN_POINT('Ctrl Pts',(64.6995701042535,1076.65330884816,487.55268582739));
#115050=CARTESIAN_POINT('Ctrl Pts',(64.6786861551085,1076.6513385752,487.667169847103));
#115051=CARTESIAN_POINT('Ctrl Pts',(64.5939433460243,1076.64861220933,487.881400968346));
#115052=CARTESIAN_POINT('Ctrl Pts',(64.5309643521006,1076.64788279605,487.979087238798));
#115053=CARTESIAN_POINT('Ctrl Pts',(64.3710574006373,1076.64781958489,488.144446523562));
#115054=CARTESIAN_POINT('Ctrl Pts',(64.2757425146998,1076.64848382618,488.210573030146));
#115055=CARTESIAN_POINT('Ctrl Pts',(64.0651859252744,1076.6510846175,488.302319929318));
#115056=CARTESIAN_POINT('Ctrl Pts',(63.9519985665621,1076.65299295402,488.327098272006));
#115057=CARTESIAN_POINT('Ctrl Pts',(63.8313589702029,1076.65546939683,488.329530126905));
#115058=CARTESIAN_POINT('Ctrl Pts',(63.8254582594845,1076.65559161903,488.329589538096));
#115059=CARTESIAN_POINT('Ctrl Pts',(63.8195601713296,1076.65571487055,488.329589538096));
#115060=CARTESIAN_POINT('Origin',(61.0059658728171,1067.7251047501,499.690312664149));
#115061=CARTESIAN_POINT('',(61.0059658728373,1078.41010379242,498.414868543013));
#115062=CARTESIAN_POINT('Ctrl Pts',(61.0060185765775,1078.28341943821,500.965756784196));
#115063=CARTESIAN_POINT('Ctrl Pts',(61.1593612507269,1078.27681519819,500.965750447787));
#115064=CARTESIAN_POINT('Ctrl Pts',(61.3115040629282,1078.27167163102,500.938090417076));
#115065=CARTESIAN_POINT('Ctrl Pts',(61.5294627507336,1078.26656240556,500.856081999369));
#115066=CARTESIAN_POINT('Ctrl Pts',(61.6010381099983,1078.26530678887,500.821223191467));
#115067=CARTESIAN_POINT('Ctrl Pts',(61.6976461112628,1078.26424350508,500.762444921767));
#115068=CARTESIAN_POINT('Ctrl Pts',(61.7256796492391,1078.26401878141,500.743831194445));
#115069=CARTESIAN_POINT('Ctrl Pts',(61.7698766977493,1078.26380403502,500.711896878635));
#115070=CARTESIAN_POINT('Ctrl Pts',(61.7865053405924,1078.26375737041,500.699248837616));
#115071=CARTESIAN_POINT('Ctrl Pts',(61.8204286188542,1078.26373448196,500.672105388278));
#115072=CARTESIAN_POINT('Ctrl Pts',(61.8376643467884,1078.26376418367,500.657547982924));
#115073=CARTESIAN_POINT('Ctrl Pts',(61.8771326449426,1078.26393115789,500.622377443948));
#115074=CARTESIAN_POINT('Ctrl Pts',(61.8990341574984,1078.26410183812,500.601413804347));
#115075=CARTESIAN_POINT('Ctrl Pts',(61.9664003251663,1078.26488344987,500.532167311465));
#115076=CARTESIAN_POINT('Ctrl Pts',(62.0088536330547,1078.265775407,500.481115101989));
#115077=CARTESIAN_POINT('Ctrl Pts',(62.1453603527211,1078.27018479766,500.288186707831));
#115078=CARTESIAN_POINT('Ctrl Pts',(62.2147960369423,1078.27558509874,500.13117825464));
#115079=CARTESIAN_POINT('Ctrl Pts',(62.2816743671612,1078.28876887451,499.828216932716));
#115080=CARTESIAN_POINT('Ctrl Pts',(62.2890924237342,1078.29588017964,499.687178604723));
#115081=CARTESIAN_POINT('Ctrl Pts',(62.256439448631,1078.31236603524,499.396730274855));
#115082=CARTESIAN_POINT('Ctrl Pts',(62.2125768553997,1078.32174728379,499.249920461796));
#115083=CARTESIAN_POINT('Ctrl Pts',(62.0702775780052,1078.34182773481,498.968781844095));
#115084=CARTESIAN_POINT('Ctrl Pts',(61.9693673546002,1078.35238842155,498.838708946376));
#115085=CARTESIAN_POINT('Ctrl Pts',(61.7200846157815,1078.37300114546,498.620202575887));
#115086=CARTESIAN_POINT('Ctrl Pts',(61.5727161461335,1078.38282688788,498.535354569588));
#115087=CARTESIAN_POINT('Ctrl Pts',(61.260545411812,1078.3998060434,498.430212896559));
#115088=CARTESIAN_POINT('Ctrl Pts',(61.0996084303574,1078.40691089988,498.408154756107));
#115089=CARTESIAN_POINT('Ctrl Pts',(60.7774262686565,1078.41819074401,498.425151614357));
#115090=CARTESIAN_POINT('Ctrl Pts',(60.6191169232872,1078.42225765181,498.46424738999));
#115091=CARTESIAN_POINT('Ctrl Pts',(60.4175197813752,1078.4254743782,498.557119647779));
#115092=CARTESIAN_POINT('Ctrl Pts',(60.3645978106156,1078.42610383578,498.586209932429));
#115093=CARTESIAN_POINT('Ctrl Pts',(60.2898897929974,1078.42666703254,498.634466124367));
#115094=CARTESIAN_POINT('Ctrl Pts',(60.2663773999814,1078.42679236439,498.65080038069));
#115095=CARTESIAN_POINT('Ctrl Pts',(60.2256701710816,1078.42691530889,498.681160831159));
#115096=CARTESIAN_POINT('Ctrl Pts',(60.2082543284669,1078.42693534288,498.694870501367));
#115097=CARTESIAN_POINT('Ctrl Pts',(60.1729246832527,1078.42690717033,498.724204699766));
#115098=CARTESIAN_POINT('Ctrl Pts',(60.1550725821967,1078.42685394242,498.739890219775));
#115099=CARTESIAN_POINT('Ctrl Pts',(60.1106336194392,1078.42661942927,498.781192129821));
#115100=CARTESIAN_POINT('Ctrl Pts',(60.0847019742475,1078.42638369646,498.80748044149));
#115101=CARTESIAN_POINT('Ctrl Pts',(59.9880828274185,1078.42510196671,498.914328021156));
#115102=CARTESIAN_POINT('Ctrl Pts',(59.9265263277214,1078.42337382139,499.00253129405));
#115103=CARTESIAN_POINT('Ctrl Pts',(59.8175027708732,1078.4179502462,499.210164535695));
#115104=CARTESIAN_POINT('Ctrl Pts',(59.7755245946314,1078.4139748903,499.331166481984));
#115105=CARTESIAN_POINT('Ctrl Pts',(59.7260759691088,1078.40357059609,499.596148970225));
#115106=CARTESIAN_POINT('Ctrl Pts',(59.7235616529909,1078.39698056187,499.739296046524));
#115107=CARTESIAN_POINT('Ctrl Pts',(59.7675829640332,1078.38138825678,500.032233432546));
#115108=CARTESIAN_POINT('Ctrl Pts',(59.8179011397374,1078.37235473804,500.179167782539));
#115109=CARTESIAN_POINT('Ctrl Pts',(59.9740981591699,1078.35249435977,500.458066544377));
#115110=CARTESIAN_POINT('Ctrl Pts',(60.0824211082803,1078.3417682257,500.585442094107));
#115111=CARTESIAN_POINT('Ctrl Pts',(60.3125864214195,1078.3230338029,500.768497513091));
#115112=CARTESIAN_POINT('Ctrl Pts',(60.4246410377411,1078.31506352744,500.832823128112));
#115113=CARTESIAN_POINT('Ctrl Pts',(60.6915600712771,1078.2984543899,500.936433156734));
#115114=CARTESIAN_POINT('Ctrl Pts',(60.8480764598553,1078.29022176935,500.965763310663));
#115115=CARTESIAN_POINT('Ctrl Pts',(61.0060185765775,1078.28341943821,500.965756784196));
#115116=CARTESIAN_POINT('',(61.0059658727952,1076.40646512577,498.414868543013));
#115117=CARTESIAN_POINT('',(61.0059658728171,1067.7251047501,498.414868543013));
#115118=CARTESIAN_POINT('Ctrl Pts',(61.0060409438501,1076.27845846789,500.965756783076));
#115119=CARTESIAN_POINT('Ctrl Pts',(60.8393532119705,1076.28571097349,500.965766594105));
#115120=CARTESIAN_POINT('Ctrl Pts',(60.6743383448293,1076.29456922384,500.933101074979));
#115121=CARTESIAN_POINT('Ctrl Pts',(60.3658759786924,1076.31431410998,500.806082350595));
#115122=CARTESIAN_POINT('Ctrl Pts',(60.2254417397641,1076.32501352991,500.712770698471));
#115123=CARTESIAN_POINT('Ctrl Pts',(60.0477651021946,1076.34127535239,500.536232428695));
#115124=CARTESIAN_POINT('Ctrl Pts',(59.9944560145889,1076.34669397231,500.471707366279));
#115125=CARTESIAN_POINT('Ctrl Pts',(59.8533562014058,1076.3628483696,500.262049498931));
#115126=CARTESIAN_POINT('Ctrl Pts',(59.7877280301588,1076.37316917685,500.104218976959));
#115127=CARTESIAN_POINT('Ctrl Pts',(59.7220854218885,1076.39168201607,499.772829033881));
#115128=CARTESIAN_POINT('Ctrl Pts',(59.7224140897275,1076.39970620851,499.602593824359));
#115129=CARTESIAN_POINT('Ctrl Pts',(59.789407417764,1076.41262948071,499.27159316087));
#115130=CARTESIAN_POINT('Ctrl Pts',(59.8555699434147,1076.41739720942,499.114151420653));
#115131=CARTESIAN_POINT('Ctrl Pts',(60.0458503641121,1076.42316730663,498.833723887449));
#115132=CARTESIAN_POINT('Ctrl Pts',(60.1682419741281,1076.42410175589,498.713690040939));
#115133=CARTESIAN_POINT('Ctrl Pts',(60.4526371074538,1076.42199349074,498.528710937925));
#115134=CARTESIAN_POINT('Ctrl Pts',(60.611715179383,1076.41897648336,498.46555300937));
#115135=CARTESIAN_POINT('Ctrl Pts',(60.9445258790086,1076.40925873538,498.405216296368));
#115136=CARTESIAN_POINT('Ctrl Pts',(61.1148816736779,1076.40266455816,498.408382360996));
#115137=CARTESIAN_POINT('Ctrl Pts',(61.4445191497671,1076.3865296403,498.480795906462));
#115138=CARTESIAN_POINT('Ctrl Pts',(61.6005313489561,1076.37714081322,498.54938606952));
#115139=CARTESIAN_POINT('Ctrl Pts',(61.8063860563556,1076.36186638373,498.693850425921));
#115140=CARTESIAN_POINT('Ctrl Pts',(61.8693451359274,1076.35666909398,498.747878073002));
#115141=CARTESIAN_POINT('Ctrl Pts',(61.9850024580324,1076.34597130689,498.868508828113));
#115142=CARTESIAN_POINT('Ctrl Pts',(62.0371982269214,1076.340492805,498.935042374393));
#115143=CARTESIAN_POINT('Ctrl Pts',(62.1723241765287,1076.32413980981,499.147679462465));
#115144=CARTESIAN_POINT('Ctrl Pts',(62.2334714492597,1076.31342738866,499.305484806729));
#115145=CARTESIAN_POINT('Ctrl Pts',(62.2911976389649,1076.29370015856,499.635615898861));
#115146=CARTESIAN_POINT('Ctrl Pts',(62.2872777130916,1076.28487779503,499.804751501161));
#115147=CARTESIAN_POINT('Ctrl Pts',(62.2142893581537,1076.27054739291,500.13152385481));
#115148=CARTESIAN_POINT('Ctrl Pts',(62.1460960247155,1076.26517470197,500.286010253355));
#115149=CARTESIAN_POINT('Ctrl Pts',(61.9541860296279,1076.25879133627,500.559478245958));
#115150=CARTESIAN_POINT('Ctrl Pts',(61.8325311071289,1076.2578313534,500.675892842116));
#115151=CARTESIAN_POINT('Ctrl Pts',(61.5515524611975,1076.26050472866,500.855134842823));
#115152=CARTESIAN_POINT('Ctrl Pts',(61.3950511192112,1076.26410238746,500.916306047607));
#115153=CARTESIAN_POINT('Ctrl Pts',(61.1569191730779,1076.27223850714,500.95904288288));
#115154=CARTESIAN_POINT('Ctrl Pts',(61.0815476100229,1076.275173208,500.965752338849));
#115155=CARTESIAN_POINT('Ctrl Pts',(61.0060409438501,1076.27845846789,500.965756783076));
#115156=CARTESIAN_POINT('Origin',(61.0059658728171,1067.7251047501,499.690312664149));
#115157=CARTESIAN_POINT('',(61.0059658728171,1076.31052966192,500.365756785285));
#115158=CARTESIAN_POINT('',(61.005965872817,1076.37831455598,499.014868543013));
#115159=CARTESIAN_POINT('Ctrl Pts',(61.0059658728171,1076.31052966192,500.365756785285));
#115160=CARTESIAN_POINT('Ctrl Pts',(60.9602270007978,1076.31246147104,500.365756785285));
#115161=CARTESIAN_POINT('Ctrl Pts',(60.9145063088114,1076.314628575,500.361110802308));
#115162=CARTESIAN_POINT('Ctrl Pts',(60.782887332266,1076.32155472217,500.333962078073));
#115163=CARTESIAN_POINT('Ctrl Pts',(60.7006346737792,1076.32676762466,500.299255965846));
#115164=CARTESIAN_POINT('Ctrl Pts',(60.5907950691867,1076.33508722384,500.22492833398));
#115165=CARTESIAN_POINT('Ctrl Pts',(60.5566920535575,1076.33792506562,500.196606332976));
#115166=CARTESIAN_POINT('Ctrl Pts',(60.4945641776638,1076.34363858974,500.133756645256));
#115167=CARTESIAN_POINT('Ctrl Pts',(60.4666770488451,1076.3465006828,500.099387198059));
#115168=CARTESIAN_POINT('Ctrl Pts',(60.3928025512871,1076.35508766922,499.987528047546));
#115169=CARTESIAN_POINT('Ctrl Pts',(60.3587199228918,1076.36062081203,499.903354392186));
#115170=CARTESIAN_POINT('Ctrl Pts',(60.3255613131223,1076.37060790071,499.726756820627));
#115171=CARTESIAN_POINT('Ctrl Pts',(60.3267372252089,1076.37496650124,499.636099560964));
#115172=CARTESIAN_POINT('Ctrl Pts',(60.364532008823,1076.38197773769,499.460361040129));
#115173=CARTESIAN_POINT('Ctrl Pts',(60.4008255387522,1076.38455869322,499.377055787549));
#115174=CARTESIAN_POINT('Ctrl Pts',(60.5040542188223,1076.38761361433,499.229402268924));
#115175=CARTESIAN_POINT('Ctrl Pts',(60.5699940769635,1076.38805350169,499.166591258357));
#115176=CARTESIAN_POINT('Ctrl Pts',(60.7225779565673,1076.38671338192,499.070609103443));
#115177=CARTESIAN_POINT('Ctrl Pts',(60.8076510813114,1076.38494860617,499.038388159638));
#115178=CARTESIAN_POINT('Ctrl Pts',(60.9327006851329,1076.38104556125,499.017853175409));
#115179=CARTESIAN_POINT('Ctrl Pts',(60.9693057062944,1076.37975511911,499.014868543013));
#115180=CARTESIAN_POINT('Ctrl Pts',(61.0059658728168,1076.37831455598,499.014868543013));
#115181=CARTESIAN_POINT('',(61.0059658728171,1082.7251047501,499.014868543013));
#115182=CARTESIAN_POINT('',(61.0059658728171,1067.7251047501,499.014868543013));
#115183=CARTESIAN_POINT('Origin',(61.0059658728171,1082.7251047501,499.690312664149));
#115184=CARTESIAN_POINT('Ctrl Pts',(61.0059658728168,1076.37831455598,499.014868543013));
#115185=CARTESIAN_POINT('Ctrl Pts',(61.006088218702,1076.37830974839,499.014868543013));
#115186=CARTESIAN_POINT('Ctrl Pts',(61.0062105652016,1076.37830493914,499.014868576095));
#115187=CARTESIAN_POINT('Ctrl Pts',(61.0063329123016,1076.3783001282,499.014868642579));
#115188=CARTESIAN_POINT('Ctrl Pts',(61.0961419167745,1076.37476865911,499.014917445233));
#115189=CARTESIAN_POINT('Ctrl Pts',(61.1850092423183,1076.3703858054,499.032876840093));
#115190=CARTESIAN_POINT('Ctrl Pts',(61.3506539455567,1076.36036131963,499.102515794653));
#115191=CARTESIAN_POINT('Ctrl Pts',(61.4257566948979,1076.35481535028,499.15357903573));
#115192=CARTESIAN_POINT('Ctrl Pts',(61.5194648340624,1076.34622638151,499.249308564313));
#115193=CARTESIAN_POINT('Ctrl Pts',(61.5471291275999,1076.3433698427,499.283731790389));
#115194=CARTESIAN_POINT('Ctrl Pts',(61.6202954907906,1076.33473058531,499.395601181472));
#115195=CARTESIAN_POINT('Ctrl Pts',(61.6539441512043,1076.32905986884,499.479632579587));
#115196=CARTESIAN_POINT('Ctrl Pts',(61.6862786245079,1076.31871981181,499.654937752871));
#115197=CARTESIAN_POINT('Ctrl Pts',(61.6850535659793,1076.3141402482,499.744430501955));
#115198=CARTESIAN_POINT('Ctrl Pts',(61.6481138312494,1076.30669523748,499.917682732522));
#115199=CARTESIAN_POINT('Ctrl Pts',(61.6128399843051,1076.3038992998,499.999772676156));
#115200=CARTESIAN_POINT('Ctrl Pts',(61.512718568371,1076.30052576457,500.145531948238));
#115201=CARTESIAN_POINT('Ctrl Pts',(61.4489237809329,1076.29997641375,500.20781971664));
#115202=CARTESIAN_POINT('Ctrl Pts',(61.3010433856369,1076.30122143156,500.304266069869));
#115203=CARTESIAN_POINT('Ctrl Pts',(61.2184267132202,1076.30300096174,500.33750867518));
#115204=CARTESIAN_POINT('Ctrl Pts',(61.0901970097171,1076.30717218938,500.361819299098));
#115205=CARTESIAN_POINT('Ctrl Pts',(61.0480737369782,1076.30875121064,500.365756785285));
#115206=CARTESIAN_POINT('Ctrl Pts',(61.0059658728171,1076.31052966192,500.365756785285));
#115207=CARTESIAN_POINT('Origin',(56.6885840720975,1067.7251047501,512.850041810019));
#115208=CARTESIAN_POINT('',(56.6885840720974,1077.75968243012,511.751210674027));
#115209=CARTESIAN_POINT('Ctrl Pts',(56.6886081290873,1077.56894204485,513.948872945749));
#115210=CARTESIAN_POINT('Ctrl Pts',(56.8261231132141,1077.56103093171,513.948869935098));
#115211=CARTESIAN_POINT('Ctrl Pts',(56.9625179305558,1077.55546951976,513.923052854808));
#115212=CARTESIAN_POINT('Ctrl Pts',(57.1274950322521,1077.55176837792,513.858184947821));
#115213=CARTESIAN_POINT('Ctrl Pts',(57.1635121568085,1077.55116671106,513.841726874955));
#115214=CARTESIAN_POINT('Ctrl Pts',(57.2187463512769,1077.55057719113,513.812786266466));
#115215=CARTESIAN_POINT('Ctrl Pts',(57.2385936460081,1077.55043736053,513.801587100646));
#115216=CARTESIAN_POINT('Ctrl Pts',(57.274530730328,1077.55031926557,513.779808688972));
#115217=CARTESIAN_POINT('Ctrl Pts',(57.2907180079139,1077.55031925992,513.769408253724));
#115218=CARTESIAN_POINT('Ctrl Pts',(57.3254383039349,1077.55043724832,513.745789730864));
#115219=CARTESIAN_POINT('Ctrl Pts',(57.3438502323476,1077.55057679087,513.732410137908));
#115220=CARTESIAN_POINT('Ctrl Pts',(57.3938577369024,1077.55117441997,513.693641767044));
#115221=CARTESIAN_POINT('Ctrl Pts',(57.4244816451797,1077.55179569627,513.667064454835));
#115222=CARTESIAN_POINT('Ctrl Pts',(57.5580686446764,1077.55572960633,513.537514192885));
#115223=CARTESIAN_POINT('Ctrl Pts',(57.6413148447348,1077.56180565762,513.416489384173));
#115224=CARTESIAN_POINT('Ctrl Pts',(57.7450816461198,1077.57750896273,513.17436109799));
#115225=CARTESIAN_POINT('Ctrl Pts',(57.7737566562579,1077.58614944444,513.05914475885));
#115226=CARTESIAN_POINT('Ctrl Pts',(57.7943342947576,1077.60680865319,512.813268635681));
#115227=CARTESIAN_POINT('Ctrl Pts',(57.7824020047724,1077.61890753672,512.684053791606));
#115228=CARTESIAN_POINT('Ctrl Pts',(57.7118340754916,1077.64552211447,512.426249200563));
#115229=CARTESIAN_POINT('Ctrl Pts',(57.6502812306567,1077.65992011515,512.300707521847));
#115230=CARTESIAN_POINT('Ctrl Pts',(57.4794488624528,1077.68910225513,512.07336758671));
#115231=CARTESIAN_POINT('Ctrl Pts',(57.3694753385046,1077.7035880436,511.975327672765));
#115232=CARTESIAN_POINT('Ctrl Pts',(57.1215812723172,1077.72954363832,511.830291800281));
#115233=CARTESIAN_POINT('Ctrl Pts',(56.9869522514092,1077.74086067208,511.783071169242));
#115234=CARTESIAN_POINT('Ctrl Pts',(56.7198346616448,1077.7586006036,511.744170714597));
#115235=CARTESIAN_POINT('Ctrl Pts',(56.5903714491967,1077.76524234396,511.748075249157));
#115236=CARTESIAN_POINT('Ctrl Pts',(56.3865624964544,1077.7726436181,511.790541123025));
#115237=CARTESIAN_POINT('Ctrl Pts',(56.3106526789005,1077.77465788857,511.815182822459));
#115238=CARTESIAN_POINT('Ctrl Pts',(56.2097457973579,1077.77628301304,511.860543376455));
#115239=CARTESIAN_POINT('Ctrl Pts',(56.1819869597731,1077.77660963499,511.87446363521));
#115240=CARTESIAN_POINT('Ctrl Pts',(56.1369670513964,1077.77693574781,511.89948026704));
#115241=CARTESIAN_POINT('Ctrl Pts',(56.1193613932389,1077.77700871986,511.909917274788));
#115242=CARTESIAN_POINT('Ctrl Pts',(56.0856188660735,1077.77704051168,511.931216084456));
#115243=CARTESIAN_POINT('Ctrl Pts',(56.0694587463262,1077.7770048533,511.942026624961));
#115244=CARTESIAN_POINT('Ctrl Pts',(56.0323237123983,1077.77680174403,511.968321068902));
#115245=CARTESIAN_POINT('Ctrl Pts',(56.0115965806802,1077.77659359619,511.984133625794));
#115246=CARTESIAN_POINT('Ctrl Pts',(55.9476059417592,1077.77564186145,512.03665456934));
#115247=CARTESIAN_POINT('Ctrl Pts',(55.9066186050281,1077.7745579944,512.075977497988));
#115248=CARTESIAN_POINT('Ctrl Pts',(55.7718916726251,1077.76918120536,512.226900584202));
#115249=CARTESIAN_POINT('Ctrl Pts',(55.6975541818714,1077.76257849438,512.353628038415));
#115250=CARTESIAN_POINT('Ctrl Pts',(55.6104694429214,1077.74608656393,512.605545779289));
#115251=CARTESIAN_POINT('Ctrl Pts',(55.5901279684423,1077.7370413497,512.725719525586));
#115252=CARTESIAN_POINT('Ctrl Pts',(55.5893552004997,1077.71560635979,512.978428314551));
#115253=CARTESIAN_POINT('Ctrl Pts',(55.6126484753009,1077.70316050526,513.109084826551));
#115254=CARTESIAN_POINT('Ctrl Pts',(55.707782491818,1077.67583170941,513.36537363583));
#115255=CARTESIAN_POINT('Ctrl Pts',(55.7823949292631,1077.66108130366,513.487498046795));
#115256=CARTESIAN_POINT('Ctrl Pts',(55.967260464845,1077.63306249184,513.689412387421));
#115257=CARTESIAN_POINT('Ctrl Pts',(56.0732526704201,1077.61998236202,513.769963117753));
#115258=CARTESIAN_POINT('Ctrl Pts',(56.2594534447348,1077.60103419945,513.86451717195));
#115259=CARTESIAN_POINT('Ctrl Pts',(56.3313290710501,1077.5944937807,513.892008434028));
#115260=CARTESIAN_POINT('Ctrl Pts',(56.497805996776,1077.5810230906,513.936391378811));
#115261=CARTESIAN_POINT('Ctrl Pts',(56.59296919302,1077.57444406668,513.948875039596));
#115262=CARTESIAN_POINT('Ctrl Pts',(56.6886081290873,1077.56894204485,513.948872945749));
#115263=CARTESIAN_POINT('',(56.6885840720726,1075.74962658425,511.751210674027));
#115264=CARTESIAN_POINT('',(56.6885840720975,1067.7251047501,511.751210674027));
#115265=CARTESIAN_POINT('Ctrl Pts',(56.688665939873,1075.55713627063,513.948872942962));
#115266=CARTESIAN_POINT('Ctrl Pts',(56.545178338593,1075.56546486824,513.948883633423));
#115267=CARTESIAN_POINT('Ctrl Pts',(56.4032254515711,1075.57621265454,513.920792057026));
#115268=CARTESIAN_POINT('Ctrl Pts',(56.137487060598,1075.60126725074,513.81154703054));
#115269=CARTESIAN_POINT('Ctrl Pts',(56.0163641408127,1075.61535423461,513.731100016272));
#115270=CARTESIAN_POINT('Ctrl Pts',(55.863120128512,1075.63749302432,513.578898554677));
#115271=CARTESIAN_POINT('Ctrl Pts',(55.8171142560329,1075.64499509613,513.523214503998));
#115272=CARTESIAN_POINT('Ctrl Pts',(55.7368450001395,1075.65997707953,513.403909826976));
#115273=CARTESIAN_POINT('Ctrl Pts',(55.7027169832874,1075.66742250756,513.340598178089));
#115274=CARTESIAN_POINT('Ctrl Pts',(55.6187164697901,1075.68957947368,513.139965011894));
#115275=CARTESIAN_POINT('Ctrl Pts',(55.5896951964811,1075.70365286938,512.995563315431));
#115276=CARTESIAN_POINT('Ctrl Pts',(55.5898106614579,1075.72864668678,512.704120985872));
#115277=CARTESIAN_POINT('Ctrl Pts',(55.618761220439,1075.73933512329,512.559942790098));
#115278=CARTESIAN_POINT('Ctrl Pts',(55.7314955667793,1075.75601604001,512.290817644665));
#115279=CARTESIAN_POINT('Ctrl Pts',(55.814231570036,1075.76183417675,512.168634566489));
#115280=CARTESIAN_POINT('Ctrl Pts',(56.0206828343934,1075.76774660283,511.965823938307));
#115281=CARTESIAN_POINT('Ctrl Pts',(56.1414700414339,1075.7678990289,511.886402274529));
#115282=CARTESIAN_POINT('Ctrl Pts',(56.4070000636937,1075.76263714728,511.778250402562));
#115283=CARTESIAN_POINT('Ctrl Pts',(56.5491486730179,1075.75726195637,511.750709334383));
#115284=CARTESIAN_POINT('Ctrl Pts',(56.8382667326121,1075.74143131156,511.751734533559));
#115285=CARTESIAN_POINT('Ctrl Pts',(56.9823492838177,1075.73104815858,511.781255765029));
#115286=CARTESIAN_POINT('Ctrl Pts',(57.25077628193,1075.70654473072,511.894709152754));
#115287=CARTESIAN_POINT('Ctrl Pts',(57.372416941745,1075.69265311821,511.977671978499));
#115288=CARTESIAN_POINT('Ctrl Pts',(57.5769230252388,1075.6630478409,512.186834707922));
#115289=CARTESIAN_POINT('Ctrl Pts',(57.6574878086284,1075.64760781311,512.31133209373));
#115290=CARTESIAN_POINT('Ctrl Pts',(57.7646463823465,1075.61747936737,512.583870217935));
#115291=CARTESIAN_POINT('Ctrl Pts',(57.7904938275083,1075.60307749624,512.729172590082));
#115292=CARTESIAN_POINT('Ctrl Pts',(57.7837973641008,1075.57748263647,513.019629825418));
#115293=CARTESIAN_POINT('Ctrl Pts',(57.7520835582338,1075.56649753112,513.161980597539));
#115294=CARTESIAN_POINT('Ctrl Pts',(57.6355578208295,1075.54944468611,513.425637637228));
#115295=CARTESIAN_POINT('Ctrl Pts',(57.5522289267554,1075.54351604955,513.544482780541));
#115296=CARTESIAN_POINT('Ctrl Pts',(57.3448504471021,1075.53759642069,513.742922434999));
#115297=CARTESIAN_POINT('Ctrl Pts',(57.2230770502388,1075.53763572485,513.820731366586));
#115298=CARTESIAN_POINT('Ctrl Pts',(56.9619228712105,1075.54357025731,513.923162562141));
#115299=CARTESIAN_POINT('Ctrl Pts',(56.825850053433,1075.5491735528,513.948862722139));
#115300=CARTESIAN_POINT('Ctrl Pts',(56.688665939873,1075.55713627063,513.948872942962));
#115301=CARTESIAN_POINT('Origin',(56.6885840720975,1067.7251047501,512.850041810019));
#115302=CARTESIAN_POINT('',(56.6885840720975,1075.61138997104,513.348872946012));
#115303=CARTESIAN_POINT('',(56.6885840720978,1075.69877322724,512.351210674027));
#115304=CARTESIAN_POINT('Ctrl Pts',(56.6885840720976,1075.61138997104,513.348872946012));
#115305=CARTESIAN_POINT('Ctrl Pts',(56.6856353917996,1075.61155830615,513.348872946012));
#115306=CARTESIAN_POINT('Ctrl Pts',(56.6826856497571,1075.61172901146,513.348846800787));
#115307=CARTESIAN_POINT('Ctrl Pts',(56.6145283054266,1075.6157267927,513.347637551156));
#115308=CARTESIAN_POINT('Ctrl Pts',(56.550247139395,1075.6206265607,513.333706769179));
#115309=CARTESIAN_POINT('Ctrl Pts',(56.4304095372942,1075.63202017548,513.28185968679));
#115310=CARTESIAN_POINT('Ctrl Pts',(56.3760567804463,1075.63841378756,513.244295287237));
#115311=CARTESIAN_POINT('Ctrl Pts',(56.2841232541272,1075.65193539467,513.149517112086));
#115312=CARTESIAN_POINT('Ctrl Pts',(56.247773763792,1075.65894372933,513.092860533435));
#115313=CARTESIAN_POINT('Ctrl Pts',(56.1995769763763,1075.67247229934,512.968843972007));
#115314=CARTESIAN_POINT('Ctrl Pts',(56.1881045044952,1075.67886399388,512.902720402242));
#115315=CARTESIAN_POINT('Ctrl Pts',(56.1917799382474,1075.69018089434,512.769881583919));
#115316=CARTESIAN_POINT('Ctrl Pts',(56.2068480293014,1075.69499713634,512.704481362263));
#115317=CARTESIAN_POINT('Ctrl Pts',(56.2615232716968,1075.70236414649,512.583997057215));
#115318=CARTESIAN_POINT('Ctrl Pts',(56.3003133012152,1075.70486596451,512.530013671785));
#115319=CARTESIAN_POINT('Ctrl Pts',(56.3960612796101,1075.70725109424,512.440788863679));
#115320=CARTESIAN_POINT('Ctrl Pts',(56.4518198103308,1075.70714518084,512.406195279986));
#115321=CARTESIAN_POINT('Ctrl Pts',(56.5688319756226,1075.70446970291,512.362088715319));
#115322=CARTESIAN_POINT('Ctrl Pts',(56.6283527037088,1075.70211063064,512.351241331275));
#115323=CARTESIAN_POINT('Ctrl Pts',(56.6883296349369,1075.69878733113,512.351210739033));
#115324=CARTESIAN_POINT('Ctrl Pts',(56.6884144485161,1075.69878263164,512.351210695772));
#115325=CARTESIAN_POINT('Ctrl Pts',(56.6884992609062,1075.69877793035,512.351210674027));
#115326=CARTESIAN_POINT('Ctrl Pts',(56.688584072098,1075.69877322724,512.351210674027));
#115327=CARTESIAN_POINT('',(56.6885840720975,1082.7251047501,512.351210674027));
#115328=CARTESIAN_POINT('',(56.6885840720975,1067.7251047501,512.351210674027));
#115329=CARTESIAN_POINT('Origin',(56.6885840720975,1082.7251047501,512.850041810019));
#115330=CARTESIAN_POINT('Ctrl Pts',(56.688584072098,1075.69877322724,512.351210674027));
#115331=CARTESIAN_POINT('Ctrl Pts',(56.7550184269763,1075.69508918153,512.351210674027));
#115332=CARTESIAN_POINT('Ctrl Pts',(56.8207179252903,1075.69029351969,512.364480756885));
#115333=CARTESIAN_POINT('Ctrl Pts',(56.9431511449826,1075.67900838172,512.41593311774));
#115334=CARTESIAN_POINT('Ctrl Pts',(56.9986424001624,1075.6726255336,512.453676334347));
#115335=CARTESIAN_POINT('Ctrl Pts',(57.0917047797326,1075.65910658288,512.548764302263));
#115336=CARTESIAN_POINT('Ctrl Pts',(57.1283045669644,1075.65209891217,512.605257041306));
#115337=CARTESIAN_POINT('Ctrl Pts',(57.1772166247705,1075.63842106371,512.729462828353));
#115338=CARTESIAN_POINT('Ctrl Pts',(57.188976740676,1075.63188566127,512.795998323866));
#115339=CARTESIAN_POINT('Ctrl Pts',(57.1855601054695,1075.62037662518,512.928332734584));
#115340=CARTESIAN_POINT('Ctrl Pts',(57.17101361606,1075.61548204284,512.992847771813));
#115341=CARTESIAN_POINT('Ctrl Pts',(57.1178833131381,1075.60790188226,513.112304719604));
#115342=CARTESIAN_POINT('Ctrl Pts',(57.0799660849343,1075.60527804921,513.166130164001));
#115343=CARTESIAN_POINT('Ctrl Pts',(56.9856739717083,1075.60267072458,513.255989818789));
#115344=CARTESIAN_POINT('Ctrl Pts',(56.9303155975767,1075.60270252346,513.291201547692));
#115345=CARTESIAN_POINT('Ctrl Pts',(56.8119498459242,1075.6053660802,513.337344559212));
#115346=CARTESIAN_POINT('Ctrl Pts',(56.750501019099,1075.60785523846,513.348872946012));
#115347=CARTESIAN_POINT('Ctrl Pts',(56.6885840720976,1075.61138997104,513.348872946012));
#115348=CARTESIAN_POINT('Origin',(49.7050859019682,1067.7251047501,524.96881684456));
#115349=CARTESIAN_POINT('',(49.7050859019681,1076.94955520377,523.878276095832));
#115350=CARTESIAN_POINT('Ctrl Pts',(49.7051010956667,1076.68713161255,526.059357593183));
#115351=CARTESIAN_POINT('Ctrl Pts',(49.8088196058972,1076.68081788784,526.059356148149));
#115352=CARTESIAN_POINT('Ctrl Pts',(49.9120885769206,1076.67634163785,526.044558198505));
#115353=CARTESIAN_POINT('Ctrl Pts',(50.0459481856418,1076.67300727781,526.005330350595));
#115354=CARTESIAN_POINT('Ctrl Pts',(50.0796158220323,1076.67239233822,525.993646226015));
#115355=CARTESIAN_POINT('Ctrl Pts',(50.132975025126,1076.67178502937,525.972146286058));
#115356=CARTESIAN_POINT('Ctrl Pts',(50.1530443720276,1076.67164427072,525.963348054894));
#115357=CARTESIAN_POINT('Ctrl Pts',(50.1906690054537,1076.67154917841,525.945483576024));
#115358=CARTESIAN_POINT('Ctrl Pts',(50.2082691325682,1076.6715777997,525.936533477392));
#115359=CARTESIAN_POINT('Ctrl Pts',(50.2475560463489,1076.67180942963,525.915193424795));
#115360=CARTESIAN_POINT('Ctrl Pts',(50.2690788279477,1076.67205652408,525.902526837374));
#115361=CARTESIAN_POINT('Ctrl Pts',(50.3317132132919,1076.67313964998,525.862709087758));
#115362=CARTESIAN_POINT('Ctrl Pts',(50.3714324424752,1076.67431347612,525.83350483112));
#115363=CARTESIAN_POINT('Ctrl Pts',(50.5193153002078,1076.68068267819,525.708518676353));
#115364=CARTESIAN_POINT('Ctrl Pts',(50.6098380401068,1076.68920035861,525.594469904896));
#115365=CARTESIAN_POINT('Ctrl Pts',(50.7297357974363,1076.71059995738,525.360591608081));
#115366=CARTESIAN_POINT('Ctrl Pts',(50.7662173654937,1076.72230872815,525.246873664953));
#115367=CARTESIAN_POINT('Ctrl Pts',(50.8027980978875,1076.75001560668,525.001616850204));
#115368=CARTESIAN_POINT('Ctrl Pts',(50.7989167301965,1076.76609517129,524.871305558032));
#115369=CARTESIAN_POINT('Ctrl Pts',(50.7437473135572,1076.80123160075,524.608400609267));
#115370=CARTESIAN_POINT('Ctrl Pts',(50.6892153615724,1076.82011769004,524.47871760199));
#115371=CARTESIAN_POINT('Ctrl Pts',(50.5313246102264,1076.85783773953,524.242481790271));
#115372=CARTESIAN_POINT('Ctrl Pts',(50.4276399916915,1076.87628991027,524.139216212707));
#115373=CARTESIAN_POINT('Ctrl Pts',(50.1911042395142,1076.90880615558,523.982787576683));
#115374=CARTESIAN_POINT('Ctrl Pts',(50.0618738851153,1076.92274392356,523.928965892714));
#115375=CARTESIAN_POINT('Ctrl Pts',(49.7950978369668,1076.94484043791,523.873833716397));
#115376=CARTESIAN_POINT('Ctrl Pts',(49.6603852961936,1076.95301660898,523.871010226687));
#115377=CARTESIAN_POINT('Ctrl Pts',(49.4669169638779,1076.96054213026,523.9027808114));
#115378=CARTESIAN_POINT('Ctrl Pts',(49.4064240516526,1076.96225868753,523.91812041938));
#115379=CARTESIAN_POINT('Ctrl Pts',(49.3242060255788,1076.96368973258,523.946652212118));
#115380=CARTESIAN_POINT('Ctrl Pts',(49.3011368386674,1076.96398683188,523.955547236706));
#115381=CARTESIAN_POINT('Ctrl Pts',(49.2615022695362,1076.9643131366,523.972398566672));
#115382=CARTESIAN_POINT('Ctrl Pts',(49.2447994750683,1076.96439158913,523.980003289559));
#115383=CARTESIAN_POINT('Ctrl Pts',(49.2104144860873,1076.96442869639,523.996718783239));
#115384=CARTESIAN_POINT('Ctrl Pts',(49.192773902446,1076.96437678838,524.005898961466));
#115385=CARTESIAN_POINT('Ctrl Pts',(49.1519569226844,1076.96408778106,524.028579440257));
#115386=CARTESIAN_POINT('Ctrl Pts',(49.1290090154073,1076.9637925443,524.042461993219));
#115387=CARTESIAN_POINT('Ctrl Pts',(49.057371330461,1076.96243744104,524.089491811313));
#115388=CARTESIAN_POINT('Ctrl Pts',(49.0108570925859,1076.96088780839,524.125733641707));
#115389=CARTESIAN_POINT('Ctrl Pts',(48.8612232473619,1076.95345476994,524.263129374957));
#115390=CARTESIAN_POINT('Ctrl Pts',(48.7755058867875,1076.94462518507,524.380708499751));
#115391=CARTESIAN_POINT('Ctrl Pts',(48.6645189513374,1076.92276844206,524.620881359219));
#115392=CARTESIAN_POINT('Ctrl Pts',(48.6325026062703,1076.91080305764,524.737897999566));
#115393=CARTESIAN_POINT('Ctrl Pts',(48.6068359257461,1076.8825797593,524.98826281284));
#115394=CARTESIAN_POINT('Ctrl Pts',(48.6171692821046,1076.8662535282,525.120123908447));
#115395=CARTESIAN_POINT('Ctrl Pts',(48.6866792696424,1076.83056210063,525.383751228586));
#115396=CARTESIAN_POINT('Ctrl Pts',(48.7490851406893,1076.81137652074,525.51230254272));
#115397=CARTESIAN_POINT('Ctrl Pts',(48.9188277218414,1076.7739993112,525.737448347857));
#115398=CARTESIAN_POINT('Ctrl Pts',(49.0243149715656,1076.75612946937,525.832315979849));
#115399=CARTESIAN_POINT('Ctrl Pts',(49.2171396635911,1076.73042006772,525.947716364382));
#115400=CARTESIAN_POINT('Ctrl Pts',(49.2940365919188,1076.72152431293,525.982425429634));
#115401=CARTESIAN_POINT('Ctrl Pts',(49.4810873207852,1076.70289412714,526.041979076823));
#115402=CARTESIAN_POINT('Ctrl Pts',(49.592681813386,1076.69397498504,526.059359159437));
#115403=CARTESIAN_POINT('Ctrl Pts',(49.7051010956667,1076.68713161255,526.059357593183));
#115404=CARTESIAN_POINT('',(49.7050859019402,1074.93236944137,523.878276095832));
#115405=CARTESIAN_POINT('',(49.7050859019682,1067.7251047501,523.878276095832));
#115406=CARTESIAN_POINT('Ctrl Pts',(49.7045327815809,1074.66780810413,526.059357453018));
#115407=CARTESIAN_POINT('Ctrl Pts',(49.5625720018367,1074.67652953238,526.059285450746));
#115408=CARTESIAN_POINT('Ctrl Pts',(49.4222337317669,1074.6885690479,526.03149985231));
#115409=CARTESIAN_POINT('Ctrl Pts',(49.1590551093703,1074.7179348791,525.923575693812));
#115410=CARTESIAN_POINT('Ctrl Pts',(49.0389404221457,1074.73502905751,525.843944797542));
#115411=CARTESIAN_POINT('Ctrl Pts',(48.8866461967813,1074.76269718284,525.693103719675));
#115412=CARTESIAN_POINT('Ctrl Pts',(48.8407632584335,1074.77223284,525.637677149076));
#115413=CARTESIAN_POINT('Ctrl Pts',(48.7606636865352,1074.7915328718,525.518791458315));
#115414=CARTESIAN_POINT('Ctrl Pts',(48.7266027627846,1074.80125310818,525.455618460512));
#115415=CARTESIAN_POINT('Ctrl Pts',(48.6429153207276,1074.8305179077,525.255502964398));
#115416=CARTESIAN_POINT('Ctrl Pts',(48.6141566330179,1074.84959607476,525.11145403381));
#115417=CARTESIAN_POINT('Ctrl Pts',(48.6149386387002,1074.88435927607,524.821397837244));
#115418=CARTESIAN_POINT('Ctrl Pts',(48.6440366075017,1074.89973770998,524.678190775981));
#115419=CARTESIAN_POINT('Ctrl Pts',(48.7566128360411,1074.92484835885,524.411541627296));
#115420=CARTESIAN_POINT('Ctrl Pts',(48.838790490427,1074.93434730158,524.290726991862));
#115421=CARTESIAN_POINT('Ctrl Pts',(49.0447128969339,1074.94613771329,524.08921518635));
#115422=CARTESIAN_POINT('Ctrl Pts',(49.1658542694596,1074.9483909307,524.010144969033));
#115423=CARTESIAN_POINT('Ctrl Pts',(49.4304649275366,1074.94544904026,523.903936701423));
#115424=CARTESIAN_POINT('Ctrl Pts',(49.570991037753,1074.94036278595,523.877332045742));
#115425=CARTESIAN_POINT('Ctrl Pts',(49.857416713149,1074.92329557957,523.879293889884));
#115426=CARTESIAN_POINT('Ctrl Pts',(50.0003887150679,1074.9113327437,523.909133788143));
#115427=CARTESIAN_POINT('Ctrl Pts',(50.2666680223075,1074.88201441875,524.022791742783));
#115428=CARTESIAN_POINT('Ctrl Pts',(50.3872229444195,1074.86492275914,524.105737641097));
#115429=CARTESIAN_POINT('Ctrl Pts',(50.5374275697886,1074.83730943705,524.260624802096));
#115430=CARTESIAN_POINT('Ctrl Pts',(50.5817735933465,1074.82793436821,524.316329727833));
#115431=CARTESIAN_POINT('Ctrl Pts',(50.6591441952577,1074.80884541381,524.435772126998));
#115432=CARTESIAN_POINT('Ctrl Pts',(50.6919459063807,1074.7991730995,524.499274702747));
#115433=CARTESIAN_POINT('Ctrl Pts',(50.7725931602685,1074.76968516607,524.70188856101));
#115434=CARTESIAN_POINT('Ctrl Pts',(50.7988337714617,1074.7502503453,524.847940784062));
#115435=CARTESIAN_POINT('Ctrl Pts',(50.7918754877078,1074.71502421092,525.13852279965));
#115436=CARTESIAN_POINT('Ctrl Pts',(50.7600934763545,1074.6994930169,525.280276126511));
#115437=CARTESIAN_POINT('Ctrl Pts',(50.6435681777698,1074.67425178988,525.542296465004));
#115438=CARTESIAN_POINT('Ctrl Pts',(50.5605041258705,1074.66473437469,525.660196468658));
#115439=CARTESIAN_POINT('Ctrl Pts',(50.3541867038513,1074.65305420016,525.856532132437));
#115440=CARTESIAN_POINT('Ctrl Pts',(50.233396864555,1074.6509444254,525.93333098338));
#115441=CARTESIAN_POINT('Ctrl Pts',(49.9746818113774,1074.65433161193,526.034203506374));
#115442=CARTESIAN_POINT('Ctrl Pts',(49.8401329657222,1074.6594774421,526.059426229206));
#115443=CARTESIAN_POINT('Ctrl Pts',(49.7045327815809,1074.66780810413,526.059357453018));
#115444=CARTESIAN_POINT('Origin',(49.7050859019682,1067.7251047501,524.96881684456));
#115445=CARTESIAN_POINT('',(49.7050859019682,1074.74227702453,525.459357593288));
#115446=CARTESIAN_POINT('',(49.7050859019685,1074.86129916363,524.478276095832));
#115447=CARTESIAN_POINT('Ctrl Pts',(49.7050859019682,1074.74227702453,525.459357593288));
#115448=CARTESIAN_POINT('Ctrl Pts',(49.7042385243676,1074.74232843758,525.459357593288));
#115449=CARTESIAN_POINT('Ctrl Pts',(49.7033910526429,1074.74238012467,525.459355397603));
#115450=CARTESIAN_POINT('Ctrl Pts',(49.6386219609656,1074.74635089057,525.459019703593));
#115451=CARTESIAN_POINT('Ctrl Pts',(49.5754894174681,1074.75174807733,525.446200007164));
#115452=CARTESIAN_POINT('Ctrl Pts',(49.4572417247623,1074.76491503881,525.397005248761));
#115453=CARTESIAN_POINT('Ctrl Pts',(49.403354017794,1074.77258043984,525.360871069239));
#115454=CARTESIAN_POINT('Ctrl Pts',(49.3352444927388,1074.78498960951,525.292676140412));
#115455=CARTESIAN_POINT('Ctrl Pts',(49.3147929353546,1074.78925799106,525.267710480105));
#115456=CARTESIAN_POINT('Ctrl Pts',(49.279098864582,1074.79791017122,525.214173023116));
#115457=CARTESIAN_POINT('Ctrl Pts',(49.2639332817146,1074.80227438928,525.18572430995));
#115458=CARTESIAN_POINT('Ctrl Pts',(49.2266561959728,1074.81545990107,525.095424886765));
#115459=CARTESIAN_POINT('Ctrl Pts',(49.2140178972823,1074.82408227959,525.03039670124));
#115460=CARTESIAN_POINT('Ctrl Pts',(49.2151031724537,1074.83982449383,524.899459650653));
#115461=CARTESIAN_POINT('Ctrl Pts',(49.2286758037565,1074.84680058392,524.834821027198));
#115462=CARTESIAN_POINT('Ctrl Pts',(49.2801672148551,1074.85810553264,524.715348895732));
#115463=CARTESIAN_POINT('Ctrl Pts',(49.3172319860543,1074.86235798359,524.661579615519));
#115464=CARTESIAN_POINT('Ctrl Pts',(49.4095276776769,1074.86760490442,524.572157907458));
#115465=CARTESIAN_POINT('Ctrl Pts',(49.4635318492254,1074.86859727634,524.537133276184));
#115466=CARTESIAN_POINT('Ctrl Pts',(49.5807062159694,1074.86726255741,524.490217355236));
#115467=CARTESIAN_POINT('Ctrl Pts',(49.6425127344436,1074.86501864792,524.478307291072));
#115468=CARTESIAN_POINT('Ctrl Pts',(49.7048408686823,1074.86131373627,524.478276157118));
#115469=CARTESIAN_POINT('Ctrl Pts',(49.7049225476157,1074.86130888111,524.478276116317));
#115470=CARTESIAN_POINT('Ctrl Pts',(49.7050042253808,1074.86130402357,524.478276095832));
#115471=CARTESIAN_POINT('Ctrl Pts',(49.7050859019687,1074.86129916363,524.478276095832));
#115472=CARTESIAN_POINT('',(49.7050859019682,1082.7251047501,524.478276095832));
#115473=CARTESIAN_POINT('',(49.7050859019682,1067.7251047501,524.478276095832));
#115474=CARTESIAN_POINT('Origin',(49.7050859019682,1082.7251047501,524.96881684456));
#115475=CARTESIAN_POINT('Ctrl Pts',(49.7050859019687,1074.86129916363,524.478276095832));
#115476=CARTESIAN_POINT('Ctrl Pts',(49.7690222839905,1074.85749480846,524.478276095832));
#115477=CARTESIAN_POINT('Ctrl Pts',(49.8322378137251,1074.8522284988,524.490773982374));
#115478=CARTESIAN_POINT('Ctrl Pts',(49.9518571609206,1074.83918388506,524.539828474315));
#115479=CARTESIAN_POINT('Ctrl Pts',(50.0068143051841,1074.83146919783,524.576564320064));
#115480=CARTESIAN_POINT('Ctrl Pts',(50.0755035950335,1074.81900529293,524.645632418096));
#115481=CARTESIAN_POINT('Ctrl Pts',(50.0958136304354,1074.8147772041,524.670508815552));
#115482=CARTESIAN_POINT('Ctrl Pts',(50.1313241442475,1074.80617701668,524.723905292744));
#115483=CARTESIAN_POINT('Ctrl Pts',(50.1464325591112,1074.80182393296,524.752313818214));
#115484=CARTESIAN_POINT('Ctrl Pts',(50.1837270944111,1074.78858807754,524.842856832629));
#115485=CARTESIAN_POINT('Ctrl Pts',(50.1963126327165,1074.7798774798,524.908201722288));
#115486=CARTESIAN_POINT('Ctrl Pts',(50.1948930021439,1074.76399887641,525.039146675381));
#115487=CARTESIAN_POINT('Ctrl Pts',(50.1812690455078,1074.75696291534,525.103481856568));
#115488=CARTESIAN_POINT('Ctrl Pts',(50.129968273002,1074.74554619808,525.222227936558));
#115489=CARTESIAN_POINT('Ctrl Pts',(50.093202375989,1074.74123492869,525.275625525989));
#115490=CARTESIAN_POINT('Ctrl Pts',(50.0013970852732,1074.73586449067,525.364916401852));
#115491=CARTESIAN_POINT('Ctrl Pts',(49.9474434653618,1074.73483245957,525.400052791796));
#115492=CARTESIAN_POINT('Ctrl Pts',(49.8299711124248,1074.73616947686,525.447336148879));
#115493=CARTESIAN_POINT('Ctrl Pts',(49.7677861562045,1074.73847280419,525.459357593288));
#115494=CARTESIAN_POINT('Ctrl Pts',(49.7050859019682,1074.74227702453,525.459357593288));
#115495=CARTESIAN_POINT('Origin',(75.4882582191912,1067.7251047501,472.809444687437));
#115496=CARTESIAN_POINT('',(75.4882582192226,1078.69210669589,471.331141555243));
#115497=CARTESIAN_POINT('Ctrl Pts',(75.4883591791963,1078.65110304669,474.287747816183));
#115498=CARTESIAN_POINT('Ctrl Pts',(75.6738846076919,1078.64642022966,474.287735145812));
#115499=CARTESIAN_POINT('Ctrl Pts',(75.8577731642089,1078.64215344441,474.25279772366));
#115500=CARTESIAN_POINT('Ctrl Pts',(76.2028476993047,1078.63519237295,474.116771245797));
#115501=CARTESIAN_POINT('Ctrl Pts',(76.3609960447903,1078.63256354019,474.016954115307));
#115502=CARTESIAN_POINT('Ctrl Pts',(76.5486284066885,1078.63044231687,473.84194790386));
#115503=CARTESIAN_POINT('Ctrl Pts',(76.5971122148997,1078.63001746006,473.789695126768));
#115504=CARTESIAN_POINT('Ctrl Pts',(76.6599317411793,1078.62965774124,473.711340567205));
#115505=CARTESIAN_POINT('Ctrl Pts',(76.6775400349786,1078.62958172096,473.687991095779));
#115506=CARTESIAN_POINT('Ctrl Pts',(76.7085227237751,1078.62949534906,473.644266605918));
#115507=CARTESIAN_POINT('Ctrl Pts',(76.7221080656931,1078.62947615609,473.624053584186));
#115508=CARTESIAN_POINT('Ctrl Pts',(76.7485175895551,1078.62947796131,473.582582632352));
#115509=CARTESIAN_POINT('Ctrl Pts',(76.7613180723559,1078.62949973388,473.56131872677));
#115510=CARTESIAN_POINT('Ctrl Pts',(76.7912100487528,1078.62960359524,473.508709076028));
#115511=CARTESIAN_POINT('Ctrl Pts',(76.8077130885578,1078.62970791169,473.47704710312));
#115512=CARTESIAN_POINT('Ctrl Pts',(76.8612782639026,1078.6302211234,473.364517282206));
#115513=CARTESIAN_POINT('Ctrl Pts',(76.8921774655035,1078.63085155159,473.2809314245));
#115514=CARTESIAN_POINT('Ctrl Pts',(76.9476616566716,1078.63295707426,473.075600852574));
#115515=CARTESIAN_POINT('Ctrl Pts',(76.9648138863255,1078.63465835563,472.952545948046));
#115516=CARTESIAN_POINT('Ctrl Pts',(76.9684843419805,1078.63942569333,472.672302980661));
#115517=CARTESIAN_POINT('Ctrl Pts',(76.945666676569,1078.64270286122,472.516474557731));
#115518=CARTESIAN_POINT('Ctrl Pts',(76.8476704098332,1078.65041112291,472.203941880989));
#115519=CARTESIAN_POINT('Ctrl Pts',(76.7685599201206,1078.65485959935,472.050855059878));
#115520=CARTESIAN_POINT('Ctrl Pts',(76.5539017011356,1078.66433878016,471.768528614668));
#115521=CARTESIAN_POINT('Ctrl Pts',(76.4164840386204,1078.66930162597,471.644326190103));
#115522=CARTESIAN_POINT('Ctrl Pts',(76.0912980893407,1078.67907857565,471.445345791837));
#115523=CARTESIAN_POINT('Ctrl Pts',(75.9037669536843,1078.68375251818,471.377039649236));
#115524=CARTESIAN_POINT('Ctrl Pts',(75.5189195473925,1078.6917736033,471.319095987988));
#115525=CARTESIAN_POINT('Ctrl Pts',(75.3257234847783,1078.69508675301,471.327665340448));
#115526=CARTESIAN_POINT('Ctrl Pts',(74.9743722653524,1078.70008698208,471.412953117287));
#115527=CARTESIAN_POINT('Ctrl Pts',(74.8173451207834,1078.70188330224,471.481232786763));
#115528=CARTESIAN_POINT('Ctrl Pts',(74.5666181739271,1078.70413599813,471.646296258331));
#115529=CARTESIAN_POINT('Ctrl Pts',(74.4677945957722,1078.70479808836,471.731952485555));
#115530=CARTESIAN_POINT('Ctrl Pts',(74.3528508500848,1078.70527814465,471.861766235987));
#115531=CARTESIAN_POINT('Ctrl Pts',(74.3256580871193,1078.70536409373,471.89533020559));
#115532=CARTESIAN_POINT('Ctrl Pts',(74.2843529187854,1078.70544864801,471.951143061264));
#115533=CARTESIAN_POINT('Ctrl Pts',(74.2692975379912,1078.70546825953,471.972662450159));
#115534=CARTESIAN_POINT('Ctrl Pts',(74.2418698223851,1078.70548202789,472.014178476528));
#115535=CARTESIAN_POINT('Ctrl Pts',(74.2293856857682,1078.70547863999,472.034091653993));
#115536=CARTESIAN_POINT('Ctrl Pts',(74.2022918730305,1078.70544866441,472.079689031923));
#115537=CARTESIAN_POINT('Ctrl Pts',(74.1879667654673,1078.70541634643,472.105530705662));
#115538=CARTESIAN_POINT('Ctrl Pts',(74.147897836739,1078.70527436976,472.183215423094));
#115539=CARTESIAN_POINT('Ctrl Pts',(74.1244130703106,1078.70512045451,472.236159924138));
#115540=CARTESIAN_POINT('Ctrl Pts',(74.0347841579004,1078.70417420876,472.475152694407));
#115541=CARTESIAN_POINT('Ctrl Pts',(74.0031867137151,1078.70275493028,472.671979498503));
#115542=CARTESIAN_POINT('Ctrl Pts',(74.0176317392622,1078.69883959814,473.029132484725));
#115543=CARTESIAN_POINT('Ctrl Pts',(74.0500373477484,1078.69661836051,473.186965030117));
#115544=CARTESIAN_POINT('Ctrl Pts',(74.1693318751837,1078.69096939555,473.499570856544));
#115545=CARTESIAN_POINT('Ctrl Pts',(74.2599415360653,1078.68749082197,473.650320590085));
#115546=CARTESIAN_POINT('Ctrl Pts',(74.4981372593134,1078.67929894864,473.923108964409));
#115547=CARTESIAN_POINT('Ctrl Pts',(74.6473337685029,1078.67458300061,474.039659012687));
#115548=CARTESIAN_POINT('Ctrl Pts',(74.9138363613299,1078.66667163302,474.176163692336));
#115549=CARTESIAN_POINT('Ctrl Pts',(75.0188120815975,1078.66365965535,474.215681286133));
#115550=CARTESIAN_POINT('Ctrl Pts',(75.2453036469157,1078.65739862494,474.272721080618));
#115551=CARTESIAN_POINT('Ctrl Pts',(75.3665981398743,1078.65417639719,474.287756131795));
#115552=CARTESIAN_POINT('Ctrl Pts',(75.4883591791963,1078.65110304669,474.287747816183));
#115553=CARTESIAN_POINT('',(75.4882582191714,1076.6916225261,471.331141555244));
#115554=CARTESIAN_POINT('',(75.4882582191912,1067.7251047501,471.331141555244));
#115555=CARTESIAN_POINT('Ctrl Pts',(75.487416119239,1076.65015733518,474.287747579784));
#115556=CARTESIAN_POINT('Ctrl Pts',(75.2941477495985,1076.65509390806,474.287637486456));
#115557=CARTESIAN_POINT('Ctrl Pts',(75.1027674812067,1076.66038695946,474.249627667376));
#115558=CARTESIAN_POINT('Ctrl Pts',(74.7454004369792,1076.67085061937,474.102089954927));
#115559=CARTESIAN_POINT('Ctrl Pts',(74.582864262089,1076.67591723991,473.993943445776));
#115560=CARTESIAN_POINT('Ctrl Pts',(74.3073819627376,1076.68518114485,473.719940057585));
#115561=CARTESIAN_POINT('Ctrl Pts',(74.1976138837424,1076.68928141582,473.556249372343));
#115562=CARTESIAN_POINT('Ctrl Pts',(74.048125694059,1076.69614758041,473.195944211236));
#115563=CARTESIAN_POINT('Ctrl Pts',(74.0097657378391,1076.69885579239,473.00291543298));
#115564=CARTESIAN_POINT('Ctrl Pts',(74.0101469157191,1076.70288797094,472.611989528244));
#115565=CARTESIAN_POINT('Ctrl Pts',(74.0493216181602,1076.70417222778,472.417951918973));
#115566=CARTESIAN_POINT('Ctrl Pts',(74.2013211842234,1076.70537226395,472.055889894595));
#115567=CARTESIAN_POINT('Ctrl Pts',(74.3128635434451,1076.70527492564,471.891567320269));
#115568=CARTESIAN_POINT('Ctrl Pts',(74.5931205500648,1076.7036766014,471.616773061266));
#115569=CARTESIAN_POINT('Ctrl Pts',(74.7588236214776,1076.70219294848,471.50880710114));
#115570=CARTESIAN_POINT('Ctrl Pts',(75.1217122397172,1076.6977548676,471.364112829601));
#115571=CARTESIAN_POINT('Ctrl Pts',(75.3151722554871,1076.69484316653,471.328440445533));
#115572=CARTESIAN_POINT('Ctrl Pts',(75.7053422696635,1076.68758955606,471.33416999898));
#115573=CARTESIAN_POINT('Ctrl Pts',(75.898212919866,1076.68330767376,471.37574715457));
#115574=CARTESIAN_POINT('Ctrl Pts',(76.1654707024127,1076.67615770782,471.491877270918));
#115575=CARTESIAN_POINT('Ctrl Pts',(76.2495993877647,1076.67369664673,471.538634153267));
#115576=CARTESIAN_POINT('Ctrl Pts',(76.4897797850506,1076.66599625282,471.704583745673));
#115577=CARTESIAN_POINT('Ctrl Pts',(76.6272274923538,1076.66059878149,471.846890075095));
#115578=CARTESIAN_POINT('Ctrl Pts',(76.8376279573087,1076.65019591766,472.175223471903));
#115579=CARTESIAN_POINT('Ctrl Pts',(76.9091447621676,1076.64529430033,472.357642143143));
#115580=CARTESIAN_POINT('Ctrl Pts',(76.9776049539143,1076.63692598836,472.739650764687));
#115581=CARTESIAN_POINT('Ctrl Pts',(76.9739027906418,1076.63354729511,472.935528786523));
#115582=CARTESIAN_POINT('Ctrl Pts',(76.891101144393,1076.62908213527,473.314360346499));
#115583=CARTESIAN_POINT('Ctrl Pts',(76.8129350538818,1076.62803950129,473.493655297899));
#115584=CARTESIAN_POINT('Ctrl Pts',(76.5921399911397,1076.62854799809,473.811538877061));
#115585=CARTESIAN_POINT('Ctrl Pts',(76.4517926810517,1076.63008793845,473.947136320226));
#115586=CARTESIAN_POINT('Ctrl Pts',(76.1270588505246,1076.63541758085,474.156515194196));
#115587=CARTESIAN_POINT('Ctrl Pts',(75.9458490738619,1076.63914850194,474.228339926111));
#115588=CARTESIAN_POINT('Ctrl Pts',(75.6673873722677,1076.64564977036,474.279617326469));
#115589=CARTESIAN_POINT('Ctrl Pts',(75.5774921057094,1076.64785656205,474.287798890638));
#115590=CARTESIAN_POINT('Ctrl Pts',(75.487416119239,1076.65015733518,474.287747579784));
#115591=CARTESIAN_POINT('Origin',(75.4882582191912,1067.7251047501,472.809444687437));
#115592=CARTESIAN_POINT('',(75.4882582191912,1076.65987181774,473.68774781963));
#115593=CARTESIAN_POINT('',(75.4882582191939,1076.68449717364,471.931141555244));
#115594=CARTESIAN_POINT('Ctrl Pts',(75.4882582191911,1076.65987181774,473.68774781963));
#115595=CARTESIAN_POINT('Ctrl Pts',(75.3795548737725,1076.66248986587,473.68774781963));
#115596=CARTESIAN_POINT('Ctrl Pts',(75.2717368513576,1076.66532867394,473.667566390282));
#115597=CARTESIAN_POINT('Ctrl Pts',(75.0631502138089,1076.67124953729,473.586564628072));
#115598=CARTESIAN_POINT('Ctrl Pts',(74.9651901345204,1076.67427623391,473.52431053641));
#115599=CARTESIAN_POINT('Ctrl Pts',(74.7976946551806,1076.67998948559,473.364526163751));
#115600=CARTESIAN_POINT('Ctrl Pts',(74.7302215487056,1076.68261510257,473.268113306397));
#115601=CARTESIAN_POINT('Ctrl Pts',(74.6368674030413,1076.68714518856,473.054628849557));
#115602=CARTESIAN_POINT('Ctrl Pts',(74.6118897284744,1076.68900781701,472.939686161403));
#115603=CARTESIAN_POINT('Ctrl Pts',(74.6082293322471,1076.6918454184,472.706296121146));
#115604=CARTESIAN_POINT('Ctrl Pts',(74.6297641493946,1076.69279138027,472.590172895777));
#115605=CARTESIAN_POINT('Ctrl Pts',(74.7171461708703,1076.69371340958,472.372934854634));
#115606=CARTESIAN_POINT('Ctrl Pts',(74.7822155095578,1076.6936791762,472.274039933481));
#115607=CARTESIAN_POINT('Ctrl Pts',(74.9471113267483,1076.6926208934,472.107843477452));
#115608=CARTESIAN_POINT('Ctrl Pts',(75.0451981403042,1076.69160862419,472.042124578511));
#115609=CARTESIAN_POINT('Ctrl Pts',(75.2595247999158,1076.68866381459,471.953692750837));
#115610=CARTESIAN_POINT('Ctrl Pts',(75.3733480631393,1076.68677275628,471.931141555244));
#115611=CARTESIAN_POINT('Ctrl Pts',(75.4882582191967,1076.68449717364,471.931141555244));
#115612=CARTESIAN_POINT('',(75.4882582191912,1082.7251047501,471.931141555244));
#115613=CARTESIAN_POINT('',(75.4882582191912,1067.7251047501,471.931141555244));
#115614=CARTESIAN_POINT('Origin',(75.4882582191912,1082.7251047501,472.809444687437));
#115615=CARTESIAN_POINT('Ctrl Pts',(75.4882582191967,1076.68449717364,471.931141555244));
#115616=CARTESIAN_POINT('Ctrl Pts',(75.4897687748842,1076.68446725989,471.931141555244));
#115617=CARTESIAN_POINT('Ctrl Pts',(75.4912795183942,1076.68443727978,471.931145452152));
#115618=CARTESIAN_POINT('Ctrl Pts',(75.6093545818292,1076.68208921839,471.93175475067));
#115619=CARTESIAN_POINT('Ctrl Pts',(75.7246341896332,1076.67941978365,471.955555118033));
#115620=CARTESIAN_POINT('Ctrl Pts',(75.884478497529,1076.67508939696,472.023511770839));
#115621=CARTESIAN_POINT('Ctrl Pts',(75.9347534318612,1076.67361895054,472.050944275815));
#115622=CARTESIAN_POINT('Ctrl Pts',(76.0782617178249,1076.6690746825,472.148492106724));
#115623=CARTESIAN_POINT('Ctrl Pts',(76.1605597090188,1076.6659615896,472.232406066685));
#115624=CARTESIAN_POINT('Ctrl Pts',(76.2869862583745,1076.66005651707,472.42641082651));
#115625=CARTESIAN_POINT('Ctrl Pts',(76.3302816653696,1076.65732080599,472.534342839857));
#115626=CARTESIAN_POINT('Ctrl Pts',(76.3606717240375,1076.65399831874,472.696395274421));
#115627=CARTESIAN_POINT('Ctrl Pts',(76.3656697823108,1076.65308034466,472.745924848059));
#115628=CARTESIAN_POINT('Ctrl Pts',(76.3664524173893,1076.65226038285,472.795612035064));
#115629=CARTESIAN_POINT('Ctrl Pts',(76.3682654495979,1076.6503608805,472.910716089134));
#115630=CARTESIAN_POINT('Ctrl Pts',(76.3474312203528,1076.64901622478,473.025068011928));
#115631=CARTESIAN_POINT('Ctrl Pts',(76.2628817863424,1076.64767305316,473.239092129448));
#115632=CARTESIAN_POINT('Ctrl Pts',(76.2000401080296,1076.64768681701,473.336706577559));
#115633=CARTESIAN_POINT('Ctrl Pts',(76.0403984525932,1076.64908105315,473.502087076357));
#115634=CARTESIAN_POINT('Ctrl Pts',(75.9451775833408,1076.65044569815,473.568281919729));
#115635=CARTESIAN_POINT('Ctrl Pts',(75.7346737785574,1076.65427288339,473.660261316522));
#115636=CARTESIAN_POINT('Ctrl Pts',(75.6214226622723,1076.65669614696,473.685157609897));
#115637=CARTESIAN_POINT('Ctrl Pts',(75.5004853717269,1076.65957810674,473.687684017164));
#115638=CARTESIAN_POINT('Ctrl Pts',(75.494370395865,1076.65972461001,473.68774781963));
#115639=CARTESIAN_POINT('Ctrl Pts',(75.4882582191911,1076.65987181774,473.68774781963));
#115640=CARTESIAN_POINT('Origin',(75.2807843499779,1067.7251047501,485.365998005138));
#115641=CARTESIAN_POINT('',(75.2807843500077,1078.39877300636,484.090553884001));
#115642=CARTESIAN_POINT('Ctrl Pts',(75.2809045366249,1078.29623865226,486.641442120612));
#115643=CARTESIAN_POINT('Ctrl Pts',(75.4339105238594,1078.2882023348,486.641427702672));
#115644=CARTESIAN_POINT('Ctrl Pts',(75.5857297123117,1078.28130556259,486.613880856192));
#115645=CARTESIAN_POINT('Ctrl Pts',(75.870023368324,1078.27070260712,486.507146698662));
#115646=CARTESIAN_POINT('Ctrl Pts',(76.0005273852905,1078.26703110727,486.429678545514));
#115647=CARTESIAN_POINT('Ctrl Pts',(76.1462977300508,1078.26464544065,486.303765465089));
#115648=CARTESIAN_POINT('Ctrl Pts',(76.1767035328239,1078.26426694378,486.274761038957));
#115649=CARTESIAN_POINT('Ctrl Pts',(76.222190991114,1078.26389723177,486.226863869023));
#115650=CARTESIAN_POINT('Ctrl Pts',(76.2382613847249,1078.26380971897,486.208953664539));
#115651=CARTESIAN_POINT('Ctrl Pts',(76.2669222035402,1078.2637355859,486.175133845931));
#115652=CARTESIAN_POINT('Ctrl Pts',(76.2796581257944,1078.26373526559,486.159357857223));
#115653=CARTESIAN_POINT('Ctrl Pts',(76.3066136640089,1078.26380783491,486.124289470864));
#115654=CARTESIAN_POINT('Ctrl Pts',(76.3206764811848,1078.26389403399,486.104886405074));
#115655=CARTESIAN_POINT('Ctrl Pts',(76.3582619371465,1078.26426397549,486.049828044096));
#115656=CARTESIAN_POINT('Ctrl Pts',(76.3805521187458,1078.26464929531,486.013371236718));
#115657=CARTESIAN_POINT('Ctrl Pts',(76.4819964712389,1078.26729100411,485.827041527426));
#115658=CARTESIAN_POINT('Ctrl Pts',(76.5325310650515,1078.27168449475,485.663600881729));
#115659=CARTESIAN_POINT('Ctrl Pts',(76.5634527384567,1078.28312828342,485.35973230746));
#115660=CARTESIAN_POINT('Ctrl Pts',(76.555468701051,1078.28941048786,485.223055576913));
#115661=CARTESIAN_POINT('Ctrl Pts',(76.493947627413,1078.30441416594,484.945199741084));
#115662=CARTESIAN_POINT('Ctrl Pts',(76.4367295935245,1078.31319121105,484.80688854445));
#115663=CARTESIAN_POINT('Ctrl Pts',(76.2713755449846,1078.33240508195,484.546870966901));
#115664=CARTESIAN_POINT('Ctrl Pts',(76.1611861636037,1078.34274706974,484.429446477995));
#115665=CARTESIAN_POINT('Ctrl Pts',(75.8956885425243,1078.36366888313,484.235866696622));
#115666=CARTESIAN_POINT('Ctrl Pts',(75.740707945171,1078.37402252915,484.16441542305));
#115667=CARTESIAN_POINT('Ctrl Pts',(75.416129209437,1078.39256448877,484.087115759469));
#115668=CARTESIAN_POINT('Ctrl Pts',(75.2500504972073,1078.400632639,484.080326399211));
#115669=CARTESIAN_POINT('Ctrl Pts',(74.9448587649636,1078.41307129196,484.127185420217));
#115670=CARTESIAN_POINT('Ctrl Pts',(74.8071835967028,1078.41769217654,484.173007260694));
#115671=CARTESIAN_POINT('Ctrl Pts',(74.5863103151216,1078.42343536162,484.290936006579));
#115672=CARTESIAN_POINT('Ctrl Pts',(74.4991717021453,1078.42513500507,484.352519283816));
#115673=CARTESIAN_POINT('Ctrl Pts',(74.393953385885,1078.42639080901,484.448611206889));
#115674=CARTESIAN_POINT('Ctrl Pts',(74.3682783263774,1078.42662066942,484.474145699792));
#115675=CARTESIAN_POINT('Ctrl Pts',(74.3285856906966,1078.42684757054,484.517132085187));
#115676=CARTESIAN_POINT('Ctrl Pts',(74.3138804350274,1078.42690004787,484.533920807439));
#115677=CARTESIAN_POINT('Ctrl Pts',(74.286734267309,1078.42693505528,484.566605058894));
#115678=CARTESIAN_POINT('Ctrl Pts',(74.2742153570082,1078.42692380996,484.582427006257));
#115679=CARTESIAN_POINT('Ctrl Pts',(74.2466507154517,1078.42683500459,484.619015682967));
#115680=CARTESIAN_POINT('Ctrl Pts',(74.2318454130292,1078.42674032887,484.63995251557));
#115681=CARTESIAN_POINT('Ctrl Pts',(74.1894275853905,1078.42632234144,484.703945707616));
#115682=CARTESIAN_POINT('Ctrl Pts',(74.1637638439162,1078.42586570848,484.748229684603));
#115683=CARTESIAN_POINT('Ctrl Pts',(74.0648826850275,1078.42313516236,484.945270423876));
#115684=CARTESIAN_POINT('Ctrl Pts',(74.0198471286397,1078.41913259009,485.110188562167));
#115685=CARTESIAN_POINT('Ctrl Pts',(73.9988927945721,1078.40868075659,485.416812705358));
#115686=CARTESIAN_POINT('Ctrl Pts',(74.0119178351324,1078.40288387409,485.555162740193));
#115687=CARTESIAN_POINT('Ctrl Pts',(74.0849456541348,1078.38880698269,485.834418461351));
#115688=CARTESIAN_POINT('Ctrl Pts',(74.1485603018477,1078.38045633912,485.972207522359));
#115689=CARTESIAN_POINT('Ctrl Pts',(74.3273945550068,1078.36171231311,486.228590057464));
#115690=CARTESIAN_POINT('Ctrl Pts',(74.444574647628,1078.35137807255,486.34260277014));
#115691=CARTESIAN_POINT('Ctrl Pts',(74.6771583592216,1078.33348784218,486.495571379258));
#115692=CARTESIAN_POINT('Ctrl Pts',(74.7826912782624,1078.3260535696,486.54591668702));
#115693=CARTESIAN_POINT('Ctrl Pts',(75.0187903984343,1078.31079932443,486.621140681863));
#115694=CARTESIAN_POINT('Ctrl Pts',(75.1494377303241,1078.30314366958,486.641454508888));
#115695=CARTESIAN_POINT('Ctrl Pts',(75.2809045366249,1078.29623865226,486.641442120612));
#115696=CARTESIAN_POINT('',(75.280784349959,1076.3950142966,484.090553884002));
#115697=CARTESIAN_POINT('',(75.2807843499779,1067.7251047501,484.090553884002));
#115698=CARTESIAN_POINT('Ctrl Pts',(75.2808777508431,1076.29141182132,486.641442122854));
#115699=CARTESIAN_POINT('Ctrl Pts',(75.1140408641621,1076.30026491392,486.641454340332));
#115700=CARTESIAN_POINT('Ctrl Pts',(74.9488638013435,1076.31032003874,486.60873234125));
#115701=CARTESIAN_POINT('Ctrl Pts',(74.7175248930847,1076.32622456351,486.513371472444));
#115702=CARTESIAN_POINT('Ctrl Pts',(74.6436555185119,1076.3316297301,486.474056100849));
#115703=CARTESIAN_POINT('Ctrl Pts',(74.5046433536862,1076.34247314129,486.381545150379));
#115704=CARTESIAN_POINT('Ctrl Pts',(74.4398334068195,1076.34788563694,486.32856406927));
#115705=CARTESIAN_POINT('Ctrl Pts',(74.2606645043229,1076.36400774368,486.150091497939));
#115706=CARTESIAN_POINT('Ctrl Pts',(74.1656350644278,1076.37427869745,486.007807887029));
#115707=CARTESIAN_POINT('Ctrl Pts',(74.0370711249052,1076.39263302296,485.695166642793));
#115708=CARTESIAN_POINT('Ctrl Pts',(74.0044762480409,1076.40055173042,485.528028987161));
#115709=CARTESIAN_POINT('Ctrl Pts',(74.0062403464886,1076.41322435377,485.190386718522));
#115710=CARTESIAN_POINT('Ctrl Pts',(74.0406838301846,1076.41785252816,485.023239054337));
#115711=CARTESIAN_POINT('Ctrl Pts',(74.1729601823872,1076.42333201726,484.711620713509));
#115712=CARTESIAN_POINT('Ctrl Pts',(74.2696286622621,1076.42412110499,484.570351064309));
#115713=CARTESIAN_POINT('Ctrl Pts',(74.5123785638704,1076.42173533607,484.334025774632));
#115714=CARTESIAN_POINT('Ctrl Pts',(74.655952339171,1076.41858835557,484.241286129291));
#115715=CARTESIAN_POINT('Ctrl Pts',(74.9703980447938,1076.40863309289,484.117442564739));
#115716=CARTESIAN_POINT('Ctrl Pts',(75.1380594259484,1076.40192964516,484.087397190795));
#115717=CARTESIAN_POINT('Ctrl Pts',(75.4756191035355,1076.38560017553,484.094242855806));
#115718=CARTESIAN_POINT('Ctrl Pts',(75.6421777359095,1076.3761242814,484.131219186376));
#115719=CARTESIAN_POINT('Ctrl Pts',(75.8724659623747,1076.360753094,484.233062024092));
#115720=CARTESIAN_POINT('Ctrl Pts',(75.9448308854703,1076.35552822348,484.273903400199));
#115721=CARTESIAN_POINT('Ctrl Pts',(76.0817938114949,1076.34479762919,484.369877130782));
#115722=CARTESIAN_POINT('Ctrl Pts',(76.1459002725335,1076.33931456702,484.425016201848));
#115723=CARTESIAN_POINT('Ctrl Pts',(76.3197225732954,1076.32296952879,484.60740907976));
#115724=CARTESIAN_POINT('Ctrl Pts',(76.4103329637795,1076.31229321409,484.750375695436));
#115725=CARTESIAN_POINT('Ctrl Pts',(76.531015683909,1076.29270145854,485.063100721387));
#115726=CARTESIAN_POINT('Ctrl Pts',(76.5599740863891,1076.28397745739,485.229825189004));
#115727=CARTESIAN_POINT('Ctrl Pts',(76.5517185072052,1076.26989613149,485.564613960329));
#115728=CARTESIAN_POINT('Ctrl Pts',(76.5147572621712,1076.26467144202,485.729414367033));
#115729=CARTESIAN_POINT('Ctrl Pts',(76.3794759900474,1076.25861045035,486.034912615537));
#115730=CARTESIAN_POINT('Ctrl Pts',(76.2826908660345,1076.25782084881,486.172695017995));
#115731=CARTESIAN_POINT('Ctrl Pts',(76.0418008954033,1076.26082762739,486.402974827879));
#115732=CARTESIAN_POINT('Ctrl Pts',(75.9001483641354,1076.26458439457,486.493307150367));
#115733=CARTESIAN_POINT('Ctrl Pts',(75.597171675997,1076.27580070577,486.611757669751));
#115734=CARTESIAN_POINT('Ctrl Pts',(75.4396886644151,1076.28298462186,486.64143049312));
#115735=CARTESIAN_POINT('Ctrl Pts',(75.280877750843,1076.29141182132,486.641442122854));
#115736=CARTESIAN_POINT('Origin',(75.2807843499779,1067.7251047501,485.365998005138));
#115737=CARTESIAN_POINT('',(75.2807843499779,1076.31720630032,486.041442126274));
#115738=CARTESIAN_POINT('',(75.2807843499785,1076.3720597734,484.690553884002));
#115739=CARTESIAN_POINT('Ctrl Pts',(75.2807843499779,1076.31720630032,486.041442126274));
#115740=CARTESIAN_POINT('Ctrl Pts',(75.2805672485108,1076.31721754179,486.041442126274));
#115741=CARTESIAN_POINT('Ctrl Pts',(75.2803501421419,1076.31722878769,486.041442021603));
#115742=CARTESIAN_POINT('Ctrl Pts',(75.1917003815966,1076.32182247007,486.041356538139));
#115743=CARTESIAN_POINT('Ctrl Pts',(75.1041680787943,1076.32705182337,486.02390559196));
#115744=CARTESIAN_POINT('Ctrl Pts',(74.9816429630424,1076.33538467202,485.973200491599));
#115745=CARTESIAN_POINT('Ctrl Pts',(74.9425425067788,1076.33822522788,485.952319110587));
#115746=CARTESIAN_POINT('Ctrl Pts',(74.868992635477,1076.3439444394,485.90321982519));
#115747=CARTESIAN_POINT('Ctrl Pts',(74.8347173484263,1076.3468095166,485.875118918327));
#115748=CARTESIAN_POINT('Ctrl Pts',(74.7397583913188,1076.35539801353,485.780263711893));
#115749=CARTESIAN_POINT('Ctrl Pts',(74.6894174042909,1076.36092308838,485.704551273704));
#115750=CARTESIAN_POINT('Ctrl Pts',(74.6214844176693,1076.37087259255,485.538063460784));
#115751=CARTESIAN_POINT('Ctrl Pts',(74.6044647353718,1076.37520300687,485.448984739103));
#115752=CARTESIAN_POINT('Ctrl Pts',(74.6062854402542,1076.38214292305,485.269286881598));
#115753=CARTESIAN_POINT('Ctrl Pts',(74.6251235199639,1076.38468343182,485.180471439936));
#115754=CARTESIAN_POINT('Ctrl Pts',(74.6965420898417,1076.38765532396,485.015297584075));
#115755=CARTESIAN_POINT('Ctrl Pts',(74.7484371702031,1076.38805488841,484.940630010926));
#115756=CARTESIAN_POINT('Ctrl Pts',(74.8784083840739,1076.38664140941,484.8160754338));
#115757=CARTESIAN_POINT('Ctrl Pts',(74.9551487084894,1076.3848437304,484.767436661445));
#115758=CARTESIAN_POINT('Ctrl Pts',(75.1163020148837,1076.37946891737,484.70569604598));
#115759=CARTESIAN_POINT('Ctrl Pts',(75.1982066679893,1076.37609316992,484.690553884002));
#115760=CARTESIAN_POINT('Ctrl Pts',(75.2807843499796,1076.3720597734,484.690553884002));
#115761=CARTESIAN_POINT('',(75.2807843499779,1082.7251047501,484.690553884002));
#115762=CARTESIAN_POINT('',(75.2807843499779,1067.7251047501,484.690553884002));
#115763=CARTESIAN_POINT('Origin',(75.2807843499779,1082.7251047501,485.365998005138));
#115764=CARTESIAN_POINT('Ctrl Pts',(75.280789999719,1076.37205949745,484.690553884025));
#115765=CARTESIAN_POINT('Ctrl Pts',(75.3707000073535,1076.36766793225,484.690554636076));
#115766=CARTESIAN_POINT('Ctrl Pts',(75.4596792503472,1076.36257979634,484.70850687006));
#115767=CARTESIAN_POINT('Ctrl Pts',(75.583088663004,1076.3543701819,484.760379032669));
#115768=CARTESIAN_POINT('Ctrl Pts',(75.6218987573435,1076.35158916811,484.781359211578));
#115769=CARTESIAN_POINT('Ctrl Pts',(75.6949764250228,1076.34593312118,484.830631809924));
#115770=CARTESIAN_POINT('Ctrl Pts',(75.72905860543,1076.3430712256,484.858827298119));
#115771=CARTESIAN_POINT('Ctrl Pts',(75.8232814843969,1076.33443099212,484.953744755188));
#115772=CARTESIAN_POINT('Ctrl Pts',(75.8731450516467,1076.32877074794,485.029291833927));
#115773=CARTESIAN_POINT('Ctrl Pts',(75.9400871324703,1076.31846592261,485.194532351811));
#115774=CARTESIAN_POINT('Ctrl Pts',(75.9568871292005,1076.31391088546,485.282465231146));
#115775=CARTESIAN_POINT('Ctrl Pts',(75.9555319465901,1076.3065277786,485.459647670252));
#115776=CARTESIAN_POINT('Ctrl Pts',(75.9374739089418,1076.30376858818,485.54717153329));
#115777=CARTESIAN_POINT('Ctrl Pts',(75.8686767856061,1076.30047573724,485.710100362392));
#115778=CARTESIAN_POINT('Ctrl Pts',(75.8186964139097,1076.29996918873,485.783941474256));
#115779=CARTESIAN_POINT('Ctrl Pts',(75.6932153305394,1076.30129870733,485.908131174528));
#115780=CARTESIAN_POINT('Ctrl Pts',(75.6189735970548,1076.30311868741,485.957291787176));
#115781=CARTESIAN_POINT('Ctrl Pts',(75.4559510433341,1076.30882414188,486.024250034985));
#115782=CARTESIAN_POINT('Ctrl Pts',(75.3687702480181,1076.31265041163,486.041442126274));
#115783=CARTESIAN_POINT('Ctrl Pts',(75.2807843499779,1076.31720630032,486.041442126274));
#115784=CARTESIAN_POINT('Origin',(73.793809237574,1067.7251047501,499.135789645571));
#115785=CARTESIAN_POINT('',(73.7938092375738,1077.74530255756,498.036958509579));
#115786=CARTESIAN_POINT('Ctrl Pts',(73.7933312060954,1077.58423708672,500.234620677583));
#115787=CARTESIAN_POINT('Ctrl Pts',(73.9124417122508,1077.57535459326,500.234672494987));
#115788=CARTESIAN_POINT('Ctrl Pts',(74.0308689479815,1077.56794487714,500.215357137192));
#115789=CARTESIAN_POINT('Ctrl Pts',(74.2455323814251,1077.55730469832,500.143192444516));
#115790=CARTESIAN_POINT('Ctrl Pts',(74.3416181649181,1077.55378480492,500.094351536102));
#115791=CARTESIAN_POINT('Ctrl Pts',(74.4565106494304,1077.55132489931,500.012934102364));
#115792=CARTESIAN_POINT('Ctrl Pts',(74.4829842327755,1077.55090110402,499.99229046815));
#115793=CARTESIAN_POINT('Ctrl Pts',(74.5235558786957,1077.55048740021,499.957552367046));
#115794=CARTESIAN_POINT('Ctrl Pts',(74.5382860581984,1077.55039106666,499.944231613654));
#115795=CARTESIAN_POINT('Ctrl Pts',(74.5651350992939,1077.55031863288,499.918595112909));
#115796=CARTESIAN_POINT('Ctrl Pts',(74.5773400221384,1077.55032849672,499.906378700872));
#115797=CARTESIAN_POINT('Ctrl Pts',(74.6040202414769,1077.55044811783,499.878383895092));
#115798=CARTESIAN_POINT('Ctrl Pts',(74.6183322385584,1077.5505812347,499.862460048817));
#115799=CARTESIAN_POINT('Ctrl Pts',(74.6583280431628,1077.55115878803,499.815255968473));
#115800=CARTESIAN_POINT('Ctrl Pts',(74.6827587200317,1077.55177444295,499.782964649903));
#115801=CARTESIAN_POINT('Ctrl Pts',(74.7871428356671,1077.55570285974,499.627898763944));
#115802=CARTESIAN_POINT('Ctrl Pts',(74.8437564074959,1077.56181746199,499.491359554758));
#115803=CARTESIAN_POINT('Ctrl Pts',(74.8947463817484,1077.5775952898,499.232123340022));
#115804=CARTESIAN_POINT('Ctrl Pts',(74.8987087598206,1077.58623675781,499.113576373838));
#115805=CARTESIAN_POINT('Ctrl Pts',(74.8675108231822,1077.60689745236,498.868971232424));
#115806=CARTESIAN_POINT('Ctrl Pts',(74.8288763505096,1077.6189982519,498.745127096819));
#115807=CARTESIAN_POINT('Ctrl Pts',(74.7060676945397,1077.64561593364,498.50775612588));
#115808=CARTESIAN_POINT('Ctrl Pts',(74.6196650193212,1077.66001519281,498.397824330894));
#115809=CARTESIAN_POINT('Ctrl Pts',(74.4051453040325,1077.6891943188,498.211151157411));
#115810=CARTESIAN_POINT('Ctrl Pts',(74.2771365204911,1077.70367567654,498.138227235733));
#115811=CARTESIAN_POINT('Ctrl Pts',(74.0045179663677,1077.72961144853,498.04815261718));
#115812=CARTESIAN_POINT('Ctrl Pts',(73.8630878151982,1077.74091504749,498.03006538966));
#115813=CARTESIAN_POINT('Ctrl Pts',(73.5963567766027,1077.75846984418,498.047537720141));
#115814=CARTESIAN_POINT('Ctrl Pts',(73.4729816321844,1077.76500965731,498.07730234913));
#115815=CARTESIAN_POINT('Ctrl Pts',(73.2807891581509,1077.77257860996,498.160501310288));
#115816=CARTESIAN_POINT('Ctrl Pts',(73.2082936732639,1077.77469880566,498.202218013958));
#115817=CARTESIAN_POINT('Ctrl Pts',(73.1171600973508,1077.77631811587,498.269493681862));
#115818=CARTESIAN_POINT('Ctrl Pts',(73.0938526270263,1077.77662537978,498.288214489695));
#115819=CARTESIAN_POINT('Ctrl Pts',(73.0570919810898,1077.77693018569,498.320292888793));
#115820=CARTESIAN_POINT('Ctrl Pts',(73.0431705850289,1077.77699998709,498.333088641093));
#115821=CARTESIAN_POINT('Ctrl Pts',(73.0170663092033,1077.77704117233,498.358355477605));
#115822=CARTESIAN_POINT('Ctrl Pts',(73.0048365180837,1077.77701983419,498.3707697071));
#115823=CARTESIAN_POINT('Ctrl Pts',(72.9774240097596,1077.7768764149,498.399952407309));
#115824=CARTESIAN_POINT('Ctrl Pts',(72.9624537206654,1077.77672625258,498.41690909654));
#115825=CARTESIAN_POINT('Ctrl Pts',(72.9181924867336,1077.77605439487,498.470276373843));
#115826=CARTESIAN_POINT('Ctrl Pts',(72.8906941389063,1077.77530802723,498.50809954657));
#115827=CARTESIAN_POINT('Ctrl Pts',(72.7876611654125,1077.77103914359,498.670665207963));
#115828=CARTESIAN_POINT('Ctrl Pts',(72.7349598832007,1077.76503245415,498.807987674773));
#115829=CARTESIAN_POINT('Ctrl Pts',(72.6905343401532,1077.74961802217,499.069095452969));
#115830=CARTESIAN_POINT('Ctrl Pts',(72.689826709024,1077.74112156295,499.189088494081));
#115831=CARTESIAN_POINT('Ctrl Pts',(72.7286200299827,1077.72071914054,499.43538852032));
#115832=CARTESIAN_POINT('Ctrl Pts',(72.7715699371,1077.70872794931,499.559305581308));
#115833=CARTESIAN_POINT('Ctrl Pts',(72.9036580323554,1077.68212244327,499.795134127343));
#115834=CARTESIAN_POINT('Ctrl Pts',(72.9949874731787,1077.66761150533,499.903233977721));
#115835=CARTESIAN_POINT('Ctrl Pts',(73.1930481878229,1077.64141292084,500.062914038606));
#115836=CARTESIAN_POINT('Ctrl Pts',(73.2926259662991,1077.62985494095,500.12032369341));
#115837=CARTESIAN_POINT('Ctrl Pts',(73.5249304671283,1077.60607303618,500.209686272067));
#115838=CARTESIAN_POINT('Ctrl Pts',(73.6584913990223,1077.59429257002,500.234562017361));
#115839=CARTESIAN_POINT('Ctrl Pts',(73.7933312060954,1077.58423708672,500.234620677583));
#115840=CARTESIAN_POINT('',(73.7938092375516,1075.73511330977,498.036958509579));
#115841=CARTESIAN_POINT('',(73.793809237574,1067.7251047501,498.036958509579));
#115842=CARTESIAN_POINT('Ctrl Pts',(73.7943431628175,1075.57249684997,500.234620651846));
#115843=CARTESIAN_POINT('Ctrl Pts',(73.6506175246825,1075.58330219327,500.23469048856));
#115844=CARTESIAN_POINT('Ctrl Pts',(73.5084060437648,1075.59608072594,500.206563734191));
#115845=CARTESIAN_POINT('Ctrl Pts',(73.2422667990826,1075.62408715031,500.097069246554));
#115846=CARTESIAN_POINT('Ctrl Pts',(73.120965264772,1075.63906256478,500.016420972424));
#115847=CARTESIAN_POINT('Ctrl Pts',(72.9676850470399,1075.66158528276,499.863893253268));
#115848=CARTESIAN_POINT('Ctrl Pts',(72.9217478532435,1075.6690461048,499.808194085901));
#115849=CARTESIAN_POINT('Ctrl Pts',(72.8001152687884,1075.69119911753,499.627072426163));
#115850=CARTESIAN_POINT('Ctrl Pts',(72.7435967681914,1075.70521824599,499.490618477095));
#115851=CARTESIAN_POINT('Ctrl Pts',(72.6874998082093,1075.72998009466,499.204202457804));
#115852=CARTESIAN_POINT('Ctrl Pts',(72.6881438427515,1075.74050139934,499.05713036763));
#115853=CARTESIAN_POINT('Ctrl Pts',(72.7468740496821,1075.75677397741,498.77169592508));
#115854=CARTESIAN_POINT('Ctrl Pts',(72.8043087950933,1075.76236876971,498.636207548035));
#115855=CARTESIAN_POINT('Ctrl Pts',(72.9688874035406,1075.76790839337,498.395375264388));
#115856=CARTESIAN_POINT('Ctrl Pts',(73.0743576562249,1075.76779510899,498.292523538431));
#115857=CARTESIAN_POINT('Ctrl Pts',(73.3192403672629,1075.76181406095,498.134053144044));
#115858=CARTESIAN_POINT('Ctrl Pts',(73.4561199949375,1075.75600891844,498.08004344579));
#115859=CARTESIAN_POINT('Ctrl Pts',(73.7429349984395,1075.7393569208,498.028496799552));
#115860=CARTESIAN_POINT('Ctrl Pts',(73.8899851476081,1075.72866956609,498.031546297141));
#115861=CARTESIAN_POINT('Ctrl Pts',(74.174944804702,1075.70364040769,498.094830441354));
#115862=CARTESIAN_POINT('Ctrl Pts',(74.3099702953708,1075.68952223951,498.154781690339));
#115863=CARTESIAN_POINT('Ctrl Pts',(74.4878092140052,1075.66731262955,498.280834008654));
#115864=CARTESIAN_POINT('Ctrl Pts',(74.5421696666241,1075.65986224754,498.327990547762));
#115865=CARTESIAN_POINT('Ctrl Pts',(74.6920987469502,1075.63714734461,498.486260647984));
#115866=CARTESIAN_POINT('Ctrl Pts',(74.7705033963861,1075.62200641361,498.61146960579));
#115867=CARTESIAN_POINT('Ctrl Pts',(74.8730752789762,1075.59392129564,498.883739892678));
#115868=CARTESIAN_POINT('Ctrl Pts',(74.8968920458942,1075.58122242146,499.027943543766));
#115869=CARTESIAN_POINT('Ctrl Pts',(74.8871731536858,1075.56000737385,499.316724330229));
#115870=CARTESIAN_POINT('Ctrl Pts',(74.8540577792207,1075.55167687336,499.458485925363));
#115871=CARTESIAN_POINT('Ctrl Pts',(74.7351518794729,1075.54063425143,499.720481415376));
#115872=CARTESIAN_POINT('Ctrl Pts',(74.6508834236155,1075.5379977505,499.838244773477));
#115873=CARTESIAN_POINT('Ctrl Pts',(74.4421058838755,1075.53880709932,500.034452359883));
#115874=CARTESIAN_POINT('Ctrl Pts',(74.3198178645823,1075.54222455647,500.111064665783));
#115875=CARTESIAN_POINT('Ctrl Pts',(74.061089762638,1075.55425587424,500.210023985928));
#115876=CARTESIAN_POINT('Ctrl Pts',(73.9282217980015,1075.56243180778,500.23455559982));
#115877=CARTESIAN_POINT('Ctrl Pts',(73.7943431628175,1075.57249684997,500.234620651846));
#115878=CARTESIAN_POINT('Origin',(73.793809237574,1067.7251047501,499.135789645571));
#115879=CARTESIAN_POINT('',(73.793809237574,1075.61827177418,499.634620781564));
#115880=CARTESIAN_POINT('',(73.7938092375747,1075.69207332612,498.636958509579));
#115881=CARTESIAN_POINT('Ctrl Pts',(73.7938092375739,1075.61827177418,499.634620781564));
#115882=CARTESIAN_POINT('Ctrl Pts',(73.7913850280998,1075.61845153324,499.634620781564));
#115883=CARTESIAN_POINT('Ctrl Pts',(73.7889601060211,1075.61863265287,499.634603109896));
#115884=CARTESIAN_POINT('Ctrl Pts',(73.721225695092,1075.62372835527,499.633615217395));
#115885=CARTESIAN_POINT('Ctrl Pts',(73.6567987396114,1075.62952376564,499.619846996068));
#115886=CARTESIAN_POINT('Ctrl Pts',(73.5366576718624,1075.64222522068,499.568229107957));
#115887=CARTESIAN_POINT('Ctrl Pts',(73.4821309605372,1075.64901660974,499.530734949376));
#115888=CARTESIAN_POINT('Ctrl Pts',(73.3898621684334,1075.66278401858,499.43597876458));
#115889=CARTESIAN_POINT('Ctrl Pts',(73.3533473110501,1075.66962750127,499.379280500382));
#115890=CARTESIAN_POINT('Ctrl Pts',(73.3049263756146,1075.68227121177,499.255132621402));
#115891=CARTESIAN_POINT('Ctrl Pts',(73.2933698982706,1075.6879534161,499.188952422037));
#115892=CARTESIAN_POINT('Ctrl Pts',(73.2969399182935,1075.69740214851,499.056065581121));
#115893=CARTESIAN_POINT('Ctrl Pts',(73.3119394658212,1075.70108093001,498.990695929044));
#115894=CARTESIAN_POINT('Ctrl Pts',(73.366709024541,1075.70594176922,498.869661300972));
#115895=CARTESIAN_POINT('Ctrl Pts',(73.4058829075062,1075.70707737461,498.815231302157));
#115896=CARTESIAN_POINT('Ctrl Pts',(73.502255851258,1075.70663762081,498.725841807686));
#115897=CARTESIAN_POINT('Ctrl Pts',(73.5580969989074,1075.70512317638,498.69138749117));
#115898=CARTESIAN_POINT('Ctrl Pts',(73.6749146300443,1075.69988437989,498.647662390977));
#115899=CARTESIAN_POINT('Ctrl Pts',(73.7341467464272,1075.69639019611,498.636958509579));
#115900=CARTESIAN_POINT('Ctrl Pts',(73.7938092375755,1075.69207332612,498.636958509579));
#115901=CARTESIAN_POINT('',(73.793809237574,1082.7251047501,498.636958509579));
#115902=CARTESIAN_POINT('',(73.793809237574,1067.7251047501,498.636958509579));
#115903=CARTESIAN_POINT('Origin',(73.793809237574,1082.7251047501,499.135789645571));
#115904=CARTESIAN_POINT('Ctrl Pts',(73.7938092375755,1075.69207332612,498.636958509579));
#115905=CARTESIAN_POINT('Ctrl Pts',(73.7938800001328,1075.6920682061,498.636958509579));
#115906=CARTESIAN_POINT('Ctrl Pts',(73.7939507632939,1075.69206308491,498.636958524932));
#115907=CARTESIAN_POINT('Ctrl Pts',(73.7940215270573,1075.69205796258,498.636958555047));
#115908=CARTESIAN_POINT('Ctrl Pts',(73.8606121962174,1075.68723770921,498.636986894369));
#115909=CARTESIAN_POINT('Ctrl Pts',(73.9264607334969,1075.68148464659,498.650347571099));
#115910=CARTESIAN_POINT('Ctrl Pts',(74.0492569028667,1075.66874103527,498.70215111076));
#115911=CARTESIAN_POINT('Ctrl Pts',(74.1049458244209,1075.66186959979,498.74021065917));
#115912=CARTESIAN_POINT('Ctrl Pts',(74.1981819534008,1075.64794210248,498.836115794799));
#115913=CARTESIAN_POINT('Ctrl Pts',(74.2347495868739,1075.64102167646,498.893096125891));
#115914=CARTESIAN_POINT('Ctrl Pts',(74.282658541406,1075.62827460122,499.016788074975));
#115915=CARTESIAN_POINT('Ctrl Pts',(74.2940762066304,1075.62254889527,499.082087367716));
#115916=CARTESIAN_POINT('Ctrl Pts',(74.2909250966268,1075.6129706565,499.21310637812));
#115917=CARTESIAN_POINT('Ctrl Pts',(74.2765328430183,1075.60920138255,499.277548944007));
#115918=CARTESIAN_POINT('Ctrl Pts',(74.2237659659103,1075.604155167,499.3969506414));
#115919=CARTESIAN_POINT('Ctrl Pts',(74.1860540023914,1075.60291434053,499.450778478515));
#115920=CARTESIAN_POINT('Ctrl Pts',(74.0921557874047,1075.60313681649,499.540810307316));
#115921=CARTESIAN_POINT('Ctrl Pts',(74.0369543903032,1075.6045910064,499.576159751426));
#115922=CARTESIAN_POINT('Ctrl Pts',(73.9182848271023,1075.60991048372,499.622883923426));
#115923=CARTESIAN_POINT('Ctrl Pts',(73.8562836600276,1075.61363919447,499.634620781564));
#115924=CARTESIAN_POINT('Ctrl Pts',(73.7938092375739,1075.61827177418,499.634620781564));
#115925=CARTESIAN_POINT('Origin',(69.4825522658044,1067.7251047501,512.441691281815));
#115926=CARTESIAN_POINT('',(69.4825522658043,1076.93351373127,511.351150533087));
#115927=CARTESIAN_POINT('Ctrl Pts',(69.4826078971758,1076.70383791337,513.532232029124));
#115928=CARTESIAN_POINT('Ctrl Pts',(69.6122669881504,1076.69283316808,513.53222541487));
#115929=CARTESIAN_POINT('Ctrl Pts',(69.741060928863,1076.68435581015,513.509095376724));
#115930=CARTESIAN_POINT('Ctrl Pts',(69.9252523092832,1076.67604351272,513.440551985081));
#115931=CARTESIAN_POINT('Ctrl Pts',(69.9853778208891,1076.67402815309,513.411680414185));
#115932=CARTESIAN_POINT('Ctrl Pts',(70.0659665877485,1076.67235331882,513.363457985195));
#115933=CARTESIAN_POINT('Ctrl Pts',(70.0888854128759,1076.67200602563,513.348546524656));
#115934=CARTESIAN_POINT('Ctrl Pts',(70.124835040167,1076.67167395825,513.323184078409));
#115935=CARTESIAN_POINT('Ctrl Pts',(70.1382272484212,1076.67160062657,513.313268612612));
#115936=CARTESIAN_POINT('Ctrl Pts',(70.1654174322554,1076.67155755931,513.292155757156));
#115937=CARTESIAN_POINT('Ctrl Pts',(70.1791792986112,1076.67159500289,513.280920348107));
#115938=CARTESIAN_POINT('Ctrl Pts',(70.2104971720501,1076.6718205056,513.254050609814));
#115939=CARTESIAN_POINT('Ctrl Pts',(70.2278337040877,1076.67205325521,513.238175394666));
#115940=CARTESIAN_POINT('Ctrl Pts',(70.2805377597367,1076.67310876059,513.186685545547));
#115941=CARTESIAN_POINT('Ctrl Pts',(70.313961178618,1076.6743000496,513.149189903141));
#115942=CARTESIAN_POINT('Ctrl Pts',(70.433096754109,1076.68071441277,512.995396899938));
#115943=CARTESIAN_POINT('Ctrl Pts',(70.4978496578637,1076.68924152534,512.864994581949));
#115944=CARTESIAN_POINT('Ctrl Pts',(70.5663203402181,1076.71064373906,512.61141627984));
#115945=CARTESIAN_POINT('Ctrl Pts',(70.5783051673573,1076.72234162312,512.492743699219));
#115946=CARTESIAN_POINT('Ctrl Pts',(70.563071319087,1076.75002822772,512.245448508246));
#115947=CARTESIAN_POINT('Ctrl Pts',(70.5321875212895,1076.76610081385,512.118852361795));
#115948=CARTESIAN_POINT('Ctrl Pts',(70.423597375804,1076.80122707127,511.873231550895));
#115949=CARTESIAN_POINT('Ctrl Pts',(70.343309627338,1076.82011063196,511.757732408011));
#115950=CARTESIAN_POINT('Ctrl Pts',(70.1397826128885,1076.85782792288,511.559489641262));
#115951=CARTESIAN_POINT('Ctrl Pts',(70.0169040425762,1076.87627986179,511.480032211021));
#115952=CARTESIAN_POINT('Ctrl Pts',(69.7531366181056,1076.90878354048,511.376224666224));
#115953=CARTESIAN_POINT('Ctrl Pts',(69.6156653127265,1076.92271222959,511.350437098259));
#115954=CARTESIAN_POINT('Ctrl Pts',(69.346538439072,1076.94455379086,511.351849166121));
#115955=CARTESIAN_POINT('Ctrl Pts',(69.217258819437,1076.95260568815,511.37587845933));
#115956=CARTESIAN_POINT('Ctrl Pts',(69.0345315832573,1076.96033083147,511.445315644274));
#115957=CARTESIAN_POINT('Ctrl Pts',(68.976051749935,1076.96216491322,511.47372976735));
#115958=CARTESIAN_POINT('Ctrl Pts',(68.8973958977383,1076.96369723817,511.521042754245));
#115959=CARTESIAN_POINT('Ctrl Pts',(68.8748803697039,1076.96401668945,511.535746077119));
#115960=CARTESIAN_POINT('Ctrl Pts',(68.8394765478094,1076.96432238444,511.560780253401));
#115961=CARTESIAN_POINT('Ctrl Pts',(68.8262402256117,1076.96438970056,511.57059706391));
#115962=CARTESIAN_POINT('Ctrl Pts',(68.7993082234047,1076.96442783105,511.591533821189));
#115963=CARTESIAN_POINT('Ctrl Pts',(68.7856498519398,1076.96439152585,511.602693579264));
#115964=CARTESIAN_POINT('Ctrl Pts',(68.7544786491073,1076.96417654197,511.62944897881));
#115965=CARTESIAN_POINT('Ctrl Pts',(68.7371868096006,1076.96395496499,511.645287492151));
#115966=CARTESIAN_POINT('Ctrl Pts',(68.684337732467,1076.96294594852,511.696924573239));
#115967=CARTESIAN_POINT('Ctrl Pts',(68.6507528556428,1076.96180203104,511.734632888165));
#115968=CARTESIAN_POINT('Ctrl Pts',(68.5315755127396,1076.95565562866,511.888728652044));
#115969=CARTESIAN_POINT('Ctrl Pts',(68.4669153471803,1076.94750162141,512.019194209781));
#115970=CARTESIAN_POINT('Ctrl Pts',(68.3985531773248,1076.92686605912,512.273197251867));
#115971=CARTESIAN_POINT('Ctrl Pts',(68.3866861996268,1076.91552292664,512.392249928602));
#115972=CARTESIAN_POINT('Ctrl Pts',(68.4024229816617,1076.88846020786,512.640424938139));
#115973=CARTESIAN_POINT('Ctrl Pts',(68.4337620374989,1076.87263882435,512.767474808657));
#115974=CARTESIAN_POINT('Ctrl Pts',(68.5436959760718,1076.8377331556,513.013954870388));
#115975=CARTESIAN_POINT('Ctrl Pts',(68.6249513056033,1076.81879458981,513.12975867381));
#115976=CARTESIAN_POINT('Ctrl Pts',(68.815604926498,1076.78344747383,513.313466635032));
#115977=CARTESIAN_POINT('Ctrl Pts',(68.919582257624,1076.76723503197,513.383988540194));
#115978=CARTESIAN_POINT('Ctrl Pts',(69.0976126242619,1076.74366820895,513.464471225474));
#115979=CARTESIAN_POINT('Ctrl Pts',(69.1646234271701,1076.73558041456,513.487250429895));
#115980=CARTESIAN_POINT('Ctrl Pts',(69.3150133891904,1076.71909139178,513.522539992064));
#115981=CARTESIAN_POINT('Ctrl Pts',(69.3986264979972,1076.71096578925,513.532236313237));
#115982=CARTESIAN_POINT('Ctrl Pts',(69.4826078971757,1076.70383791337,513.532232029124));
#115983=CARTESIAN_POINT('',(69.4825522657769,1074.91619351132,511.351150533086));
#115984=CARTESIAN_POINT('',(69.4825522658044,1067.7251047501,511.351150533086));
#115985=CARTESIAN_POINT('Ctrl Pts',(69.4820444016945,1074.68466440541,513.532231912287));
#115986=CARTESIAN_POINT('Ctrl Pts',(69.3394705209171,1074.69687223284,513.532165515717));
#115987=CARTESIAN_POINT('Ctrl Pts',(69.1985379162362,1074.71192877342,513.504145529219));
#115988=CARTESIAN_POINT('Ctrl Pts',(68.9344311812239,1074.74606446002,513.395339502725));
#115989=CARTESIAN_POINT('Ctrl Pts',(68.8139383864327,1074.76485862075,513.315053679255));
#115990=CARTESIAN_POINT('Ctrl Pts',(68.6619976213376,1074.79379438774,513.163531925989));
#115991=CARTESIAN_POINT('Ctrl Pts',(68.6165657547483,1074.80347559918,513.108348181927));
#115992=CARTESIAN_POINT('Ctrl Pts',(68.4961976649056,1074.8325900277,512.92887515516));
#115993=CARTESIAN_POINT('Ctrl Pts',(68.4402223128954,1074.85151852095,512.793644469373));
#115994=CARTESIAN_POINT('Ctrl Pts',(68.3846015740659,1074.88595897511,512.509637830926));
#115995=CARTESIAN_POINT('Ctrl Pts',(68.3852108393213,1074.90115966746,512.363650922729));
#115996=CARTESIAN_POINT('Ctrl Pts',(68.443601734931,1074.92589973294,512.079989476065));
#115997=CARTESIAN_POINT('Ctrl Pts',(68.5007943994584,1074.93519072691,511.945190126555));
#115998=CARTESIAN_POINT('Ctrl Pts',(68.6628914927086,1074.94642867149,511.708550178006));
#115999=CARTESIAN_POINT('Ctrl Pts',(68.764964210655,1074.94843806051,511.60836412095));
#116000=CARTESIAN_POINT('Ctrl Pts',(69.0019088635042,1074.94515900181,511.452559146278));
#116001=CARTESIAN_POINT('Ctrl Pts',(69.1343968809284,1074.93989756299,511.398561240073));
#116002=CARTESIAN_POINT('Ctrl Pts',(69.4156680715146,1074.9224947882,511.343590363771));
#116003=CARTESIAN_POINT('Ctrl Pts',(69.5618379405238,1074.91037210208,511.344477112535));
#116004=CARTESIAN_POINT('Ctrl Pts',(69.8451847015609,1074.88081983878,511.403062532666));
#116005=CARTESIAN_POINT('Ctrl Pts',(69.9795342445981,1074.86367019389,511.460293514152));
#116006=CARTESIAN_POINT('Ctrl Pts',(70.1571436095353,1074.83603585489,511.581909187756));
#116007=CARTESIAN_POINT('Ctrl Pts',(70.2115395624646,1074.8266691463,511.627523778567));
#116008=CARTESIAN_POINT('Ctrl Pts',(70.3108605259358,1074.80762135251,511.728787369085));
#116009=CARTESIAN_POINT('Ctrl Pts',(70.3555302526697,1074.79798169931,511.784245543407));
#116010=CARTESIAN_POINT('Ctrl Pts',(70.4747269729781,1074.76860477466,511.966004496857));
#116011=CARTESIAN_POINT('Ctrl Pts',(70.5295976336062,1074.74926883606,512.103373722146));
#116012=CARTESIAN_POINT('Ctrl Pts',(70.5812274960528,1074.71422832265,512.388845353581));
#116013=CARTESIAN_POINT('Ctrl Pts',(70.5786812208422,1074.69878838845,512.533982227166));
#116014=CARTESIAN_POINT('Ctrl Pts',(70.517467466125,1074.67375549784,512.813910243385));
#116015=CARTESIAN_POINT('Ctrl Pts',(70.4599660560575,1074.66435260242,512.946048139922));
#116016=CARTESIAN_POINT('Ctrl Pts',(70.2976701742277,1074.65290348342,513.179891536469));
#116017=CARTESIAN_POINT('Ctrl Pts',(70.1949339328048,1074.65091110759,513.279484386364));
#116018=CARTESIAN_POINT('Ctrl Pts',(69.9572467919293,1074.65459479166,513.433643157594));
#116019=CARTESIAN_POINT('Ctrl Pts',(69.8247872974603,1074.66021707146,513.486728871373));
#116020=CARTESIAN_POINT('Ctrl Pts',(69.6187299662236,1074.67364883709,513.525862309228));
#116021=CARTESIAN_POINT('Ctrl Pts',(69.5504341427086,1074.67880856315,513.532263761348));
#116022=CARTESIAN_POINT('Ctrl Pts',(69.4820444016944,1074.68466440541,513.532231912287));
#116023=CARTESIAN_POINT('Origin',(69.4825522658044,1067.7251047501,512.441691281815));
#116024=CARTESIAN_POINT('',(69.4825522658045,1074.74977363876,512.932232030543));
#116025=CARTESIAN_POINT('',(69.4825522658044,1074.85393827482,511.951150533086));
#116026=CARTESIAN_POINT('Ctrl Pts',(69.4825522658045,1074.74977363876,512.932232030543));
#116027=CARTESIAN_POINT('Ctrl Pts',(69.449079001942,1074.75260930569,512.932232030543));
#116028=CARTESIAN_POINT('Ctrl Pts',(69.4156422604509,1074.75580684056,512.928805735255));
#116029=CARTESIAN_POINT('Ctrl Pts',(69.3196946475562,1074.76605381396,512.908872049097));
#116030=CARTESIAN_POINT('Ctrl Pts',(69.2599081233851,1074.7738132317,512.883491244156));
#116031=CARTESIAN_POINT('Ctrl Pts',(69.1802249341963,1074.78629861362,512.829324110509));
#116032=CARTESIAN_POINT('Ctrl Pts',(69.1555178518989,1074.79057166016,512.808717383512));
#116033=CARTESIAN_POINT('Ctrl Pts',(69.1105321240183,1074.79921186373,512.763028191438));
#116034=CARTESIAN_POINT('Ctrl Pts',(69.090346984417,1074.80355955703,512.738054954091));
#116035=CARTESIAN_POINT('Ctrl Pts',(69.0368499035733,1074.81667515841,512.656736030347));
#116036=CARTESIAN_POINT('Ctrl Pts',(69.0121780541397,1074.82522094721,512.595505966556));
#116037=CARTESIAN_POINT('Ctrl Pts',(68.9883421325934,1074.84078388337,512.467035695293));
#116038=CARTESIAN_POINT('Ctrl Pts',(68.9893356107765,1074.8476554736,512.401053500535));
#116039=CARTESIAN_POINT('Ctrl Pts',(69.017058142962,1074.85872061286,512.27401364987));
#116040=CARTESIAN_POINT('Ctrl Pts',(69.0431699591804,1074.86283865761,512.214168299575));
#116041=CARTESIAN_POINT('Ctrl Pts',(69.1166676980363,1074.86779966899,512.108797235077));
#116042=CARTESIAN_POINT('Ctrl Pts',(69.1629663043581,1074.86864416037,512.064120133381));
#116043=CARTESIAN_POINT('Ctrl Pts',(69.2701100198263,1074.86700441952,511.994964613161));
#116044=CARTESIAN_POINT('Ctrl Pts',(69.3298661792914,1074.86453637549,511.971192686971));
#116045=CARTESIAN_POINT('Ctrl Pts',(69.4221751405219,1074.858671246,511.953941216856));
#116046=CARTESIAN_POINT('Ctrl Pts',(69.4523419826411,1074.85645423452,511.951150631426));
#116047=CARTESIAN_POINT('Ctrl Pts',(69.4825506689621,1074.85393840781,511.951150533089));
#116048=CARTESIAN_POINT('',(69.4825522658044,1082.7251047501,511.951150533086));
#116049=CARTESIAN_POINT('',(69.4825522658044,1067.7251047501,511.951150533086));
#116050=CARTESIAN_POINT('Origin',(69.4825522658044,1082.7251047501,512.441691281815));
#116051=CARTESIAN_POINT('Ctrl Pts',(69.4825522658042,1074.85393827482,511.951150533086));
#116052=CARTESIAN_POINT('Ctrl Pts',(69.5480076026392,1074.8484870293,511.951150533086));
#116053=CARTESIAN_POINT('Ctrl Pts',(69.6126865705572,1074.84171403297,511.964248612907));
#116054=CARTESIAN_POINT('Ctrl Pts',(69.7331209623984,1074.82629764847,512.014929237526));
#116055=CARTESIAN_POINT('Ctrl Pts',(69.7876777637123,1074.81779887447,512.052086079148));
#116056=CARTESIAN_POINT('Ctrl Pts',(69.8556816419551,1074.80471537265,512.121648042885));
#116057=CARTESIAN_POINT('Ctrl Pts',(69.8757492299989,1074.80037531797,512.146650205093));
#116058=CARTESIAN_POINT('Ctrl Pts',(69.9291246522644,1074.78720272623,512.228362682958));
#116059=CARTESIAN_POINT('Ctrl Pts',(69.9536570560271,1074.77856974081,512.289994969465));
#116060=CARTESIAN_POINT('Ctrl Pts',(69.9768429254042,1074.76288232822,512.418650406565));
#116061=CARTESIAN_POINT('Ctrl Pts',(69.9755636053974,1074.7559614686,512.484375975875));
#116062=CARTESIAN_POINT('Ctrl Pts',(69.9475407365004,1074.74482450298,512.61056883289));
#116063=CARTESIAN_POINT('Ctrl Pts',(69.9215175585826,1074.74067272418,512.669872078126));
#116064=CARTESIAN_POINT('Ctrl Pts',(69.8482518897609,1074.73563614165,512.774790752987));
#116065=CARTESIAN_POINT('Ctrl Pts',(69.8019190784616,1074.73477696069,512.819450070359));
#116066=CARTESIAN_POINT('Ctrl Pts',(69.6947818169604,1074.7364624146,512.888508879183));
#116067=CARTESIAN_POINT('Ctrl Pts',(69.6350868502195,1074.7389856868,512.912228790736));
#116068=CARTESIAN_POINT('Ctrl Pts',(69.542803701313,1074.744964776,512.929459774938));
#116069=CARTESIAN_POINT('Ctrl Pts',(69.5126632077471,1074.74722280885,512.932232030543));
#116070=CARTESIAN_POINT('Ctrl Pts',(69.4825522658045,1074.74977363876,512.932232030543));
#116071=CARTESIAN_POINT('Origin',(83.8577571500221,1067.7251047501,456.061503599423));
#116072=CARTESIAN_POINT('',(83.8577571500471,1078.68595559847,454.58320046723));
#116073=CARTESIAN_POINT('Ctrl Pts',(83.857895722855,1078.6591843157,457.539806725122));
#116074=CARTESIAN_POINT('Ctrl Pts',(84.0501826867988,1078.65404884633,457.539788700571));
#116075=CARTESIAN_POINT('Ctrl Pts',(84.2406408333334,1078.64908129588,457.502253888277));
#116076=CARTESIAN_POINT('Ctrl Pts',(84.5743214387011,1078.64088084795,457.365440788119));
#116077=CARTESIAN_POINT('Ctrl Pts',(84.718037646745,1078.63757322054,457.275440178014));
#116078=CARTESIAN_POINT('Ctrl Pts',(84.9597562330392,1078.63267847603,457.059157454937));
#116079=CARTESIAN_POINT('Ctrl Pts',(85.0588207078151,1078.6310153872,456.937383861936));
#116080=CARTESIAN_POINT('Ctrl Pts',(85.1596304165353,1078.62990767214,456.7633181193));
#116081=CARTESIAN_POINT('Ctrl Pts',(85.1804514808721,1078.6297267007,456.723241749134));
#116082=CARTESIAN_POINT('Ctrl Pts',(85.2104913314188,1078.62954871999,456.658317834723));
#116083=CARTESIAN_POINT('Ctrl Pts',(85.2209326799639,1078.62950655315,456.634067548322));
#116084=CARTESIAN_POINT('Ctrl Pts',(85.239011086755,1078.62947224598,456.588777709061));
#116085=CARTESIAN_POINT('Ctrl Pts',(85.2468305538254,1078.6294734533,456.567819215659));
#116086=CARTESIAN_POINT('Ctrl Pts',(85.2630399000802,1078.62951352662,456.521167252621));
#116087=CARTESIAN_POINT('Ctrl Pts',(85.27120684045,1078.62956017016,456.495404797611));
#116088=CARTESIAN_POINT('Ctrl Pts',(85.292214551982,1078.62976095209,456.422230426666));
#116089=CARTESIAN_POINT('Ctrl Pts',(85.3034053828301,1078.6299716987,456.37438217292));
#116090=CARTESIAN_POINT('Ctrl Pts',(85.3473339019269,1078.63142373511,456.132884567486));
#116091=CARTESIAN_POINT('Ctrl Pts',(85.3436337191116,1078.63385382327,455.934638312188));
#116092=CARTESIAN_POINT('Ctrl Pts',(85.2673723068792,1078.6400585357,455.589076190886));
#116093=CARTESIAN_POINT('Ctrl Pts',(85.2090444140144,1078.64342875293,455.441649644837));
#116094=CARTESIAN_POINT('Ctrl Pts',(85.0407378233742,1078.65129476155,455.15846130064));
#116095=CARTESIAN_POINT('Ctrl Pts',(84.9278135471952,1078.65580171458,455.027142050148));
#116096=CARTESIAN_POINT('Ctrl Pts',(84.6521900266623,1078.66535009839,454.801228067949));
#116097=CARTESIAN_POINT('Ctrl Pts',(84.4888587419943,1078.67031854076,454.712010624993));
#116098=CARTESIAN_POINT('Ctrl Pts',(84.1272415690971,1078.67997968496,454.594866421756));
#116099=CARTESIAN_POINT('Ctrl Pts',(83.9310060435655,1078.68454131793,454.572111169916));
#116100=CARTESIAN_POINT('Ctrl Pts',(83.5456899038228,1078.69237044383,454.60394709358));
#116101=CARTESIAN_POINT('Ctrl Pts',(83.3601782355851,1078.69559819491,454.65641279354));
#116102=CARTESIAN_POINT('Ctrl Pts',(83.0422820629693,1078.70038697822,454.81743061677));
#116103=CARTESIAN_POINT('Ctrl Pts',(82.9083529441599,1078.70208456588,454.916360716088));
#116104=CARTESIAN_POINT('Ctrl Pts',(82.7052131785727,1078.70421724732,455.127035596776));
#116105=CARTESIAN_POINT('Ctrl Pts',(82.6290517179936,1078.70484431844,455.229715316369));
#116106=CARTESIAN_POINT('Ctrl Pts',(82.5467639482396,1078.70529344552,455.377107029814));
#116107=CARTESIAN_POINT('Ctrl Pts',(82.5280715782491,1078.70537283249,455.414172053926));
#116108=CARTESIAN_POINT('Ctrl Pts',(82.5006240037821,1078.70545074768,455.474819214385));
#116109=CARTESIAN_POINT('Ctrl Pts',(82.4908677776319,1078.70546882236,455.49792362392));
#116110=CARTESIAN_POINT('Ctrl Pts',(82.4743523585173,1078.70548110583,455.539990396581));
#116111=CARTESIAN_POINT('Ctrl Pts',(82.4673837486615,1078.70547932534,455.558863924635));
#116112=CARTESIAN_POINT('Ctrl Pts',(82.4519822322641,1078.70545819374,455.60335088314));
#116113=CARTESIAN_POINT('Ctrl Pts',(82.4438605960793,1078.70543307706,455.629064511982));
#116114=CARTESIAN_POINT('Ctrl Pts',(82.4227439641766,1078.70532439608,455.702894709613));
#116115=CARTESIAN_POINT('Ctrl Pts',(82.4114723624004,1078.70520943202,455.751465743107));
#116116=CARTESIAN_POINT('Ctrl Pts',(82.3679412476656,1078.70441873335,455.994161466607));
#116117=CARTESIAN_POINT('Ctrl Pts',(82.3722126048156,1078.70310566954,456.192805463357));
#116118=CARTESIAN_POINT('Ctrl Pts',(82.4498696732354,1078.69940825983,456.539333448924));
#116119=CARTESIAN_POINT('Ctrl Pts',(82.5091214958284,1078.69730138823,456.687320321736));
#116120=CARTESIAN_POINT('Ctrl Pts',(82.6799381027615,1078.69189796453,456.971514598402));
#116121=CARTESIAN_POINT('Ctrl Pts',(82.7945553185853,1078.68854615125,457.103124026201));
#116122=CARTESIAN_POINT('Ctrl Pts',(83.0589086833123,1078.68103416303,457.316474892323));
#116123=CARTESIAN_POINT('Ctrl Pts',(83.2052366795662,1078.67696202899,457.398411926288));
#116124=CARTESIAN_POINT('Ctrl Pts',(83.5212696691922,1078.66826446424,457.510881285026));
#116125=CARTESIAN_POINT('Ctrl Pts',(83.6889634141074,1078.66369604484,457.539822560459));
#116126=CARTESIAN_POINT('Ctrl Pts',(83.857895722855,1078.6591843157,457.539806725122));
#116127=CARTESIAN_POINT('',(83.8577571500032,1076.68539762474,454.58320046723));
#116128=CARTESIAN_POINT('',(83.8577571500221,1067.7251047501,454.58320046723));
#116129=CARTESIAN_POINT('Ctrl Pts',(83.8571954838192,1076.65832806552,457.539806624917));
#116130=CARTESIAN_POINT('Ctrl Pts',(83.6639119834466,1076.66355105368,457.539733188816));
#116131=CARTESIAN_POINT('Ctrl Pts',(83.4725026434182,1076.66883992384,457.5017536051));
#116132=CARTESIAN_POINT('Ctrl Pts',(83.1151092303283,1076.67882739148,457.354265983379));
#116133=CARTESIAN_POINT('Ctrl Pts',(82.9525718107223,1076.68342942717,457.246159064353));
#116134=CARTESIAN_POINT('Ctrl Pts',(82.6771709865733,1076.69149751766,456.972338653538));
#116135=CARTESIAN_POINT('Ctrl Pts',(82.5674425843615,1076.69487994061,456.808833048692));
#116136=CARTESIAN_POINT('Ctrl Pts',(82.4177379379093,1076.7002538874,456.44854537559));
#116137=CARTESIAN_POINT('Ctrl Pts',(82.3792750403163,1076.70220032726,456.255288785364));
#116138=CARTESIAN_POINT('Ctrl Pts',(82.3796349258613,1076.70472115355,455.864260269205));
#116139=CARTESIAN_POINT('Ctrl Pts',(82.4187468703183,1076.70527147427,455.670349959404));
#116140=CARTESIAN_POINT('Ctrl Pts',(82.5702395422862,1076.70500246619,455.309168589201));
#116141=CARTESIAN_POINT('Ctrl Pts',(82.6810802262658,1076.70418581685,455.145458431561));
#116142=CARTESIAN_POINT('Ctrl Pts',(82.9595479947621,1076.70111661657,454.871279807384));
#116143=CARTESIAN_POINT('Ctrl Pts',(83.1242181473936,1076.69889278287,454.7633022341));
#116144=CARTESIAN_POINT('Ctrl Pts',(83.4861185286791,1076.69296530367,454.61742433396));
#116145=CARTESIAN_POINT('Ctrl Pts',(83.6798175416097,1076.68931013321,454.581027832075));
#116146=CARTESIAN_POINT('Ctrl Pts',(83.9707694676161,1076.68291524758,454.584416412143));
#116147=CARTESIAN_POINT('Ctrl Pts',(84.0662279375089,1076.68067306608,454.594841687333));
#116148=CARTESIAN_POINT('Ctrl Pts',(84.2555261586187,1076.67591578607,454.634379563519));
#116149=CARTESIAN_POINT('Ctrl Pts',(84.3488386880646,1076.67340794898,454.663740659378));
#116150=CARTESIAN_POINT('Ctrl Pts',(84.6169810283324,1076.66569950907,454.778304904097));
#116151=CARTESIAN_POINT('Ctrl Pts',(84.7786502908841,1076.66035445157,454.888910304203));
#116152=CARTESIAN_POINT('Ctrl Pts',(85.0501368360057,1076.65001067064,455.166344833762));
#116153=CARTESIAN_POINT('Ctrl Pts',(85.1572813234135,1076.6451186208,455.330528614358));
#116154=CARTESIAN_POINT('Ctrl Pts',(85.3019583596872,1076.63678412459,455.690892624565));
#116155=CARTESIAN_POINT('Ctrl Pts',(85.3381013789166,1076.63342948226,455.883563481951));
#116156=CARTESIAN_POINT('Ctrl Pts',(85.3338456226123,1076.62902403533,456.271481836929));
#116157=CARTESIAN_POINT('Ctrl Pts',(85.2936440839372,1076.62801568502,456.46295270076));
#116158=CARTESIAN_POINT('Ctrl Pts',(85.1418631734501,1076.62859370268,456.819001944414));
#116159=CARTESIAN_POINT('Ctrl Pts',(85.031945038628,1076.63016690374,456.980202608986));
#116160=CARTESIAN_POINT('Ctrl Pts',(84.7565214178857,1076.63555268389,457.250976790726));
#116161=CARTESIAN_POINT('Ctrl Pts',(84.5937449471793,1076.63930519792,457.358011815409));
#116162=CARTESIAN_POINT('Ctrl Pts',(84.237882256376,1076.64816033336,457.502844080452));
#116163=CARTESIAN_POINT('Ctrl Pts',(84.0484294235124,1076.65316046145,457.539879282308));
#116164=CARTESIAN_POINT('Ctrl Pts',(83.8571954838192,1076.65832806552,457.539806624917));
#116165=CARTESIAN_POINT('Origin',(83.8577571500221,1067.7251047501,456.061503599423));
#116166=CARTESIAN_POINT('',(83.8577571500221,1076.66449392106,456.939806731617));
#116167=CARTESIAN_POINT('',(83.8577571500243,1076.68056431803,455.18320046723));
#116168=CARTESIAN_POINT('Ctrl Pts',(83.8577571500221,1076.66449392106,456.939806731616));
#116169=CARTESIAN_POINT('Ctrl Pts',(83.7491563869114,1076.66731144614,456.939806731616));
#116170=CARTESIAN_POINT('Ctrl Pts',(83.64143436695,1076.67021713204,456.919663328342));
#116171=CARTESIAN_POINT('Ctrl Pts',(83.4329170859451,1076.67603402612,456.838768819911));
#116172=CARTESIAN_POINT('Ctrl Pts',(83.3349402934638,1076.67887787434,456.776552656778));
#116173=CARTESIAN_POINT('Ctrl Pts',(83.1673710954663,1076.68403158457,456.616811491697));
#116174=CARTESIAN_POINT('Ctrl Pts',(83.0998519482754,1076.68628429903,456.520396479986));
#116175=CARTESIAN_POINT('Ctrl Pts',(83.0064065376708,1076.68996027735,456.306855913284));
#116176=CARTESIAN_POINT('Ctrl Pts',(82.9813977169083,1076.69135025765,456.19185765644));
#116177=CARTESIAN_POINT('Ctrl Pts',(82.9777244290133,1076.69319196447,455.958576204661));
#116178=CARTESIAN_POINT('Ctrl Pts',(82.9991882680623,1076.69362560699,455.842615681471));
#116179=CARTESIAN_POINT('Ctrl Pts',(83.0861994999065,1076.69351107157,455.625904651252));
#116180=CARTESIAN_POINT('Ctrl Pts',(83.1508707555719,1076.69296406066,455.527314243881));
#116181=CARTESIAN_POINT('Ctrl Pts',(83.3148040429077,1076.69090032807,455.361364456753));
#116182=CARTESIAN_POINT('Ctrl Pts',(83.4123680647117,1076.68940369389,455.295593094294));
#116183=CARTESIAN_POINT('Ctrl Pts',(83.6269699886546,1076.68554041562,455.206164115548));
#116184=CARTESIAN_POINT('Ctrl Pts',(83.7418004079885,1076.68321289986,455.18320046723));
#116185=CARTESIAN_POINT('Ctrl Pts',(83.8577571500265,1076.68056431803,455.18320046723));
#116186=CARTESIAN_POINT('',(83.8577571500221,1082.7251047501,455.18320046723));
#116187=CARTESIAN_POINT('',(83.8577571500221,1067.7251047501,455.18320046723));
#116188=CARTESIAN_POINT('Origin',(83.8577571500221,1082.7251047501,456.061503599423));
#116189=CARTESIAN_POINT('Ctrl Pts',(83.8577571500264,1076.68056431803,455.18320046723));
#116190=CARTESIAN_POINT('Ctrl Pts',(83.8583775614648,1076.68055014713,455.18320046723));
#116191=CARTESIAN_POINT('Ctrl Pts',(83.8589980051472,1076.68053596712,455.183201124595));
#116192=CARTESIAN_POINT('Ctrl Pts',(83.9167484364247,1076.67921531978,455.183323511558));
#116193=CARTESIAN_POINT('Ctrl Pts',(83.973729065245,1076.67784084955,455.189018396919));
#116194=CARTESIAN_POINT('Ctrl Pts',(84.0866258061812,1076.67496599451,455.211562807171));
#116195=CARTESIAN_POINT('Ctrl Pts',(84.142235845964,1076.67347102156,455.228525885965));
#116196=CARTESIAN_POINT('Ctrl Pts',(84.3020804656356,1076.66893066948,455.295174012744));
#116197=CARTESIAN_POINT('Ctrl Pts',(84.398644774739,1076.6658514267,455.359987187322));
#116198=CARTESIAN_POINT('Ctrl Pts',(84.5612830577236,1076.65998142773,455.523221426675));
#116199=CARTESIAN_POINT('Ctrl Pts',(84.6257688330966,1076.65724973988,455.620076851781));
#116200=CARTESIAN_POINT('Ctrl Pts',(84.7117989206522,1076.65271883418,455.828666388698));
#116201=CARTESIAN_POINT('Ctrl Pts',(84.7342768823954,1076.65092765027,455.937741862609));
#116202=CARTESIAN_POINT('Ctrl Pts',(84.7359583932156,1076.64970293009,456.048125689504));
#116203=CARTESIAN_POINT('Ctrl Pts',(84.7377114048492,1076.64842613264,456.163203231901));
#116204=CARTESIAN_POINT('Ctrl Pts',(84.7168283306949,1076.64779110094,456.277514211922));
#116205=CARTESIAN_POINT('Ctrl Pts',(84.632235179076,1076.64791761215,456.491389717655));
#116206=CARTESIAN_POINT('Ctrl Pts',(84.5694184676888,1076.64867542544,456.588907253751));
#116207=CARTESIAN_POINT('Ctrl Pts',(84.4098843528329,1076.65144475292,456.75414263032));
#116208=CARTESIAN_POINT('Ctrl Pts',(84.3147370841928,1076.65342659934,456.820291355855));
#116209=CARTESIAN_POINT('Ctrl Pts',(84.1043647865005,1076.65825257172,456.91225928783));
#116210=CARTESIAN_POINT('Ctrl Pts',(83.9911573508748,1076.66104800146,456.937175987832));
#116211=CARTESIAN_POINT('Ctrl Pts',(83.8701655771886,1076.66417236966,456.93974102359));
#116212=CARTESIAN_POINT('Ctrl Pts',(83.8639599301777,1076.66433299688,456.939806731616));
#116213=CARTESIAN_POINT('Ctrl Pts',(83.8577571500221,1076.66449392106,456.939806731616));
#116214=CARTESIAN_POINT('Origin',(86.2654713137628,1067.7251047501,468.386802343567));
#116215=CARTESIAN_POINT('',(86.2654713137801,1078.38513071259,467.111358222431));
#116216=CARTESIAN_POINT('Ctrl Pts',(86.2657852622204,1078.31122975657,469.662246426064));
#116217=CARTESIAN_POINT('Ctrl Pts',(86.4293026174469,1078.30152800511,469.662206176537));
#116218=CARTESIAN_POINT('Ctrl Pts',(86.5913564979556,1078.29272124248,469.630720814669));
#116219=CARTESIAN_POINT('Ctrl Pts',(86.8771104038815,1078.27890818702,469.51531799073));
#116220=CARTESIAN_POINT('Ctrl Pts',(87.0010080273735,1078.27368093332,469.438782944172));
#116221=CARTESIAN_POINT('Ctrl Pts',(87.1845084955334,1078.26743513783,469.276830663847));
#116222=CARTESIAN_POINT('Ctrl Pts',(87.2515171699036,1078.26563813553,469.20197029594));
#116223=CARTESIAN_POINT('Ctrl Pts',(87.3287326703871,1078.26430944613,469.092069028911));
#116224=CARTESIAN_POINT('Ctrl Pts',(87.3472491563598,1078.26406575919,469.063324775724));
#116225=CARTESIAN_POINT('Ctrl Pts',(87.3753205107532,1078.26382535787,469.015642474366));
#116226=CARTESIAN_POINT('Ctrl Pts',(87.3855968720574,1078.26376994913,468.997149697114));
#116227=CARTESIAN_POINT('Ctrl Pts',(87.4043122313338,1078.2637340015,468.961404405957));
#116228=CARTESIAN_POINT('Ctrl Pts',(87.4128308217793,1078.26374701227,468.944200157969));
#116229=CARTESIAN_POINT('Ctrl Pts',(87.4313377728443,1078.26384518279,468.904599750075));
#116230=CARTESIAN_POINT('Ctrl Pts',(87.4410750442437,1078.2639493232,468.882094785677));
#116231=CARTESIAN_POINT('Ctrl Pts',(87.468463229481,1078.26441083778,468.813428202348));
#116232=CARTESIAN_POINT('Ctrl Pts',(87.4840856653855,1078.26491761532,468.766509914351));
#116233=CARTESIAN_POINT('Ctrl Pts',(87.5410400564051,1078.26802511382,468.555253403917));
#116234=CARTESIAN_POINT('Ctrl Pts',(87.552098884957,1078.27269527593,468.38460081847));
#116235=CARTESIAN_POINT('Ctrl Pts',(87.5112581261407,1078.28461173621,468.080880886857));
#116236=CARTESIAN_POINT('Ctrl Pts',(87.4711738657788,1078.29112017823,467.948819592391));
#116237=CARTESIAN_POINT('Ctrl Pts',(87.3451063275319,1078.30653492293,467.691463710751));
#116238=CARTESIAN_POINT('Ctrl Pts',(87.2562627253326,1078.31548411419,467.569846163314));
#116239=CARTESIAN_POINT('Ctrl Pts',(87.0325714867284,1078.3349540528,467.355253190721));
#116240=CARTESIAN_POINT('Ctrl Pts',(86.8967577700272,1078.34536821816,467.266975472739));
#116241=CARTESIAN_POINT('Ctrl Pts',(86.5918757201393,1078.36623672665,467.142326464495));
#116242=CARTESIAN_POINT('Ctrl Pts',(86.4244251035465,1078.37646189505,467.110079125792));
#116243=CARTESIAN_POINT('Ctrl Pts',(86.0917677391716,1078.39460656449,467.112674756566));
#116244=CARTESIAN_POINT('Ctrl Pts',(85.9297263499821,1078.40242275936,467.145477650272));
#116245=CARTESIAN_POINT('Ctrl Pts',(85.6438360406098,1078.41444363172,467.263641401564));
#116246=CARTESIAN_POINT('Ctrl Pts',(85.5198491895828,1078.41886952241,467.341818930712));
#116247=CARTESIAN_POINT('Ctrl Pts',(85.3396895087518,1078.42398312233,467.504144282614));
#116248=CARTESIAN_POINT('Ctrl Pts',(85.275289481429,1078.42540855033,467.577048896656));
#116249=CARTESIAN_POINT('Ctrl Pts',(85.2005866668197,1078.4264705406,467.684021425547));
#116250=CARTESIAN_POINT('Ctrl Pts',(85.1824928022474,1078.42666681158,467.712237347808));
#116251=CARTESIAN_POINT('Ctrl Pts',(85.1549758934935,1078.42686075099,467.759114244863));
#116252=CARTESIAN_POINT('Ctrl Pts',(85.1448634543236,1078.42690540145,467.777351395219));
#116253=CARTESIAN_POINT('Ctrl Pts',(85.1264023954751,1078.42693384648,467.812659132235));
#116254=CARTESIAN_POINT('Ctrl Pts',(85.1179792311707,1078.4269227042,467.829684450228));
#116255=CARTESIAN_POINT('Ctrl Pts',(85.099630581685,1078.42684091163,467.868954728429));
#116256=CARTESIAN_POINT('Ctrl Pts',(85.0899558199228,1078.42675437259,467.891308574778));
#116257=CARTESIAN_POINT('Ctrl Pts',(85.0626207102447,1078.42636969244,467.959782320886));
#116258=CARTESIAN_POINT('Ctrl Pts',(85.0469932150047,1078.42594586247,468.006662213625));
#116259=CARTESIAN_POINT('Ctrl Pts',(84.9899689910333,1078.42333734457,468.217856632479));
#116260=CARTESIAN_POINT('Ctrl Pts',(84.9788404704766,1078.41940782907,468.388513222671));
#116261=CARTESIAN_POINT('Ctrl Pts',(85.0196343830212,1078.40909248344,468.692729001687));
#116262=CARTESIAN_POINT('Ctrl Pts',(85.0598810477708,1078.40336881025,468.825243477131));
#116263=CARTESIAN_POINT('Ctrl Pts',(85.1866963835772,1078.38943448805,469.083644742128));
#116264=CARTESIAN_POINT('Ctrl Pts',(85.2762164602593,1078.38114900311,469.20576072949));
#116265=CARTESIAN_POINT('Ctrl Pts',(85.501864338204,1078.36251506303,469.421121871411));
#116266=CARTESIAN_POINT('Ctrl Pts',(85.639015606967,1078.35222191931,469.509500663051));
#116267=CARTESIAN_POINT('Ctrl Pts',(85.9405155358859,1078.33133210487,469.630926748259));
#116268=CARTESIAN_POINT('Ctrl Pts',(86.1023854601413,1078.3209245334,469.662286646656));
#116269=CARTESIAN_POINT('Ctrl Pts',(86.2657852622204,1078.31122975657,469.662246426064));
#116270=CARTESIAN_POINT('',(86.2654713137447,1076.38122798592,467.111358222431));
#116271=CARTESIAN_POINT('',(86.2654713137628,1067.7251047501,467.111358222431));
#116272=CARTESIAN_POINT('Ctrl Pts',(86.2659892652717,1076.3065438716,469.662246359534));
#116273=CARTESIAN_POINT('Ctrl Pts',(86.0990110388632,1076.31655262552,469.662314168567));
#116274=CARTESIAN_POINT('Ctrl Pts',(85.9336598964842,1076.3273118429,469.629591248244));
#116275=CARTESIAN_POINT('Ctrl Pts',(85.7021327202753,1076.34357417979,469.534138393049));
#116276=CARTESIAN_POINT('Ctrl Pts',(85.6282420575696,1076.34897918251,469.494805264416));
#116277=CARTESIAN_POINT('Ctrl Pts',(85.4175456889382,1076.3650722077,469.354553963634));
#116278=CARTESIAN_POINT('Ctrl Pts',(85.2964793286387,1076.37529935133,469.233328924411));
#116279=CARTESIAN_POINT('Ctrl Pts',(85.1094441551327,1076.39350676399,468.951419131407));
#116280=CARTESIAN_POINT('Ctrl Pts',(85.0449708655218,1076.40132620614,468.793756169916));
#116281=CARTESIAN_POINT('Ctrl Pts',(84.9811268117638,1076.41376165968,468.462324009853));
#116282=CARTESIAN_POINT('Ctrl Pts',(84.9824054704497,1076.41825857064,468.291845287455));
#116283=CARTESIAN_POINT('Ctrl Pts',(85.0513882282358,1076.42346813979,467.960915715412));
#116284=CARTESIAN_POINT('Ctrl Pts',(85.1185202239477,1076.4241245211,467.803805578061));
#116285=CARTESIAN_POINT('Ctrl Pts',(85.3100788862593,1076.42149000419,467.52509062931));
#116286=CARTESIAN_POINT('Ctrl Pts',(85.4325239584889,1076.41822820435,467.406242546533));
#116287=CARTESIAN_POINT('Ctrl Pts',(85.7163259414703,1076.40806435727,467.223335420329));
#116288=CARTESIAN_POINT('Ctrl Pts',(85.8748006196462,1076.40126404783,467.161015982234));
#116289=CARTESIAN_POINT('Ctrl Pts',(86.207338620264,1076.38475895787,467.101491973826));
#116290=CARTESIAN_POINT('Ctrl Pts',(86.3781587396811,1076.37520173521,467.105136950802));
#116291=CARTESIAN_POINT('Ctrl Pts',(86.6243099064432,1076.35973799447,467.160061550193));
#116292=CARTESIAN_POINT('Ctrl Pts',(86.7034162619302,1076.35448602985,467.186027677112));
#116293=CARTESIAN_POINT('Ctrl Pts',(86.8566195534566,1076.34372468397,467.2534819613));
#116294=CARTESIAN_POINT('Ctrl Pts',(86.9302484684515,1076.33823863164,467.295041298377));
#116295=CARTESIAN_POINT('Ctrl Pts',(87.1363509583598,1076.32190336354,467.440003227648));
#116296=CARTESIAN_POINT('Ctrl Pts',(87.2531466267127,1076.31126142937,467.562557477571));
#116297=CARTESIAN_POINT('Ctrl Pts',(87.4325825032181,1076.29179595377,467.845790468995));
#116298=CARTESIAN_POINT('Ctrl Pts',(87.4935301684182,1076.28316302257,468.003711654092));
#116299=CARTESIAN_POINT('Ctrl Pts',(87.5507426137669,1076.26931200386,468.333770842427));
#116300=CARTESIAN_POINT('Ctrl Pts',(87.5466236263288,1076.26422399356,468.50265306745));
#116301=CARTESIAN_POINT('Ctrl Pts',(87.4734851819258,1076.25846048254,468.828699693846));
#116302=CARTESIAN_POINT('Ctrl Pts',(87.4054162907907,1076.25782771373,468.982706349862));
#116303=CARTESIAN_POINT('Ctrl Pts',(87.2140597338252,1076.26114034261,469.255500400334));
#116304=CARTESIAN_POINT('Ctrl Pts',(87.0927642320039,1076.26504221223,469.371694400366));
#116305=CARTESIAN_POINT('Ctrl Pts',(86.8123871363491,1076.27677433783,469.550998739777));
#116306=CARTESIAN_POINT('Ctrl Pts',(86.6559935268662,1076.28449022634,469.612329798631));
#116307=CARTESIAN_POINT('Ctrl Pts',(86.4176130659882,1076.29763161351,469.655412796818));
#116308=CARTESIAN_POINT('Ctrl Pts',(86.3418720166314,1076.30199542357,469.662215543924));
#116309=CARTESIAN_POINT('Ctrl Pts',(86.2659892652717,1076.3065438716,469.662246359534));
#116310=CARTESIAN_POINT('Origin',(86.2654713137628,1067.7251047501,468.386802343567));
#116311=CARTESIAN_POINT('',(86.2654713137628,1076.32506388483,469.062246464703));
#116312=CARTESIAN_POINT('',(86.265471313763,1076.36458696229,467.711358222431));
#116313=CARTESIAN_POINT('Ctrl Pts',(86.2654713137628,1076.32506388483,469.062246464703));
#116314=CARTESIAN_POINT('Ctrl Pts',(86.221131644048,1076.3276742955,469.062246464703));
#116315=CARTESIAN_POINT('Ctrl Pts',(86.176799990606,1076.33040428046,469.057880406972));
#116316=CARTESIAN_POINT('Ctrl Pts',(86.0897630260982,1076.33600127725,469.040489378451));
#116317=CARTESIAN_POINT('Ctrl Pts',(86.0473582127218,1076.33884722441,469.027588123505));
#116318=CARTESIAN_POINT('Ctrl Pts',(85.9656683713897,1076.344570484,468.993679184451));
#116319=CARTESIAN_POINT('Ctrl Pts',(85.9265785304812,1076.34743421304,468.972748761436));
#116320=CARTESIAN_POINT('Ctrl Pts',(85.8149132408429,1076.35601217159,468.898021572604));
#116321=CARTESIAN_POINT('Ctrl Pts',(85.7507762389027,1076.36151517799,468.833394967447));
#116322=CARTESIAN_POINT('Ctrl Pts',(85.6518576691523,1076.37138378073,468.683054671894));
#116323=CARTESIAN_POINT('Ctrl Pts',(85.617934073741,1076.37565746368,468.598922112967));
#116324=CARTESIAN_POINT('Ctrl Pts',(85.5850142199041,1076.38245893128,468.422331719813));
#116325=CARTESIAN_POINT('Ctrl Pts',(85.586316150721,1076.38492157503,468.331651468764));
#116326=CARTESIAN_POINT('Ctrl Pts',(85.6243420134699,1076.38773247282,468.156037181576));
#116327=CARTESIAN_POINT('Ctrl Pts',(85.660695250463,1076.38805223879,468.07288106433));
#116328=CARTESIAN_POINT('Ctrl Pts',(85.7637996490437,1076.3864893365,467.925692998336));
#116329=CARTESIAN_POINT('Ctrl Pts',(85.8294991820277,1076.3846226682,467.863144660363));
#116330=CARTESIAN_POINT('Ctrl Pts',(85.9814878905492,1076.37889956016,467.767410140476));
#116331=CARTESIAN_POINT('Ctrl Pts',(86.0662529747926,1076.37509888885,467.735194004088));
#116332=CARTESIAN_POINT('Ctrl Pts',(86.1913820877741,1076.36867438578,467.714410473312));
#116333=CARTESIAN_POINT('Ctrl Pts',(86.2283981852657,1076.36667970469,467.711358222431));
#116334=CARTESIAN_POINT('Ctrl Pts',(86.2654713137633,1076.36458696229,467.711358222431));
#116335=CARTESIAN_POINT('',(86.2654713137628,1082.7251047501,467.711358222431));
#116336=CARTESIAN_POINT('',(86.2654713137628,1067.7251047501,467.711358222431));
#116337=CARTESIAN_POINT('Origin',(86.2654713137628,1082.7251047501,468.386802343567));
#116338=CARTESIAN_POINT('Ctrl Pts',(86.2654713137633,1076.36458696229,467.711358222431));
#116339=CARTESIAN_POINT('Ctrl Pts',(86.2655409522252,1076.36458303127,467.711358222431));
#116340=CARTESIAN_POINT('Ctrl Pts',(86.2656105908878,1076.36457909989,467.711358233502));
#116341=CARTESIAN_POINT('Ctrl Pts',(86.2656802297497,1076.36457516817,467.711358255042));
#116342=CARTESIAN_POINT('Ctrl Pts',(86.355911849862,1076.35948081317,467.711386163862));
#116343=CARTESIAN_POINT('Ctrl Pts',(86.4452075118274,1076.3538758243,467.729494157835));
#116344=CARTESIAN_POINT('Ctrl Pts',(86.5694496717781,1076.34520358804,467.781973253651));
#116345=CARTESIAN_POINT('Ctrl Pts',(86.6087819724189,1076.34230438781,467.803399558533));
#116346=CARTESIAN_POINT('Ctrl Pts',(86.7190276781068,1076.33369870382,467.878490567791));
#116347=CARTESIAN_POINT('Ctrl Pts',(86.7818100803589,1076.32812258751,467.942398193927));
#116348=CARTESIAN_POINT('Ctrl Pts',(86.8790362657067,1076.31794553537,468.090789963433));
#116349=CARTESIAN_POINT('Ctrl Pts',(86.9125709066619,1076.3134428523,468.173824515392));
#116350=CARTESIAN_POINT('Ctrl Pts',(86.9455813375285,1076.30618997006,468.347959352503));
#116351=CARTESIAN_POINT('Ctrl Pts',(86.9448195947062,1076.30350728791,468.437345199056));
#116352=CARTESIAN_POINT('Ctrl Pts',(86.9088741993592,1076.30038067367,468.610537551847));
#116353=CARTESIAN_POINT('Ctrl Pts',(86.8741385265952,1076.29996176381,468.69266301623));
#116354=CARTESIAN_POINT('Ctrl Pts',(86.7750897341507,1076.30146354208,468.838791458384));
#116355=CARTESIAN_POINT('Ctrl Pts',(86.7117868827548,1076.3033659806,468.901389393473));
#116356=CARTESIAN_POINT('Ctrl Pts',(86.56467718958,1076.30922539268,468.998757270787));
#116357=CARTESIAN_POINT('Ctrl Pts',(86.4822796861326,1076.3131263705,469.0325537748));
#116358=CARTESIAN_POINT('Ctrl Pts',(86.3527307934431,1076.32004288636,469.058019934114));
#116359=CARTESIAN_POINT('Ctrl Pts',(86.3090971729148,1076.32249549835,469.062246464703));
#116360=CARTESIAN_POINT('Ctrl Pts',(86.2654713137628,1076.32506388483,469.062246464703));
#116361=CARTESIAN_POINT('Origin',(87.6738908373847,1067.7251047501,482.164850509085));
#116362=CARTESIAN_POINT('',(87.6738908373846,1077.72740193357,481.066019373093));
#116363=CARTESIAN_POINT('Ctrl Pts',(87.6740206312035,1077.60297233385,483.263681637412));
#116364=CARTESIAN_POINT('Ctrl Pts',(87.8111078912392,1077.59090326144,483.263665444679));
#116365=CARTESIAN_POINT('Ctrl Pts',(87.947120297585,1077.58034241541,483.237995402536));
#116366=CARTESIAN_POINT('Ctrl Pts',(88.2018528738531,1077.56352493692,483.138120241511));
#116367=CARTESIAN_POINT('Ctrl Pts',(88.3184574072474,1077.5573852086,483.065176719914));
#116368=CARTESIAN_POINT('Ctrl Pts',(88.4570329518924,1077.55249541496,482.937395245085));
#116369=CARTESIAN_POINT('Ctrl Pts',(88.4927347895459,1077.55152977756,482.899447681179));
#116370=CARTESIAN_POINT('Ctrl Pts',(88.5385563920844,1077.55073133453,482.8432329801));
#116371=CARTESIAN_POINT('Ctrl Pts',(88.5510499554212,1077.55056682287,482.826999449908));
#116372=CARTESIAN_POINT('Ctrl Pts',(88.572016367431,1077.55038679093,482.798121078688));
#116373=CARTESIAN_POINT('Ctrl Pts',(88.5806936239008,1077.55034382916,482.785632108351));
#116374=CARTESIAN_POINT('Ctrl Pts',(88.5982462673749,1077.55032467976,482.759215300122));
#116375=CARTESIAN_POINT('Ctrl Pts',(88.6070724459055,1077.55035454002,482.745259456535));
#116376=CARTESIAN_POINT('Ctrl Pts',(88.6271168118163,1077.55051865362,482.711925668892));
#116377=CARTESIAN_POINT('Ctrl Pts',(88.638063627853,1077.55068623542,482.692393653871));
#116378=CARTESIAN_POINT('Ctrl Pts',(88.6715312240695,1077.55146427346,482.628152446531));
#116379=CARTESIAN_POINT('Ctrl Pts',(88.6915935803461,1077.5523652021,482.582241053861));
#116380=CARTESIAN_POINT('Ctrl Pts',(88.7575650094331,1077.55728247949,482.397915688518));
#116381=CARTESIAN_POINT('Ctrl Pts',(88.7788497727581,1077.56391333966,482.252414060837));
#116382=CARTESIAN_POINT('Ctrl Pts',(88.7649338993396,1077.58057500221,481.98795427312));
#116383=CARTESIAN_POINT('Ctrl Pts',(88.7393040393277,1077.58966491729,481.870717581574));
#116384=CARTESIAN_POINT('Ctrl Pts',(88.6475136601557,1077.61115073085,481.639123730004));
#116385=CARTESIAN_POINT('Ctrl Pts',(88.578579094557,1077.62360428328,481.527806123344));
#116386=CARTESIAN_POINT('Ctrl Pts',(88.3985409779626,1077.65076097294,481.327081251066));
#116387=CARTESIAN_POINT('Ctrl Pts',(88.2861888347545,1077.66532303483,481.241778560504));
#116388=CARTESIAN_POINT('Ctrl Pts',(88.0303906645026,1077.69441375866,481.115314135174));
#116389=CARTESIAN_POINT('Ctrl Pts',(87.8882923742511,1077.70863879979,481.077328391473));
#116390=CARTESIAN_POINT('Ctrl Pts',(87.6032966241837,1077.73374848996,481.05941248711));
#116391=CARTESIAN_POINT('Ctrl Pts',(87.4632323965882,1077.74452188966,481.077343357942));
#116392=CARTESIAN_POINT('Ctrl Pts',(87.2081666536232,1077.76124407805,481.161338661643));
#116393=CARTESIAN_POINT('Ctrl Pts',(87.0940421833216,1077.76738954126,481.22264216562));
#116394=CARTESIAN_POINT('Ctrl Pts',(86.9373214824395,1077.77366309305,481.346352945659));
#116395=CARTESIAN_POINT('Ctrl Pts',(86.885966737377,1077.77523806423,481.39566106034));
#116396=CARTESIAN_POINT('Ctrl Pts',(86.8223721562136,1077.77647482148,481.469827931667));
#116397=CARTESIAN_POINT('Ctrl Pts',(86.8057621118243,1077.77671668394,481.490689508232));
#116398=CARTESIAN_POINT('Ctrl Pts',(86.7796539289241,1077.77695716748,481.526047486838));
#116399=CARTESIAN_POINT('Ctrl Pts',(86.7697109074471,1077.77701135261,481.540200517127));
#116400=CARTESIAN_POINT('Ctrl Pts',(86.7510753823337,1077.77703794793,481.568104417005));
#116401=CARTESIAN_POINT('Ctrl Pts',(86.7423460381145,1077.77701505015,481.581825170085));
#116402=CARTESIAN_POINT('Ctrl Pts',(86.7227395151829,1077.77687846258,481.614207800903));
#116403=CARTESIAN_POINT('Ctrl Pts',(86.7121018345921,1077.77673747912,481.633006445475));
#116404=CARTESIAN_POINT('Ctrl Pts',(86.6803193986995,1077.77609440414,481.693247465911));
#116405=CARTESIAN_POINT('Ctrl Pts',(86.661250042485,1077.77536405011,481.735721841062));
#116406=CARTESIAN_POINT('Ctrl Pts',(86.5937730347837,1077.77115622372,481.915791865297));
#116407=CARTESIAN_POINT('Ctrl Pts',(86.5703289296778,1077.76518874474,482.061035824494));
#116408=CARTESIAN_POINT('Ctrl Pts',(86.580366437141,1077.74984985467,482.325527842935));
#116409=CARTESIAN_POINT('Ctrl Pts',(86.6041948654783,1077.74139736497,482.442911986737));
#116410=CARTESIAN_POINT('Ctrl Pts',(86.6923952079399,1077.72107857569,482.675748734811));
#116411=CARTESIAN_POINT('Ctrl Pts',(86.759674563606,1077.70912391434,482.788156688546));
#116412=CARTESIAN_POINT('Ctrl Pts',(86.9369334168585,1077.68257735879,482.991871882107));
#116413=CARTESIAN_POINT('Ctrl Pts',(87.0482874353572,1077.66808642387,483.079002105188));
#116414=CARTESIAN_POINT('Ctrl Pts',(87.2468622285877,1077.64510456924,483.180709496343));
#116415=CARTESIAN_POINT('Ctrl Pts',(87.3248255496704,1077.6366457401,483.210069231924));
#116416=CARTESIAN_POINT('Ctrl Pts',(87.4931599888644,1077.61951268012,483.252491707867));
#116417=CARTESIAN_POINT('Ctrl Pts',(87.5833947489484,1077.61095097705,483.263692342132));
#116418=CARTESIAN_POINT('Ctrl Pts',(87.6740206312035,1077.60297233385,483.263681637412));
#116419=CARTESIAN_POINT('',(87.6738908373588,1075.71704703142,481.066019373093));
#116420=CARTESIAN_POINT('',(87.6738908373847,1067.7251047501,481.066019373093));
#116421=CARTESIAN_POINT('Ctrl Pts',(87.6734764141951,1075.59152636934,483.263681566928));
#116422=CARTESIAN_POINT('Ctrl Pts',(87.5292769610456,1075.60434077903,483.263627182228));
#116423=CARTESIAN_POINT('Ctrl Pts',(87.3865888632646,1075.61859675302,483.235190481196));
#116424=CARTESIAN_POINT('Ctrl Pts',(87.1181456506469,1075.64852695256,483.124041830118));
#116425=CARTESIAN_POINT('Ctrl Pts',(86.9953185741151,1075.66393157655,483.041462726015));
#116426=CARTESIAN_POINT('Ctrl Pts',(86.7900265506239,1075.69343560738,482.833719639797));
#116427=CARTESIAN_POINT('Ctrl Pts',(86.7092408291913,1075.70726261736,482.710851473547));
#116428=CARTESIAN_POINT('Ctrl Pts',(86.6003467446628,1075.73162894803,482.440728071573));
#116429=CARTESIAN_POINT('Ctrl Pts',(86.5732339670936,1075.74193644529,482.296159388352));
#116430=CARTESIAN_POINT('Ctrl Pts',(86.5770822421847,1075.75775246956,482.004127373511));
#116431=CARTESIAN_POINT('Ctrl Pts',(86.6081899068073,1075.76308729527,481.859634643593));
#116432=CARTESIAN_POINT('Ctrl Pts',(86.7240214239792,1075.76797693463,481.594163314984));
#116433=CARTESIAN_POINT('Ctrl Pts',(86.8063947943622,1075.76760933368,481.475370492346));
#116434=CARTESIAN_POINT('Ctrl Pts',(87.0123398616821,1075.76133151365,481.275807533555));
#116435=CARTESIAN_POINT('Ctrl Pts',(87.1339717779872,1075.75546724528,481.19713241487));
#116436=CARTESIAN_POINT('Ctrl Pts',(87.4025778338071,1075.73874752703,481.090112345591));
#116437=CARTESIAN_POINT('Ctrl Pts',(87.5472218895445,1075.7279777464,481.063694070379));
#116438=CARTESIAN_POINT('Ctrl Pts',(87.8384255124702,1075.7028704515,481.068670891156));
#116439=CARTESIAN_POINT('Ctrl Pts',(87.982128630667,1075.68876933436,481.10013883438));
#116440=CARTESIAN_POINT('Ctrl Pts',(88.1808335292629,1075.66663079743,481.187333292501));
#116441=CARTESIAN_POINT('Ctrl Pts',(88.2432738679707,1075.65921506883,481.222337088777));
#116442=CARTESIAN_POINT('Ctrl Pts',(88.4227006748425,1075.63643163934,481.347296047487));
#116443=CARTESIAN_POINT('Ctrl Pts',(88.5254396337985,1075.62120195041,481.454914625536));
#116444=CARTESIAN_POINT('Ctrl Pts',(88.68086350819,1075.5931267396,481.701915668365));
#116445=CARTESIAN_POINT('Ctrl Pts',(88.7330142254566,1075.58050893989,481.838294430055));
#116446=CARTESIAN_POINT('Ctrl Pts',(88.7813084100526,1075.55948538804,482.122868329802));
#116447=CARTESIAN_POINT('Ctrl Pts',(88.777306778482,1075.55126245121,482.268226562851));
#116448=CARTESIAN_POINT('Ctrl Pts',(88.7134875328229,1075.54043862233,482.548523774093));
#116449=CARTESIAN_POINT('Ctrl Pts',(88.6546335203854,1075.53791396469,482.680736199129));
#116450=CARTESIAN_POINT('Ctrl Pts',(88.4895906495717,1075.53894046124,482.914869217121));
#116451=CARTESIAN_POINT('Ctrl Pts',(88.3851680557,1075.54246634591,483.014521711206));
#116452=CARTESIAN_POINT('Ctrl Pts',(88.1438160023445,1075.55509807103,483.168414464634));
#116453=CARTESIAN_POINT('Ctrl Pts',(88.009185497361,1075.56409226403,483.221007869021));
#116454=CARTESIAN_POINT('Ctrl Pts',(87.8040425953351,1075.58024751605,483.257904290828));
#116455=CARTESIAN_POINT('Ctrl Pts',(87.7388081660356,1075.58572060645,483.263706206742));
#116456=CARTESIAN_POINT('Ctrl Pts',(87.6734764141951,1075.59152636934,483.263681566928));
#116457=CARTESIAN_POINT('Origin',(87.6738908373847,1067.7251047501,482.164850509085));
#116458=CARTESIAN_POINT('',(87.6738908373847,1075.62676689012,482.663681645078));
#116459=CARTESIAN_POINT('',(87.6738908373844,1075.68376086233,481.666019373093));
#116460=CARTESIAN_POINT('Ctrl Pts',(87.6738908373847,1075.62676689012,482.663681645078));
#116461=CARTESIAN_POINT('Ctrl Pts',(87.6405437266238,1075.62969674438,482.663681645078));
#116462=CARTESIAN_POINT('Ctrl Pts',(87.6072155162424,1075.63281359472,482.660337682329));
#116463=CARTESIAN_POINT('Ctrl Pts',(87.5090710985346,1075.6425588954,482.640364150143));
#116464=CARTESIAN_POINT('Ctrl Pts',(87.4470775639424,1075.64947758236,482.614104143471));
#116465=CARTESIAN_POINT('Ctrl Pts',(87.3373126205476,1075.66331998747,482.538955909657));
#116466=CARTESIAN_POINT('Ctrl Pts',(87.2905424987636,1075.67011069185,482.490874696734));
#116467=CARTESIAN_POINT('Ctrl Pts',(87.2186324786873,1075.68265728098,482.379260249585));
#116468=CARTESIAN_POINT('Ctrl Pts',(87.1941545739213,1075.68829322328,482.316842132766));
#116469=CARTESIAN_POINT('Ctrl Pts',(87.1710842150568,1075.6976622135,482.185889203247));
#116470=CARTESIAN_POINT('Ctrl Pts',(87.1727519968497,1075.70129929393,482.118670489896));
#116471=CARTESIAN_POINT('Ctrl Pts',(87.2020814466865,1075.7059997038,481.99033977916));
#116472=CARTESIAN_POINT('Ctrl Pts',(87.2288175142528,1075.70707762621,481.93038736364));
#116473=CARTESIAN_POINT('Ctrl Pts',(87.3038208703414,1075.70662936817,481.824099411465));
#116474=CARTESIAN_POINT('Ctrl Pts',(87.3513394876768,1075.7051076779,481.778823797502));
#116475=CARTESIAN_POINT('Ctrl Pts',(87.4612261556118,1075.69962458665,481.708930741842));
#116476=CARTESIAN_POINT('Ctrl Pts',(87.5225600535927,1075.69570776398,481.685087421994));
#116477=CARTESIAN_POINT('Ctrl Pts',(87.6154826379312,1075.68864767134,481.668587802623));
#116478=CARTESIAN_POINT('Ctrl Pts',(87.6446651300579,1075.68628043382,481.666019373093));
#116479=CARTESIAN_POINT('Ctrl Pts',(87.6738908373842,1075.68376086233,481.666019373093));
#116480=CARTESIAN_POINT('',(87.6738908373847,1082.7251047501,481.666019373093));
#116481=CARTESIAN_POINT('',(87.6738908373847,1067.7251047501,481.666019373093));
#116482=CARTESIAN_POINT('Origin',(87.6738908373847,1082.7251047501,482.164850509085));
#116483=CARTESIAN_POINT('Ctrl Pts',(87.6738908373842,1075.68376086233,481.666019373093));
#116484=CARTESIAN_POINT('Ctrl Pts',(87.6738972500494,1075.68376030949,481.666019373093));
#116485=CARTESIAN_POINT('Ctrl Pts',(87.6739036627171,1075.68375975665,481.666019373132));
#116486=CARTESIAN_POINT('Ctrl Pts',(87.6739100753865,1075.68375920379,481.66601937338));
#116487=CARTESIAN_POINT('Ctrl Pts',(87.7403307301844,1075.67803287809,481.666021934973));
#116488=CARTESIAN_POINT('Ctrl Pts',(87.8060356353594,1075.67160013665,481.67928947701));
#116489=CARTESIAN_POINT('Ctrl Pts',(87.8971153636982,1075.66151731301,481.717572405829));
#116490=CARTESIAN_POINT('Ctrl Pts',(87.9257468068423,1075.6581462725,481.733046125472));
#116491=CARTESIAN_POINT('Ctrl Pts',(88.0079443108267,1075.64782497327,481.788441285301));
#116492=CARTESIAN_POINT('Ctrl Pts',(88.0552181071588,1075.64094345281,481.836411863289));
#116493=CARTESIAN_POINT('Ctrl Pts',(88.1278106129164,1075.62818139214,481.947676929813));
#116494=CARTESIAN_POINT('Ctrl Pts',(88.1526103480024,1075.62241655307,482.009764891465));
#116495=CARTESIAN_POINT('Ctrl Pts',(88.1763173761705,1075.61284437028,482.139150533971));
#116496=CARTESIAN_POINT('Ctrl Pts',(88.1753770175085,1075.60910239877,482.205101727012));
#116497=CARTESIAN_POINT('Ctrl Pts',(88.1481307969692,1075.60410850654,482.332658491556));
#116498=CARTESIAN_POINT('Ctrl Pts',(88.1222289247291,1075.60289338895,482.393021430533));
#116499=CARTESIAN_POINT('Ctrl Pts',(88.0487332535141,1075.60316451165,482.500331856297));
#116500=CARTESIAN_POINT('Ctrl Pts',(88.0019108728425,1075.60464340461,482.546230003847));
#116501=CARTESIAN_POINT('Ctrl Pts',(87.8931985020239,1075.61011317454,482.617594768251));
#116502=CARTESIAN_POINT('Ctrl Pts',(87.8323409444093,1075.6140569638,482.642292553746));
#116503=CARTESIAN_POINT('Ctrl Pts',(87.7372504496691,1075.62137033106,482.660665506466));
#116504=CARTESIAN_POINT('Ctrl Pts',(87.7055621192307,1075.62398427304,482.663681645078));
#116505=CARTESIAN_POINT('Ctrl Pts',(87.6738908373847,1075.62676689012,482.663681645078));
#116506=CARTESIAN_POINT('Origin',(86.2232976813476,1067.7251047501,496.076346996727));
#116507=CARTESIAN_POINT('',(86.2232976813475,1076.9124877279,494.985806247999));
#116508=CARTESIAN_POINT('Ctrl Pts',(86.2234201885755,1076.72559507709,497.166887738574));
#116509=CARTESIAN_POINT('Ctrl Pts',(86.3524097961115,1076.71205555844,497.166873248369));
#116510=CARTESIAN_POINT('Ctrl Pts',(86.480576174896,1076.70055077558,497.143973457267));
#116511=CARTESIAN_POINT('Ctrl Pts',(86.7226977502226,1076.68283926357,497.054338875221));
#116512=CARTESIAN_POINT('Ctrl Pts',(86.8347360052163,1076.67675512922,496.988530372314));
#116513=CARTESIAN_POINT('Ctrl Pts',(86.9563728152243,1076.67302111874,496.884336703862));
#116514=CARTESIAN_POINT('Ctrl Pts',(86.9791203061111,1076.67247634535,496.863099231561));
#116515=CARTESIAN_POINT('Ctrl Pts',(87.0150778334672,1076.67187843183,496.826527300309));
#116516=CARTESIAN_POINT('Ctrl Pts',(87.0288231866282,1076.67171992683,496.811748253903));
#116517=CARTESIAN_POINT('Ctrl Pts',(87.0527719620715,1076.67157337985,496.784520813728));
#116518=CARTESIAN_POINT('Ctrl Pts',(87.0631246265751,1076.67155727495,496.772212245553));
#116519=CARTESIAN_POINT('Ctrl Pts',(87.0844921179883,1076.67162681908,496.745636138793));
#116520=CARTESIAN_POINT('Ctrl Pts',(87.0954329115812,1076.67172494994,496.731315646235));
#116521=CARTESIAN_POINT('Ctrl Pts',(87.1235095640396,1076.67214795092,496.69261431479));
#116522=CARTESIAN_POINT('Ctrl Pts',(87.1400083661517,1076.67257890471,496.667792751873));
#116523=CARTESIAN_POINT('Ctrl Pts',(87.2083308298922,1076.67521735423,496.555265770314));
#116524=CARTESIAN_POINT('Ctrl Pts',(87.2486980622296,1076.67918721935,496.461287481939));
#116525=CARTESIAN_POINT('Ctrl Pts',(87.3041125094595,1076.69113009959,496.257998890933));
#116526=CARTESIAN_POINT('Ctrl Pts',(87.3168160464308,1076.69929813708,496.149273692147));
#116527=CARTESIAN_POINT('Ctrl Pts',(87.3092617857711,1076.72018567046,495.918906240303));
#116528=CARTESIAN_POINT('Ctrl Pts',(87.2849248909177,1076.73318443667,495.798910476036));
#116529=CARTESIAN_POINT('Ctrl Pts',(87.1940481680738,1076.76321722936,495.562156814412));
#116530=CARTESIAN_POINT('Ctrl Pts',(87.1246914887283,1076.78026547521,495.448512857642));
#116531=CARTESIAN_POINT('Ctrl Pts',(86.9420708702739,1076.81680859389,495.243947432705));
#116532=CARTESIAN_POINT('Ctrl Pts',(86.8274301421062,1076.83606120584,495.157344153586));
#116533=CARTESIAN_POINT('Ctrl Pts',(86.5699757981875,1076.87316869743,495.032423992116));
#116534=CARTESIAN_POINT('Ctrl Pts',(86.4292727160451,1076.89066379218,494.995771917294));
#116535=CARTESIAN_POINT('Ctrl Pts',(86.1520096037281,1076.92024691669,494.979977090931));
#116536=CARTESIAN_POINT('Ctrl Pts',(86.0182260605291,1076.9323936938,494.996919913663));
#116537=CARTESIAN_POINT('Ctrl Pts',(85.754889645979,1076.95197768784,495.081258135025));
#116538=CARTESIAN_POINT('Ctrl Pts',(85.6287943502149,1076.95886674519,495.151003283154));
#116539=CARTESIAN_POINT('Ctrl Pts',(85.4948783411836,1076.96291995805,495.264106667049));
#116540=CARTESIAN_POINT('Ctrl Pts',(85.4710646908169,1076.96348255808,495.286109662743));
#116541=CARTESIAN_POINT('Ctrl Pts',(85.4338410843614,1076.96409366395,495.32371313831));
#116542=CARTESIAN_POINT('Ctrl Pts',(85.4198312838338,1076.96425497732,495.338687696573));
#116543=CARTESIAN_POINT('Ctrl Pts',(85.3956531535167,1076.96440748111,495.366037406025));
#116544=CARTESIAN_POINT('Ctrl Pts',(85.3853198319258,1076.96442822542,495.378257956122));
#116545=CARTESIAN_POINT('Ctrl Pts',(85.3642047971045,1076.96437496726,495.404374023749));
#116546=CARTESIAN_POINT('Ctrl Pts',(85.3534828868134,1076.96429141355,495.4183116884));
#116547=CARTESIAN_POINT('Ctrl Pts',(85.3263965849636,1076.96392829633,495.45534115173));
#116548=CARTESIAN_POINT('Ctrl Pts',(85.3105867106407,1076.96356046012,495.478820164385));
#116549=CARTESIAN_POINT('Ctrl Pts',(85.2481877839852,1076.9614176983,495.579752102493));
#116550=CARTESIAN_POINT('Ctrl Pts',(85.2104302273405,1076.95833555419,495.662187103763));
#116551=CARTESIAN_POINT('Ctrl Pts',(85.1510913618141,1076.94858126176,495.850301666348));
#116552=CARTESIAN_POINT('Ctrl Pts',(85.1341308980016,1076.94140598426,495.956389671081));
#116553=CARTESIAN_POINT('Ctrl Pts',(85.1313766008971,1076.92258946607,496.183610851459));
#116554=CARTESIAN_POINT('Ctrl Pts',(85.1498936846263,1076.91062344118,496.303330037062));
#116555=CARTESIAN_POINT('Ctrl Pts',(85.2285475665924,1076.88239890454,496.542169211195));
#116556=CARTESIAN_POINT('Ctrl Pts',(85.2917526328625,1076.86606951276,496.658298576247));
#116557=CARTESIAN_POINT('Ctrl Pts',(85.4627335065793,1076.83037150634,496.870620253821));
#116558=CARTESIAN_POINT('Ctrl Pts',(85.5721659738896,1076.811182402,496.962545314751));
#116559=CARTESIAN_POINT('Ctrl Pts',(85.7716424590892,1076.78098187998,497.07270832065));
#116560=CARTESIAN_POINT('Ctrl Pts',(85.8519245211287,1076.76980240617,497.105340155335));
#116561=CARTESIAN_POINT('Ctrl Pts',(86.0290587067681,1076.74710795817,497.153847856076));
#116562=CARTESIAN_POINT('Ctrl Pts',(86.1259690214058,1076.7358241329,497.16689868587));
#116563=CARTESIAN_POINT('Ctrl Pts',(86.2234201885755,1076.72559507709,497.166887738574));
#116564=CARTESIAN_POINT('',(86.223297681327,1074.89499160754,494.985806247999));
#116565=CARTESIAN_POINT('',(86.2232976813476,1067.7251047501,494.985806247999));
#116566=CARTESIAN_POINT('Ctrl Pts',(86.2233659408369,1074.70655738266,497.166887743319));
#116567=CARTESIAN_POINT('Ctrl Pts',(86.0803109173772,1074.72169708915,497.166896697467));
#116568=CARTESIAN_POINT('Ctrl Pts',(85.938853039836,1074.739081694,497.138761309409));
#116569=CARTESIAN_POINT('Ctrl Pts',(85.7406870749057,1074.76700945455,497.056914296415));
#116570=CARTESIAN_POINT('Ctrl Pts',(85.6772676320875,1074.77659254706,497.023062448602));
#116571=CARTESIAN_POINT('Ctrl Pts',(85.5582047487984,1074.7959229432,496.943549312242));
#116572=CARTESIAN_POINT('Ctrl Pts',(85.5028064575396,1074.80562619512,496.898102180657));
#116573=CARTESIAN_POINT('Ctrl Pts',(85.3496454429075,1074.83475784732,496.744974796333));
#116574=CARTESIAN_POINT('Ctrl Pts',(85.2684330580968,1074.85363670812,496.62283397562));
#116575=CARTESIAN_POINT('Ctrl Pts',(85.1589809956636,1074.8878324657,496.354495851551));
#116576=CARTESIAN_POINT('Ctrl Pts',(85.1314496167889,1074.90284549871,496.211037453975));
#116577=CARTESIAN_POINT('Ctrl Pts',(85.1341568903704,1074.92710203794,495.921551916974));
#116578=CARTESIAN_POINT('Ctrl Pts',(85.164257561941,1074.93611353415,495.778461490953));
#116579=CARTESIAN_POINT('Ctrl Pts',(85.27756399223,1074.94679051999,495.515157651623));
#116580=CARTESIAN_POINT('Ctrl Pts',(85.358395700729,1074.94851346881,495.397146356174));
#116581=CARTESIAN_POINT('Ctrl Pts',(85.5608242107753,1074.94466507112,495.198550289736));
#116582=CARTESIAN_POINT('Ctrl Pts',(85.6803908911938,1074.93912728222,495.120010733015));
#116583=CARTESIAN_POINT('Ctrl Pts',(85.9456637895418,1074.9212164551,495.011831856432));
#116584=CARTESIAN_POINT('Ctrl Pts',(86.0891610405896,1074.90887126502,494.984492764252));
#116585=CARTESIAN_POINT('Ctrl Pts',(86.37863716269,1074.87892711957,494.987222700849));
#116586=CARTESIAN_POINT('Ctrl Pts',(86.5217505346063,1074.86160048812,495.017512633713));
#116587=CARTESIAN_POINT('Ctrl Pts',(86.7198448431444,1074.83377040269,495.102815010389));
#116588=CARTESIAN_POINT('Ctrl Pts',(86.7821549224923,1074.8243469137,495.137201058864));
#116589=CARTESIAN_POINT('Ctrl Pts',(86.8994061884456,1074.80520795178,495.217723154351));
#116590=CARTESIAN_POINT('Ctrl Pts',(86.9540537293406,1074.79553430232,495.26372613206));
#116591=CARTESIAN_POINT('Ctrl Pts',(87.1062621169359,1074.76611453062,495.419712469126));
#116592=CARTESIAN_POINT('Ctrl Pts',(87.1865717931367,1074.74682286749,495.544391033771));
#116593=CARTESIAN_POINT('Ctrl Pts',(87.2917921724487,1074.71205820369,495.815179799298));
#116594=CARTESIAN_POINT('Ctrl Pts',(87.3169440053454,1074.6968373674,495.958177480026));
#116595=CARTESIAN_POINT('Ctrl Pts',(87.3101560755106,1074.67234277346,496.244694824896));
#116596=CARTESIAN_POINT('Ctrl Pts',(87.2788618340179,1074.66325286937,496.385379091055));
#116597=CARTESIAN_POINT('Ctrl Pts',(87.1640524130299,1074.65247828509,496.645852898545));
#116598=CARTESIAN_POINT('Ctrl Pts',(87.0821614426303,1074.65083964695,496.763174927283));
#116599=CARTESIAN_POINT('Ctrl Pts',(86.8782047774325,1074.65521976434,496.959746556909));
#116600=CARTESIAN_POINT('Ctrl Pts',(86.7583012027278,1074.6611775755,497.037070803745));
#116601=CARTESIAN_POINT('Ctrl Pts',(86.4984665135315,1074.67969380481,497.140652703391));
#116602=CARTESIAN_POINT('Ctrl Pts',(86.3614278650871,1074.6919461026,497.166879101701));
#116603=CARTESIAN_POINT('Ctrl Pts',(86.2233659408369,1074.70655738266,497.166887743319));
#116604=CARTESIAN_POINT('Origin',(86.2232976813476,1067.7251047501,496.076346996727));
#116605=CARTESIAN_POINT('',(86.2232976813475,1074.75955377087,496.566887745455));
#116606=CARTESIAN_POINT('',(86.2232976813475,1074.84430822541,495.585806247999));
#116607=CARTESIAN_POINT('Ctrl Pts',(86.2232976813475,1074.75955377087,496.566887745455));
#116608=CARTESIAN_POINT('Ctrl Pts',(86.2226440593275,1074.75962237626,496.566887745455));
#116609=CARTESIAN_POINT('Ctrl Pts',(86.2219903858984,1074.75969109957,496.566886439075));
#116610=CARTESIAN_POINT('Ctrl Pts',(86.156936183418,1074.76654170787,496.566626372241));
#116611=CARTESIAN_POINT('Ctrl Pts',(86.0933076663028,1074.77433382017,496.553691462151));
#116612=CARTESIAN_POINT('Ctrl Pts',(86.0043705346255,1074.78685722683,496.516501857578));
#116613=CARTESIAN_POINT('Ctrl Pts',(85.9759897465591,1074.79114664136,496.50120329209));
#116614=CARTESIAN_POINT('Ctrl Pts',(85.9226764809709,1074.79981475687,496.465305525912));
#116615=CARTESIAN_POINT('Ctrl Pts',(85.8978599907607,1074.80417389155,496.444792691315));
#116616=CARTESIAN_POINT('Ctrl Pts',(85.8291081585573,1074.81730799618,496.375560257888));
#116617=CARTESIAN_POINT('Ctrl Pts',(85.7927021199992,1074.82584734057,496.320310092879));
#116618=CARTESIAN_POINT('Ctrl Pts',(85.7438543031066,1074.84134511513,496.198921929108));
#116619=CARTESIAN_POINT('Ctrl Pts',(85.7317757644832,1074.84816107792,496.134009919116));
#116620=CARTESIAN_POINT('Ctrl Pts',(85.7338479894099,1074.85908486631,496.003971718148));
#116621=CARTESIAN_POINT('Ctrl Pts',(85.7476145889624,1074.86312067503,495.940158239953));
#116622=CARTESIAN_POINT('Ctrl Pts',(85.7988303780936,1074.86790886816,495.822341948628));
#116623=CARTESIAN_POINT('Ctrl Pts',(85.8353891435477,1074.86866356488,495.769389890237));
#116624=CARTESIAN_POINT('Ctrl Pts',(85.9267488713175,1074.86684566662,495.680424992944));
#116625=CARTESIAN_POINT('Ctrl Pts',(85.9806190019375,1074.86429169331,495.645316174372));
#116626=CARTESIAN_POINT('Ctrl Pts',(86.0980899150621,1074.85622254089,495.597883000476));
#116627=CARTESIAN_POINT('Ctrl Pts',(86.1604532385391,1074.85081360277,495.585806247999));
#116628=CARTESIAN_POINT('Ctrl Pts',(86.2232976813474,1074.84430822541,495.585806247999));
#116629=CARTESIAN_POINT('',(86.2232976813476,1082.7251047501,495.585806247999));
#116630=CARTESIAN_POINT('',(86.2232976813476,1067.7251047501,495.585806247999));
#116631=CARTESIAN_POINT('Origin',(86.2232976813476,1082.7251047501,496.076346996727));
#116632=CARTESIAN_POINT('Ctrl Pts',(86.2232976813474,1074.84430822541,495.585806247999));
#116633=CARTESIAN_POINT('Ctrl Pts',(86.2233019494077,1074.8443077836,495.585806247999));
#116634=CARTESIAN_POINT('Ctrl Pts',(86.2233062174703,1074.84430734178,495.585806248042));
#116635=CARTESIAN_POINT('Ctrl Pts',(86.2233104855349,1074.84430689996,495.585806248154));
#116636=CARTESIAN_POINT('Ctrl Pts',(86.2888311471117,1074.8375243441,495.585807958388));
#116637=CARTESIAN_POINT('Ctrl Pts',(86.3535917320136,1074.82968248953,495.598934670239));
#116638=CARTESIAN_POINT('Ctrl Pts',(86.4433153117649,1074.81710255258,495.6367467866));
#116639=CARTESIAN_POINT('Ctrl Pts',(86.4715312206027,1074.8128490095,495.652041918061));
#116640=CARTESIAN_POINT('Ctrl Pts',(86.5246181303704,1074.80422349754,495.687933598277));
#116641=CARTESIAN_POINT('Ctrl Pts',(86.5493630162513,1074.79987063099,495.708460720927));
#116642=CARTESIAN_POINT('Ctrl Pts',(86.6181958536365,1074.78667374477,495.777999013993));
#116643=CARTESIAN_POINT('Ctrl Pts',(86.6546383624893,1074.77804081921,495.833618109012));
#116644=CARTESIAN_POINT('Ctrl Pts',(86.7030654206161,1074.76240822645,495.955203405332));
#116645=CARTESIAN_POINT('Ctrl Pts',(86.7149169782775,1074.75553756712,496.019854259707));
#116646=CARTESIAN_POINT('Ctrl Pts',(86.7126255587337,1074.74451778519,496.149112216989));
#116647=CARTESIAN_POINT('Ctrl Pts',(86.6989445841481,1074.74043286006,496.212433045587));
#116648=CARTESIAN_POINT('Ctrl Pts',(86.6480524086574,1074.73554231507,496.329873683035));
#116649=CARTESIAN_POINT('Ctrl Pts',(86.6115468864515,1074.73476019736,496.382875657183));
#116650=CARTESIAN_POINT('Ctrl Pts',(86.5203271726244,1074.7365981839,496.471896694175));
#116651=CARTESIAN_POINT('Ctrl Pts',(86.4665679794862,1074.73919466779,496.507032781713));
#116652=CARTESIAN_POINT('Ctrl Pts',(86.3489982345556,1074.74740833894,496.554716480634));
#116653=CARTESIAN_POINT('Ctrl Pts',(86.2863874353879,1074.7529317518,496.566887745455));
#116654=CARTESIAN_POINT('Ctrl Pts',(86.2232976813475,1074.75955377087,496.566887745455));
#116655=CARTESIAN_POINT('Origin',(88.5622696992333,1067.7251047501,437.939428532945));
#116656=CARTESIAN_POINT('',(88.5622696992515,1078.67883079978,436.461125400751));
#116657=CARTESIAN_POINT('Ctrl Pts',(88.5624504403869,1078.66748248367,439.417731654089));
#116658=CARTESIAN_POINT('Ctrl Pts',(88.757345015015,1078.66228612236,439.417707825776));
#116659=CARTESIAN_POINT('Ctrl Pts',(88.9503273060786,1078.6569937597,439.379142881179));
#116660=CARTESIAN_POINT('Ctrl Pts',(89.3025589141094,1078.64726732473,439.232555684521));
#116661=CARTESIAN_POINT('Ctrl Pts',(89.4597375327993,1078.64289971757,439.128868216047));
#116662=CARTESIAN_POINT('Ctrl Pts',(89.7209953868401,1078.6358690912,438.874527370835));
#116663=CARTESIAN_POINT('Ctrl Pts',(89.8250665607932,1078.63319830216,438.72835683181));
#116664=CARTESIAN_POINT('Ctrl Pts',(89.9360868402136,1078.63073122799,438.491667515965));
#116665=CARTESIAN_POINT('Ctrl Pts',(89.9650602475366,1078.63016532841,438.413264597878));
#116666=CARTESIAN_POINT('Ctrl Pts',(89.9963785571602,1078.62969541958,438.299823872625));
#116667=CARTESIAN_POINT('Ctrl Pts',(90.0043425517052,1078.62959797718,438.266504855865));
#116668=CARTESIAN_POINT('Ctrl Pts',(90.0152946475143,1078.6295048698,438.212441453156));
#116669=CARTESIAN_POINT('Ctrl Pts',(90.0190116220425,1078.62948435833,438.191857783571));
#116670=CARTESIAN_POINT('Ctrl Pts',(90.0257937762046,1078.62947257754,438.149134691943));
#116671=CARTESIAN_POINT('Ctrl Pts',(90.0287961599801,1078.62948340464,438.126990619487));
#116672=CARTESIAN_POINT('Ctrl Pts',(90.0346138172216,1078.62954793693,438.075307226615));
#116673=CARTESIAN_POINT('Ctrl Pts',(90.0370440215606,1078.62961451857,438.045734279213));
#116674=CARTESIAN_POINT('Ctrl Pts',(90.0418964547107,1078.62991783137,437.952310614242));
#116675=CARTESIAN_POINT('Ctrl Pts',(90.0410711413001,1078.63026201202,437.888365873144));
#116676=CARTESIAN_POINT('Ctrl Pts',(90.0208508646909,1078.63220780497,437.628662782334));
#116677=CARTESIAN_POINT('Ctrl Pts',(89.9666401589069,1078.63492363913,437.437664654653));
#116678=CARTESIAN_POINT('Ctrl Pts',(89.8034269765363,1078.64159556978,437.120572201635));
#116679=CARTESIAN_POINT('Ctrl Pts',(89.7075560654635,1078.64517893324,436.991109043046));
#116680=CARTESIAN_POINT('Ctrl Pts',(89.4681195341764,1078.65339775563,436.758298803338));
#116681=CARTESIAN_POINT('Ctrl Pts',(89.3229983760408,1078.65802967811,436.660006815832));
#116682=CARTESIAN_POINT('Ctrl Pts',(88.9937644666912,1078.66771358045,436.513248057597));
#116683=CARTESIAN_POINT('Ctrl Pts',(88.810531607163,1078.67268076812,436.470228677978));
#116684=CARTESIAN_POINT('Ctrl Pts',(88.4289595182711,1078.68215611944,436.454244500458));
#116685=CARTESIAN_POINT('Ctrl Pts',(88.2340670620951,1078.6865383815,436.484837421534));
#116686=CARTESIAN_POINT('Ctrl Pts',(87.8733545189762,1078.69393353298,436.617865550892));
#116687=CARTESIAN_POINT('Ctrl Pts',(87.7101300913676,1078.69692399872,436.71672727955));
#116688=CARTESIAN_POINT('Ctrl Pts',(87.4425068272208,1078.70139236637,436.959082917338));
#116689=CARTESIAN_POINT('Ctrl Pts',(87.3361587463948,1078.70295379596,437.09586366536));
#116690=CARTESIAN_POINT('Ctrl Pts',(87.2083715890297,1078.70459376192,437.337282044604));
#116691=CARTESIAN_POINT('Ctrl Pts',(87.1703383730882,1078.70501319292,437.431345881074));
#116692=CARTESIAN_POINT('Ctrl Pts',(87.1319459917568,1078.7053363797,437.564037213949));
#116693=CARTESIAN_POINT('Ctrl Pts',(87.1230131209069,1078.70539825704,437.59989199811));
#116694=CARTESIAN_POINT('Ctrl Pts',(87.1105851978113,1078.70545965385,437.659160541457));
#116695=CARTESIAN_POINT('Ctrl Pts',(87.1062925734953,1078.70547360007,437.682390308681));
#116696=CARTESIAN_POINT('Ctrl Pts',(87.0990865422115,1078.70548123484,437.727396825959));
#116697=CARTESIAN_POINT('Ctrl Pts',(87.0960983146865,1078.70547627664,437.749155395497));
#116698=CARTESIAN_POINT('Ctrl Pts',(87.0903143381137,1078.70544484624,437.799582626489));
#116699=CARTESIAN_POINT('Ctrl Pts',(87.0878694684239,1078.70541216515,437.828282591387));
#116700=CARTESIAN_POINT('Ctrl Pts',(87.0828839198283,1078.70526441035,437.91759478844));
#116701=CARTESIAN_POINT('Ctrl Pts',(87.083233658455,1078.7050984122,437.978304538025));
#116702=CARTESIAN_POINT('Ctrl Pts',(87.1005846110692,1078.70410859516,438.235789588208));
#116703=CARTESIAN_POINT('Ctrl Pts',(87.1531793757567,1078.70266328467,438.428114147403));
#116704=CARTESIAN_POINT('Ctrl Pts',(87.3140974976532,1078.69869682965,438.747605160651));
#116705=CARTESIAN_POINT('Ctrl Pts',(87.4090274351938,1078.69644991752,438.878103900114));
#116706=CARTESIAN_POINT('Ctrl Pts',(87.6473447712769,1078.69074624572,439.113669287901));
#116707=CARTESIAN_POINT('Ctrl Pts',(87.7924536974861,1078.68723915733,439.213518635821));
#116708=CARTESIAN_POINT('Ctrl Pts',(88.0476778660629,1078.68086743532,439.329285867746));
#116709=CARTESIAN_POINT('Ctrl Pts',(88.1481322858348,1078.67831845493,439.362452438779));
#116710=CARTESIAN_POINT('Ctrl Pts',(88.3535252766991,1078.67301211949,439.406653678577));
#116711=CARTESIAN_POINT('Ctrl Pts',(88.4578420533073,1078.67027159659,439.417744443781));
#116712=CARTESIAN_POINT('Ctrl Pts',(88.5624504403869,1078.66748248367,439.417731654089));
#116713=CARTESIAN_POINT('',(88.5622696992118,1076.67818780051,436.461125400751));
#116714=CARTESIAN_POINT('',(88.5622696992333,1067.7251047501,436.461125400751));
#116715=CARTESIAN_POINT('Ctrl Pts',(88.5617352524017,1076.66672428354,439.41773156853));
#116716=CARTESIAN_POINT('Ctrl Pts',(88.3683809758935,1076.67194009027,439.41766166569));
#116717=CARTESIAN_POINT('Ctrl Pts',(88.1768972564217,1076.67695651917,439.379657888919));
#116718=CARTESIAN_POINT('Ctrl Pts',(87.8176643094205,1076.68608108643,439.231354792517));
#116719=CARTESIAN_POINT('Ctrl Pts',(87.6536988854534,1076.69009296818,439.121807155248));
#116720=CARTESIAN_POINT('Ctrl Pts',(87.3780890166092,1076.69676616586,438.845568983184));
#116721=CARTESIAN_POINT('Ctrl Pts',(87.2690504815552,1076.69937242687,438.681699088468));
#116722=CARTESIAN_POINT('Ctrl Pts',(87.1204864835168,1076.70320006966,438.320226613705));
#116723=CARTESIAN_POINT('Ctrl Pts',(87.0827691330013,1076.70438483802,438.126049449173));
#116724=CARTESIAN_POINT('Ctrl Pts',(87.0852248910072,1076.70538860172,437.733826789366));
#116725=CARTESIAN_POINT('Ctrl Pts',(87.1255605943168,1076.70519705504,437.539678770042));
#116726=CARTESIAN_POINT('Ctrl Pts',(87.2794221082317,1076.70340929647,437.179207364597));
#116727=CARTESIAN_POINT('Ctrl Pts',(87.3911426333467,1076.70183157579,437.016340666353));
#116728=CARTESIAN_POINT('Ctrl Pts',(87.6709541381621,1076.69720280529,436.744061410256));
#116729=CARTESIAN_POINT('Ctrl Pts',(87.8360887993002,1076.69419419588,436.637123174694));
#116730=CARTESIAN_POINT('Ctrl Pts',(88.1991432641097,1076.68675386757,436.493110421715));
#116731=CARTESIAN_POINT('Ctrl Pts',(88.3936214801836,1076.68238210076,436.457792522723));
#116732=CARTESIAN_POINT('Ctrl Pts',(88.6868856082326,1076.67509357414,436.463157910341));
#116733=CARTESIAN_POINT('Ctrl Pts',(88.7840415346486,1076.67256602926,436.474600731023));
#116734=CARTESIAN_POINT('Ctrl Pts',(89.0688325908674,1076.66481721658,436.537142277561));
#116735=CARTESIAN_POINT('Ctrl Pts',(89.2482781730382,1076.65946977958,436.615644168988));
#116736=CARTESIAN_POINT('Ctrl Pts',(89.5666905284698,1076.64918330829,436.837523430681));
#116737=CARTESIAN_POINT('Ctrl Pts',(89.7025484344164,1076.64435046856,436.978788202611));
#116738=CARTESIAN_POINT('Ctrl Pts',(89.9118735393716,1076.6361906598,437.305702102426));
#116739=CARTESIAN_POINT('Ctrl Pts',(89.9833289645815,1076.6329495055,437.488161197479));
#116740=CARTESIAN_POINT('Ctrl Pts',(90.0515895250753,1076.62880161083,437.869913486374));
#116741=CARTESIAN_POINT('Ctrl Pts',(90.0478755907697,1076.62793474189,438.065464302928));
#116742=CARTESIAN_POINT('Ctrl Pts',(89.9653350825308,1076.62879179068,438.443550743642));
#116743=CARTESIAN_POINT('Ctrl Pts',(89.8874864742292,1076.63050034395,438.622454655504));
#116744=CARTESIAN_POINT('Ctrl Pts',(89.6674995590258,1076.63612200071,438.939984840519));
#116745=CARTESIAN_POINT('Ctrl Pts',(89.527548801666,1076.63997328647,439.075593198019));
#116746=CARTESIAN_POINT('Ctrl Pts',(89.203370742823,1076.64901305868,439.285412825144));
#116747=CARTESIAN_POINT('Ctrl Pts',(89.022228488455,1076.65410849205,439.357566614862));
#116748=CARTESIAN_POINT('Ctrl Pts',(88.7431027765002,1076.66180103145,439.409435422911));
#116749=CARTESIAN_POINT('Ctrl Pts',(88.6525139055784,1076.6642754941,439.417764387486));
#116750=CARTESIAN_POINT('Ctrl Pts',(88.5617352524017,1076.66672428354,439.41773156853));
#116751=CARTESIAN_POINT('Origin',(88.5622696992333,1067.7251047501,437.939428532945));
#116752=CARTESIAN_POINT('',(88.5622696992333,1076.6693343871,438.817731665138));
#116753=CARTESIAN_POINT('',(88.5622696993117,1076.67614304338,437.061125400752));
#116754=CARTESIAN_POINT('Ctrl Pts',(88.5622696992333,1076.6693343871,438.817731665138));
#116755=CARTESIAN_POINT('Ctrl Pts',(88.4536517533704,1076.67220897669,438.817731665138));
#116756=CARTESIAN_POINT('Ctrl Pts',(88.3459099310249,1076.67504496281,438.797581873877));
#116757=CARTESIAN_POINT('Ctrl Pts',(88.1358308853606,1076.68054698191,438.71606497484));
#116758=CARTESIAN_POINT('Ctrl Pts',(88.0365939392436,1076.68313022806,438.652648202581));
#116759=CARTESIAN_POINT('Ctrl Pts',(87.8687859378155,1076.68755634743,438.490849384969));
#116760=CARTESIAN_POINT('Ctrl Pts',(87.8018434510697,1076.68935896266,438.394114717533));
#116761=CARTESIAN_POINT('Ctrl Pts',(87.7094694558756,1076.69206732777,438.179843760435));
#116762=CARTESIAN_POINT('Ctrl Pts',(87.6850841716801,1076.69294615635,438.064388079985));
#116763=CARTESIAN_POINT('Ctrl Pts',(87.6829222669053,1076.69373261675,437.830517802458));
#116764=CARTESIAN_POINT('Ctrl Pts',(87.7052427320025,1076.69363180558,437.714443996672));
#116765=CARTESIAN_POINT('Ctrl Pts',(87.7939562708241,1076.69244392786,437.498129167194));
#116766=CARTESIAN_POINT('Ctrl Pts',(87.8593627160175,1076.6913694884,437.400011721706));
#116767=CARTESIAN_POINT('Ctrl Pts',(88.0244931402338,1076.68828756065,437.235314081606));
#116768=CARTESIAN_POINT('Ctrl Pts',(88.1224915206422,1076.68631006592,437.170290791429));
#116769=CARTESIAN_POINT('Ctrl Pts',(88.335721505322,1076.68163482803,437.083241244989));
#116770=CARTESIAN_POINT('Ctrl Pts',(88.4484747365534,1076.67899668761,437.061125400731));
#116771=CARTESIAN_POINT('Ctrl Pts',(88.56226969939,1076.67614304338,437.061125400751));
#116772=CARTESIAN_POINT('',(88.5622696992333,1082.7251047501,437.061125400751));
#116773=CARTESIAN_POINT('',(88.5622696992333,1067.7251047501,437.061125400751));
#116774=CARTESIAN_POINT('Origin',(88.5622696992333,1082.7251047501,437.939428532945));
#116775=CARTESIAN_POINT('Ctrl Pts',(88.56226969939,1076.67614304338,437.061125400751));
#116776=CARTESIAN_POINT('Ctrl Pts',(88.5651433688951,1076.67607098017,437.061125400752));
#116777=CARTESIAN_POINT('Ctrl Pts',(88.5680177027814,1076.6759987816,437.061139504034));
#116778=CARTESIAN_POINT('Ctrl Pts',(88.6288907643527,1076.67446722831,437.06173716517));
#116779=CARTESIAN_POINT('Ctrl Pts',(88.6866892952071,1076.67296430677,437.068050272989));
#116780=CARTESIAN_POINT('Ctrl Pts',(88.8561391256731,1076.6684109272,437.103771672063));
#116781=CARTESIAN_POINT('Ctrl Pts',(88.9630724197748,1076.66533696018,437.149466870854));
#116782=CARTESIAN_POINT('Ctrl Pts',(89.1532244248137,1076.65950966314,437.279534086036));
#116783=CARTESIAN_POINT('Ctrl Pts',(89.2345977229757,1076.65681496627,437.362656120586));
#116784=CARTESIAN_POINT('Ctrl Pts',(89.3605927294946,1076.65228848288,437.555549579377));
#116785=CARTESIAN_POINT('Ctrl Pts',(89.4040047099736,1076.6505028898,437.663442066641));
#116786=CARTESIAN_POINT('Ctrl Pts',(89.4346526918423,1076.648845267,437.825935577347));
#116787=CARTESIAN_POINT('Ctrl Pts',(89.4397101202682,1076.6484648082,437.875936544235));
#116788=CARTESIAN_POINT('Ctrl Pts',(89.4404716297984,1076.64821331939,437.926095822328));
#116789=CARTESIAN_POINT('Ctrl Pts',(89.442217060216,1076.64763689034,438.041064218952));
#116790=CARTESIAN_POINT('Ctrl Pts',(89.4213693793535,1076.64774924074,438.155263251906));
#116791=CARTESIAN_POINT('Ctrl Pts',(89.3369086710337,1076.6493305304,438.369011200203));
#116792=CARTESIAN_POINT('Ctrl Pts',(89.2741615572938,1076.65078152744,438.466508778896));
#116793=CARTESIAN_POINT('Ctrl Pts',(89.1147209668251,1076.65475310104,438.63181621552));
#116794=CARTESIAN_POINT('Ctrl Pts',(89.019566207292,1076.65723294942,438.698032125079));
#116795=CARTESIAN_POINT('Ctrl Pts',(88.8091103257634,1076.66278330872,438.790128042062));
#116796=CARTESIAN_POINT('Ctrl Pts',(88.6958206984086,1076.66579840644,438.81508978528));
#116797=CARTESIAN_POINT('Ctrl Pts',(88.574718553124,1076.66900488633,438.817665528259));
#116798=CARTESIAN_POINT('Ctrl Pts',(88.5684926881341,1076.66916969481,438.817731665138));
#116799=CARTESIAN_POINT('Ctrl Pts',(88.5622696992333,1076.6693343871,438.817731665138));
#116800=CARTESIAN_POINT('Origin',(93.479943233478,1067.7251047501,449.494798005067));
#116801=CARTESIAN_POINT('',(93.4799432334968,1078.36968470723,448.219353883931));
#116802=CARTESIAN_POINT('Ctrl Pts',(93.4801826298566,1078.32767378068,450.770242103737));
#116803=CARTESIAN_POINT('Ctrl Pts',(93.6475477114777,1078.31708652496,450.770210689898));
#116804=CARTESIAN_POINT('Ctrl Pts',(93.8133273471716,1078.30697943726,450.737236796184));
#116805=CARTESIAN_POINT('Ctrl Pts',(94.1110529047082,1078.2897292958,450.613914363091));
#116806=CARTESIAN_POINT('Ctrl Pts',(94.2421511453505,1078.28256593783,450.52910739579));
#116807=CARTESIAN_POINT('Ctrl Pts',(94.47314148915,1078.27107922897,450.311336576597));
#116808=CARTESIAN_POINT('Ctrl Pts',(94.5690466207419,1078.2670225275,450.178217006567));
#116809=CARTESIAN_POINT('Ctrl Pts',(94.6529474756453,1078.26462949725,449.996986510507));
#116810=CARTESIAN_POINT('Ctrl Pts',(94.6670491949256,1078.26429572532,449.962678154495));
#116811=CARTESIAN_POINT('Ctrl Pts',(94.6876349920122,1078.26393260025,449.905642734319));
#116812=CARTESIAN_POINT('Ctrl Pts',(94.695017938818,1078.26383669483,449.88326454698));
#116813=CARTESIAN_POINT('Ctrl Pts',(94.7070736130371,1078.2637464853,449.843007189547));
#116814=CARTESIAN_POINT('Ctrl Pts',(94.7119856793705,1078.26373470009,449.825206870223));
#116815=CARTESIAN_POINT('Ctrl Pts',(94.7215007826988,1078.26376851037,449.787556473735));
#116816=CARTESIAN_POINT('Ctrl Pts',(94.7260180969208,1078.26382015393,449.767690103934));
#116817=CARTESIAN_POINT('Ctrl Pts',(94.7365988617227,1078.2640440848,449.715393549379));
#116818=CARTESIAN_POINT('Ctrl Pts',(94.7418832817774,1078.26427119927,449.682821937226));
#116819=CARTESIAN_POINT('Ctrl Pts',(94.7589553049056,1078.26561079862,449.543642638043));
#116820=CARTESIAN_POINT('Ctrl Pts',(94.7585335793055,1078.26756089624,449.435996084373));
#116821=CARTESIAN_POINT('Ctrl Pts',(94.7284219549179,1078.27366930619,449.205341470702));
#116822=CARTESIAN_POINT('Ctrl Pts',(94.6939422154392,1078.27811235492,449.084100176053));
#116823=CARTESIAN_POINT('Ctrl Pts',(94.5844834156256,1078.28959207689,448.84170975938));
#116824=CARTESIAN_POINT('Ctrl Pts',(94.505828263565,1078.29679879806,448.724040549938));
#116825=CARTESIAN_POINT('Ctrl Pts',(94.3052850705498,1078.31345024192,448.510525371881));
#116826=CARTESIAN_POINT('Ctrl Pts',(94.1819070491363,1078.32289717681,448.419061114382));
#116827=CARTESIAN_POINT('Ctrl Pts',(93.8987475672184,1078.34306554176,448.279021051198));
#116828=CARTESIAN_POINT('Ctrl Pts',(93.7395370223165,1078.35364313157,448.235382198108));
#116829=CARTESIAN_POINT('Ctrl Pts',(93.4086729706007,1078.37418974403,448.210282468943));
#116830=CARTESIAN_POINT('Ctrl Pts',(93.2400015141554,1078.3839347676,448.230867165947));
#116831=CARTESIAN_POINT('Ctrl Pts',(92.9282270374595,1078.40067106426,448.333779738091));
#116832=CARTESIAN_POINT('Ctrl Pts',(92.7870323122245,1078.40763067077,448.412086778063));
#116833=CARTESIAN_POINT('Ctrl Pts',(92.5426094346535,1078.41853937265,448.615536314068));
#116834=CARTESIAN_POINT('Ctrl Pts',(92.4410186940592,1078.42243686271,448.738256576007));
#116835=CARTESIAN_POINT('Ctrl Pts',(92.3353775377774,1078.42553735098,448.928833482709));
#116836=CARTESIAN_POINT('Ctrl Pts',(92.3100600450754,1078.42614826811,448.983211849712));
#116837=CARTESIAN_POINT('Ctrl Pts',(92.2791929794852,1078.42667705712,449.063916897381));
#116838=CARTESIAN_POINT('Ctrl Pts',(92.2705014079795,1078.42679127977,449.088952966193));
#116839=CARTESIAN_POINT('Ctrl Pts',(92.2570433252745,1078.42690397541,449.132003527251));
#116840=CARTESIAN_POINT('Ctrl Pts',(92.2518801726277,1078.42692676637,449.149884769434));
#116841=CARTESIAN_POINT('Ctrl Pts',(92.2422504584826,1078.42692490095,449.186198345056));
#116842=CARTESIAN_POINT('Ctrl Pts',(92.2378000171455,1078.42689934546,449.204630150487));
#116843=CARTESIAN_POINT('Ctrl Pts',(92.2279502619266,1078.42677699351,449.249816463611));
#116844=CARTESIAN_POINT('Ctrl Pts',(92.2229956135971,1078.42665386618,449.276658109654));
#116845=CARTESIAN_POINT('Ctrl Pts',(92.2086628326856,1078.42604427424,449.371207953038));
#116846=CARTESIAN_POINT('Ctrl Pts',(92.2038678680935,1078.42529103033,449.43948895891));
#116847=CARTESIAN_POINT('Ctrl Pts',(92.2063028295234,1078.42156955022,449.677955713005));
#116848=CARTESIAN_POINT('Ctrl Pts',(92.2420651811146,1078.41701467454,449.845987096239));
#116849=CARTESIAN_POINT('Ctrl Pts',(92.3655792799109,1078.40555094395,450.130958778107));
#116850=CARTESIAN_POINT('Ctrl Pts',(92.4423770957565,1078.39926377994,450.249741709368));
#116851=CARTESIAN_POINT('Ctrl Pts',(92.639781211349,1078.38424392151,450.466503842991));
#116852=CARTESIAN_POINT('Ctrl Pts',(92.7620390281582,1078.37546379632,450.560007998539));
#116853=CARTESIAN_POINT('Ctrl Pts',(92.9872034922823,1078.35992787438,450.6754956304));
#116854=CARTESIAN_POINT('Ctrl Pts',(93.0816361975551,1078.3535620404,450.710605327249));
#116855=CARTESIAN_POINT('Ctrl Pts',(93.2777354264199,1078.34062038903,450.758186876195));
#116856=CARTESIAN_POINT('Ctrl Pts',(93.3787783042975,1078.33408846118,450.770261136972));
#116857=CARTESIAN_POINT('Ctrl Pts',(93.4801826298566,1078.32767378068,450.770242103737));
#116858=CARTESIAN_POINT('',(93.4799432334501,1076.36561958492,448.219353883931));
#116859=CARTESIAN_POINT('',(93.479943233478,1067.7251047501,448.219353883931));
#116860=CARTESIAN_POINT('Ctrl Pts',(93.4801397319905,1076.32317311768,450.770242111067));
#116861=CARTESIAN_POINT('Ctrl Pts',(93.3966391800305,1076.32851006915,450.770254975397));
#116862=CARTESIAN_POINT('Ctrl Pts',(93.3133414971078,1076.3339303567,450.762067917032));
#116863=CARTESIAN_POINT('Ctrl Pts',(93.1497499971195,1076.34475870276,450.729572381437));
#116864=CARTESIAN_POINT('Ctrl Pts',(93.0698354885403,1076.35014117197,450.705379818211));
#116865=CARTESIAN_POINT('Ctrl Pts',(92.836739106239,1076.36612940808,450.609059066668));
#116866=CARTESIAN_POINT('Ctrl Pts',(92.6949442321963,1076.37625737627,450.514159482743));
#116867=CARTESIAN_POINT('Ctrl Pts',(92.456901802598,1076.39427452854,450.274886685455));
#116868=CARTESIAN_POINT('Ctrl Pts',(92.3628568939185,1076.40199774594,450.133007941772));
#116869=CARTESIAN_POINT('Ctrl Pts',(92.2351340378411,1076.41424292262,449.820165117067));
#116870=CARTESIAN_POINT('Ctrl Pts',(92.202969309497,1076.41863513552,449.652218865655));
#116871=CARTESIAN_POINT('Ctrl Pts',(92.2061462687408,1076.42360522909,449.312901654591));
#116872=CARTESIAN_POINT('Ctrl Pts',(92.2416938301822,1076.42412210169,449.144959103998));
#116873=CARTESIAN_POINT('Ctrl Pts',(92.376375543339,1076.42117660296,448.83324001666));
#116874=CARTESIAN_POINT('Ctrl Pts',(92.4740078374944,1076.41775112604,448.692557144687));
#116875=CARTESIAN_POINT('Ctrl Pts',(92.7179325220569,1076.40727311881,448.458181072377));
#116876=CARTESIAN_POINT('Ctrl Pts',(92.8615712173566,1076.40033668268,448.366608964887));
#116877=CARTESIAN_POINT('Ctrl Pts',(93.176148830756,1076.38362615321,448.244617868714));
#116878=CARTESIAN_POINT('Ctrl Pts',(93.3440045530336,1076.37400987909,448.215452292248));
#116879=CARTESIAN_POINT('Ctrl Pts',(93.6826596272493,1076.35313032174,448.224129279082));
#116880=CARTESIAN_POINT('Ctrl Pts',(93.8501126669127,1076.34205873386,448.262460176437));
#116881=CARTESIAN_POINT('Ctrl Pts',(94.1577977508267,1076.32020256933,448.401478309504));
#116882=CARTESIAN_POINT('Ctrl Pts',(94.2954475977977,1076.30962762166,448.499905468882));
#116883=CARTESIAN_POINT('Ctrl Pts',(94.5246944317019,1076.29039063412,448.744273655185));
#116884=CARTESIAN_POINT('Ctrl Pts',(94.6141375007907,1076.28191586489,448.887805261111));
#116885=CARTESIAN_POINT('Ctrl Pts',(94.7322757779242,1076.2684440228,449.200946253375));
#116886=CARTESIAN_POINT('Ctrl Pts',(94.7599828200759,1076.26357300931,449.367436284188));
#116887=CARTESIAN_POINT('Ctrl Pts',(94.7495666775411,1076.25826497393,449.701213616718));
#116888=CARTESIAN_POINT('Ctrl Pts',(94.7117462240708,1076.25786835316,449.865224565764));
#116889=CARTESIAN_POINT('Ctrl Pts',(94.5752357038917,1076.26163815408,450.169195636705));
#116890=CARTESIAN_POINT('Ctrl Pts',(94.4779667113281,1076.26575996905,450.306213464761));
#116891=CARTESIAN_POINT('Ctrl Pts',(94.236224075899,1076.27788545298,450.535259222229));
#116892=CARTESIAN_POINT('Ctrl Pts',(94.0940336295003,1076.28577278385,450.625005130405));
#116893=CARTESIAN_POINT('Ctrl Pts',(93.7923508974505,1076.3035555458,450.74129559664));
#116894=CARTESIAN_POINT('Ctrl Pts',(93.6368948719087,1076.31315408721,450.770217960928));
#116895=CARTESIAN_POINT('Ctrl Pts',(93.4801397319905,1076.32317311768,450.770242111067));
#116896=CARTESIAN_POINT('Origin',(93.479943233478,1067.7251047501,449.494798005067));
#116897=CARTESIAN_POINT('',(93.479943233478,1076.33373423278,450.170242126204));
#116898=CARTESIAN_POINT('',(93.4799432334781,1076.35619778296,448.819353883931));
#116899=CARTESIAN_POINT('Ctrl Pts',(93.479943233478,1076.33373423278,450.170242126204));
#116900=CARTESIAN_POINT('Ctrl Pts',(93.4371754633824,1076.33643869804,450.170242126204));
#116901=CARTESIAN_POINT('Ctrl Pts',(93.3945029447023,1076.33919408693,450.166180168351));
#116902=CARTESIAN_POINT('Ctrl Pts',(93.3092123998598,1076.34481486458,450.149793282562));
#116903=CARTESIAN_POINT('Ctrl Pts',(93.2668405035828,1076.34766755124,450.137258346407));
#116904=CARTESIAN_POINT('Ctrl Pts',(93.1427944673026,1076.35620649091,450.086927080627));
#116905=CARTESIAN_POINT('Ctrl Pts',(93.0671353424771,1076.36167909722,450.036908765151));
#116906=CARTESIAN_POINT('Ctrl Pts',(92.9398637726623,1076.3715038067,449.910238678341));
#116907=CARTESIAN_POINT('Ctrl Pts',(92.8894860433503,1076.37576103081,449.834870332213));
#116908=CARTESIAN_POINT('Ctrl Pts',(92.8210536335252,1076.38253942125,449.668565823741));
#116909=CARTESIAN_POINT('Ctrl Pts',(92.8037738169076,1076.38498913436,449.57926606267));
#116910=CARTESIAN_POINT('Ctrl Pts',(92.8052559516844,1076.38773096296,449.400921098179));
#116911=CARTESIAN_POINT('Ctrl Pts',(92.8232839999973,1076.38803946154,449.313647021995));
#116912=CARTESIAN_POINT('Ctrl Pts',(92.8919407583486,1076.38652986799,449.15086205297));
#116913=CARTESIAN_POINT('Ctrl Pts',(92.9419423208957,1076.38472322065,449.076961826822));
#116914=CARTESIAN_POINT('Ctrl Pts',(93.0685981587866,1076.3791301043,448.951570441442));
#116915=CARTESIAN_POINT('Ctrl Pts',(93.144416855151,1076.37536546497,448.901745636581));
#116916=CARTESIAN_POINT('Ctrl Pts',(93.3079194127563,1076.3664986175,448.835930620374));
#116917=CARTESIAN_POINT('Ctrl Pts',(93.3935461910011,1076.36153221488,448.819353883931));
#116918=CARTESIAN_POINT('Ctrl Pts',(93.4799432334782,1076.35619778296,448.819353883931));
#116919=CARTESIAN_POINT('',(93.479943233478,1082.7251047501,448.819353883931));
#116920=CARTESIAN_POINT('',(93.479943233478,1067.7251047501,448.819353883931));
#116921=CARTESIAN_POINT('Origin',(93.479943233478,1082.7251047501,449.494798005067));
#116922=CARTESIAN_POINT('Ctrl Pts',(93.4799432334782,1076.35619778296,448.819353883931));
#116923=CARTESIAN_POINT('Ctrl Pts',(93.4799582875746,1076.35619685347,448.819353883931));
#116924=CARTESIAN_POINT('Ctrl Pts',(93.4799733416942,1076.35619592397,448.819353884573));
#116925=CARTESIAN_POINT('Ctrl Pts',(93.4799883958374,1076.35619499446,448.81935388558));
#116926=CARTESIAN_POINT('Ctrl Pts',(93.5239130761171,1076.35348288653,448.819356822524));
#116927=CARTESIAN_POINT('Ctrl Pts',(93.5677293071545,1076.35069484535,448.823644427834));
#116928=CARTESIAN_POINT('Ctrl Pts',(93.6539989035039,1076.34503745886,448.840682570169));
#116929=CARTESIAN_POINT('Ctrl Pts',(93.6962459378029,1076.34218124833,448.853412412776));
#116930=CARTESIAN_POINT('Ctrl Pts',(93.819820025376,1076.33356167836,448.904257531836));
#116931=CARTESIAN_POINT('Ctrl Pts',(93.8950974830939,1076.32793422957,448.954512861949));
#116932=CARTESIAN_POINT('Ctrl Pts',(94.0209077297674,1076.31774179405,449.080757673004));
#116933=CARTESIAN_POINT('Ctrl Pts',(94.0705124222885,1076.31326426424,449.155221544693));
#116934=CARTESIAN_POINT('Ctrl Pts',(94.1380576308787,1076.30606768474,449.318924767482));
#116935=CARTESIAN_POINT('Ctrl Pts',(94.1554180377051,1076.30341556689,449.406537685414));
#116936=CARTESIAN_POINT('Ctrl Pts',(94.1553566605395,1076.30034980644,449.583324463453));
#116937=CARTESIAN_POINT('Ctrl Pts',(94.1380145459098,1076.29996170617,449.670764062105));
#116938=CARTESIAN_POINT('Ctrl Pts',(94.0706868754874,1076.30152307186,449.833963248197));
#116939=CARTESIAN_POINT('Ctrl Pts',(94.0213835798089,1076.30345527971,449.90813282625));
#116940=CARTESIAN_POINT('Ctrl Pts',(93.8970065888715,1076.30937099208,450.03339265262));
#116941=CARTESIAN_POINT('Ctrl Pts',(93.82310625867,1076.31329879062,450.083230605174));
#116942=CARTESIAN_POINT('Ctrl Pts',(93.6601858134117,1076.3225953758,450.151735095738));
#116943=CARTESIAN_POINT('Ctrl Pts',(93.572697535404,1076.32787696942,450.16966190179));
#116944=CARTESIAN_POINT('Ctrl Pts',(93.4828271644317,1076.33355192919,450.170237509001));
#116945=CARTESIAN_POINT('Ctrl Pts',(93.4813851448154,1076.33364305199,450.170242126204));
#116946=CARTESIAN_POINT('Ctrl Pts',(93.479943233478,1076.33373423278,450.170242126204));
#116947=CARTESIAN_POINT('Origin',(97.7222027015969,1067.7251047501,462.678935876427));
#116948=CARTESIAN_POINT('',(97.7222027015967,1077.70670509264,461.580104740434));
#116949=CARTESIAN_POINT('Ctrl Pts',(97.7223774853707,1077.62439637431,463.777766998518));
#116950=CARTESIAN_POINT('Ctrl Pts',(97.8652488471286,1077.61047146469,463.777744272919));
#116951=CARTESIAN_POINT('Ctrl Pts',(98.0068778787342,1077.59763005528,463.749857219864));
#116952=CARTESIAN_POINT('Ctrl Pts',(98.2526249076054,1077.57726328201,463.649034000485));
#116953=CARTESIAN_POINT('Ctrl Pts',(98.3574905237846,1077.56938265876,463.583865810438));
#116954=CARTESIAN_POINT('Ctrl Pts',(98.5370653843179,1077.55767770435,463.425313758873));
#116955=CARTESIAN_POINT('Ctrl Pts',(98.6118031240287,1077.55375460285,463.334466346593));
#116956=CARTESIAN_POINT('Ctrl Pts',(98.6868906872435,1077.55125604233,463.206021931477));
#116957=CARTESIAN_POINT('Ctrl Pts',(98.7017513688048,1077.55086778332,463.177861979705));
#116958=CARTESIAN_POINT('Ctrl Pts',(98.723157007946,1077.55048929999,463.132644603069));
#116959=CARTESIAN_POINT('Ctrl Pts',(98.7305347726689,1077.55039988936,463.116002901385));
#116960=CARTESIAN_POINT('Ctrl Pts',(98.7433633565128,1077.55032428066,463.085009950598));
#116961=CARTESIAN_POINT('Ctrl Pts',(98.7489333403759,1077.5503240831,463.070713150755));
#116962=CARTESIAN_POINT('Ctrl Pts',(98.7604385804056,1077.55039873526,463.039249475392));
#116963=CARTESIAN_POINT('Ctrl Pts',(98.7662512017515,1077.55048736259,463.022042773026));
#116964=CARTESIAN_POINT('Ctrl Pts',(98.7812747130292,1077.55086882627,462.973645347321));
#116965=CARTESIAN_POINT('Ctrl Pts',(98.7895309708941,1077.55126752842,462.942179720779));
#116966=CARTESIAN_POINT('Ctrl Pts',(98.8256759145672,1077.55417681668,462.774435855143));
#116967=CARTESIAN_POINT('Ctrl Pts',(98.8288759297638,1077.55930118692,462.634237323956));
#116968=CARTESIAN_POINT('Ctrl Pts',(98.7868430771987,1077.57316198976,462.383526553364));
#116969=CARTESIAN_POINT('Ctrl Pts',(98.7500126803987,1077.58104747223,462.273609643655));
#116970=CARTESIAN_POINT('Ctrl Pts',(98.6383090863358,1077.60028657507,462.059057600028));
#116971=CARTESIAN_POINT('Ctrl Pts',(98.560797625596,1077.61176560098,461.957680001032));
#116972=CARTESIAN_POINT('Ctrl Pts',(98.3674511948929,1077.63739383679,461.779071930105));
#116973=CARTESIAN_POINT('Ctrl Pts',(98.2506922038987,1077.65146467942,461.705910199451));
#116974=CARTESIAN_POINT('Ctrl Pts',(97.9865450051201,1077.68074653231,461.602266454776));
#116975=CARTESIAN_POINT('Ctrl Pts',(97.8400508784254,1077.69567544329,461.576554671687));
#116976=CARTESIAN_POINT('Ctrl Pts',(97.5502102397836,1077.72284129563,461.584316882894));
#116977=CARTESIAN_POINT('Ctrl Pts',(97.409604703891,1077.73489848313,461.615861291594));
#116978=CARTESIAN_POINT('Ctrl Pts',(97.1698005802234,1077.75347127226,461.721600828075));
#116979=CARTESIAN_POINT('Ctrl Pts',(97.069200000847,1077.76045186913,461.787157714475));
#116980=CARTESIAN_POINT('Ctrl Pts',(96.8984418442197,1077.77065893617,461.943156169815));
#116981=CARTESIAN_POINT('Ctrl Pts',(96.8277981069749,1077.77403230737,462.030850174253));
#116982=CARTESIAN_POINT('Ctrl Pts',(96.7560163178606,1077.77621092353,462.154645142902));
#116983=CARTESIAN_POINT('Ctrl Pts',(96.7415657161512,1077.77655464805,462.182198335974));
#116984=CARTESIAN_POINT('Ctrl Pts',(96.72065487641,1077.77689079144,462.22654950586));
#116985=CARTESIAN_POINT('Ctrl Pts',(96.7134051362498,1077.7769702779,462.242955417096));
#116986=CARTESIAN_POINT('Ctrl Pts',(96.7013379646493,1077.77703368948,462.272177657662));
#116987=CARTESIAN_POINT('Ctrl Pts',(96.696352470503,1077.77703579725,462.28492018693));
#116988=CARTESIAN_POINT('Ctrl Pts',(96.685532330415,1077.77698284557,462.314174342721));
#116989=CARTESIAN_POINT('Ctrl Pts',(96.6798518613852,1077.77691163816,462.330738878175));
#116990=CARTESIAN_POINT('Ctrl Pts',(96.6655000931725,1077.77660560186,462.376093948235));
#116991=CARTESIAN_POINT('Ctrl Pts',(96.6576109573208,1077.77629020204,462.405114944635));
#116992=CARTESIAN_POINT('Ctrl Pts',(96.6255903096901,1077.77419969049,462.545405709047));
#116993=CARTESIAN_POINT('Ctrl Pts',(96.6176693930722,1077.77082065323,462.659606965961));
#116994=CARTESIAN_POINT('Ctrl Pts',(96.6369579321418,1077.76091280199,462.884263300539));
#116995=CARTESIAN_POINT('Ctrl Pts',(96.6634346560488,1077.75449909266,462.993405676657));
#116996=CARTESIAN_POINT('Ctrl Pts',(96.7530884914899,1077.7381816032,463.211563535045));
#116997=CARTESIAN_POINT('Ctrl Pts',(96.8194456910075,1077.72808106501,463.317570621166));
#116998=CARTESIAN_POINT('Ctrl Pts',(96.991592198616,1077.70471527976,463.510655144333));
#116999=CARTESIAN_POINT('Ctrl Pts',(97.0988195395435,1077.69144661683,463.593759639793));
#117000=CARTESIAN_POINT('Ctrl Pts',(97.2945945973171,1077.66893027088,463.694785591453));
#117001=CARTESIAN_POINT('Ctrl Pts',(97.3752305141564,1077.66003853043,463.725075789592));
#117002=CARTESIAN_POINT('Ctrl Pts',(97.5448563663803,1077.64207150673,463.766998119792));
#117003=CARTESIAN_POINT('Ctrl Pts',(97.6334417894073,1077.63306446226,463.777781144929));
#117004=CARTESIAN_POINT('Ctrl Pts',(97.7223774853707,1077.62439637431,463.777766998518));
#117005=CARTESIAN_POINT('',(97.7222027015771,1075.6961592181,461.580104740434));
#117006=CARTESIAN_POINT('',(97.7222027015969,1067.7251047501,461.580104740434));
#117007=CARTESIAN_POINT('Ctrl Pts',(97.7213962340406,1075.61319330111,463.777766716473));
#117008=CARTESIAN_POINT('Ctrl Pts',(97.5770261561073,1075.62739687131,463.777660758595));
#117009=CARTESIAN_POINT('Ctrl Pts',(97.4341242719184,1075.64244589601,463.749104628276));
#117010=CARTESIAN_POINT('Ctrl Pts',(97.1656082188661,1075.67268771489,463.637621917011));
#117011=CARTESIAN_POINT('Ctrl Pts',(97.0428695849892,1075.68758788676,463.554963927471));
#117012=CARTESIAN_POINT('Ctrl Pts',(96.837686314047,1075.71492195647,463.346959379739));
#117013=CARTESIAN_POINT('Ctrl Pts',(96.756960917834,1075.72710923841,463.223924830604));
#117014=CARTESIAN_POINT('Ctrl Pts',(96.6483007962585,1075.7472871335,462.953466622021));
#117015=CARTESIAN_POINT('Ctrl Pts',(96.6213648162697,1075.75508627585,462.8087842277));
#117016=CARTESIAN_POINT('Ctrl Pts',(96.6256133146802,1075.76531543224,462.516949278297));
#117017=CARTESIAN_POINT('Ctrl Pts',(96.656816480121,1075.76763690043,462.372790660382));
#117018=CARTESIAN_POINT('Ctrl Pts',(96.7738060454817,1075.76644992584,462.105082237661));
#117019=CARTESIAN_POINT('Ctrl Pts',(96.8583708276482,1075.76295468752,461.984297679999));
#117020=CARTESIAN_POINT('Ctrl Pts',(97.0695415973137,1075.75052545678,461.782986595226));
#117021=CARTESIAN_POINT('Ctrl Pts',(97.1939544639372,1075.7417206361,461.704478040095));
#117022=CARTESIAN_POINT('Ctrl Pts',(97.4662404315634,1075.71981663867,461.600412100679));
#117023=CARTESIAN_POINT('Ctrl Pts',(97.6114601384691,1075.70692132068,461.576034860562));
#117024=CARTESIAN_POINT('Ctrl Pts',(97.8285214474085,1075.68587135561,461.582926702863));
#117025=CARTESIAN_POINT('Ctrl Pts',(97.8995578343671,1075.67869690786,461.592161096067));
#117026=CARTESIAN_POINT('Ctrl Pts',(98.0390806357657,1075.66402382542,461.624343517563));
#117027=CARTESIAN_POINT('Ctrl Pts',(98.1072333201016,1075.65655780719,461.647273957167));
#117028=CARTESIAN_POINT('Ctrl Pts',(98.3060072031474,1075.63385069365,461.736611056026));
#117029=CARTESIAN_POINT('Ctrl Pts',(98.4261202769493,1075.6187994765,461.822583420046));
#117030=CARTESIAN_POINT('Ctrl Pts',(98.6244761046872,1075.59106783417,462.03533062314));
#117031=CARTESIAN_POINT('Ctrl Pts',(98.7013213763591,1075.57862690897,462.15957890916));
#117032=CARTESIAN_POINT('Ctrl Pts',(98.802151146019,1075.55805915997,462.430202485468));
#117033=CARTESIAN_POINT('Ctrl Pts',(98.825461828968,1075.55011041699,462.573807692676));
#117034=CARTESIAN_POINT('Ctrl Pts',(98.8152523198532,1075.53989503967,462.861188426707));
#117035=CARTESIAN_POINT('Ctrl Pts',(98.782185188029,1075.53769666475,463.002099720797));
#117036=CARTESIAN_POINT('Ctrl Pts',(98.6638974462999,1075.53937606489,463.26296984945));
#117037=CARTESIAN_POINT('Ctrl Pts',(98.5800032503363,1075.54321998508,463.380378597254));
#117038=CARTESIAN_POINT('Ctrl Pts',(98.3718309816341,1075.55643045529,463.576673547403));
#117039=CARTESIAN_POINT('Ctrl Pts',(98.2495045334886,1075.56567869409,463.653524192746));
#117040=CARTESIAN_POINT('Ctrl Pts',(97.9899832981551,1075.58763380002,463.753158562953));
#117041=CARTESIAN_POINT('Ctrl Pts',(97.8561966645764,1075.59993122211,463.777865650877));
#117042=CARTESIAN_POINT('Ctrl Pts',(97.7213962340406,1075.61319330111,463.777766716473));
#117043=CARTESIAN_POINT('Origin',(97.7222027015969,1067.7251047501,462.678935876427));
#117044=CARTESIAN_POINT('',(97.7222027015969,1075.63649232379,463.177767012419));
#117045=CARTESIAN_POINT('',(97.7222027015972,1075.6741872497,462.180104740434));
#117046=CARTESIAN_POINT('Ctrl Pts',(97.7222027015969,1075.63649232379,463.177767012419));
#117047=CARTESIAN_POINT('Ctrl Pts',(97.6572569350772,1075.64283239013,463.177767012419));
#117048=CARTESIAN_POINT('Ctrl Pts',(97.5929472946405,1075.6495721601,463.165083811798));
#117049=CARTESIAN_POINT('Ctrl Pts',(97.4712302351422,1075.66326292133,463.115154326405));
#117050=CARTESIAN_POINT('Ctrl Pts',(97.4152347351747,1075.67008164955,463.077749631703));
#117051=CARTESIAN_POINT('Ctrl Pts',(97.3214347213736,1075.68266182711,462.983286339805));
#117052=CARTESIAN_POINT('Ctrl Pts',(97.2844710857069,1075.68830516242,462.927233885765));
#117053=CARTESIAN_POINT('Ctrl Pts',(97.2347461427881,1075.69766744456,462.803943202293));
#117054=CARTESIAN_POINT('Ctrl Pts',(97.2224316028057,1075.70129708935,462.737970559391));
#117055=CARTESIAN_POINT('Ctrl Pts',(97.2244011812662,1075.705997423,462.606444795298));
#117056=CARTESIAN_POINT('Ctrl Pts',(97.2380806517,1075.70707708838,462.542216119828));
#117057=CARTESIAN_POINT('Ctrl Pts',(97.2893356417546,1075.70663047217,462.422640387586));
#117058=CARTESIAN_POINT('Ctrl Pts',(97.3263853081653,1075.70511021377,462.368480132492));
#117059=CARTESIAN_POINT('Ctrl Pts',(97.4202147779464,1075.69957691317,462.276369805907));
#117060=CARTESIAN_POINT('Ctrl Pts',(97.4764713908016,1075.69556253835,462.239782288104));
#117061=CARTESIAN_POINT('Ctrl Pts',(97.5966624666558,1075.68582134651,462.19207681243));
#117062=CARTESIAN_POINT('Ctrl Pts',(97.6589621544798,1075.68028190558,462.180158261962));
#117063=CARTESIAN_POINT('Ctrl Pts',(97.7217791146744,1075.67422807885,462.180104920357));
#117064=CARTESIAN_POINT('Ctrl Pts',(97.7219203119211,1075.67421447132,462.180104800458));
#117065=CARTESIAN_POINT('Ctrl Pts',(97.7220615075749,1075.67420086161,462.180104740434));
#117066=CARTESIAN_POINT('Ctrl Pts',(97.7222027015975,1075.6741872497,462.180104740434));
#117067=CARTESIAN_POINT('',(97.7222027015969,1082.7251047501,462.180104740434));
#117068=CARTESIAN_POINT('',(97.7222027015969,1067.7251047501,462.180104740434));
#117069=CARTESIAN_POINT('Origin',(97.7222027015969,1082.7251047501,462.678935876427));
#117070=CARTESIAN_POINT('Ctrl Pts',(97.7222027015975,1075.6741872497,462.180104740434));
#117071=CARTESIAN_POINT('Ctrl Pts',(97.754609689393,1075.67106303118,462.180104740434));
#117072=CARTESIAN_POINT('Ctrl Pts',(97.7869307534788,1075.66782351289,462.183262736636));
#117073=CARTESIAN_POINT('Ctrl Pts',(97.850693653922,1075.66118268563,462.19583607518));
#117074=CARTESIAN_POINT('Ctrl Pts',(97.8819805854774,1075.65779584215,462.205263039015));
#117075=CARTESIAN_POINT('Ctrl Pts',(97.973996019334,1075.64743399608,462.243148976887));
#117076=CARTESIAN_POINT('Ctrl Pts',(98.0301420491263,1075.64053600106,462.280827109893));
#117077=CARTESIAN_POINT('Ctrl Pts',(98.1232581986539,1075.62785013386,462.375148449897));
#117078=CARTESIAN_POINT('Ctrl Pts',(98.1597193537219,1075.62216301585,462.430485544627));
#117079=CARTESIAN_POINT('Ctrl Pts',(98.2089844657867,1075.61268012852,462.551883093394));
#117080=CARTESIAN_POINT('Ctrl Pts',(98.2214434684478,1075.60896646353,462.616701334425));
#117081=CARTESIAN_POINT('Ctrl Pts',(98.2206060480949,1075.60403958664,462.747201156494));
#117082=CARTESIAN_POINT('Ctrl Pts',(98.2074623439131,1075.60286166937,462.811581640935));
#117083=CARTESIAN_POINT('Ctrl Pts',(98.1572135606402,1075.60320924604,462.931559153335));
#117084=CARTESIAN_POINT('Ctrl Pts',(98.1206638117141,1075.60472521221,462.985977292797));
#117085=CARTESIAN_POINT('Ctrl Pts',(98.0286985689788,1075.61026144565,463.077844669439));
#117086=CARTESIAN_POINT('Ctrl Pts',(97.9741443597817,1075.61423299495,463.114340784303));
#117087=CARTESIAN_POINT('Ctrl Pts',(97.8538834137291,1075.62412149214,463.164489182562));
#117088=CARTESIAN_POINT('Ctrl Pts',(97.7892776797568,1075.62995335678,463.17752150349));
#117089=CARTESIAN_POINT('Ctrl Pts',(97.7234368912988,1075.63637188279,463.177765867431));
#117090=CARTESIAN_POINT('Ctrl Pts',(97.7228197677316,1075.63643208521,463.177767012419));
#117091=CARTESIAN_POINT('Ctrl Pts',(97.7222027015969,1075.63649232379,463.177767012419));
#117092=CARTESIAN_POINT('Origin',(99.1956712429292,1067.7251047501,476.588028064191));
#117093=CARTESIAN_POINT('',(99.1956712429291,1076.88734730071,475.497487315463));
#117094=CARTESIAN_POINT('Ctrl Pts',(99.1958465811725,1076.75140941306,477.678568798823));
#117095=CARTESIAN_POINT('Ctrl Pts',(99.3351617747574,1076.7346540188,477.678546399586));
#117096=CARTESIAN_POINT('Ctrl Pts',(99.4734108960095,1076.71964145972,477.651828116974));
#117097=CARTESIAN_POINT('Ctrl Pts',(99.7161417774516,1076.69644564892,477.554078976883));
#117098=CARTESIAN_POINT('Ctrl Pts',(99.8209503002571,1076.68780224914,477.489830406464));
#117099=CARTESIAN_POINT('Ctrl Pts',(99.9771448754437,1076.67750000721,477.353420953028));
#117100=CARTESIAN_POINT('Ctrl Pts',(100.034524803286,1076.67455478323,477.290073020182));
#117101=CARTESIAN_POINT('Ctrl Pts',(100.100082677636,1076.67244456217,477.198020799036));
#117102=CARTESIAN_POINT('Ctrl Pts',(100.115331571195,1076.67207042614,477.174778670863));
#117103=CARTESIAN_POINT('Ctrl Pts',(100.13838380948,1076.67170327014,477.136532058407));
#117104=CARTESIAN_POINT('Ctrl Pts',(100.146754487306,1076.67161830386,477.121885998868));
#117105=CARTESIAN_POINT('Ctrl Pts',(100.161250987515,1076.67156200304,477.095097703538));
#117106=CARTESIAN_POINT('Ctrl Pts',(100.167495713823,1076.6715718113,477.083024082478));
#117107=CARTESIAN_POINT('Ctrl Pts',(100.181620291774,1076.67167681384,477.054417309451));
#117108=CARTESIAN_POINT('Ctrl Pts',(100.189312418226,1076.67180046132,477.037796490646));
#117109=CARTESIAN_POINT('Ctrl Pts',(100.210170509832,1076.67233666983,476.98957729023));
#117110=CARTESIAN_POINT('Ctrl Pts',(100.222270962653,1076.67290662092,476.957545393931));
#117111=CARTESIAN_POINT('Ctrl Pts',(100.277467201558,1076.67702217729,476.787656350893));
#117112=CARTESIAN_POINT('Ctrl Pts',(100.294314996694,1076.68419826844,476.642980662656));
#117113=CARTESIAN_POINT('Ctrl Pts',(100.273215456004,1076.70320492643,476.384279417923));
#117114=CARTESIAN_POINT('Ctrl Pts',(100.245620457751,1076.71370283127,476.271565322794));
#117115=CARTESIAN_POINT('Ctrl Pts',(100.151824386149,1076.73914623861,476.04844949399));
#117116=CARTESIAN_POINT('Ctrl Pts',(100.08269373915,1076.75424250037,475.941123726815));
#117117=CARTESIAN_POINT('Ctrl Pts',(99.9039530308407,1076.78783564412,475.74757637163));
#117118=CARTESIAN_POINT('Ctrl Pts',(99.792997548431,1076.80622580733,475.665426877847));
#117119=CARTESIAN_POINT('Ctrl Pts',(99.538988806265,1076.84405326829,475.542793526404));
#117120=CARTESIAN_POINT('Ctrl Pts',(99.3967517492221,1076.86313019544,475.506354948691));
#117121=CARTESIAN_POINT('Ctrl Pts',(99.1107527556563,1076.89770522881,475.491710286497));
#117122=CARTESIAN_POINT('Ctrl Pts',(98.9697771982252,1076.91298595081,475.511822942385));
#117123=CARTESIAN_POINT('Ctrl Pts',(98.7228795308952,1076.93655323769,475.597980489552));
#117124=CARTESIAN_POINT('Ctrl Pts',(98.6165747687278,1076.94538168441,475.656123314795));
#117125=CARTESIAN_POINT('Ctrl Pts',(98.4429096462419,1076.95725957267,475.792600900962));
#117126=CARTESIAN_POINT('Ctrl Pts',(98.3728785958174,1076.96096863199,475.865261488284));
#117127=CARTESIAN_POINT('Ctrl Pts',(98.2965084980456,1076.96344766329,475.970253245765));
#117128=CARTESIAN_POINT('Ctrl Pts',(98.2802182803277,1076.96385410512,475.994660144318));
#117129=CARTESIAN_POINT('Ctrl Pts',(98.2559131364058,1076.96425457595,476.034463937463));
#117130=CARTESIAN_POINT('Ctrl Pts',(98.2472480027526,1076.96434931872,476.04944481332));
#117131=CARTESIAN_POINT('Ctrl Pts',(98.2317871277339,1076.96442531801,476.077705784519));
#117132=CARTESIAN_POINT('Ctrl Pts',(98.224900370466,1076.96442045686,476.090931163826));
#117133=CARTESIAN_POINT('Ctrl Pts',(98.2102834441325,1076.96432123259,476.120464624055));
#117134=CARTESIAN_POINT('Ctrl Pts',(98.202682663047,1076.96420828806,476.136831502438));
#117135=CARTESIAN_POINT('Ctrl Pts',(98.1821749620315,1076.96371932022,476.18402218748));
#117136=CARTESIAN_POINT('Ctrl Pts',(98.1702748581943,1076.96320143568,476.215258297867));
#117137=CARTESIAN_POINT('Ctrl Pts',(98.1147447674314,1076.95939189429,476.383920280059));
#117138=CARTESIAN_POINT('Ctrl Pts',(98.0973062344002,1076.9526395624,476.528286014376));
#117139=CARTESIAN_POINT('Ctrl Pts',(98.1172160619302,1076.93453986928,476.786949066574));
#117140=CARTESIAN_POINT('Ctrl Pts',(98.1443316871356,1076.92447492308,476.899877821638));
#117141=CARTESIAN_POINT('Ctrl Pts',(98.2373240012515,1076.89985495387,477.123773319765));
#117142=CARTESIAN_POINT('Ctrl Pts',(98.3062050670795,1076.88513004011,477.231626860478));
#117143=CARTESIAN_POINT('Ctrl Pts',(98.4848475972005,1076.85201768475,477.426421706207));
#117144=CARTESIAN_POINT('Ctrl Pts',(98.596019935673,1076.83370848726,477.509196004444));
#117145=CARTESIAN_POINT('Ctrl Pts',(98.7912373214412,1076.80456106505,477.603932553809));
#117146=CARTESIAN_POINT('Ctrl Pts',(98.8665394631734,1076.79389458265,477.630767999022));
#117147=CARTESIAN_POINT('Ctrl Pts',(99.0265397562579,1076.77237044624,477.668699342284));
#117148=CARTESIAN_POINT('Ctrl Pts',(99.1110212610301,1076.76161132748,477.678582437124));
#117149=CARTESIAN_POINT('Ctrl Pts',(99.1958465811724,1076.75140941306,477.678568798823));
#117150=CARTESIAN_POINT('',(99.1956712429125,1074.86964135584,475.497487315462));
#117151=CARTESIAN_POINT('',(99.1956712429292,1067.7251047501,475.497487315462));
#117152=CARTESIAN_POINT('Ctrl Pts',(99.1952643927994,1074.73264861964,477.678568737027));
#117153=CARTESIAN_POINT('Ctrl Pts',(99.0517460771263,1074.75005615301,477.67851519437));
#117154=CARTESIAN_POINT('Ctrl Pts',(98.9097698670427,1074.76900244351,477.650133765574));
#117155=CARTESIAN_POINT('Ctrl Pts',(98.7113786882859,1074.79803574604,477.567751158396));
#117156=CARTESIAN_POINT('Ctrl Pts',(98.6481671702273,1074.8077433162,477.533880670059));
#117157=CARTESIAN_POINT('Ctrl Pts',(98.4681042010753,1074.83684315306,477.413257926984));
#117158=CARTESIAN_POINT('Ctrl Pts',(98.3646996972244,1074.85564381212,477.309090431949));
#117159=CARTESIAN_POINT('Ctrl Pts',(98.2053095581982,1074.88957139567,477.066908547697));
#117160=CARTESIAN_POINT('Ctrl Pts',(98.1505262447493,1074.90439905785,476.931469881838));
#117161=CARTESIAN_POINT('Ctrl Pts',(98.0971762665379,1074.92820415866,476.646984446269));
#117162=CARTESIAN_POINT('Ctrl Pts',(98.0990043535727,1074.93695809786,476.500856558028));
#117163=CARTESIAN_POINT('Ctrl Pts',(98.1591409803313,1074.94710326793,476.220670198977));
#117164=CARTESIAN_POINT('Ctrl Pts',(98.2155816401616,1074.94855352414,476.089238716457));
#117165=CARTESIAN_POINT('Ctrl Pts',(98.3757013610401,1074.94416584569,475.855191509198));
#117166=CARTESIAN_POINT('Ctrl Pts',(98.4777903545748,1074.9383661131,475.754977821258));
#117167=CARTESIAN_POINT('Ctrl Pts',(98.7170546997745,1074.91997135385,475.597477159545));
#117168=CARTESIAN_POINT('Ctrl Pts',(98.8525072930294,1074.90741099956,475.542863991436));
#117169=CARTESIAN_POINT('Ctrl Pts',(99.1371075425808,1074.87710181334,475.489426290735));
#117170=CARTESIAN_POINT('Ctrl Pts',(99.2835000073978,1074.85962400353,475.491430677514));
#117171=CARTESIAN_POINT('Ctrl Pts',(99.4945554115769,1074.8316404046,475.536836580004));
#117172=CARTESIAN_POINT('Ctrl Pts',(99.5624190940086,1074.82217675517,475.558550211646));
#117173=CARTESIAN_POINT('Ctrl Pts',(99.6931910602662,1074.80298217493,475.614968030021));
#117174=CARTESIAN_POINT('Ctrl Pts',(99.7557834634978,1074.79329335006,475.649600604602));
#117175=CARTESIAN_POINT('Ctrl Pts',(99.9342486124761,1074.76407509348,475.772602348726));
#117176=CARTESIAN_POINT('Ctrl Pts',(100.036371341694,1074.74503432885,475.878296152674));
#117177=CARTESIAN_POINT('Ctrl Pts',(100.192042063617,1074.71064395715,476.122051110436));
#117178=CARTESIAN_POINT('Ctrl Pts',(100.24479599716,1074.69557213169,476.257324526878));
#117179=CARTESIAN_POINT('Ctrl Pts',(100.294422682368,1074.67143879966,476.539592348336));
#117180=CARTESIAN_POINT('Ctrl Pts',(100.291374202805,1074.66255692892,476.683674581217));
#117181=CARTESIAN_POINT('Ctrl Pts',(100.229978789766,1074.65222651072,476.961607860377));
#117182=CARTESIAN_POINT('Ctrl Pts',(100.172738965682,1074.65081939223,477.092718628694));
#117183=CARTESIAN_POINT('Ctrl Pts',(100.011398926172,1074.6556532975,477.325513495924));
#117184=CARTESIAN_POINT('Ctrl Pts',(99.9090348548584,1074.66182947456,477.424883587504));
#117185=CARTESIAN_POINT('Ctrl Pts',(99.6716504411043,1074.68097646112,477.57944521021));
#117186=CARTESIAN_POINT('Ctrl Pts',(99.5387978489786,1074.69379625042,477.632821930371));
#117187=CARTESIAN_POINT('Ctrl Pts',(99.3322582714828,1074.71642671158,477.672157205324));
#117188=CARTESIAN_POINT('Ctrl Pts',(99.2638100766752,1074.72433461963,477.678594309498));
#117189=CARTESIAN_POINT('Ctrl Pts',(99.1952643927994,1074.73264861964,477.678568737027));
#117190=CARTESIAN_POINT('Origin',(99.1956712429292,1067.7251047501,476.588028064191));
#117191=CARTESIAN_POINT('',(99.1956712429292,1074.77118038462,477.078568812919));
#117192=CARTESIAN_POINT('',(99.1956712429291,1074.8328201009,476.097487315462));
#117193=CARTESIAN_POINT('Ctrl Pts',(99.1956712429292,1074.77118038462,477.078568812919));
#117194=CARTESIAN_POINT('Ctrl Pts',(99.1626961372876,1074.7751548492,477.078568812919));
#117195=CARTESIAN_POINT('Ctrl Pts',(99.1297477646064,1074.7793322153,477.075243758096));
#117196=CARTESIAN_POINT('Ctrl Pts',(99.0657858437502,1074.78785081691,477.062155481617));
#117197=CARTESIAN_POINT('Ctrl Pts',(99.0349616082967,1074.7921556658,477.052611997444));
#117198=CARTESIAN_POINT('Ctrl Pts',(98.9756735887002,1074.80084234471,477.02764702067));
#117199=CARTESIAN_POINT('Ctrl Pts',(98.9473408483259,1074.80520455892,477.012287419544));
#117200=CARTESIAN_POINT('Ctrl Pts',(98.8664725268024,1074.81832574806,476.957552677079));
#117201=CARTESIAN_POINT('Ctrl Pts',(98.8200739716366,1074.82682834479,476.910307871755));
#117202=CARTESIAN_POINT('Ctrl Pts',(98.7487547995675,1074.84219589629,476.8005306581));
#117203=CARTESIAN_POINT('Ctrl Pts',(98.7244136738683,1074.84892064961,476.739145109896));
#117204=CARTESIAN_POINT('Ctrl Pts',(98.7014411623352,1074.85962464656,476.611139004963));
#117205=CARTESIAN_POINT('Ctrl Pts',(98.7026768247695,1074.86353531181,476.545884627614));
#117206=CARTESIAN_POINT('Ctrl Pts',(98.7302649995425,1074.86806023038,476.420433380235));
#117207=CARTESIAN_POINT('Ctrl Pts',(98.7559520265371,1074.86867885329,476.361440805009));
#117208=CARTESIAN_POINT('Ctrl Pts',(98.8284834149077,1074.86659269479,476.256563420427));
#117209=CARTESIAN_POINT('Ctrl Pts',(98.874591640806,1074.86390876541,476.211746241645));
#117210=CARTESIAN_POINT('Ctrl Pts',(98.9815985143537,1074.85553641748,476.142036772301));
#117211=CARTESIAN_POINT('Ctrl Pts',(99.041523297757,1074.84991135535,476.117977723604));
#117212=CARTESIAN_POINT('Ctrl Pts',(99.1344242837301,1074.83994515504,476.100359062507));
#117213=CARTESIAN_POINT('Ctrl Pts',(99.165025857401,1074.8364766822,476.097487315462));
#117214=CARTESIAN_POINT('Ctrl Pts',(99.1956712429291,1074.8328201009,476.097487315462));
#117215=CARTESIAN_POINT('',(99.1956712429292,1082.7251047501,476.097487315462));
#117216=CARTESIAN_POINT('',(99.1956712429292,1067.7251047501,476.097487315462));
#117217=CARTESIAN_POINT('Origin',(99.1956712429292,1082.7251047501,476.588028064191));
#117218=CARTESIAN_POINT('Ctrl Pts',(99.1956712429291,1074.8328201009,476.097487315462));
#117219=CARTESIAN_POINT('Ctrl Pts',(99.1956805572333,1074.83281898953,476.097487315462));
#117220=CARTESIAN_POINT('Ctrl Pts',(99.1956898715415,1074.83281787814,476.097487315729));
#117221=CARTESIAN_POINT('Ctrl Pts',(99.1956991858538,1074.83281676673,476.097487316259));
#117222=CARTESIAN_POINT('Ctrl Pts',(99.2613415340014,1074.82498413957,476.097491055479));
#117223=CARTESIAN_POINT('Ctrl Pts',(99.3262541257414,1074.81639903078,476.11066932637));
#117224=CARTESIAN_POINT('Ctrl Pts',(99.4161889769876,1074.80323755955,476.148672372801));
#117225=CARTESIAN_POINT('Ctrl Pts',(99.4444713012855,1074.79887903672,476.164046852538));
#117226=CARTESIAN_POINT('Ctrl Pts',(99.5255279562476,1074.78568733498,476.21903124286));
#117227=CARTESIAN_POINT('Ctrl Pts',(99.5720685022878,1074.77708580007,476.266615523325));
#117228=CARTESIAN_POINT('Ctrl Pts',(99.6430606853371,1074.76157824561,476.376620403901));
#117229=CARTESIAN_POINT('Ctrl Pts',(99.667154531816,1074.75479754371,476.437754037079));
#117230=CARTESIAN_POINT('Ctrl Pts',(99.68984303202,1074.74399030679,476.565003513488));
#117231=CARTESIAN_POINT('Ctrl Pts',(99.6886378745193,1074.74002593788,476.629767038152));
#117232=CARTESIAN_POINT('Ctrl Pts',(99.6613707160498,1074.73539219092,476.754808810447));
#117233=CARTESIAN_POINT('Ctrl Pts',(99.6357837972584,1074.73474383589,476.813852869771));
#117234=CARTESIAN_POINT('Ctrl Pts',(99.5634706639402,1074.73684468048,476.91879929773));
#117235=CARTESIAN_POINT('Ctrl Pts',(99.5175072957653,1074.73956811237,476.963649574576));
#117236=CARTESIAN_POINT('Ctrl Pts',(99.4108081536497,1074.74805522612,477.033491876358));
#117237=CARTESIAN_POINT('Ctrl Pts',(99.3510457986267,1074.7537529146,477.057659621408));
#117238=CARTESIAN_POINT('Ctrl Pts',(99.257774605815,1074.76387774655,477.075622838188));
#117239=CARTESIAN_POINT('Ctrl Pts',(99.2267110811289,1074.76743917635,477.078568812919));
#117240=CARTESIAN_POINT('Ctrl Pts',(99.1956712429292,1074.77118038462,477.078568812919));
#117241=CARTESIAN_POINT('Origin',(89.3961860936685,1067.7251047501,419.235241127771));
#117242=CARTESIAN_POINT('',(89.396186093693,1078.67097321562,417.756937995578));
#117243=CARTESIAN_POINT('Ctrl Pts',(89.396365151478,1078.67555522044,420.713544249121));
#117244=CARTESIAN_POINT('Ctrl Pts',(89.5926021620978,1078.67059400202,420.713520480133));
#117245=CARTESIAN_POINT('Ctrl Pts',(89.7868803865718,1078.66530429547,420.674422855112));
#117246=CARTESIAN_POINT('Ctrl Pts',(90.1455321466403,1078.65489274438,420.524033233358));
#117247=CARTESIAN_POINT('Ctrl Pts',(90.3069592237574,1078.64987437859,420.415496758054));
#117248=CARTESIAN_POINT('Ctrl Pts',(90.5639905174958,1078.64146838599,420.157719986072));
#117249=CARTESIAN_POINT('Ctrl Pts',(90.6629652919494,1078.63802999079,420.016274572357));
#117250=CARTESIAN_POINT('Ctrl Pts',(90.804684180364,1078.63284103783,419.712966951113));
#117251=CARTESIAN_POINT('Ctrl Pts',(90.848840040397,1078.63105791976,419.554444544646));
#117252=CARTESIAN_POINT('Ctrl Pts',(90.8709486226905,1078.62990837589,419.347020229116));
#117253=CARTESIAN_POINT('Ctrl Pts',(90.8736746801494,1078.62972718661,419.301924041295));
#117254=CARTESIAN_POINT('Ctrl Pts',(90.8747098060535,1078.62955017467,419.230865850681));
#117255=CARTESIAN_POINT('Ctrl Pts',(90.8744060075422,1078.62950828556,419.204952494405));
#117256=CARTESIAN_POINT('Ctrl Pts',(90.872589819542,1078.62947295042,419.157196933325));
#117257=CARTESIAN_POINT('Ctrl Pts',(90.8712730476324,1078.62947298505,419.135354510003));
#117258=CARTESIAN_POINT('Ctrl Pts',(90.8673372935181,1078.62950848713,419.087705502361));
#117259=CARTESIAN_POINT('Ctrl Pts',(90.8645229743418,1078.62955051107,419.061922303702));
#117260=CARTESIAN_POINT('Ctrl Pts',(90.8547740306395,1078.62973121858,418.990165251602));
#117261=CARTESIAN_POINT('Ctrl Pts',(90.8463470880121,1078.62992003612,418.944425048915));
#117262=CARTESIAN_POINT('Ctrl Pts',(90.7911382054936,1078.63128073333,418.707940641688));
#117263=CARTESIAN_POINT('Ctrl Pts',(90.7088465874481,1078.63365394497,418.52753381423));
#117264=CARTESIAN_POINT('Ctrl Pts',(90.5016993951744,1078.63976416674,418.241329873439));
#117265=CARTESIAN_POINT('Ctrl Pts',(90.390004512142,1078.64308916845,418.129647228667));
#117266=CARTESIAN_POINT('Ctrl Pts',(90.1239555920498,1078.65087862969,417.937115791031));
#117267=CARTESIAN_POINT('Ctrl Pts',(89.9686248448788,1078.65535749821,417.86152813034));
#117268=CARTESIAN_POINT('Ctrl Pts',(89.6268884115708,1078.66487281626,417.76349378516));
#117269=CARTESIAN_POINT('Ctrl Pts',(89.4420129126725,1078.66983874007,417.746226030568));
#117270=CARTESIAN_POINT('Ctrl Pts',(89.0639182086915,1078.67953229188,417.781535349483));
#117271=CARTESIAN_POINT('Ctrl Pts',(88.874632708023,1078.68412829493,417.838225318654));
#117272=CARTESIAN_POINT('Ctrl Pts',(88.5329987312695,1078.69204165862,418.019971931558));
#117273=CARTESIAN_POINT('Ctrl Pts',(88.3831434860232,1078.69531632402,418.141749270905));
#117274=CARTESIAN_POINT('Ctrl Pts',(88.1541684632275,1078.70019975614,418.416443957324));
#117275=CARTESIAN_POINT('Ctrl Pts',(88.0699986809484,1078.70194026103,418.561247774263));
#117276=CARTESIAN_POINT('Ctrl Pts',(87.9653313245738,1078.70416950108,418.840871856981));
#117277=CARTESIAN_POINT('Ctrl Pts',(87.935797782561,1078.70483204222,418.97040285699));
#117278=CARTESIAN_POINT('Ctrl Pts',(87.9201609548036,1078.70529363473,419.143353153028));
#117279=CARTESIAN_POINT('Ctrl Pts',(87.9181668201181,1078.70537280198,419.184717394828));
#117280=CARTESIAN_POINT('Ctrl Pts',(87.9177594267779,1078.70545007456,419.250676894304));
#117281=CARTESIAN_POINT('Ctrl Pts',(87.9182200869431,1078.70546803235,419.275243079408));
#117282=CARTESIAN_POINT('Ctrl Pts',(87.9202278843457,1078.70548141821,419.321184556132));
#117283=CARTESIAN_POINT('Ctrl Pts',(87.9216279949986,1078.70547943627,419.342559915636));
#117284=CARTESIAN_POINT('Ctrl Pts',(87.9258105320442,1078.7054565499,419.390436345672));
#117285=CARTESIAN_POINT('Ctrl Pts',(87.9288459703438,1078.705431156,419.416907881017));
#117286=CARTESIAN_POINT('Ctrl Pts',(87.9397257594501,1078.70532051258,419.493448103484));
#117287=CARTESIAN_POINT('Ctrl Pts',(87.9494309089539,1078.70520204724,419.543213467121));
#117288=CARTESIAN_POINT('Ctrl Pts',(88.0093787827409,1078.70439483503,419.784003892429));
#117289=CARTESIAN_POINT('Ctrl Pts',(88.0949997063828,1078.703065199,419.964134396414));
#117290=CARTESIAN_POINT('Ctrl Pts',(88.3085843445926,1078.69933176009,420.248968168345));
#117291=CARTESIAN_POINT('Ctrl Pts',(88.4234942861283,1078.69721030295,420.359690718077));
#117292=CARTESIAN_POINT('Ctrl Pts',(88.6833424792936,1078.69203228291,420.539884312143));
#117293=CARTESIAN_POINT('Ctrl Pts',(88.826444223292,1078.68901136644,420.60842325218));
#117294=CARTESIAN_POINT('Ctrl Pts',(89.1136032323245,1078.68250947261,420.693192330588));
#117295=CARTESIAN_POINT('Ctrl Pts',(89.2546213004758,1078.67913875548,420.713561417686));
#117296=CARTESIAN_POINT('Ctrl Pts',(89.396365151478,1078.67555522044,420.713544249121));
#117297=CARTESIAN_POINT('',(89.3961860936479,1076.67023697645,417.756937995578));
#117298=CARTESIAN_POINT('',(89.3961860936685,1067.7251047501,417.756937995578));
#117299=CARTESIAN_POINT('Ctrl Pts',(89.3958628075866,1076.67488613727,420.713544224615));
#117300=CARTESIAN_POINT('Ctrl Pts',(89.2003037329778,1076.67988828043,420.713501458333));
#117301=CARTESIAN_POINT('Ctrl Pts',(89.0066716658443,1076.68446185602,420.674654572202));
#117302=CARTESIAN_POINT('Ctrl Pts',(88.6465876150618,1076.69236398927,420.52418675266));
#117303=CARTESIAN_POINT('Ctrl Pts',(88.4835370452158,1076.69562704742,420.414375969499));
#117304=CARTESIAN_POINT('Ctrl Pts',(88.2086750915665,1076.70077456957,420.137175558416));
#117305=CARTESIAN_POINT('Ctrl Pts',(88.0998441334391,1076.70260977851,419.972242292839));
#117306=CARTESIAN_POINT('Ctrl Pts',(87.9522924601903,1076.70490671658,419.608479072034));
#117307=CARTESIAN_POINT('Ctrl Pts',(87.915474988846,1076.7053429627,419.413092822487));
#117308=CARTESIAN_POINT('Ctrl Pts',(87.920531048797,1076.70482948334,419.019707987937));
#117309=CARTESIAN_POINT('Ctrl Pts',(87.9622279083649,1076.70388566694,418.82563928336));
#117310=CARTESIAN_POINT('Ctrl Pts',(88.1185225555899,1076.700547807,418.46644147806));
#117311=CARTESIAN_POINT('Ctrl Pts',(88.2310752264399,1076.69818923817,418.30465679144));
#117312=CARTESIAN_POINT('Ctrl Pts',(88.5122114751986,1076.69200409886,418.034448108022));
#117313=CARTESIAN_POINT('Ctrl Pts',(88.6779244245936,1076.68823293265,417.928563692943));
#117314=CARTESIAN_POINT('Ctrl Pts',(88.9483676843181,1076.68169997947,417.823164216011));
#117315=CARTESIAN_POINT('Ctrl Pts',(89.0405086630507,1076.67941956102,417.79718861429));
#117316=CARTESIAN_POINT('Ctrl Pts',(89.2289885462388,1076.67463308011,417.763289757598));
#117317=CARTESIAN_POINT('Ctrl Pts',(89.3248999771645,1076.67213721909,417.755540694822));
#117318=CARTESIAN_POINT('Ctrl Pts',(89.6167681764678,1076.66436230015,417.760417007292));
#117319=CARTESIAN_POINT('Ctrl Pts',(89.8100648471479,1076.65896009628,417.802597665003));
#117320=CARTESIAN_POINT('Ctrl Pts',(90.1672018754771,1076.64866396056,417.959093496439));
#117321=CARTESIAN_POINT('Ctrl Pts',(90.3278536181244,1076.64387183281,418.071186420475));
#117322=CARTESIAN_POINT('Ctrl Pts',(90.5966378383839,1076.63582738994,418.350982375037));
#117323=CARTESIAN_POINT('Ctrl Pts',(90.7021831269147,1076.63265953329,418.515948775082));
#117324=CARTESIAN_POINT('Ctrl Pts',(90.8434262157542,1076.6286746025,418.87694085061));
#117325=CARTESIAN_POINT('Ctrl Pts',(90.8778696214137,1076.62789620056,419.069408129626));
#117326=CARTESIAN_POINT('Ctrl Pts',(90.8705930944519,1076.62892628264,419.456296678916));
#117327=CARTESIAN_POINT('Ctrl Pts',(90.8290910361996,1076.63071870553,419.646965769265));
#117328=CARTESIAN_POINT('Ctrl Pts',(90.6751354860759,1076.63648673964,420.001381795169));
#117329=CARTESIAN_POINT('Ctrl Pts',(90.5642152194989,1076.64039978275,420.161728568667));
#117330=CARTESIAN_POINT('Ctrl Pts',(90.2869293510888,1076.64952914099,420.430775575771));
#117331=CARTESIAN_POINT('Ctrl Pts',(90.1231898942228,1076.65465149798,420.536849901135));
#117332=CARTESIAN_POINT('Ctrl Pts',(89.8570914339161,1076.66242227576,420.642948213038));
#117333=CARTESIAN_POINT('Ctrl Pts',(89.7674132497588,1076.66496255713,420.669208868241));
#117334=CARTESIAN_POINT('Ctrl Pts',(89.5835906501358,1076.66999866792,420.704625199847));
#117335=CARTESIAN_POINT('Ctrl Pts',(89.4898334440527,1076.67248249235,420.713564774798));
#117336=CARTESIAN_POINT('Ctrl Pts',(89.3958628075866,1076.67488613727,420.713544224615));
#117337=CARTESIAN_POINT('Origin',(89.3961860936685,1067.7251047501,419.235241127771));
#117338=CARTESIAN_POINT('',(89.3961860936685,1076.67415347727,420.113544259965));
#117339=CARTESIAN_POINT('',(89.3961860936854,1076.67140064346,418.356937995578));
#117340=CARTESIAN_POINT('Ctrl Pts',(89.3961860936685,1076.67415347727,420.113544259965));
#117341=CARTESIAN_POINT('Ctrl Pts',(89.2860749511209,1076.67698690193,420.113544259965));
#117342=CARTESIAN_POINT('Ctrl Pts',(89.1768740162537,1076.67966401957,420.092836616295));
#117343=CARTESIAN_POINT('Ctrl Pts',(88.9660596953361,1076.68460580211,420.009801445987));
#117344=CARTESIAN_POINT('Ctrl Pts',(88.8673463593847,1076.6867908605,419.946074527012));
#117345=CARTESIAN_POINT('Ctrl Pts',(88.700164984497,1076.690328816,419.783527140741));
#117346=CARTESIAN_POINT('Ctrl Pts',(88.6334878189784,1076.69164609358,419.686191896892));
#117347=CARTESIAN_POINT('Ctrl Pts',(88.5419256009336,1076.69333443435,419.470665020016));
#117348=CARTESIAN_POINT('Ctrl Pts',(88.5181485291833,1076.69368635659,419.354556242671));
#117349=CARTESIAN_POINT('Ctrl Pts',(88.5176220514905,1076.69339780757,419.119972542679));
#117350=CARTESIAN_POINT('Ctrl Pts',(88.5408361739458,1076.69276073735,419.003860581854));
#117351=CARTESIAN_POINT('Ctrl Pts',(88.631242643307,1076.69051636158,418.788156268158));
#117352=CARTESIAN_POINT('Ctrl Pts',(88.697313779647,1076.68893376231,418.690632858346));
#117353=CARTESIAN_POINT('Ctrl Pts',(88.8634648455413,1076.68490757212,418.527314785467));
#117354=CARTESIAN_POINT('Ctrl Pts',(88.9618126163982,1076.68250310554,418.463057119944));
#117355=CARTESIAN_POINT('Ctrl Pts',(89.1226742179782,1076.67846342243,418.398670771847));
#117356=CARTESIAN_POINT('Ctrl Pts',(89.1774695150229,1076.67707208457,418.382702881811));
#117357=CARTESIAN_POINT('Ctrl Pts',(89.2870916290989,1076.67425368401,418.36203000487));
#117358=CARTESIAN_POINT('Ctrl Pts',(89.3415825686882,1076.67283665557,418.356937995576));
#117359=CARTESIAN_POINT('Ctrl Pts',(89.3961860937022,1076.67140064346,418.356937995578));
#117360=CARTESIAN_POINT('',(89.3961860936685,1082.7251047501,418.356937995578));
#117361=CARTESIAN_POINT('',(89.3961860936685,1067.7251047501,418.356937995578));
#117362=CARTESIAN_POINT('Origin',(89.3961860936685,1082.7251047501,419.235241127771));
#117363=CARTESIAN_POINT('Ctrl Pts',(89.3961860937022,1076.67140064346,418.356937995578));
#117364=CARTESIAN_POINT('Ctrl Pts',(89.3986607406576,1076.67133556299,418.356937995578));
#117365=CARTESIAN_POINT('Ctrl Pts',(89.4011356188665,1076.67127044396,418.356948454172));
#117366=CARTESIAN_POINT('Ctrl Pts',(89.5199913397858,1076.66814155448,418.357953214332));
#117367=CARTESIAN_POINT('Ctrl Pts',(89.6350256668046,1076.6650379992,418.382059894481));
#117368=CARTESIAN_POINT('Ctrl Pts',(89.8478551468005,1076.6592102296,418.473224245885));
#117369=CARTESIAN_POINT('Ctrl Pts',(89.9437637384592,1076.65654094439,418.53893899094));
#117370=CARTESIAN_POINT('Ctrl Pts',(90.1047307400064,1076.65208210947,418.703609080853));
#117371=CARTESIAN_POINT('Ctrl Pts',(90.1682412701848,1076.6503379917,418.800957168843));
#117372=CARTESIAN_POINT('Ctrl Pts',(90.2512204196791,1076.64819395911,419.00747937103));
#117373=CARTESIAN_POINT('Ctrl Pts',(90.2726467436591,1076.64773102208,419.113681003135));
#117374=CARTESIAN_POINT('Ctrl Pts',(90.2743755221586,1076.64787624781,419.221108905413));
#117375=CARTESIAN_POINT('Ctrl Pts',(90.2762246161387,1076.64803158062,419.336013323445));
#117376=CARTESIAN_POINT('Ctrl Pts',(90.2555044101713,1076.64887998737,419.450166271211));
#117377=CARTESIAN_POINT('Ctrl Pts',(90.1713002092023,1076.65181242532,419.663974429493));
#117378=CARTESIAN_POINT('Ctrl Pts',(90.108641187565,1076.65386587201,419.76156620233));
#117379=CARTESIAN_POINT('Ctrl Pts',(89.9492837723896,1076.65880378749,419.927128576555));
#117380=CARTESIAN_POINT('Ctrl Pts',(89.8541034515488,1076.66163849817,419.993485350182));
#117381=CARTESIAN_POINT('Ctrl Pts',(89.643558053945,1076.66761007176,420.085795385248));
#117382=CARTESIAN_POINT('Ctrl Pts',(89.5302118704862,1076.67068771278,420.110839572154));
#117383=CARTESIAN_POINT('Ctrl Pts',(89.4089026814889,1076.67382581652,420.113475248774));
#117384=CARTESIAN_POINT('Ctrl Pts',(89.4025428706656,1076.67398990211,420.113544259965));
#117385=CARTESIAN_POINT('Ctrl Pts',(89.3961860936685,1076.67415347727,420.113544259965));
#117386=CARTESIAN_POINT('Origin',(96.608893067355,1067.7251047501,429.515656233126));
#117387=CARTESIAN_POINT('',(96.6088930673831,1078.35304757369,428.24021211199));
#117388=CARTESIAN_POINT('Ctrl Pts',(96.6091598698775,1078.34476504118,430.791100326357));
#117389=CARTESIAN_POINT('Ctrl Pts',(96.7780589842411,1078.33391689068,430.791064995361));
#117390=CARTESIAN_POINT('Ctrl Pts',(96.9453022942696,1078.32309025058,430.757480637883));
#117391=CARTESIAN_POINT('Ctrl Pts',(97.252542525453,1078.30313955902,430.628940999755));
#117392=CARTESIAN_POINT('Ctrl Pts',(97.3903484268822,1078.29416340589,430.536956076821));
#117393=CARTESIAN_POINT('Ctrl Pts',(97.6068876450851,1078.2801769268,430.322235083317));
#117394=CARTESIAN_POINT('Ctrl Pts',(97.6897643941568,1078.27488130207,430.207252763852));
#117395=CARTESIAN_POINT('Ctrl Pts',(97.8017564083411,1078.26794934715,429.980780131298));
#117396=CARTESIAN_POINT('Ctrl Pts',(97.8379361604888,1078.26581462932,429.874437867473));
#117397=CARTESIAN_POINT('Ctrl Pts',(97.8665541867106,1078.26433515541,429.730712377094));
#117398=CARTESIAN_POINT('Ctrl Pts',(97.8719370554832,1078.26408218529,429.696434049079));
#117399=CARTESIAN_POINT('Ctrl Pts',(97.8782736194658,1078.26383542025,429.641564880119));
#117400=CARTESIAN_POINT('Ctrl Pts',(97.8801374016113,1078.26377805036,429.621097325731));
#117401=CARTESIAN_POINT('Ctrl Pts',(97.8826983900408,1078.2637352564,429.582726152118));
#117402=CARTESIAN_POINT('Ctrl Pts',(97.8835144878876,1078.26374153488,429.564835576519));
#117403=CARTESIAN_POINT('Ctrl Pts',(97.8844998735435,1078.26381441373,429.524665335253));
#117404=CARTESIAN_POINT('Ctrl Pts',(97.884462661919,1078.26389534235,429.502386557595));
#117405=CARTESIAN_POINT('Ctrl Pts',(97.8826598355887,1078.26424784371,429.437705113659));
#117406=CARTESIAN_POINT('Ctrl Pts',(97.8793617789237,1078.26462545867,429.395376595322));
#117407=CARTESIAN_POINT('Ctrl Pts',(97.8522924709095,1078.26724264127,429.184464150602));
#117408=CARTESIAN_POINT('Ctrl Pts',(97.7970543993223,1078.27164299534,429.021724858507));
#117409=CARTESIAN_POINT('Ctrl Pts',(97.643273015679,1078.28310168061,428.757184750735));
#117410=CARTESIAN_POINT('Ctrl Pts',(97.5566731991259,1078.28937029402,428.651417211364));
#117411=CARTESIAN_POINT('Ctrl Pts',(97.3439662424416,1078.30434876736,428.462814941456));
#117412=CARTESIAN_POINT('Ctrl Pts',(97.2165371116341,1078.31311606194,428.384483139707));
#117413=CARTESIAN_POINT('Ctrl Pts',(96.9301900342652,1078.33231516005,428.271071750476));
#117414=CARTESIAN_POINT('Ctrl Pts',(96.7721146000858,1078.34265289184,428.240675042645));
#117415=CARTESIAN_POINT('Ctrl Pts',(96.4435935292681,1078.36357468578,428.239732727962));
#117416=CARTESIAN_POINT('Ctrl Pts',(96.2761721401171,1078.37393269022,428.272825621434));
#117417=CARTESIAN_POINT('Ctrl Pts',(95.9680216748652,1078.39248535877,428.400697928381));
#117418=CARTESIAN_POINT('Ctrl Pts',(95.8295845387844,1078.40056007298,428.492638938362));
#117419=CARTESIAN_POINT('Ctrl Pts',(95.6124230489633,1078.41287657546,428.707219678173));
#117420=CARTESIAN_POINT('Ctrl Pts',(95.5294171079926,1078.41742446496,428.821916780123));
#117421=CARTESIAN_POINT('Ctrl Pts',(95.4165788203255,1078.42336782487,429.048889145251));
#117422=CARTESIAN_POINT('Ctrl Pts',(95.3799756824197,1078.42518293578,429.15613878423));
#117423=CARTESIAN_POINT('Ctrl Pts',(95.3512065708384,1078.42643117177,429.300759728285));
#117424=CARTESIAN_POINT('Ctrl Pts',(95.3458379126787,1078.42664263812,429.33496982924));
#117425=CARTESIAN_POINT('Ctrl Pts',(95.3395283160829,1078.42684858651,429.389613878104));
#117426=CARTESIAN_POINT('Ctrl Pts',(95.3376753841892,1078.42689649,429.409924712243));
#117427=CARTESIAN_POINT('Ctrl Pts',(95.3351141541855,1078.42693294889,429.448097447928));
#117428=CARTESIAN_POINT('Ctrl Pts',(95.3342927853368,1078.42692811649,429.465946779611));
#117429=CARTESIAN_POINT('Ctrl Pts',(95.3332975045362,1078.42686857656,429.505792232258));
#117430=CARTESIAN_POINT('Ctrl Pts',(95.3333170549708,1078.42680262111,429.527787446515));
#117431=CARTESIAN_POINT('Ctrl Pts',(95.3350230576038,1078.42651543316,429.591546673648));
#117432=CARTESIAN_POINT('Ctrl Pts',(95.338193352319,1078.4262080599,429.633241306722));
#117433=CARTESIAN_POINT('Ctrl Pts',(95.3646146130976,1078.42404864329,429.843466252332));
#117434=CARTESIAN_POINT('Ctrl Pts',(95.4193650307878,1078.42037893309,430.006253541714));
#117435=CARTESIAN_POINT('Ctrl Pts',(95.5724958984442,1078.41053361279,430.271426216472));
#117436=CARTESIAN_POINT('Ctrl Pts',(95.6590386556319,1078.40506236998,430.37766705163));
#117437=CARTESIAN_POINT('Ctrl Pts',(95.8720884163574,1078.39162279519,430.567380500981));
#117438=CARTESIAN_POINT('Ctrl Pts',(95.9999857653115,1078.38356658276,430.646235777515));
#117439=CARTESIAN_POINT('Ctrl Pts',(96.2883505717373,1078.36529272026,430.760639839526));
#117440=CARTESIAN_POINT('Ctrl Pts',(96.4480465416396,1078.35511312168,430.79113402869));
#117441=CARTESIAN_POINT('Ctrl Pts',(96.6091598698775,1078.34476504118,430.791100326357));
#117442=CARTESIAN_POINT('',(96.6088930673352,1076.3488082978,428.24021211199));
#117443=CARTESIAN_POINT('',(96.608893067355,1067.7251047501,428.24021211199));
#117444=CARTESIAN_POINT('Ctrl Pts',(96.6091161516571,1076.34044219187,430.791100334753));
#117445=CARTESIAN_POINT('Ctrl Pts',(96.5257062042077,1076.34585531859,430.791114923749));
#117446=CARTESIAN_POINT('Ctrl Pts',(96.4424911049163,1076.35123612761,430.782947365478));
#117447=CARTESIAN_POINT('Ctrl Pts',(96.194791856356,1076.3671952592,430.733800607917));
#117448=CARTESIAN_POINT('Ctrl Pts',(96.0370589157469,1076.37727408663,430.66821601593));
#117449=CARTESIAN_POINT('Ctrl Pts',(95.7568651334049,1076.3951358746,430.479614349123));
#117450=CARTESIAN_POINT('Ctrl Pts',(95.6370223540367,1076.40275653031,430.358672128692));
#117451=CARTESIAN_POINT('Ctrl Pts',(95.4510449959223,1076.4147596279,430.076680552373));
#117452=CARTESIAN_POINT('Ctrl Pts',(95.386912852988,1076.41901866201,429.918339734609));
#117453=CARTESIAN_POINT('Ctrl Pts',(95.3241009777672,1076.42371559229,429.585332395619));
#117454=CARTESIAN_POINT('Ctrl Pts',(95.3262351364234,1076.42409823989,429.413985449834));
#117455=CARTESIAN_POINT('Ctrl Pts',(95.3973581420346,1076.42090102356,429.082506550211));
#117456=CARTESIAN_POINT('Ctrl Pts',(95.4654991720177,1076.41735930617,428.925689250503));
#117457=CARTESIAN_POINT('Ctrl Pts',(95.6586502079043,1076.40667050234,428.648325624693));
#117458=CARTESIAN_POINT('Ctrl Pts',(95.7815504819943,1076.39963671498,428.530421550854));
#117459=CARTESIAN_POINT('Ctrl Pts',(96.0663045449067,1076.38275178711,428.349073138491));
#117460=CARTESIAN_POINT('Ctrl Pts',(96.2254321069276,1076.37305628671,428.287552070561));
#117461=CARTESIAN_POINT('Ctrl Pts',(96.5598377418726,1076.35205431126,428.229806745443));
#117462=CARTESIAN_POINT('Ctrl Pts',(96.7319221687995,1076.3409408836,428.234770116977));
#117463=CARTESIAN_POINT('Ctrl Pts',(97.0611532241657,1076.31908585922,428.311370086237));
#117464=CARTESIAN_POINT('Ctrl Pts',(97.2153462197109,1076.30855281656,428.381159049807));
#117465=CARTESIAN_POINT('Ctrl Pts',(97.4877985936292,1076.28945991678,428.576330749339));
#117466=CARTESIAN_POINT('Ctrl Pts',(97.6034704741582,1076.28108626243,428.699771245375));
#117467=CARTESIAN_POINT('Ctrl Pts',(97.7802554189951,1076.26786524973,428.984048732891));
#117468=CARTESIAN_POINT('Ctrl Pts',(97.8397958318671,1076.26314114355,429.142011296511));
#117469=CARTESIAN_POINT('Ctrl Pts',(97.8944277253633,1076.25814920103,429.471480852004));
#117470=CARTESIAN_POINT('Ctrl Pts',(97.8891910980265,1076.25791770276,429.639711562067));
#117471=CARTESIAN_POINT('Ctrl Pts',(97.8143459148466,1076.26200684184,429.964377877794));
#117472=CARTESIAN_POINT('Ctrl Pts',(97.7455690186523,1076.26627897936,430.117655123041));
#117473=CARTESIAN_POINT('Ctrl Pts',(97.5529961184477,1076.27866570818,430.389255396033));
#117474=CARTESIAN_POINT('Ctrl Pts',(97.4309970420768,1076.2866612289,430.504901473221));
#117475=CARTESIAN_POINT('Ctrl Pts',(97.1491933464996,1076.30516104736,430.68300221619));
#117476=CARTESIAN_POINT('Ctrl Pts',(96.9919835153256,1076.31549077737,430.743595488476));
#117477=CARTESIAN_POINT('Ctrl Pts',(96.7554587177488,1076.33092979891,430.784766387279));
#117478=CARTESIAN_POINT('Ctrl Pts',(96.6823552564843,1076.33568913103,430.791087524709));
#117479=CARTESIAN_POINT('Ctrl Pts',(96.6091161516571,1076.34044219187,430.791100334753));
#117480=CARTESIAN_POINT('Origin',(96.608893067355,1067.7251047501,429.515656233126));
#117481=CARTESIAN_POINT('',(96.608893067355,1076.34281999372,430.191100354262));
#117482=CARTESIAN_POINT('',(96.608893067355,1076.34724098047,428.84021211199));
#117483=CARTESIAN_POINT('Ctrl Pts',(96.608893067355,1076.34281999372,430.191100354262));
#117484=CARTESIAN_POINT('Ctrl Pts',(96.5658147920971,1076.34560871382,430.191100354262));
#117485=CARTESIAN_POINT('Ctrl Pts',(96.52283114131,1076.34839238715,430.186979197945));
#117486=CARTESIAN_POINT('Ctrl Pts',(96.3922695285492,1076.35685180461,430.161706409238));
#117487=CARTESIAN_POINT('Ctrl Pts',(96.3082778772544,1076.36229842477,430.127167221171));
#117488=CARTESIAN_POINT('Ctrl Pts',(96.158884077575,1076.3720341645,430.027293685815));
#117489=CARTESIAN_POINT('Ctrl Pts',(96.0949243857349,1076.37623042713,429.963014350603));
#117490=CARTESIAN_POINT('Ctrl Pts',(95.9958047352578,1076.38286170464,429.813040719218));
#117491=CARTESIAN_POINT('Ctrl Pts',(95.9616820843232,1076.38522898994,429.728826775021));
#117492=CARTESIAN_POINT('Ctrl Pts',(95.9284231983361,1076.38783123599,429.551810006037));
#117493=CARTESIAN_POINT('Ctrl Pts',(95.929674749872,1076.3880374266,429.460795811302));
#117494=CARTESIAN_POINT('Ctrl Pts',(95.9678012182744,1076.38623910634,429.284719321792));
#117495=CARTESIAN_POINT('Ctrl Pts',(96.0042519996463,1076.38425464593,429.201439533524));
#117496=CARTESIAN_POINT('Ctrl Pts',(96.1075236577383,1076.37831335311,429.054218441719));
#117497=CARTESIAN_POINT('Ctrl Pts',(96.1732545550311,1076.3744182383,428.99172570101));
#117498=CARTESIAN_POINT('Ctrl Pts',(96.3253360597475,1076.36516534383,428.896058513761));
#117499=CARTESIAN_POINT('Ctrl Pts',(96.4101984234306,1076.35989647234,428.863876652953));
#117500=CARTESIAN_POINT('Ctrl Pts',(96.5352179471671,1076.35196907944,428.843230577298));
#117501=CARTESIAN_POINT('Ctrl Pts',(96.5720256934705,1076.34961643708,428.84021211199));
#117502=CARTESIAN_POINT('Ctrl Pts',(96.6088930673551,1076.34724098047,428.84021211199));
#117503=CARTESIAN_POINT('',(96.608893067355,1082.7251047501,428.84021211199));
#117504=CARTESIAN_POINT('',(96.608893067355,1067.7251047501,428.84021211199));
#117505=CARTESIAN_POINT('Origin',(96.608893067355,1082.7251047501,429.515656233126));
#117506=CARTESIAN_POINT('Ctrl Pts',(96.6088930673551,1076.34724098047,428.84021211199));
#117507=CARTESIAN_POINT('Ctrl Pts',(96.6089025413445,1076.34724037004,428.84021211199));
#117508=CARTESIAN_POINT('Ctrl Pts',(96.6089120153378,1076.34723975961,428.840212112183));
#117509=CARTESIAN_POINT('Ctrl Pts',(96.6089214893351,1076.34723914917,428.840212112582));
#117510=CARTESIAN_POINT('Ctrl Pts',(96.6530279814733,1076.34439724654,428.840213968537));
#117511=CARTESIAN_POINT('Ctrl Pts',(96.6970284556051,1076.34153498234,428.84453604931));
#117512=CARTESIAN_POINT('Ctrl Pts',(96.8281870782537,1076.33292169698,428.870548295092));
#117513=CARTESIAN_POINT('Ctrl Pts',(96.9117602770266,1076.32731966516,428.905301673286));
#117514=CARTESIAN_POINT('Ctrl Pts',(97.0596241144492,1076.31720948098,429.004855233394));
#117515=CARTESIAN_POINT('Ctrl Pts',(97.1227030254683,1076.31278797405,429.068344596971));
#117516=CARTESIAN_POINT('Ctrl Pts',(97.2206312431141,1076.30572917975,429.21594679194));
#117517=CARTESIAN_POINT('Ctrl Pts',(97.2545974685802,1076.30315738567,429.298573106462));
#117518=CARTESIAN_POINT('Ctrl Pts',(97.2886875845159,1076.30026500213,429.47206387651));
#117519=CARTESIAN_POINT('Ctrl Pts',(97.2885599604648,1076.29996784546,429.561209221119));
#117520=CARTESIAN_POINT('Ctrl Pts',(97.2540221793563,1076.30170717808,429.734327758894));
#117521=CARTESIAN_POINT('Ctrl Pts',(97.2199798348334,1076.30372425459,429.816610854075));
#117522=CARTESIAN_POINT('Ctrl Pts',(97.1221665855661,1076.30979055424,429.963509334998));
#117523=CARTESIAN_POINT('Ctrl Pts',(97.0593064093363,1076.31378244562,430.026672537639));
#117524=CARTESIAN_POINT('Ctrl Pts',(96.9127352398344,1076.32317802229,430.125352966867));
#117525=CARTESIAN_POINT('Ctrl Pts',(96.830382000739,1076.32849361908,430.159848746053));
#117526=CARTESIAN_POINT('Ctrl Pts',(96.7004128191174,1076.33689663328,430.186331298869));
#117527=CARTESIAN_POINT('Ctrl Pts',(96.6563141293245,1076.33975020148,430.190883463694));
#117528=CARTESIAN_POINT('Ctrl Pts',(96.6110243655397,1076.34268202248,430.191097832485));
#117529=CARTESIAN_POINT('Ctrl Pts',(96.6099586874942,1076.34275100961,430.191100354262));
#117530=CARTESIAN_POINT('Ctrl Pts',(96.608893067355,1076.34281999372,430.191100354262));
#117531=CARTESIAN_POINT('Origin',(103.499585384595,1067.7251047501,441.529673720836));
#117532=CARTESIAN_POINT('',(103.499585384619,1077.68406953396,440.430842584843));
#117533=CARTESIAN_POINT('Ctrl Pts',(103.499860694173,1077.64747802966,442.628504822339));
#117534=CARTESIAN_POINT('Ctrl Pts',(103.645111118182,1077.63259627413,442.628468430183));
#117535=CARTESIAN_POINT('Ctrl Pts',(103.789010605813,1077.6182221956,442.59963215631));
#117536=CARTESIAN_POINT('Ctrl Pts',(104.050498000161,1077.59291668959,442.490382015408));
#117537=CARTESIAN_POINT('Ctrl Pts',(104.16677498141,1077.58206970272,442.413639589368));
#117538=CARTESIAN_POINT('Ctrl Pts',(104.359583798264,1077.56505944824,442.226046984409));
#117539=CARTESIAN_POINT('Ctrl Pts',(104.436358856901,1077.55881466678,442.11877473147));
#117540=CARTESIAN_POINT('Ctrl Pts',(104.518663846431,1077.55312454052,441.94518193482));
#117541=CARTESIAN_POINT('Ctrl Pts',(104.540205315743,1077.5518391956,441.887836893985));
#117542=CARTESIAN_POINT('Ctrl Pts',(104.563392351372,1077.55080368086,441.805932189706));
#117543=CARTESIAN_POINT('Ctrl Pts',(104.569163545854,1077.55059555095,441.782669040295));
#117544=CARTESIAN_POINT('Ctrl Pts',(104.577163463826,1077.55039678927,441.745221169366));
#117545=CARTESIAN_POINT('Ctrl Pts',(104.579882835002,1077.55035237811,441.731149882642));
#117546=CARTESIAN_POINT('Ctrl Pts',(104.584899611622,1077.55032279103,441.702157590973));
#117547=CARTESIAN_POINT('Ctrl Pts',(104.587166314174,1077.55034089549,441.68723442818));
#117548=CARTESIAN_POINT('Ctrl Pts',(104.591680524313,1077.55045929991,441.652742416295));
#117549=CARTESIAN_POINT('Ctrl Pts',(104.593710695626,1077.55058295171,441.633150648677));
#117550=CARTESIAN_POINT('Ctrl Pts',(104.598359693779,1077.55114022538,441.572398295951));
#117551=CARTESIAN_POINT('Ctrl Pts',(104.599188774366,1077.55176452249,441.531140496396));
#117552=CARTESIAN_POINT('Ctrl Pts',(104.592420560346,1077.55570449242,441.344100048161));
#117553=CARTESIAN_POINT('Ctrl Pts',(104.558150384969,1077.56179060128,441.200883163092));
#117554=CARTESIAN_POINT('Ctrl Pts',(104.447618586277,1077.57749669874,440.96176623425));
#117555=CARTESIAN_POINT('Ctrl Pts',(104.381422833653,1077.58610740631,440.863638806983));
#117556=CARTESIAN_POINT('Ctrl Pts',(104.212974784091,1077.60671063103,440.684055240918));
#117557=CARTESIAN_POINT('Ctrl Pts',(104.109177244887,1077.61878817036,440.606447398284));
#117558=CARTESIAN_POINT('Ctrl Pts',(103.870735432718,1077.64536986028,440.486185842388));
#117559=CARTESIAN_POINT('Ctrl Pts',(103.736382388567,1077.65975812971,440.447760953317));
#117560=CARTESIAN_POINT('Ctrl Pts',(103.453241190359,1077.68893717594,440.422179988729));
#117561=CARTESIAN_POINT('Ctrl Pts',(103.306772389159,1077.70342984835,440.438087269816));
#117562=CARTESIAN_POINT('Ctrl Pts',(103.033089922435,1077.72939661722,440.524821449055));
#117563=CARTESIAN_POINT('Ctrl Pts',(102.907899993219,1077.74071983741,440.593016016293));
#117564=CARTESIAN_POINT('Ctrl Pts',(102.705109527106,1077.75805565959,440.760852622276));
#117565=CARTESIAN_POINT('Ctrl Pts',(102.62474411354,1077.76446595137,440.853676109533));
#117566=CARTESIAN_POINT('Ctrl Pts',(102.514059557075,1077.77241712264,441.035314010731));
#117567=CARTESIAN_POINT('Ctrl Pts',(102.476624965789,1077.77475443465,441.118316870278));
#117568=CARTESIAN_POINT('Ctrl Pts',(102.44146198237,1077.77637828602,441.232009394482));
#117569=CARTESIAN_POINT('Ctrl Pts',(102.43415352809,1077.77665665588,441.259332703226));
#117570=CARTESIAN_POINT('Ctrl Pts',(102.424194427279,1077.77692835425,441.303296789513));
#117571=CARTESIAN_POINT('Ctrl Pts',(102.42085837831,1077.77699146764,441.319768308307));
#117572=CARTESIAN_POINT('Ctrl Pts',(102.41531823909,1077.77703812473,441.350760055114));
#117573=CARTESIAN_POINT('Ctrl Pts',(102.413024933617,1077.77703071548,441.365260435083));
#117574=CARTESIAN_POINT('Ctrl Pts',(102.408525571024,1077.77694853396,441.397940717941));
#117575=CARTESIAN_POINT('Ctrl Pts',(102.406482085994,1077.77685756898,441.416138424035));
#117576=CARTESIAN_POINT('Ctrl Pts',(102.401855078273,1077.77646055183,441.469290527423));
#117577=CARTESIAN_POINT('Ctrl Pts',(102.400487948646,1077.77603414678,441.504326058925));
#117578=CARTESIAN_POINT('Ctrl Pts',(102.4020877338,1077.7729759697,441.685711092669));
#117579=CARTESIAN_POINT('Ctrl Pts',(102.432600355618,1077.76767656071,441.830237547501));
#117580=CARTESIAN_POINT('Ctrl Pts',(102.536710317238,1077.75353427765,442.071868559446));
#117581=CARTESIAN_POINT('Ctrl Pts',(102.599789433246,1077.74570263645,442.171100762973));
#117582=CARTESIAN_POINT('Ctrl Pts',(102.762352164988,1077.72657612096,442.354530854693));
#117583=CARTESIAN_POINT('Ctrl Pts',(102.863580427146,1077.71515985653,442.434853135299));
#117584=CARTESIAN_POINT('Ctrl Pts',(103.057063159085,1077.69398375268,442.539647893311));
#117585=CARTESIAN_POINT('Ctrl Pts',(103.143009302606,1077.68475074002,442.573089765098));
#117586=CARTESIAN_POINT('Ctrl Pts',(103.319643890586,1077.66608556445,442.617424205756));
#117587=CARTESIAN_POINT('Ctrl Pts',(103.409582050061,1077.6567276048,442.628527441443));
#117588=CARTESIAN_POINT('Ctrl Pts',(103.499860694173,1077.64747802966,442.628504822339));
#117589=CARTESIAN_POINT('',(103.499585384576,1075.67331547342,440.430842584843));
#117590=CARTESIAN_POINT('',(103.499585384595,1067.7251047501,440.430842584843));
#117591=CARTESIAN_POINT('Ctrl Pts',(103.499274463467,1075.63644950196,442.62850481284));
#117592=CARTESIAN_POINT('Ctrl Pts',(103.427257073541,1075.64389599565,442.628484435069));
#117593=CARTESIAN_POINT('Ctrl Pts',(103.355417684151,1075.65141634246,442.621384084784));
#117594=CARTESIAN_POINT('Ctrl Pts',(103.141451896906,1075.67409110447,442.578736761835));
#117595=CARTESIAN_POINT('Ctrl Pts',(103.00516743923,1075.68891256557,442.521836809897));
#117596=CARTESIAN_POINT('Ctrl Pts',(102.76346360034,1075.71605248958,442.358359915889));
#117597=CARTESIAN_POINT('Ctrl Pts',(102.660217219451,1075.72812379484,442.25364715078));
#117598=CARTESIAN_POINT('Ctrl Pts',(102.500503022171,1075.74804648779,442.009784639939));
#117599=CARTESIAN_POINT('Ctrl Pts',(102.445632435157,1075.75570175893,441.873078335723));
#117600=CARTESIAN_POINT('Ctrl Pts',(102.392738789125,1075.76556424131,441.587100897914));
#117601=CARTESIAN_POINT('Ctrl Pts',(102.394806535939,1075.76771622652,441.44082761082));
#117602=CARTESIAN_POINT('Ctrl Pts',(102.455286709802,1075.76629090132,441.158968232738));
#117603=CARTESIAN_POINT('Ctrl Pts',(102.51249188648,1075.76278859546,441.026093096148));
#117604=CARTESIAN_POINT('Ctrl Pts',(102.676073269864,1075.75043099469,440.787688685539));
#117605=CARTESIAN_POINT('Ctrl Pts',(102.781666879871,1075.74160185034,440.685144574812));
#117606=CARTESIAN_POINT('Ctrl Pts',(103.026590908685,1075.71966684757,440.527192912908));
#117607=CARTESIAN_POINT('Ctrl Pts',(103.163525373555,1075.70677087799,440.47341623255));
#117608=CARTESIAN_POINT('Ctrl Pts',(103.377100443955,1075.68573219168,440.435359798528));
#117609=CARTESIAN_POINT('Ctrl Pts',(103.44841135433,1075.67856529576,440.429718598257));
#117610=CARTESIAN_POINT('Ctrl Pts',(103.59134490727,1075.66391272026,440.432341345033));
#117611=CARTESIAN_POINT('Ctrl Pts',(103.662639108214,1075.65645961681,440.440651271714));
#117612=CARTESIAN_POINT('Ctrl Pts',(103.876865904172,1075.63361876489,440.48713891478));
#117613=CARTESIAN_POINT('Ctrl Pts',(104.01340727035,1075.61842751581,440.547205576925));
#117614=CARTESIAN_POINT('Ctrl Pts',(104.25201284105,1075.59062294275,440.715939607113));
#117615=CARTESIAN_POINT('Ctrl Pts',(104.352499763948,1075.57822704031,440.821911344669));
#117616=CARTESIAN_POINT('Ctrl Pts',(104.506254203105,1075.5577670559,441.066252704841));
#117617=CARTESIAN_POINT('Ctrl Pts',(104.558300614325,1075.54987967195,441.202048164075));
#117618=CARTESIAN_POINT('Ctrl Pts',(104.606836644657,1075.53979213193,441.485399575454));
#117619=CARTESIAN_POINT('Ctrl Pts',(104.603175506552,1075.53765998793,441.630062853594));
#117620=CARTESIAN_POINT('Ctrl Pts',(104.540538158766,1075.53946911503,441.909550504499));
#117621=CARTESIAN_POINT('Ctrl Pts',(104.482323453435,1075.54337712613,442.041604688478));
#117622=CARTESIAN_POINT('Ctrl Pts',(104.31847971329,1075.55670754947,442.276249936995));
#117623=CARTESIAN_POINT('Ctrl Pts',(104.214335601615,1075.56601176743,442.376441487126));
#117624=CARTESIAN_POINT('Ctrl Pts',(103.973025804153,1075.58875984639,442.531668586423));
#117625=CARTESIAN_POINT('Ctrl Pts',(103.837984657249,1075.6020071227,442.584925014224));
#117626=CARTESIAN_POINT('Ctrl Pts',(103.631515481982,1075.62285393917,442.622563338287));
#117627=CARTESIAN_POINT('Ctrl Pts',(103.565454977384,1075.62960653279,442.62852353903));
#117628=CARTESIAN_POINT('Ctrl Pts',(103.499274463467,1075.63644950196,442.62850481284));
#117629=CARTESIAN_POINT('Origin',(103.499585384595,1067.7251047501,441.529673720836));
#117630=CARTESIAN_POINT('',(103.499585384595,1075.64701319545,442.028504856828));
#117631=CARTESIAN_POINT('',(103.499585384595,1075.66376111901,441.030842584843));
#117632=CARTESIAN_POINT('Ctrl Pts',(103.499585384595,1075.64701319545,442.028504856828));
#117633=CARTESIAN_POINT('Ctrl Pts',(103.499575443353,1075.64701421976,442.028504856828));
#117634=CARTESIAN_POINT('Ctrl Pts',(103.499565502105,1075.64701524408,442.028504856513));
#117635=CARTESIAN_POINT('Ctrl Pts',(103.466919470037,1075.65037901643,442.028502904697));
#117636=CARTESIAN_POINT('Ctrl Pts',(103.434363758874,1075.65378175874,442.025298132306));
#117637=CARTESIAN_POINT('Ctrl Pts',(103.337113753866,1075.66409266761,442.00597215801));
#117638=CARTESIAN_POINT('Ctrl Pts',(103.275087078802,1075.67087185248,441.980080458876));
#117639=CARTESIAN_POINT('Ctrl Pts',(103.164983052293,1075.68334498511,441.905545705399));
#117640=CARTESIAN_POINT('Ctrl Pts',(103.117939128761,1075.68892082593,441.857700281519));
#117641=CARTESIAN_POINT('Ctrl Pts',(103.045358487654,1075.69812876426,441.74629941969));
#117642=CARTESIAN_POINT('Ctrl Pts',(103.020539627964,1075.70166991111,441.683878905855));
#117643=CARTESIAN_POINT('Ctrl Pts',(102.997142800598,1075.70617246218,441.554390485282));
#117644=CARTESIAN_POINT('Ctrl Pts',(102.998198250127,1075.70714788565,441.488746093747));
#117645=CARTESIAN_POINT('Ctrl Pts',(103.025459847927,1075.70649369283,441.361543849802));
#117646=CARTESIAN_POINT('Ctrl Pts',(103.051389544962,1075.70487101264,441.301253869449));
#117647=CARTESIAN_POINT('Ctrl Pts',(103.125004608819,1075.69920085749,441.193851859608));
#117648=CARTESIAN_POINT('Ctrl Pts',(103.172040786718,1075.69520012457,441.147854409471));
#117649=CARTESIAN_POINT('Ctrl Pts',(103.28218497472,1075.68521075879,441.075809535943));
#117650=CARTESIAN_POINT('Ctrl Pts',(103.34451076681,1075.67928094454,441.050933876175));
#117651=CARTESIAN_POINT('Ctrl Pts',(103.439368402523,1075.66988058255,441.033579969333));
#117652=CARTESIAN_POINT('Ctrl Pts',(103.469341848508,1075.66685978171,441.030855574593));
#117653=CARTESIAN_POINT('Ctrl Pts',(103.499370369833,1075.66378314963,441.030842631183));
#117654=CARTESIAN_POINT('Ctrl Pts',(103.499442041806,1075.66377580633,441.03084260029));
#117655=CARTESIAN_POINT('Ctrl Pts',(103.499513713395,1075.66376846279,441.030842584843));
#117656=CARTESIAN_POINT('Ctrl Pts',(103.499585384595,1075.66376111901,441.030842584843));
#117657=CARTESIAN_POINT('',(103.499585384595,1082.7251047501,441.030842584843));
#117658=CARTESIAN_POINT('',(103.499585384595,1067.7251047501,441.030842584843));
#117659=CARTESIAN_POINT('Origin',(103.499585384595,1082.7251047501,441.529673720836));
#117660=CARTESIAN_POINT('Ctrl Pts',(103.499585384595,1075.66376111901,441.030842584843));
#117661=CARTESIAN_POINT('Ctrl Pts',(103.532060611507,1075.66043354591,441.030842584843));
#117662=CARTESIAN_POINT('Ctrl Pts',(103.564455810833,1075.65705545975,441.034013912775));
#117663=CARTESIAN_POINT('Ctrl Pts',(103.661850094858,1075.64671898749,441.053264220225));
#117664=CARTESIAN_POINT('Ctrl Pts',(103.724152924491,1075.6398520434,441.079259655313));
#117665=CARTESIAN_POINT('Ctrl Pts',(103.834235296593,1075.62719741521,441.153887815884));
#117666=CARTESIAN_POINT('Ctrl Pts',(103.881103112898,1075.62152146925,441.201547987854));
#117667=CARTESIAN_POINT('Ctrl Pts',(103.952997527745,1075.61216832407,441.311701420194));
#117668=CARTESIAN_POINT('Ctrl Pts',(103.977634544781,1075.60855460844,441.372897386145));
#117669=CARTESIAN_POINT('Ctrl Pts',(104.001826508974,1075.60384253857,441.50108260297));
#117670=CARTESIAN_POINT('Ctrl Pts',(104.001275424936,1075.60277788747,441.566767408293));
#117671=CARTESIAN_POINT('Ctrl Pts',(103.974984361348,1075.60335067882,441.694141624082));
#117672=CARTESIAN_POINT('Ctrl Pts',(103.949551691095,1075.60497755678,441.75456574776));
#117673=CARTESIAN_POINT('Ctrl Pts',(103.876901269081,1075.61072008804,441.862396457139));
#117674=CARTESIAN_POINT('Ctrl Pts',(103.830337481106,1075.6147859128,441.908697009938));
#117675=CARTESIAN_POINT('Ctrl Pts',(103.721868130933,1075.62483343728,441.9810013349));
#117676=CARTESIAN_POINT('Ctrl Pts',(103.660922918955,1075.63072855163,442.00618346961));
#117677=CARTESIAN_POINT('Ctrl Pts',(103.564858078166,1075.64033609418,442.025295009983));
#117678=CARTESIAN_POINT('Ctrl Pts',(103.532257199036,1075.64364679602,442.028504856828));
#117679=CARTESIAN_POINT('Ctrl Pts',(103.499585384595,1075.64701319545,442.028504856828));
#117680=CARTESIAN_POINT('Origin',(107.832717977554,1067.7251047501,454.828467536887));
#117681=CARTESIAN_POINT('',(107.832717977553,1076.85914687694,453.73792678816));
#117682=CARTESIAN_POINT('Ctrl Pts',(107.832971536831,1076.78010498484,455.919008256138));
#117683=CARTESIAN_POINT('Ctrl Pts',(107.976293244521,1076.76145240728,455.918974932716));
#117684=CARTESIAN_POINT('Ctrl Pts',(108.118399363473,1076.74390174584,455.890688248432));
#117685=CARTESIAN_POINT('Ctrl Pts',(108.37179267808,1076.71451997644,455.785420615026));
#117686=CARTESIAN_POINT('Ctrl Pts',(108.482684606891,1076.70255123353,455.71391068143));
#117687=CARTESIAN_POINT('Ctrl Pts',(108.679564754118,1076.68339266947,455.529442953307));
#117688=CARTESIAN_POINT('Ctrl Pts',(108.76187320898,1076.67670328487,455.416064819364));
#117689=CARTESIAN_POINT('Ctrl Pts',(108.833425746483,1076.67291107026,455.262937671884));
#117690=CARTESIAN_POINT('Ctrl Pts',(108.845007218833,1076.67240572149,455.235224438535));
#117691=CARTESIAN_POINT('Ctrl Pts',(108.861958322215,1076.67185990988,455.189434183184));
#117692=CARTESIAN_POINT('Ctrl Pts',(108.868028563725,1076.67171637646,455.171636064354));
#117693=CARTESIAN_POINT('Ctrl Pts',(108.877981463478,1076.67158017788,455.139780425035));
#117694=CARTESIAN_POINT('Ctrl Pts',(108.882047957335,1076.67156084973,455.125785662428));
#117695=CARTESIAN_POINT('Ctrl Pts',(108.889968807407,1076.67160443307,455.09633576917));
#117696=CARTESIAN_POINT('Ctrl Pts',(108.893767450016,1076.67167513581,455.080869424165));
#117697=CARTESIAN_POINT('Ctrl Pts',(108.902759896149,1076.67198347318,455.040454799156));
#117698=CARTESIAN_POINT('Ctrl Pts',(108.907420149256,1076.67229571784,455.015399081513));
#117699=CARTESIAN_POINT('Ctrl Pts',(108.923198026648,1076.67410834938,454.910190488869));
#117700=CARTESIAN_POINT('Ctrl Pts',(108.926250263164,1076.67670990839,454.829127156987));
#117701=CARTESIAN_POINT('Ctrl Pts',(108.912698862536,1076.68532799887,454.644795911623));
#117702=CARTESIAN_POINT('Ctrl Pts',(108.890287235635,1076.69206269198,454.542818239556));
#117703=CARTESIAN_POINT('Ctrl Pts',(108.812358334415,1076.71000836084,454.33494918969));
#117704=CARTESIAN_POINT('Ctrl Pts',(108.753195588104,1076.72158975816,454.231895257354));
#117705=CARTESIAN_POINT('Ctrl Pts',(108.597336430079,1076.74906156974,454.040231380331));
#117706=CARTESIAN_POINT('Ctrl Pts',(108.498800674608,1076.76504438467,453.955416786063));
#117707=CARTESIAN_POINT('Ctrl Pts',(108.268110439784,1076.80003438503,453.818973439859));
#117708=CARTESIAN_POINT('Ctrl Pts',(108.135890091922,1076.81887779136,453.771717561882));
#117709=CARTESIAN_POINT('Ctrl Pts',(107.855266020332,1076.85661706485,453.728587014278));
#117710=CARTESIAN_POINT('Ctrl Pts',(107.709041231693,1076.87513160685,453.735290159195));
#117711=CARTESIAN_POINT('Ctrl Pts',(107.433875004523,1076.90781956673,453.804067820478));
#117712=CARTESIAN_POINT('Ctrl Pts',(107.306889381564,1076.92186363973,453.863016890868));
#117713=CARTESIAN_POINT('Ctrl Pts',(107.093475367213,1076.94345106512,454.017143888293));
#117714=CARTESIAN_POINT('Ctrl Pts',(107.005775803873,1076.95136420361,454.106687994877));
#117715=CARTESIAN_POINT('Ctrl Pts',(106.892531043737,1076.95985674309,454.270855283648));
#117716=CARTESIAN_POINT('Ctrl Pts',(106.856465869863,1076.9620786582,454.336712183565));
#117717=CARTESIAN_POINT('Ctrl Pts',(106.817521675084,1076.96371792995,454.429332414074));
#117718=CARTESIAN_POINT('Ctrl Pts',(106.808445806467,1076.9640180105,454.453235549723));
#117719=CARTESIAN_POINT('Ctrl Pts',(106.795113662979,1076.96431392402,454.492449893638));
#117720=CARTESIAN_POINT('Ctrl Pts',(106.790337472132,1076.96438197488,454.507572746395));
#117721=CARTESIAN_POINT('Ctrl Pts',(106.781848177851,1076.96442545437,454.536645673666));
#117722=CARTESIAN_POINT('Ctrl Pts',(106.778078965015,1076.96440866715,454.550575672544));
#117723=CARTESIAN_POINT('Ctrl Pts',(106.770110107113,1076.96428478677,454.582528587587));
#117724=CARTESIAN_POINT('Ctrl Pts',(106.766090614728,1076.96415356452,454.600591490269));
#117725=CARTESIAN_POINT('Ctrl Pts',(106.755297878057,1076.96356896003,454.655665996039));
#117726=CARTESIAN_POINT('Ctrl Pts',(106.74997914225,1076.96292322275,454.692930011779));
#117727=CARTESIAN_POINT('Ctrl Pts',(106.73359348296,1076.95857765652,454.874386330028));
#117728=CARTESIAN_POINT('Ctrl Pts',(106.749367691084,1076.9514635675,455.01937028733));
#117729=CARTESIAN_POINT('Ctrl Pts',(106.827870501434,1076.93270628244,455.267901842644));
#117730=CARTESIAN_POINT('Ctrl Pts',(106.880406277064,1076.92232823087,455.372390030318));
#117731=CARTESIAN_POINT('Ctrl Pts',(107.023110276428,1076.89710289102,455.570194855512));
#117732=CARTESIAN_POINT('Ctrl Pts',(107.115460432949,1076.88210142741,455.659781991592));
#117733=CARTESIAN_POINT('Ctrl Pts',(107.311017983575,1076.85224734,455.792273036469));
#117734=CARTESIAN_POINT('Ctrl Pts',(107.409562028757,1076.83785939066,455.839411681416));
#117735=CARTESIAN_POINT('Ctrl Pts',(107.616921296845,1076.80876215893,455.902914512555));
#117736=CARTESIAN_POINT('Ctrl Pts',(107.724632667405,1076.79420472728,455.919033445776));
#117737=CARTESIAN_POINT('Ctrl Pts',(107.832971536831,1076.78010498484,455.919008256138));
#117738=CARTESIAN_POINT('',(107.832717977524,1074.84120620429,453.737926788159));
#117739=CARTESIAN_POINT('',(107.832717977554,1067.7251047501,453.737926788159));
#117740=CARTESIAN_POINT('Ctrl Pts',(107.832913167154,1074.76151756941,455.919008268147));
#117741=CARTESIAN_POINT('Ctrl Pts',(107.761364680361,1074.77090615704,455.919021074199));
#117742=CARTESIAN_POINT('Ctrl Pts',(107.690007241569,1074.7805072353,455.911992639033));
#117743=CARTESIAN_POINT('Ctrl Pts',(107.549993601512,1074.79981575487,455.884129554535));
#117744=CARTESIAN_POINT('Ctrl Pts',(107.481641060263,1074.80947954401,455.863408111629));
#117745=CARTESIAN_POINT('Ctrl Pts',(107.282079838548,1074.83843075412,455.780842033004));
#117746=CARTESIAN_POINT('Ctrl Pts',(107.1605628438,1074.85709833395,455.699395202276));
#117747=CARTESIAN_POINT('Ctrl Pts',(106.956789546625,1074.89075928502,455.493949390514));
#117748=CARTESIAN_POINT('Ctrl Pts',(106.876320330313,1074.9054469374,455.372119822143));
#117749=CARTESIAN_POINT('Ctrl Pts',(106.767561384308,1074.92896688559,455.103616175412));
#117750=CARTESIAN_POINT('Ctrl Pts',(106.740399210943,1074.93755992791,454.959669784576));
#117751=CARTESIAN_POINT('Ctrl Pts',(106.744089173054,1074.94731695781,454.67282620598));
#117752=CARTESIAN_POINT('Ctrl Pts',(106.773480886195,1074.94856290909,454.532882477924));
#117753=CARTESIAN_POINT('Ctrl Pts',(106.884264397555,1074.94377444183,454.271823333038));
#117754=CARTESIAN_POINT('Ctrl Pts',(106.964608960224,1074.93777693391,454.153392027821));
#117755=CARTESIAN_POINT('Ctrl Pts',(107.168200687902,1074.91901003619,453.951710582853));
#117756=CARTESIAN_POINT('Ctrl Pts',(107.290291937445,1074.90627884597,453.87142850615));
#117757=CARTESIAN_POINT('Ctrl Pts',(107.558549872016,1074.87572560015,453.763059868814));
#117758=CARTESIAN_POINT('Ctrl Pts',(107.702131789146,1074.85818938898,453.736178496687));
#117759=CARTESIAN_POINT('Ctrl Pts',(107.917463658781,1074.83019045815,453.738916049534));
#117760=CARTESIAN_POINT('Ctrl Pts',(107.988067088475,1074.82073763901,453.746726052469));
#117761=CARTESIAN_POINT('Ctrl Pts',(108.12696748848,1074.80158989798,453.775969661687));
#117762=CARTESIAN_POINT('Ctrl Pts',(108.194945731411,1074.79193686762,453.797387563067));
#117763=CARTESIAN_POINT('Ctrl Pts',(108.395041151581,1074.76264162941,453.882682931718));
#117764=CARTESIAN_POINT('Ctrl Pts',(108.516929903128,1074.7435246556,453.966693540862));
#117765=CARTESIAN_POINT('Ctrl Pts',(108.718078675198,1074.70925152903,454.175788192346));
#117766=CARTESIAN_POINT('Ctrl Pts',(108.796325451983,1074.69434260757,454.297946150964));
#117767=CARTESIAN_POINT('Ctrl Pts',(108.900425519118,1074.67058456738,454.564710628252));
#117768=CARTESIAN_POINT('Ctrl Pts',(108.925782033253,1074.66191095239,454.706449742708));
#117769=CARTESIAN_POINT('Ctrl Pts',(108.920362005906,1074.65200819628,454.990860435801));
#117770=CARTESIAN_POINT('Ctrl Pts',(108.890099436397,1074.65082000139,455.130630123571));
#117771=CARTESIAN_POINT('Ctrl Pts',(108.777834792077,1074.65607970017,455.390664360931));
#117772=CARTESIAN_POINT('Ctrl Pts',(108.697039268529,1074.66246419161,455.508302532283));
#117773=CARTESIAN_POINT('Ctrl Pts',(108.494652339104,1074.68199695735,455.706727884768));
#117774=CARTESIAN_POINT('Ctrl Pts',(108.37480824893,1074.69499371989,455.785286066671));
#117775=CARTESIAN_POINT('Ctrl Pts',(108.112958319505,1074.72568614054,455.891770153792));
#117776=CARTESIAN_POINT('Ctrl Pts',(107.973506051147,1074.74306898062,455.918983104237));
#117777=CARTESIAN_POINT('Ctrl Pts',(107.832913167154,1074.76151756941,455.919008268147));
#117778=CARTESIAN_POINT('Origin',(107.832717977554,1067.7251047501,454.828467536887));
#117779=CARTESIAN_POINT('',(107.832717977554,1074.78413642061,455.319008285615));
#117780=CARTESIAN_POINT('',(107.832717977554,1074.8199670159,454.337926788159));
#117781=CARTESIAN_POINT('Ctrl Pts',(107.832717977554,1074.78413642061,455.319008285615));
#117782=CARTESIAN_POINT('Ctrl Pts',(107.80132417306,1074.78824117862,455.319008285615));
#117783=CARTESIAN_POINT('Ctrl Pts',(107.77001005431,1074.79244177835,455.315994575158));
#117784=CARTESIAN_POINT('Ctrl Pts',(107.707766885313,1074.80100537068,455.303907485118));
#117785=CARTESIAN_POINT('Ctrl Pts',(107.676999512641,1074.80535060123,455.294737716767));
#117786=CARTESIAN_POINT('Ctrl Pts',(107.586891108525,1074.81842493241,455.257958976559));
#117787=CARTESIAN_POINT('Ctrl Pts',(107.531906586075,1074.82689694455,455.221435086252));
#117788=CARTESIAN_POINT('Ctrl Pts',(107.439558776845,1074.84222992862,455.128988095712));
#117789=CARTESIAN_POINT('Ctrl Pts',(107.403041771232,1074.84894717126,455.074014804486));
#117790=CARTESIAN_POINT('Ctrl Pts',(107.354029797519,1074.85964148896,454.953589742402));
#117791=CARTESIAN_POINT('Ctrl Pts',(107.341703043795,1074.86354839834,454.889494764361));
#117792=CARTESIAN_POINT('Ctrl Pts',(107.342671627679,1074.86806437088,454.761060606083));
#117793=CARTESIAN_POINT('Ctrl Pts',(107.355558844303,1074.868678798,454.698037234446));
#117794=CARTESIAN_POINT('Ctrl Pts',(107.404752322777,1074.8665853144,454.580387569291));
#117795=CARTESIAN_POINT('Ctrl Pts',(107.440572432291,1074.86389653181,454.526963801322));
#117796=CARTESIAN_POINT('Ctrl Pts',(107.530841728602,1074.85551182968,454.43653428028));
#117797=CARTESIAN_POINT('Ctrl Pts',(107.584516325315,1074.84987837628,454.400553573597));
#117798=CARTESIAN_POINT('Ctrl Pts',(107.703501609517,1074.83627639932,454.350799989405));
#117799=CARTESIAN_POINT('Ctrl Pts',(107.767834298285,1074.82840098098,454.337926788159));
#117800=CARTESIAN_POINT('Ctrl Pts',(107.832717977554,1074.8199670159,454.337926788159));
#117801=CARTESIAN_POINT('',(107.832717977554,1082.7251047501,454.337926788159));
#117802=CARTESIAN_POINT('',(107.832717977554,1067.7251047501,454.337926788159));
#117803=CARTESIAN_POINT('Origin',(107.832717977554,1082.7251047501,454.828467536887));
#117804=CARTESIAN_POINT('Ctrl Pts',(107.832717977554,1074.8199670159,454.337926788159));
#117805=CARTESIAN_POINT('Ctrl Pts',(107.832731662808,1074.81996523701,454.337926788159));
#117806=CARTESIAN_POINT('Ctrl Pts',(107.832745348086,1074.81996345809,454.337926788733));
#117807=CARTESIAN_POINT('Ctrl Pts',(107.832759033389,1074.81996167915,454.337926789878));
#117808=CARTESIAN_POINT('Ctrl Pts',(107.864720572838,1074.81580702779,454.337929464901));
#117809=CARTESIAN_POINT('Ctrl Pts',(107.896595272592,1074.81154558869,454.341055820378));
#117810=CARTESIAN_POINT('Ctrl Pts',(107.959313103048,1074.80292319969,454.353465016089));
#117811=CARTESIAN_POINT('Ctrl Pts',(107.990014750329,1074.79858131692,454.362729932292));
#117812=CARTESIAN_POINT('Ctrl Pts',(108.080279548172,1074.78543850234,454.399922020564));
#117813=CARTESIAN_POINT('Ctrl Pts',(108.135392458427,1074.77687321478,454.436877219524));
#117814=CARTESIAN_POINT('Ctrl Pts',(108.22728102955,1074.76141574975,454.52985399325));
#117815=CARTESIAN_POINT('Ctrl Pts',(108.263391166522,1074.75465297741,454.584748587818));
#117816=CARTESIAN_POINT('Ctrl Pts',(108.311662403432,1074.74389147749,454.70460246635));
#117817=CARTESIAN_POINT('Ctrl Pts',(108.323757055971,1074.73995263477,454.768191978922));
#117818=CARTESIAN_POINT('Ctrl Pts',(108.322732874622,1074.73536732846,454.896108010189));
#117819=CARTESIAN_POINT('Ctrl Pts',(108.30981429028,1074.73474283866,454.959130700503));
#117820=CARTESIAN_POINT('Ctrl Pts',(108.260588473304,1074.73688951362,455.076692195476));
#117821=CARTESIAN_POINT('Ctrl Pts',(108.224798394672,1074.73963642042,455.130039055872));
#117822=CARTESIAN_POINT('Ctrl Pts',(108.134656224412,1074.748169808,455.22033612801));
#117823=CARTESIAN_POINT('Ctrl Pts',(108.081081628074,1074.7538909484,455.256271530422));
#117824=CARTESIAN_POINT('Ctrl Pts',(107.962788666784,1074.76759438969,455.305820312635));
#117825=CARTESIAN_POINT('Ctrl Pts',(107.899100568906,1074.77546674313,455.318728063144));
#117826=CARTESIAN_POINT('Ctrl Pts',(107.834120646257,1074.78395307392,455.319006781636));
#117827=CARTESIAN_POINT('Ctrl Pts',(107.833419292021,1074.78404472334,455.319008285615));
#117828=CARTESIAN_POINT('Ctrl Pts',(107.832717977554,1074.78413642061,455.319008285615));
#117829=CARTESIAN_POINT('Origin',(86.323060185316,1067.7251047501,400.766404126158));
#117830=CARTESIAN_POINT('',(86.3230601853348,1078.66271960918,399.288100993964));
#117831=CARTESIAN_POINT('Ctrl Pts',(86.3231885187679,1078.68302856617,402.244707252781));
#117832=CARTESIAN_POINT('Ctrl Pts',(86.511377124993,1078.67873167388,402.244690915879));
#117833=CARTESIAN_POINT('Ctrl Pts',(86.6978340159513,1078.67397014017,402.208740216216));
#117834=CARTESIAN_POINT('Ctrl Pts',(87.0536990953585,1078.66381065772,402.066262785444));
#117835=CARTESIAN_POINT('Ctrl Pts',(87.2187302999287,1078.65849687174,401.95856262917));
#117836=CARTESIAN_POINT('Ctrl Pts',(87.4924700757981,1078.64859018114,401.690140995185));
#117837=CARTESIAN_POINT('Ctrl Pts',(87.6004762133578,1078.64407489731,401.533884827865));
#117838=CARTESIAN_POINT('Ctrl Pts',(87.7457832568328,1078.63684031022,401.203503049251));
#117839=CARTESIAN_POINT('Ctrl Pts',(87.7870777909925,1078.63406309525,401.034465919139));
#117840=CARTESIAN_POINT('Ctrl Pts',(87.8046994174545,1078.63111786495,400.762906393987));
#117841=CARTESIAN_POINT('Ctrl Pts',(87.8011109419465,1078.63034964539,400.66328299183));
#117842=CARTESIAN_POINT('Ctrl Pts',(87.7824754248551,1078.62974695291,400.527928373313));
#117843=CARTESIAN_POINT('Ctrl Pts',(87.776013699419,1078.62962913559,400.491286635201));
#117844=CARTESIAN_POINT('Ctrl Pts',(87.7631011112122,1078.62951198781,400.43137780273));
#117845=CARTESIAN_POINT('Ctrl Pts',(87.7574503625128,1078.62948555144,400.407955625885));
#117846=CARTESIAN_POINT('Ctrl Pts',(87.7453884988887,1078.62947240838,400.362827544823));
#117847=CARTESIAN_POINT('Ctrl Pts',(87.7390463566941,1078.62948337884,400.341110051006));
#117848=CARTESIAN_POINT('Ctrl Pts',(87.7231399691271,1078.62954918519,400.290949855368));
#117849=CARTESIAN_POINT('Ctrl Pts',(87.7132032005472,1078.62961714908,400.262635772914));
#117850=CARTESIAN_POINT('Ctrl Pts',(87.6792290728415,1078.62992641556,400.174509103744));
#117851=CARTESIAN_POINT('Ctrl Pts',(87.6521388856902,1078.63027691097,400.115955521755));
#117852=CARTESIAN_POINT('Ctrl Pts',(87.5272739895007,1078.63224469689,399.886682816148));
#117853=CARTESIAN_POINT('Ctrl Pts',(87.3997291574734,1078.63497295119,399.734506182838));
#117854=CARTESIAN_POINT('Ctrl Pts',(87.1210596675006,1078.64166554795,399.511718491457));
#117855=CARTESIAN_POINT('Ctrl Pts',(86.9805224613034,1078.64525865084,399.432696435072));
#117856=CARTESIAN_POINT('Ctrl Pts',(86.6665992891594,1078.6534933482,399.318078559461));
#117857=CARTESIAN_POINT('Ctrl Pts',(86.4938682118272,1078.65813069637,399.287726539262));
#117858=CARTESIAN_POINT('Ctrl Pts',(86.1332105510088,1078.6678200902,399.288509831046));
#117859=CARTESIAN_POINT('Ctrl Pts',(85.9483204421648,1078.67278681185,399.32425700736));
#117860=CARTESIAN_POINT('Ctrl Pts',(85.5935550584435,1078.68225291729,399.465881124098));
#117861=CARTESIAN_POINT('Ctrl Pts',(85.4282673175356,1078.68662673938,399.573553508469));
#117862=CARTESIAN_POINT('Ctrl Pts',(85.153666317123,1078.69400196367,399.84248969958));
#117863=CARTESIAN_POINT('Ctrl Pts',(85.0452372845045,1078.69698172471,399.999412656643));
#117864=CARTESIAN_POINT('Ctrl Pts',(84.8998834356383,1078.70144204265,400.330738224604));
#117865=CARTESIAN_POINT('Ctrl Pts',(84.8587408193982,1078.70300006463,400.499929000067));
#117866=CARTESIAN_POINT('Ctrl Pts',(84.8414343245999,1078.70461262791,400.771480271008));
#117867=CARTESIAN_POINT('Ctrl Pts',(84.8451197289468,1078.70502006977,400.870966338669));
#117868=CARTESIAN_POINT('Ctrl Pts',(84.863816927806,1078.70533761821,401.005885381117));
#117869=CARTESIAN_POINT('Ctrl Pts',(84.8702500342564,1078.70539915638,401.042238908333));
#117870=CARTESIAN_POINT('Ctrl Pts',(84.8830600391271,1078.70546027805,401.101585490668));
#117871=CARTESIAN_POINT('Ctrl Pts',(84.8886447678288,1078.70547408537,401.124732716756));
#117872=CARTESIAN_POINT('Ctrl Pts',(84.9005335922015,1078.70548116609,401.169262293854));
#117873=CARTESIAN_POINT('Ctrl Pts',(84.9067670820064,1078.70547569812,401.190656947926));
#117874=CARTESIAN_POINT('Ctrl Pts',(84.9223508278997,1078.7054423641,401.239964673893));
#117875=CARTESIAN_POINT('Ctrl Pts',(84.9320559174966,1078.70540788476,401.267755720552));
#117876=CARTESIAN_POINT('Ctrl Pts',(84.9650280379881,1078.70525120238,401.353826576474));
#117877=CARTESIAN_POINT('Ctrl Pts',(84.9911789878627,1078.70507413942,401.41092633258));
#117878=CARTESIAN_POINT('Ctrl Pts',(85.1138777067444,1078.70404785706,401.639247301699));
#117879=CARTESIAN_POINT('Ctrl Pts',(85.2404466466818,1078.70258809057,401.792036317088));
#117880=CARTESIAN_POINT('Ctrl Pts',(85.5180154432927,1078.69859591862,402.016634821358));
#117881=CARTESIAN_POINT('Ctrl Pts',(85.6584935110152,1078.69632929459,402.096637478305));
#117882=CARTESIAN_POINT('Ctrl Pts',(85.9736132389365,1078.69057521564,402.213493079599));
#117883=CARTESIAN_POINT('Ctrl Pts',(86.1477101532214,1078.68703524676,402.24472248629));
#117884=CARTESIAN_POINT('Ctrl Pts',(86.3231885187679,1078.68302856617,402.244707252781));
#117885=CARTESIAN_POINT('',(86.3230601852944,1076.66188598601,399.288100993964));
#117886=CARTESIAN_POINT('',(86.323060185316,1067.7251047501,399.288100993964));
#117887=CARTESIAN_POINT('',(86.323060185316,1076.68243856932,402.244707258351));
#117888=CARTESIAN_POINT('Ctrl Pts',(86.323060185316,1076.68243856932,402.244707258351));
#117889=CARTESIAN_POINT('Ctrl Pts',(86.2781747730325,1076.68347561579,402.244707258351));
#117890=CARTESIAN_POINT('Ctrl Pts',(86.2336323361814,1076.68447645497,402.242667270048));
#117891=CARTESIAN_POINT('Ctrl Pts',(86.1894286980019,1076.68544312929,402.238655047791));
#117892=CARTESIAN_POINT('Ctrl Pts',(86.1447882829812,1076.68641935534,402.234603180704));
#117893=CARTESIAN_POINT('Ctrl Pts',(86.1004924641547,1076.68736073805,402.228539911076));
#117894=CARTESIAN_POINT('Ctrl Pts',(86.0565337239154,1076.688269381,402.220482458307));
#117895=CARTESIAN_POINT('Ctrl Pts',(86.049311585819,1076.68841866519,402.219158670676));
#117896=CARTESIAN_POINT('Ctrl Pts',(86.0420985572702,1076.68856706566,402.217780941709));
#117897=CARTESIAN_POINT('Ctrl Pts',(86.0348946237282,1076.68871459173,402.216349214693));
#117898=CARTESIAN_POINT('Ctrl Pts',(85.996765109473,1076.68949542867,402.208771263655));
#117899=CARTESIAN_POINT('Ctrl Pts',(85.958725481398,1076.69025451741,402.199643312767));
#117900=CARTESIAN_POINT('Ctrl Pts',(85.92103295674,1076.69098826324,402.188991296821));
#117901=CARTESIAN_POINT('Ctrl Pts',(85.8833768031073,1076.69172130105,402.178349559432));
#117902=CARTESIAN_POINT('Ctrl Pts',(85.846067682979,1076.69242904483,402.166186817494));
#117903=CARTESIAN_POINT('Ctrl Pts',(85.8093508310832,1076.69310791027,402.152579746354));
#117904=CARTESIAN_POINT('Ctrl Pts',(85.791761404465,1076.6934331248,402.146061197869));
#117905=CARTESIAN_POINT('Ctrl Pts',(85.7743076779248,1076.69375171191,402.139211922037));
#117906=CARTESIAN_POINT('Ctrl Pts',(85.7570150942891,1076.69406327753,402.132044307749));
#117907=CARTESIAN_POINT('Ctrl Pts',(85.7152840314043,1076.69481515849,402.114747172231));
#117908=CARTESIAN_POINT('Ctrl Pts',(85.6745594924959,1076.6955259268,402.095630482121));
#117909=CARTESIAN_POINT('Ctrl Pts',(85.6348252209055,1076.69619803782,402.0747285448));
#117910=CARTESIAN_POINT('Ctrl Pts',(85.5949967567797,1076.69687174212,402.053777058151));
#117911=CARTESIAN_POINT('Ctrl Pts',(85.5561624134356,1076.69750660564,402.031031427587));
#117912=CARTESIAN_POINT('Ctrl Pts',(85.5183279992,1076.69810510126,402.006479228432));
#117913=CARTESIAN_POINT('Ctrl Pts',(85.5129365550676,1076.69819038752,402.002980514028));
#117914=CARTESIAN_POINT('Ctrl Pts',(85.5075654650637,1076.69827493527,401.999445043196));
#117915=CARTESIAN_POINT('Ctrl Pts',(85.5022147979378,1076.69835875168,401.99587271082));
#117916=CARTESIAN_POINT('Ctrl Pts',(85.4720809220624,1076.69883078871,401.975754056855));
#117917=CARTESIAN_POINT('Ctrl Pts',(85.4425301022561,1076.69927989956,401.954417787375));
#117918=CARTESIAN_POINT('Ctrl Pts',(85.4137805664492,1076.69970448713,401.931990127003));
#117919=CARTESIAN_POINT('Ctrl Pts',(85.3850243052947,1076.70012917403,401.909557220153));
#117920=CARTESIAN_POINT('Ctrl Pts',(85.3570701847616,1076.70052932618,401.886032751249));
#117921=CARTESIAN_POINT('Ctrl Pts',(85.3301054815449,1076.70090334536,401.861584981958));
#117922=CARTESIAN_POINT('Ctrl Pts',(85.3121382809558,1076.70115256293,401.845294872207));
#117923=CARTESIAN_POINT('Ctrl Pts',(85.2946097069164,1076.70139017782,401.828595697225));
#117924=CARTESIAN_POINT('Ctrl Pts',(85.2775660305127,1076.70161571723,401.811546280568));
#117925=CARTESIAN_POINT('Ctrl Pts',(85.2424743437808,1076.70208008641,401.776442775073));
#117926=CARTESIAN_POINT('Ctrl Pts',(85.2090706729493,1076.70249853921,401.73948581198));
#117927=CARTESIAN_POINT('Ctrl Pts',(85.1775876281939,1076.70287118893,401.700894774336));
#117928=CARTESIAN_POINT('Ctrl Pts',(85.1461227436608,1076.70324362368,401.662325996986));
#117929=CARTESIAN_POINT('Ctrl Pts',(85.1165766905558,1076.70357030818,401.622125482738));
#117930=CARTESIAN_POINT('Ctrl Pts',(85.0891433844455,1076.70385135552,401.580547528257));
#117931=CARTESIAN_POINT('Ctrl Pts',(85.0616894197992,1076.7041326145,401.538938263673));
#117932=CARTESIAN_POINT('Ctrl Pts',(85.0363517220966,1076.70436816757,401.495950004178));
#117933=CARTESIAN_POINT('Ctrl Pts',(85.0132805743846,1076.70455812808,401.451865665152));
#117934=CARTESIAN_POINT('Ctrl Pts',(84.9928181668511,1076.70472660905,401.412766105727));
#117935=CARTESIAN_POINT('Ctrl Pts',(84.9741381915511,1076.70485922517,401.372804988911));
#117936=CARTESIAN_POINT('Ctrl Pts',(84.9573137963501,1076.70495605553,401.332192913321));
#117937=CARTESIAN_POINT('Ctrl Pts',(84.9384373945459,1076.70506469592,401.286627539482));
#117938=CARTESIAN_POINT('Ctrl Pts',(84.9217916099113,1076.70512901854,401.23998628075));
#117939=CARTESIAN_POINT('Ctrl Pts',(84.9075126608846,1076.70514893364,401.192555926258));
#117940=CARTESIAN_POINT('Ctrl Pts',(84.8932441338425,1076.70516883421,401.14516019045));
#117941=CARTESIAN_POINT('Ctrl Pts',(84.8813392198776,1076.70514439207,401.096977085023));
#117942=CARTESIAN_POINT('Ctrl Pts',(84.8718854375303,1076.70507551768,401.04831191612));
#117943=CARTESIAN_POINT('Ctrl Pts',(84.8624265602351,1076.70500660617,400.999620519991));
#117944=CARTESIAN_POINT('Ctrl Pts',(84.8554215850028,1076.7048932145,400.950447149187));
#117945=CARTESIAN_POINT('Ctrl Pts',(84.8509069838721,1076.70473525298,400.901107883088));
#117946=CARTESIAN_POINT('Ctrl Pts',(84.8468157491852,1076.70459210465,400.856395512925));
#117947=CARTESIAN_POINT('Ctrl Pts',(84.8447690760854,1076.70441235379,400.811547360364));
#117948=CARTESIAN_POINT('Ctrl Pts',(84.8447571060139,1076.70419593364,400.766799573503));
#117949=CARTESIAN_POINT('Ctrl Pts',(84.8447473670697,1076.70401985251,400.730392422381));
#117950=CARTESIAN_POINT('Ctrl Pts',(84.8460868290201,1076.70381787846,400.693768275429));
#117951=CARTESIAN_POINT('Ctrl Pts',(84.8487976378466,1076.70359075187,400.65717916664));
#117952=CARTESIAN_POINT('Ctrl Pts',(84.8515071072191,1076.70336373751,400.620608137115));
#117953=CARTESIAN_POINT('Ctrl Pts',(84.8555865653958,1076.70311159546,400.584072701866));
#117954=CARTESIAN_POINT('Ctrl Pts',(84.8610060230901,1076.702835065,400.547822842946));
#117955=CARTESIAN_POINT('Ctrl Pts',(84.8645262241826,1076.70265544504,400.524276798273));
#117956=CARTESIAN_POINT('Ctrl Pts',(84.8686107167369,1076.70246553528,400.50085118465));
#117957=CARTESIAN_POINT('Ctrl Pts',(84.8732396922764,1076.70226553832,400.477612352357));
#117958=CARTESIAN_POINT('Ctrl Pts',(84.8820608692554,1076.70188441544,400.433327423501));
#117959=CARTESIAN_POINT('Ctrl Pts',(84.8928711226574,1076.70146702708,400.389624982645));
#117960=CARTESIAN_POINT('Ctrl Pts',(84.9056472680785,1076.7010111334,400.346498454964));
#117961=CARTESIAN_POINT('Ctrl Pts',(84.9184092539294,1076.70055574497,400.303419723631));
#117962=CARTESIAN_POINT('Ctrl Pts',(84.9331330539135,1076.70006193652,400.260914727335));
#117963=CARTESIAN_POINT('Ctrl Pts',(84.9498449798141,1076.69952747563,400.218991895722));
#117964=CARTESIAN_POINT('Ctrl Pts',(84.952221111862,1076.699451485,400.213031231204));
#117965=CARTESIAN_POINT('Ctrl Pts',(84.9546375125551,1076.69937467257,400.207082373412));
#117966=CARTESIAN_POINT('Ctrl Pts',(84.9570943332091,1076.69929703189,400.201145387587));
#117967=CARTESIAN_POINT('Ctrl Pts',(84.9717199476879,1076.69883483188,400.165802121608));
#117968=CARTESIAN_POINT('Ctrl Pts',(84.9877730909188,1076.69834274521,400.130902979445));
#117969=CARTESIAN_POINT('Ctrl Pts',(85.0051613822483,1076.69782306189,400.096685606535));
#117970=CARTESIAN_POINT('Ctrl Pts',(85.0225647163828,1076.69730292899,400.062438631794));
#117971=CARTESIAN_POINT('Ctrl Pts',(85.0413052391773,1076.69675515167,400.028875150433));
#117972=CARTESIAN_POINT('Ctrl Pts',(85.0612437929392,1076.69618202591,399.996209642549));
#117973=CARTESIAN_POINT('Ctrl Pts',(85.0718285068446,1076.69587777253,399.97886861272));
#117974=CARTESIAN_POINT('Ctrl Pts',(85.0827500869924,1076.69556637547,399.961780196826));
#117975=CARTESIAN_POINT('Ctrl Pts',(85.0939828637915,1076.69524817822,399.94497300405));
#117976=CARTESIAN_POINT('Ctrl Pts',(85.1188605168078,1076.69454345481,399.907749482428));
#117977=CARTESIAN_POINT('Ctrl Pts',(85.1453867556051,1076.69380278896,399.871711793279));
#117978=CARTESIAN_POINT('Ctrl Pts',(85.1735698409287,1076.69302336567,399.836860098791));
#117979=CARTESIAN_POINT('Ctrl Pts',(85.2015102136936,1076.69225065478,399.802308546884));
#117980=CARTESIAN_POINT('Ctrl Pts',(85.2310796490996,1076.69143985114,399.768921984926));
#117981=CARTESIAN_POINT('Ctrl Pts',(85.2623219763971,1076.69058821188,399.736736897005));
#117982=CARTESIAN_POINT('Ctrl Pts',(85.2673789151792,1076.69045036403,399.731527361307));
#117983=CARTESIAN_POINT('Ctrl Pts',(85.2724797471146,1076.69031144632,399.726349393422));
#117984=CARTESIAN_POINT('Ctrl Pts',(85.277624729216,1076.69017144712,399.721203256573));
#117985=CARTESIAN_POINT('Ctrl Pts',(85.3270311525582,1076.68882705761,399.671785744376));
#117986=CARTESIAN_POINT('Ctrl Pts',(85.3796355268857,1076.68740530391,399.62617214953));
#117987=CARTESIAN_POINT('Ctrl Pts',(85.4350174597331,1076.68591198077,399.584557999036));
#117988=CARTESIAN_POINT('Ctrl Pts',(85.4932534022695,1076.68434170188,399.5407993371));
#117989=CARTESIAN_POINT('Ctrl Pts',(85.5545622562959,1076.68269228709,399.50146084956));
#117990=CARTESIAN_POINT('Ctrl Pts',(85.618505362964,1076.680970474,399.466795472388));
#117991=CARTESIAN_POINT('Ctrl Pts',(85.6635875331991,1076.67975653438,399.44235514541));
#117992=CARTESIAN_POINT('Ctrl Pts',(85.7099803264848,1076.67850660736,399.420238305068));
#117993=CARTESIAN_POINT('Ctrl Pts',(85.7575354277989,1076.67722305418,399.40054838733));
#117994=CARTESIAN_POINT('Ctrl Pts',(85.7992620443115,1076.67609681682,399.383271720392));
#117995=CARTESIAN_POINT('Ctrl Pts',(85.841552596285,1076.67495402394,399.367996775221));
#117996=CARTESIAN_POINT('Ctrl Pts',(85.8843932112835,1076.67379476451,399.354684806836));
#117997=CARTESIAN_POINT('Ctrl Pts',(85.9273698567947,1076.67263182411,399.34133056936));
#117998=CARTESIAN_POINT('Ctrl Pts',(85.9709009592765,1076.67145231241,399.329951487713));
#117999=CARTESIAN_POINT('Ctrl Pts',(86.0149906391529,1076.67025631923,399.320557209856));
#118000=CARTESIAN_POINT('Ctrl Pts',(86.0212994704472,1076.67008518351,399.319212974327));
#118001=CARTESIAN_POINT('Ctrl Pts',(86.0276197554638,1076.66991371033,399.317909463193));
#118002=CARTESIAN_POINT('Ctrl Pts',(86.0339515196089,1076.66974189995,399.316646791268));
#118003=CARTESIAN_POINT('Ctrl Pts',(86.069346529021,1076.6687814678,399.309588365905));
#118004=CARTESIAN_POINT('Ctrl Pts',(86.1051948127433,1076.66780773598,399.303791735915));
#118005=CARTESIAN_POINT('Ctrl Pts',(86.1412531880335,1076.66682790792,399.299323226414));
#118006=CARTESIAN_POINT('Ctrl Pts',(86.1773155013337,1076.66584797285,399.294854228899));
#118007=CARTESIAN_POINT('Ctrl Pts',(86.2135873733398,1076.6648619402,399.291713745247));
#118008=CARTESIAN_POINT('Ctrl Pts',(86.2498176838234,1076.66387701573,399.289916507982));
#118009=CARTESIAN_POINT('Ctrl Pts',(86.2742766985505,1076.66321209507,399.288703196471));
#118010=CARTESIAN_POINT('Ctrl Pts',(86.2987166153919,1076.66254767947,399.288100993965));
#118011=CARTESIAN_POINT('Ctrl Pts',(86.3230601852944,1076.66188598601,399.288100993964));
#118012=CARTESIAN_POINT('Ctrl Pts',(86.3230601852944,1076.66188598601,399.288100993964));
#118013=CARTESIAN_POINT('Ctrl Pts',(86.5193488915849,1076.65655057493,399.288100993962));
#118014=CARTESIAN_POINT('Ctrl Pts',(86.7136832635768,1076.65127220747,399.327193099627));
#118015=CARTESIAN_POINT('Ctrl Pts',(87.0726851878742,1076.64181642315,399.47772843703));
#118016=CARTESIAN_POINT('Ctrl Pts',(87.2343467825304,1076.63772009232,399.586492581294));
#118017=CARTESIAN_POINT('Ctrl Pts',(87.5068579887354,1076.63149362544,399.860136871519));
#118018=CARTESIAN_POINT('Ctrl Pts',(87.6150361758342,1076.62943100754,400.022425360104));
#118019=CARTESIAN_POINT('Ctrl Pts',(87.7630166637178,1076.62783207451,400.379867168201));
#118020=CARTESIAN_POINT('Ctrl Pts',(87.8012156409061,1076.62831903304,400.571623049732));
#118021=CARTESIAN_POINT('Ctrl Pts',(87.8015097065115,1076.63176047436,400.95836775111));
#118022=CARTESIAN_POINT('Ctrl Pts',(87.7638255065369,1076.63467101274,401.149610492304));
#118023=CARTESIAN_POINT('Ctrl Pts',(87.6171026682516,1076.64228909187,401.506739872023));
#118024=CARTESIAN_POINT('Ctrl Pts',(87.509483419049,1076.646916496,401.669195699455));
#118025=CARTESIAN_POINT('Ctrl Pts',(87.2377712112084,1076.65696241842,401.943698001443));
#118026=CARTESIAN_POINT('Ctrl Pts',(87.07622419366,1076.66227879963,402.053050768127));
#118027=CARTESIAN_POINT('Ctrl Pts',(86.8058328361515,1076.67017479352,402.167250190758));
#118028=CARTESIAN_POINT('Ctrl Pts',(86.7097073453473,1076.67282204102,402.196769066544));
#118029=CARTESIAN_POINT('Ctrl Pts',(86.5164033827763,1076.67783862898,402.235201840842));
#118030=CARTESIAN_POINT('Ctrl Pts',(86.4198549618292,1076.6802021928,402.244707258351));
#118031=CARTESIAN_POINT('Ctrl Pts',(86.323060185316,1076.68243856932,402.244707258351));
#118032=CARTESIAN_POINT('Origin',(86.323060185316,1067.7251047501,400.766404126158));
#118033=CARTESIAN_POINT('',(86.323060185316,1076.67873408293,401.644707258351));
#118034=CARTESIAN_POINT('',(86.3230601934255,1076.66654097378,399.888100993964));
#118035=CARTESIAN_POINT('Ctrl Pts',(86.323060185316,1076.67873408293,401.644707258351));
#118036=CARTESIAN_POINT('Ctrl Pts',(86.2703365558132,1076.67999434393,401.644707258351));
#118037=CARTESIAN_POINT('Ctrl Pts',(86.2175900991985,1076.68120258287,401.639959906646));
#118038=CARTESIAN_POINT('Ctrl Pts',(86.0508799772341,1076.68486336245,401.609553687992));
#118039=CARTESIAN_POINT('Ctrl Pts',(85.9415805432687,1076.6870210946,401.566066376273));
#118040=CARTESIAN_POINT('Ctrl Pts',(85.7462055632267,1076.69049162001,401.438903899627));
#118041=CARTESIAN_POINT('Ctrl Pts',(85.6621011671413,1076.69177193059,401.356448727894));
#118042=CARTESIAN_POINT('Ctrl Pts',(85.5308559925965,1076.69338560833,401.163264956452));
#118043=CARTESIAN_POINT('Ctrl Pts',(85.4851196212203,1076.69370245253,401.054401013379));
#118044=CARTESIAN_POINT('Ctrl Pts',(85.4389747655909,1076.69335051842,400.82523873274));
#118045=CARTESIAN_POINT('Ctrl Pts',(85.4389975443721,1076.69268545099,400.70723855402));
#118046=CARTESIAN_POINT('Ctrl Pts',(85.4851488405695,1076.6903905254,400.478480005544));
#118047=CARTESIAN_POINT('Ctrl Pts',(85.5306973091888,1076.68878349222,400.369977469653));
#118048=CARTESIAN_POINT('Ctrl Pts',(85.6615055835276,1076.6847086655,400.177036919966));
#118049=CARTESIAN_POINT('Ctrl Pts',(85.7454867969112,1076.68227796102,400.094530632461));
#118050=CARTESIAN_POINT('Ctrl Pts',(85.8909526465541,1076.67820342884,399.999617090543));
#118051=CARTESIAN_POINT('Ctrl Pts',(85.9417217547294,1076.67680058898,399.973145035766));
#118052=CARTESIAN_POINT('Ctrl Pts',(86.0484920846018,1076.67388088735,399.930107152951));
#118053=CARTESIAN_POINT('Ctrl Pts',(86.1043003340706,1076.67236973109,399.913805613415));
#118054=CARTESIAN_POINT('Ctrl Pts',(86.2147707440104,1076.66940637569,399.893106551994));
#118055=CARTESIAN_POINT('Ctrl Pts',(86.2689219404621,1076.66796623408,399.888100992965));
#118056=CARTESIAN_POINT('Ctrl Pts',(86.3230602015351,1076.66654097378,399.888100993964));
#118057=CARTESIAN_POINT('',(86.323060185316,1082.7251047501,399.888100993964));
#118058=CARTESIAN_POINT('',(86.323060185316,1067.7251047501,399.888100993964));
#118059=CARTESIAN_POINT('Origin',(86.323060185316,1082.7251047501,400.766404126158));
#118060=CARTESIAN_POINT('Ctrl Pts',(86.3230602015351,1076.66654097378,399.888100993964));
#118061=CARTESIAN_POINT('Ctrl Pts',(86.3835602978918,1076.66494822988,399.888100995082));
#118062=CARTESIAN_POINT('Ctrl Pts',(86.4440442396713,1076.66337405196,399.894352178612));
#118063=CARTESIAN_POINT('Ctrl Pts',(86.6162978831962,1076.65896256379,399.930519125098));
#118064=CARTESIAN_POINT('Ctrl Pts',(86.7233134227448,1076.65631211925,399.97615557805));
#118065=CARTESIAN_POINT('Ctrl Pts',(86.9135845116199,1076.65190698282,400.106126773335));
#118066=CARTESIAN_POINT('Ctrl Pts',(86.9950035821248,1076.65019723603,400.189185963914));
#118067=CARTESIAN_POINT('Ctrl Pts',(87.1210520559765,1076.64805927605,400.381876011175));
#118068=CARTESIAN_POINT('Ctrl Pts',(87.1645076941637,1076.64765153742,400.489600926454));
#118069=CARTESIAN_POINT('Ctrl Pts',(87.195329481483,1076.64806700802,400.652003725408));
#118070=CARTESIAN_POINT('Ctrl Pts',(87.2004447812257,1076.64832486168,400.70208215275));
#118071=CARTESIAN_POINT('Ctrl Pts',(87.2012504124973,1076.64870978558,400.752321622694));
#118072=CARTESIAN_POINT('Ctrl Pts',(87.2030916191839,1076.64958949878,400.867139966079));
#118073=CARTESIAN_POINT('Ctrl Pts',(87.1823974007777,1076.65112258767,400.981204654637));
#118074=CARTESIAN_POINT('Ctrl Pts',(87.0983016656521,1076.65523027365,401.194890512925));
#118075=CARTESIAN_POINT('Ctrl Pts',(87.0357107310818,1076.65776283178,401.292451292755));
#118076=CARTESIAN_POINT('Ctrl Pts',(86.8764915534712,1076.66338249602,401.458019541839));
#118077=CARTESIAN_POINT('Ctrl Pts',(86.7813684669782,1076.6664135884,401.524408367226));
#118078=CARTESIAN_POINT('Ctrl Pts',(86.6236024554262,1076.67097304646,401.593680827278));
#118079=CARTESIAN_POINT('Ctrl Pts',(86.5688985800898,1076.67248410541,401.611552632287));
#118080=CARTESIAN_POINT('Ctrl Pts',(86.4503735200599,1076.67561408443,401.637783076379));
#118081=CARTESIAN_POINT('Ctrl Pts',(86.386733500936,1076.67721208991,401.644707258351));
#118082=CARTESIAN_POINT('Ctrl Pts',(86.323060185316,1076.67873408293,401.644707258351));
#118083=CARTESIAN_POINT('Origin',(95.5155706932862,1067.7251047501,409.322561393736));
#118084=CARTESIAN_POINT('',(95.5155706933088,1078.33592031499,408.047117272599));
#118085=CARTESIAN_POINT('Ctrl Pts',(95.5157708467647,1078.36173587679,410.598005499167));
#118086=CARTESIAN_POINT('Ctrl Pts',(95.6818456189848,1078.35138272575,410.597979437309));
#118087=CARTESIAN_POINT('Ctrl Pts',(95.846320998692,1078.34061900062,410.5655169649));
#118088=CARTESIAN_POINT('Ctrl Pts',(96.1550572043217,1078.31940202197,410.438773886002));
#118089=CARTESIAN_POINT('Ctrl Pts',(96.2961429969713,1078.30915868367,410.345111475783));
#118090=CARTESIAN_POINT('Ctrl Pts',(96.5262341735934,1078.29144359458,410.116223207326));
#118091=CARTESIAN_POINT('Ctrl Pts',(96.6160958137961,1078.28398795017,409.98605322132));
#118092=CARTESIAN_POINT('Ctrl Pts',(96.7478900226055,1078.27185634106,409.691035758722));
#118093=CARTESIAN_POINT('Ctrl Pts',(96.7853912837021,1078.26749239219,409.527434387064));
#118094=CARTESIAN_POINT('Ctrl Pts',(96.7916613111768,1078.26479235547,409.320553344349));
#118095=CARTESIAN_POINT('Ctrl Pts',(96.790948682325,1078.26439437466,409.279870660457));
#118096=CARTESIAN_POINT('Ctrl Pts',(96.7867088842337,1078.26397330139,409.215069130938));
#118097=CARTESIAN_POINT('Ctrl Pts',(96.784433022949,1078.26386384006,409.190897814286));
#118098=CARTESIAN_POINT('Ctrl Pts',(96.7792129087214,1078.26375578654,409.148471473705));
#118099=CARTESIAN_POINT('Ctrl Pts',(96.7765589847555,1078.26373696293,409.130188108744));
#118100=CARTESIAN_POINT('Ctrl Pts',(96.7702825434915,1078.26375561822,409.09269687742));
#118101=CARTESIAN_POINT('Ctrl Pts',(96.7666137692975,1078.26379641053,409.073501680161));
#118102=CARTESIAN_POINT('Ctrl Pts',(96.7562134955821,1078.26397855988,409.025141302091));
#118103=CARTESIAN_POINT('Ctrl Pts',(96.748893867157,1078.26416179124,408.996115116325));
#118104=CARTESIAN_POINT('Ctrl Pts',(96.7167486679843,1078.26514854897,408.885251096893));
#118105=CARTESIAN_POINT('Ctrl Pts',(96.6847417155487,1078.2664698986,408.805739397829));
#118106=CARTESIAN_POINT('Ctrl Pts',(96.5890202668801,1078.27101453864,408.623277459538));
#118107=CARTESIAN_POINT('Ctrl Pts',(96.518173715774,1078.27477282283,408.525024934341));
#118108=CARTESIAN_POINT('Ctrl Pts',(96.3394301153674,1078.28485574914,408.33927001983));
#118109=CARTESIAN_POINT('Ctrl Pts',(96.2289188733061,1078.29139780745,408.256392798646));
#118110=CARTESIAN_POINT('Ctrl Pts',(95.9748429615258,1078.3068731441,408.123305858752));
#118111=CARTESIAN_POINT('Ctrl Pts',(95.8311486695084,1078.3158476971,408.077758970819));
#118112=CARTESIAN_POINT('Ctrl Pts',(95.523583801791,1078.33535479415,408.037058711165));
#118113=CARTESIAN_POINT('Ctrl Pts',(95.3617187997048,1078.34577900403,408.046273854795));
#118114=CARTESIAN_POINT('Ctrl Pts',(95.0420855861173,1078.36663663872,408.126290569185));
#118115=CARTESIAN_POINT('Ctrl Pts',(94.8880501038049,1078.37684060563,408.199396782662));
#118116=CARTESIAN_POINT('Ctrl Pts',(94.6216044936282,1078.39491960971,408.39825515004));
#118117=CARTESIAN_POINT('Ctrl Pts',(94.5105001323017,1078.40269454033,408.520446453725));
#118118=CARTESIAN_POINT('Ctrl Pts',(94.350454285991,1078.41460470566,408.783898272124));
#118119=CARTESIAN_POINT('Ctrl Pts',(94.2969284648118,1078.41897537158,408.919341038538));
#118120=CARTESIAN_POINT('Ctrl Pts',(94.247274087537,1078.42404571228,409.156223439857));
#118121=CARTESIAN_POINT('Ctrl Pts',(94.2382751790723,1078.42546105857,409.253537466283));
#118122=CARTESIAN_POINT('Ctrl Pts',(94.2411673834591,1078.4264927777,409.383527933655));
#118123=CARTESIAN_POINT('Ctrl Pts',(94.2431422157397,1078.42667908012,409.416084339831));
#118124=CARTESIAN_POINT('Ctrl Pts',(94.2483381277004,1078.42686245503,409.468436387324));
#118125=CARTESIAN_POINT('Ctrl Pts',(94.2507819359811,1078.42690480424,409.488293992395));
#118126=CARTESIAN_POINT('Ctrl Pts',(94.2563164209592,1078.42693323704,409.525937795906));
#118127=CARTESIAN_POINT('Ctrl Pts',(94.2593195755141,1078.42692442566,409.543731944702));
#118128=CARTESIAN_POINT('Ctrl Pts',(94.2669889144042,1078.42685384478,409.583953367182));
#118129=CARTESIAN_POINT('Ctrl Pts',(94.2718837455851,1078.42677846831,409.606330647218));
#118130=CARTESIAN_POINT('Ctrl Pts',(94.2883467413373,1078.42644521499,409.672945647874));
#118131=CARTESIAN_POINT('Ctrl Pts',(94.3016931476827,1078.42608061037,409.716704588679));
#118132=CARTESIAN_POINT('Ctrl Pts',(94.3754706640813,1078.42369665795,409.918953739349));
#118133=CARTESIAN_POINT('Ctrl Pts',(94.4647569250254,1078.41989967285,410.065041142623));
#118134=CARTESIAN_POINT('Ctrl Pts',(94.6729760200097,1078.40982746045,410.289788849472));
#118135=CARTESIAN_POINT('Ctrl Pts',(94.7815364596466,1078.40423244603,410.374543694537));
#118136=CARTESIAN_POINT('Ctrl Pts',(95.0000289934117,1078.3923269411,410.49458042913));
#118137=CARTESIAN_POINT('Ctrl Pts',(95.10533012359,1078.38637181487,410.535451565601));
#118138=CARTESIAN_POINT('Ctrl Pts',(95.3132100058356,1078.37417482621,410.585932618435));
#118139=CARTESIAN_POINT('Ctrl Pts',(95.4143185766654,1078.36806044169,410.598021419915));
#118140=CARTESIAN_POINT('Ctrl Pts',(95.5157708467647,1078.36173587679,410.598005499167));
#118141=CARTESIAN_POINT('',(95.515570693267,1076.33150256053,408.0471172726));
#118142=CARTESIAN_POINT('',(95.5155706932862,1067.7251047501,408.0471172726));
#118143=CARTESIAN_POINT('Ctrl Pts',(95.5152393238831,1076.35762093081,410.598005471826));
#118144=CARTESIAN_POINT('Ctrl Pts',(95.3462068216855,1076.3682676787,410.597961555985));
#118145=CARTESIAN_POINT('Ctrl Pts',(95.1788077616908,1076.37827883585,410.56431576052));
#118146=CARTESIAN_POINT('Ctrl Pts',(94.8673437761854,1076.39596881353,410.433853171452));
#118147=CARTESIAN_POINT('Ctrl Pts',(94.7262614520925,1076.40348614202,410.338533835159));
#118148=CARTESIAN_POINT('Ctrl Pts',(94.4889398941508,1076.41525764072,410.09806679161));
#118149=CARTESIAN_POINT('Ctrl Pts',(94.3952089412524,1076.41938944838,409.955172995849));
#118150=CARTESIAN_POINT('Ctrl Pts',(94.2688186385361,1076.4238178205,409.640635468617));
#118151=CARTESIAN_POINT('Ctrl Pts',(94.2376021102377,1076.42406178306,409.472093703902));
#118152=CARTESIAN_POINT('Ctrl Pts',(94.2429641604886,1076.42058948996,409.133059848678));
#118153=CARTESIAN_POINT('Ctrl Pts',(94.2793402074269,1076.41691485914,408.965985053345));
#118154=CARTESIAN_POINT('Ctrl Pts',(94.4149212921026,1076.40598072977,408.656384811212));
#118155=CARTESIAN_POINT('Ctrl Pts',(94.5125647178691,1076.39883715225,408.516857732209));
#118156=CARTESIAN_POINT('Ctrl Pts',(94.756648226872,1076.38176911232,408.283640659087));
#118157=CARTESIAN_POINT('Ctrl Pts',(94.9007928616087,1076.37200195597,408.192370202695));
#118158=CARTESIAN_POINT('Ctrl Pts',(95.2176270772563,1076.35090892827,408.070742322079));
#118159=CARTESIAN_POINT('Ctrl Pts',(95.3874168679025,1076.3397775118,408.042175011207));
#118160=CARTESIAN_POINT('Ctrl Pts',(95.7252721625835,1076.31795289155,408.053361722937));
#118161=CARTESIAN_POINT('Ctrl Pts',(95.8900811076927,1076.30746694685,408.091866282138));
#118162=CARTESIAN_POINT('Ctrl Pts',(96.1952413370978,1076.28852989874,408.230384756731));
#118163=CARTESIAN_POINT('Ctrl Pts',(96.3326784552892,1076.28026335186,408.328990890009));
#118164=CARTESIAN_POINT('Ctrl Pts',(96.561303952101,1076.26730168083,408.573474622017));
#118165=CARTESIAN_POINT('Ctrl Pts',(96.6503925565104,1076.26272699978,408.71683592043));
#118166=CARTESIAN_POINT('Ctrl Pts',(96.7680017223648,1076.25805157737,409.029368217875));
#118167=CARTESIAN_POINT('Ctrl Pts',(96.7955605163017,1076.25798414124,409.195390865539));
#118168=CARTESIAN_POINT('Ctrl Pts',(96.7852559247905,1076.26238928213,409.528395735921));
#118169=CARTESIAN_POINT('Ctrl Pts',(96.7475859808118,1076.26681076826,409.692119201418));
#118170=CARTESIAN_POINT('Ctrl Pts',(96.6114758770957,1076.27945864058,409.995988321167));
#118171=CARTESIAN_POINT('Ctrl Pts',(96.5142708974298,1076.28756378237,410.133156880886));
#118172=CARTESIAN_POINT('Ctrl Pts',(96.272427198426,1076.30622741002,410.362655425657));
#118173=CARTESIAN_POINT('Ctrl Pts',(96.1299714925185,1076.3166096792,410.452655243967));
#118174=CARTESIAN_POINT('Ctrl Pts',(95.9014745265624,1076.33238731036,410.540725233353));
#118175=CARTESIAN_POINT('Ctrl Pts',(95.8262539165507,1076.33746266407,410.562045378037));
#118176=CARTESIAN_POINT('Ctrl Pts',(95.6722912265138,1076.34761456986,410.590778526715));
#118177=CARTESIAN_POINT('Ctrl Pts',(95.5938506946242,1076.35266948399,410.598025895617));
#118178=CARTESIAN_POINT('Ctrl Pts',(95.5152393238831,1076.35762093081,410.598005471826));
#118179=CARTESIAN_POINT('Origin',(95.5155706932862,1067.7251047501,409.322561393736));
#118180=CARTESIAN_POINT('',(95.5155706932862,1076.35191524971,409.998005514872));
#118181=CARTESIAN_POINT('',(95.5155706932863,1076.33810018128,408.6471172726));
#118182=CARTESIAN_POINT('Ctrl Pts',(95.5155706932862,1076.35191524971,409.998005514872));
#118183=CARTESIAN_POINT('Ctrl Pts',(95.4268631047514,1076.3575378307,409.998005514872));
#118184=CARTESIAN_POINT('Ctrl Pts',(95.3389823525427,1076.36287753048,409.980530058774));
#118185=CARTESIAN_POINT('Ctrl Pts',(95.1740512569251,1076.37246855803,409.912176126145));
#118186=CARTESIAN_POINT('Ctrl Pts',(95.0987775398121,1076.37661271161,409.861613003879));
#118187=CARTESIAN_POINT('Ctrl Pts',(94.9722814177744,1076.38312432879,409.733846983442));
#118188=CARTESIAN_POINT('Ctrl Pts',(94.9223727036056,1076.38542472252,409.657887972189));
#118189=CARTESIAN_POINT('Ctrl Pts',(94.8552103879287,1076.38788498739,409.490713375327));
#118190=CARTESIAN_POINT('Ctrl Pts',(94.8386874965241,1076.38801741199,409.401177587466));
#118191=CARTESIAN_POINT('Ctrl Pts',(94.8417602983214,1076.38607341608,409.221013227405));
#118192=CARTESIAN_POINT('Ctrl Pts',(94.8612822612857,1076.38401880293,409.132216377598));
#118193=CARTESIAN_POINT('Ctrl Pts',(94.9338840883269,1076.37795001218,408.967686475133));
#118194=CARTESIAN_POINT('Ctrl Pts',(94.9861728002878,1076.37399904601,408.893584305718));
#118195=CARTESIAN_POINT('Ctrl Pts',(95.1166832878363,1076.36465634994,408.770118356905));
#118196=CARTESIAN_POINT('Ctrl Pts',(95.1936383730592,1076.35935448643,408.722016209618));
#118197=CARTESIAN_POINT('Ctrl Pts',(95.3536793712844,1076.34862033023,408.661802104452));
#118198=CARTESIAN_POINT('Ctrl Pts',(95.4341694303066,1076.3433362448,408.647147294093));
#118199=CARTESIAN_POINT('Ctrl Pts',(95.5153212013006,1076.33811622929,408.647117318678));
#118200=CARTESIAN_POINT('Ctrl Pts',(95.5154043660395,1076.3381108798,408.647117287959));
#118201=CARTESIAN_POINT('Ctrl Pts',(95.5154875300362,1076.33810553046,408.6471172726));
#118202=CARTESIAN_POINT('Ctrl Pts',(95.5155706932864,1076.33810018128,408.6471172726));
#118203=CARTESIAN_POINT('',(95.5155706932862,1082.7251047501,408.6471172726));
#118204=CARTESIAN_POINT('',(95.5155706932862,1067.7251047501,408.6471172726));
#118205=CARTESIAN_POINT('Origin',(95.5155706932862,1082.7251047501,409.322561393736));
#118206=CARTESIAN_POINT('Ctrl Pts',(95.5155706932864,1076.33810018128,408.6471172726));
#118207=CARTESIAN_POINT('Ctrl Pts',(95.6050888462091,1076.33234224998,408.6471172726));
#118208=CARTESIAN_POINT('Ctrl Pts',(95.6937419908893,1076.32676984405,408.664913370058));
#118209=CARTESIAN_POINT('Ctrl Pts',(95.8580878010066,1076.31674152892,408.73370087287));
#118210=CARTESIAN_POINT('Ctrl Pts',(95.93232579778,1076.31237213147,408.783671656049));
#118211=CARTESIAN_POINT('Ctrl Pts',(96.0571375631939,1076.30543870016,408.909338698087));
#118212=CARTESIAN_POINT('Ctrl Pts',(96.1065556297645,1076.30293886113,408.983748504815));
#118213=CARTESIAN_POINT('Ctrl Pts',(96.1738144023741,1076.30019943501,409.147246984151));
#118214=CARTESIAN_POINT('Ctrl Pts',(96.1910713569332,1076.29998186512,409.234699493124));
#118215=CARTESIAN_POINT('Ctrl Pts',(96.1909580358862,1076.30187621358,409.411224565421));
#118216=CARTESIAN_POINT('Ctrl Pts',(96.1736151391932,1076.30396742989,409.498568174232));
#118217=CARTESIAN_POINT('Ctrl Pts',(96.1063230347709,1076.31016595517,409.661729965477));
#118218=CARTESIAN_POINT('Ctrl Pts',(96.0569808708569,1076.31421480077,409.735945468884));
#118219=CARTESIAN_POINT('Ctrl Pts',(95.9324502998172,1076.32369904763,409.86132215265));
#118220=CARTESIAN_POINT('Ctrl Pts',(95.8583941731649,1076.32904547513,409.911216828379));
#118221=CARTESIAN_POINT('Ctrl Pts',(95.7360696308699,1076.33747218958,409.962531130631));
#118222=CARTESIAN_POINT('Ctrl Pts',(95.6937025115112,1076.3403297286,409.975592635954));
#118223=CARTESIAN_POINT('Ctrl Pts',(95.6071250341514,1076.34604948107,409.993225142205));
#118224=CARTESIAN_POINT('Ctrl Pts',(95.5631235614272,1076.34889814964,409.997773289301));
#118225=CARTESIAN_POINT('Ctrl Pts',(95.5178516334647,1076.35177063834,409.998002626737));
#118226=CARTESIAN_POINT('Ctrl Pts',(95.5167110950412,1076.35184296727,409.998005514872));
#118227=CARTESIAN_POINT('Ctrl Pts',(95.5155706932862,1076.35191524971,409.998005514872));
#118228=CARTESIAN_POINT('Origin',(104.753539540173,1067.7251047501,419.641388283931));
#118229=CARTESIAN_POINT('',(104.753539540203,1077.66045630879,418.542557147938));
#118230=CARTESIAN_POINT('Ctrl Pts',(104.753337989031,1077.67124291073,420.740219401439));
#118231=CARTESIAN_POINT('Ctrl Pts',(104.900057040271,1077.65614840032,420.740246313119));
#118232=CARTESIAN_POINT('Ctrl Pts',(105.045339494299,1077.64093797211,420.710887479148));
#118233=CARTESIAN_POINT('Ctrl Pts',(105.312516336785,1077.61248223269,420.598193937028));
#118234=CARTESIAN_POINT('Ctrl Pts',(105.43241877665,1077.59946383205,420.517244645325));
#118235=CARTESIAN_POINT('Ctrl Pts',(105.621401545446,1077.57853531814,420.32683144979));
#118236=CARTESIAN_POINT('Ctrl Pts',(105.693683172648,1077.5703353697,420.223797724618));
#118237=CARTESIAN_POINT('Ctrl Pts',(105.799112991354,1077.55798113396,420.000603992107));
#118238=CARTESIAN_POINT('Ctrl Pts',(105.832489688039,1077.55381500438,419.882548921654));
#118239=CARTESIAN_POINT('Ctrl Pts',(105.848952660687,1077.55129454079,419.732674653752));
#118240=CARTESIAN_POINT('Ctrl Pts',(105.850972785091,1077.55093225463,419.703866746693));
#118241=CARTESIAN_POINT('Ctrl Pts',(105.852428174474,1077.55053513875,419.65632548408));
#118242=CARTESIAN_POINT('Ctrl Pts',(105.852523267621,1077.55042996759,419.63762785047));
#118243=CARTESIAN_POINT('Ctrl Pts',(105.851837017862,1077.55033270959,419.604048396105));
#118244=CARTESIAN_POINT('Ctrl Pts',(105.851230137569,1077.55032197808,419.589167868126));
#118245=CARTESIAN_POINT('Ctrl Pts',(105.849302102183,1077.55036792785,419.557645716235));
#118246=CARTESIAN_POINT('Ctrl Pts',(105.847903805087,1077.5504329001,419.541012705523));
#118247=CARTESIAN_POINT('Ctrl Pts',(105.84318525221,1077.55071337619,419.49693792828));
#118248=CARTESIAN_POINT('Ctrl Pts',(105.83920769182,1077.55099956616,419.469579595451));
#118249=CARTESIAN_POINT('Ctrl Pts',(105.816907725988,1077.55276765661,419.348472261398));
#118250=CARTESIAN_POINT('Ctrl Pts',(105.787446389403,1077.55545267616,419.257233179425));
#118251=CARTESIAN_POINT('Ctrl Pts',(105.700341275358,1077.56380784206,419.073350382954));
#118252=CARTESIAN_POINT('Ctrl Pts',(105.639982010274,1077.5697778904,418.983142259288));
#118253=CARTESIAN_POINT('Ctrl Pts',(105.486013291688,1077.58525013152,418.813360339748));
#118254=CARTESIAN_POINT('Ctrl Pts',(105.390265249364,1077.59499159045,418.73768516913));
#118255=CARTESIAN_POINT('Ctrl Pts',(105.168861991658,1077.61765178481,418.615576761589));
#118256=CARTESIAN_POINT('Ctrl Pts',(105.043079533405,1077.63059258579,418.573254642765));
#118257=CARTESIAN_POINT('Ctrl Pts',(104.772769955003,1077.65846054535,418.533635647527));
#118258=CARTESIAN_POINT('Ctrl Pts',(104.629979601619,1077.67321148739,418.540377563639));
#118259=CARTESIAN_POINT('Ctrl Pts',(104.351458636077,1077.70203924284,418.608521521727));
#118260=CARTESIAN_POINT('Ctrl Pts',(104.218632435707,1077.71581753649,418.670605939101));
#118261=CARTESIAN_POINT('Ctrl Pts',(103.991259135625,1077.73955344112,418.838166468809));
#118262=CARTESIAN_POINT('Ctrl Pts',(103.896959638166,1077.7494780425,418.939550694101));
#118263=CARTESIAN_POINT('Ctrl Pts',(103.751832614709,1077.76505147781,419.169984413909));
#118264=CARTESIAN_POINT('Ctrl Pts',(103.701518069179,1077.77064053063,419.296516377219));
#118265=CARTESIAN_POINT('Ctrl Pts',(103.665516933398,1077.77507197987,419.479338792007));
#118266=CARTESIAN_POINT('Ctrl Pts',(103.659145621184,1077.77594280979,419.530228916064));
#118267=CARTESIAN_POINT('Ctrl Pts',(103.65514842758,1077.7766828898,419.603317531618));
#118268=CARTESIAN_POINT('Ctrl Pts',(103.65460683322,1077.77683993463,419.625283385923));
#118269=CARTESIAN_POINT('Ctrl Pts',(103.654797677955,1077.7769894068,419.661051367562));
#118270=CARTESIAN_POINT('Ctrl Pts',(103.655131283486,1077.77702131537,419.674849047804));
#118271=CARTESIAN_POINT('Ctrl Pts',(103.656372282436,1077.77703413892,419.703683511127));
#118272=CARTESIAN_POINT('Ctrl Pts',(103.657329146783,1077.77701013077,419.718715243145));
#118273=CARTESIAN_POINT('Ctrl Pts',(103.660323033302,1077.7768807378,419.754218226528));
#118274=CARTESIAN_POINT('Ctrl Pts',(103.662626495215,1077.77674883046,419.774661040391));
#118275=CARTESIAN_POINT('Ctrl Pts',(103.672030997665,1077.7761308177,419.841261851752));
#118276=CARTESIAN_POINT('Ctrl Pts',(103.681499536177,1077.77540831961,419.887029439237));
#118277=CARTESIAN_POINT('Ctrl Pts',(103.732479124479,1077.77123006641,420.072889265702));
#118278=CARTESIAN_POINT('Ctrl Pts',(103.798771233643,1077.76527569804,420.20451944097));
#118279=CARTESIAN_POINT('Ctrl Pts',(103.962124804672,1077.74996187958,420.412906061734));
#118280=CARTESIAN_POINT('Ctrl Pts',(104.050155865404,1077.74153430367,420.493904256605));
#118281=CARTESIAN_POINT('Ctrl Pts',(104.242901321601,1077.72272849526,420.620788193795));
#118282=CARTESIAN_POINT('Ctrl Pts',(104.345261722085,1077.71259696246,420.667669086737));
#118283=CARTESIAN_POINT('Ctrl Pts',(104.550623988338,1077.6919728297,420.726094557412));
#118284=CARTESIAN_POINT('Ctrl Pts',(104.651750685918,1077.68169425015,420.740200767968));
#118285=CARTESIAN_POINT('Ctrl Pts',(104.753337989031,1077.67124291073,420.740219401439));
#118286=CARTESIAN_POINT('',(104.753539540154,1075.64948580966,418.542557147938));
#118287=CARTESIAN_POINT('',(104.753539540173,1067.7251047501,418.542557147938));
#118288=CARTESIAN_POINT('Ctrl Pts',(104.753780331061,1075.66032526247,420.740219393541));
#118289=CARTESIAN_POINT('Ctrl Pts',(104.608017390083,1075.67545936333,420.740251335108));
#118290=CARTESIAN_POINT('Ctrl Pts',(104.463616745573,1075.69018993346,420.711279234496));
#118291=CARTESIAN_POINT('Ctrl Pts',(104.194951603842,1075.71712622813,420.598748997557));
#118292=CARTESIAN_POINT('Ctrl Pts',(104.073213737543,1075.72908278922,420.516486776639));
#118293=CARTESIAN_POINT('Ctrl Pts',(103.868511886586,1075.74876355436,420.308816329664));
#118294=CARTESIAN_POINT('Ctrl Pts',(103.787693667013,1075.75628352042,420.185398144544));
#118295=CARTESIAN_POINT('Ctrl Pts',(103.68018647117,1075.76577533426,419.916766300725));
#118296=CARTESIAN_POINT('Ctrl Pts',(103.653464740972,1075.76776781884,419.774714435164));
#118297=CARTESIAN_POINT('Ctrl Pts',(103.656042550634,1075.76614840311,419.488119056161));
#118298=CARTESIAN_POINT('Ctrl Pts',(103.685384927727,1075.76254544142,419.346429673682));
#118299=CARTESIAN_POINT('Ctrl Pts',(103.797781076754,1075.74999313514,419.079899130659));
#118300=CARTESIAN_POINT('Ctrl Pts',(103.880695003253,1075.74106943032,418.95815433516));
#118301=CARTESIAN_POINT('Ctrl Pts',(104.088875957801,1075.71899043143,418.754339373639));
#118302=CARTESIAN_POINT('Ctrl Pts',(104.212042704123,1075.70605456884,418.674258481696));
#118303=CARTESIAN_POINT('Ctrl Pts',(104.413276182018,1075.6849934789,418.594141672999));
#118304=CARTESIAN_POINT('Ctrl Pts',(104.481849030662,1075.67782790398,418.574297114894));
#118305=CARTESIAN_POINT('Ctrl Pts',(104.622050555195,1075.66319241087,418.548117027916));
#118306=CARTESIAN_POINT('Ctrl Pts',(104.69336763863,1075.65575504721,418.54188424412));
#118307=CARTESIAN_POINT('Ctrl Pts',(104.912040589968,1075.63297156441,418.544120805526));
#118308=CARTESIAN_POINT('Ctrl Pts',(105.057573541504,1075.61783475013,418.575217732282));
#118309=CARTESIAN_POINT('Ctrl Pts',(105.325079724885,1075.59013380257,418.691846022237));
#118310=CARTESIAN_POINT('Ctrl Pts',(105.444929098913,1075.57778939103,418.77516108264));
#118311=CARTESIAN_POINT('Ctrl Pts',(105.645011802497,1075.5574505081,418.983060248187));
#118312=CARTESIAN_POINT('Ctrl Pts',(105.723529884179,1075.54963116592,419.105373244616));
#118313=CARTESIAN_POINT('Ctrl Pts',(105.828633711985,1075.53968325811,419.372823013811));
#118314=CARTESIAN_POINT('Ctrl Pts',(105.854469043342,1075.53762287042,419.515167045892));
#118315=CARTESIAN_POINT('Ctrl Pts',(105.850010428383,1075.53957190013,419.801536839165));
#118316=CARTESIAN_POINT('Ctrl Pts',(105.81987321488,1075.54354935951,419.942695662963));
#118317=CARTESIAN_POINT('Ctrl Pts',(105.707147584058,1075.55701077624,420.205849421708));
#118318=CARTESIAN_POINT('Ctrl Pts',(105.625507553164,1075.56637704818,420.325183367221));
#118319=CARTESIAN_POINT('Ctrl Pts',(105.420671355516,1075.58923218899,420.526316245184));
#118320=CARTESIAN_POINT('Ctrl Pts',(105.299193802991,1075.60252338783,420.605936850527));
#118321=CARTESIAN_POINT('Ctrl Pts',(105.100901594778,1075.62380745086,420.686230699525));
#118322=CARTESIAN_POINT('Ctrl Pts',(105.03348467881,1075.63098393756,420.706274568668));
#118323=CARTESIAN_POINT('Ctrl Pts',(104.895171228648,1075.64558403776,420.733349890659));
#118324=CARTESIAN_POINT('Ctrl Pts',(104.824558764112,1075.65297656371,420.740203883603));
#118325=CARTESIAN_POINT('Ctrl Pts',(104.753780331061,1075.66032526247,420.740219393541));
#118326=CARTESIAN_POINT('Origin',(104.753539540173,1067.7251047501,419.641388283931));
#118327=CARTESIAN_POINT('',(104.753539540173,1075.65786345153,420.140219419923));
#118328=CARTESIAN_POINT('',(104.753539540173,1075.6529321444,419.142557147938));
#118329=CARTESIAN_POINT('Ctrl Pts',(104.753539540173,1075.65786345153,420.140219419923));
#118330=CARTESIAN_POINT('Ctrl Pts',(104.687308095507,1075.66474562987,420.140219419923));
#118331=CARTESIAN_POINT('Ctrl Pts',(104.6217006974,1075.67147329423,420.127028753312));
#118332=CARTESIAN_POINT('Ctrl Pts',(104.499402998231,1075.68384521078,420.075722277205));
#118333=CARTESIAN_POINT('Ctrl Pts',(104.443910813031,1075.68936866123,420.038097664375));
#118334=CARTESIAN_POINT('Ctrl Pts',(104.351273826184,1075.69841656153,419.94363288491));
#118335=CARTESIAN_POINT('Ctrl Pts',(104.314888857087,1075.70186926393,419.887903677498));
#118336=CARTESIAN_POINT('Ctrl Pts',(104.266247826669,1075.70625322989,419.766304749997));
#118337=CARTESIAN_POINT('Ctrl Pts',(104.254127516133,1075.70717766645,419.70179843261));
#118338=CARTESIAN_POINT('Ctrl Pts',(104.2553322653,1075.70642279515,419.571718340932));
#118339=CARTESIAN_POINT('Ctrl Pts',(104.268652931906,1075.70475016815,419.507442009579));
#118340=CARTESIAN_POINT('Ctrl Pts',(104.319266761738,1075.69898536685,419.387422063991));
#118341=CARTESIAN_POINT('Ctrl Pts',(104.356155572995,1075.69494004472,419.332905003089));
#118342=CARTESIAN_POINT('Ctrl Pts',(104.449605432924,1075.68488233212,419.240305082476));
#118343=CARTESIAN_POINT('Ctrl Pts',(104.5056018145,1075.67893304666,419.203489809737));
#118344=CARTESIAN_POINT('Ctrl Pts',(104.59652450694,1075.66935129237,419.166851252507));
#118345=CARTESIAN_POINT('Ctrl Pts',(104.62700921512,1075.66614981598,419.15783042343));
#118346=CARTESIAN_POINT('Ctrl Pts',(104.689569604725,1075.65959990815,419.14564039129));
#118347=CARTESIAN_POINT('Ctrl Pts',(104.721518529795,1075.6562649377,419.142557147938));
#118348=CARTESIAN_POINT('Ctrl Pts',(104.753539540173,1075.6529321444,419.142557147938));
#118349=CARTESIAN_POINT('',(104.753539540173,1082.7251047501,419.142557147938));
#118350=CARTESIAN_POINT('',(104.753539540173,1067.7251047501,419.142557147938));
#118351=CARTESIAN_POINT('Origin',(104.753539540173,1082.7251047501,419.641388283931));
#118352=CARTESIAN_POINT('Ctrl Pts',(104.753539540173,1075.6529321444,419.142557147938));
#118353=CARTESIAN_POINT('Ctrl Pts',(104.753554883302,1075.65293054746,419.142557147938));
#118354=CARTESIAN_POINT('Ctrl Pts',(104.753570226448,1075.65292895053,419.14255714865));
#118355=CARTESIAN_POINT('Ctrl Pts',(104.753585569611,1075.65292735359,419.142557150066));
#118356=CARTESIAN_POINT('Ctrl Pts',(104.820236507847,1075.64599024648,419.142563300253));
#118357=CARTESIAN_POINT('Ctrl Pts',(104.886245227159,1075.63916129711,419.155927665713));
#118358=CARTESIAN_POINT('Ctrl Pts',(105.008600799258,1075.62659969549,419.207627952597));
#118359=CARTESIAN_POINT('Ctrl Pts',(105.063844999928,1075.62097982271,419.2452423481));
#118360=CARTESIAN_POINT('Ctrl Pts',(105.15578253575,1075.61176696558,419.339246517142));
#118361=CARTESIAN_POINT('Ctrl Pts',(105.191850127128,1075.60823474515,419.394430821737));
#118362=CARTESIAN_POINT('Ctrl Pts',(105.240552991933,1075.60369561211,419.515377191944));
#118363=CARTESIAN_POINT('Ctrl Pts',(105.252822055778,1075.60272146629,419.579884890652));
#118364=CARTESIAN_POINT('Ctrl Pts',(105.251894482801,1075.60347331626,419.709928517852));
#118365=CARTESIAN_POINT('Ctrl Pts',(105.238738326434,1075.60518842731,419.774163933337));
#118366=CARTESIAN_POINT('Ctrl Pts',(105.188503374222,1075.61109544875,419.894139303052));
#118367=CARTESIAN_POINT('Ctrl Pts',(105.15183985976,1075.61523693659,419.948662143914));
#118368=CARTESIAN_POINT('Ctrl Pts',(105.059485096615,1075.62541254168,420.040774108678));
#118369=CARTESIAN_POINT('Ctrl Pts',(105.004574740326,1075.63135882211,420.077368044466));
#118370=CARTESIAN_POINT('Ctrl Pts',(104.914082025973,1075.64101053315,420.114804766002));
#118371=CARTESIAN_POINT('Ctrl Pts',(104.88278861588,1075.64432587833,420.124286571065));
#118372=CARTESIAN_POINT('Ctrl Pts',(104.818882512722,1075.65105180129,420.136990864592));
#118373=CARTESIAN_POINT('Ctrl Pts',(104.78641959614,1075.65444670141,420.140197247639));
#118374=CARTESIAN_POINT('Ctrl Pts',(104.753764951171,1075.65784002859,420.140219381712));
#118375=CARTESIAN_POINT('Ctrl Pts',(104.753652244768,1075.65785174028,420.140219419923));
#118376=CARTESIAN_POINT('Ctrl Pts',(104.753539540173,1075.65786345153,420.140219419923));
#118377=CARTESIAN_POINT('Origin',(111.756957497769,1067.7251047501,431.748662623815));
#118378=CARTESIAN_POINT('',(111.756957497785,1076.82908683398,430.658121875088));
#118379=CARTESIAN_POINT('Ctrl Pts',(111.75727025721,1076.81040039708,432.839203327695));
#118380=CARTESIAN_POINT('Ctrl Pts',(111.902381742046,1076.79092321827,432.839161710737));
#118381=CARTESIAN_POINT('Ctrl Pts',(112.046147905152,1076.77177761504,432.810156830667));
#118382=CARTESIAN_POINT('Ctrl Pts',(112.308989063476,1076.73713110618,432.69950342034));
#118383=CARTESIAN_POINT('Ctrl Pts',(112.426451522639,1076.72183019829,432.620864925895));
#118384=CARTESIAN_POINT('Ctrl Pts',(112.610205488221,1076.69835402504,432.438136469508));
#118385=CARTESIAN_POINT('Ctrl Pts',(112.680329885432,1076.68960723474,432.34099987065));
#118386=CARTESIAN_POINT('Ctrl Pts',(112.775480883036,1076.67824727762,432.149686176776));
#118387=CARTESIAN_POINT('Ctrl Pts',(112.806413414772,1076.67479002866,432.059908091913));
#118388=CARTESIAN_POINT('Ctrl Pts',(112.830928519096,1076.67247594805,431.940060959275));
#118389=CARTESIAN_POINT('Ctrl Pts',(112.835445613322,1076.67209561867,431.912707390979));
#118390=CARTESIAN_POINT('Ctrl Pts',(112.840971520463,1076.67172067452,431.868921685871));
#118391=CARTESIAN_POINT('Ctrl Pts',(112.842659079724,1076.67163207462,431.852589222748));
#118392=CARTESIAN_POINT('Ctrl Pts',(112.845117214313,1076.6715618758,431.822073228129));
#118393=CARTESIAN_POINT('Ctrl Pts',(112.845980687728,1076.6715674332,431.807900935848));
#118394=CARTESIAN_POINT('Ctrl Pts',(112.84728008644,1076.67166416966,431.776475037786));
#118395=CARTESIAN_POINT('Ctrl Pts',(112.847583645854,1076.67177352059,431.759220087844));
#118396=CARTESIAN_POINT('Ctrl Pts',(112.847279913083,1076.6722479771,431.709761661606));
#118397=CARTESIAN_POINT('Ctrl Pts',(112.845655753014,1076.67275233942,431.677585353316));
#118398=CARTESIAN_POINT('Ctrl Pts',(112.828979890943,1076.6765753079,431.502040475541));
#118399=CARTESIAN_POINT('Ctrl Pts',(112.78705630706,1076.6835436819,431.362841729849));
#118400=CARTESIAN_POINT('Ctrl Pts',(112.665394732555,1076.70217029938,431.134469564144));
#118401=CARTESIAN_POINT('Ctrl Pts',(112.595729305969,1076.71248370333,431.042347247913));
#118402=CARTESIAN_POINT('Ctrl Pts',(112.422010651828,1076.73757576167,430.875178388979));
#118403=CARTESIAN_POINT('Ctrl Pts',(112.316453851464,1076.75251609532,430.804123561165));
#118404=CARTESIAN_POINT('Ctrl Pts',(112.07657617303,1076.78585597769,430.69711021615));
#118405=CARTESIAN_POINT('Ctrl Pts',(111.942611320986,1076.8041585093,430.665418413196));
#118406=CARTESIAN_POINT('Ctrl Pts',(111.661168067832,1076.84196882221,430.652659141278));
#118407=CARTESIAN_POINT('Ctrl Pts',(111.5160160997,1076.86112237415,430.675158454265));
#118408=CARTESIAN_POINT('Ctrl Pts',(111.247033082611,1076.8959726345,430.774403056583));
#118409=CARTESIAN_POINT('Ctrl Pts',(111.125137220351,1076.91144094223,430.84859073697));
#118410=CARTESIAN_POINT('Ctrl Pts',(110.936862817124,1076.93477697119,431.020901325329));
#118411=CARTESIAN_POINT('Ctrl Pts',(110.865437059576,1076.94339940202,431.110347351822));
#118412=CARTESIAN_POINT('Ctrl Pts',(110.754005580943,1076.95636331188,431.306192426863));
#118413=CARTESIAN_POINT('Ctrl Pts',(110.714031538733,1076.96071523188,431.410974238829));
#118414=CARTESIAN_POINT('Ctrl Pts',(110.684999757307,1076.96338113125,431.546398510142));
#118415=CARTESIAN_POINT('Ctrl Pts',(110.680332206982,1076.96376999925,431.572928853762));
#118416=CARTESIAN_POINT('Ctrl Pts',(110.674247574482,1076.96419759711,431.617028146599));
#118417=CARTESIAN_POINT('Ctrl Pts',(110.672265543499,1076.96431093093,431.634505692611));
#118418=CARTESIAN_POINT('Ctrl Pts',(110.669456605958,1076.96441482982,431.666079052284));
#118419=CARTESIAN_POINT('Ctrl Pts',(110.668479088377,1076.96442522452,431.68015721576));
#118420=CARTESIAN_POINT('Ctrl Pts',(110.666980413094,1076.96437101206,431.710156565671));
#118421=CARTESIAN_POINT('Ctrl Pts',(110.666534329686,1076.96429659172,431.726078025884));
#118422=CARTESIAN_POINT('Ctrl Pts',(110.666274409588,1076.96397574151,431.768642355027));
#118423=CARTESIAN_POINT('Ctrl Pts',(110.667087901174,1076.96364739238,431.795276875441));
#118424=CARTESIAN_POINT('Ctrl Pts',(110.67523109658,1076.96157361978,431.916336904323));
#118425=CARTESIAN_POINT('Ctrl Pts',(110.693862561181,1076.95836105401,432.009539071371));
#118426=CARTESIAN_POINT('Ctrl Pts',(110.75862031329,1076.94828780795,432.200363156414));
#118427=CARTESIAN_POINT('Ctrl Pts',(110.807642981491,1076.94106358344,432.295895149266));
#118428=CARTESIAN_POINT('Ctrl Pts',(110.939756315756,1076.92214738207,432.480777916079));
#118429=CARTESIAN_POINT('Ctrl Pts',(111.025516972836,1076.91012897666,432.566419021153));
#118430=CARTESIAN_POINT('Ctrl Pts',(111.218727770251,1076.88340794796,432.704338833626));
#118431=CARTESIAN_POINT('Ctrl Pts',(111.324343496112,1076.86895036648,432.756530884704));
#118432=CARTESIAN_POINT('Ctrl Pts',(111.54017868944,1076.83962445961,432.822973548804));
#118433=CARTESIAN_POINT('Ctrl Pts',(111.648436672709,1076.82500827728,432.839234540405));
#118434=CARTESIAN_POINT('Ctrl Pts',(111.75727025721,1076.81040039708,432.839203327695));
#118435=CARTESIAN_POINT('',(111.756957497753,1074.81089668524,430.658121875087));
#118436=CARTESIAN_POINT('',(111.756957497769,1067.7251047501,430.658121875087));
#118437=CARTESIAN_POINT('Ctrl Pts',(111.756676799939,1074.79213585482,432.839203336419));
#118438=CARTESIAN_POINT('Ctrl Pts',(111.685336789338,1074.80179067849,432.839184973981));
#118439=CARTESIAN_POINT('Ctrl Pts',(111.61416304056,1074.81146046818,432.832166367726));
#118440=CARTESIAN_POINT('Ctrl Pts',(111.402102858394,1074.84038596573,432.789980057988));
#118441=CARTESIAN_POINT('Ctrl Pts',(111.26691656466,1074.85898197916,432.733657466272));
#118442=CARTESIAN_POINT('Ctrl Pts',(111.026953109172,1074.89238584326,432.571596577775));
#118443=CARTESIAN_POINT('Ctrl Pts',(110.924330817354,1074.90689346776,432.46768798791));
#118444=CARTESIAN_POINT('Ctrl Pts',(110.765555579852,1074.92997212448,432.225478463408));
#118445=CARTESIAN_POINT('Ctrl Pts',(110.710988485895,1074.9383146646,432.089670289979));
#118446=CARTESIAN_POINT('Ctrl Pts',(110.658843592089,1074.94756386189,431.807701263431));
#118447=CARTESIAN_POINT('Ctrl Pts',(110.660460841978,1074.94855131792,431.664709323906));
#118448=CARTESIAN_POINT('Ctrl Pts',(110.718360677713,1074.94325334289,431.387091065484));
#118449=CARTESIAN_POINT('Ctrl Pts',(110.774139435225,1074.93700976715,431.255300249266));
#118450=CARTESIAN_POINT('Ctrl Pts',(110.934594932809,1074.91779174939,431.01791303319));
#118451=CARTESIAN_POINT('Ctrl Pts',(111.038708429017,1074.90486215894,430.915441976632));
#118452=CARTESIAN_POINT('Ctrl Pts',(111.2808515148,1074.87396993153,430.756881120247));
#118453=CARTESIAN_POINT('Ctrl Pts',(111.41662418256,1074.85628999999,430.702541711662));
#118454=CARTESIAN_POINT('Ctrl Pts',(111.628661045039,1074.82814366381,430.663370031491));
#118455=CARTESIAN_POINT('Ctrl Pts',(111.699550933579,1074.81865134874,430.657324632177));
#118456=CARTESIAN_POINT('Ctrl Pts',(111.841732594009,1074.79944746737,430.659090819334));
#118457=CARTESIAN_POINT('Ctrl Pts',(111.912707084578,1074.78977810564,430.666952673787));
#118458=CARTESIAN_POINT('Ctrl Pts',(112.125858871651,1074.76048623674,430.711991224333));
#118459=CARTESIAN_POINT('Ctrl Pts',(112.261882570826,1074.74143505668,430.770953595469));
#118460=CARTESIAN_POINT('Ctrl Pts',(112.499774167161,1074.70743783601,430.937442051952));
#118461=CARTESIAN_POINT('Ctrl Pts',(112.600121881773,1074.69272932387,431.042214961932));
#118462=CARTESIAN_POINT('Ctrl Pts',(112.753729407214,1074.66945233698,431.283891616949));
#118463=CARTESIAN_POINT('Ctrl Pts',(112.805948745228,1074.6610538322,431.418070304207));
#118464=CARTESIAN_POINT('Ctrl Pts',(112.855496719518,1074.65173543934,431.698163389931));
#118465=CARTESIAN_POINT('Ctrl Pts',(112.852768146603,1074.65085045777,431.841129578785));
#118466=CARTESIAN_POINT('Ctrl Pts',(112.792797957082,1074.65670190277,432.117909946033));
#118467=CARTESIAN_POINT('Ctrl Pts',(112.736226830982,1074.66336973984,432.248915791649));
#118468=CARTESIAN_POINT('Ctrl Pts',(112.575953438042,1074.68341185282,432.482653942603));
#118469=CARTESIAN_POINT('Ctrl Pts',(112.473527027896,1074.6966302517,432.582863203708));
#118470=CARTESIAN_POINT('Ctrl Pts',(112.2352762265,1074.72791877231,432.739115643008));
#118471=CARTESIAN_POINT('Ctrl Pts',(112.101390509769,1074.74573701192,432.79319551915));
#118472=CARTESIAN_POINT('Ctrl Pts',(111.893683261218,1074.77362868244,432.832771180604));
#118473=CARTESIAN_POINT('Ctrl Pts',(111.825247851777,1074.78285576909,432.839220986145));
#118474=CARTESIAN_POINT('Ctrl Pts',(111.756676799939,1074.79213585482,432.839203336419));
#118475=CARTESIAN_POINT('Origin',(111.756957497769,1067.7251047501,431.748662623815));
#118476=CARTESIAN_POINT('',(111.756957497769,1074.79784893105,432.239203372544));
#118477=CARTESIAN_POINT('',(111.756957497769,1074.80630411877,431.258121875087));
#118478=CARTESIAN_POINT('Ctrl Pts',(111.756957497769,1074.79784893105,432.239203372544));
#118479=CARTESIAN_POINT('Ctrl Pts',(111.725374838794,1074.80211913335,432.239203372544));
#118480=CARTESIAN_POINT('Ctrl Pts',(111.693862381834,1074.80640164172,432.236153273107));
#118481=CARTESIAN_POINT('Ctrl Pts',(111.598702625693,1074.81940105083,432.217553834054));
#118482=CARTESIAN_POINT('Ctrl Pts',(111.537627148781,1074.82783931817,432.192301833779));
#118483=CARTESIAN_POINT('Ctrl Pts',(111.429107335121,1074.84304638832,432.119341812944));
#118484=CARTESIAN_POINT('Ctrl Pts',(111.382666546665,1074.84967409467,432.072427251562));
#118485=CARTESIAN_POINT('Ctrl Pts',(111.31136320506,1074.86015249039,431.963702187915));
#118486=CARTESIAN_POINT('Ctrl Pts',(111.286918958097,1074.86393667771,431.903199231883));
#118487=CARTESIAN_POINT('Ctrl Pts',(111.263109129291,1074.86819548905,431.777002839856));
#118488=CARTESIAN_POINT('Ctrl Pts',(111.263604197717,1074.86867731751,431.712678298726));
#118489=CARTESIAN_POINT('Ctrl Pts',(111.289189338445,1074.86632293511,431.58775498063));
#118490=CARTESIAN_POINT('Ctrl Pts',(111.314036076062,1074.86350825481,431.528429468777));
#118491=CARTESIAN_POINT('Ctrl Pts',(111.385170426667,1074.85489419562,431.422296119667));
#118492=CARTESIAN_POINT('Ctrl Pts',(111.430897821905,1074.84915945784,431.376642252814));
#118493=CARTESIAN_POINT('Ctrl Pts',(111.538405098834,1074.83534679618,431.304643113215));
#118494=CARTESIAN_POINT('Ctrl Pts',(111.599484517994,1074.82735137497,431.279516718815));
#118495=CARTESIAN_POINT('Ctrl Pts',(111.694308950933,1074.81473253188,431.261134356665));
#118496=CARTESIAN_POINT('Ctrl Pts',(111.725507307599,1074.81055040783,431.258133896878));
#118497=CARTESIAN_POINT('Ctrl Pts',(111.756769426889,1074.80632951177,431.258121911136));
#118498=CARTESIAN_POINT('Ctrl Pts',(111.756832117468,1074.80632104752,431.258121887101));
#118499=CARTESIAN_POINT('Ctrl Pts',(111.756894807763,1074.80631258319,431.258121875087));
#118500=CARTESIAN_POINT('Ctrl Pts',(111.756957497769,1074.80630411877,431.258121875087));
#118501=CARTESIAN_POINT('',(111.756957497769,1082.7251047501,431.258121875087));
#118502=CARTESIAN_POINT('',(111.756957497769,1067.7251047501,431.258121875087));
#118503=CARTESIAN_POINT('Origin',(111.756957497769,1082.7251047501,431.748662623815));
#118504=CARTESIAN_POINT('Ctrl Pts',(111.756957497769,1074.80630411877,431.258121875087));
#118505=CARTESIAN_POINT('Ctrl Pts',(111.78894086001,1074.80198571955,431.258121875087));
#118506=CARTESIAN_POINT('Ctrl Pts',(111.82084916161,1074.79764588071,431.261249858237));
#118507=CARTESIAN_POINT('Ctrl Pts',(111.916695267811,1074.78451351391,431.280225632813));
#118508=CARTESIAN_POINT('Ctrl Pts',(111.978012474172,1074.77597625463,431.305828974978));
#118509=CARTESIAN_POINT('Ctrl Pts',(112.086225850602,1074.76063819376,431.379298041251));
#118510=CARTESIAN_POINT('Ctrl Pts',(112.132271420881,1074.75396260125,431.426148010146));
#118511=CARTESIAN_POINT('Ctrl Pts',(112.202836977189,1074.74340516081,431.534368544303));
#118512=CARTESIAN_POINT('Ctrl Pts',(112.227019608748,1074.73958151596,431.594410285604));
#118513=CARTESIAN_POINT('Ctrl Pts',(112.250793234647,1074.73524139378,431.720097888902));
#118514=CARTESIAN_POINT('Ctrl Pts',(112.250327396791,1074.73474438414,431.784424990654));
#118515=CARTESIAN_POINT('Ctrl Pts',(112.224812517838,1074.73714097658,431.90928651105));
#118516=CARTESIAN_POINT('Ctrl Pts',(112.20003784051,1074.74000803974,431.96855198485));
#118517=CARTESIAN_POINT('Ctrl Pts',(112.12910604374,1074.74875875828,432.074596453481));
#118518=CARTESIAN_POINT('Ctrl Pts',(112.083512174581,1074.75457511682,432.120230132115));
#118519=CARTESIAN_POINT('Ctrl Pts',(111.97706736352,1074.76843142764,432.191760203727));
#118520=CARTESIAN_POINT('Ctrl Pts',(111.917087983988,1074.77635989495,432.216765724299));
#118521=CARTESIAN_POINT('Ctrl Pts',(111.822579290969,1074.78900032703,432.235855343108));
#118522=CARTESIAN_POINT('Ctrl Pts',(111.790538507449,1074.79330923836,432.239105481057));
#118523=CARTESIAN_POINT('Ctrl Pts',(111.757932,1074.79771717655,432.239202646579));
#118524=CARTESIAN_POINT('Ctrl Pts',(111.757444740529,1074.79778305233,432.239203372544));
#118525=CARTESIAN_POINT('Ctrl Pts',(111.756957497769,1074.79784893105,432.239203372544));
#118526=CARTESIAN_POINT('Origin',(79.4772023228649,1067.7251047501,383.340094328387));
#118527=CARTESIAN_POINT('',(79.4772023228812,1078.65448750233,381.861791196193));
#118528=CARTESIAN_POINT('Ctrl Pts',(79.4773064989971,1078.68961796465,384.81839745691));
#118529=CARTESIAN_POINT('Ctrl Pts',(79.6578339946104,1078.68607426205,384.818384735123));
#118530=CARTESIAN_POINT('Ctrl Pts',(79.836830601856,1078.68200456401,384.785303885374));
#118531=CARTESIAN_POINT('Ctrl Pts',(80.1867059151628,1078.67273509248,384.651451899359));
#118532=CARTESIAN_POINT('Ctrl Pts',(80.3525634585585,1078.66756101805,384.547071048555));
#118533=CARTESIAN_POINT('Ctrl Pts',(80.6340875241951,1078.65714773939,384.280556940427));
#118534=CARTESIAN_POINT('Ctrl Pts',(80.7471708722345,1078.65201364776,384.121143869101));
#118535=CARTESIAN_POINT('Ctrl Pts',(80.8991655963413,1078.64310803231,383.781853449734));
#118536=CARTESIAN_POINT('Ctrl Pts',(80.9420212089376,1078.63933893738,383.60738718419));
#118537=CARTESIAN_POINT('Ctrl Pts',(80.9635643432908,1078.63342109524,383.25183193677));
#118538=CARTESIAN_POINT('Ctrl Pts',(80.9421538036005,1078.63132275943,383.073660644745));
#118539=CARTESIAN_POINT('Ctrl Pts',(80.876512373027,1078.63000398959,382.861269826507));
#118540=CARTESIAN_POINT('Ctrl Pts',(80.861540351744,1078.62980609948,382.819565948513));
#118541=CARTESIAN_POINT('Ctrl Pts',(80.8337123673341,1078.62958784562,382.751791404895));
#118542=CARTESIAN_POINT('Ctrl Pts',(80.8219202799108,1078.62952980079,382.725315137572));
#118543=CARTESIAN_POINT('Ctrl Pts',(80.7992811203725,1078.62947641101,382.6782574625));
#118544=CARTESIAN_POINT('Ctrl Pts',(80.7887120002637,1078.62947093756,382.657552937272));
#118545=CARTESIAN_POINT('Ctrl Pts',(80.7652055631167,1078.62949821313,382.614068408584));
#118546=CARTESIAN_POINT('Ctrl Pts',(80.7521420397551,1078.62953588972,382.591365607003));
#118547=CARTESIAN_POINT('Ctrl Pts',(80.7157428543219,1078.6296979789,382.531825721137));
#118548=CARTESIAN_POINT('Ctrl Pts',(80.6913691662945,1078.62986333655,382.495653907294));
#118549=CARTESIAN_POINT('Ctrl Pts',(80.5758348535649,1078.6308813964,382.339560419491));
#118550=CARTESIAN_POINT('Ctrl Pts',(80.4682669407166,1078.63242196648,382.232913962992));
#118551=CARTESIAN_POINT('Ctrl Pts',(80.2243706001013,1078.63681483155,382.055608510863));
#118552=CARTESIAN_POINT('Ctrl Pts',(80.0894106673181,1078.63964278792,381.986078311478));
#118553=CARTESIAN_POINT('Ctrl Pts',(79.7880964850754,1078.64655843017,381.885257431442));
#118554=CARTESIAN_POINT('Ctrl Pts',(79.6220920608436,1078.6506949489,381.859484017786));
#118555=CARTESIAN_POINT('Ctrl Pts',(79.2756447960113,1078.65976047334,381.864613338933));
#118556=CARTESIAN_POINT('Ctrl Pts',(79.0979539302923,1078.66464635616,381.900011030537));
#118557=CARTESIAN_POINT('Ctrl Pts',(78.7518267241186,1078.67449913495,382.037642641232));
#118558=CARTESIAN_POINT('Ctrl Pts',(78.5883205091446,1078.67934851276,382.143245868681));
#118559=CARTESIAN_POINT('Ctrl Pts',(78.3103492235038,1078.68806918596,382.411977945481));
#118560=CARTESIAN_POINT('Ctrl Pts',(78.1988380884844,1078.69185427754,382.572800338836));
#118561=CARTESIAN_POINT('Ctrl Pts',(78.0504301882596,1078.69784731183,382.914073895328));
#118562=CARTESIAN_POINT('Ctrl Pts',(78.0094874103787,1078.70011438911,383.089115733394));
#118563=CARTESIAN_POINT('Ctrl Pts',(77.9921229956226,1078.70345252035,383.440919095969));
#118564=CARTESIAN_POINT('Ctrl Pts',(78.0142688186805,1078.70453002803,383.614783512436));
#118565=CARTESIAN_POINT('Ctrl Pts',(78.0791043739633,1078.70520849499,383.82238078746));
#118566=CARTESIAN_POINT('Ctrl Pts',(78.0939237557013,1078.70531014815,383.863371046404));
#118567=CARTESIAN_POINT('Ctrl Pts',(78.1214133705135,1078.70542214587,383.930036077492));
#118568=CARTESIAN_POINT('Ctrl Pts',(78.1330571157045,1078.7054518573,383.956104567591));
#118569=CARTESIAN_POINT('Ctrl Pts',(78.15539559675,1078.70547912024,384.002462978809));
#118570=CARTESIAN_POINT('Ctrl Pts',(78.165821570848,1078.70548185375,384.022872311212));
#118571=CARTESIAN_POINT('Ctrl Pts',(78.1890011987403,1078.70546766206,384.06575632791));
#118572=CARTESIAN_POINT('Ctrl Pts',(78.2018782188641,1078.70544819287,384.088155758255));
#118573=CARTESIAN_POINT('Ctrl Pts',(78.2377454160883,1078.70536440756,384.146925951444));
#118574=CARTESIAN_POINT('Ctrl Pts',(78.2617473919494,1078.70527893162,384.182649959848));
#118575=CARTESIAN_POINT('Ctrl Pts',(78.3753391430794,1078.70475016454,384.33674133563));
#118576=CARTESIAN_POINT('Ctrl Pts',(78.4808951230963,1078.70394945669,384.442264202522));
#118577=CARTESIAN_POINT('Ctrl Pts',(78.7219575096514,1078.70150403823,384.619854943717));
#118578=CARTESIAN_POINT('Ctrl Pts',(78.8565358187346,1078.69985736615,384.690261845773));
#118579=CARTESIAN_POINT('Ctrl Pts',(79.1532792153285,1078.69553142343,384.791605819647));
#118580=CARTESIAN_POINT('Ctrl Pts',(79.3147437498588,1078.69280902447,384.818408912719));
#118581=CARTESIAN_POINT('Ctrl Pts',(79.4773064989971,1078.68961796465,384.81839745691));
#118582=CARTESIAN_POINT('',(79.4772023228652,1076.65355727679,381.861791196194));
#118583=CARTESIAN_POINT('',(79.4772023228649,1067.7251047501,381.861791196194));
#118584=CARTESIAN_POINT('',(79.4772023228649,1076.68910595681,384.81839746058));
#118585=CARTESIAN_POINT('Ctrl Pts',(79.4772023228649,1076.68910595681,384.81839746058));
#118586=CARTESIAN_POINT('Ctrl Pts',(79.4323165774695,1076.68999757484,384.81839746058));
#118587=CARTESIAN_POINT('Ctrl Pts',(79.3877738363708,1076.69084832688,384.81635744192));
#118588=CARTESIAN_POINT('Ctrl Pts',(79.3435699272914,1076.69166091905,384.81234516758));
#118589=CARTESIAN_POINT('Ctrl Pts',(79.2989291589977,1076.69248154192,384.808293240661));
#118590=CARTESIAN_POINT('Ctrl Pts',(79.2546330221333,1076.69326324693,384.802229881876));
#118591=CARTESIAN_POINT('Ctrl Pts',(79.2106740020746,1076.69400882121,384.794172319716));
#118592=CARTESIAN_POINT('Ctrl Pts',(79.2034450509487,1076.69413142904,384.792847273731));
#118593=CARTESIAN_POINT('Ctrl Pts',(79.1962252274782,1076.69425305979,384.791468184736));
#118594=CARTESIAN_POINT('Ctrl Pts',(79.189014517095,1076.69437372585,384.790034995883));
#118595=CARTESIAN_POINT('Ctrl Pts',(79.1508933289145,1076.69501165655,384.782458091654));
#118596=CARTESIAN_POINT('Ctrl Pts',(79.1128619636276,1076.6956246815,384.77333184482));
#118597=CARTESIAN_POINT('Ctrl Pts',(79.0751776100142,1076.69621034861,384.762682209999));
#118598=CARTESIAN_POINT('Ctrl Pts',(79.0375295333672,1076.69679545193,384.752042827084));
#118599=CARTESIAN_POINT('Ctrl Pts',(79.0002284001745,1076.69735325007,384.739883108458));
#118600=CARTESIAN_POINT('Ctrl Pts',(78.9635194136748,1076.69788129803,384.726279748689));
#118601=CARTESIAN_POINT('Ctrl Pts',(78.9459072244516,1076.69813464418,384.719753146645));
#118602=CARTESIAN_POINT('Ctrl Pts',(78.9284311173179,1076.69838114221,384.712894976343));
#118603=CARTESIAN_POINT('Ctrl Pts',(78.9111166457398,1076.6986205221,384.705717686713));
#118604=CARTESIAN_POINT('Ctrl Pts',(78.8693868293314,1076.69919745444,384.688419614566));
#118605=CARTESIAN_POINT('Ctrl Pts',(78.8286635630319,1076.69973316404,384.669302084844));
#118606=CARTESIAN_POINT('Ctrl Pts',(78.7889305802416,1076.70022999697,384.648399399446));
#118607=CARTESIAN_POINT('Ctrl Pts',(78.7491034394834,1076.70072800729,384.627447179524));
#118608=CARTESIAN_POINT('Ctrl Pts',(78.7102704342413,1076.70118695647,384.604700910479));
#118609=CARTESIAN_POINT('Ctrl Pts',(78.6724373642652,1076.70160920733,384.580148162727));
#118610=CARTESIAN_POINT('Ctrl Pts',(78.6670397817217,1076.70166944918,384.57664526215));
#118611=CARTESIAN_POINT('Ctrl Pts',(78.6616626012551,1076.70172894405,384.573105520616));
#118612=CARTESIAN_POINT('Ctrl Pts',(78.6563058918429,1076.70178769882,384.569528832616));
#118613=CARTESIAN_POINT('Ctrl Pts',(78.6261684482637,1076.7021182597,384.54940598769));
#118614=CARTESIAN_POINT('Ctrl Pts',(78.5966145481867,1076.70242534945,384.528065374972));
#118615=CARTESIAN_POINT('Ctrl Pts',(78.5678623889557,1076.7027080878,384.505633274648));
#118616=CARTESIAN_POINT('Ctrl Pts',(78.5391033511076,1076.70299089379,384.483195807706));
#118617=CARTESIAN_POINT('Ctrl Pts',(78.5111469194186,1076.70324933674,384.459666670504));
#118618=CARTESIAN_POINT('Ctrl Pts',(78.4841803351657,1076.70348253576,384.435214176896));
#118619=CARTESIAN_POINT('Ctrl Pts',(78.4662182055165,1076.70363786693,384.418926653926));
#118620=CARTESIAN_POINT('Ctrl Pts',(78.4486945839047,1076.70378199803,384.402230329042));
#118621=CARTESIAN_POINT('Ctrl Pts',(78.4316556816896,1076.70391466873,384.385183976111));
#118622=CARTESIAN_POINT('Ctrl Pts',(78.3965683871994,1076.70418787037,384.350081338761));
#118623=CARTESIAN_POINT('Ctrl Pts',(78.3631689880996,1076.70441584811,384.313125644738));
#118624=CARTESIAN_POINT('Ctrl Pts',(78.3316900422146,1076.70459872642,384.27453628246));
#118625=CARTESIAN_POINT('Ctrl Pts',(78.3002292294129,1076.70478149938,384.235969149139));
#118626=CARTESIAN_POINT('Ctrl Pts',(78.2706870783422,1076.70491922485,384.195770682281));
#118627=CARTESIAN_POINT('Ctrl Pts',(78.2432574468465,1076.70501202707,384.154195178159));
#118628=CARTESIAN_POINT('Ctrl Pts',(78.2158071059045,1076.70510489936,384.112588284419));
#118629=CARTESIAN_POINT('Ctrl Pts',(78.1904728123462,1076.70515278055,384.069602794041));
#118630=CARTESIAN_POINT('Ctrl Pts',(78.1674047872852,1076.70515579517,384.025521615881));
#118631=CARTESIAN_POINT('Ctrl Pts',(78.1469356867591,1076.70515847014,383.986406777716));
#118632=CARTESIAN_POINT('Ctrl Pts',(78.1282504482097,1076.7051258187,383.946429892694));
#118633=CARTESIAN_POINT('Ctrl Pts',(78.1114222681008,1076.70505792785,383.905801843505));
#118634=CARTESIAN_POINT('Ctrl Pts',(78.092545671038,1076.70498177295,383.86022832878));
#118635=CARTESIAN_POINT('Ctrl Pts',(78.0759005429512,1076.7048607265,383.813578976737));
#118636=CARTESIAN_POINT('Ctrl Pts',(78.0616230533806,1076.70469467634,383.766140666781));
#118637=CARTESIAN_POINT('Ctrl Pts',(78.0473559677274,1076.70452874718,383.718736924824));
#118638=CARTESIAN_POINT('Ctrl Pts',(78.0354533023461,1076.70431787986,383.670545949035));
#118639=CARTESIAN_POINT('Ctrl Pts',(78.0260025224258,1076.70406196247,383.621873124356));
#118640=CARTESIAN_POINT('Ctrl Pts',(78.0165466406782,1076.70380590693,383.573174024561));
#118641=CARTESIAN_POINT('Ctrl Pts',(78.0095454198943,1076.70350475266,383.523993164022));
#118642=CARTESIAN_POINT('Ctrl Pts',(78.0050352763836,1076.70315838755,383.474646689596));
#118643=CARTESIAN_POINT('Ctrl Pts',(78.0009506314825,1076.70284469943,383.429955689261));
#118644=CARTESIAN_POINT('Ctrl Pts',(77.9989085705711,1076.7024939287,383.385129306266));
#118645=CARTESIAN_POINT('Ctrl Pts',(77.9988992229576,1076.70210599207,383.340403289638));
#118646=CARTESIAN_POINT('Ctrl Pts',(77.9988916155266,1076.701790275,383.304003615509));
#118647=CARTESIAN_POINT('Ctrl Pts',(78.0002326693678,1076.70144728133,383.267387185696));
#118648=CARTESIAN_POINT('Ctrl Pts',(78.0029444698945,1076.70107842819,383.230806023397));
#118649=CARTESIAN_POINT('Ctrl Pts',(78.005654947569,1076.70070975499,383.194242705874));
#118650=CARTESIAN_POINT('Ctrl Pts',(78.0097348316084,1076.70031524755,383.157715212124));
#118651=CARTESIAN_POINT('Ctrl Pts',(78.0151540721176,1076.69989632095,383.121473507926));
#118652=CARTESIAN_POINT('Ctrl Pts',(78.0186769104227,1076.69962399299,383.097914180087));
#118653=CARTESIAN_POINT('Ctrl Pts',(78.022764660728,1076.69934134599,383.074475563693));
#118654=CARTESIAN_POINT('Ctrl Pts',(78.0273974478024,1076.69904876866,383.051224158765));
#118655=CARTESIAN_POINT('Ctrl Pts',(78.0362211421981,1076.69849152033,383.006939090605));
#118656=CARTESIAN_POINT('Ctrl Pts',(78.0470339763282,1076.69789823608,382.963236436771));
#118657=CARTESIAN_POINT('Ctrl Pts',(78.0598128163726,1076.69726649033,382.920109641121));
#118658=CARTESIAN_POINT('Ctrl Pts',(78.0725773291265,1076.69663545287,382.877031198069));
#118659=CARTESIAN_POINT('Ctrl Pts',(78.0873037191838,1076.69596604009,382.834526420395));
#118660=CARTESIAN_POINT('Ctrl Pts',(78.1040183448495,1076.69525583455,382.792603768492));
#118661=CARTESIAN_POINT('Ctrl Pts',(78.1063929514182,1076.69515493736,382.786647918413));
#118662=CARTESIAN_POINT('Ctrl Pts',(78.1088077641602,1076.69505321684,382.780703855331));
#118663=CARTESIAN_POINT('Ctrl Pts',(78.1112629341433,1076.69495066606,382.774771644434));
#118664=CARTESIAN_POINT('Ctrl Pts',(78.1258989119271,1076.69433933124,382.739408020941));
#118665=CARTESIAN_POINT('Ctrl Pts',(78.1419638050131,1076.69369808852,382.70448981176));
#118666=CARTESIAN_POINT('Ctrl Pts',(78.1593650916418,1076.69303031757,382.670254659022));
#118667=CARTESIAN_POINT('Ctrl Pts',(78.1767815203228,1076.69236196556,382.635989715931));
#118668=CARTESIAN_POINT('Ctrl Pts',(78.1955363984234,1076.69166703914,382.602409562577));
#118669=CARTESIAN_POINT('Ctrl Pts',(78.2154904348338,1076.69094892683,382.569728660503));
#118670=CARTESIAN_POINT('Ctrl Pts',(78.2260517243111,1076.69056884373,382.55243128467));
#118671=CARTESIAN_POINT('Ctrl Pts',(78.2369481848875,1076.69018226538,382.535385372116));
#118672=CARTESIAN_POINT('Ctrl Pts',(78.2481543628143,1076.6897896942,382.51861927548));
#118673=CARTESIAN_POINT('Ctrl Pts',(78.2730325534311,1076.68891816951,382.481397829352));
#118674=CARTESIAN_POINT('Ctrl Pts',(78.299559302157,1076.68801358794,382.445362019445));
#118675=CARTESIAN_POINT('Ctrl Pts',(78.3277429257228,1076.68707374922,382.41051203242));
#118676=CARTESIAN_POINT('Ctrl Pts',(78.3556834593331,1076.68614201682,382.375962634203));
#118677=CARTESIAN_POINT('Ctrl Pts',(78.3852530400077,1076.68517563284,382.342578026162));
#118678=CARTESIAN_POINT('Ctrl Pts',(78.4164955420233,1076.68417245347,382.310394723779));
#118679=CARTESIAN_POINT('Ctrl Pts',(78.4215509809009,1076.68401012614,382.305187051295));
#118680=CARTESIAN_POINT('Ctrl Pts',(78.4266502871599,1076.68384683538,382.300010923153));
#118681=CARTESIAN_POINT('Ctrl Pts',(78.4317937177455,1076.68368257211,382.294866602485));
#118682=CARTESIAN_POINT('Ctrl Pts',(78.4811168907444,1076.68210736162,382.24553489399));
#118683=CARTESIAN_POINT('Ctrl Pts',(78.5336262529255,1076.68046914874,382.19999488545));
#118684=CARTESIAN_POINT('Ctrl Pts',(78.5889038618298,1076.67877789683,382.158440404949));
#118685=CARTESIAN_POINT('Ctrl Pts',(78.646998755554,1076.67700044839,382.114768054132));
#118686=CARTESIAN_POINT('Ctrl Pts',(78.7081529543673,1076.67516441677,382.075495751653));
#118687=CARTESIAN_POINT('Ctrl Pts',(78.7719313713774,1076.6732813677,382.040874163965));
#118688=CARTESIAN_POINT('Ctrl Pts',(78.8172395161129,1076.6719436509,382.016279011255));
#118689=CARTESIAN_POINT('Ctrl Pts',(78.8638732351684,1076.67058220593,381.994031511756));
#118690=CARTESIAN_POINT('Ctrl Pts',(78.9116821341399,1076.66920117927,381.974236697886));
#118691=CARTESIAN_POINT('Ctrl Pts',(78.9534074216605,1076.66799588621,381.956960744707));
#118692=CARTESIAN_POINT('Ctrl Pts',(78.9956969695686,1076.66678565021,381.941686228821));
#118693=CARTESIAN_POINT('Ctrl Pts',(79.0385369690515,1076.66557138359,381.928374505612));
#118694=CARTESIAN_POINT('Ctrl Pts',(79.0815117452,1076.66435329684,381.915020903091));
#118695=CARTESIAN_POINT('Ctrl Pts',(79.1250413371005,1076.66313115407,381.903642156297));
#118696=CARTESIAN_POINT('Ctrl Pts',(79.1691299093578,1076.66190587627,381.894248023039));
#118697=CARTESIAN_POINT('Ctrl Pts',(79.1754387204867,1076.66173054634,381.892903778728));
#118698=CARTESIAN_POINT('Ctrl Pts',(79.1817589940561,1076.66155515221,381.891600256707));
#118699=CARTESIAN_POINT('Ctrl Pts',(79.1880907555688,1076.6613796966,381.890337572131));
#118700=CARTESIAN_POINT('Ctrl Pts',(79.2234843642184,1076.6603989257,381.883279352451));
#118701=CARTESIAN_POINT('Ctrl Pts',(79.259331463925,1076.65941372101,381.877482778857));
#118702=CARTESIAN_POINT('Ctrl Pts',(79.295388881851,1076.65843163133,381.873014227193));
#118703=CARTESIAN_POINT('Ctrl Pts',(79.3314500263962,1076.65744944014,381.868545213694));
#118704=CARTESIAN_POINT('Ctrl Pts',(79.3677209539181,1076.65647036461,381.865404600017));
#118705=CARTESIAN_POINT('Ctrl Pts',(79.4039505509298,1076.6555019559,381.863607170108));
#118706=CARTESIAN_POINT('Ctrl Pts',(79.4284125670731,1076.65484809189,381.862393555742));
#118707=CARTESIAN_POINT('Ctrl Pts',(79.4528555850251,1076.65419909074,381.861791196194));
#118708=CARTESIAN_POINT('Ctrl Pts',(79.4772023228649,1076.65355727679,381.861791196194));
#118709=CARTESIAN_POINT('Ctrl Pts',(79.4772023228652,1076.65355727679,381.861791196194));
#118710=CARTESIAN_POINT('Ctrl Pts',(79.6729707687277,1076.64839654768,381.861791196194));
#118711=CARTESIAN_POINT('Ctrl Pts',(79.866806416513,1076.64358157986,381.900676359504));
#118712=CARTESIAN_POINT('Ctrl Pts',(80.2255548712202,1076.63559755373,382.050669534883));
#118713=CARTESIAN_POINT('Ctrl Pts',(80.3873767252618,1076.632490266,382.159314096149));
#118714=CARTESIAN_POINT('Ctrl Pts',(80.660352144368,1076.62860861734,382.432929539083));
#118715=CARTESIAN_POINT('Ctrl Pts',(80.7687708768473,1076.62787984994,382.595349081387));
#118716=CARTESIAN_POINT('Ctrl Pts',(80.9170871154754,1076.62900365002,382.953166720926));
#118717=CARTESIAN_POINT('Ctrl Pts',(80.955367665541,1076.63085058817,383.145157575024));
#118718=CARTESIAN_POINT('Ctrl Pts',(80.9556418926109,1076.63671612003,383.532075796931));
#118719=CARTESIAN_POINT('Ctrl Pts',(80.9179706056803,1076.64066296239,383.723259023923));
#118720=CARTESIAN_POINT('Ctrl Pts',(80.7712549670908,1076.64983688938,384.080439810865));
#118721=CARTESIAN_POINT('Ctrl Pts',(80.6635672715775,1076.65496970436,384.242987364763));
#118722=CARTESIAN_POINT('Ctrl Pts',(80.4597270928463,1076.66283262355,384.448856776867));
#118723=CARTESIAN_POINT('Ctrl Pts',(80.3852058085155,1076.66546317263,384.510666375708));
#118724=CARTESIAN_POINT('Ctrl Pts',(80.178978583346,1076.67214380466,384.650094652687));
#118725=CARTESIAN_POINT('Ctrl Pts',(80.0403270719585,1076.67609393888,384.715406827373));
#118726=CARTESIAN_POINT('Ctrl Pts',(79.7587501365082,1076.68317131549,384.798185252103));
#118727=CARTESIAN_POINT('Ctrl Pts',(79.6183469796841,1076.6863022355,384.81839746058));
#118728=CARTESIAN_POINT('Ctrl Pts',(79.4772023228649,1076.68910595681,384.81839746058));
#118729=CARTESIAN_POINT('Origin',(79.4772023228649,1067.7251047501,383.340094328387));
#118730=CARTESIAN_POINT('',(79.4772023228649,1076.68289265596,384.21839746058));
#118731=CARTESIAN_POINT('',(79.4772023229628,1076.66179580958,382.461791196194));
#118732=CARTESIAN_POINT('Ctrl Pts',(79.4772023228649,1076.68289265596,384.21839746058));
#118733=CARTESIAN_POINT('Ctrl Pts',(79.3652526559606,1076.68526371833,384.21839746058));
#118734=CARTESIAN_POINT('Ctrl Pts',(79.2542783682972,1076.68729633286,384.196992809842));
#118735=CARTESIAN_POINT('Ctrl Pts',(79.0420083774302,1076.69064094287,384.111866380992));
#118736=CARTESIAN_POINT('Ctrl Pts',(78.9434550090199,1076.69188875241,384.047301429353));
#118737=CARTESIAN_POINT('Ctrl Pts',(78.7771243994947,1076.69343485552,383.883223559309));
#118738=CARTESIAN_POINT('Ctrl Pts',(78.7110935093777,1076.69371708435,383.785264270313));
#118739=CARTESIAN_POINT('Ctrl Pts',(78.6213255463339,1076.69329477762,383.569333997618));
#118740=CARTESIAN_POINT('Ctrl Pts',(78.598450481321,1076.69259474931,383.453539462766));
#118741=CARTESIAN_POINT('Ctrl Pts',(78.5993599252962,1076.69023161065,383.220140723507));
#118742=CARTESIAN_POINT('Ctrl Pts',(78.6230011791956,1076.688592191,383.104862932747));
#118743=CARTESIAN_POINT('Ctrl Pts',(78.7139033442099,1076.68445895829,382.890227975624));
#118744=CARTESIAN_POINT('Ctrl Pts',(78.7802792285221,1076.68200293971,382.793011066017));
#118745=CARTESIAN_POINT('Ctrl Pts',(78.9045559895815,1076.67790004802,382.671697262365));
#118746=CARTESIAN_POINT('Ctrl Pts',(78.9492196479396,1076.67648948421,382.635883802985));
#118747=CARTESIAN_POINT('Ctrl Pts',(79.0456063271205,1076.67355785249,382.572953389854));
#118748=CARTESIAN_POINT('Ctrl Pts',(79.0971921818112,1076.67204256838,382.546134345015));
#118749=CARTESIAN_POINT('Ctrl Pts',(79.2548033101116,1076.6675615439,382.483097553544));
#118750=CARTESIAN_POINT('Ctrl Pts',(79.3655095007989,1076.66459268337,382.461791196169));
#118751=CARTESIAN_POINT('Ctrl Pts',(79.4772023230607,1076.66179580958,382.461791196194));
#118752=CARTESIAN_POINT('',(79.4772023228649,1082.7251047501,382.461791196194));
#118753=CARTESIAN_POINT('',(79.4772023228649,1067.7251047501,382.461791196194));
#118754=CARTESIAN_POINT('Origin',(79.4772023228649,1082.7251047501,383.340094328387));
#118755=CARTESIAN_POINT('Ctrl Pts',(79.4772023230607,1076.66179580958,382.461791196194));
#118756=CARTESIAN_POINT('Ctrl Pts',(79.4806295203402,1076.66170998994,382.461791196194));
#118757=CARTESIAN_POINT('Ctrl Pts',(79.4840576466145,1076.66162433483,382.461811255905));
#118758=CARTESIAN_POINT('Ctrl Pts',(79.6026910282681,1076.65866671775,382.46320045041));
#118759=CARTESIAN_POINT('Ctrl Pts',(79.7165197423068,1076.65604185539,382.487204617594));
#118760=CARTESIAN_POINT('Ctrl Pts',(79.9283760477523,1076.65170526073,382.577778928352));
#118761=CARTESIAN_POINT('Ctrl Pts',(80.0243554599845,1076.65003774835,382.643452765418));
#118762=CARTESIAN_POINT('Ctrl Pts',(80.1853883939126,1076.64799329725,382.808001150205));
#118763=CARTESIAN_POINT('Ctrl Pts',(80.2489203113362,1076.64763587441,382.90523468599));
#118764=CARTESIAN_POINT('Ctrl Pts',(80.3321322595537,1076.64829141853,383.111827764756));
#118765=CARTESIAN_POINT('Ctrl Pts',(80.353651967693,1076.64921177656,383.218254704458));
#118766=CARTESIAN_POINT('Ctrl Pts',(80.3553908959406,1076.65066400983,383.325909049407));
#118767=CARTESIAN_POINT('Ctrl Pts',(80.3572452836985,1076.65221266695,383.440711313171));
#118768=CARTESIAN_POINT('Ctrl Pts',(80.3365703578649,1076.65433562453,383.554761917856));
#118769=CARTESIAN_POINT('Ctrl Pts',(80.2525014000806,1076.65937701402,383.768488947881));
#118770=CARTESIAN_POINT('Ctrl Pts',(80.1898930480443,1076.66224474932,383.866098161961));
#118771=CARTESIAN_POINT('Ctrl Pts',(80.070492135499,1076.6667429314,383.990262667662));
#118772=CARTESIAN_POINT('Ctrl Pts',(80.0267418154695,1076.66826425098,384.027639208293));
#118773=CARTESIAN_POINT('Ctrl Pts',(79.9325698297907,1076.671300918,384.093322675064));
#118774=CARTESIAN_POINT('Ctrl Pts',(79.8823730763377,1076.67280895582,384.121470869562));
#118775=CARTESIAN_POINT('Ctrl Pts',(79.7227328060416,1076.67728776372,384.191442760892));
#118776=CARTESIAN_POINT('Ctrl Pts',(79.6073729687394,1076.68010796009,384.216528949717));
#118777=CARTESIAN_POINT('Ctrl Pts',(79.4860569412789,1076.68270462264,384.2183639967));
#118778=CARTESIAN_POINT('Ctrl Pts',(79.4816288695732,1076.68279890295,384.21839746058));
#118779=CARTESIAN_POINT('Ctrl Pts',(79.4772023228649,1076.68289265596,384.21839746058));
#118780=CARTESIAN_POINT('Origin',(90.2477595453611,1067.7251047501,389.798048628597));
#118781=CARTESIAN_POINT('',(90.247759545381,1078.31906551735,388.522604507461));
#118782=CARTESIAN_POINT('Ctrl Pts',(90.2479786339883,1078.37784002205,391.073492730917));
#118783=CARTESIAN_POINT('Ctrl Pts',(90.4072924505591,1078.36862711137,391.073465364884));
#118784=CARTESIAN_POINT('Ctrl Pts',(90.5651682441571,1078.35867651224,391.04358936537));
#118785=CARTESIAN_POINT('Ctrl Pts',(90.8708245606265,1078.33764550322,390.923717765228));
#118786=CARTESIAN_POINT('Ctrl Pts',(91.0144009896261,1078.32673821539,390.831301921722));
#118787=CARTESIAN_POINT('Ctrl Pts',(91.2543335457832,1078.30637295623,390.598576482715));
#118788=CARTESIAN_POINT('Ctrl Pts',(91.349470918864,1078.29708085559,390.461603592906));
#118789=CARTESIAN_POINT('Ctrl Pts',(91.4710866406911,1078.28258950731,390.184252922138));
#118790=CARTESIAN_POINT('Ctrl Pts',(91.5056040894251,1078.27706243863,390.050110186705));
#118791=CARTESIAN_POINT('Ctrl Pts',(91.5295394970062,1078.26895950706,389.785640309555));
#118792=CARTESIAN_POINT('Ctrl Pts',(91.5218465334233,1078.26624929792,389.657232693508));
#118793=CARTESIAN_POINT('Ctrl Pts',(91.4874399942531,1078.26444461193,389.495849786554));
#118794=CARTESIAN_POINT('Ctrl Pts',(91.4781338812537,1078.2641499748,389.459949707738));
#118795=CARTESIAN_POINT('Ctrl Pts',(91.4609077209896,1078.2638600006,389.403710981464));
#118796=CARTESIAN_POINT('Ctrl Pts',(91.4540075087571,1078.26379133505,389.383082922125));
#118797=CARTESIAN_POINT('Ctrl Pts',(91.4402753035378,1078.2637358018,389.345273516858));
#118798=CARTESIAN_POINT('Ctrl Pts',(91.433590732954,1078.26373819292,389.328044873608));
#118799=CARTESIAN_POINT('Ctrl Pts',(91.4179825826874,1078.2638051891,389.29027191666));
#118800=CARTESIAN_POINT('Ctrl Pts',(91.4088874543157,1078.26388285747,389.269805206658));
#118801=CARTESIAN_POINT('Ctrl Pts',(91.3816603437648,1078.26421798979,389.212641533564));
#118802=CARTESIAN_POINT('Ctrl Pts',(91.3622948430431,1078.26457087267,389.176563819338));
#118803=CARTESIAN_POINT('Ctrl Pts',(91.2535722341533,1078.26708713355,388.995493658735));
#118804=CARTESIAN_POINT('Ctrl Pts',(91.1375907889607,1078.27142677805,388.868575846934));
#118805=CARTESIAN_POINT('Ctrl Pts',(90.8906327389324,1078.28278379058,388.688149139343));
#118806=CARTESIAN_POINT('Ctrl Pts',(90.7690566330834,1078.28900378146,388.626132389191));
#118807=CARTESIAN_POINT('Ctrl Pts',(90.4989402363623,1078.30389328142,388.538818864234));
#118808=CARTESIAN_POINT('Ctrl Pts',(90.3509870841868,1078.31262280569,388.518176868577));
#118809=CARTESIAN_POINT('Ctrl Pts',(90.0435750160734,1078.33176483397,388.52900630582));
#118810=CARTESIAN_POINT('Ctrl Pts',(89.8867552869763,1078.34208576919,388.564423401423));
#118811=CARTESIAN_POINT('Ctrl Pts',(89.5854871661062,1078.36301604762,388.695003523307));
#118812=CARTESIAN_POINT('Ctrl Pts',(89.4452958580764,1078.37340027826,388.792369144175));
#118813=CARTESIAN_POINT('Ctrl Pts',(89.2139757836579,1078.39203626485,389.033065941907));
#118814=CARTESIAN_POINT('Ctrl Pts',(89.1238577013517,1078.40016459864,389.172916564038));
#118815=CARTESIAN_POINT('Ctrl Pts',(89.0106452550058,1078.41260133766,389.45715746681));
#118816=CARTESIAN_POINT('Ctrl Pts',(88.980534804604,1078.41720851734,389.5960066182));
#118817=CARTESIAN_POINT('Ctrl Pts',(88.9683368003032,1078.42325841467,389.850514311394));
#118818=CARTESIAN_POINT('Ctrl Pts',(88.9780938792126,1078.42511565541,389.964272834517));
#118819=CARTESIAN_POINT('Ctrl Pts',(89.0105033558247,1078.42640768506,390.109835672536));
#118820=CARTESIAN_POINT('Ctrl Pts',(89.0196454770702,1078.42662929179,390.144097686916));
#118821=CARTESIAN_POINT('Ctrl Pts',(89.0364608738141,1078.42684554273,390.197991983752));
#118822=CARTESIAN_POINT('Ctrl Pts',(89.0432135346738,1078.42689582628,390.217891543741));
#118823=CARTESIAN_POINT('Ctrl Pts',(89.0567634727298,1078.42693336289,390.254799274328));
#118824=CARTESIAN_POINT('Ctrl Pts',(89.0634414568015,1078.42692789351,390.271845486051));
#118825=CARTESIAN_POINT('Ctrl Pts',(89.079238194387,1078.42686416128,390.309745144983));
#118826=CARTESIAN_POINT('Ctrl Pts',(89.0885528293671,1078.42679340296,390.330510131756));
#118827=CARTESIAN_POINT('Ctrl Pts',(89.1171692155467,1078.42648547983,390.389989377509));
#118828=CARTESIAN_POINT('Ctrl Pts',(89.1378904746825,1078.42615605807,390.427984199798));
#118829=CARTESIAN_POINT('Ctrl Pts',(89.2494796056993,1078.42390412141,390.609936239275));
#118830=CARTESIAN_POINT('Ctrl Pts',(89.3665830158952,1078.42017199153,390.73571927123));
#118831=CARTESIAN_POINT('Ctrl Pts',(89.6158695138219,1078.41020970893,390.914346516717));
#118832=CARTESIAN_POINT('Ctrl Pts',(89.7388957093978,1078.4046794162,390.975521365935));
#118833=CARTESIAN_POINT('Ctrl Pts',(89.9918960393226,1078.3921179301,391.054150890187));
#118834=CARTESIAN_POINT('Ctrl Pts',(90.1195896616231,1078.38526458923,391.073514784854));
#118835=CARTESIAN_POINT('Ctrl Pts',(90.2479786339883,1078.37784002205,391.073492730917));
#118836=CARTESIAN_POINT('',(90.2477595453332,1076.31447289884,388.522604507461));
#118837=CARTESIAN_POINT('',(90.2477595453611,1067.7251047501,388.522604507461));
#118838=CARTESIAN_POINT('Ctrl Pts',(90.2473924269198,1076.37389480859,391.073492696899));
#118839=CARTESIAN_POINT('Ctrl Pts',(90.0786678211981,1076.38375238938,391.07344413192));
#118840=CARTESIAN_POINT('Ctrl Pts',(89.9115576809659,1076.39258810219,391.039916041364));
#118841=CARTESIAN_POINT('Ctrl Pts',(89.6001222777372,1076.40737676698,390.909708654403));
#118842=CARTESIAN_POINT('Ctrl Pts',(89.4588627501205,1076.41319074441,390.814365881412));
#118843=CARTESIAN_POINT('Ctrl Pts',(89.2212821771998,1076.4212058014,390.573782629421));
#118844=CARTESIAN_POINT('Ctrl Pts',(89.1274746485026,1076.42332030174,390.430817231719));
#118845=CARTESIAN_POINT('Ctrl Pts',(89.0011623088369,1076.42359751866,390.116542235314));
#118846=CARTESIAN_POINT('Ctrl Pts',(88.9699388158943,1076.4217570164,389.9483936573));
#118847=CARTESIAN_POINT('Ctrl Pts',(88.974966989438,1076.41426223305,389.610248087243));
#118848=CARTESIAN_POINT('Ctrl Pts',(89.0109791987585,1076.40868962099,389.443635792331));
#118849=CARTESIAN_POINT('Ctrl Pts',(89.1457249137492,1076.39432665083,389.134141610723));
#118850=CARTESIAN_POINT('Ctrl Pts',(89.2431414882275,1076.38567244326,388.994335807397));
#118851=CARTESIAN_POINT('Ctrl Pts',(89.4875261158289,1076.36615484006,388.759933106992));
#118852=CARTESIAN_POINT('Ctrl Pts',(89.632428630942,1076.35546600574,388.668012091641));
#118853=CARTESIAN_POINT('Ctrl Pts',(89.9490985165273,1076.33352043879,388.546562565143));
#118854=CARTESIAN_POINT('Ctrl Pts',(90.1176726428313,1076.3224810292,388.51800816092));
#118855=CARTESIAN_POINT('Ctrl Pts',(90.454422931293,1076.30172067755,388.528349923876));
#118856=CARTESIAN_POINT('Ctrl Pts',(90.6193498029185,1076.2921906145,388.566462382039));
#118857=CARTESIAN_POINT('Ctrl Pts',(90.9247820613952,1076.27603432292,388.70424411318));
#118858=CARTESIAN_POINT('Ctrl Pts',(91.0623730244936,1076.26956346593,388.802450032287));
#118859=CARTESIAN_POINT('Ctrl Pts',(91.291415537799,1076.26077000566,389.046115902754));
#118860=CARTESIAN_POINT('Ctrl Pts',(91.3807791954783,1076.25852248664,389.18902839898));
#118861=CARTESIAN_POINT('Ctrl Pts',(91.4992089951027,1076.25864459449,389.500791779399));
#118862=CARTESIAN_POINT('Ctrl Pts',(91.5272777349046,1076.26100037752,389.666514235576));
#118863=CARTESIAN_POINT('Ctrl Pts',(91.5181766731156,1076.26995313121,389.999301759715));
#118864=CARTESIAN_POINT('Ctrl Pts',(91.4811032128848,1076.27645944988,390.163127478227));
#118865=CARTESIAN_POINT('Ctrl Pts',(91.3460764523357,1076.29262394204,390.467566296283));
#118866=CARTESIAN_POINT('Ctrl Pts',(91.2492760870129,1076.30212968719,390.60519176657));
#118867=CARTESIAN_POINT('Ctrl Pts',(91.0080112746451,1076.32272303391,390.83568287336));
#118868=CARTESIAN_POINT('Ctrl Pts',(90.8657207867423,1076.33361480845,390.926224837942));
#118869=CARTESIAN_POINT('Ctrl Pts',(90.5625742841719,1076.3546622751,391.044116987762));
#118870=CARTESIAN_POINT('Ctrl Pts',(90.4056823246697,1076.36464686607,391.073538258395));
#118871=CARTESIAN_POINT('Ctrl Pts',(90.2473924269198,1076.37389480859,391.073492696899));
#118872=CARTESIAN_POINT('Origin',(90.2477595453611,1067.7251047501,389.798048628597));
#118873=CARTESIAN_POINT('',(90.2477595453611,1076.3606248843,390.473492749734));
#118874=CARTESIAN_POINT('',(90.2477595453612,1076.32917837425,389.122604507461));
#118875=CARTESIAN_POINT('Ctrl Pts',(90.2477595453611,1076.3606248843,390.473492749734));
#118876=CARTESIAN_POINT('Ctrl Pts',(90.2043920721301,1076.36319732881,390.473492749734));
#118877=CARTESIAN_POINT('Ctrl Pts',(90.1610125495164,1076.36566376778,390.469316146937));
#118878=CARTESIAN_POINT('Ctrl Pts',(90.0301266378503,1076.37278298611,390.443741260242));
#118879=CARTESIAN_POINT('Ctrl Pts',(89.9463009289524,1076.3768891315,390.409127887364));
#118880=CARTESIAN_POINT('Ctrl Pts',(89.7970259838005,1076.38330872468,390.309068283425));
#118881=CARTESIAN_POINT('Ctrl Pts',(89.7330857382475,1076.38555825709,390.244614648894));
#118882=CARTESIAN_POINT('Ctrl Pts',(89.6341405527321,1076.38791588244,390.094351645691));
#118883=CARTESIAN_POINT('Ctrl Pts',(89.6001639605402,1076.3879988915,390.010048714635));
#118884=CARTESIAN_POINT('Ctrl Pts',(89.5672600607563,1076.38596507471,389.833156887381));
#118885=CARTESIAN_POINT('Ctrl Pts',(89.5686397960403,1076.38386995074,389.742366687895));
#118886=CARTESIAN_POINT('Ctrl Pts',(89.6068257228187,1076.37772919497,389.566750407836));
#118887=CARTESIAN_POINT('Ctrl Pts',(89.6432272718938,1076.37374505058,389.483686272504));
#118888=CARTESIAN_POINT('Ctrl Pts',(89.7464541356269,1076.36434306899,389.336510143142));
#118889=CARTESIAN_POINT('Ctrl Pts',(89.8123271951584,1076.35901407682,389.27391686985));
#118890=CARTESIAN_POINT('Ctrl Pts',(89.9650841166153,1076.34766646312,389.177968647693));
#118891=CARTESIAN_POINT('Ctrl Pts',(90.0505569705632,1076.34175694847,389.145733736912));
#118892=CARTESIAN_POINT('Ctrl Pts',(90.1754297270574,1076.33367615497,389.125520878135));
#118893=CARTESIAN_POINT('Ctrl Pts',(90.2114348409469,1076.33140664045,389.122618319795));
#118894=CARTESIAN_POINT('Ctrl Pts',(90.2475017958103,1076.32919418435,389.12260455664));
#118895=CARTESIAN_POINT('Ctrl Pts',(90.2475877131029,1076.32918891392,389.122604523854));
#118896=CARTESIAN_POINT('Ctrl Pts',(90.2476736296214,1076.32918364389,389.122604507461));
#118897=CARTESIAN_POINT('Ctrl Pts',(90.2477595453612,1076.32917837425,389.122604507461));
#118898=CARTESIAN_POINT('',(90.2477595453611,1082.7251047501,389.122604507461));
#118899=CARTESIAN_POINT('',(90.2477595453611,1067.7251047501,389.122604507461));
#118900=CARTESIAN_POINT('Origin',(90.2477595453611,1082.7251047501,389.798048628597));
#118901=CARTESIAN_POINT('Ctrl Pts',(90.2477595453612,1076.32917837425,389.122604507461));
#118902=CARTESIAN_POINT('Ctrl Pts',(90.3363441354781,1076.32374504016,389.122604507461));
#118903=CARTESIAN_POINT('Ctrl Pts',(90.4241007966864,1076.31872897983,389.140031364471));
#118904=CARTESIAN_POINT('Ctrl Pts',(90.587837013375,1076.31016472553,389.207782768556));
#118905=CARTESIAN_POINT('Ctrl Pts',(90.6622418995852,1076.30669931367,389.257416805097));
#118906=CARTESIAN_POINT('Ctrl Pts',(90.7875044729904,1076.30185856023,389.382464264245));
#118907=CARTESIAN_POINT('Ctrl Pts',(90.8372022803927,1076.3005257356,389.456584447126));
#118908=CARTESIAN_POINT('Ctrl Pts',(90.9051620205711,1076.30020727945,389.619631964433));
#118909=CARTESIAN_POINT('Ctrl Pts',(90.9228181857498,1076.30122032886,389.706932955501));
#118910=CARTESIAN_POINT('Ctrl Pts',(90.9235767550121,1076.30545578206,389.883377994996));
#118911=CARTESIAN_POINT('Ctrl Pts',(90.9066640330344,1076.30863653759,389.970801489982));
#118912=CARTESIAN_POINT('Ctrl Pts',(90.8401661034984,1076.31671697932,390.134333828792));
#118913=CARTESIAN_POINT('Ctrl Pts',(90.7911515887479,1076.32154108136,390.208837027244));
#118914=CARTESIAN_POINT('Ctrl Pts',(90.6671338231893,1076.33215574363,390.334878350438));
#118915=CARTESIAN_POINT('Ctrl Pts',(90.593254242526,1076.33784599028,390.385151674791));
#118916=CARTESIAN_POINT('Ctrl Pts',(90.471117276196,1076.34643557514,390.437024038278));
#118917=CARTESIAN_POINT('Ctrl Pts',(90.4288363024025,1076.3492860713,390.450267765535));
#118918=CARTESIAN_POINT('Ctrl Pts',(90.3401321550213,1076.35502446918,390.468754036599));
#118919=CARTESIAN_POINT('Ctrl Pts',(90.2939526865699,1076.35788482859,390.473492749734));
#118920=CARTESIAN_POINT('Ctrl Pts',(90.2477595453611,1076.3606248843,390.473492749734));
#118921=CARTESIAN_POINT('Origin',(101.429261354593,1067.7251047501,397.970702670951));
#118922=CARTESIAN_POINT('',(101.429261354616,1077.63689261564,396.871871534958));
#118923=CARTESIAN_POINT('Ctrl Pts',(101.429493570798,1077.6944933282,399.069533782406));
#118924=CARTESIAN_POINT('Ctrl Pts',(101.570114169588,1077.68059568689,399.069504065026));
#118925=CARTESIAN_POINT('Ctrl Pts',(101.709401215988,1077.66602446619,399.042481726076));
#118926=CARTESIAN_POINT('Ctrl Pts',(101.974745505556,1077.63660140021,398.935609334865));
#118927=CARTESIAN_POINT('Ctrl Pts',(102.097645727388,1077.62203792686,398.85495706354));
#118928=CARTESIAN_POINT('Ctrl Pts',(102.300390061509,1077.59607657363,398.654778498191));
#118929=CARTESIAN_POINT('Ctrl Pts',(102.38008642834,1077.58480050336,398.538884121675));
#118930=CARTESIAN_POINT('Ctrl Pts',(102.486863479351,1077.56724256247,398.294764832151));
#118931=CARTESIAN_POINT('Ctrl Pts',(102.517235416251,1077.56073649119,398.170454293728));
#118932=CARTESIAN_POINT('Ctrl Pts',(102.530485929281,1077.5539583423,397.971211786179));
#118933=CARTESIAN_POINT('Ctrl Pts',(102.528118025575,1077.55222622028,397.898488200265));
#118934=CARTESIAN_POINT('Ctrl Pts',(102.515183338414,1077.5509077762,397.800768043311));
#118935=CARTESIAN_POINT('Ctrl Pts',(102.510863688064,1077.55065819879,397.775150056597));
#118936=CARTESIAN_POINT('Ctrl Pts',(102.502325967931,1077.55041101339,397.733566093651));
#118937=CARTESIAN_POINT('Ctrl Pts',(102.498649030552,1077.55035468184,397.717500322744));
#118938=CARTESIAN_POINT('Ctrl Pts',(102.490877245652,1077.5503226105,397.686741376454));
#118939=CARTESIAN_POINT('Ctrl Pts',(102.486835124766,1077.55034116017,397.672038920362));
#118940=CARTESIAN_POINT('Ctrl Pts',(102.476813549706,1077.55046219606,397.638346744497));
#118941=CARTESIAN_POINT('Ctrl Pts',(102.47062145392,1077.55058857402,397.61942617132));
#118942=CARTESIAN_POINT('Ctrl Pts',(102.449874079969,1077.55115830721,397.561411632438));
#118943=CARTESIAN_POINT('Ctrl Pts',(102.433605780676,1077.5517967795,397.522973810068));
#118944=CARTESIAN_POINT('Ctrl Pts',(102.350770301885,1077.55579018709,397.354632119186));
#118945=CARTESIAN_POINT('Ctrl Pts',(102.260963329105,1077.56190750512,397.237947552194));
#118946=CARTESIAN_POINT('Ctrl Pts',(102.062286967439,1077.5776687232,397.064839397336));
#118947=CARTESIAN_POINT('Ctrl Pts',(101.961669014374,1077.58630768889,397.002299025535));
#118948=CARTESIAN_POINT('Ctrl Pts',(101.734340889773,1077.60696342372,396.907245255332));
#118949=CARTESIAN_POINT('Ctrl Pts',(101.607799466399,1077.61906353407,396.878872319039));
#118950=CARTESIAN_POINT('Ctrl Pts',(101.340870322989,1077.64568030702,396.866697678955));
#118951=CARTESIAN_POINT('Ctrl Pts',(101.202482023023,1077.66007960346,396.886636115246));
#118952=CARTESIAN_POINT('Ctrl Pts',(100.933620267909,1077.6892557907,396.979225792778));
#118953=CARTESIAN_POINT('Ctrl Pts',(100.806507605167,1077.70373406477,397.053689947072));
#118954=CARTESIAN_POINT('Ctrl Pts',(100.592365051029,1077.72965371775,397.244801758827));
#118955=CARTESIAN_POINT('Ctrl Pts',(100.506089086297,1077.74094623503,397.358204768748));
#118956=CARTESIAN_POINT('Ctrl Pts',(100.38954102776,1077.75825520151,397.594700476585));
#118957=CARTESIAN_POINT('Ctrl Pts',(100.354127119112,1077.76465594977,397.712778277675));
#118958=CARTESIAN_POINT('Ctrl Pts',(100.327844372379,1077.7724947124,397.922933852471));
#118959=CARTESIAN_POINT('Ctrl Pts',(100.327600168607,1077.77477782493,398.012573491737));
#118960=CARTESIAN_POINT('Ctrl Pts',(100.34157339482,1077.77638028477,398.129331870532));
#118961=CARTESIAN_POINT('Ctrl Pts',(100.346012245204,1077.77665805758,398.15724974196));
#118962=CARTESIAN_POINT('Ctrl Pts',(100.354818878955,1077.77692965227,398.201546788563));
#118963=CARTESIAN_POINT('Ctrl Pts',(100.358497412579,1077.77699268152,398.218049050297));
#118964=CARTESIAN_POINT('Ctrl Pts',(100.365790839327,1077.7770364592,398.247545643728));
#118965=CARTESIAN_POINT('Ctrl Pts',(100.369266953818,1077.77703128813,398.260570639017));
#118966=CARTESIAN_POINT('Ctrl Pts',(100.377936098852,1077.77696183636,398.290809289014));
#118967=CARTESIAN_POINT('Ctrl Pts',(100.383313660878,1077.77687842146,398.307965845557));
#118968=CARTESIAN_POINT('Ctrl Pts',(100.39975632701,1077.77651792379,398.356240863478));
#118969=CARTESIAN_POINT('Ctrl Pts',(100.411806143182,1077.77613738196,398.387001811308));
#118970=CARTESIAN_POINT('Ctrl Pts',(100.484498084542,1077.77328380231,398.550474620684));
#118971=CARTESIAN_POINT('Ctrl Pts',(100.569691975595,1077.76813744088,398.670561399635));
#118972=CARTESIAN_POINT('Ctrl Pts',(100.760535136054,1077.75427983179,398.850364712881));
#118973=CARTESIAN_POINT('Ctrl Pts',(100.857419397221,1077.74657847039,398.916194746146));
#118974=CARTESIAN_POINT('Ctrl Pts',(101.039521930982,1077.73103980715,399.001589257506));
#118975=CARTESIAN_POINT('Ctrl Pts',(101.120183985121,1077.72385589326,399.028568136013));
#118976=CARTESIAN_POINT('Ctrl Pts',(101.27757129444,1077.70927321966,399.061671103831));
#118977=CARTESIAN_POINT('Ctrl Pts',(101.353445151774,1077.70200925161,399.069549853735));
#118978=CARTESIAN_POINT('Ctrl Pts',(101.429493570798,1077.6944933282,399.069533782406));
#118979=CARTESIAN_POINT('',(101.429261354572,1075.62570687173,396.871871534959));
#118980=CARTESIAN_POINT('',(101.429261354593,1067.7251047501,396.871871534959));
#118981=CARTESIAN_POINT('Ctrl Pts',(101.428824109534,1075.68390181721,399.06953371995));
#118982=CARTESIAN_POINT('Ctrl Pts',(101.283118147846,1075.69843181531,399.069475740871));
#118983=CARTESIAN_POINT('Ctrl Pts',(101.13874912924,1075.71195732163,399.040437274791));
#118984=CARTESIAN_POINT('Ctrl Pts',(100.869966130838,1075.73547780411,398.927676464783));
#118985=CARTESIAN_POINT('Ctrl Pts',(100.748147277168,1075.74525357799,398.845216604272));
#118986=CARTESIAN_POINT('Ctrl Pts',(100.543500785851,1075.75984986348,398.637170030997));
#118987=CARTESIAN_POINT('Ctrl Pts',(100.462816124142,1075.76451724927,398.513641006511));
#118988=CARTESIAN_POINT('Ctrl Pts',(100.355577104622,1075.76806198767,398.244832180365));
#118989=CARTESIAN_POINT('Ctrl Pts',(100.329030698117,1075.7670195189,398.102712524122));
#118990=CARTESIAN_POINT('Ctrl Pts',(100.331972350312,1075.75936870649,397.813495563413));
#118991=CARTESIAN_POINT('Ctrl Pts',(100.36255146929,1075.75272765045,397.669334337659));
#118992=CARTESIAN_POINT('Ctrl Pts',(100.478051834914,1075.73458193086,397.401599442797));
#118993=CARTESIAN_POINT('Ctrl Pts',(100.561787929872,1075.72325879679,397.280713035585));
#118994=CARTESIAN_POINT('Ctrl Pts',(100.771752308137,1075.69725319785,397.07824217027));
#118995=CARTESIAN_POINT('Ctrl Pts',(100.896119724191,1075.68280793521,396.998843706387));
#118996=CARTESIAN_POINT('Ctrl Pts',(101.099118750661,1075.66037880992,396.92019080175));
#118997=CARTESIAN_POINT('Ctrl Pts',(101.168337372211,1075.65290133642,396.900895733485));
#118998=CARTESIAN_POINT('Ctrl Pts',(101.382892660413,1075.63022365326,396.863162951671));
#118999=CARTESIAN_POINT('Ctrl Pts',(101.530533126309,1075.61528668515,396.866810028771));
#119000=CARTESIAN_POINT('Ctrl Pts',(101.814062762848,1075.58797342294,396.931360455569));
#119001=CARTESIAN_POINT('Ctrl Pts',(101.947377545443,1075.57582990881,396.990936590587));
#119002=CARTESIAN_POINT('Ctrl Pts',(102.182729390908,1075.55599730865,397.158041962838));
#119003=CARTESIAN_POINT('Ctrl Pts',(102.282654681582,1075.54847789514,397.263649463309));
#119004=CARTESIAN_POINT('Ctrl Pts',(102.435678626395,1075.53918627221,397.506933630482));
#119005=CARTESIAN_POINT('Ctrl Pts',(102.487527926722,1075.53747427039,397.641995746359));
#119006=CARTESIAN_POINT('Ctrl Pts',(102.536384974375,1075.5401145013,397.924169840587));
#119007=CARTESIAN_POINT('Ctrl Pts',(102.533023360652,1075.54442675161,398.06843602517));
#119008=CARTESIAN_POINT('Ctrl Pts',(102.471234631415,1075.55849440184,398.347879580521));
#119009=CARTESIAN_POINT('Ctrl Pts',(102.413246441751,1075.5681258234,398.480273664585));
#119010=CARTESIAN_POINT('Ctrl Pts',(102.249486945095,1075.59140627521,398.715940073188));
#119011=CARTESIAN_POINT('Ctrl Pts',(102.14499270199,1075.60485359843,398.816758062767));
#119012=CARTESIAN_POINT('Ctrl Pts',(101.963519900669,1075.62647206832,398.933615686175));
#119013=CARTESIAN_POINT('Ctrl Pts',(101.89918202132,1075.63388506018,398.966596438669));
#119014=CARTESIAN_POINT('Ctrl Pts',(101.768280558606,1075.64849837418,399.018175774439));
#119015=CARTESIAN_POINT('Ctrl Pts',(101.702254414096,1075.6556606865,399.037290202223));
#119016=CARTESIAN_POINT('Ctrl Pts',(101.56697018122,1075.66992994431,399.063060186457));
#119017=CARTESIAN_POINT('Ctrl Pts',(101.497979788506,1075.67700551817,399.069561238265));
#119018=CARTESIAN_POINT('Ctrl Pts',(101.428824109533,1075.68390181721,399.06953371995));
#119019=CARTESIAN_POINT('Origin',(101.429261354593,1067.7251047501,397.970702670951));
#119020=CARTESIAN_POINT('',(101.429261354593,1075.66856733728,398.469533806944));
#119021=CARTESIAN_POINT('',(101.429261354593,1075.64217240143,397.471871534959));
#119022=CARTESIAN_POINT('Ctrl Pts',(101.429261354593,1075.66856733728,398.469533806944));
#119023=CARTESIAN_POINT('Ctrl Pts',(101.396725259188,1075.67182918461,398.469533806944));
#119024=CARTESIAN_POINT('Ctrl Pts',(101.364178506132,1075.67500282734,398.466350650069));
#119025=CARTESIAN_POINT('Ctrl Pts',(101.266977566166,1075.68420943944,398.447046565021));
#119026=CARTESIAN_POINT('Ctrl Pts',(101.205032551033,1075.6897021991,398.421233424481));
#119027=CARTESIAN_POINT('Ctrl Pts',(101.094874904145,1075.69870538601,398.346778844227));
#119028=CARTESIAN_POINT('Ctrl Pts',(101.047762299093,1075.70212737812,398.298911441355));
#119029=CARTESIAN_POINT('Ctrl Pts',(100.975899018794,1075.70637630619,398.188697938427));
#119030=CARTESIAN_POINT('Ctrl Pts',(100.951367518801,1075.70721976277,398.127804081999));
#119031=CARTESIAN_POINT('Ctrl Pts',(100.927061625673,1075.70630237684,398.00000569481));
#119032=CARTESIAN_POINT('Ctrl Pts',(100.927528876131,1075.70455067681,397.934375840882));
#119033=CARTESIAN_POINT('Ctrl Pts',(100.953630317649,1075.69864101878,397.806803050874));
#119034=CARTESIAN_POINT('Ctrl Pts',(100.979102284652,1075.69453192855,397.746138789854));
#119035=CARTESIAN_POINT('Ctrl Pts',(101.052616408138,1075.68435848275,397.636941267692));
#119036=CARTESIAN_POINT('Ctrl Pts',(101.100398225715,1075.67835508124,397.589793552283));
#119037=CARTESIAN_POINT('Ctrl Pts',(101.183162262418,1075.66864061709,397.535586954051));
#119038=CARTESIAN_POINT('Ctrl Pts',(101.212043073601,1075.66534555193,397.520474218651));
#119039=CARTESIAN_POINT('Ctrl Pts',(101.271649811749,1075.65871997472,397.496359259037));
#119040=CARTESIAN_POINT('Ctrl Pts',(101.302189757706,1075.65540641244,397.487281858555));
#119041=CARTESIAN_POINT('Ctrl Pts',(101.364879120949,1075.64876173334,397.475003708015));
#119042=CARTESIAN_POINT('Ctrl Pts',(101.396901311918,1075.64544559241,397.471888121455));
#119043=CARTESIAN_POINT('Ctrl Pts',(101.429004655058,1075.64219836474,397.471871601006));
#119044=CARTESIAN_POINT('Ctrl Pts',(101.429090222574,1075.64218970965,397.471871556973));
#119045=CARTESIAN_POINT('Ctrl Pts',(101.429175789089,1075.64218105522,397.471871534959));
#119046=CARTESIAN_POINT('Ctrl Pts',(101.429261354593,1075.64217240143,397.471871534959));
#119047=CARTESIAN_POINT('',(101.429261354593,1082.7251047501,397.471871534959));
#119048=CARTESIAN_POINT('',(101.429261354593,1067.7251047501,397.471871534959));
#119049=CARTESIAN_POINT('Origin',(101.429261354593,1082.7251047501,397.970702670951));
#119050=CARTESIAN_POINT('Ctrl Pts',(101.429261354593,1075.64217240143,397.471871534959));
#119051=CARTESIAN_POINT('Ctrl Pts',(101.495421950748,1075.63548115745,397.471871534959));
#119052=CARTESIAN_POINT('Ctrl Pts',(101.560978599971,1075.62917816881,397.485034008547));
#119053=CARTESIAN_POINT('Ctrl Pts',(101.682419981123,1075.61818275567,397.535935948996));
#119054=CARTESIAN_POINT('Ctrl Pts',(101.737249774835,1075.61357707225,397.572869047254));
#119055=CARTESIAN_POINT('Ctrl Pts',(101.829287030385,1075.60666323584,397.665652088365));
#119056=CARTESIAN_POINT('Ctrl Pts',(101.865692713758,1075.60440995756,397.720473476261));
#119057=CARTESIAN_POINT('Ctrl Pts',(101.915264791931,1075.60257310897,397.840873822758));
#119058=CARTESIAN_POINT('Ctrl Pts',(101.928023384354,1075.60299801806,397.905210534623));
#119059=CARTESIAN_POINT('Ctrl Pts',(101.928161096421,1075.60647968227,398.035194002776));
#119060=CARTESIAN_POINT('Ctrl Pts',(101.915517978015,1075.60950367989,398.099548383412));
#119061=CARTESIAN_POINT('Ctrl Pts',(101.866221262996,1075.61776614351,398.220012152439));
#119062=CARTESIAN_POINT('Ctrl Pts',(101.829930797645,1075.62293418494,398.274900719215));
#119063=CARTESIAN_POINT('Ctrl Pts',(101.73814313638,1075.63473796658,398.367837084625));
#119064=CARTESIAN_POINT('Ctrl Pts',(101.683408510518,1075.64126910735,398.404894731071));
#119065=CARTESIAN_POINT('Ctrl Pts',(101.593043672638,1075.65140156573,398.443009268326));
#119066=CARTESIAN_POINT('Ctrl Pts',(101.561793158021,1075.65480771647,398.452712395339));
#119067=CARTESIAN_POINT('Ctrl Pts',(101.496660735388,1075.66171451687,398.466117623723));
#119068=CARTESIAN_POINT('Ctrl Pts',(101.46296676434,1075.66518826246,398.469533806944));
#119069=CARTESIAN_POINT('Ctrl Pts',(101.429261354593,1075.66856733728,398.469533806944));
#119070=CARTESIAN_POINT('Origin',(110.796881705952,1067.7251047501,408.357311548868));
#119071=CARTESIAN_POINT('',(110.79688170597,1076.79846644782,407.266770800141));
#119072=CARTESIAN_POINT('Ctrl Pts',(110.797596068878,1076.84090759235,409.447852063623));
#119073=CARTESIAN_POINT('Ctrl Pts',(110.940798490479,1076.82194611934,409.447758258304));
#119074=CARTESIAN_POINT('Ctrl Pts',(111.082602685119,1076.80252747935,409.419458867192));
#119075=CARTESIAN_POINT('Ctrl Pts',(111.347547647025,1076.76496011306,409.309506201558));
#119076=CARTESIAN_POINT('Ctrl Pts',(111.468196495587,1076.7471620535,409.228716494913));
#119077=CARTESIAN_POINT('Ctrl Pts',(111.663174628467,1076.71701008936,409.032843373741));
#119078=CARTESIAN_POINT('Ctrl Pts',(111.738859542695,1076.7045810305,408.922638121687));
#119079=CARTESIAN_POINT('Ctrl Pts',(111.850538649928,1076.68446048781,408.672117681504));
#119080=CARTESIAN_POINT('Ctrl Pts',(111.882517354936,1076.67733136566,408.532763321516));
#119081=CARTESIAN_POINT('Ctrl Pts',(111.887907789629,1076.67312014269,408.35848053537));
#119082=CARTESIAN_POINT('Ctrl Pts',(111.887456463124,1076.67253121684,408.325903660198));
#119083=CARTESIAN_POINT('Ctrl Pts',(111.884521713249,1076.6719325176,408.275919304519));
#119084=CARTESIAN_POINT('Ctrl Pts',(111.883075271443,1076.67178095054,408.258472999811));
#119085=CARTESIAN_POINT('Ctrl Pts',(111.879652867879,1076.67160909169,408.226548432727));
#119086=CARTESIAN_POINT('Ctrl Pts',(111.877804756182,1076.67157122571,408.212060906793));
#119087=CARTESIAN_POINT('Ctrl Pts',(111.873479467553,1076.67157620347,408.18284269891));
#119088=CARTESIAN_POINT('Ctrl Pts',(111.870989531762,1076.67162088662,408.168117223433));
#119089=CARTESIAN_POINT('Ctrl Pts',(111.864156962088,1076.67183338189,408.132211687618));
#119090=CARTESIAN_POINT('Ctrl Pts',(111.859485544345,1076.67204730599,408.111101412548));
#119091=CARTESIAN_POINT('Ctrl Pts',(111.840716041769,1076.6731171682,408.036821405501));
#119092=CARTESIAN_POINT('Ctrl Pts',(111.823230749441,1076.67445279373,407.984606899442));
#119093=CARTESIAN_POINT('Ctrl Pts',(111.745848355034,1076.68130575353,407.800912492653));
#119094=CARTESIAN_POINT('Ctrl Pts',(111.664032941405,1076.6900207055,407.680514225089));
#119095=CARTESIAN_POINT('Ctrl Pts',(111.47660366712,1076.7117353652,407.496275756476));
#119096=CARTESIAN_POINT('Ctrl Pts',(111.378919935215,1076.72357163678,407.427495958239));
#119097=CARTESIAN_POINT('Ctrl Pts',(111.155543420406,1076.75151197595,407.319304807177));
#119098=CARTESIAN_POINT('Ctrl Pts',(111.029813890956,1076.76769471878,407.284107570939));
#119099=CARTESIAN_POINT('Ctrl Pts',(110.761934560225,1076.80298809342,407.258414106273));
#119100=CARTESIAN_POINT('Ctrl Pts',(110.62160256584,1076.8219212525,407.271923152553));
#119101=CARTESIAN_POINT('Ctrl Pts',(110.348934538908,1076.8595917202,407.352549191111));
#119102=CARTESIAN_POINT('Ctrl Pts',(110.219603083,1076.87794711436,407.420804922885));
#119103=CARTESIAN_POINT('Ctrl Pts',(110.000530428149,1076.91013053916,407.599619671674));
#119104=CARTESIAN_POINT('Ctrl Pts',(109.911078128603,1076.92385613248,407.706355951291));
#119105=CARTESIAN_POINT('Ctrl Pts',(109.782567297638,1076.9450121476,407.937372447147));
#119106=CARTESIAN_POINT('Ctrl Pts',(109.740768013442,1076.95272737992,408.057510368056));
#119107=CARTESIAN_POINT('Ctrl Pts',(109.709490002801,1076.9604471158,408.249856803403));
#119108=CARTESIAN_POINT('Ctrl Pts',(109.704885749696,1076.96234661771,408.318346506131));
#119109=CARTESIAN_POINT('Ctrl Pts',(109.707401418855,1076.96378737287,408.411231851096));
#119110=CARTESIAN_POINT('Ctrl Pts',(109.708880866583,1076.96405911113,408.435599411419));
#119111=CARTESIAN_POINT('Ctrl Pts',(109.712631138036,1076.96432803011,408.475289733741));
#119112=CARTESIAN_POINT('Ctrl Pts',(109.714412642405,1076.96438930685,408.490649034774));
#119113=CARTESIAN_POINT('Ctrl Pts',(109.718468114861,1076.96442438148,408.520122708937));
#119114=CARTESIAN_POINT('Ctrl Pts',(109.720694191577,1076.96440444519,408.534240291552));
#119115=CARTESIAN_POINT('Ctrl Pts',(109.72646223583,1076.96427375415,408.566664952867));
#119116=CARTESIAN_POINT('Ctrl Pts',(109.730197472961,1076.96413721157,408.584932737935));
#119117=CARTESIAN_POINT('Ctrl Pts',(109.743198805031,1076.9635215027,408.641135341062));
#119118=CARTESIAN_POINT('Ctrl Pts',(109.75403409151,1076.96283139683,408.678670724879));
#119119=CARTESIAN_POINT('Ctrl Pts',(109.814372691947,1076.95831109599,408.852164245958));
#119120=CARTESIAN_POINT('Ctrl Pts',(109.888540162546,1076.95108732914,408.977816204453));
#119121=CARTESIAN_POINT('Ctrl Pts',(110.062727173184,1076.93213260548,409.172108767722));
#119122=CARTESIAN_POINT('Ctrl Pts',(110.153883205898,1076.92165881263,409.245769799526));
#119123=CARTESIAN_POINT('Ctrl Pts',(110.341538697821,1076.89917000054,409.353270798214));
#119124=CARTESIAN_POINT('Ctrl Pts',(110.434606194538,1076.88768352365,409.390746166895));
#119125=CARTESIAN_POINT('Ctrl Pts',(110.618468559949,1076.86437474434,409.43690112176));
#119126=CARTESIAN_POINT('Ctrl Pts',(110.707891313523,1076.85278542428,409.447910825082));
#119127=CARTESIAN_POINT('Ctrl Pts',(110.797596068878,1076.84090759235,409.447852063623));
#119128=CARTESIAN_POINT('',(110.796881705933,1074.78002293647,407.26677080014));
#119129=CARTESIAN_POINT('',(110.796881705952,1067.7251047501,407.26677080014));
#119130=CARTESIAN_POINT('Ctrl Pts',(110.797104296965,1074.82288111126,409.44785227488));
#119131=CARTESIAN_POINT('Ctrl Pts',(110.652438844663,1074.84219373867,409.447881802644));
#119132=CARTESIAN_POINT('Ctrl Pts',(110.509041163128,1074.86067712467,409.41912529087));
#119133=CARTESIAN_POINT('Ctrl Pts',(110.242179317219,1074.89380419229,409.307272717847));
#119134=CARTESIAN_POINT('Ctrl Pts',(110.121210562518,1074.90814599874,409.225486400346));
#119135=CARTESIAN_POINT('Ctrl Pts',(109.918968855179,1074.93074023296,409.019984542716));
#119136=CARTESIAN_POINT('Ctrl Pts',(109.83936521802,1074.93882396886,408.898726784053));
#119137=CARTESIAN_POINT('Ctrl Pts',(109.732560159946,1074.9477078735,408.63399921831));
#119138=CARTESIAN_POINT('Ctrl Pts',(109.705652335196,1074.94852919444,408.49356864231));
#119139=CARTESIAN_POINT('Ctrl Pts',(109.707057740186,1074.94290529174,408.209967554164));
#119140=CARTESIAN_POINT('Ctrl Pts',(109.735462484341,1074.93650257059,408.069675734858));
#119141=CARTESIAN_POINT('Ctrl Pts',(109.84542065414,1074.91699009266,407.805042530233));
#119142=CARTESIAN_POINT('Ctrl Pts',(109.927041106778,1074.90392926951,407.683873081696));
#119143=CARTESIAN_POINT('Ctrl Pts',(110.132663885017,1074.87283895158,407.480336697443));
#119144=CARTESIAN_POINT('Ctrl Pts',(110.254768731147,1074.85509826984,407.400089688862));
#119145=CARTESIAN_POINT('Ctrl Pts',(110.454534828223,1074.82691355067,407.319473955404));
#119146=CARTESIAN_POINT('Ctrl Pts',(110.522711679009,1074.81741858841,407.29942049743));
#119147=CARTESIAN_POINT('Ctrl Pts',(110.662207018169,1074.79822716727,407.27278280803));
#119148=CARTESIAN_POINT('Ctrl Pts',(110.733225327124,1074.78857285774,407.266307963273));
#119149=CARTESIAN_POINT('Ctrl Pts',(110.950836314104,1074.75934327395,407.267802286347));
#119150=CARTESIAN_POINT('Ctrl Pts',(111.095764470464,1074.74036228006,407.298306539936));
#119151=CARTESIAN_POINT('Ctrl Pts',(111.36201243672,1074.70654289296,407.413666149387));
#119152=CARTESIAN_POINT('Ctrl Pts',(111.481279983993,1074.69194134382,407.496162584562));
#119153=CARTESIAN_POINT('Ctrl Pts',(111.680159312817,1074.66891163819,407.702046636736));
#119154=CARTESIAN_POINT('Ctrl Pts',(111.758204460931,1074.66065081163,407.822974454505));
#119155=CARTESIAN_POINT('Ctrl Pts',(111.862928670743,1074.65161706806,408.087354033574));
#119156=CARTESIAN_POINT('Ctrl Pts',(111.88894651253,1074.65087800413,408.227935717224));
#119157=CARTESIAN_POINT('Ctrl Pts',(111.885761555839,1074.65701288816,408.51111919239));
#119158=CARTESIAN_POINT('Ctrl Pts',(111.856631937355,1074.66381808078,408.650835991852));
#119159=CARTESIAN_POINT('Ctrl Pts',(111.746500202022,1074.68411125413,408.912052886199));
#119160=CARTESIAN_POINT('Ctrl Pts',(111.666228687497,1074.69744235606,409.030820038809));
#119161=CARTESIAN_POINT('Ctrl Pts',(111.464078426709,1074.72891417179,409.231754012385));
#119162=CARTESIAN_POINT('Ctrl Pts',(111.343705581201,1074.74680083847,409.311608728508));
#119163=CARTESIAN_POINT('Ctrl Pts',(111.14622773306,1074.77501547182,409.392793530291));
#119164=CARTESIAN_POINT('Ctrl Pts',(111.078476928241,1074.78452761695,409.413230826971));
#119165=CARTESIAN_POINT('Ctrl Pts',(110.939390232132,1074.80372666124,409.440843814289));
#119166=CARTESIAN_POINT('Ctrl Pts',(110.86833802526,1074.81337151217,409.447837735315));
#119167=CARTESIAN_POINT('Ctrl Pts',(110.797104296965,1074.82288111126,409.44785227488));
#119168=CARTESIAN_POINT('Origin',(110.796881705952,1067.7251047501,408.357311548868));
#119169=CARTESIAN_POINT('',(110.796881705952,1074.81171529132,408.847852297596));
#119170=CARTESIAN_POINT('',(110.796881705952,1074.79242545665,407.86677080014));
#119171=CARTESIAN_POINT('Ctrl Pts',(110.796881705952,1074.81171529132,408.847852297596));
#119172=CARTESIAN_POINT('Ctrl Pts',(110.732230902365,1074.82036176743,408.847852297596));
#119173=CARTESIAN_POINT('Ctrl Pts',(110.668137201305,1074.82866376,408.835071239047));
#119174=CARTESIAN_POINT('Ctrl Pts',(110.548079367316,1074.84367802719,408.785079045369));
#119175=CARTESIAN_POINT('Ctrl Pts',(110.493348101575,1074.85023254509,408.748186842145));
#119176=CARTESIAN_POINT('Ctrl Pts',(110.402117569826,1074.86054008216,408.655567616644));
#119177=CARTESIAN_POINT('Ctrl Pts',(110.366286408721,1074.8642284773,408.601041247894));
#119178=CARTESIAN_POINT('Ctrl Pts',(110.318190424013,1074.86828640209,408.481983554045));
#119179=CARTESIAN_POINT('Ctrl Pts',(110.306058615111,1074.86866517485,408.418821584829));
#119180=CARTESIAN_POINT('Ctrl Pts',(110.306633608904,1074.86610898353,408.291303235435));
#119181=CARTESIAN_POINT('Ctrl Pts',(110.319362355406,1074.8631961676,408.228242712091));
#119182=CARTESIAN_POINT('Ctrl Pts',(110.368313422293,1074.85440131949,408.110180529535));
#119183=CARTESIAN_POINT('Ctrl Pts',(110.404219439568,1074.84858498955,408.056422718336));
#119184=CARTESIAN_POINT('Ctrl Pts',(110.495510813699,1074.83464611687,407.964773307526));
#119185=CARTESIAN_POINT('Ctrl Pts',(110.550425655568,1074.82661064083,407.928187191488));
#119186=CARTESIAN_POINT('Ctrl Pts',(110.640080283218,1074.81391187333,407.891430867615));
#119187=CARTESIAN_POINT('Ctrl Pts',(110.670443074312,1074.80967184199,407.882291851998));
#119188=CARTESIAN_POINT('Ctrl Pts',(110.73280598265,1074.801079668,407.869925255115));
#119189=CARTESIAN_POINT('Ctrl Pts',(110.764681141398,1074.79674591179,407.866786851268));
#119190=CARTESIAN_POINT('Ctrl Pts',(110.796636258659,1074.792458388,407.866770861555));
#119191=CARTESIAN_POINT('Ctrl Pts',(110.796718075338,1074.79244741039,407.866770820616));
#119192=CARTESIAN_POINT('Ctrl Pts',(110.796799891105,1074.79243643327,407.86677080014));
#119193=CARTESIAN_POINT('Ctrl Pts',(110.796881705952,1074.79242545665,407.86677080014));
#119194=CARTESIAN_POINT('',(110.796881705952,1082.7251047501,407.86677080014));
#119195=CARTESIAN_POINT('',(110.796881705952,1067.7251047501,407.86677080014));
#119196=CARTESIAN_POINT('Origin',(110.796881705952,1082.7251047501,408.357311548868));
#119197=CARTESIAN_POINT('Ctrl Pts',(110.796881705952,1074.79242545665,407.86677080014));
#119198=CARTESIAN_POINT('Ctrl Pts',(110.862448424036,1074.78362875217,407.86677080014));
#119199=CARTESIAN_POINT('Ctrl Pts',(110.927424711471,1074.77515064853,407.87991650284));
#119200=CARTESIAN_POINT('Ctrl Pts',(111.047742741636,1074.75994924986,407.930797048961));
#119201=CARTESIAN_POINT('Ctrl Pts',(111.102033244182,1074.75335292131,407.967751717849));
#119202=CARTESIAN_POINT('Ctrl Pts',(111.192335164697,1074.7429825256,408.060085497495));
#119203=CARTESIAN_POINT('Ctrl Pts',(111.227759642654,1074.73926380156,408.114222684894));
#119204=CARTESIAN_POINT('Ctrl Pts',(111.27561552072,1074.73514222284,408.232803372901));
#119205=CARTESIAN_POINT('Ctrl Pts',(111.287725651519,1074.73475766369,408.295968305641));
#119206=CARTESIAN_POINT('Ctrl Pts',(111.287107750214,1074.7373736331,408.423406605835));
#119207=CARTESIAN_POINT('Ctrl Pts',(111.274389220315,1074.74034695761,408.486382547684));
#119208=CARTESIAN_POINT('Ctrl Pts',(111.225528705733,1074.74929199442,408.60427926035));
#119209=CARTESIAN_POINT('Ctrl Pts',(111.189707559974,1074.75519534922,408.6579641971));
#119210=CARTESIAN_POINT('Ctrl Pts',(111.099232079229,1074.76919354963,408.748938714261));
#119211=CARTESIAN_POINT('Ctrl Pts',(111.045258313269,1074.77717531092,408.785184830353));
#119212=CARTESIAN_POINT('Ctrl Pts',(110.956297730916,1074.78985619173,408.822334846439));
#119213=CARTESIAN_POINT('Ctrl Pts',(110.925549031485,1074.79416760951,408.83176266743));
#119214=CARTESIAN_POINT('Ctrl Pts',(110.862723959561,1074.80283806631,408.844466863021));
#119215=CARTESIAN_POINT('Ctrl Pts',(110.830790115671,1074.80717767322,408.84772577844));
#119216=CARTESIAN_POINT('Ctrl Pts',(110.798136690445,1074.81154742282,408.847851093668));
#119217=CARTESIAN_POINT('Ctrl Pts',(110.797509171956,1074.81163137327,408.847852297596));
#119218=CARTESIAN_POINT('Ctrl Pts',(110.796881705952,1074.81171529132,408.847852297596));
#119219=CARTESIAN_POINT('Origin',(69.1578093449752,1067.7251047501,367.717925093334));
#119220=CARTESIAN_POINT('',(69.1578093449994,1078.64674583663,366.23962196114));
#119221=CARTESIAN_POINT('',(69.1578093449753,1078.69514019783,369.196228225527));
#119222=CARTESIAN_POINT('Ctrl Pts',(69.1578093449994,1078.64674583663,366.23962196114));
#119223=CARTESIAN_POINT('Ctrl Pts',(69.0296449594974,1078.64978215304,366.239621961138));
#119224=CARTESIAN_POINT('Ctrl Pts',(68.9020372739768,1078.65305477435,366.256287402465));
#119225=CARTESIAN_POINT('Ctrl Pts',(68.6682202561937,1078.65943950329,366.318415431848));
#119226=CARTESIAN_POINT('Ctrl Pts',(68.5620016043582,1078.66250668231,366.360229385106));
#119227=CARTESIAN_POINT('Ctrl Pts',(68.2929599044742,1078.67068017121,366.503851637143));
#119228=CARTESIAN_POINT('Ctrl Pts',(68.1433397887672,1078.67566912136,366.62577319367));
#119229=CARTESIAN_POINT('Ctrl Pts',(67.9073232828472,1078.68448653439,366.909636845607));
#119230=CARTESIAN_POINT('Ctrl Pts',(67.8191858166255,1078.68830218495,367.065897950557));
#119231=CARTESIAN_POINT('Ctrl Pts',(67.70719855906,1078.69461389355,367.389196055409));
#119232=CARTESIAN_POINT('Ctrl Pts',(67.6796760452616,1078.69714927108,367.552210845489));
#119233=CARTESIAN_POINT('Ctrl Pts',(67.6793262989304,1078.70137772082,367.891909047171));
#119234=CARTESIAN_POINT('Ctrl Pts',(67.7104015479753,1078.70297179684,368.066058318319));
#119235=CARTESIAN_POINT('Ctrl Pts',(67.8049247097742,1078.70459182585,368.321657185957));
#119236=CARTESIAN_POINT('Ctrl Pts',(67.8474429188161,1078.70499568347,368.409104794057));
#119237=CARTESIAN_POINT('Ctrl Pts',(67.9185829621773,1078.70532619632,368.52490184275));
#119238=CARTESIAN_POINT('Ctrl Pts',(67.9402469233516,1078.70539357062,368.557231508571));
#119239=CARTESIAN_POINT('Ctrl Pts',(67.9784442733099,1078.70546072103,368.609637745062));
#119240=CARTESIAN_POINT('Ctrl Pts',(67.9942772144347,1078.70547551981,368.630200494422));
#119241=CARTESIAN_POINT('Ctrl Pts',(68.0263437354676,1078.70548089504,368.669652666604));
#119242=CARTESIAN_POINT('Ctrl Pts',(68.0425297450801,1078.70547243057,368.688569834165));
#119243=CARTESIAN_POINT('Ctrl Pts',(68.0817827631551,1078.70542631421,368.732167417706));
#119244=CARTESIAN_POINT('Ctrl Pts',(68.1052332637385,1078.70537934681,368.756483847911));
#119245=CARTESIAN_POINT('Ctrl Pts',(68.183526721153,1078.70516165467,368.832290230457));
#119246=CARTESIAN_POINT('Ctrl Pts',(68.24147084426,1078.70491031437,368.880405174778));
#119247=CARTESIAN_POINT('Ctrl Pts',(68.463348284611,1078.70362891227,369.037706880796));
#119248=CARTESIAN_POINT('Ctrl Pts',(68.6449874630025,1078.7020157938,369.118321248062));
#119249=CARTESIAN_POINT('Ctrl Pts',(68.9423791004867,1078.69836935129,369.18442071346));
#119250=CARTESIAN_POINT('Ctrl Pts',(69.049929047363,1078.69686402144,369.196228225527));
#119251=CARTESIAN_POINT('Ctrl Pts',(69.1578093449753,1078.69514019783,369.196228225527));
#119252=CARTESIAN_POINT('',(69.1578093449571,1076.64572521568,366.239621961141));
#119253=CARTESIAN_POINT('',(69.1578093449752,1067.7251047501,366.23962196114));
#119254=CARTESIAN_POINT('',(69.1578093449752,1076.6946925711,369.196228225527));
#119255=CARTESIAN_POINT('Ctrl Pts',(69.1578093449752,1076.6946925711,369.196228225527));
#119256=CARTESIAN_POINT('Ctrl Pts',(69.1129243695232,1076.69541844176,369.196228225527));
#119257=CARTESIAN_POINT('Ctrl Pts',(69.0683825043262,1076.6961017847,369.19418827694));
#119258=CARTESIAN_POINT('Ctrl Pts',(69.0241795694995,1076.69674557598,369.190176170344));
#119259=CARTESIAN_POINT('Ctrl Pts',(68.9795394951775,1076.69739573396,369.186124386513));
#119260=CARTESIAN_POINT('Ctrl Pts',(68.9352441571163,1076.69800555415,369.18006124436));
#119261=CARTESIAN_POINT('Ctrl Pts',(68.8912860273357,1076.69857810177,369.172004001718));
#119262=CARTESIAN_POINT('Ctrl Pts',(68.8840484801668,1076.69867236966,369.170677405842));
#119263=CARTESIAN_POINT('Ctrl Pts',(68.8768200852097,1076.69876562716,369.169296638954));
#119264=CARTESIAN_POINT('Ctrl Pts',(68.8696008277746,1076.69885788794,369.167861644106));
#119265=CARTESIAN_POINT('Ctrl Pts',(68.8314853405077,1076.69934499682,369.160285307016));
#119266=CARTESIAN_POINT('Ctrl Pts',(68.793459694709,1076.69980569616,369.151160086375));
#119267=CARTESIAN_POINT('Ctrl Pts',(68.7557810565234,1076.70023844489,369.140511964473));
#119268=CARTESIAN_POINT('Ctrl Pts',(68.7181385859787,1076.70067077823,369.129874063679));
#119269=CARTESIAN_POINT('Ctrl Pts',(68.6808430566933,1076.7010752146,369.117716304634));
#119270=CARTESIAN_POINT('Ctrl Pts',(68.6441396458052,1076.70145021738,369.104115408841));
#119271=CARTESIAN_POINT('Ctrl Pts',(68.6265107180164,1076.70163033407,369.097582795006));
#119272=CARTESIAN_POINT('Ctrl Pts',(68.6090181661426,1076.70180366057,369.090717997316));
#119273=CARTESIAN_POINT('Ctrl Pts',(68.5916876243133,1076.70197002661,369.083533510138));
#119274=CARTESIAN_POINT('Ctrl Pts',(68.5499591554298,1076.70237060267,369.066234705946));
#119275=CARTESIAN_POINT('Ctrl Pts',(68.5092372895722,1076.70273123869,369.04711656848));
#119276=CARTESIAN_POINT('Ctrl Pts',(68.4695057440446,1076.7030537665,369.026213403913));
#119277=CARTESIAN_POINT('Ctrl Pts',(68.4296799567572,1076.70337705933,369.005260657811));
#119278=CARTESIAN_POINT('Ctrl Pts',(68.3908483463713,1076.70366206297,368.982513983927));
#119279=CARTESIAN_POINT('Ctrl Pts',(68.3530166957146,1076.7039106223,368.957960956665));
#119280=CARTESIAN_POINT('Ctrl Pts',(68.347613722873,1076.7039461206,368.954454386448));
#119281=CARTESIAN_POINT('Ctrl Pts',(68.3422311949065,1076.70398087557,368.950910901442));
#119282=CARTESIAN_POINT('Ctrl Pts',(68.336869180964,1076.70401489258,368.947330395814));
#119283=CARTESIAN_POINT('Ctrl Pts',(68.3067288594723,1076.70420610496,368.927204079115));
#119284=CARTESIAN_POINT('Ctrl Pts',(68.277172490896,1076.70437365221,368.905859877632));
#119285=CARTESIAN_POINT('Ctrl Pts',(68.2484182459181,1076.70451718386,368.883424119334));
#119286=CARTESIAN_POINT('Ctrl Pts',(68.2196569893529,1076.7046607505,368.860982890183));
#119287=CARTESIAN_POINT('Ctrl Pts',(68.1916987292402,1076.70478028982,368.837449911598));
#119288=CARTESIAN_POINT('Ctrl Pts',(68.1647306760372,1076.70487545108,368.812993542314));
#119289=CARTESIAN_POINT('Ctrl Pts',(68.1467730472035,1076.70493881757,368.796708406754));
#119290=CARTESIAN_POINT('Ctrl Pts',(68.1292538177756,1076.70499137475,368.780014703662));
#119291=CARTESIAN_POINT('Ctrl Pts',(68.1122191473878,1076.70503301906,368.762971163783));
#119292=CARTESIAN_POINT('Ctrl Pts',(68.0771355036054,1076.70511878734,368.727869252899));
#119293=CARTESIAN_POINT('Ctrl Pts',(68.0437396734568,1076.70515964597,368.690914637454));
#119294=CARTESIAN_POINT('Ctrl Pts',(68.0122641653214,1076.70515559111,368.652326715777));
#119295=CARTESIAN_POINT('Ctrl Pts',(67.9808067613756,1076.70515153857,368.613760989232));
#119296=CARTESIAN_POINT('Ctrl Pts',(67.9512678913311,1076.7051026242,368.573564288066));
#119297=CARTESIAN_POINT('Ctrl Pts',(67.9238413581347,1076.70500884412,368.531990912605));
#119298=CARTESIAN_POINT('Ctrl Pts',(67.8963940645984,1076.70491499307,368.490386068442));
#119299=CARTESIAN_POINT('Ctrl Pts',(67.8710626435722,1076.70477620837,368.447402985898));
#119300=CARTESIAN_POINT('Ctrl Pts',(67.8479972570152,1076.70459248618,368.403324571658));
#119301=CARTESIAN_POINT('Ctrl Pts',(67.8275232175205,1076.70442940478,368.364198273393));
#119302=CARTESIAN_POINT('Ctrl Pts',(67.8088341266088,1076.70423091595,368.324209594824));
#119303=CARTESIAN_POINT('Ctrl Pts',(67.7920032094858,1076.70399701699,368.283569638001));
#119304=CARTESIAN_POINT('Ctrl Pts',(67.7731266905889,1076.70373469034,368.237990368177));
#119305=CARTESIAN_POINT('Ctrl Pts',(67.756482261278,1076.70342600895,368.191335359111));
#119306=CARTESIAN_POINT('Ctrl Pts',(67.7422060389957,1076.70307117226,368.143891560033));
#119307=CARTESIAN_POINT('Ctrl Pts',(67.727940201487,1076.70271659368,368.096482272405));
#119308=CARTESIAN_POINT('Ctrl Pts',(67.7160393578063,1076.70231592693,368.048285916623));
#119309=CARTESIAN_POINT('Ctrl Pts',(67.7065909166684,1076.70186937099,367.999607936253));
#119310=CARTESIAN_POINT('Ctrl Pts',(67.6971373622955,1076.70142257339,367.950903612707));
#119311=CARTESIAN_POINT('Ctrl Pts',(67.690138992944,1076.70092983692,367.901717751667));
#119312=CARTESIAN_POINT('Ctrl Pts',(67.6856321660866,1076.70039136092,367.852366547552));
#119313=CARTESIAN_POINT('Ctrl Pts',(67.6815524693982,1076.69990391845,367.807692556212));
#119314=CARTESIAN_POINT('Ctrl Pts',(67.6795137893469,1076.69937899545,367.762883532693));
#119315=CARTESIAN_POINT('Ctrl Pts',(67.6795062338911,1076.69881673977,367.71817491663));
#119316=CARTESIAN_POINT('Ctrl Pts',(67.6795000833663,1076.69835903508,367.681779832221));
#119317=CARTESIAN_POINT('Ctrl Pts',(67.6808422638254,1076.69787293693,367.6451681948));
#119318=CARTESIAN_POINT('Ctrl Pts',(67.6835548113673,1076.69736076001,367.608592020619));
#119319=CARTESIAN_POINT('Ctrl Pts',(67.6862660494103,1076.69684883035,367.57203350381));
#119320=CARTESIAN_POINT('Ctrl Pts',(67.6903463283445,1076.69631084708,367.535511006626));
#119321=CARTESIAN_POINT('Ctrl Pts',(67.6957655489489,1076.69574912154,367.499274483562));
#119322=CARTESIAN_POINT('Ctrl Pts',(67.6992897940453,1076.69538381837,367.475709030512));
#119323=CARTESIAN_POINT('Ctrl Pts',(67.7033792317309,1076.69500847411,367.452264464278));
#119324=CARTESIAN_POINT('Ctrl Pts',(67.708013947672,1076.69462372445,367.429007360041));
#119325=CARTESIAN_POINT('Ctrl Pts',(67.7168391423511,1076.69389110337,367.384722343402));
#119326=CARTESIAN_POINT('Ctrl Pts',(67.7276535011892,1076.69312395991,367.341019701624));
#119327=CARTESIAN_POINT('Ctrl Pts',(67.7404339194266,1076.69232010618,367.297892887779));
#119328=CARTESIAN_POINT('Ctrl Pts',(67.7531999187991,1076.69151715936,367.254814729595));
#119329=CARTESIAN_POINT('Ctrl Pts',(67.7679278213293,1076.69067758506,367.212310198549));
#119330=CARTESIAN_POINT('Ctrl Pts',(67.7846440120623,1076.68979920278,367.170387771191));
#119331=CARTESIAN_POINT('Ctrl Pts',(67.7870168346456,1076.68967451856,367.164436984677));
#119332=CARTESIAN_POINT('Ctrl Pts',(67.789429796553,1076.68954905239,367.15849796482));
#119333=CARTESIAN_POINT('Ctrl Pts',(67.7918830485335,1076.68942279803,367.152570776695));
#119334=CARTESIAN_POINT('Ctrl Pts',(67.8065254954997,1076.68866923799,367.117193840911));
#119335=CARTESIAN_POINT('Ctrl Pts',(67.8225977706757,1076.68788737807,367.082263123204));
#119336=CARTESIAN_POINT('Ctrl Pts',(67.8400072677222,1076.68708182782,367.048016266821));
#119337=CARTESIAN_POINT('Ctrl Pts',(67.8574319591611,1076.68627557453,367.013739520994));
#119338=CARTESIAN_POINT('Ctrl Pts',(67.8761959365134,1076.68544558954,366.980148374759));
#119339=CARTESIAN_POINT('Ctrl Pts',(67.8961598287834,1076.68459649448,366.947457281582));
#119340=CARTESIAN_POINT('Ctrl Pts',(67.9067045072196,1076.68414801309,366.930190254661));
#119341=CARTESIAN_POINT('Ctrl Pts',(67.9175831835706,1076.68369420032,366.913173875774));
#119342=CARTESIAN_POINT('Ctrl Pts',(67.9287705538774,1076.68323573722,366.896436322486));
#119343=CARTESIAN_POINT('Ctrl Pts',(67.9536480055309,1076.68221624886,366.859216881161));
#119344=CARTESIAN_POINT('Ctrl Pts',(67.9801739456007,1076.68116933278,366.823182839392));
#119345=CARTESIAN_POINT('Ctrl Pts',(68.008356743339,1076.68009372025,366.788334394561));
#119346=CARTESIAN_POINT('Ctrl Pts',(68.0362961581857,1076.67902739656,366.753786896263));
#119347=CARTESIAN_POINT('Ctrl Pts',(68.0658645682457,1076.67793286991,366.720403941188));
#119348=CARTESIAN_POINT('Ctrl Pts',(68.0971058920654,1076.67680890415,366.688222060592));
#119349=CARTESIAN_POINT('Ctrl Pts',(68.1021604648095,1076.67662705633,366.683015313994));
#119350=CARTESIAN_POINT('Ctrl Pts',(68.1072588930011,1076.67644443789,366.677840097268));
#119351=CARTESIAN_POINT('Ctrl Pts',(68.1124014336536,1076.67626104361,366.672696673514));
#119352=CARTESIAN_POINT('Ctrl Pts',(68.1616662374676,1076.67450415265,366.623423409718));
#119353=CARTESIAN_POINT('Ctrl Pts',(68.2141095020647,1076.67270591134,366.577933034726));
#119354=CARTESIAN_POINT('Ctrl Pts',(68.2693151663366,1076.67088010323,366.53641832434));
#119355=CARTESIAN_POINT('Ctrl Pts',(68.3272964798804,1076.66896249652,366.492816323145));
#119356=CARTESIAN_POINT('Ctrl Pts',(68.3883266438417,1076.66701448131,366.45359774211));
#119357=CARTESIAN_POINT('Ctrl Pts',(68.451973582526,1076.66505202649,366.41901169087));
#119358=CARTESIAN_POINT('Ctrl Pts',(68.497452943878,1076.66364974079,366.394297988144));
#119359=CARTESIAN_POINT('Ctrl Pts',(68.5442696367321,1076.66224008235,366.371950199882));
#119360=CARTESIAN_POINT('Ctrl Pts',(68.5922717248266,1076.66082887737,366.352074680276));
#119361=CARTESIAN_POINT('Ctrl Pts',(68.6339957019783,1076.65960224147,366.334798645861));
#119362=CARTESIAN_POINT('Ctrl Pts',(68.67628421805,1076.65838450843,366.319523819645));
#119363=CARTESIAN_POINT('Ctrl Pts',(68.7191235128161,1076.65717723202,366.306211633982));
#119364=CARTESIAN_POINT('Ctrl Pts',(68.7620966106071,1076.65596618483,366.29285786942));
#119365=CARTESIAN_POINT('Ctrl Pts',(68.805624828294,1076.6547656597,366.281478718402));
#119366=CARTESIAN_POINT('Ctrl Pts',(68.8497123649171,1076.65357722502,366.2720840227));
#119367=CARTESIAN_POINT('Ctrl Pts',(68.8560243419479,1076.65340707778,366.2707389917));
#119368=CARTESIAN_POINT('Ctrl Pts',(68.8623478003799,1076.65323717837,366.269434722546));
#119369=CARTESIAN_POINT('Ctrl Pts',(68.868682765832,1076.65306753139,366.268171330833));
#119370=CARTESIAN_POINT('Ctrl Pts',(68.9040718768512,1076.65211982992,366.261113627054));
#119371=CARTESIAN_POINT('Ctrl Pts',(68.9399147782392,1076.65117790773,366.255317170565));
#119372=CARTESIAN_POINT('Ctrl Pts',(68.9759683148074,1076.65024912806,366.250848411493));
#119373=CARTESIAN_POINT('Ctrl Pts',(69.0120253008042,1076.64932025953,366.246379224872));
#119374=CARTESIAN_POINT('Ctrl Pts',(69.0482923836453,1076.64840453604,366.243238093264));
#119375=CARTESIAN_POINT('Ctrl Pts',(69.0845184620344,1076.64750932295,366.241439875958));
#119376=CARTESIAN_POINT('Ctrl Pts',(69.1089934386633,1076.64690450123,366.240224968672));
#119377=CARTESIAN_POINT('Ctrl Pts',(69.1334495417676,1076.64630904166,366.239621961141));
#119378=CARTESIAN_POINT('Ctrl Pts',(69.1578093449571,1076.64572521568,366.23962196114));
#119379=CARTESIAN_POINT('Ctrl Pts',(69.1578093449571,1076.64572521568,366.23962196114));
#119380=CARTESIAN_POINT('Ctrl Pts',(69.352931273687,1076.64104877185,366.239621961138));
#119381=CARTESIAN_POINT('Ctrl Pts',(69.5461424200158,1076.63700733176,366.278250654702));
#119382=CARTESIAN_POINT('Ctrl Pts',(69.904617273348,1076.63102126722,366.427584991751));
#119383=CARTESIAN_POINT('Ctrl Pts',(70.0666751927357,1076.62911941045,366.536116840485));
#119384=CARTESIAN_POINT('Ctrl Pts',(70.3402320110238,1076.62785827307,366.809749322705));
#119385=CARTESIAN_POINT('Ctrl Pts',(70.4489338813008,1076.62851936261,366.972337429951));
#119386=CARTESIAN_POINT('Ctrl Pts',(70.5976113015266,1076.63229212897,367.330569118657));
#119387=CARTESIAN_POINT('Ctrl Pts',(70.635978789656,1076.63536880311,367.522789870244));
#119388=CARTESIAN_POINT('Ctrl Pts',(70.6362446921766,1076.64325078239,367.909901156615));
#119389=CARTESIAN_POINT('Ctrl Pts',(70.5985838608918,1076.64796333925,368.101050258007));
#119390=CARTESIAN_POINT('Ctrl Pts',(70.4518734837467,1076.65810199654,368.458266969645));
#119391=CARTESIAN_POINT('Ctrl Pts',(70.3441445489206,1076.66342525502,368.62087363203));
#119392=CARTESIAN_POINT('Ctrl Pts',(70.1402224447557,1076.67118325305,368.826787579702));
#119393=CARTESIAN_POINT('Ctrl Pts',(70.0656838951687,1076.67371436516,368.888598425619));
#119394=CARTESIAN_POINT('Ctrl Pts',(69.8595005831698,1076.67999687825,369.027960622456));
#119395=CARTESIAN_POINT('Ctrl Pts',(69.7209274126418,1076.68357129267,369.093230903822));
#119396=CARTESIAN_POINT('Ctrl Pts',(69.4394106335367,1076.68976760015,369.176008313024));
#119397=CARTESIAN_POINT('Ctrl Pts',(69.2989808746828,1076.69240957396,369.196228225527));
#119398=CARTESIAN_POINT('Ctrl Pts',(69.1578093449752,1076.6946925711,369.196228225527));
#119399=CARTESIAN_POINT('Ctrl Pts',(69.1578093449753,1078.69514019783,369.196228225527));
#119400=CARTESIAN_POINT('Ctrl Pts',(69.2026895040078,1078.69442305597,369.196228225527));
#119401=CARTESIAN_POINT('Ctrl Pts',(69.2472253980492,1078.69367481439,369.194188714804));
#119402=CARTESIAN_POINT('Ctrl Pts',(69.2914212403612,1078.69289411521,369.190177793132));
#119403=CARTESIAN_POINT('Ctrl Pts',(69.336057578074,1078.69210563488,369.186126895018));
#119404=CARTESIAN_POINT('Ctrl Pts',(69.380347982333,1078.69128404672,369.180065092482));
#119405=CARTESIAN_POINT('Ctrl Pts',(69.4243000771816,1078.69042795185,369.172009974041));
#119406=CARTESIAN_POINT('Ctrl Pts',(69.4315466965742,1078.69028680286,369.170681883134));
#119407=CARTESIAN_POINT('Ctrl Pts',(69.4387841084827,1078.69014471585,369.169299491733));
#119408=CARTESIAN_POINT('Ctrl Pts',(69.4460123282472,1078.69000168453,369.167862744092));
#119409=CARTESIAN_POINT('Ctrl Pts',(69.4841481969199,1078.68924705566,369.160282507028));
#119410=CARTESIAN_POINT('Ctrl Pts',(69.5221930517588,1078.68846212262,369.151151951091));
#119411=CARTESIAN_POINT('Ctrl Pts',(69.5598897116961,1078.68765110172,369.140497245933));
#119412=CARTESIAN_POINT('Ctrl Pts',(69.5975507316531,1078.68684084759,369.129852614174));
#119413=CARTESIAN_POINT('Ctrl Pts',(69.6348636152083,1078.68600455491,369.117686835009));
#119414=CARTESIAN_POINT('Ctrl Pts',(69.6715831858082,1078.68514642804,369.104076813431));
#119415=CARTESIAN_POINT('Ctrl Pts',(69.6891632639869,1078.68473558616,369.097560799233));
#119416=CARTESIAN_POINT('Ctrl Pts',(69.7066075675586,1078.68431973951,369.090714478063));
#119417=CARTESIAN_POINT('Ctrl Pts',(69.7238907087858,1078.6838993495,369.083550239631));
#119418=CARTESIAN_POINT('Ctrl Pts',(69.7656195477865,1078.68288434957,369.066252727092));
#119419=CARTESIAN_POINT('Ctrl Pts',(69.8063408444482,1078.68184536983,369.047136277935));
#119420=CARTESIAN_POINT('Ctrl Pts',(69.8460709945219,1078.680781756,369.026235474098));
#119421=CARTESIAN_POINT('Ctrl Pts',(69.8858984397647,1078.67971553749,369.00528348628));
#119422=CARTESIAN_POINT('Ctrl Pts',(69.9247307253615,1078.67862456408,368.982537971681));
#119423=CARTESIAN_POINT('Ctrl Pts',(69.9625622349569,1078.67750817665,368.957986759832));
#119424=CARTESIAN_POINT('Ctrl Pts',(69.9679489099638,1078.67734921878,368.954491012486));
#119425=CARTESIAN_POINT('Ctrl Pts',(69.9733152466221,1078.67718974567,368.950958585688));
#119426=CARTESIAN_POINT('Ctrl Pts',(69.9786611769871,1078.67702975542,368.947389375261));
#119427=CARTESIAN_POINT('Ctrl Pts',(70.0088029708973,1078.67612768734,368.927265206454));
#119428=CARTESIAN_POINT('Ctrl Pts',(70.0383607050039,1078.6752067494,368.905923237811));
#119429=CARTESIAN_POINT('Ctrl Pts',(70.0671162296579,1078.6742734662,368.883489823463));
#119430=CARTESIAN_POINT('Ctrl Pts',(70.0958788993767,1078.6733399511,368.861050834944));
#119431=CARTESIAN_POINT('Ctrl Pts',(70.123838479359,1078.6723940846,368.837520198105));
#119432=CARTESIAN_POINT('Ctrl Pts',(70.1508077805883,1078.67144239617,368.81306629771));
#119433=CARTESIAN_POINT('Ctrl Pts',(70.1687464501386,1078.67080937924,368.796800750647));
#119434=CARTESIAN_POINT('Ctrl Pts',(70.1862476557113,1078.67017378653,368.78012759345));
#119435=CARTESIAN_POINT('Ctrl Pts',(70.2032653927109,1078.66953753953,368.763105366256));
#119436=CARTESIAN_POINT('Ctrl Pts',(70.2383773093518,1078.66822480028,368.727984185201));
#119437=CARTESIAN_POINT('Ctrl Pts',(70.2717988799081,1078.66689541973,368.691008063464));
#119438=CARTESIAN_POINT('Ctrl Pts',(70.303297459044,1078.66555961571,368.652396671917));
#119439=CARTESIAN_POINT('Ctrl Pts',(70.3347779802083,1078.66422457749,368.61380741608));
#119440=CARTESIAN_POINT('Ctrl Pts',(70.3643372941782,1078.66288312317,368.573585218041));
#119441=CARTESIAN_POINT('Ctrl Pts',(70.3917814682312,1078.66154545297,368.531984642556));
#119442=CARTESIAN_POINT('Ctrl Pts',(70.4192463413744,1078.66020677388,368.490352690864));
#119443=CARTESIAN_POINT('Ctrl Pts',(70.4445925464701,1078.65887188463,368.447340802391));
#119444=CARTESIAN_POINT('Ctrl Pts',(70.4676697967241,1078.65755100857,368.403232139552));
#119445=CARTESIAN_POINT('Ctrl Pts',(70.4880669909355,1078.65638353129,368.364245997251));
#119446=CARTESIAN_POINT('Ctrl Pts',(70.5066921717936,1078.65522700137,368.324403695189));
#119447=CARTESIAN_POINT('Ctrl Pts',(70.5234728961012,1078.65408847797,368.283913799739));
#119448=CARTESIAN_POINT('Ctrl Pts',(70.5423509878215,1078.65280765429,368.238363205733));
#119449=CARTESIAN_POINT('Ctrl Pts',(70.5590001328656,1078.65154335145,368.191736150675));
#119450=CARTESIAN_POINT('Ctrl Pts',(70.5732838951057,1078.6503058413,368.144319216869));
#119451=CARTESIAN_POINT('Ctrl Pts',(70.5875571559638,1078.64906924097,368.09693714386));
#119452=CARTESIAN_POINT('Ctrl Pts',(70.5994682789034,1078.64785939396,368.048766927578));
#119453=CARTESIAN_POINT('Ctrl Pts',(70.608929510515,1078.64668654949,368.00011371078));
#119454=CARTESIAN_POINT('Ctrl Pts',(70.618395766857,1078.64551308214,367.951434654926));
#119455=CARTESIAN_POINT('Ctrl Pts',(70.6254094006007,1078.64437665664,367.902272693871));
#119456=CARTESIAN_POINT('Ctrl Pts',(70.6299336955014,1078.64328753856,367.852943785523));
#119457=CARTESIAN_POINT('Ctrl Pts',(70.6340334740229,1078.64230061286,367.808243428147));
#119458=CARTESIAN_POINT('Ctrl Pts',(70.6360897811352,1078.64135253334,367.763406441123));
#119459=CARTESIAN_POINT('Ctrl Pts',(70.636112290058,1078.64045093853,367.718668875577));
#119460=CARTESIAN_POINT('Ctrl Pts',(70.6361306194975,1078.63971675292,367.682238233956));
#119461=CARTESIAN_POINT('Ctrl Pts',(70.6347980636925,1078.63900781863,367.64558925659));
#119462=CARTESIAN_POINT('Ctrl Pts',(70.6320921581352,1078.63832976351,367.608974014984));
#119463=CARTESIAN_POINT('Ctrl Pts',(70.6293876811409,1078.63765206636,367.572378104124));
#119464=CARTESIAN_POINT('Ctrl Pts',(70.625311306697,1078.63700521579,367.535816484357));
#119465=CARTESIAN_POINT('Ctrl Pts',(70.6198927054709,1078.63639483075,367.499539201815));
#119466=CARTESIAN_POINT('Ctrl Pts',(70.6163845710028,1078.6359996526,367.476052405134));
#119467=CARTESIAN_POINT('Ctrl Pts',(70.6123149010517,1078.63561975927,367.452684733468));
#119468=CARTESIAN_POINT('Ctrl Pts',(70.6077032114111,1078.63525667561,367.429501920333));
#119469=CARTESIAN_POINT('Ctrl Pts',(70.5988938480721,1078.63456310423,367.385217538674));
#119470=CARTESIAN_POINT('Ctrl Pts',(70.588095576243,1078.63392774252,367.341515392521));
#119471=CARTESIAN_POINT('Ctrl Pts',(70.5753316548135,1078.63335222651,367.298388859185));
#119472=CARTESIAN_POINT('Ctrl Pts',(70.5625816171825,1078.63277733651,367.255309236206));
#119473=CARTESIAN_POINT('Ctrl Pts',(70.5478699270497,1078.63226216208,367.21280307215));
#119474=CARTESIAN_POINT('Ctrl Pts',(70.5311703381008,1078.63180833392,367.170878721247));
#119475=CARTESIAN_POINT('Ctrl Pts',(70.5287932953106,1078.63174373539,367.164911150646));
#119476=CARTESIAN_POINT('Ctrl Pts',(70.5263758980182,1078.63168037979,367.158955406119));
#119477=CARTESIAN_POINT('Ctrl Pts',(70.5239179945542,1078.63161827185,367.153011552871));
#119478=CARTESIAN_POINT('Ctrl Pts',(70.5093450285995,1078.6312500324,367.117770310779));
#119479=CARTESIAN_POINT('Ctrl Pts',(70.4933514000306,1078.63092718475,367.082966502713));
#119480=CARTESIAN_POINT('Ctrl Pts',(70.4760287367767,1078.63065157815,367.048837815222));
#119481=CARTESIAN_POINT('Ctrl Pts',(70.4586916236253,1078.63037574165,367.014680658896));
#119482=CARTESIAN_POINT('Ctrl Pts',(70.4400235261928,1078.63014722503,366.981200293855));
#119483=CARTESIAN_POINT('Ctrl Pts',(70.420162889289,1078.62996788219,366.948611321319));
#119484=CARTESIAN_POINT('Ctrl Pts',(70.4094681278935,1078.6298713078,366.931062473964));
#119485=CARTESIAN_POINT('Ctrl Pts',(70.3984283410797,1078.62978899241,366.913771648191));
#119486=CARTESIAN_POINT('Ctrl Pts',(70.3870702416581,1078.62972122551,366.896768714476));
#119487=CARTESIAN_POINT('Ctrl Pts',(70.3622003491434,1078.62957284193,366.859538794378));
#119488=CARTESIAN_POINT('Ctrl Pts',(70.3356819388416,1078.62949150588,366.823495001307));
#119489=CARTESIAN_POINT('Ctrl Pts',(70.3075069097702,1078.62947843671,366.78863737677));
#119490=CARTESIAN_POINT('Ctrl Pts',(70.2795732684654,1078.62946547951,366.754078392709));
#119491=CARTESIAN_POINT('Ctrl Pts',(70.2500106423273,1078.62951962446,366.72068467377));
#119492=CARTESIAN_POINT('Ctrl Pts',(70.2187753212431,1078.62964205983,366.688492556518));
#119493=CARTESIAN_POINT('Ctrl Pts',(70.2137096637967,1078.62966191606,366.683271728532));
#119494=CARTESIAN_POINT('Ctrl Pts',(70.20859994706,1078.62968356842,366.678082594804));
#119495=CARTESIAN_POINT('Ctrl Pts',(70.2034459129137,1078.62970702199,366.672925419438));
#119496=CARTESIAN_POINT('Ctrl Pts',(70.153642759543,1078.62993365258,366.62309191263));
#119497=CARTESIAN_POINT('Ctrl Pts',(70.1005834878078,1078.63032599499,366.577120035045));
#119498=CARTESIAN_POINT('Ctrl Pts',(70.0446997169128,1078.63087440028,366.535213962577));
#119499=CARTESIAN_POINT('Ctrl Pts',(69.9858388820021,1078.63145202045,366.491075451989));
#119500=CARTESIAN_POINT('Ctrl Pts',(69.9238428387631,1078.63220277408,366.451445317227));
#119501=CARTESIAN_POINT('Ctrl Pts',(69.8591657617108,1078.63311538654,366.41658757856));
#119502=CARTESIAN_POINT('Ctrl Pts',(69.8151253679448,1078.63373680937,366.392851989282));
#119503=CARTESIAN_POINT('Ctrl Pts',(69.7698407589187,1078.63443328001,366.371329815705));
#119504=CARTESIAN_POINT('Ctrl Pts',(69.7234507243797,1078.63520123882,366.352117646964));
#119505=CARTESIAN_POINT('Ctrl Pts',(69.6817292201314,1078.63589191295,366.334838923469));
#119506=CARTESIAN_POINT('Ctrl Pts',(69.6394448286438,1078.63663436471,366.319561988434));
#119507=CARTESIAN_POINT('Ctrl Pts',(69.5966115042897,1078.63742637666,366.306247787561));
#119508=CARTESIAN_POINT('Ctrl Pts',(69.5536388323326,1078.63822096521,366.292890272236));
#119509=CARTESIAN_POINT('Ctrl Pts',(69.5101127552433,1078.63906543694,366.281507975003));
#119510=CARTESIAN_POINT('Ctrl Pts',(69.4660291753488,1078.63995755266,366.27211020656));
#119511=CARTESIAN_POINT('Ctrl Pts',(69.4596877970459,1078.6400858826,366.270758347091));
#119512=CARTESIAN_POINT('Ctrl Pts',(69.4533348654621,1078.64021519842,366.269447638946));
#119513=CARTESIAN_POINT('Ctrl Pts',(69.4469703547381,1078.64034549345,366.268178197808));
#119514=CARTESIAN_POINT('Ctrl Pts',(69.4115753791297,1078.64107010364,366.261118450401));
#119515=CARTESIAN_POINT('Ctrl Pts',(69.3757272816245,1078.64182781151,366.255320538375));
#119516=CARTESIAN_POINT('Ctrl Pts',(69.3396692499277,1078.64261197157,366.250850751106));
#119517=CARTESIAN_POINT('Ctrl Pts',(69.3036070482776,1078.64339622231,366.246380446926));
#119518=CARTESIAN_POINT('Ctrl Pts',(69.2673354426477,1078.64420693137,366.24323867791));
#119519=CARTESIAN_POINT('Ctrl Pts',(69.23110555833,1078.64503745094,366.241440140562));
#119520=CARTESIAN_POINT('Ctrl Pts',(69.2066284800311,1078.64559855383,366.240225040368));
#119521=CARTESIAN_POINT('Ctrl Pts',(69.1821706012387,1078.64616869906,366.239621961141));
#119522=CARTESIAN_POINT('Ctrl Pts',(69.1578093449994,1078.64674583663,366.23962196114));
#119523=CARTESIAN_POINT('Origin',(69.1578093449752,1067.7251047501,367.717925093334));
#119524=CARTESIAN_POINT('',(69.1578093449752,1076.68648464657,368.596228225527));
#119525=CARTESIAN_POINT('',(69.1578093460768,1076.65741108276,366.83962196114));
#119526=CARTESIAN_POINT('Ctrl Pts',(69.1578093449752,1076.68648464657,368.596228225527));
#119527=CARTESIAN_POINT('Ctrl Pts',(69.1033913216514,1076.68745213356,368.596228225527));
#119528=CARTESIAN_POINT('Ctrl Pts',(69.0489568302921,1076.68833127394,368.591170819637));
#119529=CARTESIAN_POINT('Ctrl Pts',(68.8806783358555,1076.690788854,368.559470806678));
#119530=CARTESIAN_POINT('Ctrl Pts',(68.7715682797969,1076.69200219795,368.515308799181));
#119531=CARTESIAN_POINT('Ctrl Pts',(68.5767947391705,1076.69347843089,368.386857203596));
#119532=CARTESIAN_POINT('Ctrl Pts',(68.4931144571871,1076.69372679574,368.303782852469));
#119533=CARTESIAN_POINT('Ctrl Pts',(68.3631859945438,1076.6932401161,368.109848421111));
#119534=CARTESIAN_POINT('Ctrl Pts',(68.3182074810282,1076.692509962,368.000940182514));
#119535=CARTESIAN_POINT('Ctrl Pts',(68.2734740550392,1076.69009005642,367.772113640544));
#119536=CARTESIAN_POINT('Ctrl Pts',(68.2740910388,1076.68842327646,367.654486218947));
#119537=CARTESIAN_POINT('Ctrl Pts',(68.3212194444405,1076.68423805352,367.426110114958));
#119538=CARTESIAN_POINT('Ctrl Pts',(68.3673558816376,1076.68175664377,367.317651689982));
#119539=CARTESIAN_POINT('Ctrl Pts',(68.4656778165328,1076.67762249391,367.174193405861));
#119540=CARTESIAN_POINT('Ctrl Pts',(68.5025586164138,1076.67620237088,367.130271796045));
#119541=CARTESIAN_POINT('Ctrl Pts',(68.5848923080706,1076.67325751785,367.049684240538));
#119542=CARTESIAN_POINT('Ctrl Pts',(68.6302535863163,1076.67173882008,367.013322693962));
#119543=CARTESIAN_POINT('Ctrl Pts',(68.7754303711597,1076.66716266438,366.918879626459));
#119544=CARTESIAN_POINT('Ctrl Pts',(68.8834192681614,1076.66410705643,366.875667143876));
#119545=CARTESIAN_POINT('Ctrl Pts',(69.0499335363381,1076.65990656262,366.844589377721));
#119546=CARTESIAN_POINT('Ctrl Pts',(69.1038777531703,1076.65861970931,366.839621961005));
#119547=CARTESIAN_POINT('Ctrl Pts',(69.1578093471783,1076.65741108276,366.839621961141));
#119548=CARTESIAN_POINT('',(69.1578093449752,1082.7251047501,366.83962196114));
#119549=CARTESIAN_POINT('',(69.1578093449752,1067.7251047501,366.83962196114));
#119550=CARTESIAN_POINT('Origin',(69.1578093449752,1082.7251047501,367.717925093334));
#119551=CARTESIAN_POINT('Ctrl Pts',(69.1578093471783,1076.65741108276,366.839621961141));
#119552=CARTESIAN_POINT('Ctrl Pts',(69.2185893566547,1076.65604898073,366.839621961293));
#119553=CARTESIAN_POINT('Ctrl Pts',(69.2793533349976,1076.65478627884,366.845931115126));
#119554=CARTESIAN_POINT('Ctrl Pts',(69.4518434428587,1076.65151826913,366.882320930328));
#119555=CARTESIAN_POINT('Ctrl Pts',(69.5588086901154,1076.64989055328,366.928055881927));
#119556=CARTESIAN_POINT('Ctrl Pts',(69.7488354249485,1076.64793522068,367.058121529201));
#119557=CARTESIAN_POINT('Ctrl Pts',(69.8300894466683,1076.64762590062,367.141129793432));
#119558=CARTESIAN_POINT('Ctrl Pts',(69.9558650303434,1076.64839705208,367.333586542729));
#119559=CARTESIAN_POINT('Ctrl Pts',(69.9992304916355,1076.64946717695,367.441127444555));
#119560=CARTESIAN_POINT('Ctrl Pts',(70.0300594458653,1076.65185531037,367.603360484574));
#119561=CARTESIAN_POINT('Ctrl Pts',(70.0351869866777,1076.65269087043,367.653477995551));
#119562=CARTESIAN_POINT('Ctrl Pts',(70.0359981836434,1076.65362084856,367.703756266315));
#119563=CARTESIAN_POINT('Ctrl Pts',(70.0378500058754,1076.65574382761,367.818532853905));
#119564=CARTESIAN_POINT('Ctrl Pts',(70.0171825981728,1076.6583288395,367.932558929511));
#119565=CARTESIAN_POINT('Ctrl Pts',(69.9331307082613,1076.66401532473,368.146283551002));
#119566=CARTESIAN_POINT('Ctrl Pts',(69.8705162180584,1076.667060243,368.243911836661));
#119567=CARTESIAN_POINT('Ctrl Pts',(69.7510970754531,1076.67161375661,368.36809574681));
#119568=CARTESIAN_POINT('Ctrl Pts',(69.7073423318817,1076.67311852531,368.405475708202));
#119569=CARTESIAN_POINT('Ctrl Pts',(69.5642433266447,1076.67758605903,368.505281356192));
#119570=CARTESIAN_POINT('Ctrl Pts',(69.4558031000024,1076.68039187618,368.552383553611));
#119571=CARTESIAN_POINT('Ctrl Pts',(69.280854745882,1076.68418363178,368.589761703587));
#119572=CARTESIAN_POINT('Ctrl Pts',(69.2193425741478,1076.68539065977,368.596228225527));
#119573=CARTESIAN_POINT('Ctrl Pts',(69.1578093449752,1076.68648464657,368.596228225527));
#119574=CARTESIAN_POINT('Origin',(81.0356882485065,1067.7251047501,371.795432834555));
#119575=CARTESIAN_POINT('',(81.0356882485327,1078.30327084026,370.519988713418));
#119576=CARTESIAN_POINT('Ctrl Pts',(81.0358308103573,1078.39242989444,373.070876947723));
#119577=CARTESIAN_POINT('Ctrl Pts',(81.1884057339834,1078.38464480654,373.070859893771));
#119578=CARTESIAN_POINT('Ctrl Pts',(81.3397012484411,1078.37589925079,373.043466129561));
#119579=CARTESIAN_POINT('Ctrl Pts',(81.6362004968986,1078.35649977253,372.932561804349));
#119580=CARTESIAN_POINT('Ctrl Pts',(81.7773347281252,1078.34592815118,372.84597014097));
#119581=CARTESIAN_POINT('Ctrl Pts',(82.0221333562771,1078.32463994517,372.621261163093));
#119582=CARTESIAN_POINT('Ctrl Pts',(82.1223789098522,1078.31413379904,372.484049947285));
#119583=CARTESIAN_POINT('Ctrl Pts',(82.2604701861183,1078.29547983935,372.18579151591));
#119584=CARTESIAN_POINT('Ctrl Pts',(82.2998253150436,1078.28741255873,372.028814535696));
#119585=CARTESIAN_POINT('Ctrl Pts',(82.3180263290313,1078.27452947834,371.712080372361));
#119586=CARTESIAN_POINT('Ctrl Pts',(82.2980863433854,1078.26975656345,371.555181212364));
#119587=CARTESIAN_POINT('Ctrl Pts',(82.230290382327,1078.26569525718,371.343864336666));
#119588=CARTESIAN_POINT('Ctrl Pts',(82.2057103902217,1078.26483747344,371.283536647818));
#119589=CARTESIAN_POINT('Ctrl Pts',(82.1637902669127,1078.26409447237,371.199639910996));
#119590=CARTESIAN_POINT('Ctrl Pts',(82.1500816406033,1078.26393383565,371.174376650431));
#119591=CARTESIAN_POINT('Ctrl Pts',(82.1253259030924,1078.26377515,371.132218174737));
#119592=CARTESIAN_POINT('Ctrl Pts',(82.1147099969581,1078.26374289513,371.11508294322));
#119593=CARTESIAN_POINT('Ctrl Pts',(82.092485921406,1078.26374479798,371.081040332632));
#119594=CARTESIAN_POINT('Ctrl Pts',(82.0808671468127,1078.26378010454,371.064146957027));
#119595=CARTESIAN_POINT('Ctrl Pts',(82.0515881305638,1078.26394965979,371.023700129456));
#119596=CARTESIAN_POINT('Ctrl Pts',(82.0335101567194,1078.26412026554,371.000464073211));
#119597=CARTESIAN_POINT('Ctrl Pts',(81.9677303517599,1078.26496011535,370.921698343161));
#119598=CARTESIAN_POINT('Ctrl Pts',(81.916071287035,1078.26599219976,370.869669134888));
#119599=CARTESIAN_POINT('Ctrl Pts',(81.7305123881603,1078.27081199972,370.712431814371));
#119600=CARTESIAN_POINT('Ctrl Pts',(81.5801518157617,1078.2763930109,370.629589776234));
#119601=CARTESIAN_POINT('Ctrl Pts',(81.2836407110295,1078.28987780946,370.536414934771));
#119602=CARTESIAN_POINT('Ctrl Pts',(81.1432081065826,1078.29712579653,370.516753914293));
#119603=CARTESIAN_POINT('Ctrl Pts',(80.8499294205669,1078.31384887624,370.524396367248));
#119604=CARTESIAN_POINT('Ctrl Pts',(80.6993718381563,1078.32332341751,370.555709947107));
#119605=CARTESIAN_POINT('Ctrl Pts',(80.4061269803256,1078.34352829353,370.674173509885));
#119606=CARTESIAN_POINT('Ctrl Pts',(80.2675152898507,1078.35411256255,370.764177743707));
#119607=CARTESIAN_POINT('Ctrl Pts',(80.0287193674031,1078.3746344643,370.994770384816));
#119608=CARTESIAN_POINT('Ctrl Pts',(79.9319894839163,1078.38434908772,371.134426379589));
#119609=CARTESIAN_POINT('Ctrl Pts',(79.8016793128289,1078.40100311338,371.435544837902));
#119610=CARTESIAN_POINT('Ctrl Pts',(79.7663144653885,1078.40791454577,371.592892921503));
#119611=CARTESIAN_POINT('Ctrl Pts',(79.7555594008279,1078.41884473075,371.9138956309));
#119612=CARTESIAN_POINT('Ctrl Pts',(79.7807739763514,1078.42274345753,372.074677947513));
#119613=CARTESIAN_POINT('Ctrl Pts',(79.8544181503619,1078.42567992686,372.279743248795));
#119614=CARTESIAN_POINT('Ctrl Pts',(79.8770507726827,1078.426226461,372.331637364107));
#119615=CARTESIAN_POINT('Ctrl Pts',(79.9149836863006,1078.42670601796,372.40490167505));
#119616=CARTESIAN_POINT('Ctrl Pts',(79.9276143978122,1078.42681086608,372.427574705602));
#119617=CARTESIAN_POINT('Ctrl Pts',(79.9510629483887,1078.42691439707,372.466801468702));
#119618=CARTESIAN_POINT('Ctrl Pts',(79.9615904440653,1078.42693243513,372.483518435096));
#119619=CARTESIAN_POINT('Ctrl Pts',(79.9840364482984,1078.42691457718,372.517390040069));
#119620=CARTESIAN_POINT('Ctrl Pts',(79.9959966323434,1078.42687554582,372.534509998901));
#119621=CARTESIAN_POINT('Ctrl Pts',(80.0272844313338,1078.4267014353,372.577032364982));
#119622=CARTESIAN_POINT('Ctrl Pts',(80.0471550020037,1078.42652657543,372.602017026243));
#119623=CARTESIAN_POINT('Ctrl Pts',(80.1267268383092,1078.42559156516,372.694705612336));
#119624=CARTESIAN_POINT('Ctrl Pts',(80.1926097137023,1078.42434897808,372.756743560868));
#119625=CARTESIAN_POINT('Ctrl Pts',(80.3621654348938,1078.42014608295,372.885463580501));
#119626=CARTESIAN_POINT('Ctrl Pts',(80.4700191567871,1078.41675140564,372.945131146269));
#119627=CARTESIAN_POINT('Ctrl Pts',(80.7289068154651,1078.40704746284,373.042994997205));
#119628=CARTESIAN_POINT('Ctrl Pts',(80.8817622928742,1078.4002911925,373.070894168621));
#119629=CARTESIAN_POINT('Ctrl Pts',(81.0358308103573,1078.39242989444,373.070876947723));
#119630=CARTESIAN_POINT('',(81.0356882484902,1076.29851503552,370.519988713418));
#119631=CARTESIAN_POINT('',(81.0356882485065,1067.7251047501,370.519988713418));
#119632=CARTESIAN_POINT('Ctrl Pts',(81.0350565731442,1076.38864406689,373.070876799269));
#119633=CARTESIAN_POINT('Ctrl Pts',(80.8664862906615,1076.39733226541,373.070793313285));
#119634=CARTESIAN_POINT('Ctrl Pts',(80.6995315644439,1076.40467581067,373.037291772264));
#119635=CARTESIAN_POINT('Ctrl Pts',(80.3878190702641,1076.41605389929,372.907023308189));
#119636=CARTESIAN_POINT('Ctrl Pts',(80.2462379881508,1076.41997082751,372.811387209307));
#119637=CARTESIAN_POINT('Ctrl Pts',(80.0083555405032,1076.42395235266,372.570101428271));
#119638=CARTESIAN_POINT('Ctrl Pts',(79.9145584601887,1076.42397030439,372.426774287735));
#119639=CARTESIAN_POINT('Ctrl Pts',(79.7886672873119,1076.42005915076,372.112191055772));
#119640=CARTESIAN_POINT('Ctrl Pts',(79.7577013174188,1076.41617589414,371.944158949024));
#119641=CARTESIAN_POINT('Ctrl Pts',(79.7631060572532,1076.40485953809,371.606355933519));
#119642=CARTESIAN_POINT('Ctrl Pts',(79.7992394641575,1076.39754357679,371.439949186657));
#119643=CARTESIAN_POINT('Ctrl Pts',(79.9342772081048,1076.38018301084,371.130405535808));
#119644=CARTESIAN_POINT('Ctrl Pts',(80.0320561229994,1076.37029650381,370.990413983824));
#119645=CARTESIAN_POINT('Ctrl Pts',(80.2142332201473,1076.35452936383,370.816218435966));
#119646=CARTESIAN_POINT('Ctrl Pts',(80.2796872431149,1076.34920883116,370.764845732684));
#119647=CARTESIAN_POINT('Ctrl Pts',(80.4923704658847,1076.33287422385,370.629148188538));
#119648=CARTESIAN_POINT('Ctrl Pts',(80.6518029340403,1076.32184527168,370.5674030045));
#119649=CARTESIAN_POINT('Ctrl Pts',(80.9837668752778,1076.30114301383,370.510077213482));
#119650=CARTESIAN_POINT('Ctrl Pts',(81.1529565440444,1076.29165948219,370.514369669047));
#119651=CARTESIAN_POINT('Ctrl Pts',(81.479741220954,1076.27562556121,370.588133207905));
#119652=CARTESIAN_POINT('Ctrl Pts',(81.6341893472203,1076.26922910276,370.656751372915));
#119653=CARTESIAN_POINT('Ctrl Pts',(81.9073817641115,1076.26059966692,370.849513871025));
#119654=CARTESIAN_POINT('Ctrl Pts',(82.0235678754709,1076.25844036517,370.971585818619));
#119655=CARTESIAN_POINT('Ctrl Pts',(82.2021010434889,1076.25873859831,371.253243552757));
#119656=CARTESIAN_POINT('Ctrl Pts',(82.2628343095997,1076.26118130393,371.409971277465));
#119657=CARTESIAN_POINT('Ctrl Pts',(82.3206615205412,1076.27029388232,371.737851187403));
#119658=CARTESIAN_POINT('Ctrl Pts',(82.3171892246466,1076.27687221552,371.905812334753));
#119659=CARTESIAN_POINT('Ctrl Pts',(82.2459237164212,1076.29315510069,372.231203944968));
#119660=CARTESIAN_POINT('Ctrl Pts',(82.1786575957118,1076.30270616538,372.385474573604));
#119661=CARTESIAN_POINT('Ctrl Pts',(81.9884413495885,1076.32335627142,372.659687639345));
#119662=CARTESIAN_POINT('Ctrl Pts',(81.8671613616621,1076.33425872348,372.776920528879));
#119663=CARTESIAN_POINT('Ctrl Pts',(81.5841304790166,1076.35603408549,372.959375490447));
#119664=CARTESIAN_POINT('Ctrl Pts',(81.4245552059327,1076.36668916406,373.021955669117));
#119665=CARTESIAN_POINT('Ctrl Pts',(81.1839937467045,1076.3807211026,373.064415325453));
#119666=CARTESIAN_POINT('Ctrl Pts',(81.1096012482494,1076.38480199623,373.070913718206));
#119667=CARTESIAN_POINT('Ctrl Pts',(81.0350565731442,1076.38864406688,373.070876799269));
#119668=CARTESIAN_POINT('Origin',(81.0356882485065,1067.7251047501,371.795432834555));
#119669=CARTESIAN_POINT('',(81.0356882485065,1076.36858155369,372.470876955691));
#119670=CARTESIAN_POINT('',(81.0356882485072,1076.32087957987,371.119988713418));
#119671=CARTESIAN_POINT('Ctrl Pts',(81.0356882485065,1076.36858155369,372.470876955691));
#119672=CARTESIAN_POINT('Ctrl Pts',(80.9466770371988,1076.37328023044,372.470876955691));
#119673=CARTESIAN_POINT('Ctrl Pts',(80.858496420118,1076.37729165449,372.453281738094));
#119674=CARTESIAN_POINT('Ctrl Pts',(80.6931986193752,1076.38356420663,372.384512535967));
#119675=CARTESIAN_POINT('Ctrl Pts',(80.6178670477176,1076.38574621753,372.333715093343));
#119676=CARTESIAN_POINT('Ctrl Pts',(80.4914463209232,1076.38795918467,372.205482579773));
#119677=CARTESIAN_POINT('Ctrl Pts',(80.441669457937,1076.38796586462,372.129321688419));
#119678=CARTESIAN_POINT('Ctrl Pts',(80.3749629387847,1076.38577894784,371.962060009786));
#119679=CARTESIAN_POINT('Ctrl Pts',(80.3586739916778,1076.3836093465,371.872672515698));
#119680=CARTESIAN_POINT('Ctrl Pts',(80.3620505018149,1076.37733324501,371.692930128103));
#119681=CARTESIAN_POINT('Ctrl Pts',(80.3816374802864,1076.37329081345,371.604382799259));
#119682=CARTESIAN_POINT('Ctrl Pts',(80.4543124070447,1076.36379836162,371.440021372384));
#119683=CARTESIAN_POINT('Ctrl Pts',(80.5067431586288,1076.35843882412,371.365871375587));
#119684=CARTESIAN_POINT('Ctrl Pts',(80.6041627856006,1076.34998549194,371.273943714408));
#119685=CARTESIAN_POINT('Ctrl Pts',(80.6390795219818,1076.34715044972,371.246920070266));
#119686=CARTESIAN_POINT('Ctrl Pts',(80.75227468855,1076.33850025317,371.175807294144));
#119687=CARTESIAN_POINT('Ctrl Pts',(80.8369215519361,1076.33272090615,371.143700506065));
#119688=CARTESIAN_POINT('Ctrl Pts',(80.9618312322459,1076.32508481194,371.123022719963));
#119689=CARTESIAN_POINT('Ctrl Pts',(80.9987260469959,1076.32293230681,371.119988713418));
#119690=CARTESIAN_POINT('Ctrl Pts',(81.0356882485079,1076.32087957987,371.119988713418));
#119691=CARTESIAN_POINT('',(81.0356882485065,1082.7251047501,371.119988713418));
#119692=CARTESIAN_POINT('',(81.0356882485065,1067.7251047501,371.119988713418));
#119693=CARTESIAN_POINT('Origin',(81.0356882485065,1082.7251047501,371.795432834555));
#119694=CARTESIAN_POINT('Ctrl Pts',(81.0356882485079,1076.32087957987,371.119988713418));
#119695=CARTESIAN_POINT('Ctrl Pts',(81.0357054443659,1076.32087862488,371.119988713418));
#119696=CARTESIAN_POINT('Ctrl Pts',(81.0357226402371,1076.32087766989,371.119988713433));
#119697=CARTESIAN_POINT('Ctrl Pts',(81.0357398361243,1076.32087671495,371.119988714746));
#119698=CARTESIAN_POINT('Ctrl Pts',(81.1243435443242,1076.31595626447,371.119995482045));
#119699=CARTESIAN_POINT('Ctrl Pts',(81.2121212293695,1076.31167662248,371.1374365346));
#119700=CARTESIAN_POINT('Ctrl Pts',(81.3757717600072,1076.30495878294,371.20518644674));
#119701=CARTESIAN_POINT('Ctrl Pts',(81.4500812808145,1076.30258252459,371.254752409407));
#119702=CARTESIAN_POINT('Ctrl Pts',(81.5752349561495,1076.30010567544,371.379610221861));
#119703=CARTESIAN_POINT('Ctrl Pts',(81.624909378144,1076.30002439202,371.453617243076));
#119704=CARTESIAN_POINT('Ctrl Pts',(81.6929459822121,1076.30218324274,371.616489854028));
#119705=CARTESIAN_POINT('Ctrl Pts',(81.7106653117081,1076.30440012159,371.703751217166));
#119706=CARTESIAN_POINT('Ctrl Pts',(81.711581903132,1076.31082095477,371.880232247626));
#119707=CARTESIAN_POINT('Ctrl Pts',(81.6947185259169,1076.31496437524,371.967740683178));
#119708=CARTESIAN_POINT('Ctrl Pts',(81.6282500105839,1076.32459376466,372.131471779847));
#119709=CARTESIAN_POINT('Ctrl Pts',(81.5791991967838,1076.32998936313,372.206089947184));
#119710=CARTESIAN_POINT('Ctrl Pts',(81.4861691653524,1076.33845164833,372.300653578167));
#119711=CARTESIAN_POINT('Ctrl Pts',(81.4521293101644,1076.34131459263,372.329059735823));
#119712=CARTESIAN_POINT('Ctrl Pts',(81.3790581437592,1076.34703343511,372.378759987772));
#119713=CARTESIAN_POINT('Ctrl Pts',(81.3402091740787,1076.3498758091,372.39994986762));
#119714=CARTESIAN_POINT('Ctrl Pts',(81.2168163045953,1076.35834006927,372.452318629312));
#119715=CARTESIAN_POINT('Ctrl Pts',(81.1278547392712,1076.36370538279,372.470577877855));
#119716=CARTESIAN_POINT('Ctrl Pts',(81.0371671841974,1076.36850344002,372.470875741445));
#119717=CARTESIAN_POINT('Ctrl Pts',(81.0364276876917,1076.36854252056,372.470876955691));
#119718=CARTESIAN_POINT('Ctrl Pts',(81.0356882485065,1076.36858155369,372.470876955691));
#119719=CARTESIAN_POINT('Origin',(93.672037736222,1067.7251047501,377.464729830671));
#119720=CARTESIAN_POINT('',(93.6720377362532,1077.61442735557,376.365898694678));
#119721=CARTESIAN_POINT('Ctrl Pts',(93.6722192570493,1077.71636978598,378.563560951671));
#119722=CARTESIAN_POINT('Ctrl Pts',(93.8069726126999,1077.70416449936,378.563538691161));
#119723=CARTESIAN_POINT('Ctrl Pts',(93.940501286018,1077.69085765877,378.538730121288));
#119724=CARTESIAN_POINT('Ctrl Pts',(94.2016485877809,1077.66224246217,378.43838866533));
#119725=CARTESIAN_POINT('Ctrl Pts',(94.3255105403184,1077.64712923762,378.359985369633));
#119726=CARTESIAN_POINT('Ctrl Pts',(94.5347285823885,1077.61827030834,378.160376146465));
#119727=CARTESIAN_POINT('Ctrl Pts',(94.6184400607495,1077.60478587765,378.04139872997));
#119728=CARTESIAN_POINT('Ctrl Pts',(94.7296608502277,1077.58235612848,377.790162862338));
#119729=CARTESIAN_POINT('Ctrl Pts',(94.7608616898128,1077.5732810015,377.66220907866));
#119730=CARTESIAN_POINT('Ctrl Pts',(94.7768578192544,1077.55920490251,377.400090184243));
#119731=CARTESIAN_POINT('Ctrl Pts',(94.761151718272,1077.5543550064,377.268059088689));
#119732=CARTESIAN_POINT('Ctrl Pts',(94.7132900568707,1077.55143784041,377.112337778839));
#119733=CARTESIAN_POINT('Ctrl Pts',(94.7029581550161,1077.55102180196,377.08316740982));
#119734=CARTESIAN_POINT('Ctrl Pts',(94.6839831446964,1077.55056687306,377.03602026585));
#119735=CARTESIAN_POINT('Ctrl Pts',(94.6760580635762,1077.55044644325,377.017775007529));
#119736=CARTESIAN_POINT('Ctrl Pts',(94.6609820194468,1077.5503341694,376.985494206524));
#119737=CARTESIAN_POINT('Ctrl Pts',(94.6540163884814,1077.55032075154,376.971378526587));
#119738=CARTESIAN_POINT('Ctrl Pts',(94.638659320679,1077.5503688821,376.941872610019));
#119739=CARTESIAN_POINT('Ctrl Pts',(94.6301980774744,1077.55043909865,376.9265238189));
#119740=CARTESIAN_POINT('Ctrl Pts',(94.6069027087987,1077.5507426925,376.886557620365));
#119741=CARTESIAN_POINT('Ctrl Pts',(94.591464265452,1077.55105160028,376.862309430856));
#119742=CARTESIAN_POINT('Ctrl Pts',(94.5201593218287,1077.55291754057,376.759451893077));
#119743=CARTESIAN_POINT('Ctrl Pts',(94.4550541510353,1077.55569270544,376.687813708108));
#119744=CARTESIAN_POINT('Ctrl Pts',(94.2985320845842,1077.56426327506,376.555481884181));
#119745=CARTESIAN_POINT('Ctrl Pts',(94.2057097935229,1077.57034920252,376.498092424018));
#119746=CARTESIAN_POINT('Ctrl Pts',(93.9942661857174,1077.58605697478,376.407181231617));
#119747=CARTESIAN_POINT('Ctrl Pts',(93.875350856341,1077.59590936187,376.378058458468));
#119748=CARTESIAN_POINT('Ctrl Pts',(93.6225289033882,1077.61876654283,376.35910222023));
#119749=CARTESIAN_POINT('Ctrl Pts',(93.4902316494238,1077.63178686478,376.373046808699));
#119750=CARTESIAN_POINT('Ctrl Pts',(93.2274118087518,1077.65976644178,376.449898376105));
#119751=CARTESIAN_POINT('Ctrl Pts',(93.1001687450403,1077.67454334546,376.515757354355));
#119752=CARTESIAN_POINT('Ctrl Pts',(92.875384414685,1077.70331172652,376.694145559379));
#119753=CARTESIAN_POINT('Ctrl Pts',(92.7806737081482,1077.71700711364,376.80595132329));
#119754=CARTESIAN_POINT('Ctrl Pts',(92.6442788952363,1077.74049955449,377.052639481322));
#119755=CARTESIAN_POINT('Ctrl Pts',(92.6009804713983,1077.75027787408,377.183641342492));
#119756=CARTESIAN_POINT('Ctrl Pts',(92.5645515134517,1077.76578290103,377.456560579428));
#119757=CARTESIAN_POINT('Ctrl Pts',(92.5723172959504,1077.77132429832,377.596096035243));
#119758=CARTESIAN_POINT('Ctrl Pts',(92.617145577569,1077.77537339781,377.775874390503));
#119759=CARTESIAN_POINT('Ctrl Pts',(92.631313516235,1077.77610400737,377.820401539368));
#119760=CARTESIAN_POINT('Ctrl Pts',(92.6552155756255,1077.77672037922,377.881704528439));
#119761=CARTESIAN_POINT('Ctrl Pts',(92.6626225706082,1077.77685015094,377.899328791607));
#119762=CARTESIAN_POINT('Ctrl Pts',(92.6770338023038,1077.77699746021,377.931260024202));
#119763=CARTESIAN_POINT('Ctrl Pts',(92.683896484605,1077.77703011922,377.94562495789));
#119764=CARTESIAN_POINT('Ctrl Pts',(92.6983841906382,1077.77702681335,377.974329900841));
#119765=CARTESIAN_POINT('Ctrl Pts',(92.7060198356745,1077.77698946814,377.988660046438));
#119766=CARTESIAN_POINT('Ctrl Pts',(92.7254306868201,1077.77681124326,378.023221273012));
#119767=CARTESIAN_POINT('Ctrl Pts',(92.7375399568977,1077.77663198026,378.043255067068));
#119768=CARTESIAN_POINT('Ctrl Pts',(92.7822988664053,1077.7757428724,378.112228474618));
#119769=CARTESIAN_POINT('Ctrl Pts',(92.8182241127524,1077.77464221183,378.158912856635));
#119770=CARTESIAN_POINT('Ctrl Pts',(92.955485621408,1077.7692326222,378.310420338624));
#119771=CARTESIAN_POINT('Ctrl Pts',(93.0736737001234,1077.76264378489,378.39775559986));
#119772=CARTESIAN_POINT('Ctrl Pts',(93.2844673200733,1077.74825829438,378.496651028051));
#119773=CARTESIAN_POINT('Ctrl Pts',(93.3677105903819,1077.74204282004,378.524182025668));
#119774=CARTESIAN_POINT('Ctrl Pts',(93.5253735340906,1077.72931031049,378.556211222365));
#119775=CARTESIAN_POINT('Ctrl Pts',(93.5987219805113,1077.72302680259,378.563573093014));
#119776=CARTESIAN_POINT('Ctrl Pts',(93.6722192570494,1077.71636978598,378.563560951671));
#119777=CARTESIAN_POINT('',(93.6720377362221,1075.60303707734,376.365898694679));
#119778=CARTESIAN_POINT('',(93.672037736222,1067.7251047501,376.365898694679));
#119779=CARTESIAN_POINT('Ctrl Pts',(93.6718533219435,1075.70594646218,378.563560951189));
#119780=CARTESIAN_POINT('Ctrl Pts',(93.5264011728922,1075.71923995543,378.563536540292));
#119781=CARTESIAN_POINT('Ctrl Pts',(93.3822507739243,1075.73099086691,378.534632194512));
#119782=CARTESIAN_POINT('Ctrl Pts',(93.1132797204475,1075.75015626527,378.422064723482));
#119783=CARTESIAN_POINT('Ctrl Pts',(92.9911786947583,1075.75737768,378.339487097749));
#119784=CARTESIAN_POINT('Ctrl Pts',(92.7871558505531,1075.76630049765,378.132106267149));
#119785=CARTESIAN_POINT('Ctrl Pts',(92.7069670767,1075.767959732,378.009765079275));
#119786=CARTESIAN_POINT('Ctrl Pts',(92.5992293667541,1075.76555675552,377.742355363055));
#119787=CARTESIAN_POINT('Ctrl Pts',(92.5722187985566,1075.76157684131,377.600200246242));
#119788=CARTESIAN_POINT('Ctrl Pts',(92.5742681550686,1075.74832304881,377.311065603305));
#119789=CARTESIAN_POINT('Ctrl Pts',(92.6043371897209,1075.73908663897,377.166993298332));
#119790=CARTESIAN_POINT('Ctrl Pts',(92.7188044499007,1075.71647031607,376.899016341679));
#119791=CARTESIAN_POINT('Ctrl Pts',(92.80213277933,1075.70330675867,376.777796144562));
#119792=CARTESIAN_POINT('Ctrl Pts',(92.957757529143,1075.68200378671,376.626679273154));
#119793=CARTESIAN_POINT('Ctrl Pts',(93.0136780383686,1075.67477205783,376.58207328005));
#119794=CARTESIAN_POINT('Ctrl Pts',(93.1335681882368,1075.66003685109,376.504204542886));
#119795=CARTESIAN_POINT('Ctrl Pts',(93.1972919032829,1075.65256627695,376.471163708906));
#119796=CARTESIAN_POINT('Ctrl Pts',(93.3994687805416,1075.62990018571,376.390253784415));
#119797=CARTESIAN_POINT('Ctrl Pts',(93.5447127617592,1075.61497447705,376.363538608292));
#119798=CARTESIAN_POINT('Ctrl Pts',(93.8354181602545,1075.58770264304,376.368553787696));
#119799=CARTESIAN_POINT('Ctrl Pts',(93.978088294476,1075.57558818508,376.399502214301));
#119800=CARTESIAN_POINT('Ctrl Pts',(94.2426651545265,1075.55582408963,376.51472645125));
#119801=CARTESIAN_POINT('Ctrl Pts',(94.3621119467305,1075.54834330311,376.597554918917));
#119802=CARTESIAN_POINT('Ctrl Pts',(94.5617904319835,1075.5391317027,376.804204799827));
#119803=CARTESIAN_POINT('Ctrl Pts',(94.6402580869334,1075.53746098628,376.925729772193));
#119804=CARTESIAN_POINT('Ctrl Pts',(94.7460161189048,1075.54018185347,377.191853128827));
#119805=CARTESIAN_POINT('Ctrl Pts',(94.7723507116371,1075.54453380114,377.333746448445));
#119806=CARTESIAN_POINT('Ctrl Pts',(94.7692532755111,1075.55867537877,377.619964173259));
#119807=CARTESIAN_POINT('Ctrl Pts',(94.7396711864189,1075.56834103044,377.761473666155));
#119808=CARTESIAN_POINT('Ctrl Pts',(94.6277405914666,1075.59167914103,378.025791613268));
#119809=CARTESIAN_POINT('Ctrl Pts',(94.5461379024299,1075.60514926797,378.145934458013));
#119810=CARTESIAN_POINT('Ctrl Pts',(94.3924695673108,1075.62678943036,378.297563876846));
#119811=CARTESIAN_POINT('Ctrl Pts',(94.3362606254359,1075.63420691134,378.343045695243));
#119812=CARTESIAN_POINT('Ctrl Pts',(94.2159504354054,1075.64916839968,378.422204779237));
#119813=CARTESIAN_POINT('Ctrl Pts',(94.1521513402626,1075.65667739653,378.455734718383));
#119814=CARTESIAN_POINT('Ctrl Pts',(93.9542201423241,1075.67878305921,378.536126584217));
#119815=CARTESIAN_POINT('Ctrl Pts',(93.813744660885,1075.69297840658,378.563584764483));
#119816=CARTESIAN_POINT('Ctrl Pts',(93.6718533219435,1075.70594646218,378.563560951189));
#119817=CARTESIAN_POINT('Origin',(93.672037736222,1067.7251047501,377.464729830671));
#119818=CARTESIAN_POINT('',(93.6720377362219,1075.67866049267,377.963560966664));
#119819=CARTESIAN_POINT('',(93.672037736222,1075.63195590694,376.965898694679));
#119820=CARTESIAN_POINT('Ctrl Pts',(93.6720377362219,1075.67866049267,377.963560966664));
#119821=CARTESIAN_POINT('Ctrl Pts',(93.6058998860328,1075.684763007,377.963560966664));
#119822=CARTESIAN_POINT('Ctrl Pts',(93.5403511446652,1075.69018085178,377.950407548697));
#119823=CARTESIAN_POINT('Ctrl Pts',(93.4179092189567,1075.69904625754,377.899093828582));
#119824=CARTESIAN_POINT('Ctrl Pts',(93.3622879773617,1075.70239783057,377.861369755518));
#119825=CARTESIAN_POINT('Ctrl Pts',(93.2701945710849,1075.70649147921,377.767352417574));
#119826=CARTESIAN_POINT('Ctrl Pts',(93.234208934487,1075.70725376,377.712455394587));
#119827=CARTESIAN_POINT('Ctrl Pts',(93.1853227757369,1075.70617538341,377.591902707691));
#119828=CARTESIAN_POINT('Ctrl Pts',(93.1729159538782,1075.70434469343,377.52744659807));
#119829=CARTESIAN_POINT('Ctrl Pts',(93.1735087932216,1075.69828795475,377.397205779866));
#119830=CARTESIAN_POINT('Ctrl Pts',(93.1866054048728,1075.69411175676,377.332706721366));
#119831=CARTESIAN_POINT('Ctrl Pts',(93.2372996771602,1075.68382886917,377.21124250193));
#119832=CARTESIAN_POINT('Ctrl Pts',(93.274893086152,1075.67778614536,377.155676442994));
#119833=CARTESIAN_POINT('Ctrl Pts',(93.3453758446788,1075.66803744424,377.086337562461));
#119834=CARTESIAN_POINT('Ctrl Pts',(93.3707100698784,1075.66473559238,377.065869730989));
#119835=CARTESIAN_POINT('Ctrl Pts',(93.4250289965021,1075.65802442011,377.030128954924));
#119836=CARTESIAN_POINT('Ctrl Pts',(93.4538948022533,1075.65463035487,377.014946826748));
#119837=CARTESIAN_POINT('Ctrl Pts',(93.5437056075,1075.64455376019,376.978402820946));
#119838=CARTESIAN_POINT('Ctrl Pts',(93.6075511765563,1075.63799913074,376.965898694679));
#119839=CARTESIAN_POINT('Ctrl Pts',(93.672037736222,1075.63195590694,376.965898694679));
#119840=CARTESIAN_POINT('',(93.672037736222,1082.7251047501,376.965898694679));
#119841=CARTESIAN_POINT('',(93.672037736222,1067.7251047501,376.965898694679));
#119842=CARTESIAN_POINT('Origin',(93.672037736222,1082.7251047501,377.464729830671));
#119843=CARTESIAN_POINT('Ctrl Pts',(93.672037736222,1075.63195590694,376.965898694679));
#119844=CARTESIAN_POINT('Ctrl Pts',(93.6720484915353,1075.63195489903,376.965898694679));
#119845=CARTESIAN_POINT('Ctrl Pts',(93.6720592468665,1075.63195389113,376.965898695025));
#119846=CARTESIAN_POINT('Ctrl Pts',(93.6720700022155,1075.63195288325,376.965898695721));
#119847=CARTESIAN_POINT('Ctrl Pts',(93.7381764088161,1075.62575805452,376.965902971695));
#119848=CARTESIAN_POINT('Ctrl Pts',(93.8036919268756,1075.62021962966,376.979048112777));
#119849=CARTESIAN_POINT('Ctrl Pts',(93.9249685551116,1075.61120428251,377.029854466407));
#119850=CARTESIAN_POINT('Ctrl Pts',(93.979678677085,1075.60778648756,377.066656469242));
#119851=CARTESIAN_POINT('Ctrl Pts',(94.0716200681311,1075.603496699,377.159123318087));
#119852=CARTESIAN_POINT('Ctrl Pts',(94.1080262747016,1075.60265471042,377.213772593599));
#119853=CARTESIAN_POINT('Ctrl Pts',(94.1577777270919,1075.6036696957,377.333919423654));
#119854=CARTESIAN_POINT('Ctrl Pts',(94.1706559676332,1075.60551295254,377.3982030184));
#119855=CARTESIAN_POINT('Ctrl Pts',(94.1710772677511,1075.61165428562,377.528248779548));
#119856=CARTESIAN_POINT('Ctrl Pts',(94.1585298528844,1075.61589956251,377.592730355597));
#119857=CARTESIAN_POINT('Ctrl Pts',(94.1093259777868,1075.6262445344,377.713505120068));
#119858=CARTESIAN_POINT('Ctrl Pts',(94.0730001144866,1075.63225474547,377.768580069253));
#119859=CARTESIAN_POINT('Ctrl Pts',(94.0041977852763,1075.64197104994,377.838320117501));
#119860=CARTESIAN_POINT('Ctrl Pts',(93.9790269289867,1075.64530535397,377.859263394115));
#119861=CARTESIAN_POINT('Ctrl Pts',(93.9250115168889,1075.65205820513,377.895890811382));
#119862=CARTESIAN_POINT('Ctrl Pts',(93.8962977328366,1075.65546102669,377.91149925783));
#119863=CARTESIAN_POINT('Ctrl Pts',(93.8050509164328,1075.66574049287,377.950072140307));
#119864=CARTESIAN_POINT('Ctrl Pts',(93.7392424435488,1075.67245522381,377.963470859681));
#119865=CARTESIAN_POINT('Ctrl Pts',(93.6724858533722,1075.67861913784,377.963560815709));
#119866=CARTESIAN_POINT('Ctrl Pts',(93.6722617914164,1075.67863981918,377.963560966664));
#119867=CARTESIAN_POINT('Ctrl Pts',(93.6720377362219,1075.67866049267,377.963560966664));
#119868=CARTESIAN_POINT('Origin',(104.994450521159,1067.7251047501,385.676728598176));
#119869=CARTESIAN_POINT('',(104.994450521181,1076.76862933859,384.586187849449));
#119870=CARTESIAN_POINT('Ctrl Pts',(104.994633285524,1076.87046141638,386.76726933159));
#119871=CARTESIAN_POINT('Ctrl Pts',(105.131833259839,1076.85333286283,386.767246338165));
#119872=CARTESIAN_POINT('Ctrl Pts',(105.267718545062,1076.83509138601,386.741333633219));
#119873=CARTESIAN_POINT('Ctrl Pts',(105.530325094078,1076.79716254288,386.63757987829));
#119874=CARTESIAN_POINT('Ctrl Pts',(105.653538059104,1076.77780942427,386.557668010356));
#119875=CARTESIAN_POINT('Ctrl Pts',(105.858143402187,1076.74234604782,386.357287723099));
#119876=CARTESIAN_POINT('Ctrl Pts',(105.938900147509,1076.72647291626,386.239988648573));
#119877=CARTESIAN_POINT('Ctrl Pts',(106.043387948015,1076.70163546465,385.998859661691));
#119878=CARTESIAN_POINT('Ctrl Pts',(106.072793049309,1076.69219014714,385.87994369037));
#119879=CARTESIAN_POINT('Ctrl Pts',(106.089667233352,1076.6793090253,385.655445393521));
#119880=CARTESIAN_POINT('Ctrl Pts',(106.082737437329,1076.67524695972,385.55177151307));
#119881=CARTESIAN_POINT('Ctrl Pts',(106.055200125584,1076.67258699994,385.421877171064));
#119882=CARTESIAN_POINT('Ctrl Pts',(106.047963832544,1076.67216051198,385.393446127906));
#119883=CARTESIAN_POINT('Ctrl Pts',(106.034704465905,1076.67174196399,385.348942751733));
#119884=CARTESIAN_POINT('Ctrl Pts',(106.029434046577,1076.67164299811,385.332663259662));
#119885=CARTESIAN_POINT('Ctrl Pts',(106.01899629093,1076.67156241664,385.302836808276));
#119886=CARTESIAN_POINT('Ctrl Pts',(106.013937755519,1076.67156516685,385.289256166582));
#119887=CARTESIAN_POINT('Ctrl Pts',(106.002169479634,1076.67165893655,385.259489458096));
#119888=CARTESIAN_POINT('Ctrl Pts',(105.995337394395,1076.67176826091,385.243356421428));
#119889=CARTESIAN_POINT('Ctrl Pts',(105.974960017513,1076.67224037247,385.198293275171));
#119890=CARTESIAN_POINT('Ctrl Pts',(105.960529291255,1076.67273749297,385.169786125775));
#119891=CARTESIAN_POINT('Ctrl Pts',(105.874194892632,1076.67652888274,385.016349175557));
#119892=CARTESIAN_POINT('Ctrl Pts',(105.779405815304,1076.68347640333,384.906142161435));
#119893=CARTESIAN_POINT('Ctrl Pts',(105.575566594723,1076.70206856823,384.746786035878));
#119894=CARTESIAN_POINT('Ctrl Pts',(105.474525489599,1076.71236791538,384.690855692307));
#119895=CARTESIAN_POINT('Ctrl Pts',(105.247953699509,1076.73743328187,384.608552052302));
#119896=CARTESIAN_POINT('Ctrl Pts',(105.122669325942,1076.75236128811,384.586432904679));
#119897=CARTESIAN_POINT('Ctrl Pts',(104.860053917182,1076.78568102768,384.58592683987));
#119898=CARTESIAN_POINT('Ctrl Pts',(104.72477820044,1076.80397641313,384.611292371405));
#119899=CARTESIAN_POINT('Ctrl Pts',(104.462369570083,1076.84178556993,384.713769297562));
#119900=CARTESIAN_POINT('Ctrl Pts',(104.338813916159,1076.86094567878,384.793209576895));
#119901=CARTESIAN_POINT('Ctrl Pts',(104.133173658214,1076.89582103737,384.99304978521));
#119902=CARTESIAN_POINT('Ctrl Pts',(104.051829332693,1076.91130668487,385.110335141414));
#119903=CARTESIAN_POINT('Ctrl Pts',(103.9493959124,1076.93472860304,385.344783563755));
#119904=CARTESIAN_POINT('Ctrl Pts',(103.920335107035,1076.94340083518,385.456122569877));
#119905=CARTESIAN_POINT('Ctrl Pts',(103.898341977279,1076.95632730457,385.679937638596));
#119906=CARTESIAN_POINT('Ctrl Pts',(103.904281400433,1076.96065170195,385.79087886747));
#119907=CARTESIAN_POINT('Ctrl Pts',(103.932945111882,1076.96340025134,385.928496425229));
#119908=CARTESIAN_POINT('Ctrl Pts',(103.940279985098,1076.96382644933,385.957629889771));
#119909=CARTESIAN_POINT('Ctrl Pts',(103.953690200165,1076.9642419062,386.00290731595));
#119910=CARTESIAN_POINT('Ctrl Pts',(103.958960841991,1076.96434001242,386.019271660269));
#119911=CARTESIAN_POINT('Ctrl Pts',(103.968910185781,1076.9644190025,386.047830336804));
#119912=CARTESIAN_POINT('Ctrl Pts',(103.97342510192,1076.96442241269,386.060077753699));
#119913=CARTESIAN_POINT('Ctrl Pts',(103.984192208757,1076.96436037941,386.087744436638));
#119914=CARTESIAN_POINT('Ctrl Pts',(103.990579517295,1076.96427578225,386.103107385609));
#119915=CARTESIAN_POINT('Ctrl Pts',(104.008814937133,1076.96391202882,386.144284037777));
#119916=CARTESIAN_POINT('Ctrl Pts',(104.021323346397,1076.9635377495,386.169789331306));
#119917=CARTESIAN_POINT('Ctrl Pts',(104.085327406492,1076.96107813431,386.288351459443));
#119918=CARTESIAN_POINT('Ctrl Pts',(104.149224725981,1076.95713113042,386.373974107909));
#119919=CARTESIAN_POINT('Ctrl Pts',(104.301834591077,1076.94529580539,386.526146918114));
#119920=CARTESIAN_POINT('Ctrl Pts',(104.390313940337,1076.93736524954,386.59116430131));
#119921=CARTESIAN_POINT('Ctrl Pts',(104.571110202303,1076.91937906314,386.686247035992));
#119922=CARTESIAN_POINT('Ctrl Pts',(104.660724526256,1076.90979923496,386.719288662887));
#119923=CARTESIAN_POINT('Ctrl Pts',(104.832603767784,1076.89024419292,386.758248009956));
#119924=CARTESIAN_POINT('Ctrl Pts',(104.913525354245,1076.88058723128,386.767282924516));
#119925=CARTESIAN_POINT('Ctrl Pts',(104.994633285524,1076.87046141638,386.76726933159));
#119926=CARTESIAN_POINT('',(104.994450521159,1074.74993967683,384.586187849448));
#119927=CARTESIAN_POINT('',(104.994450521159,1067.7251047501,384.586187849448));
#119928=CARTESIAN_POINT('Ctrl Pts',(104.993488433118,1074.85275892785,386.767268922521));
#119929=CARTESIAN_POINT('Ctrl Pts',(104.848894050105,1074.87095330795,386.767141359584));
#119930=CARTESIAN_POINT('Ctrl Pts',(104.705538610491,1074.88756311335,386.738257385749));
#119931=CARTESIAN_POINT('Ctrl Pts',(104.438687030779,1074.91567748798,386.626080293747));
#119932=CARTESIAN_POINT('Ctrl Pts',(104.317764632415,1074.92692549908,386.544119650505));
#119933=CARTESIAN_POINT('Ctrl Pts',(104.115898398542,1074.94251123594,386.338505252222));
#119934=CARTESIAN_POINT('Ctrl Pts',(104.036584485142,1074.94676743849,386.217424362304));
#119935=CARTESIAN_POINT('Ctrl Pts',(103.929993585147,1074.94781847454,385.952935140033));
#119936=CARTESIAN_POINT('Ctrl Pts',(103.903175231259,1074.94469329364,385.812505239435));
#119937=CARTESIAN_POINT('Ctrl Pts',(103.904692652719,1074.93132865139,385.526049797475));
#119938=CARTESIAN_POINT('Ctrl Pts',(103.93432703878,1074.92106172641,385.382974201478));
#119939=CARTESIAN_POINT('Ctrl Pts',(104.047585187939,1074.89462196658,385.116602069858));
#119940=CARTESIAN_POINT('Ctrl Pts',(104.130245107814,1074.8786936825,384.996058232639));
#119941=CARTESIAN_POINT('Ctrl Pts',(104.338162169601,1074.84312401658,384.793680168606));
#119942=CARTESIAN_POINT('Ctrl Pts',(104.461731642368,1074.82379728769,384.714110364067));
#119943=CARTESIAN_POINT('Ctrl Pts',(104.73363518047,1074.784287512,384.607741245521));
#119944=CARTESIAN_POINT('Ctrl Pts',(104.879567783969,1074.76447519522,384.582376661305));
#119945=CARTESIAN_POINT('Ctrl Pts',(105.169986449437,1074.72767768233,384.590840635096));
#119946=CARTESIAN_POINT('Ctrl Pts',(105.311734870644,1074.71098974609,384.623437323337));
#119947=CARTESIAN_POINT('Ctrl Pts',(105.573464807664,1074.68286566589,384.741611689425));
#119948=CARTESIAN_POINT('Ctrl Pts',(105.6910983992,1074.67165698388,384.825544961858));
#119949=CARTESIAN_POINT('Ctrl Pts',(105.886435982201,1074.65632244418,385.03346829857));
#119950=CARTESIAN_POINT('Ctrl Pts',(105.962559155349,1074.65228317652,385.154959248906));
#119951=CARTESIAN_POINT('Ctrl Pts',(106.06371306275,1074.65190767947,385.419886601982));
#119952=CARTESIAN_POINT('Ctrl Pts',(106.087946901198,1074.65553960046,385.560513977255));
#119953=CARTESIAN_POINT('Ctrl Pts',(106.081449055933,1074.67000160222,385.843526770489));
#119954=CARTESIAN_POINT('Ctrl Pts',(106.050584602473,1074.68071050683,385.983067765841));
#119955=CARTESIAN_POINT('Ctrl Pts',(105.937020596228,1074.7078463793,386.243487413592));
#119956=CARTESIAN_POINT('Ctrl Pts',(105.85492648638,1074.72406183403,386.361644029438));
#119957=CARTESIAN_POINT('Ctrl Pts',(105.649393385778,1074.7598564498,386.560450824642));
#119958=CARTESIAN_POINT('Ctrl Pts',(105.527488624727,1074.77913013045,386.638879168424));
#119959=CARTESIAN_POINT('Ctrl Pts',(105.330629273114,1074.80778502169,386.716392154147));
#119960=CARTESIAN_POINT('Ctrl Pts',(105.265058168699,1074.81698560129,386.735355511107));
#119961=CARTESIAN_POINT('Ctrl Pts',(105.130707495125,1074.83517037925,386.760898443258));
#119962=CARTESIAN_POINT('Ctrl Pts',(105.062187610499,1074.84411447763,386.767329529778));
#119963=CARTESIAN_POINT('Ctrl Pts',(104.993488433118,1074.85275892785,386.767268922522));
#119964=CARTESIAN_POINT('Origin',(104.994450521159,1067.7251047501,385.676728598176));
#119965=CARTESIAN_POINT('',(104.994450521159,1074.82513013623,386.167269346904));
#119966=CARTESIAN_POINT('',(104.994450521159,1074.77893852154,385.186187849448));
#119967=CARTESIAN_POINT('Ctrl Pts',(104.994450521159,1074.82513013623,386.167269346904));
#119968=CARTESIAN_POINT('Ctrl Pts',(104.961419275554,1074.82930714217,386.167269346904));
#119969=CARTESIAN_POINT('Ctrl Pts',(104.928372056375,1074.83332530481,386.163933201317));
#119970=CARTESIAN_POINT('Ctrl Pts',(104.831883977299,1074.84457534412,386.144127822702));
#119971=CARTESIAN_POINT('Ctrl Pts',(104.771100254234,1074.85102591974,386.118354154493));
#119972=CARTESIAN_POINT('Ctrl Pts',(104.663869618342,1074.86108560777,386.04484503087));
#119973=CARTESIAN_POINT('Ctrl Pts',(104.618302621517,1074.86463432453,385.99817313082));
#119974=CARTESIAN_POINT('Ctrl Pts',(104.548366762419,1074.86840152833,385.890500793405));
#119975=CARTESIAN_POINT('Ctrl Pts',(104.524399009584,1074.86863103434,385.830813769502));
#119976=CARTESIAN_POINT('Ctrl Pts',(104.500619619116,1074.86578258252,385.705541217366));
#119977=CARTESIAN_POINT('Ctrl Pts',(104.501073431236,1074.86273014935,385.641222927864));
#119978=CARTESIAN_POINT('Ctrl Pts',(104.526837632459,1074.85358833337,385.514693139946));
#119979=CARTESIAN_POINT('Ctrl Pts',(104.552589963409,1074.84750928077,385.453910247323));
#119980=CARTESIAN_POINT('Ctrl Pts',(104.626388233192,1074.8331465811,385.345880995702));
#119981=CARTESIAN_POINT('Ctrl Pts',(104.673807640141,1074.82499455012,385.299771707557));
#119982=CARTESIAN_POINT('Ctrl Pts',(104.784046408763,1074.80769812398,385.228755129994));
#119983=CARTESIAN_POINT('Ctrl Pts',(104.845888373133,1074.7987138235,385.204629265908));
#119984=CARTESIAN_POINT('Ctrl Pts',(104.938305311029,1074.78620333812,385.188603019807));
#119985=CARTESIAN_POINT('Ctrl Pts',(104.966346558262,1074.78251941681,385.186187849448));
#119986=CARTESIAN_POINT('Ctrl Pts',(104.994450521159,1074.77893852154,385.186187849448));
#119987=CARTESIAN_POINT('',(104.994450521159,1082.7251047501,385.186187849448));
#119988=CARTESIAN_POINT('',(104.994450521159,1067.7251047501,385.186187849448));
#119989=CARTESIAN_POINT('Origin',(104.994450521159,1082.7251047501,385.676728598176));
#119990=CARTESIAN_POINT('Ctrl Pts',(104.994450521159,1074.77893852154,385.186187849448));
#119991=CARTESIAN_POINT('Ctrl Pts',(104.994464257439,1074.77893677132,385.186187849448));
#119992=CARTESIAN_POINT('Ctrl Pts',(104.994477993734,1074.77893502112,385.186187850023));
#119993=CARTESIAN_POINT('Ctrl Pts',(104.994491730044,1074.77893327095,385.186187851177));
#119994=CARTESIAN_POINT('Ctrl Pts',(105.059640385892,1074.77063253974,385.186193324124));
#119995=CARTESIAN_POINT('Ctrl Pts',(105.124238028413,1074.76299834931,385.199177344179));
#119996=CARTESIAN_POINT('Ctrl Pts',(105.243714845829,1074.75010145091,385.249381071327));
#119997=CARTESIAN_POINT('Ctrl Pts',(105.297582269794,1074.74492664549,385.285709133516));
#119998=CARTESIAN_POINT('Ctrl Pts',(105.387874370596,1074.73768627985,385.376856186067));
#119999=CARTESIAN_POINT('Ctrl Pts',(105.423554179795,1074.73566461898,385.430581951871));
#120000=CARTESIAN_POINT('Ctrl Pts',(105.472206670697,1074.73503589283,385.548540810414));
#120001=CARTESIAN_POINT('Ctrl Pts',(105.484780053331,1074.73642066584,385.611525372796));
#120002=CARTESIAN_POINT('Ctrl Pts',(105.485197961527,1074.74242685904,385.738943318982));
#120003=CARTESIAN_POINT('Ctrl Pts',(105.472950987099,1074.74699876339,385.802095233921));
#120004=CARTESIAN_POINT('Ctrl Pts',(105.424901815903,1074.75876995799,385.920588122722));
#120005=CARTESIAN_POINT('Ctrl Pts',(105.389351189106,1074.76587783325,385.974693766438));
#120006=CARTESIAN_POINT('Ctrl Pts',(105.298329439124,1074.78187046461,386.067408110274));
#120007=CARTESIAN_POINT('Ctrl Pts',(105.24319545496,1074.79064456718,386.104614012243));
#120008=CARTESIAN_POINT('Ctrl Pts',(105.152746248563,1074.80389813393,386.142136541162));
#120009=CARTESIAN_POINT('Ctrl Pts',(105.121934370952,1074.80824743372,386.151502715335));
#120010=CARTESIAN_POINT('Ctrl Pts',(105.05876146013,1074.81684508775,386.164106074168));
#120011=CARTESIAN_POINT('Ctrl Pts',(105.026613563918,1074.82106291994,386.167269346904));
#120012=CARTESIAN_POINT('Ctrl Pts',(104.994450521159,1074.82513013623,386.167269346904));
#120013=CARTESIAN_POINT('Origin',(55.815888242722,1067.7251047501,354.582660180055));
#120014=CARTESIAN_POINT('',(55.8158882427517,1078.63997504936,353.104357047861));
#120015=CARTESIAN_POINT('Ctrl Pts',(57.2939968241464,1078.64787169026,354.606642927438));
#120016=CARTESIAN_POINT('Ctrl Pts',(57.2969184316135,1078.64352236629,354.426577941565));
#120017=CARTESIAN_POINT('Ctrl Pts',(57.266912218914,1078.63966729243,354.247472367867));
#120018=CARTESIAN_POINT('Ctrl Pts',(57.145828661031,1078.63368068486,353.913962040012));
#120019=CARTESIAN_POINT('Ctrl Pts',(57.0575700354636,1078.63155159986,353.761604601839));
#120020=CARTESIAN_POINT('Ctrl Pts',(56.9104943662943,1078.63007661884,353.587655299811));
#120021=CARTESIAN_POINT('Ctrl Pts',(56.8740669522224,1078.62982565291,353.548999118833));
#120022=CARTESIAN_POINT('Ctrl Pts',(56.8129432314803,1078.62957717498,353.490760801996));
#120023=CARTESIAN_POINT('Ctrl Pts',(56.789564844328,1078.62951801421,353.469863349694));
#120024=CARTESIAN_POINT('Ctrl Pts',(56.7450898180418,1078.62947008869,353.432583392865));
#120025=CARTESIAN_POINT('Ctrl Pts',(56.7241795261188,1078.62947216577,353.415998648908));
#120026=CARTESIAN_POINT('Ctrl Pts',(56.676976352036,1078.62953006807,353.380598655119));
#120027=CARTESIAN_POINT('Ctrl Pts',(56.6504920054245,1078.62959713719,353.362061477982));
#120028=CARTESIAN_POINT('Ctrl Pts',(56.5742373535414,1078.62988507737,353.312331596955));
#120029=CARTESIAN_POINT('Ctrl Pts',(56.5231862823401,1078.63018663483,353.283215133532));
#120030=CARTESIAN_POINT('Ctrl Pts',(56.2939538201222,1078.63199098522,353.169994991084));
#120031=CARTESIAN_POINT('Ctrl Pts',(56.1017200431752,1078.63463960227,353.118946086318));
#120032=CARTESIAN_POINT('Ctrl Pts',(55.745589600636,1078.64121184432,353.097401602526));
#120033=CARTESIAN_POINT('Ctrl Pts',(55.585518832982,1078.64475387938,353.113695084757));
#120034=CARTESIAN_POINT('Ctrl Pts',(55.2635527974551,1078.652906188,353.200470502829));
#120035=CARTESIAN_POINT('Ctrl Pts',(55.1051858181154,1078.65751512975,353.274829427366));
#120036=CARTESIAN_POINT('Ctrl Pts',(54.8113020715414,1078.66717696182,353.482283652066));
#120037=CARTESIAN_POINT('Ctrl Pts',(54.6808733268301,1078.67214756829,353.617379678643));
#120038=CARTESIAN_POINT('Ctrl Pts',(54.4719245610859,1078.6816697907,353.936645493797));
#120039=CARTESIAN_POINT('Ctrl Pts',(54.3983791070371,1078.68609408375,354.119788496336));
#120040=CARTESIAN_POINT('Ctrl Pts',(54.3278338269869,1078.69359342704,354.498491252392));
#120041=CARTESIAN_POINT('Ctrl Pts',(54.3293240155054,1078.69664048303,354.690013471633));
#120042=CARTESIAN_POINT('Ctrl Pts',(54.4021872456954,1078.70126943562,355.04988143644));
#120043=CARTESIAN_POINT('Ctrl Pts',(54.4683972021584,1078.70290214987,355.215998798835));
#120044=CARTESIAN_POINT('Ctrl Pts',(54.613838310897,1078.70455694528,355.44860008299));
#120045=CARTESIAN_POINT('Ctrl Pts',(54.6731883621541,1078.70496900646,355.525535153428));
#120046=CARTESIAN_POINT('Ctrl Pts',(54.767589425649,1078.70531607425,355.625786162928));
#120047=CARTESIAN_POINT('Ctrl Pts',(54.7967540417351,1078.70538890873,355.654298045532));
#120048=CARTESIAN_POINT('Ctrl Pts',(54.84576976925,1078.70545858904,355.698403792387));
#120049=CARTESIAN_POINT('Ctrl Pts',(54.8649067311524,1078.70547382994,355.714759038956));
#120050=CARTESIAN_POINT('Ctrl Pts',(54.9054491574829,1078.70548191424,355.747654584633));
#120051=CARTESIAN_POINT('Ctrl Pts',(54.9269098935684,1078.70547300861,355.76411216166));
#120052=CARTESIAN_POINT('Ctrl Pts',(54.978011082835,1078.70542165694,355.801119013134));
#120053=CARTESIAN_POINT('Ctrl Pts',(55.0079761274488,1078.70536904224,355.821190790078));
#120054=CARTESIAN_POINT('Ctrl Pts',(55.1046488053296,1078.70512954056,355.880943465592));
#120055=CARTESIAN_POINT('Ctrl Pts',(55.1737621594419,1078.70485839347,355.916479883787));
#120056=CARTESIAN_POINT('Ctrl Pts',(55.4267538566271,1078.7035121241,356.022321300206));
#120057=CARTESIAN_POINT('Ctrl Pts',(55.6214916457768,1078.70186102409,356.061259217013));
#120058=CARTESIAN_POINT('Ctrl Pts',(55.981739897164,1078.6974773684,356.060713995291));
#120059=CARTESIAN_POINT('Ctrl Pts',(56.1441760343487,1078.69499804822,356.033305645742));
#120060=CARTESIAN_POINT('Ctrl Pts',(56.4664743251616,1078.68880333957,355.921910257738));
#120061=CARTESIAN_POINT('Ctrl Pts',(56.6223443169839,1078.68504706121,355.834249011311));
#120062=CARTESIAN_POINT('Ctrl Pts',(56.9057054315686,1078.67633804477,355.599516228649));
#120063=CARTESIAN_POINT('Ctrl Pts',(57.0275736034234,1078.67139544533,355.450710142807));
#120064=CARTESIAN_POINT('Ctrl Pts',(57.1705702404536,1078.66331797367,355.184833116585));
#120065=CARTESIAN_POINT('Ctrl Pts',(57.2120608397622,1078.66031418798,355.081135640913));
#120066=CARTESIAN_POINT('Ctrl Pts',(57.2743500699509,1078.65407101206,354.854084693676));
#120067=CARTESIAN_POINT('Ctrl Pts',(57.2919833333689,1078.65086912363,354.730738718023));
#120068=CARTESIAN_POINT('Ctrl Pts',(57.2939968241464,1078.64787169026,354.606642927438));
#120069=CARTESIAN_POINT('',(55.8158882427049,1076.63887570959,353.104357047862));
#120070=CARTESIAN_POINT('',(55.815888242722,1067.7251047501,353.104357047862));
#120071=CARTESIAN_POINT('Ctrl Pts',(55.8159488750934,1076.69909976501,356.060963311005));
#120072=CARTESIAN_POINT('Ctrl Pts',(55.6205302673948,1076.70150112669,356.060971326069));
#120073=CARTESIAN_POINT('Ctrl Pts',(55.4270293164456,1076.7031613472,356.022230223064));
#120074=CARTESIAN_POINT('Ctrl Pts',(55.0656195798272,1076.70511406965,355.871443026767));
#120075=CARTESIAN_POINT('Ctrl Pts',(54.9014037352093,1076.70538694798,355.760617365159));
#120076=CARTESIAN_POINT('Ctrl Pts',(54.6260845612497,1076.70455121485,355.481597781454));
#120077=CARTESIAN_POINT('Ctrl Pts',(54.5176090973004,1076.70345118471,355.316274419462));
#120078=CARTESIAN_POINT('Ctrl Pts',(54.3717074783901,1076.69979801304,354.953778924329));
#120079=CARTESIAN_POINT('Ctrl Pts',(54.335408016863,1076.69727930961,354.760307636342));
#120080=CARTESIAN_POINT('Ctrl Pts',(54.3399685391359,1076.6907742897,354.370081298712));
#120081=CARTESIAN_POINT('Ctrl Pts',(54.3809338631428,1076.68684116129,354.177166361784));
#120082=CARTESIAN_POINT('Ctrl Pts',(54.4961456775211,1076.68009878215,353.90971080636));
#120083=CARTESIAN_POINT('Ctrl Pts',(54.5425784356717,1076.67775331901,353.825519238522));
#120084=CARTESIAN_POINT('Ctrl Pts',(54.652036610934,1076.67282477512,353.665953010365));
#120085=CARTESIAN_POINT('Ctrl Pts',(54.7150682705674,1076.67025030537,353.591147526017));
#120086=CARTESIAN_POINT('Ctrl Pts',(54.924069295383,1076.66241063477,353.387803372566));
#120087=CARTESIAN_POINT('Ctrl Pts',(55.088417322061,1076.65707067033,353.281195099306));
#120088=CARTESIAN_POINT('Ctrl Pts',(55.4490082435505,1076.64696688877,353.13750612433));
#120089=CARTESIAN_POINT('Ctrl Pts',(55.6417743015555,1076.64230806022,353.101861096665));
#120090=CARTESIAN_POINT('Ctrl Pts',(56.0299605837615,1076.63464889073,353.107123027127));
#120091=CARTESIAN_POINT('Ctrl Pts',(56.2216071052081,1076.6317288412,353.147933582595));
#120092=CARTESIAN_POINT('Ctrl Pts',(56.5778045152464,1076.62830445861,353.301111942892));
#120093=CARTESIAN_POINT('Ctrl Pts',(56.7389539407118,1076.62783146734,353.411833886296));
#120094=CARTESIAN_POINT('Ctrl Pts',(57.0090681159595,1076.62945740592,353.688776930316));
#120095=CARTESIAN_POINT('Ctrl Pts',(57.1155430882697,1076.63153277978,353.85218504));
#120096=CARTESIAN_POINT('Ctrl Pts',(57.2595455391089,1076.63778079007,354.210520645505));
#120097=CARTESIAN_POINT('Ctrl Pts',(57.295744328831,1076.64188570826,354.401971590899));
#120098=CARTESIAN_POINT('Ctrl Pts',(57.2925349242128,1076.65127643338,354.788087702466));
#120099=CARTESIAN_POINT('Ctrl Pts',(57.2530932340981,1076.65646600966,354.97904706042));
#120100=CARTESIAN_POINT('Ctrl Pts',(57.1405307400976,1076.66434065629,355.246009099696));
#120101=CARTESIAN_POINT('Ctrl Pts',(57.0943714723888,1076.66696296708,355.331118890569));
#120102=CARTESIAN_POINT('Ctrl Pts',(56.9861041145873,1076.67210986742,355.491124314132));
#120103=CARTESIAN_POINT('Ctrl Pts',(56.9242534152109,1076.67462204577,355.565635106593));
#120104=CARTESIAN_POINT('Ctrl Pts',(56.7162992535386,1076.68193309578,355.771366953678));
#120105=CARTESIAN_POINT('Ctrl Pts',(56.5510024355483,1076.68634792033,355.880111642091));
#120106=CARTESIAN_POINT('Ctrl Pts',(56.1934713067884,1076.69377697856,356.024454103851));
#120107=CARTESIAN_POINT('Ctrl Pts',(56.0055962117159,1076.69676932242,356.060955532649));
#120108=CARTESIAN_POINT('Ctrl Pts',(55.8159488750934,1076.69909976501,356.060963311005));
#120109=CARTESIAN_POINT('Origin',(55.815888242722,1067.7251047501,354.582660180055));
#120110=CARTESIAN_POINT('',(55.815888242722,1076.68940454296,355.460963312248));
#120111=CARTESIAN_POINT('',(55.8158882427295,1076.65362934538,353.704357047862));
#120112=CARTESIAN_POINT('Ctrl Pts',(55.815888242722,1076.68940454296,355.460963312248));
#120113=CARTESIAN_POINT('Ctrl Pts',(55.7020152112483,1076.69098784474,355.460963312248));
#120114=CARTESIAN_POINT('Ctrl Pts',(55.5891889227174,1076.69213028676,355.438817072165));
#120115=CARTESIAN_POINT('Ctrl Pts',(55.3754742486306,1076.69352199293,355.351506169293));
#120116=CARTESIAN_POINT('Ctrl Pts',(55.2771422558615,1076.6937347303,355.28611011008));
#120117=CARTESIAN_POINT('Ctrl Pts',(55.1119513573992,1076.69317380385,355.120743520564));
#120118=CARTESIAN_POINT('Ctrl Pts',(55.0467101966484,1076.69240603686,355.022460759002));
#120119=CARTESIAN_POINT('Ctrl Pts',(54.9586126127917,1076.68991215862,354.806421275002));
#120120=CARTESIAN_POINT('Ctrl Pts',(54.9365246902861,1076.68821059589,354.690861218791));
#120121=CARTESIAN_POINT('Ctrl Pts',(54.9387250458333,1076.68396437041,354.457744922806));
#120122=CARTESIAN_POINT('Ctrl Pts',(54.9630448406274,1076.68145810191,354.342505892462));
#120123=CARTESIAN_POINT('Ctrl Pts',(55.0317542656464,1076.67729810155,354.182888163623));
#120124=CARTESIAN_POINT('Ctrl Pts',(55.0594259513635,1076.6758715647,354.132717645012));
#120125=CARTESIAN_POINT('Ctrl Pts',(55.1245972640669,1076.67291653756,354.037777734949));
#120126=CARTESIAN_POINT('Ctrl Pts',(55.1620755956594,1076.67139407967,353.993330914934));
#120127=CARTESIAN_POINT('Ctrl Pts',(55.2862506747189,1076.66681439603,353.8726119167));
#120128=CARTESIAN_POINT('Ctrl Pts',(55.3838375411703,1076.66376624872,353.809344060017));
#120129=CARTESIAN_POINT('Ctrl Pts',(55.594289888278,1076.65818353779,353.725509099961));
#120130=CARTESIAN_POINT('Ctrl Pts',(55.7046005627282,1076.65568877212,353.70435704786));
#120131=CARTESIAN_POINT('Ctrl Pts',(55.815888242737,1076.65362934538,353.704357047862));
#120132=CARTESIAN_POINT('',(55.815888242722,1082.7251047501,353.704357047862));
#120133=CARTESIAN_POINT('',(55.815888242722,1067.7251047501,353.704357047862));
#120134=CARTESIAN_POINT('Origin',(55.815888242722,1082.7251047501,354.582660180055));
#120135=CARTESIAN_POINT('Ctrl Pts',(55.815888242737,1076.65362934538,353.704357047862));
#120136=CARTESIAN_POINT('Ctrl Pts',(55.8197649584117,1076.65355760507,353.704357047862));
#120137=CARTESIAN_POINT('Ctrl Pts',(55.8236428596713,1076.65348639333,353.704382714809));
#120138=CARTESIAN_POINT('Ctrl Pts',(55.94269192059,1076.6513172319,353.705959702638));
#120139=CARTESIAN_POINT('Ctrl Pts',(56.0564524851715,1076.64973468531,353.730125629126));
#120140=CARTESIAN_POINT('Ctrl Pts',(56.2680142300927,1076.64787775109,353.820931480909));
#120141=CARTESIAN_POINT('Ctrl Pts',(56.3637850202993,1076.64762079416,353.886629799102));
#120142=CARTESIAN_POINT('Ctrl Pts',(56.524435932203,1076.64849385808,354.051086024939));
#120143=CARTESIAN_POINT('Ctrl Pts',(56.5878053142086,1076.64961279919,354.148203815499));
#120144=CARTESIAN_POINT('Ctrl Pts',(56.6708758297469,1076.65291270086,354.354622230776));
#120145=CARTESIAN_POINT('Ctrl Pts',(56.692362346411,1076.65499271175,354.461025189534));
#120146=CARTESIAN_POINT('Ctrl Pts',(56.6940795884859,1076.65740429285,354.568647605487));
#120147=CARTESIAN_POINT('Ctrl Pts',(56.695912136676,1076.65997780223,354.683496447389));
#120148=CARTESIAN_POINT('Ctrl Pts',(56.675197332517,1076.66287848519,354.797591719143));
#120149=CARTESIAN_POINT('Ctrl Pts',(56.6120843920517,1076.66739708317,354.957871277574));
#120150=CARTESIAN_POINT('Ctrl Pts',(56.5858662871713,1076.66892038143,355.009093597327));
#120151=CARTESIAN_POINT('Ctrl Pts',(56.5238073760246,1076.6719520213,355.105692665344));
#120152=CARTESIAN_POINT('Ctrl Pts',(56.488114175994,1076.67345306842,355.150837026364));
#120153=CARTESIAN_POINT('Ctrl Pts',(56.3671601182725,1076.67789849534,355.276329231394));
#120154=CARTESIAN_POINT('Ctrl Pts',(56.2700564020598,1076.68068038924,355.343456793896));
#120155=CARTESIAN_POINT('Ctrl Pts',(56.0556557242177,1076.68557767416,355.435591881462));
#120156=CARTESIAN_POINT('Ctrl Pts',(55.9405592226238,1076.6876493049,355.45983816675));
#120157=CARTESIAN_POINT('Ctrl Pts',(55.8213514717962,1076.68932833524,355.460950571655));
#120158=CARTESIAN_POINT('Ctrl Pts',(55.8186195561669,1076.68936656651,355.460963312248));
#120159=CARTESIAN_POINT('Ctrl Pts',(55.815888242722,1076.68940454296,355.460963312248));
#120160=CARTESIAN_POINT('Origin',(68.2819685228176,1067.7251047501,356.101514707942));
#120161=CARTESIAN_POINT('',(68.2819685228382,1078.28930526318,354.826070586805));
#120162=CARTESIAN_POINT('Ctrl Pts',(68.282008024927,1078.40494025576,357.376958828466));
#120163=CARTESIAN_POINT('Ctrl Pts',(68.4272802061516,1078.39879186158,357.376954329204));
#120164=CARTESIAN_POINT('Ctrl Pts',(68.5714409895716,1078.39156248641,357.352130990053));
#120165=CARTESIAN_POINT('Ctrl Pts',(68.8561106303347,1078.37478862654,357.251176962716));
#120166=CARTESIAN_POINT('Ctrl Pts',(68.9929803058314,1078.36524410491,357.171936387957));
#120167=CARTESIAN_POINT('Ctrl Pts',(69.2401787937585,1078.34460608442,356.960049394559));
#120168=CARTESIAN_POINT('Ctrl Pts',(69.3452663176645,1078.33364968231,356.825841584997));
#120169=CARTESIAN_POINT('Ctrl Pts',(69.4961240041268,1078.31268843434,356.526205651141));
#120170=CARTESIAN_POINT('Ctrl Pts',(69.541194980926,1078.30287538035,356.364037485814));
#120171=CARTESIAN_POINT('Ctrl Pts',(69.5651287858941,1078.2865830692,356.047718379383));
#120172=CARTESIAN_POINT('Ctrl Pts',(69.5498492769712,1078.28000210315,355.896805757738));
#120173=CARTESIAN_POINT('Ctrl Pts',(69.4699812033245,1078.27021904016,355.616505019617));
#120174=CARTESIAN_POINT('Ctrl Pts',(69.4091767994855,1078.26689651899,355.48830280211));
#120175=CARTESIAN_POINT('Ctrl Pts',(69.3047154976682,1078.26463988305,355.338300271891));
#120176=CARTESIAN_POINT('Ctrl Pts',(69.2791342029159,1078.26426398515,355.305167754843));
#120177=CARTESIAN_POINT('Ctrl Pts',(69.2359820433617,1078.26389295801,355.254624979299));
#120178=CARTESIAN_POINT('Ctrl Pts',(69.219454788941,1078.26380487357,355.236365282305));
#120179=CARTESIAN_POINT('Ctrl Pts',(69.1879157711236,1078.26373353825,355.203485953658));
#120180=CARTESIAN_POINT('Ctrl Pts',(69.1730524688451,1078.26373657647,355.188735730667));
#120181=CARTESIAN_POINT('Ctrl Pts',(69.1393978101969,1078.26382249366,355.156942920723));
#120182=CARTESIAN_POINT('Ctrl Pts',(69.120447626172,1078.26392208629,355.140081602065));
#120183=CARTESIAN_POINT('Ctrl Pts',(69.0655988363193,1078.26435079336,355.094134514308));
#120184=CARTESIAN_POINT('Ctrl Pts',(69.0286061874164,1078.26480094747,355.06641895646));
#120185=CARTESIAN_POINT('Ctrl Pts',(68.8491710423865,1078.26770141377,354.946615701958));
#120186=CARTESIAN_POINT('Ctrl Pts',(68.6908265634068,1078.27225783199,354.881551543092));
#120187=CARTESIAN_POINT('Ctrl Pts',(68.3900923339753,1078.28398741261,354.823313845346));
#120188=CARTESIAN_POINT('Ctrl Pts',(68.2524605328724,1078.29040904682,354.819098072872));
#120189=CARTESIAN_POINT('Ctrl Pts',(67.9689162741077,1078.30566702941,354.856118564548));
#120190=CARTESIAN_POINT('Ctrl Pts',(67.8255586356722,1078.31455037641,354.901231276389));
#120191=CARTESIAN_POINT('Ctrl Pts',(67.551168832755,1078.33392323053,355.043992272885));
#120192=CARTESIAN_POINT('Ctrl Pts',(67.424251565182,1078.34431063248,355.144048758361));
#120193=CARTESIAN_POINT('Ctrl Pts',(67.2084156789855,1078.36520467754,355.392456335813));
#120194=CARTESIAN_POINT('Ctrl Pts',(67.1240363732813,1078.3754831245,355.540711432959));
#120195=CARTESIAN_POINT('Ctrl Pts',(67.0194583715021,1078.39379384599,355.857015045418));
#120196=CARTESIAN_POINT('Ctrl Pts',(66.9984817094128,1078.40171497849,356.021443183465));
#120197=CARTESIAN_POINT('Ctrl Pts',(67.0189659068121,1078.41399803443,356.332295928338));
#120198=CARTESIAN_POINT('Ctrl Pts',(67.0540164470797,1078.41855445889,356.476470869262));
#120199=CARTESIAN_POINT('Ctrl Pts',(67.1516738658537,1078.4238111331,356.700335628744));
#120200=CARTESIAN_POINT('Ctrl Pts',(67.2004345792778,1078.42527979935,356.784479161516));
#120201=CARTESIAN_POINT('Ctrl Pts',(67.279503240532,1078.42641945879,356.890874824266));
#120202=CARTESIAN_POINT('Ctrl Pts',(67.301934253527,1078.42663933128,356.918557511908));
#120203=CARTESIAN_POINT('Ctrl Pts',(67.3405656922861,1078.42685775384,356.962350020648));
#120204=CARTESIAN_POINT('Ctrl Pts',(67.3560918682947,1078.42690746137,356.979027758045));
#120205=CARTESIAN_POINT('Ctrl Pts',(67.3868844889647,1078.42693479388,357.010376653845));
#120206=CARTESIAN_POINT('Ctrl Pts',(67.4020859106746,1078.42691729389,357.025101223384));
#120207=CARTESIAN_POINT('Ctrl Pts',(67.4380042430564,1078.42680614552,357.058200851031));
#120208=CARTESIAN_POINT('Ctrl Pts',(67.4589671476937,1078.42669071757,357.076293039177));
#120209=CARTESIAN_POINT('Ctrl Pts',(67.5255308873736,1078.42617220858,357.130062458145));
#120210=CARTESIAN_POINT('Ctrl Pts',(67.5729821404391,1078.42559337644,357.163327385636));
#120211=CARTESIAN_POINT('Ctrl Pts',(67.6866109848778,1078.42374837165,357.231962589286));
#120212=CARTESIAN_POINT('Ctrl Pts',(67.7539742470069,1078.42233401632,357.264950568641));
#120213=CARTESIAN_POINT('Ctrl Pts',(67.9700757138016,1078.41683452277,357.348124314899));
#120214=CARTESIAN_POINT('Ctrl Pts',(68.1254001479995,1078.41156841368,357.376963678809));
#120215=CARTESIAN_POINT('Ctrl Pts',(68.282008024927,1078.40494025576,357.376958828466));
#120216=CARTESIAN_POINT('',(68.2819685228178,1076.28440570417,354.826070586806));
#120217=CARTESIAN_POINT('',(68.2819685228176,1067.7251047501,354.826070586806));
#120218=CARTESIAN_POINT('Ctrl Pts',(68.2828783104664,1076.40120959841,357.376958504597));
#120219=CARTESIAN_POINT('Ctrl Pts',(68.1139567583433,1076.40843995203,357.37707899814));
#120220=CARTESIAN_POINT('Ctrl Pts',(67.9466278649383,1076.41406505978,357.343639921872));
#120221=CARTESIAN_POINT('Ctrl Pts',(67.6339827215819,1076.42166979259,357.213131289088));
#120222=CARTESIAN_POINT('Ctrl Pts',(67.4919227930535,1076.4235606558,357.117102529378));
#120223=CARTESIAN_POINT('Ctrl Pts',(67.2537522745128,1076.42336444091,356.875047956837));
#120224=CARTESIAN_POINT('Ctrl Pts',(67.1600452959416,1076.42127982381,356.731479350378));
#120225=CARTESIAN_POINT('Ctrl Pts',(67.0346165639685,1076.4133081298,356.416836516397));
#120226=CARTESIAN_POINT('Ctrl Pts',(67.003877767371,1076.40751346596,356.24903397595));
#120227=CARTESIAN_POINT('Ctrl Pts',(67.0095239001937,1076.39276767705,355.911567035652));
#120228=CARTESIAN_POINT('Ctrl Pts',(67.0457543452616,1076.38396179721,355.745243186752));
#120229=CARTESIAN_POINT('Ctrl Pts',(67.1462960048837,1076.369313427,355.515147547741));
#120230=CARTESIAN_POINT('Ctrl Pts',(67.1866324669658,1076.36428440595,355.442869201086));
#120231=CARTESIAN_POINT('Ctrl Pts',(67.2808780688924,1076.35391284183,355.306878818267));
#120232=CARTESIAN_POINT('Ctrl Pts',(67.3346184608261,1076.34859344092,355.243520334193));
#120233=CARTESIAN_POINT('Ctrl Pts',(67.5156475588365,1076.33225853127,355.067994680925));
#120234=CARTESIAN_POINT('Ctrl Pts',(67.6594388532063,1076.3212403891,354.975512882304));
#120235=CARTESIAN_POINT('Ctrl Pts',(67.9730905331906,1076.30059636382,354.852750475746));
#120236=CARTESIAN_POINT('Ctrl Pts',(68.1396460975408,1076.29115894958,354.822999083903));
#120237=CARTESIAN_POINT('Ctrl Pts',(68.4744759275764,1076.27524404749,354.829635769033));
#120238=CARTESIAN_POINT('Ctrl Pts',(68.6394985229903,1076.2689190114,354.865816191403));
#120239=CARTESIAN_POINT('Ctrl Pts',(68.9457644325333,1076.26044482447,354.99970932176));
#120240=CARTESIAN_POINT('Ctrl Pts',(69.0840834178632,1076.25836832752,355.095915883548));
#120241=CARTESIAN_POINT('Ctrl Pts',(69.3155747813728,1076.25883093411,355.335910886107));
#120242=CARTESIAN_POINT('Ctrl Pts',(69.4065789781513,1076.26135484848,355.477237605242));
#120243=CARTESIAN_POINT('Ctrl Pts',(69.5291562007942,1076.27061731939,355.786853877496));
#120244=CARTESIAN_POINT('Ctrl Pts',(69.5595173346668,1076.27726386798,355.952136508149));
#120245=CARTESIAN_POINT('Ctrl Pts',(69.5550756438495,1076.29365984583,356.285321351552));
#120246=CARTESIAN_POINT('Ctrl Pts',(69.5201498404082,1076.30325476694,356.450019900906));
#120247=CARTESIAN_POINT('Ctrl Pts',(69.3888204583184,1076.32396004204,356.756926860179));
#120248=CARTESIAN_POINT('Ctrl Pts',(69.2935198658765,1076.33487293518,356.896147746133));
#120249=CARTESIAN_POINT('Ctrl Pts',(69.0530584958274,1076.35661504826,357.131498335221));
#120250=CARTESIAN_POINT('Ctrl Pts',(68.9095899511603,1076.36722761946,357.2247075545));
#120251=CARTESIAN_POINT('Ctrl Pts',(68.602778087315,1076.3861212556,357.346356448884));
#120252=CARTESIAN_POINT('Ctrl Pts',(68.4435885401786,1076.39433071424,357.376843868278));
#120253=CARTESIAN_POINT('Ctrl Pts',(68.2828783104664,1076.40120959841,357.376958504597));
#120254=CARTESIAN_POINT('Origin',(68.2819685228176,1067.7251047501,356.101514707942));
#120255=CARTESIAN_POINT('',(68.2819685228176,1076.37545952532,356.776958829078));
#120256=CARTESIAN_POINT('',(68.2819685228177,1076.31358867648,355.426070586806));
#120257=CARTESIAN_POINT('Ctrl Pts',(68.2819685228176,1076.37545952532,356.776958829078));
#120258=CARTESIAN_POINT('Ctrl Pts',(68.2814488826747,1076.37548245635,356.776958829078));
#120259=CARTESIAN_POINT('Ctrl Pts',(68.2809292117553,1076.37550536127,356.776958229415));
#120260=CARTESIAN_POINT('Ctrl Pts',(68.1905059800451,1076.3794860582,356.776749520431));
#120261=CARTESIAN_POINT('Ctrl Pts',(68.1015116578338,1076.38258242533,356.758594310527));
#120262=CARTESIAN_POINT('Ctrl Pts',(67.9364242674877,1076.38672767774,356.688710918134));
#120263=CARTESIAN_POINT('Ctrl Pts',(67.8618880002053,1076.38775102954,356.637925606172));
#120264=CARTESIAN_POINT('Ctrl Pts',(67.7375745412074,1076.38761756947,356.510983791035));
#120265=CARTESIAN_POINT('Ctrl Pts',(67.6887506463528,1076.38648584552,356.436354826076));
#120266=CARTESIAN_POINT('Ctrl Pts',(67.6219904881311,1076.38215781662,356.271057086154));
#120267=CARTESIAN_POINT('Ctrl Pts',(67.6053146123236,1076.37896661029,356.181789805928));
#120268=CARTESIAN_POINT('Ctrl Pts',(67.6078691598746,1076.37089386361,356.002143801593));
#120269=CARTESIAN_POINT('Ctrl Pts',(67.627028665527,1076.36609359528,355.913560241435));
#120270=CARTESIAN_POINT('Ctrl Pts',(67.680475129787,1076.35818119408,355.791098857711));
#120271=CARTESIAN_POINT('Ctrl Pts',(67.7019159684127,1076.35547748858,355.752673156844));
#120272=CARTESIAN_POINT('Ctrl Pts',(67.7519892924917,1076.34993029553,355.68046763933));
#120273=CARTESIAN_POINT('Ctrl Pts',(67.7805173901468,1076.34709959059,355.646866496652));
#120274=CARTESIAN_POINT('Ctrl Pts',(67.8770853906298,1076.33840108898,355.553358074326));
#120275=CARTESIAN_POINT('Ctrl Pts',(67.954054961846,1076.33257086589,355.504117765021));
#120276=CARTESIAN_POINT('Ctrl Pts',(68.1160982976483,1076.32211248113,355.441482222345));
#120277=CARTESIAN_POINT('Ctrl Pts',(68.1986617481032,1076.31751514527,355.426070586806));
#120278=CARTESIAN_POINT('Ctrl Pts',(68.2819685228178,1076.31358867648,355.426070586806));
#120279=CARTESIAN_POINT('',(68.2819685228176,1082.7251047501,355.426070586806));
#120280=CARTESIAN_POINT('',(68.2819685228176,1067.7251047501,355.426070586806));
#120281=CARTESIAN_POINT('Origin',(68.2819685228176,1082.7251047501,356.101514707942));
#120282=CARTESIAN_POINT('Ctrl Pts',(68.2819685228178,1076.31358867648,355.426070586806));
#120283=CARTESIAN_POINT('Ctrl Pts',(68.2820960517956,1076.3135826657,355.426070586806));
#120284=CARTESIAN_POINT('Ctrl Pts',(68.2822235825154,1076.3135766565,355.426070622914));
#120285=CARTESIAN_POINT('Ctrl Pts',(68.2823511149623,1076.31357064887,355.426070695152));
#120286=CARTESIAN_POINT('Ctrl Pts',(68.3708482950225,1076.30940184007,355.426120822646));
#120287=CARTESIAN_POINT('Ctrl Pts',(68.4585121162839,1076.30607015087,355.443562902922));
#120288=CARTESIAN_POINT('Ctrl Pts',(68.6219598404336,1076.30152420804,355.51123144722));
#120289=CARTESIAN_POINT('Ctrl Pts',(68.6961761521499,1076.30034993916,355.560713989813));
#120290=CARTESIAN_POINT('Ctrl Pts',(68.8212687860782,1076.30035029981,355.685381908252));
#120291=CARTESIAN_POINT('Ctrl Pts',(68.8709521077544,1076.30152159786,355.759309061297));
#120292=CARTESIAN_POINT('Ctrl Pts',(68.9391073604367,1076.30605164107,355.92210943135));
#120293=CARTESIAN_POINT('Ctrl Pts',(68.9568921450285,1076.30936685706,356.009404789735));
#120294=CARTESIAN_POINT('Ctrl Pts',(68.957911846463,1076.31767337057,356.186036349548));
#120295=CARTESIAN_POINT('Ctrl Pts',(68.9410550673682,1076.3225870389,356.273669451315));
#120296=CARTESIAN_POINT('Ctrl Pts',(68.8745184277081,1076.33332184607,356.437597389258));
#120297=CARTESIAN_POINT('Ctrl Pts',(68.8254035959997,1076.33904115829,356.512296353457));
#120298=CARTESIAN_POINT('Ctrl Pts',(68.7001941369294,1076.35058538137,356.639474188949));
#120299=CARTESIAN_POINT('Ctrl Pts',(68.6249180721111,1076.35629672746,356.690330819141));
#120300=CARTESIAN_POINT('Ctrl Pts',(68.4595535166777,1076.36681187013,356.759271270782));
#120301=CARTESIAN_POINT('Ctrl Pts',(68.3712149398878,1076.37152119931,356.776958829078));
#120302=CARTESIAN_POINT('Ctrl Pts',(68.2819685228176,1076.37545952532,356.776958829078));
#120303=CARTESIAN_POINT('Origin',(81.8208965804709,1067.7251047501,359.019679174786));
#120304=CARTESIAN_POINT('',(81.8208965804941,1077.59408165984,357.920848038793));
#120305=CARTESIAN_POINT('Ctrl Pts',(81.8210035103925,1077.7359053691,360.118510305575));
#120306=CARTESIAN_POINT('Ctrl Pts',(81.9496451149812,1077.72579923846,360.118497787149));
#120307=CARTESIAN_POINT('Ctrl Pts',(82.0771867011425,1077.71429950911,360.095896627786));
#120308=CARTESIAN_POINT('Ctrl Pts',(82.3281251504515,1077.68850385192,360.004253756816));
#120309=CARTESIAN_POINT('Ctrl Pts',(82.4481865036554,1077.67428181328,359.932450106309));
#120310=CARTESIAN_POINT('Ctrl Pts',(82.6606388749049,1077.64490797405,359.743242171231));
#120311=CARTESIAN_POINT('Ctrl Pts',(82.7492199475112,1077.63002722378,359.625452369551));
#120312=CARTESIAN_POINT('Ctrl Pts',(82.8731938158463,1077.60287609857,359.366210021708));
#120313=CARTESIAN_POINT('Ctrl Pts',(82.9090582715662,1077.59078693907,359.227983574739));
#120314=CARTESIAN_POINT('Ctrl Pts',(82.9251667013517,1077.5719472468,358.964074781048));
#120315=CARTESIAN_POINT('Ctrl Pts',(82.9120606293678,1077.56483506721,358.841034095682));
#120316=CARTESIAN_POINT('Ctrl Pts',(82.853763293938,1077.55582794555,358.633407710144));
#120317=CARTESIAN_POINT('Ctrl Pts',(82.8175121955166,1077.55311661812,358.547673633375));
#120318=CARTESIAN_POINT('Ctrl Pts',(82.7555063823544,1077.55115313016,358.440996830497));
#120319=CARTESIAN_POINT('Ctrl Pts',(82.7390063568056,1077.55080121932,358.415160050793));
#120320=CARTESIAN_POINT('Ctrl Pts',(82.7107543559653,1077.55045507672,358.374751864592));
#120321=CARTESIAN_POINT('Ctrl Pts',(82.6996735929003,1077.55037484604,358.359732907036));
#120322=CARTESIAN_POINT('Ctrl Pts',(82.6779419959406,1077.5503191592,358.33179619459));
#120323=CARTESIAN_POINT('Ctrl Pts',(82.6673680872842,1077.55033373728,358.318825534113));
#120324=CARTESIAN_POINT('Ctrl Pts',(82.6428038034306,1077.55045913375,358.290060551153));
#120325=CARTESIAN_POINT('Ctrl Pts',(82.6286466693954,1077.55059402165,358.27441775756));
#120326=CARTESIAN_POINT('Ctrl Pts',(82.5852591569209,1077.55118740004,358.229166628975));
#120327=CARTESIAN_POINT('Ctrl Pts',(82.5547908274227,1077.55183251712,358.20080260558));
#120328=CARTESIAN_POINT('Ctrl Pts',(82.4106550737012,1077.55585407554,358.08113972463));
#120329=CARTESIAN_POINT('Ctrl Pts',(82.2812029852015,1077.56198574477,358.011350846977));
#120330=CARTESIAN_POINT('Ctrl Pts',(82.0291910157458,1077.57777641674,357.934338306733));
#120331=CARTESIAN_POINT('Ctrl Pts',(81.9116317904677,1077.5864420575,357.918283630983));
#120332=CARTESIAN_POINT('Ctrl Pts',(81.6650306041736,1077.60714755689,357.924349784796));
#120333=CARTESIAN_POINT('Ctrl Pts',(81.5378381430728,1077.61926818079,357.950159267881));
#120334=CARTESIAN_POINT('Ctrl Pts',(81.2890745397625,1077.64591669128,358.048172727042));
#120335=CARTESIAN_POINT('Ctrl Pts',(81.1708569576794,1077.66032572816,358.122964382053));
#120336=CARTESIAN_POINT('Ctrl Pts',(80.9632831192145,1077.68950104246,358.317409025053));
#120337=CARTESIAN_POINT('Ctrl Pts',(80.8777158067086,1077.70396833387,358.437319646737));
#120338=CARTESIAN_POINT('Ctrl Pts',(80.7603979468685,1077.72985602794,358.699258395091));
#120339=CARTESIAN_POINT('Ctrl Pts',(80.7280108804241,1077.74112813057,358.838017680069));
#120340=CARTESIAN_POINT('Ctrl Pts',(80.7182084206833,1077.75856839595,359.10417984325));
#120341=CARTESIAN_POINT('Ctrl Pts',(80.7349613879902,1077.7650481351,359.229086414236));
#120342=CARTESIAN_POINT('Ctrl Pts',(80.7976633685545,1077.77261700745,359.428981992576));
#120343=CARTESIAN_POINT('Ctrl Pts',(80.8320695343832,1077.77474977431,359.506263043289));
#120344=CARTESIAN_POINT('Ctrl Pts',(80.8898797516962,1077.77634355938,359.60405389632));
#120345=CARTESIAN_POINT('Ctrl Pts',(80.9057719866548,1077.77663908646,359.628639984643));
#120346=CARTESIAN_POINT('Ctrl Pts',(80.9331332808851,1077.77693110665,359.667474600064));
#120347=CARTESIAN_POINT('Ctrl Pts',(80.9440090002506,1077.77699826099,359.682122209562));
#120348=CARTESIAN_POINT('Ctrl Pts',(80.9654900791558,1077.77704056504,359.709596764533));
#120349=CARTESIAN_POINT('Ctrl Pts',(80.9760319875259,1077.77702329249,359.722466753914));
#120350=CARTESIAN_POINT('Ctrl Pts',(81.0007632700304,1077.77689835445,359.751298684624));
#120351=CARTESIAN_POINT('Ctrl Pts',(81.0151337479807,1077.77676647162,359.767096047392));
#120352=CARTESIAN_POINT('Ctrl Pts',(81.0600518878109,1077.77618036699,359.813672225824));
#120353=CARTESIAN_POINT('Ctrl Pts',(81.0919668509945,1077.77553457729,359.843068768853));
#120354=CARTESIAN_POINT('Ctrl Pts',(81.1684310725808,1077.77349360069,359.905561940639));
#120355=CARTESIAN_POINT('Ctrl Pts',(81.2139123191459,1077.77194299733,359.937321360241));
#120356=CARTESIAN_POINT('Ctrl Pts',(81.3532701792501,1077.76625859978,360.019729940068));
#120357=CARTESIAN_POINT('Ctrl Pts',(81.4522984247743,1077.76109302637,360.060296548066));
#120358=CARTESIAN_POINT('Ctrl Pts',(81.6424277467173,1077.74921977244,360.107610906314));
#120359=CARTESIAN_POINT('Ctrl Pts',(81.7315768295082,1077.74293076125,360.118519007902));
#120360=CARTESIAN_POINT('Ctrl Pts',(81.8210035103925,1077.7359053691,360.118510305575));
#120361=CARTESIAN_POINT('',(81.8208965804711,1075.58250670589,357.920848038793));
#120362=CARTESIAN_POINT('',(81.8208965804709,1067.7251047501,357.920848038793));
#120363=CARTESIAN_POINT('Ctrl Pts',(81.8203364796409,1075.72568197611,360.11851016803));
#120364=CARTESIAN_POINT('Ctrl Pts',(81.6748513000131,1075.73721127236,360.118436010702));
#120365=CARTESIAN_POINT('Ctrl Pts',(81.5306805462196,1075.74672849855,360.089469144153));
#120366=CARTESIAN_POINT('Ctrl Pts',(81.2618461305948,1075.76073707659,359.976824306072));
#120367=CARTESIAN_POINT('Ctrl Pts',(81.1399103591242,1075.7650899466,359.894302916234));
#120368=CARTESIAN_POINT('Ctrl Pts',(80.9352730099284,1075.768047685,359.686305972091));
#120369=CARTESIAN_POINT('Ctrl Pts',(80.8546944157296,1075.76662105825,359.562964091174));
#120370=CARTESIAN_POINT('Ctrl Pts',(80.7464431802241,1075.75810450695,359.292141971266));
#120371=CARTESIAN_POINT('Ctrl Pts',(80.7198546155749,1075.75110285212,359.147451758713));
#120372=CARTESIAN_POINT('Ctrl Pts',(80.7245685152145,1075.73231752799,358.856066705015));
#120373=CARTESIAN_POINT('Ctrl Pts',(80.7559361766191,1075.72071042844,358.71230042189));
#120374=CARTESIAN_POINT('Ctrl Pts',(80.873125219009,1075.69423688013,358.444657028142));
#120375=CARTESIAN_POINT('Ctrl Pts',(80.9581686919438,1075.67960707372,358.32356797675));
#120376=CARTESIAN_POINT('Ctrl Pts',(81.1165287884067,1075.65702132493,358.173233928333));
#120377=CARTESIAN_POINT('Ctrl Pts',(81.1734298595951,1075.64951009384,358.128954821535));
#120378=CARTESIAN_POINT('Ctrl Pts',(81.3578182002398,1075.62685045887,358.012531732351));
#120379=CARTESIAN_POINT('Ctrl Pts',(81.4957887389163,1075.61203371471,357.959897319903));
#120380=CARTESIAN_POINT('Ctrl Pts',(81.7826337015554,1075.58512819763,357.912046817121));
#120381=CARTESIAN_POINT('Ctrl Pts',(81.9286185636597,1075.57326760528,357.91659604885));
#120382=CARTESIAN_POINT('Ctrl Pts',(82.2098166212493,1075.5541349373,357.981952412458));
#120383=CARTESIAN_POINT('Ctrl Pts',(82.3423401505379,1075.54702471785,358.041772051681));
#120384=CARTESIAN_POINT('Ctrl Pts',(82.5761994330248,1075.53861721898,358.20883287706));
#120385=CARTESIAN_POINT('Ctrl Pts',(82.6753882754589,1075.53737025829,358.314121354662));
#120386=CARTESIAN_POINT('Ctrl Pts',(82.8276040985836,1075.54092604795,358.55662369521));
#120387=CARTESIAN_POINT('Ctrl Pts',(82.879210882916,1075.54567967013,358.691347940956));
#120388=CARTESIAN_POINT('Ctrl Pts',(82.9280594719914,1075.56054356659,358.973272901754));
#120389=CARTESIAN_POINT('Ctrl Pts',(82.9246469618963,1075.57052259812,359.117740886092));
#120390=CARTESIAN_POINT('Ctrl Pts',(82.8625822165472,1075.59435807866,359.397878520871));
#120391=CARTESIAN_POINT('Ctrl Pts',(82.8041739820782,1075.60800756338,359.530800078522));
#120392=CARTESIAN_POINT('Ctrl Pts',(82.6806331736267,1075.62980163666,359.707782908721));
#120393=CARTESIAN_POINT('Ctrl Pts',(82.6336243995114,1075.63725178508,359.762716196854));
#120394=CARTESIAN_POINT('Ctrl Pts',(82.5295312429813,1075.65226318573,359.862572687651));
#120395=CARTESIAN_POINT('Ctrl Pts',(82.4726866690676,1075.65978957021,359.907261992778));
#120396=CARTESIAN_POINT('Ctrl Pts',(82.2884884512699,1075.68231542504,360.02476940505));
#120397=CARTESIAN_POINT('Ctrl Pts',(82.1505373258723,1075.69681693572,360.078092773233));
#120398=CARTESIAN_POINT('Ctrl Pts',(81.9447607738923,1075.71547192738,360.11327867515));
#120399=CARTESIAN_POINT('Ctrl Pts',(81.8826168770904,1075.72074642765,360.11854191386));
#120400=CARTESIAN_POINT('Ctrl Pts',(81.8203364796409,1075.72568197611,360.11851016803));
#120401=CARTESIAN_POINT('Origin',(81.8208965804709,1067.7251047501,359.019679174786));
#120402=CARTESIAN_POINT('',(81.8208965804709,1075.68770968364,359.518510310778));
#120403=CARTESIAN_POINT('',(81.8208965804708,1075.62273721903,358.520848038793));
#120404=CARTESIAN_POINT('Ctrl Pts',(81.8208965804709,1075.68770968364,359.518510310778));
#120405=CARTESIAN_POINT('Ctrl Pts',(81.7879945785618,1075.6903532399,359.518510310778));
#120406=CARTESIAN_POINT('Ctrl Pts',(81.7550763799472,1075.69278479065,359.515255218438));
#120407=CARTESIAN_POINT('Ctrl Pts',(81.6575716992867,1075.69934037109,359.495663082824));
#120408=CARTESIAN_POINT('Ctrl Pts',(81.5957192253617,1075.70262161683,359.46972951162));
#120409=CARTESIAN_POINT('Ctrl Pts',(81.4863399484057,1075.70660325775,359.395478948915));
#120410=CARTESIAN_POINT('Ctrl Pts',(81.4397720828946,1075.70729150202,359.348162169015));
#120411=CARTESIAN_POINT('Ctrl Pts',(81.3680599741735,1075.70601502793,359.238772116286));
#120412=CARTESIAN_POINT('Ctrl Pts',(81.343401036283,1075.70409193481,359.177956954028));
#120413=CARTESIAN_POINT('Ctrl Pts',(81.3185003947358,1075.69780607712,359.048870127068));
#120414=CARTESIAN_POINT('Ctrl Pts',(81.3190988368862,1075.69345140553,358.981783870762));
#120415=CARTESIAN_POINT('Ctrl Pts',(81.3465173653583,1075.68286651085,358.85164093288));
#120416=CARTESIAN_POINT('Ctrl Pts',(81.3731663997571,1075.67673446555,358.7899068656));
#120417=CARTESIAN_POINT('Ctrl Pts',(81.4296859052742,1075.66688857504,358.708472190585));
#120418=CARTESIAN_POINT('Ctrl Pts',(81.4508538977159,1075.66355900733,358.683579325378));
#120419=CARTESIAN_POINT('Ctrl Pts',(81.4977877577823,1075.65680419623,358.638233899828));
#120420=CARTESIAN_POINT('Ctrl Pts',(81.5234558602621,1075.65339438285,358.61789717551));
#120421=CARTESIAN_POINT('Ctrl Pts',(81.6067070831681,1075.64312404903,358.564315958701));
#120422=CARTESIAN_POINT('Ctrl Pts',(81.6691226552038,1075.63642650157,358.539880240271));
#120423=CARTESIAN_POINT('Ctrl Pts',(81.7629342065803,1075.62766038669,358.523388114674));
#120424=CARTESIAN_POINT('Ctrl Pts',(81.7917338964536,1075.62513259164,358.520865178427));
#120425=CARTESIAN_POINT('Ctrl Pts',(81.8206019166418,1075.62276141663,358.520848125837));
#120426=CARTESIAN_POINT('Ctrl Pts',(81.8207001391889,1075.62275334878,358.520848067817));
#120427=CARTESIAN_POINT('Ctrl Pts',(81.8207983604694,1075.62274528291,358.520848038793));
#120428=CARTESIAN_POINT('Ctrl Pts',(81.8208965804707,1075.62273721903,358.520848038793));
#120429=CARTESIAN_POINT('',(81.8208965804709,1082.7251047501,358.520848038793));
#120430=CARTESIAN_POINT('',(81.8208965804709,1067.7251047501,358.520848038793));
#120431=CARTESIAN_POINT('Origin',(81.8208965804709,1082.7251047501,359.019679174786));
#120432=CARTESIAN_POINT('Ctrl Pts',(81.8208965804707,1075.62273721903,358.520848038793));
#120433=CARTESIAN_POINT('Ctrl Pts',(81.886228206205,1075.61737347788,358.520848038793));
#120434=CARTESIAN_POINT('Ctrl Pts',(81.9509939035222,1075.61288729907,358.533682714537));
#120435=CARTESIAN_POINT('Ctrl Pts',(82.0717020651763,1075.60623432872,358.583589329763));
#120436=CARTESIAN_POINT('Ctrl Pts',(82.1264928596674,1075.60412300937,358.620056055585));
#120437=CARTESIAN_POINT('Ctrl Pts',(82.2187957612182,1075.60258075092,358.711895613239));
#120438=CARTESIAN_POINT('Ctrl Pts',(82.255453124008,1075.60315492614,358.766277803405));
#120439=CARTESIAN_POINT('Ctrl Pts',(82.3058747440072,1075.60692094092,358.886058668206));
#120440=CARTESIAN_POINT('Ctrl Pts',(82.3191209577567,1075.61007699176,358.950275056747));
#120441=CARTESIAN_POINT('Ctrl Pts',(82.3202966963971,1075.61856836367,359.080395035986));
#120442=CARTESIAN_POINT('Ctrl Pts',(82.308088585028,1075.6238310256,359.145035623558));
#120443=CARTESIAN_POINT('Ctrl Pts',(82.2594537562011,1075.63577470265,359.266234841303));
#120444=CARTESIAN_POINT('Ctrl Pts',(82.2233441044727,1075.64234981651,359.321587259796));
#120445=CARTESIAN_POINT('Ctrl Pts',(82.154738941984,1075.65251450466,359.391771376562));
#120446=CARTESIAN_POINT('Ctrl Pts',(82.1296175665403,1075.65593017312,359.412864444856));
#120447=CARTESIAN_POINT('Ctrl Pts',(82.0475879396677,1075.66623581512,359.468999918754));
#120448=CARTESIAN_POINT('Ctrl Pts',(81.9855377649109,1075.67295302678,359.495264246264));
#120449=CARTESIAN_POINT('Ctrl Pts',(81.8873987449316,1075.68214848607,359.515183930342));
#120450=CARTESIAN_POINT('Ctrl Pts',(81.8541559389162,1075.68503741509,359.518510310778));
#120451=CARTESIAN_POINT('Ctrl Pts',(81.8208965804709,1075.68770968364,359.518510310778));
#120452=CARTESIAN_POINT('Origin',(94.6032580293201,1067.7251047501,364.698164080197));
#120453=CARTESIAN_POINT('',(94.603258029345,1076.74090351967,363.607623331469));
#120454=CARTESIAN_POINT('Ctrl Pts',(94.6034039085428,1076.89760555679,365.788704819168));
#120455=CARTESIAN_POINT('Ctrl Pts',(94.7345715164352,1076.88291957311,365.788687273167));
#120456=CARTESIAN_POINT('Ctrl Pts',(94.8645131843872,1076.86663458984,365.765007633727));
#120457=CARTESIAN_POINT('Ctrl Pts',(95.1194451714134,1076.8310043412,365.669165482204));
#120458=CARTESIAN_POINT('Ctrl Pts',(95.2409065605302,1076.81183546033,365.594092782859));
#120459=CARTESIAN_POINT('Ctrl Pts',(95.4504462837096,1076.77394048259,365.399853698011));
#120460=CARTESIAN_POINT('Ctrl Pts',(95.5358649587737,1076.75558261267,365.281629155982));
#120461=CARTESIAN_POINT('Ctrl Pts',(95.6520812154778,1076.72364186116,365.026360743801));
#120462=CARTESIAN_POINT('Ctrl Pts',(95.6848675699349,1076.71011204164,364.893053069973));
#120463=CARTESIAN_POINT('Ctrl Pts',(95.6993864053341,1076.68872730221,364.62404129982));
#120464=CARTESIAN_POINT('Ctrl Pts',(95.6821801915352,1076.68093172327,364.490785253847));
#120465=CARTESIAN_POINT('Ctrl Pts',(95.625009822732,1076.67452023046,364.313305550669));
#120466=CARTESIAN_POINT('Ctrl Pts',(95.6050800208169,1076.67321231869,364.264057828994));
#120467=CARTESIAN_POINT('Ctrl Pts',(95.5715298011371,1076.67209630214,364.195916599161));
#120468=CARTESIAN_POINT('Ctrl Pts',(95.560777705991,1076.67185854829,364.175709371293));
#120469=CARTESIAN_POINT('Ctrl Pts',(95.5422287287133,1076.67163221522,364.143347936837));
#120470=CARTESIAN_POINT('Ctrl Pts',(95.5348128341495,1076.67158400599,364.130984582994));
#120471=CARTESIAN_POINT('Ctrl Pts',(95.5187805069463,1076.67156534444,364.105419519539));
#120472=CARTESIAN_POINT('Ctrl Pts',(95.5101186477741,1076.67160256858,364.092250443705));
#120473=CARTESIAN_POINT('Ctrl Pts',(95.4889328370921,1076.67180192759,364.06151302807));
#120474=CARTESIAN_POINT('Ctrl Pts',(95.4761673802746,1076.67200500754,364.044120026008));
#120475=CARTESIAN_POINT('Ctrl Pts',(95.4326666278011,1076.67295764359,363.988393840474));
#120476=CARTESIAN_POINT('Ctrl Pts',(95.3998624117891,1076.67407276017,363.951764783842));
#120477=CARTESIAN_POINT('Ctrl Pts',(95.2610071374953,1076.68023247673,363.816330678941));
#120478=CARTESIAN_POINT('Ctrl Pts',(95.1383344063074,1076.68863564959,363.736994062286));
#120479=CARTESIAN_POINT('Ctrl Pts',(94.8940154330133,1076.70981701248,363.640471722811));
#120480=CARTESIAN_POINT('Ctrl Pts',(94.7779025299033,1076.72137604043,363.615263249293));
#120481=CARTESIAN_POINT('Ctrl Pts',(94.5312467376063,1076.74880671727,363.602370560171));
#120482=CARTESIAN_POINT('Ctrl Pts',(94.4022859908853,1076.76477130994,363.618587666129));
#120483=CARTESIAN_POINT('Ctrl Pts',(94.1464455761988,1076.79973329141,363.69818720285));
#120484=CARTESIAN_POINT('Ctrl Pts',(94.0227620182876,1076.81856805543,363.764545231607));
#120485=CARTESIAN_POINT('Ctrl Pts',(93.8025779388021,1076.85631439853,363.94373611102));
#120486=CARTESIAN_POINT('Ctrl Pts',(93.7094662193629,1076.87484481459,364.05670241198));
#120487=CARTESIAN_POINT('Ctrl Pts',(93.5758711658185,1076.90758767687,364.307041190962));
#120488=CARTESIAN_POINT('Ctrl Pts',(93.5344142658805,1076.92166706804,364.440881622791));
#120489=CARTESIAN_POINT('Ctrl Pts',(93.5055131619185,1076.94342908994,364.704071881101));
#120490=CARTESIAN_POINT('Ctrl Pts',(93.5134809992833,1076.95143159331,364.830604631922));
#120491=CARTESIAN_POINT('Ctrl Pts',(93.5600296450457,1076.95985923957,365.02420022273));
#120492=CARTESIAN_POINT('Ctrl Pts',(93.5842352256024,1076.96203225347,365.093417911572));
#120493=CARTESIAN_POINT('Ctrl Pts',(93.6263102562109,1076.96368941769,365.183489651022));
#120494=CARTESIAN_POINT('Ctrl Pts',(93.6382727170041,1076.96400364626,365.206859832407));
#120495=CARTESIAN_POINT('Ctrl Pts',(93.6591888633484,1076.96431490137,365.244323484867));
#120496=CARTESIAN_POINT('Ctrl Pts',(93.6676426918722,1076.96438582107,365.258682270905));
#120497=CARTESIAN_POINT('Ctrl Pts',(93.6845445728684,1076.96442611252,365.285941486676));
#120498=CARTESIAN_POINT('Ctrl Pts',(93.6929436471067,1076.96440268446,365.298867349726));
#120499=CARTESIAN_POINT('Ctrl Pts',(93.7129282675081,1076.96425008642,365.328240751172));
#120500=CARTESIAN_POINT('Ctrl Pts',(93.7247003152812,1076.96409087818,365.344554052353));
#120501=CARTESIAN_POINT('Ctrl Pts',(93.7624725316358,1076.96337400637,365.393958078733));
#120502=CARTESIAN_POINT('Ctrl Pts',(93.7899381971193,1076.96257174082,365.4258724012));
#120503=CARTESIAN_POINT('Ctrl Pts',(93.9196394980028,1076.95762238231,365.5600453961));
#120504=CARTESIAN_POINT('Ctrl Pts',(94.0396461207868,1076.95014294675,365.642843885717));
#120505=CARTESIAN_POINT('Ctrl Pts',(94.2465145052762,1076.93342147644,365.73188247013));
#120506=CARTESIAN_POINT('Ctrl Pts',(94.32417754157,1076.92644267633,365.755485767671));
#120507=CARTESIAN_POINT('Ctrl Pts',(94.4695833862916,1076.91213653877,365.782556602382));
#120508=CARTESIAN_POINT('Ctrl Pts',(94.5364491625008,1076.9051020441,365.788713775556));
#120509=CARTESIAN_POINT('Ctrl Pts',(94.6034039085428,1076.89760555679,365.788704819168));
#120510=CARTESIAN_POINT('',(94.6032580293202,1074.72198576327,363.607623331468));
#120511=CARTESIAN_POINT('',(94.6032580293201,1067.7251047501,363.607623331468));
#120512=CARTESIAN_POINT('Ctrl Pts',(94.6024843825279,1074.88008894717,365.788704554506));
#120513=CARTESIAN_POINT('Ctrl Pts',(94.4580905763941,1074.89638168322,365.788602119239));
#120514=CARTESIAN_POINT('Ctrl Pts',(94.3149041808003,1074.91041844163,365.759822716901));
#120515=CARTESIAN_POINT('Ctrl Pts',(94.0478148968823,1074.93239665398,365.647754598289));
#120516=CARTESIAN_POINT('Ctrl Pts',(93.9266353324091,1074.94011908936,365.565643651049));
#120517=CARTESIAN_POINT('Ctrl Pts',(93.7257672460261,1074.94807140394,365.360998186142));
#120518=CARTESIAN_POINT('Ctrl Pts',(93.6471830436114,1074.94839699918,365.24154621693));
#120519=CARTESIAN_POINT('Ctrl Pts',(93.5399736185817,1074.94180138391,364.978981084259));
#120520=CARTESIAN_POINT('Ctrl Pts',(93.5125448378681,1074.93493078036,364.83848532818));
#120521=CARTESIAN_POINT('Ctrl Pts',(93.5128953027451,1074.9145632267,364.551947282319));
#120522=CARTESIAN_POINT('Ctrl Pts',(93.5419373637495,1074.90112683102,364.408801334487));
#120523=CARTESIAN_POINT('Ctrl Pts',(93.6540884616984,1074.86941262532,364.14192291546));
#120524=CARTESIAN_POINT('Ctrl Pts',(93.7363418777446,1074.85142241365,364.020906732474));
#120525=CARTESIAN_POINT('Ctrl Pts',(93.943818278137,1074.81314300848,363.81742414112));
#120526=CARTESIAN_POINT('Ctrl Pts',(94.0674115956666,1074.7931995908,363.737215533729));
#120527=CARTESIAN_POINT('Ctrl Pts',(94.3382107013227,1074.75430992866,363.630397256631));
#120528=CARTESIAN_POINT('Ctrl Pts',(94.4827771833473,1074.73572547102,363.604566296967));
#120529=CARTESIAN_POINT('Ctrl Pts',(94.771631845205,1074.70273517309,363.611205121975));
#120530=CARTESIAN_POINT('Ctrl Pts',(94.9131470606423,1074.68858566121,363.642731415956));
#120531=CARTESIAN_POINT('Ctrl Pts',(95.1748321497686,1074.66662099108,363.75856755272));
#120532=CARTESIAN_POINT('Ctrl Pts',(95.2926172799575,1074.65896115871,363.841179675866));
#120533=CARTESIAN_POINT('Ctrl Pts',(95.4891311884377,1074.65118912929,364.046586066743));
#120534=CARTESIAN_POINT('Ctrl Pts',(95.5661545114112,1074.65109939044,364.166979738535));
#120535=CARTESIAN_POINT('Ctrl Pts',(95.6698641777838,1074.65849322358,364.430451950522));
#120536=CARTESIAN_POINT('Ctrl Pts',(95.6955094012144,1074.66589885394,364.57084618374));
#120537=CARTESIAN_POINT('Ctrl Pts',(95.6918976183761,1074.68726700068,364.854330615544));
#120538=CARTESIAN_POINT('Ctrl Pts',(95.6622668743928,1074.70106418117,364.994624476514));
#120539=CARTESIAN_POINT('Ctrl Pts',(95.5506493052697,1074.73326922215,365.256968123332));
#120540=CARTESIAN_POINT('Ctrl Pts',(95.4691819321429,1074.75141521818,365.37631789352));
#120541=CARTESIAN_POINT('Ctrl Pts',(95.3160734736272,1074.77995980457,365.526594003809));
#120542=CARTESIAN_POINT('Ctrl Pts',(95.2601887561047,1074.7896376246,365.57157168583));
#120543=CARTESIAN_POINT('Ctrl Pts',(95.1406646726612,1074.80898201746,365.649770123526));
#120544=CARTESIAN_POINT('Ctrl Pts',(95.0773227458251,1074.81860525188,365.682860159408));
#120545=CARTESIAN_POINT('Ctrl Pts',(94.8814544432978,1074.84661074313,365.761863484231));
#120546=CARTESIAN_POINT('Ctrl Pts',(94.7427005524783,1074.86426759646,365.788804026092));
#120547=CARTESIAN_POINT('Ctrl Pts',(94.602484382528,1074.88008894717,365.788704554506));
#120548=CARTESIAN_POINT('Origin',(94.6032580293201,1067.7251047501,364.698164080197));
#120549=CARTESIAN_POINT('',(94.6032580293201,1074.83751173097,365.188704828925));
#120550=CARTESIAN_POINT('',(94.6032580293198,1074.76643751182,364.207623331468));
#120551=CARTESIAN_POINT('Ctrl Pts',(94.6032580293201,1074.83751173097,365.188704828925));
#120552=CARTESIAN_POINT('Ctrl Pts',(94.5389061106776,1074.84482891857,365.188704828925));
#120553=CARTESIAN_POINT('Ctrl Pts',(94.4750626242078,1074.85116271567,365.176041667615));
#120554=CARTESIAN_POINT('Ctrl Pts',(94.355799041386,1074.86113145739,365.126600282273));
#120555=CARTESIAN_POINT('Ctrl Pts',(94.301577574366,1074.86466829042,365.090341076152));
#120556=CARTESIAN_POINT('Ctrl Pts',(94.2109220617968,1074.86841034894,364.999429988502));
#120557=CARTESIAN_POINT('Ctrl Pts',(94.1751501476945,1074.86862713673,364.945981842153));
#120558=CARTESIAN_POINT('Ctrl Pts',(94.1260143351309,1074.86575397584,364.82831382425));
#120559=CARTESIAN_POINT('Ctrl Pts',(94.113177601997,1074.86268898348,364.765276774419));
#120560=CARTESIAN_POINT('Ctrl Pts',(94.1122778758208,1074.85361851103,364.637475867034));
#120561=CARTESIAN_POINT('Ctrl Pts',(94.124409879171,1074.8476812996,364.573978135957));
#120562=CARTESIAN_POINT('Ctrl Pts',(94.1728220578349,1074.833538774,364.453940275409));
#120563=CARTESIAN_POINT('Ctrl Pts',(94.2092053512491,1074.82542114712,364.398796248784));
#120564=CARTESIAN_POINT('Ctrl Pts',(94.2778158189421,1074.81260148508,364.329731172231));
#120565=CARTESIAN_POINT('Ctrl Pts',(94.3025463005061,1074.80829768802,364.309284998983));
#120566=CARTESIAN_POINT('Ctrl Pts',(94.355671400612,1074.79963006164,364.273477049086));
#120567=CARTESIAN_POINT('Ctrl Pts',(94.3839538127132,1074.79528551796,364.258204655916));
#120568=CARTESIAN_POINT('Ctrl Pts',(94.4734209271869,1074.78231080277,364.220680126695));
#120569=CARTESIAN_POINT('Ctrl Pts',(94.5377780281442,1074.77397382395,364.207675108751));
#120570=CARTESIAN_POINT('Ctrl Pts',(94.6028689869237,1074.766482277,364.207623485824));
#120571=CARTESIAN_POINT('Ctrl Pts',(94.6029986698093,1074.76646735134,364.207623382974));
#120572=CARTESIAN_POINT('Ctrl Pts',(94.6031283506174,1074.76645242961,364.207623331468));
#120573=CARTESIAN_POINT('Ctrl Pts',(94.6032580293194,1074.76643751182,364.207623331468));
#120574=CARTESIAN_POINT('',(94.6032580293201,1082.7251047501,364.207623331468));
#120575=CARTESIAN_POINT('',(94.6032580293201,1067.7251047501,364.207623331468));
#120576=CARTESIAN_POINT('Origin',(94.6032580293201,1082.7251047501,364.698164080197));
#120577=CARTESIAN_POINT('Ctrl Pts',(94.6032580293194,1074.76643751182,364.207623331468));
#120578=CARTESIAN_POINT('Ctrl Pts',(94.6680332572963,1074.75898599329,364.207623331468));
#120579=CARTESIAN_POINT('Ctrl Pts',(94.732282812711,1074.75251641632,364.22045357071));
#120580=CARTESIAN_POINT('Ctrl Pts',(94.8513221203709,1074.74241360936,364.270156160834));
#120581=CARTESIAN_POINT('Ctrl Pts',(94.9050646308186,1074.73883903866,364.306169283017));
#120582=CARTESIAN_POINT('Ctrl Pts',(94.9954062537941,1074.73502183265,364.396654863073));
#120583=CARTESIAN_POINT('Ctrl Pts',(95.0312087567533,1074.73479450522,364.450076096674));
#120584=CARTESIAN_POINT('Ctrl Pts',(95.0803863796765,1074.73771692571,364.567632508475));
#120585=CARTESIAN_POINT('Ctrl Pts',(95.0932612525265,1074.74083680898,364.6305720752));
#120586=CARTESIAN_POINT('Ctrl Pts',(95.0943071710892,1074.75004537671,364.75818118997));
#120587=CARTESIAN_POINT('Ctrl Pts',(95.0822883095453,1074.7560633823,364.821590601207));
#120588=CARTESIAN_POINT('Ctrl Pts',(95.0345111409291,1074.77024359054,364.940668529626));
#120589=CARTESIAN_POINT('Ctrl Pts',(94.9989705004992,1074.77829084204,364.995113303414));
#120590=CARTESIAN_POINT('Ctrl Pts',(94.9315400724301,1074.7910311435,365.064078933143));
#120591=CARTESIAN_POINT('Ctrl Pts',(94.9068770365164,1074.79535855075,365.08478716013));
#120592=CARTESIAN_POINT('Ctrl Pts',(94.853912051573,1074.80404676007,365.121048452993));
#120593=CARTESIAN_POINT('Ctrl Pts',(94.8257343886553,1074.80838806796,365.136528568761));
#120594=CARTESIAN_POINT('Ctrl Pts',(94.7361499980262,1074.82138885907,365.17486371948));
#120595=CARTESIAN_POINT('Ctrl Pts',(94.6714494675528,1074.82973127462,365.188339619355));
#120596=CARTESIAN_POINT('Ctrl Pts',(94.6050444588179,1074.83730842527,365.18870238954));
#120597=CARTESIAN_POINT('Ctrl Pts',(94.6041511950963,1074.83741017283,365.188704828925));
#120598=CARTESIAN_POINT('Ctrl Pts',(94.6032580293201,1074.83751173097,365.188704828925));
#120599=CARTESIAN_POINT('Origin',(40.0345449899143,1067.7251047501,344.508373695255));
#120600=CARTESIAN_POINT('',(40.0345449899354,1078.63462185218,343.030070563061));
#120601=CARTESIAN_POINT('Ctrl Pts',(40.0345298081687,1078.70265697563,345.98667682737));
#120602=CARTESIAN_POINT('Ctrl Pts',(40.1870769959575,1078.70139267951,345.986678393986));
#120603=CARTESIAN_POINT('Ctrl Pts',(40.3387045132084,1078.69970637529,345.963067796558));
#120604=CARTESIAN_POINT('Ctrl Pts',(40.6443100614649,1078.69522348719,345.865531202951));
#120605=CARTESIAN_POINT('Ctrl Pts',(40.7946868828938,1078.69235957377,345.787384514896));
#120606=CARTESIAN_POINT('Ctrl Pts',(41.0731536536299,1078.68537357539,345.575890364103));
#120607=CARTESIAN_POINT('Ctrl Pts',(41.1962041796893,1078.68122519747,345.440489855969));
#120608=CARTESIAN_POINT('Ctrl Pts',(41.3942627051156,1078.67182114612,345.120395956006));
#120609=CARTESIAN_POINT('Ctrl Pts',(41.4630461188509,1078.66659597651,344.935906577345));
#120610=CARTESIAN_POINT('Ctrl Pts',(41.5247801004033,1078.65617516795,344.552542153899));
#120611=CARTESIAN_POINT('Ctrl Pts',(41.5177816248192,1078.65108473326,344.35748835509));
#120612=CARTESIAN_POINT('Ctrl Pts',(41.4327450684474,1078.64233694907,343.996615763979));
#120613=CARTESIAN_POINT('Ctrl Pts',(41.3612884748127,1078.63867249004,343.832636670864));
#120614=CARTESIAN_POINT('Ctrl Pts',(41.1751693589469,1078.63331757418,343.554987476488));
#120615=CARTESIAN_POINT('Ctrl Pts',(41.0676812309894,1078.63148296546,343.439447183941));
#120616=CARTESIAN_POINT('Ctrl Pts',(40.900837799776,1078.63009065238,343.309240123584));
#120617=CARTESIAN_POINT('Ctrl Pts',(40.8557842742147,1078.62982884019,343.277946656458));
#120618=CARTESIAN_POINT('Ctrl Pts',(40.7803487871408,1078.62956909741,343.231543233202));
#120619=CARTESIAN_POINT('Ctrl Pts',(40.7510034224305,1078.62950848805,343.214848799138));
#120620=CARTESIAN_POINT('Ctrl Pts',(40.6942129493864,1078.62946662967,343.185066887409));
#120621=CARTESIAN_POINT('Ctrl Pts',(40.6668851573709,1078.6294780536,343.171792745258));
#120622=CARTESIAN_POINT('Ctrl Pts',(40.6042326255494,1078.62957444674,343.143711907255));
#120623=CARTESIAN_POINT('Ctrl Pts',(40.5687023967708,1078.62967776305,343.129416972725));
#120624=CARTESIAN_POINT('Ctrl Pts',(40.4622711798401,1078.63012789365,343.091327746049));
#120625=CARTESIAN_POINT('Ctrl Pts',(40.3900764676671,1078.63061242729,343.071513947266));
#120626=CARTESIAN_POINT('Ctrl Pts',(40.1235794022449,1078.63302242121,343.019697593838));
#120627=CARTESIAN_POINT('Ctrl Pts',(39.9249134544416,1078.63599068713,343.021076484672));
#120628=CARTESIAN_POINT('Ctrl Pts',(39.5729307101086,1078.64308306182,343.094577439807));
#120629=CARTESIAN_POINT('Ctrl Pts',(39.4200998508842,1078.64686751981,343.153988802032));
#120630=CARTESIAN_POINT('Ctrl Pts',(39.1286721787148,1078.65540846637,343.326949504323));
#120631=CARTESIAN_POINT('Ctrl Pts',(38.9945511780422,1078.66014661647,343.443113584532));
#120632=CARTESIAN_POINT('Ctrl Pts',(38.7656111355713,1078.669929276,343.726871526025));
#120633=CARTESIAN_POINT('Ctrl Pts',(38.676366399166,1078.67487810754,343.894945216506));
#120634=CARTESIAN_POINT('Ctrl Pts',(38.5639733887957,1078.68414479644,344.261723965494));
#120635=CARTESIAN_POINT('Ctrl Pts',(38.5442910887746,1078.68834557585,344.457684168192));
#120636=CARTESIAN_POINT('Ctrl Pts',(38.5813876113478,1078.69532059509,344.838189453119));
#120637=CARTESIAN_POINT('Ctrl Pts',(38.634805416616,1078.69808858127,345.019432170996));
#120638=CARTESIAN_POINT('Ctrl Pts',(38.8090992727656,1078.70241362814,345.357446072826));
#120639=CARTESIAN_POINT('Ctrl Pts',(38.9303211481427,1078.7038969122,345.510039693333));
#120640=CARTESIAN_POINT('Ctrl Pts',(39.1226285262451,1078.70497375118,345.67340753571));
#120641=CARTESIAN_POINT('Ctrl Pts',(39.1700835710925,1078.70516294444,345.709041005679));
#120642=CARTESIAN_POINT('Ctrl Pts',(39.2513688025827,1078.70537039742,345.762753910481));
#120643=CARTESIAN_POINT('Ctrl Pts',(39.2839893481535,1078.70542545781,345.782540442394));
#120644=CARTESIAN_POINT('Ctrl Pts',(39.3435674557254,1078.70547731213,345.815595916527));
#120645=CARTESIAN_POINT('Ctrl Pts',(39.3702333284403,1078.70548401993,345.829346785688));
#120646=CARTESIAN_POINT('Ctrl Pts',(39.4271176663775,1078.70546425427,345.856522157912));
#120647=CARTESIAN_POINT('Ctrl Pts',(39.4574055970158,1078.70543434374,345.869763554872));
#120648=CARTESIAN_POINT('Ctrl Pts',(39.5373721782761,1078.7053054182,345.901575027128));
#120649=CARTESIAN_POINT('Ctrl Pts',(39.587651027545,1078.70517570101,345.918507205525));
#120650=CARTESIAN_POINT('Ctrl Pts',(39.7676148496473,1078.70453971941,345.968518380772));
#120651=CARTESIAN_POINT('Ctrl Pts',(39.9007648912784,1078.70376560612,345.986675453643));
#120652=CARTESIAN_POINT('Ctrl Pts',(40.0345298081687,1078.70265697563,345.98667682737));
#120653=CARTESIAN_POINT('',(40.0345449898976,1076.63346048996,343.030070563062));
#120654=CARTESIAN_POINT('',(40.0345449899143,1067.7251047501,343.030070563062));
#120655=CARTESIAN_POINT('Ctrl Pts',(40.0345647694422,1076.70230005615,345.986676827316));
#120656=CARTESIAN_POINT('Ctrl Pts',(39.8381690817314,1076.70394762921,345.986679455068));
#120657=CARTESIAN_POINT('Ctrl Pts',(39.6437235768841,1076.70486623863,345.947544487483));
#120658=CARTESIAN_POINT('Ctrl Pts',(39.2812618398217,1076.70533123689,345.795472409541));
#120659=CARTESIAN_POINT('Ctrl Pts',(39.1169027655019,1076.70487241795,345.683954438994));
#120660=CARTESIAN_POINT('Ctrl Pts',(38.8422407547009,1076.70253132886,345.403939431545));
#120661=CARTESIAN_POINT('Ctrl Pts',(38.7343551487054,1076.70067430054,345.238530258621));
#120662=CARTESIAN_POINT('Ctrl Pts',(38.5895216200697,1076.6954824908,344.876090383321));
#120663=CARTESIAN_POINT('Ctrl Pts',(38.5537025844545,1076.69219612885,344.682744773146));
#120664=CARTESIAN_POINT('Ctrl Pts',(38.5590755428721,1076.68424813219,344.292265910432));
#120665=CARTESIAN_POINT('Ctrl Pts',(38.6006335398305,1076.67965161652,344.098981965935));
#120666=CARTESIAN_POINT('Ctrl Pts',(38.7175062361582,1076.67212935267,343.829909392309));
#120667=CARTESIAN_POINT('Ctrl Pts',(38.7651558928275,1076.66954215796,343.74446561809));
#120668=CARTESIAN_POINT('Ctrl Pts',(38.931623387017,1076.66168215188,343.505094156789));
#120669=CARTESIAN_POINT('Ctrl Pts',(39.0726414234504,1076.65635074054,343.369185675713));
#120670=CARTESIAN_POINT('Ctrl Pts',(39.3991621772117,1076.64631592817,343.159551097859));
#120671=CARTESIAN_POINT('Ctrl Pts',(39.5815172535644,1076.64171670725,343.08787721764));
#120672=CARTESIAN_POINT('Ctrl Pts',(39.9633978584457,1076.6342187386,343.019100194819));
#120673=CARTESIAN_POINT('Ctrl Pts',(40.159205054712,1076.63139847529,343.022618519874));
#120674=CARTESIAN_POINT('Ctrl Pts',(40.5379335556789,1076.62819188702,343.104998264033));
#120675=CARTESIAN_POINT('Ctrl Pts',(40.7172015103969,1076.6278351644,343.182913632582));
#120676=CARTESIAN_POINT('Ctrl Pts',(41.0351944871715,1076.62968477286,343.403195653141));
#120677=CARTESIAN_POINT('Ctrl Pts',(41.1709204276943,1076.63186629871,343.543303964137));
#120678=CARTESIAN_POINT('Ctrl Pts',(41.3807213749652,1076.63829496575,343.867685954405));
#120679=CARTESIAN_POINT('Ctrl Pts',(41.4528055038673,1076.64247319015,344.048811916474));
#120680=CARTESIAN_POINT('Ctrl Pts',(41.5232926801648,1076.65196438147,344.428654534693));
#120681=CARTESIAN_POINT('Ctrl Pts',(41.5209540579369,1076.65718006625,344.623734821265));
#120682=CARTESIAN_POINT('Ctrl Pts',(41.461261755044,1076.66505854813,344.907362481619));
#120683=CARTESIAN_POINT('Ctrl Pts',(41.4321470439931,1076.66767583019,344.99972042017));
#120684=CARTESIAN_POINT('Ctrl Pts',(41.3563368966256,1076.67280097439,345.177379111665));
#120685=CARTESIAN_POINT('Ctrl Pts',(41.3098333686639,1076.67529657552,345.262258612636));
#120686=CARTESIAN_POINT('Ctrl Pts',(41.1452079246329,1076.68253558073,345.50335243865));
#120687=CARTESIAN_POINT('Ctrl Pts',(41.0041200277274,1076.68688658498,345.641285195669));
#120688=CARTESIAN_POINT('Ctrl Pts',(40.6769876094355,1076.69429247959,345.853953686285));
#120689=CARTESIAN_POINT('Ctrl Pts',(40.4942945461983,1076.69728591065,345.926808178478));
#120690=CARTESIAN_POINT('Ctrl Pts',(40.2142754775636,1076.70064097964,345.978464690868));
#120691=CARTESIAN_POINT('Ctrl Pts',(40.1245146495462,1076.7015454622,345.986675623797));
#120692=CARTESIAN_POINT('Ctrl Pts',(40.0345647694422,1076.70230005615,345.986676827316));
#120693=CARTESIAN_POINT('Origin',(40.0345449899143,1067.7251047501,344.508373695255));
#120694=CARTESIAN_POINT('',(40.0345449899143,1076.69158153387,345.386676827448));
#120695=CARTESIAN_POINT('',(40.034544986754,1076.65067043015,343.630070563062));
#120696=CARTESIAN_POINT('Ctrl Pts',(40.0345449899143,1076.69158153387,345.386676827448));
#120697=CARTESIAN_POINT('Ctrl Pts',(39.9786335213035,1076.69212537235,345.386676827448));
#120698=CARTESIAN_POINT('Ctrl Pts',(39.9227111060459,1076.69256032714,345.38133799963));
#120699=CARTESIAN_POINT('Ctrl Pts',(39.7524248425115,1076.69355902828,345.348358848986));
#120700=CARTESIAN_POINT('Ctrl Pts',(39.6429228985649,1076.69373899373,345.303231742983));
#120701=CARTESIAN_POINT('Ctrl Pts',(39.448278352782,1076.69310701969,345.172761769052));
#120702=CARTESIAN_POINT('Ctrl Pts',(39.3650471625921,1076.69230229399,345.088797046905));
#120703=CARTESIAN_POINT('Ctrl Pts',(39.2366872348667,1076.68973511117,344.893628048601));
#120704=CARTESIAN_POINT('Ctrl Pts',(39.1926679333464,1076.687999699,344.784486146156));
#120705=CARTESIAN_POINT('Ctrl Pts',(39.1498113885486,1076.68369650378,344.55549678087));
#120706=CARTESIAN_POINT('Ctrl Pts',(39.1513641080747,1076.68116920148,344.437928321518));
#120707=CARTESIAN_POINT('Ctrl Pts',(39.1877575310469,1076.67698995566,344.268331674107));
#120708=CARTESIAN_POINT('Ctrl Pts',(39.205126676018,1076.67555954236,344.213867043996));
#120709=CARTESIAN_POINT('Ctrl Pts',(39.2502520250954,1076.67261762342,344.10890519359));
#120710=CARTESIAN_POINT('Ctrl Pts',(39.2779349695538,1076.67111286994,344.058671909614));
#120711=CARTESIAN_POINT('Ctrl Pts',(39.3761497672044,1076.6665198648,343.915517746365));
#120712=CARTESIAN_POINT('Ctrl Pts',(39.4604198919524,1076.6634462406,343.833581805168));
#120713=CARTESIAN_POINT('Ctrl Pts',(39.6549650142604,1076.65777816535,343.707999929808));
#120714=CARTESIAN_POINT('Ctrl Pts',(39.763074061024,1076.65523628195,343.665173713736));
#120715=CARTESIAN_POINT('Ctrl Pts',(39.9286757203146,1076.6522249091,343.634854570039));
#120716=CARTESIAN_POINT('Ctrl Pts',(39.9816183328414,1076.65138505455,343.630070563443));
#120717=CARTESIAN_POINT('Ctrl Pts',(40.0345449835937,1076.65067043015,343.630070563062));
#120718=CARTESIAN_POINT('',(40.0345449899143,1082.7251047501,343.630070563062));
#120719=CARTESIAN_POINT('',(40.0345449899143,1067.7251047501,343.630070563062));
#120720=CARTESIAN_POINT('Origin',(40.0345449899143,1082.7251047501,344.508373695255));
#120721=CARTESIAN_POINT('Ctrl Pts',(40.0345449835937,1076.65067043015,343.630070563062));
#120722=CARTESIAN_POINT('Ctrl Pts',(40.0962035459098,1076.64983790604,343.630070562618));
#120723=CARTESIAN_POINT('Ctrl Pts',(40.1578404465244,1076.64917544013,343.636563440191));
#120724=CARTESIAN_POINT('Ctrl Pts',(40.3308810453299,1076.64782522135,343.673611547947));
#120725=CARTESIAN_POINT('Ctrl Pts',(40.4375233994829,1076.64762160324,343.719544297305));
#120726=CARTESIAN_POINT('Ctrl Pts',(40.6269430771155,1076.64859800546,343.849829191404));
#120727=CARTESIAN_POINT('Ctrl Pts',(40.7079102894806,1076.6497664633,343.932880149146));
#120728=CARTESIAN_POINT('Ctrl Pts',(40.8332649402529,1076.65325914728,344.125415059333));
#120729=CARTESIAN_POINT('Ctrl Pts',(40.8764455468128,1076.6555473135,344.233036523614));
#120730=CARTESIAN_POINT('Ctrl Pts',(40.9068968632132,1076.65933360956,344.394815192062));
#120731=CARTESIAN_POINT('Ctrl Pts',(40.9119290308596,1076.66053770417,344.444418012714));
#120732=CARTESIAN_POINT('Ctrl Pts',(40.9127333929343,1076.66178363424,344.494177892296));
#120733=CARTESIAN_POINT('Ctrl Pts',(40.9145913478028,1076.66466154447,344.609115696348));
#120734=CARTESIAN_POINT('Ctrl Pts',(40.8938666841488,1076.66772012843,344.723306089928));
#120735=CARTESIAN_POINT('Ctrl Pts',(40.8307220192165,1076.67226453346,344.883616932722));
#120736=CARTESIAN_POINT('Ctrl Pts',(40.8045283503295,1076.67376017027,344.934790321281));
#120737=CARTESIAN_POINT('Ctrl Pts',(40.7105285925089,1076.67817941879,345.081133380678));
#120738=CARTESIAN_POINT('Ctrl Pts',(40.6286166916474,1076.68093604389,345.165708538019));
#120739=CARTESIAN_POINT('Ctrl Pts',(40.4366974478299,1076.68578220386,345.297829447687));
#120740=CARTESIAN_POINT('Ctrl Pts',(40.3286359851419,1076.68782722287,345.344125209233));
#120741=CARTESIAN_POINT('Ctrl Pts',(40.1553017976055,1076.69027980393,345.380449449774));
#120742=CARTESIAN_POINT('Ctrl Pts',(40.0949297780623,1076.69099418439,345.386676827448));
#120743=CARTESIAN_POINT('Ctrl Pts',(40.0345449899143,1076.69158153387,345.386676827448));
#120744=CARTESIAN_POINT('Origin',(52.543999119444,1067.7251047501,343.402193778667));
#120745=CARTESIAN_POINT('',(52.5439991194616,1078.27787179661,342.12674965753));
#120746=CARTESIAN_POINT('Ctrl Pts',(52.5439470409818,1078.414918165,344.67763789874));
#120747=CARTESIAN_POINT('Ctrl Pts',(52.6806287622999,1078.41052452383,344.677643479677));
#120748=CARTESIAN_POINT('Ctrl Pts',(52.8163853250807,1078.40503088569,344.65567846108));
#120749=CARTESIAN_POINT('Ctrl Pts',(53.0877764056428,1078.39154679656,344.5655398441));
#120750=CARTESIAN_POINT('Ctrl Pts',(53.2201162054865,1078.3834727294,344.493938536534));
#120751=CARTESIAN_POINT('Ctrl Pts',(53.4629019934239,1078.36520134234,344.301195872381));
#120752=CARTESIAN_POINT('Ctrl Pts',(53.5687394638358,1078.35504826614,344.178388505717));
#120753=CARTESIAN_POINT('Ctrl Pts',(53.7333383278594,1078.33388013324,343.892865438981));
#120754=CARTESIAN_POINT('Ctrl Pts',(53.7878043824023,1078.32305394832,343.731206514432));
#120755=CARTESIAN_POINT('Ctrl Pts',(53.8299759183017,1078.30309729252,343.400679940482));
#120756=CARTESIAN_POINT('Ctrl Pts',(53.8191019530346,1078.29411629439,343.235191379999));
#120757=CARTESIAN_POINT('Ctrl Pts',(53.7391934951799,1078.27978612663,342.932863065434));
#120758=CARTESIAN_POINT('Ctrl Pts',(53.6765468888482,1078.27428018031,342.797109888813));
#120759=CARTESIAN_POINT('Ctrl Pts',(53.5357022654691,1078.26778955493,342.594101148773));
#120760=CARTESIAN_POINT('Ctrl Pts',(53.4702493947951,1078.26592976164,342.519836287121));
#120761=CARTESIAN_POINT('Ctrl Pts',(53.3684220975573,1078.26443171191,342.428258731446));
#120762=CARTESIAN_POINT('Ctrl Pts',(53.3388244100163,1078.26413114032,342.403957521689));
#120763=CARTESIAN_POINT('Ctrl Pts',(53.2880554917141,1078.26383087659,342.365965283963));
#120764=CARTESIAN_POINT('Ctrl Pts',(53.2674921492526,1078.26376336979,342.351504848028));
#120765=CARTESIAN_POINT('Ctrl Pts',(53.2266567979879,1078.26373244668,342.324556416679));
#120766=CARTESIAN_POINT('Ctrl Pts',(53.2064359306392,1078.26376367514,342.31200973171));
#120767=CARTESIAN_POINT('Ctrl Pts',(53.1584316695823,1078.26394450058,342.284052910683));
#120768=CARTESIAN_POINT('Ctrl Pts',(53.1304003051289,1078.26413017116,342.26910068918));
#120769=CARTESIAN_POINT('Ctrl Pts',(53.0402284246735,1078.26497458922,342.225245110275));
#120770=CARTESIAN_POINT('Ctrl Pts',(52.9763066088944,1078.26593088975,342.200295062625));
#120771=CARTESIAN_POINT('Ctrl Pts',(52.7478690818006,1078.2705386644,342.131722806857));
#120772=CARTESIAN_POINT('Ctrl Pts',(52.5769645665709,1078.27604053758,342.115907675524));
#120773=CARTESIAN_POINT('Ctrl Pts',(52.268016297067,1078.28940144417,342.149027699748));
#120774=CARTESIAN_POINT('Ctrl Pts',(52.131482905164,1078.29660142415,342.18712348529));
#120775=CARTESIAN_POINT('Ctrl Pts',(51.865880749568,1078.31324185179,342.311253696498));
#120776=CARTESIAN_POINT('Ctrl Pts',(51.7404935650894,1078.3226834259,342.400018787585));
#120777=CARTESIAN_POINT('Ctrl Pts',(51.5192208871175,1078.34284470951,342.625455281768));
#120778=CARTESIAN_POINT('Ctrl Pts',(51.4281787326337,1078.35342112333,342.763097396756));
#120779=CARTESIAN_POINT('Ctrl Pts',(51.3012247989589,1078.37398239285,343.069650137752));
#120780=CARTESIAN_POINT('Ctrl Pts',(51.2682200221517,1078.38374276718,343.236379318044));
#120781=CARTESIAN_POINT('Ctrl Pts',(51.2688793490305,1078.40054058862,343.56526497517));
#120782=CARTESIAN_POINT('Ctrl Pts',(51.2994994186301,1078.40753814576,343.724340385699));
#120783=CARTESIAN_POINT('Ctrl Pts',(51.4200335928109,1078.41874857271,344.027373443867));
#120784=CARTESIAN_POINT('Ctrl Pts',(51.5105682129547,1078.42276773402,344.167827510623));
#120785=CARTESIAN_POINT('Ctrl Pts',(51.6632745076855,1078.42569550122,344.326344748451));
#120786=CARTESIAN_POINT('Ctrl Pts',(51.7035848423353,1078.42622028533,344.363149096999));
#120787=CARTESIAN_POINT('Ctrl Pts',(51.7684815765133,1078.42671193573,344.41518498354));
#120788=CARTESIAN_POINT('Ctrl Pts',(51.7914328720423,1078.42682522576,344.432350422273));
#120789=CARTESIAN_POINT('Ctrl Pts',(51.8339428942365,1078.42692850034,344.461964535543));
#120790=CARTESIAN_POINT('Ctrl Pts',(51.8532998285876,1078.42693794926,344.474680791104));
#120791=CARTESIAN_POINT('Ctrl Pts',(51.8952905869465,1078.42687980587,344.500657456102));
#120792=CARTESIAN_POINT('Ctrl Pts',(51.9180089549087,1078.42680186758,344.513760920601));
#120793=CARTESIAN_POINT('Ctrl Pts',(51.9797073234866,1078.42646826494,344.546855462759));
#120794=CARTESIAN_POINT('Ctrl Pts',(52.0193394914607,1078.42612873875,344.565554300254));
#120795=CARTESIAN_POINT('Ctrl Pts',(52.1978811024911,1078.4240594286,344.638809653504));
#120796=CARTESIAN_POINT('Ctrl Pts',(52.3447533564488,1078.42096974804,344.67077594215));
#120797=CARTESIAN_POINT('Ctrl Pts',(52.5104912914418,1078.41597667431,344.677307423537));
#120798=CARTESIAN_POINT('Ctrl Pts',(52.5272186158717,1078.41545590111,344.677637215691));
#120799=CARTESIAN_POINT('Ctrl Pts',(52.5439470409818,1078.414918165,344.677637898739));
#120800=CARTESIAN_POINT('',(52.5439991194251,1076.27285491302,342.12674965753));
#120801=CARTESIAN_POINT('',(52.543999119444,1067.7251047501,342.126749657531));
#120802=CARTESIAN_POINT('Ctrl Pts',(52.5448741578425,1076.41130048726,344.677637599636));
#120803=CARTESIAN_POINT('Ctrl Pts',(52.3760585255815,1076.4167911207,344.67775341827));
#120804=CARTESIAN_POINT('Ctrl Pts',(52.2088482972886,1076.42049246151,344.644351612941));
#120805=CARTESIAN_POINT('Ctrl Pts',(51.8969113527991,1076.42404043833,344.514231820045));
#120806=CARTESIAN_POINT('Ctrl Pts',(51.7553423336663,1076.42384876801,344.418741966092));
#120807=CARTESIAN_POINT('Ctrl Pts',(51.5178702888806,1076.41954871692,344.178292808864));
#120808=CARTESIAN_POINT('Ctrl Pts',(51.4242785122984,1076.41548646548,344.035808714357));
#120809=CARTESIAN_POINT('Ctrl Pts',(51.2980352713163,1076.40384472051,343.722815650814));
#120810=CARTESIAN_POINT('Ctrl Pts',(51.2666181326482,1076.3963770296,343.555427530059));
#120811=CARTESIAN_POINT('Ctrl Pts',(51.2706886250048,1076.37874428829,343.217261708239));
#120812=CARTESIAN_POINT('Ctrl Pts',(51.3065307289596,1076.36873442188,343.049834047307));
#120813=CARTESIAN_POINT('Ctrl Pts',(51.407604560614,1076.35276810011,342.816974900379));
#120814=CARTESIAN_POINT('Ctrl Pts',(51.4487844347974,1076.34734114316,342.743121125799));
#120815=CARTESIAN_POINT('Ctrl Pts',(51.5926665317801,1076.33100148369,342.536271250745));
#120816=CARTESIAN_POINT('Ctrl Pts',(51.7145906311547,1076.32011487132,342.418857721563));
#120817=CARTESIAN_POINT('Ctrl Pts',(51.9968842888048,1076.2996593575,342.237923173106));
#120818=CARTESIAN_POINT('Ctrl Pts',(52.1545332014154,1076.29029077785,342.176135972092));
#120819=CARTESIAN_POINT('Ctrl Pts',(52.4844665501504,1076.27456705509,342.117189794759));
#120820=CARTESIAN_POINT('Ctrl Pts',(52.6535123759482,1076.26836276017,342.120464788608));
#120821=CARTESIAN_POINT('Ctrl Pts',(52.980196402225,1076.26016733156,342.192089869105));
#120822=CARTESIAN_POINT('Ctrl Pts',(53.1346721618463,1076.25824420501,342.259503616586));
#120823=CARTESIAN_POINT('Ctrl Pts',(53.4085097230585,1076.25901715282,342.449777353806));
#120824=CARTESIAN_POINT('Ctrl Pts',(53.525287599844,1076.26169208717,342.570612864856));
#120825=CARTESIAN_POINT('Ctrl Pts',(53.7058022611237,1076.27122502918,342.8502324545));
#120826=CARTESIAN_POINT('Ctrl Pts',(53.7677911877719,1076.2779866748,343.006293756194));
#120827=CARTESIAN_POINT('Ctrl Pts',(53.8284633256784,1076.2945610217,343.333678621171));
#120828=CARTESIAN_POINT('Ctrl Pts',(53.8264053467256,1076.30421755588,343.501892394966));
#120829=CARTESIAN_POINT('Ctrl Pts',(53.7576888084343,1076.32499206789,343.828362276718));
#120830=CARTESIAN_POINT('Ctrl Pts',(53.691504005586,1076.33591258319,343.983474542858));
#120831=CARTESIAN_POINT('Ctrl Pts',(53.503066844489,1076.35747764861,344.259447919595));
#120832=CARTESIAN_POINT('Ctrl Pts',(53.382571470997,1076.36791606443,344.377650827589));
#120833=CARTESIAN_POINT('Ctrl Pts',(53.1014708282764,1076.38707781672,344.561706105059));
#120834=CARTESIAN_POINT('Ctrl Pts',(52.9432602796086,1076.39559959136,344.62525367013));
#120835=CARTESIAN_POINT('Ctrl Pts',(52.7005954176518,1076.40586432971,344.670384508208));
#120836=CARTESIAN_POINT('Ctrl Pts',(52.6228257610832,1076.40876515523,344.677584119706));
#120837=CARTESIAN_POINT('Ctrl Pts',(52.5448741578425,1076.41130048726,344.677637599636));
#120838=CARTESIAN_POINT('Origin',(52.543999119444,1067.7251047501,343.402193778667));
#120839=CARTESIAN_POINT('',(52.543999119444,1076.38098512892,344.077637899803));
#120840=CARTESIAN_POINT('',(52.5439991194442,1076.3076507295,342.726749657531));
#120841=CARTESIAN_POINT('Ctrl Pts',(52.543999119444,1076.38098512892,344.077637899803));
#120842=CARTESIAN_POINT('Ctrl Pts',(52.5433807264998,1076.38100599235,344.077637899803));
#120843=CARTESIAN_POINT('Ctrl Pts',(52.542762289986,1076.3810268122,344.077637050562));
#120844=CARTESIAN_POINT('Ctrl Pts',(52.4523875817405,1076.38406271807,344.077388808654));
#120845=CARTESIAN_POINT('Ctrl Pts',(52.3635521603753,1076.38609930809,344.059253661504));
#120846=CARTESIAN_POINT('Ctrl Pts',(52.1981297309606,1076.3880170916,343.989276229176));
#120847=CARTESIAN_POINT('Ctrl Pts',(52.1232170008691,1076.38787904209,343.938135262467));
#120848=CARTESIAN_POINT('Ctrl Pts',(51.9977994361851,1076.38542237209,343.809568380947));
#120849=CARTESIAN_POINT('Ctrl Pts',(51.9485567483193,1076.38312830049,343.733445801916));
#120850=CARTESIAN_POINT('Ctrl Pts',(51.8826782488512,1076.37662930272,343.566366025876));
#120851=CARTESIAN_POINT('Ctrl Pts',(51.8667406204239,1076.37248613241,343.477071121541));
#120852=CARTESIAN_POINT('Ctrl Pts',(51.8707060407776,1076.36282170416,343.297156301785));
#120853=CARTESIAN_POINT('Ctrl Pts',(51.890726046444,1076.35738996094,343.20833338735));
#120854=CARTESIAN_POINT('Ctrl Pts',(51.9458353864727,1076.3488351946,343.08529995842));
#120855=CARTESIAN_POINT('Ctrl Pts',(51.9681033615599,1076.34595007169,343.046433614101));
#120856=CARTESIAN_POINT('Ctrl Pts',(52.0455468991329,1076.33731465088,342.937823430901));
#120857=CARTESIAN_POINT('Ctrl Pts',(52.110786128562,1076.33162386015,342.876431855099));
#120858=CARTESIAN_POINT('Ctrl Pts',(52.2612458989706,1076.32103007045,342.782402809608));
#120859=CARTESIAN_POINT('Ctrl Pts',(52.3450082375807,1076.31622956707,342.750653784727));
#120860=CARTESIAN_POINT('Ctrl Pts',(52.4693696608681,1076.3105451118,342.729847663679));
#120861=CARTESIAN_POINT('Ctrl Pts',(52.5066490854813,1076.30901319594,342.726749657531));
#120862=CARTESIAN_POINT('Ctrl Pts',(52.5439991194443,1076.3076507295,342.726749657531));
#120863=CARTESIAN_POINT('',(52.543999119444,1082.7251047501,342.72674965753));
#120864=CARTESIAN_POINT('',(52.543999119444,1067.7251047501,342.72674965753));
#120865=CARTESIAN_POINT('Origin',(52.543999119444,1082.7251047501,343.402193778667));
#120866=CARTESIAN_POINT('Ctrl Pts',(52.5439991194443,1076.3076507295,342.726749657531));
#120867=CARTESIAN_POINT('Ctrl Pts',(52.5441477900375,1076.30764530625,342.726749657531));
#120868=CARTESIAN_POINT('Ctrl Pts',(52.5442964617491,1076.30763988567,342.726749706442));
#120869=CARTESIAN_POINT('Ctrl Pts',(52.5444451345556,1076.30763446778,342.726749804615));
#120870=CARTESIAN_POINT('Ctrl Pts',(52.6329197611313,1076.30441030596,342.726808226946));
#120871=CARTESIAN_POINT('Ctrl Pts',(52.7205517733353,1076.30218341099,342.744249612993));
#120872=CARTESIAN_POINT('Ctrl Pts',(52.8839167860554,1076.3000238337,342.811876149376));
#120873=CARTESIAN_POINT('Ctrl Pts',(52.9580808165592,1076.30010657371,342.861310328468));
#120874=CARTESIAN_POINT('Ctrl Pts',(53.0831251884017,1076.30258187268,342.985844757017));
#120875=CARTESIAN_POINT('Ctrl Pts',(53.1328063450898,1076.30494745181,343.059702544723));
#120876=CARTESIAN_POINT('Ctrl Pts',(53.2010284385821,1076.3116279873,343.222391644339));
#120877=CARTESIAN_POINT('Ctrl Pts',(53.2188641763637,1076.31587973779,343.309666606089));
#120878=CARTESIAN_POINT('Ctrl Pts',(53.2199960970929,1076.32567177348,343.486302900883));
#120879=CARTESIAN_POINT('Ctrl Pts',(53.2031883434355,1076.33112027135,343.573973116125));
#120880=CARTESIAN_POINT('Ctrl Pts',(53.1367204121467,1076.34245755723,343.737976388051));
#120881=CARTESIAN_POINT('Ctrl Pts',(53.0876321814311,1076.34823836342,343.812721321394));
#120882=CARTESIAN_POINT('Ctrl Pts',(52.9623579357704,1076.35944707001,343.940071688636));
#120883=CARTESIAN_POINT('Ctrl Pts',(52.8869687016715,1076.36475686067,343.991021635442));
#120884=CARTESIAN_POINT('Ctrl Pts',(52.7214919960114,1076.37405943928,344.059968834246));
#120885=CARTESIAN_POINT('Ctrl Pts',(52.6331988197174,1076.37797569543,344.077637899803));
#120886=CARTESIAN_POINT('Ctrl Pts',(52.543999119444,1076.38098512892,344.077637899803));
#120887=CARTESIAN_POINT('Origin',(66.3937896239309,1067.7251047501,343.44168792613));
#120888=CARTESIAN_POINT('',(66.3937896239499,1077.5767973048,342.342856790137));
#120889=CARTESIAN_POINT('Ctrl Pts',(66.393844446936,1077.75229507912,344.540519060755));
#120890=CARTESIAN_POINT('Ctrl Pts',(66.5156047808145,1077.74457990434,344.540512985874));
#120891=CARTESIAN_POINT('Ctrl Pts',(66.6364164896922,1077.73532362626,344.520270125798));
#120892=CARTESIAN_POINT('Ctrl Pts',(66.8764648242798,1077.71349668689,344.437659106797));
#120893=CARTESIAN_POINT('Ctrl Pts',(66.9926823993953,1077.70088000448,344.372395271678));
#120894=CARTESIAN_POINT('Ctrl Pts',(67.2041742539876,1077.67328602451,344.197326472306));
#120895=CARTESIAN_POINT('Ctrl Pts',(67.2951792475751,1077.65845261111,344.086051003281));
#120896=CARTESIAN_POINT('Ctrl Pts',(67.4308913778546,1077.62913740611,343.832688323854));
#120897=CARTESIAN_POINT('Ctrl Pts',(67.4734312399676,1077.61494537538,343.692466422285));
#120898=CARTESIAN_POINT('Ctrl Pts',(67.5007105882041,1077.59022872158,343.411663502516));
#120899=CARTESIAN_POINT('Ctrl Pts',(67.4883765111924,1077.57975612923,343.273978206053));
#120900=CARTESIAN_POINT('Ctrl Pts',(67.4125482135635,1077.5628407334,343.006484785892));
#120901=CARTESIAN_POINT('Ctrl Pts',(67.3484012867948,1077.55667540388,342.879507191737));
#120902=CARTESIAN_POINT('Ctrl Pts',(67.2363297287251,1077.55230747336,342.735077440396));
#120903=CARTESIAN_POINT('Ctrl Pts',(67.2088793297651,1077.55155832973,342.703581066852));
#120904=CARTESIAN_POINT('Ctrl Pts',(67.1640309920068,1077.55079498211,342.657684895358));
#120905=CARTESIAN_POINT('Ctrl Pts',(67.1478742767711,1077.55060127544,342.642132478529));
#120906=CARTESIAN_POINT('Ctrl Pts',(67.1174314726128,1077.55038077762,342.614572503704));
#120907=CARTESIAN_POINT('Ctrl Pts',(67.103294019441,1077.55033139913,342.602413851488));
#120908=CARTESIAN_POINT('Ctrl Pts',(67.0741661943938,1077.55033423748,342.578625234909));
#120909=CARTESIAN_POINT('Ctrl Pts',(67.0591704618174,1077.55038821109,342.567012089965));
#120910=CARTESIAN_POINT('Ctrl Pts',(67.0219534853485,1077.55064734677,342.539701329928));
#120911=CARTESIAN_POINT('Ctrl Pts',(66.9994360342243,1077.55090789771,342.524430069476));
#120912=CARTESIAN_POINT('Ctrl Pts',(66.919336635988,1077.55218540012,342.474343177823));
#120913=CARTESIAN_POINT('Ctrl Pts',(66.8591547614701,1077.55374852366,342.443997143634));
#120914=CARTESIAN_POINT('Ctrl Pts',(66.660270835929,1077.56072099858,342.365636889656));
#120915=CARTESIAN_POINT('Ctrl Pts',(66.5147068104391,1077.56842132315,342.339779830423));
#120916=CARTESIAN_POINT('Ctrl Pts',(66.2463109020279,1077.58696107329,342.345962596173));
#120917=CARTESIAN_POINT('Ctrl Pts',(66.1255671040911,1077.59694354704,342.369134434207));
#120918=CARTESIAN_POINT('Ctrl Pts',(65.8870664179928,1077.62003066478,342.457718359591));
#120919=CARTESIAN_POINT('Ctrl Pts',(65.7723544065373,1077.6331425326,342.525857453649));
#120920=CARTESIAN_POINT('Ctrl Pts',(65.5652017859656,1077.66124856549,342.70607871717));
#120921=CARTESIAN_POINT('Ctrl Pts',(65.4769899780966,1077.67605320035,342.819460488795));
#120922=CARTESIAN_POINT('Ctrl Pts',(65.3475510385666,1077.70475009774,343.075883486354));
#120923=CARTESIAN_POINT('Ctrl Pts',(65.3084313242539,1077.71834953237,343.216990505056));
#120924=CARTESIAN_POINT('Ctrl Pts',(65.2879561572984,1077.7415744366,343.497635090311));
#120925=CARTESIAN_POINT('Ctrl Pts',(65.3033975496496,1077.75119426144,343.634327110823));
#120926=CARTESIAN_POINT('Ctrl Pts',(65.3860847421763,1077.76673889436,343.903094257173));
#120927=CARTESIAN_POINT('Ctrl Pts',(65.455557862181,1077.77225539152,344.031721937204));
#120928=CARTESIAN_POINT('Ctrl Pts',(65.5706513000055,1077.77568245297,344.170471871437));
#120929=CARTESIAN_POINT('Ctrl Pts',(65.594554333178,1077.77618819588,344.196609138093));
#120930=CARTESIAN_POINT('Ctrl Pts',(65.6358849765145,1077.7767426396,344.237635048401));
#120931=CARTESIAN_POINT('Ctrl Pts',(65.652588831005,1077.77688970836,344.253212852171));
#120932=CARTESIAN_POINT('Ctrl Pts',(65.683366751852,1077.77702686598,344.280172335808));
#120933=CARTESIAN_POINT('Ctrl Pts',(65.6972592660129,1077.77704324397,344.29174805819));
#120934=CARTESIAN_POINT('Ctrl Pts',(65.7271922708986,1077.77698438626,344.315462593795));
#120935=CARTESIAN_POINT('Ctrl Pts',(65.74329306933,1077.77689868224,344.327514329823));
#120936=CARTESIAN_POINT('Ctrl Pts',(65.7865323385124,1077.77652918998,344.358064821957));
#120937=CARTESIAN_POINT('Ctrl Pts',(65.814183915158,1077.77615455756,344.375799824849));
#120938=CARTESIAN_POINT('Ctrl Pts',(65.9355059909989,1077.77393712333,344.446149514732));
#120939=CARTESIAN_POINT('Ctrl Pts',(66.0357869149437,1077.77070578318,344.486093316765));
#120940=CARTESIAN_POINT('Ctrl Pts',(66.2233615474464,1077.76231076593,344.530580163756));
#120941=CARTESIAN_POINT('Ctrl Pts',(66.3084805240333,1077.75770404577,344.540523319741));
#120942=CARTESIAN_POINT('Ctrl Pts',(66.393844446936,1077.75229507912,344.540519060755));
#120943=CARTESIAN_POINT('',(66.3937896239311,1075.56506587574,342.342856790137));
#120944=CARTESIAN_POINT('',(66.3937896239309,1067.7251047501,342.342856790137));
#120945=CARTESIAN_POINT('Ctrl Pts',(66.3932272216318,1075.74221012263,344.540518918198));
#120946=CARTESIAN_POINT('Ctrl Pts',(66.2474802543578,1075.75152431216,344.540444322168));
#120947=CARTESIAN_POINT('Ctrl Pts',(66.103078919897,1075.75843983839,344.511372802697));
#120948=CARTESIAN_POINT('Ctrl Pts',(65.8336989264172,1075.76676134646,344.398294360709));
#120949=CARTESIAN_POINT('Ctrl Pts',(65.7115269763156,1075.76807547437,344.315375098008));
#120950=CARTESIAN_POINT('Ctrl Pts',(65.5068551547325,1075.76487056035,344.106616976573));
#120951=CARTESIAN_POINT('Ctrl Pts',(65.4264460255889,1075.76038790145,343.982967587889));
#120952=CARTESIAN_POINT('Ctrl Pts',(65.3187398076029,1075.74613160246,343.7117951189));
#120953=CARTESIAN_POINT('Ctrl Pts',(65.2924759146155,1075.73650629327,343.567057759706));
#120954=CARTESIAN_POINT('Ctrl Pts',(65.2978182202965,1075.71323086363,343.275602151053));
#120955=CARTESIAN_POINT('Ctrl Pts',(65.3295437562049,1075.69979682563,343.131771747123));
#120956=CARTESIAN_POINT('Ctrl Pts',(65.4171797226662,1075.67821918432,342.932986273977));
#120957=CARTESIAN_POINT('Ctrl Pts',(65.452341935033,1075.67091610097,342.870534494126));
#120958=CARTESIAN_POINT('Ctrl Pts',(65.5344480859605,1075.65608241569,342.75312801349));
#120959=CARTESIAN_POINT('Ctrl Pts',(65.5812512531236,1075.64858516863,342.69847617303));
#120960=CARTESIAN_POINT('Ctrl Pts',(65.7384930843161,1075.62595622194,342.54761293775));
#120961=CARTESIAN_POINT('Ctrl Pts',(65.8631256982616,1075.61117448687,342.468432654874));
#120962=CARTESIAN_POINT('Ctrl Pts',(66.1345163634118,1075.58438902696,342.364157470795));
#120963=CARTESIAN_POINT('Ctrl Pts',(66.2783887558511,1075.57261072206,342.339390174486));
#120964=CARTESIAN_POINT('Ctrl Pts',(66.566849366719,1075.55367179737,342.347079732253));
#120965=CARTESIAN_POINT('Ctrl Pts',(66.7086065581168,1075.5466708528,342.379107852499));
#120966=CARTESIAN_POINT('Ctrl Pts',(66.9711281072818,1075.53849079615,342.495841035501));
#120967=CARTESIAN_POINT('Ctrl Pts',(67.0893930388519,1075.53736121238,342.57907879815));
#120968=CARTESIAN_POINT('Ctrl Pts',(67.287157616269,1075.54114581463,342.786110836944));
#120969=CARTESIAN_POINT('Ctrl Pts',(67.3647506911734,1075.54601098546,342.90776706945));
#120970=CARTESIAN_POINT('Ctrl Pts',(67.4691769431824,1075.56107977074,343.174248689843));
#120971=CARTESIAN_POINT('Ctrl Pts',(67.4948053120897,1075.57115155937,343.316533160801));
#120972=CARTESIAN_POINT('Ctrl Pts',(67.4901297386214,1075.59513940164,343.603554794462));
#120973=CARTESIAN_POINT('Ctrl Pts',(67.4595134358805,1075.60884679079,343.745548817247));
#120974=CARTESIAN_POINT('Ctrl Pts',(67.3738733608471,1075.63069259695,343.943754995825));
#120975=CARTESIAN_POINT('Ctrl Pts',(67.3388066801131,1075.63815275872,344.006997741652));
#120976=CARTESIAN_POINT('Ctrl Pts',(67.2568961660437,1075.6531536218,344.125541247711));
#120977=CARTESIAN_POINT('Ctrl Pts',(67.210269256498,1075.66065939707,344.180586074322));
#120978=CARTESIAN_POINT('Ctrl Pts',(67.053711728565,1075.68311375052,344.332344363354));
#120979=CARTESIAN_POINT('Ctrl Pts',(66.9295361570051,1075.69755011896,344.412149796458));
#120980=CARTESIAN_POINT('Ctrl Pts',(66.6659000552012,1075.72273875493,344.515040382875));
#120981=CARTESIAN_POINT('Ctrl Pts',(66.5302251879546,1075.73345505178,344.540589036325));
#120982=CARTESIAN_POINT('Ctrl Pts',(66.3932272216318,1075.74221012263,344.540518918198));
#120983=CARTESIAN_POINT('Origin',(66.3937896239309,1067.7251047501,343.44168792613));
#120984=CARTESIAN_POINT('',(66.3937896239309,1075.69533039084,343.940519062122));
#120985=CARTESIAN_POINT('',(66.3937896239307,1075.61493016275,342.942856790137));
#120986=CARTESIAN_POINT('Ctrl Pts',(66.3937896239309,1075.69533039084,343.940519062122));
#120987=CARTESIAN_POINT('Ctrl Pts',(66.3936857389102,1075.69533714603,343.940519062122));
#120988=CARTESIAN_POINT('Ctrl Pts',(66.3935818520956,1075.69534389873,343.94051902967));
#120989=CARTESIAN_POINT('Ctrl Pts',(66.3270401237183,1075.69966748105,343.940477455626));
#120990=CARTESIAN_POINT('Ctrl Pts',(66.2612210191196,1075.70287960374,343.927163298428));
#120991=CARTESIAN_POINT('Ctrl Pts',(66.1400081066437,1075.70668362999,343.876030984594));
#120992=CARTESIAN_POINT('Ctrl Pts',(66.0856109827812,1075.70729671465,343.839290514662));
#120993=CARTESIAN_POINT('Ctrl Pts',(65.9939584714249,1075.70592219778,343.746973765016));
#120994=CARTESIAN_POINT('Ctrl Pts',(65.9576216472256,1075.70394746083,343.692312800562));
#120995=CARTESIAN_POINT('Ctrl Pts',(65.9073820050535,1075.69756411103,343.570782221173));
#120996=CARTESIAN_POINT('Ctrl Pts',(65.8945458337568,1075.69316420124,343.504904016412));
#120997=CARTESIAN_POINT('Ctrl Pts',(65.8953923813694,1075.68251179053,343.37195999464));
#120998=CARTESIAN_POINT('Ctrl Pts',(65.9091289550251,1075.67636087266,343.306221376174));
#120999=CARTESIAN_POINT('Ctrl Pts',(65.9481307274171,1075.66650499341,343.215236903949));
#121000=CARTESIAN_POINT('Ctrl Pts',(65.9638492653669,1075.66317600945,343.186653888216));
#121001=CARTESIAN_POINT('Ctrl Pts',(66.0006561980104,1075.65642883476,343.132913877559));
#121002=CARTESIAN_POINT('Ctrl Pts',(66.0216703849935,1075.65302603371,343.107887747318));
#121003=CARTESIAN_POINT('Ctrl Pts',(66.0927979615361,1075.64271090725,343.038312395468));
#121004=CARTESIAN_POINT('Ctrl Pts',(66.1495729191216,1075.63597265537,343.001601506029));
#121005=CARTESIAN_POINT('Ctrl Pts',(66.2697411886632,1075.62416188221,342.954555511029));
#121006=CARTESIAN_POINT('Ctrl Pts',(66.3313197546715,1075.61910513006,342.94289143163));
#121007=CARTESIAN_POINT('Ctrl Pts',(66.3935123918432,1075.61494868444,342.942856867238));
#121008=CARTESIAN_POINT('Ctrl Pts',(66.3936048036805,1075.61494250839,342.942856815879));
#121009=CARTESIAN_POINT('Ctrl Pts',(66.3936972143795,1075.61493633449,342.942856790137));
#121010=CARTESIAN_POINT('Ctrl Pts',(66.3937896239304,1075.61493016275,342.942856790137));
#121011=CARTESIAN_POINT('',(66.3937896239309,1082.7251047501,342.942856790137));
#121012=CARTESIAN_POINT('',(66.3937896239309,1067.7251047501,342.942856790137));
#121013=CARTESIAN_POINT('Origin',(66.3937896239309,1082.7251047501,343.44168792613));
#121014=CARTESIAN_POINT('Ctrl Pts',(66.3937896239304,1075.61493016275,342.942856790137));
#121015=CARTESIAN_POINT('Ctrl Pts',(66.4589533147248,1075.61057808795,342.942856790137));
#121016=CARTESIAN_POINT('Ctrl Pts',(66.5235459705353,1075.60729823447,342.955625539973));
#121017=CARTESIAN_POINT('Ctrl Pts',(66.6440165015387,1075.60329532221,343.005284692942));
#121018=CARTESIAN_POINT('Ctrl Pts',(66.6987277318149,1075.60260290825,343.041591128476));
#121019=CARTESIAN_POINT('Ctrl Pts',(66.7910831321971,1075.60391406314,343.133123469872));
#121020=CARTESIAN_POINT('Ctrl Pts',(66.8278269578003,1075.60590102542,343.187411743355));
#121021=CARTESIAN_POINT('Ctrl Pts',(66.8785310374756,1075.61230429113,343.307150947806));
#121022=CARTESIAN_POINT('Ctrl Pts',(66.8919118393908,1075.61666534876,343.371458683115));
#121023=CARTESIAN_POINT('Ctrl Pts',(66.8932790056263,1075.62719848133,343.501853998062));
#121024=CARTESIAN_POINT('Ctrl Pts',(66.8810979459664,1075.63327925175,343.56669291016));
#121025=CARTESIAN_POINT('Ctrl Pts',(66.8446327996808,1075.64306395291,343.657657305404));
#121026=CARTESIAN_POINT('Ctrl Pts',(66.8295081670838,1075.64641669883,343.686740724506));
#121027=CARTESIAN_POINT('Ctrl Pts',(66.7938191334769,1075.65319311943,343.74147932882));
#121028=CARTESIAN_POINT('Ctrl Pts',(66.7733449568916,1075.65660102139,343.767012808854));
#121029=CARTESIAN_POINT('Ctrl Pts',(66.7040105152463,1075.66687236542,343.837949850398));
#121030=CARTESIAN_POINT('Ctrl Pts',(66.6484158564627,1075.67355077613,343.875780188069));
#121031=CARTESIAN_POINT('Ctrl Pts',(66.5258839728004,1075.68567659138,343.927257184211));
#121032=CARTESIAN_POINT('Ctrl Pts',(66.4602034002325,1075.69101179288,343.940519062122));
#121033=CARTESIAN_POINT('Ctrl Pts',(66.3937896239309,1075.69533039084,343.940519062122));
#121034=CARTESIAN_POINT('Origin',(80.0774492048022,1067.7251047501,346.338481930687));
#121035=CARTESIAN_POINT('',(80.0774492048332,1076.71653899679,345.247941181959));
#121036=CARTESIAN_POINT('Ctrl Pts',(80.0774862161661,1076.9212633053,347.429022678787));
#121037=CARTESIAN_POINT('Ctrl Pts',(80.2021222418157,1076.90950098152,347.429018448822));
#121038=CARTESIAN_POINT('Ctrl Pts',(80.3256605239218,1076.89583373553,347.407650156297));
#121039=CARTESIAN_POINT('Ctrl Pts',(80.5699985990722,1076.86454049355,347.320777825101));
#121040=CARTESIAN_POINT('Ctrl Pts',(80.6876112503,1076.84693371904,347.252349941046));
#121041=CARTESIAN_POINT('Ctrl Pts',(80.8999983458895,1076.80940010752,347.069172492099));
#121042=CARTESIAN_POINT('Ctrl Pts',(80.9901724003361,1076.78975347167,346.952862829086));
#121043=CARTESIAN_POINT('Ctrl Pts',(81.1180192331078,1076.75293679588,346.694550975318));
#121044=CARTESIAN_POINT('Ctrl Pts',(81.1556736200037,1076.73605787768,346.555548346587));
#121045=CARTESIAN_POINT('Ctrl Pts',(81.1740311378466,1076.70871655558,346.287633171766));
#121046=CARTESIAN_POINT('Ctrl Pts',(81.1608924211059,1076.69793181172,346.161504102804));
#121047=CARTESIAN_POINT('Ctrl Pts',(81.0937106174324,1076.68187202188,345.925206689725));
#121048=CARTESIAN_POINT('Ctrl Pts',(81.0422696197197,1076.67645739526,345.816220218082));
#121049=CARTESIAN_POINT('Ctrl Pts',(80.954871778068,1076.67291909723,345.689987089237));
#121050=CARTESIAN_POINT('Ctrl Pts',(80.9344018195415,1076.67235413996,345.663168199325));
#121051=CARTESIAN_POINT('Ctrl Pts',(80.9001939403582,1076.67180071413,345.622416442801));
#121052=CARTESIAN_POINT('Ctrl Pts',(80.8872702293781,1076.67166965193,345.607832472062));
#121053=CARTESIAN_POINT('Ctrl Pts',(80.8638040799272,1076.6715650625,345.58273969905));
#121054=CARTESIAN_POINT('Ctrl Pts',(80.8534245708629,1076.67156160475,345.572086116607));
#121055=CARTESIAN_POINT('Ctrl Pts',(80.829272568673,1076.67164906389,345.548290179324));
#121056=CARTESIAN_POINT('Ctrl Pts',(80.8153676395287,1076.67176663643,345.535289719132));
#121057=CARTESIAN_POINT('Ctrl Pts',(80.7767076367494,1076.67227144132,345.500996081948));
#121058=CARTESIAN_POINT('Ctrl Pts',(80.7513272062193,1076.67279113894,345.480441759747));
#121059=CARTESIAN_POINT('Ctrl Pts',(80.6266659516045,1076.67620264786,345.388430654137));
#121060=CARTESIAN_POINT('Ctrl Pts',(80.5168429989352,1076.68166430112,345.332939718575));
#121061=CARTESIAN_POINT('Ctrl Pts',(80.2926834941226,1076.69698303526,345.263478914974));
#121062=CARTESIAN_POINT('Ctrl Pts',(80.1807647002479,1076.70636891199,345.247053057343));
#121063=CARTESIAN_POINT('Ctrl Pts',(79.9439600129226,1076.72967133889,345.249003870407));
#121064=CARTESIAN_POINT('Ctrl Pts',(79.8207213725019,1076.74379757481,345.271340812334));
#121065=CARTESIAN_POINT('Ctrl Pts',(79.5775385247131,1076.77578286523,345.359963177364));
#121066=CARTESIAN_POINT('Ctrl Pts',(79.4607415971847,1076.7935925419,345.429067615163));
#121067=CARTESIAN_POINT('Ctrl Pts',(79.2503495668522,1076.83111960669,345.613072547751));
#121068=CARTESIAN_POINT('Ctrl Pts',(79.1612564043964,1076.85052630989,345.729426103173));
#121069=CARTESIAN_POINT('Ctrl Pts',(79.0349882716665,1076.88662159092,345.987954979939));
#121070=CARTESIAN_POINT('Ctrl Pts',(78.9980559790793,1076.9030227927,346.127241921194));
#121071=CARTESIAN_POINT('Ctrl Pts',(78.981157704172,1076.92937822644,346.395425618788));
#121072=CARTESIAN_POINT('Ctrl Pts',(78.995011499467,1076.93967409601,346.52155125629));
#121073=CARTESIAN_POINT('Ctrl Pts',(79.063141240306,1076.95481244733,346.756110474455));
#121074=CARTESIAN_POINT('Ctrl Pts',(79.1143343080273,1076.95985541406,346.863543473075));
#121075=CARTESIAN_POINT('Ctrl Pts',(79.2009074300033,1076.96315645615,346.988150699005));
#121076=CARTESIAN_POINT('Ctrl Pts',(79.2212195178538,1076.96368449461,347.014696499386));
#121077=CARTESIAN_POINT('Ctrl Pts',(79.2551481772751,1076.96420162873,347.055052310515));
#121078=CARTESIAN_POINT('Ctrl Pts',(79.2679668532749,1076.96432402151,347.06950207222));
#121079=CARTESIAN_POINT('Ctrl Pts',(79.2912376489969,1076.96442142945,347.094370770387));
#121080=CARTESIAN_POINT('Ctrl Pts',(79.301529867698,1076.96442444433,347.104932015753));
#121081=CARTESIAN_POINT('Ctrl Pts',(79.325475171283,1076.96434204236,347.128526422866));
#121082=CARTESIAN_POINT('Ctrl Pts',(79.3392585456271,1076.96423166111,347.141420142427));
#121083=CARTESIAN_POINT('Ctrl Pts',(79.3775700528827,1076.96375815884,347.175438165737));
#121084=CARTESIAN_POINT('Ctrl Pts',(79.4027134025562,1076.96327100895,347.195837054384));
#121085=CARTESIAN_POINT('Ctrl Pts',(79.5260322643498,1076.96007646042,347.28709834934));
#121086=CARTESIAN_POINT('Ctrl Pts',(79.6345701952546,1076.95496847895,347.342346363548));
#121087=CARTESIAN_POINT('Ctrl Pts',(79.8559841104131,1076.94057462712,347.412081134828));
#121088=CARTESIAN_POINT('Ctrl Pts',(79.9664798597703,1076.93173935103,347.429026446181));
#121089=CARTESIAN_POINT('Ctrl Pts',(80.0774862161661,1076.9212633053,347.429022678787));
#121090=CARTESIAN_POINT('',(80.0774492048021,1074.69742129942,345.247941181958));
#121091=CARTESIAN_POINT('',(80.0774492048022,1067.7251047501,345.247941181958));
#121092=CARTESIAN_POINT('Ctrl Pts',(80.0781137458199,1074.9037808193,347.42902247694));
#121093=CARTESIAN_POINT('Ctrl Pts',(79.9334466289482,1074.91755562924,347.429110632519));
#121094=CARTESIAN_POINT('Ctrl Pts',(79.7899751621157,1074.9284898498,347.400411437874));
#121095=CARTESIAN_POINT('Ctrl Pts',(79.5254490843108,1074.94327057592,347.289612618674));
#121096=CARTESIAN_POINT('Ctrl Pts',(79.4065916812818,1074.94713161862,347.209891653313));
#121097=CARTESIAN_POINT('Ctrl Pts',(79.2060658521217,1074.94755442777,347.009346371445));
#121098=CARTESIAN_POINT('Ctrl Pts',(79.1264022916102,1074.9441185709,346.890598141408));
#121099=CARTESIAN_POINT('Ctrl Pts',(79.0166350565131,1074.93028306558,346.628703085767));
#121100=CARTESIAN_POINT('Ctrl Pts',(78.9879263739783,1074.91998207438,346.488070119579));
#121101=CARTESIAN_POINT('Ctrl Pts',(78.9859242803638,1074.89351348247,346.201340752291));
#121102=CARTESIAN_POINT('Ctrl Pts',(79.0137424215749,1074.87749855487,346.058069531191));
#121103=CARTESIAN_POINT('Ctrl Pts',(79.1235861989138,1074.84186845908,345.790323711697));
#121104=CARTESIAN_POINT('Ctrl Pts',(79.2048518700485,1074.82257431892,345.668524335293));
#121105=CARTESIAN_POINT('Ctrl Pts',(79.4108424343549,1074.78319878757,345.46313421656));
#121106=CARTESIAN_POINT('Ctrl Pts',(79.5339549215185,1074.76348460309,345.381790061626));
#121107=CARTESIAN_POINT('Ctrl Pts',(79.8037781608253,1074.72672636237,345.272957371469));
#121108=CARTESIAN_POINT('Ctrl Pts',(79.947699847112,1074.71000823119,345.245992427068));
#121109=CARTESIAN_POINT('Ctrl Pts',(80.2356656514258,1074.68204977285,345.250074345777));
#121110=CARTESIAN_POINT('Ctrl Pts',(80.3768755282356,1074.67099564023,345.280116708461));
#121111=CARTESIAN_POINT('Ctrl Pts',(80.6387431159376,1074.65598367746,345.392781516202));
#121112=CARTESIAN_POINT('Ctrl Pts',(80.7569490114497,1074.65211172391,345.473765989537));
#121113=CARTESIAN_POINT('Ctrl Pts',(80.9553827767437,1074.65206476887,345.676266937325));
#121114=CARTESIAN_POINT('Ctrl Pts',(81.0337311360745,1074.655860176,345.795555777806));
#121115=CARTESIAN_POINT('Ctrl Pts',(81.1407526310339,1074.67063283288,346.057762614982));
#121116=CARTESIAN_POINT('Ctrl Pts',(81.168134940995,1074.68149026881,346.198137657933));
#121117=CARTESIAN_POINT('Ctrl Pts',(81.1678423651269,1074.70888881994,346.482476047229));
#121118=CARTESIAN_POINT('Ctrl Pts',(81.1396252966577,1074.72521645264,346.623698286506));
#121119=CARTESIAN_POINT('Ctrl Pts',(81.0292947954484,1074.76148410104,346.890431916308));
#121120=CARTESIAN_POINT('Ctrl Pts',(80.9468371392338,1074.78115616437,347.01285012048));
#121121=CARTESIAN_POINT('Ctrl Pts',(80.7395671019805,1074.82055590851,347.217048915134));
#121122=CARTESIAN_POINT('Ctrl Pts',(80.6170155088918,1074.83991514004,347.297235108876));
#121123=CARTESIAN_POINT('Ctrl Pts',(80.3539046017529,1074.87501442923,347.402418178793));
#121124=CARTESIAN_POINT('Ctrl Pts',(80.2167606810137,1074.89057923471,347.42893798987));
#121125=CARTESIAN_POINT('Ctrl Pts',(80.0781137458199,1074.9037808193,347.42902247694));
#121126=CARTESIAN_POINT('Origin',(80.0774492048022,1067.7251047501,346.338481930687));
#121127=CARTESIAN_POINT('',(80.0774492048022,1074.84832662855,346.829022679415));
#121128=CARTESIAN_POINT('',(80.0774492048022,1074.75547652073,345.847941181958));
#121129=CARTESIAN_POINT('Ctrl Pts',(80.0774492048022,1074.84832662855,346.829022679415));
#121130=CARTESIAN_POINT('Ctrl Pts',(80.0448262837344,1074.85146078003,346.829022679415));
#121131=CARTESIAN_POINT('Ctrl Pts',(80.0121774599946,1074.85428931932,346.82576858999));
#121132=CARTESIAN_POINT('Ctrl Pts',(79.9173773701227,1074.86158169795,346.806551318557));
#121133=CARTESIAN_POINT('Ctrl Pts',(79.8577669540331,1074.86496734547,346.78173228012));
#121134=CARTESIAN_POINT('Ctrl Pts',(79.7516219069293,1074.86847995328,346.710670330104));
#121135=CARTESIAN_POINT('Ctrl Pts',(79.7060940777251,1074.86858860055,346.665259594229));
#121136=CARTESIAN_POINT('Ctrl Pts',(79.6348796406192,1074.86550463963,346.559470199017));
#121137=CARTESIAN_POINT('Ctrl Pts',(79.6099534868352,1074.86233716934,346.500139824643));
#121138=CARTESIAN_POINT('Ctrl Pts',(79.5840705163992,1074.85307807046,346.374918800676));
#121139=CARTESIAN_POINT('Ctrl Pts',(79.5835615662606,1074.84705566208,346.310230045752));
#121140=CARTESIAN_POINT('Ctrl Pts',(79.6075899148517,1074.83278916591,346.183118039608));
#121141=CARTESIAN_POINT('Ctrl Pts',(79.6324412816207,1074.82463920019,346.122027803914));
#121142=CARTESIAN_POINT('Ctrl Pts',(79.7045910480179,1074.80738198665,346.013072575906));
#121143=CARTESIAN_POINT('Ctrl Pts',(79.7512860855446,1074.79843440899,345.966284796809));
#121144=CARTESIAN_POINT('Ctrl Pts',(79.8604184380882,1074.78096377653,345.893695992609));
#121145=CARTESIAN_POINT('Ctrl Pts',(79.9218656775853,1074.77260759018,345.868640899455));
#121146=CARTESIAN_POINT('Ctrl Pts',(80.0164631193384,1074.76169513746,345.850792958124));
#121147=CARTESIAN_POINT('Ctrl Pts',(80.0469102527727,1074.75845540067,345.847941181958));
#121148=CARTESIAN_POINT('Ctrl Pts',(80.0774492048022,1074.75547652073,345.847941181958));
#121149=CARTESIAN_POINT('',(80.0774492048022,1082.7251047501,345.847941181958));
#121150=CARTESIAN_POINT('',(80.0774492048022,1067.7251047501,345.847941181958));
#121151=CARTESIAN_POINT('Origin',(80.0774492048022,1082.7251047501,346.338481930687));
#121152=CARTESIAN_POINT('Ctrl Pts',(80.0774492048022,1074.75547652073,345.847941181958));
#121153=CARTESIAN_POINT('Ctrl Pts',(80.0775388926569,1074.75546777226,345.847941181958));
#121154=CARTESIAN_POINT('Ctrl Pts',(80.0776285813035,1074.75545902603,345.847941206553));
#121155=CARTESIAN_POINT('Ctrl Pts',(80.077718270732,1074.75545028205,345.847941255749));
#121156=CARTESIAN_POINT('Ctrl Pts',(80.141896953241,1074.74919339174,345.847976458328));
#121157=CARTESIAN_POINT('Ctrl Pts',(80.2055508752481,1074.74417955805,345.860606346322));
#121158=CARTESIAN_POINT('Ctrl Pts',(80.3239842080001,1074.73728505508,345.90962237699));
#121159=CARTESIAN_POINT('Ctrl Pts',(80.3776497106477,1074.73544608304,345.945301405553));
#121160=CARTESIAN_POINT('Ctrl Pts',(80.4681858369132,1074.73518183834,346.0351519956));
#121161=CARTESIAN_POINT('Ctrl Pts',(80.5041882971281,1074.73674795505,346.088345403766));
#121162=CARTESIAN_POINT('Ctrl Pts',(80.5539774203366,1074.74309711386,346.205696589049));
#121163=CARTESIAN_POINT('Ctrl Pts',(80.567162622304,1074.74782998118,346.26871759626));
#121164=CARTESIAN_POINT('Ctrl Pts',(80.5687495278745,1074.75988222632,346.396699556429));
#121165=CARTESIAN_POINT('Ctrl Pts',(80.5568964923362,1074.76710791374,346.460424134477));
#121166=CARTESIAN_POINT('Ctrl Pts',(80.5088924221565,1074.78323359995,346.580959464777));
#121167=CARTESIAN_POINT('Ctrl Pts',(80.4726313521396,1074.7920133588,346.636404740842));
#121168=CARTESIAN_POINT('Ctrl Pts',(80.4041238268715,1074.80521790094,346.705819008354));
#121169=CARTESIAN_POINT('Ctrl Pts',(80.3794855574961,1074.80954079106,346.726331785911));
#121170=CARTESIAN_POINT('Ctrl Pts',(80.2990547436627,1074.82247169893,346.780948487007));
#121171=CARTESIAN_POINT('Ctrl Pts',(80.2382523658034,1074.83074194295,346.80650742751));
#121172=CARTESIAN_POINT('Ctrl Pts',(80.1422619523651,1074.84179563017,346.825808794145));
#121173=CARTESIAN_POINT('Ctrl Pts',(80.1098683705286,1074.84521205226,346.829022679415));
#121174=CARTESIAN_POINT('Ctrl Pts',(80.0774492048022,1074.84832662855,346.829022679415));
#121175=CARTESIAN_POINT('Origin',(22.5035000139866,1067.7251047501,337.93536030011));
#121176=CARTESIAN_POINT('',(22.5035000140068,1078.63105472707,336.457057167916));
#121177=CARTESIAN_POINT('Ctrl Pts',(22.5033438253408,1078.70463574344,339.413663424052));
#121178=CARTESIAN_POINT('Ctrl Pts',(22.6998393579387,1078.70375115027,339.413684184592));
#121179=CARTESIAN_POINT('Ctrl Pts',(22.8943758673387,1078.7021830175,339.374527560636));
#121180=CARTESIAN_POINT('Ctrl Pts',(23.2260457576551,1078.69795923647,339.235338949005));
#121181=CARTESIAN_POINT('Ctrl Pts',(23.3650392043164,1078.69555654171,339.147697921552));
#121182=CARTESIAN_POINT('Ctrl Pts',(23.6188702233219,1078.68952231744,338.921552645424));
#121183=CARTESIAN_POINT('Ctrl Pts',(23.7286905091169,1078.68584933042,338.781248797633));
#121184=CARTESIAN_POINT('Ctrl Pts',(23.8996139680247,1078.67729456531,338.457116205948));
#121185=CARTESIAN_POINT('Ctrl Pts',(23.9549739161666,1078.67241988861,338.273858498662));
#121186=CARTESIAN_POINT('Ctrl Pts',(23.993946068272,1078.66216121608,337.891234536368));
#121187=CARTESIAN_POINT('Ctrl Pts',(23.9751491699249,1078.65686956334,337.695303155037));
#121188=CARTESIAN_POINT('Ctrl Pts',(23.8647860477522,1078.64713360485,337.329217038423));
#121189=CARTESIAN_POINT('Ctrl Pts',(23.7770464117301,1078.64275882396,337.161668900629));
#121190=CARTESIAN_POINT('Ctrl Pts',(23.5377313979699,1078.63538889654,336.860870933825));
#121191=CARTESIAN_POINT('Ctrl Pts',(23.3855479512426,1078.63255547997,336.732794403445));
#121192=CARTESIAN_POINT('Ctrl Pts',(23.1537881881404,1078.63041906278,336.606067547748));
#121193=CARTESIAN_POINT('Ctrl Pts',(23.0927109542506,1078.63002173119,336.577890361605));
#121194=CARTESIAN_POINT('Ctrl Pts',(22.9925613722135,1078.62962914115,336.539724871977));
#121195=CARTESIAN_POINT('Ctrl Pts',(22.9546313787496,1078.6295363605,336.527006732112));
#121196=CARTESIAN_POINT('Ctrl Pts',(22.8826391492461,1078.62946389862,336.506074612261));
#121197=CARTESIAN_POINT('Ctrl Pts',(22.8487097479939,1078.62947153563,336.497502761961));
#121198=CARTESIAN_POINT('Ctrl Pts',(22.7727872377825,1078.6295804406,336.481164371475));
#121199=CARTESIAN_POINT('Ctrl Pts',(22.7306971316394,1078.62970188202,336.473996947489));
#121200=CARTESIAN_POINT('Ctrl Pts',(22.6102597817211,1078.63022070365,336.45881756648));
#121201=CARTESIAN_POINT('Ctrl Pts',(22.5315032163279,1078.63076385718,336.455228048553));
#121202=CARTESIAN_POINT('Ctrl Pts',(22.2564445706053,1078.63335212975,336.464659975376));
#121203=CARTESIAN_POINT('Ctrl Pts',(22.0633677201798,1078.63640804246,336.510485687278));
#121204=CARTESIAN_POINT('Ctrl Pts',(21.735934141379,1078.6436481339,336.661339136317));
#121205=CARTESIAN_POINT('Ctrl Pts',(21.5994184030165,1078.64750785798,336.754294071997));
#121206=CARTESIAN_POINT('Ctrl Pts',(21.3532341336299,1078.65616651653,336.990081719004));
#121207=CARTESIAN_POINT('Ctrl Pts',(21.2484887016351,1078.66094145711,337.134356113793));
#121208=CARTESIAN_POINT('Ctrl Pts',(21.0895331219666,1078.67075352981,337.464267130856));
#121209=CARTESIAN_POINT('Ctrl Pts',(21.0408757487221,1078.67569103634,337.649062160451));
#121210=CARTESIAN_POINT('Ctrl Pts',(21.0155710478685,1078.68487172237,338.032484083151));
#121211=CARTESIAN_POINT('Ctrl Pts',(21.0413204969999,1078.68900202211,338.227603192364));
#121212=CARTESIAN_POINT('Ctrl Pts',(21.1643989648315,1078.69582054318,338.588852624159));
#121213=CARTESIAN_POINT('Ctrl Pts',(21.2575618128547,1078.69850742647,338.7526047337));
#121214=CARTESIAN_POINT('Ctrl Pts',(21.498624319817,1078.70259042803,339.035239076157));
#121215=CARTESIAN_POINT('Ctrl Pts',(21.6438028711614,1078.70397036597,339.152090625918));
#121216=CARTESIAN_POINT('Ctrl Pts',(21.8639160723917,1078.70501767913,339.269719614016));
#121217=CARTESIAN_POINT('Ctrl Pts',(21.9230370295853,1078.70521343792,339.296479391541));
#121218=CARTESIAN_POINT('Ctrl Pts',(22.0203369658017,1078.70540677569,339.333023816273));
#121219=CARTESIAN_POINT('Ctrl Pts',(22.0574822187452,1078.70545205528,339.345317025429));
#121220=CARTESIAN_POINT('Ctrl Pts',(22.1279356211446,1078.7054856114,339.365570378957));
#121221=CARTESIAN_POINT('Ctrl Pts',(22.1611180321196,1078.70548032346,339.37387483295));
#121222=CARTESIAN_POINT('Ctrl Pts',(22.2359580776211,1078.70542160349,339.389868348979));
#121223=CARTESIAN_POINT('Ctrl Pts',(22.2777185955029,1078.70535704877,339.396933115691));
#121224=CARTESIAN_POINT('Ctrl Pts',(22.3806336989986,1078.70511991689,339.409827045523));
#121225=CARTESIAN_POINT('Ctrl Pts',(22.4419589121447,1078.70491208904,339.41365693849));
#121226=CARTESIAN_POINT('Ctrl Pts',(22.5033438253408,1078.70463574344,339.413663424052));
#121227=CARTESIAN_POINT('',(22.5035000139672,1076.62985213807,336.457057167916));
#121228=CARTESIAN_POINT('',(22.5035000139866,1067.7251047501,336.457057167916));
#121229=CARTESIAN_POINT('Ctrl Pts',(22.5035260490889,1076.70430235654,339.413663432074));
#121230=CARTESIAN_POINT('Ctrl Pts',(22.3076788371628,1076.70519520394,339.413666881233));
#121231=CARTESIAN_POINT('Ctrl Pts',(22.1137677330167,1076.70538754263,339.374750988217));
#121232=CARTESIAN_POINT('Ctrl Pts',(21.7527313031503,1076.70439216947,339.223748601578));
#121233=CARTESIAN_POINT('Ctrl Pts',(21.5891218480039,1076.70321411592,339.11328534297));
#121234=CARTESIAN_POINT('Ctrl Pts',(21.3147874457625,1076.69940261299,338.835542643899));
#121235=CARTESIAN_POINT('Ctrl Pts',(21.206597453164,1076.69680306849,338.671160869024));
#121236=CARTESIAN_POINT('Ctrl Pts',(21.0599426673985,1076.69013715911,338.30924466156));
#121237=CARTESIAN_POINT('Ctrl Pts',(21.0231932299689,1076.68612319168,338.115164727295));
#121238=CARTESIAN_POINT('Ctrl Pts',(21.0273720866854,1076.67693757734,337.723704893172));
#121239=CARTESIAN_POINT('Ctrl Pts',(21.0683744972371,1076.67185192883,337.530194015843));
#121240=CARTESIAN_POINT('Ctrl Pts',(21.2226910821344,1076.66132785084,337.172098605117));
#121241=CARTESIAN_POINT('Ctrl Pts',(21.3338390723428,1076.65599830827,337.010733148387));
#121242=CARTESIAN_POINT('Ctrl Pts',(21.6122223415557,1076.64599102733,336.740069375323));
#121243=CARTESIAN_POINT('Ctrl Pts',(21.7767966931952,1076.64141768865,336.633435040405));
#121244=CARTESIAN_POINT('Ctrl Pts',(22.1376408798258,1076.63399700659,336.489954508475));
#121245=CARTESIAN_POINT('Ctrl Pts',(22.3303783413942,1076.63122725497,336.45445156041));
#121246=CARTESIAN_POINT('Ctrl Pts',(22.7180943579612,1076.62813692179,336.459953621801));
#121247=CARTESIAN_POINT('Ctrl Pts',(22.9092997859577,1076.62784337958,336.500716264339));
#121248=CARTESIAN_POINT('Ctrl Pts',(23.2646560876052,1076.62981478918,336.653437586307));
#121249=CARTESIAN_POINT('Ctrl Pts',(23.4254392124878,1076.63205207791,336.763736146618));
#121250=CARTESIAN_POINT('Ctrl Pts',(23.6953603606003,1076.63857096145,337.039770842792));
#121251=CARTESIAN_POINT('Ctrl Pts',(23.801945903119,1076.64278211273,337.202804356312));
#121252=CARTESIAN_POINT('Ctrl Pts',(23.9465274573639,1076.65231326441,337.560737575826));
#121253=CARTESIAN_POINT('Ctrl Pts',(23.9830708203088,1076.65753584508,337.752231578144));
#121254=CARTESIAN_POINT('Ctrl Pts',(23.9811187188208,1076.66540907678,338.041903382089));
#121255=CARTESIAN_POINT('Ctrl Pts',(23.9710044060804,1076.6680227192,338.138189482373));
#121256=CARTESIAN_POINT('Ctrl Pts',(23.9321348193541,1076.67313785636,338.327424681259));
#121257=CARTESIAN_POINT('Ctrl Pts',(23.9034696544849,1076.67562702131,338.419919623396));
#121258=CARTESIAN_POINT('Ctrl Pts',(23.7899135097339,1076.68285475593,338.689654095926));
#121259=CARTESIAN_POINT('Ctrl Pts',(23.678644083091,1076.68719199501,338.853436943178));
#121260=CARTESIAN_POINT('Ctrl Pts',(23.3995246799656,1076.69454406291,339.127208323104));
#121261=CARTESIAN_POINT('Ctrl Pts',(23.2347606929472,1076.69750180075,339.234832374726));
#121262=CARTESIAN_POINT('Ctrl Pts',(22.878880550176,1076.70194543775,339.377585959403));
#121263=CARTESIAN_POINT('Ctrl Pts',(22.6920707453321,1076.70344280057,339.413660111523));
#121264=CARTESIAN_POINT('Ctrl Pts',(22.5035260490889,1076.70430235654,339.413663432074));
#121265=CARTESIAN_POINT('Origin',(22.5035000139866,1067.7251047501,337.93536030011));
#121266=CARTESIAN_POINT('',(22.5035000139866,1076.69297254634,338.813663432303));
#121267=CARTESIAN_POINT('',(22.5035000139359,1076.64871264505,337.057057167916));
#121268=CARTESIAN_POINT('Ctrl Pts',(22.5035000139866,1076.69297254634,338.813663432303));
#121269=CARTESIAN_POINT('Ctrl Pts',(22.3878767363282,1076.69359423243,338.813663432303));
#121270=CARTESIAN_POINT('Ctrl Pts',(22.2733708709006,1076.69373416697,338.790831450123));
#121271=CARTESIAN_POINT('Ctrl Pts',(22.0588653938933,1076.6930455795,338.701727736787));
#121272=CARTESIAN_POINT('Ctrl Pts',(21.9611437701684,1076.69221489214,338.635979444957));
#121273=CARTESIAN_POINT('Ctrl Pts',(21.7972022392667,1076.68960067082,338.47026886885));
#121274=CARTESIAN_POINT('Ctrl Pts',(21.7325714022931,1076.68784156337,338.37199507179));
#121275=CARTESIAN_POINT('Ctrl Pts',(21.6452933652732,1076.68348938718,338.15567604397));
#121276=CARTESIAN_POINT('Ctrl Pts',(21.6236359871019,1076.68093454894,338.039733910526));
#121277=CARTESIAN_POINT('Ctrl Pts',(21.6269271605318,1076.67528671955,337.806589730332));
#121278=CARTESIAN_POINT('Ctrl Pts',(21.651684659901,1076.67225026564,337.691698814802));
#121279=CARTESIAN_POINT('Ctrl Pts',(21.7440712650905,1076.66612043095,337.479336588598));
#121280=CARTESIAN_POINT('Ctrl Pts',(21.810373419722,1076.66308830352,337.383756695907));
#121281=CARTESIAN_POINT('Ctrl Pts',(21.9761262991321,1076.65748436421,337.223617330552));
#121282=CARTESIAN_POINT('Ctrl Pts',(22.0739834480995,1076.65496945098,337.160621496983));
#121283=CARTESIAN_POINT('Ctrl Pts',(22.2838754306421,1076.65100816475,337.077829047932));
#121284=CARTESIAN_POINT('Ctrl Pts',(22.3932172379869,1076.64955887,337.057057167929));
#121285=CARTESIAN_POINT('Ctrl Pts',(22.5035000138852,1076.64871264505,337.057057167917));
#121286=CARTESIAN_POINT('',(22.5035000139866,1082.7251047501,337.057057167916));
#121287=CARTESIAN_POINT('',(22.5035000139866,1067.7251047501,337.057057167916));
#121288=CARTESIAN_POINT('Origin',(22.5035000139866,1082.7251047501,337.93536030011));
#121289=CARTESIAN_POINT('Ctrl Pts',(22.5035000138852,1076.64871264505,337.057057167916));
#121290=CARTESIAN_POINT('Ctrl Pts',(22.5083455647385,1076.64867546403,337.057057167916));
#121291=CARTESIAN_POINT('Ctrl Pts',(22.5131929321026,1076.64863944285,337.057097266808));
#121292=CARTESIAN_POINT('Ctrl Pts',(22.633052817737,1076.64777788057,337.059081997554));
#121293=CARTESIAN_POINT('Ctrl Pts',(22.746577983698,1076.64762843378,337.08356157286));
#121294=CARTESIAN_POINT('Ctrl Pts',(22.9575589611612,1076.64870989134,337.174811135971));
#121295=CARTESIAN_POINT('Ctrl Pts',(23.0529995289714,1076.64992730021,337.240628668182));
#121296=CARTESIAN_POINT('Ctrl Pts',(23.2130964306104,1076.65350239392,337.405207037073));
#121297=CARTESIAN_POINT('Ctrl Pts',(23.2762234220587,1076.65582284456,337.502365674146));
#121298=CARTESIAN_POINT('Ctrl Pts',(23.3586278483235,1076.6609686024,337.708182993632));
#121299=CARTESIAN_POINT('Ctrl Pts',(23.3799111548858,1076.66370395421,337.813890257395));
#121300=CARTESIAN_POINT('Ctrl Pts',(23.381682622606,1076.66651885184,337.920810456847));
#121301=CARTESIAN_POINT('Ctrl Pts',(23.3826335120876,1076.66802983425,337.978203144207));
#121302=CARTESIAN_POINT('Ctrl Pts',(23.3779558593717,1076.66955366055,338.035551066894));
#121303=CARTESIAN_POINT('Ctrl Pts',(23.3574760532041,1076.67257789149,338.14852043641));
#121304=CARTESIAN_POINT('Ctrl Pts',(23.3417211491484,1076.67407102164,338.203870679632));
#121305=CARTESIAN_POINT('Ctrl Pts',(23.2777947269055,1076.67848416595,338.366141427581));
#121306=CARTESIAN_POINT('Ctrl Pts',(23.2135880123276,1076.68123002284,338.46534386836));
#121307=CARTESIAN_POINT('Ctrl Pts',(23.0504339278554,1076.68603251116,338.632390075667));
#121308=CARTESIAN_POINT('Ctrl Pts',(22.9532592893986,1076.68804699463,338.698712717894));
#121309=CARTESIAN_POINT('Ctrl Pts',(22.7386428959933,1076.69120466253,338.789590833938));
#121310=CARTESIAN_POINT('Ctrl Pts',(22.623326353342,1076.69231903148,338.813224537003));
#121311=CARTESIAN_POINT('Ctrl Pts',(22.5056741696389,1076.69296081386,338.813661414268));
#121312=CARTESIAN_POINT('Ctrl Pts',(22.5045870424311,1076.69296670158,338.813663432303));
#121313=CARTESIAN_POINT('Ctrl Pts',(22.5035000139866,1076.69297254634,338.813663432303));
#121314=CARTESIAN_POINT('Origin',(34.5096048204692,1067.7251047501,334.252491309441));
#121315=CARTESIAN_POINT('',(34.5096048204916,1078.26956110846,332.977047188305));
#121316=CARTESIAN_POINT('Ctrl Pts',(34.5096147511975,1078.42202229817,335.527935430539));
#121317=CARTESIAN_POINT('Ctrl Pts',(34.6788900809127,1078.41848212202,335.527934112545));
#121318=CARTESIAN_POINT('Ctrl Pts',(34.8464284900048,1078.4131107714,335.494234862051));
#121319=CARTESIAN_POINT('Ctrl Pts',(35.1359547877757,1078.40014346458,335.372934139495));
#121320=CARTESIAN_POINT('Ctrl Pts',(35.2589154610803,1078.39307233246,335.294707124768));
#121321=CARTESIAN_POINT('Ctrl Pts',(35.4818542978442,1078.37658785593,335.092666420833));
#121322=CARTESIAN_POINT('Ctrl Pts',(35.5773303002289,1078.36716823394,334.967405662373));
#121323=CARTESIAN_POINT('Ctrl Pts',(35.7235798016571,1078.34671690063,334.678196417761));
#121324=CARTESIAN_POINT('Ctrl Pts',(35.7690250311635,1078.33581296784,334.514829661878));
#121325=CARTESIAN_POINT('Ctrl Pts',(35.7939442785044,1078.31474731809,334.180726523008));
#121326=CARTESIAN_POINT('Ctrl Pts',(35.7735107608398,1078.30478590551,334.013217513336));
#121327=CARTESIAN_POINT('Ctrl Pts',(35.6732223167888,1078.28795050828,333.70797182205));
#121328=CARTESIAN_POINT('Ctrl Pts',(35.5989622077366,1078.28103732217,333.5714310054));
#121329=CARTESIAN_POINT('Ctrl Pts',(35.4155791059637,1078.27094007561,333.344226731133));
#121330=CARTESIAN_POINT('Ctrl Pts',(35.3122412652377,1078.26750497797,333.25172802105));
#121331=CARTESIAN_POINT('Ctrl Pts',(35.1553934425796,1078.26489491942,333.151561732247));
#121332=CARTESIAN_POINT('Ctrl Pts',(35.1132568748934,1078.26440402831,333.127905410159));
#121333=CARTESIAN_POINT('Ctrl Pts',(35.0431913814379,1078.26391702572,333.093644634156));
#121334=CARTESIAN_POINT('Ctrl Pts',(35.0160556824621,1078.26380335544,333.081531108159));
#121335=CARTESIAN_POINT('Ctrl Pts',(34.9637699943256,1078.26372442065,333.060348324321));
#121336=CARTESIAN_POINT('Ctrl Pts',(34.9387096191683,1078.2637453383,333.051100461356));
#121337=CARTESIAN_POINT('Ctrl Pts',(34.8814984999493,1078.26392411984,333.032006872119));
#121338=CARTESIAN_POINT('Ctrl Pts',(34.8492119449382,1078.26411591185,333.022631926122));
#121339=CARTESIAN_POINT('Ctrl Pts',(34.7531149081119,1078.26495074532,332.998801609938));
#121340=CARTESIAN_POINT('Ctrl Pts',(34.6885241418035,1078.26584788466,332.987967011555));
#121341=CARTESIAN_POINT('Ctrl Pts',(34.4540959154272,1078.27028355316,332.966968894671));
#121342=CARTESIAN_POINT('Ctrl Pts',(34.2835286720398,1078.27571016965,332.985803391606));
#121343=CARTESIAN_POINT('Ctrl Pts',(33.9875839019163,1078.28895387294,333.080280780492));
#121344=CARTESIAN_POINT('Ctrl Pts',(33.8615088215039,1078.29610909007,333.145003815832));
#121345=CARTESIAN_POINT('Ctrl Pts',(33.6263666062539,1078.31267232065,333.319836449441));
#121346=CARTESIAN_POINT('Ctrl Pts',(33.5214296212414,1078.32208286624,333.431854167036));
#121347=CARTESIAN_POINT('Ctrl Pts',(33.3500320209256,1078.34220280928,333.696781295865));
#121348=CARTESIAN_POINT('Ctrl Pts',(33.2884764937801,1078.35277145748,333.849659006327));
#121349=CARTESIAN_POINT('Ctrl Pts',(33.2254191467029,1078.37336833541,334.175263302984));
#121350=CARTESIAN_POINT('Ctrl Pts',(33.2264379303475,1078.38317088678,334.345296792578));
#121351=CARTESIAN_POINT('Ctrl Pts',(33.2930446394784,1078.40010063959,334.668064508785));
#121352=CARTESIAN_POINT('Ctrl Pts',(33.3552300229392,1078.40717753,334.818330797793));
#121353=CARTESIAN_POINT('Ctrl Pts',(33.5370927722223,1078.41866703403,335.095004549569));
#121354=CARTESIAN_POINT('Ctrl Pts',(33.6578343919329,1078.42280636336,335.216920579092));
#121355=CARTESIAN_POINT('Ctrl Pts',(33.8427374050399,1078.42572190528,335.34098853853));
#121356=CARTESIAN_POINT('Ctrl Pts',(33.8883070459096,1078.42622474696,335.367627096213));
#121357=CARTESIAN_POINT('Ctrl Pts',(33.9629561123523,1078.4267216759,335.405264287277));
#121358=CARTESIAN_POINT('Ctrl Pts',(33.9910117492956,1078.42684008769,335.418154900283));
#121359=CARTESIAN_POINT('Ctrl Pts',(34.0413320849543,1078.42693406491,335.439098731677));
#121360=CARTESIAN_POINT('Ctrl Pts',(34.0634049784836,1078.42693656199,335.447573830197));
#121361=CARTESIAN_POINT('Ctrl Pts',(34.1142066581152,1078.42685506576,335.465475852172));
#121362=CARTESIAN_POINT('Ctrl Pts',(34.1430605655501,1078.42674681612,335.474504603571));
#121363=CARTESIAN_POINT('Ctrl Pts',(34.2217440071173,1078.42628615239,335.49608784527));
#121364=CARTESIAN_POINT('Ctrl Pts',(34.2720544852055,1078.42581637568,335.506670602497));
#121365=CARTESIAN_POINT('Ctrl Pts',(34.3846975793669,1078.42437984733,335.523342615151));
#121366=CARTESIAN_POINT('Ctrl Pts',(34.4471161568302,1078.42332937601,335.527935917159));
#121367=CARTESIAN_POINT('Ctrl Pts',(34.5096147511975,1078.42202229817,335.527935430539));
#121368=CARTESIAN_POINT('',(34.5096048204403,1076.26445914773,332.977047188305));
#121369=CARTESIAN_POINT('',(34.5096048204692,1067.7251047501,332.977047188305));
#121370=CARTESIAN_POINT('Ctrl Pts',(34.5102109201886,1076.41849772182,335.527935286566));
#121371=CARTESIAN_POINT('Ctrl Pts',(34.340802513415,1076.42208285403,335.528015790602));
#121372=CARTESIAN_POINT('Ctrl Pts',(34.1730438365003,1076.42374639349,335.49434307368));
#121373=CARTESIAN_POINT('Ctrl Pts',(33.8605337398837,1076.42310943455,335.36341668331));
#121374=CARTESIAN_POINT('Ctrl Pts',(33.7189220406696,1076.42081641364,335.267504925686));
#121375=CARTESIAN_POINT('Ctrl Pts',(33.4818233026479,1076.41246193248,335.026393198278));
#121376=CARTESIAN_POINT('Ctrl Pts',(33.388563752612,1076.40649108723,334.883750708962));
#121377=CARTESIAN_POINT('Ctrl Pts',(33.2629400687953,1076.39142866753,334.5704421047));
#121378=CARTESIAN_POINT('Ctrl Pts',(33.2318666463486,1076.38247877826,334.402859557023));
#121379=CARTESIAN_POINT('Ctrl Pts',(33.2354824664854,1076.36766235584,334.151400656831));
#121380=CARTESIAN_POINT('Ctrl Pts',(33.2447238528446,1076.36258362599,334.068970626844));
#121381=CARTESIAN_POINT('Ctrl Pts',(33.2791157729686,1076.35212829543,333.906711076648));
#121382=CARTESIAN_POINT('Ctrl Pts',(33.3042586837665,1076.34677504228,333.827277996471));
#121383=CARTESIAN_POINT('Ctrl Pts',(33.4035232894238,1076.33040323854,333.59522743218));
#121384=CARTESIAN_POINT('Ctrl Pts',(33.5004296136776,1076.31941991101,333.454373892106));
#121385=CARTESIAN_POINT('Ctrl Pts',(33.7423609597917,1076.29894476336,333.21993421309));
#121386=CARTESIAN_POINT('Ctrl Pts',(33.8845533658297,1076.28963946483,333.12812963202));
#121387=CARTESIAN_POINT('Ctrl Pts',(34.1960783506563,1076.2740769255,333.004912336979));
#121388=CARTESIAN_POINT('Ctrl Pts',(34.3623240049718,1076.26796854383,332.9745620649));
#121389=CARTESIAN_POINT('Ctrl Pts',(34.6965963480527,1076.2599801983,332.979841362785));
#121390=CARTESIAN_POINT('Ctrl Pts',(34.8613404043709,1076.25816692957,333.015195519091));
#121391=CARTESIAN_POINT('Ctrl Pts',(35.1675090936512,1076.25915691969,333.147211945058));
#121392=CARTESIAN_POINT('Ctrl Pts',(35.3059899336232,1076.26193861752,333.242427561267));
#121393=CARTESIAN_POINT('Ctrl Pts',(35.5385438700153,1076.27166771401,333.480639647995));
#121394=CARTESIAN_POINT('Ctrl Pts',(35.6303460932242,1076.27851813776,333.621329378398));
#121395=CARTESIAN_POINT('Ctrl Pts',(35.7548949936911,1076.29523851775,333.930277026068));
#121396=CARTESIAN_POINT('Ctrl Pts',(35.7862914377388,1076.30495095122,334.095633422479));
#121397=CARTESIAN_POINT('Ctrl Pts',(35.7837278835445,1076.32579386364,334.429373808202));
#121398=CARTESIAN_POINT('Ctrl Pts',(35.7496234062969,1076.33672577133,334.594579542738));
#121399=CARTESIAN_POINT('Ctrl Pts',(35.6186724076319,1076.35843100728,334.904803232953));
#121400=CARTESIAN_POINT('Ctrl Pts',(35.5221498569416,1076.3689855776,335.046418752925));
#121401=CARTESIAN_POINT('Ctrl Pts',(35.2800739986142,1076.38812047267,335.282815051021));
#121402=CARTESIAN_POINT('Ctrl Pts',(35.1372193674678,1076.39652954069,335.37558137405));
#121403=CARTESIAN_POINT('Ctrl Pts',(34.8308026336779,1076.41000443043,335.497279305095));
#121404=CARTESIAN_POINT('Ctrl Pts',(34.6712631505156,1076.41508942852,335.527858753442));
#121405=CARTESIAN_POINT('Ctrl Pts',(34.5102109201886,1076.41849772182,335.527935286566));
#121406=CARTESIAN_POINT('Origin',(34.5096048204692,1067.7251047501,334.252491309441));
#121407=CARTESIAN_POINT('',(34.5096048204692,1076.38494400861,334.927935430577));
#121408=CARTESIAN_POINT('',(34.5096048204691,1076.30335139737,333.577047188305));
#121409=CARTESIAN_POINT('Ctrl Pts',(34.5096048204692,1076.38494400861,334.927935430577));
#121410=CARTESIAN_POINT('Ctrl Pts',(34.5076204863166,1076.38498777139,334.927935430577));
#121411=CARTESIAN_POINT('Ctrl Pts',(34.505635719696,1076.38503103526,334.927926686154));
#121412=CARTESIAN_POINT('Ctrl Pts',(34.4136515499107,1076.38701252793,334.927115786453));
#121413=CARTESIAN_POINT('Ctrl Pts',(34.3247019053225,1076.38788513909,334.908341647077));
#121414=CARTESIAN_POINT('Ctrl Pts',(34.1594034672164,1076.38741377614,334.837029001987));
#121415=CARTESIAN_POINT('Ctrl Pts',(34.0847309499407,1076.3860749365,334.785222161754));
#121416=CARTESIAN_POINT('Ctrl Pts',(33.960171830601,1076.38132376325,334.655508926247));
#121417=CARTESIAN_POINT('Ctrl Pts',(33.911510309296,1076.37796080277,334.578944121455));
#121418=CARTESIAN_POINT('Ctrl Pts',(33.846960452068,1076.36959080339,334.411256518578));
#121419=CARTESIAN_POINT('Ctrl Pts',(33.8317482226124,1076.3646644461,334.321796648458));
#121420=CARTESIAN_POINT('Ctrl Pts',(33.83580476543,1076.35661574422,334.188042091632));
#121421=CARTESIAN_POINT('Ctrl Pts',(33.8414312719777,1076.3538746385,334.144308576499));
#121422=CARTESIAN_POINT('Ctrl Pts',(33.8611295966575,1076.34827017143,334.058457123008));
#121423=CARTESIAN_POINT('Ctrl Pts',(33.8751765830277,1076.34541975035,334.016546567831));
#121424=CARTESIAN_POINT('Ctrl Pts',(33.9298550244792,1076.3367634241,333.894513470876));
#121425=CARTESIAN_POINT('Ctrl Pts',(33.9824256775183,1076.33102829037,333.820814073603));
#121426=CARTESIAN_POINT('Ctrl Pts',(34.1125602101747,1076.32045290633,333.698922122255));
#121427=CARTESIAN_POINT('Ctrl Pts',(34.1885855586371,1076.31570608637,333.651623978921));
#121428=CARTESIAN_POINT('Ctrl Pts',(34.347662912495,1076.30816746905,333.591731499172));
#121429=CARTESIAN_POINT('Ctrl Pts',(34.4282875005316,1076.30530761802,333.577047188305));
#121430=CARTESIAN_POINT('Ctrl Pts',(34.509604820469,1076.30335139737,333.577047188305));
#121431=CARTESIAN_POINT('',(34.5096048204692,1082.7251047501,333.577047188305));
#121432=CARTESIAN_POINT('',(34.5096048204692,1067.7251047501,333.577047188305));
#121433=CARTESIAN_POINT('Origin',(34.5096048204692,1082.7251047501,334.252491309441));
#121434=CARTESIAN_POINT('Ctrl Pts',(34.509604820469,1076.30335139737,333.577047188305));
#121435=CARTESIAN_POINT('Ctrl Pts',(34.5097104357425,1076.30334885662,333.577047188305));
#121436=CARTESIAN_POINT('Ctrl Pts',(34.5098160521846,1076.3033463174,333.577047213136));
#121437=CARTESIAN_POINT('Ctrl Pts',(34.5099216697866,1076.3033437797,333.577047262681));
#121438=CARTESIAN_POINT('Ctrl Pts',(34.5982697152156,1076.3012210189,333.577088706532));
#121439=CARTESIAN_POINT('Ctrl Pts',(34.6857691725621,1076.30020595607,333.594463525176));
#121440=CARTESIAN_POINT('Ctrl Pts',(34.8489964149025,1076.30052704744,333.66187938198));
#121441=CARTESIAN_POINT('Ctrl Pts',(34.9231439920578,1076.30185616366,333.711206804535));
#121442=CARTESIAN_POINT('Ctrl Pts',(35.0483053469897,1076.30667596252,333.835580321072));
#121443=CARTESIAN_POINT('Ctrl Pts',(35.0980858579031,1076.31012002537,333.909429616361));
#121444=CARTESIAN_POINT('Ctrl Pts',(35.1665194890139,1076.31863717469,334.072209307536));
#121445=CARTESIAN_POINT('Ctrl Pts',(35.1844379846351,1076.32363062344,334.159603982343));
#121446=CARTESIAN_POINT('Ctrl Pts',(35.1856305787911,1076.33446701535,334.336475996902));
#121447=CARTESIAN_POINT('Ctrl Pts',(35.1688126803986,1076.3402072694,334.424264869087));
#121448=CARTESIAN_POINT('Ctrl Pts',(35.1016905359036,1076.35174522374,334.589801169872));
#121449=CARTESIAN_POINT('Ctrl Pts',(35.051457375514,1076.35742799787,334.665705040811));
#121450=CARTESIAN_POINT('Ctrl Pts',(34.9243861831326,1076.36785261679,334.7930861097));
#121451=CARTESIAN_POINT('Ctrl Pts',(34.8489091855288,1076.37249601905,334.843397942504));
#121452=CARTESIAN_POINT('Ctrl Pts',(34.684486155862,1076.38009119671,334.9107908759));
#121453=CARTESIAN_POINT('Ctrl Pts',(34.5974694356268,1076.3830062301,334.927935430577));
#121454=CARTESIAN_POINT('Ctrl Pts',(34.5096048204692,1076.38494400861,334.927935430577));
#121455=CARTESIAN_POINT('Origin',(48.0649554680753,1067.7251047501,331.411589053766));
#121456=CARTESIAN_POINT('',(48.0649554680963,1077.56338652908,330.312757917773));
#121457=CARTESIAN_POINT('Ctrl Pts',(48.0649716197798,1077.7648831442,332.510420189639));
#121458=CARTESIAN_POINT('Ctrl Pts',(48.178352154084,1077.75970685431,332.51041852306));
#121459=CARTESIAN_POINT('Ctrl Pts',(48.2909673304275,1077.75299736048,332.492869337076));
#121460=CARTESIAN_POINT('Ctrl Pts',(48.5182099272391,1077.73608180198,332.420395537207));
#121461=CARTESIAN_POINT('Ctrl Pts',(48.6300971783606,1077.72570234581,332.362217480017));
#121462=CARTESIAN_POINT('Ctrl Pts',(48.8375449886251,1077.70183999985,332.204606627412));
#121463=CARTESIAN_POINT('Ctrl Pts',(48.9292536117016,1077.68837022053,332.103487055596));
#121464=CARTESIAN_POINT('Ctrl Pts',(49.076808191232,1077.6595310852,331.864194664782));
#121465=CARTESIAN_POINT('Ctrl Pts',(49.1278923488863,1077.64437043363,331.726036229211));
#121466=CARTESIAN_POINT('Ctrl Pts',(49.1727821420296,1077.61567136738,331.439938839538));
#121467=CARTESIAN_POINT('Ctrl Pts',(49.1670087823169,1077.6023817782,331.294844533771));
#121468=CARTESIAN_POINT('Ctrl Pts',(49.1030881065632,1077.58048206346,331.028806169293));
#121469=CARTESIAN_POINT('Ctrl Pts',(49.0506916953905,1077.5717112608,330.908968998611));
#121470=CARTESIAN_POINT('Ctrl Pts',(48.9137468474225,1077.55899518548,330.704082580428));
#121471=CARTESIAN_POINT('Ctrl Pts',(48.8339446140538,1077.55472994776,330.618054006717));
#121472=CARTESIAN_POINT('Ctrl Pts',(48.7118554226231,1077.55163429195,330.522533033387));
#121473=CARTESIAN_POINT('Ctrl Pts',(48.6804372721054,1077.55107968466,330.500500263895));
#121474=CARTESIAN_POINT('Ctrl Pts',(48.6284098270173,1077.5505342769,330.467936946777));
#121475=CARTESIAN_POINT('Ctrl Pts',(48.6085110774363,1077.55040687991,330.456336492958));
#121476=CARTESIAN_POINT('Ctrl Pts',(48.5721328957578,1077.55031714434,330.436633984257));
#121477=CARTESIAN_POINT('Ctrl Pts',(48.5557874136468,1077.55032651203,330.428303575575));
#121478=CARTESIAN_POINT('Ctrl Pts',(48.5172560827631,1077.55046276867,330.409866525129));
#121479=CARTESIAN_POINT('Ctrl Pts',(48.4949276757087,1077.55062723603,330.400081408223));
#121480=CARTESIAN_POINT('Ctrl Pts',(48.4312248328205,1077.55133327342,330.374655159362));
#121481=CARTESIAN_POINT('Ctrl Pts',(48.3892090526295,1077.55207222191,330.360758931861));
#121482=CARTESIAN_POINT('Ctrl Pts',(48.2053273015861,1077.5564524783,330.312021908459));
#121483=CARTESIAN_POINT('Ctrl Pts',(48.0582476593478,1077.5628157921,330.303147962668));
#121484=CARTESIAN_POINT('Ctrl Pts',(47.7960385763287,1077.57903617972,330.33955486139));
#121485=CARTESIAN_POINT('Ctrl Pts',(47.6817784495743,1077.58792245681,330.374910895428));
#121486=CARTESIAN_POINT('Ctrl Pts',(47.4595029378342,1077.60903606065,330.485501826043));
#121487=CARTESIAN_POINT('Ctrl Pts',(47.3547201557304,1077.62132926004,330.56321930683));
#121488=CARTESIAN_POINT('Ctrl Pts',(47.1703253790053,1077.6482429037,330.758551376419));
#121489=CARTESIAN_POINT('Ctrl Pts',(47.0948590130962,1077.66273278756,330.877055188268));
#121490=CARTESIAN_POINT('Ctrl Pts',(46.9898151758799,1077.69187966943,331.141904072517));
#121491=CARTESIAN_POINT('Ctrl Pts',(46.9635360839081,1077.70623475282,331.286757043586));
#121492=CARTESIAN_POINT('Ctrl Pts',(46.9690147760831,1077.73177127797,331.573235184765));
#121493=CARTESIAN_POINT('Ctrl Pts',(46.9986860515326,1077.74281768748,331.712185253558));
#121494=CARTESIAN_POINT('Ctrl Pts',(47.1056810555825,1077.7602775885,331.963615565543));
#121495=CARTESIAN_POINT('Ctrl Pts',(47.1791061162971,1077.76678995776,332.075112078044));
#121496=CARTESIAN_POINT('Ctrl Pts',(47.3189767550015,1077.7733420861,332.221422522343));
#121497=CARTESIAN_POINT('Ctrl Pts',(47.3719924400894,1077.77497059055,332.267229676188));
#121498=CARTESIAN_POINT('Ctrl Pts',(47.4536558318971,1077.77636730149,332.325184020711));
#121499=CARTESIAN_POINT('Ctrl Pts',(47.479011047914,1077.77666611122,332.341649425967));
#121500=CARTESIAN_POINT('Ctrl Pts',(47.5213221343044,1077.77695163752,332.366707850815));
#121501=CARTESIAN_POINT('Ctrl Pts',(47.5378779011577,1077.77701312378,332.375942915218));
#121502=CARTESIAN_POINT('Ctrl Pts',(47.5729061019401,1077.77703996846,332.394310551927));
#121503=CARTESIAN_POINT('Ctrl Pts',(47.5914130828635,1077.77699652618,332.403361065396));
#121504=CARTESIAN_POINT('Ctrl Pts',(47.6355333725391,1077.77675929222,332.423420667363));
#121505=CARTESIAN_POINT('Ctrl Pts',(47.6613322255803,1077.77651792696,332.433985616383));
#121506=CARTESIAN_POINT('Ctrl Pts',(47.7452564333032,1077.77540886323,332.464681620272));
#121507=CARTESIAN_POINT('Ctrl Pts',(47.8046708492155,1077.77413896231,332.480916341996));
#121508=CARTESIAN_POINT('Ctrl Pts',(47.9310591630673,1077.77044888337,332.504291375912));
#121509=CARTESIAN_POINT('Ctrl Pts',(47.9979557989091,1077.76794269333,332.510421174704));
#121510=CARTESIAN_POINT('Ctrl Pts',(48.0649716197798,1077.7648831442,332.510420189639));
#121511=CARTESIAN_POINT('',(48.0649554680754,1075.55153395083,330.312757917773));
#121512=CARTESIAN_POINT('',(48.0649554680753,1067.7251047501,330.312757917773));
#121513=CARTESIAN_POINT('Ctrl Pts',(48.0649874847738,1075.75487488712,332.510420189292));
#121514=CARTESIAN_POINT('Ctrl Pts',(47.9186934725305,1075.76161608273,332.510424451868));
#121515=CARTESIAN_POINT('Ctrl Pts',(47.77378732338,1075.76566123828,332.481212826068));
#121516=CARTESIAN_POINT('Ctrl Pts',(47.5067627381033,1075.76791600253,332.36886332233));
#121517=CARTESIAN_POINT('Ctrl Pts',(47.3868749072479,1075.76622817133,332.288026427572));
#121518=CARTESIAN_POINT('Ctrl Pts',(47.1828382832594,1075.75732351336,332.082895532957));
#121519=CARTESIAN_POINT('Ctrl Pts',(47.1015698117973,1075.75008447038,331.95986121963));
#121520=CARTESIAN_POINT('Ctrl Pts',(46.9919493351637,1075.73088939794,331.689650946595));
#121521=CARTESIAN_POINT('Ctrl Pts',(46.9646269580503,1075.71912894922,331.545217250679));
#121522=CARTESIAN_POINT('Ctrl Pts',(46.9677551381208,1075.69247091493,331.253735442318));
#121523=CARTESIAN_POINT('Ctrl Pts',(46.998428562372,1075.67781839374,331.109531855694));
#121524=CARTESIAN_POINT('Ctrl Pts',(47.0847385615665,1075.65527800369,330.909857236068));
#121525=CARTESIAN_POINT('Ctrl Pts',(47.119517409326,1075.64779663082,330.847047921984));
#121526=CARTESIAN_POINT('Ctrl Pts',(47.2430714473924,1075.62519853705,330.667756621868));
#121527=CARTESIAN_POINT('Ctrl Pts',(47.3492014365594,1075.61044739057,330.565111949947));
#121528=CARTESIAN_POINT('Ctrl Pts',(47.5939727676699,1075.58376638424,330.408369154433));
#121529=CARTESIAN_POINT('Ctrl Pts',(47.7298416619558,1075.57205931713,330.355153140756));
#121530=CARTESIAN_POINT('Ctrl Pts',(48.0138021853828,1075.55328624887,330.304574479363));
#121531=CARTESIAN_POINT('Ctrl Pts',(48.1590369585093,1075.54637812743,330.307363022654));
#121532=CARTESIAN_POINT('Ctrl Pts',(48.4396166961066,1075.53838981627,330.368723946942));
#121533=CARTESIAN_POINT('Ctrl Pts',(48.5722161574972,1075.53735884485,330.426380120262));
#121534=CARTESIAN_POINT('Ctrl Pts',(48.8076871283584,1075.54133536622,330.589247538962));
#121535=CARTESIAN_POINT('Ctrl Pts',(48.9082472702065,1075.54629435517,330.692768456006));
#121536=CARTESIAN_POINT('Ctrl Pts',(49.064329507079,1075.56153603297,330.93278602151));
#121537=CARTESIAN_POINT('Ctrl Pts',(49.1181445935129,1075.57168658861,331.067044682633));
#121538=CARTESIAN_POINT('Ctrl Pts',(49.1714343129085,1075.5958042192,331.349249458987));
#121539=CARTESIAN_POINT('Ctrl Pts',(49.170049411285,1075.60956112074,331.494569515375));
#121540=CARTESIAN_POINT('Ctrl Pts',(49.1260696578948,1075.63144476061,331.705978096679));
#121541=CARTESIAN_POINT('Ctrl Pts',(49.1044752427592,1075.63890669277,331.774940051196));
#121542=CARTESIAN_POINT('Ctrl Pts',(49.0482183160794,1075.65388793986,331.907348066901));
#121543=CARTESIAN_POINT('Ctrl Pts',(49.0137391194163,1075.66137241396,331.970510972076));
#121544=CARTESIAN_POINT('Ctrl Pts',(48.8913182184056,1075.68375750389,332.150376217104));
#121545=CARTESIAN_POINT('Ctrl Pts',(48.7860710315865,1075.69813484908,332.253449521655));
#121546=CARTESIAN_POINT('Ctrl Pts',(48.5417130443118,1075.72398963666,332.412232229124));
#121547=CARTESIAN_POINT('Ctrl Pts',(48.4051043623622,1075.73522779827,332.466560848604));
#121548=CARTESIAN_POINT('Ctrl Pts',(48.1968430398588,1075.74826246404,332.504468511868));
#121549=CARTESIAN_POINT('Ctrl Pts',(48.1309961998813,1075.75183322017,332.510418265992));
#121550=CARTESIAN_POINT('Ctrl Pts',(48.0649874847738,1075.75487488712,332.510420189292));
#121551=CARTESIAN_POINT('Origin',(48.0649554680753,1067.7251047501,331.411589053766));
#121552=CARTESIAN_POINT('',(48.0649554680753,1075.70120171291,331.910420189758));
#121553=CARTESIAN_POINT('',(48.0649554680763,1075.60888786087,330.912757917773));
#121554=CARTESIAN_POINT('Ctrl Pts',(48.0649554680753,1075.70120171291,331.910420189758));
#121555=CARTESIAN_POINT('Ctrl Pts',(48.0306710331432,1075.7028123358,331.910420189758));
#121556=CARTESIAN_POINT('Ctrl Pts',(47.9963809644694,1075.70409991635,331.906885757966));
#121557=CARTESIAN_POINT('Ctrl Pts',(47.899017501197,1075.7068113055,331.886480708058));
#121558=CARTESIAN_POINT('Ctrl Pts',(47.838605396802,1075.70731189829,331.860839012816));
#121559=CARTESIAN_POINT('Ctrl Pts',(47.7309687707835,1075.70571568726,331.787780017816));
#121560=CARTESIAN_POINT('Ctrl Pts',(47.6848282042222,1075.70363260956,331.741074234883));
#121561=CARTESIAN_POINT('Ctrl Pts',(47.6129305960903,1075.6971102356,331.63242461102));
#121562=CARTESIAN_POINT('Ctrl Pts',(47.5879750129836,1075.6927246489,331.571489610806));
#121563=CARTESIAN_POINT('Ctrl Pts',(47.5626553064818,1075.68209624682,331.442322121797));
#121564=CARTESIAN_POINT('Ctrl Pts',(47.5630437078385,1075.67592344304,331.375255516538));
#121565=CARTESIAN_POINT('Ctrl Pts',(47.5831174809899,1075.66605577145,331.278472134671));
#121566=CARTESIAN_POINT('Ctrl Pts',(47.5928059226919,1075.66272723371,331.247388089204));
#121567=CARTESIAN_POINT('Ctrl Pts',(47.6181011662297,1075.65598822601,331.187509268941));
#121568=CARTESIAN_POINT('Ctrl Pts',(47.6336593298329,1075.65259309782,331.158855648727));
#121569=CARTESIAN_POINT('Ctrl Pts',(47.6893341221625,1075.64230630239,331.076625907071));
#121570=CARTESIAN_POINT('Ctrl Pts',(47.7375191470671,1075.63559657088,331.029375263062));
#121571=CARTESIAN_POINT('Ctrl Pts',(47.8485629393243,1075.62353502493,330.957392611238));
#121572=CARTESIAN_POINT('Ctrl Pts',(47.9100422347544,1075.61827364809,330.932904458574));
#121573=CARTESIAN_POINT('Ctrl Pts',(48.0043710097193,1075.61208154299,330.915523963248));
#121574=CARTESIAN_POINT('Ctrl Pts',(48.0346206392831,1075.61035734689,330.912757917773));
#121575=CARTESIAN_POINT('Ctrl Pts',(48.0649554680778,1075.60888786087,330.912757917773));
#121576=CARTESIAN_POINT('',(48.0649554680753,1082.7251047501,330.912757917773));
#121577=CARTESIAN_POINT('',(48.0649554680753,1067.7251047501,330.912757917773));
#121578=CARTESIAN_POINT('Origin',(48.0649554680753,1082.7251047501,331.411589053766));
#121579=CARTESIAN_POINT('Ctrl Pts',(48.0649636762499,1075.60888746326,330.912757917841));
#121580=CARTESIAN_POINT('Ctrl Pts',(48.1300654628176,1075.60573388934,330.912758989078));
#121581=CARTESIAN_POINT('Ctrl Pts',(48.1945770351577,1075.60380209979,330.925504507233));
#121582=CARTESIAN_POINT('Ctrl Pts',(48.3149247369696,1075.60262406827,330.975046456933));
#121583=CARTESIAN_POINT('Ctrl Pts',(48.3695851031577,1075.60338155543,331.011275263444));
#121584=CARTESIAN_POINT('Ctrl Pts',(48.462007986295,1075.60749709355,331.102697530493));
#121585=CARTESIAN_POINT('Ctrl Pts',(48.4988235568122,1075.61081819815,331.157013265499));
#121586=CARTESIAN_POINT('Ctrl Pts',(48.54968213026,1075.61960069567,331.276917082956));
#121587=CARTESIAN_POINT('Ctrl Pts',(48.5631047536,1075.624987281,331.34139428124));
#121588=CARTESIAN_POINT('Ctrl Pts',(48.5644345106547,1075.63723543239,331.473389224999));
#121589=CARTESIAN_POINT('Ctrl Pts',(48.5516724214059,1075.64400915804,331.539635813471));
#121590=CARTESIAN_POINT('Ctrl Pts',(48.5138825399483,1075.65432757827,331.631492619645));
#121591=CARTESIAN_POINT('Ctrl Pts',(48.4985721202037,1075.65772548985,331.660325500007));
#121592=CARTESIAN_POINT('Ctrl Pts',(48.4438364840096,1075.66794837201,331.742785713353));
#121593=CARTESIAN_POINT('Ctrl Pts',(48.396409921061,1075.67456732752,331.790258573698));
#121594=CARTESIAN_POINT('Ctrl Pts',(48.2857635303348,1075.68654875824,331.863784226594));
#121595=CARTESIAN_POINT('Ctrl Pts',(48.2236579472687,1075.69179636756,331.889153178431));
#121596=CARTESIAN_POINT('Ctrl Pts',(48.1274943987379,1075.69799473505,331.907479517654));
#121597=CARTESIAN_POINT('Ctrl Pts',(48.0962272775363,1075.69973261789,331.910420189758));
#121598=CARTESIAN_POINT('Ctrl Pts',(48.0649554680753,1075.70120171291,331.910420189758));
#121599=CARTESIAN_POINT('Origin',(62.0518715958009,1067.7251047501,331.400088359109));
#121600=CARTESIAN_POINT('',(62.0518715958319,1076.69664647652,330.309547610381));
#121601=CARTESIAN_POINT('Ctrl Pts',(62.051916276496,1076.94042940536,332.490629106922));
#121602=CARTESIAN_POINT('Ctrl Pts',(62.1689467597441,1076.9319000034,332.49062431205));
#121603=CARTESIAN_POINT('Ctrl Pts',(62.2850515643844,1076.92135625036,332.471782941714));
#121604=CARTESIAN_POINT('Ctrl Pts',(62.5175406903148,1076.89581200022,332.394515759891));
#121605=CARTESIAN_POINT('Ctrl Pts',(62.6310201944877,1076.88066974096,332.33295422707));
#121606=CARTESIAN_POINT('Ctrl Pts',(62.8394604484178,1076.846863144,332.167003639001));
#121607=CARTESIAN_POINT('Ctrl Pts',(62.930330983206,1076.82830242782,332.06094370315));
#121608=CARTESIAN_POINT('Ctrl Pts',(63.0708677040734,1076.79026494312,331.814790810824));
#121609=CARTESIAN_POINT('Ctrl Pts',(63.1169988033058,1076.77114287074,331.675589569795));
#121610=CARTESIAN_POINT('Ctrl Pts',(63.1513190413059,1076.73657033434,331.392472888326));
#121611=CARTESIAN_POINT('Ctrl Pts',(63.1413081417149,1076.72131894172,331.251450726646));
#121612=CARTESIAN_POINT('Ctrl Pts',(63.0720818267986,1076.69736837096,330.994895270063));
#121613=CARTESIAN_POINT('Ctrl Pts',(63.0187160747209,1076.68832780491,330.88017768393));
#121614=CARTESIAN_POINT('Ctrl Pts',(62.899835283627,1076.67786000366,330.709430009114));
#121615=CARTESIAN_POINT('Ctrl Pts',(62.8452953736487,1076.67491669758,330.647397028657));
#121616=CARTESIAN_POINT('Ctrl Pts',(62.7615123585332,1076.67260892928,330.571456052561));
#121617=CARTESIAN_POINT('Ctrl Pts',(62.7379046939632,1076.67215873912,330.551807495784));
#121618=CARTESIAN_POINT('Ctrl Pts',(62.6977604198812,1076.67171059519,330.521169333621));
#121619=CARTESIAN_POINT('Ctrl Pts',(62.6816990465148,1076.67160888888,330.50958937468));
#121620=CARTESIAN_POINT('Ctrl Pts',(62.6500336421708,1076.67155548727,330.488044703156));
#121621=CARTESIAN_POINT('Ctrl Pts',(62.6344739316891,1076.67159442429,330.478027637488));
#121622=CARTESIAN_POINT('Ctrl Pts',(62.5978413736133,1076.67183458392,330.455741838846));
#121623=CARTESIAN_POINT('Ctrl Pts',(62.5765977291325,1076.67208333596,330.443774746252));
#121624=CARTESIAN_POINT('Ctrl Pts',(62.5091956281057,1076.67320688124,330.408727739606));
#121625=CARTESIAN_POINT('Ctrl Pts',(62.4617984909764,1076.67446909744,330.388209592741));
#121626=CARTESIAN_POINT('Ctrl Pts',(62.2769377920682,1076.68111883128,330.323305189534));
#121627=CARTESIAN_POINT('Ctrl Pts',(62.1327875076142,1076.6897742696,330.303065934061));
#121628=CARTESIAN_POINT('Ctrl Pts',(61.8702586788995,1076.71140682714,330.318211972485));
#121629=CARTESIAN_POINT('Ctrl Pts',(61.7535533797444,1076.72322357857,330.344452723208));
#121630=CARTESIAN_POINT('Ctrl Pts',(61.5232586626982,1076.75112863505,330.437451679091));
#121631=CARTESIAN_POINT('Ctrl Pts',(61.4127560950302,1076.76729379384,330.507026288529));
#121632=CARTESIAN_POINT('Ctrl Pts',(61.2139210672944,1076.80255994862,330.688314858694));
#121633=CARTESIAN_POINT('Ctrl Pts',(61.1297600389307,1076.82148441762,330.801351381263));
#121634=CARTESIAN_POINT('Ctrl Pts',(61.0064643877677,1076.85917076983,331.057543244206));
#121635=CARTESIAN_POINT('Ctrl Pts',(60.9702207203452,1076.87755070318,331.199251640443));
#121636=CARTESIAN_POINT('Ctrl Pts',(60.9556738464336,1076.90983274036,331.482017924519));
#121637=CARTESIAN_POINT('Ctrl Pts',(60.9748427048558,1076.92362227454,331.620293430687));
#121638=CARTESIAN_POINT('Ctrl Pts',(61.0621953451036,1076.94537653608,331.876936286487));
#121639=CARTESIAN_POINT('Ctrl Pts',(61.1274646747224,1076.95338504239,331.9937210282));
#121640=CARTESIAN_POINT('Ctrl Pts',(61.2509721729956,1076.96067487758,332.142734368523));
#121641=CARTESIAN_POINT('Ctrl Pts',(61.2935487614635,1076.96232006156,332.186163227701));
#121642=CARTESIAN_POINT('Ctrl Pts',(61.3597305078431,1076.96374168654,332.24325583806));
#121643=CARTESIAN_POINT('Ctrl Pts',(61.3805621655427,1076.96404818618,332.259933980456));
#121644=CARTESIAN_POINT('Ctrl Pts',(61.4155782452409,1076.96433999831,332.285919270919));
#121645=CARTESIAN_POINT('Ctrl Pts',(61.4294040470271,1076.96440171869,332.295688603362));
#121646=CARTESIAN_POINT('Ctrl Pts',(61.4588680779628,1076.96442293528,332.315495929317));
#121647=CARTESIAN_POINT('Ctrl Pts',(61.4745465235254,1076.96437188357,332.325463927271));
#121648=CARTESIAN_POINT('Ctrl Pts',(61.5123307337301,1076.96410340793,332.348152111356));
#121649=CARTESIAN_POINT('Ctrl Pts',(61.534642267143,1076.96383117136,332.360506455053));
#121650=CARTESIAN_POINT('Ctrl Pts',(61.6090517280108,1076.96255840619,332.398363215552));
#121651=CARTESIAN_POINT('Ctrl Pts',(61.662740225478,1076.9610741055,332.420488006479));
#121652=CARTESIAN_POINT('Ctrl Pts',(61.8259551604238,1076.95494829649,332.472991398032));
#121653=CARTESIAN_POINT('Ctrl Pts',(61.9386477587942,1076.94868462819,332.490633747662));
#121654=CARTESIAN_POINT('Ctrl Pts',(62.051916276496,1076.94042940536,332.490629106922));
#121655=CARTESIAN_POINT('',(62.0518715958011,1074.67736588017,330.309547610381));
#121656=CARTESIAN_POINT('',(62.0518715958009,1067.7251047501,330.309547610381));
#121657=CARTESIAN_POINT('Ctrl Pts',(62.0518920858522,1074.9231689021,332.490629107645));
#121658=CARTESIAN_POINT('Ctrl Pts',(61.9072766880482,1074.9337967205,332.490631824808));
#121659=CARTESIAN_POINT('Ctrl Pts',(61.7639282422094,1074.94112803438,332.461868316459));
#121660=CARTESIAN_POINT('Ctrl Pts',(61.4996256396725,1074.94829122717,332.35107001861));
#121661=CARTESIAN_POINT('Ctrl Pts',(61.3809087112088,1074.9482181156,332.271380194124));
#121662=CARTESIAN_POINT('Ctrl Pts',(61.1803663694778,1074.94084440522,332.070843453706));
#121663=CARTESIAN_POINT('Ctrl Pts',(61.100660326611,1074.93360139843,331.951939984251));
#121664=CARTESIAN_POINT('Ctrl Pts',(60.9899959889945,1074.91255576933,331.687646155658));
#121665=CARTESIAN_POINT('Ctrl Pts',(60.9613228924259,1074.89882163901,331.544430066913));
#121666=CARTESIAN_POINT('Ctrl Pts',(60.9613388548559,1074.86660946104,331.254722168143));
#121667=CARTESIAN_POINT('Ctrl Pts',(60.9903839082085,1074.84841713424,331.111065437832));
#121668=CARTESIAN_POINT('Ctrl Pts',(61.0741556946148,1074.8198039495,330.911805339064));
#121669=CARTESIAN_POINT('Ctrl Pts',(61.1081062745881,1074.81020402191,330.849042381779));
#121670=CARTESIAN_POINT('Ctrl Pts',(61.2299476471322,1074.78070840419,330.668499216895));
#121671=CARTESIAN_POINT('Ctrl Pts',(61.3357050178387,1074.76096641421,330.564660631712));
#121672=CARTESIAN_POINT('Ctrl Pts',(61.5795997859539,1074.72451459745,330.406653089535));
#121673=CARTESIAN_POINT('Ctrl Pts',(61.7147457076355,1074.70809339683,330.352983008506));
#121674=CARTESIAN_POINT('Ctrl Pts',(61.9971928860336,1074.68064821233,330.301591792456));
#121675=CARTESIAN_POINT('Ctrl Pts',(62.1416183696132,1074.66984339509,330.303841104559));
#121676=CARTESIAN_POINT('Ctrl Pts',(62.4203883616412,1074.65539081775,330.363939536672));
#121677=CARTESIAN_POINT('Ctrl Pts',(62.5520072922979,1074.65182117772,330.42063815083));
#121678=CARTESIAN_POINT('Ctrl Pts',(62.7857347125334,1074.65238493327,330.581104864286));
#121679=CARTESIAN_POINT('Ctrl Pts',(62.8855793518802,1074.65648012115,330.683035833256));
#121680=CARTESIAN_POINT('Ctrl Pts',(63.0410814226853,1074.67180421789,330.919606615128));
#121681=CARTESIAN_POINT('Ctrl Pts',(63.0949950473784,1074.68290651985,331.052000355747));
#121682=CARTESIAN_POINT('Ctrl Pts',(63.1495440183203,1074.71070786131,331.330909671221));
#121683=CARTESIAN_POINT('Ctrl Pts',(63.149121740666,1074.72718943165,331.474850097114));
#121684=CARTESIAN_POINT('Ctrl Pts',(63.092896486172,1074.76334686442,331.755324436365));
#121685=CARTESIAN_POINT('Ctrl Pts',(63.0371047486052,1074.78271234783,331.889164603409));
#121686=CARTESIAN_POINT('Ctrl Pts',(62.8759167863411,1074.82184081789,332.129056530396));
#121687=CARTESIAN_POINT('Ctrl Pts',(62.7713671965666,1074.84123833865,332.232454513835));
#121688=CARTESIAN_POINT('Ctrl Pts',(62.5285877224576,1074.87703484017,332.391508195153));
#121689=CARTESIAN_POINT('Ctrl Pts',(62.3929410695632,1074.89311730865,332.446020732886));
#121690=CARTESIAN_POINT('Ctrl Pts',(62.1849547481319,1074.91270964417,332.484520659806));
#121691=CARTESIAN_POINT('Ctrl Pts',(62.1185199715278,1074.91827240366,332.490627855781));
#121692=CARTESIAN_POINT('Ctrl Pts',(62.0518920858522,1074.9231689021,332.490629107645));
#121693=CARTESIAN_POINT('Origin',(62.0518715958009,1067.7251047501,331.400088359109));
#121694=CARTESIAN_POINT('',(62.0518715958009,1074.85711166046,331.890629107838));
#121695=CARTESIAN_POINT('',(62.0518715957995,1074.74654397689,330.909547610381));
#121696=CARTESIAN_POINT('Ctrl Pts',(62.051871595801,1074.85711166046,331.890629107838));
#121697=CARTESIAN_POINT('Ctrl Pts',(62.0508414461873,1074.85718823713,331.890629107838));
#121698=CARTESIAN_POINT('Ctrl Pts',(62.0498111098117,1074.8572644638,331.890625862824));
#121699=CARTESIAN_POINT('Ctrl Pts',(61.9842804536085,1074.8620894158,331.890212932986));
#121700=CARTESIAN_POINT('Ctrl Pts',(61.9204148249089,1074.86536582664,331.877088205641));
#121701=CARTESIAN_POINT('Ctrl Pts',(61.8021903547936,1074.86856750923,331.827110421472));
#121702=CARTESIAN_POINT('Ctrl Pts',(61.7489041167558,1074.86850855109,331.791111240611));
#121703=CARTESIAN_POINT('Ctrl Pts',(61.659006187408,1074.86509854825,331.700684959973));
#121704=CARTESIAN_POINT('Ctrl Pts',(61.6233336316729,1074.86177673475,331.64714692349));
#121705=CARTESIAN_POINT('Ctrl Pts',(61.5737682166001,1074.85214402318,331.527897368748));
#121706=CARTESIAN_POINT('Ctrl Pts',(61.561038995203,1074.84584993916,331.46311795312));
#121707=CARTESIAN_POINT('Ctrl Pts',(61.5616343725284,1074.83114636991,331.33226118111));
#121708=CARTESIAN_POINT('Ctrl Pts',(61.5750848572269,1074.82287118521,331.267471907523));
#121709=CARTESIAN_POINT('Ctrl Pts',(61.6134133509576,1074.80991482127,331.177795982349));
#121710=CARTESIAN_POINT('Ctrl Pts',(61.6288841399801,1074.80558139531,331.149607902732));
#121711=CARTESIAN_POINT('Ctrl Pts',(61.684147017624,1074.79232851443,331.068818318877));
#121712=CARTESIAN_POINT('Ctrl Pts',(61.7318809974185,1074.78350501292,331.022492357096));
#121713=CARTESIAN_POINT('Ctrl Pts',(61.8421902947146,1074.76719952519,330.951870066679));
#121714=CARTESIAN_POINT('Ctrl Pts',(61.9035280093915,1074.75985750452,330.927979432424));
#121715=CARTESIAN_POINT('Ctrl Pts',(61.9955737695265,1074.75108054626,330.911977110688));
#121716=CARTESIAN_POINT('Ctrl Pts',(62.0236815926941,1074.74867782624,330.909548068142));
#121717=CARTESIAN_POINT('Ctrl Pts',(62.0518636290663,1074.74654457992,330.909547610446));
#121718=CARTESIAN_POINT('',(62.0518715958009,1082.7251047501,330.909547610381));
#121719=CARTESIAN_POINT('',(62.0518715958009,1067.7251047501,330.909547610381));
#121720=CARTESIAN_POINT('Origin',(62.0518715958009,1082.7251047501,331.400088359109));
#121721=CARTESIAN_POINT('Ctrl Pts',(62.0518715957962,1074.74654397689,330.909547610381));
#121722=CARTESIAN_POINT('Ctrl Pts',(62.115868350468,1074.74169984421,330.90954761038));
#121723=CARTESIAN_POINT('Ctrl Pts',(62.179320075241,1074.73831573489,330.92206916904));
#121724=CARTESIAN_POINT('Ctrl Pts',(62.2975373009314,1074.73489722521,330.970744933648));
#121725=CARTESIAN_POINT('Ctrl Pts',(62.3511527164464,1074.73487485355,331.00623768826));
#121726=CARTESIAN_POINT('Ctrl Pts',(62.4418284087802,1074.73819498118,331.095747096567));
#121727=CARTESIAN_POINT('Ctrl Pts',(62.4779637585687,1074.74150435431,331.148858725687));
#121728=CARTESIAN_POINT('Ctrl Pts',(62.5281132346037,1074.7510522655,331.266201330322));
#121729=CARTESIAN_POINT('Ctrl Pts',(62.5414636331938,1074.7572172371,331.329347871775));
#121730=CARTESIAN_POINT('Ctrl Pts',(62.5432727372191,1074.77162897249,331.457648809979));
#121731=CARTESIAN_POINT('Ctrl Pts',(62.5314601012918,1074.77975838652,331.521593733552));
#121732=CARTESIAN_POINT('Ctrl Pts',(62.4833880269776,1074.79702613393,331.64246581233));
#121733=CARTESIAN_POINT('Ctrl Pts',(62.4470523632795,1074.80601828966,331.698057412042));
#121734=CARTESIAN_POINT('Ctrl Pts',(62.3548570296498,1074.82341668373,331.791383377283));
#121735=CARTESIAN_POINT('Ctrl Pts',(62.2999617822409,1074.83166156739,331.828321795356));
#121736=CARTESIAN_POINT('Ctrl Pts',(62.1799911633698,1074.84616489195,331.877939340832));
#121737=CARTESIAN_POINT('Ctrl Pts',(62.116296600872,1074.85232259687,331.890629107838));
#121738=CARTESIAN_POINT('Ctrl Pts',(62.051871595801,1074.85711166046,331.890629107838));
#121739=CARTESIAN_POINT('Origin',(3.98894410367401,1067.7251047501,335.150892220804));
#121740=CARTESIAN_POINT('',(3.98894410369655,1078.62952598896,333.672589088611));
#121741=CARTESIAN_POINT('Ctrl Pts',(3.98892918962189,1078.70545283844,336.629195352922));
#121742=CARTESIAN_POINT('Ctrl Pts',(4.03786747477723,1078.70541435023,336.629195846643));
#121743=CARTESIAN_POINT('Ctrl Pts',(4.08677555468786,1078.70533301832,336.626766232996));
#121744=CARTESIAN_POINT('Ctrl Pts',(4.22075614699632,1078.70499063064,336.613420428748));
#121745=CARTESIAN_POINT('Ctrl Pts',(4.30513902806456,1078.704641378,336.597524920551));
#121746=CARTESIAN_POINT('Ctrl Pts',(4.57794731394422,1078.70304196814,336.52111207434));
#121747=CARTESIAN_POINT('Ctrl Pts',(4.75561762870029,1078.70123172322,336.430202147003));
#121748=CARTESIAN_POINT('Ctrl Pts',(5.04060446999527,1078.69650897887,336.203133442749));
#121749=CARTESIAN_POINT('Ctrl Pts',(5.15252223361214,1078.69384077107,336.077866790619));
#121750=CARTESIAN_POINT('Ctrl Pts',(5.3366583079901,1078.68725393482,335.784397588403));
#121751=CARTESIAN_POINT('Ctrl Pts',(5.40360494039046,1078.68330483038,335.616069770505));
#121752=CARTESIAN_POINT('Ctrl Pts',(5.47638562696601,1078.67425120324,335.250950368245));
#121753=CARTESIAN_POINT('Ctrl Pts',(5.47675254686655,1078.66916769866,335.056472056768));
#121754=CARTESIAN_POINT('Ctrl Pts',(5.40256039196515,1078.65877688197,334.676754766409));
#121755=CARTESIAN_POINT('Ctrl Pts',(5.32808988340935,1078.65357279211,334.495293135256));
#121756=CARTESIAN_POINT('Ctrl Pts',(5.11867226978488,1078.64429345339,334.179752629101));
#121757=CARTESIAN_POINT('Ctrl Pts',(4.98881021210526,1078.64026181465,334.046503035112));
#121758=CARTESIAN_POINT('Ctrl Pts',(4.7067037902564,1078.63429626432,333.848649819207));
#121759=CARTESIAN_POINT('Ctrl Pts',(4.56154612480652,1078.63219749884,333.778614155116));
#121760=CARTESIAN_POINT('Ctrl Pts',(4.34326559247139,1078.63038211411,333.714093153353));
#121761=CARTESIAN_POINT('Ctrl Pts',(4.27730718287703,1078.62999143848,333.699416335752));
#121762=CARTESIAN_POINT('Ctrl Pts',(4.1661353663951,1078.62959503315,333.682558523943));
#121763=CARTESIAN_POINT('Ctrl Pts',(4.12140975412106,1078.6295044828,333.677849972551));
#121764=CARTESIAN_POINT('Ctrl Pts',(4.03402577116883,1078.62946143129,333.672663026376));
#121765=CARTESIAN_POINT('Ctrl Pts',(3.99142324262148,1078.62950194538,333.671977837842));
#121766=CARTESIAN_POINT('Ctrl Pts',(3.89258045832872,1078.62973820764,333.674659556288));
#121767=CARTESIAN_POINT('Ctrl Pts',(3.83644371024871,1078.62997954585,333.679398978925));
#121768=CARTESIAN_POINT('Ctrl Pts',(3.66586755016836,1078.63103848406,333.703667783558));
#121769=CARTESIAN_POINT('Ctrl Pts',(3.55334610772653,1078.63219297376,333.733468664245));
#121770=CARTESIAN_POINT('Ctrl Pts',(3.26184166844232,1078.63638726145,333.848704653796));
#121771=CARTESIAN_POINT('Ctrl Pts',(3.09461816678822,1078.64014081387,333.957351726536));
#121772=CARTESIAN_POINT('Ctrl Pts',(2.83228962003559,1078.64848060665,334.214702922275));
#121773=CARTESIAN_POINT('Ctrl Pts',(2.73235499249032,1078.65281241297,334.353848566448));
#121774=CARTESIAN_POINT('Ctrl Pts',(2.57893055794889,1078.66214975565,334.670869898601));
#121775=CARTESIAN_POINT('Ctrl Pts',(2.5305635037259,1078.66709716785,334.848094398121));
#121776=CARTESIAN_POINT('Ctrl Pts',(2.49961085669172,1078.67693717591,335.224181933052));
#121777=CARTESIAN_POINT('Ctrl Pts',(2.52228959250107,1078.68170139175,335.419997076885));
#121778=CARTESIAN_POINT('Ctrl Pts',(2.64179380622852,1078.690076523,335.789546881013));
#121779=CARTESIAN_POINT('Ctrl Pts',(2.73668484288976,1078.69362319307,335.959934329484));
#121780=CARTESIAN_POINT('Ctrl Pts',(2.97658100153028,1078.69914702624,336.242704702269));
#121781=CARTESIAN_POINT('Ctrl Pts',(3.11498027446472,1078.70118871564,336.356348738234));
#121782=CARTESIAN_POINT('Ctrl Pts',(3.38118618246868,1078.70371203262,336.504456515524));
#121783=CARTESIAN_POINT('Ctrl Pts',(3.49965089958669,1078.70446244868,336.55164167264));
#121784=CARTESIAN_POINT('Ctrl Pts',(3.68054300568547,1078.70514283027,336.59790144199));
#121785=CARTESIAN_POINT('Ctrl Pts',(3.73924715800365,1078.70529591923,336.60917833755));
#121786=CARTESIAN_POINT('Ctrl Pts',(3.84050345373653,1078.70544857856,336.622334362943));
#121787=CARTESIAN_POINT('Ctrl Pts',(3.88275021557812,1078.70547971821,336.625985257367));
#121788=CARTESIAN_POINT('Ctrl Pts',(3.94636085655102,1078.70547819981,336.628735205219));
#121789=CARTESIAN_POINT('Ctrl Pts',(3.967643781809,1078.70546957865,336.629195138182));
#121790=CARTESIAN_POINT('Ctrl Pts',(3.98892918962189,1078.70545283844,336.629195352922));
#121791=CARTESIAN_POINT('',(3.98894410365689,1076.62830575618,333.672589088611));
#121792=CARTESIAN_POINT('',(3.98894410367401,1067.7251047501,333.672589088611));
#121793=CARTESIAN_POINT('Ctrl Pts',(3.98878836967398,1076.70513034802,336.629195344795));
#121794=CARTESIAN_POINT('Ctrl Pts',(3.7930202123859,1076.70528585575,336.629174721312));
#121795=CARTESIAN_POINT('Ctrl Pts',(3.59919331969724,1076.70475707765,336.590266460707));
#121796=CARTESIAN_POINT('Ctrl Pts',(3.23859265166785,1076.70228199228,336.439463716588));
#121797=CARTESIAN_POINT('Ctrl Pts',(3.075274785619,1076.70035886093,336.329300839745));
#121798=CARTESIAN_POINT('Ctrl Pts',(2.80088043015867,1076.69503122865,336.051964074437));
#121799=CARTESIAN_POINT('Ctrl Pts',(2.69249236033706,1076.6916707662,335.887526388395));
#121800=CARTESIAN_POINT('Ctrl Pts',(2.54517248907245,1076.68357204508,335.524528027989));
#121801=CARTESIAN_POINT('Ctrl Pts',(2.50832320045053,1076.67889691296,335.329310069862));
#121802=CARTESIAN_POINT('Ctrl Pts',(2.51315100918465,1076.66880288985,334.938648120785));
#121803=CARTESIAN_POINT('Ctrl Pts',(2.55370690269806,1076.66349351796,334.747030171959));
#121804=CARTESIAN_POINT('Ctrl Pts',(2.70656038072564,1076.65300750955,334.390255602793));
#121805=CARTESIAN_POINT('Ctrl Pts',(2.81743887061719,1076.64793808138,334.228580517299));
#121806=CARTESIAN_POINT('Ctrl Pts',(3.095369869255,1076.63903923649,333.95731938209));
#121807=CARTESIAN_POINT('Ctrl Pts',(3.25972780495756,1076.63530369453,333.850374268239));
#121808=CARTESIAN_POINT('Ctrl Pts',(3.62009120867445,1076.63000627701,333.706275428726));
#121809=CARTESIAN_POINT('Ctrl Pts',(3.8125361211168,1076.62849720654,333.6704000379));
#121810=CARTESIAN_POINT('Ctrl Pts',(4.19976287471065,1076.62806931342,333.674978342989));
#121811=CARTESIAN_POINT('Ctrl Pts',(4.39078290107999,1076.62914776945,333.715173933314));
#121812=CARTESIAN_POINT('Ctrl Pts',(4.74617483270904,1076.63365995214,333.866669597516));
#121813=CARTESIAN_POINT('Ctrl Pts',(4.90716816144421,1076.63704150804,333.976380078437));
#121814=CARTESIAN_POINT('Ctrl Pts',(5.1779123931955,1076.64538915298,334.251456192178));
#121815=CARTESIAN_POINT('Ctrl Pts',(5.28505196529667,1076.65026846074,334.414192486284));
#121816=CARTESIAN_POINT('Ctrl Pts',(5.43083042257437,1076.6605739556,334.771837263306));
#121817=CARTESIAN_POINT('Ctrl Pts',(5.4679805068262,1076.66589594301,334.963353327041));
#121818=CARTESIAN_POINT('Ctrl Pts',(5.46686421438338,1076.67354941954,335.253186362826));
#121819=CARTESIAN_POINT('Ctrl Pts',(5.45702436219599,1076.67602885489,335.349520432207));
#121820=CARTESIAN_POINT('Ctrl Pts',(5.39896579566468,1076.68321919339,335.636318864411));
#121821=CARTESIAN_POINT('Ctrl Pts',(5.32224942252514,1076.6875225925,335.818804368267));
#121822=CARTESIAN_POINT('Ctrl Pts',(5.10273419738406,1076.6948015051,336.142270875995));
#121823=CARTESIAN_POINT('Ctrl Pts',(4.96247867826358,1076.69772050267,336.280316098033));
#121824=CARTESIAN_POINT('Ctrl Pts',(4.63614714833236,1076.70216533599,336.494266421958));
#121825=CARTESIAN_POINT('Ctrl Pts',(4.45319269068329,1076.70365284641,336.567932575272));
#121826=CARTESIAN_POINT('Ctrl Pts',(4.1713828408152,1076.70483439467,336.620738883684));
#121827=CARTESIAN_POINT('Ctrl Pts',(4.08018360826906,1076.70505774854,336.629204972959));
#121828=CARTESIAN_POINT('Ctrl Pts',(3.98878836967398,1076.70513034802,336.629195344795));
#121829=CARTESIAN_POINT('Origin',(3.98894410367401,1067.7251047501,335.150892220804));
#121830=CARTESIAN_POINT('',(3.98894410367403,1076.69355479191,336.029195352998));
#121831=CARTESIAN_POINT('',(3.98894410317932,1076.64787682225,334.272589088611));
#121832=CARTESIAN_POINT('Ctrl Pts',(3.98894410367403,1076.69355479191,336.029195352998));
#121833=CARTESIAN_POINT('Ctrl Pts',(3.93091475126699,1076.69360970332,336.029195352998));
#121834=CARTESIAN_POINT('Ctrl Pts',(3.87288505415834,1076.69354277828,336.023444360572));
#121835=CARTESIAN_POINT('Ctrl Pts',(3.70138881123196,1076.69297135146,335.988942426484));
#121836=CARTESIAN_POINT('Ctrl Pts',(3.59278219407908,1076.69210617214,335.943401124292));
#121837=CARTESIAN_POINT('Ctrl Pts',(3.39982045431152,1076.68942545344,335.812645313259));
#121838=CARTESIAN_POINT('Ctrl Pts',(3.31735426483233,1076.68763485745,335.728774569024));
#121839=CARTESIAN_POINT('Ctrl Pts',(3.18975861923189,1076.68322620786,335.533471034364));
#121840=CARTESIAN_POINT('Ctrl Pts',(3.14601743550809,1076.68064682687,335.423904157034));
#121841=CARTESIAN_POINT('Ctrl Pts',(3.10403796131332,1076.67496401598,335.19451813196));
#121842=CARTESIAN_POINT('Ctrl Pts',(3.10605029308206,1076.67191761824,335.0770058293));
#121843=CARTESIAN_POINT('Ctrl Pts',(3.15551202014162,1076.66578701744,334.850756746851));
#121844=CARTESIAN_POINT('Ctrl Pts',(3.20202687940525,1076.66276395548,334.744132968252));
#121845=CARTESIAN_POINT('Ctrl Pts',(3.33359160165528,1076.65719862283,334.554893473413));
#121846=CARTESIAN_POINT('Ctrl Pts',(3.41738042736138,1076.65471290943,334.47412045959));
#121847=CARTESIAN_POINT('Ctrl Pts',(3.61131803505323,1076.65074150661,334.349589423035));
#121848=CARTESIAN_POINT('Ctrl Pts',(3.71956672676871,1076.64929614901,334.307016244285));
#121849=CARTESIAN_POINT('Ctrl Pts',(3.88455002691543,1076.64816214277,334.277240351956));
#121850=CARTESIAN_POINT('Ctrl Pts',(3.93675683209862,1076.64794813166,334.27258908867));
#121851=CARTESIAN_POINT('Ctrl Pts',(3.98894410268463,1076.64787682225,334.272589088611));
#121852=CARTESIAN_POINT('',(3.98894410367401,1082.7251047501,334.272589088611));
#121853=CARTESIAN_POINT('',(3.98894410367401,1067.7251047501,334.272589088611));
#121854=CARTESIAN_POINT('Origin',(3.98894410367401,1082.7251047501,335.150892220804));
#121855=CARTESIAN_POINT('Ctrl Pts',(3.98894410268463,1076.64787682225,334.272589088611));
#121856=CARTESIAN_POINT('Ctrl Pts',(4.05123528120277,1076.64779170673,334.272589088541));
#121857=CARTESIAN_POINT('Ctrl Pts',(4.11349862889648,1076.64791000709,334.27921590747));
#121858=CARTESIAN_POINT('Ctrl Pts',(4.28690692430041,1076.6488211043,334.316733106288));
#121859=CARTESIAN_POINT('Ctrl Pts',(4.39329327861196,1076.65008504048,334.362791891777));
#121860=CARTESIAN_POINT('Ctrl Pts',(4.5822611944483,1076.65373968478,334.493196024519));
#121861=CARTESIAN_POINT('Ctrl Pts',(4.66303086930762,1076.65609242238,334.576268200363));
#121862=CARTESIAN_POINT('Ctrl Pts',(4.78808835047346,1076.66146718022,334.768826134735));
#121863=CARTESIAN_POINT('Ctrl Pts',(4.83114447161027,1076.66443548735,334.876478862489));
#121864=CARTESIAN_POINT('Ctrl Pts',(4.86138277028479,1076.66877929985,335.038087607017));
#121865=CARTESIAN_POINT('Ctrl Pts',(4.86635837388089,1076.67009391629,335.087501981756));
#121866=CARTESIAN_POINT('Ctrl Pts',(4.86713848754261,1076.67139771689,335.137071361129));
#121867=CARTESIAN_POINT('Ctrl Pts',(4.86804189137142,1076.67290757181,335.194474749012));
#121868=CARTESIAN_POINT('Ctrl Pts',(4.86331485679127,1076.67439610009,335.251829481203));
#121869=CARTESIAN_POINT('Ctrl Pts',(4.83205951683594,1076.67878878755,335.423390817771));
#121870=CARTESIAN_POINT('Ctrl Pts',(4.78831343977695,1076.68151307608,335.533136456035));
#121871=CARTESIAN_POINT('Ctrl Pts',(4.66066562184075,1076.68626326664,335.728625856977));
#121872=CARTESIAN_POINT('Ctrl Pts',(4.57820143998906,1076.68824752279,335.81253020833));
#121873=CARTESIAN_POINT('Ctrl Pts',(4.38528525337268,1076.69134030004,335.943304162282));
#121874=CARTESIAN_POINT('Ctrl Pts',(4.27673716279811,1076.69242055267,335.988854081877));
#121875=CARTESIAN_POINT('Ctrl Pts',(4.10520212664494,1076.69332251958,336.023424552889));
#121876=CARTESIAN_POINT('Ctrl Pts',(4.04707328810597,1076.69349978603,336.029195352998));
#121877=CARTESIAN_POINT('Ctrl Pts',(3.98894410367403,1076.69355479191,336.029195352998));
#121878=CARTESIAN_POINT('Origin',(14.9669751953833,1067.7251047501,329.052293203314));
#121879=CARTESIAN_POINT('',(14.9669751953994,1078.26481065249,327.776849082177));
#121880=CARTESIAN_POINT('Ctrl Pts',(14.9670414268982,1078.42603035398,330.327737322731));
#121881=CARTESIAN_POINT('Ctrl Pts',(15.0508755418035,1078.42527386653,330.327732969376));
#121882=CARTESIAN_POINT('Ctrl Pts',(15.1344986130066,1078.42404243283,330.319463080818));
#121883=CARTESIAN_POINT('Ctrl Pts',(15.3828386223669,1078.41892060072,330.269880459933));
#121884=CARTESIAN_POINT('Ctrl Pts',(15.5406646352344,1078.41365256733,330.203947377001));
#121885=CARTESIAN_POINT('Ctrl Pts',(15.800795671808,1078.40085954674,330.028209766681));
#121886=CARTESIAN_POINT('Ctrl Pts',(15.9059480870898,1078.39386610398,329.927492297754));
#121887=CARTESIAN_POINT('Ctrl Pts',(16.0847682905068,1078.37752469092,329.686025913971));
#121888=CARTESIAN_POINT('Ctrl Pts',(16.1537883367907,1078.36816846601,329.544766148022));
#121889=CARTESIAN_POINT('Ctrl Pts',(16.2405793382962,1078.34781444111,329.233253811105));
#121890=CARTESIAN_POINT('Ctrl Pts',(16.2533118075247,1078.33694000721,329.064612431137));
#121891=CARTESIAN_POINT('Ctrl Pts',(16.2128969673545,1078.31582579914,328.732243032528));
#121892=CARTESIAN_POINT('Ctrl Pts',(16.1602070366504,1078.30578990794,328.5716870269));
#121893=CARTESIAN_POINT('Ctrl Pts',(16.0013166061144,1078.28866933711,328.28988839172));
#121894=CARTESIAN_POINT('Ctrl Pts',(15.9003079684194,1078.28157845807,328.169088801628));
#121895=CARTESIAN_POINT('Ctrl Pts',(15.6764154780689,1078.27138138027,327.983881540676));
#121896=CARTESIAN_POINT('Ctrl Pts',(15.559980959649,1078.26792199564,327.915116530907));
#121897=CARTESIAN_POINT('Ctrl Pts',(15.385990907775,1078.26508680129,327.846494022059));
#121898=CARTESIAN_POINT('Ctrl Pts',(15.3358973241739,1078.26450956568,327.830236409693));
#121899=CARTESIAN_POINT('Ctrl Pts',(15.2520136569127,1078.26392919189,327.808642599197));
#121900=CARTESIAN_POINT('Ctrl Pts',(15.2187604003336,1078.2637954118,327.801486259334));
#121901=CARTESIAN_POINT('Ctrl Pts',(15.1541280676858,1078.26371955065,327.790259133371));
#121902=CARTESIAN_POINT('Ctrl Pts',(15.1228053640728,1078.26376461733,327.786010006042));
#121903=CARTESIAN_POINT('Ctrl Pts',(15.0504839633303,1078.26405564935,327.77892339476));
#121904=CARTESIAN_POINT('Ctrl Pts',(15.0094419579447,1078.26435761509,327.776894914863));
#121905=CARTESIAN_POINT('Ctrl Pts',(14.8849931185867,1078.26568508702,327.776758351789));
#121906=CARTESIAN_POINT('Ctrl Pts',(14.8018126880519,1078.26713253849,327.784843607977));
#121907=CARTESIAN_POINT('Ctrl Pts',(14.5537424610274,1078.27313282264,327.83380074425));
#121908=CARTESIAN_POINT('Ctrl Pts',(14.3957239243208,1078.27929053976,327.899421225175));
#121909=CARTESIAN_POINT('Ctrl Pts',(14.1357208939644,1078.29378738404,328.07428420265));
#121910=CARTESIAN_POINT('Ctrl Pts',(14.0307570734049,1078.30155384578,328.174253138317));
#121911=CARTESIAN_POINT('Ctrl Pts',(13.8520496664264,1078.31915947966,328.413770259329));
#121912=CARTESIAN_POINT('Ctrl Pts',(13.7828031126072,1078.32896464567,328.553803466007));
#121913=CARTESIAN_POINT('Ctrl Pts',(13.6948406554323,1078.34958137226,328.862514498121));
#121914=CARTESIAN_POINT('Ctrl Pts',(13.6809575238583,1078.36021843774,329.02962463015));
#121915=CARTESIAN_POINT('Ctrl Pts',(13.7182230595974,1078.38034586136,329.361274643958));
#121916=CARTESIAN_POINT('Ctrl Pts',(13.7695958184114,1078.38963305736,329.522580854854));
#121917=CARTESIAN_POINT('Ctrl Pts',(13.9268499640947,1078.4051665969,329.807041172956));
#121918=CARTESIAN_POINT('Ctrl Pts',(14.0278029367714,1078.41143660226,329.929500549406));
#121919=CARTESIAN_POINT('Ctrl Pts',(14.2531259830977,1078.42038043295,330.118020163101));
#121920=CARTESIAN_POINT('Ctrl Pts',(14.3710980251748,1078.42336651719,330.188206407939));
#121921=CARTESIAN_POINT('Ctrl Pts',(14.5470803108169,1078.42579036702,330.257795593266));
#121922=CARTESIAN_POINT('Ctrl Pts',(14.5973608879206,1078.4262785311,330.274149724578));
#121923=CARTESIAN_POINT('Ctrl Pts',(14.6812541583739,1078.42676739415,330.295782058203));
#121924=CARTESIAN_POINT('Ctrl Pts',(14.7143194977419,1078.42688008699,330.302919517373));
#121925=CARTESIAN_POINT('Ctrl Pts',(14.7783391756695,1078.42694625575,330.314095875837));
#121926=CARTESIAN_POINT('Ctrl Pts',(14.8092350207692,1078.42691145009,330.318329364288));
#121927=CARTESIAN_POINT('Ctrl Pts',(14.8801998610739,1078.426679681,330.325415061572));
#121928=CARTESIAN_POINT('Ctrl Pts',(14.9203103683575,1078.42643908147,330.327515346321));
#121929=CARTESIAN_POINT('Ctrl Pts',(14.9626486368974,1078.42606966526,330.327731877347));
#121930=CARTESIAN_POINT('Ctrl Pts',(14.9648450320519,1078.42605017341,330.327737436785));
#121931=CARTESIAN_POINT('Ctrl Pts',(14.9670414268982,1078.42603035398,330.327737322731));
#121932=CARTESIAN_POINT('',(14.9669751953554,1076.25966013686,327.776849082178));
#121933=CARTESIAN_POINT('',(14.9669751953833,1067.7251047501,327.776849082178));
#121934=CARTESIAN_POINT('Ctrl Pts',(14.9669818897757,1076.42256163736,330.327737324433));
#121935=CARTESIAN_POINT('Ctrl Pts',(14.7973915322079,1076.42410781104,330.327738214557));
#121936=CARTESIAN_POINT('Ctrl Pts',(14.6294952652309,1076.42367255477,330.293914196354));
#121937=CARTESIAN_POINT('Ctrl Pts',(14.3171888818399,1076.41887675521,330.162764125605));
#121938=CARTESIAN_POINT('Ctrl Pts',(14.1758534955704,1076.4145717933,330.06691872567));
#121939=CARTESIAN_POINT('Ctrl Pts',(13.9391054826949,1076.40248529862,329.826047172991));
#121940=CARTESIAN_POINT('Ctrl Pts',(13.8459413763126,1076.39482645647,329.683524440797));
#121941=CARTESIAN_POINT('Ctrl Pts',(13.7201763700816,1076.37689844833,329.369956021304));
#121942=CARTESIAN_POINT('Ctrl Pts',(13.6890849546996,1076.36679130366,329.201895792141));
#121943=CARTESIAN_POINT('Ctrl Pts',(13.6929566703232,1076.35082650684,328.949614980448));
#121944=CARTESIAN_POINT('Ctrl Pts',(13.7023526050109,1076.34546178853,328.866836214588));
#121945=CARTESIAN_POINT('Ctrl Pts',(13.7551310672895,1076.32908051219,328.620038786145));
#121946=CARTESIAN_POINT('Ctrl Pts',(13.8231346388622,1076.31812610706,328.463180210707));
#121947=CARTESIAN_POINT('Ctrl Pts',(14.0154443533977,1076.29778257473,328.186602895354));
#121948=CARTESIAN_POINT('Ctrl Pts',(14.1373073185298,1076.28857790361,328.069173828211));
#121949=CARTESIAN_POINT('Ctrl Pts',(14.4192675079826,1076.27327608476,327.88835237167));
#121950=CARTESIAN_POINT('Ctrl Pts',(14.5765366991904,1076.26732491336,327.826592684308));
#121951=CARTESIAN_POINT('Ctrl Pts',(14.9055193028814,1076.25968212144,327.767451429315));
#121952=CARTESIAN_POINT('Ctrl Pts',(15.0739592792332,1076.25805376913,327.770433937849));
#121953=CARTESIAN_POINT('Ctrl Pts',(15.3997830801189,1076.25941081277,327.841030809865));
#121954=CARTESIAN_POINT('Ctrl Pts',(15.5539987330769,1076.26237164526,327.907802579917));
#121955=CARTESIAN_POINT('Ctrl Pts',(15.8280758297298,1076.27242547397,328.09679163355));
#121956=CARTESIAN_POINT('Ctrl Pts',(15.9452593815558,1076.27941898224,328.217192535579));
#121957=CARTESIAN_POINT('Ctrl Pts',(16.126974089001,1076.29636844751,328.496431438403));
#121958=CARTESIAN_POINT('Ctrl Pts',(16.1896186643221,1076.30616474413,328.652684640968));
#121959=CARTESIAN_POINT('Ctrl Pts',(16.2358663161956,1076.32185850349,328.898537767218));
#121960=CARTESIAN_POINT('Ctrl Pts',(16.2432063861972,1076.32722385042,328.981883410289));
#121961=CARTESIAN_POINT('Ctrl Pts',(16.2414983319426,1076.33804693771,329.14884085682));
#121962=CARTESIAN_POINT('Ctrl Pts',(16.2324459257184,1076.34347900151,329.232056830215));
#121963=CARTESIAN_POINT('Ctrl Pts',(16.1805702870738,1076.35975331527,329.479704078509));
#121964=CARTESIAN_POINT('Ctrl Pts',(16.1130768669453,1076.37024051315,329.637076535622));
#121965=CARTESIAN_POINT('Ctrl Pts',(15.9210142141033,1076.38919409139,329.915419032512));
#121966=CARTESIAN_POINT('Ctrl Pts',(15.7986708492355,1076.39749028877,330.033873879393));
#121967=CARTESIAN_POINT('Ctrl Pts',(15.5147036387591,1076.41103039056,330.216457158506));
#121968=CARTESIAN_POINT('Ctrl Pts',(15.3558558765118,1076.4161414139,330.278706558088));
#121969=CARTESIAN_POINT('Ctrl Pts',(15.1160129447032,1076.42082132936,330.321193333598));
#121970=CARTESIAN_POINT('Ctrl Pts',(15.0415718435788,1076.42188159266,330.327736932934));
#121971=CARTESIAN_POINT('Ctrl Pts',(14.9669818897757,1076.42256163736,330.327737324433));
#121972=CARTESIAN_POINT('Origin',(14.9669751953833,1067.7251047501,329.052293203314));
#121973=CARTESIAN_POINT('',(14.9669751953833,1076.38718569293,329.72773732445));
#121974=CARTESIAN_POINT('',(14.9669751953839,1076.30090002967,328.376849082178));
#121975=CARTESIAN_POINT('Ctrl Pts',(14.9669751953833,1076.38718569293,329.72773732445));
#121976=CARTESIAN_POINT('Ctrl Pts',(14.9194354684686,1076.38763918504,329.72773732445));
#121977=CARTESIAN_POINT('Ctrl Pts',(14.8719081858183,1076.3877866468,329.722718311536));
#121978=CARTESIAN_POINT('Ctrl Pts',(14.7371605195918,1076.38731020095,329.69378916954));
#121979=CARTESIAN_POINT('Ctrl Pts',(14.6538046338945,1076.38589623523,329.65747948583));
#121980=CARTESIAN_POINT('Ctrl Pts',(14.5063694136426,1076.38100410945,329.554432181541));
#121981=CARTESIAN_POINT('Ctrl Pts',(14.4437471384081,1076.37757731989,329.488781690384));
#121982=CARTESIAN_POINT('Ctrl Pts',(14.3478389426105,1076.36910032337,329.33684759343));
#121983=CARTESIAN_POINT('Ctrl Pts',(14.3155307410438,1076.3641322677,329.252068096327));
#121984=CARTESIAN_POINT('Ctrl Pts',(14.2935059757345,1076.35604253381,329.120104927158));
#121985=CARTESIAN_POINT('Ctrl Pts',(14.2905207933502,1076.35329154602,329.076123350273));
#121986=CARTESIAN_POINT('Ctrl Pts',(14.2931443375162,1076.34767485741,328.988105006611));
#121987=CARTESIAN_POINT('Ctrl Pts',(14.2987684474515,1076.34482214203,328.944276252203));
#121988=CARTESIAN_POINT('Ctrl Pts',(14.3286558647562,1076.33616895413,328.813953637626));
#121989=CARTESIAN_POINT('Ctrl Pts',(14.365881272224,1076.33045126678,328.731436764397));
#121990=CARTESIAN_POINT('Ctrl Pts',(14.4698049177082,1076.31994204415,328.586564729992));
#121991=CARTESIAN_POINT('Ctrl Pts',(14.5351649459538,1076.31524289661,328.525384325979));
#121992=CARTESIAN_POINT('Ctrl Pts',(14.6856790386531,1076.30750211623,328.431866759496));
#121993=CARTESIAN_POINT('Ctrl Pts',(14.7693259695929,1076.30453310428,328.400371241936));
#121994=CARTESIAN_POINT('Ctrl Pts',(14.8931461334107,1076.30187437154,328.379880400079));
#121995=CARTESIAN_POINT('Ctrl Pts',(14.9300237741418,1076.30128645698,328.376849082178));
#121996=CARTESIAN_POINT('Ctrl Pts',(14.966975195385,1076.30090002967,328.376849082178));
#121997=CARTESIAN_POINT('',(14.9669751953833,1082.7251047501,328.376849082178));
#121998=CARTESIAN_POINT('',(14.9669751953833,1067.7251047501,328.376849082178));
#121999=CARTESIAN_POINT('Origin',(14.9669751953833,1082.7251047501,329.052293203314));
#122000=CARTESIAN_POINT('Ctrl Pts',(14.9669835900019,1076.30089994188,328.37684908223));
#122001=CARTESIAN_POINT('Ctrl Pts',(15.0552529225584,1076.29997691983,328.376850179267));
#122002=CARTESIAN_POINT('Ctrl Pts',(15.1426683856137,1076.3002189197,328.394154081871));
#122003=CARTESIAN_POINT('Ctrl Pts',(15.3058514613236,1076.30299993899,328.461385760682));
#122004=CARTESIAN_POINT('Ctrl Pts',(15.3800287689552,1076.30551021201,328.510642195034));
#122005=CARTESIAN_POINT('Ctrl Pts',(15.5053418329324,1076.31244578406,328.634935009798));
#122006=CARTESIAN_POINT('Ctrl Pts',(15.5552218458248,1076.31680594787,328.708810684804));
#122007=CARTESIAN_POINT('Ctrl Pts',(15.6238180723971,1076.3267621582,328.871704004732));
#122008=CARTESIAN_POINT('Ctrl Pts',(15.6417942447796,1076.33226457382,328.959195813127));
#122009=CARTESIAN_POINT('Ctrl Pts',(15.6427078900658,1076.34079539611,329.091873747251));
#122010=CARTESIAN_POINT('Ctrl Pts',(15.638666851738,1076.34366543975,329.136028245512));
#122011=CARTESIAN_POINT('Ctrl Pts',(15.6133842956322,1076.35233006512,329.267904706217));
#122012=CARTESIAN_POINT('Ctrl Pts',(15.5789119379269,1076.35798780034,329.352081595718));
#122013=CARTESIAN_POINT('Ctrl Pts',(15.4791310258456,1076.36833895204,329.501714414155));
#122014=CARTESIAN_POINT('Ctrl Pts',(15.4149168999795,1076.37293438836,329.565755076838));
#122015=CARTESIAN_POINT('Ctrl Pts',(15.2651186974525,1076.38050188352,329.665000015237));
#122016=CARTESIAN_POINT('Ctrl Pts',(15.1810292835317,1076.38339912944,329.699201532241));
#122017=CARTESIAN_POINT('Ctrl Pts',(15.0511420367375,1076.38614310924,329.723805255119));
#122018=CARTESIAN_POINT('Ctrl Pts',(15.0090537415224,1076.38678429624,329.72773732445));
#122019=CARTESIAN_POINT('Ctrl Pts',(14.9669751953833,1076.38718569293,329.72773732445));
#122020=CARTESIAN_POINT('Origin',(27.6354521170193,1067.7251047501,323.455155605234));
#122021=CARTESIAN_POINT('',(27.635452117036,1077.55448697719,322.356324469241));
#122022=CARTESIAN_POINT('Ctrl Pts',(27.6354554833944,1077.77317479141,324.553986741222));
#122023=CARTESIAN_POINT('Ctrl Pts',(27.78209499346,1077.76933775153,324.553986291977));
#122024=CARTESIAN_POINT('Ctrl Pts',(27.9271434753266,1077.76272537266,324.524634563112));
#122025=CARTESIAN_POINT('Ctrl Pts',(28.1739870805,1077.74618397533,324.420638081256));
#122026=CARTESIAN_POINT('Ctrl Pts',(28.2772138623149,1077.73712735143,324.355305784982));
#122027=CARTESIAN_POINT('Ctrl Pts',(28.465932012245,1077.71567121148,324.186672230339));
#122028=CARTESIAN_POINT('Ctrl Pts',(28.5475671410015,1077.70321917219,324.081903618919));
#122029=CARTESIAN_POINT('Ctrl Pts',(28.6745324689479,1077.67588242266,323.839673648655));
#122030=CARTESIAN_POINT('Ctrl Pts',(28.7154272804537,1077.6611311179,323.702514468041));
#122031=CARTESIAN_POINT('Ctrl Pts',(28.7431770865928,1077.6317537095,323.416840957285));
#122032=CARTESIAN_POINT('Ctrl Pts',(28.7284304245995,1077.61741873458,323.270839115508));
#122033=CARTESIAN_POINT('Ctrl Pts',(28.6449444884221,1077.59219529833,322.999639008381));
#122034=CARTESIAN_POINT('Ctrl Pts',(28.579593209094,1077.58139708564,322.876155530717));
#122035=CARTESIAN_POINT('Ctrl Pts',(28.4015541037616,1077.5636020172,322.653994853476));
#122036=CARTESIAN_POINT('Ctrl Pts',(28.2883036486213,1077.55702439445,322.559263112266));
#122037=CARTESIAN_POINT('Ctrl Pts',(28.1185711617126,1077.55230238832,322.46711842826));
#122038=CARTESIAN_POINT('Ctrl Pts',(28.0760381468249,1077.55146969942,322.447432193482));
#122039=CARTESIAN_POINT('Ctrl Pts',(28.0069992603195,1077.55065580183,322.420688068669));
#122040=CARTESIAN_POINT('Ctrl Pts',(27.9812674154294,1077.55046431554,322.41180416452));
#122041=CARTESIAN_POINT('Ctrl Pts',(27.9327826170647,1077.55030907866,322.397055880877));
#122042=CARTESIAN_POINT('Ctrl Pts',(27.9101206603123,1077.55031762918,322.390948086064));
#122043=CARTESIAN_POINT('Ctrl Pts',(27.8597731958885,1077.55051373314,322.37909402679));
#122044=CARTESIAN_POINT('Ctrl Pts',(27.8320270728602,1077.55073743386,322.373681308994));
#122045=CARTESIAN_POINT('Ctrl Pts',(27.7533536848727,1077.55169445846,322.361461484103));
#122046=CARTESIAN_POINT('Ctrl Pts',(27.7021202585493,1077.5526937123,322.357147642689));
#122047=CARTESIAN_POINT('Ctrl Pts',(27.504547116373,1077.55797550645,322.354391246003));
#122048=CARTESIAN_POINT('Ctrl Pts',(27.3594979330312,1077.56486021906,322.381564525387));
#122049=CARTESIAN_POINT('Ctrl Pts',(27.1123086761813,1077.58201058351,322.481355677257));
#122050=CARTESIAN_POINT('Ctrl Pts',(27.0087976084889,1077.59135801052,322.544540131769));
#122051=CARTESIAN_POINT('Ctrl Pts',(26.8186156075235,1077.61331288489,322.708616137735));
#122052=CARTESIAN_POINT('Ctrl Pts',(26.7356818667534,1077.62595896572,322.811017313524));
#122053=CARTESIAN_POINT('Ctrl Pts',(26.604985371743,1077.65340077059,323.048579265206));
#122054=CARTESIAN_POINT('Ctrl Pts',(26.5614979401041,1077.66804161175,323.183517000024));
#122055=CARTESIAN_POINT('Ctrl Pts',(26.5271042354151,1077.69706815676,323.467368269408));
#122056=CARTESIAN_POINT('Ctrl Pts',(26.5384377477433,1077.71115022112,323.613901157408));
#122057=CARTESIAN_POINT('Ctrl Pts',(26.6160006262472,1077.73585151202,323.888296295945));
#122058=CARTESIAN_POINT('Ctrl Pts',(26.6792043795877,1077.74637213626,324.014221197783));
#122059=CARTESIAN_POINT('Ctrl Pts',(26.8506198362845,1077.76335470198,324.237120432146));
#122060=CARTESIAN_POINT('Ctrl Pts',(26.9577336417413,1077.76960833789,324.331617522846));
#122061=CARTESIAN_POINT('Ctrl Pts',(27.1261596779175,1077.77465431793,324.430308089278));
#122062=CARTESIAN_POINT('Ctrl Pts',(27.1743178349814,1077.77566096828,324.453983851187));
#122063=CARTESIAN_POINT('Ctrl Pts',(27.2505559288919,1077.77661378816,324.484769082922));
#122064=CARTESIAN_POINT('Ctrl Pts',(27.2775036728934,1077.77683515168,324.494444786114));
#122065=CARTESIAN_POINT('Ctrl Pts',(27.3270076596723,1077.77703575534,324.510065177338));
#122066=CARTESIAN_POINT('Ctrl Pts',(27.3494333768748,1077.77705237694,324.516365045468));
#122067=CARTESIAN_POINT('Ctrl Pts',(27.3977436051221,1077.77693106367,324.528293693508));
#122068=CARTESIAN_POINT('Ctrl Pts',(27.423665293593,1077.77677172099,324.533708792302));
#122069=CARTESIAN_POINT('Ctrl Pts',(27.4933860815695,1077.77609332228,324.545663100758));
#122070=CARTESIAN_POINT('Ctrl Pts',(27.5374238124978,1077.77540513588,324.550499888846));
#122071=CARTESIAN_POINT('Ctrl Pts',(27.5995585848569,1077.77407183489,324.553547051538));
#122072=CARTESIAN_POINT('Ctrl Pts',(27.6175061940963,1077.77364446114,324.553986796211));
#122073=CARTESIAN_POINT('Ctrl Pts',(27.6354554833944,1077.77317479141,324.553986741221));
#122074=CARTESIAN_POINT('',(27.635452116996,1075.54255412639,322.356324469242));
#122075=CARTESIAN_POINT('',(27.6354521170193,1067.7251047501,322.356324469242));
#122076=CARTESIAN_POINT('Ctrl Pts',(27.6354637578243,1075.7632441652,324.553986741165));
#122077=CARTESIAN_POINT('Ctrl Pts',(27.4893848818429,1075.76710221568,324.553988288697));
#122078=CARTESIAN_POINT('Ctrl Pts',(27.3447413669374,1075.76810235755,324.524859733852));
#122079=CARTESIAN_POINT('Ctrl Pts',(27.0753847867248,1075.76428525466,324.411752571686));
#122080=CARTESIAN_POINT('Ctrl Pts',(26.9534410681139,1075.75951030705,324.328977880892));
#122081=CARTESIAN_POINT('Ctrl Pts',(26.7491438613275,1075.74472243282,324.120844299191));
#122082=CARTESIAN_POINT('Ctrl Pts',(26.6688433354455,1075.7348596376,323.997622254667));
#122083=CARTESIAN_POINT('Ctrl Pts',(26.5607566653673,1075.71118587656,323.726812293878));
#122084=CARTESIAN_POINT('Ctrl Pts',(26.5342459186675,1075.69759180768,323.581819681718));
#122085=CARTESIAN_POINT('Ctrl Pts',(26.5380357036236,1075.67585756518,323.364425471326));
#122086=CARTESIAN_POINT('Ctrl Pts',(26.546275071122,1075.66851545085,323.293154931303));
#122087=CARTESIAN_POINT('Ctrl Pts',(26.576551672069,1075.6536322625,323.152955190422));
#122088=CARTESIAN_POINT('Ctrl Pts',(26.5985785079818,1075.64612482737,323.084361186689));
#122089=CARTESIAN_POINT('Ctrl Pts',(26.6852172837086,1075.62353484456,322.884339423397));
#122090=CARTESIAN_POINT('Ctrl Pts',(26.7694851961867,1075.60885159091,322.763109239036));
#122091=CARTESIAN_POINT('Ctrl Pts',(26.979357587787,1075.58238452567,322.561941176326));
#122092=CARTESIAN_POINT('Ctrl Pts',(27.1024258318607,1075.57082202732,322.483425754171));
#122093=CARTESIAN_POINT('Ctrl Pts',(27.3713583443627,1075.55240563357,322.378881570527));
#122094=CARTESIAN_POINT('Ctrl Pts',(27.5144402415721,1075.54570557635,322.353550160154));
#122095=CARTESIAN_POINT('Ctrl Pts',(27.8016371369334,1075.53816692316,322.359562940599));
#122096=CARTESIAN_POINT('Ctrl Pts',(27.9428784569236,1075.53737148428,322.390524849676));
#122097=CARTESIAN_POINT('Ctrl Pts',(28.2053399882139,1075.54180882458,322.504832444295));
#122098=CARTESIAN_POINT('Ctrl Pts',(28.3239729793978,1075.54698711339,322.586955359263));
#122099=CARTESIAN_POINT('Ctrl Pts',(28.5234273573164,1075.56261813331,322.792219089591));
#122100=CARTESIAN_POINT('Ctrl Pts',(28.6021500792818,1075.57293440965,322.913494049916));
#122101=CARTESIAN_POINT('Ctrl Pts',(28.7089690590344,1075.59730911865,323.179967444967));
#122102=CARTESIAN_POINT('Ctrl Pts',(28.7357146877056,1075.61115506102,323.322762436554));
#122103=CARTESIAN_POINT('Ctrl Pts',(28.7334763005315,1075.63311520331,323.538696203443));
#122104=CARTESIAN_POINT('Ctrl Pts',(28.7256236824297,1075.64059723465,323.610588873429));
#122105=CARTESIAN_POINT('Ctrl Pts',(28.6959788472949,1075.65561155148,323.751625342745));
#122106=CARTESIAN_POINT('Ctrl Pts',(28.6742851296499,1075.6631089484,323.820448464849));
#122107=CARTESIAN_POINT('Ctrl Pts',(28.5886406650049,1075.68548973464,324.021024212218));
#122108=CARTESIAN_POINT('Ctrl Pts',(28.5050027746342,1075.6998135266,324.142697999747));
#122109=CARTESIAN_POINT('Ctrl Pts',(28.2953907973526,1075.72544481533,324.345707774317));
#122110=CARTESIAN_POINT('Ctrl Pts',(28.1716927693333,1075.7365204612,324.425274518019));
#122111=CARTESIAN_POINT('Ctrl Pts',(27.9084124987656,1075.75354880344,324.528316300412));
#122112=CARTESIAN_POINT('Ctrl Pts',(27.7725918425639,1075.75962251169,324.553985288457));
#122113=CARTESIAN_POINT('Ctrl Pts',(27.6354637578243,1075.7632441652,324.553986741165));
#122114=CARTESIAN_POINT('Origin',(27.6354521170193,1067.7251047501,323.455155605234));
#122115=CARTESIAN_POINT('',(27.6354521170193,1075.70507826342,323.953986741227));
#122116=CARTESIAN_POINT('',(27.6354521170193,1075.60488526556,322.956324469242));
#122117=CARTESIAN_POINT('Ctrl Pts',(27.6354521170193,1075.70507826342,323.953986741227));
#122118=CARTESIAN_POINT('Ctrl Pts',(27.634044503031,1075.70511623235,323.953986741227));
#122119=CARTESIAN_POINT('Ctrl Pts',(27.6326365788117,1075.70515362057,323.953980783171));
#122120=CARTESIAN_POINT('Ctrl Pts',(27.5662202751841,1075.70688953137,323.953418398493));
#122121=CARTESIAN_POINT('Ctrl Pts',(27.501934139173,1075.70731419297,323.940164730451));
#122122=CARTESIAN_POINT('Ctrl Pts',(27.382030109535,1075.70556779413,323.889715649661));
#122123=CARTESIAN_POINT('Ctrl Pts',(27.3276115070596,1075.70341274803,323.853011731308));
#122124=CARTESIAN_POINT('Ctrl Pts',(27.234877522119,1075.69669649567,323.759780973222));
#122125=CARTESIAN_POINT('Ctrl Pts',(27.197921958113,1075.6921483109,323.703765212779));
#122126=CARTESIAN_POINT('Ctrl Pts',(27.1480534878934,1075.68125181367,323.580493573235));
#122127=CARTESIAN_POINT('Ctrl Pts',(27.135713339052,1075.67500623829,323.514435177438));
#122128=CARTESIAN_POINT('Ctrl Pts',(27.1371431232632,1075.66506192422,323.415382620928));
#122129=CARTESIAN_POINT('Ctrl Pts',(27.1408029297177,1075.66171215883,323.382939317489));
#122130=CARTESIAN_POINT('Ctrl Pts',(27.1544047637778,1075.65494142215,323.319174211982));
#122131=CARTESIAN_POINT('Ctrl Pts',(27.1643286318015,1075.65153595021,323.288002183825));
#122132=CARTESIAN_POINT('Ctrl Pts',(27.2036824476216,1075.64124433757,323.196526028818));
#122133=CARTESIAN_POINT('Ctrl Pts',(27.2422663137376,1075.63456288874,323.140942034853));
#122134=CARTESIAN_POINT('Ctrl Pts',(27.3380542535881,1075.62263149001,323.049350748552));
#122135=CARTESIAN_POINT('Ctrl Pts',(27.3939003959041,1075.61746697062,323.013802116999));
#122136=CARTESIAN_POINT('Ctrl Pts',(27.5125646838575,1075.6094812346,322.967784142417));
#122137=CARTESIAN_POINT('Ctrl Pts',(27.5737163233485,1075.60660692522,322.956324469242));
#122138=CARTESIAN_POINT('Ctrl Pts',(27.6354521170193,1075.60488526556,322.956324469242));
#122139=CARTESIAN_POINT('',(27.6354521170193,1082.7251047501,322.956324469242));
#122140=CARTESIAN_POINT('',(27.6354521170193,1067.7251047501,322.956324469242));
#122141=CARTESIAN_POINT('Origin',(27.6354521170193,1082.7251047501,323.455155605234));
#122142=CARTESIAN_POINT('Ctrl Pts',(27.6354526343093,1075.60488525113,322.956324469242));
#122143=CARTESIAN_POINT('Ctrl Pts',(27.7004736444753,1075.60307198173,322.956324536669));
#122144=CARTESIAN_POINT('Ctrl Pts',(27.7648809908801,1075.60257292419,322.969037435341));
#122145=CARTESIAN_POINT('Ctrl Pts',(27.8851394872723,1075.60426457263,323.018451535124));
#122146=CARTESIAN_POINT('Ctrl Pts',(27.9397996373544,1075.60643549965,323.054635109211));
#122147=CARTESIAN_POINT('Ctrl Pts',(28.0323199462946,1075.6131730729,323.146009206826));
#122148=CARTESIAN_POINT('Ctrl Pts',(28.0692064098541,1075.61768166637,323.200369259097));
#122149=CARTESIAN_POINT('Ctrl Pts',(28.1201754896558,1075.62845341682,323.320417951284));
#122150=CARTESIAN_POINT('Ctrl Pts',(28.1336271886545,1075.63462291697,323.385018683961));
#122151=CARTESIAN_POINT('Ctrl Pts',(28.1345768312166,1075.64448793891,323.483043289621));
#122152=CARTESIAN_POINT('Ctrl Pts',(28.1316735317111,1075.64785881459,323.515709779067));
#122153=CARTESIAN_POINT('Ctrl Pts',(28.1195251090723,1075.65465299698,323.579946749933));
#122154=CARTESIAN_POINT('Ctrl Pts',(28.1103170093908,1075.65806050761,323.611370153617));
#122155=CARTESIAN_POINT('Ctrl Pts',(28.0732135116152,1075.66830142562,323.703406689827));
#122156=CARTESIAN_POINT('Ctrl Pts',(28.0362007253373,1075.67492087552,323.759581440303));
#122157=CARTESIAN_POINT('Ctrl Pts',(27.9424006803349,1075.68686729279,323.853933002792));
#122158=CARTESIAN_POINT('Ctrl Pts',(27.8866104873441,1075.69208213468,323.891249257643));
#122159=CARTESIAN_POINT('Ctrl Pts',(27.7649500282382,1075.70032657103,323.941251252787));
#122160=CARTESIAN_POINT('Ctrl Pts',(27.7005326457111,1075.70332278349,323.953986741227));
#122161=CARTESIAN_POINT('Ctrl Pts',(27.6354521170193,1075.70507826342,323.953986741227));
#122162=CARTESIAN_POINT('Origin',(41.3143294401475,1067.7251047501,320.535862846908));
#122163=CARTESIAN_POINT('',(41.3143294401746,1076.68214102844,319.44532209818));
#122164=CARTESIAN_POINT('Ctrl Pts',(41.3143428194402,1076.95432942362,321.626403595554));
#122165=CARTESIAN_POINT('Ctrl Pts',(41.4218166275092,1076.94912750026,321.626402277012));
#122166=CARTESIAN_POINT('Ctrl Pts',(41.5285827596115,1076.9420159031,321.610514544172));
#122167=CARTESIAN_POINT('Ctrl Pts',(41.7465386926837,1076.92332534773,321.544328843047));
#122168=CARTESIAN_POINT('Ctrl Pts',(41.8551072169579,1076.91143255922,321.49047694153));
#122169=CARTESIAN_POINT('Ctrl Pts',(42.0589629662026,1076.88334386355,321.34333706984));
#122170=CARTESIAN_POINT('Ctrl Pts',(42.1505005855932,1076.86707680082,321.248068199629));
#122171=CARTESIAN_POINT('Ctrl Pts',(42.3011116436337,1076.83147654984,321.021183105947));
#122172=CARTESIAN_POINT('Ctrl Pts',(42.355651873213,1076.81231902425,320.889292817876));
#122173=CARTESIAN_POINT('Ctrl Pts',(42.4119342200797,1076.77440537764,320.609182994267));
#122174=CARTESIAN_POINT('Ctrl Pts',(42.41202397689,1076.75601805803,320.463273429836));
#122175=CARTESIAN_POINT('Ctrl Pts',(42.3567504731207,1076.72393887002,320.187633286867));
#122176=CARTESIAN_POINT('Ctrl Pts',(42.3049909651277,1076.71031809491,320.059822407833));
#122177=CARTESIAN_POINT('Ctrl Pts',(42.154338259021,1076.68820754652,319.826247547805));
#122178=CARTESIAN_POINT('Ctrl Pts',(42.0555296045438,1076.6801007609,319.723525029405));
#122179=CARTESIAN_POINT('Ctrl Pts',(41.9050007143757,1076.67427562563,319.618159098336));
#122180=CARTESIAN_POINT('Ctrl Pts',(41.8689131970497,1076.67326327875,319.595910218023));
#122181=CARTESIAN_POINT('Ctrl Pts',(41.8079915436222,1076.67215899292,319.563084875167));
#122182=CARTESIAN_POINT('Ctrl Pts',(41.7839041937303,1076.67186608549,319.551231457372));
#122183=CARTESIAN_POINT('Ctrl Pts',(41.7403350435942,1076.67158708966,319.531753994512));
#122184=CARTESIAN_POINT('Ctrl Pts',(41.7210262273562,1076.67154742382,319.523779301169));
#122185=CARTESIAN_POINT('Ctrl Pts',(41.6801633928604,1076.67163704969,319.508260998845));
#122186=CARTESIAN_POINT('Ctrl Pts',(41.6585780577322,1076.67178232638,319.500830056112));
#122187=CARTESIAN_POINT('Ctrl Pts',(41.6020992464047,1076.67241313776,319.483349027432));
#122188=CARTESIAN_POINT('Ctrl Pts',(41.5669122236252,1076.67304852764,319.474355366001));
#122189=CARTESIAN_POINT('Ctrl Pts',(41.4234207721387,1076.67660184293,319.445217862265));
#122190=CARTESIAN_POINT('Ctrl Pts',(41.3128898742779,1076.68151244776,319.439794759528));
#122191=CARTESIAN_POINT('Ctrl Pts',(41.0916870010979,1076.69558248906,319.46238955167));
#122192=CARTESIAN_POINT('Ctrl Pts',(40.9824491401439,1076.70474597225,319.491016072199));
#122193=CARTESIAN_POINT('Ctrl Pts',(40.7657586636322,1076.72761581736,319.585197821066));
#122194=CARTESIAN_POINT('Ctrl Pts',(40.6613385128956,1076.74153617064,319.653698614563));
#122195=CARTESIAN_POINT('Ctrl Pts',(40.4725764169351,1076.77317112897,319.829642607107));
#122196=CARTESIAN_POINT('Ctrl Pts',(40.3921978359933,1076.79084654215,319.938436490654));
#122197=CARTESIAN_POINT('Ctrl Pts',(40.2704151628547,1076.8282082524,320.188890633183));
#122198=CARTESIAN_POINT('Ctrl Pts',(40.233653008625,1076.84759758869,320.330131809515));
#122199=CARTESIAN_POINT('Ctrl Pts',(40.2174761305333,1076.88394167024,320.617160634091));
#122200=CARTESIAN_POINT('Ctrl Pts',(40.23754079299,1076.90058842704,320.760227311747));
#122201=CARTESIAN_POINT('Ctrl Pts',(40.3273217429563,1076.92777313096,321.017237138234));
#122202=CARTESIAN_POINT('Ctrl Pts',(40.3911610969451,1076.93854377822,321.130641097368));
#122203=CARTESIAN_POINT('Ctrl Pts',(40.5462268939571,1076.95395216355,321.31838197958));
#122204=CARTESIAN_POINT('Ctrl Pts',(40.6323826063517,1076.95906139893,321.394530103112));
#122205=CARTESIAN_POINT('Ctrl Pts',(40.7612065228253,1076.96281648845,321.476502172275));
#122206=CARTESIAN_POINT('Ctrl Pts',(40.7945994162274,1076.96349816862,321.495356845758));
#122207=CARTESIAN_POINT('Ctrl Pts',(40.849669187214,1076.96416938875,321.522730056165));
#122208=CARTESIAN_POINT('Ctrl Pts',(40.8707427482178,1076.96432584328,321.532380259352));
#122209=CARTESIAN_POINT('Ctrl Pts',(40.9091990554738,1076.96443342747,321.548528681394));
#122210=CARTESIAN_POINT('Ctrl Pts',(40.9264699651473,1076.96441935669,321.555268433267));
#122211=CARTESIAN_POINT('Ctrl Pts',(40.9671501679068,1076.96424215797,321.569959809575));
#122212=CARTESIAN_POINT('Ctrl Pts',(40.9906739658815,1076.96403096218,321.577561951523));
#122213=CARTESIAN_POINT('Ctrl Pts',(41.0577482813037,1076.96312542355,321.596746803453));
#122214=CARTESIAN_POINT('Ctrl Pts',(41.1017807062377,1076.9621774666,321.606437629254));
#122215=CARTESIAN_POINT('Ctrl Pts',(41.201900545872,1076.95923915612,321.622052494203));
#122216=CARTESIAN_POINT('Ctrl Pts',(41.2580901248877,1076.95705215404,321.62640428569));
#122217=CARTESIAN_POINT('Ctrl Pts',(41.3143428194403,1076.95432942362,321.626403595554));
#122218=CARTESIAN_POINT('',(41.3143294401476,1074.66274184067,319.445322098179));
#122219=CARTESIAN_POINT('',(41.3143294401475,1067.7251047501,319.445322098179));
#122220=CARTESIAN_POINT('Ctrl Pts',(41.314812718535,1074.93716077403,321.626403488553));
#122221=CARTESIAN_POINT('Ctrl Pts',(41.1715706204318,1074.94415975441,321.626466966985));
#122222=CARTESIAN_POINT('Ctrl Pts',(41.0296257881001,1074.94761527766,321.598307263943));
#122223=CARTESIAN_POINT('Ctrl Pts',(40.7661667853346,1074.94706138158,321.489219256244));
#122224=CARTESIAN_POINT('Ctrl Pts',(40.6471136149637,1074.94314345929,321.410015151242));
#122225=CARTESIAN_POINT('Ctrl Pts',(40.4436327271655,1074.9282686863,321.208304548177));
#122226=CARTESIAN_POINT('Ctrl Pts',(40.3622271759297,1074.91729988569,321.086920184947));
#122227=CARTESIAN_POINT('Ctrl Pts',(40.2514001287905,1074.88966635459,320.819529671462));
#122228=CARTESIAN_POINT('Ctrl Pts',(40.22323779074,1074.87325991693,320.676134756145));
#122229=CARTESIAN_POINT('Ctrl Pts',(40.2240712253127,1074.84635165742,320.460731515587));
#122230=CARTESIAN_POINT('Ctrl Pts',(40.2312612710062,1074.83715955598,320.390050263008));
#122231=CARTESIAN_POINT('Ctrl Pts',(40.2592825923277,1074.81832765418,320.250884592581));
#122232=CARTESIAN_POINT('Ctrl Pts',(40.2801031120063,1074.8087284771,320.182721629814));
#122233=CARTESIAN_POINT('Ctrl Pts',(40.3636445847771,1074.77926437491,319.981852006162));
#122234=CARTESIAN_POINT('Ctrl Pts',(40.4465935118131,1074.7595824578,319.85923951023));
#122235=CARTESIAN_POINT('Ctrl Pts',(40.6540803439798,1074.72330166367,319.656084325281));
#122236=CARTESIAN_POINT('Ctrl Pts',(40.7758210107337,1074.70699060038,319.576655842871));
#122237=CARTESIAN_POINT('Ctrl Pts',(41.0423110224472,1074.67981823942,319.47018350843));
#122238=CARTESIAN_POINT('Ctrl Pts',(41.1842336149242,1074.669172538,319.443677603048));
#122239=CARTESIAN_POINT('Ctrl Pts',(41.4692836080394,1074.65506020246,319.447107815698));
#122240=CARTESIAN_POINT('Ctrl Pts',(41.6095117397283,1074.65166939933,319.476470135398));
#122241=CARTESIAN_POINT('Ctrl Pts',(41.8704724359342,1074.65258759188,319.587181347956));
#122242=CARTESIAN_POINT('Ctrl Pts',(41.9886136753546,1074.65685765158,319.66720053904));
#122243=CARTESIAN_POINT('Ctrl Pts',(42.1881325358432,1074.67250856062,319.868119441079));
#122244=CARTESIAN_POINT('Ctrl Pts',(42.2673412716932,1074.68376186316,319.987179146882));
#122245=CARTESIAN_POINT('Ctrl Pts',(42.3763256559622,1074.7118212103,320.249764494128));
#122246=CARTESIAN_POINT('Ctrl Pts',(42.4045472972949,1074.72840748582,320.390979483382));
#122247=CARTESIAN_POINT('Ctrl Pts',(42.4051904739248,1074.7647076447,320.677135393134));
#122248=CARTESIAN_POINT('Ctrl Pts',(42.3770995356429,1074.78410874865,320.819433855955));
#122249=CARTESIAN_POINT('Ctrl Pts',(42.2668478998924,1074.82320033299,321.086396971585));
#122250=CARTESIAN_POINT('Ctrl Pts',(42.1850879715168,1074.84252574672,321.208338340571));
#122251=CARTESIAN_POINT('Ctrl Pts',(41.9790840161114,1074.87814078714,321.41236025411));
#122252=CARTESIAN_POINT('Ctrl Pts',(41.8571019468562,1074.89411356443,321.492772676195));
#122253=CARTESIAN_POINT('Ctrl Pts',(41.5932926861952,1074.92022809525,321.599323040952));
#122254=CARTESIAN_POINT('Ctrl Pts',(41.4548180418782,1074.93031994633,321.626341444513));
#122255=CARTESIAN_POINT('Ctrl Pts',(41.314812718535,1074.93716077403,321.626403488553));
#122256=CARTESIAN_POINT('Origin',(41.3143294401475,1067.7251047501,320.535862846908));
#122257=CARTESIAN_POINT('',(41.3143294401474,1074.86349252611,321.026403595636));
#122258=CARTESIAN_POINT('',(41.3143294401486,1074.74003968768,320.045322098179));
#122259=CARTESIAN_POINT('Ctrl Pts',(41.3143294401475,1074.86349252611,321.026403595636));
#122260=CARTESIAN_POINT('Ctrl Pts',(41.3128461441749,1074.86356585894,321.026403595636));
#122261=CARTESIAN_POINT('Ctrl Pts',(41.311362475265,1074.86363837087,321.026396867861));
#122262=CARTESIAN_POINT('Ctrl Pts',(41.2461231309153,1074.86678989609,321.025804888836));
#122263=CARTESIAN_POINT('Ctrl Pts',(41.1830517971698,1074.86828664131,321.012801589578));
#122264=CARTESIAN_POINT('Ctrl Pts',(41.0654668578589,1074.8679427817,320.96336554765));
#122265=CARTESIAN_POINT('Ctrl Pts',(41.0121363364488,1074.86611110015,320.927474302055));
#122266=CARTESIAN_POINT('Ctrl Pts',(40.9219662375796,1074.8593183105,320.837152945459));
#122267=CARTESIAN_POINT('Ctrl Pts',(40.8861257096163,1074.85440853092,320.783534500662));
#122268=CARTESIAN_POINT('Ctrl Pts',(40.8363689843546,1074.84197415737,320.66421014995));
#122269=CARTESIAN_POINT('Ctrl Pts',(40.8235619957307,1074.83450870245,320.599426216224));
#122270=CARTESIAN_POINT('Ctrl Pts',(40.8239043346288,1074.82229754514,320.502134287703));
#122271=CARTESIAN_POINT('Ctrl Pts',(40.8271483246973,1074.81813395482,320.47023476108));
#122272=CARTESIAN_POINT('Ctrl Pts',(40.8398022570964,1074.80962223017,320.407485629597));
#122273=CARTESIAN_POINT('Ctrl Pts',(40.8491966197144,1074.80529284422,320.376779305835));
#122274=CARTESIAN_POINT('Ctrl Pts',(40.8867898432869,1074.7920577392,320.28654447439));
#122275=CARTESIAN_POINT('Ctrl Pts',(40.9240193757248,1074.78325330532,320.231528258088));
#122276=CARTESIAN_POINT('Ctrl Pts',(41.017513513941,1074.76698530552,320.139926546507));
#122277=CARTESIAN_POINT('Ctrl Pts',(41.0726737877535,1074.75966276451,320.104012551252));
#122278=CARTESIAN_POINT('Ctrl Pts',(41.1908666812368,1074.74776277432,320.057097400236));
#122279=CARTESIAN_POINT('Ctrl Pts',(41.2522651499211,1074.7431707449,320.045322098179));
#122280=CARTESIAN_POINT('Ctrl Pts',(41.3143294401506,1074.74003968768,320.045322098179));
#122281=CARTESIAN_POINT('',(41.3143294401475,1082.7251047501,320.045322098179));
#122282=CARTESIAN_POINT('',(41.3143294401475,1067.7251047501,320.045322098179));
#122283=CARTESIAN_POINT('Origin',(41.3143294401475,1082.7251047501,320.535862846908));
#122284=CARTESIAN_POINT('Ctrl Pts',(41.3143357717175,1074.74003936826,320.04532209822));
#122285=CARTESIAN_POINT('Ctrl Pts',(41.3781299766579,1074.73682114373,320.045322921633));
#122286=CARTESIAN_POINT('Ctrl Pts',(41.4413545263827,1074.73521147509,320.057768195823));
#122287=CARTESIAN_POINT('Ctrl Pts',(41.5593563747643,1074.73540889194,320.106158929656));
#122288=CARTESIAN_POINT('Ctrl Pts',(41.6129569156641,1074.73720296111,320.141535103922));
#122289=CARTESIAN_POINT('Ctrl Pts',(41.7038314946861,1074.74397664506,320.230906139878));
#122290=CARTESIAN_POINT('Ctrl Pts',(41.7401150978535,1074.74890226474,320.284085696526));
#122291=CARTESIAN_POINT('Ctrl Pts',(41.7905321071453,1074.76127962073,320.40171467661));
#122292=CARTESIAN_POINT('Ctrl Pts',(41.8039575734674,1074.76863453191,320.465124426693));
#122293=CARTESIAN_POINT('Ctrl Pts',(41.8057157905573,1074.78495844504,320.595010761301));
#122294=CARTESIAN_POINT('Ctrl Pts',(41.793362062695,1074.79380651393,320.660267504426));
#122295=CARTESIAN_POINT('Ctrl Pts',(41.7438144368007,1074.81156672865,320.781750903608));
#122296=CARTESIAN_POINT('Ctrl Pts',(41.7071739584895,1074.82031168915,320.836867395503));
#122297=CARTESIAN_POINT('Ctrl Pts',(41.6145238676394,1074.83649756601,320.929277488738));
#122298=CARTESIAN_POINT('Ctrl Pts',(41.5594893696512,1074.84378943367,320.965764438528));
#122299=CARTESIAN_POINT('Ctrl Pts',(41.4402856454316,1074.85573639902,321.014145779283));
#122300=CARTESIAN_POINT('Ctrl Pts',(41.3776473147849,1074.86036214679,321.026403595636));
#122301=CARTESIAN_POINT('Ctrl Pts',(41.3143294401475,1074.86349252611,321.026403595636));
#122302=CARTESIAN_POINT('Origin',(-14.6999478050467,1067.7251047501,336.276664073765));
#122303=CARTESIAN_POINT('',(-14.6999478050671,1076.62893223815,334.798360941572));
#122304=CARTESIAN_POINT('',(-14.6999478050467,1067.7251047501,334.798360941572));
#122305=CARTESIAN_POINT('Ctrl Pts',(-14.7001323799959,1076.70479648561,
337.754967194436));
#122306=CARTESIAN_POINT('Ctrl Pts',(-14.8957174153601,1076.70421870621,
337.754942774479));
#122307=CARTESIAN_POINT('Ctrl Pts',(-15.0893628551477,1076.70295890393,
337.716103585662));
#122308=CARTESIAN_POINT('Ctrl Pts',(-15.4496590785385,1076.69897902633,
337.565577962594));
#122309=CARTESIAN_POINT('Ctrl Pts',(-15.6128648691738,1076.69629503056,
337.45562172281));
#122310=CARTESIAN_POINT('Ctrl Pts',(-15.8877068483204,1076.68946791284,
337.178254670474));
#122311=CARTESIAN_POINT('Ctrl Pts',(-15.9964363629675,1076.68537915515,
337.013376391187));
#122312=CARTESIAN_POINT('Ctrl Pts',(-16.143526651107,1076.6760751074,336.650605313986));
#122313=CARTESIAN_POINT('Ctrl Pts',(-16.1803177063381,1076.67094723356,
336.456248500635));
#122314=CARTESIAN_POINT('Ctrl Pts',(-16.1760250080137,1076.66039506669,
336.066348106327));
#122315=CARTESIAN_POINT('Ctrl Pts',(-16.135702478106,1076.65507972852,335.874609375946));
#122316=CARTESIAN_POINT('Ctrl Pts',(-15.9832429731908,1076.64516680223,
335.517560480363));
#122317=CARTESIAN_POINT('Ctrl Pts',(-15.8725418398901,1076.64067274634,
335.35573025354));
#122318=CARTESIAN_POINT('Ctrl Pts',(-15.5950090525183,1076.63346531469,
335.084230376839));
#122319=CARTESIAN_POINT('Ctrl Pts',(-15.4309223292167,1076.6308271039,334.977156605108));
#122320=CARTESIAN_POINT('Ctrl Pts',(-15.0711758210652,1076.62802354181,
334.832693752177));
#122321=CARTESIAN_POINT('Ctrl Pts',(-14.8790874762117,1076.62788220176,
334.796539023342));
#122322=CARTESIAN_POINT('Ctrl Pts',(-14.492366869078,1076.63014395414,334.800319623269));
#122323=CARTESIAN_POINT('Ctrl Pts',(-14.3014805265477,1076.63251681089,
334.840037186407));
#122324=CARTESIAN_POINT('Ctrl Pts',(-13.9459269105799,1076.63926185274,
334.9905549053));
#122325=CARTESIAN_POINT('Ctrl Pts',(-13.7846630300826,1076.64356169163,
335.099860498032));
#122326=CARTESIAN_POINT('Ctrl Pts',(-13.5131316530228,1076.65320905303,
335.374359106864));
#122327=CARTESIAN_POINT('Ctrl Pts',(-13.405521946531,1076.65845805784,335.536971833433));
#122328=CARTESIAN_POINT('Ctrl Pts',(-13.2955725337978,1076.66632703601,
335.805028646334));
#122329=CARTESIAN_POINT('Ctrl Pts',(-13.2677636227205,1076.66893183358,
335.897772577147));
#122330=CARTESIAN_POINT('Ctrl Pts',(-13.2306355304937,1076.6740168994,336.08736641753));
#122331=CARTESIAN_POINT('Ctrl Pts',(-13.2214072090968,1076.67648492476,
336.183762191161));
#122332=CARTESIAN_POINT('Ctrl Pts',(-13.2221400186975,1076.68362806364,
336.476172445074));
#122333=CARTESIAN_POINT('Ctrl Pts',(-13.2615276495364,1076.68788966242,
336.66995329469));
#122334=CARTESIAN_POINT('Ctrl Pts',(-13.4131658664563,1076.69508381343,
337.030019992103));
#122335=CARTESIAN_POINT('Ctrl Pts',(-13.5235705203483,1076.69795956421,
337.192904836477));
#122336=CARTESIAN_POINT('Ctrl Pts',(-13.8016209096952,1076.70232020223,
337.466871387134));
#122337=CARTESIAN_POINT('Ctrl Pts',(-13.9666897463278,1076.70376629342,
337.575094380905));
#122338=CARTESIAN_POINT('Ctrl Pts',(-14.323521881502,1076.7052676937,337.718701187015));
#122339=CARTESIAN_POINT('Ctrl Pts',(-14.5109563147374,1076.70535533222,
337.754990814194));
#122340=CARTESIAN_POINT('Ctrl Pts',(-14.7001323799959,1076.70479648561,
337.754967194436));
#122341=CARTESIAN_POINT('Origin',(-14.6999478050467,1067.7251047501,336.276664073765));
#122342=CARTESIAN_POINT('',(-14.6999478050467,1076.69331989119,337.154967205958));
#122343=CARTESIAN_POINT('',(-14.6999478049914,1076.64821521145,335.398360941572));
#122344=CARTESIAN_POINT('Ctrl Pts',(-14.6999478050467,1076.69331989119,
337.154967205958));
#122345=CARTESIAN_POINT('Ctrl Pts',(-14.7009690133301,1076.69331631968,
337.154967205958));
#122346=CARTESIAN_POINT('Ctrl Pts',(-14.7019903090399,1076.6933127102,337.154965424911));
#122347=CARTESIAN_POINT('Ctrl Pts',(-14.8197051797538,1076.69289233503,
337.154554784525));
#122348=CARTESIAN_POINT('Ctrl Pts',(-14.9351523343786,1076.69199137635,
337.130895378293));
#122349=CARTESIAN_POINT('Ctrl Pts',(-15.149848331648,1076.68924131929,337.03992980832));
#122350=CARTESIAN_POINT('Ctrl Pts',(-15.2469926280456,1076.68741838492,
336.973603155994));
#122351=CARTESIAN_POINT('Ctrl Pts',(-15.4099403752669,1076.68295357097,
336.806722403128));
#122352=CARTESIAN_POINT('Ctrl Pts',(-15.4740387894439,1076.68035136175,
336.707745689171));
#122353=CARTESIAN_POINT('Ctrl Pts',(-15.5596391832146,1076.67463626738,
336.490889282691));
#122354=CARTESIAN_POINT('Ctrl Pts',(-15.5804295691151,1076.67158052066,
336.375214774509));
#122355=CARTESIAN_POINT('Ctrl Pts',(-15.5757351879597,1076.665450948,336.143680355862));
#122356=CARTESIAN_POINT('Ctrl Pts',(-15.5507610283096,1076.66243812165,
336.030074047769));
#122357=CARTESIAN_POINT('Ctrl Pts',(-15.4583672024248,1076.65691398668,
335.818955908892));
#122358=CARTESIAN_POINT('Ctrl Pts',(-15.3918314957487,1076.6544588038,335.723493769938));
#122359=CARTESIAN_POINT('Ctrl Pts',(-15.2257389425843,1076.65056444469,
335.563764242563));
#122360=CARTESIAN_POINT('Ctrl Pts',(-15.1278164029263,1076.64916478105,
335.50102621267));
#122361=CARTESIAN_POINT('Ctrl Pts',(-14.9183826869667,1076.64773857793,
335.41890461113));
#122362=CARTESIAN_POINT('Ctrl Pts',(-14.8096227972511,1076.64766396979,
335.398360941558));
#122363=CARTESIAN_POINT('Ctrl Pts',(-14.6999478049361,1076.64821521145,
335.398360941572));
#122364=CARTESIAN_POINT('',(-14.6999478050467,1082.7251047501,335.398360941572));
#122365=CARTESIAN_POINT('',(-14.6999478050467,1067.7251047501,335.398360941572));
#122366=CARTESIAN_POINT('Origin',(-14.6999478050467,1082.7251047501,336.276664073765));
#122367=CARTESIAN_POINT('Ctrl Pts',(-14.6999478049361,1076.64821521145,
335.398360941572));
#122368=CARTESIAN_POINT('Ctrl Pts',(-14.6947111011966,1076.64824153184,
335.398360941572));
#122369=CARTESIAN_POINT('Ctrl Pts',(-14.6894723111497,1076.6482692717,335.398407775651));
#122370=CARTESIAN_POINT('Ctrl Pts',(-14.569409954258,1076.64893731845,335.40055643325));
#122371=CARTESIAN_POINT('Ctrl Pts',(-14.4561050216884,1076.65024750165,
335.42511110646));
#122372=CARTESIAN_POINT('Ctrl Pts',(-14.2454119130326,1076.65398123313,
335.516406631954));
#122373=CARTESIAN_POINT('Ctrl Pts',(-14.1500509251862,1076.65636615552,
335.582254989699));
#122374=CARTESIAN_POINT('Ctrl Pts',(-13.9900092290904,1076.66178631504,
335.746948899337));
#122375=CARTESIAN_POINT('Ctrl Pts',(-13.9268930265349,1076.66476739208,
335.844234325778));
#122376=CARTESIAN_POINT('Ctrl Pts',(-13.8645400063229,1076.66921265106,
336.000356130546));
#122377=CARTESIAN_POINT('Ctrl Pts',(-13.8493270604945,1076.67062404865,
336.051504898227));
#122378=CARTESIAN_POINT('Ctrl Pts',(-13.8282750640927,1076.67342571959,
336.156322335976));
#122379=CARTESIAN_POINT('Ctrl Pts',(-13.8225521104539,1076.67480987164,
336.209787600263));
#122380=CARTESIAN_POINT('Ctrl Pts',(-13.8217442258762,1076.67615522911,
336.263440399819));
#122381=CARTESIAN_POINT('Ctrl Pts',(-13.8199848288176,1076.67908512532,
336.380284538617));
#122382=CARTESIAN_POINT('Ctrl Pts',(-13.8415618709421,1076.68178577728,
336.496319632915));
#122383=CARTESIAN_POINT('Ctrl Pts',(-13.9287208200021,1076.68648279568,
336.712773304373));
#122384=CARTESIAN_POINT('Ctrl Pts',(-13.9932886641846,1076.6884375335,336.811096708633));
#122385=CARTESIAN_POINT('Ctrl Pts',(-14.1571383012838,1076.69146843165,
336.976935330054));
#122386=CARTESIAN_POINT('Ctrl Pts',(-14.2548352530162,1076.692516146,337.042757206605));
#122387=CARTESIAN_POINT('Ctrl Pts',(-14.4694686493758,1076.69364587763,
337.132064727983));
#122388=CARTESIAN_POINT('Ctrl Pts',(-14.5841461198548,1076.69372488816,
337.154967205958));
#122389=CARTESIAN_POINT('Ctrl Pts',(-14.6999478050467,1076.69331989119,
337.154967205958));
#122390=CARTESIAN_POINT('Origin',(-5.22978306525612,1067.7251047501,328.028873070842));
#122391=CARTESIAN_POINT('',(-5.22978306527338,1076.25871334817,326.753428949706));
#122392=CARTESIAN_POINT('',(-5.22978306525612,1067.7251047501,326.753428949706));
#122393=CARTESIAN_POINT('Ctrl Pts',(-5.22980002134218,1076.42335631864,
329.304317191865));
#122394=CARTESIAN_POINT('Ctrl Pts',(-5.39871008864912,1076.42281868721,
329.304314946331));
#122395=CARTESIAN_POINT('Ctrl Pts',(-5.5659217275966,1076.42032080269,329.27075924164));
#122396=CARTESIAN_POINT('Ctrl Pts',(-5.87732970737173,1076.41159226847,
329.140578640962));
#122397=CARTESIAN_POINT('Ctrl Pts',(-6.01845082508294,1076.40544851869,
329.045323293699));
#122398=CARTESIAN_POINT('Ctrl Pts',(-6.25583188549957,1076.39007218768,
328.805140032806));
#122399=CARTESIAN_POINT('Ctrl Pts',(-6.34957526252597,1076.38097658469,
328.662428174666));
#122400=CARTESIAN_POINT('Ctrl Pts',(-6.4437826020366,1076.36598863353,328.428685660021));
#122401=CARTESIAN_POINT('Ctrl Pts',(-6.46721545286191,1076.36085853699,
328.348877497224));
#122402=CARTESIAN_POINT('Ctrl Pts',(-6.49850324657515,1076.35025697929,
328.18450719843));
#122403=CARTESIAN_POINT('Ctrl Pts',(-6.50601640248389,1076.34480694621,
328.100286993975));
#122404=CARTESIAN_POINT('Ctrl Pts',(-6.5034629094911,1076.32844751407,327.848318943459));
#122405=CARTESIAN_POINT('Ctrl Pts',(-6.46873196795216,1076.31761440162,
327.682634354775));
#122406=CARTESIAN_POINT('Ctrl Pts',(-6.33715013572135,1076.29740617211,
327.374196116182));
#122407=CARTESIAN_POINT('Ctrl Pts',(-6.24157877707444,1076.2882291901,327.234407631844));
#122408=CARTESIAN_POINT('Ctrl Pts',(-6.0019832135847,1076.27300620447,327.000047598259));
#122409=CARTESIAN_POINT('Ctrl Pts',(-5.8604023862094,1076.26710555059,326.907652267113));
#122410=CARTESIAN_POINT('Ctrl Pts',(-5.5500800430281,1076.25958131043,326.783072665468));
#122411=CARTESIAN_POINT('Ctrl Pts',(-5.38448313634122,1076.25801833975,
326.751888435179));
#122412=CARTESIAN_POINT('Ctrl Pts',(-5.05111387272699,1076.25950720414,
326.75508203554));
#122413=CARTESIAN_POINT('Ctrl Pts',(-4.88661425568984,1076.26253097892,
326.789245222799));
#122414=CARTESIAN_POINT('Ctrl Pts',(-4.58007283918707,1076.27269469094,
326.918772839875));
#122415=CARTESIAN_POINT('Ctrl Pts',(-4.44100867108024,1076.27973281541,
327.01288271623));
#122416=CARTESIAN_POINT('Ctrl Pts',(-4.20660263042861,1076.29674796525,
327.249354942443));
#122417=CARTESIAN_POINT('Ctrl Pts',(-4.11362655130575,1076.30656481447,
327.389571834589));
#122418=CARTESIAN_POINT('Ctrl Pts',(-4.01849713856952,1076.32227319417,
327.620818220311));
#122419=CARTESIAN_POINT('Ctrl Pts',(-3.99440092444456,1076.3276417906,327.700922507677));
#122420=CARTESIAN_POINT('Ctrl Pts',(-3.96219290797154,1076.33846635749,
327.864725572457));
#122421=CARTESIAN_POINT('Ctrl Pts',(-3.95416735250404,1076.34389666082,
327.948038155783));
#122422=CARTESIAN_POINT('Ctrl Pts',(-3.9546907780537,1076.36000641825,328.198680620265));
#122423=CARTESIAN_POINT('Ctrl Pts',(-3.98789229642846,1076.37033621946,
328.364177170258));
#122424=CARTESIAN_POINT('Ctrl Pts',(-4.11689228092931,1076.38917183608,
328.674403822433));
#122425=CARTESIAN_POINT('Ctrl Pts',(-4.21199517874441,1076.39747873865,
328.815883529567));
#122426=CARTESIAN_POINT('Ctrl Pts',(-4.45169695792621,1076.41101550019,
329.05345514243));
#122427=CARTESIAN_POINT('Ctrl Pts',(-4.59384341222352,1076.41612139346,
329.14726512928));
#122428=CARTESIAN_POINT('Ctrl Pts',(-4.90250109010282,1076.42253561259,
329.272525358247));
#122429=CARTESIAN_POINT('Ctrl Pts',(-5.06537340948472,1076.42387967949,
329.304319377796));
#122430=CARTESIAN_POINT('Ctrl Pts',(-5.22980002134219,1076.42335631864,
329.304317191866));
#122431=CARTESIAN_POINT('Origin',(-5.22978306525612,1067.7251047501,328.028873070842));
#122432=CARTESIAN_POINT('',(-5.22978306525612,1076.38762615333,328.704317191978));
#122433=CARTESIAN_POINT('',(-5.22978306525612,1076.30041692086,327.353428949706));
#122434=CARTESIAN_POINT('Ctrl Pts',(-5.22978306525612,1076.38762615333,
328.704317191978));
#122435=CARTESIAN_POINT('Ctrl Pts',(-5.23150159288228,1076.38762042817,
328.704317191978));
#122436=CARTESIAN_POINT('Ctrl Pts',(-5.23322043819156,1076.38761429833,
328.704310633325));
#122437=CARTESIAN_POINT('Ctrl Pts',(-5.32469806735429,1076.38726656726,
328.703612251232));
#122438=CARTESIAN_POINT('Ctrl Pts',(-5.41340925249523,1076.38583007508,
328.685041934543));
#122439=CARTESIAN_POINT('Ctrl Pts',(-5.57840986133551,1076.38090364662,
328.61431840182));
#122440=CARTESIAN_POINT('Ctrl Pts',(-5.65303014191035,1076.37746078315,
328.562855613516));
#122441=CARTESIAN_POINT('Ctrl Pts',(-5.77797587655441,1076.36894858366,
328.433615026693));
#122442=CARTESIAN_POINT('Ctrl Pts',(-5.82696387717909,1076.36395756775,
328.357042943192));
#122443=CARTESIAN_POINT('Ctrl Pts',(-5.87545701961128,1076.35583555273,
328.232036422869));
#122444=CARTESIAN_POINT('Ctrl Pts',(-5.8873412449498,1076.35307295674,328.189455342913));
#122445=CARTESIAN_POINT('Ctrl Pts',(-5.90273979728353,1076.3474050146,328.10202024457));
#122446=CARTESIAN_POINT('Ctrl Pts',(-5.90610384351652,1076.34451200176,
328.057355719052));
#122447=CARTESIAN_POINT('Ctrl Pts',(-5.90290750237631,1076.33588076271,
327.923997444573));
#122448=CARTESIAN_POINT('Ctrl Pts',(-5.88332825018665,1076.33023000309,
327.836572457998));
#122449=CARTESIAN_POINT('Ctrl Pts',(-5.81149381182939,1076.31979054399,
327.674326511174));
#122450=CARTESIAN_POINT('Ctrl Pts',(-5.75995094481466,1076.31510288466,
327.601059445507));
#122451=CARTESIAN_POINT('Ctrl Pts',(-5.63157738022333,1076.3073944345,327.478757479008));
#122452=CARTESIAN_POINT('Ctrl Pts',(-5.55605322117435,1076.30444602716,
327.430855883987));
#122453=CARTESIAN_POINT('Ctrl Pts',(-5.3957101543754,1076.30085281192,327.368848489771));
#122454=CARTESIAN_POINT('Ctrl Pts',(-5.31311406372096,1076.30011236494,
327.353430235009));
#122455=CARTESIAN_POINT('Ctrl Pts',(-5.2297934839294,1076.30041688277,327.353428949791));
#122456=CARTESIAN_POINT('Ctrl Pts',(-5.22979001103696,1076.30041689547,
327.353428949737));
#122457=CARTESIAN_POINT('Ctrl Pts',(-5.22978653814587,1076.30041690816,
327.353428949706));
#122458=CARTESIAN_POINT('Ctrl Pts',(-5.22978306525612,1076.30041692086,
327.353428949706));
#122459=CARTESIAN_POINT('',(-5.22978306525612,1082.7251047501,327.353428949706));
#122460=CARTESIAN_POINT('',(-5.22978306525612,1067.7251047501,327.353428949706));
#122461=CARTESIAN_POINT('Origin',(-5.22978306525612,1082.7251047501,328.028873070842));
#122462=CARTESIAN_POINT('Ctrl Pts',(-5.22978306525612,1076.30041692086,
327.353428949706));
#122463=CARTESIAN_POINT('Ctrl Pts',(-5.14157676647768,1076.30073938674,
327.353428949706));
#122464=CARTESIAN_POINT('Ctrl Pts',(-5.05423792967729,1076.30222686055,
327.370706767218));
#122465=CARTESIAN_POINT('Ctrl Pts',(-4.89112798246151,1076.30733494484,
327.43784075922));
#122466=CARTESIAN_POINT('Ctrl Pts',(-4.81694914848848,1076.31090587175,
327.487058810574));
#122467=CARTESIAN_POINT('Ctrl Pts',(-4.69157712628812,1076.31962785362,
327.611300922366));
#122468=CARTESIAN_POINT('Ctrl Pts',(-4.64164741770922,1076.32469737144,
327.685189581609));
#122469=CARTESIAN_POINT('Ctrl Pts',(-4.59018686609572,1076.33288805052,
327.807297470601));
#122470=CARTESIAN_POINT('Ctrl Pts',(-4.57706081607156,1076.33569860303,
327.849618819418));
#122471=CARTESIAN_POINT('Ctrl Pts',(-4.55926121635584,1076.34139282905,
327.936237453764));
#122472=CARTESIAN_POINT('Ctrl Pts',(-4.554635302571,1076.34426301577,327.980330348298));
#122473=CARTESIAN_POINT('Ctrl Pts',(-4.55378680854414,1076.35282244118,
328.113133712064));
#122474=CARTESIAN_POINT('Ctrl Pts',(-4.57065005764883,1076.35836941536,
328.200980577174));
#122475=CARTESIAN_POINT('Ctrl Pts',(-4.63782053446517,1076.36860395823,
328.366334551107));
#122476=CARTESIAN_POINT('Ctrl Pts',(-4.68792980095587,1076.37317792213,
328.44203993191));
#122477=CARTESIAN_POINT('Ctrl Pts',(-4.81475200576151,1076.38067821524,
328.569263487384));
#122478=CARTESIAN_POINT('Ctrl Pts',(-4.89013394019629,1076.38353503896,
328.619568660416));
#122479=CARTESIAN_POINT('Ctrl Pts',(-5.05459613291234,1076.38715314282,
328.687115392195));
#122480=CARTESIAN_POINT('Ctrl Pts',(-5.14177299919702,1076.38791935332,
328.704317191978));
#122481=CARTESIAN_POINT('Ctrl Pts',(-5.22978306525612,1076.38762615333,
328.704317191978));
#122482=CARTESIAN_POINT('Origin',(5.99814689883732,1067.7251047501,319.92012190144));
#122483=CARTESIAN_POINT('',(5.99814689885421,1077.55052528867,318.821290765448));
#122484=CARTESIAN_POINT('Ctrl Pts',(5.99813818557661,1077.77685023714,321.018953037398));
#122485=CARTESIAN_POINT('Ctrl Pts',(6.03402897129008,1077.77664671849,321.018953321997));
#122486=CARTESIAN_POINT('Ctrl Pts',(6.06989643802268,1077.77626924974,321.017195170753));
#122487=CARTESIAN_POINT('Ctrl Pts',(6.17620552639777,1077.77463143461,321.00674815849));
#122488=CARTESIAN_POINT('Ctrl Pts',(6.24594597955941,1077.77287303179,320.992993074577));
#122489=CARTESIAN_POINT('Ctrl Pts',(6.45377180865714,1077.76550514219,320.930652940034));
#122490=CARTESIAN_POINT('Ctrl Pts',(6.58379753294961,1077.7578662106,320.86124351676));
#122491=CARTESIAN_POINT('Ctrl Pts',(6.79256249897359,1077.73947535801,320.689435887432));
#122492=CARTESIAN_POINT('Ctrl Pts',(6.87449189597205,1077.72947345924,320.594591294463));
#122493=CARTESIAN_POINT('Ctrl Pts',(7.00828522979832,1077.70628616274,320.373040185438));
#122494=CARTESIAN_POINT('Ctrl Pts',(7.05604257103551,1077.69309841382,320.246205023341));
#122495=CARTESIAN_POINT('Ctrl Pts',(7.10524446530176,1077.66466058666,319.971700421772));
#122496=CARTESIAN_POINT('Ctrl Pts',(7.10242385109399,1077.64959635674,319.825760756618));
#122497=CARTESIAN_POINT('Ctrl Pts',(7.04047630273029,1077.62059346521,319.543525880911));
#122498=CARTESIAN_POINT('Ctrl Pts',(6.98200714074261,1077.60692740777,319.409869716104));
#122499=CARTESIAN_POINT('Ctrl Pts',(6.82220397605965,1077.58375388275,319.180872799465));
#122500=CARTESIAN_POINT('Ctrl Pts',(6.72543431367814,1077.57422145046,319.085448010837));
#122501=CARTESIAN_POINT('Ctrl Pts',(6.51859700134971,1077.56060975366,318.945576404004));
#122502=CARTESIAN_POINT('Ctrl Pts',(6.41395855628505,1077.55601580324,318.896530792454));
#122503=CARTESIAN_POINT('Ctrl Pts',(6.25908125103286,1077.55217888507,318.851717900121));
#122504=CARTESIAN_POINT('Ctrl Pts',(6.21382852968329,1077.55138256315,318.841671041601));
#122505=CARTESIAN_POINT('Ctrl Pts',(6.13810911774021,1077.55057980112,318.829819094664));
#122506=CARTESIAN_POINT('Ctrl Pts',(6.10796415248247,1077.55039594371,318.826371517131));
#122507=CARTESIAN_POINT('Ctrl Pts',(6.04934396738986,1077.55030002877,318.822115593108));
#122508=CARTESIAN_POINT('Ctrl Pts',(6.02090449053742,1077.55037183287,318.821158275126));
#122509=CARTESIAN_POINT('Ctrl Pts',(5.95516186915943,1077.55081059801,318.821498507502));
#122510=CARTESIAN_POINT('Ctrl Pts',(5.91789992129018,1077.55126218835,318.823590490068));
#122511=CARTESIAN_POINT('Ctrl Pts',(5.80468741502161,1077.55325336375,318.835748275193));
#122512=CARTESIAN_POINT('Ctrl Pts',(5.72964185224664,1077.55543241902,318.851856583078));
#122513=CARTESIAN_POINT('Ctrl Pts',(5.5180690553479,1077.56409248179,318.920978794798));
#122514=CARTESIAN_POINT('Ctrl Pts',(5.38980380252459,1077.57259517038,318.993514882065));
#122515=CARTESIAN_POINT('Ctrl Pts',(5.18501286018711,1077.59256525408,319.170555573244));
#122516=CARTESIAN_POINT('Ctrl Pts',(5.10520765179409,1077.60328663014,319.26770684178));
#122517=CARTESIAN_POINT('Ctrl Pts',(4.97682703080281,1077.62765395393,319.492986858509));
#122518=CARTESIAN_POINT('Ctrl Pts',(4.93226986812911,1077.64126162121,319.621100347007));
#122519=CARTESIAN_POINT('Ctrl Pts',(4.89011008043779,1077.67001296525,319.896780935986));
#122520=CARTESIAN_POINT('Ctrl Pts',(4.89663199986748,1077.68492539953,320.042505340985));
#122521=CARTESIAN_POINT('Ctrl Pts',(4.96566438556969,1077.71307929742,320.322880898688));
#122522=CARTESIAN_POINT('Ctrl Pts',(5.027419178452,1077.7260593628,320.454904094474));
#122523=CARTESIAN_POINT('Ctrl Pts',(5.19233780381988,1077.7476326199,320.679074630057));
#122524=CARTESIAN_POINT('Ctrl Pts',(5.29073536817695,1077.75630093277,320.771572677047));
#122525=CARTESIAN_POINT('Ctrl Pts',(5.49533855247392,1077.76823964554,320.90325598723));
#122526=CARTESIAN_POINT('Ctrl Pts',(5.59557219190474,1077.77214426792,320.94838508845));
#122527=CARTESIAN_POINT('Ctrl Pts',(5.74421632212992,1077.77543953415,320.990157912074));
#122528=CARTESIAN_POINT('Ctrl Pts',(5.7882815736842,1077.77613099893,320.999665830365));
#122529=CARTESIAN_POINT('Ctrl Pts',(5.86233075455628,1077.77682681649,321.010936056465));
#122530=CARTESIAN_POINT('Ctrl Pts',(5.89202334245002,1077.77698389273,321.014224004991));
#122531=CARTESIAN_POINT('Ctrl Pts',(5.94721680696162,1077.77705135174,321.018067459556));
#122532=CARTESIAN_POINT('Ctrl Pts',(5.97267374842211,1077.77699463319,321.018952835476));
#122533=CARTESIAN_POINT('Ctrl Pts',(5.99813818557661,1077.77685023714,321.018953037398));
#122534=CARTESIAN_POINT('',(5.99814689882034,1075.53855673557,318.821290765448));
#122535=CARTESIAN_POINT('',(5.99814689883732,1067.7251047501,318.821290765448));
#122536=CARTESIAN_POINT('Ctrl Pts',(5.99814215972078,1075.76695402288,321.018953037423));
#122537=CARTESIAN_POINT('Ctrl Pts',(5.8520632422525,1075.76779012951,321.018952407403));
#122538=CARTESIAN_POINT('Ctrl Pts',(5.70748007846799,1075.76571137799,320.989822594062));
#122539=CARTESIAN_POINT('Ctrl Pts',(5.43836269523627,1075.75594245909,320.876859596151));
#122540=CARTESIAN_POINT('Ctrl Pts',(5.31656708136263,1075.74835604039,320.794240606573));
#122541=CARTESIAN_POINT('Ctrl Pts',(5.11225111323726,1075.72854766061,320.586373200309));
#122542=CARTESIAN_POINT('Ctrl Pts',(5.03184052795361,1075.71651409246,320.463144520239));
#122543=CARTESIAN_POINT('Ctrl Pts',(4.92340990019868,1075.68940727686,320.191876799852));
#122544=CARTESIAN_POINT('Ctrl Pts',(4.89681414578907,1075.67457833951,320.046343626292));
#122545=CARTESIAN_POINT('Ctrl Pts',(4.90082033537793,1075.65189539804,319.828060324323));
#122546=CARTESIAN_POINT('Ctrl Pts',(4.90919448778044,1075.64438522352,319.75646364717));
#122547=CARTESIAN_POINT('Ctrl Pts',(4.95560403582249,1075.62183169916,319.543456432126));
#122548=CARTESIAN_POINT('Ctrl Pts',(5.01488014313486,1075.60722242713,319.408252145682));
#122549=CARTESIAN_POINT('Ctrl Pts',(5.1819575818043,1075.58098895896,319.170373367996));
#122550=CARTESIAN_POINT('Ctrl Pts',(5.28754186240645,1075.56958294292,319.069585267379));
#122551=CARTESIAN_POINT('Ctrl Pts',(5.53119986459102,1075.55154162309,318.915101627791));
#122552=CARTESIAN_POINT('Ctrl Pts',(5.66667436248557,1075.54505598575,318.86262643622));
#122553=CARTESIAN_POINT('Ctrl Pts',(5.94958340526732,1075.53797150875,318.813063661307));
#122554=CARTESIAN_POINT('Ctrl Pts',(6.09412503465963,1075.53741155264,318.81616050575));
#122555=CARTESIAN_POINT('Ctrl Pts',(6.37370239329595,1075.54230703978,318.877603496269));
#122556=CARTESIAN_POINT('Ctrl Pts',(6.50596325036728,1075.54770443986,318.935259734272));
#122557=CARTESIAN_POINT('Ctrl Pts',(6.74132532924915,1075.56372765755,319.098127177709));
#122558=CARTESIAN_POINT('Ctrl Pts',(6.84200443907265,1075.57421391683,319.201921968478));
#122559=CARTESIAN_POINT('Ctrl Pts',(6.99830220519505,1075.59885591519,319.442773031183));
#122560=CARTESIAN_POINT('Ctrl Pts',(7.05213167518135,1075.61279646497,319.577734835983));
#122561=CARTESIAN_POINT('Ctrl Pts',(7.09163764881545,1075.63483204805,319.790065273794));
#122562=CARTESIAN_POINT('Ctrl Pts',(7.0978154874518,1075.64232752601,319.862126551262));
#122563=CARTESIAN_POINT('Ctrl Pts',(7.09596075417271,1075.65734489128,320.006231284631));
#122564=CARTESIAN_POINT('Ctrl Pts',(7.0879657580583,1075.66483193062,320.077941104531));
#122565=CARTESIAN_POINT('Ctrl Pts',(7.04266969368658,1075.68714864385,320.291260197174));
#122566=CARTESIAN_POINT('Ctrl Pts',(6.98410971497628,1075.70138589349,320.426785277514));
#122567=CARTESIAN_POINT('Ctrl Pts',(6.81765790554724,1075.72677144719,320.666448688881));
#122568=CARTESIAN_POINT('Ctrl Pts',(6.71165676234959,1075.73769031499,320.768407327162));
#122569=CARTESIAN_POINT('Ctrl Pts',(6.46581951217859,1075.75488418721,320.925084279348));
#122570=CARTESIAN_POINT('Ctrl Pts',(6.3284757494544,1075.76099042824,320.978238176426));
#122571=CARTESIAN_POINT('Ctrl Pts',(6.12305966386463,1075.76570599713,321.013617894088));
#122572=CARTESIAN_POINT('Ctrl Pts',(6.06066155676042,1075.76659618286,321.018953307061));
#122573=CARTESIAN_POINT('Ctrl Pts',(5.99814215972077,1075.76695402288,321.018953037423));
#122574=CARTESIAN_POINT('Origin',(5.99814689883732,1067.7251047501,319.92012190144));
#122575=CARTESIAN_POINT('',(5.99814689883734,1075.70679891916,320.418953037433));
#122576=CARTESIAN_POINT('',(5.99814689883732,1075.60310529675,319.421290765448));
#122577=CARTESIAN_POINT('Ctrl Pts',(5.99814689883733,1075.70679891916,320.418953037433));
#122578=CARTESIAN_POINT('Ctrl Pts',(5.96441846974092,1075.70699626532,320.418953037433));
#122579=CARTESIAN_POINT('Ctrl Pts',(5.93069536794872,1075.70684424762,320.415532205603));
#122580=CARTESIAN_POINT('Ctrl Pts',(5.83377706009526,1075.70537201006,320.395567176941));
#122581=CARTESIAN_POINT('Ctrl Pts',(5.77327328762252,1075.70312564208,320.37010782257));
#122582=CARTESIAN_POINT('Ctrl Pts',(5.66422493924436,1075.69624140982,320.296622433145));
#122583=CARTESIAN_POINT('Ctrl Pts',(5.61711214887369,1075.69161867454,320.248834122477));
#122584=CARTESIAN_POINT('Ctrl Pts',(5.54428472231775,1075.68060086452,320.137557262403));
#122585=CARTESIAN_POINT('Ctrl Pts',(5.51936898699363,1075.6743093303,320.075128000783));
#122586=CARTESIAN_POINT('Ctrl Pts',(5.50157357306298,1075.66432386098,319.977648817592));
#122587=CARTESIAN_POINT('Ctrl Pts',(5.49887761981519,1075.6609649492,319.94510039372));
#122588=CARTESIAN_POINT('Ctrl Pts',(5.49987058814139,1075.65418528476,319.879885292506));
#122589=CARTESIAN_POINT('Ctrl Pts',(5.50357083567267,1075.65078007968,319.84736919866));
#122590=CARTESIAN_POINT('Ctrl Pts',(5.52447286235389,1075.6405052714,319.749977334952));
#122591=CARTESIAN_POINT('Ctrl Pts',(5.55157271801686,1075.6338558112,319.687960042484));
#122592=CARTESIAN_POINT('Ctrl Pts',(5.62782968782083,1075.62202739303,319.579552702453));
#122593=CARTESIAN_POINT('Ctrl Pts',(5.67573429197332,1075.61693167691,319.53387141516));
#122594=CARTESIAN_POINT('Ctrl Pts',(5.78626645296075,1075.60888384346,319.463839833566));
#122595=CARTESIAN_POINT('Ctrl Pts',(5.8477201001261,1075.60599824989,319.440047475464));
#122596=CARTESIAN_POINT('Ctrl Pts',(5.94048365436939,1075.60371931919,319.423795457181));
#122597=CARTESIAN_POINT('Ctrl Pts',(5.96928596170959,1075.6032800873,319.421290779236));
#122598=CARTESIAN_POINT('Ctrl Pts',(5.99814666053062,1075.6031052982,319.421290765448));
#122599=CARTESIAN_POINT('',(5.99814689883732,1082.7251047501,319.421290765448));
#122600=CARTESIAN_POINT('',(5.99814689883732,1067.7251047501,319.421290765448));
#122601=CARTESIAN_POINT('Origin',(5.99814689883732,1082.7251047501,319.92012190144));
#122602=CARTESIAN_POINT('Ctrl Pts',(5.99814689883732,1075.60310529675,319.421290765448));
#122603=CARTESIAN_POINT('Ctrl Pts',(6.06311539178196,1075.60271183123,319.421290765448));
#122604=CARTESIAN_POINT('Ctrl Pts',(6.12744245729569,1075.60366470266,319.433982617426));
#122605=CARTESIAN_POINT('Ctrl Pts',(6.24768404791999,1075.60814847313,319.483322509358));
#122606=CARTESIAN_POINT('Ctrl Pts',(6.30239155130446,1075.6116386024,319.519518727233));
#122607=CARTESIAN_POINT('Ctrl Pts',(6.39505069803708,1075.62070993086,319.61099203887));
#122608=CARTESIAN_POINT('Ctrl Pts',(6.43200846161313,1075.62621351316,319.665481246679));
#122609=CARTESIAN_POINT('Ctrl Pts',(6.48300583552815,1075.63851005159,319.785811662801));
#122610=CARTESIAN_POINT('Ctrl Pts',(6.49642641021656,1075.64519299541,319.850573521958));
#122611=CARTESIAN_POINT('Ctrl Pts',(6.49722829744655,1075.65540057616,319.948712305593));
#122612=CARTESIAN_POINT('Ctrl Pts',(6.49428573182464,1075.65880628682,319.981327562342));
#122613=CARTESIAN_POINT('Ctrl Pts',(6.47572426394299,1075.66902696246,320.078815924131));
#122614=CARTESIAN_POINT('Ctrl Pts',(6.45030022400967,1075.67561331809,320.141102859008));
#122615=CARTESIAN_POINT('Ctrl Pts',(6.37656230478856,1075.68745878926,320.251848514706));
#122616=CARTESIAN_POINT('Ctrl Pts',(6.32906250043543,1075.69260689519,320.299269679326));
#122617=CARTESIAN_POINT('Ctrl Pts',(6.21823285328952,1075.70078131365,320.372675577079));
#122618=CARTESIAN_POINT('Ctrl Pts',(6.15605483786203,1075.70372887614,320.397951468107));
#122619=CARTESIAN_POINT('Ctrl Pts',(6.06011541117237,1075.70614157331,320.416066641399));
#122620=CARTESIAN_POINT('Ctrl Pts',(6.0291289075029,1075.70661764241,320.418953037433));
#122621=CARTESIAN_POINT('Ctrl Pts',(5.99814689883733,1075.70679891916,320.418953037433));
#122622=CARTESIAN_POINT('Origin',(18.7711528398115,1067.7251047501,314.220624181303));
#122623=CARTESIAN_POINT('',(18.7711528398304,1076.67369445817,313.130083432575));
#122624=CARTESIAN_POINT('Ctrl Pts',(18.7711740718832,1076.96239192968,315.311164929825));
#122625=CARTESIAN_POINT('Ctrl Pts',(18.8565499206275,1076.96051699849,315.311163267617));
#122626=CARTESIAN_POINT('Ctrl Pts',(18.9415846564319,1076.95735423103,315.301135976198));
#122627=CARTESIAN_POINT('Ctrl Pts',(19.1311831022978,1076.94732452807,315.255843937261));
#122628=CARTESIAN_POINT('Ctrl Pts',(19.2332557852884,1076.93971748319,315.214459674833));
#122629=CARTESIAN_POINT('Ctrl Pts',(19.4322313852995,1076.91999789434,315.096477580774));
#122630=CARTESIAN_POINT('Ctrl Pts',(19.5257834587689,1076.90760984435,315.01723865809));
#122631=CARTESIAN_POINT('Ctrl Pts',(19.6896281664456,1076.87860994378,314.823276719968));
#122632=CARTESIAN_POINT('Ctrl Pts',(19.7558161700798,1076.8619549548,314.707608257872));
#122633=CARTESIAN_POINT('Ctrl Pts',(19.8470622156246,1076.82577039875,314.448668701238));
#122634=CARTESIAN_POINT('Ctrl Pts',(19.8676238443435,1076.80644410249,314.30628029851));
#122635=CARTESIAN_POINT('Ctrl Pts',(19.8527409615674,1076.76870378821,314.02017626805));
#122636=CARTESIAN_POINT('Ctrl Pts',(19.8168462631533,1076.75065099957,313.879104658375));
#122637=CARTESIAN_POINT('Ctrl Pts',(19.6959591480312,1076.71958386177,313.627087015878));
#122638=CARTESIAN_POINT('Ctrl Pts',(19.6152440639234,1076.70658793918,313.516934170119));
#122639=CARTESIAN_POINT('Ctrl Pts',(19.4206920631347,1076.68647743287,313.334909402774));
#122640=CARTESIAN_POINT('Ctrl Pts',(19.3097508668743,1076.67934092959,313.26334533726));
#122641=CARTESIAN_POINT('Ctrl Pts',(19.1467556238646,1076.67394628016,313.195804475051));
#122642=CARTESIAN_POINT('Ctrl Pts',(19.1038406874721,1076.67293970615,313.181079460163));
#122643=CARTESIAN_POINT('Ctrl Pts',(19.0336632541015,1076.67194328844,313.161794376889));
#122644=CARTESIAN_POINT('Ctrl Pts',(19.006934431174,1076.67170933742,313.155523503489));
#122645=CARTESIAN_POINT('Ctrl Pts',(18.958493776337,1076.67154464163,313.146071967829));
#122646=CARTESIAN_POINT('Ctrl Pts',(18.9368697139823,1076.67156228046,313.142525390757));
#122647=CARTESIAN_POINT('Ctrl Pts',(18.8863227687454,1076.67181449815,313.135791946905));
#122648=CARTESIAN_POINT('Ctrl Pts',(18.8573514578252,1076.67211815113,313.133106501733));
#122649=CARTESIAN_POINT('Ctrl Pts',(18.7760127610326,1076.6734137555,313.128837595686));
#122650=CARTESIAN_POINT('Ctrl Pts',(18.7235995544648,1076.67476037677,313.129864090982));
#122651=CARTESIAN_POINT('Ctrl Pts',(18.5272316905924,1076.68172290723,313.14788783336));
#122652=CARTESIAN_POINT('Ctrl Pts',(18.387274609478,1076.69060574131,313.189709918569));
#122653=CARTESIAN_POINT('Ctrl Pts',(18.1537486489474,1076.71268883386,313.3137173955));
#122654=CARTESIAN_POINT('Ctrl Pts',(18.0579679195659,1076.72474532902,313.386985085639));
#122655=CARTESIAN_POINT('Ctrl Pts',(17.8869006773265,1076.75308924173,313.569195688427));
#122656=CARTESIAN_POINT('Ctrl Pts',(17.8155509647045,1076.76943533832,313.679315750208));
#122657=CARTESIAN_POINT('Ctrl Pts',(17.7111546376568,1076.80497054691,313.92852096586));
#122658=CARTESIAN_POINT('Ctrl Pts',(17.6824280302455,1076.82397007963,314.06701414303));
#122659=CARTESIAN_POINT('Ctrl Pts',(17.6789078331298,1076.86159801367,314.351718371588));
#122660=CARTESIAN_POINT('Ctrl Pts',(17.7058887326829,1076.8798450509,314.495380783429));
#122661=CARTESIAN_POINT('Ctrl Pts',(17.8120190855963,1076.91175911336,314.757641847138));
#122662=CARTESIAN_POINT('Ctrl Pts',(17.8876879721164,1076.92532286863,314.874791524117));
#122663=CARTESIAN_POINT('Ctrl Pts',(18.0817104693889,1076.94733857193,315.077447522578));
#122664=CARTESIAN_POINT('Ctrl Pts',(18.1992413928995,1076.95543054713,315.160035366346));
#122665=CARTESIAN_POINT('Ctrl Pts',(18.3746981532943,1076.96161699663,315.237750606446));
#122666=CARTESIAN_POINT('Ctrl Pts',(18.4212117517483,1076.96278147958,315.254677246983));
#122667=CARTESIAN_POINT('Ctrl Pts',(18.4961788547779,1076.96392961285,315.27631592709));
#122668=CARTESIAN_POINT('Ctrl Pts',(18.5239370633942,1076.96420373902,315.28315901993));
#122669=CARTESIAN_POINT('Ctrl Pts',(18.575504662916,1076.96443793567,315.293741098617));
#122670=CARTESIAN_POINT('Ctrl Pts',(18.5992296758164,1076.96444072701,315.297796665258));
#122671=CARTESIAN_POINT('Ctrl Pts',(18.6510687077741,1076.96422007506,315.304901642252));
#122672=CARTESIAN_POINT('Ctrl Pts',(18.6792053473891,1076.96395716417,315.307649170701));
#122673=CARTESIAN_POINT('Ctrl Pts',(18.7286471402936,1076.96324547549,315.310543772322));
#122674=CARTESIAN_POINT('Ctrl Pts',(18.7499090730405,1076.96285892837,315.31116534384));
#122675=CARTESIAN_POINT('Ctrl Pts',(18.7711740718832,1076.96239192968,315.311164929825));
#122676=CARTESIAN_POINT('',(18.7711528397839,1074.65422628875,313.130083432575));
#122677=CARTESIAN_POINT('',(18.7711528398115,1067.7251047501,313.130083432575));
#122678=CARTESIAN_POINT('Ctrl Pts',(18.7711532049613,1074.94531438668,315.311164930032));
#122679=CARTESIAN_POINT('Ctrl Pts',(18.6295126016433,1074.94845071869,315.311164977458));
#122680=CARTESIAN_POINT('Ctrl Pts',(18.489229947793,1074.94796418247,315.283570179508));
#122681=CARTESIAN_POINT('Ctrl Pts',(18.2267237729283,1074.93978639499,315.176157584916));
#122682=CARTESIAN_POINT('Ctrl Pts',(18.1072149318836,1074.93215740244,315.097287744657));
#122683=CARTESIAN_POINT('Ctrl Pts',(17.9029672783477,1074.91041133747,314.896289324538));
#122684=CARTESIAN_POINT('Ctrl Pts',(17.8211634545652,1074.89637264129,314.77528758755));
#122685=CARTESIAN_POINT('Ctrl Pts',(17.7092090647952,1074.86368561375,314.50812596384));
#122686=CARTESIAN_POINT('Ctrl Pts',(17.6804647626921,1074.845328699,314.364440658711));
#122687=CARTESIAN_POINT('Ctrl Pts',(17.6806852961651,1074.81659288248,314.148331197341));
#122688=CARTESIAN_POINT('Ctrl Pts',(17.6877266598991,1074.8069732511,314.077340547243));
#122689=CARTESIAN_POINT('Ctrl Pts',(17.7302684298483,1074.77748284186,313.863797989307));
#122690=CARTESIAN_POINT('Ctrl Pts',(17.7876191912421,1074.7578316948,313.72718186224));
#122691=CARTESIAN_POINT('Ctrl Pts',(17.9513659157638,1074.72172657867,313.487216582186));
#122692=CARTESIAN_POINT('Ctrl Pts',(18.0551863687773,1074.70555474421,313.385482955735));
#122693=CARTESIAN_POINT('Ctrl Pts',(18.29564469102,1074.67873327706,313.228880973402));
#122694=CARTESIAN_POINT('Ctrl Pts',(18.4296096178777,1074.66829510334,313.175092557974));
#122695=CARTESIAN_POINT('Ctrl Pts',(18.7097753803758,1074.65463487909,313.122613565655));
#122696=CARTESIAN_POINT('Ctrl Pts',(18.8530190433782,1074.65148405588,313.123930813235));
#122697=CARTESIAN_POINT('Ctrl Pts',(19.1305877934054,1074.65288064726,313.181347029997));
#122698=CARTESIAN_POINT('Ctrl Pts',(19.2621108319926,1074.65738529076,313.236657969319));
#122699=CARTESIAN_POINT('Ctrl Pts',(19.4971345229847,1074.67346948716,313.394569742299));
#122700=CARTESIAN_POINT('Ctrl Pts',(19.5981458415991,1074.68491825309,313.49580068736));
#122701=CARTESIAN_POINT('Ctrl Pts',(19.7564893702803,1074.71330363923,313.731948520451));
#122702=CARTESIAN_POINT('Ctrl Pts',(19.8118442657399,1074.73001744375,313.86490971987));
#122703=CARTESIAN_POINT('Ctrl Pts',(19.8542934928333,1074.75731680167,314.074892457734));
#122704=CARTESIAN_POINT('Ctrl Pts',(19.861529504772,1074.76676550202,314.146451478113));
#122705=CARTESIAN_POINT('Ctrl Pts',(19.8618518685598,1074.78596641096,314.289763692645));
#122706=CARTESIAN_POINT('Ctrl Pts',(19.8549625708726,1074.79567461623,314.361192331446));
#122707=CARTESIAN_POINT('Ctrl Pts',(19.8130360169185,1074.8250147734,314.574003122828));
#122708=CARTESIAN_POINT('Ctrl Pts',(19.7567052206923,1074.84428996541,314.70965518479));
#122709=CARTESIAN_POINT('Ctrl Pts',(19.5945503301769,1074.87970950716,314.950124265562));
#122710=CARTESIAN_POINT('Ctrl Pts',(19.4906374493414,1074.89553987892,315.052867407687));
#122711=CARTESIAN_POINT('Ctrl Pts',(19.2486324127144,1074.92175013034,315.211672874505));
#122712=CARTESIAN_POINT('Ctrl Pts',(19.1130654563246,1074.93188496957,315.266273233153));
#122713=CARTESIAN_POINT('Ctrl Pts',(18.9048291638458,1074.94155174826,315.305004789759));
#122714=CARTESIAN_POINT('Ctrl Pts',(18.8380754588461,1074.94383253471,315.311164907624));
#122715=CARTESIAN_POINT('Ctrl Pts',(18.7711532049613,1074.94531438668,315.311164930032));
#122716=CARTESIAN_POINT('Origin',(18.7711528398115,1067.7251047501,314.220624181303));
#122717=CARTESIAN_POINT('',(18.7711528398116,1074.86719845859,314.711164930032));
#122718=CARTESIAN_POINT('',(18.771152839812,1074.73625576269,313.730083432575));
#122719=CARTESIAN_POINT('Ctrl Pts',(18.7711528398116,1074.86719845859,314.711164930032));
#122720=CARTESIAN_POINT('Ctrl Pts',(18.7385480853299,1074.86793038454,314.711164930032));
#122721=CARTESIAN_POINT('Ctrl Pts',(18.7059390521038,1074.86823314263,314.70791427713));
#122722=CARTESIAN_POINT('Ctrl Pts',(18.6113554544388,1074.86782827932,314.688765320027));
#122723=CARTESIAN_POINT('Ctrl Pts',(18.5520019098276,1074.86590240622,314.664079613653));
#122724=CARTESIAN_POINT('Ctrl Pts',(18.445809349119,1074.85893388317,314.593285686387));
#122725=CARTESIAN_POINT('Ctrl Pts',(18.4001099060201,1074.8539440585,314.547773970777));
#122726=CARTESIAN_POINT('Ctrl Pts',(18.3278152053011,1074.84137102067,314.440565017267));
#122727=CARTESIAN_POINT('Ctrl Pts',(18.3024956026649,1074.83384807965,314.379547469962));
#122728=CARTESIAN_POINT('Ctrl Pts',(18.283676651615,1074.82157631196,314.284047924447));
#122729=CARTESIAN_POINT('Ctrl Pts',(18.2805795723888,1074.81739646137,314.252114230671));
#122730=CARTESIAN_POINT('Ctrl Pts',(18.2806451986833,1074.80886056661,314.188056780906));
#122731=CARTESIAN_POINT('Ctrl Pts',(18.2838218962225,1074.80452333255,314.156076775462));
#122732=CARTESIAN_POINT('Ctrl Pts',(18.302963549083,1074.791280049,314.060141259098));
#122733=CARTESIAN_POINT('Ctrl Pts',(18.3286834286998,1074.78249115736,313.998837836215));
#122734=CARTESIAN_POINT('Ctrl Pts',(18.4024071876352,1074.76630381678,313.890639135883));
#122735=CARTESIAN_POINT('Ctrl Pts',(18.4494365092931,1074.75904405019,313.844606638804));
#122736=CARTESIAN_POINT('Ctrl Pts',(18.5580244506283,1074.74708388726,313.774167856831));
#122737=CARTESIAN_POINT('Ctrl Pts',(18.6182659084927,1074.74245928634,313.750095322647));
#122738=CARTESIAN_POINT('Ctrl Pts',(18.7110831417207,1074.73800637966,313.732848716439));
#122739=CARTESIAN_POINT('Ctrl Pts',(18.7410768438834,1074.73694555396,313.730083432575));
#122740=CARTESIAN_POINT('Ctrl Pts',(18.7711528398128,1074.73625576269,313.730083432575));
#122741=CARTESIAN_POINT('',(18.7711528398115,1082.7251047501,313.730083432575));
#122742=CARTESIAN_POINT('',(18.7711528398115,1067.7251047501,313.730083432575));
#122743=CARTESIAN_POINT('Origin',(18.7711528398115,1082.7251047501,314.220624181303));
#122744=CARTESIAN_POINT('Ctrl Pts',(18.7711586301647,1074.7362556299,313.730083432609));
#122745=CARTESIAN_POINT('Ctrl Pts',(18.8348430630451,1074.7347951324,313.730084184342));
#122746=CARTESIAN_POINT('Ctrl Pts',(18.8979158494026,1074.73502164797,313.742486465278));
#122747=CARTESIAN_POINT('Ctrl Pts',(19.0158429155388,1074.73882248562,313.790718113182));
#122748=CARTESIAN_POINT('Ctrl Pts',(19.0694925402283,1074.74236107298,313.826079148332));
#122749=CARTESIAN_POINT('Ctrl Pts',(19.1605784364352,1074.7523200418,313.915526407697));
#122750=CARTESIAN_POINT('Ctrl Pts',(19.1969823754605,1074.75866387993,313.968872448428));
#122751=CARTESIAN_POINT('Ctrl Pts',(19.2475053338174,1074.77335681989,314.086903594016));
#122752=CARTESIAN_POINT('Ctrl Pts',(19.2609156300818,1074.78158534014,314.150575152938));
#122753=CARTESIAN_POINT('Ctrl Pts',(19.2620328545287,1074.79446778855,314.247095450945));
#122754=CARTESIAN_POINT('Ctrl Pts',(19.2592433843294,1074.79881998562,314.279199203387));
#122755=CARTESIAN_POINT('Ctrl Pts',(19.2412905284059,1074.81203868588,314.375201128204));
#122756=CARTESIAN_POINT('Ctrl Pts',(19.2164540477036,1074.82077499339,314.436593985981));
#122757=CARTESIAN_POINT('Ctrl Pts',(19.1442117511555,1074.83691514523,314.545771484838));
#122758=CARTESIAN_POINT('Ctrl Pts',(19.0976099832201,1074.84417083407,314.592573906919));
#122759=CARTESIAN_POINT('Ctrl Pts',(18.9887695707287,1074.85622054663,314.665071771415));
#122760=CARTESIAN_POINT('Ctrl Pts',(18.927683439345,1074.86090184323,314.690107358892));
#122761=CARTESIAN_POINT('Ctrl Pts',(18.8329207682236,1074.86542665211,314.708247913804));
#122762=CARTESIAN_POINT('Ctrl Pts',(18.8020387239465,1074.86650511861,314.711164930032));
#122763=CARTESIAN_POINT('Ctrl Pts',(18.7711528398116,1074.86719845859,314.711164930032));
#122764=CARTESIAN_POINT('Origin',(-32.7463814565112,1067.7251047501,341.263474226965));
#122765=CARTESIAN_POINT('',(-32.7463814565318,1076.63168654751,339.785171094771));
#122766=CARTESIAN_POINT('',(-32.7463814565112,1067.7251047501,339.785171094771));
#122767=CARTESIAN_POINT('Ctrl Pts',(-32.7470870485927,1076.70329236998,
342.741777190769));
#122768=CARTESIAN_POINT('Ctrl Pts',(-32.9423914885626,1076.70197251887,
342.741683972214));
#122769=CARTESIAN_POINT('Ctrl Pts',(-33.1357477776511,1076.69996211391,
342.702888100506));
#122770=CARTESIAN_POINT('Ctrl Pts',(-33.4957903882059,1076.69446217964,
342.55256025233));
#122771=CARTESIAN_POINT('Ctrl Pts',(-33.6589997362473,1076.69102122284,
342.44265849417));
#122772=CARTESIAN_POINT('Ctrl Pts',(-33.9343950040687,1076.68278802472,
342.164883295513));
#122773=CARTESIAN_POINT('Ctrl Pts',(-34.0434534885546,1076.67806211271,
341.99934777928));
#122774=CARTESIAN_POINT('Ctrl Pts',(-34.1904010961292,1076.66785445784,
341.635723945508));
#122775=CARTESIAN_POINT('Ctrl Pts',(-34.226969885446,1076.66247571627,341.441290303896));
#122776=CARTESIAN_POINT('Ctrl Pts',(-34.2222006804835,1076.65197963566,
341.051339442137));
#122777=CARTESIAN_POINT('Ctrl Pts',(-34.1816369203232,1076.64696787535,
340.859626242509));
#122778=CARTESIAN_POINT('Ctrl Pts',(-34.0287522855682,1076.63825541818,
340.502836086486));
#122779=CARTESIAN_POINT('Ctrl Pts',(-33.9179210750424,1076.6346464259,340.341220182126));
#122780=CARTESIAN_POINT('Ctrl Pts',(-33.6403510676973,1076.6296453929,340.070263234071));
#122781=CARTESIAN_POINT('Ctrl Pts',(-33.4764013116883,1076.62830318012,
339.96346991672));
#122782=CARTESIAN_POINT('Ctrl Pts',(-33.1170599009339,1076.62821181225,
339.819396893368));
#122783=CARTESIAN_POINT('Ctrl Pts',(-32.925226969539,1076.62945743532,339.783349057752));
#122784=CARTESIAN_POINT('Ctrl Pts',(-32.5388448250334,1076.63426868405,
339.787132334209));
#122785=CARTESIAN_POINT('Ctrl Pts',(-32.3480268118459,1076.63778014823,
339.826825916564));
#122786=CARTESIAN_POINT('Ctrl Pts',(-31.9923956996128,1076.64632548213,
339.977323938767));
#122787=CARTESIAN_POINT('Ctrl Pts',(-31.8310124580455,1076.65127082582,
340.086712346266));
#122788=CARTESIAN_POINT('Ctrl Pts',(-31.5593083828433,1076.66163684506,
340.361472537787));
#122789=CARTESIAN_POINT('Ctrl Pts',(-31.4516537547339,1076.66695266425,
340.524264482069));
#122790=CARTESIAN_POINT('Ctrl Pts',(-31.3039330523849,1076.67717046794,
340.884919591891));
#122791=CARTESIAN_POINT('Ctrl Pts',(-31.2664474452449,1076.68196158429,
341.079721979092));
#122792=CARTESIAN_POINT('Ctrl Pts',(-31.269804627352,1076.69034599917,341.47103163766));
#122793=CARTESIAN_POINT('Ctrl Pts',(-31.3099952016447,1076.69387164049,
341.663677597622));
#122794=CARTESIAN_POINT('Ctrl Pts',(-31.4629309126439,1076.69954362996,
342.0225846597));
#122795=CARTESIAN_POINT('Ctrl Pts',(-31.5742902131587,1076.70164036403,
342.18526696593));
#122796=CARTESIAN_POINT('Ctrl Pts',(-31.8545217810664,1076.70445798862,
342.45866714017));
#122797=CARTESIAN_POINT('Ctrl Pts',(-32.0209035674124,1076.70515030379,
342.566387699169));
#122798=CARTESIAN_POINT('Ctrl Pts',(-32.3765474074373,1076.70516218888,
342.706815634382));
#122799=CARTESIAN_POINT('Ctrl Pts',(-32.5609957573799,1076.70454995941,
342.7418660119));
#122800=CARTESIAN_POINT('Ctrl Pts',(-32.7470870485927,1076.70329236998,
342.741777190769));
#122801=CARTESIAN_POINT('Origin',(-32.7463814565112,1067.7251047501,341.263474226965));
#122802=CARTESIAN_POINT('',(-32.7463814565112,1076.69227114041,342.141777359158));
#122803=CARTESIAN_POINT('',(-32.7463814563977,1076.64970661189,340.385171094772));
#122804=CARTESIAN_POINT('Ctrl Pts',(-32.7463814565112,1076.69227114041,
342.141777359158));
#122805=CARTESIAN_POINT('Ctrl Pts',(-32.7476268445788,1076.69226131304,
342.141777359158));
#122806=CARTESIAN_POINT('Ctrl Pts',(-32.7488723621132,1076.69225142971,
342.141774710315));
#122807=CARTESIAN_POINT('Ctrl Pts',(-32.8667671123006,1076.69131071209,
342.141273148912));
#122808=CARTESIAN_POINT('Ctrl Pts',(-32.9821514820699,1076.68990936895,
342.117543144741));
#122809=CARTESIAN_POINT('Ctrl Pts',(-33.1967235692852,1076.68621385391,
342.026475417372));
#122810=CARTESIAN_POINT('Ctrl Pts',(-33.2938069723275,1076.68395473799,
341.960109667909));
#122811=CARTESIAN_POINT('Ctrl Pts',(-33.45676683502,1076.67874629255,341.793043322698));
#122812=CARTESIAN_POINT('Ctrl Pts',(-33.5208812683237,1076.67584407161,
341.693867602432));
#122813=CARTESIAN_POINT('Ctrl Pts',(-33.6063087830092,1076.66976369463,
341.476752963199));
#122814=CARTESIAN_POINT('Ctrl Pts',(-33.6269735772364,1076.66664714384,
341.361047467887));
#122815=CARTESIAN_POINT('Ctrl Pts',(-33.6220192032145,1076.66069232682,
341.129518889262));
#122816=CARTESIAN_POINT('Ctrl Pts',(-33.5969222871173,1076.65791120844,
341.015949009934));
#122817=CARTESIAN_POINT('Ctrl Pts',(-33.5043246500839,1076.653140776,340.804993273576));
#122818=CARTESIAN_POINT('Ctrl Pts',(-33.4377304794073,1076.65120014331,
340.709648472046));
#122819=CARTESIAN_POINT('Ctrl Pts',(-33.2716177131071,1076.64853964147,
340.550182843906));
#122820=CARTESIAN_POINT('Ctrl Pts',(-33.1737465768415,1076.64784604426,
340.487575726962));
#122821=CARTESIAN_POINT('Ctrl Pts',(-32.9645139181643,1076.64785395915,
340.405656643403));
#122822=CARTESIAN_POINT('Ctrl Pts',(-32.8559011532274,1076.64849047604,
340.385171094743));
#122823=CARTESIAN_POINT('Ctrl Pts',(-32.7463814562842,1076.64970661189,
340.385171094771));
#122824=CARTESIAN_POINT('',(-32.7463814565112,1082.7251047501,340.385171094771));
#122825=CARTESIAN_POINT('',(-32.7463814565112,1067.7251047501,340.385171094771));
#122826=CARTESIAN_POINT('Origin',(-32.7463814565112,1082.7251047501,341.263474226965));
#122827=CARTESIAN_POINT('Ctrl Pts',(-32.7463814562842,1076.64970661189,
340.385171094771));
#122828=CARTESIAN_POINT('Ctrl Pts',(-32.7410877836287,1076.64976539424,
340.385171094773));
#122829=CARTESIAN_POINT('Ctrl Pts',(-32.7357919920265,1076.6498255239,340.385218953388));
#122830=CARTESIAN_POINT('Ctrl Pts',(-32.6156783143586,1076.65121930985,
340.387391924009));
#122831=CARTESIAN_POINT('Ctrl Pts',(-32.5023849415872,1076.65315679928,
340.4119664611));
#122832=CARTESIAN_POINT('Ctrl Pts',(-32.2916472160877,1076.65791509622,
340.50332418109));
#122833=CARTESIAN_POINT('Ctrl Pts',(-32.19624116946,1076.66068784022,340.56924510938));
#122834=CARTESIAN_POINT('Ctrl Pts',(-32.0361639662629,1076.66659587187,
340.734116874935));
#122835=CARTESIAN_POINT('Ctrl Pts',(-31.9730575347923,1076.66967254534,
340.831504332081));
#122836=CARTESIAN_POINT('Ctrl Pts',(-31.890930205726,1076.67545878808,341.037551927229));
#122837=CARTESIAN_POINT('Ctrl Pts',(-31.8698088465635,1076.67813105007,
341.143224669835));
#122838=CARTESIAN_POINT('Ctrl Pts',(-31.8681802914946,1076.68057177695,
341.250091186051));
#122839=CARTESIAN_POINT('Ctrl Pts',(-31.8664057517647,1076.68323129207,
341.366537281396));
#122840=CARTESIAN_POINT('Ctrl Pts',(-31.8878091293091,1076.68556652517,
341.4821886438));
#122841=CARTESIAN_POINT('Ctrl Pts',(-31.9745374154931,1076.68943079159,
341.69852433212));
#122842=CARTESIAN_POINT('Ctrl Pts',(-32.0390473530326,1076.6909235103,341.797040381191));
#122843=CARTESIAN_POINT('Ctrl Pts',(-32.2030559898266,1076.69297894973,
341.96340568665));
#122844=CARTESIAN_POINT('Ctrl Pts',(-32.3010287740737,1076.69352027147,
342.029482453987));
#122845=CARTESIAN_POINT('Ctrl Pts',(-32.5159752164315,1076.69361847209,
342.118890353154));
#122846=CARTESIAN_POINT('Ctrl Pts',(-32.6306190082936,1076.69318462243,
342.141777359158));
#122847=CARTESIAN_POINT('Ctrl Pts',(-32.7463814565112,1076.69227114041,
342.141777359158));
#122848=CARTESIAN_POINT('Origin',(-25.1979747106603,1067.7251047501,331.226959282729));
#122849=CARTESIAN_POINT('',(-25.1979747106792,1076.26166943286,329.951515161593));
#122850=CARTESIAN_POINT('',(-25.1979747106603,1067.7251047501,329.951515161593));
#122851=CARTESIAN_POINT('Ctrl Pts',(-25.1980032377211,1076.42086980393,
332.502403403546));
#122852=CARTESIAN_POINT('Ctrl Pts',(-25.36705969148,1076.41826882087,332.502399622366));
#122853=CARTESIAN_POINT('Ctrl Pts',(-25.5343921697909,1076.41376902618,
332.468784797302));
#122854=CARTESIAN_POINT('Ctrl Pts',(-25.8458881365049,1076.40132876238,
332.338455592051));
#122855=CARTESIAN_POINT('Ctrl Pts',(-25.9869961492942,1076.39351219026,
332.243138053092));
#122856=CARTESIAN_POINT('Ctrl Pts',(-26.2245078606825,1076.37532289726,
332.002649118291));
#122857=CARTESIAN_POINT('Ctrl Pts',(-26.3183251064285,1076.3651134342,331.859611292541));
#122858=CARTESIAN_POINT('Ctrl Pts',(-26.4129107652612,1076.34898533397,
331.624205262477));
#122859=CARTESIAN_POINT('Ctrl Pts',(-26.4365172614667,1076.34352500537,
331.543005334542));
#122860=CARTESIAN_POINT('Ctrl Pts',(-26.4825679162042,1076.32716353809,
331.295293385328));
#122861=CARTESIAN_POINT('Ctrl Pts',(-26.4804270245162,1076.31636411902,
331.126052751354));
#122862=CARTESIAN_POINT('Ctrl Pts',(-26.4108043557608,1076.29629617508,
330.798150060569));
#122863=CARTESIAN_POINT('Ctrl Pts',(-26.3440301995677,1076.28722377961,
330.64263696166));
#122864=CARTESIAN_POINT('Ctrl Pts',(-26.1542812502165,1076.27226345453,
330.366600016229));
#122865=CARTESIAN_POINT('Ctrl Pts',(-26.0332861584661,1076.26651779982,
330.248677000342));
#122866=CARTESIAN_POINT('Ctrl Pts',(-25.7530239795191,1076.25932675635,
330.0665671552));
#122867=CARTESIAN_POINT('Ctrl Pts',(-25.5966355803637,1076.25793970918,
330.003983116595));
#122868=CARTESIAN_POINT('Ctrl Pts',(-25.2689795137375,1076.25977446275,
329.942657018773));
#122869=CARTESIAN_POINT('Ctrl Pts',(-25.1009567331692,1076.26296704667,
329.944369712011));
#122870=CARTESIAN_POINT('Ctrl Pts',(-24.7750493429435,1076.27343781723,
330.012212322424));
#122871=CARTESIAN_POINT('Ctrl Pts',(-24.6203360176324,1076.2806128095,330.07771394198));
#122872=CARTESIAN_POINT('Ctrl Pts',(-24.3445146671539,1076.29784880489,
330.264573161085));
#122873=CARTESIAN_POINT('Ctrl Pts',(-24.2261483303946,1076.30774747809,
330.384284884773));
#122874=CARTESIAN_POINT('Ctrl Pts',(-24.0881316782512,1076.32352699544,
330.592944913446));
#122875=CARTESIAN_POINT('Ctrl Pts',(-24.049028858082,1076.32890941553,330.666916761111));
#122876=CARTESIAN_POINT('Ctrl Pts',(-23.9858266572107,1076.33974392426,
330.821462373265));
#122877=CARTESIAN_POINT('Ctrl Pts',(-23.9618841178172,1076.34517029959,
330.901672657433));
#122878=CARTESIAN_POINT('Ctrl Pts',(-23.9136159982493,1076.36139485872,
331.150048110655));
#122879=CARTESIAN_POINT('Ctrl Pts',(-23.9147658066077,1076.37180532051,
331.321279810547));
#122880=CARTESIAN_POINT('Ctrl Pts',(-23.9837983035842,1076.39053694666,
331.652348720763));
#122881=CARTESIAN_POINT('Ctrl Pts',(-24.0506083409084,1076.39869042679,
331.80900113857));
#122882=CARTESIAN_POINT('Ctrl Pts',(-24.2415044822947,1076.4118984853,332.087450762062));
#122883=CARTESIAN_POINT('Ctrl Pts',(-24.363752916489,1076.41682377266,332.206442664842));
#122884=CARTESIAN_POINT('Ctrl Pts',(-24.6479982924025,1076.42293360066,
332.39014394625));
#122885=CARTESIAN_POINT('Ctrl Pts',(-24.8072436045823,1076.42404946741,
332.452850820141));
#122886=CARTESIAN_POINT('Ctrl Pts',(-25.0480040306134,1076.42279725656,
332.495778924567));
#122887=CARTESIAN_POINT('Ctrl Pts',(-25.1229325560726,1076.42202478836,
332.502405082605));
#122888=CARTESIAN_POINT('Ctrl Pts',(-25.1980032377211,1076.42086980393,
332.502403403546));
#122889=CARTESIAN_POINT('Origin',(-25.1979747106603,1067.7251047501,331.226959282729));
#122890=CARTESIAN_POINT('',(-25.1979747106603,1076.38624898044,331.902403403865));
#122891=CARTESIAN_POINT('',(-25.1979747106602,1076.3019258569,330.551515161593));
#122892=CARTESIAN_POINT('Ctrl Pts',(-25.1979747106603,1076.38624898044,
331.902403403865));
#122893=CARTESIAN_POINT('Ctrl Pts',(-25.2471812358611,1076.38545783245,
331.902403403865));
#122894=CARTESIAN_POINT('Ctrl Pts',(-25.2963568705416,1076.38434577168,
331.897026203571));
#122895=CARTESIAN_POINT('Ctrl Pts',(-25.4323214908925,1076.3803418051,331.866786924668));
#122896=CARTESIAN_POINT('Ctrl Pts',(-25.5152270241464,1076.37679013501,
331.82998264202));
#122897=CARTESIAN_POINT('Ctrl Pts',(-25.6618430249056,1076.36810176254,
331.726092728421));
#122898=CARTESIAN_POINT('Ctrl Pts',(-25.7240629546574,1076.36304832444,
331.660004822544));
#122899=CARTESIAN_POINT('Ctrl Pts',(-25.7947649861978,1076.35487229256,
331.546338881351));
#122900=CARTESIAN_POINT('Ctrl Pts',(-25.8143011508075,1076.35209936297,
331.506785957527));
#122901=CARTESIAN_POINT('Ctrl Pts',(-25.8454405672376,1076.34645311229,
331.424341249773));
#122902=CARTESIAN_POINT('Ctrl Pts',(-25.8569487026477,1076.34359288809,
331.381635759692));
#122903=CARTESIAN_POINT('Ctrl Pts',(-25.8789581544592,1076.33494671822,
331.249717581615));
#122904=CARTESIAN_POINT('Ctrl Pts',(-25.875969789591,1076.32926836339,331.159245492184));
#122905=CARTESIAN_POINT('Ctrl Pts',(-25.8350622871002,1076.31890066796,
330.985710803517));
#122906=CARTESIAN_POINT('Ctrl Pts',(-25.7979324441916,1076.31430177259,
330.904245617303));
#122907=CARTESIAN_POINT('Ctrl Pts',(-25.6943862091979,1076.30681073806,
330.760449535376));
#122908=CARTESIAN_POINT('Ctrl Pts',(-25.6290457199438,1076.30398861186,
330.699470787555));
#122909=CARTESIAN_POINT('Ctrl Pts',(-25.4787036906503,1076.30056020518,
330.606301500901));
#122910=CARTESIAN_POINT('Ctrl Pts',(-25.3952258217971,1076.29998235526,
330.574947530313));
#122911=CARTESIAN_POINT('Ctrl Pts',(-25.2716845042923,1076.30082579969,
330.554536759418));
#122912=CARTESIAN_POINT('Ctrl Pts',(-25.2348649592348,1076.3012770248,330.551515771758));
#122913=CARTESIAN_POINT('Ctrl Pts',(-25.1979858830973,1076.30192566039,
330.551515161756));
#122914=CARTESIAN_POINT('Ctrl Pts',(-25.1979821589501,1076.30192572589,
330.551515161694));
#122915=CARTESIAN_POINT('Ctrl Pts',(-25.1979784348043,1076.30192579139,
330.551515161593));
#122916=CARTESIAN_POINT('Ctrl Pts',(-25.1979747106602,1076.3019258569,330.551515161593));
#122917=CARTESIAN_POINT('',(-25.1979747106603,1082.7251047501,330.551515161593));
#122918=CARTESIAN_POINT('',(-25.1979747106603,1067.7251047501,330.551515161593));
#122919=CARTESIAN_POINT('Origin',(-25.1979747106603,1082.7251047501,331.226959282729));
#122920=CARTESIAN_POINT('Ctrl Pts',(-25.1979747106602,1076.3019258569,330.551515161593));
#122921=CARTESIAN_POINT('Ctrl Pts',(-25.109754694076,1076.30347758071,330.551515161593));
#122922=CARTESIAN_POINT('Ctrl Pts',(-25.0224144977182,1076.30613837089,
330.568798147374));
#122923=CARTESIAN_POINT('Ctrl Pts',(-24.8592059024046,1076.31333459836,
330.635974818503));
#122924=CARTESIAN_POINT('Ctrl Pts',(-24.784940815646,1076.31780258741,330.685278616937));
#122925=CARTESIAN_POINT('Ctrl Pts',(-24.6594569177532,1076.32791710315,
330.809761185901));
#122926=CARTESIAN_POINT('Ctrl Pts',(-24.609502878529,1076.33346843719,330.88381207894));
#122927=CARTESIAN_POINT('Ctrl Pts',(-24.5581135217446,1076.34202464141,
331.006144925782));
#122928=CARTESIAN_POINT('Ctrl Pts',(-24.5450295698096,1076.34489499932,
331.048510411215));
#122929=CARTESIAN_POINT('Ctrl Pts',(-24.5181676135318,1076.35353733772,
331.180085689814));
#122930=CARTESIAN_POINT('Ctrl Pts',(-24.5179767652101,1076.35914812453,
331.271059263526));
#122931=CARTESIAN_POINT('Ctrl Pts',(-24.5532474129041,1076.36934944255,
331.447438544772));
#122932=CARTESIAN_POINT('Ctrl Pts',(-24.5882335394392,1076.37384368879,
331.531117263122));
#122933=CARTESIAN_POINT('Ctrl Pts',(-24.6889438876951,1076.38116825472,
331.679932907919));
#122934=CARTESIAN_POINT('Ctrl Pts',(-24.7536613715196,1076.3839264696,331.743576301247));
#122935=CARTESIAN_POINT('Ctrl Pts',(-24.9043545433581,1076.38736353833,
331.841869194931));
#122936=CARTESIAN_POINT('Ctrl Pts',(-24.9888282224768,1076.3880059005,331.875486363782));
#122937=CARTESIAN_POINT('Ctrl Pts',(-25.1172929206417,1076.38733026166,
331.898791292979));
#122938=CARTESIAN_POINT('Ctrl Pts',(-25.1576441914772,1076.38689741901,
331.902403403865));
#122939=CARTESIAN_POINT('Ctrl Pts',(-25.1979747106603,1076.38624898044,
331.902403403865));
#122940=CARTESIAN_POINT('Origin',(-15.9013061211259,1067.7251047501,320.960985878213));
#122941=CARTESIAN_POINT('',(-15.901306121144,1075.53973422622,319.862154742221));
#122942=CARTESIAN_POINT('',(-15.9013061211259,1067.7251047501,319.862154742221));
#122943=CARTESIAN_POINT('Ctrl Pts',(-15.9013183816517,1075.76586210742,
322.059817014137));
#122944=CARTESIAN_POINT('Ctrl Pts',(-16.0472269922218,1075.76364690165,
322.05981538612));
#122945=CARTESIAN_POINT('Ctrl Pts',(-16.1915897472063,1075.75858015459,
322.030753759462));
#122946=CARTESIAN_POINT('Ctrl Pts',(-16.4604451299536,1075.74326344712,
321.918087664903));
#122947=CARTESIAN_POINT('Ctrl Pts',(-16.58220670375,1075.73316467281,321.835613218183));
#122948=CARTESIAN_POINT('Ctrl Pts',(-16.7868653598449,1075.70909583708,
321.627761662381));
#122949=CARTESIAN_POINT('Ctrl Pts',(-16.8675413122869,1075.69534327377,
321.504242453182));
#122950=CARTESIAN_POINT('Ctrl Pts',(-16.9482963891639,1075.67345610172,
321.302129034095));
#122951=CARTESIAN_POINT('Ctrl Pts',(-16.9683097655656,1075.66607632406,
321.233138440417));
#122952=CARTESIAN_POINT('Ctrl Pts',(-16.9948448527741,1075.65105120479,
321.091049237343));
#122953=CARTESIAN_POINT('Ctrl Pts',(-17.0010635249007,1075.64343914419,
321.018237504974));
#122954=CARTESIAN_POINT('Ctrl Pts',(-16.9979651957292,1075.62094467287,
320.800574562154));
#122955=CARTESIAN_POINT('Ctrl Pts',(-16.9673098121961,1075.60650474725,
320.657538248775));
#122956=CARTESIAN_POINT('Ctrl Pts',(-16.852353782415,1075.58047494831,320.391952227302));
#122957=CARTESIAN_POINT('Ctrl Pts',(-16.7693475035747,1075.56912651833,
320.271870856426));
#122958=CARTESIAN_POINT('Ctrl Pts',(-16.5619837108859,1075.55122442585,
320.071259986371));
#122959=CARTESIAN_POINT('Ctrl Pts',(-16.439927446826,1075.54481883454,319.992451446599));
#122960=CARTESIAN_POINT('Ctrl Pts',(-16.1728997908162,1075.5379049811,319.886661577952));
#122961=CARTESIAN_POINT('Ctrl Pts',(-16.0307255945619,1075.53743358193,
319.860444336545));
#122962=CARTESIAN_POINT('Ctrl Pts',(-15.7445118197114,1075.54250111157,
319.864035640628));
#122963=CARTESIAN_POINT('Ctrl Pts',(-15.6033283901581,1075.54798015182,
319.893728990274));
#122964=CARTESIAN_POINT('Ctrl Pts',(-15.3398915156939,1075.56414806262,
320.00558002081));
#122965=CARTESIAN_POINT('Ctrl Pts',(-15.2202951230251,1075.57469598467,
320.086841748472));
#122966=CARTESIAN_POINT('Ctrl Pts',(-15.018490373626,1075.59943336025,320.291055452454));
#122967=CARTESIAN_POINT('Ctrl Pts',(-14.9384574793007,1075.6134067287,320.412320353851));
#122968=CARTESIAN_POINT('Ctrl Pts',(-14.8567867324523,1075.63546720063,
320.612251183191));
#122969=CARTESIAN_POINT('Ctrl Pts',(-14.8361484273098,1075.64296696986,
320.681569384525));
#122970=CARTESIAN_POINT('Ctrl Pts',(-14.8087834485469,1075.6579890958,320.823107614848));
#122971=CARTESIAN_POINT('Ctrl Pts',(-14.802095746972,1075.66547659229,320.894994585311));
#122972=CARTESIAN_POINT('Ctrl Pts',(-14.8032947200149,1075.687779544,321.113173425508));
#122973=CARTESIAN_POINT('Ctrl Pts',(-14.8332484575461,1075.7019896304,321.257806786604));
#122974=CARTESIAN_POINT('Ctrl Pts',(-14.9478420172994,1075.72728452876,
321.526238004055));
#122975=CARTESIAN_POINT('Ctrl Pts',(-15.031047423577,1075.73814208654,321.647525124861));
#122976=CARTESIAN_POINT('Ctrl Pts',(-15.2400991870558,1075.75518944082,
321.850623175349));
#122977=CARTESIAN_POINT('Ctrl Pts',(-15.3638024185795,1075.76121419415,
321.930417864329));
#122978=CARTESIAN_POINT('Ctrl Pts',(-15.6275412594093,1075.76746576582,
322.034011522529));
#122979=CARTESIAN_POINT('Ctrl Pts',(-15.7638192353197,1075.76794963948,
322.059818548324));
#122980=CARTESIAN_POINT('Ctrl Pts',(-15.9013183816517,1075.76586210742,
322.059817014137));
#122981=CARTESIAN_POINT('Origin',(-15.9013061211259,1067.7251047501,320.960985878213));
#122982=CARTESIAN_POINT('',(-15.9013061211259,1075.70629239322,321.459817014206));
#122983=CARTESIAN_POINT('',(-15.9013061211256,1075.60362949862,320.462154742221));
#122984=CARTESIAN_POINT('Ctrl Pts',(-15.9013061211259,1075.70629239322,
321.459817014206));
#122985=CARTESIAN_POINT('Ctrl Pts',(-15.9027535012539,1075.70626993847,
321.459817014206));
#122986=CARTESIAN_POINT('Ctrl Pts',(-15.9042011776659,1075.70624684176,
321.459810714755));
#122987=CARTESIAN_POINT('Ctrl Pts',(-15.9707105043603,1075.70515642044,
321.459231640583));
#122988=CARTESIAN_POINT('Ctrl Pts',(-16.0349930669914,1075.70281517994,
321.445942636561));
#122989=CARTESIAN_POINT('Ctrl Pts',(-16.156182577991,1075.69575713627,321.394914764689));
#122990=CARTESIAN_POINT('Ctrl Pts',(-16.2116400238405,1075.69105759309,
321.35713204646));
#122991=CARTESIAN_POINT('Ctrl Pts',(-16.304622580305,1075.6799136683,321.262000551855));
#122992=CARTESIAN_POINT('Ctrl Pts',(-16.3411480830573,1075.67357315667,
321.205525304293));
#122993=CARTESIAN_POINT('Ctrl Pts',(-16.3774474234298,1075.6635429136,321.113253709203));
#122994=CARTESIAN_POINT('Ctrl Pts',(-16.3863796690735,1075.66017364307,
321.081812503107));
#122995=CARTESIAN_POINT('Ctrl Pts',(-16.3979926987541,1075.6533829733,321.017577036737));
#122996=CARTESIAN_POINT('Ctrl Pts',(-16.4006327713848,1075.64997719005,
320.984928600088));
#122997=CARTESIAN_POINT('Ctrl Pts',(-16.3989004958387,1075.63979069932,
320.885965480553));
#122998=CARTESIAN_POINT('Ctrl Pts',(-16.3845348923151,1075.63324025375,
320.820523772531));
#122999=CARTESIAN_POINT('Ctrl Pts',(-16.3313385075833,1075.62155424489,
320.699845122897));
#123000=CARTESIAN_POINT('Ctrl Pts',(-16.2933462146483,1075.61651332255,
320.645638342996));
#123001=CARTESIAN_POINT('Ctrl Pts',(-16.198733867935,1075.60859541564,320.555247933136));
#123002=CARTESIAN_POINT('Ctrl Pts',(-16.1431566091223,1075.60578355299,
320.519842299189));
#123003=CARTESIAN_POINT('Ctrl Pts',(-16.024595193168,1075.60285688101,320.473681964203));
#123004=CARTESIAN_POINT('Ctrl Pts',(-15.9632237991125,1075.6026355528,320.462154742221));
#123005=CARTESIAN_POINT('Ctrl Pts',(-15.9013061211248,1075.60362949862,
320.462154742221));
#123006=CARTESIAN_POINT('',(-15.9013061211259,1082.7251047501,320.462154742221));
#123007=CARTESIAN_POINT('',(-15.9013061211259,1067.7251047501,320.462154742221));
#123008=CARTESIAN_POINT('Origin',(-15.9013061211259,1082.7251047501,320.960985878213));
#123009=CARTESIAN_POINT('Ctrl Pts',(-15.9013021674381,1075.60362956209,
320.462154742237));
#123010=CARTESIAN_POINT('Ctrl Pts',(-15.8363273247354,1075.60467263752,
320.462155257221));
#123011=CARTESIAN_POINT('Ctrl Pts',(-15.7720200532064,1075.60703351656,
320.474849655884));
#123012=CARTESIAN_POINT('Ctrl Pts',(-15.6517121538532,1075.61411388871,
320.524202822739));
#123013=CARTESIAN_POINT('Ctrl Pts',(-15.5969274629695,1075.61877242025,
320.560469438888));
#123014=CARTESIAN_POINT('Ctrl Pts',(-15.5041480528897,1075.62978368196,
320.652153043733));
#123015=CARTESIAN_POINT('Ctrl Pts',(-15.46714933412,1075.63604037615,320.706806078424));
#123016=CARTESIAN_POINT('Ctrl Pts',(-15.429011929669,1075.64598127082,320.797148681718));
#123017=CARTESIAN_POINT('Ctrl Pts',(-15.4192811049715,1075.64936875669,
320.828487821771));
#123018=CARTESIAN_POINT('Ctrl Pts',(-15.4061097386104,1075.65617680393,
320.892565172555));
#123019=CARTESIAN_POINT('Ctrl Pts',(-15.4026908943796,1075.65958154805,
320.925153009441));
#123020=CARTESIAN_POINT('Ctrl Pts',(-15.4020652237601,1075.66978294967,
321.024436226829));
#123021=CARTESIAN_POINT('Ctrl Pts',(-15.4149851501882,1075.67633558523,
321.090488908085));
#123022=CARTESIAN_POINT('Ctrl Pts',(-15.4659668956417,1075.68807447895,
321.213415530183));
#123023=CARTESIAN_POINT('Ctrl Pts',(-15.503419072807,1075.69315134413,321.269116239206));
#123024=CARTESIAN_POINT('Ctrl Pts',(-15.5979744807591,1075.7011562374,321.362519086056));
#123025=CARTESIAN_POINT('Ctrl Pts',(-15.6540756517758,1075.70400819849,
321.39931121727));
#123026=CARTESIAN_POINT('Ctrl Pts',(-15.7747893415874,1075.70702747658,
321.447674869886));
#123027=CARTESIAN_POINT('Ctrl Pts',(-15.8377621891094,1075.70727821804,
321.459817014206));
#123028=CARTESIAN_POINT('Ctrl Pts',(-15.9013061211259,1075.70629239322,
321.459817014206));
#123029=CARTESIAN_POINT('Origin',(-4.59241321360898,1067.7251047501,312.73037859586));
#123030=CARTESIAN_POINT('',(-4.5924132136256,1074.6522152412,311.639837847132));
#123031=CARTESIAN_POINT('',(-4.59241321360898,1067.7251047501,311.639837847132));
#123032=CARTESIAN_POINT('Ctrl Pts',(-4.59242154314923,1074.94723110711,
313.820919344557));
#123033=CARTESIAN_POINT('Ctrl Pts',(-4.73417441665283,1074.94646331085,
313.82091826185));
#123034=CARTESIAN_POINT('Ctrl Pts',(-4.87446768389953,1074.94206003125,
313.793280638671));
#123035=CARTESIAN_POINT('Ctrl Pts',(-5.13950864065852,1074.9262762585,313.684810857126));
#123036=CARTESIAN_POINT('Ctrl Pts',(-5.2610613528356,1074.91489969795,313.60389685957));
#123037=CARTESIAN_POINT('Ctrl Pts',(-5.46586598942681,1074.88655943134,
313.399274617924));
#123038=CARTESIAN_POINT('Ctrl Pts',(-5.54686784141405,1074.86984878477,
313.277399654976));
#123039=CARTESIAN_POINT('Ctrl Pts',(-5.62860101239182,1074.84260840697,
313.077717779237));
#123040=CARTESIAN_POINT('Ctrl Pts',(-5.64901645007429,1074.83332330149,
313.009502701119));
#123041=CARTESIAN_POINT('Ctrl Pts',(-5.67635023549569,1074.81434541568,
312.869828260613));
#123042=CARTESIAN_POINT('Ctrl Pts',(-5.68314655426807,1074.80469370511,
312.798670210033));
#123043=CARTESIAN_POINT('Ctrl Pts',(-5.68254464419452,1074.77515502237,
312.580535231193));
#123044=CARTESIAN_POINT('Ctrl Pts',(-5.65248779637873,1074.75553601166,
312.435175883673));
#123045=CARTESIAN_POINT('Ctrl Pts',(-5.53774437308449,1074.71965851928,
312.167982761174));
#123046=CARTESIAN_POINT('Ctrl Pts',(-5.45537699260935,1074.70367302368,
312.048200548254));
#123047=CARTESIAN_POINT('Ctrl Pts',(-5.24943671602821,1074.6773203616,311.848345273121));
#123048=CARTESIAN_POINT('Ctrl Pts',(-5.12828913258207,1074.66715917283,
311.769845770818));
#123049=CARTESIAN_POINT('Ctrl Pts',(-4.86342142412553,1074.65410276184,
311.664570774242));
#123050=CARTESIAN_POINT('Ctrl Pts',(-4.72260569605938,1074.65127210857,
311.6383706536));
#123051=CARTESIAN_POINT('Ctrl Pts',(-4.43921361249575,1074.65330593362,
311.641426329821));
#123052=CARTESIAN_POINT('Ctrl Pts',(-4.29953671467465,1074.65812173189,
311.670451496656));
#123053=CARTESIAN_POINT('Ctrl Pts',(-4.03859143543839,1074.67477760158,
311.7802760977));
#123054=CARTESIAN_POINT('Ctrl Pts',(-3.920026596784,1074.68648206998,311.860217895112));
#123055=CARTESIAN_POINT('Ctrl Pts',(-3.71928348622794,1074.71529000323,
312.06154683786));
#123056=CARTESIAN_POINT('Ctrl Pts',(-3.63941913700345,1074.7321666632,312.181401833915));
#123057=CARTESIAN_POINT('Ctrl Pts',(-3.5574261244455,1074.75962418542,312.379331949081));
#123058=CARTESIAN_POINT('Ctrl Pts',(-3.53657934187177,1074.76911108084,
312.448175008495));
#123059=CARTESIAN_POINT('Ctrl Pts',(-3.50871996467179,1074.78836976263,
312.588860340566));
#123060=CARTESIAN_POINT('Ctrl Pts',(-3.50176299797697,1074.79809774018,
312.660382283191));
#123061=CARTESIAN_POINT('Ctrl Pts',(-3.50209860283686,1074.82744712561,
312.877561022191));
#123062=CARTESIAN_POINT('Ctrl Pts',(-3.53143919505767,1074.84666254094,
313.021677024456));
#123063=CARTESIAN_POINT('Ctrl Pts',(-3.64469868835762,1074.88182214959,
313.288955618368));
#123064=CARTESIAN_POINT('Ctrl Pts',(-3.72708461848955,1074.89745764829,
313.409725430513));
#123065=CARTESIAN_POINT('Ctrl Pts',(-3.93424897340151,1074.92317009665,
313.611828490723));
#123066=CARTESIAN_POINT('Ctrl Pts',(-4.05677723349741,1074.93301348281,
313.691288427238));
#123067=CARTESIAN_POINT('Ctrl Pts',(-4.31905539402455,1074.94529213272,
313.79498192967));
#123068=CARTESIAN_POINT('Ctrl Pts',(-4.45509219391934,1074.9479749436,313.820920393477));
#123069=CARTESIAN_POINT('Ctrl Pts',(-4.59242154314923,1074.94723110711,
313.820919344557));
#123070=CARTESIAN_POINT('Origin',(-4.59241321360898,1067.7251047501,312.73037859586));
#123071=CARTESIAN_POINT('',(-4.59241321360898,1074.8680726283,313.220919344589));
#123072=CARTESIAN_POINT('',(-4.59241321360906,1074.73536251872,312.239837847132));
#123073=CARTESIAN_POINT('Ctrl Pts',(-4.59241321360898,1074.8680726283,313.220919344589));
#123074=CARTESIAN_POINT('Ctrl Pts',(-4.59343259811277,1074.86806703061,
313.220919344589));
#123075=CARTESIAN_POINT('Ctrl Pts',(-4.59445214105991,1074.86806100691,
313.220916167041));
#123076=CARTESIAN_POINT('Ctrl Pts',(-4.65919666386597,1074.86765146619,
313.220512464842));
#123077=CARTESIAN_POINT('Ctrl Pts',(-4.72218589708467,1074.86559231559,
313.207702474031));
#123078=CARTESIAN_POINT('Ctrl Pts',(-4.84000296423593,1074.85837634849,
313.158658728959));
#123079=CARTESIAN_POINT('Ctrl Pts',(-4.89359922392605,1074.85327469048,
313.122789291614));
#123080=CARTESIAN_POINT('Ctrl Pts',(-4.98520338088352,1074.84050617101,
313.031452684482));
#123081=CARTESIAN_POINT('Ctrl Pts',(-5.02181171024764,1074.83290009585,
312.976388746648));
#123082=CARTESIAN_POINT('Ctrl Pts',(-5.05865719923982,1074.82053899349,
312.886182966118));
#123083=CARTESIAN_POINT('Ctrl Pts',(-5.06783727646721,1074.8163344332,312.855393246639));
#123084=CARTESIAN_POINT('Ctrl Pts',(-5.08007526073578,1074.80776045823,
312.792409544954));
#123085=CARTESIAN_POINT('Ctrl Pts',(-5.08308941819944,1074.80340996283,
312.760354062892));
#123086=CARTESIAN_POINT('Ctrl Pts',(-5.08266187334577,1074.79015019368,
312.66236355755));
#123087=CARTESIAN_POINT('Ctrl Pts',(-5.06910752841617,1074.78138135226,
312.597165597613));
#123088=CARTESIAN_POINT('Ctrl Pts',(-5.01733907562667,1074.76531240295,
312.47680634019));
#123089=CARTESIAN_POINT('Ctrl Pts',(-4.97996812233148,1074.75814666573,
312.422662009554));
#123090=CARTESIAN_POINT('Ctrl Pts',(-4.88683250062607,1074.74641467959,
312.332805671349));
#123091=CARTESIAN_POINT('Ctrl Pts',(-4.83229404821456,1074.74192219264,
312.297679426263));
#123092=CARTESIAN_POINT('Ctrl Pts',(-4.71513682801718,1074.73626345487,
312.251460229922));
#123093=CARTESIAN_POINT('Ctrl Pts',(-4.6540664253156,1074.73501655744,312.239838061364));
#123094=CARTESIAN_POINT('Ctrl Pts',(-4.59241491815632,1074.73536250915,
312.239837847135));
#123095=CARTESIAN_POINT('',(-4.59241321360898,1082.7251047501,312.239837847132));
#123096=CARTESIAN_POINT('',(-4.59241321360898,1067.7251047501,312.239837847132));
#123097=CARTESIAN_POINT('Origin',(-4.59241321360898,1082.7251047501,312.73037859586));
#123098=CARTESIAN_POINT('Ctrl Pts',(-4.59241321360922,1074.73536251872,
312.239837847132));
#123099=CARTESIAN_POINT('Ctrl Pts',(-4.52875064557946,1074.73571978555,
312.239837847132));
#123100=CARTESIAN_POINT('Ctrl Pts',(-4.46574735051964,1074.73776821706,
312.252229509161));
#123101=CARTESIAN_POINT('Ctrl Pts',(-4.34776850179519,1074.7450132071,312.300425563072));
#123102=CARTESIAN_POINT('Ctrl Pts',(-4.29401920231488,1074.75015182552,
312.335858802838));
#123103=CARTESIAN_POINT('Ctrl Pts',(-4.20273370102847,1074.76288605867,
312.425558610257));
#123104=CARTESIAN_POINT('Ctrl Pts',(-4.16624547770014,1074.77038146574,
312.479137556319));
#123105=CARTESIAN_POINT('Ctrl Pts',(-4.128484121288,1074.78262864972,312.56777786159));
#123106=CARTESIAN_POINT('Ctrl Pts',(-4.11881011052542,1074.78686288898,
312.598592580366));
#123107=CARTESIAN_POINT('Ctrl Pts',(-4.10564643941886,1074.79547983249,
312.661638793863));
#123108=CARTESIAN_POINT('Ctrl Pts',(-4.10218535791044,1074.79984300773,
312.693727376496));
#123109=CARTESIAN_POINT('Ctrl Pts',(-4.10129632511921,1074.81307368021,
312.791531019133));
#123110=CARTESIAN_POINT('Ctrl Pts',(-4.11386954858357,1074.82178992049,
312.856651742813));
#123111=CARTESIAN_POINT('Ctrl Pts',(-4.16383161852702,1074.83782658645,
312.977796257153));
#123112=CARTESIAN_POINT('Ctrl Pts',(-4.20059282629724,1074.84500106704,
313.032706154599));
#123113=CARTESIAN_POINT('Ctrl Pts',(-4.29347628013839,1074.85683857716,
313.124739868));
#123114=CARTESIAN_POINT('Ctrl Pts',(-4.34856892267024,1074.86139424134,
313.161016716072));
#123115=CARTESIAN_POINT('Ctrl Pts',(-4.4674544550444,1074.86714703548,313.208867730578));
#123116=CARTESIAN_POINT('Ctrl Pts',(-4.52963335727786,1074.86841736828,
313.220919344589));
#123117=CARTESIAN_POINT('Ctrl Pts',(-4.59241321360898,1074.8680726283,313.220919344589));
#123118=CARTESIAN_POINT('Origin',(-49.3616411037539,1067.7251047501,349.893375147338));
#123119=CARTESIAN_POINT('',(-49.3616411037758,1076.63637248492,348.415072015145));
#123120=CARTESIAN_POINT('',(-49.3616411037539,1067.7251047501,348.415072015145));
#123121=CARTESIAN_POINT('Ctrl Pts',(-49.3624372582816,1076.70060106622,
351.371678065143));
#123122=CARTESIAN_POINT('Ctrl Pts',(-49.5573261371424,1076.6985286974,351.371573105827));
#123123=CARTESIAN_POINT('Ctrl Pts',(-49.7502737386378,1076.69575821467,
351.332930288383));
#123124=CARTESIAN_POINT('Ctrl Pts',(-50.1107340574847,1076.68876623073,
351.182757831355));
#123125=CARTESIAN_POINT('Ctrl Pts',(-50.2745829485658,1076.68460066891,
351.072432238936));
#123126=CARTESIAN_POINT('Ctrl Pts',(-50.5500125666934,1076.67517733427,
350.794222637883));
#123127=CARTESIAN_POINT('Ctrl Pts',(-50.6587901775009,1076.67000872495,
350.629005017809));
#123128=CARTESIAN_POINT('Ctrl Pts',(-50.8049247452241,1076.65943419735,
350.267498610164));
#123129=CARTESIAN_POINT('Ctrl Pts',(-50.8415216207758,1076.65413721465,
350.075015038867));
#123130=CARTESIAN_POINT('Ctrl Pts',(-50.838261778393,1076.64432889098,349.686809038781));
#123131=CARTESIAN_POINT('Ctrl Pts',(-50.7983972091676,1076.63992013039,
349.494851033114));
#123132=CARTESIAN_POINT('Ctrl Pts',(-50.6468018068872,1076.63293865188,
349.137477534985));
#123133=CARTESIAN_POINT('Ctrl Pts',(-50.5366114824806,1076.63043852341,
348.975511260837));
#123134=CARTESIAN_POINT('Ctrl Pts',(-50.2602807225132,1076.62793377259,
348.703713849592));
#123135=CARTESIAN_POINT('Ctrl Pts',(-50.0969595379003,1076.62794991829,
348.596396391019));
#123136=CARTESIAN_POINT('Ctrl Pts',(-49.7386548966553,1076.63050995024,
348.450967511084));
#123137=CARTESIAN_POINT('Ctrl Pts',(-49.5472065995713,1076.63302082595,
348.414106937213));
#123138=CARTESIAN_POINT('Ctrl Pts',(-49.1610999938002,1076.63999363883,
348.416075018567));
#123139=CARTESIAN_POINT('Ctrl Pts',(-48.970157576568,1076.64438124009,348.454847472195));
#123140=CARTESIAN_POINT('Ctrl Pts',(-48.6138111271898,1076.65414039512,
348.603627656267));
#123141=CARTESIAN_POINT('Ctrl Pts',(-48.4518556663351,1076.65941239181,
348.712280146129));
#123142=CARTESIAN_POINT('Ctrl Pts',(-48.178794140413,1076.66989527097,348.985831772015));
#123143=CARTESIAN_POINT('Ctrl Pts',(-48.0703593694701,1076.6750017051,349.148150999423));
#123144=CARTESIAN_POINT('Ctrl Pts',(-47.9212624073684,1076.68439492229,
349.507424230142));
#123145=CARTESIAN_POINT('Ctrl Pts',(-47.8828801681462,1076.68858075922,
349.701217613954));
#123146=CARTESIAN_POINT('Ctrl Pts',(-47.8838021698197,1076.69561581394,
350.091731480461));
#123147=CARTESIAN_POINT('Ctrl Pts',(-47.9227879557564,1076.69840881142,
350.284606960883));
#123148=CARTESIAN_POINT('Ctrl Pts',(-48.0736060068292,1076.70260581189,
350.644772576739));
#123149=CARTESIAN_POINT('Ctrl Pts',(-48.1842076763103,1076.7039716175,350.80840891566));
#123150=CARTESIAN_POINT('Ctrl Pts',(-48.4630809225606,1076.70533906345,
351.083518673881));
#123151=CARTESIAN_POINT('Ctrl Pts',(-48.6287430128023,1076.70532690411,
351.19211005852));
#123152=CARTESIAN_POINT('Ctrl Pts',(-48.9861537457672,1076.70393342627,
351.335635161093));
#123153=CARTESIAN_POINT('Ctrl Pts',(-49.1734369125114,1076.70261081877,
351.371779853132));
#123154=CARTESIAN_POINT('Ctrl Pts',(-49.3624372582816,1076.70060106622,
351.371678065143));
#123155=CARTESIAN_POINT('Origin',(-49.3616411037539,1067.7251047501,349.893375147338));
#123156=CARTESIAN_POINT('',(-49.3616411037539,1076.69042463418,350.771678279532));
#123157=CARTESIAN_POINT('',(-49.3616411037048,1076.65225835227,349.015072015145));
#123158=CARTESIAN_POINT('Ctrl Pts',(-49.3616411037539,1076.69042463418,
350.771678279532));
#123159=CARTESIAN_POINT('Ctrl Pts',(-49.3625704187744,1076.69041333812,
350.771678279532));
#123160=CARTESIAN_POINT('Ctrl Pts',(-49.3634998059874,1076.69040201185,
350.771676804597));
#123161=CARTESIAN_POINT('Ctrl Pts',(-49.4809116296106,1076.6889674243,350.771304080901));
#123162=CARTESIAN_POINT('Ctrl Pts',(-49.5961581176758,1076.6870980418,350.747765838718));
#123163=CARTESIAN_POINT('Ctrl Pts',(-49.8110004431342,1076.68255175518,
350.657001385538));
#123164=CARTESIAN_POINT('Ctrl Pts',(-49.9084153153564,1076.67991546678,
350.590572237286));
#123165=CARTESIAN_POINT('Ctrl Pts',(-50.0713045452949,1076.67415320759,
350.423789609162));
#123166=CARTESIAN_POINT('Ctrl Pts',(-50.1352663641717,1076.67108484349,
350.325190465426));
#123167=CARTESIAN_POINT('Ctrl Pts',(-50.2205951676991,1076.66495902319,
350.109905191831));
#123168=CARTESIAN_POINT('Ctrl Pts',(-50.2415618915099,1076.66196233688,
349.995495063625));
#123169=CARTESIAN_POINT('Ctrl Pts',(-50.2381316140452,1076.65650070811,
349.765084242071));
#123170=CARTESIAN_POINT('Ctrl Pts',(-50.2137590463193,1076.65409128658,
349.651315422922));
#123171=CARTESIAN_POINT('Ctrl Pts',(-50.1224986918316,1076.6503118739,349.439751385887));
#123172=CARTESIAN_POINT('Ctrl Pts',(-50.0565270679309,1076.64898016664,
349.343997948549));
#123173=CARTESIAN_POINT('Ctrl Pts',(-49.891513023805,1076.64766604219,349.1835328555));
#123174=CARTESIAN_POINT('Ctrl Pts',(-49.7941231829853,1076.64769517389,
349.120329542137));
#123175=CARTESIAN_POINT('Ctrl Pts',(-49.583695091253,1076.64909847968,349.036310411531));
#123176=CARTESIAN_POINT('Ctrl Pts',(-49.4731558007671,1076.65041868008,
349.015072015133));
#123177=CARTESIAN_POINT('Ctrl Pts',(-49.3616411036557,1076.65225835227,
349.015072015145));
#123178=CARTESIAN_POINT('',(-49.3616411037539,1082.7251047501,349.015072015145));
#123179=CARTESIAN_POINT('',(-49.3616411037539,1067.7251047501,349.015072015145));
#123180=CARTESIAN_POINT('Origin',(-49.3616411037539,1082.7251047501,349.893375147338));
#123181=CARTESIAN_POINT('Ctrl Pts',(-49.3616411036557,1076.65225835227,
349.015072015145));
#123182=CARTESIAN_POINT('Ctrl Pts',(-49.358388971609,1076.65231200311,349.015072015146));
#123183=CARTESIAN_POINT('Ctrl Pts',(-49.3551360099501,1076.65236609375,
349.015090077852));
#123184=CARTESIAN_POINT('Ctrl Pts',(-49.237082057938,1076.65434454469,349.016401844435));
#123185=CARTESIAN_POINT('Ctrl Pts',(-49.1236465415889,1076.65677534514,
349.040174079882));
#123186=CARTESIAN_POINT('Ctrl Pts',(-48.9122815362571,1076.6622589491,349.130033646003));
#123187=CARTESIAN_POINT('Ctrl Pts',(-48.8163994673081,1076.66525699316,
349.195289044838));
#123188=CARTESIAN_POINT('Ctrl Pts',(-48.6551513088489,1076.67133890587,
349.359051416487));
#123189=CARTESIAN_POINT('Ctrl Pts',(-48.5913579463045,1076.67436309738,
349.456002597264));
#123190=CARTESIAN_POINT('Ctrl Pts',(-48.5070154856061,1076.67988048972,
349.663384664));
#123191=CARTESIAN_POINT('Ctrl Pts',(-48.4851032457939,1076.68234651501,
349.771045990123));
#123192=CARTESIAN_POINT('Ctrl Pts',(-48.4834403150115,1076.68450315177,
349.879967437887));
#123193=CARTESIAN_POINT('Ctrl Pts',(-48.48166237498,1076.68680894276,349.996421955609));
#123194=CARTESIAN_POINT('Ctrl Pts',(-48.5030657737506,1076.68871900412,
350.112081873623));
#123195=CARTESIAN_POINT('Ctrl Pts',(-48.5898341393267,1076.69165504541,
350.328517937336));
#123196=CARTESIAN_POINT('Ctrl Pts',(-48.6544168509016,1076.69265298522,
350.427108128113));
#123197=CARTESIAN_POINT('Ctrl Pts',(-48.8184786592588,1076.69368492031,
350.593416341232));
#123198=CARTESIAN_POINT('Ctrl Pts',(-48.9163750845321,1076.69370826272,
350.659417789244));
#123199=CARTESIAN_POINT('Ctrl Pts',(-49.1312263548964,1076.69277304321,
350.748789351629));
#123200=CARTESIAN_POINT('Ctrl Pts',(-49.2458735547687,1076.69183181851,
350.771678279532));
#123201=CARTESIAN_POINT('Ctrl Pts',(-49.3616411037539,1076.69042463418,
350.771678279532));
#123202=CARTESIAN_POINT('Origin',(-44.0648939479107,1067.7251047501,338.506780125395));
#123203=CARTESIAN_POINT('',(-44.0648939479323,1076.26837051893,337.231336004259));
#123204=CARTESIAN_POINT('',(-44.0648939479107,1067.7251047501,337.231336004259));
#123205=CARTESIAN_POINT('Ctrl Pts',(-44.0649261075141,1076.4151789643,339.782224246126));
#123206=CARTESIAN_POINT('Ctrl Pts',(-44.2336598940819,1076.41060464631,
339.782219991599));
#123207=CARTESIAN_POINT('Ctrl Pts',(-44.4006651244362,1076.40426367171,
339.748733322867));
#123208=CARTESIAN_POINT('Ctrl Pts',(-44.7122484929901,1076.38855220908,
339.618652496492));
#123209=CARTESIAN_POINT('Ctrl Pts',(-44.8536809853667,1076.37932519515,
339.52319728587));
#123210=CARTESIAN_POINT('Ctrl Pts',(-45.0306315424271,1076.36420574997,
339.344027076611));
#123211=CARTESIAN_POINT('Ctrl Pts',(-45.0829933660694,1076.35904397866,
339.279503945446));
#123212=CARTESIAN_POINT('Ctrl Pts',(-45.1752520753158,1076.34839634336,
339.140008453564));
#123213=CARTESIAN_POINT('Ctrl Pts',(-45.2146887254062,1076.34293216348,
339.065210168011));
#123214=CARTESIAN_POINT('Ctrl Pts',(-45.309571491767,1076.32656966431,338.831790783897));
#123215=CARTESIAN_POINT('Ctrl Pts',(-45.3414761794732,1076.31578487138,
338.665554696912));
#123216=CARTESIAN_POINT('Ctrl Pts',(-45.3391385409566,1076.29577801926,
338.330304067015));
#123217=CARTESIAN_POINT('Ctrl Pts',(-45.3049515910949,1076.28675174734,
338.164518416843));
#123218=CARTESIAN_POINT('Ctrl Pts',(-45.1744747321936,1076.2719115661,337.855950572801));
#123219=CARTESIAN_POINT('Ctrl Pts',(-45.079605021859,1076.26623866432,337.716115255821));
#123220=CARTESIAN_POINT('Ctrl Pts',(-44.8415852495467,1076.259208809,337.481430483732));
#123221=CARTESIAN_POINT('Ctrl Pts',(-44.7009398145652,1076.25790804247,
337.38872474482));
#123222=CARTESIAN_POINT('Ctrl Pts',(-44.3922760685759,1076.25991350823,
337.262879219626));
#123223=CARTESIAN_POINT('Ctrl Pts',(-44.227347641951,1076.26318826141,337.230829011179));
#123224=CARTESIAN_POINT('Ctrl Pts',(-43.8945015931953,1076.27380526315,
337.231855349343));
#123225=CARTESIAN_POINT('Ctrl Pts',(-43.7298146663088,1076.28104267337,
337.264949285428));
#123226=CARTESIAN_POINT('Ctrl Pts',(-43.4221342121765,1076.29837523064,
337.39258424967));
#123227=CARTESIAN_POINT('Ctrl Pts',(-43.2821552025762,1076.30830719036,
337.486065369304));
#123228=CARTESIAN_POINT('Ctrl Pts',(-43.1050532123365,1076.32411306166,
337.662723940361));
#123229=CARTESIAN_POINT('Ctrl Pts',(-43.0518889994096,1076.32950057698,
337.727328676111));
#123230=CARTESIAN_POINT('Ctrl Pts',(-42.9589294291105,1076.34033751772,
337.866020596402));
#123231=CARTESIAN_POINT('Ctrl Pts',(-42.9193609705127,1076.34576122432,
337.939783417094));
#123232=CARTESIAN_POINT('Ctrl Pts',(-42.8221237512356,1076.36197546012,
338.173521564673));
#123233=CARTESIAN_POINT('Ctrl Pts',(-42.7888468807461,1076.37236605329,
338.341636945681));
#123234=CARTESIAN_POINT('Ctrl Pts',(-42.7900653299466,1076.39102444614,
338.680003284053));
#123235=CARTESIAN_POINT('Ctrl Pts',(-42.8241096351059,1076.39912655215,
338.846913054497));
#123236=CARTESIAN_POINT('Ctrl Pts',(-42.9552802592578,1076.4122089099,339.157939313282));
#123237=CARTESIAN_POINT('Ctrl Pts',(-43.0511214816866,1076.41706360979,
339.298959797462));
#123238=CARTESIAN_POINT('Ctrl Pts',(-43.2925182921174,1076.42302688752,
339.535782995973));
#123239=CARTESIAN_POINT('Ctrl Pts',(-43.4357602165995,1076.42407033161,
339.629103391144));
#123240=CARTESIAN_POINT('Ctrl Pts',(-43.7432075571928,1076.42224124413,
339.751529034989));
#123241=CARTESIAN_POINT('Ctrl Pts',(-43.9033505103276,1076.41955922611,
339.782228320163));
#123242=CARTESIAN_POINT('Ctrl Pts',(-44.064926107514,1076.4151789643,339.782224246126));
#123243=CARTESIAN_POINT('Origin',(-44.0648939479107,1067.7251047501,338.506780125395));
#123244=CARTESIAN_POINT('',(-44.0648939479107,1076.38310559156,339.182224246531));
#123245=CARTESIAN_POINT('',(-44.0648939479116,1076.3053526307,337.831336004259));
#123246=CARTESIAN_POINT('Ctrl Pts',(-44.0648939479107,1076.38310559156,
339.182224246531));
#123247=CARTESIAN_POINT('Ctrl Pts',(-44.0701053267806,1076.38295851287,
339.182224246531));
#123248=CARTESIAN_POINT('Ctrl Pts',(-44.07531929434,1076.382807996,339.182163934248));
#123249=CARTESIAN_POINT('Ctrl Pts',(-44.1703403507942,1076.3800033562,339.179962995578));
#123250=CARTESIAN_POINT('Ctrl Pts',(-44.2587997309686,1076.37639117361,
339.159989869285));
#123251=CARTESIAN_POINT('Ctrl Pts',(-44.422867070002,1076.36759865339,339.086586505214));
#123252=CARTESIAN_POINT('Ctrl Pts',(-44.4968037028826,1076.36250120841,
339.033812918612));
#123253=CARTESIAN_POINT('Ctrl Pts',(-44.5883168675794,1076.35427915154,
338.935959179585));
#123254=CARTESIAN_POINT('Ctrl Pts',(-44.6151895017533,1076.35149386377,
338.900912515337));
#123255=CARTESIAN_POINT('Ctrl Pts',(-44.6620541643205,1076.34579761963,
338.825560558424));
#123256=CARTESIAN_POINT('Ctrl Pts',(-44.6818289598925,1076.34289924136,
338.785370116022));
#123257=CARTESIAN_POINT('Ctrl Pts',(-44.7285808174976,1076.33428482065,
338.660445497062));
#123258=CARTESIAN_POINT('Ctrl Pts',(-44.743010021877,1076.32868756283,338.572034526306));
#123259=CARTESIAN_POINT('Ctrl Pts',(-44.7368560300366,1076.31843825193,
338.394749413042));
#123260=CARTESIAN_POINT('Ctrl Pts',(-44.7163664259211,1076.31388509559,
338.307582723559));
#123261=CARTESIAN_POINT('Ctrl Pts',(-44.6429157475108,1076.30650787739,
338.14629644736));
#123262=CARTESIAN_POINT('Ctrl Pts',(-44.5907474285419,1076.30375264393,
338.073714035702));
#123263=CARTESIAN_POINT('Ctrl Pts',(-44.461504086302,1076.30046952909,337.952952110373));
#123264=CARTESIAN_POINT('Ctrl Pts',(-44.3857627848415,1076.29996838611,
337.905888769468));
#123265=CARTESIAN_POINT('Ctrl Pts',(-44.2269518232933,1076.30125692338,
337.846034014573));
#123266=CARTESIAN_POINT('Ctrl Pts',(-44.1462502246026,1076.30285836369,
337.831336791843));
#123267=CARTESIAN_POINT('Ctrl Pts',(-44.0649004869312,1076.30535243022,
337.831336004291));
#123268=CARTESIAN_POINT('',(-44.0648939479107,1082.7251047501,337.831336004259));
#123269=CARTESIAN_POINT('',(-44.0648939479107,1067.7251047501,337.831336004259));
#123270=CARTESIAN_POINT('Origin',(-44.0648939479107,1082.7251047501,338.506780125395));
#123271=CARTESIAN_POINT('Ctrl Pts',(-44.0648939479131,1076.3053526307,337.831336004259));
#123272=CARTESIAN_POINT('Ctrl Pts',(-43.9766448134179,1076.30805827353,
337.831336004259));
#123273=CARTESIAN_POINT('Ctrl Pts',(-43.889288750267,1076.31176270499,337.848628616159));
#123274=CARTESIAN_POINT('Ctrl Pts',(-43.7260036952492,1076.32070212658,
337.915854565925));
#123275=CARTESIAN_POINT('Ctrl Pts',(-43.6516833975952,1076.3258532554,337.965220516065));
#123276=CARTESIAN_POINT('Ctrl Pts',(-43.5576135704436,1076.33411829575,
338.058621136685));
#123277=CARTESIAN_POINT('Ctrl Pts',(-43.5293733861181,1076.33694500713,
338.092778854888));
#123278=CARTESIAN_POINT('Ctrl Pts',(-43.4799654418549,1076.34265482929,
338.166133842445));
#123279=CARTESIAN_POINT('Ctrl Pts',(-43.4589184628472,1076.34552439997,
338.205159436198));
#123280=CARTESIAN_POINT('Ctrl Pts',(-43.4070362814347,1076.35415686086,
338.32909816132));
#123281=CARTESIAN_POINT('Ctrl Pts',(-43.3892155291544,1076.35974582471,
338.41838465554));
#123282=CARTESIAN_POINT('Ctrl Pts',(-43.3896877983555,1076.36987042931,
338.598348130609));
#123283=CARTESIAN_POINT('Ctrl Pts',(-43.4078277279341,1076.37431118753,
338.68723528674));
#123284=CARTESIAN_POINT('Ctrl Pts',(-43.4778407350897,1076.38150504704,
338.852695445679));
#123285=CARTESIAN_POINT('Ctrl Pts',(-43.5289898388636,1076.38418867834,
338.927619124806));
#123286=CARTESIAN_POINT('Ctrl Pts',(-43.6576940453655,1076.38746799743,
339.053129768485));
#123287=CARTESIAN_POINT('Ctrl Pts',(-43.733965202815,1076.38802990554,339.102429483049));
#123288=CARTESIAN_POINT('Ctrl Pts',(-43.8964582207888,1076.38697465127,
339.16634457229));
#123289=CARTESIAN_POINT('Ctrl Pts',(-43.980335296259,1076.38549205715,339.182224246531));
#123290=CARTESIAN_POINT('Ctrl Pts',(-44.0648939479107,1076.38310559156,
339.182224246531));
#123291=CARTESIAN_POINT('Origin',(-37.1057957606635,1067.7251047501,326.532256785149));
#123292=CARTESIAN_POINT('',(-37.1057957606863,1075.54602985383,325.433425649156));
#123293=CARTESIAN_POINT('',(-37.1057957606635,1067.7251047501,325.433425649156));
#123294=CARTESIAN_POINT('Ctrl Pts',(-37.1058073123272,1075.76001085596,
327.63108792108));
#123295=CARTESIAN_POINT('Ctrl Pts',(-37.2518284405106,1075.75482651318,
327.631086386007));
#123296=CARTESIAN_POINT('Ctrl Pts',(-37.3962598046139,1075.74695417433,
327.601981034185));
#123297=CARTESIAN_POINT('Ctrl Pts',(-37.6650853491754,1075.72665806207,
327.489263457504));
#123298=CARTESIAN_POINT('Ctrl Pts',(-37.7867990112802,1075.71443564425,
327.406797640552));
#123299=CARTESIAN_POINT('Ctrl Pts',(-37.9914435144782,1075.68708110747,
327.198924779726));
#123300=CARTESIAN_POINT('Ctrl Pts',(-38.0721596202323,1075.67219889787,
327.075320147664));
#123301=CARTESIAN_POINT('Ctrl Pts',(-38.180945642096,1075.64166922648,326.802791977858));
#123302=CARTESIAN_POINT('Ctrl Pts',(-38.2075079548967,1075.62631399735,
326.656321017783));
#123303=CARTESIAN_POINT('Ctrl Pts',(-38.2013114880832,1075.59771489936,
326.364408113399));
#123304=CARTESIAN_POINT('Ctrl Pts',(-38.169749465209,1075.58470882455,326.221764156176));
#123305=CARTESIAN_POINT('Ctrl Pts',(-38.0532988666014,1075.56269452548,
325.957446292491));
#123306=CARTESIAN_POINT('Ctrl Pts',(-37.9698350118053,1075.55388054548,
325.838221115935));
#123307=CARTESIAN_POINT('Ctrl Pts',(-37.7620152173118,1075.54176321282,
325.639303563615));
#123308=CARTESIAN_POINT('Ctrl Pts',(-37.6399766875971,1075.53854797351,
325.561342179345));
#123309=CARTESIAN_POINT('Ctrl Pts',(-37.3731357590198,1075.53819317261,
325.456886005567));
#123310=CARTESIAN_POINT('Ctrl Pts',(-37.2310757442444,1075.54103782532,
325.431272211773));
#123311=CARTESIAN_POINT('Ctrl Pts',(-36.9449401196969,1075.55240702316,
325.435867034869));
#123312=CARTESIAN_POINT('Ctrl Pts',(-36.8036954486044,1075.56082839968,
325.466140682772));
#123313=CARTESIAN_POINT('Ctrl Pts',(-36.5401773185045,1075.58211239206,
325.579268049508));
#123314=CARTESIAN_POINT('Ctrl Pts',(-36.4205720923164,1075.59479213284,
325.661335190783));
#123315=CARTESIAN_POINT('Ctrl Pts',(-36.2192627347873,1075.62267128543,
325.867176742192));
#123316=CARTESIAN_POINT('Ctrl Pts',(-36.1396820771978,1075.63761886704,
325.989239640643));
#123317=CARTESIAN_POINT('Ctrl Pts',(-36.0592605433807,1075.66012338436,
326.189708769316));
#123318=CARTESIAN_POINT('Ctrl Pts',(-36.0391332125001,1075.66756631343,
326.258745241083));
#123319=CARTESIAN_POINT('Ctrl Pts',(-35.9989565568231,1075.68971399939,
326.472477529121));
#123320=CARTESIAN_POINT('Ctrl Pts',(-36.0007730411933,1075.70377809693,
326.61973599735));
#123321=CARTESIAN_POINT('Ctrl Pts',(-36.0618194981078,1075.72874992371,
326.904693915371));
#123322=CARTESIAN_POINT('Ctrl Pts',(-36.1202761882012,1075.73942548664,
327.039631897666));
#123323=CARTESIAN_POINT('Ctrl Pts',(-36.2867996883745,1075.75607775343,
327.279251163207));
#123324=CARTESIAN_POINT('Ctrl Pts',(-36.393269326976,1075.76187977416,327.3814441553));
#123325=CARTESIAN_POINT('Ctrl Pts',(-36.6375840605244,1075.76775699067,
327.536602841777));
#123326=CARTESIAN_POINT('Ctrl Pts',(-36.7723094344706,1075.76789137202,
327.589007226966));
#123327=CARTESIAN_POINT('Ctrl Pts',(-36.9768529295806,1075.76405293402,
327.625404456655));
#123328=CARTESIAN_POINT('Ctrl Pts',(-37.0412749341261,1075.76230201733,
327.631088599489));
#123329=CARTESIAN_POINT('Ctrl Pts',(-37.1058073123272,1075.76001085596,
327.63108792108));
#123330=CARTESIAN_POINT('Origin',(-37.1057957606635,1067.7251047501,326.532256785149));
#123331=CARTESIAN_POINT('',(-37.1057957606635,1075.70357965628,327.031087921141));
#123332=CARTESIAN_POINT('',(-37.1057957606635,1075.60643384366,326.033425649156));
#123333=CARTESIAN_POINT('Ctrl Pts',(-37.1057957606635,1075.70357965628,
327.031087921141));
#123334=CARTESIAN_POINT('Ctrl Pts',(-37.140106488576,1075.7023363494,327.031087921141));
#123335=CARTESIAN_POINT('Ctrl Pts',(-37.1743956888152,1075.70075395455,
327.027547901333));
#123336=CARTESIAN_POINT('Ctrl Pts',(-37.273219899766,1075.69517982228,327.006837474669));
#123337=CARTESIAN_POINT('Ctrl Pts',(-37.3348755442173,1075.69039082338,
326.980322296078));
#123338=CARTESIAN_POINT('Ctrl Pts',(-37.444177405344,1075.67911765527,326.904750563201));
#123339=CARTESIAN_POINT('Ctrl Pts',(-37.4907178407904,1075.67274226759,
326.856410606957));
#123340=CARTESIAN_POINT('Ctrl Pts',(-37.5622347215614,1075.65923254556,
326.74423882876));
#123341=CARTESIAN_POINT('Ctrl Pts',(-37.5864371812949,1075.65222653652,
326.681440921334));
#123342=CARTESIAN_POINT('Ctrl Pts',(-37.6087771550836,1075.63854469637,
326.549854573336));
#123343=CARTESIAN_POINT('Ctrl Pts',(-37.6066148687186,1075.63200363463,
326.482331093145));
#123344=CARTESIAN_POINT('Ctrl Pts',(-37.5760845179854,1075.62047616974,
326.35353043989));
#123345=CARTESIAN_POINT('Ctrl Pts',(-37.5485935844269,1075.61556928953,
326.293380523485));
#123346=CARTESIAN_POINT('Ctrl Pts',(-37.4720539903056,1075.60796033873,
326.187387836821));
#123347=CARTESIAN_POINT('Ctrl Pts',(-37.4238868403951,1075.60532031765,
326.142500625099));
#123348=CARTESIAN_POINT('Ctrl Pts',(-37.3131435041877,1075.60267900704,
326.073930327446));
#123349=CARTESIAN_POINT('Ctrl Pts',(-37.2517311074801,1075.60269334399,
326.050843199775));
#123350=CARTESIAN_POINT('Ctrl Pts',(-37.1605723102931,1075.60460678886,
326.035684601278));
#123351=CARTESIAN_POINT('Ctrl Pts',(-37.1332046641734,1075.60540804463,
326.033425719712));
#123352=CARTESIAN_POINT('Ctrl Pts',(-37.1057970447751,1075.6064337956,326.033425649158));
#123353=CARTESIAN_POINT('',(-37.1057957606635,1082.7251047501,326.033425649156));
#123354=CARTESIAN_POINT('',(-37.1057957606635,1067.7251047501,326.033425649156));
#123355=CARTESIAN_POINT('Origin',(-37.1057957606635,1082.7251047501,326.532256785149));
#123356=CARTESIAN_POINT('Ctrl Pts',(-37.1057957606636,1075.60643384366,
326.033425649156));
#123357=CARTESIAN_POINT('Ctrl Pts',(-37.0407169455499,1075.6088694843,326.033425649156));
#123358=CARTESIAN_POINT('Ctrl Pts',(-36.9763277968887,1075.61253673435,
326.046159525286));
#123359=CARTESIAN_POINT('Ctrl Pts',(-36.8558063188034,1075.6219137584,326.095671962726));
#123360=CARTESIAN_POINT('Ctrl Pts',(-36.8008960338681,1075.62754321943,
326.132105180252));
#123361=CARTESIAN_POINT('Ctrl Pts',(-36.7071388769123,1075.64013808892,
326.225060758133));
#123362=CARTESIAN_POINT('Ctrl Pts',(-36.6696435445463,1075.64700825431,
326.281138031886));
#123363=CARTESIAN_POINT('Ctrl Pts',(-36.6319410649877,1075.65734999268,
326.373025779382));
#123364=CARTESIAN_POINT('Ctrl Pts',(-36.622558756964,1075.6607360617,326.404291296112));
#123365=CARTESIAN_POINT('Ctrl Pts',(-36.6035095940503,1075.67086637644,
326.501416618221));
#123366=CARTESIAN_POINT('Ctrl Pts',(-36.6038605143582,1075.67734593208,
326.568529010141));
#123367=CARTESIAN_POINT('Ctrl Pts',(-36.6308674213977,1075.68891197812,
326.698635881763));
#123368=CARTESIAN_POINT('Ctrl Pts',(-36.6572112485464,1075.69388735971,
326.760353983765));
#123369=CARTESIAN_POINT('Ctrl Pts',(-36.7322444818216,1075.70162342845,
326.869335007153));
#123370=CARTESIAN_POINT('Ctrl Pts',(-36.7799438054035,1075.70433043034,
326.915656103613));
#123371=CARTESIAN_POINT('Ctrl Pts',(-36.8899237168445,1075.70714178724,
326.986631850417));
#123372=CARTESIAN_POINT('Ctrl Pts',(-36.9509059692144,1075.70725318984,
327.010866369372));
#123373=CARTESIAN_POINT('Ctrl Pts',(-37.0449053721231,1075.70551868177,
327.028302317338));
#123374=CARTESIAN_POINT('Ctrl Pts',(-37.0753590365554,1075.70468258213,
327.031087921141));
#123375=CARTESIAN_POINT('Ctrl Pts',(-37.1057957606635,1075.70357965628,
327.031087921141));
#123376=CARTESIAN_POINT('Origin',(-27.7552687727512,1067.7251047501,316.130256973654));
#123377=CARTESIAN_POINT('',(-27.7552687727736,1074.65680240674,315.039716224926));
#123378=CARTESIAN_POINT('',(-27.7552687727512,1067.7251047501,315.039716224926));
#123379=CARTESIAN_POINT('Ctrl Pts',(-27.7552727853641,1074.94285712098,
317.220797722375));
#123380=CARTESIAN_POINT('Ctrl Pts',(-27.8973584452209,1074.93820301204,
317.220797199575));
#123381=CARTESIAN_POINT('Ctrl Pts',(-28.0378937657681,1074.93004129443,
317.193032001366));
#123382=CARTESIAN_POINT('Ctrl Pts',(-28.3030665935802,1074.90733597777,
317.084292366754));
#123383=CARTESIAN_POINT('Ctrl Pts',(-28.4245787743323,1074.89288518666,
317.003270315551));
#123384=CARTESIAN_POINT('Ctrl Pts',(-28.6292838197719,1074.85956610145,
316.798433088887));
#123385=CARTESIAN_POINT('Ctrl Pts',(-28.7102642929308,1074.84099679104,
316.676382741362));
#123386=CARTESIAN_POINT('Ctrl Pts',(-28.7918734176438,1074.81211645738,
316.476365811308));
#123387=CARTESIAN_POINT('Ctrl Pts',(-28.8122365366506,1074.8024781713,316.408029337154));
#123388=CARTESIAN_POINT('Ctrl Pts',(-28.85373449036,1074.77302037737,316.194396321065));
#123389=CARTESIAN_POINT('Ctrl Pts',(-28.8524287703557,1074.75351190795,
316.046308775394));
#123390=CARTESIAN_POINT('Ctrl Pts',(-28.7918689412043,1074.71791835285,
315.762327358554));
#123391=CARTESIAN_POINT('Ctrl Pts',(-28.7343987300333,1074.70210609435,
315.628907896589));
#123392=CARTESIAN_POINT('Ctrl Pts',(-28.5713852237671,1074.67617142822,
315.392974176405));
#123393=CARTESIAN_POINT('Ctrl Pts',(-28.4679187224216,1074.66624974281,
315.29247203694));
#123394=CARTESIAN_POINT('Ctrl Pts',(-28.2287806000093,1074.65369806997,
315.137703554575));
#123395=CARTESIAN_POINT('Ctrl Pts',(-28.0958312668207,1074.65113008374,
315.084585446537));
#123396=CARTESIAN_POINT('Ctrl Pts',(-27.8173253647566,1074.65368051675,
315.032329998061));
#123397=CARTESIAN_POINT('Ctrl Pts',(-27.6746487315551,1074.65875008991,
315.033567962164));
#123398=CARTESIAN_POINT('Ctrl Pts',(-27.3971930839227,1074.67587815065,
315.090438759667));
#123399=CARTESIAN_POINT('Ctrl Pts',(-27.2652386157998,1074.68779999794,
315.145787840477));
#123400=CARTESIAN_POINT('Ctrl Pts',(-27.0289748507789,1074.7169759611,315.304291257733));
#123401=CARTESIAN_POINT('Ctrl Pts',(-26.9272378234838,1074.73399973998,
315.406398978482));
#123402=CARTESIAN_POINT('Ctrl Pts',(-26.8082980716652,1074.76159306632,
315.584664699751));
#123403=CARTESIAN_POINT('Ctrl Pts',(-26.7744856246139,1074.77110284607,
315.648093801851));
#123404=CARTESIAN_POINT('Ctrl Pts',(-26.7198903389802,1074.79035914604,
315.780429150949));
#123405=CARTESIAN_POINT('Ctrl Pts',(-26.6991939337255,1074.80006156145,
315.849021623245));
#123406=CARTESIAN_POINT('Ctrl Pts',(-26.6572695965763,1074.82929992101,
316.061489943875));
#123407=CARTESIAN_POINT('Ctrl Pts',(-26.6578452791933,1074.84839480724,
316.208149109684));
#123408=CARTESIAN_POINT('Ctrl Pts',(-26.7163654965046,1074.88327995893,
316.491938847863));
#123409=CARTESIAN_POINT('Ctrl Pts',(-26.7733835538738,1074.89875909424,
316.626412377309));
#123410=CARTESIAN_POINT('Ctrl Pts',(-26.9368389624288,1074.92413906852,
316.865353924037));
#123411=CARTESIAN_POINT('Ctrl Pts',(-27.0415458977297,1074.93379587298,
316.967462358757));
#123412=CARTESIAN_POINT('Ctrl Pts',(-27.2823376330203,1074.94583858414,
317.123073465832));
#123413=CARTESIAN_POINT('Ctrl Pts',(-27.4152213834633,1074.94826787575,
317.176081451513));
#123414=CARTESIAN_POINT('Ctrl Pts',(-27.6207763410728,1074.946463579,317.214566103836));
#123415=CARTESIAN_POINT('Ctrl Pts',(-27.6879608245359,1074.94506196839,
317.220797970047));
#123416=CARTESIAN_POINT('Ctrl Pts',(-27.7552727853641,1074.94285712098,
317.220797722375));
#123417=CARTESIAN_POINT('Origin',(-27.7552687727512,1067.7251047501,316.130256973654));
#123418=CARTESIAN_POINT('',(-27.7552687727512,1074.86607808781,316.620797722383));
#123419=CARTESIAN_POINT('',(-27.7552687727512,1074.73740020174,315.639716224926));
#123420=CARTESIAN_POINT('Ctrl Pts',(-27.7552687727512,1074.86607808781,
316.620797722383));
#123421=CARTESIAN_POINT('Ctrl Pts',(-27.7884696064037,1074.86497585636,
316.620797722383));
#123422=CARTESIAN_POINT('Ctrl Pts',(-27.8216492971736,1074.86343664612,
316.617427003901));
#123423=CARTESIAN_POINT('Ctrl Pts',(-27.9170085408949,1074.85771584,316.59777272351));
#123424=CARTESIAN_POINT('Ctrl Pts',(-27.9764850729975,1074.85248196319,
316.572714128191));
#123425=CARTESIAN_POINT('Ctrl Pts',(-28.0837233019206,1074.83949904116,
316.500440952334));
#123426=CARTESIAN_POINT('Ctrl Pts',(-28.1300673257111,1074.831818402,316.453397041095));
#123427=CARTESIAN_POINT('Ctrl Pts',(-28.1833214032295,1074.81939504425,
316.371970184342));
#123428=CARTESIAN_POINT('Ctrl Pts',(-28.198167470537,1074.8151797047,316.343548883207));
#123429=CARTESIAN_POINT('Ctrl Pts',(-28.222132474559,1074.8066020564,316.284188817218));
#123430=CARTESIAN_POINT('Ctrl Pts',(-28.2311863850425,1074.8022586878,316.25337819008));
#123431=CARTESIAN_POINT('Ctrl Pts',(-28.2494497329859,1074.78904135798,
316.157349397889));
#123432=CARTESIAN_POINT('Ctrl Pts',(-28.2486406854603,1074.78032991429,
316.090923533509));
#123433=CARTESIAN_POINT('Ctrl Pts',(-28.2209875291239,1074.76440635846,
315.9630313853));
#123434=CARTESIAN_POINT('Ctrl Pts',(-28.1947220220795,1074.75732954294,
315.902733652316));
#123435=CARTESIAN_POINT('Ctrl Pts',(-28.1206277481484,1074.74581605109,
315.796710376851));
#123436=CARTESIAN_POINT('Ctrl Pts',(-28.0739006966746,1074.74144915903,
315.751788809119));
#123437=CARTESIAN_POINT('Ctrl Pts',(-27.9660563149437,1074.73595691929,
315.682749211619));
#123438=CARTESIAN_POINT('Ctrl Pts',(-27.9061520431679,1074.73486034789,
315.659156489425));
#123439=CARTESIAN_POINT('Ctrl Pts',(-27.81430495024,1074.73575206587,315.642385335104));
#123440=CARTESIAN_POINT('Ctrl Pts',(-27.7848132644947,1074.73639847351,
315.639716237778));
#123441=CARTESIAN_POINT('Ctrl Pts',(-27.755268986145,1074.73740019451,315.639716224926));
#123442=CARTESIAN_POINT('',(-27.7552687727512,1082.7251047501,315.639716224926));
#123443=CARTESIAN_POINT('',(-27.7552687727512,1067.7251047501,315.639716224926));
#123444=CARTESIAN_POINT('Origin',(-27.7552687727512,1082.7251047501,316.130256973654));
#123445=CARTESIAN_POINT('Ctrl Pts',(-27.7552687727512,1074.73740020174,
315.639716224926));
#123446=CARTESIAN_POINT('Ctrl Pts',(-27.6915062829793,1074.73956212063,
315.639716224926));
#123447=CARTESIAN_POINT('Ctrl Pts',(-27.6284419276466,1074.74334710473,
315.652146476916));
#123448=CARTESIAN_POINT('Ctrl Pts',(-27.5102192567908,1074.753745222,315.70049679494));
#123449=CARTESIAN_POINT('Ctrl Pts',(-27.4562985012817,1074.76027853999,
315.736134215707));
#123450=CARTESIAN_POINT('Ctrl Pts',(-27.3638940977153,1074.77541819911,
315.827279615052));
#123451=CARTESIAN_POINT('Ctrl Pts',(-27.3268432956719,1074.78393176463,
315.882460540546));
#123452=CARTESIAN_POINT('Ctrl Pts',(-27.2895397096046,1074.79706746359,
315.972911992357));
#123453=CARTESIAN_POINT('Ctrl Pts',(-27.2802430053885,1074.80142252945,
316.003721191227));
#123454=CARTESIAN_POINT('Ctrl Pts',(-27.2613460142679,1074.81459913811,
316.099406401156));
#123455=CARTESIAN_POINT('Ctrl Pts',(-27.2616284401372,1074.82323949055,
316.165544848401));
#123456=CARTESIAN_POINT('Ctrl Pts',(-27.2881526839442,1074.83907391969,
316.29363484863));
#123457=CARTESIAN_POINT('Ctrl Pts',(-27.3140306965928,1074.84612183971,
316.354369608848));
#123458=CARTESIAN_POINT('Ctrl Pts',(-27.3877637173149,1074.85760796943,
316.461532688281));
#123459=CARTESIAN_POINT('Ctrl Pts',(-27.4345898663682,1074.86196601396,
316.50707588247));
#123460=CARTESIAN_POINT('Ctrl Pts',(-27.5425300250943,1074.86743669456,
316.576838097611));
#123461=CARTESIAN_POINT('Ctrl Pts',(-27.6023149030358,1074.86854575969,
316.600686958105));
#123462=CARTESIAN_POINT('Ctrl Pts',(-27.694858086976,1074.86772161904,316.618009572747));
#123463=CARTESIAN_POINT('Ctrl Pts',(-27.7250721744106,1074.86708058192,
316.620797722383));
#123464=CARTESIAN_POINT('Ctrl Pts',(-27.7552687727512,1074.86607808781,
316.620797722383));
#123465=CARTESIAN_POINT('Origin',(-63.8195601713292,1067.7251047501,361.789198753807));
#123466=CARTESIAN_POINT('',(-63.8195601713524,1076.6426633433,360.310895621613));
#123467=CARTESIAN_POINT('',(-63.8195601713292,1067.7251047501,360.310895621613));
#123468=CARTESIAN_POINT('Ctrl Pts',(-63.8201632810582,1076.69670629135,
363.267501762973));
#123469=CARTESIAN_POINT('Ctrl Pts',(-64.015353854477,1076.69386865944,363.267422130224));
#123470=CARTESIAN_POINT('Ctrl Pts',(-64.2085968376498,1076.69033702687,
363.228685102967));
#123471=CARTESIAN_POINT('Ctrl Pts',(-64.5706194753776,1076.68192930682,
363.077661357673));
#123472=CARTESIAN_POINT('Ctrl Pts',(-64.735509565079,1076.67711908905,362.966166911613));
#123473=CARTESIAN_POINT('Ctrl Pts',(-65.0096989131915,1076.66686056675,
362.687302338553));
#123474=CARTESIAN_POINT('Ctrl Pts',(-65.1171648687651,1076.66152410503,
362.523529083437));
#123475=CARTESIAN_POINT('Ctrl Pts',(-65.2627692911948,1076.65111675822,
362.163678711344));
#123476=CARTESIAN_POINT('Ctrl Pts',(-65.2994325087523,1076.64615292214,
361.971061474138));
#123477=CARTESIAN_POINT('Ctrl Pts',(-65.2961912983331,1076.63759819319,
361.582681058723));
#123478=CARTESIAN_POINT('Ctrl Pts',(-65.256325482641,1076.63409755005,361.390693151394));
#123479=CARTESIAN_POINT('Ctrl Pts',(-65.1047862765125,1076.6293551382,361.033458505376));
#123480=CARTESIAN_POINT('Ctrl Pts',(-64.9947309899203,1076.62815957435,
360.871632163452));
#123481=CARTESIAN_POINT('Ctrl Pts',(-64.7188321430135,1076.628364894,360.60005985534));
#123482=CARTESIAN_POINT('Ctrl Pts',(-64.5558209929454,1076.62975614991,
360.492797899789));
#123483=CARTESIAN_POINT('Ctrl Pts',(-64.1980757816965,1076.63482298825,
360.347206975795));
#123484=CARTESIAN_POINT('Ctrl Pts',(-64.00683986861,1076.6384411848,360.310169143266));
#123485=CARTESIAN_POINT('Ctrl Pts',(-63.6208982831683,1076.64714170327,
360.311644008145));
#123486=CARTESIAN_POINT('Ctrl Pts',(-63.4298961045216,1076.65213408422,
360.350175191289));
#123487=CARTESIAN_POINT('Ctrl Pts',(-63.0732830495466,1076.66253495407,
360.498541330444));
#123488=CARTESIAN_POINT('Ctrl Pts',(-62.9111308706323,1076.66783855036,
360.607046398371));
#123489=CARTESIAN_POINT('Ctrl Pts',(-62.6377034902941,1076.67790751942,
360.880364469796));
#123490=CARTESIAN_POINT('Ctrl Pts',(-62.5290851983599,1076.68257505022,
361.042574576914));
#123491=CARTESIAN_POINT('Ctrl Pts',(-62.3797882542706,1076.69080186221,
361.401241248447));
#123492=CARTESIAN_POINT('Ctrl Pts',(-62.3412016120399,1076.69427503924,
361.594470437375));
#123493=CARTESIAN_POINT('Ctrl Pts',(-62.3413125454988,1076.69982894111,
361.984626181701));
#123494=CARTESIAN_POINT('Ctrl Pts',(-62.3799534221957,1076.7018646516,362.177716371857));
#123495=CARTESIAN_POINT('Ctrl Pts',(-62.5302048996037,1076.70456231898,
362.538348616852));
#123496=CARTESIAN_POINT('Ctrl Pts',(-62.6405679067661,1076.70519950057,
362.702238464813));
#123497=CARTESIAN_POINT('Ctrl Pts',(-62.9186743733461,1076.70510896687,
362.977498579521));
#123498=CARTESIAN_POINT('Ctrl Pts',(-63.0836594593772,1076.70438212369,
363.08615667722));
#123499=CARTESIAN_POINT('Ctrl Pts',(-63.4413841836492,1076.70153441586,
363.230923411168));
#123500=CARTESIAN_POINT('Ctrl Pts',(-63.6298963787954,1076.69947234416,
363.267579386992));
#123501=CARTESIAN_POINT('Ctrl Pts',(-63.8201632810582,1076.69670629135,
363.267501762973));
#123502=CARTESIAN_POINT('Origin',(-63.8195601713292,1067.7251047501,361.789198753807));
#123503=CARTESIAN_POINT('',(-63.8195601713292,1076.68781395203,362.667501886));
#123504=CARTESIAN_POINT('',(-63.8195601713159,1076.65571487055,360.910895621613));
#123505=CARTESIAN_POINT('Ctrl Pts',(-63.8195601713292,1076.68781395203,
362.667501886));
#123506=CARTESIAN_POINT('Ctrl Pts',(-63.8199454877377,1076.68780771864,
362.667501886));
#123507=CARTESIAN_POINT('Ctrl Pts',(-63.8203308166387,1076.6878014804,362.667501632439));
#123508=CARTESIAN_POINT('Ctrl Pts',(-63.9373488144158,1076.68590561051,
362.66734761803));
#123509=CARTESIAN_POINT('Ctrl Pts',(-64.0527834853948,1076.68360606599,
362.643963785317));
#123510=CARTESIAN_POINT('Ctrl Pts',(-64.268441678792,1076.67832383068,362.553198415436));
#123511=CARTESIAN_POINT('Ctrl Pts',(-64.3663936634442,1076.67538804155,
362.486451144002));
#123512=CARTESIAN_POINT('Ctrl Pts',(-64.5287569903648,1076.66930624779,
362.319976532879));
#123513=CARTESIAN_POINT('Ctrl Pts',(-64.5921817907566,1076.66622437169,
362.222490044308));
#123514=CARTESIAN_POINT('Ctrl Pts',(-64.6778083774569,1076.6603259619,362.008539966662));
#123515=CARTESIAN_POINT('Ctrl Pts',(-64.6991574664424,1076.65756875994,
361.894137712006));
#123516=CARTESIAN_POINT('Ctrl Pts',(-64.6964480560042,1076.65286913567,
361.663635011196));
#123517=CARTESIAN_POINT('Ctrl Pts',(-64.6724242359687,1076.65097478949,
361.549771841494));
#123518=CARTESIAN_POINT('Ctrl Pts',(-64.5818293995344,1076.64842252704,
361.337966531035));
#123519=CARTESIAN_POINT('Ctrl Pts',(-64.5161979903458,1076.64778936419,
361.242058726776));
#123520=CARTESIAN_POINT('Ctrl Pts',(-64.3518317690396,1076.64791989456,
361.081170561096));
#123521=CARTESIAN_POINT('Ctrl Pts',(-64.2547513026543,1076.64867960996,
361.017691267961));
#123522=CARTESIAN_POINT('Ctrl Pts',(-64.0437424557757,1076.65142648614,
360.932548615098));
#123523=CARTESIAN_POINT('Ctrl Pts',(-63.9321584635616,1076.65336191998,
360.91089562161));
#123524=CARTESIAN_POINT('Ctrl Pts',(-63.8195601713027,1076.65571487055,
360.910895621613));
#123525=CARTESIAN_POINT('',(-63.8195601713292,1082.7251047501,360.910895621613));
#123526=CARTESIAN_POINT('',(-63.8195601713292,1067.7251047501,360.910895621613));
#123527=CARTESIAN_POINT('Origin',(-63.8195601713292,1082.7251047501,361.789198753807));
#123528=CARTESIAN_POINT('Ctrl Pts',(-63.8195601713027,1076.65571487055,
360.910895621613));
#123529=CARTESIAN_POINT('Ctrl Pts',(-63.8174430765292,1076.65575911118,
360.910895621613));
#123530=CARTESIAN_POINT('Ctrl Pts',(-63.8153256231689,1076.65580349898,
360.910903276298));
#123531=CARTESIAN_POINT('Ctrl Pts',(-63.6984101531963,1076.65826207426,
360.911748888507));
#123532=CARTESIAN_POINT('Ctrl Pts',(-63.5848877566488,1076.66105759599,
360.935078370482));
#123533=CARTESIAN_POINT('Ctrl Pts',(-63.3731563508884,1076.66698821698,
361.024121575518));
#123534=CARTESIAN_POINT('Ctrl Pts',(-63.2770008061881,1076.67006465605,
361.08902112782));
#123535=CARTESIAN_POINT('Ctrl Pts',(-63.1151044300733,1076.67604241627,
361.252194543827));
#123536=CARTESIAN_POINT('Ctrl Pts',(-63.0509377109618,1076.67888594666,
361.348911073015));
#123537=CARTESIAN_POINT('Ctrl Pts',(-62.9653862248395,1076.68389356872,
361.557012103622));
#123538=CARTESIAN_POINT('Ctrl Pts',(-62.9430405935998,1076.68603911317,
361.665748668285));
#123539=CARTESIAN_POINT('Ctrl Pts',(-62.941359524766,1076.68781868475,361.775781734884));
#123540=CARTESIAN_POINT('Ctrl Pts',(-62.939580259543,1076.68970220658,361.892242170563));
#123541=CARTESIAN_POINT('Ctrl Pts',(-62.9609847548429,1076.69114215142,
362.007907060518));
#123542=CARTESIAN_POINT('Ctrl Pts',(-63.0477360763869,1076.6930879473,362.224297014507));
#123543=CARTESIAN_POINT('Ctrl Pts',(-63.1122801435149,1076.69357534904,
362.322845446417));
#123544=CARTESIAN_POINT('Ctrl Pts',(-63.2760938107374,1076.69357125405,
362.488961579553));
#123545=CARTESIAN_POINT('Ctrl Pts',(-63.3737312609862,1076.69307979762,
362.554874514465));
#123546=CARTESIAN_POINT('Ctrl Pts',(-63.5885326016093,1076.69112928325,
362.644489116581));
#123547=CARTESIAN_POINT('Ctrl Pts',(-63.7034794771557,1076.68969182472,
362.667501886));
#123548=CARTESIAN_POINT('Ctrl Pts',(-63.8195601713292,1076.68781395203,
362.667501886));
#123549=CARTESIAN_POINT('Origin',(-61.0059658728168,1067.7251047501,349.55017249556));
#123550=CARTESIAN_POINT('',(-61.0059658728379,1076.2784617343,348.274728374424));
#123551=CARTESIAN_POINT('',(-61.0059658728168,1067.7251047501,348.274728374424));
#123552=CARTESIAN_POINT('Ctrl Pts',(-61.0067058992696,1076.40643702417,
350.825616402011));
#123553=CARTESIAN_POINT('Ctrl Pts',(-61.1753054387743,1076.40003226263,
350.825518578721));
#123554=CARTESIAN_POINT('Ctrl Pts',(-61.3421566834799,1076.39205183224,
350.791992768892));
#123555=CARTESIAN_POINT('Ctrl Pts',(-61.6536284043553,1076.37361992364,
350.661873794951));
#123556=CARTESIAN_POINT('Ctrl Pts',(-61.7950931069933,1076.36333748561,
350.566339211117));
#123557=CARTESIAN_POINT('Ctrl Pts',(-61.9720986104835,1076.34724752692,
350.38697296011));
#123558=CARTESIAN_POINT('Ctrl Pts',(-62.0244933194174,1076.34186431443,
350.322343709386));
#123559=CARTESIAN_POINT('Ctrl Pts',(-62.1635103492835,1076.32548494157,
350.111860644301));
#123560=CARTESIAN_POINT('Ctrl Pts',(-62.2277644014619,1076.31462480656,
349.953446951942));
#123561=CARTESIAN_POINT('Ctrl Pts',(-62.2903191259055,1076.29467144139,
349.622542312494));
#123562=CARTESIAN_POINT('Ctrl Pts',(-62.2887286016733,1076.28575627957,
349.453405539597));
#123563=CARTESIAN_POINT('Ctrl Pts',(-62.2202731715604,1076.27118931772,
349.125717544534));
#123564=CARTESIAN_POINT('Ctrl Pts',(-62.1542350328075,1076.26567540096,
348.97032575603));
#123565=CARTESIAN_POINT('Ctrl Pts',(-61.9661507403253,1076.2589831158,348.694243238935));
#123566=CARTESIAN_POINT('Ctrl Pts',(-61.8461220668367,1076.25785922442,
348.576151501845));
#123567=CARTESIAN_POINT('Ctrl Pts',(-61.5676355023932,1076.26021061205,
348.393016521291));
#123568=CARTESIAN_POINT('Ctrl Pts',(-61.4119736280636,1076.26365396946,
348.32967540113));
#123569=CARTESIAN_POINT('Ctrl Pts',(-61.0850425665927,1076.2745774365,348.266328573456));
#123570=CARTESIAN_POINT('Ctrl Pts',(-60.9169365353592,1076.28195160997,
348.266997869564));
#123571=CARTESIAN_POINT('Ctrl Pts',(-60.5901574624181,1076.2995040843,348.332913182217));
#123572=CARTESIAN_POINT('Ctrl Pts',(-60.4346530062398,1076.30951689685,
348.397703227076));
#123573=CARTESIAN_POINT('Ctrl Pts',(-60.2267010518738,1076.32539106199,
348.537021220366));
#123574=CARTESIAN_POINT('Ctrl Pts',(-60.1620682096721,1076.33079084241,
348.590190938777));
#123575=CARTESIAN_POINT('Ctrl Pts',(-60.0442138254672,1076.34162485025,
348.70830501263));
#123576=CARTESIAN_POINT('Ctrl Pts',(-59.9912546462302,1076.34703336414,
348.772953133667));
#123577=CARTESIAN_POINT('Ctrl Pts',(-59.8511883005758,1076.3631541683,348.982891484046));
#123578=CARTESIAN_POINT('Ctrl Pts',(-59.7862395156745,1076.3734464042,349.140762520099));
#123579=CARTESIAN_POINT('Ctrl Pts',(-59.7218127162375,1076.39190480177,
349.472121104942));
#123580=CARTESIAN_POINT('Ctrl Pts',(-59.7227297197432,1076.39990174225,
349.642303386525));
#123581=CARTESIAN_POINT('Ctrl Pts',(-59.7908666233923,1076.41277231975,
349.973164318111));
#123582=CARTESIAN_POINT('Ctrl Pts',(-59.8576467141859,1076.41751133487,
350.130502875937));
#123583=CARTESIAN_POINT('Ctrl Pts',(-60.049186292316,1076.4232156542,350.410533120237));
#123584=CARTESIAN_POINT('Ctrl Pts',(-60.1722347424379,1076.42411128731,
350.530247317855));
#123585=CARTESIAN_POINT('Ctrl Pts',(-60.4577789939867,1076.42191503209,
350.714237017071));
#123586=CARTESIAN_POINT('Ctrl Pts',(-60.6173197527075,1076.41885092961,
350.776747981925));
#123587=CARTESIAN_POINT('Ctrl Pts',(-60.8577860580678,1076.41177372177,
350.819171155113));
#123588=CARTESIAN_POINT('Ctrl Pts',(-60.9321818678592,1076.40926804406,
350.825659641666));
#123589=CARTESIAN_POINT('Ctrl Pts',(-61.0067058992696,1076.40643702417,
350.825616402011));
#123590=CARTESIAN_POINT('Origin',(-61.0059658728168,1067.7251047501,349.55017249556));
#123591=CARTESIAN_POINT('',(-61.0059658728168,1076.37831455598,350.225616616696));
#123592=CARTESIAN_POINT('',(-61.0059658728176,1076.31052966192,348.874728374424));
#123593=CARTESIAN_POINT('Ctrl Pts',(-61.0059658728168,1076.37831455598,
350.225616616696));
#123594=CARTESIAN_POINT('Ctrl Pts',(-61.0542344883888,1076.37641783823,
350.225616616696));
#123595=CARTESIAN_POINT('Ctrl Pts',(-61.1024739458748,1076.37426575044,
350.220442463225));
#123596=CARTESIAN_POINT('Ctrl Pts',(-61.2375448907151,1076.36748370411,
350.190994170549));
#123597=CARTESIAN_POINT('Ctrl Pts',(-61.3205272413257,1076.3623903405,350.154591162086));
#123598=CARTESIAN_POINT('Ctrl Pts',(-61.4298965737918,1076.35418408558,
350.077842621852));
#123599=CARTESIAN_POINT('Ctrl Pts',(-61.4632927026525,1076.35140697668,
350.049176012208));
#123600=CARTESIAN_POINT('Ctrl Pts',(-61.5241091075068,1076.34576283651,
349.985704802513));
#123601=CARTESIAN_POINT('Ctrl Pts',(-61.5513731195263,1076.34290888727,
349.951036121775));
#123602=CARTESIAN_POINT('Ctrl Pts',(-61.6233351775406,1076.33427925253,
349.838460636607));
#123603=CARTESIAN_POINT('Ctrl Pts',(-61.6561045403002,1076.32862479538,
349.754086858265));
#123604=CARTESIAN_POINT('Ctrl Pts',(-61.686605946541,1076.31834160321,349.578482398263));
#123605=CARTESIAN_POINT('Ctrl Pts',(-61.6844541768283,1076.31380158068,
349.489032894533));
#123606=CARTESIAN_POINT('Ctrl Pts',(-61.6457414101539,1076.30645221666,
349.316219681921));
#123607=CARTESIAN_POINT('Ctrl Pts',(-61.6096384270678,1076.30371138074,
349.234520008511));
#123608=CARTESIAN_POINT('Ctrl Pts',(-61.5080577167856,1076.30045505201,
349.089819711671));
#123609=CARTESIAN_POINT('Ctrl Pts',(-61.4436415274147,1076.2999669893,349.028192578388));
#123610=CARTESIAN_POINT('Ctrl Pts',(-61.2947930869919,1076.30133225723,
348.933252667705));
#123611=CARTESIAN_POINT('Ctrl Pts',(-61.2118340721429,1076.30317014007,
348.900848177727));
#123612=CARTESIAN_POINT('Ctrl Pts',(-61.0858364824871,1076.30733713304,
348.878287309241));
#123613=CARTESIAN_POINT('Ctrl Pts',(-61.0461204817631,1076.30883480827,
348.874750038688));
#123614=CARTESIAN_POINT('Ctrl Pts',(-61.0063319687469,1076.31051420464,
348.874728472955));
#123615=CARTESIAN_POINT('Ctrl Pts',(-61.0062099350874,1076.31051935545,
348.874728406812));
#123616=CARTESIAN_POINT('Ctrl Pts',(-61.0060879031079,1076.3105245079,348.874728374424));
#123617=CARTESIAN_POINT('Ctrl Pts',(-61.0059658728184,1076.31052966192,
348.874728374424));
#123618=CARTESIAN_POINT('',(-61.0059658728168,1082.7251047501,348.874728374424));
#123619=CARTESIAN_POINT('',(-61.0059658728168,1067.7251047501,348.874728374424));
#123620=CARTESIAN_POINT('Origin',(-61.0059658728168,1082.7251047501,349.55017249556));
#123621=CARTESIAN_POINT('Ctrl Pts',(-61.0059658728184,1076.31052966192,
348.874728374424));
#123622=CARTESIAN_POINT('Ctrl Pts',(-60.9176998992336,1076.31425762907,
348.874728374424));
#123623=CARTESIAN_POINT('Ctrl Pts',(-60.8303188655872,1076.31882699849,
348.892029359859));
#123624=CARTESIAN_POINT('Ctrl Pts',(-60.6668950091229,1076.3290905237,348.959330175153));
#123625=CARTESIAN_POINT('Ctrl Pts',(-60.5924665285989,1076.33468917506,
349.008807530495));
#123626=CARTESIAN_POINT('Ctrl Pts',(-60.498438361391,1076.34325793899,349.102305160194));
#123627=CARTESIAN_POINT('Ctrl Pts',(-60.470288271324,1076.3461174665,349.136386371444));
#123628=CARTESIAN_POINT('Ctrl Pts',(-60.3955131618802,1076.35470522712,
349.247458253658));
#123629=CARTESIAN_POINT('Ctrl Pts',(-60.3607078687554,1076.36024970119,
349.331224569256));
#123630=CARTESIAN_POINT('Ctrl Pts',(-60.3259345653945,1076.37028351035,
349.507381430532));
#123631=CARTESIAN_POINT('Ctrl Pts',(-60.3262625962687,1076.37467621228,
349.598017605762));
#123632=CARTESIAN_POINT('Ctrl Pts',(-60.3624093399875,1076.38177287548,
349.774140873562));
#123633=CARTESIAN_POINT('Ctrl Pts',(-60.3979554426796,1076.38440248887,
349.857840918896));
#123634=CARTESIAN_POINT('Ctrl Pts',(-60.4993860991622,1076.38754143813,
350.005778792616));
#123635=CARTESIAN_POINT('Ctrl Pts',(-60.5639999398497,1076.38803790272,
350.068697607441));
#123636=CARTESIAN_POINT('Ctrl Pts',(-60.7131856289696,1076.38685709905,
350.165246944526));
#123637=CARTESIAN_POINT('Ctrl Pts',(-60.7960814594361,1076.38521365448,
350.198230481894));
#123638=CARTESIAN_POINT('Ctrl Pts',(-60.9236336325516,1076.38136334764,
350.221855237295));
#123639=CARTESIAN_POINT('Ctrl Pts',(-60.9648103509532,1076.37993176433,
350.225616616696));
#123640=CARTESIAN_POINT('Ctrl Pts',(-61.0059658728168,1076.37831455598,
350.225616616696));
#123641=CARTESIAN_POINT('Origin',(-56.6885840720973,1067.7251047501,336.39044334969));
#123642=CARTESIAN_POINT('',(-56.6885840721218,1075.55714102284,335.291612213697));
#123643=CARTESIAN_POINT('',(-56.6885840720973,1067.7251047501,335.291612213697));
#123644=CARTESIAN_POINT('Ctrl Pts',(-56.6886635173097,1075.7496222582,337.48927448281));
#123645=CARTESIAN_POINT('Ctrl Pts',(-56.8344491670304,1075.74168330395,
337.489263942544));
#123646=CARTESIAN_POINT('Ctrl Pts',(-56.9786320037909,1075.73133837871,
337.460243990801));
#123647=CARTESIAN_POINT('Ctrl Pts',(-57.2475658978346,1075.70688580914,
337.347677049276));
#123648=CARTESIAN_POINT('Ctrl Pts',(-57.3695861217295,1075.69300350249,
337.265045372198));
#123649=CARTESIAN_POINT('Ctrl Pts',(-57.5749594347056,1075.66339060859,
337.056311688249));
#123650=CARTESIAN_POINT('Ctrl Pts',(-57.6559843038123,1075.64793365169,
336.931896070108));
#123651=CARTESIAN_POINT('Ctrl Pts',(-57.7639354792398,1075.61777360276,
336.65947572204));
#123652=CARTESIAN_POINT('Ctrl Pts',(-57.7901696681622,1075.60335669269,
336.514237357354));
#123653=CARTESIAN_POINT('Ctrl Pts',(-57.7842422704277,1075.57771444552,
336.223721630292));
#123654=CARTESIAN_POINT('Ctrl Pts',(-57.7528904562715,1075.56669838166,
336.081251353044));
#123655=CARTESIAN_POINT('Ctrl Pts',(-57.6370095854657,1075.5495764937,335.817234847899));
#123656=CARTESIAN_POINT('Ctrl Pts',(-57.5539600000379,1075.54361036534,
335.698153927165));
#123657=CARTESIAN_POINT('Ctrl Pts',(-57.3470413252792,1075.53761512669,
335.49917586878));
#123658=CARTESIAN_POINT('Ctrl Pts',(-57.2254514661288,1075.53761608331,
335.421063600339));
#123659=CARTESIAN_POINT('Ctrl Pts',(-56.95925442656,1075.54359724004,335.315904740578));
#123660=CARTESIAN_POINT('Ctrl Pts',(-56.8173162673525,1075.54951253567,
335.289869092651));
#123661=CARTESIAN_POINT('Ctrl Pts',(-56.5310162291635,1075.56646030936,
335.293544430829));
#123662=CARTESIAN_POINT('Ctrl Pts',(-56.3894500677497,1075.57734646249,
335.323461203079));
#123663=CARTESIAN_POINT('Ctrl Pts',(-56.1251606816273,1075.60261266604,
335.436110316585));
#123664=CARTESIAN_POINT('Ctrl Pts',(-56.0050879379537,1075.61677082831,
335.518104474796));
#123665=CARTESIAN_POINT('Ctrl Pts',(-55.853772697369,1075.63896636136,335.67230559026));
#123666=CARTESIAN_POINT('Ctrl Pts',(-55.8084513356478,1075.64648240489,
335.72863011673));
#123667=CARTESIAN_POINT('Ctrl Pts',(-55.7296691301273,1075.6614740001,335.849084447118));
#123668=CARTESIAN_POINT('Ctrl Pts',(-55.6963413169535,1075.66891505494,
335.912903460578));
#123669=CARTESIAN_POINT('Ctrl Pts',(-55.614934311832,1075.69102574124,336.114798853958));
#123670=CARTESIAN_POINT('Ctrl Pts',(-55.5878255203469,1075.70502787136,
336.259687746594));
#123671=CARTESIAN_POINT('Ctrl Pts',(-55.5918854306654,1075.72980139543,
336.551226849469));
#123672=CARTESIAN_POINT('Ctrl Pts',(-55.6227885558044,1075.74034514702,
336.695011167313));
#123673=CARTESIAN_POINT('Ctrl Pts',(-55.7391227224178,1075.75668550736,
336.962493602663));
#123674=CARTESIAN_POINT('Ctrl Pts',(-55.8234249357666,1075.76231514086,
337.083461673728));
#123675=CARTESIAN_POINT('Ctrl Pts',(-56.0346902733854,1075.76790695523,
337.285567862994));
#123676=CARTESIAN_POINT('Ctrl Pts',(-56.1595183826974,1075.7678056593,337.364565226893));
#123677=CARTESIAN_POINT('Ctrl Pts',(-56.4215339292318,1075.76206186809,
337.464750987201));
#123678=CARTESIAN_POINT('Ctrl Pts',(-56.554578478896,1075.75692403987,337.489284177124));
#123679=CARTESIAN_POINT('Ctrl Pts',(-56.6886635173097,1075.7496222582,337.48927448281));
#123680=CARTESIAN_POINT('Origin',(-56.6885840720973,1067.7251047501,336.39044334969));
#123681=CARTESIAN_POINT('',(-56.6885840720973,1075.69877322724,336.889274485682));
#123682=CARTESIAN_POINT('',(-56.6885840720972,1075.61138997104,335.891612213697));
#123683=CARTESIAN_POINT('Ctrl Pts',(-56.6885840720972,1075.69877322723,
336.889274485682));
#123684=CARTESIAN_POINT('Ctrl Pts',(-56.6894491464213,1075.69872525547,
336.889274485682));
#123685=CARTESIAN_POINT('Ctrl Pts',(-56.6903143202152,1075.69867708276,
336.889272235361));
#123686=CARTESIAN_POINT('Ctrl Pts',(-56.7576970253416,1075.69490999697,
336.888921625651));
#123687=CARTESIAN_POINT('Ctrl Pts',(-56.8234066897673,1075.69008096533,
336.875275915875));
#123688=CARTESIAN_POINT('Ctrl Pts',(-56.9456757698671,1075.67873876071,
336.82307097793));
#123689=CARTESIAN_POINT('Ctrl Pts',(-57.0009960109743,1075.67233343206,
336.78496672716));
#123690=CARTESIAN_POINT('Ctrl Pts',(-57.0935839815181,1075.65878126756,
336.689209466401));
#123691=CARTESIAN_POINT('Ctrl Pts',(-57.1298751391389,1075.65176327744,
336.632409856439));
#123692=CARTESIAN_POINT('Ctrl Pts',(-57.178022099384,1075.63808674825,336.507744699949));
#123693=CARTESIAN_POINT('Ctrl Pts',(-57.189342428336,1075.63156314422,336.44106872803));
#123694=CARTESIAN_POINT('Ctrl Pts',(-57.1850034196467,1075.62010134744,
336.308688392635));
#123695=CARTESIAN_POINT('Ctrl Pts',(-57.1700042031795,1075.61524035459,
336.244265817626));
#123696=CARTESIAN_POINT('Ctrl Pts',(-57.1160293855711,1075.60773979562,
336.125167635418));
#123697=CARTESIAN_POINT('Ctrl Pts',(-57.0777297314247,1075.60516108071,
336.071604451795));
#123698=CARTESIAN_POINT('Ctrl Pts',(-56.9828002514258,1075.60264920655,
335.982407647644));
#123699=CARTESIAN_POINT('Ctrl Pts',(-56.9271946859133,1075.60273012714,
335.947587982151));
#123700=CARTESIAN_POINT('Ctrl Pts',(-56.8096376474247,1075.6054603161,335.902713493885));
#123701=CARTESIAN_POINT('Ctrl Pts',(-56.7493441376742,1075.60792128284,
335.891612213697));
#123702=CARTESIAN_POINT('Ctrl Pts',(-56.6885840720971,1075.61138997104,
335.891612213697));
#123703=CARTESIAN_POINT('',(-56.6885840720973,1082.7251047501,335.891612213697));
#123704=CARTESIAN_POINT('',(-56.6885840720973,1067.7251047501,335.891612213697));
#123705=CARTESIAN_POINT('Origin',(-56.6885840720973,1082.7251047501,336.39044334969));
#123706=CARTESIAN_POINT('Ctrl Pts',(-56.6885840720971,1075.61138997104,
335.891612213697));
#123707=CARTESIAN_POINT('Ctrl Pts',(-56.6884990384235,1075.61139482547,
335.891612213697));
#123708=CARTESIAN_POINT('Ctrl Pts',(-56.6884140038361,1075.61139968187,
335.891612235446));
#123709=CARTESIAN_POINT('Ctrl Pts',(-56.6883289683429,1075.61140454024,
335.891612278933));
#123710=CARTESIAN_POINT('Ctrl Pts',(-56.6231385591007,1075.61512909418,
335.891645617508));
#123711=CARTESIAN_POINT('Ctrl Pts',(-56.5586528662546,1075.61994219145,
335.904456408237));
#123712=CARTESIAN_POINT('Ctrl Pts',(-56.4379784929127,1075.63119943098,
335.95419283561));
#123713=CARTESIAN_POINT('Ctrl Pts',(-56.3830001270856,1075.63754486953,
335.990788440737));
#123714=CARTESIAN_POINT('Ctrl Pts',(-56.3135139750078,1075.64755079746,
336.059955081574));
#123715=CARTESIAN_POINT('Ctrl Pts',(-56.292680101939,1075.65094353892,336.085222649743));
#123716=CARTESIAN_POINT('Ctrl Pts',(-56.2562895994222,1075.65774040457,
336.139411092992));
#123717=CARTESIAN_POINT('Ctrl Pts',(-56.2408071720882,1075.6611288352,336.168200308803));
#123718=CARTESIAN_POINT('Ctrl Pts',(-56.202639353073,1075.67125571532,336.259641747662));
#123719=CARTESIAN_POINT('Ctrl Pts',(-56.1895345233825,1075.67772119746,
336.325533686445));
#123720=CARTESIAN_POINT('Ctrl Pts',(-56.1899762510962,1075.68923225219,
336.458485848432));
#123721=CARTESIAN_POINT('Ctrl Pts',(-56.2034468466609,1075.69416854804,
336.524230057133));
#123722=CARTESIAN_POINT('Ctrl Pts',(-56.2551726678914,1075.70181310519,
336.646013731805));
#123723=CARTESIAN_POINT('Ctrl Pts',(-56.2926424310386,1075.70446900306,
336.700933185089));
#123724=CARTESIAN_POINT('Ctrl Pts',(-56.3862038139609,1075.70717419258,
336.792468298214));
#123725=CARTESIAN_POINT('Ctrl Pts',(-56.4411098868677,1075.7072312694,336.828409888256));
#123726=CARTESIAN_POINT('Ctrl Pts',(-56.560888664013,1075.70478130846,336.876910908503));
#123727=CARTESIAN_POINT('Ctrl Pts',(-56.6244631064969,1075.70232898642,
336.889274485682));
#123728=CARTESIAN_POINT('Ctrl Pts',(-56.6885840720972,1075.69877322723,
336.889274485682));
#123729=CARTESIAN_POINT('Origin',(-49.705085901968,1067.7251047501,324.271668315149));
#123730=CARTESIAN_POINT('',(-49.7050859019928,1074.6677741402,323.181127566421));
#123731=CARTESIAN_POINT('',(-49.705085901968,1067.7251047501,323.18112756642));
#123732=CARTESIAN_POINT('Ctrl Pts',(-49.7045317577611,1074.93240199134,
325.362208923087));
#123733=CARTESIAN_POINT('Ctrl Pts',(-49.8493940963802,1074.92389728949,
325.362282533024));
#123734=CARTESIAN_POINT('Ctrl Pts',(-49.9925804253556,1074.91204851772,
325.333496298155));
#123735=CARTESIAN_POINT('Ctrl Pts',(-50.2596848576552,1074.88292013809,
325.221803446226));
#123736=CARTESIAN_POINT('Ctrl Pts',(-50.3808423955098,1074.86590266617,
325.139751063587));
#123737=CARTESIAN_POINT('Ctrl Pts',(-50.532177739072,1074.83836158758,324.985984200759));
#123738=CARTESIAN_POINT('Ctrl Pts',(-50.5769308665596,1074.82900398012,
324.930611673339));
#123739=CARTESIAN_POINT('Ctrl Pts',(-50.6551767204814,1074.80993652455,
324.811752310003));
#123740=CARTESIAN_POINT('Ctrl Pts',(-50.6884446502032,1074.80026814903,
324.748498673531));
#123741=CARTESIAN_POINT('Ctrl Pts',(-50.7705871361969,1074.77076949046,
324.546494173401));
#123742=CARTESIAN_POINT('Ctrl Pts',(-50.7979071668757,1074.75129755642,
324.400644472631));
#123743=CARTESIAN_POINT('Ctrl Pts',(-50.7931038296754,1074.71593933622,
324.110008868538));
#123744=CARTESIAN_POINT('Ctrl Pts',(-50.762366670685,1074.70031598856,323.968007650524));
#123745=CARTESIAN_POINT('Ctrl Pts',(-50.6477606925917,1074.67485058289,
323.705101200891));
#123746=CARTESIAN_POINT('Ctrl Pts',(-50.5655508166102,1074.66520380374,
323.586574474836));
#123747=CARTESIAN_POINT('Ctrl Pts',(-50.3606452792527,1074.65324773146,
323.388709663174));
#123748=CARTESIAN_POINT('Ctrl Pts',(-50.2404042163707,1074.65099377426,
323.311022651359));
#123749=CARTESIAN_POINT('Ctrl Pts',(-49.9771820655242,1074.65416583854,
323.206185028552));
#123750=CARTESIAN_POINT('Ctrl Pts',(-49.8369519245457,1074.65953702178,
323.179958494126));
#123751=CARTESIAN_POINT('Ctrl Pts',(-49.5537773989021,1074.67721516714,
323.182383161852));
#123752=CARTESIAN_POINT('Ctrl Pts',(-49.4136533650652,1074.68938063811,
323.211304456397));
#123753=CARTESIAN_POINT('Ctrl Pts',(-49.1513265559742,1074.71895400281,
323.321368276287));
#123754=CARTESIAN_POINT('Ctrl Pts',(-49.0318440509625,1074.73612774369,
323.401983991196));
#123755=CARTESIAN_POINT('Ctrl Pts',(-48.8807642619317,1074.76387098562,
323.554082316392));
#123756=CARTESIAN_POINT('Ctrl Pts',(-48.8353309354415,1074.77342371778,
323.609886543423));
#123757=CARTESIAN_POINT('Ctrl Pts',(-48.7562044287484,1074.79274070763,
323.729424328376));
#123758=CARTESIAN_POINT('Ctrl Pts',(-48.7226624192436,1074.80246079913,
323.792869135357));
#123759=CARTESIAN_POINT('Ctrl Pts',(-48.6406171815644,1074.83170117203,
323.993644130364));
#123760=CARTESIAN_POINT('Ctrl Pts',(-48.6130333909722,1074.85073155292,
324.137910845684));
#123761=CARTESIAN_POINT('Ctrl Pts',(-48.6161728279485,1074.88534490407,
324.427938350528));
#123762=CARTESIAN_POINT('Ctrl Pts',(-48.6464318479754,1074.90062277419,
324.57090020764));
#123763=CARTESIAN_POINT('Ctrl Pts',(-48.7611674737408,1074.92549253054,
324.836623993457));
#123764=CARTESIAN_POINT('Ctrl Pts',(-48.8443224720443,1074.93485329814,
324.95676596895));
#123765=CARTESIAN_POINT('Ctrl Pts',(-49.0518694102871,1074.94634854687,
325.156597439565));
#123766=CARTESIAN_POINT('Ctrl Pts',(-49.1736447811957,1074.94844781702,
325.234679494678));
#123767=CARTESIAN_POINT('Ctrl Pts',(-49.4338131682571,1074.94526662733,
325.336665715075));
#123768=CARTESIAN_POINT('Ctrl Pts',(-49.5686259828435,1074.9403808636,325.362139864312));
#123769=CARTESIAN_POINT('Ctrl Pts',(-49.7045317577611,1074.93240199134,
325.362208923086));
#123770=CARTESIAN_POINT('Origin',(-49.705085901968,1067.7251047501,324.271668315149));
#123771=CARTESIAN_POINT('',(-49.705085901968,1074.86129916363,324.762209063877));
#123772=CARTESIAN_POINT('',(-49.7050859019679,1074.74227702453,323.78112756642));
#123773=CARTESIAN_POINT('Ctrl Pts',(-49.705085901968,1074.86129916363,324.762209063877));
#123774=CARTESIAN_POINT('Ctrl Pts',(-49.7055456137983,1074.86127180977,
324.762209063877));
#123775=CARTESIAN_POINT('Ctrl Pts',(-49.7060053538754,1074.8612443764,324.762208417647));
#123776=CARTESIAN_POINT('Ctrl Pts',(-49.7704871387181,1074.8573857354,324.762027118034));
#123777=CARTESIAN_POINT('Ctrl Pts',(-49.8337492093071,1074.85209112191,
324.749317746845));
#123778=CARTESIAN_POINT('Ctrl Pts',(-49.95328548125,1074.83899921727,324.699832482791));
#123779=CARTESIAN_POINT('Ctrl Pts',(-50.0081234310176,1074.83126901174,
324.662911112905));
#123780=CARTESIAN_POINT('Ctrl Pts',(-50.076586183687,1074.81878982457,324.593608006074));
#123781=CARTESIAN_POINT('Ctrl Pts',(-50.0968144814737,1074.8145579582,324.568661180176));
#123782=CARTESIAN_POINT('Ctrl Pts',(-50.132148608211,1074.80595291254,324.515139825244));
#123783=CARTESIAN_POINT('Ctrl Pts',(-50.1471626873319,1074.80159876538,
324.486677142847));
#123784=CARTESIAN_POINT('Ctrl Pts',(-50.1841533638763,1074.78836440411,
324.395999925204));
#123785=CARTESIAN_POINT('Ctrl Pts',(-50.1965174791759,1074.77966095661,
324.330606792812));
#123786=CARTESIAN_POINT('Ctrl Pts',(-50.1946492706973,1074.76380931707,
324.199665063864));
#123787=CARTESIAN_POINT('Ctrl Pts',(-50.1808066576286,1074.75679257532,
324.135380605636));
#123788=CARTESIAN_POINT('Ctrl Pts',(-50.1291047977023,1074.74542206639,
324.016815791196));
#123789=CARTESIAN_POINT('Ctrl Pts',(-50.0921597962372,1074.74113726211,
323.963546121838));
#123790=CARTESIAN_POINT('Ctrl Pts',(-50.0000569991088,1074.73582341612,
323.87457009062));
#123791=CARTESIAN_POINT('Ctrl Pts',(-49.945987103598,1074.73482100748,323.839617587412));
#123792=CARTESIAN_POINT('Ctrl Pts',(-49.8288825190181,1074.7362099424,323.792939821709));
#123793=CARTESIAN_POINT('Ctrl Pts',(-49.7672384927223,1074.73850603265,
323.78112756642));
#123794=CARTESIAN_POINT('Ctrl Pts',(-49.7050859019678,1074.74227702453,
323.78112756642));
#123795=CARTESIAN_POINT('',(-49.705085901968,1082.7251047501,323.78112756642));
#123796=CARTESIAN_POINT('',(-49.705085901968,1067.7251047501,323.78112756642));
#123797=CARTESIAN_POINT('Origin',(-49.705085901968,1082.7251047501,324.271668315149));
#123798=CARTESIAN_POINT('Ctrl Pts',(-49.7050859019678,1074.74227702453,
323.78112756642));
#123799=CARTESIAN_POINT('Ctrl Pts',(-49.7050040619518,1074.74228199002,
323.78112756642));
#123800=CARTESIAN_POINT('Ctrl Pts',(-49.7049222210541,1074.74228695807,
323.781127586905));
#123801=CARTESIAN_POINT('Ctrl Pts',(-49.704840379282,1074.74229192867,323.781127627868));
#123802=CARTESIAN_POINT('Ctrl Pts',(-49.6409234603641,1074.74617387742,
323.781159619205));
#123803=CARTESIAN_POINT('Ctrl Pts',(-49.5777366215018,1074.75153806376,
323.793681432173));
#123804=CARTESIAN_POINT('Ctrl Pts',(-49.4592687194716,1074.7646501543,323.842313969592));
#123805=CARTESIAN_POINT('Ctrl Pts',(-49.405216469586,1074.77229422411,323.878188920965));
#123806=CARTESIAN_POINT('Ctrl Pts',(-49.3367866694145,1074.78468339727,
323.946056024522));
#123807=CARTESIAN_POINT('Ctrl Pts',(-49.3162152533231,1074.7889476124,323.970926284283));
#123808=CARTESIAN_POINT('Ctrl Pts',(-49.2802643853385,1074.79759568054,
324.024299075212));
#123809=CARTESIAN_POINT('Ctrl Pts',(-49.2649627538341,1074.80195995729,
324.05267901216));
#123810=CARTESIAN_POINT('Ctrl Pts',(-49.2272555687101,1074.81515184372,
324.142812399));
#123811=CARTESIAN_POINT('Ctrl Pts',(-49.2143109374341,1074.82378669253,
324.207788204707));
#123812=CARTESIAN_POINT('Ctrl Pts',(-49.2147844903059,1074.83956781397,
324.338738520539));
#123813=CARTESIAN_POINT('Ctrl Pts',(-49.2280561837372,1074.84657003657,
324.403442530516));
#123814=CARTESIAN_POINT('Ctrl Pts',(-49.2789933276834,1074.85793777556,
324.523158854203));
#123815=CARTESIAN_POINT('Ctrl Pts',(-49.3158103692566,1074.86222611825,
324.577103343054));
#123816=CARTESIAN_POINT('Ctrl Pts',(-49.4076961864532,1074.867549275,324.66695634815));
#123817=CARTESIAN_POINT('Ctrl Pts',(-49.4615405481388,1074.86858127356,
324.702232199905));
#123818=CARTESIAN_POINT('Ctrl Pts',(-49.579287383854,1074.86731575151,324.750008315291));
#123819=CARTESIAN_POINT('Ctrl Pts',(-49.641919981638,1074.86505767464,324.762209063877));
#123820=CARTESIAN_POINT('Ctrl Pts',(-49.705085901968,1074.86129916363,324.762209063877));
#123821=CARTESIAN_POINT('Origin',(-75.4882582191906,1067.7251047501,376.431040472272));
#123822=CARTESIAN_POINT('',(-75.4882582192121,1076.65013582838,374.952737340079));
#123823=CARTESIAN_POINT('',(-75.4882582191906,1067.7251047501,374.952737340079));
#123824=CARTESIAN_POINT('Ctrl Pts',(-75.4874144218056,1076.69163799014,
377.909343363651));
#123825=CARTESIAN_POINT('Ctrl Pts',(-75.6827415468976,1076.68805926486,
377.909454854008));
#123826=CARTESIAN_POINT('Ctrl Pts',(-75.8761542728031,1076.68382657079,
377.870852981114));
#123827=CARTESIAN_POINT('Ctrl Pts',(-76.1450544222639,1076.67673305976,
377.758899442763));
#123828=CARTESIAN_POINT('Ctrl Pts',(-76.2298494272729,1076.67428790979,
377.71347265165));
#123829=CARTESIAN_POINT('Ctrl Pts',(-76.4725288914479,1076.66662134139,
377.551296525591));
#123830=CARTESIAN_POINT('Ctrl Pts',(-76.6121646848941,1076.66122864575,
377.411140205371));
#123831=CARTESIAN_POINT('Ctrl Pts',(-76.8276270320169,1076.65079155497,
377.086116262237));
#123832=CARTESIAN_POINT('Ctrl Pts',(-76.9019628475037,1076.64585154935,
376.904834607344));
#123833=CARTESIAN_POINT('Ctrl Pts',(-76.976343040882,1076.63736503469,376.523937251217));
#123834=CARTESIAN_POINT('Ctrl Pts',(-76.9756806703523,1076.63390778129,
376.328021630331));
#123835=CARTESIAN_POINT('Ctrl Pts',(-76.8987620580907,1076.62926059287,
375.947933113412));
#123836=CARTESIAN_POINT('Ctrl Pts',(-76.8233781015899,1076.62811659682,
375.767433720505));
#123837=CARTESIAN_POINT('Ctrl Pts',(-76.6075137538433,1076.62842293834,
375.446144237223));
#123838=CARTESIAN_POINT('Ctrl Pts',(-76.4692692472796,1076.62986423688,
375.308380913045));
#123839=CARTESIAN_POINT('Ctrl Pts',(-76.1477920876477,1076.63502127057,
375.0939982024));
#123840=CARTESIAN_POINT('Ctrl Pts',(-75.9677090415123,1076.63867986198,
375.019381249661));
#123841=CARTESIAN_POINT('Ctrl Pts',(-75.5889785768878,1076.64744328673,
374.943575341487));
#123842=CARTESIAN_POINT('Ctrl Pts',(-75.393962310733,1076.65245758771,374.943156778212));
#123843=CARTESIAN_POINT('Ctrl Pts',(-75.0146544172071,1076.66287850511,
375.017371038021));
#123844=CARTESIAN_POINT('Ctrl Pts',(-74.8340193331443,1076.66817983416,
375.091363129787));
#123845=CARTESIAN_POINT('Ctrl Pts',(-74.5092349614717,1076.67829380086,
375.306172695358));
#123846=CARTESIAN_POINT('Ctrl Pts',(-74.3688437965922,1076.68299767023,
375.445782028953));
#123847=CARTESIAN_POINT('Ctrl Pts',(-74.1514358922739,1076.6911867403,375.770570104066));
#123848=CARTESIAN_POINT('Ctrl Pts',(-74.0761343683581,1076.6946052898,375.952260659721));
#123849=CARTESIAN_POINT('Ctrl Pts',(-74.0001947561923,1076.70006327117,
376.33498595089));
#123850=CARTESIAN_POINT('Ctrl Pts',(-74.0005382583571,1076.70205315722,
376.53230337495));
#123851=CARTESIAN_POINT('Ctrl Pts',(-74.0781654507825,1076.70465848027,
376.916465918374));
#123852=CARTESIAN_POINT('Ctrl Pts',(-74.155111593748,1076.70524644866,377.099412513354));
#123853=CARTESIAN_POINT('Ctrl Pts',(-74.3759678646567,1076.70504468597,
377.424402041657));
#123854=CARTESIAN_POINT('Ctrl Pts',(-74.5176392126666,1076.70425718784,
377.56323022199));
#123855=CARTESIAN_POINT('Ctrl Pts',(-74.8459572862212,1076.70124211397,
377.776755326571));
#123856=CARTESIAN_POINT('Ctrl Pts',(-75.0290990036184,1076.69904580999,
377.849724978353));
#123857=CARTESIAN_POINT('Ctrl Pts',(-75.3089626614887,1076.69476517686,
377.90114657676));
#123858=CARTESIAN_POINT('Ctrl Pts',(-75.398095676438,1076.69327446153,377.909292381593));
#123859=CARTESIAN_POINT('Ctrl Pts',(-75.4874144218056,1076.69163799014,
377.909343363651));
#123860=CARTESIAN_POINT('Origin',(-75.4882582191906,1067.7251047501,376.431040472272));
#123861=CARTESIAN_POINT('',(-75.4882582191906,1076.68449717364,377.309343604465));
#123862=CARTESIAN_POINT('',(-75.4882582226568,1076.65987181757,375.552737340079));
#123863=CARTESIAN_POINT('Ctrl Pts',(-75.4882582191906,1076.68449717364,
377.309343604465));
#123864=CARTESIAN_POINT('Ctrl Pts',(-75.4897648571436,1076.68446733747,
377.309343604465));
#123865=CARTESIAN_POINT('Ctrl Pts',(-75.4912716819592,1076.68443743529,
377.309339727744));
#123866=CARTESIAN_POINT('Ctrl Pts',(-75.6093360531358,1076.68208961198,
377.308732064741));
#123867=CARTESIAN_POINT('Ctrl Pts',(-75.7246094171306,1076.67942037264,
377.284935973877));
#123868=CARTESIAN_POINT('Ctrl Pts',(-75.8844460862234,1076.67509031527,
377.216989422195));
#123869=CARTESIAN_POINT('Ctrl Pts',(-75.9347184963435,1076.67361999382,
377.189561131168));
#123870=CARTESIAN_POINT('Ctrl Pts',(-76.0782280956566,1076.66907587537,
377.09202303258));
#123871=CARTESIAN_POINT('Ctrl Pts',(-76.1605302317935,1076.66596277885,
377.008113398505));
#123872=CARTESIAN_POINT('Ctrl Pts',(-76.2869658349762,1076.66005765652,
376.814116483053));
#123873=CARTESIAN_POINT('Ctrl Pts',(-76.3302664836154,1076.65732189573,
376.706188177514));
#123874=CARTESIAN_POINT('Ctrl Pts',(-76.3727349171275,1076.65268004244,
376.479798994131));
#123875=CARTESIAN_POINT('Ctrl Pts',(-76.3715039989058,1076.65082128705,
376.363534746148));
#123876=CARTESIAN_POINT('Ctrl Pts',(-76.3242646963916,1076.64834691408,
376.138216821916));
#123877=CARTESIAN_POINT('Ctrl Pts',(-76.2787611106823,1076.64775567246,
376.031341632903));
#123878=CARTESIAN_POINT('Ctrl Pts',(-76.1492160697001,1076.64796899716,
375.841331760484));
#123879=CARTESIAN_POINT('Ctrl Pts',(-76.0664771514959,1076.64876963235,
375.760009501673));
#123880=CARTESIAN_POINT('Ctrl Pts',(-75.8744368915971,1076.65161652036,
375.633874306666));
#123881=CARTESIAN_POINT('Ctrl Pts',(-75.7670035037809,1076.65363282658,
375.590263956964));
#123882=CARTESIAN_POINT('Ctrl Pts',(-75.5994049531778,1076.65725865743,
375.558010997993));
#123883=CARTESIAN_POINT('Ctrl Pts',(-75.5438273738724,1076.65853347143,
375.552737340517));
#123884=CARTESIAN_POINT('Ctrl Pts',(-75.488258226123,1076.65987181757,375.552737340079));
#123885=CARTESIAN_POINT('',(-75.4882582191906,1082.7251047501,375.552737340079));
#123886=CARTESIAN_POINT('',(-75.4882582191906,1067.7251047501,375.552737340079));
#123887=CARTESIAN_POINT('Origin',(-75.4882582191906,1082.7251047501,376.431040472272));
#123888=CARTESIAN_POINT('Ctrl Pts',(-75.488258226123,1076.65987181757,375.552737340079));
#123889=CARTESIAN_POINT('Ctrl Pts',(-75.4294792692097,1076.66128746984,
375.552737339615));
#123890=CARTESIAN_POINT('Ctrl Pts',(-75.3707097446567,1076.66277414839,
375.558637895176));
#123891=CARTESIAN_POINT('Ctrl Pts',(-75.2002026530587,1076.66728030078,
375.593391578033));
#123892=CARTESIAN_POINT('Ctrl Pts',(-75.0931566296768,1076.67035816284,
375.638243891762));
#123893=CARTESIAN_POINT('Ctrl Pts',(-74.9009299959585,1076.67636918568,
375.767643214141));
#123894=CARTESIAN_POINT('Ctrl Pts',(-74.8180309293281,1076.67923939418,
375.851516328865));
#123895=CARTESIAN_POINT('Ctrl Pts',(-74.6900978634223,1076.68436902491,
376.046457031318));
#123896=CARTESIAN_POINT('Ctrl Pts',(-74.6462082735092,1076.68658173662,
376.15550562242));
#123897=CARTESIAN_POINT('Ctrl Pts',(-74.615791802267,1076.6891393847,376.318519839637));
#123898=CARTESIAN_POINT('Ctrl Pts',(-74.6108434045295,1076.68982209035,
376.367779090221));
#123899=CARTESIAN_POINT('Ctrl Pts',(-74.6100642504227,1076.69042296099,
376.417193261711));
#123900=CARTESIAN_POINT('Ctrl Pts',(-74.6082205493547,1076.69184479247,
376.534121299387));
#123901=CARTESIAN_POINT('Ctrl Pts',(-74.629748032955,1076.69279098358,376.650252553386));
#123902=CARTESIAN_POINT('Ctrl Pts',(-74.7171221748697,1076.69371338343,
376.867510329167));
#123903=CARTESIAN_POINT('Ctrl Pts',(-74.7821919157866,1076.69367926517,
376.966416082538));
#123904=CARTESIAN_POINT('Ctrl Pts',(-74.9470930001565,1076.6926210733,377.132628559757));
#123905=CARTESIAN_POINT('Ctrl Pts',(-75.0451835742738,1076.69160880458,
377.198353097151));
#123906=CARTESIAN_POINT('Ctrl Pts',(-75.2595179757525,1076.68866392777,
377.286791042517));
#123907=CARTESIAN_POINT('Ctrl Pts',(-75.3733445800223,1076.68677282525,
377.309343604465));
#123908=CARTESIAN_POINT('Ctrl Pts',(-75.4882582191906,1076.68449717364,
377.309343604465));
#123909=CARTESIAN_POINT('Origin',(-75.2807843499774,1067.7251047501,363.874487154571));
#123910=CARTESIAN_POINT('',(-75.2807843499963,1076.29141677771,362.599043033435));
#123911=CARTESIAN_POINT('',(-75.2807843499774,1067.7251047501,362.599043033435));
#123912=CARTESIAN_POINT('Ctrl Pts',(-75.2808749340257,1076.39500999161,
365.149931272491));
#123913=CARTESIAN_POINT('Ctrl Pts',(-75.4498210414911,1076.38698060872,
365.149919273672));
#123914=CARTESIAN_POINT('Ctrl Pts',(-75.6170307065239,1076.3776224465,365.116340771465));
#123915=CARTESIAN_POINT('Ctrl Pts',(-75.8492390085435,1076.36237274116,
365.019250115279));
#123916=CARTESIAN_POINT('Ctrl Pts',(-75.9223784283126,1076.35717939432,
364.979917908772));
#123917=CARTESIAN_POINT('Ctrl Pts',(-76.061238436746,1076.34648830333,364.886793904917));
#123918=CARTESIAN_POINT('Ctrl Pts',(-76.1264620246764,1076.34101262697,
364.832976554995));
#123919=CARTESIAN_POINT('Ctrl Pts',(-76.3039794736953,1076.32465583089,
364.654179688324));
#123920=CARTESIAN_POINT('Ctrl Pts',(-76.3974933459678,1076.31392645234,
364.513102161657));
#123921=CARTESIAN_POINT('Ctrl Pts',(-76.5245527179282,1076.29413631785,
364.202917882855));
#123922=CARTESIAN_POINT('Ctrl Pts',(-76.5569187050774,1076.28526892554,
364.036817935459));
#123923=CARTESIAN_POINT('Ctrl Pts',(-76.5555176995462,1076.270828232,363.701911407914));
#123924=CARTESIAN_POINT('Ctrl Pts',(-76.5219309210856,1076.26539150449,
363.536371154417));
#123925=CARTESIAN_POINT('Ctrl Pts',(-76.3929024521023,1076.25887218167,
363.228135518878));
#123926=CARTESIAN_POINT('Ctrl Pts',(-76.2989352653415,1076.25784107666,
363.088386334433));
#123927=CARTESIAN_POINT('Ctrl Pts',(-76.0627598804327,1076.26037567887,
362.853220905376));
#123928=CARTESIAN_POINT('Ctrl Pts',(-75.9229653443812,1076.26390607121,
362.760015899581));
#123929=CARTESIAN_POINT('Ctrl Pts',(-75.6154483973887,1076.27498166654,
362.632519442779));
#123930=CARTESIAN_POINT('Ctrl Pts',(-75.4506912723202,1076.2824186827,362.59950854281));
#123931=CARTESIAN_POINT('Ctrl Pts',(-75.1174768044228,1076.30006499764,
362.598586018667));
#123932=CARTESIAN_POINT('Ctrl Pts',(-74.9522100684297,1076.31010806948,
362.630863635212));
#123933=CARTESIAN_POINT('Ctrl Pts',(-74.7206134221463,1076.32600344859,
362.725602622322));
#123934=CARTESIAN_POINT('Ctrl Pts',(-74.6466383907175,1076.33140704741,
362.764719246028));
#123935=CARTESIAN_POINT('Ctrl Pts',(-74.5073775810664,1076.34225027004,
362.856856148271));
#123936=CARTESIAN_POINT('Ctrl Pts',(-74.4424252380534,1076.34766414583,
362.909662853596));
#123937=CARTESIAN_POINT('Ctrl Pts',(-74.2627876179995,1076.3637936282,363.087642402728));
#123938=CARTESIAN_POINT('Ctrl Pts',(-74.1673821801803,1076.37407487544,
363.22965523587));
#123939=CARTESIAN_POINT('Ctrl Pts',(-74.0379745778915,1076.39245960072,
363.541926165913));
#123940=CARTESIAN_POINT('Ctrl Pts',(-74.0049244006597,1076.4003979401,363.708969289003));
#123941=CARTESIAN_POINT('Ctrl Pts',(-74.0057646263549,1076.41311637904,
364.046622539015));
#123942=CARTESIAN_POINT('Ctrl Pts',(-74.0397555211792,1076.41776996181,
364.213875922484));
#123943=CARTESIAN_POINT('Ctrl Pts',(-74.1712035330894,1076.42330258773,
364.525888642469));
#123944=CARTESIAN_POINT('Ctrl Pts',(-74.2675100910345,1076.42411854434,
364.667440380937));
#123945=CARTESIAN_POINT('Ctrl Pts',(-74.5096750297681,1076.42178479807,
364.904445368011));
#123946=CARTESIAN_POINT('Ctrl Pts',(-74.6530304154158,1076.41866250436,
364.997575027204));
#123947=CARTESIAN_POINT('Ctrl Pts',(-74.9601457853265,1076.40897481434,
365.119446518862));
#123948=CARTESIAN_POINT('Ctrl Pts',(-75.1198146387644,1076.40266459105,
365.149942711246));
#123949=CARTESIAN_POINT('Ctrl Pts',(-75.2808749340257,1076.39500999161,
365.149931272491));
#123950=CARTESIAN_POINT('Origin',(-75.2807843499774,1067.7251047501,363.874487154571));
#123951=CARTESIAN_POINT('',(-75.2807843499774,1076.3720597734,364.549931275707));
#123952=CARTESIAN_POINT('',(-75.2807843499778,1076.31720630032,363.199043033435));
#123953=CARTESIAN_POINT('Ctrl Pts',(-75.2807843499774,1076.3720597734,364.549931275707));
#123954=CARTESIAN_POINT('Ctrl Pts',(-75.2877215036647,1076.3717209374,364.549931275707));
#123955=CARTESIAN_POINT('Ctrl Pts',(-75.2946629386578,1076.37137748182,
364.549824404112));
#123956=CARTESIAN_POINT('Ctrl Pts',(-75.3914829118915,1076.366525004,364.546838321674));
#123957=CARTESIAN_POINT('Ctrl Pts',(-75.4798767778265,1076.36134974017,
364.526148301032));
#123958=CARTESIAN_POINT('Ctrl Pts',(-75.6016450178768,1076.35305791868,
364.470483346753));
#123959=CARTESIAN_POINT('Ctrl Pts',(-75.6397969140367,1076.3502576311,364.448309786551));
#123960=CARTESIAN_POINT('Ctrl Pts',(-75.711775200249,1076.34454471581,364.396472028127));
#123961=CARTESIAN_POINT('Ctrl Pts',(-75.7453531963788,1076.34164487273,
364.366825559236));
#123962=CARTESIAN_POINT('Ctrl Pts',(-75.836106514004,1076.33305189152,364.269086326673));
#123963=CARTESIAN_POINT('Ctrl Pts',(-75.8830807748402,1076.3275018733,364.192822000742));
#123964=CARTESIAN_POINT('Ctrl Pts',(-75.9448261000479,1076.3174107107,364.026563492133));
#123965=CARTESIAN_POINT('Ctrl Pts',(-75.9590418127969,1076.31296668752,
363.938187175942));
#123966=CARTESIAN_POINT('Ctrl Pts',(-75.9525027664394,1076.30585423698,
363.761146251404));
#123967=CARTESIAN_POINT('Ctrl Pts',(-75.9318978026455,1076.30325185463,
363.674204671663));
#123968=CARTESIAN_POINT('Ctrl Pts',(-75.8583863822407,1076.30029495885,
363.513380867354));
#123969=CARTESIAN_POINT('Ctrl Pts',(-75.8062816866164,1076.2999643101,363.441040688944));
#123970=CARTESIAN_POINT('Ctrl Pts',(-75.6772478077877,1076.30163836959,
363.320569784331));
#123971=CARTESIAN_POINT('Ctrl Pts',(-75.6016066419786,1076.30362398676,
363.273593808685));
#123972=CARTESIAN_POINT('Ctrl Pts',(-75.4429036913969,1076.30940021779,
363.213749865197));
#123973=CARTESIAN_POINT('Ctrl Pts',(-75.3621640822628,1076.3129924975,363.199043538177));
#123974=CARTESIAN_POINT('Ctrl Pts',(-75.2807885393945,1076.3172060834,363.199043033448));
#123975=CARTESIAN_POINT('',(-75.2807843499774,1082.7251047501,363.199043033435));
#123976=CARTESIAN_POINT('',(-75.2807843499774,1067.7251047501,363.199043033435));
#123977=CARTESIAN_POINT('Origin',(-75.2807843499774,1082.7251047501,363.874487154571));
#123978=CARTESIAN_POINT('Ctrl Pts',(-75.2807843499784,1076.31720630032,
363.199043033435));
#123979=CARTESIAN_POINT('Ctrl Pts',(-75.1923494186631,1076.32178543985,
363.199043033435));
#123980=CARTESIAN_POINT('Ctrl Pts',(-75.1048022879565,1076.3270122528,363.216409353866));
#123981=CARTESIAN_POINT('Ctrl Pts',(-74.9822262069248,1076.33534324347,
363.266997652347));
#123982=CARTESIAN_POINT('Ctrl Pts',(-74.9431054264288,1076.33818342375,
363.287841643676));
#123983=CARTESIAN_POINT('Ctrl Pts',(-74.8695141570817,1076.34390194688,
363.336866565203));
#123984=CARTESIAN_POINT('Ctrl Pts',(-74.8352170575663,1076.34676671064,
363.364929475761));
#123985=CARTESIAN_POINT('Ctrl Pts',(-74.7401777376837,1076.35535527583,
363.459676970117));
#123986=CARTESIAN_POINT('Ctrl Pts',(-74.6897666533623,1076.36088163242,
363.53532779201));
#123987=CARTESIAN_POINT('Ctrl Pts',(-74.6216654575394,1076.3708364867,363.701730874945));
#123988=CARTESIAN_POINT('Ctrl Pts',(-74.60455276562,1076.37517080223,363.790788986676));
#123989=CARTESIAN_POINT('Ctrl Pts',(-74.6061837746983,1076.3821204472,363.970494750931));
#123990=CARTESIAN_POINT('Ctrl Pts',(-74.624931632915,1076.38466645676,364.059338537434));
#123991=CARTESIAN_POINT('Ctrl Pts',(-74.6961917881948,1076.38764967982,
364.224607327379));
#123992=CARTESIAN_POINT('Ctrl Pts',(-74.7480225687572,1076.38805479619,
364.299339070781));
#123993=CARTESIAN_POINT('Ctrl Pts',(-74.8778961562943,1076.38665154554,
364.424036680836));
#123994=CARTESIAN_POINT('Ctrl Pts',(-74.954602951011,1076.38485851261,364.472753221244));
#123995=CARTESIAN_POINT('Ctrl Pts',(-75.1159547584908,1076.37948362869,
364.534734942781));
#123996=CARTESIAN_POINT('Ctrl Pts',(-75.1980651866747,1076.37610008038,
364.549931275707));
#123997=CARTESIAN_POINT('Ctrl Pts',(-75.2807843499774,1076.3720597734,364.549931275707));
#123998=CARTESIAN_POINT('Origin',(-73.7938092375736,1067.7251047501,350.104695514138));
#123999=CARTESIAN_POINT('',(-73.7938092376029,1075.57253700026,349.005864378145));
#124000=CARTESIAN_POINT('',(-73.7938092375736,1067.7251047501,349.005864378145));
#124001=CARTESIAN_POINT('Ctrl Pts',(-73.7943438286108,1075.73507520609,
351.203526520088));
#124002=CARTESIAN_POINT('Ctrl Pts',(-73.9403170085117,1075.72466814698,
351.203455502841));
#124003=CARTESIAN_POINT('Ctrl Pts',(-74.084675960195,1075.71222254048,351.174300992785));
#124004=CARTESIAN_POINT('Ctrl Pts',(-74.2849583459431,1075.69163544522,
351.090248581891));
#124005=CARTESIAN_POINT('Ctrl Pts',(-74.3480101216659,1075.68457833148,
351.056219174524));
#124006=CARTESIAN_POINT('Ctrl Pts',(-74.5296165654477,1075.66239714621,
350.934006536723));
#124007=CARTESIAN_POINT('Ctrl Pts',(-74.6341208385784,1075.64688776811,
350.827910232112));
#124008=CARTESIAN_POINT('Ctrl Pts',(-74.7935894751206,1075.61685947417,
350.583058284819));
#124009=CARTESIAN_POINT('Ctrl Pts',(-74.8479057527387,1075.60261206263,
350.447227919341));
#124010=CARTESIAN_POINT('Ctrl Pts',(-74.9005698938151,1075.57717485605,
350.162682866827));
#124011=CARTESIAN_POINT('Ctrl Pts',(-74.8986315070578,1075.56621986658,
350.016749704869));
#124012=CARTESIAN_POINT('Ctrl Pts',(-74.8384004917684,1075.54924950489,
349.734665488139));
#124013=CARTESIAN_POINT('Ctrl Pts',(-74.7810666738733,1075.54337181776,
349.601231042371));
#124014=CARTESIAN_POINT('Ctrl Pts',(-74.6185071053364,1075.53756791743,
349.364561147917));
#124015=CARTESIAN_POINT('Ctrl Pts',(-74.5151683413827,1075.53766809888,
349.263526373816));
#124016=CARTESIAN_POINT('Ctrl Pts',(-74.2756832064865,1075.54384041196,
349.106856863847));
#124017=CARTESIAN_POINT('Ctrl Pts',(-74.1419546455288,1075.54984400915,
349.052736057625));
#124018=CARTESIAN_POINT('Ctrl Pts',(-73.8609052025502,1075.56694315995,
348.998578412881));
#124019=CARTESIAN_POINT('Ctrl Pts',(-73.7162781603625,1075.57789026887,
348.999298161707));
#124020=CARTESIAN_POINT('Ctrl Pts',(-73.4347958345081,1075.60324547587,
349.056224428512));
#124021=CARTESIAN_POINT('Ctrl Pts',(-73.3006816519036,1075.61743115363,
349.112247540691));
#124022=CARTESIAN_POINT('Ctrl Pts',(-73.0612986408069,1075.64708439173,
349.272991388969));
#124023=CARTESIAN_POINT('Ctrl Pts',(-72.958399197672,1075.66227779007,349.376410086018));
#124024=CARTESIAN_POINT('Ctrl Pts',(-72.797612000534,1075.6917527953,349.618511135587));
#124025=CARTESIAN_POINT('Ctrl Pts',(-72.7417953372785,1075.70573900701,
349.755246162285));
#124026=CARTESIAN_POINT('Ctrl Pts',(-72.6871649626123,1075.73041142659,
350.041937314009));
#124027=CARTESIAN_POINT('Ctrl Pts',(-72.6885603814981,1075.7408770953,350.189001738921));
#124028=CARTESIAN_POINT('Ctrl Pts',(-72.7487463610536,1075.75702253198,
350.4741281338));
#124029=CARTESIAN_POINT('Ctrl Pts',(-72.8068707077791,1075.76254706029,
350.609318738545));
#124030=CARTESIAN_POINT('Ctrl Pts',(-72.9726685012712,1075.76793996582,
350.849299583654));
#124031=CARTESIAN_POINT('Ctrl Pts',(-73.0786544439614,1075.76775184252,
350.951607007295));
#124032=CARTESIAN_POINT('Ctrl Pts',(-73.3243233086004,1075.76162585565,
351.108823140814));
#124033=CARTESIAN_POINT('Ctrl Pts',(-73.4614663626373,1075.75575198615,
351.16213559445));
#124034=CARTESIAN_POINT('Ctrl Pts',(-73.6674877868136,1075.74371243895,
351.198088647224));
#124035=CARTESIAN_POINT('Ctrl Pts',(-73.7308714385672,1075.7396004272,351.20355739997));
#124036=CARTESIAN_POINT('Ctrl Pts',(-73.7943438286108,1075.73507520609,
351.203526520089));
#124037=CARTESIAN_POINT('Origin',(-73.7938092375736,1067.7251047501,350.104695514138));
#124038=CARTESIAN_POINT('',(-73.7938092375736,1075.69207332612,350.60352665013));
#124039=CARTESIAN_POINT('',(-73.7938092375736,1075.61827177418,349.605864378145));
#124040=CARTESIAN_POINT('Ctrl Pts',(-73.7938092375736,1075.69207332612,
350.60352665013));
#124041=CARTESIAN_POINT('Ctrl Pts',(-73.7979495129483,1075.69177375716,
350.60352665013));
#124042=CARTESIAN_POINT('Ctrl Pts',(-73.802091793159,1075.69147023046,350.603475104143));
#124043=CARTESIAN_POINT('Ctrl Pts',(-73.8728178240604,1075.68622244654,
350.60171277064));
#124044=CARTESIAN_POINT('Ctrl Pts',(-73.9383329755696,1075.68037315732,
350.586738379904));
#124045=CARTESIAN_POINT('Ctrl Pts',(-74.0286377306387,1075.67080350965,
350.546000300336));
#124046=CARTESIAN_POINT('Ctrl Pts',(-74.0569482506047,1075.66754082214,
350.529726126065));
#124047=CARTESIAN_POINT('Ctrl Pts',(-74.1100452604125,1075.66086906725,
350.4918561257));
#124048=CARTESIAN_POINT('Ctrl Pts',(-74.134699477728,1075.65747511528,350.470334703564));
#124049=CARTESIAN_POINT('Ctrl Pts',(-74.2029959977506,1075.64709855625,
350.397763736712));
#124050=CARTESIAN_POINT('Ctrl Pts',(-74.238638821479,1075.64019996183,350.340188220393));
#124051=CARTESIAN_POINT('Ctrl Pts',(-74.2845288500381,1075.62754140758,
350.215728271492));
#124052=CARTESIAN_POINT('Ctrl Pts',(-74.2948822435841,1075.62188043308,
350.150258958649));
#124053=CARTESIAN_POINT('Ctrl Pts',(-74.2896041219376,1075.61246458717,
350.019325521818));
#124054=CARTESIAN_POINT('Ctrl Pts',(-74.2741718712292,1075.60879116,349.95513669967));
#124055=CARTESIAN_POINT('Ctrl Pts',(-74.2194898641718,1075.60395376277,
349.836623196663));
#124056=CARTESIAN_POINT('Ctrl Pts',(-74.1809195751678,1075.60282391206,
349.783420087652));
#124057=CARTESIAN_POINT('Ctrl Pts',(-74.0855925349758,1075.60326819831,
349.694921376715));
#124058=CARTESIAN_POINT('Ctrl Pts',(-74.0298308188195,1075.60483147094,
349.660467354418));
#124059=CARTESIAN_POINT('Ctrl Pts',(-73.9130462923001,1075.61022799793,
349.61664313576));
#124060=CARTESIAN_POINT('Ctrl Pts',(-73.8537514928858,1075.61382884438,
349.6058898588));
#124061=CARTESIAN_POINT('Ctrl Pts',(-73.7940216604385,1075.61825602602,
349.605864423372));
#124062=CARTESIAN_POINT('Ctrl Pts',(-73.793950852004,1075.61826127435,349.605864393219));
#124063=CARTESIAN_POINT('Ctrl Pts',(-73.7938800443809,1075.61826652374,
349.605864378145));
#124064=CARTESIAN_POINT('Ctrl Pts',(-73.7938092375737,1075.61827177418,
349.605864378145));
#124065=CARTESIAN_POINT('',(-73.7938092375736,1082.7251047501,349.605864378145));
#124066=CARTESIAN_POINT('',(-73.7938092375736,1067.7251047501,349.605864378145));
#124067=CARTESIAN_POINT('Origin',(-73.7938092375736,1082.7251047501,350.104695514138));
#124068=CARTESIAN_POINT('Ctrl Pts',(-73.7938092375737,1075.61827177418,
349.605864378145));
#124069=CARTESIAN_POINT('Ctrl Pts',(-73.7285772438854,1075.62310883226,
349.605864378145));
#124070=CARTESIAN_POINT('Ctrl Pts',(-73.6640377663185,1075.6288410551,349.618658646094));
#124071=CARTESIAN_POINT('Ctrl Pts',(-73.543216236694,1075.64145773073,349.668423827516));
#124072=CARTESIAN_POINT('Ctrl Pts',(-73.4881375880883,1075.64822967675,
349.705085037028));
#124073=CARTESIAN_POINT('Ctrl Pts',(-73.3944413635905,1075.66200138751,
349.798437137012));
#124074=CARTESIAN_POINT('Ctrl Pts',(-73.3570671295821,1075.66886930196,
349.854590499074));
#124075=CARTESIAN_POINT('Ctrl Pts',(-73.306774695344,1075.68159917132,349.978015673703));
#124076=CARTESIAN_POINT('Ctrl Pts',(-73.2942236093973,1075.68734219416,
350.04402356237));
#124077=CARTESIAN_POINT('Ctrl Pts',(-73.2957998750605,1075.69694028833,
350.176956305832));
#124078=CARTESIAN_POINT('Ctrl Pts',(-73.3098168227983,1075.7007063751,350.242543762047));
#124079=CARTESIAN_POINT('Ctrl Pts',(-73.3627627989532,1075.7057576137,350.364382063199));
#124080=CARTESIAN_POINT('Ctrl Pts',(-73.4011122848796,1075.70699463425,
350.419391136037));
#124081=CARTESIAN_POINT('Ctrl Pts',(-73.4961277294539,1075.70675684485,
350.510214825593));
#124082=CARTESIAN_POINT('Ctrl Pts',(-73.5514432522579,1075.70534097152,
350.54550420152));
#124083=CARTESIAN_POINT('Ctrl Pts',(-73.669974095671,1075.70017464118,350.591913631098));
#124084=CARTESIAN_POINT('Ctrl Pts',(-73.7316658307316,1075.69656970236,
350.60352665013));
#124085=CARTESIAN_POINT('Ctrl Pts',(-73.7938092375736,1075.69207332612,
350.60352665013));
#124086=CARTESIAN_POINT('Origin',(-69.4825522658041,1067.7251047501,336.798793877895));
#124087=CARTESIAN_POINT('',(-69.482552265823,1074.68462093241,335.708253129166));
#124088=CARTESIAN_POINT('',(-69.4825522658041,1067.7251047501,335.708253129166));
#124089=CARTESIAN_POINT('Ctrl Pts',(-69.482044588625,1074.91623532639,337.889334508454));
#124090=CARTESIAN_POINT('Ctrl Pts',(-69.6268448872223,1074.90431233596,
337.889401917045));
#124091=CARTESIAN_POINT('Ctrl Pts',(-69.7699610523262,1074.88948709449,
337.860634556447));
#124092=CARTESIAN_POINT('Ctrl Pts',(-70.0368352563637,1074.85562701002,
337.749084359417));
#124093=CARTESIAN_POINT('Ctrl Pts',(-70.1579277482776,1074.83690116048,
337.66716268673));
#124094=CARTESIAN_POINT('Ctrl Pts',(-70.3092460076959,1074.80795475402,
337.513563586279));
#124095=CARTESIAN_POINT('Ctrl Pts',(-70.3540051655982,1074.79832384645,
337.458253465507));
#124096=CARTESIAN_POINT('Ctrl Pts',(-70.4735436314901,1074.76896404509,
337.27691019806));
#124097=CARTESIAN_POINT('Ctrl Pts',(-70.5287184548299,1074.74962867978,
337.13977603213));
#124098=CARTESIAN_POINT('Ctrl Pts',(-70.5810814878598,1074.71455491498,
336.854557003272));
#124099=CARTESIAN_POINT('Ctrl Pts',(-70.5789216965246,1074.69908367227,
336.70942848117));
#124100=CARTESIAN_POINT('Ctrl Pts',(-70.5184644809355,1074.67397221671,
336.429363436276));
#124101=CARTESIAN_POINT('Ctrl Pts',(-70.4613246199309,1074.66452295267,
336.297081656758));
#124102=CARTESIAN_POINT('Ctrl Pts',(-70.2996719412468,1074.65297235618,
336.062810712616));
#124103=CARTESIAN_POINT('Ctrl Pts',(-70.197208708713,1074.65092631395,335.962940541778));
#124104=CARTESIAN_POINT('Ctrl Pts',(-69.9599373338993,1074.65450377585,
335.808133153499));
#124105=CARTESIAN_POINT('Ctrl Pts',(-69.8276153228959,1074.66007498532,
335.754685532963));
#124106=CARTESIAN_POINT('Ctrl Pts',(-69.5493717095422,1074.67812828618,
335.701064215748));
#124107=CARTESIAN_POINT('Ctrl Pts',(-69.4061566135024,1074.69046942786,
335.701749622818));
#124108=CARTESIAN_POINT('Ctrl Pts',(-69.126998138824,1074.72034296465,335.75795645933));
#124109=CARTESIAN_POINT('Ctrl Pts',(-68.9938302321287,1074.73763799905,
335.813502389317));
#124110=CARTESIAN_POINT('Ctrl Pts',(-68.8158524427427,1074.76546282371,
335.932820391935));
#124111=CARTESIAN_POINT('Ctrl Pts',(-68.7605056092299,1074.77500173065,
335.978403244282));
#124112=CARTESIAN_POINT('Ctrl Pts',(-68.6597463291446,1074.79425731883,
336.079526422682));
#124113=CARTESIAN_POINT('Ctrl Pts',(-68.6145238193859,1074.80393019429,
336.134804249594));
#124114=CARTESIAN_POINT('Ctrl Pts',(-68.4947890010657,1074.83301338696,
336.314503657827));
#124115=CARTESIAN_POINT('Ctrl Pts',(-68.4392432986122,1074.85191119827,
336.449796131516));
#124116=CARTESIAN_POINT('Ctrl Pts',(-68.3844244251128,1074.88628567302,
336.733828681667));
#124117=CARTESIAN_POINT('Ctrl Pts',(-68.3854281483946,1074.90145000531,
336.879787802314));
#124118=CARTESIAN_POINT('Ctrl Pts',(-68.4445847243561,1074.9261138144,337.163333469513));
#124119=CARTESIAN_POINT('Ctrl Pts',(-68.5021762038381,1074.93536178919,
337.298037043689));
#124120=CARTESIAN_POINT('Ctrl Pts',(-68.664979268859,1074.94649842765,337.534260766224));
#124121=CARTESIAN_POINT('Ctrl Pts',(-68.7673286622167,1074.94845439328,
337.634149339983));
#124122=CARTESIAN_POINT('Ctrl Pts',(-69.004712556087,1074.94507002068,337.789285191735));
#124123=CARTESIAN_POINT('Ctrl Pts',(-69.1373636244834,1074.9397565634,337.842910728574));
#124124=CARTESIAN_POINT('Ctrl Pts',(-69.3442431971288,1074.92689252331,
337.882730528295));
#124125=CARTESIAN_POINT('Ctrl Pts',(-69.4130907838078,1074.92191304641,
337.889302408528));
#124126=CARTESIAN_POINT('Ctrl Pts',(-69.482044588625,1074.91623532639,337.889334508454));
#124127=CARTESIAN_POINT('Origin',(-69.4825522658041,1067.7251047501,336.798793877895));
#124128=CARTESIAN_POINT('',(-69.4825522658041,1074.85393827482,337.289334626623));
#124129=CARTESIAN_POINT('',(-69.4825522658041,1074.74977363876,336.308253129166));
#124130=CARTESIAN_POINT('Ctrl Pts',(-69.4825522658041,1074.85393827482,
337.289334626623));
#124131=CARTESIAN_POINT('Ctrl Pts',(-69.5156608898946,1074.85118092534,
337.289334626623));
#124132=CARTESIAN_POINT('Ctrl Pts',(-69.5487365376258,1074.84807154848,
337.285982577554));
#124133=CARTESIAN_POINT('Ctrl Pts',(-69.6453218199865,1074.83792315234,
337.266139960999));
#124134=CARTESIAN_POINT('Ctrl Pts',(-69.7060039722654,1074.830128241,337.240326933441));
#124135=CARTESIAN_POINT('Ctrl Pts',(-69.7861436696537,1074.81760734305,
337.185423455841));
#124136=CARTESIAN_POINT('Ctrl Pts',(-69.8106551502927,1074.81337335087,
337.164850184747));
#124137=CARTESIAN_POINT('Ctrl Pts',(-69.8553503056872,1074.80478387879,
337.119220492057));
#124138=CARTESIAN_POINT('Ctrl Pts',(-69.8754283392612,1074.80044735509,
337.094259376792));
#124139=CARTESIAN_POINT('Ctrl Pts',(-69.9288586827907,1074.7872828606,337.012665023113));
#124140=CARTESIAN_POINT('Ctrl Pts',(-69.95345227519,1074.7786526084,336.951105668282));
#124141=CARTESIAN_POINT('Ctrl Pts',(-69.9768104861118,1074.7629587941,336.82252465352));
#124142=CARTESIAN_POINT('Ctrl Pts',(-69.975622761632,1074.75602992107,336.756795840196));
#124143=CARTESIAN_POINT('Ctrl Pts',(-69.9477765303257,1074.74487453043,
336.630569671525));
#124144=CARTESIAN_POINT('Ctrl Pts',(-69.9218399501277,1074.74071220095,
336.571236267911));
#124145=CARTESIAN_POINT('Ctrl Pts',(-69.8487299623223,1074.73565201654,
336.466220536245));
#124146=CARTESIAN_POINT('Ctrl Pts',(-69.8024632954533,1074.7347802369,336.421496203756));
#124147=CARTESIAN_POINT('Ctrl Pts',(-69.6954251653061,1074.73644059973,
336.352281990104));
#124148=CARTESIAN_POINT('Ctrl Pts',(-69.6357611873031,1074.73895190826,
336.328475021556));
#124149=CARTESIAN_POINT('Ctrl Pts',(-69.5433400443614,1074.74492535713,
336.311081847338));
#124150=CARTESIAN_POINT('Ctrl Pts',(-69.5129674837563,1074.7471970323,336.308253129166));
#124151=CARTESIAN_POINT('Ctrl Pts',(-69.4825522658041,1074.74977363876,
336.308253129166));
#124152=CARTESIAN_POINT('',(-69.4825522658041,1082.7251047501,336.308253129166));
#124153=CARTESIAN_POINT('',(-69.4825522658041,1067.7251047501,336.308253129166));
#124154=CARTESIAN_POINT('Origin',(-69.4825522658041,1082.7251047501,336.798793877895));
#124155=CARTESIAN_POINT('Ctrl Pts',(-69.48255183749,1074.74977367504,336.308253129166));
#124156=CARTESIAN_POINT('Ctrl Pts',(-69.4183527172007,1074.75521226996,
336.308253185222));
#124157=CARTESIAN_POINT('Ctrl Pts',(-69.3548876880576,1074.76193077302,
336.320853926478));
#124158=CARTESIAN_POINT('Ctrl Pts',(-69.234964446525,1074.77733067317,336.370251892038));
#124159=CARTESIAN_POINT('Ctrl Pts',(-69.1799132064186,1074.78590878087,
336.407205839001));
#124160=CARTESIAN_POINT('Ctrl Pts',(-69.1112824361735,1074.79905699663,
336.476592740311));
#124161=CARTESIAN_POINT('Ctrl Pts',(-69.0910539250758,1074.8034013946,336.50149956963));
#124162=CARTESIAN_POINT('Ctrl Pts',(-69.0373963429084,1074.81651113423,
336.582632990236));
#124163=CARTESIAN_POINT('Ctrl Pts',(-69.012584813969,1074.82505786061,336.643759086384));
#124164=CARTESIAN_POINT('Ctrl Pts',(-68.988414035207,1074.84063673182,336.772111408957));
#124165=CARTESIAN_POINT('Ctrl Pts',(-68.9892279760228,1074.84752250316,
336.838084476661));
#124166=CARTESIAN_POINT('Ctrl Pts',(-69.0165987816869,1074.85862426497,
336.965191865952));
#124167=CARTESIAN_POINT('Ctrl Pts',(-69.0425474794926,1074.86276376567,
337.025111727045));
#124168=CARTESIAN_POINT('Ctrl Pts',(-69.1157573489778,1074.86776989741,
337.130684087977));
#124169=CARTESIAN_POINT('Ctrl Pts',(-69.1619316104886,1074.86863787131,
337.175486532404));
#124170=CARTESIAN_POINT('Ctrl Pts',(-69.2688854443816,1074.86704482667,
337.244936442028));
#124171=CARTESIAN_POINT('Ctrl Pts',(-69.3285787197443,1074.86459932949,
337.268873137344));
#124172=CARTESIAN_POINT('Ctrl Pts',(-69.4213566312991,1074.85873207417,
337.286474621064));
#124173=CARTESIAN_POINT('Ctrl Pts',(-69.4519685163185,1074.85648534792,
337.289334626623));
#124174=CARTESIAN_POINT('Ctrl Pts',(-69.4825522658041,1074.85393827482,
337.289334626623));
#124175=CARTESIAN_POINT('Origin',(-83.8577571500213,1067.7251047501,393.178981560286));
#124176=CARTESIAN_POINT('',(-83.857757150042,1076.65831288829,391.700678428093));
#124177=CARTESIAN_POINT('',(-83.8577571500213,1067.7251047501,391.700678428093));
#124178=CARTESIAN_POINT('Ctrl Pts',(-83.8571940935802,1076.6854098979,394.657284585251));
#124179=CARTESIAN_POINT('Ctrl Pts',(-83.9528543621346,1076.68332503261,
394.657321020359));
#124180=CARTESIAN_POINT('Ctrl Pts',(-84.0482896858879,1076.68110226508,
394.648072189946));
#124181=CARTESIAN_POINT('Ctrl Pts',(-84.237925298588,1076.67637636788,394.610895081188));
#124182=CARTESIAN_POINT('Ctrl Pts',(-84.3315968557539,1076.6738799666,394.582683514737));
#124183=CARTESIAN_POINT('Ctrl Pts',(-84.6011130072004,1076.66619665297,
394.471434048908));
#124184=CARTESIAN_POINT('Ctrl Pts',(-84.7641144709483,1076.66085524092,
394.362842571996));
#124185=CARTESIAN_POINT('Ctrl Pts',(-85.038951478879,1076.65048514005,394.088837035227));
#124186=CARTESIAN_POINT('Ctrl Pts',(-85.1480925625414,1076.64556313726,
393.926042650183));
#124187=CARTESIAN_POINT('Ctrl Pts',(-85.29720850228,1076.63713488144,393.567607409226));
#124188=CARTESIAN_POINT('Ctrl Pts',(-85.3357493456625,1076.63371736493,
393.375454127138));
#124189=CARTESIAN_POINT('Ctrl Pts',(-85.3363669002121,1076.62916473982,
392.987575080872));
#124190=CARTESIAN_POINT('Ctrl Pts',(-85.2985786646413,1076.6280741197,392.795625867869));
#124191=CARTESIAN_POINT('Ctrl Pts',(-85.1512839784971,1076.62848785611,
392.437677318038));
#124192=CARTESIAN_POINT('Ctrl Pts',(-85.0433812733427,1076.6299813596,392.27508309293));
#124193=CARTESIAN_POINT('Ctrl Pts',(-84.7713116447634,1076.63522890501,
392.00082100113));
#124194=CARTESIAN_POINT('Ctrl Pts',(-84.6098376407021,1076.63892452082,
391.89173373863));
#124195=CARTESIAN_POINT('Ctrl Pts',(-84.2540359013528,1076.6477403855,391.741749309456));
#124196=CARTESIAN_POINT('Ctrl Pts',(-84.0631087233663,1076.65276963375,
391.702331024677));
#124197=CARTESIAN_POINT('Ctrl Pts',(-83.6767164193077,1076.66319957231,
391.699125773987));
#124198=CARTESIAN_POINT('Ctrl Pts',(-83.484959280491,1076.66849503082,391.735453626999));
#124199=CARTESIAN_POINT('Ctrl Pts',(-83.12350095616,1076.67858982704,391.880984179758));
#124200=CARTESIAN_POINT('Ctrl Pts',(-82.9577796125186,1076.68327916066,
391.989873201615));
#124201=CARTESIAN_POINT('Ctrl Pts',(-82.6796118544,1076.69142377176,392.265014015731));
#124202=CARTESIAN_POINT('Ctrl Pts',(-82.5695033304998,1076.6948139835,392.428132767469));
#124203=CARTESIAN_POINT('Ctrl Pts',(-82.4187788222995,1076.70020865997,
392.7880223399));
#124204=CARTESIAN_POINT('Ctrl Pts',(-82.3797726792368,1076.70216608927,
392.981307429118));
#124205=CARTESIAN_POINT('Ctrl Pts',(-82.379137778424,1076.70470788168,393.372764725265));
#124206=CARTESIAN_POINT('Ctrl Pts',(-82.4178747972533,1076.70526678929,
393.56706340159));
#124207=CARTESIAN_POINT('Ctrl Pts',(-82.5688901593564,1076.70501100144,
393.92907705046));
#124208=CARTESIAN_POINT('Ctrl Pts',(-82.6796238666232,1076.7041989837,394.093214087362));
#124209=CARTESIAN_POINT('Ctrl Pts',(-82.9579861578556,1076.70113667203,
394.368040577126));
#124210=CARTESIAN_POINT('Ctrl Pts',(-83.1225997395357,1076.69891644088,
394.476281318645));
#124211=CARTESIAN_POINT('Ctrl Pts',(-83.4794127948176,1076.69307788233,
394.62059810628));
#124212=CARTESIAN_POINT('Ctrl Pts',(-83.6674202830168,1076.68954591838,
394.657212304152));
#124213=CARTESIAN_POINT('Ctrl Pts',(-83.8571940935802,1076.6854098979,394.657284585251));
#124214=CARTESIAN_POINT('Origin',(-83.8577571500213,1067.7251047501,393.178981560286));
#124215=CARTESIAN_POINT('',(-83.8577571500214,1076.68056431803,394.057284692479));
#124216=CARTESIAN_POINT('',(-83.8577571500214,1076.66449392106,392.300678428093));
#124217=CARTESIAN_POINT('Ctrl Pts',(-83.8577571500213,1076.68056431803,
394.057284692479));
#124218=CARTESIAN_POINT('Ctrl Pts',(-83.8670327327715,1076.68035245333,
394.057284692479));
#124219=CARTESIAN_POINT('Ctrl Pts',(-83.8763143809642,1076.68013857438,
394.057137756963));
#124220=CARTESIAN_POINT('Ctrl Pts',(-83.9426550514218,1076.67859627437,
394.05503375308));
#124221=CARTESIAN_POINT('Ctrl Pts',(-83.9993979702626,1076.67720503007,
394.047666006467));
#124222=CARTESIAN_POINT('Ctrl Pts',(-84.1115404391114,1076.67430293354,
394.021818713267));
#124223=CARTESIAN_POINT('Ctrl Pts',(-84.1666289995102,1076.67279760102,
394.003225708839));
#124224=CARTESIAN_POINT('Ctrl Pts',(-84.3244367217557,1076.66824031985,
393.931904175525));
#124225=CARTESIAN_POINT('Ctrl Pts',(-84.4190457650727,1076.6651682811,393.864282995571));
#124226=CARTESIAN_POINT('Ctrl Pts',(-84.5767883879247,1076.65935515809,
393.696363226682));
#124227=CARTESIAN_POINT('Ctrl Pts',(-84.6383872444461,1076.65667261187,
393.597681479671));
#124228=CARTESIAN_POINT('Ctrl Pts',(-84.7199568441604,1076.65217975208,
393.382194701899));
#124229=CARTESIAN_POINT('Ctrl Pts',(-84.7391506937016,1076.65041529028,
393.267485487742));
#124230=CARTESIAN_POINT('Ctrl Pts',(-84.7321658922115,1076.6481548133,393.037337041536));
#124231=CARTESIAN_POINT('Ctrl Pts',(-84.706112537041,1076.64768065755,392.924132305296));
#124232=CARTESIAN_POINT('Ctrl Pts',(-84.6119096269206,1076.6481273546,392.714362857543));
#124233=CARTESIAN_POINT('Ctrl Pts',(-84.5447339090463,1076.64904152667,
392.619806061394));
#124234=CARTESIAN_POINT('Ctrl Pts',(-84.3778492305326,1076.65208950437,
392.461971183699));
#124235=CARTESIAN_POINT('Ctrl Pts',(-84.2797698970617,1076.65419121897,
392.400199755891));
#124236=CARTESIAN_POINT('Ctrl Pts',(-84.0721098264575,1076.65904314149,
392.320461958781));
#124237=CARTESIAN_POINT('Ctrl Pts',(-83.9653858733157,1076.66170161447,
392.300678428093));
#124238=CARTESIAN_POINT('Ctrl Pts',(-83.8577571500214,1076.66449392106,
392.300678428093));
#124239=CARTESIAN_POINT('',(-83.8577571500213,1082.7251047501,392.300678428093));
#124240=CARTESIAN_POINT('',(-83.8577571500213,1067.7251047501,392.300678428093));
#124241=CARTESIAN_POINT('Origin',(-83.8577571500213,1082.7251047501,393.178981560286));
#124242=CARTESIAN_POINT('Ctrl Pts',(-83.8577571500215,1076.66449392106,
392.300678428093));
#124243=CARTESIAN_POINT('Ctrl Pts',(-83.8576325991735,1076.66449715239,
392.300678428093));
#124244=CARTESIAN_POINT('Ctrl Pts',(-83.8575080471139,1076.66450038391,
392.300678454586));
#124245=CARTESIAN_POINT('Ctrl Pts',(-83.8573834938509,1076.6645036156,392.300678507575));
#124246=CARTESIAN_POINT('Ctrl Pts',(-83.7424453681473,1076.66748583276,
392.300727405663));
#124247=CARTESIAN_POINT('Ctrl Pts',(-83.6286264789588,1076.67056282292,
392.323337722145));
#124248=CARTESIAN_POINT('Ctrl Pts',(-83.4143101513657,1076.67656701639,
392.411878073479));
#124249=CARTESIAN_POINT('Ctrl Pts',(-83.3162179447018,1076.67943066473,
392.477675041555));
#124250=CARTESIAN_POINT('Ctrl Pts',(-83.1519124801383,1076.68453543471,
392.64347795714));
#124251=CARTESIAN_POINT('Ctrl Pts',(-83.0871956578491,1076.68673069361,
392.74169562649));
#124252=CARTESIAN_POINT('Ctrl Pts',(-82.999794699067,1076.69028414284,392.957803100277));
#124253=CARTESIAN_POINT('Ctrl Pts',(-82.9780358079161,1076.69160888867,
393.073567321889));
#124254=CARTESIAN_POINT('Ctrl Pts',(-82.9810196179529,1076.69331446352,
393.307153084358));
#124255=CARTESIAN_POINT('Ctrl Pts',(-83.0058604890839,1076.69367765092,
393.422639927147));
#124256=CARTESIAN_POINT('Ctrl Pts',(-83.0992918588072,1076.69341808685,
393.637035353046));
#124257=CARTESIAN_POINT('Ctrl Pts',(-83.1669243560869,1076.69279811395,
393.733807464251));
#124258=CARTESIAN_POINT('Ctrl Pts',(-83.3358456582448,1076.6905903592,393.894949496057));
#124259=CARTESIAN_POINT('Ctrl Pts',(-83.4353550347065,1076.68902491243,
393.957811127997));
#124260=CARTESIAN_POINT('Ctrl Pts',(-83.6444027165045,1076.68518587222,
394.037700648553));
#124261=CARTESIAN_POINT('Ctrl Pts',(-83.7506757699026,1076.68301017665,
394.057284692479));
#124262=CARTESIAN_POINT('Ctrl Pts',(-83.8577571500213,1076.68056431803,
394.057284692479));
#124263=CARTESIAN_POINT('Origin',(-86.2654713137621,1067.7251047501,380.853682816142));
#124264=CARTESIAN_POINT('',(-86.2654713137811,1076.3065749206,379.578238695006));
#124265=CARTESIAN_POINT('',(-86.2654713137621,1067.7251047501,379.578238695006));
#124266=CARTESIAN_POINT('Ctrl Pts',(-86.2659855827959,1076.38119950511,
382.1291268336));
#124267=CARTESIAN_POINT('Ctrl Pts',(-86.4358682980053,1076.37179008192,
382.129058335556));
#124268=CARTESIAN_POINT('Ctrl Pts',(-86.6039911709605,1076.36136063546,
382.095050328875));
#124269=CARTESIAN_POINT('Ctrl Pts',(-86.838212942953,1076.34506250357,381.996415866367));
#124270=CARTESIAN_POINT('Ctrl Pts',(-86.9125062498822,1076.33958092772,
381.956051590261));
#124271=CARTESIAN_POINT('Ctrl Pts',(-87.120926270196,1076.32323213126,381.814441036432));
#124272=CARTESIAN_POINT('Ctrl Pts',(-87.2396860582528,1076.31254531983,
381.693793545343));
#124273=CARTESIAN_POINT('Ctrl Pts',(-87.4236826281354,1076.29291722146,
381.413497063116));
#124274=CARTESIAN_POINT('Ctrl Pts',(-87.4871785906302,1076.2841681821,381.256573626955));
#124275=CARTESIAN_POINT('Ctrl Pts',(-87.5497217275718,1076.27002873665,
380.927454436253));
#124276=CARTESIAN_POINT('Ctrl Pts',(-87.5483281141395,1076.26477160671,
380.75850570807));
#124277=CARTESIAN_POINT('Ctrl Pts',(-87.4804422415383,1076.25864463005,
380.431281106168));
#124278=CARTESIAN_POINT('Ctrl Pts',(-87.4148505403703,1076.25782123202,
380.276177917597));
#124279=CARTESIAN_POINT('Ctrl Pts',(-87.2278806424649,1076.26076272105,
380.000320821711));
#124280=CARTESIAN_POINT('Ctrl Pts',(-87.1084596581209,1076.2644873009,379.882189185605));
#124281=CARTESIAN_POINT('Ctrl Pts',(-86.8309951438903,1076.27590558092,
379.698412639541));
#124282=CARTESIAN_POINT('Ctrl Pts',(-86.6756168158444,1076.28348750493,
379.634583953848));
#124283=CARTESIAN_POINT('Ctrl Pts',(-86.3488023339255,1076.30135488652,
379.570080743726));
#124284=CARTESIAN_POINT('Ctrl Pts',(-86.1804566596807,1076.31147216406,
379.570203373631));
#124285=CARTESIAN_POINT('Ctrl Pts',(-85.9350741103993,1076.327421904,379.618950564278));
#124286=CARTESIAN_POINT('Ctrl Pts',(-85.8549948440434,1076.33283452927,
379.643214275629));
#124287=CARTESIAN_POINT('Ctrl Pts',(-85.7007056878628,1076.34367716873,
379.707048541646));
#124288=CARTESIAN_POINT('Ctrl Pts',(-85.6268640325357,1076.34908143445,
379.746473557798));
#124289=CARTESIAN_POINT('Ctrl Pts',(-85.416338610646,1076.36517058836,379.886989368421));
#124290=CARTESIAN_POINT('Ctrl Pts',(-85.2954204815106,1076.37539263519,
380.008368862177));
#124291=CARTESIAN_POINT('Ctrl Pts',(-85.1087361966729,1076.39358550485,
380.290517624953));
#124292=CARTESIAN_POINT('Ctrl Pts',(-85.0444606327581,1076.40139571981,
380.44826213456));
#124293=CARTESIAN_POINT('Ctrl Pts',(-84.9810339300332,1076.41380990982,
380.779769772346));
#124294=CARTESIAN_POINT('Ctrl Pts',(-84.9825257112795,1076.41829511191,
380.950241206266));
#124295=CARTESIAN_POINT('Ctrl Pts',(-85.0519167131888,1076.42348028237,
381.28106874482));
#124296=CARTESIAN_POINT('Ctrl Pts',(-85.1192376968099,1076.4241243296,381.438085739406));
#124297=CARTESIAN_POINT('Ctrl Pts',(-85.3111237528364,1076.42146587903,
381.716549588247));
#124298=CARTESIAN_POINT('Ctrl Pts',(-85.4337045468094,1076.41819268183,
381.835242468119));
#124299=CARTESIAN_POINT('Ctrl Pts',(-85.7177150601958,1076.40800779872,
382.017804202035));
#124300=CARTESIAN_POINT('Ctrl Pts',(-85.8762627837711,1076.40119785151,
382.079934047725));
#124301=CARTESIAN_POINT('Ctrl Pts',(-86.1161074105835,1076.38928422029,
382.122571135187));
#124302=CARTESIAN_POINT('Ctrl Pts',(-86.1909810984377,1076.38535383554,
382.129157075996));
#124303=CARTESIAN_POINT('Ctrl Pts',(-86.265985582796,1076.38119950511,382.1291268336));
#124304=CARTESIAN_POINT('Origin',(-86.2654713137621,1067.7251047501,380.853682816142));
#124305=CARTESIAN_POINT('',(-86.2654713137621,1076.36458696229,381.529126937278));
#124306=CARTESIAN_POINT('',(-86.2654713137623,1076.32506388483,380.178238695006));
#124307=CARTESIAN_POINT('Ctrl Pts',(-86.2654713137621,1076.36458696229,
381.529126937278));
#124308=CARTESIAN_POINT('Ctrl Pts',(-86.3176203844329,1076.36164319747,
381.529126937278));
#124309=CARTESIAN_POINT('Ctrl Pts',(-86.3697119936323,1076.35851489311,
381.523087338792));
#124310=CARTESIAN_POINT('Ctrl Pts',(-86.4636268773205,1076.3525165865,381.500911826086));
#124311=CARTESIAN_POINT('Ctrl Pts',(-86.5054630782866,1076.34970353828,
381.486592295606));
#124312=CARTESIAN_POINT('Ctrl Pts',(-86.5862544493745,1076.34397809118,
381.449769217969));
#124313=CARTESIAN_POINT('Ctrl Pts',(-86.6249698706937,1076.34107874961,
381.427252031763));
#124314=CARTESIAN_POINT('Ctrl Pts',(-86.7330705388248,1076.33249670945,
381.349107136058));
#124315=CARTESIAN_POINT('Ctrl Pts',(-86.7940420633252,1076.32696821287,
381.28346691746));
#124316=CARTESIAN_POINT('Ctrl Pts',(-86.8870760472062,1076.31694808952,
381.132415059668));
#124317=CARTESIAN_POINT('Ctrl Pts',(-86.9182729858075,1076.31255312352,
381.048481114142));
#124318=CARTESIAN_POINT('Ctrl Pts',(-86.9463994247123,1076.30556164688,
380.873509680982));
#124319=CARTESIAN_POINT('Ctrl Pts',(-86.9431418328645,1076.30302988497,
380.784194133374));
#124320=CARTESIAN_POINT('Ctrl Pts',(-86.9023852566707,1076.30022562937,
380.612097881493));
#124321=CARTESIAN_POINT('Ctrl Pts',(-86.8653797104945,1076.29997496699,
380.530985347912));
#124322=CARTESIAN_POINT('Ctrl Pts',(-86.7623125829652,1076.30180520775,
380.387685650732));
#124323=CARTESIAN_POINT('Ctrl Pts',(-86.6972952692519,1076.30386493615,
380.326876916281));
#124324=CARTESIAN_POINT('Ctrl Pts',(-86.5475324764006,1076.31000530059,
380.233637770325));
#124325=CARTESIAN_POINT('Ctrl Pts',(-86.464218835407,1076.31402749585,380.202144991004));
#124326=CARTESIAN_POINT('Ctrl Pts',(-86.340372603284,1076.32074018736,380.181364110388));
#124327=CARTESIAN_POINT('Ctrl Pts',(-86.3030552747707,1076.32285151909,
380.178250175801));
#124328=CARTESIAN_POINT('Ctrl Pts',(-86.2656782137016,1076.32505170487,
380.178238726578));
#124329=CARTESIAN_POINT('Ctrl Pts',(-86.2656092465274,1076.3250557646,380.178238705453));
#124330=CARTESIAN_POINT('Ctrl Pts',(-86.2655402798804,1076.32505982459,
380.178238695006));
#124331=CARTESIAN_POINT('Ctrl Pts',(-86.2654713137625,1076.32506388483,
380.178238695006));
#124332=CARTESIAN_POINT('',(-86.2654713137621,1082.7251047501,380.178238695006));
#124333=CARTESIAN_POINT('',(-86.2654713137621,1067.7251047501,380.178238695006));
#124334=CARTESIAN_POINT('Origin',(-86.2654713137621,1082.7251047501,380.853682816142));
#124335=CARTESIAN_POINT('Ctrl Pts',(-86.2654713137625,1076.32506388483,
380.178238695006));
#124336=CARTESIAN_POINT('Ctrl Pts',(-86.1770509574414,1076.33026945905,
380.178238695006));
#124337=CARTESIAN_POINT('Ctrl Pts',(-86.0895006637669,1076.33589992213,
380.195600640667));
#124338=CARTESIAN_POINT('Ctrl Pts',(-85.9669065670266,1076.34448117668,
380.246195871646));
#124339=CARTESIAN_POINT('Ctrl Pts',(-85.9277742439781,1076.34734529568,
380.267046474723));
#124340=CARTESIAN_POINT('Ctrl Pts',(-85.8159507223342,1076.35592662903,
380.341549771814));
#124341=CARTESIAN_POINT('Ctrl Pts',(-85.7516777695141,1076.36143430001,
380.406051840836));
#124342=CARTESIAN_POINT('Ctrl Pts',(-85.6524526681669,1076.37131553153,
380.556200724508));
#124343=CARTESIAN_POINT('Ctrl Pts',(-85.6183599087259,1076.37559710457,
380.640266770774));
#124344=CARTESIAN_POINT('Ctrl Pts',(-85.5850873944973,1076.3824166311,380.816788623762));
#124345=CARTESIAN_POINT('Ctrl Pts',(-85.5862070859935,1076.38488938295,
380.907467173279));
#124346=CARTESIAN_POINT('Ctrl Pts',(-85.6238764233128,1076.38772183095,
381.083147878936));
#124347=CARTESIAN_POINT('Ctrl Pts',(-85.6600581347183,1076.38805288534,
381.166371898665));
#124348=CARTESIAN_POINT('Ctrl Pts',(-85.7628554500964,1076.38651252053,
381.313761929224));
#124349=CARTESIAN_POINT('Ctrl Pts',(-85.8284231525437,1076.38465683894,
381.376442053706));
#124350=CARTESIAN_POINT('Ctrl Pts',(-85.9802096773907,1076.37895394214,
381.472487243089));
#124351=CARTESIAN_POINT('Ctrl Pts',(-86.0649071745352,1076.37516222332,
381.504878057641));
#124352=CARTESIAN_POINT('Ctrl Pts',(-86.1905403956323,1076.36871995438,
381.526012303071));
#124353=CARTESIAN_POINT('Ctrl Pts',(-86.2280206704145,1076.36670101505,
381.529126937278));
#124354=CARTESIAN_POINT('Ctrl Pts',(-86.2654713137621,1076.36458696229,
381.529126937278));
#124355=CARTESIAN_POINT('Origin',(-87.6738908373841,1067.7251047501,367.075634650624));
#124356=CARTESIAN_POINT('',(-87.6738908374021,1075.59148954561,365.976803514631));
#124357=CARTESIAN_POINT('',(-87.6738908373841,1067.7251047501,365.976803514631));
#124358=CARTESIAN_POINT('Ctrl Pts',(-87.6734743951659,1075.7170825134,368.174465707703));
#124359=CARTESIAN_POINT('Ctrl Pts',(-87.819343312233,1075.70465571775,368.174520990065));
#124360=CARTESIAN_POINT('Ctrl Pts',(-87.9636575725919,1075.6906511942,368.145532263478));
#124361=CARTESIAN_POINT('Ctrl Pts',(-88.1639583242107,1075.66858130876,
368.061723796441));
#124362=CARTESIAN_POINT('Ctrl Pts',(-88.2270334907758,1075.66117542291,
368.027773599668));
#124363=CARTESIAN_POINT('Ctrl Pts',(-88.4086864406982,1075.63838489597,
367.905823706016));
#124364=CARTESIAN_POINT('Ctrl Pts',(-88.5132999336648,1075.62309825929,
367.799900398979));
#124365=CARTESIAN_POINT('Ctrl Pts',(-88.6729366183675,1075.59481458622,
367.555450155456));
#124366=CARTESIAN_POINT('Ctrl Pts',(-88.7273878484798,1075.58204853035,
367.419926572265));
#124367=CARTESIAN_POINT('Ctrl Pts',(-88.7804597333168,1075.56065085913,
367.136108631691));
#124368=CARTESIAN_POINT('Ctrl Pts',(-88.7788827440092,1075.55220640037,
366.990645907562));
#124369=CARTESIAN_POINT('Ctrl Pts',(-88.7197058693303,1075.54090098764,
366.709236914304));
#124370=CARTESIAN_POINT('Ctrl Pts',(-88.6630334350074,1075.53812041122,
366.576030986879));
#124371=CARTESIAN_POINT('Ctrl Pts',(-88.5018533127044,1075.5386369226,366.339176513656));
#124372=CARTESIAN_POINT('Ctrl Pts',(-88.3990911692971,1075.54191181696,
366.237815058458));
#124373=CARTESIAN_POINT('Ctrl Pts',(-88.160345480136,1075.55407916221,366.07998436106));
#124374=CARTESIAN_POINT('Ctrl Pts',(-88.0266449019473,1075.56286283703,
366.02518536982));
#124375=CARTESIAN_POINT('Ctrl Pts',(-87.7451843872829,1075.58475377391,
365.969720362314));
#124376=CARTESIAN_POINT('Ctrl Pts',(-87.6000649909103,1075.59767257472,
365.96991986028));
#124377=CARTESIAN_POINT('Ctrl Pts',(-87.3175958345444,1075.62587011806,
366.026189090554));
#124378=CARTESIAN_POINT('Ctrl Pts',(-87.1829606302508,1075.64089300229,
366.082032503143));
#124379=CARTESIAN_POINT('Ctrl Pts',(-86.9415902402265,1075.6711193491,366.243468766865));
#124380=CARTESIAN_POINT('Ctrl Pts',(-86.8375236448611,1075.68603306015,
366.348108637216));
#124381=CARTESIAN_POINT('Ctrl Pts',(-86.6768162114639,1075.71350487496,
366.591463032114));
#124382=CARTESIAN_POINT('Ctrl Pts',(-86.6214830441957,1075.72581151788,
366.727644750228));
#124383=CARTESIAN_POINT('Ctrl Pts',(-86.5671441103932,1075.74631830682,
367.014025689984));
#124384=CARTESIAN_POINT('Ctrl Pts',(-86.5687179818675,1075.75431392225,
367.161369995145));
#124385=CARTESIAN_POINT('Ctrl Pts',(-86.6292282425146,1075.76490486689,
367.445891003711));
#124386=CARTESIAN_POINT('Ctrl Pts',(-86.6870868365479,1075.76743884215,
367.580267337248));
#124387=CARTESIAN_POINT('Ctrl Pts',(-86.8507785005654,1075.76677452854,
367.817567181624));
#124388=CARTESIAN_POINT('Ctrl Pts',(-86.9544469095452,1075.76364524551,
367.918455254543));
#124389=CARTESIAN_POINT('Ctrl Pts',(-87.1968443215546,1075.75198819898,
368.07621785947));
#124390=CARTESIAN_POINT('Ctrl Pts',(-87.3337235930814,1075.74347543984,
368.130599225017));
#124391=CARTESIAN_POINT('Ctrl Pts',(-87.5419143744327,1075.7279425631,368.168499682902));
#124392=CARTESIAN_POINT('Ctrl Pts',(-87.6076419361123,1075.72269088105,
368.174440758085));
#124393=CARTESIAN_POINT('Ctrl Pts',(-87.673474395166,1075.7170825134,368.174465707703));
#124394=CARTESIAN_POINT('Origin',(-87.6738908373841,1067.7251047501,367.075634650624));
#124395=CARTESIAN_POINT('',(-87.6738908373841,1075.68376086233,367.574465786616));
#124396=CARTESIAN_POINT('',(-87.6738908373842,1075.62676689012,366.576803514631));
#124397=CARTESIAN_POINT('Ctrl Pts',(-87.6738908373841,1075.68376086233,
367.574465786616));
#124398=CARTESIAN_POINT('Ctrl Pts',(-87.6769953171298,1075.68349322266,
367.574465786616));
#124399=CARTESIAN_POINT('Ctrl Pts',(-87.6801009614361,1075.68322380588,
367.574436805534));
#124400=CARTESIAN_POINT('Ctrl Pts',(-87.7496697673629,1075.67715100789,
367.573137261163));
#124401=CARTESIAN_POINT('Ctrl Pts',(-87.8151691130928,1075.67066331402,
367.558625056895));
#124402=CARTESIAN_POINT('Ctrl Pts',(-87.9055907621926,1075.66053419269,
367.518584251856));
#124403=CARTESIAN_POINT('Ctrl Pts',(-87.9339536640393,1075.65715335191,
367.502549366014));
#124404=CARTESIAN_POINT('Ctrl Pts',(-88.0151640038816,1075.64682142456,
367.445523969457));
#124405=CARTESIAN_POINT('Ctrl Pts',(-88.061552503808,1075.63995957008,367.396588511813));
#124406=CARTESIAN_POINT('Ctrl Pts',(-88.1319807875865,1075.62729936569,
367.283863784303));
#124407=CARTESIAN_POINT('Ctrl Pts',(-88.1555546455449,1075.62161404733,
367.221313695564));
#124408=CARTESIAN_POINT('Ctrl Pts',(-88.1767238053739,1075.61223872528,
367.09150150772));
#124409=CARTESIAN_POINT('Ctrl Pts',(-88.1744934763366,1075.60861202125,
367.025583724268));
#124410=CARTESIAN_POINT('Ctrl Pts',(-88.1447600013157,1075.60387016661,
366.898589417079));
#124411=CARTESIAN_POINT('Ctrl Pts',(-88.1176848205915,1075.60278928111,
366.8387486077));
#124412=CARTESIAN_POINT('Ctrl Pts',(-88.0421128711325,1075.60332914552,
366.73290012093));
#124413=CARTESIAN_POINT('Ctrl Pts',(-87.9944058423625,1075.6049400738,366.687927485667));
#124414=CARTESIAN_POINT('Ctrl Pts',(-87.884326747752,1075.6106538794,366.618699183331));
#124415=CARTESIAN_POINT('Ctrl Pts',(-87.822999222578,1075.61470748199,366.595193289664));
#124416=CARTESIAN_POINT('Ctrl Pts',(-87.7309262673952,1075.62189435976,
366.579259278205));
#124417=CARTESIAN_POINT('Ctrl Pts',(-87.7025481394435,1075.62424984986,
366.576817171752));
#124418=CARTESIAN_POINT('Ctrl Pts',(-87.6741295580651,1075.62674591951,
366.576803571751));
#124419=CARTESIAN_POINT('Ctrl Pts',(-87.674049983502,1075.62675290873,366.576803533669));
#124420=CARTESIAN_POINT('Ctrl Pts',(-87.6739704099395,1075.62675989893,
366.576803514631));
#124421=CARTESIAN_POINT('Ctrl Pts',(-87.6738908373843,1075.62676689012,
366.576803514631));
#124422=CARTESIAN_POINT('',(-87.6738908373841,1082.7251047501,366.576803514631));
#124423=CARTESIAN_POINT('',(-87.6738908373841,1067.7251047501,366.576803514631));
#124424=CARTESIAN_POINT('Origin',(-87.6738908373841,1082.7251047501,367.075634650624));
#124425=CARTESIAN_POINT('Ctrl Pts',(-87.6738908373843,1075.62676689012,
366.576803514631));
#124426=CARTESIAN_POINT('Ctrl Pts',(-87.6084744953582,1075.63251432502,
366.576803514631));
#124427=CARTESIAN_POINT('Ctrl Pts',(-87.5437388459447,1075.63892740047,
366.589670546865));
#124428=CARTESIAN_POINT('Ctrl Pts',(-87.4218180103966,1075.65246164864,
366.640058854636));
#124429=CARTESIAN_POINT('Ctrl Pts',(-87.3659830474847,1075.65946279612,
366.677563307127));
#124430=CARTESIAN_POINT('Ctrl Pts',(-87.272497503493,1075.6729528367,366.772120662268));
#124431=CARTESIAN_POINT('Ctrl Pts',(-87.2356857889018,1075.67931362939,
366.828194063365));
#124432=CARTESIAN_POINT('Ctrl Pts',(-87.1862113655451,1075.69055153046,
366.951500387343));
#124433=CARTESIAN_POINT('Ctrl Pts',(-87.1740123991004,1075.69531957854,
367.017500520854));
#124434=CARTESIAN_POINT('Ctrl Pts',(-87.1762354342323,1075.70257536774,
367.149793398211));
#124435=CARTESIAN_POINT('Ctrl Pts',(-87.1903430344116,1075.70501561211,
367.214750349486));
#124436=CARTESIAN_POINT('Ctrl Pts',(-87.2426809623601,1075.70727323407,
367.334701272723));
#124437=CARTESIAN_POINT('Ctrl Pts',(-87.2800698378778,1075.70710257816,
367.388622980891));
#124438=CARTESIAN_POINT('Ctrl Pts',(-87.3735040727621,1075.7041932488,367.479169595807));
#124439=CARTESIAN_POINT('Ctrl Pts',(-87.428652808903,1075.70147855512,367.51486012164));
#124440=CARTESIAN_POINT('Ctrl Pts',(-87.5479317826372,1075.69392442781,
367.562446644088));
#124441=CARTESIAN_POINT('Ctrl Pts',(-87.6106698370051,1075.68921119508,
367.574465786616));
#124442=CARTESIAN_POINT('Ctrl Pts',(-87.6738908373841,1075.68376086233,
367.574465786616));
#124443=CARTESIAN_POINT('Origin',(-86.223297681347,1067.7251047501,353.164138162982));
#124444=CARTESIAN_POINT('',(-86.2232976813637,1074.70656460683,352.073597414254));
#124445=CARTESIAN_POINT('',(-86.223297681347,1067.7251047501,352.073597414254));
#124446=CARTESIAN_POINT('Ctrl Pts',(-86.2233677532852,1074.89498441646,
354.254678909459));
#124447=CARTESIAN_POINT('Ctrl Pts',(-86.368344875043,1074.88010584553,354.254669594055));
#124448=CARTESIAN_POINT('Ctrl Pts',(-86.5116511349023,1074.86288057737,
354.22575525816));
#124449=CARTESIAN_POINT('Ctrl Pts',(-86.7104163792378,1074.83515588272,
354.142417373206));
#124450=CARTESIAN_POINT('Ctrl Pts',(-86.7730009159911,1074.82576075823,
354.10866651405));
#124451=CARTESIAN_POINT('Ctrl Pts',(-86.8909172515992,1074.8066630244,354.029372714505));
#124452=CARTESIAN_POINT('Ctrl Pts',(-86.9459561835566,1074.79700205051,
353.983961631481));
#124453=CARTESIAN_POINT('Ctrl Pts',(-87.0995725072276,1074.76758689865,
353.829646561973));
#124454=CARTESIAN_POINT('Ctrl Pts',(-87.1810712521107,1074.74825609641,
353.705899263475));
#124455=CARTESIAN_POINT('Ctrl Pts',(-87.2890357889482,1074.71331643717,
353.436335052299));
#124456=CARTESIAN_POINT('Ctrl Pts',(-87.31566387096,1074.6979657045,353.293605735661));
#124457=CARTESIAN_POINT('Ctrl Pts',(-87.3118383319029,1074.6731550123,353.007029673786));
#124458=CARTESIAN_POINT('Ctrl Pts',(-87.2819977757527,1074.6638825771,352.866020866224));
#124459=CARTESIAN_POINT('Ctrl Pts',(-87.1698735233297,1074.65271742962,
352.604358888485));
#124460=CARTESIAN_POINT('Ctrl Pts',(-87.0891892390927,1074.65087475215,
352.486187985245));
#124461=CARTESIAN_POINT('Ctrl Pts',(-86.8872485135896,1074.65485404087,
352.28751481358));
#124462=CARTESIAN_POINT('Ctrl Pts',(-86.7681391494087,1074.66061843664,
352.208957451225));
#124463=CARTESIAN_POINT('Ctrl Pts',(-86.5060753862408,1074.67901964644,
352.101358585668));
#124464=CARTESIAN_POINT('Ctrl Pts',(-86.3656006334892,1074.69151155488,
352.073688597946));
#124465=CARTESIAN_POINT('Ctrl Pts',(-86.0809227651831,1074.72162523263,
352.07350573436));
#124466=CARTESIAN_POINT('Ctrl Pts',(-85.9394289842916,1074.73900736629,
352.101567128908));
#124467=CARTESIAN_POINT('Ctrl Pts',(-85.7412472838941,1074.76692708733,
352.183298954599));
#124468=CARTESIAN_POINT('Ctrl Pts',(-85.6778517635491,1074.7765025099,352.217089791856));
#124469=CARTESIAN_POINT('Ctrl Pts',(-85.5588289393753,1074.79581686684,
352.296462570153));
#124470=CARTESIAN_POINT('Ctrl Pts',(-85.5034449821349,1074.80551182402,
352.341828958228));
#124471=CARTESIAN_POINT('Ctrl Pts',(-85.3502759860123,1074.83462368291,
352.494710311079));
#124472=CARTESIAN_POINT('Ctrl Pts',(-85.2690056712539,1074.85349436744,
352.616680404154));
#124473=CARTESIAN_POINT('Ctrl Pts',(-85.1593032350647,1074.88769575649,
352.884772454204));
#124474=CARTESIAN_POINT('Ctrl Pts',(-85.1316110871613,1074.90272070902,
353.028172840797));
#124475=CARTESIAN_POINT('Ctrl Pts',(-85.1339738033433,1074.92701700662,
353.317706236598));
#124476=CARTESIAN_POINT('Ctrl Pts',(-85.1639327013078,1074.93605189535,
353.460901381754));
#124477=CARTESIAN_POINT('Ctrl Pts',(-85.2770016280364,1074.94676759518,
353.724376683253));
#124478=CARTESIAN_POINT('Ctrl Pts',(-85.3577098365307,1074.94850940341,
353.842463017781));
#124479=CARTESIAN_POINT('Ctrl Pts',(-85.5599368404702,1074.94469892628,
354.04126579189));
#124480=CARTESIAN_POINT('Ctrl Pts',(-85.6794317190385,1074.93917903281,
354.119930596787));
#124481=CARTESIAN_POINT('Ctrl Pts',(-85.9417525597329,1074.92149346684,
354.227210035181));
#124482=CARTESIAN_POINT('Ctrl Pts',(-86.082003853221,1074.90949217319,354.254687992699));
#124483=CARTESIAN_POINT('Ctrl Pts',(-86.2233677532852,1074.89498441646,
354.254678909459));
#124484=CARTESIAN_POINT('Origin',(-86.223297681347,1067.7251047501,353.164138162982));
#124485=CARTESIAN_POINT('',(-86.223297681347,1074.84430822541,353.654678911711));
#124486=CARTESIAN_POINT('',(-86.223297681347,1074.75955377087,352.673597414254));
#124487=CARTESIAN_POINT('Ctrl Pts',(-86.223297681347,1074.84430822541,353.654678911711));
#124488=CARTESIAN_POINT('Ctrl Pts',(-86.2235616057638,1074.84428090512,
353.654678911711));
#124489=CARTESIAN_POINT('Ctrl Pts',(-86.2238255387521,1074.84425356549,
353.654678698713));
#124490=CARTESIAN_POINT('Ctrl Pts',(-86.2895776205274,1074.8374380034,353.654572565875));
#124491=CARTESIAN_POINT('Ctrl Pts',(-86.3542861322824,1074.82959371022,
353.641356063634));
#124492=CARTESIAN_POINT('Ctrl Pts',(-86.4439064652634,1074.81701539543,
353.603440338078));
#124493=CARTESIAN_POINT('Ctrl Pts',(-86.4720819309782,1074.81276372674,
353.588118861306));
#124494=CARTESIAN_POINT('Ctrl Pts',(-86.5250816008154,1074.80414390752,
353.552189237157));
#124495=CARTESIAN_POINT('Ctrl Pts',(-86.549780679976,1074.79979483259,353.531651378652));
#124496=CARTESIAN_POINT('Ctrl Pts',(-86.6184848412624,1074.78660945671,
353.462092690839));
#124497=CARTESIAN_POINT('Ctrl Pts',(-86.6548482908479,1074.77798532736,
353.406480662891));
#124498=CARTESIAN_POINT('Ctrl Pts',(-86.7031609604075,1074.76236519994,
353.284902225443));
#124499=CARTESIAN_POINT('Ctrl Pts',(-86.7149612752407,1074.75549914626,
353.220242998242));
#124500=CARTESIAN_POINT('Ctrl Pts',(-86.7125683266654,1074.74449113462,
353.090998295684));
#124501=CARTESIAN_POINT('Ctrl Pts',(-86.6988418164033,1074.74041282319,
353.027698486224));
#124502=CARTESIAN_POINT('Ctrl Pts',(-86.647870655823,1074.73553498482,352.910308239208));
#124503=CARTESIAN_POINT('Ctrl Pts',(-86.6113299191538,1074.73475915941,
352.857335800884));
#124504=CARTESIAN_POINT('Ctrl Pts',(-86.5200480541649,1074.73660923987,
352.768378295057));
#124505=CARTESIAN_POINT('Ctrl Pts',(-86.466260113021,1074.7392118728,352.733278000128));
#124506=CARTESIAN_POINT('Ctrl Pts',(-86.3487726254677,1074.74742840115,
352.685726662078));
#124507=CARTESIAN_POINT('Ctrl Pts',(-86.2862830539244,1074.75294285452,
352.673599117021));
#124508=CARTESIAN_POINT('Ctrl Pts',(-86.2233109440985,1074.7595523788,352.673597414443));
#124509=CARTESIAN_POINT('Ctrl Pts',(-86.223306523178,1074.75955284282,352.673597414323));
#124510=CARTESIAN_POINT('Ctrl Pts',(-86.2233021022608,1074.75955330684,
352.673597414254));
#124511=CARTESIAN_POINT('Ctrl Pts',(-86.223297681347,1074.75955377087,352.673597414254));
#124512=CARTESIAN_POINT('',(-86.223297681347,1082.7251047501,352.673597414254));
#124513=CARTESIAN_POINT('',(-86.223297681347,1067.7251047501,352.673597414254));
#124514=CARTESIAN_POINT('Origin',(-86.223297681347,1082.7251047501,353.164138162982));
#124515=CARTESIAN_POINT('Ctrl Pts',(-86.223297681347,1074.75955377087,352.673597414254));
#124516=CARTESIAN_POINT('Ctrl Pts',(-86.1588957466318,1074.76631351889,
352.673597414254));
#124517=CARTESIAN_POINT('Ctrl Pts',(-86.0952156099574,1074.7740892792,352.686278215375));
#124518=CARTESIAN_POINT('Ctrl Pts',(-86.0061506826996,1074.78659502971,
352.723103946718));
#124519=CARTESIAN_POINT('Ctrl Pts',(-85.9777275016174,1074.79087817074,
352.738276741612));
#124520=CARTESIAN_POINT('Ctrl Pts',(-85.9243073248254,1074.79953640906,
352.773926837269));
#124521=CARTESIAN_POINT('Ctrl Pts',(-85.8994258824298,1074.8038919747,352.794317643984));
#124522=CARTESIAN_POINT('Ctrl Pts',(-85.8304291692944,1074.81702219254,
352.863202457608));
#124523=CARTESIAN_POINT('Ctrl Pts',(-85.7938052904732,1074.82556721703,
352.91825082026));
#124524=CARTESIAN_POINT('Ctrl Pts',(-85.744424273489,1074.84109704224,353.039360492071));
#124525=CARTESIAN_POINT('Ctrl Pts',(-85.7320488061634,1074.84793826289,
353.104205426397));
#124526=CARTESIAN_POINT('Ctrl Pts',(-85.7335174022278,1074.85892494984,
353.234245441724));
#124527=CARTESIAN_POINT('Ctrl Pts',(-85.7469894804082,1074.86299706639,
353.298126973912));
#124528=CARTESIAN_POINT('Ctrl Pts',(-85.7976627926436,1074.86786162508,
353.416181240793));
#124529=CARTESIAN_POINT('Ctrl Pts',(-85.8339757250197,1074.86865593611,
353.469300526993));
#124530=CARTESIAN_POINT('Ctrl Pts',(-85.9249247406229,1074.86691646873,
353.558687620525));
#124531=CARTESIAN_POINT('Ctrl Pts',(-85.9786346967291,1074.86440039348,
353.594046282404));
#124532=CARTESIAN_POINT('Ctrl Pts',(-86.0965964857103,1074.85635183583,
353.642310203414));
#124533=CARTESIAN_POINT('Ctrl Pts',(-86.1596982074619,1074.85089176023,
353.654678911711));
#124534=CARTESIAN_POINT('Ctrl Pts',(-86.223297681347,1074.84430822541,353.654678911711));
#124535=CARTESIAN_POINT('Origin',(-88.5622696992325,1067.7251047501,411.301056626764));
#124536=CARTESIAN_POINT('',(-88.5622696992586,1076.66670986628,409.822753494571));
#124537=CARTESIAN_POINT('',(-88.5622696992325,1067.7251047501,409.822753494571));
#124538=CARTESIAN_POINT('Ctrl Pts',(-88.5617321436617,1076.67820104542,
412.779359661222));
#124539=CARTESIAN_POINT('Ctrl Pts',(-88.6593215347776,1076.67579673124,
412.779395147668));
#124540=CARTESIAN_POINT('Ctrl Pts',(-88.7566727307759,1076.67328588799,
412.769767089839));
#124541=CARTESIAN_POINT('Ctrl Pts',(-89.042583966656,1076.66557155864,412.712549655407));
#124542=CARTESIAN_POINT('Ctrl Pts',(-89.2234665533449,1076.66022627971,
412.637407100015));
#124543=CARTESIAN_POINT('Ctrl Pts',(-89.5459795296261,1076.6498915022,412.421493205337));
#124544=CARTESIAN_POINT('Ctrl Pts',(-89.6844588836696,1076.64500852948,
412.282771260311));
#124545=CARTESIAN_POINT('Ctrl Pts',(-89.8998609967692,1076.63669979489,
411.959768945481));
#124546=CARTESIAN_POINT('Ctrl Pts',(-89.9747075202018,1076.63336149731,
411.778637893389));
#124547=CARTESIAN_POINT('Ctrl Pts',(-90.0500502281694,1076.6289920861,411.398152893131));
#124548=CARTESIAN_POINT('Ctrl Pts',(-90.0499578729967,1076.62800326179,
411.202532384846));
#124549=CARTESIAN_POINT('Ctrl Pts',(-89.9744103265577,1076.6286195008,410.822940806752));
#124550=CARTESIAN_POINT('Ctrl Pts',(-89.8998750714784,1076.63021145483,
410.642618530076));
#124551=CARTESIAN_POINT('Ctrl Pts',(-89.6857907183491,1076.63563055537,
410.321087709615));
#124552=CARTESIAN_POINT('Ctrl Pts',(-89.5483835651257,1076.6393976063,410.182930557444));
#124553=CARTESIAN_POINT('Ctrl Pts',(-89.2281854038617,1076.64831647696,
409.967179654828));
#124554=CARTESIAN_POINT('Ctrl Pts',(-89.0484431140305,1076.65337636157,
409.891695090916));
#124555=CARTESIAN_POINT('Ctrl Pts',(-88.6699221160384,1076.66382623327,
409.814059840246));
#124556=CARTESIAN_POINT('Ctrl Pts',(-88.4747593446922,1076.66911090161,
409.812737768367));
#124557=CARTESIAN_POINT('Ctrl Pts',(-88.0920481922756,1076.67915233789,
409.885849219094));
#124558=CARTESIAN_POINT('Ctrl Pts',(-87.9084634367413,1076.68379948386,
409.960733286966));
#124559=CARTESIAN_POINT('Ctrl Pts',(-87.5824741873546,1076.69184601093,
410.177061009378));
#124560=CARTESIAN_POINT('Ctrl Pts',(-87.4429740478766,1076.69518140116,
410.315890982764));
#124561=CARTESIAN_POINT('Ctrl Pts',(-87.2256775268126,1076.70046426318,
410.639973285762));
#124562=CARTESIAN_POINT('Ctrl Pts',(-87.1501329207538,1076.70236580788,
410.82211529469));
#124563=CARTESIAN_POINT('Ctrl Pts',(-87.0740410935017,1076.70479706172,
411.206062452591));
#124564=CARTESIAN_POINT('Ctrl Pts',(-87.0745786619321,1076.70530259369,
411.404134500205));
#124565=CARTESIAN_POINT('Ctrl Pts',(-87.1528946154287,1076.7049395419,411.788341793998));
#124566=CARTESIAN_POINT('Ctrl Pts',(-87.2298311414188,1076.70407471558,
411.970675986506));
#124567=CARTESIAN_POINT('Ctrl Pts',(-87.4498085532559,1076.70090442615,
412.293961508813));
#124568=CARTESIAN_POINT('Ctrl Pts',(-87.5903808308169,1076.69862961784,
412.431921643145));
#124569=CARTESIAN_POINT('Ctrl Pts',(-87.9169957376771,1076.69260314726,
412.645328977771));
#124570=CARTESIAN_POINT('Ctrl Pts',(-88.0998395526459,1076.68890193453,
412.718658746031));
#124571=CARTESIAN_POINT('Ctrl Pts',(-88.380707200547,1076.68256419721,412.770963442842));
#124572=CARTESIAN_POINT('Ctrl Pts',(-88.4711236397969,1076.68043337116,
412.779326713237));
#124573=CARTESIAN_POINT('Ctrl Pts',(-88.5617321436617,1076.67820104542,
412.779359661222));
#124574=CARTESIAN_POINT('Origin',(-88.5622696992325,1067.7251047501,411.301056626764));
#124575=CARTESIAN_POINT('',(-88.5622696992324,1076.67614304338,412.179359758958));
#124576=CARTESIAN_POINT('',(-88.5622696992325,1076.6693343871,410.422753494571));
#124577=CARTESIAN_POINT('Ctrl Pts',(-88.5622696992324,1076.67614304338,
412.179359758958));
#124578=CARTESIAN_POINT('Ctrl Pts',(-88.5713478733904,1076.67591538937,
412.179359758958));
#124579=CARTESIAN_POINT('Ctrl Pts',(-88.5804283472778,1076.67568649302,
412.179219010571));
#124580=CARTESIAN_POINT('Ctrl Pts',(-88.6474792402766,1076.67398748811,
412.177138610937));
#124581=CARTESIAN_POINT('Ctrl Pts',(-88.7051293905032,1076.67247775111,
412.169602100923));
#124582=CARTESIAN_POINT('Ctrl Pts',(-88.8737893149981,1076.66791373208,
412.130296477369));
#124583=CARTESIAN_POINT('Ctrl Pts',(-88.9797364074945,1076.6648459483,412.082341167464));
#124584=CARTESIAN_POINT('Ctrl Pts',(-89.1671040340671,1076.65906117588,
411.948255948921));
#124585=CARTESIAN_POINT('Ctrl Pts',(-89.2467038093409,1076.65640251678,
411.863413100359));
#124586=CARTESIAN_POINT('Ctrl Pts',(-89.368581097211,1076.65197505532,411.667862894601));
#124587=CARTESIAN_POINT('Ctrl Pts',(-89.4096903733426,1076.6502514299,411.559061855057));
#124588=CARTESIAN_POINT('Ctrl Pts',(-89.4475377483728,1076.64808248081,
411.331937846654));
#124589=CARTESIAN_POINT('Ctrl Pts',(-89.4439674757885,1076.64765798086,
411.215831833517));
#124590=CARTESIAN_POINT('Ctrl Pts',(-89.3923040979717,1076.6482028578,410.991770890877));
#124591=CARTESIAN_POINT('Ctrl Pts',(-89.3447778078736,1076.64916448576,
410.88597406025));
#124592=CARTESIAN_POINT('Ctrl Pts',(-89.2117409049548,1076.65229599655,
410.698740149001));
#124593=CARTESIAN_POINT('Ctrl Pts',(-89.1275355879964,1076.65443295928,
410.619097196889));
#124594=CARTESIAN_POINT('Ctrl Pts',(-88.9332206535198,1076.65949516651,
410.49669052188));
#124595=CARTESIAN_POINT('Ctrl Pts',(-88.8249678993894,1076.66236952584,
410.455127182263));
#124596=CARTESIAN_POINT('Ctrl Pts',(-88.6624094006598,1076.6666814505,410.427042847244));
#124597=CARTESIAN_POINT('Ctrl Pts',(-88.612385243038,1076.66800807202,410.422753494571));
#124598=CARTESIAN_POINT('Ctrl Pts',(-88.5622696992325,1076.6693343871,410.422753494571));
#124599=CARTESIAN_POINT('',(-88.5622696992325,1082.7251047501,410.422753494571));
#124600=CARTESIAN_POINT('',(-88.5622696992325,1067.7251047501,410.422753494571));
#124601=CARTESIAN_POINT('Origin',(-88.5622696992325,1082.7251047501,411.301056626764));
#124602=CARTESIAN_POINT('Ctrl Pts',(-88.5622696992325,1076.6693343871,410.422753494571));
#124603=CARTESIAN_POINT('Ctrl Pts',(-88.5621479139323,1076.66933761017,
410.422753494571));
#124604=CARTESIAN_POINT('Ctrl Pts',(-88.5620261280924,1076.66934083323,
410.422753519901));
#124605=CARTESIAN_POINT('Ctrl Pts',(-88.5619043417208,1076.6693440563,410.422753570562));
#124606=CARTESIAN_POINT('Ctrl Pts',(-88.5044934230413,1076.67086343007,
410.422777452422));
#124607=CARTESIAN_POINT('Ctrl Pts',(-88.447222416631,1076.67237543949,410.428430336649));
#124608=CARTESIAN_POINT('Ctrl Pts',(-88.2762036933014,1076.67687629903,
410.46244962376));
#124609=CARTESIAN_POINT('Ctrl Pts',(-88.167193098939,1076.67972253554,410.507953514121));
#124610=CARTESIAN_POINT('Ctrl Pts',(-87.9738090385764,1076.68478130384,
410.638714698088));
#124611=CARTESIAN_POINT('Ctrl Pts',(-87.8912507914937,1076.68694853699,
410.722507068956));
#124612=CARTESIAN_POINT('Ctrl Pts',(-87.763563118689,1076.69043999321,410.917539359605));
#124613=CARTESIAN_POINT('Ctrl Pts',(-87.7197486379689,1076.69173149826,
411.026870139116));
#124614=CARTESIAN_POINT('Ctrl Pts',(-87.6773361005266,1076.69336831006,
411.256548822462));
#124615=CARTESIAN_POINT('Ctrl Pts',(-87.6792766294144,1076.69369681906,
411.37462478389));
#124616=CARTESIAN_POINT('Ctrl Pts',(-87.7292636477229,1076.69336814375,
411.603004899497));
#124617=CARTESIAN_POINT('Ctrl Pts',(-87.7767813386656,1076.69271443728,
411.711030619459));
#124618=CARTESIAN_POINT('Ctrl Pts',(-87.9111132566874,1076.6904414756,411.901882998739));
#124619=CARTESIAN_POINT('Ctrl Pts',(-87.9964854077183,1076.68884491687,
411.98287954438));
#124620=CARTESIAN_POINT('Ctrl Pts',(-88.1938844886558,1076.68478930375,
412.106846868462));
#124621=CARTESIAN_POINT('Ctrl Pts',(-88.3039599660869,1076.6823672592,412.148569736987));
#124622=CARTESIAN_POINT('Ctrl Pts',(-88.466341671572,1076.67851541078,412.175425510553));
#124623=CARTESIAN_POINT('Ctrl Pts',(-88.51427354557,1076.67734664628,412.179359758958));
#124624=CARTESIAN_POINT('Ctrl Pts',(-88.5622696992324,1076.67614304338,
412.179359758958));
#124625=CARTESIAN_POINT('Origin',(-93.4799432334773,1067.7251047501,399.745687154642));
#124626=CARTESIAN_POINT('',(-93.4799432334936,1076.32318567709,398.470243033506));
#124627=CARTESIAN_POINT('',(-93.4799432334773,1067.7251047501,398.470243033506));
#124628=CARTESIAN_POINT('Ctrl Pts',(-93.4801333950918,1076.36560796598,
401.021131261602));
#124629=CARTESIAN_POINT('Ctrl Pts',(-93.5629569069197,1076.36054728635,
401.021118913078));
#124630=CARTESIAN_POINT('Ctrl Pts',(-93.6455745583778,1076.35532421901,
401.013039155634));
#124631=CARTESIAN_POINT('Ctrl Pts',(-93.8095771701939,1076.34459454335,
400.980683159562));
#124632=CARTESIAN_POINT('Ctrl Pts',(-93.8905125998491,1076.33911044844,
400.9561853359));
#124633=CARTESIAN_POINT('Ctrl Pts',(-94.1232432929026,1076.32276821168,
400.859692860781));
#124634=CARTESIAN_POINT('Ctrl Pts',(-94.2639251192673,1076.31209976449,
400.765607436634));
#124635=CARTESIAN_POINT('Ctrl Pts',(-94.5007585398004,1076.29253532213,
400.52846982775));
#124636=CARTESIAN_POINT('Ctrl Pts',(-94.5946705888021,1076.28383022148,
400.387746201942));
#124637=CARTESIAN_POINT('Ctrl Pts',(-94.7225496399746,1076.26979329303,
400.07831192922));
#124638=CARTESIAN_POINT('Ctrl Pts',(-94.75542733347,1076.26459362006,399.912686407884));
#124639=CARTESIAN_POINT('Ctrl Pts',(-94.7553474338139,1076.25858411173,
399.578625581044));
#124640=CARTESIAN_POINT('Ctrl Pts',(-94.7226047752679,1076.25782102401,
399.413476123076));
#124641=CARTESIAN_POINT('Ctrl Pts',(-94.5955203019502,1076.2608791342,399.105405733507));
#124642=CARTESIAN_POINT('Ctrl Pts',(-94.5025336228493,1076.26466104138,
398.965461683089));
#124643=CARTESIAN_POINT('Ctrl Pts',(-94.2680295445492,1076.27618487448,
398.729115270103));
#124644=CARTESIAN_POINT('Ctrl Pts',(-94.1287405064727,1076.28381516539,
398.635049761835));
#124645=CARTESIAN_POINT('Ctrl Pts',(-93.8216056398943,1076.30176140672,
398.505575588351));
#124646=CARTESIAN_POINT('Ctrl Pts',(-93.6566292623946,1076.31190817482,
398.471575353977));
#124647=CARTESIAN_POINT('Ctrl Pts',(-93.4063476511197,1076.32788248785,
398.469633711281));
#124648=CARTESIAN_POINT('Ctrl Pts',(-93.3229984130479,1076.33329885397,
398.477185653582));
#124649=CARTESIAN_POINT('Ctrl Pts',(-93.1590300742001,1076.34413759169,
398.508458706518));
#124650=CARTESIAN_POINT('Ctrl Pts',(-93.0787977205017,1076.34953425454,
398.532096181547));
#124651=CARTESIAN_POINT('Ctrl Pts',(-92.8446604858417,1076.36557149516,
398.626856400855));
#124652=CARTESIAN_POINT('Ctrl Pts',(-92.7020073105663,1076.37574404396,
398.720887726704));
#124653=CARTESIAN_POINT('Ctrl Pts',(-92.4621703824325,1076.39385563328,
398.958730167123));
#124654=CARTESIAN_POINT('Ctrl Pts',(-92.3671563759896,1076.40163019714,
399.100001437337));
#124655=CARTESIAN_POINT('Ctrl Pts',(-92.2374009785951,1076.41398301362,
399.411854727107));
#124656=CARTESIAN_POINT('Ctrl Pts',(-92.2041160776654,1076.41843466233,
399.57940203307));
#124657=CARTESIAN_POINT('Ctrl Pts',(-92.2048899521654,1076.42353646164,
399.918302816354));
#124658=CARTESIAN_POINT('Ctrl Pts',(-92.2391437461501,1076.42412648457,
400.086242677537));
#124659=CARTESIAN_POINT('Ctrl Pts',(-92.3712558622388,1076.42133698604,
400.398581387896));
#124660=CARTESIAN_POINT('Ctrl Pts',(-92.4676687942551,1076.41799107729,
400.53987567314));
#124661=CARTESIAN_POINT('Ctrl Pts',(-92.7095487807018,1076.40766356967,
400.776087030306));
#124662=CARTESIAN_POINT('Ctrl Pts',(-92.8524308286309,1076.40079297176,
400.868816421315));
#124663=CARTESIAN_POINT('Ctrl Pts',(-93.1590792330014,1076.38455917893,
400.990609035014));
#124664=CARTESIAN_POINT('Ctrl Pts',(-93.3189077425315,1076.37545917075,
401.021155299449));
#124665=CARTESIAN_POINT('Ctrl Pts',(-93.4801333950918,1076.36560796598,
401.021131261602));
#124666=CARTESIAN_POINT('Origin',(-93.4799432334773,1067.7251047501,399.745687154642));
#124667=CARTESIAN_POINT('',(-93.4799432334773,1076.35619778296,400.421131275778));
#124668=CARTESIAN_POINT('',(-93.4799432334773,1076.33373423278,399.070243033506));
#124669=CARTESIAN_POINT('Ctrl Pts',(-93.4799432334773,1076.35619778296,
400.421131275778));
#124670=CARTESIAN_POINT('Ctrl Pts',(-93.4883532932941,1076.35567851875,
400.421131275778));
#124671=CARTESIAN_POINT('Ctrl Pts',(-93.4967694338094,1076.35515585416,
400.420974204448));
#124672=CARTESIAN_POINT('Ctrl Pts',(-93.5953782260296,1076.34899626522,
400.417286217715));
#124673=CARTESIAN_POINT('Ctrl Pts',(-93.6839797165283,1076.34310966564,
400.395870128729));
#124674=CARTESIAN_POINT('Ctrl Pts',(-93.8469288872262,1076.33156782656,
400.319772606978));
#124675=CARTESIAN_POINT('Ctrl Pts',(-93.9197814455157,1076.32602460709,
400.266074232109));
#124676=CARTESIAN_POINT('Ctrl Pts',(-94.0395870715425,1076.31610126246,
400.1341101629));
#124677=CARTESIAN_POINT('Ctrl Pts',(-94.0856782668617,1076.31180516189,
400.057409911078));
#124678=CARTESIAN_POINT('Ctrl Pts',(-94.1455327743756,1076.30504731657,
399.890727925973));
#124679=CARTESIAN_POINT('Ctrl Pts',(-94.1587945357534,1076.30264794552,
399.802401964556));
#124680=CARTESIAN_POINT('Ctrl Pts',(-94.1505032189142,1076.30012159766,
399.625819649506));
#124681=CARTESIAN_POINT('Ctrl Pts',(-94.1291125066518,1076.3000145825,399.53929278628));
#124682=CARTESIAN_POINT('Ctrl Pts',(-94.0542779032438,1076.30212357938,
399.379423555318));
#124683=CARTESIAN_POINT('Ctrl Pts',(-94.0015873571222,1076.30431699002,
399.307636848827));
#124684=CARTESIAN_POINT('Ctrl Pts',(-93.871542184645,1076.31069679075,399.188304816762));
#124685=CARTESIAN_POINT('Ctrl Pts',(-93.795413342083,1076.31482310402,399.141956126631));
#124686=CARTESIAN_POINT('Ctrl Pts',(-93.6380415729123,1076.32393226757,
399.084226239711));
#124687=CARTESIAN_POINT('Ctrl Pts',(-93.5593007106689,1076.32871601054,
399.07024530662));
#124688=CARTESIAN_POINT('Ctrl Pts',(-93.479962584241,1076.33373300911,399.070243033671));
#124689=CARTESIAN_POINT('Ctrl Pts',(-93.4799561339841,1076.333733417,399.070243033486));
#124690=CARTESIAN_POINT('Ctrl Pts',(-93.4799496837297,1076.33373382489,
399.070243033506));
#124691=CARTESIAN_POINT('Ctrl Pts',(-93.4799432334775,1076.33373423278,
399.070243033506));
#124692=CARTESIAN_POINT('',(-93.4799432334773,1082.7251047501,399.070243033506));
#124693=CARTESIAN_POINT('',(-93.4799432334773,1067.7251047501,399.070243033506));
#124694=CARTESIAN_POINT('Origin',(-93.4799432334773,1082.7251047501,399.745687154642));
#124695=CARTESIAN_POINT('Ctrl Pts',(-93.4799432334775,1076.33373423278,
399.070243033506));
#124696=CARTESIAN_POINT('Ctrl Pts',(-93.435721437085,1076.33653064493,399.070243033506));
#124697=CARTESIAN_POINT('Ctrl Pts',(-93.3916084193459,1076.33938105541,
399.074585875597));
#124698=CARTESIAN_POINT('Ctrl Pts',(-93.3049435932713,1076.34510035486,
399.091815221194));
#124699=CARTESIAN_POINT('Ctrl Pts',(-93.2625942045437,1076.34795567402,
399.104646568976));
#124700=CARTESIAN_POINT('Ctrl Pts',(-93.1387348822979,1076.35649513563,
399.155872324731));
#124701=CARTESIAN_POINT('Ctrl Pts',(-93.0633358533861,1076.36195946124,
399.20647345938));
#124702=CARTESIAN_POINT('Ctrl Pts',(-92.9368881130846,1076.37174713727,
399.334139596107));
#124703=CARTESIAN_POINT('Ctrl Pts',(-92.8870437902805,1076.37597700716,
399.409885692517));
#124704=CARTESIAN_POINT('Ctrl Pts',(-92.8198410747591,1076.38268695544,
399.576626213071));
#124705=CARTESIAN_POINT('Ctrl Pts',(-92.8032084878391,1076.38509827905,
399.665965229687));
#124706=CARTESIAN_POINT('Ctrl Pts',(-92.8059480411021,1076.38779313137,
399.846089904278));
#124707=CARTESIAN_POINT('Ctrl Pts',(-92.8253479181109,1076.38804668744,
399.935044626837));
#124708=CARTESIAN_POINT('Ctrl Pts',(-92.8978823718494,1076.38634035124,
400.100002885482));
#124709=CARTESIAN_POINT('Ctrl Pts',(-92.950244411421,1076.38439963927,400.174343344076));
#124710=CARTESIAN_POINT('Ctrl Pts',(-93.0808636745382,1076.37853760764,
400.29798447593));
#124711=CARTESIAN_POINT('Ctrl Pts',(-93.1577576535785,1076.37467765188,
400.346088105425));
#124712=CARTESIAN_POINT('Ctrl Pts',(-93.31798331091,1076.36591425995,400.40646485887));
#124713=CARTESIAN_POINT('Ctrl Pts',(-93.3986794334962,1076.36121527194,
400.421131275778));
#124714=CARTESIAN_POINT('Ctrl Pts',(-93.4799432334773,1076.35619778296,
400.421131275778));
#124715=CARTESIAN_POINT('Origin',(-99.1956712429286,1067.7251047501,372.652457095519));
#124716=CARTESIAN_POINT('',(-99.1956712429516,1074.73259927686,371.56191634679));
#124717=CARTESIAN_POINT('',(-99.1956712429286,1067.7251047501,371.56191634679));
#124718=CARTESIAN_POINT('Ctrl Pts',(-99.1952613378211,1074.86968995685,
373.742997767211));
#124719=CARTESIAN_POINT('Ctrl Pts',(-99.3408017340122,1074.85243551291,
373.743052471958));
#124720=CARTESIAN_POINT('Ctrl Pts',(-99.4847391278243,1074.83348174949,
373.713974810929));
#124721=CARTESIAN_POINT('Ctrl Pts',(-99.6843997937052,1074.80431537499,
373.629961568344));
#124722=CARTESIAN_POINT('Ctrl Pts',(-99.7472934042108,1074.79462839847,
373.595899336245));
#124723=CARTESIAN_POINT('Ctrl Pts',(-99.9280501618477,1074.76519211283,
373.473711540432));
#124724=CARTESIAN_POINT('Ctrl Pts',(-100.031958218192,1074.74591713644,
373.367679291368));
#124725=CARTESIAN_POINT('Ctrl Pts',(-100.189659947538,1074.7112567494,373.123497891547));
#124726=CARTESIAN_POINT('Ctrl Pts',(-100.243105198812,1074.69611853186,
372.988482528436));
#124727=CARTESIAN_POINT('Ctrl Pts',(-100.294165847614,1074.6718263573,372.706443612323));
#124728=CARTESIAN_POINT('Ctrl Pts',(-100.291844411895,1074.66285387972,
372.562331202692));
#124729=CARTESIAN_POINT('Ctrl Pts',(-100.231839953063,1074.65233192603,
372.284067747315));
#124730=CARTESIAN_POINT('Ctrl Pts',(-100.175253863595,1074.65082544753,
372.152661609642));
#124731=CARTESIAN_POINT('Ctrl Pts',(-100.01507247592,1074.65546506098,371.91905605327));
#124732=CARTESIAN_POINT('Ctrl Pts',(-99.9132074593707,1074.66154741341,
371.819176381304));
#124733=CARTESIAN_POINT('Ctrl Pts',(-99.6766085323472,1074.68052379203,
371.663437476209));
#124734=CARTESIAN_POINT('Ctrl Pts',(-99.5440372268615,1074.69326789544,
371.609400162372));
#124735=CARTESIAN_POINT('Ctrl Pts',(-99.2646770342454,1074.72378710895,
371.554738587819));
#124736=CARTESIAN_POINT('Ctrl Pts',(-99.1204299995402,1074.74131861624,
371.555197654905));
#124737=CARTESIAN_POINT('Ctrl Pts',(-98.9101695674117,1074.76938287174,
371.597506382811));
#124738=CARTESIAN_POINT('Ctrl Pts',(-98.8413848604377,1074.77899988353,
371.618577184547));
#124739=CARTESIAN_POINT('Ctrl Pts',(-98.709181303031,1074.79836792181,371.67382322579));
#124740=CARTESIAN_POINT('Ctrl Pts',(-98.6460451247645,1074.80807485702,
371.707835919492));
#124741=CARTESIAN_POINT('Ctrl Pts',(-98.4662524538523,1074.83716615011,
371.828863517514));
#124742=CARTESIAN_POINT('Ctrl Pts',(-98.3630814106523,1074.85595247211,
371.933263557887));
#124743=CARTESIAN_POINT('Ctrl Pts',(-98.2042354166269,1074.88983619223,
372.175804495964));
#124744=CARTESIAN_POINT('Ctrl Pts',(-98.1497567703304,1074.90463482366,
372.311365818768));
#124745=CARTESIAN_POINT('Ctrl Pts',(-98.0970469897061,1074.9283709619,372.595967805245));
#124746=CARTESIAN_POINT('Ctrl Pts',(-98.0992031312702,1074.93708574653,
372.742087826904));
#124747=CARTESIAN_POINT('Ctrl Pts',(-98.1599660416553,1074.94714886773,
373.022134517035));
#124748=CARTESIAN_POINT('Ctrl Pts',(-98.2167003806437,1074.94855697519,
373.153437943663));
#124749=CARTESIAN_POINT('Ctrl Pts',(-98.377342780694,1074.94408613779,373.387126542476));
#124750=CARTESIAN_POINT('Ctrl Pts',(-98.4796569838478,1074.93824599315,
373.48711237768));
#124751=CARTESIAN_POINT('Ctrl Pts',(-98.7192730786927,1074.91977646349,
373.644076669666));
#124752=CARTESIAN_POINT('Ctrl Pts',(-98.8548463810203,1074.90718271451,
373.698386081222));
#124753=CARTESIAN_POINT('Ctrl Pts',(-99.0623199847187,1074.88505662857,
373.73686213158));
#124754=CARTESIAN_POINT('Ctrl Pts',(-99.1287448150628,1074.87757577854,
373.742972765427));
#124755=CARTESIAN_POINT('Ctrl Pts',(-99.1952613378212,1074.86968995685,
373.742997767211));
#124756=CARTESIAN_POINT('Origin',(-99.1956712429286,1067.7251047501,372.652457095519));
#124757=CARTESIAN_POINT('',(-99.1956712429286,1074.8328201009,373.142997844247));
#124758=CARTESIAN_POINT('',(-99.1956712429286,1074.77118038462,372.16191634679));
#124759=CARTESIAN_POINT('Ctrl Pts',(-99.1956712429286,1074.8328201009,373.142997844247));
#124760=CARTESIAN_POINT('Ctrl Pts',(-99.2307558172767,1074.82863383938,
373.142997844247));
#124761=CARTESIAN_POINT('Ctrl Pts',(-99.2658013664893,1074.82421250411,
373.13923374202));
#124762=CARTESIAN_POINT('Ctrl Pts',(-99.3315287933037,1074.81545469225,
373.124898801776));
#124763=CARTESIAN_POINT('Ctrl Pts',(-99.3621030623619,1074.81117487194,
373.115012649334));
#124764=CARTESIAN_POINT('Ctrl Pts',(-99.4209335720955,1074.80251702725,
373.089399514846));
#124765=CARTESIAN_POINT('Ctrl Pts',(-99.4490523457672,1074.79815824675,
373.07371702756));
#124766=CARTESIAN_POINT('Ctrl Pts',(-99.5295155813452,1074.78498078999,
373.017850813383));
#124767=CARTESIAN_POINT('Ctrl Pts',(-99.5755408836341,1074.77640830922,
372.969759798282));
#124768=CARTESIAN_POINT('Ctrl Pts',(-99.6450929902016,1074.7610483231,372.85936697056));
#124769=CARTESIAN_POINT('Ctrl Pts',(-99.6684363547394,1074.7543712077,372.798445232698));
#124770=CARTESIAN_POINT('Ctrl Pts',(-99.6900123648613,1074.7437156369,372.671474620523));
#124771=CARTESIAN_POINT('Ctrl Pts',(-99.6882828172453,1074.73981601127,
372.606732697218));
#124772=CARTESIAN_POINT('Ctrl Pts',(-99.6600111766514,1074.73531901636,
372.481929375305));
#124773=CARTESIAN_POINT('Ctrl Pts',(-99.6339517209293,1074.73474154548,
372.423098988367));
#124774=CARTESIAN_POINT('Ctrl Pts',(-99.5608011538376,1074.73698123031,
372.318740912569));
#124775=CARTESIAN_POINT('Ctrl Pts',(-99.5144777954332,1074.7397717411,372.274260968877));
#124776=CARTESIAN_POINT('Ctrl Pts',(-99.4072144933072,1074.74838106255,
372.205274422036));
#124777=CARTESIAN_POINT('Ctrl Pts',(-99.347252102839,1074.75413301401,372.181586395893));
#124778=CARTESIAN_POINT('Ctrl Pts',(-99.2552154208791,1074.76417188024,
372.164631224256));
#124779=CARTESIAN_POINT('Ctrl Pts',(-99.2254770900566,1074.76758801247,
372.161918025972));
#124780=CARTESIAN_POINT('Ctrl Pts',(-99.1956988915339,1074.7711770522,372.161916347568));
#124781=CARTESIAN_POINT('Ctrl Pts',(-99.1956896753178,1074.77117816299,
372.161916347048));
#124782=CARTESIAN_POINT('Ctrl Pts',(-99.195680459116,1074.7711792738,372.16191634679));
#124783=CARTESIAN_POINT('Ctrl Pts',(-99.1956712429286,1074.77118038462,
372.16191634679));
#124784=CARTESIAN_POINT('',(-99.1956712429286,1082.7251047501,372.16191634679));
#124785=CARTESIAN_POINT('',(-99.1956712429286,1067.7251047501,372.16191634679));
#124786=CARTESIAN_POINT('Origin',(-99.1956712429286,1082.7251047501,372.652457095519));
#124787=CARTESIAN_POINT('Ctrl Pts',(-99.1956712429286,1074.77118038462,
372.16191634679));
#124788=CARTESIAN_POINT('Ctrl Pts',(-99.1297340660699,1074.77912774276,
372.16191634679));
#124789=CARTESIAN_POINT('Ctrl Pts',(-99.0645312222755,1074.7878101565,372.1752096209));
#124790=CARTESIAN_POINT('Ctrl Pts',(-98.9743517036196,1074.80104262714,
372.213502073698));
#124791=CARTESIAN_POINT('Ctrl Pts',(-98.9460644227095,1074.80540462821,
372.228947359956));
#124792=CARTESIAN_POINT('Ctrl Pts',(-98.8653599029516,1074.8185211102,372.283926582666));
#124793=CARTESIAN_POINT('Ctrl Pts',(-98.8191031316056,1074.82701527461,
372.33131186045));
#124794=CARTESIAN_POINT('Ctrl Pts',(-98.7481151465056,1074.84235637596,
372.441305120991));
#124795=CARTESIAN_POINT('Ctrl Pts',(-98.7239595772774,1074.84906341277,
372.502763622427));
#124796=CARTESIAN_POINT('Ctrl Pts',(-98.7013740385812,1074.85972531503,
372.630836062828));
#124797=CARTESIAN_POINT('Ctrl Pts',(-98.7028062655346,1074.86361216937,
372.696083679091));
#124798=CARTESIAN_POINT('Ctrl Pts',(-98.7307701748566,1074.86808704829,
372.821447784717));
#124799=CARTESIAN_POINT('Ctrl Pts',(-98.7566336507401,1074.8686798691,372.880361708791));
#124800=CARTESIAN_POINT('Ctrl Pts',(-98.8294783216542,1074.86654297423,
372.985020790852));
#124801=CARTESIAN_POINT('Ctrl Pts',(-98.8757212820671,1074.86383445787,
373.029699944009));
#124802=CARTESIAN_POINT('Ctrl Pts',(-98.9829389375818,1074.85541703767,
373.099089660562));
#124803=CARTESIAN_POINT('Ctrl Pts',(-99.042938015002,1074.84977184277,373.12296932195));
#124804=CARTESIAN_POINT('Ctrl Pts',(-99.1354780105686,1074.83982609407,
373.140230847772));
#124805=CARTESIAN_POINT('Ctrl Pts',(-99.1655889700239,1074.83640949208,
373.142997844247));
#124806=CARTESIAN_POINT('Ctrl Pts',(-99.1956712429286,1074.8328201009,373.142997844247));
#124807=CARTESIAN_POINT('Origin',(-97.7222027015963,1067.7251047501,386.561549283282));
#124808=CARTESIAN_POINT('',(-97.7222027016186,1075.61311396869,385.46271814729));
#124809=CARTESIAN_POINT('',(-97.7222027015963,1067.7251047501,385.46271814729));
#124810=CARTESIAN_POINT('Ctrl Pts',(-97.7213988942016,1075.69623611514,
387.660380125278));
#124811=CARTESIAN_POINT('Ctrl Pts',(-97.7927939677333,1075.68940709858,
387.660432351595));
#124812=CARTESIAN_POINT('Ctrl Pts',(-97.8640028065381,1075.68231205992,
387.653526301707));
#124813=CARTESIAN_POINT('Ctrl Pts',(-98.0042962639257,1075.66775644269,
387.625965942542));
#124814=CARTESIAN_POINT('Ctrl Pts',(-98.0730487518634,1075.66032808101,
387.605323305624));
#124815=CARTESIAN_POINT('Ctrl Pts',(-98.2758843532508,1075.6374862955,387.52210313036));
#124816=CARTESIAN_POINT('Ctrl Pts',(-98.3998385255858,1075.62218947111,
387.439084648386));
#124817=CARTESIAN_POINT('Ctrl Pts',(-98.6053228124055,1075.59396881424,
387.231195397763));
#124818=CARTESIAN_POINT('Ctrl Pts',(-98.6857602946434,1075.58127100407,
387.1092371073));
#124819=CARTESIAN_POINT('Ctrl Pts',(-98.7944472760788,1075.56005240322,
386.841647480565));
#124820=CARTESIAN_POINT('Ctrl Pts',(-98.8219370424237,1075.55171700464,
386.698755938379));
#124821=CARTESIAN_POINT('Ctrl Pts',(-98.8200911789728,1075.54065643482,
386.411143056393));
#124822=CARTESIAN_POINT('Ctrl Pts',(-98.7911263244649,1075.53800826563,
386.269295043914));
#124823=CARTESIAN_POINT('Ctrl Pts',(-98.6804305013425,1075.5387916389,386.005053410384));
#124824=CARTESIAN_POINT('Ctrl Pts',(-98.5999634160729,1075.54219713368,
385.885244836217));
#124825=CARTESIAN_POINT('Ctrl Pts',(-98.3975468297286,1075.55460304053,
385.682995241437));
#124826=CARTESIAN_POINT('Ctrl Pts',(-98.2775037975997,1075.5634916692,385.602639121292));
#124827=CARTESIAN_POINT('Ctrl Pts',(-98.0128524825785,1075.58555280984,
385.492138136355));
#124828=CARTESIAN_POINT('Ctrl Pts',(-97.8706550702968,1075.59853521395,
385.463366061341));
#124829=CARTESIAN_POINT('Ctrl Pts',(-97.5826998525611,1075.62681310325,
385.462088309446));
#124830=CARTESIAN_POINT('Ctrl Pts',(-97.4396440456053,1075.64185219423,
385.489908949946));
#124831=CARTESIAN_POINT('Ctrl Pts',(-97.1706666046853,1075.67209073474,
385.599963242149));
#124832=CARTESIAN_POINT('Ctrl Pts',(-97.0475985821659,1075.68699859297,
385.681895667295));
#124833=CARTESIAN_POINT('Ctrl Pts',(-96.841400767303,1075.71438832665,385.888646192269));
#124834=CARTESIAN_POINT('Ctrl Pts',(-96.7600209710137,1075.72662181786,
386.011188802362));
#124835=CARTESIAN_POINT('Ctrl Pts',(-96.6498379179535,1075.74692429867,
386.28104276992));
#124836=CARTESIAN_POINT('Ctrl Pts',(-96.6220888699548,1075.75479732189,
386.42563596903));
#124837=CARTESIAN_POINT('Ctrl Pts',(-96.624747375387,1075.76518408089,386.717694008871));
#124838=CARTESIAN_POINT('Ctrl Pts',(-96.6552215892545,1075.76758459124,
386.862159174312));
#124839=CARTESIAN_POINT('Ctrl Pts',(-96.7698335321823,1075.76655483237,
387.128091212793));
#124840=CARTESIAN_POINT('Ctrl Pts',(-96.8517548533546,1075.76324894579,
387.247307224677));
#124841=CARTESIAN_POINT('Ctrl Pts',(-97.0585089197345,1075.75126299893,
387.449365585822));
#124842=CARTESIAN_POINT('Ctrl Pts',(-97.1819905856914,1075.7426053114,387.52943428261));
#124843=CARTESIAN_POINT('Ctrl Pts',(-97.4460777276447,1075.72150585643,
387.634096632222));
#124844=CARTESIAN_POINT('Ctrl Pts',(-97.5831723197036,1075.70945763757,
387.660279010949));
#124845=CARTESIAN_POINT('Ctrl Pts',(-97.7213988942016,1075.69623611513,
387.660380125278));
#124846=CARTESIAN_POINT('Origin',(-97.7222027015963,1067.7251047501,386.561549283282));
#124847=CARTESIAN_POINT('',(-97.7222027015962,1075.6741872497,387.060380419275));
#124848=CARTESIAN_POINT('',(-97.7222027015963,1075.63649232378,386.06271814729));
#124849=CARTESIAN_POINT('Ctrl Pts',(-97.7222027015961,1075.6741872497,387.060380419275));
#124850=CARTESIAN_POINT('Ctrl Pts',(-97.7249263879499,1075.67392467079,
387.060380419275));
#124851=CARTESIAN_POINT('Ctrl Pts',(-97.7276509946975,1075.67366113051,
387.060358111756));
#124852=CARTESIAN_POINT('Ctrl Pts',(-97.762899977707,1075.67024032216,387.05978046529));
#124853=CARTESIAN_POINT('Ctrl Pts',(-97.7952848834862,1075.66697284493,
387.056067683896));
#124854=CARTESIAN_POINT('Ctrl Pts',(-97.8589146873207,1075.66030116281,
387.042385392596));
#124855=CARTESIAN_POINT('Ctrl Pts',(-97.8900104669429,1075.65691209393,
387.032435413474));
#124856=CARTESIAN_POINT('Ctrl Pts',(-97.9812941539065,1075.64656074511,
386.993028306789));
#124857=CARTESIAN_POINT('Ctrl Pts',(-98.036754080926,1075.63969324207,386.954445759814));
#124858=CARTESIAN_POINT('Ctrl Pts',(-98.128239041283,1075.62710710462,386.858642086529));
#124859=CARTESIAN_POINT('Ctrl Pts',(-98.1637678945812,1075.62148792769,
386.802725766566));
#124860=CARTESIAN_POINT('Ctrl Pts',(-98.211006819578,1075.61217335651,386.680571496346));
#124861=CARTESIAN_POINT('Ctrl Pts',(-98.2223941639612,1075.60855815078,
386.615582502864));
#124862=CARTESIAN_POINT('Ctrl Pts',(-98.2194229250556,1075.60384387592,
386.485153884733));
#124863=CARTESIAN_POINT('Ctrl Pts',(-98.2052336626134,1075.60277834611,
386.421012651017));
#124864=CARTESIAN_POINT('Ctrl Pts',(-98.1530459549406,1075.60334973963,
386.301881037638));
#124865=CARTESIAN_POINT('Ctrl Pts',(-98.1156137934597,1075.60497579798,
386.24806332025));
#124866=CARTESIAN_POINT('Ctrl Pts',(-98.0221507717359,1075.61071633582,
386.157690755954));
#124867=CARTESIAN_POINT('Ctrl Pts',(-97.9669908054845,1075.61478079353,
386.122079993755));
#124868=CARTESIAN_POINT('Ctrl Pts',(-97.8478871855469,1075.62465919293,
386.074690770394));
#124869=CARTESIAN_POINT('Ctrl Pts',(-97.7853021333535,1075.63033249837,
386.06271814729));
#124870=CARTESIAN_POINT('Ctrl Pts',(-97.7222027015964,1075.63649232378,
386.06271814729));
#124871=CARTESIAN_POINT('',(-97.7222027015963,1082.7251047501,386.06271814729));
#124872=CARTESIAN_POINT('',(-97.7222027015963,1067.7251047501,386.06271814729));
#124873=CARTESIAN_POINT('Origin',(-97.7222027015963,1082.7251047501,386.561549283282));
#124874=CARTESIAN_POINT('Ctrl Pts',(-97.7222027015964,1075.63649232378,
386.06271814729));
#124875=CARTESIAN_POINT('Ctrl Pts',(-97.7221511724957,1075.6364973541,386.06271814729));
#124876=CARTESIAN_POINT('Ctrl Pts',(-97.722099643052,1075.63650238475,386.062718155274));
#124877=CARTESIAN_POINT('Ctrl Pts',(-97.7220481132671,1075.63650741572,
386.062718171243));
#124878=CARTESIAN_POINT('Ctrl Pts',(-97.6893287168738,1075.63970188354,
386.062728311021));
#124879=CARTESIAN_POINT('Ctrl Pts',(-97.656698034032,1075.64300505106,386.065957603219));
#124880=CARTESIAN_POINT('Ctrl Pts',(-97.592592556617,1075.64972746131,386.078744203233));
#124881=CARTESIAN_POINT('Ctrl Pts',(-97.5612650171618,1075.65313098461,
386.088264651513));
#124882=CARTESIAN_POINT('Ctrl Pts',(-97.4695991206023,1075.6634566299,386.126283525766));
#124883=CARTESIAN_POINT('Ctrl Pts',(-97.413798364603,1075.67026241494,386.163856256138));
#124884=CARTESIAN_POINT('Ctrl Pts',(-97.3203918518557,1075.68281384094,
386.25858229628));
#124885=CARTESIAN_POINT('Ctrl Pts',(-97.2836336377487,1075.68844110033,
386.314739948528));
#124886=CARTESIAN_POINT('Ctrl Pts',(-97.2343187412388,1075.69777017507,
386.438203499131));
#124887=CARTESIAN_POINT('Ctrl Pts',(-97.222225460169,1075.70138131606,386.504250147017));
#124888=CARTESIAN_POINT('Ctrl Pts',(-97.2246604112321,1075.70603775601,
386.635792573754));
#124889=CARTESIAN_POINT('Ctrl Pts',(-97.2385639595588,1075.70709399248,
386.699965336072));
#124890=CARTESIAN_POINT('Ctrl Pts',(-97.2902347119164,1075.70660095883,
386.819358321241));
#124891=CARTESIAN_POINT('Ctrl Pts',(-97.327476342736,1075.70505768393,386.873391808103));
#124892=CARTESIAN_POINT('Ctrl Pts',(-97.420701095975,1075.6995360576,386.964267241999));
#124893=CARTESIAN_POINT('Ctrl Pts',(-97.4758256104629,1075.69560341623,
387.000146838782));
#124894=CARTESIAN_POINT('Ctrl Pts',(-97.5954245965813,1075.6859325459,387.04820135808));
#124895=CARTESIAN_POINT('Ctrl Pts',(-97.6585624263007,1075.68032253532,
387.060380419275));
#124896=CARTESIAN_POINT('Ctrl Pts',(-97.7222027015961,1075.6741872497,387.060380419275));
#124897=CARTESIAN_POINT('Origin',(-9.69136378659147,1067.7251047501,441.167646863288));
#124898=CARTESIAN_POINT('',(-9.69136378659147,1078.73142393294,440.067288797613));
#124899=CARTESIAN_POINT('Origin',(-9.69136378659147,1078.73142393294,441.167646863288));
#124900=CARTESIAN_POINT('',(-9.69136378659147,1076.73142393294,440.067288797613));
#124901=CARTESIAN_POINT('',(-9.69136378659147,1067.7251047501,440.067288797613));
#124902=CARTESIAN_POINT('Origin',(-9.69136378659147,1076.73142393294,441.167646863288));
#124903=CARTESIAN_POINT('Origin',(-9.69136378659147,1067.7251047501,441.167646863288));
#124904=CARTESIAN_POINT('',(-9.69136378659147,1076.73142393294,440.667288797613));
#124905=CARTESIAN_POINT('Origin',(-9.69136378659147,1076.73142393294,441.167646863288));
#124906=CARTESIAN_POINT('',(-9.69136378659147,1082.7251047501,440.667288797613));
#124907=CARTESIAN_POINT('',(-9.69136378659147,1067.7251047501,440.667288797613));
#124908=CARTESIAN_POINT('Origin',(-9.69136378659147,1082.7251047501,441.167646863288));
#124909=CARTESIAN_POINT('Origin',(-16.2097648263481,1067.7251047501,446.721728083052));
#124910=CARTESIAN_POINT('',(-16.2097648263481,1078.73142393294,445.507696516315));
#124911=CARTESIAN_POINT('Origin',(-16.2097648263481,1078.73142393294,446.721728083052));
#124912=CARTESIAN_POINT('',(-16.2097648263481,1076.73142393294,445.507696516315));
#124913=CARTESIAN_POINT('',(-16.2097648263481,1067.7251047501,445.507696516315));
#124914=CARTESIAN_POINT('Origin',(-16.2097648263481,1076.73142393294,446.721728083052));
#124915=CARTESIAN_POINT('Origin',(-16.2097648263481,1067.7251047501,446.721728083052));
#124916=CARTESIAN_POINT('',(-16.2097648263481,1076.73142393294,446.107696516315));
#124917=CARTESIAN_POINT('Origin',(-16.2097648263481,1076.73142393294,446.721728083052));
#124918=CARTESIAN_POINT('',(-16.2097648263481,1082.7251047501,446.107696516315));
#124919=CARTESIAN_POINT('',(-16.2097648263481,1067.7251047501,446.107696516315));
#124920=CARTESIAN_POINT('Origin',(-16.2097648263481,1082.7251047501,446.721728083052));
#124921=CARTESIAN_POINT('Origin',(-23.3029185074263,1067.7251047501,450.258118980149));
#124922=CARTESIAN_POINT('',(-23.3029185074263,1078.73142393294,448.929311016575));
#124923=CARTESIAN_POINT('Origin',(-23.3029185074263,1078.73142393294,450.258118980149));
#124924=CARTESIAN_POINT('',(-23.3029185074263,1076.73142393294,448.929311016575));
#124925=CARTESIAN_POINT('',(-23.3029185074263,1067.7251047501,448.929311016575));
#124926=CARTESIAN_POINT('Origin',(-23.3029185074263,1076.73142393294,450.258118980149));
#124927=CARTESIAN_POINT('Origin',(-23.3029185074263,1067.7251047501,450.258118980149));
#124928=CARTESIAN_POINT('',(-23.3029185074263,1076.73142393294,449.529311016575));
#124929=CARTESIAN_POINT('Origin',(-23.3029185074263,1076.73142393294,450.258118980149));
#124930=CARTESIAN_POINT('',(-23.3029185074263,1082.7251047501,449.529311016575));
#124931=CARTESIAN_POINT('',(-23.3029185074263,1067.7251047501,449.529311016575));
#124932=CARTESIAN_POINT('Origin',(-23.3029185074263,1082.7251047501,450.258118980149));
#124933=CARTESIAN_POINT('Origin',(-32.1589076220707,1067.7251047501,452.997442536411));
#124934=CARTESIAN_POINT('',(-32.1589076220707,1078.73142393294,451.536325534594));
#124935=CARTESIAN_POINT('Origin',(-32.1589076220707,1078.73142393294,452.997442536411));
#124936=CARTESIAN_POINT('',(-32.1589076220707,1076.73142393294,451.536325534594));
#124937=CARTESIAN_POINT('',(-32.1589076220707,1067.7251047501,451.536325534594));
#124938=CARTESIAN_POINT('Origin',(-32.1589076220707,1076.73142393294,452.997442536411));
#124939=CARTESIAN_POINT('Origin',(-32.1589076220707,1067.7251047501,452.997442536411));
#124940=CARTESIAN_POINT('',(-32.1589076220707,1076.73142393294,452.136325534594));
#124941=CARTESIAN_POINT('Origin',(-32.1589076220707,1076.73142393294,452.997442536411));
#124942=CARTESIAN_POINT('',(-32.1589076220707,1082.7251047501,452.136325534594));
#124943=CARTESIAN_POINT('',(-32.1589076220707,1067.7251047501,452.136325534594));
#124944=CARTESIAN_POINT('Origin',(-32.1589076220707,1082.7251047501,452.997442536411));
#124945=CARTESIAN_POINT('Origin',(-41.0676411737315,1067.7251047501,453.455473148425));
#124946=CARTESIAN_POINT('',(-41.0676411737315,1078.73142393294,451.8349911058));
#124947=CARTESIAN_POINT('Origin',(-41.0676411737315,1078.73142393294,453.455473148425));
#124948=CARTESIAN_POINT('',(-41.0676411737315,1076.73142393294,451.8349911058));
#124949=CARTESIAN_POINT('',(-41.0676411737315,1067.7251047501,451.8349911058));
#124950=CARTESIAN_POINT('Origin',(-41.0676411737315,1076.73142393294,453.455473148425));
#124951=CARTESIAN_POINT('Origin',(-41.0676411737315,1067.7251047501,453.455473148425));
#124952=CARTESIAN_POINT('',(-41.0676411737315,1076.73142393294,452.4349911058));
#124953=CARTESIAN_POINT('Origin',(-41.0676411737315,1076.73142393294,453.455473148425));
#124954=CARTESIAN_POINT('',(-41.0676411737315,1082.7251047501,452.4349911058));
#124955=CARTESIAN_POINT('',(-41.0676411737315,1067.7251047501,452.4349911058));
#124956=CARTESIAN_POINT('Origin',(-41.0676411737315,1082.7251047501,453.455473148425));
#124957=CARTESIAN_POINT('Origin',(-51.2135807025652,1067.7251047501,452.701475992022));
#124958=CARTESIAN_POINT('',(-51.2135807025652,1078.73142393294,451.000475768939));
#124959=CARTESIAN_POINT('Origin',(-51.2135807025652,1078.73142393294,452.701475992022));
#124960=CARTESIAN_POINT('',(-51.2135807025652,1076.73142393294,451.000475768939));
#124961=CARTESIAN_POINT('',(-51.2135807025652,1067.7251047501,451.000475768939));
#124962=CARTESIAN_POINT('Origin',(-51.2135807025652,1076.73142393294,452.701475992022));
#124963=CARTESIAN_POINT('Origin',(-51.2135807025652,1067.7251047501,452.701475992022));
#124964=CARTESIAN_POINT('',(-51.2135807025652,1076.73142393294,451.600475768939));
#124965=CARTESIAN_POINT('Origin',(-51.2135807025652,1076.73142393294,452.701475992022));
#124966=CARTESIAN_POINT('',(-51.2135807025652,1082.7251047501,451.600475768939));
#124967=CARTESIAN_POINT('',(-51.2135807025652,1067.7251047501,451.600475768939));
#124968=CARTESIAN_POINT('Origin',(-51.2135807025652,1082.7251047501,452.701475992022));
#124969=CARTESIAN_POINT('Origin',(-60.6270981054984,1067.7251047501,449.74779979654));
#124970=CARTESIAN_POINT('',(-60.6270981054984,1078.73142393294,448.026525164496));
#124971=CARTESIAN_POINT('Origin',(-60.6270981054984,1078.73142393294,449.74779979654));
#124972=CARTESIAN_POINT('',(-60.6270981054984,1076.73142393294,448.026525164496));
#124973=CARTESIAN_POINT('',(-60.6270981054984,1067.7251047501,448.026525164496));
#124974=CARTESIAN_POINT('Origin',(-60.6270981054984,1076.73142393294,449.74779979654));
#124975=CARTESIAN_POINT('Origin',(-60.6270981054984,1067.7251047501,449.74779979654));
#124976=CARTESIAN_POINT('',(-60.6270981054984,1076.73142393294,448.626525164496));
#124977=CARTESIAN_POINT('Origin',(-60.6270981054984,1076.73142393294,449.74779979654));
#124978=CARTESIAN_POINT('',(-60.6270981054984,1082.7251047501,448.626525164496));
#124979=CARTESIAN_POINT('',(-60.6270981054984,1067.7251047501,448.626525164496));
#124980=CARTESIAN_POINT('Origin',(-60.6270981054984,1082.7251047501,449.74779979654));
#124981=CARTESIAN_POINT('Origin',(-71.0377028430569,1067.7251047501,445.125673808251));
#124982=CARTESIAN_POINT('',(-71.0377028430569,1078.73142393294,443.343681153846));
#124983=CARTESIAN_POINT('Origin',(-71.0377028430569,1078.73142393294,445.125673808251));
#124984=CARTESIAN_POINT('',(-71.0377028430569,1076.73142393294,443.343681153846));
#124985=CARTESIAN_POINT('',(-71.0377028430569,1067.7251047501,443.343681153846));
#124986=CARTESIAN_POINT('Origin',(-71.0377028430569,1076.73142393294,445.125673808251));
#124987=CARTESIAN_POINT('Origin',(-71.0377028430569,1067.7251047501,445.125673808251));
#124988=CARTESIAN_POINT('',(-71.0377028430569,1076.73142393294,443.943681153846));
#124989=CARTESIAN_POINT('Origin',(-71.0377028430569,1076.73142393294,445.125673808251));
#124990=CARTESIAN_POINT('',(-71.0377028430569,1082.7251047501,443.943681153846));
#124991=CARTESIAN_POINT('',(-71.0377028430569,1067.7251047501,443.943681153846));
#124992=CARTESIAN_POINT('Origin',(-71.0377028430569,1082.7251047501,445.125673808251));
#124993=CARTESIAN_POINT('Origin',(-80.1058740725522,1067.7251047501,438.515078960781));
#124994=CARTESIAN_POINT('',(-80.1058740725522,1078.73142393294,436.85419815086));
#124995=CARTESIAN_POINT('Origin',(-80.1058740725522,1078.73142393294,438.515078960781));
#124996=CARTESIAN_POINT('',(-80.1058740725522,1076.73142393294,436.85419815086));
#124997=CARTESIAN_POINT('',(-80.1058740725522,1067.7251047501,436.85419815086));
#124998=CARTESIAN_POINT('Origin',(-80.1058740725522,1076.73142393294,438.515078960781));
#124999=CARTESIAN_POINT('Origin',(-80.1058740725522,1067.7251047501,438.515078960781));
#125000=CARTESIAN_POINT('',(-80.1058740725522,1076.73142393294,437.45419815086));
#125001=CARTESIAN_POINT('Origin',(-80.1058740725522,1076.73142393294,438.515078960781));
#125002=CARTESIAN_POINT('',(-80.1058740725522,1082.7251047501,437.45419815086));
#125003=CARTESIAN_POINT('',(-80.1058740725522,1067.7251047501,437.45419815086));
#125004=CARTESIAN_POINT('Origin',(-80.1058740725522,1082.7251047501,438.515078960781));
#125005=CARTESIAN_POINT('Origin',(-6.03918543247926,1067.7251047501,442.820994209267));
#125006=CARTESIAN_POINT('',(-6.03918543247926,1078.73142393294,441.720636143593));
#125007=CARTESIAN_POINT('Origin',(-6.03918543247926,1078.73142393294,442.820994209267));
#125008=CARTESIAN_POINT('',(-6.03918543247926,1076.73142393294,441.720636143593));
#125009=CARTESIAN_POINT('',(-6.03918543247926,1067.7251047501,441.720636143593));
#125010=CARTESIAN_POINT('Origin',(-6.03918543247926,1076.73142393294,442.820994209267));
#125011=CARTESIAN_POINT('Origin',(-6.03918543247926,1067.7251047501,442.820994209267));
#125012=CARTESIAN_POINT('',(-6.03918543247926,1076.73142393294,442.320636143593));
#125013=CARTESIAN_POINT('Origin',(-6.03918543247926,1076.73142393294,442.820994209267));
#125014=CARTESIAN_POINT('',(-6.03918543247926,1082.7251047501,442.320636143593));
#125015=CARTESIAN_POINT('',(-6.03918543247926,1067.7251047501,442.320636143593));
#125016=CARTESIAN_POINT('Origin',(-6.03918543247926,1082.7251047501,442.820994209267));
#125017=CARTESIAN_POINT('Origin',(-11.2603853527976,1067.7251047501,449.608957210264));
#125018=CARTESIAN_POINT('',(-11.2603853527976,1078.73142393294,448.394925643527));
#125019=CARTESIAN_POINT('Origin',(-11.2603853527976,1078.73142393294,449.608957210264));
#125020=CARTESIAN_POINT('',(-11.2603853527976,1076.73142393294,448.394925643527));
#125021=CARTESIAN_POINT('',(-11.2603853527976,1067.7251047501,448.394925643527));
#125022=CARTESIAN_POINT('Origin',(-11.2603853527976,1076.73142393294,449.608957210264));
#125023=CARTESIAN_POINT('Origin',(-11.2603853527976,1067.7251047501,449.608957210264));
#125024=CARTESIAN_POINT('',(-11.2603853527976,1076.73142393294,448.994925643527));
#125025=CARTESIAN_POINT('Origin',(-11.2603853527976,1076.73142393294,449.608957210264));
#125026=CARTESIAN_POINT('',(-11.2603853527976,1082.7251047501,448.994925643527));
#125027=CARTESIAN_POINT('',(-11.2603853527976,1067.7251047501,448.994925643527));
#125028=CARTESIAN_POINT('Origin',(-11.2603853527976,1082.7251047501,449.608957210264));
#125029=CARTESIAN_POINT('Origin',(-17.4632795967725,1067.7251047501,454.54281905658));
#125030=CARTESIAN_POINT('',(-17.4632795967725,1078.73142393294,453.214011093006));
#125031=CARTESIAN_POINT('Origin',(-17.4632795967725,1078.73142393294,454.54281905658));
#125032=CARTESIAN_POINT('',(-17.4632795967725,1076.73142393294,453.214011093006));
#125033=CARTESIAN_POINT('',(-17.4632795967725,1067.7251047501,453.214011093006));
#125034=CARTESIAN_POINT('Origin',(-17.4632795967725,1076.73142393294,454.54281905658));
#125035=CARTESIAN_POINT('Origin',(-17.4632795967725,1067.7251047501,454.54281905658));
#125036=CARTESIAN_POINT('',(-17.4632795967725,1076.73142393294,453.814011093006));
#125037=CARTESIAN_POINT('Origin',(-17.4632795967725,1076.73142393294,454.54281905658));
#125038=CARTESIAN_POINT('',(-17.4632795967725,1082.7251047501,453.814011093006));
#125039=CARTESIAN_POINT('',(-17.4632795967725,1067.7251047501,453.814011093006));
#125040=CARTESIAN_POINT('Origin',(-17.4632795967725,1082.7251047501,454.54281905658));
#125041=CARTESIAN_POINT('Origin',(-25.5562067091073,1067.7251047501,459.06354549146));
#125042=CARTESIAN_POINT('',(-25.5562067091073,1078.73142393294,457.602428489643));
#125043=CARTESIAN_POINT('Origin',(-25.5562067091073,1078.73142393294,459.06354549146));
#125044=CARTESIAN_POINT('',(-25.5562067091073,1076.73142393294,457.602428489643));
#125045=CARTESIAN_POINT('',(-25.5562067091073,1067.7251047501,457.602428489643));
#125046=CARTESIAN_POINT('Origin',(-25.5562067091073,1076.73142393294,459.06354549146));
#125047=CARTESIAN_POINT('Origin',(-25.5562067091073,1067.7251047501,459.06354549146));
#125048=CARTESIAN_POINT('',(-25.5562067091073,1076.73142393294,458.202428489643));
#125049=CARTESIAN_POINT('Origin',(-25.5562067091073,1076.73142393294,459.06354549146));
#125050=CARTESIAN_POINT('',(-25.5562067091073,1082.7251047501,458.202428489643));
#125051=CARTESIAN_POINT('',(-25.5562067091073,1067.7251047501,458.202428489643));
#125052=CARTESIAN_POINT('Origin',(-25.5562067091073,1082.7251047501,459.06354549146));
#125053=CARTESIAN_POINT('Origin',(-34.1750331392509,1067.7251047501,461.363796891435));
#125054=CARTESIAN_POINT('',(-34.1750331392509,1078.73142393294,459.743314848811));
#125055=CARTESIAN_POINT('Origin',(-34.1750331392509,1078.73142393294,461.363796891435));
#125056=CARTESIAN_POINT('',(-34.1750331392509,1076.73142393294,459.743314848811));
#125057=CARTESIAN_POINT('',(-34.1750331392509,1067.7251047501,459.743314848811));
#125058=CARTESIAN_POINT('Origin',(-34.1750331392509,1076.73142393294,461.363796891435));
#125059=CARTESIAN_POINT('Origin',(-34.1750331392509,1067.7251047501,461.363796891435));
#125060=CARTESIAN_POINT('',(-34.1750331392509,1076.73142393294,460.343314848811));
#125061=CARTESIAN_POINT('Origin',(-34.1750331392509,1076.73142393294,461.363796891435));
#125062=CARTESIAN_POINT('',(-34.1750331392509,1082.7251047501,460.343314848811));
#125063=CARTESIAN_POINT('',(-34.1750331392509,1067.7251047501,460.343314848811));
#125064=CARTESIAN_POINT('Origin',(-34.1750331392509,1082.7251047501,461.363796891435));
#125065=CARTESIAN_POINT('Origin',(-44.2560243702294,1067.7251047501,462.735735824314));
#125066=CARTESIAN_POINT('',(-44.2560243702294,1078.73142393294,461.034735601231));
#125067=CARTESIAN_POINT('Origin',(-44.2560243702294,1078.73142393294,462.735735824314));
#125068=CARTESIAN_POINT('',(-44.2560243702294,1076.73142393294,461.034735601231));
#125069=CARTESIAN_POINT('',(-44.2560243702294,1067.7251047501,461.034735601231));
#125070=CARTESIAN_POINT('Origin',(-44.2560243702294,1076.73142393294,462.735735824314));
#125071=CARTESIAN_POINT('Origin',(-44.2560243702294,1067.7251047501,462.735735824314));
#125072=CARTESIAN_POINT('',(-44.2560243702294,1076.73142393294,461.634735601231));
#125073=CARTESIAN_POINT('Origin',(-44.2560243702294,1076.73142393294,462.735735824314));
#125074=CARTESIAN_POINT('',(-44.2560243702294,1082.7251047501,461.634735601231));
#125075=CARTESIAN_POINT('',(-44.2560243702294,1067.7251047501,461.634735601231));
#125076=CARTESIAN_POINT('Origin',(-44.2560243702294,1082.7251047501,462.735735824314));
#125077=CARTESIAN_POINT('Origin',(-54.0779376443053,1067.7251047501,461.803784860145));
#125078=CARTESIAN_POINT('',(-54.0779376443053,1078.73142393294,460.082510228102));
#125079=CARTESIAN_POINT('Origin',(-54.0779376443053,1078.73142393294,461.803784860145));
#125080=CARTESIAN_POINT('',(-54.0779376443053,1076.73142393294,460.082510228102));
#125081=CARTESIAN_POINT('',(-54.0779376443053,1067.7251047501,460.082510228102));
#125082=CARTESIAN_POINT('Origin',(-54.0779376443053,1076.73142393294,461.803784860145));
#125083=CARTESIAN_POINT('Origin',(-54.0779376443053,1067.7251047501,461.803784860145));
#125084=CARTESIAN_POINT('',(-54.0779376443053,1076.73142393294,460.682510228102));
#125085=CARTESIAN_POINT('Origin',(-54.0779376443053,1076.73142393294,461.803784860145));
#125086=CARTESIAN_POINT('',(-54.0779376443053,1082.7251047501,460.682510228102));
#125087=CARTESIAN_POINT('',(-54.0779376443053,1067.7251047501,460.682510228102));
#125088=CARTESIAN_POINT('Origin',(-54.0779376443053,1082.7251047501,461.803784860145));
#125089=CARTESIAN_POINT('Origin',(-65.222039719934,1067.7251047501,459.447149847832));
#125090=CARTESIAN_POINT('',(-65.222039719934,1078.73142393294,457.665157193427));
#125091=CARTESIAN_POINT('Origin',(-65.222039719934,1078.73142393294,459.447149847832));
#125092=CARTESIAN_POINT('',(-65.222039719934,1076.73142393294,457.665157193427));
#125093=CARTESIAN_POINT('',(-65.222039719934,1067.7251047501,457.665157193427));
#125094=CARTESIAN_POINT('Origin',(-65.222039719934,1076.73142393294,459.447149847832));
#125095=CARTESIAN_POINT('Origin',(-65.222039719934,1067.7251047501,459.447149847832));
#125096=CARTESIAN_POINT('',(-65.222039719934,1076.73142393294,458.265157193427));
#125097=CARTESIAN_POINT('Origin',(-65.222039719934,1076.73142393294,459.447149847832));
#125098=CARTESIAN_POINT('',(-65.222039719934,1082.7251047501,458.265157193427));
#125099=CARTESIAN_POINT('',(-65.222039719934,1067.7251047501,458.265157193427));
#125100=CARTESIAN_POINT('Origin',(-65.222039719934,1082.7251047501,459.447149847832));
#125101=CARTESIAN_POINT('Origin',(-75.4664696031568,1067.7251047501,454.866391171305));
#125102=CARTESIAN_POINT('',(-75.4664696031568,1078.73142393294,453.205510361384));
#125103=CARTESIAN_POINT('Origin',(-75.4664696031568,1078.73142393294,454.866391171305));
#125104=CARTESIAN_POINT('',(-75.4664696031568,1076.73142393294,453.205510361384));
#125105=CARTESIAN_POINT('',(-75.4664696031568,1067.7251047501,453.205510361384));
#125106=CARTESIAN_POINT('Origin',(-75.4664696031568,1076.73142393294,454.866391171305));
#125107=CARTESIAN_POINT('Origin',(-75.4664696031568,1067.7251047501,454.866391171305));
#125108=CARTESIAN_POINT('',(-75.4664696031568,1076.73142393294,453.805510361384));
#125109=CARTESIAN_POINT('Origin',(-75.4664696031568,1076.73142393294,454.866391171305));
#125110=CARTESIAN_POINT('',(-75.4664696031568,1082.7251047501,453.805510361384));
#125111=CARTESIAN_POINT('',(-75.4664696031568,1067.7251047501,453.805510361384));
#125112=CARTESIAN_POINT('Origin',(-75.4664696031568,1082.7251047501,454.866391171305));
#125113=CARTESIAN_POINT('Origin',(-2.12306569574067,1067.7251047501,443.678881372145));
#125114=CARTESIAN_POINT('',(-2.12306569574067,1078.73142393294,442.578523306471));
#125115=CARTESIAN_POINT('Origin',(-2.12306569574067,1078.73142393294,443.678881372145));
#125116=CARTESIAN_POINT('',(-2.12306569574067,1076.73142393294,442.578523306471));
#125117=CARTESIAN_POINT('',(-2.12306569574067,1067.7251047501,442.578523306471));
#125118=CARTESIAN_POINT('Origin',(-2.12306569574067,1076.73142393294,443.678881372145));
#125119=CARTESIAN_POINT('Origin',(-2.12306569574067,1067.7251047501,443.678881372145));
#125120=CARTESIAN_POINT('',(-2.12306569574067,1076.73142393294,443.178523306471));
#125121=CARTESIAN_POINT('Origin',(-2.12306569574067,1076.73142393294,443.678881372145));
#125122=CARTESIAN_POINT('',(-2.12306569574067,1082.7251047501,443.178523306471));
#125123=CARTESIAN_POINT('',(-2.12306569574067,1067.7251047501,443.178523306471));
#125124=CARTESIAN_POINT('Origin',(-2.12306569574067,1082.7251047501,443.678881372145));
#125125=CARTESIAN_POINT('Origin',(-5.818873006006,1067.7251047501,451.404059598971));
#125126=CARTESIAN_POINT('',(-5.818873006006,1078.73142393294,450.190028032234));
#125127=CARTESIAN_POINT('Origin',(-5.818873006006,1078.73142393294,451.404059598971));
#125128=CARTESIAN_POINT('',(-5.818873006006,1076.73142393294,450.190028032234));
#125129=CARTESIAN_POINT('',(-5.818873006006,1067.7251047501,450.190028032234));
#125130=CARTESIAN_POINT('Origin',(-5.818873006006,1076.73142393294,451.404059598971));
#125131=CARTESIAN_POINT('Origin',(-5.818873006006,1067.7251047501,451.404059598971));
#125132=CARTESIAN_POINT('',(-5.818873006006,1076.73142393294,450.790028032234));
#125133=CARTESIAN_POINT('Origin',(-5.818873006006,1076.73142393294,451.404059598971));
#125134=CARTESIAN_POINT('',(-5.818873006006,1082.7251047501,450.790028032234));
#125135=CARTESIAN_POINT('',(-5.818873006006,1067.7251047501,450.790028032234));
#125136=CARTESIAN_POINT('Origin',(-5.818873006006,1082.7251047501,451.404059598971));
#125137=CARTESIAN_POINT('Origin',(-10.8604115696268,1067.7251047501,457.519758956525));
#125138=CARTESIAN_POINT('',(-10.8604115696268,1078.73142393294,456.190950992952));
#125139=CARTESIAN_POINT('Origin',(-10.8604115696268,1078.73142393294,457.519758956525));
#125140=CARTESIAN_POINT('',(-10.8604115696268,1076.73142393294,456.190950992952));
#125141=CARTESIAN_POINT('',(-10.8604115696268,1067.7251047501,456.190950992952));
#125142=CARTESIAN_POINT('Origin',(-10.8604115696268,1076.73142393294,457.519758956525));
#125143=CARTESIAN_POINT('Origin',(-10.8604115696268,1067.7251047501,457.519758956525));
#125144=CARTESIAN_POINT('',(-10.8604115696268,1076.73142393294,456.790950992952));
#125145=CARTESIAN_POINT('Origin',(-10.8604115696268,1076.73142393294,457.519758956525));
#125146=CARTESIAN_POINT('',(-10.8604115696268,1082.7251047501,456.790950992952));
#125147=CARTESIAN_POINT('',(-10.8604115696268,1067.7251047501,456.790950992952));
#125148=CARTESIAN_POINT('Origin',(-10.8604115696268,1082.7251047501,457.519758956525));
#125149=CARTESIAN_POINT('Origin',(-17.8365769306701,1067.7251047501,463.624310831968));
#125150=CARTESIAN_POINT('',(-17.8365769306701,1078.73142393294,462.163193830151));
#125151=CARTESIAN_POINT('Origin',(-17.8365769306701,1078.73142393294,463.624310831968));
#125152=CARTESIAN_POINT('',(-17.8365769306701,1076.73142393294,462.163193830151));
#125153=CARTESIAN_POINT('',(-17.8365769306701,1067.7251047501,462.163193830151));
#125154=CARTESIAN_POINT('Origin',(-17.8365769306701,1076.73142393294,463.624310831968));
#125155=CARTESIAN_POINT('Origin',(-17.8365769306701,1067.7251047501,463.624310831968));
#125156=CARTESIAN_POINT('',(-17.8365769306701,1076.73142393294,462.763193830151));
#125157=CARTESIAN_POINT('Origin',(-17.8365769306701,1076.73142393294,463.624310831968));
#125158=CARTESIAN_POINT('',(-17.8365769306701,1082.7251047501,462.763193830151));
#125159=CARTESIAN_POINT('',(-17.8365769306701,1067.7251047501,462.763193830151));
#125160=CARTESIAN_POINT('Origin',(-17.8365769306701,1082.7251047501,463.624310831968));
#125161=CARTESIAN_POINT('Origin',(-25.7888121665815,1067.7251047501,467.666250995894));
#125162=CARTESIAN_POINT('',(-25.7888121665815,1078.73142393294,466.04576895327));
#125163=CARTESIAN_POINT('Origin',(-25.7888121665815,1078.73142393294,467.666250995894));
#125164=CARTESIAN_POINT('',(-25.7888121665815,1076.73142393294,466.04576895327));
#125165=CARTESIAN_POINT('',(-25.7888121665815,1067.7251047501,466.04576895327));
#125166=CARTESIAN_POINT('Origin',(-25.7888121665815,1076.73142393294,467.666250995894));
#125167=CARTESIAN_POINT('Origin',(-25.7888121665815,1067.7251047501,467.666250995894));
#125168=CARTESIAN_POINT('',(-25.7888121665815,1076.73142393294,466.64576895327));
#125169=CARTESIAN_POINT('Origin',(-25.7888121665815,1076.73142393294,467.666250995894));
#125170=CARTESIAN_POINT('',(-25.7888121665815,1082.7251047501,466.64576895327));
#125171=CARTESIAN_POINT('',(-25.7888121665815,1067.7251047501,466.64576895327));
#125172=CARTESIAN_POINT('Origin',(-25.7888121665815,1082.7251047501,467.666250995894));
#125173=CARTESIAN_POINT('Origin',(-35.3642674089481,1067.7251047501,471.104165703395));
#125174=CARTESIAN_POINT('',(-35.3642674089481,1078.73142393294,469.403165480312));
#125175=CARTESIAN_POINT('Origin',(-35.3642674089481,1078.73142393294,471.104165703395));
#125176=CARTESIAN_POINT('',(-35.3642674089481,1076.73142393294,469.403165480312));
#125177=CARTESIAN_POINT('',(-35.3642674089481,1067.7251047501,469.403165480312));
#125178=CARTESIAN_POINT('Origin',(-35.3642674089481,1076.73142393294,471.104165703395));
#125179=CARTESIAN_POINT('Origin',(-35.3642674089481,1067.7251047501,471.104165703395));
#125180=CARTESIAN_POINT('',(-35.3642674089481,1076.73142393294,470.003165480312));
#125181=CARTESIAN_POINT('Origin',(-35.3642674089481,1076.73142393294,471.104165703395));
#125182=CARTESIAN_POINT('',(-35.3642674089481,1082.7251047501,470.003165480312));
#125183=CARTESIAN_POINT('',(-35.3642674089481,1067.7251047501,470.003165480312));
#125184=CARTESIAN_POINT('Origin',(-35.3642674089481,1082.7251047501,471.104165703395));
#125185=CARTESIAN_POINT('Origin',(-45.1653118133206,1067.7251047501,472.23467069967));
#125186=CARTESIAN_POINT('',(-45.1653118133206,1078.73142393294,470.513396067626));
#125187=CARTESIAN_POINT('Origin',(-45.1653118133206,1078.73142393294,472.23467069967));
#125188=CARTESIAN_POINT('',(-45.1653118133206,1076.73142393294,470.513396067626));
#125189=CARTESIAN_POINT('',(-45.1653118133206,1067.7251047501,470.513396067626));
#125190=CARTESIAN_POINT('Origin',(-45.1653118133206,1076.73142393294,472.23467069967));
#125191=CARTESIAN_POINT('Origin',(-45.1653118133206,1067.7251047501,472.23467069967));
#125192=CARTESIAN_POINT('',(-45.1653118133206,1076.73142393294,471.113396067626));
#125193=CARTESIAN_POINT('Origin',(-45.1653118133206,1076.73142393294,472.23467069967));
#125194=CARTESIAN_POINT('',(-45.1653118133206,1082.7251047501,471.113396067626));
#125195=CARTESIAN_POINT('',(-45.1653118133206,1067.7251047501,471.113396067626));
#125196=CARTESIAN_POINT('Origin',(-45.1653118133206,1082.7251047501,472.23467069967));
#125197=CARTESIAN_POINT('Origin',(-56.5558604909797,1067.7251047501,472.24652292176));
#125198=CARTESIAN_POINT('',(-56.5558604909797,1078.73142393294,470.464530267355));
#125199=CARTESIAN_POINT('Origin',(-56.5558604909797,1078.73142393294,472.24652292176));
#125200=CARTESIAN_POINT('',(-56.5558604909797,1076.73142393294,470.464530267355));
#125201=CARTESIAN_POINT('',(-56.5558604909797,1067.7251047501,470.464530267355));
#125202=CARTESIAN_POINT('Origin',(-56.5558604909797,1076.73142393294,472.24652292176));
#125203=CARTESIAN_POINT('Origin',(-56.5558604909797,1067.7251047501,472.24652292176));
#125204=CARTESIAN_POINT('',(-56.5558604909797,1076.73142393294,471.064530267355));
#125205=CARTESIAN_POINT('Origin',(-56.5558604909797,1076.73142393294,472.24652292176));
#125206=CARTESIAN_POINT('',(-56.5558604909797,1082.7251047501,471.064530267355));
#125207=CARTESIAN_POINT('',(-56.5558604909797,1067.7251047501,471.064530267355));
#125208=CARTESIAN_POINT('Origin',(-56.5558604909797,1082.7251047501,472.24652292176));
#125209=CARTESIAN_POINT('Origin',(-67.5288182838046,1067.7251047501,469.89580155126));
#125210=CARTESIAN_POINT('',(-67.5288182838046,1078.73142393294,468.234920741339));
#125211=CARTESIAN_POINT('Origin',(-67.5288182838046,1078.73142393294,469.89580155126));
#125212=CARTESIAN_POINT('',(-67.5288182838046,1076.73142393294,468.234920741339));
#125213=CARTESIAN_POINT('',(-67.5288182838046,1067.7251047501,468.234920741339));
#125214=CARTESIAN_POINT('Origin',(-67.5288182838046,1076.73142393294,469.89580155126));
#125215=CARTESIAN_POINT('Origin',(-67.5288182838046,1067.7251047501,469.89580155126));
#125216=CARTESIAN_POINT('',(-67.5288182838046,1076.73142393294,468.834920741339));
#125217=CARTESIAN_POINT('Origin',(-67.5288182838046,1076.73142393294,469.89580155126));
#125218=CARTESIAN_POINT('',(-67.5288182838046,1082.7251047501,468.834920741339));
#125219=CARTESIAN_POINT('',(-67.5288182838046,1067.7251047501,468.834920741339));
#125220=CARTESIAN_POINT('Origin',(-67.5288182838046,1082.7251047501,469.89580155126));
#125221=CARTESIAN_POINT('Origin',(1.88584219950125,1067.7251047501,443.703814566305));
#125222=CARTESIAN_POINT('',(1.88584219950125,1078.73142393294,442.60345650063));
#125223=CARTESIAN_POINT('Origin',(1.88584219950125,1078.73142393294,443.703814566305));
#125224=CARTESIAN_POINT('',(1.88584219950125,1076.73142393294,442.60345650063));
#125225=CARTESIAN_POINT('',(1.88584219950125,1067.7251047501,442.60345650063));
#125226=CARTESIAN_POINT('Origin',(1.88584219950125,1076.73142393294,443.703814566305));
#125227=CARTESIAN_POINT('Origin',(1.88584219950125,1067.7251047501,443.703814566305));
#125228=CARTESIAN_POINT('',(1.88584219950125,1076.73142393294,443.20345650063));
#125229=CARTESIAN_POINT('Origin',(1.88584219950125,1076.73142393294,443.703814566305));
#125230=CARTESIAN_POINT('',(1.88584219950125,1082.7251047501,443.20345650063));
#125231=CARTESIAN_POINT('',(1.88584219950125,1067.7251047501,443.20345650063));
#125232=CARTESIAN_POINT('Origin',(1.88584219950125,1082.7251047501,443.703814566305));
#125233=CARTESIAN_POINT('Origin',(-0.123047986801322,1067.7251047501,452.02858066093));
#125234=CARTESIAN_POINT('',(-0.123047986801322,1078.73142393294,450.814549094193));
#125235=CARTESIAN_POINT('Origin',(-0.123047986801322,1078.73142393294,452.02858066093));
#125236=CARTESIAN_POINT('',(-0.123047986801322,1076.73142393294,450.814549094193));
#125237=CARTESIAN_POINT('',(-0.123047986801322,1067.7251047501,450.814549094193));
#125238=CARTESIAN_POINT('Origin',(-0.123047986801322,1076.73142393294,452.02858066093));
#125239=CARTESIAN_POINT('Origin',(-0.123047986801322,1067.7251047501,452.02858066093));
#125240=CARTESIAN_POINT('',(-0.123047986801322,1076.73142393294,451.414549094192));
#125241=CARTESIAN_POINT('Origin',(-0.123047986801322,1076.73142393294,452.02858066093));
#125242=CARTESIAN_POINT('',(-0.123047986801322,1082.7251047501,451.414549094192));
#125243=CARTESIAN_POINT('',(-0.123047986801322,1067.7251047501,451.414549094192));
#125244=CARTESIAN_POINT('Origin',(-0.123047986801322,1082.7251047501,452.02858066093));
#125245=CARTESIAN_POINT('Origin',(-3.78289144285191,1067.7251047501,459.058832121416));
#125246=CARTESIAN_POINT('',(-3.78289144285191,1078.73142393294,457.730024157842));
#125247=CARTESIAN_POINT('Origin',(-3.78289144285191,1078.73142393294,459.058832121416));
#125248=CARTESIAN_POINT('',(-3.78289144285191,1076.73142393294,457.730024157842));
#125249=CARTESIAN_POINT('',(-3.78289144285191,1067.7251047501,457.730024157842));
#125250=CARTESIAN_POINT('Origin',(-3.78289144285191,1076.73142393294,459.058832121416));
#125251=CARTESIAN_POINT('Origin',(-3.78289144285191,1067.7251047501,459.058832121416));
#125252=CARTESIAN_POINT('',(-3.78289144285191,1076.73142393294,458.330024157842));
#125253=CARTESIAN_POINT('Origin',(-3.78289144285191,1076.73142393294,459.058832121416));
#125254=CARTESIAN_POINT('',(-3.78289144285191,1082.7251047501,458.330024157842));
#125255=CARTESIAN_POINT('',(-3.78289144285191,1067.7251047501,458.330024157842));
#125256=CARTESIAN_POINT('Origin',(-3.78289144285191,1082.7251047501,459.058832121416));
#125257=CARTESIAN_POINT('Origin',(-9.33740315097062,1067.7251047501,466.480411227574));
#125258=CARTESIAN_POINT('',(-9.33740315097062,1078.73142393294,465.019294225757));
#125259=CARTESIAN_POINT('Origin',(-9.33740315097062,1078.73142393294,466.480411227574));
#125260=CARTESIAN_POINT('',(-9.33740315097062,1076.73142393294,465.019294225757));
#125261=CARTESIAN_POINT('',(-9.33740315097062,1067.7251047501,465.019294225757));
#125262=CARTESIAN_POINT('Origin',(-9.33740315097062,1076.73142393294,466.480411227574));
#125263=CARTESIAN_POINT('Origin',(-9.33740315097062,1067.7251047501,466.480411227574));
#125264=CARTESIAN_POINT('',(-9.33740315097062,1076.73142393294,465.619294225757));
#125265=CARTESIAN_POINT('Origin',(-9.33740315097062,1076.73142393294,466.480411227574));
#125266=CARTESIAN_POINT('',(-9.33740315097062,1082.7251047501,465.619294225757));
#125267=CARTESIAN_POINT('',(-9.33740315097062,1067.7251047501,465.619294225757));
#125268=CARTESIAN_POINT('Origin',(-9.33740315097062,1082.7251047501,466.480411227574));
#125269=CARTESIAN_POINT('Origin',(-16.2754963537821,1067.7251047501,472.087387974907));
#125270=CARTESIAN_POINT('',(-16.2754963537821,1078.73142393294,470.466905932282));
#125271=CARTESIAN_POINT('Origin',(-16.2754963537821,1078.73142393294,472.087387974907));
#125272=CARTESIAN_POINT('',(-16.2754963537821,1076.73142393294,470.466905932282));
#125273=CARTESIAN_POINT('',(-16.2754963537821,1067.7251047501,470.466905932282));
#125274=CARTESIAN_POINT('Origin',(-16.2754963537821,1076.73142393294,472.087387974907));
#125275=CARTESIAN_POINT('Origin',(-16.2754963537821,1067.7251047501,472.087387974907));
#125276=CARTESIAN_POINT('',(-16.2754963537821,1076.73142393294,471.066905932282));
#125277=CARTESIAN_POINT('Origin',(-16.2754963537821,1076.73142393294,472.087387974907));
#125278=CARTESIAN_POINT('',(-16.2754963537821,1082.7251047501,471.066905932282));
#125279=CARTESIAN_POINT('',(-16.2754963537821,1067.7251047501,471.066905932282));
#125280=CARTESIAN_POINT('Origin',(-16.2754963537821,1082.7251047501,472.087387974907));
#125281=CARTESIAN_POINT('Origin',(-24.9269222653132,1067.7251047501,477.441025087366));
#125282=CARTESIAN_POINT('',(-24.9269222653132,1078.73142393294,475.740024864283));
#125283=CARTESIAN_POINT('Origin',(-24.9269222653132,1078.73142393294,477.441025087366));
#125284=CARTESIAN_POINT('',(-24.9269222653132,1076.73142393294,475.740024864283));
#125285=CARTESIAN_POINT('',(-24.9269222653132,1067.7251047501,475.740024864283));
#125286=CARTESIAN_POINT('Origin',(-24.9269222653132,1076.73142393294,477.441025087366));
#125287=CARTESIAN_POINT('Origin',(-24.9269222653132,1067.7251047501,477.441025087366));
#125288=CARTESIAN_POINT('',(-24.9269222653132,1076.73142393294,476.340024864283));
#125289=CARTESIAN_POINT('Origin',(-24.9269222653132,1076.73142393294,477.441025087366));
#125290=CARTESIAN_POINT('',(-24.9269222653132,1082.7251047501,476.340024864283));
#125291=CARTESIAN_POINT('',(-24.9269222653132,1067.7251047501,476.340024864283));
#125292=CARTESIAN_POINT('Origin',(-24.9269222653132,1082.7251047501,477.441025087366));
#125293=CARTESIAN_POINT('Origin',(-34.2787451288822,1067.7251047501,480.584577550983));
#125294=CARTESIAN_POINT('',(-34.2787451288822,1078.73142393294,478.863302918939));
#125295=CARTESIAN_POINT('Origin',(-34.2787451288822,1078.73142393294,480.584577550983));
#125296=CARTESIAN_POINT('',(-34.2787451288822,1076.73142393294,478.863302918939));
#125297=CARTESIAN_POINT('',(-34.2787451288822,1067.7251047501,478.863302918939));
#125298=CARTESIAN_POINT('Origin',(-34.2787451288822,1076.73142393294,480.584577550983));
#125299=CARTESIAN_POINT('Origin',(-34.2787451288822,1067.7251047501,480.584577550983));
#125300=CARTESIAN_POINT('',(-34.2787451288822,1076.73142393294,479.463302918939));
#125301=CARTESIAN_POINT('Origin',(-34.2787451288822,1076.73142393294,480.584577550983));
#125302=CARTESIAN_POINT('',(-34.2787451288822,1082.7251047501,479.463302918939));
#125303=CARTESIAN_POINT('',(-34.2787451288822,1067.7251047501,479.463302918939));
#125304=CARTESIAN_POINT('Origin',(-34.2787451288822,1082.7251047501,480.584577550983));
#125305=CARTESIAN_POINT('Origin',(-45.4179187734414,1067.7251047501,482.964399008498));
#125306=CARTESIAN_POINT('',(-45.4179187734414,1078.73142393294,481.182406354093));
#125307=CARTESIAN_POINT('Origin',(-45.4179187734414,1078.73142393294,482.964399008498));
#125308=CARTESIAN_POINT('',(-45.4179187734414,1076.73142393294,481.182406354093));
#125309=CARTESIAN_POINT('',(-45.4179187734414,1067.7251047501,481.182406354093));
#125310=CARTESIAN_POINT('Origin',(-45.4179187734414,1076.73142393294,482.964399008498));
#125311=CARTESIAN_POINT('Origin',(-45.4179187734414,1067.7251047501,482.964399008498));
#125312=CARTESIAN_POINT('',(-45.4179187734414,1076.73142393294,481.782406354093));
#125313=CARTESIAN_POINT('Origin',(-45.4179187734414,1076.73142393294,482.964399008498));
#125314=CARTESIAN_POINT('',(-45.4179187734414,1082.7251047501,481.782406354093));
#125315=CARTESIAN_POINT('',(-45.4179187734414,1067.7251047501,481.782406354093));
#125316=CARTESIAN_POINT('Origin',(-45.4179187734414,1082.7251047501,482.964399008498));
#125317=CARTESIAN_POINT('Origin',(-56.6398335662286,1067.7251047501,482.946452747927));
#125318=CARTESIAN_POINT('',(-56.6398335662286,1078.73142393294,481.285571938007));
#125319=CARTESIAN_POINT('Origin',(-56.6398335662286,1078.73142393294,482.946452747927));
#125320=CARTESIAN_POINT('',(-56.6398335662286,1076.73142393294,481.285571938007));
#125321=CARTESIAN_POINT('',(-56.6398335662286,1067.7251047501,481.285571938007));
#125322=CARTESIAN_POINT('Origin',(-56.6398335662286,1076.73142393294,482.946452747927));
#125323=CARTESIAN_POINT('Origin',(-56.6398335662286,1067.7251047501,482.946452747927));
#125324=CARTESIAN_POINT('',(-56.6398335662286,1076.73142393294,481.885571938007));
#125325=CARTESIAN_POINT('Origin',(-56.6398335662286,1076.73142393294,482.946452747927));
#125326=CARTESIAN_POINT('',(-56.6398335662286,1082.7251047501,481.885571938007));
#125327=CARTESIAN_POINT('',(-56.6398335662286,1067.7251047501,481.885571938007));
#125328=CARTESIAN_POINT('Origin',(-56.6398335662286,1082.7251047501,482.946452747927));
#125329=CARTESIAN_POINT('Origin',(5.81232974134988,1067.7251047501,442.894704091518));
#125330=CARTESIAN_POINT('',(5.81232974134988,1078.73142393294,441.794346025843));
#125331=CARTESIAN_POINT('Origin',(5.81232974134988,1078.73142393294,442.894704091518));
#125332=CARTESIAN_POINT('',(5.81232974134988,1076.73142393294,441.794346025843));
#125333=CARTESIAN_POINT('',(5.81232974134988,1067.7251047501,441.794346025843));
#125334=CARTESIAN_POINT('Origin',(5.81232974134988,1076.73142393294,442.894704091518));
#125335=CARTESIAN_POINT('Origin',(5.81232974134988,1067.7251047501,442.894704091518));
#125336=CARTESIAN_POINT('',(5.81232974134988,1076.73142393294,442.394346025843));
#125337=CARTESIAN_POINT('Origin',(5.81232974134988,1076.73142393294,442.894704091518));
#125338=CARTESIAN_POINT('',(5.81232974134988,1082.7251047501,442.394346025843));
#125339=CARTESIAN_POINT('',(5.81232974134988,1067.7251047501,442.394346025843));
#125340=CARTESIAN_POINT('Origin',(5.81232974134988,1082.7251047501,442.894704091518));
#125341=CARTESIAN_POINT('Origin',(5.57815481987611,1067.7251047501,451.455225828947));
#125342=CARTESIAN_POINT('',(5.57815481987611,1078.73142393294,450.24119426221));
#125343=CARTESIAN_POINT('Origin',(5.57815481987611,1078.73142393294,451.455225828947));
#125344=CARTESIAN_POINT('',(5.57815481987611,1076.73142393294,450.24119426221));
#125345=CARTESIAN_POINT('',(5.57815481987611,1067.7251047501,450.24119426221));
#125346=CARTESIAN_POINT('Origin',(5.57815481987611,1076.73142393294,451.455225828947));
#125347=CARTESIAN_POINT('Origin',(5.57815481987611,1067.7251047501,451.455225828947));
#125348=CARTESIAN_POINT('',(5.57815481987611,1076.73142393294,450.84119426221));
#125349=CARTESIAN_POINT('Origin',(5.57815481987611,1076.73142393294,451.455225828947));
#125350=CARTESIAN_POINT('',(5.57815481987611,1082.7251047501,450.84119426221));
#125351=CARTESIAN_POINT('',(5.57815481987611,1067.7251047501,450.84119426221));
#125352=CARTESIAN_POINT('Origin',(5.57815481987611,1082.7251047501,451.455225828947));
#125353=CARTESIAN_POINT('Origin',(3.45995919230269,1067.7251047501,459.092773668652));
#125354=CARTESIAN_POINT('',(3.45995919230269,1078.73142393294,457.763965705079));
#125355=CARTESIAN_POINT('Origin',(3.45995919230269,1078.73142393294,459.092773668652));
#125356=CARTESIAN_POINT('',(3.45995919230269,1076.73142393294,457.763965705079));
#125357=CARTESIAN_POINT('',(3.45995919230269,1067.7251047501,457.763965705079));
#125358=CARTESIAN_POINT('Origin',(3.45995919230269,1076.73142393294,459.092773668652));
#125359=CARTESIAN_POINT('Origin',(3.45995919230269,1067.7251047501,459.092773668652));
#125360=CARTESIAN_POINT('',(3.45995919230269,1076.73142393294,458.363965705079));
#125361=CARTESIAN_POINT('Origin',(3.45995919230269,1076.73142393294,459.092773668652));
#125362=CARTESIAN_POINT('',(3.45995919230269,1082.7251047501,458.363965705079));
#125363=CARTESIAN_POINT('',(3.45995919230269,1067.7251047501,458.363965705079));
#125364=CARTESIAN_POINT('Origin',(3.45995919230269,1082.7251047501,459.092773668652));
#125365=CARTESIAN_POINT('Origin',(-0.430140047742333,1067.7251047501,467.507021385899));
#125366=CARTESIAN_POINT('',(-0.430140047742334,1078.73142393294,466.045904384082));
#125367=CARTESIAN_POINT('Origin',(-0.430140047742333,1078.73142393294,467.507021385899));
#125368=CARTESIAN_POINT('',(-0.430140047742334,1076.73142393294,466.045904384082));
#125369=CARTESIAN_POINT('',(-0.430140047742334,1067.7251047501,466.045904384082));
#125370=CARTESIAN_POINT('Origin',(-0.430140047742333,1076.73142393294,467.507021385899));
#125371=CARTESIAN_POINT('Origin',(-0.430140047742333,1067.7251047501,467.507021385899));
#125372=CARTESIAN_POINT('',(-0.430140047742333,1076.73142393294,466.645904384082));
#125373=CARTESIAN_POINT('Origin',(-0.430140047742333,1076.73142393294,467.507021385899));
#125374=CARTESIAN_POINT('',(-0.430140047742333,1082.7251047501,466.645904384082));
#125375=CARTESIAN_POINT('',(-0.430140047742333,1067.7251047501,466.645904384082));
#125376=CARTESIAN_POINT('Origin',(-0.430140047742333,1082.7251047501,467.507021385899));
#125377=CARTESIAN_POINT('Origin',(-6.05086325182613,1067.7251047501,474.433982927521));
#125378=CARTESIAN_POINT('',(-6.05086325182613,1078.73142393294,472.813500884896));
#125379=CARTESIAN_POINT('Origin',(-6.05086325182613,1078.73142393294,474.433982927521));
#125380=CARTESIAN_POINT('',(-6.05086325182613,1076.73142393294,472.813500884896));
#125381=CARTESIAN_POINT('',(-6.05086325182613,1067.7251047501,472.813500884896));
#125382=CARTESIAN_POINT('Origin',(-6.05086325182613,1076.73142393294,474.433982927521));
#125383=CARTESIAN_POINT('Origin',(-6.05086325182613,1067.7251047501,474.433982927521));
#125384=CARTESIAN_POINT('',(-6.05086325182613,1076.73142393294,473.413500884896));
#125385=CARTESIAN_POINT('Origin',(-6.05086325182613,1076.73142393294,474.433982927521));
#125386=CARTESIAN_POINT('',(-6.05086325182613,1082.7251047501,473.413500884896));
#125387=CARTESIAN_POINT('',(-6.05086325182613,1067.7251047501,473.413500884896));
#125388=CARTESIAN_POINT('Origin',(-6.05086325182613,1082.7251047501,474.433982927521));
#125389=CARTESIAN_POINT('Origin',(-13.4001510060405,1067.7251047501,481.469362813523));
#125390=CARTESIAN_POINT('',(-13.4001510060405,1078.73142393294,479.76836259044));
#125391=CARTESIAN_POINT('Origin',(-13.4001510060405,1078.73142393294,481.469362813523));
#125392=CARTESIAN_POINT('',(-13.4001510060405,1076.73142393294,479.76836259044));
#125393=CARTESIAN_POINT('',(-13.4001510060405,1067.7251047501,479.76836259044));
#125394=CARTESIAN_POINT('Origin',(-13.4001510060405,1076.73142393294,481.469362813523));
#125395=CARTESIAN_POINT('Origin',(-13.4001510060405,1067.7251047501,481.469362813523));
#125396=CARTESIAN_POINT('',(-13.4001510060405,1076.73142393294,480.36836259044));
#125397=CARTESIAN_POINT('Origin',(-13.4001510060405,1076.73142393294,481.469362813523));
#125398=CARTESIAN_POINT('',(-13.4001510060405,1082.7251047501,480.36836259044));
#125399=CARTESIAN_POINT('',(-13.4001510060405,1067.7251047501,480.36836259044));
#125400=CARTESIAN_POINT('Origin',(-13.4001510060405,1082.7251047501,481.469362813523));
#125401=CARTESIAN_POINT('Origin',(-21.8940327946431,1067.7251047501,486.488574417384));
#125402=CARTESIAN_POINT('',(-21.8940327946431,1078.73142393294,484.76729978534));
#125403=CARTESIAN_POINT('Origin',(-21.8940327946431,1078.73142393294,486.488574417384));
#125404=CARTESIAN_POINT('',(-21.8940327946431,1076.73142393294,484.76729978534));
#125405=CARTESIAN_POINT('',(-21.8940327946431,1067.7251047501,484.76729978534));
#125406=CARTESIAN_POINT('Origin',(-21.8940327946431,1076.73142393294,486.488574417384));
#125407=CARTESIAN_POINT('Origin',(-21.8940327946431,1067.7251047501,486.488574417384));
#125408=CARTESIAN_POINT('',(-21.8940327946431,1076.73142393294,485.36729978534));
#125409=CARTESIAN_POINT('Origin',(-21.8940327946431,1076.73142393294,486.488574417384));
#125410=CARTESIAN_POINT('',(-21.8940327946431,1082.7251047501,485.36729978534));
#125411=CARTESIAN_POINT('',(-21.8940327946431,1067.7251047501,485.36729978534));
#125412=CARTESIAN_POINT('Origin',(-21.8940327946431,1082.7251047501,486.488574417384));
#125413=CARTESIAN_POINT('Origin',(-32.2949960661494,1067.7251047501,491.13235549298));
#125414=CARTESIAN_POINT('',(-32.2949960661494,1078.73142393294,489.350362838575));
#125415=CARTESIAN_POINT('Origin',(-32.2949960661494,1078.73142393294,491.13235549298));
#125416=CARTESIAN_POINT('',(-32.2949960661494,1076.73142393294,489.350362838575));
#125417=CARTESIAN_POINT('',(-32.2949960661494,1067.7251047501,489.350362838575));
#125418=CARTESIAN_POINT('Origin',(-32.2949960661494,1076.73142393294,491.13235549298));
#125419=CARTESIAN_POINT('Origin',(-32.2949960661494,1067.7251047501,491.13235549298));
#125420=CARTESIAN_POINT('',(-32.2949960661494,1076.73142393294,489.950362838575));
#125421=CARTESIAN_POINT('Origin',(-32.2949960661494,1076.73142393294,491.13235549298));
#125422=CARTESIAN_POINT('',(-32.2949960661494,1082.7251047501,489.950362838575));
#125423=CARTESIAN_POINT('',(-32.2949960661494,1067.7251047501,489.950362838575));
#125424=CARTESIAN_POINT('Origin',(-32.2949960661494,1082.7251047501,491.13235549298));
#125425=CARTESIAN_POINT('Origin',(-43.2754163337326,1067.7251047501,493.447968680042));
#125426=CARTESIAN_POINT('',(-43.2754163337326,1078.73142393294,491.787087870121));
#125427=CARTESIAN_POINT('Origin',(-43.2754163337326,1078.73142393294,493.447968680042));
#125428=CARTESIAN_POINT('',(-43.2754163337326,1076.73142393294,491.787087870121));
#125429=CARTESIAN_POINT('',(-43.2754163337326,1067.7251047501,491.787087870121));
#125430=CARTESIAN_POINT('Origin',(-43.2754163337326,1076.73142393294,493.447968680042));
#125431=CARTESIAN_POINT('Origin',(-43.2754163337326,1067.7251047501,493.447968680042));
#125432=CARTESIAN_POINT('',(-43.2754163337326,1076.73142393294,492.387087870121));
#125433=CARTESIAN_POINT('Origin',(-43.2754163337326,1076.73142393294,493.447968680042));
#125434=CARTESIAN_POINT('',(-43.2754163337326,1082.7251047501,492.387087870121));
#125435=CARTESIAN_POINT('',(-43.2754163337326,1067.7251047501,492.387087870121));
#125436=CARTESIAN_POINT('Origin',(-43.2754163337326,1082.7251047501,493.447968680042));
#125437=CARTESIAN_POINT('Origin',(9.48479058284935,1067.7251047501,441.286911958076));
#125438=CARTESIAN_POINT('',(9.48479058284935,1078.73142393294,440.186553892402));
#125439=CARTESIAN_POINT('Origin',(9.48479058284935,1078.73142393294,441.286911958076));
#125440=CARTESIAN_POINT('',(9.48479058284935,1076.73142393294,440.186553892402));
#125441=CARTESIAN_POINT('',(9.48479058284935,1067.7251047501,440.186553892402));
#125442=CARTESIAN_POINT('Origin',(9.48479058284935,1076.73142393294,441.286911958076));
#125443=CARTESIAN_POINT('Origin',(9.48479058284935,1067.7251047501,441.286911958076));
#125444=CARTESIAN_POINT('',(9.48479058284935,1076.73142393294,440.786553892401));
#125445=CARTESIAN_POINT('Origin',(9.48479058284935,1076.73142393294,441.286911958076));
#125446=CARTESIAN_POINT('',(9.48479058284935,1082.7251047501,440.786553892401));
#125447=CARTESIAN_POINT('',(9.48479058284935,1067.7251047501,440.786553892401));
#125448=CARTESIAN_POINT('Origin',(9.48479058284935,1082.7251047501,441.286911958076));
#125449=CARTESIAN_POINT('Origin',(11.0355654939687,1067.7251047501,449.709053460442));
#125450=CARTESIAN_POINT('',(11.0355654939687,1078.73142393294,448.495021893705));
#125451=CARTESIAN_POINT('Origin',(11.0355654939687,1078.73142393294,449.709053460442));
#125452=CARTESIAN_POINT('',(11.0355654939687,1076.73142393294,448.495021893705));
#125453=CARTESIAN_POINT('',(11.0355654939687,1067.7251047501,448.495021893705));
#125454=CARTESIAN_POINT('Origin',(11.0355654939687,1076.73142393294,449.709053460442));
#125455=CARTESIAN_POINT('Origin',(11.0355654939687,1067.7251047501,449.709053460442));
#125456=CARTESIAN_POINT('',(11.0355654939687,1076.73142393294,449.095021893705));
#125457=CARTESIAN_POINT('Origin',(11.0355654939687,1076.73142393294,449.709053460442));
#125458=CARTESIAN_POINT('',(11.0355654939687,1082.7251047501,449.095021893705));
#125459=CARTESIAN_POINT('',(11.0355654939687,1067.7251047501,449.095021893705));
#125460=CARTESIAN_POINT('Origin',(11.0355654939687,1082.7251047501,449.709053460442));
#125461=CARTESIAN_POINT('Origin',(10.5515930080276,1067.7251047501,457.620100189752));
#125462=CARTESIAN_POINT('',(10.5515930080276,1078.73142393294,456.291292226178));
#125463=CARTESIAN_POINT('Origin',(10.5515930080276,1078.73142393294,457.620100189752));
#125464=CARTESIAN_POINT('',(10.5515930080276,1076.73142393294,456.291292226178));
#125465=CARTESIAN_POINT('',(10.5515930080276,1067.7251047501,456.291292226178));
#125466=CARTESIAN_POINT('Origin',(10.5515930080276,1076.73142393294,457.620100189752));
#125467=CARTESIAN_POINT('Origin',(10.5515930080276,1067.7251047501,457.620100189752));
#125468=CARTESIAN_POINT('',(10.5515930080276,1076.73142393294,456.891292226178));
#125469=CARTESIAN_POINT('Origin',(10.5515930080276,1076.73142393294,457.620100189752));
#125470=CARTESIAN_POINT('',(10.5515930080276,1082.7251047501,456.891292226178));
#125471=CARTESIAN_POINT('',(10.5515930080276,1067.7251047501,456.891292226178));
#125472=CARTESIAN_POINT('Origin',(10.5515930080276,1082.7251047501,457.620100189752));
#125473=CARTESIAN_POINT('Origin',(8.49592223961343,1067.7251047501,466.659273516803));
#125474=CARTESIAN_POINT('',(8.49592223961343,1078.73142393294,465.198156514986));
#125475=CARTESIAN_POINT('Origin',(8.49592223961343,1078.73142393294,466.659273516803));
#125476=CARTESIAN_POINT('',(8.49592223961343,1076.73142393294,465.198156514986));
#125477=CARTESIAN_POINT('',(8.49592223961343,1067.7251047501,465.198156514986));
#125478=CARTESIAN_POINT('Origin',(8.49592223961343,1076.73142393294,466.659273516803));
#125479=CARTESIAN_POINT('Origin',(8.49592223961343,1067.7251047501,466.659273516803));
#125480=CARTESIAN_POINT('',(8.49592223961343,1076.73142393294,465.798156514986));
#125481=CARTESIAN_POINT('Origin',(8.49592223961343,1076.73142393294,466.659273516803));
#125482=CARTESIAN_POINT('',(8.49592223961343,1082.7251047501,465.798156514986));
#125483=CARTESIAN_POINT('',(8.49592223961343,1067.7251047501,465.798156514986));
#125484=CARTESIAN_POINT('Origin',(8.49592223961343,1082.7251047501,466.659273516803));
#125485=CARTESIAN_POINT('Origin',(4.43822160949819,1067.7251047501,474.603478394095));
#125486=CARTESIAN_POINT('',(4.43822160949819,1078.73142393294,472.982996351471));
#125487=CARTESIAN_POINT('Origin',(4.43822160949819,1078.73142393294,474.603478394095));
#125488=CARTESIAN_POINT('',(4.43822160949819,1076.73142393294,472.982996351471));
#125489=CARTESIAN_POINT('',(4.43822160949819,1067.7251047501,472.982996351471));
#125490=CARTESIAN_POINT('Origin',(4.43822160949819,1076.73142393294,474.603478394095));
#125491=CARTESIAN_POINT('Origin',(4.43822160949819,1067.7251047501,474.603478394095));
#125492=CARTESIAN_POINT('',(4.43822160949819,1076.73142393294,473.582996351471));
#125493=CARTESIAN_POINT('Origin',(4.43822160949819,1076.73142393294,474.603478394095));
#125494=CARTESIAN_POINT('',(4.43822160949819,1082.7251047501,473.582996351471));
#125495=CARTESIAN_POINT('',(4.43822160949819,1067.7251047501,473.582996351471));
#125496=CARTESIAN_POINT('Origin',(4.43822160949819,1082.7251047501,474.603478394095));
#125497=CARTESIAN_POINT('Origin',(-1.28772884674494,1067.7251047501,483.013121193124));
#125498=CARTESIAN_POINT('',(-1.28772884674494,1078.73142393294,481.312120970041));
#125499=CARTESIAN_POINT('Origin',(-1.28772884674494,1078.73142393294,483.013121193124));
#125500=CARTESIAN_POINT('',(-1.28772884674494,1076.73142393294,481.312120970041));
#125501=CARTESIAN_POINT('',(-1.28772884674494,1067.7251047501,481.312120970041));
#125502=CARTESIAN_POINT('Origin',(-1.28772884674494,1076.73142393294,483.013121193124));
#125503=CARTESIAN_POINT('Origin',(-1.28772884674494,1067.7251047501,483.013121193124));
#125504=CARTESIAN_POINT('',(-1.28772884674494,1076.73142393294,481.912120970041));
#125505=CARTESIAN_POINT('Origin',(-1.28772884674494,1076.73142393294,483.013121193124));
#125506=CARTESIAN_POINT('',(-1.28772884674494,1082.7251047501,481.912120970041));
#125507=CARTESIAN_POINT('',(-1.28772884674494,1067.7251047501,481.912120970041));
#125508=CARTESIAN_POINT('Origin',(-1.28772884674494,1082.7251047501,483.013121193124));
#125509=CARTESIAN_POINT('Origin',(-8.5524461680524,1067.7251047501,489.68862830529));
#125510=CARTESIAN_POINT('',(-8.5524461680524,1078.73142393294,487.967353673247));
#125511=CARTESIAN_POINT('Origin',(-8.5524461680524,1078.73142393294,489.68862830529));
#125512=CARTESIAN_POINT('',(-8.5524461680524,1076.73142393294,487.967353673247));
#125513=CARTESIAN_POINT('',(-8.5524461680524,1067.7251047501,487.967353673247));
#125514=CARTESIAN_POINT('Origin',(-8.5524461680524,1076.73142393294,489.68862830529));
#125515=CARTESIAN_POINT('Origin',(-8.5524461680524,1067.7251047501,489.68862830529));
#125516=CARTESIAN_POINT('',(-8.5524461680524,1076.73142393294,488.567353673247));
#125517=CARTESIAN_POINT('Origin',(-8.5524461680524,1076.73142393294,489.68862830529));
#125518=CARTESIAN_POINT('',(-8.5524461680524,1082.7251047501,488.567353673247));
#125519=CARTESIAN_POINT('',(-8.5524461680524,1067.7251047501,488.567353673247));
#125520=CARTESIAN_POINT('Origin',(-8.5524461680524,1082.7251047501,489.68862830529));
#125521=CARTESIAN_POINT('Origin',(-17.760627062182,1067.7251047501,496.39341348263));
#125522=CARTESIAN_POINT('',(-17.760627062182,1078.73142393294,494.611420828225));
#125523=CARTESIAN_POINT('Origin',(-17.760627062182,1078.73142393294,496.39341348263));
#125524=CARTESIAN_POINT('',(-17.760627062182,1076.73142393294,494.611420828225));
#125525=CARTESIAN_POINT('',(-17.760627062182,1067.7251047501,494.611420828225));
#125526=CARTESIAN_POINT('Origin',(-17.760627062182,1076.73142393294,496.39341348263));
#125527=CARTESIAN_POINT('Origin',(-17.760627062182,1067.7251047501,496.39341348263));
#125528=CARTESIAN_POINT('',(-17.760627062182,1076.73142393294,495.211420828225));
#125529=CARTESIAN_POINT('Origin',(-17.760627062182,1076.73142393294,496.39341348263));
#125530=CARTESIAN_POINT('',(-17.760627062182,1082.7251047501,495.211420828225));
#125531=CARTESIAN_POINT('',(-17.760627062182,1067.7251047501,495.211420828225));
#125532=CARTESIAN_POINT('Origin',(-17.760627062182,1082.7251047501,496.39341348263));
#125533=CARTESIAN_POINT('Origin',(-28.0196557489654,1067.7251047501,500.941382709505));
#125534=CARTESIAN_POINT('',(-28.0196557489654,1078.73142393294,499.280501899584));
#125535=CARTESIAN_POINT('Origin',(-28.0196557489654,1078.73142393294,500.941382709505));
#125536=CARTESIAN_POINT('',(-28.0196557489654,1076.73142393294,499.280501899584));
#125537=CARTESIAN_POINT('',(-28.0196557489654,1067.7251047501,499.280501899584));
#125538=CARTESIAN_POINT('Origin',(-28.0196557489654,1076.73142393294,500.941382709505));
#125539=CARTESIAN_POINT('Origin',(-28.0196557489654,1067.7251047501,500.941382709505));
#125540=CARTESIAN_POINT('',(-28.0196557489654,1076.73142393294,499.880501899584));
#125541=CARTESIAN_POINT('Origin',(-28.0196557489654,1076.73142393294,500.941382709505));
#125542=CARTESIAN_POINT('',(-28.0196557489654,1082.7251047501,499.880501899584));
#125543=CARTESIAN_POINT('',(-28.0196557489654,1067.7251047501,499.880501899584));
#125544=CARTESIAN_POINT('Origin',(-28.0196557489654,1082.7251047501,500.941382709505));
#125545=CARTESIAN_POINT('Origin',(12.7427205628033,1067.7251047501,438.950706397253));
#125546=CARTESIAN_POINT('',(12.7427205628033,1078.73142393294,437.850348331578));
#125547=CARTESIAN_POINT('Origin',(12.7427205628033,1078.73142393294,438.950706397253));
#125548=CARTESIAN_POINT('',(12.7427205628033,1076.73142393294,437.850348331578));
#125549=CARTESIAN_POINT('',(12.7427205628033,1067.7251047501,437.850348331578));
#125550=CARTESIAN_POINT('Origin',(12.7427205628033,1076.73142393294,438.950706397253));
#125551=CARTESIAN_POINT('Origin',(12.7427205628033,1067.7251047501,438.950706397253));
#125552=CARTESIAN_POINT('',(12.7427205628033,1076.73142393294,438.450348331578));
#125553=CARTESIAN_POINT('Origin',(12.7427205628033,1076.73142393294,438.950706397253));
#125554=CARTESIAN_POINT('',(12.7427205628033,1082.7251047501,438.450348331578));
#125555=CARTESIAN_POINT('',(12.7427205628033,1067.7251047501,438.450348331578));
#125556=CARTESIAN_POINT('Origin',(12.7427205628033,1082.7251047501,438.950706397253));
#125557=CARTESIAN_POINT('Origin',(16.0106690014563,1067.7251047501,446.866379666985));
#125558=CARTESIAN_POINT('',(16.0106690014563,1078.73142393294,445.652348100247));
#125559=CARTESIAN_POINT('Origin',(16.0106690014563,1078.73142393294,446.866379666985));
#125560=CARTESIAN_POINT('',(16.0106690014563,1076.73142393294,445.652348100247));
#125561=CARTESIAN_POINT('',(16.0106690014563,1067.7251047501,445.652348100247));
#125562=CARTESIAN_POINT('Origin',(16.0106690014563,1076.73142393294,446.866379666985));
#125563=CARTESIAN_POINT('Origin',(16.0106690014563,1067.7251047501,446.866379666985));
#125564=CARTESIAN_POINT('',(16.0106690014563,1076.73142393294,446.252348100247));
#125565=CARTESIAN_POINT('Origin',(16.0106690014563,1076.73142393294,446.866379666985));
#125566=CARTESIAN_POINT('',(16.0106690014563,1082.7251047501,446.252348100247));
#125567=CARTESIAN_POINT('',(16.0106690014563,1067.7251047501,446.252348100247));
#125568=CARTESIAN_POINT('Origin',(16.0106690014563,1082.7251047501,446.866379666985));
#125569=CARTESIAN_POINT('Origin',(17.1820715771408,1067.7251047501,454.705174582413));
#125570=CARTESIAN_POINT('',(17.1820715771408,1078.73142393294,453.376366618839));
#125571=CARTESIAN_POINT('Origin',(17.1820715771408,1078.73142393294,454.705174582413));
#125572=CARTESIAN_POINT('',(17.1820715771408,1076.73142393294,453.376366618839));
#125573=CARTESIAN_POINT('',(17.1820715771408,1067.7251047501,453.376366618839));
#125574=CARTESIAN_POINT('Origin',(17.1820715771408,1076.73142393294,454.705174582413));
#125575=CARTESIAN_POINT('Origin',(17.1820715771408,1067.7251047501,454.705174582413));
#125576=CARTESIAN_POINT('',(17.1820715771408,1076.73142393294,453.976366618839));
#125577=CARTESIAN_POINT('Origin',(17.1820715771408,1076.73142393294,454.705174582413));
#125578=CARTESIAN_POINT('',(17.1820715771408,1082.7251047501,453.976366618839));
#125579=CARTESIAN_POINT('',(17.1820715771408,1067.7251047501,453.976366618839));
#125580=CARTESIAN_POINT('Origin',(17.1820715771408,1082.7251047501,454.705174582413));
#125581=CARTESIAN_POINT('Origin',(17.05067195714,1067.7251047501,463.974218270111));
#125582=CARTESIAN_POINT('',(17.05067195714,1078.73142393294,462.513101268294));
#125583=CARTESIAN_POINT('Origin',(17.05067195714,1078.73142393294,463.974218270111));
#125584=CARTESIAN_POINT('',(17.05067195714,1076.73142393294,462.513101268294));
#125585=CARTESIAN_POINT('',(17.05067195714,1067.7251047501,462.513101268294));
#125586=CARTESIAN_POINT('Origin',(17.05067195714,1076.73142393294,463.974218270111));
#125587=CARTESIAN_POINT('Origin',(17.05067195714,1067.7251047501,463.974218270111));
#125588=CARTESIAN_POINT('',(17.05067195714,1076.73142393294,463.113101268294));
#125589=CARTESIAN_POINT('Origin',(17.05067195714,1076.73142393294,463.974218270111));
#125590=CARTESIAN_POINT('',(17.05067195714,1082.7251047501,463.113101268294));
#125591=CARTESIAN_POINT('',(17.05067195714,1067.7251047501,463.113101268294));
#125592=CARTESIAN_POINT('Origin',(17.05067195714,1082.7251047501,463.974218270111));
#125593=CARTESIAN_POINT('Origin',(14.7333348895372,1067.7251047501,472.588466609411));
#125594=CARTESIAN_POINT('',(14.7333348895372,1078.73142393294,470.967984566787));
#125595=CARTESIAN_POINT('Origin',(14.7333348895372,1078.73142393294,472.588466609411));
#125596=CARTESIAN_POINT('',(14.7333348895372,1076.73142393294,470.967984566787));
#125597=CARTESIAN_POINT('',(14.7333348895372,1067.7251047501,470.967984566787));
#125598=CARTESIAN_POINT('Origin',(14.7333348895372,1076.73142393294,472.588466609411));
#125599=CARTESIAN_POINT('Origin',(14.7333348895372,1067.7251047501,472.588466609411));
#125600=CARTESIAN_POINT('',(14.7333348895372,1076.73142393294,471.567984566787));
#125601=CARTESIAN_POINT('Origin',(14.7333348895372,1076.73142393294,472.588466609411));
#125602=CARTESIAN_POINT('',(14.7333348895372,1082.7251047501,471.567984566787));
#125603=CARTESIAN_POINT('',(14.7333348895372,1067.7251047501,471.567984566787));
#125604=CARTESIAN_POINT('Origin',(14.7333348895372,1082.7251047501,472.588466609411));
#125605=CARTESIAN_POINT('Origin',(10.8809732423619,1067.7251047501,482.004830577206));
#125606=CARTESIAN_POINT('',(10.8809732423619,1078.73142393294,480.303830354124));
#125607=CARTESIAN_POINT('Origin',(10.8809732423619,1078.73142393294,482.004830577206));
#125608=CARTESIAN_POINT('',(10.8809732423619,1076.73142393294,480.303830354124));
#125609=CARTESIAN_POINT('',(10.8809732423619,1067.7251047501,480.303830354124));
#125610=CARTESIAN_POINT('Origin',(10.8809732423619,1076.73142393294,482.004830577206));
#125611=CARTESIAN_POINT('Origin',(10.8809732423619,1067.7251047501,482.004830577206));
#125612=CARTESIAN_POINT('',(10.8809732423619,1076.73142393294,480.903830354123));
#125613=CARTESIAN_POINT('Origin',(10.8809732423619,1076.73142393294,482.004830577206));
#125614=CARTESIAN_POINT('',(10.8809732423619,1082.7251047501,480.903830354123));
#125615=CARTESIAN_POINT('',(10.8809732423619,1067.7251047501,480.903830354123));
#125616=CARTESIAN_POINT('Origin',(10.8809732423619,1082.7251047501,482.004830577206));
#125617=CARTESIAN_POINT('Origin',(5.16292339527213,1067.7251047501,490.044881504239));
#125618=CARTESIAN_POINT('',(5.16292339527213,1078.73142393294,488.323606872196));
#125619=CARTESIAN_POINT('Origin',(5.16292339527213,1078.73142393294,490.044881504239));
#125620=CARTESIAN_POINT('',(5.16292339527213,1076.73142393294,488.323606872196));
#125621=CARTESIAN_POINT('',(5.16292339527213,1067.7251047501,488.323606872196));
#125622=CARTESIAN_POINT('Origin',(5.16292339527213,1076.73142393294,490.044881504239));
#125623=CARTESIAN_POINT('Origin',(5.16292339527213,1067.7251047501,490.044881504239));
#125624=CARTESIAN_POINT('',(5.16292339527213,1076.73142393294,488.923606872196));
#125625=CARTESIAN_POINT('Origin',(5.16292339527213,1076.73142393294,490.044881504239));
#125626=CARTESIAN_POINT('',(5.16292339527213,1082.7251047501,488.923606872196));
#125627=CARTESIAN_POINT('',(5.16292339527213,1067.7251047501,488.923606872196));
#125628=CARTESIAN_POINT('Origin',(5.16292339527213,1082.7251047501,490.044881504239));
#125629=CARTESIAN_POINT('Origin',(-2.45003343065298,1067.7251047501,498.517639497944));
#125630=CARTESIAN_POINT('',(-2.45003343065298,1078.73142393294,496.735646843539));
#125631=CARTESIAN_POINT('Origin',(-2.45003343065298,1078.73142393294,498.517639497944));
#125632=CARTESIAN_POINT('',(-2.45003343065298,1076.73142393294,496.735646843539));
#125633=CARTESIAN_POINT('',(-2.45003343065298,1067.7251047501,496.735646843539));
#125634=CARTESIAN_POINT('Origin',(-2.45003343065298,1076.73142393294,498.517639497944));
#125635=CARTESIAN_POINT('Origin',(-2.45003343065298,1067.7251047501,498.517639497944));
#125636=CARTESIAN_POINT('',(-2.45003343065298,1076.73142393294,497.335646843539));
#125637=CARTESIAN_POINT('Origin',(-2.45003343065298,1076.73142393294,498.517639497944));
#125638=CARTESIAN_POINT('',(-2.45003343065298,1082.7251047501,497.335646843539));
#125639=CARTESIAN_POINT('',(-2.45003343065298,1067.7251047501,497.335646843539));
#125640=CARTESIAN_POINT('Origin',(-2.45003343065298,1082.7251047501,498.517639497944));
#125641=CARTESIAN_POINT('Origin',(-11.5393017547428,1067.7251047501,505.09919668584));
#125642=CARTESIAN_POINT('',(-11.5393017547428,1078.73142393294,503.438315875919));
#125643=CARTESIAN_POINT('Origin',(-11.5393017547428,1078.73142393294,505.09919668584));
#125644=CARTESIAN_POINT('',(-11.5393017547428,1076.73142393294,503.438315875919));
#125645=CARTESIAN_POINT('',(-11.5393017547428,1067.7251047501,503.438315875919));
#125646=CARTESIAN_POINT('Origin',(-11.5393017547428,1076.73142393294,505.09919668584));
#125647=CARTESIAN_POINT('Origin',(-11.5393017547428,1067.7251047501,505.09919668584));
#125648=CARTESIAN_POINT('',(-11.5393017547428,1076.73142393294,504.038315875919));
#125649=CARTESIAN_POINT('Origin',(-11.5393017547428,1076.73142393294,505.09919668584));
#125650=CARTESIAN_POINT('',(-11.5393017547428,1082.7251047501,504.038315875919));
#125651=CARTESIAN_POINT('',(-11.5393017547428,1067.7251047501,504.038315875919));
#125652=CARTESIAN_POINT('Origin',(-11.5393017547428,1082.7251047501,505.09919668584));
#125653=CARTESIAN_POINT('Origin',(15.4437325078056,1067.7251047501,435.988190802415));
#125654=CARTESIAN_POINT('',(15.4437325078056,1078.73142393294,434.88783273674));
#125655=CARTESIAN_POINT('Origin',(15.4437325078056,1078.73142393294,435.988190802415));
#125656=CARTESIAN_POINT('',(15.4437325078056,1076.73142393294,434.88783273674));
#125657=CARTESIAN_POINT('',(15.4437325078056,1067.7251047501,434.88783273674));
#125658=CARTESIAN_POINT('Origin',(15.4437325078056,1076.73142393294,435.988190802415));
#125659=CARTESIAN_POINT('Origin',(15.4437325078056,1067.7251047501,435.988190802415));
#125660=CARTESIAN_POINT('',(15.4437325078056,1076.73142393294,435.48783273674));
#125661=CARTESIAN_POINT('Origin',(15.4437325078056,1076.73142393294,435.988190802415));
#125662=CARTESIAN_POINT('',(15.4437325078056,1082.7251047501,435.48783273674));
#125663=CARTESIAN_POINT('',(15.4437325078056,1067.7251047501,435.48783273674));
#125664=CARTESIAN_POINT('Origin',(15.4437325078056,1082.7251047501,435.988190802415));
#125665=CARTESIAN_POINT('Origin',(20.2860294458665,1067.7251047501,443.05144293401));
#125666=CARTESIAN_POINT('',(20.2860294458665,1078.73142393294,441.837411367273));
#125667=CARTESIAN_POINT('Origin',(20.2860294458665,1078.73142393294,443.05144293401));
#125668=CARTESIAN_POINT('',(20.2860294458665,1076.73142393294,441.837411367273));
#125669=CARTESIAN_POINT('',(20.2860294458665,1067.7251047501,441.837411367273));
#125670=CARTESIAN_POINT('Origin',(20.2860294458665,1076.73142393294,443.05144293401));
#125671=CARTESIAN_POINT('Origin',(20.2860294458665,1067.7251047501,443.05144293401));
#125672=CARTESIAN_POINT('',(20.2860294458665,1076.73142393294,442.437411367273));
#125673=CARTESIAN_POINT('Origin',(20.2860294458665,1076.73142393294,443.05144293401));
#125674=CARTESIAN_POINT('',(20.2860294458665,1082.7251047501,442.437411367273));
#125675=CARTESIAN_POINT('',(20.2860294458665,1067.7251047501,442.437411367273));
#125676=CARTESIAN_POINT('Origin',(20.2860294458665,1082.7251047501,443.05144293401));
#125677=CARTESIAN_POINT('Origin',(23.0616111696061,1067.7251047501,450.475393083042));
#125678=CARTESIAN_POINT('',(23.0616111696061,1078.73142393294,449.146585119468));
#125679=CARTESIAN_POINT('Origin',(23.0616111696061,1078.73142393294,450.475393083042));
#125680=CARTESIAN_POINT('',(23.0616111696061,1076.73142393294,449.146585119468));
#125681=CARTESIAN_POINT('',(23.0616111696061,1067.7251047501,449.146585119468));
#125682=CARTESIAN_POINT('Origin',(23.0616111696061,1076.73142393294,450.475393083042));
#125683=CARTESIAN_POINT('Origin',(23.0616111696061,1067.7251047501,450.475393083042));
#125684=CARTESIAN_POINT('',(23.0616111696061,1076.73142393294,449.746585119468));
#125685=CARTESIAN_POINT('Origin',(23.0616111696061,1076.73142393294,450.475393083042));
#125686=CARTESIAN_POINT('',(23.0616111696061,1082.7251047501,449.746585119468));
#125687=CARTESIAN_POINT('',(23.0616111696061,1067.7251047501,449.746585119468));
#125688=CARTESIAN_POINT('Origin',(23.0616111696061,1082.7251047501,450.475393083042));
#125689=CARTESIAN_POINT('Origin',(24.8602254919379,1067.7251047501,459.569205444427));
#125690=CARTESIAN_POINT('',(24.8602254919379,1078.73142393294,458.108088442611));
#125691=CARTESIAN_POINT('Origin',(24.8602254919379,1078.73142393294,459.569205444427));
#125692=CARTESIAN_POINT('',(24.8602254919379,1076.73142393294,458.108088442611));
#125693=CARTESIAN_POINT('',(24.8602254919379,1067.7251047501,458.108088442611));
#125694=CARTESIAN_POINT('Origin',(24.8602254919379,1076.73142393294,459.569205444427));
#125695=CARTESIAN_POINT('Origin',(24.8602254919379,1067.7251047501,459.569205444427));
#125696=CARTESIAN_POINT('',(24.8602254919379,1076.73142393294,458.708088442611));
#125697=CARTESIAN_POINT('Origin',(24.8602254919379,1076.73142393294,459.569205444427));
#125698=CARTESIAN_POINT('',(24.8602254919379,1082.7251047501,458.708088442611));
#125699=CARTESIAN_POINT('',(24.8602254919379,1067.7251047501,458.708088442611));
#125700=CARTESIAN_POINT('Origin',(24.8602254919379,1082.7251047501,459.569205444427));
#125701=CARTESIAN_POINT('Origin',(24.3845307365188,1067.7251047501,468.477013257559));
#125702=CARTESIAN_POINT('',(24.3845307365188,1078.73142393294,466.856531214935));
#125703=CARTESIAN_POINT('Origin',(24.3845307365188,1078.73142393294,468.477013257559));
#125704=CARTESIAN_POINT('',(24.3845307365188,1076.73142393294,466.856531214935));
#125705=CARTESIAN_POINT('',(24.3845307365188,1067.7251047501,466.856531214935));
#125706=CARTESIAN_POINT('Origin',(24.3845307365188,1076.73142393294,468.477013257559));
#125707=CARTESIAN_POINT('Origin',(24.3845307365188,1067.7251047501,468.477013257559));
#125708=CARTESIAN_POINT('',(24.3845307365188,1076.73142393294,467.456531214935));
#125709=CARTESIAN_POINT('Origin',(24.3845307365188,1076.73142393294,468.477013257559));
#125710=CARTESIAN_POINT('',(24.3845307365188,1082.7251047501,467.456531214935));
#125711=CARTESIAN_POINT('',(24.3845307365188,1067.7251047501,467.456531214935));
#125712=CARTESIAN_POINT('Origin',(24.3845307365188,1082.7251047501,468.477013257559));
#125713=CARTESIAN_POINT('Origin',(22.5741245880751,1067.7251047501,478.488558104));
#125714=CARTESIAN_POINT('',(22.5741245880751,1078.73142393294,476.787557880917));
#125715=CARTESIAN_POINT('Origin',(22.5741245880751,1078.73142393294,478.488558104));
#125716=CARTESIAN_POINT('',(22.5741245880751,1076.73142393294,476.787557880917));
#125717=CARTESIAN_POINT('',(22.5741245880751,1067.7251047501,476.787557880917));
#125718=CARTESIAN_POINT('Origin',(22.5741245880751,1076.73142393294,478.488558104));
#125719=CARTESIAN_POINT('Origin',(22.5741245880751,1067.7251047501,478.488558104));
#125720=CARTESIAN_POINT('',(22.5741245880751,1076.73142393294,477.387557880917));
#125721=CARTESIAN_POINT('Origin',(22.5741245880751,1076.73142393294,478.488558104));
#125722=CARTESIAN_POINT('',(22.5741245880751,1082.7251047501,477.387557880917));
#125723=CARTESIAN_POINT('',(22.5741245880751,1067.7251047501,477.387557880917));
#125724=CARTESIAN_POINT('Origin',(22.5741245880751,1082.7251047501,478.488558104));
#125725=CARTESIAN_POINT('Origin',(18.6526484317682,1067.7251047501,487.541764039943));
#125726=CARTESIAN_POINT('',(18.6526484317682,1078.73142393294,485.8204894079));
#125727=CARTESIAN_POINT('Origin',(18.6526484317682,1078.73142393294,487.541764039943));
#125728=CARTESIAN_POINT('',(18.6526484317682,1076.73142393294,485.8204894079));
#125729=CARTESIAN_POINT('',(18.6526484317682,1067.7251047501,485.8204894079));
#125730=CARTESIAN_POINT('Origin',(18.6526484317682,1076.73142393294,487.541764039943));
#125731=CARTESIAN_POINT('Origin',(18.6526484317682,1067.7251047501,487.541764039943));
#125732=CARTESIAN_POINT('',(18.6526484317682,1076.73142393294,486.4204894079));
#125733=CARTESIAN_POINT('Origin',(18.6526484317682,1076.73142393294,487.541764039943));
#125734=CARTESIAN_POINT('',(18.6526484317682,1082.7251047501,486.4204894079));
#125735=CARTESIAN_POINT('',(18.6526484317682,1067.7251047501,486.4204894079));
#125736=CARTESIAN_POINT('Origin',(18.6526484317682,1082.7251047501,487.541764039943));
#125737=CARTESIAN_POINT('Origin',(12.9676384183603,1067.7251047501,497.412194668885));
#125738=CARTESIAN_POINT('',(12.9676384183603,1078.73142393294,495.63020201448));
#125739=CARTESIAN_POINT('Origin',(12.9676384183603,1078.73142393294,497.412194668885));
#125740=CARTESIAN_POINT('',(12.9676384183603,1076.73142393294,495.63020201448));
#125741=CARTESIAN_POINT('',(12.9676384183603,1067.7251047501,495.63020201448));
#125742=CARTESIAN_POINT('Origin',(12.9676384183603,1076.73142393294,497.412194668885));
#125743=CARTESIAN_POINT('Origin',(12.9676384183603,1067.7251047501,497.412194668885));
#125744=CARTESIAN_POINT('',(12.9676384183603,1076.73142393294,496.23020201448));
#125745=CARTESIAN_POINT('Origin',(12.9676384183603,1076.73142393294,497.412194668885));
#125746=CARTESIAN_POINT('',(12.9676384183603,1082.7251047501,496.23020201448));
#125747=CARTESIAN_POINT('',(12.9676384183603,1067.7251047501,496.23020201448));
#125748=CARTESIAN_POINT('Origin',(12.9676384183603,1082.7251047501,497.412194668885));
#125749=CARTESIAN_POINT('Origin',(5.4453750978754,1067.7251047501,505.739694186875));
#125750=CARTESIAN_POINT('',(5.4453750978754,1078.73142393294,504.078813376954));
#125751=CARTESIAN_POINT('Origin',(5.4453750978754,1078.73142393294,505.739694186875));
#125752=CARTESIAN_POINT('',(5.4453750978754,1076.73142393294,504.078813376954));
#125753=CARTESIAN_POINT('',(5.4453750978754,1067.7251047501,504.078813376954));
#125754=CARTESIAN_POINT('Origin',(5.4453750978754,1076.73142393294,505.739694186875));
#125755=CARTESIAN_POINT('Origin',(5.4453750978754,1067.7251047501,505.739694186875));
#125756=CARTESIAN_POINT('',(5.4453750978754,1076.73142393294,504.678813376955));
#125757=CARTESIAN_POINT('Origin',(5.4453750978754,1076.73142393294,505.739694186875));
#125758=CARTESIAN_POINT('',(5.4453750978754,1082.7251047501,504.678813376955));
#125759=CARTESIAN_POINT('',(5.4453750978754,1067.7251047501,504.678813376955));
#125760=CARTESIAN_POINT('Origin',(5.4453750978754,1082.7251047501,505.739694186875));
#125761=CARTESIAN_POINT('Origin',(17.4697792349661,1067.7251047501,432.528841320783));
#125762=CARTESIAN_POINT('',(17.4697792349661,1078.73142393294,431.428483255108));
#125763=CARTESIAN_POINT('Origin',(17.4697792349661,1078.73142393294,432.528841320783));
#125764=CARTESIAN_POINT('',(17.4697792349661,1076.73142393294,431.428483255108));
#125765=CARTESIAN_POINT('',(17.4697792349661,1067.7251047501,431.428483255108));
#125766=CARTESIAN_POINT('Origin',(17.4697792349661,1076.73142393294,432.528841320783));
#125767=CARTESIAN_POINT('Origin',(17.4697792349661,1067.7251047501,432.528841320783));
#125768=CARTESIAN_POINT('',(17.4697792349661,1076.73142393294,432.028483255108));
#125769=CARTESIAN_POINT('Origin',(17.4697792349661,1076.73142393294,432.528841320783));
#125770=CARTESIAN_POINT('',(17.4697792349661,1082.7251047501,432.028483255108));
#125771=CARTESIAN_POINT('',(17.4697792349661,1067.7251047501,432.028483255108));
#125772=CARTESIAN_POINT('Origin',(17.4697792349661,1082.7251047501,432.528841320783));
#125773=CARTESIAN_POINT('Origin',(23.6747930603231,1067.7251047501,438.430974302847));
#125774=CARTESIAN_POINT('',(23.6747930603231,1078.73142393294,437.21694273611));
#125775=CARTESIAN_POINT('Origin',(23.6747930603231,1078.73142393294,438.430974302847));
#125776=CARTESIAN_POINT('',(23.6747930603231,1076.73142393294,437.21694273611));
#125777=CARTESIAN_POINT('',(23.6747930603231,1067.7251047501,437.21694273611));
#125778=CARTESIAN_POINT('Origin',(23.6747930603231,1076.73142393294,438.430974302847));
#125779=CARTESIAN_POINT('Origin',(23.6747930603231,1067.7251047501,438.430974302847));
#125780=CARTESIAN_POINT('',(23.6747930603231,1076.73142393294,437.81694273611));
#125781=CARTESIAN_POINT('Origin',(23.6747930603231,1076.73142393294,438.430974302847));
#125782=CARTESIAN_POINT('',(23.6747930603231,1082.7251047501,437.81694273611));
#125783=CARTESIAN_POINT('',(23.6747930603231,1067.7251047501,437.81694273611));
#125784=CARTESIAN_POINT('Origin',(23.6747930603231,1082.7251047501,438.430974302847));
#125785=CARTESIAN_POINT('Origin',(27.9332476920715,1067.7251047501,445.115617439904));
#125786=CARTESIAN_POINT('',(27.9332476920715,1078.73142393294,443.786809476331));
#125787=CARTESIAN_POINT('Origin',(27.9332476920715,1078.73142393294,445.115617439904));
#125788=CARTESIAN_POINT('',(27.9332476920715,1076.73142393294,443.786809476331));
#125789=CARTESIAN_POINT('',(27.9332476920715,1067.7251047501,443.786809476331));
#125790=CARTESIAN_POINT('Origin',(27.9332476920715,1076.73142393294,445.115617439904));
#125791=CARTESIAN_POINT('Origin',(27.9332476920715,1067.7251047501,445.115617439904));
#125792=CARTESIAN_POINT('',(27.9332476920715,1076.73142393294,444.386809476331));
#125793=CARTESIAN_POINT('Origin',(27.9332476920715,1076.73142393294,445.115617439904));
#125794=CARTESIAN_POINT('',(27.9332476920715,1082.7251047501,444.386809476331));
#125795=CARTESIAN_POINT('',(27.9332476920715,1067.7251047501,444.386809476331));
#125796=CARTESIAN_POINT('Origin',(27.9332476920715,1082.7251047501,445.115617439904));
#125797=CARTESIAN_POINT('Origin',(31.583267880141,1067.7251047501,453.636755237832));
#125798=CARTESIAN_POINT('',(31.583267880141,1078.73142393294,452.175638236015));
#125799=CARTESIAN_POINT('Origin',(31.583267880141,1078.73142393294,453.636755237832));
#125800=CARTESIAN_POINT('',(31.583267880141,1076.73142393294,452.175638236015));
#125801=CARTESIAN_POINT('',(31.583267880141,1067.7251047501,452.175638236015));
#125802=CARTESIAN_POINT('Origin',(31.583267880141,1076.73142393294,453.636755237832));
#125803=CARTESIAN_POINT('Origin',(31.583267880141,1067.7251047501,453.636755237832));
#125804=CARTESIAN_POINT('',(31.583267880141,1076.73142393294,452.775638236015));
#125805=CARTESIAN_POINT('Origin',(31.583267880141,1076.73142393294,453.636755237832));
#125806=CARTESIAN_POINT('',(31.583267880141,1082.7251047501,452.775638236015));
#125807=CARTESIAN_POINT('',(31.583267880141,1067.7251047501,452.775638236015));
#125808=CARTESIAN_POINT('Origin',(31.583267880141,1082.7251047501,453.636755237832));
#125809=CARTESIAN_POINT('Origin',(32.9700055803541,1067.7251047501,462.448808578957));
#125810=CARTESIAN_POINT('',(32.9700055803541,1078.73142393294,460.828326536333));
#125811=CARTESIAN_POINT('Origin',(32.9700055803541,1078.73142393294,462.448808578957));
#125812=CARTESIAN_POINT('',(32.9700055803541,1076.73142393294,460.828326536333));
#125813=CARTESIAN_POINT('',(32.9700055803541,1067.7251047501,460.828326536333));
#125814=CARTESIAN_POINT('Origin',(32.9700055803541,1076.73142393294,462.448808578957));
#125815=CARTESIAN_POINT('Origin',(32.9700055803541,1067.7251047501,462.448808578957));
#125816=CARTESIAN_POINT('',(32.9700055803541,1076.73142393294,461.428326536333));
#125817=CARTESIAN_POINT('Origin',(32.9700055803541,1076.73142393294,462.448808578957));
#125818=CARTESIAN_POINT('',(32.9700055803541,1082.7251047501,461.428326536333));
#125819=CARTESIAN_POINT('',(32.9700055803541,1067.7251047501,461.428326536333));
#125820=CARTESIAN_POINT('Origin',(32.9700055803541,1082.7251047501,462.448808578957));
#125821=CARTESIAN_POINT('Origin',(33.2806783666214,1067.7251047501,472.617981753532));
#125822=CARTESIAN_POINT('',(33.2806783666214,1078.73142393294,470.916981530449));
#125823=CARTESIAN_POINT('Origin',(33.2806783666214,1078.73142393294,472.617981753532));
#125824=CARTESIAN_POINT('',(33.2806783666214,1076.73142393294,470.916981530449));
#125825=CARTESIAN_POINT('',(33.2806783666214,1067.7251047501,470.916981530449));
#125826=CARTESIAN_POINT('Origin',(33.2806783666214,1076.73142393294,472.617981753532));
#125827=CARTESIAN_POINT('Origin',(33.2806783666214,1067.7251047501,472.617981753532));
#125828=CARTESIAN_POINT('',(33.2806783666214,1076.73142393294,471.516981530449));
#125829=CARTESIAN_POINT('Origin',(33.2806783666214,1076.73142393294,472.617981753532));
#125830=CARTESIAN_POINT('',(33.2806783666214,1082.7251047501,471.516981530449));
#125831=CARTESIAN_POINT('',(33.2806783666214,1067.7251047501,471.516981530449));
#125832=CARTESIAN_POINT('Origin',(33.2806783666214,1082.7251047501,472.617981753532));
#125833=CARTESIAN_POINT('Origin',(31.3271632264583,1067.7251047501,482.288674156883));
#125834=CARTESIAN_POINT('',(31.3271632264583,1078.73142393294,480.56739952484));
#125835=CARTESIAN_POINT('Origin',(31.3271632264583,1078.73142393294,482.288674156883));
#125836=CARTESIAN_POINT('',(31.3271632264583,1076.73142393294,480.56739952484));
#125837=CARTESIAN_POINT('',(31.3271632264583,1067.7251047501,480.56739952484));
#125838=CARTESIAN_POINT('Origin',(31.3271632264583,1076.73142393294,482.288674156883));
#125839=CARTESIAN_POINT('Origin',(31.3271632264583,1067.7251047501,482.288674156883));
#125840=CARTESIAN_POINT('',(31.3271632264583,1076.73142393294,481.16739952484));
#125841=CARTESIAN_POINT('Origin',(31.3271632264583,1076.73142393294,482.288674156883));
#125842=CARTESIAN_POINT('',(31.3271632264583,1082.7251047501,481.16739952484));
#125843=CARTESIAN_POINT('',(31.3271632264583,1067.7251047501,481.16739952484));
#125844=CARTESIAN_POINT('Origin',(31.3271632264583,1082.7251047501,482.288674156883));
#125845=CARTESIAN_POINT('Origin',(27.8185622428584,1067.7251047501,493.125392238995));
#125846=CARTESIAN_POINT('',(27.8185622428584,1078.73142393294,491.34339958459));
#125847=CARTESIAN_POINT('Origin',(27.8185622428584,1078.73142393294,493.125392238995));
#125848=CARTESIAN_POINT('',(27.8185622428584,1076.73142393294,491.34339958459));
#125849=CARTESIAN_POINT('',(27.8185622428584,1067.7251047501,491.34339958459));
#125850=CARTESIAN_POINT('Origin',(27.8185622428584,1076.73142393294,493.125392238995));
#125851=CARTESIAN_POINT('Origin',(27.8185622428584,1067.7251047501,493.125392238995));
#125852=CARTESIAN_POINT('',(27.8185622428584,1076.73142393294,491.94339958459));
#125853=CARTESIAN_POINT('Origin',(27.8185622428584,1076.73142393294,493.125392238995));
#125854=CARTESIAN_POINT('',(27.8185622428584,1082.7251047501,491.94339958459));
#125855=CARTESIAN_POINT('',(27.8185622428584,1067.7251047501,491.94339958459));
#125856=CARTESIAN_POINT('Origin',(27.8185622428584,1082.7251047501,493.125392238995));
#125857=CARTESIAN_POINT('Origin',(22.1920629289076,1067.7251047501,502.834882398368));
#125858=CARTESIAN_POINT('',(22.1920629289076,1078.73142393294,501.174001588447));
#125859=CARTESIAN_POINT('Origin',(22.1920629289076,1078.73142393294,502.834882398368));
#125860=CARTESIAN_POINT('',(22.1920629289076,1076.73142393294,501.174001588447));
#125861=CARTESIAN_POINT('',(22.1920629289076,1067.7251047501,501.174001588447));
#125862=CARTESIAN_POINT('Origin',(22.1920629289076,1076.73142393294,502.834882398368));
#125863=CARTESIAN_POINT('Origin',(22.1920629289076,1067.7251047501,502.834882398368));
#125864=CARTESIAN_POINT('',(22.1920629289076,1076.73142393294,501.774001588447));
#125865=CARTESIAN_POINT('Origin',(22.1920629289076,1076.73142393294,502.834882398368));
#125866=CARTESIAN_POINT('',(22.1920629289076,1082.7251047501,501.774001588447));
#125867=CARTESIAN_POINT('',(22.1920629289076,1067.7251047501,501.774001588447));
#125868=CARTESIAN_POINT('Origin',(22.1920629289076,1082.7251047501,502.834882398368));
#125869=CARTESIAN_POINT('Origin',(18.7323127802571,1067.7251047501,428.723848124506));
#125870=CARTESIAN_POINT('',(18.7323127802571,1078.73142393294,427.623490058831));
#125871=CARTESIAN_POINT('Origin',(18.7323127802571,1078.73142393294,428.723848124506));
#125872=CARTESIAN_POINT('',(18.7323127802571,1076.73142393294,427.623490058831));
#125873=CARTESIAN_POINT('',(18.7323127802571,1067.7251047501,427.623490058831));
#125874=CARTESIAN_POINT('Origin',(18.7323127802571,1076.73142393294,428.723848124506));
#125875=CARTESIAN_POINT('Origin',(18.7323127802571,1067.7251047501,428.723848124506));
#125876=CARTESIAN_POINT('',(18.7323127802571,1076.73142393294,428.223490058831));
#125877=CARTESIAN_POINT('Origin',(18.7323127802571,1076.73142393294,428.723848124506));
#125878=CARTESIAN_POINT('',(18.7323127802571,1082.7251047501,428.223490058831));
#125879=CARTESIAN_POINT('',(18.7323127802571,1067.7251047501,428.223490058831));
#125880=CARTESIAN_POINT('Origin',(18.7323127802571,1082.7251047501,428.723848124506));
#125881=CARTESIAN_POINT('Origin',(26.0288546137823,1067.7251047501,433.206910424145));
#125882=CARTESIAN_POINT('',(26.0288546137823,1078.73142393294,431.992878857408));
#125883=CARTESIAN_POINT('Origin',(26.0288546137823,1078.73142393294,433.206910424145));
#125884=CARTESIAN_POINT('',(26.0288546137823,1076.73142393294,431.992878857408));
#125885=CARTESIAN_POINT('',(26.0288546137823,1067.7251047501,431.992878857408));
#125886=CARTESIAN_POINT('Origin',(26.0288546137823,1076.73142393294,433.206910424145));
#125887=CARTESIAN_POINT('Origin',(26.0288546137823,1067.7251047501,433.206910424145));
#125888=CARTESIAN_POINT('',(26.0288546137823,1076.73142393294,432.592878857408));
#125889=CARTESIAN_POINT('Origin',(26.0288546137823,1076.73142393294,433.206910424145));
#125890=CARTESIAN_POINT('',(26.0288546137823,1082.7251047501,432.592878857408));
#125891=CARTESIAN_POINT('',(26.0288546137823,1067.7251047501,432.592878857408));
#125892=CARTESIAN_POINT('Origin',(26.0288546137823,1082.7251047501,433.206910424145));
#125893=CARTESIAN_POINT('Origin',(31.5840672517996,1067.7251047501,438.860095567662));
#125894=CARTESIAN_POINT('',(31.5840672517996,1078.73142393294,437.531287604089));
#125895=CARTESIAN_POINT('Origin',(31.5840672517996,1078.73142393294,438.860095567662));
#125896=CARTESIAN_POINT('',(31.5840672517996,1076.73142393294,437.531287604089));
#125897=CARTESIAN_POINT('',(31.5840672517996,1067.7251047501,437.531287604089));
#125898=CARTESIAN_POINT('Origin',(31.5840672517996,1076.73142393294,438.860095567662));
#125899=CARTESIAN_POINT('Origin',(31.5840672517996,1067.7251047501,438.860095567662));
#125900=CARTESIAN_POINT('',(31.5840672517996,1076.73142393294,438.131287604089));
#125901=CARTESIAN_POINT('Origin',(31.5840672517996,1076.73142393294,438.860095567662));
#125902=CARTESIAN_POINT('',(31.5840672517996,1082.7251047501,438.131287604089));
#125903=CARTESIAN_POINT('',(31.5840672517996,1067.7251047501,438.131287604089));
#125904=CARTESIAN_POINT('Origin',(31.5840672517996,1082.7251047501,438.860095567662));
#125905=CARTESIAN_POINT('Origin',(36.9259699086481,1067.7251047501,446.436144191407));
#125906=CARTESIAN_POINT('',(36.9259699086481,1078.73142393294,444.97502718959));
#125907=CARTESIAN_POINT('Origin',(36.9259699086481,1078.73142393294,446.436144191407));
#125908=CARTESIAN_POINT('',(36.9259699086481,1076.73142393294,444.97502718959));
#125909=CARTESIAN_POINT('',(36.9259699086481,1067.7251047501,444.97502718959));
#125910=CARTESIAN_POINT('Origin',(36.9259699086481,1076.73142393294,446.436144191407));
#125911=CARTESIAN_POINT('Origin',(36.9259699086481,1067.7251047501,446.436144191407));
#125912=CARTESIAN_POINT('',(36.9259699086481,1076.73142393294,445.57502718959));
#125913=CARTESIAN_POINT('Origin',(36.9259699086481,1076.73142393294,446.436144191407));
#125914=CARTESIAN_POINT('',(36.9259699086481,1082.7251047501,445.57502718959));
#125915=CARTESIAN_POINT('',(36.9259699086481,1067.7251047501,445.57502718959));
#125916=CARTESIAN_POINT('Origin',(36.9259699086481,1082.7251047501,446.436144191407));
#125917=CARTESIAN_POINT('Origin',(40.1145329726883,1067.7251047501,454.767314044595));
#125918=CARTESIAN_POINT('',(40.1145329726883,1078.73142393294,453.14683200197));
#125919=CARTESIAN_POINT('Origin',(40.1145329726883,1078.73142393294,454.767314044595));
#125920=CARTESIAN_POINT('',(40.1145329726883,1076.73142393294,453.14683200197));
#125921=CARTESIAN_POINT('',(40.1145329726883,1067.7251047501,453.14683200197));
#125922=CARTESIAN_POINT('Origin',(40.1145329726883,1076.73142393294,454.767314044595));
#125923=CARTESIAN_POINT('Origin',(40.1145329726883,1067.7251047501,454.767314044595));
#125924=CARTESIAN_POINT('',(40.1145329726883,1076.73142393294,453.74683200197));
#125925=CARTESIAN_POINT('Origin',(40.1145329726883,1076.73142393294,454.767314044595));
#125926=CARTESIAN_POINT('',(40.1145329726883,1082.7251047501,453.74683200197));
#125927=CARTESIAN_POINT('',(40.1145329726883,1067.7251047501,453.74683200197));
#125928=CARTESIAN_POINT('Origin',(40.1145329726883,1082.7251047501,454.767314044595));
#125929=CARTESIAN_POINT('Origin',(42.5327068021333,1067.7251047501,464.649673882468));
#125930=CARTESIAN_POINT('',(42.5327068021333,1078.73142393294,462.948673659385));
#125931=CARTESIAN_POINT('Origin',(42.5327068021333,1078.73142393294,464.649673882468));
#125932=CARTESIAN_POINT('',(42.5327068021333,1076.73142393294,462.948673659385));
#125933=CARTESIAN_POINT('',(42.5327068021333,1067.7251047501,462.948673659385));
#125934=CARTESIAN_POINT('Origin',(42.5327068021333,1076.73142393294,464.649673882468));
#125935=CARTESIAN_POINT('Origin',(42.5327068021333,1067.7251047501,464.649673882468));
#125936=CARTESIAN_POINT('',(42.5327068021333,1076.73142393294,463.548673659385));
#125937=CARTESIAN_POINT('Origin',(42.5327068021333,1076.73142393294,464.649673882468));
#125938=CARTESIAN_POINT('',(42.5327068021333,1082.7251047501,463.548673659385));
#125939=CARTESIAN_POINT('',(42.5327068021333,1067.7251047501,463.548673659385));
#125940=CARTESIAN_POINT('Origin',(42.5327068021333,1082.7251047501,464.649673882468));
#125941=CARTESIAN_POINT('Origin',(42.6325306637449,1067.7251047501,474.51519709007));
#125942=CARTESIAN_POINT('',(42.6325306637449,1078.73142393294,472.793922458026));
#125943=CARTESIAN_POINT('Origin',(42.6325306637449,1078.73142393294,474.51519709007));
#125944=CARTESIAN_POINT('',(42.6325306637449,1076.73142393294,472.793922458026));
#125945=CARTESIAN_POINT('',(42.6325306637449,1067.7251047501,472.793922458026));
#125946=CARTESIAN_POINT('Origin',(42.6325306637449,1076.73142393294,474.51519709007));
#125947=CARTESIAN_POINT('Origin',(42.6325306637449,1067.7251047501,474.51519709007));
#125948=CARTESIAN_POINT('',(42.6325306637449,1076.73142393294,473.393922458026));
#125949=CARTESIAN_POINT('Origin',(42.6325306637449,1076.73142393294,474.51519709007));
#125950=CARTESIAN_POINT('',(42.6325306637449,1082.7251047501,473.393922458026));
#125951=CARTESIAN_POINT('',(42.6325306637449,1067.7251047501,473.393922458026));
#125952=CARTESIAN_POINT('Origin',(42.6325306637449,1082.7251047501,474.51519709007));
#125953=CARTESIAN_POINT('Origin',(41.4536814090717,1067.7251047501,485.844586044821));
#125954=CARTESIAN_POINT('',(41.4536814090717,1078.73142393294,484.062593390416));
#125955=CARTESIAN_POINT('Origin',(41.4536814090717,1078.73142393294,485.844586044821));
#125956=CARTESIAN_POINT('',(41.4536814090717,1076.73142393294,484.062593390416));
#125957=CARTESIAN_POINT('',(41.4536814090717,1067.7251047501,484.062593390416));
#125958=CARTESIAN_POINT('Origin',(41.4536814090717,1076.73142393294,485.844586044821));
#125959=CARTESIAN_POINT('Origin',(41.4536814090717,1067.7251047501,485.844586044821));
#125960=CARTESIAN_POINT('',(41.4536814090717,1076.73142393294,484.662593390416));
#125961=CARTESIAN_POINT('Origin',(41.4536814090717,1076.73142393294,485.844586044821));
#125962=CARTESIAN_POINT('',(41.4536814090717,1082.7251047501,484.662593390416));
#125963=CARTESIAN_POINT('',(41.4536814090717,1067.7251047501,484.662593390416));
#125964=CARTESIAN_POINT('Origin',(41.4536814090717,1082.7251047501,485.844586044821));
#125965=CARTESIAN_POINT('Origin',(37.9688511206139,1067.7251047501,496.511715534309));
#125966=CARTESIAN_POINT('',(37.9688511206139,1078.73142393294,494.850834724388));
#125967=CARTESIAN_POINT('Origin',(37.9688511206139,1078.73142393294,496.511715534309));
#125968=CARTESIAN_POINT('',(37.9688511206139,1076.73142393294,494.850834724388));
#125969=CARTESIAN_POINT('',(37.9688511206139,1067.7251047501,494.850834724388));
#125970=CARTESIAN_POINT('Origin',(37.9688511206139,1076.73142393294,496.511715534309));
#125971=CARTESIAN_POINT('Origin',(37.9688511206139,1067.7251047501,496.511715534309));
#125972=CARTESIAN_POINT('',(37.9688511206139,1076.73142393294,495.450834724388));
#125973=CARTESIAN_POINT('Origin',(37.9688511206139,1076.73142393294,496.511715534309));
#125974=CARTESIAN_POINT('',(37.9688511206139,1082.7251047501,495.450834724388));
#125975=CARTESIAN_POINT('',(37.9688511206139,1067.7251047501,495.450834724388));
#125976=CARTESIAN_POINT('Origin',(37.9688511206139,1082.7251047501,496.511715534309));
#125977=CARTESIAN_POINT('Origin',(19.1761543694413,1067.7251047501,424.739507674643));
#125978=CARTESIAN_POINT('',(19.1761543694413,1078.73142393294,423.639149608968));
#125979=CARTESIAN_POINT('Origin',(19.1761543694413,1078.73142393294,424.739507674643));
#125980=CARTESIAN_POINT('',(19.1761543694413,1076.73142393294,423.639149608968));
#125981=CARTESIAN_POINT('',(19.1761543694413,1067.7251047501,423.639149608968));
#125982=CARTESIAN_POINT('Origin',(19.1761543694413,1076.73142393294,424.739507674643));
#125983=CARTESIAN_POINT('Origin',(19.1761543694413,1067.7251047501,424.739507674643));
#125984=CARTESIAN_POINT('',(19.1761543694413,1076.73142393294,424.239149608968));
#125985=CARTESIAN_POINT('Origin',(19.1761543694413,1076.73142393294,424.739507674643));
#125986=CARTESIAN_POINT('',(19.1761543694413,1082.7251047501,424.239149608968));
#125987=CARTESIAN_POINT('',(19.1761543694413,1067.7251047501,424.239149608968));
#125988=CARTESIAN_POINT('Origin',(19.1761543694413,1082.7251047501,424.739507674643));
#125989=CARTESIAN_POINT('Origin',(27.2453303203172,1067.7251047501,427.607567957245));
#125990=CARTESIAN_POINT('',(27.2453303203172,1078.73142393294,426.393536390508));
#125991=CARTESIAN_POINT('Origin',(27.2453303203172,1078.73142393294,427.607567957245));
#125992=CARTESIAN_POINT('',(27.2453303203172,1076.73142393294,426.393536390508));
#125993=CARTESIAN_POINT('',(27.2453303203172,1067.7251047501,426.393536390508));
#125994=CARTESIAN_POINT('Origin',(27.2453303203172,1076.73142393294,427.607567957245));
#125995=CARTESIAN_POINT('Origin',(27.2453303203172,1067.7251047501,427.607567957245));
#125996=CARTESIAN_POINT('',(27.2453303203172,1076.73142393294,426.993536390508));
#125997=CARTESIAN_POINT('Origin',(27.2453303203172,1076.73142393294,427.607567957245));
#125998=CARTESIAN_POINT('',(27.2453303203172,1082.7251047501,426.993536390508));
#125999=CARTESIAN_POINT('',(27.2453303203172,1067.7251047501,426.993536390508));
#126000=CARTESIAN_POINT('Origin',(27.2453303203172,1082.7251047501,427.607567957245));
#126001=CARTESIAN_POINT('Origin',(33.8545115154544,1067.7251047501,431.982223789457));
#126002=CARTESIAN_POINT('',(33.8545115154544,1078.73142393294,430.653415825884));
#126003=CARTESIAN_POINT('Origin',(33.8545115154544,1078.73142393294,431.982223789457));
#126004=CARTESIAN_POINT('',(33.8545115154544,1076.73142393294,430.653415825884));
#126005=CARTESIAN_POINT('',(33.8545115154544,1067.7251047501,430.653415825884));
#126006=CARTESIAN_POINT('Origin',(33.8545115154544,1076.73142393294,431.982223789457));
#126007=CARTESIAN_POINT('Origin',(33.8545115154544,1067.7251047501,431.982223789457));
#126008=CARTESIAN_POINT('',(33.8545115154544,1076.73142393294,431.253415825884));
#126009=CARTESIAN_POINT('Origin',(33.8545115154544,1076.73142393294,431.982223789457));
#126010=CARTESIAN_POINT('',(33.8545115154544,1082.7251047501,431.253415825884));
#126011=CARTESIAN_POINT('',(33.8545115154544,1067.7251047501,431.253415825884));
#126012=CARTESIAN_POINT('Origin',(33.8545115154544,1082.7251047501,431.982223789457));
#126013=CARTESIAN_POINT('Origin',(40.6548298616846,1067.7251047501,438.282073560247));
#126014=CARTESIAN_POINT('',(40.6548298616846,1078.73142393294,436.82095655843));
#126015=CARTESIAN_POINT('Origin',(40.6548298616846,1078.73142393294,438.282073560247));
#126016=CARTESIAN_POINT('',(40.6548298616846,1076.73142393294,436.82095655843));
#126017=CARTESIAN_POINT('',(40.6548298616846,1067.7251047501,436.82095655843));
#126018=CARTESIAN_POINT('Origin',(40.6548298616846,1076.73142393294,438.282073560247));
#126019=CARTESIAN_POINT('Origin',(40.6548298616846,1067.7251047501,438.282073560247));
#126020=CARTESIAN_POINT('',(40.6548298616846,1076.73142393294,437.42095655843));
#126021=CARTESIAN_POINT('Origin',(40.6548298616846,1076.73142393294,438.282073560247));
#126022=CARTESIAN_POINT('',(40.6548298616846,1082.7251047501,437.42095655843));
#126023=CARTESIAN_POINT('',(40.6548298616846,1067.7251047501,437.42095655843));
#126024=CARTESIAN_POINT('Origin',(40.6548298616846,1082.7251047501,438.282073560247));
#126025=CARTESIAN_POINT('Origin',(45.5058627832302,1067.7251047501,445.768247825525));
#126026=CARTESIAN_POINT('',(45.5058627832302,1078.73142393294,444.1477657829));
#126027=CARTESIAN_POINT('Origin',(45.5058627832302,1078.73142393294,445.768247825525));
#126028=CARTESIAN_POINT('',(45.5058627832302,1076.73142393294,444.1477657829));
#126029=CARTESIAN_POINT('',(45.5058627832302,1067.7251047501,444.1477657829));
#126030=CARTESIAN_POINT('Origin',(45.5058627832302,1076.73142393294,445.768247825525));
#126031=CARTESIAN_POINT('Origin',(45.5058627832302,1067.7251047501,445.768247825525));
#126032=CARTESIAN_POINT('',(45.5058627832302,1076.73142393294,444.7477657829));
#126033=CARTESIAN_POINT('Origin',(45.5058627832302,1076.73142393294,445.768247825525));
#126034=CARTESIAN_POINT('',(45.5058627832302,1082.7251047501,444.7477657829));
#126035=CARTESIAN_POINT('',(45.5058627832302,1067.7251047501,444.7477657829));
#126036=CARTESIAN_POINT('Origin',(45.5058627832302,1082.7251047501,445.768247825525));
#126037=CARTESIAN_POINT('Origin',(49.9258518558208,1067.7251047501,454.931887780957));
#126038=CARTESIAN_POINT('',(49.9258518558208,1078.73142393294,453.230887557874));
#126039=CARTESIAN_POINT('Origin',(49.9258518558208,1078.73142393294,454.931887780957));
#126040=CARTESIAN_POINT('',(49.9258518558208,1076.73142393294,453.230887557874));
#126041=CARTESIAN_POINT('',(49.9258518558208,1067.7251047501,453.230887557874));
#126042=CARTESIAN_POINT('Origin',(49.9258518558208,1076.73142393294,454.931887780957));
#126043=CARTESIAN_POINT('Origin',(49.9258518558208,1067.7251047501,454.931887780957));
#126044=CARTESIAN_POINT('',(49.9258518558208,1076.73142393294,453.830887557874));
#126045=CARTESIAN_POINT('Origin',(49.9258518558208,1076.73142393294,454.931887780957));
#126046=CARTESIAN_POINT('',(49.9258518558208,1082.7251047501,453.830887557874));
#126047=CARTESIAN_POINT('',(49.9258518558208,1067.7251047501,453.830887557874));
#126048=CARTESIAN_POINT('Origin',(49.9258518558208,1082.7251047501,454.931887780957));
#126049=CARTESIAN_POINT('Origin',(52.0746519374465,1067.7251047501,464.561071088605));
#126050=CARTESIAN_POINT('',(52.0746519374465,1078.73142393294,462.839796456561));
#126051=CARTESIAN_POINT('Origin',(52.0746519374465,1078.73142393294,464.561071088605));
#126052=CARTESIAN_POINT('',(52.0746519374465,1076.73142393294,462.839796456561));
#126053=CARTESIAN_POINT('',(52.0746519374465,1067.7251047501,462.839796456561));
#126054=CARTESIAN_POINT('Origin',(52.0746519374465,1076.73142393294,464.561071088605));
#126055=CARTESIAN_POINT('Origin',(52.0746519374465,1067.7251047501,464.561071088605));
#126056=CARTESIAN_POINT('',(52.0746519374465,1076.73142393294,463.439796456561));
#126057=CARTESIAN_POINT('Origin',(52.0746519374465,1076.73142393294,464.561071088605));
#126058=CARTESIAN_POINT('',(52.0746519374465,1082.7251047501,463.439796456561));
#126059=CARTESIAN_POINT('',(52.0746519374465,1067.7251047501,463.439796456561));
#126060=CARTESIAN_POINT('Origin',(52.0746519374465,1082.7251047501,464.561071088605));
#126061=CARTESIAN_POINT('Origin',(53.2770757808756,1067.7251047501,475.887982254234));
#126062=CARTESIAN_POINT('',(53.2770757808756,1078.73142393294,474.105989599829));
#126063=CARTESIAN_POINT('Origin',(53.2770757808756,1078.73142393294,475.887982254234));
#126064=CARTESIAN_POINT('',(53.2770757808756,1076.73142393294,474.105989599829));
#126065=CARTESIAN_POINT('',(53.2770757808756,1067.7251047501,474.105989599829));
#126066=CARTESIAN_POINT('Origin',(53.2770757808756,1076.73142393294,475.887982254234));
#126067=CARTESIAN_POINT('Origin',(53.2770757808756,1067.7251047501,475.887982254234));
#126068=CARTESIAN_POINT('',(53.2770757808756,1076.73142393294,474.705989599829));
#126069=CARTESIAN_POINT('Origin',(53.2770757808756,1076.73142393294,475.887982254234));
#126070=CARTESIAN_POINT('',(53.2770757808756,1082.7251047501,474.705989599829));
#126071=CARTESIAN_POINT('',(53.2770757808756,1067.7251047501,474.705989599829));
#126072=CARTESIAN_POINT('Origin',(53.2770757808756,1082.7251047501,475.887982254234));
#126073=CARTESIAN_POINT('Origin',(52.0862183235875,1067.7251047501,487.046546328579));
#126074=CARTESIAN_POINT('',(52.0862183235875,1078.73142393294,485.385665518658));
#126075=CARTESIAN_POINT('Origin',(52.0862183235875,1078.73142393294,487.046546328579));
#126076=CARTESIAN_POINT('',(52.0862183235875,1076.73142393294,485.385665518658));
#126077=CARTESIAN_POINT('',(52.0862183235875,1067.7251047501,485.385665518658));
#126078=CARTESIAN_POINT('Origin',(52.0862183235875,1076.73142393294,487.046546328579));
#126079=CARTESIAN_POINT('Origin',(52.0862183235875,1067.7251047501,487.046546328579));
#126080=CARTESIAN_POINT('',(52.0862183235875,1076.73142393294,485.985665518658));
#126081=CARTESIAN_POINT('Origin',(52.0862183235875,1076.73142393294,487.046546328579));
#126082=CARTESIAN_POINT('',(52.0862183235875,1082.7251047501,485.985665518658));
#126083=CARTESIAN_POINT('',(52.0862183235875,1067.7251047501,485.985665518658));
#126084=CARTESIAN_POINT('Origin',(52.0862183235875,1082.7251047501,487.046546328579));
#126085=CARTESIAN_POINT('Origin',(18.7819059952831,1067.7251047501,420.74995476784));
#126086=CARTESIAN_POINT('',(18.7819059952831,1078.73142393294,419.649596702165));
#126087=CARTESIAN_POINT('Origin',(18.7819059952831,1078.73142393294,420.74995476784));
#126088=CARTESIAN_POINT('',(18.7819059952831,1076.73142393294,419.649596702165));
#126089=CARTESIAN_POINT('',(18.7819059952831,1067.7251047501,419.649596702165));
#126090=CARTESIAN_POINT('Origin',(18.7819059952831,1076.73142393294,420.74995476784));
#126091=CARTESIAN_POINT('Origin',(18.7819059952831,1067.7251047501,420.74995476784));
#126092=CARTESIAN_POINT('',(18.7819059952831,1076.73142393294,420.249596702165));
#126093=CARTESIAN_POINT('Origin',(18.7819059952831,1076.73142393294,420.74995476784));
#126094=CARTESIAN_POINT('',(18.7819059952831,1082.7251047501,420.249596702165));
#126095=CARTESIAN_POINT('',(18.7819059952831,1067.7251047501,420.249596702165));
#126096=CARTESIAN_POINT('Origin',(18.7819059952831,1082.7251047501,420.74995476784));
#126097=CARTESIAN_POINT('Origin',(27.2710543542544,1067.7251047501,421.877665036574));
#126098=CARTESIAN_POINT('',(27.2710543542544,1078.73142393294,420.663633469837));
#126099=CARTESIAN_POINT('Origin',(27.2710543542544,1078.73142393294,421.877665036574));
#126100=CARTESIAN_POINT('',(27.2710543542544,1076.73142393294,420.663633469837));
#126101=CARTESIAN_POINT('',(27.2710543542544,1067.7251047501,420.663633469837));
#126102=CARTESIAN_POINT('Origin',(27.2710543542544,1076.73142393294,421.877665036574));
#126103=CARTESIAN_POINT('Origin',(27.2710543542544,1067.7251047501,421.877665036574));
#126104=CARTESIAN_POINT('',(27.2710543542544,1076.73142393294,421.263633469837));
#126105=CARTESIAN_POINT('Origin',(27.2710543542544,1076.73142393294,421.877665036574));
#126106=CARTESIAN_POINT('',(27.2710543542544,1082.7251047501,421.263633469837));
#126107=CARTESIAN_POINT('',(27.2710543542544,1067.7251047501,421.263633469837));
#126108=CARTESIAN_POINT('Origin',(27.2710543542544,1082.7251047501,421.877665036574));
#126109=CARTESIAN_POINT('Origin',(34.6453511739137,1067.7251047501,424.782598105687));
#126110=CARTESIAN_POINT('',(34.6453511739137,1078.73142393294,423.453790142114));
#126111=CARTESIAN_POINT('Origin',(34.6453511739137,1078.73142393294,424.782598105687));
#126112=CARTESIAN_POINT('',(34.6453511739137,1076.73142393294,423.453790142114));
#126113=CARTESIAN_POINT('',(34.6453511739137,1067.7251047501,423.453790142114));
#126114=CARTESIAN_POINT('Origin',(34.6453511739137,1076.73142393294,424.782598105687));
#126115=CARTESIAN_POINT('Origin',(34.6453511739137,1067.7251047501,424.782598105687));
#126116=CARTESIAN_POINT('',(34.6453511739137,1076.73142393294,424.053790142114));
#126117=CARTESIAN_POINT('Origin',(34.6453511739137,1076.73142393294,424.782598105687));
#126118=CARTESIAN_POINT('',(34.6453511739137,1082.7251047501,424.053790142114));
#126119=CARTESIAN_POINT('',(34.6453511739137,1067.7251047501,424.053790142114));
#126120=CARTESIAN_POINT('Origin',(34.6453511739137,1082.7251047501,424.782598105687));
#126121=CARTESIAN_POINT('Origin',(42.6068786662477,1067.7251047501,429.530915358505));
#126122=CARTESIAN_POINT('',(42.6068786662477,1078.73142393294,428.069798356688));
#126123=CARTESIAN_POINT('Origin',(42.6068786662477,1078.73142393294,429.530915358505));
#126124=CARTESIAN_POINT('',(42.6068786662477,1076.73142393294,428.069798356688));
#126125=CARTESIAN_POINT('',(42.6068786662477,1067.7251047501,428.069798356688));
#126126=CARTESIAN_POINT('Origin',(42.6068786662477,1076.73142393294,429.530915358505));
#126127=CARTESIAN_POINT('Origin',(42.6068786662477,1067.7251047501,429.530915358505));
#126128=CARTESIAN_POINT('',(42.6068786662477,1076.73142393294,428.669798356688));
#126129=CARTESIAN_POINT('Origin',(42.6068786662477,1076.73142393294,429.530915358505));
#126130=CARTESIAN_POINT('',(42.6068786662477,1082.7251047501,428.669798356688));
#126131=CARTESIAN_POINT('',(42.6068786662477,1067.7251047501,428.669798356688));
#126132=CARTESIAN_POINT('Origin',(42.6068786662477,1082.7251047501,429.530915358505));
#126133=CARTESIAN_POINT('Origin',(48.9083680287886,1067.7251047501,435.84491229783));
#126134=CARTESIAN_POINT('',(48.9083680287886,1078.73142393294,434.224430255206));
#126135=CARTESIAN_POINT('Origin',(48.9083680287886,1078.73142393294,435.84491229783));
#126136=CARTESIAN_POINT('',(48.9083680287886,1076.73142393294,434.224430255206));
#126137=CARTESIAN_POINT('',(48.9083680287886,1067.7251047501,434.224430255206));
#126138=CARTESIAN_POINT('Origin',(48.9083680287886,1076.73142393294,435.84491229783));
#126139=CARTESIAN_POINT('Origin',(48.9083680287886,1067.7251047501,435.84491229783));
#126140=CARTESIAN_POINT('',(48.9083680287886,1076.73142393294,434.824430255206));
#126141=CARTESIAN_POINT('Origin',(48.9083680287886,1076.73142393294,435.84491229783));
#126142=CARTESIAN_POINT('',(48.9083680287886,1082.7251047501,434.824430255206));
#126143=CARTESIAN_POINT('',(48.9083680287886,1067.7251047501,434.824430255206));
#126144=CARTESIAN_POINT('Origin',(48.9083680287886,1082.7251047501,435.84491229783));
#126145=CARTESIAN_POINT('Origin',(55.1369976125917,1067.7251047501,443.889337332746));
#126146=CARTESIAN_POINT('',(55.1369976125917,1078.73142393294,442.188337109664));
#126147=CARTESIAN_POINT('Origin',(55.1369976125917,1078.73142393294,443.889337332746));
#126148=CARTESIAN_POINT('',(55.1369976125917,1076.73142393294,442.188337109664));
#126149=CARTESIAN_POINT('',(55.1369976125917,1067.7251047501,442.188337109664));
#126150=CARTESIAN_POINT('Origin',(55.1369976125917,1076.73142393294,443.889337332746));
#126151=CARTESIAN_POINT('Origin',(55.1369976125917,1067.7251047501,443.889337332746));
#126152=CARTESIAN_POINT('',(55.1369976125917,1076.73142393294,442.788337109663));
#126153=CARTESIAN_POINT('Origin',(55.1369976125917,1076.73142393294,443.889337332746));
#126154=CARTESIAN_POINT('',(55.1369976125917,1082.7251047501,442.788337109663));
#126155=CARTESIAN_POINT('',(55.1369976125917,1067.7251047501,442.788337109663));
#126156=CARTESIAN_POINT('Origin',(55.1369976125917,1082.7251047501,443.889337332746));
#126157=CARTESIAN_POINT('Origin',(59.2408610395779,1067.7251047501,452.861339223948));
#126158=CARTESIAN_POINT('',(59.2408610395779,1078.73142393294,451.140064591905));
#126159=CARTESIAN_POINT('Origin',(59.2408610395779,1078.73142393294,452.861339223948));
#126160=CARTESIAN_POINT('',(59.2408610395779,1076.73142393294,451.140064591905));
#126161=CARTESIAN_POINT('',(59.2408610395779,1067.7251047501,451.140064591905));
#126162=CARTESIAN_POINT('Origin',(59.2408610395779,1076.73142393294,452.861339223948));
#126163=CARTESIAN_POINT('Origin',(59.2408610395779,1067.7251047501,452.861339223948));
#126164=CARTESIAN_POINT('',(59.2408610395779,1076.73142393294,451.740064591905));
#126165=CARTESIAN_POINT('Origin',(59.2408610395779,1076.73142393294,452.861339223948));
#126166=CARTESIAN_POINT('',(59.2408610395779,1082.7251047501,451.740064591905));
#126167=CARTESIAN_POINT('',(59.2408610395779,1067.7251047501,451.740064591905));
#126168=CARTESIAN_POINT('Origin',(59.2408610395779,1082.7251047501,452.861339223948));
#126169=CARTESIAN_POINT('Origin',(62.7720062892815,1067.7251047501,463.690732229966));
#126170=CARTESIAN_POINT('',(62.7720062892815,1078.73142393294,461.908739575561));
#126171=CARTESIAN_POINT('Origin',(62.7720062892815,1078.73142393294,463.690732229966));
#126172=CARTESIAN_POINT('',(62.7720062892815,1076.73142393294,461.908739575561));
#126173=CARTESIAN_POINT('',(62.7720062892815,1067.7251047501,461.908739575561));
#126174=CARTESIAN_POINT('Origin',(62.7720062892815,1076.73142393294,463.690732229966));
#126175=CARTESIAN_POINT('Origin',(62.7720062892815,1067.7251047501,463.690732229966));
#126176=CARTESIAN_POINT('',(62.7720062892815,1076.73142393294,462.508739575561));
#126177=CARTESIAN_POINT('Origin',(62.7720062892815,1076.73142393294,463.690732229966));
#126178=CARTESIAN_POINT('',(62.7720062892815,1082.7251047501,462.508739575561));
#126179=CARTESIAN_POINT('',(62.7720062892815,1067.7251047501,462.508739575561));
#126180=CARTESIAN_POINT('Origin',(62.7720062892815,1082.7251047501,463.690732229966));
#126181=CARTESIAN_POINT('Origin',(63.9271678484146,1067.7251047501,474.853048094389));
#126182=CARTESIAN_POINT('',(63.9271678484146,1078.73142393294,473.192167284468));
#126183=CARTESIAN_POINT('Origin',(63.9271678484146,1078.73142393294,474.853048094389));
#126184=CARTESIAN_POINT('',(63.9271678484146,1076.73142393294,473.192167284468));
#126185=CARTESIAN_POINT('',(63.9271678484146,1067.7251047501,473.192167284468));
#126186=CARTESIAN_POINT('Origin',(63.9271678484146,1076.73142393294,474.853048094389));
#126187=CARTESIAN_POINT('Origin',(63.9271678484146,1067.7251047501,474.853048094389));
#126188=CARTESIAN_POINT('',(63.9271678484146,1076.73142393294,473.792167284468));
#126189=CARTESIAN_POINT('Origin',(63.9271678484146,1076.73142393294,474.853048094389));
#126190=CARTESIAN_POINT('',(63.9271678484146,1082.7251047501,473.792167284468));
#126191=CARTESIAN_POINT('',(63.9271678484146,1067.7251047501,473.792167284468));
#126192=CARTESIAN_POINT('Origin',(63.9271678484146,1082.7251047501,474.853048094389));
#126193=CARTESIAN_POINT('Origin',(17.5667982035468,1067.7251047501,416.929552010124));
#126194=CARTESIAN_POINT('',(17.5667982035468,1078.73142393294,415.829193944449));
#126195=CARTESIAN_POINT('Origin',(17.5667982035468,1078.73142393294,416.929552010124));
#126196=CARTESIAN_POINT('',(17.5667982035468,1076.73142393294,415.829193944449));
#126197=CARTESIAN_POINT('',(17.5667982035468,1067.7251047501,415.829193944449));
#126198=CARTESIAN_POINT('Origin',(17.5667982035468,1076.73142393294,416.929552010124));
#126199=CARTESIAN_POINT('Origin',(17.5667982035468,1067.7251047501,416.929552010124));
#126200=CARTESIAN_POINT('',(17.5667982035468,1076.73142393294,416.429193944449));
#126201=CARTESIAN_POINT('Origin',(17.5667982035468,1076.73142393294,416.929552010124));
#126202=CARTESIAN_POINT('',(17.5667982035468,1082.7251047501,416.429193944449));
#126203=CARTESIAN_POINT('',(17.5667982035468,1067.7251047501,416.429193944449));
#126204=CARTESIAN_POINT('Origin',(17.5667982035468,1082.7251047501,416.929552010124));
#126205=CARTESIAN_POINT('Origin',(26.104902451873,1067.7251047501,416.267625914893));
#126206=CARTESIAN_POINT('',(26.104902451873,1078.73142393294,415.053594348156));
#126207=CARTESIAN_POINT('Origin',(26.104902451873,1078.73142393294,416.267625914893));
#126208=CARTESIAN_POINT('',(26.104902451873,1076.73142393294,415.053594348156));
#126209=CARTESIAN_POINT('',(26.104902451873,1067.7251047501,415.053594348156));
#126210=CARTESIAN_POINT('Origin',(26.104902451873,1076.73142393294,416.267625914893));
#126211=CARTESIAN_POINT('Origin',(26.104902451873,1067.7251047501,416.267625914893));
#126212=CARTESIAN_POINT('',(26.104902451873,1076.73142393294,415.653594348156));
#126213=CARTESIAN_POINT('Origin',(26.104902451873,1076.73142393294,416.267625914893));
#126214=CARTESIAN_POINT('',(26.104902451873,1082.7251047501,415.653594348156));
#126215=CARTESIAN_POINT('',(26.104902451873,1067.7251047501,415.653594348156));
#126216=CARTESIAN_POINT('Origin',(26.104902451873,1082.7251047501,416.267625914893));
#126217=CARTESIAN_POINT('Origin',(33.9220227392334,1067.7251047501,417.57587670637));
#126218=CARTESIAN_POINT('',(33.9220227392334,1078.73142393294,416.247068742797));
#126219=CARTESIAN_POINT('Origin',(33.9220227392334,1078.73142393294,417.57587670637));
#126220=CARTESIAN_POINT('',(33.9220227392334,1076.73142393294,416.247068742797));
#126221=CARTESIAN_POINT('',(33.9220227392334,1067.7251047501,416.247068742797));
#126222=CARTESIAN_POINT('Origin',(33.9220227392334,1076.73142393294,417.57587670637));
#126223=CARTESIAN_POINT('Origin',(33.9220227392334,1067.7251047501,417.57587670637));
#126224=CARTESIAN_POINT('',(33.9220227392334,1076.73142393294,416.847068742797));
#126225=CARTESIAN_POINT('Origin',(33.9220227392334,1076.73142393294,417.57587670637));
#126226=CARTESIAN_POINT('',(33.9220227392334,1082.7251047501,416.847068742797));
#126227=CARTESIAN_POINT('',(33.9220227392334,1067.7251047501,416.847068742797));
#126228=CARTESIAN_POINT('Origin',(33.9220227392334,1082.7251047501,417.57587670637));
#126229=CARTESIAN_POINT('Origin',(42.6968024226085,1067.7251047501,420.565137192314));
#126230=CARTESIAN_POINT('',(42.6968024226085,1078.73142393294,419.104020190497));
#126231=CARTESIAN_POINT('Origin',(42.6968024226085,1078.73142393294,420.565137192314));
#126232=CARTESIAN_POINT('',(42.6968024226085,1076.73142393294,419.104020190497));
#126233=CARTESIAN_POINT('',(42.6968024226085,1067.7251047501,419.104020190497));
#126234=CARTESIAN_POINT('Origin',(42.6968024226085,1076.73142393294,420.565137192314));
#126235=CARTESIAN_POINT('Origin',(42.6968024226085,1067.7251047501,420.565137192314));
#126236=CARTESIAN_POINT('',(42.6968024226085,1076.73142393294,419.704020190497));
#126237=CARTESIAN_POINT('Origin',(42.6968024226085,1076.73142393294,420.565137192314));
#126238=CARTESIAN_POINT('',(42.6968024226085,1082.7251047501,419.704020190497));
#126239=CARTESIAN_POINT('',(42.6968024226085,1067.7251047501,419.704020190497));
#126240=CARTESIAN_POINT('Origin',(42.6968024226085,1082.7251047501,420.565137192314));
#126241=CARTESIAN_POINT('Origin',(50.1733429031008,1067.7251047501,425.431004841519));
#126242=CARTESIAN_POINT('',(50.1733429031008,1078.73142393294,423.810522798895));
#126243=CARTESIAN_POINT('Origin',(50.1733429031008,1078.73142393294,425.431004841519));
#126244=CARTESIAN_POINT('',(50.1733429031008,1076.73142393294,423.810522798895));
#126245=CARTESIAN_POINT('',(50.1733429031008,1067.7251047501,423.810522798895));
#126246=CARTESIAN_POINT('Origin',(50.1733429031008,1076.73142393294,425.431004841519));
#126247=CARTESIAN_POINT('Origin',(50.1733429031008,1067.7251047501,425.431004841519));
#126248=CARTESIAN_POINT('',(50.1733429031008,1076.73142393294,424.410522798895));
#126249=CARTESIAN_POINT('Origin',(50.1733429031008,1076.73142393294,425.431004841519));
#126250=CARTESIAN_POINT('',(50.1733429031008,1082.7251047501,424.410522798895));
#126251=CARTESIAN_POINT('',(50.1733429031008,1067.7251047501,424.410522798895));
#126252=CARTESIAN_POINT('Origin',(50.1733429031008,1082.7251047501,425.431004841519));
#126253=CARTESIAN_POINT('Origin',(57.9383919970236,1067.7251047501,432.00463498046));
#126254=CARTESIAN_POINT('',(57.9383919970236,1078.73142393294,430.303634757377));
#126255=CARTESIAN_POINT('Origin',(57.9383919970236,1078.73142393294,432.00463498046));
#126256=CARTESIAN_POINT('',(57.9383919970236,1076.73142393294,430.303634757377));
#126257=CARTESIAN_POINT('',(57.9383919970236,1067.7251047501,430.303634757377));
#126258=CARTESIAN_POINT('Origin',(57.9383919970236,1076.73142393294,432.00463498046));
#126259=CARTESIAN_POINT('Origin',(57.9383919970236,1067.7251047501,432.00463498046));
#126260=CARTESIAN_POINT('',(57.9383919970236,1076.73142393294,430.903634757377));
#126261=CARTESIAN_POINT('Origin',(57.9383919970236,1076.73142393294,432.00463498046));
#126262=CARTESIAN_POINT('',(57.9383919970236,1082.7251047501,430.903634757377));
#126263=CARTESIAN_POINT('',(57.9383919970236,1067.7251047501,430.903634757377));
#126264=CARTESIAN_POINT('Origin',(57.9383919970236,1082.7251047501,432.00463498046));
#126265=CARTESIAN_POINT('Origin',(63.8179602450892,1067.7251047501,439.927335920128));
#126266=CARTESIAN_POINT('',(63.8179602450892,1078.73142393294,438.206061288084));
#126267=CARTESIAN_POINT('Origin',(63.8179602450892,1078.73142393294,439.927335920128));
#126268=CARTESIAN_POINT('',(63.8179602450892,1076.73142393294,438.206061288084));
#126269=CARTESIAN_POINT('',(63.8179602450892,1067.7251047501,438.206061288084));
#126270=CARTESIAN_POINT('Origin',(63.8179602450892,1076.73142393294,439.927335920128));
#126271=CARTESIAN_POINT('Origin',(63.8179602450892,1067.7251047501,439.927335920128));
#126272=CARTESIAN_POINT('',(63.8179602450892,1076.73142393294,438.806061288084));
#126273=CARTESIAN_POINT('Origin',(63.8179602450892,1076.73142393294,439.927335920128));
#126274=CARTESIAN_POINT('',(63.8179602450892,1082.7251047501,438.806061288084));
#126275=CARTESIAN_POINT('',(63.8179602450892,1067.7251047501,438.806061288084));
#126276=CARTESIAN_POINT('Origin',(63.8179602450892,1082.7251047501,439.927335920128));
#126277=CARTESIAN_POINT('Origin',(69.5234989093405,1067.7251047501,449.785914326979));
#126278=CARTESIAN_POINT('',(69.5234989093405,1078.73142393294,448.003921672574));
#126279=CARTESIAN_POINT('Origin',(69.5234989093405,1078.73142393294,449.785914326979));
#126280=CARTESIAN_POINT('',(69.5234989093405,1076.73142393294,448.003921672574));
#126281=CARTESIAN_POINT('',(69.5234989093405,1067.7251047501,448.003921672574));
#126282=CARTESIAN_POINT('Origin',(69.5234989093405,1076.73142393294,449.785914326979));
#126283=CARTESIAN_POINT('Origin',(69.5234989093405,1067.7251047501,449.785914326979));
#126284=CARTESIAN_POINT('',(69.5234989093405,1076.73142393294,448.603921672574));
#126285=CARTESIAN_POINT('Origin',(69.5234989093405,1076.73142393294,449.785914326979));
#126286=CARTESIAN_POINT('',(69.5234989093405,1082.7251047501,448.603921672574));
#126287=CARTESIAN_POINT('',(69.5234989093405,1067.7251047501,448.603921672574));
#126288=CARTESIAN_POINT('Origin',(69.5234989093405,1082.7251047501,449.785914326979));
#126289=CARTESIAN_POINT('Origin',(72.9741933816806,1067.7251047501,460.46413521547));
#126290=CARTESIAN_POINT('',(72.9741933816806,1078.73142393294,458.803254405549));
#126291=CARTESIAN_POINT('Origin',(72.9741933816806,1078.73142393294,460.46413521547));
#126292=CARTESIAN_POINT('',(72.9741933816806,1076.73142393294,458.803254405549));
#126293=CARTESIAN_POINT('',(72.9741933816806,1067.7251047501,458.803254405549));
#126294=CARTESIAN_POINT('Origin',(72.9741933816806,1076.73142393294,460.46413521547));
#126295=CARTESIAN_POINT('Origin',(72.9741933816806,1067.7251047501,460.46413521547));
#126296=CARTESIAN_POINT('',(72.9741933816806,1076.73142393294,459.403254405549));
#126297=CARTESIAN_POINT('Origin',(72.9741933816806,1076.73142393294,460.46413521547));
#126298=CARTESIAN_POINT('',(72.9741933816806,1082.7251047501,459.403254405549));
#126299=CARTESIAN_POINT('',(72.9741933816806,1067.7251047501,459.403254405549));
#126300=CARTESIAN_POINT('Origin',(72.9741933816806,1082.7251047501,460.46413521547));
#126301=CARTESIAN_POINT('Origin',(15.5839370354653,1067.7251047501,413.445269334333));
#126302=CARTESIAN_POINT('',(15.5839370354653,1078.73142393294,412.344911268658));
#126303=CARTESIAN_POINT('Origin',(15.5839370354653,1078.73142393294,413.445269334333));
#126304=CARTESIAN_POINT('',(15.5839370354653,1076.73142393294,412.344911268658));
#126305=CARTESIAN_POINT('',(15.5839370354653,1067.7251047501,412.344911268658));
#126306=CARTESIAN_POINT('Origin',(15.5839370354653,1076.73142393294,413.445269334333));
#126307=CARTESIAN_POINT('Origin',(15.5839370354653,1067.7251047501,413.445269334333));
#126308=CARTESIAN_POINT('',(15.5839370354653,1076.73142393294,412.944911268658));
#126309=CARTESIAN_POINT('Origin',(15.5839370354653,1076.73142393294,413.445269334333));
#126310=CARTESIAN_POINT('',(15.5839370354653,1082.7251047501,412.944911268658));
#126311=CARTESIAN_POINT('',(15.5839370354653,1067.7251047501,412.944911268658));
#126312=CARTESIAN_POINT('Origin',(15.5839370354653,1082.7251047501,413.445269334333));
#126313=CARTESIAN_POINT('Origin',(23.7978410471248,1067.7251047501,411.022636221772));
#126314=CARTESIAN_POINT('',(23.7978410471248,1078.73142393294,409.808604655035));
#126315=CARTESIAN_POINT('Origin',(23.7978410471248,1078.73142393294,411.022636221772));
#126316=CARTESIAN_POINT('',(23.7978410471248,1076.73142393294,409.808604655035));
#126317=CARTESIAN_POINT('',(23.7978410471248,1067.7251047501,409.808604655035));
#126318=CARTESIAN_POINT('Origin',(23.7978410471248,1076.73142393294,411.022636221772));
#126319=CARTESIAN_POINT('Origin',(23.7978410471248,1067.7251047501,411.022636221772));
#126320=CARTESIAN_POINT('',(23.7978410471248,1076.73142393294,410.408604655034));
#126321=CARTESIAN_POINT('Origin',(23.7978410471248,1076.73142393294,411.022636221772));
#126322=CARTESIAN_POINT('',(23.7978410471248,1082.7251047501,410.408604655034));
#126323=CARTESIAN_POINT('',(23.7978410471248,1067.7251047501,410.408604655034));
#126324=CARTESIAN_POINT('Origin',(23.7978410471248,1082.7251047501,411.022636221772));
#126325=CARTESIAN_POINT('Origin',(31.7161391349238,1067.7251047501,410.677027898342));
#126326=CARTESIAN_POINT('',(31.7161391349238,1078.73142393294,409.348219934769));
#126327=CARTESIAN_POINT('Origin',(31.7161391349238,1078.73142393294,410.677027898342));
#126328=CARTESIAN_POINT('',(31.7161391349238,1076.73142393294,409.348219934769));
#126329=CARTESIAN_POINT('',(31.7161391349238,1067.7251047501,409.348219934769));
#126330=CARTESIAN_POINT('Origin',(31.7161391349238,1076.73142393294,410.677027898342));
#126331=CARTESIAN_POINT('Origin',(31.7161391349238,1067.7251047501,410.677027898342));
#126332=CARTESIAN_POINT('',(31.7161391349238,1076.73142393294,409.948219934769));
#126333=CARTESIAN_POINT('Origin',(31.7161391349238,1076.73142393294,410.677027898342));
#126334=CARTESIAN_POINT('',(31.7161391349238,1082.7251047501,409.948219934769));
#126335=CARTESIAN_POINT('',(31.7161391349238,1067.7251047501,409.948219934769));
#126336=CARTESIAN_POINT('Origin',(31.7161391349238,1082.7251047501,410.677027898342));
#126337=CARTESIAN_POINT('Origin',(40.920671031112,1067.7251047501,411.776586590112));
#126338=CARTESIAN_POINT('',(40.920671031112,1078.73142393294,410.315469588295));
#126339=CARTESIAN_POINT('Origin',(40.920671031112,1078.73142393294,411.776586590112));
#126340=CARTESIAN_POINT('',(40.920671031112,1076.73142393294,410.315469588295));
#126341=CARTESIAN_POINT('',(40.920671031112,1067.7251047501,410.315469588295));
#126342=CARTESIAN_POINT('Origin',(40.920671031112,1076.73142393294,411.776586590112));
#126343=CARTESIAN_POINT('Origin',(40.920671031112,1067.7251047501,411.776586590112));
#126344=CARTESIAN_POINT('',(40.920671031112,1076.73142393294,410.915469588295));
#126345=CARTESIAN_POINT('Origin',(40.920671031112,1076.73142393294,411.776586590112));
#126346=CARTESIAN_POINT('',(40.920671031112,1082.7251047501,410.915469588295));
#126347=CARTESIAN_POINT('',(40.920671031112,1067.7251047501,410.915469588295));
#126348=CARTESIAN_POINT('Origin',(40.920671031112,1082.7251047501,411.776586590112));
#126349=CARTESIAN_POINT('Origin',(49.2455019341365,1067.7251047501,414.981663183905));
#126350=CARTESIAN_POINT('',(49.2455019341365,1078.73142393294,413.36118114128));
#126351=CARTESIAN_POINT('Origin',(49.2455019341365,1078.73142393294,414.981663183905));
#126352=CARTESIAN_POINT('',(49.2455019341365,1076.73142393294,413.36118114128));
#126353=CARTESIAN_POINT('',(49.2455019341365,1067.7251047501,413.36118114128));
#126354=CARTESIAN_POINT('Origin',(49.2455019341365,1076.73142393294,414.981663183905));
#126355=CARTESIAN_POINT('Origin',(49.2455019341365,1067.7251047501,414.981663183905));
#126356=CARTESIAN_POINT('',(49.2455019341365,1076.73142393294,413.96118114128));
#126357=CARTESIAN_POINT('Origin',(49.2455019341365,1076.73142393294,414.981663183905));
#126358=CARTESIAN_POINT('',(49.2455019341365,1082.7251047501,413.96118114128));
#126359=CARTESIAN_POINT('',(49.2455019341365,1067.7251047501,413.96118114128));
#126360=CARTESIAN_POINT('Origin',(49.2455019341365,1082.7251047501,414.981663183905));
#126361=CARTESIAN_POINT('Origin',(58.207600631935,1067.7251047501,419.79719924602));
#126362=CARTESIAN_POINT('',(58.207600631935,1078.73142393294,418.096199022937));
#126363=CARTESIAN_POINT('Origin',(58.207600631935,1078.73142393294,419.79719924602));
#126364=CARTESIAN_POINT('',(58.207600631935,1076.73142393294,418.096199022937));
#126365=CARTESIAN_POINT('',(58.207600631935,1067.7251047501,418.096199022937));
#126366=CARTESIAN_POINT('Origin',(58.207600631935,1076.73142393294,419.79719924602));
#126367=CARTESIAN_POINT('Origin',(58.207600631935,1067.7251047501,419.79719924602));
#126368=CARTESIAN_POINT('',(58.207600631935,1076.73142393294,418.696199022937));
#126369=CARTESIAN_POINT('Origin',(58.207600631935,1076.73142393294,419.79719924602));
#126370=CARTESIAN_POINT('',(58.207600631935,1082.7251047501,418.696199022937));
#126371=CARTESIAN_POINT('',(58.207600631935,1067.7251047501,418.696199022937));
#126372=CARTESIAN_POINT('Origin',(58.207600631935,1082.7251047501,419.79719924602));
#126373=CARTESIAN_POINT('Origin',(65.6059083553409,1067.7251047501,426.324339185754));
#126374=CARTESIAN_POINT('',(65.6059083553409,1078.73142393294,424.603064553711));
#126375=CARTESIAN_POINT('Origin',(65.6059083553409,1078.73142393294,426.324339185754));
#126376=CARTESIAN_POINT('',(65.6059083553409,1076.73142393294,424.603064553711));
#126377=CARTESIAN_POINT('',(65.6059083553409,1067.7251047501,424.603064553711));
#126378=CARTESIAN_POINT('Origin',(65.6059083553409,1076.73142393294,426.324339185754));
#126379=CARTESIAN_POINT('Origin',(65.6059083553409,1067.7251047501,426.324339185754));
#126380=CARTESIAN_POINT('',(65.6059083553409,1076.73142393294,425.203064553711));
#126381=CARTESIAN_POINT('Origin',(65.6059083553409,1076.73142393294,426.324339185754));
#126382=CARTESIAN_POINT('',(65.6059083553409,1082.7251047501,425.203064553711));
#126383=CARTESIAN_POINT('',(65.6059083553409,1067.7251047501,425.203064553711));
#126384=CARTESIAN_POINT('Origin',(65.6059083553409,1082.7251047501,426.324339185754));
#126385=CARTESIAN_POINT('Origin',(73.2364810163002,1067.7251047501,434.781235810351));
#126386=CARTESIAN_POINT('',(73.2364810163002,1078.73142393294,432.999243155946));
#126387=CARTESIAN_POINT('Origin',(73.2364810163002,1078.73142393294,434.781235810351));
#126388=CARTESIAN_POINT('',(73.2364810163002,1076.73142393294,432.999243155946));
#126389=CARTESIAN_POINT('',(73.2364810163002,1067.7251047501,432.999243155946));
#126390=CARTESIAN_POINT('Origin',(73.2364810163002,1076.73142393294,434.781235810351));
#126391=CARTESIAN_POINT('Origin',(73.2364810163002,1067.7251047501,434.781235810351));
#126392=CARTESIAN_POINT('',(73.2364810163002,1076.73142393294,433.599243155946));
#126393=CARTESIAN_POINT('Origin',(73.2364810163002,1076.73142393294,434.781235810351));
#126394=CARTESIAN_POINT('',(73.2364810163002,1082.7251047501,433.599243155946));
#126395=CARTESIAN_POINT('',(73.2364810163002,1067.7251047501,433.599243155946));
#126396=CARTESIAN_POINT('Origin',(73.2364810163002,1082.7251047501,434.781235810351));
#126397=CARTESIAN_POINT('Origin',(78.8318964951367,1067.7251047501,444.508672230294));
#126398=CARTESIAN_POINT('',(78.8318964951367,1078.73142393294,442.847791420374));
#126399=CARTESIAN_POINT('Origin',(78.8318964951367,1078.73142393294,444.508672230294));
#126400=CARTESIAN_POINT('',(78.8318964951367,1076.73142393294,442.847791420374));
#126401=CARTESIAN_POINT('',(78.8318964951367,1067.7251047501,442.847791420374));
#126402=CARTESIAN_POINT('Origin',(78.8318964951367,1076.73142393294,444.508672230294));
#126403=CARTESIAN_POINT('Origin',(78.8318964951367,1067.7251047501,444.508672230294));
#126404=CARTESIAN_POINT('',(78.8318964951367,1076.73142393294,443.447791420374));
#126405=CARTESIAN_POINT('Origin',(78.8318964951367,1076.73142393294,444.508672230294));
#126406=CARTESIAN_POINT('',(78.8318964951367,1082.7251047501,443.447791420374));
#126407=CARTESIAN_POINT('',(78.8318964951367,1067.7251047501,443.447791420374));
#126408=CARTESIAN_POINT('Origin',(78.8318964951367,1082.7251047501,444.508672230294));
#126409=CARTESIAN_POINT('Origin',(12.9199830389075,1067.7251047501,410.449386612842));
#126410=CARTESIAN_POINT('',(12.9199830389075,1078.73142393294,409.349028547167));
#126411=CARTESIAN_POINT('Origin',(12.9199830389075,1078.73142393294,410.449386612842));
#126412=CARTESIAN_POINT('',(12.9199830389075,1076.73142393294,409.349028547167));
#126413=CARTESIAN_POINT('',(12.9199830389075,1067.7251047501,409.349028547167));
#126414=CARTESIAN_POINT('Origin',(12.9199830389075,1076.73142393294,410.449386612842));
#126415=CARTESIAN_POINT('Origin',(12.9199830389075,1067.7251047501,410.449386612842));
#126416=CARTESIAN_POINT('',(12.9199830389075,1076.73142393294,409.949028547167));
#126417=CARTESIAN_POINT('Origin',(12.9199830389075,1076.73142393294,410.449386612842));
#126418=CARTESIAN_POINT('',(12.9199830389075,1082.7251047501,409.949028547167));
#126419=CARTESIAN_POINT('',(12.9199830389075,1067.7251047501,409.949028547167));
#126420=CARTESIAN_POINT('Origin',(12.9199830389075,1082.7251047501,410.449386612842));
#126421=CARTESIAN_POINT('Origin',(20.4506997939064,1067.7251047501,406.371927175053));
#126422=CARTESIAN_POINT('',(20.4506997939064,1078.73142393294,405.157895608316));
#126423=CARTESIAN_POINT('Origin',(20.4506997939064,1078.73142393294,406.371927175053));
#126424=CARTESIAN_POINT('',(20.4506997939064,1076.73142393294,405.157895608316));
#126425=CARTESIAN_POINT('',(20.4506997939064,1067.7251047501,405.157895608316));
#126426=CARTESIAN_POINT('Origin',(20.4506997939064,1076.73142393294,406.371927175053));
#126427=CARTESIAN_POINT('Origin',(20.4506997939064,1067.7251047501,406.371927175053));
#126428=CARTESIAN_POINT('',(20.4506997939064,1076.73142393294,405.757895608316));
#126429=CARTESIAN_POINT('Origin',(20.4506997939064,1076.73142393294,406.371927175053));
#126430=CARTESIAN_POINT('',(20.4506997939064,1082.7251047501,405.757895608316));
#126431=CARTESIAN_POINT('',(20.4506997939064,1067.7251047501,405.757895608316));
#126432=CARTESIAN_POINT('Origin',(20.4506997939064,1082.7251047501,406.371927175053));
#126433=CARTESIAN_POINT('Origin',(28.1241080594971,1067.7251047501,404.387564478864));
#126434=CARTESIAN_POINT('',(28.1241080594971,1078.73142393294,403.058756515291));
#126435=CARTESIAN_POINT('Origin',(28.1241080594971,1078.73142393294,404.387564478864));
#126436=CARTESIAN_POINT('',(28.1241080594971,1076.73142393294,403.058756515291));
#126437=CARTESIAN_POINT('',(28.1241080594971,1067.7251047501,403.058756515291));
#126438=CARTESIAN_POINT('Origin',(28.1241080594971,1076.73142393294,404.387564478864));
#126439=CARTESIAN_POINT('Origin',(28.1241080594971,1067.7251047501,404.387564478864));
#126440=CARTESIAN_POINT('',(28.1241080594971,1076.73142393294,403.658756515291));
#126441=CARTESIAN_POINT('Origin',(28.1241080594971,1076.73142393294,404.387564478864));
#126442=CARTESIAN_POINT('',(28.1241080594971,1082.7251047501,403.658756515291));
#126443=CARTESIAN_POINT('',(28.1241080594971,1067.7251047501,403.658756515291));
#126444=CARTESIAN_POINT('Origin',(28.1241080594971,1082.7251047501,404.387564478864));
#126445=CARTESIAN_POINT('Origin',(37.3561099563906,1067.7251047501,403.549365385362));
#126446=CARTESIAN_POINT('',(37.3561099563906,1078.73142393294,402.088248383545));
#126447=CARTESIAN_POINT('Origin',(37.3561099563906,1078.73142393294,403.549365385362));
#126448=CARTESIAN_POINT('',(37.3561099563906,1076.73142393294,402.088248383545));
#126449=CARTESIAN_POINT('',(37.3561099563906,1067.7251047501,402.088248383545));
#126450=CARTESIAN_POINT('Origin',(37.3561099563906,1076.73142393294,403.549365385362));
#126451=CARTESIAN_POINT('Origin',(37.3561099563906,1067.7251047501,403.549365385362));
#126452=CARTESIAN_POINT('',(37.3561099563906,1076.73142393294,402.688248383545));
#126453=CARTESIAN_POINT('Origin',(37.3561099563906,1076.73142393294,403.549365385362));
#126454=CARTESIAN_POINT('',(37.3561099563906,1082.7251047501,402.688248383545));
#126455=CARTESIAN_POINT('',(37.3561099563906,1067.7251047501,402.688248383545));
#126456=CARTESIAN_POINT('Origin',(37.3561099563906,1082.7251047501,403.549365385362));
#126457=CARTESIAN_POINT('Origin',(46.1653962245145,1067.7251047501,404.953573696928));
#126458=CARTESIAN_POINT('',(46.1653962245145,1078.73142393294,403.333091654304));
#126459=CARTESIAN_POINT('Origin',(46.1653962245145,1078.73142393294,404.953573696928));
#126460=CARTESIAN_POINT('',(46.1653962245145,1076.73142393294,403.333091654304));
#126461=CARTESIAN_POINT('',(46.1653962245145,1067.7251047501,403.333091654304));
#126462=CARTESIAN_POINT('Origin',(46.1653962245145,1076.73142393294,404.953573696928));
#126463=CARTESIAN_POINT('Origin',(46.1653962245145,1067.7251047501,404.953573696928));
#126464=CARTESIAN_POINT('',(46.1653962245145,1076.73142393294,403.933091654304));
#126465=CARTESIAN_POINT('Origin',(46.1653962245145,1076.73142393294,404.953573696928));
#126466=CARTESIAN_POINT('',(46.1653962245145,1082.7251047501,403.933091654304));
#126467=CARTESIAN_POINT('',(46.1653962245145,1067.7251047501,403.933091654304));
#126468=CARTESIAN_POINT('Origin',(46.1653962245145,1082.7251047501,404.953573696928));
#126469=CARTESIAN_POINT('Origin',(55.9328578081739,1067.7251047501,407.800553648799));
#126470=CARTESIAN_POINT('',(55.9328578081739,1078.73142393294,406.099553425716));
#126471=CARTESIAN_POINT('Origin',(55.9328578081739,1078.73142393294,407.800553648799));
#126472=CARTESIAN_POINT('',(55.9328578081739,1076.73142393294,406.099553425716));
#126473=CARTESIAN_POINT('',(55.9328578081739,1067.7251047501,406.099553425716));
#126474=CARTESIAN_POINT('Origin',(55.9328578081739,1076.73142393294,407.800553648799));
#126475=CARTESIAN_POINT('Origin',(55.9328578081739,1067.7251047501,407.800553648799));
#126476=CARTESIAN_POINT('',(55.9328578081739,1076.73142393294,406.699553425716));
#126477=CARTESIAN_POINT('Origin',(55.9328578081739,1076.73142393294,407.800553648799));
#126478=CARTESIAN_POINT('',(55.9328578081739,1082.7251047501,406.699553425716));
#126479=CARTESIAN_POINT('',(55.9328578081739,1067.7251047501,406.699553425716));
#126480=CARTESIAN_POINT('Origin',(55.9328578081739,1082.7251047501,407.800553648799));
#126481=CARTESIAN_POINT('Origin',(64.5265634583882,1067.7251047501,412.64686525254));
#126482=CARTESIAN_POINT('',(64.5265634583882,1078.73142393294,410.925590620497));
#126483=CARTESIAN_POINT('Origin',(64.5265634583882,1078.73142393294,412.64686525254));
#126484=CARTESIAN_POINT('',(64.5265634583882,1076.73142393294,410.925590620497));
#126485=CARTESIAN_POINT('',(64.5265634583882,1067.7251047501,410.925590620497));
#126486=CARTESIAN_POINT('Origin',(64.5265634583882,1076.73142393294,412.64686525254));
#126487=CARTESIAN_POINT('Origin',(64.5265634583882,1067.7251047501,412.64686525254));
#126488=CARTESIAN_POINT('',(64.5265634583882,1076.73142393294,411.525590620497));
#126489=CARTESIAN_POINT('Origin',(64.5265634583882,1076.73142393294,412.64686525254));
#126490=CARTESIAN_POINT('',(64.5265634583882,1082.7251047501,411.525590620497));
#126491=CARTESIAN_POINT('',(64.5265634583882,1067.7251047501,411.525590620497));
#126492=CARTESIAN_POINT('Origin',(64.5265634583882,1082.7251047501,412.64686525254));
#126493=CARTESIAN_POINT('Origin',(73.7486774752213,1067.7251047501,419.332473131695));
#126494=CARTESIAN_POINT('',(73.7486774752213,1078.73142393294,417.55048047729));
#126495=CARTESIAN_POINT('Origin',(73.7486774752213,1078.73142393294,419.332473131695));
#126496=CARTESIAN_POINT('',(73.7486774752213,1076.73142393294,417.55048047729));
#126497=CARTESIAN_POINT('',(73.7486774752213,1067.7251047501,417.55048047729));
#126498=CARTESIAN_POINT('Origin',(73.7486774752213,1076.73142393294,419.332473131695));
#126499=CARTESIAN_POINT('Origin',(73.7486774752213,1067.7251047501,419.332473131695));
#126500=CARTESIAN_POINT('',(73.7486774752213,1076.73142393294,418.15048047729));
#126501=CARTESIAN_POINT('Origin',(73.7486774752213,1076.73142393294,419.332473131695));
#126502=CARTESIAN_POINT('',(73.7486774752213,1082.7251047501,418.15048047729));
#126503=CARTESIAN_POINT('',(73.7486774752213,1067.7251047501,418.15048047729));
#126504=CARTESIAN_POINT('Origin',(73.7486774752213,1082.7251047501,419.332473131695));
#126505=CARTESIAN_POINT('Origin',(81.2442674543467,1067.7251047501,427.683989434121));
#126506=CARTESIAN_POINT('',(81.2442674543467,1078.73142393294,426.0231086242));
#126507=CARTESIAN_POINT('Origin',(81.2442674543467,1078.73142393294,427.683989434121));
#126508=CARTESIAN_POINT('',(81.2442674543467,1076.73142393294,426.0231086242));
#126509=CARTESIAN_POINT('',(81.2442674543467,1067.7251047501,426.0231086242));
#126510=CARTESIAN_POINT('Origin',(81.2442674543467,1076.73142393294,427.683989434121));
#126511=CARTESIAN_POINT('Origin',(81.2442674543467,1067.7251047501,427.683989434121));
#126512=CARTESIAN_POINT('',(81.2442674543467,1076.73142393294,426.6231086242));
#126513=CARTESIAN_POINT('Origin',(81.2442674543467,1076.73142393294,427.683989434121));
#126514=CARTESIAN_POINT('',(81.2442674543467,1082.7251047501,426.6231086242));
#126515=CARTESIAN_POINT('',(81.2442674543467,1067.7251047501,426.6231086242));
#126516=CARTESIAN_POINT('Origin',(81.2442674543467,1082.7251047501,427.683989434121));
#126517=CARTESIAN_POINT('Origin',(9.69136378659227,1067.7251047501,408.072838296421));
#126518=CARTESIAN_POINT('',(9.69136378659227,1078.73142393294,406.972480230746));
#126519=CARTESIAN_POINT('Origin',(9.69136378659227,1078.73142393294,408.072838296421));
#126520=CARTESIAN_POINT('',(9.69136378659227,1076.73142393294,406.972480230746));
#126521=CARTESIAN_POINT('',(9.69136378659227,1067.7251047501,406.972480230746));
#126522=CARTESIAN_POINT('Origin',(9.69136378659227,1076.73142393294,408.072838296421));
#126523=CARTESIAN_POINT('Origin',(9.69136378659227,1067.7251047501,408.072838296421));
#126524=CARTESIAN_POINT('',(9.69136378659227,1076.73142393294,407.572480230746));
#126525=CARTESIAN_POINT('Origin',(9.69136378659227,1076.73142393294,408.072838296421));
#126526=CARTESIAN_POINT('',(9.69136378659227,1082.7251047501,407.572480230746));
#126527=CARTESIAN_POINT('',(9.69136378659227,1067.7251047501,407.572480230746));
#126528=CARTESIAN_POINT('Origin',(9.69136378659227,1082.7251047501,408.072838296421));
#126529=CARTESIAN_POINT('Origin',(16.2097648263488,1067.7251047501,402.518757076657));
#126530=CARTESIAN_POINT('',(16.2097648263488,1078.73142393294,401.30472550992));
#126531=CARTESIAN_POINT('Origin',(16.2097648263488,1078.73142393294,402.518757076657));
#126532=CARTESIAN_POINT('',(16.2097648263488,1076.73142393294,401.30472550992));
#126533=CARTESIAN_POINT('',(16.2097648263488,1067.7251047501,401.30472550992));
#126534=CARTESIAN_POINT('Origin',(16.2097648263488,1076.73142393294,402.518757076657));
#126535=CARTESIAN_POINT('Origin',(16.2097648263488,1067.7251047501,402.518757076657));
#126536=CARTESIAN_POINT('',(16.2097648263488,1076.73142393294,401.90472550992));
#126537=CARTESIAN_POINT('Origin',(16.2097648263488,1076.73142393294,402.518757076657));
#126538=CARTESIAN_POINT('',(16.2097648263488,1082.7251047501,401.90472550992));
#126539=CARTESIAN_POINT('',(16.2097648263488,1067.7251047501,401.90472550992));
#126540=CARTESIAN_POINT('Origin',(16.2097648263488,1082.7251047501,402.518757076657));
#126541=CARTESIAN_POINT('Origin',(23.302918507427,1067.7251047501,398.98236617956));
#126542=CARTESIAN_POINT('',(23.302918507427,1078.73142393294,397.653558215986));
#126543=CARTESIAN_POINT('Origin',(23.302918507427,1078.73142393294,398.98236617956));
#126544=CARTESIAN_POINT('',(23.302918507427,1076.73142393294,397.653558215986));
#126545=CARTESIAN_POINT('',(23.302918507427,1067.7251047501,397.653558215986));
#126546=CARTESIAN_POINT('Origin',(23.302918507427,1076.73142393294,398.98236617956));
#126547=CARTESIAN_POINT('Origin',(23.302918507427,1067.7251047501,398.98236617956));
#126548=CARTESIAN_POINT('',(23.302918507427,1076.73142393294,398.253558215986));
#126549=CARTESIAN_POINT('Origin',(23.302918507427,1076.73142393294,398.98236617956));
#126550=CARTESIAN_POINT('',(23.302918507427,1082.7251047501,398.253558215986));
#126551=CARTESIAN_POINT('',(23.302918507427,1067.7251047501,398.253558215986));
#126552=CARTESIAN_POINT('Origin',(23.302918507427,1082.7251047501,398.98236617956));
#126553=CARTESIAN_POINT('Origin',(32.1589076220714,1067.7251047501,396.243042623298));
#126554=CARTESIAN_POINT('',(32.1589076220714,1078.73142393294,394.781925621481));
#126555=CARTESIAN_POINT('Origin',(32.1589076220714,1078.73142393294,396.243042623298));
#126556=CARTESIAN_POINT('',(32.1589076220714,1076.73142393294,394.781925621481));
#126557=CARTESIAN_POINT('',(32.1589076220714,1067.7251047501,394.781925621481));
#126558=CARTESIAN_POINT('Origin',(32.1589076220714,1076.73142393294,396.243042623298));
#126559=CARTESIAN_POINT('Origin',(32.1589076220714,1067.7251047501,396.243042623298));
#126560=CARTESIAN_POINT('',(32.1589076220714,1076.73142393294,395.381925621481));
#126561=CARTESIAN_POINT('Origin',(32.1589076220714,1076.73142393294,396.243042623298));
#126562=CARTESIAN_POINT('',(32.1589076220714,1082.7251047501,395.381925621481));
#126563=CARTESIAN_POINT('',(32.1589076220714,1067.7251047501,395.381925621481));
#126564=CARTESIAN_POINT('Origin',(32.1589076220714,1082.7251047501,396.243042623298));
#126565=CARTESIAN_POINT('Origin',(41.0676411737322,1067.7251047501,395.785012011284));
#126566=CARTESIAN_POINT('',(41.0676411737322,1078.73142393294,394.164529968659));
#126567=CARTESIAN_POINT('Origin',(41.0676411737322,1078.73142393294,395.785012011284));
#126568=CARTESIAN_POINT('',(41.0676411737322,1076.73142393294,394.164529968659));
#126569=CARTESIAN_POINT('',(41.0676411737322,1067.7251047501,394.164529968659));
#126570=CARTESIAN_POINT('Origin',(41.0676411737322,1076.73142393294,395.785012011284));
#126571=CARTESIAN_POINT('Origin',(41.0676411737322,1067.7251047501,395.785012011284));
#126572=CARTESIAN_POINT('',(41.0676411737322,1076.73142393294,394.764529968659));
#126573=CARTESIAN_POINT('Origin',(41.0676411737322,1076.73142393294,395.785012011284));
#126574=CARTESIAN_POINT('',(41.0676411737322,1082.7251047501,394.764529968659));
#126575=CARTESIAN_POINT('',(41.0676411737322,1067.7251047501,394.764529968659));
#126576=CARTESIAN_POINT('Origin',(41.0676411737322,1082.7251047501,395.785012011284));
#126577=CARTESIAN_POINT('Origin',(51.2135807025659,1067.7251047501,396.539009167687));
#126578=CARTESIAN_POINT('',(51.2135807025659,1078.73142393294,394.838008944604));
#126579=CARTESIAN_POINT('Origin',(51.2135807025659,1078.73142393294,396.539009167687));
#126580=CARTESIAN_POINT('',(51.2135807025659,1076.73142393294,394.838008944604));
#126581=CARTESIAN_POINT('',(51.2135807025659,1067.7251047501,394.838008944604));
#126582=CARTESIAN_POINT('Origin',(51.2135807025659,1076.73142393294,396.539009167687));
#126583=CARTESIAN_POINT('Origin',(51.2135807025659,1067.7251047501,396.539009167687));
#126584=CARTESIAN_POINT('',(51.2135807025659,1076.73142393294,395.438008944604));
#126585=CARTESIAN_POINT('Origin',(51.2135807025659,1076.73142393294,396.539009167687));
#126586=CARTESIAN_POINT('',(51.2135807025659,1082.7251047501,395.438008944604));
#126587=CARTESIAN_POINT('',(51.2135807025659,1067.7251047501,395.438008944604));
#126588=CARTESIAN_POINT('Origin',(51.2135807025659,1082.7251047501,396.539009167687));
#126589=CARTESIAN_POINT('Origin',(60.6270981054991,1067.7251047501,399.492685363169));
#126590=CARTESIAN_POINT('',(60.6270981054991,1078.73142393294,397.771410731125));
#126591=CARTESIAN_POINT('Origin',(60.6270981054991,1078.73142393294,399.492685363169));
#126592=CARTESIAN_POINT('',(60.6270981054991,1076.73142393294,397.771410731125));
#126593=CARTESIAN_POINT('',(60.6270981054991,1067.7251047501,397.771410731125));
#126594=CARTESIAN_POINT('Origin',(60.6270981054991,1076.73142393294,399.492685363169));
#126595=CARTESIAN_POINT('Origin',(60.6270981054991,1067.7251047501,399.492685363169));
#126596=CARTESIAN_POINT('',(60.6270981054991,1076.73142393294,398.371410731125));
#126597=CARTESIAN_POINT('Origin',(60.6270981054991,1076.73142393294,399.492685363169));
#126598=CARTESIAN_POINT('',(60.6270981054991,1082.7251047501,398.371410731125));
#126599=CARTESIAN_POINT('',(60.6270981054991,1067.7251047501,398.371410731125));
#126600=CARTESIAN_POINT('Origin',(60.6270981054991,1082.7251047501,399.492685363169));
#126601=CARTESIAN_POINT('Origin',(71.0377028430577,1067.7251047501,404.114811351457));
#126602=CARTESIAN_POINT('',(71.0377028430577,1078.73142393294,402.332818697052));
#126603=CARTESIAN_POINT('Origin',(71.0377028430577,1078.73142393294,404.114811351457));
#126604=CARTESIAN_POINT('',(71.0377028430577,1076.73142393294,402.332818697052));
#126605=CARTESIAN_POINT('',(71.0377028430577,1067.7251047501,402.332818697052));
#126606=CARTESIAN_POINT('Origin',(71.0377028430577,1076.73142393294,404.114811351457));
#126607=CARTESIAN_POINT('Origin',(71.0377028430577,1067.7251047501,404.114811351457));
#126608=CARTESIAN_POINT('',(71.0377028430577,1076.73142393294,402.932818697052));
#126609=CARTESIAN_POINT('Origin',(71.0377028430577,1076.73142393294,404.114811351457));
#126610=CARTESIAN_POINT('',(71.0377028430577,1082.7251047501,402.932818697052));
#126611=CARTESIAN_POINT('',(71.0377028430577,1067.7251047501,402.932818697052));
#126612=CARTESIAN_POINT('Origin',(71.0377028430577,1082.7251047501,404.114811351457));
#126613=CARTESIAN_POINT('Origin',(80.105874072553,1067.7251047501,410.725406198927));
#126614=CARTESIAN_POINT('',(80.105874072553,1078.73142393294,409.064525389007));
#126615=CARTESIAN_POINT('Origin',(80.105874072553,1078.73142393294,410.725406198927));
#126616=CARTESIAN_POINT('',(80.105874072553,1076.73142393294,409.064525389007));
#126617=CARTESIAN_POINT('',(80.105874072553,1067.7251047501,409.064525389007));
#126618=CARTESIAN_POINT('Origin',(80.105874072553,1076.73142393294,410.725406198927));
#126619=CARTESIAN_POINT('Origin',(80.105874072553,1067.7251047501,410.725406198927));
#126620=CARTESIAN_POINT('',(80.105874072553,1076.73142393294,409.664525389007));
#126621=CARTESIAN_POINT('Origin',(80.105874072553,1076.73142393294,410.725406198927));
#126622=CARTESIAN_POINT('',(80.105874072553,1082.7251047501,409.664525389007));
#126623=CARTESIAN_POINT('',(80.105874072553,1067.7251047501,409.664525389007));
#126624=CARTESIAN_POINT('Origin',(80.105874072553,1082.7251047501,410.725406198927));
#126625=CARTESIAN_POINT('Origin',(6.03918543248003,1067.7251047501,406.419490950441));
#126626=CARTESIAN_POINT('',(6.03918543248003,1078.73142393294,405.319132884767));
#126627=CARTESIAN_POINT('Origin',(6.03918543248003,1078.73142393294,406.419490950441));
#126628=CARTESIAN_POINT('',(6.03918543248003,1076.73142393294,405.319132884767));
#126629=CARTESIAN_POINT('',(6.03918543248003,1067.7251047501,405.319132884767));
#126630=CARTESIAN_POINT('Origin',(6.03918543248003,1076.73142393294,406.419490950441));
#126631=CARTESIAN_POINT('Origin',(6.03918543248003,1067.7251047501,406.419490950441));
#126632=CARTESIAN_POINT('',(6.03918543248003,1076.73142393294,405.919132884767));
#126633=CARTESIAN_POINT('Origin',(6.03918543248003,1076.73142393294,406.419490950441));
#126634=CARTESIAN_POINT('',(6.03918543248003,1082.7251047501,405.919132884767));
#126635=CARTESIAN_POINT('',(6.03918543248003,1067.7251047501,405.919132884767));
#126636=CARTESIAN_POINT('Origin',(6.03918543248003,1082.7251047501,406.419490950441));
#126637=CARTESIAN_POINT('Origin',(11.2603853527983,1067.7251047501,399.631527949444));
#126638=CARTESIAN_POINT('',(11.2603853527983,1078.73142393294,398.417496382707));
#126639=CARTESIAN_POINT('Origin',(11.2603853527983,1078.73142393294,399.631527949444));
#126640=CARTESIAN_POINT('',(11.2603853527983,1076.73142393294,398.417496382707));
#126641=CARTESIAN_POINT('',(11.2603853527983,1067.7251047501,398.417496382707));
#126642=CARTESIAN_POINT('Origin',(11.2603853527983,1076.73142393294,399.631527949444));
#126643=CARTESIAN_POINT('Origin',(11.2603853527983,1067.7251047501,399.631527949444));
#126644=CARTESIAN_POINT('',(11.2603853527983,1076.73142393294,399.017496382707));
#126645=CARTESIAN_POINT('Origin',(11.2603853527983,1076.73142393294,399.631527949444));
#126646=CARTESIAN_POINT('',(11.2603853527983,1082.7251047501,399.017496382707));
#126647=CARTESIAN_POINT('',(11.2603853527983,1067.7251047501,399.017496382707));
#126648=CARTESIAN_POINT('Origin',(11.2603853527983,1082.7251047501,399.631527949444));
#126649=CARTESIAN_POINT('Origin',(17.4632795967732,1067.7251047501,394.697666103129));
#126650=CARTESIAN_POINT('',(17.4632795967732,1078.73142393294,393.368858139556));
#126651=CARTESIAN_POINT('Origin',(17.4632795967732,1078.73142393294,394.697666103129));
#126652=CARTESIAN_POINT('',(17.4632795967732,1076.73142393294,393.368858139556));
#126653=CARTESIAN_POINT('',(17.4632795967732,1067.7251047501,393.368858139556));
#126654=CARTESIAN_POINT('Origin',(17.4632795967732,1076.73142393294,394.697666103129));
#126655=CARTESIAN_POINT('Origin',(17.4632795967732,1067.7251047501,394.697666103129));
#126656=CARTESIAN_POINT('',(17.4632795967732,1076.73142393294,393.968858139556));
#126657=CARTESIAN_POINT('Origin',(17.4632795967732,1076.73142393294,394.697666103129));
#126658=CARTESIAN_POINT('',(17.4632795967732,1082.7251047501,393.968858139556));
#126659=CARTESIAN_POINT('',(17.4632795967732,1067.7251047501,393.968858139556));
#126660=CARTESIAN_POINT('Origin',(17.4632795967732,1082.7251047501,394.697666103129));
#126661=CARTESIAN_POINT('Origin',(25.5562067091079,1067.7251047501,390.176939668248));
#126662=CARTESIAN_POINT('',(25.5562067091079,1078.73142393294,388.715822666431));
#126663=CARTESIAN_POINT('Origin',(25.5562067091079,1078.73142393294,390.176939668248));
#126664=CARTESIAN_POINT('',(25.5562067091079,1076.73142393294,388.715822666431));
#126665=CARTESIAN_POINT('',(25.5562067091079,1067.7251047501,388.715822666431));
#126666=CARTESIAN_POINT('Origin',(25.5562067091079,1076.73142393294,390.176939668248));
#126667=CARTESIAN_POINT('Origin',(25.5562067091079,1067.7251047501,390.176939668248));
#126668=CARTESIAN_POINT('',(25.5562067091079,1076.73142393294,389.315822666431));
#126669=CARTESIAN_POINT('Origin',(25.5562067091079,1076.73142393294,390.176939668248));
#126670=CARTESIAN_POINT('',(25.5562067091079,1082.7251047501,389.315822666431));
#126671=CARTESIAN_POINT('',(25.5562067091079,1067.7251047501,389.315822666431));
#126672=CARTESIAN_POINT('Origin',(25.5562067091079,1082.7251047501,390.176939668248));
#126673=CARTESIAN_POINT('Origin',(34.1750331392515,1067.7251047501,387.876688268273));
#126674=CARTESIAN_POINT('',(34.1750331392515,1078.73142393294,386.256206225648));
#126675=CARTESIAN_POINT('Origin',(34.1750331392515,1078.73142393294,387.876688268273));
#126676=CARTESIAN_POINT('',(34.1750331392515,1076.73142393294,386.256206225648));
#126677=CARTESIAN_POINT('',(34.1750331392515,1067.7251047501,386.256206225648));
#126678=CARTESIAN_POINT('Origin',(34.1750331392515,1076.73142393294,387.876688268273));
#126679=CARTESIAN_POINT('Origin',(34.1750331392515,1067.7251047501,387.876688268273));
#126680=CARTESIAN_POINT('',(34.1750331392515,1076.73142393294,386.856206225649));
#126681=CARTESIAN_POINT('Origin',(34.1750331392515,1076.73142393294,387.876688268273));
#126682=CARTESIAN_POINT('',(34.1750331392515,1082.7251047501,386.856206225649));
#126683=CARTESIAN_POINT('',(34.1750331392515,1067.7251047501,386.856206225649));
#126684=CARTESIAN_POINT('Origin',(34.1750331392515,1082.7251047501,387.876688268273));
#126685=CARTESIAN_POINT('Origin',(44.25602437023,1067.7251047501,386.504749335394));
#126686=CARTESIAN_POINT('',(44.25602437023,1078.73142393294,384.803749112311));
#126687=CARTESIAN_POINT('Origin',(44.25602437023,1078.73142393294,386.504749335394));
#126688=CARTESIAN_POINT('',(44.25602437023,1076.73142393294,384.803749112311));
#126689=CARTESIAN_POINT('',(44.25602437023,1067.7251047501,384.803749112311));
#126690=CARTESIAN_POINT('Origin',(44.25602437023,1076.73142393294,386.504749335394));
#126691=CARTESIAN_POINT('Origin',(44.25602437023,1067.7251047501,386.504749335394));
#126692=CARTESIAN_POINT('',(44.25602437023,1076.73142393294,385.403749112311));
#126693=CARTESIAN_POINT('Origin',(44.25602437023,1076.73142393294,386.504749335394));
#126694=CARTESIAN_POINT('',(44.25602437023,1082.7251047501,385.403749112311));
#126695=CARTESIAN_POINT('',(44.25602437023,1067.7251047501,385.403749112311));
#126696=CARTESIAN_POINT('Origin',(44.25602437023,1082.7251047501,386.504749335394));
#126697=CARTESIAN_POINT('Origin',(54.0779376443059,1067.7251047501,387.436700299563));
#126698=CARTESIAN_POINT('',(54.0779376443059,1078.73142393294,385.71542566752));
#126699=CARTESIAN_POINT('Origin',(54.0779376443059,1078.73142393294,387.436700299563));
#126700=CARTESIAN_POINT('',(54.0779376443059,1076.73142393294,385.71542566752));
#126701=CARTESIAN_POINT('',(54.0779376443059,1067.7251047501,385.71542566752));
#126702=CARTESIAN_POINT('Origin',(54.0779376443059,1076.73142393294,387.436700299563));
#126703=CARTESIAN_POINT('Origin',(54.0779376443059,1067.7251047501,387.436700299563));
#126704=CARTESIAN_POINT('',(54.0779376443059,1076.73142393294,386.31542566752));
#126705=CARTESIAN_POINT('Origin',(54.0779376443059,1076.73142393294,387.436700299563));
#126706=CARTESIAN_POINT('',(54.0779376443059,1082.7251047501,386.31542566752));
#126707=CARTESIAN_POINT('',(54.0779376443059,1067.7251047501,386.31542566752));
#126708=CARTESIAN_POINT('Origin',(54.0779376443059,1082.7251047501,387.436700299563));
#126709=CARTESIAN_POINT('Origin',(65.2220397199346,1067.7251047501,389.793335311876));
#126710=CARTESIAN_POINT('',(65.2220397199346,1078.73142393294,388.011342657471));
#126711=CARTESIAN_POINT('Origin',(65.2220397199346,1078.73142393294,389.793335311876));
#126712=CARTESIAN_POINT('',(65.2220397199346,1076.73142393294,388.011342657471));
#126713=CARTESIAN_POINT('',(65.2220397199346,1067.7251047501,388.011342657471));
#126714=CARTESIAN_POINT('Origin',(65.2220397199346,1076.73142393294,389.793335311876));
#126715=CARTESIAN_POINT('Origin',(65.2220397199346,1067.7251047501,389.793335311876));
#126716=CARTESIAN_POINT('',(65.2220397199346,1076.73142393294,388.611342657471));
#126717=CARTESIAN_POINT('Origin',(65.2220397199346,1076.73142393294,389.793335311876));
#126718=CARTESIAN_POINT('',(65.2220397199346,1082.7251047501,388.611342657471));
#126719=CARTESIAN_POINT('',(65.2220397199346,1067.7251047501,388.611342657471));
#126720=CARTESIAN_POINT('Origin',(65.2220397199346,1082.7251047501,389.793335311876));
#126721=CARTESIAN_POINT('Origin',(75.4664696031574,1067.7251047501,394.374093988403));
#126722=CARTESIAN_POINT('',(75.4664696031574,1078.73142393294,392.713213178482));
#126723=CARTESIAN_POINT('Origin',(75.4664696031574,1078.73142393294,394.374093988403));
#126724=CARTESIAN_POINT('',(75.4664696031574,1076.73142393294,392.713213178482));
#126725=CARTESIAN_POINT('',(75.4664696031574,1067.7251047501,392.713213178482));
#126726=CARTESIAN_POINT('Origin',(75.4664696031574,1076.73142393294,394.374093988403));
#126727=CARTESIAN_POINT('Origin',(75.4664696031574,1067.7251047501,394.374093988403));
#126728=CARTESIAN_POINT('',(75.4664696031574,1076.73142393294,393.313213178482));
#126729=CARTESIAN_POINT('Origin',(75.4664696031574,1076.73142393294,394.374093988403));
#126730=CARTESIAN_POINT('',(75.4664696031574,1082.7251047501,393.313213178482));
#126731=CARTESIAN_POINT('',(75.4664696031574,1067.7251047501,393.313213178482));
#126732=CARTESIAN_POINT('Origin',(75.4664696031574,1082.7251047501,394.374093988403));
#126733=CARTESIAN_POINT('Origin',(2.12306569574147,1067.7251047501,405.561603787563));
#126734=CARTESIAN_POINT('',(2.12306569574147,1078.73142393294,404.461245721888));
#126735=CARTESIAN_POINT('Origin',(2.12306569574147,1078.73142393294,405.561603787563));
#126736=CARTESIAN_POINT('',(2.12306569574147,1076.73142393294,404.461245721888));
#126737=CARTESIAN_POINT('',(2.12306569574147,1067.7251047501,404.461245721888));
#126738=CARTESIAN_POINT('Origin',(2.12306569574147,1076.73142393294,405.561603787563));
#126739=CARTESIAN_POINT('Origin',(2.12306569574147,1067.7251047501,405.561603787563));
#126740=CARTESIAN_POINT('',(2.12306569574147,1076.73142393294,405.061245721888));
#126741=CARTESIAN_POINT('Origin',(2.12306569574147,1076.73142393294,405.561603787563));
#126742=CARTESIAN_POINT('',(2.12306569574147,1082.7251047501,405.061245721888));
#126743=CARTESIAN_POINT('',(2.12306569574147,1067.7251047501,405.061245721888));
#126744=CARTESIAN_POINT('Origin',(2.12306569574147,1082.7251047501,405.561603787563));
#126745=CARTESIAN_POINT('Origin',(5.81887300600675,1067.7251047501,397.836425560737));
#126746=CARTESIAN_POINT('',(5.81887300600675,1078.73142393294,396.622393994));
#126747=CARTESIAN_POINT('Origin',(5.81887300600675,1078.73142393294,397.836425560737));
#126748=CARTESIAN_POINT('',(5.81887300600675,1076.73142393294,396.622393994));
#126749=CARTESIAN_POINT('',(5.81887300600675,1067.7251047501,396.622393994));
#126750=CARTESIAN_POINT('Origin',(5.81887300600675,1076.73142393294,397.836425560737));
#126751=CARTESIAN_POINT('Origin',(5.81887300600675,1067.7251047501,397.836425560737));
#126752=CARTESIAN_POINT('',(5.81887300600675,1076.73142393294,397.222393994));
#126753=CARTESIAN_POINT('Origin',(5.81887300600675,1076.73142393294,397.836425560737));
#126754=CARTESIAN_POINT('',(5.81887300600675,1082.7251047501,397.222393994));
#126755=CARTESIAN_POINT('',(5.81887300600675,1067.7251047501,397.222393994));
#126756=CARTESIAN_POINT('Origin',(5.81887300600675,1082.7251047501,397.836425560737));
#126757=CARTESIAN_POINT('Origin',(10.8604115696276,1067.7251047501,391.720726203183));
#126758=CARTESIAN_POINT('',(10.8604115696276,1078.73142393294,390.39191823961));
#126759=CARTESIAN_POINT('Origin',(10.8604115696276,1078.73142393294,391.720726203183));
#126760=CARTESIAN_POINT('',(10.8604115696276,1076.73142393294,390.39191823961));
#126761=CARTESIAN_POINT('',(10.8604115696276,1067.7251047501,390.39191823961));
#126762=CARTESIAN_POINT('Origin',(10.8604115696276,1076.73142393294,391.720726203183));
#126763=CARTESIAN_POINT('Origin',(10.8604115696276,1067.7251047501,391.720726203183));
#126764=CARTESIAN_POINT('',(10.8604115696276,1076.73142393294,390.99191823961));
#126765=CARTESIAN_POINT('Origin',(10.8604115696276,1076.73142393294,391.720726203183));
#126766=CARTESIAN_POINT('',(10.8604115696276,1082.7251047501,390.99191823961));
#126767=CARTESIAN_POINT('',(10.8604115696276,1067.7251047501,390.99191823961));
#126768=CARTESIAN_POINT('Origin',(10.8604115696276,1082.7251047501,391.720726203183));
#126769=CARTESIAN_POINT('Origin',(17.8365769306708,1067.7251047501,385.61617432774));
#126770=CARTESIAN_POINT('',(17.8365769306708,1078.73142393294,384.155057325923));
#126771=CARTESIAN_POINT('Origin',(17.8365769306708,1078.73142393294,385.61617432774));
#126772=CARTESIAN_POINT('',(17.8365769306708,1076.73142393294,384.155057325923));
#126773=CARTESIAN_POINT('',(17.8365769306708,1067.7251047501,384.155057325923));
#126774=CARTESIAN_POINT('Origin',(17.8365769306708,1076.73142393294,385.61617432774));
#126775=CARTESIAN_POINT('Origin',(17.8365769306708,1067.7251047501,385.61617432774));
#126776=CARTESIAN_POINT('',(17.8365769306708,1076.73142393294,384.755057325923));
#126777=CARTESIAN_POINT('Origin',(17.8365769306708,1076.73142393294,385.61617432774));
#126778=CARTESIAN_POINT('',(17.8365769306708,1082.7251047501,384.755057325923));
#126779=CARTESIAN_POINT('',(17.8365769306708,1067.7251047501,384.755057325923));
#126780=CARTESIAN_POINT('Origin',(17.8365769306708,1082.7251047501,385.61617432774));
#126781=CARTESIAN_POINT('Origin',(25.7888121665822,1067.7251047501,381.574234163814));
#126782=CARTESIAN_POINT('',(25.7888121665822,1078.73142393294,379.953752121189));
#126783=CARTESIAN_POINT('Origin',(25.7888121665822,1078.73142393294,381.574234163814));
#126784=CARTESIAN_POINT('',(25.7888121665822,1076.73142393294,379.953752121189));
#126785=CARTESIAN_POINT('',(25.7888121665822,1067.7251047501,379.953752121189));
#126786=CARTESIAN_POINT('Origin',(25.7888121665822,1076.73142393294,381.574234163814));
#126787=CARTESIAN_POINT('Origin',(25.7888121665822,1067.7251047501,381.574234163814));
#126788=CARTESIAN_POINT('',(25.7888121665822,1076.73142393294,380.55375212119));
#126789=CARTESIAN_POINT('Origin',(25.7888121665822,1076.73142393294,381.574234163814));
#126790=CARTESIAN_POINT('',(25.7888121665822,1082.7251047501,380.55375212119));
#126791=CARTESIAN_POINT('',(25.7888121665822,1067.7251047501,380.55375212119));
#126792=CARTESIAN_POINT('Origin',(25.7888121665822,1082.7251047501,381.574234163814));
#126793=CARTESIAN_POINT('Origin',(35.3642674089487,1067.7251047501,378.136319456314));
#126794=CARTESIAN_POINT('',(35.3642674089487,1078.73142393294,376.435319233231));
#126795=CARTESIAN_POINT('Origin',(35.3642674089487,1078.73142393294,378.136319456314));
#126796=CARTESIAN_POINT('',(35.3642674089487,1076.73142393294,376.435319233231));
#126797=CARTESIAN_POINT('',(35.3642674089487,1067.7251047501,376.435319233231));
#126798=CARTESIAN_POINT('Origin',(35.3642674089487,1076.73142393294,378.136319456314));
#126799=CARTESIAN_POINT('Origin',(35.3642674089487,1067.7251047501,378.136319456314));
#126800=CARTESIAN_POINT('',(35.3642674089487,1076.73142393294,377.035319233231));
#126801=CARTESIAN_POINT('Origin',(35.3642674089487,1076.73142393294,378.136319456314));
#126802=CARTESIAN_POINT('',(35.3642674089487,1082.7251047501,377.035319233231));
#126803=CARTESIAN_POINT('',(35.3642674089487,1067.7251047501,377.035319233231));
#126804=CARTESIAN_POINT('Origin',(35.3642674089487,1082.7251047501,378.136319456314));
#126805=CARTESIAN_POINT('Origin',(45.1653118133212,1067.7251047501,377.005814460039));
#126806=CARTESIAN_POINT('',(45.1653118133212,1078.73142393294,375.284539827995));
#126807=CARTESIAN_POINT('Origin',(45.1653118133212,1078.73142393294,377.005814460039));
#126808=CARTESIAN_POINT('',(45.1653118133212,1076.73142393294,375.284539827995));
#126809=CARTESIAN_POINT('',(45.1653118133212,1067.7251047501,375.284539827995));
#126810=CARTESIAN_POINT('Origin',(45.1653118133212,1076.73142393294,377.005814460039));
#126811=CARTESIAN_POINT('Origin',(45.1653118133212,1067.7251047501,377.005814460039));
#126812=CARTESIAN_POINT('',(45.1653118133212,1076.73142393294,375.884539827995));
#126813=CARTESIAN_POINT('Origin',(45.1653118133212,1076.73142393294,377.005814460039));
#126814=CARTESIAN_POINT('',(45.1653118133212,1082.7251047501,375.884539827995));
#126815=CARTESIAN_POINT('',(45.1653118133212,1067.7251047501,375.884539827995));
#126816=CARTESIAN_POINT('Origin',(45.1653118133212,1082.7251047501,377.005814460039));
#126817=CARTESIAN_POINT('Origin',(56.5558604909803,1067.7251047501,376.993962237948));
#126818=CARTESIAN_POINT('',(56.5558604909803,1078.73142393294,375.211969583543));
#126819=CARTESIAN_POINT('Origin',(56.5558604909803,1078.73142393294,376.993962237948));
#126820=CARTESIAN_POINT('',(56.5558604909803,1076.73142393294,375.211969583543));
#126821=CARTESIAN_POINT('',(56.5558604909803,1067.7251047501,375.211969583543));
#126822=CARTESIAN_POINT('Origin',(56.5558604909803,1076.73142393294,376.993962237948));
#126823=CARTESIAN_POINT('Origin',(56.5558604909803,1067.7251047501,376.993962237948));
#126824=CARTESIAN_POINT('',(56.5558604909803,1076.73142393294,375.811969583543));
#126825=CARTESIAN_POINT('Origin',(56.5558604909803,1076.73142393294,376.993962237948));
#126826=CARTESIAN_POINT('',(56.5558604909803,1082.7251047501,375.811969583543));
#126827=CARTESIAN_POINT('',(56.5558604909803,1067.7251047501,375.811969583543));
#126828=CARTESIAN_POINT('Origin',(56.5558604909803,1082.7251047501,376.993962237948));
#126829=CARTESIAN_POINT('Origin',(67.5288182838053,1067.7251047501,379.344683608449));
#126830=CARTESIAN_POINT('',(67.5288182838053,1078.73142393294,377.683802798528));
#126831=CARTESIAN_POINT('Origin',(67.5288182838053,1078.73142393294,379.344683608449));
#126832=CARTESIAN_POINT('',(67.5288182838053,1076.73142393294,377.683802798528));
#126833=CARTESIAN_POINT('',(67.5288182838053,1067.7251047501,377.683802798528));
#126834=CARTESIAN_POINT('Origin',(67.5288182838053,1076.73142393294,379.344683608449));
#126835=CARTESIAN_POINT('Origin',(67.5288182838053,1067.7251047501,379.344683608449));
#126836=CARTESIAN_POINT('',(67.5288182838053,1076.73142393294,378.283802798528));
#126837=CARTESIAN_POINT('Origin',(67.5288182838053,1076.73142393294,379.344683608449));
#126838=CARTESIAN_POINT('',(67.5288182838053,1082.7251047501,378.283802798528));
#126839=CARTESIAN_POINT('',(67.5288182838053,1067.7251047501,378.283802798528));
#126840=CARTESIAN_POINT('Origin',(67.5288182838053,1082.7251047501,379.344683608449));
#126841=CARTESIAN_POINT('Origin',(-1.88584219950044,1067.7251047501,405.536670593404));
#126842=CARTESIAN_POINT('',(-1.88584219950044,1078.73142393294,404.436312527729));
#126843=CARTESIAN_POINT('Origin',(-1.88584219950044,1078.73142393294,405.536670593404));
#126844=CARTESIAN_POINT('',(-1.88584219950044,1076.73142393294,404.436312527729));
#126845=CARTESIAN_POINT('',(-1.88584219950044,1067.7251047501,404.436312527729));
#126846=CARTESIAN_POINT('Origin',(-1.88584219950044,1076.73142393294,405.536670593404));
#126847=CARTESIAN_POINT('Origin',(-1.88584219950044,1067.7251047501,405.536670593404));
#126848=CARTESIAN_POINT('',(-1.88584219950044,1076.73142393294,405.036312527729));
#126849=CARTESIAN_POINT('Origin',(-1.88584219950044,1076.73142393294,405.536670593404));
#126850=CARTESIAN_POINT('',(-1.88584219950044,1082.7251047501,405.036312527729));
#126851=CARTESIAN_POINT('',(-1.88584219950044,1067.7251047501,405.036312527729));
#126852=CARTESIAN_POINT('Origin',(-1.88584219950044,1082.7251047501,405.536670593404));
#126853=CARTESIAN_POINT('Origin',(0.123047986802127,1067.7251047501,397.211904498779));
#126854=CARTESIAN_POINT('',(0.123047986802127,1078.73142393294,395.997872932042));
#126855=CARTESIAN_POINT('Origin',(0.123047986802127,1078.73142393294,397.211904498779));
#126856=CARTESIAN_POINT('',(0.123047986802127,1076.73142393294,395.997872932042));
#126857=CARTESIAN_POINT('',(0.123047986802127,1067.7251047501,395.997872932042));
#126858=CARTESIAN_POINT('Origin',(0.123047986802127,1076.73142393294,397.211904498779));
#126859=CARTESIAN_POINT('Origin',(0.123047986802127,1067.7251047501,397.211904498779));
#126860=CARTESIAN_POINT('',(0.123047986802127,1076.73142393294,396.597872932042));
#126861=CARTESIAN_POINT('Origin',(0.123047986802127,1076.73142393294,397.211904498779));
#126862=CARTESIAN_POINT('',(0.123047986802127,1082.7251047501,396.597872932042));
#126863=CARTESIAN_POINT('',(0.123047986802127,1067.7251047501,396.597872932042));
#126864=CARTESIAN_POINT('Origin',(0.123047986802127,1082.7251047501,397.211904498779));
#126865=CARTESIAN_POINT('Origin',(3.7828914428526,1067.7251047501,390.181653038293));
#126866=CARTESIAN_POINT('',(3.7828914428526,1078.73142393294,388.85284507472));
#126867=CARTESIAN_POINT('Origin',(3.7828914428526,1078.73142393294,390.181653038293));
#126868=CARTESIAN_POINT('',(3.7828914428526,1076.73142393294,388.85284507472));
#126869=CARTESIAN_POINT('',(3.7828914428526,1067.7251047501,388.85284507472));
#126870=CARTESIAN_POINT('Origin',(3.7828914428526,1076.73142393294,390.181653038293));
#126871=CARTESIAN_POINT('Origin',(3.7828914428526,1067.7251047501,390.181653038293));
#126872=CARTESIAN_POINT('',(3.7828914428526,1076.73142393294,389.45284507472));
#126873=CARTESIAN_POINT('Origin',(3.7828914428526,1076.73142393294,390.181653038293));
#126874=CARTESIAN_POINT('',(3.7828914428526,1082.7251047501,389.45284507472));
#126875=CARTESIAN_POINT('',(3.7828914428526,1067.7251047501,389.45284507472));
#126876=CARTESIAN_POINT('Origin',(3.7828914428526,1082.7251047501,390.181653038293));
#126877=CARTESIAN_POINT('Origin',(9.33740315097129,1067.7251047501,382.760073932135));
#126878=CARTESIAN_POINT('',(9.33740315097129,1078.73142393294,381.298956930318));
#126879=CARTESIAN_POINT('Origin',(9.33740315097129,1078.73142393294,382.760073932135));
#126880=CARTESIAN_POINT('',(9.33740315097129,1076.73142393294,381.298956930318));
#126881=CARTESIAN_POINT('',(9.33740315097129,1067.7251047501,381.298956930318));
#126882=CARTESIAN_POINT('Origin',(9.33740315097129,1076.73142393294,382.760073932135));
#126883=CARTESIAN_POINT('Origin',(9.33740315097129,1067.7251047501,382.760073932135));
#126884=CARTESIAN_POINT('',(9.33740315097129,1076.73142393294,381.898956930318));
#126885=CARTESIAN_POINT('Origin',(9.33740315097129,1076.73142393294,382.760073932135));
#126886=CARTESIAN_POINT('',(9.33740315097129,1082.7251047501,381.898956930318));
#126887=CARTESIAN_POINT('',(9.33740315097129,1067.7251047501,381.898956930318));
#126888=CARTESIAN_POINT('Origin',(9.33740315097129,1082.7251047501,382.760073932135));
#126889=CARTESIAN_POINT('Origin',(16.2754963537827,1067.7251047501,377.153097184802));
#126890=CARTESIAN_POINT('',(16.2754963537827,1078.73142393294,375.532615142177));
#126891=CARTESIAN_POINT('Origin',(16.2754963537827,1078.73142393294,377.153097184802));
#126892=CARTESIAN_POINT('',(16.2754963537827,1076.73142393294,375.532615142177));
#126893=CARTESIAN_POINT('',(16.2754963537827,1067.7251047501,375.532615142177));
#126894=CARTESIAN_POINT('Origin',(16.2754963537827,1076.73142393294,377.153097184802));
#126895=CARTESIAN_POINT('Origin',(16.2754963537827,1067.7251047501,377.153097184802));
#126896=CARTESIAN_POINT('',(16.2754963537827,1076.73142393294,376.132615142177));
#126897=CARTESIAN_POINT('Origin',(16.2754963537827,1076.73142393294,377.153097184802));
#126898=CARTESIAN_POINT('',(16.2754963537827,1082.7251047501,376.132615142177));
#126899=CARTESIAN_POINT('',(16.2754963537827,1067.7251047501,376.132615142177));
#126900=CARTESIAN_POINT('Origin',(16.2754963537827,1082.7251047501,377.153097184802));
#126901=CARTESIAN_POINT('Origin',(24.9269222653138,1067.7251047501,371.799460072343));
#126902=CARTESIAN_POINT('',(24.9269222653138,1078.73142393294,370.09845984926));
#126903=CARTESIAN_POINT('Origin',(24.9269222653138,1078.73142393294,371.799460072343));
#126904=CARTESIAN_POINT('',(24.9269222653138,1076.73142393294,370.09845984926));
#126905=CARTESIAN_POINT('',(24.9269222653138,1067.7251047501,370.09845984926));
#126906=CARTESIAN_POINT('Origin',(24.9269222653138,1076.73142393294,371.799460072343));
#126907=CARTESIAN_POINT('Origin',(24.9269222653138,1067.7251047501,371.799460072343));
#126908=CARTESIAN_POINT('',(24.9269222653138,1076.73142393294,370.69845984926));
#126909=CARTESIAN_POINT('Origin',(24.9269222653138,1076.73142393294,371.799460072343));
#126910=CARTESIAN_POINT('',(24.9269222653138,1082.7251047501,370.69845984926));
#126911=CARTESIAN_POINT('',(24.9269222653138,1067.7251047501,370.69845984926));
#126912=CARTESIAN_POINT('Origin',(24.9269222653138,1082.7251047501,371.799460072343));
#126913=CARTESIAN_POINT('Origin',(34.2787451288828,1067.7251047501,368.655907608726));
#126914=CARTESIAN_POINT('',(34.2787451288828,1078.73142393294,366.934632976682));
#126915=CARTESIAN_POINT('Origin',(34.2787451288828,1078.73142393294,368.655907608726));
#126916=CARTESIAN_POINT('',(34.2787451288828,1076.73142393294,366.934632976682));
#126917=CARTESIAN_POINT('',(34.2787451288828,1067.7251047501,366.934632976682));
#126918=CARTESIAN_POINT('Origin',(34.2787451288828,1076.73142393294,368.655907608726));
#126919=CARTESIAN_POINT('Origin',(34.2787451288828,1067.7251047501,368.655907608726));
#126920=CARTESIAN_POINT('',(34.2787451288828,1076.73142393294,367.534632976682));
#126921=CARTESIAN_POINT('Origin',(34.2787451288828,1076.73142393294,368.655907608726));
#126922=CARTESIAN_POINT('',(34.2787451288828,1082.7251047501,367.534632976682));
#126923=CARTESIAN_POINT('',(34.2787451288828,1067.7251047501,367.534632976682));
#126924=CARTESIAN_POINT('Origin',(34.2787451288828,1082.7251047501,368.655907608726));
#126925=CARTESIAN_POINT('Origin',(45.4179187734419,1067.7251047501,366.27608615121));
#126926=CARTESIAN_POINT('',(45.4179187734419,1078.73142393294,364.494093496805));
#126927=CARTESIAN_POINT('Origin',(45.4179187734419,1078.73142393294,366.27608615121));
#126928=CARTESIAN_POINT('',(45.4179187734419,1076.73142393294,364.494093496805));
#126929=CARTESIAN_POINT('',(45.4179187734419,1067.7251047501,364.494093496805));
#126930=CARTESIAN_POINT('Origin',(45.4179187734419,1076.73142393294,366.27608615121));
#126931=CARTESIAN_POINT('Origin',(45.4179187734419,1067.7251047501,366.27608615121));
#126932=CARTESIAN_POINT('',(45.4179187734419,1076.73142393294,365.094093496805));
#126933=CARTESIAN_POINT('Origin',(45.4179187734419,1076.73142393294,366.27608615121));
#126934=CARTESIAN_POINT('',(45.4179187734419,1082.7251047501,365.094093496805));
#126935=CARTESIAN_POINT('',(45.4179187734419,1067.7251047501,365.094093496805));
#126936=CARTESIAN_POINT('Origin',(45.4179187734419,1082.7251047501,366.27608615121));
#126937=CARTESIAN_POINT('Origin',(56.6398335662292,1067.7251047501,366.294032411781));
#126938=CARTESIAN_POINT('',(56.6398335662292,1078.73142393294,364.63315160186));
#126939=CARTESIAN_POINT('Origin',(56.6398335662292,1078.73142393294,366.294032411781));
#126940=CARTESIAN_POINT('',(56.6398335662292,1076.73142393294,364.63315160186));
#126941=CARTESIAN_POINT('',(56.6398335662292,1067.7251047501,364.63315160186));
#126942=CARTESIAN_POINT('Origin',(56.6398335662292,1076.73142393294,366.294032411781));
#126943=CARTESIAN_POINT('Origin',(56.6398335662292,1067.7251047501,366.294032411781));
#126944=CARTESIAN_POINT('',(56.6398335662292,1076.73142393294,365.23315160186));
#126945=CARTESIAN_POINT('Origin',(56.6398335662292,1076.73142393294,366.294032411781));
#126946=CARTESIAN_POINT('',(56.6398335662292,1082.7251047501,365.23315160186));
#126947=CARTESIAN_POINT('',(56.6398335662292,1067.7251047501,365.23315160186));
#126948=CARTESIAN_POINT('Origin',(56.6398335662292,1082.7251047501,366.294032411781));
#126949=CARTESIAN_POINT('Origin',(-5.81232974134926,1067.7251047501,406.345781068191));
#126950=CARTESIAN_POINT('',(-5.81232974134926,1078.73142393294,405.245423002516));
#126951=CARTESIAN_POINT('Origin',(-5.81232974134926,1078.73142393294,406.345781068191));
#126952=CARTESIAN_POINT('',(-5.81232974134926,1076.73142393294,405.245423002516));
#126953=CARTESIAN_POINT('',(-5.81232974134926,1067.7251047501,405.245423002516));
#126954=CARTESIAN_POINT('Origin',(-5.81232974134926,1076.73142393294,406.345781068191));
#126955=CARTESIAN_POINT('Origin',(-5.81232974134926,1067.7251047501,406.345781068191));
#126956=CARTESIAN_POINT('',(-5.81232974134926,1076.73142393294,405.845423002516));
#126957=CARTESIAN_POINT('Origin',(-5.81232974134926,1076.73142393294,406.345781068191));
#126958=CARTESIAN_POINT('',(-5.81232974134926,1082.7251047501,405.845423002516));
#126959=CARTESIAN_POINT('',(-5.81232974134926,1067.7251047501,405.845423002516));
#126960=CARTESIAN_POINT('Origin',(-5.81232974134926,1082.7251047501,406.345781068191));
#126961=CARTESIAN_POINT('Origin',(-5.5781548198755,1067.7251047501,397.785259330762));
#126962=CARTESIAN_POINT('',(-5.5781548198755,1078.73142393294,396.571227764025));
#126963=CARTESIAN_POINT('Origin',(-5.5781548198755,1078.73142393294,397.785259330762));
#126964=CARTESIAN_POINT('',(-5.5781548198755,1076.73142393294,396.571227764025));
#126965=CARTESIAN_POINT('',(-5.5781548198755,1067.7251047501,396.571227764025));
#126966=CARTESIAN_POINT('Origin',(-5.5781548198755,1076.73142393294,397.785259330762));
#126967=CARTESIAN_POINT('Origin',(-5.5781548198755,1067.7251047501,397.785259330762));
#126968=CARTESIAN_POINT('',(-5.5781548198755,1076.73142393294,397.171227764025));
#126969=CARTESIAN_POINT('Origin',(-5.5781548198755,1076.73142393294,397.785259330762));
#126970=CARTESIAN_POINT('',(-5.5781548198755,1082.7251047501,397.171227764025));
#126971=CARTESIAN_POINT('',(-5.5781548198755,1067.7251047501,397.171227764025));
#126972=CARTESIAN_POINT('Origin',(-5.5781548198755,1082.7251047501,397.785259330762));
#126973=CARTESIAN_POINT('Origin',(-3.45995919230213,1067.7251047501,390.147711491056));
#126974=CARTESIAN_POINT('',(-3.45995919230213,1078.73142393294,388.818903527483));
#126975=CARTESIAN_POINT('Origin',(-3.45995919230213,1078.73142393294,390.147711491056));
#126976=CARTESIAN_POINT('',(-3.45995919230213,1076.73142393294,388.818903527483));
#126977=CARTESIAN_POINT('',(-3.45995919230213,1067.7251047501,388.818903527483));
#126978=CARTESIAN_POINT('Origin',(-3.45995919230213,1076.73142393294,390.147711491056));
#126979=CARTESIAN_POINT('Origin',(-3.45995919230213,1067.7251047501,390.147711491056));
#126980=CARTESIAN_POINT('',(-3.45995919230213,1076.73142393294,389.418903527483));
#126981=CARTESIAN_POINT('Origin',(-3.45995919230213,1076.73142393294,390.147711491056));
#126982=CARTESIAN_POINT('',(-3.45995919230213,1082.7251047501,389.418903527483));
#126983=CARTESIAN_POINT('',(-3.45995919230213,1067.7251047501,389.418903527483));
#126984=CARTESIAN_POINT('Origin',(-3.45995919230213,1082.7251047501,390.147711491056));
#126985=CARTESIAN_POINT('Origin',(0.430140047742833,1067.7251047501,381.733463773809));
#126986=CARTESIAN_POINT('',(0.430140047742833,1078.73142393294,380.272346771993));
#126987=CARTESIAN_POINT('Origin',(0.430140047742833,1078.73142393294,381.733463773809));
#126988=CARTESIAN_POINT('',(0.430140047742833,1076.73142393294,380.272346771993));
#126989=CARTESIAN_POINT('',(0.430140047742833,1067.7251047501,380.272346771993));
#126990=CARTESIAN_POINT('Origin',(0.430140047742833,1076.73142393294,381.733463773809));
#126991=CARTESIAN_POINT('Origin',(0.430140047742833,1067.7251047501,381.733463773809));
#126992=CARTESIAN_POINT('',(0.430140047742833,1076.73142393294,380.872346771993));
#126993=CARTESIAN_POINT('Origin',(0.430140047742833,1076.73142393294,381.733463773809));
#126994=CARTESIAN_POINT('',(0.430140047742833,1082.7251047501,380.872346771993));
#126995=CARTESIAN_POINT('',(0.430140047742833,1067.7251047501,380.872346771993));
#126996=CARTESIAN_POINT('Origin',(0.430140047742833,1082.7251047501,381.733463773809));
#126997=CARTESIAN_POINT('Origin',(6.05086325182658,1067.7251047501,374.806502232188));
#126998=CARTESIAN_POINT('',(6.05086325182658,1078.73142393294,373.186020189563));
#126999=CARTESIAN_POINT('Origin',(6.05086325182658,1078.73142393294,374.806502232188));
#127000=CARTESIAN_POINT('',(6.05086325182658,1076.73142393294,373.186020189563));
#127001=CARTESIAN_POINT('',(6.05086325182658,1067.7251047501,373.186020189563));
#127002=CARTESIAN_POINT('Origin',(6.05086325182658,1076.73142393294,374.806502232188));
#127003=CARTESIAN_POINT('Origin',(6.05086325182658,1067.7251047501,374.806502232188));
#127004=CARTESIAN_POINT('',(6.05086325182658,1076.73142393294,373.786020189563));
#127005=CARTESIAN_POINT('Origin',(6.05086325182658,1076.73142393294,374.806502232188));
#127006=CARTESIAN_POINT('',(6.05086325182658,1082.7251047501,373.786020189563));
#127007=CARTESIAN_POINT('',(6.05086325182658,1067.7251047501,373.786020189563));
#127008=CARTESIAN_POINT('Origin',(6.05086325182658,1082.7251047501,374.806502232188));
#127009=CARTESIAN_POINT('Origin',(13.4001510060409,1067.7251047501,367.771122346186));
#127010=CARTESIAN_POINT('',(13.4001510060409,1078.73142393294,366.070122123103));
#127011=CARTESIAN_POINT('Origin',(13.4001510060409,1078.73142393294,367.771122346186));
#127012=CARTESIAN_POINT('',(13.4001510060409,1076.73142393294,366.070122123103));
#127013=CARTESIAN_POINT('',(13.4001510060409,1067.7251047501,366.070122123103));
#127014=CARTESIAN_POINT('Origin',(13.4001510060409,1076.73142393294,367.771122346186));
#127015=CARTESIAN_POINT('Origin',(13.4001510060409,1067.7251047501,367.771122346186));
#127016=CARTESIAN_POINT('',(13.4001510060409,1076.73142393294,366.670122123103));
#127017=CARTESIAN_POINT('Origin',(13.4001510060409,1076.73142393294,367.771122346186));
#127018=CARTESIAN_POINT('',(13.4001510060409,1082.7251047501,366.670122123103));
#127019=CARTESIAN_POINT('',(13.4001510060409,1067.7251047501,366.670122123103));
#127020=CARTESIAN_POINT('Origin',(13.4001510060409,1082.7251047501,367.771122346186));
#127021=CARTESIAN_POINT('Origin',(21.8940327946435,1067.7251047501,362.751910742325));
#127022=CARTESIAN_POINT('',(21.8940327946435,1078.73142393294,361.030636110281));
#127023=CARTESIAN_POINT('Origin',(21.8940327946435,1078.73142393294,362.751910742325));
#127024=CARTESIAN_POINT('',(21.8940327946435,1076.73142393294,361.030636110281));
#127025=CARTESIAN_POINT('',(21.8940327946435,1067.7251047501,361.030636110281));
#127026=CARTESIAN_POINT('Origin',(21.8940327946435,1076.73142393294,362.751910742325));
#127027=CARTESIAN_POINT('Origin',(21.8940327946435,1067.7251047501,362.751910742325));
#127028=CARTESIAN_POINT('',(21.8940327946435,1076.73142393294,361.630636110281));
#127029=CARTESIAN_POINT('Origin',(21.8940327946435,1076.73142393294,362.751910742325));
#127030=CARTESIAN_POINT('',(21.8940327946435,1082.7251047501,361.630636110281));
#127031=CARTESIAN_POINT('',(21.8940327946435,1067.7251047501,361.630636110281));
#127032=CARTESIAN_POINT('Origin',(21.8940327946435,1082.7251047501,362.751910742325));
#127033=CARTESIAN_POINT('Origin',(32.2949960661498,1067.7251047501,358.108129666728));
#127034=CARTESIAN_POINT('',(32.2949960661498,1078.73142393294,356.326137012323));
#127035=CARTESIAN_POINT('Origin',(32.2949960661498,1078.73142393294,358.108129666728));
#127036=CARTESIAN_POINT('',(32.2949960661498,1076.73142393294,356.326137012323));
#127037=CARTESIAN_POINT('',(32.2949960661498,1067.7251047501,356.326137012323));
#127038=CARTESIAN_POINT('Origin',(32.2949960661498,1076.73142393294,358.108129666728));
#127039=CARTESIAN_POINT('Origin',(32.2949960661498,1067.7251047501,358.108129666728));
#127040=CARTESIAN_POINT('',(32.2949960661498,1076.73142393294,356.926137012323));
#127041=CARTESIAN_POINT('Origin',(32.2949960661498,1076.73142393294,358.108129666728));
#127042=CARTESIAN_POINT('',(32.2949960661498,1082.7251047501,356.926137012323));
#127043=CARTESIAN_POINT('',(32.2949960661498,1067.7251047501,356.926137012323));
#127044=CARTESIAN_POINT('Origin',(32.2949960661498,1082.7251047501,358.108129666728));
#127045=CARTESIAN_POINT('Origin',(43.2754163337329,1067.7251047501,355.792516479666));
#127046=CARTESIAN_POINT('',(43.2754163337329,1078.73142393294,354.131635669746));
#127047=CARTESIAN_POINT('Origin',(43.2754163337329,1078.73142393294,355.792516479666));
#127048=CARTESIAN_POINT('',(43.2754163337329,1076.73142393294,354.131635669746));
#127049=CARTESIAN_POINT('',(43.2754163337329,1067.7251047501,354.131635669746));
#127050=CARTESIAN_POINT('Origin',(43.2754163337329,1076.73142393294,355.792516479666));
#127051=CARTESIAN_POINT('Origin',(43.2754163337329,1067.7251047501,355.792516479666));
#127052=CARTESIAN_POINT('',(43.2754163337329,1076.73142393294,354.731635669746));
#127053=CARTESIAN_POINT('Origin',(43.2754163337329,1076.73142393294,355.792516479666));
#127054=CARTESIAN_POINT('',(43.2754163337329,1082.7251047501,354.731635669746));
#127055=CARTESIAN_POINT('',(43.2754163337329,1067.7251047501,354.731635669746));
#127056=CARTESIAN_POINT('Origin',(43.2754163337329,1082.7251047501,355.792516479666));
#127057=CARTESIAN_POINT('Origin',(-9.48479058284857,1067.7251047501,407.953573201632));
#127058=CARTESIAN_POINT('',(-9.48479058284857,1078.73142393294,406.853215135958));
#127059=CARTESIAN_POINT('Origin',(-9.48479058284857,1078.73142393294,407.953573201632));
#127060=CARTESIAN_POINT('',(-9.48479058284857,1076.73142393294,406.853215135958));
#127061=CARTESIAN_POINT('',(-9.48479058284857,1067.7251047501,406.853215135958));
#127062=CARTESIAN_POINT('Origin',(-9.48479058284857,1076.73142393294,407.953573201632));
#127063=CARTESIAN_POINT('Origin',(-9.48479058284857,1067.7251047501,407.953573201632));
#127064=CARTESIAN_POINT('',(-9.48479058284857,1076.73142393294,407.453215135958));
#127065=CARTESIAN_POINT('Origin',(-9.48479058284857,1076.73142393294,407.953573201632));
#127066=CARTESIAN_POINT('',(-9.48479058284857,1082.7251047501,407.453215135958));
#127067=CARTESIAN_POINT('',(-9.48479058284857,1067.7251047501,407.453215135958));
#127068=CARTESIAN_POINT('Origin',(-9.48479058284857,1082.7251047501,407.953573201632));
#127069=CARTESIAN_POINT('Origin',(-11.0355654939679,1067.7251047501,399.531431699266));
#127070=CARTESIAN_POINT('',(-11.0355654939679,1078.73142393294,398.317400132529));
#127071=CARTESIAN_POINT('Origin',(-11.0355654939679,1078.73142393294,399.531431699266));
#127072=CARTESIAN_POINT('',(-11.0355654939679,1076.73142393294,398.317400132529));
#127073=CARTESIAN_POINT('',(-11.0355654939679,1067.7251047501,398.317400132529));
#127074=CARTESIAN_POINT('Origin',(-11.0355654939679,1076.73142393294,399.531431699266));
#127075=CARTESIAN_POINT('Origin',(-11.0355654939679,1067.7251047501,399.531431699266));
#127076=CARTESIAN_POINT('',(-11.0355654939679,1076.73142393294,398.917400132529));
#127077=CARTESIAN_POINT('Origin',(-11.0355654939679,1076.73142393294,399.531431699266));
#127078=CARTESIAN_POINT('',(-11.0355654939679,1082.7251047501,398.917400132529));
#127079=CARTESIAN_POINT('',(-11.0355654939679,1067.7251047501,398.917400132529));
#127080=CARTESIAN_POINT('Origin',(-11.0355654939679,1082.7251047501,399.531431699266));
#127081=CARTESIAN_POINT('Origin',(-10.5515930080269,1067.7251047501,391.620384969957));
#127082=CARTESIAN_POINT('',(-10.5515930080269,1078.73142393294,390.291577006384));
#127083=CARTESIAN_POINT('Origin',(-10.5515930080269,1078.73142393294,391.620384969957));
#127084=CARTESIAN_POINT('',(-10.5515930080269,1076.73142393294,390.291577006384));
#127085=CARTESIAN_POINT('',(-10.5515930080269,1067.7251047501,390.291577006384));
#127086=CARTESIAN_POINT('Origin',(-10.5515930080269,1076.73142393294,391.620384969957));
#127087=CARTESIAN_POINT('Origin',(-10.5515930080269,1067.7251047501,391.620384969957));
#127088=CARTESIAN_POINT('',(-10.5515930080269,1076.73142393294,390.891577006384));
#127089=CARTESIAN_POINT('Origin',(-10.5515930080269,1076.73142393294,391.620384969957));
#127090=CARTESIAN_POINT('',(-10.5515930080269,1082.7251047501,390.891577006384));
#127091=CARTESIAN_POINT('',(-10.5515930080269,1067.7251047501,390.891577006384));
#127092=CARTESIAN_POINT('Origin',(-10.5515930080269,1082.7251047501,391.620384969957));
#127093=CARTESIAN_POINT('Origin',(-8.49592223961282,1067.7251047501,382.581211642906));
#127094=CARTESIAN_POINT('',(-8.49592223961282,1078.73142393294,381.120094641089));
#127095=CARTESIAN_POINT('Origin',(-8.49592223961282,1078.73142393294,382.581211642906));
#127096=CARTESIAN_POINT('',(-8.49592223961282,1076.73142393294,381.120094641089));
#127097=CARTESIAN_POINT('',(-8.49592223961282,1067.7251047501,381.120094641089));
#127098=CARTESIAN_POINT('Origin',(-8.49592223961282,1076.73142393294,382.581211642906));
#127099=CARTESIAN_POINT('Origin',(-8.49592223961282,1067.7251047501,382.581211642906));
#127100=CARTESIAN_POINT('',(-8.49592223961282,1076.73142393294,381.720094641089));
#127101=CARTESIAN_POINT('Origin',(-8.49592223961282,1076.73142393294,382.581211642906));
#127102=CARTESIAN_POINT('',(-8.49592223961282,1082.7251047501,381.720094641089));
#127103=CARTESIAN_POINT('',(-8.49592223961282,1067.7251047501,381.720094641089));
#127104=CARTESIAN_POINT('Origin',(-8.49592223961282,1082.7251047501,382.581211642906));
#127105=CARTESIAN_POINT('Origin',(-4.43822160949764,1067.7251047501,374.637006765614));
#127106=CARTESIAN_POINT('',(-4.43822160949764,1078.73142393294,373.016524722989));
#127107=CARTESIAN_POINT('Origin',(-4.43822160949764,1078.73142393294,374.637006765614));
#127108=CARTESIAN_POINT('',(-4.43822160949764,1076.73142393294,373.016524722989));
#127109=CARTESIAN_POINT('',(-4.43822160949764,1067.7251047501,373.016524722989));
#127110=CARTESIAN_POINT('Origin',(-4.43822160949764,1076.73142393294,374.637006765614));
#127111=CARTESIAN_POINT('Origin',(-4.43822160949764,1067.7251047501,374.637006765614));
#127112=CARTESIAN_POINT('',(-4.43822160949764,1076.73142393294,373.616524722989));
#127113=CARTESIAN_POINT('Origin',(-4.43822160949764,1076.73142393294,374.637006765614));
#127114=CARTESIAN_POINT('',(-4.43822160949764,1082.7251047501,373.616524722989));
#127115=CARTESIAN_POINT('',(-4.43822160949764,1067.7251047501,373.616524722989));
#127116=CARTESIAN_POINT('Origin',(-4.43822160949764,1082.7251047501,374.637006765614));
#127117=CARTESIAN_POINT('Origin',(1.28772884674538,1067.7251047501,366.227363966584));
#127118=CARTESIAN_POINT('',(1.28772884674538,1078.73142393294,364.526363743502));
#127119=CARTESIAN_POINT('Origin',(1.28772884674538,1078.73142393294,366.227363966584));
#127120=CARTESIAN_POINT('',(1.28772884674538,1076.73142393294,364.526363743502));
#127121=CARTESIAN_POINT('',(1.28772884674538,1067.7251047501,364.526363743502));
#127122=CARTESIAN_POINT('Origin',(1.28772884674538,1076.73142393294,366.227363966584));
#127123=CARTESIAN_POINT('Origin',(1.28772884674538,1067.7251047501,366.227363966584));
#127124=CARTESIAN_POINT('',(1.28772884674538,1076.73142393294,365.126363743502));
#127125=CARTESIAN_POINT('Origin',(1.28772884674538,1076.73142393294,366.227363966584));
#127126=CARTESIAN_POINT('',(1.28772884674538,1082.7251047501,365.126363743502));
#127127=CARTESIAN_POINT('',(1.28772884674538,1067.7251047501,365.126363743502));
#127128=CARTESIAN_POINT('Origin',(1.28772884674538,1082.7251047501,366.227363966584));
#127129=CARTESIAN_POINT('Origin',(8.55244616805279,1067.7251047501,359.551856854418));
#127130=CARTESIAN_POINT('',(8.55244616805279,1078.73142393294,357.830582222375));
#127131=CARTESIAN_POINT('Origin',(8.55244616805279,1078.73142393294,359.551856854418));
#127132=CARTESIAN_POINT('',(8.55244616805279,1076.73142393294,357.830582222375));
#127133=CARTESIAN_POINT('',(8.55244616805279,1067.7251047501,357.830582222375));
#127134=CARTESIAN_POINT('Origin',(8.55244616805279,1076.73142393294,359.551856854418));
#127135=CARTESIAN_POINT('Origin',(8.55244616805279,1067.7251047501,359.551856854418));
#127136=CARTESIAN_POINT('',(8.55244616805279,1076.73142393294,358.430582222375));
#127137=CARTESIAN_POINT('Origin',(8.55244616805279,1076.73142393294,359.551856854418));
#127138=CARTESIAN_POINT('',(8.55244616805279,1082.7251047501,358.430582222375));
#127139=CARTESIAN_POINT('',(8.55244616805279,1067.7251047501,358.430582222375));
#127140=CARTESIAN_POINT('Origin',(8.55244616805279,1082.7251047501,359.551856854418));
#127141=CARTESIAN_POINT('Origin',(17.7606270621823,1067.7251047501,352.847071677078));
#127142=CARTESIAN_POINT('',(17.7606270621823,1078.73142393294,351.065079022673));
#127143=CARTESIAN_POINT('Origin',(17.7606270621823,1078.73142393294,352.847071677078));
#127144=CARTESIAN_POINT('',(17.7606270621823,1076.73142393294,351.065079022673));
#127145=CARTESIAN_POINT('',(17.7606270621823,1067.7251047501,351.065079022673));
#127146=CARTESIAN_POINT('Origin',(17.7606270621823,1076.73142393294,352.847071677078));
#127147=CARTESIAN_POINT('Origin',(17.7606270621823,1067.7251047501,352.847071677078));
#127148=CARTESIAN_POINT('',(17.7606270621823,1076.73142393294,351.665079022673));
#127149=CARTESIAN_POINT('Origin',(17.7606270621823,1076.73142393294,352.847071677078));
#127150=CARTESIAN_POINT('',(17.7606270621823,1082.7251047501,351.665079022673));
#127151=CARTESIAN_POINT('',(17.7606270621823,1067.7251047501,351.665079022673));
#127152=CARTESIAN_POINT('Origin',(17.7606270621823,1082.7251047501,352.847071677078));
#127153=CARTESIAN_POINT('Origin',(28.0196557489657,1067.7251047501,348.299102450203));
#127154=CARTESIAN_POINT('',(28.0196557489657,1078.73142393294,346.638221640282));
#127155=CARTESIAN_POINT('Origin',(28.0196557489657,1078.73142393294,348.299102450203));
#127156=CARTESIAN_POINT('',(28.0196557489657,1076.73142393294,346.638221640282));
#127157=CARTESIAN_POINT('',(28.0196557489657,1067.7251047501,346.638221640282));
#127158=CARTESIAN_POINT('Origin',(28.0196557489657,1076.73142393294,348.299102450203));
#127159=CARTESIAN_POINT('Origin',(28.0196557489657,1067.7251047501,348.299102450203));
#127160=CARTESIAN_POINT('',(28.0196557489657,1076.73142393294,347.238221640282));
#127161=CARTESIAN_POINT('Origin',(28.0196557489657,1076.73142393294,348.299102450203));
#127162=CARTESIAN_POINT('',(28.0196557489657,1082.7251047501,347.238221640282));
#127163=CARTESIAN_POINT('',(28.0196557489657,1067.7251047501,347.238221640282));
#127164=CARTESIAN_POINT('Origin',(28.0196557489657,1082.7251047501,348.299102450203));
#127165=CARTESIAN_POINT('Origin',(-12.7427205628026,1067.7251047501,410.289778762456));
#127166=CARTESIAN_POINT('',(-12.7427205628026,1078.73142393294,409.189420696781));
#127167=CARTESIAN_POINT('Origin',(-12.7427205628026,1078.73142393294,410.289778762456));
#127168=CARTESIAN_POINT('',(-12.7427205628026,1076.73142393294,409.189420696781));
#127169=CARTESIAN_POINT('',(-12.7427205628026,1067.7251047501,409.189420696781));
#127170=CARTESIAN_POINT('Origin',(-12.7427205628026,1076.73142393294,410.289778762456));
#127171=CARTESIAN_POINT('Origin',(-12.7427205628026,1067.7251047501,410.289778762456));
#127172=CARTESIAN_POINT('',(-12.7427205628026,1076.73142393294,409.789420696781));
#127173=CARTESIAN_POINT('Origin',(-12.7427205628026,1076.73142393294,410.289778762456));
#127174=CARTESIAN_POINT('',(-12.7427205628026,1082.7251047501,409.789420696781));
#127175=CARTESIAN_POINT('',(-12.7427205628026,1067.7251047501,409.789420696781));
#127176=CARTESIAN_POINT('Origin',(-12.7427205628026,1082.7251047501,410.289778762456));
#127177=CARTESIAN_POINT('Origin',(-16.0106690014555,1067.7251047501,402.374105492724));
#127178=CARTESIAN_POINT('',(-16.0106690014555,1078.73142393294,401.160073925987));
#127179=CARTESIAN_POINT('Origin',(-16.0106690014555,1078.73142393294,402.374105492724));
#127180=CARTESIAN_POINT('',(-16.0106690014555,1076.73142393294,401.160073925987));
#127181=CARTESIAN_POINT('',(-16.0106690014555,1067.7251047501,401.160073925987));
#127182=CARTESIAN_POINT('Origin',(-16.0106690014555,1076.73142393294,402.374105492724));
#127183=CARTESIAN_POINT('Origin',(-16.0106690014555,1067.7251047501,402.374105492724));
#127184=CARTESIAN_POINT('',(-16.0106690014555,1076.73142393294,401.760073925987));
#127185=CARTESIAN_POINT('Origin',(-16.0106690014555,1076.73142393294,402.374105492724));
#127186=CARTESIAN_POINT('',(-16.0106690014555,1082.7251047501,401.760073925987));
#127187=CARTESIAN_POINT('',(-16.0106690014555,1067.7251047501,401.760073925987));
#127188=CARTESIAN_POINT('Origin',(-16.0106690014555,1082.7251047501,402.374105492724));
#127189=CARTESIAN_POINT('Origin',(-17.1820715771402,1067.7251047501,394.535310577296));
#127190=CARTESIAN_POINT('',(-17.1820715771402,1078.73142393294,393.206502613723));
#127191=CARTESIAN_POINT('Origin',(-17.1820715771402,1078.73142393294,394.535310577296));
#127192=CARTESIAN_POINT('',(-17.1820715771402,1076.73142393294,393.206502613723));
#127193=CARTESIAN_POINT('',(-17.1820715771402,1067.7251047501,393.206502613723));
#127194=CARTESIAN_POINT('Origin',(-17.1820715771402,1076.73142393294,394.535310577296));
#127195=CARTESIAN_POINT('Origin',(-17.1820715771402,1067.7251047501,394.535310577296));
#127196=CARTESIAN_POINT('',(-17.1820715771402,1076.73142393294,393.806502613723));
#127197=CARTESIAN_POINT('Origin',(-17.1820715771402,1076.73142393294,394.535310577296));
#127198=CARTESIAN_POINT('',(-17.1820715771402,1082.7251047501,393.806502613723));
#127199=CARTESIAN_POINT('',(-17.1820715771402,1067.7251047501,393.806502613723));
#127200=CARTESIAN_POINT('Origin',(-17.1820715771402,1082.7251047501,394.535310577296));
#127201=CARTESIAN_POINT('Origin',(-17.0506719571394,1067.7251047501,385.266266889598));
#127202=CARTESIAN_POINT('',(-17.0506719571394,1078.73142393294,383.805149887781));
#127203=CARTESIAN_POINT('Origin',(-17.0506719571394,1078.73142393294,385.266266889598));
#127204=CARTESIAN_POINT('',(-17.0506719571394,1076.73142393294,383.805149887781));
#127205=CARTESIAN_POINT('',(-17.0506719571394,1067.7251047501,383.805149887781));
#127206=CARTESIAN_POINT('Origin',(-17.0506719571394,1076.73142393294,385.266266889598));
#127207=CARTESIAN_POINT('Origin',(-17.0506719571394,1067.7251047501,385.266266889598));
#127208=CARTESIAN_POINT('',(-17.0506719571394,1076.73142393294,384.405149887781));
#127209=CARTESIAN_POINT('Origin',(-17.0506719571394,1076.73142393294,385.266266889598));
#127210=CARTESIAN_POINT('',(-17.0506719571394,1082.7251047501,384.405149887781));
#127211=CARTESIAN_POINT('',(-17.0506719571394,1067.7251047501,384.405149887781));
#127212=CARTESIAN_POINT('Origin',(-17.0506719571394,1082.7251047501,385.266266889598));
#127213=CARTESIAN_POINT('Origin',(-14.7333348895366,1067.7251047501,376.652018550297));
#127214=CARTESIAN_POINT('',(-14.7333348895366,1078.73142393294,375.031536507673));
#127215=CARTESIAN_POINT('Origin',(-14.7333348895366,1078.73142393294,376.652018550297));
#127216=CARTESIAN_POINT('',(-14.7333348895366,1076.73142393294,375.031536507673));
#127217=CARTESIAN_POINT('',(-14.7333348895366,1067.7251047501,375.031536507673));
#127218=CARTESIAN_POINT('Origin',(-14.7333348895366,1076.73142393294,376.652018550297));
#127219=CARTESIAN_POINT('Origin',(-14.7333348895366,1067.7251047501,376.652018550297));
#127220=CARTESIAN_POINT('',(-14.7333348895366,1076.73142393294,375.631536507673));
#127221=CARTESIAN_POINT('Origin',(-14.7333348895366,1076.73142393294,376.652018550297));
#127222=CARTESIAN_POINT('',(-14.7333348895366,1082.7251047501,375.631536507673));
#127223=CARTESIAN_POINT('',(-14.7333348895366,1067.7251047501,375.631536507673));
#127224=CARTESIAN_POINT('Origin',(-14.7333348895366,1082.7251047501,376.652018550297));
#127225=CARTESIAN_POINT('Origin',(-10.8809732423614,1067.7251047501,367.235654582502));
#127226=CARTESIAN_POINT('',(-10.8809732423614,1078.73142393294,365.53465435942));
#127227=CARTESIAN_POINT('Origin',(-10.8809732423614,1078.73142393294,367.235654582502));
#127228=CARTESIAN_POINT('',(-10.8809732423614,1076.73142393294,365.53465435942));
#127229=CARTESIAN_POINT('',(-10.8809732423614,1067.7251047501,365.53465435942));
#127230=CARTESIAN_POINT('Origin',(-10.8809732423614,1076.73142393294,367.235654582502));
#127231=CARTESIAN_POINT('Origin',(-10.8809732423614,1067.7251047501,367.235654582502));
#127232=CARTESIAN_POINT('',(-10.8809732423614,1076.73142393294,366.13465435942));
#127233=CARTESIAN_POINT('Origin',(-10.8809732423614,1076.73142393294,367.235654582502));
#127234=CARTESIAN_POINT('',(-10.8809732423614,1082.7251047501,366.13465435942));
#127235=CARTESIAN_POINT('',(-10.8809732423614,1067.7251047501,366.13465435942));
#127236=CARTESIAN_POINT('Origin',(-10.8809732423614,1082.7251047501,367.235654582502));
#127237=CARTESIAN_POINT('Origin',(-5.16292339527169,1067.7251047501,359.19560365547));
#127238=CARTESIAN_POINT('',(-5.16292339527169,1078.73142393294,357.474329023426));
#127239=CARTESIAN_POINT('Origin',(-5.16292339527169,1078.73142393294,359.19560365547));
#127240=CARTESIAN_POINT('',(-5.16292339527169,1076.73142393294,357.474329023426));
#127241=CARTESIAN_POINT('',(-5.16292339527169,1067.7251047501,357.474329023426));
#127242=CARTESIAN_POINT('Origin',(-5.16292339527169,1076.73142393294,359.19560365547));
#127243=CARTESIAN_POINT('Origin',(-5.16292339527169,1067.7251047501,359.19560365547));
#127244=CARTESIAN_POINT('',(-5.16292339527169,1076.73142393294,358.074329023426));
#127245=CARTESIAN_POINT('Origin',(-5.16292339527169,1076.73142393294,359.19560365547));
#127246=CARTESIAN_POINT('',(-5.16292339527169,1082.7251047501,358.074329023426));
#127247=CARTESIAN_POINT('',(-5.16292339527169,1067.7251047501,358.074329023426));
#127248=CARTESIAN_POINT('Origin',(-5.16292339527169,1082.7251047501,359.19560365547));
#127249=CARTESIAN_POINT('Origin',(2.45003343065336,1067.7251047501,350.722845661765));
#127250=CARTESIAN_POINT('',(2.45003343065336,1078.73142393294,348.94085300736));
#127251=CARTESIAN_POINT('Origin',(2.45003343065336,1078.73142393294,350.722845661765));
#127252=CARTESIAN_POINT('',(2.45003343065336,1076.73142393294,348.94085300736));
#127253=CARTESIAN_POINT('',(2.45003343065336,1067.7251047501,348.94085300736));
#127254=CARTESIAN_POINT('Origin',(2.45003343065336,1076.73142393294,350.722845661765));
#127255=CARTESIAN_POINT('Origin',(2.45003343065336,1067.7251047501,350.722845661765));
#127256=CARTESIAN_POINT('',(2.45003343065336,1076.73142393294,349.54085300736));
#127257=CARTESIAN_POINT('Origin',(2.45003343065336,1076.73142393294,350.722845661765));
#127258=CARTESIAN_POINT('',(2.45003343065336,1082.7251047501,349.54085300736));
#127259=CARTESIAN_POINT('',(2.45003343065336,1067.7251047501,349.54085300736));
#127260=CARTESIAN_POINT('Origin',(2.45003343065336,1082.7251047501,350.722845661765));
#127261=CARTESIAN_POINT('Origin',(11.539301754743,1067.7251047501,344.141288473869));
#127262=CARTESIAN_POINT('',(11.539301754743,1078.73142393294,342.480407663948));
#127263=CARTESIAN_POINT('Origin',(11.539301754743,1078.73142393294,344.141288473869));
#127264=CARTESIAN_POINT('',(11.539301754743,1076.73142393294,342.480407663948));
#127265=CARTESIAN_POINT('',(11.539301754743,1067.7251047501,342.480407663948));
#127266=CARTESIAN_POINT('Origin',(11.539301754743,1076.73142393294,344.141288473869));
#127267=CARTESIAN_POINT('Origin',(11.539301754743,1067.7251047501,344.141288473869));
#127268=CARTESIAN_POINT('',(11.539301754743,1076.73142393294,343.080407663948));
#127269=CARTESIAN_POINT('Origin',(11.539301754743,1076.73142393294,344.141288473869));
#127270=CARTESIAN_POINT('',(11.539301754743,1082.7251047501,343.080407663948));
#127271=CARTESIAN_POINT('',(11.539301754743,1067.7251047501,343.080407663948));
#127272=CARTESIAN_POINT('Origin',(11.539301754743,1082.7251047501,344.141288473869));
#127273=CARTESIAN_POINT('Origin',(-15.4437325078047,1067.7251047501,413.252294357294));
#127274=CARTESIAN_POINT('',(-15.4437325078047,1078.73142393294,412.151936291619));
#127275=CARTESIAN_POINT('Origin',(-15.4437325078047,1078.73142393294,413.252294357294));
#127276=CARTESIAN_POINT('',(-15.4437325078047,1076.73142393294,412.151936291619));
#127277=CARTESIAN_POINT('',(-15.4437325078047,1067.7251047501,412.151936291619));
#127278=CARTESIAN_POINT('Origin',(-15.4437325078047,1076.73142393294,413.252294357294));
#127279=CARTESIAN_POINT('Origin',(-15.4437325078047,1067.7251047501,413.252294357294));
#127280=CARTESIAN_POINT('',(-15.4437325078047,1076.73142393294,412.751936291619));
#127281=CARTESIAN_POINT('Origin',(-15.4437325078047,1076.73142393294,413.252294357294));
#127282=CARTESIAN_POINT('',(-15.4437325078047,1082.7251047501,412.751936291619));
#127283=CARTESIAN_POINT('',(-15.4437325078047,1067.7251047501,412.751936291619));
#127284=CARTESIAN_POINT('Origin',(-15.4437325078047,1082.7251047501,413.252294357294));
#127285=CARTESIAN_POINT('Origin',(-20.2860294458657,1067.7251047501,406.189042225699));
#127286=CARTESIAN_POINT('',(-20.2860294458657,1078.73142393294,404.975010658962));
#127287=CARTESIAN_POINT('Origin',(-20.2860294458657,1078.73142393294,406.189042225699));
#127288=CARTESIAN_POINT('',(-20.2860294458657,1076.73142393294,404.975010658962));
#127289=CARTESIAN_POINT('',(-20.2860294458657,1067.7251047501,404.975010658962));
#127290=CARTESIAN_POINT('Origin',(-20.2860294458657,1076.73142393294,406.189042225699));
#127291=CARTESIAN_POINT('Origin',(-20.2860294458657,1067.7251047501,406.189042225699));
#127292=CARTESIAN_POINT('',(-20.2860294458657,1076.73142393294,405.575010658962));
#127293=CARTESIAN_POINT('Origin',(-20.2860294458657,1076.73142393294,406.189042225699));
#127294=CARTESIAN_POINT('',(-20.2860294458657,1082.7251047501,405.575010658962));
#127295=CARTESIAN_POINT('',(-20.2860294458657,1067.7251047501,405.575010658962));
#127296=CARTESIAN_POINT('Origin',(-20.2860294458657,1082.7251047501,406.189042225699));
#127297=CARTESIAN_POINT('Origin',(-23.0616111696053,1067.7251047501,398.765092076667));
#127298=CARTESIAN_POINT('',(-23.0616111696053,1078.73142393294,397.436284113094));
#127299=CARTESIAN_POINT('Origin',(-23.0616111696053,1078.73142393294,398.765092076667));
#127300=CARTESIAN_POINT('',(-23.0616111696053,1076.73142393294,397.436284113094));
#127301=CARTESIAN_POINT('',(-23.0616111696053,1067.7251047501,397.436284113094));
#127302=CARTESIAN_POINT('Origin',(-23.0616111696053,1076.73142393294,398.765092076667));
#127303=CARTESIAN_POINT('Origin',(-23.0616111696053,1067.7251047501,398.765092076667));
#127304=CARTESIAN_POINT('',(-23.0616111696053,1076.73142393294,398.036284113094));
#127305=CARTESIAN_POINT('Origin',(-23.0616111696053,1076.73142393294,398.765092076667));
#127306=CARTESIAN_POINT('',(-23.0616111696053,1082.7251047501,398.036284113094));
#127307=CARTESIAN_POINT('',(-23.0616111696053,1067.7251047501,398.036284113094));
#127308=CARTESIAN_POINT('Origin',(-23.0616111696053,1082.7251047501,398.765092076667));
#127309=CARTESIAN_POINT('Origin',(-24.8602254919372,1067.7251047501,389.671279715281));
#127310=CARTESIAN_POINT('',(-24.8602254919372,1078.73142393294,388.210162713464));
#127311=CARTESIAN_POINT('Origin',(-24.8602254919372,1078.73142393294,389.671279715281));
#127312=CARTESIAN_POINT('',(-24.8602254919372,1076.73142393294,388.210162713464));
#127313=CARTESIAN_POINT('',(-24.8602254919372,1067.7251047501,388.210162713464));
#127314=CARTESIAN_POINT('Origin',(-24.8602254919372,1076.73142393294,389.671279715281));
#127315=CARTESIAN_POINT('Origin',(-24.8602254919372,1067.7251047501,389.671279715281));
#127316=CARTESIAN_POINT('',(-24.8602254919372,1076.73142393294,388.810162713464));
#127317=CARTESIAN_POINT('Origin',(-24.8602254919372,1076.73142393294,389.671279715281));
#127318=CARTESIAN_POINT('',(-24.8602254919372,1082.7251047501,388.810162713464));
#127319=CARTESIAN_POINT('',(-24.8602254919372,1067.7251047501,388.810162713464));
#127320=CARTESIAN_POINT('Origin',(-24.8602254919372,1082.7251047501,389.671279715281));
#127321=CARTESIAN_POINT('Origin',(-24.3845307365182,1067.7251047501,380.763471902149));
#127322=CARTESIAN_POINT('',(-24.3845307365182,1078.73142393294,379.142989859525));
#127323=CARTESIAN_POINT('Origin',(-24.3845307365182,1078.73142393294,380.763471902149));
#127324=CARTESIAN_POINT('',(-24.3845307365182,1076.73142393294,379.142989859525));
#127325=CARTESIAN_POINT('',(-24.3845307365182,1067.7251047501,379.142989859525));
#127326=CARTESIAN_POINT('Origin',(-24.3845307365182,1076.73142393294,380.763471902149));
#127327=CARTESIAN_POINT('Origin',(-24.3845307365182,1067.7251047501,380.763471902149));
#127328=CARTESIAN_POINT('',(-24.3845307365182,1076.73142393294,379.742989859525));
#127329=CARTESIAN_POINT('Origin',(-24.3845307365182,1076.73142393294,380.763471902149));
#127330=CARTESIAN_POINT('',(-24.3845307365182,1082.7251047501,379.742989859525));
#127331=CARTESIAN_POINT('',(-24.3845307365182,1067.7251047501,379.742989859525));
#127332=CARTESIAN_POINT('Origin',(-24.3845307365182,1082.7251047501,380.763471902149));
#127333=CARTESIAN_POINT('Origin',(-22.5741245880745,1067.7251047501,370.751927055709));
#127334=CARTESIAN_POINT('',(-22.5741245880745,1078.73142393294,369.050926832626));
#127335=CARTESIAN_POINT('Origin',(-22.5741245880745,1078.73142393294,370.751927055709));
#127336=CARTESIAN_POINT('',(-22.5741245880745,1076.73142393294,369.050926832626));
#127337=CARTESIAN_POINT('',(-22.5741245880745,1067.7251047501,369.050926832626));
#127338=CARTESIAN_POINT('Origin',(-22.5741245880745,1076.73142393294,370.751927055709));
#127339=CARTESIAN_POINT('Origin',(-22.5741245880745,1067.7251047501,370.751927055709));
#127340=CARTESIAN_POINT('',(-22.5741245880745,1076.73142393294,369.650926832626));
#127341=CARTESIAN_POINT('Origin',(-22.5741245880745,1076.73142393294,370.751927055709));
#127342=CARTESIAN_POINT('',(-22.5741245880745,1082.7251047501,369.650926832626));
#127343=CARTESIAN_POINT('',(-22.5741245880745,1067.7251047501,369.650926832626));
#127344=CARTESIAN_POINT('Origin',(-22.5741245880745,1082.7251047501,370.751927055709));
#127345=CARTESIAN_POINT('Origin',(-18.6526484317677,1067.7251047501,361.698721119765));
#127346=CARTESIAN_POINT('',(-18.6526484317677,1078.73142393294,359.977446487722));
#127347=CARTESIAN_POINT('Origin',(-18.6526484317677,1078.73142393294,361.698721119765));
#127348=CARTESIAN_POINT('',(-18.6526484317677,1076.73142393294,359.977446487722));
#127349=CARTESIAN_POINT('',(-18.6526484317677,1067.7251047501,359.977446487722));
#127350=CARTESIAN_POINT('Origin',(-18.6526484317677,1076.73142393294,361.698721119765));
#127351=CARTESIAN_POINT('Origin',(-18.6526484317677,1067.7251047501,361.698721119765));
#127352=CARTESIAN_POINT('',(-18.6526484317677,1076.73142393294,360.577446487722));
#127353=CARTESIAN_POINT('Origin',(-18.6526484317677,1076.73142393294,361.698721119765));
#127354=CARTESIAN_POINT('',(-18.6526484317677,1082.7251047501,360.577446487722));
#127355=CARTESIAN_POINT('',(-18.6526484317677,1067.7251047501,360.577446487722));
#127356=CARTESIAN_POINT('Origin',(-18.6526484317677,1082.7251047501,361.698721119765));
#127357=CARTESIAN_POINT('Origin',(-12.9676384183599,1067.7251047501,351.828290490824));
#127358=CARTESIAN_POINT('',(-12.9676384183599,1078.73142393294,350.046297836419));
#127359=CARTESIAN_POINT('Origin',(-12.9676384183599,1078.73142393294,351.828290490824));
#127360=CARTESIAN_POINT('',(-12.9676384183599,1076.73142393294,350.046297836419));
#127361=CARTESIAN_POINT('',(-12.9676384183599,1067.7251047501,350.046297836419));
#127362=CARTESIAN_POINT('Origin',(-12.9676384183599,1076.73142393294,351.828290490824));
#127363=CARTESIAN_POINT('Origin',(-12.9676384183599,1067.7251047501,351.828290490824));
#127364=CARTESIAN_POINT('',(-12.9676384183599,1076.73142393294,350.646297836419));
#127365=CARTESIAN_POINT('Origin',(-12.9676384183599,1076.73142393294,351.828290490824));
#127366=CARTESIAN_POINT('',(-12.9676384183599,1082.7251047501,350.646297836419));
#127367=CARTESIAN_POINT('',(-12.9676384183599,1067.7251047501,350.646297836419));
#127368=CARTESIAN_POINT('Origin',(-12.9676384183599,1082.7251047501,351.828290490824));
#127369=CARTESIAN_POINT('Origin',(-5.44537509787502,1067.7251047501,343.500790972833));
#127370=CARTESIAN_POINT('',(-5.44537509787502,1078.73142393294,341.839910162913));
#127371=CARTESIAN_POINT('Origin',(-5.44537509787502,1078.73142393294,343.500790972833));
#127372=CARTESIAN_POINT('',(-5.44537509787502,1076.73142393294,341.839910162913));
#127373=CARTESIAN_POINT('',(-5.44537509787502,1067.7251047501,341.839910162913));
#127374=CARTESIAN_POINT('Origin',(-5.44537509787502,1076.73142393294,343.500790972833));
#127375=CARTESIAN_POINT('Origin',(-5.44537509787502,1067.7251047501,343.500790972833));
#127376=CARTESIAN_POINT('',(-5.44537509787502,1076.73142393294,342.439910162913));
#127377=CARTESIAN_POINT('Origin',(-5.44537509787502,1076.73142393294,343.500790972833));
#127378=CARTESIAN_POINT('',(-5.44537509787502,1082.7251047501,342.439910162913));
#127379=CARTESIAN_POINT('',(-5.44537509787502,1067.7251047501,342.439910162913));
#127380=CARTESIAN_POINT('Origin',(-5.44537509787502,1082.7251047501,343.500790972833));
#127381=CARTESIAN_POINT('Origin',(-17.4697792349653,1067.7251047501,416.711643838926));
#127382=CARTESIAN_POINT('',(-17.4697792349653,1078.73142393294,415.611285773251));
#127383=CARTESIAN_POINT('Origin',(-17.4697792349653,1078.73142393294,416.711643838926));
#127384=CARTESIAN_POINT('',(-17.4697792349653,1076.73142393294,415.611285773251));
#127385=CARTESIAN_POINT('',(-17.4697792349653,1067.7251047501,415.611285773251));
#127386=CARTESIAN_POINT('Origin',(-17.4697792349653,1076.73142393294,416.711643838926));
#127387=CARTESIAN_POINT('Origin',(-17.4697792349653,1067.7251047501,416.711643838926));
#127388=CARTESIAN_POINT('',(-17.4697792349653,1076.73142393294,416.211285773251));
#127389=CARTESIAN_POINT('Origin',(-17.4697792349653,1076.73142393294,416.711643838926));
#127390=CARTESIAN_POINT('',(-17.4697792349653,1082.7251047501,416.211285773251));
#127391=CARTESIAN_POINT('',(-17.4697792349653,1067.7251047501,416.211285773251));
#127392=CARTESIAN_POINT('Origin',(-17.4697792349653,1082.7251047501,416.711643838926));
#127393=CARTESIAN_POINT('Origin',(-23.6747930603223,1067.7251047501,410.809510856862));
#127394=CARTESIAN_POINT('',(-23.6747930603223,1078.73142393294,409.595479290125));
#127395=CARTESIAN_POINT('Origin',(-23.6747930603223,1078.73142393294,410.809510856862));
#127396=CARTESIAN_POINT('',(-23.6747930603223,1076.73142393294,409.595479290125));
#127397=CARTESIAN_POINT('',(-23.6747930603223,1067.7251047501,409.595479290125));
#127398=CARTESIAN_POINT('Origin',(-23.6747930603223,1076.73142393294,410.809510856862));
#127399=CARTESIAN_POINT('Origin',(-23.6747930603223,1067.7251047501,410.809510856862));
#127400=CARTESIAN_POINT('',(-23.6747930603223,1076.73142393294,410.195479290125));
#127401=CARTESIAN_POINT('Origin',(-23.6747930603223,1076.73142393294,410.809510856862));
#127402=CARTESIAN_POINT('',(-23.6747930603223,1082.7251047501,410.195479290125));
#127403=CARTESIAN_POINT('',(-23.6747930603223,1067.7251047501,410.195479290125));
#127404=CARTESIAN_POINT('Origin',(-23.6747930603223,1082.7251047501,410.809510856862));
#127405=CARTESIAN_POINT('Origin',(-27.9332476920707,1067.7251047501,404.124867719805));
#127406=CARTESIAN_POINT('',(-27.9332476920707,1078.73142393294,402.796059756232));
#127407=CARTESIAN_POINT('Origin',(-27.9332476920707,1078.73142393294,404.124867719805));
#127408=CARTESIAN_POINT('',(-27.9332476920707,1076.73142393294,402.796059756232));
#127409=CARTESIAN_POINT('',(-27.9332476920707,1067.7251047501,402.796059756232));
#127410=CARTESIAN_POINT('Origin',(-27.9332476920707,1076.73142393294,404.124867719805));
#127411=CARTESIAN_POINT('Origin',(-27.9332476920707,1067.7251047501,404.124867719805));
#127412=CARTESIAN_POINT('',(-27.9332476920707,1076.73142393294,403.396059756232));
#127413=CARTESIAN_POINT('Origin',(-27.9332476920707,1076.73142393294,404.124867719805));
#127414=CARTESIAN_POINT('',(-27.9332476920707,1082.7251047501,403.396059756232));
#127415=CARTESIAN_POINT('',(-27.9332476920707,1067.7251047501,403.396059756232));
#127416=CARTESIAN_POINT('Origin',(-27.9332476920707,1082.7251047501,404.124867719805));
#127417=CARTESIAN_POINT('Origin',(-31.5832678801404,1067.7251047501,395.603729921877));
#127418=CARTESIAN_POINT('',(-31.5832678801404,1078.73142393294,394.14261292006));
#127419=CARTESIAN_POINT('Origin',(-31.5832678801404,1078.73142393294,395.603729921877));
#127420=CARTESIAN_POINT('',(-31.5832678801404,1076.73142393294,394.14261292006));
#127421=CARTESIAN_POINT('',(-31.5832678801404,1067.7251047501,394.14261292006));
#127422=CARTESIAN_POINT('Origin',(-31.5832678801404,1076.73142393294,395.603729921877));
#127423=CARTESIAN_POINT('Origin',(-31.5832678801404,1067.7251047501,395.603729921877));
#127424=CARTESIAN_POINT('',(-31.5832678801404,1076.73142393294,394.74261292006));
#127425=CARTESIAN_POINT('Origin',(-31.5832678801404,1076.73142393294,395.603729921877));
#127426=CARTESIAN_POINT('',(-31.5832678801404,1082.7251047501,394.74261292006));
#127427=CARTESIAN_POINT('',(-31.5832678801404,1067.7251047501,394.74261292006));
#127428=CARTESIAN_POINT('Origin',(-31.5832678801404,1082.7251047501,395.603729921877));
#127429=CARTESIAN_POINT('Origin',(-32.9700055803535,1067.7251047501,386.791676580752));
#127430=CARTESIAN_POINT('',(-32.9700055803535,1078.73142393294,385.171194538127));
#127431=CARTESIAN_POINT('Origin',(-32.9700055803535,1078.73142393294,386.791676580752));
#127432=CARTESIAN_POINT('',(-32.9700055803535,1076.73142393294,385.171194538127));
#127433=CARTESIAN_POINT('',(-32.9700055803535,1067.7251047501,385.171194538127));
#127434=CARTESIAN_POINT('Origin',(-32.9700055803535,1076.73142393294,386.791676580752));
#127435=CARTESIAN_POINT('Origin',(-32.9700055803535,1067.7251047501,386.791676580752));
#127436=CARTESIAN_POINT('',(-32.9700055803535,1076.73142393294,385.771194538127));
#127437=CARTESIAN_POINT('Origin',(-32.9700055803535,1076.73142393294,386.791676580752));
#127438=CARTESIAN_POINT('',(-32.9700055803535,1082.7251047501,385.771194538127));
#127439=CARTESIAN_POINT('',(-32.9700055803535,1067.7251047501,385.771194538127));
#127440=CARTESIAN_POINT('Origin',(-32.9700055803535,1082.7251047501,386.791676580752));
#127441=CARTESIAN_POINT('Origin',(-33.2806783666209,1067.7251047501,376.622503406177));
#127442=CARTESIAN_POINT('',(-33.2806783666209,1078.73142393294,374.921503183094));
#127443=CARTESIAN_POINT('Origin',(-33.2806783666209,1078.73142393294,376.622503406177));
#127444=CARTESIAN_POINT('',(-33.2806783666209,1076.73142393294,374.921503183094));
#127445=CARTESIAN_POINT('',(-33.2806783666209,1067.7251047501,374.921503183094));
#127446=CARTESIAN_POINT('Origin',(-33.2806783666209,1076.73142393294,376.622503406177));
#127447=CARTESIAN_POINT('Origin',(-33.2806783666209,1067.7251047501,376.622503406177));
#127448=CARTESIAN_POINT('',(-33.2806783666209,1076.73142393294,375.521503183094));
#127449=CARTESIAN_POINT('Origin',(-33.2806783666209,1076.73142393294,376.622503406177));
#127450=CARTESIAN_POINT('',(-33.2806783666209,1082.7251047501,375.521503183094));
#127451=CARTESIAN_POINT('',(-33.2806783666209,1067.7251047501,375.521503183094));
#127452=CARTESIAN_POINT('Origin',(-33.2806783666209,1082.7251047501,376.622503406177));
#127453=CARTESIAN_POINT('Origin',(-31.3271632264578,1067.7251047501,366.951811002826));
#127454=CARTESIAN_POINT('',(-31.3271632264578,1078.73142393294,365.230536370782));
#127455=CARTESIAN_POINT('Origin',(-31.3271632264578,1078.73142393294,366.951811002826));
#127456=CARTESIAN_POINT('',(-31.3271632264578,1076.73142393294,365.230536370782));
#127457=CARTESIAN_POINT('',(-31.3271632264578,1067.7251047501,365.230536370782));
#127458=CARTESIAN_POINT('Origin',(-31.3271632264578,1076.73142393294,366.951811002826));
#127459=CARTESIAN_POINT('Origin',(-31.3271632264578,1067.7251047501,366.951811002826));
#127460=CARTESIAN_POINT('',(-31.3271632264578,1076.73142393294,365.830536370782));
#127461=CARTESIAN_POINT('Origin',(-31.3271632264578,1076.73142393294,366.951811002826));
#127462=CARTESIAN_POINT('',(-31.3271632264578,1082.7251047501,365.830536370782));
#127463=CARTESIAN_POINT('',(-31.3271632264578,1067.7251047501,365.830536370782));
#127464=CARTESIAN_POINT('Origin',(-31.3271632264578,1082.7251047501,366.951811002826));
#127465=CARTESIAN_POINT('Origin',(-27.818562242858,1067.7251047501,356.115092920714));
#127466=CARTESIAN_POINT('',(-27.818562242858,1078.73142393294,354.333100266309));
#127467=CARTESIAN_POINT('Origin',(-27.818562242858,1078.73142393294,356.115092920714));
#127468=CARTESIAN_POINT('',(-27.818562242858,1076.73142393294,354.333100266309));
#127469=CARTESIAN_POINT('',(-27.818562242858,1067.7251047501,354.333100266309));
#127470=CARTESIAN_POINT('Origin',(-27.818562242858,1076.73142393294,356.115092920714));
#127471=CARTESIAN_POINT('Origin',(-27.818562242858,1067.7251047501,356.115092920714));
#127472=CARTESIAN_POINT('',(-27.818562242858,1076.73142393294,354.933100266309));
#127473=CARTESIAN_POINT('Origin',(-27.818562242858,1076.73142393294,356.115092920714));
#127474=CARTESIAN_POINT('',(-27.818562242858,1082.7251047501,354.933100266309));
#127475=CARTESIAN_POINT('',(-27.818562242858,1067.7251047501,354.933100266309));
#127476=CARTESIAN_POINT('Origin',(-27.818562242858,1082.7251047501,356.115092920714));
#127477=CARTESIAN_POINT('Origin',(-22.1920629289073,1067.7251047501,346.405602761341));
#127478=CARTESIAN_POINT('',(-22.1920629289073,1078.73142393294,344.74472195142));
#127479=CARTESIAN_POINT('Origin',(-22.1920629289073,1078.73142393294,346.405602761341));
#127480=CARTESIAN_POINT('',(-22.1920629289073,1076.73142393294,344.74472195142));
#127481=CARTESIAN_POINT('',(-22.1920629289073,1067.7251047501,344.74472195142));
#127482=CARTESIAN_POINT('Origin',(-22.1920629289073,1076.73142393294,346.405602761341));
#127483=CARTESIAN_POINT('Origin',(-22.1920629289073,1067.7251047501,346.405602761341));
#127484=CARTESIAN_POINT('',(-22.1920629289073,1076.73142393294,345.34472195142));
#127485=CARTESIAN_POINT('Origin',(-22.1920629289073,1076.73142393294,346.405602761341));
#127486=CARTESIAN_POINT('',(-22.1920629289073,1082.7251047501,345.34472195142));
#127487=CARTESIAN_POINT('',(-22.1920629289073,1067.7251047501,345.34472195142));
#127488=CARTESIAN_POINT('Origin',(-22.1920629289073,1082.7251047501,346.405602761341));
#127489=CARTESIAN_POINT('Origin',(-18.7323127802563,1067.7251047501,420.516637035203));
#127490=CARTESIAN_POINT('',(-18.7323127802563,1078.73142393294,419.416278969528));
#127491=CARTESIAN_POINT('Origin',(-18.7323127802563,1078.73142393294,420.516637035203));
#127492=CARTESIAN_POINT('',(-18.7323127802563,1076.73142393294,419.416278969528));
#127493=CARTESIAN_POINT('',(-18.7323127802563,1067.7251047501,419.416278969528));
#127494=CARTESIAN_POINT('Origin',(-18.7323127802563,1076.73142393294,420.516637035203));
#127495=CARTESIAN_POINT('Origin',(-18.7323127802563,1067.7251047501,420.516637035203));
#127496=CARTESIAN_POINT('',(-18.7323127802563,1076.73142393294,420.016278969528));
#127497=CARTESIAN_POINT('Origin',(-18.7323127802563,1076.73142393294,420.516637035203));
#127498=CARTESIAN_POINT('',(-18.7323127802563,1082.7251047501,420.016278969528));
#127499=CARTESIAN_POINT('',(-18.7323127802563,1067.7251047501,420.016278969528));
#127500=CARTESIAN_POINT('Origin',(-18.7323127802563,1082.7251047501,420.516637035203));
#127501=CARTESIAN_POINT('Origin',(-26.0288546137815,1067.7251047501,416.033574735563));
#127502=CARTESIAN_POINT('',(-26.0288546137815,1078.73142393294,414.819543168826));
#127503=CARTESIAN_POINT('Origin',(-26.0288546137815,1078.73142393294,416.033574735563));
#127504=CARTESIAN_POINT('',(-26.0288546137815,1076.73142393294,414.819543168826));
#127505=CARTESIAN_POINT('',(-26.0288546137815,1067.7251047501,414.819543168826));
#127506=CARTESIAN_POINT('Origin',(-26.0288546137815,1076.73142393294,416.033574735563));
#127507=CARTESIAN_POINT('Origin',(-26.0288546137815,1067.7251047501,416.033574735563));
#127508=CARTESIAN_POINT('',(-26.0288546137815,1076.73142393294,415.419543168826));
#127509=CARTESIAN_POINT('Origin',(-26.0288546137815,1076.73142393294,416.033574735563));
#127510=CARTESIAN_POINT('',(-26.0288546137815,1082.7251047501,415.419543168826));
#127511=CARTESIAN_POINT('',(-26.0288546137815,1067.7251047501,415.419543168826));
#127512=CARTESIAN_POINT('Origin',(-26.0288546137815,1082.7251047501,416.033574735563));
#127513=CARTESIAN_POINT('Origin',(-31.5840672517988,1067.7251047501,410.380389592047));
#127514=CARTESIAN_POINT('',(-31.5840672517988,1078.73142393294,409.051581628474));
#127515=CARTESIAN_POINT('Origin',(-31.5840672517988,1078.73142393294,410.380389592047));
#127516=CARTESIAN_POINT('',(-31.5840672517988,1076.73142393294,409.051581628474));
#127517=CARTESIAN_POINT('',(-31.5840672517988,1067.7251047501,409.051581628474));
#127518=CARTESIAN_POINT('Origin',(-31.5840672517988,1076.73142393294,410.380389592047));
#127519=CARTESIAN_POINT('Origin',(-31.5840672517988,1067.7251047501,410.380389592047));
#127520=CARTESIAN_POINT('',(-31.5840672517988,1076.73142393294,409.651581628474));
#127521=CARTESIAN_POINT('Origin',(-31.5840672517988,1076.73142393294,410.380389592047));
#127522=CARTESIAN_POINT('',(-31.5840672517988,1082.7251047501,409.651581628474));
#127523=CARTESIAN_POINT('',(-31.5840672517988,1067.7251047501,409.651581628474));
#127524=CARTESIAN_POINT('Origin',(-31.5840672517988,1082.7251047501,410.380389592047));
#127525=CARTESIAN_POINT('Origin',(-36.9259699086473,1067.7251047501,402.804340968302));
#127526=CARTESIAN_POINT('',(-36.9259699086473,1078.73142393294,401.343223966485));
#127527=CARTESIAN_POINT('Origin',(-36.9259699086473,1078.73142393294,402.804340968302));
#127528=CARTESIAN_POINT('',(-36.9259699086473,1076.73142393294,401.343223966485));
#127529=CARTESIAN_POINT('',(-36.9259699086473,1067.7251047501,401.343223966485));
#127530=CARTESIAN_POINT('Origin',(-36.9259699086473,1076.73142393294,402.804340968302));
#127531=CARTESIAN_POINT('Origin',(-36.9259699086473,1067.7251047501,402.804340968302));
#127532=CARTESIAN_POINT('',(-36.9259699086473,1076.73142393294,401.943223966485));
#127533=CARTESIAN_POINT('Origin',(-36.9259699086473,1076.73142393294,402.804340968302));
#127534=CARTESIAN_POINT('',(-36.9259699086473,1082.7251047501,401.943223966485));
#127535=CARTESIAN_POINT('',(-36.9259699086473,1067.7251047501,401.943223966485));
#127536=CARTESIAN_POINT('Origin',(-36.9259699086473,1082.7251047501,402.804340968302));
#127537=CARTESIAN_POINT('Origin',(-40.1145329726876,1067.7251047501,394.473171115114));
#127538=CARTESIAN_POINT('',(-40.1145329726876,1078.73142393294,392.85268907249));
#127539=CARTESIAN_POINT('Origin',(-40.1145329726876,1078.73142393294,394.473171115114));
#127540=CARTESIAN_POINT('',(-40.1145329726876,1076.73142393294,392.85268907249));
#127541=CARTESIAN_POINT('',(-40.1145329726876,1067.7251047501,392.85268907249));
#127542=CARTESIAN_POINT('Origin',(-40.1145329726876,1076.73142393294,394.473171115114));
#127543=CARTESIAN_POINT('Origin',(-40.1145329726876,1067.7251047501,394.473171115114));
#127544=CARTESIAN_POINT('',(-40.1145329726876,1076.73142393294,393.45268907249));
#127545=CARTESIAN_POINT('Origin',(-40.1145329726876,1076.73142393294,394.473171115114));
#127546=CARTESIAN_POINT('',(-40.1145329726876,1082.7251047501,393.45268907249));
#127547=CARTESIAN_POINT('',(-40.1145329726876,1067.7251047501,393.45268907249));
#127548=CARTESIAN_POINT('Origin',(-40.1145329726876,1082.7251047501,394.473171115114));
#127549=CARTESIAN_POINT('Origin',(-42.5327068021327,1067.7251047501,384.590811277241));
#127550=CARTESIAN_POINT('',(-42.5327068021327,1078.73142393294,382.889811054159));
#127551=CARTESIAN_POINT('Origin',(-42.5327068021327,1078.73142393294,384.590811277241));
#127552=CARTESIAN_POINT('',(-42.5327068021327,1076.73142393294,382.889811054159));
#127553=CARTESIAN_POINT('',(-42.5327068021327,1067.7251047501,382.889811054159));
#127554=CARTESIAN_POINT('Origin',(-42.5327068021327,1076.73142393294,384.590811277241));
#127555=CARTESIAN_POINT('Origin',(-42.5327068021327,1067.7251047501,384.590811277241));
#127556=CARTESIAN_POINT('',(-42.5327068021327,1076.73142393294,383.489811054159));
#127557=CARTESIAN_POINT('Origin',(-42.5327068021327,1076.73142393294,384.590811277241));
#127558=CARTESIAN_POINT('',(-42.5327068021327,1082.7251047501,383.489811054159));
#127559=CARTESIAN_POINT('',(-42.5327068021327,1067.7251047501,383.489811054159));
#127560=CARTESIAN_POINT('Origin',(-42.5327068021327,1082.7251047501,384.590811277241));
#127561=CARTESIAN_POINT('Origin',(-42.6325306637444,1067.7251047501,374.725288069639));
#127562=CARTESIAN_POINT('',(-42.6325306637444,1078.73142393294,373.004013437596));
#127563=CARTESIAN_POINT('Origin',(-42.6325306637444,1078.73142393294,374.725288069639));
#127564=CARTESIAN_POINT('',(-42.6325306637444,1076.73142393294,373.004013437596));
#127565=CARTESIAN_POINT('',(-42.6325306637444,1067.7251047501,373.004013437596));
#127566=CARTESIAN_POINT('Origin',(-42.6325306637444,1076.73142393294,374.725288069639));
#127567=CARTESIAN_POINT('Origin',(-42.6325306637444,1067.7251047501,374.725288069639));
#127568=CARTESIAN_POINT('',(-42.6325306637444,1076.73142393294,373.604013437596));
#127569=CARTESIAN_POINT('Origin',(-42.6325306637444,1076.73142393294,374.725288069639));
#127570=CARTESIAN_POINT('',(-42.6325306637444,1082.7251047501,373.604013437596));
#127571=CARTESIAN_POINT('',(-42.6325306637444,1067.7251047501,373.604013437596));
#127572=CARTESIAN_POINT('Origin',(-42.6325306637444,1082.7251047501,374.725288069639));
#127573=CARTESIAN_POINT('Origin',(-41.4536814090712,1067.7251047501,363.395899114888));
#127574=CARTESIAN_POINT('',(-41.4536814090712,1078.73142393294,361.613906460483));
#127575=CARTESIAN_POINT('Origin',(-41.4536814090712,1078.73142393294,363.395899114888));
#127576=CARTESIAN_POINT('',(-41.4536814090712,1076.73142393294,361.613906460483));
#127577=CARTESIAN_POINT('',(-41.4536814090712,1067.7251047501,361.613906460483));
#127578=CARTESIAN_POINT('Origin',(-41.4536814090712,1076.73142393294,363.395899114888));
#127579=CARTESIAN_POINT('Origin',(-41.4536814090712,1067.7251047501,363.395899114888));
#127580=CARTESIAN_POINT('',(-41.4536814090712,1076.73142393294,362.213906460483));
#127581=CARTESIAN_POINT('Origin',(-41.4536814090712,1076.73142393294,363.395899114888));
#127582=CARTESIAN_POINT('',(-41.4536814090712,1082.7251047501,362.213906460483));
#127583=CARTESIAN_POINT('',(-41.4536814090712,1067.7251047501,362.213906460483));
#127584=CARTESIAN_POINT('Origin',(-41.4536814090712,1082.7251047501,363.395899114888));
#127585=CARTESIAN_POINT('Origin',(-37.9688511206135,1067.7251047501,352.7287696254));
#127586=CARTESIAN_POINT('',(-37.9688511206135,1078.73142393294,351.067888815479));
#127587=CARTESIAN_POINT('Origin',(-37.9688511206135,1078.73142393294,352.7287696254));
#127588=CARTESIAN_POINT('',(-37.9688511206135,1076.73142393294,351.067888815479));
#127589=CARTESIAN_POINT('',(-37.9688511206135,1067.7251047501,351.067888815479));
#127590=CARTESIAN_POINT('Origin',(-37.9688511206135,1076.73142393294,352.7287696254));
#127591=CARTESIAN_POINT('Origin',(-37.9688511206135,1067.7251047501,352.7287696254));
#127592=CARTESIAN_POINT('',(-37.9688511206135,1076.73142393294,351.667888815479));
#127593=CARTESIAN_POINT('Origin',(-37.9688511206135,1076.73142393294,352.7287696254));
#127594=CARTESIAN_POINT('',(-37.9688511206135,1082.7251047501,351.667888815479));
#127595=CARTESIAN_POINT('',(-37.9688511206135,1067.7251047501,351.667888815479));
#127596=CARTESIAN_POINT('Origin',(-37.9688511206135,1082.7251047501,352.7287696254));
#127597=CARTESIAN_POINT('Origin',(-19.1761543694403,1067.7251047501,424.500977485066));
#127598=CARTESIAN_POINT('',(-19.1761543694403,1078.73142393294,423.400619419391));
#127599=CARTESIAN_POINT('Origin',(-19.1761543694403,1078.73142393294,424.500977485066));
#127600=CARTESIAN_POINT('',(-19.1761543694403,1076.73142393294,423.400619419391));
#127601=CARTESIAN_POINT('',(-19.1761543694403,1067.7251047501,423.400619419391));
#127602=CARTESIAN_POINT('Origin',(-19.1761543694403,1076.73142393294,424.500977485066));
#127603=CARTESIAN_POINT('Origin',(-19.1761543694403,1067.7251047501,424.500977485066));
#127604=CARTESIAN_POINT('',(-19.1761543694403,1076.73142393294,424.000619419391));
#127605=CARTESIAN_POINT('Origin',(-19.1761543694403,1076.73142393294,424.500977485066));
#127606=CARTESIAN_POINT('',(-19.1761543694403,1082.7251047501,424.000619419391));
#127607=CARTESIAN_POINT('',(-19.1761543694403,1067.7251047501,424.000619419391));
#127608=CARTESIAN_POINT('Origin',(-19.1761543694403,1082.7251047501,424.500977485066));
#127609=CARTESIAN_POINT('Origin',(-27.2453303203163,1067.7251047501,421.632917202464));
#127610=CARTESIAN_POINT('',(-27.2453303203163,1078.73142393294,420.418885635727));
#127611=CARTESIAN_POINT('Origin',(-27.2453303203163,1078.73142393294,421.632917202464));
#127612=CARTESIAN_POINT('',(-27.2453303203163,1076.73142393294,420.418885635727));
#127613=CARTESIAN_POINT('',(-27.2453303203163,1067.7251047501,420.418885635727));
#127614=CARTESIAN_POINT('Origin',(-27.2453303203163,1076.73142393294,421.632917202464));
#127615=CARTESIAN_POINT('Origin',(-27.2453303203163,1067.7251047501,421.632917202464));
#127616=CARTESIAN_POINT('',(-27.2453303203163,1076.73142393294,421.018885635727));
#127617=CARTESIAN_POINT('Origin',(-27.2453303203163,1076.73142393294,421.632917202464));
#127618=CARTESIAN_POINT('',(-27.2453303203163,1082.7251047501,421.018885635727));
#127619=CARTESIAN_POINT('',(-27.2453303203163,1067.7251047501,421.018885635727));
#127620=CARTESIAN_POINT('Origin',(-27.2453303203163,1082.7251047501,421.632917202464));
#127621=CARTESIAN_POINT('Origin',(-33.8545115154534,1067.7251047501,417.258261370252));
#127622=CARTESIAN_POINT('',(-33.8545115154534,1078.73142393294,415.929453406678));
#127623=CARTESIAN_POINT('Origin',(-33.8545115154534,1078.73142393294,417.258261370252));
#127624=CARTESIAN_POINT('',(-33.8545115154534,1076.73142393294,415.929453406678));
#127625=CARTESIAN_POINT('',(-33.8545115154534,1067.7251047501,415.929453406678));
#127626=CARTESIAN_POINT('Origin',(-33.8545115154534,1076.73142393294,417.258261370252));
#127627=CARTESIAN_POINT('Origin',(-33.8545115154534,1067.7251047501,417.258261370252));
#127628=CARTESIAN_POINT('',(-33.8545115154534,1076.73142393294,416.529453406679));
#127629=CARTESIAN_POINT('Origin',(-33.8545115154534,1076.73142393294,417.258261370252));
#127630=CARTESIAN_POINT('',(-33.8545115154534,1082.7251047501,416.529453406679));
#127631=CARTESIAN_POINT('',(-33.8545115154534,1067.7251047501,416.529453406679));
#127632=CARTESIAN_POINT('Origin',(-33.8545115154534,1082.7251047501,417.258261370252));
#127633=CARTESIAN_POINT('Origin',(-40.6548298616837,1067.7251047501,410.958411599462));
#127634=CARTESIAN_POINT('',(-40.6548298616837,1078.73142393294,409.497294597646));
#127635=CARTESIAN_POINT('Origin',(-40.6548298616837,1078.73142393294,410.958411599462));
#127636=CARTESIAN_POINT('',(-40.6548298616837,1076.73142393294,409.497294597646));
#127637=CARTESIAN_POINT('',(-40.6548298616837,1067.7251047501,409.497294597646));
#127638=CARTESIAN_POINT('Origin',(-40.6548298616837,1076.73142393294,410.958411599462));
#127639=CARTESIAN_POINT('Origin',(-40.6548298616837,1067.7251047501,410.958411599462));
#127640=CARTESIAN_POINT('',(-40.6548298616837,1076.73142393294,410.097294597645));
#127641=CARTESIAN_POINT('Origin',(-40.6548298616837,1076.73142393294,410.958411599462));
#127642=CARTESIAN_POINT('',(-40.6548298616837,1082.7251047501,410.097294597645));
#127643=CARTESIAN_POINT('',(-40.6548298616837,1067.7251047501,410.097294597645));
#127644=CARTESIAN_POINT('Origin',(-40.6548298616837,1082.7251047501,410.958411599462));
#127645=CARTESIAN_POINT('Origin',(-45.5058627832294,1067.7251047501,403.472237334184));
#127646=CARTESIAN_POINT('',(-45.5058627832294,1078.73142393294,401.85175529156));
#127647=CARTESIAN_POINT('Origin',(-45.5058627832294,1078.73142393294,403.472237334184));
#127648=CARTESIAN_POINT('',(-45.5058627832294,1076.73142393294,401.85175529156));
#127649=CARTESIAN_POINT('',(-45.5058627832294,1067.7251047501,401.85175529156));
#127650=CARTESIAN_POINT('Origin',(-45.5058627832294,1076.73142393294,403.472237334184));
#127651=CARTESIAN_POINT('Origin',(-45.5058627832294,1067.7251047501,403.472237334184));
#127652=CARTESIAN_POINT('',(-45.5058627832294,1076.73142393294,402.45175529156));
#127653=CARTESIAN_POINT('Origin',(-45.5058627832294,1076.73142393294,403.472237334184));
#127654=CARTESIAN_POINT('',(-45.5058627832294,1082.7251047501,402.45175529156));
#127655=CARTESIAN_POINT('',(-45.5058627832294,1067.7251047501,402.45175529156));
#127656=CARTESIAN_POINT('Origin',(-45.5058627832294,1082.7251047501,403.472237334184));
#127657=CARTESIAN_POINT('Origin',(-49.92585185582,1067.7251047501,394.308597378752));
#127658=CARTESIAN_POINT('',(-49.92585185582,1078.73142393294,392.607597155669));
#127659=CARTESIAN_POINT('Origin',(-49.92585185582,1078.73142393294,394.308597378752));
#127660=CARTESIAN_POINT('',(-49.92585185582,1076.73142393294,392.607597155669));
#127661=CARTESIAN_POINT('',(-49.92585185582,1067.7251047501,392.607597155669));
#127662=CARTESIAN_POINT('Origin',(-49.92585185582,1076.73142393294,394.308597378752));
#127663=CARTESIAN_POINT('Origin',(-49.92585185582,1067.7251047501,394.308597378752));
#127664=CARTESIAN_POINT('',(-49.92585185582,1076.73142393294,393.207597155669));
#127665=CARTESIAN_POINT('Origin',(-49.92585185582,1076.73142393294,394.308597378752));
#127666=CARTESIAN_POINT('',(-49.92585185582,1082.7251047501,393.207597155669));
#127667=CARTESIAN_POINT('',(-49.92585185582,1067.7251047501,393.207597155669));
#127668=CARTESIAN_POINT('Origin',(-49.92585185582,1082.7251047501,394.308597378752));
#127669=CARTESIAN_POINT('Origin',(-52.0746519374459,1067.7251047501,384.679414071104));
#127670=CARTESIAN_POINT('',(-52.0746519374459,1078.73142393294,382.958139439061));
#127671=CARTESIAN_POINT('Origin',(-52.0746519374459,1078.73142393294,384.679414071104));
#127672=CARTESIAN_POINT('',(-52.0746519374459,1076.73142393294,382.958139439061));
#127673=CARTESIAN_POINT('',(-52.0746519374459,1067.7251047501,382.958139439061));
#127674=CARTESIAN_POINT('Origin',(-52.0746519374459,1076.73142393294,384.679414071104));
#127675=CARTESIAN_POINT('Origin',(-52.0746519374459,1067.7251047501,384.679414071104));
#127676=CARTESIAN_POINT('',(-52.0746519374459,1076.73142393294,383.558139439061));
#127677=CARTESIAN_POINT('Origin',(-52.0746519374459,1076.73142393294,384.679414071104));
#127678=CARTESIAN_POINT('',(-52.0746519374459,1082.7251047501,383.558139439061));
#127679=CARTESIAN_POINT('',(-52.0746519374459,1067.7251047501,383.558139439061));
#127680=CARTESIAN_POINT('Origin',(-52.0746519374459,1082.7251047501,384.679414071104));
#127681=CARTESIAN_POINT('Origin',(-53.277075780875,1067.7251047501,373.352502905475));
#127682=CARTESIAN_POINT('',(-53.277075780875,1078.73142393294,371.57051025107));
#127683=CARTESIAN_POINT('Origin',(-53.277075780875,1078.73142393294,373.352502905475));
#127684=CARTESIAN_POINT('',(-53.277075780875,1076.73142393294,371.57051025107));
#127685=CARTESIAN_POINT('',(-53.277075780875,1067.7251047501,371.57051025107));
#127686=CARTESIAN_POINT('Origin',(-53.277075780875,1076.73142393294,373.352502905475));
#127687=CARTESIAN_POINT('Origin',(-53.277075780875,1067.7251047501,373.352502905475));
#127688=CARTESIAN_POINT('',(-53.277075780875,1076.73142393294,372.17051025107));
#127689=CARTESIAN_POINT('Origin',(-53.277075780875,1076.73142393294,373.352502905475));
#127690=CARTESIAN_POINT('',(-53.277075780875,1082.7251047501,372.17051025107));
#127691=CARTESIAN_POINT('',(-53.277075780875,1067.7251047501,372.17051025107));
#127692=CARTESIAN_POINT('Origin',(-53.277075780875,1082.7251047501,373.352502905475));
#127693=CARTESIAN_POINT('Origin',(-52.086218323587,1067.7251047501,362.19393883113));
#127694=CARTESIAN_POINT('',(-52.086218323587,1078.73142393294,360.53305802121));
#127695=CARTESIAN_POINT('Origin',(-52.086218323587,1078.73142393294,362.19393883113));
#127696=CARTESIAN_POINT('',(-52.086218323587,1076.73142393294,360.53305802121));
#127697=CARTESIAN_POINT('',(-52.086218323587,1067.7251047501,360.53305802121));
#127698=CARTESIAN_POINT('Origin',(-52.086218323587,1076.73142393294,362.19393883113));
#127699=CARTESIAN_POINT('Origin',(-52.086218323587,1067.7251047501,362.19393883113));
#127700=CARTESIAN_POINT('',(-52.086218323587,1076.73142393294,361.133058021209));
#127701=CARTESIAN_POINT('Origin',(-52.086218323587,1076.73142393294,362.19393883113));
#127702=CARTESIAN_POINT('',(-52.086218323587,1082.7251047501,361.133058021209));
#127703=CARTESIAN_POINT('',(-52.086218323587,1067.7251047501,361.133058021209));
#127704=CARTESIAN_POINT('Origin',(-52.086218323587,1082.7251047501,362.19393883113));
#127705=CARTESIAN_POINT('Origin',(-18.7819059952821,1067.7251047501,428.490530391869));
#127706=CARTESIAN_POINT('',(-18.7819059952821,1078.73142393294,427.390172326194));
#127707=CARTESIAN_POINT('Origin',(-18.7819059952821,1078.73142393294,428.490530391869));
#127708=CARTESIAN_POINT('',(-18.7819059952821,1076.73142393294,427.390172326194));
#127709=CARTESIAN_POINT('',(-18.7819059952821,1067.7251047501,427.390172326194));
#127710=CARTESIAN_POINT('Origin',(-18.7819059952821,1076.73142393294,428.490530391869));
#127711=CARTESIAN_POINT('Origin',(-18.7819059952821,1067.7251047501,428.490530391869));
#127712=CARTESIAN_POINT('',(-18.7819059952821,1076.73142393294,427.990172326194));
#127713=CARTESIAN_POINT('Origin',(-18.7819059952821,1076.73142393294,428.490530391869));
#127714=CARTESIAN_POINT('',(-18.7819059952821,1082.7251047501,427.990172326194));
#127715=CARTESIAN_POINT('',(-18.7819059952821,1067.7251047501,427.990172326194));
#127716=CARTESIAN_POINT('Origin',(-18.7819059952821,1082.7251047501,428.490530391869));
#127717=CARTESIAN_POINT('Origin',(-27.2710543542534,1067.7251047501,427.362820123134));
#127718=CARTESIAN_POINT('',(-27.2710543542534,1078.73142393294,426.148788556397));
#127719=CARTESIAN_POINT('Origin',(-27.2710543542534,1078.73142393294,427.362820123134));
#127720=CARTESIAN_POINT('',(-27.2710543542534,1076.73142393294,426.148788556397));
#127721=CARTESIAN_POINT('',(-27.2710543542534,1067.7251047501,426.148788556397));
#127722=CARTESIAN_POINT('Origin',(-27.2710543542534,1076.73142393294,427.362820123134));
#127723=CARTESIAN_POINT('Origin',(-27.2710543542534,1067.7251047501,427.362820123134));
#127724=CARTESIAN_POINT('',(-27.2710543542534,1076.73142393294,426.748788556397));
#127725=CARTESIAN_POINT('Origin',(-27.2710543542534,1076.73142393294,427.362820123134));
#127726=CARTESIAN_POINT('',(-27.2710543542534,1082.7251047501,426.748788556397));
#127727=CARTESIAN_POINT('',(-27.2710543542534,1067.7251047501,426.748788556397));
#127728=CARTESIAN_POINT('Origin',(-27.2710543542534,1082.7251047501,427.362820123134));
#127729=CARTESIAN_POINT('Origin',(-34.6453511739129,1067.7251047501,424.457887054022));
#127730=CARTESIAN_POINT('',(-34.6453511739129,1078.73142393294,423.129079090448));
#127731=CARTESIAN_POINT('Origin',(-34.6453511739129,1078.73142393294,424.457887054022));
#127732=CARTESIAN_POINT('',(-34.6453511739129,1076.73142393294,423.129079090448));
#127733=CARTESIAN_POINT('',(-34.6453511739129,1067.7251047501,423.129079090448));
#127734=CARTESIAN_POINT('Origin',(-34.6453511739129,1076.73142393294,424.457887054022));
#127735=CARTESIAN_POINT('Origin',(-34.6453511739129,1067.7251047501,424.457887054022));
#127736=CARTESIAN_POINT('',(-34.6453511739129,1076.73142393294,423.729079090448));
#127737=CARTESIAN_POINT('Origin',(-34.6453511739129,1076.73142393294,424.457887054022));
#127738=CARTESIAN_POINT('',(-34.6453511739129,1082.7251047501,423.729079090448));
#127739=CARTESIAN_POINT('',(-34.6453511739129,1067.7251047501,423.729079090448));
#127740=CARTESIAN_POINT('Origin',(-34.6453511739129,1082.7251047501,424.457887054022));
#127741=CARTESIAN_POINT('Origin',(-42.6068786662468,1067.7251047501,419.709569801204));
#127742=CARTESIAN_POINT('',(-42.6068786662468,1078.73142393294,418.248452799388));
#127743=CARTESIAN_POINT('Origin',(-42.6068786662468,1078.73142393294,419.709569801204));
#127744=CARTESIAN_POINT('',(-42.6068786662468,1076.73142393294,418.248452799388));
#127745=CARTESIAN_POINT('',(-42.6068786662468,1067.7251047501,418.248452799388));
#127746=CARTESIAN_POINT('Origin',(-42.6068786662468,1076.73142393294,419.709569801204));
#127747=CARTESIAN_POINT('Origin',(-42.6068786662468,1067.7251047501,419.709569801204));
#127748=CARTESIAN_POINT('',(-42.6068786662468,1076.73142393294,418.848452799388));
#127749=CARTESIAN_POINT('Origin',(-42.6068786662468,1076.73142393294,419.709569801204));
#127750=CARTESIAN_POINT('',(-42.6068786662468,1082.7251047501,418.848452799388));
#127751=CARTESIAN_POINT('',(-42.6068786662468,1067.7251047501,418.848452799388));
#127752=CARTESIAN_POINT('Origin',(-42.6068786662468,1082.7251047501,419.709569801204));
#127753=CARTESIAN_POINT('Origin',(-48.9083680287877,1067.7251047501,413.395572861879));
#127754=CARTESIAN_POINT('',(-48.9083680287877,1078.73142393294,411.775090819254));
#127755=CARTESIAN_POINT('Origin',(-48.9083680287877,1078.73142393294,413.395572861879));
#127756=CARTESIAN_POINT('',(-48.9083680287877,1076.73142393294,411.775090819254));
#127757=CARTESIAN_POINT('',(-48.9083680287877,1067.7251047501,411.775090819254));
#127758=CARTESIAN_POINT('Origin',(-48.9083680287877,1076.73142393294,413.395572861879));
#127759=CARTESIAN_POINT('Origin',(-48.9083680287877,1067.7251047501,413.395572861879));
#127760=CARTESIAN_POINT('',(-48.9083680287877,1076.73142393294,412.375090819254));
#127761=CARTESIAN_POINT('Origin',(-48.9083680287877,1076.73142393294,413.395572861879));
#127762=CARTESIAN_POINT('',(-48.9083680287877,1082.7251047501,412.375090819254));
#127763=CARTESIAN_POINT('',(-48.9083680287877,1067.7251047501,412.375090819254));
#127764=CARTESIAN_POINT('Origin',(-48.9083680287877,1082.7251047501,413.395572861879));
#127765=CARTESIAN_POINT('Origin',(-55.136997612591,1067.7251047501,405.351147826963));
#127766=CARTESIAN_POINT('',(-55.136997612591,1078.73142393294,403.65014760388));
#127767=CARTESIAN_POINT('Origin',(-55.136997612591,1078.73142393294,405.351147826963));
#127768=CARTESIAN_POINT('',(-55.136997612591,1076.73142393294,403.65014760388));
#127769=CARTESIAN_POINT('',(-55.136997612591,1067.7251047501,403.65014760388));
#127770=CARTESIAN_POINT('Origin',(-55.136997612591,1076.73142393294,405.351147826963));
#127771=CARTESIAN_POINT('Origin',(-55.136997612591,1067.7251047501,405.351147826963));
#127772=CARTESIAN_POINT('',(-55.136997612591,1076.73142393294,404.25014760388));
#127773=CARTESIAN_POINT('Origin',(-55.136997612591,1076.73142393294,405.351147826963));
#127774=CARTESIAN_POINT('',(-55.136997612591,1082.7251047501,404.25014760388));
#127775=CARTESIAN_POINT('',(-55.136997612591,1067.7251047501,404.25014760388));
#127776=CARTESIAN_POINT('Origin',(-55.136997612591,1082.7251047501,405.351147826963));
#127777=CARTESIAN_POINT('Origin',(-59.2408610395772,1067.7251047501,396.379145935761));
#127778=CARTESIAN_POINT('',(-59.2408610395772,1078.73142393294,394.657871303717));
#127779=CARTESIAN_POINT('Origin',(-59.2408610395772,1078.73142393294,396.379145935761));
#127780=CARTESIAN_POINT('',(-59.2408610395772,1076.73142393294,394.657871303717));
#127781=CARTESIAN_POINT('',(-59.2408610395772,1067.7251047501,394.657871303717));
#127782=CARTESIAN_POINT('Origin',(-59.2408610395772,1076.73142393294,396.379145935761));
#127783=CARTESIAN_POINT('Origin',(-59.2408610395772,1067.7251047501,396.379145935761));
#127784=CARTESIAN_POINT('',(-59.2408610395772,1076.73142393294,395.257871303717));
#127785=CARTESIAN_POINT('Origin',(-59.2408610395772,1076.73142393294,396.379145935761));
#127786=CARTESIAN_POINT('',(-59.2408610395772,1082.7251047501,395.257871303717));
#127787=CARTESIAN_POINT('',(-59.2408610395772,1067.7251047501,395.257871303717));
#127788=CARTESIAN_POINT('Origin',(-59.2408610395772,1082.7251047501,396.379145935761));
#127789=CARTESIAN_POINT('Origin',(-62.7720062892809,1067.7251047501,385.549752929743));
#127790=CARTESIAN_POINT('',(-62.7720062892809,1078.73142393294,383.767760275338));
#127791=CARTESIAN_POINT('Origin',(-62.7720062892809,1078.73142393294,385.549752929743));
#127792=CARTESIAN_POINT('',(-62.7720062892809,1076.73142393294,383.767760275338));
#127793=CARTESIAN_POINT('',(-62.7720062892809,1067.7251047501,383.767760275338));
#127794=CARTESIAN_POINT('Origin',(-62.7720062892809,1076.73142393294,385.549752929743));
#127795=CARTESIAN_POINT('Origin',(-62.7720062892809,1067.7251047501,385.549752929743));
#127796=CARTESIAN_POINT('',(-62.7720062892809,1076.73142393294,384.367760275338));
#127797=CARTESIAN_POINT('Origin',(-62.7720062892809,1076.73142393294,385.549752929743));
#127798=CARTESIAN_POINT('',(-62.7720062892809,1082.7251047501,384.367760275338));
#127799=CARTESIAN_POINT('',(-62.7720062892809,1067.7251047501,384.367760275338));
#127800=CARTESIAN_POINT('Origin',(-62.7720062892809,1082.7251047501,385.549752929743));
#127801=CARTESIAN_POINT('Origin',(-63.9271678484141,1067.7251047501,374.38743706532));
#127802=CARTESIAN_POINT('',(-63.9271678484141,1078.73142393294,372.726556255399));
#127803=CARTESIAN_POINT('Origin',(-63.9271678484141,1078.73142393294,374.38743706532));
#127804=CARTESIAN_POINT('',(-63.9271678484141,1076.73142393294,372.726556255399));
#127805=CARTESIAN_POINT('',(-63.9271678484141,1067.7251047501,372.726556255399));
#127806=CARTESIAN_POINT('Origin',(-63.9271678484141,1076.73142393294,374.38743706532));
#127807=CARTESIAN_POINT('Origin',(-63.9271678484141,1067.7251047501,374.38743706532));
#127808=CARTESIAN_POINT('',(-63.9271678484141,1076.73142393294,373.326556255399));
#127809=CARTESIAN_POINT('Origin',(-63.9271678484141,1076.73142393294,374.38743706532));
#127810=CARTESIAN_POINT('',(-63.9271678484141,1082.7251047501,373.326556255399));
#127811=CARTESIAN_POINT('',(-63.9271678484141,1067.7251047501,373.326556255399));
#127812=CARTESIAN_POINT('Origin',(-63.9271678484141,1082.7251047501,374.38743706532));
#127813=CARTESIAN_POINT('Origin',(-17.5667982035458,1067.7251047501,432.310933149585));
#127814=CARTESIAN_POINT('',(-17.5667982035458,1078.73142393294,431.21057508391));
#127815=CARTESIAN_POINT('Origin',(-17.5667982035458,1078.73142393294,432.310933149585));
#127816=CARTESIAN_POINT('',(-17.5667982035458,1076.73142393294,431.21057508391));
#127817=CARTESIAN_POINT('',(-17.5667982035458,1067.7251047501,431.21057508391));
#127818=CARTESIAN_POINT('Origin',(-17.5667982035458,1076.73142393294,432.310933149585));
#127819=CARTESIAN_POINT('Origin',(-17.5667982035458,1067.7251047501,432.310933149585));
#127820=CARTESIAN_POINT('',(-17.5667982035458,1076.73142393294,431.81057508391));
#127821=CARTESIAN_POINT('Origin',(-17.5667982035458,1076.73142393294,432.310933149585));
#127822=CARTESIAN_POINT('',(-17.5667982035458,1082.7251047501,431.81057508391));
#127823=CARTESIAN_POINT('',(-17.5667982035458,1067.7251047501,431.81057508391));
#127824=CARTESIAN_POINT('Origin',(-17.5667982035458,1082.7251047501,432.310933149585));
#127825=CARTESIAN_POINT('Origin',(-26.104902451872,1067.7251047501,432.972859244816));
#127826=CARTESIAN_POINT('',(-26.104902451872,1078.73142393294,431.758827678079));
#127827=CARTESIAN_POINT('Origin',(-26.104902451872,1078.73142393294,432.972859244816));
#127828=CARTESIAN_POINT('',(-26.104902451872,1076.73142393294,431.758827678079));
#127829=CARTESIAN_POINT('',(-26.104902451872,1067.7251047501,431.758827678079));
#127830=CARTESIAN_POINT('Origin',(-26.104902451872,1076.73142393294,432.972859244816));
#127831=CARTESIAN_POINT('Origin',(-26.104902451872,1067.7251047501,432.972859244816));
#127832=CARTESIAN_POINT('',(-26.104902451872,1076.73142393294,432.358827678079));
#127833=CARTESIAN_POINT('Origin',(-26.104902451872,1076.73142393294,432.972859244816));
#127834=CARTESIAN_POINT('',(-26.104902451872,1082.7251047501,432.358827678079));
#127835=CARTESIAN_POINT('',(-26.104902451872,1067.7251047501,432.358827678079));
#127836=CARTESIAN_POINT('Origin',(-26.104902451872,1082.7251047501,432.972859244816));
#127837=CARTESIAN_POINT('Origin',(-33.9220227392324,1067.7251047501,431.664608453338));
#127838=CARTESIAN_POINT('',(-33.9220227392324,1078.73142393294,430.335800489765));
#127839=CARTESIAN_POINT('Origin',(-33.9220227392324,1078.73142393294,431.664608453338));
#127840=CARTESIAN_POINT('',(-33.9220227392324,1076.73142393294,430.335800489765));
#127841=CARTESIAN_POINT('',(-33.9220227392324,1067.7251047501,430.335800489765));
#127842=CARTESIAN_POINT('Origin',(-33.9220227392324,1076.73142393294,431.664608453338));
#127843=CARTESIAN_POINT('Origin',(-33.9220227392324,1067.7251047501,431.664608453338));
#127844=CARTESIAN_POINT('',(-33.9220227392324,1076.73142393294,430.935800489765));
#127845=CARTESIAN_POINT('Origin',(-33.9220227392324,1076.73142393294,431.664608453338));
#127846=CARTESIAN_POINT('',(-33.9220227392324,1082.7251047501,430.935800489765));
#127847=CARTESIAN_POINT('',(-33.9220227392324,1067.7251047501,430.935800489765));
#127848=CARTESIAN_POINT('Origin',(-33.9220227392324,1082.7251047501,431.664608453338));
#127849=CARTESIAN_POINT('Origin',(-42.6968024226075,1067.7251047501,428.675347967396));
#127850=CARTESIAN_POINT('',(-42.6968024226075,1078.73142393294,427.214230965579));
#127851=CARTESIAN_POINT('Origin',(-42.6968024226075,1078.73142393294,428.675347967396));
#127852=CARTESIAN_POINT('',(-42.6968024226075,1076.73142393294,427.214230965579));
#127853=CARTESIAN_POINT('',(-42.6968024226075,1067.7251047501,427.214230965579));
#127854=CARTESIAN_POINT('Origin',(-42.6968024226075,1076.73142393294,428.675347967396));
#127855=CARTESIAN_POINT('Origin',(-42.6968024226075,1067.7251047501,428.675347967396));
#127856=CARTESIAN_POINT('',(-42.6968024226075,1076.73142393294,427.814230965579));
#127857=CARTESIAN_POINT('Origin',(-42.6968024226075,1076.73142393294,428.675347967396));
#127858=CARTESIAN_POINT('',(-42.6968024226075,1082.7251047501,427.814230965579));
#127859=CARTESIAN_POINT('',(-42.6968024226075,1067.7251047501,427.814230965579));
#127860=CARTESIAN_POINT('Origin',(-42.6968024226075,1082.7251047501,428.675347967396));
#127861=CARTESIAN_POINT('Origin',(-50.1733429030999,1067.7251047501,423.80948031819));
#127862=CARTESIAN_POINT('',(-50.1733429030999,1078.73142393294,422.188998275565));
#127863=CARTESIAN_POINT('Origin',(-50.1733429030999,1078.73142393294,423.80948031819));
#127864=CARTESIAN_POINT('',(-50.1733429030999,1076.73142393294,422.188998275565));
#127865=CARTESIAN_POINT('',(-50.1733429030999,1067.7251047501,422.188998275565));
#127866=CARTESIAN_POINT('Origin',(-50.1733429030999,1076.73142393294,423.80948031819));
#127867=CARTESIAN_POINT('Origin',(-50.1733429030999,1067.7251047501,423.80948031819));
#127868=CARTESIAN_POINT('',(-50.1733429030999,1076.73142393294,422.788998275565));
#127869=CARTESIAN_POINT('Origin',(-50.1733429030999,1076.73142393294,423.80948031819));
#127870=CARTESIAN_POINT('',(-50.1733429030999,1082.7251047501,422.788998275565));
#127871=CARTESIAN_POINT('',(-50.1733429030999,1067.7251047501,422.788998275565));
#127872=CARTESIAN_POINT('Origin',(-50.1733429030999,1082.7251047501,423.80948031819));
#127873=CARTESIAN_POINT('Origin',(-57.9383919970227,1067.7251047501,417.23585017925));
#127874=CARTESIAN_POINT('',(-57.9383919970227,1078.73142393294,415.534849956167));
#127875=CARTESIAN_POINT('Origin',(-57.9383919970227,1078.73142393294,417.23585017925));
#127876=CARTESIAN_POINT('',(-57.9383919970227,1076.73142393294,415.534849956167));
#127877=CARTESIAN_POINT('',(-57.9383919970227,1067.7251047501,415.534849956167));
#127878=CARTESIAN_POINT('Origin',(-57.9383919970227,1076.73142393294,417.23585017925));
#127879=CARTESIAN_POINT('Origin',(-57.9383919970227,1067.7251047501,417.23585017925));
#127880=CARTESIAN_POINT('',(-57.9383919970227,1076.73142393294,416.134849956167));
#127881=CARTESIAN_POINT('Origin',(-57.9383919970227,1076.73142393294,417.23585017925));
#127882=CARTESIAN_POINT('',(-57.9383919970227,1082.7251047501,416.134849956167));
#127883=CARTESIAN_POINT('',(-57.9383919970227,1067.7251047501,416.134849956167));
#127884=CARTESIAN_POINT('Origin',(-57.9383919970227,1082.7251047501,417.23585017925));
#127885=CARTESIAN_POINT('Origin',(-63.8179602450884,1067.7251047501,409.313149239581));
#127886=CARTESIAN_POINT('',(-63.8179602450884,1078.73142393294,407.591874607538));
#127887=CARTESIAN_POINT('Origin',(-63.8179602450884,1078.73142393294,409.313149239581));
#127888=CARTESIAN_POINT('',(-63.8179602450884,1076.73142393294,407.591874607538));
#127889=CARTESIAN_POINT('',(-63.8179602450884,1067.7251047501,407.591874607538));
#127890=CARTESIAN_POINT('Origin',(-63.8179602450884,1076.73142393294,409.313149239581));
#127891=CARTESIAN_POINT('Origin',(-63.8179602450884,1067.7251047501,409.313149239581));
#127892=CARTESIAN_POINT('',(-63.8179602450884,1076.73142393294,408.191874607538));
#127893=CARTESIAN_POINT('Origin',(-63.8179602450884,1076.73142393294,409.313149239581));
#127894=CARTESIAN_POINT('',(-63.8179602450884,1082.7251047501,408.191874607538));
#127895=CARTESIAN_POINT('',(-63.8179602450884,1067.7251047501,408.191874607538));
#127896=CARTESIAN_POINT('Origin',(-63.8179602450884,1082.7251047501,409.313149239581));
#127897=CARTESIAN_POINT('Origin',(-69.5234989093398,1067.7251047501,399.45457083273));
#127898=CARTESIAN_POINT('',(-69.5234989093398,1078.73142393294,397.672578178326));
#127899=CARTESIAN_POINT('Origin',(-69.5234989093398,1078.73142393294,399.45457083273));
#127900=CARTESIAN_POINT('',(-69.5234989093398,1076.73142393294,397.672578178326));
#127901=CARTESIAN_POINT('',(-69.5234989093398,1067.7251047501,397.672578178326));
#127902=CARTESIAN_POINT('Origin',(-69.5234989093398,1076.73142393294,399.45457083273));
#127903=CARTESIAN_POINT('Origin',(-69.5234989093398,1067.7251047501,399.45457083273));
#127904=CARTESIAN_POINT('',(-69.5234989093398,1076.73142393294,398.272578178326));
#127905=CARTESIAN_POINT('Origin',(-69.5234989093398,1076.73142393294,399.45457083273));
#127906=CARTESIAN_POINT('',(-69.5234989093398,1082.7251047501,398.272578178326));
#127907=CARTESIAN_POINT('',(-69.5234989093398,1067.7251047501,398.272578178326));
#127908=CARTESIAN_POINT('Origin',(-69.5234989093398,1082.7251047501,399.45457083273));
#127909=CARTESIAN_POINT('Origin',(-72.9741933816799,1067.7251047501,388.776349944239));
#127910=CARTESIAN_POINT('',(-72.9741933816799,1078.73142393294,387.115469134319));
#127911=CARTESIAN_POINT('Origin',(-72.9741933816799,1078.73142393294,388.776349944239));
#127912=CARTESIAN_POINT('',(-72.9741933816799,1076.73142393294,387.115469134319));
#127913=CARTESIAN_POINT('',(-72.9741933816799,1067.7251047501,387.115469134319));
#127914=CARTESIAN_POINT('Origin',(-72.9741933816799,1076.73142393294,388.776349944239));
#127915=CARTESIAN_POINT('Origin',(-72.9741933816799,1067.7251047501,388.776349944239));
#127916=CARTESIAN_POINT('',(-72.9741933816799,1076.73142393294,387.715469134319));
#127917=CARTESIAN_POINT('Origin',(-72.9741933816799,1076.73142393294,388.776349944239));
#127918=CARTESIAN_POINT('',(-72.9741933816799,1082.7251047501,387.715469134319));
#127919=CARTESIAN_POINT('',(-72.9741933816799,1067.7251047501,387.715469134319));
#127920=CARTESIAN_POINT('Origin',(-72.9741933816799,1082.7251047501,388.776349944239));
#127921=CARTESIAN_POINT('Origin',(-15.5839370354643,1067.7251047501,435.795215825376));
#127922=CARTESIAN_POINT('',(-15.5839370354643,1078.73142393294,434.694857759701));
#127923=CARTESIAN_POINT('Origin',(-15.5839370354643,1078.73142393294,435.795215825376));
#127924=CARTESIAN_POINT('',(-15.5839370354643,1076.73142393294,434.694857759701));
#127925=CARTESIAN_POINT('',(-15.5839370354643,1067.7251047501,434.694857759701));
#127926=CARTESIAN_POINT('Origin',(-15.5839370354643,1076.73142393294,435.795215825376));
#127927=CARTESIAN_POINT('Origin',(-15.5839370354643,1067.7251047501,435.795215825376));
#127928=CARTESIAN_POINT('',(-15.5839370354643,1076.73142393294,435.294857759701));
#127929=CARTESIAN_POINT('Origin',(-15.5839370354643,1076.73142393294,435.795215825376));
#127930=CARTESIAN_POINT('',(-15.5839370354643,1082.7251047501,435.294857759701));
#127931=CARTESIAN_POINT('',(-15.5839370354643,1067.7251047501,435.294857759701));
#127932=CARTESIAN_POINT('Origin',(-15.5839370354643,1082.7251047501,435.795215825376));
#127933=CARTESIAN_POINT('Origin',(-23.7978410471238,1067.7251047501,438.217848937937));
#127934=CARTESIAN_POINT('',(-23.7978410471238,1078.73142393294,437.0038173712));
#127935=CARTESIAN_POINT('Origin',(-23.7978410471238,1078.73142393294,438.217848937937));
#127936=CARTESIAN_POINT('',(-23.7978410471238,1076.73142393294,437.0038173712));
#127937=CARTESIAN_POINT('',(-23.7978410471238,1067.7251047501,437.0038173712));
#127938=CARTESIAN_POINT('Origin',(-23.7978410471238,1076.73142393294,438.217848937937));
#127939=CARTESIAN_POINT('Origin',(-23.7978410471238,1067.7251047501,438.217848937937));
#127940=CARTESIAN_POINT('',(-23.7978410471238,1076.73142393294,437.6038173712));
#127941=CARTESIAN_POINT('Origin',(-23.7978410471238,1076.73142393294,438.217848937937));
#127942=CARTESIAN_POINT('',(-23.7978410471238,1082.7251047501,437.6038173712));
#127943=CARTESIAN_POINT('',(-23.7978410471238,1067.7251047501,437.6038173712));
#127944=CARTESIAN_POINT('Origin',(-23.7978410471238,1082.7251047501,438.217848937937));
#127945=CARTESIAN_POINT('Origin',(-31.7161391349227,1067.7251047501,438.563457261366));
#127946=CARTESIAN_POINT('',(-31.7161391349227,1078.73142393294,437.234649297793));
#127947=CARTESIAN_POINT('Origin',(-31.7161391349227,1078.73142393294,438.563457261366));
#127948=CARTESIAN_POINT('',(-31.7161391349227,1076.73142393294,437.234649297793));
#127949=CARTESIAN_POINT('',(-31.7161391349227,1067.7251047501,437.234649297793));
#127950=CARTESIAN_POINT('Origin',(-31.7161391349227,1076.73142393294,438.563457261366));
#127951=CARTESIAN_POINT('Origin',(-31.7161391349227,1067.7251047501,438.563457261366));
#127952=CARTESIAN_POINT('',(-31.7161391349227,1076.73142393294,437.834649297793));
#127953=CARTESIAN_POINT('Origin',(-31.7161391349227,1076.73142393294,438.563457261366));
#127954=CARTESIAN_POINT('',(-31.7161391349227,1082.7251047501,437.834649297793));
#127955=CARTESIAN_POINT('',(-31.7161391349227,1067.7251047501,437.834649297793));
#127956=CARTESIAN_POINT('Origin',(-31.7161391349227,1082.7251047501,438.563457261366));
#127957=CARTESIAN_POINT('Origin',(-40.9206710311109,1067.7251047501,437.463898569597));
#127958=CARTESIAN_POINT('',(-40.9206710311109,1078.73142393294,436.00278156778));
#127959=CARTESIAN_POINT('Origin',(-40.9206710311109,1078.73142393294,437.463898569597));
#127960=CARTESIAN_POINT('',(-40.9206710311109,1076.73142393294,436.00278156778));
#127961=CARTESIAN_POINT('',(-40.9206710311109,1067.7251047501,436.00278156778));
#127962=CARTESIAN_POINT('Origin',(-40.9206710311109,1076.73142393294,437.463898569597));
#127963=CARTESIAN_POINT('Origin',(-40.9206710311109,1067.7251047501,437.463898569597));
#127964=CARTESIAN_POINT('',(-40.9206710311109,1076.73142393294,436.60278156778));
#127965=CARTESIAN_POINT('Origin',(-40.9206710311109,1076.73142393294,437.463898569597));
#127966=CARTESIAN_POINT('',(-40.9206710311109,1082.7251047501,436.60278156778));
#127967=CARTESIAN_POINT('',(-40.9206710311109,1067.7251047501,436.60278156778));
#127968=CARTESIAN_POINT('Origin',(-40.9206710311109,1082.7251047501,437.463898569597));
#127969=CARTESIAN_POINT('Origin',(-49.2455019341356,1067.7251047501,434.258821975804));
#127970=CARTESIAN_POINT('',(-49.2455019341356,1078.73142393294,432.63833993318));
#127971=CARTESIAN_POINT('Origin',(-49.2455019341356,1078.73142393294,434.258821975804));
#127972=CARTESIAN_POINT('',(-49.2455019341356,1076.73142393294,432.63833993318));
#127973=CARTESIAN_POINT('',(-49.2455019341356,1067.7251047501,432.63833993318));
#127974=CARTESIAN_POINT('Origin',(-49.2455019341356,1076.73142393294,434.258821975804));
#127975=CARTESIAN_POINT('Origin',(-49.2455019341356,1067.7251047501,434.258821975804));
#127976=CARTESIAN_POINT('',(-49.2455019341356,1076.73142393294,433.23833993318));
#127977=CARTESIAN_POINT('Origin',(-49.2455019341356,1076.73142393294,434.258821975804));
#127978=CARTESIAN_POINT('',(-49.2455019341356,1082.7251047501,433.23833993318));
#127979=CARTESIAN_POINT('',(-49.2455019341356,1067.7251047501,433.23833993318));
#127980=CARTESIAN_POINT('Origin',(-49.2455019341356,1082.7251047501,434.258821975804));
#127981=CARTESIAN_POINT('Origin',(-58.207600631934,1067.7251047501,429.443285913689));
#127982=CARTESIAN_POINT('',(-58.207600631934,1078.73142393294,427.742285690606));
#127983=CARTESIAN_POINT('Origin',(-58.207600631934,1078.73142393294,429.443285913689));
#127984=CARTESIAN_POINT('',(-58.207600631934,1076.73142393294,427.742285690606));
#127985=CARTESIAN_POINT('',(-58.207600631934,1067.7251047501,427.742285690606));
#127986=CARTESIAN_POINT('Origin',(-58.207600631934,1076.73142393294,429.443285913689));
#127987=CARTESIAN_POINT('Origin',(-58.207600631934,1067.7251047501,429.443285913689));
#127988=CARTESIAN_POINT('',(-58.207600631934,1076.73142393294,428.342285690606));
#127989=CARTESIAN_POINT('Origin',(-58.207600631934,1076.73142393294,429.443285913689));
#127990=CARTESIAN_POINT('',(-58.207600631934,1082.7251047501,428.342285690606));
#127991=CARTESIAN_POINT('',(-58.207600631934,1067.7251047501,428.342285690606));
#127992=CARTESIAN_POINT('Origin',(-58.207600631934,1082.7251047501,429.443285913689));
#127993=CARTESIAN_POINT('Origin',(-65.60590835534,1067.7251047501,422.916145973955));
#127994=CARTESIAN_POINT('',(-65.60590835534,1078.73142393294,421.194871341911));
#127995=CARTESIAN_POINT('Origin',(-65.60590835534,1078.73142393294,422.916145973955));
#127996=CARTESIAN_POINT('',(-65.60590835534,1076.73142393294,421.194871341911));
#127997=CARTESIAN_POINT('',(-65.60590835534,1067.7251047501,421.194871341911));
#127998=CARTESIAN_POINT('Origin',(-65.60590835534,1076.73142393294,422.916145973955));
#127999=CARTESIAN_POINT('Origin',(-65.60590835534,1067.7251047501,422.916145973955));
#128000=CARTESIAN_POINT('',(-65.60590835534,1076.73142393294,421.794871341911));
#128001=CARTESIAN_POINT('Origin',(-65.60590835534,1076.73142393294,422.916145973955));
#128002=CARTESIAN_POINT('',(-65.60590835534,1082.7251047501,421.794871341911));
#128003=CARTESIAN_POINT('',(-65.60590835534,1067.7251047501,421.794871341911));
#128004=CARTESIAN_POINT('Origin',(-65.60590835534,1082.7251047501,422.916145973955));
#128005=CARTESIAN_POINT('Origin',(-73.2364810162993,1067.7251047501,414.459249349358));
#128006=CARTESIAN_POINT('',(-73.2364810162993,1078.73142393294,412.677256694953));
#128007=CARTESIAN_POINT('Origin',(-73.2364810162993,1078.73142393294,414.459249349358));
#128008=CARTESIAN_POINT('',(-73.2364810162993,1076.73142393294,412.677256694953));
#128009=CARTESIAN_POINT('',(-73.2364810162993,1067.7251047501,412.677256694953));
#128010=CARTESIAN_POINT('Origin',(-73.2364810162993,1076.73142393294,414.459249349358));
#128011=CARTESIAN_POINT('Origin',(-73.2364810162993,1067.7251047501,414.459249349358));
#128012=CARTESIAN_POINT('',(-73.2364810162993,1076.73142393294,413.277256694953));
#128013=CARTESIAN_POINT('Origin',(-73.2364810162993,1076.73142393294,414.459249349358));
#128014=CARTESIAN_POINT('',(-73.2364810162993,1082.7251047501,413.277256694953));
#128015=CARTESIAN_POINT('',(-73.2364810162993,1067.7251047501,413.277256694953));
#128016=CARTESIAN_POINT('Origin',(-73.2364810162993,1082.7251047501,414.459249349358));
#128017=CARTESIAN_POINT('Origin',(-78.8318964951359,1067.7251047501,404.731812929415));
#128018=CARTESIAN_POINT('',(-78.8318964951359,1078.73142393294,403.070932119494));
#128019=CARTESIAN_POINT('Origin',(-78.8318964951359,1078.73142393294,404.731812929415));
#128020=CARTESIAN_POINT('',(-78.8318964951359,1076.73142393294,403.070932119494));
#128021=CARTESIAN_POINT('',(-78.8318964951359,1067.7251047501,403.070932119494));
#128022=CARTESIAN_POINT('Origin',(-78.8318964951359,1076.73142393294,404.731812929415));
#128023=CARTESIAN_POINT('Origin',(-78.8318964951359,1067.7251047501,404.731812929415));
#128024=CARTESIAN_POINT('',(-78.8318964951359,1076.73142393294,403.670932119494));
#128025=CARTESIAN_POINT('Origin',(-78.8318964951359,1076.73142393294,404.731812929415));
#128026=CARTESIAN_POINT('',(-78.8318964951359,1082.7251047501,403.670932119494));
#128027=CARTESIAN_POINT('',(-78.8318964951359,1067.7251047501,403.670932119494));
#128028=CARTESIAN_POINT('Origin',(-78.8318964951359,1082.7251047501,404.731812929415));
#128029=CARTESIAN_POINT('Origin',(-12.9199830389064,1067.7251047501,438.791098546867));
#128030=CARTESIAN_POINT('',(-12.9199830389064,1078.73142393294,437.690740481192));
#128031=CARTESIAN_POINT('Origin',(-12.9199830389064,1078.73142393294,438.791098546867));
#128032=CARTESIAN_POINT('',(-12.9199830389064,1076.73142393294,437.690740481192));
#128033=CARTESIAN_POINT('',(-12.9199830389064,1067.7251047501,437.690740481192));
#128034=CARTESIAN_POINT('Origin',(-12.9199830389064,1076.73142393294,438.791098546867));
#128035=CARTESIAN_POINT('Origin',(-12.9199830389064,1067.7251047501,438.791098546867));
#128036=CARTESIAN_POINT('',(-12.9199830389064,1076.73142393294,438.290740481192));
#128037=CARTESIAN_POINT('Origin',(-12.9199830389064,1076.73142393294,438.791098546867));
#128038=CARTESIAN_POINT('',(-12.9199830389064,1082.7251047501,438.290740481192));
#128039=CARTESIAN_POINT('',(-12.9199830389064,1067.7251047501,438.290740481192));
#128040=CARTESIAN_POINT('Origin',(-12.9199830389064,1082.7251047501,438.791098546867));
#128041=CARTESIAN_POINT('Origin',(-20.4506997939053,1067.7251047501,442.868557984656));
#128042=CARTESIAN_POINT('',(-20.4506997939053,1078.73142393294,441.654526417919));
#128043=CARTESIAN_POINT('Origin',(-20.4506997939053,1078.73142393294,442.868557984656));
#128044=CARTESIAN_POINT('',(-20.4506997939053,1076.73142393294,441.654526417919));
#128045=CARTESIAN_POINT('',(-20.4506997939053,1067.7251047501,441.654526417919));
#128046=CARTESIAN_POINT('Origin',(-20.4506997939053,1076.73142393294,442.868557984656));
#128047=CARTESIAN_POINT('Origin',(-20.4506997939053,1067.7251047501,442.868557984656));
#128048=CARTESIAN_POINT('',(-20.4506997939053,1076.73142393294,442.254526417919));
#128049=CARTESIAN_POINT('Origin',(-20.4506997939053,1076.73142393294,442.868557984656));
#128050=CARTESIAN_POINT('',(-20.4506997939053,1082.7251047501,442.254526417919));
#128051=CARTESIAN_POINT('',(-20.4506997939053,1067.7251047501,442.254526417919));
#128052=CARTESIAN_POINT('Origin',(-20.4506997939053,1082.7251047501,442.868557984656));
#128053=CARTESIAN_POINT('Origin',(-28.1241080594961,1067.7251047501,444.852920680845));
#128054=CARTESIAN_POINT('',(-28.1241080594961,1078.73142393294,443.524112717272));
#128055=CARTESIAN_POINT('Origin',(-28.1241080594961,1078.73142393294,444.852920680845));
#128056=CARTESIAN_POINT('',(-28.1241080594961,1076.73142393294,443.524112717272));
#128057=CARTESIAN_POINT('',(-28.1241080594961,1067.7251047501,443.524112717272));
#128058=CARTESIAN_POINT('Origin',(-28.1241080594961,1076.73142393294,444.852920680845));
#128059=CARTESIAN_POINT('Origin',(-28.1241080594961,1067.7251047501,444.852920680845));
#128060=CARTESIAN_POINT('',(-28.1241080594961,1076.73142393294,444.124112717272));
#128061=CARTESIAN_POINT('Origin',(-28.1241080594961,1076.73142393294,444.852920680845));
#128062=CARTESIAN_POINT('',(-28.1241080594961,1082.7251047501,444.124112717272));
#128063=CARTESIAN_POINT('',(-28.1241080594961,1067.7251047501,444.124112717272));
#128064=CARTESIAN_POINT('Origin',(-28.1241080594961,1082.7251047501,444.852920680845));
#128065=CARTESIAN_POINT('Origin',(-37.3561099563896,1067.7251047501,445.691119774347));
#128066=CARTESIAN_POINT('',(-37.3561099563896,1078.73142393294,444.23000277253));
#128067=CARTESIAN_POINT('Origin',(-37.3561099563896,1078.73142393294,445.691119774347));
#128068=CARTESIAN_POINT('',(-37.3561099563896,1076.73142393294,444.23000277253));
#128069=CARTESIAN_POINT('',(-37.3561099563896,1067.7251047501,444.23000277253));
#128070=CARTESIAN_POINT('Origin',(-37.3561099563896,1076.73142393294,445.691119774347));
#128071=CARTESIAN_POINT('Origin',(-37.3561099563896,1067.7251047501,445.691119774347));
#128072=CARTESIAN_POINT('',(-37.3561099563896,1076.73142393294,444.83000277253));
#128073=CARTESIAN_POINT('Origin',(-37.3561099563896,1076.73142393294,445.691119774347));
#128074=CARTESIAN_POINT('',(-37.3561099563896,1082.7251047501,444.83000277253));
#128075=CARTESIAN_POINT('',(-37.3561099563896,1067.7251047501,444.83000277253));
#128076=CARTESIAN_POINT('Origin',(-37.3561099563896,1082.7251047501,445.691119774347));
#128077=CARTESIAN_POINT('Origin',(-46.1653962245135,1067.7251047501,444.286911462781));
#128078=CARTESIAN_POINT('',(-46.1653962245135,1078.73142393294,442.666429420156));
#128079=CARTESIAN_POINT('Origin',(-46.1653962245135,1078.73142393294,444.286911462781));
#128080=CARTESIAN_POINT('',(-46.1653962245135,1076.73142393294,442.666429420156));
#128081=CARTESIAN_POINT('',(-46.1653962245135,1067.7251047501,442.666429420156));
#128082=CARTESIAN_POINT('Origin',(-46.1653962245135,1076.73142393294,444.286911462781));
#128083=CARTESIAN_POINT('Origin',(-46.1653962245135,1067.7251047501,444.286911462781));
#128084=CARTESIAN_POINT('',(-46.1653962245135,1076.73142393294,443.266429420156));
#128085=CARTESIAN_POINT('Origin',(-46.1653962245135,1076.73142393294,444.286911462781));
#128086=CARTESIAN_POINT('',(-46.1653962245135,1082.7251047501,443.266429420156));
#128087=CARTESIAN_POINT('',(-46.1653962245135,1067.7251047501,443.266429420156));
#128088=CARTESIAN_POINT('Origin',(-46.1653962245135,1082.7251047501,444.286911462781));
#128089=CARTESIAN_POINT('Origin',(-55.9328578081729,1067.7251047501,441.43993151091));
#128090=CARTESIAN_POINT('',(-55.9328578081729,1078.73142393294,439.738931287827));
#128091=CARTESIAN_POINT('Origin',(-55.9328578081729,1078.73142393294,441.43993151091));
#128092=CARTESIAN_POINT('',(-55.9328578081729,1076.73142393294,439.738931287827));
#128093=CARTESIAN_POINT('',(-55.9328578081729,1067.7251047501,439.738931287827));
#128094=CARTESIAN_POINT('Origin',(-55.9328578081729,1076.73142393294,441.43993151091));
#128095=CARTESIAN_POINT('Origin',(-55.9328578081729,1067.7251047501,441.43993151091));
#128096=CARTESIAN_POINT('',(-55.9328578081729,1076.73142393294,440.338931287827));
#128097=CARTESIAN_POINT('Origin',(-55.9328578081729,1076.73142393294,441.43993151091));
#128098=CARTESIAN_POINT('',(-55.9328578081729,1082.7251047501,440.338931287827));
#128099=CARTESIAN_POINT('',(-55.9328578081729,1067.7251047501,440.338931287827));
#128100=CARTESIAN_POINT('Origin',(-55.9328578081729,1082.7251047501,441.43993151091));
#128101=CARTESIAN_POINT('Origin',(-64.5265634583872,1067.7251047501,436.593619907169));
#128102=CARTESIAN_POINT('',(-64.5265634583872,1078.73142393294,434.872345275125));
#128103=CARTESIAN_POINT('Origin',(-64.5265634583872,1078.73142393294,436.593619907169));
#128104=CARTESIAN_POINT('',(-64.5265634583872,1076.73142393294,434.872345275125));
#128105=CARTESIAN_POINT('',(-64.5265634583872,1067.7251047501,434.872345275125));
#128106=CARTESIAN_POINT('Origin',(-64.5265634583872,1076.73142393294,436.593619907169));
#128107=CARTESIAN_POINT('Origin',(-64.5265634583872,1067.7251047501,436.593619907169));
#128108=CARTESIAN_POINT('',(-64.5265634583872,1076.73142393294,435.472345275125));
#128109=CARTESIAN_POINT('Origin',(-64.5265634583872,1076.73142393294,436.593619907169));
#128110=CARTESIAN_POINT('',(-64.5265634583872,1082.7251047501,435.472345275125));
#128111=CARTESIAN_POINT('',(-64.5265634583872,1067.7251047501,435.472345275125));
#128112=CARTESIAN_POINT('Origin',(-64.5265634583872,1082.7251047501,436.593619907169));
#128113=CARTESIAN_POINT('Origin',(-73.7486774752203,1067.7251047501,429.908012028014));
#128114=CARTESIAN_POINT('',(-73.7486774752203,1078.73142393294,428.126019373609));
#128115=CARTESIAN_POINT('Origin',(-73.7486774752203,1078.73142393294,429.908012028014));
#128116=CARTESIAN_POINT('',(-73.7486774752203,1076.73142393294,428.126019373609));
#128117=CARTESIAN_POINT('',(-73.7486774752203,1067.7251047501,428.126019373609));
#128118=CARTESIAN_POINT('Origin',(-73.7486774752203,1076.73142393294,429.908012028014));
#128119=CARTESIAN_POINT('Origin',(-73.7486774752203,1067.7251047501,429.908012028014));
#128120=CARTESIAN_POINT('',(-73.7486774752203,1076.73142393294,428.726019373609));
#128121=CARTESIAN_POINT('Origin',(-73.7486774752203,1076.73142393294,429.908012028014));
#128122=CARTESIAN_POINT('',(-73.7486774752203,1082.7251047501,428.726019373609));
#128123=CARTESIAN_POINT('',(-73.7486774752203,1067.7251047501,428.726019373609));
#128124=CARTESIAN_POINT('Origin',(-73.7486774752203,1082.7251047501,429.908012028014));
#128125=CARTESIAN_POINT('Origin',(-81.2442674543458,1067.7251047501,421.556495725588));
#128126=CARTESIAN_POINT('',(-81.2442674543458,1078.73142393294,419.895614915668));
#128127=CARTESIAN_POINT('Origin',(-81.2442674543458,1078.73142393294,421.556495725588));
#128128=CARTESIAN_POINT('',(-81.2442674543458,1076.73142393294,419.895614915668));
#128129=CARTESIAN_POINT('',(-81.2442674543458,1067.7251047501,419.895614915668));
#128130=CARTESIAN_POINT('Origin',(-81.2442674543458,1076.73142393294,421.556495725588));
#128131=CARTESIAN_POINT('Origin',(-81.2442674543458,1067.7251047501,421.556495725588));
#128132=CARTESIAN_POINT('',(-81.2442674543458,1076.73142393294,420.495614915667));
#128133=CARTESIAN_POINT('Origin',(-81.2442674543458,1076.73142393294,421.556495725588));
#128134=CARTESIAN_POINT('',(-81.2442674543458,1082.7251047501,420.495614915667));
#128135=CARTESIAN_POINT('',(-81.2442674543458,1067.7251047501,420.495614915667));
#128136=CARTESIAN_POINT('Origin',(-81.2442674543458,1082.7251047501,421.556495725588));
#128137=CARTESIAN_POINT('Origin',(0.,1074.88309437944,424.620242579854));
#128138=CARTESIAN_POINT('',(-1.56039672537847E-14,1074.88309437944,552.036304620344));
#128139=CARTESIAN_POINT('Origin',(-1.55427349138273E-14,1074.88309437944,
551.536304620344));
#128140=CARTESIAN_POINT('Origin',(0.,1074.88309437944,424.620242579854));
#128141=CARTESIAN_POINT('Origin',(0.,1074.39201604106,424.620242579854));
#128142=CARTESIAN_POINT('Origin',(0.,1118.16413742548,424.620242579854));
#128143=CARTESIAN_POINT('',(-1.56039672537847E-14,1075.04643807976,552.036304620344));
#128144=CARTESIAN_POINT('',(-1.56039672537847E-14,1118.16413742548,552.036304620344));
#128145=CARTESIAN_POINT('Origin',(0.,1075.04643807976,424.620242579854));
#128146=CARTESIAN_POINT('Origin',(0.,1122.00270384563,424.620242579854));
#128147=CARTESIAN_POINT('',(-1.45329701922362E-15,1121.50270384563,436.487313315967));
#128148=CARTESIAN_POINT('Origin',(0.,1121.50270384563,424.620242579854));
#128149=CARTESIAN_POINT('',(-1.51452935918098E-15,1122.00270384563,436.987313315967));
#128150=CARTESIAN_POINT('Origin',(-1.45329701922361E-15,1122.00270384563,
436.487313315967));
#128151=CARTESIAN_POINT('',(1.51452935918099E-15,1122.00270384563,412.253171843741));
#128152=CARTESIAN_POINT('Origin',(0.,1122.00270384563,424.620242579854));
#128153=CARTESIAN_POINT('Origin',(0.,1122.00270384563,424.620242579854));
#128154=CARTESIAN_POINT('Origin',(0.,1133.64517683891,424.620242579854));
#128155=CARTESIAN_POINT('',(-1.45329701922361E-15,1134.14517683891,412.753171843741));
#128156=CARTESIAN_POINT('Origin',(0.,1134.14517683891,424.620242579854));
#128157=CARTESIAN_POINT('',(-1.51452935918099E-15,1133.64517683891,412.253171843741));
#128158=CARTESIAN_POINT('Origin',(-1.45329701922361E-15,1133.64517683891,
412.753171843741));
#128159=CARTESIAN_POINT('Origin',(0.,1133.64517683891,424.620242579854));
#128160=CARTESIAN_POINT('Origin',(0.,1134.14517683891,424.620242579854));
#128161=CARTESIAN_POINT('',(-1.51452935918099E-15,1134.14517683891,412.253171843741));
#128162=CARTESIAN_POINT('Origin',(0.,1109.29344889777,424.620242579854));
#128163=CARTESIAN_POINT('',(0.,1118.15413742548,435.663222162066));
#128164=CARTESIAN_POINT('Origin',(0.,1118.15413742548,424.620242579854));
#128165=CARTESIAN_POINT('Origin',(0.,1117.65413742548,424.620242579854));
#128166=CARTESIAN_POINT('',(-2.03875185873375E-15,1117.69439144477,441.267914873231));
#128167=CARTESIAN_POINT('Origin',(0.,1117.69439144477,424.620242579854));
#128168=CARTESIAN_POINT('',(-1.97771828143355E-15,1118.15413742548,440.769537893495));
#128169=CARTESIAN_POINT('Origin',(-1.97771828143355E-15,1117.65413742548,
440.769537893495));
#128170=CARTESIAN_POINT('Origin',(0.,1118.15413742548,424.620242579854));
#128171=CARTESIAN_POINT('Origin',(0.,1075.18041267597,424.620242579854));
#128172=CARTESIAN_POINT('',(-1.59204083889156E-14,1075.18041267597,294.620242579854));
#128173=CARTESIAN_POINT('Origin',(0.,1075.18041267597,424.620242579854));
#128174=CARTESIAN_POINT('',(-1.57979437090009E-14,1074.18041267597,295.620242579854));
#128175=CARTESIAN_POINT('Origin',(-1.57979437090009E-14,1075.18041267597,
295.620242579854));
#128176=CARTESIAN_POINT('Origin',(0.,1074.18041267597,424.620242579854));
#128177=CARTESIAN_POINT('Origin',(0.,1075.04643807976,424.620242579854));
#128178=CARTESIAN_POINT('',(-1.5665199593742E-14,1074.18041267597,552.536304620344));
#128179=CARTESIAN_POINT('Origin',(-1.57264319336994E-14,1075.04643807976,
553.036304620344));
#128180=CARTESIAN_POINT('Origin',(0.,1074.18041267597,424.620242579854));
#128181=CARTESIAN_POINT('Origin',(0.,1094.6328882123,424.620242579854));
#128182=CARTESIAN_POINT('',(-2.2668647037689E-15,1094.6328882123,443.130597609134));
#128183=CARTESIAN_POINT('Origin',(0.,1094.6328882123,424.620242579854));
#128184=CARTESIAN_POINT('',(-2.2668647037689E-15,1094.6328882123,443.130597609134));
#128185=CARTESIAN_POINT('Origin',(0.,1093.6328882123,424.620242579854));
#128186=CARTESIAN_POINT('',(1.59204083889156E-14,1093.6328882123,294.620242579854));
#128187=CARTESIAN_POINT('',(-1.59204083889156E-14,1093.6328882123,554.620242579854));
#128188=CARTESIAN_POINT('Origin',(0.,1093.6328882123,424.620242579854));
#128189=CARTESIAN_POINT('Origin',(0.,1093.6328882123,424.620242579854));
#128190=CARTESIAN_POINT('',(-1.57979437090009E-14,1094.6328882123,553.620242579854));
#128191=CARTESIAN_POINT('Origin',(-1.57979437090009E-14,1093.6328882123,
553.620242579854));
#128192=CARTESIAN_POINT('Origin',(0.,1094.6328882123,424.620242579854));
#128193=CARTESIAN_POINT('Origin',(0.,1118.15413742548,424.620242579854));
#128194=CARTESIAN_POINT('',(-1.59204083889156E-14,1118.15413742548,294.620242579854));
#128195=CARTESIAN_POINT('Origin',(-89.3961860936676,1067.7251047501,430.005244031937));
#128196=CARTESIAN_POINT('',(-89.3961860936676,1076.67140064346,430.88354716413));
#128197=CARTESIAN_POINT('',(-89.3961860936687,1076.67415347727,429.126940899744));
#128198=CARTESIAN_POINT('Ctrl Pts',(-89.3961860936676,1076.67140064346,
430.88354716413));
#128199=CARTESIAN_POINT('Ctrl Pts',(-89.405023436492,1076.67116823115,430.88354716413));
#128200=CARTESIAN_POINT('Ctrl Pts',(-89.4138630014268,1076.67093534602,
430.883413784404));
#128201=CARTESIAN_POINT('Ctrl Pts',(-89.5390342024466,1076.66763180858,
430.879633183896));
#128202=CARTESIAN_POINT('Ctrl Pts',(-89.6535182774614,1076.66453579198,
430.853031166677));
#128203=CARTESIAN_POINT('Ctrl Pts',(-89.8643186271013,1076.65875455185,
430.75725940252));
#128204=CARTESIAN_POINT('Ctrl Pts',(-89.9587775668252,1076.65612353728,
430.689473083606));
#128205=CARTESIAN_POINT('Ctrl Pts',(-90.1161258498771,1076.65176824399,
430.521339609659));
#128206=CARTESIAN_POINT('Ctrl Pts',(-90.1775034223224,1076.65008833703,
430.422634332581));
#128207=CARTESIAN_POINT('Ctrl Pts',(-90.2586432415134,1076.64801435652,
430.207265590749));
#128208=CARTESIAN_POINT('Ctrl Pts',(-90.2776597841645,1076.64764053423,
430.092708970466));
#128209=CARTESIAN_POINT('Ctrl Pts',(-90.2704609974862,1076.64828460326,
429.862893265806));
#128210=CARTESIAN_POINT('Ctrl Pts',(-90.2443592853713,1076.64929444614,
429.749861592639));
#128211=CARTESIAN_POINT('Ctrl Pts',(-90.1501312341865,1076.65251178129,
429.540291536694));
#128212=CARTESIAN_POINT('Ctrl Pts',(-90.0829218230843,1076.65468593256,
429.445776131215));
#128213=CARTESIAN_POINT('Ctrl Pts',(-89.9159003371264,1076.65980500206,
429.287940991561));
#128214=CARTESIAN_POINT('Ctrl Pts',(-89.8176790713377,1076.66269844556,
429.226162629292));
#128215=CARTESIAN_POINT('Ctrl Pts',(-89.6605146832878,1076.66710802558,
429.165961206007));
#128216=CARTESIAN_POINT('Ctrl Pts',(-89.6090347504715,1076.66852301801,
429.151452089803));
#128217=CARTESIAN_POINT('Ctrl Pts',(-89.5036687283435,1076.67135652926,
429.131884096841));
#128218=CARTESIAN_POINT('Ctrl Pts',(-89.4499887326727,1076.67276900264,
429.12694142144));
#128219=CARTESIAN_POINT('Ctrl Pts',(-89.396194610801,1076.67415325811,429.126940899785));
#128220=CARTESIAN_POINT('',(-89.3961860936676,1082.7251047501,429.126940899744));
#128221=CARTESIAN_POINT('',(-89.3961860936676,1067.7251047501,429.126940899744));
#128222=CARTESIAN_POINT('Origin',(-89.3961860936676,1082.7251047501,430.005244031937));
#128223=CARTESIAN_POINT('Ctrl Pts',(-89.3961860936707,1076.67415347727,
429.126940899744));
#128224=CARTESIAN_POINT('Ctrl Pts',(-89.2796210199493,1076.67715297711,
429.126940899743));
#128225=CARTESIAN_POINT('Ctrl Pts',(-89.1642164309715,1076.67997334784,
429.150143740078));
#128226=CARTESIAN_POINT('Ctrl Pts',(-88.9493848859387,1076.68498184303,
429.240178986333));
#128227=CARTESIAN_POINT('Ctrl Pts',(-88.8520628226455,1076.68712361318,
429.306038141905));
#128228=CARTESIAN_POINT('Ctrl Pts',(-88.6884166218447,1076.6905664082,429.472203861829));
#128229=CARTESIAN_POINT('Ctrl Pts',(-88.6238554495119,1076.69183261313,
429.570989421663));
#128230=CARTESIAN_POINT('Ctrl Pts',(-88.5370000408771,1076.69341471635,
429.788484763094));
#128231=CARTESIAN_POINT('Ctrl Pts',(-88.5157580119964,1076.6937126517,429.905083111817));
#128232=CARTESIAN_POINT('Ctrl Pts',(-88.5203404525082,1076.69331570962,
430.139583869797));
#128233=CARTESIAN_POINT('Ctrl Pts',(-88.5460623157962,1076.69262548977,
430.255126137273));
#128234=CARTESIAN_POINT('Ctrl Pts',(-88.6410887384043,1076.69027838736,
430.468755941952));
#128235=CARTESIAN_POINT('Ctrl Pts',(-88.7092298410642,1076.68864710353,
430.564800713523));
#128236=CARTESIAN_POINT('Ctrl Pts',(-88.8788436280051,1076.68453246604,
430.724487658119));
#128237=CARTESIAN_POINT('Ctrl Pts',(-88.9785650294521,1076.68208877619,
430.7866172519));
#128238=CARTESIAN_POINT('Ctrl Pts',(-89.1408075113255,1076.67800408912,
430.847528149199));
#128239=CARTESIAN_POINT('Ctrl Pts',(-89.1959526202103,1076.67660009373,
430.862312884638));
#128240=CARTESIAN_POINT('Ctrl Pts',(-89.2997610432547,1076.67392404207,
430.879571908049));
#128241=CARTESIAN_POINT('Ctrl Pts',(-89.3479404563299,1076.67266945018,
430.88354716413));
#128242=CARTESIAN_POINT('Ctrl Pts',(-89.3961860936676,1076.67140064346,
430.88354716413));
#128243=CARTESIAN_POINT('Origin',(-89.3961860936676,1067.7251047501,430.005244031937));
#128244=CARTESIAN_POINT('',(-89.3961860936954,1076.6748778677,428.526940899743));
#128245=CARTESIAN_POINT('',(-89.3961860936676,1067.7251047501,428.526940899744));
#128246=CARTESIAN_POINT('Ctrl Pts',(-89.396310882001,1076.6702336653,431.483547158863));
#128247=CARTESIAN_POINT('Ctrl Pts',(-89.5922242330258,1076.66503522431,
431.483530621186));
#128248=CARTESIAN_POINT('Ctrl Pts',(-89.786193582667,1076.65963369298,431.444568941278));
#128249=CARTESIAN_POINT('Ctrl Pts',(-90.1458826936886,1076.64929134132,
431.294031807984));
#128250=CARTESIAN_POINT('Ctrl Pts',(-90.3083768514711,1076.64445312791,
431.184623642052));
#128251=CARTESIAN_POINT('Ctrl Pts',(-90.5817833137706,1076.63627341402,
430.90932457426));
#128252=CARTESIAN_POINT('Ctrl Pts',(-90.6900606418802,1076.63301783246,
430.746123907287));
#128253=CARTESIAN_POINT('Ctrl Pts',(-90.8372870058146,1076.62883349518,
430.387498136413));
#128254=CARTESIAN_POINT('Ctrl Pts',(-90.8749203854877,1076.62794565169,
430.195609537752));
#128255=CARTESIAN_POINT('Ctrl Pts',(-90.8740514734311,1076.62876031399,
429.808623023054));
#128256=CARTESIAN_POINT('Ctrl Pts',(-90.8357080596201,1076.63044894684,
429.61728140158));
#128257=CARTESIAN_POINT('Ctrl Pts',(-90.6876309142824,1076.63603781517,
429.260360231857));
#128258=CARTESIAN_POINT('Ctrl Pts',(-90.5793801275754,1076.63987714276,
429.098204129196));
#128259=CARTESIAN_POINT('Ctrl Pts',(-90.3065942273166,1076.64890226726,
428.824617633557));
#128260=CARTESIAN_POINT('Ctrl Pts',(-90.1446436506629,1076.65399508226,
428.715854129427));
#128261=CARTESIAN_POINT('Ctrl Pts',(-89.8772431317426,1076.66184606648,
428.604067161451));
#128262=CARTESIAN_POINT('Ctrl Pts',(-89.7846756756862,1076.66448013638,
428.575632748052));
#128263=CARTESIAN_POINT('Ctrl Pts',(-89.5953138101581,1076.66968566528,
428.537231028037));
#128264=CARTESIAN_POINT('Ctrl Pts',(-89.4989728558646,1076.67224455488,
428.527357176248));
#128265=CARTESIAN_POINT('Ctrl Pts',(-89.2067578975014,1076.67973121083,
428.5261371014));
#128266=CARTESIAN_POINT('Ctrl Pts',(-89.0129151656653,1076.68431790559,
428.564149733114));
#128267=CARTESIAN_POINT('Ctrl Pts',(-88.652142016831,1076.69224877693,428.713083425865));
#128268=CARTESIAN_POINT('Ctrl Pts',(-88.4886162547277,1076.69552734412,
428.822194499984));
#128269=CARTESIAN_POINT('Ctrl Pts',(-88.2125818772706,1076.70070586114,
429.098194867347));
#128270=CARTESIAN_POINT('Ctrl Pts',(-88.1030544639645,1076.70255649978,
429.262631847192));
#128271=CARTESIAN_POINT('Ctrl Pts',(-87.9539426673206,1076.70488424405,
429.625695227485));
#128272=CARTESIAN_POINT('Ctrl Pts',(-87.9162748479842,1076.70533563943,
429.820887429998));
#128273=CARTESIAN_POINT('Ctrl Pts',(-87.9195938260601,1076.70485327614,
430.214251499443));
#128274=CARTESIAN_POINT('Ctrl Pts',(-87.9604298910247,1076.70392505077,
430.408493855319));
#128275=CARTESIAN_POINT('Ctrl Pts',(-88.1151305771591,1076.70061930047,
430.76838028918));
#128276=CARTESIAN_POINT('Ctrl Pts',(-88.2269711146128,1076.69827684766,
430.930668302977));
#128277=CARTESIAN_POINT('Ctrl Pts',(-88.5069220174034,1076.6921230587,431.202126228349));
#128278=CARTESIAN_POINT('Ctrl Pts',(-88.6721722242147,1076.68836681521,
431.308744036377));
#128279=CARTESIAN_POINT('Ctrl Pts',(-88.9391143575598,1076.68192578571,
431.414135149626));
#128280=CARTESIAN_POINT('Ctrl Pts',(-89.0278915873782,1076.67973295163,
431.43990320465));
#128281=CARTESIAN_POINT('Ctrl Pts',(-89.2100593557822,1076.67511974181,
431.474743718238));
#128282=CARTESIAN_POINT('Ctrl Pts',(-89.3030821256448,1076.67270743334,
431.483555028603));
#128283=CARTESIAN_POINT('Ctrl Pts',(-89.396310882001,1076.6702336653,431.483547158863));
#128284=CARTESIAN_POINT('Ctrl Pts',(-90.9758547056989,1076.62738724384,
428.575583521194));
#128285=CARTESIAN_POINT('Ctrl Pts',(-90.9317360093904,1076.62738724384,
429.590347144532));
#128286=CARTESIAN_POINT('Ctrl Pts',(-90.8706467446144,1076.62738724384,
430.604230654776));
#128287=CARTESIAN_POINT('Ctrl Pts',(-90.7926040105104,1076.62738724384,
431.616950261709));
#128288=CARTESIAN_POINT('Ctrl Pts',(-89.9667063292985,1076.66219983996,
428.531708957971));
#128289=CARTESIAN_POINT('Ctrl Pts',(-89.9230770190023,1076.66219983996,
429.535216330228));
#128290=CARTESIAN_POINT('Ctrl Pts',(-89.8626653860283,1076.66219983996,
430.537853352032));
#128291=CARTESIAN_POINT('Ctrl Pts',(-89.7854883398441,1076.66219983996,
431.539339381107));
#128292=CARTESIAN_POINT('Ctrl Pts',(-88.9650760950845,1076.68827166653,
428.488161259669));
#128293=CARTESIAN_POINT('Ctrl Pts',(-88.9219325248811,1076.68827166653,
429.480496239767));
#128294=CARTESIAN_POINT('Ctrl Pts',(-88.8621934753611,1076.68827166653,
430.471970559324));
#128295=CARTESIAN_POINT('Ctrl Pts',(-88.785875667733,1076.68827166653,431.462306700548));
#128296=CARTESIAN_POINT('Ctrl Pts',(-87.9709679881959,1076.70560884642,
428.44494059955));
#128297=CARTESIAN_POINT('Ctrl Pts',(-87.9283065102335,1076.70560884642,
429.426187090864));
#128298=CARTESIAN_POINT('Ctrl Pts',(-87.8692349931434,1076.70560884642,
430.406582538776));
#128299=CARTESIAN_POINT('Ctrl Pts',(-87.7937699712892,1076.70560884642,
431.385852526519));
#128300=CARTESIAN_POINT('Origin',(0.,1082.7251047501,424.620242579854));
#128301=CARTESIAN_POINT('Origin',(0.,1074.18041267597,296.704180539364));
#128302=CARTESIAN_POINT('Origin',(0.,1094.6328882123,294.620242579854));
#128303=CARTESIAN_POINT('Origin',(0.,1118.15413742548,408.009704071406));
#128304=CARTESIAN_POINT('Origin',(0.,1134.14517683891,424.620242579854));
#128305=CARTESIAN_POINT('Origin',(0.,1121.50270384563,431.789154132961));
#128306=CARTESIAN_POINT('Origin',(0.,1078.73142393294,424.620242579854));
#128307=CARTESIAN_POINT('Origin',(0.,1078.73142393294,424.620242579854));
#128308=CARTESIAN_POINT('Ctrl Pts',(-1.04233045748865E-14,1078.73142393294,
509.732983511718));
#128309=CARTESIAN_POINT('Ctrl Pts',(170.225481863728,1078.73142393294,509.732983511718));
#128310=CARTESIAN_POINT('Ctrl Pts',(170.225481863728,1078.73142393294,339.50750164799));
#128311=CARTESIAN_POINT('Ctrl Pts',(2.08466091497731E-14,1078.73142393294,
339.50750164799));
#128312=CARTESIAN_POINT('Ctrl Pts',(-1.27558853978063E-14,1078.73142393294,
528.779951376607));
#128313=CARTESIAN_POINT('Ctrl Pts',(208.319417593505,1078.73142393294,528.779951376607));
#128314=CARTESIAN_POINT('Ctrl Pts',(208.319417593505,1078.73142393294,320.460533783101));
#128315=CARTESIAN_POINT('Ctrl Pts',(2.55117707956127E-14,1078.73142393294,
320.460533783101));
#128316=CARTESIAN_POINT('Ctrl Pts',(-1.55312192834318E-14,1074.39201604106,
551.442272362198));
#128317=CARTESIAN_POINT('Ctrl Pts',(253.644059564688,1074.39201604106,551.442272362198));
#128318=CARTESIAN_POINT('Ctrl Pts',(253.644059564688,1074.39201604106,297.79821279751));
#128319=CARTESIAN_POINT('Ctrl Pts',(3.10624385668636E-14,1074.39201604106,
297.79821279751));
#128320=CARTESIAN_POINT('Origin',(0.,1082.7251047501,424.620242579854));
#128321=CARTESIAN_POINT('Origin',(0.,1076.73142393294,424.620242579854));
#128322=CARTESIAN_POINT('Origin',(0.,1082.7251047501,424.620242579854));
#128323=CARTESIAN_POINT('Origin',(0.,1076.73142393294,424.620242579854));
#128324=CARTESIAN_POINT('Origin',(0.,1082.7251047501,424.620242579854));
#128325=CARTESIAN_POINT('Origin',(0.,1076.73142393294,424.620242579854));
#128326=CARTESIAN_POINT('Origin',(0.,1082.7251047501,424.620242579854));
#128327=CARTESIAN_POINT('Origin',(0.,1076.73142393294,424.620242579854));
#128328=CARTESIAN_POINT('Origin',(0.,1082.7251047501,424.620242579854));
#128329=CARTESIAN_POINT('Origin',(0.,1076.73142393294,424.620242579854));
#128330=CARTESIAN_POINT('Origin',(0.,1082.7251047501,424.620242579854));
#128331=CARTESIAN_POINT('Origin',(0.,1076.73142393294,424.620242579854));
#128332=CARTESIAN_POINT('Origin',(0.,1082.7251047501,424.620242579854));
#128333=CARTESIAN_POINT('Origin',(0.,1076.73142393294,424.620242579854));
#128334=CARTESIAN_POINT('Origin',(0.,1082.7251047501,424.620242579854));
#128335=CARTESIAN_POINT('Origin',(0.,1076.73142393294,424.620242579854));
#128336=CARTESIAN_POINT('Origin',(0.,1082.7251047501,424.620242579854));
#128337=CARTESIAN_POINT('Origin',(0.,1076.73142393294,424.620242579854));
#128338=CARTESIAN_POINT('Origin',(0.,1082.7251047501,424.620242579854));
#128339=CARTESIAN_POINT('Origin',(0.,1076.73142393294,424.620242579854));
#128340=CARTESIAN_POINT('Origin',(0.,1082.7251047501,424.620242579854));
#128341=CARTESIAN_POINT('Origin',(0.,1076.73142393294,424.620242579854));
#128342=CARTESIAN_POINT('Origin',(0.,1082.7251047501,424.620242579854));
#128343=CARTESIAN_POINT('Origin',(0.,1076.73142393294,424.620242579854));
#128344=CARTESIAN_POINT('Origin',(0.,1082.7251047501,424.620242579854));
#128345=CARTESIAN_POINT('Origin',(0.,1076.73142393294,424.620242579854));
#128346=CARTESIAN_POINT('Origin',(0.,1082.7251047501,424.620242579854));
#128347=CARTESIAN_POINT('Origin',(0.,1076.73142393294,424.620242579854));
#128348=CARTESIAN_POINT('Origin',(0.,1082.7251047501,424.620242579854));
#128349=CARTESIAN_POINT('Origin',(0.,1076.73142393294,424.620242579854));
#128350=CARTESIAN_POINT('Origin',(0.,1082.7251047501,424.620242579854));
#128351=CARTESIAN_POINT('Origin',(0.,1076.73142393294,424.620242579854));
#128352=CARTESIAN_POINT('Origin',(0.,1082.7251047501,424.620242579854));
#128353=CARTESIAN_POINT('Origin',(0.,1076.73142393294,424.620242579854));
#128354=CARTESIAN_POINT('Origin',(0.,1082.7251047501,424.620242579854));
#128355=CARTESIAN_POINT('Origin',(0.,1076.73142393294,424.620242579854));
#128356=CARTESIAN_POINT('Origin',(0.,1082.7251047501,424.620242579854));
#128357=CARTESIAN_POINT('Origin',(0.,1076.73142393294,424.620242579854));
#128358=CARTESIAN_POINT('Origin',(0.,1082.7251047501,424.620242579854));
#128359=CARTESIAN_POINT('Origin',(0.,1076.73142393294,424.620242579854));
#128360=CARTESIAN_POINT('Origin',(0.,1082.7251047501,424.620242579854));
#128361=CARTESIAN_POINT('Origin',(0.,1076.73142393294,424.620242579854));
#128362=CARTESIAN_POINT('Origin',(0.,1082.7251047501,424.620242579854));
#128363=CARTESIAN_POINT('Origin',(0.,1076.73142393294,424.620242579854));
#128364=CARTESIAN_POINT('Origin',(0.,1082.7251047501,424.620242579854));
#128365=CARTESIAN_POINT('Origin',(0.,1076.73142393294,424.620242579854));
#128366=CARTESIAN_POINT('Origin',(0.,1082.7251047501,424.620242579854));
#128367=CARTESIAN_POINT('Origin',(0.,1076.73142393294,424.620242579854));
#128368=CARTESIAN_POINT('Origin',(0.,1082.7251047501,424.620242579854));
#128369=CARTESIAN_POINT('Origin',(0.,1076.73142393294,424.620242579854));
#128370=CARTESIAN_POINT('Origin',(0.,1082.7251047501,424.620242579854));
#128371=CARTESIAN_POINT('Origin',(0.,1076.73142393294,424.620242579854));
#128372=CARTESIAN_POINT('Origin',(0.,1082.7251047501,424.620242579854));
#128373=CARTESIAN_POINT('Origin',(0.,1076.73142393294,424.620242579854));
#128374=CARTESIAN_POINT('Origin',(0.,1082.7251047501,424.620242579854));
#128375=CARTESIAN_POINT('Origin',(0.,1076.73142393294,424.620242579854));
#128376=CARTESIAN_POINT('Origin',(0.,1082.7251047501,424.620242579854));
#128377=CARTESIAN_POINT('Origin',(0.,1076.73142393294,424.620242579854));
#128378=CARTESIAN_POINT('Origin',(0.,1082.7251047501,424.620242579854));
#128379=CARTESIAN_POINT('Origin',(0.,1076.73142393294,424.620242579854));
#128380=CARTESIAN_POINT('Origin',(0.,1082.7251047501,424.620242579854));
#128381=CARTESIAN_POINT('Origin',(0.,1076.73142393294,424.620242579854));
#128382=CARTESIAN_POINT('Origin',(0.,1082.7251047501,424.620242579854));
#128383=CARTESIAN_POINT('Origin',(0.,1076.73142393294,424.620242579854));
#128384=CARTESIAN_POINT('Origin',(0.,1082.7251047501,424.620242579854));
#128385=CARTESIAN_POINT('Origin',(0.,1076.73142393294,424.620242579854));
#128386=CARTESIAN_POINT('Origin',(0.,1082.7251047501,424.620242579854));
#128387=CARTESIAN_POINT('Origin',(0.,1076.73142393294,424.620242579854));
#128388=CARTESIAN_POINT('Origin',(0.,1082.7251047501,424.620242579854));
#128389=CARTESIAN_POINT('Origin',(0.,1076.73142393294,424.620242579854));
#128390=CARTESIAN_POINT('Origin',(0.,1082.7251047501,424.620242579854));
#128391=CARTESIAN_POINT('Origin',(0.,1076.73142393294,424.620242579854));
#128392=CARTESIAN_POINT('Origin',(0.,1082.7251047501,424.620242579854));
#128393=CARTESIAN_POINT('Origin',(0.,1076.73142393294,424.620242579854));
#128394=CARTESIAN_POINT('Origin',(0.,1082.7251047501,424.620242579854));
#128395=CARTESIAN_POINT('Origin',(0.,1076.73142393294,424.620242579854));
#128396=CARTESIAN_POINT('Origin',(0.,1082.7251047501,424.620242579854));
#128397=CARTESIAN_POINT('Origin',(0.,1076.73142393294,424.620242579854));
#128398=CARTESIAN_POINT('Origin',(0.,1082.7251047501,424.620242579854));
#128399=CARTESIAN_POINT('Origin',(0.,1076.73142393294,424.620242579854));
#128400=CARTESIAN_POINT('Origin',(0.,1082.7251047501,424.620242579854));
#128401=CARTESIAN_POINT('Origin',(0.,1076.73142393294,424.620242579854));
#128402=CARTESIAN_POINT('Origin',(0.,1082.7251047501,424.620242579854));
#128403=CARTESIAN_POINT('Origin',(0.,1076.73142393294,424.620242579854));
#128404=CARTESIAN_POINT('Origin',(0.,1082.7251047501,424.620242579854));
#128405=CARTESIAN_POINT('Origin',(0.,1076.73142393294,424.620242579854));
#128406=CARTESIAN_POINT('Origin',(0.,1082.7251047501,424.620242579854));
#128407=CARTESIAN_POINT('Origin',(0.,1076.73142393294,424.620242579854));
#128408=CARTESIAN_POINT('Origin',(0.,1082.7251047501,424.620242579854));
#128409=CARTESIAN_POINT('Origin',(0.,1076.73142393294,424.620242579854));
#128410=CARTESIAN_POINT('Origin',(0.,1082.7251047501,424.620242579854));
#128411=CARTESIAN_POINT('Origin',(0.,1076.73142393294,424.620242579854));
#128412=CARTESIAN_POINT('Origin',(0.,1082.7251047501,424.620242579854));
#128413=CARTESIAN_POINT('Origin',(0.,1076.73142393294,424.620242579854));
#128414=CARTESIAN_POINT('Origin',(0.,1082.7251047501,424.620242579854));
#128415=CARTESIAN_POINT('Origin',(0.,1076.73142393294,424.620242579854));
#128416=CARTESIAN_POINT('Origin',(0.,1082.7251047501,424.620242579854));
#128417=CARTESIAN_POINT('Origin',(0.,1076.73142393294,424.620242579854));
#128418=CARTESIAN_POINT('Origin',(0.,1082.7251047501,424.620242579854));
#128419=CARTESIAN_POINT('Origin',(0.,1076.73142393294,424.620242579854));
#128420=CARTESIAN_POINT('Origin',(0.,1082.7251047501,424.620242579854));
#128421=CARTESIAN_POINT('Origin',(0.,1076.73142393294,424.620242579854));
#128422=CARTESIAN_POINT('Origin',(0.,1082.7251047501,424.620242579854));
#128423=CARTESIAN_POINT('Origin',(0.,1076.73142393294,424.620242579854));
#128424=CARTESIAN_POINT('Origin',(0.,1082.7251047501,424.620242579854));
#128425=CARTESIAN_POINT('Origin',(0.,1076.73142393294,424.620242579854));
#128426=CARTESIAN_POINT('Origin',(0.,1082.7251047501,424.620242579854));
#128427=CARTESIAN_POINT('Origin',(0.,1076.73142393294,424.620242579854));
#128428=CARTESIAN_POINT('Origin',(0.,1082.7251047501,424.620242579854));
#128429=CARTESIAN_POINT('Origin',(0.,1076.73142393294,424.620242579854));
#128430=CARTESIAN_POINT('Origin',(0.,1082.7251047501,424.620242579854));
#128431=CARTESIAN_POINT('Origin',(0.,1076.73142393294,424.620242579854));
#128432=CARTESIAN_POINT('Origin',(0.,1082.7251047501,424.620242579854));
#128433=CARTESIAN_POINT('Origin',(0.,1076.73142393294,424.620242579854));
#128434=CARTESIAN_POINT('Origin',(0.,1082.7251047501,424.620242579854));
#128435=CARTESIAN_POINT('Origin',(0.,1076.73142393294,424.620242579854));
#128436=CARTESIAN_POINT('Origin',(0.,1082.7251047501,424.620242579854));
#128437=CARTESIAN_POINT('Origin',(0.,1076.73142393294,424.620242579854));
#128438=CARTESIAN_POINT('Origin',(0.,1082.7251047501,424.620242579854));
#128439=CARTESIAN_POINT('Origin',(0.,1076.73142393294,424.620242579854));
#128440=CARTESIAN_POINT('Origin',(0.,1082.7251047501,424.620242579854));
#128441=CARTESIAN_POINT('Origin',(0.,1076.73142393294,424.620242579854));
#128442=CARTESIAN_POINT('Origin',(0.,1082.7251047501,424.620242579854));
#128443=CARTESIAN_POINT('Origin',(0.,1076.73142393294,424.620242579854));
#128444=CARTESIAN_POINT('Origin',(0.,1082.7251047501,424.620242579854));
#128445=CARTESIAN_POINT('Origin',(0.,1076.73142393294,424.620242579854));
#128446=CARTESIAN_POINT('Origin',(0.,1082.7251047501,424.620242579854));
#128447=CARTESIAN_POINT('Origin',(0.,1076.73142393294,424.620242579854));
#128448=CARTESIAN_POINT('Origin',(0.,1082.7251047501,424.620242579854));
#128449=CARTESIAN_POINT('Origin',(0.,1076.73142393294,424.620242579854));
#128450=CARTESIAN_POINT('Origin',(0.,1082.7251047501,424.620242579854));
#128451=CARTESIAN_POINT('Origin',(0.,1076.73142393294,424.620242579854));
#128452=CARTESIAN_POINT('Origin',(0.,1082.7251047501,424.620242579854));
#128453=CARTESIAN_POINT('Origin',(0.,1076.73142393294,424.620242579854));
#128454=CARTESIAN_POINT('Origin',(0.,1082.7251047501,424.620242579854));
#128455=CARTESIAN_POINT('Origin',(0.,1076.73142393294,424.620242579854));
#128456=CARTESIAN_POINT('Origin',(0.,1082.7251047501,424.620242579854));
#128457=CARTESIAN_POINT('Origin',(0.,1076.73142393294,424.620242579854));
#128458=CARTESIAN_POINT('Origin',(0.,1082.7251047501,424.620242579854));
#128459=CARTESIAN_POINT('Origin',(0.,1076.73142393294,424.620242579854));
#128460=CARTESIAN_POINT('Origin',(0.,1082.7251047501,424.620242579854));
#128461=CARTESIAN_POINT('Origin',(0.,1076.73142393294,424.620242579854));
#128462=CARTESIAN_POINT('Origin',(0.,1082.7251047501,424.620242579854));
#128463=CARTESIAN_POINT('Origin',(0.,1076.73142393294,424.620242579854));
#128464=CARTESIAN_POINT('Origin',(0.,1082.7251047501,424.620242579854));
#128465=CARTESIAN_POINT('Origin',(0.,1076.73142393294,424.620242579854));
#128466=CARTESIAN_POINT('Origin',(0.,1082.7251047501,424.620242579854));
#128467=CARTESIAN_POINT('Origin',(0.,1076.73142393294,424.620242579854));
#128468=CARTESIAN_POINT('Origin',(0.,1082.7251047501,424.620242579854));
#128469=CARTESIAN_POINT('Origin',(0.,1076.73142393294,424.620242579854));
#128470=CARTESIAN_POINT('Origin',(0.,1082.7251047501,424.620242579854));
#128471=CARTESIAN_POINT('Origin',(0.,1076.73142393294,424.620242579854));
#128472=CARTESIAN_POINT('Origin',(0.,1082.7251047501,424.620242579854));
#128473=CARTESIAN_POINT('Origin',(0.,1076.73142393294,424.620242579854));
#128474=CARTESIAN_POINT('Origin',(0.,1082.7251047501,424.620242579854));
#128475=CARTESIAN_POINT('Origin',(0.,1076.73142393294,424.620242579854));
#128476=CARTESIAN_POINT('Origin',(0.,1082.7251047501,424.620242579854));
#128477=CARTESIAN_POINT('Origin',(0.,1076.73142393294,424.620242579854));
#128478=CARTESIAN_POINT('Origin',(0.,1082.7251047501,424.620242579854));
#128479=CARTESIAN_POINT('Origin',(0.,1076.73142393294,424.620242579854));
#128480=CARTESIAN_POINT('Origin',(0.,1082.7251047501,424.620242579854));
#128481=CARTESIAN_POINT('Origin',(0.,1076.73142393294,424.620242579854));
#128482=CARTESIAN_POINT('Origin',(0.,1082.7251047501,424.620242579854));
#128483=CARTESIAN_POINT('Origin',(0.,1076.73142393294,424.620242579854));
#128484=CARTESIAN_POINT('Origin',(0.,1082.7251047501,424.620242579854));
#128485=CARTESIAN_POINT('Origin',(0.,1076.73142393294,424.620242579854));
#128486=CARTESIAN_POINT('Origin',(0.,1082.7251047501,424.620242579854));
#128487=CARTESIAN_POINT('Origin',(0.,1076.73142393294,424.620242579854));
#128488=CARTESIAN_POINT('Origin',(0.,1082.7251047501,424.620242579854));
#128489=CARTESIAN_POINT('Origin',(0.,1076.73142393294,424.620242579854));
#128490=CARTESIAN_POINT('Origin',(0.,1082.7251047501,424.620242579854));
#128491=CARTESIAN_POINT('Origin',(0.,1076.73142393294,424.620242579854));
#128492=CARTESIAN_POINT('Origin',(0.,1082.7251047501,424.620242579854));
#128493=CARTESIAN_POINT('Origin',(0.,1076.73142393294,424.620242579854));
#128494=CARTESIAN_POINT('Origin',(0.,1082.7251047501,424.620242579854));
#128495=CARTESIAN_POINT('Origin',(0.,1076.73142393294,424.620242579854));
#128496=CARTESIAN_POINT('Origin',(0.,1082.7251047501,424.620242579854));
#128497=CARTESIAN_POINT('Origin',(0.,1076.73142393294,424.620242579854));
#128498=CARTESIAN_POINT('Origin',(0.,1082.7251047501,424.620242579854));
#128499=CARTESIAN_POINT('Origin',(0.,1076.73142393294,424.620242579854));
#128500=CARTESIAN_POINT('Origin',(0.,1082.7251047501,424.620242579854));
#128501=CARTESIAN_POINT('Origin',(0.,1076.73142393294,424.620242579854));
#128502=CARTESIAN_POINT('Origin',(0.,1082.7251047501,424.620242579854));
#128503=CARTESIAN_POINT('Origin',(0.,1076.73142393294,424.620242579854));
#128504=CARTESIAN_POINT('Origin',(0.,1082.7251047501,424.620242579854));
#128505=CARTESIAN_POINT('Origin',(0.,1076.73142393294,424.620242579854));
#128506=CARTESIAN_POINT('Origin',(0.,1082.7251047501,424.620242579854));
#128507=CARTESIAN_POINT('Origin',(0.,1076.73142393294,424.620242579854));
#128508=CARTESIAN_POINT('Origin',(0.,1082.7251047501,424.620242579854));
#128509=CARTESIAN_POINT('Origin',(0.,1076.73142393294,424.620242579854));
#128510=CARTESIAN_POINT('Origin',(0.,1082.7251047501,424.620242579854));
#128511=CARTESIAN_POINT('Origin',(0.,1076.73142393294,424.620242579854));
#128512=CARTESIAN_POINT('Origin',(0.,1082.7251047501,424.620242579854));
#128513=CARTESIAN_POINT('Origin',(0.,1076.73142393294,424.620242579854));
#128514=CARTESIAN_POINT('Origin',(0.,1082.7251047501,424.620242579854));
#128515=CARTESIAN_POINT('Origin',(0.,1076.73142393294,424.620242579854));
#128516=CARTESIAN_POINT('Origin',(0.,1082.7251047501,424.620242579854));
#128517=CARTESIAN_POINT('Origin',(0.,1076.73142393294,424.620242579854));
#128518=CARTESIAN_POINT('Origin',(0.,1082.7251047501,424.620242579854));
#128519=CARTESIAN_POINT('Origin',(0.,1076.73142393294,424.620242579854));
#128520=CARTESIAN_POINT('Origin',(0.,1082.7251047501,424.620242579854));
#128521=CARTESIAN_POINT('Origin',(0.,1076.73142393294,424.620242579854));
#128522=CARTESIAN_POINT('Origin',(0.,1082.7251047501,424.620242579854));
#128523=CARTESIAN_POINT('Origin',(0.,1076.73142393294,424.620242579854));
#128524=CARTESIAN_POINT('Origin',(0.,1082.7251047501,424.620242579854));
#128525=CARTESIAN_POINT('Origin',(0.,1076.73142393294,424.620242579854));
#128526=CARTESIAN_POINT('Origin',(0.,1082.7251047501,424.620242579854));
#128527=CARTESIAN_POINT('Origin',(0.,1076.73142393294,424.620242579854));
#128528=CARTESIAN_POINT('Origin',(0.,1082.7251047501,424.620242579854));
#128529=CARTESIAN_POINT('Origin',(0.,1076.73142393294,424.620242579854));
#128530=CARTESIAN_POINT('Origin',(0.,1082.7251047501,424.620242579854));
#128531=CARTESIAN_POINT('Origin',(0.,1076.73142393294,424.620242579854));
#128532=CARTESIAN_POINT('Origin',(0.,1082.7251047501,424.620242579854));
#128533=CARTESIAN_POINT('Origin',(0.,1076.73142393294,424.620242579854));
#128534=CARTESIAN_POINT('Origin',(0.,1082.7251047501,424.620242579854));
#128535=CARTESIAN_POINT('Origin',(0.,1076.73142393294,424.620242579854));
#128536=CARTESIAN_POINT('Origin',(0.,1082.7251047501,424.620242579854));
#128537=CARTESIAN_POINT('Origin',(0.,1076.73142393294,424.620242579854));
#128538=CARTESIAN_POINT('Origin',(0.,1082.7251047501,424.620242579854));
#128539=CARTESIAN_POINT('Origin',(0.,1076.73142393294,424.620242579854));
#128540=CARTESIAN_POINT('Origin',(0.,1082.7251047501,424.620242579854));
#128541=CARTESIAN_POINT('Origin',(0.,1076.73142393294,424.620242579854));
#128542=CARTESIAN_POINT('Origin',(0.,1082.7251047501,424.620242579854));
#128543=CARTESIAN_POINT('Origin',(0.,1076.73142393294,424.620242579854));
#128544=CARTESIAN_POINT('Origin',(0.,1082.7251047501,424.620242579854));
#128545=CARTESIAN_POINT('Origin',(0.,1076.73142393294,424.620242579854));
#128546=CARTESIAN_POINT('Origin',(0.,1082.7251047501,424.620242579854));
#128547=CARTESIAN_POINT('Origin',(0.,1076.73142393294,424.620242579854));
#128548=CARTESIAN_POINT('Origin',(0.,1082.7251047501,424.620242579854));
#128549=CARTESIAN_POINT('Origin',(0.,1076.73142393294,424.620242579854));
#128550=CARTESIAN_POINT('Origin',(0.,1082.7251047501,424.620242579854));
#128551=CARTESIAN_POINT('Origin',(0.,1076.73142393294,424.620242579854));
#128552=CARTESIAN_POINT('Origin',(0.,1082.7251047501,424.620242579854));
#128553=CARTESIAN_POINT('Origin',(0.,1076.73142393294,424.620242579854));
#128554=CARTESIAN_POINT('Origin',(0.,1082.7251047501,424.620242579854));
#128555=CARTESIAN_POINT('Origin',(0.,1076.73142393294,424.620242579854));
#128556=CARTESIAN_POINT('Origin',(0.,1082.7251047501,424.620242579854));
#128557=CARTESIAN_POINT('Origin',(0.,1076.73142393294,424.620242579854));
#128558=CARTESIAN_POINT('Origin',(0.,1082.7251047501,424.620242579854));
#128559=CARTESIAN_POINT('Origin',(0.,1076.73142393294,424.620242579854));
#128560=CARTESIAN_POINT('Origin',(0.,1082.7251047501,424.620242579854));
#128561=CARTESIAN_POINT('Origin',(0.,1076.73142393294,424.620242579854));
#128562=CARTESIAN_POINT('Origin',(0.,1082.7251047501,424.620242579854));
#128563=CARTESIAN_POINT('Origin',(0.,1076.73142393294,424.620242579854));
#128564=CARTESIAN_POINT('Origin',(0.,1082.7251047501,424.620242579854));
#128565=CARTESIAN_POINT('Origin',(0.,1076.73142393294,424.620242579854));
#128566=CARTESIAN_POINT('Origin',(0.,1082.7251047501,424.620242579854));
#128567=CARTESIAN_POINT('Origin',(0.,1076.73142393294,424.620242579854));
#128568=CARTESIAN_POINT('Origin',(0.,1082.7251047501,424.620242579854));
#128569=CARTESIAN_POINT('Origin',(0.,1076.73142393294,424.620242579854));
#128570=CARTESIAN_POINT('Origin',(0.,1082.7251047501,424.620242579854));
#128571=CARTESIAN_POINT('Origin',(0.,1076.73142393294,424.620242579854));
#128572=CARTESIAN_POINT('Origin',(0.,1082.7251047501,424.620242579854));
#128573=CARTESIAN_POINT('Origin',(0.,1076.73142393294,424.620242579854));
#128574=CARTESIAN_POINT('Origin',(0.,1082.7251047501,424.620242579854));
#128575=CARTESIAN_POINT('Origin',(0.,1076.73142393294,424.620242579854));
#128576=CARTESIAN_POINT('Origin',(0.,1082.7251047501,424.620242579854));
#128577=CARTESIAN_POINT('Origin',(0.,1076.73142393294,424.620242579854));
#128578=CARTESIAN_POINT('Origin',(0.,1082.7251047501,424.620242579854));
#128579=CARTESIAN_POINT('Origin',(0.,1076.73142393294,424.620242579854));
#128580=CARTESIAN_POINT('Origin',(0.,1082.7251047501,424.620242579854));
#128581=CARTESIAN_POINT('Origin',(0.,1076.73142393294,424.620242579854));
#128582=CARTESIAN_POINT('Origin',(0.,1082.7251047501,424.620242579854));
#128583=CARTESIAN_POINT('Origin',(0.,1076.73142393294,424.620242579854));
#128584=CARTESIAN_POINT('Origin',(0.,1082.7251047501,424.620242579854));
#128585=CARTESIAN_POINT('Origin',(0.,1076.73142393294,424.620242579854));
#128586=CARTESIAN_POINT('Origin',(0.,1082.7251047501,424.620242579854));
#128587=CARTESIAN_POINT('Origin',(0.,1076.73142393294,424.620242579854));
#128588=CARTESIAN_POINT('Origin',(0.,1082.7251047501,424.620242579854));
#128589=CARTESIAN_POINT('Origin',(0.,1076.73142393294,424.620242579854));
#128590=CARTESIAN_POINT('Origin',(0.,1082.7251047501,424.620242579854));
#128591=CARTESIAN_POINT('Origin',(0.,1076.73142393294,424.620242579854));
#128592=CARTESIAN_POINT('Origin',(0.,1082.7251047501,424.620242579854));
#128593=CARTESIAN_POINT('Origin',(0.,1076.73142393294,424.620242579854));
#128594=CARTESIAN_POINT('Origin',(0.,1082.7251047501,424.620242579854));
#128595=CARTESIAN_POINT('Origin',(0.,1076.73142393294,424.620242579854));
#128596=CARTESIAN_POINT('Origin',(0.,1082.7251047501,424.620242579854));
#128597=CARTESIAN_POINT('Origin',(0.,1076.73142393294,424.620242579854));
#128598=CARTESIAN_POINT('Origin',(0.,1082.7251047501,424.620242579854));
#128599=CARTESIAN_POINT('Origin',(0.,1076.73142393294,424.620242579854));
#128600=CARTESIAN_POINT('Origin',(0.,1082.7251047501,424.620242579854));
#128601=CARTESIAN_POINT('Origin',(0.,1076.73142393294,424.620242579854));
#128602=CARTESIAN_POINT('Origin',(0.,1082.7251047501,424.620242579854));
#128603=CARTESIAN_POINT('Origin',(0.,1076.73142393294,424.620242579854));
#128604=CARTESIAN_POINT('Origin',(0.,1082.7251047501,424.620242579854));
#128605=CARTESIAN_POINT('Origin',(0.,1076.73142393294,424.620242579854));
#128606=CARTESIAN_POINT('Origin',(0.,1082.7251047501,424.620242579854));
#128607=CARTESIAN_POINT('Origin',(0.,1076.73142393294,424.620242579854));
#128608=CARTESIAN_POINT('Origin',(0.,1082.7251047501,424.620242579854));
#128609=CARTESIAN_POINT('Origin',(0.,1076.73142393294,424.620242579854));
#128610=CARTESIAN_POINT('Origin',(0.,1082.7251047501,424.620242579854));
#128611=CARTESIAN_POINT('Origin',(0.,1076.73142393294,424.620242579854));
#128612=CARTESIAN_POINT('Origin',(0.,1082.7251047501,424.620242579854));
#128613=CARTESIAN_POINT('Origin',(0.,1076.73142393294,424.620242579854));
#128614=CARTESIAN_POINT('Origin',(0.,1082.7251047501,424.620242579854));
#128615=CARTESIAN_POINT('Origin',(0.,1076.73142393294,424.620242579854));
#128616=CARTESIAN_POINT('Origin',(0.,1082.7251047501,424.620242579854));
#128617=CARTESIAN_POINT('Origin',(0.,1076.73142393294,424.620242579854));
#128618=CARTESIAN_POINT('Origin',(0.,1082.7251047501,424.620242579854));
#128619=CARTESIAN_POINT('Origin',(0.,1076.73142393294,424.620242579854));
#128620=CARTESIAN_POINT('Origin',(0.,1082.7251047501,424.620242579854));
#128621=CARTESIAN_POINT('Origin',(0.,1076.73142393294,424.620242579854));
#128622=CARTESIAN_POINT('Origin',(0.,1082.7251047501,424.620242579854));
#128623=CARTESIAN_POINT('Origin',(0.,1076.73142393294,424.620242579854));
#128624=CARTESIAN_POINT('Origin',(0.,1082.7251047501,424.620242579854));
#128625=CARTESIAN_POINT('Origin',(0.,1076.73142393294,424.620242579854));
#128626=CARTESIAN_POINT('Origin',(0.,1082.7251047501,424.620242579854));
#128627=CARTESIAN_POINT('Origin',(0.,1076.73142393294,424.620242579854));
#128628=CARTESIAN_POINT('Origin',(0.,1082.7251047501,424.620242579854));
#128629=CARTESIAN_POINT('Origin',(0.,1076.73142393294,424.620242579854));
#128630=CARTESIAN_POINT('Origin',(0.,1082.7251047501,424.620242579854));
#128631=CARTESIAN_POINT('Origin',(0.,1076.73142393294,424.620242579854));
#128632=CARTESIAN_POINT('Origin',(0.,1082.7251047501,424.620242579854));
#128633=CARTESIAN_POINT('Origin',(0.,1076.73142393294,424.620242579854));
#128634=CARTESIAN_POINT('Origin',(0.,1082.7251047501,424.620242579854));
#128635=CARTESIAN_POINT('Origin',(0.,1076.73142393294,424.620242579854));
#128636=CARTESIAN_POINT('Origin',(0.,1082.7251047501,424.620242579854));
#128637=CARTESIAN_POINT('Origin',(0.,1076.73142393294,424.620242579854));
#128638=CARTESIAN_POINT('Origin',(0.,1082.7251047501,424.620242579854));
#128639=CARTESIAN_POINT('Origin',(0.,1076.73142393294,424.620242579854));
#128640=CARTESIAN_POINT('Origin',(0.,1082.7251047501,424.620242579854));
#128641=CARTESIAN_POINT('Origin',(0.,1076.73142393294,424.620242579854));
#128642=CARTESIAN_POINT('Origin',(0.,1082.7251047501,424.620242579854));
#128643=CARTESIAN_POINT('Origin',(0.,1076.73142393294,424.620242579854));
#128644=CARTESIAN_POINT('Origin',(0.,1082.7251047501,424.620242579854));
#128645=CARTESIAN_POINT('Origin',(0.,1076.73142393294,424.620242579854));
#128646=CARTESIAN_POINT('Origin',(0.,1082.7251047501,424.620242579854));
#128647=CARTESIAN_POINT('Origin',(0.,1076.73142393294,424.620242579854));
#128648=CARTESIAN_POINT('Origin',(0.,1082.7251047501,424.620242579854));
#128649=CARTESIAN_POINT('Origin',(0.,1076.73142393294,424.620242579854));
#128650=CARTESIAN_POINT('Origin',(0.,1082.7251047501,424.620242579854));
#128651=CARTESIAN_POINT('Origin',(0.,1076.73142393294,424.620242579854));
#128652=CARTESIAN_POINT('Origin',(0.,1082.7251047501,424.620242579854));
#128653=CARTESIAN_POINT('Origin',(0.,1076.73142393294,424.620242579854));
#128654=CARTESIAN_POINT('Origin',(0.,1082.7251047501,424.620242579854));
#128655=CARTESIAN_POINT('Origin',(0.,1076.73142393294,424.620242579854));
#128656=CARTESIAN_POINT('Origin',(0.,1082.7251047501,424.620242579854));
#128657=CARTESIAN_POINT('Origin',(0.,1076.73142393294,424.620242579854));
#128658=CARTESIAN_POINT('Origin',(0.,1082.7251047501,424.620242579854));
#128659=CARTESIAN_POINT('Origin',(0.,1076.73142393294,424.620242579854));
#128660=CARTESIAN_POINT('Origin',(0.,1082.7251047501,424.620242579854));
#128661=CARTESIAN_POINT('Origin',(0.,1076.73142393294,424.620242579854));
#128662=CARTESIAN_POINT('Origin',(0.,1082.7251047501,424.620242579854));
#128663=CARTESIAN_POINT('Origin',(0.,1076.73142393294,424.620242579854));
#128664=CARTESIAN_POINT('Origin',(0.,1082.7251047501,424.620242579854));
#128665=CARTESIAN_POINT('Origin',(0.,1076.73142393294,424.620242579854));
#128666=CARTESIAN_POINT('Origin',(0.,1082.7251047501,424.620242579854));
#128667=CARTESIAN_POINT('Origin',(0.,1076.73142393294,424.620242579854));
#128668=CARTESIAN_POINT('Origin',(0.,1082.7251047501,424.620242579854));
#128669=CARTESIAN_POINT('Origin',(0.,1076.73142393294,424.620242579854));
#128670=CARTESIAN_POINT('Origin',(0.,1082.7251047501,424.620242579854));
#128671=CARTESIAN_POINT('Origin',(0.,1076.73142393294,424.620242579854));
#128672=CARTESIAN_POINT('Origin',(0.,1082.7251047501,424.620242579854));
#128673=CARTESIAN_POINT('Origin',(0.,1076.73142393294,424.620242579854));
#128674=CARTESIAN_POINT('Origin',(0.,1082.7251047501,424.620242579854));
#128675=CARTESIAN_POINT('Origin',(0.,1076.73142393294,424.620242579854));
#128676=CARTESIAN_POINT('Origin',(0.,1082.7251047501,424.620242579854));
#128677=CARTESIAN_POINT('Origin',(0.,1076.73142393294,424.620242579854));
#128678=CARTESIAN_POINT('Origin',(0.,1082.7251047501,424.620242579854));
#128679=CARTESIAN_POINT('Origin',(0.,1076.73142393294,424.620242579854));
#128680=CARTESIAN_POINT('Origin',(0.,1082.7251047501,424.620242579854));
#128681=CARTESIAN_POINT('Origin',(0.,1076.73142393294,424.620242579854));
#128682=CARTESIAN_POINT('Origin',(0.,1082.7251047501,424.620242579854));
#128683=CARTESIAN_POINT('Origin',(0.,1076.73142393294,424.620242579854));
#128684=CARTESIAN_POINT('Origin',(0.,1082.7251047501,424.620242579854));
#128685=CARTESIAN_POINT('Origin',(0.,1076.73142393294,424.620242579854));
#128686=CARTESIAN_POINT('Origin',(0.,1082.7251047501,424.620242579854));
#128687=CARTESIAN_POINT('Origin',(0.,1076.73142393294,424.620242579854));
#128688=CARTESIAN_POINT('Origin',(0.,1082.7251047501,424.620242579854));
#128689=CARTESIAN_POINT('Origin',(0.,1076.73142393294,424.620242579854));
#128690=CARTESIAN_POINT('Origin',(0.,1082.7251047501,424.620242579854));
#128691=CARTESIAN_POINT('Origin',(0.,1076.73142393294,424.620242579854));
#128692=CARTESIAN_POINT('Origin',(0.,1082.7251047501,424.620242579854));
#128693=CARTESIAN_POINT('Origin',(0.,1076.73142393294,424.620242579854));
#128694=CARTESIAN_POINT('Origin',(0.,1082.7251047501,424.620242579854));
#128695=CARTESIAN_POINT('Origin',(0.,1076.73142393294,424.620242579854));
#128696=CARTESIAN_POINT('Origin',(0.,1082.7251047501,424.620242579854));
#128697=CARTESIAN_POINT('Origin',(0.,1076.73142393294,424.620242579854));
#128698=CARTESIAN_POINT('Origin',(0.,1082.7251047501,424.620242579854));
#128699=CARTESIAN_POINT('Origin',(0.,1076.73142393294,424.620242579854));
#128700=CARTESIAN_POINT('Origin',(0.,1082.7251047501,424.620242579854));
#128701=CARTESIAN_POINT('Origin',(0.,1076.73142393294,424.620242579854));
#128702=CARTESIAN_POINT('Origin',(0.,1082.7251047501,424.620242579854));
#128703=CARTESIAN_POINT('Origin',(0.,1076.73142393294,424.620242579854));
#128704=CARTESIAN_POINT('Origin',(0.,1082.7251047501,424.620242579854));
#128705=CARTESIAN_POINT('Origin',(0.,1076.73142393294,424.620242579854));
#128706=CARTESIAN_POINT('Origin',(0.,1082.7251047501,424.620242579854));
#128707=CARTESIAN_POINT('Origin',(0.,1076.73142393294,424.620242579854));
#128708=CARTESIAN_POINT('Origin',(0.,1082.7251047501,424.620242579854));
#128709=CARTESIAN_POINT('Origin',(0.,1076.73142393294,424.620242579854));
#128710=CARTESIAN_POINT('Origin',(0.,1082.7251047501,424.620242579854));
#128711=CARTESIAN_POINT('Origin',(0.,1076.73142393294,424.620242579854));
#128712=CARTESIAN_POINT('Origin',(0.,1082.7251047501,424.620242579854));
#128713=CARTESIAN_POINT('Origin',(0.,1076.73142393294,424.620242579854));
#128714=CARTESIAN_POINT('Origin',(0.,1082.7251047501,424.620242579854));
#128715=CARTESIAN_POINT('Origin',(0.,1076.73142393294,424.620242579854));
#128716=CARTESIAN_POINT('Origin',(0.,1082.7251047501,424.620242579854));
#128717=CARTESIAN_POINT('Origin',(0.,1076.73142393294,424.620242579854));
#128718=CARTESIAN_POINT('Origin',(0.,1082.7251047501,424.620242579854));
#128719=CARTESIAN_POINT('Origin',(0.,1076.73142393294,424.620242579854));
#128720=CARTESIAN_POINT('Origin',(0.,1082.7251047501,424.620242579854));
#128721=CARTESIAN_POINT('Origin',(0.,1076.73142393294,424.620242579854));
#128722=CARTESIAN_POINT('Origin',(0.,1082.7251047501,424.620242579854));
#128723=CARTESIAN_POINT('Origin',(0.,1076.73142393294,424.620242579854));
#128724=CARTESIAN_POINT('Origin',(0.,1082.7251047501,424.620242579854));
#128725=CARTESIAN_POINT('Origin',(0.,1076.73142393294,424.620242579854));
#128726=CARTESIAN_POINT('Origin',(0.,1082.7251047501,424.620242579854));
#128727=CARTESIAN_POINT('Origin',(0.,1076.73142393294,424.620242579854));
#128728=CARTESIAN_POINT('Origin',(0.,1082.7251047501,424.620242579854));
#128729=CARTESIAN_POINT('Origin',(0.,1076.73142393294,424.620242579854));
#128730=CARTESIAN_POINT('Origin',(0.,1082.7251047501,424.620242579854));
#128731=CARTESIAN_POINT('Origin',(0.,1076.73142393294,424.620242579854));
#128732=CARTESIAN_POINT('Origin',(0.,1082.7251047501,424.620242579854));
#128733=CARTESIAN_POINT('Origin',(0.,1076.73142393294,424.620242579854));
#128734=CARTESIAN_POINT('Origin',(0.,1082.7251047501,424.620242579854));
#128735=CARTESIAN_POINT('Origin',(0.,1076.73142393294,424.620242579854));
#128736=CARTESIAN_POINT('Origin',(0.,1082.7251047501,424.620242579854));
#128737=CARTESIAN_POINT('Origin',(0.,1076.73142393294,424.620242579854));
#128738=CARTESIAN_POINT('Origin',(0.,1082.7251047501,424.620242579854));
#128739=CARTESIAN_POINT('Origin',(0.,1076.73142393294,424.620242579854));
#128740=CARTESIAN_POINT('Origin',(0.,1082.7251047501,424.620242579854));
#128741=CARTESIAN_POINT('Origin',(0.,1076.73142393294,424.620242579854));
#128742=CARTESIAN_POINT('Origin',(0.,1082.7251047501,424.620242579854));
#128743=CARTESIAN_POINT('Origin',(0.,1076.73142393294,424.620242579854));
#128744=CARTESIAN_POINT('Origin',(0.,1082.7251047501,424.620242579854));
#128745=CARTESIAN_POINT('Origin',(0.,1076.73142393294,424.620242579854));
#128746=CARTESIAN_POINT('Origin',(0.,1082.7251047501,424.620242579854));
#128747=CARTESIAN_POINT('Origin',(0.,1076.73142393294,424.620242579854));
#128748=CARTESIAN_POINT('Origin',(0.,1082.7251047501,424.620242579854));
#128749=CARTESIAN_POINT('Origin',(0.,1076.73142393294,424.620242579854));
#128750=CARTESIAN_POINT('Origin',(0.,1082.7251047501,424.620242579854));
#128751=CARTESIAN_POINT('Origin',(0.,1076.73142393294,424.620242579854));
#128752=CARTESIAN_POINT('Origin',(0.,1082.7251047501,424.620242579854));
#128753=CARTESIAN_POINT('Origin',(0.,1076.73142393294,424.620242579854));
#128754=CARTESIAN_POINT('Origin',(0.,1082.7251047501,424.620242579854));
#128755=CARTESIAN_POINT('Origin',(0.,1076.73142393294,424.620242579854));
#128756=CARTESIAN_POINT('Origin',(0.,1082.7251047501,424.620242579854));
#128757=CARTESIAN_POINT('Origin',(0.,1076.73142393294,424.620242579854));
#128758=CARTESIAN_POINT('Origin',(0.,1082.7251047501,424.620242579854));
#128759=CARTESIAN_POINT('Origin',(0.,1076.73142393294,424.620242579854));
#128760=CARTESIAN_POINT('Origin',(0.,1082.7251047501,424.620242579854));
#128761=CARTESIAN_POINT('Origin',(0.,1076.73142393294,424.620242579854));
#128762=CARTESIAN_POINT('Origin',(0.,1082.7251047501,424.620242579854));
#128763=CARTESIAN_POINT('Origin',(0.,1076.73142393294,424.620242579854));
#128764=CARTESIAN_POINT('Origin',(0.,1082.7251047501,424.620242579854));
#128765=CARTESIAN_POINT('Origin',(0.,1076.73142393294,424.620242579854));
#128766=CARTESIAN_POINT('Origin',(0.,1082.7251047501,424.620242579854));
#128767=CARTESIAN_POINT('Origin',(0.,1076.73142393294,424.620242579854));
#128768=CARTESIAN_POINT('Origin',(0.,1082.7251047501,424.620242579854));
#128769=CARTESIAN_POINT('Origin',(0.,1076.73142393294,424.620242579854));
#128770=CARTESIAN_POINT('Origin',(0.,1082.7251047501,424.620242579854));
#128771=CARTESIAN_POINT('Origin',(0.,1076.73142393294,424.620242579854));
#128772=CARTESIAN_POINT('Origin',(0.,1082.7251047501,424.620242579854));
#128773=CARTESIAN_POINT('Origin',(0.,1076.73142393294,424.620242579854));
#128774=CARTESIAN_POINT('Origin',(0.,1082.7251047501,424.620242579854));
#128775=CARTESIAN_POINT('Origin',(0.,1076.73142393294,424.620242579854));
#128776=CARTESIAN_POINT('Origin',(0.,1082.7251047501,424.620242579854));
#128777=CARTESIAN_POINT('Origin',(0.,1076.73142393294,424.620242579854));
#128778=CARTESIAN_POINT('Origin',(0.,1082.7251047501,424.620242579854));
#128779=CARTESIAN_POINT('Origin',(0.,1076.73142393294,424.620242579854));
#128780=CARTESIAN_POINT('Origin',(0.,1082.7251047501,424.620242579854));
#128781=CARTESIAN_POINT('Origin',(0.,1076.73142393294,424.620242579854));
#128782=CARTESIAN_POINT('Origin',(0.,1082.7251047501,424.620242579854));
#128783=CARTESIAN_POINT('Origin',(0.,1076.73142393294,424.620242579854));
#128784=CARTESIAN_POINT('Origin',(0.,1082.7251047501,424.620242579854));
#128785=CARTESIAN_POINT('Origin',(0.,1076.73142393294,424.620242579854));
#128786=CARTESIAN_POINT('Origin',(0.,1082.7251047501,424.620242579854));
#128787=CARTESIAN_POINT('Origin',(0.,1076.73142393294,424.620242579854));
#128788=CARTESIAN_POINT('Origin',(0.,1082.7251047501,424.620242579854));
#128789=CARTESIAN_POINT('Origin',(0.,1076.73142393294,424.620242579854));
#128790=CARTESIAN_POINT('Origin',(0.,1082.7251047501,424.620242579854));
#128791=CARTESIAN_POINT('Origin',(0.,1076.73142393294,424.620242579854));
#128792=CARTESIAN_POINT('Origin',(0.,1082.7251047501,424.620242579854));
#128793=CARTESIAN_POINT('Origin',(0.,1076.73142393294,424.620242579854));
#128794=CARTESIAN_POINT('Origin',(0.,1082.7251047501,424.620242579854));
#128795=CARTESIAN_POINT('Origin',(0.,1076.73142393294,424.620242579854));
#128796=CARTESIAN_POINT('Origin',(0.,1082.7251047501,424.620242579854));
#128797=CARTESIAN_POINT('Origin',(0.,1076.73142393294,424.620242579854));
#128798=CARTESIAN_POINT('Origin',(0.,1082.7251047501,424.620242579854));
#128799=CARTESIAN_POINT('Origin',(0.,1076.73142393294,424.620242579854));
#128800=CARTESIAN_POINT('Origin',(0.,1082.7251047501,424.620242579854));
#128801=CARTESIAN_POINT('Origin',(0.,1076.73142393294,424.620242579854));
#128802=CARTESIAN_POINT('Origin',(0.,1082.7251047501,424.620242579854));
#128803=CARTESIAN_POINT('Origin',(0.,1076.73142393294,424.620242579854));
#128804=CARTESIAN_POINT('Origin',(0.,1082.7251047501,424.620242579854));
#128805=CARTESIAN_POINT('Origin',(0.,1076.73142393294,424.620242579854));
#128806=CARTESIAN_POINT('Origin',(0.,1082.7251047501,424.620242579854));
#128807=CARTESIAN_POINT('Origin',(0.,1076.73142393294,424.620242579854));
#128808=CARTESIAN_POINT('Origin',(0.,1082.7251047501,424.620242579854));
#128809=CARTESIAN_POINT('Origin',(0.,1076.73142393294,424.620242579854));
#128810=CARTESIAN_POINT('Origin',(0.,1082.7251047501,424.620242579854));
#128811=CARTESIAN_POINT('Origin',(0.,1076.73142393294,424.620242579854));
#128812=CARTESIAN_POINT('Origin',(0.,1082.7251047501,424.620242579854));
#128813=CARTESIAN_POINT('Origin',(0.,1076.73142393294,424.620242579854));
#128814=CARTESIAN_POINT('Origin',(0.,1082.7251047501,424.620242579854));
#128815=CARTESIAN_POINT('Origin',(0.,1076.73142393294,424.620242579854));
#128816=CARTESIAN_POINT('Origin',(0.,1082.7251047501,424.620242579854));
#128817=CARTESIAN_POINT('Origin',(0.,1076.73142393294,424.620242579854));
#128818=CARTESIAN_POINT('Origin',(0.,1082.7251047501,424.620242579854));
#128819=CARTESIAN_POINT('Origin',(0.,1076.73142393294,424.620242579854));
#128820=CARTESIAN_POINT('Origin',(0.,1082.7251047501,424.620242579854));
#128821=CARTESIAN_POINT('Origin',(0.,1076.73142393294,424.620242579854));
#128822=CARTESIAN_POINT('Origin',(0.,1082.7251047501,424.620242579854));
#128823=CARTESIAN_POINT('Origin',(0.,1076.73142393294,424.620242579854));
#128824=CARTESIAN_POINT('Origin',(0.,1082.7251047501,424.620242579854));
#128825=CARTESIAN_POINT('Origin',(0.,1076.73142393294,424.620242579854));
#128826=CARTESIAN_POINT('Origin',(0.,1082.7251047501,424.620242579854));
#128827=CARTESIAN_POINT('Origin',(0.,1076.73142393294,424.620242579854));
#128828=CARTESIAN_POINT('Origin',(0.,1082.7251047501,424.620242579854));
#128829=CARTESIAN_POINT('Origin',(0.,1076.73142393294,424.620242579854));
#128830=CARTESIAN_POINT('Origin',(0.,1082.7251047501,424.620242579854));
#128831=CARTESIAN_POINT('Origin',(0.,1076.73142393294,424.620242579854));
#128832=CARTESIAN_POINT('Origin',(0.,1082.7251047501,424.620242579854));
#128833=CARTESIAN_POINT('Origin',(0.,1076.73142393294,424.620242579854));
#128834=CARTESIAN_POINT('Origin',(0.,1082.7251047501,424.620242579854));
#128835=CARTESIAN_POINT('Origin',(0.,1076.73142393294,424.620242579854));
#128836=CARTESIAN_POINT('Origin',(0.,1082.7251047501,424.620242579854));
#128837=CARTESIAN_POINT('Origin',(0.,1076.73142393294,424.620242579854));
#128838=CARTESIAN_POINT('Origin',(0.,1082.7251047501,424.620242579854));
#128839=CARTESIAN_POINT('Origin',(0.,1076.73142393294,424.620242579854));
#128840=CARTESIAN_POINT('Origin',(0.,1082.7251047501,424.620242579854));
#128841=CARTESIAN_POINT('Origin',(0.,1076.73142393294,424.620242579854));
#128842=CARTESIAN_POINT('Origin',(0.,1082.7251047501,424.620242579854));
#128843=CARTESIAN_POINT('Origin',(0.,1076.73142393294,424.620242579854));
#128844=CARTESIAN_POINT('Origin',(0.,1082.7251047501,424.620242579854));
#128845=CARTESIAN_POINT('Origin',(0.,1076.73142393294,424.620242579854));
#128846=CARTESIAN_POINT('Origin',(0.,1082.7251047501,424.620242579854));
#128847=CARTESIAN_POINT('Origin',(0.,1076.73142393294,424.620242579854));
#128848=CARTESIAN_POINT('Origin',(0.,1082.7251047501,424.620242579854));
#128849=CARTESIAN_POINT('Origin',(0.,1076.73142393294,424.620242579854));
#128850=CARTESIAN_POINT('Origin',(0.,1082.7251047501,424.620242579854));
#128851=CARTESIAN_POINT('Origin',(0.,1076.73142393294,424.620242579854));
#128852=CARTESIAN_POINT('Origin',(0.,1082.7251047501,424.620242579854));
#128853=CARTESIAN_POINT('Origin',(0.,1076.73142393294,424.620242579854));
#128854=CARTESIAN_POINT('Origin',(0.,1082.7251047501,424.620242579854));
#128855=CARTESIAN_POINT('Origin',(0.,1076.73142393294,424.620242579854));
#128856=CARTESIAN_POINT('Origin',(0.,1082.7251047501,424.620242579854));
#128857=CARTESIAN_POINT('Origin',(0.,1076.73142393294,424.620242579854));
#128858=CARTESIAN_POINT('Origin',(0.,1082.7251047501,424.620242579854));
#128859=CARTESIAN_POINT('Origin',(0.,1076.73142393294,424.620242579854));
#128860=CARTESIAN_POINT('Origin',(0.,1082.7251047501,424.620242579854));
#128861=CARTESIAN_POINT('Ctrl Pts',(-98.3487995443478,1075.53620292392,
385.104677429649));
#128862=CARTESIAN_POINT('Ctrl Pts',(-98.629240211509,1075.53620292392,385.802655627705));
#128863=CARTESIAN_POINT('Ctrl Pts',(-98.9022349770337,1075.53620292392,
386.50357958275));
#128864=CARTESIAN_POINT('Ctrl Pts',(-99.1677529050815,1075.53620292392,
387.207369865892));
#128865=CARTESIAN_POINT('Ctrl Pts',(-97.654964079969,1075.61786654403,385.383453587804));
#128866=CARTESIAN_POINT('Ctrl Pts',(-97.9334262818979,1075.61786654403,
386.076507658373));
#128867=CARTESIAN_POINT('Ctrl Pts',(-98.2044951118669,1075.61786654403,
386.772486704074));
#128868=CARTESIAN_POINT('Ctrl Pts',(-98.4681398522829,1075.61786654403,
387.471311856374));
#128869=CARTESIAN_POINT('Ctrl Pts',(-96.9644573915014,1075.69533882439,
385.660892277053));
#128870=CARTESIAN_POINT('Ctrl Pts',(-97.240950620171,1075.69533882439,386.349045844348));
#128871=CARTESIAN_POINT('Ctrl Pts',(-97.5101027545383,1075.69533882439,
387.040103704622));
#128872=CARTESIAN_POINT('Ctrl Pts',(-97.7718832942109,1075.69533882439,
387.733987547012));
#128873=CARTESIAN_POINT('Ctrl Pts',(-96.2772807018516,1075.76862178799,
385.936993006044));
#128874=CARTESIAN_POINT('Ctrl Pts',(-96.5518144527218,1075.76862178799,
386.620269702957));
#128875=CARTESIAN_POINT('Ctrl Pts',(-96.8190591348362,1075.76862178799,
387.306430110437));
#128876=CARTESIAN_POINT('Ctrl Pts',(-97.0789844639553,1075.76862178799,
387.995396472602));
#128877=CARTESIAN_POINT('Origin',(0.,1082.7251047501,424.620242579854));
#128878=CARTESIAN_POINT('Ctrl Pts',(-99.649831526399,1074.6499846452,371.148967657458));
#128879=CARTESIAN_POINT('Ctrl Pts',(-100.003261188269,1074.6499846452,371.807624222369));
#128880=CARTESIAN_POINT('Ctrl Pts',(-100.350143399903,1074.6499846452,372.469752403044));
#128881=CARTESIAN_POINT('Ctrl Pts',(-100.690444064651,1074.6499846452,373.135287115859));
#128882=CARTESIAN_POINT('Ctrl Pts',(-98.9960442017051,1074.75386596962,
371.499784525324));
#128883=CARTESIAN_POINT('Ctrl Pts',(-99.3471550655449,1074.75386596962,
372.154119745113));
#128884=CARTESIAN_POINT('Ctrl Pts',(-99.6917614359683,1074.75386596962,
372.811903803923));
#128885=CARTESIAN_POINT('Ctrl Pts',(-100.029829440031,1074.75386596962,
373.473072045138));
#128886=CARTESIAN_POINT('Ctrl Pts',(-98.3451877959452,1074.85385082036,
371.849028686346));
#128887=CARTESIAN_POINT('Ctrl Pts',(-98.6939902568916,1074.85385082036,
372.499061933538));
#128888=CARTESIAN_POINT('Ctrl Pts',(-99.0363309886679,1074.85385082036,
373.152521345119));
#128889=CARTESIAN_POINT('Ctrl Pts',(-99.3721763410299,1074.85385082036,
373.809342689561));
#128890=CARTESIAN_POINT('Ctrl Pts',(-97.6972633477068,1074.94994100663,
372.196699583225));
#128891=CARTESIAN_POINT('Ctrl Pts',(-98.0437678045809,1074.94994100663,
372.842450237212));
#128892=CARTESIAN_POINT('Ctrl Pts',(-98.383853103888,1074.94994100663,373.4916044831));
#128893=CARTESIAN_POINT('Ctrl Pts',(-98.7174858170808,1074.94994100663,
374.144098512532));
#128894=CARTESIAN_POINT('Origin',(0.,1082.7251047501,424.620242579854));
#128895=CARTESIAN_POINT('Ctrl Pts',(-94.3883656101975,1076.25696242948,
398.145298833932));
#128896=CARTESIAN_POINT('Ctrl Pts',(-94.6250421977941,1076.25696242948,
398.989097275803));
#128897=CARTESIAN_POINT('Ctrl Pts',(-94.8503832990042,1076.25696242948,
399.835993376708));
#128898=CARTESIAN_POINT('Ctrl Pts',(-95.064348397423,1076.25696242948,400.685834864445));
#128899=CARTESIAN_POINT('Ctrl Pts',(-93.5499215982822,1076.31899804589,
398.380473560245));
#128900=CARTESIAN_POINT('Ctrl Pts',(-93.7844958074093,1076.31899804589,
399.216776610643));
#128901=CARTESIAN_POINT('Ctrl Pts',(-94.0078352223339,1076.31899804589,
400.056149803825));
#128902=CARTESIAN_POINT('Ctrl Pts',(-94.2198996865552,1076.31899804589,
400.898442220214));
#128903=CARTESIAN_POINT('Ctrl Pts',(-92.7165113242668,1076.37494427844,
398.614236376025));
#128904=CARTESIAN_POINT('Ctrl Pts',(-92.9489957769028,1076.37494427844,
399.443089034776));
#128905=CARTESIAN_POINT('Ctrl Pts',(-93.1703455229981,1076.37494427844,
400.274984485262));
#128906=CARTESIAN_POINT('Ctrl Pts',(-93.380520763795,1076.37494427844,401.109773152406));
#128907=CARTESIAN_POINT('Ctrl Pts',(-91.8881370161384,1076.42480467903,
398.846586656342));
#128908=CARTESIAN_POINT('Ctrl Pts',(-92.1185443398482,1076.42480467903,
399.668033943192));
#128909=CARTESIAN_POINT('Ctrl Pts',(-92.3379164398894,1076.42480467903,
400.492496836));
#128910=CARTESIAN_POINT('Ctrl Pts',(-92.5462138730855,1076.42480467903,
401.319827096063));
#128911=CARTESIAN_POINT('Origin',(0.,1082.7251047501,424.620242579854));
#128912=CARTESIAN_POINT('Ctrl Pts',(-89.8068600050043,1076.62748242345,
409.571133399922));
#128913=CARTESIAN_POINT('Ctrl Pts',(-89.9752215487277,1076.62748242345,
410.575845466703));
#128914=CARTESIAN_POINT('Ctrl Pts',(-90.1267006838473,1076.62748242345,
411.583241127883));
#128915=CARTESIAN_POINT('Ctrl Pts',(-90.2612547574608,1076.62748242345,
412.593036724929));
#128916=CARTESIAN_POINT('Ctrl Pts',(-88.8113461800284,1076.66225518595,
409.73795357648));
#128917=CARTESIAN_POINT('Ctrl Pts',(-88.977841427075,1076.66225518595,410.731528356505));
#128918=CARTESIAN_POINT('Ctrl Pts',(-89.1276414079163,1076.66225518595,
411.727756983141));
#128919=CARTESIAN_POINT('Ctrl Pts',(-89.2607039424593,1076.66225518595,
412.726358942227));
#128920=CARTESIAN_POINT('Ctrl Pts',(-87.8232439306037,1076.68829918657,
409.903531780993));
#128921=CARTESIAN_POINT('Ctrl Pts',(-87.9878867755057,1076.68829918657,
410.886052191082));
#128922=CARTESIAN_POINT('Ctrl Pts',(-88.1360201033303,1076.68829918657,
411.871196921468));
#128923=CARTESIAN_POINT('Ctrl Pts',(-88.267602203274,1076.68829918657,412.858688578948));
#128924=CARTESIAN_POINT('Ctrl Pts',(-86.8425571826817,1076.70562053557,
410.06786735558));
#128925=CARTESIAN_POINT('Ctrl Pts',(-87.0053615273314,1076.70562053557,
411.039416356477));
#128926=CARTESIAN_POINT('Ctrl Pts',(-87.1518407100228,1076.70562053557,
412.013560372944));
#128927=CARTESIAN_POINT('Ctrl Pts',(-87.2819534857204,1076.70562053557,
412.990025109318));
#128928=CARTESIAN_POINT('Origin',(0.,1082.7251047501,424.620242579854));
#128929=CARTESIAN_POINT('Ctrl Pts',(-86.3584302894826,1074.64930692473,
351.59570928573));
#128930=CARTESIAN_POINT('Ctrl Pts',(-86.8398187017703,1074.64930692473,
352.164996698732));
#128931=CARTESIAN_POINT('Ctrl Pts',(-87.315554525217,1074.64930692473,352.739016200472));
#128932=CARTESIAN_POINT('Ctrl Pts',(-87.7855912457502,1074.64930692473,
353.317711667395));
#128933=CARTESIAN_POINT('Ctrl Pts',(-85.7921843593031,1074.75314553403,
352.074525825614));
#128934=CARTESIAN_POINT('Ctrl Pts',(-86.2704163428741,1074.75314553403,
352.640080462562));
#128935=CARTESIAN_POINT('Ctrl Pts',(-86.743032801217,1074.75314553403,353.210336160286));
#128936=CARTESIAN_POINT('Ctrl Pts',(-87.2099875252486,1074.75314553403,
353.785237163231));
#128937=CARTESIAN_POINT('Ctrl Pts',(-85.2284753922116,1074.85309213932,
352.551197114076));
#128938=CARTESIAN_POINT('Ctrl Pts',(-85.7035650888773,1074.85309213932,
353.113035699));
#128939=CARTESIAN_POINT('Ctrl Pts',(-86.1730761578708,1074.85309213932,
353.679544455756));
#128940=CARTESIAN_POINT('Ctrl Pts',(-86.6369626937321,1074.85309213932,
354.250667995136));
#128941=CARTESIAN_POINT('Ctrl Pts',(-84.6673042866797,1074.94914854672,
353.025722391367));
#128942=CARTESIAN_POINT('Ctrl Pts',(-85.1392658432598,1074.94914854672,
353.583861654224));
#128943=CARTESIAN_POINT('Ctrl Pts',(-85.6056855036081,1074.94914854672,
354.146640339031));
#128944=CARTESIAN_POINT('Ctrl Pts',(-86.0665176645205,1074.94914854672,
354.714003421281));
#128945=CARTESIAN_POINT('Origin',(0.,1082.7251047501,424.620242579854));
#128946=CARTESIAN_POINT('Ctrl Pts',(-87.9863052406897,1075.53617638582,
365.523475655949));
#128947=CARTESIAN_POINT('Ctrl Pts',(-88.4058111505509,1075.53617638582,
366.148057624754));
#128948=CARTESIAN_POINT('Ctrl Pts',(-88.8186430196475,1075.53617638582,
366.777070893312));
#128949=CARTESIAN_POINT('Ctrl Pts',(-89.2247540438749,1075.53617638582,
367.410444148325));
#128950=CARTESIAN_POINT('Ctrl Pts',(-87.3640928236274,1075.6180360885,365.94139003578));
#128951=CARTESIAN_POINT('Ctrl Pts',(-87.780632115156,1075.6180360885,366.561555150674));
#128952=CARTESIAN_POINT('Ctrl Pts',(-88.1905445627084,1075.6180360885,367.186120228515));
#128953=CARTESIAN_POINT('Ctrl Pts',(-88.5937836931645,1075.6180360885,367.815014460311));
#128954=CARTESIAN_POINT('Ctrl Pts',(-86.7448726917102,1075.69568439305,
366.357294621277));
#128955=CARTESIAN_POINT('Ctrl Pts',(-87.1584596316867,1075.69568439305,
366.973064123375));
#128956=CARTESIAN_POINT('Ctrl Pts',(-87.5654666975011,1075.69568439305,
367.593202402318));
#128957=CARTESIAN_POINT('Ctrl Pts',(-87.965847745426,1075.69568439305,368.217639150992));
#128958=CARTESIAN_POINT('Ctrl Pts',(-86.1286459468542,1075.76912333699,
366.771188672327));
#128959=CARTESIAN_POINT('Ctrl Pts',(-86.5392948073127,1075.76912333699,
367.382583810569));
#128960=CARTESIAN_POINT('Ctrl Pts',(-86.9434105363655,1075.76912333699,
367.998316690309));
#128961=CARTESIAN_POINT('Ctrl Pts',(-87.3409473180852,1075.76912333699,
368.618317503889));
#128962=CARTESIAN_POINT('Origin',(0.,1082.7251047501,424.620242579854));
#128963=CARTESIAN_POINT('Ctrl Pts',(-86.8150232951319,1076.25735809069,
379.099381006362));
#128964=CARTESIAN_POINT('Ctrl Pts',(-87.2224634623205,1076.25735809069,
379.876429734861));
#128965=CARTESIAN_POINT('Ctrl Pts',(-87.6194349295328,1076.25735809069,
380.658878372485));
#128966=CARTESIAN_POINT('Ctrl Pts',(-88.0058661457325,1076.25735809069,
381.446585888919));
#128967=CARTESIAN_POINT('Ctrl Pts',(-86.0454051748305,1076.31924104508,
379.502924985146));
#128968=CARTESIAN_POINT('Ctrl Pts',(-86.4492333711446,1076.31924104508,
380.273085150362));
#128969=CARTESIAN_POINT('Ctrl Pts',(-86.8426856728622,1076.31924104508,
381.048597354327));
#128970=CARTESIAN_POINT('Ctrl Pts',(-87.2256911632491,1076.31924104508,
381.829321816963));
#128971=CARTESIAN_POINT('Ctrl Pts',(-85.2803982612145,1076.37505949439,
379.904051109354));
#128972=CARTESIAN_POINT('Ctrl Pts',(-85.6806361279641,1076.37505949439,
380.667363984471));
#128973=CARTESIAN_POINT('Ctrl Pts',(-86.0705903494486,1076.37505949439,
381.435981314777));
#128974=CARTESIAN_POINT('Ctrl Pts',(-86.4501906394357,1076.37505949439,
382.209764562942));
#128975=CARTESIAN_POINT('Ctrl Pts',(-84.5200045910798,1076.42481696877,
380.302758311009));
#128976=CARTESIAN_POINT('Ctrl Pts',(-84.9166737791338,1076.42481696877,
381.059265187439));
#128977=CARTESIAN_POINT('Ctrl Pts',(-85.3031510149603,1076.42481696877,
381.821029222443));
#128978=CARTESIAN_POINT('Ctrl Pts',(-85.6793666390268,1076.42481696877,
382.587913113945));
#128979=CARTESIAN_POINT('Origin',(0.,1082.7251047501,424.620242579854));
#128980=CARTESIAN_POINT('Ctrl Pts',(-84.7179661437949,1076.62733369941,
391.222638015823));
#128981=CARTESIAN_POINT('Ctrl Pts',(-85.0910907886886,1076.62733369941,
392.169123892465));
#128982=CARTESIAN_POINT('Ctrl Pts',(-85.4483030389599,1076.62733369941,
393.121729227095));
#128983=CARTESIAN_POINT('Ctrl Pts',(-85.7895025866761,1076.62733369941,
394.080186520848));
#128984=CARTESIAN_POINT('Ctrl Pts',(-83.7798178484809,1076.66209686976,
391.59247581075));
#128985=CARTESIAN_POINT('Ctrl Pts',(-84.1488105923685,1076.66209686976,
392.528480509052));
#128986=CARTESIAN_POINT('Ctrl Pts',(-84.502067152024,1076.66209686976,393.470536899799));
#128987=CARTESIAN_POINT('Ctrl Pts',(-84.8394883303031,1076.66209686976,
394.418380446348));
#128988=CARTESIAN_POINT('Ctrl Pts',(-82.8486469713158,1076.68814855513,
391.95956296065));
#128989=CARTESIAN_POINT('Ctrl Pts',(-83.2135385449476,1076.68814855513,
392.885164433709));
#128990=CARTESIAN_POINT('Ctrl Pts',(-83.5628688341843,1076.68814855513,
393.81675033767));
#128991=CARTESIAN_POINT('Ctrl Pts',(-83.8965397444081,1076.68814855513,
394.754059076083));
#128992=CARTESIAN_POINT('Ctrl Pts',(-81.924457204617,1076.70549484766,392.323898009936));
#128993=CARTESIAN_POINT('Ctrl Pts',(-82.2852783550056,1076.70549484766,
393.239174252098));
#128994=CARTESIAN_POINT('Ctrl Pts',(-82.6307118095888,1076.70549484766,
394.160368167888));
#128995=CARTESIAN_POINT('Ctrl Pts',(-82.96066056801,1076.70549484766,395.087221079007));
#128996=CARTESIAN_POINT('Origin',(0.,1082.7251047501,424.620242579854));
#128997=CARTESIAN_POINT('Ctrl Pts',(-69.2937118359578,1074.64931581022,
335.240557572053));
#128998=CARTESIAN_POINT('Ctrl Pts',(-69.8828803090973,1074.64931581022,
335.697324346259));
#128999=CARTESIAN_POINT('Ctrl Pts',(-70.4675037924513,1074.64931581022,
336.15989407989));
#129000=CARTESIAN_POINT('Ctrl Pts',(-71.0475251325708,1074.64931581022,
336.628221551608));
#129001=CARTESIAN_POINT('Ctrl Pts',(-68.8381453304565,1074.75343131481,
335.828177857977));
#129002=CARTESIAN_POINT('Ctrl Pts',(-69.4234403580071,1074.75343131481,
336.281941652004));
#129003=CARTESIAN_POINT('Ctrl Pts',(-70.0042202764792,1074.75343131481,
336.741470254319));
#129004=CARTESIAN_POINT('Ctrl Pts',(-70.5804283081752,1074.75343131481,
337.206718740888));
#129005=CARTESIAN_POINT('Ctrl Pts',(-68.3846253564385,1074.85363401426,
336.413158390099));
#129006=CARTESIAN_POINT('Ctrl Pts',(-68.9660643389952,1074.85363401426,
336.86393269417));
#129007=CARTESIAN_POINT('Ctrl Pts',(-69.5430179589482,1074.85363401426,
337.320433826776));
#129008=CARTESIAN_POINT('Ctrl Pts',(-70.1154298126631,1074.85363401426,
337.782617159852));
#129009=CARTESIAN_POINT('Ctrl Pts',(-67.933152640622,1074.94992572917,336.995498231047));
#129010=CARTESIAN_POINT('Ctrl Pts',(-68.5107529849589,1074.94992572917,
337.443296540175));
#129011=CARTESIAN_POINT('Ctrl Pts',(-69.0838975788868,1074.94992572917,
337.896783869531));
#129012=CARTESIAN_POINT('Ctrl Pts',(-69.6525303911459,1074.94992572917,
338.355915885685));
#129013=CARTESIAN_POINT('Origin',(0.,1082.7251047501,424.620242579854));
#129014=CARTESIAN_POINT('Ctrl Pts',(-73.7691873467676,1075.53681660702,
348.522397650382));
#129015=CARTESIAN_POINT('Ctrl Pts',(-74.3105270143456,1075.53681660702,
349.047171872212));
#129016=CARTESIAN_POINT('Ctrl Pts',(-74.8462364222988,1075.53681660702,
349.5776924183));
#129017=CARTESIAN_POINT('Ctrl Pts',(-75.3762545767591,1075.53681660702,
350.113898885561));
#129018=CARTESIAN_POINT('Ctrl Pts',(-73.2488932306589,1075.61843552384,
349.059115789613));
#129019=CARTESIAN_POINT('Ctrl Pts',(-73.7864148292844,1075.61843552384,
349.580188778588));
#129020=CARTESIAN_POINT('Ctrl Pts',(-74.3183458785092,1075.61843552384,
350.106967562993));
#129021=CARTESIAN_POINT('Ctrl Pts',(-74.8446258146548,1075.61843552384,
350.639392165767));
#129022=CARTESIAN_POINT('Ctrl Pts',(-72.7310946383515,1075.6958655393,349.593259629329));
#129023=CARTESIAN_POINT('Ctrl Pts',(-73.2648164809012,1075.6958655393,350.110649137936));
#129024=CARTESIAN_POINT('Ctrl Pts',(-73.7929872938091,1075.6958655393,350.633704107536));
#129025=CARTESIAN_POINT('Ctrl Pts',(-74.3155469415234,1075.6958655393,351.162364985049));
#129026=CARTESIAN_POINT('Ctrl Pts',(-72.2157924863696,1075.76910867463,
350.124828224073));
#129027=CARTESIAN_POINT('Ctrl Pts',(-72.7457328924458,1075.76910867463,
350.63855201132));
#129028=CARTESIAN_POINT('Ctrl Pts',(-73.2701615981042,1075.76910867463,
351.157901119585));
#129029=CARTESIAN_POINT('Ctrl Pts',(-73.7890188938555,1075.76910867463,
351.682816417725));
#129030=CARTESIAN_POINT('Origin',(0.,1082.7251047501,424.620242579854));
#129031=CARTESIAN_POINT('Ctrl Pts',(-75.4581277762219,1076.25692467333,
362.040205265552));
#129032=CARTESIAN_POINT('Ctrl Pts',(-76.0168599993451,1076.25692467333,
362.713916712436));
#129033=CARTESIAN_POINT('Ctrl Pts',(-76.5665200306141,1076.25692467333,
363.395050077384));
#129034=CARTESIAN_POINT('Ctrl Pts',(-77.1070092920242,1076.25692467333,
364.08348320349));
#129035=CARTESIAN_POINT('Ctrl Pts',(-74.7894053761516,1076.31881801516,
362.594799899458));
#129036=CARTESIAN_POINT('Ctrl Pts',(-75.3431860219661,1076.31881801516,
363.262540804149));
#129037=CARTESIAN_POINT('Ctrl Pts',(-75.8879748751902,1076.31881801516,
363.937637852639));
#129038=CARTESIAN_POINT('Ctrl Pts',(-76.4236742314337,1076.31881801516,
364.619969970597));
#129039=CARTESIAN_POINT('Ctrl Pts',(-74.124688384805,1076.37465035438,363.146072709264));
#129040=CARTESIAN_POINT('Ctrl Pts',(-74.6735471114934,1076.37465035438,
363.807878833181));
#129041=CARTESIAN_POINT('Ctrl Pts',(-75.2134939632922,1076.37465035438,
364.476975720596));
#129042=CARTESIAN_POINT('Ctrl Pts',(-75.744432104193,1076.37465035438,365.15324337327));
#129043=CARTESIAN_POINT('Ctrl Pts',(-73.4639785708834,1076.42442521807,
363.694022228125));
#129044=CARTESIAN_POINT('Ctrl Pts',(-74.0079450497246,1076.42442521807,
364.349929348478));
#129045=CARTESIAN_POINT('Ctrl Pts',(-74.5430790896012,1076.42442521807,
365.013062246167));
#129046=CARTESIAN_POINT('Ctrl Pts',(-75.0692847176521,1076.42442521807,
365.683301992556));
#129047=CARTESIAN_POINT('Origin',(0.,1082.7251047501,424.620242579854));
#129048=CARTESIAN_POINT('Ctrl Pts',(-75.9265346513598,1076.62732561046,
374.343629244776));
#129049=CARTESIAN_POINT('Ctrl Pts',(-76.4886562467854,1076.62732561046,
375.192531785385));
#129050=CARTESIAN_POINT('Ctrl Pts',(-77.0364633027961,1076.62732561046,
376.050741340727));
#129051=CARTESIAN_POINT('Ctrl Pts',(-77.56980176015,1076.62732561046,376.91801655737));
#129052=CARTESIAN_POINT('Ctrl Pts',(-75.0834901232,1076.6621832391,374.901871813875));
#129053=CARTESIAN_POINT('Ctrl Pts',(-75.639370244056,1076.6621832391,375.741348629405));
#129054=CARTESIAN_POINT('Ctrl Pts',(-76.1810947659015,1076.6621832391,376.590029119935));
#129055=CARTESIAN_POINT('Ctrl Pts',(-76.7085113400799,1076.6621832391,377.447674611882));
#129056=CARTESIAN_POINT('Ctrl Pts',(-74.2467324701365,1076.68828265731,
375.455951374748));
#129057=CARTESIAN_POINT('Ctrl Pts',(-74.796417661261,1076.68828265731,376.286072756096));
#129058=CARTESIAN_POINT('Ctrl Pts',(-75.3321050085058,1076.68828265731,
377.125295243352));
#129059=CARTESIAN_POINT('Ctrl Pts',(-75.8536438610429,1076.68828265731,
377.973382822797));
#129060=CARTESIAN_POINT('Ctrl Pts',(-73.4162650279748,1076.70563000628,
376.00586571851));
#129061=CARTESIAN_POINT('Ctrl Pts',(-73.9598018589024,1076.70563000628,
376.82670199387));
#129062=CARTESIAN_POINT('Ctrl Pts',(-74.4894974151786,1076.70563000628,
377.656537577094));
#129063=CARTESIAN_POINT('Ctrl Pts',(-75.0052027310409,1076.70563000628,
378.495139094332));
#129064=CARTESIAN_POINT('Origin',(0.,1082.7251047501,424.620242579854));
#129065=CARTESIAN_POINT('Ctrl Pts',(-49.1887364726124,1074.64986286691,
322.787383952035));
#129066=CARTESIAN_POINT('Ctrl Pts',(-49.861949754311,1074.64986286691,323.112568879077));
#129067=CARTESIAN_POINT('Ctrl Pts',(-50.5319053641702,1074.64986286691,
323.444413481638));
#129068=CARTESIAN_POINT('Ctrl Pts',(-51.1985374242161,1074.64986286691,
323.782885128825));
#129069=CARTESIAN_POINT('Ctrl Pts',(-48.8659612240735,1074.75376552472,
323.455608602841));
#129070=CARTESIAN_POINT('Ctrl Pts',(-49.5347568971914,1074.75376552472,
323.778659674591));
#129071=CARTESIAN_POINT('Ctrl Pts',(-50.2003162752302,1074.75376552472,
324.108326721237));
#129072=CARTESIAN_POINT('Ctrl Pts',(-50.8625739125059,1074.75376552472,
324.444577326009));
#129073=CARTESIAN_POINT('Ctrl Pts',(-48.544633221678,1074.85377033612,324.12083709594));
#129074=CARTESIAN_POINT('Ctrl Pts',(-49.2090310937035,1074.85377033612,
324.441763880088));
#129075=CARTESIAN_POINT('Ctrl Pts',(-49.8702139515621,1074.85377033612,
324.769263134453));
#129076=CARTESIAN_POINT('Ctrl Pts',(-50.5281167799212,1074.85377033612,
325.103302655427));
#129077=CARTESIAN_POINT('Ctrl Pts',(-48.2247529783561,1074.94987911127,
324.783068369438));
#129078=CARTESIAN_POINT('Ctrl Pts',(-48.8847728637976,1074.94987911127,
325.101880437067));
#129079=CARTESIAN_POINT('Ctrl Pts',(-49.5415989201024,1074.94987911127,
325.427221666245));
#129080=CARTESIAN_POINT('Ctrl Pts',(-50.19516656035,1074.94987911127,325.759060065568));
#129081=CARTESIAN_POINT('Origin',(0.,1082.7251047501,424.620242579854));
#129082=CARTESIAN_POINT('Ctrl Pts',(-56.3385706144534,1075.53620324036,
334.843123513399));
#129083=CARTESIAN_POINT('Ctrl Pts',(-56.9759578646755,1075.53620324036,
335.243108353399));
#129084=CARTESIAN_POINT('Ctrl Pts',(-57.6090494979524,1075.53620324036,
335.649858107977));
#129085=CARTESIAN_POINT('Ctrl Pts',(-58.2377737176665,1075.53620324036,
336.063326649126));
#129086=CARTESIAN_POINT('Ctrl Pts',(-55.9408904765946,1075.61791211129,
335.47683815503));
#129087=CARTESIAN_POINT('Ctrl Pts',(-56.5737785667072,1075.61791211129,
335.873999600247));
#129088=CARTESIAN_POINT('Ctrl Pts',(-57.2024013615799,1075.61791211129,
336.277878208172));
#129089=CARTESIAN_POINT('Ctrl Pts',(-57.8266875713899,1075.61791211129,
336.688428176403));
#129090=CARTESIAN_POINT('Ctrl Pts',(-55.5451193241529,1075.69542499513,
336.107510773953));
#129091=CARTESIAN_POINT('Ctrl Pts',(-56.1735298514906,1075.69542499513,
336.50186237754));
#129092=CARTESIAN_POINT('Ctrl Pts',(-56.7977052597404,1075.69542499513,
336.902883621188));
#129093=CARTESIAN_POINT('Ctrl Pts',(-57.4175747634414,1075.69542499513,
337.310529026537));
#129094=CARTESIAN_POINT('Ctrl Pts',(-55.1512578588289,1075.76874391824,
336.73514025199));
#129095=CARTESIAN_POINT('Ctrl Pts',(-55.7752124286652,1075.76874391824,
337.126695572081));
#129096=CARTESIAN_POINT('Ctrl Pts',(-56.3949619099586,1075.76874391824,
337.524873238893));
#129097=CARTESIAN_POINT('Ctrl Pts',(-57.0104360191766,1075.76874391824,
337.929628096546));
#129098=CARTESIAN_POINT('Origin',(0.,1082.7251047501,424.620242579854));
#129099=CARTESIAN_POINT('Ctrl Pts',(-60.8036583368741,1076.25693403304,
347.723691993978));
#129100=CARTESIAN_POINT('Ctrl Pts',(-61.4899622341832,1076.25693403304,
348.266366371038));
#129101=CARTESIAN_POINT('Ctrl Pts',(-62.1689399918952,1076.25693403304,
348.81817949476));
#129102=CARTESIAN_POINT('Ctrl Pts',(-62.8404699284279,1076.25693403304,
349.379032473106));
#129103=CARTESIAN_POINT('Ctrl Pts',(-60.2634899240499,1076.31897791375,
348.406826673992));
#129104=CARTESIAN_POINT('Ctrl Pts',(-60.9436968249437,1076.31897791375,
348.94468003263));
#129105=CARTESIAN_POINT('Ctrl Pts',(-61.6166426703044,1076.31897791375,
349.491590951002));
#129106=CARTESIAN_POINT('Ctrl Pts',(-62.2822068595465,1076.31897791375,
350.047461415607));
#129107=CARTESIAN_POINT('Ctrl Pts',(-59.7265648307342,1076.37493115239,
349.085859625763));
#129108=CARTESIAN_POINT('Ctrl Pts',(-60.4007113432535,1076.37493115239,
349.618920912699));
#129109=CARTESIAN_POINT('Ctrl Pts',(-61.0676614935213,1076.37493115239,
350.160959059907));
#129110=CARTESIAN_POINT('Ctrl Pts',(-61.7272957554581,1076.37493115239,
350.711876927153));
#129111=CARTESIAN_POINT('Ctrl Pts',(-59.1928844926034,1076.42479730197,
349.760789033635));
#129112=CARTESIAN_POINT('Ctrl Pts',(-59.8610072409942,1076.42479730197,
350.2890872084));
#129113=CARTESIAN_POINT('Ctrl Pts',(-60.5219979294594,1076.42479730197,
350.826282031662));
#129114=CARTESIAN_POINT('Ctrl Pts',(-61.175738099932,1076.42479730197,351.372277231172));
#129115=CARTESIAN_POINT('Origin',(0.,1082.7251047501,424.620242579854));
#129116=CARTESIAN_POINT('Ctrl Pts',(-63.8042737731188,1076.62756831568,
359.656342770107));
#129117=CARTESIAN_POINT('Ctrl Pts',(-64.5322278769664,1076.62756831568,
360.371302664328));
#129118=CARTESIAN_POINT('Ctrl Pts',(-65.2480630511544,1076.62756831568,
361.098396077204));
#129119=CARTESIAN_POINT('Ctrl Pts',(-65.9515770830636,1076.62756831568,
361.837417615835));
#129120=CARTESIAN_POINT('Ctrl Pts',(-63.0975147104926,1076.66230088097,
360.375946994384));
#129121=CARTESIAN_POINT('Ctrl Pts',(-63.8174052767486,1076.66230088097,
361.082987287695));
#129122=CARTESIAN_POINT('Ctrl Pts',(-64.5253111545621,1076.66230088097,
361.802026696842));
#129123=CARTESIAN_POINT('Ctrl Pts',(-65.2210323712204,1076.66230088097,
362.532862104058));
#129124=CARTESIAN_POINT('Ctrl Pts',(-62.3960136094621,1076.68831765292,
361.090197694985));
#129125=CARTESIAN_POINT('Ctrl Pts',(-63.1079006271289,1076.68831765292,
361.789377305565));
#129126=CARTESIAN_POINT('Ctrl Pts',(-63.8079361988774,1076.68831765292,
362.500422629057));
#129127=CARTESIAN_POINT('Ctrl Pts',(-64.4959225752375,1076.68831765292,
363.223132805903));
#129128=CARTESIAN_POINT('Ctrl Pts',(-61.6997732531278,1076.7056247282,361.799092038227));
#129129=CARTESIAN_POINT('Ctrl Pts',(-62.4037167429603,1076.7056247282,362.490469915442));
#129130=CARTESIAN_POINT('Ctrl Pts',(-63.0959410301775,1076.7056247282,363.193581103069));
#129131=CARTESIAN_POINT('Ctrl Pts',(-63.7762505718791,1076.7056247282,363.908226982823));
#129132=CARTESIAN_POINT('Origin',(0.,1082.7251047501,424.620242579854));
#129133=CARTESIAN_POINT('Ctrl Pts',(-26.9425711955054,1074.64941712613,
314.782722615003));
#129134=CARTESIAN_POINT('Ctrl Pts',(-27.6676358963114,1074.64941712613,
314.960577207214));
#129135=CARTESIAN_POINT('Ctrl Pts',(-28.3909040175034,1074.64941712613,
315.145602343865));
#129136=CARTESIAN_POINT('Ctrl Pts',(-29.1123046476605,1074.64941712613,
315.337779884526));
#129137=CARTESIAN_POINT('Ctrl Pts',(-26.7656745127426,1074.75339142399,
315.503882180053));
#129138=CARTESIAN_POINT('Ctrl Pts',(-27.4859786604659,1074.75339142399,
315.680569033404));
#129139=CARTESIAN_POINT('Ctrl Pts',(-28.2044980243675,1074.75339142399,
315.864379351593));
#129140=CARTESIAN_POINT('Ctrl Pts',(-28.9211621586091,1074.75339142399,
316.055295113295));
#129141=CARTESIAN_POINT('Ctrl Pts',(-26.5895714430747,1074.85346333329,
316.221806400802));
#129142=CARTESIAN_POINT('Ctrl Pts',(-27.3051363950251,1074.85346333329,
316.39733075413));
#129143=CARTESIAN_POINT('Ctrl Pts',(-28.0189283060266,1074.85346333329,
316.579931703908));
#129144=CARTESIAN_POINT('Ctrl Pts',(-28.7308771937348,1074.85346333329,
316.76959134738));
#129145=CARTESIAN_POINT('Ctrl Pts',(-26.4142622679364,1074.9496346674,316.936494129919));
#129146=CARTESIAN_POINT('Ctrl Pts',(-27.1251093889977,1074.9496346674,317.110861223917));
#129147=CARTESIAN_POINT('Ctrl Pts',(-27.8341951590444,1074.9496346674,317.292258257267));
#129148=CARTESIAN_POINT('Ctrl Pts',(-28.5414500571367,1074.9496346674,317.480667445246));
#129149=CARTESIAN_POINT('Origin',(0.,1082.7251047501,424.620242579854));
#129150=CARTESIAN_POINT('Ctrl Pts',(-36.4456850718535,1075.53624331041,
325.093362237882));
#129151=CARTESIAN_POINT('Ctrl Pts',(-37.152037505206,1075.53624331041,325.352020986627));
#129152=CARTESIAN_POINT('Ctrl Pts',(-37.8555964276979,1075.53624331041,
325.61818437815));
#129153=CARTESIAN_POINT('Ctrl Pts',(-38.5562821088095,1075.53624331041,
325.891822249598));
#129154=CARTESIAN_POINT('Ctrl Pts',(-36.1881437694065,1075.61803963491,
325.796663118116));
#129155=CARTESIAN_POINT('Ctrl Pts',(-36.8895048045918,1075.61803963491,
326.053494069937));
#129156=CARTESIAN_POINT('Ctrl Pts',(-37.5880920690975,1075.61803963491,
326.317776633418));
#129157=CARTESIAN_POINT('Ctrl Pts',(-38.2838263958152,1075.61803963491,
326.589480858848));
#129158=CARTESIAN_POINT('Ctrl Pts',(-35.9318400894039,1075.69563084465,
326.4965842649));
#129159=CARTESIAN_POINT('Ctrl Pts',(-36.6282337127353,1075.69563084465,
326.751596203331));
#129160=CARTESIAN_POINT('Ctrl Pts',(-37.3218732107063,1075.69563084465,
327.014006977145));
#129161=CARTESIAN_POINT('Ctrl Pts',(-38.0126799769119,1075.69563084465,
327.28378684875));
#129162=CARTESIAN_POINT('Ctrl Pts',(-35.6767744872628,1075.76901897262,
327.193124434569));
#129163=CARTESIAN_POINT('Ctrl Pts',(-36.3682246938802,1075.76901897262,
327.446326146375));
#129164=CARTESIAN_POINT('Ctrl Pts',(-37.0569403255594,1075.76901897262,
327.706874172223));
#129165=CARTESIAN_POINT('Ctrl Pts',(-37.7428433338905,1075.76901897262,
327.974738985617));
#129166=CARTESIAN_POINT('Origin',(0.,1082.7251047501,424.620242579854));
#129167=CARTESIAN_POINT('Ctrl Pts',(-43.4792032208331,1076.25720649399,
336.762554668715));
#129168=CARTESIAN_POINT('Ctrl Pts',(-44.2653215602855,1076.25720649399,
337.151590618207));
#129169=CARTESIAN_POINT('Ctrl Pts',(-45.0461479884214,1076.25720649399,
337.551141744779));
#129170=CARTESIAN_POINT('Ctrl Pts',(-45.8215418613918,1076.25720649399,
337.96113608057));
#129171=CARTESIAN_POINT('Ctrl Pts',(-43.093582895018,1076.3191283065,337.541771115382));
#129172=CARTESIAN_POINT('Ctrl Pts',(-43.8727290917508,1076.3191283065,337.927356675757));
#129173=CARTESIAN_POINT('Ctrl Pts',(-44.6466303115269,1076.3191283065,338.323364153316));
#129174=CARTESIAN_POINT('Ctrl Pts',(-45.4151471578782,1076.3191283065,338.729722218484));
#129175=CARTESIAN_POINT('Ctrl Pts',(-42.7102740907138,1076.37497993555,
338.316316709769));
#129176=CARTESIAN_POINT('Ctrl Pts',(-43.4824899377986,1076.37497993555,
338.698472563673));
#129177=CARTESIAN_POINT('Ctrl Pts',(-44.2495074609481,1076.37497993555,
339.090957633891));
#129178=CARTESIAN_POINT('Ctrl Pts',(-45.0111885035979,1076.37497993555,
339.493701225312));
#129179=CARTESIAN_POINT('Ctrl Pts',(-42.3292778294105,1076.42476491624,
339.086189387768));
#129180=CARTESIAN_POINT('Ctrl Pts',(-43.0946051383877,1076.42476491624,
339.464936226988));
#129181=CARTESIAN_POINT('Ctrl Pts',(-43.8547804949884,1076.42476491624,
339.853920140925));
#129182=CARTESIAN_POINT('Ctrl Pts',(-44.6096669750714,1076.42476491624,
340.253071065104));
#129183=CARTESIAN_POINT('Origin',(0.,1082.7251047501,424.620242579854));
#129184=CARTESIAN_POINT('Ctrl Pts',(-48.9068694848042,1076.62734888474,
347.80506396164));
#129185=CARTESIAN_POINT('Ctrl Pts',(-49.7666339575146,1076.62734888474,
348.352460838284));
#129186=CARTESIAN_POINT('Ctrl Pts',(-50.6170879148582,1076.62734888474,
348.914213769326));
#129187=CARTESIAN_POINT('Ctrl Pts',(-51.4579916683211,1076.62734888474,
349.490164432584));
#129188=CARTESIAN_POINT('Ctrl Pts',(-48.3647367445688,1076.66214464411,
348.656560361116));
#129189=CARTESIAN_POINT('Ctrl Pts',(-49.2149707264819,1076.66214464411,
349.197889342353));
#129190=CARTESIAN_POINT('Ctrl Pts',(-50.0559974001086,1076.66214464411,
349.753415241098));
#129191=CARTESIAN_POINT('Ctrl Pts',(-50.8875797338825,1076.66214464411,
350.32298149017));
#129192=CARTESIAN_POINT('Ctrl Pts',(-47.8266401655489,1076.68821130439,
349.501717396655));
#129193=CARTESIAN_POINT('Ctrl Pts',(-48.6674146108693,1076.68821130439,
350.037023657776));
#129194=CARTESIAN_POINT('Ctrl Pts',(-49.4990841866101,1076.68821130439,
350.586368884283));
#129195=CARTESIAN_POINT('Ctrl Pts',(-50.3214144983718,1076.68821130439,
351.149598250933));
#129196=CARTESIAN_POINT('Ctrl Pts',(-47.2925818857626,1076.70555497619,
350.340531710195));
#129197=CARTESIAN_POINT('Ctrl Pts',(-48.1239677862803,1076.70555497619,
350.86986045042));
#129198=CARTESIAN_POINT('Ctrl Pts',(-48.9463504871448,1076.70555497619,
351.413071389307));
#129199=CARTESIAN_POINT('Ctrl Pts',(-49.759498211332,1076.70555497619,351.970011430476));
#129200=CARTESIAN_POINT('Origin',(0.,1082.7251047501,424.620242579854));
#129201=CARTESIAN_POINT('Ctrl Pts',(-3.52018246155676,1074.6501598088,311.586656837294));
#129202=CARTESIAN_POINT('Ctrl Pts',(-4.26598294102489,1074.6501598088,311.609883153175));
#129203=CARTESIAN_POINT('Ctrl Pts',(-5.0115170308526,1074.6501598088,311.64048932623));
#129204=CARTESIAN_POINT('Ctrl Pts',(-5.75671170754627,1074.6501598088,311.678472358649));
#129205=CARTESIAN_POINT('Ctrl Pts',(-3.49714761316157,1074.75376387604,
312.326309267126));
#129206=CARTESIAN_POINT('Ctrl Pts',(-4.23806783395981,1074.75376387604,
312.349383598083));
#129207=CARTESIAN_POINT('Ctrl Pts',(-4.97872340827869,1074.75376387604,
312.379789494998));
#129208=CARTESIAN_POINT('Ctrl Pts',(-5.71904179046491,1074.75376387604,
312.417523979677));
#129209=CARTESIAN_POINT('Ctrl Pts',(-3.47421575892244,1074.85349191521,
313.062654539192));
#129210=CARTESIAN_POINT('Ctrl Pts',(-4.21027754182053,1074.85349191521,
313.085577564784));
#129211=CARTESIAN_POINT('Ctrl Pts',(-4.94607641360625,1074.85349191521,
313.11578408104));
#129212=CARTESIAN_POINT('Ctrl Pts',(-5.68154030433007,1074.85349191521,
313.153271129294));
#129213=CARTESIAN_POINT('Ctrl Pts',(-3.45138693524003,1074.94934572131,
313.795691484659));
#129214=CARTESIAN_POINT('Ctrl Pts',(-4.18261210871973,1074.94934572131,
313.818463884687));
#129215=CARTESIAN_POINT('Ctrl Pts',(-4.9135760986572,1074.94934572131,313.848471916081));
#129216=CARTESIAN_POINT('Ctrl Pts',(-5.64420730866941,1074.94934572131,
313.885712639618));
#129217=CARTESIAN_POINT('Origin',(0.,1082.7251047501,424.620242579854));
#129218=CARTESIAN_POINT('Ctrl Pts',(-14.9526527161707,1075.53640608928,
319.691742708466));
#129219=CARTESIAN_POINT('Ctrl Pts',(-15.6983726462263,1075.53640608928,
319.798010225406));
#129220=CARTESIAN_POINT('Ctrl Pts',(-16.4429173934917,1075.53640608928,
319.912221076722));
#129221=CARTESIAN_POINT('Ctrl Pts',(-17.1862023488174,1075.53640608928,
320.034362283631));
#129222=CARTESIAN_POINT('Ctrl Pts',(-14.8472166832474,1075.61802125527,
320.431627796218));
#129223=CARTESIAN_POINT('Ctrl Pts',(-15.5876782987691,1075.61802125527,
320.537145986225));
#129224=CARTESIAN_POINT('Ctrl Pts',(-16.326973018098,1075.61802125527,320.650551499564));
#129225=CARTESIAN_POINT('Ctrl Pts',(-17.0650168286911,1075.61802125527,
320.771831448972));
#129226=CARTESIAN_POINT('Ctrl Pts',(-14.7422862420094,1075.69544934262,
321.167964953172));
#129227=CARTESIAN_POINT('Ctrl Pts',(-15.4775147579075,1075.69544934262,
321.272737409452));
#129228=CARTESIAN_POINT('Ctrl Pts',(-16.2115846244738,1075.69544934262,
321.385341446608));
#129229=CARTESIAN_POINT('Ctrl Pts',(-16.9444124229112,1075.69544934262,
321.505764268456));
#129230=CARTESIAN_POINT('Ctrl Pts',(-14.6378615781037,1075.76869237125,
321.900752876572));
#129231=CARTESIAN_POINT('Ctrl Pts',(-15.367882218547,1075.76869237125,322.00478319365));
#129232=CARTESIAN_POINT('Ctrl Pts',(-16.0967524167687,1075.76869237125,
322.116589617835));
#129233=CARTESIAN_POINT('Ctrl Pts',(-16.8243893448556,1075.76869237125,
322.236159443582));
#129234=CARTESIAN_POINT('Origin',(0.,1082.7251047501,424.620242579854));
#129235=CARTESIAN_POINT('Ctrl Pts',(-24.2635631860074,1076.2570261591,329.640295684007));
#129236=CARTESIAN_POINT('Ctrl Pts',(-25.1128615239931,1076.2570261591,329.857257311813));
#129237=CARTESIAN_POINT('Ctrl Pts',(-25.9591735823918,1076.2570261591,330.085590214949));
#129238=CARTESIAN_POINT('Ctrl Pts',(-26.8023471182513,1076.2570261591,330.325253318642));
#129239=CARTESIAN_POINT('Ctrl Pts',(-24.0482616346989,1076.31899119494,
330.483095636887));
#129240=CARTESIAN_POINT('Ctrl Pts',(-24.8900237650678,1076.31899119494,
330.698132066211));
#129241=CARTESIAN_POINT('Ctrl Pts',(-25.7288261144568,1076.31899119494,
330.924438868403));
#129242=CARTESIAN_POINT('Ctrl Pts',(-26.5645177908342,1076.31899119494,
331.161975333167));
#129243=CARTESIAN_POINT('Ctrl Pts',(-23.8342513036848,1076.37487987957,
331.320841095749));
#129244=CARTESIAN_POINT('Ctrl Pts',(-24.6685224230654,1076.37487987957,
331.533963872513));
#129245=CARTESIAN_POINT('Ctrl Pts',(-25.4998601011541,1076.37487987957,
331.758256724825));
#129246=CARTESIAN_POINT('Ctrl Pts',(-26.3281147887377,1076.37487987957,
331.993679304677));
#129247=CARTESIAN_POINT('Ctrl Pts',(-23.6215327638613,1076.42469575349,
332.153529825814));
#129248=CARTESIAN_POINT('Ctrl Pts',(-24.4483580888651,1076.42469575349,
332.364750501048));
#129249=CARTESIAN_POINT('Ctrl Pts',(-25.2722761532755,1076.42469575349,
332.587041559914));
#129250=CARTESIAN_POINT('Ctrl Pts',(-26.0931387425927,1076.42469575349,
332.820363014507));
#129251=CARTESIAN_POINT('Origin',(0.,1082.7251047501,424.620242579854));
#129252=CARTESIAN_POINT('Ctrl Pts',(-31.8715411090461,1076.62737351001,
339.317673442166));
#129253=CARTESIAN_POINT('Ctrl Pts',(-32.8252407714822,1076.62737351001,
339.67400360085));
#129254=CARTESIAN_POINT('Ctrl Pts',(-33.7728311362533,1076.62737351001,
340.046275985955));
#129255=CARTESIAN_POINT('Ctrl Pts',(-34.7140457315322,1076.62737351001,
340.434385910786));
#129256=CARTESIAN_POINT('Ctrl Pts',(-31.5180618270612,1076.66218303982,
340.263742877186));
#129257=CARTESIAN_POINT('Ctrl Pts',(-32.4611842453422,1076.66218303982,
340.616121067303));
#129258=CARTESIAN_POINT('Ctrl Pts',(-33.398265122649,1076.66218303982,340.9842646726));
#129259=CARTESIAN_POINT('Ctrl Pts',(-34.3290409425265,1076.66218303982,
341.368070167436));
#129260=CARTESIAN_POINT('Ctrl Pts',(-31.1672155499358,1076.68825449303,
341.20276520776));
#129261=CARTESIAN_POINT('Ctrl Pts',(-32.099839512089,1076.68825449303,341.551220866827));
#129262=CARTESIAN_POINT('Ctrl Pts',(-33.0264891852509,1076.68825449303,
341.915266446869));
#129263=CARTESIAN_POINT('Ctrl Pts',(-33.9469039863248,1076.68825449303,
342.294799574649));
#129264=CARTESIAN_POINT('Ctrl Pts',(-30.8190036731312,1076.7055939897,342.134736699005));
#129265=CARTESIAN_POINT('Ctrl Pts',(-31.7412080089404,1076.7055939897,342.479299280142));
#129266=CARTESIAN_POINT('Ctrl Pts',(-32.6575048027661,1076.7055939897,342.83927760578));
#129267=CARTESIAN_POINT('Ctrl Pts',(-33.5676363828443,1076.7055939897,343.214570446438));
#129268=CARTESIAN_POINT('Origin',(0.,1082.7251047501,424.620242579854));
#129269=CARTESIAN_POINT('Ctrl Pts',(20.0601507246982,1074.64981245085,313.322737267786));
#129270=CARTESIAN_POINT('Ctrl Pts',(19.3253404299007,1074.64981245085,313.190295797275));
#129271=CARTESIAN_POINT('Ctrl Pts',(18.5892545990681,1074.64981245085,313.065137648924));
#129272=CARTESIAN_POINT('Ctrl Pts',(17.8519654215009,1074.64981245085,312.947275097222));
#129273=CARTESIAN_POINT('Ctrl Pts',(19.9285675901508,1074.75367623909,314.052785352531));
#129274=CARTESIAN_POINT('Ctrl Pts',(19.1985772313156,1074.75367623909,313.921212622444));
#129275=CARTESIAN_POINT('Ctrl Pts',(18.4673197032334,1074.75367623909,313.796875440081));
#129276=CARTESIAN_POINT('Ctrl Pts',(17.734866721684,1074.75367623909,313.67978599942));
#129277=CARTESIAN_POINT('Ctrl Pts',(19.7975742137943,1074.85364519094,314.779561347436));
#129278=CARTESIAN_POINT('Ctrl Pts',(19.0723821878739,1074.85364519094,314.648853464061));
#129279=CARTESIAN_POINT('Ctrl Pts',(18.3459313219943,1074.85364519094,314.525333568101));
#129280=CARTESIAN_POINT('Ctrl Pts',(17.6182928605373,1074.85364519094,314.409013773381));
#129281=CARTESIAN_POINT('Ctrl Pts',(19.667170804569,1074.94972111449,315.50306409326));
#129282=CARTESIAN_POINT('Ctrl Pts',(18.9467555008622,1074.94972111449,315.373217161506));
#129283=CARTESIAN_POINT('Ctrl Pts',(18.2250896489708,1074.94972111449,315.25051087106));
#129284=CARTESIAN_POINT('Ctrl Pts',(17.5022440240014,1074.94972111449,315.134957255955));
#129285=CARTESIAN_POINT('Origin',(0.,1082.7251047501,424.620242579854));
#129286=CARTESIAN_POINT('Ctrl Pts',(7.18925503840259,1075.53658218756,318.877419242361));
#129287=CARTESIAN_POINT('Ctrl Pts',(6.43791533520909,1075.53658218756,318.826337073603));
#129288=CARTESIAN_POINT('Ctrl Pts',(5.68607388927085,1075.53658218756,318.783265299441));
#129289=CARTESIAN_POINT('Ctrl Pts',(4.93381610082962,1075.53658218756,318.748208812317));
#129290=CARTESIAN_POINT('Ctrl Pts',(7.13853586903372,1075.61823151961,319.623419785915));
#129291=CARTESIAN_POINT('Ctrl Pts',(6.39249676033246,1075.61823151961,319.572697994575));
#129292=CARTESIAN_POINT('Ctrl Pts',(5.64595944860998,1075.61823151961,319.529930085639));
#129293=CARTESIAN_POINT('Ctrl Pts',(4.89900873162153,1075.61823151961,319.495120917034));
#129294=CARTESIAN_POINT('Ctrl Pts',(7.08806003205873,1075.69568964953,320.365841286272));
#129295=CARTESIAN_POINT('Ctrl Pts',(6.34729608749738,1075.69568964953,320.315478143388));
#129296=CARTESIAN_POINT('Ctrl Pts',(5.60603746265602,1075.69568964953,320.273012641843));
#129297=CARTESIAN_POINT('Ctrl Pts',(4.86436835569387,1075.69568964953,320.23844960521));
#129298=CARTESIAN_POINT('Ctrl Pts',(7.03782761687019,1075.76895860023,321.104682428605));
#129299=CARTESIAN_POINT('Ctrl Pts',(6.30231339675412,1075.76895860023,321.054676204581));
#129300=CARTESIAN_POINT('Ctrl Pts',(5.56630800211068,1075.76895860023,321.012511652053));
#129301=CARTESIAN_POINT('Ctrl Pts',(4.82989503439467,1075.76895860023,320.978193560413));
#129302=CARTESIAN_POINT('Origin',(0.,1082.7251047501,424.620242579854));
#129303=CARTESIAN_POINT('Ctrl Pts',(-3.98735671405646,1076.25744174455,
326.677056081815));
#129304=CARTESIAN_POINT('Ctrl Pts',(-4.86288710452009,1076.25744174455,
326.712699724886));
#129305=CARTESIAN_POINT('Ctrl Pts',(-5.73786088507023,1076.25744174455,
326.760079227486));
#129306=CARTESIAN_POINT('Ctrl Pts',(-6.61212075197863,1076.25744174455,
326.819186071675));
#129307=CARTESIAN_POINT('Ctrl Pts',(-3.95209372041479,1076.31916993005,
327.543236413901));
#129308=CARTESIAN_POINT('Ctrl Pts',(-4.81988118121196,1076.31916993005,
327.578564835223));
#129309=CARTESIAN_POINT('Ctrl Pts',(-5.68711695458773,1076.31916993005,
327.625525327631));
#129310=CARTESIAN_POINT('Ctrl Pts',(-6.5536451279611,1076.31916993005,327.684109448517));
#129311=CARTESIAN_POINT('Ctrl Pts',(-3.91704149820492,1076.37486284266,
328.404239475144));
#129312=CARTESIAN_POINT('Ctrl Pts',(-4.77713230981848,1076.37486284266,
328.439254558837));
#129313=CARTESIAN_POINT('Ctrl Pts',(-5.63667632708034,1076.37486284266,
328.485798545532));
#129314=CARTESIAN_POINT('Ctrl Pts',(-6.49551902024172,1076.37486284266,
328.5438630675));
#129315=CARTESIAN_POINT('Ctrl Pts',(-3.88220014030112,1076.42452398704,
329.260062984234));
#129316=CARTESIAN_POINT('Ctrl Pts',(-4.73464060360691,1076.42452398704,
329.29476661525));
#129317=CARTESIAN_POINT('Ctrl Pts',(-5.5865391361954,1076.42452398704,329.340896601812));
#129318=CARTESIAN_POINT('Ctrl Pts',(-6.43774258283125,1076.42452398704,
329.398444650623));
#129319=CARTESIAN_POINT('Origin',(0.,1082.7251047501,424.620242579854));
#129320=CARTESIAN_POINT('Ctrl Pts',(-13.4363545933944,1076.62739445405,
334.555392974316));
#129321=CARTESIAN_POINT('Ctrl Pts',(-14.4438874283289,1076.62739445405,
334.705702095954));
#129322=CARTESIAN_POINT('Ctrl Pts',(-15.4487564642742,1076.62739445405,
334.872894996872));
#129323=CARTESIAN_POINT('Ctrl Pts',(-16.4506787909077,1076.62739445405,
335.056924605664));
#129324=CARTESIAN_POINT('Ctrl Pts',(-13.2875689926388,1076.6621457791,335.552713539383));
#129325=CARTESIAN_POINT('Ctrl Pts',(-14.2839450530862,1076.6621457791,335.701358233903));
#129326=CARTESIAN_POINT('Ctrl Pts',(-15.2776868117514,1076.6621457791,335.866699747524));
#129327=CARTESIAN_POINT('Ctrl Pts',(-16.2685144910799,1076.6621457791,336.04869153008));
#129328=CARTESIAN_POINT('Ctrl Pts',(-13.1398899312993,1076.68818647194,
336.542616891292));
#129329=CARTESIAN_POINT('Ctrl Pts',(-14.125192191759,1076.68818647194,336.68960953727));
#129330=CARTESIAN_POINT('Ctrl Pts',(-15.1078894282686,1076.68818647194,
336.853113432622));
#129331=CARTESIAN_POINT('Ctrl Pts',(-16.0877049727428,1076.68818647194,
337.033082544543));
#129332=CARTESIAN_POINT('Ctrl Pts',(-12.993317994907,1076.70552262381,337.525099105185));
#129333=CARTESIAN_POINT('Ctrl Pts',(-13.9676294737846,1076.70552262381,
337.670452087752));
#129334=CARTESIAN_POINT('Ctrl Pts',(-14.9393649870532,1076.70552262381,
337.832132141148));
#129335=CARTESIAN_POINT('Ctrl Pts',(-15.9082509527858,1076.70552262381,
338.010093746053));
#129336=CARTESIAN_POINT('Origin',(0.,1082.7251047501,424.620242579854));
#129337=CARTESIAN_POINT('Ctrl Pts',(42.762254864373,1074.64941228744,319.922676659465));
#129338=CARTESIAN_POINT('Ctrl Pts',(42.0709027679261,1074.64941228744,319.640303575722));
#129339=CARTESIAN_POINT('Ctrl Pts',(41.3767877733801,1074.64941228744,319.364791953408));
#129340=CARTESIAN_POINT('Ctrl Pts',(40.6799779767329,1074.64941228744,319.096168821529));
#129341=CARTESIAN_POINT('Ctrl Pts',(42.4815009844214,1074.75338301753,320.61006435562));
#129342=CARTESIAN_POINT('Ctrl Pts',(41.7946879326087,1074.75338301753,320.329545181104));
#129343=CARTESIAN_POINT('Ctrl Pts',(41.1051301223943,1074.75338301753,320.055842419366));
#129344=CARTESIAN_POINT('Ctrl Pts',(40.4128952026945,1074.75338301753,319.788982921953));
#129345=CARTESIAN_POINT('Ctrl Pts',(42.2020066081244,1074.85345163594,321.294368328354));
#129346=CARTESIAN_POINT('Ctrl Pts',(41.5197122381168,1074.85345163594,321.015694746152));
#129347=CARTESIAN_POINT('Ctrl Pts',(40.8346911680273,1074.85345163594,320.743792730171));
#129348=CARTESIAN_POINT('Ctrl Pts',(40.1470106016967,1074.85345163594,320.478688955298));
#129349=CARTESIAN_POINT('Ctrl Pts',(41.9237721821172,1074.94961995582,321.97558748414));
#129350=CARTESIAN_POINT('Ctrl Pts',(41.2459761238645,1074.94961995582,321.698751174391));
#129351=CARTESIAN_POINT('Ctrl Pts',(40.5654713424437,1074.94961995582,321.428641786473));
#129352=CARTESIAN_POINT('Ctrl Pts',(39.8823245986259,1074.94961995582,321.165285819407));
#129353=CARTESIAN_POINT('Origin',(0.,1082.7251047501,424.620242579854));
#129354=CARTESIAN_POINT('Ctrl Pts',(29.0176251705041,1075.53651526506,322.682332980308));
#129355=CARTESIAN_POINT('Ctrl Pts',(28.2930779591799,1075.53651526506,322.476083514538));
#129356=CARTESIAN_POINT('Ctrl Pts',(27.5663730602314,1075.53651526506,322.27757030739));
#129357=CARTESIAN_POINT('Ctrl Pts',(26.8375930740242,1075.53651526506,322.086815922718));
#129358=CARTESIAN_POINT('Ctrl Pts',(28.8127959863172,1075.61821260512,323.401890791752));
#129359=CARTESIAN_POINT('Ctrl Pts',(28.0933631981523,1075.61821260512,323.197097196667));
#129360=CARTESIAN_POINT('Ctrl Pts',(27.3717879530167,1075.61821260512,322.999985251615));
#129361=CARTESIAN_POINT('Ctrl Pts',(26.6481522682177,1075.61821260512,322.810577361177));
#129362=CARTESIAN_POINT('Ctrl Pts',(28.6089500466826,1075.69571404777,324.117994499226));
#129363=CARTESIAN_POINT('Ctrl Pts',(27.8946071308361,1075.69571404777,323.914649786188));
#129364=CARTESIAN_POINT('Ctrl Pts',(27.1781369155606,1075.69571404777,323.718932376733));
#129365=CARTESIAN_POINT('Ctrl Pts',(26.4596208379039,1075.69571404777,323.530864516934));
#129366=CARTESIAN_POINT('Ctrl Pts',(28.4060877130153,1075.7690216193,324.830642833093));
#129367=CARTESIAN_POINT('Ctrl Pts',(27.6968101096221,1075.7690216193,324.628740010895));
#129368=CARTESIAN_POINT('Ctrl Pts',(26.9854202912027,1075.7690216193,324.434410408066));
#129369=CARTESIAN_POINT('Ctrl Pts',(26.2719991173455,1075.7690216193,324.247676112933));
#129370=CARTESIAN_POINT('Origin',(0.,1082.7251047501,424.620242579854));
#129371=CARTESIAN_POINT('Ctrl Pts',(16.464705126852,1076.25721586291,327.98535171322));
#129372=CARTESIAN_POINT('Ctrl Pts',(15.6016647874419,1076.25721586291,327.838306432023));
#129373=CARTESIAN_POINT('Ctrl Pts',(14.7367321236006,1076.25721586291,327.702835294166));
#129374=CARTESIAN_POINT('Ctrl Pts',(13.8700623477992,1076.25721586291,327.578962609995));
#129375=CARTESIAN_POINT('Ctrl Pts',(16.3187044751784,1076.31912596814,328.842260897578));
#129376=CARTESIAN_POINT('Ctrl Pts',(15.4633171396334,1076.31912596814,328.69651953933));
#129377=CARTESIAN_POINT('Ctrl Pts',(14.6060542598303,1076.31912596814,328.562249690793));
#129378=CARTESIAN_POINT('Ctrl Pts',(13.7470696718946,1076.31912596814,328.439475446738));
#129379=CARTESIAN_POINT('Ctrl Pts',(16.1735788380354,1076.37496806519,329.694034433709));
#129380=CARTESIAN_POINT('Ctrl Pts',(15.3257986401933,1076.37496806519,329.54958918371));
#129381=CARTESIAN_POINT('Ctrl Pts',(14.4761595776988,1076.37496806519,329.416513424896));
#129382=CARTESIAN_POINT('Ctrl Pts',(13.6248141185805,1076.37496806519,329.29483103776));
#129383=CARTESIAN_POINT('Ctrl Pts',(16.0293286020337,1076.42474568726,330.540670052514));
#129384=CARTESIAN_POINT('Ctrl Pts',(15.189109655467,1076.42474568726,330.397513092609));
#129385=CARTESIAN_POINT('Ctrl Pts',(14.3470484232417,1076.42474568726,330.265624220743));
#129386=CARTESIAN_POINT('Ctrl Pts',(13.5032960135423,1076.42474568726,330.14502710442));
#129387=CARTESIAN_POINT('Origin',(0.,1082.7251047501,424.620242579854));
#129388=CARTESIAN_POINT('Ctrl Pts',(5.58142985825276,1076.62751743038,333.733442928555));
#129389=CARTESIAN_POINT('Ctrl Pts',(4.56395251573579,1076.62751743038,333.670958844602));
#129390=CARTESIAN_POINT('Ctrl Pts',(3.5455694495139,1076.62751743038,333.625567945566));
#129391=CARTESIAN_POINT('Ctrl Pts',(2.52656779749708,1076.62751743038,333.597283029625));
#129392=CARTESIAN_POINT('Ctrl Pts',(5.51963911911433,1076.66223932963,334.739629993698));
#129393=CARTESIAN_POINT('Ctrl Pts',(4.51342603658942,1076.66223932963,334.677837656812));
#129394=CARTESIAN_POINT('Ctrl Pts',(3.50631725742049,1076.66223932963,334.632949270084));
#129395=CARTESIAN_POINT('Ctrl Pts',(2.49859674067911,1076.66223932963,334.604977490007));
#129396=CARTESIAN_POINT('Ctrl Pts',(5.45830781737085,1076.68825505249,335.738335679423));
#129397=CARTESIAN_POINT('Ctrl Pts',(4.46327524082663,1076.68825505249,335.677229946204));
#129398=CARTESIAN_POINT('Ctrl Pts',(3.46735692014434,1076.68825505249,335.632840335416));
#129399=CARTESIAN_POINT('Ctrl Pts',(2.470833659193,1076.68825505249,335.605179362921));
#129400=CARTESIAN_POINT('Ctrl Pts',(5.39743619607369,1076.70557068555,336.729556027934));
#129401=CARTESIAN_POINT('Ctrl Pts',(4.41350032719132,1076.70557068555,336.669131752261));
#129402=CARTESIAN_POINT('Ctrl Pts',(3.42868859208241,1076.70557068555,336.625237179069));
#129403=CARTESIAN_POINT('Ctrl Pts',(2.44327866306178,1076.70557068555,336.59788468464));
#129404=CARTESIAN_POINT('Origin',(0.,1082.7251047501,424.620242579854));
#129405=CARTESIAN_POINT('Ctrl Pts',(63.5947113611256,1074.64992056935,331.105097475553));
#129406=CARTESIAN_POINT('Ctrl Pts',(62.9766859027927,1074.64992056935,330.684811001178));
#129407=CARTESIAN_POINT('Ctrl Pts',(62.3545245459131,1074.64992056935,330.270671611968));
#129408=CARTESIAN_POINT('Ctrl Pts',(61.7282884292425,1074.64992056935,329.862720004706));
#129409=CARTESIAN_POINT('Ctrl Pts',(63.1774566783766,1074.7538085787,331.718664726155));
#129410=CARTESIAN_POINT('Ctrl Pts',(62.5634861801343,1074.7538085787,331.301135815984));
#129411=CARTESIAN_POINT('Ctrl Pts',(61.9454069196119,1074.7538085787,330.889713659005));
#129412=CARTESIAN_POINT('Ctrl Pts',(61.3232796344242,1074.7538085787,330.484438684985));
#129413=CARTESIAN_POINT('Ctrl Pts',(62.7620726301513,1074.85379973269,332.329481234516));
#129414=CARTESIAN_POINT('Ctrl Pts',(62.1521389128188,1074.85379973269,331.914697525846));
#129415=CARTESIAN_POINT('Ctrl Pts',(61.5381234478156,1074.85379973269,331.505980419214));
#129416=CARTESIAN_POINT('Ctrl Pts',(60.920086573414,1074.85379973269,331.103370078565));
#129417=CARTESIAN_POINT('Ctrl Pts',(62.3485598793522,1074.94989584082,332.937546025845));
#129418=CARTESIAN_POINT('Ctrl Pts',(61.7426447573065,1074.94989584082,332.525495151596));
#129419=CARTESIAN_POINT('Ctrl Pts',(61.132674780499,1074.94989584082,332.119470909108));
#129420=CARTESIAN_POINT('Ctrl Pts',(60.5187098896588,1074.94989584082,331.719513197707));
#129421=CARTESIAN_POINT('Origin',(0.,1082.7251047501,424.620242579854));
#129422=CARTESIAN_POINT('Ctrl Pts',(49.5794614304066,1075.53619414421,330.940680740174));
#129423=CARTESIAN_POINT('Ctrl Pts',(48.9146671134995,1075.53619414421,330.588841517755));
#129424=CARTESIAN_POINT('Ctrl Pts',(48.2461653747274,1075.53619414421,330.244098501171));
#129425=CARTESIAN_POINT('Ctrl Pts',(47.5740319583019,1075.53619414421,329.906490751336));
#129426=CARTESIAN_POINT('Ctrl Pts',(49.2289544664351,1075.61802890567,331.602957777061));
#129427=CARTESIAN_POINT('Ctrl Pts',(48.568859979477,1075.61802890567,331.253605917234));
#129428=CARTESIAN_POINT('Ctrl Pts',(47.9050842806437,1075.61802890567,330.911300095904));
#129429=CARTESIAN_POINT('Ctrl Pts',(47.2377025786657,1075.61802890567,330.576079097841));
#129430=CARTESIAN_POINT('Ctrl Pts',(48.8801326275998,1075.6956547724,332.262050798233));
#129431=CARTESIAN_POINT('Ctrl Pts',(48.2247153753147,1075.6956547724,331.915174342554));
#129432=CARTESIAN_POINT('Ctrl Pts',(47.565642995135,1075.6956547724,331.575293999225));
#129433=CARTESIAN_POINT('Ctrl Pts',(46.9029901628844,1075.6956547724,331.242448278195));
#129434=CARTESIAN_POINT('Ctrl Pts',(48.5329965342673,1075.76907378011,332.917958631515));
#129435=CARTESIAN_POINT('Ctrl Pts',(47.8822339130609,1075.76907378011,332.573545617141));
#129436=CARTESIAN_POINT('Ctrl Pts',(47.227842121885,1075.76907378011,332.236079030245));
#129437=CARTESIAN_POINT('Ctrl Pts',(46.5698953062317,1075.76907378011,331.905597107288));
#129438=CARTESIAN_POINT('Origin',(0.,1082.7251047501,424.620242579854));
#129439=CARTESIAN_POINT('Ctrl Pts',(36.19552153342,1076.25694505369,333.515806627299));
#129440=CARTESIAN_POINT('Ctrl Pts',(35.3812836960972,1076.25694505369,333.192312355412));
#129441=CARTESIAN_POINT('Ctrl Pts',(34.5627824799597,1076.25694505369,332.879762265261));
#129442=CARTESIAN_POINT('Ctrl Pts',(33.7401649782897,1076.25694505369,332.578212525388));
#129443=CARTESIAN_POINT('Ctrl Pts',(35.874500582732,1076.31888525212,334.3238190941));
#129444=CARTESIAN_POINT('Ctrl Pts',(35.0674842853553,1076.31888525212,334.003193918563));
#129445=CARTESIAN_POINT('Ctrl Pts',(34.2562424214086,1076.31888525212,333.693415859946));
#129446=CARTESIAN_POINT('Ctrl Pts',(33.4409207795923,1076.31888525212,333.394540588628));
#129447=CARTESIAN_POINT('Ctrl Pts',(35.5554039327238,1076.37475500685,335.126988079703));
#129448=CARTESIAN_POINT('Ctrl Pts',(34.7555658871084,1076.37475500685,334.809214802248));
#129449=CARTESIAN_POINT('Ctrl Pts',(33.9515398605094,1076.37475500685,334.502192158735));
#129450=CARTESIAN_POINT('Ctrl Pts',(33.143470344865,1076.37475500685,334.205975324365));
#129451=CARTESIAN_POINT('Ctrl Pts',(35.2382324337861,1076.4245578532,335.925311443665));
#129452=CARTESIAN_POINT('Ctrl Pts',(34.4455293326173,1076.4245578532,335.610372858426));
#129453=CARTESIAN_POINT('Ctrl Pts',(33.6486756092925,1076.4245578532,335.306089006244));
#129454=CARTESIAN_POINT('Ctrl Pts',(32.8478144668115,1076.4245578532,335.01251457013));
#129455=CARTESIAN_POINT('Origin',(0.,1082.7251047501,424.620242579854));
#129456=CARTESIAN_POINT('Ctrl Pts',(24.3576856453425,1076.62752897425,336.880828280042));
#129457=CARTESIAN_POINT('Ctrl Pts',(23.3746783538014,1076.62752897426,336.607931739924));
#129458=CARTESIAN_POINT('Ctrl Pts',(22.3872241095125,1076.62752897426,336.351592175542));
#129459=CARTESIAN_POINT('Ctrl Pts',(21.3956017636078,1076.62752897425,336.111881975646));
#129460=CARTESIAN_POINT('Ctrl Pts',(24.0878033771608,1076.66227769843,337.852977789029));
#129461=CARTESIAN_POINT('Ctrl Pts',(23.1156877705418,1076.66227769843,337.583104932618));
#129462=CARTESIAN_POINT('Ctrl Pts',(22.1391744832491,1076.66227769843,337.329605601256));
#129463=CARTESIAN_POINT('Ctrl Pts',(21.1585392767545,1076.66227769843,337.092551381628));
#129464=CARTESIAN_POINT('Ctrl Pts',(23.8199294505212,1076.68830582022,338.817893001901));
#129465=CARTESIAN_POINT('Ctrl Pts',(22.8586244778407,1076.68830582022,338.551021328313));
#129466=CARTESIAN_POINT('Ctrl Pts',(21.8929707299003,1076.68830582022,338.300341094244));
#129467=CARTESIAN_POINT('Ctrl Pts',(20.9232409015031,1076.68830582022,338.065923090283));
#129468=CARTESIAN_POINT('Ctrl Pts',(23.5540649287557,1076.70561944135,339.775570088405));
#129469=CARTESIAN_POINT('Ctrl Pts',(22.603489496117,1076.70561944135,339.511677084842));
#129470=CARTESIAN_POINT('Ctrl Pts',(21.6486138267775,1076.70561944135,339.263794801149));
#129471=CARTESIAN_POINT('Ctrl Pts',(20.689707571876,1076.70561944135,339.031993237788));
#129472=CARTESIAN_POINT('Origin',(0.,1082.7251047501,424.620242579854));
#129473=CARTESIAN_POINT('Ctrl Pts',(81.6513798708841,1074.64930297342,346.367961510039));
#129474=CARTESIAN_POINT('Ctrl Pts',(81.1354496615202,1074.64930297342,345.829620481053));
#129475=CARTESIAN_POINT('Ctrl Pts',(80.6142207985842,1074.64930297342,345.296408031023));
#129476=CARTESIAN_POINT('Ctrl Pts',(80.0877442598867,1074.64930297342,344.768376309793));
#129477=CARTESIAN_POINT('Ctrl Pts',(81.1145207771131,1074.75342815374,346.882471476277));
#129478=CARTESIAN_POINT('Ctrl Pts',(80.6019828169075,1074.75342815374,346.347670047937));
#129479=CARTESIAN_POINT('Ctrl Pts',(80.0841810418596,1074.75342815374,345.817963478067));
#129480=CARTESIAN_POINT('Ctrl Pts',(79.5611660946002,1074.75342815374,345.293403573624));
#129481=CARTESIAN_POINT('Ctrl Pts',(80.580073619499,1074.85363982574,347.394669913838));
#129482=CARTESIAN_POINT('Ctrl Pts',(80.0709126681616,1074.85363982574,346.863392183851));
#129483=CARTESIAN_POINT('Ctrl Pts',(79.5565225841924,1074.85363982574,346.337175743343));
#129484=CARTESIAN_POINT('Ctrl Pts',(79.0369536765479,1074.85363982574,345.816072057925));
#129485=CARTESIAN_POINT('Ctrl Pts',(80.0480392545915,1074.9499398105,347.90455600183));
#129486=CARTESIAN_POINT('Ctrl Pts',(79.5422400664198,1074.9499398105,347.376786062256));
#129487=CARTESIAN_POINT('Ctrl Pts',(79.0312462712518,1074.9499398105,346.854043994718));
#129488=CARTESIAN_POINT('Ctrl Pts',(78.5151078458766,1074.9499398105,346.336380925024));
#129489=CARTESIAN_POINT('Origin',(0.,1082.7251047501,424.620242579854));
#129490=CARTESIAN_POINT('Ctrl Pts',(67.9699229048373,1075.5361780923,343.293100500072));
#129491=CARTESIAN_POINT('Ctrl Pts',(67.3926691025201,1075.5361780923,342.810655212599));
#129492=CARTESIAN_POINT('Ctrl Pts',(66.8103116710274,1075.5361780923,342.334382990357));
#129493=CARTESIAN_POINT('Ctrl Pts',(66.2229166210398,1075.5361780923,341.864337819182));
#129494=CARTESIAN_POINT('Ctrl Pts',(67.490436446628,1075.61783741877,343.866814014015));
#129495=CARTESIAN_POINT('Ctrl Pts',(66.9172548187275,1075.61783741877,343.387772084561));
#129496=CARTESIAN_POINT('Ctrl Pts',(66.3390055646507,1075.61783741877,342.914859673117));
#129497=CARTESIAN_POINT('Ctrl Pts',(65.755754229413,1075.61783741877,342.448130384685));
#129498=CARTESIAN_POINT('Ctrl Pts',(67.013250246792,1075.69530593322,344.437775230594));
#129499=CARTESIAN_POINT('Ctrl Pts',(66.4441212577132,1075.69530593322,343.962120332102));
#129500=CARTESIAN_POINT('Ctrl Pts',(65.8699604727387,1075.69530593322,343.492551613311));
#129501=CARTESIAN_POINT('Ctrl Pts',(65.2908329734526,1075.69530593322,343.029122300212));
#129502=CARTESIAN_POINT('Ctrl Pts',(66.538365150332,1075.76858565825,345.005983138752));
#129503=CARTESIAN_POINT('Ctrl Pts',(65.9732692573033,1075.76858565825,344.533698938167));
#129504=CARTESIAN_POINT('Ctrl Pts',(65.4031772258775,1075.76858565825,344.067457787961));
#129505=CARTESIAN_POINT('Ctrl Pts',(64.8281536764424,1075.76858565825,343.607312536943));
#129506=CARTESIAN_POINT('Origin',(0.,1082.7251047501,424.620242579854));
#129507=CARTESIAN_POINT('Ctrl Pts',(54.3457421654589,1076.25743101328,343.039995893921));
#129508=CARTESIAN_POINT('Ctrl Pts',(53.6154830488532,1076.25743101328,342.553524287408));
#129509=CARTESIAN_POINT('Ctrl Pts',(52.8787582301574,1076.25743101328,342.076901225811));
#129510=CARTESIAN_POINT('Ctrl Pts',(52.1357005219295,1076.25743101328,341.610212632023));
#129511=CARTESIAN_POINT('Ctrl Pts',(53.8641626587902,1076.31928350271,343.762911312637));
#129512=CARTESIAN_POINT('Ctrl Pts',(53.1403746622963,1076.31928350271,343.280750526934));
#129513=CARTESIAN_POINT('Ctrl Pts',(52.4101782589021,1076.31928350271,342.808351014224));
#129514=CARTESIAN_POINT('Ctrl Pts',(51.6737050842604,1076.31928350271,342.345797936003));
#129515=CARTESIAN_POINT('Ctrl Pts',(53.3854673762382,1076.37507652506,344.481497124182));
#129516=CARTESIAN_POINT('Ctrl Pts',(52.6681117437203,1076.37507652506,344.003621341385));
#129517=CARTESIAN_POINT('Ctrl Pts',(51.9444046563461,1076.37507652506,343.535420082339));
#129518=CARTESIAN_POINT('Ctrl Pts',(51.2144765799112,1076.37507652506,343.076977751702));
#129519=CARTESIAN_POINT('Ctrl Pts',(52.9096575912514,1076.42481360611,345.19575141694));
#129520=CARTESIAN_POINT('Ctrl Pts',(52.1986955494624,1076.42481360611,344.722134807747));
#129521=CARTESIAN_POINT('Ctrl Pts',(51.4814386615631,1076.42481360611,344.258106495972));
#129522=CARTESIAN_POINT('Ctrl Pts',(50.7580162305439,1076.42481360611,343.803750133997));
#129523=CARTESIAN_POINT('Origin',(0.,1082.7251047501,424.620242579854));
#129524=CARTESIAN_POINT('Ctrl Pts',(42.0705803179982,1076.6273260991,343.857378571533));
#129525=CARTESIAN_POINT('Ctrl Pts',(41.1680830520137,1076.6273260991,343.387254286299));
#129526=CARTESIAN_POINT('Ctrl Pts',(40.2578330776796,1076.6273260991,342.932322266211));
#129527=CARTESIAN_POINT('Ctrl Pts',(39.3400861126556,1076.6273260991,342.492710315889));
#129528=CARTESIAN_POINT('Ctrl Pts',(41.6034762298823,1076.66218189567,344.754077967193));
#129529=CARTESIAN_POINT('Ctrl Pts',(40.7109992716585,1076.66218189567,344.289173409709));
#129530=CARTESIAN_POINT('Ctrl Pts',(39.8108556823802,1076.66218189567,343.839292439662));
#129531=CARTESIAN_POINT('Ctrl Pts',(38.9032983405081,1076.66218189567,343.404561442672));
#129532=CARTESIAN_POINT('Ctrl Pts',(41.1398553241158,1076.68828036131,345.644090700101));
#129533=CARTESIAN_POINT('Ctrl Pts',(40.257323952493,1076.68828036131,345.184366947001));
#129534=CARTESIAN_POINT('Ctrl Pts',(39.367211385235,1076.68828036131,344.739499361452));
#129535=CARTESIAN_POINT('Ctrl Pts',(38.4697676827748,1076.68828036131,344.309612920659));
#129536=CARTESIAN_POINT('Ctrl Pts',(40.6797194487766,1076.70562763633,346.527413222502));
#129537=CARTESIAN_POINT('Ctrl Pts',(39.8070589029502,1076.70562763633,346.072831329768));
#129538=CARTESIAN_POINT('Ctrl Pts',(38.9269019546913,1076.70562763633,345.632939443192));
#129539=CARTESIAN_POINT('Ctrl Pts',(38.0394958675885,1076.70562763633,345.20786114215));
#129540=CARTESIAN_POINT('Origin',(0.,1082.7251047501,424.620242579854));
#129541=CARTESIAN_POINT('Ctrl Pts',(96.1331826317623,1074.64932100267,365.048861852279));
#129542=CARTESIAN_POINT('Ctrl Pts',(95.7405047741856,1074.64932100267,364.415178836427));
#129543=CARTESIAN_POINT('Ctrl Pts',(95.3415807234807,1074.64932100267,363.78540930225));
#129544=CARTESIAN_POINT('Ctrl Pts',(94.9364494785642,1074.64932100267,363.159614816175));
#129545=CARTESIAN_POINT('Ctrl Pts',(95.5028901751477,1074.75315166316,365.439438663269));
#129546=CARTESIAN_POINT('Ctrl Pts',(95.1127868905201,1074.75315166316,364.809910358766));
#129547=CARTESIAN_POINT('Ctrl Pts',(94.7164783656206,1074.75315166316,364.184269877387));
#129548=CARTESIAN_POINT('Ctrl Pts',(94.3140033436712,1074.75315166316,363.562578381905));
#129549=CARTESIAN_POINT('Ctrl Pts',(94.8754214251531,1074.8530908892,365.828265692369));
#129550=CARTESIAN_POINT('Ctrl Pts',(94.4878811794024,1074.8530908892,365.20287348613));
#129551=CARTESIAN_POINT('Ctrl Pts',(94.0941764627675,1074.8530908892,364.581343559416));
#129552=CARTESIAN_POINT('Ctrl Pts',(93.6943457639214,1074.8530908892,363.963736673152));
#129553=CARTESIAN_POINT('Ctrl Pts',(94.2507773817279,1074.94914048649,366.215342319933));
#129554=CARTESIAN_POINT('Ctrl Pts',(93.8657886366974,1074.94914048649,365.594067592284));
#129555=CARTESIAN_POINT('Ctrl Pts',(93.4746760066368,1074.94914048649,364.976629715552));
#129556=CARTESIAN_POINT('Ctrl Pts',(93.0774777268163,1074.94914048649,364.363089050622));
#129557=CARTESIAN_POINT('Origin',(0.,1082.7251047501,424.620242579854));
#129558=CARTESIAN_POINT('Ctrl Pts',(83.3922632669072,1075.53677429,359.209329248305));
#129559=CARTESIAN_POINT('Ctrl Pts',(82.9269536714695,1075.53677429,358.616106828574));
#129560=CARTESIAN_POINT('Ctrl Pts',(82.4553408499488,1075.53677429,358.027883056991));
#129561=CARTESIAN_POINT('Ctrl Pts',(81.9774784970065,1075.53677429,357.444724904756));
#129562=CARTESIAN_POINT('Ctrl Pts',(82.8039693524285,1075.61841261373,359.670773041121));
#129563=CARTESIAN_POINT('Ctrl Pts',(82.3419423013495,1075.61841261373,359.081735531666));
#129564=CARTESIAN_POINT('Ctrl Pts',(81.8736564905372,1075.61841261373,358.497661407204));
#129565=CARTESIAN_POINT('Ctrl Pts',(81.399165235862,1075.61841261373,357.918617166484));
#129566=CARTESIAN_POINT('Ctrl Pts',(82.2184977300363,1075.69586019218,360.130003094967));
#129567=CARTESIAN_POINT('Ctrl Pts',(81.7597374755771,1075.69586019218,359.545130419022));
#129568=CARTESIAN_POINT('Ctrl Pts',(81.2947627144106,1075.69586019218,358.965186034087));
#129569=CARTESIAN_POINT('Ctrl Pts',(80.8236263854336,1075.69586019218,358.390235968727));
#129570=CARTESIAN_POINT('Ctrl Pts',(81.6358494364943,1075.76911904789,360.587018596629));
#129571=CARTESIAN_POINT('Ctrl Pts',(81.180340225131,1075.76911904789,360.006290670053));
#129572=CARTESIAN_POINT('Ctrl Pts',(80.7186605466846,1075.76911904789,359.430456109738));
#129573=CARTESIAN_POINT('Ctrl Pts',(80.2508629648956,1075.76911904789,358.859580476334));
#129574=CARTESIAN_POINT('Origin',(0.,1082.7251047501,424.620242579854));
#129575=CARTESIAN_POINT('Ctrl Pts',(70.1247710735795,1076.25692701636,356.116956881602));
#129576=CARTESIAN_POINT('Ctrl Pts',(69.5128940250494,1076.25692701636,355.490596590764));
#129577=CARTESIAN_POINT('Ctrl Pts',(68.892680340111,1076.25692701636,354.872490029181));
#129578=CARTESIAN_POINT('Ctrl Pts',(68.2642413448404,1076.25692701636,354.262748144708));
#129579=CARTESIAN_POINT('Ctrl Pts',(69.5016741105325,1076.31898349264,356.725646059818));
#129580=CARTESIAN_POINT('Ctrl Pts',(68.8952339243959,1076.31898349264,356.104851322906));
#129581=CARTESIAN_POINT('Ctrl Pts',(68.2805311774272,1076.31898349264,355.492236976348));
#129582=CARTESIAN_POINT('Ctrl Pts',(67.6576762065094,1076.31898349264,354.887912982168));
#129583=CARTESIAN_POINT('Ctrl Pts',(68.8823191228473,1076.37494694374,357.33067978785));
#129584=CARTESIAN_POINT('Ctrl Pts',(68.2812831483188,1076.37494694374,356.715417181229));
#129585=CARTESIAN_POINT('Ctrl Pts',(67.6720582436777,1076.37494694374,356.108262066495));
#129586=CARTESIAN_POINT('Ctrl Pts',(67.0547537625543,1076.37494694374,355.509323425758));
#129587=CARTESIAN_POINT('Ctrl Pts',(68.2667077672577,1076.42482092472,357.932056447273));
#129588=CARTESIAN_POINT('Ctrl Pts',(67.6710433390963,1076.42482092472,357.32229253251));
#129589=CARTESIAN_POINT('Ctrl Pts',(67.0672631664877,1076.42482092472,356.720563651793));
#129590=CARTESIAN_POINT('Ctrl Pts',(66.455475625753,1076.42482092472,356.126977813244));
#129591=CARTESIAN_POINT('Origin',(0.,1082.7251047501,424.620242579854));
#129592=CARTESIAN_POINT('Ctrl Pts',(57.9363124048121,1076.6273289632,354.363979478503));
#129593=CARTESIAN_POINT('Ctrl Pts',(57.1513185877894,1076.6273289632,353.716640081114));
#129594=CARTESIAN_POINT('Ctrl Pts',(56.3555866550415,1076.6273289632,353.082546807706));
#129595=CARTESIAN_POINT('Ctrl Pts',(55.5493400979898,1076.6273289632,352.461877751429));
#129596=CARTESIAN_POINT('Ctrl Pts',(57.2950021496325,1076.6620786573,355.141662077677));
#129597=CARTESIAN_POINT('Ctrl Pts',(56.518697608199,1076.6620786573,354.501488227712));
#129598=CARTESIAN_POINT('Ctrl Pts',(55.7317738136923,1076.6620786573,353.87441387736));
#129599=CARTESIAN_POINT('Ctrl Pts',(54.9344517836562,1076.6620786573,353.26061514842));
#129600=CARTESIAN_POINT('Ctrl Pts',(56.658459637728,1076.68812401525,355.913563089931));
#129601=CARTESIAN_POINT('Ctrl Pts',(55.8907797725189,1076.68812401525,355.280501515997));
#129602=CARTESIAN_POINT('Ctrl Pts',(55.1125986332183,1076.68812401525,354.660393907371));
#129603=CARTESIAN_POINT('Ctrl Pts',(54.3241347818846,1076.68812401525,354.053414429152));
#129604=CARTESIAN_POINT('Ctrl Pts',(56.0266873910628,1076.70547112168,356.679679457015));
#129605=CARTESIAN_POINT('Ctrl Pts',(55.2675675685421,1076.70547112168,356.053676859542));
#129606=CARTESIAN_POINT('Ctrl Pts',(54.4980635667746,1076.70547112168,355.440483783707));
#129607=CARTESIAN_POINT('Ctrl Pts',(53.7183915107343,1076.70547112168,354.840272452576));
#129608=CARTESIAN_POINT('Origin',(0.,1082.7251047501,424.620242579854));
#129609=CARTESIAN_POINT('Ctrl Pts',(106.417077534095,1074.64979188503,386.345144051125));
#129610=CARTESIAN_POINT('Ctrl Pts',(106.164069922499,1074.64979188503,385.641701560972));
#129611=CARTESIAN_POINT('Ctrl Pts',(105.904100089906,1074.64979188503,384.940802228243));
#129612=CARTESIAN_POINT('Ctrl Pts',(105.637193594043,1074.64979188503,384.242514958602));
#129613=CARTESIAN_POINT('Ctrl Pts',(105.718538992071,1074.75373114609,386.596387856552));
#129614=CARTESIAN_POINT('Ctrl Pts',(105.467192162487,1074.75373114609,385.897562874254));
#129615=CARTESIAN_POINT('Ctrl Pts',(105.208928813027,1074.75373114609,385.201264355693));
#129616=CARTESIAN_POINT('Ctrl Pts',(104.943774333653,1074.75373114609,384.507560754223));
#129617=CARTESIAN_POINT('Ctrl Pts',(105.023133571111,1074.85376994682,386.846504770316));
#129618=CARTESIAN_POINT('Ctrl Pts',(104.773440074514,1074.85376994682,386.15227658519));
#129619=CARTESIAN_POINT('Ctrl Pts',(104.516875554181,1074.85376994682,385.460558244988));
#129620=CARTESIAN_POINT('Ctrl Pts',(104.25346523306,1074.85376994682,384.771417752785));
#129621=CARTESIAN_POINT('Ctrl Pts',(104.330862382022,1074.94991009922,387.095494392893));
#129622=CARTESIAN_POINT('Ctrl Pts',(104.082814766745,1074.94991009922,386.405842286912));
#129623=CARTESIAN_POINT('Ctrl Pts',(103.827941418819,1074.94991009922,385.718683481943));
#129624=CARTESIAN_POINT('Ctrl Pts',(103.566267394931,1074.94991009922,385.034085532814));
#129625=CARTESIAN_POINT('Origin',(0.,1082.7251047501,424.620242579854));
#129626=CARTESIAN_POINT('Ctrl Pts',(95.1741262372256,1075.53621972965,377.974563935349));
#129627=CARTESIAN_POINT('Ctrl Pts',(94.8428820819214,1075.53621972965,377.298705549998));
#129628=CARTESIAN_POINT('Ctrl Pts',(94.504457797769,1075.53621972965,376.626413759651));
#129629=CARTESIAN_POINT('Ctrl Pts',(94.1588917817534,1075.53621972965,375.957764841274));
#129630=CARTESIAN_POINT('Ctrl Pts',(94.5012690776854,1075.61805523595,378.304337163415));
#129631=CARTESIAN_POINT('Ctrl Pts',(94.1723667353325,1075.61805523595,377.633256927036));
#129632=CARTESIAN_POINT('Ctrl Pts',(93.8363350258384,1075.61805523595,376.96571807073));
#129633=CARTESIAN_POINT('Ctrl Pts',(93.4932120747309,1075.61805523595,376.301796332204));
#129634=CARTESIAN_POINT('Ctrl Pts',(93.8316468671878,1075.69568168088,378.632524914424));
#129635=CARTESIAN_POINT('Ctrl Pts',(93.5050750788652,1075.69568168088,377.966199854729));
#129636=CARTESIAN_POINT('Ctrl Pts',(93.1714244410573,1075.69568168088,377.303391081404));
#129637=CARTESIAN_POINT('Ctrl Pts',(92.8307328091399,1075.69568168088,376.64417379549));
#129638=CARTESIAN_POINT('Ctrl Pts',(93.1652607966795,1075.76910110026,378.959126604684));
#129639=CARTESIAN_POINT('Ctrl Pts',(92.8410082993214,1075.76910110026,378.297533740928));
#129640=CARTESIAN_POINT('Ctrl Pts',(92.5097272259928,1075.76910110026,377.639432191111));
#129641=CARTESIAN_POINT('Ctrl Pts',(92.1714551632232,1075.76910110026,376.984896622203));
#129642=CARTESIAN_POINT('Origin',(0.,1082.7251047501,424.620242579854));
#129643=CARTESIAN_POINT('Ctrl Pts',(82.8314235492149,1076.25695287626,372.188689355832));
#129644=CARTESIAN_POINT('Ctrl Pts',(82.3633219523744,1076.25695287626,371.449181955273));
#129645=CARTESIAN_POINT('Ctrl Pts',(81.8853595906112,1076.25695287626,370.716009205381));
#129646=CARTESIAN_POINT('Ctrl Pts',(81.3976221753205,1076.25695287626,369.989302583579));
#129647=CARTESIAN_POINT('Ctrl Pts',(82.0971191044224,1076.3188643633,372.653497528022));
#129648=CARTESIAN_POINT('Ctrl Pts',(81.6331672501365,1076.3188643633,371.920545895164));
#129649=CARTESIAN_POINT('Ctrl Pts',(81.1594420470705,1076.3188643633,371.193872756));
#129650=CARTESIAN_POINT('Ctrl Pts',(80.6760284467838,1076.3188643633,370.473608422396));
#129651=CARTESIAN_POINT('Ctrl Pts',(81.3672143100217,1076.3747109331,373.115520760707));
#129652=CARTESIAN_POINT('Ctrl Pts',(80.907387334739,1076.3747109331,372.389085616086));
#129653=CARTESIAN_POINT('Ctrl Pts',(80.437873903057,1076.3747109331,371.668873144652));
#129654=CARTESIAN_POINT('Ctrl Pts',(79.958758211252,1076.3747109331,370.955012499705));
#129655=CARTESIAN_POINT('Ctrl Pts',(80.6417111094299,1076.42449611617,373.574757823721));
#129656=CARTESIAN_POINT('Ctrl Pts',(80.185984138616,1076.42449611617,372.85479987052));
#129657=CARTESIAN_POINT('Ctrl Pts',(79.7206570797905,1076.42449611617,372.141009106621));
#129658=CARTESIAN_POINT('Ctrl Pts',(79.2458133785017,1076.42449611617,371.433513533737));
#129659=CARTESIAN_POINT('Origin',(0.,1082.7251047501,424.620242579854));
#129660=CARTESIAN_POINT('Ctrl Pts',(71.2784833618073,1076.62751692106,367.955057389048));
#129661=CARTESIAN_POINT('Ctrl Pts',(70.6436506951664,1076.62751692106,367.15650869439));
#129662=CARTESIAN_POINT('Ctrl Pts',(69.9954894423832,1076.62751692106,366.368739995617));
#129663=CARTESIAN_POINT('Ctrl Pts',(69.3341826242336,1076.62751692106,365.591973734349));
#129664=CARTESIAN_POINT('Ctrl Pts',(70.4885383781271,1076.66227574332,368.583050251404));
#129665=CARTESIAN_POINT('Ctrl Pts',(69.860741255129,1076.66227574332,367.793351486007));
#129666=CARTESIAN_POINT('Ctrl Pts',(69.2197632602675,1076.66227574332,367.01431324701));
#129667=CARTESIAN_POINT('Ctrl Pts',(68.5657853859875,1076.66227574332,366.246155510821));
#129668=CARTESIAN_POINT('Ctrl Pts',(69.7044731636426,1076.68830990593,369.206368796987));
#129669=CARTESIAN_POINT('Ctrl Pts',(69.0836592168774,1076.68830990594,368.425454088489));
#129670=CARTESIAN_POINT('Ctrl Pts',(68.4498110130512,1076.68830990594,367.65508132615));
#129671=CARTESIAN_POINT('Ctrl Pts',(67.8031075313755,1076.68830990593,366.895468039513));
#129672=CARTESIAN_POINT('Ctrl Pts',(68.9262908321672,1076.70562551488,369.825010550368));
#129673=CARTESIAN_POINT('Ctrl Pts',(68.3124076664922,1076.70562551488,369.052813991523));
#129674=CARTESIAN_POINT('Ctrl Pts',(67.6856357584999,1076.70562551488,368.29104168831));
#129675=CARTESIAN_POINT('Ctrl Pts',(67.0461520892739,1076.70562551488,367.539908741765));
#129676=CARTESIAN_POINT('Origin',(0.,1082.7251047501,424.620242579854));
#129677=CARTESIAN_POINT('Ctrl Pts',(112.050974474796,1074.64949814216,409.302566991023));
#129678=CARTESIAN_POINT('Ctrl Pts',(111.949995186494,1074.64949814216,408.563889141998));
#129679=CARTESIAN_POINT('Ctrl Pts',(111.841716652463,1074.64949814216,407.826245908196));
#129680=CARTESIAN_POINT('Ctrl Pts',(111.726149460023,1074.64949814216,407.08970941532));
#129681=CARTESIAN_POINT('Ctrl Pts',(111.314975450695,1074.75351345269,409.403180076609));
#129682=CARTESIAN_POINT('Ctrl Pts',(111.214659437818,1074.75351345269,408.669354181604));
#129683=CARTESIAN_POINT('Ctrl Pts',(111.107092123798,1074.75351345269,407.936556106024));
#129684=CARTESIAN_POINT('Ctrl Pts',(110.992284026415,1074.75351345269,407.204857501819));
#129685=CARTESIAN_POINT('Ctrl Pts',(110.582279720134,1074.85362314365,409.503341592907));
#129686=CARTESIAN_POINT('Ctrl Pts',(110.482624005784,1074.85362314365,408.774345875495));
#129687=CARTESIAN_POINT('Ctrl Pts',(110.375764719695,1074.85362314365,408.046371212211));
#129688=CARTESIAN_POINT('Ctrl Pts',(110.261712310416,1074.85362314365,407.319488783379));
#129689=CARTESIAN_POINT('Ctrl Pts',(109.852888455028,1074.94982903064,409.603051379713));
#129690=CARTESIAN_POINT('Ctrl Pts',(109.753890061251,1074.94982903064,408.878864055743));
#129691=CARTESIAN_POINT('Ctrl Pts',(109.64773560988,1074.94982903064,408.155691051114));
#129692=CARTESIAN_POINT('Ctrl Pts',(109.534435480544,1074.94982903064,407.433603076653));
#129693=CARTESIAN_POINT('Origin',(0.,1082.7251047501,424.620242579854));
#129694=CARTESIAN_POINT('Ctrl Pts',(102.791080266267,1075.53629018843,398.778596009474));
#129695=CARTESIAN_POINT('Ctrl Pts',(102.607642971954,1075.53629018843,398.048932069828));
#129696=CARTESIAN_POINT('Ctrl Pts',(102.416447074636,1075.53629018843,397.321262615603));
#129697=CARTESIAN_POINT('Ctrl Pts',(102.217514250128,1075.53629018843,396.59567014245));
#129698=CARTESIAN_POINT('Ctrl Pts',(102.065499511081,1075.61799617016,398.961006792445));
#129699=CARTESIAN_POINT('Ctrl Pts',(101.883357062296,1075.61799617016,398.23649339807));
#129700=CARTESIAN_POINT('Ctrl Pts',(101.693510776862,1075.61799617016,397.51396041046));
#129701=CARTESIAN_POINT('Ctrl Pts',(101.495982177591,1075.61799617016,396.793489742946));
#129702=CARTESIAN_POINT('Ctrl Pts',(101.343401779889,1075.69550615652,399.142541944234));
#129703=CARTESIAN_POINT('Ctrl Pts',(101.162547960951,1075.69550615652,398.423154370835));
#129704=CARTESIAN_POINT('Ctrl Pts',(100.974044808825,1075.69550615652,397.705733193127));
#129705=CARTESIAN_POINT('Ctrl Pts',(100.777913694053,1075.69550615652,396.990359744918));
#129706=CARTESIAN_POINT('Ctrl Pts',(100.624788352975,1075.76882217388,399.323201142979));
#129707=CARTESIAN_POINT('Ctrl Pts',(100.445216945919,1075.76882217388,398.608914657173));
#129708=CARTESIAN_POINT('Ctrl Pts',(100.258050446143,1075.76882217388,397.896580623591));
#129709=CARTESIAN_POINT('Ctrl Pts',(100.063310072652,1075.76882217388,397.186279799312));
#129710=CARTESIAN_POINT('Origin',(0.,1082.7251047501,424.620242579854));
#129711=CARTESIAN_POINT('Ctrl Pts',(91.9219760284135,1076.25713903639,390.562197315818));
#129712=CARTESIAN_POINT('Ctrl Pts',(91.6173444167836,1076.25713903639,389.740002751079));
#129713=CARTESIAN_POINT('Ctrl Pts',(91.301709724956,1076.25713903639,388.921969095044));
#129714=CARTESIAN_POINT('Ctrl Pts',(90.9751287655975,1076.25713903639,388.108243589682));
#129715=CARTESIAN_POINT('Ctrl Pts',(91.1063834873439,1076.31909062344,390.864382809221));
#129716=CARTESIAN_POINT('Ctrl Pts',(90.8044547687648,1076.31909062344,390.049483298214));
#129717=CARTESIAN_POINT('Ctrl Pts',(90.4916205965896,1076.31909062344,389.238707777579));
#129718=CARTESIAN_POINT('Ctrl Pts',(90.1679372794056,1076.31909062344,388.432202182856));
#129719=CARTESIAN_POINT('Ctrl Pts',(90.2956818280571,1076.37496705179,391.16475618021));
#129720=CARTESIAN_POINT('Ctrl Pts',(89.9964397940304,1076.37496705179,390.357107976526));
#129721=CARTESIAN_POINT('Ctrl Pts',(89.6863893475696,1076.37496705179,389.55354706627));
#129722=CARTESIAN_POINT('Ctrl Pts',(89.3655862962055,1076.37496705179,388.754218086388));
#129723=CARTESIAN_POINT('Ctrl Pts',(89.4898732127801,1076.42477186091,391.463316627657));
#129724=CARTESIAN_POINT('Ctrl Pts',(89.1933016476416,1076.42477186091,390.662875965546));
#129725=CARTESIAN_POINT('Ctrl Pts',(88.8860181255329,1076.42477186091,389.866486121406));
#129726=CARTESIAN_POINT('Ctrl Pts',(88.5680779559518,1076.42477186091,389.074290441427));
#129727=CARTESIAN_POINT('Origin',(0.,1082.7251047501,424.620242579854));
#129728=CARTESIAN_POINT('Ctrl Pts',(81.5058918905999,1076.62736807858,384.010616614734));
#129729=CARTESIAN_POINT('Ctrl Pts',(81.0512512124329,1076.62736807858,383.098126211705));
#129730=CARTESIAN_POINT('Ctrl Pts',(80.5813525416058,1076.62736807858,382.193398561516));
#129731=CARTESIAN_POINT('Ctrl Pts',(80.0963283776399,1076.62736807858,381.296688774443));
#129732=CARTESIAN_POINT('Ctrl Pts',(80.6014836943623,1076.66219575471,384.46123040126));
#129733=CARTESIAN_POINT('Ctrl Pts',(80.1518878141374,1076.66219575471,383.558865202438));
#129734=CARTESIAN_POINT('Ctrl Pts',(79.687203247462,1076.66219575471,382.664176619158));
#129735=CARTESIAN_POINT('Ctrl Pts',(79.2075610236123,1076.66219575471,381.777416930934));
#129736=CARTESIAN_POINT('Ctrl Pts',(79.7038156058466,1076.68827669796,384.908485985732));
#129737=CARTESIAN_POINT('Ctrl Pts',(79.2592269271757,1076.68827669796,384.01617053297));
#129738=CARTESIAN_POINT('Ctrl Pts',(78.7997176065083,1076.68827669796,383.13144620039));
#129739=CARTESIAN_POINT('Ctrl Pts',(78.3254172138324,1076.68827669796,382.254562457841));
#129740=CARTESIAN_POINT('Ctrl Pts',(78.8128911989983,1076.70561703749,385.352381587462));
#129741=CARTESIAN_POINT('Ctrl Pts',(78.3732721055577,1076.70561703749,384.470040382601));
#129742=CARTESIAN_POINT('Ctrl Pts',(77.9188991521501,1076.70561703749,383.595205444841));
#129743=CARTESIAN_POINT('Ctrl Pts',(77.449900460438,1076.70561703749,382.728123455474));
#129744=CARTESIAN_POINT('Origin',(0.,1082.7251047501,424.620242579854));
#129745=CARTESIAN_POINT('Ctrl Pts',(112.785775301718,1074.64965137923,432.937298637013));
#129746=CARTESIAN_POINT('Ctrl Pts',(112.840648198164,1074.64965137923,432.193179308468));
#129747=CARTESIAN_POINT('Ctrl Pts',(112.888154506911,1074.64965137923,431.448553388621));
#129748=CARTESIAN_POINT('Ctrl Pts',(112.928289575393,1074.64965137923,430.70349380298));
#129749=CARTESIAN_POINT('Ctrl Pts',(112.045457486278,1074.75359102585,432.882706071996));
#129750=CARTESIAN_POINT('Ctrl Pts',(112.099970200931,1074.75359102585,432.143471089853));
#129751=CARTESIAN_POINT('Ctrl Pts',(112.147164681643,1074.75359102585,431.403732841637));
#129752=CARTESIAN_POINT('Ctrl Pts',(112.187036306387,1074.75359102585,430.663563774178));
#129753=CARTESIAN_POINT('Ctrl Pts',(111.308460068527,1074.85363044618,432.828358359964));
#129754=CARTESIAN_POINT('Ctrl Pts',(111.362614216836,1074.85363044618,432.093985817452));
#129755=CARTESIAN_POINT('Ctrl Pts',(111.409498268092,1074.85363044618,431.359113319182));
#129756=CARTESIAN_POINT('Ctrl Pts',(111.44910763067,1074.85363044618,430.623812835454));
#129757=CARTESIAN_POINT('Ctrl Pts',(110.574784225631,1074.94977145207,432.774255587723));
#129758=CARTESIAN_POINT('Ctrl Pts',(110.628581423621,1074.94977145207,432.044723570305));
#129759=CARTESIAN_POINT('Ctrl Pts',(110.675156444497,1074.94977145207,431.314694892525));
#129760=CARTESIAN_POINT('Ctrl Pts',(110.714504726896,1074.94977145207,430.5842410503));
#129761=CARTESIAN_POINT('Origin',(0.,1082.7251047501,424.620242579854));
#129762=CARTESIAN_POINT('Ctrl Pts',(105.917360566518,1075.53631386031,420.713368851864));
#129763=CARTESIAN_POINT('Ctrl Pts',(105.889707479413,1075.53631386031,419.963679406639));
#129764=CARTESIAN_POINT('Ctrl Pts',(105.854096729417,1075.53631386031,419.214325797191));
#129765=CARTESIAN_POINT('Ctrl Pts',(105.810532330478,1075.53631386031,418.465392488643));
#129766=CARTESIAN_POINT('Ctrl Pts',(105.169355002635,1075.61805795958,420.740959827227));
#129767=CARTESIAN_POINT('Ctrl Pts',(105.141897206112,1075.61805795958,419.996564810349));
#129768=CARTESIAN_POINT('Ctrl Pts',(105.106537945003,1075.61805795958,419.252503257522));
#129769=CARTESIAN_POINT('Ctrl Pts',(105.063281204908,1075.61805795958,418.50885903736));
#129770=CARTESIAN_POINT('Ctrl Pts',(104.424941823346,1075.69560206441,420.76841829369));
#129771=CARTESIAN_POINT('Ctrl Pts',(104.397678379499,1075.69560206441,420.029292278045));
#129772=CARTESIAN_POINT('Ctrl Pts',(104.362569399472,1075.69560206441,419.290497366114));
#129773=CARTESIAN_POINT('Ctrl Pts',(104.319618840655,1075.69560206441,418.552116832871));
#129774=CARTESIAN_POINT('Ctrl Pts',(103.684122349764,1075.76894820407,420.795744202522));
#129775=CARTESIAN_POINT('Ctrl Pts',(103.657052320342,1075.76894820407,420.061861751644));
#129776=CARTESIAN_POINT('Ctrl Pts',(103.622192413148,1075.76894820407,419.328308055539));
#129777=CARTESIAN_POINT('Ctrl Pts',(103.579546557497,1075.76894820407,418.595165798406));
#129778=CARTESIAN_POINT('Origin',(0.,1082.7251047501,424.620242579854));
#129779=CARTESIAN_POINT('Ctrl Pts',(96.9947980060726,1076.25705988878,410.413654841029));
#129780=CARTESIAN_POINT('Ctrl Pts',(96.8679299958094,1076.25705988878,409.547469571552));
#129781=CARTESIAN_POINT('Ctrl Pts',(96.7294712182359,1076.25705988878,408.683061346232));
#129782=CARTESIAN_POINT('Ctrl Pts',(96.5794465158489,1076.25705988878,407.820585258586));
#129783=CARTESIAN_POINT('Ctrl Pts',(96.1340987741442,1076.31902403782,410.539719324965));
#129784=CARTESIAN_POINT('Ctrl Pts',(96.0083565479565,1076.31902403782,409.681220292394));
#129785=CARTESIAN_POINT('Ctrl Pts',(95.8711264070311,1076.31902403782,408.824482535088));
#129786=CARTESIAN_POINT('Ctrl Pts',(95.7224329734211,1076.31902403782,407.969659770316));
#129787=CARTESIAN_POINT('Ctrl Pts',(95.2785615044095,1076.37491157774,410.665027749089));
#129788=CARTESIAN_POINT('Ctrl Pts',(95.1539383105136,1076.37491157774,409.814168855945));
#129789=CARTESIAN_POINT('Ctrl Pts',(95.0179294376044,1076.37491157774,408.965055563747));
#129790=CARTESIAN_POINT('Ctrl Pts',(94.8705592886128,1076.37491157774,408.117840221769));
#129791=CARTESIAN_POINT('Ctrl Pts',(94.4281884792105,1076.42472604926,410.789579779111));
#129792=CARTESIAN_POINT('Ctrl Pts',(94.3046775628379,1076.42472604926,409.946314907535));
#129793=CARTESIAN_POINT('Ctrl Pts',(94.1698825860548,1076.42472604926,409.104780057198));
#129794=CARTESIAN_POINT('Ctrl Pts',(94.023827733993,1076.42472604926,408.265126217639));
#129795=CARTESIAN_POINT('Origin',(0.,1082.7251047501,424.620242579854));
#129796=CARTESIAN_POINT('Ctrl Pts',(88.1662889859269,1076.62740160071,401.841294443769));
#129797=CARTESIAN_POINT('Ctrl Pts',(87.9114355350873,1076.62740160071,400.854880020173));
#129798=CARTESIAN_POINT('Ctrl Pts',(87.6400653482025,1076.62740160071,399.872881080177));
#129799=CARTESIAN_POINT('Ctrl Pts',(87.3522548453362,1076.62740160071,398.895574162713));
#129800=CARTESIAN_POINT('Ctrl Pts',(87.1890270721594,1076.66218602849,402.093783220433));
#129801=CARTESIAN_POINT('Ctrl Pts',(86.9369984943407,1076.66218602849,401.118302513777));
#129802=CARTESIAN_POINT('Ctrl Pts',(86.6686362569933,1076.66218602849,400.147188348159));
#129803=CARTESIAN_POINT('Ctrl Pts',(86.384015933118,1076.66218602849,399.180714197272));
#129804=CARTESIAN_POINT('Ctrl Pts',(86.2190403734841,1076.6882426219,402.3443923473));
#129805=CARTESIAN_POINT('Ctrl Pts',(85.9698156389513,1076.6882426219,401.379763961652));
#129806=CARTESIAN_POINT('Ctrl Pts',(85.7044389584957,1076.6882426219,400.419453538836));
#129807=CARTESIAN_POINT('Ctrl Pts',(85.4229850643604,1076.6882426219,399.463731510118));
#129808=CARTESIAN_POINT('Ctrl Pts',(85.2563327434172,1076.70557749024,402.59312082876));
#129809=CARTESIAN_POINT('Ctrl Pts',(85.0098908112967,1076.70557749024,401.639263325079));
#129810=CARTESIAN_POINT('Ctrl Pts',(84.7474772832261,1076.70557749024,400.689675570564));
#129811=CARTESIAN_POINT('Ctrl Pts',(84.4691660570007,1076.70557749024,399.744624976895));
#129812=CARTESIAN_POINT('Origin',(0.,1082.7251047501,424.620242579854));
#129813=CARTESIAN_POINT('Ctrl Pts',(108.594221951652,1074.64934918539,456.20485338271));
#129814=CARTESIAN_POINT('Ctrl Pts',(108.80254055405,1074.64934918539,455.488612277612));
#129815=CARTESIAN_POINT('Ctrl Pts',(109.003763162472,1074.64934918539,454.770345319861));
#129816=CARTESIAN_POINT('Ctrl Pts',(109.197870082341,1074.64934918539,454.050122809524));
#129817=CARTESIAN_POINT('Ctrl Pts',(107.880497720998,1074.75343155823,455.997266812811));
#129818=CARTESIAN_POINT('Ctrl Pts',(108.087447171046,1074.75343155823,455.285733127892));
#129819=CARTESIAN_POINT('Ctrl Pts',(108.2873472648,1074.75343155823,454.572186905025));
#129820=CARTESIAN_POINT('Ctrl Pts',(108.480178437124,1074.75343155823,453.856697982239));
#129821=CARTESIAN_POINT('Ctrl Pts',(107.169978746795,1074.85360355319,455.7906124912));
#129822=CARTESIAN_POINT('Ctrl Pts',(107.375565193204,1074.85360355319,455.083765085957));
#129823=CARTESIAN_POINT('Ctrl Pts',(107.574148711557,1074.85360355319,454.374918397678));
#129824=CARTESIAN_POINT('Ctrl Pts',(107.765709865577,1074.85360355319,453.664141804425));
#129825=CARTESIAN_POINT('Ctrl Pts',(106.462666166869,1074.94986698918,455.584890748814));
#129826=CARTESIAN_POINT('Ctrl Pts',(106.666895760533,1074.94986698918,454.88270847524));
#129827=CARTESIAN_POINT('Ctrl Pts',(106.86416864486,1074.94986698918,454.178540113725));
#129828=CARTESIAN_POINT('Ctrl Pts',(107.05446551185,1074.94986698918,453.472454584442));
#129829=CARTESIAN_POINT('Origin',(0.,1082.7251047501,424.620242579854));
#129830=CARTESIAN_POINT('Ctrl Pts',(104.415190336176,1075.53624138483,442.823528975234));
#129831=CARTESIAN_POINT('Ctrl Pts',(104.544378431635,1075.53624138483,442.082497972176));
#129832=CARTESIAN_POINT('Ctrl Pts',(104.665670898072,1075.53624138483,441.34013374278));
#129833=CARTESIAN_POINT('Ctrl Pts',(104.779053990598,1075.53624138483,440.596520411922));
#129834=CARTESIAN_POINT('Ctrl Pts',(103.677939602859,1075.61797203207,442.694999915424));
#129835=CARTESIAN_POINT('Ctrl Pts',(103.806215532015,1075.61797203207,441.959201155383));
#129836=CARTESIAN_POINT('Ctrl Pts',(103.926651581301,1075.61797203207,441.222078582595));
#129837=CARTESIAN_POINT('Ctrl Pts',(104.039234102877,1075.61797203207,440.483715727953));
#129838=CARTESIAN_POINT('Ctrl Pts',(102.944228902186,1075.69550432148,442.567088009382));
#129839=CARTESIAN_POINT('Ctrl Pts',(103.071597044958,1075.69550432148,441.836496368867));
#129840=CARTESIAN_POINT('Ctrl Pts',(103.191180789323,1075.69550432148,441.104590283998));
#129841=CARTESIAN_POINT('Ctrl Pts',(103.302966584025,1075.69550432148,440.371452694533));
#129842=CARTESIAN_POINT('Ctrl Pts',(102.214059535762,1075.76884028115,442.439793484022));
#129843=CARTESIAN_POINT('Ctrl Pts',(102.34052427368,1075.76884028115,441.714383830307));
#129844=CARTESIAN_POINT('Ctrl Pts',(102.459259826867,1075.76884028115,440.987669055412));
#129845=CARTESIAN_POINT('Ctrl Pts',(102.570252740182,1075.76884028115,440.259731510815));
#129846=CARTESIAN_POINT('Origin',(0.,1082.7251047501,424.620242579854));
#129847=CARTESIAN_POINT('Ctrl Pts',(97.8272190274779,1076.2571674599,430.893766563347));
#129848=CARTESIAN_POINT('Ctrl Pts',(97.8832329311818,1076.2571674599,430.020304623829));
#129849=CARTESIAN_POINT('Ctrl Pts',(97.9275442980839,1076.2571674599,429.146170869785));
#129850=CARTESIAN_POINT('Ctrl Pts',(97.9601451806249,1076.2571674599,428.271522083327));
#129851=CARTESIAN_POINT('Ctrl Pts',(96.9595108057009,1076.31909709904,430.838121637588));
#129852=CARTESIAN_POINT('Ctrl Pts',(97.0150278770789,1076.31909709904,429.972407133946));
#129853=CARTESIAN_POINT('Ctrl Pts',(97.0589462108583,1076.31909709904,429.106026774641));
#129854=CARTESIAN_POINT('Ctrl Pts',(97.0912579299732,1076.31909709904,428.239135951158));
#129855=CARTESIAN_POINT('Ctrl Pts',(96.0970043114389,1076.37495551961,430.782810291406));
#129856=CARTESIAN_POINT('Ctrl Pts',(96.1520275288957,1076.37495551961,429.924796779398));
#129857=CARTESIAN_POINT('Ctrl Pts',(96.1955551857029,1076.37495551961,429.066123334868));
#129858=CARTESIAN_POINT('Ctrl Pts',(96.2275794748654,1076.37495551961,428.206943967011));
#129859=CARTESIAN_POINT('Ctrl Pts',(95.2397018435956,1076.42474625764,430.727832672226));
#129860=CARTESIAN_POINT('Ctrl Pts',(95.2942341868524,1076.42474625764,429.877473687084));
#129861=CARTESIAN_POINT('Ctrl Pts',(95.3373735238793,1076.42474625764,429.026460656824));
#129862=CARTESIAN_POINT('Ctrl Pts',(95.3691121173291,1076.42474625764,428.174946216689));
#129863=CARTESIAN_POINT('Origin',(0.,1082.7251047501,424.620242579854));
#129864=CARTESIAN_POINT('Ctrl Pts',(90.9765429512604,1076.62736694439,420.667172948711));
#129865=CARTESIAN_POINT('Ctrl Pts',(90.9324560734266,1076.62736694439,419.652550867876));
#129866=CARTESIAN_POINT('Ctrl Pts',(90.8714034843986,1076.62736694439,418.638808197823));
#129867=CARTESIAN_POINT('Ctrl Pts',(90.7934022680253,1076.62736694439,417.62622860591));
#129868=CARTESIAN_POINT('Ctrl Pts',(89.967409109738,1076.66218229773,420.711021354171));
#129869=CARTESIAN_POINT('Ctrl Pts',(89.9238112542274,1076.66218229773,419.707653707116));
#129870=CARTESIAN_POINT('Ctrl Pts',(89.8634358752988,1076.66218229773,418.705155716205));
#129871=CARTESIAN_POINT('Ctrl Pts',(89.7862998673032,1076.66218229773,417.70380790229));
#129872=CARTESIAN_POINT('Ctrl Pts',(88.9657931412671,1076.68825720191,420.754543096574));
#129873=CARTESIAN_POINT('Ctrl Pts',(88.9226806649477,1076.68825720191,419.762346039708));
#129874=CARTESIAN_POINT('Ctrl Pts',(88.8629774510202,1076.68825720191,418.771008957019));
#129875=CARTESIAN_POINT('Ctrl Pts',(88.7867002057489,1076.68825720191,417.780809246293));
#129876=CARTESIAN_POINT('Ctrl Pts',(87.9716990307714,1076.70559777949,420.797738002768));
#129877=CARTESIAN_POINT('Ctrl Pts',(87.9290682885802,1076.70559777949,419.816627648059));
#129878=CARTESIAN_POINT('Ctrl Pts',(87.8700321918811,1076.70559777949,418.836367658269));
#129879=CARTESIAN_POINT('Ctrl Pts',(87.7946072602644,1076.70559777949,417.85723233157));
#129880=CARTESIAN_POINT('Origin',(0.,1082.7251047501,424.620242579854));
#129881=CARTESIAN_POINT('Ctrl Pts',(99.6541986370725,1074.64931753844,478.093455448501));
#129882=CARTESIAN_POINT('Ctrl Pts',(100.007599436641,1074.64931753844,477.434847678565));
#129883=CARTESIAN_POINT('Ctrl Pts',(100.354454045054,1074.64931753844,476.77276898205));
#129884=CARTESIAN_POINT('Ctrl Pts',(100.694728376414,1074.64931753844,476.107284422369));
#129885=CARTESIAN_POINT('Ctrl Pts',(99.0004381414725,1074.75320910968,477.742655636507));
#129886=CARTESIAN_POINT('Ctrl Pts',(99.3515205291227,1074.75320910968,477.088368524887));
#129887=CARTESIAN_POINT('Ctrl Pts',(99.6960996705322,1074.75320910968,476.430633256974));
#129888=CARTESIAN_POINT('Ctrl Pts',(100.034141703419,1074.75320910968,475.769514469349));
#129889=CARTESIAN_POINT('Ctrl Pts',(98.3496082045902,1074.85320468589,477.393428326146));
#129890=CARTESIAN_POINT('Ctrl Pts',(98.6983825728772,1074.85320468589,476.74344250498));
#129891=CARTESIAN_POINT('Ctrl Pts',(99.0406964473337,1074.85320468589,476.090031195739));
#129892=CARTESIAN_POINT('Ctrl Pts',(99.3765161882889,1074.85320468589,475.433258610078));
#129893=CARTESIAN_POINT('Ctrl Pts',(97.7017098648222,1074.94930607596,477.04577407461));
#129894=CARTESIAN_POINT('Ctrl Pts',(98.048186609984,1074.94930607596,476.400070169174));
#129895=CARTESIAN_POINT('Ctrl Pts',(98.3882454211516,1074.94930607596,475.750963341771));
#129896=CARTESIAN_POINT('Ctrl Pts',(98.7218528802625,1074.94930607596,475.098517381053));
#129897=CARTESIAN_POINT('Origin',(0.,1082.7251047501,424.620242579854));
#129898=CARTESIAN_POINT('Ctrl Pts',(98.3451399293708,1075.53671645102,464.132302641614));
#129899=CARTESIAN_POINT('Ctrl Pts',(98.6258712392865,1075.53671645102,463.43356509381));
#129900=CARTESIAN_POINT('Ctrl Pts',(98.8991401434067,1075.53671645102,462.731875465044));
#129901=CARTESIAN_POINT('Ctrl Pts',(99.164915605103,1075.53671645102,462.027313450004));
#129902=CARTESIAN_POINT('Ctrl Pts',(97.6512806020871,1075.61836636429,463.853531251042));
#129903=CARTESIAN_POINT('Ctrl Pts',(97.9300312545144,1075.61836636429,463.159723540801));
#129904=CARTESIAN_POINT('Ctrl Pts',(98.2013721510267,1075.61836636429,462.46298457756));
#129905=CARTESIAN_POINT('Ctrl Pts',(98.4652724739699,1075.61836636429,461.763393493733));
#129906=CARTESIAN_POINT('Ctrl Pts',(96.9607503923561,1075.69582454512,463.576097397768));
#129907=CARTESIAN_POINT('Ctrl Pts',(97.237529890434,1075.69582454512,462.887195871867));
#129908=CARTESIAN_POINT('Ctrl Pts',(97.5069520298648,1075.69582454512,462.195383820996));
#129909=CARTESIAN_POINT('Ctrl Pts',(97.7689862109179,1075.69582454512,461.500739817996));
#129910=CARTESIAN_POINT('Ctrl Pts',(96.2735505232669,1075.76909301678,463.300001573192));
#129911=CARTESIAN_POINT('Ctrl Pts',(96.5483683736258,1075.76909301678,462.615982569719));
#129912=CARTESIAN_POINT('Ctrl Pts',(96.8158810098999,1075.76909301678,461.929073669338));
#129913=CARTESIAN_POINT('Ctrl Pts',(97.0760580492314,1075.76909301678,461.239352888012));
#129914=CARTESIAN_POINT('Origin',(0.,1082.7251047501,424.620242579854));
#129915=CARTESIAN_POINT('Ctrl Pts',(94.3881599803209,1076.25694104584,451.097030807224));
#129916=CARTESIAN_POINT('Ctrl Pts',(94.6244864530644,1076.25694104584,450.254541124361));
#129917=CARTESIAN_POINT('Ctrl Pts',(94.8495125801886,1076.25694104584,449.408963032425));
#129918=CARTESIAN_POINT('Ctrl Pts',(95.0631980271476,1076.25694104584,448.560448096076));
#129919=CARTESIAN_POINT('Ctrl Pts',(93.5497242556542,1076.31897768791,450.861841508811));
#129920=CARTESIAN_POINT('Ctrl Pts',(93.7839514761455,1076.31897768791,450.026835534158));
#129921=CARTESIAN_POINT('Ctrl Pts',(94.0069787302753,1076.31897768791,449.188768584302));
#129922=CARTESIAN_POINT('Ctrl Pts',(94.2187660417838,1076.31897768791,448.347790877577));
#129923=CARTESIAN_POINT('Ctrl Pts',(92.7163221816138,1076.37492501907,450.628064197893));
#129924=CARTESIAN_POINT('Ctrl Pts',(92.9484627529684,1076.37492501907,449.8004970021));
#129925=CARTESIAN_POINT('Ctrl Pts',(93.1695031345806,1076.37492501907,448.969896100271));
#129926=CARTESIAN_POINT('Ctrl Pts',(93.379403706325,1076.37492501907,448.136410372497));
#129927=CARTESIAN_POINT('Ctrl Pts',(91.8879559861347,1076.42478659114,450.395699499429));
#129928=CARTESIAN_POINT('Ctrl Pts',(92.1180225170464,1076.42478659114,449.575526133259));
#129929=CARTESIAN_POINT('Ctrl Pts',(92.3370880319291,1076.42478659114,448.752346165445));
#129930=CARTESIAN_POINT('Ctrl Pts',(92.5451132646399,1076.42478659114,447.926307145921));
#129931=CARTESIAN_POINT('Origin',(0.,1082.7251047501,424.620242579854));
#129932=CARTESIAN_POINT('Ctrl Pts',(89.8103648304035,1076.62734440709,439.672670140951));
#129933=CARTESIAN_POINT('Ctrl Pts',(89.9786348315319,1076.62734440709,438.668686555578));
#129934=CARTESIAN_POINT('Ctrl Pts',(90.1300475661144,1076.62734440709,437.662022750337));
#129935=CARTESIAN_POINT('Ctrl Pts',(90.2645604650628,1076.62734440709,436.652961744751));
#129936=CARTESIAN_POINT('Ctrl Pts',(88.8148916651083,1076.66213832489,439.505826506167));
#129937=CARTESIAN_POINT('Ctrl Pts',(88.9812965332872,1076.66213832489,438.512971243449));
#129938=CARTESIAN_POINT('Ctrl Pts',(89.1310309836935,1076.66213832489,437.51746546887));
#129939=CARTESIAN_POINT('Ctrl Pts',(89.2640529190817,1076.66213832489,436.519589064918));
#129940=CARTESIAN_POINT('Ctrl Pts',(87.8268292096143,1076.68820444296,439.340224923707));
#129941=CARTESIAN_POINT('Ctrl Pts',(87.9913828296571,1076.68820444296,438.358415139856));
#129942=CARTESIAN_POINT('Ctrl Pts',(88.1394514897216,1076.68820444296,437.37398433099));
#129943=CARTESIAN_POINT('Ctrl Pts',(88.2709935608928,1076.68820444296,436.387209265918));
#129944=CARTESIAN_POINT('Ctrl Pts',(86.8461813891991,1076.70554887055,439.175866051459));
#129945=CARTESIAN_POINT('Ctrl Pts',(87.0088976532735,1076.70554887055,438.205018858802));
#129946=CARTESIAN_POINT('Ctrl Pts',(87.1553130234483,1076.70554887055,437.231579906705));
#129947=CARTESIAN_POINT('Ctrl Pts',(87.2853863356247,1076.70554887055,436.255822873657));
#129948=CARTESIAN_POINT('Origin',(0.,1082.7251047501,424.620242579854));
#129949=CARTESIAN_POINT('Ctrl Pts',(86.3565913854363,1074.65013798949,497.637758039474));
#129950=CARTESIAN_POINT('Ctrl Pts',(86.8384286186397,1074.65013798949,497.067897221832));
#129951=CARTESIAN_POINT('Ctrl Pts',(87.3146017276091,1074.65013798949,496.493295062873));
#129952=CARTESIAN_POINT('Ctrl Pts',(87.7850640597002,1074.65013798949,495.914007858744));
#129953=CARTESIAN_POINT('Ctrl Pts',(85.7902738736794,1074.75396819847,497.158916795206));
#129954=CARTESIAN_POINT('Ctrl Pts',(86.2689512686052,1074.75396819847,496.592793065319));
#129955=CARTESIAN_POINT('Ctrl Pts',(86.7420016840325,1074.75396819847,496.021959087338));
#129956=CARTESIAN_POINT('Ctrl Pts',(87.2093787732602,1074.75396819847,495.446470788223));
#129957=CARTESIAN_POINT('Ctrl Pts',(85.2264940110564,1074.85390548088,496.68222122195));
#129958=CARTESIAN_POINT('Ctrl Pts',(85.7020257268305,1074.85390548088,496.119817834058));
#129959=CARTESIAN_POINT('Ctrl Pts',(86.1719674413972,1074.85390548088,495.552735151966));
#129960=CARTESIAN_POINT('Ctrl Pts',(86.6362731126277,1074.85390548088,494.981028735103));
#129961=CARTESIAN_POINT('Ctrl Pts',(84.6652526963884,1074.94995164347,496.207672079691));
#129962=CARTESIAN_POINT('Ctrl Pts',(85.1376528971515,1074.94995164347,495.648972282103));
#129963=CARTESIAN_POINT('Ctrl Pts',(85.6044999084952,1074.94995164347,495.08562400483));
#129964=CARTESIAN_POINT('Ctrl Pts',(86.0657479914915,1074.94995164347,494.517682441429));
#129965=CARTESIAN_POINT('Origin',(0.,1082.7251047501,424.620242579854));
#129966=CARTESIAN_POINT('Ctrl Pts',(87.9839219813682,1075.53617027389,483.720658031948));
#129967=CARTESIAN_POINT('Ctrl Pts',(88.4030068095904,1075.53617027389,483.096758410468));
#129968=CARTESIAN_POINT('Ctrl Pts',(88.8154320139319,1075.53617027389,482.468436612539));
#129969=CARTESIAN_POINT('Ctrl Pts',(89.2211509359701,1075.53617027389,481.835763721363));
#129970=CARTESIAN_POINT('Ctrl Pts',(87.3617260771309,1075.61803025466,483.302717621872));
#129971=CARTESIAN_POINT('Ctrl Pts',(87.7778472631583,1075.61803025466,482.683230031367));
#129972=CARTESIAN_POINT('Ctrl Pts',(88.1873559201675,1075.61803025466,482.05935153672));
#129973=CARTESIAN_POINT('Ctrl Pts',(88.5902057196901,1075.61803025466,481.431152718451));
#129974=CARTESIAN_POINT('Ctrl Pts',(86.7425223803861,1075.69567883021,482.886787132494));
#129975=CARTESIAN_POINT('Ctrl Pts',(87.155694176695,1075.69567883021,482.271690355031));
#129976=CARTESIAN_POINT('Ctrl Pts',(87.5623003123638,1075.69567883021,481.652233795337));
#129977=CARTESIAN_POINT('Ctrl Pts',(87.9622947872917,1075.69567883021,481.028487533674));
#129978=CARTESIAN_POINT('Ctrl Pts',(86.1263119930219,1075.76911803806,482.472867303973));
#129979=CARTESIAN_POINT('Ctrl Pts',(86.5365486573371,1075.76911803806,481.862140113802));
#129980=CARTESIAN_POINT('Ctrl Pts',(86.9402663028226,1075.76911803806,481.247084112867));
#129981=CARTESIAN_POINT('Ctrl Pts',(87.3374192561581,1075.76911803806,480.627768883586));
#129982=CARTESIAN_POINT('Origin',(0.,1082.7251047501,424.620242579854));
#129983=CARTESIAN_POINT('Ctrl Pts',(86.8205627762618,1076.25692673602,470.143580773689));
#129984=CARTESIAN_POINT('Ctrl Pts',(87.2279599308813,1076.25692673602,469.366606772202));
#129985=CARTESIAN_POINT('Ctrl Pts',(87.6248910727604,1076.25692673602,468.584234284709));
#129986=CARTESIAN_POINT('Ctrl Pts',(88.0112846810161,1076.25692673602,467.796604282691));
#129987=CARTESIAN_POINT('Ctrl Pts',(86.0509918531742,1076.31883222028,469.740065335922));
#129988=CARTESIAN_POINT('Ctrl Pts',(86.4547778701287,1076.31883222028,468.969978373408));
#129989=CARTESIAN_POINT('Ctrl Pts',(86.8481906442906,1076.31883222028,468.194540776661));
#129990=CARTESIAN_POINT('Ctrl Pts',(87.2311592887328,1076.31883222028,467.413892267602));
#129991=CARTESIAN_POINT('Ctrl Pts',(85.286031300467,1076.37467429721,469.338967291492));
#129992=CARTESIAN_POINT('Ctrl Pts',(85.6862278134767,1076.37467429721,468.575726108856));
#129993=CARTESIAN_POINT('Ctrl Pts',(86.0761432978725,1076.37467429721,467.807181857088));
#129994=CARTESIAN_POINT('Ctrl Pts',(86.4557074968852,1076.37467429721,467.033473016034));
#129995=CARTESIAN_POINT('Ctrl Pts',(84.5256831543828,1076.42445649601,468.94028770808));
#129996=CARTESIAN_POINT('Ctrl Pts',(84.9223118067231,1076.42445649601,468.183851028003));
#129997=CARTESIAN_POINT('Ctrl Pts',(85.3087510886134,1076.42445649601,467.422158557096));
#129998=CARTESIAN_POINT('Ctrl Pts',(85.6849313696428,1076.42445649601,466.655347540621));
#129999=CARTESIAN_POINT('Origin',(0.,1082.7251047501,424.620242579854));
#130000=CARTESIAN_POINT('Ctrl Pts',(84.7123651370726,1076.62758566352,458.012113964912));
#130001=CARTESIAN_POINT('Ctrl Pts',(85.0860848089413,1076.62758566352,457.064018635447));
#130002=CARTESIAN_POINT('Ctrl Pts',(85.4438367859815,1076.62758566352,456.109783512525));
#130003=CARTESIAN_POINT('Ctrl Pts',(85.7855202534696,1076.62758566352,455.149677500182));
#130004=CARTESIAN_POINT('Ctrl Pts',(83.7741341029246,1076.66231053226,457.642282595299));
#130005=CARTESIAN_POINT('Ctrl Pts',(84.1437146459465,1076.66231053226,456.704687887084));
#130006=CARTESIAN_POINT('Ctrl Pts',(84.4975043441996,1076.66231053226,455.761021386639));
#130007=CARTESIAN_POINT('Ctrl Pts',(84.8354034995328,1076.66231053226,454.811549019754));
#130008=CARTESIAN_POINT('Ctrl Pts',(82.8428821294764,1076.68832201484,457.275202227821));
#130009=CARTESIAN_POINT('Ctrl Pts',(83.2083543326901,1076.68832201484,456.348030031658));
#130010=CARTESIAN_POINT('Ctrl Pts',(83.55821122569,1076.68832201484,455.414853538662));
#130011=CARTESIAN_POINT('Ctrl Pts',(83.8923542185919,1076.68832201484,454.475935718534));
#130012=CARTESIAN_POINT('Ctrl Pts',(81.9186129103161,1076.70562620542,456.910874318414));
#130013=CARTESIAN_POINT('Ctrl Pts',(82.2800075790548,1076.70562620542,455.994046483766));
#130014=CARTESIAN_POINT('Ctrl Pts',(82.6259611559338,1076.70562620542,455.071281341587));
#130015=CARTESIAN_POINT('Ctrl Pts',(82.956376151026,1076.70562620542,454.142838927651));
#130016=CARTESIAN_POINT('Origin',(0.,1082.7251047501,424.620242579854));
#130017=CARTESIAN_POINT('Ctrl Pts',(69.2883894728621,1074.6493363685,514.003867860922));
#130018=CARTESIAN_POINT('Ctrl Pts',(69.8780536973393,1074.6493363685,513.546772007903));
#130019=CARTESIAN_POINT('Ctrl Pts',(70.4631660048975,1074.6493363685,513.083863697306));
#130020=CARTESIAN_POINT('Ctrl Pts',(71.0436691030515,1074.6493363685,512.615188255759));
#130021=CARTESIAN_POINT('Ctrl Pts',(68.8328608071636,1074.75345063343,513.416225344342));
#130022=CARTESIAN_POINT('Ctrl Pts',(69.4186483510103,1074.75345063343,512.962134616216));
#130023=CARTESIAN_POINT('Ctrl Pts',(69.9999139040001,1074.75345063343,512.502269643857));
#130024=CARTESIAN_POINT('Ctrl Pts',(70.5766005503106,1074.75345063343,512.036675455896));
#130025=CARTESIAN_POINT('Ctrl Pts',(68.3793784899775,1074.85365214779,512.831222664682));
#130026=CARTESIAN_POINT('Ctrl Pts',(68.9613067682112,1074.85365214779,512.380123561678));
#130027=CARTESIAN_POINT('Ctrl Pts',(69.5387428472146,1074.85365214779,511.92328825612));
#130028=CARTESIAN_POINT('Ctrl Pts',(70.1116301861363,1074.85365214779,511.460761479985));
#130029=CARTESIAN_POINT('Ctrl Pts',(67.9279432479523,1074.94994273216,512.248860759335));
#130030=CARTESIAN_POINT('Ctrl Pts',(68.5060296817743,1074.94994273216,511.800739776888));
#130031=CARTESIAN_POINT('Ctrl Pts',(69.0796535735096,1074.94994273216,511.346920461842));
#130032=CARTESIAN_POINT('Ctrl Pts',(69.648758755585,1074.94994273216,510.887447250856));
#130033=CARTESIAN_POINT('Origin',(0.,1082.7251047501,424.620242579854));
#130034=CARTESIAN_POINT('Ctrl Pts',(73.7732679240495,1075.53618795423,500.72214962966));
#130035=CARTESIAN_POINT('Ctrl Pts',(74.3145652537746,1075.53618795423,500.197415434678));
#130036=CARTESIAN_POINT('Ctrl Pts',(74.8502334981649,1075.53618795423,499.666936116983));
#130037=CARTESIAN_POINT('Ctrl Pts',(75.3802116840874,1075.53618795423,499.13077205907));
#130038=CARTESIAN_POINT('Ctrl Pts',(73.2529980727088,1075.6178224785,500.185457559732));
#130039=CARTESIAN_POINT('Ctrl Pts',(73.7904780212985,1075.6178224785,499.664423937997));
#130040=CARTESIAN_POINT('Ctrl Pts',(74.3223685824477,1075.6178224785,499.13768570977));
#130041=CARTESIAN_POINT('Ctrl Pts',(74.8486092130231,1075.6178224785,498.605302831716));
#130042=CARTESIAN_POINT('Ctrl Pts',(72.7352233846767,1075.69526870155,499.651339412466));
#130043=CARTESIAN_POINT('Ctrl Pts',(73.2689042599175,1075.69526870155,499.13398861639));
#130044=CARTESIAN_POINT('Ctrl Pts',(73.7970352552249,1075.69526870155,498.610973535734));
#130045=CARTESIAN_POINT('Ctrl Pts',(74.319556255403,1075.69526870155,498.082353703368));
#130046=CARTESIAN_POINT('Ctrl Pts',(72.2199447762796,1075.76852864419,499.119796133112));
#130047=CARTESIAN_POINT('Ctrl Pts',(72.7498448926814,1075.76852864419,498.606110408591));
#130048=CARTESIAN_POINT('Ctrl Pts',(73.2742344461996,1075.76852864419,498.086800527018));
#130049=CARTESIAN_POINT('Ctrl Pts',(73.7930537475129,1075.76852864419,497.561925599512));
#130050=CARTESIAN_POINT('Origin',(0.,1082.7251047501,424.620242579854));
#130051=CARTESIAN_POINT('Ctrl Pts',(75.4567986547188,1076.25738960263,487.191656892968));
#130052=CARTESIAN_POINT('Ctrl Pts',(76.0156278790124,1076.25738960263,486.51774749324));
#130053=CARTESIAN_POINT('Ctrl Pts',(76.5653794102637,1076.25738960263,485.836412601389));
#130054=CARTESIAN_POINT('Ctrl Pts',(77.1059545926398,1076.25738960263,485.147774486581));
#130055=CARTESIAN_POINT('Ctrl Pts',(74.7879755561225,1076.3192607262,486.637045407316));
#130056=CARTESIAN_POINT('Ctrl Pts',(75.3418515104651,1076.3192607262,485.969109308615));
#130057=CARTESIAN_POINT('Ctrl Pts',(75.8867302333128,1076.3192607262,485.293813534798));
#130058=CARTESIAN_POINT('Ctrl Pts',(76.4225139432842,1076.3192607262,484.61127927128));
#130059=CARTESIAN_POINT('Ctrl Pts',(74.1231591212705,1076.3750692605,486.085756387255));
#130060=CARTESIAN_POINT('Ctrl Pts',(74.6721114788105,1076.3750692605,485.423757805816));
#130061=CARTESIAN_POINT('Ctrl Pts',(75.2121465843888,1076.3750692605,484.754464971983));
#130062=CARTESIAN_POINT('Ctrl Pts',(75.7431675258367,1076.3750692605,484.077997993913));
#130063=CARTESIAN_POINT('Ctrl Pts',(73.4623511196488,1076.42481873403,485.537791300105));
#130064=CARTESIAN_POINT('Ctrl Pts',(74.0064095666395,1076.42481873403,484.881694436359));
#130065=CARTESIAN_POINT('Ctrl Pts',(74.5416302589744,1076.42481873403,484.218368348484));
#130066=CARTESIAN_POINT('Ctrl Pts',(75.0679171484566,1076.42481873403,483.54793207387));
#130067=CARTESIAN_POINT('Origin',(0.,1082.7251047501,424.620242579854));
#130068=CARTESIAN_POINT('Ctrl Pts',(75.9228204664487,1076.62732636353,474.902424976691));
#130069=CARTESIAN_POINT('Ctrl Pts',(76.4850486031252,1076.62732636353,474.053497109058));
#130070=CARTESIAN_POINT('Ctrl Pts',(77.032960627269,1076.62732636353,473.195259720037));
#130071=CARTESIAN_POINT('Ctrl Pts',(77.5664024258491,1076.62732636353,472.327954208904));
#130072=CARTESIAN_POINT('Ctrl Pts',(75.0798167841509,1076.66218387772,474.344120310794));
#130073=CARTESIAN_POINT('Ctrl Pts',(75.6358022603651,1076.66218387772,473.504618453865));
#130074=CARTESIAN_POINT('Ctrl Pts',(76.1776305819925,1076.66218387772,472.655910443163));
#130075=CARTESIAN_POINT('Ctrl Pts',(76.7051493471851,1076.66218387772,471.798234997602));
#130076=CARTESIAN_POINT('Ctrl Pts',(74.2430996751547,1076.68828317563,473.789979118058));
#130077=CARTESIAN_POINT('Ctrl Pts',(74.7928890446091,1076.68828317564,472.959832978775));
#130078=CARTESIAN_POINT('Ctrl Pts',(75.3286790320175,1076.68828317564,472.120583282485));
#130079=CARTESIAN_POINT('Ctrl Pts',(75.8503189339542,1076.68828317563,471.27246608773));
#130080=CARTESIAN_POINT('Ctrl Pts',(73.4126724751064,1076.7056303985,473.240003607618));
#130081=CARTESIAN_POINT('Ctrl Pts',(73.9563123162048,1076.7056303985,472.419142855625));
#130082=CARTESIAN_POINT('Ctrl Pts',(74.486109361764,1076.7056303985,471.589280372132));
#130083=CARTESIAN_POINT('Ctrl Pts',(75.001914594013,1076.7056303985,470.750649575311));
#130084=CARTESIAN_POINT('Origin',(0.,1082.7251047501,424.620242579854));
#130085=CARTESIAN_POINT('Ctrl Pts',(49.1901626715064,1074.64938719149,526.456185081641));
#130086=CARTESIAN_POINT('Ctrl Pts',(49.8633080434734,1074.64938719149,526.131033376505));
#130087=CARTESIAN_POINT('Ctrl Pts',(50.5331965078962,1074.64938719149,525.799223538816));
#130088=CARTESIAN_POINT('Ctrl Pts',(51.1997622106805,1074.64938719149,525.460788187493));
#130089=CARTESIAN_POINT('Ctrl Pts',(48.8673986854593,1074.75329680596,525.787982885518));
#130090=CARTESIAN_POINT('Ctrl Pts',(49.536127176659,1074.75329680596,525.464964681365));
#130091=CARTESIAN_POINT('Ctrl Pts',(50.2016201306943,1074.75329680596,525.135332032367));
#130092=CARTESIAN_POINT('Ctrl Pts',(50.8638121255763,1074.75329680596,524.799117343409));
#130093=CARTESIAN_POINT('Ctrl Pts',(48.5460818056865,1074.85330894177,525.122776561402));
#130094=CARTESIAN_POINT('Ctrl Pts',(49.2104132191208,1074.85330894177,524.80188229272));
#130095=CARTESIAN_POINT('Ctrl Pts',(49.871530369957,1074.85330894177,524.474417071027));
#130096=CARTESIAN_POINT('Ctrl Pts',(50.529368266374,1074.85330894177,524.140413088137));
#130097=CARTESIAN_POINT('Ctrl Pts',(48.2262125450444,1074.94942540884,524.460567171033));
#130098=CARTESIAN_POINT('Ctrl Pts',(48.8861666907337,1074.94942540884,524.141787268921));
#130099=CARTESIAN_POINT('Ctrl Pts',(49.5429277525433,1074.94942540884,523.816479709689));
#130100=CARTESIAN_POINT('Ctrl Pts',(50.1964311668822,1074.94942540884,523.484676473041));
#130101=CARTESIAN_POINT('Origin',(0.,1082.7251047501,424.620242579854));
#130102=CARTESIAN_POINT('Ctrl Pts',(56.3423819173354,1075.53657255571,514.390977079417));
#130103=CARTESIAN_POINT('Ctrl Pts',(56.9789503748771,1075.53657255571,513.991450626266));
#130104=CARTESIAN_POINT('Ctrl Pts',(57.6112333937505,1075.53657255571,513.585176123069));
#130105=CARTESIAN_POINT('Ctrl Pts',(58.2391594429655,1075.53657255571,513.172199532181));
#130106=CARTESIAN_POINT('Ctrl Pts',(55.9446376610293,1075.61827500173,513.75724820931));
#130107=CARTESIAN_POINT('Ctrl Pts',(56.5767123176503,1075.61827500173,513.360542179198));
#130108=CARTESIAN_POINT('Ctrl Pts',(57.2045317882931,1075.61827500173,512.957135736324));
#130109=CARTESIAN_POINT('Ctrl Pts',(57.8280250469345,1075.61827500173,512.547074518578));
#130110=CARTESIAN_POINT('Ctrl Pts',(55.5488028719652,1075.6957808248,513.126561707506));
#130111=CARTESIAN_POINT('Ctrl Pts',(56.1764053012408,1075.6957808248,512.73266256031));
#130112=CARTESIAN_POINT('Ctrl Pts',(56.7997826519929,1075.6957808248,512.332110408945));
#130113=CARTESIAN_POINT('Ctrl Pts',(57.418864400741,1075.6957808248,511.92495056839));
#130114=CARTESIAN_POINT('Ctrl Pts',(55.154878252074,1075.76909205172,512.498918692396));
#130115=CARTESIAN_POINT('Ctrl Pts',(55.77803003551,1075.76909205172,512.107812883019));
#130116=CARTESIAN_POINT('Ctrl Pts',(56.3969867025886,1075.76909205172,511.710101249285));
#130117=CARTESIAN_POINT('Ctrl Pts',(57.0116782299466,1075.76909205172,511.305828784823));
#130118=CARTESIAN_POINT('Origin',(0.,1082.7251047501,424.620242579854));
#130119=CARTESIAN_POINT('Ctrl Pts',(60.797722754504,1076.25695168791,501.521170266194));
#130120=CARTESIAN_POINT('Ctrl Pts',(61.4850557949331,1076.25695168791,500.977766111143));
#130121=CARTESIAN_POINT('Ctrl Pts',(62.1650421640159,1076.25695168791,500.42519636708));
#130122=CARTESIAN_POINT('Ctrl Pts',(62.8375596476042,1076.25695168791,499.863560347527));
#130123=CARTESIAN_POINT('Ctrl Pts',(60.2576093626057,1076.31899406394,500.83799959777));
#130124=CARTESIAN_POINT('Ctrl Pts',(60.9388362897955,1076.31899406394,500.299422923883));
#130125=CARTESIAN_POINT('Ctrl Pts',(61.6127818118266,1076.31899406394,499.751762086029));
#130126=CARTESIAN_POINT('Ctrl Pts',(62.2793248002741,1076.31899406394,499.195115515452));
#130127=CARTESIAN_POINT('Ctrl Pts',(59.7207389454293,1076.37494586681,500.158930855427));
#130128=CARTESIAN_POINT('Ctrl Pts',(60.3958964219976,1076.37494586681,499.625152677309));
#130129=CARTESIAN_POINT('Ctrl Pts',(61.0638373677205,1076.37494586681,499.082371271375));
#130130=CARTESIAN_POINT('Ctrl Pts',(61.7244417333773,1076.37494586681,498.530684191884));
#130131=CARTESIAN_POINT('Ctrl Pts',(59.1871129384905,1076.42481064945,499.483965854899));
#130132=CARTESIAN_POINT('Ctrl Pts',(59.8562376432841,1076.42481064945,498.954957174325));
#130133=CARTESIAN_POINT('Ctrl Pts',(60.5182102994977,1076.42481064945,498.417025712973));
#130134=CARTESIAN_POINT('Ctrl Pts',(61.1729119305929,1076.42481064945,497.870268153419));
#130135=CARTESIAN_POINT('Origin',(0.,1082.7251047501,424.620242579854));
#130136=CARTESIAN_POINT('Ctrl Pts',(63.8090632272348,1076.62733705021,489.588846730312));
#130137=CARTESIAN_POINT('Ctrl Pts',(64.5369215796459,1076.62733705021,488.873978984009));
#130138=CARTESIAN_POINT('Ctrl Pts',(65.2526650562726,1076.62733705021,488.146981768371));
#130139=CARTESIAN_POINT('Ctrl Pts',(65.9560915528467,1076.62733705021,487.408060365382));
#130140=CARTESIAN_POINT('Ctrl Pts',(63.1023554131808,1076.66210456745,488.869296592774));
#130141=CARTESIAN_POINT('Ctrl Pts',(63.8221524783835,1076.66210456745,488.162346258149));
#130142=CARTESIAN_POINT('Ctrl Pts',(64.5299688443114,1076.66210456745,487.443400792327));
#130143=CARTESIAN_POINT('Ctrl Pts',(65.225604645072,1076.66210456745,486.712663203721));
#130144=CARTESIAN_POINT('Ctrl Pts',(62.4009044379396,1076.68815814051,488.15509882154));
#130145=CARTESIAN_POINT('Ctrl Pts',(63.112700179736,1076.68815814051,487.456007005007));
#130146=CARTESIAN_POINT('Ctrl Pts',(63.8126484006965,1076.68815814051,486.745053396143));
#130147=CARTESIAN_POINT('Ctrl Pts',(64.5005514566546,1076.68815814051,486.022438746702));
#130148=CARTESIAN_POINT('Ctrl Pts',(61.7047130837235,1076.7055038641,487.446256249381));
#130149=CARTESIAN_POINT('Ctrl Pts',(62.4085674976518,1076.7055038641,486.754964026185));
#130150=CARTESIAN_POINT('Ctrl Pts',(63.1007065705844,1076.7055038641,486.051942349721));
#130151=CARTESIAN_POINT('Ctrl Pts',(63.7809348634214,1076.7055038641,485.337389732007));
#130152=CARTESIAN_POINT('Origin',(0.,1082.7251047501,424.620242579854));
#130153=CARTESIAN_POINT('Ctrl Pts',(26.9469667224666,1074.64963445669,534.45508610748));
#130154=CARTESIAN_POINT('Ctrl Pts',(27.6711831580577,1074.64963445669,534.277406278721));
#130155=CARTESIAN_POINT('Ctrl Pts',(28.3936068826267,1074.64963445669,534.092572490392));
#130156=CARTESIAN_POINT('Ctrl Pts',(29.1141672297197,1074.64963445669,533.90060282267));
#130157=CARTESIAN_POINT('Ctrl Pts',(26.7700334311186,1074.75360709312,533.73391253087));
#130158=CARTESIAN_POINT('Ctrl Pts',(27.4894946748206,1074.75360709312,533.557399344622));
#130159=CARTESIAN_POINT('Ctrl Pts',(28.2071749784082,1074.75360709312,533.373779171571));
#130160=CARTESIAN_POINT('Ctrl Pts',(28.9230041394223,1074.75360709312,533.183069973182));
#130161=CARTESIAN_POINT('Ctrl Pts',(26.5938939510957,1074.85367705875,533.015974499974));
#130162=CARTESIAN_POINT('Ctrl Pts',(27.3086213370798,1074.85367705875,532.840622722093));
#130163=CARTESIAN_POINT('Ctrl Pts',(28.0215795010474,1074.85367705875,532.658210719436));
#130164=CARTESIAN_POINT('Ctrl Pts',(28.7326987024519,1074.85367705875,532.468756335282));
#130165=CARTESIAN_POINT('Ctrl Pts',(26.4185485639129,1074.94984616712,532.301273162236));
#130166=CARTESIAN_POINT('Ctrl Pts',(27.1285634339167,1074.94984616712,532.127077556726));
#130167=CARTESIAN_POINT('Ctrl Pts',(27.8368207471725,1074.94984616712,531.945868277644));
#130168=CARTESIAN_POINT('Ctrl Pts',(28.5432512229646,1074.94984616712,531.757663050624));
#130169=CARTESIAN_POINT('Origin',(0.,1082.7251047501,424.620242579854));
#130170=CARTESIAN_POINT('Ctrl Pts',(36.4415553305205,1075.53628600585,524.14821876446));
#130171=CARTESIAN_POINT('Ctrl Pts',(37.1487244658279,1075.53628600585,523.889293142135));
#130172=CARTESIAN_POINT('Ctrl Pts',(37.853093954926,1075.53628600585,523.622845611362));
#130173=CARTESIAN_POINT('Ctrl Pts',(38.5545837925167,1075.53628600585,523.348906436389));
#130174=CARTESIAN_POINT('Ctrl Pts',(36.1840447135347,1075.61808022474,523.44491424515));
#130175=CARTESIAN_POINT('Ctrl Pts',(36.8862167086625,1075.61808022474,523.187818294917));
#130176=CARTESIAN_POINT('Ctrl Pts',(37.5856088410019,1075.61808022474,522.92325358905));
#130177=CARTESIAN_POINT('Ctrl Pts',(38.2821416706041,1075.61808022474,522.651250177942));
#130178=CARTESIAN_POINT('Ctrl Pts',(35.9277715639648,1075.69566939527,522.744989456106));
#130179=CARTESIAN_POINT('Ctrl Pts',(36.6249704326731,1075.69566939527,522.489714385474));
#130180=CARTESIAN_POINT('Ctrl Pts',(37.3194091269444,1075.69566939527,522.227023456599));
#130181=CARTESIAN_POINT('Ctrl Pts',(38.0110087694628,1075.69566939527,521.95694650704));
#130182=CARTESIAN_POINT('Ctrl Pts',(35.6727363371673,1075.76905555037,522.048445640983));
#130183=CARTESIAN_POINT('Ctrl Pts',(36.3649861020524,1075.76905555037,521.794982654226));
#130184=CARTESIAN_POINT('Ctrl Pts',(37.0544952857479,1075.76905555037,521.534156451097));
#130185=CARTESIAN_POINT('Ctrl Pts',(37.7411855708526,1075.76905555037,521.265996657351));
#130186=CARTESIAN_POINT('Origin',(0.,1082.7251047501,424.620242579854));
#130187=CARTESIAN_POINT('Ctrl Pts',(43.4804114603392,1076.25699166103,512.48069772089));
#130188=CARTESIAN_POINT('Ctrl Pts',(44.2664168702271,1076.25699166103,512.09171910045));
#130189=CARTESIAN_POINT('Ctrl Pts',(45.0471320873662,1076.25699166103,511.692228648424));
#130190=CARTESIAN_POINT('Ctrl Pts',(45.8224165371904,1076.25699166103,511.282298296544));
#130191=CARTESIAN_POINT('Ctrl Pts',(43.0948065119335,1076.31892436805,511.701509458091));
#130192=CARTESIAN_POINT('Ctrl Pts',(43.8738412523786,1076.31892436805,511.315980484879));
#130193=CARTESIAN_POINT('Ctrl Pts',(44.6476327160179,1076.31892436805,510.920032903999));
#130194=CARTESIAN_POINT('Ctrl Pts',(45.4160415749672,1076.31892436805,510.513738009255));
#130195=CARTESIAN_POINT('Ctrl Pts',(42.7115128423091,1076.37478750376,510.926991574409));
#130196=CARTESIAN_POINT('Ctrl Pts',(43.4836186948302,1076.37478750376,510.544891571573));
#130197=CARTESIAN_POINT('Ctrl Pts',(44.2505279052787,1076.37478750376,510.152465626211));
#130198=CARTESIAN_POINT('Ctrl Pts',(45.01210238498,1076.37478750376,509.749784398027));
#130199=CARTESIAN_POINT('Ctrl Pts',(42.3305314727975,1076.42458460272,510.15714613364));
#130200=CARTESIAN_POINT('Ctrl Pts',(43.0957502373761,1076.42458460272,509.778454415191));
#130201=CARTESIAN_POINT('Ctrl Pts',(43.8558187132815,1076.42458460272,509.389528860335));
#130202=CARTESIAN_POINT('Ctrl Pts',(44.6106000435729,1076.42458460272,508.990439498502));
#130203=CARTESIAN_POINT('Origin',(0.,1082.7251047501,424.620242579854));
#130204=CARTESIAN_POINT('Ctrl Pts',(48.9116093958664,1076.62746842925,501.428290573206));
#130205=CARTESIAN_POINT('Ctrl Pts',(49.7696403684266,1076.62746842925,500.881893719285));
#130206=CARTESIAN_POINT('Ctrl Pts',(50.6183959633884,1076.62746842925,500.321197177589));
#130207=CARTESIAN_POINT('Ctrl Pts',(51.457637890193,1076.62746842925,499.746358365276));
#130208=CARTESIAN_POINT('Ctrl Pts',(48.3693760270001,1076.66224654234,500.576797704051));
#130209=CARTESIAN_POINT('Ctrl Pts',(49.2178948810554,1076.66224654234,500.036458197465));
#130210=CARTESIAN_POINT('Ctrl Pts',(50.0572411842092,1076.66224654234,499.481977529229));
#130211=CARTESIAN_POINT('Ctrl Pts',(50.8871792875885,1076.66224654234,498.913511371376));
#130212=CARTESIAN_POINT('Ctrl Pts',(47.8311799129396,1076.68829438222,499.731644713397));
#130213=CARTESIAN_POINT('Ctrl Pts',(48.6702574719552,1076.68829438222,499.197317453539));
#130214=CARTESIAN_POINT('Ctrl Pts',(49.5002645411595,1076.68829438222,498.649006377832));
#130215=CARTESIAN_POINT('Ctrl Pts',(50.3209680936961,1076.68829438222,498.086865426179));
#130216=CARTESIAN_POINT('Ctrl Pts',(47.2970231924259,1076.70561806076,498.892834959804));
#130217=CARTESIAN_POINT('Ctrl Pts',(48.1267303173858,1076.70561806076,498.364474822172));
#130218=CARTESIAN_POINT('Ctrl Pts',(48.9474682476122,1076.70561806076,497.822287033547));
#130219=CARTESIAN_POINT('Ctrl Pts',(49.759006558586,1076.70561806076,497.266423814698));
#130220=CARTESIAN_POINT('Origin',(0.,1082.7251047501,424.620242579854));
#130221=CARTESIAN_POINT('Ctrl Pts',(3.5173666145595,1074.64994371665,537.655460170167));
#130222=CARTESIAN_POINT('Ctrl Pts',(4.2639663124766,1074.64994371665,537.632227898775));
#130223=CARTESIAN_POINT('Ctrl Pts',(5.01029920227245,1074.64994371665,537.601600052411));
#130224=CARTESIAN_POINT('Ctrl Pts',(5.75629202757494,1074.64994371665,537.563579637354));
#130225=CARTESIAN_POINT('Ctrl Pts',(3.49435080813864,1074.75355117008,536.915816859735));
#130226=CARTESIAN_POINT('Ctrl Pts',(4.23606514834239,1074.75355117008,536.892736608169));
#130227=CARTESIAN_POINT('Ctrl Pts',(4.9775144262776,1074.75355117008,536.862309174403));
#130228=CARTESIAN_POINT('Ctrl Pts',(5.71862586492354,1074.75355117008,536.824537545045));
#130229=CARTESIAN_POINT('Ctrl Pts',(3.47143790807793,1074.85328274408,536.179480580978));
#130230=CARTESIAN_POINT('Ctrl Pts',(4.20828873357357,1074.85328274408,536.15655166954));
#130231=CARTESIAN_POINT('Ctrl Pts',(4.94487623484748,1074.85328274408,536.126323752305));
#130232=CARTESIAN_POINT('Ctrl Pts',(5.68112811208704,1074.85328274408,536.088799796296));
#130233=CARTESIAN_POINT('Ctrl Pts',(3.44862795074633,1074.94914023354,535.446452502662));
#130234=CARTESIAN_POINT('Ctrl Pts',(4.18063711225881,1074.94914023354,535.423674251413));
#130235=CARTESIAN_POINT('Ctrl Pts',(4.9123846797877,1074.94914023354,535.393644954323));
#130236=CARTESIAN_POINT('Ctrl Pts',(5.64379882858451,1074.94914023354,535.356367558921));
#130237=CARTESIAN_POINT('Origin',(0.,1082.7251047501,424.620242579854));
#130238=CARTESIAN_POINT('Ctrl Pts',(14.9520407112949,1075.53663732595,529.546690715972));
#130239=CARTESIAN_POINT('Ctrl Pts',(15.697740763202,1075.53663732595,529.440428303276));
#130240=CARTESIAN_POINT('Ctrl Pts',(16.4422656965068,1075.53663732595,529.326222824188));
#130241=CARTESIAN_POINT('Ctrl Pts',(17.185530905513,1075.53663732595,529.204087256694));
#130242=CARTESIAN_POINT('Ctrl Pts',(14.8466056747203,1075.61824626063,528.806796803797));
#130243=CARTESIAN_POINT('Ctrl Pts',(15.5870473867283,1075.61824626063,528.701283705632));
#130244=CARTESIAN_POINT('Ctrl Pts',(16.3263222665394,1075.61824626063,528.587883551991));
#130245=CARTESIAN_POINT('Ctrl Pts',(17.0643463050586,1075.61824626063,528.466609229344));
#130246=CARTESIAN_POINT('Ctrl Pts',(14.7416762402029,1075.69566794643,528.070450971049));
#130247=CARTESIAN_POINT('Ctrl Pts',(15.4768848280991,1075.69566794643,527.96568359416));
#130248=CARTESIAN_POINT('Ctrl Pts',(16.2109348304675,1075.69566794643,527.853084904116));
#130249=CARTESIAN_POINT('Ctrl Pts',(16.9437428319531,1075.69566794643,527.732667696313));
#130250=CARTESIAN_POINT('Ctrl Pts',(14.6372525933972,1075.76890440336,527.337654520564));
#130251=CARTESIAN_POINT('Ctrl Pts',(15.3672532822281,1075.76890440336,527.233629270376));
#130252=CARTESIAN_POINT('Ctrl Pts',(16.0961035924491,1075.76890440336,527.121828180663));
#130253=CARTESIAN_POINT('Ctrl Pts',(16.8237206995835,1075.76890440336,527.002263956182));
#130254=CARTESIAN_POINT('Origin',(0.,1082.7251047501,424.620242579854));
#130255=CARTESIAN_POINT('Ctrl Pts',(24.2670610153852,1076.25706953122,519.598667421324));
#130256=CARTESIAN_POINT('Ctrl Pts',(25.1150319980636,1076.25706953122,519.382010179321));
#130257=CARTESIAN_POINT('Ctrl Pts',(25.9600256331401,1076.25706953122,519.154016967454));
#130258=CARTESIAN_POINT('Ctrl Pts',(26.8018903847055,1076.25706953122,518.914728672612));
#130259=CARTESIAN_POINT('Ctrl Pts',(24.0517235332975,1076.31903292809,518.755861823849));
#130260=CARTESIAN_POINT('Ctrl Pts',(24.892169915606,1076.31903292809,518.541127123061));
#130261=CARTESIAN_POINT('Ctrl Pts',(25.7296653702625,1076.31903292809,518.315157043875));
#130262=CARTESIAN_POINT('Ctrl Pts',(26.5640597060347,1076.31903292809,518.07799211036));
#130263=CARTESIAN_POINT('Ctrl Pts',(23.837677515676,1076.37491973991,517.918110866517));
#130264=CARTESIAN_POINT('Ctrl Pts',(24.6706444256336,1076.37491973991,517.7052871767));
#130265=CARTESIAN_POINT('Ctrl Pts',(25.5006866694382,1076.37491973991,517.481328096663));
#130266=CARTESIAN_POINT('Ctrl Pts',(26.32765539247,1076.37491973991,517.246273789834));
#130267=CARTESIAN_POINT('Ctrl Pts',(23.6249235335358,1076.42473350737,517.085416784213));
#130268=CARTESIAN_POINT('Ctrl Pts',(24.4504561191147,1076.42473350737,516.874492570025));
#130269=CARTESIAN_POINT('Ctrl Pts',(25.2730901415187,1076.42473350737,516.652532350241));
#130270=CARTESIAN_POINT('Ctrl Pts',(26.0926780746722,1076.42473350737,516.419575929826));
#130271=CARTESIAN_POINT('Origin',(0.,1082.7251047501,424.620242579854));
#130272=CARTESIAN_POINT('Ctrl Pts',(31.867100541542,1076.6273958791,509.923777861397));
#130273=CARTESIAN_POINT('Ctrl Pts',(32.8224307605543,1076.6273958791,509.566892252387));
#130274=CARTESIAN_POINT('Ctrl Pts',(33.7716315198204,1076.6273958791,509.19401012103));
#130275=CARTESIAN_POINT('Ctrl Pts',(34.7144349873161,1076.6273958791,508.805236681924));
#130276=CARTESIAN_POINT('Ctrl Pts',(31.5136676399737,1076.66220181075,508.977690031747));
#130277=CARTESIAN_POINT('Ctrl Pts',(32.4584024447335,1076.66220181075,508.624762583792));
#130278=CARTESIAN_POINT('Ctrl Pts',(33.3970757706022,1076.66220181075,508.256016028355));
#130279=CARTESIAN_POINT('Ctrl Pts',(34.3294227560376,1076.66220181075,507.871554413115));
#130280=CARTESIAN_POINT('Ctrl Pts',(31.1628674174928,1076.68826959406,508.038649496315));
#130281=CARTESIAN_POINT('Ctrl Pts',(32.097085731964,1076.68826959406,507.689650725552));
#130282=CARTESIAN_POINT('Ctrl Pts',(33.0253100420179,1076.68826959406,507.325008940628));
#130283=CARTESIAN_POINT('Ctrl Pts',(33.9472784344677,1076.68826959406,506.944827030996));
#130284=CARTESIAN_POINT('Ctrl Pts',(30.8147012693935,1076.70560534914,507.1066599901));
#130285=CARTESIAN_POINT('Ctrl Pts',(31.7384820593689,1076.70560534914,506.761560397037));
#130286=CARTESIAN_POINT('Ctrl Pts',(32.6563358127511,1076.70560534914,506.400992560893));
#130287=CARTESIAN_POINT('Ctrl Pts',(33.5680035425704,1076.70560534914,506.025058221592));
#130288=CARTESIAN_POINT('Origin',(0.,1082.7251047501,424.620242579854));
#130289=CARTESIAN_POINT('Ctrl Pts',(-20.0609463067695,1074.64954802915,
535.919523414127));
#130290=CARTESIAN_POINT('Ctrl Pts',(-19.3257242373893,1074.64954802915,
536.05204224396));
#130291=CARTESIAN_POINT('Ctrl Pts',(-18.5892252109256,1074.64954802915,
536.177269699343));
#130292=CARTESIAN_POINT('Ctrl Pts',(-17.8515215358667,1074.64954802915,
536.295193485614));
#130293=CARTESIAN_POINT('Ctrl Pts',(-19.9293635146521,1074.75341498236,
535.189494535684));
#130294=CARTESIAN_POINT('Ctrl Pts',(-19.1989638784332,1074.75341498236,
535.321144154395));
#130295=CARTESIAN_POINT('Ctrl Pts',(-18.467295660886,1074.75341498236,535.44555022389));
#130296=CARTESIAN_POINT('Ctrl Pts',(-17.7344306962167,1074.75341498236,
535.562700530145));
#130297=CARTESIAN_POINT('Ctrl Pts',(-19.7983704549659,1074.85338735602,
534.462737526598));
#130298=CARTESIAN_POINT('Ctrl Pts',(-19.072771638556,1074.85338735602,534.593521829849));
#130299=CARTESIAN_POINT('Ctrl Pts',(-18.3459125790345,1074.85338735602,
534.71711019477));
#130300=CARTESIAN_POINT('Ctrl Pts',(-17.6178646384507,1074.85338735602,
534.833490487621));
#130301=CARTESIAN_POINT('Ctrl Pts',(-19.6679673366353,1074.94946695803,
533.739253545992));
#130302=CARTESIAN_POINT('Ctrl Pts',(-18.9471477190252,1074.94946695803,
533.869176430824));
#130303=CARTESIAN_POINT('Ctrl Pts',(-18.2250761589681,1074.94946695803,
533.991950773792));
#130304=CARTESIAN_POINT('Ctrl Pts',(-17.5018235484828,1074.94946695803,
534.107564521076));
#130305=CARTESIAN_POINT('Origin',(0.,1082.7251047501,424.620242579854));
#130306=CARTESIAN_POINT('Ctrl Pts',(-7.18812240170579,1075.53634869535,
530.365286015731));
#130307=CARTESIAN_POINT('Ctrl Pts',(-6.43769521904607,1075.53634869535,
530.416297034946));
#130308=CARTESIAN_POINT('Ctrl Pts',(-5.68676756649073,1075.53634869535,
530.459317276502));
#130309=CARTESIAN_POINT('Ctrl Pts',(-4.93542452985916,1075.53634869535,
530.494341865881));
#130310=CARTESIAN_POINT('Ctrl Pts',(-7.13741356032504,1075.61800315405,
529.619304195344));
#130311=CARTESIAN_POINT('Ctrl Pts',(-6.39228029043513,1075.61800315405,
529.669955355678));
#130312=CARTESIAN_POINT('Ctrl Pts',(-5.64665008123061,1075.61800315405,
529.712672109553));
#130313=CARTESIAN_POINT('Ctrl Pts',(-4.90060741829024,1075.61800315405,
529.747449616836));
#130314=CARTESIAN_POINT('Ctrl Pts',(-7.08694799094726,1075.69546670263,
528.876901168845));
#130315=CARTESIAN_POINT('Ctrl Pts',(-6.3470832366631,1075.69546670263,528.927194196695));
#130316=CARTESIAN_POINT('Ctrl Pts',(-5.60672505670767,1075.69546670263,
528.969608918849));
#130317=CARTESIAN_POINT('Ctrl Pts',(-4.86595733929864,1075.69546670263,
529.004140529394));
#130318=CARTESIAN_POINT('Ctrl Pts',(-7.03672578293973,1075.76874136376,
528.138078250924));
#130319=CARTESIAN_POINT('Ctrl Pts',(-6.3021041377675,1075.76874136376,528.188014873321));
#130320=CARTESIAN_POINT('Ctrl Pts',(-5.56699256362338,1075.76874136376,
528.230129020248));
#130321=CARTESIAN_POINT('Ctrl Pts',(-4.83147435424468,1075.76874136376,
528.264415919851));
#130322=CARTESIAN_POINT('Origin',(0.,1082.7251047501,424.620242579854));
#130323=CARTESIAN_POINT('Ctrl Pts',(3.98619775720727,1076.25727779325,522.565780470137));
#130324=CARTESIAN_POINT('Ctrl Pts',(4.86230647016848,1076.25727779325,522.530124505997));
#130325=CARTESIAN_POINT('Ctrl Pts',(5.73785795148452,1076.25727779325,522.482717457253));
#130326=CARTESIAN_POINT('Ctrl Pts',(6.61269459313368,1076.25727779325,522.42356785765));
#130327=CARTESIAN_POINT('Ctrl Pts',(3.95094675756026,1076.3190144058,521.69962220808));
#130328=CARTESIAN_POINT('Ctrl Pts',(4.81930780976492,1076.3190144058,521.664281559049));
#130329=CARTESIAN_POINT('Ctrl Pts',(5.68711655807104,1076.3190144058,521.617293743359));
#130330=CARTESIAN_POINT('Ctrl Pts',(6.55421678822626,1076.3190144058,521.558667219288));
#130331=CARTESIAN_POINT('Ctrl Pts',(3.91590644763562,1076.37471618392,520.838640838752));
#130332=CARTESIAN_POINT('Ctrl Pts',(4.7765661456427,1076.37471618392,520.803613620241));
#130333=CARTESIAN_POINT('Ctrl Pts',(5.6366784380455,1076.37471618392,520.757042531915));
#130334=CARTESIAN_POINT('Ctrl Pts',(6.49608849603066,1076.37471618392,520.698935957035));
#130335=CARTESIAN_POINT('Ctrl Pts',(3.88107692026826,1076.42438663189,519.982838643216));
#130336=CARTESIAN_POINT('Ctrl Pts',(4.73408159104051,1076.42438663189,519.948122969804));
#130337=CARTESIAN_POINT('Ctrl Pts',(5.58654372503737,1076.42438663189,519.901966102047));
#130338=CARTESIAN_POINT('Ctrl Pts',(6.4383098705505,1076.42438663189,519.84437634864));
#130339=CARTESIAN_POINT('Origin',(0.,1082.7251047501,424.620242579854));
#130340=CARTESIAN_POINT('Ctrl Pts',(13.4352335940896,1076.62753213844,514.681218805467));
#130341=CARTESIAN_POINT('Ctrl Pts',(14.4439034065725,1076.62753213844,514.530746146631));
#130342=CARTESIAN_POINT('Ctrl Pts',(15.4499032260186,1076.62753213844,514.36335088103));
#130343=CARTESIAN_POINT('Ctrl Pts',(16.4529491598105,1076.62753213844,514.179080247518));
#130344=CARTESIAN_POINT('Ctrl Pts',(13.2864477959342,1076.66226255021,513.683856598361));
#130345=CARTESIAN_POINT('Ctrl Pts',(14.2839472970061,1076.66226255021,513.535050318788));
#130346=CARTESIAN_POINT('Ctrl Pts',(15.2788063733432,1076.66226255021,513.369508838461));
#130347=CARTESIAN_POINT('Ctrl Pts',(16.2707442762401,1076.66226255021,513.187278873099));
#130348=CARTESIAN_POINT('Ctrl Pts',(13.1387686281562,1076.68828128334,512.693912514015));
#130349=CARTESIAN_POINT('Ctrl Pts',(14.1251808997112,1076.68828128334,512.546760219605));
#130350=CARTESIAN_POINT('Ctrl Pts',(15.1089820949122,1076.68828128334,512.383058736577));
#130351=CARTESIAN_POINT('Ctrl Pts',(16.0898945855816,1076.68828128334,512.202854261401));
#130352=CARTESIAN_POINT('Ctrl Pts',(12.9921966763696,1076.7055944302,511.711390478002));
#130353=CARTESIAN_POINT('Ctrl Pts',(13.9676048442678,1076.7055944302,511.565879768097));
#130354=CARTESIAN_POINT('Ctrl Pts',(14.9404310641548,1076.7055944302,511.404004487093));
#130355=CARTESIAN_POINT('Ctrl Pts',(15.9104008049853,1076.7055944302,511.22581031611));
#130356=CARTESIAN_POINT('Origin',(0.,1082.7251047501,424.620242579854));
#130357=CARTESIAN_POINT('Ctrl Pts',(-42.7617176792035,1074.64965272011,
529.316173097487));
#130358=CARTESIAN_POINT('Ctrl Pts',(-42.0711681572054,1074.64965272011,
529.598219243476));
#130359=CARTESIAN_POINT('Ctrl Pts',(-41.3778620576057,1074.64965272011,
529.87341975775));
#130360=CARTESIAN_POINT('Ctrl Pts',(-40.6818672413462,1074.64965272011,
530.141747703627));
#130361=CARTESIAN_POINT('Ctrl Pts',(-42.4809605599403,1074.75361908038,
528.628779572484));
#130362=CARTESIAN_POINT('Ctrl Pts',(-41.7949449225714,1074.75361908038,
528.908973911114));
#130363=CARTESIAN_POINT('Ctrl Pts',(-41.1061908062375,1074.75361908038,
529.182367563835));
#130364=CARTESIAN_POINT('Ctrl Pts',(-40.4147656263312,1074.75361908038,
529.448933770821));
#130365=CARTESIAN_POINT('Ctrl Pts',(-42.2014629878619,1074.8536832068,527.944469868049));
#130366=CARTESIAN_POINT('Ctrl Pts',(-41.5199608949733,1074.8536832068,528.222820706996));
#130367=CARTESIAN_POINT('Ctrl Pts',(-40.8357383405612,1074.8536832068,528.494415604201));
#130368=CARTESIAN_POINT('Ctrl Pts',(-40.148862296468,1074.8536832068,528.759227975899));
#130369=CARTESIAN_POINT('Ctrl Pts',(-41.923225409626,1074.94984691261,527.263245077761));
#130370=CARTESIAN_POINT('Ctrl Pts',(-41.2462165138558,1074.94984691261,
527.539760727644));
#130371=CARTESIAN_POINT('Ctrl Pts',(-40.5665050927797,1074.94984691261,
527.809564978243));
#130372=CARTESIAN_POINT('Ctrl Pts',(-39.8841576766896,1074.94984691261,
528.072631421062));
#130373=CARTESIAN_POINT('Origin',(0.,1082.7251047501,424.620242579854));
#130374=CARTESIAN_POINT('Ctrl Pts',(-29.0176510102205,1075.53628195624,
526.560366125851));
#130375=CARTESIAN_POINT('Ctrl Pts',(-28.2931960294411,1075.53628195624,
526.766585042148));
#130376=CARTESIAN_POINT('Ctrl Pts',(-27.5665839967992,1075.53628195624,
526.965069839135));
#130377=CARTESIAN_POINT('Ctrl Pts',(-26.8378974774944,1075.53628195624,
527.155797962909));
#130378=CARTESIAN_POINT('Ctrl Pts',(-28.8128258799699,1075.61798649467,
525.840807569036));
#130379=CARTESIAN_POINT('Ctrl Pts',(-28.0934845655498,1075.61798649467,
526.045570860397));
#130380=CARTESIAN_POINT('Ctrl Pts',(-27.3720014251182,1075.61798649467,
526.242654624806));
#130381=CARTESIAN_POINT('Ctrl Pts',(-26.6484584410766,1075.61798649467,
526.43203646756));
#130382=CARTESIAN_POINT('Ctrl Pts',(-28.6089839559804,1075.69549521486,
525.124703053615));
#130383=CARTESIAN_POINT('Ctrl Pts',(-27.8947317611819,1075.69549521486,
525.328017707364));
#130384=CARTESIAN_POINT('Ctrl Pts',(-27.1783528931352,1075.69549521486,
525.523707164464));
#130385=CARTESIAN_POINT('Ctrl Pts',(-26.4599287542417,1075.69549521486,
525.711749188647));
#130386=CARTESIAN_POINT('Ctrl Pts',(-28.4061255996499,1075.76881014303,
524.412053849191));
#130387=CARTESIAN_POINT('Ctrl Pts',(-27.6969379687123,1075.76881014303,
524.613926855221));
#130388=CARTESIAN_POINT('Ctrl Pts',(-26.9856387441757,1075.76881014303,
524.808228732752));
#130389=CARTESIAN_POINT('Ctrl Pts',(-26.2723087512395,1075.76881014303,
524.994937403189));
#130390=CARTESIAN_POINT('Origin',(0.,1082.7251047501,424.620242579854));
#130391=CARTESIAN_POINT('Ctrl Pts',(-16.4646989908154,1076.25701255651,
521.258029889561));
#130392=CARTESIAN_POINT('Ctrl Pts',(-15.6004015618574,1076.25701255651,
521.405284885795));
#130393=CARTESIAN_POINT('Ctrl Pts',(-14.7342065197343,1076.25701255651,
521.540932328162));
#130394=CARTESIAN_POINT('Ctrl Pts',(-13.8662697472228,1076.25701255651,
521.664947805186));
#130395=CARTESIAN_POINT('Ctrl Pts',(-16.3187084370332,1076.31893267559,
520.401153970147));
#130396=CARTESIAN_POINT('Ctrl Pts',(-15.4620746319505,1076.31893267559,
520.54710327361));
#130397=CARTESIAN_POINT('Ctrl Pts',(-14.603560039616,1076.31893267559,520.681547946024));
#130398=CARTESIAN_POINT('Ctrl Pts',(-13.743319160612,1076.31893267559,520.804463792367));
#130399=CARTESIAN_POINT('Ctrl Pts',(-16.173592779169,1076.37478542332,519.54941315862));
#130400=CARTESIAN_POINT('Ctrl Pts',(-15.3245766712008,1076.37478542332,
519.694064594101));
#130401=CARTESIAN_POINT('Ctrl Pts',(-14.4736965010593,1076.37478542332,
519.827313704553));
#130402=CARTESIAN_POINT('Ctrl Pts',(-13.6211053954157,1076.37478542332,
519.949136510109));
#130403=CARTESIAN_POINT('Ctrl Pts',(-16.0293524037607,1076.42457433234,
518.702809723722));
#130404=CARTESIAN_POINT('Ctrl Pts',(-15.1879080458553,1076.42457433234,
518.846171119467));
#130405=CARTESIAN_POINT('Ctrl Pts',(-14.3446162499757,1076.42457433234,
518.978231879131));
#130406=CARTESIAN_POINT('Ctrl Pts',(-13.4996287771691,1076.42457433234,
519.098968236707));
#130407=CARTESIAN_POINT('Origin',(0.,1082.7251047501,424.620242579854));
#130408=CARTESIAN_POINT('Ctrl Pts',(-5.58190196061815,1076.62744005165,
515.509263604268));
#130409=CARTESIAN_POINT('Ctrl Pts',(-4.56636243499452,1076.62744005165,
515.571632436116));
#130410=CARTESIAN_POINT('Ctrl Pts',(-3.54992031559118,1076.62744005165,
515.616973556448));
#130411=CARTESIAN_POINT('Ctrl Pts',(-2.53286108863103,1076.62744005165,
515.645274230384));
#130412=CARTESIAN_POINT('Ctrl Pts',(-5.52010923061872,1076.66217353754,
514.503104632702));
#130413=CARTESIAN_POINT('Ctrl Pts',(-4.51581192317688,1076.66217353754,
514.564783029568));
#130414=CARTESIAN_POINT('Ctrl Pts',(-3.51062201384234,1076.66217353754,
514.609622214962));
#130415=CARTESIAN_POINT('Ctrl Pts',(-2.50482182845053,1076.66217353754,
514.637609594987));
#130416=CARTESIAN_POINT('Ctrl Pts',(-5.45877592976358,1076.68820151705,
513.504426456294));
#130417=CARTESIAN_POINT('Ctrl Pts',(-4.46563725457555,1076.68820151705,
513.565419551563));
#130418=CARTESIAN_POINT('Ctrl Pts',(-3.47161589509213,1076.68820151705,
513.609760533908));
#130419=CARTESIAN_POINT('Ctrl Pts',(-2.47699104025874,1076.68820151705,
513.637436949361));
#130420=CARTESIAN_POINT('Ctrl Pts',(-5.39790230109045,1076.70553007605,
512.513233032379));
#130421=CARTESIAN_POINT('Ctrl Pts',(-4.41583862801136,1076.70553007605,
512.573545962152));
#130422=CARTESIAN_POINT('Ctrl Pts',(-3.43290211390516,1076.70553007605,
512.617392475312));
#130423=CARTESIAN_POINT('Ctrl Pts',(-2.44936883433722,1076.70553007605,
512.644760256767));
#130424=CARTESIAN_POINT('Origin',(0.,1082.7251047501,424.620242579854));
#130425=CARTESIAN_POINT('Ctrl Pts',(-63.5965651485269,1074.64936691183,
518.138908889593));
#130426=CARTESIAN_POINT('Ctrl Pts',(-62.9786024477089,1074.64936691183,
518.559149112349));
#130427=CARTESIAN_POINT('Ctrl Pts',(-62.3565048751138,1074.64936691183,
518.973243732692));
#130428=CARTESIAN_POINT('Ctrl Pts',(-61.7303335462127,1074.64936691183,
519.381152069561));
#130429=CARTESIAN_POINT('Ctrl Pts',(-63.1793148961809,1074.75326661151,
517.525342936374));
#130430=CARTESIAN_POINT('Ctrl Pts',(-62.5654065824553,1074.75326661151,
517.94282600804));
#130431=CARTESIAN_POINT('Ctrl Pts',(-61.9473905254034,1074.75326661151,
518.35420379793));
#130432=CARTESIAN_POINT('Ctrl Pts',(-61.3253274395243,1074.75326661151,
518.75943589189));
#130433=CARTESIAN_POINT('Ctrl Pts',(-62.7639351887473,1074.85326961418,
516.914527617015));
#130434=CARTESIAN_POINT('Ctrl Pts',(-62.1540630861798,1074.85326961418,
517.329265897978));
#130435=CARTESIAN_POINT('Ctrl Pts',(-61.5401102471193,1074.85326961418,
517.737939037045));
#130436=CARTESIAN_POINT('Ctrl Pts',(-60.9221369868903,1074.85326961418,
518.140506885771));
#130437=CARTESIAN_POINT('Ctrl Pts',(-62.3504266890833,1074.94937772924,
516.306463906247));
#130438=CARTESIAN_POINT('Ctrl Pts',(-61.7445726152988,1074.94937772924,
516.718469761274));
#130439=CARTESIAN_POINT('Ctrl Pts',(-61.1346646901937,1074.94937772924,
517.124450433464));
#130440=CARTESIAN_POINT('Ctrl Pts',(-60.5207628317164,1074.94937772924,
517.524366038881));
#130441=CARTESIAN_POINT('Origin',(0.,1082.7251047501,424.620242579854));
#130442=CARTESIAN_POINT('Ctrl Pts',(-49.5774617998323,1075.53622510687,
518.300541925841));
#130443=CARTESIAN_POINT('Ctrl Pts',(-48.911899503254,1075.53622510687,518.652770618153));
#130444=CARTESIAN_POINT('Ctrl Pts',(-48.2426214679627,1075.53622510687,
518.997886734541));
#130445=CARTESIAN_POINT('Ctrl Pts',(-47.569703700229,1075.53622510687,519.335851082043));
#130446=CARTESIAN_POINT('Ctrl Pts',(-49.2269716736319,1075.61805805635,
517.638264779164));
#130447=CARTESIAN_POINT('Ctrl Pts',(-48.5661146000491,1075.61805805635,
517.988003374679));
#130448=CARTESIAN_POINT('Ctrl Pts',(-47.9015680563376,1075.61805805635,
518.33067967695));
#130449=CARTESIAN_POINT('Ctrl Pts',(-47.2334075114381,1075.61805805635,
518.666254770092));
#130450=CARTESIAN_POINT('Ctrl Pts',(-48.8781665782885,1075.69568218855,
516.979171623546));
#130451=CARTESIAN_POINT('Ctrl Pts',(-48.2219921066762,1075.69568218855,
517.326432093757));
#130452=CARTESIAN_POINT('Ctrl Pts',(-47.5621543072295,1075.69568218855,
517.666680311663));
#130453=CARTESIAN_POINT('Ctrl Pts',(-46.8987281141425,1075.69568218855,
517.999877637121));
#130454=CARTESIAN_POINT('Ctrl Pts',(-48.5310471341285,1075.7690995391,516.32326363114));
#130455=CARTESIAN_POINT('Ctrl Pts',(-47.8795326351339,1075.7690995391,516.668057951947));
#130456=CARTESIAN_POINT('Ctrl Pts',(-47.2243808242627,1075.7690995391,517.005889819556));
#130457=CARTESIAN_POINT('Ctrl Pts',(-46.5656661035469,1075.7690995391,517.336720868239));
#130458=CARTESIAN_POINT('Origin',(0.,1082.7251047501,424.620242579854));
#130459=CARTESIAN_POINT('Ctrl Pts',(-36.1968662814073,1076.25723523531,
515.719760643928));
#130460=CARTESIAN_POINT('Ctrl Pts',(-35.3839173772627,1076.25723523531,
516.042772262456));
#130461=CARTESIAN_POINT('Ctrl Pts',(-34.5667178457009,1076.25723523531,
516.354873771694));
#130462=CARTESIAN_POINT('Ctrl Pts',(-33.7454140973306,1076.25723523531,
516.6560092551));
#130463=CARTESIAN_POINT('Ctrl Pts',(-35.8758056493458,1076.31916041081,
514.911721941828));
#130464=CARTESIAN_POINT('Ctrl Pts',(-35.0700674768422,1076.31916041081,
515.23186849702));
#130465=CARTESIAN_POINT('Ctrl Pts',(-34.2601163793322,1076.31916041081,
515.541201713914));
#130466=CARTESIAN_POINT('Ctrl Pts',(-33.4460974687851,1076.31916041081,
515.839666171937));
#130467=CARTESIAN_POINT('Ctrl Pts',(-35.5566697156339,1076.37501437569,
514.108527280388));
#130468=CARTESIAN_POINT('Ctrl Pts',(-34.7580990477857,1076.37501437569,
514.425825947764));
#130469=CARTESIAN_POINT('Ctrl Pts',(-33.9553529313231,1076.37501437569,
514.732407467707));
#130470=CARTESIAN_POINT('Ctrl Pts',(-33.148575187361,1076.37501437569,515.028216912643));
#130471=CARTESIAN_POINT('Ctrl Pts',(-35.2394593308914,1076.42480066596,
513.310178800431));
#130472=CARTESIAN_POINT('Ctrl Pts',(-34.448012921609,1076.42480066596,513.624646763099));
#130473=CARTESIAN_POINT('Ctrl Pts',(-33.6524283139854,1076.42480066596,
513.92849318882));
#130474=CARTESIAN_POINT('Ctrl Pts',(-32.8528480460696,1076.42480066596,
514.221663640044));
#130475=CARTESIAN_POINT('Origin',(0.,1082.7251047501,424.620242579854));
#130476=CARTESIAN_POINT('Ctrl Pts',(-24.3584940949169,1076.62734697186,
512.364914333088));
#130477=CARTESIAN_POINT('Ctrl Pts',(-23.3756297382246,1076.62734697186,
512.637763899338));
#130478=CARTESIAN_POINT('Ctrl Pts',(-22.3883200821596,1076.62734697186,
512.894062304522));
#130479=CARTESIAN_POINT('Ctrl Pts',(-21.3968438225608,1076.62734697186,
513.133737201227));
#130480=CARTESIAN_POINT('Ctrl Pts',(-24.0886312393208,1076.66212359129,
511.39280876735));
#130481=CARTESIAN_POINT('Ctrl Pts',(-23.116655839102,1076.66212359129,511.662635488148));
#130482=CARTESIAN_POINT('Ctrl Pts',(-22.1402843880881,1076.66212359129,
511.916094414863));
#130483=CARTESIAN_POINT('Ctrl Pts',(-21.1597924945025,1076.66212359129,
512.153114001606));
#130484=CARTESIAN_POINT('Ctrl Pts',(-23.8207763800282,1076.68818087236,
510.42793644747));
#130485=CARTESIAN_POINT('Ctrl Pts',(-22.8596089137046,1076.68818087236,
510.694762815213));
#130486=CARTESIAN_POINT('Ctrl Pts',(-21.8940942787144,1076.68818087236,
510.945403391459));
#130487=CARTESIAN_POINT('Ctrl Pts',(-20.9245050186402,1076.68818087236,
511.179787425878));
#130488=CARTESIAN_POINT('Ctrl Pts',(-23.5549305801114,1076.70552491543,
509.47030120287));
#130489=CARTESIAN_POINT('Ctrl Pts',(-22.6044899822098,1076.70552491543,
509.734149721862));
#130490=CARTESIAN_POINT('Ctrl Pts',(-21.6497507311271,1076.70552491543,
509.981993086825));
#130491=CARTESIAN_POINT('Ctrl Pts',(-20.6909823287917,1076.70552491543,
510.213761337017));
#130492=CARTESIAN_POINT('Origin',(0.,1082.7251047501,424.620242579854));
#130493=CARTESIAN_POINT('Ctrl Pts',(-81.6487557536238,1074.64931959703,
502.875090091892));
#130494=CARTESIAN_POINT('Ctrl Pts',(-81.1322577363025,1074.64931959703,
503.413988598556));
#130495=CARTESIAN_POINT('Ctrl Pts',(-80.6104499440739,1074.64931959703,
503.947747373989));
#130496=CARTESIAN_POINT('Ctrl Pts',(-80.0833835204045,1074.64931959703,
504.476314103383));
#130497=CARTESIAN_POINT('Ctrl Pts',(-81.1119145088187,1074.75344418584,
502.360563821863));
#130498=CARTESIAN_POINT('Ctrl Pts',(-80.5988124702359,1074.75344418584,
502.895919066386));
#130499=CARTESIAN_POINT('Ctrl Pts',(-80.0804355685597,1074.75344418584,
503.426168373453));
#130500=CARTESIAN_POINT('Ctrl Pts',(-79.5568346109878,1074.75344418584,
503.951259772227));
#130501=CARTESIAN_POINT('Ctrl Pts',(-80.5774851171265,1074.85365527957,
501.848349151023));
#130502=CARTESIAN_POINT('Ctrl Pts',(-80.0677638002541,1074.85365527957,
502.380177052129));
#130503=CARTESIAN_POINT('Ctrl Pts',(-79.5528023752549,1074.85365527957,
502.906932657731));
#130504=CARTESIAN_POINT('Ctrl Pts',(-79.0326513145686,1074.85365527957,
503.428564339414));
#130505=CARTESIAN_POINT('Ctrl Pts',(-80.045468435066,1074.94995469931,501.338446900288));
#130506=CARTESIAN_POINT('Ctrl Pts',(-79.5391125774579,1074.94995469931,
501.866763382355));
#130507=CARTESIAN_POINT('Ctrl Pts',(-79.0275512097863,1074.94995469931,
502.390041058989));
#130508=CARTESIAN_POINT('Ctrl Pts',(-78.5108344712444,1074.94995469931,
502.908228642658));
#130509=CARTESIAN_POINT('Origin',(0.,1082.7251047501,424.620242579854));
#130510=CARTESIAN_POINT('Ctrl Pts',(-67.9701058202362,1075.5367489508,505.940418806113));
#130511=CARTESIAN_POINT('Ctrl Pts',(-67.3934113371822,1075.5367489508,506.422439220457));
#130512=CARTESIAN_POINT('Ctrl Pts',(-66.8116221918185,1075.5367489508,506.898298019857));
#130513=CARTESIAN_POINT('Ctrl Pts',(-66.2248042139591,1075.5367489508,507.367941360586));
#130514=CARTESIAN_POINT('Ctrl Pts',(-67.4905656334257,1075.61839547079,
505.366691694342));
#130515=CARTESIAN_POINT('Ctrl Pts',(-66.9179398240452,1075.61839547079,
505.845311376015));
#130516=CARTESIAN_POINT('Ctrl Pts',(-66.3402552960289,1075.61839547079,
506.317812913943));
#130517=CARTESIAN_POINT('Ctrl Pts',(-65.7575774147506,1075.61839547079,
506.784142844273));
#130518=CARTESIAN_POINT('Ctrl Pts',(-67.01332620572,1075.6958504928,504.795717235868));
#130519=CARTESIAN_POINT('Ctrl Pts',(-66.4447495491506,1075.6958504928,505.270952501055));
#130520=CARTESIAN_POINT('Ctrl Pts',(-65.8711499451671,1075.6958504928,505.740112885127));
#130521=CARTESIAN_POINT('Ctrl Pts',(-65.2925922969317,1075.6958504928,506.203145302288));
#130522=CARTESIAN_POINT('Ctrl Pts',(-66.5383883823746,1075.76911603994,
504.227496441963));
#130523=CARTESIAN_POINT('Ctrl Pts',(-65.9738413505823,1075.76911603994,
504.699363612844));
#130524=CARTESIAN_POINT('Ctrl Pts',(-65.4043069700822,1075.76911603994,
505.165198956596));
#130525=CARTESIAN_POINT('Ctrl Pts',(-64.8298496840536,1075.76911603994,
505.624949763653));
#130526=CARTESIAN_POINT('Origin',(0.,1082.7251047501,424.620242579854));
#130527=CARTESIAN_POINT('Ctrl Pts',(-54.3493735289956,1076.25693128953,
506.206500653992));
#130528=CARTESIAN_POINT('Ctrl Pts',(-53.6191815405488,1076.25693128953,
506.692924202084));
#130529=CARTESIAN_POINT('Ctrl Pts',(-52.8825255487871,1076.25693128953,
507.169501748694));
#130530=CARTESIAN_POINT('Ctrl Pts',(-52.1395383098849,1076.25693128953,
507.636147407581));
#130531=CARTESIAN_POINT('Ctrl Pts',(-53.8678157746301,1076.31881191121,
505.483612924582));
#130532=CARTESIAN_POINT('Ctrl Pts',(-53.1440935868706,1076.31881191121,
505.96572656041));
#130533=CARTESIAN_POINT('Ctrl Pts',(-52.4139646695184,1076.31881191121,
506.43808143437));
#130534=CARTESIAN_POINT('Ctrl Pts',(-51.6775606024737,1076.31881191121,
506.900592421209));
#130535=CARTESIAN_POINT('Ctrl Pts',(-53.3891418081157,1076.37463393687,
504.765054177174));
#130536=CARTESIAN_POINT('Ctrl Pts',(-52.671850676921,1076.37463393687,505.242883710463));
#130537=CARTESIAN_POINT('Ctrl Pts',(-51.9482097468746,1076.37463393687,
505.711041199065));
#130538=CARTESIAN_POINT('Ctrl Pts',(-51.2183494286465,1076.37463393687,
506.169442274161));
#130539=CARTESIAN_POINT('Ctrl Pts',(-52.9133529026173,1076.42440089149,
504.050826322972));
#130540=CARTESIAN_POINT('Ctrl Pts',(-52.2024540667598,1076.42440089149,
504.52439757484));
#130541=CARTESIAN_POINT('Ctrl Pts',(-51.4852620196589,1076.42440089149,
504.988382976543));
#130542=CARTESIAN_POINT('Ctrl Pts',(-50.7619060098017,1076.42440089149,
505.442698911133));
#130543=CARTESIAN_POINT('Origin',(0.,1082.7251047501,424.620242579854));
#130544=CARTESIAN_POINT('Ctrl Pts',(-42.0660921733734,1076.62733098606,
505.385284537138));
#130545=CARTESIAN_POINT('Ctrl Pts',(-41.1625853458286,1076.62733098606,
505.855871818042));
#130546=CARTESIAN_POINT('Ctrl Pts',(-40.2513098605778,1076.62733098606,
506.311233176031));
#130547=CARTESIAN_POINT('Ctrl Pts',(-39.332522282548,1076.62733098606,506.751240406456));
#130548=CARTESIAN_POINT('Ctrl Pts',(-41.5990376134109,1076.66218595673,
504.488560378016));
#130549=CARTESIAN_POINT('Ctrl Pts',(-40.7055623091657,1076.66218595673,
504.953922787199));
#130550=CARTESIAN_POINT('Ctrl Pts',(-39.8044046016495,1076.66218595673,
505.404228324985));
#130551=CARTESIAN_POINT('Ctrl Pts',(-38.8958182071807,1076.66218595673,
505.839350210165));
#130552=CARTESIAN_POINT('Ctrl Pts',(-41.135465868248,1076.68828360045,503.598523069725));
#130553=CARTESIAN_POINT('Ctrl Pts',(-40.2519472824706,1076.68828360045,
504.058699568932));
#130554=CARTESIAN_POINT('Ctrl Pts',(-39.3608319046597,1076.68828360045,
504.503986987646));
#130555=CARTESIAN_POINT('Ctrl Pts',(-38.4623706237676,1076.68828360045,
504.934259957486));
#130556=CARTESIAN_POINT('Ctrl Pts',(-40.675378785767,1076.70563005751,502.715176160118));
#130557=CARTESIAN_POINT('Ctrl Pts',(-39.8017420739363,1076.70563005751,
503.170205731766));
#130558=CARTESIAN_POINT('Ctrl Pts',(-38.9205935377711,1076.70563005751,
503.610512752543));
#130559=CARTESIAN_POINT('Ctrl Pts',(-38.0321812601107,1076.70563005751,
504.035973256274));
#130560=CARTESIAN_POINT('Origin',(0.,1082.7251047501,424.620242579854));
#130561=CARTESIAN_POINT('Ctrl Pts',(-96.131601715426,1074.65015601416,484.182852263091));
#130562=CARTESIAN_POINT('Ctrl Pts',(-95.7386795646446,1074.65015601416,
484.817012450245));
#130563=CARTESIAN_POINT('Ctrl Pts',(-95.3395017199826,1074.65015601416,
485.447253680153));
#130564=CARTESIAN_POINT('Ctrl Pts',(-94.9341072652433,1074.65015601416,
486.073514245423));
#130565=CARTESIAN_POINT('Ctrl Pts',(-95.5012439298025,1074.7539752954,483.792286059305));
#130566=CARTESIAN_POINT('Ctrl Pts',(-95.1108982630542,1074.7539752954,484.422287907222));
#130567=CARTESIAN_POINT('Ctrl Pts',(-94.7143379224985,1074.7539752954,485.048396495429));
#130568=CARTESIAN_POINT('Ctrl Pts',(-94.3116017356569,1074.7539752954,485.670550521162));
#130569=CARTESIAN_POINT('Ctrl Pts',(-94.8737104720578,1074.85390243578,
483.40346979348));
#130570=CARTESIAN_POINT('Ctrl Pts',(-94.4859297453657,1074.85390243578,
484.029331933664));
#130571=CARTESIAN_POINT('Ctrl Pts',(-94.0919751811483,1074.85390243578,
484.651326396534));
#130572=CARTESIAN_POINT('Ctrl Pts',(-93.6918853517936,1074.85390243578,
485.269392282145));
#130573=CARTESIAN_POINT('Ctrl Pts',(-94.2490023424518,1074.94993924152,
483.01640408537));
#130574=CARTESIAN_POINT('Ctrl Pts',(-93.8637750077506,1074.94993924152,
483.638145155924));
#130575=CARTESIAN_POINT('Ctrl Pts',(-93.4724144879501,1074.94993924152,
484.256044016381));
#130576=CARTESIAN_POINT('Ctrl Pts',(-93.0749591014535,1074.94993924152,
484.870040167801));
#130577=CARTESIAN_POINT('Origin',(0.,1082.7251047501,424.620242579854));
#130578=CARTESIAN_POINT('Ctrl Pts',(-83.396532923316,1075.53617509883,490.034603122049));
#130579=CARTESIAN_POINT('Ctrl Pts',(-82.9312588738367,1075.53617509883,
490.62777933388));
#130580=CARTESIAN_POINT('Ctrl Pts',(-82.4596828994069,1075.53617509883,
491.215957928986));
#130581=CARTESIAN_POINT('Ctrl Pts',(-81.981858676633,1075.53617509883,491.799071958599));
#130582=CARTESIAN_POINT('Ctrl Pts',(-82.808284881169,1075.61782568845,489.573194617781));
#130583=CARTESIAN_POINT('Ctrl Pts',(-82.34629270132,1075.61782568845,490.162186785827));
#130584=CARTESIAN_POINT('Ctrl Pts',(-81.8780430479488,1075.61782568845,
490.746216588473));
#130585=CARTESIAN_POINT('Ctrl Pts',(-81.4035892190472,1075.61782568845,
491.325217549183));
#130586=CARTESIAN_POINT('Ctrl Pts',(-82.2228585576068,1075.69528637324,
489.113999405966));
#130587=CARTESIAN_POINT('Ctrl Pts',(-81.7641325048579,1075.69528637324,
489.698827600322));
#130588=CARTESIAN_POINT('Ctrl Pts',(-81.2991932167898,1075.69528637324,
490.278728511509));
#130589=CARTESIAN_POINT('Ctrl Pts',(-80.8280936145958,1075.69528637324,
490.853636132955));
#130590=CARTESIAN_POINT('Ctrl Pts',(-81.6402549890788,1075.76855917516,
488.65701829957));
#130591=CARTESIAN_POINT('Ctrl Pts',(-81.1847793151174,1075.76855917516,
489.237702597704));
#130592=CARTESIAN_POINT('Ctrl Pts',(-80.7231344307362,1075.76855917516,
489.813494525742));
#130593=CARTESIAN_POINT('Ctrl Pts',(-80.2553728821466,1075.76855917516,
490.384328544814));
#130594=CARTESIAN_POINT('Origin',(0.,1082.7251047501,424.620242579854));
#130595=CARTESIAN_POINT('Ctrl Pts',(-70.1200501589484,1076.25692209858,
493.128459381365));
#130596=CARTESIAN_POINT('Ctrl Pts',(-69.5084690741912,1076.25692209858,
493.754429496216));
#130597=CARTESIAN_POINT('Ctrl Pts',(-68.8885611520353,1076.25692209858,
494.372154496493));
#130598=CARTESIAN_POINT('Ctrl Pts',(-68.2604375400634,1076.25692209858,
494.981523626005));
#130599=CARTESIAN_POINT('Ctrl Pts',(-69.4969951628274,1076.31897891888,
492.519726406178));
#130600=CARTESIAN_POINT('Ctrl Pts',(-68.8908483104976,1076.31897891888,
493.140134434199));
#130601=CARTESIAN_POINT('Ctrl Pts',(-68.2764486092736,1076.31897891888,
493.752370609999));
#130602=CARTESIAN_POINT('Ctrl Pts',(-67.6539062191311,1076.31897891888,
494.356325161516));
#130603=CARTESIAN_POINT('Ctrl Pts',(-68.8776818901403,1076.37494270955,
491.914649144295));
#130604=CARTESIAN_POINT('Ctrl Pts',(-68.276936635246,1076.37494270955,492.529528488301));
#130605=CARTESIAN_POINT('Ctrl Pts',(-67.668012075628,1076.37494270955,493.136308802465));
#130606=CARTESIAN_POINT('Ctrl Pts',(-67.0510173895858,1076.37494270955,
493.734881292945));
#130607=CARTESIAN_POINT('Ctrl Pts',(-68.2621119975104,1076.42481702568,
491.313229214258));
#130608=CARTESIAN_POINT('Ctrl Pts',(-67.6667356906106,1076.42481702568,
491.922613291853));
#130609=CARTESIAN_POINT('Ctrl Pts',(-67.0632531786269,1076.42481702568,
492.523970721817));
#130610=CARTESIAN_POINT('Ctrl Pts',(-66.4517726641162,1076.42481702568,
493.117193682615));
#130611=CARTESIAN_POINT('Origin',(0.,1082.7251047501,424.620242579854));
#130612=CARTESIAN_POINT('Ctrl Pts',(-57.9374139544679,1076.6276306297,494.864246584548));
#130613=CARTESIAN_POINT('Ctrl Pts',(-57.1515529148392,1076.6276306297,495.51242655391));
#130614=CARTESIAN_POINT('Ctrl Pts',(-56.3549261816959,1076.6276306297,496.147328667886));
#130615=CARTESIAN_POINT('Ctrl Pts',(-55.5477580706169,1076.6276306297,496.768774149603));
#130616=CARTESIAN_POINT('Ctrl Pts',(-57.2959682255943,1076.66233473874,
494.086550217513));
#130617=CARTESIAN_POINT('Ctrl Pts',(-56.5188077332104,1076.66233473874,
494.727553955758));
#130618=CARTESIAN_POINT('Ctrl Pts',(-55.7310007381363,1076.66233473874,
495.355426842478));
#130619=CARTESIAN_POINT('Ctrl Pts',(-54.9327690724731,1076.66233473874,
495.969992080104));
#130620=CARTESIAN_POINT('Ctrl Pts',(-56.659292123221,1076.68833210733,493.314636601901));
#130621=CARTESIAN_POINT('Ctrl Pts',(-55.8907674830364,1076.68833210733,
493.948517469649));
#130622=CARTESIAN_POINT('Ctrl Pts',(-55.1117146447132,1076.68833210733,
494.569413396651));
#130623=CARTESIAN_POINT('Ctrl Pts',(-54.3223529753417,1076.68833210733,
495.177149549924));
#130624=CARTESIAN_POINT('Ctrl Pts',(-56.0273881706553,1076.70562882264,
492.548508796999));
#130625=CARTESIAN_POINT('Ctrl Pts',(-55.2674346533982,1076.70562882264,
493.1753201831));
#130626=CARTESIAN_POINT('Ctrl Pts',(-54.497070355813,1076.70562882264,493.789291445574));
#130627=CARTESIAN_POINT('Ctrl Pts',(-53.7165121984548,1076.70562882264,
494.390249701295));
#130628=CARTESIAN_POINT('Origin',(0.,1082.7251047501,424.620242579854));
#130629=CARTESIAN_POINT('Ctrl Pts',(-106.420074485931,1074.64935171829,
462.896296919825));
#130630=CARTESIAN_POINT('Ctrl Pts',(-106.167092369887,1074.64935171829,
463.599670767973));
#130631=CARTESIAN_POINT('Ctrl Pts',(-105.907149585896,1074.64935171829,
464.300502038928));
#130632=CARTESIAN_POINT('Ctrl Pts',(-105.640271682601,1074.64935171829,
464.998721851043));
#130633=CARTESIAN_POINT('Ctrl Pts',(-105.721561764291,1074.75329679414,
462.645063202692));
#130634=CARTESIAN_POINT('Ctrl Pts',(-105.470240154756,1074.75329679414,
463.343820294243));
#130635=CARTESIAN_POINT('Ctrl Pts',(-105.212003565226,1074.75329679414,
464.040051497392));
#130636=CARTESIAN_POINT('Ctrl Pts',(-104.946877376646,1074.75329679414,
464.733688382615));
#130637=CARTESIAN_POINT('Ctrl Pts',(-105.026181850047,1074.85334179708,
462.39495626081));
#130638=CARTESIAN_POINT('Ctrl Pts',(-104.776513299703,1074.85334179708,
463.08911730177));
#130639=CARTESIAN_POINT('Ctrl Pts',(-104.519975252404,1074.85334179708,
463.780769068272));
#130640=CARTESIAN_POINT('Ctrl Pts',(-104.256592922156,1074.85334179708,
464.469843580884));
#130641=CARTESIAN_POINT('Ctrl Pts',(-104.33393585384,1074.94948853882,462.145976493642));
#130642=CARTESIAN_POINT('Ctrl Pts',(-104.085912912726,1074.94948853882,
462.835562197359));
#130643=CARTESIAN_POINT('Ctrl Pts',(-103.831065752719,1074.94948853882,
463.522655165687));
#130644=CARTESIAN_POINT('Ctrl Pts',(-103.569419421632,1074.94948853882,
464.207187867256));
#130645=CARTESIAN_POINT('Origin',(0.,1082.7251047501,424.620242579854));
#130646=CARTESIAN_POINT('Ctrl Pts',(-95.1717412686241,1075.53619529415,
471.271295452212));
#130647=CARTESIAN_POINT('Ctrl Pts',(-94.8408681026697,1075.53619529415,
471.946302197056));
#130648=CARTESIAN_POINT('Ctrl Pts',(-94.5028326909729,1075.53619529415,
472.617750793729));
#130649=CARTESIAN_POINT('Ctrl Pts',(-94.1576732917246,1075.53619529415,
473.285565248982));
#130650=CARTESIAN_POINT('Ctrl Pts',(-94.498905235811,1075.61803121392,470.941486320606));
#130651=CARTESIAN_POINT('Ctrl Pts',(-94.1703712451766,1075.61803121392,
471.611720967617));
#130652=CARTESIAN_POINT('Ctrl Pts',(-93.8347256437568,1075.61803121392,
472.27842262151));
#130653=CARTESIAN_POINT('Ctrl Pts',(-93.4920064192681,1075.61803121392,
472.941515826288));
#130654=CARTESIAN_POINT('Ctrl Pts',(-93.8293040304781,1075.69565811578,
470.613262828874));
#130655=CARTESIAN_POINT('Ctrl Pts',(-93.5030979689936,1075.69565811578,
471.278748321106));
#130656=CARTESIAN_POINT('Ctrl Pts',(-93.1698306882401,1075.69565811578,
471.940725854334));
#130657=CARTESIAN_POINT('Ctrl Pts',(-92.8295399067608,1075.69565811578,
472.599120507228));
#130658=CARTESIAN_POINT('Ctrl Pts',(-93.1629388435215,1075.76907803551,
470.286625560767));
#130659=CARTESIAN_POINT('Ctrl Pts',(-92.8390494608762,1075.76907803551,
470.947384849718));
#130660=CARTESIAN_POINT('Ctrl Pts',(-92.5081490069488,1075.76907803551,
471.604661092798));
#130661=CARTESIAN_POINT('Ctrl Pts',(-92.1702749324093,1075.76907803551,
472.258379900757));
#130662=CARTESIAN_POINT('Origin',(0.,1082.7251047501,424.620242579854));
#130663=CARTESIAN_POINT('Ctrl Pts',(-82.8304831843315,1076.25730969014,
477.043914818581));
#130664=CARTESIAN_POINT('Ctrl Pts',(-82.3617874431307,1076.25730969014,
477.78446375482));
#130665=CARTESIAN_POINT('Ctrl Pts',(-81.8832030846018,1076.25730969014,
478.518660892212));
#130666=CARTESIAN_POINT('Ctrl Pts',(-81.394816175536,1076.25730969014,479.246374195538));
#130667=CARTESIAN_POINT('Ctrl Pts',(-82.0961025158692,1076.31920325934,
476.579122993375));
#130668=CARTESIAN_POINT('Ctrl Pts',(-81.6315622628231,1076.31920325934,
477.313106172638));
#130669=CARTESIAN_POINT('Ctrl Pts',(-81.1572210655994,1076.31920325934,
478.040793868532));
#130670=CARTESIAN_POINT('Ctrl Pts',(-80.6731642279151,1076.31920325934,
478.762055216471));
#130671=CARTESIAN_POINT('Ctrl Pts',(-81.3661224427135,1076.3750308618,476.117116318722));
#130672=CARTESIAN_POINT('Ctrl Pts',(-80.9057127770828,1076.3750308618,476.84457308469));
#130673=CARTESIAN_POINT('Ctrl Pts',(-80.4355893150649,1076.3750308618,477.565790345312));
#130674=CARTESIAN_POINT('Ctrl Pts',(-79.9558366018756,1076.3750308618,478.280638399618));
#130675=CARTESIAN_POINT('Ctrl Pts',(-80.6405449088662,1076.42479602894,
475.657896024986));
#130676=CARTESIAN_POINT('Ctrl Pts',(-80.1842409189113,1076.42479602894,
476.378865738722));
#130677=CARTESIAN_POINT('Ctrl Pts',(-79.718309754768,1076.42479602894,477.093651587527));
#130678=CARTESIAN_POINT('Ctrl Pts',(-79.242835207725,1076.42479602894,477.802125027034));
#130679=CARTESIAN_POINT('Origin',(0.,1082.7251047501,424.620242579854));
#130680=CARTESIAN_POINT('Ctrl Pts',(-71.2826353250197,1076.62733493393,
481.288691976922));
#130681=CARTESIAN_POINT('Ctrl Pts',(-70.6478912735919,1076.62733493393,
482.087129718276));
#130682=CARTESIAN_POINT('Ctrl Pts',(-69.9998230975193,1076.62733493393,
482.874791115581));
#130683=CARTESIAN_POINT('Ctrl Pts',(-69.3386137191451,1076.62733493393,
483.651453845209));
#130684=CARTESIAN_POINT('Ctrl Pts',(-70.4927453171238,1076.66212086289,
480.660743224219));
#130685=CARTESIAN_POINT('Ctrl Pts',(-69.8650349279827,1076.66212086289,
481.450333397145));
#130686=CARTESIAN_POINT('Ctrl Pts',(-69.2241480601543,1076.66212086289,
482.229266639767));
#130687=CARTESIAN_POINT('Ctrl Pts',(-68.5702656090004,1076.66212086289,
482.997323092047));
#130688=CARTESIAN_POINT('Ctrl Pts',(-69.7087339478242,1076.68818379331,
480.037467886469));
#130689=CARTESIAN_POINT('Ctrl Pts',(-69.0880048739874,1076.68818379331,
480.818276337675));
#130690=CARTESIAN_POINT('Ctrl Pts',(-68.4542458685872,1076.68818379331,
481.588546383604));
#130691=CARTESIAN_POINT('Ctrl Pts',(-67.8076358150905,1076.68818379331,
482.348060609473));
#130692=CARTESIAN_POINT('Ctrl Pts',(-68.9306043300403,1076.7055298294,479.418868438389));
#130693=CARTESIAN_POINT('Ctrl Pts',(-68.3168041968055,1076.7055298294,480.190961049452));
#130694=CARTESIAN_POINT('Ctrl Pts',(-67.6901195797166,1076.7055298294,480.952632891074));
#130695=CARTESIAN_POINT('Ctrl Pts',(-67.0507273654387,1076.7055298294,481.703668975384));
#130696=CARTESIAN_POINT('Origin',(0.,1082.7251047501,424.620242579854));
#130697=CARTESIAN_POINT('Ctrl Pts',(-112.051426574092,1074.64943926585,
439.937715424524));
#130698=CARTESIAN_POINT('Ctrl Pts',(-111.950523798461,1074.64943926585,
440.675846320489));
#130699=CARTESIAN_POINT('Ctrl Pts',(-111.842332607831,1074.64943926585,
441.412944181006));
#130700=CARTESIAN_POINT('Ctrl Pts',(-111.726863565238,1074.64943926585,
442.148937040966));
#130701=CARTESIAN_POINT('Ctrl Pts',(-111.315440883155,1074.75345395672,
439.83710589924));
#130702=CARTESIAN_POINT('Ctrl Pts',(-111.215200865699,1074.75345395672,
440.570388541202));
#130703=CARTESIAN_POINT('Ctrl Pts',(-111.107720305631,1074.75345395672,
441.302644932987));
#130704=CARTESIAN_POINT('Ctrl Pts',(-110.993009696604,1074.75345395672,
442.033803582172));
#130705=CARTESIAN_POINT('Ctrl Pts',(-110.582758353619,1074.85356318489,
439.736947917383));
#130706=CARTESIAN_POINT('Ctrl Pts',(-110.483178119828,1074.85356318489,
440.465404064685));
#130707=CARTESIAN_POINT('Ctrl Pts',(-110.376405000956,1074.85356318489,
441.192840716628));
#130708=CARTESIAN_POINT('Ctrl Pts',(-110.262449421587,1074.85356318489,
441.919186851356));
#130709=CARTESIAN_POINT('Ctrl Pts',(-109.853380157329,1074.94976876584,
439.637241639143));
#130710=CARTESIAN_POINT('Ctrl Pts',(-109.754456731637,1074.94976876584,
440.360893058848));
#130711=CARTESIAN_POINT('Ctrl Pts',(-109.648387863464,1074.94976876584,
441.083531707549));
#130712=CARTESIAN_POINT('Ctrl Pts',(-109.535183908635,1074.94976876584,
441.805087031833));
#130713=CARTESIAN_POINT('Origin',(0.,1082.7251047501,424.620242579854));
#130714=CARTESIAN_POINT('Ctrl Pts',(-102.790046090129,1075.53649189674,
450.458426927557));
#130715=CARTESIAN_POINT('Ctrl Pts',(-102.60642453742,1075.53649189674,451.188914318317));
#130716=CARTESIAN_POINT('Ctrl Pts',(-102.415026793123,1075.53649189674,
451.917402894861));
#130717=CARTESIAN_POINT('Ctrl Pts',(-102.215874605379,1075.53649189674,
452.643809880507));
#130718=CARTESIAN_POINT('Ctrl Pts',(-102.064433267001,1075.61819462687,
450.276030687822));
#130719=CARTESIAN_POINT('Ctrl Pts',(-101.882107930787,1075.61819462687,
451.001361440969));
#130720=CARTESIAN_POINT('Ctrl Pts',(-101.692061296475,1075.61819462687,
451.724707489879));
#130721=CARTESIAN_POINT('Ctrl Pts',(-101.494314958681,1075.61819462687,
452.445986642201));
#130722=CARTESIAN_POINT('Ctrl Pts',(-101.342303806185,1075.69570098791,
450.094510055804));
#130723=CARTESIAN_POINT('Ctrl Pts',(-101.161268463875,1075.69570098791,
450.814708926189));
#130724=CARTESIAN_POINT('Ctrl Pts',(-100.972566453436,1075.69570098791,
451.532937134578));
#130725=CARTESIAN_POINT('Ctrl Pts',(-100.776219216697,1075.69570098791,
452.249113070151));
#130726=CARTESIAN_POINT('Ctrl Pts',(-100.623658988146,1075.7690130065,449.913865353371));
#130727=CARTESIAN_POINT('Ctrl Pts',(-100.443907414862,1075.7690130065,450.628957104945));
#130728=CARTESIAN_POINT('Ctrl Pts',(-100.256543539801,1075.7690130065,451.342092169003));
#130729=CARTESIAN_POINT('Ctrl Pts',(-100.061588652741,1075.7690130065,452.053189513449));
#130730=CARTESIAN_POINT('Origin',(0.,1082.7251047501,424.620242579854));
#130731=CARTESIAN_POINT('Ctrl Pts',(-91.9241429483952,1076.25698153983,
458.678803283175));
#130732=CARTESIAN_POINT('Ctrl Pts',(-91.6195337915803,1076.25698153983,
459.500944180976));
#130733=CARTESIAN_POINT('Ctrl Pts',(-91.3039232474814,1076.25698153983,
460.318924852328));
#130734=CARTESIAN_POINT('Ctrl Pts',(-90.9773681143258,1076.25698153983,
461.132598090958));
#130735=CARTESIAN_POINT('Ctrl Pts',(-91.1085750045413,1076.31894086093,
458.376629453401));
#130736=CARTESIAN_POINT('Ctrl Pts',(-90.8066683963251,1076.31894086093,
459.191476165582));
#130737=CARTESIAN_POINT('Ctrl Pts',(-90.493858007161,1076.31894086093,460.002199561611));
#130738=CARTESIAN_POINT('Ctrl Pts',(-90.1702001313522,1076.31894086093,
460.808653741254));
#130739=CARTESIAN_POINT('Ctrl Pts',(-90.297897541255,1076.37482552263,458.076267582095));
#130740=CARTESIAN_POINT('Ctrl Pts',(-89.9986772760452,1076.37482552263,
458.883863847592));
#130741=CARTESIAN_POINT('Ctrl Pts',(-89.6886502509362,1076.37482552263,
459.687373485902));
#130742=CARTESIAN_POINT('Ctrl Pts',(-89.3678722593284,1076.37482552263,
460.486651895004));
#130743=CARTESIAN_POINT('Ctrl Pts',(-89.492112720497,1076.42463906393,457.77771847028));
#130744=CARTESIAN_POINT('Ctrl Pts',(-89.1955625855377,1076.42463906393,
458.578108047362));
#130745=CARTESIAN_POINT('Ctrl Pts',(-88.8883021261812,1076.42463906393,
459.374447464799));
#130746=CARTESIAN_POINT('Ctrl Pts',(-88.5703866379484,1076.42463906393,
460.16659341094));
#130747=CARTESIAN_POINT('Origin',(0.,1082.7251047501,424.620242579854));
#130748=CARTESIAN_POINT('Ctrl Pts',(-81.5036900617922,1076.62735149554,
465.235366130203));
#130749=CARTESIAN_POINT('Ctrl Pts',(-81.0498664378651,1076.62735149554,
466.14606876395));
#130750=CARTESIAN_POINT('Ctrl Pts',(-80.5808440211162,1076.62735149554,
467.049037833927));
#130751=CARTESIAN_POINT('Ctrl Pts',(-80.0967545534475,1076.62735149554,
467.944019708627));
#130752=CARTESIAN_POINT('Ctrl Pts',(-80.5993187014014,1076.66218157195,
464.784697522318));
#130753=CARTESIAN_POINT('Ctrl Pts',(-80.1505307401276,1076.66218157195,
465.685294927956));
#130754=CARTESIAN_POINT('Ctrl Pts',(-79.6867126330335,1076.66218157195,
466.578244582057));
#130755=CARTESIAN_POINT('Ctrl Pts',(-79.2079946602025,1076.66218157195,
467.463295667427));
#130756=CARTESIAN_POINT('Ctrl Pts',(-79.7016870849284,1076.6882651034,464.33738748055));
#130757=CARTESIAN_POINT('Ctrl Pts',(-79.2578972584977,1076.6882651034,465.227954966357));
#130758=CARTESIAN_POINT('Ctrl Pts',(-78.799244676422,1076.6882651034,466.110959873351));
#130759=CARTESIAN_POINT('Ctrl Pts',(-78.3258581678604,1076.6882651034,466.986154177682));
#130760=CARTESIAN_POINT('Ctrl Pts',(-78.8107987860875,1076.70560821884,
463.893437785763));
#130761=CARTESIAN_POINT('Ctrl Pts',(-78.3719695467908,1076.70560821884,
464.774050699948));
#130762=CARTESIAN_POINT('Ctrl Pts',(-77.9184436845319,1076.70560821884,
465.647185568199));
#130763=CARTESIAN_POINT('Ctrl Pts',(-77.450348588445,1076.70560821884,466.512597139021));
#130764=CARTESIAN_POINT('Origin',(0.,1082.7251047501,424.620242579854));
#130765=CARTESIAN_POINT('Ctrl Pts',(-112.787114881755,1074.64949257569,
416.305931144629));
#130766=CARTESIAN_POINT('Ctrl Pts',(-112.841951325419,1074.64949257569,
417.049810456757));
#130767=CARTESIAN_POINT('Ctrl Pts',(-112.88942602191,1074.64949257569,417.794195854089));
#130768=CARTESIAN_POINT('Ctrl Pts',(-112.929534324867,1074.64949257569,
418.539014483421));
#130769=CARTESIAN_POINT('Ctrl Pts',(-112.046792792878,1074.75343612786,
416.360505360981));
#130770=CARTESIAN_POINT('Ctrl Pts',(-112.10126929622,1074.75343612786,417.099501931967));
#130771=CARTESIAN_POINT('Ctrl Pts',(-112.148432374078,1074.75343612786,
417.839001266268));
#130772=CARTESIAN_POINT('Ctrl Pts',(-112.188277410591,1074.75343612786,
418.578930988884));
#130773=CARTESIAN_POINT('Ctrl Pts',(-111.309791102948,1074.85347945785,
416.414834807964));
#130774=CARTESIAN_POINT('Ctrl Pts',(-111.363909280326,1074.85347945785,
417.14897053726));
#130775=CARTESIAN_POINT('Ctrl Pts',(-111.410762137185,1074.85347945785,
417.883605722883));
#130776=CARTESIAN_POINT('Ctrl Pts',(-111.450345088023,1074.85347945785,
418.618668465888));
#130777=CARTESIAN_POINT('Ctrl Pts',(-110.576110989133,1074.9496243775,416.468919398801));
#130778=CARTESIAN_POINT('Ctrl Pts',(-110.629872455478,1074.9496243775,417.198216193623));
#130779=CARTESIAN_POINT('Ctrl Pts',(-110.676416489465,1074.9496243775,417.928009152689));
#130780=CARTESIAN_POINT('Ctrl Pts',(-110.715738535817,1074.9496243775,418.658226850962));
#130781=CARTESIAN_POINT('Origin',(0.,1082.7251047501,424.620242579854));
#130782=CARTESIAN_POINT('Ctrl Pts',(-105.916863873868,1075.53636233154,
428.528540576853));
#130783=CARTESIAN_POINT('Ctrl Pts',(-105.889193093616,1075.53636233154,
429.278432797824));
#130784=CARTESIAN_POINT('Ctrl Pts',(-105.853560308952,1075.53636233154,
430.027988879656));
#130785=CARTESIAN_POINT('Ctrl Pts',(-105.809969538517,1075.53636233154,
430.777124287901));
#130786=CARTESIAN_POINT('Ctrl Pts',(-105.168863810439,1075.61810436561,
428.500939616602));
#130787=CARTESIAN_POINT('Ctrl Pts',(-105.141388445201,1075.61810436561,
429.2455359913));
#130788=CARTESIAN_POINT('Ctrl Pts',(-105.106007304366,1075.61810436561,
429.989798600721));
#130789=CARTESIAN_POINT('Ctrl Pts',(-105.062724378195,1075.61810436561,
430.733643507413));
#130790=CARTESIAN_POINT('Ctrl Pts',(-104.424456094477,1075.69564644726,
428.47347121281));
#130791=CARTESIAN_POINT('Ctrl Pts',(-104.397175205751,1075.69564644726,
429.212797175083));
#130792=CARTESIAN_POINT('Ctrl Pts',(-104.3620445002,1075.69564644726,429.95179173454));
#130793=CARTESIAN_POINT('Ctrl Pts',(-104.31906793984,1075.69564644726,430.690371547858));
#130794=CARTESIAN_POINT('Ctrl Pts',(-103.683642047071,1075.7689906057,428.446135414225));
#130795=CARTESIAN_POINT('Ctrl Pts',(-103.656554696013,1075.7689906057,429.180216407274));
#130796=CARTESIAN_POINT('Ctrl Pts',(-103.621673216755,1075.7689906057,429.913968348564));
#130797=CARTESIAN_POINT('Ctrl Pts',(-103.579001543208,1075.7689906057,430.647308486031));
#130798=CARTESIAN_POINT('Origin',(0.,1082.7251047501,424.620242579854));
#130799=CARTESIAN_POINT('Ctrl Pts',(-96.9953277889122,1076.25703779475,
438.82535338608));
#130800=CARTESIAN_POINT('Ctrl Pts',(-96.8685997973428,1076.25703779475,
439.690677370524));
#130801=CARTESIAN_POINT('Ctrl Pts',(-96.7303041265953,1076.25703779475,
440.554228115619));
#130802=CARTESIAN_POINT('Ctrl Pts',(-96.580465540314,1076.25703779475,441.415850991338));
#130803=CARTESIAN_POINT('Ctrl Pts',(-96.1346410229007,1076.31900226003,
438.699304522085));
#130804=CARTESIAN_POINT('Ctrl Pts',(-96.0090375504984,1076.31900226003,
439.556950065528));
#130805=CARTESIAN_POINT('Ctrl Pts',(-95.8719690445673,1076.31900226003,
440.412838104439));
#130806=CARTESIAN_POINT('Ctrl Pts',(-95.7234600490115,1076.31900226003,
441.266815380898));
#130807=CARTESIAN_POINT('Ctrl Pts',(-95.2791160427069,1076.37489033703,
438.574011609342));
#130808=CARTESIAN_POINT('Ctrl Pts',(-95.1546303454073,1076.37489033703,
439.424024761602));
#130809=CARTESIAN_POINT('Ctrl Pts',(-95.0187816446325,1076.37489033703,
440.272296049779));
#130810=CARTESIAN_POINT('Ctrl Pts',(-94.8715942658647,1076.37489033703,
441.118673579832));
#130811=CARTESIAN_POINT('Ctrl Pts',(-94.4287551305539,1076.42470556629,
438.449474982086));
#130812=CARTESIAN_POINT('Ctrl Pts',(-94.3053804613106,1076.42470556629,
439.29190181334));
#130813=CARTESIAN_POINT('Ctrl Pts',(-94.1707442027782,1076.42470556629,
440.132602326552));
#130814=CARTESIAN_POINT('Ctrl Pts',(-94.0248704633352,1076.42470556629,
440.971425983329));
#130815=CARTESIAN_POINT('Origin',(0.,1082.7251047501,424.620242579854));
#130816=CARTESIAN_POINT('Ctrl Pts',(-88.1662720496537,1076.62742624042,
447.39639773452));
#130817=CARTESIAN_POINT('Ctrl Pts',(-87.9111819950692,1076.62742624042,
448.38384882084));
#130818=CARTESIAN_POINT('Ctrl Pts',(-87.6395405034666,1076.62742624042,
449.366875516236));
#130819=CARTESIAN_POINT('Ctrl Pts',(-87.3514242321929,1076.62742624042,
450.345200410149));
#130820=CARTESIAN_POINT('Ctrl Pts',(-87.1889865167269,1076.66220724281,
447.143933766033));
#130821=CARTESIAN_POINT('Ctrl Pts',(-86.936724026631,1076.66220724281,448.120439378095));
#130822=CARTESIAN_POINT('Ctrl Pts',(-86.6680935651391,1076.66220724281,
449.09256964172));
#130823=CARTESIAN_POINT('Ctrl Pts',(-86.383170939884,1076.66220724281,450.060050221327));
#130824=CARTESIAN_POINT('Ctrl Pts',(-86.2189765468992,1076.68826006274,
446.893349307138));
#130825=CARTESIAN_POINT('Ctrl Pts',(-85.9695205710223,1076.68826006274,
447.858990930328));
#130826=CARTESIAN_POINT('Ctrl Pts',(-85.7038787235315,1076.68826006274,
448.820305882463));
#130827=CARTESIAN_POINT('Ctrl Pts',(-85.4221259686714,1076.68826006274,
449.777022880047));
#130828=CARTESIAN_POINT('Ctrl Pts',(-85.2562459939478,1076.70559080985,
446.644645353388));
#130829=CARTESIAN_POINT('Ctrl Pts',(-85.0095754708705,1076.70559080985,
447.599504516253));
#130830=CARTESIAN_POINT('Ctrl Pts',(-84.7468998093977,1076.70559080985,
448.550085320147));
#130831=CARTESIAN_POINT('Ctrl Pts',(-84.4682931367152,1076.70559080985,
449.496119510755));
#130832=CARTESIAN_POINT('Origin',(0.,1082.7251047501,424.620242579854));
#130833=CARTESIAN_POINT('Ctrl Pts',(-108.594074399517,1074.64939441013,
393.036280926091));
#130834=CARTESIAN_POINT('Ctrl Pts',(-108.802630048851,1074.64939441013,
393.753350809485));
#130835=CARTESIAN_POINT('Ctrl Pts',(-109.004073252079,1074.64939441013,
394.47245115882));
#130836=CARTESIAN_POINT('Ctrl Pts',(-109.198384247329,1074.64939441013,
395.193511429301));
#130837=CARTESIAN_POINT('Ctrl Pts',(-107.880346429781,1074.75347617509,
393.243864599068));
#130838=CARTESIAN_POINT('Ctrl Pts',(-108.087531359755,1074.75347617509,
393.956221584131));
#130839=CARTESIAN_POINT('Ctrl Pts',(-108.287650589744,1074.75347617509,
394.67059569002));
#130840=CARTESIAN_POINT('Ctrl Pts',(-108.480684487759,1074.75347617509,
395.386916835592));
#130841=CARTESIAN_POINT('Ctrl Pts',(-107.169823753786,1074.85364752299,
393.450516030804));
#130842=CARTESIAN_POINT('Ctrl Pts',(-107.375644120187,1074.85364752299,
394.158181282776));
#130843=CARTESIAN_POINT('Ctrl Pts',(-107.574445322792,1074.85364752299,
394.867850370391));
#130844=CARTESIAN_POINT('Ctrl Pts',(-107.766207858911,1074.85364752299,
395.579453674075));
#130845=CARTESIAN_POINT('Ctrl Pts',(-106.462507509375,1074.94991027277,
393.656234890365));
#130846=CARTESIAN_POINT('Ctrl Pts',(-106.666969470178,1074.94991027277,
394.359229581998));
#130847=CARTESIAN_POINT('Ctrl Pts',(-106.864458593364,1074.94991027277,
395.064214884045));
#130848=CARTESIAN_POINT('Ctrl Pts',(-107.054955504962,1074.94991027277,
395.771121636418));
#130849=CARTESIAN_POINT('Origin',(0.,1082.7251047501,424.620242579854));
#130850=CARTESIAN_POINT('Ctrl Pts',(-104.413416366025,1075.53647952796,
406.419477816671));
#130851=CARTESIAN_POINT('Ctrl Pts',(-104.542624892593,1075.53647952796,
407.160716102985));
#130852=CARTESIAN_POINT('Ctrl Pts',(-104.663933237021,1075.53647952796,
407.903288204539));
#130853=CARTESIAN_POINT('Ctrl Pts',(-104.777327644461,1075.53647952796,
408.64710992296));
#130854=CARTESIAN_POINT('Ctrl Pts',(-103.676158825789,1075.61820324334,
406.547992441772));
#130855=CARTESIAN_POINT('Ctrl Pts',(-103.804455017872,1075.61820324334,
407.283996884248));
#130856=CARTESIAN_POINT('Ctrl Pts',(-103.924906810578,1075.61820324334,
408.021325723968));
#130857=CARTESIAN_POINT('Ctrl Pts',(-104.037500546181,1075.61820324334,
408.759895357077));
#130858=CARTESIAN_POINT('Ctrl Pts',(-102.942441438183,1075.69572847712,
406.675889967198));
#130859=CARTESIAN_POINT('Ctrl Pts',(-103.069829676616,1075.69572847712,
407.406685697633));
#130860=CARTESIAN_POINT('Ctrl Pts',(-103.189429030577,1075.69572847712,
408.138796452538));
#130861=CARTESIAN_POINT('Ctrl Pts',(-103.301225938997,1075.69572847712,
408.872139219722));
#130862=CARTESIAN_POINT('Ctrl Pts',(-102.212265504876,1075.76905725745,
406.803170166049));
#130863=CARTESIAN_POINT('Ctrl Pts',(-102.338750172103,1075.76905725745,
407.528782325481));
#130864=CARTESIAN_POINT('Ctrl Pts',(-102.45750120181,1075.76905725745,408.255700181846));
#130865=CARTESIAN_POINT('Ctrl Pts',(-102.568505129116,1075.76905725745,
408.983841311767));
#130866=CARTESIAN_POINT('Origin',(0.,1082.7251047501,424.620242579854));
#130867=CARTESIAN_POINT('Ctrl Pts',(-97.8296100732469,1076.25700990573,
418.349442191101));
#130868=CARTESIAN_POINT('Ctrl Pts',(-97.8855743077914,1076.25700990573,
419.2225299796));
#130869=CARTESIAN_POINT('Ctrl Pts',(-97.9298463187621,1076.25700990573,
420.096288682573));
#130870=CARTESIAN_POINT('Ctrl Pts',(-97.9624181728472,1076.25700990573,
420.970561727049));
#130871=CARTESIAN_POINT('Ctrl Pts',(-96.9619111406566,1076.31894843203,
418.405061004257));
#130872=CARTESIAN_POINT('Ctrl Pts',(-97.0173790008771,1076.31894843203,
419.270404947702));
#130873=CARTESIAN_POINT('Ctrl Pts',(-97.0612583416058,1076.31894843203,
420.13641385495));
#130874=CARTESIAN_POINT('Ctrl Pts',(-97.0935412998954,1076.31894843203,
421.002932541753));
#130875=CARTESIAN_POINT('Ctrl Pts',(-96.0994137067278,1076.37481601301,
418.460346405476));
#130876=CARTESIAN_POINT('Ctrl Pts',(-96.1543881681843,1076.37481601301,
419.317992925037));
#130877=CARTESIAN_POINT('Ctrl Pts',(-96.1978771925678,1076.37481601301,
420.176298493401));
#130878=CARTESIAN_POINT('Ctrl Pts',(-96.2298729868736,1076.37481601301,
421.035109306721));
#130879=CARTESIAN_POINT('Ctrl Pts',(-95.2421200702117,1076.42461618443,
418.515298247409));
#130880=CARTESIAN_POINT('Ctrl Pts',(-95.2966041097795,1076.42461618443,
419.365293784771));
#130881=CARTESIAN_POINT('Ctrl Pts',(-95.3397051727548,1076.42461618443,
420.215942491626));
#130882=CARTESIAN_POINT('Ctrl Pts',(-95.3714155356537,1076.42461618443,
421.067091936193));
#130883=CARTESIAN_POINT('',(0.,0.,0.));
#130884=CARTESIAN_POINT('',(0.,0.,0.));
#130885=CARTESIAN_POINT('',(0.,0.,0.));
#130886=CARTESIAN_POINT('',(0.,0.,0.));
#130887=CARTESIAN_POINT('',(0.,0.,0.));
#130888=CARTESIAN_POINT('',(0.,0.,0.));
#130889=CARTESIAN_POINT('',(0.,0.,0.));
#130890=CARTESIAN_POINT('',(0.,0.,0.));
#130891=UNCERTAINTY_MEASURE_WITH_UNIT(LENGTH_MEASURE(0.01),#130911,
'DISTANCE_ACCURACY_VALUE',
'Maximum model space distance between geometric entities at asserted c
onnectivities');
#130892=UNCERTAINTY_MEASURE_WITH_UNIT(LENGTH_MEASURE(0.01),#130911,
'DISTANCE_ACCURACY_VALUE',
'Maximum model space distance between geometric entities at asserted c
onnectivities');
#130893=UNCERTAINTY_MEASURE_WITH_UNIT(LENGTH_MEASURE(0.01),#130911,
'DISTANCE_ACCURACY_VALUE',
'Maximum model space distance between geometric entities at asserted c
onnectivities');
#130894=UNCERTAINTY_MEASURE_WITH_UNIT(LENGTH_MEASURE(0.01),#130911,
'DISTANCE_ACCURACY_VALUE',
'Maximum model space distance between geometric entities at asserted c
onnectivities');
#130895=UNCERTAINTY_MEASURE_WITH_UNIT(LENGTH_MEASURE(0.01),#130911,
'DISTANCE_ACCURACY_VALUE',
'Maximum model space distance between geometric entities at asserted c
onnectivities');
#130896=UNCERTAINTY_MEASURE_WITH_UNIT(LENGTH_MEASURE(0.01),#130911,
'DISTANCE_ACCURACY_VALUE',
'Maximum model space distance between geometric entities at asserted c
onnectivities');
#130897=UNCERTAINTY_MEASURE_WITH_UNIT(LENGTH_MEASURE(0.01),#130911,
'DISTANCE_ACCURACY_VALUE',
'Maximum model space distance between geometric entities at asserted c
onnectivities');
#130898=UNCERTAINTY_MEASURE_WITH_UNIT(LENGTH_MEASURE(0.01),#130911,
'DISTANCE_ACCURACY_VALUE',
'Maximum model space distance between geometric entities at asserted c
onnectivities');
#130899=UNCERTAINTY_MEASURE_WITH_UNIT(LENGTH_MEASURE(0.01),#130911,
'DISTANCE_ACCURACY_VALUE',
'Maximum model space distance between geometric entities at asserted c
onnectivities');
#130900=UNCERTAINTY_MEASURE_WITH_UNIT(LENGTH_MEASURE(0.01),#130911,
'DISTANCE_ACCURACY_VALUE',
'Maximum model space distance between geometric entities at asserted c
onnectivities');
#130901=(
GEOMETRIC_REPRESENTATION_CONTEXT(3)
GLOBAL_UNCERTAINTY_ASSIGNED_CONTEXT((#130891))
GLOBAL_UNIT_ASSIGNED_CONTEXT((#130911,#130913,#130914))
REPRESENTATION_CONTEXT('','3D')
);
#130902=(
GEOMETRIC_REPRESENTATION_CONTEXT(3)
GLOBAL_UNCERTAINTY_ASSIGNED_CONTEXT((#130892))
GLOBAL_UNIT_ASSIGNED_CONTEXT((#130911,#130913,#130914))
REPRESENTATION_CONTEXT('','3D')
);
#130903=(
GEOMETRIC_REPRESENTATION_CONTEXT(3)
GLOBAL_UNCERTAINTY_ASSIGNED_CONTEXT((#130893))
GLOBAL_UNIT_ASSIGNED_CONTEXT((#130911,#130913,#130914))
REPRESENTATION_CONTEXT('','3D')
);
#130904=(
GEOMETRIC_REPRESENTATION_CONTEXT(3)
GLOBAL_UNCERTAINTY_ASSIGNED_CONTEXT((#130894))
GLOBAL_UNIT_ASSIGNED_CONTEXT((#130911,#130913,#130914))
REPRESENTATION_CONTEXT('','3D')
);
#130905=(
GEOMETRIC_REPRESENTATION_CONTEXT(3)
GLOBAL_UNCERTAINTY_ASSIGNED_CONTEXT((#130895))
GLOBAL_UNIT_ASSIGNED_CONTEXT((#130911,#130913,#130914))
REPRESENTATION_CONTEXT('','3D')
);
#130906=(
GEOMETRIC_REPRESENTATION_CONTEXT(3)
GLOBAL_UNCERTAINTY_ASSIGNED_CONTEXT((#130896))
GLOBAL_UNIT_ASSIGNED_CONTEXT((#130911,#130913,#130914))
REPRESENTATION_CONTEXT('','3D')
);
#130907=(
GEOMETRIC_REPRESENTATION_CONTEXT(3)
GLOBAL_UNCERTAINTY_ASSIGNED_CONTEXT((#130897))
GLOBAL_UNIT_ASSIGNED_CONTEXT((#130911,#130913,#130914))
REPRESENTATION_CONTEXT('','3D')
);
#130908=(
GEOMETRIC_REPRESENTATION_CONTEXT(3)
GLOBAL_UNCERTAINTY_ASSIGNED_CONTEXT((#130898))
GLOBAL_UNIT_ASSIGNED_CONTEXT((#130911,#130913,#130914))
REPRESENTATION_CONTEXT('','3D')
);
#130909=(
GEOMETRIC_REPRESENTATION_CONTEXT(3)
GLOBAL_UNCERTAINTY_ASSIGNED_CONTEXT((#130899))
GLOBAL_UNIT_ASSIGNED_CONTEXT((#130911,#130913,#130914))
REPRESENTATION_CONTEXT('','3D')
);
#130910=(
GEOMETRIC_REPRESENTATION_CONTEXT(3)
GLOBAL_UNCERTAINTY_ASSIGNED_CONTEXT((#130900))
GLOBAL_UNIT_ASSIGNED_CONTEXT((#130911,#130913,#130914))
REPRESENTATION_CONTEXT('','3D')
);
#130911=(
LENGTH_UNIT()
NAMED_UNIT(*)
SI_UNIT(.MILLI.,.METRE.)
);
#130912=(
LENGTH_UNIT()
NAMED_UNIT(*)
SI_UNIT($,.METRE.)
);
#130913=(
NAMED_UNIT(*)
PLANE_ANGLE_UNIT()
SI_UNIT($,.RADIAN.)
);
#130914=(
NAMED_UNIT(*)
SI_UNIT($,.STERADIAN.)
SOLID_ANGLE_UNIT()
);
#130915=SHAPE_DEFINITION_REPRESENTATION(#130924,#130941);
#130916=SHAPE_DEFINITION_REPRESENTATION(#130925,#130942);
#130917=SHAPE_DEFINITION_REPRESENTATION(#130926,#130943);
#130918=SHAPE_DEFINITION_REPRESENTATION(#130927,#130944);
#130919=SHAPE_DEFINITION_REPRESENTATION(#130928,#130945);
#130920=SHAPE_DEFINITION_REPRESENTATION(#130929,#130946);
#130921=SHAPE_DEFINITION_REPRESENTATION(#130930,#130947);
#130922=SHAPE_DEFINITION_REPRESENTATION(#130931,#130948);
#130923=SHAPE_DEFINITION_REPRESENTATION(#130932,#130949);
#130924=PRODUCT_DEFINITION_SHAPE('',$,#130951);
#130925=PRODUCT_DEFINITION_SHAPE('',$,#130952);
#130926=PRODUCT_DEFINITION_SHAPE('',$,#130953);
#130927=PRODUCT_DEFINITION_SHAPE('',$,#130954);
#130928=PRODUCT_DEFINITION_SHAPE('',$,#130955);
#130929=PRODUCT_DEFINITION_SHAPE('',$,#130956);
#130930=PRODUCT_DEFINITION_SHAPE('',$,#130957);
#130931=PRODUCT_DEFINITION_SHAPE('',$,#130958);
#130932=PRODUCT_DEFINITION_SHAPE('',$,#130959);
#130933=PRODUCT_DEFINITION_SHAPE($,$,#35);
#130934=PRODUCT_DEFINITION_SHAPE($,$,#36);
#130935=PRODUCT_DEFINITION_SHAPE($,$,#37);
#130936=PRODUCT_DEFINITION_SHAPE($,$,#38);
#130937=PRODUCT_DEFINITION_SHAPE($,$,#39);
#130938=PRODUCT_DEFINITION_SHAPE($,$,#40);
#130939=PRODUCT_DEFINITION_SHAPE($,$,#41);
#130940=PRODUCT_DEFINITION_SHAPE($,$,#42);
#130941=SHAPE_REPRESENTATION('',(#45549,#51593,#51594,#51595,#51596,#51597,
#51598,#51599,#51600),#130901);
#130942=SHAPE_REPRESENTATION('',(#45550),#130902);
#130943=SHAPE_REPRESENTATION('',(#45568),#130903);
#130944=SHAPE_REPRESENTATION('',(#48137),#130904);
#130945=SHAPE_REPRESENTATION('',(#48162),#130905);
#130946=SHAPE_REPRESENTATION('',(#48574),#130906);
#130947=SHAPE_REPRESENTATION('',(#48753),#130907);
#130948=SHAPE_REPRESENTATION('',(#48892),#130908);
#130949=SHAPE_REPRESENTATION('',(#48902),#130909);
#130950=PRODUCT_DEFINITION_CONTEXT('part definition',#130979,'design');
#130951=PRODUCT_DEFINITION('W401061','MAS-616',#130960,#130950);
#130952=PRODUCT_DEFINITION('Component1','Component1',#130961,#130950);
#130953=PRODUCT_DEFINITION('Component2','Component2',#130962,#130950);
#130954=PRODUCT_DEFINITION('Component3','Component3',#130963,#130950);
#130955=PRODUCT_DEFINITION('2026-10-06-10-46-07-206','Component4',#130964,
#130950);
#130956=PRODUCT_DEFINITION('Component5','Component5',#130965,#130950);
#130957=PRODUCT_DEFINITION('Component6','Component6',#130966,#130950);
#130958=PRODUCT_DEFINITION('Component7','Component7',#130967,#130950);
#130959=PRODUCT_DEFINITION('Component8','Component8',#130968,#130950);
#130960=PRODUCT_DEFINITION_FORMATION('',$,#130981);
#130961=PRODUCT_DEFINITION_FORMATION('',$,#130982);
#130962=PRODUCT_DEFINITION_FORMATION('',$,#130983);
#130963=PRODUCT_DEFINITION_FORMATION('',$,#130984);
#130964=PRODUCT_DEFINITION_FORMATION('',$,#130985);
#130965=PRODUCT_DEFINITION_FORMATION('',$,#130986);
#130966=PRODUCT_DEFINITION_FORMATION('',$,#130987);
#130967=PRODUCT_DEFINITION_FORMATION('',$,#130988);
#130968=PRODUCT_DEFINITION_FORMATION('',$,#130989);
#130969=PRODUCT_RELATED_PRODUCT_CATEGORY('MAS-616','MAS-616',(#130981));
#130970=PRODUCT_RELATED_PRODUCT_CATEGORY('Component1','Component1',(#130982));
#130971=PRODUCT_RELATED_PRODUCT_CATEGORY('Component2','Component2',(#130983));
#130972=PRODUCT_RELATED_PRODUCT_CATEGORY('Component3','Component3',(#130984));
#130973=PRODUCT_RELATED_PRODUCT_CATEGORY('Component4','Component4',(#130985));
#130974=PRODUCT_RELATED_PRODUCT_CATEGORY('Component5','Component5',(#130986));
#130975=PRODUCT_RELATED_PRODUCT_CATEGORY('Component6','Component6',(#130987));
#130976=PRODUCT_RELATED_PRODUCT_CATEGORY('Component7','Component7',(#130988));
#130977=PRODUCT_RELATED_PRODUCT_CATEGORY('Component8','Component8',(#130989));
#130978=APPLICATION_PROTOCOL_DEFINITION('international standard',
'automotive_design',2009,#130979);
#130979=APPLICATION_CONTEXT(
'Core Data for Automotive Mechanical Design Process');
#130980=PRODUCT_CONTEXT('part definition',#130979,'mechanical');
#130981=PRODUCT('W401061','MAS-616','STEP AP214',(#130980));
#130982=PRODUCT('Component1','Component1',$,(#130980));
#130983=PRODUCT('Component2','Component2',$,(#130980));
#130984=PRODUCT('Component3','Component3',$,(#130980));
#130985=PRODUCT('2026-10-06-10-46-07-206','Component4',$,(#130980));
#130986=PRODUCT('Component5','Component5',$,(#130980));
#130987=PRODUCT('Component6','Component6',$,(#130980));
#130988=PRODUCT('Component7','Component7',$,(#130980));
#130989=PRODUCT('Component8','Component8',$,(#130980));
#130990=PRESENTATION_STYLE_ASSIGNMENT((#130992));
#130991=PRESENTATION_STYLE_ASSIGNMENT((#130993));
#130992=SURFACE_STYLE_USAGE(.BOTH.,#130994);
#130993=SURFACE_STYLE_USAGE(.BOTH.,#130995);
#130994=SURFACE_SIDE_STYLE('',(#130996));
#130995=SURFACE_SIDE_STYLE('',(#130997));
#130996=SURFACE_STYLE_FILL_AREA(#130998);
#130997=SURFACE_STYLE_FILL_AREA(#130999);
#130998=FILL_AREA_STYLE('Steel - Satin',(#131000));
#130999=FILL_AREA_STYLE('Opaque(202,209,238)',(#131001));
#131000=FILL_AREA_STYLE_COLOUR('Steel - Satin',#131002);
#131001=FILL_AREA_STYLE_COLOUR('Opaque(202,209,238)',#131003);
#131002=COLOUR_RGB('Steel - Satin', 0.66274510, 0.83137255, 0.94901961);
#131003=COLOUR_RGB('Opaque(202,209,238)', 0.40784314, 0.44705882, 0.49803922);
ENDSEC;
END-ISO-10303-21;
